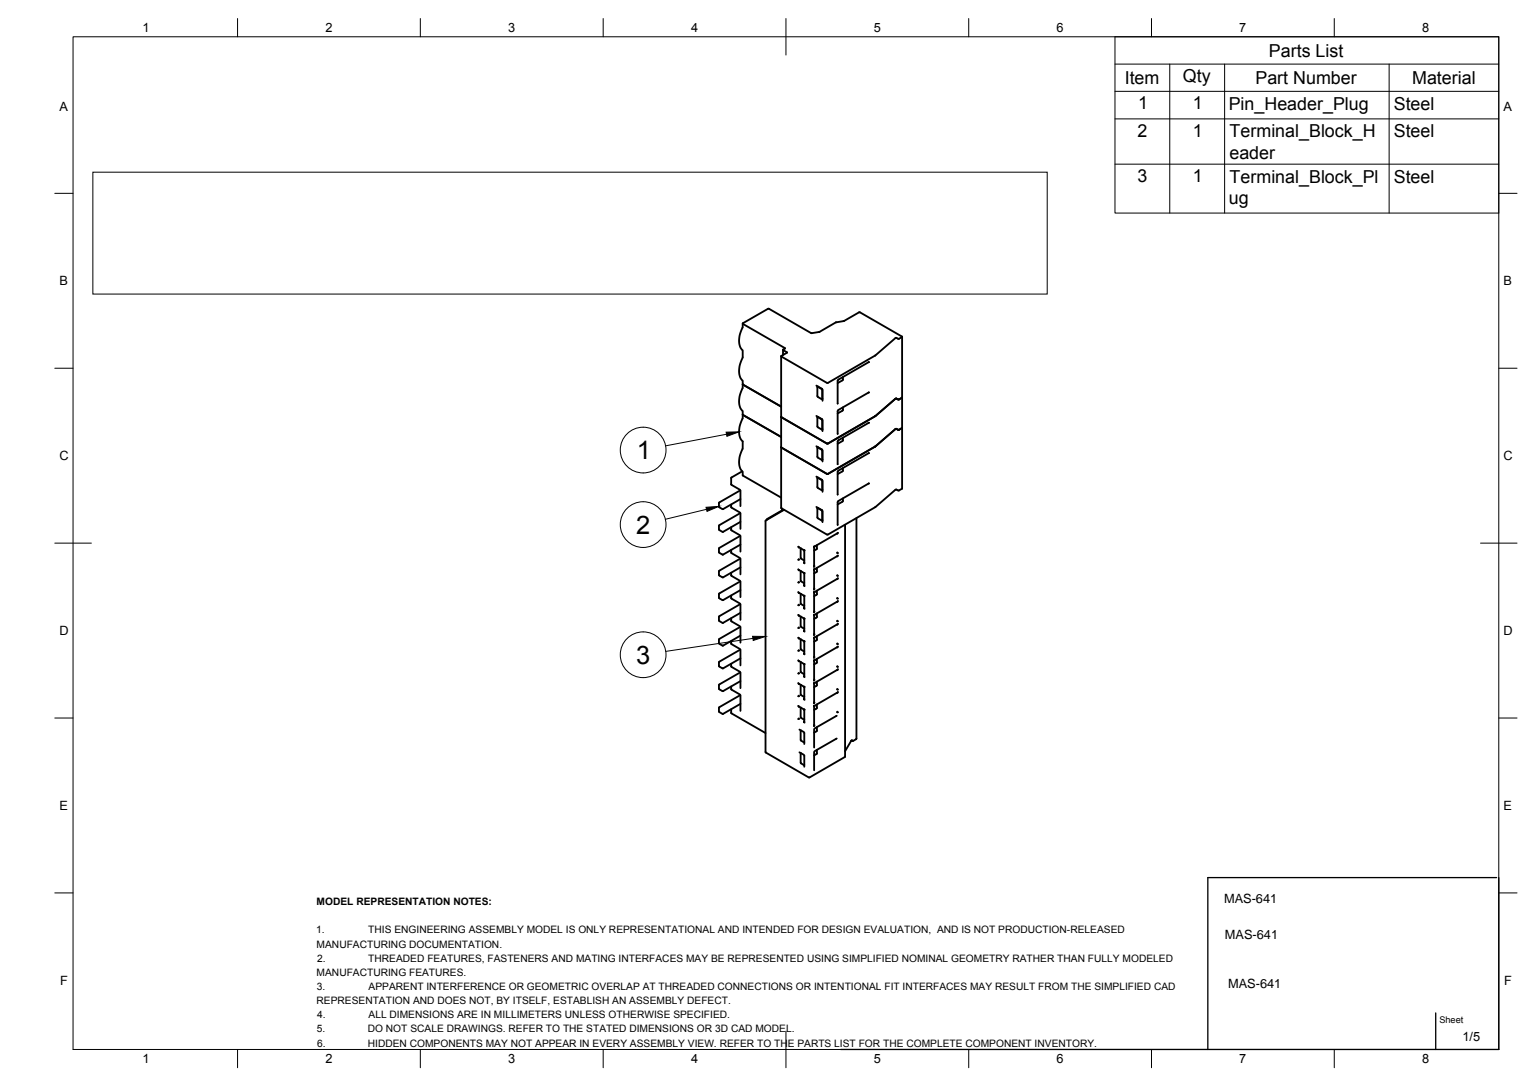
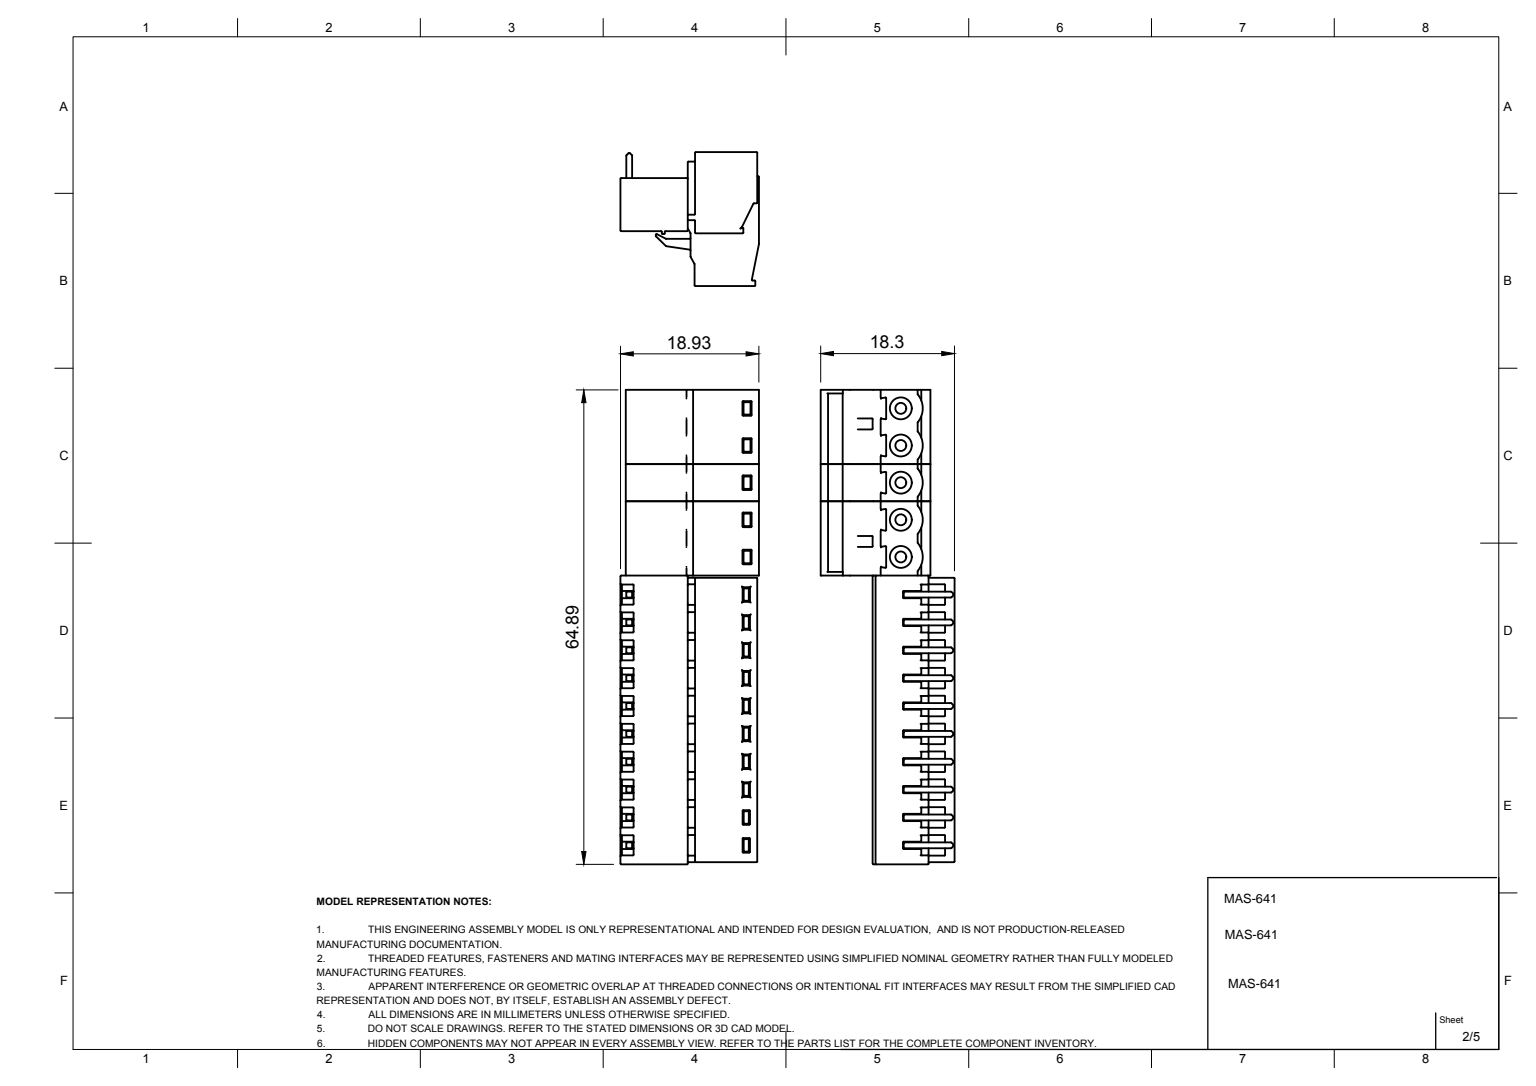
ISO-10303-21;
HEADER;
FILE_DESCRIPTION((''),'2;1');
FILE_NAME('MAS-641','2026-10-09T09:55:32-07:00',(''),(''),'','','');
FILE_SCHEMA (('AUTOMOTIVE_DESIGN { 1 0 10303 214 3 1 1 }'));
ENDSEC;
DATA;
#10 = MECHANICAL_DESIGN_GEOMETRIC_PRESENTATION_REPRESENTATION('',(#79661,
#79662,#79663,#79664,#79665,#79666,#79667,#79668,#79669,#79670,#79671,#79672,
#79673,#79674,#79675,#79676,#79677,#79678,#79679,#79680,#79681,#79682,#79683,
#79684,#79685,#79686,#79687,#79688,#79689,#79690,#79691,#79692,#79693,#79694,
#79695,#79696,#79697,#79698,#79699,#79700,#79701,#79702,#79703,#79704,#79705,
#79706,#79707,#79708,#79709,#79710,#79711,#79712,#79713,#79714,#79715,#79716,
#79717,#79718,#79719,#79720,#79721,#79722,#79723,#79724,#79725,#79726,#79727,
#79728,#79729,#79730,#79731,#79732,#79733,#79734,#79735,#79736,#79737,#79738,
#79739,#79740,#79741,#79742,#79743,#79744,#79745,#79746,#79747,#79748,#79749,
#79750,#79751,#79752,#79753,#79754,#79755,#79756,#79757,#79758,#79759,#79760,
#79761,#79762,#79763,#79764,#79765,#79766,#79767,#79768,#79769,#79770,#79771,
#79772,#79773,#79774,#79775,#79776,#79777,#79778,#79779,#79780,#79781,#79782,
#79783,#79784,#79785,#79786,#79787,#79788,#79789,#79790,#79791,#79792,#79793,
#79794,#79795,#79796,#79797,#79798,#79799,#79800,#79801,#79802,#79803,#79804,
#79805,#79806,#79807,#79808,#79809,#79810,#79811,#79812,#79813,#79814,#79815,
#79816,#79817,#79818,#79819,#79820,#79821,#79822,#79823,#79824,#79825,#79826,
#79827,#79828,#79829,#79830,#79831,#79832,#79833,#79834,#79835,#79836,#79837,
#79838,#79839,#79840,#79841,#79842,#79843,#79844,#79845,#79846,#79847,#79848,
#79849,#79850,#79851,#79852,#79853,#79854,#79855,#79856,#79857,#79858,#79859,
#79860,#79861,#79862,#79863,#79864,#79865,#79866,#79867,#79868,#79869,#79870,
#79871,#79872,#79873,#79874,#79875,#79876,#79877,#79878,#79879,#79880,#79881,
#79882,#79883,#79884,#79885,#79886,#79887,#79888,#79889,#79890,#79891,#79892,
#79893,#79894,#79895,#79896,#79897,#79898,#79899,#79900,#79901,#79902,#79903,
#79904,#79905,#79906,#79907,#79908,#79909,#79910,#79911,#79912,#79913,#79914,
#79915,#79916,#79917,#79918,#79919,#79920,#79921,#79922,#79923,#79924,#79925,
#79926,#79927,#79928,#79929,#79930,#79931,#79932,#79933,#79934,#79935,#79936,
#79937,#79938,#79939,#79940,#79941,#79942,#79943,#79944,#79945,#79946,#79947,
#79948,#79949,#79950,#79951,#79952,#79953,#79954,#79955,#79956,#79957,#79958,
#79959,#79960,#79961,#79962,#79963,#79964,#79965,#79966,#79967,#79968,#79969,
#79970,#79971,#79972,#79973,#79974,#79975,#79976,#79977,#79978,#79979,#79980,
#79981,#79982,#79983,#79984,#79985,#79986,#79987,#79988,#79989,#79990,#79991,
#79992,#79993,#79994,#79995,#79996,#79997,#79998,#79999,#80000,#80001,#80002,
#80003,#80004,#80005,#80006,#80007,#80008,#80009,#80010,#80011,#80012,#80013,
#80014,#80015,#80016,#80017,#80018,#80019,#80020,#80021,#80022,#80023,#80024,
#80025,#80026,#80027,#80028,#80029,#80030,#80031,#80032,#80033,#80034,#80035,
#80036,#80037,#80038,#80039,#80040,#80041,#80042,#80043,#80044,#80045,#80046,
#80047,#80048,#80049,#80050,#80051,#80052,#80053,#80054,#80055,#80056,#80057,
#80058,#80059,#80060,#80061,#80062,#80063,#80064,#80065,#80066,#80067,#80068,
#80069,#80070,#80071,#80072,#80073,#80074,#80075,#80076,#80077,#80078,#80079,
#80080,#80081,#80082,#80083,#80084,#80085,#80086,#80087,#80088,#80089,#80090,
#80091,#80092,#80093,#80094,#80095,#80096,#80097,#80098,#80099,#80100,#80101,
#80102,#80103,#80104,#80105,#80106,#80107,#80108,#80109,#80110,#80111,#80112,
#80113,#80114,#80115,#80116,#80117,#80118,#80119,#80120,#80121,#80122,#80123,
#80124,#80125,#80126,#80127,#80128,#80129,#80130,#80131,#80132,#80133,#80134,
#80135,#80136,#80137,#80138,#80139,#80140,#80141,#80142,#80143,#80144,#80145,
#80146,#80147,#80148,#80149,#80150,#80151,#80152,#80153,#80154,#80155,#80156,
#80157,#80158,#80159,#80160,#80161,#80162,#80163,#80164,#80165,#80166,#80167,
#80168,#80169,#80170,#80171,#80172,#80173,#80174,#80175,#80176,#80177,#80178,
#80179,#80180,#80181,#80182,#80183,#80184,#80185,#80186,#80187,#80188,#80189,
#80190,#80191,#80192,#80193,#80194,#80195,#80196,#80197,#80198,#80199,#80200,
#80201,#80202,#80203,#80204,#80205,#80206,#80207,#80208,#80209,#80210,#80211,
#80212,#80213,#80214,#80215,#80216,#80217,#80218,#80219,#80220,#80221,#80222,
#80223,#80224,#80225,#80226,#80227,#80228,#80229,#80230,#80231,#80232,#80233,
#80234,#80235,#80236,#80237,#80238,#80239,#80240,#80241,#80242,#80243,#80244,
#80245,#80246,#80247,#80248,#80249,#80250,#80251,#80252,#80253,#80254,#80255,
#80256,#80257,#80258,#80259,#80260,#80261,#80262,#80263,#80264,#80265,#80266,
#80267,#80268,#80269,#80270,#80271,#80272,#80273,#80274,#80275,#80276,#80277,
#80278,#80279,#80280,#80281,#80282,#80283,#80284,#80285,#80286,#80287,#80288,
#80289,#80290,#80291,#80292,#80293,#80294,#80295,#80296,#80297,#80298,#80299,
#80300,#80301,#80302,#80303,#80304,#80305,#80306,#80307,#80308,#80309,#80310,
#80311,#80312,#80313,#80314,#80315,#80316,#80317,#80318,#80319,#80320,#80321,
#80322,#80323,#80324,#80325,#80326,#80327,#80328,#80329,#80330,#80331,#80332,
#80333,#80334,#80335,#80336,#80337,#80338,#80339,#80340,#80341,#80342,#80343,
#80344,#80345,#80346,#80347,#80348,#80349,#80350,#80351,#80352,#80353,#80354,
#80355,#80356,#80357,#80358,#80359,#80360,#80361,#80362,#80363,#80364,#80365,
#80366,#80367,#80368,#80369,#80370,#80371,#80372,#80373,#80374,#80375,#80376,
#80377,#80378,#80379,#80380,#80381,#80382,#80383,#80384,#80385,#80386,#80387,
#80388,#80389,#80390,#80391,#80392,#80393,#80394,#80395,#80396,#80397,#80398,
#80399,#80400,#80401,#80402,#80403,#80404,#80405,#80406,#80407,#80408,#80409,
#80410,#80411,#80412,#80413,#80414,#80415,#80416,#80417,#80418,#80419,#80420,
#80421,#80422,#80423,#80424,#80425,#80426,#80427,#80428,#80429,#80430,#80431,
#80432,#80433,#80434,#80435,#80436,#80437,#80438,#80439,#80440,#80441,#80442,
#80443,#80444,#80445,#80446,#80447,#80448,#80449,#80450,#80451,#80452,#80453,
#80454,#80455,#80456,#80457,#80458,#80459,#80460,#80461,#80462,#80463,#80464,
#80465,#80466,#80467,#80468,#80469,#80470,#80471,#80472,#80473,#80474,#80475,
#80476,#80477,#80478,#80479,#80480,#80481,#80482,#80483,#80484,#80485,#80486,
#80487,#80488,#80489,#80490,#80491,#80492,#80493,#80494,#80495,#80496,#80497,
#80498,#80499,#80500,#80501,#80502,#80503,#80504,#80505,#80506,#80507,#80508,
#80509,#80510,#80511,#80512,#80513,#80514,#80515,#80516,#80517,#80518,#80519,
#80520,#80521,#80522,#80523,#80524,#80525,#80526,#80527,#80528,#80529,#80530,
#80531,#80532,#80533,#80534,#80535,#80536,#80537,#80538,#80539,#80540,#80541,
#80542,#80543,#80544,#80545,#80546,#80547,#80548,#80549,#80550,#80551,#80552,
#80553,#80554,#80555,#80556,#80557,#80558,#80559,#80560,#80561,#80562,#80563,
#80564,#80565,#80566,#80567,#80568,#80569,#80570,#80571,#80572,#80573,#80574,
#80575,#80576,#80577,#80578,#80579,#80580,#80581,#80582,#80583,#80584,#80585,
#80586,#80587,#80588,#80589,#80590,#80591,#80592,#80593,#80594,#80595,#80596,
#80597,#80598,#80599,#80600,#80601,#80602,#80603,#80604,#80605,#80606,#80607,
#80608,#80609,#80610,#80611,#80612,#80613,#80614,#80615,#80616,#80617,#80618,
#80619,#80620,#80621,#80622,#80623,#80624,#80625,#80626,#80627,#80628,#80629,
#80630,#80631,#80632,#80633,#80634,#80635,#80636,#80637,#80638,#80639,#80640,
#80641,#80642,#80643,#80644,#80645,#80646,#80647,#80648,#80649,#80650,#80651,
#80652,#80653,#80654,#80655,#80656,#80657,#80658,#80659,#80660,#80661,#80662,
#80663,#80664,#80665,#80666,#80667,#80668,#80669,#80670,#80671,#80672,#80673,
#80674,#80675,#80676,#80677,#80678,#80679,#80680,#80681,#80682,#80683,#80684,
#80685,#80686,#80687,#80688,#80689,#80690,#80691,#80692,#80693,#80694,#80695,
#80696,#80697,#80698,#80699,#80700,#80701,#80702,#80703,#80704,#80705,#80706,
#80707,#80708,#80709,#80710,#80711,#80712,#80713,#80714,#80715,#80716,#80717,
#80718,#80719,#80720,#80721,#80722,#80723,#80724,#80725,#80726,#80727,#80728,
#80729,#80730,#80731,#80732,#80733,#80734,#80735,#80736,#80737,#80738,#80739,
#80740,#80741,#80742,#80743,#80744,#80745,#80746,#80747,#80748,#80749,#80750,
#80751,#80752,#80753,#80754,#80755,#80756,#80757,#80758,#80759,#80760,#80761,
#80762,#80763,#80764,#80765,#80766,#80767,#80768,#80769,#80770,#80771,#80772,
#80773,#80774,#80775,#80776,#80777,#80778,#80779,#80780,#80781,#80782,#80783,
#80784,#80785,#80786,#80787,#80788,#80789,#80790,#80791,#80792,#80793,#80794,
#80795,#80796,#80797,#80798,#80799,#80800,#80801,#80802,#80803,#80804,#80805,
#80806,#80807,#80808,#80809,#80810,#80811,#80812,#80813,#80814,#80815,#80816,
#80817,#80818,#80819,#80820,#80821,#80822,#80823,#80824,#80825,#80826,#80827,
#80828,#80829,#80830,#80831,#80832,#80833,#80834,#80835,#80836,#80837,#80838,
#80839,#80840,#80841,#80842,#80843,#80844,#80845,#80846,#80847,#80848,#80849,
#80850,#80851,#80852,#80853,#80854,#80855,#80856,#80857,#80858,#80859,#80860,
#80861,#80862,#80863,#80864,#80865,#80866,#80867,#80868,#80869,#80870,#80871,
#80872,#80873,#80874,#80875,#80876,#80877,#80878,#80879,#80880,#80881,#80882,
#80883,#80884,#80885,#80886,#80887,#80888,#80889,#80890,#80891,#80892,#80893,
#80894,#80895,#80896,#80897,#80898,#80899,#80900,#80901,#80902,#80903,#80904,
#80905,#80906,#80907,#80908,#80909,#80910,#80911,#80912,#80913,#80914,#80915,
#80916,#80917,#80918,#80919,#80920,#80921,#80922,#80923,#80924,#80925,#80926,
#80927,#80928,#80929,#80930,#80931,#80932,#80933,#80934,#80935,#80936,#80937,
#80938,#80939,#80940,#80941,#80942,#80943,#80944,#80945,#80946,#80947,#80948,
#80949,#80950,#80951,#80952,#80953,#80954,#80955,#80956,#80957,#80958,#80959,
#80960,#80961,#80962,#80963,#80964,#80965,#80966,#80967,#80968,#80969,#80970,
#80971,#80972,#80973,#80974,#80975,#80976,#80977,#80978,#80979,#80980,#80981,
#80982,#80983,#80984,#80985,#80986,#80987,#80988,#80989,#80990,#80991,#80992,
#80993,#80994,#80995,#80996,#80997,#80998,#80999,#81000,#81001,#81002,#81003,
#81004,#81005,#81006,#81007,#81008,#81009,#81010,#81011,#81012,#81013,#81014,
#81015,#81016,#81017,#81018,#81019,#81020,#81021,#81022,#81023,#81024,#81025,
#81026,#81027,#81028,#81029,#81030,#81031,#81032,#81033,#81034,#81035,#81036,
#81037,#81038,#81039,#81040,#81041,#81042,#81043,#81044,#81045,#81046,#81047,
#81048,#81049,#81050,#81051,#81052,#81053,#81054,#81055,#81056,#81057,#81058,
#81059,#81060,#81061,#81062,#81063,#81064,#81065,#81066,#81067,#81068,#81069,
#81070,#81071,#81072,#81073,#81074,#81075,#81076,#81077,#81078,#81079,#81080,
#81081,#81082,#81083,#81084,#81085,#81086,#81087,#81088,#81089,#81090,#81091,
#81092,#81093,#81094,#81095,#81096,#81097,#81098,#81099,#81100,#81101,#81102,
#81103,#81104,#81105,#81106,#81107,#81108,#81109,#81110,#81111,#81112,#81113,
#81114,#81115,#81116,#81117,#81118,#81119,#81120,#81121,#81122,#81123,#81124,
#81125,#81126,#81127,#81128,#81129,#81130,#81131,#81132,#81133,#81134,#81135,
#81136,#81137,#81138,#81139,#81140,#81141,#81142,#81143,#81144,#81145,#81146,
#81147,#81148,#81149,#81150,#81151,#81152,#81153,#81154,#81155,#81156,#81157,
#81158,#81159,#81160,#81161,#81162,#81163,#81164,#81165,#81166,#81167,#81168,
#81169,#81170,#81171,#81172,#81173,#81174,#81175,#81176,#81177,#81178,#81179,
#81180,#81181,#81182,#81183,#81184,#81185,#81186,#81187,#81188,#81189,#81190,
#81191,#81192,#81193,#81194,#81195,#81196,#81197,#81198,#81199,#81200,#81201,
#81202,#81203,#81204,#81205,#81206,#81207,#81208,#81209,#81210,#81211,#81212,
#81213,#81214,#81215,#81216,#81217,#81218,#81219,#81220,#81221,#81222,#81223,
#81224,#81225,#81226,#81227,#81228,#81229,#81230,#81231,#81232,#81233,#81234,
#81235,#81236,#81237,#81238,#81239,#81240,#81241,#81242,#81243,#81244,#81245,
#81246,#81247,#81248,#81249,#81250,#81251,#81252,#81253,#81254,#81255,#81256,
#81257,#81258,#81259,#81260,#81261,#81262,#81263,#81264,#81265,#81266,#81267,
#81268,#81269,#81270,#81271,#81272,#81273,#81274,#81275,#81276,#81277,#81278,
#81279,#81280,#81281,#81282,#81283,#81284,#81285,#81286,#81287,#81288,#81289,
#81290,#81291,#81292,#81293,#81294,#81295,#81296,#81297,#81298,#81299,#81300,
#81301,#81302,#81303,#81304,#81305,#81306,#81307,#81308,#81309,#81310,#81311,
#81312,#81313,#81314,#81315,#81316,#81317,#81318,#81319,#81320,#81321,#81322,
#81323,#81324,#81325,#81326,#81327,#81328,#81329,#81330,#81331,#81332,#81333,
#81334,#81335,#81336,#81337,#81338,#81339,#81340,#81341,#81342,#81343,#81344,
#81345,#81346,#81347,#81348,#81349,#81350,#81351,#81352,#81353,#81354,#81355,
#81356,#81357,#81358,#81359,#81360,#81361,#81362,#81363,#81364,#81365,#81366,
#81367,#81368,#81369,#81370,#81371,#81372,#81373,#81374,#81375,#81376,#81377,
#81378,#81379,#81380,#81381,#81382,#81383,#81384,#81385,#81386,#81387,#81388,
#81389,#81390,#81391,#81392,#81393,#81394,#81395,#81396,#81397,#81398,#81399,
#81400,#81401,#81402,#81403,#81404,#81405,#81406,#81407,#81408,#81409,#81410,
#81411,#81412,#81413,#81414,#81415,#81416,#81417,#81418,#81419,#81420,#81421,
#81422,#81423,#81424,#81425,#81426,#81427,#81428,#81429,#81430,#81431,#81432,
#81433,#81434,#81435,#81436,#81437,#81438,#81439,#81440,#81441,#81442,#81443,
#81444,#81445,#81446,#81447,#81448,#81449,#81450,#81451,#81452,#81453,#81454,
#81455,#81456,#81457,#81458,#81459,#81460,#81461,#81462,#81463,#81464,#81465,
#81466,#81467,#81468,#81469,#81470,#81471,#81472,#81473,#81474,#81475,#81476,
#81477,#81478,#81479,#81480,#81481,#81482,#81483,#81484,#81485,#81486,#81487,
#81488,#81489,#81490,#81491,#81492,#81493,#81494,#81495,#81496,#81497,#81498,
#81499,#81500,#81501,#81502,#81503,#81504,#81505,#81506,#81507,#81508,#81509,
#81510,#81511,#81512,#81513,#81514,#81515,#81516,#81517,#81518,#81519,#81520,
#81521,#81522,#81523,#81524,#81525,#81526,#81527,#81528,#81529,#81530,#81531,
#81532,#81533,#81534,#81535,#81536,#81537,#81538,#81539,#81540,#81541,#81542,
#81543,#81544,#81545,#81546,#81547,#81548,#81549,#81550,#81551,#81552,#81553,
#81554,#81555,#81556,#81557,#81558,#81559,#81560,#81561,#81562,#81563,#81564,
#81565,#81566,#81567,#81568,#81569,#81570,#81571,#81572,#81573,#81574,#81575,
#81576,#81577,#81578,#81579,#81580,#81581,#81582,#81583,#81584,#81585,#81586,
#81587,#81588,#81589,#81590,#81591,#81592,#81593,#81594,#81595,#81596,#81597,
#81598,#81599,#81600,#81601,#81602,#81603,#81604,#81605,#81606,#81607,#81608,
#81609,#81610,#81611,#81612,#81613,#81614,#81615,#81616,#81617,#81618,#81619,
#81620,#81621,#81622,#81623,#81624,#81625,#81626,#81627,#81628,#81629,#81630,
#81631,#81632,#81633,#81634,#81635,#81636,#81637,#81638,#81639,#81640,#81641,
#81642,#81643,#81644,#81645,#81646,#81647,#81648,#81649,#81650,#81651,#81652,
#81653,#81654,#81655,#81656,#81657,#81658,#81659,#81660,#81661,#81662,#81663,
#81664,#81665,#81666,#81667,#81668,#81669,#81670,#81671,#81672,#81673,#81674,
#81675,#81676,#81677,#81678,#81679,#81680,#81681,#81682,#81683,#81684,#81685,
#81686,#81687,#81688,#81689,#81690,#81691,#81692,#81693,#81694,#81695,#81696,
#81697,#81698,#81699,#81700,#81701,#81702,#81703,#81704,#81705,#81706,#81707,
#81708,#81709,#81710,#81711,#81712,#81713,#81714,#81715,#81716,#81717,#81718,
#81719,#81720,#81721,#81722,#81723,#81724,#81725,#81726,#81727,#81728,#81729,
#81730,#81731,#81732,#81733,#81734,#81735,#81736,#81737,#81738,#81739,#81740,
#81741,#81742,#81743,#81744,#81745,#81746,#81747,#81748,#81749,#81750,#81751,
#81752,#81753,#81754,#81755,#81756,#81757,#81758,#81759,#81760,#81761,#81762,
#81763,#81764,#81765,#81766,#81767,#81768,#81769,#81770,#81771,#81772,#81773,
#81774,#81775,#81776,#81777,#81778,#81779,#81780,#81781,#81782,#81783,#81784,
#81785,#81786,#81787,#81788,#81789,#81790,#81791,#81792,#81793,#81794,#81795,
#81796,#81797,#81798,#81799,#81800,#81801,#81802,#81803,#81804,#81805,#81806,
#81807,#81808,#81809,#81810,#81811,#81812,#81813,#81814,#81815,#81816,#81817,
#81818,#81819,#81820,#81821,#81822,#81823,#81824,#81825,#81826,#81827,#81828,
#81829,#81830,#81831,#81832,#81833,#81834,#81835,#81836,#81837,#81838,#81839,
#81840,#81841,#81842,#81843,#81844,#81845,#81846,#81847,#81848,#81849,#81850,
#81851,#81852,#81853,#81854,#81855,#81856,#81857,#81858,#81859,#81860,#81861,
#81862,#81863,#81864,#81865,#81866,#81867,#81868,#81869,#81870,#81871,#81872,
#81873,#81874,#81875,#81876,#81877,#81878,#81879,#81880,#81881,#81882,#81883,
#81884,#81885,#81886,#81887,#81888,#81889,#81890,#81891,#81892,#81893,#81894,
#81895,#81896,#81897,#81898,#81899,#81900,#81901,#81902,#81903,#81904,#81905,
#81906,#81907,#81908,#81909,#81910,#81911,#81912,#81913,#81914,#81915,#81916,
#81917,#81918,#81919,#81920,#81921,#81922,#81923,#81924,#81925,#81926,#81927,
#81928,#81929,#81930,#81931,#81932,#81933,#81934,#81935,#81936,#81937,#81938,
#81939,#81940,#81941,#81942,#81943,#81944,#81945,#81946,#81947,#81948,#81949,
#81950,#81951,#81952,#81953,#81954,#81955,#81956,#81957,#81958,#81959,#81960,
#81961,#81962,#81963,#81964,#81965,#81966,#81967,#81968,#81969,#81970,#81971,
#81972,#81973,#81974,#81975,#81976,#81977,#81978,#81979,#81980,#81981,#81982,
#81983,#81984,#81985,#81986,#81987,#81988,#81989,#81990,#81991,#81992,#81993,
#81994,#81995,#81996,#81997,#81998,#81999,#82000,#82001,#82002,#82003,#82004,
#82005,#82006,#82007,#82008,#82009,#82010,#82011,#82012,#82013,#82014,#82015,
#82016,#82017,#82018,#82019,#82020,#82021,#82022,#82023,#82024,#82025,#82026,
#82027,#82028,#82029,#82030,#82031,#82032,#82033,#82034,#82035,#82036,#82037,
#82038,#82039,#82040,#82041,#82042,#82043,#82044,#82045,#82046,#82047,#82048,
#82049,#82050,#82051,#82052,#82053,#82054,#82055,#82056,#82057,#82058,#82059,
#82060,#82061,#82062,#82063,#82064,#82065,#82066,#82067,#82068,#82069,#82070,
#82071,#82072,#82073,#82074,#82075,#82076,#82077,#82078,#82079,#82080,#82081,
#82082,#82083,#82084,#82085,#82086,#82087,#82088,#82089,#82090,#82091,#82092,
#82093,#82094,#82095,#82096,#82097,#82098,#82099,#82100,#82101,#82102,#82103,
#82104,#82105,#82106,#82107,#82108,#82109,#82110,#82111,#82112,#82113,#82114,
#82115,#82116,#82117,#82118,#82119,#82120,#82121,#82122,#82123,#82124,#82125,
#82126,#82127,#82128,#82129,#82130,#82131,#82132,#82133,#82134,#82135,#82136,
#82137,#82138,#82139,#82140,#82141,#82142,#82143,#82144,#82145,#82146,#82147,
#82148,#82149,#82150,#82151,#82152,#82153,#82154,#82155,#82156,#82157,#82158,
#82159,#82160,#82161,#82162,#82163,#82164,#82165,#82166,#82167,#82168,#82169,
#82170,#82171,#82172,#82173,#82174,#82175,#82176,#82177,#82178,#82179,#82180,
#82181,#82182,#82183,#82184,#82185,#82186,#82187,#82188,#82189,#82190,#82191,
#82192,#82193,#82194,#82195,#82196,#82197,#82198,#82199,#82200,#82201,#82202,
#82203,#82204,#82205,#82206,#82207,#82208,#82209,#82210,#82211,#82212,#82213,
#82214,#82215,#82216,#82217,#82218,#82219,#82220,#82221,#82222,#82223,#82224,
#82225,#82226,#82227,#82228,#82229,#82230,#82231,#82232,#82233,#82234,#82235,
#82236,#82237,#82238,#82239,#82240,#82241,#82242,#82243,#82244,#82245,#82246,
#82247,#82248,#82249,#82250,#82251,#82252,#82253,#82254,#82255,#82256,#82257,
#82258,#82259,#82260,#82261,#82262,#82263,#82264,#82265,#82266,#82267,#82268,
#82269,#82270,#82271,#82272,#82273,#82274,#82275,#82276,#82277,#82278,#82279,
#82280,#82281,#82282,#82283,#82284,#82285,#82286,#82287,#82288,#82289,#82290,
#82291,#82292,#82293,#82294,#82295,#82296,#82297,#82298,#82299,#82300,#82301,
#82302,#82303,#82304,#82305,#82306,#82307,#82308,#82309,#82310,#82311,#82312,
#82313,#82314,#82315,#82316,#82317,#82318,#82319,#82320,#82321,#82322,#82323,
#82324,#82325,#82326,#82327,#82328,#82329,#82330,#82331,#82332,#82333,#82334,
#82335,#82336,#82337,#82338,#82339,#82340,#82341,#82342,#82343,#82344,#82345,
#82346,#82347,#82348,#82349,#82350,#82351,#82352,#82353,#82354,#82355,#82356,
#82357,#82358,#82359,#82360,#82361,#82362,#82363,#82364,#82365,#82366,#82367,
#82368,#82369,#82370,#82371,#82372,#82373,#82374,#82375,#82376,#82377,#82378,
#82379,#82380,#82381,#82382,#82383,#82384,#82385,#82386,#82387,#82388,#82389,
#82390,#82391,#82392,#82393,#82394,#82395,#82396,#82397,#82398,#82399,#82400,
#82401,#82402,#82403,#82404,#82405,#82406,#82407,#82408,#82409,#82410,#82411,
#82412,#82413,#82414,#82415,#82416,#82417,#82418,#82419,#82420,#82421,#82422,
#82423,#82424,#82425,#82426,#82427,#82428,#82429,#82430,#82431,#82432,#82433,
#82434,#82435,#82436,#82437,#82438,#82439,#82440,#82441,#82442,#82443,#82444,
#82445,#82446,#82447,#82448,#82449,#82450,#82451,#82452,#82453,#82454,#82455,
#82456,#82457,#82458,#82459,#82460,#82461,#82462,#82463,#82464,#82465,#82466,
#82467,#82468,#82469,#82470,#82471,#82472,#82473,#82474,#82475,#82476,#82477,
#82478,#82479,#82480,#82481,#82482,#82483,#82484,#82485,#82486,#82487,#82488,
#82489,#82490,#82491,#82492,#82493,#82494,#82495,#82496,#82497,#82498,#82499,
#82500,#82501,#82502,#82503,#82504,#82505,#82506,#82507,#82508,#82509,#82510,
#82511,#82512,#82513,#82514,#82515,#82516,#82517,#82518,#82519,#82520,#82521,
#82522,#82523,#82524,#82525,#82526,#82527,#82528,#82529,#82530,#82531,#82532,
#82533,#82534,#82535,#82536,#82537,#82538,#82539,#82540,#82541,#82542,#82543,
#82544,#82545,#82546,#82547,#82548,#82549,#82550,#82551,#82552,#82553,#82554,
#82555,#82556,#82557,#82558,#82559,#82560,#82561,#82562,#82563,#82564,#82565,
#82566,#82567,#82568,#82569,#82570,#82571,#82572,#82573,#82574,#82575,#82576,
#82577,#82578,#82579,#82580,#82581,#82582,#82583,#82584,#82585,#82586,#82587,
#82588,#82589,#82590,#82591,#82592,#82593,#82594,#82595,#82596,#82597,#82598,
#82599,#82600,#82601,#82602,#82603,#82604,#82605,#82606,#82607,#82608,#82609,
#82610,#82611,#82612,#82613,#82614,#82615,#82616,#82617,#82618,#82619,#82620,
#82621,#82622,#82623,#82624,#82625,#82626,#82627,#82628,#82629,#82630,#82631,
#82632,#82633,#82634,#82635,#82636,#82637,#82638,#82639,#82640,#82641,#82642,
#82643,#82644,#82645,#82646,#82647,#82648,#82649,#82650,#82651,#82652,#82653,
#82654,#82655,#82656,#82657,#82658,#82659,#82660,#82661,#82662,#82663,#82664,
#82665,#82666,#82667,#82668,#82669,#82670,#82671,#82672,#82673,#82674,#82675,
#82676,#82677,#82678,#82679,#82680,#82681,#82682,#82683,#82684,#82685,#82686,
#82687,#82688,#82689,#82690,#82691,#82692,#82693,#82694,#82695,#82696,#82697,
#82698,#82699,#82700,#82701,#82702,#82703,#82704,#82705,#82706,#82707,#82708,
#82709,#82710,#82711,#82712,#82713,#82714,#82715,#82716,#82717,#82718,#82719,
#82720,#82721,#82722,#82723,#82724,#82725,#82726,#82727,#82728,#82729,#82730,
#82731,#82732,#82733,#82734,#82735,#82736,#82737,#82738,#82739,#82740,#82741,
#82742,#82743,#82744,#82745,#82746,#82747,#82748,#82749,#82750,#82751,#82752,
#82753,#82754,#82755,#82756,#82757,#82758,#82759,#82760,#82761,#82762,#82763,
#82764,#82765,#82766,#82767,#82768,#82769,#82770,#82771,#82772,#82773,#82774,
#82775,#82776,#82777,#82778,#82779,#82780,#82781,#82782,#82783,#82784,#82785,
#82786,#82787,#82788,#82789,#82790,#82791,#82792,#82793,#82794,#82795,#82796,
#82797,#82798,#82799,#82800,#82801,#82802,#82803,#82804,#82805,#82806,#82807,
#82808,#82809,#82810,#82811,#82812,#82813,#82814,#82815,#82816,#82817,#82818,
#82819,#82820,#82821,#82822,#82823,#82824,#82825,#82826,#82827,#82828,#82829,
#82830,#82831,#82832,#82833,#82834,#82835,#82836,#82837,#82838,#82839,#82840,
#82841,#82842,#82843,#82844,#82845,#82846,#82847,#82848,#82849,#82850,#82851,
#82852,#82853,#82854,#82855,#82856,#82857,#82858,#82859,#82860,#82861,#82862,
#82863,#82864,#82865,#82866,#82867,#82868,#82869,#82870,#82871,#82872,#82873,
#82874,#82875,#82876,#82877,#82878,#82879,#82880,#82881,#82882,#82883,#82884,
#82885,#82886,#82887,#82888,#82889,#82890,#82891,#82892,#82893,#82894,#82895,
#82896,#82897,#82898,#82899,#82900,#82901,#82902,#82903,#82904,#82905,#82906,
#82907,#82908,#82909,#82910,#82911,#82912,#82913,#82914,#82915,#82916,#82917,
#82918,#82919,#82920,#82921,#82922,#82923,#82924,#82925,#82926,#82927,#82928,
#82929,#82930,#82931,#82932,#82933,#82934,#82935,#82936,#82937,#82938,#82939,
#82940,#82941,#82942,#82943,#82944,#82945,#82946,#82947,#82948,#82949,#82950,
#82951,#82952,#82953,#82954,#82955,#82956,#82957,#82958,#82959,#82960,#82961,
#82962,#82963,#82964,#82965,#82966,#82967,#82968,#82969,#82970,#82971,#82972,
#82973,#82974,#82975,#82976,#82977,#82978,#82979,#82980,#82981,#82982,#82983,
#82984,#82985,#82986,#82987,#82988,#82989,#82990,#82991,#82992,#82993,#82994,
#82995,#82996,#82997,#82998,#82999,#83000,#83001,#83002,#83003,#83004,#83005,
#83006,#83007,#83008,#83009,#83010,#83011,#83012,#83013,#83014,#83015,#83016,
#83017,#83018,#83019,#83020,#83021,#83022,#83023,#83024,#83025,#83026,#83027,
#83028,#83029,#83030,#83031,#83032,#83033,#83034,#83035,#83036,#83037,#83038,
#83039,#83040,#83041,#83042,#83043,#83044,#83045,#83046,#83047,#83048,#83049,
#83050,#83051,#83052,#83053,#83054,#83055,#83056,#83057,#83058,#83059,#83060,
#83061,#83062,#83063,#83064,#83065,#83066,#83067,#83068,#83069,#83070,#83071,
#83072,#83073,#83074,#83075,#83076,#83077,#83078,#83079,#83080,#83081,#83082,
#83083,#83084,#83085,#83086,#83087,#83088,#83089,#83090,#83091,#83092,#83093,
#83094,#83095,#83096,#83097,#83098,#83099,#83100,#83101,#83102,#83103,#83104,
#83105,#83106,#83107,#83108,#83109,#83110,#83111,#83112,#83113,#83114,#83115,
#83116,#83117,#83118,#83119,#83120,#83121,#83122,#83123,#83124,#83125,#83126,
#83127,#83128,#83129,#83130,#83131,#83132,#83133,#83134,#83135,#83136,#83137,
#83138,#83139,#83140,#83141,#83142,#83143,#83144,#83145,#83146,#83147,#83148,
#83149,#83150,#83151,#83152,#83153,#83154,#83155,#83156,#83157,#83158,#83159,
#83160,#83161,#83162,#83163,#83164,#83165,#83166,#83167,#83168,#83169,#83170,
#83171,#83172,#83173,#83174,#83175,#83176,#83177,#83178,#83179,#83180,#83181,
#83182,#83183,#83184,#83185,#83186,#83187,#83188,#83189,#83190,#83191,#83192,
#83193,#83194,#83195,#83196,#83197,#83198,#83199,#83200,#83201,#83202,#83203,
#83204,#83205,#83206,#83207,#83208,#83209,#83210,#83211,#83212,#83213,#83214,
#83215,#83216,#83217,#83218,#83219,#83220,#83221,#83222,#83223,#83224,#83225,
#83226,#83227,#83228,#83229,#83230,#83231,#83232,#83233,#83234,#83235,#83236,
#83237,#83238,#83239,#83240,#83241,#83242,#83243,#83244,#83245,#83246,#83247,
#83248,#83249,#83250,#83251,#83252,#83253,#83254,#83255,#83256,#83257,#83258,
#83259,#83260,#83261,#83262,#83263,#83264,#83265,#83266,#83267,#83268,#83269,
#83270,#83271,#83272,#83273,#83274,#83275,#83276,#83277,#83278,#83279,#83280,
#83281,#83282,#83283,#83284,#83285,#83286,#83287,#83288,#83289,#83290,#83291,
#83292,#83293,#83294,#83295,#83296,#83297,#83298,#83299,#83300,#83301,#83302,
#83303,#83304,#83305,#83306,#83307,#83308,#83309,#83310,#83311,#83312,#83313,
#83314,#83315,#83316,#83317,#83318,#83319,#83320,#83321,#83322,#83323,#83324,
#83325,#83326,#83327,#83328,#83329,#83330,#83331,#83332,#83333,#83334,#83335,
#83336,#83337,#83338,#83339,#83340,#83341,#83342,#83343,#83344,#83345,#83346,
#83347,#83348,#83349,#83350,#83351,#83352,#83353,#83354,#83355,#83356,#83357,
#83358,#83359,#83360,#83361,#83362,#83363,#83364,#83365,#83366,#83367,#83368,
#83369,#83370,#83371,#83372,#83373,#83374,#83375,#83376,#83377,#83378,#83379,
#83380,#83381,#83382,#83383,#83384,#83385,#83386,#83387,#83388,#83389,#83390,
#83391,#83392,#83393,#83394,#83395,#83396,#83397,#83398,#83399,#83400,#83401,
#83402,#83403,#83404,#83405,#83406,#83407,#83408,#83409,#83410,#83411,#83412,
#83413,#83414,#83415,#83416,#83417,#83418,#83419,#83420,#83421,#83422,#83423,
#83424,#83425,#83426,#83427,#83428,#83429,#83430,#83431,#83432,#83433,#83434,
#83435,#83436,#83437,#83438,#83439,#83440,#83441,#83442,#83443,#83444,#83445,
#83446,#83447,#83448,#83449,#83450,#83451,#83452,#83453,#83454,#83455,#83456,
#83457,#83458,#83459,#83460,#83461,#83462,#83463,#83464,#83465,#83466,#83467,
#83468,#83469,#83470,#83471,#83472,#83473,#83474,#83475,#83476,#83477,#83478,
#83479,#83480,#83481,#83482,#83483,#83484,#83485,#83486,#83487,#83488,#83489,
#83490,#83491,#83492,#83493,#83494,#83495,#83496,#83497,#83498,#83499,#83500,
#83501,#83502,#83503,#83504,#83505,#83506,#83507,#83508,#83509,#83510,#83511,
#83512,#83513,#83514,#83515,#83516,#83517,#83518,#83519,#83520,#83521,#83522,
#83523,#83524,#83525,#83526,#83527,#83528,#83529,#83530,#83531,#83532,#83533,
#83534,#83535,#83536,#83537,#83538,#83539,#83540,#83541,#83542,#83543,#83544,
#83545,#83546,#83547,#83548,#83549,#83550,#83551,#83552,#83553,#83554,#83555,
#83556,#83557,#83558,#83559,#83560,#83561,#83562,#83563,#83564,#83565,#83566,
#83567,#83568,#83569,#83570,#83571,#83572,#83573,#83574,#83575,#83576,#83577,
#83578,#83579,#83580,#83581,#83582,#83583,#83584,#83585,#83586,#83587,#83588,
#83589,#83590,#83591,#83592,#83593,#83594,#83595,#83596,#83597,#83598,#83599,
#83600,#83601,#83602,#83603,#83604,#83605,#83606,#83607,#83608,#83609,#83610,
#83611,#83612,#83613,#83614,#83615,#83616,#83617,#83618,#83619,#83620,#83621,
#83622,#83623,#83624,#83625,#83626,#83627,#83628,#83629,#83630,#83631,#83632,
#83633,#83634,#83635,#83636,#83637,#83638,#83639,#83640,#83641,#83642,#83643,
#83644,#83645,#83646,#83647,#83648,#83649,#83650,#83651,#83652,#83653,#83654,
#83655,#83656,#83657,#83658,#83659,#83660,#83661,#83662,#83663,#83664,#83665,
#83666,#83667,#83668,#83669,#83670,#83671,#83672,#83673,#83674,#83675,#83676,
#83677,#83678,#83679,#83680,#83681,#83682,#83683,#83684,#83685,#83686,#83687,
#83688,#83689,#83690,#83691,#83692,#83693,#83694,#83695,#83696,#83697,#83698,
#83699,#83700,#83701,#83702,#83703,#83704,#83705,#83706,#83707,#83708,#83709,
#83710,#83711,#83712,#83713,#83714,#83715,#83716,#83717,#83718,#83719,#83720,
#83721,#83722,#83723,#83724,#83725,#83726,#83727,#83728,#83729,#83730,#83731,
#83732,#83733,#83734,#83735,#83736,#83737,#83738,#83739,#83740,#83741,#83742,
#83743,#83744,#83745,#83746,#83747,#83748,#83749,#83750,#83751,#83752,#83753,
#83754,#83755,#83756,#83757,#83758,#83759,#83760,#83761,#83762,#83763,#83764,
#83765,#83766,#83767,#83768,#83769,#83770,#83771,#83772,#83773,#83774,#83775,
#83776,#83777,#83778,#83779,#83780,#83781,#83782,#83783,#83784,#83785,#83786,
#83787,#83788,#83789,#83790,#83791,#83792,#83793,#83794,#83795,#83796,#83797,
#83798,#83799,#83800,#83801,#83802,#83803,#83804,#83805,#83806,#83807,#83808,
#83809,#83810,#83811,#83812,#83813,#83814,#83815,#83816,#83817,#83818,#83819,
#83820,#83821,#83822,#83823,#83824,#83825,#83826,#83827,#83828,#83829,#83830,
#83831,#83832,#83833,#83834,#83835,#83836,#83837,#83838,#83839,#83840,#83841,
#83842,#83843,#83844,#83845,#83846,#83847,#83848,#83849,#83850,#83851,#83852,
#83853,#83854,#83855,#83856,#83857,#83858,#83859,#83860,#83861,#83862,#83863,
#83864,#83865,#83866,#83867,#83868,#83869,#83870,#83871,#83872,#83873,#83874,
#83875,#83876,#83877,#83878,#83879,#83880,#83881,#83882,#83883,#83884,#83885,
#83886,#83887,#83888,#83889,#83890,#83891,#83892,#83893,#83894,#83895,#83896,
#83897,#83898,#83899,#83900,#83901,#83902,#83903,#83904,#83905,#83906,#83907,
#83908,#83909,#83910,#83911,#83912,#83913,#83914,#83915,#83916,#83917,#83918,
#83919,#83920,#83921,#83922,#83923,#83924,#83925,#83926,#83927,#83928,#83929,
#83930,#83931,#83932,#83933,#83934,#83935,#83936,#83937,#83938,#83939,#83940,
#83941,#83942,#83943,#83944,#83945,#83946,#83947,#83948,#83949,#83950,#83951,
#83952,#83953,#83954,#83955,#83956,#83957,#83958,#83959,#83960,#83961,#83962,
#83963,#83964,#83965,#83966,#83967,#83968,#83969,#83970,#83971,#83972,#83973,
#83974,#83975,#83976,#83977,#83978,#83979,#83980,#83981,#83982,#83983,#83984,
#83985,#83986,#83987,#83988,#83989,#83990,#83991,#83992,#83993,#83994,#83995,
#83996,#83997,#83998,#83999,#84000,#84001,#84002,#84003,#84004,#84005,#84006,
#84007,#84008,#84009,#84010,#84011,#84012,#84013,#84014,#84015,#84016,#84017,
#84018,#84019,#84020,#84021,#84022,#84023,#84024,#84025,#84026,#84027,#84028,
#84029,#84030,#84031,#84032,#84033,#84034,#84035,#84036,#84037,#84038,#84039,
#84040,#84041,#84042,#84043,#84044,#84045,#84046,#84047,#84048,#84049,#84050,
#84051,#84052,#84053,#84054,#84055,#84056,#84057,#84058,#84059,#84060,#84061,
#84062,#84063,#84064,#84065,#84066,#84067,#84068,#84069,#84070,#84071,#84072,
#84073,#84074,#84075,#84076,#84077,#84078,#84079,#84080,#84081,#84082,#84083,
#84084,#84085,#84086,#84087,#84088,#84089,#84090,#84091,#84092,#84093,#84094,
#84095,#84096,#84097,#84098,#84099,#84100,#84101,#84102,#84103,#84104,#84105,
#84106,#84107,#84108,#84109,#84110,#84111,#84112,#84113,#84114,#84115,#84116,
#84117,#84118,#84119,#84120,#84121,#84122,#84123,#84124,#84125,#84126,#84127,
#84128,#84129,#84130,#84131,#84132,#84133,#84134,#84135,#84136,#84137,#84138,
#84139,#84140,#84141,#84142,#84143,#84144,#84145,#84146,#84147,#84148,#84149,
#84150,#84151,#84152,#84153,#84154,#84155,#84156,#84157,#84158,#84159,#84160,
#84161,#84162,#84163,#84164,#84165,#84166,#84167,#84168,#84169,#84170,#84171,
#84172,#84173,#84174,#84175,#84176,#84177,#84178,#84179,#84180,#84181,#84182,
#84183,#84184,#84185,#84186,#84187,#84188,#84189,#84190,#84191,#84192,#84193,
#84194,#84195,#84196,#84197,#84198,#84199,#84200,#84201,#84202,#84203,#84204,
#84205,#84206,#84207,#84208,#84209,#84210,#84211,#84212,#84213,#84214,#84215,
#84216,#84217,#84218,#84219,#84220,#84221,#84222,#84223,#84224,#84225,#84226,
#84227,#84228,#84229,#84230,#84231,#84232,#84233,#84234,#84235,#84236,#84237,
#84238,#84239,#84240,#84241,#84242,#84243,#84244,#84245,#84246,#84247,#84248,
#84249,#84250,#84251,#84252,#84253,#84254,#84255,#84256,#84257,#84258,#84259,
#84260,#84261,#84262,#84263,#84264,#84265,#84266,#84267,#84268,#84269,#84270,
#84271,#84272,#84273,#84274,#84275,#84276,#84277,#84278,#84279,#84280,#84281,
#84282,#84283,#84284,#84285,#84286,#84287,#84288,#84289,#84290,#84291,#84292,
#84293,#84294,#84295,#84296,#84297,#84298,#84299,#84300,#84301,#84302,#84303,
#84304,#84305,#84306,#84307,#84308,#84309,#84310,#84311,#84312,#84313,#84314,
#84315,#84316,#84317,#84318,#84319,#84320,#84321,#84322,#84323,#84324,#84325,
#84326,#84327,#84328,#84329,#84330,#84331,#84332,#84333,#84334,#84335,#84336,
#84337,#84338,#84339,#84340,#84341,#84342,#84343,#84344,#84345,#84346,#84347,
#84348,#84349,#84350,#84351,#84352,#84353,#84354,#84355,#84356,#84357,#84358,
#84359,#84360,#84361,#84362,#84363,#84364,#84365,#84366,#84367,#84368,#84369,
#84370,#84371,#84372,#84373,#84374,#84375,#84376,#84377,#84378,#84379,#84380,
#84381,#84382,#84383,#84384,#84385,#84386,#84387,#84388,#84389,#84390,#84391,
#84392,#84393,#84394,#84395,#84396,#84397,#84398,#84399,#84400,#84401,#84402,
#84403,#84404,#84405,#84406,#84407,#84408,#84409,#84410,#84411,#84412,#84413,
#84414,#84415,#84416,#84417,#84418,#84419,#84420,#84421,#84422,#84423,#84424,
#84425,#84426,#84427,#84428,#84429,#84430,#84431,#84432,#84433,#84434,#84435,
#84436,#84437,#84438,#84439,#84440,#84441,#84442,#84443,#84444,#84445,#84446,
#84447,#84448,#84449,#84450,#84451,#84452,#84453,#84454,#84455,#84456,#84457,
#84458,#84459,#84460,#84461,#84462,#84463,#84464,#84465,#84466,#84467,#84468,
#84469,#84470,#84471,#84472,#84473,#84474,#84475,#84476,#84477,#84478,#84479,
#84480,#84481,#84482,#84483,#84484,#84485,#84486,#84487,#84488,#84489,#84490,
#84491,#84492,#84493,#84494,#84495,#84496,#84497,#84498,#84499,#84500,#84501,
#84502,#84503,#84504,#84505,#84506,#84507,#84508,#84509,#84510,#84511,#84512,
#84513,#84514,#84515,#84516,#84517,#84518,#84519,#84520,#84521,#84522,#84523,
#84524,#84525,#84526,#84527,#84528,#84529,#84530,#84531,#84532,#84533,#84534,
#84535,#84536,#84537,#84538,#84539,#84540,#84541,#84542,#84543,#84544,#84545,
#84546,#84547,#84548,#84549,#84550,#84551,#84552,#84553,#84554,#84555,#84556,
#84557,#84558,#84559,#84560,#84561,#84562,#84563,#84564,#84565,#84566,#84567,
#84568,#84569,#84570,#84571,#84572,#84573,#84574,#84575,#84576,#84577,#84578,
#84579,#84580,#84581,#84582,#84583,#84584,#84585,#84586,#84587,#84588,#84589,
#84590,#84591,#84592,#84593,#84594,#84595,#84596,#84597,#84598,#84599,#84600,
#84601,#84602,#84603,#84604,#84605,#84606,#84607,#84608,#84609,#84610,#84611,
#84612,#84613,#84614,#84615,#84616,#84617,#84618,#84619,#84620,#84621,#84622,
#84623,#84624,#84625,#84626,#84627,#84628,#84629,#84630,#84631,#84632,#84633,
#84634,#84635,#84636,#84637,#84638,#84639,#84640,#84641,#84642,#84643,#84644,
#84645,#84646,#84647,#84648,#84649,#84650,#84651,#84652,#84653,#84654,#84655,
#84656,#84657,#84658,#84659,#84660,#84661,#84662,#84663,#84664,#84665,#84666,
#84667,#84668,#84669,#84670,#84671,#84672,#84673,#84674,#84675,#84676,#84677,
#84678,#84679,#84680,#84681,#84682,#84683,#84684,#84685,#84686,#84687,#84688,
#84689,#84690,#84691,#84692,#84693,#84694,#84695,#84696,#84697,#84698,#84699,
#84700,#84701,#84702,#84703,#84704,#84705,#84706,#84707,#84708,#84709,#84710,
#84711,#84712,#84713,#84714,#84715,#84716,#84717,#84718,#84719,#84720,#84721,
#84722,#84723,#84724,#84725,#84726,#84727,#84728,#84729,#84730,#84731,#84732,
#84733,#84734,#84735,#84736,#84737,#84738,#84739,#84740,#84741,#84742,#84743,
#84744,#84745,#84746,#84747,#84748,#84749,#84750,#84751,#84752,#84753,#84754,
#84755,#84756,#84757,#84758,#84759,#84760,#84761,#84762,#84763,#84764,#84765,
#84766,#84767,#84768,#84769,#84770,#84771,#84772,#84773,#84774,#84775,#84776,
#84777,#84778,#84779,#84780,#84781,#84782,#84783,#84784,#84785,#84786,#84787,
#84788,#84789,#84790,#84791,#84792,#84793,#84794,#84795,#84796,#84797,#84798,
#84799,#84800,#84801,#84802,#84803,#84804,#84805,#84806,#84807,#84808,#84809,
#84810,#84811,#84812,#84813,#84814,#84815,#84816,#84817,#84818,#84819,#84820,
#84821,#84822,#84823,#84824,#84825,#84826,#84827,#84828,#84829,#84830,#84831,
#84832,#84833,#84834,#84835,#84836,#84837,#84838,#84839,#84840,#84841,#84842,
#84843,#84844,#84845,#84846,#84847,#84848,#84849,#84850,#84851,#84852,#84853,
#84854,#84855,#84856,#84857,#84858,#84859,#84860,#84861,#84862,#84863,#84864,
#84865,#84866,#84867,#84868,#84869,#84870,#84871,#84872,#84873,#84874,#84875,
#84876,#84877,#84878,#84879,#84880,#84881,#84882,#84883,#84884,#84885,#84886,
#84887,#84888,#84889,#84890,#84891,#84892,#84893,#84894,#84895,#84896,#84897,
#84898,#84899,#84900,#84901,#84902,#84903,#84904,#84905,#84906,#84907,#84908,
#84909,#84910,#84911,#84912,#84913,#84914,#84915,#84916,#84917,#84918,#84919,
#84920,#84921,#84922,#84923,#84924,#84925,#84926,#84927,#84928,#84929,#84930,
#84931,#84932,#84933,#84934,#84935,#84936,#84937,#84938,#84939,#84940,#84941,
#84942,#84943,#84944,#84945,#84946,#84947,#84948,#84949,#84950,#84951,#84952,
#84953,#84954,#84955,#84956,#84957,#84958,#84959,#84960,#84961,#84962,#84963,
#84964,#84965,#84966,#84967,#84968,#84969,#84970,#84971,#84972,#84973,#84974,
#84975,#84976,#84977,#84978,#84979,#84980,#84981,#84982,#84983,#84984,#84985,
#84986,#84987,#84988,#84989,#84990,#84991,#84992,#84993,#84994,#84995,#84996,
#84997,#84998,#84999,#85000,#85001,#85002,#85003,#85004,#85005,#85006,#85007,
#85008,#85009,#85010,#85011,#85012,#85013,#85014,#85015,#85016,#85017,#85018,
#85019,#85020,#85021,#85022,#85023,#85024,#85025,#85026,#85027,#85028,#85029,
#85030,#85031,#85032,#85033,#85034,#85035,#85036,#85037,#85038,#85039,#85040,
#85041,#85042,#85043,#85044,#85045,#85046,#85047,#85048,#85049,#85050,#85051,
#85052,#85053,#85054,#85055,#85056,#85057,#85058,#85059,#85060,#85061,#85062,
#85063,#85064,#85065,#85066,#85067,#85068,#85069,#85070,#85071,#85072,#85073,
#85074,#85075,#85076,#85077,#85078,#85079,#85080,#85081,#85082,#85083,#85084,
#85085,#85086,#85087,#85088,#85089,#85090,#85091,#85092,#85093,#85094,#85095,
#85096,#85097,#85098,#85099,#85100,#85101,#85102,#85103,#85104,#85105,#85106,
#85107,#85108,#85109,#85110,#85111,#85112,#85113,#85114,#85115,#85116,#85117,
#85118,#85119,#85120,#85121,#85122,#85123,#85124,#85125,#85126,#85127,#85128,
#85129,#85130,#85131,#85132,#85133,#85134,#85135,#85136,#85137,#85138,#85139,
#85140,#85141,#85142,#85143,#85144,#85145,#85146,#85147,#85148,#85149,#85150,
#85151,#85152,#85153,#85154,#85155,#85156,#85157,#85158,#85159,#85160,#85161,
#85162,#85163,#85164,#85165,#85166,#85167,#85168,#85169,#85170,#85171,#85172,
#85173,#85174,#85175,#85176,#85177,#85178,#85179,#85180,#85181,#85182,#85183,
#85184,#85185,#85186,#85187,#85188,#85189,#85190,#85191,#85192,#85193,#85194,
#85195,#85196,#85197,#85198,#85199,#85200,#85201,#85202,#85203,#85204,#85205,
#85206,#85207,#85208,#85209,#85210,#85211,#85212,#85213,#85214,#85215,#85216,
#85217,#85218,#85219,#85220,#85221,#85222,#85223,#85224,#85225,#85226,#85227,
#85228,#85229,#85230,#85231,#85232,#85233,#85234,#85235,#85236,#85237,#85238,
#85239,#85240,#85241,#85242,#85243,#85244,#85245,#85246,#85247,#85248,#85249,
#85250,#85251,#85252,#85253,#85254,#85255,#85256,#85257,#85258,#85259,#85260,
#85261,#85262,#85263,#85264,#85265,#85266,#85267,#85268,#85269,#85270,#85271,
#85272,#85273,#85274,#85275,#85276,#85277,#85278,#85279,#85280,#85281,#85282,
#85283,#85284,#85285,#85286,#85287,#85288,#85289,#85290,#85291,#85292,#85293,
#85294,#85295,#85296,#85297,#85298,#85299,#85300,#85301,#85302,#85303,#85304,
#85305,#85306,#85307,#85308,#85309,#85310,#85311,#85312,#85313,#85314,#85315,
#85316,#85317,#85318,#85319,#85320,#85321,#85322,#85323,#85324,#85325,#85326,
#85327,#85328,#85329,#85330,#85331,#85332,#85333,#85334,#85335,#85336,#85337,
#85338,#85339,#85340,#85341,#85342,#85343,#85344,#85345,#85346,#85347,#85348,
#85349,#85350,#85351,#85352,#85353,#85354,#85355,#85356,#85357,#85358,#85359,
#85360,#85361,#85362,#85363,#85364,#85365,#85366),#170127) ;
#11 = ITEM_DEFINED_TRANSFORMATION($,$,#91123,#103077) ;
#12 = ITEM_DEFINED_TRANSFORMATION($,$,#93348,#103078) ;
#13 = ITEM_DEFINED_TRANSFORMATION($,$,#98151,#103079) ;
#14 = (
REPRESENTATION_RELATIONSHIP($,$,#170144,#170143)
REPRESENTATION_RELATIONSHIP_WITH_TRANSFORMATION(#11)
SHAPE_REPRESENTATION_RELATIONSHIP()
) ;
#15 = (
REPRESENTATION_RELATIONSHIP($,$,#170145,#170143)
REPRESENTATION_RELATIONSHIP_WITH_TRANSFORMATION(#12)
SHAPE_REPRESENTATION_RELATIONSHIP()
) ;
#16 = (
REPRESENTATION_RELATIONSHIP($,$,#170146,#170143)
REPRESENTATION_RELATIONSHIP_WITH_TRANSFORMATION(#13)
SHAPE_REPRESENTATION_RELATIONSHIP()
) ;
#17 = CONTEXT_DEPENDENT_SHAPE_REPRESENTATION(#14,#170140) ;
#18 = CONTEXT_DEPENDENT_SHAPE_REPRESENTATION(#15,#170141) ;
#19 = CONTEXT_DEPENDENT_SHAPE_REPRESENTATION(#16,#170142) ;
#20 = NEXT_ASSEMBLY_USAGE_OCCURRENCE('Pin_Header_Plug:1',
'Pin_Header_Plug:1','Pin_Header_Plug:1',#170148,#170149,
'Pin_Header_Plug:1') ;
#21 = NEXT_ASSEMBLY_USAGE_OCCURRENCE('Terminal_Block_Header:1',
'Terminal_Block_Header:1','Terminal_Block_Header:1',#170148,#170150,
'Terminal_Block_Header:1') ;
#22 = NEXT_ASSEMBLY_USAGE_OCCURRENCE('Terminal_Block_Plug:1',
'Terminal_Block_Plug:1','Terminal_Block_Plug:1',#170148,#170151,
'Terminal_Block_Plug:1') ;
#23 = SHAPE_REPRESENTATION_RELATIONSHIP('SRR','None',#170144,#26) ;
#24 = SHAPE_REPRESENTATION_RELATIONSHIP('SRR','None',#170145,#27) ;
#25 = SHAPE_REPRESENTATION_RELATIONSHIP('SRR','None',#170146,#28) ;
#26 = ADVANCED_BREP_SHAPE_REPRESENTATION('',(#29,#30,#31),#170124) ;
#27 = ADVANCED_BREP_SHAPE_REPRESENTATION('',(#32),#170125) ;
#28 = ADVANCED_BREP_SHAPE_REPRESENTATION('',(#33),#170126) ;
#29 = MANIFOLD_SOLID_BREP('Body1',#91083) ;
#30 = MANIFOLD_SOLID_BREP('Body2',#91084) ;
#31 = MANIFOLD_SOLID_BREP('Body3',#91085) ;
#32 = MANIFOLD_SOLID_BREP('Body1',#91086) ;
#33 = MANIFOLD_SOLID_BREP('Body1',#91087) ;
#34 = (
BOUNDED_SURFACE()
B_SPLINE_SURFACE(3,2,((#133940,#133941,#133942),(#133943,#133944,#133945),
(#133946,#133947,#133948),(#133949,#133950,#133951),(#133952,#133953,#133954),
(#133955,#133956,#133957)),.UNSPECIFIED.,.F.,.F.,.F.)
B_SPLINE_SURFACE_WITH_KNOTS((4,2,4),(3,3),(3.14159265358979,3.92699081698724,
4.71238898038469),(0.,1.),.UNSPECIFIED.)
GEOMETRIC_REPRESENTATION_ITEM()
RATIONAL_B_SPLINE_SURFACE(((1.,0.934721701546417,1.),(1.,0.934869636336921,
1.),(1.,0.913780519322362,1.),(1.,0.83464631504231,1.),(1.,0.776518516961033,
1.),(1.,0.707106781186548,1.)))
REPRESENTATION_ITEM('')
SURFACE()
) ;
#35 = (
BOUNDED_SURFACE()
B_SPLINE_SURFACE(3,2,((#133968,#133969,#133970),(#133971,#133972,#133973),
(#133974,#133975,#133976),(#133977,#133978,#133979)),.UNSPECIFIED.,.F.,
 .F.,.F.)
B_SPLINE_SURFACE_WITH_KNOTS((4,4),(3,3),(1.5707963267949,2.41495031290807),
(0.,1.),.UNSPECIFIED.)
GEOMETRIC_REPRESENTATION_ITEM()
RATIONAL_B_SPLINE_SURFACE(((1.,0.707106781186547,1.),(1.,0.730803471035897,
1.),(1.,0.752906082887246,1.),(1.,0.76729220397862,1.)))
REPRESENTATION_ITEM('')
SURFACE()
) ;
#36 = (
BOUNDED_SURFACE()
B_SPLINE_SURFACE(3,2,((#133996,#133997,#133998),(#133999,#134000,#134001),
(#134002,#134003,#134004),(#134005,#134006,#134007),(#134008,#134009,#134010),
(#134011,#134012,#134013)),.UNSPECIFIED.,.F.,.F.,.F.)
B_SPLINE_SURFACE_WITH_KNOTS((4,2,4),(3,3),(1.56955149927804,2.35619449019234,
3.14283748110665),(-0.00124482751686043,1.),.UNSPECIFIED.)
GEOMETRIC_REPRESENTATION_ITEM()
RATIONAL_B_SPLINE_SURFACE(((1.00073060381457,0.70654415785643,1.),(1.00062673753069,
0.748263304672891,1.),(1.00053422463656,0.785422225437728,1.),(1.00040682904418,
0.836592203069559,1.),(1.00037181710676,0.850655170404881,1.),(1.00037229282027,
0.850464094333141,1.)))
REPRESENTATION_ITEM('')
SURFACE()
) ;
#37 = (
BOUNDED_SURFACE()
B_SPLINE_SURFACE(3,2,((#134016,#134017,#134018),(#134019,#134020,#134021),
(#134022,#134023,#134024),(#134025,#134026,#134027),(#134028,#134029,#134030),
(#134031,#134032,#134033)),.UNSPECIFIED.,.F.,.F.,.F.)
B_SPLINE_SURFACE_WITH_KNOTS((4,2,4),(3,3),(4.71238898038469,5.49778714378214,
6.28318530717959),(0.,1.),.UNSPECIFIED.)
GEOMETRIC_REPRESENTATION_ITEM()
RATIONAL_B_SPLINE_SURFACE(((1.,0.707106781186548,1.),(1.,0.776518516961036,
1.),(1.,0.834646315042305,1.),(1.,0.913780519322366,1.),(1.,0.934869636336917,
1.),(1.,0.934721701546417,1.)))
REPRESENTATION_ITEM('')
SURFACE()
) ;
#38 = (
BOUNDED_SURFACE()
B_SPLINE_SURFACE(3,2,((#134041,#134042,#134043),(#134044,#134045,#134046),
(#134047,#134048,#134049),(#134050,#134051,#134052)),.UNSPECIFIED.,.F.,
 .F.,.F.)
B_SPLINE_SURFACE_WITH_KNOTS((4,4),(3,3),(0.726642340681724,1.5707963267949),
(0.,1.),.UNSPECIFIED.)
GEOMETRIC_REPRESENTATION_ITEM()
RATIONAL_B_SPLINE_SURFACE(((1.,0.76729220397862,1.),(1.,0.752906082887247,
1.),(1.,0.730803471035896,1.),(1.,0.707106781186548,1.)))
REPRESENTATION_ITEM('')
SURFACE()
) ;
#39 = (
BOUNDED_SURFACE()
B_SPLINE_SURFACE(3,2,((#134068,#134069,#134070),(#134071,#134072,#134073),
(#134074,#134075,#134076),(#134077,#134078,#134079),(#134080,#134081,#134082),
(#134083,#134084,#134085)),.UNSPECIFIED.,.F.,.F.,.F.)
B_SPLINE_SURFACE_WITH_KNOTS((4,2,4),(3,3),(-0.00124482751684684,0.785398163397448,
1.57204115431174),(-0.00124482751684684,1.),.UNSPECIFIED.)
GEOMETRIC_REPRESENTATION_ITEM()
RATIONAL_B_SPLINE_SURFACE(((1.00037229282026,0.850464094333143,1.),(1.00037181710676,
0.850655170404876,1.),(1.00040682904417,0.83659220306957,1.),(1.00053422463656,
0.785422225437723,1.),(1.00062673753069,0.748263304672901,1.),(1.00073060381456,
0.706544157856436,1.)))
REPRESENTATION_ITEM('')
SURFACE()
) ;
#40 = (
BOUNDED_SURFACE()
B_SPLINE_SURFACE(3,2,((#134097,#134098,#134099),(#134100,#134101,#134102),
(#134103,#134104,#134105),(#134106,#134107,#134108)),.UNSPECIFIED.,.F.,
 .F.,.F.)
B_SPLINE_SURFACE_WITH_KNOTS((4,4),(3,3),(1.10714871779409,1.5707963267949),
(0.,1.),.UNSPECIFIED.)
GEOMETRIC_REPRESENTATION_ITEM()
RATIONAL_B_SPLINE_SURFACE(((1.,0.743704326447946,1.),(1.,0.73267692820235,
1.),(1.,0.720087778783133,1.),(1.,0.707106781186547,1.)))
REPRESENTATION_ITEM('')
SURFACE()
) ;
#41 = (
BOUNDED_SURFACE()
B_SPLINE_SURFACE(3,2,((#134116,#134117,#134118),(#134119,#134120,#134121),
(#134122,#134123,#134124),(#134125,#134126,#134127)),.UNSPECIFIED.,.F.,
 .F.,.F.)
B_SPLINE_SURFACE_WITH_KNOTS((4,4),(3,3),(1.5707963267949,2.0344439357957),
(0.,1.),.UNSPECIFIED.)
GEOMETRIC_REPRESENTATION_ITEM()
RATIONAL_B_SPLINE_SURFACE(((1.,0.707106781186547,1.),(1.,0.720087778783132,
1.),(1.,0.73267692820235,1.),(1.,0.743704326447946,1.)))
REPRESENTATION_ITEM('')
SURFACE()
) ;
#42 = (
BOUNDED_SURFACE()
B_SPLINE_SURFACE(3,2,((#134402,#134403,#134404),(#134405,#134406,#134407),
(#134408,#134409,#134410),(#134411,#134412,#134413)),.UNSPECIFIED.,.F.,
 .F.,.F.)
B_SPLINE_SURFACE_WITH_KNOTS((4,4),(3,3),(0.000111059871785624,0.00024129664665087),
(0.,1.00030059112233),.UNSPECIFIED.)
GEOMETRIC_REPRESENTATION_ITEM()
RATIONAL_B_SPLINE_SURFACE(((1.,0.839985548969888,1.00009619784685),(1.,
0.797322032917078,1.00012184639519),(1.,0.734686009440384,1.00015950206038),
(1.,0.707018740085181,1.00017613513148)))
REPRESENTATION_ITEM('')
SURFACE()
) ;
#43 = (
BOUNDED_SURFACE()
B_SPLINE_SURFACE(3,2,((#134415,#134416,#134417),(#134418,#134419,#134420),
(#134421,#134422,#134423),(#134424,#134425,#134426)),.UNSPECIFIED.,.F.,
 .F.,.F.)
B_SPLINE_SURFACE_WITH_KNOTS((4,4),(3,3),(3.14159265358979,3.68974201455418),
(0.,1.),.UNSPECIFIED.)
GEOMETRIC_REPRESENTATION_ITEM()
RATIONAL_B_SPLINE_SURFACE(((1.,0.860789971413512,1.),(1.,0.86080954675505,
1.),(1.,0.853709425573778,1.),(1.,0.840033633436872,1.)))
REPRESENTATION_ITEM('')
SURFACE()
) ;
#44 = (
BOUNDED_SURFACE()
B_SPLINE_SURFACE(3,2,((#134432,#134433,#134434),(#134435,#134436,#134437),
(#134438,#134439,#134440),(#134441,#134442,#134443)),.UNSPECIFIED.,.F.,
 .F.,.F.)
B_SPLINE_SURFACE_WITH_KNOTS((4,4),(3,3),(2.59344329260966,3.14159265358979),
(0.,1.),.UNSPECIFIED.)
GEOMETRIC_REPRESENTATION_ITEM()
RATIONAL_B_SPLINE_SURFACE(((1.,0.840033633435697,1.),(1.,0.853709425573365,
1.),(1.,0.860809546755054,1.),(1.,0.860789971413512,1.)))
REPRESENTATION_ITEM('')
SURFACE()
) ;
#45 = (
BOUNDED_SURFACE()
B_SPLINE_SURFACE(3,2,((#134445,#134446,#134447),(#134448,#134449,#134450),
(#134451,#134452,#134453),(#134454,#134455,#134456)),.UNSPECIFIED.,.F.,
 .F.,.F.)
B_SPLINE_SURFACE_WITH_KNOTS((4,4),(3,3),(0.000111059871788868,0.00024129664665087),
(-0.000300086749770041,1.),.UNSPECIFIED.)
GEOMETRIC_REPRESENTATION_ITEM()
RATIONAL_B_SPLINE_SURFACE(((1.00009603638463,0.839985629649273,1.),(1.00012164188345,
0.797322135108583,1.),(1.0001592343459,0.734686143216499,1.),(1.0001758394994,
0.707018887812483,1.)))
REPRESENTATION_ITEM('')
SURFACE()
) ;
#46 = (
BOUNDED_SURFACE()
B_SPLINE_SURFACE(3,2,((#134540,#134541,#134542),(#134543,#134544,#134545),
(#134546,#134547,#134548),(#134549,#134550,#134551),(#134552,#134553,#134554),
(#134555,#134556,#134557),(#134558,#134559,#134560),(#134561,#134562,#134563),
(#134564,#134565,#134566),(#134567,#134568,#134569)),.UNSPECIFIED.,.F.,
 .F.,.F.)
B_SPLINE_SURFACE_WITH_KNOTS((4,2,2,2,4),(3,3),(0.00112100122803332,0.00145633576709043,
0.0015908372445872,0.00165808798333558,0.00178849406635728),(-0.000893324189270442,
1.00101552458207),.UNSPECIFIED.)
GEOMETRIC_REPRESENTATION_ITEM()
RATIONAL_B_SPLINE_SURFACE(((1.00061830890916,0.653576280075622,1.00070297498515),
(1.00045188087569,0.746821933830033,1.00051375768191),(1.00032243686652,
0.819346321742885,1.00036658868746),(1.00017052538066,0.904458700444864,
1.00019387570704),(1.00013074576008,0.926746272131238,1.0001486489963),
(1.00007983643892,0.955269549338581,1.0000907685764),(1.00006394848111,
0.964171192776746,1.00007270505389),(1.00002748579919,0.98460036292333,
1.00003124947579),(1.00001632684003,0.990852461324379,1.00001856250163),
(1.00006581963707,0.963122828765907,1.00007483243037)))
REPRESENTATION_ITEM('')
SURFACE()
) ;
#47 = (
BOUNDED_SURFACE()
B_SPLINE_SURFACE(3,2,((#134611,#134612,#134613),(#134614,#134615,#134616),
(#134617,#134618,#134619),(#134620,#134621,#134622),(#134623,#134624,#134625),
(#134626,#134627,#134628),(#134629,#134630,#134631),(#134632,#134633,#134634),
(#134635,#134636,#134637),(#134638,#134639,#134640)),.UNSPECIFIED.,.F.,
 .F.,.F.)
B_SPLINE_SURFACE_WITH_KNOTS((4,2,2,2,4),(3,3),(0.00112100122803331,0.00145633576709043,
0.00159083724458721,0.00165808798333559,0.00178849406635727),(-0.00113559264167203,
1.),.UNSPECIFIED.)
GEOMETRIC_REPRESENTATION_ITEM()
RATIONAL_B_SPLINE_SURFACE(((1.0007861837978,0.65384427084655,1.),(1.00057456947123,
0.747017790468101,1.),(1.00040998057203,0.819486074062728,1.),(1.00021682413014,
0.904532610471948,1.),(1.00016624408395,0.926802940661382,1.),(1.00010151255112,
0.955304152477056,1.),(1.00008131090948,0.964198909671164,1.),(1.00003494837236,
0.984612275966157,1.),(1.00002075968326,0.990859537791147,1.),(1.00008369009644,
0.963151356666802,0.999999999999999)))
REPRESENTATION_ITEM('')
SURFACE()
) ;
#48 = (
BOUNDED_SURFACE()
B_SPLINE_SURFACE(3,2,((#134677,#134678,#134679),(#134680,#134681,#134682),
(#134683,#134684,#134685),(#134686,#134687,#134688),(#134689,#134690,#134691),
(#134692,#134693,#134694),(#134695,#134696,#134697),(#134698,#134699,#134700),
(#134701,#134702,#134703),(#134704,#134705,#134706),(#134707,#134708,#134709),
(#134710,#134711,#134712),(#134713,#134714,#134715),(#134716,#134717,#134718),
(#134719,#134720,#134721),(#134722,#134723,#134724)),.UNSPECIFIED.,.F.,
 .F.,.F.)
B_SPLINE_SURFACE_WITH_KNOTS((4,2,2,2,2,2,2,4),(3,3),(5.62831031780675E-15,
3.85995771599554E-5,5.7899365737119E-5,6.75492600257008E-5,7.23742071699917E-5,
7.47866807421371E-5,7.59929175282099E-5,7.71991543142826E-5),(0.,1.00107899067816),
 .UNSPECIFIED.)
GEOMETRIC_REPRESENTATION_ITEM()
RATIONAL_B_SPLINE_SURFACE(((1.,0.976255617118809,1.00005123993557),(1.,
0.981339981891257,1.00004026797119),(1.,0.986086237829177,1.00003002563936),
(1.,0.992269463037034,1.00001668235464),(1.,0.994174411180039,1.00001257151206),
(1.,0.996706913506704,1.00000710641926),(1.,0.997492596832092,1.00000541092929),
(1.,0.998537621803389,1.00000315578488),(1.,0.998865045809511,1.00000244920998),
(1.,0.999323526852931,1.00000145981644),(1.,0.999468419970869,1.00000114713979),
(1.,0.99959844684718,1.00000086654422),(1.,0.999614491362717,1.00000083192045),
(1.,0.999732489024762,1.0000005772837),(1.,0.999724369239699,1.00000059480604),
(1.,1.,1.)))
REPRESENTATION_ITEM('')
SURFACE()
) ;
#49 = (
BOUNDED_SURFACE()
B_SPLINE_SURFACE(3,2,((#134726,#134727,#134728),(#134729,#134730,#134731),
(#134732,#134733,#134734),(#134735,#134736,#134737),(#134738,#134739,#134740),
(#134741,#134742,#134743),(#134744,#134745,#134746),(#134747,#134748,#134749),
(#134750,#134751,#134752),(#134753,#134754,#134755)),.UNSPECIFIED.,.F.,
 .F.,.F.)
B_SPLINE_SURFACE_WITH_KNOTS((4,2,2,2,4),(3,3),(-0.000110707928511331,0.000553539642556654,
0.000830309463834981,0.000968694374474144,0.00121778721363011),(0.,1.00563383762696),
 .UNSPECIFIED.)
GEOMETRIC_REPRESENTATION_ITEM()
RATIONAL_B_SPLINE_SURFACE(((1.,0.710139408519195,1.00326605501372),(1.,
0.691948125896918,1.00347102847876),(1.,0.728232377173825,1.00306218931854),
(1.,0.818030374423679,1.00205037464707),(1.,0.849110759469254,1.00170017096161),
(1.,0.897979778369935,1.00114953072666),(1.,0.914666724297516,1.00096150763897),
(1.,0.961090538823392,1.00043841917284),(1.,0.990973799041213,1.00010170430118),
(1.,0.9924634551618,1.00008491933977)))
REPRESENTATION_ITEM('')
SURFACE()
) ;
#50 = (
BOUNDED_SURFACE()
B_SPLINE_SURFACE(3,2,((#134757,#134758,#134759),(#134760,#134761,#134762),
(#134763,#134764,#134765),(#134766,#134767,#134768),(#134769,#134770,#134771),
(#134772,#134773,#134774),(#134775,#134776,#134777),(#134778,#134779,#134780),
(#134781,#134782,#134783),(#134784,#134785,#134786)),.UNSPECIFIED.,.F.,
 .F.,.F.)
B_SPLINE_SURFACE_WITH_KNOTS((4,2,2,2,4),(3,3),(-0.000137915648493858,0.000139027965246065,
0.000278055930499747,0.00055611186100711,0.00125013859505181),(-0.000741678185408241,
1.00283457365794),.UNSPECIFIED.)
GEOMETRIC_REPRESENTATION_ITEM()
RATIONAL_B_SPLINE_SURFACE(((1.00001340810331,0.990935328833035,1.00005135076282),
(1.00000300543757,0.997968146378466,1.00001151031642),(1.00005311279897,
0.964092605306839,1.00020341301682),(1.00012590576281,0.914880254704014,
1.00048219772916),(1.00015093966337,0.897955856705928,1.00057807332481),
(1.00022375355351,0.84872935869733,1.00085693818127),(1.00026920263019,
0.818003093714666,1.00103100044084),(1.00040494517418,0.726233102310977,
1.0015508713745),(1.00045889592378,0.689759203409617,1.00175749360019),
(1.00042429005305,0.71315481959354,1.00162495898138)))
REPRESENTATION_ITEM('')
SURFACE()
) ;
#51 = (
BOUNDED_SURFACE()
B_SPLINE_SURFACE(3,2,((#134788,#134789,#134790),(#134791,#134792,#134793),
(#134794,#134795,#134796),(#134797,#134798,#134799),(#134800,#134801,#134802),
(#134803,#134804,#134805),(#134806,#134807,#134808),(#134809,#134810,#134811),
(#134812,#134813,#134814),(#134815,#134816,#134817),(#134818,#134819,#134820),
(#134821,#134822,#134823),(#134824,#134825,#134826),(#134827,#134828,#134829),
(#134830,#134831,#134832),(#134833,#134834,#134835)),.UNSPECIFIED.,.F.,
 .F.,.F.)
B_SPLINE_SURFACE_WITH_KNOTS((4,2,2,2,2,2,2,4),(3,3),(7.77892019462184E-15,
3.88447601478312E-5,5.82671402178573E-5,6.79783302528704E-5,7.28339252703769E-5,
7.52617227791302E-5,7.64756215335068E-5,7.76895202878834E-5),(-0.00120945525754678,
1.01080070868962),.UNSPECIFIED.)
GEOMETRIC_REPRESENTATION_ITEM()
RATIONAL_B_SPLINE_SURFACE(((1.00005744302265,0.975995723233526,1.00051789333956),
(1.00004519813151,0.981112615457369,1.0004074961621),(1.00003362760161,
0.985947705765597,1.00030317887351),(1.00001854219783,0.992251590743247,
1.00016717227456),(1.00001393966879,0.994174894491123,1.0001256769106),
(1.00000788875349,0.996703449551652,1.00007112322264),(1.00000601414708,
0.997486809637524,1.00005422219392),(1.00000351698944,0.998530321282699,
1.00003170838373),(1.00000273459082,0.998857269833632,1.0000246544542),
(1.00000163903614,0.999315079966001,1.00001477718022),(1.00000129000885,
0.999460931405222,1.00001163042892),(1.0000009745592,0.999592751431242,
1.000008786406),(1.00000093560708,0.99960902873406,1.00000843522246),(1.00000065019919,
0.999728294915416,1.00000586204929),(1.00000066918571,0.99972036083143,
1.00000603322751),(1.,1.,1.)))
REPRESENTATION_ITEM('')
SURFACE()
) ;
#52 = (
BOUNDED_SURFACE()
B_SPLINE_SURFACE(3,2,((#135308,#135309,#135310),(#135311,#135312,#135313),
(#135314,#135315,#135316),(#135317,#135318,#135319),(#135320,#135321,#135322),
(#135323,#135324,#135325)),.UNSPECIFIED.,.F.,.F.,.F.)
B_SPLINE_SURFACE_WITH_KNOTS((4,2,4),(3,3),(3.14159265358979,3.92699081698724,
4.71238898038469),(0.,1.),.UNSPECIFIED.)
GEOMETRIC_REPRESENTATION_ITEM()
RATIONAL_B_SPLINE_SURFACE(((1.,0.934721701546417,1.),(1.,0.934869636336909,
1.),(1.,0.913780519322377,1.),(1.,0.834646315042295,1.),(1.,0.776518516961044,
1.),(1.,0.707106781186548,1.)))
REPRESENTATION_ITEM('')
SURFACE()
) ;
#53 = (
BOUNDED_SURFACE()
B_SPLINE_SURFACE(3,2,((#135336,#135337,#135338),(#135339,#135340,#135341),
(#135342,#135343,#135344),(#135345,#135346,#135347)),.UNSPECIFIED.,.F.,
 .F.,.F.)
B_SPLINE_SURFACE_WITH_KNOTS((4,4),(3,3),(1.5707963267949,2.41495031290807),
(0.,1.),.UNSPECIFIED.)
GEOMETRIC_REPRESENTATION_ITEM()
RATIONAL_B_SPLINE_SURFACE(((1.,0.707106781186547,1.),(1.,0.730803471035898,
1.),(1.,0.752906082887245,1.),(1.,0.76729220397862,1.)))
REPRESENTATION_ITEM('')
SURFACE()
) ;
#54 = (
BOUNDED_SURFACE()
B_SPLINE_SURFACE(3,2,((#135364,#135365,#135366),(#135367,#135368,#135369),
(#135370,#135371,#135372),(#135373,#135374,#135375),(#135376,#135377,#135378),
(#135379,#135380,#135381)),.UNSPECIFIED.,.F.,.F.,.F.)
B_SPLINE_SURFACE_WITH_KNOTS((4,2,4),(3,3),(1.5695514992781,2.35619449019234,
3.14283748110659),(-0.00124482751679711,1.),.UNSPECIFIED.)
GEOMETRIC_REPRESENTATION_ITEM()
RATIONAL_B_SPLINE_SURFACE(((1.00073060381453,0.706544157856458,1.),(1.00062673753066,
0.748263304672962,1.),(1.00053422463654,0.785422225437678,1.),(1.00040682904416,
0.836592203069638,1.),(1.00037181710674,0.850655170404834,1.),(1.00037229282025,
0.850464094333151,1.)))
REPRESENTATION_ITEM('')
SURFACE()
) ;
#55 = (
BOUNDED_SURFACE()
B_SPLINE_SURFACE(3,2,((#135384,#135385,#135386),(#135387,#135388,#135389),
(#135390,#135391,#135392),(#135393,#135394,#135395),(#135396,#135397,#135398),
(#135399,#135400,#135401)),.UNSPECIFIED.,.F.,.F.,.F.)
B_SPLINE_SURFACE_WITH_KNOTS((4,2,4),(3,3),(4.71238898038469,5.49778714378214,
6.28318530717959),(0.,1.),.UNSPECIFIED.)
GEOMETRIC_REPRESENTATION_ITEM()
RATIONAL_B_SPLINE_SURFACE(((1.,0.707106781186548,1.),(1.,0.776518516961043,
1.),(1.,0.834646315042294,1.),(1.,0.913780519322378,1.),(1.,0.934869636336909,
1.),(1.,0.934721701546417,1.)))
REPRESENTATION_ITEM('')
SURFACE()
) ;
#56 = (
BOUNDED_SURFACE()
B_SPLINE_SURFACE(3,2,((#135409,#135410,#135411),(#135412,#135413,#135414),
(#135415,#135416,#135417),(#135418,#135419,#135420)),.UNSPECIFIED.,.F.,
 .F.,.F.)
B_SPLINE_SURFACE_WITH_KNOTS((4,4),(3,3),(0.726642340681723,1.5707963267949),
(0.,1.),.UNSPECIFIED.)
GEOMETRIC_REPRESENTATION_ITEM()
RATIONAL_B_SPLINE_SURFACE(((1.,0.767292203978618,1.),(1.,0.752906082887251,
1.),(1.,0.730803471035892,1.),(1.,0.70710678118655,1.)))
REPRESENTATION_ITEM('')
SURFACE()
) ;
#57 = (
BOUNDED_SURFACE()
B_SPLINE_SURFACE(3,2,((#135436,#135437,#135438),(#135439,#135440,#135441),
(#135442,#135443,#135444),(#135445,#135446,#135447),(#135448,#135449,#135450),
(#135451,#135452,#135453)),.UNSPECIFIED.,.F.,.F.,.F.)
B_SPLINE_SURFACE_WITH_KNOTS((4,2,4),(3,3),(-0.00124482751677724,0.785398163397448,
1.57204115431167),(-0.00124482751677724,1.),.UNSPECIFIED.)
GEOMETRIC_REPRESENTATION_ITEM()
RATIONAL_B_SPLINE_SURFACE(((1.00037229282024,0.850464094333154,1.),(1.00037181710674,
0.850655170404788,1.),(1.00040682904415,0.836592203069706,1.),(1.00053422463653,
0.785422225437613,1.),(1.00062673753065,0.748263304673021,1.),(1.00073060381452,
0.706544157856467,1.)))
REPRESENTATION_ITEM('')
SURFACE()
) ;
#58 = (
BOUNDED_SURFACE()
B_SPLINE_SURFACE(3,2,((#135465,#135466,#135467),(#135468,#135469,#135470),
(#135471,#135472,#135473),(#135474,#135475,#135476)),.UNSPECIFIED.,.F.,
 .F.,.F.)
B_SPLINE_SURFACE_WITH_KNOTS((4,4),(3,3),(1.10714871779409,1.5707963267949),
(0.,1.),.UNSPECIFIED.)
GEOMETRIC_REPRESENTATION_ITEM()
RATIONAL_B_SPLINE_SURFACE(((1.,0.743704326447947,1.),(1.,0.732676928202351,
1.),(1.,0.720087778783133,1.),(1.,0.707106781186548,1.)))
REPRESENTATION_ITEM('')
SURFACE()
) ;
#59 = (
BOUNDED_SURFACE()
B_SPLINE_SURFACE(3,2,((#135484,#135485,#135486),(#135487,#135488,#135489),
(#135490,#135491,#135492),(#135493,#135494,#135495)),.UNSPECIFIED.,.F.,
 .F.,.F.)
B_SPLINE_SURFACE_WITH_KNOTS((4,4),(3,3),(1.5707963267949,2.0344439357957),
(0.,1.),.UNSPECIFIED.)
GEOMETRIC_REPRESENTATION_ITEM()
RATIONAL_B_SPLINE_SURFACE(((1.,0.707106781186548,1.),(1.,0.720087778783135,
1.),(1.,0.732676928202346,1.),(1.,0.74370432644795,1.)))
REPRESENTATION_ITEM('')
SURFACE()
) ;
#60 = (
BOUNDED_SURFACE()
B_SPLINE_SURFACE(3,2,((#135745,#135746,#135747),(#135748,#135749,#135750),
(#135751,#135752,#135753),(#135754,#135755,#135756)),.UNSPECIFIED.,.F.,
 .F.,.F.)
B_SPLINE_SURFACE_WITH_KNOTS((4,4),(3,3),(0.000111059871785624,0.00024129664665087),
(0.,1.00030059112235),.UNSPECIFIED.)
GEOMETRIC_REPRESENTATION_ITEM()
RATIONAL_B_SPLINE_SURFACE(((1.,0.839985548969885,1.00009619784685),(1.,
0.797322032917072,1.0001218463952),(1.,0.734686009440383,1.00015950206039),
(1.,0.707018740085174,1.00017613513149)))
REPRESENTATION_ITEM('')
SURFACE()
) ;
#61 = (
BOUNDED_SURFACE()
B_SPLINE_SURFACE(3,2,((#135758,#135759,#135760),(#135761,#135762,#135763),
(#135764,#135765,#135766),(#135767,#135768,#135769)),.UNSPECIFIED.,.F.,
 .F.,.F.)
B_SPLINE_SURFACE_WITH_KNOTS((4,4),(3,3),(3.14159265358979,3.68974201455419),
(0.,1.),.UNSPECIFIED.)
GEOMETRIC_REPRESENTATION_ITEM()
RATIONAL_B_SPLINE_SURFACE(((1.,0.860789971413512,1.),(1.,0.860809546755051,
1.),(1.,0.853709425573777,1.),(1.,0.840033633436872,1.)))
REPRESENTATION_ITEM('')
SURFACE()
) ;
#62 = (
BOUNDED_SURFACE()
B_SPLINE_SURFACE(3,2,((#135772,#135773,#135774),(#135775,#135776,#135777),
(#135778,#135779,#135780),(#135781,#135782,#135783)),.UNSPECIFIED.,.F.,
 .F.,.F.)
B_SPLINE_SURFACE_WITH_KNOTS((4,4),(3,3),(2.59344329260966,3.14159265358979),
(0.,1.),.UNSPECIFIED.)
GEOMETRIC_REPRESENTATION_ITEM()
RATIONAL_B_SPLINE_SURFACE(((1.,0.840033633435696,1.),(1.,0.853709425573366,
1.),(1.,0.860809546755054,1.),(1.,0.860789971413512,1.)))
REPRESENTATION_ITEM('')
SURFACE()
) ;
#63 = (
BOUNDED_SURFACE()
B_SPLINE_SURFACE(3,2,((#135785,#135786,#135787),(#135788,#135789,#135790),
(#135791,#135792,#135793),(#135794,#135795,#135796)),.UNSPECIFIED.,.F.,
 .F.,.F.)
B_SPLINE_SURFACE_WITH_KNOTS((4,4),(3,3),(0.000111059871788867,0.00024129664665087),
(-0.000300086749674745,1.),.UNSPECIFIED.)
GEOMETRIC_REPRESENTATION_ITEM()
RATIONAL_B_SPLINE_SURFACE(((1.0000960363846,0.839985629649289,1.),(1.00012164188341,
0.797322135108605,1.),(1.00015923434585,0.734686143216524,1.),(1.00017583949934,
0.707018887812511,1.)))
REPRESENTATION_ITEM('')
SURFACE()
) ;
#64 = (
BOUNDED_SURFACE()
B_SPLINE_SURFACE(3,2,((#135878,#135879,#135880),(#135881,#135882,#135883),
(#135884,#135885,#135886),(#135887,#135888,#135889),(#135890,#135891,#135892),
(#135893,#135894,#135895),(#135896,#135897,#135898),(#135899,#135900,#135901),
(#135902,#135903,#135904),(#135905,#135906,#135907)),.UNSPECIFIED.,.F.,
 .F.,.F.)
B_SPLINE_SURFACE_WITH_KNOTS((4,2,2,2,4),(3,3),(0.00112100122803333,0.00145633576709043,
0.0015908372445872,0.00165808798333558,0.00178849406635727),(-0.000893324189226138,
1.00101552458159),.UNSPECIFIED.)
GEOMETRIC_REPRESENTATION_ITEM()
RATIONAL_B_SPLINE_SURFACE(((1.00061830890913,0.653576280075824,1.00070297498481),
(1.00045188087567,0.746821933830164,1.00051375768166),(1.0003224368665,
0.819346321742989,1.00036658868727),(1.00017052538065,0.904458700444912,
1.00019387570695),(1.00013074576007,0.926746272131305,1.00014864899623),
(1.00007983643891,0.955269549338591,1.00009076857636),(1.00006394848111,
0.964171192776766,1.00007270505385),(1.00002748579919,0.984600362923336,
1.00003124947577),(1.00001632684003,0.99085246132439,1.00001856250162),
(1.00006581963707,0.963122828765912,1.00007483243033)))
REPRESENTATION_ITEM('')
SURFACE()
) ;
#65 = (
BOUNDED_SURFACE()
B_SPLINE_SURFACE(3,2,((#135948,#135949,#135950),(#135951,#135952,#135953),
(#135954,#135955,#135956),(#135957,#135958,#135959),(#135960,#135961,#135962),
(#135963,#135964,#135965),(#135966,#135967,#135968),(#135969,#135970,#135971),
(#135972,#135973,#135974),(#135975,#135976,#135977)),.UNSPECIFIED.,.F.,
 .F.,.F.)
B_SPLINE_SURFACE_WITH_KNOTS((4,2,2,2,4),(3,3),(0.00112100122803332,0.00145633576709043,
0.00159083724458721,0.00165808798333559,0.00178849406635728),(-0.00113559264173565,
1.),.UNSPECIFIED.)
GEOMETRIC_REPRESENTATION_ITEM()
RATIONAL_B_SPLINE_SURFACE(((1.00078618379784,0.653844270846546,1.),(1.00057456947127,
0.747017790468067,1.),(1.00040998057205,0.819486074062731,1.),(1.00021682413015,
0.904532610471937,1.),(1.00016624408396,0.926802940661352,1.),(1.00010151255113,
0.955304152477066,1.),(1.00008131090949,0.964198909671163,1.),(1.00003494837236,
0.984612275966154,1.),(1.00002075968326,0.990859537791153,1.),(1.00008369009645,
0.963151356666784,1.)))
REPRESENTATION_ITEM('')
SURFACE()
) ;
#66 = (
BOUNDED_SURFACE()
B_SPLINE_SURFACE(3,2,((#136014,#136015,#136016),(#136017,#136018,#136019),
(#136020,#136021,#136022),(#136023,#136024,#136025),(#136026,#136027,#136028),
(#136029,#136030,#136031),(#136032,#136033,#136034),(#136035,#136036,#136037),
(#136038,#136039,#136040),(#136041,#136042,#136043),(#136044,#136045,#136046),
(#136047,#136048,#136049),(#136050,#136051,#136052),(#136053,#136054,#136055),
(#136056,#136057,#136058),(#136059,#136060,#136061)),.UNSPECIFIED.,.F.,
 .F.,.F.)
B_SPLINE_SURFACE_WITH_KNOTS((4,2,2,2,2,2,2,4),(3,3),(5.62805281979079E-15,
3.85995771599553E-5,5.7899365737119E-5,6.75492600257008E-5,7.23742071699917E-5,
7.47866807421372E-5,7.59929175282099E-5,7.71991543142826E-5),(0.,1.00107899067844),
 .UNSPECIFIED.)
GEOMETRIC_REPRESENTATION_ITEM()
RATIONAL_B_SPLINE_SURFACE(((1.,0.976255617118803,1.00005123993559),(1.,
0.981339981891199,1.0000402679712),(1.,0.986086237829182,1.00003002563937),
(1.,0.992269463037027,1.00001668235464),(1.,0.994174411180035,1.00001257151207),
(1.,0.996706913506705,1.00000710641926),(1.,0.997492596832093,1.00000541092929),
(1.,0.998537621803387,1.00000315578488),(1.,0.998865045809509,1.00000244920998),
(1.,0.999323526852929,1.00000145981644),(1.,0.999468419970868,1.00000114713979),
(1.,0.999598446847179,1.00000086654422),(1.,0.999614491362717,1.00000083192045),
(1.,0.999732489024762,1.0000005772837),(1.,0.999724369239699,1.00000059480604),
(1.,1.,1.)))
REPRESENTATION_ITEM('')
SURFACE()
) ;
#67 = (
BOUNDED_SURFACE()
B_SPLINE_SURFACE(3,2,((#136063,#136064,#136065),(#136066,#136067,#136068),
(#136069,#136070,#136071),(#136072,#136073,#136074),(#136075,#136076,#136077),
(#136078,#136079,#136080),(#136081,#136082,#136083),(#136084,#136085,#136086),
(#136087,#136088,#136089),(#136090,#136091,#136092)),.UNSPECIFIED.,.F.,
 .F.,.F.)
B_SPLINE_SURFACE_WITH_KNOTS((4,2,2,2,4),(3,3),(-0.000110707928511331,0.000553539642556654,
0.000830309463834981,0.000968694374474145,0.00121778721363011),(0.,1.00563383762722),
 .UNSPECIFIED.)
GEOMETRIC_REPRESENTATION_ITEM()
RATIONAL_B_SPLINE_SURFACE(((1.,0.710139408519121,1.00326605501387),(1.,
0.691948125896839,1.00347102847892),(1.,0.728232377173756,1.00306218931868),
(1.,0.818030374423633,1.00205037464717),(1.,0.849110759469252,1.00170017096169),
(1.,0.897979778369892,1.00114953072671),(1.,0.914666724297501,1.00096150763901),
(1.,0.961090538823375,1.00043841917286),(1.,0.990973799041227,1.00010170430118),
(1.,0.992463455161771,1.00008491933978)))
REPRESENTATION_ITEM('')
SURFACE()
) ;
#68 = (
BOUNDED_SURFACE()
B_SPLINE_SURFACE(3,2,((#136094,#136095,#136096),(#136097,#136098,#136099),
(#136100,#136101,#136102),(#136103,#136104,#136105),(#136106,#136107,#136108),
(#136109,#136110,#136111),(#136112,#136113,#136114),(#136115,#136116,#136117),
(#136118,#136119,#136120),(#136121,#136122,#136123)),.UNSPECIFIED.,.F.,
 .F.,.F.)
B_SPLINE_SURFACE_WITH_KNOTS((4,2,2,2,4),(3,3),(-0.000137915648493859,0.000139027965246065,
0.000278055930499747,0.000556111861007111,0.00125013859505181),(-0.000741678185857755,
1.00283457365566),.UNSPECIFIED.)
GEOMETRIC_REPRESENTATION_ITEM()
RATIONAL_B_SPLINE_SURFACE(((1.00001340810332,0.990935328833157,1.00005135076278),
(1.00000300543756,0.997968146378419,1.00001151031642),(1.00005311279899,
0.96409260530692,1.00020341301665),(1.00012590576288,0.914880254704161,
1.00048219772877),(1.00015093966347,0.897955856706116,1.00057807332434),
(1.00022375355364,0.8487293586976,1.00085693818058),(1.00026920263035,0.818003093714992,
1.00103100044001),(1.00040494517442,0.726233102311489,1.00155087137326),
(1.00045889592406,0.689759203410164,1.00175749359878),(1.0004242900533,
0.713154819594072,1.00162495898007)))
REPRESENTATION_ITEM('')
SURFACE()
) ;
#69 = (
BOUNDED_SURFACE()
B_SPLINE_SURFACE(3,2,((#136125,#136126,#136127),(#136128,#136129,#136130),
(#136131,#136132,#136133),(#136134,#136135,#136136),(#136137,#136138,#136139),
(#136140,#136141,#136142),(#136143,#136144,#136145),(#136146,#136147,#136148),
(#136149,#136150,#136151),(#136152,#136153,#136154),(#136155,#136156,#136157),
(#136158,#136159,#136160),(#136161,#136162,#136163),(#136164,#136165,#136166),
(#136167,#136168,#136169),(#136170,#136171,#136172)),.UNSPECIFIED.,.F.,
 .F.,.F.)
B_SPLINE_SURFACE_WITH_KNOTS((4,2,2,2,2,2,2,4),(3,3),(7.77840519858991E-15,
3.8844760147831E-5,5.82671402178573E-5,6.79783302528705E-5,7.28339252703771E-5,
7.52617227791304E-5,7.6475621533507E-5,7.76895202878836E-5),(-0.00120945525754052,
1.01080070868977),.UNSPECIFIED.)
GEOMETRIC_REPRESENTATION_ITEM()
RATIONAL_B_SPLINE_SURFACE(((1.00005744302265,0.975995723233522,1.00051789333957),
(1.00004519813151,0.981112615457372,1.0004074961621),(1.00003362760161,
0.985947705765589,1.00030317887352),(1.00001854219783,0.992251590743248,
1.00016717227456),(1.00001393966879,0.994174894491119,1.0001256769106),
(1.00000788875349,0.996703449551654,1.00007112322264),(1.00000601414708,
0.997486809637525,1.00005422219392),(1.00000351698944,0.9985303212827,1.00003170838373),
(1.00000273459082,0.998857269833632,1.0000246544542),(1.00000163903614,
0.999315079965995,1.00001477718022),(1.00000129000885,0.999460931405222,
1.00001163042892),(1.0000009745592,0.999592751431241,1.000008786406),(1.00000093560708,
0.999609028734061,1.00000843522246),(1.00000065019919,0.999728294915418,
1.00000586204929),(1.00000066918571,0.999720360831427,1.00000603322751),
(1.,1.,1.)))
REPRESENTATION_ITEM('')
SURFACE()
) ;
#70 = (
BOUNDED_SURFACE()
B_SPLINE_SURFACE(3,2,((#136214,#136215,#136216),(#136217,#136218,#136219),
(#136220,#136221,#136222),(#136223,#136224,#136225)),.UNSPECIFIED.,.F.,
 .F.,.F.)
B_SPLINE_SURFACE_WITH_KNOTS((4,4),(3,3),(3.14159265358979,4.71238898038469),
(0.,1.),.UNSPECIFIED.)
GEOMETRIC_REPRESENTATION_ITEM()
RATIONAL_B_SPLINE_SURFACE(((1.,0.75750200074082,1.),(1.,0.758151925542941,
1.),(1.,0.735025202593057,1.),(1.,0.707106781186548,1.)))
REPRESENTATION_ITEM('')
SURFACE()
) ;
#71 = (
BOUNDED_SURFACE()
B_SPLINE_SURFACE(3,2,((#136227,#136228,#136229),(#136230,#136231,#136232),
(#136233,#136234,#136235),(#136236,#136237,#136238)),.UNSPECIFIED.,.F.,
 .F.,.F.)
B_SPLINE_SURFACE_WITH_KNOTS((4,4),(3,3),(4.71238898038469,6.28318530717959),
(0.,1.),.UNSPECIFIED.)
GEOMETRIC_REPRESENTATION_ITEM()
RATIONAL_B_SPLINE_SURFACE(((1.,0.707106781186548,1.),(1.,0.735025202593054,
1.),(1.,0.758151925542943,1.),(1.,0.75750200074082,1.)))
REPRESENTATION_ITEM('')
SURFACE()
) ;
#72 = (
BOUNDED_SURFACE()
B_SPLINE_SURFACE(3,2,((#137643,#137644,#137645),(#137646,#137647,#137648),
(#137649,#137650,#137651),(#137652,#137653,#137654),(#137655,#137656,#137657),
(#137658,#137659,#137660)),.UNSPECIFIED.,.F.,.F.,.F.)
B_SPLINE_SURFACE_WITH_KNOTS((4,2,4),(3,3),(3.14159265358979,3.92699081698724,
4.71238898038469),(0.,1.),.UNSPECIFIED.)
GEOMETRIC_REPRESENTATION_ITEM()
RATIONAL_B_SPLINE_SURFACE(((1.,0.934721701546417,1.),(1.,0.934869636336908,
1.),(1.,0.913780519322379,1.),(1.,0.834646315042289,1.),(1.,0.776518516961048,
1.),(1.,0.707106781186548,1.)))
REPRESENTATION_ITEM('')
SURFACE()
) ;
#73 = (
BOUNDED_SURFACE()
B_SPLINE_SURFACE(3,2,((#137671,#137672,#137673),(#137674,#137675,#137676),
(#137677,#137678,#137679),(#137680,#137681,#137682)),.UNSPECIFIED.,.F.,
 .F.,.F.)
B_SPLINE_SURFACE_WITH_KNOTS((4,4),(3,3),(1.5707963267949,2.41495031290807),
(0.,1.),.UNSPECIFIED.)
GEOMETRIC_REPRESENTATION_ITEM()
RATIONAL_B_SPLINE_SURFACE(((1.,0.707106781186547,1.),(1.,0.730803471035896,
1.),(1.,0.752906082887246,1.),(1.,0.767292203978619,1.)))
REPRESENTATION_ITEM('')
SURFACE()
) ;
#74 = (
BOUNDED_SURFACE()
B_SPLINE_SURFACE(3,2,((#137699,#137700,#137701),(#137702,#137703,#137704),
(#137705,#137706,#137707),(#137708,#137709,#137710),(#137711,#137712,#137713),
(#137714,#137715,#137716)),.UNSPECIFIED.,.F.,.F.,.F.)
B_SPLINE_SURFACE_WITH_KNOTS((4,2,4),(3,3),(1.56955149927807,2.35619449019234,
3.14283748110662),(-0.00124482751682279,1.),.UNSPECIFIED.)
GEOMETRIC_REPRESENTATION_ITEM()
RATIONAL_B_SPLINE_SURFACE(((1.00073060381455,0.706544157856447,1.),(1.00062673753067,
0.748263304672953,1.),(1.00053422463655,0.78542222543767,1.),(1.00040682904416,
0.836592203069634,1.),(1.00037181710675,0.850655170404833,1.),(1.00037229282025,
0.850464094333147,1.)))
REPRESENTATION_ITEM('')
SURFACE()
) ;
#75 = (
BOUNDED_SURFACE()
B_SPLINE_SURFACE(3,2,((#137719,#137720,#137721),(#137722,#137723,#137724),
(#137725,#137726,#137727),(#137728,#137729,#137730),(#137731,#137732,#137733),
(#137734,#137735,#137736)),.UNSPECIFIED.,.F.,.F.,.F.)
B_SPLINE_SURFACE_WITH_KNOTS((4,2,4),(3,3),(4.71238898038469,5.49778714378214,
6.28318530717959),(0.,1.),.UNSPECIFIED.)
GEOMETRIC_REPRESENTATION_ITEM()
RATIONAL_B_SPLINE_SURFACE(((1.,0.707106781186548,1.),(1.,0.776518516961086,
1.),(1.,0.83464631504224,1.),(1.,0.913780519322428,1.),(1.,0.934869636336872,
1.),(1.,0.934721701546417,1.)))
REPRESENTATION_ITEM('')
SURFACE()
) ;
#76 = (
BOUNDED_SURFACE()
B_SPLINE_SURFACE(3,2,((#137744,#137745,#137746),(#137747,#137748,#137749),
(#137750,#137751,#137752),(#137753,#137754,#137755)),.UNSPECIFIED.,.F.,
 .F.,.F.)
B_SPLINE_SURFACE_WITH_KNOTS((4,4),(3,3),(0.726642340681723,1.5707963267949),
(0.,1.),.UNSPECIFIED.)
GEOMETRIC_REPRESENTATION_ITEM()
RATIONAL_B_SPLINE_SURFACE(((1.,0.767292203978619,1.),(1.,0.752906082887264,
1.),(1.,0.730803471035884,1.),(1.,0.707106781186547,1.)))
REPRESENTATION_ITEM('')
SURFACE()
) ;
#77 = (
BOUNDED_SURFACE()
B_SPLINE_SURFACE(3,2,((#137771,#137772,#137773),(#137774,#137775,#137776),
(#137777,#137778,#137779),(#137780,#137781,#137782),(#137783,#137784,#137785),
(#137786,#137787,#137788)),.UNSPECIFIED.,.F.,.F.,.F.)
B_SPLINE_SURFACE_WITH_KNOTS((4,2,4),(3,3),(-0.00124482751685595,0.785398163397448,
1.57204115431175),(-0.00124482751685595,1.),.UNSPECIFIED.)
GEOMETRIC_REPRESENTATION_ITEM()
RATIONAL_B_SPLINE_SURFACE(((1.00037229282026,0.850464094333142,1.),(1.00037181710676,
0.850655170404827,1.),(1.00040682904418,0.836592203069629,1.),(1.00053422463656,
0.785422225437663,1.),(1.00062673753069,0.748263304672945,1.),(1.00073060381456,
0.706544157856431,1.)))
REPRESENTATION_ITEM('')
SURFACE()
) ;
#78 = (
BOUNDED_SURFACE()
B_SPLINE_SURFACE(3,2,((#137800,#137801,#137802),(#137803,#137804,#137805),
(#137806,#137807,#137808),(#137809,#137810,#137811)),.UNSPECIFIED.,.F.,
 .F.,.F.)
B_SPLINE_SURFACE_WITH_KNOTS((4,4),(3,3),(1.10714871779409,1.5707963267949),
(0.,1.),.UNSPECIFIED.)
GEOMETRIC_REPRESENTATION_ITEM()
RATIONAL_B_SPLINE_SURFACE(((1.,0.743704326447947,1.),(1.,0.732676928202348,
1.),(1.,0.720087778783133,1.),(1.,0.707106781186548,1.)))
REPRESENTATION_ITEM('')
SURFACE()
) ;
#79 = (
BOUNDED_SURFACE()
B_SPLINE_SURFACE(3,2,((#137819,#137820,#137821),(#137822,#137823,#137824),
(#137825,#137826,#137827),(#137828,#137829,#137830)),.UNSPECIFIED.,.F.,
 .F.,.F.)
B_SPLINE_SURFACE_WITH_KNOTS((4,4),(3,3),(1.5707963267949,2.0344439357957),
(0.,1.),.UNSPECIFIED.)
GEOMETRIC_REPRESENTATION_ITEM()
RATIONAL_B_SPLINE_SURFACE(((1.,0.707106781186548,1.),(1.,0.720087778783145,
1.),(1.,0.732676928202328,1.),(1.,0.743704326447957,1.)))
REPRESENTATION_ITEM('')
SURFACE()
) ;
#80 = (
BOUNDED_SURFACE()
B_SPLINE_SURFACE(3,2,((#138105,#138106,#138107),(#138108,#138109,#138110),
(#138111,#138112,#138113),(#138114,#138115,#138116)),.UNSPECIFIED.,.F.,
 .F.,.F.)
B_SPLINE_SURFACE_WITH_KNOTS((4,4),(3,3),(0.000111059871785624,0.000241296646650869),
(0.,1.00030059112236),.UNSPECIFIED.)
GEOMETRIC_REPRESENTATION_ITEM()
RATIONAL_B_SPLINE_SURFACE(((1.,0.839985548969886,1.00009619784686),(1.,
0.79732203291707,1.0001218463952),(1.,0.73468600944038,1.0001595020604),
(1.,0.707018740085173,1.00017613513149)))
REPRESENTATION_ITEM('')
SURFACE()
) ;
#81 = (
BOUNDED_SURFACE()
B_SPLINE_SURFACE(3,2,((#138118,#138119,#138120),(#138121,#138122,#138123),
(#138124,#138125,#138126),(#138127,#138128,#138129)),.UNSPECIFIED.,.F.,
 .F.,.F.)
B_SPLINE_SURFACE_WITH_KNOTS((4,4),(3,3),(3.14159265358979,3.68974201455418),
(0.,1.),.UNSPECIFIED.)
GEOMETRIC_REPRESENTATION_ITEM()
RATIONAL_B_SPLINE_SURFACE(((1.,0.860789971413512,1.),(1.,0.860809546755052,
1.),(1.,0.853709425573776,1.),(1.,0.840033633436873,1.)))
REPRESENTATION_ITEM('')
SURFACE()
) ;
#82 = (
BOUNDED_SURFACE()
B_SPLINE_SURFACE(3,2,((#138135,#138136,#138137),(#138138,#138139,#138140),
(#138141,#138142,#138143),(#138144,#138145,#138146)),.UNSPECIFIED.,.F.,
 .F.,.F.)
B_SPLINE_SURFACE_WITH_KNOTS((4,4),(3,3),(2.59344329260967,3.14159265358979),
(0.,1.),.UNSPECIFIED.)
GEOMETRIC_REPRESENTATION_ITEM()
RATIONAL_B_SPLINE_SURFACE(((1.,0.840033633435699,1.),(1.,0.853709425573365,
1.),(1.,0.860809546755054,1.),(1.,0.860789971413512,1.)))
REPRESENTATION_ITEM('')
SURFACE()
) ;
#83 = (
BOUNDED_SURFACE()
B_SPLINE_SURFACE(3,2,((#138148,#138149,#138150),(#138151,#138152,#138153),
(#138154,#138155,#138156),(#138157,#138158,#138159)),.UNSPECIFIED.,.F.,
 .F.,.F.)
B_SPLINE_SURFACE_WITH_KNOTS((4,4),(3,3),(0.000111059871788868,0.000241296646650869),
(-0.000300086750004719,1.),.UNSPECIFIED.)
GEOMETRIC_REPRESENTATION_ITEM()
RATIONAL_B_SPLINE_SURFACE(((1.00009603638471,0.839985629649231,1.),(1.00012164188355,
0.797322135108548,1.),(1.00015923434603,0.734686143216427,1.),(1.00017583949954,
0.707018887812415,1.)))
REPRESENTATION_ITEM('')
SURFACE()
) ;
#84 = (
BOUNDED_SURFACE()
B_SPLINE_SURFACE(3,2,((#138244,#138245,#138246),(#138247,#138248,#138249),
(#138250,#138251,#138252),(#138253,#138254,#138255),(#138256,#138257,#138258),
(#138259,#138260,#138261),(#138262,#138263,#138264),(#138265,#138266,#138267),
(#138268,#138269,#138270),(#138271,#138272,#138273)),.UNSPECIFIED.,.F.,
 .F.,.F.)
B_SPLINE_SURFACE_WITH_KNOTS((4,2,2,2,4),(3,3),(0.00112100122803336,0.00145633576709043,
0.0015908372445872,0.00165808798333558,0.00178849406635727),(-0.000893324189260702,
1.00101552458171),.UNSPECIFIED.)
GEOMETRIC_REPRESENTATION_ITEM()
RATIONAL_B_SPLINE_SURFACE(((1.00061830890916,0.653576280075716,1.0007029749849),
(1.00045188087569,0.746821933830268,1.00051375768173),(1.00032243686651,
0.819346321742879,1.00036658868733),(1.00017052538065,0.904458700444932,
1.00019387570697),(1.00013074576008,0.926746272131252,1.00014864899624),
(1.00007983643892,0.955269549338603,1.00009076857637),(1.00006394848111,
0.964171192776776,1.00007270505386),(1.00002748579919,0.984600362923306,
1.00003124947578),(1.00001632684003,0.990852461324469,1.00001856250162),
(1.00006581963707,0.963122828765763,1.00007483243035)))
REPRESENTATION_ITEM('')
SURFACE()
) ;
#85 = (
BOUNDED_SURFACE()
B_SPLINE_SURFACE(3,2,((#138314,#138315,#138316),(#138317,#138318,#138319),
(#138320,#138321,#138322),(#138323,#138324,#138325),(#138326,#138327,#138328),
(#138329,#138330,#138331),(#138332,#138333,#138334),(#138335,#138336,#138337),
(#138338,#138339,#138340),(#138341,#138342,#138343)),.UNSPECIFIED.,.F.,
 .F.,.F.)
B_SPLINE_SURFACE_WITH_KNOTS((4,2,2,2,4),(3,3),(0.00112100122803338,0.00145633576709043,
0.00159083724458721,0.00165808798333559,0.00178849406635728),(-0.00113559264167306,
1.),.UNSPECIFIED.)
GEOMETRIC_REPRESENTATION_ITEM()
RATIONAL_B_SPLINE_SURFACE(((1.0007861837978,0.653844270846518,1.),(1.00057456947124,
0.747017790468252,1.),(1.00040998057203,0.81948607406265,1.),(1.00021682413014,
0.904532610471983,1.),(1.00016624408395,0.926802940661303,1.),(1.00010151255112,
0.955304152477097,1.),(1.00008131090948,0.964198909671178,1.),(1.00003494837236,
0.984612275966134,1.),(1.00002075968324,0.990859537791216,1.),(1.00008369009644,
0.963151356666673,1.)))
REPRESENTATION_ITEM('')
SURFACE()
) ;
#86 = (
BOUNDED_SURFACE()
B_SPLINE_SURFACE(3,2,((#138380,#138381,#138382),(#138383,#138384,#138385),
(#138386,#138387,#138388),(#138389,#138390,#138391),(#138392,#138393,#138394),
(#138395,#138396,#138397),(#138398,#138399,#138400),(#138401,#138402,#138403),
(#138404,#138405,#138406),(#138407,#138408,#138409),(#138410,#138411,#138412),
(#138413,#138414,#138415),(#138416,#138417,#138418),(#138419,#138420,#138421),
(#138422,#138423,#138424),(#138425,#138426,#138427)),.UNSPECIFIED.,.F.,
 .F.,.F.)
B_SPLINE_SURFACE_WITH_KNOTS((4,2,2,2,2,2,2,4),(3,3),(5.6285407107684E-15,
3.85995771599558E-5,5.78993657371195E-5,6.75492600257013E-5,7.23742071699922E-5,
7.47866807421377E-5,7.59929175282104E-5,7.71991543142831E-5),(0.,1.00107899067822),
 .UNSPECIFIED.)
GEOMETRIC_REPRESENTATION_ITEM()
RATIONAL_B_SPLINE_SURFACE(((1.,0.976255617118807,1.00005123993558),(1.,
0.981339981891218,1.00004026797119),(1.,0.986086237829171,1.00003002563936),
(1.,0.992269463037035,1.00001668235464),(1.,0.994174411180035,1.00001257151206),
(1.,0.996706913506707,1.00000710641926),(1.,0.997492596832092,1.00000541092929),
(1.,0.998537621803386,1.00000315578488),(1.,0.998865045809506,1.00000244920998),
(1.,0.999323526852926,1.00000145981644),(1.,0.999468419970867,1.00000114713979),
(1.,0.99959844684718,1.00000086654422),(1.,0.999614491362716,1.00000083192045),
(1.,0.999732489024761,1.0000005772837),(1.,0.999724369239699,1.00000059480604),
(1.,1.,1.)))
REPRESENTATION_ITEM('')
SURFACE()
) ;
#87 = (
BOUNDED_SURFACE()
B_SPLINE_SURFACE(3,2,((#138429,#138430,#138431),(#138432,#138433,#138434),
(#138435,#138436,#138437),(#138438,#138439,#138440),(#138441,#138442,#138443),
(#138444,#138445,#138446),(#138447,#138448,#138449),(#138450,#138451,#138452),
(#138453,#138454,#138455),(#138456,#138457,#138458)),.UNSPECIFIED.,.F.,
 .F.,.F.)
B_SPLINE_SURFACE_WITH_KNOTS((4,2,2,2,4),(3,3),(-0.00011070792851133,0.000553539642556655,
0.000830309463834981,0.000968694374474145,0.00121778721363011),(0.,1.00563383762715),
 .UNSPECIFIED.)
GEOMETRIC_REPRESENTATION_ITEM()
RATIONAL_B_SPLINE_SURFACE(((1.,0.710139408519237,1.00326605501383),(1.,
0.691948125896667,1.00347102847888),(1.,0.728232377173921,1.00306218931864),
(1.,0.818030374423583,1.00205037464714),(1.,0.8491107594692,1.00170017096167),
(1.,0.897979778369929,1.0011495307267),(1.,0.914666724297522,1.000961507639),
(1.,0.961090538823349,1.00043841917286),(1.,0.990973799041317,1.00010170430118),
(1.,0.992463455161609,1.00008491933978)))
REPRESENTATION_ITEM('')
SURFACE()
) ;
#88 = (
BOUNDED_SURFACE()
B_SPLINE_SURFACE(3,2,((#138460,#138461,#138462),(#138463,#138464,#138465),
(#138466,#138467,#138468),(#138469,#138470,#138471),(#138472,#138473,#138474),
(#138475,#138476,#138477),(#138478,#138479,#138480),(#138481,#138482,#138483),
(#138484,#138485,#138486),(#138487,#138488,#138489)),.UNSPECIFIED.,.F.,
 .F.,.F.)
B_SPLINE_SURFACE_WITH_KNOTS((4,2,2,2,4),(3,3),(-0.000137915648493747,0.000139027965246066,
0.000278055930499748,0.000556111861007113,0.00125013859505175),(-0.000741678186154432,
1.00283457365368),.UNSPECIFIED.)
GEOMETRIC_REPRESENTATION_ITEM()
RATIONAL_B_SPLINE_SURFACE(((1.00001340810332,0.990935328832712,1.00005135076275),
(1.00000300543757,0.997968146378609,1.00001151031641),(1.00005311279901,
0.964092605306906,1.0002034130165),(1.00012590576293,0.914880254704336,
1.00048219772843),(1.00015093966353,0.897955856706345,1.00057807332394),
(1.00022375355373,0.848729358697742,1.00085693817998),(1.00026920263046,
0.818003093715361,1.00103100043929),(1.00040494517458,0.726233102311804,
1.00155087137217),(1.00045889592424,0.689759203410913,1.00175749359754),
(1.00042429005347,0.713154819594415,1.00162495897893)))
REPRESENTATION_ITEM('')
SURFACE()
) ;
#89 = (
BOUNDED_SURFACE()
B_SPLINE_SURFACE(3,2,((#138491,#138492,#138493),(#138494,#138495,#138496),
(#138497,#138498,#138499),(#138500,#138501,#138502),(#138503,#138504,#138505),
(#138506,#138507,#138508),(#138509,#138510,#138511),(#138512,#138513,#138514),
(#138515,#138516,#138517),(#138518,#138519,#138520),(#138521,#138522,#138523),
(#138524,#138525,#138526),(#138527,#138528,#138529),(#138530,#138531,#138532),
(#138533,#138534,#138535),(#138536,#138537,#138538)),.UNSPECIFIED.,.F.,
 .F.,.F.)
B_SPLINE_SURFACE_WITH_KNOTS((4,2,2,2,2,2,2,4),(3,3),(7.7799501866857E-15,
3.88447601478329E-5,5.82671402178594E-5,6.79783302528727E-5,7.28339252703793E-5,
7.52617227791326E-5,7.64756215335093E-5,7.76895202878859E-5),(-0.00120945525743048,
1.010800708689),.UNSPECIFIED.)
GEOMETRIC_REPRESENTATION_ITEM()
RATIONAL_B_SPLINE_SURFACE(((1.00005744302265,0.975995723233542,1.00051789333953),
(1.00004519813151,0.98111261545739,1.00040749616208),(1.00003362760161,
0.985947705765599,1.00030317887349),(1.00001854219782,0.992251590743256,
1.00016717227455),(1.00001393966879,0.994174894491125,1.0001256769106),
(1.00000788875349,0.996703449551656,1.00007112322263),(1.00000601414708,
0.997486809637528,1.00005422219392),(1.00000351698944,0.998530321282699,
1.00003170838373),(1.00000273459082,0.998857269833612,1.0000246544542),
(1.00000163903614,0.999315079966002,1.00001477718022),(1.00000129000885,
0.999460931405225,1.00001163042892),(1.0000009745592,0.99959275143124,1.000008786406),
(1.00000093560708,0.99960902873406,1.00000843522246),(1.00000065019919,
0.999728294915416,1.00000586204929),(1.00000066918571,0.99972036083143,
1.00000603322751),(1.,1.,1.)))
REPRESENTATION_ITEM('')
SURFACE()
) ;
#90 = (
BOUNDED_SURFACE()
B_SPLINE_SURFACE(3,2,((#139011,#139012,#139013),(#139014,#139015,#139016),
(#139017,#139018,#139019),(#139020,#139021,#139022),(#139023,#139024,#139025),
(#139026,#139027,#139028)),.UNSPECIFIED.,.F.,.F.,.F.)
B_SPLINE_SURFACE_WITH_KNOTS((4,2,4),(3,3),(3.14159265358979,3.92699081698724,
4.71238898038469),(0.,1.),.UNSPECIFIED.)
GEOMETRIC_REPRESENTATION_ITEM()
RATIONAL_B_SPLINE_SURFACE(((1.,0.934721701546417,1.),(1.,0.934869636336949,
1.),(1.,0.913780519322321,1.),(1.,0.834646315042351,1.),(1.,0.776518516961002,
1.),(1.,0.707106781186548,1.)))
REPRESENTATION_ITEM('')
SURFACE()
) ;
#91 = (
BOUNDED_SURFACE()
B_SPLINE_SURFACE(3,2,((#139039,#139040,#139041),(#139042,#139043,#139044),
(#139045,#139046,#139047),(#139048,#139049,#139050)),.UNSPECIFIED.,.F.,
 .F.,.F.)
B_SPLINE_SURFACE_WITH_KNOTS((4,4),(3,3),(1.5707963267949,2.41495031290807),
(0.,1.),.UNSPECIFIED.)
GEOMETRIC_REPRESENTATION_ITEM()
RATIONAL_B_SPLINE_SURFACE(((1.,0.707106781186553,1.),(1.,0.730803471035898,
1.),(1.,0.752906082887247,1.),(1.,0.76729220397862,1.)))
REPRESENTATION_ITEM('')
SURFACE()
) ;
#92 = (
BOUNDED_SURFACE()
B_SPLINE_SURFACE(3,2,((#139067,#139068,#139069),(#139070,#139071,#139072),
(#139073,#139074,#139075),(#139076,#139077,#139078),(#139079,#139080,#139081),
(#139082,#139083,#139084)),.UNSPECIFIED.,.F.,.F.,.F.)
B_SPLINE_SURFACE_WITH_KNOTS((4,2,4),(3,3),(1.56955149927814,2.35619449019234,
3.14283748110655),(-0.00124482751675719,1.),.UNSPECIFIED.)
GEOMETRIC_REPRESENTATION_ITEM()
RATIONAL_B_SPLINE_SURFACE(((1.00073060381451,0.706544157856477,1.),(1.00062673753064,
0.748263304672955,1.),(1.00053422463652,0.785422225437717,1.),(1.00040682904414,
0.83659220306961,1.),(1.00037181710673,0.850655170404864,1.),(1.00037229282023,
0.850464094333156,1.)))
REPRESENTATION_ITEM('')
SURFACE()
) ;
#93 = (
BOUNDED_SURFACE()
B_SPLINE_SURFACE(3,2,((#139087,#139088,#139089),(#139090,#139091,#139092),
(#139093,#139094,#139095),(#139096,#139097,#139098),(#139099,#139100,#139101),
(#139102,#139103,#139104)),.UNSPECIFIED.,.F.,.F.,.F.)
B_SPLINE_SURFACE_WITH_KNOTS((4,2,4),(3,3),(4.71238898038469,5.49778714378214,
6.28318530717959),(0.,1.),.UNSPECIFIED.)
GEOMETRIC_REPRESENTATION_ITEM()
RATIONAL_B_SPLINE_SURFACE(((1.,0.707106781186548,1.),(1.,0.776518516960999,
1.),(1.,0.834646315042352,1.),(1.,0.913780519322316,1.),(1.,0.934869636336956,
1.),(1.,0.934721701546417,1.)))
REPRESENTATION_ITEM('')
SURFACE()
) ;
#94 = (
BOUNDED_SURFACE()
B_SPLINE_SURFACE(3,2,((#139112,#139113,#139114),(#139115,#139116,#139117),
(#139118,#139119,#139120),(#139121,#139122,#139123)),.UNSPECIFIED.,.F.,
 .F.,.F.)
B_SPLINE_SURFACE_WITH_KNOTS((4,4),(3,3),(0.726642340681723,1.5707963267949),
(0.,1.),.UNSPECIFIED.)
GEOMETRIC_REPRESENTATION_ITEM()
RATIONAL_B_SPLINE_SURFACE(((1.,0.767292203978619,1.),(1.,0.752906082887246,
1.),(1.,0.730803471035896,1.),(1.,0.707106781186547,1.)))
REPRESENTATION_ITEM('')
SURFACE()
) ;
#95 = (
BOUNDED_SURFACE()
B_SPLINE_SURFACE(3,2,((#139139,#139140,#139141),(#139142,#139143,#139144),
(#139145,#139146,#139147),(#139148,#139149,#139150),(#139151,#139152,#139153),
(#139154,#139155,#139156)),.UNSPECIFIED.,.F.,.F.,.F.)
B_SPLINE_SURFACE_WITH_KNOTS((4,2,4),(3,3),(-0.00124482751681696,0.785398163397448,
1.57204115431171),(-0.00124482751681696,1.),.UNSPECIFIED.)
GEOMETRIC_REPRESENTATION_ITEM()
RATIONAL_B_SPLINE_SURFACE(((1.00037229282025,0.850464094333147,1.),(1.00037181710675,
0.850655170404832,1.),(1.00040682904416,0.836592203069633,1.),(1.00053422463654,
0.785422225437673,1.),(1.00062673753067,0.748263304672954,1.),(1.00073060381454,
0.706544157856449,1.)))
REPRESENTATION_ITEM('')
SURFACE()
) ;
#96 = (
BOUNDED_SURFACE()
B_SPLINE_SURFACE(3,2,((#139168,#139169,#139170),(#139171,#139172,#139173),
(#139174,#139175,#139176),(#139177,#139178,#139179)),.UNSPECIFIED.,.F.,
 .F.,.F.)
B_SPLINE_SURFACE_WITH_KNOTS((4,4),(3,3),(1.10714871779409,1.5707963267949),
(0.,1.),.UNSPECIFIED.)
GEOMETRIC_REPRESENTATION_ITEM()
RATIONAL_B_SPLINE_SURFACE(((1.,0.743704326447947,1.),(1.,0.732676928202349,
1.),(1.,0.720087778783133,1.),(1.,0.707106781186553,1.)))
REPRESENTATION_ITEM('')
SURFACE()
) ;
#97 = (
BOUNDED_SURFACE()
B_SPLINE_SURFACE(3,2,((#139187,#139188,#139189),(#139190,#139191,#139192),
(#139193,#139194,#139195),(#139196,#139197,#139198)),.UNSPECIFIED.,.F.,
 .F.,.F.)
B_SPLINE_SURFACE_WITH_KNOTS((4,4),(3,3),(1.5707963267949,2.0344439357957),
(0.,1.),.UNSPECIFIED.)
GEOMETRIC_REPRESENTATION_ITEM()
RATIONAL_B_SPLINE_SURFACE(((1.,0.707106781186548,1.),(1.,0.720087778783133,
1.),(1.,0.73267692820235,1.),(1.,0.743704326447947,1.)))
REPRESENTATION_ITEM('')
SURFACE()
) ;
#98 = (
BOUNDED_SURFACE()
B_SPLINE_SURFACE(3,2,((#139448,#139449,#139450),(#139451,#139452,#139453),
(#139454,#139455,#139456),(#139457,#139458,#139459)),.UNSPECIFIED.,.F.,
 .F.,.F.)
B_SPLINE_SURFACE_WITH_KNOTS((4,4),(3,3),(0.000111059871785622,0.000241296646650869),
(0.,1.00030059112227),.UNSPECIFIED.)
GEOMETRIC_REPRESENTATION_ITEM()
RATIONAL_B_SPLINE_SURFACE(((1.,0.839985548969898,1.00009619784683),(1.,
0.797322032917094,1.00012184639517),(1.,0.734686009440392,1.00015950206035),
(1.,0.707018740085205,1.00017613513144)))
REPRESENTATION_ITEM('')
SURFACE()
) ;
#99 = (
BOUNDED_SURFACE()
B_SPLINE_SURFACE(3,2,((#139461,#139462,#139463),(#139464,#139465,#139466),
(#139467,#139468,#139469),(#139470,#139471,#139472)),.UNSPECIFIED.,.F.,
 .F.,.F.)
B_SPLINE_SURFACE_WITH_KNOTS((4,4),(3,3),(3.14159265358979,3.68974201455418),
(0.,1.),.UNSPECIFIED.)
GEOMETRIC_REPRESENTATION_ITEM()
RATIONAL_B_SPLINE_SURFACE(((1.,0.860789971413512,1.),(1.,0.860809546755051,
1.),(1.,0.853709425573778,1.),(1.,0.840033633436873,1.)))
REPRESENTATION_ITEM('')
SURFACE()
) ;
#100 = (
BOUNDED_SURFACE()
B_SPLINE_SURFACE(3,2,((#139475,#139476,#139477),(#139478,#139479,#139480),
(#139481,#139482,#139483),(#139484,#139485,#139486)),.UNSPECIFIED.,.F.,
 .F.,.F.)
B_SPLINE_SURFACE_WITH_KNOTS((4,4),(3,3),(2.59344329260967,3.14159265358979),
(0.,1.),.UNSPECIFIED.)
GEOMETRIC_REPRESENTATION_ITEM()
RATIONAL_B_SPLINE_SURFACE(((1.,0.840033633435699,1.),(1.,0.853709425573363,
1.),(1.,0.860809546755055,1.),(1.,0.860789971413512,1.)))
REPRESENTATION_ITEM('')
SURFACE()
) ;
#101 = (
BOUNDED_SURFACE()
B_SPLINE_SURFACE(3,2,((#139488,#139489,#139490),(#139491,#139492,#139493),
(#139494,#139495,#139496),(#139497,#139498,#139499)),.UNSPECIFIED.,.F.,
 .F.,.F.)
B_SPLINE_SURFACE_WITH_KNOTS((4,4),(3,3),(0.000111059871788868,0.000241296646650869),
(-0.000300086750003606,1.),.UNSPECIFIED.)
GEOMETRIC_REPRESENTATION_ITEM()
RATIONAL_B_SPLINE_SURFACE(((1.0000960363847,0.839985629649235,1.),(1.00012164188355,
0.797322135108538,1.),(1.00015923434603,0.734686143216438,1.),(1.00017583949954,
0.707018887812415,1.)))
REPRESENTATION_ITEM('')
SURFACE()
) ;
#102 = (
BOUNDED_SURFACE()
B_SPLINE_SURFACE(3,2,((#139583,#139584,#139585),(#139586,#139587,#139588),
(#139589,#139590,#139591),(#139592,#139593,#139594),(#139595,#139596,#139597),
(#139598,#139599,#139600),(#139601,#139602,#139603),(#139604,#139605,#139606),
(#139607,#139608,#139609),(#139610,#139611,#139612)),.UNSPECIFIED.,.F.,
 .F.,.F.)
B_SPLINE_SURFACE_WITH_KNOTS((4,2,2,2,4),(3,3),(0.00112100122803331,0.00145633576709043,
0.0015908372445872,0.00165808798333558,0.00178849406635728),(-0.000893324189052896,
1.00101552458165),.UNSPECIFIED.)
GEOMETRIC_REPRESENTATION_ITEM()
RATIONAL_B_SPLINE_SURFACE(((1.00061830890902,0.653576280075841,1.00070297498485),
(1.00045188087558,0.746821933830185,1.0005137576817),(1.00032243686644,
0.819346321743005,1.0003665886873),(1.00017052538062,0.904458700444923,
1.00019387570696),(1.00013074576005,0.926746272131313,1.00014864899624),
(1.0000798364389,0.955269549338596,1.00009076857636),(1.0000639484811,0.964171192776782,
1.00007270505386),(1.00002748579918,0.984600362923314,1.00003124947578),
(1.00001632684004,0.990852461324472,1.00001856250162),(1.00006581963706,
0.963122828765752,1.00007483243035)))
REPRESENTATION_ITEM('')
SURFACE()
) ;
#103 = (
BOUNDED_SURFACE()
B_SPLINE_SURFACE(3,2,((#139651,#139652,#139653),(#139654,#139655,#139656),
(#139657,#139658,#139659),(#139660,#139661,#139662),(#139663,#139664,#139665),
(#139666,#139667,#139668),(#139669,#139670,#139671),(#139672,#139673,#139674),
(#139675,#139676,#139677),(#139678,#139679,#139680)),.UNSPECIFIED.,.F.,
 .F.,.F.)
B_SPLINE_SURFACE_WITH_KNOTS((4,2,2,2,4),(3,3),(0.00112100122803326,0.00145633576709043,
0.00159083724458721,0.00165808798333559,0.00178849406635729),(-0.00113559264180098,
1.),.UNSPECIFIED.)
GEOMETRIC_REPRESENTATION_ITEM()
RATIONAL_B_SPLINE_SURFACE(((1.00078618379789,0.653844270846382,1.),(1.0005745694713,
0.747017790468173,1.),(1.00040998057207,0.819486074062609,1.),(1.00021682413016,
0.904532610471971,1.),(1.00016624408397,0.926802940661278,1.),(1.00010151255113,
0.955304152477099,1.),(1.00008131090949,0.964198909671174,1.),(1.00003494837237,
0.984612275966134,1.),(1.00002075968325,0.990859537791216,1.),(1.00008369009645,
0.963151356666666,1.)))
REPRESENTATION_ITEM('')
SURFACE()
) ;
#104 = (
BOUNDED_SURFACE()
B_SPLINE_SURFACE(3,2,((#139717,#139718,#139719),(#139720,#139721,#139722),
(#139723,#139724,#139725),(#139726,#139727,#139728),(#139729,#139730,#139731),
(#139732,#139733,#139734),(#139735,#139736,#139737),(#139738,#139739,#139740),
(#139741,#139742,#139743),(#139744,#139745,#139746),(#139747,#139748,#139749),
(#139750,#139751,#139752),(#139753,#139754,#139755),(#139756,#139757,#139758),
(#139759,#139760,#139761),(#139762,#139763,#139764)),.UNSPECIFIED.,.F.,
 .F.,.F.)
B_SPLINE_SURFACE_WITH_KNOTS((4,2,2,2,2,2,2,4),(3,3),(5.6278630844106E-15,
3.85995771599556E-5,5.78993657371195E-5,6.75492600257015E-5,7.23742071699924E-5,
7.47866807421379E-5,7.59929175282107E-5,7.71991543142834E-5),(0.,1.00107899067813),
 .UNSPECIFIED.)
GEOMETRIC_REPRESENTATION_ITEM()
RATIONAL_B_SPLINE_SURFACE(((1.,0.976255617118809,1.00005123993557),(1.,
0.981339981891254,1.00004026797119),(1.,0.986086237829182,1.00003002563936),
(1.,0.992269463037031,1.00001668235464),(1.,0.994174411180037,1.00001257151206),
(1.,0.996706913506705,1.00000710641926),(1.,0.997492596832093,1.00000541092929),
(1.,0.99853762180339,1.00000315578488),(1.,0.998865045809501,1.00000244920998),
(1.,0.999323526852926,1.00000145981644),(1.,0.999468419970872,1.00000114713979),
(1.,0.999598446847179,1.00000086654422),(1.,0.999614491362717,1.00000083192045),
(1.,0.999732489024762,1.0000005772837),(1.,0.999724369239697,1.00000059480604),
(1.,1.,1.)))
REPRESENTATION_ITEM('')
SURFACE()
) ;
#105 = (
BOUNDED_SURFACE()
B_SPLINE_SURFACE(3,2,((#139766,#139767,#139768),(#139769,#139770,#139771),
(#139772,#139773,#139774),(#139775,#139776,#139777),(#139778,#139779,#139780),
(#139781,#139782,#139783),(#139784,#139785,#139786),(#139787,#139788,#139789),
(#139790,#139791,#139792),(#139793,#139794,#139795)),.UNSPECIFIED.,.F.,
 .F.,.F.)
B_SPLINE_SURFACE_WITH_KNOTS((4,2,2,2,4),(3,3),(-0.000110707928511331,0.000553539642556653,
0.00083030946383498,0.000968694374474144,0.00121778721363011),(0.,1.00563383762645),
 .UNSPECIFIED.)
GEOMETRIC_REPRESENTATION_ITEM()
RATIONAL_B_SPLINE_SURFACE(((1.,0.710139408519343,1.00326605501342),(1.,
0.691948125897072,1.00347102847844),(1.,0.728232377173963,1.00306218931826),
(1.,0.818030374423771,1.00205037464689),(1.,0.849110759469331,1.00170017096146),
(1.,0.897979778369987,1.00114953072656),(1.,0.914666724297546,1.00096150763888),
(1.,0.961090538823436,1.0004384191728),(1.,0.990973799041145,1.00010170430117),
(1.,0.992463455161931,1.00008491933976)))
REPRESENTATION_ITEM('')
SURFACE()
) ;
#106 = (
BOUNDED_SURFACE()
B_SPLINE_SURFACE(3,2,((#139797,#139798,#139799),(#139800,#139801,#139802),
(#139803,#139804,#139805),(#139806,#139807,#139808),(#139809,#139810,#139811),
(#139812,#139813,#139814),(#139815,#139816,#139817),(#139818,#139819,#139820),
(#139821,#139822,#139823),(#139824,#139825,#139826)),.UNSPECIFIED.,.F.,
 .F.,.F.)
B_SPLINE_SURFACE_WITH_KNOTS((4,2,2,2,4),(3,3),(-0.000137915648493774,0.000139027965246066,
0.000278055930499748,0.000556111861007112,0.00125013859505186),(-0.000741678186100512,
1.00283457365347),.UNSPECIFIED.)
GEOMETRIC_REPRESENTATION_ITEM()
RATIONAL_B_SPLINE_SURFACE(((1.00001340810332,0.990935328832901,1.00005135076275),
(1.00000300543757,0.997968146378528,1.0000115103164),(1.00005311279901,
0.964092605306946,1.00020341301648),(1.00012590576293,0.914880254704346,
1.00048219772839),(1.00015093966352,0.897955856706357,1.00057807332389),
(1.00022375355372,0.848729358697813,1.00085693817992),(1.00026920263044,
0.818003093715353,1.00103100043921),(1.00040494517455,0.726233102312007,
1.00155087137205),(1.0004588959242,0.689759203410784,1.00175749359741),
(1.00042429005344,0.713154819594625,1.00162495897881)))
REPRESENTATION_ITEM('')
SURFACE()
) ;
#107 = (
BOUNDED_SURFACE()
B_SPLINE_SURFACE(3,2,((#139828,#139829,#139830),(#139831,#139832,#139833),
(#139834,#139835,#139836),(#139837,#139838,#139839),(#139840,#139841,#139842),
(#139843,#139844,#139845),(#139846,#139847,#139848),(#139849,#139850,#139851),
(#139852,#139853,#139854),(#139855,#139856,#139857),(#139858,#139859,#139860),
(#139861,#139862,#139863),(#139864,#139865,#139866),(#139867,#139868,#139869),
(#139870,#139871,#139872),(#139873,#139874,#139875)),.UNSPECIFIED.,.F.,
 .F.,.F.)
B_SPLINE_SURFACE_WITH_KNOTS((4,2,2,2,2,2,2,4),(3,3),(7.7799501866857E-15,
3.88447601478329E-5,5.82671402178594E-5,6.79783302528727E-5,7.28339252703793E-5,
7.52617227791326E-5,7.64756215335093E-5,7.76895202878859E-5),(-0.00120945525752119,
1.01080070868862),.UNSPECIFIED.)
GEOMETRIC_REPRESENTATION_ITEM()
RATIONAL_B_SPLINE_SURFACE(((1.00005744302265,0.975995723233548,1.00051789333951),
(1.00004519813151,0.981112615457395,1.00040749616206),(1.00003362760161,
0.985947705765603,1.00030317887348),(1.00001854219783,0.992251590743258,
1.00016717227455),(1.00001393966879,0.994174894491126,1.00012567691059),
(1.00000788875349,0.996703449551657,1.00007112322263),(1.00000601414708,
0.997486809637528,1.00005422219392),(1.00000351698944,0.9985303212827,1.00003170838373),
(1.00000273459082,0.998857269833613,1.0000246544542),(1.00000163903614,
0.999315079966002,1.00001477718021),(1.00000129000885,0.999460931405225,
1.00001163042892),(1.0000009745592,0.99959275143124,1.00000878640599),(1.00000093560708,
0.99960902873406,1.00000843522246),(1.00000065019919,0.999728294915417,
1.00000586204929),(1.00000066918571,0.99972036083143,1.00000603322751),
(1.,1.,1.)))
REPRESENTATION_ITEM('')
SURFACE()
) ;
#108 = (
BOUNDED_SURFACE()
B_SPLINE_SURFACE(3,2,((#139917,#139918,#139919),(#139920,#139921,#139922),
(#139923,#139924,#139925),(#139926,#139927,#139928)),.UNSPECIFIED.,.F.,
 .F.,.F.)
B_SPLINE_SURFACE_WITH_KNOTS((4,4),(3,3),(3.14159265358979,4.71238898038469),
(0.,1.),.UNSPECIFIED.)
GEOMETRIC_REPRESENTATION_ITEM()
RATIONAL_B_SPLINE_SURFACE(((1.,0.75750200074082,1.),(1.,0.758151925542946,
1.),(1.,0.735025202593052,1.),(1.,0.707106781186548,1.)))
REPRESENTATION_ITEM('')
SURFACE()
) ;
#109 = (
BOUNDED_SURFACE()
B_SPLINE_SURFACE(3,2,((#139930,#139931,#139932),(#139933,#139934,#139935),
(#139936,#139937,#139938),(#139939,#139940,#139941)),.UNSPECIFIED.,.F.,
 .F.,.F.)
B_SPLINE_SURFACE_WITH_KNOTS((4,4),(3,3),(4.71238898038469,6.28318530717959),
(0.,1.),.UNSPECIFIED.)
GEOMETRIC_REPRESENTATION_ITEM()
RATIONAL_B_SPLINE_SURFACE(((1.,0.707106781186548,1.),(1.,0.735025202593053,
1.),(1.,0.758151925542945,1.),(1.,0.75750200074082,1.)))
REPRESENTATION_ITEM('')
SURFACE()
) ;
#110 = (
BOUNDED_SURFACE()
B_SPLINE_SURFACE(3,2,((#140939,#140940,#140941),(#140942,#140943,#140944),
(#140945,#140946,#140947),(#140948,#140949,#140950),(#140951,#140952,#140953),
(#140954,#140955,#140956)),.UNSPECIFIED.,.F.,.F.,.F.)
B_SPLINE_SURFACE_WITH_KNOTS((4,2,4),(3,3),(3.14159265358979,3.92699081698724,
4.71238898038469),(0.,1.),.UNSPECIFIED.)
GEOMETRIC_REPRESENTATION_ITEM()
RATIONAL_B_SPLINE_SURFACE(((1.,0.934721701546417,1.),(1.,0.934869636336908,
1.),(1.,0.913780519322377,1.),(1.,0.834646315042295,1.),(1.,0.776518516961044,
1.),(1.,0.707106781186548,1.)))
REPRESENTATION_ITEM('')
SURFACE()
) ;
#111 = (
BOUNDED_SURFACE()
B_SPLINE_SURFACE(3,2,((#140967,#140968,#140969),(#140970,#140971,#140972),
(#140973,#140974,#140975),(#140976,#140977,#140978)),.UNSPECIFIED.,.F.,
 .F.,.F.)
B_SPLINE_SURFACE_WITH_KNOTS((4,4),(3,3),(1.5707963267949,2.41495031290807),
(0.,1.),.UNSPECIFIED.)
GEOMETRIC_REPRESENTATION_ITEM()
RATIONAL_B_SPLINE_SURFACE(((1.,0.707106781186547,1.),(1.,0.730803471035897,
1.),(1.,0.752906082887246,1.),(1.,0.76729220397862,1.)))
REPRESENTATION_ITEM('')
SURFACE()
) ;
#112 = (
BOUNDED_SURFACE()
B_SPLINE_SURFACE(3,2,((#140995,#140996,#140997),(#140998,#140999,#141000),
(#141001,#141002,#141003),(#141004,#141005,#141006),(#141007,#141008,#141009),
(#141010,#141011,#141012)),.UNSPECIFIED.,.F.,.F.,.F.)
B_SPLINE_SURFACE_WITH_KNOTS((4,2,4),(3,3),(1.56955149927815,2.35619449019234,
3.14283748110654),(-0.00124482751675201,1.),.UNSPECIFIED.)
GEOMETRIC_REPRESENTATION_ITEM()
RATIONAL_B_SPLINE_SURFACE(((1.0007306038145,0.706544157856479,1.),(1.00062673753064,
0.748263304672957,1.),(1.00053422463652,0.785422225437718,1.),(1.00040682904414,
0.83659220306961,1.),(1.00037181710673,0.850655170404865,1.),(1.00037229282023,
0.850464094333157,1.)))
REPRESENTATION_ITEM('')
SURFACE()
) ;
#113 = (
BOUNDED_SURFACE()
B_SPLINE_SURFACE(3,2,((#141015,#141016,#141017),(#141018,#141019,#141020),
(#141021,#141022,#141023),(#141024,#141025,#141026),(#141027,#141028,#141029),
(#141030,#141031,#141032)),.UNSPECIFIED.,.F.,.F.,.F.)
B_SPLINE_SURFACE_WITH_KNOTS((4,2,4),(3,3),(4.71238898038469,5.49778714378214,
6.28318530717959),(0.,1.),.UNSPECIFIED.)
GEOMETRIC_REPRESENTATION_ITEM()
RATIONAL_B_SPLINE_SURFACE(((1.,0.707106781186548,1.),(1.,0.776518516961005,
1.),(1.,0.834646315042348,1.),(1.,0.913780519322327,1.),(1.,0.934869636336944,
1.),(1.,0.934721701546417,1.)))
REPRESENTATION_ITEM('')
SURFACE()
) ;
#114 = (
BOUNDED_SURFACE()
B_SPLINE_SURFACE(3,2,((#141040,#141041,#141042),(#141043,#141044,#141045),
(#141046,#141047,#141048),(#141049,#141050,#141051)),.UNSPECIFIED.,.F.,
 .F.,.F.)
B_SPLINE_SURFACE_WITH_KNOTS((4,4),(3,3),(0.726642340681723,1.5707963267949),
(0.,1.),.UNSPECIFIED.)
GEOMETRIC_REPRESENTATION_ITEM()
RATIONAL_B_SPLINE_SURFACE(((1.,0.76729220397862,1.),(1.,0.752906082887249,
1.),(1.,0.730803471035892,1.),(1.,0.707106781186547,1.)))
REPRESENTATION_ITEM('')
SURFACE()
) ;
#115 = (
BOUNDED_SURFACE()
B_SPLINE_SURFACE(3,2,((#141067,#141068,#141069),(#141070,#141071,#141072),
(#141073,#141074,#141075),(#141076,#141077,#141078),(#141079,#141080,#141081),
(#141082,#141083,#141084)),.UNSPECIFIED.,.F.,.F.,.F.)
B_SPLINE_SURFACE_WITH_KNOTS((4,2,4),(3,3),(-0.001244827516706,0.785398163397448,
1.5720411543116),(-0.001244827516706,1.),.UNSPECIFIED.)
GEOMETRIC_REPRESENTATION_ITEM()
RATIONAL_B_SPLINE_SURFACE(((1.00037229282022,0.850464094333164,1.),(1.00037181710672,
0.850655170404816,1.),(1.00040682904413,0.836592203069687,1.),(1.0005342246365,
0.785422225437665,1.),(1.00062673753062,0.748263304673023,1.),(1.00073060381448,
0.7065441578565,1.)))
REPRESENTATION_ITEM('')
SURFACE()
) ;
#116 = (
BOUNDED_SURFACE()
B_SPLINE_SURFACE(3,2,((#141096,#141097,#141098),(#141099,#141100,#141101),
(#141102,#141103,#141104),(#141105,#141106,#141107)),.UNSPECIFIED.,.F.,
 .F.,.F.)
B_SPLINE_SURFACE_WITH_KNOTS((4,4),(3,3),(1.10714871779409,1.5707963267949),
(0.,1.),.UNSPECIFIED.)
GEOMETRIC_REPRESENTATION_ITEM()
RATIONAL_B_SPLINE_SURFACE(((1.,0.743704326447947,1.),(1.,0.732676928202348,
1.),(1.,0.720087778783135,1.),(1.,0.707106781186548,1.)))
REPRESENTATION_ITEM('')
SURFACE()
) ;
#117 = (
BOUNDED_SURFACE()
B_SPLINE_SURFACE(3,2,((#141115,#141116,#141117),(#141118,#141119,#141120),
(#141121,#141122,#141123),(#141124,#141125,#141126)),.UNSPECIFIED.,.F.,
 .F.,.F.)
B_SPLINE_SURFACE_WITH_KNOTS((4,4),(3,3),(1.5707963267949,2.0344439357957),
(0.,1.),.UNSPECIFIED.)
GEOMETRIC_REPRESENTATION_ITEM()
RATIONAL_B_SPLINE_SURFACE(((1.,0.707106781186548,1.),(1.,0.720087778783125,
1.),(1.,0.732676928202353,1.),(1.,0.743704326447947,1.)))
REPRESENTATION_ITEM('')
SURFACE()
) ;
#118 = (
BOUNDED_SURFACE()
B_SPLINE_SURFACE(3,2,((#141394,#141395,#141396),(#141397,#141398,#141399),
(#141400,#141401,#141402),(#141403,#141404,#141405)),.UNSPECIFIED.,.F.,
 .F.,.F.)
B_SPLINE_SURFACE_WITH_KNOTS((4,4),(3,3),(0.000111059871785624,0.00024129664665087),
(0.,1.00030059112224),.UNSPECIFIED.)
GEOMETRIC_REPRESENTATION_ITEM()
RATIONAL_B_SPLINE_SURFACE(((1.,0.839985548969901,1.00009619784682),(1.,
0.797322032917093,1.00012184639516),(1.,0.734686009440409,1.00015950206034),
(1.,0.707018740085206,1.00017613513143)))
REPRESENTATION_ITEM('')
SURFACE()
) ;
#119 = (
BOUNDED_SURFACE()
B_SPLINE_SURFACE(3,2,((#141407,#141408,#141409),(#141410,#141411,#141412),
(#141413,#141414,#141415),(#141416,#141417,#141418)),.UNSPECIFIED.,.F.,
 .F.,.F.)
B_SPLINE_SURFACE_WITH_KNOTS((4,4),(3,3),(3.14159265358979,3.68974201455418),
(0.,1.),.UNSPECIFIED.)
GEOMETRIC_REPRESENTATION_ITEM()
RATIONAL_B_SPLINE_SURFACE(((1.,0.860789971413512,1.),(1.,0.860809546755051,
1.),(1.,0.853709425573777,1.),(1.,0.840033633436873,1.)))
REPRESENTATION_ITEM('')
SURFACE()
) ;
#120 = (
BOUNDED_SURFACE()
B_SPLINE_SURFACE(3,2,((#141423,#141424,#141425),(#141426,#141427,#141428),
(#141429,#141430,#141431),(#141432,#141433,#141434)),.UNSPECIFIED.,.F.,
 .F.,.F.)
B_SPLINE_SURFACE_WITH_KNOTS((4,4),(3,3),(2.59344329260965,3.14159265358979),
(0.,1.),.UNSPECIFIED.)
GEOMETRIC_REPRESENTATION_ITEM()
RATIONAL_B_SPLINE_SURFACE(((1.,0.840033633435695,1.),(1.,0.853709425573363,
1.),(1.,0.860809546755055,1.),(1.,0.860789971413512,1.)))
REPRESENTATION_ITEM('')
SURFACE()
) ;
#121 = (
BOUNDED_SURFACE()
B_SPLINE_SURFACE(3,2,((#141436,#141437,#141438),(#141439,#141440,#141441),
(#141442,#141443,#141444),(#141445,#141446,#141447)),.UNSPECIFIED.,.F.,
 .F.,.F.)
B_SPLINE_SURFACE_WITH_KNOTS((4,4),(3,3),(0.000111059871788868,0.00024129664665087),
(-0.000300086749610278,1.),.UNSPECIFIED.)
GEOMETRIC_REPRESENTATION_ITEM()
RATIONAL_B_SPLINE_SURFACE(((1.00009603638458,0.839985629649299,1.),(1.00012164188339,
0.797322135108613,1.),(1.00015923434582,0.734686143216544,1.),(1.00017583949931,
0.70701888781253,1.)))
REPRESENTATION_ITEM('')
SURFACE()
) ;
#122 = (
BOUNDED_SURFACE()
B_SPLINE_SURFACE(3,2,((#141531,#141532,#141533),(#141534,#141535,#141536),
(#141537,#141538,#141539),(#141540,#141541,#141542),(#141543,#141544,#141545),
(#141546,#141547,#141548),(#141549,#141550,#141551),(#141552,#141553,#141554),
(#141555,#141556,#141557),(#141558,#141559,#141560)),.UNSPECIFIED.,.F.,
 .F.,.F.)
B_SPLINE_SURFACE_WITH_KNOTS((4,2,2,2,4),(3,3),(0.00112100122803331,0.00145633576709043,
0.0015908372445872,0.00165808798333558,0.00178849406635726),(-0.000893324189041646,
1.00101552458189),.UNSPECIFIED.)
GEOMETRIC_REPRESENTATION_ITEM()
RATIONAL_B_SPLINE_SURFACE(((1.00061830890901,0.653576280075763,1.00070297498501),
(1.00045188087558,0.74682193383013,1.00051375768181),(1.00032243686644,
0.819346321742964,1.00036658868739),(1.00017052538061,0.904458700444901,
1.000193875707),(1.00013074576005,0.926746272131261,1.00014864899627),(1.0000798364389,
0.955269549338603,1.00009076857638),(1.0000639484811,0.964171192776774,
1.00007270505388),(1.00002748579918,0.98460036292331,1.00003124947578),
(1.00001632684003,0.990852461324468,1.00001856250162),(1.00006581963706,
0.96312282876575,1.00007483243036)))
REPRESENTATION_ITEM('')
SURFACE()
) ;
#123 = (
BOUNDED_SURFACE()
B_SPLINE_SURFACE(3,2,((#141601,#141602,#141603),(#141604,#141605,#141606),
(#141607,#141608,#141609),(#141610,#141611,#141612),(#141613,#141614,#141615),
(#141616,#141617,#141618),(#141619,#141620,#141621),(#141622,#141623,#141624),
(#141625,#141626,#141627),(#141628,#141629,#141630)),.UNSPECIFIED.,.F.,
 .F.,.F.)
B_SPLINE_SURFACE_WITH_KNOTS((4,2,2,2,4),(3,3),(0.00112100122803333,0.00145633576709044,
0.00159083724458721,0.00165808798333559,0.00178849406635728),(-0.00113559264181192,
1.),.UNSPECIFIED.)
GEOMETRIC_REPRESENTATION_ITEM()
RATIONAL_B_SPLINE_SURFACE(((1.0007861837979,0.653844270846462,0.999999999999999),
(1.00057456947131,0.747017790468138,1.),(1.00040998057208,0.819486074062655,
1.),(1.00021682413016,0.904532610471955,1.),(1.00016624408397,0.926802940661334,
1.),(1.00010151255113,0.955304152477068,1.),(1.00008131090949,0.964198909671162,
1.),(1.00003494837237,0.984612275966151,1.),(1.00002075968325,0.990859537791165,
1.),(1.00008369009645,0.963151356666752,1.)))
REPRESENTATION_ITEM('')
SURFACE()
) ;
#124 = (
BOUNDED_SURFACE()
B_SPLINE_SURFACE(3,2,((#141667,#141668,#141669),(#141670,#141671,#141672),
(#141673,#141674,#141675),(#141676,#141677,#141678),(#141679,#141680,#141681),
(#141682,#141683,#141684),(#141685,#141686,#141687),(#141688,#141689,#141690),
(#141691,#141692,#141693),(#141694,#141695,#141696),(#141697,#141698,#141699),
(#141700,#141701,#141702),(#141703,#141704,#141705),(#141706,#141707,#141708),
(#141709,#141710,#141711),(#141712,#141713,#141714)),.UNSPECIFIED.,.F.,
 .F.,.F.)
B_SPLINE_SURFACE_WITH_KNOTS((4,2,2,2,2,2,2,4),(3,3),(5.6278630844106E-15,
3.85995771599548E-5,5.78993657371183E-5,6.75492600257001E-5,7.23742071699909E-5,
7.47866807421364E-5,7.59929175282091E-5,7.71991543142818E-5),(0.,1.00107899067834),
 .UNSPECIFIED.)
GEOMETRIC_REPRESENTATION_ITEM()
RATIONAL_B_SPLINE_SURFACE(((1.,0.976255617118804,1.00005123993558),(1.,
0.981339981891258,1.00004026797119),(1.,0.986086237829169,1.00003002563937),
(1.,0.992269463037034,1.00001668235464),(1.,0.994174411180042,1.00001257151207),
(1.,0.996706913506702,1.00000710641926),(1.,0.997492596832094,1.00000541092929),
(1.,0.998537621803387,1.00000315578488),(1.,0.998865045809503,1.00000244920998),
(1.,0.999323526852936,1.00000145981644),(1.,0.999468419970867,1.00000114713979),
(1.,0.99959844684718,1.00000086654422),(1.,0.999614491362718,1.00000083192045),
(1.,0.999732489024762,1.0000005772837),(1.,0.999724369239699,1.00000059480604),
(1.,1.,1.)))
REPRESENTATION_ITEM('')
SURFACE()
) ;
#125 = (
BOUNDED_SURFACE()
B_SPLINE_SURFACE(3,2,((#141716,#141717,#141718),(#141719,#141720,#141721),
(#141722,#141723,#141724),(#141725,#141726,#141727),(#141728,#141729,#141730),
(#141731,#141732,#141733),(#141734,#141735,#141736),(#141737,#141738,#141739),
(#141740,#141741,#141742),(#141743,#141744,#141745)),.UNSPECIFIED.,.F.,
 .F.,.F.)
B_SPLINE_SURFACE_WITH_KNOTS((4,2,2,2,4),(3,3),(-0.000110707928511331,0.000553539642556653,
0.00083030946383498,0.000968694374474144,0.00121778721363011),(0.,1.00563383762648),
 .UNSPECIFIED.)
GEOMETRIC_REPRESENTATION_ITEM()
RATIONAL_B_SPLINE_SURFACE(((1.,0.710139408519336,1.00326605501343),(1.,
0.691948125897064,1.00347102847846),(1.,0.728232377173955,1.00306218931827),
(1.,0.818030374423766,1.0020503746469),(1.,0.849110759469326,1.00170017096147),
(1.,0.897979778369984,1.00114953072656),(1.,0.914666724297552,1.00096150763889),
(1.,0.961090538823421,1.00043841917281),(1.,0.990973799041186,1.00010170430117),
(1.,0.992463455161859,1.00008491933977)))
REPRESENTATION_ITEM('')
SURFACE()
) ;
#126 = (
BOUNDED_SURFACE()
B_SPLINE_SURFACE(3,2,((#141747,#141748,#141749),(#141750,#141751,#141752),
(#141753,#141754,#141755),(#141756,#141757,#141758),(#141759,#141760,#141761),
(#141762,#141763,#141764),(#141765,#141766,#141767),(#141768,#141769,#141770),
(#141771,#141772,#141773),(#141774,#141775,#141776)),.UNSPECIFIED.,.F.,
 .F.,.F.)
B_SPLINE_SURFACE_WITH_KNOTS((4,2,2,2,4),(3,3),(-0.000137915648493739,0.000139027965246064,
0.000278055930499746,0.00055611186100711,0.00125013859505175),(-0.000741678185789884,
1.00283457365337),.UNSPECIFIED.)
GEOMETRIC_REPRESENTATION_ITEM()
RATIONAL_B_SPLINE_SURFACE(((1.00001340810331,0.990935328832968,1.00005135076275),
(1.00000300543756,0.997968146378497,1.0000115103164),(1.00005311279899,
0.96409260530696,1.00020341301648),(1.00012590576287,0.914880254704378,
1.00048219772838),(1.00015093966345,0.897955856706366,1.00057807332388),
(1.00022375355362,0.848729358697935,1.00085693817989),(1.00026920263033,
0.818003093715416,1.00103100043918),(1.00040494517438,0.726233102312152,
1.001550871372),(1.00045889592401,0.689759203410882,1.00175749359735),(1.00042429005326,
0.713154819594753,1.00162495897875)))
REPRESENTATION_ITEM('')
SURFACE()
) ;
#127 = (
BOUNDED_SURFACE()
B_SPLINE_SURFACE(3,2,((#141778,#141779,#141780),(#141781,#141782,#141783),
(#141784,#141785,#141786),(#141787,#141788,#141789),(#141790,#141791,#141792),
(#141793,#141794,#141795),(#141796,#141797,#141798),(#141799,#141800,#141801),
(#141802,#141803,#141804),(#141805,#141806,#141807),(#141808,#141809,#141810),
(#141811,#141812,#141813),(#141814,#141815,#141816),(#141817,#141818,#141819),
(#141820,#141821,#141822),(#141823,#141824,#141825)),.UNSPECIFIED.,.F.,
 .F.,.F.)
B_SPLINE_SURFACE_WITH_KNOTS((4,2,2,2,2,2,2,4),(3,3),(7.77892019462184E-15,
3.88447601478307E-5,5.82671402178566E-5,6.79783302528695E-5,7.2833925270376E-5,
7.52617227791293E-5,7.64756215335059E-5,7.76895202878825E-5),(-0.0012094552576271,
1.01080070868954),.UNSPECIFIED.)
GEOMETRIC_REPRESENTATION_ITEM()
RATIONAL_B_SPLINE_SURFACE(((1.00005744302266,0.975995723233527,1.00051789333955),
(1.00004519813152,0.981112615457371,1.0004074961621),(1.00003362760161,
0.985947705765597,1.00030317887351),(1.00001854219783,0.992251590743248,
1.00016717227456),(1.00001393966879,0.994174894491124,1.0001256769106),
(1.00000788875349,0.996703449551651,1.00007112322264),(1.00000601414708,
0.997486809637525,1.00005422219392),(1.00000351698944,0.998530321282699,
1.00003170838373),(1.00000273459082,0.998857269833631,1.0000246544542),
(1.00000163903614,0.999315079965992,1.00001477718022),(1.00000129000885,
0.999460931405225,1.00001163042892),(1.0000009745592,0.99959275143124,1.000008786406),
(1.00000093560708,0.99960902873406,1.00000843522246),(1.00000065019919,
0.999728294915417,1.00000586204929),(1.00000066918571,0.99972036083143,
1.00000603322751),(1.,1.,1.)))
REPRESENTATION_ITEM('')
SURFACE()
) ;
#128 = (
BOUNDED_SURFACE()
B_SPLINE_SURFACE(3,2,((#157489,#157490,#157491),(#157492,#157493,#157494),
(#157495,#157496,#157497),(#157498,#157499,#157500),(#157501,#157502,#157503),
(#157504,#157505,#157506)),.UNSPECIFIED.,.F.,.F.,.F.)
B_SPLINE_SURFACE_WITH_KNOTS((4,2,4),(3,3),(0.,0.785398163397448,1.5707963267949),
(0.,1.),.UNSPECIFIED.)
GEOMETRIC_REPRESENTATION_ITEM()
RATIONAL_B_SPLINE_SURFACE(((1.,0.923879532511288,1.),(1.,0.924029717224457,
1.),(1.,0.903812846803813,1.),(1.,0.828237960765067,1.),(1.,0.772793297349054,
1.),(1.,0.707106781186551,1.)))
REPRESENTATION_ITEM('')
SURFACE()
) ;
#129 = (
BOUNDED_SURFACE()
B_SPLINE_SURFACE(3,2,((#157529,#157530,#157531),(#157532,#157533,#157534),
(#157535,#157536,#157537),(#157538,#157539,#157540),(#157541,#157542,#157543),
(#157544,#157545,#157546)),.UNSPECIFIED.,.F.,.F.,.F.)
B_SPLINE_SURFACE_WITH_KNOTS((4,2,4),(3,3),(1.5707963267949,2.35619449019234,
3.14159265358979),(0.,1.),.UNSPECIFIED.)
GEOMETRIC_REPRESENTATION_ITEM()
RATIONAL_B_SPLINE_SURFACE(((1.,0.707106781186551,1.),(1.,0.772793297349013,
1.),(1.,0.828237960765125,1.),(1.,0.903812846803755,1.),(1.,0.924029717224501,
1.),(1.,0.923879532511288,1.)))
REPRESENTATION_ITEM('')
SURFACE()
) ;
#130 = (
BOUNDED_SURFACE()
B_SPLINE_SURFACE(3,2,((#157548,#157549,#157550),(#157551,#157552,#157553),
(#157554,#157555,#157556),(#157557,#157558,#157559),(#157560,#157561,#157562),
(#157563,#157564,#157565)),.UNSPECIFIED.,.F.,.F.,.F.)
B_SPLINE_SURFACE_WITH_KNOTS((4,2,4),(3,3),(4.71185725581867,5.49778714378214,
6.2837170317456),(0.,1.00053172456602),.UNSPECIFIED.)
GEOMETRIC_REPRESENTATION_ITEM()
RATIONAL_B_SPLINE_SURFACE(((1.,0.70690521752879,1.00031169139202),(1.,0.729483947708843,
1.00028768006101),(1.,0.750534083362416,1.00026529431252),(1.,0.779901566764209,
1.00023406348779),(1.,0.788212408697306,1.00022522533015),(1.,0.788092590029068,
1.00022535275121)))
REPRESENTATION_ITEM('')
SURFACE()
) ;
#131 = (
BOUNDED_SURFACE()
B_SPLINE_SURFACE(3,2,((#157577,#157578,#157579),(#157580,#157581,#157582),
(#157583,#157584,#157585),(#157586,#157587,#157588),(#157589,#157590,#157591),
(#157592,#157593,#157594)),.UNSPECIFIED.,.F.,.F.,.F.)
B_SPLINE_SURFACE_WITH_KNOTS((4,2,4),(3,3),(3.14106092902388,3.92699081698724,
4.71292070495061),(0.,1.00053172456592),.UNSPECIFIED.)
GEOMETRIC_REPRESENTATION_ITEM()
RATIONAL_B_SPLINE_SURFACE(((1.,0.788092590029089,1.00022535275116),(1.,
0.788212408697304,1.0002252253301),(1.,0.77990156676426,1.00023406348774),
(1.,0.750534083362408,1.00026529431247),(1.,0.729483947708901,1.00028768006096),
(1.,0.706905217528829,1.00031169139196)))
REPRESENTATION_ITEM('')
SURFACE()
) ;
#132 = (
BOUNDED_SURFACE()
B_SPLINE_SURFACE(3,2,((#157852,#157853,#157854),(#157855,#157856,#157857),
(#157858,#157859,#157860),(#157861,#157862,#157863),(#157864,#157865,#157866),
(#157867,#157868,#157869),(#157870,#157871,#157872),(#157873,#157874,#157875),
(#157876,#157877,#157878),(#157879,#157880,#157881)),.UNSPECIFIED.,.F.,
 .F.,.F.)
B_SPLINE_SURFACE_WITH_KNOTS((4,2,2,2,4),(3,3),(-3.3881317890172E-21,5.50005871024832E-5,
0.000110001174204966,0.000165001761307449,0.000220002348409933),(-9.32574651155486E-5,
1.),.UNSPECIFIED.)
GEOMETRIC_REPRESENTATION_ITEM()
RATIONAL_B_SPLINE_SURFACE(((1.00005463405283,0.707079466707411,1.),(1.00005694771662,
0.694674755787634,1.),(1.00005645688428,0.697306353922579,1.),(1.00005591567353,
0.70020805593976,1.),(1.0000556235962,0.701774028840071,1.),(1.00005562454822,
0.701768924610627,1.),(1.00005591789343,0.700196153956614,1.),(1.00005645795057,
0.697300636998118,1.),(1.00005694973354,0.694663942070733,1.),(1.00005463405283,
0.707079466707407,1.)))
REPRESENTATION_ITEM('')
SURFACE()
) ;
#133 = (
BOUNDED_SURFACE()
B_SPLINE_SURFACE(3,2,((#157886,#157887,#157888),(#157889,#157890,#157891),
(#157892,#157893,#157894),(#157895,#157896,#157897),(#157898,#157899,#157900),
(#157901,#157902,#157903),(#157904,#157905,#157906),(#157907,#157908,#157909),
(#157910,#157911,#157912),(#157913,#157914,#157915)),.UNSPECIFIED.,.F.,
 .F.,.F.)
B_SPLINE_SURFACE_WITH_KNOTS((4,2,2,2,4),(3,3),(-1.89735380184963E-19,5.50005871024829E-5,
0.000110001174204966,0.000165001761307449,0.000220002348409932),(0.,1.00009325746512),
 .UNSPECIFIED.)
GEOMETRIC_REPRESENTATION_ITEM()
RATIONAL_B_SPLINE_SURFACE(((1.,0.707079466707407,1.00005463405283),(1.,
0.69467475578763,1.00005694771662),(1.,0.697306353922582,1.00005645688428),
(1.,0.700208055939751,1.00005591567353),(1.,0.701774028840056,1.0000556235962),
(1.,0.701768924610644,1.00005562454822),(1.,0.700196153956613,1.00005591789343),
(1.,0.697300636998124,1.00005645795057),(1.,0.694663942070735,1.00005694973354),
(1.,0.70707946670741,1.00005463405283)))
REPRESENTATION_ITEM('')
SURFACE()
) ;
#134 = (
BOUNDED_SURFACE()
B_SPLINE_SURFACE(3,2,((#163040,#163041,#163042),(#163043,#163044,#163045),
(#163046,#163047,#163048),(#163049,#163050,#163051),(#163052,#163053,#163054),
(#163055,#163056,#163057)),.UNSPECIFIED.,.F.,.F.,.F.)
B_SPLINE_SURFACE_WITH_KNOTS((4,2,4),(3,3),(0.,0.785398163397448,1.5707963267949),
(0.,1.),.UNSPECIFIED.)
GEOMETRIC_REPRESENTATION_ITEM()
RATIONAL_B_SPLINE_SURFACE(((1.,0.923879532511288,1.),(1.,0.924029717224521,
1.),(1.,0.903812846803727,1.),(1.,0.828237960765152,1.),(1.,0.772793297348994,
1.),(1.,0.707106781186548,1.)))
REPRESENTATION_ITEM('')
SURFACE()
) ;
#135 = (
BOUNDED_SURFACE()
B_SPLINE_SURFACE(3,2,((#163080,#163081,#163082),(#163083,#163084,#163085),
(#163086,#163087,#163088),(#163089,#163090,#163091),(#163092,#163093,#163094),
(#163095,#163096,#163097)),.UNSPECIFIED.,.F.,.F.,.F.)
B_SPLINE_SURFACE_WITH_KNOTS((4,2,4),(3,3),(1.5707963267949,2.35619449019234,
3.14159265358979),(0.,1.),.UNSPECIFIED.)
GEOMETRIC_REPRESENTATION_ITEM()
RATIONAL_B_SPLINE_SURFACE(((1.,0.707106781186551,1.),(1.,0.772793297348998,
1.),(1.,0.828237960765139,1.),(1.,0.90381284680374,1.),(1.,0.924029717224511,
1.),(1.,0.923879532511288,1.)))
REPRESENTATION_ITEM('')
SURFACE()
) ;
#136 = (
BOUNDED_SURFACE()
B_SPLINE_SURFACE(3,2,((#163099,#163100,#163101),(#163102,#163103,#163104),
(#163105,#163106,#163107),(#163108,#163109,#163110),(#163111,#163112,#163113),
(#163114,#163115,#163116)),.UNSPECIFIED.,.F.,.F.,.F.)
B_SPLINE_SURFACE_WITH_KNOTS((4,2,4),(3,3),(4.71185725581866,5.49778714378214,
6.28371703174562),(0.,1.00053172456603),.UNSPECIFIED.)
GEOMETRIC_REPRESENTATION_ITEM()
RATIONAL_B_SPLINE_SURFACE(((1.,0.706905217528784,1.00031169139203),(1.,
0.729483947708883,1.00028768006102),(1.,0.750534083362363,1.00026529431253),
(1.,0.779901566764257,1.00023406348779),(1.,0.788212408697267,1.00022522533015),
(1.,0.788092590029066,1.00022535275121)))
REPRESENTATION_ITEM('')
SURFACE()
) ;
#137 = (
BOUNDED_SURFACE()
B_SPLINE_SURFACE(3,2,((#163128,#163129,#163130),(#163131,#163132,#163133),
(#163134,#163135,#163136),(#163137,#163138,#163139),(#163140,#163141,#163142),
(#163143,#163144,#163145)),.UNSPECIFIED.,.F.,.F.,.F.)
B_SPLINE_SURFACE_WITH_KNOTS((4,2,4),(3,3),(3.14106092902389,3.92699081698724,
4.71292070495059),(0.,1.0005317245659),.UNSPECIFIED.)
GEOMETRIC_REPRESENTATION_ITEM()
RATIONAL_B_SPLINE_SURFACE(((1.,0.788092590029092,1.00022535275116),(1.,
0.788212408697299,1.0002252253301),(1.,0.779901566764274,1.00023406348774),
(1.,0.7505340833624,1.00026529431246),(1.,0.729483947708915,1.00028768006095),
(1.,0.706905217528834,1.00031169139195)))
REPRESENTATION_ITEM('')
SURFACE()
) ;
#138 = (
BOUNDED_SURFACE()
B_SPLINE_SURFACE(3,2,((#163546,#163547,#163548),(#163549,#163550,#163551),
(#163552,#163553,#163554),(#163555,#163556,#163557),(#163558,#163559,#163560),
(#163561,#163562,#163563),(#163564,#163565,#163566),(#163567,#163568,#163569)),
 .UNSPECIFIED.,.F.,.F.,.F.)
B_SPLINE_SURFACE_WITH_KNOTS((4,2,2,4),(3,3),(1.5707963267949,2.35619449019234,
2.74889357189107,3.14159265358979),(0.,1.),.UNSPECIFIED.)
GEOMETRIC_REPRESENTATION_ITEM()
RATIONAL_B_SPLINE_SURFACE(((1.,1.,1.),(1.,1.00267605951749,1.),(1.,0.941599607549753,
1.),(1.,0.828238301901781,1.),(1.,0.787677905717216,1.),(1.,0.726552333979994,
1.),(1.,0.706675310150435,1.),(1.,0.707106781186544,1.)))
REPRESENTATION_ITEM('')
SURFACE()
) ;
#139 = (
BOUNDED_SURFACE()
B_SPLINE_SURFACE(3,2,((#163573,#163574,#163575),(#163576,#163577,#163578),
(#163579,#163580,#163581),(#163582,#163583,#163584),(#163585,#163586,#163587),
(#163588,#163589,#163590),(#163591,#163592,#163593),(#163594,#163595,#163596)),
 .UNSPECIFIED.,.F.,.F.,.F.)
B_SPLINE_SURFACE_WITH_KNOTS((4,2,2,4),(3,3),(4.71238898038469,5.49778714378214,
5.89048622548086,6.28318530717959),(0.,1.),.UNSPECIFIED.)
GEOMETRIC_REPRESENTATION_ITEM()
RATIONAL_B_SPLINE_SURFACE(((1.,1.,1.),(1.,1.00267605951751,1.),(1.,0.941599607549725,
1.),(1.,0.828238301901795,1.),(1.,0.787677905717217,1.),(1.,0.726552333979995,
1.),(1.,0.706675310150434,1.),(1.,0.707106781186544,1.)))
REPRESENTATION_ITEM('')
SURFACE()
) ;
#140 = (
BOUNDED_SURFACE()
B_SPLINE_SURFACE(3,2,((#163601,#163602,#163603),(#163604,#163605,#163606),
(#163607,#163608,#163609),(#163610,#163611,#163612),(#163613,#163614,#163615),
(#163616,#163617,#163618),(#163619,#163620,#163621),(#163622,#163623,#163624)),
 .UNSPECIFIED.,.F.,.F.,.F.)
B_SPLINE_SURFACE_WITH_KNOTS((4,2,2,4),(3,3),(1.5707963267949,2.35619449019234,
2.74889357189107,3.14159265358979),(0.,1.),.UNSPECIFIED.)
GEOMETRIC_REPRESENTATION_ITEM()
RATIONAL_B_SPLINE_SURFACE(((1.,1.,1.),(1.,1.00267605951744,1.),(1.,0.941599607549824,
1.),(1.,0.828238301901746,1.),(1.,0.787677905717207,1.),(1.,0.726552333980003,
1.),(1.,0.706675310150422,1.),(1.,0.707106781186548,1.)))
REPRESENTATION_ITEM('')
SURFACE()
) ;
#141 = (
BOUNDED_SURFACE()
B_SPLINE_SURFACE(3,2,((#163646,#163647,#163648),(#163649,#163650,#163651),
(#163652,#163653,#163654),(#163655,#163656,#163657),(#163658,#163659,#163660),
(#163661,#163662,#163663),(#163664,#163665,#163666),(#163667,#163668,#163669)),
 .UNSPECIFIED.,.F.,.F.,.F.)
B_SPLINE_SURFACE_WITH_KNOTS((4,2,2,4),(3,3),(4.71238898038469,5.49778714378214,
5.89048622548086,6.28318530717959),(0.,1.),.UNSPECIFIED.)
GEOMETRIC_REPRESENTATION_ITEM()
RATIONAL_B_SPLINE_SURFACE(((1.,1.,1.),(1.,1.00267605951747,1.),(1.,0.941599607549785,
1.),(1.,0.828238301901765,1.),(1.,0.787677905717207,1.),(1.,0.726552333980003,
1.),(1.,0.706675310150422,1.),(1.,0.707106781186548,1.)))
REPRESENTATION_ITEM('')
SURFACE()
) ;
#142 = (
BOUNDED_SURFACE()
B_SPLINE_SURFACE(3,2,((#163670,#163671,#163672),(#163673,#163674,#163675),
(#163676,#163677,#163678),(#163679,#163680,#163681),(#163682,#163683,#163684),
(#163685,#163686,#163687),(#163688,#163689,#163690),(#163691,#163692,#163693)),
 .UNSPECIFIED.,.F.,.F.,.F.)
B_SPLINE_SURFACE_WITH_KNOTS((4,2,2,4),(3,3),(3.38657131671666,3.71802573263366,
4.04948014855067,4.71238898038469),(-0.000420825309489484,1.00042070189283),
 .UNSPECIFIED.)
GEOMETRIC_REPRESENTATION_ITEM()
RATIONAL_B_SPLINE_SURFACE(((1.00022935632051,0.727377552434629,1.00022928902823),
(1.00021435583198,0.74520775606903,1.00021429294078),(1.00019031910525,
0.773778807684193,1.00019026326634),(1.00013753195033,0.836523812238417,
1.00013749159897),(1.00010896375305,0.870481157936262,1.0001089317835),
(1.00003378452308,0.959842312830291,1.00003377461082),(0.999998875499962,
1.00133662744396,0.999998875829887),(1.,1.,1.)))
REPRESENTATION_ITEM('')
SURFACE()
) ;
#143 = (
BOUNDED_SURFACE()
B_SPLINE_SURFACE(3,2,((#163695,#163696,#163697),(#163698,#163699,#163700),
(#163701,#163702,#163703),(#163704,#163705,#163706)),.UNSPECIFIED.,.F.,
 .F.,.F.)
B_SPLINE_SURFACE_WITH_KNOTS((4,4),(3,3),(1.32581766366803,1.5707963267949),
(0.,1.),.UNSPECIFIED.)
GEOMETRIC_REPRESENTATION_ITEM()
RATIONAL_B_SPLINE_SURFACE(((1.,0.727606875108995,1.),(1.,0.721005575721677,
1.),(1.,0.714109499479742,1.),(1.,0.707106781186548,1.)))
REPRESENTATION_ITEM('')
SURFACE()
) ;
#144 = (
BOUNDED_SURFACE()
B_SPLINE_SURFACE(3,2,((#163722,#163723,#163724),(#163725,#163726,#163727),
(#163728,#163729,#163730),(#163731,#163732,#163733)),.UNSPECIFIED.,.F.,
 .F.,.F.)
B_SPLINE_SURFACE_WITH_KNOTS((4,4),(3,3),(3.92699081698724,4.71238898038469),
(0.,1.),.UNSPECIFIED.)
GEOMETRIC_REPRESENTATION_ITEM()
RATIONAL_B_SPLINE_SURFACE(((1.,0.866025403784441,1.),(1.,0.82836361504933,
1.),(1.,0.772698924407957,1.),(1.,0.707106781186548,1.)))
REPRESENTATION_ITEM('')
SURFACE()
) ;
#145 = (
BOUNDED_SURFACE()
B_SPLINE_SURFACE(3,2,((#163735,#163736,#163737),(#163738,#163739,#163740),
(#163741,#163742,#163743),(#163744,#163745,#163746)),.UNSPECIFIED.,.F.,
 .F.,.F.)
B_SPLINE_SURFACE_WITH_KNOTS((4,4),(3,3),(1.5707963267949,2.35619449019234),
(0.,1.),.UNSPECIFIED.)
GEOMETRIC_REPRESENTATION_ITEM()
RATIONAL_B_SPLINE_SURFACE(((1.,1.,1.),(1.,1.00150544078213,1.),(1.,0.943158245625731,
1.),(1.,0.866025403784441,1.)))
REPRESENTATION_ITEM('')
SURFACE()
) ;
#146 = (
BOUNDED_SURFACE()
B_SPLINE_SURFACE(3,2,((#163747,#163748,#163749),(#163750,#163751,#163752),
(#163753,#163754,#163755),(#163756,#163757,#163758)),.UNSPECIFIED.,.F.,
 .F.,.F.)
B_SPLINE_SURFACE_WITH_KNOTS((4,4),(3,3),(7.06858347057708,7.85398163397448),
(0.,1.),.UNSPECIFIED.)
GEOMETRIC_REPRESENTATION_ITEM()
RATIONAL_B_SPLINE_SURFACE(((1.,0.866025403784455,1.),(1.,0.943158245625741,
1.),(1.,1.00150544078213,1.),(1.,1.,1.)))
REPRESENTATION_ITEM('')
SURFACE()
) ;
#147 = (
BOUNDED_SURFACE()
B_SPLINE_SURFACE(3,2,((#163760,#163761,#163762),(#163763,#163764,#163765),
(#163766,#163767,#163768),(#163769,#163770,#163771)),.UNSPECIFIED.,.F.,
 .F.,.F.)
B_SPLINE_SURFACE_WITH_KNOTS((4,4),(3,3),(1.5707963267949,2.35619449019239),
(0.,1.),.UNSPECIFIED.)
GEOMETRIC_REPRESENTATION_ITEM()
RATIONAL_B_SPLINE_SURFACE(((1.,0.707106781186545,1.),(1.,0.77269892440796,
1.),(1.,0.82836361504934,1.),(1.,0.866025403784447,1.)))
REPRESENTATION_ITEM('')
SURFACE()
) ;
#148 = (
BOUNDED_SURFACE()
B_SPLINE_SURFACE(3,2,((#163787,#163788,#163789),(#163790,#163791,#163792),
(#163793,#163794,#163795),(#163796,#163797,#163798)),.UNSPECIFIED.,.F.,
 .F.,.F.)
B_SPLINE_SURFACE_WITH_KNOTS((4,4),(3,3),(4.71238898038469,4.95736764351155),
(0.,1.),.UNSPECIFIED.)
GEOMETRIC_REPRESENTATION_ITEM()
RATIONAL_B_SPLINE_SURFACE(((1.,0.707106781186548,1.),(1.,0.714109499479746,
1.),(1.,0.721005575721676,1.),(1.,0.727606875108995,1.)))
REPRESENTATION_ITEM('')
SURFACE()
) ;
#149 = (
BOUNDED_SURFACE()
B_SPLINE_SURFACE(3,2,((#163800,#163801,#163802),(#163803,#163804,#163805),
(#163806,#163807,#163808),(#163809,#163810,#163811),(#163812,#163813,#163814),
(#163815,#163816,#163817),(#163818,#163819,#163820),(#163821,#163822,#163823)),
 .UNSPECIFIED.,.F.,.F.,.F.)
B_SPLINE_SURFACE_WITH_KNOTS((4,2,2,4),(3,3),(3.38657131671666,3.71802573263366,
4.04948014855067,4.71238898038469),(-0.000420825307952133,1.00042070189548),
 .UNSPECIFIED.)
GEOMETRIC_REPRESENTATION_ITEM()
RATIONAL_B_SPLINE_SURFACE(((1.00022935631968,0.727377552434324,1.00022928902968),
(1.0002143558312,0.745207756068745,1.00021429294214),(1.00019031910455,
0.77377880768394,1.00019026326754),(1.00013753194982,0.836523812238234,
1.00013749159984),(1.00010896375265,0.87048115793612,1.00010893178419),
(1.00003378452295,0.959842312830239,1.00003377461103),(0.999998875499966,
1.00133662744397,0.99999887582988),(1.,1.,1.)))
REPRESENTATION_ITEM('')
SURFACE()
) ;
#150 = (
BOUNDED_SURFACE()
B_SPLINE_SURFACE(3,2,((#164038,#164039,#164040),(#164041,#164042,#164043),
(#164044,#164045,#164046),(#164047,#164048,#164049),(#164050,#164051,#164052),
(#164053,#164054,#164055),(#164056,#164057,#164058),(#164059,#164060,#164061)),
 .UNSPECIFIED.,.F.,.F.,.F.)
B_SPLINE_SURFACE_WITH_KNOTS((4,2,2,4),(3,3),(1.5707963267949,2.35619449019234,
2.74889357189107,3.14159265358979),(0.,1.),.UNSPECIFIED.)
GEOMETRIC_REPRESENTATION_ITEM()
RATIONAL_B_SPLINE_SURFACE(((1.,1.,1.),(1.,1.00267605951747,1.),(1.,0.941599607549782,
1.),(1.,0.828238301901767,1.),(1.,0.787677905717159,1.),(1.,0.726552333980051,
1.),(1.,0.706675310150383,1.),(1.,0.707106781186548,1.)))
REPRESENTATION_ITEM('')
SURFACE()
) ;
#151 = (
BOUNDED_SURFACE()
B_SPLINE_SURFACE(3,2,((#164065,#164066,#164067),(#164068,#164069,#164070),
(#164071,#164072,#164073),(#164074,#164075,#164076),(#164077,#164078,#164079),
(#164080,#164081,#164082),(#164083,#164084,#164085),(#164086,#164087,#164088)),
 .UNSPECIFIED.,.F.,.F.,.F.)
B_SPLINE_SURFACE_WITH_KNOTS((4,2,2,4),(3,3),(4.71238898038469,5.49778714378214,
5.89048622548086,6.28318530717959),(0.,1.),.UNSPECIFIED.)
GEOMETRIC_REPRESENTATION_ITEM()
RATIONAL_B_SPLINE_SURFACE(((1.,1.,1.),(1.,1.00267605951742,1.),(1.,0.941599607549842,
1.),(1.,0.828238301901737,1.),(1.,0.787677905717144,1.),(1.,0.726552333980065,
1.),(1.,0.706675310150372,1.),(1.,0.707106781186548,1.)))
REPRESENTATION_ITEM('')
SURFACE()
) ;
#152 = (
BOUNDED_SURFACE()
B_SPLINE_SURFACE(3,2,((#164093,#164094,#164095),(#164096,#164097,#164098),
(#164099,#164100,#164101),(#164102,#164103,#164104),(#164105,#164106,#164107),
(#164108,#164109,#164110),(#164111,#164112,#164113),(#164114,#164115,#164116)),
 .UNSPECIFIED.,.F.,.F.,.F.)
B_SPLINE_SURFACE_WITH_KNOTS((4,2,2,4),(3,3),(1.5707963267949,2.35619449019234,
2.74889357189107,3.14159265358979),(0.,1.),.UNSPECIFIED.)
GEOMETRIC_REPRESENTATION_ITEM()
RATIONAL_B_SPLINE_SURFACE(((1.,1.,1.),(1.,1.0026760595174,1.),(1.,0.941599607549881,
1.),(1.,0.828238301901717,1.),(1.,0.787677905717207,1.),(1.,0.726552333980003,
1.),(1.,0.706675310150419,1.),(1.,0.707106781186548,1.)))
REPRESENTATION_ITEM('')
SURFACE()
) ;
#153 = (
BOUNDED_SURFACE()
B_SPLINE_SURFACE(3,2,((#164138,#164139,#164140),(#164141,#164142,#164143),
(#164144,#164145,#164146),(#164147,#164148,#164149),(#164150,#164151,#164152),
(#164153,#164154,#164155),(#164156,#164157,#164158),(#164159,#164160,#164161)),
 .UNSPECIFIED.,.F.,.F.,.F.)
B_SPLINE_SURFACE_WITH_KNOTS((4,2,2,4),(3,3),(4.71238898038469,5.49778714378214,
5.89048622548086,6.28318530717959),(0.,1.),.UNSPECIFIED.)
GEOMETRIC_REPRESENTATION_ITEM()
RATIONAL_B_SPLINE_SURFACE(((1.,1.,1.),(1.,1.00267605951742,1.),(1.,0.941599607549842,
1.),(1.,0.828238301901737,1.),(1.,0.787677905717207,1.),(1.,0.726552333980003,
1.),(1.,0.706675310150423,1.),(1.,0.707106781186548,1.)))
REPRESENTATION_ITEM('')
SURFACE()
) ;
#154 = (
BOUNDED_SURFACE()
B_SPLINE_SURFACE(3,2,((#164162,#164163,#164164),(#164165,#164166,#164167),
(#164168,#164169,#164170),(#164171,#164172,#164173),(#164174,#164175,#164176),
(#164177,#164178,#164179),(#164180,#164181,#164182),(#164183,#164184,#164185)),
 .UNSPECIFIED.,.F.,.F.,.F.)
B_SPLINE_SURFACE_WITH_KNOTS((4,2,2,4),(3,3),(3.38657131671666,3.71802573263366,
4.04948014855067,4.71238898038469),(-0.000420825308263448,1.00042070189224),
 .UNSPECIFIED.)
GEOMETRIC_REPRESENTATION_ITEM()
RATIONAL_B_SPLINE_SURFACE(((1.00022935631984,0.727377552435123,1.00022928902791),
(1.00021435583136,0.745207756069495,1.00021429294048),(1.0001903191047,
0.773778807684603,1.00019026326607),(1.00013753194992,0.836523812238713,
1.00013749159878),(1.00010896375274,0.8704811579365,1.00010893178334),(1.00003378452297,
0.959842312830357,1.00003377461078),(0.999998875499966,1.00133662744397,
0.999998875829888),(1.,1.,1.)))
REPRESENTATION_ITEM('')
SURFACE()
) ;
#155 = (
BOUNDED_SURFACE()
B_SPLINE_SURFACE(3,2,((#164187,#164188,#164189),(#164190,#164191,#164192),
(#164193,#164194,#164195),(#164196,#164197,#164198)),.UNSPECIFIED.,.F.,
 .F.,.F.)
B_SPLINE_SURFACE_WITH_KNOTS((4,4),(3,3),(1.32581766366803,1.5707963267949),
(0.,1.),.UNSPECIFIED.)
GEOMETRIC_REPRESENTATION_ITEM()
RATIONAL_B_SPLINE_SURFACE(((1.,0.727606875108995,1.),(1.,0.721005575721675,
1.),(1.,0.71410949947975,1.),(1.,0.707106781186548,1.)))
REPRESENTATION_ITEM('')
SURFACE()
) ;
#156 = (
BOUNDED_SURFACE()
B_SPLINE_SURFACE(3,2,((#164214,#164215,#164216),(#164217,#164218,#164219),
(#164220,#164221,#164222),(#164223,#164224,#164225)),.UNSPECIFIED.,.F.,
 .F.,.F.)
B_SPLINE_SURFACE_WITH_KNOTS((4,4),(3,3),(3.92699081698723,4.71238898038469),
(0.,1.),.UNSPECIFIED.)
GEOMETRIC_REPRESENTATION_ITEM()
RATIONAL_B_SPLINE_SURFACE(((1.,0.866025403784441,1.),(1.,0.828363615049339,
1.),(1.,0.772698924407948,1.),(1.,0.707106781186548,1.)))
REPRESENTATION_ITEM('')
SURFACE()
) ;
#157 = (
BOUNDED_SURFACE()
B_SPLINE_SURFACE(3,2,((#164227,#164228,#164229),(#164230,#164231,#164232),
(#164233,#164234,#164235),(#164236,#164237,#164238)),.UNSPECIFIED.,.F.,
 .F.,.F.)
B_SPLINE_SURFACE_WITH_KNOTS((4,4),(3,3),(1.5707963267949,2.35619449019234),
(0.,1.),.UNSPECIFIED.)
GEOMETRIC_REPRESENTATION_ITEM()
RATIONAL_B_SPLINE_SURFACE(((1.,1.,1.),(1.,1.00150544078213,1.),(1.,0.943158245625731,
1.),(1.,0.866025403784441,1.)))
REPRESENTATION_ITEM('')
SURFACE()
) ;
#158 = (
BOUNDED_SURFACE()
B_SPLINE_SURFACE(3,2,((#164239,#164240,#164241),(#164242,#164243,#164244),
(#164245,#164246,#164247),(#164248,#164249,#164250)),.UNSPECIFIED.,.F.,
 .F.,.F.)
B_SPLINE_SURFACE_WITH_KNOTS((4,4),(3,3),(7.06858347057708,7.85398163397448),
(0.,1.),.UNSPECIFIED.)
GEOMETRIC_REPRESENTATION_ITEM()
RATIONAL_B_SPLINE_SURFACE(((1.,0.866025403784455,1.),(1.,0.943158245625741,
1.),(1.,1.00150544078213,1.),(1.,1.,1.)))
REPRESENTATION_ITEM('')
SURFACE()
) ;
#159 = (
BOUNDED_SURFACE()
B_SPLINE_SURFACE(3,2,((#164252,#164253,#164254),(#164255,#164256,#164257),
(#164258,#164259,#164260),(#164261,#164262,#164263)),.UNSPECIFIED.,.F.,
 .F.,.F.)
B_SPLINE_SURFACE_WITH_KNOTS((4,4),(3,3),(1.5707963267949,2.35619449019239),
(0.,1.),.UNSPECIFIED.)
GEOMETRIC_REPRESENTATION_ITEM()
RATIONAL_B_SPLINE_SURFACE(((1.,0.707106781186545,1.),(1.,0.772698924407959,
1.),(1.,0.828363615049342,1.),(1.,0.866025403784447,1.)))
REPRESENTATION_ITEM('')
SURFACE()
) ;
#160 = (
BOUNDED_SURFACE()
B_SPLINE_SURFACE(3,2,((#164279,#164280,#164281),(#164282,#164283,#164284),
(#164285,#164286,#164287),(#164288,#164289,#164290)),.UNSPECIFIED.,.F.,
 .F.,.F.)
B_SPLINE_SURFACE_WITH_KNOTS((4,4),(3,3),(4.71238898038469,4.95736764351155),
(0.,1.),.UNSPECIFIED.)
GEOMETRIC_REPRESENTATION_ITEM()
RATIONAL_B_SPLINE_SURFACE(((1.,0.707106781186548,1.),(1.,0.714109499479743,
1.),(1.,0.721005575721684,1.),(1.,0.727606875108989,1.)))
REPRESENTATION_ITEM('')
SURFACE()
) ;
#161 = (
BOUNDED_SURFACE()
B_SPLINE_SURFACE(3,2,((#164292,#164293,#164294),(#164295,#164296,#164297),
(#164298,#164299,#164300),(#164301,#164302,#164303),(#164304,#164305,#164306),
(#164307,#164308,#164309),(#164310,#164311,#164312),(#164313,#164314,#164315)),
 .UNSPECIFIED.,.F.,.F.,.F.)
B_SPLINE_SURFACE_WITH_KNOTS((4,2,2,4),(3,3),(3.38657131671666,3.71802573263366,
4.04948014855067,4.71238898038469),(-0.000420825308919027,1.00042070189557),
 .UNSPECIFIED.)
GEOMETRIC_REPRESENTATION_ITEM()
RATIONAL_B_SPLINE_SURFACE(((1.00022935632021,0.727377552434032,1.00022928902973),
(1.00021435583169,0.745207756068483,1.00021429294218),(1.00019031910499,
0.773778807683706,1.00019026326758),(1.00013753195014,0.836523812238065,
1.00013749159987),(1.0001089637529,0.870481157935983,1.0001089317842),(1.00003378452302,
0.959842312830197,1.00003377461104),(0.999998875499964,1.00133662744398,
0.999998875829879),(1.,1.,1.)))
REPRESENTATION_ITEM('')
SURFACE()
) ;
#162 = (
BOUNDED_SURFACE()
B_SPLINE_SURFACE(3,2,((#164530,#164531,#164532),(#164533,#164534,#164535),
(#164536,#164537,#164538),(#164539,#164540,#164541),(#164542,#164543,#164544),
(#164545,#164546,#164547),(#164548,#164549,#164550),(#164551,#164552,#164553)),
 .UNSPECIFIED.,.F.,.F.,.F.)
B_SPLINE_SURFACE_WITH_KNOTS((4,2,2,4),(3,3),(1.5707963267949,2.35619449019234,
2.74889357189107,3.14159265358979),(0.,1.),.UNSPECIFIED.)
GEOMETRIC_REPRESENTATION_ITEM()
RATIONAL_B_SPLINE_SURFACE(((1.,1.,1.),(1.,1.00267605951747,1.),(1.,0.941599607549782,
1.),(1.,0.828238301901767,1.),(1.,0.787677905717283,1.),(1.,0.726552333979927,
1.),(1.,0.706675310150483,1.),(1.,0.707106781186548,1.)))
REPRESENTATION_ITEM('')
SURFACE()
) ;
#163 = (
BOUNDED_SURFACE()
B_SPLINE_SURFACE(3,2,((#164557,#164558,#164559),(#164560,#164561,#164562),
(#164563,#164564,#164565),(#164566,#164567,#164568),(#164569,#164570,#164571),
(#164572,#164573,#164574),(#164575,#164576,#164577),(#164578,#164579,#164580)),
 .UNSPECIFIED.,.F.,.F.,.F.)
B_SPLINE_SURFACE_WITH_KNOTS((4,2,2,4),(3,3),(4.71238898038469,5.49778714378214,
5.89048622548086,6.28318530717959),(0.,1.),.UNSPECIFIED.)
GEOMETRIC_REPRESENTATION_ITEM()
RATIONAL_B_SPLINE_SURFACE(((1.,1.,1.),(1.,1.00267605951751,1.),(1.,0.941599607549728,
1.),(1.,0.828238301901794,1.),(1.,0.787677905717269,1.),(1.,0.726552333979941,
1.),(1.,0.706675310150473,1.),(1.,0.707106781186548,1.)))
REPRESENTATION_ITEM('')
SURFACE()
) ;
#164 = (
BOUNDED_SURFACE()
B_SPLINE_SURFACE(3,2,((#164585,#164586,#164587),(#164588,#164589,#164590),
(#164591,#164592,#164593),(#164594,#164595,#164596),(#164597,#164598,#164599),
(#164600,#164601,#164602),(#164603,#164604,#164605),(#164606,#164607,#164608)),
 .UNSPECIFIED.,.F.,.F.,.F.)
B_SPLINE_SURFACE_WITH_KNOTS((4,2,2,4),(3,3),(1.5707963267949,2.35619449019234,
2.74889357189107,3.14159265358979),(0.,1.),.UNSPECIFIED.)
GEOMETRIC_REPRESENTATION_ITEM()
RATIONAL_B_SPLINE_SURFACE(((1.,1.,1.),(1.,1.00267605951739,1.),(1.,0.941599607549883,
1.),(1.,0.828238301901719,1.),(1.,0.787677905717209,1.),(1.,0.726552333979999,
1.),(1.,0.706675310150425,1.),(1.,0.707106781186548,1.)))
REPRESENTATION_ITEM('')
SURFACE()
) ;
#165 = (
BOUNDED_SURFACE()
B_SPLINE_SURFACE(3,2,((#164630,#164631,#164632),(#164633,#164634,#164635),
(#164636,#164637,#164638),(#164639,#164640,#164641),(#164642,#164643,#164644),
(#164645,#164646,#164647),(#164648,#164649,#164650),(#164651,#164652,#164653)),
 .UNSPECIFIED.,.F.,.F.,.F.)
B_SPLINE_SURFACE_WITH_KNOTS((4,2,2,4),(3,3),(4.71238898038469,5.49778714378214,
5.89048622548086,6.28318530717959),(0.,1.),.UNSPECIFIED.)
GEOMETRIC_REPRESENTATION_ITEM()
RATIONAL_B_SPLINE_SURFACE(((1.,1.,1.),(1.,1.00267605951742,1.),(1.,0.941599607549841,
1.),(1.,0.82823830190174,1.),(1.,0.787677905717209,1.),(1.,0.726552333979999,
1.),(1.,0.706675310150426,1.),(1.,0.707106781186548,1.)))
REPRESENTATION_ITEM('')
SURFACE()
) ;
#166 = (
BOUNDED_SURFACE()
B_SPLINE_SURFACE(3,2,((#164654,#164655,#164656),(#164657,#164658,#164659),
(#164660,#164661,#164662),(#164663,#164664,#164665),(#164666,#164667,#164668),
(#164669,#164670,#164671),(#164672,#164673,#164674),(#164675,#164676,#164677)),
 .UNSPECIFIED.,.F.,.F.,.F.)
B_SPLINE_SURFACE_WITH_KNOTS((4,2,2,4),(3,3),(3.38657131671666,3.71802573263366,
4.04948014855067,4.71238898038469),(-0.000420825307961358,1.00042070189188),
 .UNSPECIFIED.)
GEOMETRIC_REPRESENTATION_ITEM()
RATIONAL_B_SPLINE_SURFACE(((1.00022935631968,0.727377552435299,1.00022928902772),
(1.00021435583119,0.74520775606967,1.0002142929403),(1.00019031910456,0.773778807684758,
1.00019026326591),(1.00013753194983,0.836523812238825,1.00013749159866),
(1.00010896375265,0.870481157936586,1.00010893178325),(1.00003378452295,
0.959842312830383,1.00003377461075),(0.999998875499967,1.00133662744397,
0.999998875829889),(1.,1.,1.)))
REPRESENTATION_ITEM('')
SURFACE()
) ;
#167 = (
BOUNDED_SURFACE()
B_SPLINE_SURFACE(3,2,((#164679,#164680,#164681),(#164682,#164683,#164684),
(#164685,#164686,#164687),(#164688,#164689,#164690)),.UNSPECIFIED.,.F.,
 .F.,.F.)
B_SPLINE_SURFACE_WITH_KNOTS((4,4),(3,3),(1.32581766366803,1.5707963267949),
(0.,1.),.UNSPECIFIED.)
GEOMETRIC_REPRESENTATION_ITEM()
RATIONAL_B_SPLINE_SURFACE(((1.,0.727606875108989,1.),(1.,0.721005575721685,
1.),(1.,0.714109499479745,1.),(1.,0.707106781186548,1.)))
REPRESENTATION_ITEM('')
SURFACE()
) ;
#168 = (
BOUNDED_SURFACE()
B_SPLINE_SURFACE(3,2,((#164706,#164707,#164708),(#164709,#164710,#164711),
(#164712,#164713,#164714),(#164715,#164716,#164717)),.UNSPECIFIED.,.F.,
 .F.,.F.)
B_SPLINE_SURFACE_WITH_KNOTS((4,4),(3,3),(3.92699081698723,4.71238898038469),
(0.,1.),.UNSPECIFIED.)
GEOMETRIC_REPRESENTATION_ITEM()
RATIONAL_B_SPLINE_SURFACE(((1.,0.866025403784441,1.),(1.,0.828363615049344,
1.),(1.,0.772698924407949,1.),(1.,0.707106781186548,1.)))
REPRESENTATION_ITEM('')
SURFACE()
) ;
#169 = (
BOUNDED_SURFACE()
B_SPLINE_SURFACE(3,2,((#164719,#164720,#164721),(#164722,#164723,#164724),
(#164725,#164726,#164727),(#164728,#164729,#164730)),.UNSPECIFIED.,.F.,
 .F.,.F.)
B_SPLINE_SURFACE_WITH_KNOTS((4,4),(3,3),(1.5707963267949,2.35619449019234),
(0.,1.),.UNSPECIFIED.)
GEOMETRIC_REPRESENTATION_ITEM()
RATIONAL_B_SPLINE_SURFACE(((1.,1.,1.),(1.,1.00150544078213,1.),(1.,0.943158245625731,
1.),(1.,0.866025403784441,1.)))
REPRESENTATION_ITEM('')
SURFACE()
) ;
#170 = (
BOUNDED_SURFACE()
B_SPLINE_SURFACE(3,2,((#164731,#164732,#164733),(#164734,#164735,#164736),
(#164737,#164738,#164739),(#164740,#164741,#164742)),.UNSPECIFIED.,.F.,
 .F.,.F.)
B_SPLINE_SURFACE_WITH_KNOTS((4,4),(3,3),(7.06858347057709,7.85398163397448),
(0.,1.),.UNSPECIFIED.)
GEOMETRIC_REPRESENTATION_ITEM()
RATIONAL_B_SPLINE_SURFACE(((1.,0.866025403784455,1.),(1.,0.943158245625743,
1.),(1.,1.00150544078213,1.),(1.,1.,1.)))
REPRESENTATION_ITEM('')
SURFACE()
) ;
#171 = (
BOUNDED_SURFACE()
B_SPLINE_SURFACE(3,2,((#164744,#164745,#164746),(#164747,#164748,#164749),
(#164750,#164751,#164752),(#164753,#164754,#164755)),.UNSPECIFIED.,.F.,
 .F.,.F.)
B_SPLINE_SURFACE_WITH_KNOTS((4,4),(3,3),(1.5707963267949,2.35619449019239),
(0.,1.),.UNSPECIFIED.)
GEOMETRIC_REPRESENTATION_ITEM()
RATIONAL_B_SPLINE_SURFACE(((1.,0.707106781186545,1.),(1.,0.772698924407961,
1.),(1.,0.828363615049341,1.),(1.,0.866025403784449,1.)))
REPRESENTATION_ITEM('')
SURFACE()
) ;
#172 = (
BOUNDED_SURFACE()
B_SPLINE_SURFACE(3,2,((#164771,#164772,#164773),(#164774,#164775,#164776),
(#164777,#164778,#164779),(#164780,#164781,#164782)),.UNSPECIFIED.,.F.,
 .F.,.F.)
B_SPLINE_SURFACE_WITH_KNOTS((4,4),(3,3),(4.71238898038469,4.95736764351155),
(0.,1.),.UNSPECIFIED.)
GEOMETRIC_REPRESENTATION_ITEM()
RATIONAL_B_SPLINE_SURFACE(((1.,0.707106781186548,1.),(1.,0.714109499479746,
1.),(1.,0.721005575721676,1.),(1.,0.727606875108995,1.)))
REPRESENTATION_ITEM('')
SURFACE()
) ;
#173 = (
BOUNDED_SURFACE()
B_SPLINE_SURFACE(3,2,((#164784,#164785,#164786),(#164787,#164788,#164789),
(#164790,#164791,#164792),(#164793,#164794,#164795),(#164796,#164797,#164798),
(#164799,#164800,#164801),(#164802,#164803,#164804),(#164805,#164806,#164807)),
 .UNSPECIFIED.,.F.,.F.,.F.)
B_SPLINE_SURFACE_WITH_KNOTS((4,2,2,4),(3,3),(3.38657131671666,3.71802573263366,
4.04948014855067,4.71238898038469),(-0.00042082530997056,1.00042070189335),
 .UNSPECIFIED.)
GEOMETRIC_REPRESENTATION_ITEM()
RATIONAL_B_SPLINE_SURFACE(((1.00022935632077,0.727377552434356,1.00022928902852),
(1.00021435583222,0.745207756068763,1.00021429294105),(1.00019031910547,
0.773778807683983,1.00019026326658),(1.00013753195048,0.836523812238235,
1.00013749159914),(1.00010896375318,0.870481157936081,1.00010893178364),
(1.00003378452311,0.95984231283035,1.00003377461086),(0.999998875499962,
1.00133662744389,0.999998875829885),(1.,1.,1.)))
REPRESENTATION_ITEM('')
SURFACE()
) ;
#174 = (
BOUNDED_SURFACE()
B_SPLINE_SURFACE(3,2,((#165022,#165023,#165024),(#165025,#165026,#165027),
(#165028,#165029,#165030),(#165031,#165032,#165033),(#165034,#165035,#165036),
(#165037,#165038,#165039),(#165040,#165041,#165042),(#165043,#165044,#165045)),
 .UNSPECIFIED.,.F.,.F.,.F.)
B_SPLINE_SURFACE_WITH_KNOTS((4,2,2,4),(3,3),(1.5707963267949,2.35619449019234,
2.74889357189107,3.14159265358979),(0.,1.),.UNSPECIFIED.)
GEOMETRIC_REPRESENTATION_ITEM()
RATIONAL_B_SPLINE_SURFACE(((1.,1.,1.),(1.,1.00267605951743,1.),(1.,0.941599607549841,
1.),(1.,0.82823830190174,1.),(1.,0.787677905717223,1.),(1.,0.726552333979985,
1.),(1.,0.706675310150436,1.),(1.,0.707106781186548,1.)))
REPRESENTATION_ITEM('')
SURFACE()
) ;
#175 = (
BOUNDED_SURFACE()
B_SPLINE_SURFACE(3,2,((#165049,#165050,#165051),(#165052,#165053,#165054),
(#165055,#165056,#165057),(#165058,#165059,#165060),(#165061,#165062,#165063),
(#165064,#165065,#165066),(#165067,#165068,#165069),(#165070,#165071,#165072)),
 .UNSPECIFIED.,.F.,.F.,.F.)
B_SPLINE_SURFACE_WITH_KNOTS((4,2,2,4),(3,3),(4.71238898038469,5.49778714378214,
5.89048622548086,6.28318530717959),(0.,1.),.UNSPECIFIED.)
GEOMETRIC_REPRESENTATION_ITEM()
RATIONAL_B_SPLINE_SURFACE(((1.,1.,1.),(1.,1.00267605951742,1.),(1.,0.941599607549841,
1.),(1.,0.82823830190174,1.),(1.,0.787677905717209,1.),(1.,0.726552333979999,
1.),(1.,0.706675310150426,1.),(1.,0.707106781186548,1.)))
REPRESENTATION_ITEM('')
SURFACE()
) ;
#176 = (
BOUNDED_SURFACE()
B_SPLINE_SURFACE(3,2,((#165077,#165078,#165079),(#165080,#165081,#165082),
(#165083,#165084,#165085),(#165086,#165087,#165088),(#165089,#165090,#165091),
(#165092,#165093,#165094),(#165095,#165096,#165097),(#165098,#165099,#165100)),
 .UNSPECIFIED.,.F.,.F.,.F.)
B_SPLINE_SURFACE_WITH_KNOTS((4,2,2,4),(3,3),(1.5707963267949,2.35619449019234,
2.74889357189107,3.14159265358979),(0.,1.),.UNSPECIFIED.)
GEOMETRIC_REPRESENTATION_ITEM()
RATIONAL_B_SPLINE_SURFACE(((1.,1.,1.),(1.,1.00267605951739,1.),(1.,0.941599607549883,
1.),(1.,0.828238301901719,1.),(1.,0.787677905717209,1.),(1.,0.726552333979999,
1.),(1.,0.706675310150425,1.),(1.,0.707106781186548,1.)))
REPRESENTATION_ITEM('')
SURFACE()
) ;
#177 = (
BOUNDED_SURFACE()
B_SPLINE_SURFACE(3,2,((#165122,#165123,#165124),(#165125,#165126,#165127),
(#165128,#165129,#165130),(#165131,#165132,#165133),(#165134,#165135,#165136),
(#165137,#165138,#165139),(#165140,#165141,#165142),(#165143,#165144,#165145)),
 .UNSPECIFIED.,.F.,.F.,.F.)
B_SPLINE_SURFACE_WITH_KNOTS((4,2,2,4),(3,3),(4.71238898038469,5.49778714378214,
5.89048622548086,6.28318530717959),(0.,1.),.UNSPECIFIED.)
GEOMETRIC_REPRESENTATION_ITEM()
RATIONAL_B_SPLINE_SURFACE(((1.,1.,1.),(1.,1.00267605951742,1.),(1.,0.941599607549841,
1.),(1.,0.82823830190174,1.),(1.,0.787677905717209,1.),(1.,0.726552333979999,
1.),(1.,0.706675310150426,1.),(1.,0.707106781186548,1.)))
REPRESENTATION_ITEM('')
SURFACE()
) ;
#178 = (
BOUNDED_SURFACE()
B_SPLINE_SURFACE(3,2,((#165146,#165147,#165148),(#165149,#165150,#165151),
(#165152,#165153,#165154),(#165155,#165156,#165157),(#165158,#165159,#165160),
(#165161,#165162,#165163),(#165164,#165165,#165166),(#165167,#165168,#165169)),
 .UNSPECIFIED.,.F.,.F.,.F.)
B_SPLINE_SURFACE_WITH_KNOTS((4,2,2,4),(3,3),(3.38657131671666,3.71802573263366,
4.04948014855067,4.71238898038469),(-0.000420825307131761,1.00042070189354),
 .UNSPECIFIED.)
GEOMETRIC_REPRESENTATION_ITEM()
RATIONAL_B_SPLINE_SURFACE(((1.00022935631923,0.727377552435078,1.00022928902862),
(1.00021435583078,0.745207756069438,1.00021429294114),(1.00019031910419,
0.773778807684582,1.00019026326667),(1.00013753194956,0.836523812238669,
1.0001374915992),(1.00010896375244,0.870481157936476,1.00010893178368),
(1.00003378452288,0.959842312830354,1.00003377461088),(0.999998875499969,
1.00133662744396,0.999998875829884),(1.,1.,1.)))
REPRESENTATION_ITEM('')
SURFACE()
) ;
#179 = (
BOUNDED_SURFACE()
B_SPLINE_SURFACE(3,2,((#165171,#165172,#165173),(#165174,#165175,#165176),
(#165177,#165178,#165179),(#165180,#165181,#165182)),.UNSPECIFIED.,.F.,
 .F.,.F.)
B_SPLINE_SURFACE_WITH_KNOTS((4,4),(3,3),(1.32581766366803,1.5707963267949),
(0.,1.),.UNSPECIFIED.)
GEOMETRIC_REPRESENTATION_ITEM()
RATIONAL_B_SPLINE_SURFACE(((1.,0.727606875108995,1.),(1.,0.721005575721675,
1.),(1.,0.71410949947975,1.),(1.,0.707106781186548,1.)))
REPRESENTATION_ITEM('')
SURFACE()
) ;
#180 = (
BOUNDED_SURFACE()
B_SPLINE_SURFACE(3,2,((#165198,#165199,#165200),(#165201,#165202,#165203),
(#165204,#165205,#165206),(#165207,#165208,#165209)),.UNSPECIFIED.,.F.,
 .F.,.F.)
B_SPLINE_SURFACE_WITH_KNOTS((4,4),(3,3),(3.92699081698722,4.71238898038469),
(0.,1.),.UNSPECIFIED.)
GEOMETRIC_REPRESENTATION_ITEM()
RATIONAL_B_SPLINE_SURFACE(((1.,0.866025403784442,1.),(1.,0.828363615049333,
1.),(1.,0.772698924407957,1.),(1.,0.707106781186545,1.)))
REPRESENTATION_ITEM('')
SURFACE()
) ;
#181 = (
BOUNDED_SURFACE()
B_SPLINE_SURFACE(3,2,((#165211,#165212,#165213),(#165214,#165215,#165216),
(#165217,#165218,#165219),(#165220,#165221,#165222)),.UNSPECIFIED.,.F.,
 .F.,.F.)
B_SPLINE_SURFACE_WITH_KNOTS((4,4),(3,3),(1.5707963267949,2.35619449019234),
(0.,1.),.UNSPECIFIED.)
GEOMETRIC_REPRESENTATION_ITEM()
RATIONAL_B_SPLINE_SURFACE(((1.,1.,1.),(1.,1.00150544078214,1.),(1.,0.943158245625729,
1.),(1.,0.866025403784442,1.)))
REPRESENTATION_ITEM('')
SURFACE()
) ;
#182 = (
BOUNDED_SURFACE()
B_SPLINE_SURFACE(3,2,((#165223,#165224,#165225),(#165226,#165227,#165228),
(#165229,#165230,#165231),(#165232,#165233,#165234)),.UNSPECIFIED.,.F.,
 .F.,.F.)
B_SPLINE_SURFACE_WITH_KNOTS((4,4),(3,3),(7.06858347057709,7.85398163397448),
(0.,1.),.UNSPECIFIED.)
GEOMETRIC_REPRESENTATION_ITEM()
RATIONAL_B_SPLINE_SURFACE(((1.,0.866025403784455,1.),(1.,0.943158245625743,
1.),(1.,1.00150544078213,1.),(1.,1.,1.)))
REPRESENTATION_ITEM('')
SURFACE()
) ;
#183 = (
BOUNDED_SURFACE()
B_SPLINE_SURFACE(3,2,((#165236,#165237,#165238),(#165239,#165240,#165241),
(#165242,#165243,#165244),(#165245,#165246,#165247)),.UNSPECIFIED.,.F.,
 .F.,.F.)
B_SPLINE_SURFACE_WITH_KNOTS((4,4),(3,3),(1.5707963267949,2.35619449019239),
(0.,1.),.UNSPECIFIED.)
GEOMETRIC_REPRESENTATION_ITEM()
RATIONAL_B_SPLINE_SURFACE(((1.,0.707106781186545,1.),(1.,0.772698924407961,
1.),(1.,0.828363615049341,1.),(1.,0.866025403784449,1.)))
REPRESENTATION_ITEM('')
SURFACE()
) ;
#184 = (
BOUNDED_SURFACE()
B_SPLINE_SURFACE(3,2,((#165263,#165264,#165265),(#165266,#165267,#165268),
(#165269,#165270,#165271),(#165272,#165273,#165274)),.UNSPECIFIED.,.F.,
 .F.,.F.)
B_SPLINE_SURFACE_WITH_KNOTS((4,4),(3,3),(4.71238898038469,4.95736764351155),
(0.,1.),.UNSPECIFIED.)
GEOMETRIC_REPRESENTATION_ITEM()
RATIONAL_B_SPLINE_SURFACE(((1.,0.707106781186548,1.),(1.,0.714109499479746,
1.),(1.,0.721005575721676,1.),(1.,0.727606875108995,1.)))
REPRESENTATION_ITEM('')
SURFACE()
) ;
#185 = (
BOUNDED_SURFACE()
B_SPLINE_SURFACE(3,2,((#165276,#165277,#165278),(#165279,#165280,#165281),
(#165282,#165283,#165284),(#165285,#165286,#165287),(#165288,#165289,#165290),
(#165291,#165292,#165293),(#165294,#165295,#165296),(#165297,#165298,#165299)),
 .UNSPECIFIED.,.F.,.F.,.F.)
B_SPLINE_SURFACE_WITH_KNOTS((4,2,2,4),(3,3),(3.38657131671666,3.71802573263366,
4.04948014855067,4.71238898038469),(-0.000420825309824966,1.00042070189421),
 .UNSPECIFIED.)
GEOMETRIC_REPRESENTATION_ITEM()
RATIONAL_B_SPLINE_SURFACE(((1.0002293563207,0.72737755243416,1.00022928902899),
(1.00021435583215,0.74520775606858,1.00021429294149),(1.0001903191054,0.77377880768382,
1.00019026326696),(1.00013753195043,0.836523812238119,1.00013749159943),
(1.00010896375314,0.870481157935989,1.00010893178386),(1.0000337845231,
0.959842312830321,1.00003377461093),(0.999998875499962,1.0013366274439,
0.999998875829883),(1.,1.,1.)))
REPRESENTATION_ITEM('')
SURFACE()
) ;
#186 = (
BOUNDED_SURFACE()
B_SPLINE_SURFACE(3,2,((#165514,#165515,#165516),(#165517,#165518,#165519),
(#165520,#165521,#165522),(#165523,#165524,#165525),(#165526,#165527,#165528),
(#165529,#165530,#165531),(#165532,#165533,#165534),(#165535,#165536,#165537)),
 .UNSPECIFIED.,.F.,.F.,.F.)
B_SPLINE_SURFACE_WITH_KNOTS((4,2,2,4),(3,3),(1.5707963267949,2.35619449019234,
2.74889357189107,3.14159265358979),(0.,1.),.UNSPECIFIED.)
GEOMETRIC_REPRESENTATION_ITEM()
RATIONAL_B_SPLINE_SURFACE(((1.,1.,1.),(1.,1.00267605951751,1.),(1.,0.94159960754973,
1.),(1.,0.828238301901795,1.),(1.,0.787677905717223,1.),(1.,0.726552333979985,
1.),(1.,0.706675310150446,1.),(1.,0.707106781186535,1.)))
REPRESENTATION_ITEM('')
SURFACE()
) ;
#187 = (
BOUNDED_SURFACE()
B_SPLINE_SURFACE(3,2,((#165541,#165542,#165543),(#165544,#165545,#165546),
(#165547,#165548,#165549),(#165550,#165551,#165552),(#165553,#165554,#165555),
(#165556,#165557,#165558),(#165559,#165560,#165561),(#165562,#165563,#165564)),
 .UNSPECIFIED.,.F.,.F.,.F.)
B_SPLINE_SURFACE_WITH_KNOTS((4,2,2,4),(3,3),(4.71238898038469,5.49778714378214,
5.89048622548086,6.28318530717959),(0.,1.),.UNSPECIFIED.)
GEOMETRIC_REPRESENTATION_ITEM()
RATIONAL_B_SPLINE_SURFACE(((1.,1.,1.),(1.,1.00267605951751,1.),(1.,0.94159960754973,
1.),(1.,0.828238301901796,1.),(1.,0.787677905717209,1.),(1.,0.726552333979999,
1.),(1.,0.706675310150435,1.),(1.,0.707106781186535,1.)))
REPRESENTATION_ITEM('')
SURFACE()
) ;
#188 = (
BOUNDED_SURFACE()
B_SPLINE_SURFACE(3,2,((#165569,#165570,#165571),(#165572,#165573,#165574),
(#165575,#165576,#165577),(#165578,#165579,#165580),(#165581,#165582,#165583),
(#165584,#165585,#165586),(#165587,#165588,#165589),(#165590,#165591,#165592)),
 .UNSPECIFIED.,.F.,.F.,.F.)
B_SPLINE_SURFACE_WITH_KNOTS((4,2,2,4),(3,3),(1.5707963267949,2.35619449019234,
2.74889357189107,3.14159265358979),(0.,1.),.UNSPECIFIED.)
GEOMETRIC_REPRESENTATION_ITEM()
RATIONAL_B_SPLINE_SURFACE(((1.,1.,1.),(1.,1.00267605951731,1.),(1.,0.941599607549997,
1.),(1.,0.828238301901662,1.),(1.,0.787677905717218,1.),(1.,0.726552333980008,
1.),(1.,0.706675310150421,1.),(1.,0.707106781186548,1.)))
REPRESENTATION_ITEM('')
SURFACE()
) ;
#189 = (
BOUNDED_SURFACE()
B_SPLINE_SURFACE(3,2,((#165614,#165615,#165616),(#165617,#165618,#165619),
(#165620,#165621,#165622),(#165623,#165624,#165625),(#165626,#165627,#165628),
(#165629,#165630,#165631),(#165632,#165633,#165634),(#165635,#165636,#165637)),
 .UNSPECIFIED.,.F.,.F.,.F.)
B_SPLINE_SURFACE_WITH_KNOTS((4,2,2,4),(3,3),(4.71238898038469,5.49778714378214,
5.89048622548086,6.28318530717959),(0.,1.),.UNSPECIFIED.)
GEOMETRIC_REPRESENTATION_ITEM()
RATIONAL_B_SPLINE_SURFACE(((1.,1.,1.),(1.,1.00267605951734,1.),(1.,0.941599607549954,
1.),(1.,0.828238301901683,1.),(1.,0.787677905717218,1.),(1.,0.726552333980008,
1.),(1.,0.706675310150422,1.),(1.,0.707106781186548,1.)))
REPRESENTATION_ITEM('')
SURFACE()
) ;
#190 = (
BOUNDED_SURFACE()
B_SPLINE_SURFACE(3,2,((#165638,#165639,#165640),(#165641,#165642,#165643),
(#165644,#165645,#165646),(#165647,#165648,#165649),(#165650,#165651,#165652),
(#165653,#165654,#165655),(#165656,#165657,#165658),(#165659,#165660,#165661)),
 .UNSPECIFIED.,.F.,.F.,.F.)
B_SPLINE_SURFACE_WITH_KNOTS((4,2,2,4),(3,3),(3.38657131671666,3.71802573263366,
4.04948014855067,4.71238898038469),(-0.000420825307381943,1.00042070189293),
 .UNSPECIFIED.)
GEOMETRIC_REPRESENTATION_ITEM()
RATIONAL_B_SPLINE_SURFACE(((1.00022935631936,0.727377552435165,1.00022928902829),
(1.00021435583091,0.745207756069537,1.00021429294084),(1.0001903191043,
0.773778807684663,1.00019026326638),(1.00013753194964,0.836523812238728,
1.000137491599),(1.00010896375251,0.870481157936522,1.00010893178353),(1.0000337845229,
0.959842312830368,1.00003377461083),(0.999998875499968,1.00133662744396,
0.999998875829886),(1.,1.,1.)))
REPRESENTATION_ITEM('')
SURFACE()
) ;
#191 = (
BOUNDED_SURFACE()
B_SPLINE_SURFACE(3,2,((#165663,#165664,#165665),(#165666,#165667,#165668),
(#165669,#165670,#165671),(#165672,#165673,#165674)),.UNSPECIFIED.,.F.,
 .F.,.F.)
B_SPLINE_SURFACE_WITH_KNOTS((4,4),(3,3),(1.32581766366803,1.5707963267949),
(0.,1.),.UNSPECIFIED.)
GEOMETRIC_REPRESENTATION_ITEM()
RATIONAL_B_SPLINE_SURFACE(((1.,0.727606875108984,1.),(1.,0.7210055757217,
1.),(1.,0.714109499479712,1.),(1.,0.70710678118656,1.)))
REPRESENTATION_ITEM('')
SURFACE()
) ;
#192 = (
BOUNDED_SURFACE()
B_SPLINE_SURFACE(3,2,((#165690,#165691,#165692),(#165693,#165694,#165695),
(#165696,#165697,#165698),(#165699,#165700,#165701)),.UNSPECIFIED.,.F.,
 .F.,.F.)
B_SPLINE_SURFACE_WITH_KNOTS((4,4),(3,3),(3.92699081698722,4.71238898038469),
(0.,1.),.UNSPECIFIED.)
GEOMETRIC_REPRESENTATION_ITEM()
RATIONAL_B_SPLINE_SURFACE(((1.,0.866025403784442,1.),(1.,0.82836361504934,
1.),(1.,0.772698924407942,1.),(1.,0.707106781186558,1.)))
REPRESENTATION_ITEM('')
SURFACE()
) ;
#193 = (
BOUNDED_SURFACE()
B_SPLINE_SURFACE(3,2,((#165703,#165704,#165705),(#165706,#165707,#165708),
(#165709,#165710,#165711),(#165712,#165713,#165714)),.UNSPECIFIED.,.F.,
 .F.,.F.)
B_SPLINE_SURFACE_WITH_KNOTS((4,4),(3,3),(1.5707963267949,2.35619449019234),
(0.,1.),.UNSPECIFIED.)
GEOMETRIC_REPRESENTATION_ITEM()
RATIONAL_B_SPLINE_SURFACE(((1.,1.,1.),(1.,1.00150544078214,1.),(1.,0.943158245625727,
1.),(1.,0.866025403784442,1.)))
REPRESENTATION_ITEM('')
SURFACE()
) ;
#194 = (
BOUNDED_SURFACE()
B_SPLINE_SURFACE(3,2,((#165715,#165716,#165717),(#165718,#165719,#165720),
(#165721,#165722,#165723),(#165724,#165725,#165726)),.UNSPECIFIED.,.F.,
 .F.,.F.)
B_SPLINE_SURFACE_WITH_KNOTS((4,4),(3,3),(7.06858347057709,7.85398163397448),
(0.,1.),.UNSPECIFIED.)
GEOMETRIC_REPRESENTATION_ITEM()
RATIONAL_B_SPLINE_SURFACE(((1.,0.866025403784455,1.),(1.,0.943158245625744,
1.),(1.,1.00150544078213,1.),(1.,1.,1.)))
REPRESENTATION_ITEM('')
SURFACE()
) ;
#195 = (
BOUNDED_SURFACE()
B_SPLINE_SURFACE(3,2,((#165728,#165729,#165730),(#165731,#165732,#165733),
(#165734,#165735,#165736),(#165737,#165738,#165739)),.UNSPECIFIED.,.F.,
 .F.,.F.)
B_SPLINE_SURFACE_WITH_KNOTS((4,4),(3,3),(1.5707963267949,2.35619449019239),
(0.,1.),.UNSPECIFIED.)
GEOMETRIC_REPRESENTATION_ITEM()
RATIONAL_B_SPLINE_SURFACE(((1.,0.707106781186533,1.),(1.,0.772698924407975,
1.),(1.,0.828363615049334,1.),(1.,0.866025403784449,1.)))
REPRESENTATION_ITEM('')
SURFACE()
) ;
#196 = (
BOUNDED_SURFACE()
B_SPLINE_SURFACE(3,2,((#165755,#165756,#165757),(#165758,#165759,#165760),
(#165761,#165762,#165763),(#165764,#165765,#165766)),.UNSPECIFIED.,.F.,
 .F.,.F.)
B_SPLINE_SURFACE_WITH_KNOTS((4,4),(3,3),(4.71238898038469,4.95736764351155),
(0.,1.),.UNSPECIFIED.)
GEOMETRIC_REPRESENTATION_ITEM()
RATIONAL_B_SPLINE_SURFACE(((1.,0.707106781186535,1.),(1.,0.714109499479782,
1.),(1.,0.721005575721652,1.),(1.,0.727606875109006,1.)))
REPRESENTATION_ITEM('')
SURFACE()
) ;
#197 = (
BOUNDED_SURFACE()
B_SPLINE_SURFACE(3,2,((#165768,#165769,#165770),(#165771,#165772,#165773),
(#165774,#165775,#165776),(#165777,#165778,#165779),(#165780,#165781,#165782),
(#165783,#165784,#165785),(#165786,#165787,#165788),(#165789,#165790,#165791)),
 .UNSPECIFIED.,.F.,.F.,.F.)
B_SPLINE_SURFACE_WITH_KNOTS((4,2,2,4),(3,3),(3.38657131671666,3.71802573263366,
4.04948014855067,4.71238898038469),(-0.00042082530954674,1.00042070189244),
 .UNSPECIFIED.)
GEOMETRIC_REPRESENTATION_ITEM()
RATIONAL_B_SPLINE_SURFACE(((1.00022935632055,0.727377552434729,1.00022928902802),
(1.000214355832,0.745207756069095,1.00021429294059),(1.00019031910528,0.773778807684285,
1.00019026326617),(1.00013753195035,0.836523812238453,1.00013749159884),
(1.00010896375307,0.870481157936255,1.0001089317834),(1.00003378452308,
0.959842312830403,1.00003377461079),(0.999998875499963,1.00133662744389,
0.999998875829888),(1.,1.,1.)))
REPRESENTATION_ITEM('')
SURFACE()
) ;
#198 = (
BOUNDED_SURFACE()
B_SPLINE_SURFACE(3,2,((#166006,#166007,#166008),(#166009,#166010,#166011),
(#166012,#166013,#166014),(#166015,#166016,#166017),(#166018,#166019,#166020),
(#166021,#166022,#166023),(#166024,#166025,#166026),(#166027,#166028,#166029)),
 .UNSPECIFIED.,.F.,.F.,.F.)
B_SPLINE_SURFACE_WITH_KNOTS((4,2,2,4),(3,3),(1.5707963267949,2.35619449019234,
2.74889357189107,3.14159265358979),(0.,1.),.UNSPECIFIED.)
GEOMETRIC_REPRESENTATION_ITEM()
RATIONAL_B_SPLINE_SURFACE(((1.,1.,1.),(1.,1.00267605951743,1.),(1.,0.941599607549841,
1.),(1.,0.82823830190174,1.),(1.,0.787677905717349,1.),(1.,0.726552333979859,
1.),(1.,0.706675310150533,1.),(1.,0.707106781186548,1.)))
REPRESENTATION_ITEM('')
SURFACE()
) ;
#199 = (
BOUNDED_SURFACE()
B_SPLINE_SURFACE(3,2,((#166033,#166034,#166035),(#166036,#166037,#166038),
(#166039,#166040,#166041),(#166042,#166043,#166044),(#166045,#166046,#166047),
(#166048,#166049,#166050),(#166051,#166052,#166053),(#166054,#166055,#166056)),
 .UNSPECIFIED.,.F.,.F.,.F.)
B_SPLINE_SURFACE_WITH_KNOTS((4,2,2,4),(3,3),(4.71238898038469,5.49778714378214,
5.89048622548086,6.28318530717959),(0.,1.),.UNSPECIFIED.)
GEOMETRIC_REPRESENTATION_ITEM()
RATIONAL_B_SPLINE_SURFACE(((1.,1.,1.),(1.,1.00267605951742,1.),(1.,0.941599607549841,
1.),(1.,0.82823830190174,1.),(1.,0.787677905717335,1.),(1.,0.726552333979873,
1.),(1.,0.706675310150523,1.),(1.,0.707106781186548,1.)))
REPRESENTATION_ITEM('')
SURFACE()
) ;
#200 = (
BOUNDED_SURFACE()
B_SPLINE_SURFACE(3,2,((#166061,#166062,#166063),(#166064,#166065,#166066),
(#166067,#166068,#166069),(#166070,#166071,#166072),(#166073,#166074,#166075),
(#166076,#166077,#166078),(#166079,#166080,#166081),(#166082,#166083,#166084)),
 .UNSPECIFIED.,.F.,.F.,.F.)
B_SPLINE_SURFACE_WITH_KNOTS((4,2,2,4),(3,3),(1.5707963267949,2.35619449019234,
2.74889357189107,3.14159265358979),(0.,1.),.UNSPECIFIED.)
GEOMETRIC_REPRESENTATION_ITEM()
RATIONAL_B_SPLINE_SURFACE(((1.,1.,1.),(1.,1.00267605951739,1.),(1.,0.941599607549887,
1.),(1.,0.828238301901723,1.),(1.,0.787677905717337,1.),(1.,0.726552333979871,
1.),(1.,0.706675310150514,1.),(1.,0.707106781186548,1.)))
REPRESENTATION_ITEM('')
SURFACE()
) ;
#201 = (
BOUNDED_SURFACE()
B_SPLINE_SURFACE(3,2,((#166106,#166107,#166108),(#166109,#166110,#166111),
(#166112,#166113,#166114),(#166115,#166116,#166117),(#166118,#166119,#166120),
(#166121,#166122,#166123),(#166124,#166125,#166126),(#166127,#166128,#166129)),
 .UNSPECIFIED.,.F.,.F.,.F.)
B_SPLINE_SURFACE_WITH_KNOTS((4,2,2,4),(3,3),(4.71238898038469,5.49778714378214,
5.89048622548086,6.28318530717959),(0.,1.),.UNSPECIFIED.)
GEOMETRIC_REPRESENTATION_ITEM()
RATIONAL_B_SPLINE_SURFACE(((1.,1.,1.),(1.,1.00267605951742,1.),(1.,0.941599607549844,
1.),(1.,0.828238301901744,1.),(1.,0.787677905717337,1.),(1.,0.726552333979871,
1.),(1.,0.706675310150515,1.),(1.,0.707106781186548,1.)))
REPRESENTATION_ITEM('')
SURFACE()
) ;
#202 = (
BOUNDED_SURFACE()
B_SPLINE_SURFACE(3,2,((#166130,#166131,#166132),(#166133,#166134,#166135),
(#166136,#166137,#166138),(#166139,#166140,#166141),(#166142,#166143,#166144),
(#166145,#166146,#166147),(#166148,#166149,#166150),(#166151,#166152,#166153)),
 .UNSPECIFIED.,.F.,.F.,.F.)
B_SPLINE_SURFACE_WITH_KNOTS((4,2,2,4),(3,3),(3.38657131671666,3.71802573263366,
4.04948014855067,4.71238898038469),(-0.000420825307658434,1.00042070189319),
 .UNSPECIFIED.)
GEOMETRIC_REPRESENTATION_ITEM()
RATIONAL_B_SPLINE_SURFACE(((1.00022935631952,0.727377552435029,1.00022928902843),
(1.00021435583105,0.745207756069326,1.00021429294096),(1.00019031910442,
0.773778807684626,1.00019026326651),(1.00013753194973,0.836523812238567,
1.00013749159909),(1.00010896375258,0.870481157936425,1.00010893178359),
(1.00003378452293,0.959842312830407,1.00003377461085),(0.999998875499967,
1.00133662744392,0.999998875829886),(1.,1.,1.)))
REPRESENTATION_ITEM('')
SURFACE()
) ;
#203 = (
BOUNDED_SURFACE()
B_SPLINE_SURFACE(3,2,((#166155,#166156,#166157),(#166158,#166159,#166160),
(#166161,#166162,#166163),(#166164,#166165,#166166)),.UNSPECIFIED.,.F.,
 .F.,.F.)
B_SPLINE_SURFACE_WITH_KNOTS((4,4),(3,3),(1.32581766366803,1.5707963267949),
(0.,1.),.UNSPECIFIED.)
GEOMETRIC_REPRESENTATION_ITEM()
RATIONAL_B_SPLINE_SURFACE(((1.,0.727606875108995,1.),(1.,0.72100557572167,
1.),(1.,0.714109499479753,1.),(1.,0.707106781186548,1.)))
REPRESENTATION_ITEM('')
SURFACE()
) ;
#204 = (
BOUNDED_SURFACE()
B_SPLINE_SURFACE(3,2,((#166182,#166183,#166184),(#166185,#166186,#166187),
(#166188,#166189,#166190),(#166191,#166192,#166193)),.UNSPECIFIED.,.F.,
 .F.,.F.)
B_SPLINE_SURFACE_WITH_KNOTS((4,4),(3,3),(3.92699081698722,4.71238898038469),
(0.,1.),.UNSPECIFIED.)
GEOMETRIC_REPRESENTATION_ITEM()
RATIONAL_B_SPLINE_SURFACE(((1.,0.866025403784439,1.),(1.,0.828363615049346,
1.),(1.,0.772698924407957,1.),(1.,0.707106781186545,1.)))
REPRESENTATION_ITEM('')
SURFACE()
) ;
#205 = (
BOUNDED_SURFACE()
B_SPLINE_SURFACE(3,2,((#166195,#166196,#166197),(#166198,#166199,#166200),
(#166201,#166202,#166203),(#166204,#166205,#166206)),.UNSPECIFIED.,.F.,
 .F.,.F.)
B_SPLINE_SURFACE_WITH_KNOTS((4,4),(3,3),(1.5707963267949,2.35619449019234),
(0.,1.),.UNSPECIFIED.)
GEOMETRIC_REPRESENTATION_ITEM()
RATIONAL_B_SPLINE_SURFACE(((1.,1.,1.),(1.,1.00150544078214,1.),(1.,0.943158245625728,
1.),(1.,0.866025403784442,1.)))
REPRESENTATION_ITEM('')
SURFACE()
) ;
#206 = (
BOUNDED_SURFACE()
B_SPLINE_SURFACE(3,2,((#166207,#166208,#166209),(#166210,#166211,#166212),
(#166213,#166214,#166215),(#166216,#166217,#166218)),.UNSPECIFIED.,.F.,
 .F.,.F.)
B_SPLINE_SURFACE_WITH_KNOTS((4,4),(3,3),(7.06858347057709,7.85398163397448),
(0.,1.),.UNSPECIFIED.)
GEOMETRIC_REPRESENTATION_ITEM()
RATIONAL_B_SPLINE_SURFACE(((1.,0.866025403784455,1.),(1.,0.943158245625744,
1.),(1.,1.00150544078213,1.),(1.,1.,1.)))
REPRESENTATION_ITEM('')
SURFACE()
) ;
#207 = (
BOUNDED_SURFACE()
B_SPLINE_SURFACE(3,2,((#166220,#166221,#166222),(#166223,#166224,#166225),
(#166226,#166227,#166228),(#166229,#166230,#166231)),.UNSPECIFIED.,.F.,
 .F.,.F.)
B_SPLINE_SURFACE_WITH_KNOTS((4,4),(3,3),(1.5707963267949,2.35619449019239),
(0.,1.),.UNSPECIFIED.)
GEOMETRIC_REPRESENTATION_ITEM()
RATIONAL_B_SPLINE_SURFACE(((1.,0.707106781186545,1.),(1.,0.772698924407971,
1.),(1.,0.828363615049334,1.),(1.,0.866025403784449,1.)))
REPRESENTATION_ITEM('')
SURFACE()
) ;
#208 = (
BOUNDED_SURFACE()
B_SPLINE_SURFACE(3,2,((#166247,#166248,#166249),(#166250,#166251,#166252),
(#166253,#166254,#166255),(#166256,#166257,#166258)),.UNSPECIFIED.,.F.,
 .F.,.F.)
B_SPLINE_SURFACE_WITH_KNOTS((4,4),(3,3),(4.71238898038469,4.95736764351155),
(0.,1.),.UNSPECIFIED.)
GEOMETRIC_REPRESENTATION_ITEM()
RATIONAL_B_SPLINE_SURFACE(((1.,0.707106781186548,1.),(1.,0.714109499479749,
1.),(1.,0.721005575721671,1.),(1.,0.727606875108995,1.)))
REPRESENTATION_ITEM('')
SURFACE()
) ;
#209 = (
BOUNDED_SURFACE()
B_SPLINE_SURFACE(3,2,((#166260,#166261,#166262),(#166263,#166264,#166265),
(#166266,#166267,#166268),(#166269,#166270,#166271),(#166272,#166273,#166274),
(#166275,#166276,#166277),(#166278,#166279,#166280),(#166281,#166282,#166283)),
 .UNSPECIFIED.,.F.,.F.,.F.)
B_SPLINE_SURFACE_WITH_KNOTS((4,2,2,4),(3,3),(3.38657131671666,3.71802573263366,
4.04948014855067,4.71238898038469),(-0.00042082530851535,1.00042070189436),
 .UNSPECIFIED.)
GEOMETRIC_REPRESENTATION_ITEM()
RATIONAL_B_SPLINE_SURFACE(((1.00022935631998,0.727377552434477,1.00022928902906),
(1.00021435583148,0.745207756068811,1.00021429294157),(1.00019031910481,
0.773778807684169,1.00019026326703),(1.00013753195001,0.836523812238236,
1.00013749159947),(1.0001089637528,0.870481157936111,1.0001089317839),(1.00003378452299,
0.95984231283043,1.00003377461095),(0.999998875499966,1.00133662744384,
0.999998875829883),(1.,1.,1.)))
REPRESENTATION_ITEM('')
SURFACE()
) ;
#210 = (
BOUNDED_SURFACE()
B_SPLINE_SURFACE(3,2,((#166498,#166499,#166500),(#166501,#166502,#166503),
(#166504,#166505,#166506),(#166507,#166508,#166509),(#166510,#166511,#166512),
(#166513,#166514,#166515),(#166516,#166517,#166518),(#166519,#166520,#166521)),
 .UNSPECIFIED.,.F.,.F.,.F.)
B_SPLINE_SURFACE_WITH_KNOTS((4,2,2,4),(3,3),(1.5707963267949,2.35619449019234,
2.74889357189107,3.14159265358979),(0.,1.),.UNSPECIFIED.)
GEOMETRIC_REPRESENTATION_ITEM()
RATIONAL_B_SPLINE_SURFACE(((1.,1.,1.),(1.,1.00267605951734,1.),(1.,0.941599607549954,
1.),(1.,0.828238301901683,1.),(1.,0.787677905717223,1.),(1.,0.726552333979985,
1.),(1.,0.706675310150426,1.),(1.,0.70710678118656,1.)))
REPRESENTATION_ITEM('')
SURFACE()
) ;
#211 = (
BOUNDED_SURFACE()
B_SPLINE_SURFACE(3,2,((#166525,#166526,#166527),(#166528,#166529,#166530),
(#166531,#166532,#166533),(#166534,#166535,#166536),(#166537,#166538,#166539),
(#166540,#166541,#166542),(#166543,#166544,#166545),(#166546,#166547,#166548)),
 .UNSPECIFIED.,.F.,.F.,.F.)
B_SPLINE_SURFACE_WITH_KNOTS((4,2,2,4),(3,3),(4.71238898038469,5.49778714378214,
5.89048622548086,6.28318530717959),(0.,1.),.UNSPECIFIED.)
GEOMETRIC_REPRESENTATION_ITEM()
RATIONAL_B_SPLINE_SURFACE(((1.,1.,1.),(1.,1.00267605951734,1.),(1.,0.941599607549954,
1.),(1.,0.828238301901683,1.),(1.,0.787677905717209,1.),(1.,0.726552333979999,
1.),(1.,0.706675310150416,1.),(1.,0.70710678118656,1.)))
REPRESENTATION_ITEM('')
SURFACE()
) ;
#212 = (
BOUNDED_SURFACE()
B_SPLINE_SURFACE(3,2,((#166553,#166554,#166555),(#166556,#166557,#166558),
(#166559,#166560,#166561),(#166562,#166563,#166564),(#166565,#166566,#166567),
(#166568,#166569,#166570),(#166571,#166572,#166573),(#166574,#166575,#166576)),
 .UNSPECIFIED.,.F.,.F.,.F.)
B_SPLINE_SURFACE_WITH_KNOTS((4,2,2,4),(3,3),(1.5707963267949,2.35619449019234,
2.74889357189107,3.14159265358979),(0.,1.),.UNSPECIFIED.)
GEOMETRIC_REPRESENTATION_ITEM()
RATIONAL_B_SPLINE_SURFACE(((1.,1.,1.),(1.,1.00267605951746,1.),(1.,0.941599607549799,
1.),(1.,0.828238301901763,1.),(1.,0.787677905717196,1.),(1.,0.72655233398001,
1.),(1.,0.706675310150416,1.),(1.,0.707106781186548,1.)))
REPRESENTATION_ITEM('')
SURFACE()
) ;
#213 = (
BOUNDED_SURFACE()
B_SPLINE_SURFACE(3,2,((#166598,#166599,#166600),(#166601,#166602,#166603),
(#166604,#166605,#166606),(#166607,#166608,#166609),(#166610,#166611,#166612),
(#166613,#166614,#166615),(#166616,#166617,#166618),(#166619,#166620,#166621)),
 .UNSPECIFIED.,.F.,.F.,.F.)
B_SPLINE_SURFACE_WITH_KNOTS((4,2,2,4),(3,3),(4.71238898038469,5.49778714378214,
5.89048622548086,6.28318530717959),(0.,1.),.UNSPECIFIED.)
GEOMETRIC_REPRESENTATION_ITEM()
RATIONAL_B_SPLINE_SURFACE(((1.,1.,1.),(1.,1.00267605951749,1.),(1.,0.941599607549756,
1.),(1.,0.828238301901784,1.),(1.,0.787677905717196,1.),(1.,0.72655233398001,
1.),(1.,0.706675310150417,1.),(1.,0.707106781186548,1.)))
REPRESENTATION_ITEM('')
SURFACE()
) ;
#214 = (
BOUNDED_SURFACE()
B_SPLINE_SURFACE(3,2,((#166622,#166623,#166624),(#166625,#166626,#166627),
(#166628,#166629,#166630),(#166631,#166632,#166633),(#166634,#166635,#166636),
(#166637,#166638,#166639),(#166640,#166641,#166642),(#166643,#166644,#166645)),
 .UNSPECIFIED.,.F.,.F.,.F.)
B_SPLINE_SURFACE_WITH_KNOTS((4,2,2,4),(3,3),(3.38657131671666,3.71802573263366,
4.04948014855067,4.71238898038469),(-0.000420825308972864,1.00042070189455),
 .UNSPECIFIED.)
GEOMETRIC_REPRESENTATION_ITEM()
RATIONAL_B_SPLINE_SURFACE(((1.00022935632023,0.727377552434312,1.00022928902917),
(1.00021435583172,0.745207756068707,1.00021429294166),(1.00019031910501,
0.773778807683938,1.00019026326711),(1.00013753195016,0.836523812238204,
1.00013749159953),(1.00010896375292,0.870481157936108,1.00010893178394),
(1.00003378452303,0.959842312830239,1.00003377461096),(0.999998875499964,
1.00133662744397,0.999998875829882),(1.,1.,1.)))
REPRESENTATION_ITEM('')
SURFACE()
) ;
#215 = (
BOUNDED_SURFACE()
B_SPLINE_SURFACE(3,2,((#166647,#166648,#166649),(#166650,#166651,#166652),
(#166653,#166654,#166655),(#166656,#166657,#166658)),.UNSPECIFIED.,.F.,
 .F.,.F.)
B_SPLINE_SURFACE_WITH_KNOTS((4,4),(3,3),(1.32581766366803,1.5707963267949),
(0.,1.),.UNSPECIFIED.)
GEOMETRIC_REPRESENTATION_ITEM()
RATIONAL_B_SPLINE_SURFACE(((1.,0.727606875109006,1.),(1.,0.72100557572165,
1.),(1.,0.714109499479786,1.),(1.,0.707106781186535,1.)))
REPRESENTATION_ITEM('')
SURFACE()
) ;
#216 = (
BOUNDED_SURFACE()
B_SPLINE_SURFACE(3,2,((#166674,#166675,#166676),(#166677,#166678,#166679),
(#166680,#166681,#166682),(#166683,#166684,#166685)),.UNSPECIFIED.,.F.,
 .F.,.F.)
B_SPLINE_SURFACE_WITH_KNOTS((4,4),(3,3),(3.92699081698722,4.71238898038469),
(0.,1.),.UNSPECIFIED.)
GEOMETRIC_REPRESENTATION_ITEM()
RATIONAL_B_SPLINE_SURFACE(((1.,0.866025403784442,1.),(1.,0.828363615049326,
1.),(1.,0.772698924407971,1.),(1.,0.707106781186533,1.)))
REPRESENTATION_ITEM('')
SURFACE()
) ;
#217 = (
BOUNDED_SURFACE()
B_SPLINE_SURFACE(3,2,((#166687,#166688,#166689),(#166690,#166691,#166692),
(#166693,#166694,#166695),(#166696,#166697,#166698)),.UNSPECIFIED.,.F.,
 .F.,.F.)
B_SPLINE_SURFACE_WITH_KNOTS((4,4),(3,3),(1.5707963267949,2.35619449019234),
(0.,1.),.UNSPECIFIED.)
GEOMETRIC_REPRESENTATION_ITEM()
RATIONAL_B_SPLINE_SURFACE(((1.,1.,1.),(1.,1.00150544078214,1.),(1.,0.943158245625729,
1.),(1.,0.866025403784442,1.)))
REPRESENTATION_ITEM('')
SURFACE()
) ;
#218 = (
BOUNDED_SURFACE()
B_SPLINE_SURFACE(3,2,((#166699,#166700,#166701),(#166702,#166703,#166704),
(#166705,#166706,#166707),(#166708,#166709,#166710)),.UNSPECIFIED.,.F.,
 .F.,.F.)
B_SPLINE_SURFACE_WITH_KNOTS((4,4),(3,3),(7.06858347057706,7.85398163397448),
(0.,1.),.UNSPECIFIED.)
GEOMETRIC_REPRESENTATION_ITEM()
RATIONAL_B_SPLINE_SURFACE(((1.,0.866025403784446,1.),(1.,0.943158245625744,
1.),(1.,1.00150544078213,1.),(1.,1.,1.)))
REPRESENTATION_ITEM('')
SURFACE()
) ;
#219 = (
BOUNDED_SURFACE()
B_SPLINE_SURFACE(3,2,((#166712,#166713,#166714),(#166715,#166716,#166717),
(#166718,#166719,#166720),(#166721,#166722,#166723)),.UNSPECIFIED.,.F.,
 .F.,.F.)
B_SPLINE_SURFACE_WITH_KNOTS((4,4),(3,3),(1.5707963267949,2.35619449019237),
(0.,1.),.UNSPECIFIED.)
GEOMETRIC_REPRESENTATION_ITEM()
RATIONAL_B_SPLINE_SURFACE(((1.,0.707106781186545,1.),(1.,0.772698924407959,
1.),(1.,0.828363615049336,1.),(1.,0.86602540378444,1.)))
REPRESENTATION_ITEM('')
SURFACE()
) ;
#220 = (
BOUNDED_SURFACE()
B_SPLINE_SURFACE(3,2,((#166739,#166740,#166741),(#166742,#166743,#166744),
(#166745,#166746,#166747),(#166748,#166749,#166750)),.UNSPECIFIED.,.F.,
 .F.,.F.)
B_SPLINE_SURFACE_WITH_KNOTS((4,4),(3,3),(4.71238898038469,4.95736764351155),
(0.,1.),.UNSPECIFIED.)
GEOMETRIC_REPRESENTATION_ITEM()
RATIONAL_B_SPLINE_SURFACE(((1.,0.707106781186548,1.),(1.,0.714109499479746,
1.),(1.,0.721005575721677,1.),(1.,0.727606875108994,1.)))
REPRESENTATION_ITEM('')
SURFACE()
) ;
#221 = (
BOUNDED_SURFACE()
B_SPLINE_SURFACE(3,2,((#166752,#166753,#166754),(#166755,#166756,#166757),
(#166758,#166759,#166760),(#166761,#166762,#166763),(#166764,#166765,#166766),
(#166767,#166768,#166769),(#166770,#166771,#166772),(#166773,#166774,#166775)),
 .UNSPECIFIED.,.F.,.F.,.F.)
B_SPLINE_SURFACE_WITH_KNOTS((4,2,2,4),(3,3),(3.38657131671663,3.71802573263365,
4.04948014855066,4.71238898038469),(-0.000420825310317862,1.0004207018963),
 .UNSPECIFIED.)
GEOMETRIC_REPRESENTATION_ITEM()
RATIONAL_B_SPLINE_SURFACE(((1.00022935632096,0.72737755243345,1.00022928903013),
(1.0002143558324,0.745207756067913,1.00021429294255),(1.00019031910563,
0.773778807683235,1.00019026326791),(1.0001375319506,0.83652381223769,1.00013749160011),
(1.00010896375327,0.870481157935671,1.0001089317844),(1.00003378452314,
0.959842312830171,1.0000337746111),(0.99999887549996,1.00133662744394,0.999998875829878),
(1.,1.,1.)))
REPRESENTATION_ITEM('')
SURFACE()
) ;
#222 = (
BOUNDED_SURFACE()
B_SPLINE_SURFACE(3,2,((#166990,#166991,#166992),(#166993,#166994,#166995),
(#166996,#166997,#166998),(#166999,#167000,#167001),(#167002,#167003,#167004),
(#167005,#167006,#167007),(#167008,#167009,#167010),(#167011,#167012,#167013)),
 .UNSPECIFIED.,.F.,.F.,.F.)
B_SPLINE_SURFACE_WITH_KNOTS((4,2,2,4),(3,3),(1.5707963267949,2.35619449019234,
2.74889357189107,3.14159265358979),(0.,1.),.UNSPECIFIED.)
GEOMETRIC_REPRESENTATION_ITEM()
RATIONAL_B_SPLINE_SURFACE(((1.,1.,1.),(1.,1.00267605951749,1.),(1.,0.94159960754976,
1.),(1.,0.828238301901782,1.),(1.,0.787677905717208,1.),(1.,0.726552333979998,
1.),(1.,0.706675310150427,1.),(1.,0.707106781186548,1.)))
REPRESENTATION_ITEM('')
SURFACE()
) ;
#223 = (
BOUNDED_SURFACE()
B_SPLINE_SURFACE(3,2,((#167017,#167018,#167019),(#167020,#167021,#167022),
(#167023,#167024,#167025),(#167026,#167027,#167028),(#167029,#167030,#167031),
(#167032,#167033,#167034),(#167035,#167036,#167037),(#167038,#167039,#167040)),
 .UNSPECIFIED.,.F.,.F.,.F.)
B_SPLINE_SURFACE_WITH_KNOTS((4,2,2,4),(3,3),(4.71238898038469,5.49778714378214,
5.89048622548086,6.28318530717959),(0.,1.),.UNSPECIFIED.)
GEOMETRIC_REPRESENTATION_ITEM()
RATIONAL_B_SPLINE_SURFACE(((1.,1.,1.),(1.,1.00267605951749,1.),(1.,0.941599607549756,
1.),(1.,0.828238301901784,1.),(1.,0.787677905717196,1.),(1.,0.72655233398001,
1.),(1.,0.706675310150417,1.),(1.,0.707106781186548,1.)))
REPRESENTATION_ITEM('')
SURFACE()
) ;
#224 = (
BOUNDED_SURFACE()
B_SPLINE_SURFACE(3,2,((#167045,#167046,#167047),(#167048,#167049,#167050),
(#167051,#167052,#167053),(#167054,#167055,#167056),(#167057,#167058,#167059),
(#167060,#167061,#167062),(#167063,#167064,#167065),(#167066,#167067,#167068)),
 .UNSPECIFIED.,.F.,.F.,.F.)
B_SPLINE_SURFACE_WITH_KNOTS((4,2,2,4),(3,3),(1.5707963267949,2.35619449019234,
2.74889357189107,3.14159265358979),(0.,1.),.UNSPECIFIED.)
GEOMETRIC_REPRESENTATION_ITEM()
RATIONAL_B_SPLINE_SURFACE(((1.,1.,1.),(1.,1.00267605951746,1.),(1.,0.941599607549799,
1.),(1.,0.828238301901763,1.),(1.,0.787677905717196,1.),(1.,0.72655233398001,
1.),(1.,0.706675310150416,1.),(1.,0.707106781186548,1.)))
REPRESENTATION_ITEM('')
SURFACE()
) ;
#225 = (
BOUNDED_SURFACE()
B_SPLINE_SURFACE(3,2,((#167090,#167091,#167092),(#167093,#167094,#167095),
(#167096,#167097,#167098),(#167099,#167100,#167101),(#167102,#167103,#167104),
(#167105,#167106,#167107),(#167108,#167109,#167110),(#167111,#167112,#167113)),
 .UNSPECIFIED.,.F.,.F.,.F.)
B_SPLINE_SURFACE_WITH_KNOTS((4,2,2,4),(3,3),(4.71238898038469,5.49778714378214,
5.89048622548086,6.28318530717959),(0.,1.),.UNSPECIFIED.)
GEOMETRIC_REPRESENTATION_ITEM()
RATIONAL_B_SPLINE_SURFACE(((1.,1.,1.),(1.,1.00267605951749,1.),(1.,0.941599607549756,
1.),(1.,0.828238301901784,1.),(1.,0.787677905717196,1.),(1.,0.72655233398001,
1.),(1.,0.706675310150417,1.),(1.,0.707106781186548,1.)))
REPRESENTATION_ITEM('')
SURFACE()
) ;
#226 = (
BOUNDED_SURFACE()
B_SPLINE_SURFACE(3,2,((#167114,#167115,#167116),(#167117,#167118,#167119),
(#167120,#167121,#167122),(#167123,#167124,#167125),(#167126,#167127,#167128),
(#167129,#167130,#167131),(#167132,#167133,#167134),(#167135,#167136,#167137)),
 .UNSPECIFIED.,.F.,.F.,.F.)
B_SPLINE_SURFACE_WITH_KNOTS((4,2,2,4),(3,3),(3.38657131671664,3.71802573263365,
4.04948014855067,4.71238898038469),(-0.000420825293764194,1.00042070189636),
 .UNSPECIFIED.)
GEOMETRIC_REPRESENTATION_ITEM()
RATIONAL_B_SPLINE_SURFACE(((1.00022935631194,0.727377552437947,1.00022928903016),
(1.00021435582396,0.745207756072161,1.00021429294259),(1.00019031909813,
0.773778807686912,1.00019026326795),(1.00013753194518,0.836523812240446,
1.00013749160012),(1.00010896374898,0.870481157937832,1.00010893178441),
(1.00003378452181,0.959842312830787,1.0000337746111),(0.999998875500004,
1.00133662744395,0.999998875829878),(1.,1.,1.)))
REPRESENTATION_ITEM('')
SURFACE()
) ;
#227 = (
BOUNDED_SURFACE()
B_SPLINE_SURFACE(3,2,((#167139,#167140,#167141),(#167142,#167143,#167144),
(#167145,#167146,#167147),(#167148,#167149,#167150)),.UNSPECIFIED.,.F.,
 .F.,.F.)
B_SPLINE_SURFACE_WITH_KNOTS((4,4),(3,3),(1.32581766366803,1.5707963267949),
(0.,1.),.UNSPECIFIED.)
GEOMETRIC_REPRESENTATION_ITEM()
RATIONAL_B_SPLINE_SURFACE(((1.,0.727606875108994,1.),(1.,0.721005575721676,
1.),(1.,0.714109499479749,1.),(1.,0.707106781186548,1.)))
REPRESENTATION_ITEM('')
SURFACE()
) ;
#228 = (
BOUNDED_SURFACE()
B_SPLINE_SURFACE(3,2,((#167166,#167167,#167168),(#167169,#167170,#167171),
(#167172,#167173,#167174),(#167175,#167176,#167177)),.UNSPECIFIED.,.F.,
 .F.,.F.)
B_SPLINE_SURFACE_WITH_KNOTS((4,4),(3,3),(3.92699081698722,4.71238898038469),
(0.,1.),.UNSPECIFIED.)
GEOMETRIC_REPRESENTATION_ITEM()
RATIONAL_B_SPLINE_SURFACE(((1.,0.866025403784442,1.),(1.,0.828363615049332,
1.),(1.,0.772698924407958,1.),(1.,0.707106781186545,1.)))
REPRESENTATION_ITEM('')
SURFACE()
) ;
#229 = (
BOUNDED_SURFACE()
B_SPLINE_SURFACE(3,2,((#167179,#167180,#167181),(#167182,#167183,#167184),
(#167185,#167186,#167187),(#167188,#167189,#167190)),.UNSPECIFIED.,.F.,
 .F.,.F.)
B_SPLINE_SURFACE_WITH_KNOTS((4,4),(3,3),(1.5707963267949,2.35619449019233),
(0.,1.),.UNSPECIFIED.)
GEOMETRIC_REPRESENTATION_ITEM()
RATIONAL_B_SPLINE_SURFACE(((1.,1.,1.),(1.,1.00150544078213,1.),(1.,0.943158245625741,
1.),(1.,0.866025403784444,1.)))
REPRESENTATION_ITEM('')
SURFACE()
) ;
#230 = (
BOUNDED_SURFACE()
B_SPLINE_SURFACE(3,2,((#167191,#167192,#167193),(#167194,#167195,#167196),
(#167197,#167198,#167199),(#167200,#167201,#167202)),.UNSPECIFIED.,.F.,
 .F.,.F.)
B_SPLINE_SURFACE_WITH_KNOTS((4,4),(3,3),(7.06858347057706,7.85398163397448),
(0.,1.),.UNSPECIFIED.)
GEOMETRIC_REPRESENTATION_ITEM()
RATIONAL_B_SPLINE_SURFACE(((1.,0.866025403784446,1.),(1.,0.943158245625744,
1.),(1.,1.00150544078213,1.),(1.,1.,1.)))
REPRESENTATION_ITEM('')
SURFACE()
) ;
#231 = (
BOUNDED_SURFACE()
B_SPLINE_SURFACE(3,2,((#167204,#167205,#167206),(#167207,#167208,#167209),
(#167210,#167211,#167212),(#167213,#167214,#167215)),.UNSPECIFIED.,.F.,
 .F.,.F.)
B_SPLINE_SURFACE_WITH_KNOTS((4,4),(3,3),(1.5707963267949,2.35619449019237),
(0.,1.),.UNSPECIFIED.)
GEOMETRIC_REPRESENTATION_ITEM()
RATIONAL_B_SPLINE_SURFACE(((1.,0.707106781186545,1.),(1.,0.772698924407959,
1.),(1.,0.828363615049336,1.),(1.,0.86602540378444,1.)))
REPRESENTATION_ITEM('')
SURFACE()
) ;
#232 = (
BOUNDED_SURFACE()
B_SPLINE_SURFACE(3,2,((#167231,#167232,#167233),(#167234,#167235,#167236),
(#167237,#167238,#167239),(#167240,#167241,#167242)),.UNSPECIFIED.,.F.,
 .F.,.F.)
B_SPLINE_SURFACE_WITH_KNOTS((4,4),(3,3),(4.71238898038469,4.95736764351155),
(0.,1.),.UNSPECIFIED.)
GEOMETRIC_REPRESENTATION_ITEM()
RATIONAL_B_SPLINE_SURFACE(((1.,0.707106781186548,1.),(1.,0.714109499479746,
1.),(1.,0.721005575721677,1.),(1.,0.727606875108994,1.)))
REPRESENTATION_ITEM('')
SURFACE()
) ;
#233 = (
BOUNDED_SURFACE()
B_SPLINE_SURFACE(3,2,((#167244,#167245,#167246),(#167247,#167248,#167249),
(#167250,#167251,#167252),(#167253,#167254,#167255),(#167256,#167257,#167258),
(#167259,#167260,#167261),(#167262,#167263,#167264),(#167265,#167266,#167267)),
 .UNSPECIFIED.,.F.,.F.,.F.)
B_SPLINE_SURFACE_WITH_KNOTS((4,2,2,4),(3,3),(3.38657131671663,3.71802573263365,
4.04948014855066,4.71238898038469),(-0.00042082531042703,1.00042070189448),
 .UNSPECIFIED.)
GEOMETRIC_REPRESENTATION_ITEM()
RATIONAL_B_SPLINE_SURFACE(((1.00022935632103,0.727377552433915,1.00022928902914),
(1.00021435583246,0.745207756068348,1.00021429294162),(1.00019031910567,
0.773778807683621,1.00019026326709),(1.00013753195063,0.836523812237968,
1.00013749159951),(1.00010896375329,0.870481157935892,1.00010893178393),
(1.00003378452315,0.959842312830238,1.00003377461096),(0.99999887549996,
1.00133662744394,0.999998875829883),(1.,1.,1.)))
REPRESENTATION_ITEM('')
SURFACE()
) ;
#234 = (
BOUNDED_SURFACE()
B_SPLINE_SURFACE(3,2,((#168899,#168900,#168901),(#168902,#168903,#168904),
(#168905,#168906,#168907),(#168908,#168909,#168910),(#168911,#168912,#168913),
(#168914,#168915,#168916),(#168917,#168918,#168919),(#168920,#168921,#168922),
(#168923,#168924,#168925),(#168926,#168927,#168928)),.UNSPECIFIED.,.F.,
 .F.,.F.)
B_SPLINE_SURFACE_WITH_KNOTS((4,2,2,2,4),(3,3),(-3.3881317890172E-21,5.50005871024831E-5,
0.000110001174204966,0.000165001761307449,0.000220002348409932),(-9.32574651119021E-5,
1.),.UNSPECIFIED.)
GEOMETRIC_REPRESENTATION_ITEM()
RATIONAL_B_SPLINE_SURFACE(((1.00005463405283,0.707079466707422,1.),(1.00005694771662,
0.694674755787659,1.),(1.00005645688428,0.697306353922547,1.),(1.00005591567353,
0.700208055939803,1.),(1.0000556235962,0.701774028840045,1.),(1.00005562454822,
0.70176892461066,1.),(1.00005591789343,0.70019615395662,1.),(1.00005645795057,
0.697300636998116,1.),(1.00005694973354,0.694663942070735,1.),(1.00005463405283,
0.707079466707408,1.)))
REPRESENTATION_ITEM('')
SURFACE()
) ;
#235 = (
BOUNDED_SURFACE()
B_SPLINE_SURFACE(3,2,((#168933,#168934,#168935),(#168936,#168937,#168938),
(#168939,#168940,#168941),(#168942,#168943,#168944),(#168945,#168946,#168947),
(#168948,#168949,#168950),(#168951,#168952,#168953),(#168954,#168955,#168956),
(#168957,#168958,#168959),(#168960,#168961,#168962)),.UNSPECIFIED.,.F.,
 .F.,.F.)
B_SPLINE_SURFACE_WITH_KNOTS((4,2,2,2,4),(3,3),(-3.3881317890172E-21,5.50005871024829E-5,
0.000110001174204966,0.000165001761307449,0.000220002348409932),(0.,1.00009325746509),
 .UNSPECIFIED.)
GEOMETRIC_REPRESENTATION_ITEM()
RATIONAL_B_SPLINE_SURFACE(((1.,0.707079466707414,1.00005463405282),(1.,
0.694674755787651,1.00005694771661),(1.,0.697306353922573,1.00005645688426),
(1.,0.700208055939776,1.00005591567352),(1.,0.701774028840086,1.00005562359619),
(1.,0.701768924610626,1.0000556245482),(1.,0.700196153956618,1.00005591789341),
(1.,0.697300636998131,1.00005645795056),(1.,0.694663942070735,1.00005694973353),
(1.,0.707079466707415,1.00005463405282)))
REPRESENTATION_ITEM('')
SURFACE()
) ;
#236 = (
BOUNDED_SURFACE()
B_SPLINE_SURFACE(3,2,((#168967,#168968,#168969),(#168970,#168971,#168972),
(#168973,#168974,#168975),(#168976,#168977,#168978),(#168979,#168980,#168981),
(#168982,#168983,#168984),(#168985,#168986,#168987),(#168988,#168989,#168990),
(#168991,#168992,#168993),(#168994,#168995,#168996)),.UNSPECIFIED.,.F.,
 .F.,.F.)
B_SPLINE_SURFACE_WITH_KNOTS((4,2,2,2,4),(3,3),(0.,5.5000587102484E-5,0.000110001174204968,
0.000165001761307452,0.000220002348409936),(-9.32574651108896E-5,1.),
 .UNSPECIFIED.)
GEOMETRIC_REPRESENTATION_ITEM()
RATIONAL_B_SPLINE_SURFACE(((1.00005463405283,0.707079466707377,1.),(1.00005694771662,
0.694674755787608,1.),(1.00005645688428,0.697306353922581,1.),(1.00005591567353,
0.700208055939738,1.),(1.0000556235962,0.7017740288401,1.),(1.00005562454822,
0.701768924610595,1.),(1.00005591789342,0.700196153956602,1.),(1.00005645795057,
0.697300636998131,1.),(1.00005694973354,0.694663942070724,1.),(1.00005463405283,
0.70707946670741,1.)))
REPRESENTATION_ITEM('')
SURFACE()
) ;
#237 = (
BOUNDED_SURFACE()
B_SPLINE_SURFACE(3,2,((#169001,#169002,#169003),(#169004,#169005,#169006),
(#169007,#169008,#169009),(#169010,#169011,#169012),(#169013,#169014,#169015),
(#169016,#169017,#169018),(#169019,#169020,#169021),(#169022,#169023,#169024),
(#169025,#169026,#169027),(#169028,#169029,#169030)),.UNSPECIFIED.,.F.,
 .F.,.F.)
B_SPLINE_SURFACE_WITH_KNOTS((4,2,2,2,4),(3,3),(0.,5.5000587102483E-5,0.000110001174204966,
0.000165001761307449,0.000220002348409932),(0.,1.00009325746509),
 .UNSPECIFIED.)
GEOMETRIC_REPRESENTATION_ITEM()
RATIONAL_B_SPLINE_SURFACE(((1.,0.707079466707415,1.00005463405282),(1.,
0.694674755787641,1.00005694771661),(1.,0.697306353922585,1.00005645688426),
(1.,0.700208055939766,1.00005591567351),(1.,0.701774028840102,1.00005562359619),
(1.,0.701768924610621,1.0000556245482),(1.,0.700196153956564,1.00005591789341),
(1.,0.697300636998199,1.00005645795056),(1.,0.694663942070693,1.00005694973353),
(1.,0.707079466707429,1.00005463405282)))
REPRESENTATION_ITEM('')
SURFACE()
) ;
#238 = (
BOUNDED_SURFACE()
B_SPLINE_SURFACE(3,2,((#169035,#169036,#169037),(#169038,#169039,#169040),
(#169041,#169042,#169043),(#169044,#169045,#169046),(#169047,#169048,#169049),
(#169050,#169051,#169052),(#169053,#169054,#169055),(#169056,#169057,#169058),
(#169059,#169060,#169061),(#169062,#169063,#169064)),.UNSPECIFIED.,.F.,
 .F.,.F.)
B_SPLINE_SURFACE_WITH_KNOTS((4,2,2,2,4),(3,3),(6.7762635780344E-21,5.50005871024835E-5,
0.000110001174204967,0.00016500176130745,0.000220002348409934),(-9.32574651090946E-5,
1.),.UNSPECIFIED.)
GEOMETRIC_REPRESENTATION_ITEM()
RATIONAL_B_SPLINE_SURFACE(((1.00005463405283,0.707079466707396,1.),(1.00005694771662,
0.694674755787625,1.),(1.00005645688428,0.697306353922589,1.),(1.00005591567353,
0.700208055939743,1.),(1.0000556235962,0.701774028840088,1.),(1.00005562454822,
0.701768924610605,1.),(1.00005591789342,0.700196153956601,1.),(1.00005645795057,
0.697300636998125,1.),(1.00005694973354,0.694663942070733,1.),(1.00005463405283,
0.707079466707409,1.)))
REPRESENTATION_ITEM('')
SURFACE()
) ;
#239 = (
BOUNDED_SURFACE()
B_SPLINE_SURFACE(3,2,((#169069,#169070,#169071),(#169072,#169073,#169074),
(#169075,#169076,#169077),(#169078,#169079,#169080),(#169081,#169082,#169083),
(#169084,#169085,#169086),(#169087,#169088,#169089),(#169090,#169091,#169092),
(#169093,#169094,#169095),(#169096,#169097,#169098)),.UNSPECIFIED.,.F.,
 .F.,.F.)
B_SPLINE_SURFACE_WITH_KNOTS((4,2,2,2,4),(3,3),(3.3881317890172E-21,5.50005871024834E-5,
0.000110001174204967,0.00016500176130745,0.000220002348409934),(0.,1.00009325746519),
 .UNSPECIFIED.)
GEOMETRIC_REPRESENTATION_ITEM()
RATIONAL_B_SPLINE_SURFACE(((1.,0.707079466707384,1.00005463405288),(1.,
0.694674755787592,1.00005694771667),(1.,0.697306353922578,1.00005645688433),
(1.,0.700208055939709,1.00005591567358),(1.,0.701774028840076,1.00005562359625),
(1.,0.701768924610577,1.00005562454827),(1.,0.700196153956582,1.00005591789348),
(1.,0.697300636998093,1.00005645795062),(1.,0.694663942070696,1.00005694973359),
(1.,0.70707946670737,1.00005463405288)))
REPRESENTATION_ITEM('')
SURFACE()
) ;
#240 = (
BOUNDED_SURFACE()
B_SPLINE_SURFACE(3,2,((#169103,#169104,#169105),(#169106,#169107,#169108),
(#169109,#169110,#169111),(#169112,#169113,#169114),(#169115,#169116,#169117),
(#169118,#169119,#169120),(#169121,#169122,#169123),(#169124,#169125,#169126),
(#169127,#169128,#169129),(#169130,#169131,#169132)),.UNSPECIFIED.,.F.,
 .F.,.F.)
B_SPLINE_SURFACE_WITH_KNOTS((4,2,2,2,4),(3,3),(-3.3881317890172E-21,5.50005871024834E-5,
0.000110001174204967,0.00016500176130745,0.000220002348409933),(-9.32574651049742E-5,
1.),.UNSPECIFIED.)
GEOMETRIC_REPRESENTATION_ITEM()
RATIONAL_B_SPLINE_SURFACE(((1.00005463405282,0.707079466707415,1.),(1.00005694771662,
0.694674755787666,1.),(1.00005645688427,0.697306353922507,1.),(1.00005591567352,
0.700208055939813,1.),(1.0000556235962,0.701774028840077,1.),(1.00005562454821,
0.701768924610621,1.),(1.00005591789342,0.700196153956683,1.),(1.00005645795056,
0.697300636998053,1.),(1.00005694973354,0.694663942070781,1.),(1.00005463405282,
0.707079466707411,1.)))
REPRESENTATION_ITEM('')
SURFACE()
) ;
#241 = (
BOUNDED_SURFACE()
B_SPLINE_SURFACE(3,2,((#169137,#169138,#169139),(#169140,#169141,#169142),
(#169143,#169144,#169145),(#169146,#169147,#169148),(#169149,#169150,#169151),
(#169152,#169153,#169154),(#169155,#169156,#169157),(#169158,#169159,#169160),
(#169161,#169162,#169163),(#169164,#169165,#169166)),.UNSPECIFIED.,.F.,
 .F.,.F.)
B_SPLINE_SURFACE_WITH_KNOTS((4,2,2,2,4),(3,3),(3.3881317890172E-21,5.50005871024834E-5,
0.000110001174204967,0.00016500176130745,0.000220002348409934),(0.,1.00009325746519),
 .UNSPECIFIED.)
GEOMETRIC_REPRESENTATION_ITEM()
RATIONAL_B_SPLINE_SURFACE(((1.,0.707079466707385,1.00005463405287),(1.,
0.694674755787593,1.00005694771667),(1.,0.69730635392258,1.00005645688432),
(1.,0.70020805593971,1.00005591567357),(1.,0.701774028840128,1.00005562359625),
(1.,0.701768924610516,1.00005562454826),(1.,0.700196153956523,1.00005591789347),
(1.,0.697300636998155,1.00005645795062),(1.,0.694663942070652,1.00005694973359),
(1.,0.707079466707371,1.00005463405287)))
REPRESENTATION_ITEM('')
SURFACE()
) ;
#242 = (
BOUNDED_SURFACE()
B_SPLINE_SURFACE(3,2,((#169171,#169172,#169173),(#169174,#169175,#169176),
(#169177,#169178,#169179),(#169180,#169181,#169182),(#169183,#169184,#169185),
(#169186,#169187,#169188),(#169189,#169190,#169191),(#169192,#169193,#169194),
(#169195,#169196,#169197),(#169198,#169199,#169200)),.UNSPECIFIED.,.F.,
 .F.,.F.)
B_SPLINE_SURFACE_WITH_KNOTS((4,2,2,2,4),(3,3),(-3.3881317890172E-21,5.50005871024834E-5,
0.000110001174204967,0.00016500176130745,0.000220002348409933),(-9.3257465103702E-5,
1.),.UNSPECIFIED.)
GEOMETRIC_REPRESENTATION_ITEM()
RATIONAL_B_SPLINE_SURFACE(((1.00005463405282,0.707079466707416,1.),(1.00005694771662,
0.694674755787666,1.),(1.00005645688427,0.697306353922507,1.),(1.00005591567352,
0.700208055939814,1.),(1.0000556235962,0.701774028840078,1.),(1.00005562454821,
0.701768924610622,1.),(1.00005591789342,0.700196153956684,1.),(1.00005645795056,
0.697300636998054,1.),(1.00005694973353,0.694663942070781,1.),(1.00005463405282,
0.707079466707412,1.)))
REPRESENTATION_ITEM('')
SURFACE()
) ;
#243 = (
BOUNDED_SURFACE()
B_SPLINE_SURFACE(3,2,((#169205,#169206,#169207),(#169208,#169209,#169210),
(#169211,#169212,#169213),(#169214,#169215,#169216),(#169217,#169218,#169219),
(#169220,#169221,#169222),(#169223,#169224,#169225),(#169226,#169227,#169228),
(#169229,#169230,#169231),(#169232,#169233,#169234)),.UNSPECIFIED.,.F.,
 .F.,.F.)
B_SPLINE_SURFACE_WITH_KNOTS((4,2,2,2,4),(3,3),(3.3881317890172E-21,5.50005871024832E-5,
0.000110001174204966,0.00016500176130745,0.000220002348409933),(0.,1.00009325746505),
 .UNSPECIFIED.)
GEOMETRIC_REPRESENTATION_ITEM()
RATIONAL_B_SPLINE_SURFACE(((1.,0.707079466707425,1.00005463405279),(1.,
0.694674755787719,1.00005694771658),(1.,0.697306353922511,1.00005645688424),
(1.,0.700208055939858,1.00005591567349),(1.,0.701774028840035,1.00005562359617),
(1.,0.701768924610702,1.00005562454818),(1.,0.700196153956624,1.00005591789339),
(1.,0.697300636998136,1.00005645795053),(1.,0.694663942070728,1.0000569497335),
(1.,0.707079466707431,1.00005463405279)))
REPRESENTATION_ITEM('')
SURFACE()
) ;
#244 = (
BOUNDED_SURFACE()
B_SPLINE_SURFACE(3,2,((#169239,#169240,#169241),(#169242,#169243,#169244),
(#169245,#169246,#169247),(#169248,#169249,#169250),(#169251,#169252,#169253),
(#169254,#169255,#169256),(#169257,#169258,#169259),(#169260,#169261,#169262),
(#169263,#169264,#169265),(#169266,#169267,#169268)),.UNSPECIFIED.,.F.,
 .F.,.F.)
B_SPLINE_SURFACE_WITH_KNOTS((4,2,2,2,4),(3,3),(-3.3881317890172E-21,5.50005871024834E-5,
0.000110001174204967,0.00016500176130745,0.000220002348409933),(-9.32574651063451E-5,
1.),.UNSPECIFIED.)
GEOMETRIC_REPRESENTATION_ITEM()
RATIONAL_B_SPLINE_SURFACE(((1.00005463405282,0.707079466707415,1.),(1.00005694771662,
0.694674755787663,1.),(1.00005645688427,0.697306353922506,1.),(1.00005591567352,
0.700208055939813,1.),(1.0000556235962,0.701774028840077,1.),(1.00005562454821,
0.701768924610621,1.),(1.00005591789342,0.700196153956578,1.),(1.00005645795057,
0.697300636998158,1.),(1.00005694973354,0.6946639420707,1.),(1.00005463405282,
0.707079466707411,1.)))
REPRESENTATION_ITEM('')
SURFACE()
) ;
#245 = (
BOUNDED_SURFACE()
B_SPLINE_SURFACE(3,2,((#169273,#169274,#169275),(#169276,#169277,#169278),
(#169279,#169280,#169281),(#169282,#169283,#169284),(#169285,#169286,#169287),
(#169288,#169289,#169290),(#169291,#169292,#169293),(#169294,#169295,#169296),
(#169297,#169298,#169299),(#169300,#169301,#169302)),.UNSPECIFIED.,.F.,
 .F.,.F.)
B_SPLINE_SURFACE_WITH_KNOTS((4,2,2,2,4),(3,3),(3.3881317890172E-21,5.50005871024832E-5,
0.000110001174204966,0.00016500176130745,0.000220002348409933),(0.,1.00009325746505),
 .UNSPECIFIED.)
GEOMETRIC_REPRESENTATION_ITEM()
RATIONAL_B_SPLINE_SURFACE(((1.,0.707079466707427,1.00005463405279),(1.,
0.694674755787585,1.00005694771658),(1.,0.6973063539227,1.00005645688424),
(1.,0.700208055939672,1.00005591567349),(1.,0.70177402884015,1.00005562359616),
(1.,0.701768924610591,1.00005562454818),(1.,0.700196153956506,1.00005591789339),
(1.,0.697300636998258,1.00005645795053),(1.,0.694663942070653,1.0000569497335),
(1.,0.707079466707433,1.00005463405279)))
REPRESENTATION_ITEM('')
SURFACE()
) ;
#246 = (
BOUNDED_SURFACE()
B_SPLINE_SURFACE(3,2,((#169307,#169308,#169309),(#169310,#169311,#169312),
(#169313,#169314,#169315),(#169316,#169317,#169318),(#169319,#169320,#169321),
(#169322,#169323,#169324),(#169325,#169326,#169327),(#169328,#169329,#169330),
(#169331,#169332,#169333),(#169334,#169335,#169336)),.UNSPECIFIED.,.F.,
 .F.,.F.)
B_SPLINE_SURFACE_WITH_KNOTS((4,2,2,2,4),(3,3),(-3.3881317890172E-21,5.50005871024834E-5,
0.000110001174204967,0.00016500176130745,0.000220002348409933),(-9.32574651063668E-5,
1.),.UNSPECIFIED.)
GEOMETRIC_REPRESENTATION_ITEM()
RATIONAL_B_SPLINE_SURFACE(((1.00005463405283,0.707079466707403,1.),(1.00005694771662,
0.694674755787773,1.),(1.00005645688427,0.697306353922386,1.),(1.00005591567352,
0.700208055939933,1.),(1.0000556235962,0.701774028840204,1.),(1.00005562454821,
0.701768924610519,1.),(1.00005591789342,0.700196153956681,1.),(1.00005645795057,
0.697300636998076,1.),(1.00005694973354,0.694663942070754,1.),(1.00005463405283,
0.707079466707411,1.)))
REPRESENTATION_ITEM('')
SURFACE()
) ;
#247 = (
BOUNDED_SURFACE()
B_SPLINE_SURFACE(3,2,((#169341,#169342,#169343),(#169344,#169345,#169346),
(#169347,#169348,#169349),(#169350,#169351,#169352),(#169353,#169354,#169355),
(#169356,#169357,#169358),(#169359,#169360,#169361),(#169362,#169363,#169364),
(#169365,#169366,#169367),(#169368,#169369,#169370)),.UNSPECIFIED.,.F.,
 .F.,.F.)
B_SPLINE_SURFACE_WITH_KNOTS((4,2,2,2,4),(3,3),(3.3881317890172E-21,5.50005871024832E-5,
0.000110001174204966,0.00016500176130745,0.000220002348409933),(0.,1.00009325746505),
 .UNSPECIFIED.)
GEOMETRIC_REPRESENTATION_ITEM()
RATIONAL_B_SPLINE_SURFACE(((1.,0.707079466707425,1.00005463405279),(1.,
0.694674755787727,1.00005694771658),(1.,0.69730635392251,1.00005645688424),
(1.,0.700208055939857,1.00005591567349),(1.,0.701774028839934,1.00005562359617),
(1.,0.701768924610827,1.00005562454818),(1.,0.700196153956623,1.00005591789339),
(1.,0.697300636998135,1.00005645795053),(1.,0.694663942070729,1.0000569497335),
(1.,0.707079466707418,1.00005463405279)))
REPRESENTATION_ITEM('')
SURFACE()
) ;
#248 = (
BOUNDED_SURFACE()
B_SPLINE_SURFACE(3,2,((#169375,#169376,#169377),(#169378,#169379,#169380),
(#169381,#169382,#169383),(#169384,#169385,#169386),(#169387,#169388,#169389),
(#169390,#169391,#169392),(#169393,#169394,#169395),(#169396,#169397,#169398),
(#169399,#169400,#169401),(#169402,#169403,#169404)),.UNSPECIFIED.,.F.,
 .F.,.F.)
B_SPLINE_SURFACE_WITH_KNOTS((4,2,2,2,4),(3,3),(-3.3881317890172E-21,5.50005871024821E-5,
0.000110001174204964,0.000165001761307446,0.000220002348409928),(-9.325746516207E-5,
1.),.UNSPECIFIED.)
GEOMETRIC_REPRESENTATION_ITEM()
RATIONAL_B_SPLINE_SURFACE(((1.00005463405286,0.707079466707472,1.),(1.00005694771665,
0.6946747557876,1.),(1.00005645688431,0.697306353922669,1.),(1.00005591567356,
0.700208055939717,1.),(1.00005562359623,0.701774028840023,1.),(1.00005562454825,
0.701768924610666,1.),(1.00005591789346,0.700196153956725,1.),(1.0000564579506,
0.697300636997996,1.),(1.00005694973357,0.694663942070795,1.),(1.00005463405286,
0.707079466707395,1.)))
REPRESENTATION_ITEM('')
SURFACE()
) ;
#249 = (
BOUNDED_SURFACE()
B_SPLINE_SURFACE(3,2,((#169409,#169410,#169411),(#169412,#169413,#169414),
(#169415,#169416,#169417),(#169418,#169419,#169420),(#169421,#169422,#169423),
(#169424,#169425,#169426),(#169427,#169428,#169429),(#169430,#169431,#169432),
(#169433,#169434,#169435),(#169436,#169437,#169438)),.UNSPECIFIED.,.F.,
 .F.,.F.)
B_SPLINE_SURFACE_WITH_KNOTS((4,2,2,2,4),(3,3),(3.3881317890172E-21,5.50005871024832E-5,
0.000110001174204966,0.00016500176130745,0.000220002348409933),(0.,1.00009325746505),
 .UNSPECIFIED.)
GEOMETRIC_REPRESENTATION_ITEM()
RATIONAL_B_SPLINE_SURFACE(((1.,0.707079466707427,1.00005463405279),(1.,
0.694674755787857,1.00005694771658),(1.,0.697306353922324,1.00005645688424),
(1.,0.700208055940047,1.00005591567349),(1.,0.701774028839924,1.00005562359616),
(1.,0.701768924610816,1.00005562454818),(1.,0.700196153956747,1.00005591789339),
(1.,0.697300636998016,1.00005645795053),(1.,0.694663942070808,1.0000569497335),
(1.,0.707079466707432,1.00005463405279)))
REPRESENTATION_ITEM('')
SURFACE()
) ;
#250 = (
BOUNDED_SURFACE()
B_SPLINE_SURFACE(3,2,((#169443,#169444,#169445),(#169446,#169447,#169448),
(#169449,#169450,#169451),(#169452,#169453,#169454),(#169455,#169456,#169457),
(#169458,#169459,#169460),(#169461,#169462,#169463),(#169464,#169465,#169466),
(#169467,#169468,#169469),(#169470,#169471,#169472)),.UNSPECIFIED.,.F.,
 .F.,.F.)
B_SPLINE_SURFACE_WITH_KNOTS((4,2,2,2,4),(3,3),(-3.3881317890172E-21,5.50005871024821E-5,
0.000110001174204964,0.000165001761307446,0.000220002348409928),(-9.32574651622988E-5,
1.),.UNSPECIFIED.)
GEOMETRIC_REPRESENTATION_ITEM()
RATIONAL_B_SPLINE_SURFACE(((1.00005463405286,0.707079466707472,1.),(1.00005694771665,
0.6946747557876,1.),(1.00005645688431,0.697306353922669,1.),(1.00005591567356,
0.700208055939717,1.),(1.00005562359623,0.701774028840023,1.),(1.00005562454825,
0.701768924610666,1.),(1.00005591789346,0.700196153956725,1.),(1.0000564579506,
0.697300636997996,1.),(1.00005694973357,0.694663942070795,1.),(1.00005463405286,
0.707079466707394,1.)))
REPRESENTATION_ITEM('')
SURFACE()
) ;
#251 = (
BOUNDED_SURFACE()
B_SPLINE_SURFACE(3,2,((#169477,#169478,#169479),(#169480,#169481,#169482),
(#169483,#169484,#169485),(#169486,#169487,#169488),(#169489,#169490,#169491),
(#169492,#169493,#169494),(#169495,#169496,#169497),(#169498,#169499,#169500),
(#169501,#169502,#169503),(#169504,#169505,#169506)),.UNSPECIFIED.,.F.,
 .F.,.F.)
B_SPLINE_SURFACE_WITH_KNOTS((4,2,2,2,4),(3,3),(0.,5.50005871024826E-5,0.000110001174204965,
0.000165001761307448,0.00022000234840993),(0.,1.00009325746516),
 .UNSPECIFIED.)
GEOMETRIC_REPRESENTATION_ITEM()
RATIONAL_B_SPLINE_SURFACE(((1.,0.707079466707393,1.00005463405286),(1.,
0.6946747557876,1.00005694771665),(1.,0.697306353922587,1.00005645688431),
(1.,0.700208055939715,1.00005591567356),(1.,0.701774028840065,1.00005562359623),
(1.,0.701768924610603,1.00005562454825),(1.,0.700196153956427,1.00005591789346),
(1.,0.697300636998359,1.0000564579506),(1.,0.694663942070582,1.00005694973357),
(1.,0.707079466707472,1.00005463405286)))
REPRESENTATION_ITEM('')
SURFACE()
) ;
#252 = (
BOUNDED_SURFACE()
B_SPLINE_SURFACE(3,2,((#169610,#169611,#169612),(#169613,#169614,#169615),
(#169616,#169617,#169618),(#169619,#169620,#169621),(#169622,#169623,#169624),
(#169625,#169626,#169627),(#169628,#169629,#169630),(#169631,#169632,#169633),
(#169634,#169635,#169636),(#169637,#169638,#169639)),.UNSPECIFIED.,.F.,
 .F.,.F.)
B_SPLINE_SURFACE_WITH_KNOTS((4,2,2,2,4),(3,3),(-8.470329472543E-22,1.20923255006762E-5,
2.41846510013524E-5,4.83693020027048E-5,9.67386040054096E-5),(-0.000804444758851847,
1.00077659724948),.UNSPECIFIED.)
GEOMETRIC_REPRESENTATION_ITEM()
RATIONAL_B_SPLINE_SURFACE(((1.00092876437359,0.422280884438106,1.00089658833676),
(1.00092908313811,0.422082603407448,1.00089689605803),(1.00086201767711,
0.46379931855613,1.00083215400736),(1.00071445154572,0.555589849432173,
1.00068970014494),(1.00063665558035,0.603981258051229,1.00061459933661),
(1.00042751802664,0.734071048305621,1.00041270712717),(1.00031984666358,
0.801045844505129,1.00030876592199),(1.0000701654339,0.956355009333009,
1.00006773462836),(1.00000277537655,0.998273633088197,1.00000267922663),
(1.,1.,1.)))
REPRESENTATION_ITEM('')
SURFACE()
) ;
#253 = (
BOUNDED_SURFACE()
B_SPLINE_SURFACE(3,2,((#169641,#169642,#169643),(#169644,#169645,#169646),
(#169647,#169648,#169649),(#169650,#169651,#169652),(#169653,#169654,#169655),
(#169656,#169657,#169658),(#169659,#169660,#169661),(#169662,#169663,#169664),
(#169665,#169666,#169667),(#169668,#169669,#169670)),.UNSPECIFIED.,.F.,
 .F.,.F.)
B_SPLINE_SURFACE_WITH_KNOTS((4,2,2,2,4),(3,3),(0.,9.64580201362678E-6,1.92916040272536E-5,
3.85832080545071E-5,7.71664161090142E-5),(-0.000370411631943625,1.00037041163331),
 .UNSPECIFIED.)
GEOMETRIC_REPRESENTATION_ITEM()
RATIONAL_B_SPLINE_SURFACE(((1.00032019601253,0.567623377417556,1.00032019601371),
(1.00032045653552,0.567271580252903,1.0003204565367),(1.00030818786187,
0.583838581291787,1.00030818786301),(1.00027173235979,0.63306626136058,
1.0002717323608),(1.00024819709674,0.664847099196012,1.00024819709766),
(1.00017892209811,0.758392579986913,1.00017892209877),(1.000134718753,0.818082558353675,
1.0001347187535),(1.00003314780627,0.955238866321452,1.00003314780639),
(0.999999834267815,1.00022379642419,0.999999834267814),(1.,1.,1.)))
REPRESENTATION_ITEM('')
SURFACE()
) ;
#254 = (
BOUNDED_SURFACE()
B_SPLINE_SURFACE(3,2,((#169672,#169673,#169674),(#169675,#169676,#169677),
(#169678,#169679,#169680),(#169681,#169682,#169683),(#169684,#169685,#169686),
(#169687,#169688,#169689),(#169690,#169691,#169692),(#169693,#169694,#169695),
(#169696,#169697,#169698),(#169699,#169700,#169701)),.UNSPECIFIED.,.F.,
 .F.,.F.)
B_SPLINE_SURFACE_WITH_KNOTS((4,2,2,2,4),(3,3),(0.,9.64580201362836E-6,1.92916040272567E-5,
3.85832080545134E-5,7.71664161090269E-5),(-0.000370411633304617,1.00037041163335),
 .UNSPECIFIED.)
GEOMETRIC_REPRESENTATION_ITEM()
RATIONAL_B_SPLINE_SURFACE(((1.0003201960137,0.56762337741697,1.00032019601374),
(1.00032045653669,0.567271580252287,1.00032045653673),(1.00030818786301,
0.583838581291198,1.00030818786303),(1.00027173236079,0.633066261360079,
1.00027173236081),(1.00024819709765,0.664847099195498,1.00024819709767),
(1.00017892209876,0.758392579986697,1.00017892209878),(1.0001347187535,
0.818082558353415,1.00013471875351),(1.00003314780639,0.955238866321388,
1.00003314780639),(0.999999834267815,1.0002237964242,0.999999834267813),
(1.,1.,1.)))
REPRESENTATION_ITEM('')
SURFACE()
) ;
#255 = (
BOUNDED_SURFACE()
B_SPLINE_SURFACE(3,2,((#169703,#169704,#169705),(#169706,#169707,#169708),
(#169709,#169710,#169711),(#169712,#169713,#169714),(#169715,#169716,#169717),
(#169718,#169719,#169720),(#169721,#169722,#169723),(#169724,#169725,#169726),
(#169727,#169728,#169729),(#169730,#169731,#169732)),.UNSPECIFIED.,.F.,
 .F.,.F.)
B_SPLINE_SURFACE_WITH_KNOTS((4,2,2,2,4),(3,3),(0.,9.64580201362833E-6,1.92916040272567E-5,
3.85832080545133E-5,7.71664161090267E-5),(-0.000370411633799105,1.00037041163132),
 .UNSPECIFIED.)
GEOMETRIC_REPRESENTATION_ITEM()
RATIONAL_B_SPLINE_SURFACE(((1.00032019601413,0.567623377417628,1.00032019601199),
(1.00032045653712,0.567271580252937,1.00032045653497),(1.00030818786341,
0.583838581291844,1.00030818786135),(1.00027173236115,0.63306626136063,
1.00027173235934),(1.00024819709798,0.66484709919601,1.00024819709632),
(1.000178922099,0.758392579987061,1.0001789220978),(1.00013471875369,0.818082558353688,
1.00013471875278),(1.00003314780643,0.955238866321459,1.00003314780621),
(0.999999834267814,1.00022379642419,0.999999834267815),(1.,1.,1.)))
REPRESENTATION_ITEM('')
SURFACE()
) ;
#256 = (
BOUNDED_SURFACE()
B_SPLINE_SURFACE(3,2,((#169734,#169735,#169736),(#169737,#169738,#169739),
(#169740,#169741,#169742),(#169743,#169744,#169745),(#169746,#169747,#169748),
(#169749,#169750,#169751),(#169752,#169753,#169754),(#169755,#169756,#169757),
(#169758,#169759,#169760),(#169761,#169762,#169763)),.UNSPECIFIED.,.F.,
 .F.,.F.)
B_SPLINE_SURFACE_WITH_KNOTS((4,2,2,2,4),(3,3),(-4.25210539521659E-19,9.64580201362817E-6,
1.92916040272568E-5,3.8583208054514E-5,7.71664161090284E-5),(-0.00037041163343029,
1.00037041163324),.UNSPECIFIED.)
GEOMETRIC_REPRESENTATION_ITEM()
RATIONAL_B_SPLINE_SURFACE(((1.00032019601381,0.567623377416959,1.00032019601364),
(1.0003204565368,0.56727158025228,1.00032045653663),(1.00030818786311,0.583838581291188,
1.00030818786295),(1.00027173236089,0.633066261360063,1.00027173236074),
(1.00024819709774,0.664847099195502,1.00024819709761),(1.00017892209882,
0.758392579986709,1.00017892209873),(1.00013471875355,0.818082558353424,
1.00013471875348),(1.0000331478064,0.955238866321397,1.00003314780639),
(0.999999834267814,1.00022379642418,0.999999834267814),(1.,1.,1.)))
REPRESENTATION_ITEM('')
SURFACE()
) ;
#257 = (
BOUNDED_SURFACE()
B_SPLINE_SURFACE(3,2,((#169765,#169766,#169767),(#169768,#169769,#169770),
(#169771,#169772,#169773),(#169774,#169775,#169776),(#169777,#169778,#169779),
(#169780,#169781,#169782),(#169783,#169784,#169785),(#169786,#169787,#169788),
(#169789,#169790,#169791),(#169792,#169793,#169794)),.UNSPECIFIED.,.F.,
 .F.,.F.)
B_SPLINE_SURFACE_WITH_KNOTS((4,2,2,2,4),(3,3),(-4.25210539521659E-19,9.64580201362817E-6,
1.92916040272568E-5,3.8583208054514E-5,7.71664161090284E-5),(-0.000370411633405951,
1.00037041163366),.UNSPECIFIED.)
GEOMETRIC_REPRESENTATION_ITEM()
RATIONAL_B_SPLINE_SURFACE(((1.00032019601379,0.567623377416788,1.00032019601401),
(1.00032045653678,0.567271580252109,1.00032045653699),(1.00030818786309,
0.583838581291024,1.0003081878633),(1.00027173236087,0.633066261359918,
1.00027173236105),(1.00024819709772,0.66484709919537,1.00024819709789),
(1.00017892209881,0.758392579986613,1.00017892209894),(1.00013471875354,
0.818082558353352,1.00013471875363),(1.0000331478064,0.955238866321379,
1.00003314780643),(0.999999834267814,1.00022379642418,0.999999834267814),
(1.,1.,1.)))
REPRESENTATION_ITEM('')
SURFACE()
) ;
#258 = (
BOUNDED_SURFACE()
B_SPLINE_SURFACE(3,2,((#169796,#169797,#169798),(#169799,#169800,#169801),
(#169802,#169803,#169804),(#169805,#169806,#169807),(#169808,#169809,#169810),
(#169811,#169812,#169813),(#169814,#169815,#169816),(#169817,#169818,#169819),
(#169820,#169821,#169822),(#169823,#169824,#169825)),.UNSPECIFIED.,.F.,
 .F.,.F.)
B_SPLINE_SURFACE_WITH_KNOTS((4,2,2,2,4),(3,3),(-8.92772726406033E-19,9.64580201362776E-6,
1.92916040272564E-5,3.85832080545137E-5,7.71664161090283E-5),(-0.000370411626210755,
1.00037041164027),.UNSPECIFIED.)
GEOMETRIC_REPRESENTATION_ITEM()
RATIONAL_B_SPLINE_SURFACE(((1.00032019600757,0.567623377417044,1.00032019601972),
(1.00032045653055,0.567271580252367,1.00032045654271),(1.0003081878571,
0.583838581291261,1.0003081878688),(1.00027173235558,0.633066261360144,
1.0002717323659),(1.0002481970929,0.664847099195559,1.00024819710231),(1.00017892209533,
0.758392579986733,1.00017892210213),(1.00013471875092,0.818082558353452,
1.00013471875604),(1.00003314780575,0.955238866321398,1.00003314780701),
(0.999999834267817,1.00022379642419,0.99999983426781),(1.,1.,1.)))
REPRESENTATION_ITEM('')
SURFACE()
) ;
#259 = (
BOUNDED_SURFACE()
B_SPLINE_SURFACE(3,2,((#169827,#169828,#169829),(#169830,#169831,#169832),
(#169833,#169834,#169835),(#169836,#169837,#169838),(#169839,#169840,#169841),
(#169842,#169843,#169844),(#169845,#169846,#169847),(#169848,#169849,#169850),
(#169851,#169852,#169853),(#169854,#169855,#169856)),.UNSPECIFIED.,.F.,
 .F.,.F.)
B_SPLINE_SURFACE_WITH_KNOTS((4,2,2,2,4),(3,3),(0.,9.64580201362838E-6,1.92916040272568E-5,
3.85832080545135E-5,7.71664161090271E-5),(-0.000370411640884523,1.00037041162619),
 .UNSPECIFIED.)
GEOMETRIC_REPRESENTATION_ITEM()
RATIONAL_B_SPLINE_SURFACE(((1.00032019602025,0.567623377416787,1.00032019600755),
(1.00032045654325,0.567271580252103,1.00032045653053),(1.00030818786931,
0.58383858129102,1.00030818785708),(1.00027173236636,0.633066261359912,
1.00027173235557),(1.00024819710274,0.66484709919538,1.00024819709289),
(1.00017892210243,0.758392579986544,1.00017892209533),(1.00013471875626,
0.81808255835334,1.00013471875092),(1.00003314780707,0.955238866321376,
1.00003314780575),(0.99999983426781,1.00022379642419,0.999999834267817),
(1.,1.,1.)))
REPRESENTATION_ITEM('')
SURFACE()
) ;
#260 = (
BOUNDED_SURFACE()
B_SPLINE_SURFACE(3,2,((#169858,#169859,#169860),(#169861,#169862,#169863),
(#169864,#169865,#169866),(#169867,#169868,#169869),(#169870,#169871,#169872),
(#169873,#169874,#169875),(#169876,#169877,#169878),(#169879,#169880,#169881),
(#169882,#169883,#169884),(#169885,#169886,#169887)),.UNSPECIFIED.,.F.,
 .F.,.F.)
B_SPLINE_SURFACE_WITH_KNOTS((4,2,2,2,4),(3,3),(0.,9.64580201362832E-6,1.92916040272566E-5,
3.85832080545133E-5,7.71664161090265E-5),(-0.000370411633605454,1.00037041163324),
 .UNSPECIFIED.)
GEOMETRIC_REPRESENTATION_ITEM()
RATIONAL_B_SPLINE_SURFACE(((1.00032019601396,0.567623377416892,1.00032019601364),
(1.00032045653695,0.567271580252197,1.00032045653663),(1.00030818786325,
0.583838581291129,1.00030818786294),(1.00027173236101,0.633066261360012,
1.00027173236073),(1.00024819709786,0.664847099195459,1.00024819709761),
(1.00017892209891,0.758392579986615,1.00017892209872),(1.00013471875361,
0.8180825583534,1.00013471875347),(1.00003314780642,0.955238866321366,1.00003314780638),
(0.999999834267813,1.0002237964242,0.999999834267813),(1.,1.,1.)))
REPRESENTATION_ITEM('')
SURFACE()
) ;
#261 = (
BOUNDED_SURFACE()
B_SPLINE_SURFACE(3,2,((#169893,#169894,#169895),(#169896,#169897,#169898),
(#169899,#169900,#169901),(#169902,#169903,#169904),(#169905,#169906,#169907),
(#169908,#169909,#169910),(#169911,#169912,#169913),(#169914,#169915,#169916),
(#169917,#169918,#169919),(#169920,#169921,#169922)),.UNSPECIFIED.,.F.,
 .F.,.F.)
B_SPLINE_SURFACE_WITH_KNOTS((4,2,2,2,4),(3,3),(0.,9.6458020136283E-6,1.92916040272566E-5,
3.85832080545132E-5,7.71664161090264E-5),(-0.000370411633385564,1.00037041163303),
 .UNSPECIFIED.)
GEOMETRIC_REPRESENTATION_ITEM()
RATIONAL_B_SPLINE_SURFACE(((1.00032019601377,0.567623377417072,1.00032019601346),
(1.00032045653676,0.567271580252374,1.00032045653645),(1.00030818786307,
0.58383858129131,1.00030818786277),(1.00027173236085,0.633066261360156,
1.00027173236059),(1.00024819709771,0.664847099195593,1.00024819709747),
(1.0001789220988,0.758392579986717,1.00017892209863),(1.00013471875353,
0.81808255835345,1.0001347187534),(1.0000331478064,0.955238866321428,1.00003314780636),
(0.999999834267813,1.00022379642417,0.999999834267814),(1.,1.,1.)))
REPRESENTATION_ITEM('')
SURFACE()
) ;
#262 = (
BOUNDED_SURFACE()
B_SPLINE_SURFACE(3,2,((#169928,#169929,#169930),(#169931,#169932,#169933),
(#169934,#169935,#169936),(#169937,#169938,#169939),(#169940,#169941,#169942),
(#169943,#169944,#169945),(#169946,#169947,#169948),(#169949,#169950,#169951),
(#169952,#169953,#169954),(#169955,#169956,#169957)),.UNSPECIFIED.,.F.,
 .F.,.F.)
B_SPLINE_SURFACE_WITH_KNOTS((4,2,2,2,4),(3,3),(-4.26904605416167E-19,1.20923255006779E-5,
2.41846510013563E-5,4.8369302002713E-5,9.67386040054264E-5),(-0.000768510511548604,
1.00084741984056),.UNSPECIFIED.)
GEOMETRIC_REPRESENTATION_ITEM()
RATIONAL_B_SPLINE_SURFACE(((1.00088724495747,0.422260730021251,1.00097842287518),
(1.00088754947197,0.422062442073261,1.00097875868317),(1.00082348210054,
0.463780612559125,1.00090810741463),(1.00068251275493,0.555574345656711,
1.00075265132409),(1.00060819457483,0.603967442467466,1.00067069582031),
(1.00040840629136,0.734061771058594,1.0004503762512),(1.00030554826122,
0.801038903753378,1.00033694799359),(1.00006702876336,0.95635348672563,
1.00007391698856),(1.00000265130631,0.9982735728619,1.00000292376837),(1.,
1.,1.)))
REPRESENTATION_ITEM('')
SURFACE()
) ;
#263 = (
BOUNDED_SURFACE()
B_SPLINE_SURFACE(3,2,((#170041,#170042,#170043),(#170044,#170045,#170046),
(#170047,#170048,#170049),(#170050,#170051,#170052),(#170053,#170054,#170055),
(#170056,#170057,#170058),(#170059,#170060,#170061),(#170062,#170063,#170064)),
 .UNSPECIFIED.,.F.,.F.,.F.)
B_SPLINE_SURFACE_WITH_KNOTS((4,2,2,4),(3,3),(3.40064005737571,3.72857728812795,
4.0565145188802,4.71238898038469),(0.,1.00035627873587),.UNSPECIFIED.)
GEOMETRIC_REPRESENTATION_ITEM()
RATIONAL_B_SPLINE_SURFACE(((1.,0.571144599242878,1.00030558412011),(1.,
0.605472570854249,1.00028112346745),(1.,0.655758245054346,1.00024529203457),
(1.,0.758559230914953,1.000172040424),(1.,0.810907017329345,1.00013473961766),
(1.,0.944519775683756,1.00003953284837),(1.,1.00147328708535,0.999998950198279),
(1.,1.,1.)))
REPRESENTATION_ITEM('')
SURFACE()
) ;
#264 = (
BOUNDED_SURFACE()
B_SPLINE_SURFACE(3,2,((#170066,#170067,#170068),(#170069,#170070,#170071),
(#170072,#170073,#170074),(#170075,#170076,#170077)),.UNSPECIFIED.,.F.,
 .F.,.F.)
B_SPLINE_SURFACE_WITH_KNOTS((4,4),(3,3),(0.000567067675011747,0.00061979582196747),
(0.,1.),.UNSPECIFIED.)
GEOMETRIC_REPRESENTATION_ITEM()
RATIONAL_B_SPLINE_SURFACE(((1.,0.571297336894462,1.),(1.,0.558391514685631,
1.),(1.,0.550506809043631,1.),(1.,0.550571663591217,1.)))
REPRESENTATION_ITEM('')
SURFACE()
) ;
#265 = (
BOUNDED_SURFACE()
B_SPLINE_SURFACE(3,2,((#170078,#170079,#170080),(#170081,#170082,#170083),
(#170084,#170085,#170086),(#170087,#170088,#170089),(#170090,#170091,#170092),
(#170093,#170094,#170095),(#170096,#170097,#170098),(#170099,#170100,#170101)),
 .UNSPECIFIED.,.F.,.F.,.F.)
B_SPLINE_SURFACE_WITH_KNOTS((4,2,2,4),(3,3),(6.54223271101527,6.87016994175507,
7.19810717249488,7.85398163397448),(-0.000356360340643563,1.00035627873694),
 .UNSPECIFIED.)
GEOMETRIC_REPRESENTATION_ITEM()
RATIONAL_B_SPLINE_SURFACE(((1.00030565413832,0.570991717771645,1.00030558412101),
(1.00028118788101,0.605331926871258,1.00028112346828),(1.00024534823811,
0.655635527273589,1.0002452920353),(1.00017207984346,0.758473160372548,
1.0001720404245),(1.00013477049042,0.810839608102769,1.00013473961805),
(1.00003954190649,0.944499997695579,1.00003953284848),(0.999998949957739,
1.00147381229284,0.999998950198277),(1.,1.,1.)))
REPRESENTATION_ITEM('')
SURFACE()
) ;
#266 = (
BOUNDED_SURFACE()
B_SPLINE_SURFACE(3,2,((#170103,#170104,#170105),(#170106,#170107,#170108),
(#170109,#170110,#170111),(#170112,#170113,#170114)),.UNSPECIFIED.,.F.,
 .F.,.F.)
B_SPLINE_SURFACE_WITH_KNOTS((4,4),(3,3),(0.000567067675015788,0.000619795821981054),
(0.,1.00004537587559),.UNSPECIFIED.)
GEOMETRIC_REPRESENTATION_ITEM()
RATIONAL_B_SPLINE_SURFACE(((1.,0.571277884142694,1.00003890728278),(1.,
0.558371476316907,1.0000400785619),(1.,0.55048641289642,1.00004079414521),
(1.,0.550551270386939,1.00004078825928)))
REPRESENTATION_ITEM('')
SURFACE()
) ;
#267 = ELLIPSE('',#91249,0.191322338734783,0.178429548359619) ;
#268 = ELLIPSE('',#91250,0.19132233878183,0.178429548383724) ;
#269 = ELLIPSE('',#91251,0.191322338731802,0.178429548357439) ;
#270 = ELLIPSE('',#91252,0.191322338779123,0.17842954838245) ;
#271 = ELLIPSE('',#91300,0.190951225717336,0.171364150514683) ;
#272 = ELLIPSE('',#91301,0.184110979856706,0.15942086075581) ;
#273 = ELLIPSE('',#91303,0.102944309528002,0.0999999999999975) ;
#274 = ELLIPSE('',#91304,0.102944309527982,0.0999999999999795) ;
#275 = ELLIPSE('',#91305,0.102944309527979,0.0999999999999756) ;
#276 = ELLIPSE('',#91306,0.102944309527978,0.0999999999999751) ;
#277 = ELLIPSE('',#91308,0.184110979853722,0.159420860750542) ;
#278 = ELLIPSE('',#91309,0.19095122571746,0.171364150514935) ;
#279 = ELLIPSE('',#91378,0.102447207929153,0.0855466862257129) ;
#280 = ELLIPSE('',#91388,0.102447207928901,0.0855466862253011) ;
#281 = ELLIPSE('',#91393,0.141421356237246,0.099999999999956) ;
#282 = ELLIPSE('',#91411,0.141421356237246,0.0999999999999589) ;
#283 = ELLIPSE('',#91422,0.111310931434027,0.0999999999994426) ;
#284 = ELLIPSE('',#91426,0.111310931436794,0.100000000004093) ;
#285 = ELLIPSE('',#91433,0.126113554280143,0.0912763326628817) ;
#286 = ELLIPSE('',#91447,0.126113554274935,0.0912763326607385) ;
#287 = ELLIPSE('',#91665,0.190951225717095,0.171364150514224) ;
#288 = ELLIPSE('',#91666,0.18411097985465,0.159420860752213) ;
#289 = ELLIPSE('',#91668,0.102944309528002,0.0999999999999973) ;
#290 = ELLIPSE('',#91669,0.102944309528015,0.100000000000011) ;
#291 = ELLIPSE('',#91670,0.102944309528021,0.100000000000013) ;
#292 = ELLIPSE('',#91671,0.102944309527952,0.0999999999999486) ;
#293 = ELLIPSE('',#91673,0.184110979853536,0.159420860750266) ;
#294 = ELLIPSE('',#91674,0.19095122571723,0.17136415051449) ;
#295 = ELLIPSE('',#91743,0.102447207929021,0.085546686225496) ;
#296 = ELLIPSE('',#91753,0.102447207929205,0.0855466862258343) ;
#297 = ELLIPSE('',#91758,0.14142135623734,0.100000000000021) ;
#298 = ELLIPSE('',#91776,0.141421356237089,0.0999999999998527) ;
#299 = ELLIPSE('',#91787,0.11131093143594,0.100000000002612) ;
#300 = ELLIPSE('',#91791,0.111310931435708,0.10000000000223) ;
#301 = ELLIPSE('',#91798,0.126113554274573,0.0912763326605795) ;
#302 = ELLIPSE('',#91811,0.126113554276116,0.0912763326612655) ;
#303 = ELLIPSE('',#92137,0.191322338736984,0.178429548360737) ;
#304 = ELLIPSE('',#92138,0.191322338786359,0.178429548386577) ;
#305 = ELLIPSE('',#92139,0.191322338724264,0.17842954835187) ;
#306 = ELLIPSE('',#92140,0.191322338783867,0.178429548384638) ;
#307 = ELLIPSE('',#92189,0.190951225717061,0.171364150514171) ;
#308 = ELLIPSE('',#92190,0.184110979854607,0.159420860752121) ;
#309 = ELLIPSE('',#92192,0.102944309527925,0.0999999999999341) ;
#310 = ELLIPSE('',#92193,0.102944309528208,0.100000000000198) ;
#311 = ELLIPSE('',#92194,0.102944309528197,0.100000000000187) ;
#312 = ELLIPSE('',#92195,0.10294430952777,0.0999999999997609) ;
#313 = ELLIPSE('',#92197,0.184110979849685,0.159420860743423) ;
#314 = ELLIPSE('',#92198,0.190951225717448,0.171364150514883) ;
#315 = ELLIPSE('',#92267,0.102447207929559,0.0855466862264446) ;
#316 = ELLIPSE('',#92277,0.102447207929716,0.0855466862267171) ;
#317 = ELLIPSE('',#92282,0.141421356237578,0.100000000000185) ;
#318 = ELLIPSE('',#92300,0.141421356237136,0.0999999999998538) ;
#319 = ELLIPSE('',#92311,0.111310931434914,0.100000000000826) ;
#320 = ELLIPSE('',#92315,0.111310931434193,0.099999999999555) ;
#321 = ELLIPSE('',#92322,0.12611355428909,0.0912763326666119) ;
#322 = ELLIPSE('',#92336,0.126113554268033,0.0912763326579103) ;
#323 = ELLIPSE('',#92554,0.190951225717901,0.171364150515768) ;
#324 = ELLIPSE('',#92555,0.184110979854194,0.159420860751403) ;
#325 = ELLIPSE('',#92557,0.102944309528061,0.100000000000057) ;
#326 = ELLIPSE('',#92558,0.102944309528071,0.100000000000074) ;
#327 = ELLIPSE('',#92559,0.102944309527994,0.0999999999999879) ;
#328 = ELLIPSE('',#92560,0.102944309527827,0.0999999999998399) ;
#329 = ELLIPSE('',#92562,0.184110979851928,0.159420860747419) ;
#330 = ELLIPSE('',#92563,0.190951225717375,0.17136415051477) ;
#331 = ELLIPSE('',#92632,0.102447207928804,0.0855466862251576) ;
#332 = ELLIPSE('',#92642,0.102447207929456,0.0855466862262483) ;
#333 = ELLIPSE('',#92647,0.141421356237259,0.0999999999999835) ;
#334 = ELLIPSE('',#92665,0.141421356237111,0.0999999999998622) ;
#335 = ELLIPSE('',#92676,0.111310931436081,0.100000000002901) ;
#336 = ELLIPSE('',#92680,0.111310931433336,0.0999999999981691) ;
#337 = ELLIPSE('',#92686,0.126113554288552,0.0912763326663696) ;
#338 = ELLIPSE('',#92700,0.126113554294105,0.0912763326688326) ;
#339 = ELLIPSE('',#92960,0.191322338738038,0.178429548361451) ;
#340 = ELLIPSE('',#92961,0.191322338777325,0.178429548380458) ;
#341 = ELLIPSE('',#93028,0.190951225717903,0.171364150515775) ;
#342 = ELLIPSE('',#93029,0.184110979854543,0.159420860752014) ;
#343 = ELLIPSE('',#93031,0.10294430952807,0.100000000000064) ;
#344 = ELLIPSE('',#93032,0.102944309528103,0.1000000000001) ;
#345 = ELLIPSE('',#93033,0.102944309528091,0.100000000000089) ;
#346 = ELLIPSE('',#93034,0.102944309527858,0.0999999999998653) ;
#347 = ELLIPSE('',#93036,0.184110979854767,0.159420860752386) ;
#348 = ELLIPSE('',#93037,0.190951225717425,0.171364150514857) ;
#349 = ELLIPSE('',#93106,0.102447207929024,0.0855466862255089) ;
#350 = ELLIPSE('',#93116,0.102447207928841,0.0855466862251956) ;
#351 = ELLIPSE('',#93121,0.141421356237363,0.100000000000039) ;
#352 = ELLIPSE('',#93139,0.141421356237142,0.0999999999998897) ;
#353 = ELLIPSE('',#93150,0.111310931435548,0.10000000000196) ;
#354 = ELLIPSE('',#93154,0.111310931436154,0.100000000003053) ;
#355 = ELLIPSE('',#93161,0.126113554273832,0.0912763326602602) ;
#356 = ELLIPSE('',#93175,0.126113554282611,0.0912763326639418) ;
#357 = ELLIPSE('',#93363,0.141421356226833,0.0999999999854714) ;
#358 = ELLIPSE('',#93380,0.141421356205715,0.0999999999561054) ;
#359 = ELLIPSE('',#93397,0.141421356206211,0.0999999999568741) ;
#360 = ELLIPSE('',#93414,0.14142135619891,0.0999999999469108) ;
#361 = ELLIPSE('',#93431,0.14142135620716,0.0999999999583245) ;
#362 = ELLIPSE('',#93448,0.141421356264666,0.100000000037862) ;
#363 = ELLIPSE('',#93465,0.141421356235352,0.0999999999972513) ;
#364 = ELLIPSE('',#93482,0.141421356240128,0.100000000003844) ;
#365 = ELLIPSE('',#93544,0.141421356242718,0.100000000007393) ;
#366 = ELLIPSE('',#93593,0.141421356244824,0.100000000010334) ;
#367 = ELLIPSE('',#98719,0.113705760628021,0.0999999999999901) ;
#368 = ELLIPSE('',#98720,0.149345237620599,0.0999999999999305) ;
#369 = ELLIPSE('',#98721,0.149345237620645,0.0999999999999468) ;
#370 = ELLIPSE('',#98722,0.113705760627924,0.0999999999999499) ;
#371 = ELLIPSE('',#98829,0.37480415029708,0.108393547954855) ;
#372 = ELLIPSE('',#98830,0.293533022904216,0.0776808743108713) ;
#373 = ELLIPSE('',#98841,0.0594417542785182,0.0546700434940687) ;
#374 = ELLIPSE('',#98843,0.335126724531724,0.0994337530748851) ;
#375 = ELLIPSE('',#98844,0.35994804660384,0.105243435885102) ;
#376 = ELLIPSE('',#98845,0.108850968875591,0.0580464239932984) ;
#377 = ELLIPSE('',#98864,0.0629103936951647,0.0573206382682852) ;
#378 = ELLIPSE('',#98870,0.335126724504839,0.0994337530612308) ;
#379 = ELLIPSE('',#98871,0.359948046537181,0.105243435873707) ;
#380 = ELLIPSE('',#98875,0.0702807513773626,0.0453069706635111) ;
#381 = ELLIPSE('',#98876,0.359930277252907,0.105237474483862) ;
#382 = ELLIPSE('',#98877,0.335173749742838,0.0994597385892411) ;
#383 = ELLIPSE('',#99074,0.111803398874898,0.0999999999999263) ;
#384 = ELLIPSE('',#99089,0.111803398874933,0.0999999999999485) ;
#385 = ELLIPSE('',#99211,0.113705760627989,0.0999999999999707) ;
#386 = ELLIPSE('',#99212,0.149345237619608,0.0999999999995642) ;
#387 = ELLIPSE('',#99213,0.149345237620654,0.0999999999999208) ;
#388 = ELLIPSE('',#99214,0.113705760628105,0.100000000000041) ;
#389 = ELLIPSE('',#99220,0.113705760628277,0.100000000000111) ;
#390 = ELLIPSE('',#99221,0.149345237618997,0.0999999999993761) ;
#391 = ELLIPSE('',#99222,0.149345237620065,0.0999999999997663) ;
#392 = ELLIPSE('',#99223,0.113705760628311,0.100000000000123) ;
#393 = ELLIPSE('',#99229,0.113705760628234,0.100000000000072) ;
#394 = ELLIPSE('',#99230,0.149345237619401,0.0999999999995206) ;
#395 = ELLIPSE('',#99231,0.149345237620857,0.100000000000031) ;
#396 = ELLIPSE('',#99232,0.113705760627957,0.0999999999999554) ;
#397 = ELLIPSE('',#99238,0.113705760628047,0.100000000000004) ;
#398 = ELLIPSE('',#99239,0.149345237619215,0.0999999999994726) ;
#399 = ELLIPSE('',#99240,0.14934523762126,0.10000000000015) ;
#400 = ELLIPSE('',#99241,0.113705760628205,0.100000000000077) ;
#401 = ELLIPSE('',#99247,0.113705760628038,0.0999999999999974) ;
#402 = ELLIPSE('',#99248,0.149345237619726,0.0999999999996396) ;
#403 = ELLIPSE('',#99249,0.149345237619801,0.0999999999996606) ;
#404 = ELLIPSE('',#99250,0.11370576062794,0.0999999999999675) ;
#405 = ELLIPSE('',#99256,0.113705760628114,0.100000000000042) ;
#406 = ELLIPSE('',#99257,0.149345237621322,0.100000000000178) ;
#407 = ELLIPSE('',#99258,0.14934523761991,0.0999999999997026) ;
#408 = ELLIPSE('',#99259,0.113705760627855,0.0999999999999047) ;
#409 = ELLIPSE('',#99265,0.113705760627948,0.099999999999958) ;
#410 = ELLIPSE('',#99266,0.149345237620904,0.100000000000041) ;
#411 = ELLIPSE('',#99267,0.149345237620801,0.100000000000004) ;
#412 = ELLIPSE('',#99268,0.113705760627834,0.0999999999999106) ;
#413 = ELLIPSE('',#99274,0.113705760628053,0.100000000000007) ;
#414 = ELLIPSE('',#99275,0.149345237620591,0.0999999999999292) ;
#415 = ELLIPSE('',#99276,0.149345237621263,0.100000000000161) ;
#416 = ELLIPSE('',#99277,0.113705760627995,0.0999999999999786) ;
#417 = ELLIPSE('',#99283,0.113705760627941,0.0999999999999602) ;
#418 = ELLIPSE('',#99284,0.149345237620714,0.0999999999999713) ;
#419 = ELLIPSE('',#99285,0.149345237620732,0.0999999999999782) ;
#420 = ELLIPSE('',#99286,0.113705760627987,0.0999999999999783) ;
#421 = ELLIPSE('',#99291,0.180453309435584,0.153056323384521) ;
#422 = ELLIPSE('',#99292,0.180453309425237,0.153056323367989) ;
#423 = ELLIPSE('',#99294,0.18045330947415,0.153056323451711) ;
#424 = ELLIPSE('',#99295,0.180453309589905,0.153056323648943) ;
#425 = ELLIPSE('',#99297,0.180453309654479,0.153056323758989) ;
#426 = ELLIPSE('',#99298,0.180453309391707,0.15305632331313) ;
#427 = ELLIPSE('',#99300,0.180453309365101,0.153056323267468) ;
#428 = ELLIPSE('',#99301,0.180453309556384,0.153056323594097) ;
#429 = ELLIPSE('',#99303,0.180453309198145,0.153056322983094) ;
#430 = ELLIPSE('',#99304,0.180453309480796,0.153056323464846) ;
#431 = ELLIPSE('',#99306,0.180453309173328,0.153056322941511) ;
#432 = ELLIPSE('',#99307,0.180453309202449,0.153056322990444) ;
#433 = ELLIPSE('',#99309,0.180453309242158,0.153056323057428) ;
#434 = ELLIPSE('',#99310,0.180453309451238,0.153056323414422) ;
#435 = ELLIPSE('',#99312,0.180453309481229,0.153056323465124) ;
#436 = ELLIPSE('',#99313,0.180453309451544,0.153056323414031) ;
#437 = ELLIPSE('',#99316,0.25539026404391,0.166311404124396) ;
#438 = ELLIPSE('',#99317,0.255390264039982,0.166311404121025) ;
#439 = ELLIPSE('',#99319,0.255390264047263,0.166311404128388) ;
#440 = ELLIPSE('',#99320,0.255390264044952,0.166311404125431) ;
#441 = ELLIPSE('',#99322,0.255390264049319,0.166311404131415) ;
#442 = ELLIPSE('',#99323,0.255390264043609,0.166311404123759) ;
#443 = ELLIPSE('',#99325,0.255390264047487,0.166311404129269) ;
#444 = ELLIPSE('',#99326,0.255390264041227,0.166311404120253) ;
#445 = ELLIPSE('',#99328,0.255390264048306,0.166311404130063) ;
#446 = ELLIPSE('',#99329,0.255390264042795,0.166311404122152) ;
#447 = ELLIPSE('',#99331,0.255390264044007,0.166311404124825) ;
#448 = ELLIPSE('',#99332,0.255390264041525,0.166311404120579) ;
#449 = ELLIPSE('',#99334,0.255390264028709,0.166311404112411) ;
#450 = ELLIPSE('',#99335,0.255390264039117,0.166311404117828) ;
#451 = ELLIPSE('',#99337,0.255390264033842,0.166311404118425) ;
#452 = ELLIPSE('',#99338,0.255390264029649,0.166311404113467) ;
#453 = ELLIPSE('',#100045,0.239471272541672,0.104190452490447) ;
#454 = ELLIPSE('',#100046,0.239594752726074,0.104223676986789) ;
#455 = ELLIPSE('',#100048,0.239594752697272,0.104223676980424) ;
#456 = ELLIPSE('',#100049,0.239471272492843,0.104190452477864) ;
#457 = ELLIPSE('',#100051,0.239594752684102,0.1042236769773) ;
#458 = ELLIPSE('',#100052,0.239471272466969,0.10419045247166) ;
#459 = ELLIPSE('',#100054,0.239594752734068,0.104223676990242) ;
#460 = ELLIPSE('',#100055,0.239471272561877,0.104190452494461) ;
#461 = ELLIPSE('',#100057,0.239471272527132,0.104190452486722) ;
#462 = ELLIPSE('',#100058,0.239594752734183,0.104223676988681) ;
#463 = ELLIPSE('',#100060,0.23959475268759,0.104223676978089) ;
#464 = ELLIPSE('',#100061,0.239471272489249,0.104190452477087) ;
#465 = ELLIPSE('',#100063,0.2395947526905,0.104223676978911) ;
#466 = ELLIPSE('',#100064,0.239471272497335,0.104190452479123) ;
#467 = ELLIPSE('',#100066,0.239594752708729,0.104223676983616) ;
#468 = ELLIPSE('',#100067,0.239471272526268,0.104190452487083) ;
#469 = ELLIPSE('',#100069,0.239471272514144,0.104190452483521) ;
#470 = ELLIPSE('',#100070,0.239594752716605,0.104223676986095) ;
#471 = ELLIPSE('',#100072,0.239594752699331,0.104223676981028) ;
#472 = ELLIPSE('',#100073,0.239471272496544,0.10419045247883) ;
#473 = ELLIPSE('',#100075,0.239594752723358,0.10422367698701) ;
#474 = ELLIPSE('',#100076,0.239471272495837,0.104190452478645) ;
#475 = ELLIPSE('',#100078,0.239594752698616,0.104223676981038) ;
#476 = ELLIPSE('',#100079,0.239471272522506,0.104190452485985) ;
#477 = ELLIPSE('',#100081,0.239471272517247,0.104190452484287) ;
#478 = ELLIPSE('',#100082,0.239594752720674,0.104223676987029) ;
#479 = ELLIPSE('',#100084,0.239594752709324,0.104223676983649) ;
#480 = ELLIPSE('',#100085,0.239471272554278,0.104190452493733) ;
#481 = ELLIPSE('',#100087,0.239594752719202,0.104223676985857) ;
#482 = ELLIPSE('',#100088,0.239471272507799,0.104190452481569) ;
#483 = ELLIPSE('',#100090,0.239594752706474,0.104223676983052) ;
#484 = ELLIPSE('',#100091,0.239471272527043,0.104190452487123) ;
#485 = ELLIPSE('',#100093,0.239471272527633,0.104190452486785) ;
#486 = ELLIPSE('',#100094,0.239594752719546,0.104223676986731) ;
#487 = ELLIPSE('',#100096,0.239594752703205,0.10422367698204) ;
#488 = ELLIPSE('',#100097,0.239471272482974,0.10419045247551) ;
#489 = ELLIPSE('',#100099,0.23959475271894,0.104223676985872) ;
#490 = ELLIPSE('',#100100,0.239471272513673,0.104190452482924) ;
#491 = ELLIPSE('',#100102,0.239594752701382,0.104223676981721) ;
#492 = ELLIPSE('',#100103,0.239471272535599,0.104190452489416) ;
#493 = ELLIPSE('',#100105,0.239471272525269,0.104190452486334) ;
#494 = ELLIPSE('',#100106,0.239594752716578,0.104223676986044) ;
#495 = ELLIPSE('',#100108,0.23959475276603,0.104223676998289) ;
#496 = ELLIPSE('',#100109,0.239471272489896,0.104190452477545) ;
#497 = ELLIPSE('',#100111,0.239594752717894,0.104223676985692) ;
#498 = ELLIPSE('',#100112,0.239471272524125,0.10419045248605) ;
#499 = ELLIPSE('',#100114,0.239594752691381,0.104223676979494) ;
#500 = ELLIPSE('',#100115,0.239471272558152,0.10419045249462) ;
#501 = ELLIPSE('',#100117,0.239471272517302,0.104190452484572) ;
#502 = ELLIPSE('',#100118,0.239594752726099,0.104223676988114) ;
#503 = ELLIPSE('',#100120,0.239594752760816,0.104223676997006) ;
#504 = ELLIPSE('',#100121,0.239471272488601,0.104190452477342) ;
#505 = ELLIPSE('',#100123,0.239594752734497,0.104223676990487) ;
#506 = ELLIPSE('',#100124,0.239471272528897,0.104190452487192) ;
#507 = ELLIPSE('',#100126,0.239594752719834,0.104223676986734) ;
#508 = ELLIPSE('',#100127,0.239471272551583,0.104190452493005) ;
#509 = ELLIPSE('',#100129,0.239471272526413,0.1041904524868) ;
#510 = ELLIPSE('',#100130,0.239594752719693,0.104223676986493) ;
#511 = ELLIPSE('',#100132,0.23959475272552,0.104223676988002) ;
#512 = ELLIPSE('',#100133,0.23947127255968,0.104190452495628) ;
#513 = ELLIPSE('',#100135,0.239594752745901,0.104223676993333) ;
#514 = ELLIPSE('',#100136,0.239471272534012,0.104190452488509) ;
#515 = ELLIPSE('',#100138,0.239594752723728,0.104223676987511) ;
#516 = ELLIPSE('',#100139,0.239471272544375,0.10419045249119) ;
#517 = ELLIPSE('',#100231,0.111803398874902,0.0999999999999214) ;
#518 = ELLIPSE('',#100246,0.111803398875015,0.100000000000024) ;
#519 = ELLIPSE('',#100249,0.19738899237826,0.0801201351308594) ;
#520 = ELLIPSE('',#100250,0.197388988783904,0.0801201312644544) ;
#521 = ELLIPSE('',#100251,0.111803398883664,0.100000000015977) ;
#522 = ELLIPSE('',#100252,0.236436524449966,0.104276779744234) ;
#523 = ELLIPSE('',#100253,0.222726289984573,0.0995178910570516) ;
#524 = ELLIPSE('',#100255,0.222704123466412,0.099498796196121) ;
#525 = ELLIPSE('',#100256,0.236408404049101,0.104269413800199) ;
#526 = ELLIPSE('',#100257,0.236436524432732,0.104276779737213) ;
#527 = ELLIPSE('',#100258,0.222726289984934,0.0995178910577687) ;
#528 = ELLIPSE('',#100260,0.197388992378616,0.0801201351309043) ;
#529 = ELLIPSE('',#100261,0.197388992379545,0.080120135131515) ;
#530 = ELLIPSE('',#100263,0.222704123474636,0.0994987962024968) ;
#531 = ELLIPSE('',#100264,0.236408404032557,0.104269413795424) ;
#532 = ELLIPSE('',#100265,0.111803398978043,0.100000000180811) ;
#533 = ELLIPSE('',#100266,0.197388988784215,0.080120131264687) ;
#534 = ELLIPSE('',#100267,0.197388992379424,0.0801201351317529) ;
#535 = ELLIPSE('',#100269,0.197388992379045,0.0801201351315553) ;
#536 = ELLIPSE('',#100270,0.197388988782772,0.0801201312636463) ;
#537 = ELLIPSE('',#100271,0.111803398854216,0.0999999999644239) ;
#538 = ELLIPSE('',#100272,0.236436524483533,0.104276779754402) ;
#539 = ELLIPSE('',#100273,0.222726289977912,0.0995178910519717) ;
#540 = ELLIPSE('',#100275,0.2227041234645,0.0994987961949076) ;
#541 = ELLIPSE('',#100276,0.236408403975384,0.104269413775528) ;
#542 = ELLIPSE('',#100277,0.236436524415503,0.104276779732904) ;
#543 = ELLIPSE('',#100278,0.222726289980937,0.0995178910544354) ;
#544 = ELLIPSE('',#100280,0.197388992380326,0.0801201351322599) ;
#545 = ELLIPSE('',#100281,0.197388992379516,0.0801201351314597) ;
#546 = ELLIPSE('',#100283,0.222704123471206,0.0994987961995229) ;
#547 = ELLIPSE('',#100284,0.236408404041556,0.104269413798962) ;
#548 = ELLIPSE('',#100285,0.1118033989916,0.100000000205665) ;
#549 = ELLIPSE('',#100286,0.197388988782326,0.0801201312633943) ;
#550 = ELLIPSE('',#100287,0.197388992380803,0.0801201351327621) ;
#551 = ELLIPSE('',#100289,0.197388992379311,0.0801201351317526) ;
#552 = ELLIPSE('',#100290,0.197388988782863,0.0801201312636897) ;
#553 = ELLIPSE('',#100291,0.111803398885653,0.100000000017746) ;
#554 = ELLIPSE('',#100292,0.236436524510541,0.104276779762262) ;
#555 = ELLIPSE('',#100293,0.222726289989238,0.0995178910616732) ;
#556 = ELLIPSE('',#100295,0.222704123468478,0.099498796197896) ;
#557 = ELLIPSE('',#100296,0.236408403942723,0.10426941376595) ;
#558 = ELLIPSE('',#100297,0.236436524607894,0.10427677979644) ;
#559 = ELLIPSE('',#100298,0.222726289996681,0.0995178910669966) ;
#560 = ELLIPSE('',#100300,0.197388992379108,0.0801201351314067) ;
#561 = ELLIPSE('',#100301,0.197388992378061,0.0801201351307853) ;
#562 = ELLIPSE('',#100303,0.222704123464741,0.0994987961955434) ;
#563 = ELLIPSE('',#100304,0.236408404096636,0.104269413815376) ;
#564 = ELLIPSE('',#100305,0.111803399145635,0.100000000475424) ;
#565 = ELLIPSE('',#100306,0.197388988779542,0.0801201312609667) ;
#566 = ELLIPSE('',#100307,0.197388992378485,0.0801201351306929) ;
#567 = ELLIPSE('',#100309,0.197388992378957,0.0801201351310294) ;
#568 = ELLIPSE('',#100310,0.19738898878374,0.0801201312642938) ;
#569 = ELLIPSE('',#100311,0.111803399036703,0.100000000285152) ;
#570 = ELLIPSE('',#100312,0.236436524495273,0.104276779757397) ;
#571 = ELLIPSE('',#100313,0.222726289990922,0.099517891062712) ;
#572 = ELLIPSE('',#100315,0.222704123464531,0.0994987961947874) ;
#573 = ELLIPSE('',#100316,0.236408404057535,0.10426941380379) ;
#574 = ELLIPSE('',#100317,0.236436524486579,0.104276779756148) ;
#575 = ELLIPSE('',#100318,0.222726289984491,0.0995178910572093) ;
#576 = ELLIPSE('',#100320,0.197388992378839,0.0801201351314571) ;
#577 = ELLIPSE('',#100321,0.197388992377843,0.0801201351307153) ;
#578 = ELLIPSE('',#100323,0.222704123467226,0.0994987961965839) ;
#579 = ELLIPSE('',#100324,0.236408404080475,0.104269413810236) ;
#580 = ELLIPSE('',#100325,0.111803399487092,0.100000001075964) ;
#581 = ELLIPSE('',#100326,0.197388988782072,0.080120131262859) ;
#582 = ELLIPSE('',#100327,0.197388992379507,0.0801201351315046) ;
#583 = ELLIPSE('',#100329,0.19738899237792,0.0801201351302709) ;
#584 = ELLIPSE('',#100330,0.197388988782827,0.0801201312637812) ;
#585 = ELLIPSE('',#100331,0.111803399293401,0.100000000733944) ;
#586 = ELLIPSE('',#100332,0.236436524534394,0.104276779769979) ;
#587 = ELLIPSE('',#100333,0.22272629000147,0.0995178910705121) ;
#588 = ELLIPSE('',#100335,0.222704123464496,0.0994987961947227) ;
#589 = ELLIPSE('',#100336,0.236408403913088,0.104269413756808) ;
#590 = ELLIPSE('',#100337,0.236436524427347,0.104276779737167) ;
#591 = ELLIPSE('',#100338,0.222726289994107,0.0995178910649231) ;
#592 = ELLIPSE('',#100340,0.197388992379256,0.0801201351317907) ;
#593 = ELLIPSE('',#100341,0.19738899237989,0.0801201351321866) ;
#594 = ELLIPSE('',#100343,0.222704123455483,0.0994987961875182) ;
#595 = ELLIPSE('',#100344,0.236408404037391,0.104269413796386) ;
#596 = ELLIPSE('',#100345,0.111803399309713,0.100000000765477) ;
#597 = ELLIPSE('',#100346,0.197388988785316,0.0801201312652288) ;
#598 = ELLIPSE('',#100347,0.197388992379548,0.0801201351314808) ;
#599 = ELLIPSE('',#100349,0.19738899237924,0.0801201351312266) ;
#600 = ELLIPSE('',#100350,0.197388988776506,0.0801201312591199) ;
#601 = ELLIPSE('',#100351,0.111803398888132,0.100000000025592) ;
#602 = ELLIPSE('',#100352,0.236436524490662,0.104276779756003) ;
#603 = ELLIPSE('',#100353,0.222726290011381,0.0995178910787348) ;
#604 = ELLIPSE('',#100355,0.222704123464471,0.0994987961944618) ;
#605 = ELLIPSE('',#100356,0.236408403978192,0.104269413778509) ;
#606 = ELLIPSE('',#100357,0.236436524480116,0.104276779754641) ;
#607 = ELLIPSE('',#100358,0.222726289983351,0.0995178910561129) ;
#608 = ELLIPSE('',#100360,0.197388992377652,0.080120135130641) ;
#609 = ELLIPSE('',#100361,0.197388992377957,0.0801201351307889) ;
#610 = ELLIPSE('',#100363,0.222704123465533,0.0994987961961162) ;
#611 = ELLIPSE('',#100364,0.236408404086778,0.104269413812232) ;
#612 = ELLIPSE('',#100365,0.111803400137024,0.100000002213876) ;
#613 = ELLIPSE('',#100366,0.1973889887795,0.0801201312608118) ;
#614 = ELLIPSE('',#100367,0.197388992378253,0.0801201351305352) ;
#615 = ELLIPSE('',#100369,0.197388992377339,0.080120135129837) ;
#616 = ELLIPSE('',#100370,0.197388988783307,0.0801201312640243) ;
#617 = ELLIPSE('',#100371,0.11180339860087,0.0999999995158049) ;
#618 = ELLIPSE('',#100372,0.236436524487559,0.104276779755015) ;
#619 = ELLIPSE('',#100373,0.222726290004162,0.0995178910729244) ;
#620 = ELLIPSE('',#100375,0.222704123462615,0.0994987961928787) ;
#621 = ELLIPSE('',#100376,0.236408404066321,0.104269413806983) ;
#622 = ELLIPSE('',#100377,0.236436524282318,0.104276779688654) ;
#623 = ELLIPSE('',#100378,0.222726289995458,0.0995178910658395) ;
#624 = ELLIPSE('',#100380,0.197388992379746,0.0801201351321519) ;
#625 = ELLIPSE('',#100381,0.197388992378042,0.0801201351301879) ;
#626 = ELLIPSE('',#100383,0.222704123484497,0.099498796209647) ;
#627 = ELLIPSE('',#100384,0.236408404052811,0.104269413801709) ;
#628 = ELLIPSE('',#100385,0.111803399379941,0.100000000890385) ;
#629 = ELLIPSE('',#100386,0.197388988782014,0.0801201312627937) ;
#630 = ELLIPSE('',#100387,0.197388992380941,0.0801201351337526) ;
#631 = ELLIPSE('',#100389,0.19738899238036,0.0801201351332252) ;
#632 = ELLIPSE('',#100390,0.197388988775444,0.0801201312580623) ;
#633 = ELLIPSE('',#100391,0.111803398688121,0.0999999996752641) ;
#634 = ELLIPSE('',#100392,0.236436524475147,0.104276779747239) ;
#635 = ELLIPSE('',#100393,0.222726289922601,0.0995178910101093) ;
#636 = ELLIPSE('',#100395,0.222704123486384,0.0994987962122068) ;
#637 = ELLIPSE('',#100396,0.236408404061106,0.104269413803139) ;
#638 = ELLIPSE('',#100397,0.236436524346302,0.104276779709588) ;
#639 = ELLIPSE('',#100398,0.22272628996843,0.0995178910441956) ;
#640 = ELLIPSE('',#100400,0.197388992380072,0.0801201351314788) ;
#641 = ELLIPSE('',#100401,0.197388992377762,0.0801201351300403) ;
#642 = ELLIPSE('',#100403,0.22270412347746,0.0994987962033312) ;
#643 = ELLIPSE('',#100404,0.236408404072224,0.104269413808533) ;
#644 = ELLIPSE('',#100405,0.11180339854823,0.0999999994295695) ;
#645 = ELLIPSE('',#100406,0.197388988782537,0.0801201312629481) ;
#646 = ELLIPSE('',#100407,0.197388992380398,0.0801201351334049) ;
#647 = FACE_BOUND('',#22787,.T.) ;
#648 = FACE_BOUND('',#22800,.T.) ;
#649 = FACE_BOUND('',#22801,.T.) ;
#650 = FACE_BOUND('',#22807,.T.) ;
#651 = FACE_BOUND('',#22808,.T.) ;
#652 = FACE_BOUND('',#22809,.T.) ;
#653 = FACE_BOUND('',#22810,.T.) ;
#654 = FACE_BOUND('',#22815,.T.) ;
#655 = FACE_BOUND('',#22816,.T.) ;
#656 = FACE_BOUND('',#22818,.T.) ;
#657 = FACE_BOUND('',#22819,.T.) ;
#658 = FACE_BOUND('',#22839,.T.) ;
#659 = FACE_BOUND('',#22858,.T.) ;
#660 = FACE_BOUND('',#23042,.T.) ;
#661 = FACE_BOUND('',#23061,.T.) ;
#662 = FACE_BOUND('',#23250,.T.) ;
#663 = FACE_BOUND('',#23263,.T.) ;
#664 = FACE_BOUND('',#23264,.T.) ;
#665 = FACE_BOUND('',#23270,.T.) ;
#666 = FACE_BOUND('',#23271,.T.) ;
#667 = FACE_BOUND('',#23272,.T.) ;
#668 = FACE_BOUND('',#23273,.T.) ;
#669 = FACE_BOUND('',#23278,.T.) ;
#670 = FACE_BOUND('',#23279,.T.) ;
#671 = FACE_BOUND('',#23281,.T.) ;
#672 = FACE_BOUND('',#23282,.T.) ;
#673 = FACE_BOUND('',#23302,.T.) ;
#674 = FACE_BOUND('',#23321,.T.) ;
#675 = FACE_BOUND('',#23505,.T.) ;
#676 = FACE_BOUND('',#23524,.T.) ;
#677 = FACE_BOUND('',#23706,.T.) ;
#678 = FACE_BOUND('',#23716,.T.) ;
#679 = FACE_BOUND('',#23717,.T.) ;
#680 = FACE_BOUND('',#23722,.T.) ;
#681 = FACE_BOUND('',#23724,.T.) ;
#682 = FACE_BOUND('',#23745,.T.) ;
#683 = FACE_BOUND('',#23764,.T.) ;
#684 = FACE_BOUND('',#24047,.T.) ;
#685 = FACE_BOUND('',#24048,.T.) ;
#686 = FACE_BOUND('',#24049,.T.) ;
#687 = FACE_BOUND('',#24050,.T.) ;
#688 = FACE_BOUND('',#24051,.T.) ;
#689 = FACE_BOUND('',#24052,.T.) ;
#690 = FACE_BOUND('',#24053,.T.) ;
#691 = FACE_BOUND('',#24054,.T.) ;
#692 = FACE_BOUND('',#24055,.T.) ;
#693 = FACE_BOUND('',#24056,.T.) ;
#694 = FACE_BOUND('',#24093,.T.) ;
#695 = FACE_BOUND('',#24095,.T.) ;
#696 = FACE_BOUND('',#24382,.T.) ;
#697 = FACE_BOUND('',#24411,.T.) ;
#698 = FACE_BOUND('',#24440,.T.) ;
#699 = FACE_BOUND('',#24469,.T.) ;
#700 = FACE_BOUND('',#24498,.T.) ;
#701 = FACE_BOUND('',#24527,.T.) ;
#702 = FACE_BOUND('',#24556,.T.) ;
#703 = FACE_BOUND('',#24585,.T.) ;
#704 = FACE_BOUND('',#24614,.T.) ;
#705 = FACE_BOUND('',#24616,.T.) ;
#706 = FACE_BOUND('',#24618,.T.) ;
#707 = FACE_BOUND('',#24620,.T.) ;
#708 = FACE_BOUND('',#24622,.T.) ;
#709 = FACE_BOUND('',#24624,.T.) ;
#710 = FACE_BOUND('',#24626,.T.) ;
#711 = FACE_BOUND('',#24628,.T.) ;
#712 = FACE_BOUND('',#24630,.T.) ;
#713 = FACE_BOUND('',#24632,.T.) ;
#714 = FACE_BOUND('',#26275,.T.) ;
#715 = FACE_BOUND('',#26276,.T.) ;
#716 = FACE_BOUND('',#26277,.T.) ;
#717 = FACE_BOUND('',#26278,.T.) ;
#718 = FACE_BOUND('',#26279,.T.) ;
#719 = FACE_BOUND('',#26280,.T.) ;
#720 = FACE_BOUND('',#26281,.T.) ;
#721 = FACE_BOUND('',#26282,.T.) ;
#722 = FACE_BOUND('',#26283,.T.) ;
#723 = FACE_BOUND('',#26284,.T.) ;
#724 = FACE_BOUND('',#26285,.T.) ;
#725 = FACE_BOUND('',#26286,.T.) ;
#726 = FACE_BOUND('',#26287,.T.) ;
#727 = FACE_BOUND('',#26288,.T.) ;
#728 = FACE_BOUND('',#26289,.T.) ;
#729 = FACE_BOUND('',#26290,.T.) ;
#730 = FACE_BOUND('',#26291,.T.) ;
#731 = FACE_BOUND('',#26292,.T.) ;
#732 = FACE_BOUND('',#26293,.T.) ;
#733 = FACE_BOUND('',#26294,.T.) ;
#734 = FACE_BOUND('',#26296,.T.) ;
#735 = FACE_BOUND('',#26298,.T.) ;
#736 = FACE_BOUND('',#26300,.T.) ;
#737 = FACE_BOUND('',#26302,.T.) ;
#738 = FACE_BOUND('',#26304,.T.) ;
#739 = FACE_BOUND('',#26306,.T.) ;
#740 = FACE_BOUND('',#26308,.T.) ;
#741 = FACE_BOUND('',#26310,.T.) ;
#742 = FACE_BOUND('',#26312,.T.) ;
#743 = FACE_BOUND('',#26337,.T.) ;
#744 = FACE_BOUND('',#26338,.T.) ;
#745 = FACE_BOUND('',#26339,.T.) ;
#746 = FACE_BOUND('',#26340,.T.) ;
#747 = FACE_BOUND('',#26341,.T.) ;
#748 = FACE_BOUND('',#26342,.T.) ;
#749 = FACE_BOUND('',#26343,.T.) ;
#750 = FACE_BOUND('',#26344,.T.) ;
#751 = FACE_BOUND('',#26345,.T.) ;
#752 = FACE_BOUND('',#26346,.T.) ;
#753 = FACE_BOUND('',#26348,.T.) ;
#754 = FACE_BOUND('',#26356,.T.) ;
#755 = FACE_BOUND('',#26357,.T.) ;
#756 = FACE_BOUND('',#26358,.T.) ;
#757 = FACE_BOUND('',#26359,.T.) ;
#758 = FACE_BOUND('',#26360,.T.) ;
#759 = FACE_BOUND('',#26361,.T.) ;
#760 = FACE_BOUND('',#26362,.T.) ;
#761 = FACE_BOUND('',#26363,.T.) ;
#762 = FACE_BOUND('',#26364,.T.) ;
#763 = FACE_BOUND('',#26365,.T.) ;
#764 = FACE_BOUND('',#26380,.T.) ;
#765 = FACE_BOUND('',#26396,.T.) ;
#766 = FACE_BOUND('',#26403,.T.) ;
#767 = FACE_BOUND('',#26715,.T.) ;
#768 = FACE_BOUND('',#26721,.T.) ;
#769 = FACE_BOUND('',#26727,.T.) ;
#770 = FACE_BOUND('',#26733,.T.) ;
#771 = FACE_BOUND('',#26739,.T.) ;
#772 = FACE_BOUND('',#26745,.T.) ;
#773 = FACE_BOUND('',#26751,.T.) ;
#774 = FACE_BOUND('',#26757,.T.) ;
#775 = FACE_BOUND('',#26763,.T.) ;
#776 = FACE_BOUND('',#26817,.T.) ;
#777 = FACE_BOUND('',#26822,.T.) ;
#778 = FACE_BOUND('',#26827,.T.) ;
#779 = FACE_BOUND('',#26832,.T.) ;
#780 = FACE_BOUND('',#26837,.T.) ;
#781 = FACE_BOUND('',#26842,.T.) ;
#782 = FACE_BOUND('',#26847,.T.) ;
#783 = FACE_BOUND('',#26852,.T.) ;
#784 = FACE_BOUND('',#26857,.T.) ;
#785 = FACE_BOUND('',#26904,.T.) ;
#786 = FACE_BOUND('',#26910,.T.) ;
#787 = FACE_BOUND('',#26916,.T.) ;
#788 = FACE_BOUND('',#26922,.T.) ;
#789 = FACE_BOUND('',#26928,.T.) ;
#790 = FACE_BOUND('',#26934,.T.) ;
#791 = FACE_BOUND('',#26940,.T.) ;
#792 = FACE_BOUND('',#26946,.T.) ;
#793 = FACE_BOUND('',#26952,.T.) ;
#794 = PLANE('',#91213) ;
#795 = PLANE('',#91216) ;
#796 = PLANE('',#91217) ;
#797 = PLANE('',#91218) ;
#798 = PLANE('',#91232) ;
#799 = PLANE('',#91235) ;
#800 = PLANE('',#91236) ;
#801 = PLANE('',#91237) ;
#802 = PLANE('',#91238) ;
#803 = PLANE('',#91247) ;
#804 = PLANE('',#91248) ;
#805 = PLANE('',#91253) ;
#806 = PLANE('',#91254) ;
#807 = PLANE('',#91255) ;
#808 = PLANE('',#91264) ;
#809 = PLANE('',#91265) ;
#810 = PLANE('',#91266) ;
#811 = PLANE('',#91267) ;
#812 = PLANE('',#91268) ;
#813 = PLANE('',#91277) ;
#814 = PLANE('',#91278) ;
#815 = PLANE('',#91279) ;
#816 = PLANE('',#91281) ;
#817 = PLANE('',#91282) ;
#818 = PLANE('',#91297) ;
#819 = PLANE('',#91298) ;
#820 = PLANE('',#91299) ;
#821 = PLANE('',#91302) ;
#822 = PLANE('',#91307) ;
#823 = PLANE('',#91310) ;
#824 = PLANE('',#91311) ;
#825 = PLANE('',#91312) ;
#826 = PLANE('',#91313) ;
#827 = PLANE('',#91314) ;
#828 = PLANE('',#91315) ;
#829 = PLANE('',#91316) ;
#830 = PLANE('',#91317) ;
#831 = PLANE('',#91318) ;
#832 = PLANE('',#91325) ;
#833 = PLANE('',#91328) ;
#834 = PLANE('',#91331) ;
#835 = PLANE('',#91334) ;
#836 = PLANE('',#91335) ;
#837 = PLANE('',#91336) ;
#838 = PLANE('',#91337) ;
#839 = PLANE('',#91338) ;
#840 = PLANE('',#91339) ;
#841 = PLANE('',#91340) ;
#842 = PLANE('',#91341) ;
#843 = PLANE('',#91342) ;
#844 = PLANE('',#91343) ;
#845 = PLANE('',#91344) ;
#846 = PLANE('',#91351) ;
#847 = PLANE('',#91354) ;
#848 = PLANE('',#91357) ;
#849 = PLANE('',#91360) ;
#850 = PLANE('',#91361) ;
#851 = PLANE('',#91362) ;
#852 = PLANE('',#91363) ;
#853 = PLANE('',#91364) ;
#854 = PLANE('',#91365) ;
#855 = PLANE('',#91367) ;
#856 = PLANE('',#91629) ;
#857 = PLANE('',#91630) ;
#858 = PLANE('',#91634) ;
#859 = PLANE('',#91638) ;
#860 = PLANE('',#91642) ;
#861 = PLANE('',#91646) ;
#862 = PLANE('',#91647) ;
#863 = PLANE('',#91649) ;
#864 = PLANE('',#91651) ;
#865 = PLANE('',#91653) ;
#866 = PLANE('',#91654) ;
#867 = PLANE('',#91655) ;
#868 = PLANE('',#91656) ;
#869 = PLANE('',#91662) ;
#870 = PLANE('',#91663) ;
#871 = PLANE('',#91664) ;
#872 = PLANE('',#91667) ;
#873 = PLANE('',#91672) ;
#874 = PLANE('',#91675) ;
#875 = PLANE('',#91676) ;
#876 = PLANE('',#91677) ;
#877 = PLANE('',#91678) ;
#878 = PLANE('',#91679) ;
#879 = PLANE('',#91680) ;
#880 = PLANE('',#91681) ;
#881 = PLANE('',#91682) ;
#882 = PLANE('',#91683) ;
#883 = PLANE('',#91690) ;
#884 = PLANE('',#91693) ;
#885 = PLANE('',#91696) ;
#886 = PLANE('',#91699) ;
#887 = PLANE('',#91700) ;
#888 = PLANE('',#91701) ;
#889 = PLANE('',#91702) ;
#890 = PLANE('',#91703) ;
#891 = PLANE('',#91704) ;
#892 = PLANE('',#91705) ;
#893 = PLANE('',#91706) ;
#894 = PLANE('',#91707) ;
#895 = PLANE('',#91708) ;
#896 = PLANE('',#91709) ;
#897 = PLANE('',#91716) ;
#898 = PLANE('',#91719) ;
#899 = PLANE('',#91722) ;
#900 = PLANE('',#91725) ;
#901 = PLANE('',#91726) ;
#902 = PLANE('',#91727) ;
#903 = PLANE('',#91728) ;
#904 = PLANE('',#91729) ;
#905 = PLANE('',#91730) ;
#906 = PLANE('',#91732) ;
#907 = PLANE('',#92102) ;
#908 = PLANE('',#92105) ;
#909 = PLANE('',#92106) ;
#910 = PLANE('',#92107) ;
#911 = PLANE('',#92121) ;
#912 = PLANE('',#92123) ;
#913 = PLANE('',#92124) ;
#914 = PLANE('',#92125) ;
#915 = PLANE('',#92126) ;
#916 = PLANE('',#92135) ;
#917 = PLANE('',#92136) ;
#918 = PLANE('',#92141) ;
#919 = PLANE('',#92142) ;
#920 = PLANE('',#92143) ;
#921 = PLANE('',#92152) ;
#922 = PLANE('',#92153) ;
#923 = PLANE('',#92154) ;
#924 = PLANE('',#92155) ;
#925 = PLANE('',#92156) ;
#926 = PLANE('',#92165) ;
#927 = PLANE('',#92166) ;
#928 = PLANE('',#92167) ;
#929 = PLANE('',#92170) ;
#930 = PLANE('',#92171) ;
#931 = PLANE('',#92186) ;
#932 = PLANE('',#92187) ;
#933 = PLANE('',#92188) ;
#934 = PLANE('',#92191) ;
#935 = PLANE('',#92196) ;
#936 = PLANE('',#92199) ;
#937 = PLANE('',#92200) ;
#938 = PLANE('',#92201) ;
#939 = PLANE('',#92202) ;
#940 = PLANE('',#92203) ;
#941 = PLANE('',#92204) ;
#942 = PLANE('',#92205) ;
#943 = PLANE('',#92206) ;
#944 = PLANE('',#92207) ;
#945 = PLANE('',#92214) ;
#946 = PLANE('',#92217) ;
#947 = PLANE('',#92220) ;
#948 = PLANE('',#92223) ;
#949 = PLANE('',#92224) ;
#950 = PLANE('',#92225) ;
#951 = PLANE('',#92226) ;
#952 = PLANE('',#92227) ;
#953 = PLANE('',#92228) ;
#954 = PLANE('',#92229) ;
#955 = PLANE('',#92230) ;
#956 = PLANE('',#92231) ;
#957 = PLANE('',#92232) ;
#958 = PLANE('',#92233) ;
#959 = PLANE('',#92240) ;
#960 = PLANE('',#92243) ;
#961 = PLANE('',#92246) ;
#962 = PLANE('',#92249) ;
#963 = PLANE('',#92250) ;
#964 = PLANE('',#92251) ;
#965 = PLANE('',#92252) ;
#966 = PLANE('',#92253) ;
#967 = PLANE('',#92254) ;
#968 = PLANE('',#92256) ;
#969 = PLANE('',#92518) ;
#970 = PLANE('',#92519) ;
#971 = PLANE('',#92523) ;
#972 = PLANE('',#92527) ;
#973 = PLANE('',#92531) ;
#974 = PLANE('',#92535) ;
#975 = PLANE('',#92536) ;
#976 = PLANE('',#92538) ;
#977 = PLANE('',#92540) ;
#978 = PLANE('',#92541) ;
#979 = PLANE('',#92542) ;
#980 = PLANE('',#92543) ;
#981 = PLANE('',#92545) ;
#982 = PLANE('',#92551) ;
#983 = PLANE('',#92552) ;
#984 = PLANE('',#92553) ;
#985 = PLANE('',#92556) ;
#986 = PLANE('',#92561) ;
#987 = PLANE('',#92564) ;
#988 = PLANE('',#92565) ;
#989 = PLANE('',#92566) ;
#990 = PLANE('',#92567) ;
#991 = PLANE('',#92568) ;
#992 = PLANE('',#92569) ;
#993 = PLANE('',#92570) ;
#994 = PLANE('',#92571) ;
#995 = PLANE('',#92572) ;
#996 = PLANE('',#92579) ;
#997 = PLANE('',#92582) ;
#998 = PLANE('',#92585) ;
#999 = PLANE('',#92588) ;
#1000 = PLANE('',#92589) ;
#1001 = PLANE('',#92590) ;
#1002 = PLANE('',#92591) ;
#1003 = PLANE('',#92592) ;
#1004 = PLANE('',#92593) ;
#1005 = PLANE('',#92594) ;
#1006 = PLANE('',#92595) ;
#1007 = PLANE('',#92596) ;
#1008 = PLANE('',#92597) ;
#1009 = PLANE('',#92598) ;
#1010 = PLANE('',#92605) ;
#1011 = PLANE('',#92608) ;
#1012 = PLANE('',#92611) ;
#1013 = PLANE('',#92614) ;
#1014 = PLANE('',#92615) ;
#1015 = PLANE('',#92616) ;
#1016 = PLANE('',#92617) ;
#1017 = PLANE('',#92618) ;
#1018 = PLANE('',#92619) ;
#1019 = PLANE('',#92621) ;
#1020 = PLANE('',#92948) ;
#1021 = PLANE('',#92950) ;
#1022 = PLANE('',#92951) ;
#1023 = PLANE('',#92952) ;
#1024 = PLANE('',#92953) ;
#1025 = PLANE('',#92958) ;
#1026 = PLANE('',#92959) ;
#1027 = PLANE('',#92962) ;
#1028 = PLANE('',#92963) ;
#1029 = PLANE('',#92964) ;
#1030 = PLANE('',#92965) ;
#1031 = PLANE('',#92966) ;
#1032 = PLANE('',#92967) ;
#1033 = PLANE('',#92968) ;
#1034 = PLANE('',#92973) ;
#1035 = PLANE('',#92974) ;
#1036 = PLANE('',#92975) ;
#1037 = PLANE('',#92976) ;
#1038 = PLANE('',#92977) ;
#1039 = PLANE('',#92982) ;
#1040 = PLANE('',#92983) ;
#1041 = PLANE('',#92984) ;
#1042 = PLANE('',#92986) ;
#1043 = PLANE('',#92987) ;
#1044 = PLANE('',#93006) ;
#1045 = PLANE('',#93025) ;
#1046 = PLANE('',#93026) ;
#1047 = PLANE('',#93027) ;
#1048 = PLANE('',#93030) ;
#1049 = PLANE('',#93035) ;
#1050 = PLANE('',#93038) ;
#1051 = PLANE('',#93039) ;
#1052 = PLANE('',#93040) ;
#1053 = PLANE('',#93041) ;
#1054 = PLANE('',#93042) ;
#1055 = PLANE('',#93043) ;
#1056 = PLANE('',#93044) ;
#1057 = PLANE('',#93045) ;
#1058 = PLANE('',#93046) ;
#1059 = PLANE('',#93053) ;
#1060 = PLANE('',#93056) ;
#1061 = PLANE('',#93059) ;
#1062 = PLANE('',#93062) ;
#1063 = PLANE('',#93063) ;
#1064 = PLANE('',#93064) ;
#1065 = PLANE('',#93065) ;
#1066 = PLANE('',#93066) ;
#1067 = PLANE('',#93067) ;
#1068 = PLANE('',#93068) ;
#1069 = PLANE('',#93069) ;
#1070 = PLANE('',#93070) ;
#1071 = PLANE('',#93071) ;
#1072 = PLANE('',#93072) ;
#1073 = PLANE('',#93079) ;
#1074 = PLANE('',#93082) ;
#1075 = PLANE('',#93085) ;
#1076 = PLANE('',#93088) ;
#1077 = PLANE('',#93089) ;
#1078 = PLANE('',#93090) ;
#1079 = PLANE('',#93091) ;
#1080 = PLANE('',#93092) ;
#1081 = PLANE('',#93093) ;
#1082 = PLANE('',#93095) ;
#1083 = PLANE('',#93599) ;
#1084 = PLANE('',#93604) ;
#1085 = PLANE('',#93609) ;
#1086 = PLANE('',#93614) ;
#1087 = PLANE('',#93619) ;
#1088 = PLANE('',#93624) ;
#1089 = PLANE('',#93629) ;
#1090 = PLANE('',#93634) ;
#1091 = PLANE('',#93639) ;
#1092 = PLANE('',#93644) ;
#1093 = PLANE('',#93646) ;
#1094 = PLANE('',#93648) ;
#1095 = PLANE('',#93650) ;
#1096 = PLANE('',#93652) ;
#1097 = PLANE('',#93654) ;
#1098 = PLANE('',#93656) ;
#1099 = PLANE('',#93658) ;
#1100 = PLANE('',#93660) ;
#1101 = PLANE('',#93662) ;
#1102 = PLANE('',#93664) ;
#1103 = PLANE('',#93666) ;
#1104 = PLANE('',#93668) ;
#1105 = PLANE('',#93670) ;
#1106 = PLANE('',#93672) ;
#1107 = PLANE('',#93674) ;
#1108 = PLANE('',#93676) ;
#1109 = PLANE('',#93678) ;
#1110 = PLANE('',#93707) ;
#1111 = PLANE('',#93712) ;
#1112 = PLANE('',#93714) ;
#1113 = PLANE('',#93722) ;
#1114 = PLANE('',#93746) ;
#1115 = PLANE('',#93770) ;
#1116 = PLANE('',#93774) ;
#1117 = PLANE('',#93778) ;
#1118 = PLANE('',#93782) ;
#1119 = PLANE('',#93786) ;
#1120 = PLANE('',#93790) ;
#1121 = PLANE('',#93891) ;
#1122 = PLANE('',#93894) ;
#1123 = PLANE('',#93897) ;
#1124 = PLANE('',#93900) ;
#1125 = PLANE('',#93901) ;
#1126 = PLANE('',#93902) ;
#1127 = PLANE('',#93903) ;
#1128 = PLANE('',#93904) ;
#1129 = PLANE('',#93908) ;
#1130 = PLANE('',#93912) ;
#1131 = PLANE('',#93916) ;
#1132 = PLANE('',#93919) ;
#1133 = PLANE('',#93920) ;
#1134 = PLANE('',#93924) ;
#1135 = PLANE('',#93928) ;
#1136 = PLANE('',#93932) ;
#1137 = PLANE('',#93936) ;
#1138 = PLANE('',#93940) ;
#1139 = PLANE('',#93950) ;
#1140 = PLANE('',#93954) ;
#1141 = PLANE('',#93958) ;
#1142 = PLANE('',#93959) ;
#1143 = PLANE('',#93965) ;
#1144 = PLANE('',#94240) ;
#1145 = PLANE('',#94241) ;
#1146 = PLANE('',#94242) ;
#1147 = PLANE('',#94243) ;
#1148 = PLANE('',#94244) ;
#1149 = PLANE('',#94245) ;
#1150 = PLANE('',#94248) ;
#1151 = PLANE('',#94257) ;
#1152 = PLANE('',#94258) ;
#1153 = PLANE('',#94259) ;
#1154 = PLANE('',#94260) ;
#1155 = PLANE('',#94261) ;
#1156 = PLANE('',#94262) ;
#1157 = PLANE('',#94263) ;
#1158 = PLANE('',#94264) ;
#1159 = PLANE('',#94265) ;
#1160 = PLANE('',#94266) ;
#1161 = PLANE('',#94267) ;
#1162 = PLANE('',#94380) ;
#1163 = PLANE('',#94383) ;
#1164 = PLANE('',#94386) ;
#1165 = PLANE('',#94389) ;
#1166 = PLANE('',#94392) ;
#1167 = PLANE('',#94395) ;
#1168 = PLANE('',#94398) ;
#1169 = PLANE('',#94401) ;
#1170 = PLANE('',#94404) ;
#1171 = PLANE('',#94407) ;
#1172 = PLANE('',#94408) ;
#1173 = PLANE('',#94409) ;
#1174 = PLANE('',#94410) ;
#1175 = PLANE('',#94411) ;
#1176 = PLANE('',#94412) ;
#1177 = PLANE('',#94413) ;
#1178 = PLANE('',#94414) ;
#1179 = PLANE('',#94415) ;
#1180 = PLANE('',#94416) ;
#1181 = PLANE('',#94417) ;
#1182 = PLANE('',#94418) ;
#1183 = PLANE('',#94419) ;
#1184 = PLANE('',#94420) ;
#1185 = PLANE('',#94421) ;
#1186 = PLANE('',#94422) ;
#1187 = PLANE('',#94423) ;
#1188 = PLANE('',#94424) ;
#1189 = PLANE('',#94425) ;
#1190 = PLANE('',#94426) ;
#1191 = PLANE('',#94427) ;
#1192 = PLANE('',#94428) ;
#1193 = PLANE('',#94429) ;
#1194 = PLANE('',#94430) ;
#1195 = PLANE('',#94431) ;
#1196 = PLANE('',#94432) ;
#1197 = PLANE('',#94433) ;
#1198 = PLANE('',#94434) ;
#1199 = PLANE('',#94435) ;
#1200 = PLANE('',#94436) ;
#1201 = PLANE('',#94437) ;
#1202 = PLANE('',#94438) ;
#1203 = PLANE('',#94439) ;
#1204 = PLANE('',#94440) ;
#1205 = PLANE('',#94441) ;
#1206 = PLANE('',#94442) ;
#1207 = PLANE('',#94443) ;
#1208 = PLANE('',#94444) ;
#1209 = PLANE('',#94445) ;
#1210 = PLANE('',#94446) ;
#1211 = PLANE('',#94447) ;
#1212 = PLANE('',#94448) ;
#1213 = PLANE('',#94449) ;
#1214 = PLANE('',#94450) ;
#1215 = PLANE('',#94451) ;
#1216 = PLANE('',#94455) ;
#1217 = PLANE('',#94459) ;
#1218 = PLANE('',#94463) ;
#1219 = PLANE('',#94466) ;
#1220 = PLANE('',#94467) ;
#1221 = PLANE('',#94471) ;
#1222 = PLANE('',#94475) ;
#1223 = PLANE('',#94479) ;
#1224 = PLANE('',#94483) ;
#1225 = PLANE('',#94487) ;
#1226 = PLANE('',#94497) ;
#1227 = PLANE('',#94501) ;
#1228 = PLANE('',#94505) ;
#1229 = PLANE('',#94506) ;
#1230 = PLANE('',#94515) ;
#1231 = PLANE('',#94519) ;
#1232 = PLANE('',#94523) ;
#1233 = PLANE('',#94526) ;
#1234 = PLANE('',#94527) ;
#1235 = PLANE('',#94531) ;
#1236 = PLANE('',#94535) ;
#1237 = PLANE('',#94539) ;
#1238 = PLANE('',#94543) ;
#1239 = PLANE('',#94547) ;
#1240 = PLANE('',#94557) ;
#1241 = PLANE('',#94561) ;
#1242 = PLANE('',#94565) ;
#1243 = PLANE('',#94566) ;
#1244 = PLANE('',#94575) ;
#1245 = PLANE('',#94579) ;
#1246 = PLANE('',#94583) ;
#1247 = PLANE('',#94586) ;
#1248 = PLANE('',#94587) ;
#1249 = PLANE('',#94591) ;
#1250 = PLANE('',#94595) ;
#1251 = PLANE('',#94599) ;
#1252 = PLANE('',#94603) ;
#1253 = PLANE('',#94607) ;
#1254 = PLANE('',#94617) ;
#1255 = PLANE('',#94621) ;
#1256 = PLANE('',#94625) ;
#1257 = PLANE('',#94626) ;
#1258 = PLANE('',#94635) ;
#1259 = PLANE('',#94639) ;
#1260 = PLANE('',#94643) ;
#1261 = PLANE('',#94646) ;
#1262 = PLANE('',#94647) ;
#1263 = PLANE('',#94651) ;
#1264 = PLANE('',#94655) ;
#1265 = PLANE('',#94659) ;
#1266 = PLANE('',#94663) ;
#1267 = PLANE('',#94667) ;
#1268 = PLANE('',#94677) ;
#1269 = PLANE('',#94681) ;
#1270 = PLANE('',#94685) ;
#1271 = PLANE('',#94686) ;
#1272 = PLANE('',#94695) ;
#1273 = PLANE('',#94699) ;
#1274 = PLANE('',#94703) ;
#1275 = PLANE('',#94706) ;
#1276 = PLANE('',#94707) ;
#1277 = PLANE('',#94711) ;
#1278 = PLANE('',#94715) ;
#1279 = PLANE('',#94719) ;
#1280 = PLANE('',#94723) ;
#1281 = PLANE('',#94727) ;
#1282 = PLANE('',#94737) ;
#1283 = PLANE('',#94741) ;
#1284 = PLANE('',#94745) ;
#1285 = PLANE('',#94746) ;
#1286 = PLANE('',#94755) ;
#1287 = PLANE('',#94759) ;
#1288 = PLANE('',#94763) ;
#1289 = PLANE('',#94766) ;
#1290 = PLANE('',#94767) ;
#1291 = PLANE('',#94771) ;
#1292 = PLANE('',#94775) ;
#1293 = PLANE('',#94779) ;
#1294 = PLANE('',#94783) ;
#1295 = PLANE('',#94787) ;
#1296 = PLANE('',#94797) ;
#1297 = PLANE('',#94801) ;
#1298 = PLANE('',#94805) ;
#1299 = PLANE('',#94806) ;
#1300 = PLANE('',#94815) ;
#1301 = PLANE('',#94819) ;
#1302 = PLANE('',#94823) ;
#1303 = PLANE('',#94826) ;
#1304 = PLANE('',#94827) ;
#1305 = PLANE('',#94831) ;
#1306 = PLANE('',#94835) ;
#1307 = PLANE('',#94839) ;
#1308 = PLANE('',#94843) ;
#1309 = PLANE('',#94847) ;
#1310 = PLANE('',#94857) ;
#1311 = PLANE('',#94861) ;
#1312 = PLANE('',#94865) ;
#1313 = PLANE('',#94866) ;
#1314 = PLANE('',#94875) ;
#1315 = PLANE('',#94879) ;
#1316 = PLANE('',#94883) ;
#1317 = PLANE('',#94886) ;
#1318 = PLANE('',#94887) ;
#1319 = PLANE('',#94891) ;
#1320 = PLANE('',#94895) ;
#1321 = PLANE('',#94899) ;
#1322 = PLANE('',#94903) ;
#1323 = PLANE('',#94907) ;
#1324 = PLANE('',#94917) ;
#1325 = PLANE('',#94921) ;
#1326 = PLANE('',#94925) ;
#1327 = PLANE('',#94926) ;
#1328 = PLANE('',#94935) ;
#1329 = PLANE('',#94939) ;
#1330 = PLANE('',#94943) ;
#1331 = PLANE('',#94946) ;
#1332 = PLANE('',#94947) ;
#1333 = PLANE('',#94951) ;
#1334 = PLANE('',#94955) ;
#1335 = PLANE('',#94959) ;
#1336 = PLANE('',#94963) ;
#1337 = PLANE('',#94967) ;
#1338 = PLANE('',#94977) ;
#1339 = PLANE('',#94981) ;
#1340 = PLANE('',#94985) ;
#1341 = PLANE('',#94986) ;
#1342 = PLANE('',#94992) ;
#1343 = PLANE('',#94997) ;
#1344 = PLANE('',#95002) ;
#1345 = PLANE('',#95007) ;
#1346 = PLANE('',#95012) ;
#1347 = PLANE('',#95017) ;
#1348 = PLANE('',#95022) ;
#1349 = PLANE('',#95027) ;
#1350 = PLANE('',#95032) ;
#1351 = PLANE('',#96891) ;
#1352 = PLANE('',#96892) ;
#1353 = PLANE('',#96893) ;
#1354 = PLANE('',#96894) ;
#1355 = PLANE('',#96895) ;
#1356 = PLANE('',#96896) ;
#1357 = PLANE('',#96899) ;
#1358 = PLANE('',#96908) ;
#1359 = PLANE('',#96909) ;
#1360 = PLANE('',#96910) ;
#1361 = PLANE('',#96911) ;
#1362 = PLANE('',#96912) ;
#1363 = PLANE('',#96913) ;
#1364 = PLANE('',#96914) ;
#1365 = PLANE('',#96915) ;
#1366 = PLANE('',#96916) ;
#1367 = PLANE('',#96917) ;
#1368 = PLANE('',#96918) ;
#1369 = PLANE('',#96919) ;
#1370 = PLANE('',#96920) ;
#1371 = PLANE('',#96923) ;
#1372 = PLANE('',#96932) ;
#1373 = PLANE('',#96933) ;
#1374 = PLANE('',#96934) ;
#1375 = PLANE('',#96935) ;
#1376 = PLANE('',#96936) ;
#1377 = PLANE('',#96937) ;
#1378 = PLANE('',#96938) ;
#1379 = PLANE('',#96939) ;
#1380 = PLANE('',#96940) ;
#1381 = PLANE('',#96941) ;
#1382 = PLANE('',#96942) ;
#1383 = PLANE('',#96943) ;
#1384 = PLANE('',#96944) ;
#1385 = PLANE('',#96947) ;
#1386 = PLANE('',#96956) ;
#1387 = PLANE('',#96957) ;
#1388 = PLANE('',#96958) ;
#1389 = PLANE('',#96959) ;
#1390 = PLANE('',#96960) ;
#1391 = PLANE('',#96961) ;
#1392 = PLANE('',#96962) ;
#1393 = PLANE('',#96963) ;
#1394 = PLANE('',#96964) ;
#1395 = PLANE('',#96965) ;
#1396 = PLANE('',#96966) ;
#1397 = PLANE('',#96967) ;
#1398 = PLANE('',#96968) ;
#1399 = PLANE('',#96971) ;
#1400 = PLANE('',#96980) ;
#1401 = PLANE('',#96981) ;
#1402 = PLANE('',#96982) ;
#1403 = PLANE('',#96983) ;
#1404 = PLANE('',#96984) ;
#1405 = PLANE('',#96985) ;
#1406 = PLANE('',#96986) ;
#1407 = PLANE('',#96987) ;
#1408 = PLANE('',#96988) ;
#1409 = PLANE('',#96989) ;
#1410 = PLANE('',#96990) ;
#1411 = PLANE('',#96991) ;
#1412 = PLANE('',#96992) ;
#1413 = PLANE('',#96995) ;
#1414 = PLANE('',#97004) ;
#1415 = PLANE('',#97005) ;
#1416 = PLANE('',#97006) ;
#1417 = PLANE('',#97007) ;
#1418 = PLANE('',#97008) ;
#1419 = PLANE('',#97009) ;
#1420 = PLANE('',#97010) ;
#1421 = PLANE('',#97011) ;
#1422 = PLANE('',#97012) ;
#1423 = PLANE('',#97013) ;
#1424 = PLANE('',#97014) ;
#1425 = PLANE('',#97015) ;
#1426 = PLANE('',#97016) ;
#1427 = PLANE('',#97019) ;
#1428 = PLANE('',#97028) ;
#1429 = PLANE('',#97029) ;
#1430 = PLANE('',#97030) ;
#1431 = PLANE('',#97031) ;
#1432 = PLANE('',#97032) ;
#1433 = PLANE('',#97033) ;
#1434 = PLANE('',#97034) ;
#1435 = PLANE('',#97035) ;
#1436 = PLANE('',#97036) ;
#1437 = PLANE('',#97037) ;
#1438 = PLANE('',#97038) ;
#1439 = PLANE('',#97039) ;
#1440 = PLANE('',#97040) ;
#1441 = PLANE('',#97043) ;
#1442 = PLANE('',#97052) ;
#1443 = PLANE('',#97053) ;
#1444 = PLANE('',#97054) ;
#1445 = PLANE('',#97055) ;
#1446 = PLANE('',#97056) ;
#1447 = PLANE('',#97057) ;
#1448 = PLANE('',#97058) ;
#1449 = PLANE('',#97059) ;
#1450 = PLANE('',#97060) ;
#1451 = PLANE('',#97061) ;
#1452 = PLANE('',#97062) ;
#1453 = PLANE('',#97063) ;
#1454 = PLANE('',#97064) ;
#1455 = PLANE('',#97067) ;
#1456 = PLANE('',#97076) ;
#1457 = PLANE('',#97077) ;
#1458 = PLANE('',#97078) ;
#1459 = PLANE('',#97079) ;
#1460 = PLANE('',#97080) ;
#1461 = PLANE('',#97081) ;
#1462 = PLANE('',#97082) ;
#1463 = PLANE('',#97083) ;
#1464 = PLANE('',#97084) ;
#1465 = PLANE('',#97085) ;
#1466 = PLANE('',#97086) ;
#1467 = PLANE('',#97087) ;
#1468 = PLANE('',#97088) ;
#1469 = PLANE('',#97091) ;
#1470 = PLANE('',#97100) ;
#1471 = PLANE('',#97101) ;
#1472 = PLANE('',#97102) ;
#1473 = PLANE('',#97103) ;
#1474 = PLANE('',#97104) ;
#1475 = PLANE('',#97105) ;
#1476 = PLANE('',#97106) ;
#1477 = PLANE('',#97107) ;
#1478 = PLANE('',#97108) ;
#1479 = PLANE('',#97109) ;
#1480 = PLANE('',#97110) ;
#1481 = PLANE('',#97111) ;
#1482 = PLANE('',#97112) ;
#1483 = PLANE('',#97113) ;
#1484 = PLANE('',#97114) ;
#1485 = PLANE('',#97115) ;
#1486 = PLANE('',#97116) ;
#1487 = PLANE('',#97117) ;
#1488 = PLANE('',#97118) ;
#1489 = PLANE('',#97119) ;
#1490 = PLANE('',#97120) ;
#1491 = PLANE('',#97121) ;
#1492 = PLANE('',#97122) ;
#1493 = PLANE('',#97123) ;
#1494 = PLANE('',#97124) ;
#1495 = PLANE('',#97125) ;
#1496 = PLANE('',#97126) ;
#1497 = PLANE('',#97127) ;
#1498 = PLANE('',#97128) ;
#1499 = PLANE('',#97129) ;
#1500 = PLANE('',#97130) ;
#1501 = PLANE('',#97131) ;
#1502 = PLANE('',#97132) ;
#1503 = PLANE('',#97133) ;
#1504 = PLANE('',#97134) ;
#1505 = PLANE('',#97135) ;
#1506 = PLANE('',#97136) ;
#1507 = PLANE('',#97137) ;
#1508 = PLANE('',#97138) ;
#1509 = PLANE('',#97139) ;
#1510 = PLANE('',#97140) ;
#1511 = PLANE('',#97141) ;
#1512 = PLANE('',#97142) ;
#1513 = PLANE('',#98472) ;
#1514 = PLANE('',#98523) ;
#1515 = PLANE('',#98528) ;
#1516 = PLANE('',#98533) ;
#1517 = PLANE('',#98538) ;
#1518 = PLANE('',#98543) ;
#1519 = PLANE('',#98548) ;
#1520 = PLANE('',#98553) ;
#1521 = PLANE('',#98558) ;
#1522 = PLANE('',#98563) ;
#1523 = PLANE('',#98568) ;
#1524 = PLANE('',#98569) ;
#1525 = PLANE('',#98570) ;
#1526 = PLANE('',#98571) ;
#1527 = PLANE('',#98572) ;
#1528 = PLANE('',#98573) ;
#1529 = PLANE('',#98574) ;
#1530 = PLANE('',#98575) ;
#1531 = PLANE('',#98576) ;
#1532 = PLANE('',#98577) ;
#1533 = PLANE('',#98618) ;
#1534 = PLANE('',#98622) ;
#1535 = PLANE('',#98626) ;
#1536 = PLANE('',#98630) ;
#1537 = PLANE('',#98634) ;
#1538 = PLANE('',#98638) ;
#1539 = PLANE('',#98642) ;
#1540 = PLANE('',#98646) ;
#1541 = PLANE('',#98650) ;
#1542 = PLANE('',#98654) ;
#1543 = PLANE('',#98655) ;
#1544 = PLANE('',#98684) ;
#1545 = PLANE('',#98685) ;
#1546 = PLANE('',#98690) ;
#1547 = PLANE('',#98691) ;
#1548 = PLANE('',#98692) ;
#1549 = PLANE('',#98696) ;
#1550 = PLANE('',#98697) ;
#1551 = PLANE('',#98698) ;
#1552 = PLANE('',#98699) ;
#1553 = PLANE('',#98708) ;
#1554 = PLANE('',#98712) ;
#1555 = PLANE('',#98716) ;
#1556 = PLANE('',#98717) ;
#1557 = PLANE('',#98718) ;
#1558 = PLANE('',#98723) ;
#1559 = PLANE('',#98724) ;
#1560 = PLANE('',#98725) ;
#1561 = PLANE('',#98726) ;
#1562 = PLANE('',#98727) ;
#1563 = PLANE('',#98728) ;
#1564 = PLANE('',#98729) ;
#1565 = PLANE('',#98730) ;
#1566 = PLANE('',#98731) ;
#1567 = PLANE('',#98736) ;
#1568 = PLANE('',#98737) ;
#1569 = PLANE('',#98738) ;
#1570 = PLANE('',#98739) ;
#1571 = PLANE('',#98740) ;
#1572 = PLANE('',#98741) ;
#1573 = PLANE('',#98744) ;
#1574 = PLANE('',#98745) ;
#1575 = PLANE('',#98749) ;
#1576 = PLANE('',#98750) ;
#1577 = PLANE('',#98754) ;
#1578 = PLANE('',#98755) ;
#1579 = PLANE('',#98756) ;
#1580 = PLANE('',#98760) ;
#1581 = PLANE('',#98762) ;
#1582 = PLANE('',#98763) ;
#1583 = PLANE('',#98764) ;
#1584 = PLANE('',#98765) ;
#1585 = PLANE('',#98766) ;
#1586 = PLANE('',#98767) ;
#1587 = PLANE('',#98772) ;
#1588 = PLANE('',#98773) ;
#1589 = PLANE('',#98774) ;
#1590 = PLANE('',#98775) ;
#1591 = PLANE('',#98776) ;
#1592 = PLANE('',#98777) ;
#1593 = PLANE('',#98778) ;
#1594 = PLANE('',#98779) ;
#1595 = PLANE('',#98780) ;
#1596 = PLANE('',#98785) ;
#1597 = PLANE('',#98786) ;
#1598 = PLANE('',#98794) ;
#1599 = PLANE('',#98798) ;
#1600 = PLANE('',#98802) ;
#1601 = PLANE('',#98806) ;
#1602 = PLANE('',#98807) ;
#1603 = PLANE('',#99208) ;
#1604 = PLANE('',#99209) ;
#1605 = PLANE('',#99210) ;
#1606 = PLANE('',#99215) ;
#1607 = PLANE('',#99216) ;
#1608 = PLANE('',#99217) ;
#1609 = PLANE('',#99218) ;
#1610 = PLANE('',#99219) ;
#1611 = PLANE('',#99224) ;
#1612 = PLANE('',#99225) ;
#1613 = PLANE('',#99226) ;
#1614 = PLANE('',#99227) ;
#1615 = PLANE('',#99228) ;
#1616 = PLANE('',#99233) ;
#1617 = PLANE('',#99234) ;
#1618 = PLANE('',#99235) ;
#1619 = PLANE('',#99236) ;
#1620 = PLANE('',#99237) ;
#1621 = PLANE('',#99242) ;
#1622 = PLANE('',#99243) ;
#1623 = PLANE('',#99244) ;
#1624 = PLANE('',#99245) ;
#1625 = PLANE('',#99246) ;
#1626 = PLANE('',#99251) ;
#1627 = PLANE('',#99252) ;
#1628 = PLANE('',#99253) ;
#1629 = PLANE('',#99254) ;
#1630 = PLANE('',#99255) ;
#1631 = PLANE('',#99260) ;
#1632 = PLANE('',#99261) ;
#1633 = PLANE('',#99262) ;
#1634 = PLANE('',#99263) ;
#1635 = PLANE('',#99264) ;
#1636 = PLANE('',#99269) ;
#1637 = PLANE('',#99270) ;
#1638 = PLANE('',#99271) ;
#1639 = PLANE('',#99272) ;
#1640 = PLANE('',#99273) ;
#1641 = PLANE('',#99278) ;
#1642 = PLANE('',#99279) ;
#1643 = PLANE('',#99280) ;
#1644 = PLANE('',#99281) ;
#1645 = PLANE('',#99282) ;
#1646 = PLANE('',#99287) ;
#1647 = PLANE('',#99288) ;
#1648 = PLANE('',#99289) ;
#1649 = PLANE('',#99290) ;
#1650 = PLANE('',#99293) ;
#1651 = PLANE('',#99296) ;
#1652 = PLANE('',#99299) ;
#1653 = PLANE('',#99302) ;
#1654 = PLANE('',#99305) ;
#1655 = PLANE('',#99308) ;
#1656 = PLANE('',#99311) ;
#1657 = PLANE('',#99314) ;
#1658 = PLANE('',#99315) ;
#1659 = PLANE('',#99318) ;
#1660 = PLANE('',#99321) ;
#1661 = PLANE('',#99324) ;
#1662 = PLANE('',#99327) ;
#1663 = PLANE('',#99330) ;
#1664 = PLANE('',#99333) ;
#1665 = PLANE('',#99336) ;
#1666 = PLANE('',#99339) ;
#1667 = PLANE('',#99340) ;
#1668 = PLANE('',#99341) ;
#1669 = PLANE('',#99342) ;
#1670 = PLANE('',#99343) ;
#1671 = PLANE('',#99344) ;
#1672 = PLANE('',#99345) ;
#1673 = PLANE('',#99346) ;
#1674 = PLANE('',#99347) ;
#1675 = PLANE('',#99348) ;
#1676 = PLANE('',#99349) ;
#1677 = PLANE('',#99350) ;
#1678 = PLANE('',#99351) ;
#1679 = PLANE('',#99352) ;
#1680 = PLANE('',#99353) ;
#1681 = PLANE('',#99354) ;
#1682 = PLANE('',#99355) ;
#1683 = PLANE('',#99356) ;
#1684 = PLANE('',#99357) ;
#1685 = PLANE('',#99358) ;
#1686 = PLANE('',#99359) ;
#1687 = PLANE('',#99360) ;
#1688 = PLANE('',#99361) ;
#1689 = PLANE('',#99362) ;
#1690 = PLANE('',#99363) ;
#1691 = PLANE('',#99364) ;
#1692 = PLANE('',#99365) ;
#1693 = PLANE('',#99366) ;
#1694 = PLANE('',#99367) ;
#1695 = PLANE('',#99368) ;
#1696 = PLANE('',#99369) ;
#1697 = PLANE('',#99370) ;
#1698 = PLANE('',#99371) ;
#1699 = PLANE('',#99372) ;
#1700 = PLANE('',#99373) ;
#1701 = PLANE('',#99374) ;
#1702 = PLANE('',#99375) ;
#1703 = PLANE('',#99380) ;
#1704 = PLANE('',#99381) ;
#1705 = PLANE('',#99382) ;
#1706 = PLANE('',#99383) ;
#1707 = PLANE('',#99384) ;
#1708 = PLANE('',#99389) ;
#1709 = PLANE('',#99390) ;
#1710 = PLANE('',#99391) ;
#1711 = PLANE('',#99392) ;
#1712 = PLANE('',#99393) ;
#1713 = PLANE('',#99398) ;
#1714 = PLANE('',#99399) ;
#1715 = PLANE('',#99400) ;
#1716 = PLANE('',#99401) ;
#1717 = PLANE('',#99402) ;
#1718 = PLANE('',#99407) ;
#1719 = PLANE('',#99408) ;
#1720 = PLANE('',#99409) ;
#1721 = PLANE('',#99410) ;
#1722 = PLANE('',#99411) ;
#1723 = PLANE('',#99416) ;
#1724 = PLANE('',#99417) ;
#1725 = PLANE('',#99418) ;
#1726 = PLANE('',#99419) ;
#1727 = PLANE('',#99420) ;
#1728 = PLANE('',#99425) ;
#1729 = PLANE('',#99426) ;
#1730 = PLANE('',#99427) ;
#1731 = PLANE('',#99428) ;
#1732 = PLANE('',#99429) ;
#1733 = PLANE('',#99434) ;
#1734 = PLANE('',#99435) ;
#1735 = PLANE('',#99436) ;
#1736 = PLANE('',#99437) ;
#1737 = PLANE('',#99438) ;
#1738 = PLANE('',#99443) ;
#1739 = PLANE('',#99444) ;
#1740 = PLANE('',#99445) ;
#1741 = PLANE('',#99446) ;
#1742 = PLANE('',#99447) ;
#1743 = PLANE('',#99452) ;
#1744 = PLANE('',#99453) ;
#1745 = PLANE('',#99454) ;
#1746 = PLANE('',#99455) ;
#1747 = PLANE('',#99456) ;
#1748 = PLANE('',#99457) ;
#1749 = PLANE('',#99458) ;
#1750 = PLANE('',#99459) ;
#1751 = PLANE('',#99460) ;
#1752 = PLANE('',#99461) ;
#1753 = PLANE('',#99462) ;
#1754 = PLANE('',#99463) ;
#1755 = PLANE('',#99464) ;
#1756 = PLANE('',#99465) ;
#1757 = PLANE('',#99469) ;
#1758 = PLANE('',#99470) ;
#1759 = PLANE('',#99474) ;
#1760 = PLANE('',#99475) ;
#1761 = PLANE('',#99479) ;
#1762 = PLANE('',#99480) ;
#1763 = PLANE('',#99484) ;
#1764 = PLANE('',#99485) ;
#1765 = PLANE('',#99489) ;
#1766 = PLANE('',#99490) ;
#1767 = PLANE('',#99494) ;
#1768 = PLANE('',#99495) ;
#1769 = PLANE('',#99499) ;
#1770 = PLANE('',#99500) ;
#1771 = PLANE('',#99504) ;
#1772 = PLANE('',#99505) ;
#1773 = PLANE('',#99509) ;
#1774 = PLANE('',#99510) ;
#1775 = PLANE('',#99514) ;
#1776 = PLANE('',#99515) ;
#1777 = PLANE('',#99519) ;
#1778 = PLANE('',#99520) ;
#1779 = PLANE('',#99524) ;
#1780 = PLANE('',#99525) ;
#1781 = PLANE('',#99529) ;
#1782 = PLANE('',#99530) ;
#1783 = PLANE('',#99534) ;
#1784 = PLANE('',#99535) ;
#1785 = PLANE('',#99539) ;
#1786 = PLANE('',#99540) ;
#1787 = PLANE('',#99544) ;
#1788 = PLANE('',#99545) ;
#1789 = PLANE('',#99549) ;
#1790 = PLANE('',#99550) ;
#1791 = PLANE('',#99554) ;
#1792 = PLANE('',#99555) ;
#1793 = PLANE('',#99556) ;
#1794 = PLANE('',#99560) ;
#1795 = PLANE('',#99562) ;
#1796 = PLANE('',#99563) ;
#1797 = PLANE('',#99567) ;
#1798 = PLANE('',#99569) ;
#1799 = PLANE('',#99570) ;
#1800 = PLANE('',#99574) ;
#1801 = PLANE('',#99576) ;
#1802 = PLANE('',#99577) ;
#1803 = PLANE('',#99581) ;
#1804 = PLANE('',#99583) ;
#1805 = PLANE('',#99584) ;
#1806 = PLANE('',#99588) ;
#1807 = PLANE('',#99590) ;
#1808 = PLANE('',#99591) ;
#1809 = PLANE('',#99595) ;
#1810 = PLANE('',#99597) ;
#1811 = PLANE('',#99598) ;
#1812 = PLANE('',#99602) ;
#1813 = PLANE('',#99604) ;
#1814 = PLANE('',#99605) ;
#1815 = PLANE('',#99609) ;
#1816 = PLANE('',#99611) ;
#1817 = PLANE('',#99612) ;
#1818 = PLANE('',#99616) ;
#1819 = PLANE('',#99618) ;
#1820 = PLANE('',#99619) ;
#1821 = PLANE('',#99620) ;
#1822 = PLANE('',#99621) ;
#1823 = PLANE('',#99622) ;
#1824 = PLANE('',#99623) ;
#1825 = PLANE('',#99624) ;
#1826 = PLANE('',#99625) ;
#1827 = PLANE('',#99626) ;
#1828 = PLANE('',#99627) ;
#1829 = PLANE('',#99628) ;
#1830 = PLANE('',#99629) ;
#1831 = PLANE('',#99630) ;
#1832 = PLANE('',#99631) ;
#1833 = PLANE('',#99632) ;
#1834 = PLANE('',#99633) ;
#1835 = PLANE('',#99634) ;
#1836 = PLANE('',#99635) ;
#1837 = PLANE('',#99636) ;
#1838 = PLANE('',#99637) ;
#1839 = PLANE('',#99638) ;
#1840 = PLANE('',#99639) ;
#1841 = PLANE('',#99640) ;
#1842 = PLANE('',#99641) ;
#1843 = PLANE('',#99642) ;
#1844 = PLANE('',#99643) ;
#1845 = PLANE('',#99644) ;
#1846 = PLANE('',#99645) ;
#1847 = PLANE('',#99646) ;
#1848 = PLANE('',#99647) ;
#1849 = PLANE('',#99648) ;
#1850 = PLANE('',#99649) ;
#1851 = PLANE('',#99650) ;
#1852 = PLANE('',#99651) ;
#1853 = PLANE('',#99652) ;
#1854 = PLANE('',#99653) ;
#1855 = PLANE('',#99654) ;
#1856 = PLANE('',#99655) ;
#1857 = PLANE('',#99656) ;
#1858 = PLANE('',#99657) ;
#1859 = PLANE('',#99658) ;
#1860 = PLANE('',#99659) ;
#1861 = PLANE('',#99660) ;
#1862 = PLANE('',#99661) ;
#1863 = PLANE('',#99662) ;
#1864 = PLANE('',#99663) ;
#1865 = PLANE('',#99668) ;
#1866 = PLANE('',#99669) ;
#1867 = PLANE('',#99670) ;
#1868 = PLANE('',#99671) ;
#1869 = PLANE('',#99672) ;
#1870 = PLANE('',#99677) ;
#1871 = PLANE('',#99678) ;
#1872 = PLANE('',#99679) ;
#1873 = PLANE('',#99680) ;
#1874 = PLANE('',#99681) ;
#1875 = PLANE('',#99686) ;
#1876 = PLANE('',#99687) ;
#1877 = PLANE('',#99688) ;
#1878 = PLANE('',#99689) ;
#1879 = PLANE('',#99690) ;
#1880 = PLANE('',#99695) ;
#1881 = PLANE('',#99696) ;
#1882 = PLANE('',#99697) ;
#1883 = PLANE('',#99698) ;
#1884 = PLANE('',#99699) ;
#1885 = PLANE('',#99704) ;
#1886 = PLANE('',#99705) ;
#1887 = PLANE('',#99706) ;
#1888 = PLANE('',#99707) ;
#1889 = PLANE('',#99708) ;
#1890 = PLANE('',#99713) ;
#1891 = PLANE('',#99714) ;
#1892 = PLANE('',#99715) ;
#1893 = PLANE('',#99716) ;
#1894 = PLANE('',#99717) ;
#1895 = PLANE('',#99722) ;
#1896 = PLANE('',#99723) ;
#1897 = PLANE('',#99724) ;
#1898 = PLANE('',#99725) ;
#1899 = PLANE('',#99726) ;
#1900 = PLANE('',#99731) ;
#1901 = PLANE('',#99732) ;
#1902 = PLANE('',#99733) ;
#1903 = PLANE('',#99734) ;
#1904 = PLANE('',#99735) ;
#1905 = PLANE('',#99740) ;
#1906 = PLANE('',#99741) ;
#1907 = PLANE('',#99742) ;
#1908 = PLANE('',#99743) ;
#1909 = PLANE('',#99744) ;
#1910 = PLANE('',#99745) ;
#1911 = PLANE('',#99746) ;
#1912 = PLANE('',#99747) ;
#1913 = PLANE('',#99748) ;
#1914 = PLANE('',#99749) ;
#1915 = PLANE('',#99750) ;
#1916 = PLANE('',#99751) ;
#1917 = PLANE('',#99752) ;
#1918 = PLANE('',#99753) ;
#1919 = PLANE('',#99754) ;
#1920 = PLANE('',#99755) ;
#1921 = PLANE('',#99756) ;
#1922 = PLANE('',#99757) ;
#1923 = PLANE('',#99758) ;
#1924 = PLANE('',#99759) ;
#1925 = PLANE('',#99760) ;
#1926 = PLANE('',#99761) ;
#1927 = PLANE('',#99762) ;
#1928 = PLANE('',#99763) ;
#1929 = PLANE('',#99764) ;
#1930 = PLANE('',#99765) ;
#1931 = PLANE('',#99766) ;
#1932 = PLANE('',#99767) ;
#1933 = PLANE('',#99768) ;
#1934 = PLANE('',#99769) ;
#1935 = PLANE('',#99770) ;
#1936 = PLANE('',#99771) ;
#1937 = PLANE('',#99772) ;
#1938 = PLANE('',#99773) ;
#1939 = PLANE('',#99774) ;
#1940 = PLANE('',#99775) ;
#1941 = PLANE('',#99776) ;
#1942 = PLANE('',#99777) ;
#1943 = PLANE('',#99778) ;
#1944 = PLANE('',#99779) ;
#1945 = PLANE('',#99780) ;
#1946 = PLANE('',#99781) ;
#1947 = PLANE('',#99782) ;
#1948 = PLANE('',#99783) ;
#1949 = PLANE('',#99784) ;
#1950 = PLANE('',#99785) ;
#1951 = PLANE('',#99786) ;
#1952 = PLANE('',#99787) ;
#1953 = PLANE('',#99788) ;
#1954 = PLANE('',#99792) ;
#1955 = PLANE('',#99796) ;
#1956 = PLANE('',#99800) ;
#1957 = PLANE('',#99804) ;
#1958 = PLANE('',#99805) ;
#1959 = PLANE('',#99809) ;
#1960 = PLANE('',#99813) ;
#1961 = PLANE('',#99817) ;
#1962 = PLANE('',#99821) ;
#1963 = PLANE('',#99822) ;
#1964 = PLANE('',#99826) ;
#1965 = PLANE('',#99830) ;
#1966 = PLANE('',#99834) ;
#1967 = PLANE('',#99838) ;
#1968 = PLANE('',#99839) ;
#1969 = PLANE('',#99843) ;
#1970 = PLANE('',#99847) ;
#1971 = PLANE('',#99851) ;
#1972 = PLANE('',#99855) ;
#1973 = PLANE('',#99856) ;
#1974 = PLANE('',#99860) ;
#1975 = PLANE('',#99864) ;
#1976 = PLANE('',#99868) ;
#1977 = PLANE('',#99872) ;
#1978 = PLANE('',#99873) ;
#1979 = PLANE('',#99877) ;
#1980 = PLANE('',#99881) ;
#1981 = PLANE('',#99885) ;
#1982 = PLANE('',#99889) ;
#1983 = PLANE('',#99890) ;
#1984 = PLANE('',#99894) ;
#1985 = PLANE('',#99898) ;
#1986 = PLANE('',#99902) ;
#1987 = PLANE('',#99906) ;
#1988 = PLANE('',#99907) ;
#1989 = PLANE('',#99911) ;
#1990 = PLANE('',#99915) ;
#1991 = PLANE('',#99919) ;
#1992 = PLANE('',#99923) ;
#1993 = PLANE('',#99924) ;
#1994 = PLANE('',#99928) ;
#1995 = PLANE('',#99932) ;
#1996 = PLANE('',#99936) ;
#1997 = PLANE('',#99940) ;
#1998 = PLANE('',#99941) ;
#1999 = B_SPLINE_CURVE_WITH_KNOTS('',3,(#132623,#132624,#132625,#132626,#132627,
#132628,#132629,#132630,#132631,#132632),.UNSPECIFIED.,.F.,.F.,(4,2,2,2,
4),(0.0155454932989835,0.0194994353522834,0.0234533774055832,0.0272081302045205,
0.0309628830034577),.UNSPECIFIED.) ;
#2000 = B_SPLINE_CURVE_WITH_KNOTS('',3,(#132636,#132637,#132638,#132639,#132640,
#132641,#132642,#132643,#132644,#132645),.UNSPECIFIED.,.F.,.F.,(4,2,2,2,
4),(-0.0304888223793686,-0.0267236306519753,-0.0229584389245819,-0.0190821381960852,
-0.0152058374675885),.UNSPECIFIED.) ;
#2001 = B_SPLINE_CURVE_WITH_KNOTS('',3,(#132649,#132650,#132651,#132652,#132653,
#132654,#132655,#132656,#132657,#132658),.UNSPECIFIED.,.F.,.F.,(4,2,2,2,
4),(-0.0457718072911488,-0.041895506562652,-0.0380192058341553,-0.034254014106762,
-0.0304888223793686),.UNSPECIFIED.) ;
#2002 = B_SPLINE_CURVE_WITH_KNOTS('',3,(#132662,#132663,#132664,#132665,#132666,
#132667,#132668,#132669,#132670,#132671,#132672,#132673,#132674,#132675,
#132676,#132677,#132678,#132679,#132680,#132681,#132682,#132683,#132684,
#132685,#132686,#132687,#132688,#132689,#132690,#132691,#132692),
 .UNSPECIFIED.,.F.,.F.,(4,3,3,3,3,3,3,3,3,3,4),(0.,1.73748728562045E-5,
3.26506729531324E-5,5.02804002574634E-5,6.52741227887637E-5,8.3439070256478E-5,
9.83241608049985E-5,0.00011756895656783,0.00013250051079383,0.000151525967767889,
0.000159849152172774),.UNSPECIFIED.) ;
#2003 = B_SPLINE_CURVE_WITH_KNOTS('',3,(#132696,#132697,#132698,#132699,#132700,
#132701,#132702,#132703,#132704,#132705),.UNSPECIFIED.,.F.,.F.,(4,2,2,2,
4),(0.0155454932989835,0.0194994353522834,0.0234533774055832,0.0272081302045204,
0.0309628830034577),.UNSPECIFIED.) ;
#2004 = B_SPLINE_CURVE_WITH_KNOTS('',3,(#132709,#132710,#132711,#132712,#132713,
#132714,#132715,#132716,#132717,#132718),.UNSPECIFIED.,.F.,.F.,(4,2,2,2,
4),(-0.0304888223793686,-0.0267236306519752,-0.0229584389245819,-0.0190821381960852,
-0.0152058374675885),.UNSPECIFIED.) ;
#2005 = B_SPLINE_CURVE_WITH_KNOTS('',3,(#132722,#132723,#132724,#132725,#132726,
#132727,#132728,#132729,#132730,#132731),.UNSPECIFIED.,.F.,.F.,(4,2,2,2,
4),(-0.0457718072911488,-0.0418955065626521,-0.0380192058341553,-0.034254014106762,
-0.0304888223793686),.UNSPECIFIED.) ;
#2006 = B_SPLINE_CURVE_WITH_KNOTS('',3,(#132735,#132736,#132737,#132738,#132739,
#132740,#132741,#132742,#132743,#132744,#132745,#132746,#132747,#132748,
#132749,#132750,#132751,#132752,#132753,#132754,#132755,#132756,#132757,
#132758,#132759,#132760,#132761,#132762,#132763,#132764,#132765),
 .UNSPECIFIED.,.F.,.F.,(4,3,3,3,3,3,3,3,3,3,4),(0.,1.73748728562068E-5,
3.26506729531323E-5,5.02804002574648E-5,6.52741227887635E-5,8.34390702564692E-5,
9.83241608049985E-5,0.000117568956567848,0.00013250051079383,0.000151525967767866,
0.000159849152172774),.UNSPECIFIED.) ;
#2007 = B_SPLINE_CURVE_WITH_KNOTS('',3,(#132848,#132849,#132850,#132851,#132852,
#132853,#132854,#132855,#132856,#132857),.UNSPECIFIED.,.F.,.F.,(4,2,2,2,
4),(0.0155454932989836,0.0194994353522834,0.0234533774055832,0.0272081302045205,
0.0309628830034577),.UNSPECIFIED.) ;
#2008 = B_SPLINE_CURVE_WITH_KNOTS('',3,(#132861,#132862,#132863,#132864,#132865,
#132866,#132867,#132868,#132869,#132870),.UNSPECIFIED.,.F.,.F.,(4,2,2,2,
4),(-0.0304888223793686,-0.0267236306519753,-0.0229584389245819,-0.0190821381960852,
-0.0152058374675885),.UNSPECIFIED.) ;
#2009 = B_SPLINE_CURVE_WITH_KNOTS('',3,(#132874,#132875,#132876,#132877,#132878,
#132879,#132880,#132881,#132882,#132883),.UNSPECIFIED.,.F.,.F.,(4,2,2,2,
4),(-0.0457718072911489,-0.0418955065626522,-0.0380192058341554,-0.0342540141067621,
-0.0304888223793687),.UNSPECIFIED.) ;
#2010 = B_SPLINE_CURVE_WITH_KNOTS('',3,(#132887,#132888,#132889,#132890,#132891,
#132892,#132893,#132894,#132895,#132896,#132897,#132898,#132899,#132900,
#132901,#132902,#132903,#132904,#132905,#132906,#132907,#132908,#132909,
#132910,#132911,#132912,#132913,#132914,#132915,#132916,#132917),
 .UNSPECIFIED.,.F.,.F.,(4,3,3,3,3,3,3,3,3,3,4),(0.,1.73748728562045E-5,
3.26506729531323E-5,5.02804002574719E-5,6.52741227887636E-5,8.34390702564519E-5,
9.83241608049985E-5,0.000117568956567851,0.00013250051079383,0.00015152596776785,
0.000159849152172774),.UNSPECIFIED.) ;
#2011 = B_SPLINE_CURVE_WITH_KNOTS('',3,(#132921,#132922,#132923,#132924,#132925,
#132926,#132927,#132928,#132929,#132930),.UNSPECIFIED.,.F.,.F.,(4,2,2,2,
4),(0.0155454932989836,0.0194994353522834,0.0234533774055832,0.0272081302045205,
0.0309628830034577),.UNSPECIFIED.) ;
#2012 = B_SPLINE_CURVE_WITH_KNOTS('',3,(#132934,#132935,#132936,#132937,#132938,
#132939,#132940,#132941,#132942,#132943),.UNSPECIFIED.,.F.,.F.,(4,2,2,2,
4),(-0.0304888223793687,-0.0267236306519753,-0.022958438924582,-0.0190821381960853,
-0.0152058374675885),.UNSPECIFIED.) ;
#2013 = B_SPLINE_CURVE_WITH_KNOTS('',3,(#132947,#132948,#132949,#132950,#132951,
#132952,#132953,#132954,#132955,#132956),.UNSPECIFIED.,.F.,.F.,(4,2,2,2,
4),(-0.0457718072911488,-0.0418955065626521,-0.0380192058341554,-0.034254014106762,
-0.0304888223793687),.UNSPECIFIED.) ;
#2014 = B_SPLINE_CURVE_WITH_KNOTS('',3,(#132960,#132961,#132962,#132963,#132964,
#132965,#132966,#132967,#132968,#132969,#132970,#132971,#132972,#132973,
#132974,#132975,#132976,#132977,#132978,#132979,#132980,#132981,#132982,
#132983,#132984,#132985,#132986,#132987,#132988,#132989,#132990),
 .UNSPECIFIED.,.F.,.F.,(4,3,3,3,3,3,3,3,3,3,4),(0.,1.73748728562037E-5,
3.26506729531323E-5,5.02804002574677E-5,6.52741227887636E-5,8.34390702564633E-5,
9.83241608049985E-5,0.000117568956567858,0.00013250051079383,0.000151525967767868,
0.000159849152172774),.UNSPECIFIED.) ;
#2015 = B_SPLINE_CURVE_WITH_KNOTS('',3,(#133008,#133009,#133010,#133011),
 .UNSPECIFIED.,.F.,.F.,(4,4),(0.,1.5707963267949),.UNSPECIFIED.) ;
#2016 = B_SPLINE_CURVE_WITH_KNOTS('',3,(#133015,#133016,#133017,#133018),
 .UNSPECIFIED.,.F.,.F.,(4,4),(1.5707963267949,3.14159265358979),
 .UNSPECIFIED.) ;
#2017 = B_SPLINE_CURVE_WITH_KNOTS('',3,(#133260,#133261,#133262,#133263,#133264,
#133265),.UNSPECIFIED.,.F.,.F.,(4,2,4),(3.14159265358979,3.92699081698724,
4.71238898038469),.UNSPECIFIED.) ;
#2018 = B_SPLINE_CURVE_WITH_KNOTS('',3,(#133269,#133270,#133271,#133272,#133273,
#133274),.UNSPECIFIED.,.F.,.F.,(4,2,4),(3.14159265358979,3.92699081698724,
4.71238898038469),.UNSPECIFIED.) ;
#2019 = B_SPLINE_CURVE_WITH_KNOTS('',3,(#133278,#133279,#133280,#133281,#133282,
#133283),.UNSPECIFIED.,.F.,.F.,(4,2,4),(4.71238898038469,5.49778714378214,
6.28318530717959),.UNSPECIFIED.) ;
#2020 = B_SPLINE_CURVE_WITH_KNOTS('',3,(#133286,#133287,#133288,#133289,#133290,
#133291),.UNSPECIFIED.,.F.,.F.,(4,2,4),(4.71238898038469,5.49778714378214,
6.28318530717959),.UNSPECIFIED.) ;
#2021 = B_SPLINE_CURVE_WITH_KNOTS('',3,(#133296,#133297,#133298,#133299,#133300,
#133301),.UNSPECIFIED.,.F.,.F.,(4,2,4),(3.14159265358979,3.92699081698724,
4.71238898038469),.UNSPECIFIED.) ;
#2022 = B_SPLINE_CURVE_WITH_KNOTS('',3,(#133305,#133306,#133307,#133308,#133309,
#133310),.UNSPECIFIED.,.F.,.F.,(4,2,4),(3.14159265358979,3.92699081698724,
4.71238898038469),.UNSPECIFIED.) ;
#2023 = B_SPLINE_CURVE_WITH_KNOTS('',3,(#133314,#133315,#133316,#133317,#133318,
#133319),.UNSPECIFIED.,.F.,.F.,(4,2,4),(4.71238898038469,5.49778714378214,
6.28318530717959),.UNSPECIFIED.) ;
#2024 = B_SPLINE_CURVE_WITH_KNOTS('',3,(#133322,#133323,#133324,#133325,#133326,
#133327),.UNSPECIFIED.,.F.,.F.,(4,2,4),(4.71238898038469,5.49778714378214,
6.28318530717959),.UNSPECIFIED.) ;
#2025 = B_SPLINE_CURVE_WITH_KNOTS('',3,(#133381,#133382,#133383,#133384,#133385,
#133386,#133387,#133388,#133389,#133390,#133391,#133392,#133393,#133394,
#133395,#133396,#133397,#133398,#133399,#133400,#133401,#133402,#133403,
#133404,#133405,#133406,#133407,#133408),.UNSPECIFIED.,.F.,.F.,(4,3,3,3,
3,3,3,3,3,4),(2.16840434497101E-19,0.00010866297864345,0.0002173259572869,
0.000239795331094194,0.000268321712743107,0.000359692996641291,0.000370380550777844,
0.000402443213187502,0.000469559030214579,0.000479590662188387),
 .UNSPECIFIED.) ;
#2026 = B_SPLINE_CURVE_WITH_KNOTS('',3,(#133410,#133411,#133412,#133413,#133414,
#133415,#133416,#133417,#133418,#133419),.UNSPECIFIED.,.F.,.F.,(4,2,2,2,
4),(4.46821448257462E-15,0.000139027965256961,0.000278055930509455,0.000556111861014442,
0.00111222372202442),.UNSPECIFIED.) ;
#2027 = B_SPLINE_CURVE_WITH_KNOTS('',3,(#133421,#133422,#133423,#133424,#133425,
#133426,#133427,#133428,#133429,#133430,#133431,#133432,#133433,#133434,
#133435,#133436,#133437,#133438,#133439,#133440,#133441,#133442,#133443,
#133444,#133445),.UNSPECIFIED.,.F.,.F.,(4,3,3,3,3,3,3,3,4),(0.,0.000553539642553921,
0.000830309463830882,0.000968694374469362,0.000985992488299172,0.00104653588670351,
0.00108059154830595,0.00109383541670689,0.00110707928510784),
 .UNSPECIFIED.) ;
#2028 = B_SPLINE_CURVE_WITH_KNOTS('',3,(#133447,#133448,#133449,#133450,#133451,
#133452,#133453,#133454,#133455,#133456,#133457,#133458,#133459,#133460,
#133461,#133462),.UNSPECIFIED.,.F.,.F.,(4,2,2,2,2,2,2,4),(2.46381126959653E-5,
3.49307346223092E-5,0.000103812737360936,0.000147753773859884,0.000241616793832017,
0.000270869435023803,0.000448933238085274,0.000517100757351641),
 .UNSPECIFIED.) ;
#2029 = B_SPLINE_CURVE_WITH_KNOTS('',3,(#133474,#133475,#133476,#133477,#133478,
#133479,#133480,#133481,#133482,#133483,#133484,#133485,#133486,#133487,
#133488,#133489,#133490,#133491,#133492,#133493,#133494,#133495,#133496,
#133497,#133498,#133499,#133500,#133501),.UNSPECIFIED.,.F.,.F.,(4,3,3,3,
3,3,3,3,3,4),(0.,0.000108662978644149,0.000217325957288299,0.000239795331094193,
0.000268321712743106,0.00035969299664129,0.000370380550777843,0.000402443213187502,
0.000469559030214579,0.000479590662188388),.UNSPECIFIED.) ;
#2030 = B_SPLINE_CURVE_WITH_KNOTS('',3,(#133503,#133504,#133505,#133506,#133507,
#133508,#133509,#133510,#133511,#133512),.UNSPECIFIED.,.F.,.F.,(4,2,2,2,
4),(4.4671593419464E-15,0.000139027965256961,0.000278055930509454,0.000556111861014442,
0.00111222372202441),.UNSPECIFIED.) ;
#2031 = B_SPLINE_CURVE_WITH_KNOTS('',3,(#133514,#133515,#133516,#133517,#133518,
#133519,#133520,#133521,#133522,#133523,#133524,#133525,#133526,#133527,
#133528,#133529,#133530,#133531,#133532,#133533,#133534,#133535,#133536,
#133537,#133538),.UNSPECIFIED.,.F.,.F.,(4,3,3,3,3,3,3,3,4),(0.,0.000553539642553921,
0.000830309463830883,0.000968694374469362,0.000985992488299172,0.00104653588670351,
0.00108059154830595,0.00109383541670689,0.00110707928510784),
 .UNSPECIFIED.) ;
#2032 = B_SPLINE_CURVE_WITH_KNOTS('',3,(#133540,#133541,#133542,#133543,#133544,
#133545,#133546,#133547,#133548,#133549,#133550,#133551,#133552,#133553,
#133554,#133555),.UNSPECIFIED.,.F.,.F.,(4,2,2,2,2,2,2,4),(2.46381126959657E-5,
3.49307346223102E-5,0.000103812737360935,0.000147753773859885,0.000241616793832018,
0.000270869435023804,0.000448933238082175,0.00051710075735164),
 .UNSPECIFIED.) ;
#2033 = B_SPLINE_CURVE_WITH_KNOTS('',3,(#133959,#133960,#133961,#133962,#133963,
#133964),.UNSPECIFIED.,.F.,.F.,(4,2,4),(1.5707963267949,2.35619449019234,
3.14159265358979),.UNSPECIFIED.) ;
#2034 = B_SPLINE_CURVE_WITH_KNOTS('',3,(#134035,#134036,#134037,#134038,#134039,
#134040),.UNSPECIFIED.,.F.,.F.,(4,2,4),(0.,0.785398163397445,1.57079632679489),
 .UNSPECIFIED.) ;
#2035 = B_SPLINE_CURVE_WITH_KNOTS('',3,(#134134,#134135,#134136,#134137,#134138,
#134139,#134140,#134141,#134142,#134143,#134144,#134145,#134146,#134147,
#134148,#134149,#134150,#134151,#134152),.UNSPECIFIED.,.F.,.F.,(4,3,3,3,
3,3,4),(5.8575878041605E-5,6.39772274846954E-5,8.50081925564311E-5,0.000101719137060913,
0.000115369906146044,0.000121992710600423,0.000127737589255657),
 .UNSPECIFIED.) ;
#2036 = B_SPLINE_CURVE_WITH_KNOTS('',3,(#134159,#134160,#134161,#134162,#134163,
#134164,#134165,#134166,#134167,#134168,#134169,#134170,#134171,#134172),
 .UNSPECIFIED.,.F.,.F.,(4,2,2,2,2,2,4),(0.000106030898883045,0.000114450588602972,
0.0001358619160635,0.000155180925252374,0.000169070632935497,0.000187290067688934,
0.000202757041675869),.UNSPECIFIED.) ;
#2037 = B_SPLINE_CURVE_WITH_KNOTS('',3,(#134173,#134174,#134175,#134176,#134177,
#134178,#134179,#134180,#134181,#134182,#134183,#134184,#134185,#134186),
 .UNSPECIFIED.,.F.,.F.,(4,2,2,2,2,2,4),(0.,1.81852425157699E-5,3.36231897823057E-5,
5.26817905680866E-5,7.3668643005217E-5,8.81407292049458E-5,9.65446177718808E-5),
 .UNSPECIFIED.) ;
#2038 = B_SPLINE_CURVE_WITH_KNOTS('',3,(#134196,#134197,#134198,#134199,#134200,
#134201,#134202,#134203,#134204,#134205,#134206,#134207,#134208,#134209,
#134210,#134211,#134212,#134213,#134214),.UNSPECIFIED.,.F.,.F.,(4,3,3,3,
3,3,4),(0.,1.26126247467577E-5,2.08447799633808E-5,2.61321988210988E-5,
4.72564717706651E-5,6.39499555081058E-5,6.93621596435636E-5),
 .UNSPECIFIED.) ;
#2039 = B_SPLINE_CURVE_WITH_KNOTS('',3,(#134324,#134325,#134326,#134327,#134328,
#134329,#134330,#134331,#134332,#134333,#134334,#134335),.UNSPECIFIED.,
 .F.,.F.,(4,2,2,2,2,4),(2.16840434497101E-19,0.000230913708713648,0.000346370563070472,
0.000404098990248884,0.00043296320383809,0.000461827417427296),
 .UNSPECIFIED.) ;
#2040 = B_SPLINE_CURVE_WITH_KNOTS('',3,(#134362,#134363,#134364,#134365,#134366,
#134367,#134368,#134369,#134370,#134371,#134372,#134373),.UNSPECIFIED.,
 .F.,.F.,(4,2,2,2,2,4),(0.,2.92942635586613E-5,5.85885271173226E-5,0.000117177054234646,
0.000234354108469295,0.000468708216938589),.UNSPECIFIED.) ;
#2041 = B_SPLINE_CURVE_WITH_KNOTS('',3,(#134463,#134464,#134465,#134466,#134467,
#134468,#134469,#134470,#134471,#134472,#134473,#134474),.UNSPECIFIED.,
 .F.,.F.,(4,2,2,2,2,4),(7.70621319460113E-10,0.000528455713264078,0.000792683184585458,
0.000924796920246148,0.000990853788076493,0.00105691065590684),
 .UNSPECIFIED.) ;
#2042 = B_SPLINE_CURVE_WITH_KNOTS('',3,(#134475,#134476,#134477,#134478,#134479,
#134480,#134481,#134482,#134483,#134484,#134485,#134486,#134487,#134488,
#134489,#134490,#134491,#134492,#134493,#134494,#134495,#134496,#134497,
#134498,#134499,#134500,#134501,#134502),.UNSPECIFIED.,.F.,.F.,(4,2,2,2,
2,2,2,2,2,2,2,2,2,4),(0.,1.88814447164022E-5,2.66390109708352E-5,2.82246506940909E-5,
2.82548001019668E-5,4.36852952398544E-5,4.37205777570019E-5,4.63087975636132E-5,
5.19857273366478E-5,5.63013930903595E-5,5.77982263345347E-5,5.8493669267456E-5,
5.96281966878496E-5,6.07824730943691E-5),.UNSPECIFIED.) ;
#2043 = B_SPLINE_CURVE_WITH_KNOTS('',3,(#134504,#134505,#134506,#134507,#134508,
#134509,#134510,#134511,#134512,#134513,#134514,#134515,#134516,#134517,
#134518,#134519,#134520,#134521,#134522,#134523,#134524,#134525),
 .UNSPECIFIED.,.F.,.F.,(4,2,2,2,2,2,2,2,2,2,4),(-2.98424671548918E-6,-1.83179854035004E-6,
-6.78494605943823E-7,0.,1.61207185756534E-6,5.98431127542647E-6,1.25056665528015E-5,
1.40350946485193E-5,2.93914218611999E-5,4.85423642734616E-5,5.82245408950306E-5),
 .UNSPECIFIED.) ;
#2044 = B_SPLINE_CURVE_WITH_KNOTS('',3,(#134526,#134527,#134528,#134529,#134530,
#134531,#134532,#134533,#134534,#134535,#134536,#134537),.UNSPECIFIED.,
 .F.,.F.,(4,2,2,2,2,4),(0.,6.61189708719518E-5,0.000132237941743904,0.000264475883487807,
0.000528951766975614,0.00105790353395123),.UNSPECIFIED.) ;
#2045 = B_SPLINE_CURVE_WITH_KNOTS('',3,(#134570,#134571,#134572,#134573,#134574,
#134575,#134576,#134577,#134578,#134579,#134580,#134581,#134582,#134583,
#134584,#134585,#134586,#134587,#134588,#134589,#134590,#134591,#134592,
#134593,#134594,#134595,#134596,#134597,#134598,#134599,#134600,#134601,
#134602,#134603,#134604,#134605,#134606,#134607),.UNSPECIFIED.,.F.,.F.,
(4,2,2,2,2,2,2,2,2,2,2,2,2,2,2,2,2,2,4),(4.08242498362039E-13,1.91825894880777E-5,
2.29499826201368E-5,2.74799101222728E-5,3.52358269328764E-5,4.12198651829317E-5,
4.25319315563255E-5,4.54442131893302E-5,4.69409045132628E-5,4.80898427132611E-5,
4.9446473946099E-5,4.96432742482141E-5,5.04298720437356E-5,5.14115331535164E-5,
5.17333590635578E-5,5.22889985287821E-5,5.29242843672018E-5,5.37719008581487E-5,
5.49598202435906E-5),.UNSPECIFIED.) ;
#2046 = B_SPLINE_CURVE_WITH_KNOTS('',3,(#134641,#134642,#134643,#134644,#134645,
#134646,#134647,#134648,#134649,#134650,#134651,#134652,#134653,#134654,
#134655,#134656,#134657,#134658,#134659,#134660,#134661,#134662,#134663,
#134664,#134665,#134666,#134667,#134668,#134669,#134670,#134671,#134672,
#134673,#134674,#134675,#134676),.UNSPECIFIED.,.F.,.F.,(4,2,2,2,2,2,2,2,
2,2,2,2,2,2,2,2,2,4),(-2.90335387328764E-6,-1.36780202085548E-6,-6.41515161605833E-7,
-6.4061093095502E-8,3.81173304657634E-7,1.44450314270962E-6,2.24472183150878E-6,
2.5078329807616E-6,3.96662365739235E-6,5.28616271355818E-6,8.35978425194598E-6,
9.71024741494835E-6,1.08366011880723E-5,1.65505252295058E-5,2.45765562494323E-5,
2.90642498315122E-5,4.41638722239744E-5,5.20477084101052E-5),
 .UNSPECIFIED.) ;
#2047 = B_SPLINE_CURVE_WITH_KNOTS('',3,(#135327,#135328,#135329,#135330,#135331,
#135332),.UNSPECIFIED.,.F.,.F.,(4,2,4),(1.5707963267949,2.35619449019234,
3.14159265358979),.UNSPECIFIED.) ;
#2048 = B_SPLINE_CURVE_WITH_KNOTS('',3,(#135403,#135404,#135405,#135406,#135407,
#135408),.UNSPECIFIED.,.F.,.F.,(4,2,4),(0.,0.785398163397448,1.57079632679489),
 .UNSPECIFIED.) ;
#2049 = B_SPLINE_CURVE_WITH_KNOTS('',3,(#135502,#135503,#135504,#135505,#135506,
#135507,#135508,#135509,#135510,#135511,#135512,#135513,#135514,#135515,
#135516,#135517,#135518,#135519,#135520),.UNSPECIFIED.,.F.,.F.,(4,3,3,3,
3,3,4),(5.85758780416049E-5,6.39772274846956E-5,8.50081925566845E-5,0.000101719137060913,
0.000115369906146169,0.000121992710600423,0.000127737589255657),
 .UNSPECIFIED.) ;
#2050 = B_SPLINE_CURVE_WITH_KNOTS('',3,(#135527,#135528,#135529,#135530,#135531,
#135532,#135533,#135534,#135535,#135536,#135537,#135538,#135539,#135540),
 .UNSPECIFIED.,.F.,.F.,(4,2,2,2,2,2,4),(0.000106030898883045,0.000114450588602972,
0.000135861916063515,0.000155180925252387,0.000169070632935497,0.000187290067688863,
0.000202757041675869),.UNSPECIFIED.) ;
#2051 = B_SPLINE_CURVE_WITH_KNOTS('',3,(#135541,#135542,#135543,#135544,#135545,
#135546,#135547,#135548,#135549,#135550,#135551,#135552,#135553,#135554),
 .UNSPECIFIED.,.F.,.F.,(4,2,2,2,2,2,4),(0.,1.81852425155684E-5,3.36231897823057E-5,
5.26817905680615E-5,7.36686430051892E-5,8.81407292049454E-5,9.65446177718809E-5),
 .UNSPECIFIED.) ;
#2052 = B_SPLINE_CURVE_WITH_KNOTS('',3,(#135563,#135564,#135565,#135566,#135567,
#135568,#135569,#135570,#135571,#135572,#135573,#135574,#135575,#135576,
#135577,#135578,#135579,#135580,#135581),.UNSPECIFIED.,.F.,.F.,(4,3,3,3,
3,3,4),(0.,1.26126247467848E-5,2.08447799633808E-5,2.61321988210988E-5,
4.72564717709744E-5,6.39499555081057E-5,6.93621596435632E-5),
 .UNSPECIFIED.) ;
#2053 = B_SPLINE_CURVE_WITH_KNOTS('',3,(#135691,#135692,#135693,#135694,#135695,
#135696,#135697,#135698,#135699,#135700,#135701,#135702),.UNSPECIFIED.,
 .F.,.F.,(4,2,2,2,2,4),(4.33680868994202E-19,0.000230913708713649,0.000346370563070474,
0.000404098990248885,0.000432963203838091,0.000461827417427296),
 .UNSPECIFIED.) ;
#2054 = B_SPLINE_CURVE_WITH_KNOTS('',3,(#135723,#135724,#135725,#135726,#135727,
#135728,#135729,#135730,#135731,#135732,#135733,#135734),.UNSPECIFIED.,
 .F.,.F.,(4,2,2,2,2,4),(0.,2.92942635586604E-5,5.85885271173207E-5,0.000117177054234645,
0.000234354108469293,0.000468708216938593),.UNSPECIFIED.) ;
#2055 = B_SPLINE_CURVE_WITH_KNOTS('',3,(#135803,#135804,#135805,#135806,#135807,
#135808,#135809,#135810,#135811,#135812,#135813,#135814),.UNSPECIFIED.,
 .F.,.F.,(4,2,2,2,2,4),(7.70621318557099E-10,0.000528455713264077,0.000792683184585457,
0.000924796920246147,0.000990853788076492,0.00105691065590684),
 .UNSPECIFIED.) ;
#2056 = B_SPLINE_CURVE_WITH_KNOTS('',3,(#135815,#135816,#135817,#135818,#135819,
#135820,#135821,#135822,#135823,#135824,#135825,#135826,#135827,#135828,
#135829,#135830,#135831,#135832,#135833,#135834,#135835,#135836,#135837,
#135838,#135839,#135840,#135841,#135842),.UNSPECIFIED.,.F.,.F.,(4,2,2,2,
2,2,2,2,2,2,2,2,2,4),(0.,1.88814447164821E-5,2.66390109708352E-5,2.82246506940927E-5,
2.82548001019694E-5,4.36852952398541E-5,4.37205777570016E-5,4.63087975636134E-5,
5.19857273366473E-5,5.63013930903587E-5,5.77982263345345E-5,5.84936692674544E-5,
5.96281966878474E-5,6.07824730943697E-5),.UNSPECIFIED.) ;
#2057 = B_SPLINE_CURVE_WITH_KNOTS('',3,(#135844,#135845,#135846,#135847,#135848,
#135849,#135850,#135851,#135852,#135853,#135854,#135855,#135856,#135857,
#135858,#135859,#135860,#135861,#135862,#135863,#135864,#135865),
 .UNSPECIFIED.,.F.,.F.,(4,2,2,2,2,2,2,2,2,2,4),(-2.98424671548898E-6,-1.83179854035005E-6,
-6.78494605944079E-7,0.,1.61207185756418E-6,5.9843112754236E-6,1.25056665528019E-5,
1.40350946485009E-5,2.93914218611391E-5,4.85423642729475E-5,5.82245408950306E-5),
 .UNSPECIFIED.) ;
#2058 = B_SPLINE_CURVE_WITH_KNOTS('',3,(#135866,#135867,#135868,#135869,#135870,
#135871,#135872,#135873,#135874,#135875,#135876,#135877),.UNSPECIFIED.,
 .F.,.F.,(4,2,2,2,2,4),(0.,6.61189708719504E-5,0.000132237941743901,0.000264475883487804,
0.000528951766975613,0.00105790353395123),.UNSPECIFIED.) ;
#2059 = B_SPLINE_CURVE_WITH_KNOTS('',3,(#135908,#135909,#135910,#135911,#135912,
#135913,#135914,#135915,#135916,#135917,#135918,#135919,#135920,#135921,
#135922,#135923,#135924,#135925,#135926,#135927,#135928,#135929,#135930,
#135931,#135932,#135933,#135934,#135935,#135936,#135937,#135938,#135939,
#135940,#135941,#135942,#135943,#135944,#135945),.UNSPECIFIED.,.F.,.F.,
(4,2,2,2,2,2,2,2,2,2,2,2,2,2,2,2,2,2,4),(4.08242998125434E-13,1.91825894890263E-5,
2.29499826201337E-5,2.74799101222727E-5,3.52358269328724E-5,4.12198651829315E-5,
4.25319315563219E-5,4.54442131893529E-5,4.694090451326E-5,4.8089842713261E-5,
4.94464739460923E-5,4.9643274248211E-5,5.04298720437361E-5,5.14115331535221E-5,
5.17333590635549E-5,5.22889985287794E-5,5.29242843671993E-5,5.3771900858147E-5,
5.49598202435904E-5),.UNSPECIFIED.) ;
#2060 = B_SPLINE_CURVE_WITH_KNOTS('',3,(#135978,#135979,#135980,#135981,#135982,
#135983,#135984,#135985,#135986,#135987,#135988,#135989,#135990,#135991,
#135992,#135993,#135994,#135995,#135996,#135997,#135998,#135999,#136000,
#136001,#136002,#136003,#136004,#136005,#136006,#136007,#136008,#136009,
#136010,#136011,#136012,#136013),.UNSPECIFIED.,.F.,.F.,(4,2,2,2,2,2,2,2,
2,2,2,2,2,2,2,2,2,4),(-2.90335387328765E-6,-1.36780202088648E-6,-6.41515161635526E-7,
-6.40610931249841E-8,3.81173304645144E-7,1.44450314269772E-6,2.24472183150306E-6,
2.5078329807503E-6,3.96662365739234E-6,5.28616271355017E-6,8.35978425189786E-6,
9.71024741494142E-6,1.08366011880723E-5,1.65505252294989E-5,2.45765562494323E-5,
2.9064249831501E-5,4.41638722239248E-5,5.20477084101053E-5),
 .UNSPECIFIED.) ;
#2061 = B_SPLINE_CURVE_WITH_KNOTS('',3,(#136198,#136199,#136200,#136201),
 .UNSPECIFIED.,.F.,.F.,(4,4),(3.14159265358979,4.71238898038469),
 .UNSPECIFIED.) ;
#2062 = B_SPLINE_CURVE_WITH_KNOTS('',3,(#136206,#136207,#136208,#136209),
 .UNSPECIFIED.,.F.,.F.,(4,4),(4.71238898038469,6.28318530717959),
 .UNSPECIFIED.) ;
#2063 = B_SPLINE_CURVE_WITH_KNOTS('',3,(#136326,#136327,#136328,#136329,#136330,
#136331,#136332,#136333,#136334,#136335),.UNSPECIFIED.,.F.,.F.,(4,2,2,2,
4),(0.0155454932989846,0.0194994353522841,0.0234533774055837,0.0272081302045207,
0.0309628830034577),.UNSPECIFIED.) ;
#2064 = B_SPLINE_CURVE_WITH_KNOTS('',3,(#136339,#136340,#136341,#136342,#136343,
#136344,#136345,#136346,#136347,#136348),.UNSPECIFIED.,.F.,.F.,(4,2,2,2,
4),(-0.0304888223793687,-0.0267236306519748,-0.0229584389245809,-0.0190821381960837,
-0.0152058374675865),.UNSPECIFIED.) ;
#2065 = B_SPLINE_CURVE_WITH_KNOTS('',3,(#136352,#136353,#136354,#136355,#136356,
#136357,#136358,#136359,#136360,#136361),.UNSPECIFIED.,.F.,.F.,(4,2,2,2,
4),(-0.0457718072911502,-0.0418955065626531,-0.038019205834156,-0.0342540141067624,
-0.0304888223793687),.UNSPECIFIED.) ;
#2066 = B_SPLINE_CURVE_WITH_KNOTS('',3,(#136365,#136366,#136367,#136368,#136369,
#136370,#136371,#136372,#136373,#136374,#136375,#136376,#136377,#136378,
#136379,#136380,#136381,#136382,#136383,#136384,#136385,#136386,#136387,
#136388,#136389,#136390,#136391,#136392,#136393,#136394,#136395),
 .UNSPECIFIED.,.F.,.F.,(4,3,3,3,3,3,3,3,3,3,4),(0.,1.73748728561907E-5,
3.26506729531324E-5,5.02804002574635E-5,6.52741227887648E-5,8.34390702564386E-5,
9.83241608050006E-5,0.000117568956567835,0.000132500510793831,0.000151525967767874,
0.000159849152172776),.UNSPECIFIED.) ;
#2067 = B_SPLINE_CURVE_WITH_KNOTS('',3,(#136399,#136400,#136401,#136402,#136403,
#136404,#136405,#136406,#136407,#136408),.UNSPECIFIED.,.F.,.F.,(4,2,2,2,
4),(0.015545493298985,0.0194994353522845,0.023453377405584,0.0272081302045209,
0.0309628830034578),.UNSPECIFIED.) ;
#2068 = B_SPLINE_CURVE_WITH_KNOTS('',3,(#136412,#136413,#136414,#136415,#136416,
#136417,#136418,#136419,#136420,#136421),.UNSPECIFIED.,.F.,.F.,(4,2,2,2,
4),(-0.0304888223793687,-0.0267236306519748,-0.0229584389245809,-0.0190821381960837,
-0.0152058374675865),.UNSPECIFIED.) ;
#2069 = B_SPLINE_CURVE_WITH_KNOTS('',3,(#136425,#136426,#136427,#136428,#136429,
#136430,#136431,#136432,#136433,#136434),.UNSPECIFIED.,.F.,.F.,(4,2,2,2,
4),(-0.0457718072911503,-0.0418955065626532,-0.0380192058341561,-0.0342540141067624,
-0.0304888223793688),.UNSPECIFIED.) ;
#2070 = B_SPLINE_CURVE_WITH_KNOTS('',3,(#136438,#136439,#136440,#136441,#136442,
#136443,#136444,#136445,#136446,#136447,#136448,#136449,#136450,#136451,
#136452,#136453,#136454,#136455,#136456,#136457,#136458,#136459,#136460,
#136461,#136462,#136463,#136464,#136465,#136466,#136467,#136468),
 .UNSPECIFIED.,.F.,.F.,(4,3,3,3,3,3,3,3,3,3,4),(0.,1.73748728562053E-5,
3.26506729531322E-5,5.02804002574541E-5,6.52741227887639E-5,8.34390702564725E-5,
9.8324160804999E-5,0.000117568956567813,0.00013250051079383,0.000151525967767858,
0.000159849152172774),.UNSPECIFIED.) ;
#2071 = B_SPLINE_CURVE_WITH_KNOTS('',3,(#136551,#136552,#136553,#136554,#136555,
#136556,#136557,#136558,#136559,#136560),.UNSPECIFIED.,.F.,.F.,(4,2,2,2,
4),(0.0155454932989845,0.019499435352284,0.0234533774055836,0.0272081302045206,
0.0309628830034576),.UNSPECIFIED.) ;
#2072 = B_SPLINE_CURVE_WITH_KNOTS('',3,(#136564,#136565,#136566,#136567,#136568,
#136569,#136570,#136571,#136572,#136573),.UNSPECIFIED.,.F.,.F.,(4,2,2,2,
4),(-0.0304888223793686,-0.0267236306519753,-0.0229584389245819,-0.0190821381960852,
-0.0152058374675885),.UNSPECIFIED.) ;
#2073 = B_SPLINE_CURVE_WITH_KNOTS('',3,(#136577,#136578,#136579,#136580,#136581,
#136582,#136583,#136584,#136585,#136586),.UNSPECIFIED.,.F.,.F.,(4,2,2,2,
4),(-0.04577180729115,-0.041895506562653,-0.0380192058341561,-0.0342540141067623,
-0.0304888223793686),.UNSPECIFIED.) ;
#2074 = B_SPLINE_CURVE_WITH_KNOTS('',3,(#136590,#136591,#136592,#136593,#136594,
#136595,#136596,#136597,#136598,#136599,#136600,#136601,#136602,#136603,
#136604,#136605,#136606,#136607,#136608,#136609,#136610,#136611,#136612,
#136613,#136614,#136615,#136616,#136617,#136618,#136619,#136620),
 .UNSPECIFIED.,.F.,.F.,(4,3,3,3,3,3,3,3,3,3,4),(0.,1.73748728562061E-5,
3.26506729531324E-5,5.02804002574579E-5,6.52741227887648E-5,8.34390702564438E-5,
9.83241608050006E-5,0.000117568956567808,0.000132500510793831,0.000151525967767823,
0.000159849152172776),.UNSPECIFIED.) ;
#2075 = B_SPLINE_CURVE_WITH_KNOTS('',3,(#136624,#136625,#136626,#136627,#136628,
#136629,#136630,#136631,#136632,#136633),.UNSPECIFIED.,.F.,.F.,(4,2,2,2,
4),(0.0155454932989848,0.0194994353522843,0.0234533774055838,0.0272081302045207,
0.0309628830034576),.UNSPECIFIED.) ;
#2076 = B_SPLINE_CURVE_WITH_KNOTS('',3,(#136637,#136638,#136639,#136640,#136641,
#136642,#136643,#136644,#136645,#136646),.UNSPECIFIED.,.F.,.F.,(4,2,2,2,
4),(-0.0304888223793686,-0.0267236306519748,-0.0229584389245809,-0.0190821381960837,
-0.0152058374675865),.UNSPECIFIED.) ;
#2077 = B_SPLINE_CURVE_WITH_KNOTS('',3,(#136650,#136651,#136652,#136653,#136654,
#136655,#136656,#136657,#136658,#136659),.UNSPECIFIED.,.F.,.F.,(4,2,2,2,
4),(-0.04577180729115,-0.041895506562653,-0.038019205834156,-0.0342540141067624,
-0.0304888223793687),.UNSPECIFIED.) ;
#2078 = B_SPLINE_CURVE_WITH_KNOTS('',3,(#136663,#136664,#136665,#136666,#136667,
#136668,#136669,#136670,#136671,#136672,#136673,#136674,#136675,#136676,
#136677,#136678,#136679,#136680,#136681,#136682,#136683,#136684,#136685,
#136686,#136687,#136688,#136689,#136690,#136691,#136692,#136693),
 .UNSPECIFIED.,.F.,.F.,(4,3,3,3,3,3,3,3,3,3,4),(0.,1.73748728562032E-5,
3.26506729531328E-5,5.02804002574436E-5,6.52741227887643E-5,8.34390702564541E-5,
9.83241608049997E-5,0.000117568956567832,0.00013250051079383,0.000151525967767753,
0.000159849152172774),.UNSPECIFIED.) ;
#2079 = B_SPLINE_CURVE_WITH_KNOTS('',3,(#136711,#136712,#136713,#136714),
 .UNSPECIFIED.,.F.,.F.,(4,4),(0.,1.5707963267949),.UNSPECIFIED.) ;
#2080 = B_SPLINE_CURVE_WITH_KNOTS('',3,(#136718,#136719,#136720,#136721),
 .UNSPECIFIED.,.F.,.F.,(4,4),(1.5707963267949,3.14159265358979),
 .UNSPECIFIED.) ;
#2081 = B_SPLINE_CURVE_WITH_KNOTS('',3,(#136963,#136964,#136965,#136966,#136967,
#136968),.UNSPECIFIED.,.F.,.F.,(4,2,4),(3.14159265358979,3.92699081698724,
4.71238898038469),.UNSPECIFIED.) ;
#2082 = B_SPLINE_CURVE_WITH_KNOTS('',3,(#136972,#136973,#136974,#136975,#136976,
#136977),.UNSPECIFIED.,.F.,.F.,(4,2,4),(3.14159265358979,3.92699081698724,
4.71238898038469),.UNSPECIFIED.) ;
#2083 = B_SPLINE_CURVE_WITH_KNOTS('',3,(#136981,#136982,#136983,#136984,#136985,
#136986),.UNSPECIFIED.,.F.,.F.,(4,2,4),(4.71238898038469,5.49778714378214,
6.28318530717959),.UNSPECIFIED.) ;
#2084 = B_SPLINE_CURVE_WITH_KNOTS('',3,(#136989,#136990,#136991,#136992,#136993,
#136994),.UNSPECIFIED.,.F.,.F.,(4,2,4),(4.71238898038469,5.49778714378214,
6.28318530717959),.UNSPECIFIED.) ;
#2085 = B_SPLINE_CURVE_WITH_KNOTS('',3,(#136999,#137000,#137001,#137002,#137003,
#137004),.UNSPECIFIED.,.F.,.F.,(4,2,4),(3.14159265358979,3.92699081698724,
4.71238898038469),.UNSPECIFIED.) ;
#2086 = B_SPLINE_CURVE_WITH_KNOTS('',3,(#137008,#137009,#137010,#137011,#137012,
#137013),.UNSPECIFIED.,.F.,.F.,(4,2,4),(3.14159265358979,3.92699081698724,
4.71238898038469),.UNSPECIFIED.) ;
#2087 = B_SPLINE_CURVE_WITH_KNOTS('',3,(#137017,#137018,#137019,#137020,#137021,
#137022),.UNSPECIFIED.,.F.,.F.,(4,2,4),(4.71238898038469,5.49778714378214,
6.28318530717959),.UNSPECIFIED.) ;
#2088 = B_SPLINE_CURVE_WITH_KNOTS('',3,(#137025,#137026,#137027,#137028,#137029,
#137030),.UNSPECIFIED.,.F.,.F.,(4,2,4),(4.71238898038469,5.49778714378214,
6.28318530717959),.UNSPECIFIED.) ;
#2089 = B_SPLINE_CURVE_WITH_KNOTS('',3,(#137084,#137085,#137086,#137087,#137088,
#137089,#137090,#137091,#137092,#137093,#137094,#137095,#137096,#137097,
#137098,#137099,#137100,#137101,#137102,#137103,#137104,#137105,#137106,
#137107,#137108,#137109,#137110,#137111),.UNSPECIFIED.,.F.,.F.,(4,3,3,3,
3,3,3,3,3,4),(0.,0.000108662978650454,0.000217325957300909,0.000239795331094189,
0.00026832171274309,0.000359692996641288,0.000370380550777836,0.000402443213187482,
0.000469559030214573,0.000479590662188388),.UNSPECIFIED.) ;
#2090 = B_SPLINE_CURVE_WITH_KNOTS('',3,(#137113,#137114,#137115,#137116,#137117,
#137118,#137119,#137120,#137121,#137122),.UNSPECIFIED.,.F.,.F.,(4,2,2,2,
4),(4.46893664505693E-15,0.00013902796525696,0.000278055930509451,0.000556111861014443,
0.00111222372202442),.UNSPECIFIED.) ;
#2091 = B_SPLINE_CURVE_WITH_KNOTS('',3,(#137124,#137125,#137126,#137127,#137128,
#137129,#137130,#137131,#137132,#137133,#137134,#137135,#137136,#137137,
#137138,#137139,#137140,#137141,#137142,#137143,#137144,#137145,#137146,
#137147,#137148),.UNSPECIFIED.,.F.,.F.,(4,3,3,3,3,3,3,3,4),(0.,0.000553539642553915,
0.000830309463830878,0.000968694374469359,0.000985992488299169,0.0010465358867035,
0.00108059154830594,0.00109383541670689,0.00110707928510784),
 .UNSPECIFIED.) ;
#2092 = B_SPLINE_CURVE_WITH_KNOTS('',3,(#137150,#137151,#137152,#137153,#137154,
#137155,#137156,#137157,#137158,#137159,#137160,#137161,#137162,#137163,
#137164,#137165),.UNSPECIFIED.,.F.,.F.,(4,2,2,2,2,2,2,4),(2.46381126959637E-5,
3.49307346222979E-5,0.000103812737360902,0.00014775377385988,0.000241616793832009,
0.000270869435023796,0.000448933238137038,0.000517100757351638),
 .UNSPECIFIED.) ;
#2093 = B_SPLINE_CURVE_WITH_KNOTS('',3,(#137169,#137170,#137171,#137172,#137173,
#137174,#137175,#137176,#137177,#137178,#137179,#137180,#137181,#137182,
#137183,#137184,#137185,#137186,#137187,#137188,#137189,#137190,#137191,
#137192,#137193,#137194,#137195,#137196),.UNSPECIFIED.,.F.,.F.,(4,3,3,3,
3,3,3,3,3,4),(0.,0.000108662978648,0.000217325957296001,0.000239795331094189,
0.000268321712743099,0.000359692996641288,0.000370380550777836,0.00040244321318748,
0.000469559030214573,0.000479590662188388),.UNSPECIFIED.) ;
#2094 = B_SPLINE_CURVE_WITH_KNOTS('',3,(#137198,#137199,#137200,#137201,#137202,
#137203,#137204,#137205,#137206,#137207),.UNSPECIFIED.,.F.,.F.,(4,2,2,2,
4),(4.46893664505693E-15,0.00013902796525696,0.00027805593050945,0.000556111861014442,
0.00111222372202442),.UNSPECIFIED.) ;
#2095 = B_SPLINE_CURVE_WITH_KNOTS('',3,(#137209,#137210,#137211,#137212,#137213,
#137214,#137215,#137216,#137217,#137218,#137219,#137220,#137221,#137222,
#137223,#137224,#137225,#137226,#137227,#137228,#137229,#137230,#137231,
#137232,#137233),.UNSPECIFIED.,.F.,.F.,(4,3,3,3,3,3,3,3,4),(0.,0.000553539642553922,
0.00083030946383088,0.000968694374469362,0.000985992488299172,0.00104653588670351,
0.00108059154830595,0.00109383541670689,0.00110707928510784),
 .UNSPECIFIED.) ;
#2096 = B_SPLINE_CURVE_WITH_KNOTS('',3,(#137235,#137236,#137237,#137238,#137239,
#137240,#137241,#137242,#137243,#137244,#137245,#137246,#137247,#137248,
#137249,#137250),.UNSPECIFIED.,.F.,.F.,(4,2,2,2,2,2,2,4),(2.46381126959657E-5,
3.49307346222963E-5,0.000103812737360898,0.000147753773859885,0.000241616793832011,
0.000270869435023803,0.000448933238140248,0.00051710075735164),
 .UNSPECIFIED.) ;
#2097 = B_SPLINE_CURVE_WITH_KNOTS('',3,(#137662,#137663,#137664,#137665,#137666,
#137667),.UNSPECIFIED.,.F.,.F.,(4,2,4),(1.5707963267949,2.35619449019234,
3.14159265358979),.UNSPECIFIED.) ;
#2098 = B_SPLINE_CURVE_WITH_KNOTS('',3,(#137738,#137739,#137740,#137741,#137742,
#137743),.UNSPECIFIED.,.F.,.F.,(4,2,4),(0.,0.785398163397447,1.57079632679489),
 .UNSPECIFIED.) ;
#2099 = B_SPLINE_CURVE_WITH_KNOTS('',3,(#137837,#137838,#137839,#137840,#137841,
#137842,#137843,#137844,#137845,#137846,#137847,#137848,#137849,#137850,
#137851,#137852,#137853,#137854,#137855),.UNSPECIFIED.,.F.,.F.,(4,3,3,3,
3,3,4),(5.85758780416038E-5,6.39772274846938E-5,8.50081925559283E-5,0.000101719137060913,
0.000115369906146282,0.000121992710600423,0.000127737589255657),
 .UNSPECIFIED.) ;
#2100 = B_SPLINE_CURVE_WITH_KNOTS('',3,(#137862,#137863,#137864,#137865,#137866,
#137867,#137868,#137869,#137870,#137871,#137872,#137873,#137874,#137875),
 .UNSPECIFIED.,.F.,.F.,(4,2,2,2,2,2,4),(0.000106030898883045,0.000114450588602971,
0.000135861916063415,0.000155180925252132,0.000169070632935497,0.000187290067688046,
0.000202757041675868),.UNSPECIFIED.) ;
#2101 = B_SPLINE_CURVE_WITH_KNOTS('',3,(#137876,#137877,#137878,#137879,#137880,
#137881,#137882,#137883,#137884,#137885,#137886,#137887,#137888,#137889),
 .UNSPECIFIED.,.F.,.F.,(4,2,2,2,2,2,4),(0.,1.81852425150456E-5,3.36231897823044E-5,
5.26817905679537E-5,7.36686430049931E-5,8.81407292049456E-5,9.65446177718811E-5),
 .UNSPECIFIED.) ;
#2102 = B_SPLINE_CURVE_WITH_KNOTS('',3,(#137899,#137900,#137901,#137902,#137903,
#137904,#137905,#137906,#137907,#137908,#137909,#137910,#137911,#137912,
#137913,#137914,#137915,#137916,#137917),.UNSPECIFIED.,.F.,.F.,(4,3,3,3,
3,3,4),(0.,1.26126247466114E-5,2.08447799633796E-5,2.61321988210975E-5,
4.72564717703709E-5,6.3949955508106E-5,6.93621596435493E-5),
 .UNSPECIFIED.) ;
#2103 = B_SPLINE_CURVE_WITH_KNOTS('',3,(#138027,#138028,#138029,#138030,#138031,
#138032,#138033,#138034,#138035,#138036,#138037,#138038),.UNSPECIFIED.,
 .F.,.F.,(4,2,2,2,2,4),(0.,0.000230913708713649,0.000346370563070478,0.000404098990248888,
0.000432963203838092,0.000461827417427297),.UNSPECIFIED.) ;
#2104 = B_SPLINE_CURVE_WITH_KNOTS('',3,(#138065,#138066,#138067,#138068,#138069,
#138070,#138071,#138072,#138073,#138074,#138075,#138076),.UNSPECIFIED.,
 .F.,.F.,(4,2,2,2,2,4),(0.,2.92942635586651E-5,5.85885271173302E-5,0.00011717705423465,
0.000234354108469299,0.000468708216938598),.UNSPECIFIED.) ;
#2105 = B_SPLINE_CURVE_WITH_KNOTS('',3,(#138166,#138167,#138168,#138169,#138170,
#138171,#138172,#138173,#138174,#138175,#138176,#138177),.UNSPECIFIED.,
 .F.,.F.,(4,2,2,2,2,4),(7.70621319424336E-10,0.000528455713264088,0.000792683184585472,
0.00092479692024616,0.000990853788076498,0.00105691065590684),
 .UNSPECIFIED.) ;
#2106 = B_SPLINE_CURVE_WITH_KNOTS('',3,(#138178,#138179,#138180,#138181,#138182,
#138183,#138184,#138185,#138186,#138187,#138188,#138189,#138190,#138191,
#138192,#138193,#138194,#138195,#138196,#138197,#138198,#138199,#138200,
#138201,#138202,#138203,#138204,#138205),.UNSPECIFIED.,.F.,.F.,(4,2,2,2,
2,2,2,2,2,2,2,2,2,4),(0.,1.88814447163025E-5,2.66390109708352E-5,2.82246506940943E-5,
2.82548001019656E-5,4.36852952398557E-5,4.3720577757044E-5,4.63087975636134E-5,
5.19857273366473E-5,5.63013930903634E-5,5.77982263345347E-5,5.84936692674664E-5,
5.96281966878638E-5,6.07824730943714E-5),.UNSPECIFIED.) ;
#2107 = B_SPLINE_CURVE_WITH_KNOTS('',3,(#138207,#138208,#138209,#138210,#138211,
#138212,#138213,#138214,#138215,#138216,#138217,#138218,#138219,#138220,
#138221,#138222,#138223,#138224,#138225,#138226,#138227,#138228),
 .UNSPECIFIED.,.F.,.F.,(4,2,2,2,2,2,2,2,2,2,4),(-2.98424671549139E-6,-1.83179854035283E-6,
-6.78494605945076E-7,0.,1.61207185756484E-6,5.98431127542434E-6,1.25056665527988E-5,
1.40350946484969E-5,2.93914218611264E-5,4.85423642724965E-5,5.82245408950303E-5),
 .UNSPECIFIED.) ;
#2108 = B_SPLINE_CURVE_WITH_KNOTS('',3,(#138229,#138230,#138231,#138232,#138233,
#138234,#138235,#138236,#138237,#138238,#138239,#138240),.UNSPECIFIED.,
 .F.,.F.,(4,2,2,2,2,4),(0.,6.61189708719449E-5,0.00013223794174389,0.00026447588348779,
0.000528951766975601,0.00105790353395122),.UNSPECIFIED.) ;
#2109 = B_SPLINE_CURVE_WITH_KNOTS('',3,(#138274,#138275,#138276,#138277,#138278,
#138279,#138280,#138281,#138282,#138283,#138284,#138285,#138286,#138287,
#138288,#138289,#138290,#138291,#138292,#138293,#138294,#138295,#138296,
#138297,#138298,#138299,#138300,#138301,#138302,#138303,#138304,#138305,
#138306,#138307,#138308,#138309,#138310,#138311),.UNSPECIFIED.,.F.,.F.,
(4,2,2,2,2,2,2,2,2,2,2,2,2,2,2,2,2,2,4),(4.08239077498685E-13,1.91825894886969E-5,
2.29499826201334E-5,2.74799101222721E-5,3.52358269328737E-5,4.1219865182931E-5,
4.25319315563233E-5,4.54442131892892E-5,4.69409045132602E-5,4.80898427132604E-5,
4.94464739460608E-5,4.9643274248212E-5,5.04298720437271E-5,5.14115331534997E-5,
5.17333590635563E-5,5.22889985287807E-5,5.29242843672003E-5,5.37719008581471E-5,
5.49598202435899E-5),.UNSPECIFIED.) ;
#2110 = B_SPLINE_CURVE_WITH_KNOTS('',3,(#138344,#138345,#138346,#138347,#138348,
#138349,#138350,#138351,#138352,#138353,#138354,#138355,#138356,#138357,
#138358,#138359,#138360,#138361,#138362,#138363,#138364,#138365,#138366,
#138367,#138368,#138369,#138370,#138371,#138372,#138373,#138374,#138375,
#138376,#138377,#138378,#138379),.UNSPECIFIED.,.F.,.F.,(4,2,2,2,2,2,2,2,
2,2,2,2,2,2,2,2,2,4),(-2.90335387328777E-6,-1.36780202097199E-6,-6.41515161704647E-7,
-6.40610931867504E-8,3.8117330464249E-7,1.44450314269995E-6,2.24472183151459E-6,
2.50783298075742E-6,3.9666236573922E-6,5.28616271357864E-6,8.35978425016734E-6,
9.71024741498647E-6,1.08366011880722E-5,1.65505252295115E-5,2.45765562494321E-5,
2.90642498314919E-5,4.41638722245607E-5,5.20477084101079E-5),
 .UNSPECIFIED.) ;
#2111 = B_SPLINE_CURVE_WITH_KNOTS('',3,(#139030,#139031,#139032,#139033,#139034,
#139035),.UNSPECIFIED.,.F.,.F.,(4,2,4),(1.5707963267949,2.35619449019234,
3.14159265358979),.UNSPECIFIED.) ;
#2112 = B_SPLINE_CURVE_WITH_KNOTS('',3,(#139106,#139107,#139108,#139109,#139110,
#139111),.UNSPECIFIED.,.F.,.F.,(4,2,4),(0.,0.785398163397446,1.57079632679489),
 .UNSPECIFIED.) ;
#2113 = B_SPLINE_CURVE_WITH_KNOTS('',3,(#139204,#139205,#139206,#139207,#139208,
#139209,#139210,#139211,#139212,#139213,#139214,#139215,#139216,#139217,
#139218,#139219,#139220,#139221,#139222),.UNSPECIFIED.,.F.,.F.,(4,3,3,3,
3,3,4),(5.85758780416038E-5,6.39772274846938E-5,8.5008192556256E-5,0.000101719137060913,
0.000115369906146167,0.000121992710600423,0.000127737589255657),
 .UNSPECIFIED.) ;
#2114 = B_SPLINE_CURVE_WITH_KNOTS('',3,(#139229,#139230,#139231,#139232,#139233,
#139234,#139235,#139236,#139237,#139238,#139239,#139240,#139241,#139242),
 .UNSPECIFIED.,.F.,.F.,(4,2,2,2,2,2,4),(0.000106030898883045,0.000114450588602972,
0.00013586191606343,0.000155180925252192,0.000169070632935497,0.00018729006768833,
0.000202757041675869),.UNSPECIFIED.) ;
#2115 = B_SPLINE_CURVE_WITH_KNOTS('',3,(#139243,#139244,#139245,#139246,#139247,
#139248,#139249,#139250,#139251,#139252,#139253,#139254,#139255,#139256),
 .UNSPECIFIED.,.F.,.F.,(4,2,2,2,2,2,4),(0.,1.81852425150232E-5,3.36231897823044E-5,
5.26817905679335E-5,7.36686430049626E-5,8.81407292049456E-5,9.65446177718811E-5),
 .UNSPECIFIED.) ;
#2116 = B_SPLINE_CURVE_WITH_KNOTS('',3,(#139266,#139267,#139268,#139269,#139270,
#139271,#139272,#139273,#139274,#139275,#139276,#139277,#139278,#139279,
#139280,#139281,#139282,#139283,#139284),.UNSPECIFIED.,.F.,.F.,(4,3,3,3,
3,3,4),(0.,1.26126247466293E-5,2.08447799633812E-5,2.61321988210992E-5,
4.72564717703644E-5,6.39499555081068E-5,6.93621596435509E-5),
 .UNSPECIFIED.) ;
#2117 = B_SPLINE_CURVE_WITH_KNOTS('',3,(#139394,#139395,#139396,#139397,#139398,
#139399,#139400,#139401,#139402,#139403,#139404,#139405),.UNSPECIFIED.,
 .F.,.F.,(4,2,2,2,2,4),(0.,0.000230913708713646,0.000346370563070469,0.00040409899024888,
0.000432963203838088,0.000461827417427296),.UNSPECIFIED.) ;
#2118 = B_SPLINE_CURVE_WITH_KNOTS('',3,(#139426,#139427,#139428,#139429,#139430,
#139431,#139432,#139433,#139434,#139435,#139436,#139437),.UNSPECIFIED.,
 .F.,.F.,(4,2,2,2,2,4),(0.,2.92942635586651E-5,5.85885271173302E-5,0.00011717705423465,
0.000234354108469299,0.000468708216938598),.UNSPECIFIED.) ;
#2119 = B_SPLINE_CURVE_WITH_KNOTS('',3,(#139506,#139507,#139508,#139509,#139510,
#139511,#139512,#139513,#139514,#139515,#139516,#139517),.UNSPECIFIED.,
 .F.,.F.,(4,2,2,2,2,4),(7.70621319424336E-10,0.000528455713264091,0.000792683184585474,
0.00092479692024616,0.000990853788076498,0.00105691065590684),
 .UNSPECIFIED.) ;
#2120 = B_SPLINE_CURVE_WITH_KNOTS('',3,(#139518,#139519,#139520,#139521,#139522,
#139523,#139524,#139525,#139526,#139527,#139528,#139529,#139530,#139531,
#139532,#139533,#139534,#139535,#139536,#139537,#139538,#139539,#139540,
#139541,#139542,#139543,#139544,#139545),.UNSPECIFIED.,.F.,.F.,(4,2,2,2,
2,2,2,2,2,2,2,2,2,4),(0.,1.88814447163332E-5,2.66390109708352E-5,2.82246506940923E-5,
2.82548001019634E-5,4.36852952398549E-5,4.37205777570411E-5,4.63087975636134E-5,
5.1985727336649E-5,5.6301393090365E-5,5.77982263345347E-5,5.84936692674662E-5,
5.96281966878616E-5,6.07824730943714E-5),.UNSPECIFIED.) ;
#2121 = B_SPLINE_CURVE_WITH_KNOTS('',3,(#139547,#139548,#139549,#139550,#139551,
#139552,#139553,#139554,#139555,#139556,#139557,#139558,#139559,#139560,
#139561,#139562,#139563,#139564,#139565,#139566,#139567,#139568),
 .UNSPECIFIED.,.F.,.F.,(4,2,2,2,2,2,2,2,2,2,4),(-2.98424671548978E-6,-1.83179854034966E-6,
-6.78494605943072E-7,0.,1.6120718575636E-6,5.9843112754229E-6,1.25056665528019E-5,
1.40350946485183E-5,2.93914218612042E-5,4.85423642734593E-5,5.82245408950314E-5),
 .UNSPECIFIED.) ;
#2122 = B_SPLINE_CURVE_WITH_KNOTS('',3,(#139569,#139570,#139571,#139572,#139573,
#139574,#139575,#139576,#139577,#139578,#139579,#139580),.UNSPECIFIED.,
 .F.,.F.,(4,2,2,2,2,4),(0.,6.61189708719511E-5,0.000132237941743902,0.000264475883487804,
0.000528951766975613,0.00105790353395123),.UNSPECIFIED.) ;
#2123 = B_SPLINE_CURVE_WITH_KNOTS('',3,(#139613,#139614,#139615,#139616,#139617,
#139618,#139619,#139620,#139621,#139622,#139623,#139624,#139625,#139626,
#139627,#139628,#139629,#139630,#139631,#139632,#139633,#139634,#139635,
#139636,#139637,#139638,#139639,#139640,#139641,#139642,#139643,#139644,
#139645,#139646,#139647,#139648,#139649,#139650),.UNSPECIFIED.,.F.,.F.,
(4,2,2,2,2,2,2,2,2,2,2,2,2,2,2,2,2,2,4),(4.08242776004549E-13,1.91825894880122E-5,
2.29499826201316E-5,2.7479910122273E-5,3.52358269328682E-5,4.1219865182932E-5,
4.25319315563182E-5,4.54442131889642E-5,4.6940904513264E-5,4.80898427132615E-5,
4.94464739459852E-5,4.96432742482264E-5,5.04298720437672E-5,5.14115331535745E-5,
5.17333590635751E-5,5.22889985288004E-5,5.2924284367221E-5,5.37719008581647E-5,
5.4959820243591E-5),.UNSPECIFIED.) ;
#2124 = B_SPLINE_CURVE_WITH_KNOTS('',3,(#139681,#139682,#139683,#139684,#139685,
#139686,#139687,#139688,#139689,#139690,#139691,#139692,#139693,#139694,
#139695,#139696,#139697,#139698,#139699,#139700,#139701,#139702,#139703,
#139704,#139705,#139706,#139707,#139708,#139709,#139710,#139711,#139712,
#139713,#139714,#139715,#139716),.UNSPECIFIED.,.F.,.F.,(4,2,2,2,2,2,2,2,
2,2,2,2,2,2,2,2,2,4),(-2.90335387328777E-6,-1.36780202111177E-6,-6.41515161821873E-7,
-6.40610932957299E-8,3.81173304625258E-7,1.44450314268527E-6,2.24472183149534E-6,
2.50783298074528E-6,3.9666236573922E-6,5.28616271357869E-6,8.35978424998975E-6,
9.71024741500059E-6,1.08366011880722E-5,1.65505252295281E-5,2.45765562494321E-5,
2.90642498314901E-5,4.41638722228978E-5,5.20477084101061E-5),
 .UNSPECIFIED.) ;
#2125 = B_SPLINE_CURVE_WITH_KNOTS('',3,(#139901,#139902,#139903,#139904),
 .UNSPECIFIED.,.F.,.F.,(4,4),(3.14159265358979,4.71238898038469),
 .UNSPECIFIED.) ;
#2126 = B_SPLINE_CURVE_WITH_KNOTS('',3,(#139909,#139910,#139911,#139912),
 .UNSPECIFIED.,.F.,.F.,(4,4),(4.71238898038469,6.28318530717959),
 .UNSPECIFIED.) ;
#2127 = B_SPLINE_CURVE_WITH_KNOTS('',3,(#140038,#140039,#140040,#140041,#140042,
#140043,#140044,#140045,#140046,#140047),.UNSPECIFIED.,.F.,.F.,(4,2,2,2,
4),(0.0155454932989836,0.0194994353522834,0.0234533774055832,0.0272081302045205,
0.0309628830034577),.UNSPECIFIED.) ;
#2128 = B_SPLINE_CURVE_WITH_KNOTS('',3,(#140051,#140052,#140053,#140054,#140055,
#140056,#140057,#140058,#140059,#140060),.UNSPECIFIED.,.F.,.F.,(4,2,2,2,
4),(-0.0304888223793687,-0.0267236306519753,-0.0229584389245819,-0.0190821381960852,
-0.0152058374675885),.UNSPECIFIED.) ;
#2129 = B_SPLINE_CURVE_WITH_KNOTS('',3,(#140064,#140065,#140066,#140067,#140068,
#140069,#140070,#140071,#140072,#140073),.UNSPECIFIED.,.F.,.F.,(4,2,2,2,
4),(-0.0457718072911489,-0.0418955065626522,-0.0380192058341555,-0.0342540141067621,
-0.0304888223793687),.UNSPECIFIED.) ;
#2130 = B_SPLINE_CURVE_WITH_KNOTS('',3,(#140077,#140078,#140079,#140080,#140081,
#140082,#140083,#140084,#140085,#140086,#140087,#140088,#140089,#140090,
#140091,#140092,#140093,#140094,#140095,#140096,#140097,#140098,#140099,
#140100,#140101,#140102,#140103,#140104,#140105,#140106,#140107),
 .UNSPECIFIED.,.F.,.F.,(4,3,3,3,3,3,3,3,3,3,4),(0.,1.73748728562024E-5,
3.26506729531322E-5,5.028040025746E-5,6.5274122788763E-5,8.34390702564348E-5,
9.83241608049979E-5,0.000117568956567809,0.000132500510793829,0.000151525967767831,
0.000159849152172774),.UNSPECIFIED.) ;
#2131 = B_SPLINE_CURVE_WITH_KNOTS('',3,(#140111,#140112,#140113,#140114,#140115,
#140116,#140117,#140118,#140119,#140120),.UNSPECIFIED.,.F.,.F.,(4,2,2,2,
4),(0.0155454932989836,0.0194994353522835,0.0234533774055833,0.0272081302045205,
0.0309628830034578),.UNSPECIFIED.) ;
#2132 = B_SPLINE_CURVE_WITH_KNOTS('',3,(#140124,#140125,#140126,#140127,#140128,
#140129,#140130,#140131,#140132,#140133),.UNSPECIFIED.,.F.,.F.,(4,2,2,2,
4),(-0.0304888223793687,-0.0267236306519753,-0.022958438924582,-0.0190821381960853,
-0.0152058374675886),.UNSPECIFIED.) ;
#2133 = B_SPLINE_CURVE_WITH_KNOTS('',3,(#140137,#140138,#140139,#140140,#140141,
#140142,#140143,#140144,#140145,#140146),.UNSPECIFIED.,.F.,.F.,(4,2,2,2,
4),(-0.0457718072911489,-0.0418955065626522,-0.0380192058341554,-0.0342540141067621,
-0.0304888223793687),.UNSPECIFIED.) ;
#2134 = B_SPLINE_CURVE_WITH_KNOTS('',3,(#140150,#140151,#140152,#140153,#140154,
#140155,#140156,#140157,#140158,#140159,#140160,#140161,#140162,#140163,
#140164,#140165,#140166,#140167,#140168,#140169,#140170,#140171,#140172,
#140173,#140174,#140175,#140176,#140177,#140178,#140179,#140180),
 .UNSPECIFIED.,.F.,.F.,(4,3,3,3,3,3,3,3,3,3,4),(0.,1.73748728562086E-5,
3.2650672953132E-5,5.02804002574591E-5,6.52741227887635E-5,8.34390702564457E-5,
9.83241608049975E-5,0.000117568956567842,0.000132500510793829,0.000151525967767912,
0.000159849152172773),.UNSPECIFIED.) ;
#2135 = B_SPLINE_CURVE_WITH_KNOTS('',3,(#140373,#140374,#140375,#140376,#140377,
#140378),.UNSPECIFIED.,.F.,.F.,(4,2,4),(3.14159265358979,3.92699081698724,
4.71238898038469),.UNSPECIFIED.) ;
#2136 = B_SPLINE_CURVE_WITH_KNOTS('',3,(#140382,#140383,#140384,#140385,#140386,
#140387),.UNSPECIFIED.,.F.,.F.,(4,2,4),(3.14159265358979,3.92699081698724,
4.71238898038469),.UNSPECIFIED.) ;
#2137 = B_SPLINE_CURVE_WITH_KNOTS('',3,(#140391,#140392,#140393,#140394,#140395,
#140396),.UNSPECIFIED.,.F.,.F.,(4,2,4),(4.71238898038469,5.49778714378214,
6.28318530717959),.UNSPECIFIED.) ;
#2138 = B_SPLINE_CURVE_WITH_KNOTS('',3,(#140399,#140400,#140401,#140402,#140403,
#140404),.UNSPECIFIED.,.F.,.F.,(4,2,4),(4.71238898038469,5.49778714378214,
6.28318530717959),.UNSPECIFIED.) ;
#2139 = B_SPLINE_CURVE_WITH_KNOTS('',3,(#140442,#140443,#140444,#140445,#140446,
#140447,#140448,#140449,#140450,#140451,#140452,#140453,#140454,#140455,
#140456,#140457,#140458,#140459,#140460,#140461,#140462,#140463,#140464,
#140465,#140466,#140467,#140468,#140469),.UNSPECIFIED.,.F.,.F.,(4,3,3,3,
3,3,3,3,3,4),(0.,0.000108662978633385,0.00021732595726677,0.000239795331094194,
0.000268321712743107,0.000359692996641291,0.000370380550777844,0.000402443213187504,
0.000469559030214583,0.000479590662188388),.UNSPECIFIED.) ;
#2140 = B_SPLINE_CURVE_WITH_KNOTS('',3,(#140471,#140472,#140473,#140474,#140475,
#140476,#140477,#140478,#140479,#140480),.UNSPECIFIED.,.F.,.F.,(4,2,2,2,
4),(4.46838099282933E-15,0.000139027965256961,0.000278055930509455,0.000556111861014441,
0.00111222372202441),.UNSPECIFIED.) ;
#2141 = B_SPLINE_CURVE_WITH_KNOTS('',3,(#140482,#140483,#140484,#140485,#140486,
#140487,#140488,#140489,#140490,#140491,#140492,#140493,#140494,#140495,
#140496,#140497,#140498,#140499,#140500,#140501,#140502,#140503,#140504,
#140505,#140506),.UNSPECIFIED.,.F.,.F.,(4,3,3,3,3,3,3,3,4),(0.,0.000553539642553922,
0.000830309463830885,0.000968694374469364,0.000985992488299174,0.00104653588670351,
0.00108059154830595,0.0010938354167069,0.00110707928510784),
 .UNSPECIFIED.) ;
#2142 = B_SPLINE_CURVE_WITH_KNOTS('',3,(#140508,#140509,#140510,#140511,#140512,
#140513,#140514,#140515,#140516,#140517,#140518,#140519,#140520,#140521,
#140522,#140523),.UNSPECIFIED.,.F.,.F.,(4,2,2,2,2,2,2,4),(2.46381126959657E-5,
3.49307346223165E-5,0.000103812737360941,0.000147753773859885,0.000241616793832021,
0.000270869435023803,0.00044893323810819,0.00051710075735164),
 .UNSPECIFIED.) ;
#2143 = B_SPLINE_CURVE_WITH_KNOTS('',3,(#140958,#140959,#140960,#140961,#140962,
#140963),.UNSPECIFIED.,.F.,.F.,(4,2,4),(1.5707963267949,2.35619449019235,
3.14159265358979),.UNSPECIFIED.) ;
#2144 = B_SPLINE_CURVE_WITH_KNOTS('',3,(#141034,#141035,#141036,#141037,#141038,
#141039),.UNSPECIFIED.,.F.,.F.,(4,2,4),(0.,0.785398163397447,1.57079632679489),
 .UNSPECIFIED.) ;
#2145 = B_SPLINE_CURVE_WITH_KNOTS('',3,(#141133,#141134,#141135,#141136,#141137,
#141138,#141139,#141140,#141141,#141142,#141143,#141144,#141145,#141146,
#141147,#141148,#141149,#141150,#141151),.UNSPECIFIED.,.F.,.F.,(4,3,3,3,
3,3,4),(5.85758780416056E-5,6.39772274846961E-5,8.50081925558201E-5,0.000101719137060913,
0.000115369906146294,0.000121992710600423,0.000127737589255657),
 .UNSPECIFIED.) ;
#2146 = B_SPLINE_CURVE_WITH_KNOTS('',3,(#141158,#141159,#141160,#141161,#141162,
#141163,#141164,#141165,#141166,#141167,#141168,#141169,#141170,#141171),
 .UNSPECIFIED.,.F.,.F.,(4,2,2,2,2,2,4),(0.000106030898883045,0.000114450588602972,
0.000135861916063444,0.00015518092525221,0.000169070632935497,0.00018729006768838,
0.000202757041675869),.UNSPECIFIED.) ;
#2147 = B_SPLINE_CURVE_WITH_KNOTS('',3,(#141172,#141173,#141174,#141175,#141176,
#141177,#141178,#141179,#141180,#141181,#141182,#141183,#141184,#141185),
 .UNSPECIFIED.,.F.,.F.,(4,2,2,2,2,2,4),(0.,1.81852425165316E-5,3.36231897823057E-5,
5.26817905682147E-5,7.36686430054364E-5,8.81407292049455E-5,9.65446177718808E-5),
 .UNSPECIFIED.) ;
#2148 = B_SPLINE_CURVE_WITH_KNOTS('',3,(#141195,#141196,#141197,#141198,#141199,
#141200,#141201,#141202,#141203,#141204,#141205,#141206,#141207,#141208,
#141209,#141210,#141211,#141212,#141213),.UNSPECIFIED.,.F.,.F.,(4,3,3,3,
3,3,4),(0.,1.2612624746691E-5,2.08447799633812E-5,2.61321988210992E-5,4.72564717707153E-5,
6.39499555081056E-5,6.93621596435645E-5),.UNSPECIFIED.) ;
#2149 = B_SPLINE_CURVE_WITH_KNOTS('',3,(#141323,#141324,#141325,#141326,#141327,
#141328,#141329,#141330,#141331,#141332,#141333,#141334),.UNSPECIFIED.,
 .F.,.F.,(4,2,2,2,2,4),(0.,0.000230913708713651,0.000346370563070476,0.000404098990248888,
0.000432963203838092,0.000461827417427296),.UNSPECIFIED.) ;
#2150 = B_SPLINE_CURVE_WITH_KNOTS('',3,(#141359,#141360,#141361,#141362,#141363,
#141364,#141365,#141366,#141367,#141368,#141369,#141370),.UNSPECIFIED.,
 .F.,.F.,(4,2,2,2,2,4),(0.,2.92942635586625E-5,5.85885271173251E-5,0.000117177054234649,
0.000234354108469297,0.000468708216938592),.UNSPECIFIED.) ;
#2151 = B_SPLINE_CURVE_WITH_KNOTS('',3,(#141454,#141455,#141456,#141457,#141458,
#141459,#141460,#141461,#141462,#141463,#141464,#141465),.UNSPECIFIED.,
 .F.,.F.,(4,2,2,2,2,4),(7.70621319424336E-10,0.000528455713264076,0.000792683184585456,
0.000924796920246147,0.000990853788076492,0.00105691065590684),
 .UNSPECIFIED.) ;
#2152 = B_SPLINE_CURVE_WITH_KNOTS('',3,(#141466,#141467,#141468,#141469,#141470,
#141471,#141472,#141473,#141474,#141475,#141476,#141477,#141478,#141479,
#141480,#141481,#141482,#141483,#141484,#141485,#141486,#141487,#141488,
#141489,#141490,#141491,#141492,#141493),.UNSPECIFIED.,.F.,.F.,(4,2,2,2,
2,2,2,2,2,2,2,2,2,4),(0.,1.88814447164933E-5,2.66390109708352E-5,2.82246506940905E-5,
2.8254800101963E-5,4.36852952398535E-5,4.37205777570259E-5,4.63087975636133E-5,
5.19857273366466E-5,5.63013930903582E-5,5.77982263345344E-5,5.84936692674549E-5,
5.96281966878481E-5,6.07824730943679E-5),.UNSPECIFIED.) ;
#2153 = B_SPLINE_CURVE_WITH_KNOTS('',3,(#141495,#141496,#141497,#141498,#141499,
#141500,#141501,#141502,#141503,#141504,#141505,#141506,#141507,#141508,
#141509,#141510,#141511,#141512,#141513,#141514,#141515,#141516),
 .UNSPECIFIED.,.F.,.F.,(4,2,2,2,2,2,2,2,2,2,4),(-2.98424671548817E-6,-1.8317985403492E-6,
-6.78494605942832E-7,0.,1.61207185756534E-6,5.98431127542578E-6,1.25056665528019E-5,
1.40350946485201E-5,2.93914218612042E-5,4.85423642732289E-5,5.82245408950313E-5),
 .UNSPECIFIED.) ;
#2154 = B_SPLINE_CURVE_WITH_KNOTS('',3,(#141517,#141518,#141519,#141520,#141521,
#141522,#141523,#141524,#141525,#141526,#141527,#141528),.UNSPECIFIED.,
 .F.,.F.,(4,2,2,2,2,4),(0.,6.6118970871953E-5,0.000132237941743906,0.000264475883487812,
0.000528951766975618,0.00105790353395123),.UNSPECIFIED.) ;
#2155 = B_SPLINE_CURVE_WITH_KNOTS('',3,(#141561,#141562,#141563,#141564,#141565,
#141566,#141567,#141568,#141569,#141570,#141571,#141572,#141573,#141574,
#141575,#141576,#141577,#141578,#141579,#141580,#141581,#141582,#141583,
#141584,#141585,#141586,#141587,#141588,#141589,#141590,#141591,#141592,
#141593,#141594,#141595,#141596,#141597,#141598),.UNSPECIFIED.,.F.,.F.,
(4,2,2,2,2,2,2,2,2,2,2,2,2,2,2,2,2,2,4),(4.08242331775179E-13,1.91825894882532E-5,
2.29499826201334E-5,2.7479910122273E-5,3.52358269328724E-5,4.1219865182932E-5,
4.25319315563226E-5,4.54442131889474E-5,4.69409045132582E-5,4.80898427132615E-5,
4.9446473946197E-5,4.96432742482032E-5,5.04298720437313E-5,5.1411533153523E-5,
5.17333590635443E-5,5.2288998528769E-5,5.29242843671897E-5,5.37719008581445E-5,
5.4959820243591E-5),.UNSPECIFIED.) ;
#2156 = B_SPLINE_CURVE_WITH_KNOTS('',3,(#141631,#141632,#141633,#141634,#141635,
#141636,#141637,#141638,#141639,#141640,#141641,#141642,#141643,#141644,
#141645,#141646,#141647,#141648,#141649,#141650,#141651,#141652,#141653,
#141654,#141655,#141656,#141657,#141658,#141659,#141660,#141661,#141662,
#141663,#141664,#141665,#141666),.UNSPECIFIED.,.F.,.F.,(4,2,2,2,2,2,2,2,
2,2,2,2,2,2,2,2,2,4),(-2.90335387328765E-6,-1.36780202118156E-6,-6.41515161884124E-7,
-6.40610933545424E-8,3.81173304600826E-7,1.44450314266245E-6,2.2447218314835E-6,
2.50783298072407E-6,3.96662365739231E-6,5.28616271356407E-6,8.35978425208288E-6,
9.71024741497824E-6,1.08366011880723E-5,1.65505252295101E-5,2.45765562494322E-5,
2.90642498314973E-5,4.41638722243032E-5,5.20477084101071E-5),
 .UNSPECIFIED.) ;
#2157 = B_SPLINE_CURVE_WITH_KNOTS('',3,(#141862,#141863,#141864,#141865,#141866,
#141867,#141868,#141869),.UNSPECIFIED.,.F.,.F.,(4,2,2,4),(-0.0212593174733862,
-0.0176486602253693,-0.0143243289552082,-0.0134403252720105),
 .UNSPECIFIED.) ;
#2158 = B_SPLINE_CURVE_WITH_KNOTS('',3,(#141905,#141906,#141907,#141908,#141909,
#141910,#141911,#141912),.UNSPECIFIED.,.F.,.F.,(4,2,2,4),(-0.021259317482921,
-0.0176486602328459,-0.0143243289609224,-0.0134403252772803),
 .UNSPECIFIED.) ;
#2159 = B_SPLINE_CURVE_WITH_KNOTS('',3,(#141948,#141949,#141950,#141951,#141952,
#141953,#141954,#141955),.UNSPECIFIED.,.F.,.F.,(4,2,2,4),(-0.0212593174877944,
-0.0176486602368674,-0.0143243289641644,-0.0134403252803157),
 .UNSPECIFIED.) ;
#2160 = B_SPLINE_CURVE_WITH_KNOTS('',3,(#141991,#141992,#141993,#141994,#141995,
#141996,#141997,#141998),.UNSPECIFIED.,.F.,.F.,(4,2,2,4),(-0.0212593174829433,
-0.0176486602328601,-0.014324328960934,-0.0134403252772914),
 .UNSPECIFIED.) ;
#2161 = B_SPLINE_CURVE_WITH_KNOTS('',3,(#142034,#142035,#142036,#142037,#142038,
#142039,#142040,#142041),.UNSPECIFIED.,.F.,.F.,(4,2,2,4),(-0.0212593174732112,
-0.0176486602254681,-0.0143243289554829,-0.0134403252723181),
 .UNSPECIFIED.) ;
#2162 = B_SPLINE_CURVE_WITH_KNOTS('',3,(#142077,#142078,#142079,#142080,#142081,
#142082,#142083,#142084),.UNSPECIFIED.,.F.,.F.,(4,2,2,4),(-0.0212593174781932,
-0.0176486602293651,-0.0143243289584549,-0.0134403252750573),
 .UNSPECIFIED.) ;
#2163 = B_SPLINE_CURVE_WITH_KNOTS('',3,(#142120,#142121,#142122,#142123,#142124,
#142125,#142126,#142127),.UNSPECIFIED.,.F.,.F.,(4,2,2,4),(-0.0212593174830444,
-0.0176486602331658,-0.0143243289613579,-0.0134403252777338),
 .UNSPECIFIED.) ;
#2164 = B_SPLINE_CURVE_WITH_KNOTS('',3,(#142163,#142164,#142165,#142166,#142167,
#142168,#142169,#142170),.UNSPECIFIED.,.F.,.F.,(4,2,2,4),(-0.021259317485983,
-0.017648660235379,-0.0143243289629727,-0.0134403252792024),
 .UNSPECIFIED.) ;
#2165 = B_SPLINE_CURVE_WITH_KNOTS('',3,(#142287,#142288,#142289,#142290,#142291,
#142292,#142293,#142294),.UNSPECIFIED.,.F.,.F.,(4,2,2,4),(-0.0212593174838741,
-0.0176486602337396,-0.0143243289617316,-0.0134403252780616),
 .UNSPECIFIED.) ;
#2166 = B_SPLINE_CURVE_WITH_KNOTS('',3,(#142411,#142412,#142413,#142414,#142415,
#142416,#142417,#142418),.UNSPECIFIED.,.F.,.F.,(4,2,2,4),(-0.021259317485706,
-0.0176486602351398,-0.0143243289627718,-0.013440325279013),
 .UNSPECIFIED.) ;
#2167 = B_SPLINE_CURVE_WITH_KNOTS('',3,(#144015,#144016,#144017,#144018,#144019,
#144020,#144021,#144022),.UNSPECIFIED.,.F.,.F.,(4,2,2,4),(-0.052701717162025,
-0.0518504523811948,-0.0480303917439054,-0.04467544736819),
 .UNSPECIFIED.) ;
#2168 = B_SPLINE_CURVE_WITH_KNOTS('',3,(#144026,#144027,#144028,#144029,#144030,
#144031,#144032,#144033,#144034,#144035,#144036,#144037,#144038,#144039,
#144040,#144041,#144042,#144043,#144044,#144045,#144046,#144047,#144048,
#144049,#144050,#144051,#144052,#144053,#144054,#144055,#144056),
 .UNSPECIFIED.,.F.,.F.,(4,3,3,3,3,3,3,3,3,3,4),(0.,1.7911486298437E-5,3.35636550441565E-5,
5.14128838689559E-5,6.71346369544057E-5,8.50076921954425E-5,0.000100614915215922,
0.000118595988596762,0.000134133865285036,0.000151845157316713,0.0001565184788544),
 .UNSPECIFIED.) ;
#2169 = B_SPLINE_CURVE_WITH_KNOTS('',3,(#144058,#144059,#144060,#144061,#144062,
#144063,#144064,#144065,#144066,#144067,#144068,#144069,#144070,#144071,
#144072,#144073,#144074,#144075,#144076,#144077,#144078,#144079),
 .UNSPECIFIED.,.F.,.F.,(4,2,2,2,2,2,2,2,2,2,4),(-0.0842935807175857,-0.0841564124762399,
-0.0836958438579189,-0.0829341784875174,-0.0805923611130053,-0.0773601159115686,
-0.0742136752654363,-0.071123820447877,-0.0675672289498007,-0.0637829215046486,
-0.0629274139192696),.UNSPECIFIED.) ;
#2170 = B_SPLINE_CURVE_WITH_KNOTS('',3,(#147077,#147078,#147079,#147080,#147081,
#147082,#147083,#147084),.UNSPECIFIED.,.F.,.F.,(4,2,2,4),(-0.0527017171620382,
-0.0518504523812081,-0.0480303917439178,-0.0446754473682008),
 .UNSPECIFIED.) ;
#2171 = B_SPLINE_CURVE_WITH_KNOTS('',3,(#147088,#147089,#147090,#147091,#147092,
#147093,#147094,#147095,#147096,#147097,#147098,#147099,#147100,#147101,
#147102,#147103,#147104,#147105,#147106,#147107,#147108,#147109,#147110,
#147111,#147112,#147113,#147114,#147115,#147116,#147117,#147118),
 .UNSPECIFIED.,.F.,.F.,(4,3,3,3,3,3,3,3,3,3,4),(0.,1.79114862984415E-5,
3.35636550441565E-5,5.14128838689557E-5,6.7134636954406E-5,8.50076921954395E-5,
0.000100614915215921,0.000118595988596772,0.000134133865285036,0.000151845157316653,
0.0001565184788544),.UNSPECIFIED.) ;
#2172 = B_SPLINE_CURVE_WITH_KNOTS('',3,(#147120,#147121,#147122,#147123,#147124,
#147125,#147126,#147127,#147128,#147129,#147130,#147131,#147132,#147133,
#147134,#147135,#147136,#147137,#147138,#147139,#147140,#147141),
 .UNSPECIFIED.,.F.,.F.,(4,2,2,2,2,2,2,2,2,2,4),(-0.0842935807153196,-0.0841564124739783,
-0.0836958438556783,-0.0829341784853091,-0.0805923611108952,-0.0773601159095917,
-0.0742136752635866,-0.0711238204461505,-0.0675672289482145,-0.0637829215032092,
-0.062927413917864),.UNSPECIFIED.) ;
#2173 = B_SPLINE_CURVE_WITH_KNOTS('',3,(#147781,#147782,#147783,#147784,#147785,
#147786,#147787,#147788),.UNSPECIFIED.,.F.,.F.,(4,2,2,4),(-0.0527017171621304,
-0.0518504523813015,-0.0480303917440028,-0.0446754473682719),
 .UNSPECIFIED.) ;
#2174 = B_SPLINE_CURVE_WITH_KNOTS('',3,(#147792,#147793,#147794,#147795,#147796,
#147797,#147798,#147799,#147800,#147801,#147802,#147803,#147804,#147805,
#147806,#147807,#147808,#147809,#147810,#147811,#147812,#147813,#147814,
#147815,#147816,#147817,#147818,#147819,#147820,#147821,#147822),
 .UNSPECIFIED.,.F.,.F.,(4,3,3,3,3,3,3,3,3,3,4),(0.,1.79114862984384E-5,
3.35636550441566E-5,5.14128838689606E-5,6.7134636954406E-5,8.50076921954722E-5,
0.000100614915215922,0.000118595988596755,0.000134133865285036,0.00015184515731678,
0.0001565184788544),.UNSPECIFIED.) ;
#2175 = B_SPLINE_CURVE_WITH_KNOTS('',3,(#147824,#147825,#147826,#147827,#147828,
#147829,#147830,#147831,#147832,#147833,#147834,#147835,#147836,#147837,
#147838,#147839,#147840,#147841,#147842,#147843,#147844,#147845),
 .UNSPECIFIED.,.F.,.F.,(4,2,2,2,2,2,2,2,2,2,4),(-0.0842935807419127,-0.0841564125005222,
-0.0836958438819682,-0.082934178511186,-0.0805923611355419,-0.0773601159325885,
-0.0742136752850249,-0.0711238204661043,-0.0675672289665108,-0.0637829215197928,
-0.0629274139340661),.UNSPECIFIED.) ;
#2176 = B_SPLINE_CURVE_WITH_KNOTS('',3,(#148008,#148009,#148010,#148011,#148012,
#148013,#148014,#148015),.UNSPECIFIED.,.F.,.F.,(4,2,2,4),(-0.0527017171621393,
-0.0518504523813096,-0.0480303917440155,-0.0446754473682944),
 .UNSPECIFIED.) ;
#2177 = B_SPLINE_CURVE_WITH_KNOTS('',3,(#148019,#148020,#148021,#148022,#148023,
#148024,#148025,#148026,#148027,#148028,#148029,#148030,#148031,#148032,
#148033,#148034,#148035,#148036,#148037,#148038,#148039,#148040,#148041,
#148042,#148043,#148044,#148045,#148046,#148047,#148048,#148049),
 .UNSPECIFIED.,.F.,.F.,(4,3,3,3,3,3,3,3,3,3,4),(0.,1.7911486298444E-5,3.35636550441567E-5,
5.14128838689174E-5,6.71346369544062E-5,8.50076921954515E-5,0.000100614915215921,
0.000118595988596814,0.000134133865285036,0.000151845157316771,0.0001565184788544),
 .UNSPECIFIED.) ;
#2178 = B_SPLINE_CURVE_WITH_KNOTS('',3,(#148051,#148052,#148053,#148054,#148055,
#148056,#148057,#148058,#148059,#148060,#148061,#148062,#148063,#148064,
#148065,#148066,#148067,#148068,#148069,#148070,#148071,#148072),
 .UNSPECIFIED.,.F.,.F.,(4,2,2,2,2,2,2,2,2,2,4),(-0.0842935808351552,-0.0841564125935704,
-0.0836958439740798,-0.0829341786018125,-0.0805923612217205,-0.077360116012801,
-0.0742136753596006,-0.0711238205353107,-0.0675672290297288,-0.0637829215768355,
-0.0629274139897445),.UNSPECIFIED.) ;
#2179 = B_SPLINE_CURVE_WITH_KNOTS('',3,(#148235,#148236,#148237,#148238,#148239,
#148240,#148241,#148242),.UNSPECIFIED.,.F.,.F.,(4,2,2,4),(-0.0527017171620452,
-0.0518504523812172,-0.0480303917439374,-0.04467544736823),
 .UNSPECIFIED.) ;
#2180 = B_SPLINE_CURVE_WITH_KNOTS('',3,(#148246,#148247,#148248,#148249,#148250,
#148251,#148252,#148253,#148254,#148255,#148256,#148257,#148258,#148259,
#148260,#148261,#148262,#148263,#148264,#148265,#148266,#148267,#148268,
#148269,#148270,#148271,#148272,#148273,#148274,#148275,#148276),
 .UNSPECIFIED.,.F.,.F.,(4,3,3,3,3,3,3,3,3,3,4),(0.,1.79114862984569E-5,
3.35636550441567E-5,5.14128838689565E-5,6.71346369544062E-5,8.50076921954284E-5,
0.000100614915215921,0.000118595988596684,0.000134133865285036,0.000151845157316633,
0.0001565184788544),.UNSPECIFIED.) ;
#2181 = B_SPLINE_CURVE_WITH_KNOTS('',3,(#148278,#148279,#148280,#148281,#148282,
#148283,#148284,#148285,#148286,#148287,#148288,#148289,#148290,#148291,
#148292,#148293,#148294,#148295,#148296,#148297,#148298,#148299),
 .UNSPECIFIED.,.F.,.F.,(4,2,2,2,2,2,2,2,2,2,4),(-0.0842935807861705,-0.0841564125446822,
-0.08369584392567,-0.0829341785541707,-0.0805923611763772,-0.0773601159705437,
-0.0742136753202586,-0.0711238204987475,-0.0675672289962676,-0.0637829215465878,
-0.0629274139602073),.UNSPECIFIED.) ;
#2182 = B_SPLINE_CURVE_WITH_KNOTS('',3,(#148462,#148463,#148464,#148465,#148466,
#148467,#148468,#148469),.UNSPECIFIED.,.F.,.F.,(4,2,2,4),(-0.0527017171621833,
-0.0518504523813524,-0.0480303917440445,-0.044675447368305),
 .UNSPECIFIED.) ;
#2183 = B_SPLINE_CURVE_WITH_KNOTS('',3,(#148473,#148474,#148475,#148476,#148477,
#148478,#148479,#148480,#148481,#148482,#148483,#148484,#148485,#148486,
#148487,#148488,#148489,#148490,#148491,#148492,#148493,#148494,#148495,
#148496,#148497,#148498,#148499,#148500,#148501,#148502,#148503),
 .UNSPECIFIED.,.F.,.F.,(4,3,3,3,3,3,3,3,3,3,4),(0.,1.791148629847E-5,3.35636550441561E-5,
5.14128838689644E-5,6.71346369544058E-5,8.50076921954764E-5,0.000100614915215921,
0.000118595988596817,0.000134133865285032,0.000151845157316703,0.000156518478854398),
 .UNSPECIFIED.) ;
#2184 = B_SPLINE_CURVE_WITH_KNOTS('',3,(#148505,#148506,#148507,#148508,#148509,
#148510,#148511,#148512,#148513,#148514,#148515,#148516,#148517,#148518,
#148519,#148520,#148521,#148522,#148523,#148524,#148525,#148526),
 .UNSPECIFIED.,.F.,.F.,(4,2,2,2,2,2,2,2,2,2,4),(-0.0842935807861705,-0.0841564125446822,
-0.08369584392567,-0.0829341785541707,-0.0805923611763772,-0.0773601159705437,
-0.0742136753202586,-0.0711238204987475,-0.0675672289962676,-0.0637829215465878,
-0.0629274139602073),.UNSPECIFIED.) ;
#2185 = B_SPLINE_CURVE_WITH_KNOTS('',3,(#148689,#148690,#148691,#148692,#148693,
#148694,#148695,#148696),.UNSPECIFIED.,.F.,.F.,(4,2,2,4),(-0.0527017171619057,
-0.0518504523810739,-0.0480303917437878,-0.0446754473680843),
 .UNSPECIFIED.) ;
#2186 = B_SPLINE_CURVE_WITH_KNOTS('',3,(#148700,#148701,#148702,#148703,#148704,
#148705,#148706,#148707,#148708,#148709,#148710,#148711,#148712,#148713,
#148714,#148715,#148716,#148717,#148718,#148719,#148720,#148721,#148722,
#148723,#148724,#148725,#148726,#148727,#148728,#148729,#148730),
 .UNSPECIFIED.,.F.,.F.,(4,3,3,3,3,3,3,3,3,3,4),(0.,1.79114862984022E-5,
3.35636550441561E-5,5.14128838690747E-5,6.71346369544058E-5,8.50076921955029E-5,
0.000100614915215921,0.000118595988596949,0.000134133865285032,0.000151845157316721,
0.000156518478854398),.UNSPECIFIED.) ;
#2187 = B_SPLINE_CURVE_WITH_KNOTS('',3,(#148732,#148733,#148734,#148735,#148736,
#148737,#148738,#148739,#148740,#148741,#148742,#148743,#148744,#148745,
#148746,#148747,#148748,#148749,#148750,#148751,#148752,#148753),
 .UNSPECIFIED.,.F.,.F.,(4,2,2,2,2,2,2,2,2,2,4),(-0.0842935806846017,-0.0841564124433096,
-0.0836958438252493,-0.0829341784552694,-0.0805923610820353,-0.0773601158823278,
-0.0742136752378489,-0.07112382042188,-0.0675672289255957,-0.0637829214823062,
-0.0629274138973503),.UNSPECIFIED.) ;
#2188 = B_SPLINE_CURVE_WITH_KNOTS('',3,(#148916,#148917,#148918,#148919,#148920,
#148921,#148922,#148923),.UNSPECIFIED.,.F.,.F.,(4,2,2,4),(-0.0527017171620534,
-0.0518504523812236,-0.0480303917439217,-0.0446754473681886),
 .UNSPECIFIED.) ;
#2189 = B_SPLINE_CURVE_WITH_KNOTS('',3,(#148927,#148928,#148929,#148930,#148931,
#148932,#148933,#148934,#148935,#148936,#148937,#148938,#148939,#148940,
#148941,#148942,#148943,#148944,#148945,#148946,#148947,#148948,#148949,
#148950,#148951,#148952,#148953,#148954,#148955,#148956,#148957),
 .UNSPECIFIED.,.F.,.F.,(4,3,3,3,3,3,3,3,3,3,4),(0.,1.79114862984111E-5,
3.35636550441561E-5,5.1412883869035E-5,6.71346369544058E-5,8.50076921954072E-5,
0.000100614915215921,0.000118595988596959,0.000134133865285032,0.000151845157317271,
0.000156518478854398),.UNSPECIFIED.) ;
#2190 = B_SPLINE_CURVE_WITH_KNOTS('',3,(#148959,#148960,#148961,#148962,#148963,
#148964,#148965,#148966,#148967,#148968,#148969,#148970,#148971,#148972,
#148973,#148974,#148975,#148976,#148977,#148978,#148979,#148980),
 .UNSPECIFIED.,.F.,.F.,(4,2,2,2,2,2,2,2,2,2,4),(-0.0842935807784001,-0.0841564125369118,
-0.0836958439179285,-0.0829341785465007,-0.080592361168928,-0.0773601159633862,
-0.0742136753133782,-0.071123820492143,-0.0675672289899856,-0.063782921540619,
-0.0629274139542864),.UNSPECIFIED.) ;
#2191 = B_SPLINE_CURVE_WITH_KNOTS('',3,(#149143,#149144,#149145,#149146,#149147,
#149148,#149149,#149150),.UNSPECIFIED.,.F.,.F.,(4,2,2,4),(-0.0527017171619366,
-0.0518504523811075,-0.0480303917438238,-0.0446754473681228),
 .UNSPECIFIED.) ;
#2192 = B_SPLINE_CURVE_WITH_KNOTS('',3,(#149154,#149155,#149156,#149157,#149158,
#149159,#149160,#149161,#149162,#149163,#149164,#149165,#149166,#149167,
#149168,#149169,#149170,#149171,#149172,#149173,#149174,#149175,#149176,
#149177,#149178,#149179,#149180,#149181,#149182,#149183,#149184),
 .UNSPECIFIED.,.F.,.F.,(4,3,3,3,3,3,3,3,3,3,4),(0.,1.7911486298388E-5,3.35636550441561E-5,
5.14128838690249E-5,6.71346369544058E-5,8.50076921954834E-5,0.000100614915215921,
0.000118595988596784,0.000134133865285032,0.000151845157317113,0.000156518478854398),
 .UNSPECIFIED.) ;
#2193 = B_SPLINE_CURVE_WITH_KNOTS('',3,(#149186,#149187,#149188,#149189,#149190,
#149191,#149192,#149193,#149194,#149195,#149196,#149197,#149198,#149199,
#149200,#149201,#149202,#149203,#149204,#149205,#149206,#149207),
 .UNSPECIFIED.,.F.,.F.,(4,2,2,2,2,2,2,2,2,2,4),(-0.0842935807784001,-0.0841564125369118,
-0.0836958439179285,-0.0829341785465007,-0.080592361168928,-0.0773601159633862,
-0.0742136753133782,-0.071123820492143,-0.0675672289899856,-0.063782921540619,
-0.0629274139542864),.UNSPECIFIED.) ;
#2194 = B_SPLINE_CURVE_WITH_KNOTS('',3,(#149370,#149371,#149372,#149373,#149374,
#149375,#149376,#149377),.UNSPECIFIED.,.F.,.F.,(4,2,2,4),(-0.0527017171617456,
-0.0518504523809185,-0.0480303917436524,-0.0446754473679689),
 .UNSPECIFIED.) ;
#2195 = B_SPLINE_CURVE_WITH_KNOTS('',3,(#149381,#149382,#149383,#149384,#149385,
#149386,#149387,#149388,#149389,#149390,#149391,#149392,#149393,#149394,
#149395,#149396,#149397,#149398,#149399,#149400,#149401,#149402,#149403,
#149404,#149405,#149406,#149407,#149408,#149409,#149410,#149411),
 .UNSPECIFIED.,.F.,.F.,(4,3,3,3,3,3,3,3,3,3,4),(0.,1.79114862983986E-5,
3.35636550441583E-5,5.14128838688763E-5,6.71346369544075E-5,8.5007692195462E-5,
0.000100614915215918,0.000118595988596873,0.000134133865285036,0.000151845157315814,
0.000156518478854401),.UNSPECIFIED.) ;
#2196 = B_SPLINE_CURVE_WITH_KNOTS('',3,(#149413,#149414,#149415,#149416,#149417,
#149418,#149419,#149420,#149421,#149422,#149423,#149424,#149425,#149426,
#149427,#149428,#149429,#149430,#149431,#149432,#149433,#149434),
 .UNSPECIFIED.,.F.,.F.,(4,2,2,2,2,2,2,2,2,2,4),(-0.0842935807784001,-0.0841564125369118,
-0.0836958439179285,-0.0829341785465007,-0.080592361168928,-0.0773601159633862,
-0.0742136753133782,-0.071123820492143,-0.0675672289899856,-0.063782921540619,
-0.0629274139542864),.UNSPECIFIED.) ;
#2197 = B_SPLINE_CURVE_WITH_KNOTS('',3,(#152042,#152043,#152044,#152045,#152046,
#152047,#152048,#152049,#152050,#152051,#152052,#152053,#152054,#152055,
#152056,#152057,#152058,#152059,#152060,#152061,#152062,#152063,#152064,
#152065,#152066,#152067,#152068,#152069,#152070,#152071,#152072,#152073,
#152074,#152075,#152076,#152077,#152078,#152079,#152080,#152081,#152082,
#152083,#152084,#152085,#152086,#152087,#152088,#152089,#152090,#152091,
#152092,#152093,#152094,#152095,#152096,#152097,#152098,#152099,#152100,
#152101,#152102,#152103,#152104,#152105,#152106,#152107,#152108,#152109,
#152110,#152111,#152112,#152113,#152114,#152115,#152116,#152117,#152118,
#152119,#152120),.UNSPECIFIED.,.F.,.F.,(4,2,2,2,2,2,2,2,2,1,2,2,2,2,2,2,
2,2,1,2,2,2,2,2,2,2,2,2,2,1,2,2,2,2,2,2,2,2,2,2,4),(-2.04439259789017E-6,
0.,1.16813469870535E-6,2.3362693974107E-6,4.67253879482139E-6,9.34507758964279E-6,
1.56893443514872E-5,2.5897054707271E-5,3.53798289796446E-5,3.67345110185551E-5,
3.74570081059741E-5,3.91084300200745E-5,4.3512221791009E-5,4.45654530819768E-5,
6.26353541277857E-5,6.56193588433549E-5,7.12078702674521E-5,7.16407948146347E-5,
7.25009999533889E-5,7.34840915405366E-5,7.61056691062638E-5,8.65919793691728E-5,
8.89786567925481E-5,9.40446697643188E-5,9.57333407549091E-5,9.79849020756961E-5,
0.000106991147358844,0.000113571562047159,0.000119834164740902,0.000121170237394284,
0.000122506310047666,0.00012517845535443,0.000130522745967958,0.000132049686143252,
0.000136121526610702,0.000138121518246153,0.000141418986123913,0.000147599170335016,
0.000149659231738717,0.000157899477353521,0.000165007876130274),
 .UNSPECIFIED.) ;
#2198 = B_SPLINE_CURVE_WITH_KNOTS('',3,(#152123,#152124,#152125,#152126,#152127,
#152128,#152129,#152130,#152131,#152132,#152133,#152134,#152135,#152136,
#152137,#152138,#152139,#152140,#152141,#152142,#152143,#152144,#152145,
#152146,#152147,#152148,#152149,#152150,#152151,#152152,#152153,#152154,
#152155,#152156,#152157,#152158,#152159,#152160,#152161,#152162,#152163,
#152164,#152165,#152166,#152167,#152168,#152169,#152170,#152171,#152172),
 .UNSPECIFIED.,.F.,.F.,(4,2,2,2,2,2,2,2,2,2,2,2,2,2,2,2,2,2,2,2,2,2,2,2,
4),(-2.08053324537705E-6,4.2351647362715E-22,1.73126834661496E-6,3.96468142042611E-6,
7.52178969731147E-6,1.32303807352218E-5,2.25750184175543E-5,3.87948997653528E-5,
5.72367363101908E-5,6.41156850334219E-5,7.29633420205792E-5,7.57300836966956E-5,
9.46996266571652E-5,9.75514675378546E-5,0.000111620796538317,0.000116439892133749,
0.000117409636556728,0.000134179897042086,0.000142027094744281,0.000142768074549618,
0.000154973322944091,0.000157365523939564,0.000159579629273015,0.000173553148900826,
0.000174961243144783),.UNSPECIFIED.) ;
#2199 = B_SPLINE_CURVE_WITH_KNOTS('',3,(#152186,#152187,#152188,#152189,#152190,
#152191,#152192,#152193,#152194,#152195,#152196,#152197,#152198,#152199,
#152200,#152201,#152202,#152203,#152204,#152205,#152206,#152207,#152208,
#152209,#152210,#152211,#152212,#152213,#152214,#152215,#152216,#152217,
#152218,#152219,#152220,#152221,#152222,#152223,#152224,#152225,#152226,
#152227,#152228,#152229,#152230,#152231,#152232,#152233,#152234,#152235,
#152236,#152237,#152238,#152239,#152240,#152241,#152242,#152243,#152244,
#152245,#152246,#152247,#152248,#152249,#152250,#152251,#152252,#152253,
#152254,#152255,#152256,#152257,#152258,#152259,#152260,#152261,#152262,
#152263,#152264),.UNSPECIFIED.,.F.,.F.,(4,2,2,2,2,2,2,2,2,1,2,2,2,2,2,2,
2,2,1,2,2,2,2,2,2,2,2,2,2,1,2,2,2,2,2,2,2,2,2,2,4),(-2.0443925978901E-6,
-4.2351647362715E-22,1.16813469870574E-6,2.33626939741147E-6,4.67253879482294E-6,
9.34507758964589E-6,1.56893443514892E-5,2.5897054707273E-5,3.53798289796464E-5,
3.67345110185569E-5,3.74570081059758E-5,3.91084300200762E-5,4.35122217910106E-5,
4.45654530819776E-5,6.26353541267333E-5,6.56193588433769E-5,7.12078702674526E-5,
7.16407948146629E-5,7.2500999953418E-5,7.34840915405668E-5,7.61056691062967E-5,
8.65919793692166E-5,8.89786567925514E-5,9.40446697643274E-5,9.57333407549194E-5,
9.79849020757087E-5,0.000106991147358866,0.000113571562047158,0.000119834164740905,
0.000121170237394289,0.000122506310047672,0.000125178455354439,0.000130522745967973,
0.000132049686143269,0.000136121526610723,0.000138121518246146,0.000141418986123914,
0.000147599170335021,0.000149659231738723,0.000157899477353533,0.000165007876130275),
 .UNSPECIFIED.) ;
#2200 = B_SPLINE_CURVE_WITH_KNOTS('',3,(#152267,#152268,#152269,#152270,#152271,
#152272,#152273,#152274,#152275,#152276,#152277,#152278,#152279,#152280,
#152281,#152282,#152283,#152284,#152285,#152286,#152287,#152288,#152289,
#152290,#152291,#152292,#152293,#152294,#152295,#152296,#152297,#152298,
#152299,#152300,#152301,#152302,#152303,#152304,#152305,#152306,#152307,
#152308,#152309,#152310,#152311,#152312,#152313,#152314,#152315,#152316,
#152317,#152318,#152319,#152320,#152321,#152322,#152323,#152324,#152325,
#152326,#152327,#152328,#152329,#152330,#152331,#152332,#152333,#152334,
#152335,#152336,#152337,#152338,#152339,#152340,#152341,#152342,#152343,
#152344,#152345,#152346,#152347),.UNSPECIFIED.,.F.,.F.,(4,2,2,2,2,2,2,2,
2,2,1,2,2,2,2,2,2,2,2,1,2,2,2,2,2,2,2,2,2,2,1,2,2,2,2,2,2,2,2,2,2,4),(-2.04439259788975E-6,
-1.02219629894488E-6,0.,1.16813469870559E-6,2.33626939741118E-6,4.67253879482236E-6,
9.34507758964471E-6,1.56893443514874E-5,2.58970547072708E-5,3.53798289796441E-5,
3.67345110185546E-5,3.74570081059735E-5,3.91084300200739E-5,4.35122217910083E-5,
4.45654530819754E-5,6.26353541276203E-5,6.56193588433579E-5,7.12078702674436E-5,
7.1640794814638E-5,7.25009999533923E-5,7.348409154054E-5,7.61056691062674E-5,
8.65919793691769E-5,8.89786567925471E-5,9.40446697643204E-5,9.57333407549114E-5,
9.79849020756996E-5,0.000106991147358852,0.000113571562047158,0.000119834164740902,
0.000121170237394284,0.000122506310047666,0.00012517845535443,0.000130522745967958,
0.000132049686143252,0.000136121526610702,0.000138121518246153,0.000141418986123913,
0.000147599170335002,0.000149659231738699,0.000157899477353485,0.000165007876130273),
 .UNSPECIFIED.) ;
#2201 = B_SPLINE_CURVE_WITH_KNOTS('',3,(#152361,#152362,#152363,#152364,#152365,
#152366,#152367,#152368,#152369,#152370,#152371,#152372,#152373,#152374,
#152375,#152376,#152377,#152378,#152379,#152380,#152381,#152382,#152383,
#152384,#152385,#152386,#152387,#152388,#152389,#152390,#152391,#152392,
#152393,#152394,#152395,#152396,#152397,#152398,#152399,#152400,#152401,
#152402,#152403,#152404,#152405,#152406,#152407,#152408,#152409,#152410,
#152411,#152412,#152413,#152414,#152415,#152416,#152417,#152418,#152419,
#152420,#152421,#152422,#152423,#152424,#152425,#152426,#152427,#152428,
#152429,#152430,#152431,#152432,#152433,#152434,#152435,#152436,#152437,
#152438,#152439,#152440,#152441,#152442),.UNSPECIFIED.,.F.,.F.,(4,2,1,2,
2,2,2,2,2,2,2,1,2,2,2,2,2,2,2,2,1,2,2,2,2,2,2,2,2,2,2,1,2,2,2,2,2,2,2,2,
2,2,4),(-2.04439246668907E-6,-1.98050532921559E-6,-1.02219629894998E-6,
0.,1.16813469870384E-6,2.33626939740767E-6,4.67253879481535E-6,9.34507758963069E-6,
1.56893443514762E-5,2.58970547072613E-5,3.53798289796358E-5,3.67345110185464E-5,
3.74570081059654E-5,3.9108430020066E-5,4.35122217910009E-5,4.45654530819649E-5,
6.26353541268739E-5,6.56193588433615E-5,7.12078702674378E-5,7.16407948146413E-5,
7.25009999533956E-5,7.34840915405433E-5,7.61056691062706E-5,8.65919793691797E-5,
8.89786567925395E-5,9.40446697643135E-5,9.57333407549048E-5,9.79849020756933E-5,
0.000106991147358847,0.000113571562047149,0.000119834164740893,0.000121170237394276,
0.00012250631004766,0.000125178455354427,0.000130522745967961,0.000132049686143256,
0.000136121526610711,0.00013812151824614,0.000141418986123901,0.000147599170334991,
0.000149659231738688,0.000157899477353475,0.000165007876130261),
 .UNSPECIFIED.) ;
#2202 = B_SPLINE_CURVE_WITH_KNOTS('',3,(#152445,#152446,#152447,#152448,#152449,
#152450,#152451,#152452,#152453,#152454,#152455,#152456,#152457,#152458,
#152459,#152460,#152461,#152462,#152463,#152464,#152465,#152466,#152467,
#152468,#152469,#152470,#152471,#152472,#152473,#152474,#152475,#152476,
#152477,#152478,#152479,#152480,#152481,#152482,#152483,#152484,#152485,
#152486,#152487,#152488,#152489,#152490,#152491,#152492,#152493,#152494,
#152495,#152496,#152497,#152498,#152499,#152500,#152501,#152502,#152503,
#152504,#152505,#152506,#152507,#152508,#152509,#152510,#152511,#152512,
#152513,#152514,#152515,#152516,#152517,#152518,#152519,#152520,#152521,
#152522,#152523),.UNSPECIFIED.,.F.,.F.,(4,2,2,2,2,2,2,2,2,1,2,2,2,2,2,2,
2,2,1,2,2,2,2,2,2,2,2,2,2,1,2,2,2,2,2,2,2,2,2,2,4),(-2.04439259788986E-6,
0.,1.16813469870571E-6,2.33626939741142E-6,4.67253879482284E-6,9.34507758964569E-6,
1.56893443514882E-5,2.58970547072723E-5,3.53798289796464E-5,3.6734511018557E-5,
3.7457008105976E-5,3.91084300200765E-5,4.35122217910112E-5,4.45654530819765E-5,
6.26353541265572E-5,6.56193588433932E-5,7.12078702674494E-5,7.16407948146812E-5,
7.25009999534366E-5,7.34840915405856E-5,7.61056691063164E-5,8.65919793692397E-5,
8.89786567925485E-5,9.40446697643211E-5,9.57333407549119E-5,9.79849020756997E-5,
0.000106991147358851,0.000113571562047157,0.000119834164740902,0.000121170237394286,
0.000122506310047671,0.000125178455354439,0.000130522745967977,0.000132049686143273,
0.00013612152661073,0.00013812151824615,0.000141418986123912,0.000147599170335004,
0.000149659231738701,0.000157899477353491,0.000165007876130273),
 .UNSPECIFIED.) ;
#2203 = B_SPLINE_CURVE_WITH_KNOTS('',3,(#152537,#152538,#152539,#152540,#152541,
#152542,#152543,#152544,#152545,#152546,#152547,#152548,#152549,#152550,
#152551,#152552,#152553,#152554,#152555,#152556,#152557,#152558,#152559,
#152560,#152561,#152562,#152563,#152564,#152565,#152566,#152567,#152568,
#152569,#152570,#152571,#152572,#152573,#152574,#152575,#152576,#152577,
#152578,#152579,#152580,#152581,#152582,#152583,#152584,#152585,#152586,
#152587,#152588,#152589,#152590,#152591,#152592,#152593,#152594,#152595,
#152596,#152597,#152598,#152599,#152600,#152601,#152602,#152603,#152604,
#152605,#152606,#152607,#152608,#152609,#152610,#152611,#152612,#152613,
#152614,#152615,#152616),.UNSPECIFIED.,.F.,.F.,(4,1,2,2,2,2,2,2,2,2,1,2,
2,2,2,2,2,2,2,1,2,2,2,2,2,2,2,2,2,2,1,2,2,2,2,2,2,2,2,2,2,4),(-2.04439259788173E-6,
-1.02219629894086E-6,0.,1.16813469870681E-6,2.33626939741361E-6,4.67253879482722E-6,
9.34507758965445E-6,1.56893443514986E-5,2.58970547072802E-5,3.53798289796539E-5,
3.67345110185645E-5,3.74570081059834E-5,3.91084300200839E-5,4.35122217910184E-5,
4.45654530819858E-5,6.26353541299918E-5,6.56193588433716E-5,7.1207870267458E-5,
7.16407948146529E-5,7.25009999534074E-5,7.34840915405553E-5,7.61056691062832E-5,
8.65919793691949E-5,8.89786567925583E-5,9.40446697643248E-5,9.57333407549136E-5,
9.79849020756987E-5,0.000106991147358839,0.000113571562047167,0.000119834164740911,
0.000121170237394293,0.000122506310047674,0.000125178455354437,0.000130522745967964,
0.000132049686143257,0.000136121526610706,0.000138121518246156,0.00014141898612392,
0.000147599170335024,0.000149659231738725,0.00015789947735353,0.000165007876130282),
 .UNSPECIFIED.) ;
#2204 = B_SPLINE_CURVE_WITH_KNOTS('',3,(#152619,#152620,#152621,#152622,#152623,
#152624,#152625,#152626,#152627,#152628,#152629,#152630,#152631,#152632,
#152633,#152634,#152635,#152636,#152637,#152638,#152639,#152640,#152641,
#152642,#152643,#152644,#152645,#152646,#152647,#152648,#152649,#152650,
#152651,#152652,#152653,#152654,#152655,#152656,#152657,#152658,#152659,
#152660,#152661,#152662,#152663,#152664,#152665,#152666,#152667,#152668,
#152669,#152670,#152671,#152672,#152673,#152674,#152675,#152676,#152677,
#152678,#152679,#152680,#152681,#152682,#152683,#152684,#152685,#152686,
#152687,#152688,#152689,#152690,#152691,#152692,#152693,#152694,#152695,
#152696,#152697,#152698,#152699),.UNSPECIFIED.,.F.,.F.,(4,2,2,2,2,2,2,2,
2,2,1,2,2,2,2,2,2,2,2,1,2,2,2,2,2,2,2,2,2,2,1,2,2,2,2,2,2,2,2,2,2,4),(-2.0443925978812E-6,
-1.0221962989406E-6,4.2351647362715E-22,1.1681346987067E-6,2.33626939741339E-6,
4.67253879482678E-6,9.34507758965356E-6,1.56893443514987E-5,2.58970547072825E-5,
3.53798289796548E-5,3.67345110185651E-5,3.7457008105984E-5,3.91084300200842E-5,
4.35122217910181E-5,4.45654530819845E-5,6.2635354127915E-5,6.56193588433688E-5,
7.12078702674513E-5,7.16407948146474E-5,7.25009999534015E-5,7.3484091540549E-5,
7.61056691062757E-5,8.65919793691826E-5,8.89786567925572E-5,9.40446697643321E-5,
9.57333407549237E-5,9.79849020757126E-5,0.000106991147358868,0.000113571562047162,
0.000119834164740911,0.000121170237394293,0.000122506310047674,0.000125178455354437,
0.000130522745967964,0.000132049686143257,0.000136121526610706,0.000138121518246158,
0.000141418986123922,0.00014759917033502,0.00014965923173872,0.000157899477353517,
0.000165007876130284),.UNSPECIFIED.) ;
#2205 = B_SPLINE_CURVE_WITH_KNOTS('',3,(#152713,#152714,#152715,#152716,#152717,
#152718,#152719,#152720,#152721,#152722,#152723,#152724,#152725,#152726,
#152727,#152728,#152729,#152730,#152731,#152732,#152733,#152734,#152735,
#152736,#152737,#152738,#152739,#152740,#152741,#152742,#152743,#152744,
#152745,#152746,#152747,#152748,#152749,#152750,#152751,#152752,#152753,
#152754,#152755,#152756,#152757,#152758,#152759,#152760,#152761,#152762,
#152763,#152764,#152765,#152766,#152767,#152768,#152769,#152770,#152771,
#152772,#152773,#152774,#152775,#152776,#152777,#152778,#152779,#152780,
#152781,#152782,#152783,#152784,#152785,#152786,#152787,#152788,#152789,
#152790,#152791),.UNSPECIFIED.,.F.,.F.,(4,2,2,2,2,2,2,2,2,1,2,2,2,2,2,2,
2,2,1,2,2,2,2,2,2,2,2,2,2,1,2,2,2,2,2,2,2,2,2,2,4),(-2.04439259789012E-6,
-4.2351647362715E-22,1.16813469870576E-6,2.33626939741152E-6,4.67253879482304E-6,
9.34507758964607E-6,1.56893443514891E-5,2.5897054707274E-5,3.53798289796481E-5,
3.67345110185587E-5,3.74570081059777E-5,3.91084300200782E-5,4.35122217910129E-5,
4.45654530819766E-5,6.26353541292069E-5,6.56193588434199E-5,7.12078702674474E-5,
7.16407948147103E-5,7.25009999534661E-5,7.34840915406156E-5,7.61056691063475E-5,
8.6591979369275E-5,8.89786567925508E-5,9.40446697643281E-5,9.57333407549205E-5,
9.79849020757104E-5,0.00010699114735887,0.000113571562047157,0.000119834164740904,
0.00012117023739429,0.000122506310047677,0.00012517845535445,0.000130522745967996,
0.000132049686143294,0.000136121526610758,0.000138121518246149,0.000141418986123913,
0.000147599170334991,0.000149659231738683,0.000157899477353454,0.000165007876130274),
 .UNSPECIFIED.) ;
#2206 = B_SPLINE_CURVE_WITH_KNOTS('',3,(#152794,#152795,#152796,#152797,#152798,
#152799,#152800,#152801,#152802,#152803,#152804,#152805,#152806,#152807,
#152808,#152809,#152810,#152811,#152812,#152813,#152814,#152815,#152816,
#152817,#152818,#152819,#152820,#152821,#152822,#152823,#152824,#152825,
#152826,#152827,#152828,#152829,#152830,#152831,#152832,#152833,#152834,
#152835,#152836,#152837,#152838,#152839,#152840,#152841,#152842,#152843,
#152844,#152845,#152846,#152847,#152848,#152849,#152850,#152851,#152852,
#152853,#152854,#152855,#152856,#152857,#152858,#152859,#152860,#152861,
#152862,#152863,#152864,#152865,#152866,#152867,#152868,#152869,#152870,
#152871,#152872,#152873,#152874),.UNSPECIFIED.,.F.,.F.,(4,2,2,2,2,2,2,2,
2,2,1,2,2,2,2,2,2,2,2,1,2,2,2,2,2,2,2,2,2,2,1,2,2,2,2,2,2,2,2,2,2,4),(-2.04439259790034E-6,
-1.02219629895017E-6,0.,1.16813469870406E-6,2.33626939740812E-6,4.67253879481623E-6,
9.34507758963246E-6,1.56893443514797E-5,2.58970547072656E-5,3.53798289796408E-5,
3.67345110185516E-5,3.74570081059706E-5,3.91084300200713E-5,4.35122217910066E-5,
4.45654530819667E-5,6.26353541284101E-5,6.5619358843395E-5,7.12078702674452E-5,
7.1640794814688E-5,7.25009999534442E-5,7.34840915405941E-5,7.61056691063271E-5,
8.65919793692592E-5,8.89786567925412E-5,9.40446697643201E-5,9.5733340754913E-5,
9.79849020757036E-5,0.000106991147358866,0.000113571562047154,0.000119834164740894,
0.000121170237394276,0.000122506310047659,0.000125178455354423,0.000130522745967953,
0.000132049686143247,0.000136121526610698,0.000138121518246142,0.000141418986123903,
0.000147599170334999,0.000149659231738698,0.000157899477353493,0.000165007876130263),
 .UNSPECIFIED.) ;
#2207 = B_SPLINE_CURVE_WITH_KNOTS('',3,(#152888,#152889,#152890,#152891,#152892,
#152893,#152894,#152895,#152896,#152897,#152898,#152899,#152900,#152901,
#152902,#152903,#152904,#152905,#152906,#152907,#152908,#152909,#152910,
#152911,#152912,#152913,#152914,#152915,#152916,#152917,#152918,#152919,
#152920,#152921,#152922,#152923,#152924,#152925,#152926,#152927,#152928,
#152929,#152930,#152931,#152932,#152933,#152934,#152935,#152936,#152937,
#152938,#152939,#152940,#152941,#152942,#152943,#152944,#152945,#152946,
#152947,#152948,#152949,#152950,#152951,#152952,#152953,#152954,#152955,
#152956,#152957,#152958,#152959,#152960,#152961,#152962,#152963,#152964,
#152965,#152966),.UNSPECIFIED.,.F.,.F.,(4,2,2,2,2,2,2,2,2,1,2,2,2,2,2,2,
2,2,1,2,2,2,2,2,2,2,2,2,2,1,2,2,2,2,2,2,2,2,2,2,4),(-2.04439259789012E-6,
-4.2351647362715E-22,1.16813469870576E-6,2.33626939741152E-6,4.67253879482304E-6,
9.34507758964607E-6,1.56893443514891E-5,2.5897054707274E-5,3.53798289796481E-5,
3.67345110185587E-5,3.74570081059777E-5,3.91084300200782E-5,4.35122217910129E-5,
4.45654530819766E-5,6.26353541312969E-5,6.56193588434229E-5,7.12078702674478E-5,
7.16407948147216E-5,7.25009999534786E-5,7.34840915406294E-5,7.61056691063649E-5,
8.65919793693069E-5,8.89786567925508E-5,9.4044669764314E-5,9.57333407549018E-5,
9.79849020756854E-5,0.00010699114735882,0.00011357156204716,0.000119834164740904,
0.000121170237394285,0.000122506310047666,0.000125178455354429,0.000130522745967953,
0.000132049686143246,0.000136121526610693,0.000138121518246146,0.000141418986123913,
0.00014759917033499,0.000149659231738683,0.000157899477353452,0.000165007876130274),
 .UNSPECIFIED.) ;
#2208 = B_SPLINE_CURVE_WITH_KNOTS('',3,(#152969,#152970,#152971,#152972,#152973,
#152974,#152975,#152976,#152977,#152978,#152979,#152980,#152981,#152982,
#152983,#152984,#152985,#152986,#152987,#152988,#152989,#152990,#152991,
#152992,#152993,#152994,#152995,#152996,#152997,#152998,#152999,#153000,
#153001,#153002,#153003,#153004,#153005,#153006,#153007,#153008,#153009,
#153010,#153011,#153012,#153013,#153014,#153015,#153016,#153017,#153018,
#153019,#153020,#153021,#153022,#153023,#153024,#153025,#153026,#153027,
#153028,#153029,#153030,#153031,#153032,#153033,#153034,#153035,#153036,
#153037,#153038,#153039,#153040,#153041,#153042,#153043,#153044,#153045,
#153046,#153047,#153048,#153049),.UNSPECIFIED.,.F.,.F.,(4,2,2,2,2,2,2,2,
2,2,1,2,2,2,2,2,2,2,2,1,2,2,2,2,2,2,2,2,2,2,1,2,2,2,2,2,2,2,2,2,2,4),(-2.04439259789012E-6,
-1.02219629894506E-6,-4.2351647362715E-22,1.16813469870576E-6,2.33626939741152E-6,
4.67253879482304E-6,9.34507758964607E-6,1.56893443514891E-5,2.5897054707274E-5,
3.53798289796481E-5,3.67345110185587E-5,3.74570081059777E-5,3.91084300200782E-5,
4.35122217910129E-5,4.45654530819766E-5,6.26353541222793E-5,6.56193588434281E-5,
7.12078702674497E-5,7.16407948147244E-5,7.2500999953481E-5,7.34840915406315E-5,
7.61056691063659E-5,8.65919793693037E-5,8.89786567925508E-5,9.40446697643295E-5,
9.57333407549224E-5,9.79849020757129E-5,0.000106991147358875,0.000113571562047159,
0.000119834164740904,0.000121170237394286,0.000122506310047668,0.000125178455354432,
0.00013052274596796,0.000132049686143254,0.000136121526610704,0.000138121518246146,
0.000141418986123913,0.000147599170335,0.000149659231738696,0.000157899477353478,
0.000165007876130274),.UNSPECIFIED.) ;
#2209 = B_SPLINE_CURVE_WITH_KNOTS('',3,(#153063,#153064,#153065,#153066,#153067,
#153068,#153069,#153070,#153071,#153072,#153073,#153074,#153075,#153076,
#153077,#153078,#153079,#153080,#153081,#153082,#153083,#153084,#153085,
#153086,#153087,#153088,#153089,#153090,#153091,#153092,#153093,#153094,
#153095,#153096,#153097,#153098,#153099,#153100,#153101,#153102,#153103,
#153104,#153105,#153106,#153107,#153108,#153109,#153110,#153111,#153112,
#153113,#153114,#153115,#153116,#153117,#153118,#153119,#153120,#153121,
#153122,#153123,#153124,#153125,#153126,#153127,#153128,#153129,#153130,
#153131,#153132,#153133,#153134,#153135,#153136,#153137,#153138,#153139,
#153140,#153141),.UNSPECIFIED.,.F.,.F.,(4,2,2,2,2,2,2,2,2,1,2,2,2,2,2,2,
2,2,1,2,2,2,2,2,2,2,2,2,2,1,2,2,2,2,2,2,2,2,2,2,4),(-2.04439259789117E-6,
4.2351647362715E-22,1.16813469870585E-6,2.3362693974117E-6,4.67253879482341E-6,
9.34507758964682E-6,1.56893443514892E-5,2.58970547072705E-5,3.53798289796436E-5,
3.67345110185541E-5,3.7457008105973E-5,3.91084300200733E-5,4.35122217910076E-5,
4.45654530819785E-5,6.26353541292637E-5,6.56193588433652E-5,7.12078702674523E-5,
7.16407948146479E-5,7.25009999534026E-5,7.34840915405508E-5,7.61056691062794E-5,
8.65919793691936E-5,8.89786567925488E-5,9.40446697643019E-5,9.57333407548862E-5,
9.79849020756654E-5,0.000106991147358782,0.000113571562047156,0.000119834164740906,
0.000121170237394291,0.000122506310047676,0.000125178455354446,0.000130522745967985,
0.000132049686143282,0.000136121526610741,0.000138121518246147,0.000141418986123914,
0.000147599170334984,0.000149659231738674,0.000157899477353434,0.000165007876130277),
 .UNSPECIFIED.) ;
#2210 = B_SPLINE_CURVE_WITH_KNOTS('',3,(#153144,#153145,#153146,#153147,#153148,
#153149,#153150,#153151,#153152,#153153,#153154,#153155,#153156,#153157,
#153158,#153159,#153160,#153161,#153162,#153163,#153164,#153165,#153166,
#153167,#153168,#153169,#153170,#153171,#153172,#153173,#153174,#153175,
#153176,#153177,#153178,#153179,#153180,#153181,#153182,#153183,#153184,
#153185,#153186,#153187,#153188,#153189,#153190,#153191,#153192,#153193,
#153194,#153195,#153196,#153197,#153198,#153199,#153200,#153201,#153202,
#153203,#153204,#153205,#153206,#153207,#153208,#153209,#153210,#153211,
#153212,#153213,#153214,#153215,#153216,#153217,#153218,#153219,#153220,
#153221,#153222,#153223,#153224),.UNSPECIFIED.,.F.,.F.,(4,2,2,2,2,2,2,2,
2,2,1,2,2,2,2,2,2,2,2,1,2,2,2,2,2,2,2,2,2,2,1,2,2,2,2,2,2,2,2,2,2,4),(-2.04439259789012E-6,
-1.02219629894506E-6,-4.2351647362715E-22,1.16813469870576E-6,2.33626939741152E-6,
4.67253879482304E-6,9.34507758964607E-6,1.56893443514891E-5,2.5897054707274E-5,
3.53798289796481E-5,3.67345110185587E-5,3.74570081059777E-5,3.91084300200782E-5,
4.35122217910129E-5,4.45654530819766E-5,6.26353541228085E-5,6.56193588434328E-5,
7.12078702674523E-5,7.16407948147346E-5,7.2500999953492E-5,7.34840915406433E-5,
7.61056691063801E-5,8.65919793693274E-5,8.89786567925508E-5,9.40446697643413E-5,
9.57333407549381E-5,9.79849020757339E-5,0.000106991147358917,0.000113571562047154,
0.000119834164740904,0.000121170237394293,0.000122506310047682,0.000125178455354461,
0.000130522745968017,0.000132049686143319,0.000136121526610791,0.000138121518246147,
0.000141418986123913,0.000147599170334984,0.000149659231738674,0.000157899477353436,
0.000165007876130274),.UNSPECIFIED.) ;
#2211 = B_SPLINE_CURVE_WITH_KNOTS('',3,(#153238,#153239,#153240,#153241,#153242,
#153243,#153244,#153245,#153246,#153247,#153248,#153249,#153250,#153251,
#153252,#153253,#153254,#153255,#153256,#153257,#153258,#153259,#153260,
#153261,#153262,#153263,#153264,#153265,#153266,#153267,#153268,#153269,
#153270,#153271,#153272,#153273,#153274,#153275,#153276,#153277,#153278,
#153279,#153280,#153281,#153282,#153283,#153284,#153285,#153286,#153287,
#153288,#153289,#153290,#153291,#153292,#153293,#153294,#153295,#153296,
#153297,#153298,#153299,#153300,#153301,#153302,#153303,#153304,#153305,
#153306,#153307,#153308,#153309,#153310,#153311,#153312,#153313,#153314,
#153315,#153316,#153317,#153318),.UNSPECIFIED.,.F.,.F.,(4,2,2,2,2,2,2,2,
2,2,1,2,2,2,2,2,2,2,2,1,2,2,2,2,2,2,2,2,2,2,1,2,2,2,2,2,2,2,2,2,2,4),(-2.04439259788935E-6,
-1.02219629894467E-6,0.,1.16813469870576E-6,2.33626939741152E-6,4.67253879482303E-6,
9.34507758964606E-6,1.56893443514906E-5,2.5897054707276E-5,3.53798289796491E-5,
3.67345110185596E-5,3.74570081059785E-5,3.91084300200788E-5,4.35122217910131E-5,
4.45654530819802E-5,6.26353541287885E-5,6.56193588433466E-5,7.12078702674531E-5,
7.16407948146223E-5,7.25009999533759E-5,7.3484091540523E-5,7.61056691062484E-5,
8.65919793691503E-5,8.89786567925503E-5,9.40446697643058E-5,9.57333407548909E-5,
9.79849020756711E-5,0.000106991147358792,0.000113571562047162,0.000119834164740905,
0.000121170237394295,0.000122506310047685,0.000125178455354465,0.000130522745968025,
0.000132049686143328,0.000136121526610802,0.000138121518246146,0.000141418986123915,
0.000147599170335001,0.000149659231738696,0.000157899477353478,0.000165007876130276),
 .UNSPECIFIED.) ;
#2212 = B_SPLINE_CURVE_WITH_KNOTS('',3,(#153321,#153322,#153323,#153324,#153325,
#153326,#153327,#153328,#153329,#153330,#153331,#153332,#153333,#153334,
#153335,#153336,#153337,#153338,#153339,#153340,#153341,#153342,#153343,
#153344,#153345,#153346,#153347,#153348,#153349,#153350,#153351,#153352,
#153353,#153354,#153355,#153356,#153357,#153358,#153359,#153360,#153361,
#153362,#153363,#153364,#153365,#153366,#153367,#153368,#153369,#153370,
#153371,#153372,#153373,#153374,#153375,#153376,#153377,#153378,#153379,
#153380,#153381,#153382,#153383,#153384,#153385,#153386,#153387,#153388,
#153389,#153390,#153391,#153392,#153393,#153394,#153395,#153396,#153397,
#153398,#153399,#153400),.UNSPECIFIED.,.F.,.F.,(4,1,2,2,2,2,2,2,2,2,1,2,
2,2,2,2,2,2,2,1,2,2,2,2,2,2,2,2,2,2,1,2,2,2,2,2,2,2,2,2,2,4),(-2.04439259788868E-6,
-1.02219629894434E-6,0.,1.16813469870521E-6,2.33626939741041E-6,4.67253879482083E-6,
9.34507758964166E-6,1.56893443514874E-5,2.58970547072727E-5,3.53798289796463E-5,
3.67345110185568E-5,3.74570081059758E-5,3.91084300200762E-5,4.35122217910107E-5,
4.45654530819764E-5,6.26353541299785E-5,6.56193588432828E-5,7.1207870267458E-5,
7.16407948145442E-5,7.25009999532958E-5,7.34840915404405E-5,7.61056691061598E-5,
8.65919793690367E-5,8.89786567925501E-5,9.40446697643433E-5,9.57333407549411E-5,
9.7984902075738E-5,0.000106991147358926,0.000113571562047156,0.0001198341647409,
0.000121170237394275,0.00012250631004765,0.000125178455354399,0.000130522745967899,
0.000132049686143184,0.000136121526610612,0.000138121518246142,0.000141418986123913,
0.000147599170335002,0.000149659231738699,0.000157899477353484,0.000165007876130273),
 .UNSPECIFIED.) ;
#2213 = B_SPLINE_CURVE_WITH_KNOTS('',3,(#153414,#153415,#153416,#153417,#153418,
#153419,#153420,#153421,#153422,#153423,#153424,#153425,#153426,#153427,
#153428,#153429,#153430,#153431,#153432,#153433,#153434,#153435,#153436,
#153437,#153438,#153439,#153440,#153441,#153442,#153443,#153444,#153445,
#153446,#153447,#153448,#153449,#153450,#153451,#153452,#153453,#153454,
#153455,#153456,#153457,#153458,#153459,#153460,#153461,#153462,#153463,
#153464,#153465,#153466,#153467,#153468,#153469,#153470,#153471,#153472,
#153473,#153474,#153475,#153476,#153477,#153478,#153479,#153480,#153481,
#153482,#153483,#153484,#153485,#153486,#153487,#153488,#153489,#153490,
#153491,#153492,#153493),.UNSPECIFIED.,.F.,.F.,(4,1,2,2,2,2,2,2,2,2,1,2,
2,2,2,2,2,2,2,1,2,2,2,2,2,2,2,2,2,2,1,2,2,2,2,2,2,2,2,2,2,4),(-2.04439259788983E-6,
-1.02219629894492E-6,0.,1.16813469870562E-6,2.33626939741123E-6,4.67253879482247E-6,
9.34507758964493E-6,1.56893443514854E-5,2.58970547072686E-5,3.537982897964E-5,
3.67345110185502E-5,3.7457008105969E-5,3.9108430020069E-5,4.35122217910025E-5,
4.45654530819757E-5,6.26353541202787E-5,6.56193588433876E-5,7.12078702674454E-5,
7.16407948146769E-5,7.25009999534325E-5,7.34840915405817E-5,7.61056691063131E-5,
8.65919793692386E-5,8.89786567925425E-5,9.40446697643215E-5,9.57333407549146E-5,
9.79849020757052E-5,0.000106991147358868,0.000113571562047158,0.000119834164740895,
0.000121170237394282,0.000122506310047669,0.000125178455354443,0.000130522745967992,
0.000132049686143291,0.000136121526610757,0.000138121518246138,0.000141418986123904,
0.000147599170334986,0.000149659231738681,0.000157899477353457,0.000165007876130264),
 .UNSPECIFIED.) ;
#2214 = B_SPLINE_CURVE_WITH_KNOTS('',3,(#153496,#153497,#153498,#153499,#153500,
#153501,#153502,#153503,#153504,#153505,#153506,#153507,#153508,#153509,
#153510,#153511,#153512,#153513,#153514,#153515,#153516,#153517,#153518,
#153519,#153520,#153521,#153522,#153523,#153524,#153525,#153526,#153527,
#153528,#153529,#153530,#153531,#153532,#153533,#153534,#153535,#153536,
#153537,#153538,#153539,#153540,#153541,#153542,#153543,#153544,#153545,
#153546,#153547,#153548,#153549,#153550,#153551,#153552,#153553,#153554,
#153555,#153556,#153557,#153558,#153559,#153560,#153561,#153562,#153563,
#153564,#153565,#153566,#153567,#153568,#153569,#153570,#153571,#153572,
#153573,#153574),.UNSPECIFIED.,.F.,.F.,(4,2,2,2,2,2,2,2,2,1,2,2,2,2,2,2,
2,2,1,2,2,2,2,2,2,2,2,2,2,1,2,2,2,2,2,2,2,2,2,2,4),(-2.04439259789041E-6,
0.,1.16813469870559E-6,2.33626939741119E-6,4.67253879482237E-6,9.34507758964474E-6,
1.56893443514909E-5,2.5897054707274E-5,3.53798289796484E-5,3.6734511018559E-5,
3.74570081059781E-5,3.91084300200786E-5,4.35122217910135E-5,4.4565453081976E-5,
6.26353541290543E-5,6.56193588433348E-5,7.12078702674495E-5,7.16407948146086E-5,
7.2500999953362E-5,7.34840915405088E-5,7.61056691062334E-5,8.6591979369132E-5,
8.89786567925493E-5,9.4044669764311E-5,9.57333407548982E-5,9.79849020756812E-5,
0.000106991147358813,0.00011357156204716,0.000119834164740903,0.000121170237394283,
0.000122506310047663,0.000125178455354423,0.000130522745967942,0.000132049686143234,
0.000136121526610677,0.000138121518246148,0.000141418986123912,0.000147599170335,
0.000149659231738696,0.000157899477353481,0.000165007876130272),
 .UNSPECIFIED.) ;
#2215 = B_SPLINE_CURVE_WITH_KNOTS('',3,(#153588,#153589,#153590,#153591,#153592,
#153593,#153594,#153595,#153596,#153597,#153598,#153599,#153600,#153601,
#153602,#153603,#153604,#153605,#153606,#153607,#153608,#153609,#153610,
#153611,#153612,#153613,#153614,#153615,#153616,#153617,#153618,#153619,
#153620,#153621,#153622,#153623,#153624,#153625,#153626,#153627,#153628,
#153629,#153630,#153631,#153632,#153633,#153634,#153635,#153636,#153637),
 .UNSPECIFIED.,.F.,.F.,(4,2,2,2,2,2,2,2,2,2,2,2,2,2,2,2,2,2,2,2,2,2,2,2,
4),(-2.0805332453777E-6,-4.2351647362715E-22,1.73126834661512E-6,3.9646814204225E-6,
7.52178969731448E-6,1.32303807352205E-5,2.25750184175528E-5,3.87948997653525E-5,
5.72571304993316E-5,6.41156850332471E-5,7.29633420187519E-5,7.57300836966873E-5,
9.46996265562493E-5,9.75514675378132E-5,0.000111620796538463,0.000116439892133737,
0.00011740963655672,0.000134179897041995,0.000142027094744273,0.000142768074549612,
0.000154973322948364,0.000157365523939684,0.000159579629273007,0.000173553148905421,
0.000174961243144775),.UNSPECIFIED.) ;
#2216 = B_SPLINE_CURVE_WITH_KNOTS('',3,(#153640,#153641,#153642,#153643,#153644,
#153645,#153646,#153647,#153648,#153649,#153650,#153651,#153652,#153653,
#153654,#153655,#153656,#153657,#153658,#153659,#153660,#153661,#153662,
#153663,#153664,#153665,#153666,#153667,#153668,#153669,#153670,#153671,
#153672,#153673,#153674,#153675,#153676,#153677,#153678,#153679,#153680,
#153681,#153682,#153683,#153684,#153685,#153686,#153687,#153688,#153689,
#153690,#153691,#153692,#153693,#153694,#153695,#153696,#153697,#153698,
#153699,#153700,#153701,#153702,#153703,#153704,#153705,#153706,#153707,
#153708,#153709,#153710,#153711,#153712,#153713,#153714,#153715,#153716,
#153717,#153718),.UNSPECIFIED.,.F.,.F.,(4,2,2,2,2,2,2,2,2,1,2,2,2,2,2,2,
2,2,1,2,2,2,2,2,2,2,2,2,2,1,2,2,2,2,2,2,2,2,2,2,4),(-2.04439259789194E-6,
0.,1.16813469870674E-6,2.33626939741348E-6,4.67253879482696E-6,9.34507758965391E-6,
1.5689344351494E-5,2.58970547072731E-5,3.5379828979644E-5,3.67345110185541E-5,
3.74570081059728E-5,3.91084300200728E-5,4.3512221791006E-5,4.45654530819813E-5,
6.26353541219344E-5,6.56193588435038E-5,7.12078702674442E-5,7.16407948148223E-5,
7.25009999535821E-5,7.34840915407362E-5,7.61056691064803E-5,8.65919793694568E-5,
8.8978656792545E-5,9.4044669764307E-5,9.57333407548944E-5,9.79849020756775E-5,
0.00010699114735881,0.000113571562047152,0.000119834164740901,0.000121170237394268,
0.000122506310047635,0.000125178455354369,0.000130522745967838,0.000132049686143115,
0.000136121526610519,0.000138121518246145,0.000141418986123913,0.000147599170334989,
0.000149659231738682,0.00015789947735345,0.000165007876130276),
 .UNSPECIFIED.) ;
#2217 = B_SPLINE_CURVE_WITH_KNOTS('',3,(#153914,#153915,#153916,#153917,#153918,
#153919,#153920,#153921,#153922,#153923),.UNSPECIFIED.,.F.,.F.,(4,2,2,2,
4),(0.015568479421891,0.0195166960586068,0.0234649126953226,0.0272193439053862,
0.0309737751154498),.UNSPECIFIED.) ;
#2218 = B_SPLINE_CURVE_WITH_KNOTS('',3,(#153927,#153928,#153929,#153930,#153931,
#153932,#153933,#153934,#153935,#153936),.UNSPECIFIED.,.F.,.F.,(4,2,2,2,
4),(-0.0304066187772768,-0.0266397364244227,-0.0228728540715686,-0.0190171760180443,
-0.0151614979645201),.UNSPECIFIED.) ;
#2219 = B_SPLINE_CURVE_WITH_KNOTS('',3,(#153940,#153941,#153942,#153943,#153944,
#153945,#153946,#153947,#153948,#153949),.UNSPECIFIED.,.F.,.F.,(4,2,2,2,
4),(-0.045651798047763,-0.0418195667444863,-0.0379873354412096,-0.0341969771092432,
-0.0304066187772768),.UNSPECIFIED.) ;
#2220 = B_SPLINE_CURVE_WITH_KNOTS('',3,(#153953,#153954,#153955,#153956,#153957,
#153958,#153959,#153960,#153961,#153962,#153963,#153964,#153965,#153966,
#153967,#153968,#153969,#153970,#153971,#153972,#153973,#153974,#153975,
#153976,#153977,#153978,#153979,#153980,#153981,#153982,#153983),
 .UNSPECIFIED.,.F.,.F.,(4,3,3,3,3,3,3,3,3,3,4),(0.,1.7421454496146E-5,3.27267941377286E-5,
5.03532648038955E-5,6.54304063451112E-5,8.35242149508461E-5,9.84987277349577E-5,
0.000117634019508126,0.000132578862231984,0.000151533502617316,0.000159722162354116),
 .UNSPECIFIED.) ;
#2221 = B_SPLINE_CURVE_WITH_KNOTS('',3,(#153987,#153988,#153989,#153990,#153991,
#153992,#153993,#153994,#153995,#153996),.UNSPECIFIED.,.F.,.F.,(4,2,2,2,
4),(0.015568479421891,0.0195166960586069,0.0234649126953227,0.0272193439053863,
0.0309737751154499),.UNSPECIFIED.) ;
#2222 = B_SPLINE_CURVE_WITH_KNOTS('',3,(#154000,#154001,#154002,#154003,#154004,
#154005,#154006,#154007,#154008,#154009),.UNSPECIFIED.,.F.,.F.,(4,2,2,2,
4),(-0.0304066810505573,-0.0266163227185909,-0.0228259643866245,-0.0189937330833478,
-0.0151615017800711),.UNSPECIFIED.) ;
#2223 = B_SPLINE_CURVE_WITH_KNOTS('',3,(#154013,#154014,#154015,#154016,#154017,
#154018,#154019,#154020,#154021,#154022),.UNSPECIFIED.,.F.,.F.,(4,2,2,2,
4),(-0.045651801863314,-0.0417961238097898,-0.0379404457562656,-0.0341735634034114,
-0.0304066810505573),.UNSPECIFIED.) ;
#2224 = B_SPLINE_CURVE_WITH_KNOTS('',3,(#154026,#154027,#154028,#154029,#154030,
#154031,#154032,#154033,#154034,#154035,#154036,#154037,#154038,#154039,
#154040,#154041,#154042,#154043,#154044,#154045,#154046,#154047,#154048,
#154049,#154050,#154051,#154052,#154053,#154054,#154055,#154056),
 .UNSPECIFIED.,.F.,.F.,(4,3,3,3,3,3,3,3,3,3,4),(0.,1.74214544961505E-5,
3.27267941377285E-5,5.03532648039079E-5,6.54304063451121E-5,8.35242149508558E-5,
9.84987277349571E-5,0.000117634019508131,0.000132578862231983,0.0001515335026173,
0.000159722162354115),.UNSPECIFIED.) ;
#2225 = B_SPLINE_CURVE_WITH_KNOTS('',3,(#154064,#154065,#154066,#154067,#154068,
#154069,#154070,#154071,#154072,#154073),.UNSPECIFIED.,.F.,.F.,(4,2,2,2,
4),(0.0155684794218909,0.0195166960586067,0.0234649126953226,0.0272193439053862,
0.0309737751154498),.UNSPECIFIED.) ;
#2226 = B_SPLINE_CURVE_WITH_KNOTS('',3,(#154077,#154078,#154079,#154080,#154081,
#154082,#154083,#154084,#154085,#154086),.UNSPECIFIED.,.F.,.F.,(4,2,2,2,
4),(-0.0304066187772767,-0.0266397364244226,-0.0228728540715685,-0.0190171760180443,
-0.0151614979645201),.UNSPECIFIED.) ;
#2227 = B_SPLINE_CURVE_WITH_KNOTS('',3,(#154090,#154091,#154092,#154093,#154094,
#154095,#154096,#154097,#154098,#154099),.UNSPECIFIED.,.F.,.F.,(4,2,2,2,
4),(-0.0456517980477629,-0.0418195667444862,-0.0379873354412095,-0.0341969771092431,
-0.0304066187772767),.UNSPECIFIED.) ;
#2228 = B_SPLINE_CURVE_WITH_KNOTS('',3,(#154103,#154104,#154105,#154106,#154107,
#154108,#154109,#154110,#154111,#154112,#154113,#154114,#154115,#154116,
#154117,#154118,#154119,#154120,#154121,#154122,#154123,#154124,#154125,
#154126,#154127,#154128,#154129,#154130,#154131,#154132,#154133),
 .UNSPECIFIED.,.F.,.F.,(4,3,3,3,3,3,3,3,3,3,4),(0.,1.74214544961512E-5,
3.27267941377284E-5,5.0353264803915E-5,6.54304063451114E-5,8.35242149508516E-5,
9.84987277349568E-5,0.000117634019508137,0.000132578862231983,0.0001515335026173,
0.000159722162354115),.UNSPECIFIED.) ;
#2229 = B_SPLINE_CURVE_WITH_KNOTS('',3,(#154137,#154138,#154139,#154140,#154141,
#154142,#154143,#154144,#154145,#154146),.UNSPECIFIED.,.F.,.F.,(4,2,2,2,
4),(0.0155684794218909,0.0195166960586068,0.0234649126953226,0.0272193439053862,
0.0309737751154498),.UNSPECIFIED.) ;
#2230 = B_SPLINE_CURVE_WITH_KNOTS('',3,(#154150,#154151,#154152,#154153,#154154,
#154155,#154156,#154157,#154158,#154159),.UNSPECIFIED.,.F.,.F.,(4,2,2,2,
4),(-0.0304066810505572,-0.0266163227185908,-0.0228259643866244,-0.0189937330833477,
-0.015161501780071),.UNSPECIFIED.) ;
#2231 = B_SPLINE_CURVE_WITH_KNOTS('',3,(#154163,#154164,#154165,#154166,#154167,
#154168,#154169,#154170,#154171,#154172),.UNSPECIFIED.,.F.,.F.,(4,2,2,2,
4),(-0.0456518018633139,-0.0417961238097897,-0.0379404457562655,-0.0341735634034114,
-0.0304066810505572),.UNSPECIFIED.) ;
#2232 = B_SPLINE_CURVE_WITH_KNOTS('',3,(#154176,#154177,#154178,#154179,#154180,
#154181,#154182,#154183,#154184,#154185,#154186,#154187,#154188,#154189,
#154190,#154191,#154192,#154193,#154194,#154195,#154196,#154197,#154198,
#154199,#154200,#154201,#154202,#154203,#154204,#154205,#154206),
 .UNSPECIFIED.,.F.,.F.,(4,3,3,3,3,3,3,3,3,3,4),(0.,1.74214544961498E-5,
3.27267941377288E-5,5.03532648039088E-5,6.54304063451117E-5,8.35242149508504E-5,
9.84987277349565E-5,0.000117634019508152,0.000132578862231984,0.000151533502617308,
0.000159722162354116),.UNSPECIFIED.) ;
#2233 = B_SPLINE_CURVE_WITH_KNOTS('',3,(#154214,#154215,#154216,#154217,#154218,
#154219,#154220,#154221,#154222,#154223),.UNSPECIFIED.,.F.,.F.,(4,2,2,2,
4),(0.015568479421891,0.0195166960586068,0.0234649126953226,0.0272193439053862,
0.0309737751154498),.UNSPECIFIED.) ;
#2234 = B_SPLINE_CURVE_WITH_KNOTS('',3,(#154227,#154228,#154229,#154230,#154231,
#154232,#154233,#154234,#154235,#154236),.UNSPECIFIED.,.F.,.F.,(4,2,2,2,
4),(-0.0304066187772769,-0.0266397364244227,-0.0228728540715686,-0.0190171760180443,
-0.0151614979645201),.UNSPECIFIED.) ;
#2235 = B_SPLINE_CURVE_WITH_KNOTS('',3,(#154240,#154241,#154242,#154243,#154244,
#154245,#154246,#154247,#154248,#154249),.UNSPECIFIED.,.F.,.F.,(4,2,2,2,
4),(-0.0456517980477632,-0.0418195667444864,-0.0379873354412097,-0.0341969771092433,
-0.0304066187772769),.UNSPECIFIED.) ;
#2236 = B_SPLINE_CURVE_WITH_KNOTS('',3,(#154253,#154254,#154255,#154256,#154257,
#154258,#154259,#154260,#154261,#154262,#154263,#154264,#154265,#154266,
#154267,#154268,#154269,#154270,#154271,#154272,#154273,#154274,#154275,
#154276,#154277,#154278,#154279,#154280,#154281,#154282,#154283),
 .UNSPECIFIED.,.F.,.F.,(4,3,3,3,3,3,3,3,3,3,4),(0.,1.74214544961577E-5,
3.27267941377284E-5,5.0353264803909E-5,6.54304063451126E-5,8.35242149508578E-5,
9.84987277349568E-5,0.000117634019508136,0.000132578862231983,0.000151533502617318,
0.000159722162354101),.UNSPECIFIED.) ;
#2237 = B_SPLINE_CURVE_WITH_KNOTS('',3,(#154287,#154288,#154289,#154290,#154291,
#154292,#154293,#154294,#154295,#154296),.UNSPECIFIED.,.F.,.F.,(4,2,2,2,
4),(0.015568479421891,0.0195166960586068,0.0234649126953226,0.0272193439053862,
0.0309737751154499),.UNSPECIFIED.) ;
#2238 = B_SPLINE_CURVE_WITH_KNOTS('',3,(#154300,#154301,#154302,#154303,#154304,
#154305,#154306,#154307,#154308,#154309),.UNSPECIFIED.,.F.,.F.,(4,2,2,2,
4),(-0.0304066810505573,-0.0266163227185909,-0.0228259643866245,-0.0189937330833478,
-0.0151615017800711),.UNSPECIFIED.) ;
#2239 = B_SPLINE_CURVE_WITH_KNOTS('',3,(#154313,#154314,#154315,#154316,#154317,
#154318,#154319,#154320,#154321,#154322),.UNSPECIFIED.,.F.,.F.,(4,2,2,2,
4),(-0.045651801863314,-0.0417961238097898,-0.0379404457562655,-0.0341735634034114,
-0.0304066810505573),.UNSPECIFIED.) ;
#2240 = B_SPLINE_CURVE_WITH_KNOTS('',3,(#154326,#154327,#154328,#154329,#154330,
#154331,#154332,#154333,#154334,#154335,#154336,#154337,#154338,#154339,
#154340,#154341,#154342,#154343,#154344,#154345,#154346,#154347,#154348,
#154349,#154350,#154351,#154352,#154353,#154354,#154355,#154356),
 .UNSPECIFIED.,.F.,.F.,(4,3,3,3,3,3,3,3,3,3,4),(0.,1.74214544961458E-5,
3.27267941377285E-5,5.03532648039101E-5,6.54304063451128E-5,8.35242149508591E-5,
9.84987277349573E-5,0.000117634019508134,0.000132578862231983,0.000151533502617299,
0.000159722162354101),.UNSPECIFIED.) ;
#2241 = B_SPLINE_CURVE_WITH_KNOTS('',3,(#154364,#154365,#154366,#154367,#154368,
#154369,#154370,#154371,#154372,#154373),.UNSPECIFIED.,.F.,.F.,(4,2,2,2,
4),(0.015568479421891,0.0195166960586068,0.0234649126953226,0.0272193439053863,
0.0309737751154499),.UNSPECIFIED.) ;
#2242 = B_SPLINE_CURVE_WITH_KNOTS('',3,(#154377,#154378,#154379,#154380,#154381,
#154382,#154383,#154384,#154385,#154386),.UNSPECIFIED.,.F.,.F.,(4,2,2,2,
4),(-0.0304066187772769,-0.0266397364244227,-0.0228728540715686,-0.0190171760180443,
-0.0151614979645201),.UNSPECIFIED.) ;
#2243 = B_SPLINE_CURVE_WITH_KNOTS('',3,(#154390,#154391,#154392,#154393,#154394,
#154395,#154396,#154397,#154398,#154399),.UNSPECIFIED.,.F.,.F.,(4,2,2,2,
4),(-0.0456517980477631,-0.0418195667444864,-0.0379873354412096,-0.0341969771092433,
-0.0304066187772769),.UNSPECIFIED.) ;
#2244 = B_SPLINE_CURVE_WITH_KNOTS('',3,(#154403,#154404,#154405,#154406,#154407,
#154408,#154409,#154410,#154411,#154412,#154413,#154414,#154415,#154416,
#154417,#154418,#154419,#154420,#154421,#154422,#154423,#154424,#154425,
#154426,#154427,#154428,#154429,#154430,#154431,#154432,#154433),
 .UNSPECIFIED.,.F.,.F.,(4,3,3,3,3,3,3,3,3,3,4),(0.,1.74214544961475E-5,
3.27267941377288E-5,5.03532648039243E-5,6.54304063451135E-5,8.35242149508581E-5,
9.84987277349581E-5,0.000117634019508135,0.000132578862231985,0.000151533502617287,
0.000159722162354101),.UNSPECIFIED.) ;
#2245 = B_SPLINE_CURVE_WITH_KNOTS('',3,(#154437,#154438,#154439,#154440,#154441,
#154442,#154443,#154444,#154445,#154446),.UNSPECIFIED.,.F.,.F.,(4,2,2,2,
4),(0.015568479421891,0.0195166960586068,0.0234649126953226,0.0272193439053862,
0.0309737751154498),.UNSPECIFIED.) ;
#2246 = B_SPLINE_CURVE_WITH_KNOTS('',3,(#154450,#154451,#154452,#154453,#154454,
#154455,#154456,#154457,#154458,#154459),.UNSPECIFIED.,.F.,.F.,(4,2,2,2,
4),(-0.0304066810505574,-0.026616322718591,-0.0228259643866246,-0.0189937330833478,
-0.0151615017800711),.UNSPECIFIED.) ;
#2247 = B_SPLINE_CURVE_WITH_KNOTS('',3,(#154463,#154464,#154465,#154466,#154467,
#154468,#154469,#154470,#154471,#154472),.UNSPECIFIED.,.F.,.F.,(4,2,2,2,
4),(-0.0456518018633141,-0.0417961238097898,-0.0379404457562656,-0.0341735634034115,
-0.0304066810505573),.UNSPECIFIED.) ;
#2248 = B_SPLINE_CURVE_WITH_KNOTS('',3,(#154476,#154477,#154478,#154479,#154480,
#154481,#154482,#154483,#154484,#154485,#154486,#154487,#154488,#154489,
#154490,#154491,#154492,#154493,#154494,#154495,#154496,#154497,#154498,
#154499,#154500,#154501,#154502,#154503,#154504,#154505,#154506),
 .UNSPECIFIED.,.F.,.F.,(4,3,3,3,3,3,3,3,3,3,4),(0.,1.74214544961482E-5,
3.27267941377286E-5,5.03532648038853E-5,6.54304063451119E-5,8.3524214950871E-5,
9.84987277349562E-5,0.000117634019508187,0.000132578862231985,0.000151533502617321,
0.000159722162354102),.UNSPECIFIED.) ;
#2249 = B_SPLINE_CURVE_WITH_KNOTS('',3,(#154514,#154515,#154516,#154517,#154518,
#154519,#154520,#154521,#154522,#154523),.UNSPECIFIED.,.F.,.F.,(4,2,2,2,
4),(0.0155684794218922,0.0195166960586076,0.023464912695323,0.0272193439053864,
0.0309737751154497),.UNSPECIFIED.) ;
#2250 = B_SPLINE_CURVE_WITH_KNOTS('',3,(#154527,#154528,#154529,#154530,#154531,
#154532,#154533,#154534,#154535,#154536),.UNSPECIFIED.,.F.,.F.,(4,2,2,2,
4),(-0.0304066187772768,-0.0266397364244227,-0.0228728540715685,-0.0190171760180443,
-0.0151614979645201),.UNSPECIFIED.) ;
#2251 = B_SPLINE_CURVE_WITH_KNOTS('',3,(#154540,#154541,#154542,#154543,#154544,
#154545,#154546,#154547,#154548,#154549),.UNSPECIFIED.,.F.,.F.,(4,2,2,2,
4),(-0.0456517980477629,-0.0418195667444862,-0.0379873354412095,-0.0341969771092431,
-0.0304066187772767),.UNSPECIFIED.) ;
#2252 = B_SPLINE_CURVE_WITH_KNOTS('',3,(#154553,#154554,#154555,#154556,#154557,
#154558,#154559,#154560,#154561,#154562,#154563,#154564,#154565,#154566,
#154567,#154568,#154569,#154570,#154571,#154572,#154573,#154574,#154575,
#154576,#154577,#154578,#154579,#154580,#154581,#154582,#154583),
 .UNSPECIFIED.,.F.,.F.,(4,3,3,3,3,3,3,3,3,3,4),(0.,1.74214544961346E-5,
3.27267941377278E-5,5.03532648038744E-5,6.54304063451099E-5,8.35242149508715E-5,
9.84987277349543E-5,0.000117634019508116,0.000132578862231983,0.000151533502617351,
0.000159722162354115),.UNSPECIFIED.) ;
#2253 = B_SPLINE_CURVE_WITH_KNOTS('',3,(#154587,#154588,#154589,#154590,#154591,
#154592,#154593,#154594,#154595,#154596),.UNSPECIFIED.,.F.,.F.,(4,2,2,2,
4),(0.0155684794218919,0.0195166960586074,0.0234649126953229,0.0272193439053863,
0.0309737751154497),.UNSPECIFIED.) ;
#2254 = B_SPLINE_CURVE_WITH_KNOTS('',3,(#154600,#154601,#154602,#154603,#154604,
#154605,#154606,#154607,#154608,#154609),.UNSPECIFIED.,.F.,.F.,(4,2,2,2,
4),(-0.0304066810505573,-0.0266163227185909,-0.0228259643866245,-0.0189937330833478,
-0.0151615017800711),.UNSPECIFIED.) ;
#2255 = B_SPLINE_CURVE_WITH_KNOTS('',3,(#154613,#154614,#154615,#154616,#154617,
#154618,#154619,#154620,#154621,#154622),.UNSPECIFIED.,.F.,.F.,(4,2,2,2,
4),(-0.0456518018633141,-0.0417961238097899,-0.0379404457562657,-0.0341735634034116,
-0.0304066810505575),.UNSPECIFIED.) ;
#2256 = B_SPLINE_CURVE_WITH_KNOTS('',3,(#154626,#154627,#154628,#154629,#154630,
#154631,#154632,#154633,#154634,#154635,#154636,#154637,#154638,#154639,
#154640,#154641,#154642,#154643,#154644,#154645,#154646,#154647,#154648,
#154649,#154650,#154651,#154652,#154653,#154654,#154655,#154656),
 .UNSPECIFIED.,.F.,.F.,(4,3,3,3,3,3,3,3,3,3,4),(0.,1.74214544961505E-5,
3.27267941377287E-5,5.03532648039035E-5,6.54304063451121E-5,8.35242149508726E-5,
9.84987277349566E-5,0.000117634019508169,0.000132578862231986,0.000151533502617341,
0.000159722162354098),.UNSPECIFIED.) ;
#2257 = B_SPLINE_CURVE_WITH_KNOTS('',3,(#154664,#154665,#154666,#154667,#154668,
#154669,#154670,#154671,#154672,#154673),.UNSPECIFIED.,.F.,.F.,(4,2,2,2,
4),(0.0155684794218919,0.0195166960586075,0.023464912695323,0.0272193439053864,
0.0309737751154497),.UNSPECIFIED.) ;
#2258 = B_SPLINE_CURVE_WITH_KNOTS('',3,(#154677,#154678,#154679,#154680,#154681,
#154682,#154683,#154684,#154685,#154686),.UNSPECIFIED.,.F.,.F.,(4,2,2,2,
4),(-0.0304066187772767,-0.0266397364244226,-0.0228728540715685,-0.0190171760180443,
-0.0151614979645201),.UNSPECIFIED.) ;
#2259 = B_SPLINE_CURVE_WITH_KNOTS('',3,(#154690,#154691,#154692,#154693,#154694,
#154695,#154696,#154697,#154698,#154699),.UNSPECIFIED.,.F.,.F.,(4,2,2,2,
4),(-0.0456517980477628,-0.0418195667444863,-0.0379873354412098,-0.0341969771092433,
-0.0304066187772768),.UNSPECIFIED.) ;
#2260 = B_SPLINE_CURVE_WITH_KNOTS('',3,(#154703,#154704,#154705,#154706,#154707,
#154708,#154709,#154710,#154711,#154712,#154713,#154714,#154715,#154716,
#154717,#154718,#154719,#154720,#154721,#154722,#154723,#154724,#154725,
#154726,#154727,#154728,#154729,#154730,#154731,#154732,#154733),
 .UNSPECIFIED.,.F.,.F.,(4,3,3,3,3,3,3,3,3,3,4),(0.,1.74214544961313E-5,
3.27267941377278E-5,5.03532648038729E-5,6.54304063451099E-5,8.35242149508288E-5,
9.84987277349543E-5,0.000117634019508168,0.000132578862231983,0.000151533502617396,
0.000159722162354101),.UNSPECIFIED.) ;
#2261 = B_SPLINE_CURVE_WITH_KNOTS('',3,(#154737,#154738,#154739,#154740,#154741,
#154742,#154743,#154744,#154745,#154746),.UNSPECIFIED.,.F.,.F.,(4,2,2,2,
4),(0.0155684794218909,0.0195166960586067,0.0234649126953226,0.0272193439053862,
0.0309737751154498),.UNSPECIFIED.) ;
#2262 = B_SPLINE_CURVE_WITH_KNOTS('',3,(#154750,#154751,#154752,#154753,#154754,
#154755,#154756,#154757,#154758,#154759),.UNSPECIFIED.,.F.,.F.,(4,2,2,2,
4),(-0.0304066810505572,-0.0266163227185908,-0.0228259643866244,-0.0189937330833477,
-0.0151615017800711),.UNSPECIFIED.) ;
#2263 = B_SPLINE_CURVE_WITH_KNOTS('',3,(#154763,#154764,#154765,#154766,#154767,
#154768,#154769,#154770,#154771,#154772),.UNSPECIFIED.,.F.,.F.,(4,2,2,2,
4),(-0.0456518018633141,-0.0417961238097899,-0.0379404457562657,-0.0341735634034116,
-0.0304066810505575),.UNSPECIFIED.) ;
#2264 = B_SPLINE_CURVE_WITH_KNOTS('',3,(#154776,#154777,#154778,#154779,#154780,
#154781,#154782,#154783,#154784,#154785,#154786,#154787,#154788,#154789,
#154790,#154791,#154792,#154793,#154794,#154795,#154796,#154797,#154798,
#154799,#154800,#154801,#154802,#154803,#154804,#154805,#154806),
 .UNSPECIFIED.,.F.,.F.,(4,3,3,3,3,3,3,3,3,3,4),(0.,1.74214544961324E-5,
3.27267941377287E-5,5.03532648039218E-5,6.54304063451121E-5,8.35242149508849E-5,
9.84987277349566E-5,0.000117634019508209,0.000132578862231986,0.000151533502617305,
0.000159722162354113),.UNSPECIFIED.) ;
#2265 = B_SPLINE_CURVE_WITH_KNOTS('',3,(#154814,#154815,#154816,#154817,#154818,
#154819,#154820,#154821,#154822,#154823),.UNSPECIFIED.,.F.,.F.,(4,2,2,2,
4),(0.0155684794218922,0.0195166960586077,0.0234649126953232,0.0272193439053865,
0.0309737751154498),.UNSPECIFIED.) ;
#2266 = B_SPLINE_CURVE_WITH_KNOTS('',3,(#154827,#154828,#154829,#154830,#154831,
#154832,#154833,#154834,#154835,#154836),.UNSPECIFIED.,.F.,.F.,(4,2,2,2,
4),(-0.0304066187772767,-0.0266397364244226,-0.0228728540715685,-0.0190171760180443,
-0.0151614979645201),.UNSPECIFIED.) ;
#2267 = B_SPLINE_CURVE_WITH_KNOTS('',3,(#154840,#154841,#154842,#154843,#154844,
#154845,#154846,#154847,#154848,#154849),.UNSPECIFIED.,.F.,.F.,(4,2,2,2,
4),(-0.0456517980477626,-0.0418195667444861,-0.0379873354412096,-0.0341969771092432,
-0.0304066187772767),.UNSPECIFIED.) ;
#2268 = B_SPLINE_CURVE_WITH_KNOTS('',3,(#154853,#154854,#154855,#154856,#154857,
#154858,#154859,#154860,#154861,#154862,#154863,#154864,#154865,#154866,
#154867,#154868,#154869,#154870,#154871,#154872,#154873,#154874,#154875,
#154876,#154877,#154878,#154879,#154880,#154881,#154882,#154883),
 .UNSPECIFIED.,.F.,.F.,(4,3,3,3,3,3,3,3,3,3,4),(0.,1.74214544961345E-5,
3.27267941377278E-5,5.03532648038844E-5,6.54304063451099E-5,8.3524214950855E-5,
9.84987277349543E-5,0.000117634019508163,0.000132578862231983,0.00015153350261733,
0.000159722162354115),.UNSPECIFIED.) ;
#2269 = B_SPLINE_CURVE_WITH_KNOTS('',3,(#154887,#154888,#154889,#154890,#154891,
#154892,#154893,#154894,#154895,#154896),.UNSPECIFIED.,.F.,.F.,(4,2,2,2,
4),(0.0155684794218909,0.0195166960586067,0.0234649126953226,0.0272193439053862,
0.0309737751154498),.UNSPECIFIED.) ;
#2270 = B_SPLINE_CURVE_WITH_KNOTS('',3,(#154900,#154901,#154902,#154903,#154904,
#154905,#154906,#154907,#154908,#154909),.UNSPECIFIED.,.F.,.F.,(4,2,2,2,
4),(-0.0304066810505572,-0.0266163227185908,-0.0228259643866244,-0.0189937330833477,
-0.0151615017800711),.UNSPECIFIED.) ;
#2271 = B_SPLINE_CURVE_WITH_KNOTS('',3,(#154913,#154914,#154915,#154916,#154917,
#154918,#154919,#154920,#154921,#154922),.UNSPECIFIED.,.F.,.F.,(4,2,2,2,
4),(-0.0456518018633141,-0.0417961238097899,-0.0379404457562657,-0.0341735634034116,
-0.0304066810505575),.UNSPECIFIED.) ;
#2272 = B_SPLINE_CURVE_WITH_KNOTS('',3,(#154926,#154927,#154928,#154929,#154930,
#154931,#154932,#154933,#154934,#154935,#154936,#154937,#154938,#154939,
#154940,#154941,#154942,#154943,#154944,#154945,#154946,#154947,#154948,
#154949,#154950,#154951,#154952,#154953,#154954,#154955,#154956),
 .UNSPECIFIED.,.F.,.F.,(4,3,3,3,3,3,3,3,3,3,4),(0.,1.74214544961354E-5,
3.27267941377287E-5,5.03532648039094E-5,6.54304063451121E-5,8.35242149508793E-5,
9.84987277349566E-5,0.000117634019508197,0.000132578862231986,0.000151533502617206,
0.000159722162354098),.UNSPECIFIED.) ;
#2273 = B_SPLINE_CURVE_WITH_KNOTS('',3,(#154964,#154965,#154966,#154967,#154968,
#154969,#154970,#154971,#154972,#154973),.UNSPECIFIED.,.F.,.F.,(4,2,2,2,
4),(0.0155684794218921,0.0195166960586076,0.0234649126953232,0.0272193439053865,
0.0309737751154498),.UNSPECIFIED.) ;
#2274 = B_SPLINE_CURVE_WITH_KNOTS('',3,(#154977,#154978,#154979,#154980,#154981,
#154982,#154983,#154984,#154985,#154986),.UNSPECIFIED.,.F.,.F.,(4,2,2,2,
4),(-0.0304066187772767,-0.0266397364244226,-0.0228728540715685,-0.0190171760180442,
-0.01516149796452),.UNSPECIFIED.) ;
#2275 = B_SPLINE_CURVE_WITH_KNOTS('',3,(#154990,#154991,#154992,#154993,#154994,
#154995,#154996,#154997,#154998,#154999),.UNSPECIFIED.,.F.,.F.,(4,2,2,2,
4),(-0.0456517980477622,-0.0418195667444857,-0.0379873354412092,-0.0341969771092428,
-0.0304066187772765),.UNSPECIFIED.) ;
#2276 = B_SPLINE_CURVE_WITH_KNOTS('',3,(#155003,#155004,#155005,#155006,#155007,
#155008,#155009,#155010,#155011,#155012,#155013,#155014,#155015,#155016,
#155017,#155018,#155019,#155020,#155021,#155022,#155023,#155024,#155025,
#155026,#155027,#155028,#155029,#155030,#155031,#155032,#155033),
 .UNSPECIFIED.,.F.,.F.,(4,3,3,3,3,3,3,3,3,3,4),(0.,1.74214544961244E-5,
3.27267941377278E-5,5.03532648038767E-5,6.54304063451099E-5,8.3524214950855E-5,
9.84987277349543E-5,0.000117634019508207,0.000132578862231983,0.000151533502617196,
0.000159722162354101),.UNSPECIFIED.) ;
#2277 = B_SPLINE_CURVE_WITH_KNOTS('',3,(#155037,#155038,#155039,#155040,#155041,
#155042,#155043,#155044,#155045,#155046),.UNSPECIFIED.,.F.,.F.,(4,2,2,2,
4),(0.015568479421892,0.0195166960586076,0.0234649126953231,0.0272193439053864,
0.0309737751154497),.UNSPECIFIED.) ;
#2278 = B_SPLINE_CURVE_WITH_KNOTS('',3,(#155050,#155051,#155052,#155053,#155054,
#155055,#155056,#155057,#155058,#155059),.UNSPECIFIED.,.F.,.F.,(4,2,2,2,
4),(-0.0304066810505572,-0.0266163227185908,-0.0228259643866244,-0.0189937330833477,
-0.0151615017800711),.UNSPECIFIED.) ;
#2279 = B_SPLINE_CURVE_WITH_KNOTS('',3,(#155063,#155064,#155065,#155066,#155067,
#155068,#155069,#155070,#155071,#155072),.UNSPECIFIED.,.F.,.F.,(4,2,2,2,
4),(-0.0456518018633141,-0.0417961238097899,-0.0379404457562657,-0.0341735634034116,
-0.0304066810505575),.UNSPECIFIED.) ;
#2280 = B_SPLINE_CURVE_WITH_KNOTS('',3,(#155076,#155077,#155078,#155079,#155080,
#155081,#155082,#155083,#155084,#155085,#155086,#155087,#155088,#155089,
#155090,#155091,#155092,#155093,#155094,#155095,#155096,#155097,#155098,
#155099,#155100,#155101,#155102,#155103,#155104,#155105,#155106),
 .UNSPECIFIED.,.F.,.F.,(4,3,3,3,3,3,3,3,3,3,4),(0.,1.74214544961202E-5,
3.27267941377275E-5,5.03532648039345E-5,6.54304063451101E-5,8.35242149508574E-5,
9.84987277349543E-5,0.000117634019508031,0.000132578862231981,0.000151533502617366,
0.000159722162354098),.UNSPECIFIED.) ;
#2281 = B_SPLINE_CURVE_WITH_KNOTS('',3,(#155114,#155115,#155116,#155117,#155118,
#155119,#155120,#155121,#155122,#155123),.UNSPECIFIED.,.F.,.F.,(4,2,2,2,
4),(0.0155684794218921,0.0195166960586076,0.0234649126953232,0.0272193439053865,
0.0309737751154498),.UNSPECIFIED.) ;
#2282 = B_SPLINE_CURVE_WITH_KNOTS('',3,(#155127,#155128,#155129,#155130,#155131,
#155132,#155133,#155134,#155135,#155136),.UNSPECIFIED.,.F.,.F.,(4,2,2,2,
4),(-0.0304066187772767,-0.0266397364244226,-0.0228728540715685,-0.0190171760180442,
-0.01516149796452),.UNSPECIFIED.) ;
#2283 = B_SPLINE_CURVE_WITH_KNOTS('',3,(#155140,#155141,#155142,#155143,#155144,
#155145,#155146,#155147,#155148,#155149),.UNSPECIFIED.,.F.,.F.,(4,2,2,2,
4),(-0.0456517980477626,-0.041819566744486,-0.0379873354412094,-0.034196977109243,
-0.0304066187772766),.UNSPECIFIED.) ;
#2284 = B_SPLINE_CURVE_WITH_KNOTS('',3,(#155153,#155154,#155155,#155156,#155157,
#155158,#155159,#155160,#155161,#155162,#155163,#155164,#155165,#155166,
#155167,#155168,#155169,#155170,#155171,#155172,#155173,#155174,#155175,
#155176,#155177,#155178,#155179,#155180,#155181,#155182,#155183),
 .UNSPECIFIED.,.F.,.F.,(4,3,3,3,3,3,3,3,3,3,4),(0.,1.74214544961506E-5,
3.27267941377281E-5,5.03532648039511E-5,6.54304063451099E-5,8.35242149508654E-5,
9.84987277349558E-5,0.000117634019508106,0.000132578862231983,0.000151533502617118,
0.000159722162354107),.UNSPECIFIED.) ;
#2285 = B_SPLINE_CURVE_WITH_KNOTS('',3,(#155187,#155188,#155189,#155190,#155191,
#155192,#155193,#155194,#155195,#155196),.UNSPECIFIED.,.F.,.F.,(4,2,2,2,
4),(0.0155684794218909,0.0195166960586068,0.0234649126953227,0.0272193439053862,
0.0309737751154498),.UNSPECIFIED.) ;
#2286 = B_SPLINE_CURVE_WITH_KNOTS('',3,(#155200,#155201,#155202,#155203,#155204,
#155205,#155206,#155207,#155208,#155209),.UNSPECIFIED.,.F.,.F.,(4,2,2,2,
4),(-0.0304066810505572,-0.0266163227185907,-0.0228259643866243,-0.0189937330833476,
-0.0151615017800709),.UNSPECIFIED.) ;
#2287 = B_SPLINE_CURVE_WITH_KNOTS('',3,(#155213,#155214,#155215,#155216,#155217,
#155218,#155219,#155220,#155221,#155222),.UNSPECIFIED.,.F.,.F.,(4,2,2,2,
4),(-0.0456518018633141,-0.0417961238097899,-0.0379404457562657,-0.0341735634034116,
-0.0304066810505575),.UNSPECIFIED.) ;
#2288 = B_SPLINE_CURVE_WITH_KNOTS('',3,(#155226,#155227,#155228,#155229,#155230,
#155231,#155232,#155233,#155234,#155235,#155236,#155237,#155238,#155239,
#155240,#155241,#155242,#155243,#155244,#155245,#155246,#155247,#155248,
#155249,#155250,#155251,#155252,#155253,#155254,#155255,#155256),
 .UNSPECIFIED.,.F.,.F.,(4,3,3,3,3,3,3,3,3,3,4),(0.,1.74214544961235E-5,
3.27267941377286E-5,5.03532648039153E-5,6.54304063451125E-5,8.35242149508653E-5,
9.84987277349577E-5,0.000117634019508158,0.000132578862231986,0.000151533502617377,
0.000159722162354107),.UNSPECIFIED.) ;
#2289 = B_SPLINE_CURVE_WITH_KNOTS('',3,(#155354,#155355,#155356,#155357,#155358,
#155359,#155360,#155361,#155362,#155363),.UNSPECIFIED.,.F.,.F.,(4,2,2,2,
4),(0.015568479421891,0.0195166960586068,0.0234649126953226,0.0272193439053862,
0.0309737751154498),.UNSPECIFIED.) ;
#2290 = B_SPLINE_CURVE_WITH_KNOTS('',3,(#155367,#155368,#155369,#155370,#155371,
#155372,#155373,#155374,#155375,#155376),.UNSPECIFIED.,.F.,.F.,(4,2,2,2,
4),(-0.0304066187772769,-0.0266397364244227,-0.0228728540715685,-0.0190171760180443,
-0.0151614979645201),.UNSPECIFIED.) ;
#2291 = B_SPLINE_CURVE_WITH_KNOTS('',3,(#155380,#155381,#155382,#155383,#155384,
#155385,#155386,#155387,#155388,#155389),.UNSPECIFIED.,.F.,.F.,(4,2,2,2,
4),(-0.0456517980477631,-0.0418195667444864,-0.0379873354412096,-0.0341969771092432,
-0.0304066187772769),.UNSPECIFIED.) ;
#2292 = B_SPLINE_CURVE_WITH_KNOTS('',3,(#155393,#155394,#155395,#155396,#155397,
#155398,#155399,#155400,#155401,#155402,#155403,#155404,#155405,#155406,
#155407,#155408,#155409,#155410,#155411,#155412,#155413,#155414,#155415,
#155416,#155417,#155418,#155419,#155420,#155421,#155422,#155423),
 .UNSPECIFIED.,.F.,.F.,(4,3,3,3,3,3,3,3,3,3,4),(0.,1.74214544961506E-5,
3.27267941377286E-5,5.03532648039032E-5,6.54304063451112E-5,8.35242149508585E-5,
9.8498727734957E-5,0.000117634019508128,0.000132578862231984,0.000151533502617294,
0.000159722162354116),.UNSPECIFIED.) ;
#2293 = B_SPLINE_CURVE_WITH_KNOTS('',3,(#155427,#155428,#155429,#155430,#155431,
#155432,#155433,#155434,#155435,#155436),.UNSPECIFIED.,.F.,.F.,(4,2,2,2,
4),(0.015568479421891,0.0195166960586068,0.0234649126953226,0.0272193439053862,
0.0309737751154498),.UNSPECIFIED.) ;
#2294 = B_SPLINE_CURVE_WITH_KNOTS('',3,(#155440,#155441,#155442,#155443,#155444,
#155445,#155446,#155447,#155448,#155449),.UNSPECIFIED.,.F.,.F.,(4,2,2,2,
4),(-0.0304066810505573,-0.0266163227185909,-0.0228259643866245,-0.0189937330833478,
-0.0151615017800711),.UNSPECIFIED.) ;
#2295 = B_SPLINE_CURVE_WITH_KNOTS('',3,(#155453,#155454,#155455,#155456,#155457,
#155458,#155459,#155460,#155461,#155462),.UNSPECIFIED.,.F.,.F.,(4,2,2,2,
4),(-0.045651801863314,-0.0417961238097898,-0.0379404457562656,-0.0341735634034115,
-0.0304066810505573),.UNSPECIFIED.) ;
#2296 = B_SPLINE_CURVE_WITH_KNOTS('',3,(#155466,#155467,#155468,#155469,#155470,
#155471,#155472,#155473,#155474,#155475,#155476,#155477,#155478,#155479,
#155480,#155481,#155482,#155483,#155484,#155485,#155486,#155487,#155488,
#155489,#155490,#155491,#155492,#155493,#155494,#155495,#155496),
 .UNSPECIFIED.,.F.,.F.,(4,3,3,3,3,3,3,3,3,3,4),(0.,1.74214544961524E-5,
3.27267941377286E-5,5.03532648039125E-5,6.54304063451117E-5,8.35242149508611E-5,
9.84987277349575E-5,0.000117634019508132,0.000132578862231984,0.000151533502617307,
0.000159722162354116),.UNSPECIFIED.) ;
#2297 = B_SPLINE_CURVE_WITH_KNOTS('',3,(#156379,#156380,#156381,#156382,#156383,
#156384),.UNSPECIFIED.,.F.,.F.,(4,2,4),(3.14159265358979,3.92699081698724,
4.71238898038469),.UNSPECIFIED.) ;
#2298 = B_SPLINE_CURVE_WITH_KNOTS('',3,(#156388,#156389,#156390,#156391,#156392,
#156393),.UNSPECIFIED.,.F.,.F.,(4,2,4),(4.71238898038469,5.49778714378214,
6.28318530717959),.UNSPECIFIED.) ;
#2299 = B_SPLINE_CURVE_WITH_KNOTS('',3,(#156397,#156398,#156399,#156400,#156401,
#156402),.UNSPECIFIED.,.F.,.F.,(4,2,4),(0.,0.785398163397448,1.5707963267949),
 .UNSPECIFIED.) ;
#2300 = B_SPLINE_CURVE_WITH_KNOTS('',3,(#156406,#156407,#156408,#156409,#156410,
#156411),.UNSPECIFIED.,.F.,.F.,(4,2,4),(1.5707963267949,2.35619449019234,
3.14159265358979),.UNSPECIFIED.) ;
#2301 = B_SPLINE_CURVE_WITH_KNOTS('',3,(#156479,#156480,#156481,#156482,#156483,
#156484),.UNSPECIFIED.,.F.,.F.,(4,2,4),(3.14159265358979,3.92699081698724,
4.71238898038469),.UNSPECIFIED.) ;
#2302 = B_SPLINE_CURVE_WITH_KNOTS('',3,(#156488,#156489,#156490,#156491,#156492,
#156493),.UNSPECIFIED.,.F.,.F.,(4,2,4),(4.71238898038469,5.49778714378214,
6.28318530717959),.UNSPECIFIED.) ;
#2303 = B_SPLINE_CURVE_WITH_KNOTS('',3,(#156497,#156498,#156499,#156500,#156501,
#156502),.UNSPECIFIED.,.F.,.F.,(4,2,4),(0.,0.785398163397448,1.5707963267949),
 .UNSPECIFIED.) ;
#2304 = B_SPLINE_CURVE_WITH_KNOTS('',3,(#156506,#156507,#156508,#156509,#156510,
#156511),.UNSPECIFIED.,.F.,.F.,(4,2,4),(1.5707963267949,2.35619449019234,
3.14159265358979),.UNSPECIFIED.) ;
#2305 = B_SPLINE_CURVE_WITH_KNOTS('',3,(#157479,#157480,#157481,#157482,#157483,
#157484),.UNSPECIFIED.,.F.,.F.,(4,2,4),(4.71238898038469,5.49778714378214,
6.28318530717959),.UNSPECIFIED.) ;
#2306 = B_SPLINE_CURVE_WITH_KNOTS('',3,(#157514,#157515,#157516,#157517,#157518,
#157519),.UNSPECIFIED.,.F.,.F.,(4,2,4),(3.14159265358979,3.92699081698724,
4.71238898038469),.UNSPECIFIED.) ;
#2307 = B_SPLINE_CURVE_WITH_KNOTS('',3,(#157689,#157690,#157691,#157692,#157693,
#157694,#157695,#157696,#157697,#157698,#157699,#157700,#157701,#157702,
#157703,#157704,#157705,#157706,#157707,#157708,#157709,#157710,#157711,
#157712,#157713,#157714,#157715,#157716,#157717,#157718,#157719,#157720,
#157721,#157722),.UNSPECIFIED.,.F.,.F.,(4,2,2,2,2,2,2,2,2,2,2,2,2,2,2,2,
4),(0.,8.71783727051651E-6,1.76441105356865E-5,3.58270994901032E-5,4.83658434534696E-5,
6.68919645678521E-5,7.05613987999434E-5,8.27232142756399E-5,9.8736263280299E-5,
0.000104111574538336,0.000114567411933631,0.000115616565506963,0.000123791392829713,
0.00012426720927833,0.000126967031952651,0.00013254691974501,0.000134871234237328),
 .UNSPECIFIED.) ;
#2308 = B_SPLINE_CURVE_WITH_KNOTS('',3,(#157729,#157730,#157731,#157732,#157733,
#157734,#157735,#157736,#157737,#157738,#157739,#157740,#157741,#157742,
#157743,#157744,#157745,#157746,#157747,#157748,#157749,#157750,#157751,
#157752,#157753,#157754),.UNSPECIFIED.,.F.,.F.,(4,2,2,2,2,2,2,2,2,2,2,2,
4),(0.,5.70004774914365E-6,8.25511347640861E-6,9.93040049428829E-6,2.64556965229606E-5,
3.0587336112473E-5,4.24593515817714E-5,6.43784914888441E-5,7.66562101644909E-5,
9.74321373320278E-5,9.92796257088233E-5,0.000111632960404945,0.000135309975333051),
 .UNSPECIFIED.) ;
#2309 = B_SPLINE_CURVE_WITH_KNOTS('',3,(#157757,#157758,#157759,#157760,#157761,
#157762,#157763,#157764,#157765,#157766,#157767,#157768,#157769,#157770,
#157771,#157772,#157773,#157774,#157775,#157776,#157777,#157778,#157779,
#157780,#157781,#157782,#157783,#157784,#157785,#157786,#157787,#157788,
#157789,#157790,#157791,#157792,#157793,#157794,#157795,#157796,#157797,
#157798,#157799,#157800,#157801,#157802,#157803,#157804,#157805,#157806,
#157807,#157808,#157809,#157810,#157811),.UNSPECIFIED.,.F.,.F.,(4,3,3,3,
3,3,3,3,3,3,3,3,3,3,3,3,3,3,4),(0.,1.96170179200463E-5,2.35258500143173E-5,
3.58003153605657E-5,5.29187212185648E-5,5.64435994881288E-5,5.82792926524093E-5,
7.046492538053E-5,8.72923312905478E-5,9.05038369578109E-5,9.22578228185112E-5,
0.000103663146463144,0.000113866005521512,0.000117768598772948,0.000124579094175181,
0.000129312863866852,0.000130178750830806,0.000132692979584748,0.000134419842078312),
 .UNSPECIFIED.) ;
#2310 = B_SPLINE_CURVE_WITH_KNOTS('',3,(#157820,#157821,#157822,#157823,#157824,
#157825,#157826,#157827,#157828,#157829,#157830,#157831,#157832,#157833,
#157834,#157835,#157836,#157837,#157838,#157839,#157840,#157841,#157842,
#157843,#157844,#157845),.UNSPECIFIED.,.F.,.F.,(4,2,2,2,2,2,2,2,2,2,2,2,
4),(2.16840434497101E-19,5.55321021973507E-6,8.2551134764302E-6,1.91711188535186E-5,
3.04852632940551E-5,5.08165579103458E-5,5.19149958125389E-5,6.39742577536716E-5,
8.61162395509796E-5,9.85980048375157E-5,0.000117622240611177,0.000125683481931498,
0.000134262298488522),.UNSPECIFIED.) ;
#2311 = B_SPLINE_CURVE_WITH_KNOTS('',3,(#161903,#161904,#161905,#161906,#161907,
#161908,#161909,#161910,#161911,#161912,#161913,#161914,#161915,#161916),
 .UNSPECIFIED.,.F.,.F.,(4,2,2,2,2,2,4),(0.784956998631289,0.966941694311738,
1.14311721215536,1.16348181627601,1.34745079132926,1.51752882030803,1.5707963267949),
 .UNSPECIFIED.) ;
#2312 = B_SPLINE_CURVE_WITH_KNOTS('',3,(#161918,#161919,#161920,#161921,#161922,
#161923,#161924,#161925,#161926,#161927,#161928,#161929,#161930,#161931),
 .UNSPECIFIED.,.F.,.F.,(4,2,2,2,2,2,4),(1.5707963267949,1.74016540886056,
1.92604436639238,2.10178657601615,2.12292067848492,2.30714825223632,2.35663565495862),
 .UNSPECIFIED.) ;
#2313 = B_SPLINE_CURVE_WITH_KNOTS('',3,(#161935,#161936,#161937,#161938,#161939,
#161940,#161941,#161942,#161943,#161944,#161945,#161946,#161947,#161948),
 .UNSPECIFIED.,.F.,.F.,(4,2,2,2,2,2,4),(1.5707963267949,1.74016540886327,
1.92604436640156,2.10178657606191,2.12292067849459,2.30714825224118,2.35663565495873),
 .UNSPECIFIED.) ;
#2314 = B_SPLINE_CURVE_WITH_KNOTS('',3,(#161952,#161953,#161954,#161955,#161956,
#161957,#161958,#161959,#161960,#161961,#161962,#161963,#161964,#161965),
 .UNSPECIFIED.,.F.,.F.,(4,2,2,2,2,2,4),(3.92654965222093,4.10853434790149,
4.28470986572121,4.30507446986523,4.48904344491852,4.65912147389766,4.71238898038469),
 .UNSPECIFIED.) ;
#2315 = B_SPLINE_CURVE_WITH_KNOTS('',3,(#161968,#161969,#161970,#161971,#161972,
#161973,#161974,#161975,#161976,#161977,#161978,#161979,#161980,#161981),
 .UNSPECIFIED.,.F.,.F.,(4,2,2,2,2,2,4),(4.71238898038469,4.88175806245295,
5.06763701999115,5.24337922965399,5.26451333208407,5.44874090583052,5.49822830854846),
 .UNSPECIFIED.) ;
#2316 = B_SPLINE_CURVE_WITH_KNOTS('',3,(#161985,#161986,#161987,#161988,#161989,
#161990,#161991,#161992,#161993,#161994,#161995,#161996,#161997,#161998),
 .UNSPECIFIED.,.F.,.F.,(4,2,2,2,2,2,4),(0.784956998631145,0.96694169431173,
1.14311721212928,1.16348181627549,1.34745079132874,1.51752882030789,1.5707963267949),
 .UNSPECIFIED.) ;
#2317 = B_SPLINE_CURVE_WITH_KNOTS('',3,(#162001,#162002,#162003,#162004,#162005,
#162006,#162007,#162008,#162009,#162010,#162011,#162012,#162013,#162014),
 .UNSPECIFIED.,.F.,.F.,(4,2,2,2,2,2,4),(4.71238898038469,4.88175806245252,
5.06763701999072,5.24337922963828,5.26451333208419,5.44874090583056,5.49822830854825),
 .UNSPECIFIED.) ;
#2318 = B_SPLINE_CURVE_WITH_KNOTS('',3,(#162018,#162019,#162020,#162021,#162022,
#162023,#162024,#162025,#162026,#162027,#162028,#162029,#162030,#162031),
 .UNSPECIFIED.,.F.,.F.,(4,2,2,2,2,2,4),(3.92654965222105,4.1085343479052,
4.28470986576985,4.30507446986799,4.48904344491476,4.65912147389089,4.71238898038469),
 .UNSPECIFIED.) ;
#2319 = B_SPLINE_CURVE_WITH_KNOTS('',3,(#162035,#162036,#162037,#162038,#162039,
#162040,#162041,#162042,#162043,#162044,#162045,#162046,#162047,#162048),
 .UNSPECIFIED.,.F.,.F.,(4,2,2,2,2,2,4),(0.784956998631336,0.966941694311724,
1.14311721213576,1.16348181627607,1.34745079132915,1.51752882030789,1.5707963267949),
 .UNSPECIFIED.) ;
#2320 = B_SPLINE_CURVE_WITH_KNOTS('',3,(#162050,#162051,#162052,#162053,#162054,
#162055,#162056,#162057,#162058,#162059,#162060,#162061,#162062,#162063),
 .UNSPECIFIED.,.F.,.F.,(4,2,2,2,2,2,4),(1.5707963267949,1.74016540886059,
1.92604436639241,2.10178657602066,2.122920678485,2.30714825223642,2.35663565495861),
 .UNSPECIFIED.) ;
#2321 = B_SPLINE_CURVE_WITH_KNOTS('',3,(#162067,#162068,#162069,#162070,#162071,
#162072,#162073,#162074,#162075,#162076,#162077,#162078,#162079,#162080),
 .UNSPECIFIED.,.F.,.F.,(4,2,2,2,2,2,4),(1.5707963267949,1.74016540886221,
1.92604436639984,2.10178657605964,2.12292067849308,2.30714825223984,2.3566356549586),
 .UNSPECIFIED.) ;
#2322 = B_SPLINE_CURVE_WITH_KNOTS('',3,(#162084,#162085,#162086,#162087,#162088,
#162089,#162090,#162091,#162092,#162093,#162094,#162095,#162096,#162097),
 .UNSPECIFIED.,.F.,.F.,(4,2,2,2,2,2,4),(3.92654965222098,4.10853434790153,
4.28470986572269,4.30507446986533,4.48904344491862,4.6591214738977,4.71238898038469),
 .UNSPECIFIED.) ;
#2323 = B_SPLINE_CURVE_WITH_KNOTS('',3,(#162100,#162101,#162102,#162103,#162104,
#162105,#162106,#162107,#162108,#162109,#162110,#162111,#162112,#162113),
 .UNSPECIFIED.,.F.,.F.,(4,2,2,2,2,2,4),(4.71238898038469,4.88175806245294,
5.06763701999115,5.24337922965432,5.26451333208408,5.44874090583055,5.49822830854844),
 .UNSPECIFIED.) ;
#2324 = B_SPLINE_CURVE_WITH_KNOTS('',3,(#162117,#162118,#162119,#162120,#162121,
#162122,#162123,#162124,#162125,#162126,#162127,#162128,#162129,#162130),
 .UNSPECIFIED.,.F.,.F.,(4,2,2,2,2,2,4),(0.784956998631396,0.96694169431207,
1.14311721213661,1.16348181627586,1.34745079132829,1.51752882030632,1.5707963267949),
 .UNSPECIFIED.) ;
#2325 = B_SPLINE_CURVE_WITH_KNOTS('',3,(#162133,#162134,#162135,#162136,#162137,
#162138,#162139,#162140,#162141,#162142,#162143,#162144,#162145,#162146),
 .UNSPECIFIED.,.F.,.F.,(4,2,2,2,2,2,4),(4.71238898038469,4.88175806245104,
5.06763701998726,5.243379229698,5.26451333208011,5.44874090582758,5.49822830854818),
 .UNSPECIFIED.) ;
#2326 = B_SPLINE_CURVE_WITH_KNOTS('',3,(#162150,#162151,#162152,#162153,#162154,
#162155,#162156,#162157,#162158,#162159,#162160,#162161,#162162,#162163),
 .UNSPECIFIED.,.F.,.F.,(4,2,2,2,2,2,4),(3.92654965222123,4.1085343479017,
4.28470986568251,4.30507446986548,4.48904344491786,4.65912147389568,4.71238898038469),
 .UNSPECIFIED.) ;
#2327 = B_SPLINE_CURVE_WITH_KNOTS('',3,(#162167,#162168,#162169,#162170,#162171,
#162172,#162173,#162174,#162175,#162176,#162177,#162178,#162179,#162180),
 .UNSPECIFIED.,.F.,.F.,(4,2,2,2,2,2,4),(0.784956998631411,0.966941694312594,
1.14311721209517,1.16348181627623,1.3474507913276,1.51752882030504,1.5707963267949),
 .UNSPECIFIED.) ;
#2328 = B_SPLINE_CURVE_WITH_KNOTS('',3,(#162182,#162183,#162184,#162185,#162186,
#162187,#162188,#162189,#162190,#162191,#162192,#162193,#162194,#162195),
 .UNSPECIFIED.,.F.,.F.,(4,2,2,2,2,2,4),(1.5707963267949,1.74016540886207,
1.92604436639947,2.10178657612721,2.12292067849245,2.30714825223912,2.35663565495845),
 .UNSPECIFIED.) ;
#2329 = B_SPLINE_CURVE_WITH_KNOTS('',3,(#162199,#162200,#162201,#162202,#162203,
#162204,#162205,#162206,#162207,#162208,#162209,#162210,#162211,#162212),
 .UNSPECIFIED.,.F.,.F.,(4,2,2,2,2,2,4),(1.5707963267949,1.74016540886209,
1.92604436639968,2.10178657607307,2.12292067849299,2.30714825223981,2.35663565495851),
 .UNSPECIFIED.) ;
#2330 = B_SPLINE_CURVE_WITH_KNOTS('',3,(#162216,#162217,#162218,#162219,#162220,
#162221,#162222,#162223,#162224,#162225,#162226,#162227,#162228,#162229),
 .UNSPECIFIED.,.F.,.F.,(4,2,2,2,2,2,4),(3.92654965222121,4.10853434790169,
4.28470986572592,4.30507446986558,4.48904344491809,4.65912147389607,4.71238898038469),
 .UNSPECIFIED.) ;
#2331 = B_SPLINE_CURVE_WITH_KNOTS('',3,(#162232,#162233,#162234,#162235,#162236,
#162237,#162238,#162239,#162240,#162241,#162242,#162243,#162244,#162245),
 .UNSPECIFIED.,.F.,.F.,(4,2,2,2,2,2,4),(4.71238898038469,4.88175806245171,
5.06763701998878,5.24337922965182,5.26451333208185,5.44874090582863,5.49822830854819),
 .UNSPECIFIED.) ;
#2332 = B_SPLINE_CURVE_WITH_KNOTS('',3,(#162249,#162250,#162251,#162252,#162253,
#162254,#162255,#162256,#162257,#162258,#162259,#162260,#162261,#162262),
 .UNSPECIFIED.,.F.,.F.,(4,2,2,2,2,2,4),(0.784956998631413,0.966941694312171,
1.14311721212413,1.163481816276,1.34745079132843,1.51752882030641,1.5707963267949),
 .UNSPECIFIED.) ;
#2333 = B_SPLINE_CURVE_WITH_KNOTS('',3,(#162265,#162266,#162267,#162268,#162269,
#162270,#162271,#162272,#162273,#162274,#162275,#162276,#162277,#162278),
 .UNSPECIFIED.,.F.,.F.,(4,2,2,2,2,2,4),(4.71238898038469,4.88175806245124,
5.06763701998751,5.24337922969634,5.2645133320804,5.44874090582779,5.49822830854818),
 .UNSPECIFIED.) ;
#2334 = B_SPLINE_CURVE_WITH_KNOTS('',3,(#162282,#162283,#162284,#162285,#162286,
#162287,#162288,#162289,#162290,#162291,#162292,#162293,#162294,#162295),
 .UNSPECIFIED.,.F.,.F.,(4,2,2,2,2,2,4),(3.92654965222121,4.10853434790165,
4.28470986568095,4.30507446986543,4.48904344491779,4.65912147389564,4.71238898038469),
 .UNSPECIFIED.) ;
#2335 = B_SPLINE_CURVE_WITH_KNOTS('',3,(#162299,#162300,#162301,#162302,#162303,
#162304,#162305,#162306,#162307,#162308,#162309,#162310,#162311,#162312),
 .UNSPECIFIED.,.F.,.F.,(4,2,2,2,2,2,4),(0.784956998631375,0.966941694312727,
1.14311721209632,1.16348181627625,1.34745079132752,1.51752882030494,1.5707963267949),
 .UNSPECIFIED.) ;
#2336 = B_SPLINE_CURVE_WITH_KNOTS('',3,(#162314,#162315,#162316,#162317,#162318,
#162319,#162320,#162321,#162322,#162323,#162324,#162325,#162326,#162327),
 .UNSPECIFIED.,.F.,.F.,(4,2,2,2,2,2,4),(1.5707963267949,1.74016540886203,
1.9260443663994,2.10178657612866,2.1229206784924,2.30714825223906,2.35663565495846),
 .UNSPECIFIED.) ;
#2337 = B_SPLINE_CURVE_WITH_KNOTS('',3,(#162331,#162332,#162333,#162334,#162335,
#162336,#162337,#162338,#162339,#162340,#162341,#162342,#162343,#162344),
 .UNSPECIFIED.,.F.,.F.,(4,2,2,2,2,2,4),(1.5707963267949,1.74016540886207,
1.92604436639964,2.10178657606564,2.122920678493,2.30714825223986,2.35663565495852),
 .UNSPECIFIED.) ;
#2338 = B_SPLINE_CURVE_WITH_KNOTS('',3,(#162348,#162349,#162350,#162351,#162352,
#162353,#162354,#162355,#162356,#162357,#162358,#162359,#162360,#162361),
 .UNSPECIFIED.,.F.,.F.,(4,2,2,2,2,2,4),(3.92654965222121,4.10853434790162,
4.28470986571305,4.30507446986553,4.48904344491808,4.65912147389608,4.71238898038469),
 .UNSPECIFIED.) ;
#2339 = B_SPLINE_CURVE_WITH_KNOTS('',3,(#162364,#162365,#162366,#162367,#162368,
#162369,#162370,#162371,#162372,#162373,#162374,#162375,#162376,#162377),
 .UNSPECIFIED.,.F.,.F.,(4,2,2,2,2,2,4),(4.71238898038469,4.88175806245168,
5.06763701998876,5.24337922964848,5.26451333208179,5.44874090582859,5.49822830854817),
 .UNSPECIFIED.) ;
#2340 = B_SPLINE_CURVE_WITH_KNOTS('',3,(#162381,#162382,#162383,#162384,#162385,
#162386,#162387,#162388,#162389,#162390,#162391,#162392,#162393,#162394),
 .UNSPECIFIED.,.F.,.F.,(4,2,2,2,2,2,4),(0.784956998631362,0.966941694311931,
1.14311721213235,1.16348181627574,1.34745079132811,1.51752882030616,1.5707963267949),
 .UNSPECIFIED.) ;
#2341 = B_SPLINE_CURVE_WITH_KNOTS('',3,(#162397,#162398,#162399,#162400,#162401,
#162402,#162403,#162404,#162405,#162406,#162407,#162408,#162409,#162410),
 .UNSPECIFIED.,.F.,.F.,(4,2,2,2,2,2,4),(4.71238898038469,4.88175806245117,
5.06763701998738,5.24337922970193,5.26451333208026,5.44874090582769,5.49822830854819),
 .UNSPECIFIED.) ;
#2342 = B_SPLINE_CURVE_WITH_KNOTS('',3,(#162414,#162415,#162416,#162417,#162418,
#162419,#162420,#162421,#162422,#162423,#162424,#162425,#162426,#162427),
 .UNSPECIFIED.,.F.,.F.,(4,2,2,2,2,2,4),(3.92654965222123,4.1085343479017,
4.28470986570811,4.30507446986548,4.48904344491786,4.65912147389568,4.71238898038469),
 .UNSPECIFIED.) ;
#2343 = B_SPLINE_CURVE_WITH_KNOTS('',3,(#162431,#162432,#162433,#162434,#162435,
#162436,#162437,#162438,#162439,#162440,#162441,#162442,#162443,#162444),
 .UNSPECIFIED.,.F.,.F.,(4,2,2,2,2,2,4),(0.784956998631398,0.966941694312289,
1.14311721210181,1.16348181627595,1.34745079132735,1.51752882030477,1.5707963267949),
 .UNSPECIFIED.) ;
#2344 = B_SPLINE_CURVE_WITH_KNOTS('',3,(#162446,#162447,#162448,#162449,#162450,
#162451,#162452,#162453,#162454,#162455,#162456,#162457,#162458,#162459),
 .UNSPECIFIED.,.F.,.F.,(4,2,2,2,2,2,4),(1.5707963267949,1.74016540886207,
1.92604436639947,2.10178657613724,2.12292067849245,2.3071482522391,2.35663565495846),
 .UNSPECIFIED.) ;
#2345 = B_SPLINE_CURVE_WITH_KNOTS('',3,(#162463,#162464,#162465,#162466,#162467,
#162468,#162469,#162470,#162471,#162472,#162473,#162474,#162475,#162476),
 .UNSPECIFIED.,.F.,.F.,(4,2,2,2,2,2,4),(1.5707963267949,1.74016540886204,
1.9260443663996,2.10178657605896,2.12292067849293,2.30714825223977,2.35663565495851),
 .UNSPECIFIED.) ;
#2346 = B_SPLINE_CURVE_WITH_KNOTS('',3,(#162480,#162481,#162482,#162483,#162484,
#162485,#162486,#162487,#162488,#162489,#162490,#162491,#162492,#162493),
 .UNSPECIFIED.,.F.,.F.,(4,2,2,2,2,2,4),(3.92654965222119,4.10853434790172,
4.28470986572196,4.3050744698657,4.48904344491821,4.6591214738962,4.71238898038469),
 .UNSPECIFIED.) ;
#2347 = B_SPLINE_CURVE_WITH_KNOTS('',3,(#162496,#162497,#162498,#162499,#162500,
#162501,#162502,#162503,#162504,#162505,#162506,#162507,#162508,#162509),
 .UNSPECIFIED.,.F.,.F.,(4,2,2,2,2,2,4),(4.71238898038469,4.88175806245162,
5.06763701998873,5.2433792296528,5.26451333208183,5.44874090582879,5.49822830854821),
 .UNSPECIFIED.) ;
#2348 = B_SPLINE_CURVE_WITH_KNOTS('',3,(#162513,#162514,#162515,#162516,#162517,
#162518,#162519,#162520,#162521,#162522,#162523,#162524,#162525,#162526),
 .UNSPECIFIED.,.F.,.F.,(4,2,2,2,2,2,4),(0.784956998631419,0.966941694312359,
1.14311721212337,1.16348181627619,1.34745079132836,1.51752882030628,1.5707963267949),
 .UNSPECIFIED.) ;
#2349 = B_SPLINE_CURVE_WITH_KNOTS('',3,(#162529,#162530,#162531,#162532,#162533,
#162534,#162535,#162536,#162537,#162538,#162539,#162540,#162541,#162542),
 .UNSPECIFIED.,.F.,.F.,(4,2,2,2,2,2,4),(4.71238898038469,4.88175806245117,
5.06763701998736,5.24337922970041,5.26451333208017,5.44874090582767,5.49822830854818),
 .UNSPECIFIED.) ;
#2350 = B_SPLINE_CURVE_WITH_KNOTS('',3,(#162546,#162547,#162548,#162549,#162550,
#162551,#162552,#162553,#162554,#162555,#162556,#162557,#162558,#162559),
 .UNSPECIFIED.,.F.,.F.,(4,2,2,2,2,2,4),(3.92654965222123,4.10853434790176,
4.28470986571068,4.30507446986555,4.48904344491787,4.65912147389569,4.71238898038469),
 .UNSPECIFIED.) ;
#2351 = B_SPLINE_CURVE_WITH_KNOTS('',3,(#162563,#162564,#162565,#162566,#162567,
#162568,#162569,#162570,#162571,#162572,#162573,#162574,#162575,#162576),
 .UNSPECIFIED.,.F.,.F.,(4,2,2,2,2,2,4),(0.784956998631419,0.966941694312394,
1.14311721209636,1.16348181627596,1.34745079132737,1.51752882030475,1.5707963267949),
 .UNSPECIFIED.) ;
#2352 = B_SPLINE_CURVE_WITH_KNOTS('',3,(#162578,#162579,#162580,#162581,#162582,
#162583,#162584,#162585,#162586,#162587,#162588,#162589,#162590,#162591),
 .UNSPECIFIED.,.F.,.F.,(4,2,2,2,2,2,4),(1.5707963267949,1.74016540886206,
1.92604436639944,2.1017865761314,2.1229206784924,2.30714825223909,2.35663565495846),
 .UNSPECIFIED.) ;
#2353 = B_SPLINE_CURVE_WITH_KNOTS('',3,(#162595,#162596,#162597,#162598,#162599,
#162600,#162601,#162602,#162603,#162604,#162605,#162606,#162607,#162608),
 .UNSPECIFIED.,.F.,.F.,(4,2,2,2,2,2,4),(1.5707963267949,1.74016540886189,
1.92604436639889,2.10178657606285,2.12292067849207,2.30714825223932,2.35663565495855),
 .UNSPECIFIED.) ;
#2354 = B_SPLINE_CURVE_WITH_KNOTS('',3,(#162612,#162613,#162614,#162615,#162616,
#162617,#162618,#162619,#162620,#162621,#162622,#162623,#162624,#162625),
 .UNSPECIFIED.,.F.,.F.,(4,2,2,2,2,2,4),(3.92654965222116,4.10853434790171,
4.28470986572152,4.30507446986565,4.48904344491819,4.65912147389622,4.71238898038469),
 .UNSPECIFIED.) ;
#2355 = B_SPLINE_CURVE_WITH_KNOTS('',3,(#162628,#162629,#162630,#162631,#162632,
#162633,#162634,#162635,#162636,#162637,#162638,#162639,#162640,#162641),
 .UNSPECIFIED.,.F.,.F.,(4,2,2,2,2,2,4),(4.71238898038469,4.88175806245176,
5.06763701998884,5.24337922965909,5.26451333208186,5.44874090582875,5.49822830854823),
 .UNSPECIFIED.) ;
#2356 = B_SPLINE_CURVE_WITH_KNOTS('',3,(#162645,#162646,#162647,#162648,#162649,
#162650,#162651,#162652,#162653,#162654,#162655,#162656,#162657,#162658),
 .UNSPECIFIED.,.F.,.F.,(4,2,2,2,2,2,4),(0.784956998631252,0.966941694313067,
1.14311721213665,1.16348181627663,1.34745079132838,1.51752882030642,1.5707963267949),
 .UNSPECIFIED.) ;
#2357 = B_SPLINE_CURVE_WITH_KNOTS('',3,(#162661,#162662,#162663,#162664,#162665,
#162666,#162667,#162668,#162669,#162670,#162671,#162672,#162673,#162674),
 .UNSPECIFIED.,.F.,.F.,(4,2,2,2,2,2,4),(4.71238898038469,4.88175806245219,
5.06763701999001,5.24337922963567,5.26451333208336,5.44874090582993,5.4982283085483),
 .UNSPECIFIED.) ;
#2358 = B_SPLINE_CURVE_WITH_KNOTS('',3,(#162678,#162679,#162680,#162681,#162682,
#162683,#162684,#162685,#162686,#162687,#162688,#162689,#162690,#162691),
 .UNSPECIFIED.,.F.,.F.,(4,2,2,2,2,2,4),(3.92654965222115,4.10853434790203,
4.28470986568823,4.3050744698658,4.48904344491754,4.65912147389529,4.71238898038469),
 .UNSPECIFIED.) ;
#2359 = B_SPLINE_CURVE_WITH_KNOTS('',3,(#162695,#162696,#162697,#162698,#162699,
#162700,#162701,#162702,#162703,#162704,#162705,#162706,#162707,#162708),
 .UNSPECIFIED.,.F.,.F.,(4,2,2,2,2,2,4),(0.784956998631286,0.966941694311768,
1.14311721213309,1.16348181627596,1.34745079132886,1.5175288203073,1.5707963267949),
 .UNSPECIFIED.) ;
#2360 = B_SPLINE_CURVE_WITH_KNOTS('',3,(#162710,#162711,#162712,#162713,#162714,
#162715,#162716,#162717,#162718,#162719,#162720,#162721,#162722,#162723),
 .UNSPECIFIED.,.F.,.F.,(4,2,2,2,2,2,4),(1.5707963267949,1.74016540886205,
1.926044366399,2.10178657613527,2.12292067849206,2.30714825223934,2.35663565495854),
 .UNSPECIFIED.) ;
#2361 = B_SPLINE_CURVE_WITH_KNOTS('',3,(#162727,#162728,#162729,#162730,#162731,
#162732,#162733,#162734,#162735,#162736,#162737,#162738,#162739,#162740),
 .UNSPECIFIED.,.F.,.F.,(4,2,2,2,2,2,4),(1.5707963267949,1.74016540886187,
1.9260443663989,2.10178657606494,2.1229206784921,2.30714825223936,2.35663565495855),
 .UNSPECIFIED.) ;
#2362 = B_SPLINE_CURVE_WITH_KNOTS('',3,(#162744,#162745,#162746,#162747,#162748,
#162749,#162750,#162751,#162752,#162753,#162754,#162755,#162756,#162757),
 .UNSPECIFIED.,.F.,.F.,(4,2,2,2,2,2,4),(3.92654965222115,4.10853434790176,
4.28470986571692,4.3050744698657,4.48904344491822,4.65912147389629,4.71238898038469),
 .UNSPECIFIED.) ;
#2363 = B_SPLINE_CURVE_WITH_KNOTS('',3,(#162760,#162761,#162762,#162763,#162764,
#162765,#162766,#162767,#162768,#162769,#162770,#162771,#162772,#162773),
 .UNSPECIFIED.,.F.,.F.,(4,2,2,2,2,2,4),(4.71238898038469,4.88175806245178,
5.06763701998822,5.24337922965634,5.26451333208117,5.44874090582883,5.4982283085483),
 .UNSPECIFIED.) ;
#2364 = B_SPLINE_CURVE_WITH_KNOTS('',3,(#162777,#162778,#162779,#162780,#162781,
#162782,#162783,#162784,#162785,#162786,#162787,#162788,#162789,#162790),
 .UNSPECIFIED.,.F.,.F.,(4,2,2,2,2,2,4),(0.784956998631253,0.966941694312816,
1.1431172121299,1.16348181627639,1.34745079132795,1.51752882030599,1.5707963267949),
 .UNSPECIFIED.) ;
#2365 = B_SPLINE_CURVE_WITH_KNOTS('',3,(#162793,#162794,#162795,#162796,#162797,
#162798,#162799,#162800,#162801,#162802,#162803,#162804,#162805,#162806),
 .UNSPECIFIED.,.F.,.F.,(4,2,2,2,2,2,4),(4.71238898038469,4.88175806245208,
5.06763701998989,5.24337922963223,5.26451333208325,5.4487409058299,5.49822830854831),
 .UNSPECIFIED.) ;
#2366 = B_SPLINE_CURVE_WITH_KNOTS('',3,(#162810,#162811,#162812,#162813,#162814,
#162815,#162816,#162817,#162818,#162819,#162820,#162821,#162822,#162823),
 .UNSPECIFIED.,.F.,.F.,(4,2,2,2,2,2,4),(3.92654965222114,4.10853434790186,
4.2847098656881,4.30507446986561,4.48904344491734,4.65912147389511,4.71238898038469),
 .UNSPECIFIED.) ;
#2367 = B_SPLINE_CURVE_WITH_KNOTS('',3,(#162827,#162828,#162829,#162830,#162831,
#162832,#162833,#162834,#162835,#162836,#162837,#162838,#162839,#162840),
 .UNSPECIFIED.,.F.,.F.,(4,2,2,2,2,2,4),(0.784956998631275,0.966941694311846,
1.14311721212765,1.16348181627603,1.34745079132913,1.51752882030757,1.5707963267949),
 .UNSPECIFIED.) ;
#2368 = B_SPLINE_CURVE_WITH_KNOTS('',3,(#162842,#162843,#162844,#162845,#162846,
#162847,#162848,#162849,#162850,#162851,#162852,#162853,#162854,#162855),
 .UNSPECIFIED.,.F.,.F.,(4,2,2,2,2,2,4),(1.5707963267949,1.74016540886206,
1.92604436639903,2.10178657606026,2.12292067849211,2.30714825223937,2.35663565495855),
 .UNSPECIFIED.) ;
#2369 = B_SPLINE_CURVE_WITH_KNOTS('',3,(#162859,#162860,#162861,#162862,#162863,
#162864,#162865,#162866,#162867,#162868,#162869,#162870,#162871,#162872),
 .UNSPECIFIED.,.F.,.F.,(4,2,2,2,2,2,4),(1.5707963267949,1.74016540886233,
1.92604436640004,2.10178657606526,2.12292067849322,2.30714825223986,2.35663565495855),
 .UNSPECIFIED.) ;
#2370 = B_SPLINE_CURVE_WITH_KNOTS('',3,(#162876,#162877,#162878,#162879,#162880,
#162881,#162882,#162883,#162884,#162885,#162886,#162887,#162888,#162889),
 .UNSPECIFIED.,.F.,.F.,(4,2,2,2,2,2,4),(3.92654965222116,4.10853434790169,
4.28470986572823,4.30507446986562,4.48904344491821,4.65912147389623,4.71238898038469),
 .UNSPECIFIED.) ;
#2371 = B_SPLINE_CURVE_WITH_KNOTS('',3,(#162892,#162893,#162894,#162895,#162896,
#162897,#162898,#162899,#162900,#162901,#162902,#162903,#162904,#162905),
 .UNSPECIFIED.,.F.,.F.,(4,2,2,2,2,2,4),(4.71238898038469,4.88175806245184,
5.06763701998833,5.24337922965272,5.26451333208122,5.44874090582878,5.49822830854832),
 .UNSPECIFIED.) ;
#2372 = B_SPLINE_CURVE_WITH_KNOTS('',3,(#162909,#162910,#162911,#162912,#162913,
#162914,#162915,#162916,#162917,#162918,#162919,#162920,#162921,#162922),
 .UNSPECIFIED.,.F.,.F.,(4,2,2,2,2,2,4),(0.784956998631356,0.966941694311965,
1.14311721213089,1.16348181627574,1.34745079132755,1.51752882030535,1.5707963267949),
 .UNSPECIFIED.) ;
#2373 = B_SPLINE_CURVE_WITH_KNOTS('',3,(#162925,#162926,#162927,#162928,#162929,
#162930,#162931,#162932,#162933,#162934,#162935,#162936,#162937,#162938),
 .UNSPECIFIED.,.F.,.F.,(4,2,2,2,2,2,4),(4.71238898038469,4.88175806245187,
5.06763701998943,5.24337922964722,5.26451333208265,5.44874090582937,5.49822830854828),
 .UNSPECIFIED.) ;
#2374 = B_SPLINE_CURVE_WITH_KNOTS('',3,(#162942,#162943,#162944,#162945,#162946,
#162947,#162948,#162949,#162950,#162951,#162952,#162953,#162954,#162955),
 .UNSPECIFIED.,.F.,.F.,(4,2,2,2,2,2,4),(3.92654965222114,4.10853434790249,
4.28470986571866,4.30507446986622,4.48904344491771,4.65912147389542,4.71238898038469),
 .UNSPECIFIED.) ;
#2375 = B_SPLINE_CURVE_WITH_KNOTS('',3,(#163030,#163031,#163032,#163033,#163034,
#163035),.UNSPECIFIED.,.F.,.F.,(4,2,4),(4.71238898038469,5.49778714378214,
6.28318530717959),.UNSPECIFIED.) ;
#2376 = B_SPLINE_CURVE_WITH_KNOTS('',3,(#163065,#163066,#163067,#163068,#163069,
#163070),.UNSPECIFIED.,.F.,.F.,(4,2,4),(3.14159265358979,3.92699081698724,
4.71238898038469),.UNSPECIFIED.) ;
#2377 = B_SPLINE_CURVE_WITH_KNOTS('',3,(#167426,#167427,#167428,#167429,#167430,
#167431,#167432,#167433,#167434,#167435,#167436,#167437,#167438,#167439,
#167440,#167441,#167442,#167443,#167444,#167445,#167446,#167447,#167448,
#167449,#167450,#167451),.UNSPECIFIED.,.F.,.F.,(4,2,2,2,2,2,2,2,2,2,2,2,
4),(6.1331736667335E-19,5.70004774914534E-6,8.25511347640713E-6,9.93040049428836E-6,
2.64556965228396E-5,3.0587336112471E-5,4.24593515817707E-5,6.43784914888407E-5,
7.6656210164489E-5,9.74321373319979E-5,9.92796257088188E-5,0.000111632960404942,
0.000135309975333047),.UNSPECIFIED.) ;
#2378 = B_SPLINE_CURVE_WITH_KNOTS('',3,(#167458,#167459,#167460,#167461,#167462,
#167463,#167464,#167465,#167466,#167467,#167468,#167469,#167470,#167471,
#167472,#167473,#167474,#167475,#167476,#167477,#167478,#167479,#167480,
#167481,#167482,#167483,#167484,#167485,#167486,#167487,#167488,#167489,
#167490,#167491),.UNSPECIFIED.,.F.,.F.,(4,2,2,2,2,2,2,2,2,2,2,2,2,2,2,2,
4),(0.,8.71783727051893E-6,1.76441105360345E-5,3.58270994901034E-5,4.83658434534685E-5,
6.68919645679043E-5,7.05613987999435E-5,8.27232142756391E-5,9.87362632805838E-5,
0.000104111574538336,0.000114567411933464,0.000115616565506961,0.000123791392829615,
0.000124267209278334,0.000126967031952647,0.000132546919744955,0.000134871234237328),
 .UNSPECIFIED.) ;
#2379 = B_SPLINE_CURVE_WITH_KNOTS('',3,(#167493,#167494,#167495,#167496,#167497,
#167498,#167499,#167500,#167501,#167502,#167503,#167504,#167505,#167506,
#167507,#167508,#167509,#167510,#167511,#167512,#167513,#167514,#167515,
#167516,#167517,#167518),.UNSPECIFIED.,.F.,.F.,(4,2,2,2,2,2,2,2,2,2,2,2,
4),(4.33680868994202E-19,5.700047749144E-6,8.25511347640865E-6,9.93040049428814E-6,
2.64556965230734E-5,3.05873361124735E-5,4.24593515817708E-5,6.43784914888414E-5,
7.66562101644896E-5,9.74321373319674E-5,9.92796257088195E-5,0.000111632960404942,
0.000135309975333047),.UNSPECIFIED.) ;
#2380 = B_SPLINE_CURVE_WITH_KNOTS('',3,(#167522,#167523,#167524,#167525,#167526,
#167527,#167528,#167529,#167530,#167531,#167532,#167533,#167534,#167535,
#167536,#167537,#167538,#167539,#167540,#167541,#167542,#167543,#167544,
#167545,#167546,#167547),.UNSPECIFIED.,.F.,.F.,(4,2,2,2,2,2,2,2,2,2,2,2,
4),(9.69739903612216E-19,5.70004774917064E-6,8.25511347641042E-6,9.93040049429001E-6,
2.64556965230525E-5,3.05873361124729E-5,4.24593515817735E-5,6.43784914888468E-5,
7.6656210164492E-5,9.74321373319885E-5,9.92796257088266E-5,0.000111632960404945,
0.000135309975333051),.UNSPECIFIED.) ;
#2381 = B_SPLINE_CURVE_WITH_KNOTS('',3,(#167554,#167555,#167556,#167557,#167558,
#167559,#167560,#167561,#167562,#167563,#167564,#167565,#167566,#167567,
#167568,#167569,#167570,#167571,#167572,#167573,#167574,#167575,#167576,
#167577,#167578,#167579,#167580,#167581,#167582,#167583,#167584,#167585,
#167586,#167587),.UNSPECIFIED.,.F.,.F.,(4,2,2,2,2,2,2,2,2,2,2,2,2,2,2,2,
4),(0.,8.71783727085515E-6,1.7644110536621E-5,3.58270994901043E-5,4.83658434534726E-5,
6.68919645677967E-5,7.05613987999456E-5,8.27232142756448E-5,9.87362632804046E-5,
0.000104111574538337,0.00011456741193359,0.000115616565506969,0.000123791392829788,
0.000124267209278257,0.00012696703195266,0.000132546919745185,0.000134871234237334),
 .UNSPECIFIED.) ;
#2382 = B_SPLINE_CURVE_WITH_KNOTS('',3,(#167591,#167592,#167593,#167594,#167595,
#167596,#167597,#167598,#167599,#167600,#167601,#167602,#167603,#167604,
#167605,#167606,#167607,#167608,#167609,#167610,#167611,#167612,#167613,
#167614,#167615,#167616),.UNSPECIFIED.,.F.,.F.,(4,2,2,2,2,2,2,2,2,2,2,2,
4),(9.69739903612216E-19,5.70004774915885E-6,8.25511347641042E-6,9.93040049429001E-6,
2.64556965230698E-5,3.05873361124735E-5,4.24593515817735E-5,6.43784914888452E-5,
7.6656210164492E-5,9.74321373321103E-5,9.92796257088256E-5,0.000111632960404945,
0.000135309975333051),.UNSPECIFIED.) ;
#2383 = B_SPLINE_CURVE_WITH_KNOTS('',3,(#167623,#167624,#167625,#167626,#167627,
#167628,#167629,#167630,#167631,#167632,#167633,#167634,#167635,#167636,
#167637,#167638,#167639,#167640,#167641,#167642,#167643,#167644,#167645,
#167646,#167647,#167648,#167649,#167650,#167651,#167652,#167653,#167654,
#167655,#167656),.UNSPECIFIED.,.F.,.F.,(4,2,2,2,2,2,2,2,2,2,2,2,2,2,2,2,
4),(0.,8.717837270643E-6,1.76441105351036E-5,3.58270994901016E-5,4.83658434534694E-5,
6.68919645660009E-5,7.05613987999433E-5,8.27232142756404E-5,9.8736263280134E-5,
0.000104111574538333,0.000114567411932816,0.000115616565506965,0.000123791392829682,
0.000124267209278245,0.000126967031952653,0.000132546919745188,0.00013487123423733),
 .UNSPECIFIED.) ;
#2384 = B_SPLINE_CURVE_WITH_KNOTS('',3,(#167660,#167661,#167662,#167663,#167664,
#167665,#167666,#167667,#167668,#167669,#167670,#167671,#167672,#167673,
#167674,#167675,#167676,#167677,#167678,#167679,#167680,#167681,#167682,
#167683,#167684,#167685),.UNSPECIFIED.,.F.,.F.,(4,2,2,2,2,2,2,2,2,2,2,2,
4),(0.,5.70004774913574E-6,8.2551134764029E-6,9.93040049428637E-6,2.64556965229031E-5,
3.05873361124737E-5,4.24593515817696E-5,6.43784914888402E-5,7.66562101644865E-5,
9.74321373305911E-5,9.92796257088035E-5,0.000111632960404936,0.00013530997533304),
 .UNSPECIFIED.) ;
#2385 = B_SPLINE_CURVE_WITH_KNOTS('',3,(#167692,#167693,#167694,#167695,#167696,
#167697,#167698,#167699,#167700,#167701,#167702,#167703,#167704,#167705,
#167706,#167707,#167708,#167709,#167710,#167711,#167712,#167713,#167714,
#167715,#167716,#167717,#167718,#167719,#167720,#167721,#167722,#167723,
#167724,#167725),.UNSPECIFIED.,.F.,.F.,(4,2,2,2,2,2,2,2,2,2,2,2,2,2,2,2,
4),(0.,1.27221745291788E-5,3.17734837391886E-5,3.5827099490101E-5,4.83658434534691E-5,
6.6891964566145E-5,7.0561398799944E-5,8.272321427564E-5,9.87362632794886E-5,
0.00010411157453835,0.000114567411933352,0.000115616565506964,0.000123791392830442,
0.00012426720927844,0.000126967031952657,0.000132546919744853,0.000134871234237328),
 .UNSPECIFIED.) ;
#2386 = B_SPLINE_CURVE_WITH_KNOTS('',3,(#167729,#167730,#167731,#167732,#167733,
#167734,#167735,#167736,#167737,#167738,#167739,#167740,#167741,#167742,
#167743,#167744,#167745,#167746,#167747,#167748,#167749,#167750,#167751,
#167752,#167753,#167754),.UNSPECIFIED.,.F.,.F.,(4,2,2,2,2,2,2,2,2,2,2,2,
4),(0.,5.70004774912575E-6,8.2551134764029E-6,9.93040049428637E-6,2.64556965228879E-5,
3.05873361124728E-5,4.24593515817696E-5,6.43784914888337E-5,7.66562101644865E-5,
9.74321373308457E-5,9.92796257088009E-5,0.000111632960404936,0.00013530997533304),
 .UNSPECIFIED.) ;
#2387 = B_SPLINE_CURVE_WITH_KNOTS('',3,(#167761,#167762,#167763,#167764,#167765,
#167766,#167767,#167768,#167769,#167770,#167771,#167772,#167773,#167774,
#167775,#167776,#167777,#167778,#167779,#167780,#167781,#167782,#167783,
#167784,#167785,#167786,#167787,#167788,#167789,#167790,#167791,#167792,
#167793,#167794),.UNSPECIFIED.,.F.,.F.,(4,2,2,2,2,2,2,2,2,2,2,2,2,2,2,2,
4),(0.,8.71783727022481E-6,1.7644110536595E-5,3.58270994901018E-5,4.83658434534691E-5,
6.68919645661972E-5,7.05613987999443E-5,8.272321427564E-5,9.87362632793253E-5,
0.00010411157453835,0.000114567411933539,0.000115616565506964,0.000123791392830457,
0.000124267209278436,0.000126967031952657,0.000132546919744863,0.000134871234237328),
 .UNSPECIFIED.) ;
#2388 = B_SPLINE_CURVE_WITH_KNOTS('',3,(#167798,#167799,#167800,#167801,#167802,
#167803,#167804,#167805,#167806,#167807,#167808,#167809,#167810,#167811,
#167812,#167813,#167814,#167815,#167816,#167817,#167818,#167819,#167820,
#167821,#167822,#167823),.UNSPECIFIED.,.F.,.F.,(4,2,2,2,2,2,2,2,2,2,2,2,
4),(0.,5.70004774913546E-6,8.2551134764029E-6,9.93040049428637E-6,2.64556965229398E-5,
3.05873361124753E-5,4.24593515817696E-5,6.43784914888368E-5,7.66562101644865E-5,
9.74321373310438E-5,9.92796257088069E-5,0.000111632960404936,0.00013530997533304),
 .UNSPECIFIED.) ;
#2389 = B_SPLINE_CURVE_WITH_KNOTS('',3,(#167830,#167831,#167832,#167833,#167834,
#167835,#167836,#167837,#167838,#167839,#167840,#167841,#167842,#167843,
#167844,#167845,#167846,#167847,#167848,#167849,#167850,#167851,#167852,
#167853,#167854,#167855,#167856,#167857,#167858,#167859,#167860,#167861,
#167862,#167863),.UNSPECIFIED.,.F.,.F.,(4,2,2,2,2,2,2,2,2,2,2,2,2,2,2,2,
4),(0.,8.7178372714199E-6,1.76441105365042E-5,3.58270994900995E-5,4.83658434534691E-5,
6.68919645658283E-5,7.0561398799945E-5,8.272321427564E-5,9.87362632792552E-5,
0.000104111574538349,0.000114567411933256,0.000115616565506964,0.000123791392830476,
0.000124267209278436,0.000126967031952657,0.000132546919744827,0.000134871234237328),
 .UNSPECIFIED.) ;
#2390 = B_SPLINE_CURVE_WITH_KNOTS('',3,(#167867,#167868,#167869,#167870,#167871,
#167872,#167873,#167874,#167875,#167876,#167877,#167878,#167879,#167880,
#167881,#167882,#167883,#167884,#167885,#167886,#167887,#167888,#167889,
#167890,#167891,#167892),.UNSPECIFIED.,.F.,.F.,(4,2,2,2,2,2,2,2,2,2,2,2,
4),(0.,5.7000477491356E-6,8.2551134764029E-6,9.93040049428637E-6,2.64556965228419E-5,
3.05873361124732E-5,4.24593515817696E-5,6.43784914888367E-5,7.66562101644865E-5,
9.74321373305317E-5,9.92796257088022E-5,0.000111632960404936,0.00013530997533304),
 .UNSPECIFIED.) ;
#2391 = B_SPLINE_CURVE_WITH_KNOTS('',3,(#167899,#167900,#167901,#167902,#167903,
#167904,#167905,#167906,#167907,#167908,#167909,#167910,#167911,#167912,
#167913,#167914,#167915,#167916,#167917,#167918,#167919,#167920,#167921,
#167922,#167923,#167924,#167925,#167926,#167927,#167928,#167929,#167930,
#167931,#167932),.UNSPECIFIED.,.F.,.F.,(4,2,2,2,2,2,2,2,2,2,2,2,2,2,2,2,
4),(0.,1.27221745291788E-5,3.17734837391183E-5,3.58270994901062E-5,4.83658434534691E-5,
6.68919645661017E-5,7.05613987999452E-5,8.272321427564E-5,9.87362632793197E-5,
0.000104111574538349,0.00011456741193351,0.000115616565506964,0.000123791392830282,
0.000124267209278427,0.000126967031952657,0.000132546919744846,0.000134871234237328),
 .UNSPECIFIED.) ;
#2392 = B_SPLINE_CURVE_WITH_KNOTS('',3,(#167936,#167937,#167938,#167939,#167940,
#167941,#167942,#167943,#167944,#167945,#167946,#167947,#167948,#167949,
#167950,#167951,#167952,#167953,#167954,#167955,#167956,#167957,#167958,
#167959,#167960,#167961),.UNSPECIFIED.,.F.,.F.,(4,2,2,2,2,2,2,2,2,2,2,2,
4),(5.65450672847475E-18,5.70004774919696E-6,8.25511347639078E-6,9.93040049428371E-6,
2.64556965223417E-5,3.05873361124641E-5,4.24593515817652E-5,6.43784914888292E-5,
7.66562101644793E-5,9.74321373329595E-5,9.92796257088198E-5,0.000111632960404932,
0.000135309975333043),.UNSPECIFIED.) ;
#2393 = B_SPLINE_CURVE_WITH_KNOTS('',3,(#167968,#167969,#167970,#167971,#167972,
#167973,#167974,#167975,#167976,#167977,#167978,#167979,#167980,#167981,
#167982,#167983,#167984,#167985,#167986,#167987,#167988,#167989,#167990,
#167991,#167992,#167993,#167994,#167995,#167996,#167997,#167998,#167999,
#168000,#168001),.UNSPECIFIED.,.F.,.F.,(4,2,2,2,2,2,2,2,2,2,2,2,2,2,2,2,
4),(0.,1.27221745291825E-5,3.17734837389246E-5,3.58270994900963E-5,4.8365843453465E-5,
6.68919645660607E-5,7.05613987999433E-5,8.27232142756395E-5,9.87362632792754E-5,
0.000104111574538343,0.000114567411932696,0.000115616565506954,0.000123791392829404,
0.000124267209278547,0.000126967031952634,0.000132546919744699,0.000134871234237319),
 .UNSPECIFIED.) ;
#2394 = B_SPLINE_CURVE_WITH_KNOTS('',3,(#168008,#168009,#168010,#168011,#168012,
#168013,#168014,#168015,#168016,#168017,#168018,#168019,#168020,#168021,
#168022,#168023,#168024,#168025,#168026,#168027,#168028,#168029,#168030,
#168031,#168032,#168033,#168034,#168035,#168036,#168037,#168038,#168039,
#168040,#168041),.UNSPECIFIED.,.F.,.F.,(4,2,2,2,2,2,2,2,2,2,2,2,2,2,2,2,
4),(0.,1.27221745291825E-5,3.17734837389621E-5,3.58270994901002E-5,4.8365843453465E-5,
6.68919645658703E-5,7.05613987999433E-5,8.27232142756395E-5,9.87362632795784E-5,
0.000104111574538341,0.000114567411933155,0.000115616565506954,0.000123791392830688,
0.00012426720927855,0.000126967031952634,0.000132546919744675,0.000134871234237319),
 .UNSPECIFIED.) ;
#2395 = B_SPLINE_CURVE_WITH_KNOTS('',3,(#168044,#168045,#168046,#168047,#168048,
#168049,#168050,#168051,#168052,#168053,#168054,#168055,#168056,#168057,
#168058,#168059,#168060,#168061,#168062,#168063,#168064,#168065,#168066,
#168067,#168068,#168069,#168070,#168071,#168072,#168073,#168074,#168075,
#168076,#168077,#168078,#168079,#168080,#168081,#168082,#168083,#168084,
#168085,#168086,#168087,#168088,#168089,#168090,#168091,#168092,#168093,
#168094,#168095,#168096,#168097,#168098),.UNSPECIFIED.,.F.,.F.,(4,3,3,3,
3,3,3,3,3,3,3,3,3,3,3,3,3,3,4),(0.,1.96170179200497E-5,2.35258500143173E-5,
3.58003153605656E-5,5.29187212186161E-5,5.64435994880342E-5,5.827929265241E-5,
7.04649253805291E-5,8.72923312913114E-5,9.05038369578067E-5,9.22578228185119E-5,
0.000103663146463146,0.00011386600552152,0.000117768598772948,0.000124579094175181,
0.000129312863866763,0.000130178750830829,0.000132692979584749,0.000134419842078313),
 .UNSPECIFIED.) ;
#2396 = B_SPLINE_CURVE_WITH_KNOTS('',3,(#168107,#168108,#168109,#168110,#168111,
#168112,#168113,#168114,#168115,#168116,#168117,#168118,#168119,#168120,
#168121,#168122,#168123,#168124,#168125,#168126,#168127,#168128,#168129,
#168130,#168131,#168132),.UNSPECIFIED.,.F.,.F.,(4,2,2,2,2,2,2,2,2,2,2,2,
4),(0.,5.55321021973765E-6,8.25511347643081E-6,1.91711188535185E-5,3.04852632940538E-5,
5.08165579102967E-5,5.19149958125378E-5,6.39742577536705E-5,8.61162395509785E-5,
9.85980048375137E-5,0.000117622240611127,0.000125683481931241,0.00013426229848852),
 .UNSPECIFIED.) ;
#2397 = B_SPLINE_CURVE_WITH_KNOTS('',3,(#168139,#168140,#168141,#168142,#168143,
#168144,#168145,#168146,#168147,#168148,#168149,#168150,#168151,#168152,
#168153,#168154,#168155,#168156,#168157,#168158,#168159,#168160,#168161,
#168162,#168163,#168164,#168165,#168166,#168167,#168168,#168169,#168170,
#168171,#168172,#168173,#168174,#168175,#168176,#168177,#168178,#168179,
#168180,#168181,#168182,#168183,#168184,#168185,#168186,#168187,#168188,
#168189,#168190,#168191,#168192,#168193),.UNSPECIFIED.,.F.,.F.,(4,3,3,3,
3,3,3,3,3,3,3,3,3,3,3,3,3,3,4),(0.,1.96170179200542E-5,2.35258500143173E-5,
3.58003153605654E-5,5.29187212186038E-5,5.64435994880909E-5,5.8279292652409E-5,
7.04649253805292E-5,8.72923312915481E-5,9.05038369577458E-5,9.22578228185104E-5,
0.000103663146463144,0.000113866005521528,0.000117768598772953,0.00012457909417518,
0.000129312863866768,0.00013017875083082,0.000132692979584748,0.000134419842078312),
 .UNSPECIFIED.) ;
#2398 = B_SPLINE_CURVE_WITH_KNOTS('',3,(#168202,#168203,#168204,#168205,#168206,
#168207,#168208,#168209,#168210,#168211,#168212,#168213,#168214,#168215,
#168216,#168217,#168218,#168219,#168220,#168221,#168222,#168223,#168224,
#168225,#168226,#168227),.UNSPECIFIED.,.F.,.F.,(4,2,2,2,2,2,2,2,2,2,2,2,
4),(0.,5.55321021971803E-6,8.2551134764307E-6,1.91711188535182E-5,3.04852632940564E-5,
5.08165579104009E-5,5.1914995812538E-5,6.39742577536707E-5,8.61162395509773E-5,
9.85980048375135E-5,0.000117622240611135,0.000125683481931497,0.00013426229848852),
 .UNSPECIFIED.) ;
#2399 = B_SPLINE_CURVE_WITH_KNOTS('',3,(#168234,#168235,#168236,#168237,#168238,
#168239,#168240,#168241,#168242,#168243,#168244,#168245,#168246,#168247,
#168248,#168249,#168250,#168251,#168252,#168253,#168254,#168255,#168256,
#168257,#168258,#168259,#168260,#168261,#168262,#168263,#168264,#168265,
#168266,#168267,#168268,#168269,#168270,#168271,#168272,#168273,#168274,
#168275,#168276,#168277,#168278,#168279,#168280,#168281,#168282,#168283,
#168284,#168285,#168286,#168287,#168288),.UNSPECIFIED.,.F.,.F.,(4,3,3,3,
3,3,3,3,3,3,3,3,3,3,3,3,3,3,4),(0.,1.96170179192311E-5,2.35258500143173E-5,
3.58003153605661E-5,5.29187212162782E-5,5.6443599488185E-5,5.82792926524099E-5,
7.046492538053E-5,8.72923312900606E-5,9.05038369578505E-5,9.22578228185119E-5,
0.000103663146463143,0.000113866005521194,0.000117768598772959,0.000124579094175181,
0.000129312863866605,0.000130178750830851,0.000132692979584745,0.000134419842078313),
 .UNSPECIFIED.) ;
#2400 = B_SPLINE_CURVE_WITH_KNOTS('',3,(#168297,#168298,#168299,#168300,#168301,
#168302,#168303,#168304,#168305,#168306,#168307,#168308,#168309,#168310,
#168311,#168312,#168313,#168314,#168315,#168316,#168317,#168318,#168319,
#168320,#168321,#168322),.UNSPECIFIED.,.F.,.F.,(4,2,2,2,2,2,2,2,2,2,2,2,
4),(0.,5.55321021971055E-6,8.25511347643257E-6,1.91711188535176E-5,3.04852632940549E-5,
5.08165579107018E-5,5.19149958125369E-5,6.39742577536715E-5,8.61162395509772E-5,
9.85980048375149E-5,0.000117622240611143,0.00012568348193157,0.00013426229848852),
 .UNSPECIFIED.) ;
#2401 = B_SPLINE_CURVE_WITH_KNOTS('',3,(#168329,#168330,#168331,#168332,#168333,
#168334,#168335,#168336,#168337,#168338,#168339,#168340,#168341,#168342,
#168343,#168344,#168345,#168346,#168347,#168348,#168349,#168350,#168351,
#168352,#168353,#168354,#168355,#168356,#168357,#168358,#168359,#168360,
#168361,#168362,#168363,#168364,#168365,#168366,#168367,#168368,#168369,
#168370,#168371,#168372,#168373,#168374,#168375,#168376,#168377,#168378,
#168379,#168380,#168381,#168382,#168383),.UNSPECIFIED.,.F.,.F.,(4,3,3,3,
3,3,3,3,3,3,3,3,3,3,3,3,3,3,4),(0.,1.96170179203663E-5,2.35258500143174E-5,
3.58003153605658E-5,5.2918721219628E-5,5.64435994880167E-5,5.82792926524091E-5,
7.04649253805322E-5,8.72923312915083E-5,9.05038369581538E-5,9.2257822818511E-5,
0.000103663146463142,0.00011386600552163,0.000117768598772992,0.000124579094175182,
0.000129312863867062,0.0001301787508309,0.000132692979584746,0.000134419842078314),
 .UNSPECIFIED.) ;
#2402 = B_SPLINE_CURVE_WITH_KNOTS('',3,(#168392,#168393,#168394,#168395,#168396,
#168397,#168398,#168399,#168400,#168401,#168402,#168403,#168404,#168405,
#168406,#168407,#168408,#168409,#168410,#168411,#168412,#168413,#168414,
#168415,#168416,#168417),.UNSPECIFIED.,.F.,.F.,(4,2,2,2,2,2,2,2,2,2,2,2,
4),(0.,5.55321021972969E-6,8.25511347643257E-6,1.91711188535176E-5,3.04852632940556E-5,
5.08165579107454E-5,5.19149958125369E-5,6.39742577536697E-5,8.61162395509772E-5,
9.85980048375132E-5,0.000117622240611155,0.00012568348193195,0.00013426229848852),
 .UNSPECIFIED.) ;
#2403 = B_SPLINE_CURVE_WITH_KNOTS('',3,(#168424,#168425,#168426,#168427,#168428,
#168429,#168430,#168431,#168432,#168433,#168434,#168435,#168436,#168437,
#168438,#168439,#168440,#168441,#168442,#168443,#168444,#168445,#168446,
#168447,#168448,#168449,#168450,#168451,#168452,#168453,#168454,#168455,
#168456,#168457,#168458,#168459,#168460,#168461,#168462,#168463,#168464,
#168465,#168466,#168467,#168468,#168469,#168470,#168471,#168472,#168473,
#168474,#168475,#168476,#168477,#168478),.UNSPECIFIED.,.F.,.F.,(4,3,3,3,
3,3,3,3,3,3,3,3,3,3,3,3,3,3,4),(0.,1.96170179208962E-5,2.35258500143174E-5,
3.58003153605662E-5,5.29187212198585E-5,5.64435994880185E-5,5.82792926524091E-5,
7.04649253805333E-5,8.72923312910633E-5,9.05038369581232E-5,9.2257822818511E-5,
0.000103663146463146,0.000113866005521589,0.000117768598772995,0.000124579094175182,
0.000129312863867127,0.000130178750830904,0.000132692979584746,0.000134419842078314),
 .UNSPECIFIED.) ;
#2404 = B_SPLINE_CURVE_WITH_KNOTS('',3,(#168487,#168488,#168489,#168490,#168491,
#168492,#168493,#168494,#168495,#168496,#168497,#168498,#168499,#168500,
#168501,#168502,#168503,#168504,#168505,#168506,#168507,#168508,#168509,
#168510,#168511,#168512),.UNSPECIFIED.,.F.,.F.,(4,2,2,2,2,2,2,2,2,2,2,2,
4),(0.,5.55321021973998E-6,8.25511347643153E-6,1.91711188535163E-5,3.0485263294052E-5,
5.0816557910318E-5,5.19149958125372E-5,6.39742577536688E-5,8.61162395509784E-5,
9.85980048375113E-5,0.000117622240611307,0.000125683481932561,0.000134262298488521),
 .UNSPECIFIED.) ;
#2405 = B_SPLINE_CURVE_WITH_KNOTS('',3,(#168519,#168520,#168521,#168522,#168523,
#168524,#168525,#168526,#168527,#168528,#168529,#168530,#168531,#168532,
#168533,#168534,#168535,#168536,#168537,#168538,#168539,#168540,#168541,
#168542,#168543,#168544,#168545,#168546,#168547,#168548,#168549,#168550,
#168551,#168552,#168553,#168554,#168555,#168556,#168557,#168558,#168559,
#168560,#168561,#168562,#168563,#168564,#168565,#168566,#168567,#168568,
#168569,#168570,#168571,#168572,#168573),.UNSPECIFIED.,.F.,.F.,(4,3,3,3,
3,3,3,3,3,3,3,3,3,3,3,3,3,3,4),(0.,1.96170179192042E-5,2.35258500143174E-5,
3.58003153605655E-5,5.2918721218618E-5,5.64435994880514E-5,5.82792926524091E-5,
7.04649253805306E-5,8.72923312917556E-5,9.05038369587251E-5,9.2257822818511E-5,
0.000103663146463134,0.000113866005521224,0.000117768598772955,0.000124579094175182,
0.0001293128638668,0.000130178750830747,0.000132692979584746,0.000134419842078314),
 .UNSPECIFIED.) ;
#2406 = B_SPLINE_CURVE_WITH_KNOTS('',3,(#168582,#168583,#168584,#168585,#168586,
#168587,#168588,#168589,#168590,#168591,#168592,#168593,#168594,#168595,
#168596,#168597,#168598,#168599,#168600,#168601,#168602,#168603,#168604,
#168605,#168606,#168607),.UNSPECIFIED.,.F.,.F.,(4,2,2,2,2,2,2,2,2,2,2,2,
4),(0.,5.55321021976979E-6,8.25511347643153E-6,1.91711188535163E-5,3.0485263294054E-5,
5.08165579104287E-5,5.19149958125372E-5,6.39742577536726E-5,8.61162395509784E-5,
9.85980048375128E-5,0.000117622240611284,0.000125683481932007,0.000134262298488521),
 .UNSPECIFIED.) ;
#2407 = B_SPLINE_CURVE_WITH_KNOTS('',3,(#168614,#168615,#168616,#168617,#168618,
#168619,#168620,#168621,#168622,#168623,#168624,#168625,#168626,#168627,
#168628,#168629,#168630,#168631,#168632,#168633,#168634,#168635,#168636,
#168637,#168638,#168639,#168640,#168641,#168642,#168643,#168644,#168645,
#168646,#168647,#168648,#168649,#168650,#168651,#168652,#168653,#168654,
#168655,#168656,#168657,#168658,#168659,#168660,#168661,#168662,#168663,
#168664,#168665,#168666,#168667,#168668),.UNSPECIFIED.,.F.,.F.,(4,3,3,3,
3,3,3,3,3,3,3,3,3,3,3,3,3,3,4),(0.,1.96170179208898E-5,2.35258500143174E-5,
3.58003153605655E-5,5.29187212199216E-5,5.64435994880236E-5,5.82792926524091E-5,
7.04649253805303E-5,8.7292331290714E-5,9.05038369585905E-5,9.2257822818511E-5,
0.000103663146463137,0.00011386600552116,0.000117768598772957,0.000124579094175182,
0.000129312863866651,0.000130178750830784,0.000132692979584746,0.000134419842078314),
 .UNSPECIFIED.) ;
#2408 = B_SPLINE_CURVE_WITH_KNOTS('',3,(#168677,#168678,#168679,#168680,#168681,
#168682,#168683,#168684,#168685,#168686,#168687,#168688,#168689,#168690,
#168691,#168692,#168693,#168694,#168695,#168696,#168697,#168698,#168699,
#168700,#168701,#168702),.UNSPECIFIED.,.F.,.F.,(4,2,2,2,2,2,2,2,2,2,2,2,
4),(0.,5.55321021976964E-6,8.25511347643153E-6,1.91711188535163E-5,3.04852632940513E-5,
5.08165579102757E-5,5.19149958125372E-5,6.39742577536695E-5,8.61162395509784E-5,
9.85980048375118E-5,0.000117622240611266,0.000125683481932165,0.000134262298488521),
 .UNSPECIFIED.) ;
#2409 = B_SPLINE_CURVE_WITH_KNOTS('',3,(#168709,#168710,#168711,#168712,#168713,
#168714,#168715,#168716,#168717,#168718,#168719,#168720,#168721,#168722,
#168723,#168724,#168725,#168726,#168727,#168728,#168729,#168730,#168731,
#168732,#168733,#168734,#168735,#168736,#168737,#168738,#168739,#168740,
#168741,#168742,#168743,#168744,#168745,#168746,#168747,#168748,#168749,
#168750,#168751,#168752,#168753,#168754,#168755,#168756,#168757,#168758,
#168759,#168760,#168761,#168762,#168763),.UNSPECIFIED.,.F.,.F.,(4,3,3,3,
3,3,3,3,3,3,3,3,3,3,3,3,3,3,4),(0.,1.96170179198987E-5,2.35258500143176E-5,
3.58003153605645E-5,5.29187212179511E-5,5.64435994874837E-5,5.82792926524096E-5,
7.04649253805232E-5,8.72923312922054E-5,9.05038369575662E-5,9.22578228185116E-5,
0.000103663146463143,0.000113866005521635,0.000117768598772949,0.000124579094175177,
0.000129312863866761,0.000130178750830864,0.000132692979584753,0.000134419842078312),
 .UNSPECIFIED.) ;
#2410 = B_SPLINE_CURVE_WITH_KNOTS('',3,(#168772,#168773,#168774,#168775,#168776,
#168777,#168778,#168779,#168780,#168781,#168782,#168783,#168784,#168785,
#168786,#168787,#168788,#168789,#168790,#168791,#168792,#168793,#168794,
#168795,#168796,#168797),.UNSPECIFIED.,.F.,.F.,(4,2,2,2,2,2,2,2,2,2,2,2,
4),(0.,5.55321021972859E-6,8.25511347643153E-6,1.91711188535163E-5,3.0485263294052E-5,
5.08165579103031E-5,5.19149958125372E-5,6.39742577536713E-5,8.61162395509784E-5,
9.85980048375125E-5,0.000117622240611228,0.000125683481931749,0.000134262298488521),
 .UNSPECIFIED.) ;
#2411 = B_SPLINE_CURVE_WITH_KNOTS('',3,(#168804,#168805,#168806,#168807,#168808,
#168809,#168810,#168811,#168812,#168813,#168814,#168815,#168816,#168817,
#168818,#168819,#168820,#168821,#168822,#168823,#168824,#168825,#168826,
#168827,#168828,#168829,#168830,#168831,#168832,#168833,#168834,#168835,
#168836,#168837,#168838,#168839,#168840,#168841,#168842,#168843,#168844,
#168845,#168846,#168847,#168848,#168849,#168850,#168851,#168852,#168853,
#168854,#168855,#168856,#168857,#168858),.UNSPECIFIED.,.F.,.F.,(4,3,3,3,
3,3,3,3,3,3,3,3,3,3,3,3,3,3,4),(0.,1.96170179200225E-5,2.35258500143176E-5,
3.58003153605643E-5,5.29187212193709E-5,5.64435994873347E-5,5.82792926524096E-5,
7.04649253805203E-5,8.72923312916406E-5,9.05038369574672E-5,9.22578228185116E-5,
0.000103663146463146,0.000113866005521278,0.000117768598772934,0.000124579094175177,
0.00012931286386678,0.00013017875083066,0.000132692979584753,0.000134419842078312),
 .UNSPECIFIED.) ;
#2412 = B_SPLINE_CURVE_WITH_KNOTS('',3,(#168867,#168868,#168869,#168870,#168871,
#168872,#168873,#168874,#168875,#168876,#168877,#168878,#168879,#168880,
#168881,#168882,#168883,#168884,#168885,#168886,#168887,#168888,#168889,
#168890,#168891,#168892),.UNSPECIFIED.,.F.,.F.,(4,2,2,2,2,2,2,2,2,2,2,2,
4),(0.,5.55321021961745E-6,8.25511347643483E-6,1.91711188535197E-5,3.04852632940677E-5,
5.08165579107201E-5,5.19149958125403E-5,6.39742577536799E-5,8.61162395509805E-5,
9.85980048375172E-5,0.000117622240610844,0.000125683481932884,0.000134262298488518),
 .UNSPECIFIED.) ;
#2413 = B_SPLINE_CURVE_WITH_KNOTS('',3,(#169558,#169559,#169560,#169561,#169562,
#169563,#169564,#169565,#169566,#169567,#169568,#169569,#169570,#169571,
#169572,#169573,#169574,#169575,#169576,#169577,#169578,#169579,#169580,
#169581,#169582,#169583,#169584,#169585,#169586,#169587,#169588,#169589,
#169590,#169591,#169592,#169593,#169594,#169595,#169596,#169597,#169598,
#169599,#169600,#169601,#169602,#169603,#169604,#169605,#169606,#169607),
 .UNSPECIFIED.,.F.,.F.,(4,2,2,2,2,2,2,2,2,2,2,2,2,2,2,2,2,2,2,2,2,2,2,2,
4),(-2.08039868634433E-6,0.,1.80285080514979E-6,4.0751335740202E-6,7.68982405736938E-6,
1.34802948057236E-5,2.29326054193163E-5,3.92630132602966E-5,5.80367880477344E-5,
6.50818237188975E-5,7.31401178077086E-5,7.59246603911382E-5,9.50727127604295E-5,
9.80359284023885E-5,0.000112225222383658,0.000116796661227539,0.000117770724301747,
0.000134602167593749,0.000142446541904567,0.000143188584796264,0.000155450849073387,
0.000157760323312202,0.000160014008022128,0.000173898693194695,0.000175397121695959),
 .UNSPECIFIED.) ;
#2414 = B_SPLINE_CURVE_WITH_KNOTS('',3,(#169958,#169959,#169960,#169961,#169962,
#169963,#169964,#169965,#169966,#169967,#169968,#169969,#169970,#169971,
#169972,#169973,#169974,#169975,#169976,#169977,#169978,#169979,#169980,
#169981,#169982,#169983,#169984,#169985,#169986,#169987,#169988,#169989,
#169990,#169991,#169992,#169993,#169994,#169995,#169996,#169997,#169998,
#169999,#170000,#170001,#170002,#170003,#170004,#170005,#170006,#170007),
 .UNSPECIFIED.,.F.,.F.,(4,2,2,2,2,2,2,2,2,2,2,2,2,2,2,2,2,2,2,2,2,2,2,2,
4),(-2.08039868634673E-6,0.,1.80285080513718E-6,4.07513357401502E-6,7.68982405736462E-6,
1.34802948057175E-5,2.29326054193016E-5,3.92630132602916E-5,5.80367882596256E-5,
6.50818237191735E-5,7.31401178093195E-5,7.59246603911372E-5,9.50727128359684E-5,
9.80359284024087E-5,0.000112225222382539,0.000116796661227535,0.00011777072430175,
0.000134602167593809,0.000142446541904572,0.000143188584796265,0.000155450849073815,
0.000157760323312273,0.000160014008022131,0.000173898693194877,0.000175397121695963),
 .UNSPECIFIED.) ;
#2415 = CONICAL_SURFACE('',#91158,1.5,0.78539816339745) ;
#2416 = CONICAL_SURFACE('',#91204,1.5,0.78539816339745) ;
#2417 = CONICAL_SURFACE('',#92047,1.5,0.78539816339745) ;
#2418 = CONICAL_SURFACE('',#92093,1.5,0.78539816339745) ;
#2419 = CONICAL_SURFACE('',#92939,1.5,0.78539816339745) ;
#2420 = CONICAL_SURFACE('',#98416,1.,0.78539816339745) ;
#2421 = CONICAL_SURFACE('',#98418,1.,0.78539816339745) ;
#2422 = CONICAL_SURFACE('',#98420,1.,0.78539816339745) ;
#2423 = CONICAL_SURFACE('',#98422,1.,0.78539816339745) ;
#2424 = CONICAL_SURFACE('',#98424,1.,0.78539816339745) ;
#2425 = CONICAL_SURFACE('',#98426,1.,0.78539816339745) ;
#2426 = CONICAL_SURFACE('',#98428,1.,0.78539816339745) ;
#2427 = CONICAL_SURFACE('',#98430,0.999999999999999,0.78539816339745) ;
#2428 = CONICAL_SURFACE('',#98432,1.,0.78539816339745) ;
#2429 = CONICAL_SURFACE('',#98469,1.,0.78539816339745) ;
#2430 = LINE('',#132601,#7984) ;
#2431 = LINE('',#132604,#7985) ;
#2432 = LINE('',#132615,#7986) ;
#2433 = LINE('',#132617,#7987) ;
#2434 = LINE('',#132634,#7988) ;
#2435 = LINE('',#132660,#7989) ;
#2436 = LINE('',#132707,#7990) ;
#2437 = LINE('',#132733,#7991) ;
#2438 = LINE('',#132767,#7992) ;
#2439 = LINE('',#132782,#7993) ;
#2440 = LINE('',#132785,#7994) ;
#2441 = LINE('',#132826,#7995) ;
#2442 = LINE('',#132829,#7996) ;
#2443 = LINE('',#132840,#7997) ;
#2444 = LINE('',#132842,#7998) ;
#2445 = LINE('',#132859,#7999) ;
#2446 = LINE('',#132885,#8000) ;
#2447 = LINE('',#132932,#8001) ;
#2448 = LINE('',#132958,#8002) ;
#2449 = LINE('',#132992,#8003) ;
#2450 = LINE('',#132996,#8004) ;
#2451 = LINE('',#132998,#8005) ;
#2452 = LINE('',#133000,#8006) ;
#2453 = LINE('',#133001,#8007) ;
#2454 = LINE('',#133006,#8008) ;
#2455 = LINE('',#133013,#8009) ;
#2456 = LINE('',#133020,#8010) ;
#2457 = LINE('',#133023,#8011) ;
#2458 = LINE('',#133027,#8012) ;
#2459 = LINE('',#133029,#8013) ;
#2460 = LINE('',#133031,#8014) ;
#2461 = LINE('',#133032,#8015) ;
#2462 = LINE('',#133036,#8016) ;
#2463 = LINE('',#133038,#8017) ;
#2464 = LINE('',#133040,#8018) ;
#2465 = LINE('',#133041,#8019) ;
#2466 = LINE('',#133045,#8020) ;
#2467 = LINE('',#133047,#8021) ;
#2468 = LINE('',#133049,#8022) ;
#2469 = LINE('',#133050,#8023) ;
#2470 = LINE('',#133054,#8024) ;
#2471 = LINE('',#133067,#8025) ;
#2472 = LINE('',#133071,#8026) ;
#2473 = LINE('',#133078,#8027) ;
#2474 = LINE('',#133081,#8028) ;
#2475 = LINE('',#133085,#8029) ;
#2476 = LINE('',#133087,#8030) ;
#2477 = LINE('',#133089,#8031) ;
#2478 = LINE('',#133090,#8032) ;
#2479 = LINE('',#133092,#8033) ;
#2480 = LINE('',#133094,#8034) ;
#2481 = LINE('',#133096,#8035) ;
#2482 = LINE('',#133097,#8036) ;
#2483 = LINE('',#133099,#8037) ;
#2484 = LINE('',#133101,#8038) ;
#2485 = LINE('',#133103,#8039) ;
#2486 = LINE('',#133105,#8040) ;
#2487 = LINE('',#133107,#8041) ;
#2488 = LINE('',#133115,#8042) ;
#2489 = LINE('',#133123,#8043) ;
#2490 = LINE('',#133125,#8044) ;
#2491 = LINE('',#133126,#8045) ;
#2492 = LINE('',#133128,#8046) ;
#2493 = LINE('',#133131,#8047) ;
#2494 = LINE('',#133132,#8048) ;
#2495 = LINE('',#133133,#8049) ;
#2496 = LINE('',#133135,#8050) ;
#2497 = LINE('',#133138,#8051) ;
#2498 = LINE('',#133141,#8052) ;
#2499 = LINE('',#133143,#8053) ;
#2500 = LINE('',#133145,#8054) ;
#2501 = LINE('',#133146,#8055) ;
#2502 = LINE('',#133150,#8056) ;
#2503 = LINE('',#133152,#8057) ;
#2504 = LINE('',#133156,#8058) ;
#2505 = LINE('',#133160,#8059) ;
#2506 = LINE('',#133164,#8060) ;
#2507 = LINE('',#133168,#8061) ;
#2508 = LINE('',#133170,#8062) ;
#2509 = LINE('',#133171,#8063) ;
#2510 = LINE('',#133175,#8064) ;
#2511 = LINE('',#133176,#8065) ;
#2512 = LINE('',#133177,#8066) ;
#2513 = LINE('',#133180,#8067) ;
#2514 = LINE('',#133182,#8068) ;
#2515 = LINE('',#133183,#8069) ;
#2516 = LINE('',#133184,#8070) ;
#2517 = LINE('',#133188,#8071) ;
#2518 = LINE('',#133190,#8072) ;
#2519 = LINE('',#133192,#8073) ;
#2520 = LINE('',#133193,#8074) ;
#2521 = LINE('',#133198,#8075) ;
#2522 = LINE('',#133202,#8076) ;
#2523 = LINE('',#133206,#8077) ;
#2524 = LINE('',#133209,#8078) ;
#2525 = LINE('',#133214,#8079) ;
#2526 = LINE('',#133218,#8080) ;
#2527 = LINE('',#133222,#8081) ;
#2528 = LINE('',#133225,#8082) ;
#2529 = LINE('',#133229,#8083) ;
#2530 = LINE('',#133231,#8084) ;
#2531 = LINE('',#133233,#8085) ;
#2532 = LINE('',#133234,#8086) ;
#2533 = LINE('',#133238,#8087) ;
#2534 = LINE('',#133239,#8088) ;
#2535 = LINE('',#133240,#8089) ;
#2536 = LINE('',#133243,#8090) ;
#2537 = LINE('',#133245,#8091) ;
#2538 = LINE('',#133246,#8092) ;
#2539 = LINE('',#133250,#8093) ;
#2540 = LINE('',#133252,#8094) ;
#2541 = LINE('',#133254,#8095) ;
#2542 = LINE('',#133255,#8096) ;
#2543 = LINE('',#133258,#8097) ;
#2544 = LINE('',#133267,#8098) ;
#2545 = LINE('',#133276,#8099) ;
#2546 = LINE('',#133285,#8100) ;
#2547 = LINE('',#133294,#8101) ;
#2548 = LINE('',#133303,#8102) ;
#2549 = LINE('',#133312,#8103) ;
#2550 = LINE('',#133321,#8104) ;
#2551 = LINE('',#133331,#8105) ;
#2552 = LINE('',#133333,#8106) ;
#2553 = LINE('',#133335,#8107) ;
#2554 = LINE('',#133336,#8108) ;
#2555 = LINE('',#133341,#8109) ;
#2556 = LINE('',#133345,#8110) ;
#2557 = LINE('',#133349,#8111) ;
#2558 = LINE('',#133352,#8112) ;
#2559 = LINE('',#133357,#8113) ;
#2560 = LINE('',#133361,#8114) ;
#2561 = LINE('',#133365,#8115) ;
#2562 = LINE('',#133368,#8116) ;
#2563 = LINE('',#133372,#8117) ;
#2564 = LINE('',#133374,#8118) ;
#2565 = LINE('',#133376,#8119) ;
#2566 = LINE('',#133377,#8120) ;
#2567 = LINE('',#133464,#8121) ;
#2568 = LINE('',#133466,#8122) ;
#2569 = LINE('',#133468,#8123) ;
#2570 = LINE('',#133470,#8124) ;
#2571 = LINE('',#133472,#8125) ;
#2572 = LINE('',#133556,#8126) ;
#2573 = LINE('',#133560,#8127) ;
#2574 = LINE('',#133562,#8128) ;
#2575 = LINE('',#133565,#8129) ;
#2576 = LINE('',#133569,#8130) ;
#2577 = LINE('',#133571,#8131) ;
#2578 = LINE('',#133573,#8132) ;
#2579 = LINE('',#133574,#8133) ;
#2580 = LINE('',#133593,#8134) ;
#2581 = LINE('',#133595,#8135) ;
#2582 = LINE('',#133597,#8136) ;
#2583 = LINE('',#133598,#8137) ;
#2584 = LINE('',#133602,#8138) ;
#2585 = LINE('',#133604,#8139) ;
#2586 = LINE('',#133606,#8140) ;
#2587 = LINE('',#133607,#8141) ;
#2588 = LINE('',#133613,#8142) ;
#2589 = LINE('',#133615,#8143) ;
#2590 = LINE('',#133617,#8144) ;
#2591 = LINE('',#133621,#8145) ;
#2592 = LINE('',#133623,#8146) ;
#2593 = LINE('',#133624,#8147) ;
#2594 = LINE('',#133628,#8148) ;
#2595 = LINE('',#133632,#8149) ;
#2596 = LINE('',#133637,#8150) ;
#2597 = LINE('',#133643,#8151) ;
#2598 = LINE('',#133645,#8152) ;
#2599 = LINE('',#133649,#8153) ;
#2600 = LINE('',#133651,#8154) ;
#2601 = LINE('',#133652,#8155) ;
#2602 = LINE('',#133655,#8156) ;
#2603 = LINE('',#133657,#8157) ;
#2604 = LINE('',#133658,#8158) ;
#2605 = LINE('',#133661,#8159) ;
#2606 = LINE('',#133663,#8160) ;
#2607 = LINE('',#133664,#8161) ;
#2608 = LINE('',#133668,#8162) ;
#2609 = LINE('',#133670,#8163) ;
#2610 = LINE('',#133672,#8164) ;
#2611 = LINE('',#133674,#8165) ;
#2612 = LINE('',#133676,#8166) ;
#2613 = LINE('',#133677,#8167) ;
#2614 = LINE('',#133681,#8168) ;
#2615 = LINE('',#133683,#8169) ;
#2616 = LINE('',#133685,#8170) ;
#2617 = LINE('',#133687,#8171) ;
#2618 = LINE('',#133689,#8172) ;
#2619 = LINE('',#133690,#8173) ;
#2620 = LINE('',#133694,#8174) ;
#2621 = LINE('',#133696,#8175) ;
#2622 = LINE('',#133698,#8176) ;
#2623 = LINE('',#133699,#8177) ;
#2624 = LINE('',#133703,#8178) ;
#2625 = LINE('',#133705,#8179) ;
#2626 = LINE('',#133707,#8180) ;
#2627 = LINE('',#133708,#8181) ;
#2628 = LINE('',#133712,#8182) ;
#2629 = LINE('',#133714,#8183) ;
#2630 = LINE('',#133716,#8184) ;
#2631 = LINE('',#133717,#8185) ;
#2632 = LINE('',#133721,#8186) ;
#2633 = LINE('',#133723,#8187) ;
#2634 = LINE('',#133725,#8188) ;
#2635 = LINE('',#133726,#8189) ;
#2636 = LINE('',#133730,#8190) ;
#2637 = LINE('',#133732,#8191) ;
#2638 = LINE('',#133734,#8192) ;
#2639 = LINE('',#133735,#8193) ;
#2640 = LINE('',#133738,#8194) ;
#2641 = LINE('',#133742,#8195) ;
#2642 = LINE('',#133746,#8196) ;
#2643 = LINE('',#133750,#8197) ;
#2644 = LINE('',#133756,#8198) ;
#2645 = LINE('',#133757,#8199) ;
#2646 = LINE('',#133760,#8200) ;
#2647 = LINE('',#133761,#8201) ;
#2648 = LINE('',#133765,#8202) ;
#2649 = LINE('',#133768,#8203) ;
#2650 = LINE('',#133769,#8204) ;
#2651 = LINE('',#133773,#8205) ;
#2652 = LINE('',#133776,#8206) ;
#2653 = LINE('',#133777,#8207) ;
#2654 = LINE('',#133781,#8208) ;
#2655 = LINE('',#133783,#8209) ;
#2656 = LINE('',#133786,#8210) ;
#2657 = LINE('',#133788,#8211) ;
#2658 = LINE('',#133789,#8212) ;
#2659 = LINE('',#133791,#8213) ;
#2660 = LINE('',#133792,#8214) ;
#2661 = LINE('',#133794,#8215) ;
#2662 = LINE('',#133795,#8216) ;
#2663 = LINE('',#133799,#8217) ;
#2664 = LINE('',#133801,#8218) ;
#2665 = LINE('',#133803,#8219) ;
#2666 = LINE('',#133804,#8220) ;
#2667 = LINE('',#133808,#8221) ;
#2668 = LINE('',#133810,#8222) ;
#2669 = LINE('',#133812,#8223) ;
#2670 = LINE('',#133813,#8224) ;
#2671 = LINE('',#133817,#8225) ;
#2672 = LINE('',#133819,#8226) ;
#2673 = LINE('',#133821,#8227) ;
#2674 = LINE('',#133822,#8228) ;
#2675 = LINE('',#133826,#8229) ;
#2676 = LINE('',#133828,#8230) ;
#2677 = LINE('',#133830,#8231) ;
#2678 = LINE('',#133831,#8232) ;
#2679 = LINE('',#133835,#8233) ;
#2680 = LINE('',#133837,#8234) ;
#2681 = LINE('',#133839,#8235) ;
#2682 = LINE('',#133840,#8236) ;
#2683 = LINE('',#133843,#8237) ;
#2684 = LINE('',#133847,#8238) ;
#2685 = LINE('',#133851,#8239) ;
#2686 = LINE('',#133855,#8240) ;
#2687 = LINE('',#133859,#8241) ;
#2688 = LINE('',#133862,#8242) ;
#2689 = LINE('',#133865,#8243) ;
#2690 = LINE('',#133866,#8244) ;
#2691 = LINE('',#133870,#8245) ;
#2692 = LINE('',#133873,#8246) ;
#2693 = LINE('',#133874,#8247) ;
#2694 = LINE('',#133878,#8248) ;
#2695 = LINE('',#133881,#8249) ;
#2696 = LINE('',#133882,#8250) ;
#2697 = LINE('',#133886,#8251) ;
#2698 = LINE('',#133888,#8252) ;
#2699 = LINE('',#133892,#8253) ;
#2700 = LINE('',#133894,#8254) ;
#2701 = LINE('',#133896,#8255) ;
#2702 = LINE('',#133897,#8256) ;
#2703 = LINE('',#133899,#8257) ;
#2704 = LINE('',#133901,#8258) ;
#2705 = LINE('',#133903,#8259) ;
#2706 = LINE('',#133904,#8260) ;
#2707 = LINE('',#133907,#8261) ;
#2708 = LINE('',#133909,#8262) ;
#2709 = LINE('',#133910,#8263) ;
#2710 = LINE('',#133913,#8264) ;
#2711 = LINE('',#133914,#8265) ;
#2712 = LINE('',#133915,#8266) ;
#2713 = LINE('',#133918,#8267) ;
#2714 = LINE('',#133922,#8268) ;
#2715 = LINE('',#133924,#8269) ;
#2716 = LINE('',#133925,#8270) ;
#2717 = LINE('',#133936,#8271) ;
#2718 = LINE('',#133939,#8272) ;
#2719 = LINE('',#134840,#8273) ;
#2720 = LINE('',#134842,#8274) ;
#2721 = LINE('',#134844,#8275) ;
#2722 = LINE('',#134845,#8276) ;
#2723 = LINE('',#134850,#8277) ;
#2724 = LINE('',#134854,#8278) ;
#2725 = LINE('',#134856,#8279) ;
#2726 = LINE('',#134857,#8280) ;
#2727 = LINE('',#134862,#8281) ;
#2728 = LINE('',#134866,#8282) ;
#2729 = LINE('',#134868,#8283) ;
#2730 = LINE('',#134869,#8284) ;
#2731 = LINE('',#134874,#8285) ;
#2732 = LINE('',#134878,#8286) ;
#2733 = LINE('',#134880,#8287) ;
#2734 = LINE('',#134881,#8288) ;
#2735 = LINE('',#134886,#8289) ;
#2736 = LINE('',#134890,#8290) ;
#2737 = LINE('',#134892,#8291) ;
#2738 = LINE('',#134893,#8292) ;
#2739 = LINE('',#134899,#8293) ;
#2740 = LINE('',#134901,#8294) ;
#2741 = LINE('',#134903,#8295) ;
#2742 = LINE('',#134905,#8296) ;
#2743 = LINE('',#134907,#8297) ;
#2744 = LINE('',#134908,#8298) ;
#2745 = LINE('',#134912,#8299) ;
#2746 = LINE('',#134914,#8300) ;
#2747 = LINE('',#134916,#8301) ;
#2748 = LINE('',#134918,#8302) ;
#2749 = LINE('',#134922,#8303) ;
#2750 = LINE('',#134923,#8304) ;
#2751 = LINE('',#134929,#8305) ;
#2752 = LINE('',#134931,#8306) ;
#2753 = LINE('',#134932,#8307) ;
#2754 = LINE('',#134936,#8308) ;
#2755 = LINE('',#134938,#8309) ;
#2756 = LINE('',#134939,#8310) ;
#2757 = LINE('',#134940,#8311) ;
#2758 = LINE('',#134942,#8312) ;
#2759 = LINE('',#134946,#8313) ;
#2760 = LINE('',#134948,#8314) ;
#2761 = LINE('',#134950,#8315) ;
#2762 = LINE('',#134951,#8316) ;
#2763 = LINE('',#134961,#8317) ;
#2764 = LINE('',#134963,#8318) ;
#2765 = LINE('',#134965,#8319) ;
#2766 = LINE('',#134966,#8320) ;
#2767 = LINE('',#134970,#8321) ;
#2768 = LINE('',#134972,#8322) ;
#2769 = LINE('',#134974,#8323) ;
#2770 = LINE('',#134975,#8324) ;
#2771 = LINE('',#134981,#8325) ;
#2772 = LINE('',#134983,#8326) ;
#2773 = LINE('',#134985,#8327) ;
#2774 = LINE('',#134989,#8328) ;
#2775 = LINE('',#134991,#8329) ;
#2776 = LINE('',#134992,#8330) ;
#2777 = LINE('',#134996,#8331) ;
#2778 = LINE('',#135000,#8332) ;
#2779 = LINE('',#135005,#8333) ;
#2780 = LINE('',#135011,#8334) ;
#2781 = LINE('',#135013,#8335) ;
#2782 = LINE('',#135017,#8336) ;
#2783 = LINE('',#135019,#8337) ;
#2784 = LINE('',#135020,#8338) ;
#2785 = LINE('',#135023,#8339) ;
#2786 = LINE('',#135025,#8340) ;
#2787 = LINE('',#135026,#8341) ;
#2788 = LINE('',#135029,#8342) ;
#2789 = LINE('',#135031,#8343) ;
#2790 = LINE('',#135032,#8344) ;
#2791 = LINE('',#135036,#8345) ;
#2792 = LINE('',#135038,#8346) ;
#2793 = LINE('',#135040,#8347) ;
#2794 = LINE('',#135042,#8348) ;
#2795 = LINE('',#135044,#8349) ;
#2796 = LINE('',#135045,#8350) ;
#2797 = LINE('',#135049,#8351) ;
#2798 = LINE('',#135051,#8352) ;
#2799 = LINE('',#135053,#8353) ;
#2800 = LINE('',#135055,#8354) ;
#2801 = LINE('',#135057,#8355) ;
#2802 = LINE('',#135058,#8356) ;
#2803 = LINE('',#135062,#8357) ;
#2804 = LINE('',#135064,#8358) ;
#2805 = LINE('',#135066,#8359) ;
#2806 = LINE('',#135067,#8360) ;
#2807 = LINE('',#135071,#8361) ;
#2808 = LINE('',#135073,#8362) ;
#2809 = LINE('',#135075,#8363) ;
#2810 = LINE('',#135076,#8364) ;
#2811 = LINE('',#135080,#8365) ;
#2812 = LINE('',#135082,#8366) ;
#2813 = LINE('',#135084,#8367) ;
#2814 = LINE('',#135085,#8368) ;
#2815 = LINE('',#135089,#8369) ;
#2816 = LINE('',#135091,#8370) ;
#2817 = LINE('',#135093,#8371) ;
#2818 = LINE('',#135094,#8372) ;
#2819 = LINE('',#135098,#8373) ;
#2820 = LINE('',#135100,#8374) ;
#2821 = LINE('',#135102,#8375) ;
#2822 = LINE('',#135103,#8376) ;
#2823 = LINE('',#135106,#8377) ;
#2824 = LINE('',#135110,#8378) ;
#2825 = LINE('',#135114,#8379) ;
#2826 = LINE('',#135118,#8380) ;
#2827 = LINE('',#135124,#8381) ;
#2828 = LINE('',#135125,#8382) ;
#2829 = LINE('',#135128,#8383) ;
#2830 = LINE('',#135129,#8384) ;
#2831 = LINE('',#135133,#8385) ;
#2832 = LINE('',#135136,#8386) ;
#2833 = LINE('',#135137,#8387) ;
#2834 = LINE('',#135141,#8388) ;
#2835 = LINE('',#135144,#8389) ;
#2836 = LINE('',#135145,#8390) ;
#2837 = LINE('',#135149,#8391) ;
#2838 = LINE('',#135151,#8392) ;
#2839 = LINE('',#135154,#8393) ;
#2840 = LINE('',#135156,#8394) ;
#2841 = LINE('',#135157,#8395) ;
#2842 = LINE('',#135159,#8396) ;
#2843 = LINE('',#135160,#8397) ;
#2844 = LINE('',#135162,#8398) ;
#2845 = LINE('',#135163,#8399) ;
#2846 = LINE('',#135167,#8400) ;
#2847 = LINE('',#135169,#8401) ;
#2848 = LINE('',#135171,#8402) ;
#2849 = LINE('',#135172,#8403) ;
#2850 = LINE('',#135176,#8404) ;
#2851 = LINE('',#135178,#8405) ;
#2852 = LINE('',#135180,#8406) ;
#2853 = LINE('',#135181,#8407) ;
#2854 = LINE('',#135185,#8408) ;
#2855 = LINE('',#135187,#8409) ;
#2856 = LINE('',#135189,#8410) ;
#2857 = LINE('',#135190,#8411) ;
#2858 = LINE('',#135194,#8412) ;
#2859 = LINE('',#135196,#8413) ;
#2860 = LINE('',#135198,#8414) ;
#2861 = LINE('',#135199,#8415) ;
#2862 = LINE('',#135203,#8416) ;
#2863 = LINE('',#135205,#8417) ;
#2864 = LINE('',#135207,#8418) ;
#2865 = LINE('',#135208,#8419) ;
#2866 = LINE('',#135211,#8420) ;
#2867 = LINE('',#135215,#8421) ;
#2868 = LINE('',#135219,#8422) ;
#2869 = LINE('',#135223,#8423) ;
#2870 = LINE('',#135227,#8424) ;
#2871 = LINE('',#135230,#8425) ;
#2872 = LINE('',#135233,#8426) ;
#2873 = LINE('',#135234,#8427) ;
#2874 = LINE('',#135238,#8428) ;
#2875 = LINE('',#135241,#8429) ;
#2876 = LINE('',#135242,#8430) ;
#2877 = LINE('',#135246,#8431) ;
#2878 = LINE('',#135249,#8432) ;
#2879 = LINE('',#135250,#8433) ;
#2880 = LINE('',#135254,#8434) ;
#2881 = LINE('',#135256,#8435) ;
#2882 = LINE('',#135260,#8436) ;
#2883 = LINE('',#135262,#8437) ;
#2884 = LINE('',#135264,#8438) ;
#2885 = LINE('',#135265,#8439) ;
#2886 = LINE('',#135267,#8440) ;
#2887 = LINE('',#135269,#8441) ;
#2888 = LINE('',#135271,#8442) ;
#2889 = LINE('',#135272,#8443) ;
#2890 = LINE('',#135275,#8444) ;
#2891 = LINE('',#135277,#8445) ;
#2892 = LINE('',#135278,#8446) ;
#2893 = LINE('',#135281,#8447) ;
#2894 = LINE('',#135282,#8448) ;
#2895 = LINE('',#135283,#8449) ;
#2896 = LINE('',#135286,#8450) ;
#2897 = LINE('',#135290,#8451) ;
#2898 = LINE('',#135292,#8452) ;
#2899 = LINE('',#135293,#8453) ;
#2900 = LINE('',#135304,#8454) ;
#2901 = LINE('',#135307,#8455) ;
#2902 = LINE('',#136304,#8456) ;
#2903 = LINE('',#136307,#8457) ;
#2904 = LINE('',#136318,#8458) ;
#2905 = LINE('',#136320,#8459) ;
#2906 = LINE('',#136337,#8460) ;
#2907 = LINE('',#136363,#8461) ;
#2908 = LINE('',#136410,#8462) ;
#2909 = LINE('',#136436,#8463) ;
#2910 = LINE('',#136470,#8464) ;
#2911 = LINE('',#136485,#8465) ;
#2912 = LINE('',#136488,#8466) ;
#2913 = LINE('',#136529,#8467) ;
#2914 = LINE('',#136532,#8468) ;
#2915 = LINE('',#136543,#8469) ;
#2916 = LINE('',#136545,#8470) ;
#2917 = LINE('',#136562,#8471) ;
#2918 = LINE('',#136588,#8472) ;
#2919 = LINE('',#136635,#8473) ;
#2920 = LINE('',#136661,#8474) ;
#2921 = LINE('',#136695,#8475) ;
#2922 = LINE('',#136699,#8476) ;
#2923 = LINE('',#136701,#8477) ;
#2924 = LINE('',#136703,#8478) ;
#2925 = LINE('',#136704,#8479) ;
#2926 = LINE('',#136709,#8480) ;
#2927 = LINE('',#136716,#8481) ;
#2928 = LINE('',#136723,#8482) ;
#2929 = LINE('',#136726,#8483) ;
#2930 = LINE('',#136730,#8484) ;
#2931 = LINE('',#136732,#8485) ;
#2932 = LINE('',#136734,#8486) ;
#2933 = LINE('',#136735,#8487) ;
#2934 = LINE('',#136739,#8488) ;
#2935 = LINE('',#136741,#8489) ;
#2936 = LINE('',#136743,#8490) ;
#2937 = LINE('',#136744,#8491) ;
#2938 = LINE('',#136748,#8492) ;
#2939 = LINE('',#136750,#8493) ;
#2940 = LINE('',#136752,#8494) ;
#2941 = LINE('',#136753,#8495) ;
#2942 = LINE('',#136758,#8496) ;
#2943 = LINE('',#136771,#8497) ;
#2944 = LINE('',#136775,#8498) ;
#2945 = LINE('',#136781,#8499) ;
#2946 = LINE('',#136783,#8500) ;
#2947 = LINE('',#136784,#8501) ;
#2948 = LINE('',#136788,#8502) ;
#2949 = LINE('',#136790,#8503) ;
#2950 = LINE('',#136792,#8504) ;
#2951 = LINE('',#136793,#8505) ;
#2952 = LINE('',#136797,#8506) ;
#2953 = LINE('',#136799,#8507) ;
#2954 = LINE('',#136800,#8508) ;
#2955 = LINE('',#136801,#8509) ;
#2956 = LINE('',#136803,#8510) ;
#2957 = LINE('',#136805,#8511) ;
#2958 = LINE('',#136806,#8512) ;
#2959 = LINE('',#136808,#8513) ;
#2960 = LINE('',#136811,#8514) ;
#2961 = LINE('',#136812,#8515) ;
#2962 = LINE('',#136814,#8516) ;
#2963 = LINE('',#136816,#8517) ;
#2964 = LINE('',#136818,#8518) ;
#2965 = LINE('',#136826,#8519) ;
#2966 = LINE('',#136834,#8520) ;
#2967 = LINE('',#136836,#8521) ;
#2968 = LINE('',#136837,#8522) ;
#2969 = LINE('',#136839,#8523) ;
#2970 = LINE('',#136842,#8524) ;
#2971 = LINE('',#136845,#8525) ;
#2972 = LINE('',#136847,#8526) ;
#2973 = LINE('',#136848,#8527) ;
#2974 = LINE('',#136849,#8528) ;
#2975 = LINE('',#136853,#8529) ;
#2976 = LINE('',#136855,#8530) ;
#2977 = LINE('',#136857,#8531) ;
#2978 = LINE('',#136861,#8532) ;
#2979 = LINE('',#136865,#8533) ;
#2980 = LINE('',#136869,#8534) ;
#2981 = LINE('',#136873,#8535) ;
#2982 = LINE('',#136874,#8536) ;
#2983 = LINE('',#136877,#8537) ;
#2984 = LINE('',#136879,#8538) ;
#2985 = LINE('',#136880,#8539) ;
#2986 = LINE('',#136883,#8540) ;
#2987 = LINE('',#136885,#8541) ;
#2988 = LINE('',#136886,#8542) ;
#2989 = LINE('',#136887,#8543) ;
#2990 = LINE('',#136891,#8544) ;
#2991 = LINE('',#136893,#8545) ;
#2992 = LINE('',#136895,#8546) ;
#2993 = LINE('',#136896,#8547) ;
#2994 = LINE('',#136901,#8548) ;
#2995 = LINE('',#136905,#8549) ;
#2996 = LINE('',#136909,#8550) ;
#2997 = LINE('',#136912,#8551) ;
#2998 = LINE('',#136917,#8552) ;
#2999 = LINE('',#136921,#8553) ;
#3000 = LINE('',#136925,#8554) ;
#3001 = LINE('',#136928,#8555) ;
#3002 = LINE('',#136932,#8556) ;
#3003 = LINE('',#136934,#8557) ;
#3004 = LINE('',#136936,#8558) ;
#3005 = LINE('',#136937,#8559) ;
#3006 = LINE('',#136940,#8560) ;
#3007 = LINE('',#136942,#8561) ;
#3008 = LINE('',#136943,#8562) ;
#3009 = LINE('',#136946,#8563) ;
#3010 = LINE('',#136948,#8564) ;
#3011 = LINE('',#136949,#8565) ;
#3012 = LINE('',#136953,#8566) ;
#3013 = LINE('',#136955,#8567) ;
#3014 = LINE('',#136957,#8568) ;
#3015 = LINE('',#136958,#8569) ;
#3016 = LINE('',#136961,#8570) ;
#3017 = LINE('',#136970,#8571) ;
#3018 = LINE('',#136979,#8572) ;
#3019 = LINE('',#136988,#8573) ;
#3020 = LINE('',#136997,#8574) ;
#3021 = LINE('',#137006,#8575) ;
#3022 = LINE('',#137015,#8576) ;
#3023 = LINE('',#137024,#8577) ;
#3024 = LINE('',#137034,#8578) ;
#3025 = LINE('',#137036,#8579) ;
#3026 = LINE('',#137038,#8580) ;
#3027 = LINE('',#137039,#8581) ;
#3028 = LINE('',#137044,#8582) ;
#3029 = LINE('',#137048,#8583) ;
#3030 = LINE('',#137052,#8584) ;
#3031 = LINE('',#137055,#8585) ;
#3032 = LINE('',#137060,#8586) ;
#3033 = LINE('',#137064,#8587) ;
#3034 = LINE('',#137068,#8588) ;
#3035 = LINE('',#137071,#8589) ;
#3036 = LINE('',#137075,#8590) ;
#3037 = LINE('',#137077,#8591) ;
#3038 = LINE('',#137079,#8592) ;
#3039 = LINE('',#137080,#8593) ;
#3040 = LINE('',#137167,#8594) ;
#3041 = LINE('',#137252,#8595) ;
#3042 = LINE('',#137254,#8596) ;
#3043 = LINE('',#137256,#8597) ;
#3044 = LINE('',#137258,#8598) ;
#3045 = LINE('',#137259,#8599) ;
#3046 = LINE('',#137263,#8600) ;
#3047 = LINE('',#137267,#8601) ;
#3048 = LINE('',#137272,#8602) ;
#3049 = LINE('',#137274,#8603) ;
#3050 = LINE('',#137276,#8604) ;
#3051 = LINE('',#137277,#8605) ;
#3052 = LINE('',#137296,#8606) ;
#3053 = LINE('',#137298,#8607) ;
#3054 = LINE('',#137300,#8608) ;
#3055 = LINE('',#137301,#8609) ;
#3056 = LINE('',#137305,#8610) ;
#3057 = LINE('',#137307,#8611) ;
#3058 = LINE('',#137309,#8612) ;
#3059 = LINE('',#137310,#8613) ;
#3060 = LINE('',#137316,#8614) ;
#3061 = LINE('',#137318,#8615) ;
#3062 = LINE('',#137320,#8616) ;
#3063 = LINE('',#137324,#8617) ;
#3064 = LINE('',#137326,#8618) ;
#3065 = LINE('',#137327,#8619) ;
#3066 = LINE('',#137331,#8620) ;
#3067 = LINE('',#137335,#8621) ;
#3068 = LINE('',#137340,#8622) ;
#3069 = LINE('',#137346,#8623) ;
#3070 = LINE('',#137348,#8624) ;
#3071 = LINE('',#137352,#8625) ;
#3072 = LINE('',#137354,#8626) ;
#3073 = LINE('',#137355,#8627) ;
#3074 = LINE('',#137358,#8628) ;
#3075 = LINE('',#137360,#8629) ;
#3076 = LINE('',#137361,#8630) ;
#3077 = LINE('',#137364,#8631) ;
#3078 = LINE('',#137366,#8632) ;
#3079 = LINE('',#137367,#8633) ;
#3080 = LINE('',#137371,#8634) ;
#3081 = LINE('',#137373,#8635) ;
#3082 = LINE('',#137375,#8636) ;
#3083 = LINE('',#137377,#8637) ;
#3084 = LINE('',#137379,#8638) ;
#3085 = LINE('',#137380,#8639) ;
#3086 = LINE('',#137384,#8640) ;
#3087 = LINE('',#137386,#8641) ;
#3088 = LINE('',#137388,#8642) ;
#3089 = LINE('',#137390,#8643) ;
#3090 = LINE('',#137392,#8644) ;
#3091 = LINE('',#137393,#8645) ;
#3092 = LINE('',#137397,#8646) ;
#3093 = LINE('',#137399,#8647) ;
#3094 = LINE('',#137401,#8648) ;
#3095 = LINE('',#137402,#8649) ;
#3096 = LINE('',#137406,#8650) ;
#3097 = LINE('',#137408,#8651) ;
#3098 = LINE('',#137410,#8652) ;
#3099 = LINE('',#137411,#8653) ;
#3100 = LINE('',#137415,#8654) ;
#3101 = LINE('',#137417,#8655) ;
#3102 = LINE('',#137419,#8656) ;
#3103 = LINE('',#137420,#8657) ;
#3104 = LINE('',#137424,#8658) ;
#3105 = LINE('',#137426,#8659) ;
#3106 = LINE('',#137428,#8660) ;
#3107 = LINE('',#137429,#8661) ;
#3108 = LINE('',#137433,#8662) ;
#3109 = LINE('',#137435,#8663) ;
#3110 = LINE('',#137437,#8664) ;
#3111 = LINE('',#137438,#8665) ;
#3112 = LINE('',#137441,#8666) ;
#3113 = LINE('',#137445,#8667) ;
#3114 = LINE('',#137449,#8668) ;
#3115 = LINE('',#137453,#8669) ;
#3116 = LINE('',#137459,#8670) ;
#3117 = LINE('',#137460,#8671) ;
#3118 = LINE('',#137463,#8672) ;
#3119 = LINE('',#137464,#8673) ;
#3120 = LINE('',#137468,#8674) ;
#3121 = LINE('',#137471,#8675) ;
#3122 = LINE('',#137472,#8676) ;
#3123 = LINE('',#137476,#8677) ;
#3124 = LINE('',#137479,#8678) ;
#3125 = LINE('',#137480,#8679) ;
#3126 = LINE('',#137484,#8680) ;
#3127 = LINE('',#137486,#8681) ;
#3128 = LINE('',#137489,#8682) ;
#3129 = LINE('',#137491,#8683) ;
#3130 = LINE('',#137492,#8684) ;
#3131 = LINE('',#137494,#8685) ;
#3132 = LINE('',#137495,#8686) ;
#3133 = LINE('',#137497,#8687) ;
#3134 = LINE('',#137498,#8688) ;
#3135 = LINE('',#137502,#8689) ;
#3136 = LINE('',#137504,#8690) ;
#3137 = LINE('',#137506,#8691) ;
#3138 = LINE('',#137507,#8692) ;
#3139 = LINE('',#137511,#8693) ;
#3140 = LINE('',#137513,#8694) ;
#3141 = LINE('',#137515,#8695) ;
#3142 = LINE('',#137516,#8696) ;
#3143 = LINE('',#137520,#8697) ;
#3144 = LINE('',#137522,#8698) ;
#3145 = LINE('',#137524,#8699) ;
#3146 = LINE('',#137525,#8700) ;
#3147 = LINE('',#137529,#8701) ;
#3148 = LINE('',#137531,#8702) ;
#3149 = LINE('',#137533,#8703) ;
#3150 = LINE('',#137534,#8704) ;
#3151 = LINE('',#137538,#8705) ;
#3152 = LINE('',#137540,#8706) ;
#3153 = LINE('',#137542,#8707) ;
#3154 = LINE('',#137543,#8708) ;
#3155 = LINE('',#137546,#8709) ;
#3156 = LINE('',#137550,#8710) ;
#3157 = LINE('',#137554,#8711) ;
#3158 = LINE('',#137558,#8712) ;
#3159 = LINE('',#137562,#8713) ;
#3160 = LINE('',#137565,#8714) ;
#3161 = LINE('',#137568,#8715) ;
#3162 = LINE('',#137569,#8716) ;
#3163 = LINE('',#137573,#8717) ;
#3164 = LINE('',#137576,#8718) ;
#3165 = LINE('',#137577,#8719) ;
#3166 = LINE('',#137581,#8720) ;
#3167 = LINE('',#137584,#8721) ;
#3168 = LINE('',#137585,#8722) ;
#3169 = LINE('',#137589,#8723) ;
#3170 = LINE('',#137591,#8724) ;
#3171 = LINE('',#137595,#8725) ;
#3172 = LINE('',#137597,#8726) ;
#3173 = LINE('',#137599,#8727) ;
#3174 = LINE('',#137600,#8728) ;
#3175 = LINE('',#137602,#8729) ;
#3176 = LINE('',#137604,#8730) ;
#3177 = LINE('',#137606,#8731) ;
#3178 = LINE('',#137607,#8732) ;
#3179 = LINE('',#137610,#8733) ;
#3180 = LINE('',#137612,#8734) ;
#3181 = LINE('',#137613,#8735) ;
#3182 = LINE('',#137616,#8736) ;
#3183 = LINE('',#137617,#8737) ;
#3184 = LINE('',#137618,#8738) ;
#3185 = LINE('',#137621,#8739) ;
#3186 = LINE('',#137625,#8740) ;
#3187 = LINE('',#137627,#8741) ;
#3188 = LINE('',#137628,#8742) ;
#3189 = LINE('',#137639,#8743) ;
#3190 = LINE('',#137642,#8744) ;
#3191 = LINE('',#138543,#8745) ;
#3192 = LINE('',#138545,#8746) ;
#3193 = LINE('',#138547,#8747) ;
#3194 = LINE('',#138548,#8748) ;
#3195 = LINE('',#138553,#8749) ;
#3196 = LINE('',#138557,#8750) ;
#3197 = LINE('',#138559,#8751) ;
#3198 = LINE('',#138560,#8752) ;
#3199 = LINE('',#138565,#8753) ;
#3200 = LINE('',#138569,#8754) ;
#3201 = LINE('',#138571,#8755) ;
#3202 = LINE('',#138572,#8756) ;
#3203 = LINE('',#138577,#8757) ;
#3204 = LINE('',#138581,#8758) ;
#3205 = LINE('',#138583,#8759) ;
#3206 = LINE('',#138584,#8760) ;
#3207 = LINE('',#138589,#8761) ;
#3208 = LINE('',#138593,#8762) ;
#3209 = LINE('',#138595,#8763) ;
#3210 = LINE('',#138596,#8764) ;
#3211 = LINE('',#138602,#8765) ;
#3212 = LINE('',#138604,#8766) ;
#3213 = LINE('',#138606,#8767) ;
#3214 = LINE('',#138608,#8768) ;
#3215 = LINE('',#138610,#8769) ;
#3216 = LINE('',#138611,#8770) ;
#3217 = LINE('',#138615,#8771) ;
#3218 = LINE('',#138617,#8772) ;
#3219 = LINE('',#138619,#8773) ;
#3220 = LINE('',#138621,#8774) ;
#3221 = LINE('',#138625,#8775) ;
#3222 = LINE('',#138626,#8776) ;
#3223 = LINE('',#138630,#8777) ;
#3224 = LINE('',#138632,#8778) ;
#3225 = LINE('',#138634,#8779) ;
#3226 = LINE('',#138635,#8780) ;
#3227 = LINE('',#138637,#8781) ;
#3228 = LINE('',#138640,#8782) ;
#3229 = LINE('',#138642,#8783) ;
#3230 = LINE('',#138644,#8784) ;
#3231 = LINE('',#138645,#8785) ;
#3232 = LINE('',#138649,#8786) ;
#3233 = LINE('',#138651,#8787) ;
#3234 = LINE('',#138654,#8788) ;
#3235 = LINE('',#138664,#8789) ;
#3236 = LINE('',#138666,#8790) ;
#3237 = LINE('',#138668,#8791) ;
#3238 = LINE('',#138669,#8792) ;
#3239 = LINE('',#138673,#8793) ;
#3240 = LINE('',#138675,#8794) ;
#3241 = LINE('',#138677,#8795) ;
#3242 = LINE('',#138678,#8796) ;
#3243 = LINE('',#138684,#8797) ;
#3244 = LINE('',#138686,#8798) ;
#3245 = LINE('',#138688,#8799) ;
#3246 = LINE('',#138692,#8800) ;
#3247 = LINE('',#138694,#8801) ;
#3248 = LINE('',#138695,#8802) ;
#3249 = LINE('',#138699,#8803) ;
#3250 = LINE('',#138703,#8804) ;
#3251 = LINE('',#138708,#8805) ;
#3252 = LINE('',#138714,#8806) ;
#3253 = LINE('',#138716,#8807) ;
#3254 = LINE('',#138720,#8808) ;
#3255 = LINE('',#138722,#8809) ;
#3256 = LINE('',#138723,#8810) ;
#3257 = LINE('',#138726,#8811) ;
#3258 = LINE('',#138728,#8812) ;
#3259 = LINE('',#138729,#8813) ;
#3260 = LINE('',#138732,#8814) ;
#3261 = LINE('',#138734,#8815) ;
#3262 = LINE('',#138735,#8816) ;
#3263 = LINE('',#138739,#8817) ;
#3264 = LINE('',#138741,#8818) ;
#3265 = LINE('',#138743,#8819) ;
#3266 = LINE('',#138745,#8820) ;
#3267 = LINE('',#138747,#8821) ;
#3268 = LINE('',#138748,#8822) ;
#3269 = LINE('',#138752,#8823) ;
#3270 = LINE('',#138754,#8824) ;
#3271 = LINE('',#138756,#8825) ;
#3272 = LINE('',#138758,#8826) ;
#3273 = LINE('',#138760,#8827) ;
#3274 = LINE('',#138761,#8828) ;
#3275 = LINE('',#138765,#8829) ;
#3276 = LINE('',#138767,#8830) ;
#3277 = LINE('',#138769,#8831) ;
#3278 = LINE('',#138770,#8832) ;
#3279 = LINE('',#138774,#8833) ;
#3280 = LINE('',#138776,#8834) ;
#3281 = LINE('',#138778,#8835) ;
#3282 = LINE('',#138779,#8836) ;
#3283 = LINE('',#138783,#8837) ;
#3284 = LINE('',#138785,#8838) ;
#3285 = LINE('',#138787,#8839) ;
#3286 = LINE('',#138788,#8840) ;
#3287 = LINE('',#138792,#8841) ;
#3288 = LINE('',#138794,#8842) ;
#3289 = LINE('',#138796,#8843) ;
#3290 = LINE('',#138797,#8844) ;
#3291 = LINE('',#138801,#8845) ;
#3292 = LINE('',#138803,#8846) ;
#3293 = LINE('',#138805,#8847) ;
#3294 = LINE('',#138806,#8848) ;
#3295 = LINE('',#138809,#8849) ;
#3296 = LINE('',#138813,#8850) ;
#3297 = LINE('',#138817,#8851) ;
#3298 = LINE('',#138821,#8852) ;
#3299 = LINE('',#138827,#8853) ;
#3300 = LINE('',#138828,#8854) ;
#3301 = LINE('',#138831,#8855) ;
#3302 = LINE('',#138832,#8856) ;
#3303 = LINE('',#138836,#8857) ;
#3304 = LINE('',#138839,#8858) ;
#3305 = LINE('',#138840,#8859) ;
#3306 = LINE('',#138844,#8860) ;
#3307 = LINE('',#138847,#8861) ;
#3308 = LINE('',#138848,#8862) ;
#3309 = LINE('',#138852,#8863) ;
#3310 = LINE('',#138854,#8864) ;
#3311 = LINE('',#138857,#8865) ;
#3312 = LINE('',#138859,#8866) ;
#3313 = LINE('',#138860,#8867) ;
#3314 = LINE('',#138862,#8868) ;
#3315 = LINE('',#138863,#8869) ;
#3316 = LINE('',#138865,#8870) ;
#3317 = LINE('',#138866,#8871) ;
#3318 = LINE('',#138870,#8872) ;
#3319 = LINE('',#138872,#8873) ;
#3320 = LINE('',#138874,#8874) ;
#3321 = LINE('',#138875,#8875) ;
#3322 = LINE('',#138879,#8876) ;
#3323 = LINE('',#138881,#8877) ;
#3324 = LINE('',#138883,#8878) ;
#3325 = LINE('',#138884,#8879) ;
#3326 = LINE('',#138888,#8880) ;
#3327 = LINE('',#138890,#8881) ;
#3328 = LINE('',#138892,#8882) ;
#3329 = LINE('',#138893,#8883) ;
#3330 = LINE('',#138897,#8884) ;
#3331 = LINE('',#138899,#8885) ;
#3332 = LINE('',#138901,#8886) ;
#3333 = LINE('',#138902,#8887) ;
#3334 = LINE('',#138906,#8888) ;
#3335 = LINE('',#138908,#8889) ;
#3336 = LINE('',#138910,#8890) ;
#3337 = LINE('',#138911,#8891) ;
#3338 = LINE('',#138914,#8892) ;
#3339 = LINE('',#138918,#8893) ;
#3340 = LINE('',#138922,#8894) ;
#3341 = LINE('',#138926,#8895) ;
#3342 = LINE('',#138930,#8896) ;
#3343 = LINE('',#138933,#8897) ;
#3344 = LINE('',#138936,#8898) ;
#3345 = LINE('',#138937,#8899) ;
#3346 = LINE('',#138941,#8900) ;
#3347 = LINE('',#138944,#8901) ;
#3348 = LINE('',#138945,#8902) ;
#3349 = LINE('',#138949,#8903) ;
#3350 = LINE('',#138952,#8904) ;
#3351 = LINE('',#138953,#8905) ;
#3352 = LINE('',#138957,#8906) ;
#3353 = LINE('',#138959,#8907) ;
#3354 = LINE('',#138963,#8908) ;
#3355 = LINE('',#138965,#8909) ;
#3356 = LINE('',#138967,#8910) ;
#3357 = LINE('',#138968,#8911) ;
#3358 = LINE('',#138970,#8912) ;
#3359 = LINE('',#138972,#8913) ;
#3360 = LINE('',#138974,#8914) ;
#3361 = LINE('',#138975,#8915) ;
#3362 = LINE('',#138978,#8916) ;
#3363 = LINE('',#138980,#8917) ;
#3364 = LINE('',#138981,#8918) ;
#3365 = LINE('',#138984,#8919) ;
#3366 = LINE('',#138985,#8920) ;
#3367 = LINE('',#138986,#8921) ;
#3368 = LINE('',#138989,#8922) ;
#3369 = LINE('',#138993,#8923) ;
#3370 = LINE('',#138995,#8924) ;
#3371 = LINE('',#138996,#8925) ;
#3372 = LINE('',#139007,#8926) ;
#3373 = LINE('',#139010,#8927) ;
#3374 = LINE('',#139972,#8928) ;
#3375 = LINE('',#139975,#8929) ;
#3376 = LINE('',#140016,#8930) ;
#3377 = LINE('',#140019,#8931) ;
#3378 = LINE('',#140030,#8932) ;
#3379 = LINE('',#140032,#8933) ;
#3380 = LINE('',#140049,#8934) ;
#3381 = LINE('',#140075,#8935) ;
#3382 = LINE('',#140122,#8936) ;
#3383 = LINE('',#140148,#8937) ;
#3384 = LINE('',#140182,#8938) ;
#3385 = LINE('',#140188,#8939) ;
#3386 = LINE('',#140190,#8940) ;
#3387 = LINE('',#140191,#8941) ;
#3388 = LINE('',#140195,#8942) ;
#3389 = LINE('',#140197,#8943) ;
#3390 = LINE('',#140199,#8944) ;
#3391 = LINE('',#140200,#8945) ;
#3392 = LINE('',#140204,#8946) ;
#3393 = LINE('',#140206,#8947) ;
#3394 = LINE('',#140207,#8948) ;
#3395 = LINE('',#140208,#8949) ;
#3396 = LINE('',#140210,#8950) ;
#3397 = LINE('',#140212,#8951) ;
#3398 = LINE('',#140214,#8952) ;
#3399 = LINE('',#140216,#8953) ;
#3400 = LINE('',#140218,#8954) ;
#3401 = LINE('',#140226,#8955) ;
#3402 = LINE('',#140228,#8956) ;
#3403 = LINE('',#140229,#8957) ;
#3404 = LINE('',#140231,#8958) ;
#3405 = LINE('',#140234,#8959) ;
#3406 = LINE('',#140237,#8960) ;
#3407 = LINE('',#140239,#8961) ;
#3408 = LINE('',#140241,#8962) ;
#3409 = LINE('',#140242,#8963) ;
#3410 = LINE('',#140246,#8964) ;
#3411 = LINE('',#140248,#8965) ;
#3412 = LINE('',#140252,#8966) ;
#3413 = LINE('',#140256,#8967) ;
#3414 = LINE('',#140258,#8968) ;
#3415 = LINE('',#140259,#8969) ;
#3416 = LINE('',#140263,#8970) ;
#3417 = LINE('',#140265,#8971) ;
#3418 = LINE('',#140267,#8972) ;
#3419 = LINE('',#140268,#8973) ;
#3420 = LINE('',#140272,#8974) ;
#3421 = LINE('',#140274,#8975) ;
#3422 = LINE('',#140276,#8976) ;
#3423 = LINE('',#140277,#8977) ;
#3424 = LINE('',#140281,#8978) ;
#3425 = LINE('',#140283,#8979) ;
#3426 = LINE('',#140285,#8980) ;
#3427 = LINE('',#140286,#8981) ;
#3428 = LINE('',#140290,#8982) ;
#3429 = LINE('',#140292,#8983) ;
#3430 = LINE('',#140294,#8984) ;
#3431 = LINE('',#140295,#8985) ;
#3432 = LINE('',#140299,#8986) ;
#3433 = LINE('',#140301,#8987) ;
#3434 = LINE('',#140303,#8988) ;
#3435 = LINE('',#140304,#8989) ;
#3436 = LINE('',#140308,#8990) ;
#3437 = LINE('',#140310,#8991) ;
#3438 = LINE('',#140312,#8992) ;
#3439 = LINE('',#140313,#8993) ;
#3440 = LINE('',#140317,#8994) ;
#3441 = LINE('',#140319,#8995) ;
#3442 = LINE('',#140321,#8996) ;
#3443 = LINE('',#140322,#8997) ;
#3444 = LINE('',#140327,#8998) ;
#3445 = LINE('',#140331,#8999) ;
#3446 = LINE('',#140335,#9000) ;
#3447 = LINE('',#140338,#9001) ;
#3448 = LINE('',#140342,#9002) ;
#3449 = LINE('',#140344,#9003) ;
#3450 = LINE('',#140346,#9004) ;
#3451 = LINE('',#140347,#9005) ;
#3452 = LINE('',#140350,#9006) ;
#3453 = LINE('',#140352,#9007) ;
#3454 = LINE('',#140353,#9008) ;
#3455 = LINE('',#140356,#9009) ;
#3456 = LINE('',#140358,#9010) ;
#3457 = LINE('',#140359,#9011) ;
#3458 = LINE('',#140363,#9012) ;
#3459 = LINE('',#140365,#9013) ;
#3460 = LINE('',#140367,#9014) ;
#3461 = LINE('',#140368,#9015) ;
#3462 = LINE('',#140371,#9016) ;
#3463 = LINE('',#140380,#9017) ;
#3464 = LINE('',#140389,#9018) ;
#3465 = LINE('',#140398,#9019) ;
#3466 = LINE('',#140408,#9020) ;
#3467 = LINE('',#140410,#9021) ;
#3468 = LINE('',#140412,#9022) ;
#3469 = LINE('',#140413,#9023) ;
#3470 = LINE('',#140418,#9024) ;
#3471 = LINE('',#140422,#9025) ;
#3472 = LINE('',#140426,#9026) ;
#3473 = LINE('',#140429,#9027) ;
#3474 = LINE('',#140433,#9028) ;
#3475 = LINE('',#140435,#9029) ;
#3476 = LINE('',#140437,#9030) ;
#3477 = LINE('',#140438,#9031) ;
#3478 = LINE('',#140525,#9032) ;
#3479 = LINE('',#140527,#9033) ;
#3480 = LINE('',#140529,#9034) ;
#3481 = LINE('',#140531,#9035) ;
#3482 = LINE('',#140532,#9036) ;
#3483 = LINE('',#140536,#9037) ;
#3484 = LINE('',#140538,#9038) ;
#3485 = LINE('',#140541,#9039) ;
#3486 = LINE('',#140545,#9040) ;
#3487 = LINE('',#140547,#9041) ;
#3488 = LINE('',#140549,#9042) ;
#3489 = LINE('',#140550,#9043) ;
#3490 = LINE('',#140592,#9044) ;
#3491 = LINE('',#140594,#9045) ;
#3492 = LINE('',#140596,#9046) ;
#3493 = LINE('',#140597,#9047) ;
#3494 = LINE('',#140601,#9048) ;
#3495 = LINE('',#140603,#9049) ;
#3496 = LINE('',#140605,#9050) ;
#3497 = LINE('',#140606,#9051) ;
#3498 = LINE('',#140612,#9052) ;
#3499 = LINE('',#140614,#9053) ;
#3500 = LINE('',#140616,#9054) ;
#3501 = LINE('',#140620,#9055) ;
#3502 = LINE('',#140622,#9056) ;
#3503 = LINE('',#140623,#9057) ;
#3504 = LINE('',#140627,#9058) ;
#3505 = LINE('',#140631,#9059) ;
#3506 = LINE('',#140636,#9060) ;
#3507 = LINE('',#140642,#9061) ;
#3508 = LINE('',#140644,#9062) ;
#3509 = LINE('',#140648,#9063) ;
#3510 = LINE('',#140650,#9064) ;
#3511 = LINE('',#140651,#9065) ;
#3512 = LINE('',#140654,#9066) ;
#3513 = LINE('',#140656,#9067) ;
#3514 = LINE('',#140657,#9068) ;
#3515 = LINE('',#140660,#9069) ;
#3516 = LINE('',#140662,#9070) ;
#3517 = LINE('',#140663,#9071) ;
#3518 = LINE('',#140667,#9072) ;
#3519 = LINE('',#140669,#9073) ;
#3520 = LINE('',#140671,#9074) ;
#3521 = LINE('',#140673,#9075) ;
#3522 = LINE('',#140675,#9076) ;
#3523 = LINE('',#140676,#9077) ;
#3524 = LINE('',#140680,#9078) ;
#3525 = LINE('',#140682,#9079) ;
#3526 = LINE('',#140684,#9080) ;
#3527 = LINE('',#140686,#9081) ;
#3528 = LINE('',#140688,#9082) ;
#3529 = LINE('',#140689,#9083) ;
#3530 = LINE('',#140693,#9084) ;
#3531 = LINE('',#140695,#9085) ;
#3532 = LINE('',#140697,#9086) ;
#3533 = LINE('',#140698,#9087) ;
#3534 = LINE('',#140702,#9088) ;
#3535 = LINE('',#140704,#9089) ;
#3536 = LINE('',#140706,#9090) ;
#3537 = LINE('',#140707,#9091) ;
#3538 = LINE('',#140711,#9092) ;
#3539 = LINE('',#140713,#9093) ;
#3540 = LINE('',#140715,#9094) ;
#3541 = LINE('',#140716,#9095) ;
#3542 = LINE('',#140720,#9096) ;
#3543 = LINE('',#140722,#9097) ;
#3544 = LINE('',#140724,#9098) ;
#3545 = LINE('',#140725,#9099) ;
#3546 = LINE('',#140729,#9100) ;
#3547 = LINE('',#140731,#9101) ;
#3548 = LINE('',#140733,#9102) ;
#3549 = LINE('',#140734,#9103) ;
#3550 = LINE('',#140737,#9104) ;
#3551 = LINE('',#140741,#9105) ;
#3552 = LINE('',#140745,#9106) ;
#3553 = LINE('',#140749,#9107) ;
#3554 = LINE('',#140755,#9108) ;
#3555 = LINE('',#140756,#9109) ;
#3556 = LINE('',#140759,#9110) ;
#3557 = LINE('',#140760,#9111) ;
#3558 = LINE('',#140764,#9112) ;
#3559 = LINE('',#140767,#9113) ;
#3560 = LINE('',#140768,#9114) ;
#3561 = LINE('',#140772,#9115) ;
#3562 = LINE('',#140775,#9116) ;
#3563 = LINE('',#140776,#9117) ;
#3564 = LINE('',#140780,#9118) ;
#3565 = LINE('',#140782,#9119) ;
#3566 = LINE('',#140785,#9120) ;
#3567 = LINE('',#140787,#9121) ;
#3568 = LINE('',#140788,#9122) ;
#3569 = LINE('',#140790,#9123) ;
#3570 = LINE('',#140791,#9124) ;
#3571 = LINE('',#140793,#9125) ;
#3572 = LINE('',#140794,#9126) ;
#3573 = LINE('',#140798,#9127) ;
#3574 = LINE('',#140800,#9128) ;
#3575 = LINE('',#140802,#9129) ;
#3576 = LINE('',#140803,#9130) ;
#3577 = LINE('',#140807,#9131) ;
#3578 = LINE('',#140809,#9132) ;
#3579 = LINE('',#140811,#9133) ;
#3580 = LINE('',#140812,#9134) ;
#3581 = LINE('',#140816,#9135) ;
#3582 = LINE('',#140818,#9136) ;
#3583 = LINE('',#140820,#9137) ;
#3584 = LINE('',#140821,#9138) ;
#3585 = LINE('',#140825,#9139) ;
#3586 = LINE('',#140827,#9140) ;
#3587 = LINE('',#140829,#9141) ;
#3588 = LINE('',#140830,#9142) ;
#3589 = LINE('',#140834,#9143) ;
#3590 = LINE('',#140836,#9144) ;
#3591 = LINE('',#140838,#9145) ;
#3592 = LINE('',#140839,#9146) ;
#3593 = LINE('',#140842,#9147) ;
#3594 = LINE('',#140846,#9148) ;
#3595 = LINE('',#140850,#9149) ;
#3596 = LINE('',#140854,#9150) ;
#3597 = LINE('',#140858,#9151) ;
#3598 = LINE('',#140861,#9152) ;
#3599 = LINE('',#140864,#9153) ;
#3600 = LINE('',#140865,#9154) ;
#3601 = LINE('',#140869,#9155) ;
#3602 = LINE('',#140872,#9156) ;
#3603 = LINE('',#140873,#9157) ;
#3604 = LINE('',#140877,#9158) ;
#3605 = LINE('',#140880,#9159) ;
#3606 = LINE('',#140881,#9160) ;
#3607 = LINE('',#140885,#9161) ;
#3608 = LINE('',#140887,#9162) ;
#3609 = LINE('',#140891,#9163) ;
#3610 = LINE('',#140893,#9164) ;
#3611 = LINE('',#140895,#9165) ;
#3612 = LINE('',#140896,#9166) ;
#3613 = LINE('',#140898,#9167) ;
#3614 = LINE('',#140900,#9168) ;
#3615 = LINE('',#140902,#9169) ;
#3616 = LINE('',#140903,#9170) ;
#3617 = LINE('',#140906,#9171) ;
#3618 = LINE('',#140908,#9172) ;
#3619 = LINE('',#140909,#9173) ;
#3620 = LINE('',#140912,#9174) ;
#3621 = LINE('',#140913,#9175) ;
#3622 = LINE('',#140914,#9176) ;
#3623 = LINE('',#140917,#9177) ;
#3624 = LINE('',#140921,#9178) ;
#3625 = LINE('',#140923,#9179) ;
#3626 = LINE('',#140924,#9180) ;
#3627 = LINE('',#140935,#9181) ;
#3628 = LINE('',#140938,#9182) ;
#3629 = LINE('',#141855,#9183) ;
#3630 = LINE('',#141859,#9184) ;
#3631 = LINE('',#141861,#9185) ;
#3632 = LINE('',#141898,#9186) ;
#3633 = LINE('',#141902,#9187) ;
#3634 = LINE('',#141904,#9188) ;
#3635 = LINE('',#141941,#9189) ;
#3636 = LINE('',#141945,#9190) ;
#3637 = LINE('',#141947,#9191) ;
#3638 = LINE('',#141984,#9192) ;
#3639 = LINE('',#141988,#9193) ;
#3640 = LINE('',#141990,#9194) ;
#3641 = LINE('',#142027,#9195) ;
#3642 = LINE('',#142031,#9196) ;
#3643 = LINE('',#142033,#9197) ;
#3644 = LINE('',#142070,#9198) ;
#3645 = LINE('',#142074,#9199) ;
#3646 = LINE('',#142076,#9200) ;
#3647 = LINE('',#142113,#9201) ;
#3648 = LINE('',#142117,#9202) ;
#3649 = LINE('',#142119,#9203) ;
#3650 = LINE('',#142156,#9204) ;
#3651 = LINE('',#142160,#9205) ;
#3652 = LINE('',#142162,#9206) ;
#3653 = LINE('',#142280,#9207) ;
#3654 = LINE('',#142284,#9208) ;
#3655 = LINE('',#142286,#9209) ;
#3656 = LINE('',#142296,#9210) ;
#3657 = LINE('',#142298,#9211) ;
#3658 = LINE('',#142300,#9212) ;
#3659 = LINE('',#142302,#9213) ;
#3660 = LINE('',#142304,#9214) ;
#3661 = LINE('',#142306,#9215) ;
#3662 = LINE('',#142308,#9216) ;
#3663 = LINE('',#142310,#9217) ;
#3664 = LINE('',#142312,#9218) ;
#3665 = LINE('',#142317,#9219) ;
#3666 = LINE('',#142318,#9220) ;
#3667 = LINE('',#142323,#9221) ;
#3668 = LINE('',#142324,#9222) ;
#3669 = LINE('',#142329,#9223) ;
#3670 = LINE('',#142330,#9224) ;
#3671 = LINE('',#142335,#9225) ;
#3672 = LINE('',#142336,#9226) ;
#3673 = LINE('',#142341,#9227) ;
#3674 = LINE('',#142342,#9228) ;
#3675 = LINE('',#142347,#9229) ;
#3676 = LINE('',#142348,#9230) ;
#3677 = LINE('',#142353,#9231) ;
#3678 = LINE('',#142354,#9232) ;
#3679 = LINE('',#142359,#9233) ;
#3680 = LINE('',#142360,#9234) ;
#3681 = LINE('',#142365,#9235) ;
#3682 = LINE('',#142366,#9236) ;
#3683 = LINE('',#142404,#9237) ;
#3684 = LINE('',#142408,#9238) ;
#3685 = LINE('',#142410,#9239) ;
#3686 = LINE('',#142420,#9240) ;
#3687 = LINE('',#142425,#9241) ;
#3688 = LINE('',#142426,#9242) ;
#3689 = LINE('',#142430,#9243) ;
#3690 = LINE('',#142434,#9244) ;
#3691 = LINE('',#142439,#9245) ;
#3692 = LINE('',#142441,#9246) ;
#3693 = LINE('',#142443,#9247) ;
#3694 = LINE('',#142445,#9248) ;
#3695 = LINE('',#142447,#9249) ;
#3696 = LINE('',#142452,#9250) ;
#3697 = LINE('',#142456,#9251) ;
#3698 = LINE('',#142461,#9252) ;
#3699 = LINE('',#142463,#9253) ;
#3700 = LINE('',#142465,#9254) ;
#3701 = LINE('',#142467,#9255) ;
#3702 = LINE('',#142469,#9256) ;
#3703 = LINE('',#142474,#9257) ;
#3704 = LINE('',#142478,#9258) ;
#3705 = LINE('',#142483,#9259) ;
#3706 = LINE('',#142485,#9260) ;
#3707 = LINE('',#142487,#9261) ;
#3708 = LINE('',#142489,#9262) ;
#3709 = LINE('',#142491,#9263) ;
#3710 = LINE('',#142496,#9264) ;
#3711 = LINE('',#142500,#9265) ;
#3712 = LINE('',#142505,#9266) ;
#3713 = LINE('',#142507,#9267) ;
#3714 = LINE('',#142509,#9268) ;
#3715 = LINE('',#142511,#9269) ;
#3716 = LINE('',#142513,#9270) ;
#3717 = LINE('',#142518,#9271) ;
#3718 = LINE('',#142522,#9272) ;
#3719 = LINE('',#142527,#9273) ;
#3720 = LINE('',#142529,#9274) ;
#3721 = LINE('',#142531,#9275) ;
#3722 = LINE('',#142533,#9276) ;
#3723 = LINE('',#142535,#9277) ;
#3724 = LINE('',#142540,#9278) ;
#3725 = LINE('',#142544,#9279) ;
#3726 = LINE('',#142549,#9280) ;
#3727 = LINE('',#142551,#9281) ;
#3728 = LINE('',#142553,#9282) ;
#3729 = LINE('',#142555,#9283) ;
#3730 = LINE('',#142557,#9284) ;
#3731 = LINE('',#142562,#9285) ;
#3732 = LINE('',#142566,#9286) ;
#3733 = LINE('',#142571,#9287) ;
#3734 = LINE('',#142573,#9288) ;
#3735 = LINE('',#142575,#9289) ;
#3736 = LINE('',#142577,#9290) ;
#3737 = LINE('',#142579,#9291) ;
#3738 = LINE('',#142584,#9292) ;
#3739 = LINE('',#142588,#9293) ;
#3740 = LINE('',#142593,#9294) ;
#3741 = LINE('',#142595,#9295) ;
#3742 = LINE('',#142597,#9296) ;
#3743 = LINE('',#142599,#9297) ;
#3744 = LINE('',#142601,#9298) ;
#3745 = LINE('',#142606,#9299) ;
#3746 = LINE('',#142610,#9300) ;
#3747 = LINE('',#142615,#9301) ;
#3748 = LINE('',#142617,#9302) ;
#3749 = LINE('',#142619,#9303) ;
#3750 = LINE('',#142621,#9304) ;
#3751 = LINE('',#142623,#9305) ;
#3752 = LINE('',#142630,#9306) ;
#3753 = LINE('',#142632,#9307) ;
#3754 = LINE('',#142634,#9308) ;
#3755 = LINE('',#142635,#9309) ;
#3756 = LINE('',#142641,#9310) ;
#3757 = LINE('',#142643,#9311) ;
#3758 = LINE('',#142645,#9312) ;
#3759 = LINE('',#142646,#9313) ;
#3760 = LINE('',#142652,#9314) ;
#3761 = LINE('',#142654,#9315) ;
#3762 = LINE('',#142656,#9316) ;
#3763 = LINE('',#142657,#9317) ;
#3764 = LINE('',#142663,#9318) ;
#3765 = LINE('',#142665,#9319) ;
#3766 = LINE('',#142667,#9320) ;
#3767 = LINE('',#142668,#9321) ;
#3768 = LINE('',#142674,#9322) ;
#3769 = LINE('',#142676,#9323) ;
#3770 = LINE('',#142678,#9324) ;
#3771 = LINE('',#142679,#9325) ;
#3772 = LINE('',#142685,#9326) ;
#3773 = LINE('',#142687,#9327) ;
#3774 = LINE('',#142689,#9328) ;
#3775 = LINE('',#142690,#9329) ;
#3776 = LINE('',#142696,#9330) ;
#3777 = LINE('',#142698,#9331) ;
#3778 = LINE('',#142700,#9332) ;
#3779 = LINE('',#142701,#9333) ;
#3780 = LINE('',#142707,#9334) ;
#3781 = LINE('',#142709,#9335) ;
#3782 = LINE('',#142711,#9336) ;
#3783 = LINE('',#142712,#9337) ;
#3784 = LINE('',#142718,#9338) ;
#3785 = LINE('',#142720,#9339) ;
#3786 = LINE('',#142722,#9340) ;
#3787 = LINE('',#142723,#9341) ;
#3788 = LINE('',#142729,#9342) ;
#3789 = LINE('',#142731,#9343) ;
#3790 = LINE('',#142733,#9344) ;
#3791 = LINE('',#142734,#9345) ;
#3792 = LINE('',#142740,#9346) ;
#3793 = LINE('',#142742,#9347) ;
#3794 = LINE('',#142744,#9348) ;
#3795 = LINE('',#142745,#9349) ;
#3796 = LINE('',#142751,#9350) ;
#3797 = LINE('',#142753,#9351) ;
#3798 = LINE('',#142755,#9352) ;
#3799 = LINE('',#142756,#9353) ;
#3800 = LINE('',#142762,#9354) ;
#3801 = LINE('',#142764,#9355) ;
#3802 = LINE('',#142766,#9356) ;
#3803 = LINE('',#142767,#9357) ;
#3804 = LINE('',#142773,#9358) ;
#3805 = LINE('',#142775,#9359) ;
#3806 = LINE('',#142777,#9360) ;
#3807 = LINE('',#142778,#9361) ;
#3808 = LINE('',#142784,#9362) ;
#3809 = LINE('',#142786,#9363) ;
#3810 = LINE('',#142788,#9364) ;
#3811 = LINE('',#142789,#9365) ;
#3812 = LINE('',#142795,#9366) ;
#3813 = LINE('',#142797,#9367) ;
#3814 = LINE('',#142799,#9368) ;
#3815 = LINE('',#142800,#9369) ;
#3816 = LINE('',#142806,#9370) ;
#3817 = LINE('',#142808,#9371) ;
#3818 = LINE('',#142810,#9372) ;
#3819 = LINE('',#142811,#9373) ;
#3820 = LINE('',#142817,#9374) ;
#3821 = LINE('',#142819,#9375) ;
#3822 = LINE('',#142821,#9376) ;
#3823 = LINE('',#142822,#9377) ;
#3824 = LINE('',#142826,#9378) ;
#3825 = LINE('',#142830,#9379) ;
#3826 = LINE('',#142835,#9380) ;
#3827 = LINE('',#142839,#9381) ;
#3828 = LINE('',#142844,#9382) ;
#3829 = LINE('',#142848,#9383) ;
#3830 = LINE('',#142853,#9384) ;
#3831 = LINE('',#142857,#9385) ;
#3832 = LINE('',#142862,#9386) ;
#3833 = LINE('',#142866,#9387) ;
#3834 = LINE('',#142871,#9388) ;
#3835 = LINE('',#142875,#9389) ;
#3836 = LINE('',#142880,#9390) ;
#3837 = LINE('',#142884,#9391) ;
#3838 = LINE('',#142889,#9392) ;
#3839 = LINE('',#142893,#9393) ;
#3840 = LINE('',#142898,#9394) ;
#3841 = LINE('',#142902,#9395) ;
#3842 = LINE('',#142907,#9396) ;
#3843 = LINE('',#142911,#9397) ;
#3844 = LINE('',#142916,#9398) ;
#3845 = LINE('',#142918,#9399) ;
#3846 = LINE('',#142920,#9400) ;
#3847 = LINE('',#142922,#9401) ;
#3848 = LINE('',#142924,#9402) ;
#3849 = LINE('',#142931,#9403) ;
#3850 = LINE('',#142933,#9404) ;
#3851 = LINE('',#142935,#9405) ;
#3852 = LINE('',#142936,#9406) ;
#3853 = LINE('',#142942,#9407) ;
#3854 = LINE('',#142944,#9408) ;
#3855 = LINE('',#142946,#9409) ;
#3856 = LINE('',#142947,#9410) ;
#3857 = LINE('',#142951,#9411) ;
#3858 = LINE('',#142955,#9412) ;
#3859 = LINE('',#142960,#9413) ;
#3860 = LINE('',#142964,#9414) ;
#3861 = LINE('',#142971,#9415) ;
#3862 = LINE('',#142973,#9416) ;
#3863 = LINE('',#142974,#9417) ;
#3864 = LINE('',#142975,#9418) ;
#3865 = LINE('',#142977,#9419) ;
#3866 = LINE('',#142981,#9420) ;
#3867 = LINE('',#142984,#9421) ;
#3868 = LINE('',#142986,#9422) ;
#3869 = LINE('',#142990,#9423) ;
#3870 = LINE('',#142993,#9424) ;
#3871 = LINE('',#142995,#9425) ;
#3872 = LINE('',#142999,#9426) ;
#3873 = LINE('',#143002,#9427) ;
#3874 = LINE('',#143004,#9428) ;
#3875 = LINE('',#143008,#9429) ;
#3876 = LINE('',#143011,#9430) ;
#3877 = LINE('',#143013,#9431) ;
#3878 = LINE('',#143017,#9432) ;
#3879 = LINE('',#143020,#9433) ;
#3880 = LINE('',#143022,#9434) ;
#3881 = LINE('',#143026,#9435) ;
#3882 = LINE('',#143029,#9436) ;
#3883 = LINE('',#143031,#9437) ;
#3884 = LINE('',#143035,#9438) ;
#3885 = LINE('',#143038,#9439) ;
#3886 = LINE('',#143040,#9440) ;
#3887 = LINE('',#143044,#9441) ;
#3888 = LINE('',#143047,#9442) ;
#3889 = LINE('',#143049,#9443) ;
#3890 = LINE('',#143053,#9444) ;
#3891 = LINE('',#143056,#9445) ;
#3892 = LINE('',#143058,#9446) ;
#3893 = LINE('',#143061,#9447) ;
#3894 = LINE('',#143066,#9448) ;
#3895 = LINE('',#143072,#9449) ;
#3896 = LINE('',#143074,#9450) ;
#3897 = LINE('',#143078,#9451) ;
#3898 = LINE('',#143081,#9452) ;
#3899 = LINE('',#143083,#9453) ;
#3900 = LINE('',#143087,#9454) ;
#3901 = LINE('',#143090,#9455) ;
#3902 = LINE('',#143092,#9456) ;
#3903 = LINE('',#143096,#9457) ;
#3904 = LINE('',#143099,#9458) ;
#3905 = LINE('',#143101,#9459) ;
#3906 = LINE('',#143105,#9460) ;
#3907 = LINE('',#143108,#9461) ;
#3908 = LINE('',#143110,#9462) ;
#3909 = LINE('',#143114,#9463) ;
#3910 = LINE('',#143117,#9464) ;
#3911 = LINE('',#143119,#9465) ;
#3912 = LINE('',#143123,#9466) ;
#3913 = LINE('',#143126,#9467) ;
#3914 = LINE('',#143128,#9468) ;
#3915 = LINE('',#143132,#9469) ;
#3916 = LINE('',#143135,#9470) ;
#3917 = LINE('',#143137,#9471) ;
#3918 = LINE('',#143141,#9472) ;
#3919 = LINE('',#143144,#9473) ;
#3920 = LINE('',#143146,#9474) ;
#3921 = LINE('',#143150,#9475) ;
#3922 = LINE('',#143153,#9476) ;
#3923 = LINE('',#143155,#9477) ;
#3924 = LINE('',#143157,#9478) ;
#3925 = LINE('',#143158,#9479) ;
#3926 = LINE('',#143160,#9480) ;
#3927 = LINE('',#143163,#9481) ;
#3928 = LINE('',#143167,#9482) ;
#3929 = LINE('',#143173,#9483) ;
#3930 = LINE('',#143174,#9484) ;
#3931 = LINE('',#143175,#9485) ;
#3932 = LINE('',#143179,#9486) ;
#3933 = LINE('',#143185,#9487) ;
#3934 = LINE('',#143186,#9488) ;
#3935 = LINE('',#143187,#9489) ;
#3936 = LINE('',#143191,#9490) ;
#3937 = LINE('',#143197,#9491) ;
#3938 = LINE('',#143198,#9492) ;
#3939 = LINE('',#143199,#9493) ;
#3940 = LINE('',#143203,#9494) ;
#3941 = LINE('',#143209,#9495) ;
#3942 = LINE('',#143210,#9496) ;
#3943 = LINE('',#143211,#9497) ;
#3944 = LINE('',#143215,#9498) ;
#3945 = LINE('',#143221,#9499) ;
#3946 = LINE('',#143222,#9500) ;
#3947 = LINE('',#143223,#9501) ;
#3948 = LINE('',#143227,#9502) ;
#3949 = LINE('',#143231,#9503) ;
#3950 = LINE('',#143232,#9504) ;
#3951 = LINE('',#143237,#9505) ;
#3952 = LINE('',#143239,#9506) ;
#3953 = LINE('',#143241,#9507) ;
#3954 = LINE('',#143245,#9508) ;
#3955 = LINE('',#143248,#9509) ;
#3956 = LINE('',#143250,#9510) ;
#3957 = LINE('',#143254,#9511) ;
#3958 = LINE('',#143256,#9512) ;
#3959 = LINE('',#143258,#9513) ;
#3960 = LINE('',#143262,#9514) ;
#3961 = LINE('',#143266,#9515) ;
#3962 = LINE('',#143274,#9516) ;
#3963 = LINE('',#143277,#9517) ;
#3964 = LINE('',#143282,#9518) ;
#3965 = LINE('',#143284,#9519) ;
#3966 = LINE('',#143286,#9520) ;
#3967 = LINE('',#143290,#9521) ;
#3968 = LINE('',#143293,#9522) ;
#3969 = LINE('',#143295,#9523) ;
#3970 = LINE('',#143299,#9524) ;
#3971 = LINE('',#143301,#9525) ;
#3972 = LINE('',#143303,#9526) ;
#3973 = LINE('',#143307,#9527) ;
#3974 = LINE('',#143311,#9528) ;
#3975 = LINE('',#143319,#9529) ;
#3976 = LINE('',#143322,#9530) ;
#3977 = LINE('',#143327,#9531) ;
#3978 = LINE('',#143329,#9532) ;
#3979 = LINE('',#143331,#9533) ;
#3980 = LINE('',#143335,#9534) ;
#3981 = LINE('',#143338,#9535) ;
#3982 = LINE('',#143340,#9536) ;
#3983 = LINE('',#143344,#9537) ;
#3984 = LINE('',#143346,#9538) ;
#3985 = LINE('',#143348,#9539) ;
#3986 = LINE('',#143352,#9540) ;
#3987 = LINE('',#143356,#9541) ;
#3988 = LINE('',#143364,#9542) ;
#3989 = LINE('',#143367,#9543) ;
#3990 = LINE('',#143372,#9544) ;
#3991 = LINE('',#143374,#9545) ;
#3992 = LINE('',#143376,#9546) ;
#3993 = LINE('',#143380,#9547) ;
#3994 = LINE('',#143383,#9548) ;
#3995 = LINE('',#143385,#9549) ;
#3996 = LINE('',#143389,#9550) ;
#3997 = LINE('',#143391,#9551) ;
#3998 = LINE('',#143393,#9552) ;
#3999 = LINE('',#143397,#9553) ;
#4000 = LINE('',#143401,#9554) ;
#4001 = LINE('',#143409,#9555) ;
#4002 = LINE('',#143412,#9556) ;
#4003 = LINE('',#143417,#9557) ;
#4004 = LINE('',#143419,#9558) ;
#4005 = LINE('',#143421,#9559) ;
#4006 = LINE('',#143425,#9560) ;
#4007 = LINE('',#143428,#9561) ;
#4008 = LINE('',#143430,#9562) ;
#4009 = LINE('',#143434,#9563) ;
#4010 = LINE('',#143436,#9564) ;
#4011 = LINE('',#143438,#9565) ;
#4012 = LINE('',#143442,#9566) ;
#4013 = LINE('',#143446,#9567) ;
#4014 = LINE('',#143454,#9568) ;
#4015 = LINE('',#143457,#9569) ;
#4016 = LINE('',#143462,#9570) ;
#4017 = LINE('',#143464,#9571) ;
#4018 = LINE('',#143466,#9572) ;
#4019 = LINE('',#143470,#9573) ;
#4020 = LINE('',#143473,#9574) ;
#4021 = LINE('',#143475,#9575) ;
#4022 = LINE('',#143479,#9576) ;
#4023 = LINE('',#143481,#9577) ;
#4024 = LINE('',#143483,#9578) ;
#4025 = LINE('',#143487,#9579) ;
#4026 = LINE('',#143491,#9580) ;
#4027 = LINE('',#143499,#9581) ;
#4028 = LINE('',#143502,#9582) ;
#4029 = LINE('',#143507,#9583) ;
#4030 = LINE('',#143509,#9584) ;
#4031 = LINE('',#143511,#9585) ;
#4032 = LINE('',#143515,#9586) ;
#4033 = LINE('',#143518,#9587) ;
#4034 = LINE('',#143520,#9588) ;
#4035 = LINE('',#143524,#9589) ;
#4036 = LINE('',#143526,#9590) ;
#4037 = LINE('',#143528,#9591) ;
#4038 = LINE('',#143532,#9592) ;
#4039 = LINE('',#143536,#9593) ;
#4040 = LINE('',#143544,#9594) ;
#4041 = LINE('',#143547,#9595) ;
#4042 = LINE('',#143552,#9596) ;
#4043 = LINE('',#143554,#9597) ;
#4044 = LINE('',#143556,#9598) ;
#4045 = LINE('',#143560,#9599) ;
#4046 = LINE('',#143563,#9600) ;
#4047 = LINE('',#143565,#9601) ;
#4048 = LINE('',#143569,#9602) ;
#4049 = LINE('',#143571,#9603) ;
#4050 = LINE('',#143573,#9604) ;
#4051 = LINE('',#143577,#9605) ;
#4052 = LINE('',#143581,#9606) ;
#4053 = LINE('',#143589,#9607) ;
#4054 = LINE('',#143592,#9608) ;
#4055 = LINE('',#143597,#9609) ;
#4056 = LINE('',#143599,#9610) ;
#4057 = LINE('',#143601,#9611) ;
#4058 = LINE('',#143605,#9612) ;
#4059 = LINE('',#143608,#9613) ;
#4060 = LINE('',#143610,#9614) ;
#4061 = LINE('',#143614,#9615) ;
#4062 = LINE('',#143616,#9616) ;
#4063 = LINE('',#143618,#9617) ;
#4064 = LINE('',#143622,#9618) ;
#4065 = LINE('',#143626,#9619) ;
#4066 = LINE('',#143634,#9620) ;
#4067 = LINE('',#143637,#9621) ;
#4068 = LINE('',#143642,#9622) ;
#4069 = LINE('',#143644,#9623) ;
#4070 = LINE('',#143646,#9624) ;
#4071 = LINE('',#143650,#9625) ;
#4072 = LINE('',#143653,#9626) ;
#4073 = LINE('',#143655,#9627) ;
#4074 = LINE('',#143659,#9628) ;
#4075 = LINE('',#143661,#9629) ;
#4076 = LINE('',#143663,#9630) ;
#4077 = LINE('',#143667,#9631) ;
#4078 = LINE('',#143671,#9632) ;
#4079 = LINE('',#143679,#9633) ;
#4080 = LINE('',#143682,#9634) ;
#4081 = LINE('',#143686,#9635) ;
#4082 = LINE('',#143688,#9636) ;
#4083 = LINE('',#143690,#9637) ;
#4084 = LINE('',#143692,#9638) ;
#4085 = LINE('',#143696,#9639) ;
#4086 = LINE('',#143698,#9640) ;
#4087 = LINE('',#143700,#9641) ;
#4088 = LINE('',#143703,#9642) ;
#4089 = LINE('',#143707,#9643) ;
#4090 = LINE('',#143709,#9644) ;
#4091 = LINE('',#143711,#9645) ;
#4092 = LINE('',#143713,#9646) ;
#4093 = LINE('',#143717,#9647) ;
#4094 = LINE('',#143719,#9648) ;
#4095 = LINE('',#143721,#9649) ;
#4096 = LINE('',#143724,#9650) ;
#4097 = LINE('',#143728,#9651) ;
#4098 = LINE('',#143730,#9652) ;
#4099 = LINE('',#143732,#9653) ;
#4100 = LINE('',#143734,#9654) ;
#4101 = LINE('',#143736,#9655) ;
#4102 = LINE('',#143738,#9656) ;
#4103 = LINE('',#143742,#9657) ;
#4104 = LINE('',#143745,#9658) ;
#4105 = LINE('',#143749,#9659) ;
#4106 = LINE('',#143751,#9660) ;
#4107 = LINE('',#143753,#9661) ;
#4108 = LINE('',#143754,#9662) ;
#4109 = LINE('',#143757,#9663) ;
#4110 = LINE('',#143759,#9664) ;
#4111 = LINE('',#143760,#9665) ;
#4112 = LINE('',#143764,#9666) ;
#4113 = LINE('',#143766,#9667) ;
#4114 = LINE('',#143768,#9668) ;
#4115 = LINE('',#143769,#9669) ;
#4116 = LINE('',#143773,#9670) ;
#4117 = LINE('',#143775,#9671) ;
#4118 = LINE('',#143777,#9672) ;
#4119 = LINE('',#143778,#9673) ;
#4120 = LINE('',#143782,#9674) ;
#4121 = LINE('',#143784,#9675) ;
#4122 = LINE('',#143786,#9676) ;
#4123 = LINE('',#143787,#9677) ;
#4124 = LINE('',#143791,#9678) ;
#4125 = LINE('',#143795,#9679) ;
#4126 = LINE('',#143799,#9680) ;
#4127 = LINE('',#143801,#9681) ;
#4128 = LINE('',#143802,#9682) ;
#4129 = LINE('',#143807,#9683) ;
#4130 = LINE('',#143811,#9684) ;
#4131 = LINE('',#143813,#9685) ;
#4132 = LINE('',#143814,#9686) ;
#4133 = LINE('',#143819,#9687) ;
#4134 = LINE('',#143822,#9688) ;
#4135 = LINE('',#143824,#9689) ;
#4136 = LINE('',#143825,#9690) ;
#4137 = LINE('',#143828,#9691) ;
#4138 = LINE('',#143831,#9692) ;
#4139 = LINE('',#143832,#9693) ;
#4140 = LINE('',#143835,#9694) ;
#4141 = LINE('',#143837,#9695) ;
#4142 = LINE('',#143838,#9696) ;
#4143 = LINE('',#143843,#9697) ;
#4144 = LINE('',#143847,#9698) ;
#4145 = LINE('',#143849,#9699) ;
#4146 = LINE('',#143850,#9700) ;
#4147 = LINE('',#143855,#9701) ;
#4148 = LINE('',#143859,#9702) ;
#4149 = LINE('',#143861,#9703) ;
#4150 = LINE('',#143862,#9704) ;
#4151 = LINE('',#143867,#9705) ;
#4152 = LINE('',#143871,#9706) ;
#4153 = LINE('',#143873,#9707) ;
#4154 = LINE('',#143874,#9708) ;
#4155 = LINE('',#143879,#9709) ;
#4156 = LINE('',#143883,#9710) ;
#4157 = LINE('',#143885,#9711) ;
#4158 = LINE('',#143886,#9712) ;
#4159 = LINE('',#143891,#9713) ;
#4160 = LINE('',#143895,#9714) ;
#4161 = LINE('',#143897,#9715) ;
#4162 = LINE('',#143898,#9716) ;
#4163 = LINE('',#143903,#9717) ;
#4164 = LINE('',#143909,#9718) ;
#4165 = LINE('',#143915,#9719) ;
#4166 = LINE('',#143919,#9720) ;
#4167 = LINE('',#143921,#9721) ;
#4168 = LINE('',#143922,#9722) ;
#4169 = LINE('',#143927,#9723) ;
#4170 = LINE('',#143931,#9724) ;
#4171 = LINE('',#143933,#9725) ;
#4172 = LINE('',#143934,#9726) ;
#4173 = LINE('',#143939,#9727) ;
#4174 = LINE('',#143942,#9728) ;
#4175 = LINE('',#143943,#9729) ;
#4176 = LINE('',#143949,#9730) ;
#4177 = LINE('',#143953,#9731) ;
#4178 = LINE('',#143955,#9732) ;
#4179 = LINE('',#143957,#9733) ;
#4180 = LINE('',#143961,#9734) ;
#4181 = LINE('',#143963,#9735) ;
#4182 = LINE('',#143965,#9736) ;
#4183 = LINE('',#143969,#9737) ;
#4184 = LINE('',#143973,#9738) ;
#4185 = LINE('',#143975,#9739) ;
#4186 = LINE('',#143976,#9740) ;
#4187 = LINE('',#143978,#9741) ;
#4188 = LINE('',#143979,#9742) ;
#4189 = LINE('',#143983,#9743) ;
#4190 = LINE('',#143987,#9744) ;
#4191 = LINE('',#143991,#9745) ;
#4192 = LINE('',#143995,#9746) ;
#4193 = LINE('',#144023,#9747) ;
#4194 = LINE('',#144080,#9748) ;
#4195 = LINE('',#144105,#9749) ;
#4196 = LINE('',#144137,#9750) ;
#4197 = LINE('',#144163,#9751) ;
#4198 = LINE('',#144344,#9752) ;
#4199 = LINE('',#144346,#9753) ;
#4200 = LINE('',#144348,#9754) ;
#4201 = LINE('',#144349,#9755) ;
#4202 = LINE('',#144353,#9756) ;
#4203 = LINE('',#144355,#9757) ;
#4204 = LINE('',#144357,#9758) ;
#4205 = LINE('',#144358,#9759) ;
#4206 = LINE('',#144362,#9760) ;
#4207 = LINE('',#144364,#9761) ;
#4208 = LINE('',#144366,#9762) ;
#4209 = LINE('',#144367,#9763) ;
#4210 = LINE('',#144371,#9764) ;
#4211 = LINE('',#144373,#9765) ;
#4212 = LINE('',#144375,#9766) ;
#4213 = LINE('',#144376,#9767) ;
#4214 = LINE('',#144380,#9768) ;
#4215 = LINE('',#144382,#9769) ;
#4216 = LINE('',#144384,#9770) ;
#4217 = LINE('',#144385,#9771) ;
#4218 = LINE('',#144389,#9772) ;
#4219 = LINE('',#144394,#9773) ;
#4220 = LINE('',#144395,#9774) ;
#4221 = LINE('',#144399,#9775) ;
#4222 = LINE('',#144404,#9776) ;
#4223 = LINE('',#144405,#9777) ;
#4224 = LINE('',#144415,#9778) ;
#4225 = LINE('',#144417,#9779) ;
#4226 = LINE('',#144419,#9780) ;
#4227 = LINE('',#144420,#9781) ;
#4228 = LINE('',#144424,#9782) ;
#4229 = LINE('',#144425,#9783) ;
#4230 = LINE('',#144426,#9784) ;
#4231 = LINE('',#144429,#9785) ;
#4232 = LINE('',#144431,#9786) ;
#4233 = LINE('',#144432,#9787) ;
#4234 = LINE('',#144436,#9788) ;
#4235 = LINE('',#144438,#9789) ;
#4236 = LINE('',#144440,#9790) ;
#4237 = LINE('',#144441,#9791) ;
#4238 = LINE('',#144445,#9792) ;
#4239 = LINE('',#144447,#9793) ;
#4240 = LINE('',#144449,#9794) ;
#4241 = LINE('',#144450,#9795) ;
#4242 = LINE('',#144454,#9796) ;
#4243 = LINE('',#144455,#9797) ;
#4244 = LINE('',#144456,#9798) ;
#4245 = LINE('',#144459,#9799) ;
#4246 = LINE('',#144461,#9800) ;
#4247 = LINE('',#144462,#9801) ;
#4248 = LINE('',#144466,#9802) ;
#4249 = LINE('',#144468,#9803) ;
#4250 = LINE('',#144470,#9804) ;
#4251 = LINE('',#144471,#9805) ;
#4252 = LINE('',#144475,#9806) ;
#4253 = LINE('',#144477,#9807) ;
#4254 = LINE('',#144479,#9808) ;
#4255 = LINE('',#144480,#9809) ;
#4256 = LINE('',#144484,#9810) ;
#4257 = LINE('',#144486,#9811) ;
#4258 = LINE('',#144488,#9812) ;
#4259 = LINE('',#144489,#9813) ;
#4260 = LINE('',#144493,#9814) ;
#4261 = LINE('',#144495,#9815) ;
#4262 = LINE('',#144497,#9816) ;
#4263 = LINE('',#144498,#9817) ;
#4264 = LINE('',#144614,#9818) ;
#4265 = LINE('',#144616,#9819) ;
#4266 = LINE('',#144618,#9820) ;
#4267 = LINE('',#144620,#9821) ;
#4268 = LINE('',#144622,#9822) ;
#4269 = LINE('',#144624,#9823) ;
#4270 = LINE('',#144628,#9824) ;
#4271 = LINE('',#144631,#9825) ;
#4272 = LINE('',#144635,#9826) ;
#4273 = LINE('',#144637,#9827) ;
#4274 = LINE('',#144639,#9828) ;
#4275 = LINE('',#144641,#9829) ;
#4276 = LINE('',#144643,#9830) ;
#4277 = LINE('',#144645,#9831) ;
#4278 = LINE('',#144649,#9832) ;
#4279 = LINE('',#144652,#9833) ;
#4280 = LINE('',#144656,#9834) ;
#4281 = LINE('',#144658,#9835) ;
#4282 = LINE('',#144660,#9836) ;
#4283 = LINE('',#144662,#9837) ;
#4284 = LINE('',#144664,#9838) ;
#4285 = LINE('',#144666,#9839) ;
#4286 = LINE('',#144670,#9840) ;
#4287 = LINE('',#144673,#9841) ;
#4288 = LINE('',#144677,#9842) ;
#4289 = LINE('',#144679,#9843) ;
#4290 = LINE('',#144681,#9844) ;
#4291 = LINE('',#144683,#9845) ;
#4292 = LINE('',#144685,#9846) ;
#4293 = LINE('',#144687,#9847) ;
#4294 = LINE('',#144691,#9848) ;
#4295 = LINE('',#144694,#9849) ;
#4296 = LINE('',#144698,#9850) ;
#4297 = LINE('',#144700,#9851) ;
#4298 = LINE('',#144702,#9852) ;
#4299 = LINE('',#144704,#9853) ;
#4300 = LINE('',#144706,#9854) ;
#4301 = LINE('',#144708,#9855) ;
#4302 = LINE('',#144712,#9856) ;
#4303 = LINE('',#144715,#9857) ;
#4304 = LINE('',#144719,#9858) ;
#4305 = LINE('',#144721,#9859) ;
#4306 = LINE('',#144723,#9860) ;
#4307 = LINE('',#144725,#9861) ;
#4308 = LINE('',#144727,#9862) ;
#4309 = LINE('',#144729,#9863) ;
#4310 = LINE('',#144733,#9864) ;
#4311 = LINE('',#144736,#9865) ;
#4312 = LINE('',#144740,#9866) ;
#4313 = LINE('',#144742,#9867) ;
#4314 = LINE('',#144744,#9868) ;
#4315 = LINE('',#144746,#9869) ;
#4316 = LINE('',#144748,#9870) ;
#4317 = LINE('',#144750,#9871) ;
#4318 = LINE('',#144754,#9872) ;
#4319 = LINE('',#144757,#9873) ;
#4320 = LINE('',#144761,#9874) ;
#4321 = LINE('',#144763,#9875) ;
#4322 = LINE('',#144765,#9876) ;
#4323 = LINE('',#144767,#9877) ;
#4324 = LINE('',#144769,#9878) ;
#4325 = LINE('',#144771,#9879) ;
#4326 = LINE('',#144775,#9880) ;
#4327 = LINE('',#144778,#9881) ;
#4328 = LINE('',#144782,#9882) ;
#4329 = LINE('',#144784,#9883) ;
#4330 = LINE('',#144786,#9884) ;
#4331 = LINE('',#144788,#9885) ;
#4332 = LINE('',#144790,#9886) ;
#4333 = LINE('',#144792,#9887) ;
#4334 = LINE('',#144796,#9888) ;
#4335 = LINE('',#144799,#9889) ;
#4336 = LINE('',#144803,#9890) ;
#4337 = LINE('',#144805,#9891) ;
#4338 = LINE('',#144807,#9892) ;
#4339 = LINE('',#144808,#9893) ;
#4340 = LINE('',#144811,#9894) ;
#4341 = LINE('',#144813,#9895) ;
#4342 = LINE('',#144814,#9896) ;
#4343 = LINE('',#144818,#9897) ;
#4344 = LINE('',#144820,#9898) ;
#4345 = LINE('',#144822,#9899) ;
#4346 = LINE('',#144823,#9900) ;
#4347 = LINE('',#144827,#9901) ;
#4348 = LINE('',#144829,#9902) ;
#4349 = LINE('',#144831,#9903) ;
#4350 = LINE('',#144832,#9904) ;
#4351 = LINE('',#144836,#9905) ;
#4352 = LINE('',#144838,#9906) ;
#4353 = LINE('',#144840,#9907) ;
#4354 = LINE('',#144841,#9908) ;
#4355 = LINE('',#144845,#9909) ;
#4356 = LINE('',#144847,#9910) ;
#4357 = LINE('',#144849,#9911) ;
#4358 = LINE('',#144850,#9912) ;
#4359 = LINE('',#144853,#9913) ;
#4360 = LINE('',#144855,#9914) ;
#4361 = LINE('',#144856,#9915) ;
#4362 = LINE('',#144860,#9916) ;
#4363 = LINE('',#144862,#9917) ;
#4364 = LINE('',#144864,#9918) ;
#4365 = LINE('',#144865,#9919) ;
#4366 = LINE('',#144869,#9920) ;
#4367 = LINE('',#144871,#9921) ;
#4368 = LINE('',#144873,#9922) ;
#4369 = LINE('',#144874,#9923) ;
#4370 = LINE('',#144878,#9924) ;
#4371 = LINE('',#144880,#9925) ;
#4372 = LINE('',#144882,#9926) ;
#4373 = LINE('',#144883,#9927) ;
#4374 = LINE('',#144887,#9928) ;
#4375 = LINE('',#144889,#9929) ;
#4376 = LINE('',#144891,#9930) ;
#4377 = LINE('',#144892,#9931) ;
#4378 = LINE('',#144895,#9932) ;
#4379 = LINE('',#144897,#9933) ;
#4380 = LINE('',#144898,#9934) ;
#4381 = LINE('',#144902,#9935) ;
#4382 = LINE('',#144904,#9936) ;
#4383 = LINE('',#144906,#9937) ;
#4384 = LINE('',#144907,#9938) ;
#4385 = LINE('',#144911,#9939) ;
#4386 = LINE('',#144913,#9940) ;
#4387 = LINE('',#144915,#9941) ;
#4388 = LINE('',#144916,#9942) ;
#4389 = LINE('',#144920,#9943) ;
#4390 = LINE('',#144922,#9944) ;
#4391 = LINE('',#144924,#9945) ;
#4392 = LINE('',#144925,#9946) ;
#4393 = LINE('',#144929,#9947) ;
#4394 = LINE('',#144931,#9948) ;
#4395 = LINE('',#144933,#9949) ;
#4396 = LINE('',#144934,#9950) ;
#4397 = LINE('',#144937,#9951) ;
#4398 = LINE('',#144939,#9952) ;
#4399 = LINE('',#144940,#9953) ;
#4400 = LINE('',#144944,#9954) ;
#4401 = LINE('',#144946,#9955) ;
#4402 = LINE('',#144948,#9956) ;
#4403 = LINE('',#144949,#9957) ;
#4404 = LINE('',#144953,#9958) ;
#4405 = LINE('',#144955,#9959) ;
#4406 = LINE('',#144957,#9960) ;
#4407 = LINE('',#144958,#9961) ;
#4408 = LINE('',#144962,#9962) ;
#4409 = LINE('',#144964,#9963) ;
#4410 = LINE('',#144966,#9964) ;
#4411 = LINE('',#144967,#9965) ;
#4412 = LINE('',#144971,#9966) ;
#4413 = LINE('',#144973,#9967) ;
#4414 = LINE('',#144975,#9968) ;
#4415 = LINE('',#144976,#9969) ;
#4416 = LINE('',#144979,#9970) ;
#4417 = LINE('',#144981,#9971) ;
#4418 = LINE('',#144982,#9972) ;
#4419 = LINE('',#144986,#9973) ;
#4420 = LINE('',#144988,#9974) ;
#4421 = LINE('',#144990,#9975) ;
#4422 = LINE('',#144991,#9976) ;
#4423 = LINE('',#144995,#9977) ;
#4424 = LINE('',#144997,#9978) ;
#4425 = LINE('',#144999,#9979) ;
#4426 = LINE('',#145000,#9980) ;
#4427 = LINE('',#145004,#9981) ;
#4428 = LINE('',#145006,#9982) ;
#4429 = LINE('',#145008,#9983) ;
#4430 = LINE('',#145009,#9984) ;
#4431 = LINE('',#145013,#9985) ;
#4432 = LINE('',#145015,#9986) ;
#4433 = LINE('',#145017,#9987) ;
#4434 = LINE('',#145018,#9988) ;
#4435 = LINE('',#145021,#9989) ;
#4436 = LINE('',#145023,#9990) ;
#4437 = LINE('',#145024,#9991) ;
#4438 = LINE('',#145028,#9992) ;
#4439 = LINE('',#145030,#9993) ;
#4440 = LINE('',#145032,#9994) ;
#4441 = LINE('',#145033,#9995) ;
#4442 = LINE('',#145037,#9996) ;
#4443 = LINE('',#145039,#9997) ;
#4444 = LINE('',#145041,#9998) ;
#4445 = LINE('',#145042,#9999) ;
#4446 = LINE('',#145046,#10000) ;
#4447 = LINE('',#145048,#10001) ;
#4448 = LINE('',#145050,#10002) ;
#4449 = LINE('',#145051,#10003) ;
#4450 = LINE('',#145055,#10004) ;
#4451 = LINE('',#145057,#10005) ;
#4452 = LINE('',#145059,#10006) ;
#4453 = LINE('',#145060,#10007) ;
#4454 = LINE('',#145063,#10008) ;
#4455 = LINE('',#145065,#10009) ;
#4456 = LINE('',#145066,#10010) ;
#4457 = LINE('',#145070,#10011) ;
#4458 = LINE('',#145072,#10012) ;
#4459 = LINE('',#145074,#10013) ;
#4460 = LINE('',#145075,#10014) ;
#4461 = LINE('',#145079,#10015) ;
#4462 = LINE('',#145081,#10016) ;
#4463 = LINE('',#145083,#10017) ;
#4464 = LINE('',#145084,#10018) ;
#4465 = LINE('',#145088,#10019) ;
#4466 = LINE('',#145090,#10020) ;
#4467 = LINE('',#145092,#10021) ;
#4468 = LINE('',#145093,#10022) ;
#4469 = LINE('',#145097,#10023) ;
#4470 = LINE('',#145099,#10024) ;
#4471 = LINE('',#145101,#10025) ;
#4472 = LINE('',#145102,#10026) ;
#4473 = LINE('',#145105,#10027) ;
#4474 = LINE('',#145107,#10028) ;
#4475 = LINE('',#145108,#10029) ;
#4476 = LINE('',#145112,#10030) ;
#4477 = LINE('',#145114,#10031) ;
#4478 = LINE('',#145116,#10032) ;
#4479 = LINE('',#145117,#10033) ;
#4480 = LINE('',#145121,#10034) ;
#4481 = LINE('',#145123,#10035) ;
#4482 = LINE('',#145125,#10036) ;
#4483 = LINE('',#145126,#10037) ;
#4484 = LINE('',#145130,#10038) ;
#4485 = LINE('',#145132,#10039) ;
#4486 = LINE('',#145134,#10040) ;
#4487 = LINE('',#145135,#10041) ;
#4488 = LINE('',#145139,#10042) ;
#4489 = LINE('',#145141,#10043) ;
#4490 = LINE('',#145143,#10044) ;
#4491 = LINE('',#145144,#10045) ;
#4492 = LINE('',#145147,#10046) ;
#4493 = LINE('',#145149,#10047) ;
#4494 = LINE('',#145150,#10048) ;
#4495 = LINE('',#145154,#10049) ;
#4496 = LINE('',#145156,#10050) ;
#4497 = LINE('',#145158,#10051) ;
#4498 = LINE('',#145159,#10052) ;
#4499 = LINE('',#145163,#10053) ;
#4500 = LINE('',#145165,#10054) ;
#4501 = LINE('',#145167,#10055) ;
#4502 = LINE('',#145168,#10056) ;
#4503 = LINE('',#145172,#10057) ;
#4504 = LINE('',#145174,#10058) ;
#4505 = LINE('',#145176,#10059) ;
#4506 = LINE('',#145177,#10060) ;
#4507 = LINE('',#145181,#10061) ;
#4508 = LINE('',#145185,#10062) ;
#4509 = LINE('',#145189,#10063) ;
#4510 = LINE('',#145191,#10064) ;
#4511 = LINE('',#145192,#10065) ;
#4512 = LINE('',#145197,#10066) ;
#4513 = LINE('',#145201,#10067) ;
#4514 = LINE('',#145203,#10068) ;
#4515 = LINE('',#145204,#10069) ;
#4516 = LINE('',#145209,#10070) ;
#4517 = LINE('',#145212,#10071) ;
#4518 = LINE('',#145214,#10072) ;
#4519 = LINE('',#145215,#10073) ;
#4520 = LINE('',#145218,#10074) ;
#4521 = LINE('',#145221,#10075) ;
#4522 = LINE('',#145222,#10076) ;
#4523 = LINE('',#145225,#10077) ;
#4524 = LINE('',#145227,#10078) ;
#4525 = LINE('',#145228,#10079) ;
#4526 = LINE('',#145233,#10080) ;
#4527 = LINE('',#145237,#10081) ;
#4528 = LINE('',#145239,#10082) ;
#4529 = LINE('',#145240,#10083) ;
#4530 = LINE('',#145245,#10084) ;
#4531 = LINE('',#145249,#10085) ;
#4532 = LINE('',#145251,#10086) ;
#4533 = LINE('',#145252,#10087) ;
#4534 = LINE('',#145257,#10088) ;
#4535 = LINE('',#145261,#10089) ;
#4536 = LINE('',#145263,#10090) ;
#4537 = LINE('',#145264,#10091) ;
#4538 = LINE('',#145269,#10092) ;
#4539 = LINE('',#145273,#10093) ;
#4540 = LINE('',#145275,#10094) ;
#4541 = LINE('',#145276,#10095) ;
#4542 = LINE('',#145281,#10096) ;
#4543 = LINE('',#145285,#10097) ;
#4544 = LINE('',#145287,#10098) ;
#4545 = LINE('',#145288,#10099) ;
#4546 = LINE('',#145293,#10100) ;
#4547 = LINE('',#145299,#10101) ;
#4548 = LINE('',#145305,#10102) ;
#4549 = LINE('',#145309,#10103) ;
#4550 = LINE('',#145311,#10104) ;
#4551 = LINE('',#145312,#10105) ;
#4552 = LINE('',#145317,#10106) ;
#4553 = LINE('',#145321,#10107) ;
#4554 = LINE('',#145323,#10108) ;
#4555 = LINE('',#145324,#10109) ;
#4556 = LINE('',#145329,#10110) ;
#4557 = LINE('',#145332,#10111) ;
#4558 = LINE('',#145333,#10112) ;
#4559 = LINE('',#145339,#10113) ;
#4560 = LINE('',#145343,#10114) ;
#4561 = LINE('',#145345,#10115) ;
#4562 = LINE('',#145347,#10116) ;
#4563 = LINE('',#145351,#10117) ;
#4564 = LINE('',#145353,#10118) ;
#4565 = LINE('',#145355,#10119) ;
#4566 = LINE('',#145359,#10120) ;
#4567 = LINE('',#145363,#10121) ;
#4568 = LINE('',#145365,#10122) ;
#4569 = LINE('',#145366,#10123) ;
#4570 = LINE('',#145368,#10124) ;
#4571 = LINE('',#145369,#10125) ;
#4572 = LINE('',#145373,#10126) ;
#4573 = LINE('',#145377,#10127) ;
#4574 = LINE('',#145381,#10128) ;
#4575 = LINE('',#145383,#10129) ;
#4576 = LINE('',#145384,#10130) ;
#4577 = LINE('',#145389,#10131) ;
#4578 = LINE('',#145393,#10132) ;
#4579 = LINE('',#145395,#10133) ;
#4580 = LINE('',#145396,#10134) ;
#4581 = LINE('',#145401,#10135) ;
#4582 = LINE('',#145404,#10136) ;
#4583 = LINE('',#145406,#10137) ;
#4584 = LINE('',#145407,#10138) ;
#4585 = LINE('',#145410,#10139) ;
#4586 = LINE('',#145413,#10140) ;
#4587 = LINE('',#145414,#10141) ;
#4588 = LINE('',#145417,#10142) ;
#4589 = LINE('',#145419,#10143) ;
#4590 = LINE('',#145420,#10144) ;
#4591 = LINE('',#145425,#10145) ;
#4592 = LINE('',#145429,#10146) ;
#4593 = LINE('',#145431,#10147) ;
#4594 = LINE('',#145432,#10148) ;
#4595 = LINE('',#145437,#10149) ;
#4596 = LINE('',#145441,#10150) ;
#4597 = LINE('',#145443,#10151) ;
#4598 = LINE('',#145444,#10152) ;
#4599 = LINE('',#145449,#10153) ;
#4600 = LINE('',#145453,#10154) ;
#4601 = LINE('',#145455,#10155) ;
#4602 = LINE('',#145456,#10156) ;
#4603 = LINE('',#145461,#10157) ;
#4604 = LINE('',#145465,#10158) ;
#4605 = LINE('',#145467,#10159) ;
#4606 = LINE('',#145468,#10160) ;
#4607 = LINE('',#145473,#10161) ;
#4608 = LINE('',#145477,#10162) ;
#4609 = LINE('',#145479,#10163) ;
#4610 = LINE('',#145480,#10164) ;
#4611 = LINE('',#145485,#10165) ;
#4612 = LINE('',#145491,#10166) ;
#4613 = LINE('',#145497,#10167) ;
#4614 = LINE('',#145501,#10168) ;
#4615 = LINE('',#145503,#10169) ;
#4616 = LINE('',#145504,#10170) ;
#4617 = LINE('',#145509,#10171) ;
#4618 = LINE('',#145513,#10172) ;
#4619 = LINE('',#145515,#10173) ;
#4620 = LINE('',#145516,#10174) ;
#4621 = LINE('',#145521,#10175) ;
#4622 = LINE('',#145524,#10176) ;
#4623 = LINE('',#145525,#10177) ;
#4624 = LINE('',#145531,#10178) ;
#4625 = LINE('',#145535,#10179) ;
#4626 = LINE('',#145537,#10180) ;
#4627 = LINE('',#145539,#10181) ;
#4628 = LINE('',#145543,#10182) ;
#4629 = LINE('',#145545,#10183) ;
#4630 = LINE('',#145547,#10184) ;
#4631 = LINE('',#145551,#10185) ;
#4632 = LINE('',#145555,#10186) ;
#4633 = LINE('',#145557,#10187) ;
#4634 = LINE('',#145558,#10188) ;
#4635 = LINE('',#145560,#10189) ;
#4636 = LINE('',#145561,#10190) ;
#4637 = LINE('',#145565,#10191) ;
#4638 = LINE('',#145569,#10192) ;
#4639 = LINE('',#145573,#10193) ;
#4640 = LINE('',#145575,#10194) ;
#4641 = LINE('',#145576,#10195) ;
#4642 = LINE('',#145581,#10196) ;
#4643 = LINE('',#145585,#10197) ;
#4644 = LINE('',#145587,#10198) ;
#4645 = LINE('',#145588,#10199) ;
#4646 = LINE('',#145593,#10200) ;
#4647 = LINE('',#145596,#10201) ;
#4648 = LINE('',#145598,#10202) ;
#4649 = LINE('',#145599,#10203) ;
#4650 = LINE('',#145602,#10204) ;
#4651 = LINE('',#145605,#10205) ;
#4652 = LINE('',#145606,#10206) ;
#4653 = LINE('',#145609,#10207) ;
#4654 = LINE('',#145611,#10208) ;
#4655 = LINE('',#145612,#10209) ;
#4656 = LINE('',#145617,#10210) ;
#4657 = LINE('',#145621,#10211) ;
#4658 = LINE('',#145623,#10212) ;
#4659 = LINE('',#145624,#10213) ;
#4660 = LINE('',#145629,#10214) ;
#4661 = LINE('',#145633,#10215) ;
#4662 = LINE('',#145635,#10216) ;
#4663 = LINE('',#145636,#10217) ;
#4664 = LINE('',#145641,#10218) ;
#4665 = LINE('',#145645,#10219) ;
#4666 = LINE('',#145647,#10220) ;
#4667 = LINE('',#145648,#10221) ;
#4668 = LINE('',#145653,#10222) ;
#4669 = LINE('',#145657,#10223) ;
#4670 = LINE('',#145659,#10224) ;
#4671 = LINE('',#145660,#10225) ;
#4672 = LINE('',#145665,#10226) ;
#4673 = LINE('',#145669,#10227) ;
#4674 = LINE('',#145671,#10228) ;
#4675 = LINE('',#145672,#10229) ;
#4676 = LINE('',#145677,#10230) ;
#4677 = LINE('',#145683,#10231) ;
#4678 = LINE('',#145689,#10232) ;
#4679 = LINE('',#145693,#10233) ;
#4680 = LINE('',#145695,#10234) ;
#4681 = LINE('',#145696,#10235) ;
#4682 = LINE('',#145701,#10236) ;
#4683 = LINE('',#145705,#10237) ;
#4684 = LINE('',#145707,#10238) ;
#4685 = LINE('',#145708,#10239) ;
#4686 = LINE('',#145713,#10240) ;
#4687 = LINE('',#145716,#10241) ;
#4688 = LINE('',#145717,#10242) ;
#4689 = LINE('',#145723,#10243) ;
#4690 = LINE('',#145727,#10244) ;
#4691 = LINE('',#145729,#10245) ;
#4692 = LINE('',#145731,#10246) ;
#4693 = LINE('',#145735,#10247) ;
#4694 = LINE('',#145737,#10248) ;
#4695 = LINE('',#145739,#10249) ;
#4696 = LINE('',#145743,#10250) ;
#4697 = LINE('',#145747,#10251) ;
#4698 = LINE('',#145749,#10252) ;
#4699 = LINE('',#145750,#10253) ;
#4700 = LINE('',#145752,#10254) ;
#4701 = LINE('',#145753,#10255) ;
#4702 = LINE('',#145757,#10256) ;
#4703 = LINE('',#145761,#10257) ;
#4704 = LINE('',#145765,#10258) ;
#4705 = LINE('',#145767,#10259) ;
#4706 = LINE('',#145768,#10260) ;
#4707 = LINE('',#145773,#10261) ;
#4708 = LINE('',#145777,#10262) ;
#4709 = LINE('',#145779,#10263) ;
#4710 = LINE('',#145780,#10264) ;
#4711 = LINE('',#145785,#10265) ;
#4712 = LINE('',#145788,#10266) ;
#4713 = LINE('',#145790,#10267) ;
#4714 = LINE('',#145791,#10268) ;
#4715 = LINE('',#145794,#10269) ;
#4716 = LINE('',#145797,#10270) ;
#4717 = LINE('',#145798,#10271) ;
#4718 = LINE('',#145801,#10272) ;
#4719 = LINE('',#145803,#10273) ;
#4720 = LINE('',#145804,#10274) ;
#4721 = LINE('',#145809,#10275) ;
#4722 = LINE('',#145813,#10276) ;
#4723 = LINE('',#145815,#10277) ;
#4724 = LINE('',#145816,#10278) ;
#4725 = LINE('',#145821,#10279) ;
#4726 = LINE('',#145825,#10280) ;
#4727 = LINE('',#145827,#10281) ;
#4728 = LINE('',#145828,#10282) ;
#4729 = LINE('',#145833,#10283) ;
#4730 = LINE('',#145837,#10284) ;
#4731 = LINE('',#145839,#10285) ;
#4732 = LINE('',#145840,#10286) ;
#4733 = LINE('',#145845,#10287) ;
#4734 = LINE('',#145849,#10288) ;
#4735 = LINE('',#145851,#10289) ;
#4736 = LINE('',#145852,#10290) ;
#4737 = LINE('',#145857,#10291) ;
#4738 = LINE('',#145861,#10292) ;
#4739 = LINE('',#145863,#10293) ;
#4740 = LINE('',#145864,#10294) ;
#4741 = LINE('',#145869,#10295) ;
#4742 = LINE('',#145875,#10296) ;
#4743 = LINE('',#145881,#10297) ;
#4744 = LINE('',#145885,#10298) ;
#4745 = LINE('',#145887,#10299) ;
#4746 = LINE('',#145888,#10300) ;
#4747 = LINE('',#145893,#10301) ;
#4748 = LINE('',#145897,#10302) ;
#4749 = LINE('',#145899,#10303) ;
#4750 = LINE('',#145900,#10304) ;
#4751 = LINE('',#145905,#10305) ;
#4752 = LINE('',#145908,#10306) ;
#4753 = LINE('',#145909,#10307) ;
#4754 = LINE('',#145915,#10308) ;
#4755 = LINE('',#145919,#10309) ;
#4756 = LINE('',#145921,#10310) ;
#4757 = LINE('',#145923,#10311) ;
#4758 = LINE('',#145927,#10312) ;
#4759 = LINE('',#145929,#10313) ;
#4760 = LINE('',#145931,#10314) ;
#4761 = LINE('',#145935,#10315) ;
#4762 = LINE('',#145939,#10316) ;
#4763 = LINE('',#145941,#10317) ;
#4764 = LINE('',#145942,#10318) ;
#4765 = LINE('',#145944,#10319) ;
#4766 = LINE('',#145945,#10320) ;
#4767 = LINE('',#145949,#10321) ;
#4768 = LINE('',#145953,#10322) ;
#4769 = LINE('',#145957,#10323) ;
#4770 = LINE('',#145959,#10324) ;
#4771 = LINE('',#145960,#10325) ;
#4772 = LINE('',#145965,#10326) ;
#4773 = LINE('',#145969,#10327) ;
#4774 = LINE('',#145971,#10328) ;
#4775 = LINE('',#145972,#10329) ;
#4776 = LINE('',#145977,#10330) ;
#4777 = LINE('',#145980,#10331) ;
#4778 = LINE('',#145982,#10332) ;
#4779 = LINE('',#145983,#10333) ;
#4780 = LINE('',#145986,#10334) ;
#4781 = LINE('',#145989,#10335) ;
#4782 = LINE('',#145990,#10336) ;
#4783 = LINE('',#145993,#10337) ;
#4784 = LINE('',#145995,#10338) ;
#4785 = LINE('',#145996,#10339) ;
#4786 = LINE('',#146001,#10340) ;
#4787 = LINE('',#146005,#10341) ;
#4788 = LINE('',#146007,#10342) ;
#4789 = LINE('',#146008,#10343) ;
#4790 = LINE('',#146013,#10344) ;
#4791 = LINE('',#146017,#10345) ;
#4792 = LINE('',#146019,#10346) ;
#4793 = LINE('',#146020,#10347) ;
#4794 = LINE('',#146025,#10348) ;
#4795 = LINE('',#146029,#10349) ;
#4796 = LINE('',#146031,#10350) ;
#4797 = LINE('',#146032,#10351) ;
#4798 = LINE('',#146037,#10352) ;
#4799 = LINE('',#146041,#10353) ;
#4800 = LINE('',#146043,#10354) ;
#4801 = LINE('',#146044,#10355) ;
#4802 = LINE('',#146049,#10356) ;
#4803 = LINE('',#146053,#10357) ;
#4804 = LINE('',#146055,#10358) ;
#4805 = LINE('',#146056,#10359) ;
#4806 = LINE('',#146061,#10360) ;
#4807 = LINE('',#146067,#10361) ;
#4808 = LINE('',#146073,#10362) ;
#4809 = LINE('',#146077,#10363) ;
#4810 = LINE('',#146079,#10364) ;
#4811 = LINE('',#146080,#10365) ;
#4812 = LINE('',#146085,#10366) ;
#4813 = LINE('',#146089,#10367) ;
#4814 = LINE('',#146091,#10368) ;
#4815 = LINE('',#146092,#10369) ;
#4816 = LINE('',#146097,#10370) ;
#4817 = LINE('',#146100,#10371) ;
#4818 = LINE('',#146101,#10372) ;
#4819 = LINE('',#146107,#10373) ;
#4820 = LINE('',#146111,#10374) ;
#4821 = LINE('',#146113,#10375) ;
#4822 = LINE('',#146115,#10376) ;
#4823 = LINE('',#146119,#10377) ;
#4824 = LINE('',#146121,#10378) ;
#4825 = LINE('',#146123,#10379) ;
#4826 = LINE('',#146127,#10380) ;
#4827 = LINE('',#146131,#10381) ;
#4828 = LINE('',#146133,#10382) ;
#4829 = LINE('',#146134,#10383) ;
#4830 = LINE('',#146136,#10384) ;
#4831 = LINE('',#146137,#10385) ;
#4832 = LINE('',#146141,#10386) ;
#4833 = LINE('',#146145,#10387) ;
#4834 = LINE('',#146149,#10388) ;
#4835 = LINE('',#146151,#10389) ;
#4836 = LINE('',#146152,#10390) ;
#4837 = LINE('',#146157,#10391) ;
#4838 = LINE('',#146161,#10392) ;
#4839 = LINE('',#146163,#10393) ;
#4840 = LINE('',#146164,#10394) ;
#4841 = LINE('',#146169,#10395) ;
#4842 = LINE('',#146172,#10396) ;
#4843 = LINE('',#146174,#10397) ;
#4844 = LINE('',#146175,#10398) ;
#4845 = LINE('',#146178,#10399) ;
#4846 = LINE('',#146181,#10400) ;
#4847 = LINE('',#146182,#10401) ;
#4848 = LINE('',#146185,#10402) ;
#4849 = LINE('',#146187,#10403) ;
#4850 = LINE('',#146188,#10404) ;
#4851 = LINE('',#146193,#10405) ;
#4852 = LINE('',#146197,#10406) ;
#4853 = LINE('',#146199,#10407) ;
#4854 = LINE('',#146200,#10408) ;
#4855 = LINE('',#146205,#10409) ;
#4856 = LINE('',#146209,#10410) ;
#4857 = LINE('',#146211,#10411) ;
#4858 = LINE('',#146212,#10412) ;
#4859 = LINE('',#146217,#10413) ;
#4860 = LINE('',#146221,#10414) ;
#4861 = LINE('',#146223,#10415) ;
#4862 = LINE('',#146224,#10416) ;
#4863 = LINE('',#146229,#10417) ;
#4864 = LINE('',#146233,#10418) ;
#4865 = LINE('',#146235,#10419) ;
#4866 = LINE('',#146236,#10420) ;
#4867 = LINE('',#146241,#10421) ;
#4868 = LINE('',#146245,#10422) ;
#4869 = LINE('',#146247,#10423) ;
#4870 = LINE('',#146248,#10424) ;
#4871 = LINE('',#146253,#10425) ;
#4872 = LINE('',#146259,#10426) ;
#4873 = LINE('',#146265,#10427) ;
#4874 = LINE('',#146269,#10428) ;
#4875 = LINE('',#146271,#10429) ;
#4876 = LINE('',#146272,#10430) ;
#4877 = LINE('',#146277,#10431) ;
#4878 = LINE('',#146281,#10432) ;
#4879 = LINE('',#146283,#10433) ;
#4880 = LINE('',#146284,#10434) ;
#4881 = LINE('',#146289,#10435) ;
#4882 = LINE('',#146292,#10436) ;
#4883 = LINE('',#146293,#10437) ;
#4884 = LINE('',#146299,#10438) ;
#4885 = LINE('',#146303,#10439) ;
#4886 = LINE('',#146305,#10440) ;
#4887 = LINE('',#146307,#10441) ;
#4888 = LINE('',#146311,#10442) ;
#4889 = LINE('',#146313,#10443) ;
#4890 = LINE('',#146315,#10444) ;
#4891 = LINE('',#146319,#10445) ;
#4892 = LINE('',#146323,#10446) ;
#4893 = LINE('',#146325,#10447) ;
#4894 = LINE('',#146326,#10448) ;
#4895 = LINE('',#146328,#10449) ;
#4896 = LINE('',#146329,#10450) ;
#4897 = LINE('',#146333,#10451) ;
#4898 = LINE('',#146337,#10452) ;
#4899 = LINE('',#146341,#10453) ;
#4900 = LINE('',#146343,#10454) ;
#4901 = LINE('',#146344,#10455) ;
#4902 = LINE('',#146349,#10456) ;
#4903 = LINE('',#146353,#10457) ;
#4904 = LINE('',#146355,#10458) ;
#4905 = LINE('',#146356,#10459) ;
#4906 = LINE('',#146361,#10460) ;
#4907 = LINE('',#146364,#10461) ;
#4908 = LINE('',#146366,#10462) ;
#4909 = LINE('',#146367,#10463) ;
#4910 = LINE('',#146370,#10464) ;
#4911 = LINE('',#146373,#10465) ;
#4912 = LINE('',#146374,#10466) ;
#4913 = LINE('',#146377,#10467) ;
#4914 = LINE('',#146379,#10468) ;
#4915 = LINE('',#146380,#10469) ;
#4916 = LINE('',#146385,#10470) ;
#4917 = LINE('',#146389,#10471) ;
#4918 = LINE('',#146391,#10472) ;
#4919 = LINE('',#146392,#10473) ;
#4920 = LINE('',#146397,#10474) ;
#4921 = LINE('',#146401,#10475) ;
#4922 = LINE('',#146403,#10476) ;
#4923 = LINE('',#146404,#10477) ;
#4924 = LINE('',#146409,#10478) ;
#4925 = LINE('',#146413,#10479) ;
#4926 = LINE('',#146415,#10480) ;
#4927 = LINE('',#146416,#10481) ;
#4928 = LINE('',#146421,#10482) ;
#4929 = LINE('',#146425,#10483) ;
#4930 = LINE('',#146427,#10484) ;
#4931 = LINE('',#146428,#10485) ;
#4932 = LINE('',#146433,#10486) ;
#4933 = LINE('',#146437,#10487) ;
#4934 = LINE('',#146439,#10488) ;
#4935 = LINE('',#146440,#10489) ;
#4936 = LINE('',#146445,#10490) ;
#4937 = LINE('',#146451,#10491) ;
#4938 = LINE('',#146457,#10492) ;
#4939 = LINE('',#146461,#10493) ;
#4940 = LINE('',#146463,#10494) ;
#4941 = LINE('',#146464,#10495) ;
#4942 = LINE('',#146469,#10496) ;
#4943 = LINE('',#146473,#10497) ;
#4944 = LINE('',#146475,#10498) ;
#4945 = LINE('',#146476,#10499) ;
#4946 = LINE('',#146481,#10500) ;
#4947 = LINE('',#146484,#10501) ;
#4948 = LINE('',#146485,#10502) ;
#4949 = LINE('',#146491,#10503) ;
#4950 = LINE('',#146495,#10504) ;
#4951 = LINE('',#146497,#10505) ;
#4952 = LINE('',#146499,#10506) ;
#4953 = LINE('',#146503,#10507) ;
#4954 = LINE('',#146505,#10508) ;
#4955 = LINE('',#146507,#10509) ;
#4956 = LINE('',#146511,#10510) ;
#4957 = LINE('',#146515,#10511) ;
#4958 = LINE('',#146517,#10512) ;
#4959 = LINE('',#146518,#10513) ;
#4960 = LINE('',#146520,#10514) ;
#4961 = LINE('',#146521,#10515) ;
#4962 = LINE('',#146525,#10516) ;
#4963 = LINE('',#146529,#10517) ;
#4964 = LINE('',#146533,#10518) ;
#4965 = LINE('',#146535,#10519) ;
#4966 = LINE('',#146536,#10520) ;
#4967 = LINE('',#146541,#10521) ;
#4968 = LINE('',#146545,#10522) ;
#4969 = LINE('',#146547,#10523) ;
#4970 = LINE('',#146548,#10524) ;
#4971 = LINE('',#146553,#10525) ;
#4972 = LINE('',#146556,#10526) ;
#4973 = LINE('',#146558,#10527) ;
#4974 = LINE('',#146559,#10528) ;
#4975 = LINE('',#146562,#10529) ;
#4976 = LINE('',#146565,#10530) ;
#4977 = LINE('',#146566,#10531) ;
#4978 = LINE('',#146569,#10532) ;
#4979 = LINE('',#146571,#10533) ;
#4980 = LINE('',#146572,#10534) ;
#4981 = LINE('',#146577,#10535) ;
#4982 = LINE('',#146581,#10536) ;
#4983 = LINE('',#146583,#10537) ;
#4984 = LINE('',#146584,#10538) ;
#4985 = LINE('',#146589,#10539) ;
#4986 = LINE('',#146593,#10540) ;
#4987 = LINE('',#146595,#10541) ;
#4988 = LINE('',#146596,#10542) ;
#4989 = LINE('',#146601,#10543) ;
#4990 = LINE('',#146605,#10544) ;
#4991 = LINE('',#146607,#10545) ;
#4992 = LINE('',#146608,#10546) ;
#4993 = LINE('',#146613,#10547) ;
#4994 = LINE('',#146617,#10548) ;
#4995 = LINE('',#146619,#10549) ;
#4996 = LINE('',#146620,#10550) ;
#4997 = LINE('',#146625,#10551) ;
#4998 = LINE('',#146629,#10552) ;
#4999 = LINE('',#146631,#10553) ;
#5000 = LINE('',#146632,#10554) ;
#5001 = LINE('',#146637,#10555) ;
#5002 = LINE('',#146643,#10556) ;
#5003 = LINE('',#146649,#10557) ;
#5004 = LINE('',#146653,#10558) ;
#5005 = LINE('',#146655,#10559) ;
#5006 = LINE('',#146656,#10560) ;
#5007 = LINE('',#146661,#10561) ;
#5008 = LINE('',#146665,#10562) ;
#5009 = LINE('',#146667,#10563) ;
#5010 = LINE('',#146668,#10564) ;
#5011 = LINE('',#146673,#10565) ;
#5012 = LINE('',#146676,#10566) ;
#5013 = LINE('',#146677,#10567) ;
#5014 = LINE('',#146683,#10568) ;
#5015 = LINE('',#146687,#10569) ;
#5016 = LINE('',#146689,#10570) ;
#5017 = LINE('',#146691,#10571) ;
#5018 = LINE('',#146695,#10572) ;
#5019 = LINE('',#146697,#10573) ;
#5020 = LINE('',#146699,#10574) ;
#5021 = LINE('',#146703,#10575) ;
#5022 = LINE('',#146707,#10576) ;
#5023 = LINE('',#146709,#10577) ;
#5024 = LINE('',#146710,#10578) ;
#5025 = LINE('',#146712,#10579) ;
#5026 = LINE('',#146713,#10580) ;
#5027 = LINE('',#146717,#10581) ;
#5028 = LINE('',#146721,#10582) ;
#5029 = LINE('',#146725,#10583) ;
#5030 = LINE('',#146727,#10584) ;
#5031 = LINE('',#146728,#10585) ;
#5032 = LINE('',#146733,#10586) ;
#5033 = LINE('',#146737,#10587) ;
#5034 = LINE('',#146739,#10588) ;
#5035 = LINE('',#146740,#10589) ;
#5036 = LINE('',#146745,#10590) ;
#5037 = LINE('',#146748,#10591) ;
#5038 = LINE('',#146750,#10592) ;
#5039 = LINE('',#146751,#10593) ;
#5040 = LINE('',#146754,#10594) ;
#5041 = LINE('',#146757,#10595) ;
#5042 = LINE('',#146758,#10596) ;
#5043 = LINE('',#146761,#10597) ;
#5044 = LINE('',#146763,#10598) ;
#5045 = LINE('',#146764,#10599) ;
#5046 = LINE('',#146769,#10600) ;
#5047 = LINE('',#146773,#10601) ;
#5048 = LINE('',#146775,#10602) ;
#5049 = LINE('',#146776,#10603) ;
#5050 = LINE('',#146781,#10604) ;
#5051 = LINE('',#146785,#10605) ;
#5052 = LINE('',#146787,#10606) ;
#5053 = LINE('',#146788,#10607) ;
#5054 = LINE('',#146793,#10608) ;
#5055 = LINE('',#146797,#10609) ;
#5056 = LINE('',#146799,#10610) ;
#5057 = LINE('',#146800,#10611) ;
#5058 = LINE('',#146805,#10612) ;
#5059 = LINE('',#146809,#10613) ;
#5060 = LINE('',#146811,#10614) ;
#5061 = LINE('',#146812,#10615) ;
#5062 = LINE('',#146817,#10616) ;
#5063 = LINE('',#146821,#10617) ;
#5064 = LINE('',#146823,#10618) ;
#5065 = LINE('',#146824,#10619) ;
#5066 = LINE('',#146829,#10620) ;
#5067 = LINE('',#146835,#10621) ;
#5068 = LINE('',#146841,#10622) ;
#5069 = LINE('',#146845,#10623) ;
#5070 = LINE('',#146847,#10624) ;
#5071 = LINE('',#146848,#10625) ;
#5072 = LINE('',#146853,#10626) ;
#5073 = LINE('',#146857,#10627) ;
#5074 = LINE('',#146859,#10628) ;
#5075 = LINE('',#146860,#10629) ;
#5076 = LINE('',#146865,#10630) ;
#5077 = LINE('',#146868,#10631) ;
#5078 = LINE('',#146869,#10632) ;
#5079 = LINE('',#146875,#10633) ;
#5080 = LINE('',#146879,#10634) ;
#5081 = LINE('',#146881,#10635) ;
#5082 = LINE('',#146883,#10636) ;
#5083 = LINE('',#146887,#10637) ;
#5084 = LINE('',#146889,#10638) ;
#5085 = LINE('',#146891,#10639) ;
#5086 = LINE('',#146895,#10640) ;
#5087 = LINE('',#146899,#10641) ;
#5088 = LINE('',#146901,#10642) ;
#5089 = LINE('',#146902,#10643) ;
#5090 = LINE('',#146904,#10644) ;
#5091 = LINE('',#146905,#10645) ;
#5092 = LINE('',#146909,#10646) ;
#5093 = LINE('',#146913,#10647) ;
#5094 = LINE('',#146917,#10648) ;
#5095 = LINE('',#146921,#10649) ;
#5096 = LINE('',#146926,#10650) ;
#5097 = LINE('',#146930,#10651) ;
#5098 = LINE('',#146934,#10652) ;
#5099 = LINE('',#146938,#10653) ;
#5100 = LINE('',#146943,#10654) ;
#5101 = LINE('',#146947,#10655) ;
#5102 = LINE('',#146951,#10656) ;
#5103 = LINE('',#146955,#10657) ;
#5104 = LINE('',#146960,#10658) ;
#5105 = LINE('',#146964,#10659) ;
#5106 = LINE('',#146968,#10660) ;
#5107 = LINE('',#146972,#10661) ;
#5108 = LINE('',#146977,#10662) ;
#5109 = LINE('',#146981,#10663) ;
#5110 = LINE('',#146985,#10664) ;
#5111 = LINE('',#146989,#10665) ;
#5112 = LINE('',#146994,#10666) ;
#5113 = LINE('',#146998,#10667) ;
#5114 = LINE('',#147002,#10668) ;
#5115 = LINE('',#147006,#10669) ;
#5116 = LINE('',#147011,#10670) ;
#5117 = LINE('',#147015,#10671) ;
#5118 = LINE('',#147019,#10672) ;
#5119 = LINE('',#147023,#10673) ;
#5120 = LINE('',#147028,#10674) ;
#5121 = LINE('',#147032,#10675) ;
#5122 = LINE('',#147036,#10676) ;
#5123 = LINE('',#147040,#10677) ;
#5124 = LINE('',#147045,#10678) ;
#5125 = LINE('',#147049,#10679) ;
#5126 = LINE('',#147053,#10680) ;
#5127 = LINE('',#147057,#10681) ;
#5128 = LINE('',#147085,#10682) ;
#5129 = LINE('',#147142,#10683) ;
#5130 = LINE('',#147167,#10684) ;
#5131 = LINE('',#147199,#10685) ;
#5132 = LINE('',#147225,#10686) ;
#5133 = LINE('',#147789,#10687) ;
#5134 = LINE('',#147846,#10688) ;
#5135 = LINE('',#147871,#10689) ;
#5136 = LINE('',#147903,#10690) ;
#5137 = LINE('',#147929,#10691) ;
#5138 = LINE('',#148016,#10692) ;
#5139 = LINE('',#148073,#10693) ;
#5140 = LINE('',#148098,#10694) ;
#5141 = LINE('',#148130,#10695) ;
#5142 = LINE('',#148156,#10696) ;
#5143 = LINE('',#148243,#10697) ;
#5144 = LINE('',#148300,#10698) ;
#5145 = LINE('',#148325,#10699) ;
#5146 = LINE('',#148357,#10700) ;
#5147 = LINE('',#148383,#10701) ;
#5148 = LINE('',#148470,#10702) ;
#5149 = LINE('',#148527,#10703) ;
#5150 = LINE('',#148552,#10704) ;
#5151 = LINE('',#148584,#10705) ;
#5152 = LINE('',#148610,#10706) ;
#5153 = LINE('',#148697,#10707) ;
#5154 = LINE('',#148754,#10708) ;
#5155 = LINE('',#148779,#10709) ;
#5156 = LINE('',#148811,#10710) ;
#5157 = LINE('',#148837,#10711) ;
#5158 = LINE('',#148924,#10712) ;
#5159 = LINE('',#148981,#10713) ;
#5160 = LINE('',#149006,#10714) ;
#5161 = LINE('',#149038,#10715) ;
#5162 = LINE('',#149064,#10716) ;
#5163 = LINE('',#149151,#10717) ;
#5164 = LINE('',#149208,#10718) ;
#5165 = LINE('',#149233,#10719) ;
#5166 = LINE('',#149265,#10720) ;
#5167 = LINE('',#149291,#10721) ;
#5168 = LINE('',#149378,#10722) ;
#5169 = LINE('',#149435,#10723) ;
#5170 = LINE('',#149460,#10724) ;
#5171 = LINE('',#149492,#10725) ;
#5172 = LINE('',#149518,#10726) ;
#5173 = LINE('',#149582,#10727) ;
#5174 = LINE('',#149584,#10728) ;
#5175 = LINE('',#149586,#10729) ;
#5176 = LINE('',#149587,#10730) ;
#5177 = LINE('',#149591,#10731) ;
#5178 = LINE('',#149593,#10732) ;
#5179 = LINE('',#149595,#10733) ;
#5180 = LINE('',#149596,#10734) ;
#5181 = LINE('',#149600,#10735) ;
#5182 = LINE('',#149602,#10736) ;
#5183 = LINE('',#149604,#10737) ;
#5184 = LINE('',#149605,#10738) ;
#5185 = LINE('',#149609,#10739) ;
#5186 = LINE('',#149611,#10740) ;
#5187 = LINE('',#149613,#10741) ;
#5188 = LINE('',#149614,#10742) ;
#5189 = LINE('',#149618,#10743) ;
#5190 = LINE('',#149620,#10744) ;
#5191 = LINE('',#149622,#10745) ;
#5192 = LINE('',#149623,#10746) ;
#5193 = LINE('',#149627,#10747) ;
#5194 = LINE('',#149632,#10748) ;
#5195 = LINE('',#149633,#10749) ;
#5196 = LINE('',#149637,#10750) ;
#5197 = LINE('',#149642,#10751) ;
#5198 = LINE('',#149643,#10752) ;
#5199 = LINE('',#149653,#10753) ;
#5200 = LINE('',#149655,#10754) ;
#5201 = LINE('',#149657,#10755) ;
#5202 = LINE('',#149658,#10756) ;
#5203 = LINE('',#149662,#10757) ;
#5204 = LINE('',#149663,#10758) ;
#5205 = LINE('',#149664,#10759) ;
#5206 = LINE('',#149667,#10760) ;
#5207 = LINE('',#149669,#10761) ;
#5208 = LINE('',#149670,#10762) ;
#5209 = LINE('',#149674,#10763) ;
#5210 = LINE('',#149676,#10764) ;
#5211 = LINE('',#149678,#10765) ;
#5212 = LINE('',#149679,#10766) ;
#5213 = LINE('',#149683,#10767) ;
#5214 = LINE('',#149685,#10768) ;
#5215 = LINE('',#149687,#10769) ;
#5216 = LINE('',#149688,#10770) ;
#5217 = LINE('',#149692,#10771) ;
#5218 = LINE('',#149693,#10772) ;
#5219 = LINE('',#149694,#10773) ;
#5220 = LINE('',#149697,#10774) ;
#5221 = LINE('',#149699,#10775) ;
#5222 = LINE('',#149700,#10776) ;
#5223 = LINE('',#149704,#10777) ;
#5224 = LINE('',#149706,#10778) ;
#5225 = LINE('',#149708,#10779) ;
#5226 = LINE('',#149709,#10780) ;
#5227 = LINE('',#149713,#10781) ;
#5228 = LINE('',#149715,#10782) ;
#5229 = LINE('',#149717,#10783) ;
#5230 = LINE('',#149718,#10784) ;
#5231 = LINE('',#149722,#10785) ;
#5232 = LINE('',#149724,#10786) ;
#5233 = LINE('',#149726,#10787) ;
#5234 = LINE('',#149727,#10788) ;
#5235 = LINE('',#149731,#10789) ;
#5236 = LINE('',#149733,#10790) ;
#5237 = LINE('',#149735,#10791) ;
#5238 = LINE('',#149736,#10792) ;
#5239 = LINE('',#149740,#10793) ;
#5240 = LINE('',#149742,#10794) ;
#5241 = LINE('',#149744,#10795) ;
#5242 = LINE('',#149745,#10796) ;
#5243 = LINE('',#149749,#10797) ;
#5244 = LINE('',#149754,#10798) ;
#5245 = LINE('',#149755,#10799) ;
#5246 = LINE('',#149759,#10800) ;
#5247 = LINE('',#149764,#10801) ;
#5248 = LINE('',#149765,#10802) ;
#5249 = LINE('',#149775,#10803) ;
#5250 = LINE('',#149777,#10804) ;
#5251 = LINE('',#149779,#10805) ;
#5252 = LINE('',#149780,#10806) ;
#5253 = LINE('',#149784,#10807) ;
#5254 = LINE('',#149785,#10808) ;
#5255 = LINE('',#149786,#10809) ;
#5256 = LINE('',#149789,#10810) ;
#5257 = LINE('',#149791,#10811) ;
#5258 = LINE('',#149792,#10812) ;
#5259 = LINE('',#149796,#10813) ;
#5260 = LINE('',#149798,#10814) ;
#5261 = LINE('',#149800,#10815) ;
#5262 = LINE('',#149801,#10816) ;
#5263 = LINE('',#149805,#10817) ;
#5264 = LINE('',#149807,#10818) ;
#5265 = LINE('',#149809,#10819) ;
#5266 = LINE('',#149810,#10820) ;
#5267 = LINE('',#149814,#10821) ;
#5268 = LINE('',#149815,#10822) ;
#5269 = LINE('',#149816,#10823) ;
#5270 = LINE('',#149819,#10824) ;
#5271 = LINE('',#149821,#10825) ;
#5272 = LINE('',#149822,#10826) ;
#5273 = LINE('',#149826,#10827) ;
#5274 = LINE('',#149828,#10828) ;
#5275 = LINE('',#149830,#10829) ;
#5276 = LINE('',#149831,#10830) ;
#5277 = LINE('',#149835,#10831) ;
#5278 = LINE('',#149837,#10832) ;
#5279 = LINE('',#149839,#10833) ;
#5280 = LINE('',#149840,#10834) ;
#5281 = LINE('',#149844,#10835) ;
#5282 = LINE('',#149846,#10836) ;
#5283 = LINE('',#149848,#10837) ;
#5284 = LINE('',#149849,#10838) ;
#5285 = LINE('',#149853,#10839) ;
#5286 = LINE('',#149855,#10840) ;
#5287 = LINE('',#149857,#10841) ;
#5288 = LINE('',#149858,#10842) ;
#5289 = LINE('',#149862,#10843) ;
#5290 = LINE('',#149864,#10844) ;
#5291 = LINE('',#149866,#10845) ;
#5292 = LINE('',#149867,#10846) ;
#5293 = LINE('',#149871,#10847) ;
#5294 = LINE('',#149876,#10848) ;
#5295 = LINE('',#149877,#10849) ;
#5296 = LINE('',#149881,#10850) ;
#5297 = LINE('',#149886,#10851) ;
#5298 = LINE('',#149887,#10852) ;
#5299 = LINE('',#149897,#10853) ;
#5300 = LINE('',#149899,#10854) ;
#5301 = LINE('',#149901,#10855) ;
#5302 = LINE('',#149902,#10856) ;
#5303 = LINE('',#149906,#10857) ;
#5304 = LINE('',#149907,#10858) ;
#5305 = LINE('',#149908,#10859) ;
#5306 = LINE('',#149911,#10860) ;
#5307 = LINE('',#149913,#10861) ;
#5308 = LINE('',#149914,#10862) ;
#5309 = LINE('',#149918,#10863) ;
#5310 = LINE('',#149920,#10864) ;
#5311 = LINE('',#149922,#10865) ;
#5312 = LINE('',#149923,#10866) ;
#5313 = LINE('',#149927,#10867) ;
#5314 = LINE('',#149929,#10868) ;
#5315 = LINE('',#149931,#10869) ;
#5316 = LINE('',#149932,#10870) ;
#5317 = LINE('',#149936,#10871) ;
#5318 = LINE('',#149937,#10872) ;
#5319 = LINE('',#149938,#10873) ;
#5320 = LINE('',#149941,#10874) ;
#5321 = LINE('',#149943,#10875) ;
#5322 = LINE('',#149944,#10876) ;
#5323 = LINE('',#149948,#10877) ;
#5324 = LINE('',#149950,#10878) ;
#5325 = LINE('',#149952,#10879) ;
#5326 = LINE('',#149953,#10880) ;
#5327 = LINE('',#149957,#10881) ;
#5328 = LINE('',#149959,#10882) ;
#5329 = LINE('',#149961,#10883) ;
#5330 = LINE('',#149962,#10884) ;
#5331 = LINE('',#149966,#10885) ;
#5332 = LINE('',#149968,#10886) ;
#5333 = LINE('',#149970,#10887) ;
#5334 = LINE('',#149971,#10888) ;
#5335 = LINE('',#149975,#10889) ;
#5336 = LINE('',#149977,#10890) ;
#5337 = LINE('',#149979,#10891) ;
#5338 = LINE('',#149980,#10892) ;
#5339 = LINE('',#149984,#10893) ;
#5340 = LINE('',#149986,#10894) ;
#5341 = LINE('',#149988,#10895) ;
#5342 = LINE('',#149989,#10896) ;
#5343 = LINE('',#149993,#10897) ;
#5344 = LINE('',#149998,#10898) ;
#5345 = LINE('',#149999,#10899) ;
#5346 = LINE('',#150003,#10900) ;
#5347 = LINE('',#150008,#10901) ;
#5348 = LINE('',#150009,#10902) ;
#5349 = LINE('',#150019,#10903) ;
#5350 = LINE('',#150021,#10904) ;
#5351 = LINE('',#150023,#10905) ;
#5352 = LINE('',#150024,#10906) ;
#5353 = LINE('',#150028,#10907) ;
#5354 = LINE('',#150029,#10908) ;
#5355 = LINE('',#150030,#10909) ;
#5356 = LINE('',#150033,#10910) ;
#5357 = LINE('',#150035,#10911) ;
#5358 = LINE('',#150036,#10912) ;
#5359 = LINE('',#150040,#10913) ;
#5360 = LINE('',#150042,#10914) ;
#5361 = LINE('',#150044,#10915) ;
#5362 = LINE('',#150045,#10916) ;
#5363 = LINE('',#150049,#10917) ;
#5364 = LINE('',#150051,#10918) ;
#5365 = LINE('',#150053,#10919) ;
#5366 = LINE('',#150054,#10920) ;
#5367 = LINE('',#150058,#10921) ;
#5368 = LINE('',#150059,#10922) ;
#5369 = LINE('',#150060,#10923) ;
#5370 = LINE('',#150063,#10924) ;
#5371 = LINE('',#150065,#10925) ;
#5372 = LINE('',#150066,#10926) ;
#5373 = LINE('',#150070,#10927) ;
#5374 = LINE('',#150072,#10928) ;
#5375 = LINE('',#150074,#10929) ;
#5376 = LINE('',#150075,#10930) ;
#5377 = LINE('',#150079,#10931) ;
#5378 = LINE('',#150081,#10932) ;
#5379 = LINE('',#150083,#10933) ;
#5380 = LINE('',#150084,#10934) ;
#5381 = LINE('',#150088,#10935) ;
#5382 = LINE('',#150090,#10936) ;
#5383 = LINE('',#150092,#10937) ;
#5384 = LINE('',#150093,#10938) ;
#5385 = LINE('',#150097,#10939) ;
#5386 = LINE('',#150099,#10940) ;
#5387 = LINE('',#150101,#10941) ;
#5388 = LINE('',#150102,#10942) ;
#5389 = LINE('',#150106,#10943) ;
#5390 = LINE('',#150108,#10944) ;
#5391 = LINE('',#150110,#10945) ;
#5392 = LINE('',#150111,#10946) ;
#5393 = LINE('',#150115,#10947) ;
#5394 = LINE('',#150120,#10948) ;
#5395 = LINE('',#150121,#10949) ;
#5396 = LINE('',#150125,#10950) ;
#5397 = LINE('',#150130,#10951) ;
#5398 = LINE('',#150131,#10952) ;
#5399 = LINE('',#150141,#10953) ;
#5400 = LINE('',#150143,#10954) ;
#5401 = LINE('',#150145,#10955) ;
#5402 = LINE('',#150146,#10956) ;
#5403 = LINE('',#150150,#10957) ;
#5404 = LINE('',#150151,#10958) ;
#5405 = LINE('',#150152,#10959) ;
#5406 = LINE('',#150155,#10960) ;
#5407 = LINE('',#150157,#10961) ;
#5408 = LINE('',#150158,#10962) ;
#5409 = LINE('',#150162,#10963) ;
#5410 = LINE('',#150164,#10964) ;
#5411 = LINE('',#150166,#10965) ;
#5412 = LINE('',#150167,#10966) ;
#5413 = LINE('',#150171,#10967) ;
#5414 = LINE('',#150173,#10968) ;
#5415 = LINE('',#150175,#10969) ;
#5416 = LINE('',#150176,#10970) ;
#5417 = LINE('',#150180,#10971) ;
#5418 = LINE('',#150181,#10972) ;
#5419 = LINE('',#150182,#10973) ;
#5420 = LINE('',#150185,#10974) ;
#5421 = LINE('',#150187,#10975) ;
#5422 = LINE('',#150188,#10976) ;
#5423 = LINE('',#150192,#10977) ;
#5424 = LINE('',#150194,#10978) ;
#5425 = LINE('',#150196,#10979) ;
#5426 = LINE('',#150197,#10980) ;
#5427 = LINE('',#150201,#10981) ;
#5428 = LINE('',#150203,#10982) ;
#5429 = LINE('',#150205,#10983) ;
#5430 = LINE('',#150206,#10984) ;
#5431 = LINE('',#150210,#10985) ;
#5432 = LINE('',#150212,#10986) ;
#5433 = LINE('',#150214,#10987) ;
#5434 = LINE('',#150215,#10988) ;
#5435 = LINE('',#150219,#10989) ;
#5436 = LINE('',#150221,#10990) ;
#5437 = LINE('',#150223,#10991) ;
#5438 = LINE('',#150224,#10992) ;
#5439 = LINE('',#150228,#10993) ;
#5440 = LINE('',#150230,#10994) ;
#5441 = LINE('',#150232,#10995) ;
#5442 = LINE('',#150233,#10996) ;
#5443 = LINE('',#150237,#10997) ;
#5444 = LINE('',#150242,#10998) ;
#5445 = LINE('',#150243,#10999) ;
#5446 = LINE('',#150247,#11000) ;
#5447 = LINE('',#150252,#11001) ;
#5448 = LINE('',#150253,#11002) ;
#5449 = LINE('',#150263,#11003) ;
#5450 = LINE('',#150265,#11004) ;
#5451 = LINE('',#150267,#11005) ;
#5452 = LINE('',#150268,#11006) ;
#5453 = LINE('',#150272,#11007) ;
#5454 = LINE('',#150273,#11008) ;
#5455 = LINE('',#150274,#11009) ;
#5456 = LINE('',#150277,#11010) ;
#5457 = LINE('',#150279,#11011) ;
#5458 = LINE('',#150280,#11012) ;
#5459 = LINE('',#150284,#11013) ;
#5460 = LINE('',#150286,#11014) ;
#5461 = LINE('',#150288,#11015) ;
#5462 = LINE('',#150289,#11016) ;
#5463 = LINE('',#150293,#11017) ;
#5464 = LINE('',#150295,#11018) ;
#5465 = LINE('',#150297,#11019) ;
#5466 = LINE('',#150298,#11020) ;
#5467 = LINE('',#150302,#11021) ;
#5468 = LINE('',#150303,#11022) ;
#5469 = LINE('',#150304,#11023) ;
#5470 = LINE('',#150307,#11024) ;
#5471 = LINE('',#150309,#11025) ;
#5472 = LINE('',#150310,#11026) ;
#5473 = LINE('',#150314,#11027) ;
#5474 = LINE('',#150316,#11028) ;
#5475 = LINE('',#150318,#11029) ;
#5476 = LINE('',#150319,#11030) ;
#5477 = LINE('',#150323,#11031) ;
#5478 = LINE('',#150325,#11032) ;
#5479 = LINE('',#150327,#11033) ;
#5480 = LINE('',#150328,#11034) ;
#5481 = LINE('',#150332,#11035) ;
#5482 = LINE('',#150334,#11036) ;
#5483 = LINE('',#150336,#11037) ;
#5484 = LINE('',#150337,#11038) ;
#5485 = LINE('',#150341,#11039) ;
#5486 = LINE('',#150343,#11040) ;
#5487 = LINE('',#150345,#11041) ;
#5488 = LINE('',#150346,#11042) ;
#5489 = LINE('',#150350,#11043) ;
#5490 = LINE('',#150352,#11044) ;
#5491 = LINE('',#150354,#11045) ;
#5492 = LINE('',#150355,#11046) ;
#5493 = LINE('',#150359,#11047) ;
#5494 = LINE('',#150364,#11048) ;
#5495 = LINE('',#150365,#11049) ;
#5496 = LINE('',#150369,#11050) ;
#5497 = LINE('',#150374,#11051) ;
#5498 = LINE('',#150375,#11052) ;
#5499 = LINE('',#150385,#11053) ;
#5500 = LINE('',#150387,#11054) ;
#5501 = LINE('',#150389,#11055) ;
#5502 = LINE('',#150390,#11056) ;
#5503 = LINE('',#150394,#11057) ;
#5504 = LINE('',#150395,#11058) ;
#5505 = LINE('',#150396,#11059) ;
#5506 = LINE('',#150399,#11060) ;
#5507 = LINE('',#150401,#11061) ;
#5508 = LINE('',#150402,#11062) ;
#5509 = LINE('',#150406,#11063) ;
#5510 = LINE('',#150408,#11064) ;
#5511 = LINE('',#150410,#11065) ;
#5512 = LINE('',#150411,#11066) ;
#5513 = LINE('',#150415,#11067) ;
#5514 = LINE('',#150417,#11068) ;
#5515 = LINE('',#150419,#11069) ;
#5516 = LINE('',#150420,#11070) ;
#5517 = LINE('',#150424,#11071) ;
#5518 = LINE('',#150425,#11072) ;
#5519 = LINE('',#150426,#11073) ;
#5520 = LINE('',#150429,#11074) ;
#5521 = LINE('',#150431,#11075) ;
#5522 = LINE('',#150432,#11076) ;
#5523 = LINE('',#150436,#11077) ;
#5524 = LINE('',#150438,#11078) ;
#5525 = LINE('',#150440,#11079) ;
#5526 = LINE('',#150441,#11080) ;
#5527 = LINE('',#150445,#11081) ;
#5528 = LINE('',#150447,#11082) ;
#5529 = LINE('',#150449,#11083) ;
#5530 = LINE('',#150450,#11084) ;
#5531 = LINE('',#150454,#11085) ;
#5532 = LINE('',#150456,#11086) ;
#5533 = LINE('',#150458,#11087) ;
#5534 = LINE('',#150459,#11088) ;
#5535 = LINE('',#150463,#11089) ;
#5536 = LINE('',#150465,#11090) ;
#5537 = LINE('',#150467,#11091) ;
#5538 = LINE('',#150468,#11092) ;
#5539 = LINE('',#150472,#11093) ;
#5540 = LINE('',#150474,#11094) ;
#5541 = LINE('',#150476,#11095) ;
#5542 = LINE('',#150477,#11096) ;
#5543 = LINE('',#150481,#11097) ;
#5544 = LINE('',#150486,#11098) ;
#5545 = LINE('',#150487,#11099) ;
#5546 = LINE('',#150491,#11100) ;
#5547 = LINE('',#150496,#11101) ;
#5548 = LINE('',#150497,#11102) ;
#5549 = LINE('',#150507,#11103) ;
#5550 = LINE('',#150509,#11104) ;
#5551 = LINE('',#150511,#11105) ;
#5552 = LINE('',#150512,#11106) ;
#5553 = LINE('',#150516,#11107) ;
#5554 = LINE('',#150517,#11108) ;
#5555 = LINE('',#150518,#11109) ;
#5556 = LINE('',#150521,#11110) ;
#5557 = LINE('',#150523,#11111) ;
#5558 = LINE('',#150524,#11112) ;
#5559 = LINE('',#150528,#11113) ;
#5560 = LINE('',#150530,#11114) ;
#5561 = LINE('',#150532,#11115) ;
#5562 = LINE('',#150533,#11116) ;
#5563 = LINE('',#150537,#11117) ;
#5564 = LINE('',#150539,#11118) ;
#5565 = LINE('',#150541,#11119) ;
#5566 = LINE('',#150542,#11120) ;
#5567 = LINE('',#150546,#11121) ;
#5568 = LINE('',#150547,#11122) ;
#5569 = LINE('',#150548,#11123) ;
#5570 = LINE('',#150551,#11124) ;
#5571 = LINE('',#150553,#11125) ;
#5572 = LINE('',#150554,#11126) ;
#5573 = LINE('',#150558,#11127) ;
#5574 = LINE('',#150560,#11128) ;
#5575 = LINE('',#150562,#11129) ;
#5576 = LINE('',#150563,#11130) ;
#5577 = LINE('',#150567,#11131) ;
#5578 = LINE('',#150569,#11132) ;
#5579 = LINE('',#150571,#11133) ;
#5580 = LINE('',#150572,#11134) ;
#5581 = LINE('',#150576,#11135) ;
#5582 = LINE('',#150578,#11136) ;
#5583 = LINE('',#150580,#11137) ;
#5584 = LINE('',#150581,#11138) ;
#5585 = LINE('',#150585,#11139) ;
#5586 = LINE('',#150587,#11140) ;
#5587 = LINE('',#150589,#11141) ;
#5588 = LINE('',#150590,#11142) ;
#5589 = LINE('',#150594,#11143) ;
#5590 = LINE('',#150596,#11144) ;
#5591 = LINE('',#150598,#11145) ;
#5592 = LINE('',#150599,#11146) ;
#5593 = LINE('',#150603,#11147) ;
#5594 = LINE('',#150608,#11148) ;
#5595 = LINE('',#150609,#11149) ;
#5596 = LINE('',#150613,#11150) ;
#5597 = LINE('',#150618,#11151) ;
#5598 = LINE('',#150619,#11152) ;
#5599 = LINE('',#150629,#11153) ;
#5600 = LINE('',#150631,#11154) ;
#5601 = LINE('',#150633,#11155) ;
#5602 = LINE('',#150634,#11156) ;
#5603 = LINE('',#150638,#11157) ;
#5604 = LINE('',#150639,#11158) ;
#5605 = LINE('',#150640,#11159) ;
#5606 = LINE('',#150643,#11160) ;
#5607 = LINE('',#150645,#11161) ;
#5608 = LINE('',#150646,#11162) ;
#5609 = LINE('',#150650,#11163) ;
#5610 = LINE('',#150652,#11164) ;
#5611 = LINE('',#150654,#11165) ;
#5612 = LINE('',#150655,#11166) ;
#5613 = LINE('',#150659,#11167) ;
#5614 = LINE('',#150661,#11168) ;
#5615 = LINE('',#150663,#11169) ;
#5616 = LINE('',#150664,#11170) ;
#5617 = LINE('',#150668,#11171) ;
#5618 = LINE('',#150669,#11172) ;
#5619 = LINE('',#150670,#11173) ;
#5620 = LINE('',#150673,#11174) ;
#5621 = LINE('',#150675,#11175) ;
#5622 = LINE('',#150676,#11176) ;
#5623 = LINE('',#150680,#11177) ;
#5624 = LINE('',#150682,#11178) ;
#5625 = LINE('',#150684,#11179) ;
#5626 = LINE('',#150685,#11180) ;
#5627 = LINE('',#150689,#11181) ;
#5628 = LINE('',#150691,#11182) ;
#5629 = LINE('',#150693,#11183) ;
#5630 = LINE('',#150694,#11184) ;
#5631 = LINE('',#150698,#11185) ;
#5632 = LINE('',#150700,#11186) ;
#5633 = LINE('',#150702,#11187) ;
#5634 = LINE('',#150703,#11188) ;
#5635 = LINE('',#150707,#11189) ;
#5636 = LINE('',#150709,#11190) ;
#5637 = LINE('',#150711,#11191) ;
#5638 = LINE('',#150712,#11192) ;
#5639 = LINE('',#150716,#11193) ;
#5640 = LINE('',#150718,#11194) ;
#5641 = LINE('',#150720,#11195) ;
#5642 = LINE('',#150721,#11196) ;
#5643 = LINE('',#150725,#11197) ;
#5644 = LINE('',#150727,#11198) ;
#5645 = LINE('',#150729,#11199) ;
#5646 = LINE('',#150730,#11200) ;
#5647 = LINE('',#150734,#11201) ;
#5648 = LINE('',#150736,#11202) ;
#5649 = LINE('',#150738,#11203) ;
#5650 = LINE('',#150739,#11204) ;
#5651 = LINE('',#150743,#11205) ;
#5652 = LINE('',#150745,#11206) ;
#5653 = LINE('',#150747,#11207) ;
#5654 = LINE('',#150748,#11208) ;
#5655 = LINE('',#150752,#11209) ;
#5656 = LINE('',#150754,#11210) ;
#5657 = LINE('',#150756,#11211) ;
#5658 = LINE('',#150757,#11212) ;
#5659 = LINE('',#150761,#11213) ;
#5660 = LINE('',#150763,#11214) ;
#5661 = LINE('',#150765,#11215) ;
#5662 = LINE('',#150766,#11216) ;
#5663 = LINE('',#150770,#11217) ;
#5664 = LINE('',#150772,#11218) ;
#5665 = LINE('',#150774,#11219) ;
#5666 = LINE('',#150775,#11220) ;
#5667 = LINE('',#150779,#11221) ;
#5668 = LINE('',#150781,#11222) ;
#5669 = LINE('',#150783,#11223) ;
#5670 = LINE('',#150784,#11224) ;
#5671 = LINE('',#150788,#11225) ;
#5672 = LINE('',#150790,#11226) ;
#5673 = LINE('',#150792,#11227) ;
#5674 = LINE('',#150793,#11228) ;
#5675 = LINE('',#150797,#11229) ;
#5676 = LINE('',#150799,#11230) ;
#5677 = LINE('',#150801,#11231) ;
#5678 = LINE('',#150802,#11232) ;
#5679 = LINE('',#150806,#11233) ;
#5680 = LINE('',#150808,#11234) ;
#5681 = LINE('',#150810,#11235) ;
#5682 = LINE('',#150811,#11236) ;
#5683 = LINE('',#150815,#11237) ;
#5684 = LINE('',#150817,#11238) ;
#5685 = LINE('',#150819,#11239) ;
#5686 = LINE('',#150820,#11240) ;
#5687 = LINE('',#150824,#11241) ;
#5688 = LINE('',#150826,#11242) ;
#5689 = LINE('',#150828,#11243) ;
#5690 = LINE('',#150829,#11244) ;
#5691 = LINE('',#150833,#11245) ;
#5692 = LINE('',#150835,#11246) ;
#5693 = LINE('',#150837,#11247) ;
#5694 = LINE('',#150838,#11248) ;
#5695 = LINE('',#150842,#11249) ;
#5696 = LINE('',#150844,#11250) ;
#5697 = LINE('',#150846,#11251) ;
#5698 = LINE('',#150847,#11252) ;
#5699 = LINE('',#150851,#11253) ;
#5700 = LINE('',#150853,#11254) ;
#5701 = LINE('',#150855,#11255) ;
#5702 = LINE('',#150856,#11256) ;
#5703 = LINE('',#150860,#11257) ;
#5704 = LINE('',#150862,#11258) ;
#5705 = LINE('',#150864,#11259) ;
#5706 = LINE('',#150865,#11260) ;
#5707 = LINE('',#150869,#11261) ;
#5708 = LINE('',#150871,#11262) ;
#5709 = LINE('',#150873,#11263) ;
#5710 = LINE('',#150874,#11264) ;
#5711 = LINE('',#150878,#11265) ;
#5712 = LINE('',#150880,#11266) ;
#5713 = LINE('',#150882,#11267) ;
#5714 = LINE('',#150883,#11268) ;
#5715 = LINE('',#150887,#11269) ;
#5716 = LINE('',#150889,#11270) ;
#5717 = LINE('',#150891,#11271) ;
#5718 = LINE('',#150892,#11272) ;
#5719 = LINE('',#150896,#11273) ;
#5720 = LINE('',#150898,#11274) ;
#5721 = LINE('',#150900,#11275) ;
#5722 = LINE('',#150901,#11276) ;
#5723 = LINE('',#150905,#11277) ;
#5724 = LINE('',#150907,#11278) ;
#5725 = LINE('',#150909,#11279) ;
#5726 = LINE('',#150910,#11280) ;
#5727 = LINE('',#150914,#11281) ;
#5728 = LINE('',#150916,#11282) ;
#5729 = LINE('',#150918,#11283) ;
#5730 = LINE('',#150919,#11284) ;
#5731 = LINE('',#150923,#11285) ;
#5732 = LINE('',#150925,#11286) ;
#5733 = LINE('',#150927,#11287) ;
#5734 = LINE('',#150928,#11288) ;
#5735 = LINE('',#150932,#11289) ;
#5736 = LINE('',#150934,#11290) ;
#5737 = LINE('',#150936,#11291) ;
#5738 = LINE('',#150937,#11292) ;
#5739 = LINE('',#150941,#11293) ;
#5740 = LINE('',#150943,#11294) ;
#5741 = LINE('',#150945,#11295) ;
#5742 = LINE('',#150946,#11296) ;
#5743 = LINE('',#150950,#11297) ;
#5744 = LINE('',#150952,#11298) ;
#5745 = LINE('',#150954,#11299) ;
#5746 = LINE('',#150955,#11300) ;
#5747 = LINE('',#150959,#11301) ;
#5748 = LINE('',#150961,#11302) ;
#5749 = LINE('',#150963,#11303) ;
#5750 = LINE('',#150964,#11304) ;
#5751 = LINE('',#150968,#11305) ;
#5752 = LINE('',#150970,#11306) ;
#5753 = LINE('',#150972,#11307) ;
#5754 = LINE('',#150973,#11308) ;
#5755 = LINE('',#150977,#11309) ;
#5756 = LINE('',#150979,#11310) ;
#5757 = LINE('',#150981,#11311) ;
#5758 = LINE('',#150982,#11312) ;
#5759 = LINE('',#150986,#11313) ;
#5760 = LINE('',#150988,#11314) ;
#5761 = LINE('',#150990,#11315) ;
#5762 = LINE('',#150991,#11316) ;
#5763 = LINE('',#150995,#11317) ;
#5764 = LINE('',#150997,#11318) ;
#5765 = LINE('',#150999,#11319) ;
#5766 = LINE('',#151000,#11320) ;
#5767 = LINE('',#152015,#11321) ;
#5768 = LINE('',#152018,#11322) ;
#5769 = LINE('',#153721,#11323) ;
#5770 = LINE('',#153722,#11324) ;
#5771 = LINE('',#153725,#11325) ;
#5772 = LINE('',#153726,#11326) ;
#5773 = LINE('',#153729,#11327) ;
#5774 = LINE('',#153730,#11328) ;
#5775 = LINE('',#153733,#11329) ;
#5776 = LINE('',#153734,#11330) ;
#5777 = LINE('',#153737,#11331) ;
#5778 = LINE('',#153738,#11332) ;
#5779 = LINE('',#153741,#11333) ;
#5780 = LINE('',#153742,#11334) ;
#5781 = LINE('',#153745,#11335) ;
#5782 = LINE('',#153746,#11336) ;
#5783 = LINE('',#153925,#11337) ;
#5784 = LINE('',#153951,#11338) ;
#5785 = LINE('',#153998,#11339) ;
#5786 = LINE('',#154024,#11340) ;
#5787 = LINE('',#154058,#11341) ;
#5788 = LINE('',#154075,#11342) ;
#5789 = LINE('',#154101,#11343) ;
#5790 = LINE('',#154148,#11344) ;
#5791 = LINE('',#154174,#11345) ;
#5792 = LINE('',#154208,#11346) ;
#5793 = LINE('',#154225,#11347) ;
#5794 = LINE('',#154251,#11348) ;
#5795 = LINE('',#154298,#11349) ;
#5796 = LINE('',#154324,#11350) ;
#5797 = LINE('',#154358,#11351) ;
#5798 = LINE('',#154375,#11352) ;
#5799 = LINE('',#154401,#11353) ;
#5800 = LINE('',#154448,#11354) ;
#5801 = LINE('',#154474,#11355) ;
#5802 = LINE('',#154508,#11356) ;
#5803 = LINE('',#154525,#11357) ;
#5804 = LINE('',#154551,#11358) ;
#5805 = LINE('',#154598,#11359) ;
#5806 = LINE('',#154624,#11360) ;
#5807 = LINE('',#154658,#11361) ;
#5808 = LINE('',#154675,#11362) ;
#5809 = LINE('',#154701,#11363) ;
#5810 = LINE('',#154748,#11364) ;
#5811 = LINE('',#154774,#11365) ;
#5812 = LINE('',#154808,#11366) ;
#5813 = LINE('',#154825,#11367) ;
#5814 = LINE('',#154851,#11368) ;
#5815 = LINE('',#154898,#11369) ;
#5816 = LINE('',#154924,#11370) ;
#5817 = LINE('',#154958,#11371) ;
#5818 = LINE('',#154975,#11372) ;
#5819 = LINE('',#155001,#11373) ;
#5820 = LINE('',#155048,#11374) ;
#5821 = LINE('',#155074,#11375) ;
#5822 = LINE('',#155108,#11376) ;
#5823 = LINE('',#155125,#11377) ;
#5824 = LINE('',#155151,#11378) ;
#5825 = LINE('',#155198,#11379) ;
#5826 = LINE('',#155224,#11380) ;
#5827 = LINE('',#155258,#11381) ;
#5828 = LINE('',#155262,#11382) ;
#5829 = LINE('',#155266,#11383) ;
#5830 = LINE('',#155270,#11384) ;
#5831 = LINE('',#155274,#11385) ;
#5832 = LINE('',#155278,#11386) ;
#5833 = LINE('',#155282,#11387) ;
#5834 = LINE('',#155286,#11388) ;
#5835 = LINE('',#155290,#11389) ;
#5836 = LINE('',#155294,#11390) ;
#5837 = LINE('',#155296,#11391) ;
#5838 = LINE('',#155298,#11392) ;
#5839 = LINE('',#155300,#11393) ;
#5840 = LINE('',#155302,#11394) ;
#5841 = LINE('',#155304,#11395) ;
#5842 = LINE('',#155306,#11396) ;
#5843 = LINE('',#155308,#11397) ;
#5844 = LINE('',#155310,#11398) ;
#5845 = LINE('',#155312,#11399) ;
#5846 = LINE('',#155333,#11400) ;
#5847 = LINE('',#155334,#11401) ;
#5848 = LINE('',#155338,#11402) ;
#5849 = LINE('',#155339,#11403) ;
#5850 = LINE('',#155343,#11404) ;
#5851 = LINE('',#155344,#11405) ;
#5852 = LINE('',#155347,#11406) ;
#5853 = LINE('',#155348,#11407) ;
#5854 = LINE('',#155365,#11408) ;
#5855 = LINE('',#155391,#11409) ;
#5856 = LINE('',#155438,#11410) ;
#5857 = LINE('',#155464,#11411) ;
#5858 = LINE('',#155498,#11412) ;
#5859 = LINE('',#155502,#11413) ;
#5860 = LINE('',#155504,#11414) ;
#5861 = LINE('',#155508,#11415) ;
#5862 = LINE('',#155510,#11416) ;
#5863 = LINE('',#155512,#11417) ;
#5864 = LINE('',#155513,#11418) ;
#5865 = LINE('',#155525,#11419) ;
#5866 = LINE('',#155527,#11420) ;
#5867 = LINE('',#155528,#11421) ;
#5868 = LINE('',#155533,#11422) ;
#5869 = LINE('',#155537,#11423) ;
#5870 = LINE('',#155541,#11424) ;
#5871 = LINE('',#155544,#11425) ;
#5872 = LINE('',#155549,#11426) ;
#5873 = LINE('',#155553,#11427) ;
#5874 = LINE('',#155557,#11428) ;
#5875 = LINE('',#155560,#11429) ;
#5876 = LINE('',#155565,#11430) ;
#5877 = LINE('',#155569,#11431) ;
#5878 = LINE('',#155573,#11432) ;
#5879 = LINE('',#155576,#11433) ;
#5880 = LINE('',#155581,#11434) ;
#5881 = LINE('',#155585,#11435) ;
#5882 = LINE('',#155589,#11436) ;
#5883 = LINE('',#155592,#11437) ;
#5884 = LINE('',#155597,#11438) ;
#5885 = LINE('',#155601,#11439) ;
#5886 = LINE('',#155605,#11440) ;
#5887 = LINE('',#155608,#11441) ;
#5888 = LINE('',#155613,#11442) ;
#5889 = LINE('',#155617,#11443) ;
#5890 = LINE('',#155621,#11444) ;
#5891 = LINE('',#155624,#11445) ;
#5892 = LINE('',#155629,#11446) ;
#5893 = LINE('',#155633,#11447) ;
#5894 = LINE('',#155637,#11448) ;
#5895 = LINE('',#155640,#11449) ;
#5896 = LINE('',#155645,#11450) ;
#5897 = LINE('',#155649,#11451) ;
#5898 = LINE('',#155653,#11452) ;
#5899 = LINE('',#155656,#11453) ;
#5900 = LINE('',#155661,#11454) ;
#5901 = LINE('',#155665,#11455) ;
#5902 = LINE('',#155669,#11456) ;
#5903 = LINE('',#155672,#11457) ;
#5904 = LINE('',#155677,#11458) ;
#5905 = LINE('',#155681,#11459) ;
#5906 = LINE('',#155685,#11460) ;
#5907 = LINE('',#155688,#11461) ;
#5908 = LINE('',#155692,#11462) ;
#5909 = LINE('',#155694,#11463) ;
#5910 = LINE('',#155696,#11464) ;
#5911 = LINE('',#155697,#11465) ;
#5912 = LINE('',#155700,#11466) ;
#5913 = LINE('',#155704,#11467) ;
#5914 = LINE('',#155708,#11468) ;
#5915 = LINE('',#155712,#11469) ;
#5916 = LINE('',#155717,#11470) ;
#5917 = LINE('',#155719,#11471) ;
#5918 = LINE('',#155721,#11472) ;
#5919 = LINE('',#155722,#11473) ;
#5920 = LINE('',#155725,#11474) ;
#5921 = LINE('',#155729,#11475) ;
#5922 = LINE('',#155733,#11476) ;
#5923 = LINE('',#155737,#11477) ;
#5924 = LINE('',#155742,#11478) ;
#5925 = LINE('',#155744,#11479) ;
#5926 = LINE('',#155746,#11480) ;
#5927 = LINE('',#155747,#11481) ;
#5928 = LINE('',#155750,#11482) ;
#5929 = LINE('',#155754,#11483) ;
#5930 = LINE('',#155758,#11484) ;
#5931 = LINE('',#155762,#11485) ;
#5932 = LINE('',#155767,#11486) ;
#5933 = LINE('',#155769,#11487) ;
#5934 = LINE('',#155771,#11488) ;
#5935 = LINE('',#155772,#11489) ;
#5936 = LINE('',#155775,#11490) ;
#5937 = LINE('',#155779,#11491) ;
#5938 = LINE('',#155783,#11492) ;
#5939 = LINE('',#155787,#11493) ;
#5940 = LINE('',#155792,#11494) ;
#5941 = LINE('',#155794,#11495) ;
#5942 = LINE('',#155796,#11496) ;
#5943 = LINE('',#155797,#11497) ;
#5944 = LINE('',#155800,#11498) ;
#5945 = LINE('',#155804,#11499) ;
#5946 = LINE('',#155808,#11500) ;
#5947 = LINE('',#155812,#11501) ;
#5948 = LINE('',#155817,#11502) ;
#5949 = LINE('',#155819,#11503) ;
#5950 = LINE('',#155821,#11504) ;
#5951 = LINE('',#155822,#11505) ;
#5952 = LINE('',#155825,#11506) ;
#5953 = LINE('',#155829,#11507) ;
#5954 = LINE('',#155833,#11508) ;
#5955 = LINE('',#155837,#11509) ;
#5956 = LINE('',#155842,#11510) ;
#5957 = LINE('',#155844,#11511) ;
#5958 = LINE('',#155846,#11512) ;
#5959 = LINE('',#155847,#11513) ;
#5960 = LINE('',#155850,#11514) ;
#5961 = LINE('',#155854,#11515) ;
#5962 = LINE('',#155858,#11516) ;
#5963 = LINE('',#155862,#11517) ;
#5964 = LINE('',#155867,#11518) ;
#5965 = LINE('',#155869,#11519) ;
#5966 = LINE('',#155871,#11520) ;
#5967 = LINE('',#155872,#11521) ;
#5968 = LINE('',#155875,#11522) ;
#5969 = LINE('',#155879,#11523) ;
#5970 = LINE('',#155883,#11524) ;
#5971 = LINE('',#155887,#11525) ;
#5972 = LINE('',#155892,#11526) ;
#5973 = LINE('',#155894,#11527) ;
#5974 = LINE('',#155896,#11528) ;
#5975 = LINE('',#155897,#11529) ;
#5976 = LINE('',#155900,#11530) ;
#5977 = LINE('',#155904,#11531) ;
#5978 = LINE('',#155908,#11532) ;
#5979 = LINE('',#155912,#11533) ;
#5980 = LINE('',#155915,#11534) ;
#5981 = LINE('',#155917,#11535) ;
#5982 = LINE('',#155919,#11536) ;
#5983 = LINE('',#155921,#11537) ;
#5984 = LINE('',#155923,#11538) ;
#5985 = LINE('',#155925,#11539) ;
#5986 = LINE('',#155927,#11540) ;
#5987 = LINE('',#155929,#11541) ;
#5988 = LINE('',#155931,#11542) ;
#5989 = LINE('',#155935,#11543) ;
#5990 = LINE('',#155937,#11544) ;
#5991 = LINE('',#155939,#11545) ;
#5992 = LINE('',#155941,#11546) ;
#5993 = LINE('',#155943,#11547) ;
#5994 = LINE('',#155949,#11548) ;
#5995 = LINE('',#155955,#11549) ;
#5996 = LINE('',#155961,#11550) ;
#5997 = LINE('',#155967,#11551) ;
#5998 = LINE('',#155973,#11552) ;
#5999 = LINE('',#155979,#11553) ;
#6000 = LINE('',#155985,#11554) ;
#6001 = LINE('',#155991,#11555) ;
#6002 = LINE('',#155997,#11556) ;
#6003 = LINE('',#156003,#11557) ;
#6004 = LINE('',#156009,#11558) ;
#6005 = LINE('',#156015,#11559) ;
#6006 = LINE('',#156021,#11560) ;
#6007 = LINE('',#156027,#11561) ;
#6008 = LINE('',#156033,#11562) ;
#6009 = LINE('',#156039,#11563) ;
#6010 = LINE('',#156045,#11564) ;
#6011 = LINE('',#156051,#11565) ;
#6012 = LINE('',#156057,#11566) ;
#6013 = LINE('',#156066,#11567) ;
#6014 = LINE('',#156068,#11568) ;
#6015 = LINE('',#156070,#11569) ;
#6016 = LINE('',#156072,#11570) ;
#6017 = LINE('',#156074,#11571) ;
#6018 = LINE('',#156083,#11572) ;
#6019 = LINE('',#156085,#11573) ;
#6020 = LINE('',#156087,#11574) ;
#6021 = LINE('',#156089,#11575) ;
#6022 = LINE('',#156091,#11576) ;
#6023 = LINE('',#156100,#11577) ;
#6024 = LINE('',#156102,#11578) ;
#6025 = LINE('',#156104,#11579) ;
#6026 = LINE('',#156106,#11580) ;
#6027 = LINE('',#156108,#11581) ;
#6028 = LINE('',#156117,#11582) ;
#6029 = LINE('',#156119,#11583) ;
#6030 = LINE('',#156121,#11584) ;
#6031 = LINE('',#156123,#11585) ;
#6032 = LINE('',#156125,#11586) ;
#6033 = LINE('',#156134,#11587) ;
#6034 = LINE('',#156136,#11588) ;
#6035 = LINE('',#156138,#11589) ;
#6036 = LINE('',#156140,#11590) ;
#6037 = LINE('',#156142,#11591) ;
#6038 = LINE('',#156151,#11592) ;
#6039 = LINE('',#156153,#11593) ;
#6040 = LINE('',#156155,#11594) ;
#6041 = LINE('',#156157,#11595) ;
#6042 = LINE('',#156159,#11596) ;
#6043 = LINE('',#156168,#11597) ;
#6044 = LINE('',#156170,#11598) ;
#6045 = LINE('',#156172,#11599) ;
#6046 = LINE('',#156174,#11600) ;
#6047 = LINE('',#156176,#11601) ;
#6048 = LINE('',#156185,#11602) ;
#6049 = LINE('',#156187,#11603) ;
#6050 = LINE('',#156189,#11604) ;
#6051 = LINE('',#156191,#11605) ;
#6052 = LINE('',#156193,#11606) ;
#6053 = LINE('',#156202,#11607) ;
#6054 = LINE('',#156204,#11608) ;
#6055 = LINE('',#156206,#11609) ;
#6056 = LINE('',#156208,#11610) ;
#6057 = LINE('',#156210,#11611) ;
#6058 = LINE('',#156217,#11612) ;
#6059 = LINE('',#156219,#11613) ;
#6060 = LINE('',#156221,#11614) ;
#6061 = LINE('',#156222,#11615) ;
#6062 = LINE('',#156226,#11616) ;
#6063 = LINE('',#156228,#11617) ;
#6064 = LINE('',#156230,#11618) ;
#6065 = LINE('',#156232,#11619) ;
#6066 = LINE('',#156236,#11620) ;
#6067 = LINE('',#156240,#11621) ;
#6068 = LINE('',#156242,#11622) ;
#6069 = LINE('',#156244,#11623) ;
#6070 = LINE('',#156248,#11624) ;
#6071 = LINE('',#156252,#11625) ;
#6072 = LINE('',#156254,#11626) ;
#6073 = LINE('',#156256,#11627) ;
#6074 = LINE('',#156260,#11628) ;
#6075 = LINE('',#156264,#11629) ;
#6076 = LINE('',#156266,#11630) ;
#6077 = LINE('',#156268,#11631) ;
#6078 = LINE('',#156272,#11632) ;
#6079 = LINE('',#156276,#11633) ;
#6080 = LINE('',#156278,#11634) ;
#6081 = LINE('',#156280,#11635) ;
#6082 = LINE('',#156284,#11636) ;
#6083 = LINE('',#156288,#11637) ;
#6084 = LINE('',#156290,#11638) ;
#6085 = LINE('',#156292,#11639) ;
#6086 = LINE('',#156296,#11640) ;
#6087 = LINE('',#156300,#11641) ;
#6088 = LINE('',#156302,#11642) ;
#6089 = LINE('',#156304,#11643) ;
#6090 = LINE('',#156308,#11644) ;
#6091 = LINE('',#156312,#11645) ;
#6092 = LINE('',#156314,#11646) ;
#6093 = LINE('',#156316,#11647) ;
#6094 = LINE('',#156320,#11648) ;
#6095 = LINE('',#156324,#11649) ;
#6096 = LINE('',#156326,#11650) ;
#6097 = LINE('',#156328,#11651) ;
#6098 = LINE('',#156332,#11652) ;
#6099 = LINE('',#156336,#11653) ;
#6100 = LINE('',#156338,#11654) ;
#6101 = LINE('',#156340,#11655) ;
#6102 = LINE('',#156344,#11656) ;
#6103 = LINE('',#156348,#11657) ;
#6104 = LINE('',#156350,#11658) ;
#6105 = LINE('',#156351,#11659) ;
#6106 = LINE('',#156355,#11660) ;
#6107 = LINE('',#156361,#11661) ;
#6108 = LINE('',#156371,#11662) ;
#6109 = LINE('',#156373,#11663) ;
#6110 = LINE('',#156375,#11664) ;
#6111 = LINE('',#156376,#11665) ;
#6112 = LINE('',#156386,#11666) ;
#6113 = LINE('',#156395,#11667) ;
#6114 = LINE('',#156404,#11668) ;
#6115 = LINE('',#156412,#11669) ;
#6116 = LINE('',#156415,#11670) ;
#6117 = LINE('',#156417,#11671) ;
#6118 = LINE('',#156419,#11672) ;
#6119 = LINE('',#156420,#11673) ;
#6120 = LINE('',#156423,#11674) ;
#6121 = LINE('',#156425,#11675) ;
#6122 = LINE('',#156427,#11676) ;
#6123 = LINE('',#156428,#11677) ;
#6124 = LINE('',#156431,#11678) ;
#6125 = LINE('',#156433,#11679) ;
#6126 = LINE('',#156435,#11680) ;
#6127 = LINE('',#156436,#11681) ;
#6128 = LINE('',#156439,#11682) ;
#6129 = LINE('',#156441,#11683) ;
#6130 = LINE('',#156443,#11684) ;
#6131 = LINE('',#156444,#11685) ;
#6132 = LINE('',#156447,#11686) ;
#6133 = LINE('',#156449,#11687) ;
#6134 = LINE('',#156451,#11688) ;
#6135 = LINE('',#156452,#11689) ;
#6136 = LINE('',#156455,#11690) ;
#6137 = LINE('',#156457,#11691) ;
#6138 = LINE('',#156459,#11692) ;
#6139 = LINE('',#156460,#11693) ;
#6140 = LINE('',#156463,#11694) ;
#6141 = LINE('',#156465,#11695) ;
#6142 = LINE('',#156467,#11696) ;
#6143 = LINE('',#156468,#11697) ;
#6144 = LINE('',#156471,#11698) ;
#6145 = LINE('',#156473,#11699) ;
#6146 = LINE('',#156475,#11700) ;
#6147 = LINE('',#156476,#11701) ;
#6148 = LINE('',#156486,#11702) ;
#6149 = LINE('',#156495,#11703) ;
#6150 = LINE('',#156504,#11704) ;
#6151 = LINE('',#156512,#11705) ;
#6152 = LINE('',#156516,#11706) ;
#6153 = LINE('',#156518,#11707) ;
#6154 = LINE('',#156520,#11708) ;
#6155 = LINE('',#156521,#11709) ;
#6156 = LINE('',#156524,#11710) ;
#6157 = LINE('',#156528,#11711) ;
#6158 = LINE('',#156532,#11712) ;
#6159 = LINE('',#156536,#11713) ;
#6160 = LINE('',#156541,#11714) ;
#6161 = LINE('',#156543,#11715) ;
#6162 = LINE('',#156545,#11716) ;
#6163 = LINE('',#156546,#11717) ;
#6164 = LINE('',#156548,#11718) ;
#6165 = LINE('',#156552,#11719) ;
#6166 = LINE('',#156554,#11720) ;
#6167 = LINE('',#156556,#11721) ;
#6168 = LINE('',#156558,#11722) ;
#6169 = LINE('',#156565,#11723) ;
#6170 = LINE('',#156569,#11724) ;
#6171 = LINE('',#156571,#11725) ;
#6172 = LINE('',#156573,#11726) ;
#6173 = LINE('',#156574,#11727) ;
#6174 = LINE('',#156577,#11728) ;
#6175 = LINE('',#156579,#11729) ;
#6176 = LINE('',#156580,#11730) ;
#6177 = LINE('',#156584,#11731) ;
#6178 = LINE('',#156586,#11732) ;
#6179 = LINE('',#156588,#11733) ;
#6180 = LINE('',#156589,#11734) ;
#6181 = LINE('',#156593,#11735) ;
#6182 = LINE('',#156595,#11736) ;
#6183 = LINE('',#156597,#11737) ;
#6184 = LINE('',#156598,#11738) ;
#6185 = LINE('',#156601,#11739) ;
#6186 = LINE('',#156603,#11740) ;
#6187 = LINE('',#156605,#11741) ;
#6188 = LINE('',#156606,#11742) ;
#6189 = LINE('',#156609,#11743) ;
#6190 = LINE('',#156611,#11744) ;
#6191 = LINE('',#156613,#11745) ;
#6192 = LINE('',#156614,#11746) ;
#6193 = LINE('',#156617,#11747) ;
#6194 = LINE('',#156619,#11748) ;
#6195 = LINE('',#156621,#11749) ;
#6196 = LINE('',#156622,#11750) ;
#6197 = LINE('',#156625,#11751) ;
#6198 = LINE('',#156627,#11752) ;
#6199 = LINE('',#156629,#11753) ;
#6200 = LINE('',#156630,#11754) ;
#6201 = LINE('',#156633,#11755) ;
#6202 = LINE('',#156635,#11756) ;
#6203 = LINE('',#156637,#11757) ;
#6204 = LINE('',#156638,#11758) ;
#6205 = LINE('',#156641,#11759) ;
#6206 = LINE('',#156643,#11760) ;
#6207 = LINE('',#156645,#11761) ;
#6208 = LINE('',#156646,#11762) ;
#6209 = LINE('',#156649,#11763) ;
#6210 = LINE('',#156651,#11764) ;
#6211 = LINE('',#156653,#11765) ;
#6212 = LINE('',#156654,#11766) ;
#6213 = LINE('',#156657,#11767) ;
#6214 = LINE('',#156659,#11768) ;
#6215 = LINE('',#156661,#11769) ;
#6216 = LINE('',#156662,#11770) ;
#6217 = LINE('',#156667,#11771) ;
#6218 = LINE('',#156671,#11772) ;
#6219 = LINE('',#156675,#11773) ;
#6220 = LINE('',#156678,#11774) ;
#6221 = LINE('',#156683,#11775) ;
#6222 = LINE('',#156687,#11776) ;
#6223 = LINE('',#156691,#11777) ;
#6224 = LINE('',#156694,#11778) ;
#6225 = LINE('',#156698,#11779) ;
#6226 = LINE('',#156700,#11780) ;
#6227 = LINE('',#156702,#11781) ;
#6228 = LINE('',#156706,#11782) ;
#6229 = LINE('',#156708,#11783) ;
#6230 = LINE('',#156710,#11784) ;
#6231 = LINE('',#156714,#11785) ;
#6232 = LINE('',#156716,#11786) ;
#6233 = LINE('',#156718,#11787) ;
#6234 = LINE('',#156720,#11788) ;
#6235 = LINE('',#156724,#11789) ;
#6236 = LINE('',#156725,#11790) ;
#6237 = LINE('',#156729,#11791) ;
#6238 = LINE('',#156731,#11792) ;
#6239 = LINE('',#156733,#11793) ;
#6240 = LINE('',#156735,#11794) ;
#6241 = LINE('',#156737,#11795) ;
#6242 = LINE('',#156741,#11796) ;
#6243 = LINE('',#156743,#11797) ;
#6244 = LINE('',#156745,#11798) ;
#6245 = LINE('',#156747,#11799) ;
#6246 = LINE('',#156751,#11800) ;
#6247 = LINE('',#156753,#11801) ;
#6248 = LINE('',#156755,#11802) ;
#6249 = LINE('',#156760,#11803) ;
#6250 = LINE('',#156762,#11804) ;
#6251 = LINE('',#156764,#11805) ;
#6252 = LINE('',#156765,#11806) ;
#6253 = LINE('',#156769,#11807) ;
#6254 = LINE('',#156771,#11808) ;
#6255 = LINE('',#156773,#11809) ;
#6256 = LINE('',#156774,#11810) ;
#6257 = LINE('',#156778,#11811) ;
#6258 = LINE('',#156782,#11812) ;
#6259 = LINE('',#156786,#11813) ;
#6260 = LINE('',#156791,#11814) ;
#6261 = LINE('',#156793,#11815) ;
#6262 = LINE('',#156794,#11816) ;
#6263 = LINE('',#156798,#11817) ;
#6264 = LINE('',#156800,#11818) ;
#6265 = LINE('',#156802,#11819) ;
#6266 = LINE('',#156803,#11820) ;
#6267 = LINE('',#156807,#11821) ;
#6268 = LINE('',#156808,#11822) ;
#6269 = LINE('',#156810,#11823) ;
#6270 = LINE('',#156812,#11824) ;
#6271 = LINE('',#156813,#11825) ;
#6272 = LINE('',#156817,#11826) ;
#6273 = LINE('',#156818,#11827) ;
#6274 = LINE('',#156820,#11828) ;
#6275 = LINE('',#156822,#11829) ;
#6276 = LINE('',#156823,#11830) ;
#6277 = LINE('',#156827,#11831) ;
#6278 = LINE('',#156829,#11832) ;
#6279 = LINE('',#156831,#11833) ;
#6280 = LINE('',#156832,#11834) ;
#6281 = LINE('',#156836,#11835) ;
#6282 = LINE('',#156838,#11836) ;
#6283 = LINE('',#156840,#11837) ;
#6284 = LINE('',#156841,#11838) ;
#6285 = LINE('',#156845,#11839) ;
#6286 = LINE('',#156847,#11840) ;
#6287 = LINE('',#156849,#11841) ;
#6288 = LINE('',#156850,#11842) ;
#6289 = LINE('',#156854,#11843) ;
#6290 = LINE('',#156856,#11844) ;
#6291 = LINE('',#156858,#11845) ;
#6292 = LINE('',#156859,#11846) ;
#6293 = LINE('',#156863,#11847) ;
#6294 = LINE('',#156865,#11848) ;
#6295 = LINE('',#156867,#11849) ;
#6296 = LINE('',#156868,#11850) ;
#6297 = LINE('',#156871,#11851) ;
#6298 = LINE('',#156875,#11852) ;
#6299 = LINE('',#156879,#11853) ;
#6300 = LINE('',#156883,#11854) ;
#6301 = LINE('',#156887,#11855) ;
#6302 = LINE('',#156889,#11856) ;
#6303 = LINE('',#156890,#11857) ;
#6304 = LINE('',#156893,#11858) ;
#6305 = LINE('',#156895,#11859) ;
#6306 = LINE('',#156896,#11860) ;
#6307 = LINE('',#156900,#11861) ;
#6308 = LINE('',#156901,#11862) ;
#6309 = LINE('',#156902,#11863) ;
#6310 = LINE('',#156905,#11864) ;
#6311 = LINE('',#156907,#11865) ;
#6312 = LINE('',#156908,#11866) ;
#6313 = LINE('',#156912,#11867) ;
#6314 = LINE('',#156914,#11868) ;
#6315 = LINE('',#156916,#11869) ;
#6316 = LINE('',#156917,#11870) ;
#6317 = LINE('',#156920,#11871) ;
#6318 = LINE('',#156922,#11872) ;
#6319 = LINE('',#156925,#11873) ;
#6320 = LINE('',#156927,#11874) ;
#6321 = LINE('',#156931,#11875) ;
#6322 = LINE('',#156932,#11876) ;
#6323 = LINE('',#156936,#11877) ;
#6324 = LINE('',#156938,#11878) ;
#6325 = LINE('',#156940,#11879) ;
#6326 = LINE('',#156941,#11880) ;
#6327 = LINE('',#156949,#11881) ;
#6328 = LINE('',#156951,#11882) ;
#6329 = LINE('',#156953,#11883) ;
#6330 = LINE('',#156955,#11884) ;
#6331 = LINE('',#156959,#11885) ;
#6332 = LINE('',#156961,#11886) ;
#6333 = LINE('',#156962,#11887) ;
#6334 = LINE('',#156966,#11888) ;
#6335 = LINE('',#156968,#11889) ;
#6336 = LINE('',#156970,#11890) ;
#6337 = LINE('',#156971,#11891) ;
#6338 = LINE('',#156975,#11892) ;
#6339 = LINE('',#156981,#11893) ;
#6340 = LINE('',#156983,#11894) ;
#6341 = LINE('',#156985,#11895) ;
#6342 = LINE('',#156989,#11896) ;
#6343 = LINE('',#156991,#11897) ;
#6344 = LINE('',#156992,#11898) ;
#6345 = LINE('',#156995,#11899) ;
#6346 = LINE('',#156997,#11900) ;
#6347 = LINE('',#156998,#11901) ;
#6348 = LINE('',#157002,#11902) ;
#6349 = LINE('',#157004,#11903) ;
#6350 = LINE('',#157006,#11904) ;
#6351 = LINE('',#157007,#11905) ;
#6352 = LINE('',#157011,#11906) ;
#6353 = LINE('',#157013,#11907) ;
#6354 = LINE('',#157015,#11908) ;
#6355 = LINE('',#157016,#11909) ;
#6356 = LINE('',#157020,#11910) ;
#6357 = LINE('',#157024,#11911) ;
#6358 = LINE('',#157029,#11912) ;
#6359 = LINE('',#157033,#11913) ;
#6360 = LINE('',#157035,#11914) ;
#6361 = LINE('',#157037,#11915) ;
#6362 = LINE('',#157038,#11916) ;
#6363 = LINE('',#157043,#11917) ;
#6364 = LINE('',#157045,#11918) ;
#6365 = LINE('',#157047,#11919) ;
#6366 = LINE('',#157048,#11920) ;
#6367 = LINE('',#157052,#11921) ;
#6368 = LINE('',#157054,#11922) ;
#6369 = LINE('',#157056,#11923) ;
#6370 = LINE('',#157057,#11924) ;
#6371 = LINE('',#157061,#11925) ;
#6372 = LINE('',#157063,#11926) ;
#6373 = LINE('',#157065,#11927) ;
#6374 = LINE('',#157066,#11928) ;
#6375 = LINE('',#157070,#11929) ;
#6376 = LINE('',#157072,#11930) ;
#6377 = LINE('',#157074,#11931) ;
#6378 = LINE('',#157075,#11932) ;
#6379 = LINE('',#157079,#11933) ;
#6380 = LINE('',#157081,#11934) ;
#6381 = LINE('',#157083,#11935) ;
#6382 = LINE('',#157084,#11936) ;
#6383 = LINE('',#157087,#11937) ;
#6384 = LINE('',#157091,#11938) ;
#6385 = LINE('',#157095,#11939) ;
#6386 = LINE('',#157099,#11940) ;
#6387 = LINE('',#157104,#11941) ;
#6388 = LINE('',#157105,#11942) ;
#6389 = LINE('',#157106,#11943) ;
#6390 = LINE('',#157110,#11944) ;
#6391 = LINE('',#157111,#11945) ;
#6392 = LINE('',#157112,#11946) ;
#6393 = LINE('',#157115,#11947) ;
#6394 = LINE('',#157117,#11948) ;
#6395 = LINE('',#157118,#11949) ;
#6396 = LINE('',#157122,#11950) ;
#6397 = LINE('',#157123,#11951) ;
#6398 = LINE('',#157124,#11952) ;
#6399 = LINE('',#157128,#11953) ;
#6400 = LINE('',#157130,#11954) ;
#6401 = LINE('',#157132,#11955) ;
#6402 = LINE('',#157133,#11956) ;
#6403 = LINE('',#157135,#11957) ;
#6404 = LINE('',#157137,#11958) ;
#6405 = LINE('',#157138,#11959) ;
#6406 = LINE('',#157140,#11960) ;
#6407 = LINE('',#157141,#11961) ;
#6408 = LINE('',#157143,#11962) ;
#6409 = LINE('',#157144,#11963) ;
#6410 = LINE('',#157151,#11964) ;
#6411 = LINE('',#157153,#11965) ;
#6412 = LINE('',#157154,#11966) ;
#6413 = LINE('',#157158,#11967) ;
#6414 = LINE('',#157159,#11968) ;
#6415 = LINE('',#157160,#11969) ;
#6416 = LINE('',#157168,#11970) ;
#6417 = LINE('',#157172,#11971) ;
#6418 = LINE('',#157176,#11972) ;
#6419 = LINE('',#157178,#11973) ;
#6420 = LINE('',#157179,#11974) ;
#6421 = LINE('',#157184,#11975) ;
#6422 = LINE('',#157188,#11976) ;
#6423 = LINE('',#157190,#11977) ;
#6424 = LINE('',#157191,#11978) ;
#6425 = LINE('',#157196,#11979) ;
#6426 = LINE('',#157200,#11980) ;
#6427 = LINE('',#157202,#11981) ;
#6428 = LINE('',#157203,#11982) ;
#6429 = LINE('',#157208,#11983) ;
#6430 = LINE('',#157211,#11984) ;
#6431 = LINE('',#157212,#11985) ;
#6432 = LINE('',#157216,#11986) ;
#6433 = LINE('',#157218,#11987) ;
#6434 = LINE('',#157220,#11988) ;
#6435 = LINE('',#157221,#11989) ;
#6436 = LINE('',#157921,#11990) ;
#6437 = LINE('',#157923,#11991) ;
#6438 = LINE('',#157925,#11992) ;
#6439 = LINE('',#157926,#11993) ;
#6440 = LINE('',#157930,#11994) ;
#6441 = LINE('',#157932,#11995) ;
#6442 = LINE('',#157934,#11996) ;
#6443 = LINE('',#157935,#11997) ;
#6444 = LINE('',#157939,#11998) ;
#6445 = LINE('',#157943,#11999) ;
#6446 = LINE('',#157947,#12000) ;
#6447 = LINE('',#157952,#12001) ;
#6448 = LINE('',#157954,#12002) ;
#6449 = LINE('',#157955,#12003) ;
#6450 = LINE('',#157959,#12004) ;
#6451 = LINE('',#157961,#12005) ;
#6452 = LINE('',#157963,#12006) ;
#6453 = LINE('',#157964,#12007) ;
#6454 = LINE('',#157968,#12008) ;
#6455 = LINE('',#157970,#12009) ;
#6456 = LINE('',#157972,#12010) ;
#6457 = LINE('',#157973,#12011) ;
#6458 = LINE('',#157977,#12012) ;
#6459 = LINE('',#157979,#12013) ;
#6460 = LINE('',#157981,#12014) ;
#6461 = LINE('',#157982,#12015) ;
#6462 = LINE('',#157986,#12016) ;
#6463 = LINE('',#157990,#12017) ;
#6464 = LINE('',#157994,#12018) ;
#6465 = LINE('',#157999,#12019) ;
#6466 = LINE('',#158001,#12020) ;
#6467 = LINE('',#158002,#12021) ;
#6468 = LINE('',#158006,#12022) ;
#6469 = LINE('',#158008,#12023) ;
#6470 = LINE('',#158010,#12024) ;
#6471 = LINE('',#158011,#12025) ;
#6472 = LINE('',#158015,#12026) ;
#6473 = LINE('',#158017,#12027) ;
#6474 = LINE('',#158019,#12028) ;
#6475 = LINE('',#158020,#12029) ;
#6476 = LINE('',#158024,#12030) ;
#6477 = LINE('',#158026,#12031) ;
#6478 = LINE('',#158028,#12032) ;
#6479 = LINE('',#158029,#12033) ;
#6480 = LINE('',#158033,#12034) ;
#6481 = LINE('',#158037,#12035) ;
#6482 = LINE('',#158041,#12036) ;
#6483 = LINE('',#158046,#12037) ;
#6484 = LINE('',#158048,#12038) ;
#6485 = LINE('',#158049,#12039) ;
#6486 = LINE('',#158053,#12040) ;
#6487 = LINE('',#158055,#12041) ;
#6488 = LINE('',#158057,#12042) ;
#6489 = LINE('',#158058,#12043) ;
#6490 = LINE('',#158062,#12044) ;
#6491 = LINE('',#158064,#12045) ;
#6492 = LINE('',#158066,#12046) ;
#6493 = LINE('',#158067,#12047) ;
#6494 = LINE('',#158071,#12048) ;
#6495 = LINE('',#158073,#12049) ;
#6496 = LINE('',#158075,#12050) ;
#6497 = LINE('',#158076,#12051) ;
#6498 = LINE('',#158080,#12052) ;
#6499 = LINE('',#158084,#12053) ;
#6500 = LINE('',#158088,#12054) ;
#6501 = LINE('',#158093,#12055) ;
#6502 = LINE('',#158095,#12056) ;
#6503 = LINE('',#158096,#12057) ;
#6504 = LINE('',#158100,#12058) ;
#6505 = LINE('',#158102,#12059) ;
#6506 = LINE('',#158104,#12060) ;
#6507 = LINE('',#158105,#12061) ;
#6508 = LINE('',#158109,#12062) ;
#6509 = LINE('',#158111,#12063) ;
#6510 = LINE('',#158113,#12064) ;
#6511 = LINE('',#158114,#12065) ;
#6512 = LINE('',#158118,#12066) ;
#6513 = LINE('',#158120,#12067) ;
#6514 = LINE('',#158122,#12068) ;
#6515 = LINE('',#158123,#12069) ;
#6516 = LINE('',#158127,#12070) ;
#6517 = LINE('',#158131,#12071) ;
#6518 = LINE('',#158135,#12072) ;
#6519 = LINE('',#158140,#12073) ;
#6520 = LINE('',#158142,#12074) ;
#6521 = LINE('',#158143,#12075) ;
#6522 = LINE('',#158147,#12076) ;
#6523 = LINE('',#158149,#12077) ;
#6524 = LINE('',#158151,#12078) ;
#6525 = LINE('',#158152,#12079) ;
#6526 = LINE('',#158156,#12080) ;
#6527 = LINE('',#158158,#12081) ;
#6528 = LINE('',#158160,#12082) ;
#6529 = LINE('',#158161,#12083) ;
#6530 = LINE('',#158165,#12084) ;
#6531 = LINE('',#158167,#12085) ;
#6532 = LINE('',#158169,#12086) ;
#6533 = LINE('',#158170,#12087) ;
#6534 = LINE('',#158174,#12088) ;
#6535 = LINE('',#158178,#12089) ;
#6536 = LINE('',#158182,#12090) ;
#6537 = LINE('',#158187,#12091) ;
#6538 = LINE('',#158189,#12092) ;
#6539 = LINE('',#158190,#12093) ;
#6540 = LINE('',#158194,#12094) ;
#6541 = LINE('',#158196,#12095) ;
#6542 = LINE('',#158198,#12096) ;
#6543 = LINE('',#158199,#12097) ;
#6544 = LINE('',#158203,#12098) ;
#6545 = LINE('',#158205,#12099) ;
#6546 = LINE('',#158207,#12100) ;
#6547 = LINE('',#158208,#12101) ;
#6548 = LINE('',#158212,#12102) ;
#6549 = LINE('',#158214,#12103) ;
#6550 = LINE('',#158216,#12104) ;
#6551 = LINE('',#158217,#12105) ;
#6552 = LINE('',#158221,#12106) ;
#6553 = LINE('',#158225,#12107) ;
#6554 = LINE('',#158229,#12108) ;
#6555 = LINE('',#158234,#12109) ;
#6556 = LINE('',#158236,#12110) ;
#6557 = LINE('',#158237,#12111) ;
#6558 = LINE('',#158241,#12112) ;
#6559 = LINE('',#158243,#12113) ;
#6560 = LINE('',#158245,#12114) ;
#6561 = LINE('',#158246,#12115) ;
#6562 = LINE('',#158250,#12116) ;
#6563 = LINE('',#158252,#12117) ;
#6564 = LINE('',#158254,#12118) ;
#6565 = LINE('',#158255,#12119) ;
#6566 = LINE('',#158259,#12120) ;
#6567 = LINE('',#158261,#12121) ;
#6568 = LINE('',#158263,#12122) ;
#6569 = LINE('',#158264,#12123) ;
#6570 = LINE('',#158268,#12124) ;
#6571 = LINE('',#158272,#12125) ;
#6572 = LINE('',#158276,#12126) ;
#6573 = LINE('',#158281,#12127) ;
#6574 = LINE('',#158283,#12128) ;
#6575 = LINE('',#158284,#12129) ;
#6576 = LINE('',#158288,#12130) ;
#6577 = LINE('',#158290,#12131) ;
#6578 = LINE('',#158292,#12132) ;
#6579 = LINE('',#158293,#12133) ;
#6580 = LINE('',#158297,#12134) ;
#6581 = LINE('',#158299,#12135) ;
#6582 = LINE('',#158301,#12136) ;
#6583 = LINE('',#158302,#12137) ;
#6584 = LINE('',#158306,#12138) ;
#6585 = LINE('',#158308,#12139) ;
#6586 = LINE('',#158310,#12140) ;
#6587 = LINE('',#158311,#12141) ;
#6588 = LINE('',#158315,#12142) ;
#6589 = LINE('',#158319,#12143) ;
#6590 = LINE('',#158323,#12144) ;
#6591 = LINE('',#158328,#12145) ;
#6592 = LINE('',#158330,#12146) ;
#6593 = LINE('',#158331,#12147) ;
#6594 = LINE('',#158335,#12148) ;
#6595 = LINE('',#158337,#12149) ;
#6596 = LINE('',#158339,#12150) ;
#6597 = LINE('',#158340,#12151) ;
#6598 = LINE('',#158344,#12152) ;
#6599 = LINE('',#158345,#12153) ;
#6600 = LINE('',#158347,#12154) ;
#6601 = LINE('',#158349,#12155) ;
#6602 = LINE('',#158350,#12156) ;
#6603 = LINE('',#158354,#12157) ;
#6604 = LINE('',#158358,#12158) ;
#6605 = LINE('',#158359,#12159) ;
#6606 = LINE('',#158361,#12160) ;
#6607 = LINE('',#158363,#12161) ;
#6608 = LINE('',#158368,#12162) ;
#6609 = LINE('',#158372,#12163) ;
#6610 = LINE('',#158373,#12164) ;
#6611 = LINE('',#158375,#12165) ;
#6612 = LINE('',#158377,#12166) ;
#6613 = LINE('',#158382,#12167) ;
#6614 = LINE('',#158386,#12168) ;
#6615 = LINE('',#158387,#12169) ;
#6616 = LINE('',#158389,#12170) ;
#6617 = LINE('',#158391,#12171) ;
#6618 = LINE('',#158396,#12172) ;
#6619 = LINE('',#158400,#12173) ;
#6620 = LINE('',#158401,#12174) ;
#6621 = LINE('',#158403,#12175) ;
#6622 = LINE('',#158405,#12176) ;
#6623 = LINE('',#158410,#12177) ;
#6624 = LINE('',#158414,#12178) ;
#6625 = LINE('',#158415,#12179) ;
#6626 = LINE('',#158417,#12180) ;
#6627 = LINE('',#158419,#12181) ;
#6628 = LINE('',#158424,#12182) ;
#6629 = LINE('',#158428,#12183) ;
#6630 = LINE('',#158429,#12184) ;
#6631 = LINE('',#158431,#12185) ;
#6632 = LINE('',#158433,#12186) ;
#6633 = LINE('',#158438,#12187) ;
#6634 = LINE('',#158442,#12188) ;
#6635 = LINE('',#158443,#12189) ;
#6636 = LINE('',#158445,#12190) ;
#6637 = LINE('',#158447,#12191) ;
#6638 = LINE('',#158452,#12192) ;
#6639 = LINE('',#158456,#12193) ;
#6640 = LINE('',#158457,#12194) ;
#6641 = LINE('',#158459,#12195) ;
#6642 = LINE('',#158461,#12196) ;
#6643 = LINE('',#158466,#12197) ;
#6644 = LINE('',#158467,#12198) ;
#6645 = LINE('',#158469,#12199) ;
#6646 = LINE('',#158471,#12200) ;
#6647 = LINE('',#158472,#12201) ;
#6648 = LINE('',#158476,#12202) ;
#6649 = LINE('',#158480,#12203) ;
#6650 = LINE('',#158481,#12204) ;
#6651 = LINE('',#158483,#12205) ;
#6652 = LINE('',#158485,#12206) ;
#6653 = LINE('',#158490,#12207) ;
#6654 = LINE('',#158494,#12208) ;
#6655 = LINE('',#158495,#12209) ;
#6656 = LINE('',#158497,#12210) ;
#6657 = LINE('',#158499,#12211) ;
#6658 = LINE('',#158504,#12212) ;
#6659 = LINE('',#158508,#12213) ;
#6660 = LINE('',#158509,#12214) ;
#6661 = LINE('',#158511,#12215) ;
#6662 = LINE('',#158513,#12216) ;
#6663 = LINE('',#158518,#12217) ;
#6664 = LINE('',#158522,#12218) ;
#6665 = LINE('',#158523,#12219) ;
#6666 = LINE('',#158525,#12220) ;
#6667 = LINE('',#158527,#12221) ;
#6668 = LINE('',#158532,#12222) ;
#6669 = LINE('',#158536,#12223) ;
#6670 = LINE('',#158537,#12224) ;
#6671 = LINE('',#158539,#12225) ;
#6672 = LINE('',#158541,#12226) ;
#6673 = LINE('',#158546,#12227) ;
#6674 = LINE('',#158550,#12228) ;
#6675 = LINE('',#158551,#12229) ;
#6676 = LINE('',#158553,#12230) ;
#6677 = LINE('',#158555,#12231) ;
#6678 = LINE('',#158560,#12232) ;
#6679 = LINE('',#158564,#12233) ;
#6680 = LINE('',#158565,#12234) ;
#6681 = LINE('',#158567,#12235) ;
#6682 = LINE('',#158569,#12236) ;
#6683 = LINE('',#158574,#12237) ;
#6684 = LINE('',#158578,#12238) ;
#6685 = LINE('',#158579,#12239) ;
#6686 = LINE('',#158581,#12240) ;
#6687 = LINE('',#158583,#12241) ;
#6688 = LINE('',#158588,#12242) ;
#6689 = LINE('',#158590,#12243) ;
#6690 = LINE('',#158592,#12244) ;
#6691 = LINE('',#158593,#12245) ;
#6692 = LINE('',#158597,#12246) ;
#6693 = LINE('',#158599,#12247) ;
#6694 = LINE('',#158601,#12248) ;
#6695 = LINE('',#158602,#12249) ;
#6696 = LINE('',#158606,#12250) ;
#6697 = LINE('',#158608,#12251) ;
#6698 = LINE('',#158610,#12252) ;
#6699 = LINE('',#158611,#12253) ;
#6700 = LINE('',#158615,#12254) ;
#6701 = LINE('',#158617,#12255) ;
#6702 = LINE('',#158619,#12256) ;
#6703 = LINE('',#158620,#12257) ;
#6704 = LINE('',#158624,#12258) ;
#6705 = LINE('',#158626,#12259) ;
#6706 = LINE('',#158628,#12260) ;
#6707 = LINE('',#158629,#12261) ;
#6708 = LINE('',#158633,#12262) ;
#6709 = LINE('',#158635,#12263) ;
#6710 = LINE('',#158637,#12264) ;
#6711 = LINE('',#158638,#12265) ;
#6712 = LINE('',#158642,#12266) ;
#6713 = LINE('',#158644,#12267) ;
#6714 = LINE('',#158646,#12268) ;
#6715 = LINE('',#158647,#12269) ;
#6716 = LINE('',#158651,#12270) ;
#6717 = LINE('',#158653,#12271) ;
#6718 = LINE('',#158655,#12272) ;
#6719 = LINE('',#158656,#12273) ;
#6720 = LINE('',#158660,#12274) ;
#6721 = LINE('',#158662,#12275) ;
#6722 = LINE('',#158664,#12276) ;
#6723 = LINE('',#158665,#12277) ;
#6724 = LINE('',#158669,#12278) ;
#6725 = LINE('',#158671,#12279) ;
#6726 = LINE('',#158673,#12280) ;
#6727 = LINE('',#158674,#12281) ;
#6728 = LINE('',#158678,#12282) ;
#6729 = LINE('',#158680,#12283) ;
#6730 = LINE('',#158682,#12284) ;
#6731 = LINE('',#158683,#12285) ;
#6732 = LINE('',#158687,#12286) ;
#6733 = LINE('',#158689,#12287) ;
#6734 = LINE('',#158691,#12288) ;
#6735 = LINE('',#158692,#12289) ;
#6736 = LINE('',#158696,#12290) ;
#6737 = LINE('',#158698,#12291) ;
#6738 = LINE('',#158700,#12292) ;
#6739 = LINE('',#158701,#12293) ;
#6740 = LINE('',#158705,#12294) ;
#6741 = LINE('',#158707,#12295) ;
#6742 = LINE('',#158709,#12296) ;
#6743 = LINE('',#158710,#12297) ;
#6744 = LINE('',#158714,#12298) ;
#6745 = LINE('',#158716,#12299) ;
#6746 = LINE('',#158718,#12300) ;
#6747 = LINE('',#158719,#12301) ;
#6748 = LINE('',#158723,#12302) ;
#6749 = LINE('',#158725,#12303) ;
#6750 = LINE('',#158727,#12304) ;
#6751 = LINE('',#158728,#12305) ;
#6752 = LINE('',#158732,#12306) ;
#6753 = LINE('',#158734,#12307) ;
#6754 = LINE('',#158736,#12308) ;
#6755 = LINE('',#158737,#12309) ;
#6756 = LINE('',#158741,#12310) ;
#6757 = LINE('',#158743,#12311) ;
#6758 = LINE('',#158745,#12312) ;
#6759 = LINE('',#158746,#12313) ;
#6760 = LINE('',#158750,#12314) ;
#6761 = LINE('',#158752,#12315) ;
#6762 = LINE('',#158754,#12316) ;
#6763 = LINE('',#158755,#12317) ;
#6764 = LINE('',#158759,#12318) ;
#6765 = LINE('',#158761,#12319) ;
#6766 = LINE('',#158763,#12320) ;
#6767 = LINE('',#158764,#12321) ;
#6768 = LINE('',#158768,#12322) ;
#6769 = LINE('',#158770,#12323) ;
#6770 = LINE('',#158772,#12324) ;
#6771 = LINE('',#158773,#12325) ;
#6772 = LINE('',#158777,#12326) ;
#6773 = LINE('',#158779,#12327) ;
#6774 = LINE('',#158781,#12328) ;
#6775 = LINE('',#158782,#12329) ;
#6776 = LINE('',#158786,#12330) ;
#6777 = LINE('',#158788,#12331) ;
#6778 = LINE('',#158790,#12332) ;
#6779 = LINE('',#158791,#12333) ;
#6780 = LINE('',#158795,#12334) ;
#6781 = LINE('',#158797,#12335) ;
#6782 = LINE('',#158799,#12336) ;
#6783 = LINE('',#158800,#12337) ;
#6784 = LINE('',#158804,#12338) ;
#6785 = LINE('',#158806,#12339) ;
#6786 = LINE('',#158808,#12340) ;
#6787 = LINE('',#158809,#12341) ;
#6788 = LINE('',#158813,#12342) ;
#6789 = LINE('',#158815,#12343) ;
#6790 = LINE('',#158817,#12344) ;
#6791 = LINE('',#158818,#12345) ;
#6792 = LINE('',#158822,#12346) ;
#6793 = LINE('',#158824,#12347) ;
#6794 = LINE('',#158826,#12348) ;
#6795 = LINE('',#158827,#12349) ;
#6796 = LINE('',#158831,#12350) ;
#6797 = LINE('',#158833,#12351) ;
#6798 = LINE('',#158835,#12352) ;
#6799 = LINE('',#158836,#12353) ;
#6800 = LINE('',#158840,#12354) ;
#6801 = LINE('',#158842,#12355) ;
#6802 = LINE('',#158844,#12356) ;
#6803 = LINE('',#158845,#12357) ;
#6804 = LINE('',#158849,#12358) ;
#6805 = LINE('',#158851,#12359) ;
#6806 = LINE('',#158853,#12360) ;
#6807 = LINE('',#158854,#12361) ;
#6808 = LINE('',#158858,#12362) ;
#6809 = LINE('',#158860,#12363) ;
#6810 = LINE('',#158862,#12364) ;
#6811 = LINE('',#158863,#12365) ;
#6812 = LINE('',#158867,#12366) ;
#6813 = LINE('',#158869,#12367) ;
#6814 = LINE('',#158871,#12368) ;
#6815 = LINE('',#158872,#12369) ;
#6816 = LINE('',#158876,#12370) ;
#6817 = LINE('',#158878,#12371) ;
#6818 = LINE('',#158880,#12372) ;
#6819 = LINE('',#158881,#12373) ;
#6820 = LINE('',#158885,#12374) ;
#6821 = LINE('',#158887,#12375) ;
#6822 = LINE('',#158889,#12376) ;
#6823 = LINE('',#158890,#12377) ;
#6824 = LINE('',#158894,#12378) ;
#6825 = LINE('',#158896,#12379) ;
#6826 = LINE('',#158898,#12380) ;
#6827 = LINE('',#158899,#12381) ;
#6828 = LINE('',#158903,#12382) ;
#6829 = LINE('',#158905,#12383) ;
#6830 = LINE('',#158907,#12384) ;
#6831 = LINE('',#158908,#12385) ;
#6832 = LINE('',#158912,#12386) ;
#6833 = LINE('',#158914,#12387) ;
#6834 = LINE('',#158916,#12388) ;
#6835 = LINE('',#158917,#12389) ;
#6836 = LINE('',#158920,#12390) ;
#6837 = LINE('',#158924,#12391) ;
#6838 = LINE('',#158928,#12392) ;
#6839 = LINE('',#158932,#12393) ;
#6840 = LINE('',#158936,#12394) ;
#6841 = LINE('',#158938,#12395) ;
#6842 = LINE('',#158939,#12396) ;
#6843 = LINE('',#158942,#12397) ;
#6844 = LINE('',#158944,#12398) ;
#6845 = LINE('',#158945,#12399) ;
#6846 = LINE('',#158949,#12400) ;
#6847 = LINE('',#158950,#12401) ;
#6848 = LINE('',#158951,#12402) ;
#6849 = LINE('',#158954,#12403) ;
#6850 = LINE('',#158956,#12404) ;
#6851 = LINE('',#158957,#12405) ;
#6852 = LINE('',#158961,#12406) ;
#6853 = LINE('',#158963,#12407) ;
#6854 = LINE('',#158965,#12408) ;
#6855 = LINE('',#158966,#12409) ;
#6856 = LINE('',#158969,#12410) ;
#6857 = LINE('',#158973,#12411) ;
#6858 = LINE('',#158977,#12412) ;
#6859 = LINE('',#158981,#12413) ;
#6860 = LINE('',#158985,#12414) ;
#6861 = LINE('',#158987,#12415) ;
#6862 = LINE('',#158988,#12416) ;
#6863 = LINE('',#158991,#12417) ;
#6864 = LINE('',#158993,#12418) ;
#6865 = LINE('',#158994,#12419) ;
#6866 = LINE('',#158998,#12420) ;
#6867 = LINE('',#158999,#12421) ;
#6868 = LINE('',#159000,#12422) ;
#6869 = LINE('',#159003,#12423) ;
#6870 = LINE('',#159005,#12424) ;
#6871 = LINE('',#159006,#12425) ;
#6872 = LINE('',#159010,#12426) ;
#6873 = LINE('',#159012,#12427) ;
#6874 = LINE('',#159014,#12428) ;
#6875 = LINE('',#159015,#12429) ;
#6876 = LINE('',#159018,#12430) ;
#6877 = LINE('',#159022,#12431) ;
#6878 = LINE('',#159026,#12432) ;
#6879 = LINE('',#159030,#12433) ;
#6880 = LINE('',#159034,#12434) ;
#6881 = LINE('',#159036,#12435) ;
#6882 = LINE('',#159037,#12436) ;
#6883 = LINE('',#159040,#12437) ;
#6884 = LINE('',#159042,#12438) ;
#6885 = LINE('',#159043,#12439) ;
#6886 = LINE('',#159047,#12440) ;
#6887 = LINE('',#159048,#12441) ;
#6888 = LINE('',#159049,#12442) ;
#6889 = LINE('',#159052,#12443) ;
#6890 = LINE('',#159054,#12444) ;
#6891 = LINE('',#159055,#12445) ;
#6892 = LINE('',#159059,#12446) ;
#6893 = LINE('',#159061,#12447) ;
#6894 = LINE('',#159063,#12448) ;
#6895 = LINE('',#159064,#12449) ;
#6896 = LINE('',#159067,#12450) ;
#6897 = LINE('',#159071,#12451) ;
#6898 = LINE('',#159075,#12452) ;
#6899 = LINE('',#159079,#12453) ;
#6900 = LINE('',#159083,#12454) ;
#6901 = LINE('',#159085,#12455) ;
#6902 = LINE('',#159086,#12456) ;
#6903 = LINE('',#159089,#12457) ;
#6904 = LINE('',#159091,#12458) ;
#6905 = LINE('',#159092,#12459) ;
#6906 = LINE('',#159096,#12460) ;
#6907 = LINE('',#159097,#12461) ;
#6908 = LINE('',#159098,#12462) ;
#6909 = LINE('',#159101,#12463) ;
#6910 = LINE('',#159103,#12464) ;
#6911 = LINE('',#159104,#12465) ;
#6912 = LINE('',#159108,#12466) ;
#6913 = LINE('',#159110,#12467) ;
#6914 = LINE('',#159112,#12468) ;
#6915 = LINE('',#159113,#12469) ;
#6916 = LINE('',#159116,#12470) ;
#6917 = LINE('',#159120,#12471) ;
#6918 = LINE('',#159124,#12472) ;
#6919 = LINE('',#159128,#12473) ;
#6920 = LINE('',#159132,#12474) ;
#6921 = LINE('',#159134,#12475) ;
#6922 = LINE('',#159135,#12476) ;
#6923 = LINE('',#159138,#12477) ;
#6924 = LINE('',#159140,#12478) ;
#6925 = LINE('',#159141,#12479) ;
#6926 = LINE('',#159145,#12480) ;
#6927 = LINE('',#159146,#12481) ;
#6928 = LINE('',#159147,#12482) ;
#6929 = LINE('',#159150,#12483) ;
#6930 = LINE('',#159152,#12484) ;
#6931 = LINE('',#159153,#12485) ;
#6932 = LINE('',#159157,#12486) ;
#6933 = LINE('',#159159,#12487) ;
#6934 = LINE('',#159161,#12488) ;
#6935 = LINE('',#159162,#12489) ;
#6936 = LINE('',#159165,#12490) ;
#6937 = LINE('',#159169,#12491) ;
#6938 = LINE('',#159173,#12492) ;
#6939 = LINE('',#159177,#12493) ;
#6940 = LINE('',#159181,#12494) ;
#6941 = LINE('',#159183,#12495) ;
#6942 = LINE('',#159184,#12496) ;
#6943 = LINE('',#159187,#12497) ;
#6944 = LINE('',#159189,#12498) ;
#6945 = LINE('',#159190,#12499) ;
#6946 = LINE('',#159194,#12500) ;
#6947 = LINE('',#159195,#12501) ;
#6948 = LINE('',#159196,#12502) ;
#6949 = LINE('',#159199,#12503) ;
#6950 = LINE('',#159201,#12504) ;
#6951 = LINE('',#159202,#12505) ;
#6952 = LINE('',#159206,#12506) ;
#6953 = LINE('',#159208,#12507) ;
#6954 = LINE('',#159210,#12508) ;
#6955 = LINE('',#159211,#12509) ;
#6956 = LINE('',#159214,#12510) ;
#6957 = LINE('',#159218,#12511) ;
#6958 = LINE('',#159222,#12512) ;
#6959 = LINE('',#159226,#12513) ;
#6960 = LINE('',#159230,#12514) ;
#6961 = LINE('',#159232,#12515) ;
#6962 = LINE('',#159233,#12516) ;
#6963 = LINE('',#159236,#12517) ;
#6964 = LINE('',#159238,#12518) ;
#6965 = LINE('',#159239,#12519) ;
#6966 = LINE('',#159243,#12520) ;
#6967 = LINE('',#159244,#12521) ;
#6968 = LINE('',#159245,#12522) ;
#6969 = LINE('',#159248,#12523) ;
#6970 = LINE('',#159250,#12524) ;
#6971 = LINE('',#159251,#12525) ;
#6972 = LINE('',#159255,#12526) ;
#6973 = LINE('',#159257,#12527) ;
#6974 = LINE('',#159259,#12528) ;
#6975 = LINE('',#159260,#12529) ;
#6976 = LINE('',#159263,#12530) ;
#6977 = LINE('',#159267,#12531) ;
#6978 = LINE('',#159271,#12532) ;
#6979 = LINE('',#159275,#12533) ;
#6980 = LINE('',#159279,#12534) ;
#6981 = LINE('',#159281,#12535) ;
#6982 = LINE('',#159282,#12536) ;
#6983 = LINE('',#159285,#12537) ;
#6984 = LINE('',#159287,#12538) ;
#6985 = LINE('',#159288,#12539) ;
#6986 = LINE('',#159292,#12540) ;
#6987 = LINE('',#159293,#12541) ;
#6988 = LINE('',#159294,#12542) ;
#6989 = LINE('',#159297,#12543) ;
#6990 = LINE('',#159299,#12544) ;
#6991 = LINE('',#159300,#12545) ;
#6992 = LINE('',#159304,#12546) ;
#6993 = LINE('',#159306,#12547) ;
#6994 = LINE('',#159308,#12548) ;
#6995 = LINE('',#159309,#12549) ;
#6996 = LINE('',#159312,#12550) ;
#6997 = LINE('',#159316,#12551) ;
#6998 = LINE('',#159320,#12552) ;
#6999 = LINE('',#159324,#12553) ;
#7000 = LINE('',#159328,#12554) ;
#7001 = LINE('',#159330,#12555) ;
#7002 = LINE('',#159331,#12556) ;
#7003 = LINE('',#159334,#12557) ;
#7004 = LINE('',#159336,#12558) ;
#7005 = LINE('',#159337,#12559) ;
#7006 = LINE('',#159341,#12560) ;
#7007 = LINE('',#159342,#12561) ;
#7008 = LINE('',#159343,#12562) ;
#7009 = LINE('',#159346,#12563) ;
#7010 = LINE('',#159348,#12564) ;
#7011 = LINE('',#159349,#12565) ;
#7012 = LINE('',#159353,#12566) ;
#7013 = LINE('',#159355,#12567) ;
#7014 = LINE('',#159357,#12568) ;
#7015 = LINE('',#159358,#12569) ;
#7016 = LINE('',#159362,#12570) ;
#7017 = LINE('',#159364,#12571) ;
#7018 = LINE('',#159366,#12572) ;
#7019 = LINE('',#159367,#12573) ;
#7020 = LINE('',#159371,#12574) ;
#7021 = LINE('',#159373,#12575) ;
#7022 = LINE('',#159375,#12576) ;
#7023 = LINE('',#159376,#12577) ;
#7024 = LINE('',#159380,#12578) ;
#7025 = LINE('',#159382,#12579) ;
#7026 = LINE('',#159384,#12580) ;
#7027 = LINE('',#159385,#12581) ;
#7028 = LINE('',#159389,#12582) ;
#7029 = LINE('',#159391,#12583) ;
#7030 = LINE('',#159393,#12584) ;
#7031 = LINE('',#159394,#12585) ;
#7032 = LINE('',#159398,#12586) ;
#7033 = LINE('',#159400,#12587) ;
#7034 = LINE('',#159402,#12588) ;
#7035 = LINE('',#159403,#12589) ;
#7036 = LINE('',#159407,#12590) ;
#7037 = LINE('',#159409,#12591) ;
#7038 = LINE('',#159411,#12592) ;
#7039 = LINE('',#159412,#12593) ;
#7040 = LINE('',#159416,#12594) ;
#7041 = LINE('',#159418,#12595) ;
#7042 = LINE('',#159420,#12596) ;
#7043 = LINE('',#159421,#12597) ;
#7044 = LINE('',#159425,#12598) ;
#7045 = LINE('',#159427,#12599) ;
#7046 = LINE('',#159429,#12600) ;
#7047 = LINE('',#159430,#12601) ;
#7048 = LINE('',#159438,#12602) ;
#7049 = LINE('',#159440,#12603) ;
#7050 = LINE('',#159442,#12604) ;
#7051 = LINE('',#159444,#12605) ;
#7052 = LINE('',#159448,#12606) ;
#7053 = LINE('',#159450,#12607) ;
#7054 = LINE('',#159451,#12608) ;
#7055 = LINE('',#159455,#12609) ;
#7056 = LINE('',#159457,#12610) ;
#7057 = LINE('',#159459,#12611) ;
#7058 = LINE('',#159460,#12612) ;
#7059 = LINE('',#159464,#12613) ;
#7060 = LINE('',#159470,#12614) ;
#7061 = LINE('',#159472,#12615) ;
#7062 = LINE('',#159474,#12616) ;
#7063 = LINE('',#159478,#12617) ;
#7064 = LINE('',#159480,#12618) ;
#7065 = LINE('',#159481,#12619) ;
#7066 = LINE('',#159485,#12620) ;
#7067 = LINE('',#159487,#12621) ;
#7068 = LINE('',#159489,#12622) ;
#7069 = LINE('',#159490,#12623) ;
#7070 = LINE('',#159498,#12624) ;
#7071 = LINE('',#159500,#12625) ;
#7072 = LINE('',#159502,#12626) ;
#7073 = LINE('',#159504,#12627) ;
#7074 = LINE('',#159508,#12628) ;
#7075 = LINE('',#159510,#12629) ;
#7076 = LINE('',#159511,#12630) ;
#7077 = LINE('',#159515,#12631) ;
#7078 = LINE('',#159517,#12632) ;
#7079 = LINE('',#159519,#12633) ;
#7080 = LINE('',#159520,#12634) ;
#7081 = LINE('',#159524,#12635) ;
#7082 = LINE('',#159530,#12636) ;
#7083 = LINE('',#159532,#12637) ;
#7084 = LINE('',#159534,#12638) ;
#7085 = LINE('',#159538,#12639) ;
#7086 = LINE('',#159540,#12640) ;
#7087 = LINE('',#159541,#12641) ;
#7088 = LINE('',#159545,#12642) ;
#7089 = LINE('',#159547,#12643) ;
#7090 = LINE('',#159549,#12644) ;
#7091 = LINE('',#159550,#12645) ;
#7092 = LINE('',#159558,#12646) ;
#7093 = LINE('',#159560,#12647) ;
#7094 = LINE('',#159562,#12648) ;
#7095 = LINE('',#159564,#12649) ;
#7096 = LINE('',#159568,#12650) ;
#7097 = LINE('',#159570,#12651) ;
#7098 = LINE('',#159571,#12652) ;
#7099 = LINE('',#159575,#12653) ;
#7100 = LINE('',#159577,#12654) ;
#7101 = LINE('',#159579,#12655) ;
#7102 = LINE('',#159580,#12656) ;
#7103 = LINE('',#159584,#12657) ;
#7104 = LINE('',#159590,#12658) ;
#7105 = LINE('',#159592,#12659) ;
#7106 = LINE('',#159594,#12660) ;
#7107 = LINE('',#159598,#12661) ;
#7108 = LINE('',#159600,#12662) ;
#7109 = LINE('',#159601,#12663) ;
#7110 = LINE('',#159605,#12664) ;
#7111 = LINE('',#159607,#12665) ;
#7112 = LINE('',#159609,#12666) ;
#7113 = LINE('',#159610,#12667) ;
#7114 = LINE('',#159618,#12668) ;
#7115 = LINE('',#159620,#12669) ;
#7116 = LINE('',#159622,#12670) ;
#7117 = LINE('',#159624,#12671) ;
#7118 = LINE('',#159628,#12672) ;
#7119 = LINE('',#159630,#12673) ;
#7120 = LINE('',#159631,#12674) ;
#7121 = LINE('',#159635,#12675) ;
#7122 = LINE('',#159637,#12676) ;
#7123 = LINE('',#159639,#12677) ;
#7124 = LINE('',#159640,#12678) ;
#7125 = LINE('',#159644,#12679) ;
#7126 = LINE('',#159650,#12680) ;
#7127 = LINE('',#159652,#12681) ;
#7128 = LINE('',#159654,#12682) ;
#7129 = LINE('',#159658,#12683) ;
#7130 = LINE('',#159660,#12684) ;
#7131 = LINE('',#159661,#12685) ;
#7132 = LINE('',#159665,#12686) ;
#7133 = LINE('',#159667,#12687) ;
#7134 = LINE('',#159669,#12688) ;
#7135 = LINE('',#159670,#12689) ;
#7136 = LINE('',#159678,#12690) ;
#7137 = LINE('',#159680,#12691) ;
#7138 = LINE('',#159682,#12692) ;
#7139 = LINE('',#159684,#12693) ;
#7140 = LINE('',#159688,#12694) ;
#7141 = LINE('',#159690,#12695) ;
#7142 = LINE('',#159691,#12696) ;
#7143 = LINE('',#159695,#12697) ;
#7144 = LINE('',#159697,#12698) ;
#7145 = LINE('',#159699,#12699) ;
#7146 = LINE('',#159700,#12700) ;
#7147 = LINE('',#159704,#12701) ;
#7148 = LINE('',#159710,#12702) ;
#7149 = LINE('',#159712,#12703) ;
#7150 = LINE('',#159714,#12704) ;
#7151 = LINE('',#159718,#12705) ;
#7152 = LINE('',#159720,#12706) ;
#7153 = LINE('',#159721,#12707) ;
#7154 = LINE('',#159725,#12708) ;
#7155 = LINE('',#159727,#12709) ;
#7156 = LINE('',#159729,#12710) ;
#7157 = LINE('',#159730,#12711) ;
#7158 = LINE('',#159738,#12712) ;
#7159 = LINE('',#159740,#12713) ;
#7160 = LINE('',#159742,#12714) ;
#7161 = LINE('',#159744,#12715) ;
#7162 = LINE('',#159748,#12716) ;
#7163 = LINE('',#159750,#12717) ;
#7164 = LINE('',#159751,#12718) ;
#7165 = LINE('',#159755,#12719) ;
#7166 = LINE('',#159757,#12720) ;
#7167 = LINE('',#159759,#12721) ;
#7168 = LINE('',#159760,#12722) ;
#7169 = LINE('',#159764,#12723) ;
#7170 = LINE('',#159770,#12724) ;
#7171 = LINE('',#159772,#12725) ;
#7172 = LINE('',#159774,#12726) ;
#7173 = LINE('',#159778,#12727) ;
#7174 = LINE('',#159780,#12728) ;
#7175 = LINE('',#159781,#12729) ;
#7176 = LINE('',#159785,#12730) ;
#7177 = LINE('',#159787,#12731) ;
#7178 = LINE('',#159789,#12732) ;
#7179 = LINE('',#159790,#12733) ;
#7180 = LINE('',#159798,#12734) ;
#7181 = LINE('',#159800,#12735) ;
#7182 = LINE('',#159802,#12736) ;
#7183 = LINE('',#159804,#12737) ;
#7184 = LINE('',#159808,#12738) ;
#7185 = LINE('',#159810,#12739) ;
#7186 = LINE('',#159811,#12740) ;
#7187 = LINE('',#159815,#12741) ;
#7188 = LINE('',#159817,#12742) ;
#7189 = LINE('',#159819,#12743) ;
#7190 = LINE('',#159820,#12744) ;
#7191 = LINE('',#159824,#12745) ;
#7192 = LINE('',#159830,#12746) ;
#7193 = LINE('',#159832,#12747) ;
#7194 = LINE('',#159834,#12748) ;
#7195 = LINE('',#159838,#12749) ;
#7196 = LINE('',#159840,#12750) ;
#7197 = LINE('',#159841,#12751) ;
#7198 = LINE('',#159845,#12752) ;
#7199 = LINE('',#159847,#12753) ;
#7200 = LINE('',#159849,#12754) ;
#7201 = LINE('',#159850,#12755) ;
#7202 = LINE('',#159858,#12756) ;
#7203 = LINE('',#159860,#12757) ;
#7204 = LINE('',#159862,#12758) ;
#7205 = LINE('',#159864,#12759) ;
#7206 = LINE('',#159868,#12760) ;
#7207 = LINE('',#159870,#12761) ;
#7208 = LINE('',#159871,#12762) ;
#7209 = LINE('',#159875,#12763) ;
#7210 = LINE('',#159877,#12764) ;
#7211 = LINE('',#159879,#12765) ;
#7212 = LINE('',#159880,#12766) ;
#7213 = LINE('',#159884,#12767) ;
#7214 = LINE('',#159890,#12768) ;
#7215 = LINE('',#159892,#12769) ;
#7216 = LINE('',#159894,#12770) ;
#7217 = LINE('',#159898,#12771) ;
#7218 = LINE('',#159900,#12772) ;
#7219 = LINE('',#159901,#12773) ;
#7220 = LINE('',#159905,#12774) ;
#7221 = LINE('',#159907,#12775) ;
#7222 = LINE('',#159909,#12776) ;
#7223 = LINE('',#159910,#12777) ;
#7224 = LINE('',#159918,#12778) ;
#7225 = LINE('',#159920,#12779) ;
#7226 = LINE('',#159922,#12780) ;
#7227 = LINE('',#159924,#12781) ;
#7228 = LINE('',#159928,#12782) ;
#7229 = LINE('',#159930,#12783) ;
#7230 = LINE('',#159931,#12784) ;
#7231 = LINE('',#159935,#12785) ;
#7232 = LINE('',#159937,#12786) ;
#7233 = LINE('',#159939,#12787) ;
#7234 = LINE('',#159940,#12788) ;
#7235 = LINE('',#159944,#12789) ;
#7236 = LINE('',#159950,#12790) ;
#7237 = LINE('',#159952,#12791) ;
#7238 = LINE('',#159954,#12792) ;
#7239 = LINE('',#159958,#12793) ;
#7240 = LINE('',#159960,#12794) ;
#7241 = LINE('',#159961,#12795) ;
#7242 = LINE('',#159965,#12796) ;
#7243 = LINE('',#159967,#12797) ;
#7244 = LINE('',#159969,#12798) ;
#7245 = LINE('',#159970,#12799) ;
#7246 = LINE('',#159974,#12800) ;
#7247 = LINE('',#159976,#12801) ;
#7248 = LINE('',#159978,#12802) ;
#7249 = LINE('',#159979,#12803) ;
#7250 = LINE('',#159983,#12804) ;
#7251 = LINE('',#159985,#12805) ;
#7252 = LINE('',#159987,#12806) ;
#7253 = LINE('',#159988,#12807) ;
#7254 = LINE('',#159992,#12808) ;
#7255 = LINE('',#159996,#12809) ;
#7256 = LINE('',#160001,#12810) ;
#7257 = LINE('',#160005,#12811) ;
#7258 = LINE('',#160007,#12812) ;
#7259 = LINE('',#160009,#12813) ;
#7260 = LINE('',#160010,#12814) ;
#7261 = LINE('',#160014,#12815) ;
#7262 = LINE('',#160016,#12816) ;
#7263 = LINE('',#160018,#12817) ;
#7264 = LINE('',#160019,#12818) ;
#7265 = LINE('',#160023,#12819) ;
#7266 = LINE('',#160025,#12820) ;
#7267 = LINE('',#160027,#12821) ;
#7268 = LINE('',#160028,#12822) ;
#7269 = LINE('',#160032,#12823) ;
#7270 = LINE('',#160036,#12824) ;
#7271 = LINE('',#160041,#12825) ;
#7272 = LINE('',#160045,#12826) ;
#7273 = LINE('',#160047,#12827) ;
#7274 = LINE('',#160049,#12828) ;
#7275 = LINE('',#160050,#12829) ;
#7276 = LINE('',#160054,#12830) ;
#7277 = LINE('',#160056,#12831) ;
#7278 = LINE('',#160058,#12832) ;
#7279 = LINE('',#160059,#12833) ;
#7280 = LINE('',#160063,#12834) ;
#7281 = LINE('',#160065,#12835) ;
#7282 = LINE('',#160067,#12836) ;
#7283 = LINE('',#160068,#12837) ;
#7284 = LINE('',#160072,#12838) ;
#7285 = LINE('',#160076,#12839) ;
#7286 = LINE('',#160081,#12840) ;
#7287 = LINE('',#160085,#12841) ;
#7288 = LINE('',#160087,#12842) ;
#7289 = LINE('',#160089,#12843) ;
#7290 = LINE('',#160090,#12844) ;
#7291 = LINE('',#160094,#12845) ;
#7292 = LINE('',#160096,#12846) ;
#7293 = LINE('',#160098,#12847) ;
#7294 = LINE('',#160099,#12848) ;
#7295 = LINE('',#160103,#12849) ;
#7296 = LINE('',#160105,#12850) ;
#7297 = LINE('',#160107,#12851) ;
#7298 = LINE('',#160108,#12852) ;
#7299 = LINE('',#160112,#12853) ;
#7300 = LINE('',#160116,#12854) ;
#7301 = LINE('',#160121,#12855) ;
#7302 = LINE('',#160125,#12856) ;
#7303 = LINE('',#160127,#12857) ;
#7304 = LINE('',#160129,#12858) ;
#7305 = LINE('',#160130,#12859) ;
#7306 = LINE('',#160134,#12860) ;
#7307 = LINE('',#160136,#12861) ;
#7308 = LINE('',#160138,#12862) ;
#7309 = LINE('',#160139,#12863) ;
#7310 = LINE('',#160143,#12864) ;
#7311 = LINE('',#160145,#12865) ;
#7312 = LINE('',#160147,#12866) ;
#7313 = LINE('',#160148,#12867) ;
#7314 = LINE('',#160152,#12868) ;
#7315 = LINE('',#160156,#12869) ;
#7316 = LINE('',#160161,#12870) ;
#7317 = LINE('',#160165,#12871) ;
#7318 = LINE('',#160167,#12872) ;
#7319 = LINE('',#160169,#12873) ;
#7320 = LINE('',#160170,#12874) ;
#7321 = LINE('',#160174,#12875) ;
#7322 = LINE('',#160176,#12876) ;
#7323 = LINE('',#160178,#12877) ;
#7324 = LINE('',#160179,#12878) ;
#7325 = LINE('',#160183,#12879) ;
#7326 = LINE('',#160185,#12880) ;
#7327 = LINE('',#160187,#12881) ;
#7328 = LINE('',#160188,#12882) ;
#7329 = LINE('',#160192,#12883) ;
#7330 = LINE('',#160196,#12884) ;
#7331 = LINE('',#160201,#12885) ;
#7332 = LINE('',#160205,#12886) ;
#7333 = LINE('',#160207,#12887) ;
#7334 = LINE('',#160209,#12888) ;
#7335 = LINE('',#160210,#12889) ;
#7336 = LINE('',#160214,#12890) ;
#7337 = LINE('',#160216,#12891) ;
#7338 = LINE('',#160218,#12892) ;
#7339 = LINE('',#160219,#12893) ;
#7340 = LINE('',#160223,#12894) ;
#7341 = LINE('',#160225,#12895) ;
#7342 = LINE('',#160227,#12896) ;
#7343 = LINE('',#160228,#12897) ;
#7344 = LINE('',#160232,#12898) ;
#7345 = LINE('',#160236,#12899) ;
#7346 = LINE('',#160241,#12900) ;
#7347 = LINE('',#160245,#12901) ;
#7348 = LINE('',#160247,#12902) ;
#7349 = LINE('',#160249,#12903) ;
#7350 = LINE('',#160250,#12904) ;
#7351 = LINE('',#160254,#12905) ;
#7352 = LINE('',#160256,#12906) ;
#7353 = LINE('',#160258,#12907) ;
#7354 = LINE('',#160259,#12908) ;
#7355 = LINE('',#160263,#12909) ;
#7356 = LINE('',#160265,#12910) ;
#7357 = LINE('',#160267,#12911) ;
#7358 = LINE('',#160268,#12912) ;
#7359 = LINE('',#160272,#12913) ;
#7360 = LINE('',#160276,#12914) ;
#7361 = LINE('',#160281,#12915) ;
#7362 = LINE('',#160285,#12916) ;
#7363 = LINE('',#160287,#12917) ;
#7364 = LINE('',#160289,#12918) ;
#7365 = LINE('',#160290,#12919) ;
#7366 = LINE('',#160294,#12920) ;
#7367 = LINE('',#160296,#12921) ;
#7368 = LINE('',#160298,#12922) ;
#7369 = LINE('',#160299,#12923) ;
#7370 = LINE('',#160303,#12924) ;
#7371 = LINE('',#160305,#12925) ;
#7372 = LINE('',#160307,#12926) ;
#7373 = LINE('',#160308,#12927) ;
#7374 = LINE('',#160312,#12928) ;
#7375 = LINE('',#160316,#12929) ;
#7376 = LINE('',#160321,#12930) ;
#7377 = LINE('',#160325,#12931) ;
#7378 = LINE('',#160327,#12932) ;
#7379 = LINE('',#160329,#12933) ;
#7380 = LINE('',#160330,#12934) ;
#7381 = LINE('',#160343,#12935) ;
#7382 = LINE('',#160345,#12936) ;
#7383 = LINE('',#160347,#12937) ;
#7384 = LINE('',#160348,#12938) ;
#7385 = LINE('',#160352,#12939) ;
#7386 = LINE('',#160354,#12940) ;
#7387 = LINE('',#160356,#12941) ;
#7388 = LINE('',#160357,#12942) ;
#7389 = LINE('',#160361,#12943) ;
#7390 = LINE('',#160363,#12944) ;
#7391 = LINE('',#160365,#12945) ;
#7392 = LINE('',#160366,#12946) ;
#7393 = LINE('',#160370,#12947) ;
#7394 = LINE('',#160372,#12948) ;
#7395 = LINE('',#160374,#12949) ;
#7396 = LINE('',#160375,#12950) ;
#7397 = LINE('',#160379,#12951) ;
#7398 = LINE('',#160381,#12952) ;
#7399 = LINE('',#160383,#12953) ;
#7400 = LINE('',#160384,#12954) ;
#7401 = LINE('',#160388,#12955) ;
#7402 = LINE('',#160390,#12956) ;
#7403 = LINE('',#160392,#12957) ;
#7404 = LINE('',#160393,#12958) ;
#7405 = LINE('',#160397,#12959) ;
#7406 = LINE('',#160399,#12960) ;
#7407 = LINE('',#160401,#12961) ;
#7408 = LINE('',#160402,#12962) ;
#7409 = LINE('',#160406,#12963) ;
#7410 = LINE('',#160408,#12964) ;
#7411 = LINE('',#160410,#12965) ;
#7412 = LINE('',#160411,#12966) ;
#7413 = LINE('',#160415,#12967) ;
#7414 = LINE('',#160417,#12968) ;
#7415 = LINE('',#160419,#12969) ;
#7416 = LINE('',#160420,#12970) ;
#7417 = LINE('',#160424,#12971) ;
#7418 = LINE('',#160426,#12972) ;
#7419 = LINE('',#160428,#12973) ;
#7420 = LINE('',#160429,#12974) ;
#7421 = LINE('',#160433,#12975) ;
#7422 = LINE('',#160435,#12976) ;
#7423 = LINE('',#160437,#12977) ;
#7424 = LINE('',#160438,#12978) ;
#7425 = LINE('',#160442,#12979) ;
#7426 = LINE('',#160444,#12980) ;
#7427 = LINE('',#160446,#12981) ;
#7428 = LINE('',#160447,#12982) ;
#7429 = LINE('',#160451,#12983) ;
#7430 = LINE('',#160453,#12984) ;
#7431 = LINE('',#160455,#12985) ;
#7432 = LINE('',#160456,#12986) ;
#7433 = LINE('',#160460,#12987) ;
#7434 = LINE('',#160462,#12988) ;
#7435 = LINE('',#160464,#12989) ;
#7436 = LINE('',#160465,#12990) ;
#7437 = LINE('',#160469,#12991) ;
#7438 = LINE('',#160471,#12992) ;
#7439 = LINE('',#160473,#12993) ;
#7440 = LINE('',#160474,#12994) ;
#7441 = LINE('',#160478,#12995) ;
#7442 = LINE('',#160480,#12996) ;
#7443 = LINE('',#160482,#12997) ;
#7444 = LINE('',#160483,#12998) ;
#7445 = LINE('',#160487,#12999) ;
#7446 = LINE('',#160489,#13000) ;
#7447 = LINE('',#160491,#13001) ;
#7448 = LINE('',#160492,#13002) ;
#7449 = LINE('',#160496,#13003) ;
#7450 = LINE('',#160498,#13004) ;
#7451 = LINE('',#160500,#13005) ;
#7452 = LINE('',#160501,#13006) ;
#7453 = LINE('',#160505,#13007) ;
#7454 = LINE('',#160507,#13008) ;
#7455 = LINE('',#160509,#13009) ;
#7456 = LINE('',#160510,#13010) ;
#7457 = LINE('',#160514,#13011) ;
#7458 = LINE('',#160516,#13012) ;
#7459 = LINE('',#160518,#13013) ;
#7460 = LINE('',#160519,#13014) ;
#7461 = LINE('',#160523,#13015) ;
#7462 = LINE('',#160525,#13016) ;
#7463 = LINE('',#160527,#13017) ;
#7464 = LINE('',#160528,#13018) ;
#7465 = LINE('',#160532,#13019) ;
#7466 = LINE('',#160534,#13020) ;
#7467 = LINE('',#160536,#13021) ;
#7468 = LINE('',#160537,#13022) ;
#7469 = LINE('',#160541,#13023) ;
#7470 = LINE('',#160543,#13024) ;
#7471 = LINE('',#160545,#13025) ;
#7472 = LINE('',#160546,#13026) ;
#7473 = LINE('',#160550,#13027) ;
#7474 = LINE('',#160552,#13028) ;
#7475 = LINE('',#160554,#13029) ;
#7476 = LINE('',#160555,#13030) ;
#7477 = LINE('',#160559,#13031) ;
#7478 = LINE('',#160561,#13032) ;
#7479 = LINE('',#160563,#13033) ;
#7480 = LINE('',#160564,#13034) ;
#7481 = LINE('',#160568,#13035) ;
#7482 = LINE('',#160570,#13036) ;
#7483 = LINE('',#160572,#13037) ;
#7484 = LINE('',#160573,#13038) ;
#7485 = LINE('',#160577,#13039) ;
#7486 = LINE('',#160579,#13040) ;
#7487 = LINE('',#160581,#13041) ;
#7488 = LINE('',#160582,#13042) ;
#7489 = LINE('',#160586,#13043) ;
#7490 = LINE('',#160588,#13044) ;
#7491 = LINE('',#160590,#13045) ;
#7492 = LINE('',#160591,#13046) ;
#7493 = LINE('',#160595,#13047) ;
#7494 = LINE('',#160597,#13048) ;
#7495 = LINE('',#160599,#13049) ;
#7496 = LINE('',#160600,#13050) ;
#7497 = LINE('',#160604,#13051) ;
#7498 = LINE('',#160606,#13052) ;
#7499 = LINE('',#160608,#13053) ;
#7500 = LINE('',#160609,#13054) ;
#7501 = LINE('',#160613,#13055) ;
#7502 = LINE('',#160615,#13056) ;
#7503 = LINE('',#160617,#13057) ;
#7504 = LINE('',#160618,#13058) ;
#7505 = LINE('',#160622,#13059) ;
#7506 = LINE('',#160624,#13060) ;
#7507 = LINE('',#160626,#13061) ;
#7508 = LINE('',#160627,#13062) ;
#7509 = LINE('',#160631,#13063) ;
#7510 = LINE('',#160633,#13064) ;
#7511 = LINE('',#160635,#13065) ;
#7512 = LINE('',#160636,#13066) ;
#7513 = LINE('',#160640,#13067) ;
#7514 = LINE('',#160642,#13068) ;
#7515 = LINE('',#160644,#13069) ;
#7516 = LINE('',#160645,#13070) ;
#7517 = LINE('',#160649,#13071) ;
#7518 = LINE('',#160651,#13072) ;
#7519 = LINE('',#160653,#13073) ;
#7520 = LINE('',#160654,#13074) ;
#7521 = LINE('',#160658,#13075) ;
#7522 = LINE('',#160660,#13076) ;
#7523 = LINE('',#160662,#13077) ;
#7524 = LINE('',#160663,#13078) ;
#7525 = LINE('',#160667,#13079) ;
#7526 = LINE('',#160669,#13080) ;
#7527 = LINE('',#160671,#13081) ;
#7528 = LINE('',#160672,#13082) ;
#7529 = LINE('',#160675,#13083) ;
#7530 = LINE('',#160679,#13084) ;
#7531 = LINE('',#160683,#13085) ;
#7532 = LINE('',#160687,#13086) ;
#7533 = LINE('',#160692,#13087) ;
#7534 = LINE('',#160693,#13088) ;
#7535 = LINE('',#160694,#13089) ;
#7536 = LINE('',#160698,#13090) ;
#7537 = LINE('',#160699,#13091) ;
#7538 = LINE('',#160700,#13092) ;
#7539 = LINE('',#160703,#13093) ;
#7540 = LINE('',#160705,#13094) ;
#7541 = LINE('',#160706,#13095) ;
#7542 = LINE('',#160710,#13096) ;
#7543 = LINE('',#160711,#13097) ;
#7544 = LINE('',#160712,#13098) ;
#7545 = LINE('',#160716,#13099) ;
#7546 = LINE('',#160718,#13100) ;
#7547 = LINE('',#160720,#13101) ;
#7548 = LINE('',#160721,#13102) ;
#7549 = LINE('',#160724,#13103) ;
#7550 = LINE('',#160728,#13104) ;
#7551 = LINE('',#160732,#13105) ;
#7552 = LINE('',#160736,#13106) ;
#7553 = LINE('',#160741,#13107) ;
#7554 = LINE('',#160742,#13108) ;
#7555 = LINE('',#160743,#13109) ;
#7556 = LINE('',#160747,#13110) ;
#7557 = LINE('',#160748,#13111) ;
#7558 = LINE('',#160749,#13112) ;
#7559 = LINE('',#160752,#13113) ;
#7560 = LINE('',#160754,#13114) ;
#7561 = LINE('',#160755,#13115) ;
#7562 = LINE('',#160759,#13116) ;
#7563 = LINE('',#160760,#13117) ;
#7564 = LINE('',#160761,#13118) ;
#7565 = LINE('',#160765,#13119) ;
#7566 = LINE('',#160767,#13120) ;
#7567 = LINE('',#160769,#13121) ;
#7568 = LINE('',#160770,#13122) ;
#7569 = LINE('',#160773,#13123) ;
#7570 = LINE('',#160777,#13124) ;
#7571 = LINE('',#160781,#13125) ;
#7572 = LINE('',#160785,#13126) ;
#7573 = LINE('',#160790,#13127) ;
#7574 = LINE('',#160791,#13128) ;
#7575 = LINE('',#160792,#13129) ;
#7576 = LINE('',#160796,#13130) ;
#7577 = LINE('',#160797,#13131) ;
#7578 = LINE('',#160798,#13132) ;
#7579 = LINE('',#160801,#13133) ;
#7580 = LINE('',#160803,#13134) ;
#7581 = LINE('',#160804,#13135) ;
#7582 = LINE('',#160808,#13136) ;
#7583 = LINE('',#160809,#13137) ;
#7584 = LINE('',#160810,#13138) ;
#7585 = LINE('',#160814,#13139) ;
#7586 = LINE('',#160816,#13140) ;
#7587 = LINE('',#160818,#13141) ;
#7588 = LINE('',#160819,#13142) ;
#7589 = LINE('',#160822,#13143) ;
#7590 = LINE('',#160826,#13144) ;
#7591 = LINE('',#160830,#13145) ;
#7592 = LINE('',#160834,#13146) ;
#7593 = LINE('',#160839,#13147) ;
#7594 = LINE('',#160840,#13148) ;
#7595 = LINE('',#160841,#13149) ;
#7596 = LINE('',#160845,#13150) ;
#7597 = LINE('',#160846,#13151) ;
#7598 = LINE('',#160847,#13152) ;
#7599 = LINE('',#160850,#13153) ;
#7600 = LINE('',#160852,#13154) ;
#7601 = LINE('',#160853,#13155) ;
#7602 = LINE('',#160857,#13156) ;
#7603 = LINE('',#160858,#13157) ;
#7604 = LINE('',#160859,#13158) ;
#7605 = LINE('',#160863,#13159) ;
#7606 = LINE('',#160865,#13160) ;
#7607 = LINE('',#160867,#13161) ;
#7608 = LINE('',#160868,#13162) ;
#7609 = LINE('',#160871,#13163) ;
#7610 = LINE('',#160875,#13164) ;
#7611 = LINE('',#160879,#13165) ;
#7612 = LINE('',#160883,#13166) ;
#7613 = LINE('',#160888,#13167) ;
#7614 = LINE('',#160889,#13168) ;
#7615 = LINE('',#160890,#13169) ;
#7616 = LINE('',#160894,#13170) ;
#7617 = LINE('',#160895,#13171) ;
#7618 = LINE('',#160896,#13172) ;
#7619 = LINE('',#160899,#13173) ;
#7620 = LINE('',#160901,#13174) ;
#7621 = LINE('',#160902,#13175) ;
#7622 = LINE('',#160906,#13176) ;
#7623 = LINE('',#160907,#13177) ;
#7624 = LINE('',#160908,#13178) ;
#7625 = LINE('',#160912,#13179) ;
#7626 = LINE('',#160914,#13180) ;
#7627 = LINE('',#160916,#13181) ;
#7628 = LINE('',#160917,#13182) ;
#7629 = LINE('',#160920,#13183) ;
#7630 = LINE('',#160924,#13184) ;
#7631 = LINE('',#160928,#13185) ;
#7632 = LINE('',#160932,#13186) ;
#7633 = LINE('',#160937,#13187) ;
#7634 = LINE('',#160938,#13188) ;
#7635 = LINE('',#160939,#13189) ;
#7636 = LINE('',#160943,#13190) ;
#7637 = LINE('',#160944,#13191) ;
#7638 = LINE('',#160945,#13192) ;
#7639 = LINE('',#160948,#13193) ;
#7640 = LINE('',#160950,#13194) ;
#7641 = LINE('',#160951,#13195) ;
#7642 = LINE('',#160955,#13196) ;
#7643 = LINE('',#160956,#13197) ;
#7644 = LINE('',#160957,#13198) ;
#7645 = LINE('',#160961,#13199) ;
#7646 = LINE('',#160963,#13200) ;
#7647 = LINE('',#160965,#13201) ;
#7648 = LINE('',#160966,#13202) ;
#7649 = LINE('',#160969,#13203) ;
#7650 = LINE('',#160973,#13204) ;
#7651 = LINE('',#160977,#13205) ;
#7652 = LINE('',#160981,#13206) ;
#7653 = LINE('',#160986,#13207) ;
#7654 = LINE('',#160987,#13208) ;
#7655 = LINE('',#160988,#13209) ;
#7656 = LINE('',#160992,#13210) ;
#7657 = LINE('',#160993,#13211) ;
#7658 = LINE('',#160994,#13212) ;
#7659 = LINE('',#160997,#13213) ;
#7660 = LINE('',#160999,#13214) ;
#7661 = LINE('',#161000,#13215) ;
#7662 = LINE('',#161004,#13216) ;
#7663 = LINE('',#161005,#13217) ;
#7664 = LINE('',#161006,#13218) ;
#7665 = LINE('',#161010,#13219) ;
#7666 = LINE('',#161012,#13220) ;
#7667 = LINE('',#161014,#13221) ;
#7668 = LINE('',#161015,#13222) ;
#7669 = LINE('',#161018,#13223) ;
#7670 = LINE('',#161022,#13224) ;
#7671 = LINE('',#161026,#13225) ;
#7672 = LINE('',#161030,#13226) ;
#7673 = LINE('',#161035,#13227) ;
#7674 = LINE('',#161036,#13228) ;
#7675 = LINE('',#161037,#13229) ;
#7676 = LINE('',#161041,#13230) ;
#7677 = LINE('',#161042,#13231) ;
#7678 = LINE('',#161043,#13232) ;
#7679 = LINE('',#161046,#13233) ;
#7680 = LINE('',#161048,#13234) ;
#7681 = LINE('',#161049,#13235) ;
#7682 = LINE('',#161053,#13236) ;
#7683 = LINE('',#161054,#13237) ;
#7684 = LINE('',#161055,#13238) ;
#7685 = LINE('',#161059,#13239) ;
#7686 = LINE('',#161061,#13240) ;
#7687 = LINE('',#161063,#13241) ;
#7688 = LINE('',#161064,#13242) ;
#7689 = LINE('',#161067,#13243) ;
#7690 = LINE('',#161071,#13244) ;
#7691 = LINE('',#161075,#13245) ;
#7692 = LINE('',#161079,#13246) ;
#7693 = LINE('',#161084,#13247) ;
#7694 = LINE('',#161085,#13248) ;
#7695 = LINE('',#161086,#13249) ;
#7696 = LINE('',#161090,#13250) ;
#7697 = LINE('',#161091,#13251) ;
#7698 = LINE('',#161092,#13252) ;
#7699 = LINE('',#161095,#13253) ;
#7700 = LINE('',#161097,#13254) ;
#7701 = LINE('',#161098,#13255) ;
#7702 = LINE('',#161102,#13256) ;
#7703 = LINE('',#161103,#13257) ;
#7704 = LINE('',#161104,#13258) ;
#7705 = LINE('',#161108,#13259) ;
#7706 = LINE('',#161110,#13260) ;
#7707 = LINE('',#161112,#13261) ;
#7708 = LINE('',#161113,#13262) ;
#7709 = LINE('',#161117,#13263) ;
#7710 = LINE('',#161119,#13264) ;
#7711 = LINE('',#161121,#13265) ;
#7712 = LINE('',#161122,#13266) ;
#7713 = LINE('',#161126,#13267) ;
#7714 = LINE('',#161128,#13268) ;
#7715 = LINE('',#161130,#13269) ;
#7716 = LINE('',#161131,#13270) ;
#7717 = LINE('',#161135,#13271) ;
#7718 = LINE('',#161137,#13272) ;
#7719 = LINE('',#161139,#13273) ;
#7720 = LINE('',#161140,#13274) ;
#7721 = LINE('',#161144,#13275) ;
#7722 = LINE('',#161146,#13276) ;
#7723 = LINE('',#161148,#13277) ;
#7724 = LINE('',#161149,#13278) ;
#7725 = LINE('',#161153,#13279) ;
#7726 = LINE('',#161155,#13280) ;
#7727 = LINE('',#161157,#13281) ;
#7728 = LINE('',#161158,#13282) ;
#7729 = LINE('',#161162,#13283) ;
#7730 = LINE('',#161164,#13284) ;
#7731 = LINE('',#161166,#13285) ;
#7732 = LINE('',#161167,#13286) ;
#7733 = LINE('',#161171,#13287) ;
#7734 = LINE('',#161173,#13288) ;
#7735 = LINE('',#161175,#13289) ;
#7736 = LINE('',#161176,#13290) ;
#7737 = LINE('',#161180,#13291) ;
#7738 = LINE('',#161182,#13292) ;
#7739 = LINE('',#161184,#13293) ;
#7740 = LINE('',#161185,#13294) ;
#7741 = LINE('',#161187,#13295) ;
#7742 = LINE('',#161189,#13296) ;
#7743 = LINE('',#161191,#13297) ;
#7744 = LINE('',#161193,#13298) ;
#7745 = LINE('',#161195,#13299) ;
#7746 = LINE('',#161197,#13300) ;
#7747 = LINE('',#161199,#13301) ;
#7748 = LINE('',#161201,#13302) ;
#7749 = LINE('',#161203,#13303) ;
#7750 = LINE('',#161205,#13304) ;
#7751 = LINE('',#161206,#13305) ;
#7752 = LINE('',#161208,#13306) ;
#7753 = LINE('',#161209,#13307) ;
#7754 = LINE('',#161211,#13308) ;
#7755 = LINE('',#161212,#13309) ;
#7756 = LINE('',#161214,#13310) ;
#7757 = LINE('',#161215,#13311) ;
#7758 = LINE('',#161217,#13312) ;
#7759 = LINE('',#161218,#13313) ;
#7760 = LINE('',#161220,#13314) ;
#7761 = LINE('',#161221,#13315) ;
#7762 = LINE('',#161223,#13316) ;
#7763 = LINE('',#161224,#13317) ;
#7764 = LINE('',#161226,#13318) ;
#7765 = LINE('',#161227,#13319) ;
#7766 = LINE('',#161229,#13320) ;
#7767 = LINE('',#161230,#13321) ;
#7768 = LINE('',#161232,#13322) ;
#7769 = LINE('',#161233,#13323) ;
#7770 = LINE('',#161235,#13324) ;
#7771 = LINE('',#161236,#13325) ;
#7772 = LINE('',#161238,#13326) ;
#7773 = LINE('',#161239,#13327) ;
#7774 = LINE('',#161241,#13328) ;
#7775 = LINE('',#161242,#13329) ;
#7776 = LINE('',#161244,#13330) ;
#7777 = LINE('',#161245,#13331) ;
#7778 = LINE('',#161247,#13332) ;
#7779 = LINE('',#161248,#13333) ;
#7780 = LINE('',#161250,#13334) ;
#7781 = LINE('',#161251,#13335) ;
#7782 = LINE('',#161253,#13336) ;
#7783 = LINE('',#161254,#13337) ;
#7784 = LINE('',#161256,#13338) ;
#7785 = LINE('',#161257,#13339) ;
#7786 = LINE('',#161259,#13340) ;
#7787 = LINE('',#161260,#13341) ;
#7788 = LINE('',#161262,#13342) ;
#7789 = LINE('',#161263,#13343) ;
#7790 = LINE('',#161265,#13344) ;
#7791 = LINE('',#161266,#13345) ;
#7792 = LINE('',#161268,#13346) ;
#7793 = LINE('',#161269,#13347) ;
#7794 = LINE('',#161271,#13348) ;
#7795 = LINE('',#161272,#13349) ;
#7796 = LINE('',#161274,#13350) ;
#7797 = LINE('',#161275,#13351) ;
#7798 = LINE('',#161277,#13352) ;
#7799 = LINE('',#161278,#13353) ;
#7800 = LINE('',#161280,#13354) ;
#7801 = LINE('',#161281,#13355) ;
#7802 = LINE('',#161283,#13356) ;
#7803 = LINE('',#161284,#13357) ;
#7804 = LINE('',#161288,#13358) ;
#7805 = LINE('',#161292,#13359) ;
#7806 = LINE('',#161296,#13360) ;
#7807 = LINE('',#161298,#13361) ;
#7808 = LINE('',#161299,#13362) ;
#7809 = LINE('',#161304,#13363) ;
#7810 = LINE('',#161308,#13364) ;
#7811 = LINE('',#161310,#13365) ;
#7812 = LINE('',#161311,#13366) ;
#7813 = LINE('',#161316,#13367) ;
#7814 = LINE('',#161320,#13368) ;
#7815 = LINE('',#161322,#13369) ;
#7816 = LINE('',#161323,#13370) ;
#7817 = LINE('',#161328,#13371) ;
#7818 = LINE('',#161331,#13372) ;
#7819 = LINE('',#161332,#13373) ;
#7820 = LINE('',#161336,#13374) ;
#7821 = LINE('',#161338,#13375) ;
#7822 = LINE('',#161340,#13376) ;
#7823 = LINE('',#161341,#13377) ;
#7824 = LINE('',#161345,#13378) ;
#7825 = LINE('',#161349,#13379) ;
#7826 = LINE('',#161353,#13380) ;
#7827 = LINE('',#161355,#13381) ;
#7828 = LINE('',#161356,#13382) ;
#7829 = LINE('',#161361,#13383) ;
#7830 = LINE('',#161365,#13384) ;
#7831 = LINE('',#161367,#13385) ;
#7832 = LINE('',#161368,#13386) ;
#7833 = LINE('',#161373,#13387) ;
#7834 = LINE('',#161377,#13388) ;
#7835 = LINE('',#161379,#13389) ;
#7836 = LINE('',#161380,#13390) ;
#7837 = LINE('',#161385,#13391) ;
#7838 = LINE('',#161388,#13392) ;
#7839 = LINE('',#161389,#13393) ;
#7840 = LINE('',#161393,#13394) ;
#7841 = LINE('',#161395,#13395) ;
#7842 = LINE('',#161397,#13396) ;
#7843 = LINE('',#161398,#13397) ;
#7844 = LINE('',#161402,#13398) ;
#7845 = LINE('',#161406,#13399) ;
#7846 = LINE('',#161410,#13400) ;
#7847 = LINE('',#161412,#13401) ;
#7848 = LINE('',#161413,#13402) ;
#7849 = LINE('',#161418,#13403) ;
#7850 = LINE('',#161422,#13404) ;
#7851 = LINE('',#161424,#13405) ;
#7852 = LINE('',#161425,#13406) ;
#7853 = LINE('',#161430,#13407) ;
#7854 = LINE('',#161434,#13408) ;
#7855 = LINE('',#161436,#13409) ;
#7856 = LINE('',#161437,#13410) ;
#7857 = LINE('',#161442,#13411) ;
#7858 = LINE('',#161445,#13412) ;
#7859 = LINE('',#161446,#13413) ;
#7860 = LINE('',#161450,#13414) ;
#7861 = LINE('',#161452,#13415) ;
#7862 = LINE('',#161454,#13416) ;
#7863 = LINE('',#161455,#13417) ;
#7864 = LINE('',#161459,#13418) ;
#7865 = LINE('',#161463,#13419) ;
#7866 = LINE('',#161467,#13420) ;
#7867 = LINE('',#161469,#13421) ;
#7868 = LINE('',#161470,#13422) ;
#7869 = LINE('',#161475,#13423) ;
#7870 = LINE('',#161479,#13424) ;
#7871 = LINE('',#161481,#13425) ;
#7872 = LINE('',#161482,#13426) ;
#7873 = LINE('',#161487,#13427) ;
#7874 = LINE('',#161491,#13428) ;
#7875 = LINE('',#161493,#13429) ;
#7876 = LINE('',#161494,#13430) ;
#7877 = LINE('',#161499,#13431) ;
#7878 = LINE('',#161502,#13432) ;
#7879 = LINE('',#161503,#13433) ;
#7880 = LINE('',#161507,#13434) ;
#7881 = LINE('',#161509,#13435) ;
#7882 = LINE('',#161511,#13436) ;
#7883 = LINE('',#161512,#13437) ;
#7884 = LINE('',#161516,#13438) ;
#7885 = LINE('',#161520,#13439) ;
#7886 = LINE('',#161524,#13440) ;
#7887 = LINE('',#161526,#13441) ;
#7888 = LINE('',#161527,#13442) ;
#7889 = LINE('',#161532,#13443) ;
#7890 = LINE('',#161536,#13444) ;
#7891 = LINE('',#161538,#13445) ;
#7892 = LINE('',#161539,#13446) ;
#7893 = LINE('',#161544,#13447) ;
#7894 = LINE('',#161548,#13448) ;
#7895 = LINE('',#161550,#13449) ;
#7896 = LINE('',#161551,#13450) ;
#7897 = LINE('',#161556,#13451) ;
#7898 = LINE('',#161559,#13452) ;
#7899 = LINE('',#161560,#13453) ;
#7900 = LINE('',#161564,#13454) ;
#7901 = LINE('',#161566,#13455) ;
#7902 = LINE('',#161568,#13456) ;
#7903 = LINE('',#161569,#13457) ;
#7904 = LINE('',#161573,#13458) ;
#7905 = LINE('',#161577,#13459) ;
#7906 = LINE('',#161581,#13460) ;
#7907 = LINE('',#161583,#13461) ;
#7908 = LINE('',#161584,#13462) ;
#7909 = LINE('',#161589,#13463) ;
#7910 = LINE('',#161593,#13464) ;
#7911 = LINE('',#161595,#13465) ;
#7912 = LINE('',#161596,#13466) ;
#7913 = LINE('',#161601,#13467) ;
#7914 = LINE('',#161605,#13468) ;
#7915 = LINE('',#161607,#13469) ;
#7916 = LINE('',#161608,#13470) ;
#7917 = LINE('',#161613,#13471) ;
#7918 = LINE('',#161616,#13472) ;
#7919 = LINE('',#161617,#13473) ;
#7920 = LINE('',#161621,#13474) ;
#7921 = LINE('',#161623,#13475) ;
#7922 = LINE('',#161625,#13476) ;
#7923 = LINE('',#161626,#13477) ;
#7924 = LINE('',#161630,#13478) ;
#7925 = LINE('',#161634,#13479) ;
#7926 = LINE('',#161638,#13480) ;
#7927 = LINE('',#161640,#13481) ;
#7928 = LINE('',#161641,#13482) ;
#7929 = LINE('',#161646,#13483) ;
#7930 = LINE('',#161650,#13484) ;
#7931 = LINE('',#161652,#13485) ;
#7932 = LINE('',#161653,#13486) ;
#7933 = LINE('',#161658,#13487) ;
#7934 = LINE('',#161662,#13488) ;
#7935 = LINE('',#161664,#13489) ;
#7936 = LINE('',#161665,#13490) ;
#7937 = LINE('',#161670,#13491) ;
#7938 = LINE('',#161673,#13492) ;
#7939 = LINE('',#161674,#13493) ;
#7940 = LINE('',#161678,#13494) ;
#7941 = LINE('',#161680,#13495) ;
#7942 = LINE('',#161682,#13496) ;
#7943 = LINE('',#161683,#13497) ;
#7944 = LINE('',#161687,#13498) ;
#7945 = LINE('',#161691,#13499) ;
#7946 = LINE('',#161695,#13500) ;
#7947 = LINE('',#161697,#13501) ;
#7948 = LINE('',#161698,#13502) ;
#7949 = LINE('',#161703,#13503) ;
#7950 = LINE('',#161707,#13504) ;
#7951 = LINE('',#161709,#13505) ;
#7952 = LINE('',#161710,#13506) ;
#7953 = LINE('',#161715,#13507) ;
#7954 = LINE('',#161719,#13508) ;
#7955 = LINE('',#161721,#13509) ;
#7956 = LINE('',#161722,#13510) ;
#7957 = LINE('',#161727,#13511) ;
#7958 = LINE('',#161730,#13512) ;
#7959 = LINE('',#161731,#13513) ;
#7960 = LINE('',#161735,#13514) ;
#7961 = LINE('',#161737,#13515) ;
#7962 = LINE('',#161739,#13516) ;
#7963 = LINE('',#161740,#13517) ;
#7964 = LINE('',#161744,#13518) ;
#7965 = LINE('',#161748,#13519) ;
#7966 = LINE('',#161752,#13520) ;
#7967 = LINE('',#161754,#13521) ;
#7968 = LINE('',#161755,#13522) ;
#7969 = LINE('',#161760,#13523) ;
#7970 = LINE('',#161764,#13524) ;
#7971 = LINE('',#161766,#13525) ;
#7972 = LINE('',#161767,#13526) ;
#7973 = LINE('',#161772,#13527) ;
#7974 = LINE('',#161776,#13528) ;
#7975 = LINE('',#161778,#13529) ;
#7976 = LINE('',#161779,#13530) ;
#7977 = LINE('',#161784,#13531) ;
#7978 = LINE('',#161787,#13532) ;
#7979 = LINE('',#161788,#13533) ;
#7980 = LINE('',#161792,#13534) ;
#7981 = LINE('',#161794,#13535) ;
#7982 = LINE('',#161796,#13536) ;
#7983 = LINE('',#161797,#13537) ;
#7984 = VECTOR('',#103142,1000.) ;
#7985 = VECTOR('',#103145,1000.) ;
#7986 = VECTOR('',#103158,1.5) ;
#7987 = VECTOR('',#103161,1.5) ;
#7988 = VECTOR('',#103166,1000.) ;
#7989 = VECTOR('',#103169,1000.) ;
#7990 = VECTOR('',#103172,1000.) ;
#7991 = VECTOR('',#103175,1000.) ;
#7992 = VECTOR('',#103178,1.9) ;
#7993 = VECTOR('',#103193,1000.) ;
#7994 = VECTOR('',#103196,1000.) ;
#7995 = VECTOR('',#103245,1000.) ;
#7996 = VECTOR('',#103248,1000.) ;
#7997 = VECTOR('',#103261,1.5) ;
#7998 = VECTOR('',#103264,1.5) ;
#7999 = VECTOR('',#103269,1000.) ;
#8000 = VECTOR('',#103272,1000.) ;
#8001 = VECTOR('',#103275,1000.) ;
#8002 = VECTOR('',#103278,1000.) ;
#8003 = VECTOR('',#103281,1.9) ;
#8004 = VECTOR('',#103284,1000.) ;
#8005 = VECTOR('',#103285,1000.) ;
#8006 = VECTOR('',#103286,1000.) ;
#8007 = VECTOR('',#103287,1000.) ;
#8008 = VECTOR('',#103290,1000.) ;
#8009 = VECTOR('',#103291,1000.) ;
#8010 = VECTOR('',#103292,1000.) ;
#8011 = VECTOR('',#103295,1000.) ;
#8012 = VECTOR('',#103298,1000.) ;
#8013 = VECTOR('',#103299,1000.) ;
#8014 = VECTOR('',#103300,1000.) ;
#8015 = VECTOR('',#103301,1000.) ;
#8016 = VECTOR('',#103304,1000.) ;
#8017 = VECTOR('',#103305,1000.) ;
#8018 = VECTOR('',#103306,1000.) ;
#8019 = VECTOR('',#103307,1000.) ;
#8020 = VECTOR('',#103310,1000.) ;
#8021 = VECTOR('',#103311,1000.) ;
#8022 = VECTOR('',#103312,1000.) ;
#8023 = VECTOR('',#103313,1000.) ;
#8024 = VECTOR('',#103316,1000.) ;
#8025 = VECTOR('',#103337,1000.) ;
#8026 = VECTOR('',#103340,1000.) ;
#8027 = VECTOR('',#103347,1000.) ;
#8028 = VECTOR('',#103350,1000.) ;
#8029 = VECTOR('',#103353,1000.) ;
#8030 = VECTOR('',#103354,1000.) ;
#8031 = VECTOR('',#103355,1000.) ;
#8032 = VECTOR('',#103356,1000.) ;
#8033 = VECTOR('',#103359,1000.) ;
#8034 = VECTOR('',#103360,1000.) ;
#8035 = VECTOR('',#103361,1000.) ;
#8036 = VECTOR('',#103362,1000.) ;
#8037 = VECTOR('',#103365,1000.) ;
#8038 = VECTOR('',#103368,1000.) ;
#8039 = VECTOR('',#103369,1000.) ;
#8040 = VECTOR('',#103370,1000.) ;
#8041 = VECTOR('',#103371,1000.) ;
#8042 = VECTOR('',#103378,1000.) ;
#8043 = VECTOR('',#103385,1000.) ;
#8044 = VECTOR('',#103386,1000.) ;
#8045 = VECTOR('',#103387,1000.) ;
#8046 = VECTOR('',#103388,1000.) ;
#8047 = VECTOR('',#103391,1000.) ;
#8048 = VECTOR('',#103392,1000.) ;
#8049 = VECTOR('',#103393,1000.) ;
#8050 = VECTOR('',#103394,1000.) ;
#8051 = VECTOR('',#103397,1000.) ;
#8052 = VECTOR('',#103400,1000.) ;
#8053 = VECTOR('',#103401,1000.) ;
#8054 = VECTOR('',#103402,1000.) ;
#8055 = VECTOR('',#103403,1000.) ;
#8056 = VECTOR('',#103406,1000.) ;
#8057 = VECTOR('',#103407,1000.) ;
#8058 = VECTOR('',#103410,1000.) ;
#8059 = VECTOR('',#103413,1000.) ;
#8060 = VECTOR('',#103416,1000.) ;
#8061 = VECTOR('',#103419,1000.) ;
#8062 = VECTOR('',#103420,1000.) ;
#8063 = VECTOR('',#103421,1000.) ;
#8064 = VECTOR('',#103424,1000.) ;
#8065 = VECTOR('',#103425,1000.) ;
#8066 = VECTOR('',#103426,1000.) ;
#8067 = VECTOR('',#103429,1000.) ;
#8068 = VECTOR('',#103430,1000.) ;
#8069 = VECTOR('',#103431,1000.) ;
#8070 = VECTOR('',#103432,1000.) ;
#8071 = VECTOR('',#103435,1000.) ;
#8072 = VECTOR('',#103436,1000.) ;
#8073 = VECTOR('',#103437,1000.) ;
#8074 = VECTOR('',#103438,1000.) ;
#8075 = VECTOR('',#103441,1000.) ;
#8076 = VECTOR('',#103444,1000.) ;
#8077 = VECTOR('',#103447,1000.) ;
#8078 = VECTOR('',#103450,1000.) ;
#8079 = VECTOR('',#103453,1000.) ;
#8080 = VECTOR('',#103456,1000.) ;
#8081 = VECTOR('',#103459,1000.) ;
#8082 = VECTOR('',#103462,1000.) ;
#8083 = VECTOR('',#103465,1000.) ;
#8084 = VECTOR('',#103466,1000.) ;
#8085 = VECTOR('',#103467,1000.) ;
#8086 = VECTOR('',#103468,1000.) ;
#8087 = VECTOR('',#103471,1000.) ;
#8088 = VECTOR('',#103472,1000.) ;
#8089 = VECTOR('',#103473,1000.) ;
#8090 = VECTOR('',#103476,1000.) ;
#8091 = VECTOR('',#103477,1000.) ;
#8092 = VECTOR('',#103478,1000.) ;
#8093 = VECTOR('',#103481,1000.) ;
#8094 = VECTOR('',#103482,1000.) ;
#8095 = VECTOR('',#103483,1000.) ;
#8096 = VECTOR('',#103484,1000.) ;
#8097 = VECTOR('',#103485,1000.) ;
#8098 = VECTOR('',#103486,1000.) ;
#8099 = VECTOR('',#103487,1000.) ;
#8100 = VECTOR('',#103488,1000.) ;
#8101 = VECTOR('',#103489,1000.) ;
#8102 = VECTOR('',#103490,1000.) ;
#8103 = VECTOR('',#103491,1000.) ;
#8104 = VECTOR('',#103492,1000.) ;
#8105 = VECTOR('',#103495,1000.) ;
#8106 = VECTOR('',#103496,1000.) ;
#8107 = VECTOR('',#103497,1000.) ;
#8108 = VECTOR('',#103498,1000.) ;
#8109 = VECTOR('',#103501,1000.) ;
#8110 = VECTOR('',#103504,1000.) ;
#8111 = VECTOR('',#103507,1000.) ;
#8112 = VECTOR('',#103510,1000.) ;
#8113 = VECTOR('',#103513,1000.) ;
#8114 = VECTOR('',#103516,1000.) ;
#8115 = VECTOR('',#103519,1000.) ;
#8116 = VECTOR('',#103522,1000.) ;
#8117 = VECTOR('',#103525,1000.) ;
#8118 = VECTOR('',#103526,1000.) ;
#8119 = VECTOR('',#103527,1000.) ;
#8120 = VECTOR('',#103528,1000.) ;
#8121 = VECTOR('',#103531,1000.) ;
#8122 = VECTOR('',#103532,1000.) ;
#8123 = VECTOR('',#103533,1000.) ;
#8124 = VECTOR('',#103534,1000.) ;
#8125 = VECTOR('',#103535,1000.) ;
#8126 = VECTOR('',#103536,1000.) ;
#8127 = VECTOR('',#103539,1000.) ;
#8128 = VECTOR('',#103540,1000.) ;
#8129 = VECTOR('',#103543,1000.) ;
#8130 = VECTOR('',#103546,1000.) ;
#8131 = VECTOR('',#103547,1000.) ;
#8132 = VECTOR('',#103548,1000.) ;
#8133 = VECTOR('',#103549,1000.) ;
#8134 = VECTOR('',#103582,1000.) ;
#8135 = VECTOR('',#103583,1000.) ;
#8136 = VECTOR('',#103584,1000.) ;
#8137 = VECTOR('',#103585,1000.) ;
#8138 = VECTOR('',#103588,1000.) ;
#8139 = VECTOR('',#103589,1000.) ;
#8140 = VECTOR('',#103590,1000.) ;
#8141 = VECTOR('',#103591,1000.) ;
#8142 = VECTOR('',#103596,1000.) ;
#8143 = VECTOR('',#103597,1000.) ;
#8144 = VECTOR('',#103598,1000.) ;
#8145 = VECTOR('',#103601,1000.) ;
#8146 = VECTOR('',#103602,1000.) ;
#8147 = VECTOR('',#103603,1000.) ;
#8148 = VECTOR('',#103606,1000.) ;
#8149 = VECTOR('',#103609,1000.) ;
#8150 = VECTOR('',#103614,1000.) ;
#8151 = VECTOR('',#103621,1000.) ;
#8152 = VECTOR('',#103622,1000.) ;
#8153 = VECTOR('',#103625,1000.) ;
#8154 = VECTOR('',#103626,1000.) ;
#8155 = VECTOR('',#103627,1000.) ;
#8156 = VECTOR('',#103630,1000.) ;
#8157 = VECTOR('',#103631,1000.) ;
#8158 = VECTOR('',#103632,1000.) ;
#8159 = VECTOR('',#103635,1000.) ;
#8160 = VECTOR('',#103636,1000.) ;
#8161 = VECTOR('',#103637,1000.) ;
#8162 = VECTOR('',#103640,1000.) ;
#8163 = VECTOR('',#103641,1000.) ;
#8164 = VECTOR('',#103642,1000.) ;
#8165 = VECTOR('',#103643,1000.) ;
#8166 = VECTOR('',#103644,1000.) ;
#8167 = VECTOR('',#103645,1000.) ;
#8168 = VECTOR('',#103648,1000.) ;
#8169 = VECTOR('',#103649,1000.) ;
#8170 = VECTOR('',#103650,1000.) ;
#8171 = VECTOR('',#103651,1000.) ;
#8172 = VECTOR('',#103652,1000.) ;
#8173 = VECTOR('',#103653,1000.) ;
#8174 = VECTOR('',#103656,1000.) ;
#8175 = VECTOR('',#103657,1000.) ;
#8176 = VECTOR('',#103658,1000.) ;
#8177 = VECTOR('',#103659,1000.) ;
#8178 = VECTOR('',#103662,1000.) ;
#8179 = VECTOR('',#103663,1000.) ;
#8180 = VECTOR('',#103664,1000.) ;
#8181 = VECTOR('',#103665,1000.) ;
#8182 = VECTOR('',#103668,1000.) ;
#8183 = VECTOR('',#103669,1000.) ;
#8184 = VECTOR('',#103670,1000.) ;
#8185 = VECTOR('',#103671,1000.) ;
#8186 = VECTOR('',#103674,1000.) ;
#8187 = VECTOR('',#103675,1000.) ;
#8188 = VECTOR('',#103676,1000.) ;
#8189 = VECTOR('',#103677,1000.) ;
#8190 = VECTOR('',#103680,1000.) ;
#8191 = VECTOR('',#103681,1000.) ;
#8192 = VECTOR('',#103682,1000.) ;
#8193 = VECTOR('',#103683,1000.) ;
#8194 = VECTOR('',#103684,1000.) ;
#8195 = VECTOR('',#103687,1000.) ;
#8196 = VECTOR('',#103690,1000.) ;
#8197 = VECTOR('',#103693,1000.) ;
#8198 = VECTOR('',#103700,1000.) ;
#8199 = VECTOR('',#103701,1000.) ;
#8200 = VECTOR('',#103704,1000.) ;
#8201 = VECTOR('',#103705,1000.) ;
#8202 = VECTOR('',#103710,1000.) ;
#8203 = VECTOR('',#103713,1000.) ;
#8204 = VECTOR('',#103714,1000.) ;
#8205 = VECTOR('',#103719,1000.) ;
#8206 = VECTOR('',#103722,1000.) ;
#8207 = VECTOR('',#103723,1000.) ;
#8208 = VECTOR('',#103728,1000.) ;
#8209 = VECTOR('',#103731,1000.) ;
#8210 = VECTOR('',#103736,1000.) ;
#8211 = VECTOR('',#103739,1000.) ;
#8212 = VECTOR('',#103740,1000.) ;
#8213 = VECTOR('',#103743,1000.) ;
#8214 = VECTOR('',#103744,1000.) ;
#8215 = VECTOR('',#103747,1000.) ;
#8216 = VECTOR('',#103748,1000.) ;
#8217 = VECTOR('',#103751,1000.) ;
#8218 = VECTOR('',#103752,1000.) ;
#8219 = VECTOR('',#103753,1000.) ;
#8220 = VECTOR('',#103754,1000.) ;
#8221 = VECTOR('',#103757,1000.) ;
#8222 = VECTOR('',#103758,1000.) ;
#8223 = VECTOR('',#103759,1000.) ;
#8224 = VECTOR('',#103760,1000.) ;
#8225 = VECTOR('',#103763,1000.) ;
#8226 = VECTOR('',#103764,1000.) ;
#8227 = VECTOR('',#103765,1000.) ;
#8228 = VECTOR('',#103766,1000.) ;
#8229 = VECTOR('',#103769,1000.) ;
#8230 = VECTOR('',#103770,1000.) ;
#8231 = VECTOR('',#103771,1000.) ;
#8232 = VECTOR('',#103772,1000.) ;
#8233 = VECTOR('',#103775,1000.) ;
#8234 = VECTOR('',#103776,1000.) ;
#8235 = VECTOR('',#103777,1000.) ;
#8236 = VECTOR('',#103778,1000.) ;
#8237 = VECTOR('',#103779,1000.) ;
#8238 = VECTOR('',#103782,1000.) ;
#8239 = VECTOR('',#103785,1000.) ;
#8240 = VECTOR('',#103788,1000.) ;
#8241 = VECTOR('',#103793,1000.) ;
#8242 = VECTOR('',#103796,1000.) ;
#8243 = VECTOR('',#103799,1000.) ;
#8244 = VECTOR('',#103800,1000.) ;
#8245 = VECTOR('',#103805,1000.) ;
#8246 = VECTOR('',#103808,1000.) ;
#8247 = VECTOR('',#103809,1000.) ;
#8248 = VECTOR('',#103814,1000.) ;
#8249 = VECTOR('',#103817,1000.) ;
#8250 = VECTOR('',#103818,1000.) ;
#8251 = VECTOR('',#103823,1000.) ;
#8252 = VECTOR('',#103826,1000.) ;
#8253 = VECTOR('',#103829,1000.) ;
#8254 = VECTOR('',#103830,1000.) ;
#8255 = VECTOR('',#103831,1000.) ;
#8256 = VECTOR('',#103832,1000.) ;
#8257 = VECTOR('',#103835,1000.) ;
#8258 = VECTOR('',#103836,1000.) ;
#8259 = VECTOR('',#103837,1000.) ;
#8260 = VECTOR('',#103838,1000.) ;
#8261 = VECTOR('',#103841,1000.) ;
#8262 = VECTOR('',#103842,1000.) ;
#8263 = VECTOR('',#103843,1000.) ;
#8264 = VECTOR('',#103846,1000.) ;
#8265 = VECTOR('',#103847,1000.) ;
#8266 = VECTOR('',#103848,1000.) ;
#8267 = VECTOR('',#103851,1000.) ;
#8268 = VECTOR('',#103854,1000.) ;
#8269 = VECTOR('',#103855,1000.) ;
#8270 = VECTOR('',#103856,1000.) ;
#8271 = VECTOR('',#103867,1000.) ;
#8272 = VECTOR('',#103870,1000.) ;
#8273 = VECTOR('',#104387,1000.) ;
#8274 = VECTOR('',#104388,1000.) ;
#8275 = VECTOR('',#104389,1000.) ;
#8276 = VECTOR('',#104390,1000.) ;
#8277 = VECTOR('',#104395,1000.) ;
#8278 = VECTOR('',#104400,1000.) ;
#8279 = VECTOR('',#104401,1000.) ;
#8280 = VECTOR('',#104402,1000.) ;
#8281 = VECTOR('',#104407,1000.) ;
#8282 = VECTOR('',#104412,1000.) ;
#8283 = VECTOR('',#104413,1000.) ;
#8284 = VECTOR('',#104414,1000.) ;
#8285 = VECTOR('',#104419,1000.) ;
#8286 = VECTOR('',#104424,1000.) ;
#8287 = VECTOR('',#104425,1000.) ;
#8288 = VECTOR('',#104426,1000.) ;
#8289 = VECTOR('',#104431,1000.) ;
#8290 = VECTOR('',#104436,1000.) ;
#8291 = VECTOR('',#104437,1000.) ;
#8292 = VECTOR('',#104438,1000.) ;
#8293 = VECTOR('',#104443,1000.) ;
#8294 = VECTOR('',#104444,1000.) ;
#8295 = VECTOR('',#104445,1000.) ;
#8296 = VECTOR('',#104446,1000.) ;
#8297 = VECTOR('',#104447,1000.) ;
#8298 = VECTOR('',#104448,1000.) ;
#8299 = VECTOR('',#104451,1000.) ;
#8300 = VECTOR('',#104452,1000.) ;
#8301 = VECTOR('',#104453,1000.) ;
#8302 = VECTOR('',#104454,1000.) ;
#8303 = VECTOR('',#104457,1000.) ;
#8304 = VECTOR('',#104458,1000.) ;
#8305 = VECTOR('',#104463,1000.) ;
#8306 = VECTOR('',#104464,1000.) ;
#8307 = VECTOR('',#104465,1000.) ;
#8308 = VECTOR('',#104468,1000.) ;
#8309 = VECTOR('',#104469,1000.) ;
#8310 = VECTOR('',#104470,1000.) ;
#8311 = VECTOR('',#104471,1000.) ;
#8312 = VECTOR('',#104474,1000.) ;
#8313 = VECTOR('',#104477,1000.) ;
#8314 = VECTOR('',#104478,1000.) ;
#8315 = VECTOR('',#104479,1000.) ;
#8316 = VECTOR('',#104480,1000.) ;
#8317 = VECTOR('',#104495,1000.) ;
#8318 = VECTOR('',#104496,1000.) ;
#8319 = VECTOR('',#104497,1000.) ;
#8320 = VECTOR('',#104498,1000.) ;
#8321 = VECTOR('',#104501,1000.) ;
#8322 = VECTOR('',#104502,1000.) ;
#8323 = VECTOR('',#104503,1000.) ;
#8324 = VECTOR('',#104504,1000.) ;
#8325 = VECTOR('',#104509,1000.) ;
#8326 = VECTOR('',#104510,1000.) ;
#8327 = VECTOR('',#104511,1000.) ;
#8328 = VECTOR('',#104514,1000.) ;
#8329 = VECTOR('',#104515,1000.) ;
#8330 = VECTOR('',#104516,1000.) ;
#8331 = VECTOR('',#104519,1000.) ;
#8332 = VECTOR('',#104522,1000.) ;
#8333 = VECTOR('',#104527,1000.) ;
#8334 = VECTOR('',#104534,1000.) ;
#8335 = VECTOR('',#104535,1000.) ;
#8336 = VECTOR('',#104538,1000.) ;
#8337 = VECTOR('',#104539,1000.) ;
#8338 = VECTOR('',#104540,1000.) ;
#8339 = VECTOR('',#104543,1000.) ;
#8340 = VECTOR('',#104544,1000.) ;
#8341 = VECTOR('',#104545,1000.) ;
#8342 = VECTOR('',#104548,1000.) ;
#8343 = VECTOR('',#104549,1000.) ;
#8344 = VECTOR('',#104550,1000.) ;
#8345 = VECTOR('',#104553,1000.) ;
#8346 = VECTOR('',#104554,1000.) ;
#8347 = VECTOR('',#104555,1000.) ;
#8348 = VECTOR('',#104556,1000.) ;
#8349 = VECTOR('',#104557,1000.) ;
#8350 = VECTOR('',#104558,1000.) ;
#8351 = VECTOR('',#104561,1000.) ;
#8352 = VECTOR('',#104562,1000.) ;
#8353 = VECTOR('',#104563,1000.) ;
#8354 = VECTOR('',#104564,1000.) ;
#8355 = VECTOR('',#104565,1000.) ;
#8356 = VECTOR('',#104566,1000.) ;
#8357 = VECTOR('',#104569,1000.) ;
#8358 = VECTOR('',#104570,1000.) ;
#8359 = VECTOR('',#104571,1000.) ;
#8360 = VECTOR('',#104572,1000.) ;
#8361 = VECTOR('',#104575,1000.) ;
#8362 = VECTOR('',#104576,1000.) ;
#8363 = VECTOR('',#104577,1000.) ;
#8364 = VECTOR('',#104578,1000.) ;
#8365 = VECTOR('',#104581,1000.) ;
#8366 = VECTOR('',#104582,1000.) ;
#8367 = VECTOR('',#104583,1000.) ;
#8368 = VECTOR('',#104584,1000.) ;
#8369 = VECTOR('',#104587,1000.) ;
#8370 = VECTOR('',#104588,1000.) ;
#8371 = VECTOR('',#104589,1000.) ;
#8372 = VECTOR('',#104590,1000.) ;
#8373 = VECTOR('',#104593,1000.) ;
#8374 = VECTOR('',#104594,1000.) ;
#8375 = VECTOR('',#104595,1000.) ;
#8376 = VECTOR('',#104596,1000.) ;
#8377 = VECTOR('',#104597,1000.) ;
#8378 = VECTOR('',#104600,1000.) ;
#8379 = VECTOR('',#104603,1000.) ;
#8380 = VECTOR('',#104606,1000.) ;
#8381 = VECTOR('',#104613,1000.) ;
#8382 = VECTOR('',#104614,1000.) ;
#8383 = VECTOR('',#104617,1000.) ;
#8384 = VECTOR('',#104618,1000.) ;
#8385 = VECTOR('',#104623,1000.) ;
#8386 = VECTOR('',#104626,1000.) ;
#8387 = VECTOR('',#104627,1000.) ;
#8388 = VECTOR('',#104632,1000.) ;
#8389 = VECTOR('',#104635,1000.) ;
#8390 = VECTOR('',#104636,1000.) ;
#8391 = VECTOR('',#104641,1000.) ;
#8392 = VECTOR('',#104644,1000.) ;
#8393 = VECTOR('',#104649,1000.) ;
#8394 = VECTOR('',#104652,1000.) ;
#8395 = VECTOR('',#104653,1000.) ;
#8396 = VECTOR('',#104656,1000.) ;
#8397 = VECTOR('',#104657,1000.) ;
#8398 = VECTOR('',#104660,1000.) ;
#8399 = VECTOR('',#104661,1000.) ;
#8400 = VECTOR('',#104664,1000.) ;
#8401 = VECTOR('',#104665,1000.) ;
#8402 = VECTOR('',#104666,1000.) ;
#8403 = VECTOR('',#104667,1000.) ;
#8404 = VECTOR('',#104670,1000.) ;
#8405 = VECTOR('',#104671,1000.) ;
#8406 = VECTOR('',#104672,1000.) ;
#8407 = VECTOR('',#104673,1000.) ;
#8408 = VECTOR('',#104676,1000.) ;
#8409 = VECTOR('',#104677,1000.) ;
#8410 = VECTOR('',#104678,1000.) ;
#8411 = VECTOR('',#104679,1000.) ;
#8412 = VECTOR('',#104682,1000.) ;
#8413 = VECTOR('',#104683,1000.) ;
#8414 = VECTOR('',#104684,1000.) ;
#8415 = VECTOR('',#104685,1000.) ;
#8416 = VECTOR('',#104688,1000.) ;
#8417 = VECTOR('',#104689,1000.) ;
#8418 = VECTOR('',#104690,1000.) ;
#8419 = VECTOR('',#104691,1000.) ;
#8420 = VECTOR('',#104692,1000.) ;
#8421 = VECTOR('',#104695,1000.) ;
#8422 = VECTOR('',#104698,1000.) ;
#8423 = VECTOR('',#104701,1000.) ;
#8424 = VECTOR('',#104706,1000.) ;
#8425 = VECTOR('',#104709,1000.) ;
#8426 = VECTOR('',#104712,1000.) ;
#8427 = VECTOR('',#104713,1000.) ;
#8428 = VECTOR('',#104718,1000.) ;
#8429 = VECTOR('',#104721,1000.) ;
#8430 = VECTOR('',#104722,1000.) ;
#8431 = VECTOR('',#104727,1000.) ;
#8432 = VECTOR('',#104730,1000.) ;
#8433 = VECTOR('',#104731,1000.) ;
#8434 = VECTOR('',#104736,1000.) ;
#8435 = VECTOR('',#104739,1000.) ;
#8436 = VECTOR('',#104742,1000.) ;
#8437 = VECTOR('',#104743,1000.) ;
#8438 = VECTOR('',#104744,1000.) ;
#8439 = VECTOR('',#104745,1000.) ;
#8440 = VECTOR('',#104748,1000.) ;
#8441 = VECTOR('',#104749,1000.) ;
#8442 = VECTOR('',#104750,1000.) ;
#8443 = VECTOR('',#104751,1000.) ;
#8444 = VECTOR('',#104754,1000.) ;
#8445 = VECTOR('',#104755,1000.) ;
#8446 = VECTOR('',#104756,1000.) ;
#8447 = VECTOR('',#104759,1000.) ;
#8448 = VECTOR('',#104760,1000.) ;
#8449 = VECTOR('',#104761,1000.) ;
#8450 = VECTOR('',#104764,1000.) ;
#8451 = VECTOR('',#104767,1000.) ;
#8452 = VECTOR('',#104768,1000.) ;
#8453 = VECTOR('',#104769,1000.) ;
#8454 = VECTOR('',#104780,1000.) ;
#8455 = VECTOR('',#104783,1000.) ;
#8456 = VECTOR('',#105392,1000.) ;
#8457 = VECTOR('',#105395,1000.) ;
#8458 = VECTOR('',#105408,1.5) ;
#8459 = VECTOR('',#105411,1.5) ;
#8460 = VECTOR('',#105416,1000.) ;
#8461 = VECTOR('',#105419,1000.) ;
#8462 = VECTOR('',#105422,1000.) ;
#8463 = VECTOR('',#105425,1000.) ;
#8464 = VECTOR('',#105428,1.9) ;
#8465 = VECTOR('',#105443,1000.) ;
#8466 = VECTOR('',#105446,1000.) ;
#8467 = VECTOR('',#105495,1000.) ;
#8468 = VECTOR('',#105498,1000.) ;
#8469 = VECTOR('',#105511,1.5) ;
#8470 = VECTOR('',#105514,1.5) ;
#8471 = VECTOR('',#105519,1000.) ;
#8472 = VECTOR('',#105522,1000.) ;
#8473 = VECTOR('',#105525,1000.) ;
#8474 = VECTOR('',#105528,1000.) ;
#8475 = VECTOR('',#105531,1.9) ;
#8476 = VECTOR('',#105534,1000.) ;
#8477 = VECTOR('',#105535,1000.) ;
#8478 = VECTOR('',#105536,1000.) ;
#8479 = VECTOR('',#105537,1000.) ;
#8480 = VECTOR('',#105540,1000.) ;
#8481 = VECTOR('',#105541,1000.) ;
#8482 = VECTOR('',#105542,1000.) ;
#8483 = VECTOR('',#105545,1000.) ;
#8484 = VECTOR('',#105548,1000.) ;
#8485 = VECTOR('',#105549,1000.) ;
#8486 = VECTOR('',#105550,1000.) ;
#8487 = VECTOR('',#105551,1000.) ;
#8488 = VECTOR('',#105554,1000.) ;
#8489 = VECTOR('',#105555,1000.) ;
#8490 = VECTOR('',#105556,1000.) ;
#8491 = VECTOR('',#105557,1000.) ;
#8492 = VECTOR('',#105560,1000.) ;
#8493 = VECTOR('',#105561,1000.) ;
#8494 = VECTOR('',#105562,1000.) ;
#8495 = VECTOR('',#105563,1000.) ;
#8496 = VECTOR('',#105568,1000.) ;
#8497 = VECTOR('',#105587,1000.) ;
#8498 = VECTOR('',#105592,1000.) ;
#8499 = VECTOR('',#105597,1000.) ;
#8500 = VECTOR('',#105598,1000.) ;
#8501 = VECTOR('',#105599,1000.) ;
#8502 = VECTOR('',#105602,1000.) ;
#8503 = VECTOR('',#105603,1000.) ;
#8504 = VECTOR('',#105604,1000.) ;
#8505 = VECTOR('',#105605,1000.) ;
#8506 = VECTOR('',#105608,1000.) ;
#8507 = VECTOR('',#105609,1000.) ;
#8508 = VECTOR('',#105610,1000.) ;
#8509 = VECTOR('',#105611,1000.) ;
#8510 = VECTOR('',#105614,1000.) ;
#8511 = VECTOR('',#105617,1000.) ;
#8512 = VECTOR('',#105618,1000.) ;
#8513 = VECTOR('',#105619,1000.) ;
#8514 = VECTOR('',#105622,1000.) ;
#8515 = VECTOR('',#105623,1000.) ;
#8516 = VECTOR('',#105624,1000.) ;
#8517 = VECTOR('',#105625,1000.) ;
#8518 = VECTOR('',#105626,1000.) ;
#8519 = VECTOR('',#105633,1000.) ;
#8520 = VECTOR('',#105640,1000.) ;
#8521 = VECTOR('',#105641,1000.) ;
#8522 = VECTOR('',#105642,1000.) ;
#8523 = VECTOR('',#105643,1000.) ;
#8524 = VECTOR('',#105646,1000.) ;
#8525 = VECTOR('',#105649,1000.) ;
#8526 = VECTOR('',#105650,1000.) ;
#8527 = VECTOR('',#105651,1000.) ;
#8528 = VECTOR('',#105652,1000.) ;
#8529 = VECTOR('',#105655,1000.) ;
#8530 = VECTOR('',#105656,1000.) ;
#8531 = VECTOR('',#105657,1000.) ;
#8532 = VECTOR('',#105660,1000.) ;
#8533 = VECTOR('',#105663,1000.) ;
#8534 = VECTOR('',#105666,1000.) ;
#8535 = VECTOR('',#105669,1000.) ;
#8536 = VECTOR('',#105670,1000.) ;
#8537 = VECTOR('',#105673,1000.) ;
#8538 = VECTOR('',#105674,1000.) ;
#8539 = VECTOR('',#105675,1000.) ;
#8540 = VECTOR('',#105678,1000.) ;
#8541 = VECTOR('',#105679,1000.) ;
#8542 = VECTOR('',#105680,1000.) ;
#8543 = VECTOR('',#105681,1000.) ;
#8544 = VECTOR('',#105684,1000.) ;
#8545 = VECTOR('',#105685,1000.) ;
#8546 = VECTOR('',#105686,1000.) ;
#8547 = VECTOR('',#105687,1000.) ;
#8548 = VECTOR('',#105690,1000.) ;
#8549 = VECTOR('',#105693,1000.) ;
#8550 = VECTOR('',#105696,1000.) ;
#8551 = VECTOR('',#105699,1000.) ;
#8552 = VECTOR('',#105702,1000.) ;
#8553 = VECTOR('',#105705,1000.) ;
#8554 = VECTOR('',#105708,1000.) ;
#8555 = VECTOR('',#105711,1000.) ;
#8556 = VECTOR('',#105714,1000.) ;
#8557 = VECTOR('',#105715,1000.) ;
#8558 = VECTOR('',#105716,1000.) ;
#8559 = VECTOR('',#105717,1000.) ;
#8560 = VECTOR('',#105720,1000.) ;
#8561 = VECTOR('',#105721,1000.) ;
#8562 = VECTOR('',#105722,1000.) ;
#8563 = VECTOR('',#105725,1000.) ;
#8564 = VECTOR('',#105726,1000.) ;
#8565 = VECTOR('',#105727,1000.) ;
#8566 = VECTOR('',#105730,1000.) ;
#8567 = VECTOR('',#105731,1000.) ;
#8568 = VECTOR('',#105732,1000.) ;
#8569 = VECTOR('',#105733,1000.) ;
#8570 = VECTOR('',#105734,1000.) ;
#8571 = VECTOR('',#105735,1000.) ;
#8572 = VECTOR('',#105736,1000.) ;
#8573 = VECTOR('',#105737,1000.) ;
#8574 = VECTOR('',#105738,1000.) ;
#8575 = VECTOR('',#105739,1000.) ;
#8576 = VECTOR('',#105740,1000.) ;
#8577 = VECTOR('',#105741,1000.) ;
#8578 = VECTOR('',#105744,1000.) ;
#8579 = VECTOR('',#105745,1000.) ;
#8580 = VECTOR('',#105746,1000.) ;
#8581 = VECTOR('',#105747,1000.) ;
#8582 = VECTOR('',#105750,1000.) ;
#8583 = VECTOR('',#105753,1000.) ;
#8584 = VECTOR('',#105756,1000.) ;
#8585 = VECTOR('',#105759,1000.) ;
#8586 = VECTOR('',#105762,1000.) ;
#8587 = VECTOR('',#105765,1000.) ;
#8588 = VECTOR('',#105768,1000.) ;
#8589 = VECTOR('',#105771,1000.) ;
#8590 = VECTOR('',#105774,1000.) ;
#8591 = VECTOR('',#105775,1000.) ;
#8592 = VECTOR('',#105776,1000.) ;
#8593 = VECTOR('',#105777,1000.) ;
#8594 = VECTOR('',#105780,1000.) ;
#8595 = VECTOR('',#105781,1000.) ;
#8596 = VECTOR('',#105782,1000.) ;
#8597 = VECTOR('',#105783,1000.) ;
#8598 = VECTOR('',#105784,1000.) ;
#8599 = VECTOR('',#105785,1000.) ;
#8600 = VECTOR('',#105788,1000.) ;
#8601 = VECTOR('',#105791,1000.) ;
#8602 = VECTOR('',#105796,1000.) ;
#8603 = VECTOR('',#105797,1000.) ;
#8604 = VECTOR('',#105798,1000.) ;
#8605 = VECTOR('',#105799,1000.) ;
#8606 = VECTOR('',#105832,1000.) ;
#8607 = VECTOR('',#105833,1000.) ;
#8608 = VECTOR('',#105834,1000.) ;
#8609 = VECTOR('',#105835,1000.) ;
#8610 = VECTOR('',#105838,1000.) ;
#8611 = VECTOR('',#105839,1000.) ;
#8612 = VECTOR('',#105840,1000.) ;
#8613 = VECTOR('',#105841,1000.) ;
#8614 = VECTOR('',#105846,1000.) ;
#8615 = VECTOR('',#105847,1000.) ;
#8616 = VECTOR('',#105848,1000.) ;
#8617 = VECTOR('',#105851,1000.) ;
#8618 = VECTOR('',#105852,1000.) ;
#8619 = VECTOR('',#105853,1000.) ;
#8620 = VECTOR('',#105856,1000.) ;
#8621 = VECTOR('',#105859,1000.) ;
#8622 = VECTOR('',#105864,1000.) ;
#8623 = VECTOR('',#105871,1000.) ;
#8624 = VECTOR('',#105872,1000.) ;
#8625 = VECTOR('',#105875,1000.) ;
#8626 = VECTOR('',#105876,1000.) ;
#8627 = VECTOR('',#105877,1000.) ;
#8628 = VECTOR('',#105880,1000.) ;
#8629 = VECTOR('',#105881,1000.) ;
#8630 = VECTOR('',#105882,1000.) ;
#8631 = VECTOR('',#105885,1000.) ;
#8632 = VECTOR('',#105886,1000.) ;
#8633 = VECTOR('',#105887,1000.) ;
#8634 = VECTOR('',#105890,1000.) ;
#8635 = VECTOR('',#105891,1000.) ;
#8636 = VECTOR('',#105892,1000.) ;
#8637 = VECTOR('',#105893,1000.) ;
#8638 = VECTOR('',#105894,1000.) ;
#8639 = VECTOR('',#105895,1000.) ;
#8640 = VECTOR('',#105898,1000.) ;
#8641 = VECTOR('',#105899,1000.) ;
#8642 = VECTOR('',#105900,1000.) ;
#8643 = VECTOR('',#105901,1000.) ;
#8644 = VECTOR('',#105902,1000.) ;
#8645 = VECTOR('',#105903,1000.) ;
#8646 = VECTOR('',#105906,1000.) ;
#8647 = VECTOR('',#105907,1000.) ;
#8648 = VECTOR('',#105908,1000.) ;
#8649 = VECTOR('',#105909,1000.) ;
#8650 = VECTOR('',#105912,1000.) ;
#8651 = VECTOR('',#105913,1000.) ;
#8652 = VECTOR('',#105914,1000.) ;
#8653 = VECTOR('',#105915,1000.) ;
#8654 = VECTOR('',#105918,1000.) ;
#8655 = VECTOR('',#105919,1000.) ;
#8656 = VECTOR('',#105920,1000.) ;
#8657 = VECTOR('',#105921,1000.) ;
#8658 = VECTOR('',#105924,1000.) ;
#8659 = VECTOR('',#105925,1000.) ;
#8660 = VECTOR('',#105926,1000.) ;
#8661 = VECTOR('',#105927,1000.) ;
#8662 = VECTOR('',#105930,1000.) ;
#8663 = VECTOR('',#105931,1000.) ;
#8664 = VECTOR('',#105932,1000.) ;
#8665 = VECTOR('',#105933,1000.) ;
#8666 = VECTOR('',#105934,1000.) ;
#8667 = VECTOR('',#105937,1000.) ;
#8668 = VECTOR('',#105940,1000.) ;
#8669 = VECTOR('',#105943,1000.) ;
#8670 = VECTOR('',#105950,1000.) ;
#8671 = VECTOR('',#105951,1000.) ;
#8672 = VECTOR('',#105954,1000.) ;
#8673 = VECTOR('',#105955,1000.) ;
#8674 = VECTOR('',#105960,1000.) ;
#8675 = VECTOR('',#105963,1000.) ;
#8676 = VECTOR('',#105964,1000.) ;
#8677 = VECTOR('',#105969,1000.) ;
#8678 = VECTOR('',#105972,1000.) ;
#8679 = VECTOR('',#105973,1000.) ;
#8680 = VECTOR('',#105978,1000.) ;
#8681 = VECTOR('',#105981,1000.) ;
#8682 = VECTOR('',#105986,1000.) ;
#8683 = VECTOR('',#105989,1000.) ;
#8684 = VECTOR('',#105990,1000.) ;
#8685 = VECTOR('',#105993,1000.) ;
#8686 = VECTOR('',#105994,1000.) ;
#8687 = VECTOR('',#105997,1000.) ;
#8688 = VECTOR('',#105998,1000.) ;
#8689 = VECTOR('',#106001,1000.) ;
#8690 = VECTOR('',#106002,1000.) ;
#8691 = VECTOR('',#106003,1000.) ;
#8692 = VECTOR('',#106004,1000.) ;
#8693 = VECTOR('',#106007,1000.) ;
#8694 = VECTOR('',#106008,1000.) ;
#8695 = VECTOR('',#106009,1000.) ;
#8696 = VECTOR('',#106010,1000.) ;
#8697 = VECTOR('',#106013,1000.) ;
#8698 = VECTOR('',#106014,1000.) ;
#8699 = VECTOR('',#106015,1000.) ;
#8700 = VECTOR('',#106016,1000.) ;
#8701 = VECTOR('',#106019,1000.) ;
#8702 = VECTOR('',#106020,1000.) ;
#8703 = VECTOR('',#106021,1000.) ;
#8704 = VECTOR('',#106022,1000.) ;
#8705 = VECTOR('',#106025,1000.) ;
#8706 = VECTOR('',#106026,1000.) ;
#8707 = VECTOR('',#106027,1000.) ;
#8708 = VECTOR('',#106028,1000.) ;
#8709 = VECTOR('',#106029,1000.) ;
#8710 = VECTOR('',#106032,1000.) ;
#8711 = VECTOR('',#106035,1000.) ;
#8712 = VECTOR('',#106038,1000.) ;
#8713 = VECTOR('',#106043,1000.) ;
#8714 = VECTOR('',#106046,1000.) ;
#8715 = VECTOR('',#106049,1000.) ;
#8716 = VECTOR('',#106050,1000.) ;
#8717 = VECTOR('',#106055,1000.) ;
#8718 = VECTOR('',#106058,1000.) ;
#8719 = VECTOR('',#106059,1000.) ;
#8720 = VECTOR('',#106064,1000.) ;
#8721 = VECTOR('',#106067,1000.) ;
#8722 = VECTOR('',#106068,1000.) ;
#8723 = VECTOR('',#106073,1000.) ;
#8724 = VECTOR('',#106076,1000.) ;
#8725 = VECTOR('',#106079,1000.) ;
#8726 = VECTOR('',#106080,1000.) ;
#8727 = VECTOR('',#106081,1000.) ;
#8728 = VECTOR('',#106082,1000.) ;
#8729 = VECTOR('',#106085,1000.) ;
#8730 = VECTOR('',#106086,1000.) ;
#8731 = VECTOR('',#106087,1000.) ;
#8732 = VECTOR('',#106088,1000.) ;
#8733 = VECTOR('',#106091,1000.) ;
#8734 = VECTOR('',#106092,1000.) ;
#8735 = VECTOR('',#106093,1000.) ;
#8736 = VECTOR('',#106096,1000.) ;
#8737 = VECTOR('',#106097,1000.) ;
#8738 = VECTOR('',#106098,1000.) ;
#8739 = VECTOR('',#106101,1000.) ;
#8740 = VECTOR('',#106104,1000.) ;
#8741 = VECTOR('',#106105,1000.) ;
#8742 = VECTOR('',#106106,1000.) ;
#8743 = VECTOR('',#106117,1000.) ;
#8744 = VECTOR('',#106120,1000.) ;
#8745 = VECTOR('',#106637,1000.) ;
#8746 = VECTOR('',#106638,1000.) ;
#8747 = VECTOR('',#106639,1000.) ;
#8748 = VECTOR('',#106640,1000.) ;
#8749 = VECTOR('',#106645,1000.) ;
#8750 = VECTOR('',#106650,1000.) ;
#8751 = VECTOR('',#106651,1000.) ;
#8752 = VECTOR('',#106652,1000.) ;
#8753 = VECTOR('',#106657,1000.) ;
#8754 = VECTOR('',#106662,1000.) ;
#8755 = VECTOR('',#106663,1000.) ;
#8756 = VECTOR('',#106664,1000.) ;
#8757 = VECTOR('',#106669,1000.) ;
#8758 = VECTOR('',#106674,1000.) ;
#8759 = VECTOR('',#106675,1000.) ;
#8760 = VECTOR('',#106676,1000.) ;
#8761 = VECTOR('',#106681,1000.) ;
#8762 = VECTOR('',#106686,1000.) ;
#8763 = VECTOR('',#106687,1000.) ;
#8764 = VECTOR('',#106688,1000.) ;
#8765 = VECTOR('',#106693,1000.) ;
#8766 = VECTOR('',#106694,1000.) ;
#8767 = VECTOR('',#106695,1000.) ;
#8768 = VECTOR('',#106696,1000.) ;
#8769 = VECTOR('',#106697,1000.) ;
#8770 = VECTOR('',#106698,1000.) ;
#8771 = VECTOR('',#106701,1000.) ;
#8772 = VECTOR('',#106702,1000.) ;
#8773 = VECTOR('',#106703,1000.) ;
#8774 = VECTOR('',#106704,1000.) ;
#8775 = VECTOR('',#106707,1000.) ;
#8776 = VECTOR('',#106708,1000.) ;
#8777 = VECTOR('',#106711,1000.) ;
#8778 = VECTOR('',#106712,1000.) ;
#8779 = VECTOR('',#106713,1000.) ;
#8780 = VECTOR('',#106714,1000.) ;
#8781 = VECTOR('',#106717,1000.) ;
#8782 = VECTOR('',#106720,1000.) ;
#8783 = VECTOR('',#106721,1000.) ;
#8784 = VECTOR('',#106722,1000.) ;
#8785 = VECTOR('',#106723,1000.) ;
#8786 = VECTOR('',#106726,1000.) ;
#8787 = VECTOR('',#106727,1000.) ;
#8788 = VECTOR('',#106730,1000.) ;
#8789 = VECTOR('',#106745,1000.) ;
#8790 = VECTOR('',#106746,1000.) ;
#8791 = VECTOR('',#106747,1000.) ;
#8792 = VECTOR('',#106748,1000.) ;
#8793 = VECTOR('',#106751,1000.) ;
#8794 = VECTOR('',#106752,1000.) ;
#8795 = VECTOR('',#106753,1000.) ;
#8796 = VECTOR('',#106754,1000.) ;
#8797 = VECTOR('',#106759,1000.) ;
#8798 = VECTOR('',#106760,1000.) ;
#8799 = VECTOR('',#106761,1000.) ;
#8800 = VECTOR('',#106764,1000.) ;
#8801 = VECTOR('',#106765,1000.) ;
#8802 = VECTOR('',#106766,1000.) ;
#8803 = VECTOR('',#106769,1000.) ;
#8804 = VECTOR('',#106772,1000.) ;
#8805 = VECTOR('',#106777,1000.) ;
#8806 = VECTOR('',#106784,1000.) ;
#8807 = VECTOR('',#106785,1000.) ;
#8808 = VECTOR('',#106788,1000.) ;
#8809 = VECTOR('',#106789,1000.) ;
#8810 = VECTOR('',#106790,1000.) ;
#8811 = VECTOR('',#106793,1000.) ;
#8812 = VECTOR('',#106794,1000.) ;
#8813 = VECTOR('',#106795,1000.) ;
#8814 = VECTOR('',#106798,1000.) ;
#8815 = VECTOR('',#106799,1000.) ;
#8816 = VECTOR('',#106800,1000.) ;
#8817 = VECTOR('',#106803,1000.) ;
#8818 = VECTOR('',#106804,1000.) ;
#8819 = VECTOR('',#106805,1000.) ;
#8820 = VECTOR('',#106806,1000.) ;
#8821 = VECTOR('',#106807,1000.) ;
#8822 = VECTOR('',#106808,1000.) ;
#8823 = VECTOR('',#106811,1000.) ;
#8824 = VECTOR('',#106812,1000.) ;
#8825 = VECTOR('',#106813,1000.) ;
#8826 = VECTOR('',#106814,1000.) ;
#8827 = VECTOR('',#106815,1000.) ;
#8828 = VECTOR('',#106816,1000.) ;
#8829 = VECTOR('',#106819,1000.) ;
#8830 = VECTOR('',#106820,1000.) ;
#8831 = VECTOR('',#106821,1000.) ;
#8832 = VECTOR('',#106822,1000.) ;
#8833 = VECTOR('',#106825,1000.) ;
#8834 = VECTOR('',#106826,1000.) ;
#8835 = VECTOR('',#106827,1000.) ;
#8836 = VECTOR('',#106828,1000.) ;
#8837 = VECTOR('',#106831,1000.) ;
#8838 = VECTOR('',#106832,1000.) ;
#8839 = VECTOR('',#106833,1000.) ;
#8840 = VECTOR('',#106834,1000.) ;
#8841 = VECTOR('',#106837,1000.) ;
#8842 = VECTOR('',#106838,1000.) ;
#8843 = VECTOR('',#106839,1000.) ;
#8844 = VECTOR('',#106840,1000.) ;
#8845 = VECTOR('',#106843,1000.) ;
#8846 = VECTOR('',#106844,1000.) ;
#8847 = VECTOR('',#106845,1000.) ;
#8848 = VECTOR('',#106846,1000.) ;
#8849 = VECTOR('',#106847,1000.) ;
#8850 = VECTOR('',#106850,1000.) ;
#8851 = VECTOR('',#106853,1000.) ;
#8852 = VECTOR('',#106856,1000.) ;
#8853 = VECTOR('',#106863,1000.) ;
#8854 = VECTOR('',#106864,1000.) ;
#8855 = VECTOR('',#106867,1000.) ;
#8856 = VECTOR('',#106868,1000.) ;
#8857 = VECTOR('',#106873,1000.) ;
#8858 = VECTOR('',#106876,1000.) ;
#8859 = VECTOR('',#106877,1000.) ;
#8860 = VECTOR('',#106882,1000.) ;
#8861 = VECTOR('',#106885,1000.) ;
#8862 = VECTOR('',#106886,1000.) ;
#8863 = VECTOR('',#106891,1000.) ;
#8864 = VECTOR('',#106894,1000.) ;
#8865 = VECTOR('',#106899,1000.) ;
#8866 = VECTOR('',#106902,1000.) ;
#8867 = VECTOR('',#106903,1000.) ;
#8868 = VECTOR('',#106906,1000.) ;
#8869 = VECTOR('',#106907,1000.) ;
#8870 = VECTOR('',#106910,1000.) ;
#8871 = VECTOR('',#106911,1000.) ;
#8872 = VECTOR('',#106914,1000.) ;
#8873 = VECTOR('',#106915,1000.) ;
#8874 = VECTOR('',#106916,1000.) ;
#8875 = VECTOR('',#106917,1000.) ;
#8876 = VECTOR('',#106920,1000.) ;
#8877 = VECTOR('',#106921,1000.) ;
#8878 = VECTOR('',#106922,1000.) ;
#8879 = VECTOR('',#106923,1000.) ;
#8880 = VECTOR('',#106926,1000.) ;
#8881 = VECTOR('',#106927,1000.) ;
#8882 = VECTOR('',#106928,1000.) ;
#8883 = VECTOR('',#106929,1000.) ;
#8884 = VECTOR('',#106932,1000.) ;
#8885 = VECTOR('',#106933,1000.) ;
#8886 = VECTOR('',#106934,1000.) ;
#8887 = VECTOR('',#106935,1000.) ;
#8888 = VECTOR('',#106938,1000.) ;
#8889 = VECTOR('',#106939,1000.) ;
#8890 = VECTOR('',#106940,1000.) ;
#8891 = VECTOR('',#106941,1000.) ;
#8892 = VECTOR('',#106942,1000.) ;
#8893 = VECTOR('',#106945,1000.) ;
#8894 = VECTOR('',#106948,1000.) ;
#8895 = VECTOR('',#106951,1000.) ;
#8896 = VECTOR('',#106956,1000.) ;
#8897 = VECTOR('',#106959,1000.) ;
#8898 = VECTOR('',#106962,1000.) ;
#8899 = VECTOR('',#106963,1000.) ;
#8900 = VECTOR('',#106968,1000.) ;
#8901 = VECTOR('',#106971,1000.) ;
#8902 = VECTOR('',#106972,1000.) ;
#8903 = VECTOR('',#106977,1000.) ;
#8904 = VECTOR('',#106980,1000.) ;
#8905 = VECTOR('',#106981,1000.) ;
#8906 = VECTOR('',#106986,1000.) ;
#8907 = VECTOR('',#106989,1000.) ;
#8908 = VECTOR('',#106992,1000.) ;
#8909 = VECTOR('',#106993,1000.) ;
#8910 = VECTOR('',#106994,1000.) ;
#8911 = VECTOR('',#106995,1000.) ;
#8912 = VECTOR('',#106998,1000.) ;
#8913 = VECTOR('',#106999,1000.) ;
#8914 = VECTOR('',#107000,1000.) ;
#8915 = VECTOR('',#107001,1000.) ;
#8916 = VECTOR('',#107004,1000.) ;
#8917 = VECTOR('',#107005,1000.) ;
#8918 = VECTOR('',#107006,1000.) ;
#8919 = VECTOR('',#107009,1000.) ;
#8920 = VECTOR('',#107010,1000.) ;
#8921 = VECTOR('',#107011,1000.) ;
#8922 = VECTOR('',#107014,1000.) ;
#8923 = VECTOR('',#107017,1000.) ;
#8924 = VECTOR('',#107018,1000.) ;
#8925 = VECTOR('',#107019,1000.) ;
#8926 = VECTOR('',#107030,1000.) ;
#8927 = VECTOR('',#107033,1000.) ;
#8928 = VECTOR('',#107598,1000.) ;
#8929 = VECTOR('',#107601,1000.) ;
#8930 = VECTOR('',#107650,1000.) ;
#8931 = VECTOR('',#107653,1000.) ;
#8932 = VECTOR('',#107666,1.5) ;
#8933 = VECTOR('',#107669,1.5) ;
#8934 = VECTOR('',#107674,1000.) ;
#8935 = VECTOR('',#107677,1000.) ;
#8936 = VECTOR('',#107680,1000.) ;
#8937 = VECTOR('',#107683,1000.) ;
#8938 = VECTOR('',#107686,1.9) ;
#8939 = VECTOR('',#107691,1000.) ;
#8940 = VECTOR('',#107692,1000.) ;
#8941 = VECTOR('',#107693,1000.) ;
#8942 = VECTOR('',#107696,1000.) ;
#8943 = VECTOR('',#107697,1000.) ;
#8944 = VECTOR('',#107698,1000.) ;
#8945 = VECTOR('',#107699,1000.) ;
#8946 = VECTOR('',#107702,1000.) ;
#8947 = VECTOR('',#107703,1000.) ;
#8948 = VECTOR('',#107704,1000.) ;
#8949 = VECTOR('',#107705,1000.) ;
#8950 = VECTOR('',#107708,1000.) ;
#8951 = VECTOR('',#107711,1000.) ;
#8952 = VECTOR('',#107712,1000.) ;
#8953 = VECTOR('',#107713,1000.) ;
#8954 = VECTOR('',#107714,1000.) ;
#8955 = VECTOR('',#107721,1000.) ;
#8956 = VECTOR('',#107722,1000.) ;
#8957 = VECTOR('',#107723,1000.) ;
#8958 = VECTOR('',#107724,1000.) ;
#8959 = VECTOR('',#107727,1000.) ;
#8960 = VECTOR('',#107730,1000.) ;
#8961 = VECTOR('',#107731,1000.) ;
#8962 = VECTOR('',#107732,1000.) ;
#8963 = VECTOR('',#107733,1000.) ;
#8964 = VECTOR('',#107736,1000.) ;
#8965 = VECTOR('',#107737,1000.) ;
#8966 = VECTOR('',#107740,1000.) ;
#8967 = VECTOR('',#107743,1000.) ;
#8968 = VECTOR('',#107744,1000.) ;
#8969 = VECTOR('',#107745,1000.) ;
#8970 = VECTOR('',#107748,1000.) ;
#8971 = VECTOR('',#107749,1000.) ;
#8972 = VECTOR('',#107750,1000.) ;
#8973 = VECTOR('',#107751,1000.) ;
#8974 = VECTOR('',#107754,1000.) ;
#8975 = VECTOR('',#107755,1000.) ;
#8976 = VECTOR('',#107756,1000.) ;
#8977 = VECTOR('',#107757,1000.) ;
#8978 = VECTOR('',#107760,1000.) ;
#8979 = VECTOR('',#107761,1000.) ;
#8980 = VECTOR('',#107762,1000.) ;
#8981 = VECTOR('',#107763,1000.) ;
#8982 = VECTOR('',#107766,1000.) ;
#8983 = VECTOR('',#107767,1000.) ;
#8984 = VECTOR('',#107768,1000.) ;
#8985 = VECTOR('',#107769,1000.) ;
#8986 = VECTOR('',#107772,1000.) ;
#8987 = VECTOR('',#107773,1000.) ;
#8988 = VECTOR('',#107774,1000.) ;
#8989 = VECTOR('',#107775,1000.) ;
#8990 = VECTOR('',#107778,1000.) ;
#8991 = VECTOR('',#107779,1000.) ;
#8992 = VECTOR('',#107780,1000.) ;
#8993 = VECTOR('',#107781,1000.) ;
#8994 = VECTOR('',#107784,1000.) ;
#8995 = VECTOR('',#107785,1000.) ;
#8996 = VECTOR('',#107786,1000.) ;
#8997 = VECTOR('',#107787,1000.) ;
#8998 = VECTOR('',#107790,1000.) ;
#8999 = VECTOR('',#107793,1000.) ;
#9000 = VECTOR('',#107796,1000.) ;
#9001 = VECTOR('',#107799,1000.) ;
#9002 = VECTOR('',#107802,1000.) ;
#9003 = VECTOR('',#107803,1000.) ;
#9004 = VECTOR('',#107804,1000.) ;
#9005 = VECTOR('',#107805,1000.) ;
#9006 = VECTOR('',#107808,1000.) ;
#9007 = VECTOR('',#107809,1000.) ;
#9008 = VECTOR('',#107810,1000.) ;
#9009 = VECTOR('',#107813,1000.) ;
#9010 = VECTOR('',#107814,1000.) ;
#9011 = VECTOR('',#107815,1000.) ;
#9012 = VECTOR('',#107818,1000.) ;
#9013 = VECTOR('',#107819,1000.) ;
#9014 = VECTOR('',#107820,1000.) ;
#9015 = VECTOR('',#107821,1000.) ;
#9016 = VECTOR('',#107822,1000.) ;
#9017 = VECTOR('',#107823,1000.) ;
#9018 = VECTOR('',#107824,1000.) ;
#9019 = VECTOR('',#107825,1000.) ;
#9020 = VECTOR('',#107828,1000.) ;
#9021 = VECTOR('',#107829,1000.) ;
#9022 = VECTOR('',#107830,1000.) ;
#9023 = VECTOR('',#107831,1000.) ;
#9024 = VECTOR('',#107834,1000.) ;
#9025 = VECTOR('',#107837,1000.) ;
#9026 = VECTOR('',#107840,1000.) ;
#9027 = VECTOR('',#107843,1000.) ;
#9028 = VECTOR('',#107846,1000.) ;
#9029 = VECTOR('',#107847,1000.) ;
#9030 = VECTOR('',#107848,1000.) ;
#9031 = VECTOR('',#107849,1000.) ;
#9032 = VECTOR('',#107852,1000.) ;
#9033 = VECTOR('',#107853,1000.) ;
#9034 = VECTOR('',#107854,1000.) ;
#9035 = VECTOR('',#107855,1000.) ;
#9036 = VECTOR('',#107856,1000.) ;
#9037 = VECTOR('',#107859,1000.) ;
#9038 = VECTOR('',#107860,1000.) ;
#9039 = VECTOR('',#107863,1000.) ;
#9040 = VECTOR('',#107866,1000.) ;
#9041 = VECTOR('',#107867,1000.) ;
#9042 = VECTOR('',#107868,1000.) ;
#9043 = VECTOR('',#107869,1000.) ;
#9044 = VECTOR('',#107948,1000.) ;
#9045 = VECTOR('',#107949,1000.) ;
#9046 = VECTOR('',#107950,1000.) ;
#9047 = VECTOR('',#107951,1000.) ;
#9048 = VECTOR('',#107954,1000.) ;
#9049 = VECTOR('',#107955,1000.) ;
#9050 = VECTOR('',#107956,1000.) ;
#9051 = VECTOR('',#107957,1000.) ;
#9052 = VECTOR('',#107962,1000.) ;
#9053 = VECTOR('',#107963,1000.) ;
#9054 = VECTOR('',#107964,1000.) ;
#9055 = VECTOR('',#107967,1000.) ;
#9056 = VECTOR('',#107968,1000.) ;
#9057 = VECTOR('',#107969,1000.) ;
#9058 = VECTOR('',#107972,1000.) ;
#9059 = VECTOR('',#107975,1000.) ;
#9060 = VECTOR('',#107980,1000.) ;
#9061 = VECTOR('',#107987,1000.) ;
#9062 = VECTOR('',#107988,1000.) ;
#9063 = VECTOR('',#107991,1000.) ;
#9064 = VECTOR('',#107992,1000.) ;
#9065 = VECTOR('',#107993,1000.) ;
#9066 = VECTOR('',#107996,1000.) ;
#9067 = VECTOR('',#107997,1000.) ;
#9068 = VECTOR('',#107998,1000.) ;
#9069 = VECTOR('',#108001,1000.) ;
#9070 = VECTOR('',#108002,1000.) ;
#9071 = VECTOR('',#108003,1000.) ;
#9072 = VECTOR('',#108006,1000.) ;
#9073 = VECTOR('',#108007,1000.) ;
#9074 = VECTOR('',#108008,1000.) ;
#9075 = VECTOR('',#108009,1000.) ;
#9076 = VECTOR('',#108010,1000.) ;
#9077 = VECTOR('',#108011,1000.) ;
#9078 = VECTOR('',#108014,1000.) ;
#9079 = VECTOR('',#108015,1000.) ;
#9080 = VECTOR('',#108016,1000.) ;
#9081 = VECTOR('',#108017,1000.) ;
#9082 = VECTOR('',#108018,1000.) ;
#9083 = VECTOR('',#108019,1000.) ;
#9084 = VECTOR('',#108022,1000.) ;
#9085 = VECTOR('',#108023,1000.) ;
#9086 = VECTOR('',#108024,1000.) ;
#9087 = VECTOR('',#108025,1000.) ;
#9088 = VECTOR('',#108028,1000.) ;
#9089 = VECTOR('',#108029,1000.) ;
#9090 = VECTOR('',#108030,1000.) ;
#9091 = VECTOR('',#108031,1000.) ;
#9092 = VECTOR('',#108034,1000.) ;
#9093 = VECTOR('',#108035,1000.) ;
#9094 = VECTOR('',#108036,1000.) ;
#9095 = VECTOR('',#108037,1000.) ;
#9096 = VECTOR('',#108040,1000.) ;
#9097 = VECTOR('',#108041,1000.) ;
#9098 = VECTOR('',#108042,1000.) ;
#9099 = VECTOR('',#108043,1000.) ;
#9100 = VECTOR('',#108046,1000.) ;
#9101 = VECTOR('',#108047,1000.) ;
#9102 = VECTOR('',#108048,1000.) ;
#9103 = VECTOR('',#108049,1000.) ;
#9104 = VECTOR('',#108050,1000.) ;
#9105 = VECTOR('',#108053,1000.) ;
#9106 = VECTOR('',#108056,1000.) ;
#9107 = VECTOR('',#108059,1000.) ;
#9108 = VECTOR('',#108066,1000.) ;
#9109 = VECTOR('',#108067,1000.) ;
#9110 = VECTOR('',#108070,1000.) ;
#9111 = VECTOR('',#108071,1000.) ;
#9112 = VECTOR('',#108076,1000.) ;
#9113 = VECTOR('',#108079,1000.) ;
#9114 = VECTOR('',#108080,1000.) ;
#9115 = VECTOR('',#108085,1000.) ;
#9116 = VECTOR('',#108088,1000.) ;
#9117 = VECTOR('',#108089,1000.) ;
#9118 = VECTOR('',#108094,1000.) ;
#9119 = VECTOR('',#108097,1000.) ;
#9120 = VECTOR('',#108102,1000.) ;
#9121 = VECTOR('',#108105,1000.) ;
#9122 = VECTOR('',#108106,1000.) ;
#9123 = VECTOR('',#108109,1000.) ;
#9124 = VECTOR('',#108110,1000.) ;
#9125 = VECTOR('',#108113,1000.) ;
#9126 = VECTOR('',#108114,1000.) ;
#9127 = VECTOR('',#108117,1000.) ;
#9128 = VECTOR('',#108118,1000.) ;
#9129 = VECTOR('',#108119,1000.) ;
#9130 = VECTOR('',#108120,1000.) ;
#9131 = VECTOR('',#108123,1000.) ;
#9132 = VECTOR('',#108124,1000.) ;
#9133 = VECTOR('',#108125,1000.) ;
#9134 = VECTOR('',#108126,1000.) ;
#9135 = VECTOR('',#108129,1000.) ;
#9136 = VECTOR('',#108130,1000.) ;
#9137 = VECTOR('',#108131,1000.) ;
#9138 = VECTOR('',#108132,1000.) ;
#9139 = VECTOR('',#108135,1000.) ;
#9140 = VECTOR('',#108136,1000.) ;
#9141 = VECTOR('',#108137,1000.) ;
#9142 = VECTOR('',#108138,1000.) ;
#9143 = VECTOR('',#108141,1000.) ;
#9144 = VECTOR('',#108142,1000.) ;
#9145 = VECTOR('',#108143,1000.) ;
#9146 = VECTOR('',#108144,1000.) ;
#9147 = VECTOR('',#108145,1000.) ;
#9148 = VECTOR('',#108148,1000.) ;
#9149 = VECTOR('',#108151,1000.) ;
#9150 = VECTOR('',#108154,1000.) ;
#9151 = VECTOR('',#108159,1000.) ;
#9152 = VECTOR('',#108162,1000.) ;
#9153 = VECTOR('',#108165,1000.) ;
#9154 = VECTOR('',#108166,1000.) ;
#9155 = VECTOR('',#108171,1000.) ;
#9156 = VECTOR('',#108174,1000.) ;
#9157 = VECTOR('',#108175,1000.) ;
#9158 = VECTOR('',#108180,1000.) ;
#9159 = VECTOR('',#108183,1000.) ;
#9160 = VECTOR('',#108184,1000.) ;
#9161 = VECTOR('',#108189,1000.) ;
#9162 = VECTOR('',#108192,1000.) ;
#9163 = VECTOR('',#108195,1000.) ;
#9164 = VECTOR('',#108196,1000.) ;
#9165 = VECTOR('',#108197,1000.) ;
#9166 = VECTOR('',#108198,1000.) ;
#9167 = VECTOR('',#108201,1000.) ;
#9168 = VECTOR('',#108202,1000.) ;
#9169 = VECTOR('',#108203,1000.) ;
#9170 = VECTOR('',#108204,1000.) ;
#9171 = VECTOR('',#108207,1000.) ;
#9172 = VECTOR('',#108208,1000.) ;
#9173 = VECTOR('',#108209,1000.) ;
#9174 = VECTOR('',#108212,1000.) ;
#9175 = VECTOR('',#108213,1000.) ;
#9176 = VECTOR('',#108214,1000.) ;
#9177 = VECTOR('',#108217,1000.) ;
#9178 = VECTOR('',#108220,1000.) ;
#9179 = VECTOR('',#108221,1000.) ;
#9180 = VECTOR('',#108222,1000.) ;
#9181 = VECTOR('',#108233,1000.) ;
#9182 = VECTOR('',#108236,1000.) ;
#9183 = VECTOR('',#108765,1000.) ;
#9184 = VECTOR('',#108768,1000.) ;
#9185 = VECTOR('',#108769,1000.) ;
#9186 = VECTOR('',#108802,1000.) ;
#9187 = VECTOR('',#108805,1000.) ;
#9188 = VECTOR('',#108806,1000.) ;
#9189 = VECTOR('',#108839,1000.) ;
#9190 = VECTOR('',#108842,1000.) ;
#9191 = VECTOR('',#108843,1000.) ;
#9192 = VECTOR('',#108876,1000.) ;
#9193 = VECTOR('',#108879,1000.) ;
#9194 = VECTOR('',#108880,1000.) ;
#9195 = VECTOR('',#108913,1000.) ;
#9196 = VECTOR('',#108916,1000.) ;
#9197 = VECTOR('',#108917,1000.) ;
#9198 = VECTOR('',#108950,1000.) ;
#9199 = VECTOR('',#108953,1000.) ;
#9200 = VECTOR('',#108954,1000.) ;
#9201 = VECTOR('',#108987,1000.) ;
#9202 = VECTOR('',#108990,1000.) ;
#9203 = VECTOR('',#108991,1000.) ;
#9204 = VECTOR('',#109024,1000.) ;
#9205 = VECTOR('',#109027,1000.) ;
#9206 = VECTOR('',#109028,1000.) ;
#9207 = VECTOR('',#109151,1000.) ;
#9208 = VECTOR('',#109154,1000.) ;
#9209 = VECTOR('',#109155,1000.) ;
#9210 = VECTOR('',#109158,1.) ;
#9211 = VECTOR('',#109161,1.) ;
#9212 = VECTOR('',#109164,1.) ;
#9213 = VECTOR('',#109167,1.) ;
#9214 = VECTOR('',#109170,1.) ;
#9215 = VECTOR('',#109173,0.999999999999999) ;
#9216 = VECTOR('',#109176,0.999999999999999) ;
#9217 = VECTOR('',#109179,1.) ;
#9218 = VECTOR('',#109182,1.) ;
#9219 = VECTOR('',#109187,1000.) ;
#9220 = VECTOR('',#109188,1000.) ;
#9221 = VECTOR('',#109193,1000.) ;
#9222 = VECTOR('',#109194,1000.) ;
#9223 = VECTOR('',#109199,1000.) ;
#9224 = VECTOR('',#109200,1000.) ;
#9225 = VECTOR('',#109205,1000.) ;
#9226 = VECTOR('',#109206,1000.) ;
#9227 = VECTOR('',#109211,1000.) ;
#9228 = VECTOR('',#109212,1000.) ;
#9229 = VECTOR('',#109217,1000.) ;
#9230 = VECTOR('',#109218,1000.) ;
#9231 = VECTOR('',#109223,1000.) ;
#9232 = VECTOR('',#109224,1000.) ;
#9233 = VECTOR('',#109229,1000.) ;
#9234 = VECTOR('',#109230,1000.) ;
#9235 = VECTOR('',#109235,1000.) ;
#9236 = VECTOR('',#109236,1000.) ;
#9237 = VECTOR('',#109279,1000.) ;
#9238 = VECTOR('',#109282,1000.) ;
#9239 = VECTOR('',#109283,1000.) ;
#9240 = VECTOR('',#109286,1.) ;
#9241 = VECTOR('',#109291,1000.) ;
#9242 = VECTOR('',#109292,1000.) ;
#9243 = VECTOR('',#109295,1000.) ;
#9244 = VECTOR('',#109298,1000.) ;
#9245 = VECTOR('',#109303,1000.) ;
#9246 = VECTOR('',#109304,1000.) ;
#9247 = VECTOR('',#109305,1000.) ;
#9248 = VECTOR('',#109306,1000.) ;
#9249 = VECTOR('',#109307,1000.) ;
#9250 = VECTOR('',#109312,1000.) ;
#9251 = VECTOR('',#109315,1000.) ;
#9252 = VECTOR('',#109320,1000.) ;
#9253 = VECTOR('',#109321,1000.) ;
#9254 = VECTOR('',#109322,1000.) ;
#9255 = VECTOR('',#109323,1000.) ;
#9256 = VECTOR('',#109324,1000.) ;
#9257 = VECTOR('',#109329,1000.) ;
#9258 = VECTOR('',#109332,1000.) ;
#9259 = VECTOR('',#109337,1000.) ;
#9260 = VECTOR('',#109338,1000.) ;
#9261 = VECTOR('',#109339,1000.) ;
#9262 = VECTOR('',#109340,1000.) ;
#9263 = VECTOR('',#109341,1000.) ;
#9264 = VECTOR('',#109346,1000.) ;
#9265 = VECTOR('',#109349,1000.) ;
#9266 = VECTOR('',#109354,1000.) ;
#9267 = VECTOR('',#109355,1000.) ;
#9268 = VECTOR('',#109356,1000.) ;
#9269 = VECTOR('',#109357,1000.) ;
#9270 = VECTOR('',#109358,1000.) ;
#9271 = VECTOR('',#109363,1000.) ;
#9272 = VECTOR('',#109366,1000.) ;
#9273 = VECTOR('',#109371,1000.) ;
#9274 = VECTOR('',#109372,1000.) ;
#9275 = VECTOR('',#109373,1000.) ;
#9276 = VECTOR('',#109374,1000.) ;
#9277 = VECTOR('',#109375,1000.) ;
#9278 = VECTOR('',#109380,1000.) ;
#9279 = VECTOR('',#109383,1000.) ;
#9280 = VECTOR('',#109388,1000.) ;
#9281 = VECTOR('',#109389,1000.) ;
#9282 = VECTOR('',#109390,1000.) ;
#9283 = VECTOR('',#109391,1000.) ;
#9284 = VECTOR('',#109392,1000.) ;
#9285 = VECTOR('',#109397,1000.) ;
#9286 = VECTOR('',#109400,1000.) ;
#9287 = VECTOR('',#109405,1000.) ;
#9288 = VECTOR('',#109406,1000.) ;
#9289 = VECTOR('',#109407,1000.) ;
#9290 = VECTOR('',#109408,1000.) ;
#9291 = VECTOR('',#109409,1000.) ;
#9292 = VECTOR('',#109414,1000.) ;
#9293 = VECTOR('',#109417,1000.) ;
#9294 = VECTOR('',#109422,1000.) ;
#9295 = VECTOR('',#109423,1000.) ;
#9296 = VECTOR('',#109424,1000.) ;
#9297 = VECTOR('',#109425,1000.) ;
#9298 = VECTOR('',#109426,1000.) ;
#9299 = VECTOR('',#109431,1000.) ;
#9300 = VECTOR('',#109434,1000.) ;
#9301 = VECTOR('',#109439,1000.) ;
#9302 = VECTOR('',#109440,1000.) ;
#9303 = VECTOR('',#109441,1000.) ;
#9304 = VECTOR('',#109442,1000.) ;
#9305 = VECTOR('',#109443,1000.) ;
#9306 = VECTOR('',#109450,1000.) ;
#9307 = VECTOR('',#109451,1000.) ;
#9308 = VECTOR('',#109452,1000.) ;
#9309 = VECTOR('',#109453,1000.) ;
#9310 = VECTOR('',#109458,1000.) ;
#9311 = VECTOR('',#109459,1000.) ;
#9312 = VECTOR('',#109460,1000.) ;
#9313 = VECTOR('',#109461,1000.) ;
#9314 = VECTOR('',#109466,1000.) ;
#9315 = VECTOR('',#109467,1000.) ;
#9316 = VECTOR('',#109468,1000.) ;
#9317 = VECTOR('',#109469,1000.) ;
#9318 = VECTOR('',#109474,1000.) ;
#9319 = VECTOR('',#109475,1000.) ;
#9320 = VECTOR('',#109476,1000.) ;
#9321 = VECTOR('',#109477,1000.) ;
#9322 = VECTOR('',#109482,1000.) ;
#9323 = VECTOR('',#109483,1000.) ;
#9324 = VECTOR('',#109484,1000.) ;
#9325 = VECTOR('',#109485,1000.) ;
#9326 = VECTOR('',#109490,1000.) ;
#9327 = VECTOR('',#109491,1000.) ;
#9328 = VECTOR('',#109492,1000.) ;
#9329 = VECTOR('',#109493,1000.) ;
#9330 = VECTOR('',#109498,1000.) ;
#9331 = VECTOR('',#109499,1000.) ;
#9332 = VECTOR('',#109500,1000.) ;
#9333 = VECTOR('',#109501,1000.) ;
#9334 = VECTOR('',#109506,1000.) ;
#9335 = VECTOR('',#109507,1000.) ;
#9336 = VECTOR('',#109508,1000.) ;
#9337 = VECTOR('',#109509,1000.) ;
#9338 = VECTOR('',#109514,1000.) ;
#9339 = VECTOR('',#109515,1000.) ;
#9340 = VECTOR('',#109516,1000.) ;
#9341 = VECTOR('',#109517,1000.) ;
#9342 = VECTOR('',#109522,1000.) ;
#9343 = VECTOR('',#109523,1000.) ;
#9344 = VECTOR('',#109524,1000.) ;
#9345 = VECTOR('',#109525,1000.) ;
#9346 = VECTOR('',#109530,1000.) ;
#9347 = VECTOR('',#109531,1000.) ;
#9348 = VECTOR('',#109532,1000.) ;
#9349 = VECTOR('',#109533,1000.) ;
#9350 = VECTOR('',#109538,1000.) ;
#9351 = VECTOR('',#109539,1000.) ;
#9352 = VECTOR('',#109540,1000.) ;
#9353 = VECTOR('',#109541,1000.) ;
#9354 = VECTOR('',#109546,1000.) ;
#9355 = VECTOR('',#109547,1000.) ;
#9356 = VECTOR('',#109548,1000.) ;
#9357 = VECTOR('',#109549,1000.) ;
#9358 = VECTOR('',#109554,1000.) ;
#9359 = VECTOR('',#109555,1000.) ;
#9360 = VECTOR('',#109556,1000.) ;
#9361 = VECTOR('',#109557,1000.) ;
#9362 = VECTOR('',#109562,1000.) ;
#9363 = VECTOR('',#109563,1000.) ;
#9364 = VECTOR('',#109564,1000.) ;
#9365 = VECTOR('',#109565,1000.) ;
#9366 = VECTOR('',#109570,1000.) ;
#9367 = VECTOR('',#109571,1000.) ;
#9368 = VECTOR('',#109572,1000.) ;
#9369 = VECTOR('',#109573,1000.) ;
#9370 = VECTOR('',#109578,1000.) ;
#9371 = VECTOR('',#109579,1000.) ;
#9372 = VECTOR('',#109580,1000.) ;
#9373 = VECTOR('',#109581,1000.) ;
#9374 = VECTOR('',#109586,1000.) ;
#9375 = VECTOR('',#109587,1000.) ;
#9376 = VECTOR('',#109588,1000.) ;
#9377 = VECTOR('',#109589,1000.) ;
#9378 = VECTOR('',#109592,1000.) ;
#9379 = VECTOR('',#109595,1000.) ;
#9380 = VECTOR('',#109600,1000.) ;
#9381 = VECTOR('',#109603,1000.) ;
#9382 = VECTOR('',#109608,1000.) ;
#9383 = VECTOR('',#109611,1000.) ;
#9384 = VECTOR('',#109616,1000.) ;
#9385 = VECTOR('',#109619,1000.) ;
#9386 = VECTOR('',#109624,1000.) ;
#9387 = VECTOR('',#109627,1000.) ;
#9388 = VECTOR('',#109632,1000.) ;
#9389 = VECTOR('',#109635,1000.) ;
#9390 = VECTOR('',#109640,1000.) ;
#9391 = VECTOR('',#109643,1000.) ;
#9392 = VECTOR('',#109648,1000.) ;
#9393 = VECTOR('',#109651,1000.) ;
#9394 = VECTOR('',#109656,1000.) ;
#9395 = VECTOR('',#109659,1000.) ;
#9396 = VECTOR('',#109664,1000.) ;
#9397 = VECTOR('',#109667,1000.) ;
#9398 = VECTOR('',#109672,1000.) ;
#9399 = VECTOR('',#109673,1000.) ;
#9400 = VECTOR('',#109674,1000.) ;
#9401 = VECTOR('',#109675,1000.) ;
#9402 = VECTOR('',#109676,1000.) ;
#9403 = VECTOR('',#109683,1000.) ;
#9404 = VECTOR('',#109684,1000.) ;
#9405 = VECTOR('',#109685,1000.) ;
#9406 = VECTOR('',#109686,1000.) ;
#9407 = VECTOR('',#109691,1000.) ;
#9408 = VECTOR('',#109692,1000.) ;
#9409 = VECTOR('',#109693,1000.) ;
#9410 = VECTOR('',#109694,1000.) ;
#9411 = VECTOR('',#109697,1000.) ;
#9412 = VECTOR('',#109700,1000.) ;
#9413 = VECTOR('',#109705,1000.) ;
#9414 = VECTOR('',#109708,1000.) ;
#9415 = VECTOR('',#109715,1000.) ;
#9416 = VECTOR('',#109716,1000.) ;
#9417 = VECTOR('',#109717,1000.) ;
#9418 = VECTOR('',#109718,1000.) ;
#9419 = VECTOR('',#109719,1000.) ;
#9420 = VECTOR('',#109722,1000.) ;
#9421 = VECTOR('',#109725,1000.) ;
#9422 = VECTOR('',#109726,1000.) ;
#9423 = VECTOR('',#109729,1000.) ;
#9424 = VECTOR('',#109732,1000.) ;
#9425 = VECTOR('',#109733,1000.) ;
#9426 = VECTOR('',#109736,1000.) ;
#9427 = VECTOR('',#109739,1000.) ;
#9428 = VECTOR('',#109740,1000.) ;
#9429 = VECTOR('',#109743,1000.) ;
#9430 = VECTOR('',#109746,1000.) ;
#9431 = VECTOR('',#109747,1000.) ;
#9432 = VECTOR('',#109750,1000.) ;
#9433 = VECTOR('',#109753,1000.) ;
#9434 = VECTOR('',#109754,1000.) ;
#9435 = VECTOR('',#109757,1000.) ;
#9436 = VECTOR('',#109760,1000.) ;
#9437 = VECTOR('',#109761,1000.) ;
#9438 = VECTOR('',#109764,1000.) ;
#9439 = VECTOR('',#109767,1000.) ;
#9440 = VECTOR('',#109768,1000.) ;
#9441 = VECTOR('',#109771,1000.) ;
#9442 = VECTOR('',#109774,1000.) ;
#9443 = VECTOR('',#109775,1000.) ;
#9444 = VECTOR('',#109778,1000.) ;
#9445 = VECTOR('',#109781,1000.) ;
#9446 = VECTOR('',#109782,1000.) ;
#9447 = VECTOR('',#109785,1000.) ;
#9448 = VECTOR('',#109790,1000.) ;
#9449 = VECTOR('',#109797,1000.) ;
#9450 = VECTOR('',#109798,1000.) ;
#9451 = VECTOR('',#109801,1000.) ;
#9452 = VECTOR('',#109804,1000.) ;
#9453 = VECTOR('',#109805,1000.) ;
#9454 = VECTOR('',#109808,1000.) ;
#9455 = VECTOR('',#109811,1000.) ;
#9456 = VECTOR('',#109812,1000.) ;
#9457 = VECTOR('',#109815,1000.) ;
#9458 = VECTOR('',#109818,1000.) ;
#9459 = VECTOR('',#109819,1000.) ;
#9460 = VECTOR('',#109822,1000.) ;
#9461 = VECTOR('',#109825,1000.) ;
#9462 = VECTOR('',#109826,1000.) ;
#9463 = VECTOR('',#109829,1000.) ;
#9464 = VECTOR('',#109832,1000.) ;
#9465 = VECTOR('',#109833,1000.) ;
#9466 = VECTOR('',#109836,1000.) ;
#9467 = VECTOR('',#109839,1000.) ;
#9468 = VECTOR('',#109840,1000.) ;
#9469 = VECTOR('',#109843,1000.) ;
#9470 = VECTOR('',#109846,1000.) ;
#9471 = VECTOR('',#109847,1000.) ;
#9472 = VECTOR('',#109850,1000.) ;
#9473 = VECTOR('',#109853,1000.) ;
#9474 = VECTOR('',#109854,1000.) ;
#9475 = VECTOR('',#109857,1000.) ;
#9476 = VECTOR('',#109860,1000.) ;
#9477 = VECTOR('',#109861,1000.) ;
#9478 = VECTOR('',#109862,1000.) ;
#9479 = VECTOR('',#109863,1000.) ;
#9480 = VECTOR('',#109864,1000.) ;
#9481 = VECTOR('',#109867,1000.) ;
#9482 = VECTOR('',#109870,1000.) ;
#9483 = VECTOR('',#109877,1000.) ;
#9484 = VECTOR('',#109878,1000.) ;
#9485 = VECTOR('',#109879,1000.) ;
#9486 = VECTOR('',#109882,1000.) ;
#9487 = VECTOR('',#109889,1000.) ;
#9488 = VECTOR('',#109890,1000.) ;
#9489 = VECTOR('',#109891,1000.) ;
#9490 = VECTOR('',#109894,1000.) ;
#9491 = VECTOR('',#109901,1000.) ;
#9492 = VECTOR('',#109902,1000.) ;
#9493 = VECTOR('',#109903,1000.) ;
#9494 = VECTOR('',#109906,1000.) ;
#9495 = VECTOR('',#109913,1000.) ;
#9496 = VECTOR('',#109914,1000.) ;
#9497 = VECTOR('',#109915,1000.) ;
#9498 = VECTOR('',#109918,1000.) ;
#9499 = VECTOR('',#109925,1000.) ;
#9500 = VECTOR('',#109926,1000.) ;
#9501 = VECTOR('',#109927,1000.) ;
#9502 = VECTOR('',#109930,1000.) ;
#9503 = VECTOR('',#109937,1000.) ;
#9504 = VECTOR('',#109938,1000.) ;
#9505 = VECTOR('',#109941,1000.) ;
#9506 = VECTOR('',#109942,1000.) ;
#9507 = VECTOR('',#109943,1000.) ;
#9508 = VECTOR('',#109946,1000.) ;
#9509 = VECTOR('',#109949,1000.) ;
#9510 = VECTOR('',#109950,1000.) ;
#9511 = VECTOR('',#109953,1000.) ;
#9512 = VECTOR('',#109954,1000.) ;
#9513 = VECTOR('',#109955,1000.) ;
#9514 = VECTOR('',#109958,1000.) ;
#9515 = VECTOR('',#109961,1000.) ;
#9516 = VECTOR('',#109968,1000.) ;
#9517 = VECTOR('',#109971,1000.) ;
#9518 = VECTOR('',#109974,1000.) ;
#9519 = VECTOR('',#109975,1000.) ;
#9520 = VECTOR('',#109976,1000.) ;
#9521 = VECTOR('',#109979,1000.) ;
#9522 = VECTOR('',#109982,1000.) ;
#9523 = VECTOR('',#109983,1000.) ;
#9524 = VECTOR('',#109986,1000.) ;
#9525 = VECTOR('',#109987,1000.) ;
#9526 = VECTOR('',#109988,1000.) ;
#9527 = VECTOR('',#109991,1000.) ;
#9528 = VECTOR('',#109994,1000.) ;
#9529 = VECTOR('',#110001,1000.) ;
#9530 = VECTOR('',#110004,1000.) ;
#9531 = VECTOR('',#110007,1000.) ;
#9532 = VECTOR('',#110008,1000.) ;
#9533 = VECTOR('',#110009,1000.) ;
#9534 = VECTOR('',#110012,1000.) ;
#9535 = VECTOR('',#110015,1000.) ;
#9536 = VECTOR('',#110016,1000.) ;
#9537 = VECTOR('',#110019,1000.) ;
#9538 = VECTOR('',#110020,1000.) ;
#9539 = VECTOR('',#110021,1000.) ;
#9540 = VECTOR('',#110024,1000.) ;
#9541 = VECTOR('',#110027,1000.) ;
#9542 = VECTOR('',#110034,1000.) ;
#9543 = VECTOR('',#110037,1000.) ;
#9544 = VECTOR('',#110040,1000.) ;
#9545 = VECTOR('',#110041,1000.) ;
#9546 = VECTOR('',#110042,1000.) ;
#9547 = VECTOR('',#110045,1000.) ;
#9548 = VECTOR('',#110048,1000.) ;
#9549 = VECTOR('',#110049,1000.) ;
#9550 = VECTOR('',#110052,1000.) ;
#9551 = VECTOR('',#110053,1000.) ;
#9552 = VECTOR('',#110054,1000.) ;
#9553 = VECTOR('',#110057,1000.) ;
#9554 = VECTOR('',#110060,1000.) ;
#9555 = VECTOR('',#110067,1000.) ;
#9556 = VECTOR('',#110070,1000.) ;
#9557 = VECTOR('',#110073,1000.) ;
#9558 = VECTOR('',#110074,1000.) ;
#9559 = VECTOR('',#110075,1000.) ;
#9560 = VECTOR('',#110078,1000.) ;
#9561 = VECTOR('',#110081,1000.) ;
#9562 = VECTOR('',#110082,1000.) ;
#9563 = VECTOR('',#110085,1000.) ;
#9564 = VECTOR('',#110086,1000.) ;
#9565 = VECTOR('',#110087,1000.) ;
#9566 = VECTOR('',#110090,1000.) ;
#9567 = VECTOR('',#110093,1000.) ;
#9568 = VECTOR('',#110100,1000.) ;
#9569 = VECTOR('',#110103,1000.) ;
#9570 = VECTOR('',#110106,1000.) ;
#9571 = VECTOR('',#110107,1000.) ;
#9572 = VECTOR('',#110108,1000.) ;
#9573 = VECTOR('',#110111,1000.) ;
#9574 = VECTOR('',#110114,1000.) ;
#9575 = VECTOR('',#110115,1000.) ;
#9576 = VECTOR('',#110118,1000.) ;
#9577 = VECTOR('',#110119,1000.) ;
#9578 = VECTOR('',#110120,1000.) ;
#9579 = VECTOR('',#110123,1000.) ;
#9580 = VECTOR('',#110126,1000.) ;
#9581 = VECTOR('',#110133,1000.) ;
#9582 = VECTOR('',#110136,1000.) ;
#9583 = VECTOR('',#110139,1000.) ;
#9584 = VECTOR('',#110140,1000.) ;
#9585 = VECTOR('',#110141,1000.) ;
#9586 = VECTOR('',#110144,1000.) ;
#9587 = VECTOR('',#110147,1000.) ;
#9588 = VECTOR('',#110148,1000.) ;
#9589 = VECTOR('',#110151,1000.) ;
#9590 = VECTOR('',#110152,1000.) ;
#9591 = VECTOR('',#110153,1000.) ;
#9592 = VECTOR('',#110156,1000.) ;
#9593 = VECTOR('',#110159,1000.) ;
#9594 = VECTOR('',#110166,1000.) ;
#9595 = VECTOR('',#110169,1000.) ;
#9596 = VECTOR('',#110172,1000.) ;
#9597 = VECTOR('',#110173,1000.) ;
#9598 = VECTOR('',#110174,1000.) ;
#9599 = VECTOR('',#110177,1000.) ;
#9600 = VECTOR('',#110180,1000.) ;
#9601 = VECTOR('',#110181,1000.) ;
#9602 = VECTOR('',#110184,1000.) ;
#9603 = VECTOR('',#110185,1000.) ;
#9604 = VECTOR('',#110186,1000.) ;
#9605 = VECTOR('',#110189,1000.) ;
#9606 = VECTOR('',#110192,1000.) ;
#9607 = VECTOR('',#110199,1000.) ;
#9608 = VECTOR('',#110202,1000.) ;
#9609 = VECTOR('',#110205,1000.) ;
#9610 = VECTOR('',#110206,1000.) ;
#9611 = VECTOR('',#110207,1000.) ;
#9612 = VECTOR('',#110210,1000.) ;
#9613 = VECTOR('',#110213,1000.) ;
#9614 = VECTOR('',#110214,1000.) ;
#9615 = VECTOR('',#110217,1000.) ;
#9616 = VECTOR('',#110218,1000.) ;
#9617 = VECTOR('',#110219,1000.) ;
#9618 = VECTOR('',#110222,1000.) ;
#9619 = VECTOR('',#110225,1000.) ;
#9620 = VECTOR('',#110232,1000.) ;
#9621 = VECTOR('',#110235,1000.) ;
#9622 = VECTOR('',#110238,1000.) ;
#9623 = VECTOR('',#110239,1000.) ;
#9624 = VECTOR('',#110240,1000.) ;
#9625 = VECTOR('',#110243,1000.) ;
#9626 = VECTOR('',#110246,1000.) ;
#9627 = VECTOR('',#110247,1000.) ;
#9628 = VECTOR('',#110250,1000.) ;
#9629 = VECTOR('',#110251,1000.) ;
#9630 = VECTOR('',#110252,1000.) ;
#9631 = VECTOR('',#110255,1000.) ;
#9632 = VECTOR('',#110258,1000.) ;
#9633 = VECTOR('',#110265,1000.) ;
#9634 = VECTOR('',#110268,1000.) ;
#9635 = VECTOR('',#110271,1000.) ;
#9636 = VECTOR('',#110272,1000.) ;
#9637 = VECTOR('',#110273,1000.) ;
#9638 = VECTOR('',#110274,1000.) ;
#9639 = VECTOR('',#110277,1000.) ;
#9640 = VECTOR('',#110278,1000.) ;
#9641 = VECTOR('',#110279,1000.) ;
#9642 = VECTOR('',#110282,1000.) ;
#9643 = VECTOR('',#110285,1000.) ;
#9644 = VECTOR('',#110286,1000.) ;
#9645 = VECTOR('',#110287,1000.) ;
#9646 = VECTOR('',#110288,1000.) ;
#9647 = VECTOR('',#110291,1000.) ;
#9648 = VECTOR('',#110292,1000.) ;
#9649 = VECTOR('',#110293,1000.) ;
#9650 = VECTOR('',#110296,1000.) ;
#9651 = VECTOR('',#110299,1000.) ;
#9652 = VECTOR('',#110300,1000.) ;
#9653 = VECTOR('',#110301,1000.) ;
#9654 = VECTOR('',#110302,1000.) ;
#9655 = VECTOR('',#110303,1000.) ;
#9656 = VECTOR('',#110304,1000.) ;
#9657 = VECTOR('',#110307,1000.) ;
#9658 = VECTOR('',#110310,1000.) ;
#9659 = VECTOR('',#110313,1000.) ;
#9660 = VECTOR('',#110314,1000.) ;
#9661 = VECTOR('',#110315,1000.) ;
#9662 = VECTOR('',#110316,1000.) ;
#9663 = VECTOR('',#110319,1000.) ;
#9664 = VECTOR('',#110320,1000.) ;
#9665 = VECTOR('',#110321,1000.) ;
#9666 = VECTOR('',#110324,1000.) ;
#9667 = VECTOR('',#110325,1000.) ;
#9668 = VECTOR('',#110326,1000.) ;
#9669 = VECTOR('',#110327,1000.) ;
#9670 = VECTOR('',#110330,1000.) ;
#9671 = VECTOR('',#110331,1000.) ;
#9672 = VECTOR('',#110332,1000.) ;
#9673 = VECTOR('',#110333,1000.) ;
#9674 = VECTOR('',#110336,1000.) ;
#9675 = VECTOR('',#110337,1000.) ;
#9676 = VECTOR('',#110338,1000.) ;
#9677 = VECTOR('',#110339,1000.) ;
#9678 = VECTOR('',#110342,1000.) ;
#9679 = VECTOR('',#110345,1000.) ;
#9680 = VECTOR('',#110350,1000.) ;
#9681 = VECTOR('',#110351,1000.) ;
#9682 = VECTOR('',#110352,1000.) ;
#9683 = VECTOR('',#110357,1000.) ;
#9684 = VECTOR('',#110362,1000.) ;
#9685 = VECTOR('',#110363,1000.) ;
#9686 = VECTOR('',#110364,1000.) ;
#9687 = VECTOR('',#110369,1000.) ;
#9688 = VECTOR('',#110374,1000.) ;
#9689 = VECTOR('',#110375,1000.) ;
#9690 = VECTOR('',#110376,1000.) ;
#9691 = VECTOR('',#110379,1000.) ;
#9692 = VECTOR('',#110384,1000.) ;
#9693 = VECTOR('',#110385,1000.) ;
#9694 = VECTOR('',#110388,1000.) ;
#9695 = VECTOR('',#110389,1000.) ;
#9696 = VECTOR('',#110390,1000.) ;
#9697 = VECTOR('',#110395,1000.) ;
#9698 = VECTOR('',#110400,1000.) ;
#9699 = VECTOR('',#110401,1000.) ;
#9700 = VECTOR('',#110402,1000.) ;
#9701 = VECTOR('',#110407,1000.) ;
#9702 = VECTOR('',#110412,1000.) ;
#9703 = VECTOR('',#110413,1000.) ;
#9704 = VECTOR('',#110414,1000.) ;
#9705 = VECTOR('',#110419,1000.) ;
#9706 = VECTOR('',#110424,1000.) ;
#9707 = VECTOR('',#110425,1000.) ;
#9708 = VECTOR('',#110426,1000.) ;
#9709 = VECTOR('',#110431,1000.) ;
#9710 = VECTOR('',#110436,1000.) ;
#9711 = VECTOR('',#110437,1000.) ;
#9712 = VECTOR('',#110438,1000.) ;
#9713 = VECTOR('',#110443,1000.) ;
#9714 = VECTOR('',#110448,1000.) ;
#9715 = VECTOR('',#110449,1000.) ;
#9716 = VECTOR('',#110450,1000.) ;
#9717 = VECTOR('',#110455,1000.) ;
#9718 = VECTOR('',#110462,1000.) ;
#9719 = VECTOR('',#110469,1000.) ;
#9720 = VECTOR('',#110474,1000.) ;
#9721 = VECTOR('',#110475,1000.) ;
#9722 = VECTOR('',#110476,1000.) ;
#9723 = VECTOR('',#110481,1000.) ;
#9724 = VECTOR('',#110486,1000.) ;
#9725 = VECTOR('',#110487,1000.) ;
#9726 = VECTOR('',#110488,1000.) ;
#9727 = VECTOR('',#110493,1000.) ;
#9728 = VECTOR('',#110498,1000.) ;
#9729 = VECTOR('',#110499,1000.) ;
#9730 = VECTOR('',#110504,1000.) ;
#9731 = VECTOR('',#110507,1000.) ;
#9732 = VECTOR('',#110508,1000.) ;
#9733 = VECTOR('',#110509,1000.) ;
#9734 = VECTOR('',#110512,1000.) ;
#9735 = VECTOR('',#110513,1000.) ;
#9736 = VECTOR('',#110514,1000.) ;
#9737 = VECTOR('',#110517,1000.) ;
#9738 = VECTOR('',#110520,1000.) ;
#9739 = VECTOR('',#110521,1000.) ;
#9740 = VECTOR('',#110522,1000.) ;
#9741 = VECTOR('',#110523,1000.) ;
#9742 = VECTOR('',#110524,1000.) ;
#9743 = VECTOR('',#110527,1000.) ;
#9744 = VECTOR('',#110530,1000.) ;
#9745 = VECTOR('',#110533,1000.) ;
#9746 = VECTOR('',#110536,1000.) ;
#9747 = VECTOR('',#110571,1000.) ;
#9748 = VECTOR('',#110574,1000.) ;
#9749 = VECTOR('',#110621,1000.) ;
#9750 = VECTOR('',#110680,1000.) ;
#9751 = VECTOR('',#110729,1000.) ;
#9752 = VECTOR('',#111086,1000.) ;
#9753 = VECTOR('',#111087,1000.) ;
#9754 = VECTOR('',#111088,1000.) ;
#9755 = VECTOR('',#111089,1000.) ;
#9756 = VECTOR('',#111092,1000.) ;
#9757 = VECTOR('',#111093,1000.) ;
#9758 = VECTOR('',#111094,1000.) ;
#9759 = VECTOR('',#111095,1000.) ;
#9760 = VECTOR('',#111098,1000.) ;
#9761 = VECTOR('',#111099,1000.) ;
#9762 = VECTOR('',#111100,1000.) ;
#9763 = VECTOR('',#111101,1000.) ;
#9764 = VECTOR('',#111104,1000.) ;
#9765 = VECTOR('',#111105,1000.) ;
#9766 = VECTOR('',#111106,1000.) ;
#9767 = VECTOR('',#111107,1000.) ;
#9768 = VECTOR('',#111110,1000.) ;
#9769 = VECTOR('',#111111,1000.) ;
#9770 = VECTOR('',#111112,1000.) ;
#9771 = VECTOR('',#111113,1000.) ;
#9772 = VECTOR('',#111116,1000.) ;
#9773 = VECTOR('',#111121,1000.) ;
#9774 = VECTOR('',#111122,1000.) ;
#9775 = VECTOR('',#111125,1000.) ;
#9776 = VECTOR('',#111130,1000.) ;
#9777 = VECTOR('',#111131,1000.) ;
#9778 = VECTOR('',#111146,1000.) ;
#9779 = VECTOR('',#111147,1000.) ;
#9780 = VECTOR('',#111148,1000.) ;
#9781 = VECTOR('',#111149,1000.) ;
#9782 = VECTOR('',#111152,1000.) ;
#9783 = VECTOR('',#111153,1000.) ;
#9784 = VECTOR('',#111154,1000.) ;
#9785 = VECTOR('',#111157,1000.) ;
#9786 = VECTOR('',#111158,1000.) ;
#9787 = VECTOR('',#111159,1000.) ;
#9788 = VECTOR('',#111162,1000.) ;
#9789 = VECTOR('',#111163,1000.) ;
#9790 = VECTOR('',#111164,1000.) ;
#9791 = VECTOR('',#111165,1000.) ;
#9792 = VECTOR('',#111168,1000.) ;
#9793 = VECTOR('',#111169,1000.) ;
#9794 = VECTOR('',#111170,1000.) ;
#9795 = VECTOR('',#111171,1000.) ;
#9796 = VECTOR('',#111174,1000.) ;
#9797 = VECTOR('',#111175,1000.) ;
#9798 = VECTOR('',#111176,1000.) ;
#9799 = VECTOR('',#111179,1000.) ;
#9800 = VECTOR('',#111180,1000.) ;
#9801 = VECTOR('',#111181,1000.) ;
#9802 = VECTOR('',#111184,1000.) ;
#9803 = VECTOR('',#111185,1000.) ;
#9804 = VECTOR('',#111186,1000.) ;
#9805 = VECTOR('',#111187,1000.) ;
#9806 = VECTOR('',#111190,1000.) ;
#9807 = VECTOR('',#111191,1000.) ;
#9808 = VECTOR('',#111192,1000.) ;
#9809 = VECTOR('',#111193,1000.) ;
#9810 = VECTOR('',#111196,1000.) ;
#9811 = VECTOR('',#111197,1000.) ;
#9812 = VECTOR('',#111198,1000.) ;
#9813 = VECTOR('',#111199,1000.) ;
#9814 = VECTOR('',#111202,1000.) ;
#9815 = VECTOR('',#111203,1000.) ;
#9816 = VECTOR('',#111204,1000.) ;
#9817 = VECTOR('',#111205,1000.) ;
#9818 = VECTOR('',#111432,1000.) ;
#9819 = VECTOR('',#111433,1000.) ;
#9820 = VECTOR('',#111434,1000.) ;
#9821 = VECTOR('',#111435,1000.) ;
#9822 = VECTOR('',#111436,1000.) ;
#9823 = VECTOR('',#111437,1000.) ;
#9824 = VECTOR('',#111440,1000.) ;
#9825 = VECTOR('',#111443,1000.) ;
#9826 = VECTOR('',#111446,1000.) ;
#9827 = VECTOR('',#111447,1000.) ;
#9828 = VECTOR('',#111448,1000.) ;
#9829 = VECTOR('',#111449,1000.) ;
#9830 = VECTOR('',#111450,1000.) ;
#9831 = VECTOR('',#111451,1000.) ;
#9832 = VECTOR('',#111454,1000.) ;
#9833 = VECTOR('',#111457,1000.) ;
#9834 = VECTOR('',#111460,1000.) ;
#9835 = VECTOR('',#111461,1000.) ;
#9836 = VECTOR('',#111462,1000.) ;
#9837 = VECTOR('',#111463,1000.) ;
#9838 = VECTOR('',#111464,1000.) ;
#9839 = VECTOR('',#111465,1000.) ;
#9840 = VECTOR('',#111468,1000.) ;
#9841 = VECTOR('',#111471,1000.) ;
#9842 = VECTOR('',#111474,1000.) ;
#9843 = VECTOR('',#111475,1000.) ;
#9844 = VECTOR('',#111476,1000.) ;
#9845 = VECTOR('',#111477,1000.) ;
#9846 = VECTOR('',#111478,1000.) ;
#9847 = VECTOR('',#111479,1000.) ;
#9848 = VECTOR('',#111482,1000.) ;
#9849 = VECTOR('',#111485,1000.) ;
#9850 = VECTOR('',#111488,1000.) ;
#9851 = VECTOR('',#111489,1000.) ;
#9852 = VECTOR('',#111490,1000.) ;
#9853 = VECTOR('',#111491,1000.) ;
#9854 = VECTOR('',#111492,1000.) ;
#9855 = VECTOR('',#111493,1000.) ;
#9856 = VECTOR('',#111496,1000.) ;
#9857 = VECTOR('',#111499,1000.) ;
#9858 = VECTOR('',#111502,1000.) ;
#9859 = VECTOR('',#111503,1000.) ;
#9860 = VECTOR('',#111504,1000.) ;
#9861 = VECTOR('',#111505,1000.) ;
#9862 = VECTOR('',#111506,1000.) ;
#9863 = VECTOR('',#111507,1000.) ;
#9864 = VECTOR('',#111510,1000.) ;
#9865 = VECTOR('',#111513,1000.) ;
#9866 = VECTOR('',#111516,1000.) ;
#9867 = VECTOR('',#111517,1000.) ;
#9868 = VECTOR('',#111518,1000.) ;
#9869 = VECTOR('',#111519,1000.) ;
#9870 = VECTOR('',#111520,1000.) ;
#9871 = VECTOR('',#111521,1000.) ;
#9872 = VECTOR('',#111524,1000.) ;
#9873 = VECTOR('',#111527,1000.) ;
#9874 = VECTOR('',#111530,1000.) ;
#9875 = VECTOR('',#111531,1000.) ;
#9876 = VECTOR('',#111532,1000.) ;
#9877 = VECTOR('',#111533,1000.) ;
#9878 = VECTOR('',#111534,1000.) ;
#9879 = VECTOR('',#111535,1000.) ;
#9880 = VECTOR('',#111538,1000.) ;
#9881 = VECTOR('',#111541,1000.) ;
#9882 = VECTOR('',#111544,1000.) ;
#9883 = VECTOR('',#111545,1000.) ;
#9884 = VECTOR('',#111546,1000.) ;
#9885 = VECTOR('',#111547,1000.) ;
#9886 = VECTOR('',#111548,1000.) ;
#9887 = VECTOR('',#111549,1000.) ;
#9888 = VECTOR('',#111552,1000.) ;
#9889 = VECTOR('',#111555,1000.) ;
#9890 = VECTOR('',#111558,1000.) ;
#9891 = VECTOR('',#111559,1000.) ;
#9892 = VECTOR('',#111560,1000.) ;
#9893 = VECTOR('',#111561,1000.) ;
#9894 = VECTOR('',#111564,1000.) ;
#9895 = VECTOR('',#111565,1000.) ;
#9896 = VECTOR('',#111566,1000.) ;
#9897 = VECTOR('',#111569,1000.) ;
#9898 = VECTOR('',#111570,1000.) ;
#9899 = VECTOR('',#111571,1000.) ;
#9900 = VECTOR('',#111572,1000.) ;
#9901 = VECTOR('',#111575,1000.) ;
#9902 = VECTOR('',#111576,1000.) ;
#9903 = VECTOR('',#111577,1000.) ;
#9904 = VECTOR('',#111578,1000.) ;
#9905 = VECTOR('',#111581,1000.) ;
#9906 = VECTOR('',#111582,1000.) ;
#9907 = VECTOR('',#111583,1000.) ;
#9908 = VECTOR('',#111584,1000.) ;
#9909 = VECTOR('',#111587,1000.) ;
#9910 = VECTOR('',#111588,1000.) ;
#9911 = VECTOR('',#111589,1000.) ;
#9912 = VECTOR('',#111590,1000.) ;
#9913 = VECTOR('',#111593,1000.) ;
#9914 = VECTOR('',#111594,1000.) ;
#9915 = VECTOR('',#111595,1000.) ;
#9916 = VECTOR('',#111598,1000.) ;
#9917 = VECTOR('',#111599,1000.) ;
#9918 = VECTOR('',#111600,1000.) ;
#9919 = VECTOR('',#111601,1000.) ;
#9920 = VECTOR('',#111604,1000.) ;
#9921 = VECTOR('',#111605,1000.) ;
#9922 = VECTOR('',#111606,1000.) ;
#9923 = VECTOR('',#111607,1000.) ;
#9924 = VECTOR('',#111610,1000.) ;
#9925 = VECTOR('',#111611,1000.) ;
#9926 = VECTOR('',#111612,1000.) ;
#9927 = VECTOR('',#111613,1000.) ;
#9928 = VECTOR('',#111616,1000.) ;
#9929 = VECTOR('',#111617,1000.) ;
#9930 = VECTOR('',#111618,1000.) ;
#9931 = VECTOR('',#111619,1000.) ;
#9932 = VECTOR('',#111622,1000.) ;
#9933 = VECTOR('',#111623,1000.) ;
#9934 = VECTOR('',#111624,1000.) ;
#9935 = VECTOR('',#111627,1000.) ;
#9936 = VECTOR('',#111628,1000.) ;
#9937 = VECTOR('',#111629,1000.) ;
#9938 = VECTOR('',#111630,1000.) ;
#9939 = VECTOR('',#111633,1000.) ;
#9940 = VECTOR('',#111634,1000.) ;
#9941 = VECTOR('',#111635,1000.) ;
#9942 = VECTOR('',#111636,1000.) ;
#9943 = VECTOR('',#111639,1000.) ;
#9944 = VECTOR('',#111640,1000.) ;
#9945 = VECTOR('',#111641,1000.) ;
#9946 = VECTOR('',#111642,1000.) ;
#9947 = VECTOR('',#111645,1000.) ;
#9948 = VECTOR('',#111646,1000.) ;
#9949 = VECTOR('',#111647,1000.) ;
#9950 = VECTOR('',#111648,1000.) ;
#9951 = VECTOR('',#111651,1000.) ;
#9952 = VECTOR('',#111652,1000.) ;
#9953 = VECTOR('',#111653,1000.) ;
#9954 = VECTOR('',#111656,1000.) ;
#9955 = VECTOR('',#111657,1000.) ;
#9956 = VECTOR('',#111658,1000.) ;
#9957 = VECTOR('',#111659,1000.) ;
#9958 = VECTOR('',#111662,1000.) ;
#9959 = VECTOR('',#111663,1000.) ;
#9960 = VECTOR('',#111664,1000.) ;
#9961 = VECTOR('',#111665,1000.) ;
#9962 = VECTOR('',#111668,1000.) ;
#9963 = VECTOR('',#111669,1000.) ;
#9964 = VECTOR('',#111670,1000.) ;
#9965 = VECTOR('',#111671,1000.) ;
#9966 = VECTOR('',#111674,1000.) ;
#9967 = VECTOR('',#111675,1000.) ;
#9968 = VECTOR('',#111676,1000.) ;
#9969 = VECTOR('',#111677,1000.) ;
#9970 = VECTOR('',#111680,1000.) ;
#9971 = VECTOR('',#111681,1000.) ;
#9972 = VECTOR('',#111682,1000.) ;
#9973 = VECTOR('',#111685,1000.) ;
#9974 = VECTOR('',#111686,1000.) ;
#9975 = VECTOR('',#111687,1000.) ;
#9976 = VECTOR('',#111688,1000.) ;
#9977 = VECTOR('',#111691,1000.) ;
#9978 = VECTOR('',#111692,1000.) ;
#9979 = VECTOR('',#111693,1000.) ;
#9980 = VECTOR('',#111694,1000.) ;
#9981 = VECTOR('',#111697,1000.) ;
#9982 = VECTOR('',#111698,1000.) ;
#9983 = VECTOR('',#111699,1000.) ;
#9984 = VECTOR('',#111700,1000.) ;
#9985 = VECTOR('',#111703,1000.) ;
#9986 = VECTOR('',#111704,1000.) ;
#9987 = VECTOR('',#111705,1000.) ;
#9988 = VECTOR('',#111706,1000.) ;
#9989 = VECTOR('',#111709,1000.) ;
#9990 = VECTOR('',#111710,1000.) ;
#9991 = VECTOR('',#111711,1000.) ;
#9992 = VECTOR('',#111714,1000.) ;
#9993 = VECTOR('',#111715,1000.) ;
#9994 = VECTOR('',#111716,1000.) ;
#9995 = VECTOR('',#111717,1000.) ;
#9996 = VECTOR('',#111720,1000.) ;
#9997 = VECTOR('',#111721,1000.) ;
#9998 = VECTOR('',#111722,1000.) ;
#9999 = VECTOR('',#111723,1000.) ;
#10000 = VECTOR('',#111726,1000.) ;
#10001 = VECTOR('',#111727,1000.) ;
#10002 = VECTOR('',#111728,1000.) ;
#10003 = VECTOR('',#111729,1000.) ;
#10004 = VECTOR('',#111732,1000.) ;
#10005 = VECTOR('',#111733,1000.) ;
#10006 = VECTOR('',#111734,1000.) ;
#10007 = VECTOR('',#111735,1000.) ;
#10008 = VECTOR('',#111738,1000.) ;
#10009 = VECTOR('',#111739,1000.) ;
#10010 = VECTOR('',#111740,1000.) ;
#10011 = VECTOR('',#111743,1000.) ;
#10012 = VECTOR('',#111744,1000.) ;
#10013 = VECTOR('',#111745,1000.) ;
#10014 = VECTOR('',#111746,1000.) ;
#10015 = VECTOR('',#111749,1000.) ;
#10016 = VECTOR('',#111750,1000.) ;
#10017 = VECTOR('',#111751,1000.) ;
#10018 = VECTOR('',#111752,1000.) ;
#10019 = VECTOR('',#111755,1000.) ;
#10020 = VECTOR('',#111756,1000.) ;
#10021 = VECTOR('',#111757,1000.) ;
#10022 = VECTOR('',#111758,1000.) ;
#10023 = VECTOR('',#111761,1000.) ;
#10024 = VECTOR('',#111762,1000.) ;
#10025 = VECTOR('',#111763,1000.) ;
#10026 = VECTOR('',#111764,1000.) ;
#10027 = VECTOR('',#111767,1000.) ;
#10028 = VECTOR('',#111768,1000.) ;
#10029 = VECTOR('',#111769,1000.) ;
#10030 = VECTOR('',#111772,1000.) ;
#10031 = VECTOR('',#111773,1000.) ;
#10032 = VECTOR('',#111774,1000.) ;
#10033 = VECTOR('',#111775,1000.) ;
#10034 = VECTOR('',#111778,1000.) ;
#10035 = VECTOR('',#111779,1000.) ;
#10036 = VECTOR('',#111780,1000.) ;
#10037 = VECTOR('',#111781,1000.) ;
#10038 = VECTOR('',#111784,1000.) ;
#10039 = VECTOR('',#111785,1000.) ;
#10040 = VECTOR('',#111786,1000.) ;
#10041 = VECTOR('',#111787,1000.) ;
#10042 = VECTOR('',#111790,1000.) ;
#10043 = VECTOR('',#111791,1000.) ;
#10044 = VECTOR('',#111792,1000.) ;
#10045 = VECTOR('',#111793,1000.) ;
#10046 = VECTOR('',#111796,1000.) ;
#10047 = VECTOR('',#111797,1000.) ;
#10048 = VECTOR('',#111798,1000.) ;
#10049 = VECTOR('',#111801,1000.) ;
#10050 = VECTOR('',#111802,1000.) ;
#10051 = VECTOR('',#111803,1000.) ;
#10052 = VECTOR('',#111804,1000.) ;
#10053 = VECTOR('',#111807,1000.) ;
#10054 = VECTOR('',#111808,1000.) ;
#10055 = VECTOR('',#111809,1000.) ;
#10056 = VECTOR('',#111810,1000.) ;
#10057 = VECTOR('',#111813,1000.) ;
#10058 = VECTOR('',#111814,1000.) ;
#10059 = VECTOR('',#111815,1000.) ;
#10060 = VECTOR('',#111816,1000.) ;
#10061 = VECTOR('',#111819,1000.) ;
#10062 = VECTOR('',#111822,1000.) ;
#10063 = VECTOR('',#111827,1000.) ;
#10064 = VECTOR('',#111828,1000.) ;
#10065 = VECTOR('',#111829,1000.) ;
#10066 = VECTOR('',#111834,1000.) ;
#10067 = VECTOR('',#111839,1000.) ;
#10068 = VECTOR('',#111840,1000.) ;
#10069 = VECTOR('',#111841,1000.) ;
#10070 = VECTOR('',#111846,1000.) ;
#10071 = VECTOR('',#111851,1000.) ;
#10072 = VECTOR('',#111852,1000.) ;
#10073 = VECTOR('',#111853,1000.) ;
#10074 = VECTOR('',#111856,1000.) ;
#10075 = VECTOR('',#111861,1000.) ;
#10076 = VECTOR('',#111862,1000.) ;
#10077 = VECTOR('',#111865,1000.) ;
#10078 = VECTOR('',#111866,1000.) ;
#10079 = VECTOR('',#111867,1000.) ;
#10080 = VECTOR('',#111872,1000.) ;
#10081 = VECTOR('',#111877,1000.) ;
#10082 = VECTOR('',#111878,1000.) ;
#10083 = VECTOR('',#111879,1000.) ;
#10084 = VECTOR('',#111884,1000.) ;
#10085 = VECTOR('',#111889,1000.) ;
#10086 = VECTOR('',#111890,1000.) ;
#10087 = VECTOR('',#111891,1000.) ;
#10088 = VECTOR('',#111896,1000.) ;
#10089 = VECTOR('',#111901,1000.) ;
#10090 = VECTOR('',#111902,1000.) ;
#10091 = VECTOR('',#111903,1000.) ;
#10092 = VECTOR('',#111908,1000.) ;
#10093 = VECTOR('',#111913,1000.) ;
#10094 = VECTOR('',#111914,1000.) ;
#10095 = VECTOR('',#111915,1000.) ;
#10096 = VECTOR('',#111920,1000.) ;
#10097 = VECTOR('',#111925,1000.) ;
#10098 = VECTOR('',#111926,1000.) ;
#10099 = VECTOR('',#111927,1000.) ;
#10100 = VECTOR('',#111932,1000.) ;
#10101 = VECTOR('',#111939,1000.) ;
#10102 = VECTOR('',#111946,1000.) ;
#10103 = VECTOR('',#111951,1000.) ;
#10104 = VECTOR('',#111952,1000.) ;
#10105 = VECTOR('',#111953,1000.) ;
#10106 = VECTOR('',#111958,1000.) ;
#10107 = VECTOR('',#111963,1000.) ;
#10108 = VECTOR('',#111964,1000.) ;
#10109 = VECTOR('',#111965,1000.) ;
#10110 = VECTOR('',#111970,1000.) ;
#10111 = VECTOR('',#111975,1000.) ;
#10112 = VECTOR('',#111976,1000.) ;
#10113 = VECTOR('',#111981,1000.) ;
#10114 = VECTOR('',#111984,1000.) ;
#10115 = VECTOR('',#111985,1000.) ;
#10116 = VECTOR('',#111986,1000.) ;
#10117 = VECTOR('',#111989,1000.) ;
#10118 = VECTOR('',#111990,1000.) ;
#10119 = VECTOR('',#111991,1000.) ;
#10120 = VECTOR('',#111994,1000.) ;
#10121 = VECTOR('',#111997,1000.) ;
#10122 = VECTOR('',#111998,1000.) ;
#10123 = VECTOR('',#111999,1000.) ;
#10124 = VECTOR('',#112000,1000.) ;
#10125 = VECTOR('',#112001,1000.) ;
#10126 = VECTOR('',#112004,1000.) ;
#10127 = VECTOR('',#112007,1000.) ;
#10128 = VECTOR('',#112012,1000.) ;
#10129 = VECTOR('',#112013,1000.) ;
#10130 = VECTOR('',#112014,1000.) ;
#10131 = VECTOR('',#112019,1000.) ;
#10132 = VECTOR('',#112024,1000.) ;
#10133 = VECTOR('',#112025,1000.) ;
#10134 = VECTOR('',#112026,1000.) ;
#10135 = VECTOR('',#112031,1000.) ;
#10136 = VECTOR('',#112036,1000.) ;
#10137 = VECTOR('',#112037,1000.) ;
#10138 = VECTOR('',#112038,1000.) ;
#10139 = VECTOR('',#112041,1000.) ;
#10140 = VECTOR('',#112046,1000.) ;
#10141 = VECTOR('',#112047,1000.) ;
#10142 = VECTOR('',#112050,1000.) ;
#10143 = VECTOR('',#112051,1000.) ;
#10144 = VECTOR('',#112052,1000.) ;
#10145 = VECTOR('',#112057,1000.) ;
#10146 = VECTOR('',#112062,1000.) ;
#10147 = VECTOR('',#112063,1000.) ;
#10148 = VECTOR('',#112064,1000.) ;
#10149 = VECTOR('',#112069,1000.) ;
#10150 = VECTOR('',#112074,1000.) ;
#10151 = VECTOR('',#112075,1000.) ;
#10152 = VECTOR('',#112076,1000.) ;
#10153 = VECTOR('',#112081,1000.) ;
#10154 = VECTOR('',#112086,1000.) ;
#10155 = VECTOR('',#112087,1000.) ;
#10156 = VECTOR('',#112088,1000.) ;
#10157 = VECTOR('',#112093,1000.) ;
#10158 = VECTOR('',#112098,1000.) ;
#10159 = VECTOR('',#112099,1000.) ;
#10160 = VECTOR('',#112100,1000.) ;
#10161 = VECTOR('',#112105,1000.) ;
#10162 = VECTOR('',#112110,1000.) ;
#10163 = VECTOR('',#112111,1000.) ;
#10164 = VECTOR('',#112112,1000.) ;
#10165 = VECTOR('',#112117,1000.) ;
#10166 = VECTOR('',#112124,1000.) ;
#10167 = VECTOR('',#112131,1000.) ;
#10168 = VECTOR('',#112136,1000.) ;
#10169 = VECTOR('',#112137,1000.) ;
#10170 = VECTOR('',#112138,1000.) ;
#10171 = VECTOR('',#112143,1000.) ;
#10172 = VECTOR('',#112148,1000.) ;
#10173 = VECTOR('',#112149,1000.) ;
#10174 = VECTOR('',#112150,1000.) ;
#10175 = VECTOR('',#112155,1000.) ;
#10176 = VECTOR('',#112160,1000.) ;
#10177 = VECTOR('',#112161,1000.) ;
#10178 = VECTOR('',#112166,1000.) ;
#10179 = VECTOR('',#112169,1000.) ;
#10180 = VECTOR('',#112170,1000.) ;
#10181 = VECTOR('',#112171,1000.) ;
#10182 = VECTOR('',#112174,1000.) ;
#10183 = VECTOR('',#112175,1000.) ;
#10184 = VECTOR('',#112176,1000.) ;
#10185 = VECTOR('',#112179,1000.) ;
#10186 = VECTOR('',#112182,1000.) ;
#10187 = VECTOR('',#112183,1000.) ;
#10188 = VECTOR('',#112184,1000.) ;
#10189 = VECTOR('',#112185,1000.) ;
#10190 = VECTOR('',#112186,1000.) ;
#10191 = VECTOR('',#112189,1000.) ;
#10192 = VECTOR('',#112192,1000.) ;
#10193 = VECTOR('',#112197,1000.) ;
#10194 = VECTOR('',#112198,1000.) ;
#10195 = VECTOR('',#112199,1000.) ;
#10196 = VECTOR('',#112204,1000.) ;
#10197 = VECTOR('',#112209,1000.) ;
#10198 = VECTOR('',#112210,1000.) ;
#10199 = VECTOR('',#112211,1000.) ;
#10200 = VECTOR('',#112216,1000.) ;
#10201 = VECTOR('',#112221,1000.) ;
#10202 = VECTOR('',#112222,1000.) ;
#10203 = VECTOR('',#112223,1000.) ;
#10204 = VECTOR('',#112226,1000.) ;
#10205 = VECTOR('',#112231,1000.) ;
#10206 = VECTOR('',#112232,1000.) ;
#10207 = VECTOR('',#112235,1000.) ;
#10208 = VECTOR('',#112236,1000.) ;
#10209 = VECTOR('',#112237,1000.) ;
#10210 = VECTOR('',#112242,1000.) ;
#10211 = VECTOR('',#112247,1000.) ;
#10212 = VECTOR('',#112248,1000.) ;
#10213 = VECTOR('',#112249,1000.) ;
#10214 = VECTOR('',#112254,1000.) ;
#10215 = VECTOR('',#112259,1000.) ;
#10216 = VECTOR('',#112260,1000.) ;
#10217 = VECTOR('',#112261,1000.) ;
#10218 = VECTOR('',#112266,1000.) ;
#10219 = VECTOR('',#112271,1000.) ;
#10220 = VECTOR('',#112272,1000.) ;
#10221 = VECTOR('',#112273,1000.) ;
#10222 = VECTOR('',#112278,1000.) ;
#10223 = VECTOR('',#112283,1000.) ;
#10224 = VECTOR('',#112284,1000.) ;
#10225 = VECTOR('',#112285,1000.) ;
#10226 = VECTOR('',#112290,1000.) ;
#10227 = VECTOR('',#112295,1000.) ;
#10228 = VECTOR('',#112296,1000.) ;
#10229 = VECTOR('',#112297,1000.) ;
#10230 = VECTOR('',#112302,1000.) ;
#10231 = VECTOR('',#112309,1000.) ;
#10232 = VECTOR('',#112316,1000.) ;
#10233 = VECTOR('',#112321,1000.) ;
#10234 = VECTOR('',#112322,1000.) ;
#10235 = VECTOR('',#112323,1000.) ;
#10236 = VECTOR('',#112328,1000.) ;
#10237 = VECTOR('',#112333,1000.) ;
#10238 = VECTOR('',#112334,1000.) ;
#10239 = VECTOR('',#112335,1000.) ;
#10240 = VECTOR('',#112340,1000.) ;
#10241 = VECTOR('',#112345,1000.) ;
#10242 = VECTOR('',#112346,1000.) ;
#10243 = VECTOR('',#112351,1000.) ;
#10244 = VECTOR('',#112354,1000.) ;
#10245 = VECTOR('',#112355,1000.) ;
#10246 = VECTOR('',#112356,1000.) ;
#10247 = VECTOR('',#112359,1000.) ;
#10248 = VECTOR('',#112360,1000.) ;
#10249 = VECTOR('',#112361,1000.) ;
#10250 = VECTOR('',#112364,1000.) ;
#10251 = VECTOR('',#112367,1000.) ;
#10252 = VECTOR('',#112368,1000.) ;
#10253 = VECTOR('',#112369,1000.) ;
#10254 = VECTOR('',#112370,1000.) ;
#10255 = VECTOR('',#112371,1000.) ;
#10256 = VECTOR('',#112374,1000.) ;
#10257 = VECTOR('',#112377,1000.) ;
#10258 = VECTOR('',#112382,1000.) ;
#10259 = VECTOR('',#112383,1000.) ;
#10260 = VECTOR('',#112384,1000.) ;
#10261 = VECTOR('',#112389,1000.) ;
#10262 = VECTOR('',#112394,1000.) ;
#10263 = VECTOR('',#112395,1000.) ;
#10264 = VECTOR('',#112396,1000.) ;
#10265 = VECTOR('',#112401,1000.) ;
#10266 = VECTOR('',#112406,1000.) ;
#10267 = VECTOR('',#112407,1000.) ;
#10268 = VECTOR('',#112408,1000.) ;
#10269 = VECTOR('',#112411,1000.) ;
#10270 = VECTOR('',#112416,1000.) ;
#10271 = VECTOR('',#112417,1000.) ;
#10272 = VECTOR('',#112420,1000.) ;
#10273 = VECTOR('',#112421,1000.) ;
#10274 = VECTOR('',#112422,1000.) ;
#10275 = VECTOR('',#112427,1000.) ;
#10276 = VECTOR('',#112432,1000.) ;
#10277 = VECTOR('',#112433,1000.) ;
#10278 = VECTOR('',#112434,1000.) ;
#10279 = VECTOR('',#112439,1000.) ;
#10280 = VECTOR('',#112444,1000.) ;
#10281 = VECTOR('',#112445,1000.) ;
#10282 = VECTOR('',#112446,1000.) ;
#10283 = VECTOR('',#112451,1000.) ;
#10284 = VECTOR('',#112456,1000.) ;
#10285 = VECTOR('',#112457,1000.) ;
#10286 = VECTOR('',#112458,1000.) ;
#10287 = VECTOR('',#112463,1000.) ;
#10288 = VECTOR('',#112468,1000.) ;
#10289 = VECTOR('',#112469,1000.) ;
#10290 = VECTOR('',#112470,1000.) ;
#10291 = VECTOR('',#112475,1000.) ;
#10292 = VECTOR('',#112480,1000.) ;
#10293 = VECTOR('',#112481,1000.) ;
#10294 = VECTOR('',#112482,1000.) ;
#10295 = VECTOR('',#112487,1000.) ;
#10296 = VECTOR('',#112494,1000.) ;
#10297 = VECTOR('',#112501,1000.) ;
#10298 = VECTOR('',#112506,1000.) ;
#10299 = VECTOR('',#112507,1000.) ;
#10300 = VECTOR('',#112508,1000.) ;
#10301 = VECTOR('',#112513,1000.) ;
#10302 = VECTOR('',#112518,1000.) ;
#10303 = VECTOR('',#112519,1000.) ;
#10304 = VECTOR('',#112520,1000.) ;
#10305 = VECTOR('',#112525,1000.) ;
#10306 = VECTOR('',#112530,1000.) ;
#10307 = VECTOR('',#112531,1000.) ;
#10308 = VECTOR('',#112536,1000.) ;
#10309 = VECTOR('',#112539,1000.) ;
#10310 = VECTOR('',#112540,1000.) ;
#10311 = VECTOR('',#112541,1000.) ;
#10312 = VECTOR('',#112544,1000.) ;
#10313 = VECTOR('',#112545,1000.) ;
#10314 = VECTOR('',#112546,1000.) ;
#10315 = VECTOR('',#112549,1000.) ;
#10316 = VECTOR('',#112552,1000.) ;
#10317 = VECTOR('',#112553,1000.) ;
#10318 = VECTOR('',#112554,1000.) ;
#10319 = VECTOR('',#112555,1000.) ;
#10320 = VECTOR('',#112556,1000.) ;
#10321 = VECTOR('',#112559,1000.) ;
#10322 = VECTOR('',#112562,1000.) ;
#10323 = VECTOR('',#112567,1000.) ;
#10324 = VECTOR('',#112568,1000.) ;
#10325 = VECTOR('',#112569,1000.) ;
#10326 = VECTOR('',#112574,1000.) ;
#10327 = VECTOR('',#112579,1000.) ;
#10328 = VECTOR('',#112580,1000.) ;
#10329 = VECTOR('',#112581,1000.) ;
#10330 = VECTOR('',#112586,1000.) ;
#10331 = VECTOR('',#112591,1000.) ;
#10332 = VECTOR('',#112592,1000.) ;
#10333 = VECTOR('',#112593,1000.) ;
#10334 = VECTOR('',#112596,1000.) ;
#10335 = VECTOR('',#112601,1000.) ;
#10336 = VECTOR('',#112602,1000.) ;
#10337 = VECTOR('',#112605,1000.) ;
#10338 = VECTOR('',#112606,1000.) ;
#10339 = VECTOR('',#112607,1000.) ;
#10340 = VECTOR('',#112612,1000.) ;
#10341 = VECTOR('',#112617,1000.) ;
#10342 = VECTOR('',#112618,1000.) ;
#10343 = VECTOR('',#112619,1000.) ;
#10344 = VECTOR('',#112624,1000.) ;
#10345 = VECTOR('',#112629,1000.) ;
#10346 = VECTOR('',#112630,1000.) ;
#10347 = VECTOR('',#112631,1000.) ;
#10348 = VECTOR('',#112636,1000.) ;
#10349 = VECTOR('',#112641,1000.) ;
#10350 = VECTOR('',#112642,1000.) ;
#10351 = VECTOR('',#112643,1000.) ;
#10352 = VECTOR('',#112648,1000.) ;
#10353 = VECTOR('',#112653,1000.) ;
#10354 = VECTOR('',#112654,1000.) ;
#10355 = VECTOR('',#112655,1000.) ;
#10356 = VECTOR('',#112660,1000.) ;
#10357 = VECTOR('',#112665,1000.) ;
#10358 = VECTOR('',#112666,1000.) ;
#10359 = VECTOR('',#112667,1000.) ;
#10360 = VECTOR('',#112672,1000.) ;
#10361 = VECTOR('',#112679,1000.) ;
#10362 = VECTOR('',#112686,1000.) ;
#10363 = VECTOR('',#112691,1000.) ;
#10364 = VECTOR('',#112692,1000.) ;
#10365 = VECTOR('',#112693,1000.) ;
#10366 = VECTOR('',#112698,1000.) ;
#10367 = VECTOR('',#112703,1000.) ;
#10368 = VECTOR('',#112704,1000.) ;
#10369 = VECTOR('',#112705,1000.) ;
#10370 = VECTOR('',#112710,1000.) ;
#10371 = VECTOR('',#112715,1000.) ;
#10372 = VECTOR('',#112716,1000.) ;
#10373 = VECTOR('',#112721,1000.) ;
#10374 = VECTOR('',#112724,1000.) ;
#10375 = VECTOR('',#112725,1000.) ;
#10376 = VECTOR('',#112726,1000.) ;
#10377 = VECTOR('',#112729,1000.) ;
#10378 = VECTOR('',#112730,1000.) ;
#10379 = VECTOR('',#112731,1000.) ;
#10380 = VECTOR('',#112734,1000.) ;
#10381 = VECTOR('',#112737,1000.) ;
#10382 = VECTOR('',#112738,1000.) ;
#10383 = VECTOR('',#112739,1000.) ;
#10384 = VECTOR('',#112740,1000.) ;
#10385 = VECTOR('',#112741,1000.) ;
#10386 = VECTOR('',#112744,1000.) ;
#10387 = VECTOR('',#112747,1000.) ;
#10388 = VECTOR('',#112752,1000.) ;
#10389 = VECTOR('',#112753,1000.) ;
#10390 = VECTOR('',#112754,1000.) ;
#10391 = VECTOR('',#112759,1000.) ;
#10392 = VECTOR('',#112764,1000.) ;
#10393 = VECTOR('',#112765,1000.) ;
#10394 = VECTOR('',#112766,1000.) ;
#10395 = VECTOR('',#112771,1000.) ;
#10396 = VECTOR('',#112776,1000.) ;
#10397 = VECTOR('',#112777,1000.) ;
#10398 = VECTOR('',#112778,1000.) ;
#10399 = VECTOR('',#112781,1000.) ;
#10400 = VECTOR('',#112786,1000.) ;
#10401 = VECTOR('',#112787,1000.) ;
#10402 = VECTOR('',#112790,1000.) ;
#10403 = VECTOR('',#112791,1000.) ;
#10404 = VECTOR('',#112792,1000.) ;
#10405 = VECTOR('',#112797,1000.) ;
#10406 = VECTOR('',#112802,1000.) ;
#10407 = VECTOR('',#112803,1000.) ;
#10408 = VECTOR('',#112804,1000.) ;
#10409 = VECTOR('',#112809,1000.) ;
#10410 = VECTOR('',#112814,1000.) ;
#10411 = VECTOR('',#112815,1000.) ;
#10412 = VECTOR('',#112816,1000.) ;
#10413 = VECTOR('',#112821,1000.) ;
#10414 = VECTOR('',#112826,1000.) ;
#10415 = VECTOR('',#112827,1000.) ;
#10416 = VECTOR('',#112828,1000.) ;
#10417 = VECTOR('',#112833,1000.) ;
#10418 = VECTOR('',#112838,1000.) ;
#10419 = VECTOR('',#112839,1000.) ;
#10420 = VECTOR('',#112840,1000.) ;
#10421 = VECTOR('',#112845,1000.) ;
#10422 = VECTOR('',#112850,1000.) ;
#10423 = VECTOR('',#112851,1000.) ;
#10424 = VECTOR('',#112852,1000.) ;
#10425 = VECTOR('',#112857,1000.) ;
#10426 = VECTOR('',#112864,1000.) ;
#10427 = VECTOR('',#112871,1000.) ;
#10428 = VECTOR('',#112876,1000.) ;
#10429 = VECTOR('',#112877,1000.) ;
#10430 = VECTOR('',#112878,1000.) ;
#10431 = VECTOR('',#112883,1000.) ;
#10432 = VECTOR('',#112888,1000.) ;
#10433 = VECTOR('',#112889,1000.) ;
#10434 = VECTOR('',#112890,1000.) ;
#10435 = VECTOR('',#112895,1000.) ;
#10436 = VECTOR('',#112900,1000.) ;
#10437 = VECTOR('',#112901,1000.) ;
#10438 = VECTOR('',#112906,1000.) ;
#10439 = VECTOR('',#112909,1000.) ;
#10440 = VECTOR('',#112910,1000.) ;
#10441 = VECTOR('',#112911,1000.) ;
#10442 = VECTOR('',#112914,1000.) ;
#10443 = VECTOR('',#112915,1000.) ;
#10444 = VECTOR('',#112916,1000.) ;
#10445 = VECTOR('',#112919,1000.) ;
#10446 = VECTOR('',#112922,1000.) ;
#10447 = VECTOR('',#112923,1000.) ;
#10448 = VECTOR('',#112924,1000.) ;
#10449 = VECTOR('',#112925,1000.) ;
#10450 = VECTOR('',#112926,1000.) ;
#10451 = VECTOR('',#112929,1000.) ;
#10452 = VECTOR('',#112932,1000.) ;
#10453 = VECTOR('',#112937,1000.) ;
#10454 = VECTOR('',#112938,1000.) ;
#10455 = VECTOR('',#112939,1000.) ;
#10456 = VECTOR('',#112944,1000.) ;
#10457 = VECTOR('',#112949,1000.) ;
#10458 = VECTOR('',#112950,1000.) ;
#10459 = VECTOR('',#112951,1000.) ;
#10460 = VECTOR('',#112956,1000.) ;
#10461 = VECTOR('',#112961,1000.) ;
#10462 = VECTOR('',#112962,1000.) ;
#10463 = VECTOR('',#112963,1000.) ;
#10464 = VECTOR('',#112966,1000.) ;
#10465 = VECTOR('',#112971,1000.) ;
#10466 = VECTOR('',#112972,1000.) ;
#10467 = VECTOR('',#112975,1000.) ;
#10468 = VECTOR('',#112976,1000.) ;
#10469 = VECTOR('',#112977,1000.) ;
#10470 = VECTOR('',#112982,1000.) ;
#10471 = VECTOR('',#112987,1000.) ;
#10472 = VECTOR('',#112988,1000.) ;
#10473 = VECTOR('',#112989,1000.) ;
#10474 = VECTOR('',#112994,1000.) ;
#10475 = VECTOR('',#112999,1000.) ;
#10476 = VECTOR('',#113000,1000.) ;
#10477 = VECTOR('',#113001,1000.) ;
#10478 = VECTOR('',#113006,1000.) ;
#10479 = VECTOR('',#113011,1000.) ;
#10480 = VECTOR('',#113012,1000.) ;
#10481 = VECTOR('',#113013,1000.) ;
#10482 = VECTOR('',#113018,1000.) ;
#10483 = VECTOR('',#113023,1000.) ;
#10484 = VECTOR('',#113024,1000.) ;
#10485 = VECTOR('',#113025,1000.) ;
#10486 = VECTOR('',#113030,1000.) ;
#10487 = VECTOR('',#113035,1000.) ;
#10488 = VECTOR('',#113036,1000.) ;
#10489 = VECTOR('',#113037,1000.) ;
#10490 = VECTOR('',#113042,1000.) ;
#10491 = VECTOR('',#113049,1000.) ;
#10492 = VECTOR('',#113056,1000.) ;
#10493 = VECTOR('',#113061,1000.) ;
#10494 = VECTOR('',#113062,1000.) ;
#10495 = VECTOR('',#113063,1000.) ;
#10496 = VECTOR('',#113068,1000.) ;
#10497 = VECTOR('',#113073,1000.) ;
#10498 = VECTOR('',#113074,1000.) ;
#10499 = VECTOR('',#113075,1000.) ;
#10500 = VECTOR('',#113080,1000.) ;
#10501 = VECTOR('',#113085,1000.) ;
#10502 = VECTOR('',#113086,1000.) ;
#10503 = VECTOR('',#113091,1000.) ;
#10504 = VECTOR('',#113094,1000.) ;
#10505 = VECTOR('',#113095,1000.) ;
#10506 = VECTOR('',#113096,1000.) ;
#10507 = VECTOR('',#113099,1000.) ;
#10508 = VECTOR('',#113100,1000.) ;
#10509 = VECTOR('',#113101,1000.) ;
#10510 = VECTOR('',#113104,1000.) ;
#10511 = VECTOR('',#113107,1000.) ;
#10512 = VECTOR('',#113108,1000.) ;
#10513 = VECTOR('',#113109,1000.) ;
#10514 = VECTOR('',#113110,1000.) ;
#10515 = VECTOR('',#113111,1000.) ;
#10516 = VECTOR('',#113114,1000.) ;
#10517 = VECTOR('',#113117,1000.) ;
#10518 = VECTOR('',#113122,1000.) ;
#10519 = VECTOR('',#113123,1000.) ;
#10520 = VECTOR('',#113124,1000.) ;
#10521 = VECTOR('',#113129,1000.) ;
#10522 = VECTOR('',#113134,1000.) ;
#10523 = VECTOR('',#113135,1000.) ;
#10524 = VECTOR('',#113136,1000.) ;
#10525 = VECTOR('',#113141,1000.) ;
#10526 = VECTOR('',#113146,1000.) ;
#10527 = VECTOR('',#113147,1000.) ;
#10528 = VECTOR('',#113148,1000.) ;
#10529 = VECTOR('',#113151,1000.) ;
#10530 = VECTOR('',#113156,1000.) ;
#10531 = VECTOR('',#113157,1000.) ;
#10532 = VECTOR('',#113160,1000.) ;
#10533 = VECTOR('',#113161,1000.) ;
#10534 = VECTOR('',#113162,1000.) ;
#10535 = VECTOR('',#113167,1000.) ;
#10536 = VECTOR('',#113172,1000.) ;
#10537 = VECTOR('',#113173,1000.) ;
#10538 = VECTOR('',#113174,1000.) ;
#10539 = VECTOR('',#113179,1000.) ;
#10540 = VECTOR('',#113184,1000.) ;
#10541 = VECTOR('',#113185,1000.) ;
#10542 = VECTOR('',#113186,1000.) ;
#10543 = VECTOR('',#113191,1000.) ;
#10544 = VECTOR('',#113196,1000.) ;
#10545 = VECTOR('',#113197,1000.) ;
#10546 = VECTOR('',#113198,1000.) ;
#10547 = VECTOR('',#113203,1000.) ;
#10548 = VECTOR('',#113208,1000.) ;
#10549 = VECTOR('',#113209,1000.) ;
#10550 = VECTOR('',#113210,1000.) ;
#10551 = VECTOR('',#113215,1000.) ;
#10552 = VECTOR('',#113220,1000.) ;
#10553 = VECTOR('',#113221,1000.) ;
#10554 = VECTOR('',#113222,1000.) ;
#10555 = VECTOR('',#113227,1000.) ;
#10556 = VECTOR('',#113234,1000.) ;
#10557 = VECTOR('',#113241,1000.) ;
#10558 = VECTOR('',#113246,1000.) ;
#10559 = VECTOR('',#113247,1000.) ;
#10560 = VECTOR('',#113248,1000.) ;
#10561 = VECTOR('',#113253,1000.) ;
#10562 = VECTOR('',#113258,1000.) ;
#10563 = VECTOR('',#113259,1000.) ;
#10564 = VECTOR('',#113260,1000.) ;
#10565 = VECTOR('',#113265,1000.) ;
#10566 = VECTOR('',#113270,1000.) ;
#10567 = VECTOR('',#113271,1000.) ;
#10568 = VECTOR('',#113276,1000.) ;
#10569 = VECTOR('',#113279,1000.) ;
#10570 = VECTOR('',#113280,1000.) ;
#10571 = VECTOR('',#113281,1000.) ;
#10572 = VECTOR('',#113284,1000.) ;
#10573 = VECTOR('',#113285,1000.) ;
#10574 = VECTOR('',#113286,1000.) ;
#10575 = VECTOR('',#113289,1000.) ;
#10576 = VECTOR('',#113292,1000.) ;
#10577 = VECTOR('',#113293,1000.) ;
#10578 = VECTOR('',#113294,1000.) ;
#10579 = VECTOR('',#113295,1000.) ;
#10580 = VECTOR('',#113296,1000.) ;
#10581 = VECTOR('',#113299,1000.) ;
#10582 = VECTOR('',#113302,1000.) ;
#10583 = VECTOR('',#113307,1000.) ;
#10584 = VECTOR('',#113308,1000.) ;
#10585 = VECTOR('',#113309,1000.) ;
#10586 = VECTOR('',#113314,1000.) ;
#10587 = VECTOR('',#113319,1000.) ;
#10588 = VECTOR('',#113320,1000.) ;
#10589 = VECTOR('',#113321,1000.) ;
#10590 = VECTOR('',#113326,1000.) ;
#10591 = VECTOR('',#113331,1000.) ;
#10592 = VECTOR('',#113332,1000.) ;
#10593 = VECTOR('',#113333,1000.) ;
#10594 = VECTOR('',#113336,1000.) ;
#10595 = VECTOR('',#113341,1000.) ;
#10596 = VECTOR('',#113342,1000.) ;
#10597 = VECTOR('',#113345,1000.) ;
#10598 = VECTOR('',#113346,1000.) ;
#10599 = VECTOR('',#113347,1000.) ;
#10600 = VECTOR('',#113352,1000.) ;
#10601 = VECTOR('',#113357,1000.) ;
#10602 = VECTOR('',#113358,1000.) ;
#10603 = VECTOR('',#113359,1000.) ;
#10604 = VECTOR('',#113364,1000.) ;
#10605 = VECTOR('',#113369,1000.) ;
#10606 = VECTOR('',#113370,1000.) ;
#10607 = VECTOR('',#113371,1000.) ;
#10608 = VECTOR('',#113376,1000.) ;
#10609 = VECTOR('',#113381,1000.) ;
#10610 = VECTOR('',#113382,1000.) ;
#10611 = VECTOR('',#113383,1000.) ;
#10612 = VECTOR('',#113388,1000.) ;
#10613 = VECTOR('',#113393,1000.) ;
#10614 = VECTOR('',#113394,1000.) ;
#10615 = VECTOR('',#113395,1000.) ;
#10616 = VECTOR('',#113400,1000.) ;
#10617 = VECTOR('',#113405,1000.) ;
#10618 = VECTOR('',#113406,1000.) ;
#10619 = VECTOR('',#113407,1000.) ;
#10620 = VECTOR('',#113412,1000.) ;
#10621 = VECTOR('',#113419,1000.) ;
#10622 = VECTOR('',#113426,1000.) ;
#10623 = VECTOR('',#113431,1000.) ;
#10624 = VECTOR('',#113432,1000.) ;
#10625 = VECTOR('',#113433,1000.) ;
#10626 = VECTOR('',#113438,1000.) ;
#10627 = VECTOR('',#113443,1000.) ;
#10628 = VECTOR('',#113444,1000.) ;
#10629 = VECTOR('',#113445,1000.) ;
#10630 = VECTOR('',#113450,1000.) ;
#10631 = VECTOR('',#113455,1000.) ;
#10632 = VECTOR('',#113456,1000.) ;
#10633 = VECTOR('',#113461,1000.) ;
#10634 = VECTOR('',#113464,1000.) ;
#10635 = VECTOR('',#113465,1000.) ;
#10636 = VECTOR('',#113466,1000.) ;
#10637 = VECTOR('',#113469,1000.) ;
#10638 = VECTOR('',#113470,1000.) ;
#10639 = VECTOR('',#113471,1000.) ;
#10640 = VECTOR('',#113474,1000.) ;
#10641 = VECTOR('',#113477,1000.) ;
#10642 = VECTOR('',#113478,1000.) ;
#10643 = VECTOR('',#113479,1000.) ;
#10644 = VECTOR('',#113480,1000.) ;
#10645 = VECTOR('',#113481,1000.) ;
#10646 = VECTOR('',#113484,1000.) ;
#10647 = VECTOR('',#113487,1000.) ;
#10648 = VECTOR('',#113490,1000.) ;
#10649 = VECTOR('',#113493,1000.) ;
#10650 = VECTOR('',#113498,1000.) ;
#10651 = VECTOR('',#113501,1000.) ;
#10652 = VECTOR('',#113504,1000.) ;
#10653 = VECTOR('',#113507,1000.) ;
#10654 = VECTOR('',#113512,1000.) ;
#10655 = VECTOR('',#113515,1000.) ;
#10656 = VECTOR('',#113518,1000.) ;
#10657 = VECTOR('',#113521,1000.) ;
#10658 = VECTOR('',#113526,1000.) ;
#10659 = VECTOR('',#113529,1000.) ;
#10660 = VECTOR('',#113532,1000.) ;
#10661 = VECTOR('',#113535,1000.) ;
#10662 = VECTOR('',#113540,1000.) ;
#10663 = VECTOR('',#113543,1000.) ;
#10664 = VECTOR('',#113546,1000.) ;
#10665 = VECTOR('',#113549,1000.) ;
#10666 = VECTOR('',#113554,1000.) ;
#10667 = VECTOR('',#113557,1000.) ;
#10668 = VECTOR('',#113560,1000.) ;
#10669 = VECTOR('',#113563,1000.) ;
#10670 = VECTOR('',#113568,1000.) ;
#10671 = VECTOR('',#113571,1000.) ;
#10672 = VECTOR('',#113574,1000.) ;
#10673 = VECTOR('',#113577,1000.) ;
#10674 = VECTOR('',#113582,1000.) ;
#10675 = VECTOR('',#113585,1000.) ;
#10676 = VECTOR('',#113588,1000.) ;
#10677 = VECTOR('',#113591,1000.) ;
#10678 = VECTOR('',#113596,1000.) ;
#10679 = VECTOR('',#113599,1000.) ;
#10680 = VECTOR('',#113602,1000.) ;
#10681 = VECTOR('',#113605,1000.) ;
#10682 = VECTOR('',#113640,1000.) ;
#10683 = VECTOR('',#113643,1000.) ;
#10684 = VECTOR('',#113690,1000.) ;
#10685 = VECTOR('',#113749,1000.) ;
#10686 = VECTOR('',#113798,1000.) ;
#10687 = VECTOR('',#114905,1000.) ;
#10688 = VECTOR('',#114908,1000.) ;
#10689 = VECTOR('',#114955,1000.) ;
#10690 = VECTOR('',#115014,1000.) ;
#10691 = VECTOR('',#115063,1000.) ;
#10692 = VECTOR('',#115216,1000.) ;
#10693 = VECTOR('',#115219,1000.) ;
#10694 = VECTOR('',#115266,1000.) ;
#10695 = VECTOR('',#115325,1000.) ;
#10696 = VECTOR('',#115374,1000.) ;
#10697 = VECTOR('',#115527,1000.) ;
#10698 = VECTOR('',#115530,1000.) ;
#10699 = VECTOR('',#115577,1000.) ;
#10700 = VECTOR('',#115636,1000.) ;
#10701 = VECTOR('',#115685,1000.) ;
#10702 = VECTOR('',#115838,1000.) ;
#10703 = VECTOR('',#115841,1000.) ;
#10704 = VECTOR('',#115888,1000.) ;
#10705 = VECTOR('',#115947,1000.) ;
#10706 = VECTOR('',#115996,1000.) ;
#10707 = VECTOR('',#116149,1000.) ;
#10708 = VECTOR('',#116152,1000.) ;
#10709 = VECTOR('',#116199,1000.) ;
#10710 = VECTOR('',#116258,1000.) ;
#10711 = VECTOR('',#116307,1000.) ;
#10712 = VECTOR('',#116460,1000.) ;
#10713 = VECTOR('',#116463,1000.) ;
#10714 = VECTOR('',#116510,1000.) ;
#10715 = VECTOR('',#116569,1000.) ;
#10716 = VECTOR('',#116618,1000.) ;
#10717 = VECTOR('',#116771,1000.) ;
#10718 = VECTOR('',#116774,1000.) ;
#10719 = VECTOR('',#116821,1000.) ;
#10720 = VECTOR('',#116880,1000.) ;
#10721 = VECTOR('',#116929,1000.) ;
#10722 = VECTOR('',#117082,1000.) ;
#10723 = VECTOR('',#117085,1000.) ;
#10724 = VECTOR('',#117132,1000.) ;
#10725 = VECTOR('',#117191,1000.) ;
#10726 = VECTOR('',#117240,1000.) ;
#10727 = VECTOR('',#117363,1000.) ;
#10728 = VECTOR('',#117364,1000.) ;
#10729 = VECTOR('',#117365,1000.) ;
#10730 = VECTOR('',#117366,1000.) ;
#10731 = VECTOR('',#117369,1000.) ;
#10732 = VECTOR('',#117370,1000.) ;
#10733 = VECTOR('',#117371,1000.) ;
#10734 = VECTOR('',#117372,1000.) ;
#10735 = VECTOR('',#117375,1000.) ;
#10736 = VECTOR('',#117376,1000.) ;
#10737 = VECTOR('',#117377,1000.) ;
#10738 = VECTOR('',#117378,1000.) ;
#10739 = VECTOR('',#117381,1000.) ;
#10740 = VECTOR('',#117382,1000.) ;
#10741 = VECTOR('',#117383,1000.) ;
#10742 = VECTOR('',#117384,1000.) ;
#10743 = VECTOR('',#117387,1000.) ;
#10744 = VECTOR('',#117388,1000.) ;
#10745 = VECTOR('',#117389,1000.) ;
#10746 = VECTOR('',#117390,1000.) ;
#10747 = VECTOR('',#117393,1000.) ;
#10748 = VECTOR('',#117398,1000.) ;
#10749 = VECTOR('',#117399,1000.) ;
#10750 = VECTOR('',#117402,1000.) ;
#10751 = VECTOR('',#117407,1000.) ;
#10752 = VECTOR('',#117408,1000.) ;
#10753 = VECTOR('',#117423,1000.) ;
#10754 = VECTOR('',#117424,1000.) ;
#10755 = VECTOR('',#117425,1000.) ;
#10756 = VECTOR('',#117426,1000.) ;
#10757 = VECTOR('',#117429,1000.) ;
#10758 = VECTOR('',#117430,1000.) ;
#10759 = VECTOR('',#117431,1000.) ;
#10760 = VECTOR('',#117434,1000.) ;
#10761 = VECTOR('',#117435,1000.) ;
#10762 = VECTOR('',#117436,1000.) ;
#10763 = VECTOR('',#117439,1000.) ;
#10764 = VECTOR('',#117440,1000.) ;
#10765 = VECTOR('',#117441,1000.) ;
#10766 = VECTOR('',#117442,1000.) ;
#10767 = VECTOR('',#117445,1000.) ;
#10768 = VECTOR('',#117446,1000.) ;
#10769 = VECTOR('',#117447,1000.) ;
#10770 = VECTOR('',#117448,1000.) ;
#10771 = VECTOR('',#117451,1000.) ;
#10772 = VECTOR('',#117452,1000.) ;
#10773 = VECTOR('',#117453,1000.) ;
#10774 = VECTOR('',#117456,1000.) ;
#10775 = VECTOR('',#117457,1000.) ;
#10776 = VECTOR('',#117458,1000.) ;
#10777 = VECTOR('',#117461,1000.) ;
#10778 = VECTOR('',#117462,1000.) ;
#10779 = VECTOR('',#117463,1000.) ;
#10780 = VECTOR('',#117464,1000.) ;
#10781 = VECTOR('',#117467,1000.) ;
#10782 = VECTOR('',#117468,1000.) ;
#10783 = VECTOR('',#117469,1000.) ;
#10784 = VECTOR('',#117470,1000.) ;
#10785 = VECTOR('',#117473,1000.) ;
#10786 = VECTOR('',#117474,1000.) ;
#10787 = VECTOR('',#117475,1000.) ;
#10788 = VECTOR('',#117476,1000.) ;
#10789 = VECTOR('',#117479,1000.) ;
#10790 = VECTOR('',#117480,1000.) ;
#10791 = VECTOR('',#117481,1000.) ;
#10792 = VECTOR('',#117482,1000.) ;
#10793 = VECTOR('',#117485,1000.) ;
#10794 = VECTOR('',#117486,1000.) ;
#10795 = VECTOR('',#117487,1000.) ;
#10796 = VECTOR('',#117488,1000.) ;
#10797 = VECTOR('',#117491,1000.) ;
#10798 = VECTOR('',#117496,1000.) ;
#10799 = VECTOR('',#117497,1000.) ;
#10800 = VECTOR('',#117500,1000.) ;
#10801 = VECTOR('',#117505,1000.) ;
#10802 = VECTOR('',#117506,1000.) ;
#10803 = VECTOR('',#117521,1000.) ;
#10804 = VECTOR('',#117522,1000.) ;
#10805 = VECTOR('',#117523,1000.) ;
#10806 = VECTOR('',#117524,1000.) ;
#10807 = VECTOR('',#117527,1000.) ;
#10808 = VECTOR('',#117528,1000.) ;
#10809 = VECTOR('',#117529,1000.) ;
#10810 = VECTOR('',#117532,1000.) ;
#10811 = VECTOR('',#117533,1000.) ;
#10812 = VECTOR('',#117534,1000.) ;
#10813 = VECTOR('',#117537,1000.) ;
#10814 = VECTOR('',#117538,1000.) ;
#10815 = VECTOR('',#117539,1000.) ;
#10816 = VECTOR('',#117540,1000.) ;
#10817 = VECTOR('',#117543,1000.) ;
#10818 = VECTOR('',#117544,1000.) ;
#10819 = VECTOR('',#117545,1000.) ;
#10820 = VECTOR('',#117546,1000.) ;
#10821 = VECTOR('',#117549,1000.) ;
#10822 = VECTOR('',#117550,1000.) ;
#10823 = VECTOR('',#117551,1000.) ;
#10824 = VECTOR('',#117554,1000.) ;
#10825 = VECTOR('',#117555,1000.) ;
#10826 = VECTOR('',#117556,1000.) ;
#10827 = VECTOR('',#117559,1000.) ;
#10828 = VECTOR('',#117560,1000.) ;
#10829 = VECTOR('',#117561,1000.) ;
#10830 = VECTOR('',#117562,1000.) ;
#10831 = VECTOR('',#117565,1000.) ;
#10832 = VECTOR('',#117566,1000.) ;
#10833 = VECTOR('',#117567,1000.) ;
#10834 = VECTOR('',#117568,1000.) ;
#10835 = VECTOR('',#117571,1000.) ;
#10836 = VECTOR('',#117572,1000.) ;
#10837 = VECTOR('',#117573,1000.) ;
#10838 = VECTOR('',#117574,1000.) ;
#10839 = VECTOR('',#117577,1000.) ;
#10840 = VECTOR('',#117578,1000.) ;
#10841 = VECTOR('',#117579,1000.) ;
#10842 = VECTOR('',#117580,1000.) ;
#10843 = VECTOR('',#117583,1000.) ;
#10844 = VECTOR('',#117584,1000.) ;
#10845 = VECTOR('',#117585,1000.) ;
#10846 = VECTOR('',#117586,1000.) ;
#10847 = VECTOR('',#117589,1000.) ;
#10848 = VECTOR('',#117594,1000.) ;
#10849 = VECTOR('',#117595,1000.) ;
#10850 = VECTOR('',#117598,1000.) ;
#10851 = VECTOR('',#117603,1000.) ;
#10852 = VECTOR('',#117604,1000.) ;
#10853 = VECTOR('',#117619,1000.) ;
#10854 = VECTOR('',#117620,1000.) ;
#10855 = VECTOR('',#117621,1000.) ;
#10856 = VECTOR('',#117622,1000.) ;
#10857 = VECTOR('',#117625,1000.) ;
#10858 = VECTOR('',#117626,1000.) ;
#10859 = VECTOR('',#117627,1000.) ;
#10860 = VECTOR('',#117630,1000.) ;
#10861 = VECTOR('',#117631,1000.) ;
#10862 = VECTOR('',#117632,1000.) ;
#10863 = VECTOR('',#117635,1000.) ;
#10864 = VECTOR('',#117636,1000.) ;
#10865 = VECTOR('',#117637,1000.) ;
#10866 = VECTOR('',#117638,1000.) ;
#10867 = VECTOR('',#117641,1000.) ;
#10868 = VECTOR('',#117642,1000.) ;
#10869 = VECTOR('',#117643,1000.) ;
#10870 = VECTOR('',#117644,1000.) ;
#10871 = VECTOR('',#117647,1000.) ;
#10872 = VECTOR('',#117648,1000.) ;
#10873 = VECTOR('',#117649,1000.) ;
#10874 = VECTOR('',#117652,1000.) ;
#10875 = VECTOR('',#117653,1000.) ;
#10876 = VECTOR('',#117654,1000.) ;
#10877 = VECTOR('',#117657,1000.) ;
#10878 = VECTOR('',#117658,1000.) ;
#10879 = VECTOR('',#117659,1000.) ;
#10880 = VECTOR('',#117660,1000.) ;
#10881 = VECTOR('',#117663,1000.) ;
#10882 = VECTOR('',#117664,1000.) ;
#10883 = VECTOR('',#117665,1000.) ;
#10884 = VECTOR('',#117666,1000.) ;
#10885 = VECTOR('',#117669,1000.) ;
#10886 = VECTOR('',#117670,1000.) ;
#10887 = VECTOR('',#117671,1000.) ;
#10888 = VECTOR('',#117672,1000.) ;
#10889 = VECTOR('',#117675,1000.) ;
#10890 = VECTOR('',#117676,1000.) ;
#10891 = VECTOR('',#117677,1000.) ;
#10892 = VECTOR('',#117678,1000.) ;
#10893 = VECTOR('',#117681,1000.) ;
#10894 = VECTOR('',#117682,1000.) ;
#10895 = VECTOR('',#117683,1000.) ;
#10896 = VECTOR('',#117684,1000.) ;
#10897 = VECTOR('',#117687,1000.) ;
#10898 = VECTOR('',#117692,1000.) ;
#10899 = VECTOR('',#117693,1000.) ;
#10900 = VECTOR('',#117696,1000.) ;
#10901 = VECTOR('',#117701,1000.) ;
#10902 = VECTOR('',#117702,1000.) ;
#10903 = VECTOR('',#117717,1000.) ;
#10904 = VECTOR('',#117718,1000.) ;
#10905 = VECTOR('',#117719,1000.) ;
#10906 = VECTOR('',#117720,1000.) ;
#10907 = VECTOR('',#117723,1000.) ;
#10908 = VECTOR('',#117724,1000.) ;
#10909 = VECTOR('',#117725,1000.) ;
#10910 = VECTOR('',#117728,1000.) ;
#10911 = VECTOR('',#117729,1000.) ;
#10912 = VECTOR('',#117730,1000.) ;
#10913 = VECTOR('',#117733,1000.) ;
#10914 = VECTOR('',#117734,1000.) ;
#10915 = VECTOR('',#117735,1000.) ;
#10916 = VECTOR('',#117736,1000.) ;
#10917 = VECTOR('',#117739,1000.) ;
#10918 = VECTOR('',#117740,1000.) ;
#10919 = VECTOR('',#117741,1000.) ;
#10920 = VECTOR('',#117742,1000.) ;
#10921 = VECTOR('',#117745,1000.) ;
#10922 = VECTOR('',#117746,1000.) ;
#10923 = VECTOR('',#117747,1000.) ;
#10924 = VECTOR('',#117750,1000.) ;
#10925 = VECTOR('',#117751,1000.) ;
#10926 = VECTOR('',#117752,1000.) ;
#10927 = VECTOR('',#117755,1000.) ;
#10928 = VECTOR('',#117756,1000.) ;
#10929 = VECTOR('',#117757,1000.) ;
#10930 = VECTOR('',#117758,1000.) ;
#10931 = VECTOR('',#117761,1000.) ;
#10932 = VECTOR('',#117762,1000.) ;
#10933 = VECTOR('',#117763,1000.) ;
#10934 = VECTOR('',#117764,1000.) ;
#10935 = VECTOR('',#117767,1000.) ;
#10936 = VECTOR('',#117768,1000.) ;
#10937 = VECTOR('',#117769,1000.) ;
#10938 = VECTOR('',#117770,1000.) ;
#10939 = VECTOR('',#117773,1000.) ;
#10940 = VECTOR('',#117774,1000.) ;
#10941 = VECTOR('',#117775,1000.) ;
#10942 = VECTOR('',#117776,1000.) ;
#10943 = VECTOR('',#117779,1000.) ;
#10944 = VECTOR('',#117780,1000.) ;
#10945 = VECTOR('',#117781,1000.) ;
#10946 = VECTOR('',#117782,1000.) ;
#10947 = VECTOR('',#117785,1000.) ;
#10948 = VECTOR('',#117790,1000.) ;
#10949 = VECTOR('',#117791,1000.) ;
#10950 = VECTOR('',#117794,1000.) ;
#10951 = VECTOR('',#117799,1000.) ;
#10952 = VECTOR('',#117800,1000.) ;
#10953 = VECTOR('',#117815,1000.) ;
#10954 = VECTOR('',#117816,1000.) ;
#10955 = VECTOR('',#117817,1000.) ;
#10956 = VECTOR('',#117818,1000.) ;
#10957 = VECTOR('',#117821,1000.) ;
#10958 = VECTOR('',#117822,1000.) ;
#10959 = VECTOR('',#117823,1000.) ;
#10960 = VECTOR('',#117826,1000.) ;
#10961 = VECTOR('',#117827,1000.) ;
#10962 = VECTOR('',#117828,1000.) ;
#10963 = VECTOR('',#117831,1000.) ;
#10964 = VECTOR('',#117832,1000.) ;
#10965 = VECTOR('',#117833,1000.) ;
#10966 = VECTOR('',#117834,1000.) ;
#10967 = VECTOR('',#117837,1000.) ;
#10968 = VECTOR('',#117838,1000.) ;
#10969 = VECTOR('',#117839,1000.) ;
#10970 = VECTOR('',#117840,1000.) ;
#10971 = VECTOR('',#117843,1000.) ;
#10972 = VECTOR('',#117844,1000.) ;
#10973 = VECTOR('',#117845,1000.) ;
#10974 = VECTOR('',#117848,1000.) ;
#10975 = VECTOR('',#117849,1000.) ;
#10976 = VECTOR('',#117850,1000.) ;
#10977 = VECTOR('',#117853,1000.) ;
#10978 = VECTOR('',#117854,1000.) ;
#10979 = VECTOR('',#117855,1000.) ;
#10980 = VECTOR('',#117856,1000.) ;
#10981 = VECTOR('',#117859,1000.) ;
#10982 = VECTOR('',#117860,1000.) ;
#10983 = VECTOR('',#117861,1000.) ;
#10984 = VECTOR('',#117862,1000.) ;
#10985 = VECTOR('',#117865,1000.) ;
#10986 = VECTOR('',#117866,1000.) ;
#10987 = VECTOR('',#117867,1000.) ;
#10988 = VECTOR('',#117868,1000.) ;
#10989 = VECTOR('',#117871,1000.) ;
#10990 = VECTOR('',#117872,1000.) ;
#10991 = VECTOR('',#117873,1000.) ;
#10992 = VECTOR('',#117874,1000.) ;
#10993 = VECTOR('',#117877,1000.) ;
#10994 = VECTOR('',#117878,1000.) ;
#10995 = VECTOR('',#117879,1000.) ;
#10996 = VECTOR('',#117880,1000.) ;
#10997 = VECTOR('',#117883,1000.) ;
#10998 = VECTOR('',#117888,1000.) ;
#10999 = VECTOR('',#117889,1000.) ;
#11000 = VECTOR('',#117892,1000.) ;
#11001 = VECTOR('',#117897,1000.) ;
#11002 = VECTOR('',#117898,1000.) ;
#11003 = VECTOR('',#117913,1000.) ;
#11004 = VECTOR('',#117914,1000.) ;
#11005 = VECTOR('',#117915,1000.) ;
#11006 = VECTOR('',#117916,1000.) ;
#11007 = VECTOR('',#117919,1000.) ;
#11008 = VECTOR('',#117920,1000.) ;
#11009 = VECTOR('',#117921,1000.) ;
#11010 = VECTOR('',#117924,1000.) ;
#11011 = VECTOR('',#117925,1000.) ;
#11012 = VECTOR('',#117926,1000.) ;
#11013 = VECTOR('',#117929,1000.) ;
#11014 = VECTOR('',#117930,1000.) ;
#11015 = VECTOR('',#117931,1000.) ;
#11016 = VECTOR('',#117932,1000.) ;
#11017 = VECTOR('',#117935,1000.) ;
#11018 = VECTOR('',#117936,1000.) ;
#11019 = VECTOR('',#117937,1000.) ;
#11020 = VECTOR('',#117938,1000.) ;
#11021 = VECTOR('',#117941,1000.) ;
#11022 = VECTOR('',#117942,1000.) ;
#11023 = VECTOR('',#117943,1000.) ;
#11024 = VECTOR('',#117946,1000.) ;
#11025 = VECTOR('',#117947,1000.) ;
#11026 = VECTOR('',#117948,1000.) ;
#11027 = VECTOR('',#117951,1000.) ;
#11028 = VECTOR('',#117952,1000.) ;
#11029 = VECTOR('',#117953,1000.) ;
#11030 = VECTOR('',#117954,1000.) ;
#11031 = VECTOR('',#117957,1000.) ;
#11032 = VECTOR('',#117958,1000.) ;
#11033 = VECTOR('',#117959,1000.) ;
#11034 = VECTOR('',#117960,1000.) ;
#11035 = VECTOR('',#117963,1000.) ;
#11036 = VECTOR('',#117964,1000.) ;
#11037 = VECTOR('',#117965,1000.) ;
#11038 = VECTOR('',#117966,1000.) ;
#11039 = VECTOR('',#117969,1000.) ;
#11040 = VECTOR('',#117970,1000.) ;
#11041 = VECTOR('',#117971,1000.) ;
#11042 = VECTOR('',#117972,1000.) ;
#11043 = VECTOR('',#117975,1000.) ;
#11044 = VECTOR('',#117976,1000.) ;
#11045 = VECTOR('',#117977,1000.) ;
#11046 = VECTOR('',#117978,1000.) ;
#11047 = VECTOR('',#117981,1000.) ;
#11048 = VECTOR('',#117986,1000.) ;
#11049 = VECTOR('',#117987,1000.) ;
#11050 = VECTOR('',#117990,1000.) ;
#11051 = VECTOR('',#117995,1000.) ;
#11052 = VECTOR('',#117996,1000.) ;
#11053 = VECTOR('',#118011,1000.) ;
#11054 = VECTOR('',#118012,1000.) ;
#11055 = VECTOR('',#118013,1000.) ;
#11056 = VECTOR('',#118014,1000.) ;
#11057 = VECTOR('',#118017,1000.) ;
#11058 = VECTOR('',#118018,1000.) ;
#11059 = VECTOR('',#118019,1000.) ;
#11060 = VECTOR('',#118022,1000.) ;
#11061 = VECTOR('',#118023,1000.) ;
#11062 = VECTOR('',#118024,1000.) ;
#11063 = VECTOR('',#118027,1000.) ;
#11064 = VECTOR('',#118028,1000.) ;
#11065 = VECTOR('',#118029,1000.) ;
#11066 = VECTOR('',#118030,1000.) ;
#11067 = VECTOR('',#118033,1000.) ;
#11068 = VECTOR('',#118034,1000.) ;
#11069 = VECTOR('',#118035,1000.) ;
#11070 = VECTOR('',#118036,1000.) ;
#11071 = VECTOR('',#118039,1000.) ;
#11072 = VECTOR('',#118040,1000.) ;
#11073 = VECTOR('',#118041,1000.) ;
#11074 = VECTOR('',#118044,1000.) ;
#11075 = VECTOR('',#118045,1000.) ;
#11076 = VECTOR('',#118046,1000.) ;
#11077 = VECTOR('',#118049,1000.) ;
#11078 = VECTOR('',#118050,1000.) ;
#11079 = VECTOR('',#118051,1000.) ;
#11080 = VECTOR('',#118052,1000.) ;
#11081 = VECTOR('',#118055,1000.) ;
#11082 = VECTOR('',#118056,1000.) ;
#11083 = VECTOR('',#118057,1000.) ;
#11084 = VECTOR('',#118058,1000.) ;
#11085 = VECTOR('',#118061,1000.) ;
#11086 = VECTOR('',#118062,1000.) ;
#11087 = VECTOR('',#118063,1000.) ;
#11088 = VECTOR('',#118064,1000.) ;
#11089 = VECTOR('',#118067,1000.) ;
#11090 = VECTOR('',#118068,1000.) ;
#11091 = VECTOR('',#118069,1000.) ;
#11092 = VECTOR('',#118070,1000.) ;
#11093 = VECTOR('',#118073,1000.) ;
#11094 = VECTOR('',#118074,1000.) ;
#11095 = VECTOR('',#118075,1000.) ;
#11096 = VECTOR('',#118076,1000.) ;
#11097 = VECTOR('',#118079,1000.) ;
#11098 = VECTOR('',#118084,1000.) ;
#11099 = VECTOR('',#118085,1000.) ;
#11100 = VECTOR('',#118088,1000.) ;
#11101 = VECTOR('',#118093,1000.) ;
#11102 = VECTOR('',#118094,1000.) ;
#11103 = VECTOR('',#118109,1000.) ;
#11104 = VECTOR('',#118110,1000.) ;
#11105 = VECTOR('',#118111,1000.) ;
#11106 = VECTOR('',#118112,1000.) ;
#11107 = VECTOR('',#118115,1000.) ;
#11108 = VECTOR('',#118116,1000.) ;
#11109 = VECTOR('',#118117,1000.) ;
#11110 = VECTOR('',#118120,1000.) ;
#11111 = VECTOR('',#118121,1000.) ;
#11112 = VECTOR('',#118122,1000.) ;
#11113 = VECTOR('',#118125,1000.) ;
#11114 = VECTOR('',#118126,1000.) ;
#11115 = VECTOR('',#118127,1000.) ;
#11116 = VECTOR('',#118128,1000.) ;
#11117 = VECTOR('',#118131,1000.) ;
#11118 = VECTOR('',#118132,1000.) ;
#11119 = VECTOR('',#118133,1000.) ;
#11120 = VECTOR('',#118134,1000.) ;
#11121 = VECTOR('',#118137,1000.) ;
#11122 = VECTOR('',#118138,1000.) ;
#11123 = VECTOR('',#118139,1000.) ;
#11124 = VECTOR('',#118142,1000.) ;
#11125 = VECTOR('',#118143,1000.) ;
#11126 = VECTOR('',#118144,1000.) ;
#11127 = VECTOR('',#118147,1000.) ;
#11128 = VECTOR('',#118148,1000.) ;
#11129 = VECTOR('',#118149,1000.) ;
#11130 = VECTOR('',#118150,1000.) ;
#11131 = VECTOR('',#118153,1000.) ;
#11132 = VECTOR('',#118154,1000.) ;
#11133 = VECTOR('',#118155,1000.) ;
#11134 = VECTOR('',#118156,1000.) ;
#11135 = VECTOR('',#118159,1000.) ;
#11136 = VECTOR('',#118160,1000.) ;
#11137 = VECTOR('',#118161,1000.) ;
#11138 = VECTOR('',#118162,1000.) ;
#11139 = VECTOR('',#118165,1000.) ;
#11140 = VECTOR('',#118166,1000.) ;
#11141 = VECTOR('',#118167,1000.) ;
#11142 = VECTOR('',#118168,1000.) ;
#11143 = VECTOR('',#118171,1000.) ;
#11144 = VECTOR('',#118172,1000.) ;
#11145 = VECTOR('',#118173,1000.) ;
#11146 = VECTOR('',#118174,1000.) ;
#11147 = VECTOR('',#118177,1000.) ;
#11148 = VECTOR('',#118182,1000.) ;
#11149 = VECTOR('',#118183,1000.) ;
#11150 = VECTOR('',#118186,1000.) ;
#11151 = VECTOR('',#118191,1000.) ;
#11152 = VECTOR('',#118192,1000.) ;
#11153 = VECTOR('',#118207,1000.) ;
#11154 = VECTOR('',#118208,1000.) ;
#11155 = VECTOR('',#118209,1000.) ;
#11156 = VECTOR('',#118210,1000.) ;
#11157 = VECTOR('',#118213,1000.) ;
#11158 = VECTOR('',#118214,1000.) ;
#11159 = VECTOR('',#118215,1000.) ;
#11160 = VECTOR('',#118218,1000.) ;
#11161 = VECTOR('',#118219,1000.) ;
#11162 = VECTOR('',#118220,1000.) ;
#11163 = VECTOR('',#118223,1000.) ;
#11164 = VECTOR('',#118224,1000.) ;
#11165 = VECTOR('',#118225,1000.) ;
#11166 = VECTOR('',#118226,1000.) ;
#11167 = VECTOR('',#118229,1000.) ;
#11168 = VECTOR('',#118230,1000.) ;
#11169 = VECTOR('',#118231,1000.) ;
#11170 = VECTOR('',#118232,1000.) ;
#11171 = VECTOR('',#118235,1000.) ;
#11172 = VECTOR('',#118236,1000.) ;
#11173 = VECTOR('',#118237,1000.) ;
#11174 = VECTOR('',#118240,1000.) ;
#11175 = VECTOR('',#118241,1000.) ;
#11176 = VECTOR('',#118242,1000.) ;
#11177 = VECTOR('',#118245,1000.) ;
#11178 = VECTOR('',#118246,1000.) ;
#11179 = VECTOR('',#118247,1000.) ;
#11180 = VECTOR('',#118248,1000.) ;
#11181 = VECTOR('',#118251,1000.) ;
#11182 = VECTOR('',#118252,1000.) ;
#11183 = VECTOR('',#118253,1000.) ;
#11184 = VECTOR('',#118254,1000.) ;
#11185 = VECTOR('',#118257,1000.) ;
#11186 = VECTOR('',#118258,1000.) ;
#11187 = VECTOR('',#118259,1000.) ;
#11188 = VECTOR('',#118260,1000.) ;
#11189 = VECTOR('',#118263,1000.) ;
#11190 = VECTOR('',#118264,1000.) ;
#11191 = VECTOR('',#118265,1000.) ;
#11192 = VECTOR('',#118266,1000.) ;
#11193 = VECTOR('',#118269,1000.) ;
#11194 = VECTOR('',#118270,1000.) ;
#11195 = VECTOR('',#118271,1000.) ;
#11196 = VECTOR('',#118272,1000.) ;
#11197 = VECTOR('',#118275,1000.) ;
#11198 = VECTOR('',#118276,1000.) ;
#11199 = VECTOR('',#118277,1000.) ;
#11200 = VECTOR('',#118278,1000.) ;
#11201 = VECTOR('',#118281,1000.) ;
#11202 = VECTOR('',#118282,1000.) ;
#11203 = VECTOR('',#118283,1000.) ;
#11204 = VECTOR('',#118284,1000.) ;
#11205 = VECTOR('',#118287,1000.) ;
#11206 = VECTOR('',#118288,1000.) ;
#11207 = VECTOR('',#118289,1000.) ;
#11208 = VECTOR('',#118290,1000.) ;
#11209 = VECTOR('',#118293,1000.) ;
#11210 = VECTOR('',#118294,1000.) ;
#11211 = VECTOR('',#118295,1000.) ;
#11212 = VECTOR('',#118296,1000.) ;
#11213 = VECTOR('',#118299,1000.) ;
#11214 = VECTOR('',#118300,1000.) ;
#11215 = VECTOR('',#118301,1000.) ;
#11216 = VECTOR('',#118302,1000.) ;
#11217 = VECTOR('',#118305,1000.) ;
#11218 = VECTOR('',#118306,1000.) ;
#11219 = VECTOR('',#118307,1000.) ;
#11220 = VECTOR('',#118308,1000.) ;
#11221 = VECTOR('',#118311,1000.) ;
#11222 = VECTOR('',#118312,1000.) ;
#11223 = VECTOR('',#118313,1000.) ;
#11224 = VECTOR('',#118314,1000.) ;
#11225 = VECTOR('',#118317,1000.) ;
#11226 = VECTOR('',#118318,1000.) ;
#11227 = VECTOR('',#118319,1000.) ;
#11228 = VECTOR('',#118320,1000.) ;
#11229 = VECTOR('',#118323,1000.) ;
#11230 = VECTOR('',#118324,1000.) ;
#11231 = VECTOR('',#118325,1000.) ;
#11232 = VECTOR('',#118326,1000.) ;
#11233 = VECTOR('',#118329,1000.) ;
#11234 = VECTOR('',#118330,1000.) ;
#11235 = VECTOR('',#118331,1000.) ;
#11236 = VECTOR('',#118332,1000.) ;
#11237 = VECTOR('',#118335,1000.) ;
#11238 = VECTOR('',#118336,1000.) ;
#11239 = VECTOR('',#118337,1000.) ;
#11240 = VECTOR('',#118338,1000.) ;
#11241 = VECTOR('',#118341,1000.) ;
#11242 = VECTOR('',#118342,1000.) ;
#11243 = VECTOR('',#118343,1000.) ;
#11244 = VECTOR('',#118344,1000.) ;
#11245 = VECTOR('',#118347,1000.) ;
#11246 = VECTOR('',#118348,1000.) ;
#11247 = VECTOR('',#118349,1000.) ;
#11248 = VECTOR('',#118350,1000.) ;
#11249 = VECTOR('',#118353,1000.) ;
#11250 = VECTOR('',#118354,1000.) ;
#11251 = VECTOR('',#118355,1000.) ;
#11252 = VECTOR('',#118356,1000.) ;
#11253 = VECTOR('',#118359,1000.) ;
#11254 = VECTOR('',#118360,1000.) ;
#11255 = VECTOR('',#118361,1000.) ;
#11256 = VECTOR('',#118362,1000.) ;
#11257 = VECTOR('',#118365,1000.) ;
#11258 = VECTOR('',#118366,1000.) ;
#11259 = VECTOR('',#118367,1000.) ;
#11260 = VECTOR('',#118368,1000.) ;
#11261 = VECTOR('',#118371,1000.) ;
#11262 = VECTOR('',#118372,1000.) ;
#11263 = VECTOR('',#118373,1000.) ;
#11264 = VECTOR('',#118374,1000.) ;
#11265 = VECTOR('',#118377,1000.) ;
#11266 = VECTOR('',#118378,1000.) ;
#11267 = VECTOR('',#118379,1000.) ;
#11268 = VECTOR('',#118380,1000.) ;
#11269 = VECTOR('',#118383,1000.) ;
#11270 = VECTOR('',#118384,1000.) ;
#11271 = VECTOR('',#118385,1000.) ;
#11272 = VECTOR('',#118386,1000.) ;
#11273 = VECTOR('',#118389,1000.) ;
#11274 = VECTOR('',#118390,1000.) ;
#11275 = VECTOR('',#118391,1000.) ;
#11276 = VECTOR('',#118392,1000.) ;
#11277 = VECTOR('',#118395,1000.) ;
#11278 = VECTOR('',#118396,1000.) ;
#11279 = VECTOR('',#118397,1000.) ;
#11280 = VECTOR('',#118398,1000.) ;
#11281 = VECTOR('',#118401,1000.) ;
#11282 = VECTOR('',#118402,1000.) ;
#11283 = VECTOR('',#118403,1000.) ;
#11284 = VECTOR('',#118404,1000.) ;
#11285 = VECTOR('',#118407,1000.) ;
#11286 = VECTOR('',#118408,1000.) ;
#11287 = VECTOR('',#118409,1000.) ;
#11288 = VECTOR('',#118410,1000.) ;
#11289 = VECTOR('',#118413,1000.) ;
#11290 = VECTOR('',#118414,1000.) ;
#11291 = VECTOR('',#118415,1000.) ;
#11292 = VECTOR('',#118416,1000.) ;
#11293 = VECTOR('',#118419,1000.) ;
#11294 = VECTOR('',#118420,1000.) ;
#11295 = VECTOR('',#118421,1000.) ;
#11296 = VECTOR('',#118422,1000.) ;
#11297 = VECTOR('',#118425,1000.) ;
#11298 = VECTOR('',#118426,1000.) ;
#11299 = VECTOR('',#118427,1000.) ;
#11300 = VECTOR('',#118428,1000.) ;
#11301 = VECTOR('',#118431,1000.) ;
#11302 = VECTOR('',#118432,1000.) ;
#11303 = VECTOR('',#118433,1000.) ;
#11304 = VECTOR('',#118434,1000.) ;
#11305 = VECTOR('',#118437,1000.) ;
#11306 = VECTOR('',#118438,1000.) ;
#11307 = VECTOR('',#118439,1000.) ;
#11308 = VECTOR('',#118440,1000.) ;
#11309 = VECTOR('',#118443,1000.) ;
#11310 = VECTOR('',#118444,1000.) ;
#11311 = VECTOR('',#118445,1000.) ;
#11312 = VECTOR('',#118446,1000.) ;
#11313 = VECTOR('',#118449,1000.) ;
#11314 = VECTOR('',#118450,1000.) ;
#11315 = VECTOR('',#118451,1000.) ;
#11316 = VECTOR('',#118452,1000.) ;
#11317 = VECTOR('',#118455,1000.) ;
#11318 = VECTOR('',#118456,1000.) ;
#11319 = VECTOR('',#118457,1000.) ;
#11320 = VECTOR('',#118458,1000.) ;
#11321 = VECTOR('',#120481,1000.) ;
#11322 = VECTOR('',#120484,1000.) ;
#11323 = VECTOR('',#120659,1000.) ;
#11324 = VECTOR('',#120660,1000.) ;
#11325 = VECTOR('',#120665,1000.) ;
#11326 = VECTOR('',#120666,1000.) ;
#11327 = VECTOR('',#120671,1000.) ;
#11328 = VECTOR('',#120672,1000.) ;
#11329 = VECTOR('',#120677,1000.) ;
#11330 = VECTOR('',#120678,1000.) ;
#11331 = VECTOR('',#120683,1000.) ;
#11332 = VECTOR('',#120684,1000.) ;
#11333 = VECTOR('',#120689,1000.) ;
#11334 = VECTOR('',#120690,1000.) ;
#11335 = VECTOR('',#120695,1000.) ;
#11336 = VECTOR('',#120696,1000.) ;
#11337 = VECTOR('',#120917,1000.) ;
#11338 = VECTOR('',#120920,1000.) ;
#11339 = VECTOR('',#120923,1000.) ;
#11340 = VECTOR('',#120926,1000.) ;
#11341 = VECTOR('',#120929,1.5) ;
#11342 = VECTOR('',#120934,1000.) ;
#11343 = VECTOR('',#120937,1000.) ;
#11344 = VECTOR('',#120940,1000.) ;
#11345 = VECTOR('',#120943,1000.) ;
#11346 = VECTOR('',#120946,1.5) ;
#11347 = VECTOR('',#120951,1000.) ;
#11348 = VECTOR('',#120954,1000.) ;
#11349 = VECTOR('',#120957,1000.) ;
#11350 = VECTOR('',#120960,1000.) ;
#11351 = VECTOR('',#120963,1.5) ;
#11352 = VECTOR('',#120968,1000.) ;
#11353 = VECTOR('',#120971,1000.) ;
#11354 = VECTOR('',#120974,1000.) ;
#11355 = VECTOR('',#120977,1000.) ;
#11356 = VECTOR('',#120980,1.5) ;
#11357 = VECTOR('',#120985,1000.) ;
#11358 = VECTOR('',#120988,1000.) ;
#11359 = VECTOR('',#120991,1000.) ;
#11360 = VECTOR('',#120994,1000.) ;
#11361 = VECTOR('',#120997,1.5) ;
#11362 = VECTOR('',#121002,1000.) ;
#11363 = VECTOR('',#121005,1000.) ;
#11364 = VECTOR('',#121008,1000.) ;
#11365 = VECTOR('',#121011,1000.) ;
#11366 = VECTOR('',#121014,1.5) ;
#11367 = VECTOR('',#121019,1000.) ;
#11368 = VECTOR('',#121022,1000.) ;
#11369 = VECTOR('',#121025,1000.) ;
#11370 = VECTOR('',#121028,1000.) ;
#11371 = VECTOR('',#121031,1.5) ;
#11372 = VECTOR('',#121036,1000.) ;
#11373 = VECTOR('',#121039,1000.) ;
#11374 = VECTOR('',#121042,1000.) ;
#11375 = VECTOR('',#121045,1000.) ;
#11376 = VECTOR('',#121048,1.5) ;
#11377 = VECTOR('',#121053,1000.) ;
#11378 = VECTOR('',#121056,1000.) ;
#11379 = VECTOR('',#121059,1000.) ;
#11380 = VECTOR('',#121062,1000.) ;
#11381 = VECTOR('',#121065,1.5) ;
#11382 = VECTOR('',#121070,1.) ;
#11383 = VECTOR('',#121075,1.) ;
#11384 = VECTOR('',#121080,1.) ;
#11385 = VECTOR('',#121085,1.) ;
#11386 = VECTOR('',#121090,1.) ;
#11387 = VECTOR('',#121095,1.) ;
#11388 = VECTOR('',#121100,1.) ;
#11389 = VECTOR('',#121105,0.999999999999999) ;
#11390 = VECTOR('',#121110,1.) ;
#11391 = VECTOR('',#121113,1.) ;
#11392 = VECTOR('',#121116,0.999999999999999) ;
#11393 = VECTOR('',#121119,1.) ;
#11394 = VECTOR('',#121122,1.) ;
#11395 = VECTOR('',#121125,1.) ;
#11396 = VECTOR('',#121128,1.) ;
#11397 = VECTOR('',#121131,1.) ;
#11398 = VECTOR('',#121134,1.) ;
#11399 = VECTOR('',#121137,1.) ;
#11400 = VECTOR('',#121166,1000.) ;
#11401 = VECTOR('',#121167,1000.) ;
#11402 = VECTOR('',#121172,1000.) ;
#11403 = VECTOR('',#121173,1000.) ;
#11404 = VECTOR('',#121178,1000.) ;
#11405 = VECTOR('',#121179,1000.) ;
#11406 = VECTOR('',#121184,1000.) ;
#11407 = VECTOR('',#121185,1000.) ;
#11408 = VECTOR('',#121190,1000.) ;
#11409 = VECTOR('',#121193,1000.) ;
#11410 = VECTOR('',#121196,1000.) ;
#11411 = VECTOR('',#121199,1000.) ;
#11412 = VECTOR('',#121202,1.5) ;
#11413 = VECTOR('',#121207,1.) ;
#11414 = VECTOR('',#121210,1.) ;
#11415 = VECTOR('',#121213,1000.) ;
#11416 = VECTOR('',#121214,1000.) ;
#11417 = VECTOR('',#121215,1000.) ;
#11418 = VECTOR('',#121216,1000.) ;
#11419 = VECTOR('',#121237,1000.) ;
#11420 = VECTOR('',#121238,1000.) ;
#11421 = VECTOR('',#121239,1000.) ;
#11422 = VECTOR('',#121242,1000.) ;
#11423 = VECTOR('',#121245,1000.) ;
#11424 = VECTOR('',#121248,1000.) ;
#11425 = VECTOR('',#121251,1000.) ;
#11426 = VECTOR('',#121254,1000.) ;
#11427 = VECTOR('',#121257,1000.) ;
#11428 = VECTOR('',#121260,1000.) ;
#11429 = VECTOR('',#121263,1000.) ;
#11430 = VECTOR('',#121266,1000.) ;
#11431 = VECTOR('',#121269,1000.) ;
#11432 = VECTOR('',#121272,1000.) ;
#11433 = VECTOR('',#121275,1000.) ;
#11434 = VECTOR('',#121278,1000.) ;
#11435 = VECTOR('',#121281,1000.) ;
#11436 = VECTOR('',#121284,1000.) ;
#11437 = VECTOR('',#121287,1000.) ;
#11438 = VECTOR('',#121290,1000.) ;
#11439 = VECTOR('',#121293,1000.) ;
#11440 = VECTOR('',#121296,1000.) ;
#11441 = VECTOR('',#121299,1000.) ;
#11442 = VECTOR('',#121302,1000.) ;
#11443 = VECTOR('',#121305,1000.) ;
#11444 = VECTOR('',#121308,1000.) ;
#11445 = VECTOR('',#121311,1000.) ;
#11446 = VECTOR('',#121314,1000.) ;
#11447 = VECTOR('',#121317,1000.) ;
#11448 = VECTOR('',#121320,1000.) ;
#11449 = VECTOR('',#121323,1000.) ;
#11450 = VECTOR('',#121326,1000.) ;
#11451 = VECTOR('',#121329,1000.) ;
#11452 = VECTOR('',#121332,1000.) ;
#11453 = VECTOR('',#121335,1000.) ;
#11454 = VECTOR('',#121338,1000.) ;
#11455 = VECTOR('',#121341,1000.) ;
#11456 = VECTOR('',#121344,1000.) ;
#11457 = VECTOR('',#121347,1000.) ;
#11458 = VECTOR('',#121350,1000.) ;
#11459 = VECTOR('',#121353,1000.) ;
#11460 = VECTOR('',#121356,1000.) ;
#11461 = VECTOR('',#121359,1000.) ;
#11462 = VECTOR('',#121362,1000.) ;
#11463 = VECTOR('',#121363,1000.) ;
#11464 = VECTOR('',#121364,1000.) ;
#11465 = VECTOR('',#121365,1000.) ;
#11466 = VECTOR('',#121366,1000.) ;
#11467 = VECTOR('',#121369,1000.) ;
#11468 = VECTOR('',#121372,1000.) ;
#11469 = VECTOR('',#121375,1000.) ;
#11470 = VECTOR('',#121380,1000.) ;
#11471 = VECTOR('',#121381,1000.) ;
#11472 = VECTOR('',#121382,1000.) ;
#11473 = VECTOR('',#121383,1000.) ;
#11474 = VECTOR('',#121384,1000.) ;
#11475 = VECTOR('',#121387,1000.) ;
#11476 = VECTOR('',#121390,1000.) ;
#11477 = VECTOR('',#121393,1000.) ;
#11478 = VECTOR('',#121398,1000.) ;
#11479 = VECTOR('',#121399,1000.) ;
#11480 = VECTOR('',#121400,1000.) ;
#11481 = VECTOR('',#121401,1000.) ;
#11482 = VECTOR('',#121402,1000.) ;
#11483 = VECTOR('',#121405,1000.) ;
#11484 = VECTOR('',#121408,1000.) ;
#11485 = VECTOR('',#121411,1000.) ;
#11486 = VECTOR('',#121416,1000.) ;
#11487 = VECTOR('',#121417,1000.) ;
#11488 = VECTOR('',#121418,1000.) ;
#11489 = VECTOR('',#121419,1000.) ;
#11490 = VECTOR('',#121420,1000.) ;
#11491 = VECTOR('',#121423,1000.) ;
#11492 = VECTOR('',#121426,1000.) ;
#11493 = VECTOR('',#121429,1000.) ;
#11494 = VECTOR('',#121434,1000.) ;
#11495 = VECTOR('',#121435,1000.) ;
#11496 = VECTOR('',#121436,1000.) ;
#11497 = VECTOR('',#121437,1000.) ;
#11498 = VECTOR('',#121438,1000.) ;
#11499 = VECTOR('',#121441,1000.) ;
#11500 = VECTOR('',#121444,1000.) ;
#11501 = VECTOR('',#121447,1000.) ;
#11502 = VECTOR('',#121452,1000.) ;
#11503 = VECTOR('',#121453,1000.) ;
#11504 = VECTOR('',#121454,1000.) ;
#11505 = VECTOR('',#121455,1000.) ;
#11506 = VECTOR('',#121456,1000.) ;
#11507 = VECTOR('',#121459,1000.) ;
#11508 = VECTOR('',#121462,1000.) ;
#11509 = VECTOR('',#121465,1000.) ;
#11510 = VECTOR('',#121470,1000.) ;
#11511 = VECTOR('',#121471,1000.) ;
#11512 = VECTOR('',#121472,1000.) ;
#11513 = VECTOR('',#121473,1000.) ;
#11514 = VECTOR('',#121474,1000.) ;
#11515 = VECTOR('',#121477,1000.) ;
#11516 = VECTOR('',#121480,1000.) ;
#11517 = VECTOR('',#121483,1000.) ;
#11518 = VECTOR('',#121488,1000.) ;
#11519 = VECTOR('',#121489,1000.) ;
#11520 = VECTOR('',#121490,1000.) ;
#11521 = VECTOR('',#121491,1000.) ;
#11522 = VECTOR('',#121492,1000.) ;
#11523 = VECTOR('',#121495,1000.) ;
#11524 = VECTOR('',#121498,1000.) ;
#11525 = VECTOR('',#121501,1000.) ;
#11526 = VECTOR('',#121506,1000.) ;
#11527 = VECTOR('',#121507,1000.) ;
#11528 = VECTOR('',#121508,1000.) ;
#11529 = VECTOR('',#121509,1000.) ;
#11530 = VECTOR('',#121510,1000.) ;
#11531 = VECTOR('',#121513,1000.) ;
#11532 = VECTOR('',#121516,1000.) ;
#11533 = VECTOR('',#121519,1000.) ;
#11534 = VECTOR('',#121524,1000.) ;
#11535 = VECTOR('',#121527,1000.) ;
#11536 = VECTOR('',#121530,1000.) ;
#11537 = VECTOR('',#121533,1000.) ;
#11538 = VECTOR('',#121536,1000.) ;
#11539 = VECTOR('',#121539,1000.) ;
#11540 = VECTOR('',#121542,1000.) ;
#11541 = VECTOR('',#121545,1000.) ;
#11542 = VECTOR('',#121548,1000.) ;
#11543 = VECTOR('',#121551,1000.) ;
#11544 = VECTOR('',#121552,1000.) ;
#11545 = VECTOR('',#121553,1000.) ;
#11546 = VECTOR('',#121554,1000.) ;
#11547 = VECTOR('',#121555,1000.) ;
#11548 = VECTOR('',#121560,1000.) ;
#11549 = VECTOR('',#121565,1000.) ;
#11550 = VECTOR('',#121570,1000.) ;
#11551 = VECTOR('',#121575,1000.) ;
#11552 = VECTOR('',#121580,1000.) ;
#11553 = VECTOR('',#121585,1000.) ;
#11554 = VECTOR('',#121590,1000.) ;
#11555 = VECTOR('',#121595,1000.) ;
#11556 = VECTOR('',#121600,1000.) ;
#11557 = VECTOR('',#121605,1000.) ;
#11558 = VECTOR('',#121610,1000.) ;
#11559 = VECTOR('',#121615,1000.) ;
#11560 = VECTOR('',#121620,1000.) ;
#11561 = VECTOR('',#121625,1000.) ;
#11562 = VECTOR('',#121630,1000.) ;
#11563 = VECTOR('',#121635,1000.) ;
#11564 = VECTOR('',#121640,1000.) ;
#11565 = VECTOR('',#121645,1000.) ;
#11566 = VECTOR('',#121650,1000.) ;
#11567 = VECTOR('',#121659,1000.) ;
#11568 = VECTOR('',#121660,1000.) ;
#11569 = VECTOR('',#121661,1000.) ;
#11570 = VECTOR('',#121662,1000.) ;
#11571 = VECTOR('',#121663,1000.) ;
#11572 = VECTOR('',#121672,1000.) ;
#11573 = VECTOR('',#121673,1000.) ;
#11574 = VECTOR('',#121674,1000.) ;
#11575 = VECTOR('',#121675,1000.) ;
#11576 = VECTOR('',#121676,1000.) ;
#11577 = VECTOR('',#121685,1000.) ;
#11578 = VECTOR('',#121686,1000.) ;
#11579 = VECTOR('',#121687,1000.) ;
#11580 = VECTOR('',#121688,1000.) ;
#11581 = VECTOR('',#121689,1000.) ;
#11582 = VECTOR('',#121698,1000.) ;
#11583 = VECTOR('',#121699,1000.) ;
#11584 = VECTOR('',#121700,1000.) ;
#11585 = VECTOR('',#121701,1000.) ;
#11586 = VECTOR('',#121702,1000.) ;
#11587 = VECTOR('',#121711,1000.) ;
#11588 = VECTOR('',#121712,1000.) ;
#11589 = VECTOR('',#121713,1000.) ;
#11590 = VECTOR('',#121714,1000.) ;
#11591 = VECTOR('',#121715,1000.) ;
#11592 = VECTOR('',#121724,1000.) ;
#11593 = VECTOR('',#121725,1000.) ;
#11594 = VECTOR('',#121726,1000.) ;
#11595 = VECTOR('',#121727,1000.) ;
#11596 = VECTOR('',#121728,1000.) ;
#11597 = VECTOR('',#121737,1000.) ;
#11598 = VECTOR('',#121738,1000.) ;
#11599 = VECTOR('',#121739,1000.) ;
#11600 = VECTOR('',#121740,1000.) ;
#11601 = VECTOR('',#121741,1000.) ;
#11602 = VECTOR('',#121750,1000.) ;
#11603 = VECTOR('',#121751,1000.) ;
#11604 = VECTOR('',#121752,1000.) ;
#11605 = VECTOR('',#121753,1000.) ;
#11606 = VECTOR('',#121754,1000.) ;
#11607 = VECTOR('',#121763,1000.) ;
#11608 = VECTOR('',#121764,1000.) ;
#11609 = VECTOR('',#121765,1000.) ;
#11610 = VECTOR('',#121766,1000.) ;
#11611 = VECTOR('',#121767,1000.) ;
#11612 = VECTOR('',#121774,1000.) ;
#11613 = VECTOR('',#121775,1000.) ;
#11614 = VECTOR('',#121776,1000.) ;
#11615 = VECTOR('',#121777,1000.) ;
#11616 = VECTOR('',#121780,1000.) ;
#11617 = VECTOR('',#121781,1000.) ;
#11618 = VECTOR('',#121782,1000.) ;
#11619 = VECTOR('',#121783,1000.) ;
#11620 = VECTOR('',#121786,1000.) ;
#11621 = VECTOR('',#121789,1000.) ;
#11622 = VECTOR('',#121790,1000.) ;
#11623 = VECTOR('',#121791,1000.) ;
#11624 = VECTOR('',#121794,1000.) ;
#11625 = VECTOR('',#121797,1000.) ;
#11626 = VECTOR('',#121798,1000.) ;
#11627 = VECTOR('',#121799,1000.) ;
#11628 = VECTOR('',#121802,1000.) ;
#11629 = VECTOR('',#121805,1000.) ;
#11630 = VECTOR('',#121806,1000.) ;
#11631 = VECTOR('',#121807,1000.) ;
#11632 = VECTOR('',#121810,1000.) ;
#11633 = VECTOR('',#121813,1000.) ;
#11634 = VECTOR('',#121814,1000.) ;
#11635 = VECTOR('',#121815,1000.) ;
#11636 = VECTOR('',#121818,1000.) ;
#11637 = VECTOR('',#121821,1000.) ;
#11638 = VECTOR('',#121822,1000.) ;
#11639 = VECTOR('',#121823,1000.) ;
#11640 = VECTOR('',#121826,1000.) ;
#11641 = VECTOR('',#121829,1000.) ;
#11642 = VECTOR('',#121830,1000.) ;
#11643 = VECTOR('',#121831,1000.) ;
#11644 = VECTOR('',#121834,1000.) ;
#11645 = VECTOR('',#121837,1000.) ;
#11646 = VECTOR('',#121838,1000.) ;
#11647 = VECTOR('',#121839,1000.) ;
#11648 = VECTOR('',#121842,1000.) ;
#11649 = VECTOR('',#121845,1000.) ;
#11650 = VECTOR('',#121846,1000.) ;
#11651 = VECTOR('',#121847,1000.) ;
#11652 = VECTOR('',#121850,1000.) ;
#11653 = VECTOR('',#121853,1000.) ;
#11654 = VECTOR('',#121854,1000.) ;
#11655 = VECTOR('',#121855,1000.) ;
#11656 = VECTOR('',#121858,1000.) ;
#11657 = VECTOR('',#121861,1000.) ;
#11658 = VECTOR('',#121862,1000.) ;
#11659 = VECTOR('',#121863,1000.) ;
#11660 = VECTOR('',#121866,1000.) ;
#11661 = VECTOR('',#121873,1000.) ;
#11662 = VECTOR('',#121884,1000.) ;
#11663 = VECTOR('',#121885,1000.) ;
#11664 = VECTOR('',#121886,1000.) ;
#11665 = VECTOR('',#121887,1000.) ;
#11666 = VECTOR('',#121888,1000.) ;
#11667 = VECTOR('',#121889,1000.) ;
#11668 = VECTOR('',#121890,1000.) ;
#11669 = VECTOR('',#121891,1000.) ;
#11670 = VECTOR('',#121892,1000.) ;
#11671 = VECTOR('',#121893,1000.) ;
#11672 = VECTOR('',#121894,1000.) ;
#11673 = VECTOR('',#121895,1000.) ;
#11674 = VECTOR('',#121896,1000.) ;
#11675 = VECTOR('',#121897,1000.) ;
#11676 = VECTOR('',#121898,1000.) ;
#11677 = VECTOR('',#121899,1000.) ;
#11678 = VECTOR('',#121900,1000.) ;
#11679 = VECTOR('',#121901,1000.) ;
#11680 = VECTOR('',#121902,1000.) ;
#11681 = VECTOR('',#121903,1000.) ;
#11682 = VECTOR('',#121904,1000.) ;
#11683 = VECTOR('',#121905,1000.) ;
#11684 = VECTOR('',#121906,1000.) ;
#11685 = VECTOR('',#121907,1000.) ;
#11686 = VECTOR('',#121908,1000.) ;
#11687 = VECTOR('',#121909,1000.) ;
#11688 = VECTOR('',#121910,1000.) ;
#11689 = VECTOR('',#121911,1000.) ;
#11690 = VECTOR('',#121912,1000.) ;
#11691 = VECTOR('',#121913,1000.) ;
#11692 = VECTOR('',#121914,1000.) ;
#11693 = VECTOR('',#121915,1000.) ;
#11694 = VECTOR('',#121916,1000.) ;
#11695 = VECTOR('',#121917,1000.) ;
#11696 = VECTOR('',#121918,1000.) ;
#11697 = VECTOR('',#121919,1000.) ;
#11698 = VECTOR('',#121920,1000.) ;
#11699 = VECTOR('',#121921,1000.) ;
#11700 = VECTOR('',#121922,1000.) ;
#11701 = VECTOR('',#121923,1000.) ;
#11702 = VECTOR('',#121924,1000.) ;
#11703 = VECTOR('',#121925,1000.) ;
#11704 = VECTOR('',#121926,1000.) ;
#11705 = VECTOR('',#121927,1000.) ;
#11706 = VECTOR('',#121930,1000.) ;
#11707 = VECTOR('',#121931,1000.) ;
#11708 = VECTOR('',#121932,1000.) ;
#11709 = VECTOR('',#121933,1000.) ;
#11710 = VECTOR('',#121934,1000.) ;
#11711 = VECTOR('',#121937,1000.) ;
#11712 = VECTOR('',#121940,1000.) ;
#11713 = VECTOR('',#121943,1000.) ;
#11714 = VECTOR('',#121948,1000.) ;
#11715 = VECTOR('',#121949,1000.) ;
#11716 = VECTOR('',#121950,1000.) ;
#11717 = VECTOR('',#121951,1000.) ;
#11718 = VECTOR('',#121954,1000.) ;
#11719 = VECTOR('',#121957,1000.) ;
#11720 = VECTOR('',#121958,1000.) ;
#11721 = VECTOR('',#121959,1000.) ;
#11722 = VECTOR('',#121960,1000.) ;
#11723 = VECTOR('',#121967,1000.) ;
#11724 = VECTOR('',#121970,1000.) ;
#11725 = VECTOR('',#121971,1000.) ;
#11726 = VECTOR('',#121972,1000.) ;
#11727 = VECTOR('',#121973,1000.) ;
#11728 = VECTOR('',#121976,1000.) ;
#11729 = VECTOR('',#121977,1000.) ;
#11730 = VECTOR('',#121978,1000.) ;
#11731 = VECTOR('',#121981,1000.) ;
#11732 = VECTOR('',#121982,1000.) ;
#11733 = VECTOR('',#121983,1000.) ;
#11734 = VECTOR('',#121984,1000.) ;
#11735 = VECTOR('',#121987,1000.) ;
#11736 = VECTOR('',#121988,1000.) ;
#11737 = VECTOR('',#121989,1000.) ;
#11738 = VECTOR('',#121990,1000.) ;
#11739 = VECTOR('',#121991,1000.) ;
#11740 = VECTOR('',#121992,1000.) ;
#11741 = VECTOR('',#121993,1000.) ;
#11742 = VECTOR('',#121994,1000.) ;
#11743 = VECTOR('',#121995,1000.) ;
#11744 = VECTOR('',#121996,1000.) ;
#11745 = VECTOR('',#121997,1000.) ;
#11746 = VECTOR('',#121998,1000.) ;
#11747 = VECTOR('',#121999,1000.) ;
#11748 = VECTOR('',#122000,1000.) ;
#11749 = VECTOR('',#122001,1000.) ;
#11750 = VECTOR('',#122002,1000.) ;
#11751 = VECTOR('',#122003,1000.) ;
#11752 = VECTOR('',#122004,1000.) ;
#11753 = VECTOR('',#122005,1000.) ;
#11754 = VECTOR('',#122006,1000.) ;
#11755 = VECTOR('',#122007,1000.) ;
#11756 = VECTOR('',#122008,1000.) ;
#11757 = VECTOR('',#122009,1000.) ;
#11758 = VECTOR('',#122010,1000.) ;
#11759 = VECTOR('',#122011,1000.) ;
#11760 = VECTOR('',#122012,1000.) ;
#11761 = VECTOR('',#122013,1000.) ;
#11762 = VECTOR('',#122014,1000.) ;
#11763 = VECTOR('',#122015,1000.) ;
#11764 = VECTOR('',#122016,1000.) ;
#11765 = VECTOR('',#122017,1000.) ;
#11766 = VECTOR('',#122018,1000.) ;
#11767 = VECTOR('',#122019,1000.) ;
#11768 = VECTOR('',#122020,1000.) ;
#11769 = VECTOR('',#122021,1000.) ;
#11770 = VECTOR('',#122022,1000.) ;
#11771 = VECTOR('',#122025,1000.) ;
#11772 = VECTOR('',#122028,1000.) ;
#11773 = VECTOR('',#122031,1000.) ;
#11774 = VECTOR('',#122034,1000.) ;
#11775 = VECTOR('',#122037,1000.) ;
#11776 = VECTOR('',#122040,1000.) ;
#11777 = VECTOR('',#122043,1000.) ;
#11778 = VECTOR('',#122046,1000.) ;
#11779 = VECTOR('',#122049,1000.) ;
#11780 = VECTOR('',#122050,1000.) ;
#11781 = VECTOR('',#122051,1000.) ;
#11782 = VECTOR('',#122054,1000.) ;
#11783 = VECTOR('',#122055,1000.) ;
#11784 = VECTOR('',#122056,1000.) ;
#11785 = VECTOR('',#122059,1000.) ;
#11786 = VECTOR('',#122060,1000.) ;
#11787 = VECTOR('',#122061,1000.) ;
#11788 = VECTOR('',#122062,1000.) ;
#11789 = VECTOR('',#122065,1000.) ;
#11790 = VECTOR('',#122066,1000.) ;
#11791 = VECTOR('',#122069,1000.) ;
#11792 = VECTOR('',#122070,1000.) ;
#11793 = VECTOR('',#122071,1000.) ;
#11794 = VECTOR('',#122072,1000.) ;
#11795 = VECTOR('',#122073,1000.) ;
#11796 = VECTOR('',#122076,1000.) ;
#11797 = VECTOR('',#122077,1000.) ;
#11798 = VECTOR('',#122078,1000.) ;
#11799 = VECTOR('',#122079,1000.) ;
#11800 = VECTOR('',#122082,1000.) ;
#11801 = VECTOR('',#122083,1000.) ;
#11802 = VECTOR('',#122084,1000.) ;
#11803 = VECTOR('',#122089,1000.) ;
#11804 = VECTOR('',#122090,1000.) ;
#11805 = VECTOR('',#122091,1000.) ;
#11806 = VECTOR('',#122092,1000.) ;
#11807 = VECTOR('',#122095,1000.) ;
#11808 = VECTOR('',#122096,1000.) ;
#11809 = VECTOR('',#122097,1000.) ;
#11810 = VECTOR('',#122098,1000.) ;
#11811 = VECTOR('',#122101,1000.) ;
#11812 = VECTOR('',#122104,1000.) ;
#11813 = VECTOR('',#122107,1000.) ;
#11814 = VECTOR('',#122114,1000.) ;
#11815 = VECTOR('',#122115,1000.) ;
#11816 = VECTOR('',#122116,1000.) ;
#11817 = VECTOR('',#122119,1000.) ;
#11818 = VECTOR('',#122120,1000.) ;
#11819 = VECTOR('',#122121,1000.) ;
#11820 = VECTOR('',#122122,1000.) ;
#11821 = VECTOR('',#122125,1000.) ;
#11822 = VECTOR('',#122126,1000.) ;
#11823 = VECTOR('',#122127,1000.) ;
#11824 = VECTOR('',#122128,1000.) ;
#11825 = VECTOR('',#122129,1000.) ;
#11826 = VECTOR('',#122132,1000.) ;
#11827 = VECTOR('',#122133,1000.) ;
#11828 = VECTOR('',#122134,1000.) ;
#11829 = VECTOR('',#122135,1000.) ;
#11830 = VECTOR('',#122136,1000.) ;
#11831 = VECTOR('',#122139,1000.) ;
#11832 = VECTOR('',#122140,1000.) ;
#11833 = VECTOR('',#122141,1000.) ;
#11834 = VECTOR('',#122142,1000.) ;
#11835 = VECTOR('',#122145,1000.) ;
#11836 = VECTOR('',#122146,1000.) ;
#11837 = VECTOR('',#122147,1000.) ;
#11838 = VECTOR('',#122148,1000.) ;
#11839 = VECTOR('',#122151,1000.) ;
#11840 = VECTOR('',#122152,1000.) ;
#11841 = VECTOR('',#122153,1000.) ;
#11842 = VECTOR('',#122154,1000.) ;
#11843 = VECTOR('',#122157,1000.) ;
#11844 = VECTOR('',#122158,1000.) ;
#11845 = VECTOR('',#122159,1000.) ;
#11846 = VECTOR('',#122160,1000.) ;
#11847 = VECTOR('',#122163,1000.) ;
#11848 = VECTOR('',#122164,1000.) ;
#11849 = VECTOR('',#122165,1000.) ;
#11850 = VECTOR('',#122166,1000.) ;
#11851 = VECTOR('',#122167,1000.) ;
#11852 = VECTOR('',#122170,1000.) ;
#11853 = VECTOR('',#122173,1000.) ;
#11854 = VECTOR('',#122176,1000.) ;
#11855 = VECTOR('',#122181,1000.) ;
#11856 = VECTOR('',#122182,1000.) ;
#11857 = VECTOR('',#122183,1000.) ;
#11858 = VECTOR('',#122186,1000.) ;
#11859 = VECTOR('',#122187,1000.) ;
#11860 = VECTOR('',#122188,1000.) ;
#11861 = VECTOR('',#122191,1000.) ;
#11862 = VECTOR('',#122192,1000.) ;
#11863 = VECTOR('',#122193,1000.) ;
#11864 = VECTOR('',#122196,1000.) ;
#11865 = VECTOR('',#122197,1000.) ;
#11866 = VECTOR('',#122198,1000.) ;
#11867 = VECTOR('',#122201,1000.) ;
#11868 = VECTOR('',#122202,1000.) ;
#11869 = VECTOR('',#122203,1000.) ;
#11870 = VECTOR('',#122204,1000.) ;
#11871 = VECTOR('',#122207,1000.) ;
#11872 = VECTOR('',#122208,1000.) ;
#11873 = VECTOR('',#122211,1000.) ;
#11874 = VECTOR('',#122212,1000.) ;
#11875 = VECTOR('',#122215,1000.) ;
#11876 = VECTOR('',#122216,1000.) ;
#11877 = VECTOR('',#122219,1000.) ;
#11878 = VECTOR('',#122220,1000.) ;
#11879 = VECTOR('',#122221,1000.) ;
#11880 = VECTOR('',#122222,1000.) ;
#11881 = VECTOR('',#122229,1000.) ;
#11882 = VECTOR('',#122230,1000.) ;
#11883 = VECTOR('',#122231,1000.) ;
#11884 = VECTOR('',#122232,1000.) ;
#11885 = VECTOR('',#122235,1000.) ;
#11886 = VECTOR('',#122236,1000.) ;
#11887 = VECTOR('',#122237,1000.) ;
#11888 = VECTOR('',#122240,1000.) ;
#11889 = VECTOR('',#122241,1000.) ;
#11890 = VECTOR('',#122242,1000.) ;
#11891 = VECTOR('',#122243,1000.) ;
#11892 = VECTOR('',#122246,1000.) ;
#11893 = VECTOR('',#122251,1000.) ;
#11894 = VECTOR('',#122252,1000.) ;
#11895 = VECTOR('',#122253,1000.) ;
#11896 = VECTOR('',#122256,1000.) ;
#11897 = VECTOR('',#122257,1000.) ;
#11898 = VECTOR('',#122258,1000.) ;
#11899 = VECTOR('',#122261,1000.) ;
#11900 = VECTOR('',#122262,1000.) ;
#11901 = VECTOR('',#122263,1000.) ;
#11902 = VECTOR('',#122266,1000.) ;
#11903 = VECTOR('',#122267,1000.) ;
#11904 = VECTOR('',#122268,1000.) ;
#11905 = VECTOR('',#122269,1000.) ;
#11906 = VECTOR('',#122272,1000.) ;
#11907 = VECTOR('',#122273,1000.) ;
#11908 = VECTOR('',#122274,1000.) ;
#11909 = VECTOR('',#122275,1000.) ;
#11910 = VECTOR('',#122278,1000.) ;
#11911 = VECTOR('',#122281,1000.) ;
#11912 = VECTOR('',#122286,1000.) ;
#11913 = VECTOR('',#122289,1000.) ;
#11914 = VECTOR('',#122290,1000.) ;
#11915 = VECTOR('',#122291,1000.) ;
#11916 = VECTOR('',#122292,1000.) ;
#11917 = VECTOR('',#122297,1000.) ;
#11918 = VECTOR('',#122298,1000.) ;
#11919 = VECTOR('',#122299,1000.) ;
#11920 = VECTOR('',#122300,1000.) ;
#11921 = VECTOR('',#122303,1000.) ;
#11922 = VECTOR('',#122304,1000.) ;
#11923 = VECTOR('',#122305,1000.) ;
#11924 = VECTOR('',#122306,1000.) ;
#11925 = VECTOR('',#122309,1000.) ;
#11926 = VECTOR('',#122310,1000.) ;
#11927 = VECTOR('',#122311,1000.) ;
#11928 = VECTOR('',#122312,1000.) ;
#11929 = VECTOR('',#122315,1000.) ;
#11930 = VECTOR('',#122316,1000.) ;
#11931 = VECTOR('',#122317,1000.) ;
#11932 = VECTOR('',#122318,1000.) ;
#11933 = VECTOR('',#122321,1000.) ;
#11934 = VECTOR('',#122322,1000.) ;
#11935 = VECTOR('',#122323,1000.) ;
#11936 = VECTOR('',#122324,1000.) ;
#11937 = VECTOR('',#122325,1000.) ;
#11938 = VECTOR('',#122328,1000.) ;
#11939 = VECTOR('',#122331,1000.) ;
#11940 = VECTOR('',#122334,1000.) ;
#11941 = VECTOR('',#122339,1000.) ;
#11942 = VECTOR('',#122340,1000.) ;
#11943 = VECTOR('',#122341,1000.) ;
#11944 = VECTOR('',#122344,1000.) ;
#11945 = VECTOR('',#122345,1000.) ;
#11946 = VECTOR('',#122346,1000.) ;
#11947 = VECTOR('',#122349,1000.) ;
#11948 = VECTOR('',#122350,1000.) ;
#11949 = VECTOR('',#122351,1000.) ;
#11950 = VECTOR('',#122354,1000.) ;
#11951 = VECTOR('',#122355,1000.) ;
#11952 = VECTOR('',#122356,1000.) ;
#11953 = VECTOR('',#122359,1000.) ;
#11954 = VECTOR('',#122360,1000.) ;
#11955 = VECTOR('',#122361,1000.) ;
#11956 = VECTOR('',#122362,1000.) ;
#11957 = VECTOR('',#122365,1000.) ;
#11958 = VECTOR('',#122368,1000.) ;
#11959 = VECTOR('',#122369,1000.) ;
#11960 = VECTOR('',#122372,1000.) ;
#11961 = VECTOR('',#122373,1000.) ;
#11962 = VECTOR('',#122376,1000.) ;
#11963 = VECTOR('',#122377,1000.) ;
#11964 = VECTOR('',#122388,1000.) ;
#11965 = VECTOR('',#122389,1000.) ;
#11966 = VECTOR('',#122390,1000.) ;
#11967 = VECTOR('',#122393,1000.) ;
#11968 = VECTOR('',#122394,1000.) ;
#11969 = VECTOR('',#122395,1000.) ;
#11970 = VECTOR('',#122406,1000.) ;
#11971 = VECTOR('',#122409,1000.) ;
#11972 = VECTOR('',#122414,1000.) ;
#11973 = VECTOR('',#122415,1000.) ;
#11974 = VECTOR('',#122416,1000.) ;
#11975 = VECTOR('',#122421,1000.) ;
#11976 = VECTOR('',#122426,1000.) ;
#11977 = VECTOR('',#122427,1000.) ;
#11978 = VECTOR('',#122428,1000.) ;
#11979 = VECTOR('',#122433,1000.) ;
#11980 = VECTOR('',#122438,1000.) ;
#11981 = VECTOR('',#122439,1000.) ;
#11982 = VECTOR('',#122440,1000.) ;
#11983 = VECTOR('',#122445,1000.) ;
#11984 = VECTOR('',#122450,1000.) ;
#11985 = VECTOR('',#122451,1000.) ;
#11986 = VECTOR('',#122454,1000.) ;
#11987 = VECTOR('',#122455,1000.) ;
#11988 = VECTOR('',#122456,1000.) ;
#11989 = VECTOR('',#122457,1000.) ;
#11990 = VECTOR('',#123260,1000.) ;
#11991 = VECTOR('',#123261,1000.) ;
#11992 = VECTOR('',#123262,1000.) ;
#11993 = VECTOR('',#123263,1000.) ;
#11994 = VECTOR('',#123266,1000.) ;
#11995 = VECTOR('',#123267,1000.) ;
#11996 = VECTOR('',#123268,1000.) ;
#11997 = VECTOR('',#123269,1000.) ;
#11998 = VECTOR('',#123272,1000.) ;
#11999 = VECTOR('',#123275,1000.) ;
#12000 = VECTOR('',#123278,1000.) ;
#12001 = VECTOR('',#123285,1000.) ;
#12002 = VECTOR('',#123286,1000.) ;
#12003 = VECTOR('',#123287,1000.) ;
#12004 = VECTOR('',#123290,1000.) ;
#12005 = VECTOR('',#123291,1000.) ;
#12006 = VECTOR('',#123292,1000.) ;
#12007 = VECTOR('',#123293,1000.) ;
#12008 = VECTOR('',#123296,1000.) ;
#12009 = VECTOR('',#123297,1000.) ;
#12010 = VECTOR('',#123298,1000.) ;
#12011 = VECTOR('',#123299,1000.) ;
#12012 = VECTOR('',#123302,1000.) ;
#12013 = VECTOR('',#123303,1000.) ;
#12014 = VECTOR('',#123304,1000.) ;
#12015 = VECTOR('',#123305,1000.) ;
#12016 = VECTOR('',#123308,1000.) ;
#12017 = VECTOR('',#123311,1000.) ;
#12018 = VECTOR('',#123314,1000.) ;
#12019 = VECTOR('',#123321,1000.) ;
#12020 = VECTOR('',#123322,1000.) ;
#12021 = VECTOR('',#123323,1000.) ;
#12022 = VECTOR('',#123326,1000.) ;
#12023 = VECTOR('',#123327,1000.) ;
#12024 = VECTOR('',#123328,1000.) ;
#12025 = VECTOR('',#123329,1000.) ;
#12026 = VECTOR('',#123332,1000.) ;
#12027 = VECTOR('',#123333,1000.) ;
#12028 = VECTOR('',#123334,1000.) ;
#12029 = VECTOR('',#123335,1000.) ;
#12030 = VECTOR('',#123338,1000.) ;
#12031 = VECTOR('',#123339,1000.) ;
#12032 = VECTOR('',#123340,1000.) ;
#12033 = VECTOR('',#123341,1000.) ;
#12034 = VECTOR('',#123344,1000.) ;
#12035 = VECTOR('',#123347,1000.) ;
#12036 = VECTOR('',#123350,1000.) ;
#12037 = VECTOR('',#123357,1000.) ;
#12038 = VECTOR('',#123358,1000.) ;
#12039 = VECTOR('',#123359,1000.) ;
#12040 = VECTOR('',#123362,1000.) ;
#12041 = VECTOR('',#123363,1000.) ;
#12042 = VECTOR('',#123364,1000.) ;
#12043 = VECTOR('',#123365,1000.) ;
#12044 = VECTOR('',#123368,1000.) ;
#12045 = VECTOR('',#123369,1000.) ;
#12046 = VECTOR('',#123370,1000.) ;
#12047 = VECTOR('',#123371,1000.) ;
#12048 = VECTOR('',#123374,1000.) ;
#12049 = VECTOR('',#123375,1000.) ;
#12050 = VECTOR('',#123376,1000.) ;
#12051 = VECTOR('',#123377,1000.) ;
#12052 = VECTOR('',#123380,1000.) ;
#12053 = VECTOR('',#123383,1000.) ;
#12054 = VECTOR('',#123386,1000.) ;
#12055 = VECTOR('',#123393,1000.) ;
#12056 = VECTOR('',#123394,1000.) ;
#12057 = VECTOR('',#123395,1000.) ;
#12058 = VECTOR('',#123398,1000.) ;
#12059 = VECTOR('',#123399,1000.) ;
#12060 = VECTOR('',#123400,1000.) ;
#12061 = VECTOR('',#123401,1000.) ;
#12062 = VECTOR('',#123404,1000.) ;
#12063 = VECTOR('',#123405,1000.) ;
#12064 = VECTOR('',#123406,1000.) ;
#12065 = VECTOR('',#123407,1000.) ;
#12066 = VECTOR('',#123410,1000.) ;
#12067 = VECTOR('',#123411,1000.) ;
#12068 = VECTOR('',#123412,1000.) ;
#12069 = VECTOR('',#123413,1000.) ;
#12070 = VECTOR('',#123416,1000.) ;
#12071 = VECTOR('',#123419,1000.) ;
#12072 = VECTOR('',#123422,1000.) ;
#12073 = VECTOR('',#123429,1000.) ;
#12074 = VECTOR('',#123430,1000.) ;
#12075 = VECTOR('',#123431,1000.) ;
#12076 = VECTOR('',#123434,1000.) ;
#12077 = VECTOR('',#123435,1000.) ;
#12078 = VECTOR('',#123436,1000.) ;
#12079 = VECTOR('',#123437,1000.) ;
#12080 = VECTOR('',#123440,1000.) ;
#12081 = VECTOR('',#123441,1000.) ;
#12082 = VECTOR('',#123442,1000.) ;
#12083 = VECTOR('',#123443,1000.) ;
#12084 = VECTOR('',#123446,1000.) ;
#12085 = VECTOR('',#123447,1000.) ;
#12086 = VECTOR('',#123448,1000.) ;
#12087 = VECTOR('',#123449,1000.) ;
#12088 = VECTOR('',#123452,1000.) ;
#12089 = VECTOR('',#123455,1000.) ;
#12090 = VECTOR('',#123458,1000.) ;
#12091 = VECTOR('',#123465,1000.) ;
#12092 = VECTOR('',#123466,1000.) ;
#12093 = VECTOR('',#123467,1000.) ;
#12094 = VECTOR('',#123470,1000.) ;
#12095 = VECTOR('',#123471,1000.) ;
#12096 = VECTOR('',#123472,1000.) ;
#12097 = VECTOR('',#123473,1000.) ;
#12098 = VECTOR('',#123476,1000.) ;
#12099 = VECTOR('',#123477,1000.) ;
#12100 = VECTOR('',#123478,1000.) ;
#12101 = VECTOR('',#123479,1000.) ;
#12102 = VECTOR('',#123482,1000.) ;
#12103 = VECTOR('',#123483,1000.) ;
#12104 = VECTOR('',#123484,1000.) ;
#12105 = VECTOR('',#123485,1000.) ;
#12106 = VECTOR('',#123488,1000.) ;
#12107 = VECTOR('',#123491,1000.) ;
#12108 = VECTOR('',#123494,1000.) ;
#12109 = VECTOR('',#123501,1000.) ;
#12110 = VECTOR('',#123502,1000.) ;
#12111 = VECTOR('',#123503,1000.) ;
#12112 = VECTOR('',#123506,1000.) ;
#12113 = VECTOR('',#123507,1000.) ;
#12114 = VECTOR('',#123508,1000.) ;
#12115 = VECTOR('',#123509,1000.) ;
#12116 = VECTOR('',#123512,1000.) ;
#12117 = VECTOR('',#123513,1000.) ;
#12118 = VECTOR('',#123514,1000.) ;
#12119 = VECTOR('',#123515,1000.) ;
#12120 = VECTOR('',#123518,1000.) ;
#12121 = VECTOR('',#123519,1000.) ;
#12122 = VECTOR('',#123520,1000.) ;
#12123 = VECTOR('',#123521,1000.) ;
#12124 = VECTOR('',#123524,1000.) ;
#12125 = VECTOR('',#123527,1000.) ;
#12126 = VECTOR('',#123530,1000.) ;
#12127 = VECTOR('',#123537,1000.) ;
#12128 = VECTOR('',#123538,1000.) ;
#12129 = VECTOR('',#123539,1000.) ;
#12130 = VECTOR('',#123542,1000.) ;
#12131 = VECTOR('',#123543,1000.) ;
#12132 = VECTOR('',#123544,1000.) ;
#12133 = VECTOR('',#123545,1000.) ;
#12134 = VECTOR('',#123548,1000.) ;
#12135 = VECTOR('',#123549,1000.) ;
#12136 = VECTOR('',#123550,1000.) ;
#12137 = VECTOR('',#123551,1000.) ;
#12138 = VECTOR('',#123554,1000.) ;
#12139 = VECTOR('',#123555,1000.) ;
#12140 = VECTOR('',#123556,1000.) ;
#12141 = VECTOR('',#123557,1000.) ;
#12142 = VECTOR('',#123560,1000.) ;
#12143 = VECTOR('',#123563,1000.) ;
#12144 = VECTOR('',#123566,1000.) ;
#12145 = VECTOR('',#123573,1000.) ;
#12146 = VECTOR('',#123574,1000.) ;
#12147 = VECTOR('',#123575,1000.) ;
#12148 = VECTOR('',#123578,1000.) ;
#12149 = VECTOR('',#123579,1000.) ;
#12150 = VECTOR('',#123580,1000.) ;
#12151 = VECTOR('',#123581,1000.) ;
#12152 = VECTOR('',#123584,1000.) ;
#12153 = VECTOR('',#123585,1000.) ;
#12154 = VECTOR('',#123586,1000.) ;
#12155 = VECTOR('',#123587,1000.) ;
#12156 = VECTOR('',#123588,1000.) ;
#12157 = VECTOR('',#123591,1000.) ;
#12158 = VECTOR('',#123594,1000.) ;
#12159 = VECTOR('',#123595,1000.) ;
#12160 = VECTOR('',#123596,1000.) ;
#12161 = VECTOR('',#123597,1000.) ;
#12162 = VECTOR('',#123602,1000.) ;
#12163 = VECTOR('',#123605,1000.) ;
#12164 = VECTOR('',#123606,1000.) ;
#12165 = VECTOR('',#123607,1000.) ;
#12166 = VECTOR('',#123608,1000.) ;
#12167 = VECTOR('',#123613,1000.) ;
#12168 = VECTOR('',#123616,1000.) ;
#12169 = VECTOR('',#123617,1000.) ;
#12170 = VECTOR('',#123618,1000.) ;
#12171 = VECTOR('',#123619,1000.) ;
#12172 = VECTOR('',#123624,1000.) ;
#12173 = VECTOR('',#123627,1000.) ;
#12174 = VECTOR('',#123628,1000.) ;
#12175 = VECTOR('',#123629,1000.) ;
#12176 = VECTOR('',#123630,1000.) ;
#12177 = VECTOR('',#123635,1000.) ;
#12178 = VECTOR('',#123638,1000.) ;
#12179 = VECTOR('',#123639,1000.) ;
#12180 = VECTOR('',#123640,1000.) ;
#12181 = VECTOR('',#123641,1000.) ;
#12182 = VECTOR('',#123646,1000.) ;
#12183 = VECTOR('',#123649,1000.) ;
#12184 = VECTOR('',#123650,1000.) ;
#12185 = VECTOR('',#123651,1000.) ;
#12186 = VECTOR('',#123652,1000.) ;
#12187 = VECTOR('',#123657,1000.) ;
#12188 = VECTOR('',#123660,1000.) ;
#12189 = VECTOR('',#123661,1000.) ;
#12190 = VECTOR('',#123662,1000.) ;
#12191 = VECTOR('',#123663,1000.) ;
#12192 = VECTOR('',#123668,1000.) ;
#12193 = VECTOR('',#123671,1000.) ;
#12194 = VECTOR('',#123672,1000.) ;
#12195 = VECTOR('',#123673,1000.) ;
#12196 = VECTOR('',#123674,1000.) ;
#12197 = VECTOR('',#123679,1000.) ;
#12198 = VECTOR('',#123680,1000.) ;
#12199 = VECTOR('',#123681,1000.) ;
#12200 = VECTOR('',#123682,1000.) ;
#12201 = VECTOR('',#123683,1000.) ;
#12202 = VECTOR('',#123686,1000.) ;
#12203 = VECTOR('',#123689,1000.) ;
#12204 = VECTOR('',#123690,1000.) ;
#12205 = VECTOR('',#123691,1000.) ;
#12206 = VECTOR('',#123692,1000.) ;
#12207 = VECTOR('',#123697,1000.) ;
#12208 = VECTOR('',#123700,1000.) ;
#12209 = VECTOR('',#123701,1000.) ;
#12210 = VECTOR('',#123702,1000.) ;
#12211 = VECTOR('',#123703,1000.) ;
#12212 = VECTOR('',#123708,1000.) ;
#12213 = VECTOR('',#123711,1000.) ;
#12214 = VECTOR('',#123712,1000.) ;
#12215 = VECTOR('',#123713,1000.) ;
#12216 = VECTOR('',#123714,1000.) ;
#12217 = VECTOR('',#123719,1000.) ;
#12218 = VECTOR('',#123722,1000.) ;
#12219 = VECTOR('',#123723,1000.) ;
#12220 = VECTOR('',#123724,1000.) ;
#12221 = VECTOR('',#123725,1000.) ;
#12222 = VECTOR('',#123730,1000.) ;
#12223 = VECTOR('',#123733,1000.) ;
#12224 = VECTOR('',#123734,1000.) ;
#12225 = VECTOR('',#123735,1000.) ;
#12226 = VECTOR('',#123736,1000.) ;
#12227 = VECTOR('',#123741,1000.) ;
#12228 = VECTOR('',#123744,1000.) ;
#12229 = VECTOR('',#123745,1000.) ;
#12230 = VECTOR('',#123746,1000.) ;
#12231 = VECTOR('',#123747,1000.) ;
#12232 = VECTOR('',#123752,1000.) ;
#12233 = VECTOR('',#123755,1000.) ;
#12234 = VECTOR('',#123756,1000.) ;
#12235 = VECTOR('',#123757,1000.) ;
#12236 = VECTOR('',#123758,1000.) ;
#12237 = VECTOR('',#123763,1000.) ;
#12238 = VECTOR('',#123766,1000.) ;
#12239 = VECTOR('',#123767,1000.) ;
#12240 = VECTOR('',#123768,1000.) ;
#12241 = VECTOR('',#123769,1000.) ;
#12242 = VECTOR('',#123774,1000.) ;
#12243 = VECTOR('',#123775,1000.) ;
#12244 = VECTOR('',#123776,1000.) ;
#12245 = VECTOR('',#123777,1000.) ;
#12246 = VECTOR('',#123780,1000.) ;
#12247 = VECTOR('',#123781,1000.) ;
#12248 = VECTOR('',#123782,1000.) ;
#12249 = VECTOR('',#123783,1000.) ;
#12250 = VECTOR('',#123786,1000.) ;
#12251 = VECTOR('',#123787,1000.) ;
#12252 = VECTOR('',#123788,1000.) ;
#12253 = VECTOR('',#123789,1000.) ;
#12254 = VECTOR('',#123792,1000.) ;
#12255 = VECTOR('',#123793,1000.) ;
#12256 = VECTOR('',#123794,1000.) ;
#12257 = VECTOR('',#123795,1000.) ;
#12258 = VECTOR('',#123798,1000.) ;
#12259 = VECTOR('',#123799,1000.) ;
#12260 = VECTOR('',#123800,1000.) ;
#12261 = VECTOR('',#123801,1000.) ;
#12262 = VECTOR('',#123804,1000.) ;
#12263 = VECTOR('',#123805,1000.) ;
#12264 = VECTOR('',#123806,1000.) ;
#12265 = VECTOR('',#123807,1000.) ;
#12266 = VECTOR('',#123810,1000.) ;
#12267 = VECTOR('',#123811,1000.) ;
#12268 = VECTOR('',#123812,1000.) ;
#12269 = VECTOR('',#123813,1000.) ;
#12270 = VECTOR('',#123816,1000.) ;
#12271 = VECTOR('',#123817,1000.) ;
#12272 = VECTOR('',#123818,1000.) ;
#12273 = VECTOR('',#123819,1000.) ;
#12274 = VECTOR('',#123822,1000.) ;
#12275 = VECTOR('',#123823,1000.) ;
#12276 = VECTOR('',#123824,1000.) ;
#12277 = VECTOR('',#123825,1000.) ;
#12278 = VECTOR('',#123828,1000.) ;
#12279 = VECTOR('',#123829,1000.) ;
#12280 = VECTOR('',#123830,1000.) ;
#12281 = VECTOR('',#123831,1000.) ;
#12282 = VECTOR('',#123834,1000.) ;
#12283 = VECTOR('',#123835,1000.) ;
#12284 = VECTOR('',#123836,1000.) ;
#12285 = VECTOR('',#123837,1000.) ;
#12286 = VECTOR('',#123840,1000.) ;
#12287 = VECTOR('',#123841,1000.) ;
#12288 = VECTOR('',#123842,1000.) ;
#12289 = VECTOR('',#123843,1000.) ;
#12290 = VECTOR('',#123846,1000.) ;
#12291 = VECTOR('',#123847,1000.) ;
#12292 = VECTOR('',#123848,1000.) ;
#12293 = VECTOR('',#123849,1000.) ;
#12294 = VECTOR('',#123852,1000.) ;
#12295 = VECTOR('',#123853,1000.) ;
#12296 = VECTOR('',#123854,1000.) ;
#12297 = VECTOR('',#123855,1000.) ;
#12298 = VECTOR('',#123858,1000.) ;
#12299 = VECTOR('',#123859,1000.) ;
#12300 = VECTOR('',#123860,1000.) ;
#12301 = VECTOR('',#123861,1000.) ;
#12302 = VECTOR('',#123864,1000.) ;
#12303 = VECTOR('',#123865,1000.) ;
#12304 = VECTOR('',#123866,1000.) ;
#12305 = VECTOR('',#123867,1000.) ;
#12306 = VECTOR('',#123870,1000.) ;
#12307 = VECTOR('',#123871,1000.) ;
#12308 = VECTOR('',#123872,1000.) ;
#12309 = VECTOR('',#123873,1000.) ;
#12310 = VECTOR('',#123876,1000.) ;
#12311 = VECTOR('',#123877,1000.) ;
#12312 = VECTOR('',#123878,1000.) ;
#12313 = VECTOR('',#123879,1000.) ;
#12314 = VECTOR('',#123882,1000.) ;
#12315 = VECTOR('',#123883,1000.) ;
#12316 = VECTOR('',#123884,1000.) ;
#12317 = VECTOR('',#123885,1000.) ;
#12318 = VECTOR('',#123888,1000.) ;
#12319 = VECTOR('',#123889,1000.) ;
#12320 = VECTOR('',#123890,1000.) ;
#12321 = VECTOR('',#123891,1000.) ;
#12322 = VECTOR('',#123894,1000.) ;
#12323 = VECTOR('',#123895,1000.) ;
#12324 = VECTOR('',#123896,1000.) ;
#12325 = VECTOR('',#123897,1000.) ;
#12326 = VECTOR('',#123900,1000.) ;
#12327 = VECTOR('',#123901,1000.) ;
#12328 = VECTOR('',#123902,1000.) ;
#12329 = VECTOR('',#123903,1000.) ;
#12330 = VECTOR('',#123906,1000.) ;
#12331 = VECTOR('',#123907,1000.) ;
#12332 = VECTOR('',#123908,1000.) ;
#12333 = VECTOR('',#123909,1000.) ;
#12334 = VECTOR('',#123912,1000.) ;
#12335 = VECTOR('',#123913,1000.) ;
#12336 = VECTOR('',#123914,1000.) ;
#12337 = VECTOR('',#123915,1000.) ;
#12338 = VECTOR('',#123918,1000.) ;
#12339 = VECTOR('',#123919,1000.) ;
#12340 = VECTOR('',#123920,1000.) ;
#12341 = VECTOR('',#123921,1000.) ;
#12342 = VECTOR('',#123924,1000.) ;
#12343 = VECTOR('',#123925,1000.) ;
#12344 = VECTOR('',#123926,1000.) ;
#12345 = VECTOR('',#123927,1000.) ;
#12346 = VECTOR('',#123930,1000.) ;
#12347 = VECTOR('',#123931,1000.) ;
#12348 = VECTOR('',#123932,1000.) ;
#12349 = VECTOR('',#123933,1000.) ;
#12350 = VECTOR('',#123936,1000.) ;
#12351 = VECTOR('',#123937,1000.) ;
#12352 = VECTOR('',#123938,1000.) ;
#12353 = VECTOR('',#123939,1000.) ;
#12354 = VECTOR('',#123942,1000.) ;
#12355 = VECTOR('',#123943,1000.) ;
#12356 = VECTOR('',#123944,1000.) ;
#12357 = VECTOR('',#123945,1000.) ;
#12358 = VECTOR('',#123948,1000.) ;
#12359 = VECTOR('',#123949,1000.) ;
#12360 = VECTOR('',#123950,1000.) ;
#12361 = VECTOR('',#123951,1000.) ;
#12362 = VECTOR('',#123954,1000.) ;
#12363 = VECTOR('',#123955,1000.) ;
#12364 = VECTOR('',#123956,1000.) ;
#12365 = VECTOR('',#123957,1000.) ;
#12366 = VECTOR('',#123960,1000.) ;
#12367 = VECTOR('',#123961,1000.) ;
#12368 = VECTOR('',#123962,1000.) ;
#12369 = VECTOR('',#123963,1000.) ;
#12370 = VECTOR('',#123966,1000.) ;
#12371 = VECTOR('',#123967,1000.) ;
#12372 = VECTOR('',#123968,1000.) ;
#12373 = VECTOR('',#123969,1000.) ;
#12374 = VECTOR('',#123972,1000.) ;
#12375 = VECTOR('',#123973,1000.) ;
#12376 = VECTOR('',#123974,1000.) ;
#12377 = VECTOR('',#123975,1000.) ;
#12378 = VECTOR('',#123978,1000.) ;
#12379 = VECTOR('',#123979,1000.) ;
#12380 = VECTOR('',#123980,1000.) ;
#12381 = VECTOR('',#123981,1000.) ;
#12382 = VECTOR('',#123984,1000.) ;
#12383 = VECTOR('',#123985,1000.) ;
#12384 = VECTOR('',#123986,1000.) ;
#12385 = VECTOR('',#123987,1000.) ;
#12386 = VECTOR('',#123990,1000.) ;
#12387 = VECTOR('',#123991,1000.) ;
#12388 = VECTOR('',#123992,1000.) ;
#12389 = VECTOR('',#123993,1000.) ;
#12390 = VECTOR('',#123994,1000.) ;
#12391 = VECTOR('',#123997,1000.) ;
#12392 = VECTOR('',#124000,1000.) ;
#12393 = VECTOR('',#124003,1000.) ;
#12394 = VECTOR('',#124008,1000.) ;
#12395 = VECTOR('',#124009,1000.) ;
#12396 = VECTOR('',#124010,1000.) ;
#12397 = VECTOR('',#124013,1000.) ;
#12398 = VECTOR('',#124014,1000.) ;
#12399 = VECTOR('',#124015,1000.) ;
#12400 = VECTOR('',#124018,1000.) ;
#12401 = VECTOR('',#124019,1000.) ;
#12402 = VECTOR('',#124020,1000.) ;
#12403 = VECTOR('',#124023,1000.) ;
#12404 = VECTOR('',#124024,1000.) ;
#12405 = VECTOR('',#124025,1000.) ;
#12406 = VECTOR('',#124028,1000.) ;
#12407 = VECTOR('',#124029,1000.) ;
#12408 = VECTOR('',#124030,1000.) ;
#12409 = VECTOR('',#124031,1000.) ;
#12410 = VECTOR('',#124032,1000.) ;
#12411 = VECTOR('',#124035,1000.) ;
#12412 = VECTOR('',#124038,1000.) ;
#12413 = VECTOR('',#124041,1000.) ;
#12414 = VECTOR('',#124046,1000.) ;
#12415 = VECTOR('',#124047,1000.) ;
#12416 = VECTOR('',#124048,1000.) ;
#12417 = VECTOR('',#124051,1000.) ;
#12418 = VECTOR('',#124052,1000.) ;
#12419 = VECTOR('',#124053,1000.) ;
#12420 = VECTOR('',#124056,1000.) ;
#12421 = VECTOR('',#124057,1000.) ;
#12422 = VECTOR('',#124058,1000.) ;
#12423 = VECTOR('',#124061,1000.) ;
#12424 = VECTOR('',#124062,1000.) ;
#12425 = VECTOR('',#124063,1000.) ;
#12426 = VECTOR('',#124066,1000.) ;
#12427 = VECTOR('',#124067,1000.) ;
#12428 = VECTOR('',#124068,1000.) ;
#12429 = VECTOR('',#124069,1000.) ;
#12430 = VECTOR('',#124070,1000.) ;
#12431 = VECTOR('',#124073,1000.) ;
#12432 = VECTOR('',#124076,1000.) ;
#12433 = VECTOR('',#124079,1000.) ;
#12434 = VECTOR('',#124084,1000.) ;
#12435 = VECTOR('',#124085,1000.) ;
#12436 = VECTOR('',#124086,1000.) ;
#12437 = VECTOR('',#124089,1000.) ;
#12438 = VECTOR('',#124090,1000.) ;
#12439 = VECTOR('',#124091,1000.) ;
#12440 = VECTOR('',#124094,1000.) ;
#12441 = VECTOR('',#124095,1000.) ;
#12442 = VECTOR('',#124096,1000.) ;
#12443 = VECTOR('',#124099,1000.) ;
#12444 = VECTOR('',#124100,1000.) ;
#12445 = VECTOR('',#124101,1000.) ;
#12446 = VECTOR('',#124104,1000.) ;
#12447 = VECTOR('',#124105,1000.) ;
#12448 = VECTOR('',#124106,1000.) ;
#12449 = VECTOR('',#124107,1000.) ;
#12450 = VECTOR('',#124108,1000.) ;
#12451 = VECTOR('',#124111,1000.) ;
#12452 = VECTOR('',#124114,1000.) ;
#12453 = VECTOR('',#124117,1000.) ;
#12454 = VECTOR('',#124122,1000.) ;
#12455 = VECTOR('',#124123,1000.) ;
#12456 = VECTOR('',#124124,1000.) ;
#12457 = VECTOR('',#124127,1000.) ;
#12458 = VECTOR('',#124128,1000.) ;
#12459 = VECTOR('',#124129,1000.) ;
#12460 = VECTOR('',#124132,1000.) ;
#12461 = VECTOR('',#124133,1000.) ;
#12462 = VECTOR('',#124134,1000.) ;
#12463 = VECTOR('',#124137,1000.) ;
#12464 = VECTOR('',#124138,1000.) ;
#12465 = VECTOR('',#124139,1000.) ;
#12466 = VECTOR('',#124142,1000.) ;
#12467 = VECTOR('',#124143,1000.) ;
#12468 = VECTOR('',#124144,1000.) ;
#12469 = VECTOR('',#124145,1000.) ;
#12470 = VECTOR('',#124146,1000.) ;
#12471 = VECTOR('',#124149,1000.) ;
#12472 = VECTOR('',#124152,1000.) ;
#12473 = VECTOR('',#124155,1000.) ;
#12474 = VECTOR('',#124160,1000.) ;
#12475 = VECTOR('',#124161,1000.) ;
#12476 = VECTOR('',#124162,1000.) ;
#12477 = VECTOR('',#124165,1000.) ;
#12478 = VECTOR('',#124166,1000.) ;
#12479 = VECTOR('',#124167,1000.) ;
#12480 = VECTOR('',#124170,1000.) ;
#12481 = VECTOR('',#124171,1000.) ;
#12482 = VECTOR('',#124172,1000.) ;
#12483 = VECTOR('',#124175,1000.) ;
#12484 = VECTOR('',#124176,1000.) ;
#12485 = VECTOR('',#124177,1000.) ;
#12486 = VECTOR('',#124180,1000.) ;
#12487 = VECTOR('',#124181,1000.) ;
#12488 = VECTOR('',#124182,1000.) ;
#12489 = VECTOR('',#124183,1000.) ;
#12490 = VECTOR('',#124184,1000.) ;
#12491 = VECTOR('',#124187,1000.) ;
#12492 = VECTOR('',#124190,1000.) ;
#12493 = VECTOR('',#124193,1000.) ;
#12494 = VECTOR('',#124198,1000.) ;
#12495 = VECTOR('',#124199,1000.) ;
#12496 = VECTOR('',#124200,1000.) ;
#12497 = VECTOR('',#124203,1000.) ;
#12498 = VECTOR('',#124204,1000.) ;
#12499 = VECTOR('',#124205,1000.) ;
#12500 = VECTOR('',#124208,1000.) ;
#12501 = VECTOR('',#124209,1000.) ;
#12502 = VECTOR('',#124210,1000.) ;
#12503 = VECTOR('',#124213,1000.) ;
#12504 = VECTOR('',#124214,1000.) ;
#12505 = VECTOR('',#124215,1000.) ;
#12506 = VECTOR('',#124218,1000.) ;
#12507 = VECTOR('',#124219,1000.) ;
#12508 = VECTOR('',#124220,1000.) ;
#12509 = VECTOR('',#124221,1000.) ;
#12510 = VECTOR('',#124222,1000.) ;
#12511 = VECTOR('',#124225,1000.) ;
#12512 = VECTOR('',#124228,1000.) ;
#12513 = VECTOR('',#124231,1000.) ;
#12514 = VECTOR('',#124236,1000.) ;
#12515 = VECTOR('',#124237,1000.) ;
#12516 = VECTOR('',#124238,1000.) ;
#12517 = VECTOR('',#124241,1000.) ;
#12518 = VECTOR('',#124242,1000.) ;
#12519 = VECTOR('',#124243,1000.) ;
#12520 = VECTOR('',#124246,1000.) ;
#12521 = VECTOR('',#124247,1000.) ;
#12522 = VECTOR('',#124248,1000.) ;
#12523 = VECTOR('',#124251,1000.) ;
#12524 = VECTOR('',#124252,1000.) ;
#12525 = VECTOR('',#124253,1000.) ;
#12526 = VECTOR('',#124256,1000.) ;
#12527 = VECTOR('',#124257,1000.) ;
#12528 = VECTOR('',#124258,1000.) ;
#12529 = VECTOR('',#124259,1000.) ;
#12530 = VECTOR('',#124260,1000.) ;
#12531 = VECTOR('',#124263,1000.) ;
#12532 = VECTOR('',#124266,1000.) ;
#12533 = VECTOR('',#124269,1000.) ;
#12534 = VECTOR('',#124274,1000.) ;
#12535 = VECTOR('',#124275,1000.) ;
#12536 = VECTOR('',#124276,1000.) ;
#12537 = VECTOR('',#124279,1000.) ;
#12538 = VECTOR('',#124280,1000.) ;
#12539 = VECTOR('',#124281,1000.) ;
#12540 = VECTOR('',#124284,1000.) ;
#12541 = VECTOR('',#124285,1000.) ;
#12542 = VECTOR('',#124286,1000.) ;
#12543 = VECTOR('',#124289,1000.) ;
#12544 = VECTOR('',#124290,1000.) ;
#12545 = VECTOR('',#124291,1000.) ;
#12546 = VECTOR('',#124294,1000.) ;
#12547 = VECTOR('',#124295,1000.) ;
#12548 = VECTOR('',#124296,1000.) ;
#12549 = VECTOR('',#124297,1000.) ;
#12550 = VECTOR('',#124298,1000.) ;
#12551 = VECTOR('',#124301,1000.) ;
#12552 = VECTOR('',#124304,1000.) ;
#12553 = VECTOR('',#124307,1000.) ;
#12554 = VECTOR('',#124312,1000.) ;
#12555 = VECTOR('',#124313,1000.) ;
#12556 = VECTOR('',#124314,1000.) ;
#12557 = VECTOR('',#124317,1000.) ;
#12558 = VECTOR('',#124318,1000.) ;
#12559 = VECTOR('',#124319,1000.) ;
#12560 = VECTOR('',#124322,1000.) ;
#12561 = VECTOR('',#124323,1000.) ;
#12562 = VECTOR('',#124324,1000.) ;
#12563 = VECTOR('',#124327,1000.) ;
#12564 = VECTOR('',#124328,1000.) ;
#12565 = VECTOR('',#124329,1000.) ;
#12566 = VECTOR('',#124332,1000.) ;
#12567 = VECTOR('',#124333,1000.) ;
#12568 = VECTOR('',#124334,1000.) ;
#12569 = VECTOR('',#124335,1000.) ;
#12570 = VECTOR('',#124338,1000.) ;
#12571 = VECTOR('',#124339,1000.) ;
#12572 = VECTOR('',#124340,1000.) ;
#12573 = VECTOR('',#124341,1000.) ;
#12574 = VECTOR('',#124344,1000.) ;
#12575 = VECTOR('',#124345,1000.) ;
#12576 = VECTOR('',#124346,1000.) ;
#12577 = VECTOR('',#124347,1000.) ;
#12578 = VECTOR('',#124350,1000.) ;
#12579 = VECTOR('',#124351,1000.) ;
#12580 = VECTOR('',#124352,1000.) ;
#12581 = VECTOR('',#124353,1000.) ;
#12582 = VECTOR('',#124356,1000.) ;
#12583 = VECTOR('',#124357,1000.) ;
#12584 = VECTOR('',#124358,1000.) ;
#12585 = VECTOR('',#124359,1000.) ;
#12586 = VECTOR('',#124362,1000.) ;
#12587 = VECTOR('',#124363,1000.) ;
#12588 = VECTOR('',#124364,1000.) ;
#12589 = VECTOR('',#124365,1000.) ;
#12590 = VECTOR('',#124368,1000.) ;
#12591 = VECTOR('',#124369,1000.) ;
#12592 = VECTOR('',#124370,1000.) ;
#12593 = VECTOR('',#124371,1000.) ;
#12594 = VECTOR('',#124374,1000.) ;
#12595 = VECTOR('',#124375,1000.) ;
#12596 = VECTOR('',#124376,1000.) ;
#12597 = VECTOR('',#124377,1000.) ;
#12598 = VECTOR('',#124380,1000.) ;
#12599 = VECTOR('',#124381,1000.) ;
#12600 = VECTOR('',#124382,1000.) ;
#12601 = VECTOR('',#124383,1000.) ;
#12602 = VECTOR('',#124390,1000.) ;
#12603 = VECTOR('',#124391,1000.) ;
#12604 = VECTOR('',#124392,1000.) ;
#12605 = VECTOR('',#124393,1000.) ;
#12606 = VECTOR('',#124396,1000.) ;
#12607 = VECTOR('',#124397,1000.) ;
#12608 = VECTOR('',#124398,1000.) ;
#12609 = VECTOR('',#124401,1000.) ;
#12610 = VECTOR('',#124402,1000.) ;
#12611 = VECTOR('',#124403,1000.) ;
#12612 = VECTOR('',#124404,1000.) ;
#12613 = VECTOR('',#124407,1000.) ;
#12614 = VECTOR('',#124412,1000.) ;
#12615 = VECTOR('',#124413,1000.) ;
#12616 = VECTOR('',#124414,1000.) ;
#12617 = VECTOR('',#124417,1000.) ;
#12618 = VECTOR('',#124418,1000.) ;
#12619 = VECTOR('',#124419,1000.) ;
#12620 = VECTOR('',#124422,1000.) ;
#12621 = VECTOR('',#124423,1000.) ;
#12622 = VECTOR('',#124424,1000.) ;
#12623 = VECTOR('',#124425,1000.) ;
#12624 = VECTOR('',#124432,1000.) ;
#12625 = VECTOR('',#124433,1000.) ;
#12626 = VECTOR('',#124434,1000.) ;
#12627 = VECTOR('',#124435,1000.) ;
#12628 = VECTOR('',#124438,1000.) ;
#12629 = VECTOR('',#124439,1000.) ;
#12630 = VECTOR('',#124440,1000.) ;
#12631 = VECTOR('',#124443,1000.) ;
#12632 = VECTOR('',#124444,1000.) ;
#12633 = VECTOR('',#124445,1000.) ;
#12634 = VECTOR('',#124446,1000.) ;
#12635 = VECTOR('',#124449,1000.) ;
#12636 = VECTOR('',#124454,1000.) ;
#12637 = VECTOR('',#124455,1000.) ;
#12638 = VECTOR('',#124456,1000.) ;
#12639 = VECTOR('',#124459,1000.) ;
#12640 = VECTOR('',#124460,1000.) ;
#12641 = VECTOR('',#124461,1000.) ;
#12642 = VECTOR('',#124464,1000.) ;
#12643 = VECTOR('',#124465,1000.) ;
#12644 = VECTOR('',#124466,1000.) ;
#12645 = VECTOR('',#124467,1000.) ;
#12646 = VECTOR('',#124474,1000.) ;
#12647 = VECTOR('',#124475,1000.) ;
#12648 = VECTOR('',#124476,1000.) ;
#12649 = VECTOR('',#124477,1000.) ;
#12650 = VECTOR('',#124480,1000.) ;
#12651 = VECTOR('',#124481,1000.) ;
#12652 = VECTOR('',#124482,1000.) ;
#12653 = VECTOR('',#124485,1000.) ;
#12654 = VECTOR('',#124486,1000.) ;
#12655 = VECTOR('',#124487,1000.) ;
#12656 = VECTOR('',#124488,1000.) ;
#12657 = VECTOR('',#124491,1000.) ;
#12658 = VECTOR('',#124496,1000.) ;
#12659 = VECTOR('',#124497,1000.) ;
#12660 = VECTOR('',#124498,1000.) ;
#12661 = VECTOR('',#124501,1000.) ;
#12662 = VECTOR('',#124502,1000.) ;
#12663 = VECTOR('',#124503,1000.) ;
#12664 = VECTOR('',#124506,1000.) ;
#12665 = VECTOR('',#124507,1000.) ;
#12666 = VECTOR('',#124508,1000.) ;
#12667 = VECTOR('',#124509,1000.) ;
#12668 = VECTOR('',#124516,1000.) ;
#12669 = VECTOR('',#124517,1000.) ;
#12670 = VECTOR('',#124518,1000.) ;
#12671 = VECTOR('',#124519,1000.) ;
#12672 = VECTOR('',#124522,1000.) ;
#12673 = VECTOR('',#124523,1000.) ;
#12674 = VECTOR('',#124524,1000.) ;
#12675 = VECTOR('',#124527,1000.) ;
#12676 = VECTOR('',#124528,1000.) ;
#12677 = VECTOR('',#124529,1000.) ;
#12678 = VECTOR('',#124530,1000.) ;
#12679 = VECTOR('',#124533,1000.) ;
#12680 = VECTOR('',#124538,1000.) ;
#12681 = VECTOR('',#124539,1000.) ;
#12682 = VECTOR('',#124540,1000.) ;
#12683 = VECTOR('',#124543,1000.) ;
#12684 = VECTOR('',#124544,1000.) ;
#12685 = VECTOR('',#124545,1000.) ;
#12686 = VECTOR('',#124548,1000.) ;
#12687 = VECTOR('',#124549,1000.) ;
#12688 = VECTOR('',#124550,1000.) ;
#12689 = VECTOR('',#124551,1000.) ;
#12690 = VECTOR('',#124558,1000.) ;
#12691 = VECTOR('',#124559,1000.) ;
#12692 = VECTOR('',#124560,1000.) ;
#12693 = VECTOR('',#124561,1000.) ;
#12694 = VECTOR('',#124564,1000.) ;
#12695 = VECTOR('',#124565,1000.) ;
#12696 = VECTOR('',#124566,1000.) ;
#12697 = VECTOR('',#124569,1000.) ;
#12698 = VECTOR('',#124570,1000.) ;
#12699 = VECTOR('',#124571,1000.) ;
#12700 = VECTOR('',#124572,1000.) ;
#12701 = VECTOR('',#124575,1000.) ;
#12702 = VECTOR('',#124580,1000.) ;
#12703 = VECTOR('',#124581,1000.) ;
#12704 = VECTOR('',#124582,1000.) ;
#12705 = VECTOR('',#124585,1000.) ;
#12706 = VECTOR('',#124586,1000.) ;
#12707 = VECTOR('',#124587,1000.) ;
#12708 = VECTOR('',#124590,1000.) ;
#12709 = VECTOR('',#124591,1000.) ;
#12710 = VECTOR('',#124592,1000.) ;
#12711 = VECTOR('',#124593,1000.) ;
#12712 = VECTOR('',#124600,1000.) ;
#12713 = VECTOR('',#124601,1000.) ;
#12714 = VECTOR('',#124602,1000.) ;
#12715 = VECTOR('',#124603,1000.) ;
#12716 = VECTOR('',#124606,1000.) ;
#12717 = VECTOR('',#124607,1000.) ;
#12718 = VECTOR('',#124608,1000.) ;
#12719 = VECTOR('',#124611,1000.) ;
#12720 = VECTOR('',#124612,1000.) ;
#12721 = VECTOR('',#124613,1000.) ;
#12722 = VECTOR('',#124614,1000.) ;
#12723 = VECTOR('',#124617,1000.) ;
#12724 = VECTOR('',#124622,1000.) ;
#12725 = VECTOR('',#124623,1000.) ;
#12726 = VECTOR('',#124624,1000.) ;
#12727 = VECTOR('',#124627,1000.) ;
#12728 = VECTOR('',#124628,1000.) ;
#12729 = VECTOR('',#124629,1000.) ;
#12730 = VECTOR('',#124632,1000.) ;
#12731 = VECTOR('',#124633,1000.) ;
#12732 = VECTOR('',#124634,1000.) ;
#12733 = VECTOR('',#124635,1000.) ;
#12734 = VECTOR('',#124642,1000.) ;
#12735 = VECTOR('',#124643,1000.) ;
#12736 = VECTOR('',#124644,1000.) ;
#12737 = VECTOR('',#124645,1000.) ;
#12738 = VECTOR('',#124648,1000.) ;
#12739 = VECTOR('',#124649,1000.) ;
#12740 = VECTOR('',#124650,1000.) ;
#12741 = VECTOR('',#124653,1000.) ;
#12742 = VECTOR('',#124654,1000.) ;
#12743 = VECTOR('',#124655,1000.) ;
#12744 = VECTOR('',#124656,1000.) ;
#12745 = VECTOR('',#124659,1000.) ;
#12746 = VECTOR('',#124664,1000.) ;
#12747 = VECTOR('',#124665,1000.) ;
#12748 = VECTOR('',#124666,1000.) ;
#12749 = VECTOR('',#124669,1000.) ;
#12750 = VECTOR('',#124670,1000.) ;
#12751 = VECTOR('',#124671,1000.) ;
#12752 = VECTOR('',#124674,1000.) ;
#12753 = VECTOR('',#124675,1000.) ;
#12754 = VECTOR('',#124676,1000.) ;
#12755 = VECTOR('',#124677,1000.) ;
#12756 = VECTOR('',#124684,1000.) ;
#12757 = VECTOR('',#124685,1000.) ;
#12758 = VECTOR('',#124686,1000.) ;
#12759 = VECTOR('',#124687,1000.) ;
#12760 = VECTOR('',#124690,1000.) ;
#12761 = VECTOR('',#124691,1000.) ;
#12762 = VECTOR('',#124692,1000.) ;
#12763 = VECTOR('',#124695,1000.) ;
#12764 = VECTOR('',#124696,1000.) ;
#12765 = VECTOR('',#124697,1000.) ;
#12766 = VECTOR('',#124698,1000.) ;
#12767 = VECTOR('',#124701,1000.) ;
#12768 = VECTOR('',#124706,1000.) ;
#12769 = VECTOR('',#124707,1000.) ;
#12770 = VECTOR('',#124708,1000.) ;
#12771 = VECTOR('',#124711,1000.) ;
#12772 = VECTOR('',#124712,1000.) ;
#12773 = VECTOR('',#124713,1000.) ;
#12774 = VECTOR('',#124716,1000.) ;
#12775 = VECTOR('',#124717,1000.) ;
#12776 = VECTOR('',#124718,1000.) ;
#12777 = VECTOR('',#124719,1000.) ;
#12778 = VECTOR('',#124726,1000.) ;
#12779 = VECTOR('',#124727,1000.) ;
#12780 = VECTOR('',#124728,1000.) ;
#12781 = VECTOR('',#124729,1000.) ;
#12782 = VECTOR('',#124732,1000.) ;
#12783 = VECTOR('',#124733,1000.) ;
#12784 = VECTOR('',#124734,1000.) ;
#12785 = VECTOR('',#124737,1000.) ;
#12786 = VECTOR('',#124738,1000.) ;
#12787 = VECTOR('',#124739,1000.) ;
#12788 = VECTOR('',#124740,1000.) ;
#12789 = VECTOR('',#124743,1000.) ;
#12790 = VECTOR('',#124748,1000.) ;
#12791 = VECTOR('',#124749,1000.) ;
#12792 = VECTOR('',#124750,1000.) ;
#12793 = VECTOR('',#124753,1000.) ;
#12794 = VECTOR('',#124754,1000.) ;
#12795 = VECTOR('',#124755,1000.) ;
#12796 = VECTOR('',#124758,1000.) ;
#12797 = VECTOR('',#124759,1000.) ;
#12798 = VECTOR('',#124760,1000.) ;
#12799 = VECTOR('',#124761,1000.) ;
#12800 = VECTOR('',#124764,1000.) ;
#12801 = VECTOR('',#124765,1000.) ;
#12802 = VECTOR('',#124766,1000.) ;
#12803 = VECTOR('',#124767,1000.) ;
#12804 = VECTOR('',#124770,1000.) ;
#12805 = VECTOR('',#124771,1000.) ;
#12806 = VECTOR('',#124772,1000.) ;
#12807 = VECTOR('',#124773,1000.) ;
#12808 = VECTOR('',#124776,1000.) ;
#12809 = VECTOR('',#124779,1000.) ;
#12810 = VECTOR('',#124784,1000.) ;
#12811 = VECTOR('',#124787,1000.) ;
#12812 = VECTOR('',#124788,1000.) ;
#12813 = VECTOR('',#124789,1000.) ;
#12814 = VECTOR('',#124790,1000.) ;
#12815 = VECTOR('',#124793,1000.) ;
#12816 = VECTOR('',#124794,1000.) ;
#12817 = VECTOR('',#124795,1000.) ;
#12818 = VECTOR('',#124796,1000.) ;
#12819 = VECTOR('',#124799,1000.) ;
#12820 = VECTOR('',#124800,1000.) ;
#12821 = VECTOR('',#124801,1000.) ;
#12822 = VECTOR('',#124802,1000.) ;
#12823 = VECTOR('',#124805,1000.) ;
#12824 = VECTOR('',#124808,1000.) ;
#12825 = VECTOR('',#124813,1000.) ;
#12826 = VECTOR('',#124816,1000.) ;
#12827 = VECTOR('',#124817,1000.) ;
#12828 = VECTOR('',#124818,1000.) ;
#12829 = VECTOR('',#124819,1000.) ;
#12830 = VECTOR('',#124822,1000.) ;
#12831 = VECTOR('',#124823,1000.) ;
#12832 = VECTOR('',#124824,1000.) ;
#12833 = VECTOR('',#124825,1000.) ;
#12834 = VECTOR('',#124828,1000.) ;
#12835 = VECTOR('',#124829,1000.) ;
#12836 = VECTOR('',#124830,1000.) ;
#12837 = VECTOR('',#124831,1000.) ;
#12838 = VECTOR('',#124834,1000.) ;
#12839 = VECTOR('',#124837,1000.) ;
#12840 = VECTOR('',#124842,1000.) ;
#12841 = VECTOR('',#124845,1000.) ;
#12842 = VECTOR('',#124846,1000.) ;
#12843 = VECTOR('',#124847,1000.) ;
#12844 = VECTOR('',#124848,1000.) ;
#12845 = VECTOR('',#124851,1000.) ;
#12846 = VECTOR('',#124852,1000.) ;
#12847 = VECTOR('',#124853,1000.) ;
#12848 = VECTOR('',#124854,1000.) ;
#12849 = VECTOR('',#124857,1000.) ;
#12850 = VECTOR('',#124858,1000.) ;
#12851 = VECTOR('',#124859,1000.) ;
#12852 = VECTOR('',#124860,1000.) ;
#12853 = VECTOR('',#124863,1000.) ;
#12854 = VECTOR('',#124866,1000.) ;
#12855 = VECTOR('',#124871,1000.) ;
#12856 = VECTOR('',#124874,1000.) ;
#12857 = VECTOR('',#124875,1000.) ;
#12858 = VECTOR('',#124876,1000.) ;
#12859 = VECTOR('',#124877,1000.) ;
#12860 = VECTOR('',#124880,1000.) ;
#12861 = VECTOR('',#124881,1000.) ;
#12862 = VECTOR('',#124882,1000.) ;
#12863 = VECTOR('',#124883,1000.) ;
#12864 = VECTOR('',#124886,1000.) ;
#12865 = VECTOR('',#124887,1000.) ;
#12866 = VECTOR('',#124888,1000.) ;
#12867 = VECTOR('',#124889,1000.) ;
#12868 = VECTOR('',#124892,1000.) ;
#12869 = VECTOR('',#124895,1000.) ;
#12870 = VECTOR('',#124900,1000.) ;
#12871 = VECTOR('',#124903,1000.) ;
#12872 = VECTOR('',#124904,1000.) ;
#12873 = VECTOR('',#124905,1000.) ;
#12874 = VECTOR('',#124906,1000.) ;
#12875 = VECTOR('',#124909,1000.) ;
#12876 = VECTOR('',#124910,1000.) ;
#12877 = VECTOR('',#124911,1000.) ;
#12878 = VECTOR('',#124912,1000.) ;
#12879 = VECTOR('',#124915,1000.) ;
#12880 = VECTOR('',#124916,1000.) ;
#12881 = VECTOR('',#124917,1000.) ;
#12882 = VECTOR('',#124918,1000.) ;
#12883 = VECTOR('',#124921,1000.) ;
#12884 = VECTOR('',#124924,1000.) ;
#12885 = VECTOR('',#124929,1000.) ;
#12886 = VECTOR('',#124932,1000.) ;
#12887 = VECTOR('',#124933,1000.) ;
#12888 = VECTOR('',#124934,1000.) ;
#12889 = VECTOR('',#124935,1000.) ;
#12890 = VECTOR('',#124938,1000.) ;
#12891 = VECTOR('',#124939,1000.) ;
#12892 = VECTOR('',#124940,1000.) ;
#12893 = VECTOR('',#124941,1000.) ;
#12894 = VECTOR('',#124944,1000.) ;
#12895 = VECTOR('',#124945,1000.) ;
#12896 = VECTOR('',#124946,1000.) ;
#12897 = VECTOR('',#124947,1000.) ;
#12898 = VECTOR('',#124950,1000.) ;
#12899 = VECTOR('',#124953,1000.) ;
#12900 = VECTOR('',#124958,1000.) ;
#12901 = VECTOR('',#124961,1000.) ;
#12902 = VECTOR('',#124962,1000.) ;
#12903 = VECTOR('',#124963,1000.) ;
#12904 = VECTOR('',#124964,1000.) ;
#12905 = VECTOR('',#124967,1000.) ;
#12906 = VECTOR('',#124968,1000.) ;
#12907 = VECTOR('',#124969,1000.) ;
#12908 = VECTOR('',#124970,1000.) ;
#12909 = VECTOR('',#124973,1000.) ;
#12910 = VECTOR('',#124974,1000.) ;
#12911 = VECTOR('',#124975,1000.) ;
#12912 = VECTOR('',#124976,1000.) ;
#12913 = VECTOR('',#124979,1000.) ;
#12914 = VECTOR('',#124982,1000.) ;
#12915 = VECTOR('',#124987,1000.) ;
#12916 = VECTOR('',#124990,1000.) ;
#12917 = VECTOR('',#124991,1000.) ;
#12918 = VECTOR('',#124992,1000.) ;
#12919 = VECTOR('',#124993,1000.) ;
#12920 = VECTOR('',#124996,1000.) ;
#12921 = VECTOR('',#124997,1000.) ;
#12922 = VECTOR('',#124998,1000.) ;
#12923 = VECTOR('',#124999,1000.) ;
#12924 = VECTOR('',#125002,1000.) ;
#12925 = VECTOR('',#125003,1000.) ;
#12926 = VECTOR('',#125004,1000.) ;
#12927 = VECTOR('',#125005,1000.) ;
#12928 = VECTOR('',#125008,1000.) ;
#12929 = VECTOR('',#125011,1000.) ;
#12930 = VECTOR('',#125016,1000.) ;
#12931 = VECTOR('',#125019,1000.) ;
#12932 = VECTOR('',#125020,1000.) ;
#12933 = VECTOR('',#125021,1000.) ;
#12934 = VECTOR('',#125022,1000.) ;
#12935 = VECTOR('',#125043,1000.) ;
#12936 = VECTOR('',#125044,1000.) ;
#12937 = VECTOR('',#125045,1000.) ;
#12938 = VECTOR('',#125046,1000.) ;
#12939 = VECTOR('',#125049,1000.) ;
#12940 = VECTOR('',#125050,1000.) ;
#12941 = VECTOR('',#125051,1000.) ;
#12942 = VECTOR('',#125052,1000.) ;
#12943 = VECTOR('',#125055,1000.) ;
#12944 = VECTOR('',#125056,1000.) ;
#12945 = VECTOR('',#125057,1000.) ;
#12946 = VECTOR('',#125058,1000.) ;
#12947 = VECTOR('',#125061,1000.) ;
#12948 = VECTOR('',#125062,1000.) ;
#12949 = VECTOR('',#125063,1000.) ;
#12950 = VECTOR('',#125064,1000.) ;
#12951 = VECTOR('',#125067,1000.) ;
#12952 = VECTOR('',#125068,1000.) ;
#12953 = VECTOR('',#125069,1000.) ;
#12954 = VECTOR('',#125070,1000.) ;
#12955 = VECTOR('',#125073,1000.) ;
#12956 = VECTOR('',#125074,1000.) ;
#12957 = VECTOR('',#125075,1000.) ;
#12958 = VECTOR('',#125076,1000.) ;
#12959 = VECTOR('',#125079,1000.) ;
#12960 = VECTOR('',#125080,1000.) ;
#12961 = VECTOR('',#125081,1000.) ;
#12962 = VECTOR('',#125082,1000.) ;
#12963 = VECTOR('',#125085,1000.) ;
#12964 = VECTOR('',#125086,1000.) ;
#12965 = VECTOR('',#125087,1000.) ;
#12966 = VECTOR('',#125088,1000.) ;
#12967 = VECTOR('',#125091,1000.) ;
#12968 = VECTOR('',#125092,1000.) ;
#12969 = VECTOR('',#125093,1000.) ;
#12970 = VECTOR('',#125094,1000.) ;
#12971 = VECTOR('',#125097,1000.) ;
#12972 = VECTOR('',#125098,1000.) ;
#12973 = VECTOR('',#125099,1000.) ;
#12974 = VECTOR('',#125100,1000.) ;
#12975 = VECTOR('',#125103,1000.) ;
#12976 = VECTOR('',#125104,1000.) ;
#12977 = VECTOR('',#125105,1000.) ;
#12978 = VECTOR('',#125106,1000.) ;
#12979 = VECTOR('',#125109,1000.) ;
#12980 = VECTOR('',#125110,1000.) ;
#12981 = VECTOR('',#125111,1000.) ;
#12982 = VECTOR('',#125112,1000.) ;
#12983 = VECTOR('',#125115,1000.) ;
#12984 = VECTOR('',#125116,1000.) ;
#12985 = VECTOR('',#125117,1000.) ;
#12986 = VECTOR('',#125118,1000.) ;
#12987 = VECTOR('',#125121,1000.) ;
#12988 = VECTOR('',#125122,1000.) ;
#12989 = VECTOR('',#125123,1000.) ;
#12990 = VECTOR('',#125124,1000.) ;
#12991 = VECTOR('',#125127,1000.) ;
#12992 = VECTOR('',#125128,1000.) ;
#12993 = VECTOR('',#125129,1000.) ;
#12994 = VECTOR('',#125130,1000.) ;
#12995 = VECTOR('',#125133,1000.) ;
#12996 = VECTOR('',#125134,1000.) ;
#12997 = VECTOR('',#125135,1000.) ;
#12998 = VECTOR('',#125136,1000.) ;
#12999 = VECTOR('',#125139,1000.) ;
#13000 = VECTOR('',#125140,1000.) ;
#13001 = VECTOR('',#125141,1000.) ;
#13002 = VECTOR('',#125142,1000.) ;
#13003 = VECTOR('',#125145,1000.) ;
#13004 = VECTOR('',#125146,1000.) ;
#13005 = VECTOR('',#125147,1000.) ;
#13006 = VECTOR('',#125148,1000.) ;
#13007 = VECTOR('',#125151,1000.) ;
#13008 = VECTOR('',#125152,1000.) ;
#13009 = VECTOR('',#125153,1000.) ;
#13010 = VECTOR('',#125154,1000.) ;
#13011 = VECTOR('',#125157,1000.) ;
#13012 = VECTOR('',#125158,1000.) ;
#13013 = VECTOR('',#125159,1000.) ;
#13014 = VECTOR('',#125160,1000.) ;
#13015 = VECTOR('',#125163,1000.) ;
#13016 = VECTOR('',#125164,1000.) ;
#13017 = VECTOR('',#125165,1000.) ;
#13018 = VECTOR('',#125166,1000.) ;
#13019 = VECTOR('',#125169,1000.) ;
#13020 = VECTOR('',#125170,1000.) ;
#13021 = VECTOR('',#125171,1000.) ;
#13022 = VECTOR('',#125172,1000.) ;
#13023 = VECTOR('',#125175,1000.) ;
#13024 = VECTOR('',#125176,1000.) ;
#13025 = VECTOR('',#125177,1000.) ;
#13026 = VECTOR('',#125178,1000.) ;
#13027 = VECTOR('',#125181,1000.) ;
#13028 = VECTOR('',#125182,1000.) ;
#13029 = VECTOR('',#125183,1000.) ;
#13030 = VECTOR('',#125184,1000.) ;
#13031 = VECTOR('',#125187,1000.) ;
#13032 = VECTOR('',#125188,1000.) ;
#13033 = VECTOR('',#125189,1000.) ;
#13034 = VECTOR('',#125190,1000.) ;
#13035 = VECTOR('',#125193,1000.) ;
#13036 = VECTOR('',#125194,1000.) ;
#13037 = VECTOR('',#125195,1000.) ;
#13038 = VECTOR('',#125196,1000.) ;
#13039 = VECTOR('',#125199,1000.) ;
#13040 = VECTOR('',#125200,1000.) ;
#13041 = VECTOR('',#125201,1000.) ;
#13042 = VECTOR('',#125202,1000.) ;
#13043 = VECTOR('',#125205,1000.) ;
#13044 = VECTOR('',#125206,1000.) ;
#13045 = VECTOR('',#125207,1000.) ;
#13046 = VECTOR('',#125208,1000.) ;
#13047 = VECTOR('',#125211,1000.) ;
#13048 = VECTOR('',#125212,1000.) ;
#13049 = VECTOR('',#125213,1000.) ;
#13050 = VECTOR('',#125214,1000.) ;
#13051 = VECTOR('',#125217,1000.) ;
#13052 = VECTOR('',#125218,1000.) ;
#13053 = VECTOR('',#125219,1000.) ;
#13054 = VECTOR('',#125220,1000.) ;
#13055 = VECTOR('',#125223,1000.) ;
#13056 = VECTOR('',#125224,1000.) ;
#13057 = VECTOR('',#125225,1000.) ;
#13058 = VECTOR('',#125226,1000.) ;
#13059 = VECTOR('',#125229,1000.) ;
#13060 = VECTOR('',#125230,1000.) ;
#13061 = VECTOR('',#125231,1000.) ;
#13062 = VECTOR('',#125232,1000.) ;
#13063 = VECTOR('',#125235,1000.) ;
#13064 = VECTOR('',#125236,1000.) ;
#13065 = VECTOR('',#125237,1000.) ;
#13066 = VECTOR('',#125238,1000.) ;
#13067 = VECTOR('',#125241,1000.) ;
#13068 = VECTOR('',#125242,1000.) ;
#13069 = VECTOR('',#125243,1000.) ;
#13070 = VECTOR('',#125244,1000.) ;
#13071 = VECTOR('',#125247,1000.) ;
#13072 = VECTOR('',#125248,1000.) ;
#13073 = VECTOR('',#125249,1000.) ;
#13074 = VECTOR('',#125250,1000.) ;
#13075 = VECTOR('',#125253,1000.) ;
#13076 = VECTOR('',#125254,1000.) ;
#13077 = VECTOR('',#125255,1000.) ;
#13078 = VECTOR('',#125256,1000.) ;
#13079 = VECTOR('',#125259,1000.) ;
#13080 = VECTOR('',#125260,1000.) ;
#13081 = VECTOR('',#125261,1000.) ;
#13082 = VECTOR('',#125262,1000.) ;
#13083 = VECTOR('',#125263,1000.) ;
#13084 = VECTOR('',#125266,1000.) ;
#13085 = VECTOR('',#125269,1000.) ;
#13086 = VECTOR('',#125272,1000.) ;
#13087 = VECTOR('',#125277,1000.) ;
#13088 = VECTOR('',#125278,1000.) ;
#13089 = VECTOR('',#125279,1000.) ;
#13090 = VECTOR('',#125282,1000.) ;
#13091 = VECTOR('',#125283,1000.) ;
#13092 = VECTOR('',#125284,1000.) ;
#13093 = VECTOR('',#125287,1000.) ;
#13094 = VECTOR('',#125288,1000.) ;
#13095 = VECTOR('',#125289,1000.) ;
#13096 = VECTOR('',#125292,1000.) ;
#13097 = VECTOR('',#125293,1000.) ;
#13098 = VECTOR('',#125294,1000.) ;
#13099 = VECTOR('',#125297,1000.) ;
#13100 = VECTOR('',#125298,1000.) ;
#13101 = VECTOR('',#125299,1000.) ;
#13102 = VECTOR('',#125300,1000.) ;
#13103 = VECTOR('',#125301,1000.) ;
#13104 = VECTOR('',#125304,1000.) ;
#13105 = VECTOR('',#125307,1000.) ;
#13106 = VECTOR('',#125310,1000.) ;
#13107 = VECTOR('',#125315,1000.) ;
#13108 = VECTOR('',#125316,1000.) ;
#13109 = VECTOR('',#125317,1000.) ;
#13110 = VECTOR('',#125320,1000.) ;
#13111 = VECTOR('',#125321,1000.) ;
#13112 = VECTOR('',#125322,1000.) ;
#13113 = VECTOR('',#125325,1000.) ;
#13114 = VECTOR('',#125326,1000.) ;
#13115 = VECTOR('',#125327,1000.) ;
#13116 = VECTOR('',#125330,1000.) ;
#13117 = VECTOR('',#125331,1000.) ;
#13118 = VECTOR('',#125332,1000.) ;
#13119 = VECTOR('',#125335,1000.) ;
#13120 = VECTOR('',#125336,1000.) ;
#13121 = VECTOR('',#125337,1000.) ;
#13122 = VECTOR('',#125338,1000.) ;
#13123 = VECTOR('',#125339,1000.) ;
#13124 = VECTOR('',#125342,1000.) ;
#13125 = VECTOR('',#125345,1000.) ;
#13126 = VECTOR('',#125348,1000.) ;
#13127 = VECTOR('',#125353,1000.) ;
#13128 = VECTOR('',#125354,1000.) ;
#13129 = VECTOR('',#125355,1000.) ;
#13130 = VECTOR('',#125358,1000.) ;
#13131 = VECTOR('',#125359,1000.) ;
#13132 = VECTOR('',#125360,1000.) ;
#13133 = VECTOR('',#125363,1000.) ;
#13134 = VECTOR('',#125364,1000.) ;
#13135 = VECTOR('',#125365,1000.) ;
#13136 = VECTOR('',#125368,1000.) ;
#13137 = VECTOR('',#125369,1000.) ;
#13138 = VECTOR('',#125370,1000.) ;
#13139 = VECTOR('',#125373,1000.) ;
#13140 = VECTOR('',#125374,1000.) ;
#13141 = VECTOR('',#125375,1000.) ;
#13142 = VECTOR('',#125376,1000.) ;
#13143 = VECTOR('',#125377,1000.) ;
#13144 = VECTOR('',#125380,1000.) ;
#13145 = VECTOR('',#125383,1000.) ;
#13146 = VECTOR('',#125386,1000.) ;
#13147 = VECTOR('',#125391,1000.) ;
#13148 = VECTOR('',#125392,1000.) ;
#13149 = VECTOR('',#125393,1000.) ;
#13150 = VECTOR('',#125396,1000.) ;
#13151 = VECTOR('',#125397,1000.) ;
#13152 = VECTOR('',#125398,1000.) ;
#13153 = VECTOR('',#125401,1000.) ;
#13154 = VECTOR('',#125402,1000.) ;
#13155 = VECTOR('',#125403,1000.) ;
#13156 = VECTOR('',#125406,1000.) ;
#13157 = VECTOR('',#125407,1000.) ;
#13158 = VECTOR('',#125408,1000.) ;
#13159 = VECTOR('',#125411,1000.) ;
#13160 = VECTOR('',#125412,1000.) ;
#13161 = VECTOR('',#125413,1000.) ;
#13162 = VECTOR('',#125414,1000.) ;
#13163 = VECTOR('',#125415,1000.) ;
#13164 = VECTOR('',#125418,1000.) ;
#13165 = VECTOR('',#125421,1000.) ;
#13166 = VECTOR('',#125424,1000.) ;
#13167 = VECTOR('',#125429,1000.) ;
#13168 = VECTOR('',#125430,1000.) ;
#13169 = VECTOR('',#125431,1000.) ;
#13170 = VECTOR('',#125434,1000.) ;
#13171 = VECTOR('',#125435,1000.) ;
#13172 = VECTOR('',#125436,1000.) ;
#13173 = VECTOR('',#125439,1000.) ;
#13174 = VECTOR('',#125440,1000.) ;
#13175 = VECTOR('',#125441,1000.) ;
#13176 = VECTOR('',#125444,1000.) ;
#13177 = VECTOR('',#125445,1000.) ;
#13178 = VECTOR('',#125446,1000.) ;
#13179 = VECTOR('',#125449,1000.) ;
#13180 = VECTOR('',#125450,1000.) ;
#13181 = VECTOR('',#125451,1000.) ;
#13182 = VECTOR('',#125452,1000.) ;
#13183 = VECTOR('',#125453,1000.) ;
#13184 = VECTOR('',#125456,1000.) ;
#13185 = VECTOR('',#125459,1000.) ;
#13186 = VECTOR('',#125462,1000.) ;
#13187 = VECTOR('',#125467,1000.) ;
#13188 = VECTOR('',#125468,1000.) ;
#13189 = VECTOR('',#125469,1000.) ;
#13190 = VECTOR('',#125472,1000.) ;
#13191 = VECTOR('',#125473,1000.) ;
#13192 = VECTOR('',#125474,1000.) ;
#13193 = VECTOR('',#125477,1000.) ;
#13194 = VECTOR('',#125478,1000.) ;
#13195 = VECTOR('',#125479,1000.) ;
#13196 = VECTOR('',#125482,1000.) ;
#13197 = VECTOR('',#125483,1000.) ;
#13198 = VECTOR('',#125484,1000.) ;
#13199 = VECTOR('',#125487,1000.) ;
#13200 = VECTOR('',#125488,1000.) ;
#13201 = VECTOR('',#125489,1000.) ;
#13202 = VECTOR('',#125490,1000.) ;
#13203 = VECTOR('',#125491,1000.) ;
#13204 = VECTOR('',#125494,1000.) ;
#13205 = VECTOR('',#125497,1000.) ;
#13206 = VECTOR('',#125500,1000.) ;
#13207 = VECTOR('',#125505,1000.) ;
#13208 = VECTOR('',#125506,1000.) ;
#13209 = VECTOR('',#125507,1000.) ;
#13210 = VECTOR('',#125510,1000.) ;
#13211 = VECTOR('',#125511,1000.) ;
#13212 = VECTOR('',#125512,1000.) ;
#13213 = VECTOR('',#125515,1000.) ;
#13214 = VECTOR('',#125516,1000.) ;
#13215 = VECTOR('',#125517,1000.) ;
#13216 = VECTOR('',#125520,1000.) ;
#13217 = VECTOR('',#125521,1000.) ;
#13218 = VECTOR('',#125522,1000.) ;
#13219 = VECTOR('',#125525,1000.) ;
#13220 = VECTOR('',#125526,1000.) ;
#13221 = VECTOR('',#125527,1000.) ;
#13222 = VECTOR('',#125528,1000.) ;
#13223 = VECTOR('',#125529,1000.) ;
#13224 = VECTOR('',#125532,1000.) ;
#13225 = VECTOR('',#125535,1000.) ;
#13226 = VECTOR('',#125538,1000.) ;
#13227 = VECTOR('',#125543,1000.) ;
#13228 = VECTOR('',#125544,1000.) ;
#13229 = VECTOR('',#125545,1000.) ;
#13230 = VECTOR('',#125548,1000.) ;
#13231 = VECTOR('',#125549,1000.) ;
#13232 = VECTOR('',#125550,1000.) ;
#13233 = VECTOR('',#125553,1000.) ;
#13234 = VECTOR('',#125554,1000.) ;
#13235 = VECTOR('',#125555,1000.) ;
#13236 = VECTOR('',#125558,1000.) ;
#13237 = VECTOR('',#125559,1000.) ;
#13238 = VECTOR('',#125560,1000.) ;
#13239 = VECTOR('',#125563,1000.) ;
#13240 = VECTOR('',#125564,1000.) ;
#13241 = VECTOR('',#125565,1000.) ;
#13242 = VECTOR('',#125566,1000.) ;
#13243 = VECTOR('',#125567,1000.) ;
#13244 = VECTOR('',#125570,1000.) ;
#13245 = VECTOR('',#125573,1000.) ;
#13246 = VECTOR('',#125576,1000.) ;
#13247 = VECTOR('',#125581,1000.) ;
#13248 = VECTOR('',#125582,1000.) ;
#13249 = VECTOR('',#125583,1000.) ;
#13250 = VECTOR('',#125586,1000.) ;
#13251 = VECTOR('',#125587,1000.) ;
#13252 = VECTOR('',#125588,1000.) ;
#13253 = VECTOR('',#125591,1000.) ;
#13254 = VECTOR('',#125592,1000.) ;
#13255 = VECTOR('',#125593,1000.) ;
#13256 = VECTOR('',#125596,1000.) ;
#13257 = VECTOR('',#125597,1000.) ;
#13258 = VECTOR('',#125598,1000.) ;
#13259 = VECTOR('',#125601,1000.) ;
#13260 = VECTOR('',#125602,1000.) ;
#13261 = VECTOR('',#125603,1000.) ;
#13262 = VECTOR('',#125604,1000.) ;
#13263 = VECTOR('',#125607,1000.) ;
#13264 = VECTOR('',#125608,1000.) ;
#13265 = VECTOR('',#125609,1000.) ;
#13266 = VECTOR('',#125610,1000.) ;
#13267 = VECTOR('',#125613,1000.) ;
#13268 = VECTOR('',#125614,1000.) ;
#13269 = VECTOR('',#125615,1000.) ;
#13270 = VECTOR('',#125616,1000.) ;
#13271 = VECTOR('',#125619,1000.) ;
#13272 = VECTOR('',#125620,1000.) ;
#13273 = VECTOR('',#125621,1000.) ;
#13274 = VECTOR('',#125622,1000.) ;
#13275 = VECTOR('',#125625,1000.) ;
#13276 = VECTOR('',#125626,1000.) ;
#13277 = VECTOR('',#125627,1000.) ;
#13278 = VECTOR('',#125628,1000.) ;
#13279 = VECTOR('',#125631,1000.) ;
#13280 = VECTOR('',#125632,1000.) ;
#13281 = VECTOR('',#125633,1000.) ;
#13282 = VECTOR('',#125634,1000.) ;
#13283 = VECTOR('',#125637,1000.) ;
#13284 = VECTOR('',#125638,1000.) ;
#13285 = VECTOR('',#125639,1000.) ;
#13286 = VECTOR('',#125640,1000.) ;
#13287 = VECTOR('',#125643,1000.) ;
#13288 = VECTOR('',#125644,1000.) ;
#13289 = VECTOR('',#125645,1000.) ;
#13290 = VECTOR('',#125646,1000.) ;
#13291 = VECTOR('',#125649,1000.) ;
#13292 = VECTOR('',#125650,1000.) ;
#13293 = VECTOR('',#125651,1000.) ;
#13294 = VECTOR('',#125652,1000.) ;
#13295 = VECTOR('',#125655,1000.) ;
#13296 = VECTOR('',#125658,1000.) ;
#13297 = VECTOR('',#125661,1000.) ;
#13298 = VECTOR('',#125664,1000.) ;
#13299 = VECTOR('',#125667,1000.) ;
#13300 = VECTOR('',#125670,1000.) ;
#13301 = VECTOR('',#125673,1000.) ;
#13302 = VECTOR('',#125676,1000.) ;
#13303 = VECTOR('',#125679,1000.) ;
#13304 = VECTOR('',#125682,1000.) ;
#13305 = VECTOR('',#125683,1000.) ;
#13306 = VECTOR('',#125686,1000.) ;
#13307 = VECTOR('',#125687,1000.) ;
#13308 = VECTOR('',#125690,1000.) ;
#13309 = VECTOR('',#125691,1000.) ;
#13310 = VECTOR('',#125694,1000.) ;
#13311 = VECTOR('',#125695,1000.) ;
#13312 = VECTOR('',#125698,1000.) ;
#13313 = VECTOR('',#125699,1000.) ;
#13314 = VECTOR('',#125702,1000.) ;
#13315 = VECTOR('',#125703,1000.) ;
#13316 = VECTOR('',#125706,1000.) ;
#13317 = VECTOR('',#125707,1000.) ;
#13318 = VECTOR('',#125710,1000.) ;
#13319 = VECTOR('',#125711,1000.) ;
#13320 = VECTOR('',#125714,1000.) ;
#13321 = VECTOR('',#125715,1000.) ;
#13322 = VECTOR('',#125718,1000.) ;
#13323 = VECTOR('',#125719,1000.) ;
#13324 = VECTOR('',#125722,1000.) ;
#13325 = VECTOR('',#125723,1000.) ;
#13326 = VECTOR('',#125726,1000.) ;
#13327 = VECTOR('',#125727,1000.) ;
#13328 = VECTOR('',#125730,1000.) ;
#13329 = VECTOR('',#125731,1000.) ;
#13330 = VECTOR('',#125734,1000.) ;
#13331 = VECTOR('',#125735,1000.) ;
#13332 = VECTOR('',#125738,1000.) ;
#13333 = VECTOR('',#125739,1000.) ;
#13334 = VECTOR('',#125742,1000.) ;
#13335 = VECTOR('',#125743,1000.) ;
#13336 = VECTOR('',#125746,1000.) ;
#13337 = VECTOR('',#125747,1000.) ;
#13338 = VECTOR('',#125750,1000.) ;
#13339 = VECTOR('',#125751,1000.) ;
#13340 = VECTOR('',#125754,1000.) ;
#13341 = VECTOR('',#125755,1000.) ;
#13342 = VECTOR('',#125758,1000.) ;
#13343 = VECTOR('',#125759,1000.) ;
#13344 = VECTOR('',#125762,1000.) ;
#13345 = VECTOR('',#125763,1000.) ;
#13346 = VECTOR('',#125766,1000.) ;
#13347 = VECTOR('',#125767,1000.) ;
#13348 = VECTOR('',#125770,1000.) ;
#13349 = VECTOR('',#125771,1000.) ;
#13350 = VECTOR('',#125774,1000.) ;
#13351 = VECTOR('',#125775,1000.) ;
#13352 = VECTOR('',#125778,1000.) ;
#13353 = VECTOR('',#125779,1000.) ;
#13354 = VECTOR('',#125782,1000.) ;
#13355 = VECTOR('',#125783,1000.) ;
#13356 = VECTOR('',#125786,1000.) ;
#13357 = VECTOR('',#125787,1000.) ;
#13358 = VECTOR('',#125790,1000.) ;
#13359 = VECTOR('',#125793,1000.) ;
#13360 = VECTOR('',#125798,1000.) ;
#13361 = VECTOR('',#125799,1000.) ;
#13362 = VECTOR('',#125800,1000.) ;
#13363 = VECTOR('',#125805,1000.) ;
#13364 = VECTOR('',#125810,1000.) ;
#13365 = VECTOR('',#125811,1000.) ;
#13366 = VECTOR('',#125812,1000.) ;
#13367 = VECTOR('',#125817,1000.) ;
#13368 = VECTOR('',#125822,1000.) ;
#13369 = VECTOR('',#125823,1000.) ;
#13370 = VECTOR('',#125824,1000.) ;
#13371 = VECTOR('',#125829,1000.) ;
#13372 = VECTOR('',#125834,1000.) ;
#13373 = VECTOR('',#125835,1000.) ;
#13374 = VECTOR('',#125838,1000.) ;
#13375 = VECTOR('',#125839,1000.) ;
#13376 = VECTOR('',#125840,1000.) ;
#13377 = VECTOR('',#125841,1000.) ;
#13378 = VECTOR('',#125844,1000.) ;
#13379 = VECTOR('',#125847,1000.) ;
#13380 = VECTOR('',#125852,1000.) ;
#13381 = VECTOR('',#125853,1000.) ;
#13382 = VECTOR('',#125854,1000.) ;
#13383 = VECTOR('',#125859,1000.) ;
#13384 = VECTOR('',#125864,1000.) ;
#13385 = VECTOR('',#125865,1000.) ;
#13386 = VECTOR('',#125866,1000.) ;
#13387 = VECTOR('',#125871,1000.) ;
#13388 = VECTOR('',#125876,1000.) ;
#13389 = VECTOR('',#125877,1000.) ;
#13390 = VECTOR('',#125878,1000.) ;
#13391 = VECTOR('',#125883,1000.) ;
#13392 = VECTOR('',#125888,1000.) ;
#13393 = VECTOR('',#125889,1000.) ;
#13394 = VECTOR('',#125892,1000.) ;
#13395 = VECTOR('',#125893,1000.) ;
#13396 = VECTOR('',#125894,1000.) ;
#13397 = VECTOR('',#125895,1000.) ;
#13398 = VECTOR('',#125898,1000.) ;
#13399 = VECTOR('',#125901,1000.) ;
#13400 = VECTOR('',#125906,1000.) ;
#13401 = VECTOR('',#125907,1000.) ;
#13402 = VECTOR('',#125908,1000.) ;
#13403 = VECTOR('',#125913,1000.) ;
#13404 = VECTOR('',#125918,1000.) ;
#13405 = VECTOR('',#125919,1000.) ;
#13406 = VECTOR('',#125920,1000.) ;
#13407 = VECTOR('',#125925,1000.) ;
#13408 = VECTOR('',#125930,1000.) ;
#13409 = VECTOR('',#125931,1000.) ;
#13410 = VECTOR('',#125932,1000.) ;
#13411 = VECTOR('',#125937,1000.) ;
#13412 = VECTOR('',#125942,1000.) ;
#13413 = VECTOR('',#125943,1000.) ;
#13414 = VECTOR('',#125946,1000.) ;
#13415 = VECTOR('',#125947,1000.) ;
#13416 = VECTOR('',#125948,1000.) ;
#13417 = VECTOR('',#125949,1000.) ;
#13418 = VECTOR('',#125952,1000.) ;
#13419 = VECTOR('',#125955,1000.) ;
#13420 = VECTOR('',#125960,1000.) ;
#13421 = VECTOR('',#125961,1000.) ;
#13422 = VECTOR('',#125962,1000.) ;
#13423 = VECTOR('',#125967,1000.) ;
#13424 = VECTOR('',#125972,1000.) ;
#13425 = VECTOR('',#125973,1000.) ;
#13426 = VECTOR('',#125974,1000.) ;
#13427 = VECTOR('',#125979,1000.) ;
#13428 = VECTOR('',#125984,1000.) ;
#13429 = VECTOR('',#125985,1000.) ;
#13430 = VECTOR('',#125986,1000.) ;
#13431 = VECTOR('',#125991,1000.) ;
#13432 = VECTOR('',#125996,1000.) ;
#13433 = VECTOR('',#125997,1000.) ;
#13434 = VECTOR('',#126000,1000.) ;
#13435 = VECTOR('',#126001,1000.) ;
#13436 = VECTOR('',#126002,1000.) ;
#13437 = VECTOR('',#126003,1000.) ;
#13438 = VECTOR('',#126006,1000.) ;
#13439 = VECTOR('',#126009,1000.) ;
#13440 = VECTOR('',#126014,1000.) ;
#13441 = VECTOR('',#126015,1000.) ;
#13442 = VECTOR('',#126016,1000.) ;
#13443 = VECTOR('',#126021,1000.) ;
#13444 = VECTOR('',#126026,1000.) ;
#13445 = VECTOR('',#126027,1000.) ;
#13446 = VECTOR('',#126028,1000.) ;
#13447 = VECTOR('',#126033,1000.) ;
#13448 = VECTOR('',#126038,1000.) ;
#13449 = VECTOR('',#126039,1000.) ;
#13450 = VECTOR('',#126040,1000.) ;
#13451 = VECTOR('',#126045,1000.) ;
#13452 = VECTOR('',#126050,1000.) ;
#13453 = VECTOR('',#126051,1000.) ;
#13454 = VECTOR('',#126054,1000.) ;
#13455 = VECTOR('',#126055,1000.) ;
#13456 = VECTOR('',#126056,1000.) ;
#13457 = VECTOR('',#126057,1000.) ;
#13458 = VECTOR('',#126060,1000.) ;
#13459 = VECTOR('',#126063,1000.) ;
#13460 = VECTOR('',#126068,1000.) ;
#13461 = VECTOR('',#126069,1000.) ;
#13462 = VECTOR('',#126070,1000.) ;
#13463 = VECTOR('',#126075,1000.) ;
#13464 = VECTOR('',#126080,1000.) ;
#13465 = VECTOR('',#126081,1000.) ;
#13466 = VECTOR('',#126082,1000.) ;
#13467 = VECTOR('',#126087,1000.) ;
#13468 = VECTOR('',#126092,1000.) ;
#13469 = VECTOR('',#126093,1000.) ;
#13470 = VECTOR('',#126094,1000.) ;
#13471 = VECTOR('',#126099,1000.) ;
#13472 = VECTOR('',#126104,1000.) ;
#13473 = VECTOR('',#126105,1000.) ;
#13474 = VECTOR('',#126108,1000.) ;
#13475 = VECTOR('',#126109,1000.) ;
#13476 = VECTOR('',#126110,1000.) ;
#13477 = VECTOR('',#126111,1000.) ;
#13478 = VECTOR('',#126114,1000.) ;
#13479 = VECTOR('',#126117,1000.) ;
#13480 = VECTOR('',#126122,1000.) ;
#13481 = VECTOR('',#126123,1000.) ;
#13482 = VECTOR('',#126124,1000.) ;
#13483 = VECTOR('',#126129,1000.) ;
#13484 = VECTOR('',#126134,1000.) ;
#13485 = VECTOR('',#126135,1000.) ;
#13486 = VECTOR('',#126136,1000.) ;
#13487 = VECTOR('',#126141,1000.) ;
#13488 = VECTOR('',#126146,1000.) ;
#13489 = VECTOR('',#126147,1000.) ;
#13490 = VECTOR('',#126148,1000.) ;
#13491 = VECTOR('',#126153,1000.) ;
#13492 = VECTOR('',#126158,1000.) ;
#13493 = VECTOR('',#126159,1000.) ;
#13494 = VECTOR('',#126162,1000.) ;
#13495 = VECTOR('',#126163,1000.) ;
#13496 = VECTOR('',#126164,1000.) ;
#13497 = VECTOR('',#126165,1000.) ;
#13498 = VECTOR('',#126168,1000.) ;
#13499 = VECTOR('',#126171,1000.) ;
#13500 = VECTOR('',#126176,1000.) ;
#13501 = VECTOR('',#126177,1000.) ;
#13502 = VECTOR('',#126178,1000.) ;
#13503 = VECTOR('',#126183,1000.) ;
#13504 = VECTOR('',#126188,1000.) ;
#13505 = VECTOR('',#126189,1000.) ;
#13506 = VECTOR('',#126190,1000.) ;
#13507 = VECTOR('',#126195,1000.) ;
#13508 = VECTOR('',#126200,1000.) ;
#13509 = VECTOR('',#126201,1000.) ;
#13510 = VECTOR('',#126202,1000.) ;
#13511 = VECTOR('',#126207,1000.) ;
#13512 = VECTOR('',#126212,1000.) ;
#13513 = VECTOR('',#126213,1000.) ;
#13514 = VECTOR('',#126216,1000.) ;
#13515 = VECTOR('',#126217,1000.) ;
#13516 = VECTOR('',#126218,1000.) ;
#13517 = VECTOR('',#126219,1000.) ;
#13518 = VECTOR('',#126222,1000.) ;
#13519 = VECTOR('',#126225,1000.) ;
#13520 = VECTOR('',#126230,1000.) ;
#13521 = VECTOR('',#126231,1000.) ;
#13522 = VECTOR('',#126232,1000.) ;
#13523 = VECTOR('',#126237,1000.) ;
#13524 = VECTOR('',#126242,1000.) ;
#13525 = VECTOR('',#126243,1000.) ;
#13526 = VECTOR('',#126244,1000.) ;
#13527 = VECTOR('',#126249,1000.) ;
#13528 = VECTOR('',#126254,1000.) ;
#13529 = VECTOR('',#126255,1000.) ;
#13530 = VECTOR('',#126256,1000.) ;
#13531 = VECTOR('',#126261,1000.) ;
#13532 = VECTOR('',#126266,1000.) ;
#13533 = VECTOR('',#126267,1000.) ;
#13534 = VECTOR('',#126270,1000.) ;
#13535 = VECTOR('',#126271,1000.) ;
#13536 = VECTOR('',#126272,1000.) ;
#13537 = VECTOR('',#126273,1000.) ;
#13538 = CYLINDRICAL_SURFACE('',#91152,0.0999999999999998) ;
#13539 = CYLINDRICAL_SURFACE('',#91160,1.5) ;
#13540 = CYLINDRICAL_SURFACE('',#91161,1.9) ;
#13541 = CYLINDRICAL_SURFACE('',#91172,0.1) ;
#13542 = CYLINDRICAL_SURFACE('',#91198,0.1) ;
#13543 = CYLINDRICAL_SURFACE('',#91206,1.5) ;
#13544 = CYLINDRICAL_SURFACE('',#91207,1.9) ;
#13545 = CYLINDRICAL_SURFACE('',#91219,0.0999999999999998) ;
#13546 = CYLINDRICAL_SURFACE('',#91222,0.0999999999999998) ;
#13547 = CYLINDRICAL_SURFACE('',#91225,0.0999999999999998) ;
#13548 = CYLINDRICAL_SURFACE('',#91228,0.0999999999999998) ;
#13549 = CYLINDRICAL_SURFACE('',#91323,0.1) ;
#13550 = CYLINDRICAL_SURFACE('',#91326,0.1) ;
#13551 = CYLINDRICAL_SURFACE('',#91329,0.1) ;
#13552 = CYLINDRICAL_SURFACE('',#91332,0.1) ;
#13553 = CYLINDRICAL_SURFACE('',#91349,0.1) ;
#13554 = CYLINDRICAL_SURFACE('',#91352,0.1) ;
#13555 = CYLINDRICAL_SURFACE('',#91355,0.1) ;
#13556 = CYLINDRICAL_SURFACE('',#91358,0.1) ;
#13557 = CYLINDRICAL_SURFACE('',#91368,3.) ;
#13558 = CYLINDRICAL_SURFACE('',#91375,0.1) ;
#13559 = CYLINDRICAL_SURFACE('',#91379,0.0999999999999997) ;
#13560 = CYLINDRICAL_SURFACE('',#91381,0.0999999999999997) ;
#13561 = CYLINDRICAL_SURFACE('',#91383,0.0999999999999998) ;
#13562 = CYLINDRICAL_SURFACE('',#91385,0.1) ;
#13563 = CYLINDRICAL_SURFACE('',#91387,0.0999999999999998) ;
#13564 = CYLINDRICAL_SURFACE('',#91389,0.0999999999999999) ;
#13565 = CYLINDRICAL_SURFACE('',#91397,0.1) ;
#13566 = CYLINDRICAL_SURFACE('',#91399,0.0999999999999999) ;
#13567 = CYLINDRICAL_SURFACE('',#91401,0.1) ;
#13568 = CYLINDRICAL_SURFACE('',#91403,0.0999999999999998) ;
#13569 = CYLINDRICAL_SURFACE('',#91405,0.0999999999999997) ;
#13570 = CYLINDRICAL_SURFACE('',#91407,0.1) ;
#13571 = CYLINDRICAL_SURFACE('',#91414,0.1) ;
#13572 = CYLINDRICAL_SURFACE('',#91416,0.0999999999999999) ;
#13573 = CYLINDRICAL_SURFACE('',#91418,0.0999999999999999) ;
#13574 = CYLINDRICAL_SURFACE('',#91420,0.1) ;
#13575 = CYLINDRICAL_SURFACE('',#91425,0.0999999999999998) ;
#13576 = CYLINDRICAL_SURFACE('',#91427,0.1) ;
#13577 = CYLINDRICAL_SURFACE('',#91430,0.1) ;
#13578 = CYLINDRICAL_SURFACE('',#91431,0.0999999999999994) ;
#13579 = CYLINDRICAL_SURFACE('',#91432,0.0999999999999998) ;
#13580 = CYLINDRICAL_SURFACE('',#91434,0.1) ;
#13581 = CYLINDRICAL_SURFACE('',#91437,0.1) ;
#13582 = CYLINDRICAL_SURFACE('',#91439,0.1) ;
#13583 = CYLINDRICAL_SURFACE('',#91440,0.1) ;
#13584 = CYLINDRICAL_SURFACE('',#91445,0.0999999999999994) ;
#13585 = CYLINDRICAL_SURFACE('',#91446,0.0999999999999998) ;
#13586 = CYLINDRICAL_SURFACE('',#91449,0.0999999999999994) ;
#13587 = CYLINDRICAL_SURFACE('',#91450,0.1) ;
#13588 = CYLINDRICAL_SURFACE('',#91454,0.1) ;
#13589 = CYLINDRICAL_SURFACE('',#91456,0.0999999999999998) ;
#13590 = CYLINDRICAL_SURFACE('',#91462,0.0999999999999998) ;
#13591 = CYLINDRICAL_SURFACE('',#91464,0.1) ;
#13592 = CYLINDRICAL_SURFACE('',#91467,0.0999999999999998) ;
#13593 = CYLINDRICAL_SURFACE('',#91476,0.1) ;
#13594 = CYLINDRICAL_SURFACE('',#91478,0.1) ;
#13595 = CYLINDRICAL_SURFACE('',#91480,0.0999999999999998) ;
#13596 = CYLINDRICAL_SURFACE('',#91483,0.1) ;
#13597 = CYLINDRICAL_SURFACE('',#91485,0.1) ;
#13598 = CYLINDRICAL_SURFACE('',#91487,0.1) ;
#13599 = CYLINDRICAL_SURFACE('',#91498,0.1) ;
#13600 = CYLINDRICAL_SURFACE('',#91500,0.1) ;
#13601 = CYLINDRICAL_SURFACE('',#91502,0.1) ;
#13602 = CYLINDRICAL_SURFACE('',#91504,0.1) ;
#13603 = CYLINDRICAL_SURFACE('',#91510,0.1) ;
#13604 = CYLINDRICAL_SURFACE('',#91511,0.0999999999999998) ;
#13605 = CYLINDRICAL_SURFACE('',#91520,0.1) ;
#13606 = CYLINDRICAL_SURFACE('',#91522,0.1) ;
#13607 = CYLINDRICAL_SURFACE('',#91524,0.0999999999999998) ;
#13608 = CYLINDRICAL_SURFACE('',#91527,0.1) ;
#13609 = CYLINDRICAL_SURFACE('',#91529,0.1) ;
#13610 = CYLINDRICAL_SURFACE('',#91531,0.0999999999999998) ;
#13611 = CYLINDRICAL_SURFACE('',#91542,0.1) ;
#13612 = CYLINDRICAL_SURFACE('',#91544,0.1) ;
#13613 = CYLINDRICAL_SURFACE('',#91546,0.1) ;
#13614 = CYLINDRICAL_SURFACE('',#91548,0.1) ;
#13615 = CYLINDRICAL_SURFACE('',#91554,0.0999999999999998) ;
#13616 = CYLINDRICAL_SURFACE('',#91557,0.1) ;
#13617 = CYLINDRICAL_SURFACE('',#91561,0.1) ;
#13618 = CYLINDRICAL_SURFACE('',#91563,0.0999999999999994) ;
#13619 = CYLINDRICAL_SURFACE('',#91569,0.0999999999999994) ;
#13620 = CYLINDRICAL_SURFACE('',#91574,0.0999999999999998) ;
#13621 = CYLINDRICAL_SURFACE('',#91576,0.1) ;
#13622 = CYLINDRICAL_SURFACE('',#91582,0.0999999999999998) ;
#13623 = CYLINDRICAL_SURFACE('',#91584,0.0999999999999998) ;
#13624 = CYLINDRICAL_SURFACE('',#91586,0.1) ;
#13625 = CYLINDRICAL_SURFACE('',#91588,0.1) ;
#13626 = CYLINDRICAL_SURFACE('',#91590,0.1) ;
#13627 = CYLINDRICAL_SURFACE('',#91592,0.1) ;
#13628 = CYLINDRICAL_SURFACE('',#91594,0.1) ;
#13629 = CYLINDRICAL_SURFACE('',#91595,0.1) ;
#13630 = CYLINDRICAL_SURFACE('',#91596,0.1) ;
#13631 = CYLINDRICAL_SURFACE('',#91597,0.0999999999999999) ;
#13632 = CYLINDRICAL_SURFACE('',#91598,0.0999999999999998) ;
#13633 = CYLINDRICAL_SURFACE('',#91600,0.0999999999999998) ;
#13634 = CYLINDRICAL_SURFACE('',#91602,0.1) ;
#13635 = CYLINDRICAL_SURFACE('',#91606,0.1) ;
#13636 = CYLINDRICAL_SURFACE('',#91612,0.1) ;
#13637 = CYLINDRICAL_SURFACE('',#91613,0.1) ;
#13638 = CYLINDRICAL_SURFACE('',#91617,0.1) ;
#13639 = CYLINDRICAL_SURFACE('',#91621,0.1) ;
#13640 = CYLINDRICAL_SURFACE('',#91623,0.1) ;
#13641 = CYLINDRICAL_SURFACE('',#91631,0.100000000000001) ;
#13642 = CYLINDRICAL_SURFACE('',#91635,0.0999999999999994) ;
#13643 = CYLINDRICAL_SURFACE('',#91639,0.100000000000001) ;
#13644 = CYLINDRICAL_SURFACE('',#91643,0.0999999999999994) ;
#13645 = CYLINDRICAL_SURFACE('',#91688,0.1) ;
#13646 = CYLINDRICAL_SURFACE('',#91691,0.1) ;
#13647 = CYLINDRICAL_SURFACE('',#91694,0.1) ;
#13648 = CYLINDRICAL_SURFACE('',#91697,0.1) ;
#13649 = CYLINDRICAL_SURFACE('',#91714,0.1) ;
#13650 = CYLINDRICAL_SURFACE('',#91717,0.1) ;
#13651 = CYLINDRICAL_SURFACE('',#91720,0.1) ;
#13652 = CYLINDRICAL_SURFACE('',#91723,0.1) ;
#13653 = CYLINDRICAL_SURFACE('',#91733,3.) ;
#13654 = CYLINDRICAL_SURFACE('',#91740,0.1) ;
#13655 = CYLINDRICAL_SURFACE('',#91744,0.0999999999999997) ;
#13656 = CYLINDRICAL_SURFACE('',#91746,0.0999999999999997) ;
#13657 = CYLINDRICAL_SURFACE('',#91748,0.0999999999999998) ;
#13658 = CYLINDRICAL_SURFACE('',#91750,0.1) ;
#13659 = CYLINDRICAL_SURFACE('',#91752,0.0999999999999998) ;
#13660 = CYLINDRICAL_SURFACE('',#91754,0.0999999999999999) ;
#13661 = CYLINDRICAL_SURFACE('',#91762,0.0999999999999998) ;
#13662 = CYLINDRICAL_SURFACE('',#91764,0.0999999999999999) ;
#13663 = CYLINDRICAL_SURFACE('',#91766,0.1) ;
#13664 = CYLINDRICAL_SURFACE('',#91768,0.1) ;
#13665 = CYLINDRICAL_SURFACE('',#91770,0.0999999999999997) ;
#13666 = CYLINDRICAL_SURFACE('',#91772,0.1) ;
#13667 = CYLINDRICAL_SURFACE('',#91779,0.0999999999999999) ;
#13668 = CYLINDRICAL_SURFACE('',#91781,0.0999999999999999) ;
#13669 = CYLINDRICAL_SURFACE('',#91783,0.0999999999999999) ;
#13670 = CYLINDRICAL_SURFACE('',#91785,0.1) ;
#13671 = CYLINDRICAL_SURFACE('',#91790,0.0999999999999998) ;
#13672 = CYLINDRICAL_SURFACE('',#91792,0.1) ;
#13673 = CYLINDRICAL_SURFACE('',#91795,0.0999999999999999) ;
#13674 = CYLINDRICAL_SURFACE('',#91796,0.0999999999999994) ;
#13675 = CYLINDRICAL_SURFACE('',#91797,0.0999999999999998) ;
#13676 = CYLINDRICAL_SURFACE('',#91799,0.1) ;
#13677 = CYLINDRICAL_SURFACE('',#91802,0.1) ;
#13678 = CYLINDRICAL_SURFACE('',#91804,0.1) ;
#13679 = CYLINDRICAL_SURFACE('',#91805,0.1) ;
#13680 = CYLINDRICAL_SURFACE('',#91810,0.0999999999999998) ;
#13681 = CYLINDRICAL_SURFACE('',#91813,0.0999999999999994) ;
#13682 = CYLINDRICAL_SURFACE('',#91814,0.0999999999999999) ;
#13683 = CYLINDRICAL_SURFACE('',#91818,0.1) ;
#13684 = CYLINDRICAL_SURFACE('',#91820,0.0999999999999998) ;
#13685 = CYLINDRICAL_SURFACE('',#91826,0.0999999999999998) ;
#13686 = CYLINDRICAL_SURFACE('',#91828,0.1) ;
#13687 = CYLINDRICAL_SURFACE('',#91831,0.0999999999999998) ;
#13688 = CYLINDRICAL_SURFACE('',#91840,0.0999999999999998) ;
#13689 = CYLINDRICAL_SURFACE('',#91842,0.1) ;
#13690 = CYLINDRICAL_SURFACE('',#91844,0.0999999999999998) ;
#13691 = CYLINDRICAL_SURFACE('',#91847,0.1) ;
#13692 = CYLINDRICAL_SURFACE('',#91849,0.1) ;
#13693 = CYLINDRICAL_SURFACE('',#91851,0.1) ;
#13694 = CYLINDRICAL_SURFACE('',#91862,0.1) ;
#13695 = CYLINDRICAL_SURFACE('',#91864,0.1) ;
#13696 = CYLINDRICAL_SURFACE('',#91866,0.1) ;
#13697 = CYLINDRICAL_SURFACE('',#91868,0.1) ;
#13698 = CYLINDRICAL_SURFACE('',#91874,0.1) ;
#13699 = CYLINDRICAL_SURFACE('',#91875,0.0999999999999998) ;
#13700 = CYLINDRICAL_SURFACE('',#91884,0.1) ;
#13701 = CYLINDRICAL_SURFACE('',#91886,0.1) ;
#13702 = CYLINDRICAL_SURFACE('',#91888,0.0999999999999998) ;
#13703 = CYLINDRICAL_SURFACE('',#91891,0.1) ;
#13704 = CYLINDRICAL_SURFACE('',#91893,0.1) ;
#13705 = CYLINDRICAL_SURFACE('',#91895,0.0999999999999998) ;
#13706 = CYLINDRICAL_SURFACE('',#91906,0.1) ;
#13707 = CYLINDRICAL_SURFACE('',#91908,0.1) ;
#13708 = CYLINDRICAL_SURFACE('',#91910,0.1) ;
#13709 = CYLINDRICAL_SURFACE('',#91912,0.1) ;
#13710 = CYLINDRICAL_SURFACE('',#91918,0.0999999999999998) ;
#13711 = CYLINDRICAL_SURFACE('',#91923,0.0999999999999998) ;
#13712 = CYLINDRICAL_SURFACE('',#91929,0.0999999999999994) ;
#13713 = CYLINDRICAL_SURFACE('',#91933,0.1) ;
#13714 = CYLINDRICAL_SURFACE('',#91935,0.1) ;
#13715 = CYLINDRICAL_SURFACE('',#91940,0.0999999999999998) ;
#13716 = CYLINDRICAL_SURFACE('',#91941,0.0999999999999998) ;
#13717 = CYLINDRICAL_SURFACE('',#91942,0.1) ;
#13718 = CYLINDRICAL_SURFACE('',#91943,0.1) ;
#13719 = CYLINDRICAL_SURFACE('',#91946,0.0999999999999999) ;
#13720 = CYLINDRICAL_SURFACE('',#91951,0.1) ;
#13721 = CYLINDRICAL_SURFACE('',#91954,0.1) ;
#13722 = CYLINDRICAL_SURFACE('',#91958,0.1) ;
#13723 = CYLINDRICAL_SURFACE('',#91969,0.0999999999999998) ;
#13724 = CYLINDRICAL_SURFACE('',#91971,0.1) ;
#13725 = CYLINDRICAL_SURFACE('',#91973,0.1) ;
#13726 = CYLINDRICAL_SURFACE('',#91975,0.1) ;
#13727 = CYLINDRICAL_SURFACE('',#91985,0.1) ;
#13728 = CYLINDRICAL_SURFACE('',#91987,0.1) ;
#13729 = CYLINDRICAL_SURFACE('',#91988,0.1) ;
#13730 = CYLINDRICAL_SURFACE('',#91991,0.1) ;
#13731 = CYLINDRICAL_SURFACE('',#91992,0.1) ;
#13732 = CYLINDRICAL_SURFACE('',#92000,0.1) ;
#13733 = CYLINDRICAL_SURFACE('',#92002,0.0999999999999998) ;
#13734 = CYLINDRICAL_SURFACE('',#92004,0.1) ;
#13735 = CYLINDRICAL_SURFACE('',#92006,0.1) ;
#13736 = CYLINDRICAL_SURFACE('',#92012,0.1) ;
#13737 = CYLINDRICAL_SURFACE('',#92041,0.0999999999999994) ;
#13738 = CYLINDRICAL_SURFACE('',#92049,1.5) ;
#13739 = CYLINDRICAL_SURFACE('',#92050,1.9) ;
#13740 = CYLINDRICAL_SURFACE('',#92061,0.1) ;
#13741 = CYLINDRICAL_SURFACE('',#92087,0.0999999999999994) ;
#13742 = CYLINDRICAL_SURFACE('',#92095,1.5) ;
#13743 = CYLINDRICAL_SURFACE('',#92096,1.9) ;
#13744 = CYLINDRICAL_SURFACE('',#92108,0.0999999999999998) ;
#13745 = CYLINDRICAL_SURFACE('',#92111,0.0999999999999998) ;
#13746 = CYLINDRICAL_SURFACE('',#92114,0.0999999999999998) ;
#13747 = CYLINDRICAL_SURFACE('',#92117,0.0999999999999998) ;
#13748 = CYLINDRICAL_SURFACE('',#92212,0.0999999999999994) ;
#13749 = CYLINDRICAL_SURFACE('',#92215,0.0999999999999994) ;
#13750 = CYLINDRICAL_SURFACE('',#92218,0.0999999999999994) ;
#13751 = CYLINDRICAL_SURFACE('',#92221,0.0999999999999994) ;
#13752 = CYLINDRICAL_SURFACE('',#92238,0.0999999999999994) ;
#13753 = CYLINDRICAL_SURFACE('',#92241,0.0999999999999994) ;
#13754 = CYLINDRICAL_SURFACE('',#92244,0.0999999999999994) ;
#13755 = CYLINDRICAL_SURFACE('',#92247,0.0999999999999994) ;
#13756 = CYLINDRICAL_SURFACE('',#92257,3.) ;
#13757 = CYLINDRICAL_SURFACE('',#92264,0.100000000000002) ;
#13758 = CYLINDRICAL_SURFACE('',#92268,0.0999999999999997) ;
#13759 = CYLINDRICAL_SURFACE('',#92270,0.0999999999999997) ;
#13760 = CYLINDRICAL_SURFACE('',#92272,0.0999999999999994) ;
#13761 = CYLINDRICAL_SURFACE('',#92274,0.1) ;
#13762 = CYLINDRICAL_SURFACE('',#92276,0.0999999999999998) ;
#13763 = CYLINDRICAL_SURFACE('',#92278,0.100000000000002) ;
#13764 = CYLINDRICAL_SURFACE('',#92286,0.0999999999999994) ;
#13765 = CYLINDRICAL_SURFACE('',#92288,0.0999999999999999) ;
#13766 = CYLINDRICAL_SURFACE('',#92290,0.1) ;
#13767 = CYLINDRICAL_SURFACE('',#92292,0.0999999999999994) ;
#13768 = CYLINDRICAL_SURFACE('',#92294,0.0999999999999997) ;
#13769 = CYLINDRICAL_SURFACE('',#92296,0.1) ;
#13770 = CYLINDRICAL_SURFACE('',#92303,0.100000000000002) ;
#13771 = CYLINDRICAL_SURFACE('',#92305,0.0999999999999999) ;
#13772 = CYLINDRICAL_SURFACE('',#92307,0.0999999999999999) ;
#13773 = CYLINDRICAL_SURFACE('',#92309,0.0999999999999994) ;
#13774 = CYLINDRICAL_SURFACE('',#92314,0.0999999999999998) ;
#13775 = CYLINDRICAL_SURFACE('',#92316,0.1) ;
#13776 = CYLINDRICAL_SURFACE('',#92319,0.100000000000002) ;
#13777 = CYLINDRICAL_SURFACE('',#92320,0.0999999999999994) ;
#13778 = CYLINDRICAL_SURFACE('',#92321,0.0999999999999998) ;
#13779 = CYLINDRICAL_SURFACE('',#92323,0.0999999999999994) ;
#13780 = CYLINDRICAL_SURFACE('',#92326,0.0999999999999994) ;
#13781 = CYLINDRICAL_SURFACE('',#92328,0.1) ;
#13782 = CYLINDRICAL_SURFACE('',#92329,0.1) ;
#13783 = CYLINDRICAL_SURFACE('',#92334,0.0999999999999994) ;
#13784 = CYLINDRICAL_SURFACE('',#92335,0.0999999999999998) ;
#13785 = CYLINDRICAL_SURFACE('',#92338,0.0999999999999994) ;
#13786 = CYLINDRICAL_SURFACE('',#92339,0.0999999999999994) ;
#13787 = CYLINDRICAL_SURFACE('',#92343,0.0999999999999994) ;
#13788 = CYLINDRICAL_SURFACE('',#92345,0.0999999999999998) ;
#13789 = CYLINDRICAL_SURFACE('',#92351,0.0999999999999998) ;
#13790 = CYLINDRICAL_SURFACE('',#92353,0.0999999999999994) ;
#13791 = CYLINDRICAL_SURFACE('',#92356,0.0999999999999998) ;
#13792 = CYLINDRICAL_SURFACE('',#92365,0.0999999999999994) ;
#13793 = CYLINDRICAL_SURFACE('',#92367,0.0999999999999994) ;
#13794 = CYLINDRICAL_SURFACE('',#92369,0.0999999999999998) ;
#13795 = CYLINDRICAL_SURFACE('',#92372,0.0999999999999994) ;
#13796 = CYLINDRICAL_SURFACE('',#92374,0.0999999999999994) ;
#13797 = CYLINDRICAL_SURFACE('',#92376,0.1) ;
#13798 = CYLINDRICAL_SURFACE('',#92387,0.0999999999999994) ;
#13799 = CYLINDRICAL_SURFACE('',#92389,0.0999999999999994) ;
#13800 = CYLINDRICAL_SURFACE('',#92391,0.0999999999999994) ;
#13801 = CYLINDRICAL_SURFACE('',#92393,0.0999999999999994) ;
#13802 = CYLINDRICAL_SURFACE('',#92399,0.1) ;
#13803 = CYLINDRICAL_SURFACE('',#92400,0.0999999999999998) ;
#13804 = CYLINDRICAL_SURFACE('',#92409,0.0999999999999994) ;
#13805 = CYLINDRICAL_SURFACE('',#92411,0.0999999999999994) ;
#13806 = CYLINDRICAL_SURFACE('',#92413,0.0999999999999998) ;
#13807 = CYLINDRICAL_SURFACE('',#92416,0.0999999999999994) ;
#13808 = CYLINDRICAL_SURFACE('',#92418,0.0999999999999994) ;
#13809 = CYLINDRICAL_SURFACE('',#92420,0.0999999999999998) ;
#13810 = CYLINDRICAL_SURFACE('',#92431,0.0999999999999994) ;
#13811 = CYLINDRICAL_SURFACE('',#92433,0.0999999999999994) ;
#13812 = CYLINDRICAL_SURFACE('',#92435,0.0999999999999994) ;
#13813 = CYLINDRICAL_SURFACE('',#92437,0.0999999999999994) ;
#13814 = CYLINDRICAL_SURFACE('',#92443,0.0999999999999998) ;
#13815 = CYLINDRICAL_SURFACE('',#92446,0.1) ;
#13816 = CYLINDRICAL_SURFACE('',#92451,0.0999999999999994) ;
#13817 = CYLINDRICAL_SURFACE('',#92453,0.0999999999999994) ;
#13818 = CYLINDRICAL_SURFACE('',#92460,0.0999999999999994) ;
#13819 = CYLINDRICAL_SURFACE('',#92464,0.0999999999999994) ;
#13820 = CYLINDRICAL_SURFACE('',#92466,0.1) ;
#13821 = CYLINDRICAL_SURFACE('',#92471,0.0999999999999998) ;
#13822 = CYLINDRICAL_SURFACE('',#92473,0.0999999999999998) ;
#13823 = CYLINDRICAL_SURFACE('',#92475,0.1) ;
#13824 = CYLINDRICAL_SURFACE('',#92477,0.1) ;
#13825 = CYLINDRICAL_SURFACE('',#92479,0.1) ;
#13826 = CYLINDRICAL_SURFACE('',#92481,0.1) ;
#13827 = CYLINDRICAL_SURFACE('',#92483,0.0999999999999995) ;
#13828 = CYLINDRICAL_SURFACE('',#92484,0.0999999999999995) ;
#13829 = CYLINDRICAL_SURFACE('',#92485,0.0999999999999995) ;
#13830 = CYLINDRICAL_SURFACE('',#92486,0.0999999999999995) ;
#13831 = CYLINDRICAL_SURFACE('',#92487,0.0999999999999998) ;
#13832 = CYLINDRICAL_SURFACE('',#92489,0.0999999999999998) ;
#13833 = CYLINDRICAL_SURFACE('',#92491,0.1) ;
#13834 = CYLINDRICAL_SURFACE('',#92495,0.0999999999999994) ;
#13835 = CYLINDRICAL_SURFACE('',#92501,0.1) ;
#13836 = CYLINDRICAL_SURFACE('',#92503,0.1) ;
#13837 = CYLINDRICAL_SURFACE('',#92506,0.0999999999999994) ;
#13838 = CYLINDRICAL_SURFACE('',#92510,0.1) ;
#13839 = CYLINDRICAL_SURFACE('',#92513,0.1) ;
#13840 = CYLINDRICAL_SURFACE('',#92520,0.100000000000001) ;
#13841 = CYLINDRICAL_SURFACE('',#92524,0.0999999999999994) ;
#13842 = CYLINDRICAL_SURFACE('',#92528,0.100000000000001) ;
#13843 = CYLINDRICAL_SURFACE('',#92532,0.0999999999999994) ;
#13844 = CYLINDRICAL_SURFACE('',#92577,0.0999999999999994) ;
#13845 = CYLINDRICAL_SURFACE('',#92580,0.0999999999999994) ;
#13846 = CYLINDRICAL_SURFACE('',#92583,0.0999999999999994) ;
#13847 = CYLINDRICAL_SURFACE('',#92586,0.0999999999999994) ;
#13848 = CYLINDRICAL_SURFACE('',#92603,0.0999999999999994) ;
#13849 = CYLINDRICAL_SURFACE('',#92606,0.0999999999999994) ;
#13850 = CYLINDRICAL_SURFACE('',#92609,0.0999999999999994) ;
#13851 = CYLINDRICAL_SURFACE('',#92612,0.0999999999999994) ;
#13852 = CYLINDRICAL_SURFACE('',#92622,3.) ;
#13853 = CYLINDRICAL_SURFACE('',#92629,0.1) ;
#13854 = CYLINDRICAL_SURFACE('',#92633,0.0999999999999997) ;
#13855 = CYLINDRICAL_SURFACE('',#92635,0.0999999999999997) ;
#13856 = CYLINDRICAL_SURFACE('',#92637,0.0999999999999994) ;
#13857 = CYLINDRICAL_SURFACE('',#92639,0.1) ;
#13858 = CYLINDRICAL_SURFACE('',#92641,0.0999999999999998) ;
#13859 = CYLINDRICAL_SURFACE('',#92643,0.100000000000002) ;
#13860 = CYLINDRICAL_SURFACE('',#92651,0.0999999999999994) ;
#13861 = CYLINDRICAL_SURFACE('',#92653,0.0999999999999999) ;
#13862 = CYLINDRICAL_SURFACE('',#92655,0.1) ;
#13863 = CYLINDRICAL_SURFACE('',#92657,0.0999999999999994) ;
#13864 = CYLINDRICAL_SURFACE('',#92659,0.0999999999999997) ;
#13865 = CYLINDRICAL_SURFACE('',#92661,0.1) ;
#13866 = CYLINDRICAL_SURFACE('',#92668,0.0999999999999999) ;
#13867 = CYLINDRICAL_SURFACE('',#92670,0.0999999999999999) ;
#13868 = CYLINDRICAL_SURFACE('',#92672,0.0999999999999999) ;
#13869 = CYLINDRICAL_SURFACE('',#92674,0.0999999999999994) ;
#13870 = CYLINDRICAL_SURFACE('',#92679,0.0999999999999998) ;
#13871 = CYLINDRICAL_SURFACE('',#92681,0.1) ;
#13872 = CYLINDRICAL_SURFACE('',#92684,0.100000000000002) ;
#13873 = CYLINDRICAL_SURFACE('',#92685,0.0999999999999998) ;
#13874 = CYLINDRICAL_SURFACE('',#92687,0.0999999999999994) ;
#13875 = CYLINDRICAL_SURFACE('',#92690,0.0999999999999994) ;
#13876 = CYLINDRICAL_SURFACE('',#92692,0.1) ;
#13877 = CYLINDRICAL_SURFACE('',#92693,0.1) ;
#13878 = CYLINDRICAL_SURFACE('',#92698,0.0999999999999994) ;
#13879 = CYLINDRICAL_SURFACE('',#92699,0.0999999999999998) ;
#13880 = CYLINDRICAL_SURFACE('',#92702,0.0999999999999994) ;
#13881 = CYLINDRICAL_SURFACE('',#92703,0.0999999999999994) ;
#13882 = CYLINDRICAL_SURFACE('',#92707,0.0999999999999994) ;
#13883 = CYLINDRICAL_SURFACE('',#92709,0.0999999999999998) ;
#13884 = CYLINDRICAL_SURFACE('',#92715,0.0999999999999998) ;
#13885 = CYLINDRICAL_SURFACE('',#92717,0.0999999999999994) ;
#13886 = CYLINDRICAL_SURFACE('',#92720,0.0999999999999998) ;
#13887 = CYLINDRICAL_SURFACE('',#92729,0.0999999999999994) ;
#13888 = CYLINDRICAL_SURFACE('',#92731,0.0999999999999994) ;
#13889 = CYLINDRICAL_SURFACE('',#92733,0.0999999999999998) ;
#13890 = CYLINDRICAL_SURFACE('',#92736,0.0999999999999994) ;
#13891 = CYLINDRICAL_SURFACE('',#92738,0.0999999999999994) ;
#13892 = CYLINDRICAL_SURFACE('',#92740,0.1) ;
#13893 = CYLINDRICAL_SURFACE('',#92751,0.0999999999999994) ;
#13894 = CYLINDRICAL_SURFACE('',#92753,0.0999999999999994) ;
#13895 = CYLINDRICAL_SURFACE('',#92755,0.0999999999999994) ;
#13896 = CYLINDRICAL_SURFACE('',#92757,0.0999999999999994) ;
#13897 = CYLINDRICAL_SURFACE('',#92763,0.1) ;
#13898 = CYLINDRICAL_SURFACE('',#92764,0.0999999999999998) ;
#13899 = CYLINDRICAL_SURFACE('',#92773,0.0999999999999994) ;
#13900 = CYLINDRICAL_SURFACE('',#92775,0.0999999999999994) ;
#13901 = CYLINDRICAL_SURFACE('',#92777,0.0999999999999998) ;
#13902 = CYLINDRICAL_SURFACE('',#92780,0.0999999999999994) ;
#13903 = CYLINDRICAL_SURFACE('',#92782,0.0999999999999994) ;
#13904 = CYLINDRICAL_SURFACE('',#92784,0.0999999999999998) ;
#13905 = CYLINDRICAL_SURFACE('',#92795,0.0999999999999994) ;
#13906 = CYLINDRICAL_SURFACE('',#92797,0.0999999999999994) ;
#13907 = CYLINDRICAL_SURFACE('',#92799,0.0999999999999994) ;
#13908 = CYLINDRICAL_SURFACE('',#92801,0.0999999999999994) ;
#13909 = CYLINDRICAL_SURFACE('',#92807,0.0999999999999998) ;
#13910 = CYLINDRICAL_SURFACE('',#92810,0.1) ;
#13911 = CYLINDRICAL_SURFACE('',#92814,0.0999999999999994) ;
#13912 = CYLINDRICAL_SURFACE('',#92816,0.0999999999999994) ;
#13913 = CYLINDRICAL_SURFACE('',#92824,0.0999999999999994) ;
#13914 = CYLINDRICAL_SURFACE('',#92829,0.1) ;
#13915 = CYLINDRICAL_SURFACE('',#92830,0.1) ;
#13916 = CYLINDRICAL_SURFACE('',#92831,0.1) ;
#13917 = CYLINDRICAL_SURFACE('',#92832,0.1) ;
#13918 = CYLINDRICAL_SURFACE('',#92835,0.0999999999999994) ;
#13919 = CYLINDRICAL_SURFACE('',#92841,0.1) ;
#13920 = CYLINDRICAL_SURFACE('',#92843,0.0999999999999994) ;
#13921 = CYLINDRICAL_SURFACE('',#92847,0.1) ;
#13922 = CYLINDRICAL_SURFACE('',#92858,0.0999999999999994) ;
#13923 = CYLINDRICAL_SURFACE('',#92860,0.1) ;
#13924 = CYLINDRICAL_SURFACE('',#92862,0.1) ;
#13925 = CYLINDRICAL_SURFACE('',#92864,0.0999999999999994) ;
#13926 = CYLINDRICAL_SURFACE('',#92874,0.1) ;
#13927 = CYLINDRICAL_SURFACE('',#92876,0.1) ;
#13928 = CYLINDRICAL_SURFACE('',#92877,0.1) ;
#13929 = CYLINDRICAL_SURFACE('',#92880,0.1) ;
#13930 = CYLINDRICAL_SURFACE('',#92881,0.1) ;
#13931 = CYLINDRICAL_SURFACE('',#92889,0.1) ;
#13932 = CYLINDRICAL_SURFACE('',#92891,0.0999999999999994) ;
#13933 = CYLINDRICAL_SURFACE('',#92893,0.0999999999999994) ;
#13934 = CYLINDRICAL_SURFACE('',#92895,0.1) ;
#13935 = CYLINDRICAL_SURFACE('',#92901,0.1) ;
#13936 = CYLINDRICAL_SURFACE('',#92907,0.1) ;
#13937 = CYLINDRICAL_SURFACE('',#92933,0.0999999999999994) ;
#13938 = CYLINDRICAL_SURFACE('',#92941,1.5) ;
#13939 = CYLINDRICAL_SURFACE('',#92942,1.9) ;
#13940 = CYLINDRICAL_SURFACE('',#93051,0.0999999999999994) ;
#13941 = CYLINDRICAL_SURFACE('',#93054,0.0999999999999994) ;
#13942 = CYLINDRICAL_SURFACE('',#93057,0.0999999999999994) ;
#13943 = CYLINDRICAL_SURFACE('',#93060,0.0999999999999994) ;
#13944 = CYLINDRICAL_SURFACE('',#93077,0.0999999999999994) ;
#13945 = CYLINDRICAL_SURFACE('',#93080,0.0999999999999994) ;
#13946 = CYLINDRICAL_SURFACE('',#93083,0.0999999999999994) ;
#13947 = CYLINDRICAL_SURFACE('',#93086,0.0999999999999994) ;
#13948 = CYLINDRICAL_SURFACE('',#93096,3.) ;
#13949 = CYLINDRICAL_SURFACE('',#93103,0.1) ;
#13950 = CYLINDRICAL_SURFACE('',#93107,0.0999999999999997) ;
#13951 = CYLINDRICAL_SURFACE('',#93109,0.0999999999999997) ;
#13952 = CYLINDRICAL_SURFACE('',#93111,0.0999999999999994) ;
#13953 = CYLINDRICAL_SURFACE('',#93113,0.1) ;
#13954 = CYLINDRICAL_SURFACE('',#93115,0.0999999999999998) ;
#13955 = CYLINDRICAL_SURFACE('',#93117,0.0999999999999999) ;
#13956 = CYLINDRICAL_SURFACE('',#93125,0.0999999999999994) ;
#13957 = CYLINDRICAL_SURFACE('',#93127,0.0999999999999999) ;
#13958 = CYLINDRICAL_SURFACE('',#93129,0.1) ;
#13959 = CYLINDRICAL_SURFACE('',#93131,0.0999999999999994) ;
#13960 = CYLINDRICAL_SURFACE('',#93133,0.0999999999999997) ;
#13961 = CYLINDRICAL_SURFACE('',#93135,0.1) ;
#13962 = CYLINDRICAL_SURFACE('',#93142,0.0999999999999999) ;
#13963 = CYLINDRICAL_SURFACE('',#93144,0.0999999999999999) ;
#13964 = CYLINDRICAL_SURFACE('',#93146,0.0999999999999999) ;
#13965 = CYLINDRICAL_SURFACE('',#93148,0.0999999999999994) ;
#13966 = CYLINDRICAL_SURFACE('',#93153,0.0999999999999998) ;
#13967 = CYLINDRICAL_SURFACE('',#93155,0.1) ;
#13968 = CYLINDRICAL_SURFACE('',#93158,0.0999999999999999) ;
#13969 = CYLINDRICAL_SURFACE('',#93159,0.0999999999999994) ;
#13970 = CYLINDRICAL_SURFACE('',#93160,0.0999999999999998) ;
#13971 = CYLINDRICAL_SURFACE('',#93162,0.0999999999999994) ;
#13972 = CYLINDRICAL_SURFACE('',#93165,0.0999999999999994) ;
#13973 = CYLINDRICAL_SURFACE('',#93167,0.1) ;
#13974 = CYLINDRICAL_SURFACE('',#93168,0.1) ;
#13975 = CYLINDRICAL_SURFACE('',#93173,0.0999999999999994) ;
#13976 = CYLINDRICAL_SURFACE('',#93174,0.0999999999999998) ;
#13977 = CYLINDRICAL_SURFACE('',#93177,0.0999999999999994) ;
#13978 = CYLINDRICAL_SURFACE('',#93178,0.0999999999999994) ;
#13979 = CYLINDRICAL_SURFACE('',#93182,0.0999999999999994) ;
#13980 = CYLINDRICAL_SURFACE('',#93184,0.0999999999999998) ;
#13981 = CYLINDRICAL_SURFACE('',#93190,0.0999999999999998) ;
#13982 = CYLINDRICAL_SURFACE('',#93192,0.0999999999999994) ;
#13983 = CYLINDRICAL_SURFACE('',#93195,0.0999999999999998) ;
#13984 = CYLINDRICAL_SURFACE('',#93204,0.0999999999999994) ;
#13985 = CYLINDRICAL_SURFACE('',#93206,0.0999999999999994) ;
#13986 = CYLINDRICAL_SURFACE('',#93208,0.0999999999999998) ;
#13987 = CYLINDRICAL_SURFACE('',#93211,0.0999999999999994) ;
#13988 = CYLINDRICAL_SURFACE('',#93213,0.0999999999999994) ;
#13989 = CYLINDRICAL_SURFACE('',#93215,0.1) ;
#13990 = CYLINDRICAL_SURFACE('',#93226,0.0999999999999994) ;
#13991 = CYLINDRICAL_SURFACE('',#93228,0.0999999999999994) ;
#13992 = CYLINDRICAL_SURFACE('',#93230,0.0999999999999994) ;
#13993 = CYLINDRICAL_SURFACE('',#93232,0.0999999999999994) ;
#13994 = CYLINDRICAL_SURFACE('',#93238,0.1) ;
#13995 = CYLINDRICAL_SURFACE('',#93239,0.0999999999999998) ;
#13996 = CYLINDRICAL_SURFACE('',#93248,0.0999999999999994) ;
#13997 = CYLINDRICAL_SURFACE('',#93250,0.0999999999999994) ;
#13998 = CYLINDRICAL_SURFACE('',#93252,0.0999999999999998) ;
#13999 = CYLINDRICAL_SURFACE('',#93255,0.0999999999999994) ;
#14000 = CYLINDRICAL_SURFACE('',#93257,0.0999999999999994) ;
#14001 = CYLINDRICAL_SURFACE('',#93259,0.0999999999999998) ;
#14002 = CYLINDRICAL_SURFACE('',#93270,0.0999999999999994) ;
#14003 = CYLINDRICAL_SURFACE('',#93272,0.0999999999999994) ;
#14004 = CYLINDRICAL_SURFACE('',#93274,0.0999999999999994) ;
#14005 = CYLINDRICAL_SURFACE('',#93276,0.0999999999999994) ;
#14006 = CYLINDRICAL_SURFACE('',#93282,0.0999999999999998) ;
#14007 = CYLINDRICAL_SURFACE('',#93285,0.1) ;
#14008 = CYLINDRICAL_SURFACE('',#93289,0.0999999999999994) ;
#14009 = CYLINDRICAL_SURFACE('',#93291,0.0999999999999994) ;
#14010 = CYLINDRICAL_SURFACE('',#93297,0.0999999999999994) ;
#14011 = CYLINDRICAL_SURFACE('',#93301,0.0999999999999994) ;
#14012 = CYLINDRICAL_SURFACE('',#93303,0.1) ;
#14013 = CYLINDRICAL_SURFACE('',#93308,0.0999999999999998) ;
#14014 = CYLINDRICAL_SURFACE('',#93309,0.0999999999999998) ;
#14015 = CYLINDRICAL_SURFACE('',#93310,0.1) ;
#14016 = CYLINDRICAL_SURFACE('',#93311,0.1) ;
#14017 = CYLINDRICAL_SURFACE('',#93312,0.1) ;
#14018 = CYLINDRICAL_SURFACE('',#93313,0.1) ;
#14019 = CYLINDRICAL_SURFACE('',#93314,0.1) ;
#14020 = CYLINDRICAL_SURFACE('',#93315,0.1) ;
#14021 = CYLINDRICAL_SURFACE('',#93316,0.1) ;
#14022 = CYLINDRICAL_SURFACE('',#93317,0.1) ;
#14023 = CYLINDRICAL_SURFACE('',#93318,0.0999999999999998) ;
#14024 = CYLINDRICAL_SURFACE('',#93319,0.0999999999999998) ;
#14025 = CYLINDRICAL_SURFACE('',#93320,0.0999999999999998) ;
#14026 = CYLINDRICAL_SURFACE('',#93321,0.0999999999999998) ;
#14027 = CYLINDRICAL_SURFACE('',#93322,0.0999999999999998) ;
#14028 = CYLINDRICAL_SURFACE('',#93323,0.0999999999999998) ;
#14029 = CYLINDRICAL_SURFACE('',#93324,0.1) ;
#14030 = CYLINDRICAL_SURFACE('',#93327,0.0999999999999994) ;
#14031 = CYLINDRICAL_SURFACE('',#93333,0.1) ;
#14032 = CYLINDRICAL_SURFACE('',#93334,0.1) ;
#14033 = CYLINDRICAL_SURFACE('',#93337,0.0999999999999994) ;
#14034 = CYLINDRICAL_SURFACE('',#93341,0.1) ;
#14035 = CYLINDRICAL_SURFACE('',#93343,0.1) ;
#14036 = CYLINDRICAL_SURFACE('',#93362,0.1) ;
#14037 = CYLINDRICAL_SURFACE('',#93379,0.1) ;
#14038 = CYLINDRICAL_SURFACE('',#93396,0.1) ;
#14039 = CYLINDRICAL_SURFACE('',#93413,0.1) ;
#14040 = CYLINDRICAL_SURFACE('',#93430,0.1) ;
#14041 = CYLINDRICAL_SURFACE('',#93447,0.1) ;
#14042 = CYLINDRICAL_SURFACE('',#93464,0.1) ;
#14043 = CYLINDRICAL_SURFACE('',#93481,0.1) ;
#14044 = CYLINDRICAL_SURFACE('',#93543,0.1) ;
#14045 = CYLINDRICAL_SURFACE('',#93547,1.) ;
#14046 = CYLINDRICAL_SURFACE('',#93548,1.) ;
#14047 = CYLINDRICAL_SURFACE('',#93549,1.) ;
#14048 = CYLINDRICAL_SURFACE('',#93550,1.) ;
#14049 = CYLINDRICAL_SURFACE('',#93551,1.) ;
#14050 = CYLINDRICAL_SURFACE('',#93552,0.999999999999999) ;
#14051 = CYLINDRICAL_SURFACE('',#93553,0.999999999999999) ;
#14052 = CYLINDRICAL_SURFACE('',#93554,1.) ;
#14053 = CYLINDRICAL_SURFACE('',#93555,1.) ;
#14054 = CYLINDRICAL_SURFACE('',#93556,0.1) ;
#14055 = CYLINDRICAL_SURFACE('',#93558,0.100000000000001) ;
#14056 = CYLINDRICAL_SURFACE('',#93560,0.100000000000001) ;
#14057 = CYLINDRICAL_SURFACE('',#93562,0.0999999999999994) ;
#14058 = CYLINDRICAL_SURFACE('',#93564,0.0999999999999994) ;
#14059 = CYLINDRICAL_SURFACE('',#93566,0.0999999999999994) ;
#14060 = CYLINDRICAL_SURFACE('',#93568,0.0999999999999994) ;
#14061 = CYLINDRICAL_SURFACE('',#93570,0.100000000000003) ;
#14062 = CYLINDRICAL_SURFACE('',#93572,0.100000000000003) ;
#14063 = CYLINDRICAL_SURFACE('',#93592,0.1) ;
#14064 = CYLINDRICAL_SURFACE('',#93596,1.) ;
#14065 = CYLINDRICAL_SURFACE('',#93597,0.1) ;
#14066 = CYLINDRICAL_SURFACE('',#93680,0.1) ;
#14067 = CYLINDRICAL_SURFACE('',#93683,0.1) ;
#14068 = CYLINDRICAL_SURFACE('',#93686,0.1) ;
#14069 = CYLINDRICAL_SURFACE('',#93689,0.1) ;
#14070 = CYLINDRICAL_SURFACE('',#93692,0.1) ;
#14071 = CYLINDRICAL_SURFACE('',#93695,0.1) ;
#14072 = CYLINDRICAL_SURFACE('',#93698,0.1) ;
#14073 = CYLINDRICAL_SURFACE('',#93701,0.1) ;
#14074 = CYLINDRICAL_SURFACE('',#93704,0.1) ;
#14075 = CYLINDRICAL_SURFACE('',#93716,0.1) ;
#14076 = CYLINDRICAL_SURFACE('',#93719,0.0999999999999994) ;
#14077 = CYLINDRICAL_SURFACE('',#93743,0.1) ;
#14078 = CYLINDRICAL_SURFACE('',#93767,0.1) ;
#14079 = CYLINDRICAL_SURFACE('',#93771,0.1) ;
#14080 = CYLINDRICAL_SURFACE('',#93775,0.1) ;
#14081 = CYLINDRICAL_SURFACE('',#93779,0.100000000000001) ;
#14082 = CYLINDRICAL_SURFACE('',#93783,0.1) ;
#14083 = CYLINDRICAL_SURFACE('',#93787,0.0999999999999994) ;
#14084 = CYLINDRICAL_SURFACE('',#93905,0.1) ;
#14085 = CYLINDRICAL_SURFACE('',#93909,0.1) ;
#14086 = CYLINDRICAL_SURFACE('',#93913,0.0999999999999994) ;
#14087 = CYLINDRICAL_SURFACE('',#93917,0.1) ;
#14088 = CYLINDRICAL_SURFACE('',#93921,0.1) ;
#14089 = CYLINDRICAL_SURFACE('',#93925,0.1) ;
#14090 = CYLINDRICAL_SURFACE('',#93929,0.1) ;
#14091 = CYLINDRICAL_SURFACE('',#93933,0.1) ;
#14092 = CYLINDRICAL_SURFACE('',#93937,0.1) ;
#14093 = CYLINDRICAL_SURFACE('',#93941,0.1) ;
#14094 = CYLINDRICAL_SURFACE('',#93944,1.65625) ;
#14095 = CYLINDRICAL_SURFACE('',#93947,0.1) ;
#14096 = CYLINDRICAL_SURFACE('',#93951,0.1) ;
#14097 = CYLINDRICAL_SURFACE('',#93955,0.1) ;
#14098 = CYLINDRICAL_SURFACE('',#93970,0.1) ;
#14099 = CYLINDRICAL_SURFACE('',#93973,0.1) ;
#14100 = CYLINDRICAL_SURFACE('',#93984,0.1) ;
#14101 = CYLINDRICAL_SURFACE('',#93986,0.1) ;
#14102 = CYLINDRICAL_SURFACE('',#93988,0.1) ;
#14103 = CYLINDRICAL_SURFACE('',#93990,0.1) ;
#14104 = CYLINDRICAL_SURFACE('',#93992,0.1) ;
#14105 = CYLINDRICAL_SURFACE('',#93994,0.1) ;
#14106 = CYLINDRICAL_SURFACE('',#94005,0.1) ;
#14107 = CYLINDRICAL_SURFACE('',#94007,0.0999999999999998) ;
#14108 = CYLINDRICAL_SURFACE('',#94009,0.1) ;
#14109 = CYLINDRICAL_SURFACE('',#94011,0.1) ;
#14110 = CYLINDRICAL_SURFACE('',#94013,0.1) ;
#14111 = CYLINDRICAL_SURFACE('',#94023,0.1) ;
#14112 = CYLINDRICAL_SURFACE('',#94030,0.1) ;
#14113 = CYLINDRICAL_SURFACE('',#94032,0.1) ;
#14114 = CYLINDRICAL_SURFACE('',#94034,0.1) ;
#14115 = CYLINDRICAL_SURFACE('',#94038,0.1) ;
#14116 = CYLINDRICAL_SURFACE('',#94040,0.1) ;
#14117 = CYLINDRICAL_SURFACE('',#94042,0.0999999999999998) ;
#14118 = CYLINDRICAL_SURFACE('',#94049,0.1) ;
#14119 = CYLINDRICAL_SURFACE('',#94056,0.1) ;
#14120 = CYLINDRICAL_SURFACE('',#94058,0.1) ;
#14121 = CYLINDRICAL_SURFACE('',#94062,0.1) ;
#14122 = CYLINDRICAL_SURFACE('',#94065,0.1) ;
#14123 = CYLINDRICAL_SURFACE('',#94067,0.1) ;
#14124 = CYLINDRICAL_SURFACE('',#94073,0.100000000000003) ;
#14125 = CYLINDRICAL_SURFACE('',#94075,0.100000000000003) ;
#14126 = CYLINDRICAL_SURFACE('',#94081,0.1) ;
#14127 = CYLINDRICAL_SURFACE('',#94083,0.1) ;
#14128 = CYLINDRICAL_SURFACE('',#94089,0.1) ;
#14129 = CYLINDRICAL_SURFACE('',#94091,0.1) ;
#14130 = CYLINDRICAL_SURFACE('',#94097,0.100000000000003) ;
#14131 = CYLINDRICAL_SURFACE('',#94099,0.100000000000003) ;
#14132 = CYLINDRICAL_SURFACE('',#94105,0.0999999999999998) ;
#14133 = CYLINDRICAL_SURFACE('',#94107,0.0999999999999998) ;
#14134 = CYLINDRICAL_SURFACE('',#94113,0.1) ;
#14135 = CYLINDRICAL_SURFACE('',#94115,0.1) ;
#14136 = CYLINDRICAL_SURFACE('',#94121,0.1) ;
#14137 = CYLINDRICAL_SURFACE('',#94123,0.1) ;
#14138 = CYLINDRICAL_SURFACE('',#94129,0.0999999999999998) ;
#14139 = CYLINDRICAL_SURFACE('',#94131,0.0999999999999998) ;
#14140 = CYLINDRICAL_SURFACE('',#94134,0.1) ;
#14141 = CYLINDRICAL_SURFACE('',#94141,0.1) ;
#14142 = CYLINDRICAL_SURFACE('',#94143,0.1) ;
#14143 = CYLINDRICAL_SURFACE('',#94149,0.1) ;
#14144 = CYLINDRICAL_SURFACE('',#94151,0.1) ;
#14145 = CYLINDRICAL_SURFACE('',#94157,0.0999999999999999) ;
#14146 = CYLINDRICAL_SURFACE('',#94165,0.1) ;
#14147 = CYLINDRICAL_SURFACE('',#94166,0.1) ;
#14148 = CYLINDRICAL_SURFACE('',#94170,0.1) ;
#14149 = CYLINDRICAL_SURFACE('',#94172,0.1) ;
#14150 = CYLINDRICAL_SURFACE('',#94178,0.0999999999999998) ;
#14151 = CYLINDRICAL_SURFACE('',#94180,0.1) ;
#14152 = CYLINDRICAL_SURFACE('',#94186,0.1) ;
#14153 = CYLINDRICAL_SURFACE('',#94187,0.1) ;
#14154 = CYLINDRICAL_SURFACE('',#94194,0.0999999999999994) ;
#14155 = CYLINDRICAL_SURFACE('',#94196,0.1) ;
#14156 = CYLINDRICAL_SURFACE('',#94202,0.1) ;
#14157 = CYLINDRICAL_SURFACE('',#94203,0.1) ;
#14158 = CYLINDRICAL_SURFACE('',#94207,0.1) ;
#14159 = CYLINDRICAL_SURFACE('',#94209,0.0999999999999994) ;
#14160 = CYLINDRICAL_SURFACE('',#94215,0.1) ;
#14161 = CYLINDRICAL_SURFACE('',#94223,0.0999999999999998) ;
#14162 = CYLINDRICAL_SURFACE('',#94225,0.0999999999999994) ;
#14163 = CYLINDRICAL_SURFACE('',#94231,0.1) ;
#14164 = CYLINDRICAL_SURFACE('',#94233,0.1) ;
#14165 = CYLINDRICAL_SURFACE('',#94239,0.1) ;
#14166 = CYLINDRICAL_SURFACE('',#94251,1.) ;
#14167 = CYLINDRICAL_SURFACE('',#94254,0.2) ;
#14168 = CYLINDRICAL_SURFACE('',#94268,0.1) ;
#14169 = CYLINDRICAL_SURFACE('',#94271,0.1) ;
#14170 = CYLINDRICAL_SURFACE('',#94277,0.1) ;
#14171 = CYLINDRICAL_SURFACE('',#94280,0.1) ;
#14172 = CYLINDRICAL_SURFACE('',#94282,0.1) ;
#14173 = CYLINDRICAL_SURFACE('',#94289,0.1) ;
#14174 = CYLINDRICAL_SURFACE('',#94291,0.1) ;
#14175 = CYLINDRICAL_SURFACE('',#94293,0.1) ;
#14176 = CYLINDRICAL_SURFACE('',#94297,0.1) ;
#14177 = CYLINDRICAL_SURFACE('',#94300,0.1) ;
#14178 = CYLINDRICAL_SURFACE('',#94302,0.1) ;
#14179 = CYLINDRICAL_SURFACE('',#94305,0.1) ;
#14180 = CYLINDRICAL_SURFACE('',#94311,0.1) ;
#14181 = CYLINDRICAL_SURFACE('',#94314,0.1) ;
#14182 = CYLINDRICAL_SURFACE('',#94316,0.1) ;
#14183 = CYLINDRICAL_SURFACE('',#94323,0.1) ;
#14184 = CYLINDRICAL_SURFACE('',#94325,0.1) ;
#14185 = CYLINDRICAL_SURFACE('',#94327,0.1) ;
#14186 = CYLINDRICAL_SURFACE('',#94331,0.1) ;
#14187 = CYLINDRICAL_SURFACE('',#94334,0.1) ;
#14188 = CYLINDRICAL_SURFACE('',#94338,0.1) ;
#14189 = CYLINDRICAL_SURFACE('',#94342,0.1) ;
#14190 = CYLINDRICAL_SURFACE('',#94346,0.1) ;
#14191 = CYLINDRICAL_SURFACE('',#94351,0.1) ;
#14192 = CYLINDRICAL_SURFACE('',#94355,0.1) ;
#14193 = CYLINDRICAL_SURFACE('',#94359,0.1) ;
#14194 = CYLINDRICAL_SURFACE('',#94362,0.1) ;
#14195 = CYLINDRICAL_SURFACE('',#94366,0.1) ;
#14196 = CYLINDRICAL_SURFACE('',#94370,0.1) ;
#14197 = CYLINDRICAL_SURFACE('',#94371,0.1) ;
#14198 = CYLINDRICAL_SURFACE('',#94375,0.1) ;
#14199 = CYLINDRICAL_SURFACE('',#94377,0.1) ;
#14200 = CYLINDRICAL_SURFACE('',#94452,0.100000000000003) ;
#14201 = CYLINDRICAL_SURFACE('',#94456,0.100000000000003) ;
#14202 = CYLINDRICAL_SURFACE('',#94460,0.0999999999999959) ;
#14203 = CYLINDRICAL_SURFACE('',#94464,0.100000000000003) ;
#14204 = CYLINDRICAL_SURFACE('',#94468,0.100000000000003) ;
#14205 = CYLINDRICAL_SURFACE('',#94472,0.100000000000003) ;
#14206 = CYLINDRICAL_SURFACE('',#94476,0.100000000000003) ;
#14207 = CYLINDRICAL_SURFACE('',#94480,0.100000000000003) ;
#14208 = CYLINDRICAL_SURFACE('',#94484,0.100000000000003) ;
#14209 = CYLINDRICAL_SURFACE('',#94488,0.100000000000003) ;
#14210 = CYLINDRICAL_SURFACE('',#94491,1.65625) ;
#14211 = CYLINDRICAL_SURFACE('',#94494,0.100000000000003) ;
#14212 = CYLINDRICAL_SURFACE('',#94498,0.100000000000003) ;
#14213 = CYLINDRICAL_SURFACE('',#94502,0.100000000000003) ;
#14214 = CYLINDRICAL_SURFACE('',#94512,0.0999999999999994) ;
#14215 = CYLINDRICAL_SURFACE('',#94516,0.0999999999999994) ;
#14216 = CYLINDRICAL_SURFACE('',#94520,0.0999999999999994) ;
#14217 = CYLINDRICAL_SURFACE('',#94524,0.0999999999999994) ;
#14218 = CYLINDRICAL_SURFACE('',#94528,0.100000000000003) ;
#14219 = CYLINDRICAL_SURFACE('',#94532,0.0999999999999994) ;
#14220 = CYLINDRICAL_SURFACE('',#94536,0.0999999999999994) ;
#14221 = CYLINDRICAL_SURFACE('',#94540,0.100000000000003) ;
#14222 = CYLINDRICAL_SURFACE('',#94544,0.100000000000003) ;
#14223 = CYLINDRICAL_SURFACE('',#94548,0.100000000000003) ;
#14224 = CYLINDRICAL_SURFACE('',#94551,1.65625) ;
#14225 = CYLINDRICAL_SURFACE('',#94554,0.0999999999999994) ;
#14226 = CYLINDRICAL_SURFACE('',#94558,0.0999999999999994) ;
#14227 = CYLINDRICAL_SURFACE('',#94562,0.0999999999999994) ;
#14228 = CYLINDRICAL_SURFACE('',#94572,0.0999999999999994) ;
#14229 = CYLINDRICAL_SURFACE('',#94576,0.0999999999999994) ;
#14230 = CYLINDRICAL_SURFACE('',#94580,0.0999999999999994) ;
#14231 = CYLINDRICAL_SURFACE('',#94584,0.0999999999999994) ;
#14232 = CYLINDRICAL_SURFACE('',#94588,0.0999999999999994) ;
#14233 = CYLINDRICAL_SURFACE('',#94592,0.0999999999999994) ;
#14234 = CYLINDRICAL_SURFACE('',#94596,0.0999999999999994) ;
#14235 = CYLINDRICAL_SURFACE('',#94600,0.0999999999999994) ;
#14236 = CYLINDRICAL_SURFACE('',#94604,0.0999999999999994) ;
#14237 = CYLINDRICAL_SURFACE('',#94608,0.0999999999999994) ;
#14238 = CYLINDRICAL_SURFACE('',#94611,1.65625) ;
#14239 = CYLINDRICAL_SURFACE('',#94614,0.0999999999999994) ;
#14240 = CYLINDRICAL_SURFACE('',#94618,0.0999999999999994) ;
#14241 = CYLINDRICAL_SURFACE('',#94622,0.0999999999999994) ;
#14242 = CYLINDRICAL_SURFACE('',#94632,0.0999999999999994) ;
#14243 = CYLINDRICAL_SURFACE('',#94636,0.0999999999999994) ;
#14244 = CYLINDRICAL_SURFACE('',#94640,0.0999999999999994) ;
#14245 = CYLINDRICAL_SURFACE('',#94644,0.0999999999999994) ;
#14246 = CYLINDRICAL_SURFACE('',#94648,0.0999999999999994) ;
#14247 = CYLINDRICAL_SURFACE('',#94652,0.0999999999999994) ;
#14248 = CYLINDRICAL_SURFACE('',#94656,0.0999999999999994) ;
#14249 = CYLINDRICAL_SURFACE('',#94660,0.0999999999999994) ;
#14250 = CYLINDRICAL_SURFACE('',#94664,0.0999999999999994) ;
#14251 = CYLINDRICAL_SURFACE('',#94668,0.0999999999999994) ;
#14252 = CYLINDRICAL_SURFACE('',#94671,1.65625) ;
#14253 = CYLINDRICAL_SURFACE('',#94674,0.0999999999999994) ;
#14254 = CYLINDRICAL_SURFACE('',#94678,0.0999999999999994) ;
#14255 = CYLINDRICAL_SURFACE('',#94682,0.0999999999999994) ;
#14256 = CYLINDRICAL_SURFACE('',#94692,0.0999999999999994) ;
#14257 = CYLINDRICAL_SURFACE('',#94696,0.0999999999999994) ;
#14258 = CYLINDRICAL_SURFACE('',#94700,0.0999999999999994) ;
#14259 = CYLINDRICAL_SURFACE('',#94704,0.0999999999999994) ;
#14260 = CYLINDRICAL_SURFACE('',#94708,0.0999999999999994) ;
#14261 = CYLINDRICAL_SURFACE('',#94712,0.0999999999999994) ;
#14262 = CYLINDRICAL_SURFACE('',#94716,0.0999999999999994) ;
#14263 = CYLINDRICAL_SURFACE('',#94720,0.0999999999999994) ;
#14264 = CYLINDRICAL_SURFACE('',#94724,0.0999999999999994) ;
#14265 = CYLINDRICAL_SURFACE('',#94728,0.0999999999999994) ;
#14266 = CYLINDRICAL_SURFACE('',#94731,1.65625) ;
#14267 = CYLINDRICAL_SURFACE('',#94734,0.0999999999999994) ;
#14268 = CYLINDRICAL_SURFACE('',#94738,0.0999999999999994) ;
#14269 = CYLINDRICAL_SURFACE('',#94742,0.0999999999999994) ;
#14270 = CYLINDRICAL_SURFACE('',#94752,0.0999999999999994) ;
#14271 = CYLINDRICAL_SURFACE('',#94756,0.0999999999999994) ;
#14272 = CYLINDRICAL_SURFACE('',#94760,0.0999999999999994) ;
#14273 = CYLINDRICAL_SURFACE('',#94764,0.100000000000001) ;
#14274 = CYLINDRICAL_SURFACE('',#94768,0.0999999999999994) ;
#14275 = CYLINDRICAL_SURFACE('',#94772,0.0999999999999994) ;
#14276 = CYLINDRICAL_SURFACE('',#94776,0.0999999999999994) ;
#14277 = CYLINDRICAL_SURFACE('',#94780,0.0999999999999994) ;
#14278 = CYLINDRICAL_SURFACE('',#94784,0.0999999999999994) ;
#14279 = CYLINDRICAL_SURFACE('',#94788,0.0999999999999994) ;
#14280 = CYLINDRICAL_SURFACE('',#94791,1.65625) ;
#14281 = CYLINDRICAL_SURFACE('',#94794,0.0999999999999994) ;
#14282 = CYLINDRICAL_SURFACE('',#94798,0.0999999999999994) ;
#14283 = CYLINDRICAL_SURFACE('',#94802,0.0999999999999994) ;
#14284 = CYLINDRICAL_SURFACE('',#94812,0.0999999999999994) ;
#14285 = CYLINDRICAL_SURFACE('',#94816,0.0999999999999994) ;
#14286 = CYLINDRICAL_SURFACE('',#94820,0.0999999999999994) ;
#14287 = CYLINDRICAL_SURFACE('',#94824,0.100000000000001) ;
#14288 = CYLINDRICAL_SURFACE('',#94828,0.100000000000001) ;
#14289 = CYLINDRICAL_SURFACE('',#94832,0.0999999999999994) ;
#14290 = CYLINDRICAL_SURFACE('',#94836,0.0999999999999994) ;
#14291 = CYLINDRICAL_SURFACE('',#94840,0.0999999999999994) ;
#14292 = CYLINDRICAL_SURFACE('',#94844,0.0999999999999994) ;
#14293 = CYLINDRICAL_SURFACE('',#94848,0.0999999999999994) ;
#14294 = CYLINDRICAL_SURFACE('',#94851,1.65625) ;
#14295 = CYLINDRICAL_SURFACE('',#94854,0.0999999999999994) ;
#14296 = CYLINDRICAL_SURFACE('',#94858,0.0999999999999994) ;
#14297 = CYLINDRICAL_SURFACE('',#94862,0.0999999999999994) ;
#14298 = CYLINDRICAL_SURFACE('',#94872,0.1) ;
#14299 = CYLINDRICAL_SURFACE('',#94876,0.1) ;
#14300 = CYLINDRICAL_SURFACE('',#94880,0.0999999999999994) ;
#14301 = CYLINDRICAL_SURFACE('',#94884,0.1) ;
#14302 = CYLINDRICAL_SURFACE('',#94888,0.100000000000001) ;
#14303 = CYLINDRICAL_SURFACE('',#94892,0.0999999999999994) ;
#14304 = CYLINDRICAL_SURFACE('',#94896,0.0999999999999994) ;
#14305 = CYLINDRICAL_SURFACE('',#94900,0.0999999999999994) ;
#14306 = CYLINDRICAL_SURFACE('',#94904,0.0999999999999994) ;
#14307 = CYLINDRICAL_SURFACE('',#94908,0.0999999999999994) ;
#14308 = CYLINDRICAL_SURFACE('',#94911,1.65625) ;
#14309 = CYLINDRICAL_SURFACE('',#94914,0.1) ;
#14310 = CYLINDRICAL_SURFACE('',#94918,0.1) ;
#14311 = CYLINDRICAL_SURFACE('',#94922,0.1) ;
#14312 = CYLINDRICAL_SURFACE('',#94932,0.0999999999999998) ;
#14313 = CYLINDRICAL_SURFACE('',#94936,0.0999999999999998) ;
#14314 = CYLINDRICAL_SURFACE('',#94940,0.0999999999999994) ;
#14315 = CYLINDRICAL_SURFACE('',#94944,0.100000000000001) ;
#14316 = CYLINDRICAL_SURFACE('',#94948,0.1) ;
#14317 = CYLINDRICAL_SURFACE('',#94952,0.1) ;
#14318 = CYLINDRICAL_SURFACE('',#94956,0.1) ;
#14319 = CYLINDRICAL_SURFACE('',#94960,0.1) ;
#14320 = CYLINDRICAL_SURFACE('',#94964,0.1) ;
#14321 = CYLINDRICAL_SURFACE('',#94968,0.1) ;
#14322 = CYLINDRICAL_SURFACE('',#94971,1.65625) ;
#14323 = CYLINDRICAL_SURFACE('',#94974,0.0999999999999998) ;
#14324 = CYLINDRICAL_SURFACE('',#94978,0.0999999999999998) ;
#14325 = CYLINDRICAL_SURFACE('',#94982,0.1) ;
#14326 = CYLINDRICAL_SURFACE('',#95037,0.1) ;
#14327 = CYLINDRICAL_SURFACE('',#95040,0.1) ;
#14328 = CYLINDRICAL_SURFACE('',#95051,0.1) ;
#14329 = CYLINDRICAL_SURFACE('',#95053,0.1) ;
#14330 = CYLINDRICAL_SURFACE('',#95055,0.1) ;
#14331 = CYLINDRICAL_SURFACE('',#95057,0.1) ;
#14332 = CYLINDRICAL_SURFACE('',#95059,0.1) ;
#14333 = CYLINDRICAL_SURFACE('',#95061,0.1) ;
#14334 = CYLINDRICAL_SURFACE('',#95072,0.1) ;
#14335 = CYLINDRICAL_SURFACE('',#95074,0.0999999999999998) ;
#14336 = CYLINDRICAL_SURFACE('',#95076,0.1) ;
#14337 = CYLINDRICAL_SURFACE('',#95078,0.1) ;
#14338 = CYLINDRICAL_SURFACE('',#95080,0.1) ;
#14339 = CYLINDRICAL_SURFACE('',#95090,0.1) ;
#14340 = CYLINDRICAL_SURFACE('',#95097,0.1) ;
#14341 = CYLINDRICAL_SURFACE('',#95099,0.1) ;
#14342 = CYLINDRICAL_SURFACE('',#95101,0.0999999999999998) ;
#14343 = CYLINDRICAL_SURFACE('',#95105,0.1) ;
#14344 = CYLINDRICAL_SURFACE('',#95107,0.1) ;
#14345 = CYLINDRICAL_SURFACE('',#95109,0.0999999999999998) ;
#14346 = CYLINDRICAL_SURFACE('',#95116,0.1) ;
#14347 = CYLINDRICAL_SURFACE('',#95123,0.1) ;
#14348 = CYLINDRICAL_SURFACE('',#95125,0.1) ;
#14349 = CYLINDRICAL_SURFACE('',#95129,0.1) ;
#14350 = CYLINDRICAL_SURFACE('',#95132,0.1) ;
#14351 = CYLINDRICAL_SURFACE('',#95134,0.1) ;
#14352 = CYLINDRICAL_SURFACE('',#95137,0.1) ;
#14353 = CYLINDRICAL_SURFACE('',#95144,0.1) ;
#14354 = CYLINDRICAL_SURFACE('',#95146,0.1) ;
#14355 = CYLINDRICAL_SURFACE('',#95152,0.1) ;
#14356 = CYLINDRICAL_SURFACE('',#95154,0.1) ;
#14357 = CYLINDRICAL_SURFACE('',#95160,0.1) ;
#14358 = CYLINDRICAL_SURFACE('',#95168,0.1) ;
#14359 = CYLINDRICAL_SURFACE('',#95169,0.1) ;
#14360 = CYLINDRICAL_SURFACE('',#95173,0.1) ;
#14361 = CYLINDRICAL_SURFACE('',#95175,0.0999999999999998) ;
#14362 = CYLINDRICAL_SURFACE('',#95181,0.0999999999999998) ;
#14363 = CYLINDRICAL_SURFACE('',#95183,0.1) ;
#14364 = CYLINDRICAL_SURFACE('',#95189,0.0999999999999998) ;
#14365 = CYLINDRICAL_SURFACE('',#95190,0.100000000000003) ;
#14366 = CYLINDRICAL_SURFACE('',#95197,0.0999999999999994) ;
#14367 = CYLINDRICAL_SURFACE('',#95199,0.1) ;
#14368 = CYLINDRICAL_SURFACE('',#95205,0.0999999999999989) ;
#14369 = CYLINDRICAL_SURFACE('',#95206,0.100000000000003) ;
#14370 = CYLINDRICAL_SURFACE('',#95210,0.1) ;
#14371 = CYLINDRICAL_SURFACE('',#95212,0.0999999999999994) ;
#14372 = CYLINDRICAL_SURFACE('',#95218,0.0999999999999989) ;
#14373 = CYLINDRICAL_SURFACE('',#95226,0.0999999999999998) ;
#14374 = CYLINDRICAL_SURFACE('',#95228,0.0999999999999994) ;
#14375 = CYLINDRICAL_SURFACE('',#95234,0.100000000000003) ;
#14376 = CYLINDRICAL_SURFACE('',#95236,0.100000000000003) ;
#14377 = CYLINDRICAL_SURFACE('',#95242,0.1) ;
#14378 = CYLINDRICAL_SURFACE('',#95243,0.0999999999999994) ;
#14379 = CYLINDRICAL_SURFACE('',#95250,0.0999999999999994) ;
#14380 = CYLINDRICAL_SURFACE('',#95252,0.1) ;
#14381 = CYLINDRICAL_SURFACE('',#95258,0.0999999999999989) ;
#14382 = CYLINDRICAL_SURFACE('',#95259,0.100000000000003) ;
#14383 = CYLINDRICAL_SURFACE('',#95263,0.1) ;
#14384 = CYLINDRICAL_SURFACE('',#95265,0.0999999999999994) ;
#14385 = CYLINDRICAL_SURFACE('',#95271,0.0999999999999989) ;
#14386 = CYLINDRICAL_SURFACE('',#95279,0.0999999999999998) ;
#14387 = CYLINDRICAL_SURFACE('',#95281,0.0999999999999994) ;
#14388 = CYLINDRICAL_SURFACE('',#95287,0.0999999999999994) ;
#14389 = CYLINDRICAL_SURFACE('',#95289,0.0999999999999994) ;
#14390 = CYLINDRICAL_SURFACE('',#95295,0.1) ;
#14391 = CYLINDRICAL_SURFACE('',#95296,0.0999999999999994) ;
#14392 = CYLINDRICAL_SURFACE('',#95303,0.0999999999999994) ;
#14393 = CYLINDRICAL_SURFACE('',#95305,0.1) ;
#14394 = CYLINDRICAL_SURFACE('',#95311,0.0999999999999989) ;
#14395 = CYLINDRICAL_SURFACE('',#95312,0.0999999999999994) ;
#14396 = CYLINDRICAL_SURFACE('',#95316,0.1) ;
#14397 = CYLINDRICAL_SURFACE('',#95318,0.0999999999999994) ;
#14398 = CYLINDRICAL_SURFACE('',#95324,0.0999999999999989) ;
#14399 = CYLINDRICAL_SURFACE('',#95332,0.0999999999999998) ;
#14400 = CYLINDRICAL_SURFACE('',#95334,0.0999999999999994) ;
#14401 = CYLINDRICAL_SURFACE('',#95340,0.0999999999999994) ;
#14402 = CYLINDRICAL_SURFACE('',#95342,0.0999999999999994) ;
#14403 = CYLINDRICAL_SURFACE('',#95348,0.1) ;
#14404 = CYLINDRICAL_SURFACE('',#95349,0.0999999999999994) ;
#14405 = CYLINDRICAL_SURFACE('',#95356,0.0999999999999994) ;
#14406 = CYLINDRICAL_SURFACE('',#95358,0.1) ;
#14407 = CYLINDRICAL_SURFACE('',#95364,0.0999999999999989) ;
#14408 = CYLINDRICAL_SURFACE('',#95365,0.0999999999999994) ;
#14409 = CYLINDRICAL_SURFACE('',#95369,0.1) ;
#14410 = CYLINDRICAL_SURFACE('',#95371,0.0999999999999994) ;
#14411 = CYLINDRICAL_SURFACE('',#95377,0.0999999999999989) ;
#14412 = CYLINDRICAL_SURFACE('',#95385,0.0999999999999998) ;
#14413 = CYLINDRICAL_SURFACE('',#95387,0.0999999999999994) ;
#14414 = CYLINDRICAL_SURFACE('',#95393,0.0999999999999994) ;
#14415 = CYLINDRICAL_SURFACE('',#95395,0.0999999999999994) ;
#14416 = CYLINDRICAL_SURFACE('',#95401,0.1) ;
#14417 = CYLINDRICAL_SURFACE('',#95402,0.0999999999999994) ;
#14418 = CYLINDRICAL_SURFACE('',#95409,0.0999999999999994) ;
#14419 = CYLINDRICAL_SURFACE('',#95411,0.1) ;
#14420 = CYLINDRICAL_SURFACE('',#95417,0.0999999999999989) ;
#14421 = CYLINDRICAL_SURFACE('',#95418,0.0999999999999994) ;
#14422 = CYLINDRICAL_SURFACE('',#95422,0.1) ;
#14423 = CYLINDRICAL_SURFACE('',#95424,0.0999999999999994) ;
#14424 = CYLINDRICAL_SURFACE('',#95430,0.0999999999999989) ;
#14425 = CYLINDRICAL_SURFACE('',#95438,0.0999999999999998) ;
#14426 = CYLINDRICAL_SURFACE('',#95440,0.0999999999999994) ;
#14427 = CYLINDRICAL_SURFACE('',#95446,0.0999999999999994) ;
#14428 = CYLINDRICAL_SURFACE('',#95448,0.0999999999999994) ;
#14429 = CYLINDRICAL_SURFACE('',#95454,0.1) ;
#14430 = CYLINDRICAL_SURFACE('',#95455,0.0999999999999994) ;
#14431 = CYLINDRICAL_SURFACE('',#95462,0.0999999999999994) ;
#14432 = CYLINDRICAL_SURFACE('',#95464,0.1) ;
#14433 = CYLINDRICAL_SURFACE('',#95470,0.0999999999999989) ;
#14434 = CYLINDRICAL_SURFACE('',#95471,0.0999999999999994) ;
#14435 = CYLINDRICAL_SURFACE('',#95475,0.1) ;
#14436 = CYLINDRICAL_SURFACE('',#95477,0.0999999999999994) ;
#14437 = CYLINDRICAL_SURFACE('',#95483,0.1) ;
#14438 = CYLINDRICAL_SURFACE('',#95491,0.0999999999999998) ;
#14439 = CYLINDRICAL_SURFACE('',#95493,0.0999999999999994) ;
#14440 = CYLINDRICAL_SURFACE('',#95499,0.0999999999999994) ;
#14441 = CYLINDRICAL_SURFACE('',#95501,0.0999999999999994) ;
#14442 = CYLINDRICAL_SURFACE('',#95507,0.1) ;
#14443 = CYLINDRICAL_SURFACE('',#95508,0.0999999999999994) ;
#14444 = CYLINDRICAL_SURFACE('',#95515,0.0999999999999994) ;
#14445 = CYLINDRICAL_SURFACE('',#95517,0.1) ;
#14446 = CYLINDRICAL_SURFACE('',#95523,0.1) ;
#14447 = CYLINDRICAL_SURFACE('',#95524,0.0999999999999994) ;
#14448 = CYLINDRICAL_SURFACE('',#95528,0.1) ;
#14449 = CYLINDRICAL_SURFACE('',#95530,0.0999999999999994) ;
#14450 = CYLINDRICAL_SURFACE('',#95536,0.1) ;
#14451 = CYLINDRICAL_SURFACE('',#95544,0.0999999999999998) ;
#14452 = CYLINDRICAL_SURFACE('',#95546,0.0999999999999994) ;
#14453 = CYLINDRICAL_SURFACE('',#95552,0.0999999999999994) ;
#14454 = CYLINDRICAL_SURFACE('',#95554,0.0999999999999994) ;
#14455 = CYLINDRICAL_SURFACE('',#95560,0.1) ;
#14456 = CYLINDRICAL_SURFACE('',#95561,0.0999999999999994) ;
#14457 = CYLINDRICAL_SURFACE('',#95568,0.0999999999999994) ;
#14458 = CYLINDRICAL_SURFACE('',#95570,0.1) ;
#14459 = CYLINDRICAL_SURFACE('',#95576,0.1) ;
#14460 = CYLINDRICAL_SURFACE('',#95577,0.0999999999999994) ;
#14461 = CYLINDRICAL_SURFACE('',#95581,0.1) ;
#14462 = CYLINDRICAL_SURFACE('',#95583,0.0999999999999994) ;
#14463 = CYLINDRICAL_SURFACE('',#95589,0.1) ;
#14464 = CYLINDRICAL_SURFACE('',#95597,0.0999999999999998) ;
#14465 = CYLINDRICAL_SURFACE('',#95599,0.0999999999999994) ;
#14466 = CYLINDRICAL_SURFACE('',#95605,0.1) ;
#14467 = CYLINDRICAL_SURFACE('',#95607,0.1) ;
#14468 = CYLINDRICAL_SURFACE('',#95613,0.1) ;
#14469 = CYLINDRICAL_SURFACE('',#95614,0.1) ;
#14470 = CYLINDRICAL_SURFACE('',#95621,0.0999999999999994) ;
#14471 = CYLINDRICAL_SURFACE('',#95623,0.1) ;
#14472 = CYLINDRICAL_SURFACE('',#95629,0.1) ;
#14473 = CYLINDRICAL_SURFACE('',#95630,0.1) ;
#14474 = CYLINDRICAL_SURFACE('',#95634,0.1) ;
#14475 = CYLINDRICAL_SURFACE('',#95636,0.0999999999999994) ;
#14476 = CYLINDRICAL_SURFACE('',#95642,0.1) ;
#14477 = CYLINDRICAL_SURFACE('',#95650,0.0999999999999998) ;
#14478 = CYLINDRICAL_SURFACE('',#95652,0.0999999999999994) ;
#14479 = CYLINDRICAL_SURFACE('',#95658,0.0999999999999998) ;
#14480 = CYLINDRICAL_SURFACE('',#95660,0.0999999999999998) ;
#14481 = CYLINDRICAL_SURFACE('',#95666,0.1) ;
#14482 = CYLINDRICAL_SURFACE('',#95667,0.1) ;
#14483 = CYLINDRICAL_SURFACE('',#95670,0.1) ;
#14484 = CYLINDRICAL_SURFACE('',#95681,0.1) ;
#14485 = CYLINDRICAL_SURFACE('',#95683,0.1) ;
#14486 = CYLINDRICAL_SURFACE('',#95685,0.1) ;
#14487 = CYLINDRICAL_SURFACE('',#95687,0.1) ;
#14488 = CYLINDRICAL_SURFACE('',#95689,0.1) ;
#14489 = CYLINDRICAL_SURFACE('',#95691,0.1) ;
#14490 = CYLINDRICAL_SURFACE('',#95702,0.1) ;
#14491 = CYLINDRICAL_SURFACE('',#95704,0.0999999999999998) ;
#14492 = CYLINDRICAL_SURFACE('',#95706,0.1) ;
#14493 = CYLINDRICAL_SURFACE('',#95708,0.1) ;
#14494 = CYLINDRICAL_SURFACE('',#95710,0.1) ;
#14495 = CYLINDRICAL_SURFACE('',#95720,0.1) ;
#14496 = CYLINDRICAL_SURFACE('',#95727,0.1) ;
#14497 = CYLINDRICAL_SURFACE('',#95729,0.1) ;
#14498 = CYLINDRICAL_SURFACE('',#95731,0.1) ;
#14499 = CYLINDRICAL_SURFACE('',#95735,0.1) ;
#14500 = CYLINDRICAL_SURFACE('',#95737,0.1) ;
#14501 = CYLINDRICAL_SURFACE('',#95739,0.0999999999999998) ;
#14502 = CYLINDRICAL_SURFACE('',#95746,0.1) ;
#14503 = CYLINDRICAL_SURFACE('',#95753,0.1) ;
#14504 = CYLINDRICAL_SURFACE('',#95755,0.1) ;
#14505 = CYLINDRICAL_SURFACE('',#95759,0.1) ;
#14506 = CYLINDRICAL_SURFACE('',#95762,0.1) ;
#14507 = CYLINDRICAL_SURFACE('',#95764,0.0999999999999994) ;
#14508 = CYLINDRICAL_SURFACE('',#95767,0.1) ;
#14509 = CYLINDRICAL_SURFACE('',#95774,0.0999999999999994) ;
#14510 = CYLINDRICAL_SURFACE('',#95776,0.0999999999999994) ;
#14511 = CYLINDRICAL_SURFACE('',#95782,0.1) ;
#14512 = CYLINDRICAL_SURFACE('',#95784,0.1) ;
#14513 = CYLINDRICAL_SURFACE('',#95790,0.1) ;
#14514 = CYLINDRICAL_SURFACE('',#95798,0.1) ;
#14515 = CYLINDRICAL_SURFACE('',#95799,0.1) ;
#14516 = CYLINDRICAL_SURFACE('',#95803,0.1) ;
#14517 = CYLINDRICAL_SURFACE('',#95805,0.1) ;
#14518 = CYLINDRICAL_SURFACE('',#95811,0.0999999999999998) ;
#14519 = CYLINDRICAL_SURFACE('',#95813,0.1) ;
#14520 = CYLINDRICAL_SURFACE('',#95819,0.1) ;
#14521 = CYLINDRICAL_SURFACE('',#95820,0.1) ;
#14522 = CYLINDRICAL_SURFACE('',#95823,0.1) ;
#14523 = CYLINDRICAL_SURFACE('',#95834,0.1) ;
#14524 = CYLINDRICAL_SURFACE('',#95836,0.1) ;
#14525 = CYLINDRICAL_SURFACE('',#95838,0.1) ;
#14526 = CYLINDRICAL_SURFACE('',#95840,0.1) ;
#14527 = CYLINDRICAL_SURFACE('',#95842,0.1) ;
#14528 = CYLINDRICAL_SURFACE('',#95844,0.1) ;
#14529 = CYLINDRICAL_SURFACE('',#95855,0.1) ;
#14530 = CYLINDRICAL_SURFACE('',#95857,0.0999999999999998) ;
#14531 = CYLINDRICAL_SURFACE('',#95859,0.1) ;
#14532 = CYLINDRICAL_SURFACE('',#95861,0.1) ;
#14533 = CYLINDRICAL_SURFACE('',#95863,0.1) ;
#14534 = CYLINDRICAL_SURFACE('',#95873,0.1) ;
#14535 = CYLINDRICAL_SURFACE('',#95880,0.1) ;
#14536 = CYLINDRICAL_SURFACE('',#95882,0.1) ;
#14537 = CYLINDRICAL_SURFACE('',#95884,0.0999999999999994) ;
#14538 = CYLINDRICAL_SURFACE('',#95888,0.1) ;
#14539 = CYLINDRICAL_SURFACE('',#95890,0.1) ;
#14540 = CYLINDRICAL_SURFACE('',#95892,0.0999999999999998) ;
#14541 = CYLINDRICAL_SURFACE('',#95899,0.1) ;
#14542 = CYLINDRICAL_SURFACE('',#95906,0.1) ;
#14543 = CYLINDRICAL_SURFACE('',#95908,0.1) ;
#14544 = CYLINDRICAL_SURFACE('',#95912,0.1) ;
#14545 = CYLINDRICAL_SURFACE('',#95915,0.1) ;
#14546 = CYLINDRICAL_SURFACE('',#95917,0.0999999999999994) ;
#14547 = CYLINDRICAL_SURFACE('',#95920,0.1) ;
#14548 = CYLINDRICAL_SURFACE('',#95927,0.0999999999999994) ;
#14549 = CYLINDRICAL_SURFACE('',#95929,0.0999999999999994) ;
#14550 = CYLINDRICAL_SURFACE('',#95935,0.1) ;
#14551 = CYLINDRICAL_SURFACE('',#95937,0.1) ;
#14552 = CYLINDRICAL_SURFACE('',#95943,0.1) ;
#14553 = CYLINDRICAL_SURFACE('',#95951,0.1) ;
#14554 = CYLINDRICAL_SURFACE('',#95952,0.1) ;
#14555 = CYLINDRICAL_SURFACE('',#95956,0.1) ;
#14556 = CYLINDRICAL_SURFACE('',#95958,0.0999999999999994) ;
#14557 = CYLINDRICAL_SURFACE('',#95964,0.0999999999999998) ;
#14558 = CYLINDRICAL_SURFACE('',#95966,0.1) ;
#14559 = CYLINDRICAL_SURFACE('',#95972,0.0999999999999994) ;
#14560 = CYLINDRICAL_SURFACE('',#95973,0.1) ;
#14561 = CYLINDRICAL_SURFACE('',#95976,0.1) ;
#14562 = CYLINDRICAL_SURFACE('',#95987,0.1) ;
#14563 = CYLINDRICAL_SURFACE('',#95989,0.1) ;
#14564 = CYLINDRICAL_SURFACE('',#95991,0.1) ;
#14565 = CYLINDRICAL_SURFACE('',#95993,0.1) ;
#14566 = CYLINDRICAL_SURFACE('',#95995,0.1) ;
#14567 = CYLINDRICAL_SURFACE('',#95997,0.1) ;
#14568 = CYLINDRICAL_SURFACE('',#96008,0.1) ;
#14569 = CYLINDRICAL_SURFACE('',#96010,0.0999999999999998) ;
#14570 = CYLINDRICAL_SURFACE('',#96012,0.1) ;
#14571 = CYLINDRICAL_SURFACE('',#96014,0.1) ;
#14572 = CYLINDRICAL_SURFACE('',#96016,0.1) ;
#14573 = CYLINDRICAL_SURFACE('',#96026,0.1) ;
#14574 = CYLINDRICAL_SURFACE('',#96033,0.1) ;
#14575 = CYLINDRICAL_SURFACE('',#96035,0.1) ;
#14576 = CYLINDRICAL_SURFACE('',#96037,0.0999999999999994) ;
#14577 = CYLINDRICAL_SURFACE('',#96041,0.1) ;
#14578 = CYLINDRICAL_SURFACE('',#96043,0.1) ;
#14579 = CYLINDRICAL_SURFACE('',#96045,0.0999999999999998) ;
#14580 = CYLINDRICAL_SURFACE('',#96052,0.1) ;
#14581 = CYLINDRICAL_SURFACE('',#96059,0.1) ;
#14582 = CYLINDRICAL_SURFACE('',#96061,0.1) ;
#14583 = CYLINDRICAL_SURFACE('',#96065,0.1) ;
#14584 = CYLINDRICAL_SURFACE('',#96068,0.1) ;
#14585 = CYLINDRICAL_SURFACE('',#96070,0.0999999999999994) ;
#14586 = CYLINDRICAL_SURFACE('',#96073,0.1) ;
#14587 = CYLINDRICAL_SURFACE('',#96080,0.0999999999999994) ;
#14588 = CYLINDRICAL_SURFACE('',#96082,0.0999999999999994) ;
#14589 = CYLINDRICAL_SURFACE('',#96088,0.1) ;
#14590 = CYLINDRICAL_SURFACE('',#96090,0.1) ;
#14591 = CYLINDRICAL_SURFACE('',#96096,0.1) ;
#14592 = CYLINDRICAL_SURFACE('',#96104,0.1) ;
#14593 = CYLINDRICAL_SURFACE('',#96105,0.1) ;
#14594 = CYLINDRICAL_SURFACE('',#96109,0.1) ;
#14595 = CYLINDRICAL_SURFACE('',#96111,0.0999999999999994) ;
#14596 = CYLINDRICAL_SURFACE('',#96117,0.0999999999999998) ;
#14597 = CYLINDRICAL_SURFACE('',#96119,0.1) ;
#14598 = CYLINDRICAL_SURFACE('',#96125,0.0999999999999994) ;
#14599 = CYLINDRICAL_SURFACE('',#96126,0.1) ;
#14600 = CYLINDRICAL_SURFACE('',#96129,0.1) ;
#14601 = CYLINDRICAL_SURFACE('',#96140,0.1) ;
#14602 = CYLINDRICAL_SURFACE('',#96142,0.1) ;
#14603 = CYLINDRICAL_SURFACE('',#96144,0.1) ;
#14604 = CYLINDRICAL_SURFACE('',#96146,0.1) ;
#14605 = CYLINDRICAL_SURFACE('',#96148,0.1) ;
#14606 = CYLINDRICAL_SURFACE('',#96150,0.1) ;
#14607 = CYLINDRICAL_SURFACE('',#96161,0.1) ;
#14608 = CYLINDRICAL_SURFACE('',#96163,0.0999999999999998) ;
#14609 = CYLINDRICAL_SURFACE('',#96165,0.1) ;
#14610 = CYLINDRICAL_SURFACE('',#96167,0.1) ;
#14611 = CYLINDRICAL_SURFACE('',#96169,0.1) ;
#14612 = CYLINDRICAL_SURFACE('',#96179,0.1) ;
#14613 = CYLINDRICAL_SURFACE('',#96186,0.1) ;
#14614 = CYLINDRICAL_SURFACE('',#96188,0.1) ;
#14615 = CYLINDRICAL_SURFACE('',#96190,0.0999999999999994) ;
#14616 = CYLINDRICAL_SURFACE('',#96194,0.1) ;
#14617 = CYLINDRICAL_SURFACE('',#96196,0.1) ;
#14618 = CYLINDRICAL_SURFACE('',#96198,0.0999999999999998) ;
#14619 = CYLINDRICAL_SURFACE('',#96205,0.1) ;
#14620 = CYLINDRICAL_SURFACE('',#96212,0.1) ;
#14621 = CYLINDRICAL_SURFACE('',#96214,0.1) ;
#14622 = CYLINDRICAL_SURFACE('',#96218,0.1) ;
#14623 = CYLINDRICAL_SURFACE('',#96221,0.1) ;
#14624 = CYLINDRICAL_SURFACE('',#96223,0.0999999999999994) ;
#14625 = CYLINDRICAL_SURFACE('',#96226,0.1) ;
#14626 = CYLINDRICAL_SURFACE('',#96233,0.0999999999999994) ;
#14627 = CYLINDRICAL_SURFACE('',#96235,0.0999999999999994) ;
#14628 = CYLINDRICAL_SURFACE('',#96241,0.1) ;
#14629 = CYLINDRICAL_SURFACE('',#96243,0.1) ;
#14630 = CYLINDRICAL_SURFACE('',#96249,0.0999999999999988) ;
#14631 = CYLINDRICAL_SURFACE('',#96257,0.1) ;
#14632 = CYLINDRICAL_SURFACE('',#96258,0.1) ;
#14633 = CYLINDRICAL_SURFACE('',#96262,0.0999999999999989) ;
#14634 = CYLINDRICAL_SURFACE('',#96264,0.0999999999999994) ;
#14635 = CYLINDRICAL_SURFACE('',#96270,0.0999999999999998) ;
#14636 = CYLINDRICAL_SURFACE('',#96272,0.1) ;
#14637 = CYLINDRICAL_SURFACE('',#96278,0.0999999999999994) ;
#14638 = CYLINDRICAL_SURFACE('',#96279,0.1) ;
#14639 = CYLINDRICAL_SURFACE('',#96282,0.1) ;
#14640 = CYLINDRICAL_SURFACE('',#96293,0.1) ;
#14641 = CYLINDRICAL_SURFACE('',#96295,0.1) ;
#14642 = CYLINDRICAL_SURFACE('',#96297,0.1) ;
#14643 = CYLINDRICAL_SURFACE('',#96299,0.1) ;
#14644 = CYLINDRICAL_SURFACE('',#96301,0.1) ;
#14645 = CYLINDRICAL_SURFACE('',#96303,0.1) ;
#14646 = CYLINDRICAL_SURFACE('',#96314,0.1) ;
#14647 = CYLINDRICAL_SURFACE('',#96316,0.0999999999999998) ;
#14648 = CYLINDRICAL_SURFACE('',#96318,0.1) ;
#14649 = CYLINDRICAL_SURFACE('',#96320,0.1) ;
#14650 = CYLINDRICAL_SURFACE('',#96322,0.1) ;
#14651 = CYLINDRICAL_SURFACE('',#96332,0.1) ;
#14652 = CYLINDRICAL_SURFACE('',#96339,0.1) ;
#14653 = CYLINDRICAL_SURFACE('',#96341,0.1) ;
#14654 = CYLINDRICAL_SURFACE('',#96343,0.0999999999999994) ;
#14655 = CYLINDRICAL_SURFACE('',#96347,0.1) ;
#14656 = CYLINDRICAL_SURFACE('',#96349,0.1) ;
#14657 = CYLINDRICAL_SURFACE('',#96351,0.0999999999999998) ;
#14658 = CYLINDRICAL_SURFACE('',#96358,0.1) ;
#14659 = CYLINDRICAL_SURFACE('',#96365,0.1) ;
#14660 = CYLINDRICAL_SURFACE('',#96367,0.1) ;
#14661 = CYLINDRICAL_SURFACE('',#96371,0.1) ;
#14662 = CYLINDRICAL_SURFACE('',#96374,0.1) ;
#14663 = CYLINDRICAL_SURFACE('',#96376,0.0999999999999994) ;
#14664 = CYLINDRICAL_SURFACE('',#96379,0.1) ;
#14665 = CYLINDRICAL_SURFACE('',#96386,0.0999999999999994) ;
#14666 = CYLINDRICAL_SURFACE('',#96388,0.0999999999999994) ;
#14667 = CYLINDRICAL_SURFACE('',#96394,0.1) ;
#14668 = CYLINDRICAL_SURFACE('',#96396,0.1) ;
#14669 = CYLINDRICAL_SURFACE('',#96402,0.0999999999999988) ;
#14670 = CYLINDRICAL_SURFACE('',#96410,0.1) ;
#14671 = CYLINDRICAL_SURFACE('',#96411,0.1) ;
#14672 = CYLINDRICAL_SURFACE('',#96415,0.0999999999999989) ;
#14673 = CYLINDRICAL_SURFACE('',#96417,0.0999999999999994) ;
#14674 = CYLINDRICAL_SURFACE('',#96423,0.0999999999999998) ;
#14675 = CYLINDRICAL_SURFACE('',#96425,0.1) ;
#14676 = CYLINDRICAL_SURFACE('',#96431,0.0999999999999994) ;
#14677 = CYLINDRICAL_SURFACE('',#96432,0.1) ;
#14678 = CYLINDRICAL_SURFACE('',#96435,0.1) ;
#14679 = CYLINDRICAL_SURFACE('',#96446,0.1) ;
#14680 = CYLINDRICAL_SURFACE('',#96448,0.1) ;
#14681 = CYLINDRICAL_SURFACE('',#96450,0.1) ;
#14682 = CYLINDRICAL_SURFACE('',#96452,0.1) ;
#14683 = CYLINDRICAL_SURFACE('',#96454,0.1) ;
#14684 = CYLINDRICAL_SURFACE('',#96456,0.1) ;
#14685 = CYLINDRICAL_SURFACE('',#96467,0.1) ;
#14686 = CYLINDRICAL_SURFACE('',#96469,0.0999999999999998) ;
#14687 = CYLINDRICAL_SURFACE('',#96471,0.1) ;
#14688 = CYLINDRICAL_SURFACE('',#96473,0.1) ;
#14689 = CYLINDRICAL_SURFACE('',#96475,0.1) ;
#14690 = CYLINDRICAL_SURFACE('',#96485,0.1) ;
#14691 = CYLINDRICAL_SURFACE('',#96492,0.1) ;
#14692 = CYLINDRICAL_SURFACE('',#96494,0.1) ;
#14693 = CYLINDRICAL_SURFACE('',#96496,0.0999999999999994) ;
#14694 = CYLINDRICAL_SURFACE('',#96500,0.1) ;
#14695 = CYLINDRICAL_SURFACE('',#96502,0.1) ;
#14696 = CYLINDRICAL_SURFACE('',#96504,0.0999999999999998) ;
#14697 = CYLINDRICAL_SURFACE('',#96511,0.1) ;
#14698 = CYLINDRICAL_SURFACE('',#96518,0.1) ;
#14699 = CYLINDRICAL_SURFACE('',#96520,0.1) ;
#14700 = CYLINDRICAL_SURFACE('',#96524,0.1) ;
#14701 = CYLINDRICAL_SURFACE('',#96527,0.1) ;
#14702 = CYLINDRICAL_SURFACE('',#96529,0.0999999999999994) ;
#14703 = CYLINDRICAL_SURFACE('',#96532,0.1) ;
#14704 = CYLINDRICAL_SURFACE('',#96539,0.0999999999999994) ;
#14705 = CYLINDRICAL_SURFACE('',#96541,0.0999999999999994) ;
#14706 = CYLINDRICAL_SURFACE('',#96547,0.1) ;
#14707 = CYLINDRICAL_SURFACE('',#96549,0.1) ;
#14708 = CYLINDRICAL_SURFACE('',#96555,0.0999999999999988) ;
#14709 = CYLINDRICAL_SURFACE('',#96563,0.1) ;
#14710 = CYLINDRICAL_SURFACE('',#96564,0.1) ;
#14711 = CYLINDRICAL_SURFACE('',#96568,0.0999999999999989) ;
#14712 = CYLINDRICAL_SURFACE('',#96570,0.0999999999999994) ;
#14713 = CYLINDRICAL_SURFACE('',#96576,0.0999999999999998) ;
#14714 = CYLINDRICAL_SURFACE('',#96578,0.1) ;
#14715 = CYLINDRICAL_SURFACE('',#96584,0.0999999999999994) ;
#14716 = CYLINDRICAL_SURFACE('',#96585,0.1) ;
#14717 = CYLINDRICAL_SURFACE('',#96588,0.1) ;
#14718 = CYLINDRICAL_SURFACE('',#96599,0.1) ;
#14719 = CYLINDRICAL_SURFACE('',#96601,0.1) ;
#14720 = CYLINDRICAL_SURFACE('',#96603,0.1) ;
#14721 = CYLINDRICAL_SURFACE('',#96605,0.1) ;
#14722 = CYLINDRICAL_SURFACE('',#96607,0.1) ;
#14723 = CYLINDRICAL_SURFACE('',#96609,0.1) ;
#14724 = CYLINDRICAL_SURFACE('',#96620,0.1) ;
#14725 = CYLINDRICAL_SURFACE('',#96622,0.0999999999999998) ;
#14726 = CYLINDRICAL_SURFACE('',#96624,0.1) ;
#14727 = CYLINDRICAL_SURFACE('',#96626,0.1) ;
#14728 = CYLINDRICAL_SURFACE('',#96628,0.1) ;
#14729 = CYLINDRICAL_SURFACE('',#96638,0.1) ;
#14730 = CYLINDRICAL_SURFACE('',#96645,0.1) ;
#14731 = CYLINDRICAL_SURFACE('',#96647,0.1) ;
#14732 = CYLINDRICAL_SURFACE('',#96649,0.0999999999999994) ;
#14733 = CYLINDRICAL_SURFACE('',#96653,0.1) ;
#14734 = CYLINDRICAL_SURFACE('',#96655,0.1) ;
#14735 = CYLINDRICAL_SURFACE('',#96657,0.0999999999999998) ;
#14736 = CYLINDRICAL_SURFACE('',#96664,0.1) ;
#14737 = CYLINDRICAL_SURFACE('',#96671,0.1) ;
#14738 = CYLINDRICAL_SURFACE('',#96673,0.1) ;
#14739 = CYLINDRICAL_SURFACE('',#96677,0.1) ;
#14740 = CYLINDRICAL_SURFACE('',#96680,0.1) ;
#14741 = CYLINDRICAL_SURFACE('',#96682,0.100000000000003) ;
#14742 = CYLINDRICAL_SURFACE('',#96685,0.1) ;
#14743 = CYLINDRICAL_SURFACE('',#96692,0.0999999999999994) ;
#14744 = CYLINDRICAL_SURFACE('',#96694,0.100000000000003) ;
#14745 = CYLINDRICAL_SURFACE('',#96700,0.1) ;
#14746 = CYLINDRICAL_SURFACE('',#96702,0.1) ;
#14747 = CYLINDRICAL_SURFACE('',#96708,0.0999999999999988) ;
#14748 = CYLINDRICAL_SURFACE('',#96716,0.1) ;
#14749 = CYLINDRICAL_SURFACE('',#96717,0.1) ;
#14750 = CYLINDRICAL_SURFACE('',#96721,0.0999999999999989) ;
#14751 = CYLINDRICAL_SURFACE('',#96723,0.0999999999999994) ;
#14752 = CYLINDRICAL_SURFACE('',#96729,0.0999999999999998) ;
#14753 = CYLINDRICAL_SURFACE('',#96731,0.1) ;
#14754 = CYLINDRICAL_SURFACE('',#96737,0.0999999999999994) ;
#14755 = CYLINDRICAL_SURFACE('',#96738,0.1) ;
#14756 = CYLINDRICAL_SURFACE('',#96741,0.1) ;
#14757 = CYLINDRICAL_SURFACE('',#96752,0.1) ;
#14758 = CYLINDRICAL_SURFACE('',#96754,0.1) ;
#14759 = CYLINDRICAL_SURFACE('',#96756,0.1) ;
#14760 = CYLINDRICAL_SURFACE('',#96758,0.1) ;
#14761 = CYLINDRICAL_SURFACE('',#96760,0.1) ;
#14762 = CYLINDRICAL_SURFACE('',#96762,0.1) ;
#14763 = CYLINDRICAL_SURFACE('',#96773,0.1) ;
#14764 = CYLINDRICAL_SURFACE('',#96775,0.0999999999999998) ;
#14765 = CYLINDRICAL_SURFACE('',#96777,0.1) ;
#14766 = CYLINDRICAL_SURFACE('',#96779,0.1) ;
#14767 = CYLINDRICAL_SURFACE('',#96781,0.1) ;
#14768 = CYLINDRICAL_SURFACE('',#96791,0.1) ;
#14769 = CYLINDRICAL_SURFACE('',#96798,0.1) ;
#14770 = CYLINDRICAL_SURFACE('',#96800,0.1) ;
#14771 = CYLINDRICAL_SURFACE('',#96802,0.100000000000003) ;
#14772 = CYLINDRICAL_SURFACE('',#96806,0.1) ;
#14773 = CYLINDRICAL_SURFACE('',#96808,0.1) ;
#14774 = CYLINDRICAL_SURFACE('',#96810,0.0999999999999998) ;
#14775 = CYLINDRICAL_SURFACE('',#96817,0.1) ;
#14776 = CYLINDRICAL_SURFACE('',#96824,0.1) ;
#14777 = CYLINDRICAL_SURFACE('',#96826,0.1) ;
#14778 = CYLINDRICAL_SURFACE('',#96830,0.1) ;
#14779 = CYLINDRICAL_SURFACE('',#96833,0.1) ;
#14780 = CYLINDRICAL_SURFACE('',#96835,0.100000000000003) ;
#14781 = CYLINDRICAL_SURFACE('',#96838,0.1) ;
#14782 = CYLINDRICAL_SURFACE('',#96845,0.100000000000003) ;
#14783 = CYLINDRICAL_SURFACE('',#96847,0.100000000000003) ;
#14784 = CYLINDRICAL_SURFACE('',#96853,0.1) ;
#14785 = CYLINDRICAL_SURFACE('',#96855,0.1) ;
#14786 = CYLINDRICAL_SURFACE('',#96861,0.0999999999999988) ;
#14787 = CYLINDRICAL_SURFACE('',#96869,0.1) ;
#14788 = CYLINDRICAL_SURFACE('',#96870,0.1) ;
#14789 = CYLINDRICAL_SURFACE('',#96874,0.0999999999999989) ;
#14790 = CYLINDRICAL_SURFACE('',#96876,0.100000000000003) ;
#14791 = CYLINDRICAL_SURFACE('',#96882,0.0999999999999998) ;
#14792 = CYLINDRICAL_SURFACE('',#96884,0.1) ;
#14793 = CYLINDRICAL_SURFACE('',#96890,0.100000000000003) ;
#14794 = CYLINDRICAL_SURFACE('',#96902,1.) ;
#14795 = CYLINDRICAL_SURFACE('',#96905,0.2) ;
#14796 = CYLINDRICAL_SURFACE('',#96926,1.) ;
#14797 = CYLINDRICAL_SURFACE('',#96929,0.2) ;
#14798 = CYLINDRICAL_SURFACE('',#96950,1.) ;
#14799 = CYLINDRICAL_SURFACE('',#96953,0.2) ;
#14800 = CYLINDRICAL_SURFACE('',#96974,1.) ;
#14801 = CYLINDRICAL_SURFACE('',#96977,0.2) ;
#14802 = CYLINDRICAL_SURFACE('',#96998,1.) ;
#14803 = CYLINDRICAL_SURFACE('',#97001,0.2) ;
#14804 = CYLINDRICAL_SURFACE('',#97022,1.) ;
#14805 = CYLINDRICAL_SURFACE('',#97025,0.2) ;
#14806 = CYLINDRICAL_SURFACE('',#97046,1.) ;
#14807 = CYLINDRICAL_SURFACE('',#97049,0.2) ;
#14808 = CYLINDRICAL_SURFACE('',#97070,1.) ;
#14809 = CYLINDRICAL_SURFACE('',#97073,0.2) ;
#14810 = CYLINDRICAL_SURFACE('',#97094,1.) ;
#14811 = CYLINDRICAL_SURFACE('',#97097,0.2) ;
#14812 = CYLINDRICAL_SURFACE('',#97143,0.0999999999999999) ;
#14813 = CYLINDRICAL_SURFACE('',#97146,0.1) ;
#14814 = CYLINDRICAL_SURFACE('',#97152,0.0999999999999999) ;
#14815 = CYLINDRICAL_SURFACE('',#97155,0.1) ;
#14816 = CYLINDRICAL_SURFACE('',#97157,0.0999999999999998) ;
#14817 = CYLINDRICAL_SURFACE('',#97164,0.0999999999999998) ;
#14818 = CYLINDRICAL_SURFACE('',#97166,0.1) ;
#14819 = CYLINDRICAL_SURFACE('',#97168,0.1) ;
#14820 = CYLINDRICAL_SURFACE('',#97172,0.1) ;
#14821 = CYLINDRICAL_SURFACE('',#97175,0.0999999999999999) ;
#14822 = CYLINDRICAL_SURFACE('',#97177,0.1) ;
#14823 = CYLINDRICAL_SURFACE('',#97180,0.1) ;
#14824 = CYLINDRICAL_SURFACE('',#97186,0.1) ;
#14825 = CYLINDRICAL_SURFACE('',#97189,0.1) ;
#14826 = CYLINDRICAL_SURFACE('',#97191,0.0999999999999998) ;
#14827 = CYLINDRICAL_SURFACE('',#97198,0.0999999999999998) ;
#14828 = CYLINDRICAL_SURFACE('',#97200,0.1) ;
#14829 = CYLINDRICAL_SURFACE('',#97202,0.1) ;
#14830 = CYLINDRICAL_SURFACE('',#97206,0.1) ;
#14831 = CYLINDRICAL_SURFACE('',#97209,0.1) ;
#14832 = CYLINDRICAL_SURFACE('',#97211,0.1) ;
#14833 = CYLINDRICAL_SURFACE('',#97214,0.1) ;
#14834 = CYLINDRICAL_SURFACE('',#97220,0.1) ;
#14835 = CYLINDRICAL_SURFACE('',#97223,0.1) ;
#14836 = CYLINDRICAL_SURFACE('',#97225,0.1) ;
#14837 = CYLINDRICAL_SURFACE('',#97232,0.1) ;
#14838 = CYLINDRICAL_SURFACE('',#97234,0.1) ;
#14839 = CYLINDRICAL_SURFACE('',#97236,0.1) ;
#14840 = CYLINDRICAL_SURFACE('',#97240,0.1) ;
#14841 = CYLINDRICAL_SURFACE('',#97243,0.1) ;
#14842 = CYLINDRICAL_SURFACE('',#97245,0.1) ;
#14843 = CYLINDRICAL_SURFACE('',#97248,0.1) ;
#14844 = CYLINDRICAL_SURFACE('',#97254,0.1) ;
#14845 = CYLINDRICAL_SURFACE('',#97257,0.1) ;
#14846 = CYLINDRICAL_SURFACE('',#97259,0.1) ;
#14847 = CYLINDRICAL_SURFACE('',#97266,0.1) ;
#14848 = CYLINDRICAL_SURFACE('',#97268,0.1) ;
#14849 = CYLINDRICAL_SURFACE('',#97270,0.1) ;
#14850 = CYLINDRICAL_SURFACE('',#97274,0.1) ;
#14851 = CYLINDRICAL_SURFACE('',#97277,0.1) ;
#14852 = CYLINDRICAL_SURFACE('',#97279,0.1) ;
#14853 = CYLINDRICAL_SURFACE('',#97282,0.1) ;
#14854 = CYLINDRICAL_SURFACE('',#97288,0.1) ;
#14855 = CYLINDRICAL_SURFACE('',#97291,0.1) ;
#14856 = CYLINDRICAL_SURFACE('',#97293,0.0999999999999994) ;
#14857 = CYLINDRICAL_SURFACE('',#97300,0.0999999999999994) ;
#14858 = CYLINDRICAL_SURFACE('',#97302,0.1) ;
#14859 = CYLINDRICAL_SURFACE('',#97304,0.1) ;
#14860 = CYLINDRICAL_SURFACE('',#97308,0.1) ;
#14861 = CYLINDRICAL_SURFACE('',#97311,0.1) ;
#14862 = CYLINDRICAL_SURFACE('',#97313,0.1) ;
#14863 = CYLINDRICAL_SURFACE('',#97316,0.1) ;
#14864 = CYLINDRICAL_SURFACE('',#97322,0.1) ;
#14865 = CYLINDRICAL_SURFACE('',#97325,0.1) ;
#14866 = CYLINDRICAL_SURFACE('',#97327,0.0999999999999994) ;
#14867 = CYLINDRICAL_SURFACE('',#97334,0.0999999999999994) ;
#14868 = CYLINDRICAL_SURFACE('',#97336,0.1) ;
#14869 = CYLINDRICAL_SURFACE('',#97338,0.1) ;
#14870 = CYLINDRICAL_SURFACE('',#97342,0.1) ;
#14871 = CYLINDRICAL_SURFACE('',#97345,0.1) ;
#14872 = CYLINDRICAL_SURFACE('',#97347,0.1) ;
#14873 = CYLINDRICAL_SURFACE('',#97350,0.1) ;
#14874 = CYLINDRICAL_SURFACE('',#97356,0.1) ;
#14875 = CYLINDRICAL_SURFACE('',#97359,0.1) ;
#14876 = CYLINDRICAL_SURFACE('',#97361,0.0999999999999994) ;
#14877 = CYLINDRICAL_SURFACE('',#97368,0.0999999999999994) ;
#14878 = CYLINDRICAL_SURFACE('',#97370,0.1) ;
#14879 = CYLINDRICAL_SURFACE('',#97372,0.1) ;
#14880 = CYLINDRICAL_SURFACE('',#97376,0.1) ;
#14881 = CYLINDRICAL_SURFACE('',#97379,0.1) ;
#14882 = CYLINDRICAL_SURFACE('',#97381,0.1) ;
#14883 = CYLINDRICAL_SURFACE('',#97384,0.1) ;
#14884 = CYLINDRICAL_SURFACE('',#97390,0.1) ;
#14885 = CYLINDRICAL_SURFACE('',#97393,0.1) ;
#14886 = CYLINDRICAL_SURFACE('',#97395,0.0999999999999994) ;
#14887 = CYLINDRICAL_SURFACE('',#97402,0.0999999999999994) ;
#14888 = CYLINDRICAL_SURFACE('',#97404,0.1) ;
#14889 = CYLINDRICAL_SURFACE('',#97406,0.1) ;
#14890 = CYLINDRICAL_SURFACE('',#97410,0.1) ;
#14891 = CYLINDRICAL_SURFACE('',#97413,0.1) ;
#14892 = CYLINDRICAL_SURFACE('',#97415,0.099999999999999) ;
#14893 = CYLINDRICAL_SURFACE('',#97418,0.1) ;
#14894 = CYLINDRICAL_SURFACE('',#97424,0.099999999999999) ;
#14895 = CYLINDRICAL_SURFACE('',#97427,0.1) ;
#14896 = CYLINDRICAL_SURFACE('',#97429,0.0999999999999994) ;
#14897 = CYLINDRICAL_SURFACE('',#97436,0.0999999999999994) ;
#14898 = CYLINDRICAL_SURFACE('',#97438,0.1) ;
#14899 = CYLINDRICAL_SURFACE('',#97440,0.099999999999999) ;
#14900 = CYLINDRICAL_SURFACE('',#97444,0.1) ;
#14901 = CYLINDRICAL_SURFACE('',#97447,0.099999999999999) ;
#14902 = CYLINDRICAL_SURFACE('',#97449,0.0999999999999989) ;
#14903 = CYLINDRICAL_SURFACE('',#97452,0.1) ;
#14904 = CYLINDRICAL_SURFACE('',#97458,0.0999999999999989) ;
#14905 = CYLINDRICAL_SURFACE('',#97461,0.1) ;
#14906 = CYLINDRICAL_SURFACE('',#97463,0.0999999999999994) ;
#14907 = CYLINDRICAL_SURFACE('',#97470,0.0999999999999994) ;
#14908 = CYLINDRICAL_SURFACE('',#97472,0.1) ;
#14909 = CYLINDRICAL_SURFACE('',#97474,0.0999999999999989) ;
#14910 = CYLINDRICAL_SURFACE('',#97478,0.1) ;
#14911 = CYLINDRICAL_SURFACE('',#97481,0.0999999999999989) ;
#14912 = CYLINDRICAL_SURFACE('',#97483,0.099999999999999) ;
#14913 = CYLINDRICAL_SURFACE('',#97486,0.1) ;
#14914 = CYLINDRICAL_SURFACE('',#97492,0.099999999999999) ;
#14915 = CYLINDRICAL_SURFACE('',#97495,0.1) ;
#14916 = CYLINDRICAL_SURFACE('',#97497,0.0999999999999994) ;
#14917 = CYLINDRICAL_SURFACE('',#97504,0.0999999999999994) ;
#14918 = CYLINDRICAL_SURFACE('',#97506,0.1) ;
#14919 = CYLINDRICAL_SURFACE('',#97508,0.099999999999999) ;
#14920 = CYLINDRICAL_SURFACE('',#97512,0.1) ;
#14921 = CYLINDRICAL_SURFACE('',#97515,0.099999999999999) ;
#14922 = CYLINDRICAL_SURFACE('',#97517,0.0999999999999989) ;
#14923 = CYLINDRICAL_SURFACE('',#97520,0.1) ;
#14924 = CYLINDRICAL_SURFACE('',#97526,0.0999999999999989) ;
#14925 = CYLINDRICAL_SURFACE('',#97529,0.1) ;
#14926 = CYLINDRICAL_SURFACE('',#97531,0.0999999999999994) ;
#14927 = CYLINDRICAL_SURFACE('',#97538,0.0999999999999994) ;
#14928 = CYLINDRICAL_SURFACE('',#97540,0.1) ;
#14929 = CYLINDRICAL_SURFACE('',#97542,0.0999999999999989) ;
#14930 = CYLINDRICAL_SURFACE('',#97546,0.1) ;
#14931 = CYLINDRICAL_SURFACE('',#97549,0.0999999999999989) ;
#14932 = CYLINDRICAL_SURFACE('',#97551,0.099999999999999) ;
#14933 = CYLINDRICAL_SURFACE('',#97554,0.1) ;
#14934 = CYLINDRICAL_SURFACE('',#97560,0.099999999999999) ;
#14935 = CYLINDRICAL_SURFACE('',#97563,0.1) ;
#14936 = CYLINDRICAL_SURFACE('',#97565,0.0999999999999994) ;
#14937 = CYLINDRICAL_SURFACE('',#97572,0.0999999999999994) ;
#14938 = CYLINDRICAL_SURFACE('',#97574,0.1) ;
#14939 = CYLINDRICAL_SURFACE('',#97576,0.099999999999999) ;
#14940 = CYLINDRICAL_SURFACE('',#97580,0.1) ;
#14941 = CYLINDRICAL_SURFACE('',#97583,0.099999999999999) ;
#14942 = CYLINDRICAL_SURFACE('',#97585,0.0999999999999989) ;
#14943 = CYLINDRICAL_SURFACE('',#97588,0.1) ;
#14944 = CYLINDRICAL_SURFACE('',#97594,0.0999999999999989) ;
#14945 = CYLINDRICAL_SURFACE('',#97597,0.1) ;
#14946 = CYLINDRICAL_SURFACE('',#97599,0.0999999999999994) ;
#14947 = CYLINDRICAL_SURFACE('',#97606,0.0999999999999994) ;
#14948 = CYLINDRICAL_SURFACE('',#97608,0.1) ;
#14949 = CYLINDRICAL_SURFACE('',#97610,0.0999999999999989) ;
#14950 = CYLINDRICAL_SURFACE('',#97614,0.1) ;
#14951 = CYLINDRICAL_SURFACE('',#97617,0.0999999999999989) ;
#14952 = CYLINDRICAL_SURFACE('',#97619,0.099999999999999) ;
#14953 = CYLINDRICAL_SURFACE('',#97622,0.1) ;
#14954 = CYLINDRICAL_SURFACE('',#97628,0.099999999999999) ;
#14955 = CYLINDRICAL_SURFACE('',#97631,0.1) ;
#14956 = CYLINDRICAL_SURFACE('',#97633,0.0999999999999994) ;
#14957 = CYLINDRICAL_SURFACE('',#97640,0.0999999999999994) ;
#14958 = CYLINDRICAL_SURFACE('',#97642,0.1) ;
#14959 = CYLINDRICAL_SURFACE('',#97644,0.099999999999999) ;
#14960 = CYLINDRICAL_SURFACE('',#97648,0.1) ;
#14961 = CYLINDRICAL_SURFACE('',#97651,0.099999999999999) ;
#14962 = CYLINDRICAL_SURFACE('',#97653,0.0999999999999989) ;
#14963 = CYLINDRICAL_SURFACE('',#97656,0.1) ;
#14964 = CYLINDRICAL_SURFACE('',#97662,0.0999999999999989) ;
#14965 = CYLINDRICAL_SURFACE('',#97665,0.1) ;
#14966 = CYLINDRICAL_SURFACE('',#97667,0.0999999999999994) ;
#14967 = CYLINDRICAL_SURFACE('',#97674,0.0999999999999994) ;
#14968 = CYLINDRICAL_SURFACE('',#97676,0.1) ;
#14969 = CYLINDRICAL_SURFACE('',#97678,0.0999999999999989) ;
#14970 = CYLINDRICAL_SURFACE('',#97682,0.1) ;
#14971 = CYLINDRICAL_SURFACE('',#97685,0.0999999999999989) ;
#14972 = CYLINDRICAL_SURFACE('',#97687,0.099999999999999) ;
#14973 = CYLINDRICAL_SURFACE('',#97690,0.1) ;
#14974 = CYLINDRICAL_SURFACE('',#97696,0.099999999999999) ;
#14975 = CYLINDRICAL_SURFACE('',#97699,0.1) ;
#14976 = CYLINDRICAL_SURFACE('',#97701,0.100000000000003) ;
#14977 = CYLINDRICAL_SURFACE('',#97708,0.100000000000003) ;
#14978 = CYLINDRICAL_SURFACE('',#97710,0.1) ;
#14979 = CYLINDRICAL_SURFACE('',#97712,0.099999999999999) ;
#14980 = CYLINDRICAL_SURFACE('',#97716,0.1) ;
#14981 = CYLINDRICAL_SURFACE('',#97719,0.099999999999999) ;
#14982 = CYLINDRICAL_SURFACE('',#97721,0.0999999999999989) ;
#14983 = CYLINDRICAL_SURFACE('',#97724,0.1) ;
#14984 = CYLINDRICAL_SURFACE('',#97730,0.0999999999999989) ;
#14985 = CYLINDRICAL_SURFACE('',#97733,0.1) ;
#14986 = CYLINDRICAL_SURFACE('',#97735,0.100000000000003) ;
#14987 = CYLINDRICAL_SURFACE('',#97742,0.100000000000003) ;
#14988 = CYLINDRICAL_SURFACE('',#97744,0.1) ;
#14989 = CYLINDRICAL_SURFACE('',#97746,0.0999999999999989) ;
#14990 = CYLINDRICAL_SURFACE('',#97750,0.1) ;
#14991 = CYLINDRICAL_SURFACE('',#97753,0.0999999999999989) ;
#14992 = CYLINDRICAL_SURFACE('',#97757,0.1) ;
#14993 = CYLINDRICAL_SURFACE('',#97761,0.1) ;
#14994 = CYLINDRICAL_SURFACE('',#97765,0.1) ;
#14995 = CYLINDRICAL_SURFACE('',#97770,0.1) ;
#14996 = CYLINDRICAL_SURFACE('',#97774,0.1) ;
#14997 = CYLINDRICAL_SURFACE('',#97778,0.1) ;
#14998 = CYLINDRICAL_SURFACE('',#97781,0.1) ;
#14999 = CYLINDRICAL_SURFACE('',#97785,0.1) ;
#15000 = CYLINDRICAL_SURFACE('',#97789,0.1) ;
#15001 = CYLINDRICAL_SURFACE('',#97790,0.1) ;
#15002 = CYLINDRICAL_SURFACE('',#97794,0.1) ;
#15003 = CYLINDRICAL_SURFACE('',#97796,0.1) ;
#15004 = CYLINDRICAL_SURFACE('',#97801,0.1) ;
#15005 = CYLINDRICAL_SURFACE('',#97805,0.1) ;
#15006 = CYLINDRICAL_SURFACE('',#97809,0.1) ;
#15007 = CYLINDRICAL_SURFACE('',#97814,0.1) ;
#15008 = CYLINDRICAL_SURFACE('',#97818,0.1) ;
#15009 = CYLINDRICAL_SURFACE('',#97822,0.1) ;
#15010 = CYLINDRICAL_SURFACE('',#97825,0.1) ;
#15011 = CYLINDRICAL_SURFACE('',#97829,0.1) ;
#15012 = CYLINDRICAL_SURFACE('',#97833,0.1) ;
#15013 = CYLINDRICAL_SURFACE('',#97834,0.1) ;
#15014 = CYLINDRICAL_SURFACE('',#97838,0.1) ;
#15015 = CYLINDRICAL_SURFACE('',#97840,0.1) ;
#15016 = CYLINDRICAL_SURFACE('',#97845,0.1) ;
#15017 = CYLINDRICAL_SURFACE('',#97849,0.1) ;
#15018 = CYLINDRICAL_SURFACE('',#97853,0.1) ;
#15019 = CYLINDRICAL_SURFACE('',#97858,0.1) ;
#15020 = CYLINDRICAL_SURFACE('',#97862,0.1) ;
#15021 = CYLINDRICAL_SURFACE('',#97866,0.1) ;
#15022 = CYLINDRICAL_SURFACE('',#97869,0.1) ;
#15023 = CYLINDRICAL_SURFACE('',#97873,0.1) ;
#15024 = CYLINDRICAL_SURFACE('',#97877,0.1) ;
#15025 = CYLINDRICAL_SURFACE('',#97878,0.1) ;
#15026 = CYLINDRICAL_SURFACE('',#97882,0.1) ;
#15027 = CYLINDRICAL_SURFACE('',#97884,0.1) ;
#15028 = CYLINDRICAL_SURFACE('',#97889,0.1) ;
#15029 = CYLINDRICAL_SURFACE('',#97893,0.1) ;
#15030 = CYLINDRICAL_SURFACE('',#97897,0.1) ;
#15031 = CYLINDRICAL_SURFACE('',#97902,0.1) ;
#15032 = CYLINDRICAL_SURFACE('',#97906,0.1) ;
#15033 = CYLINDRICAL_SURFACE('',#97910,0.1) ;
#15034 = CYLINDRICAL_SURFACE('',#97913,0.1) ;
#15035 = CYLINDRICAL_SURFACE('',#97917,0.1) ;
#15036 = CYLINDRICAL_SURFACE('',#97921,0.1) ;
#15037 = CYLINDRICAL_SURFACE('',#97922,0.1) ;
#15038 = CYLINDRICAL_SURFACE('',#97926,0.1) ;
#15039 = CYLINDRICAL_SURFACE('',#97928,0.1) ;
#15040 = CYLINDRICAL_SURFACE('',#97933,0.1) ;
#15041 = CYLINDRICAL_SURFACE('',#97937,0.1) ;
#15042 = CYLINDRICAL_SURFACE('',#97941,0.1) ;
#15043 = CYLINDRICAL_SURFACE('',#97946,0.1) ;
#15044 = CYLINDRICAL_SURFACE('',#97950,0.1) ;
#15045 = CYLINDRICAL_SURFACE('',#97954,0.1) ;
#15046 = CYLINDRICAL_SURFACE('',#97957,0.1) ;
#15047 = CYLINDRICAL_SURFACE('',#97961,0.1) ;
#15048 = CYLINDRICAL_SURFACE('',#97965,0.1) ;
#15049 = CYLINDRICAL_SURFACE('',#97966,0.1) ;
#15050 = CYLINDRICAL_SURFACE('',#97970,0.1) ;
#15051 = CYLINDRICAL_SURFACE('',#97972,0.1) ;
#15052 = CYLINDRICAL_SURFACE('',#97977,0.1) ;
#15053 = CYLINDRICAL_SURFACE('',#97981,0.1) ;
#15054 = CYLINDRICAL_SURFACE('',#97985,0.1) ;
#15055 = CYLINDRICAL_SURFACE('',#97990,0.1) ;
#15056 = CYLINDRICAL_SURFACE('',#97994,0.1) ;
#15057 = CYLINDRICAL_SURFACE('',#97998,0.1) ;
#15058 = CYLINDRICAL_SURFACE('',#98001,0.1) ;
#15059 = CYLINDRICAL_SURFACE('',#98005,0.1) ;
#15060 = CYLINDRICAL_SURFACE('',#98009,0.1) ;
#15061 = CYLINDRICAL_SURFACE('',#98010,0.1) ;
#15062 = CYLINDRICAL_SURFACE('',#98014,0.1) ;
#15063 = CYLINDRICAL_SURFACE('',#98016,0.1) ;
#15064 = CYLINDRICAL_SURFACE('',#98021,0.1) ;
#15065 = CYLINDRICAL_SURFACE('',#98025,0.1) ;
#15066 = CYLINDRICAL_SURFACE('',#98029,0.1) ;
#15067 = CYLINDRICAL_SURFACE('',#98034,0.1) ;
#15068 = CYLINDRICAL_SURFACE('',#98038,0.1) ;
#15069 = CYLINDRICAL_SURFACE('',#98042,0.1) ;
#15070 = CYLINDRICAL_SURFACE('',#98045,0.1) ;
#15071 = CYLINDRICAL_SURFACE('',#98049,0.1) ;
#15072 = CYLINDRICAL_SURFACE('',#98053,0.1) ;
#15073 = CYLINDRICAL_SURFACE('',#98054,0.1) ;
#15074 = CYLINDRICAL_SURFACE('',#98058,0.1) ;
#15075 = CYLINDRICAL_SURFACE('',#98060,0.1) ;
#15076 = CYLINDRICAL_SURFACE('',#98065,0.1) ;
#15077 = CYLINDRICAL_SURFACE('',#98069,0.1) ;
#15078 = CYLINDRICAL_SURFACE('',#98073,0.1) ;
#15079 = CYLINDRICAL_SURFACE('',#98078,0.1) ;
#15080 = CYLINDRICAL_SURFACE('',#98082,0.1) ;
#15081 = CYLINDRICAL_SURFACE('',#98086,0.1) ;
#15082 = CYLINDRICAL_SURFACE('',#98089,0.1) ;
#15083 = CYLINDRICAL_SURFACE('',#98093,0.1) ;
#15084 = CYLINDRICAL_SURFACE('',#98097,0.1) ;
#15085 = CYLINDRICAL_SURFACE('',#98098,0.1) ;
#15086 = CYLINDRICAL_SURFACE('',#98102,0.1) ;
#15087 = CYLINDRICAL_SURFACE('',#98104,0.1) ;
#15088 = CYLINDRICAL_SURFACE('',#98109,0.1) ;
#15089 = CYLINDRICAL_SURFACE('',#98113,0.1) ;
#15090 = CYLINDRICAL_SURFACE('',#98117,0.1) ;
#15091 = CYLINDRICAL_SURFACE('',#98122,0.1) ;
#15092 = CYLINDRICAL_SURFACE('',#98126,0.1) ;
#15093 = CYLINDRICAL_SURFACE('',#98130,0.1) ;
#15094 = CYLINDRICAL_SURFACE('',#98133,0.1) ;
#15095 = CYLINDRICAL_SURFACE('',#98137,0.1) ;
#15096 = CYLINDRICAL_SURFACE('',#98141,0.1) ;
#15097 = CYLINDRICAL_SURFACE('',#98142,0.1) ;
#15098 = CYLINDRICAL_SURFACE('',#98146,0.1) ;
#15099 = CYLINDRICAL_SURFACE('',#98148,0.1) ;
#15100 = CYLINDRICAL_SURFACE('',#98152,0.0999999999999998) ;
#15101 = CYLINDRICAL_SURFACE('',#98240,0.0645125000000003) ;
#15102 = CYLINDRICAL_SURFACE('',#98242,0.0645125000000003) ;
#15103 = CYLINDRICAL_SURFACE('',#98244,0.0645125000000003) ;
#15104 = CYLINDRICAL_SURFACE('',#98246,0.0645125000000003) ;
#15105 = CYLINDRICAL_SURFACE('',#98248,0.0645125000000003) ;
#15106 = CYLINDRICAL_SURFACE('',#98250,0.0645125000000003) ;
#15107 = CYLINDRICAL_SURFACE('',#98252,0.0645125000000003) ;
#15108 = CYLINDRICAL_SURFACE('',#98362,1.5) ;
#15109 = CYLINDRICAL_SURFACE('',#98368,1.5) ;
#15110 = CYLINDRICAL_SURFACE('',#98374,1.5) ;
#15111 = CYLINDRICAL_SURFACE('',#98380,1.5) ;
#15112 = CYLINDRICAL_SURFACE('',#98386,1.5) ;
#15113 = CYLINDRICAL_SURFACE('',#98392,1.5) ;
#15114 = CYLINDRICAL_SURFACE('',#98398,1.5) ;
#15115 = CYLINDRICAL_SURFACE('',#98404,1.5) ;
#15116 = CYLINDRICAL_SURFACE('',#98410,1.5) ;
#15117 = CYLINDRICAL_SURFACE('',#98434,1.) ;
#15118 = CYLINDRICAL_SURFACE('',#98435,0.999999999999999) ;
#15119 = CYLINDRICAL_SURFACE('',#98436,1.) ;
#15120 = CYLINDRICAL_SURFACE('',#98437,1.) ;
#15121 = CYLINDRICAL_SURFACE('',#98438,1.) ;
#15122 = CYLINDRICAL_SURFACE('',#98439,1.) ;
#15123 = CYLINDRICAL_SURFACE('',#98440,1.) ;
#15124 = CYLINDRICAL_SURFACE('',#98441,1.) ;
#15125 = CYLINDRICAL_SURFACE('',#98442,1.) ;
#15126 = CYLINDRICAL_SURFACE('',#98455,0.0645125000000055) ;
#15127 = CYLINDRICAL_SURFACE('',#98457,0.0645125000000061) ;
#15128 = CYLINDRICAL_SURFACE('',#98459,0.0645124999999998) ;
#15129 = CYLINDRICAL_SURFACE('',#98461,0.0645125000000003) ;
#15130 = CYLINDRICAL_SURFACE('',#98463,1.5) ;
#15131 = CYLINDRICAL_SURFACE('',#98471,1.) ;
#15132 = CYLINDRICAL_SURFACE('',#98676,0.0999999999999998) ;
#15133 = CYLINDRICAL_SURFACE('',#98679,0.0999999999999998) ;
#15134 = CYLINDRICAL_SURFACE('',#98757,1.65625) ;
#15135 = CYLINDRICAL_SURFACE('',#98781,2.25) ;
#15136 = CYLINDRICAL_SURFACE('',#98783,2.25) ;
#15137 = CYLINDRICAL_SURFACE('',#98787,2.25) ;
#15138 = CYLINDRICAL_SURFACE('',#98789,2.25) ;
#15139 = CYLINDRICAL_SURFACE('',#98791,0.0999999999999997) ;
#15140 = CYLINDRICAL_SURFACE('',#98795,0.1) ;
#15141 = CYLINDRICAL_SURFACE('',#98799,0.1) ;
#15142 = CYLINDRICAL_SURFACE('',#98803,0.0999999999999997) ;
#15143 = CYLINDRICAL_SURFACE('',#98808,0.0999999999999998) ;
#15144 = CYLINDRICAL_SURFACE('',#98814,0.0999999999999998) ;
#15145 = CYLINDRICAL_SURFACE('',#98817,0.1) ;
#15146 = CYLINDRICAL_SURFACE('',#98819,0.1) ;
#15147 = CYLINDRICAL_SURFACE('',#98821,0.100000000000003) ;
#15148 = CYLINDRICAL_SURFACE('',#98824,0.0999999999999998) ;
#15149 = CYLINDRICAL_SURFACE('',#98827,0.0999999999999998) ;
#15150 = CYLINDRICAL_SURFACE('',#98836,0.0999999999999998) ;
#15151 = CYLINDRICAL_SURFACE('',#98842,0.1) ;
#15152 = CYLINDRICAL_SURFACE('',#98847,0.0999999999999998) ;
#15153 = CYLINDRICAL_SURFACE('',#98849,0.1) ;
#15154 = CYLINDRICAL_SURFACE('',#98851,0.1) ;
#15155 = CYLINDRICAL_SURFACE('',#98853,0.100000000000003) ;
#15156 = CYLINDRICAL_SURFACE('',#98856,0.0999999999999998) ;
#15157 = CYLINDRICAL_SURFACE('',#98865,0.1) ;
#15158 = CYLINDRICAL_SURFACE('',#98867,0.100000000000003) ;
#15159 = CYLINDRICAL_SURFACE('',#98869,0.100000000000003) ;
#15160 = CYLINDRICAL_SURFACE('',#98874,0.1) ;
#15161 = CYLINDRICAL_SURFACE('',#98884,0.1) ;
#15162 = CYLINDRICAL_SURFACE('',#98886,0.0999999999999994) ;
#15163 = CYLINDRICAL_SURFACE('',#98888,0.1) ;
#15164 = CYLINDRICAL_SURFACE('',#98891,0.0999999999999994) ;
#15165 = CYLINDRICAL_SURFACE('',#98902,0.1) ;
#15166 = CYLINDRICAL_SURFACE('',#98905,0.0999999999999994) ;
#15167 = CYLINDRICAL_SURFACE('',#98907,0.1) ;
#15168 = CYLINDRICAL_SURFACE('',#98911,0.0999999999999998) ;
#15169 = CYLINDRICAL_SURFACE('',#98913,0.1) ;
#15170 = CYLINDRICAL_SURFACE('',#98921,0.1) ;
#15171 = CYLINDRICAL_SURFACE('',#98923,0.0999999999999998) ;
#15172 = CYLINDRICAL_SURFACE('',#98925,0.1) ;
#15173 = CYLINDRICAL_SURFACE('',#98927,0.1) ;
#15174 = CYLINDRICAL_SURFACE('',#98930,0.1) ;
#15175 = CYLINDRICAL_SURFACE('',#98940,0.1) ;
#15176 = CYLINDRICAL_SURFACE('',#98942,0.0999999999999998) ;
#15177 = CYLINDRICAL_SURFACE('',#98944,0.1) ;
#15178 = CYLINDRICAL_SURFACE('',#98946,0.1) ;
#15179 = CYLINDRICAL_SURFACE('',#98952,0.1) ;
#15180 = CYLINDRICAL_SURFACE('',#98955,0.1) ;
#15181 = CYLINDRICAL_SURFACE('',#98958,0.1) ;
#15182 = CYLINDRICAL_SURFACE('',#98960,0.0999999999999998) ;
#15183 = CYLINDRICAL_SURFACE('',#98966,0.1) ;
#15184 = CYLINDRICAL_SURFACE('',#98970,0.1) ;
#15185 = CYLINDRICAL_SURFACE('',#98972,0.1) ;
#15186 = CYLINDRICAL_SURFACE('',#98978,0.1) ;
#15187 = CYLINDRICAL_SURFACE('',#98980,0.0999999999999994) ;
#15188 = CYLINDRICAL_SURFACE('',#98983,0.1) ;
#15189 = CYLINDRICAL_SURFACE('',#98992,0.1) ;
#15190 = CYLINDRICAL_SURFACE('',#98994,0.1) ;
#15191 = CYLINDRICAL_SURFACE('',#98996,0.1) ;
#15192 = CYLINDRICAL_SURFACE('',#98999,0.1) ;
#15193 = CYLINDRICAL_SURFACE('',#99001,0.0999999999999998) ;
#15194 = CYLINDRICAL_SURFACE('',#99003,0.1) ;
#15195 = CYLINDRICAL_SURFACE('',#99014,0.1) ;
#15196 = CYLINDRICAL_SURFACE('',#99016,0.1) ;
#15197 = CYLINDRICAL_SURFACE('',#99018,0.0999999999999998) ;
#15198 = CYLINDRICAL_SURFACE('',#99020,0.1) ;
#15199 = CYLINDRICAL_SURFACE('',#99026,0.1) ;
#15200 = CYLINDRICAL_SURFACE('',#99027,0.1) ;
#15201 = CYLINDRICAL_SURFACE('',#99029,0.1) ;
#15202 = CYLINDRICAL_SURFACE('',#99032,0.1) ;
#15203 = CYLINDRICAL_SURFACE('',#99038,0.1) ;
#15204 = CYLINDRICAL_SURFACE('',#99040,0.1) ;
#15205 = CYLINDRICAL_SURFACE('',#99042,0.1) ;
#15206 = CYLINDRICAL_SURFACE('',#99044,0.1) ;
#15207 = CYLINDRICAL_SURFACE('',#99050,0.1) ;
#15208 = CYLINDRICAL_SURFACE('',#99051,0.1) ;
#15209 = CYLINDRICAL_SURFACE('',#99056,0.1) ;
#15210 = CYLINDRICAL_SURFACE('',#99057,0.1) ;
#15211 = CYLINDRICAL_SURFACE('',#99059,0.1) ;
#15212 = CYLINDRICAL_SURFACE('',#99065,0.1) ;
#15213 = CYLINDRICAL_SURFACE('',#99067,0.1) ;
#15214 = CYLINDRICAL_SURFACE('',#99069,0.1) ;
#15215 = CYLINDRICAL_SURFACE('',#99071,0.1) ;
#15216 = CYLINDRICAL_SURFACE('',#99073,0.1) ;
#15217 = CYLINDRICAL_SURFACE('',#99079,0.1) ;
#15218 = CYLINDRICAL_SURFACE('',#99081,0.1) ;
#15219 = CYLINDRICAL_SURFACE('',#99083,0.1) ;
#15220 = CYLINDRICAL_SURFACE('',#99085,0.1) ;
#15221 = CYLINDRICAL_SURFACE('',#99090,0.1) ;
#15222 = CYLINDRICAL_SURFACE('',#99091,0.1) ;
#15223 = CYLINDRICAL_SURFACE('',#99100,0.0999999999999998) ;
#15224 = CYLINDRICAL_SURFACE('',#99102,0.0999999999999998) ;
#15225 = CYLINDRICAL_SURFACE('',#99104,0.1) ;
#15226 = CYLINDRICAL_SURFACE('',#99107,0.0999999999999998) ;
#15227 = CYLINDRICAL_SURFACE('',#99109,0.1) ;
#15228 = CYLINDRICAL_SURFACE('',#99111,0.1) ;
#15229 = CYLINDRICAL_SURFACE('',#99122,0.0999999999999998) ;
#15230 = CYLINDRICAL_SURFACE('',#99124,0.0999999999999998) ;
#15231 = CYLINDRICAL_SURFACE('',#99126,0.0999999999999998) ;
#15232 = CYLINDRICAL_SURFACE('',#99128,0.0999999999999998) ;
#15233 = CYLINDRICAL_SURFACE('',#99134,0.1) ;
#15234 = CYLINDRICAL_SURFACE('',#99135,0.1) ;
#15235 = CYLINDRICAL_SURFACE('',#99137,0.0999999999999998) ;
#15236 = CYLINDRICAL_SURFACE('',#99140,0.1) ;
#15237 = CYLINDRICAL_SURFACE('',#99146,0.1) ;
#15238 = CYLINDRICAL_SURFACE('',#99148,0.1) ;
#15239 = CYLINDRICAL_SURFACE('',#99150,0.1) ;
#15240 = CYLINDRICAL_SURFACE('',#99152,0.1) ;
#15241 = CYLINDRICAL_SURFACE('',#99158,0.0999999999999998) ;
#15242 = CYLINDRICAL_SURFACE('',#99159,0.0999999999999994) ;
#15243 = CYLINDRICAL_SURFACE('',#99166,0.1) ;
#15244 = CYLINDRICAL_SURFACE('',#99168,0.1) ;
#15245 = CYLINDRICAL_SURFACE('',#99174,0.0999999999999994) ;
#15246 = CYLINDRICAL_SURFACE('',#99175,0.1) ;
#15247 = CYLINDRICAL_SURFACE('',#99176,0.1) ;
#15248 = CYLINDRICAL_SURFACE('',#99177,0.1) ;
#15249 = CYLINDRICAL_SURFACE('',#99178,0.1) ;
#15250 = CYLINDRICAL_SURFACE('',#99179,0.0999999999999998) ;
#15251 = CYLINDRICAL_SURFACE('',#99183,0.0999999999999998) ;
#15252 = CYLINDRICAL_SURFACE('',#99190,0.1) ;
#15253 = CYLINDRICAL_SURFACE('',#99196,0.1) ;
#15254 = CYLINDRICAL_SURFACE('',#99557,1.65625) ;
#15255 = CYLINDRICAL_SURFACE('',#99564,1.65625) ;
#15256 = CYLINDRICAL_SURFACE('',#99571,1.65625) ;
#15257 = CYLINDRICAL_SURFACE('',#99578,1.65625) ;
#15258 = CYLINDRICAL_SURFACE('',#99585,1.65625) ;
#15259 = CYLINDRICAL_SURFACE('',#99592,1.65625) ;
#15260 = CYLINDRICAL_SURFACE('',#99599,1.65625) ;
#15261 = CYLINDRICAL_SURFACE('',#99606,1.65625) ;
#15262 = CYLINDRICAL_SURFACE('',#99613,1.65625) ;
#15263 = CYLINDRICAL_SURFACE('',#99789,0.0999999999999994) ;
#15264 = CYLINDRICAL_SURFACE('',#99793,0.1) ;
#15265 = CYLINDRICAL_SURFACE('',#99797,0.1) ;
#15266 = CYLINDRICAL_SURFACE('',#99801,0.0999999999999998) ;
#15267 = CYLINDRICAL_SURFACE('',#99806,0.0999999999999994) ;
#15268 = CYLINDRICAL_SURFACE('',#99810,0.0999999999999994) ;
#15269 = CYLINDRICAL_SURFACE('',#99814,0.1) ;
#15270 = CYLINDRICAL_SURFACE('',#99818,0.0999999999999994) ;
#15271 = CYLINDRICAL_SURFACE('',#99823,0.0999999999999994) ;
#15272 = CYLINDRICAL_SURFACE('',#99827,0.0999999999999994) ;
#15273 = CYLINDRICAL_SURFACE('',#99831,0.0999999999999994) ;
#15274 = CYLINDRICAL_SURFACE('',#99835,0.0999999999999994) ;
#15275 = CYLINDRICAL_SURFACE('',#99840,0.0999999999999994) ;
#15276 = CYLINDRICAL_SURFACE('',#99844,0.0999999999999994) ;
#15277 = CYLINDRICAL_SURFACE('',#99848,0.0999999999999994) ;
#15278 = CYLINDRICAL_SURFACE('',#99852,0.0999999999999994) ;
#15279 = CYLINDRICAL_SURFACE('',#99857,0.0999999999999994) ;
#15280 = CYLINDRICAL_SURFACE('',#99861,0.0999999999999994) ;
#15281 = CYLINDRICAL_SURFACE('',#99865,0.0999999999999994) ;
#15282 = CYLINDRICAL_SURFACE('',#99869,0.0999999999999994) ;
#15283 = CYLINDRICAL_SURFACE('',#99874,0.0999999999999994) ;
#15284 = CYLINDRICAL_SURFACE('',#99878,0.0999999999999994) ;
#15285 = CYLINDRICAL_SURFACE('',#99882,0.0999999999999994) ;
#15286 = CYLINDRICAL_SURFACE('',#99886,0.0999999999999994) ;
#15287 = CYLINDRICAL_SURFACE('',#99891,0.0999999999999994) ;
#15288 = CYLINDRICAL_SURFACE('',#99895,0.0999999999999994) ;
#15289 = CYLINDRICAL_SURFACE('',#99899,0.0999999999999994) ;
#15290 = CYLINDRICAL_SURFACE('',#99903,0.0999999999999994) ;
#15291 = CYLINDRICAL_SURFACE('',#99908,0.0999999999999994) ;
#15292 = CYLINDRICAL_SURFACE('',#99912,0.0999999999999994) ;
#15293 = CYLINDRICAL_SURFACE('',#99916,0.0999999999999994) ;
#15294 = CYLINDRICAL_SURFACE('',#99920,0.0999999999999994) ;
#15295 = CYLINDRICAL_SURFACE('',#99925,0.100000000000003) ;
#15296 = CYLINDRICAL_SURFACE('',#99929,0.100000000000003) ;
#15297 = CYLINDRICAL_SURFACE('',#99933,0.100000000000003) ;
#15298 = CYLINDRICAL_SURFACE('',#99937,0.100000000000003) ;
#15299 = CYLINDRICAL_SURFACE('',#99948,0.1) ;
#15300 = CYLINDRICAL_SURFACE('',#99950,0.0999999999999994) ;
#15301 = CYLINDRICAL_SURFACE('',#99952,0.1) ;
#15302 = CYLINDRICAL_SURFACE('',#99955,0.0999999999999994) ;
#15303 = CYLINDRICAL_SURFACE('',#99966,0.0999999999999998) ;
#15304 = CYLINDRICAL_SURFACE('',#99969,0.0999999999999994) ;
#15305 = CYLINDRICAL_SURFACE('',#99971,0.0999999999999998) ;
#15306 = CYLINDRICAL_SURFACE('',#99975,0.0999999999999998) ;
#15307 = CYLINDRICAL_SURFACE('',#99977,0.1) ;
#15308 = CYLINDRICAL_SURFACE('',#99985,0.0999999999999998) ;
#15309 = CYLINDRICAL_SURFACE('',#99987,0.0999999999999998) ;
#15310 = CYLINDRICAL_SURFACE('',#99989,0.1) ;
#15311 = CYLINDRICAL_SURFACE('',#99991,0.1) ;
#15312 = CYLINDRICAL_SURFACE('',#99994,0.1) ;
#15313 = CYLINDRICAL_SURFACE('',#100004,0.0999999999999998) ;
#15314 = CYLINDRICAL_SURFACE('',#100006,0.0999999999999998) ;
#15315 = CYLINDRICAL_SURFACE('',#100008,0.1) ;
#15316 = CYLINDRICAL_SURFACE('',#100010,0.1) ;
#15317 = CYLINDRICAL_SURFACE('',#100016,0.1) ;
#15318 = CYLINDRICAL_SURFACE('',#100019,0.1) ;
#15319 = CYLINDRICAL_SURFACE('',#100021,0.0999999999999998) ;
#15320 = CYLINDRICAL_SURFACE('',#100027,0.0999999999999998) ;
#15321 = CYLINDRICAL_SURFACE('',#100031,0.1) ;
#15322 = CYLINDRICAL_SURFACE('',#100033,0.1) ;
#15323 = CYLINDRICAL_SURFACE('',#100039,0.0999999999999998) ;
#15324 = CYLINDRICAL_SURFACE('',#100041,0.0999999999999994) ;
#15325 = CYLINDRICAL_SURFACE('',#100044,0.100000000000003) ;
#15326 = CYLINDRICAL_SURFACE('',#100047,0.0999999999999998) ;
#15327 = CYLINDRICAL_SURFACE('',#100050,0.1) ;
#15328 = CYLINDRICAL_SURFACE('',#100053,0.100000000000003) ;
#15329 = CYLINDRICAL_SURFACE('',#100056,0.100000000000003) ;
#15330 = CYLINDRICAL_SURFACE('',#100059,0.0999999999999998) ;
#15331 = CYLINDRICAL_SURFACE('',#100062,0.1) ;
#15332 = CYLINDRICAL_SURFACE('',#100065,0.0999999999999994) ;
#15333 = CYLINDRICAL_SURFACE('',#100068,0.0999999999999994) ;
#15334 = CYLINDRICAL_SURFACE('',#100071,0.0999999999999998) ;
#15335 = CYLINDRICAL_SURFACE('',#100074,0.1) ;
#15336 = CYLINDRICAL_SURFACE('',#100077,0.0999999999999994) ;
#15337 = CYLINDRICAL_SURFACE('',#100080,0.0999999999999994) ;
#15338 = CYLINDRICAL_SURFACE('',#100083,0.0999999999999998) ;
#15339 = CYLINDRICAL_SURFACE('',#100086,0.1) ;
#15340 = CYLINDRICAL_SURFACE('',#100089,0.0999999999999994) ;
#15341 = CYLINDRICAL_SURFACE('',#100092,0.0999999999999994) ;
#15342 = CYLINDRICAL_SURFACE('',#100095,0.0999999999999998) ;
#15343 = CYLINDRICAL_SURFACE('',#100098,0.1) ;
#15344 = CYLINDRICAL_SURFACE('',#100101,0.0999999999999994) ;
#15345 = CYLINDRICAL_SURFACE('',#100104,0.0999999999999994) ;
#15346 = CYLINDRICAL_SURFACE('',#100107,0.0999999999999998) ;
#15347 = CYLINDRICAL_SURFACE('',#100110,0.1) ;
#15348 = CYLINDRICAL_SURFACE('',#100113,0.0999999999999994) ;
#15349 = CYLINDRICAL_SURFACE('',#100116,0.0999999999999994) ;
#15350 = CYLINDRICAL_SURFACE('',#100119,0.0999999999999998) ;
#15351 = CYLINDRICAL_SURFACE('',#100122,0.1) ;
#15352 = CYLINDRICAL_SURFACE('',#100125,0.0999999999999994) ;
#15353 = CYLINDRICAL_SURFACE('',#100128,0.0999999999999994) ;
#15354 = CYLINDRICAL_SURFACE('',#100131,0.0999999999999998) ;
#15355 = CYLINDRICAL_SURFACE('',#100134,0.1) ;
#15356 = CYLINDRICAL_SURFACE('',#100137,0.1) ;
#15357 = CYLINDRICAL_SURFACE('',#100140,0.0999999999999998) ;
#15358 = CYLINDRICAL_SURFACE('',#100149,0.1) ;
#15359 = CYLINDRICAL_SURFACE('',#100151,0.0999999999999998) ;
#15360 = CYLINDRICAL_SURFACE('',#100153,0.0999999999999998) ;
#15361 = CYLINDRICAL_SURFACE('',#100156,0.0999999999999998) ;
#15362 = CYLINDRICAL_SURFACE('',#100158,0.0999999999999998) ;
#15363 = CYLINDRICAL_SURFACE('',#100160,0.1) ;
#15364 = CYLINDRICAL_SURFACE('',#100171,0.1) ;
#15365 = CYLINDRICAL_SURFACE('',#100173,0.1) ;
#15366 = CYLINDRICAL_SURFACE('',#100175,0.0999999999999998) ;
#15367 = CYLINDRICAL_SURFACE('',#100177,0.1) ;
#15368 = CYLINDRICAL_SURFACE('',#100183,0.1) ;
#15369 = CYLINDRICAL_SURFACE('',#100184,0.0999999999999998) ;
#15370 = CYLINDRICAL_SURFACE('',#100186,0.1) ;
#15371 = CYLINDRICAL_SURFACE('',#100189,0.1) ;
#15372 = CYLINDRICAL_SURFACE('',#100195,0.0999999999999998) ;
#15373 = CYLINDRICAL_SURFACE('',#100197,0.0999999999999998) ;
#15374 = CYLINDRICAL_SURFACE('',#100199,0.1) ;
#15375 = CYLINDRICAL_SURFACE('',#100201,0.1) ;
#15376 = CYLINDRICAL_SURFACE('',#100207,0.1) ;
#15377 = CYLINDRICAL_SURFACE('',#100208,0.1) ;
#15378 = CYLINDRICAL_SURFACE('',#100213,0.0999999999999998) ;
#15379 = CYLINDRICAL_SURFACE('',#100214,0.1) ;
#15380 = CYLINDRICAL_SURFACE('',#100216,0.1) ;
#15381 = CYLINDRICAL_SURFACE('',#100222,0.1) ;
#15382 = CYLINDRICAL_SURFACE('',#100224,0.1) ;
#15383 = CYLINDRICAL_SURFACE('',#100226,0.1) ;
#15384 = CYLINDRICAL_SURFACE('',#100228,0.1) ;
#15385 = CYLINDRICAL_SURFACE('',#100230,0.1) ;
#15386 = CYLINDRICAL_SURFACE('',#100236,0.0999999999999998) ;
#15387 = CYLINDRICAL_SURFACE('',#100238,0.0999999999999998) ;
#15388 = CYLINDRICAL_SURFACE('',#100240,0.1) ;
#15389 = CYLINDRICAL_SURFACE('',#100242,0.1) ;
#15390 = CYLINDRICAL_SURFACE('',#100247,0.1) ;
#15391 = CYLINDRICAL_SURFACE('',#100248,0.1) ;
#15392 = CYLINDRICAL_SURFACE('',#100254,0.1) ;
#15393 = CYLINDRICAL_SURFACE('',#100259,0.1) ;
#15394 = CYLINDRICAL_SURFACE('',#100262,0.1) ;
#15395 = CYLINDRICAL_SURFACE('',#100268,0.1) ;
#15396 = CYLINDRICAL_SURFACE('',#100274,0.1) ;
#15397 = CYLINDRICAL_SURFACE('',#100279,0.1) ;
#15398 = CYLINDRICAL_SURFACE('',#100282,0.1) ;
#15399 = CYLINDRICAL_SURFACE('',#100288,0.1) ;
#15400 = CYLINDRICAL_SURFACE('',#100294,0.1) ;
#15401 = CYLINDRICAL_SURFACE('',#100299,0.1) ;
#15402 = CYLINDRICAL_SURFACE('',#100302,0.1) ;
#15403 = CYLINDRICAL_SURFACE('',#100308,0.1) ;
#15404 = CYLINDRICAL_SURFACE('',#100314,0.1) ;
#15405 = CYLINDRICAL_SURFACE('',#100319,0.1) ;
#15406 = CYLINDRICAL_SURFACE('',#100322,0.1) ;
#15407 = CYLINDRICAL_SURFACE('',#100328,0.1) ;
#15408 = CYLINDRICAL_SURFACE('',#100334,0.1) ;
#15409 = CYLINDRICAL_SURFACE('',#100339,0.1) ;
#15410 = CYLINDRICAL_SURFACE('',#100342,0.1) ;
#15411 = CYLINDRICAL_SURFACE('',#100348,0.1) ;
#15412 = CYLINDRICAL_SURFACE('',#100354,0.1) ;
#15413 = CYLINDRICAL_SURFACE('',#100359,0.1) ;
#15414 = CYLINDRICAL_SURFACE('',#100362,0.1) ;
#15415 = CYLINDRICAL_SURFACE('',#100368,0.1) ;
#15416 = CYLINDRICAL_SURFACE('',#100374,0.1) ;
#15417 = CYLINDRICAL_SURFACE('',#100379,0.1) ;
#15418 = CYLINDRICAL_SURFACE('',#100382,0.1) ;
#15419 = CYLINDRICAL_SURFACE('',#100388,0.1) ;
#15420 = CYLINDRICAL_SURFACE('',#100394,0.1) ;
#15421 = CYLINDRICAL_SURFACE('',#100399,0.1) ;
#15422 = CYLINDRICAL_SURFACE('',#100402,0.1) ;
#15423 = CYLINDRICAL_SURFACE('',#100408,0.1) ;
#15424 = CYLINDRICAL_SURFACE('',#100417,0.0999999999999998) ;
#15425 = CYLINDRICAL_SURFACE('',#100419,0.0999999999999998) ;
#15426 = CYLINDRICAL_SURFACE('',#100421,0.1) ;
#15427 = CYLINDRICAL_SURFACE('',#100424,0.0999999999999998) ;
#15428 = CYLINDRICAL_SURFACE('',#100426,0.1) ;
#15429 = CYLINDRICAL_SURFACE('',#100428,0.0999999999999998) ;
#15430 = CYLINDRICAL_SURFACE('',#100439,0.0999999999999998) ;
#15431 = CYLINDRICAL_SURFACE('',#100441,0.0999999999999998) ;
#15432 = CYLINDRICAL_SURFACE('',#100443,0.0999999999999998) ;
#15433 = CYLINDRICAL_SURFACE('',#100445,0.0999999999999998) ;
#15434 = CYLINDRICAL_SURFACE('',#100451,0.0999999999999998) ;
#15435 = CYLINDRICAL_SURFACE('',#100452,0.1) ;
#15436 = CYLINDRICAL_SURFACE('',#100454,0.0999999999999998) ;
#15437 = CYLINDRICAL_SURFACE('',#100457,0.0999999999999998) ;
#15438 = CYLINDRICAL_SURFACE('',#100463,0.1) ;
#15439 = CYLINDRICAL_SURFACE('',#100465,0.1) ;
#15440 = CYLINDRICAL_SURFACE('',#100467,0.0999999999999998) ;
#15441 = CYLINDRICAL_SURFACE('',#100469,0.0999999999999998) ;
#15442 = CYLINDRICAL_SURFACE('',#100475,0.0999999999999998) ;
#15443 = CYLINDRICAL_SURFACE('',#100476,0.0999999999999994) ;
#15444 = CYLINDRICAL_SURFACE('',#100483,0.0999999999999998) ;
#15445 = CYLINDRICAL_SURFACE('',#100485,0.1) ;
#15446 = CYLINDRICAL_SURFACE('',#100491,0.0999999999999994) ;
#15447 = CYLINDRICAL_SURFACE('',#100492,0.1) ;
#15448 = CYLINDRICAL_SURFACE('',#100493,0.1) ;
#15449 = CYLINDRICAL_SURFACE('',#100494,0.1) ;
#15450 = CYLINDRICAL_SURFACE('',#100495,0.1) ;
#15451 = CYLINDRICAL_SURFACE('',#100500,0.0999999999999994) ;
#15452 = CYLINDRICAL_SURFACE('',#100502,0.1) ;
#15453 = CYLINDRICAL_SURFACE('',#100506,0.1) ;
#15454 = CYLINDRICAL_SURFACE('',#100517,0.0999999999999994) ;
#15455 = CYLINDRICAL_SURFACE('',#100520,0.1) ;
#15456 = CYLINDRICAL_SURFACE('',#100522,0.0999999999999998) ;
#15457 = CYLINDRICAL_SURFACE('',#100526,0.0999999999999994) ;
#15458 = CYLINDRICAL_SURFACE('',#100528,0.0999999999999994) ;
#15459 = CYLINDRICAL_SURFACE('',#100530,0.0999999999999994) ;
#15460 = CYLINDRICAL_SURFACE('',#100539,0.1) ;
#15461 = CYLINDRICAL_SURFACE('',#100542,0.1) ;
#15462 = CYLINDRICAL_SURFACE('',#100544,0.0999999999999998) ;
#15463 = CYLINDRICAL_SURFACE('',#100546,0.0999999999999994) ;
#15464 = CYLINDRICAL_SURFACE('',#100555,0.1) ;
#15465 = CYLINDRICAL_SURFACE('',#100557,0.1) ;
#15466 = CYLINDRICAL_SURFACE('',#100559,0.0999999999999998) ;
#15467 = CYLINDRICAL_SURFACE('',#100561,0.0999999999999994) ;
#15468 = CYLINDRICAL_SURFACE('',#100567,0.0999999999999998) ;
#15469 = CYLINDRICAL_SURFACE('',#100569,0.1) ;
#15470 = CYLINDRICAL_SURFACE('',#100571,0.1) ;
#15471 = CYLINDRICAL_SURFACE('',#100574,0.1) ;
#15472 = CYLINDRICAL_SURFACE('',#100581,0.0999999999999994) ;
#15473 = CYLINDRICAL_SURFACE('',#100583,0.1) ;
#15474 = CYLINDRICAL_SURFACE('',#100590,0.1) ;
#15475 = CYLINDRICAL_SURFACE('',#100592,0.1) ;
#15476 = CYLINDRICAL_SURFACE('',#100594,0.0999999999999998) ;
#15477 = CYLINDRICAL_SURFACE('',#100596,0.0999999999999994) ;
#15478 = CYLINDRICAL_SURFACE('',#100602,0.1) ;
#15479 = CYLINDRICAL_SURFACE('',#100604,0.0999999999999994) ;
#15480 = CYLINDRICAL_SURFACE('',#100608,0.0999999999999994) ;
#15481 = CYLINDRICAL_SURFACE('',#100612,0.1) ;
#15482 = CYLINDRICAL_SURFACE('',#100614,0.1) ;
#15483 = CYLINDRICAL_SURFACE('',#100618,0.1) ;
#15484 = CYLINDRICAL_SURFACE('',#100620,0.1) ;
#15485 = CYLINDRICAL_SURFACE('',#100624,0.1) ;
#15486 = CYLINDRICAL_SURFACE('',#100629,0.0999999999999998) ;
#15487 = CYLINDRICAL_SURFACE('',#100631,0.1) ;
#15488 = CYLINDRICAL_SURFACE('',#100635,0.0999999999999994) ;
#15489 = CYLINDRICAL_SURFACE('',#100637,0.0999999999999994) ;
#15490 = CYLINDRICAL_SURFACE('',#100641,0.1) ;
#15491 = CYLINDRICAL_SURFACE('',#100647,0.1) ;
#15492 = CYLINDRICAL_SURFACE('',#100649,0.0999999999999994) ;
#15493 = CYLINDRICAL_SURFACE('',#100655,0.1) ;
#15494 = CYLINDRICAL_SURFACE('',#100657,0.0999999999999994) ;
#15495 = CYLINDRICAL_SURFACE('',#100660,0.1) ;
#15496 = CYLINDRICAL_SURFACE('',#100662,0.1) ;
#15497 = CYLINDRICAL_SURFACE('',#100665,0.0999999999999994) ;
#15498 = CYLINDRICAL_SURFACE('',#100671,0.1) ;
#15499 = CYLINDRICAL_SURFACE('',#100673,0.1) ;
#15500 = CYLINDRICAL_SURFACE('',#100675,0.0999999999999994) ;
#15501 = CYLINDRICAL_SURFACE('',#100677,0.0999999999999994) ;
#15502 = CYLINDRICAL_SURFACE('',#100683,0.1) ;
#15503 = CYLINDRICAL_SURFACE('',#100684,0.0999999999999994) ;
#15504 = CYLINDRICAL_SURFACE('',#100693,0.0999999999999998) ;
#15505 = CYLINDRICAL_SURFACE('',#100695,0.0999999999999998) ;
#15506 = CYLINDRICAL_SURFACE('',#100697,0.0999999999999994) ;
#15507 = CYLINDRICAL_SURFACE('',#100700,0.0999999999999998) ;
#15508 = CYLINDRICAL_SURFACE('',#100702,0.1) ;
#15509 = CYLINDRICAL_SURFACE('',#100704,0.1) ;
#15510 = CYLINDRICAL_SURFACE('',#100715,0.0999999999999998) ;
#15511 = CYLINDRICAL_SURFACE('',#100717,0.0999999999999998) ;
#15512 = CYLINDRICAL_SURFACE('',#100719,0.0999999999999998) ;
#15513 = CYLINDRICAL_SURFACE('',#100721,0.0999999999999998) ;
#15514 = CYLINDRICAL_SURFACE('',#100727,0.1) ;
#15515 = CYLINDRICAL_SURFACE('',#100728,0.0999999999999994) ;
#15516 = CYLINDRICAL_SURFACE('',#100730,0.0999999999999998) ;
#15517 = CYLINDRICAL_SURFACE('',#100733,0.1) ;
#15518 = CYLINDRICAL_SURFACE('',#100739,0.0999999999999994) ;
#15519 = CYLINDRICAL_SURFACE('',#100741,0.0999999999999994) ;
#15520 = CYLINDRICAL_SURFACE('',#100743,0.1) ;
#15521 = CYLINDRICAL_SURFACE('',#100745,0.1) ;
#15522 = CYLINDRICAL_SURFACE('',#100751,0.0999999999999998) ;
#15523 = CYLINDRICAL_SURFACE('',#100752,0.0999999999999994) ;
#15524 = CYLINDRICAL_SURFACE('',#100759,0.1) ;
#15525 = CYLINDRICAL_SURFACE('',#100761,0.0999999999999994) ;
#15526 = CYLINDRICAL_SURFACE('',#100767,0.0999999999999994) ;
#15527 = CYLINDRICAL_SURFACE('',#100768,0.0999999999999998) ;
#15528 = CYLINDRICAL_SURFACE('',#100769,0.0999999999999998) ;
#15529 = CYLINDRICAL_SURFACE('',#100770,0.0999999999999998) ;
#15530 = CYLINDRICAL_SURFACE('',#100771,0.0999999999999998) ;
#15531 = CYLINDRICAL_SURFACE('',#100776,0.0999999999999994) ;
#15532 = CYLINDRICAL_SURFACE('',#100778,0.0999999999999994) ;
#15533 = CYLINDRICAL_SURFACE('',#100782,0.0999999999999994) ;
#15534 = CYLINDRICAL_SURFACE('',#100793,0.0999999999999994) ;
#15535 = CYLINDRICAL_SURFACE('',#100796,0.0999999999999994) ;
#15536 = CYLINDRICAL_SURFACE('',#100798,0.0999999999999998) ;
#15537 = CYLINDRICAL_SURFACE('',#100802,0.0999999999999994) ;
#15538 = CYLINDRICAL_SURFACE('',#100804,0.0999999999999994) ;
#15539 = CYLINDRICAL_SURFACE('',#100806,0.0999999999999994) ;
#15540 = CYLINDRICAL_SURFACE('',#100815,0.1) ;
#15541 = CYLINDRICAL_SURFACE('',#100818,0.0999999999999994) ;
#15542 = CYLINDRICAL_SURFACE('',#100820,0.0999999999999998) ;
#15543 = CYLINDRICAL_SURFACE('',#100822,0.0999999999999994) ;
#15544 = CYLINDRICAL_SURFACE('',#100831,0.0999999999999994) ;
#15545 = CYLINDRICAL_SURFACE('',#100833,0.1) ;
#15546 = CYLINDRICAL_SURFACE('',#100835,0.0999999999999998) ;
#15547 = CYLINDRICAL_SURFACE('',#100837,0.0999999999999994) ;
#15548 = CYLINDRICAL_SURFACE('',#100843,0.0999999999999998) ;
#15549 = CYLINDRICAL_SURFACE('',#100845,0.1) ;
#15550 = CYLINDRICAL_SURFACE('',#100847,0.1) ;
#15551 = CYLINDRICAL_SURFACE('',#100850,0.1) ;
#15552 = CYLINDRICAL_SURFACE('',#100857,0.0999999999999994) ;
#15553 = CYLINDRICAL_SURFACE('',#100859,0.0999999999999994) ;
#15554 = CYLINDRICAL_SURFACE('',#100866,0.0999999999999994) ;
#15555 = CYLINDRICAL_SURFACE('',#100868,0.0999999999999994) ;
#15556 = CYLINDRICAL_SURFACE('',#100870,0.0999999999999998) ;
#15557 = CYLINDRICAL_SURFACE('',#100872,0.0999999999999994) ;
#15558 = CYLINDRICAL_SURFACE('',#100878,0.1) ;
#15559 = CYLINDRICAL_SURFACE('',#100880,0.0999999999999994) ;
#15560 = CYLINDRICAL_SURFACE('',#100884,0.0999999999999994) ;
#15561 = CYLINDRICAL_SURFACE('',#100888,0.1) ;
#15562 = CYLINDRICAL_SURFACE('',#100890,0.0999999999999994) ;
#15563 = CYLINDRICAL_SURFACE('',#100894,0.0999999999999994) ;
#15564 = CYLINDRICAL_SURFACE('',#100896,0.1) ;
#15565 = CYLINDRICAL_SURFACE('',#100900,0.1) ;
#15566 = CYLINDRICAL_SURFACE('',#100905,0.0999999999999998) ;
#15567 = CYLINDRICAL_SURFACE('',#100907,0.1) ;
#15568 = CYLINDRICAL_SURFACE('',#100911,0.0999999999999994) ;
#15569 = CYLINDRICAL_SURFACE('',#100913,0.0999999999999994) ;
#15570 = CYLINDRICAL_SURFACE('',#100917,0.1) ;
#15571 = CYLINDRICAL_SURFACE('',#100923,0.1) ;
#15572 = CYLINDRICAL_SURFACE('',#100925,0.0999999999999994) ;
#15573 = CYLINDRICAL_SURFACE('',#100931,0.0999999999999994) ;
#15574 = CYLINDRICAL_SURFACE('',#100933,0.0999999999999994) ;
#15575 = CYLINDRICAL_SURFACE('',#100936,0.0999999999999994) ;
#15576 = CYLINDRICAL_SURFACE('',#100938,0.1) ;
#15577 = CYLINDRICAL_SURFACE('',#100941,0.0999999999999994) ;
#15578 = CYLINDRICAL_SURFACE('',#100947,0.0999999999999994) ;
#15579 = CYLINDRICAL_SURFACE('',#100949,0.0999999999999994) ;
#15580 = CYLINDRICAL_SURFACE('',#100951,0.0999999999999994) ;
#15581 = CYLINDRICAL_SURFACE('',#100953,0.0999999999999994) ;
#15582 = CYLINDRICAL_SURFACE('',#100959,0.1) ;
#15583 = CYLINDRICAL_SURFACE('',#100960,0.0999999999999994) ;
#15584 = CYLINDRICAL_SURFACE('',#100969,0.0999999999999998) ;
#15585 = CYLINDRICAL_SURFACE('',#100971,0.0999999999999998) ;
#15586 = CYLINDRICAL_SURFACE('',#100973,0.0999999999999994) ;
#15587 = CYLINDRICAL_SURFACE('',#100976,0.0999999999999998) ;
#15588 = CYLINDRICAL_SURFACE('',#100978,0.1) ;
#15589 = CYLINDRICAL_SURFACE('',#100980,0.0999999999999994) ;
#15590 = CYLINDRICAL_SURFACE('',#100991,0.0999999999999998) ;
#15591 = CYLINDRICAL_SURFACE('',#100993,0.0999999999999998) ;
#15592 = CYLINDRICAL_SURFACE('',#100995,0.0999999999999998) ;
#15593 = CYLINDRICAL_SURFACE('',#100997,0.0999999999999998) ;
#15594 = CYLINDRICAL_SURFACE('',#101003,0.0999999999999994) ;
#15595 = CYLINDRICAL_SURFACE('',#101004,0.0999999999999994) ;
#15596 = CYLINDRICAL_SURFACE('',#101006,0.0999999999999998) ;
#15597 = CYLINDRICAL_SURFACE('',#101009,0.0999999999999994) ;
#15598 = CYLINDRICAL_SURFACE('',#101015,0.0999999999999994) ;
#15599 = CYLINDRICAL_SURFACE('',#101017,0.0999999999999994) ;
#15600 = CYLINDRICAL_SURFACE('',#101019,0.0999999999999994) ;
#15601 = CYLINDRICAL_SURFACE('',#101021,0.0999999999999994) ;
#15602 = CYLINDRICAL_SURFACE('',#101027,0.0999999999999998) ;
#15603 = CYLINDRICAL_SURFACE('',#101028,0.0999999999999994) ;
#15604 = CYLINDRICAL_SURFACE('',#101035,0.0999999999999994) ;
#15605 = CYLINDRICAL_SURFACE('',#101037,0.0999999999999994) ;
#15606 = CYLINDRICAL_SURFACE('',#101043,0.0999999999999994) ;
#15607 = CYLINDRICAL_SURFACE('',#101044,0.1) ;
#15608 = CYLINDRICAL_SURFACE('',#101045,0.1) ;
#15609 = CYLINDRICAL_SURFACE('',#101046,0.1) ;
#15610 = CYLINDRICAL_SURFACE('',#101047,0.1) ;
#15611 = CYLINDRICAL_SURFACE('',#101052,0.0999999999999994) ;
#15612 = CYLINDRICAL_SURFACE('',#101054,0.0999999999999994) ;
#15613 = CYLINDRICAL_SURFACE('',#101058,0.0999999999999994) ;
#15614 = CYLINDRICAL_SURFACE('',#101069,0.0999999999999994) ;
#15615 = CYLINDRICAL_SURFACE('',#101072,0.0999999999999994) ;
#15616 = CYLINDRICAL_SURFACE('',#101074,0.0999999999999998) ;
#15617 = CYLINDRICAL_SURFACE('',#101078,0.0999999999999994) ;
#15618 = CYLINDRICAL_SURFACE('',#101080,0.0999999999999994) ;
#15619 = CYLINDRICAL_SURFACE('',#101082,0.0999999999999994) ;
#15620 = CYLINDRICAL_SURFACE('',#101091,0.1) ;
#15621 = CYLINDRICAL_SURFACE('',#101094,0.0999999999999994) ;
#15622 = CYLINDRICAL_SURFACE('',#101096,0.0999999999999998) ;
#15623 = CYLINDRICAL_SURFACE('',#101098,0.0999999999999994) ;
#15624 = CYLINDRICAL_SURFACE('',#101107,0.0999999999999994) ;
#15625 = CYLINDRICAL_SURFACE('',#101109,0.1) ;
#15626 = CYLINDRICAL_SURFACE('',#101111,0.0999999999999998) ;
#15627 = CYLINDRICAL_SURFACE('',#101113,0.0999999999999994) ;
#15628 = CYLINDRICAL_SURFACE('',#101119,0.0999999999999998) ;
#15629 = CYLINDRICAL_SURFACE('',#101121,0.1) ;
#15630 = CYLINDRICAL_SURFACE('',#101123,0.1) ;
#15631 = CYLINDRICAL_SURFACE('',#101126,0.1) ;
#15632 = CYLINDRICAL_SURFACE('',#101133,0.0999999999999994) ;
#15633 = CYLINDRICAL_SURFACE('',#101135,0.0999999999999994) ;
#15634 = CYLINDRICAL_SURFACE('',#101142,0.0999999999999994) ;
#15635 = CYLINDRICAL_SURFACE('',#101144,0.0999999999999994) ;
#15636 = CYLINDRICAL_SURFACE('',#101146,0.0999999999999998) ;
#15637 = CYLINDRICAL_SURFACE('',#101148,0.0999999999999994) ;
#15638 = CYLINDRICAL_SURFACE('',#101154,0.1) ;
#15639 = CYLINDRICAL_SURFACE('',#101156,0.0999999999999994) ;
#15640 = CYLINDRICAL_SURFACE('',#101160,0.0999999999999994) ;
#15641 = CYLINDRICAL_SURFACE('',#101164,0.1) ;
#15642 = CYLINDRICAL_SURFACE('',#101166,0.0999999999999994) ;
#15643 = CYLINDRICAL_SURFACE('',#101170,0.0999999999999994) ;
#15644 = CYLINDRICAL_SURFACE('',#101172,0.1) ;
#15645 = CYLINDRICAL_SURFACE('',#101176,0.1) ;
#15646 = CYLINDRICAL_SURFACE('',#101181,0.0999999999999998) ;
#15647 = CYLINDRICAL_SURFACE('',#101183,0.1) ;
#15648 = CYLINDRICAL_SURFACE('',#101187,0.0999999999999994) ;
#15649 = CYLINDRICAL_SURFACE('',#101189,0.0999999999999994) ;
#15650 = CYLINDRICAL_SURFACE('',#101193,0.1) ;
#15651 = CYLINDRICAL_SURFACE('',#101199,0.1) ;
#15652 = CYLINDRICAL_SURFACE('',#101201,0.0999999999999994) ;
#15653 = CYLINDRICAL_SURFACE('',#101207,0.0999999999999994) ;
#15654 = CYLINDRICAL_SURFACE('',#101209,0.0999999999999994) ;
#15655 = CYLINDRICAL_SURFACE('',#101212,0.0999999999999994) ;
#15656 = CYLINDRICAL_SURFACE('',#101214,0.1) ;
#15657 = CYLINDRICAL_SURFACE('',#101217,0.0999999999999994) ;
#15658 = CYLINDRICAL_SURFACE('',#101223,0.0999999999999994) ;
#15659 = CYLINDRICAL_SURFACE('',#101225,0.0999999999999994) ;
#15660 = CYLINDRICAL_SURFACE('',#101227,0.0999999999999994) ;
#15661 = CYLINDRICAL_SURFACE('',#101229,0.0999999999999994) ;
#15662 = CYLINDRICAL_SURFACE('',#101235,0.1) ;
#15663 = CYLINDRICAL_SURFACE('',#101236,0.0999999999999994) ;
#15664 = CYLINDRICAL_SURFACE('',#101245,0.0999999999999998) ;
#15665 = CYLINDRICAL_SURFACE('',#101247,0.0999999999999998) ;
#15666 = CYLINDRICAL_SURFACE('',#101249,0.0999999999999994) ;
#15667 = CYLINDRICAL_SURFACE('',#101252,0.0999999999999998) ;
#15668 = CYLINDRICAL_SURFACE('',#101254,0.1) ;
#15669 = CYLINDRICAL_SURFACE('',#101256,0.0999999999999994) ;
#15670 = CYLINDRICAL_SURFACE('',#101267,0.0999999999999998) ;
#15671 = CYLINDRICAL_SURFACE('',#101269,0.0999999999999998) ;
#15672 = CYLINDRICAL_SURFACE('',#101271,0.0999999999999998) ;
#15673 = CYLINDRICAL_SURFACE('',#101273,0.0999999999999998) ;
#15674 = CYLINDRICAL_SURFACE('',#101279,0.0999999999999994) ;
#15675 = CYLINDRICAL_SURFACE('',#101280,0.0999999999999994) ;
#15676 = CYLINDRICAL_SURFACE('',#101282,0.0999999999999998) ;
#15677 = CYLINDRICAL_SURFACE('',#101285,0.0999999999999994) ;
#15678 = CYLINDRICAL_SURFACE('',#101291,0.0999999999999994) ;
#15679 = CYLINDRICAL_SURFACE('',#101293,0.0999999999999994) ;
#15680 = CYLINDRICAL_SURFACE('',#101295,0.0999999999999994) ;
#15681 = CYLINDRICAL_SURFACE('',#101297,0.0999999999999994) ;
#15682 = CYLINDRICAL_SURFACE('',#101303,0.0999999999999998) ;
#15683 = CYLINDRICAL_SURFACE('',#101304,0.0999999999999994) ;
#15684 = CYLINDRICAL_SURFACE('',#101311,0.0999999999999994) ;
#15685 = CYLINDRICAL_SURFACE('',#101313,0.0999999999999994) ;
#15686 = CYLINDRICAL_SURFACE('',#101319,0.0999999999999994) ;
#15687 = CYLINDRICAL_SURFACE('',#101320,0.1) ;
#15688 = CYLINDRICAL_SURFACE('',#101321,0.1) ;
#15689 = CYLINDRICAL_SURFACE('',#101322,0.1) ;
#15690 = CYLINDRICAL_SURFACE('',#101323,0.1) ;
#15691 = CYLINDRICAL_SURFACE('',#101328,0.0999999999999994) ;
#15692 = CYLINDRICAL_SURFACE('',#101330,0.0999999999999994) ;
#15693 = CYLINDRICAL_SURFACE('',#101334,0.0999999999999994) ;
#15694 = CYLINDRICAL_SURFACE('',#101345,0.0999999999999994) ;
#15695 = CYLINDRICAL_SURFACE('',#101348,0.0999999999999994) ;
#15696 = CYLINDRICAL_SURFACE('',#101350,0.0999999999999998) ;
#15697 = CYLINDRICAL_SURFACE('',#101354,0.0999999999999994) ;
#15698 = CYLINDRICAL_SURFACE('',#101356,0.0999999999999994) ;
#15699 = CYLINDRICAL_SURFACE('',#101358,0.0999999999999994) ;
#15700 = CYLINDRICAL_SURFACE('',#101367,0.1) ;
#15701 = CYLINDRICAL_SURFACE('',#101370,0.0999999999999994) ;
#15702 = CYLINDRICAL_SURFACE('',#101372,0.0999999999999998) ;
#15703 = CYLINDRICAL_SURFACE('',#101374,0.0999999999999994) ;
#15704 = CYLINDRICAL_SURFACE('',#101383,0.0999999999999994) ;
#15705 = CYLINDRICAL_SURFACE('',#101385,0.1) ;
#15706 = CYLINDRICAL_SURFACE('',#101387,0.0999999999999998) ;
#15707 = CYLINDRICAL_SURFACE('',#101389,0.0999999999999994) ;
#15708 = CYLINDRICAL_SURFACE('',#101395,0.0999999999999998) ;
#15709 = CYLINDRICAL_SURFACE('',#101397,0.1) ;
#15710 = CYLINDRICAL_SURFACE('',#101399,0.1) ;
#15711 = CYLINDRICAL_SURFACE('',#101402,0.1) ;
#15712 = CYLINDRICAL_SURFACE('',#101409,0.0999999999999994) ;
#15713 = CYLINDRICAL_SURFACE('',#101411,0.0999999999999994) ;
#15714 = CYLINDRICAL_SURFACE('',#101418,0.0999999999999994) ;
#15715 = CYLINDRICAL_SURFACE('',#101420,0.0999999999999994) ;
#15716 = CYLINDRICAL_SURFACE('',#101422,0.0999999999999998) ;
#15717 = CYLINDRICAL_SURFACE('',#101424,0.0999999999999994) ;
#15718 = CYLINDRICAL_SURFACE('',#101430,0.1) ;
#15719 = CYLINDRICAL_SURFACE('',#101432,0.0999999999999994) ;
#15720 = CYLINDRICAL_SURFACE('',#101436,0.0999999999999994) ;
#15721 = CYLINDRICAL_SURFACE('',#101440,0.1) ;
#15722 = CYLINDRICAL_SURFACE('',#101442,0.0999999999999994) ;
#15723 = CYLINDRICAL_SURFACE('',#101446,0.0999999999999994) ;
#15724 = CYLINDRICAL_SURFACE('',#101448,0.1) ;
#15725 = CYLINDRICAL_SURFACE('',#101452,0.1) ;
#15726 = CYLINDRICAL_SURFACE('',#101457,0.0999999999999998) ;
#15727 = CYLINDRICAL_SURFACE('',#101459,0.1) ;
#15728 = CYLINDRICAL_SURFACE('',#101463,0.0999999999999994) ;
#15729 = CYLINDRICAL_SURFACE('',#101465,0.0999999999999994) ;
#15730 = CYLINDRICAL_SURFACE('',#101469,0.1) ;
#15731 = CYLINDRICAL_SURFACE('',#101475,0.1) ;
#15732 = CYLINDRICAL_SURFACE('',#101477,0.0999999999999994) ;
#15733 = CYLINDRICAL_SURFACE('',#101483,0.0999999999999994) ;
#15734 = CYLINDRICAL_SURFACE('',#101485,0.0999999999999994) ;
#15735 = CYLINDRICAL_SURFACE('',#101488,0.0999999999999994) ;
#15736 = CYLINDRICAL_SURFACE('',#101490,0.1) ;
#15737 = CYLINDRICAL_SURFACE('',#101493,0.0999999999999994) ;
#15738 = CYLINDRICAL_SURFACE('',#101499,0.0999999999999994) ;
#15739 = CYLINDRICAL_SURFACE('',#101501,0.0999999999999994) ;
#15740 = CYLINDRICAL_SURFACE('',#101503,0.0999999999999994) ;
#15741 = CYLINDRICAL_SURFACE('',#101505,0.0999999999999994) ;
#15742 = CYLINDRICAL_SURFACE('',#101511,0.1) ;
#15743 = CYLINDRICAL_SURFACE('',#101512,0.0999999999999994) ;
#15744 = CYLINDRICAL_SURFACE('',#101521,0.0999999999999998) ;
#15745 = CYLINDRICAL_SURFACE('',#101523,0.0999999999999998) ;
#15746 = CYLINDRICAL_SURFACE('',#101525,0.0999999999999994) ;
#15747 = CYLINDRICAL_SURFACE('',#101528,0.0999999999999998) ;
#15748 = CYLINDRICAL_SURFACE('',#101530,0.1) ;
#15749 = CYLINDRICAL_SURFACE('',#101532,0.0999999999999994) ;
#15750 = CYLINDRICAL_SURFACE('',#101543,0.0999999999999998) ;
#15751 = CYLINDRICAL_SURFACE('',#101545,0.0999999999999998) ;
#15752 = CYLINDRICAL_SURFACE('',#101547,0.0999999999999998) ;
#15753 = CYLINDRICAL_SURFACE('',#101549,0.0999999999999998) ;
#15754 = CYLINDRICAL_SURFACE('',#101555,0.0999999999999994) ;
#15755 = CYLINDRICAL_SURFACE('',#101556,0.0999999999999994) ;
#15756 = CYLINDRICAL_SURFACE('',#101558,0.0999999999999998) ;
#15757 = CYLINDRICAL_SURFACE('',#101561,0.0999999999999994) ;
#15758 = CYLINDRICAL_SURFACE('',#101567,0.0999999999999994) ;
#15759 = CYLINDRICAL_SURFACE('',#101569,0.0999999999999994) ;
#15760 = CYLINDRICAL_SURFACE('',#101571,0.0999999999999994) ;
#15761 = CYLINDRICAL_SURFACE('',#101573,0.0999999999999994) ;
#15762 = CYLINDRICAL_SURFACE('',#101579,0.0999999999999998) ;
#15763 = CYLINDRICAL_SURFACE('',#101580,0.0999999999999994) ;
#15764 = CYLINDRICAL_SURFACE('',#101587,0.0999999999999994) ;
#15765 = CYLINDRICAL_SURFACE('',#101589,0.0999999999999994) ;
#15766 = CYLINDRICAL_SURFACE('',#101595,0.0999999999999994) ;
#15767 = CYLINDRICAL_SURFACE('',#101596,0.0999999999999995) ;
#15768 = CYLINDRICAL_SURFACE('',#101597,0.0999999999999995) ;
#15769 = CYLINDRICAL_SURFACE('',#101598,0.0999999999999995) ;
#15770 = CYLINDRICAL_SURFACE('',#101599,0.0999999999999995) ;
#15771 = CYLINDRICAL_SURFACE('',#101604,0.0999999999999994) ;
#15772 = CYLINDRICAL_SURFACE('',#101606,0.0999999999999994) ;
#15773 = CYLINDRICAL_SURFACE('',#101610,0.0999999999999994) ;
#15774 = CYLINDRICAL_SURFACE('',#101621,0.0999999999999994) ;
#15775 = CYLINDRICAL_SURFACE('',#101624,0.0999999999999994) ;
#15776 = CYLINDRICAL_SURFACE('',#101626,0.0999999999999998) ;
#15777 = CYLINDRICAL_SURFACE('',#101630,0.0999999999999994) ;
#15778 = CYLINDRICAL_SURFACE('',#101632,0.0999999999999994) ;
#15779 = CYLINDRICAL_SURFACE('',#101634,0.0999999999999994) ;
#15780 = CYLINDRICAL_SURFACE('',#101643,0.1) ;
#15781 = CYLINDRICAL_SURFACE('',#101646,0.0999999999999994) ;
#15782 = CYLINDRICAL_SURFACE('',#101648,0.0999999999999998) ;
#15783 = CYLINDRICAL_SURFACE('',#101650,0.0999999999999994) ;
#15784 = CYLINDRICAL_SURFACE('',#101659,0.0999999999999994) ;
#15785 = CYLINDRICAL_SURFACE('',#101661,0.1) ;
#15786 = CYLINDRICAL_SURFACE('',#101663,0.0999999999999998) ;
#15787 = CYLINDRICAL_SURFACE('',#101665,0.0999999999999994) ;
#15788 = CYLINDRICAL_SURFACE('',#101671,0.0999999999999998) ;
#15789 = CYLINDRICAL_SURFACE('',#101673,0.1) ;
#15790 = CYLINDRICAL_SURFACE('',#101675,0.1) ;
#15791 = CYLINDRICAL_SURFACE('',#101678,0.1) ;
#15792 = CYLINDRICAL_SURFACE('',#101685,0.0999999999999994) ;
#15793 = CYLINDRICAL_SURFACE('',#101687,0.0999999999999994) ;
#15794 = CYLINDRICAL_SURFACE('',#101694,0.0999999999999994) ;
#15795 = CYLINDRICAL_SURFACE('',#101696,0.0999999999999994) ;
#15796 = CYLINDRICAL_SURFACE('',#101698,0.0999999999999998) ;
#15797 = CYLINDRICAL_SURFACE('',#101700,0.0999999999999994) ;
#15798 = CYLINDRICAL_SURFACE('',#101706,0.1) ;
#15799 = CYLINDRICAL_SURFACE('',#101708,0.0999999999999994) ;
#15800 = CYLINDRICAL_SURFACE('',#101712,0.0999999999999994) ;
#15801 = CYLINDRICAL_SURFACE('',#101716,0.1) ;
#15802 = CYLINDRICAL_SURFACE('',#101718,0.0999999999999994) ;
#15803 = CYLINDRICAL_SURFACE('',#101722,0.0999999999999994) ;
#15804 = CYLINDRICAL_SURFACE('',#101724,0.1) ;
#15805 = CYLINDRICAL_SURFACE('',#101728,0.1) ;
#15806 = CYLINDRICAL_SURFACE('',#101733,0.0999999999999998) ;
#15807 = CYLINDRICAL_SURFACE('',#101735,0.1) ;
#15808 = CYLINDRICAL_SURFACE('',#101739,0.0999999999999994) ;
#15809 = CYLINDRICAL_SURFACE('',#101741,0.0999999999999994) ;
#15810 = CYLINDRICAL_SURFACE('',#101745,0.1) ;
#15811 = CYLINDRICAL_SURFACE('',#101751,0.1) ;
#15812 = CYLINDRICAL_SURFACE('',#101753,0.0999999999999994) ;
#15813 = CYLINDRICAL_SURFACE('',#101759,0.0999999999999994) ;
#15814 = CYLINDRICAL_SURFACE('',#101761,0.0999999999999994) ;
#15815 = CYLINDRICAL_SURFACE('',#101764,0.0999999999999994) ;
#15816 = CYLINDRICAL_SURFACE('',#101766,0.1) ;
#15817 = CYLINDRICAL_SURFACE('',#101769,0.0999999999999994) ;
#15818 = CYLINDRICAL_SURFACE('',#101775,0.0999999999999994) ;
#15819 = CYLINDRICAL_SURFACE('',#101777,0.0999999999999994) ;
#15820 = CYLINDRICAL_SURFACE('',#101779,0.0999999999999994) ;
#15821 = CYLINDRICAL_SURFACE('',#101781,0.0999999999999994) ;
#15822 = CYLINDRICAL_SURFACE('',#101787,0.1) ;
#15823 = CYLINDRICAL_SURFACE('',#101788,0.0999999999999994) ;
#15824 = CYLINDRICAL_SURFACE('',#101797,0.0999999999999998) ;
#15825 = CYLINDRICAL_SURFACE('',#101799,0.0999999999999998) ;
#15826 = CYLINDRICAL_SURFACE('',#101801,0.0999999999999994) ;
#15827 = CYLINDRICAL_SURFACE('',#101804,0.0999999999999998) ;
#15828 = CYLINDRICAL_SURFACE('',#101806,0.1) ;
#15829 = CYLINDRICAL_SURFACE('',#101808,0.0999999999999994) ;
#15830 = CYLINDRICAL_SURFACE('',#101819,0.0999999999999998) ;
#15831 = CYLINDRICAL_SURFACE('',#101821,0.0999999999999998) ;
#15832 = CYLINDRICAL_SURFACE('',#101823,0.0999999999999998) ;
#15833 = CYLINDRICAL_SURFACE('',#101825,0.0999999999999998) ;
#15834 = CYLINDRICAL_SURFACE('',#101831,0.0999999999999994) ;
#15835 = CYLINDRICAL_SURFACE('',#101832,0.0999999999999994) ;
#15836 = CYLINDRICAL_SURFACE('',#101834,0.0999999999999998) ;
#15837 = CYLINDRICAL_SURFACE('',#101837,0.0999999999999994) ;
#15838 = CYLINDRICAL_SURFACE('',#101843,0.0999999999999994) ;
#15839 = CYLINDRICAL_SURFACE('',#101845,0.0999999999999994) ;
#15840 = CYLINDRICAL_SURFACE('',#101847,0.0999999999999994) ;
#15841 = CYLINDRICAL_SURFACE('',#101849,0.0999999999999994) ;
#15842 = CYLINDRICAL_SURFACE('',#101855,0.0999999999999998) ;
#15843 = CYLINDRICAL_SURFACE('',#101856,0.0999999999999994) ;
#15844 = CYLINDRICAL_SURFACE('',#101863,0.0999999999999994) ;
#15845 = CYLINDRICAL_SURFACE('',#101865,0.0999999999999994) ;
#15846 = CYLINDRICAL_SURFACE('',#101871,0.0999999999999994) ;
#15847 = CYLINDRICAL_SURFACE('',#101872,0.0999999999999995) ;
#15848 = CYLINDRICAL_SURFACE('',#101873,0.0999999999999995) ;
#15849 = CYLINDRICAL_SURFACE('',#101874,0.0999999999999995) ;
#15850 = CYLINDRICAL_SURFACE('',#101875,0.0999999999999995) ;
#15851 = CYLINDRICAL_SURFACE('',#101880,0.0999999999999994) ;
#15852 = CYLINDRICAL_SURFACE('',#101882,0.0999999999999994) ;
#15853 = CYLINDRICAL_SURFACE('',#101886,0.0999999999999994) ;
#15854 = CYLINDRICAL_SURFACE('',#101897,0.0999999999999994) ;
#15855 = CYLINDRICAL_SURFACE('',#101900,0.0999999999999994) ;
#15856 = CYLINDRICAL_SURFACE('',#101902,0.0999999999999998) ;
#15857 = CYLINDRICAL_SURFACE('',#101906,0.0999999999999994) ;
#15858 = CYLINDRICAL_SURFACE('',#101908,0.0999999999999994) ;
#15859 = CYLINDRICAL_SURFACE('',#101910,0.0999999999999994) ;
#15860 = CYLINDRICAL_SURFACE('',#101919,0.1) ;
#15861 = CYLINDRICAL_SURFACE('',#101922,0.0999999999999994) ;
#15862 = CYLINDRICAL_SURFACE('',#101924,0.0999999999999998) ;
#15863 = CYLINDRICAL_SURFACE('',#101926,0.0999999999999994) ;
#15864 = CYLINDRICAL_SURFACE('',#101935,0.0999999999999994) ;
#15865 = CYLINDRICAL_SURFACE('',#101937,0.1) ;
#15866 = CYLINDRICAL_SURFACE('',#101939,0.0999999999999998) ;
#15867 = CYLINDRICAL_SURFACE('',#101941,0.0999999999999994) ;
#15868 = CYLINDRICAL_SURFACE('',#101947,0.0999999999999998) ;
#15869 = CYLINDRICAL_SURFACE('',#101949,0.1) ;
#15870 = CYLINDRICAL_SURFACE('',#101951,0.1) ;
#15871 = CYLINDRICAL_SURFACE('',#101954,0.1) ;
#15872 = CYLINDRICAL_SURFACE('',#101961,0.0999999999999994) ;
#15873 = CYLINDRICAL_SURFACE('',#101963,0.0999999999999994) ;
#15874 = CYLINDRICAL_SURFACE('',#101970,0.0999999999999994) ;
#15875 = CYLINDRICAL_SURFACE('',#101972,0.0999999999999994) ;
#15876 = CYLINDRICAL_SURFACE('',#101974,0.0999999999999998) ;
#15877 = CYLINDRICAL_SURFACE('',#101976,0.0999999999999994) ;
#15878 = CYLINDRICAL_SURFACE('',#101982,0.1) ;
#15879 = CYLINDRICAL_SURFACE('',#101984,0.0999999999999994) ;
#15880 = CYLINDRICAL_SURFACE('',#101988,0.0999999999999994) ;
#15881 = CYLINDRICAL_SURFACE('',#101992,0.1) ;
#15882 = CYLINDRICAL_SURFACE('',#101994,0.0999999999999994) ;
#15883 = CYLINDRICAL_SURFACE('',#101998,0.0999999999999994) ;
#15884 = CYLINDRICAL_SURFACE('',#102000,0.1) ;
#15885 = CYLINDRICAL_SURFACE('',#102004,0.1) ;
#15886 = CYLINDRICAL_SURFACE('',#102009,0.0999999999999998) ;
#15887 = CYLINDRICAL_SURFACE('',#102011,0.1) ;
#15888 = CYLINDRICAL_SURFACE('',#102015,0.0999999999999994) ;
#15889 = CYLINDRICAL_SURFACE('',#102017,0.0999999999999994) ;
#15890 = CYLINDRICAL_SURFACE('',#102021,0.1) ;
#15891 = CYLINDRICAL_SURFACE('',#102027,0.1) ;
#15892 = CYLINDRICAL_SURFACE('',#102029,0.0999999999999994) ;
#15893 = CYLINDRICAL_SURFACE('',#102035,0.0999999999999994) ;
#15894 = CYLINDRICAL_SURFACE('',#102037,0.0999999999999994) ;
#15895 = CYLINDRICAL_SURFACE('',#102040,0.0999999999999994) ;
#15896 = CYLINDRICAL_SURFACE('',#102042,0.1) ;
#15897 = CYLINDRICAL_SURFACE('',#102045,0.0999999999999994) ;
#15898 = CYLINDRICAL_SURFACE('',#102051,0.0999999999999994) ;
#15899 = CYLINDRICAL_SURFACE('',#102053,0.0999999999999994) ;
#15900 = CYLINDRICAL_SURFACE('',#102055,0.0999999999999994) ;
#15901 = CYLINDRICAL_SURFACE('',#102057,0.0999999999999994) ;
#15902 = CYLINDRICAL_SURFACE('',#102063,0.1) ;
#15903 = CYLINDRICAL_SURFACE('',#102064,0.0999999999999994) ;
#15904 = CYLINDRICAL_SURFACE('',#102073,0.0999999999999998) ;
#15905 = CYLINDRICAL_SURFACE('',#102075,0.0999999999999998) ;
#15906 = CYLINDRICAL_SURFACE('',#102077,0.0999999999999994) ;
#15907 = CYLINDRICAL_SURFACE('',#102080,0.0999999999999998) ;
#15908 = CYLINDRICAL_SURFACE('',#102082,0.1) ;
#15909 = CYLINDRICAL_SURFACE('',#102084,0.0999999999999994) ;
#15910 = CYLINDRICAL_SURFACE('',#102095,0.0999999999999998) ;
#15911 = CYLINDRICAL_SURFACE('',#102097,0.0999999999999998) ;
#15912 = CYLINDRICAL_SURFACE('',#102099,0.0999999999999998) ;
#15913 = CYLINDRICAL_SURFACE('',#102101,0.0999999999999998) ;
#15914 = CYLINDRICAL_SURFACE('',#102107,0.0999999999999994) ;
#15915 = CYLINDRICAL_SURFACE('',#102108,0.0999999999999994) ;
#15916 = CYLINDRICAL_SURFACE('',#102110,0.0999999999999998) ;
#15917 = CYLINDRICAL_SURFACE('',#102113,0.0999999999999994) ;
#15918 = CYLINDRICAL_SURFACE('',#102119,0.0999999999999994) ;
#15919 = CYLINDRICAL_SURFACE('',#102121,0.0999999999999994) ;
#15920 = CYLINDRICAL_SURFACE('',#102123,0.0999999999999994) ;
#15921 = CYLINDRICAL_SURFACE('',#102125,0.0999999999999994) ;
#15922 = CYLINDRICAL_SURFACE('',#102131,0.0999999999999998) ;
#15923 = CYLINDRICAL_SURFACE('',#102132,0.0999999999999994) ;
#15924 = CYLINDRICAL_SURFACE('',#102139,0.0999999999999994) ;
#15925 = CYLINDRICAL_SURFACE('',#102141,0.0999999999999994) ;
#15926 = CYLINDRICAL_SURFACE('',#102147,0.0999999999999994) ;
#15927 = CYLINDRICAL_SURFACE('',#102148,0.0999999999999995) ;
#15928 = CYLINDRICAL_SURFACE('',#102149,0.0999999999999995) ;
#15929 = CYLINDRICAL_SURFACE('',#102150,0.0999999999999995) ;
#15930 = CYLINDRICAL_SURFACE('',#102151,0.0999999999999995) ;
#15931 = CYLINDRICAL_SURFACE('',#102156,0.0999999999999994) ;
#15932 = CYLINDRICAL_SURFACE('',#102158,0.0999999999999994) ;
#15933 = CYLINDRICAL_SURFACE('',#102162,0.0999999999999994) ;
#15934 = CYLINDRICAL_SURFACE('',#102173,0.0999999999999994) ;
#15935 = CYLINDRICAL_SURFACE('',#102176,0.0999999999999994) ;
#15936 = CYLINDRICAL_SURFACE('',#102178,0.0999999999999998) ;
#15937 = CYLINDRICAL_SURFACE('',#102182,0.100000000000003) ;
#15938 = CYLINDRICAL_SURFACE('',#102184,0.0999999999999994) ;
#15939 = CYLINDRICAL_SURFACE('',#102186,0.100000000000003) ;
#15940 = CYLINDRICAL_SURFACE('',#102195,0.1) ;
#15941 = CYLINDRICAL_SURFACE('',#102198,0.0999999999999994) ;
#15942 = CYLINDRICAL_SURFACE('',#102200,0.0999999999999998) ;
#15943 = CYLINDRICAL_SURFACE('',#102202,0.100000000000003) ;
#15944 = CYLINDRICAL_SURFACE('',#102211,0.0999999999999994) ;
#15945 = CYLINDRICAL_SURFACE('',#102213,0.1) ;
#15946 = CYLINDRICAL_SURFACE('',#102215,0.0999999999999998) ;
#15947 = CYLINDRICAL_SURFACE('',#102217,0.100000000000003) ;
#15948 = CYLINDRICAL_SURFACE('',#102223,0.0999999999999998) ;
#15949 = CYLINDRICAL_SURFACE('',#102225,0.1) ;
#15950 = CYLINDRICAL_SURFACE('',#102227,0.1) ;
#15951 = CYLINDRICAL_SURFACE('',#102230,0.1) ;
#15952 = CYLINDRICAL_SURFACE('',#102237,0.100000000000003) ;
#15953 = CYLINDRICAL_SURFACE('',#102239,0.0999999999999994) ;
#15954 = CYLINDRICAL_SURFACE('',#102246,0.0999999999999994) ;
#15955 = CYLINDRICAL_SURFACE('',#102248,0.0999999999999994) ;
#15956 = CYLINDRICAL_SURFACE('',#102250,0.0999999999999998) ;
#15957 = CYLINDRICAL_SURFACE('',#102252,0.100000000000003) ;
#15958 = CYLINDRICAL_SURFACE('',#102258,0.1) ;
#15959 = CYLINDRICAL_SURFACE('',#102260,0.100000000000003) ;
#15960 = CYLINDRICAL_SURFACE('',#102264,0.100000000000003) ;
#15961 = CYLINDRICAL_SURFACE('',#102268,0.1) ;
#15962 = CYLINDRICAL_SURFACE('',#102270,0.0999999999999994) ;
#15963 = CYLINDRICAL_SURFACE('',#102274,0.0999999999999994) ;
#15964 = CYLINDRICAL_SURFACE('',#102276,0.1) ;
#15965 = CYLINDRICAL_SURFACE('',#102280,0.1) ;
#15966 = CYLINDRICAL_SURFACE('',#102285,0.0999999999999998) ;
#15967 = CYLINDRICAL_SURFACE('',#102287,0.1) ;
#15968 = CYLINDRICAL_SURFACE('',#102291,0.100000000000003) ;
#15969 = CYLINDRICAL_SURFACE('',#102293,0.0999999999999994) ;
#15970 = CYLINDRICAL_SURFACE('',#102297,0.1) ;
#15971 = CYLINDRICAL_SURFACE('',#102303,0.1) ;
#15972 = CYLINDRICAL_SURFACE('',#102305,0.0999999999999994) ;
#15973 = CYLINDRICAL_SURFACE('',#102311,0.0999999999999994) ;
#15974 = CYLINDRICAL_SURFACE('',#102313,0.0999999999999994) ;
#15975 = CYLINDRICAL_SURFACE('',#102316,0.0999999999999994) ;
#15976 = CYLINDRICAL_SURFACE('',#102318,0.1) ;
#15977 = CYLINDRICAL_SURFACE('',#102321,0.0999999999999994) ;
#15978 = CYLINDRICAL_SURFACE('',#102327,0.0999999999999994) ;
#15979 = CYLINDRICAL_SURFACE('',#102329,0.0999999999999994) ;
#15980 = CYLINDRICAL_SURFACE('',#102331,0.0999999999999994) ;
#15981 = CYLINDRICAL_SURFACE('',#102333,0.0999999999999994) ;
#15982 = CYLINDRICAL_SURFACE('',#102339,0.1) ;
#15983 = CYLINDRICAL_SURFACE('',#102340,0.100000000000003) ;
#15984 = CYLINDRICAL_SURFACE('',#102349,0.0999999999999998) ;
#15985 = CYLINDRICAL_SURFACE('',#102351,0.0999999999999998) ;
#15986 = CYLINDRICAL_SURFACE('',#102353,0.100000000000003) ;
#15987 = CYLINDRICAL_SURFACE('',#102356,0.0999999999999998) ;
#15988 = CYLINDRICAL_SURFACE('',#102358,0.1) ;
#15989 = CYLINDRICAL_SURFACE('',#102360,0.0999999999999994) ;
#15990 = CYLINDRICAL_SURFACE('',#102371,0.0999999999999998) ;
#15991 = CYLINDRICAL_SURFACE('',#102373,0.0999999999999998) ;
#15992 = CYLINDRICAL_SURFACE('',#102375,0.0999999999999998) ;
#15993 = CYLINDRICAL_SURFACE('',#102377,0.0999999999999998) ;
#15994 = CYLINDRICAL_SURFACE('',#102383,0.0999999999999994) ;
#15995 = CYLINDRICAL_SURFACE('',#102384,0.0999999999999994) ;
#15996 = CYLINDRICAL_SURFACE('',#102386,0.0999999999999998) ;
#15997 = CYLINDRICAL_SURFACE('',#102389,0.0999999999999994) ;
#15998 = CYLINDRICAL_SURFACE('',#102395,0.0999999999999994) ;
#15999 = CYLINDRICAL_SURFACE('',#102397,0.0999999999999994) ;
#16000 = CYLINDRICAL_SURFACE('',#102399,0.0999999999999994) ;
#16001 = CYLINDRICAL_SURFACE('',#102401,0.0999999999999994) ;
#16002 = CYLINDRICAL_SURFACE('',#102407,0.0999999999999998) ;
#16003 = CYLINDRICAL_SURFACE('',#102408,0.0999999999999994) ;
#16004 = CYLINDRICAL_SURFACE('',#102415,0.0999999999999994) ;
#16005 = CYLINDRICAL_SURFACE('',#102417,0.0999999999999994) ;
#16006 = CYLINDRICAL_SURFACE('',#102423,0.0999999999999994) ;
#16007 = CYLINDRICAL_SURFACE('',#102424,0.0999999999999995) ;
#16008 = CYLINDRICAL_SURFACE('',#102425,0.0999999999999995) ;
#16009 = CYLINDRICAL_SURFACE('',#102426,0.0999999999999995) ;
#16010 = CYLINDRICAL_SURFACE('',#102427,0.0999999999999995) ;
#16011 = CYLINDRICAL_SURFACE('',#102432,0.0999999999999994) ;
#16012 = CYLINDRICAL_SURFACE('',#102434,0.100000000000003) ;
#16013 = CYLINDRICAL_SURFACE('',#102438,0.100000000000003) ;
#16014 = CYLINDRICAL_SURFACE('',#102449,0.0999999999999994) ;
#16015 = CYLINDRICAL_SURFACE('',#102452,0.100000000000003) ;
#16016 = CYLINDRICAL_SURFACE('',#102454,0.0999999999999998) ;
#16017 = CYLINDRICAL_SURFACE('',#102458,0.100000000000003) ;
#16018 = CYLINDRICAL_SURFACE('',#102460,0.0999999999999994) ;
#16019 = CYLINDRICAL_SURFACE('',#102462,0.100000000000003) ;
#16020 = CYLINDRICAL_SURFACE('',#102471,0.1) ;
#16021 = CYLINDRICAL_SURFACE('',#102474,0.100000000000003) ;
#16022 = CYLINDRICAL_SURFACE('',#102476,0.0999999999999998) ;
#16023 = CYLINDRICAL_SURFACE('',#102478,0.100000000000003) ;
#16024 = CYLINDRICAL_SURFACE('',#102487,0.100000000000003) ;
#16025 = CYLINDRICAL_SURFACE('',#102489,0.1) ;
#16026 = CYLINDRICAL_SURFACE('',#102491,0.0999999999999998) ;
#16027 = CYLINDRICAL_SURFACE('',#102493,0.100000000000003) ;
#16028 = CYLINDRICAL_SURFACE('',#102499,0.0999999999999998) ;
#16029 = CYLINDRICAL_SURFACE('',#102501,0.1) ;
#16030 = CYLINDRICAL_SURFACE('',#102503,0.1) ;
#16031 = CYLINDRICAL_SURFACE('',#102506,0.1) ;
#16032 = CYLINDRICAL_SURFACE('',#102513,0.100000000000003) ;
#16033 = CYLINDRICAL_SURFACE('',#102515,0.100000000000003) ;
#16034 = CYLINDRICAL_SURFACE('',#102522,0.100000000000003) ;
#16035 = CYLINDRICAL_SURFACE('',#102524,0.100000000000003) ;
#16036 = CYLINDRICAL_SURFACE('',#102526,0.0999999999999998) ;
#16037 = CYLINDRICAL_SURFACE('',#102528,0.100000000000003) ;
#16038 = CYLINDRICAL_SURFACE('',#102534,0.1) ;
#16039 = CYLINDRICAL_SURFACE('',#102536,0.100000000000003) ;
#16040 = CYLINDRICAL_SURFACE('',#102540,0.100000000000003) ;
#16041 = CYLINDRICAL_SURFACE('',#102544,0.1) ;
#16042 = CYLINDRICAL_SURFACE('',#102546,0.0999999999999994) ;
#16043 = CYLINDRICAL_SURFACE('',#102550,0.100000000000003) ;
#16044 = CYLINDRICAL_SURFACE('',#102552,0.1) ;
#16045 = CYLINDRICAL_SURFACE('',#102556,0.1) ;
#16046 = CYLINDRICAL_SURFACE('',#102561,0.0999999999999998) ;
#16047 = CYLINDRICAL_SURFACE('',#102563,0.1) ;
#16048 = CYLINDRICAL_SURFACE('',#102567,0.100000000000003) ;
#16049 = CYLINDRICAL_SURFACE('',#102569,0.0999999999999994) ;
#16050 = CYLINDRICAL_SURFACE('',#102573,0.1) ;
#16051 = CYLINDRICAL_SURFACE('',#102579,0.1) ;
#16052 = CYLINDRICAL_SURFACE('',#102581,0.100000000000003) ;
#16053 = CYLINDRICAL_SURFACE('',#102587,0.100000000000003) ;
#16054 = CYLINDRICAL_SURFACE('',#102589,0.0999999999999994) ;
#16055 = CYLINDRICAL_SURFACE('',#102592,0.100000000000003) ;
#16056 = CYLINDRICAL_SURFACE('',#102594,0.1) ;
#16057 = CYLINDRICAL_SURFACE('',#102597,0.100000000000003) ;
#16058 = CYLINDRICAL_SURFACE('',#102603,0.100000000000003) ;
#16059 = CYLINDRICAL_SURFACE('',#102605,0.100000000000003) ;
#16060 = CYLINDRICAL_SURFACE('',#102607,0.100000000000003) ;
#16061 = CYLINDRICAL_SURFACE('',#102609,0.100000000000003) ;
#16062 = CYLINDRICAL_SURFACE('',#102615,0.1) ;
#16063 = CYLINDRICAL_SURFACE('',#102616,0.100000000000003) ;
#16064 = CYLINDRICAL_SURFACE('',#102625,0.0999999999999998) ;
#16065 = CYLINDRICAL_SURFACE('',#102627,0.0999999999999998) ;
#16066 = CYLINDRICAL_SURFACE('',#102629,0.100000000000003) ;
#16067 = CYLINDRICAL_SURFACE('',#102632,0.0999999999999998) ;
#16068 = CYLINDRICAL_SURFACE('',#102634,0.1) ;
#16069 = CYLINDRICAL_SURFACE('',#102636,0.100000000000003) ;
#16070 = CYLINDRICAL_SURFACE('',#102647,0.0999999999999998) ;
#16071 = CYLINDRICAL_SURFACE('',#102649,0.0999999999999998) ;
#16072 = CYLINDRICAL_SURFACE('',#102651,0.0999999999999998) ;
#16073 = CYLINDRICAL_SURFACE('',#102653,0.0999999999999998) ;
#16074 = CYLINDRICAL_SURFACE('',#102659,0.100000000000003) ;
#16075 = CYLINDRICAL_SURFACE('',#102660,0.100000000000003) ;
#16076 = CYLINDRICAL_SURFACE('',#102662,0.0999999999999998) ;
#16077 = CYLINDRICAL_SURFACE('',#102665,0.100000000000003) ;
#16078 = CYLINDRICAL_SURFACE('',#102671,0.100000000000003) ;
#16079 = CYLINDRICAL_SURFACE('',#102673,0.100000000000003) ;
#16080 = CYLINDRICAL_SURFACE('',#102675,0.100000000000003) ;
#16081 = CYLINDRICAL_SURFACE('',#102677,0.100000000000003) ;
#16082 = CYLINDRICAL_SURFACE('',#102683,0.0999999999999998) ;
#16083 = CYLINDRICAL_SURFACE('',#102684,0.0999999999999994) ;
#16084 = CYLINDRICAL_SURFACE('',#102691,0.100000000000003) ;
#16085 = CYLINDRICAL_SURFACE('',#102693,0.100000000000003) ;
#16086 = CYLINDRICAL_SURFACE('',#102699,0.0999999999999994) ;
#16087 = CYLINDRICAL_SURFACE('',#102700,0.0999999999999995) ;
#16088 = CYLINDRICAL_SURFACE('',#102701,0.0999999999999995) ;
#16089 = CYLINDRICAL_SURFACE('',#102702,0.0999999999999995) ;
#16090 = CYLINDRICAL_SURFACE('',#102703,0.0999999999999995) ;
#16091 = CYLINDRICAL_SURFACE('',#102704,0.0999999999999998) ;
#16092 = CYLINDRICAL_SURFACE('',#102707,0.0999999999999998) ;
#16093 = CYLINDRICAL_SURFACE('',#102710,0.0999999999999998) ;
#16094 = CYLINDRICAL_SURFACE('',#102713,0.0999999999999998) ;
#16095 = CYLINDRICAL_SURFACE('',#102716,0.0999999999999998) ;
#16096 = CYLINDRICAL_SURFACE('',#102719,0.0999999999999998) ;
#16097 = CYLINDRICAL_SURFACE('',#102722,0.0999999999999998) ;
#16098 = CYLINDRICAL_SURFACE('',#102725,0.0999999999999998) ;
#16099 = CYLINDRICAL_SURFACE('',#102728,0.0999999999999998) ;
#16100 = CYLINDRICAL_SURFACE('',#102733,0.0999999999999998) ;
#16101 = CYLINDRICAL_SURFACE('',#102741,0.0999999999999998) ;
#16102 = CYLINDRICAL_SURFACE('',#102748,0.0999999999999998) ;
#16103 = CYLINDRICAL_SURFACE('',#102755,0.0999999999999998) ;
#16104 = CYLINDRICAL_SURFACE('',#102762,0.0999999999999998) ;
#16105 = CYLINDRICAL_SURFACE('',#102769,0.0999999999999998) ;
#16106 = CYLINDRICAL_SURFACE('',#102776,0.0999999999999998) ;
#16107 = CYLINDRICAL_SURFACE('',#102783,0.0999999999999998) ;
#16108 = CYLINDRICAL_SURFACE('',#102788,0.0999999999999998) ;
#16109 = CYLINDRICAL_SURFACE('',#102795,0.1) ;
#16110 = CYLINDRICAL_SURFACE('',#102801,0.0999999999999998) ;
#16111 = CYLINDRICAL_SURFACE('',#102807,0.0999999999999994) ;
#16112 = CYLINDRICAL_SURFACE('',#102813,0.1) ;
#16113 = CYLINDRICAL_SURFACE('',#102819,0.0999999999999994) ;
#16114 = CYLINDRICAL_SURFACE('',#102825,0.0999999999999994) ;
#16115 = CYLINDRICAL_SURFACE('',#102831,0.0999999999999994) ;
#16116 = CYLINDRICAL_SURFACE('',#102837,0.0999999999999994) ;
#16117 = CYLINDRICAL_SURFACE('',#102843,0.0999999999999994) ;
#16118 = CYLINDRICAL_SURFACE('',#102849,0.0999999999999994) ;
#16119 = CYLINDRICAL_SURFACE('',#102855,0.0999999999999994) ;
#16120 = CYLINDRICAL_SURFACE('',#102861,0.0999999999999994) ;
#16121 = CYLINDRICAL_SURFACE('',#102867,0.0999999999999994) ;
#16122 = CYLINDRICAL_SURFACE('',#102873,0.0999999999999994) ;
#16123 = CYLINDRICAL_SURFACE('',#102879,0.100000000000003) ;
#16124 = CYLINDRICAL_SURFACE('',#102885,0.0999999999999994) ;
#16125 = CYLINDRICAL_SURFACE('',#102891,0.100000000000003) ;
#16126 = CYLINDRICAL_SURFACE('',#102897,0.100000000000003) ;
#16127 = CYLINDRICAL_SURFACE('',#102973,2.25) ;
#16128 = CYLINDRICAL_SURFACE('',#102975,2.25) ;
#16129 = CYLINDRICAL_SURFACE('',#102977,2.25) ;
#16130 = CYLINDRICAL_SURFACE('',#102979,2.25) ;
#16131 = CYLINDRICAL_SURFACE('',#102981,2.25) ;
#16132 = CYLINDRICAL_SURFACE('',#102983,2.25) ;
#16133 = CYLINDRICAL_SURFACE('',#102987,0.0999999999999998) ;
#16134 = CYLINDRICAL_SURFACE('',#102991,0.0999999999999998) ;
#16135 = CYLINDRICAL_SURFACE('',#102995,0.100000000000003) ;
#16136 = CYLINDRICAL_SURFACE('',#102999,0.0999999999999998) ;
#16137 = CYLINDRICAL_SURFACE('',#103006,0.1) ;
#16138 = CYLINDRICAL_SURFACE('',#103008,0.0999999999999998) ;
#16139 = CYLINDRICAL_SURFACE('',#103010,0.0999999999999998) ;
#16140 = CYLINDRICAL_SURFACE('',#103017,0.0999999999999998) ;
#16141 = CYLINDRICAL_SURFACE('',#103019,0.0999999999999998) ;
#16142 = CYLINDRICAL_SURFACE('',#103021,0.0999999999999998) ;
#16143 = CYLINDRICAL_SURFACE('',#103024,0.1) ;
#16144 = CYLINDRICAL_SURFACE('',#103035,0.0999999999999998) ;
#16145 = CYLINDRICAL_SURFACE('',#103040,0.0999999999999998) ;
#16146 = CYLINDRICAL_SURFACE('',#103045,0.1) ;
#16147 = CYLINDRICAL_SURFACE('',#103047,0.0999999999999998) ;
#16148 = CYLINDRICAL_SURFACE('',#103054,0.1) ;
#16149 = CYLINDRICAL_SURFACE('',#103056,0.0999999999999998) ;
#16150 = CYLINDRICAL_SURFACE('',#103058,0.0999999999999998) ;
#16151 = CYLINDRICAL_SURFACE('',#103060,0.0999999999999998) ;
#16152 = CYLINDRICAL_SURFACE('',#103066,0.0999999999999998) ;
#16153 = CYLINDRICAL_SURFACE('',#103068,0.0999999999999998) ;
#16154 = CYLINDRICAL_SURFACE('',#103072,0.1) ;
#16155 = SPHERICAL_SURFACE('',#91148,0.1) ;
#16156 = SPHERICAL_SURFACE('',#91154,0.1) ;
#16157 = SPHERICAL_SURFACE('',#91194,0.1) ;
#16158 = SPHERICAL_SURFACE('',#91200,0.1) ;
#16159 = SPHERICAL_SURFACE('',#91391,0.1) ;
#16160 = SPHERICAL_SURFACE('',#91409,0.1) ;
#16161 = SPHERICAL_SURFACE('',#91412,0.1) ;
#16162 = SPHERICAL_SURFACE('',#91423,0.1) ;
#16163 = SPHERICAL_SURFACE('',#91451,0.1) ;
#16164 = SPHERICAL_SURFACE('',#91458,0.1) ;
#16165 = SPHERICAL_SURFACE('',#91460,0.1) ;
#16166 = SPHERICAL_SURFACE('',#91466,0.1) ;
#16167 = SPHERICAL_SURFACE('',#91492,0.1) ;
#16168 = SPHERICAL_SURFACE('',#91494,0.1) ;
#16169 = SPHERICAL_SURFACE('',#91506,0.1) ;
#16170 = SPHERICAL_SURFACE('',#91508,0.1) ;
#16171 = SPHERICAL_SURFACE('',#91536,0.1) ;
#16172 = SPHERICAL_SURFACE('',#91538,0.1) ;
#16173 = SPHERICAL_SURFACE('',#91550,0.1) ;
#16174 = SPHERICAL_SURFACE('',#91552,0.1) ;
#16175 = SPHERICAL_SURFACE('',#91559,0.1) ;
#16176 = SPHERICAL_SURFACE('',#91579,0.1) ;
#16177 = SPHERICAL_SURFACE('',#91604,0.1) ;
#16178 = SPHERICAL_SURFACE('',#91619,0.1) ;
#16179 = SPHERICAL_SURFACE('',#91756,0.1) ;
#16180 = SPHERICAL_SURFACE('',#91774,0.1) ;
#16181 = SPHERICAL_SURFACE('',#91777,0.1) ;
#16182 = SPHERICAL_SURFACE('',#91788,0.1) ;
#16183 = SPHERICAL_SURFACE('',#91815,0.1) ;
#16184 = SPHERICAL_SURFACE('',#91822,0.1) ;
#16185 = SPHERICAL_SURFACE('',#91824,0.1) ;
#16186 = SPHERICAL_SURFACE('',#91830,0.1) ;
#16187 = SPHERICAL_SURFACE('',#91856,0.1) ;
#16188 = SPHERICAL_SURFACE('',#91858,0.1) ;
#16189 = SPHERICAL_SURFACE('',#91870,0.1) ;
#16190 = SPHERICAL_SURFACE('',#91872,0.1) ;
#16191 = SPHERICAL_SURFACE('',#91900,0.1) ;
#16192 = SPHERICAL_SURFACE('',#91902,0.1) ;
#16193 = SPHERICAL_SURFACE('',#91914,0.1) ;
#16194 = SPHERICAL_SURFACE('',#91916,0.1) ;
#16195 = SPHERICAL_SURFACE('',#91921,0.1) ;
#16196 = SPHERICAL_SURFACE('',#91937,0.1) ;
#16197 = SPHERICAL_SURFACE('',#91944,0.1) ;
#16198 = SPHERICAL_SURFACE('',#91956,0.1) ;
#16199 = SPHERICAL_SURFACE('',#91963,0.1) ;
#16200 = SPHERICAL_SURFACE('',#91966,0.1) ;
#16201 = SPHERICAL_SURFACE('',#91977,0.1) ;
#16202 = SPHERICAL_SURFACE('',#91979,0.1) ;
#16203 = SPHERICAL_SURFACE('',#91981,0.1) ;
#16204 = SPHERICAL_SURFACE('',#91983,0.1) ;
#16205 = SPHERICAL_SURFACE('',#92037,0.1) ;
#16206 = SPHERICAL_SURFACE('',#92043,0.1) ;
#16207 = SPHERICAL_SURFACE('',#92083,0.1) ;
#16208 = SPHERICAL_SURFACE('',#92089,0.1) ;
#16209 = SPHERICAL_SURFACE('',#92280,0.1) ;
#16210 = SPHERICAL_SURFACE('',#92298,0.1) ;
#16211 = SPHERICAL_SURFACE('',#92301,0.1) ;
#16212 = SPHERICAL_SURFACE('',#92312,0.1) ;
#16213 = SPHERICAL_SURFACE('',#92340,0.1) ;
#16214 = SPHERICAL_SURFACE('',#92347,0.1) ;
#16215 = SPHERICAL_SURFACE('',#92349,0.1) ;
#16216 = SPHERICAL_SURFACE('',#92355,0.1) ;
#16217 = SPHERICAL_SURFACE('',#92381,0.1) ;
#16218 = SPHERICAL_SURFACE('',#92383,0.1) ;
#16219 = SPHERICAL_SURFACE('',#92395,0.1) ;
#16220 = SPHERICAL_SURFACE('',#92397,0.1) ;
#16221 = SPHERICAL_SURFACE('',#92425,0.1) ;
#16222 = SPHERICAL_SURFACE('',#92427,0.1) ;
#16223 = SPHERICAL_SURFACE('',#92439,0.1) ;
#16224 = SPHERICAL_SURFACE('',#92441,0.1) ;
#16225 = SPHERICAL_SURFACE('',#92449,0.1) ;
#16226 = SPHERICAL_SURFACE('',#92468,0.1) ;
#16227 = SPHERICAL_SURFACE('',#92493,0.1) ;
#16228 = SPHERICAL_SURFACE('',#92508,0.1) ;
#16229 = SPHERICAL_SURFACE('',#92645,0.1) ;
#16230 = SPHERICAL_SURFACE('',#92663,0.1) ;
#16231 = SPHERICAL_SURFACE('',#92666,0.1) ;
#16232 = SPHERICAL_SURFACE('',#92677,0.1) ;
#16233 = SPHERICAL_SURFACE('',#92704,0.1) ;
#16234 = SPHERICAL_SURFACE('',#92711,0.1) ;
#16235 = SPHERICAL_SURFACE('',#92713,0.1) ;
#16236 = SPHERICAL_SURFACE('',#92719,0.1) ;
#16237 = SPHERICAL_SURFACE('',#92745,0.1) ;
#16238 = SPHERICAL_SURFACE('',#92747,0.1) ;
#16239 = SPHERICAL_SURFACE('',#92759,0.1) ;
#16240 = SPHERICAL_SURFACE('',#92761,0.1) ;
#16241 = SPHERICAL_SURFACE('',#92789,0.1) ;
#16242 = SPHERICAL_SURFACE('',#92791,0.1) ;
#16243 = SPHERICAL_SURFACE('',#92803,0.1) ;
#16244 = SPHERICAL_SURFACE('',#92805,0.1) ;
#16245 = SPHERICAL_SURFACE('',#92812,0.1) ;
#16246 = SPHERICAL_SURFACE('',#92826,0.1) ;
#16247 = SPHERICAL_SURFACE('',#92833,0.1) ;
#16248 = SPHERICAL_SURFACE('',#92845,0.1) ;
#16249 = SPHERICAL_SURFACE('',#92852,0.1) ;
#16250 = SPHERICAL_SURFACE('',#92855,0.1) ;
#16251 = SPHERICAL_SURFACE('',#92866,0.1) ;
#16252 = SPHERICAL_SURFACE('',#92868,0.1) ;
#16253 = SPHERICAL_SURFACE('',#92870,0.1) ;
#16254 = SPHERICAL_SURFACE('',#92872,0.1) ;
#16255 = SPHERICAL_SURFACE('',#92929,0.1) ;
#16256 = SPHERICAL_SURFACE('',#92935,0.1) ;
#16257 = SPHERICAL_SURFACE('',#93119,0.1) ;
#16258 = SPHERICAL_SURFACE('',#93137,0.1) ;
#16259 = SPHERICAL_SURFACE('',#93140,0.1) ;
#16260 = SPHERICAL_SURFACE('',#93151,0.1) ;
#16261 = SPHERICAL_SURFACE('',#93179,0.1) ;
#16262 = SPHERICAL_SURFACE('',#93186,0.1) ;
#16263 = SPHERICAL_SURFACE('',#93188,0.1) ;
#16264 = SPHERICAL_SURFACE('',#93194,0.1) ;
#16265 = SPHERICAL_SURFACE('',#93220,0.1) ;
#16266 = SPHERICAL_SURFACE('',#93222,0.1) ;
#16267 = SPHERICAL_SURFACE('',#93234,0.1) ;
#16268 = SPHERICAL_SURFACE('',#93236,0.1) ;
#16269 = SPHERICAL_SURFACE('',#93264,0.1) ;
#16270 = SPHERICAL_SURFACE('',#93266,0.1) ;
#16271 = SPHERICAL_SURFACE('',#93278,0.1) ;
#16272 = SPHERICAL_SURFACE('',#93280,0.1) ;
#16273 = SPHERICAL_SURFACE('',#93287,0.1) ;
#16274 = SPHERICAL_SURFACE('',#93305,0.1) ;
#16275 = SPHERICAL_SURFACE('',#93325,0.1) ;
#16276 = SPHERICAL_SURFACE('',#93339,0.1) ;
#16277 = SPHERICAL_SURFACE('',#93358,0.1) ;
#16278 = SPHERICAL_SURFACE('',#93375,0.1) ;
#16279 = SPHERICAL_SURFACE('',#93392,0.1) ;
#16280 = SPHERICAL_SURFACE('',#93409,0.1) ;
#16281 = SPHERICAL_SURFACE('',#93426,0.1) ;
#16282 = SPHERICAL_SURFACE('',#93443,0.1) ;
#16283 = SPHERICAL_SURFACE('',#93460,0.1) ;
#16284 = SPHERICAL_SURFACE('',#93477,0.1) ;
#16285 = SPHERICAL_SURFACE('',#93539,0.1) ;
#16286 = SPHERICAL_SURFACE('',#93588,0.1) ;
#16287 = SPHERICAL_SURFACE('',#93976,0.1) ;
#16288 = SPHERICAL_SURFACE('',#93979,0.1) ;
#16289 = SPHERICAL_SURFACE('',#93997,0.1) ;
#16290 = SPHERICAL_SURFACE('',#94018,0.1) ;
#16291 = SPHERICAL_SURFACE('',#94020,0.1) ;
#16292 = SPHERICAL_SURFACE('',#94025,0.1) ;
#16293 = SPHERICAL_SURFACE('',#94028,0.1) ;
#16294 = SPHERICAL_SURFACE('',#94045,0.1) ;
#16295 = SPHERICAL_SURFACE('',#94051,0.1) ;
#16296 = SPHERICAL_SURFACE('',#94069,0.1) ;
#16297 = SPHERICAL_SURFACE('',#94070,0.1) ;
#16298 = SPHERICAL_SURFACE('',#94079,0.1) ;
#16299 = SPHERICAL_SURFACE('',#94085,0.1) ;
#16300 = SPHERICAL_SURFACE('',#94093,0.1) ;
#16301 = SPHERICAL_SURFACE('',#94095,0.1) ;
#16302 = SPHERICAL_SURFACE('',#94101,0.1) ;
#16303 = SPHERICAL_SURFACE('',#94102,0.1) ;
#16304 = SPHERICAL_SURFACE('',#94111,0.1) ;
#16305 = SPHERICAL_SURFACE('',#94117,0.1) ;
#16306 = SPHERICAL_SURFACE('',#94125,0.1) ;
#16307 = SPHERICAL_SURFACE('',#94127,0.1) ;
#16308 = SPHERICAL_SURFACE('',#94133,0.1) ;
#16309 = SPHERICAL_SURFACE('',#94139,0.1) ;
#16310 = SPHERICAL_SURFACE('',#94147,0.1) ;
#16311 = SPHERICAL_SURFACE('',#94153,0.1) ;
#16312 = SPHERICAL_SURFACE('',#94155,0.1) ;
#16313 = SPHERICAL_SURFACE('',#94161,0.1) ;
#16314 = SPHERICAL_SURFACE('',#94163,0.1) ;
#16315 = SPHERICAL_SURFACE('',#94168,0.1) ;
#16316 = SPHERICAL_SURFACE('',#94174,0.1) ;
#16317 = SPHERICAL_SURFACE('',#94176,0.1) ;
#16318 = SPHERICAL_SURFACE('',#94190,0.1) ;
#16319 = SPHERICAL_SURFACE('',#94192,0.1) ;
#16320 = SPHERICAL_SURFACE('',#94227,0.1) ;
#16321 = SPHERICAL_SURFACE('',#94235,0.1) ;
#16322 = SPHERICAL_SURFACE('',#94274,0.1) ;
#16323 = SPHERICAL_SURFACE('',#94284,0.1) ;
#16324 = SPHERICAL_SURFACE('',#94286,0.1) ;
#16325 = SPHERICAL_SURFACE('',#94295,0.1) ;
#16326 = SPHERICAL_SURFACE('',#94308,0.1) ;
#16327 = SPHERICAL_SURFACE('',#94318,0.1) ;
#16328 = SPHERICAL_SURFACE('',#94320,0.1) ;
#16329 = SPHERICAL_SURFACE('',#94329,0.1) ;
#16330 = SPHERICAL_SURFACE('',#94340,0.1) ;
#16331 = SPHERICAL_SURFACE('',#94344,0.1) ;
#16332 = SPHERICAL_SURFACE('',#94353,0.1) ;
#16333 = SPHERICAL_SURFACE('',#94357,0.1) ;
#16334 = SPHERICAL_SURFACE('',#94364,0.1) ;
#16335 = SPHERICAL_SURFACE('',#94368,0.1) ;
#16336 = SPHERICAL_SURFACE('',#94373,0.1) ;
#16337 = SPHERICAL_SURFACE('',#94379,0.1) ;
#16338 = SPHERICAL_SURFACE('',#95043,0.1) ;
#16339 = SPHERICAL_SURFACE('',#95046,0.1) ;
#16340 = SPHERICAL_SURFACE('',#95064,0.1) ;
#16341 = SPHERICAL_SURFACE('',#95085,0.1) ;
#16342 = SPHERICAL_SURFACE('',#95087,0.1) ;
#16343 = SPHERICAL_SURFACE('',#95092,0.1) ;
#16344 = SPHERICAL_SURFACE('',#95095,0.1) ;
#16345 = SPHERICAL_SURFACE('',#95112,0.1) ;
#16346 = SPHERICAL_SURFACE('',#95118,0.1) ;
#16347 = SPHERICAL_SURFACE('',#95136,0.1) ;
#16348 = SPHERICAL_SURFACE('',#95142,0.1) ;
#16349 = SPHERICAL_SURFACE('',#95150,0.1) ;
#16350 = SPHERICAL_SURFACE('',#95156,0.1) ;
#16351 = SPHERICAL_SURFACE('',#95158,0.1) ;
#16352 = SPHERICAL_SURFACE('',#95164,0.1) ;
#16353 = SPHERICAL_SURFACE('',#95166,0.1) ;
#16354 = SPHERICAL_SURFACE('',#95171,0.1) ;
#16355 = SPHERICAL_SURFACE('',#95177,0.1) ;
#16356 = SPHERICAL_SURFACE('',#95179,0.1) ;
#16357 = SPHERICAL_SURFACE('',#95193,0.1) ;
#16358 = SPHERICAL_SURFACE('',#95195,0.1) ;
#16359 = SPHERICAL_SURFACE('',#95230,0.1) ;
#16360 = SPHERICAL_SURFACE('',#95238,0.1) ;
#16361 = SPHERICAL_SURFACE('',#95246,0.1) ;
#16362 = SPHERICAL_SURFACE('',#95248,0.1) ;
#16363 = SPHERICAL_SURFACE('',#95283,0.1) ;
#16364 = SPHERICAL_SURFACE('',#95291,0.1) ;
#16365 = SPHERICAL_SURFACE('',#95299,0.1) ;
#16366 = SPHERICAL_SURFACE('',#95301,0.1) ;
#16367 = SPHERICAL_SURFACE('',#95336,0.1) ;
#16368 = SPHERICAL_SURFACE('',#95344,0.1) ;
#16369 = SPHERICAL_SURFACE('',#95352,0.1) ;
#16370 = SPHERICAL_SURFACE('',#95354,0.1) ;
#16371 = SPHERICAL_SURFACE('',#95389,0.1) ;
#16372 = SPHERICAL_SURFACE('',#95397,0.1) ;
#16373 = SPHERICAL_SURFACE('',#95405,0.1) ;
#16374 = SPHERICAL_SURFACE('',#95407,0.1) ;
#16375 = SPHERICAL_SURFACE('',#95442,0.1) ;
#16376 = SPHERICAL_SURFACE('',#95450,0.1) ;
#16377 = SPHERICAL_SURFACE('',#95458,0.1) ;
#16378 = SPHERICAL_SURFACE('',#95460,0.1) ;
#16379 = SPHERICAL_SURFACE('',#95495,0.1) ;
#16380 = SPHERICAL_SURFACE('',#95503,0.1) ;
#16381 = SPHERICAL_SURFACE('',#95511,0.1) ;
#16382 = SPHERICAL_SURFACE('',#95513,0.1) ;
#16383 = SPHERICAL_SURFACE('',#95548,0.1) ;
#16384 = SPHERICAL_SURFACE('',#95556,0.1) ;
#16385 = SPHERICAL_SURFACE('',#95564,0.1) ;
#16386 = SPHERICAL_SURFACE('',#95566,0.1) ;
#16387 = SPHERICAL_SURFACE('',#95601,0.1) ;
#16388 = SPHERICAL_SURFACE('',#95609,0.1) ;
#16389 = SPHERICAL_SURFACE('',#95617,0.1) ;
#16390 = SPHERICAL_SURFACE('',#95619,0.1) ;
#16391 = SPHERICAL_SURFACE('',#95654,0.1) ;
#16392 = SPHERICAL_SURFACE('',#95662,0.1) ;
#16393 = SPHERICAL_SURFACE('',#95673,0.1) ;
#16394 = SPHERICAL_SURFACE('',#95676,0.1) ;
#16395 = SPHERICAL_SURFACE('',#95694,0.1) ;
#16396 = SPHERICAL_SURFACE('',#95715,0.1) ;
#16397 = SPHERICAL_SURFACE('',#95717,0.1) ;
#16398 = SPHERICAL_SURFACE('',#95722,0.1) ;
#16399 = SPHERICAL_SURFACE('',#95725,0.1) ;
#16400 = SPHERICAL_SURFACE('',#95742,0.1) ;
#16401 = SPHERICAL_SURFACE('',#95748,0.1) ;
#16402 = SPHERICAL_SURFACE('',#95766,0.1) ;
#16403 = SPHERICAL_SURFACE('',#95772,0.1) ;
#16404 = SPHERICAL_SURFACE('',#95780,0.1) ;
#16405 = SPHERICAL_SURFACE('',#95786,0.1) ;
#16406 = SPHERICAL_SURFACE('',#95788,0.1) ;
#16407 = SPHERICAL_SURFACE('',#95794,0.1) ;
#16408 = SPHERICAL_SURFACE('',#95796,0.1) ;
#16409 = SPHERICAL_SURFACE('',#95801,0.1) ;
#16410 = SPHERICAL_SURFACE('',#95807,0.1) ;
#16411 = SPHERICAL_SURFACE('',#95809,0.1) ;
#16412 = SPHERICAL_SURFACE('',#95826,0.1) ;
#16413 = SPHERICAL_SURFACE('',#95829,0.1) ;
#16414 = SPHERICAL_SURFACE('',#95847,0.1) ;
#16415 = SPHERICAL_SURFACE('',#95868,0.1) ;
#16416 = SPHERICAL_SURFACE('',#95870,0.1) ;
#16417 = SPHERICAL_SURFACE('',#95875,0.1) ;
#16418 = SPHERICAL_SURFACE('',#95878,0.1) ;
#16419 = SPHERICAL_SURFACE('',#95895,0.1) ;
#16420 = SPHERICAL_SURFACE('',#95901,0.1) ;
#16421 = SPHERICAL_SURFACE('',#95919,0.1) ;
#16422 = SPHERICAL_SURFACE('',#95925,0.1) ;
#16423 = SPHERICAL_SURFACE('',#95933,0.1) ;
#16424 = SPHERICAL_SURFACE('',#95939,0.1) ;
#16425 = SPHERICAL_SURFACE('',#95941,0.1) ;
#16426 = SPHERICAL_SURFACE('',#95947,0.1) ;
#16427 = SPHERICAL_SURFACE('',#95949,0.1) ;
#16428 = SPHERICAL_SURFACE('',#95954,0.1) ;
#16429 = SPHERICAL_SURFACE('',#95960,0.1) ;
#16430 = SPHERICAL_SURFACE('',#95962,0.1) ;
#16431 = SPHERICAL_SURFACE('',#95979,0.1) ;
#16432 = SPHERICAL_SURFACE('',#95982,0.1) ;
#16433 = SPHERICAL_SURFACE('',#96000,0.1) ;
#16434 = SPHERICAL_SURFACE('',#96021,0.1) ;
#16435 = SPHERICAL_SURFACE('',#96023,0.1) ;
#16436 = SPHERICAL_SURFACE('',#96028,0.1) ;
#16437 = SPHERICAL_SURFACE('',#96031,0.1) ;
#16438 = SPHERICAL_SURFACE('',#96048,0.1) ;
#16439 = SPHERICAL_SURFACE('',#96054,0.1) ;
#16440 = SPHERICAL_SURFACE('',#96072,0.1) ;
#16441 = SPHERICAL_SURFACE('',#96078,0.1) ;
#16442 = SPHERICAL_SURFACE('',#96086,0.1) ;
#16443 = SPHERICAL_SURFACE('',#96092,0.1) ;
#16444 = SPHERICAL_SURFACE('',#96094,0.1) ;
#16445 = SPHERICAL_SURFACE('',#96100,0.1) ;
#16446 = SPHERICAL_SURFACE('',#96102,0.1) ;
#16447 = SPHERICAL_SURFACE('',#96107,0.1) ;
#16448 = SPHERICAL_SURFACE('',#96113,0.1) ;
#16449 = SPHERICAL_SURFACE('',#96115,0.1) ;
#16450 = SPHERICAL_SURFACE('',#96132,0.1) ;
#16451 = SPHERICAL_SURFACE('',#96135,0.1) ;
#16452 = SPHERICAL_SURFACE('',#96153,0.1) ;
#16453 = SPHERICAL_SURFACE('',#96174,0.1) ;
#16454 = SPHERICAL_SURFACE('',#96176,0.1) ;
#16455 = SPHERICAL_SURFACE('',#96181,0.1) ;
#16456 = SPHERICAL_SURFACE('',#96184,0.1) ;
#16457 = SPHERICAL_SURFACE('',#96201,0.1) ;
#16458 = SPHERICAL_SURFACE('',#96207,0.1) ;
#16459 = SPHERICAL_SURFACE('',#96225,0.1) ;
#16460 = SPHERICAL_SURFACE('',#96231,0.1) ;
#16461 = SPHERICAL_SURFACE('',#96239,0.1) ;
#16462 = SPHERICAL_SURFACE('',#96245,0.1) ;
#16463 = SPHERICAL_SURFACE('',#96247,0.1) ;
#16464 = SPHERICAL_SURFACE('',#96253,0.1) ;
#16465 = SPHERICAL_SURFACE('',#96255,0.1) ;
#16466 = SPHERICAL_SURFACE('',#96260,0.1) ;
#16467 = SPHERICAL_SURFACE('',#96266,0.1) ;
#16468 = SPHERICAL_SURFACE('',#96268,0.1) ;
#16469 = SPHERICAL_SURFACE('',#96285,0.1) ;
#16470 = SPHERICAL_SURFACE('',#96288,0.1) ;
#16471 = SPHERICAL_SURFACE('',#96306,0.1) ;
#16472 = SPHERICAL_SURFACE('',#96327,0.1) ;
#16473 = SPHERICAL_SURFACE('',#96329,0.1) ;
#16474 = SPHERICAL_SURFACE('',#96334,0.1) ;
#16475 = SPHERICAL_SURFACE('',#96337,0.1) ;
#16476 = SPHERICAL_SURFACE('',#96354,0.1) ;
#16477 = SPHERICAL_SURFACE('',#96360,0.1) ;
#16478 = SPHERICAL_SURFACE('',#96378,0.1) ;
#16479 = SPHERICAL_SURFACE('',#96384,0.1) ;
#16480 = SPHERICAL_SURFACE('',#96392,0.1) ;
#16481 = SPHERICAL_SURFACE('',#96398,0.1) ;
#16482 = SPHERICAL_SURFACE('',#96400,0.1) ;
#16483 = SPHERICAL_SURFACE('',#96406,0.1) ;
#16484 = SPHERICAL_SURFACE('',#96408,0.1) ;
#16485 = SPHERICAL_SURFACE('',#96413,0.1) ;
#16486 = SPHERICAL_SURFACE('',#96419,0.1) ;
#16487 = SPHERICAL_SURFACE('',#96421,0.1) ;
#16488 = SPHERICAL_SURFACE('',#96438,0.1) ;
#16489 = SPHERICAL_SURFACE('',#96441,0.1) ;
#16490 = SPHERICAL_SURFACE('',#96459,0.1) ;
#16491 = SPHERICAL_SURFACE('',#96480,0.1) ;
#16492 = SPHERICAL_SURFACE('',#96482,0.1) ;
#16493 = SPHERICAL_SURFACE('',#96487,0.1) ;
#16494 = SPHERICAL_SURFACE('',#96490,0.1) ;
#16495 = SPHERICAL_SURFACE('',#96507,0.1) ;
#16496 = SPHERICAL_SURFACE('',#96513,0.1) ;
#16497 = SPHERICAL_SURFACE('',#96531,0.1) ;
#16498 = SPHERICAL_SURFACE('',#96537,0.1) ;
#16499 = SPHERICAL_SURFACE('',#96545,0.1) ;
#16500 = SPHERICAL_SURFACE('',#96551,0.1) ;
#16501 = SPHERICAL_SURFACE('',#96553,0.1) ;
#16502 = SPHERICAL_SURFACE('',#96559,0.1) ;
#16503 = SPHERICAL_SURFACE('',#96561,0.1) ;
#16504 = SPHERICAL_SURFACE('',#96566,0.1) ;
#16505 = SPHERICAL_SURFACE('',#96572,0.1) ;
#16506 = SPHERICAL_SURFACE('',#96574,0.1) ;
#16507 = SPHERICAL_SURFACE('',#96591,0.1) ;
#16508 = SPHERICAL_SURFACE('',#96594,0.1) ;
#16509 = SPHERICAL_SURFACE('',#96612,0.1) ;
#16510 = SPHERICAL_SURFACE('',#96633,0.1) ;
#16511 = SPHERICAL_SURFACE('',#96635,0.1) ;
#16512 = SPHERICAL_SURFACE('',#96640,0.1) ;
#16513 = SPHERICAL_SURFACE('',#96643,0.1) ;
#16514 = SPHERICAL_SURFACE('',#96660,0.1) ;
#16515 = SPHERICAL_SURFACE('',#96666,0.1) ;
#16516 = SPHERICAL_SURFACE('',#96684,0.1) ;
#16517 = SPHERICAL_SURFACE('',#96690,0.1) ;
#16518 = SPHERICAL_SURFACE('',#96698,0.1) ;
#16519 = SPHERICAL_SURFACE('',#96704,0.1) ;
#16520 = SPHERICAL_SURFACE('',#96706,0.1) ;
#16521 = SPHERICAL_SURFACE('',#96712,0.1) ;
#16522 = SPHERICAL_SURFACE('',#96714,0.1) ;
#16523 = SPHERICAL_SURFACE('',#96719,0.1) ;
#16524 = SPHERICAL_SURFACE('',#96725,0.1) ;
#16525 = SPHERICAL_SURFACE('',#96727,0.1) ;
#16526 = SPHERICAL_SURFACE('',#96744,0.1) ;
#16527 = SPHERICAL_SURFACE('',#96747,0.1) ;
#16528 = SPHERICAL_SURFACE('',#96765,0.1) ;
#16529 = SPHERICAL_SURFACE('',#96786,0.1) ;
#16530 = SPHERICAL_SURFACE('',#96788,0.1) ;
#16531 = SPHERICAL_SURFACE('',#96793,0.1) ;
#16532 = SPHERICAL_SURFACE('',#96796,0.1) ;
#16533 = SPHERICAL_SURFACE('',#96813,0.1) ;
#16534 = SPHERICAL_SURFACE('',#96819,0.1) ;
#16535 = SPHERICAL_SURFACE('',#96837,0.1) ;
#16536 = SPHERICAL_SURFACE('',#96843,0.1) ;
#16537 = SPHERICAL_SURFACE('',#96851,0.1) ;
#16538 = SPHERICAL_SURFACE('',#96857,0.1) ;
#16539 = SPHERICAL_SURFACE('',#96859,0.1) ;
#16540 = SPHERICAL_SURFACE('',#96865,0.1) ;
#16541 = SPHERICAL_SURFACE('',#96867,0.1) ;
#16542 = SPHERICAL_SURFACE('',#96872,0.1) ;
#16543 = SPHERICAL_SURFACE('',#96878,0.1) ;
#16544 = SPHERICAL_SURFACE('',#96880,0.1) ;
#16545 = SPHERICAL_SURFACE('',#97149,0.1) ;
#16546 = SPHERICAL_SURFACE('',#97159,0.1) ;
#16547 = SPHERICAL_SURFACE('',#97161,0.1) ;
#16548 = SPHERICAL_SURFACE('',#97170,0.1) ;
#16549 = SPHERICAL_SURFACE('',#97183,0.1) ;
#16550 = SPHERICAL_SURFACE('',#97193,0.1) ;
#16551 = SPHERICAL_SURFACE('',#97195,0.1) ;
#16552 = SPHERICAL_SURFACE('',#97204,0.1) ;
#16553 = SPHERICAL_SURFACE('',#97217,0.1) ;
#16554 = SPHERICAL_SURFACE('',#97227,0.1) ;
#16555 = SPHERICAL_SURFACE('',#97229,0.1) ;
#16556 = SPHERICAL_SURFACE('',#97238,0.1) ;
#16557 = SPHERICAL_SURFACE('',#97251,0.1) ;
#16558 = SPHERICAL_SURFACE('',#97261,0.1) ;
#16559 = SPHERICAL_SURFACE('',#97263,0.1) ;
#16560 = SPHERICAL_SURFACE('',#97272,0.1) ;
#16561 = SPHERICAL_SURFACE('',#97285,0.1) ;
#16562 = SPHERICAL_SURFACE('',#97295,0.1) ;
#16563 = SPHERICAL_SURFACE('',#97297,0.1) ;
#16564 = SPHERICAL_SURFACE('',#97306,0.1) ;
#16565 = SPHERICAL_SURFACE('',#97319,0.1) ;
#16566 = SPHERICAL_SURFACE('',#97329,0.1) ;
#16567 = SPHERICAL_SURFACE('',#97331,0.1) ;
#16568 = SPHERICAL_SURFACE('',#97340,0.1) ;
#16569 = SPHERICAL_SURFACE('',#97353,0.1) ;
#16570 = SPHERICAL_SURFACE('',#97363,0.1) ;
#16571 = SPHERICAL_SURFACE('',#97365,0.1) ;
#16572 = SPHERICAL_SURFACE('',#97374,0.1) ;
#16573 = SPHERICAL_SURFACE('',#97387,0.1) ;
#16574 = SPHERICAL_SURFACE('',#97397,0.1) ;
#16575 = SPHERICAL_SURFACE('',#97399,0.1) ;
#16576 = SPHERICAL_SURFACE('',#97408,0.1) ;
#16577 = SPHERICAL_SURFACE('',#97421,0.1) ;
#16578 = SPHERICAL_SURFACE('',#97431,0.1) ;
#16579 = SPHERICAL_SURFACE('',#97433,0.1) ;
#16580 = SPHERICAL_SURFACE('',#97442,0.1) ;
#16581 = SPHERICAL_SURFACE('',#97455,0.1) ;
#16582 = SPHERICAL_SURFACE('',#97465,0.1) ;
#16583 = SPHERICAL_SURFACE('',#97467,0.1) ;
#16584 = SPHERICAL_SURFACE('',#97476,0.1) ;
#16585 = SPHERICAL_SURFACE('',#97489,0.1) ;
#16586 = SPHERICAL_SURFACE('',#97499,0.1) ;
#16587 = SPHERICAL_SURFACE('',#97501,0.1) ;
#16588 = SPHERICAL_SURFACE('',#97510,0.1) ;
#16589 = SPHERICAL_SURFACE('',#97523,0.1) ;
#16590 = SPHERICAL_SURFACE('',#97533,0.1) ;
#16591 = SPHERICAL_SURFACE('',#97535,0.1) ;
#16592 = SPHERICAL_SURFACE('',#97544,0.1) ;
#16593 = SPHERICAL_SURFACE('',#97557,0.1) ;
#16594 = SPHERICAL_SURFACE('',#97567,0.1) ;
#16595 = SPHERICAL_SURFACE('',#97569,0.1) ;
#16596 = SPHERICAL_SURFACE('',#97578,0.1) ;
#16597 = SPHERICAL_SURFACE('',#97591,0.1) ;
#16598 = SPHERICAL_SURFACE('',#97601,0.1) ;
#16599 = SPHERICAL_SURFACE('',#97603,0.1) ;
#16600 = SPHERICAL_SURFACE('',#97612,0.1) ;
#16601 = SPHERICAL_SURFACE('',#97625,0.1) ;
#16602 = SPHERICAL_SURFACE('',#97635,0.1) ;
#16603 = SPHERICAL_SURFACE('',#97637,0.1) ;
#16604 = SPHERICAL_SURFACE('',#97646,0.1) ;
#16605 = SPHERICAL_SURFACE('',#97659,0.1) ;
#16606 = SPHERICAL_SURFACE('',#97669,0.1) ;
#16607 = SPHERICAL_SURFACE('',#97671,0.1) ;
#16608 = SPHERICAL_SURFACE('',#97680,0.1) ;
#16609 = SPHERICAL_SURFACE('',#97693,0.1) ;
#16610 = SPHERICAL_SURFACE('',#97703,0.1) ;
#16611 = SPHERICAL_SURFACE('',#97705,0.1) ;
#16612 = SPHERICAL_SURFACE('',#97714,0.1) ;
#16613 = SPHERICAL_SURFACE('',#97727,0.1) ;
#16614 = SPHERICAL_SURFACE('',#97737,0.1) ;
#16615 = SPHERICAL_SURFACE('',#97739,0.1) ;
#16616 = SPHERICAL_SURFACE('',#97748,0.1) ;
#16617 = SPHERICAL_SURFACE('',#97759,0.1) ;
#16618 = SPHERICAL_SURFACE('',#97763,0.1) ;
#16619 = SPHERICAL_SURFACE('',#97772,0.1) ;
#16620 = SPHERICAL_SURFACE('',#97776,0.1) ;
#16621 = SPHERICAL_SURFACE('',#97783,0.1) ;
#16622 = SPHERICAL_SURFACE('',#97787,0.1) ;
#16623 = SPHERICAL_SURFACE('',#97792,0.1) ;
#16624 = SPHERICAL_SURFACE('',#97798,0.1) ;
#16625 = SPHERICAL_SURFACE('',#97803,0.1) ;
#16626 = SPHERICAL_SURFACE('',#97807,0.1) ;
#16627 = SPHERICAL_SURFACE('',#97816,0.1) ;
#16628 = SPHERICAL_SURFACE('',#97820,0.1) ;
#16629 = SPHERICAL_SURFACE('',#97827,0.1) ;
#16630 = SPHERICAL_SURFACE('',#97831,0.1) ;
#16631 = SPHERICAL_SURFACE('',#97836,0.1) ;
#16632 = SPHERICAL_SURFACE('',#97842,0.1) ;
#16633 = SPHERICAL_SURFACE('',#97847,0.1) ;
#16634 = SPHERICAL_SURFACE('',#97851,0.1) ;
#16635 = SPHERICAL_SURFACE('',#97860,0.1) ;
#16636 = SPHERICAL_SURFACE('',#97864,0.1) ;
#16637 = SPHERICAL_SURFACE('',#97871,0.1) ;
#16638 = SPHERICAL_SURFACE('',#97875,0.1) ;
#16639 = SPHERICAL_SURFACE('',#97880,0.1) ;
#16640 = SPHERICAL_SURFACE('',#97886,0.1) ;
#16641 = SPHERICAL_SURFACE('',#97891,0.1) ;
#16642 = SPHERICAL_SURFACE('',#97895,0.1) ;
#16643 = SPHERICAL_SURFACE('',#97904,0.1) ;
#16644 = SPHERICAL_SURFACE('',#97908,0.1) ;
#16645 = SPHERICAL_SURFACE('',#97915,0.1) ;
#16646 = SPHERICAL_SURFACE('',#97919,0.1) ;
#16647 = SPHERICAL_SURFACE('',#97924,0.1) ;
#16648 = SPHERICAL_SURFACE('',#97930,0.1) ;
#16649 = SPHERICAL_SURFACE('',#97935,0.1) ;
#16650 = SPHERICAL_SURFACE('',#97939,0.1) ;
#16651 = SPHERICAL_SURFACE('',#97948,0.1) ;
#16652 = SPHERICAL_SURFACE('',#97952,0.1) ;
#16653 = SPHERICAL_SURFACE('',#97959,0.1) ;
#16654 = SPHERICAL_SURFACE('',#97963,0.1) ;
#16655 = SPHERICAL_SURFACE('',#97968,0.1) ;
#16656 = SPHERICAL_SURFACE('',#97974,0.1) ;
#16657 = SPHERICAL_SURFACE('',#97979,0.1) ;
#16658 = SPHERICAL_SURFACE('',#97983,0.1) ;
#16659 = SPHERICAL_SURFACE('',#97992,0.1) ;
#16660 = SPHERICAL_SURFACE('',#97996,0.1) ;
#16661 = SPHERICAL_SURFACE('',#98003,0.1) ;
#16662 = SPHERICAL_SURFACE('',#98007,0.1) ;
#16663 = SPHERICAL_SURFACE('',#98012,0.1) ;
#16664 = SPHERICAL_SURFACE('',#98018,0.1) ;
#16665 = SPHERICAL_SURFACE('',#98023,0.1) ;
#16666 = SPHERICAL_SURFACE('',#98027,0.1) ;
#16667 = SPHERICAL_SURFACE('',#98036,0.1) ;
#16668 = SPHERICAL_SURFACE('',#98040,0.1) ;
#16669 = SPHERICAL_SURFACE('',#98047,0.1) ;
#16670 = SPHERICAL_SURFACE('',#98051,0.1) ;
#16671 = SPHERICAL_SURFACE('',#98056,0.1) ;
#16672 = SPHERICAL_SURFACE('',#98062,0.1) ;
#16673 = SPHERICAL_SURFACE('',#98067,0.1) ;
#16674 = SPHERICAL_SURFACE('',#98071,0.1) ;
#16675 = SPHERICAL_SURFACE('',#98080,0.1) ;
#16676 = SPHERICAL_SURFACE('',#98084,0.1) ;
#16677 = SPHERICAL_SURFACE('',#98091,0.1) ;
#16678 = SPHERICAL_SURFACE('',#98095,0.1) ;
#16679 = SPHERICAL_SURFACE('',#98100,0.1) ;
#16680 = SPHERICAL_SURFACE('',#98106,0.1) ;
#16681 = SPHERICAL_SURFACE('',#98111,0.1) ;
#16682 = SPHERICAL_SURFACE('',#98115,0.1) ;
#16683 = SPHERICAL_SURFACE('',#98124,0.1) ;
#16684 = SPHERICAL_SURFACE('',#98128,0.1) ;
#16685 = SPHERICAL_SURFACE('',#98135,0.1) ;
#16686 = SPHERICAL_SURFACE('',#98139,0.1) ;
#16687 = SPHERICAL_SURFACE('',#98144,0.1) ;
#16688 = SPHERICAL_SURFACE('',#98150,0.1) ;
#16689 = SPHERICAL_SURFACE('',#98811,0.1) ;
#16690 = SPHERICAL_SURFACE('',#98831,0.1) ;
#16691 = SPHERICAL_SURFACE('',#98834,0.1) ;
#16692 = SPHERICAL_SURFACE('',#98839,0.1) ;
#16693 = SPHERICAL_SURFACE('',#98860,0.1) ;
#16694 = SPHERICAL_SURFACE('',#98862,0.1) ;
#16695 = SPHERICAL_SURFACE('',#98878,0.1) ;
#16696 = SPHERICAL_SURFACE('',#98894,0.1) ;
#16697 = SPHERICAL_SURFACE('',#98900,0.1) ;
#16698 = SPHERICAL_SURFACE('',#98915,0.1) ;
#16699 = SPHERICAL_SURFACE('',#98935,0.1) ;
#16700 = SPHERICAL_SURFACE('',#98938,0.1) ;
#16701 = SPHERICAL_SURFACE('',#98948,0.1) ;
#16702 = SPHERICAL_SURFACE('',#98962,0.1) ;
#16703 = SPHERICAL_SURFACE('',#99008,0.1) ;
#16704 = SPHERICAL_SURFACE('',#99010,0.1) ;
#16705 = SPHERICAL_SURFACE('',#99022,0.1) ;
#16706 = SPHERICAL_SURFACE('',#99024,0.1) ;
#16707 = SPHERICAL_SURFACE('',#99034,0.1) ;
#16708 = SPHERICAL_SURFACE('',#99036,0.1) ;
#16709 = SPHERICAL_SURFACE('',#99046,0.1) ;
#16710 = SPHERICAL_SURFACE('',#99048,0.1) ;
#16711 = SPHERICAL_SURFACE('',#99053,0.1) ;
#16712 = SPHERICAL_SURFACE('',#99063,0.1) ;
#16713 = SPHERICAL_SURFACE('',#99075,0.1) ;
#16714 = SPHERICAL_SURFACE('',#99087,0.1) ;
#16715 = SPHERICAL_SURFACE('',#99116,0.1) ;
#16716 = SPHERICAL_SURFACE('',#99118,0.1) ;
#16717 = SPHERICAL_SURFACE('',#99130,0.1) ;
#16718 = SPHERICAL_SURFACE('',#99132,0.1) ;
#16719 = SPHERICAL_SURFACE('',#99142,0.1) ;
#16720 = SPHERICAL_SURFACE('',#99144,0.1) ;
#16721 = SPHERICAL_SURFACE('',#99154,0.1) ;
#16722 = SPHERICAL_SURFACE('',#99156,0.1) ;
#16723 = SPHERICAL_SURFACE('',#99162,0.1) ;
#16724 = SPHERICAL_SURFACE('',#99164,0.1) ;
#16725 = SPHERICAL_SURFACE('',#99170,0.1) ;
#16726 = SPHERICAL_SURFACE('',#99172,0.1) ;
#16727 = SPHERICAL_SURFACE('',#99193,0.1) ;
#16728 = SPHERICAL_SURFACE('',#99199,0.1) ;
#16729 = SPHERICAL_SURFACE('',#99942,0.1) ;
#16730 = SPHERICAL_SURFACE('',#99958,0.1) ;
#16731 = SPHERICAL_SURFACE('',#99964,0.1) ;
#16732 = SPHERICAL_SURFACE('',#99979,0.1) ;
#16733 = SPHERICAL_SURFACE('',#99999,0.1) ;
#16734 = SPHERICAL_SURFACE('',#100002,0.1) ;
#16735 = SPHERICAL_SURFACE('',#100012,0.1) ;
#16736 = SPHERICAL_SURFACE('',#100023,0.1) ;
#16737 = SPHERICAL_SURFACE('',#100165,0.1) ;
#16738 = SPHERICAL_SURFACE('',#100167,0.1) ;
#16739 = SPHERICAL_SURFACE('',#100179,0.1) ;
#16740 = SPHERICAL_SURFACE('',#100181,0.1) ;
#16741 = SPHERICAL_SURFACE('',#100191,0.1) ;
#16742 = SPHERICAL_SURFACE('',#100193,0.1) ;
#16743 = SPHERICAL_SURFACE('',#100203,0.1) ;
#16744 = SPHERICAL_SURFACE('',#100205,0.1) ;
#16745 = SPHERICAL_SURFACE('',#100210,0.1) ;
#16746 = SPHERICAL_SURFACE('',#100220,0.1) ;
#16747 = SPHERICAL_SURFACE('',#100232,0.1) ;
#16748 = SPHERICAL_SURFACE('',#100244,0.1) ;
#16749 = SPHERICAL_SURFACE('',#100433,0.1) ;
#16750 = SPHERICAL_SURFACE('',#100435,0.1) ;
#16751 = SPHERICAL_SURFACE('',#100447,0.1) ;
#16752 = SPHERICAL_SURFACE('',#100449,0.1) ;
#16753 = SPHERICAL_SURFACE('',#100459,0.1) ;
#16754 = SPHERICAL_SURFACE('',#100461,0.1) ;
#16755 = SPHERICAL_SURFACE('',#100471,0.1) ;
#16756 = SPHERICAL_SURFACE('',#100473,0.1) ;
#16757 = SPHERICAL_SURFACE('',#100479,0.1) ;
#16758 = SPHERICAL_SURFACE('',#100481,0.1) ;
#16759 = SPHERICAL_SURFACE('',#100487,0.1) ;
#16760 = SPHERICAL_SURFACE('',#100489,0.1) ;
#16761 = SPHERICAL_SURFACE('',#100496,0.1) ;
#16762 = SPHERICAL_SURFACE('',#100509,0.1) ;
#16763 = SPHERICAL_SURFACE('',#100514,0.1) ;
#16764 = SPHERICAL_SURFACE('',#100537,0.1) ;
#16765 = SPHERICAL_SURFACE('',#100548,0.1) ;
#16766 = SPHERICAL_SURFACE('',#100550,0.1) ;
#16767 = SPHERICAL_SURFACE('',#100565,0.1) ;
#16768 = SPHERICAL_SURFACE('',#100579,0.1) ;
#16769 = SPHERICAL_SURFACE('',#100586,0.1) ;
#16770 = SPHERICAL_SURFACE('',#100598,0.1) ;
#16771 = SPHERICAL_SURFACE('',#100600,0.1) ;
#16772 = SPHERICAL_SURFACE('',#100606,0.1) ;
#16773 = SPHERICAL_SURFACE('',#100616,0.1) ;
#16774 = SPHERICAL_SURFACE('',#100622,0.1) ;
#16775 = SPHERICAL_SURFACE('',#100633,0.1) ;
#16776 = SPHERICAL_SURFACE('',#100639,0.1) ;
#16777 = SPHERICAL_SURFACE('',#100667,0.1) ;
#16778 = SPHERICAL_SURFACE('',#100669,0.1) ;
#16779 = SPHERICAL_SURFACE('',#100679,0.1) ;
#16780 = SPHERICAL_SURFACE('',#100681,0.1) ;
#16781 = SPHERICAL_SURFACE('',#100709,0.1) ;
#16782 = SPHERICAL_SURFACE('',#100711,0.1) ;
#16783 = SPHERICAL_SURFACE('',#100723,0.1) ;
#16784 = SPHERICAL_SURFACE('',#100725,0.1) ;
#16785 = SPHERICAL_SURFACE('',#100735,0.1) ;
#16786 = SPHERICAL_SURFACE('',#100737,0.1) ;
#16787 = SPHERICAL_SURFACE('',#100747,0.1) ;
#16788 = SPHERICAL_SURFACE('',#100749,0.1) ;
#16789 = SPHERICAL_SURFACE('',#100755,0.1) ;
#16790 = SPHERICAL_SURFACE('',#100757,0.1) ;
#16791 = SPHERICAL_SURFACE('',#100763,0.1) ;
#16792 = SPHERICAL_SURFACE('',#100765,0.1) ;
#16793 = SPHERICAL_SURFACE('',#100772,0.1) ;
#16794 = SPHERICAL_SURFACE('',#100785,0.1) ;
#16795 = SPHERICAL_SURFACE('',#100790,0.1) ;
#16796 = SPHERICAL_SURFACE('',#100813,0.1) ;
#16797 = SPHERICAL_SURFACE('',#100824,0.1) ;
#16798 = SPHERICAL_SURFACE('',#100826,0.1) ;
#16799 = SPHERICAL_SURFACE('',#100841,0.1) ;
#16800 = SPHERICAL_SURFACE('',#100855,0.1) ;
#16801 = SPHERICAL_SURFACE('',#100862,0.1) ;
#16802 = SPHERICAL_SURFACE('',#100874,0.1) ;
#16803 = SPHERICAL_SURFACE('',#100876,0.1) ;
#16804 = SPHERICAL_SURFACE('',#100882,0.1) ;
#16805 = SPHERICAL_SURFACE('',#100892,0.1) ;
#16806 = SPHERICAL_SURFACE('',#100898,0.1) ;
#16807 = SPHERICAL_SURFACE('',#100909,0.1) ;
#16808 = SPHERICAL_SURFACE('',#100915,0.1) ;
#16809 = SPHERICAL_SURFACE('',#100943,0.1) ;
#16810 = SPHERICAL_SURFACE('',#100945,0.1) ;
#16811 = SPHERICAL_SURFACE('',#100955,0.1) ;
#16812 = SPHERICAL_SURFACE('',#100957,0.1) ;
#16813 = SPHERICAL_SURFACE('',#100985,0.1) ;
#16814 = SPHERICAL_SURFACE('',#100987,0.1) ;
#16815 = SPHERICAL_SURFACE('',#100999,0.1) ;
#16816 = SPHERICAL_SURFACE('',#101001,0.1) ;
#16817 = SPHERICAL_SURFACE('',#101011,0.1) ;
#16818 = SPHERICAL_SURFACE('',#101013,0.1) ;
#16819 = SPHERICAL_SURFACE('',#101023,0.1) ;
#16820 = SPHERICAL_SURFACE('',#101025,0.1) ;
#16821 = SPHERICAL_SURFACE('',#101031,0.1) ;
#16822 = SPHERICAL_SURFACE('',#101033,0.1) ;
#16823 = SPHERICAL_SURFACE('',#101039,0.1) ;
#16824 = SPHERICAL_SURFACE('',#101041,0.1) ;
#16825 = SPHERICAL_SURFACE('',#101048,0.1) ;
#16826 = SPHERICAL_SURFACE('',#101061,0.1) ;
#16827 = SPHERICAL_SURFACE('',#101066,0.1) ;
#16828 = SPHERICAL_SURFACE('',#101089,0.1) ;
#16829 = SPHERICAL_SURFACE('',#101100,0.1) ;
#16830 = SPHERICAL_SURFACE('',#101102,0.1) ;
#16831 = SPHERICAL_SURFACE('',#101117,0.1) ;
#16832 = SPHERICAL_SURFACE('',#101131,0.1) ;
#16833 = SPHERICAL_SURFACE('',#101138,0.1) ;
#16834 = SPHERICAL_SURFACE('',#101150,0.1) ;
#16835 = SPHERICAL_SURFACE('',#101152,0.1) ;
#16836 = SPHERICAL_SURFACE('',#101158,0.1) ;
#16837 = SPHERICAL_SURFACE('',#101168,0.1) ;
#16838 = SPHERICAL_SURFACE('',#101174,0.1) ;
#16839 = SPHERICAL_SURFACE('',#101185,0.1) ;
#16840 = SPHERICAL_SURFACE('',#101191,0.1) ;
#16841 = SPHERICAL_SURFACE('',#101219,0.1) ;
#16842 = SPHERICAL_SURFACE('',#101221,0.1) ;
#16843 = SPHERICAL_SURFACE('',#101231,0.1) ;
#16844 = SPHERICAL_SURFACE('',#101233,0.1) ;
#16845 = SPHERICAL_SURFACE('',#101261,0.1) ;
#16846 = SPHERICAL_SURFACE('',#101263,0.1) ;
#16847 = SPHERICAL_SURFACE('',#101275,0.1) ;
#16848 = SPHERICAL_SURFACE('',#101277,0.1) ;
#16849 = SPHERICAL_SURFACE('',#101287,0.1) ;
#16850 = SPHERICAL_SURFACE('',#101289,0.1) ;
#16851 = SPHERICAL_SURFACE('',#101299,0.1) ;
#16852 = SPHERICAL_SURFACE('',#101301,0.1) ;
#16853 = SPHERICAL_SURFACE('',#101307,0.1) ;
#16854 = SPHERICAL_SURFACE('',#101309,0.1) ;
#16855 = SPHERICAL_SURFACE('',#101315,0.1) ;
#16856 = SPHERICAL_SURFACE('',#101317,0.1) ;
#16857 = SPHERICAL_SURFACE('',#101324,0.1) ;
#16858 = SPHERICAL_SURFACE('',#101337,0.1) ;
#16859 = SPHERICAL_SURFACE('',#101342,0.1) ;
#16860 = SPHERICAL_SURFACE('',#101365,0.1) ;
#16861 = SPHERICAL_SURFACE('',#101376,0.1) ;
#16862 = SPHERICAL_SURFACE('',#101378,0.1) ;
#16863 = SPHERICAL_SURFACE('',#101393,0.1) ;
#16864 = SPHERICAL_SURFACE('',#101407,0.1) ;
#16865 = SPHERICAL_SURFACE('',#101414,0.1) ;
#16866 = SPHERICAL_SURFACE('',#101426,0.1) ;
#16867 = SPHERICAL_SURFACE('',#101428,0.1) ;
#16868 = SPHERICAL_SURFACE('',#101434,0.1) ;
#16869 = SPHERICAL_SURFACE('',#101444,0.1) ;
#16870 = SPHERICAL_SURFACE('',#101450,0.1) ;
#16871 = SPHERICAL_SURFACE('',#101461,0.1) ;
#16872 = SPHERICAL_SURFACE('',#101467,0.1) ;
#16873 = SPHERICAL_SURFACE('',#101495,0.1) ;
#16874 = SPHERICAL_SURFACE('',#101497,0.1) ;
#16875 = SPHERICAL_SURFACE('',#101507,0.1) ;
#16876 = SPHERICAL_SURFACE('',#101509,0.1) ;
#16877 = SPHERICAL_SURFACE('',#101537,0.1) ;
#16878 = SPHERICAL_SURFACE('',#101539,0.1) ;
#16879 = SPHERICAL_SURFACE('',#101551,0.1) ;
#16880 = SPHERICAL_SURFACE('',#101553,0.1) ;
#16881 = SPHERICAL_SURFACE('',#101563,0.1) ;
#16882 = SPHERICAL_SURFACE('',#101565,0.1) ;
#16883 = SPHERICAL_SURFACE('',#101575,0.1) ;
#16884 = SPHERICAL_SURFACE('',#101577,0.1) ;
#16885 = SPHERICAL_SURFACE('',#101583,0.1) ;
#16886 = SPHERICAL_SURFACE('',#101585,0.1) ;
#16887 = SPHERICAL_SURFACE('',#101591,0.1) ;
#16888 = SPHERICAL_SURFACE('',#101593,0.1) ;
#16889 = SPHERICAL_SURFACE('',#101600,0.1) ;
#16890 = SPHERICAL_SURFACE('',#101613,0.1) ;
#16891 = SPHERICAL_SURFACE('',#101618,0.1) ;
#16892 = SPHERICAL_SURFACE('',#101641,0.1) ;
#16893 = SPHERICAL_SURFACE('',#101652,0.1) ;
#16894 = SPHERICAL_SURFACE('',#101654,0.1) ;
#16895 = SPHERICAL_SURFACE('',#101669,0.1) ;
#16896 = SPHERICAL_SURFACE('',#101683,0.1) ;
#16897 = SPHERICAL_SURFACE('',#101690,0.1) ;
#16898 = SPHERICAL_SURFACE('',#101702,0.1) ;
#16899 = SPHERICAL_SURFACE('',#101704,0.1) ;
#16900 = SPHERICAL_SURFACE('',#101710,0.1) ;
#16901 = SPHERICAL_SURFACE('',#101720,0.1) ;
#16902 = SPHERICAL_SURFACE('',#101726,0.1) ;
#16903 = SPHERICAL_SURFACE('',#101737,0.1) ;
#16904 = SPHERICAL_SURFACE('',#101743,0.1) ;
#16905 = SPHERICAL_SURFACE('',#101771,0.1) ;
#16906 = SPHERICAL_SURFACE('',#101773,0.1) ;
#16907 = SPHERICAL_SURFACE('',#101783,0.1) ;
#16908 = SPHERICAL_SURFACE('',#101785,0.1) ;
#16909 = SPHERICAL_SURFACE('',#101813,0.1) ;
#16910 = SPHERICAL_SURFACE('',#101815,0.1) ;
#16911 = SPHERICAL_SURFACE('',#101827,0.1) ;
#16912 = SPHERICAL_SURFACE('',#101829,0.1) ;
#16913 = SPHERICAL_SURFACE('',#101839,0.1) ;
#16914 = SPHERICAL_SURFACE('',#101841,0.1) ;
#16915 = SPHERICAL_SURFACE('',#101851,0.1) ;
#16916 = SPHERICAL_SURFACE('',#101853,0.1) ;
#16917 = SPHERICAL_SURFACE('',#101859,0.1) ;
#16918 = SPHERICAL_SURFACE('',#101861,0.1) ;
#16919 = SPHERICAL_SURFACE('',#101867,0.1) ;
#16920 = SPHERICAL_SURFACE('',#101869,0.1) ;
#16921 = SPHERICAL_SURFACE('',#101876,0.1) ;
#16922 = SPHERICAL_SURFACE('',#101889,0.1) ;
#16923 = SPHERICAL_SURFACE('',#101894,0.1) ;
#16924 = SPHERICAL_SURFACE('',#101917,0.1) ;
#16925 = SPHERICAL_SURFACE('',#101928,0.1) ;
#16926 = SPHERICAL_SURFACE('',#101930,0.1) ;
#16927 = SPHERICAL_SURFACE('',#101945,0.1) ;
#16928 = SPHERICAL_SURFACE('',#101959,0.1) ;
#16929 = SPHERICAL_SURFACE('',#101966,0.1) ;
#16930 = SPHERICAL_SURFACE('',#101978,0.1) ;
#16931 = SPHERICAL_SURFACE('',#101980,0.1) ;
#16932 = SPHERICAL_SURFACE('',#101986,0.1) ;
#16933 = SPHERICAL_SURFACE('',#101996,0.1) ;
#16934 = SPHERICAL_SURFACE('',#102002,0.1) ;
#16935 = SPHERICAL_SURFACE('',#102013,0.1) ;
#16936 = SPHERICAL_SURFACE('',#102019,0.1) ;
#16937 = SPHERICAL_SURFACE('',#102047,0.1) ;
#16938 = SPHERICAL_SURFACE('',#102049,0.1) ;
#16939 = SPHERICAL_SURFACE('',#102059,0.1) ;
#16940 = SPHERICAL_SURFACE('',#102061,0.1) ;
#16941 = SPHERICAL_SURFACE('',#102089,0.1) ;
#16942 = SPHERICAL_SURFACE('',#102091,0.1) ;
#16943 = SPHERICAL_SURFACE('',#102103,0.1) ;
#16944 = SPHERICAL_SURFACE('',#102105,0.1) ;
#16945 = SPHERICAL_SURFACE('',#102115,0.1) ;
#16946 = SPHERICAL_SURFACE('',#102117,0.1) ;
#16947 = SPHERICAL_SURFACE('',#102127,0.1) ;
#16948 = SPHERICAL_SURFACE('',#102129,0.1) ;
#16949 = SPHERICAL_SURFACE('',#102135,0.1) ;
#16950 = SPHERICAL_SURFACE('',#102137,0.1) ;
#16951 = SPHERICAL_SURFACE('',#102143,0.1) ;
#16952 = SPHERICAL_SURFACE('',#102145,0.1) ;
#16953 = SPHERICAL_SURFACE('',#102152,0.1) ;
#16954 = SPHERICAL_SURFACE('',#102165,0.1) ;
#16955 = SPHERICAL_SURFACE('',#102170,0.1) ;
#16956 = SPHERICAL_SURFACE('',#102193,0.1) ;
#16957 = SPHERICAL_SURFACE('',#102204,0.1) ;
#16958 = SPHERICAL_SURFACE('',#102206,0.1) ;
#16959 = SPHERICAL_SURFACE('',#102221,0.1) ;
#16960 = SPHERICAL_SURFACE('',#102235,0.1) ;
#16961 = SPHERICAL_SURFACE('',#102242,0.1) ;
#16962 = SPHERICAL_SURFACE('',#102254,0.1) ;
#16963 = SPHERICAL_SURFACE('',#102256,0.1) ;
#16964 = SPHERICAL_SURFACE('',#102262,0.1) ;
#16965 = SPHERICAL_SURFACE('',#102272,0.1) ;
#16966 = SPHERICAL_SURFACE('',#102278,0.1) ;
#16967 = SPHERICAL_SURFACE('',#102289,0.1) ;
#16968 = SPHERICAL_SURFACE('',#102295,0.1) ;
#16969 = SPHERICAL_SURFACE('',#102323,0.1) ;
#16970 = SPHERICAL_SURFACE('',#102325,0.1) ;
#16971 = SPHERICAL_SURFACE('',#102335,0.1) ;
#16972 = SPHERICAL_SURFACE('',#102337,0.1) ;
#16973 = SPHERICAL_SURFACE('',#102365,0.1) ;
#16974 = SPHERICAL_SURFACE('',#102367,0.1) ;
#16975 = SPHERICAL_SURFACE('',#102379,0.1) ;
#16976 = SPHERICAL_SURFACE('',#102381,0.1) ;
#16977 = SPHERICAL_SURFACE('',#102391,0.1) ;
#16978 = SPHERICAL_SURFACE('',#102393,0.1) ;
#16979 = SPHERICAL_SURFACE('',#102403,0.1) ;
#16980 = SPHERICAL_SURFACE('',#102405,0.1) ;
#16981 = SPHERICAL_SURFACE('',#102411,0.1) ;
#16982 = SPHERICAL_SURFACE('',#102413,0.1) ;
#16983 = SPHERICAL_SURFACE('',#102419,0.1) ;
#16984 = SPHERICAL_SURFACE('',#102421,0.1) ;
#16985 = SPHERICAL_SURFACE('',#102428,0.1) ;
#16986 = SPHERICAL_SURFACE('',#102441,0.1) ;
#16987 = SPHERICAL_SURFACE('',#102446,0.1) ;
#16988 = SPHERICAL_SURFACE('',#102469,0.1) ;
#16989 = SPHERICAL_SURFACE('',#102480,0.1) ;
#16990 = SPHERICAL_SURFACE('',#102482,0.1) ;
#16991 = SPHERICAL_SURFACE('',#102497,0.1) ;
#16992 = SPHERICAL_SURFACE('',#102511,0.1) ;
#16993 = SPHERICAL_SURFACE('',#102518,0.1) ;
#16994 = SPHERICAL_SURFACE('',#102530,0.1) ;
#16995 = SPHERICAL_SURFACE('',#102532,0.1) ;
#16996 = SPHERICAL_SURFACE('',#102538,0.1) ;
#16997 = SPHERICAL_SURFACE('',#102548,0.1) ;
#16998 = SPHERICAL_SURFACE('',#102554,0.1) ;
#16999 = SPHERICAL_SURFACE('',#102565,0.1) ;
#17000 = SPHERICAL_SURFACE('',#102571,0.1) ;
#17001 = SPHERICAL_SURFACE('',#102599,0.1) ;
#17002 = SPHERICAL_SURFACE('',#102601,0.1) ;
#17003 = SPHERICAL_SURFACE('',#102611,0.1) ;
#17004 = SPHERICAL_SURFACE('',#102613,0.1) ;
#17005 = SPHERICAL_SURFACE('',#102641,0.1) ;
#17006 = SPHERICAL_SURFACE('',#102643,0.1) ;
#17007 = SPHERICAL_SURFACE('',#102655,0.1) ;
#17008 = SPHERICAL_SURFACE('',#102657,0.1) ;
#17009 = SPHERICAL_SURFACE('',#102667,0.1) ;
#17010 = SPHERICAL_SURFACE('',#102669,0.1) ;
#17011 = SPHERICAL_SURFACE('',#102679,0.1) ;
#17012 = SPHERICAL_SURFACE('',#102681,0.1) ;
#17013 = SPHERICAL_SURFACE('',#102687,0.1) ;
#17014 = SPHERICAL_SURFACE('',#102689,0.1) ;
#17015 = SPHERICAL_SURFACE('',#102695,0.1) ;
#17016 = SPHERICAL_SURFACE('',#102697,0.1) ;
#17017 = SPHERICAL_SURFACE('',#102798,0.1) ;
#17018 = SPHERICAL_SURFACE('',#102804,0.1) ;
#17019 = SPHERICAL_SURFACE('',#102810,0.1) ;
#17020 = SPHERICAL_SURFACE('',#102816,0.1) ;
#17021 = SPHERICAL_SURFACE('',#102822,0.1) ;
#17022 = SPHERICAL_SURFACE('',#102828,0.1) ;
#17023 = SPHERICAL_SURFACE('',#102834,0.1) ;
#17024 = SPHERICAL_SURFACE('',#102840,0.1) ;
#17025 = SPHERICAL_SURFACE('',#102846,0.1) ;
#17026 = SPHERICAL_SURFACE('',#102852,0.1) ;
#17027 = SPHERICAL_SURFACE('',#102858,0.1) ;
#17028 = SPHERICAL_SURFACE('',#102864,0.1) ;
#17029 = SPHERICAL_SURFACE('',#102870,0.1) ;
#17030 = SPHERICAL_SURFACE('',#102876,0.1) ;
#17031 = SPHERICAL_SURFACE('',#102882,0.1) ;
#17032 = SPHERICAL_SURFACE('',#102888,0.1) ;
#17033 = SPHERICAL_SURFACE('',#102894,0.1) ;
#17034 = SPHERICAL_SURFACE('',#102900,0.1) ;
#17035 = SPHERICAL_SURFACE('',#102985,0.1) ;
#17036 = SPHERICAL_SURFACE('',#102993,0.1) ;
#17037 = SPHERICAL_SURFACE('',#102997,0.1) ;
#17038 = SPHERICAL_SURFACE('',#103001,0.1) ;
#17039 = SPHERICAL_SURFACE('',#103012,0.1) ;
#17040 = SPHERICAL_SURFACE('',#103022,0.1) ;
#17041 = SPHERICAL_SURFACE('',#103032,0.1) ;
#17042 = SPHERICAL_SURFACE('',#103042,0.1) ;
#17043 = SPHERICAL_SURFACE('',#103052,0.1) ;
#17044 = SPHERICAL_SURFACE('',#103062,0.1) ;
#17045 = SPHERICAL_SURFACE('',#103070,0.1) ;
#17046 = SPHERICAL_SURFACE('',#103074,0.1) ;
#17047 = FACE_OUTER_BOUND('',#22763,.T.) ;
#17048 = FACE_OUTER_BOUND('',#22764,.T.) ;
#17049 = FACE_OUTER_BOUND('',#22765,.T.) ;
#17050 = FACE_OUTER_BOUND('',#22766,.T.) ;
#17051 = FACE_OUTER_BOUND('',#22767,.T.) ;
#17052 = FACE_OUTER_BOUND('',#22768,.T.) ;
#17053 = FACE_OUTER_BOUND('',#22769,.T.) ;
#17054 = FACE_OUTER_BOUND('',#22770,.T.) ;
#17055 = FACE_OUTER_BOUND('',#22771,.T.) ;
#17056 = FACE_OUTER_BOUND('',#22772,.T.) ;
#17057 = FACE_OUTER_BOUND('',#22773,.T.) ;
#17058 = FACE_OUTER_BOUND('',#22774,.T.) ;
#17059 = FACE_OUTER_BOUND('',#22775,.T.) ;
#17060 = FACE_OUTER_BOUND('',#22776,.T.) ;
#17061 = FACE_OUTER_BOUND('',#22777,.T.) ;
#17062 = FACE_OUTER_BOUND('',#22778,.T.) ;
#17063 = FACE_OUTER_BOUND('',#22779,.T.) ;
#17064 = FACE_OUTER_BOUND('',#22780,.T.) ;
#17065 = FACE_OUTER_BOUND('',#22781,.T.) ;
#17066 = FACE_OUTER_BOUND('',#22782,.T.) ;
#17067 = FACE_OUTER_BOUND('',#22783,.T.) ;
#17068 = FACE_OUTER_BOUND('',#22784,.T.) ;
#17069 = FACE_OUTER_BOUND('',#22785,.T.) ;
#17070 = FACE_OUTER_BOUND('',#22786,.T.) ;
#17071 = FACE_OUTER_BOUND('',#22788,.T.) ;
#17072 = FACE_OUTER_BOUND('',#22789,.T.) ;
#17073 = FACE_OUTER_BOUND('',#22790,.T.) ;
#17074 = FACE_OUTER_BOUND('',#22791,.T.) ;
#17075 = FACE_OUTER_BOUND('',#22792,.T.) ;
#17076 = FACE_OUTER_BOUND('',#22793,.T.) ;
#17077 = FACE_OUTER_BOUND('',#22794,.T.) ;
#17078 = FACE_OUTER_BOUND('',#22795,.T.) ;
#17079 = FACE_OUTER_BOUND('',#22796,.T.) ;
#17080 = FACE_OUTER_BOUND('',#22797,.T.) ;
#17081 = FACE_OUTER_BOUND('',#22798,.T.) ;
#17082 = FACE_OUTER_BOUND('',#22799,.T.) ;
#17083 = FACE_OUTER_BOUND('',#22802,.T.) ;
#17084 = FACE_OUTER_BOUND('',#22803,.T.) ;
#17085 = FACE_OUTER_BOUND('',#22804,.T.) ;
#17086 = FACE_OUTER_BOUND('',#22805,.T.) ;
#17087 = FACE_OUTER_BOUND('',#22806,.T.) ;
#17088 = FACE_OUTER_BOUND('',#22811,.T.) ;
#17089 = FACE_OUTER_BOUND('',#22812,.T.) ;
#17090 = FACE_OUTER_BOUND('',#22813,.T.) ;
#17091 = FACE_OUTER_BOUND('',#22814,.T.) ;
#17092 = FACE_OUTER_BOUND('',#22817,.T.) ;
#17093 = FACE_OUTER_BOUND('',#22820,.T.) ;
#17094 = FACE_OUTER_BOUND('',#22821,.T.) ;
#17095 = FACE_OUTER_BOUND('',#22822,.T.) ;
#17096 = FACE_OUTER_BOUND('',#22823,.T.) ;
#17097 = FACE_OUTER_BOUND('',#22824,.T.) ;
#17098 = FACE_OUTER_BOUND('',#22825,.T.) ;
#17099 = FACE_OUTER_BOUND('',#22826,.T.) ;
#17100 = FACE_OUTER_BOUND('',#22827,.T.) ;
#17101 = FACE_OUTER_BOUND('',#22828,.T.) ;
#17102 = FACE_OUTER_BOUND('',#22829,.T.) ;
#17103 = FACE_OUTER_BOUND('',#22830,.T.) ;
#17104 = FACE_OUTER_BOUND('',#22831,.T.) ;
#17105 = FACE_OUTER_BOUND('',#22832,.T.) ;
#17106 = FACE_OUTER_BOUND('',#22833,.T.) ;
#17107 = FACE_OUTER_BOUND('',#22834,.T.) ;
#17108 = FACE_OUTER_BOUND('',#22835,.T.) ;
#17109 = FACE_OUTER_BOUND('',#22836,.T.) ;
#17110 = FACE_OUTER_BOUND('',#22837,.T.) ;
#17111 = FACE_OUTER_BOUND('',#22838,.T.) ;
#17112 = FACE_OUTER_BOUND('',#22840,.T.) ;
#17113 = FACE_OUTER_BOUND('',#22841,.T.) ;
#17114 = FACE_OUTER_BOUND('',#22842,.T.) ;
#17115 = FACE_OUTER_BOUND('',#22843,.T.) ;
#17116 = FACE_OUTER_BOUND('',#22844,.T.) ;
#17117 = FACE_OUTER_BOUND('',#22845,.T.) ;
#17118 = FACE_OUTER_BOUND('',#22846,.T.) ;
#17119 = FACE_OUTER_BOUND('',#22847,.T.) ;
#17120 = FACE_OUTER_BOUND('',#22848,.T.) ;
#17121 = FACE_OUTER_BOUND('',#22849,.T.) ;
#17122 = FACE_OUTER_BOUND('',#22850,.T.) ;
#17123 = FACE_OUTER_BOUND('',#22851,.T.) ;
#17124 = FACE_OUTER_BOUND('',#22852,.T.) ;
#17125 = FACE_OUTER_BOUND('',#22853,.T.) ;
#17126 = FACE_OUTER_BOUND('',#22854,.T.) ;
#17127 = FACE_OUTER_BOUND('',#22855,.T.) ;
#17128 = FACE_OUTER_BOUND('',#22856,.T.) ;
#17129 = FACE_OUTER_BOUND('',#22857,.T.) ;
#17130 = FACE_OUTER_BOUND('',#22859,.T.) ;
#17131 = FACE_OUTER_BOUND('',#22860,.T.) ;
#17132 = FACE_OUTER_BOUND('',#22861,.T.) ;
#17133 = FACE_OUTER_BOUND('',#22862,.T.) ;
#17134 = FACE_OUTER_BOUND('',#22863,.T.) ;
#17135 = FACE_OUTER_BOUND('',#22864,.T.) ;
#17136 = FACE_OUTER_BOUND('',#22865,.T.) ;
#17137 = FACE_OUTER_BOUND('',#22866,.T.) ;
#17138 = FACE_OUTER_BOUND('',#22867,.T.) ;
#17139 = FACE_OUTER_BOUND('',#22868,.T.) ;
#17140 = FACE_OUTER_BOUND('',#22869,.T.) ;
#17141 = FACE_OUTER_BOUND('',#22870,.T.) ;
#17142 = FACE_OUTER_BOUND('',#22871,.T.) ;
#17143 = FACE_OUTER_BOUND('',#22872,.T.) ;
#17144 = FACE_OUTER_BOUND('',#22873,.T.) ;
#17145 = FACE_OUTER_BOUND('',#22874,.T.) ;
#17146 = FACE_OUTER_BOUND('',#22875,.T.) ;
#17147 = FACE_OUTER_BOUND('',#22876,.T.) ;
#17148 = FACE_OUTER_BOUND('',#22877,.T.) ;
#17149 = FACE_OUTER_BOUND('',#22878,.T.) ;
#17150 = FACE_OUTER_BOUND('',#22879,.T.) ;
#17151 = FACE_OUTER_BOUND('',#22880,.T.) ;
#17152 = FACE_OUTER_BOUND('',#22881,.T.) ;
#17153 = FACE_OUTER_BOUND('',#22882,.T.) ;
#17154 = FACE_OUTER_BOUND('',#22883,.T.) ;
#17155 = FACE_OUTER_BOUND('',#22884,.T.) ;
#17156 = FACE_OUTER_BOUND('',#22885,.T.) ;
#17157 = FACE_OUTER_BOUND('',#22886,.T.) ;
#17158 = FACE_OUTER_BOUND('',#22887,.T.) ;
#17159 = FACE_OUTER_BOUND('',#22888,.T.) ;
#17160 = FACE_OUTER_BOUND('',#22889,.T.) ;
#17161 = FACE_OUTER_BOUND('',#22890,.T.) ;
#17162 = FACE_OUTER_BOUND('',#22891,.T.) ;
#17163 = FACE_OUTER_BOUND('',#22892,.T.) ;
#17164 = FACE_OUTER_BOUND('',#22893,.T.) ;
#17165 = FACE_OUTER_BOUND('',#22894,.T.) ;
#17166 = FACE_OUTER_BOUND('',#22895,.T.) ;
#17167 = FACE_OUTER_BOUND('',#22896,.T.) ;
#17168 = FACE_OUTER_BOUND('',#22897,.T.) ;
#17169 = FACE_OUTER_BOUND('',#22898,.T.) ;
#17170 = FACE_OUTER_BOUND('',#22899,.T.) ;
#17171 = FACE_OUTER_BOUND('',#22900,.T.) ;
#17172 = FACE_OUTER_BOUND('',#22901,.T.) ;
#17173 = FACE_OUTER_BOUND('',#22902,.T.) ;
#17174 = FACE_OUTER_BOUND('',#22903,.T.) ;
#17175 = FACE_OUTER_BOUND('',#22904,.T.) ;
#17176 = FACE_OUTER_BOUND('',#22905,.T.) ;
#17177 = FACE_OUTER_BOUND('',#22906,.T.) ;
#17178 = FACE_OUTER_BOUND('',#22907,.T.) ;
#17179 = FACE_OUTER_BOUND('',#22908,.T.) ;
#17180 = FACE_OUTER_BOUND('',#22909,.T.) ;
#17181 = FACE_OUTER_BOUND('',#22910,.T.) ;
#17182 = FACE_OUTER_BOUND('',#22911,.T.) ;
#17183 = FACE_OUTER_BOUND('',#22912,.T.) ;
#17184 = FACE_OUTER_BOUND('',#22913,.T.) ;
#17185 = FACE_OUTER_BOUND('',#22914,.T.) ;
#17186 = FACE_OUTER_BOUND('',#22915,.T.) ;
#17187 = FACE_OUTER_BOUND('',#22916,.T.) ;
#17188 = FACE_OUTER_BOUND('',#22917,.T.) ;
#17189 = FACE_OUTER_BOUND('',#22918,.T.) ;
#17190 = FACE_OUTER_BOUND('',#22919,.T.) ;
#17191 = FACE_OUTER_BOUND('',#22920,.T.) ;
#17192 = FACE_OUTER_BOUND('',#22921,.T.) ;
#17193 = FACE_OUTER_BOUND('',#22922,.T.) ;
#17194 = FACE_OUTER_BOUND('',#22923,.T.) ;
#17195 = FACE_OUTER_BOUND('',#22924,.T.) ;
#17196 = FACE_OUTER_BOUND('',#22925,.T.) ;
#17197 = FACE_OUTER_BOUND('',#22926,.T.) ;
#17198 = FACE_OUTER_BOUND('',#22927,.T.) ;
#17199 = FACE_OUTER_BOUND('',#22928,.T.) ;
#17200 = FACE_OUTER_BOUND('',#22929,.T.) ;
#17201 = FACE_OUTER_BOUND('',#22930,.T.) ;
#17202 = FACE_OUTER_BOUND('',#22931,.T.) ;
#17203 = FACE_OUTER_BOUND('',#22932,.T.) ;
#17204 = FACE_OUTER_BOUND('',#22933,.T.) ;
#17205 = FACE_OUTER_BOUND('',#22934,.T.) ;
#17206 = FACE_OUTER_BOUND('',#22935,.T.) ;
#17207 = FACE_OUTER_BOUND('',#22936,.T.) ;
#17208 = FACE_OUTER_BOUND('',#22937,.T.) ;
#17209 = FACE_OUTER_BOUND('',#22938,.T.) ;
#17210 = FACE_OUTER_BOUND('',#22939,.T.) ;
#17211 = FACE_OUTER_BOUND('',#22940,.T.) ;
#17212 = FACE_OUTER_BOUND('',#22941,.T.) ;
#17213 = FACE_OUTER_BOUND('',#22942,.T.) ;
#17214 = FACE_OUTER_BOUND('',#22943,.T.) ;
#17215 = FACE_OUTER_BOUND('',#22944,.T.) ;
#17216 = FACE_OUTER_BOUND('',#22945,.T.) ;
#17217 = FACE_OUTER_BOUND('',#22946,.T.) ;
#17218 = FACE_OUTER_BOUND('',#22947,.T.) ;
#17219 = FACE_OUTER_BOUND('',#22948,.T.) ;
#17220 = FACE_OUTER_BOUND('',#22949,.T.) ;
#17221 = FACE_OUTER_BOUND('',#22950,.T.) ;
#17222 = FACE_OUTER_BOUND('',#22951,.T.) ;
#17223 = FACE_OUTER_BOUND('',#22952,.T.) ;
#17224 = FACE_OUTER_BOUND('',#22953,.T.) ;
#17225 = FACE_OUTER_BOUND('',#22954,.T.) ;
#17226 = FACE_OUTER_BOUND('',#22955,.T.) ;
#17227 = FACE_OUTER_BOUND('',#22956,.T.) ;
#17228 = FACE_OUTER_BOUND('',#22957,.T.) ;
#17229 = FACE_OUTER_BOUND('',#22958,.T.) ;
#17230 = FACE_OUTER_BOUND('',#22959,.T.) ;
#17231 = FACE_OUTER_BOUND('',#22960,.T.) ;
#17232 = FACE_OUTER_BOUND('',#22961,.T.) ;
#17233 = FACE_OUTER_BOUND('',#22962,.T.) ;
#17234 = FACE_OUTER_BOUND('',#22963,.T.) ;
#17235 = FACE_OUTER_BOUND('',#22964,.T.) ;
#17236 = FACE_OUTER_BOUND('',#22965,.T.) ;
#17237 = FACE_OUTER_BOUND('',#22966,.T.) ;
#17238 = FACE_OUTER_BOUND('',#22967,.T.) ;
#17239 = FACE_OUTER_BOUND('',#22968,.T.) ;
#17240 = FACE_OUTER_BOUND('',#22969,.T.) ;
#17241 = FACE_OUTER_BOUND('',#22970,.T.) ;
#17242 = FACE_OUTER_BOUND('',#22971,.T.) ;
#17243 = FACE_OUTER_BOUND('',#22972,.T.) ;
#17244 = FACE_OUTER_BOUND('',#22973,.T.) ;
#17245 = FACE_OUTER_BOUND('',#22974,.T.) ;
#17246 = FACE_OUTER_BOUND('',#22975,.T.) ;
#17247 = FACE_OUTER_BOUND('',#22976,.T.) ;
#17248 = FACE_OUTER_BOUND('',#22977,.T.) ;
#17249 = FACE_OUTER_BOUND('',#22978,.T.) ;
#17250 = FACE_OUTER_BOUND('',#22979,.T.) ;
#17251 = FACE_OUTER_BOUND('',#22980,.T.) ;
#17252 = FACE_OUTER_BOUND('',#22981,.T.) ;
#17253 = FACE_OUTER_BOUND('',#22982,.T.) ;
#17254 = FACE_OUTER_BOUND('',#22983,.T.) ;
#17255 = FACE_OUTER_BOUND('',#22984,.T.) ;
#17256 = FACE_OUTER_BOUND('',#22985,.T.) ;
#17257 = FACE_OUTER_BOUND('',#22986,.T.) ;
#17258 = FACE_OUTER_BOUND('',#22987,.T.) ;
#17259 = FACE_OUTER_BOUND('',#22988,.T.) ;
#17260 = FACE_OUTER_BOUND('',#22989,.T.) ;
#17261 = FACE_OUTER_BOUND('',#22990,.T.) ;
#17262 = FACE_OUTER_BOUND('',#22991,.T.) ;
#17263 = FACE_OUTER_BOUND('',#22992,.T.) ;
#17264 = FACE_OUTER_BOUND('',#22993,.T.) ;
#17265 = FACE_OUTER_BOUND('',#22994,.T.) ;
#17266 = FACE_OUTER_BOUND('',#22995,.T.) ;
#17267 = FACE_OUTER_BOUND('',#22996,.T.) ;
#17268 = FACE_OUTER_BOUND('',#22997,.T.) ;
#17269 = FACE_OUTER_BOUND('',#22998,.T.) ;
#17270 = FACE_OUTER_BOUND('',#22999,.T.) ;
#17271 = FACE_OUTER_BOUND('',#23000,.T.) ;
#17272 = FACE_OUTER_BOUND('',#23001,.T.) ;
#17273 = FACE_OUTER_BOUND('',#23002,.T.) ;
#17274 = FACE_OUTER_BOUND('',#23003,.T.) ;
#17275 = FACE_OUTER_BOUND('',#23004,.T.) ;
#17276 = FACE_OUTER_BOUND('',#23005,.T.) ;
#17277 = FACE_OUTER_BOUND('',#23006,.T.) ;
#17278 = FACE_OUTER_BOUND('',#23007,.T.) ;
#17279 = FACE_OUTER_BOUND('',#23008,.T.) ;
#17280 = FACE_OUTER_BOUND('',#23009,.T.) ;
#17281 = FACE_OUTER_BOUND('',#23010,.T.) ;
#17282 = FACE_OUTER_BOUND('',#23011,.T.) ;
#17283 = FACE_OUTER_BOUND('',#23012,.T.) ;
#17284 = FACE_OUTER_BOUND('',#23013,.T.) ;
#17285 = FACE_OUTER_BOUND('',#23014,.T.) ;
#17286 = FACE_OUTER_BOUND('',#23015,.T.) ;
#17287 = FACE_OUTER_BOUND('',#23016,.T.) ;
#17288 = FACE_OUTER_BOUND('',#23017,.T.) ;
#17289 = FACE_OUTER_BOUND('',#23018,.T.) ;
#17290 = FACE_OUTER_BOUND('',#23019,.T.) ;
#17291 = FACE_OUTER_BOUND('',#23020,.T.) ;
#17292 = FACE_OUTER_BOUND('',#23021,.T.) ;
#17293 = FACE_OUTER_BOUND('',#23022,.T.) ;
#17294 = FACE_OUTER_BOUND('',#23023,.T.) ;
#17295 = FACE_OUTER_BOUND('',#23024,.T.) ;
#17296 = FACE_OUTER_BOUND('',#23025,.T.) ;
#17297 = FACE_OUTER_BOUND('',#23026,.T.) ;
#17298 = FACE_OUTER_BOUND('',#23027,.T.) ;
#17299 = FACE_OUTER_BOUND('',#23028,.T.) ;
#17300 = FACE_OUTER_BOUND('',#23029,.T.) ;
#17301 = FACE_OUTER_BOUND('',#23030,.T.) ;
#17302 = FACE_OUTER_BOUND('',#23031,.T.) ;
#17303 = FACE_OUTER_BOUND('',#23032,.T.) ;
#17304 = FACE_OUTER_BOUND('',#23033,.T.) ;
#17305 = FACE_OUTER_BOUND('',#23034,.T.) ;
#17306 = FACE_OUTER_BOUND('',#23035,.T.) ;
#17307 = FACE_OUTER_BOUND('',#23036,.T.) ;
#17308 = FACE_OUTER_BOUND('',#23037,.T.) ;
#17309 = FACE_OUTER_BOUND('',#23038,.T.) ;
#17310 = FACE_OUTER_BOUND('',#23039,.T.) ;
#17311 = FACE_OUTER_BOUND('',#23040,.T.) ;
#17312 = FACE_OUTER_BOUND('',#23041,.T.) ;
#17313 = FACE_OUTER_BOUND('',#23043,.T.) ;
#17314 = FACE_OUTER_BOUND('',#23044,.T.) ;
#17315 = FACE_OUTER_BOUND('',#23045,.T.) ;
#17316 = FACE_OUTER_BOUND('',#23046,.T.) ;
#17317 = FACE_OUTER_BOUND('',#23047,.T.) ;
#17318 = FACE_OUTER_BOUND('',#23048,.T.) ;
#17319 = FACE_OUTER_BOUND('',#23049,.T.) ;
#17320 = FACE_OUTER_BOUND('',#23050,.T.) ;
#17321 = FACE_OUTER_BOUND('',#23051,.T.) ;
#17322 = FACE_OUTER_BOUND('',#23052,.T.) ;
#17323 = FACE_OUTER_BOUND('',#23053,.T.) ;
#17324 = FACE_OUTER_BOUND('',#23054,.T.) ;
#17325 = FACE_OUTER_BOUND('',#23055,.T.) ;
#17326 = FACE_OUTER_BOUND('',#23056,.T.) ;
#17327 = FACE_OUTER_BOUND('',#23057,.T.) ;
#17328 = FACE_OUTER_BOUND('',#23058,.T.) ;
#17329 = FACE_OUTER_BOUND('',#23059,.T.) ;
#17330 = FACE_OUTER_BOUND('',#23060,.T.) ;
#17331 = FACE_OUTER_BOUND('',#23062,.T.) ;
#17332 = FACE_OUTER_BOUND('',#23063,.T.) ;
#17333 = FACE_OUTER_BOUND('',#23064,.T.) ;
#17334 = FACE_OUTER_BOUND('',#23065,.T.) ;
#17335 = FACE_OUTER_BOUND('',#23066,.T.) ;
#17336 = FACE_OUTER_BOUND('',#23067,.T.) ;
#17337 = FACE_OUTER_BOUND('',#23068,.T.) ;
#17338 = FACE_OUTER_BOUND('',#23069,.T.) ;
#17339 = FACE_OUTER_BOUND('',#23070,.T.) ;
#17340 = FACE_OUTER_BOUND('',#23071,.T.) ;
#17341 = FACE_OUTER_BOUND('',#23072,.T.) ;
#17342 = FACE_OUTER_BOUND('',#23073,.T.) ;
#17343 = FACE_OUTER_BOUND('',#23074,.T.) ;
#17344 = FACE_OUTER_BOUND('',#23075,.T.) ;
#17345 = FACE_OUTER_BOUND('',#23076,.T.) ;
#17346 = FACE_OUTER_BOUND('',#23077,.T.) ;
#17347 = FACE_OUTER_BOUND('',#23078,.T.) ;
#17348 = FACE_OUTER_BOUND('',#23079,.T.) ;
#17349 = FACE_OUTER_BOUND('',#23080,.T.) ;
#17350 = FACE_OUTER_BOUND('',#23081,.T.) ;
#17351 = FACE_OUTER_BOUND('',#23082,.T.) ;
#17352 = FACE_OUTER_BOUND('',#23083,.T.) ;
#17353 = FACE_OUTER_BOUND('',#23084,.T.) ;
#17354 = FACE_OUTER_BOUND('',#23085,.T.) ;
#17355 = FACE_OUTER_BOUND('',#23086,.T.) ;
#17356 = FACE_OUTER_BOUND('',#23087,.T.) ;
#17357 = FACE_OUTER_BOUND('',#23088,.T.) ;
#17358 = FACE_OUTER_BOUND('',#23089,.T.) ;
#17359 = FACE_OUTER_BOUND('',#23090,.T.) ;
#17360 = FACE_OUTER_BOUND('',#23091,.T.) ;
#17361 = FACE_OUTER_BOUND('',#23092,.T.) ;
#17362 = FACE_OUTER_BOUND('',#23093,.T.) ;
#17363 = FACE_OUTER_BOUND('',#23094,.T.) ;
#17364 = FACE_OUTER_BOUND('',#23095,.T.) ;
#17365 = FACE_OUTER_BOUND('',#23096,.T.) ;
#17366 = FACE_OUTER_BOUND('',#23097,.T.) ;
#17367 = FACE_OUTER_BOUND('',#23098,.T.) ;
#17368 = FACE_OUTER_BOUND('',#23099,.T.) ;
#17369 = FACE_OUTER_BOUND('',#23100,.T.) ;
#17370 = FACE_OUTER_BOUND('',#23101,.T.) ;
#17371 = FACE_OUTER_BOUND('',#23102,.T.) ;
#17372 = FACE_OUTER_BOUND('',#23103,.T.) ;
#17373 = FACE_OUTER_BOUND('',#23104,.T.) ;
#17374 = FACE_OUTER_BOUND('',#23105,.T.) ;
#17375 = FACE_OUTER_BOUND('',#23106,.T.) ;
#17376 = FACE_OUTER_BOUND('',#23107,.T.) ;
#17377 = FACE_OUTER_BOUND('',#23108,.T.) ;
#17378 = FACE_OUTER_BOUND('',#23109,.T.) ;
#17379 = FACE_OUTER_BOUND('',#23110,.T.) ;
#17380 = FACE_OUTER_BOUND('',#23111,.T.) ;
#17381 = FACE_OUTER_BOUND('',#23112,.T.) ;
#17382 = FACE_OUTER_BOUND('',#23113,.T.) ;
#17383 = FACE_OUTER_BOUND('',#23114,.T.) ;
#17384 = FACE_OUTER_BOUND('',#23115,.T.) ;
#17385 = FACE_OUTER_BOUND('',#23116,.T.) ;
#17386 = FACE_OUTER_BOUND('',#23117,.T.) ;
#17387 = FACE_OUTER_BOUND('',#23118,.T.) ;
#17388 = FACE_OUTER_BOUND('',#23119,.T.) ;
#17389 = FACE_OUTER_BOUND('',#23120,.T.) ;
#17390 = FACE_OUTER_BOUND('',#23121,.T.) ;
#17391 = FACE_OUTER_BOUND('',#23122,.T.) ;
#17392 = FACE_OUTER_BOUND('',#23123,.T.) ;
#17393 = FACE_OUTER_BOUND('',#23124,.T.) ;
#17394 = FACE_OUTER_BOUND('',#23125,.T.) ;
#17395 = FACE_OUTER_BOUND('',#23126,.T.) ;
#17396 = FACE_OUTER_BOUND('',#23127,.T.) ;
#17397 = FACE_OUTER_BOUND('',#23128,.T.) ;
#17398 = FACE_OUTER_BOUND('',#23129,.T.) ;
#17399 = FACE_OUTER_BOUND('',#23130,.T.) ;
#17400 = FACE_OUTER_BOUND('',#23131,.T.) ;
#17401 = FACE_OUTER_BOUND('',#23132,.T.) ;
#17402 = FACE_OUTER_BOUND('',#23133,.T.) ;
#17403 = FACE_OUTER_BOUND('',#23134,.T.) ;
#17404 = FACE_OUTER_BOUND('',#23135,.T.) ;
#17405 = FACE_OUTER_BOUND('',#23136,.T.) ;
#17406 = FACE_OUTER_BOUND('',#23137,.T.) ;
#17407 = FACE_OUTER_BOUND('',#23138,.T.) ;
#17408 = FACE_OUTER_BOUND('',#23139,.T.) ;
#17409 = FACE_OUTER_BOUND('',#23140,.T.) ;
#17410 = FACE_OUTER_BOUND('',#23141,.T.) ;
#17411 = FACE_OUTER_BOUND('',#23142,.T.) ;
#17412 = FACE_OUTER_BOUND('',#23143,.T.) ;
#17413 = FACE_OUTER_BOUND('',#23144,.T.) ;
#17414 = FACE_OUTER_BOUND('',#23145,.T.) ;
#17415 = FACE_OUTER_BOUND('',#23146,.T.) ;
#17416 = FACE_OUTER_BOUND('',#23147,.T.) ;
#17417 = FACE_OUTER_BOUND('',#23148,.T.) ;
#17418 = FACE_OUTER_BOUND('',#23149,.T.) ;
#17419 = FACE_OUTER_BOUND('',#23150,.T.) ;
#17420 = FACE_OUTER_BOUND('',#23151,.T.) ;
#17421 = FACE_OUTER_BOUND('',#23152,.T.) ;
#17422 = FACE_OUTER_BOUND('',#23153,.T.) ;
#17423 = FACE_OUTER_BOUND('',#23154,.T.) ;
#17424 = FACE_OUTER_BOUND('',#23155,.T.) ;
#17425 = FACE_OUTER_BOUND('',#23156,.T.) ;
#17426 = FACE_OUTER_BOUND('',#23157,.T.) ;
#17427 = FACE_OUTER_BOUND('',#23158,.T.) ;
#17428 = FACE_OUTER_BOUND('',#23159,.T.) ;
#17429 = FACE_OUTER_BOUND('',#23160,.T.) ;
#17430 = FACE_OUTER_BOUND('',#23161,.T.) ;
#17431 = FACE_OUTER_BOUND('',#23162,.T.) ;
#17432 = FACE_OUTER_BOUND('',#23163,.T.) ;
#17433 = FACE_OUTER_BOUND('',#23164,.T.) ;
#17434 = FACE_OUTER_BOUND('',#23165,.T.) ;
#17435 = FACE_OUTER_BOUND('',#23166,.T.) ;
#17436 = FACE_OUTER_BOUND('',#23167,.T.) ;
#17437 = FACE_OUTER_BOUND('',#23168,.T.) ;
#17438 = FACE_OUTER_BOUND('',#23169,.T.) ;
#17439 = FACE_OUTER_BOUND('',#23170,.T.) ;
#17440 = FACE_OUTER_BOUND('',#23171,.T.) ;
#17441 = FACE_OUTER_BOUND('',#23172,.T.) ;
#17442 = FACE_OUTER_BOUND('',#23173,.T.) ;
#17443 = FACE_OUTER_BOUND('',#23174,.T.) ;
#17444 = FACE_OUTER_BOUND('',#23175,.T.) ;
#17445 = FACE_OUTER_BOUND('',#23176,.T.) ;
#17446 = FACE_OUTER_BOUND('',#23177,.T.) ;
#17447 = FACE_OUTER_BOUND('',#23178,.T.) ;
#17448 = FACE_OUTER_BOUND('',#23179,.T.) ;
#17449 = FACE_OUTER_BOUND('',#23180,.T.) ;
#17450 = FACE_OUTER_BOUND('',#23181,.T.) ;
#17451 = FACE_OUTER_BOUND('',#23182,.T.) ;
#17452 = FACE_OUTER_BOUND('',#23183,.T.) ;
#17453 = FACE_OUTER_BOUND('',#23184,.T.) ;
#17454 = FACE_OUTER_BOUND('',#23185,.T.) ;
#17455 = FACE_OUTER_BOUND('',#23186,.T.) ;
#17456 = FACE_OUTER_BOUND('',#23187,.T.) ;
#17457 = FACE_OUTER_BOUND('',#23188,.T.) ;
#17458 = FACE_OUTER_BOUND('',#23189,.T.) ;
#17459 = FACE_OUTER_BOUND('',#23190,.T.) ;
#17460 = FACE_OUTER_BOUND('',#23191,.T.) ;
#17461 = FACE_OUTER_BOUND('',#23192,.T.) ;
#17462 = FACE_OUTER_BOUND('',#23193,.T.) ;
#17463 = FACE_OUTER_BOUND('',#23194,.T.) ;
#17464 = FACE_OUTER_BOUND('',#23195,.T.) ;
#17465 = FACE_OUTER_BOUND('',#23196,.T.) ;
#17466 = FACE_OUTER_BOUND('',#23197,.T.) ;
#17467 = FACE_OUTER_BOUND('',#23198,.T.) ;
#17468 = FACE_OUTER_BOUND('',#23199,.T.) ;
#17469 = FACE_OUTER_BOUND('',#23200,.T.) ;
#17470 = FACE_OUTER_BOUND('',#23201,.T.) ;
#17471 = FACE_OUTER_BOUND('',#23202,.T.) ;
#17472 = FACE_OUTER_BOUND('',#23203,.T.) ;
#17473 = FACE_OUTER_BOUND('',#23204,.T.) ;
#17474 = FACE_OUTER_BOUND('',#23205,.T.) ;
#17475 = FACE_OUTER_BOUND('',#23206,.T.) ;
#17476 = FACE_OUTER_BOUND('',#23207,.T.) ;
#17477 = FACE_OUTER_BOUND('',#23208,.T.) ;
#17478 = FACE_OUTER_BOUND('',#23209,.T.) ;
#17479 = FACE_OUTER_BOUND('',#23210,.T.) ;
#17480 = FACE_OUTER_BOUND('',#23211,.T.) ;
#17481 = FACE_OUTER_BOUND('',#23212,.T.) ;
#17482 = FACE_OUTER_BOUND('',#23213,.T.) ;
#17483 = FACE_OUTER_BOUND('',#23214,.T.) ;
#17484 = FACE_OUTER_BOUND('',#23215,.T.) ;
#17485 = FACE_OUTER_BOUND('',#23216,.T.) ;
#17486 = FACE_OUTER_BOUND('',#23217,.T.) ;
#17487 = FACE_OUTER_BOUND('',#23218,.T.) ;
#17488 = FACE_OUTER_BOUND('',#23219,.T.) ;
#17489 = FACE_OUTER_BOUND('',#23220,.T.) ;
#17490 = FACE_OUTER_BOUND('',#23221,.T.) ;
#17491 = FACE_OUTER_BOUND('',#23222,.T.) ;
#17492 = FACE_OUTER_BOUND('',#23223,.T.) ;
#17493 = FACE_OUTER_BOUND('',#23224,.T.) ;
#17494 = FACE_OUTER_BOUND('',#23225,.T.) ;
#17495 = FACE_OUTER_BOUND('',#23226,.T.) ;
#17496 = FACE_OUTER_BOUND('',#23227,.T.) ;
#17497 = FACE_OUTER_BOUND('',#23228,.T.) ;
#17498 = FACE_OUTER_BOUND('',#23229,.T.) ;
#17499 = FACE_OUTER_BOUND('',#23230,.T.) ;
#17500 = FACE_OUTER_BOUND('',#23231,.T.) ;
#17501 = FACE_OUTER_BOUND('',#23232,.T.) ;
#17502 = FACE_OUTER_BOUND('',#23233,.T.) ;
#17503 = FACE_OUTER_BOUND('',#23234,.T.) ;
#17504 = FACE_OUTER_BOUND('',#23235,.T.) ;
#17505 = FACE_OUTER_BOUND('',#23236,.T.) ;
#17506 = FACE_OUTER_BOUND('',#23237,.T.) ;
#17507 = FACE_OUTER_BOUND('',#23238,.T.) ;
#17508 = FACE_OUTER_BOUND('',#23239,.T.) ;
#17509 = FACE_OUTER_BOUND('',#23240,.T.) ;
#17510 = FACE_OUTER_BOUND('',#23241,.T.) ;
#17511 = FACE_OUTER_BOUND('',#23242,.T.) ;
#17512 = FACE_OUTER_BOUND('',#23243,.T.) ;
#17513 = FACE_OUTER_BOUND('',#23244,.T.) ;
#17514 = FACE_OUTER_BOUND('',#23245,.T.) ;
#17515 = FACE_OUTER_BOUND('',#23246,.T.) ;
#17516 = FACE_OUTER_BOUND('',#23247,.T.) ;
#17517 = FACE_OUTER_BOUND('',#23248,.T.) ;
#17518 = FACE_OUTER_BOUND('',#23249,.T.) ;
#17519 = FACE_OUTER_BOUND('',#23251,.T.) ;
#17520 = FACE_OUTER_BOUND('',#23252,.T.) ;
#17521 = FACE_OUTER_BOUND('',#23253,.T.) ;
#17522 = FACE_OUTER_BOUND('',#23254,.T.) ;
#17523 = FACE_OUTER_BOUND('',#23255,.T.) ;
#17524 = FACE_OUTER_BOUND('',#23256,.T.) ;
#17525 = FACE_OUTER_BOUND('',#23257,.T.) ;
#17526 = FACE_OUTER_BOUND('',#23258,.T.) ;
#17527 = FACE_OUTER_BOUND('',#23259,.T.) ;
#17528 = FACE_OUTER_BOUND('',#23260,.T.) ;
#17529 = FACE_OUTER_BOUND('',#23261,.T.) ;
#17530 = FACE_OUTER_BOUND('',#23262,.T.) ;
#17531 = FACE_OUTER_BOUND('',#23265,.T.) ;
#17532 = FACE_OUTER_BOUND('',#23266,.T.) ;
#17533 = FACE_OUTER_BOUND('',#23267,.T.) ;
#17534 = FACE_OUTER_BOUND('',#23268,.T.) ;
#17535 = FACE_OUTER_BOUND('',#23269,.T.) ;
#17536 = FACE_OUTER_BOUND('',#23274,.T.) ;
#17537 = FACE_OUTER_BOUND('',#23275,.T.) ;
#17538 = FACE_OUTER_BOUND('',#23276,.T.) ;
#17539 = FACE_OUTER_BOUND('',#23277,.T.) ;
#17540 = FACE_OUTER_BOUND('',#23280,.T.) ;
#17541 = FACE_OUTER_BOUND('',#23283,.T.) ;
#17542 = FACE_OUTER_BOUND('',#23284,.T.) ;
#17543 = FACE_OUTER_BOUND('',#23285,.T.) ;
#17544 = FACE_OUTER_BOUND('',#23286,.T.) ;
#17545 = FACE_OUTER_BOUND('',#23287,.T.) ;
#17546 = FACE_OUTER_BOUND('',#23288,.T.) ;
#17547 = FACE_OUTER_BOUND('',#23289,.T.) ;
#17548 = FACE_OUTER_BOUND('',#23290,.T.) ;
#17549 = FACE_OUTER_BOUND('',#23291,.T.) ;
#17550 = FACE_OUTER_BOUND('',#23292,.T.) ;
#17551 = FACE_OUTER_BOUND('',#23293,.T.) ;
#17552 = FACE_OUTER_BOUND('',#23294,.T.) ;
#17553 = FACE_OUTER_BOUND('',#23295,.T.) ;
#17554 = FACE_OUTER_BOUND('',#23296,.T.) ;
#17555 = FACE_OUTER_BOUND('',#23297,.T.) ;
#17556 = FACE_OUTER_BOUND('',#23298,.T.) ;
#17557 = FACE_OUTER_BOUND('',#23299,.T.) ;
#17558 = FACE_OUTER_BOUND('',#23300,.T.) ;
#17559 = FACE_OUTER_BOUND('',#23301,.T.) ;
#17560 = FACE_OUTER_BOUND('',#23303,.T.) ;
#17561 = FACE_OUTER_BOUND('',#23304,.T.) ;
#17562 = FACE_OUTER_BOUND('',#23305,.T.) ;
#17563 = FACE_OUTER_BOUND('',#23306,.T.) ;
#17564 = FACE_OUTER_BOUND('',#23307,.T.) ;
#17565 = FACE_OUTER_BOUND('',#23308,.T.) ;
#17566 = FACE_OUTER_BOUND('',#23309,.T.) ;
#17567 = FACE_OUTER_BOUND('',#23310,.T.) ;
#17568 = FACE_OUTER_BOUND('',#23311,.T.) ;
#17569 = FACE_OUTER_BOUND('',#23312,.T.) ;
#17570 = FACE_OUTER_BOUND('',#23313,.T.) ;
#17571 = FACE_OUTER_BOUND('',#23314,.T.) ;
#17572 = FACE_OUTER_BOUND('',#23315,.T.) ;
#17573 = FACE_OUTER_BOUND('',#23316,.T.) ;
#17574 = FACE_OUTER_BOUND('',#23317,.T.) ;
#17575 = FACE_OUTER_BOUND('',#23318,.T.) ;
#17576 = FACE_OUTER_BOUND('',#23319,.T.) ;
#17577 = FACE_OUTER_BOUND('',#23320,.T.) ;
#17578 = FACE_OUTER_BOUND('',#23322,.T.) ;
#17579 = FACE_OUTER_BOUND('',#23323,.T.) ;
#17580 = FACE_OUTER_BOUND('',#23324,.T.) ;
#17581 = FACE_OUTER_BOUND('',#23325,.T.) ;
#17582 = FACE_OUTER_BOUND('',#23326,.T.) ;
#17583 = FACE_OUTER_BOUND('',#23327,.T.) ;
#17584 = FACE_OUTER_BOUND('',#23328,.T.) ;
#17585 = FACE_OUTER_BOUND('',#23329,.T.) ;
#17586 = FACE_OUTER_BOUND('',#23330,.T.) ;
#17587 = FACE_OUTER_BOUND('',#23331,.T.) ;
#17588 = FACE_OUTER_BOUND('',#23332,.T.) ;
#17589 = FACE_OUTER_BOUND('',#23333,.T.) ;
#17590 = FACE_OUTER_BOUND('',#23334,.T.) ;
#17591 = FACE_OUTER_BOUND('',#23335,.T.) ;
#17592 = FACE_OUTER_BOUND('',#23336,.T.) ;
#17593 = FACE_OUTER_BOUND('',#23337,.T.) ;
#17594 = FACE_OUTER_BOUND('',#23338,.T.) ;
#17595 = FACE_OUTER_BOUND('',#23339,.T.) ;
#17596 = FACE_OUTER_BOUND('',#23340,.T.) ;
#17597 = FACE_OUTER_BOUND('',#23341,.T.) ;
#17598 = FACE_OUTER_BOUND('',#23342,.T.) ;
#17599 = FACE_OUTER_BOUND('',#23343,.T.) ;
#17600 = FACE_OUTER_BOUND('',#23344,.T.) ;
#17601 = FACE_OUTER_BOUND('',#23345,.T.) ;
#17602 = FACE_OUTER_BOUND('',#23346,.T.) ;
#17603 = FACE_OUTER_BOUND('',#23347,.T.) ;
#17604 = FACE_OUTER_BOUND('',#23348,.T.) ;
#17605 = FACE_OUTER_BOUND('',#23349,.T.) ;
#17606 = FACE_OUTER_BOUND('',#23350,.T.) ;
#17607 = FACE_OUTER_BOUND('',#23351,.T.) ;
#17608 = FACE_OUTER_BOUND('',#23352,.T.) ;
#17609 = FACE_OUTER_BOUND('',#23353,.T.) ;
#17610 = FACE_OUTER_BOUND('',#23354,.T.) ;
#17611 = FACE_OUTER_BOUND('',#23355,.T.) ;
#17612 = FACE_OUTER_BOUND('',#23356,.T.) ;
#17613 = FACE_OUTER_BOUND('',#23357,.T.) ;
#17614 = FACE_OUTER_BOUND('',#23358,.T.) ;
#17615 = FACE_OUTER_BOUND('',#23359,.T.) ;
#17616 = FACE_OUTER_BOUND('',#23360,.T.) ;
#17617 = FACE_OUTER_BOUND('',#23361,.T.) ;
#17618 = FACE_OUTER_BOUND('',#23362,.T.) ;
#17619 = FACE_OUTER_BOUND('',#23363,.T.) ;
#17620 = FACE_OUTER_BOUND('',#23364,.T.) ;
#17621 = FACE_OUTER_BOUND('',#23365,.T.) ;
#17622 = FACE_OUTER_BOUND('',#23366,.T.) ;
#17623 = FACE_OUTER_BOUND('',#23367,.T.) ;
#17624 = FACE_OUTER_BOUND('',#23368,.T.) ;
#17625 = FACE_OUTER_BOUND('',#23369,.T.) ;
#17626 = FACE_OUTER_BOUND('',#23370,.T.) ;
#17627 = FACE_OUTER_BOUND('',#23371,.T.) ;
#17628 = FACE_OUTER_BOUND('',#23372,.T.) ;
#17629 = FACE_OUTER_BOUND('',#23373,.T.) ;
#17630 = FACE_OUTER_BOUND('',#23374,.T.) ;
#17631 = FACE_OUTER_BOUND('',#23375,.T.) ;
#17632 = FACE_OUTER_BOUND('',#23376,.T.) ;
#17633 = FACE_OUTER_BOUND('',#23377,.T.) ;
#17634 = FACE_OUTER_BOUND('',#23378,.T.) ;
#17635 = FACE_OUTER_BOUND('',#23379,.T.) ;
#17636 = FACE_OUTER_BOUND('',#23380,.T.) ;
#17637 = FACE_OUTER_BOUND('',#23381,.T.) ;
#17638 = FACE_OUTER_BOUND('',#23382,.T.) ;
#17639 = FACE_OUTER_BOUND('',#23383,.T.) ;
#17640 = FACE_OUTER_BOUND('',#23384,.T.) ;
#17641 = FACE_OUTER_BOUND('',#23385,.T.) ;
#17642 = FACE_OUTER_BOUND('',#23386,.T.) ;
#17643 = FACE_OUTER_BOUND('',#23387,.T.) ;
#17644 = FACE_OUTER_BOUND('',#23388,.T.) ;
#17645 = FACE_OUTER_BOUND('',#23389,.T.) ;
#17646 = FACE_OUTER_BOUND('',#23390,.T.) ;
#17647 = FACE_OUTER_BOUND('',#23391,.T.) ;
#17648 = FACE_OUTER_BOUND('',#23392,.T.) ;
#17649 = FACE_OUTER_BOUND('',#23393,.T.) ;
#17650 = FACE_OUTER_BOUND('',#23394,.T.) ;
#17651 = FACE_OUTER_BOUND('',#23395,.T.) ;
#17652 = FACE_OUTER_BOUND('',#23396,.T.) ;
#17653 = FACE_OUTER_BOUND('',#23397,.T.) ;
#17654 = FACE_OUTER_BOUND('',#23398,.T.) ;
#17655 = FACE_OUTER_BOUND('',#23399,.T.) ;
#17656 = FACE_OUTER_BOUND('',#23400,.T.) ;
#17657 = FACE_OUTER_BOUND('',#23401,.T.) ;
#17658 = FACE_OUTER_BOUND('',#23402,.T.) ;
#17659 = FACE_OUTER_BOUND('',#23403,.T.) ;
#17660 = FACE_OUTER_BOUND('',#23404,.T.) ;
#17661 = FACE_OUTER_BOUND('',#23405,.T.) ;
#17662 = FACE_OUTER_BOUND('',#23406,.T.) ;
#17663 = FACE_OUTER_BOUND('',#23407,.T.) ;
#17664 = FACE_OUTER_BOUND('',#23408,.T.) ;
#17665 = FACE_OUTER_BOUND('',#23409,.T.) ;
#17666 = FACE_OUTER_BOUND('',#23410,.T.) ;
#17667 = FACE_OUTER_BOUND('',#23411,.T.) ;
#17668 = FACE_OUTER_BOUND('',#23412,.T.) ;
#17669 = FACE_OUTER_BOUND('',#23413,.T.) ;
#17670 = FACE_OUTER_BOUND('',#23414,.T.) ;
#17671 = FACE_OUTER_BOUND('',#23415,.T.) ;
#17672 = FACE_OUTER_BOUND('',#23416,.T.) ;
#17673 = FACE_OUTER_BOUND('',#23417,.T.) ;
#17674 = FACE_OUTER_BOUND('',#23418,.T.) ;
#17675 = FACE_OUTER_BOUND('',#23419,.T.) ;
#17676 = FACE_OUTER_BOUND('',#23420,.T.) ;
#17677 = FACE_OUTER_BOUND('',#23421,.T.) ;
#17678 = FACE_OUTER_BOUND('',#23422,.T.) ;
#17679 = FACE_OUTER_BOUND('',#23423,.T.) ;
#17680 = FACE_OUTER_BOUND('',#23424,.T.) ;
#17681 = FACE_OUTER_BOUND('',#23425,.T.) ;
#17682 = FACE_OUTER_BOUND('',#23426,.T.) ;
#17683 = FACE_OUTER_BOUND('',#23427,.T.) ;
#17684 = FACE_OUTER_BOUND('',#23428,.T.) ;
#17685 = FACE_OUTER_BOUND('',#23429,.T.) ;
#17686 = FACE_OUTER_BOUND('',#23430,.T.) ;
#17687 = FACE_OUTER_BOUND('',#23431,.T.) ;
#17688 = FACE_OUTER_BOUND('',#23432,.T.) ;
#17689 = FACE_OUTER_BOUND('',#23433,.T.) ;
#17690 = FACE_OUTER_BOUND('',#23434,.T.) ;
#17691 = FACE_OUTER_BOUND('',#23435,.T.) ;
#17692 = FACE_OUTER_BOUND('',#23436,.T.) ;
#17693 = FACE_OUTER_BOUND('',#23437,.T.) ;
#17694 = FACE_OUTER_BOUND('',#23438,.T.) ;
#17695 = FACE_OUTER_BOUND('',#23439,.T.) ;
#17696 = FACE_OUTER_BOUND('',#23440,.T.) ;
#17697 = FACE_OUTER_BOUND('',#23441,.T.) ;
#17698 = FACE_OUTER_BOUND('',#23442,.T.) ;
#17699 = FACE_OUTER_BOUND('',#23443,.T.) ;
#17700 = FACE_OUTER_BOUND('',#23444,.T.) ;
#17701 = FACE_OUTER_BOUND('',#23445,.T.) ;
#17702 = FACE_OUTER_BOUND('',#23446,.T.) ;
#17703 = FACE_OUTER_BOUND('',#23447,.T.) ;
#17704 = FACE_OUTER_BOUND('',#23448,.T.) ;
#17705 = FACE_OUTER_BOUND('',#23449,.T.) ;
#17706 = FACE_OUTER_BOUND('',#23450,.T.) ;
#17707 = FACE_OUTER_BOUND('',#23451,.T.) ;
#17708 = FACE_OUTER_BOUND('',#23452,.T.) ;
#17709 = FACE_OUTER_BOUND('',#23453,.T.) ;
#17710 = FACE_OUTER_BOUND('',#23454,.T.) ;
#17711 = FACE_OUTER_BOUND('',#23455,.T.) ;
#17712 = FACE_OUTER_BOUND('',#23456,.T.) ;
#17713 = FACE_OUTER_BOUND('',#23457,.T.) ;
#17714 = FACE_OUTER_BOUND('',#23458,.T.) ;
#17715 = FACE_OUTER_BOUND('',#23459,.T.) ;
#17716 = FACE_OUTER_BOUND('',#23460,.T.) ;
#17717 = FACE_OUTER_BOUND('',#23461,.T.) ;
#17718 = FACE_OUTER_BOUND('',#23462,.T.) ;
#17719 = FACE_OUTER_BOUND('',#23463,.T.) ;
#17720 = FACE_OUTER_BOUND('',#23464,.T.) ;
#17721 = FACE_OUTER_BOUND('',#23465,.T.) ;
#17722 = FACE_OUTER_BOUND('',#23466,.T.) ;
#17723 = FACE_OUTER_BOUND('',#23467,.T.) ;
#17724 = FACE_OUTER_BOUND('',#23468,.T.) ;
#17725 = FACE_OUTER_BOUND('',#23469,.T.) ;
#17726 = FACE_OUTER_BOUND('',#23470,.T.) ;
#17727 = FACE_OUTER_BOUND('',#23471,.T.) ;
#17728 = FACE_OUTER_BOUND('',#23472,.T.) ;
#17729 = FACE_OUTER_BOUND('',#23473,.T.) ;
#17730 = FACE_OUTER_BOUND('',#23474,.T.) ;
#17731 = FACE_OUTER_BOUND('',#23475,.T.) ;
#17732 = FACE_OUTER_BOUND('',#23476,.T.) ;
#17733 = FACE_OUTER_BOUND('',#23477,.T.) ;
#17734 = FACE_OUTER_BOUND('',#23478,.T.) ;
#17735 = FACE_OUTER_BOUND('',#23479,.T.) ;
#17736 = FACE_OUTER_BOUND('',#23480,.T.) ;
#17737 = FACE_OUTER_BOUND('',#23481,.T.) ;
#17738 = FACE_OUTER_BOUND('',#23482,.T.) ;
#17739 = FACE_OUTER_BOUND('',#23483,.T.) ;
#17740 = FACE_OUTER_BOUND('',#23484,.T.) ;
#17741 = FACE_OUTER_BOUND('',#23485,.T.) ;
#17742 = FACE_OUTER_BOUND('',#23486,.T.) ;
#17743 = FACE_OUTER_BOUND('',#23487,.T.) ;
#17744 = FACE_OUTER_BOUND('',#23488,.T.) ;
#17745 = FACE_OUTER_BOUND('',#23489,.T.) ;
#17746 = FACE_OUTER_BOUND('',#23490,.T.) ;
#17747 = FACE_OUTER_BOUND('',#23491,.T.) ;
#17748 = FACE_OUTER_BOUND('',#23492,.T.) ;
#17749 = FACE_OUTER_BOUND('',#23493,.T.) ;
#17750 = FACE_OUTER_BOUND('',#23494,.T.) ;
#17751 = FACE_OUTER_BOUND('',#23495,.T.) ;
#17752 = FACE_OUTER_BOUND('',#23496,.T.) ;
#17753 = FACE_OUTER_BOUND('',#23497,.T.) ;
#17754 = FACE_OUTER_BOUND('',#23498,.T.) ;
#17755 = FACE_OUTER_BOUND('',#23499,.T.) ;
#17756 = FACE_OUTER_BOUND('',#23500,.T.) ;
#17757 = FACE_OUTER_BOUND('',#23501,.T.) ;
#17758 = FACE_OUTER_BOUND('',#23502,.T.) ;
#17759 = FACE_OUTER_BOUND('',#23503,.T.) ;
#17760 = FACE_OUTER_BOUND('',#23504,.T.) ;
#17761 = FACE_OUTER_BOUND('',#23506,.T.) ;
#17762 = FACE_OUTER_BOUND('',#23507,.T.) ;
#17763 = FACE_OUTER_BOUND('',#23508,.T.) ;
#17764 = FACE_OUTER_BOUND('',#23509,.T.) ;
#17765 = FACE_OUTER_BOUND('',#23510,.T.) ;
#17766 = FACE_OUTER_BOUND('',#23511,.T.) ;
#17767 = FACE_OUTER_BOUND('',#23512,.T.) ;
#17768 = FACE_OUTER_BOUND('',#23513,.T.) ;
#17769 = FACE_OUTER_BOUND('',#23514,.T.) ;
#17770 = FACE_OUTER_BOUND('',#23515,.T.) ;
#17771 = FACE_OUTER_BOUND('',#23516,.T.) ;
#17772 = FACE_OUTER_BOUND('',#23517,.T.) ;
#17773 = FACE_OUTER_BOUND('',#23518,.T.) ;
#17774 = FACE_OUTER_BOUND('',#23519,.T.) ;
#17775 = FACE_OUTER_BOUND('',#23520,.T.) ;
#17776 = FACE_OUTER_BOUND('',#23521,.T.) ;
#17777 = FACE_OUTER_BOUND('',#23522,.T.) ;
#17778 = FACE_OUTER_BOUND('',#23523,.T.) ;
#17779 = FACE_OUTER_BOUND('',#23525,.T.) ;
#17780 = FACE_OUTER_BOUND('',#23526,.T.) ;
#17781 = FACE_OUTER_BOUND('',#23527,.T.) ;
#17782 = FACE_OUTER_BOUND('',#23528,.T.) ;
#17783 = FACE_OUTER_BOUND('',#23529,.T.) ;
#17784 = FACE_OUTER_BOUND('',#23530,.T.) ;
#17785 = FACE_OUTER_BOUND('',#23531,.T.) ;
#17786 = FACE_OUTER_BOUND('',#23532,.T.) ;
#17787 = FACE_OUTER_BOUND('',#23533,.T.) ;
#17788 = FACE_OUTER_BOUND('',#23534,.T.) ;
#17789 = FACE_OUTER_BOUND('',#23535,.T.) ;
#17790 = FACE_OUTER_BOUND('',#23536,.T.) ;
#17791 = FACE_OUTER_BOUND('',#23537,.T.) ;
#17792 = FACE_OUTER_BOUND('',#23538,.T.) ;
#17793 = FACE_OUTER_BOUND('',#23539,.T.) ;
#17794 = FACE_OUTER_BOUND('',#23540,.T.) ;
#17795 = FACE_OUTER_BOUND('',#23541,.T.) ;
#17796 = FACE_OUTER_BOUND('',#23542,.T.) ;
#17797 = FACE_OUTER_BOUND('',#23543,.T.) ;
#17798 = FACE_OUTER_BOUND('',#23544,.T.) ;
#17799 = FACE_OUTER_BOUND('',#23545,.T.) ;
#17800 = FACE_OUTER_BOUND('',#23546,.T.) ;
#17801 = FACE_OUTER_BOUND('',#23547,.T.) ;
#17802 = FACE_OUTER_BOUND('',#23548,.T.) ;
#17803 = FACE_OUTER_BOUND('',#23549,.T.) ;
#17804 = FACE_OUTER_BOUND('',#23550,.T.) ;
#17805 = FACE_OUTER_BOUND('',#23551,.T.) ;
#17806 = FACE_OUTER_BOUND('',#23552,.T.) ;
#17807 = FACE_OUTER_BOUND('',#23553,.T.) ;
#17808 = FACE_OUTER_BOUND('',#23554,.T.) ;
#17809 = FACE_OUTER_BOUND('',#23555,.T.) ;
#17810 = FACE_OUTER_BOUND('',#23556,.T.) ;
#17811 = FACE_OUTER_BOUND('',#23557,.T.) ;
#17812 = FACE_OUTER_BOUND('',#23558,.T.) ;
#17813 = FACE_OUTER_BOUND('',#23559,.T.) ;
#17814 = FACE_OUTER_BOUND('',#23560,.T.) ;
#17815 = FACE_OUTER_BOUND('',#23561,.T.) ;
#17816 = FACE_OUTER_BOUND('',#23562,.T.) ;
#17817 = FACE_OUTER_BOUND('',#23563,.T.) ;
#17818 = FACE_OUTER_BOUND('',#23564,.T.) ;
#17819 = FACE_OUTER_BOUND('',#23565,.T.) ;
#17820 = FACE_OUTER_BOUND('',#23566,.T.) ;
#17821 = FACE_OUTER_BOUND('',#23567,.T.) ;
#17822 = FACE_OUTER_BOUND('',#23568,.T.) ;
#17823 = FACE_OUTER_BOUND('',#23569,.T.) ;
#17824 = FACE_OUTER_BOUND('',#23570,.T.) ;
#17825 = FACE_OUTER_BOUND('',#23571,.T.) ;
#17826 = FACE_OUTER_BOUND('',#23572,.T.) ;
#17827 = FACE_OUTER_BOUND('',#23573,.T.) ;
#17828 = FACE_OUTER_BOUND('',#23574,.T.) ;
#17829 = FACE_OUTER_BOUND('',#23575,.T.) ;
#17830 = FACE_OUTER_BOUND('',#23576,.T.) ;
#17831 = FACE_OUTER_BOUND('',#23577,.T.) ;
#17832 = FACE_OUTER_BOUND('',#23578,.T.) ;
#17833 = FACE_OUTER_BOUND('',#23579,.T.) ;
#17834 = FACE_OUTER_BOUND('',#23580,.T.) ;
#17835 = FACE_OUTER_BOUND('',#23581,.T.) ;
#17836 = FACE_OUTER_BOUND('',#23582,.T.) ;
#17837 = FACE_OUTER_BOUND('',#23583,.T.) ;
#17838 = FACE_OUTER_BOUND('',#23584,.T.) ;
#17839 = FACE_OUTER_BOUND('',#23585,.T.) ;
#17840 = FACE_OUTER_BOUND('',#23586,.T.) ;
#17841 = FACE_OUTER_BOUND('',#23587,.T.) ;
#17842 = FACE_OUTER_BOUND('',#23588,.T.) ;
#17843 = FACE_OUTER_BOUND('',#23589,.T.) ;
#17844 = FACE_OUTER_BOUND('',#23590,.T.) ;
#17845 = FACE_OUTER_BOUND('',#23591,.T.) ;
#17846 = FACE_OUTER_BOUND('',#23592,.T.) ;
#17847 = FACE_OUTER_BOUND('',#23593,.T.) ;
#17848 = FACE_OUTER_BOUND('',#23594,.T.) ;
#17849 = FACE_OUTER_BOUND('',#23595,.T.) ;
#17850 = FACE_OUTER_BOUND('',#23596,.T.) ;
#17851 = FACE_OUTER_BOUND('',#23597,.T.) ;
#17852 = FACE_OUTER_BOUND('',#23598,.T.) ;
#17853 = FACE_OUTER_BOUND('',#23599,.T.) ;
#17854 = FACE_OUTER_BOUND('',#23600,.T.) ;
#17855 = FACE_OUTER_BOUND('',#23601,.T.) ;
#17856 = FACE_OUTER_BOUND('',#23602,.T.) ;
#17857 = FACE_OUTER_BOUND('',#23603,.T.) ;
#17858 = FACE_OUTER_BOUND('',#23604,.T.) ;
#17859 = FACE_OUTER_BOUND('',#23605,.T.) ;
#17860 = FACE_OUTER_BOUND('',#23606,.T.) ;
#17861 = FACE_OUTER_BOUND('',#23607,.T.) ;
#17862 = FACE_OUTER_BOUND('',#23608,.T.) ;
#17863 = FACE_OUTER_BOUND('',#23609,.T.) ;
#17864 = FACE_OUTER_BOUND('',#23610,.T.) ;
#17865 = FACE_OUTER_BOUND('',#23611,.T.) ;
#17866 = FACE_OUTER_BOUND('',#23612,.T.) ;
#17867 = FACE_OUTER_BOUND('',#23613,.T.) ;
#17868 = FACE_OUTER_BOUND('',#23614,.T.) ;
#17869 = FACE_OUTER_BOUND('',#23615,.T.) ;
#17870 = FACE_OUTER_BOUND('',#23616,.T.) ;
#17871 = FACE_OUTER_BOUND('',#23617,.T.) ;
#17872 = FACE_OUTER_BOUND('',#23618,.T.) ;
#17873 = FACE_OUTER_BOUND('',#23619,.T.) ;
#17874 = FACE_OUTER_BOUND('',#23620,.T.) ;
#17875 = FACE_OUTER_BOUND('',#23621,.T.) ;
#17876 = FACE_OUTER_BOUND('',#23622,.T.) ;
#17877 = FACE_OUTER_BOUND('',#23623,.T.) ;
#17878 = FACE_OUTER_BOUND('',#23624,.T.) ;
#17879 = FACE_OUTER_BOUND('',#23625,.T.) ;
#17880 = FACE_OUTER_BOUND('',#23626,.T.) ;
#17881 = FACE_OUTER_BOUND('',#23627,.T.) ;
#17882 = FACE_OUTER_BOUND('',#23628,.T.) ;
#17883 = FACE_OUTER_BOUND('',#23629,.T.) ;
#17884 = FACE_OUTER_BOUND('',#23630,.T.) ;
#17885 = FACE_OUTER_BOUND('',#23631,.T.) ;
#17886 = FACE_OUTER_BOUND('',#23632,.T.) ;
#17887 = FACE_OUTER_BOUND('',#23633,.T.) ;
#17888 = FACE_OUTER_BOUND('',#23634,.T.) ;
#17889 = FACE_OUTER_BOUND('',#23635,.T.) ;
#17890 = FACE_OUTER_BOUND('',#23636,.T.) ;
#17891 = FACE_OUTER_BOUND('',#23637,.T.) ;
#17892 = FACE_OUTER_BOUND('',#23638,.T.) ;
#17893 = FACE_OUTER_BOUND('',#23639,.T.) ;
#17894 = FACE_OUTER_BOUND('',#23640,.T.) ;
#17895 = FACE_OUTER_BOUND('',#23641,.T.) ;
#17896 = FACE_OUTER_BOUND('',#23642,.T.) ;
#17897 = FACE_OUTER_BOUND('',#23643,.T.) ;
#17898 = FACE_OUTER_BOUND('',#23644,.T.) ;
#17899 = FACE_OUTER_BOUND('',#23645,.T.) ;
#17900 = FACE_OUTER_BOUND('',#23646,.T.) ;
#17901 = FACE_OUTER_BOUND('',#23647,.T.) ;
#17902 = FACE_OUTER_BOUND('',#23648,.T.) ;
#17903 = FACE_OUTER_BOUND('',#23649,.T.) ;
#17904 = FACE_OUTER_BOUND('',#23650,.T.) ;
#17905 = FACE_OUTER_BOUND('',#23651,.T.) ;
#17906 = FACE_OUTER_BOUND('',#23652,.T.) ;
#17907 = FACE_OUTER_BOUND('',#23653,.T.) ;
#17908 = FACE_OUTER_BOUND('',#23654,.T.) ;
#17909 = FACE_OUTER_BOUND('',#23655,.T.) ;
#17910 = FACE_OUTER_BOUND('',#23656,.T.) ;
#17911 = FACE_OUTER_BOUND('',#23657,.T.) ;
#17912 = FACE_OUTER_BOUND('',#23658,.T.) ;
#17913 = FACE_OUTER_BOUND('',#23659,.T.) ;
#17914 = FACE_OUTER_BOUND('',#23660,.T.) ;
#17915 = FACE_OUTER_BOUND('',#23661,.T.) ;
#17916 = FACE_OUTER_BOUND('',#23662,.T.) ;
#17917 = FACE_OUTER_BOUND('',#23663,.T.) ;
#17918 = FACE_OUTER_BOUND('',#23664,.T.) ;
#17919 = FACE_OUTER_BOUND('',#23665,.T.) ;
#17920 = FACE_OUTER_BOUND('',#23666,.T.) ;
#17921 = FACE_OUTER_BOUND('',#23667,.T.) ;
#17922 = FACE_OUTER_BOUND('',#23668,.T.) ;
#17923 = FACE_OUTER_BOUND('',#23669,.T.) ;
#17924 = FACE_OUTER_BOUND('',#23670,.T.) ;
#17925 = FACE_OUTER_BOUND('',#23671,.T.) ;
#17926 = FACE_OUTER_BOUND('',#23672,.T.) ;
#17927 = FACE_OUTER_BOUND('',#23673,.T.) ;
#17928 = FACE_OUTER_BOUND('',#23674,.T.) ;
#17929 = FACE_OUTER_BOUND('',#23675,.T.) ;
#17930 = FACE_OUTER_BOUND('',#23676,.T.) ;
#17931 = FACE_OUTER_BOUND('',#23677,.T.) ;
#17932 = FACE_OUTER_BOUND('',#23678,.T.) ;
#17933 = FACE_OUTER_BOUND('',#23679,.T.) ;
#17934 = FACE_OUTER_BOUND('',#23680,.T.) ;
#17935 = FACE_OUTER_BOUND('',#23681,.T.) ;
#17936 = FACE_OUTER_BOUND('',#23682,.T.) ;
#17937 = FACE_OUTER_BOUND('',#23683,.T.) ;
#17938 = FACE_OUTER_BOUND('',#23684,.T.) ;
#17939 = FACE_OUTER_BOUND('',#23685,.T.) ;
#17940 = FACE_OUTER_BOUND('',#23686,.T.) ;
#17941 = FACE_OUTER_BOUND('',#23687,.T.) ;
#17942 = FACE_OUTER_BOUND('',#23688,.T.) ;
#17943 = FACE_OUTER_BOUND('',#23689,.T.) ;
#17944 = FACE_OUTER_BOUND('',#23690,.T.) ;
#17945 = FACE_OUTER_BOUND('',#23691,.T.) ;
#17946 = FACE_OUTER_BOUND('',#23692,.T.) ;
#17947 = FACE_OUTER_BOUND('',#23693,.T.) ;
#17948 = FACE_OUTER_BOUND('',#23694,.T.) ;
#17949 = FACE_OUTER_BOUND('',#23695,.T.) ;
#17950 = FACE_OUTER_BOUND('',#23696,.T.) ;
#17951 = FACE_OUTER_BOUND('',#23697,.T.) ;
#17952 = FACE_OUTER_BOUND('',#23698,.T.) ;
#17953 = FACE_OUTER_BOUND('',#23699,.T.) ;
#17954 = FACE_OUTER_BOUND('',#23700,.T.) ;
#17955 = FACE_OUTER_BOUND('',#23701,.T.) ;
#17956 = FACE_OUTER_BOUND('',#23702,.T.) ;
#17957 = FACE_OUTER_BOUND('',#23703,.T.) ;
#17958 = FACE_OUTER_BOUND('',#23704,.T.) ;
#17959 = FACE_OUTER_BOUND('',#23705,.T.) ;
#17960 = FACE_OUTER_BOUND('',#23707,.T.) ;
#17961 = FACE_OUTER_BOUND('',#23708,.T.) ;
#17962 = FACE_OUTER_BOUND('',#23709,.T.) ;
#17963 = FACE_OUTER_BOUND('',#23710,.T.) ;
#17964 = FACE_OUTER_BOUND('',#23711,.T.) ;
#17965 = FACE_OUTER_BOUND('',#23712,.T.) ;
#17966 = FACE_OUTER_BOUND('',#23713,.T.) ;
#17967 = FACE_OUTER_BOUND('',#23714,.T.) ;
#17968 = FACE_OUTER_BOUND('',#23715,.T.) ;
#17969 = FACE_OUTER_BOUND('',#23718,.T.) ;
#17970 = FACE_OUTER_BOUND('',#23719,.T.) ;
#17971 = FACE_OUTER_BOUND('',#23720,.T.) ;
#17972 = FACE_OUTER_BOUND('',#23721,.T.) ;
#17973 = FACE_OUTER_BOUND('',#23723,.T.) ;
#17974 = FACE_OUTER_BOUND('',#23725,.T.) ;
#17975 = FACE_OUTER_BOUND('',#23726,.T.) ;
#17976 = FACE_OUTER_BOUND('',#23727,.T.) ;
#17977 = FACE_OUTER_BOUND('',#23728,.T.) ;
#17978 = FACE_OUTER_BOUND('',#23729,.T.) ;
#17979 = FACE_OUTER_BOUND('',#23730,.T.) ;
#17980 = FACE_OUTER_BOUND('',#23731,.T.) ;
#17981 = FACE_OUTER_BOUND('',#23732,.T.) ;
#17982 = FACE_OUTER_BOUND('',#23733,.T.) ;
#17983 = FACE_OUTER_BOUND('',#23734,.T.) ;
#17984 = FACE_OUTER_BOUND('',#23735,.T.) ;
#17985 = FACE_OUTER_BOUND('',#23736,.T.) ;
#17986 = FACE_OUTER_BOUND('',#23737,.T.) ;
#17987 = FACE_OUTER_BOUND('',#23738,.T.) ;
#17988 = FACE_OUTER_BOUND('',#23739,.T.) ;
#17989 = FACE_OUTER_BOUND('',#23740,.T.) ;
#17990 = FACE_OUTER_BOUND('',#23741,.T.) ;
#17991 = FACE_OUTER_BOUND('',#23742,.T.) ;
#17992 = FACE_OUTER_BOUND('',#23743,.T.) ;
#17993 = FACE_OUTER_BOUND('',#23744,.T.) ;
#17994 = FACE_OUTER_BOUND('',#23746,.T.) ;
#17995 = FACE_OUTER_BOUND('',#23747,.T.) ;
#17996 = FACE_OUTER_BOUND('',#23748,.T.) ;
#17997 = FACE_OUTER_BOUND('',#23749,.T.) ;
#17998 = FACE_OUTER_BOUND('',#23750,.T.) ;
#17999 = FACE_OUTER_BOUND('',#23751,.T.) ;
#18000 = FACE_OUTER_BOUND('',#23752,.T.) ;
#18001 = FACE_OUTER_BOUND('',#23753,.T.) ;
#18002 = FACE_OUTER_BOUND('',#23754,.T.) ;
#18003 = FACE_OUTER_BOUND('',#23755,.T.) ;
#18004 = FACE_OUTER_BOUND('',#23756,.T.) ;
#18005 = FACE_OUTER_BOUND('',#23757,.T.) ;
#18006 = FACE_OUTER_BOUND('',#23758,.T.) ;
#18007 = FACE_OUTER_BOUND('',#23759,.T.) ;
#18008 = FACE_OUTER_BOUND('',#23760,.T.) ;
#18009 = FACE_OUTER_BOUND('',#23761,.T.) ;
#18010 = FACE_OUTER_BOUND('',#23762,.T.) ;
#18011 = FACE_OUTER_BOUND('',#23763,.T.) ;
#18012 = FACE_OUTER_BOUND('',#23765,.T.) ;
#18013 = FACE_OUTER_BOUND('',#23766,.T.) ;
#18014 = FACE_OUTER_BOUND('',#23767,.T.) ;
#18015 = FACE_OUTER_BOUND('',#23768,.T.) ;
#18016 = FACE_OUTER_BOUND('',#23769,.T.) ;
#18017 = FACE_OUTER_BOUND('',#23770,.T.) ;
#18018 = FACE_OUTER_BOUND('',#23771,.T.) ;
#18019 = FACE_OUTER_BOUND('',#23772,.T.) ;
#18020 = FACE_OUTER_BOUND('',#23773,.T.) ;
#18021 = FACE_OUTER_BOUND('',#23774,.T.) ;
#18022 = FACE_OUTER_BOUND('',#23775,.T.) ;
#18023 = FACE_OUTER_BOUND('',#23776,.T.) ;
#18024 = FACE_OUTER_BOUND('',#23777,.T.) ;
#18025 = FACE_OUTER_BOUND('',#23778,.T.) ;
#18026 = FACE_OUTER_BOUND('',#23779,.T.) ;
#18027 = FACE_OUTER_BOUND('',#23780,.T.) ;
#18028 = FACE_OUTER_BOUND('',#23781,.T.) ;
#18029 = FACE_OUTER_BOUND('',#23782,.T.) ;
#18030 = FACE_OUTER_BOUND('',#23783,.T.) ;
#18031 = FACE_OUTER_BOUND('',#23784,.T.) ;
#18032 = FACE_OUTER_BOUND('',#23785,.T.) ;
#18033 = FACE_OUTER_BOUND('',#23786,.T.) ;
#18034 = FACE_OUTER_BOUND('',#23787,.T.) ;
#18035 = FACE_OUTER_BOUND('',#23788,.T.) ;
#18036 = FACE_OUTER_BOUND('',#23789,.T.) ;
#18037 = FACE_OUTER_BOUND('',#23790,.T.) ;
#18038 = FACE_OUTER_BOUND('',#23791,.T.) ;
#18039 = FACE_OUTER_BOUND('',#23792,.T.) ;
#18040 = FACE_OUTER_BOUND('',#23793,.T.) ;
#18041 = FACE_OUTER_BOUND('',#23794,.T.) ;
#18042 = FACE_OUTER_BOUND('',#23795,.T.) ;
#18043 = FACE_OUTER_BOUND('',#23796,.T.) ;
#18044 = FACE_OUTER_BOUND('',#23797,.T.) ;
#18045 = FACE_OUTER_BOUND('',#23798,.T.) ;
#18046 = FACE_OUTER_BOUND('',#23799,.T.) ;
#18047 = FACE_OUTER_BOUND('',#23800,.T.) ;
#18048 = FACE_OUTER_BOUND('',#23801,.T.) ;
#18049 = FACE_OUTER_BOUND('',#23802,.T.) ;
#18050 = FACE_OUTER_BOUND('',#23803,.T.) ;
#18051 = FACE_OUTER_BOUND('',#23804,.T.) ;
#18052 = FACE_OUTER_BOUND('',#23805,.T.) ;
#18053 = FACE_OUTER_BOUND('',#23806,.T.) ;
#18054 = FACE_OUTER_BOUND('',#23807,.T.) ;
#18055 = FACE_OUTER_BOUND('',#23808,.T.) ;
#18056 = FACE_OUTER_BOUND('',#23809,.T.) ;
#18057 = FACE_OUTER_BOUND('',#23810,.T.) ;
#18058 = FACE_OUTER_BOUND('',#23811,.T.) ;
#18059 = FACE_OUTER_BOUND('',#23812,.T.) ;
#18060 = FACE_OUTER_BOUND('',#23813,.T.) ;
#18061 = FACE_OUTER_BOUND('',#23814,.T.) ;
#18062 = FACE_OUTER_BOUND('',#23815,.T.) ;
#18063 = FACE_OUTER_BOUND('',#23816,.T.) ;
#18064 = FACE_OUTER_BOUND('',#23817,.T.) ;
#18065 = FACE_OUTER_BOUND('',#23818,.T.) ;
#18066 = FACE_OUTER_BOUND('',#23819,.T.) ;
#18067 = FACE_OUTER_BOUND('',#23820,.T.) ;
#18068 = FACE_OUTER_BOUND('',#23821,.T.) ;
#18069 = FACE_OUTER_BOUND('',#23822,.T.) ;
#18070 = FACE_OUTER_BOUND('',#23823,.T.) ;
#18071 = FACE_OUTER_BOUND('',#23824,.T.) ;
#18072 = FACE_OUTER_BOUND('',#23825,.T.) ;
#18073 = FACE_OUTER_BOUND('',#23826,.T.) ;
#18074 = FACE_OUTER_BOUND('',#23827,.T.) ;
#18075 = FACE_OUTER_BOUND('',#23828,.T.) ;
#18076 = FACE_OUTER_BOUND('',#23829,.T.) ;
#18077 = FACE_OUTER_BOUND('',#23830,.T.) ;
#18078 = FACE_OUTER_BOUND('',#23831,.T.) ;
#18079 = FACE_OUTER_BOUND('',#23832,.T.) ;
#18080 = FACE_OUTER_BOUND('',#23833,.T.) ;
#18081 = FACE_OUTER_BOUND('',#23834,.T.) ;
#18082 = FACE_OUTER_BOUND('',#23835,.T.) ;
#18083 = FACE_OUTER_BOUND('',#23836,.T.) ;
#18084 = FACE_OUTER_BOUND('',#23837,.T.) ;
#18085 = FACE_OUTER_BOUND('',#23838,.T.) ;
#18086 = FACE_OUTER_BOUND('',#23839,.T.) ;
#18087 = FACE_OUTER_BOUND('',#23840,.T.) ;
#18088 = FACE_OUTER_BOUND('',#23841,.T.) ;
#18089 = FACE_OUTER_BOUND('',#23842,.T.) ;
#18090 = FACE_OUTER_BOUND('',#23843,.T.) ;
#18091 = FACE_OUTER_BOUND('',#23844,.T.) ;
#18092 = FACE_OUTER_BOUND('',#23845,.T.) ;
#18093 = FACE_OUTER_BOUND('',#23846,.T.) ;
#18094 = FACE_OUTER_BOUND('',#23847,.T.) ;
#18095 = FACE_OUTER_BOUND('',#23848,.T.) ;
#18096 = FACE_OUTER_BOUND('',#23849,.T.) ;
#18097 = FACE_OUTER_BOUND('',#23850,.T.) ;
#18098 = FACE_OUTER_BOUND('',#23851,.T.) ;
#18099 = FACE_OUTER_BOUND('',#23852,.T.) ;
#18100 = FACE_OUTER_BOUND('',#23853,.T.) ;
#18101 = FACE_OUTER_BOUND('',#23854,.T.) ;
#18102 = FACE_OUTER_BOUND('',#23855,.T.) ;
#18103 = FACE_OUTER_BOUND('',#23856,.T.) ;
#18104 = FACE_OUTER_BOUND('',#23857,.T.) ;
#18105 = FACE_OUTER_BOUND('',#23858,.T.) ;
#18106 = FACE_OUTER_BOUND('',#23859,.T.) ;
#18107 = FACE_OUTER_BOUND('',#23860,.T.) ;
#18108 = FACE_OUTER_BOUND('',#23861,.T.) ;
#18109 = FACE_OUTER_BOUND('',#23862,.T.) ;
#18110 = FACE_OUTER_BOUND('',#23863,.T.) ;
#18111 = FACE_OUTER_BOUND('',#23864,.T.) ;
#18112 = FACE_OUTER_BOUND('',#23865,.T.) ;
#18113 = FACE_OUTER_BOUND('',#23866,.T.) ;
#18114 = FACE_OUTER_BOUND('',#23867,.T.) ;
#18115 = FACE_OUTER_BOUND('',#23868,.T.) ;
#18116 = FACE_OUTER_BOUND('',#23869,.T.) ;
#18117 = FACE_OUTER_BOUND('',#23870,.T.) ;
#18118 = FACE_OUTER_BOUND('',#23871,.T.) ;
#18119 = FACE_OUTER_BOUND('',#23872,.T.) ;
#18120 = FACE_OUTER_BOUND('',#23873,.T.) ;
#18121 = FACE_OUTER_BOUND('',#23874,.T.) ;
#18122 = FACE_OUTER_BOUND('',#23875,.T.) ;
#18123 = FACE_OUTER_BOUND('',#23876,.T.) ;
#18124 = FACE_OUTER_BOUND('',#23877,.T.) ;
#18125 = FACE_OUTER_BOUND('',#23878,.T.) ;
#18126 = FACE_OUTER_BOUND('',#23879,.T.) ;
#18127 = FACE_OUTER_BOUND('',#23880,.T.) ;
#18128 = FACE_OUTER_BOUND('',#23881,.T.) ;
#18129 = FACE_OUTER_BOUND('',#23882,.T.) ;
#18130 = FACE_OUTER_BOUND('',#23883,.T.) ;
#18131 = FACE_OUTER_BOUND('',#23884,.T.) ;
#18132 = FACE_OUTER_BOUND('',#23885,.T.) ;
#18133 = FACE_OUTER_BOUND('',#23886,.T.) ;
#18134 = FACE_OUTER_BOUND('',#23887,.T.) ;
#18135 = FACE_OUTER_BOUND('',#23888,.T.) ;
#18136 = FACE_OUTER_BOUND('',#23889,.T.) ;
#18137 = FACE_OUTER_BOUND('',#23890,.T.) ;
#18138 = FACE_OUTER_BOUND('',#23891,.T.) ;
#18139 = FACE_OUTER_BOUND('',#23892,.T.) ;
#18140 = FACE_OUTER_BOUND('',#23893,.T.) ;
#18141 = FACE_OUTER_BOUND('',#23894,.T.) ;
#18142 = FACE_OUTER_BOUND('',#23895,.T.) ;
#18143 = FACE_OUTER_BOUND('',#23896,.T.) ;
#18144 = FACE_OUTER_BOUND('',#23897,.T.) ;
#18145 = FACE_OUTER_BOUND('',#23898,.T.) ;
#18146 = FACE_OUTER_BOUND('',#23899,.T.) ;
#18147 = FACE_OUTER_BOUND('',#23900,.T.) ;
#18148 = FACE_OUTER_BOUND('',#23901,.T.) ;
#18149 = FACE_OUTER_BOUND('',#23902,.T.) ;
#18150 = FACE_OUTER_BOUND('',#23903,.T.) ;
#18151 = FACE_OUTER_BOUND('',#23904,.T.) ;
#18152 = FACE_OUTER_BOUND('',#23905,.T.) ;
#18153 = FACE_OUTER_BOUND('',#23906,.T.) ;
#18154 = FACE_OUTER_BOUND('',#23907,.T.) ;
#18155 = FACE_OUTER_BOUND('',#23908,.T.) ;
#18156 = FACE_OUTER_BOUND('',#23909,.T.) ;
#18157 = FACE_OUTER_BOUND('',#23910,.T.) ;
#18158 = FACE_OUTER_BOUND('',#23911,.T.) ;
#18159 = FACE_OUTER_BOUND('',#23912,.T.) ;
#18160 = FACE_OUTER_BOUND('',#23913,.T.) ;
#18161 = FACE_OUTER_BOUND('',#23914,.T.) ;
#18162 = FACE_OUTER_BOUND('',#23915,.T.) ;
#18163 = FACE_OUTER_BOUND('',#23916,.T.) ;
#18164 = FACE_OUTER_BOUND('',#23917,.T.) ;
#18165 = FACE_OUTER_BOUND('',#23918,.T.) ;
#18166 = FACE_OUTER_BOUND('',#23919,.T.) ;
#18167 = FACE_OUTER_BOUND('',#23920,.T.) ;
#18168 = FACE_OUTER_BOUND('',#23921,.T.) ;
#18169 = FACE_OUTER_BOUND('',#23922,.T.) ;
#18170 = FACE_OUTER_BOUND('',#23923,.T.) ;
#18171 = FACE_OUTER_BOUND('',#23924,.T.) ;
#18172 = FACE_OUTER_BOUND('',#23925,.T.) ;
#18173 = FACE_OUTER_BOUND('',#23926,.T.) ;
#18174 = FACE_OUTER_BOUND('',#23927,.T.) ;
#18175 = FACE_OUTER_BOUND('',#23928,.T.) ;
#18176 = FACE_OUTER_BOUND('',#23929,.T.) ;
#18177 = FACE_OUTER_BOUND('',#23930,.T.) ;
#18178 = FACE_OUTER_BOUND('',#23931,.T.) ;
#18179 = FACE_OUTER_BOUND('',#23932,.T.) ;
#18180 = FACE_OUTER_BOUND('',#23933,.T.) ;
#18181 = FACE_OUTER_BOUND('',#23934,.T.) ;
#18182 = FACE_OUTER_BOUND('',#23935,.T.) ;
#18183 = FACE_OUTER_BOUND('',#23936,.T.) ;
#18184 = FACE_OUTER_BOUND('',#23937,.T.) ;
#18185 = FACE_OUTER_BOUND('',#23938,.T.) ;
#18186 = FACE_OUTER_BOUND('',#23939,.T.) ;
#18187 = FACE_OUTER_BOUND('',#23940,.T.) ;
#18188 = FACE_OUTER_BOUND('',#23941,.T.) ;
#18189 = FACE_OUTER_BOUND('',#23942,.T.) ;
#18190 = FACE_OUTER_BOUND('',#23943,.T.) ;
#18191 = FACE_OUTER_BOUND('',#23944,.T.) ;
#18192 = FACE_OUTER_BOUND('',#23945,.T.) ;
#18193 = FACE_OUTER_BOUND('',#23946,.T.) ;
#18194 = FACE_OUTER_BOUND('',#23947,.T.) ;
#18195 = FACE_OUTER_BOUND('',#23948,.T.) ;
#18196 = FACE_OUTER_BOUND('',#23949,.T.) ;
#18197 = FACE_OUTER_BOUND('',#23950,.T.) ;
#18198 = FACE_OUTER_BOUND('',#23951,.T.) ;
#18199 = FACE_OUTER_BOUND('',#23952,.T.) ;
#18200 = FACE_OUTER_BOUND('',#23953,.T.) ;
#18201 = FACE_OUTER_BOUND('',#23954,.T.) ;
#18202 = FACE_OUTER_BOUND('',#23955,.T.) ;
#18203 = FACE_OUTER_BOUND('',#23956,.T.) ;
#18204 = FACE_OUTER_BOUND('',#23957,.T.) ;
#18205 = FACE_OUTER_BOUND('',#23958,.T.) ;
#18206 = FACE_OUTER_BOUND('',#23959,.T.) ;
#18207 = FACE_OUTER_BOUND('',#23960,.T.) ;
#18208 = FACE_OUTER_BOUND('',#23961,.T.) ;
#18209 = FACE_OUTER_BOUND('',#23962,.T.) ;
#18210 = FACE_OUTER_BOUND('',#23963,.T.) ;
#18211 = FACE_OUTER_BOUND('',#23964,.T.) ;
#18212 = FACE_OUTER_BOUND('',#23965,.T.) ;
#18213 = FACE_OUTER_BOUND('',#23966,.T.) ;
#18214 = FACE_OUTER_BOUND('',#23967,.T.) ;
#18215 = FACE_OUTER_BOUND('',#23968,.T.) ;
#18216 = FACE_OUTER_BOUND('',#23969,.T.) ;
#18217 = FACE_OUTER_BOUND('',#23970,.T.) ;
#18218 = FACE_OUTER_BOUND('',#23971,.T.) ;
#18219 = FACE_OUTER_BOUND('',#23972,.T.) ;
#18220 = FACE_OUTER_BOUND('',#23973,.T.) ;
#18221 = FACE_OUTER_BOUND('',#23974,.T.) ;
#18222 = FACE_OUTER_BOUND('',#23975,.T.) ;
#18223 = FACE_OUTER_BOUND('',#23976,.T.) ;
#18224 = FACE_OUTER_BOUND('',#23977,.T.) ;
#18225 = FACE_OUTER_BOUND('',#23978,.T.) ;
#18226 = FACE_OUTER_BOUND('',#23979,.T.) ;
#18227 = FACE_OUTER_BOUND('',#23980,.T.) ;
#18228 = FACE_OUTER_BOUND('',#23981,.T.) ;
#18229 = FACE_OUTER_BOUND('',#23982,.T.) ;
#18230 = FACE_OUTER_BOUND('',#23983,.T.) ;
#18231 = FACE_OUTER_BOUND('',#23984,.T.) ;
#18232 = FACE_OUTER_BOUND('',#23985,.T.) ;
#18233 = FACE_OUTER_BOUND('',#23986,.T.) ;
#18234 = FACE_OUTER_BOUND('',#23987,.T.) ;
#18235 = FACE_OUTER_BOUND('',#23988,.T.) ;
#18236 = FACE_OUTER_BOUND('',#23989,.T.) ;
#18237 = FACE_OUTER_BOUND('',#23990,.T.) ;
#18238 = FACE_OUTER_BOUND('',#23991,.T.) ;
#18239 = FACE_OUTER_BOUND('',#23992,.T.) ;
#18240 = FACE_OUTER_BOUND('',#23993,.T.) ;
#18241 = FACE_OUTER_BOUND('',#23994,.T.) ;
#18242 = FACE_OUTER_BOUND('',#23995,.T.) ;
#18243 = FACE_OUTER_BOUND('',#23996,.T.) ;
#18244 = FACE_OUTER_BOUND('',#23997,.T.) ;
#18245 = FACE_OUTER_BOUND('',#23998,.T.) ;
#18246 = FACE_OUTER_BOUND('',#23999,.T.) ;
#18247 = FACE_OUTER_BOUND('',#24000,.T.) ;
#18248 = FACE_OUTER_BOUND('',#24001,.T.) ;
#18249 = FACE_OUTER_BOUND('',#24002,.T.) ;
#18250 = FACE_OUTER_BOUND('',#24003,.T.) ;
#18251 = FACE_OUTER_BOUND('',#24004,.T.) ;
#18252 = FACE_OUTER_BOUND('',#24005,.T.) ;
#18253 = FACE_OUTER_BOUND('',#24006,.T.) ;
#18254 = FACE_OUTER_BOUND('',#24007,.T.) ;
#18255 = FACE_OUTER_BOUND('',#24008,.T.) ;
#18256 = FACE_OUTER_BOUND('',#24009,.T.) ;
#18257 = FACE_OUTER_BOUND('',#24010,.T.) ;
#18258 = FACE_OUTER_BOUND('',#24011,.T.) ;
#18259 = FACE_OUTER_BOUND('',#24012,.T.) ;
#18260 = FACE_OUTER_BOUND('',#24013,.T.) ;
#18261 = FACE_OUTER_BOUND('',#24014,.T.) ;
#18262 = FACE_OUTER_BOUND('',#24015,.T.) ;
#18263 = FACE_OUTER_BOUND('',#24016,.T.) ;
#18264 = FACE_OUTER_BOUND('',#24017,.T.) ;
#18265 = FACE_OUTER_BOUND('',#24018,.T.) ;
#18266 = FACE_OUTER_BOUND('',#24019,.T.) ;
#18267 = FACE_OUTER_BOUND('',#24020,.T.) ;
#18268 = FACE_OUTER_BOUND('',#24021,.T.) ;
#18269 = FACE_OUTER_BOUND('',#24022,.T.) ;
#18270 = FACE_OUTER_BOUND('',#24023,.T.) ;
#18271 = FACE_OUTER_BOUND('',#24024,.T.) ;
#18272 = FACE_OUTER_BOUND('',#24025,.T.) ;
#18273 = FACE_OUTER_BOUND('',#24026,.T.) ;
#18274 = FACE_OUTER_BOUND('',#24027,.T.) ;
#18275 = FACE_OUTER_BOUND('',#24028,.T.) ;
#18276 = FACE_OUTER_BOUND('',#24029,.T.) ;
#18277 = FACE_OUTER_BOUND('',#24030,.T.) ;
#18278 = FACE_OUTER_BOUND('',#24031,.T.) ;
#18279 = FACE_OUTER_BOUND('',#24032,.T.) ;
#18280 = FACE_OUTER_BOUND('',#24033,.T.) ;
#18281 = FACE_OUTER_BOUND('',#24034,.T.) ;
#18282 = FACE_OUTER_BOUND('',#24035,.T.) ;
#18283 = FACE_OUTER_BOUND('',#24036,.T.) ;
#18284 = FACE_OUTER_BOUND('',#24037,.T.) ;
#18285 = FACE_OUTER_BOUND('',#24038,.T.) ;
#18286 = FACE_OUTER_BOUND('',#24039,.T.) ;
#18287 = FACE_OUTER_BOUND('',#24040,.T.) ;
#18288 = FACE_OUTER_BOUND('',#24041,.T.) ;
#18289 = FACE_OUTER_BOUND('',#24042,.T.) ;
#18290 = FACE_OUTER_BOUND('',#24043,.T.) ;
#18291 = FACE_OUTER_BOUND('',#24044,.T.) ;
#18292 = FACE_OUTER_BOUND('',#24045,.T.) ;
#18293 = FACE_OUTER_BOUND('',#24046,.T.) ;
#18294 = FACE_OUTER_BOUND('',#24057,.T.) ;
#18295 = FACE_OUTER_BOUND('',#24058,.T.) ;
#18296 = FACE_OUTER_BOUND('',#24059,.T.) ;
#18297 = FACE_OUTER_BOUND('',#24060,.T.) ;
#18298 = FACE_OUTER_BOUND('',#24061,.T.) ;
#18299 = FACE_OUTER_BOUND('',#24062,.T.) ;
#18300 = FACE_OUTER_BOUND('',#24063,.T.) ;
#18301 = FACE_OUTER_BOUND('',#24064,.T.) ;
#18302 = FACE_OUTER_BOUND('',#24065,.T.) ;
#18303 = FACE_OUTER_BOUND('',#24066,.T.) ;
#18304 = FACE_OUTER_BOUND('',#24067,.T.) ;
#18305 = FACE_OUTER_BOUND('',#24068,.T.) ;
#18306 = FACE_OUTER_BOUND('',#24069,.T.) ;
#18307 = FACE_OUTER_BOUND('',#24070,.T.) ;
#18308 = FACE_OUTER_BOUND('',#24071,.T.) ;
#18309 = FACE_OUTER_BOUND('',#24072,.T.) ;
#18310 = FACE_OUTER_BOUND('',#24073,.T.) ;
#18311 = FACE_OUTER_BOUND('',#24074,.T.) ;
#18312 = FACE_OUTER_BOUND('',#24075,.T.) ;
#18313 = FACE_OUTER_BOUND('',#24076,.T.) ;
#18314 = FACE_OUTER_BOUND('',#24077,.T.) ;
#18315 = FACE_OUTER_BOUND('',#24078,.T.) ;
#18316 = FACE_OUTER_BOUND('',#24079,.T.) ;
#18317 = FACE_OUTER_BOUND('',#24080,.T.) ;
#18318 = FACE_OUTER_BOUND('',#24081,.T.) ;
#18319 = FACE_OUTER_BOUND('',#24082,.T.) ;
#18320 = FACE_OUTER_BOUND('',#24083,.T.) ;
#18321 = FACE_OUTER_BOUND('',#24084,.T.) ;
#18322 = FACE_OUTER_BOUND('',#24085,.T.) ;
#18323 = FACE_OUTER_BOUND('',#24086,.T.) ;
#18324 = FACE_OUTER_BOUND('',#24087,.T.) ;
#18325 = FACE_OUTER_BOUND('',#24088,.T.) ;
#18326 = FACE_OUTER_BOUND('',#24089,.T.) ;
#18327 = FACE_OUTER_BOUND('',#24090,.T.) ;
#18328 = FACE_OUTER_BOUND('',#24091,.T.) ;
#18329 = FACE_OUTER_BOUND('',#24092,.T.) ;
#18330 = FACE_OUTER_BOUND('',#24094,.T.) ;
#18331 = FACE_OUTER_BOUND('',#24096,.T.) ;
#18332 = FACE_OUTER_BOUND('',#24097,.T.) ;
#18333 = FACE_OUTER_BOUND('',#24098,.T.) ;
#18334 = FACE_OUTER_BOUND('',#24099,.T.) ;
#18335 = FACE_OUTER_BOUND('',#24100,.T.) ;
#18336 = FACE_OUTER_BOUND('',#24101,.T.) ;
#18337 = FACE_OUTER_BOUND('',#24102,.T.) ;
#18338 = FACE_OUTER_BOUND('',#24103,.T.) ;
#18339 = FACE_OUTER_BOUND('',#24104,.T.) ;
#18340 = FACE_OUTER_BOUND('',#24105,.T.) ;
#18341 = FACE_OUTER_BOUND('',#24106,.T.) ;
#18342 = FACE_OUTER_BOUND('',#24107,.T.) ;
#18343 = FACE_OUTER_BOUND('',#24108,.T.) ;
#18344 = FACE_OUTER_BOUND('',#24109,.T.) ;
#18345 = FACE_OUTER_BOUND('',#24110,.T.) ;
#18346 = FACE_OUTER_BOUND('',#24111,.T.) ;
#18347 = FACE_OUTER_BOUND('',#24112,.T.) ;
#18348 = FACE_OUTER_BOUND('',#24113,.T.) ;
#18349 = FACE_OUTER_BOUND('',#24114,.T.) ;
#18350 = FACE_OUTER_BOUND('',#24115,.T.) ;
#18351 = FACE_OUTER_BOUND('',#24116,.T.) ;
#18352 = FACE_OUTER_BOUND('',#24117,.T.) ;
#18353 = FACE_OUTER_BOUND('',#24118,.T.) ;
#18354 = FACE_OUTER_BOUND('',#24119,.T.) ;
#18355 = FACE_OUTER_BOUND('',#24120,.T.) ;
#18356 = FACE_OUTER_BOUND('',#24121,.T.) ;
#18357 = FACE_OUTER_BOUND('',#24122,.T.) ;
#18358 = FACE_OUTER_BOUND('',#24123,.T.) ;
#18359 = FACE_OUTER_BOUND('',#24124,.T.) ;
#18360 = FACE_OUTER_BOUND('',#24125,.T.) ;
#18361 = FACE_OUTER_BOUND('',#24126,.T.) ;
#18362 = FACE_OUTER_BOUND('',#24127,.T.) ;
#18363 = FACE_OUTER_BOUND('',#24128,.T.) ;
#18364 = FACE_OUTER_BOUND('',#24129,.T.) ;
#18365 = FACE_OUTER_BOUND('',#24130,.T.) ;
#18366 = FACE_OUTER_BOUND('',#24131,.T.) ;
#18367 = FACE_OUTER_BOUND('',#24132,.T.) ;
#18368 = FACE_OUTER_BOUND('',#24133,.T.) ;
#18369 = FACE_OUTER_BOUND('',#24134,.T.) ;
#18370 = FACE_OUTER_BOUND('',#24135,.T.) ;
#18371 = FACE_OUTER_BOUND('',#24136,.T.) ;
#18372 = FACE_OUTER_BOUND('',#24137,.T.) ;
#18373 = FACE_OUTER_BOUND('',#24138,.T.) ;
#18374 = FACE_OUTER_BOUND('',#24139,.T.) ;
#18375 = FACE_OUTER_BOUND('',#24140,.T.) ;
#18376 = FACE_OUTER_BOUND('',#24141,.T.) ;
#18377 = FACE_OUTER_BOUND('',#24142,.T.) ;
#18378 = FACE_OUTER_BOUND('',#24143,.T.) ;
#18379 = FACE_OUTER_BOUND('',#24144,.T.) ;
#18380 = FACE_OUTER_BOUND('',#24145,.T.) ;
#18381 = FACE_OUTER_BOUND('',#24146,.T.) ;
#18382 = FACE_OUTER_BOUND('',#24147,.T.) ;
#18383 = FACE_OUTER_BOUND('',#24148,.T.) ;
#18384 = FACE_OUTER_BOUND('',#24149,.T.) ;
#18385 = FACE_OUTER_BOUND('',#24150,.T.) ;
#18386 = FACE_OUTER_BOUND('',#24151,.T.) ;
#18387 = FACE_OUTER_BOUND('',#24152,.T.) ;
#18388 = FACE_OUTER_BOUND('',#24153,.T.) ;
#18389 = FACE_OUTER_BOUND('',#24154,.T.) ;
#18390 = FACE_OUTER_BOUND('',#24155,.T.) ;
#18391 = FACE_OUTER_BOUND('',#24156,.T.) ;
#18392 = FACE_OUTER_BOUND('',#24157,.T.) ;
#18393 = FACE_OUTER_BOUND('',#24158,.T.) ;
#18394 = FACE_OUTER_BOUND('',#24159,.T.) ;
#18395 = FACE_OUTER_BOUND('',#24160,.T.) ;
#18396 = FACE_OUTER_BOUND('',#24161,.T.) ;
#18397 = FACE_OUTER_BOUND('',#24162,.T.) ;
#18398 = FACE_OUTER_BOUND('',#24163,.T.) ;
#18399 = FACE_OUTER_BOUND('',#24164,.T.) ;
#18400 = FACE_OUTER_BOUND('',#24165,.T.) ;
#18401 = FACE_OUTER_BOUND('',#24166,.T.) ;
#18402 = FACE_OUTER_BOUND('',#24167,.T.) ;
#18403 = FACE_OUTER_BOUND('',#24168,.T.) ;
#18404 = FACE_OUTER_BOUND('',#24169,.T.) ;
#18405 = FACE_OUTER_BOUND('',#24170,.T.) ;
#18406 = FACE_OUTER_BOUND('',#24171,.T.) ;
#18407 = FACE_OUTER_BOUND('',#24172,.T.) ;
#18408 = FACE_OUTER_BOUND('',#24173,.T.) ;
#18409 = FACE_OUTER_BOUND('',#24174,.T.) ;
#18410 = FACE_OUTER_BOUND('',#24175,.T.) ;
#18411 = FACE_OUTER_BOUND('',#24176,.T.) ;
#18412 = FACE_OUTER_BOUND('',#24177,.T.) ;
#18413 = FACE_OUTER_BOUND('',#24178,.T.) ;
#18414 = FACE_OUTER_BOUND('',#24179,.T.) ;
#18415 = FACE_OUTER_BOUND('',#24180,.T.) ;
#18416 = FACE_OUTER_BOUND('',#24181,.T.) ;
#18417 = FACE_OUTER_BOUND('',#24182,.T.) ;
#18418 = FACE_OUTER_BOUND('',#24183,.T.) ;
#18419 = FACE_OUTER_BOUND('',#24184,.T.) ;
#18420 = FACE_OUTER_BOUND('',#24185,.T.) ;
#18421 = FACE_OUTER_BOUND('',#24186,.T.) ;
#18422 = FACE_OUTER_BOUND('',#24187,.T.) ;
#18423 = FACE_OUTER_BOUND('',#24188,.T.) ;
#18424 = FACE_OUTER_BOUND('',#24189,.T.) ;
#18425 = FACE_OUTER_BOUND('',#24190,.T.) ;
#18426 = FACE_OUTER_BOUND('',#24191,.T.) ;
#18427 = FACE_OUTER_BOUND('',#24192,.T.) ;
#18428 = FACE_OUTER_BOUND('',#24193,.T.) ;
#18429 = FACE_OUTER_BOUND('',#24194,.T.) ;
#18430 = FACE_OUTER_BOUND('',#24195,.T.) ;
#18431 = FACE_OUTER_BOUND('',#24196,.T.) ;
#18432 = FACE_OUTER_BOUND('',#24197,.T.) ;
#18433 = FACE_OUTER_BOUND('',#24198,.T.) ;
#18434 = FACE_OUTER_BOUND('',#24199,.T.) ;
#18435 = FACE_OUTER_BOUND('',#24200,.T.) ;
#18436 = FACE_OUTER_BOUND('',#24201,.T.) ;
#18437 = FACE_OUTER_BOUND('',#24202,.T.) ;
#18438 = FACE_OUTER_BOUND('',#24203,.T.) ;
#18439 = FACE_OUTER_BOUND('',#24204,.T.) ;
#18440 = FACE_OUTER_BOUND('',#24205,.T.) ;
#18441 = FACE_OUTER_BOUND('',#24206,.T.) ;
#18442 = FACE_OUTER_BOUND('',#24207,.T.) ;
#18443 = FACE_OUTER_BOUND('',#24208,.T.) ;
#18444 = FACE_OUTER_BOUND('',#24209,.T.) ;
#18445 = FACE_OUTER_BOUND('',#24210,.T.) ;
#18446 = FACE_OUTER_BOUND('',#24211,.T.) ;
#18447 = FACE_OUTER_BOUND('',#24212,.T.) ;
#18448 = FACE_OUTER_BOUND('',#24213,.T.) ;
#18449 = FACE_OUTER_BOUND('',#24214,.T.) ;
#18450 = FACE_OUTER_BOUND('',#24215,.T.) ;
#18451 = FACE_OUTER_BOUND('',#24216,.T.) ;
#18452 = FACE_OUTER_BOUND('',#24217,.T.) ;
#18453 = FACE_OUTER_BOUND('',#24218,.T.) ;
#18454 = FACE_OUTER_BOUND('',#24219,.T.) ;
#18455 = FACE_OUTER_BOUND('',#24220,.T.) ;
#18456 = FACE_OUTER_BOUND('',#24221,.T.) ;
#18457 = FACE_OUTER_BOUND('',#24222,.T.) ;
#18458 = FACE_OUTER_BOUND('',#24223,.T.) ;
#18459 = FACE_OUTER_BOUND('',#24224,.T.) ;
#18460 = FACE_OUTER_BOUND('',#24225,.T.) ;
#18461 = FACE_OUTER_BOUND('',#24226,.T.) ;
#18462 = FACE_OUTER_BOUND('',#24227,.T.) ;
#18463 = FACE_OUTER_BOUND('',#24228,.T.) ;
#18464 = FACE_OUTER_BOUND('',#24229,.T.) ;
#18465 = FACE_OUTER_BOUND('',#24230,.T.) ;
#18466 = FACE_OUTER_BOUND('',#24231,.T.) ;
#18467 = FACE_OUTER_BOUND('',#24232,.T.) ;
#18468 = FACE_OUTER_BOUND('',#24233,.T.) ;
#18469 = FACE_OUTER_BOUND('',#24234,.T.) ;
#18470 = FACE_OUTER_BOUND('',#24235,.T.) ;
#18471 = FACE_OUTER_BOUND('',#24236,.T.) ;
#18472 = FACE_OUTER_BOUND('',#24237,.T.) ;
#18473 = FACE_OUTER_BOUND('',#24238,.T.) ;
#18474 = FACE_OUTER_BOUND('',#24239,.T.) ;
#18475 = FACE_OUTER_BOUND('',#24240,.T.) ;
#18476 = FACE_OUTER_BOUND('',#24241,.T.) ;
#18477 = FACE_OUTER_BOUND('',#24242,.T.) ;
#18478 = FACE_OUTER_BOUND('',#24243,.T.) ;
#18479 = FACE_OUTER_BOUND('',#24244,.T.) ;
#18480 = FACE_OUTER_BOUND('',#24245,.T.) ;
#18481 = FACE_OUTER_BOUND('',#24246,.T.) ;
#18482 = FACE_OUTER_BOUND('',#24247,.T.) ;
#18483 = FACE_OUTER_BOUND('',#24248,.T.) ;
#18484 = FACE_OUTER_BOUND('',#24249,.T.) ;
#18485 = FACE_OUTER_BOUND('',#24250,.T.) ;
#18486 = FACE_OUTER_BOUND('',#24251,.T.) ;
#18487 = FACE_OUTER_BOUND('',#24252,.T.) ;
#18488 = FACE_OUTER_BOUND('',#24253,.T.) ;
#18489 = FACE_OUTER_BOUND('',#24254,.T.) ;
#18490 = FACE_OUTER_BOUND('',#24255,.T.) ;
#18491 = FACE_OUTER_BOUND('',#24256,.T.) ;
#18492 = FACE_OUTER_BOUND('',#24257,.T.) ;
#18493 = FACE_OUTER_BOUND('',#24258,.T.) ;
#18494 = FACE_OUTER_BOUND('',#24259,.T.) ;
#18495 = FACE_OUTER_BOUND('',#24260,.T.) ;
#18496 = FACE_OUTER_BOUND('',#24261,.T.) ;
#18497 = FACE_OUTER_BOUND('',#24262,.T.) ;
#18498 = FACE_OUTER_BOUND('',#24263,.T.) ;
#18499 = FACE_OUTER_BOUND('',#24264,.T.) ;
#18500 = FACE_OUTER_BOUND('',#24265,.T.) ;
#18501 = FACE_OUTER_BOUND('',#24266,.T.) ;
#18502 = FACE_OUTER_BOUND('',#24267,.T.) ;
#18503 = FACE_OUTER_BOUND('',#24268,.T.) ;
#18504 = FACE_OUTER_BOUND('',#24269,.T.) ;
#18505 = FACE_OUTER_BOUND('',#24270,.T.) ;
#18506 = FACE_OUTER_BOUND('',#24271,.T.) ;
#18507 = FACE_OUTER_BOUND('',#24272,.T.) ;
#18508 = FACE_OUTER_BOUND('',#24273,.T.) ;
#18509 = FACE_OUTER_BOUND('',#24274,.T.) ;
#18510 = FACE_OUTER_BOUND('',#24275,.T.) ;
#18511 = FACE_OUTER_BOUND('',#24276,.T.) ;
#18512 = FACE_OUTER_BOUND('',#24277,.T.) ;
#18513 = FACE_OUTER_BOUND('',#24278,.T.) ;
#18514 = FACE_OUTER_BOUND('',#24279,.T.) ;
#18515 = FACE_OUTER_BOUND('',#24280,.T.) ;
#18516 = FACE_OUTER_BOUND('',#24281,.T.) ;
#18517 = FACE_OUTER_BOUND('',#24282,.T.) ;
#18518 = FACE_OUTER_BOUND('',#24283,.T.) ;
#18519 = FACE_OUTER_BOUND('',#24284,.T.) ;
#18520 = FACE_OUTER_BOUND('',#24285,.T.) ;
#18521 = FACE_OUTER_BOUND('',#24286,.T.) ;
#18522 = FACE_OUTER_BOUND('',#24287,.T.) ;
#18523 = FACE_OUTER_BOUND('',#24288,.T.) ;
#18524 = FACE_OUTER_BOUND('',#24289,.T.) ;
#18525 = FACE_OUTER_BOUND('',#24290,.T.) ;
#18526 = FACE_OUTER_BOUND('',#24291,.T.) ;
#18527 = FACE_OUTER_BOUND('',#24292,.T.) ;
#18528 = FACE_OUTER_BOUND('',#24293,.T.) ;
#18529 = FACE_OUTER_BOUND('',#24294,.T.) ;
#18530 = FACE_OUTER_BOUND('',#24295,.T.) ;
#18531 = FACE_OUTER_BOUND('',#24296,.T.) ;
#18532 = FACE_OUTER_BOUND('',#24297,.T.) ;
#18533 = FACE_OUTER_BOUND('',#24298,.T.) ;
#18534 = FACE_OUTER_BOUND('',#24299,.T.) ;
#18535 = FACE_OUTER_BOUND('',#24300,.T.) ;
#18536 = FACE_OUTER_BOUND('',#24301,.T.) ;
#18537 = FACE_OUTER_BOUND('',#24302,.T.) ;
#18538 = FACE_OUTER_BOUND('',#24303,.T.) ;
#18539 = FACE_OUTER_BOUND('',#24304,.T.) ;
#18540 = FACE_OUTER_BOUND('',#24305,.T.) ;
#18541 = FACE_OUTER_BOUND('',#24306,.T.) ;
#18542 = FACE_OUTER_BOUND('',#24307,.T.) ;
#18543 = FACE_OUTER_BOUND('',#24308,.T.) ;
#18544 = FACE_OUTER_BOUND('',#24309,.T.) ;
#18545 = FACE_OUTER_BOUND('',#24310,.T.) ;
#18546 = FACE_OUTER_BOUND('',#24311,.T.) ;
#18547 = FACE_OUTER_BOUND('',#24312,.T.) ;
#18548 = FACE_OUTER_BOUND('',#24313,.T.) ;
#18549 = FACE_OUTER_BOUND('',#24314,.T.) ;
#18550 = FACE_OUTER_BOUND('',#24315,.T.) ;
#18551 = FACE_OUTER_BOUND('',#24316,.T.) ;
#18552 = FACE_OUTER_BOUND('',#24317,.T.) ;
#18553 = FACE_OUTER_BOUND('',#24318,.T.) ;
#18554 = FACE_OUTER_BOUND('',#24319,.T.) ;
#18555 = FACE_OUTER_BOUND('',#24320,.T.) ;
#18556 = FACE_OUTER_BOUND('',#24321,.T.) ;
#18557 = FACE_OUTER_BOUND('',#24322,.T.) ;
#18558 = FACE_OUTER_BOUND('',#24323,.T.) ;
#18559 = FACE_OUTER_BOUND('',#24324,.T.) ;
#18560 = FACE_OUTER_BOUND('',#24325,.T.) ;
#18561 = FACE_OUTER_BOUND('',#24326,.T.) ;
#18562 = FACE_OUTER_BOUND('',#24327,.T.) ;
#18563 = FACE_OUTER_BOUND('',#24328,.T.) ;
#18564 = FACE_OUTER_BOUND('',#24329,.T.) ;
#18565 = FACE_OUTER_BOUND('',#24330,.T.) ;
#18566 = FACE_OUTER_BOUND('',#24331,.T.) ;
#18567 = FACE_OUTER_BOUND('',#24332,.T.) ;
#18568 = FACE_OUTER_BOUND('',#24333,.T.) ;
#18569 = FACE_OUTER_BOUND('',#24334,.T.) ;
#18570 = FACE_OUTER_BOUND('',#24335,.T.) ;
#18571 = FACE_OUTER_BOUND('',#24336,.T.) ;
#18572 = FACE_OUTER_BOUND('',#24337,.T.) ;
#18573 = FACE_OUTER_BOUND('',#24338,.T.) ;
#18574 = FACE_OUTER_BOUND('',#24339,.T.) ;
#18575 = FACE_OUTER_BOUND('',#24340,.T.) ;
#18576 = FACE_OUTER_BOUND('',#24341,.T.) ;
#18577 = FACE_OUTER_BOUND('',#24342,.T.) ;
#18578 = FACE_OUTER_BOUND('',#24343,.T.) ;
#18579 = FACE_OUTER_BOUND('',#24344,.T.) ;
#18580 = FACE_OUTER_BOUND('',#24345,.T.) ;
#18581 = FACE_OUTER_BOUND('',#24346,.T.) ;
#18582 = FACE_OUTER_BOUND('',#24347,.T.) ;
#18583 = FACE_OUTER_BOUND('',#24348,.T.) ;
#18584 = FACE_OUTER_BOUND('',#24349,.T.) ;
#18585 = FACE_OUTER_BOUND('',#24350,.T.) ;
#18586 = FACE_OUTER_BOUND('',#24351,.T.) ;
#18587 = FACE_OUTER_BOUND('',#24352,.T.) ;
#18588 = FACE_OUTER_BOUND('',#24353,.T.) ;
#18589 = FACE_OUTER_BOUND('',#24354,.T.) ;
#18590 = FACE_OUTER_BOUND('',#24355,.T.) ;
#18591 = FACE_OUTER_BOUND('',#24356,.T.) ;
#18592 = FACE_OUTER_BOUND('',#24357,.T.) ;
#18593 = FACE_OUTER_BOUND('',#24358,.T.) ;
#18594 = FACE_OUTER_BOUND('',#24359,.T.) ;
#18595 = FACE_OUTER_BOUND('',#24360,.T.) ;
#18596 = FACE_OUTER_BOUND('',#24361,.T.) ;
#18597 = FACE_OUTER_BOUND('',#24362,.T.) ;
#18598 = FACE_OUTER_BOUND('',#24363,.T.) ;
#18599 = FACE_OUTER_BOUND('',#24364,.T.) ;
#18600 = FACE_OUTER_BOUND('',#24365,.T.) ;
#18601 = FACE_OUTER_BOUND('',#24366,.T.) ;
#18602 = FACE_OUTER_BOUND('',#24367,.T.) ;
#18603 = FACE_OUTER_BOUND('',#24368,.T.) ;
#18604 = FACE_OUTER_BOUND('',#24369,.T.) ;
#18605 = FACE_OUTER_BOUND('',#24370,.T.) ;
#18606 = FACE_OUTER_BOUND('',#24371,.T.) ;
#18607 = FACE_OUTER_BOUND('',#24372,.T.) ;
#18608 = FACE_OUTER_BOUND('',#24373,.T.) ;
#18609 = FACE_OUTER_BOUND('',#24374,.T.) ;
#18610 = FACE_OUTER_BOUND('',#24375,.T.) ;
#18611 = FACE_OUTER_BOUND('',#24376,.T.) ;
#18612 = FACE_OUTER_BOUND('',#24377,.T.) ;
#18613 = FACE_OUTER_BOUND('',#24378,.T.) ;
#18614 = FACE_OUTER_BOUND('',#24379,.T.) ;
#18615 = FACE_OUTER_BOUND('',#24380,.T.) ;
#18616 = FACE_OUTER_BOUND('',#24381,.T.) ;
#18617 = FACE_OUTER_BOUND('',#24383,.T.) ;
#18618 = FACE_OUTER_BOUND('',#24384,.T.) ;
#18619 = FACE_OUTER_BOUND('',#24385,.T.) ;
#18620 = FACE_OUTER_BOUND('',#24386,.T.) ;
#18621 = FACE_OUTER_BOUND('',#24387,.T.) ;
#18622 = FACE_OUTER_BOUND('',#24388,.T.) ;
#18623 = FACE_OUTER_BOUND('',#24389,.T.) ;
#18624 = FACE_OUTER_BOUND('',#24390,.T.) ;
#18625 = FACE_OUTER_BOUND('',#24391,.T.) ;
#18626 = FACE_OUTER_BOUND('',#24392,.T.) ;
#18627 = FACE_OUTER_BOUND('',#24393,.T.) ;
#18628 = FACE_OUTER_BOUND('',#24394,.T.) ;
#18629 = FACE_OUTER_BOUND('',#24395,.T.) ;
#18630 = FACE_OUTER_BOUND('',#24396,.T.) ;
#18631 = FACE_OUTER_BOUND('',#24397,.T.) ;
#18632 = FACE_OUTER_BOUND('',#24398,.T.) ;
#18633 = FACE_OUTER_BOUND('',#24399,.T.) ;
#18634 = FACE_OUTER_BOUND('',#24400,.T.) ;
#18635 = FACE_OUTER_BOUND('',#24401,.T.) ;
#18636 = FACE_OUTER_BOUND('',#24402,.T.) ;
#18637 = FACE_OUTER_BOUND('',#24403,.T.) ;
#18638 = FACE_OUTER_BOUND('',#24404,.T.) ;
#18639 = FACE_OUTER_BOUND('',#24405,.T.) ;
#18640 = FACE_OUTER_BOUND('',#24406,.T.) ;
#18641 = FACE_OUTER_BOUND('',#24407,.T.) ;
#18642 = FACE_OUTER_BOUND('',#24408,.T.) ;
#18643 = FACE_OUTER_BOUND('',#24409,.T.) ;
#18644 = FACE_OUTER_BOUND('',#24410,.T.) ;
#18645 = FACE_OUTER_BOUND('',#24412,.T.) ;
#18646 = FACE_OUTER_BOUND('',#24413,.T.) ;
#18647 = FACE_OUTER_BOUND('',#24414,.T.) ;
#18648 = FACE_OUTER_BOUND('',#24415,.T.) ;
#18649 = FACE_OUTER_BOUND('',#24416,.T.) ;
#18650 = FACE_OUTER_BOUND('',#24417,.T.) ;
#18651 = FACE_OUTER_BOUND('',#24418,.T.) ;
#18652 = FACE_OUTER_BOUND('',#24419,.T.) ;
#18653 = FACE_OUTER_BOUND('',#24420,.T.) ;
#18654 = FACE_OUTER_BOUND('',#24421,.T.) ;
#18655 = FACE_OUTER_BOUND('',#24422,.T.) ;
#18656 = FACE_OUTER_BOUND('',#24423,.T.) ;
#18657 = FACE_OUTER_BOUND('',#24424,.T.) ;
#18658 = FACE_OUTER_BOUND('',#24425,.T.) ;
#18659 = FACE_OUTER_BOUND('',#24426,.T.) ;
#18660 = FACE_OUTER_BOUND('',#24427,.T.) ;
#18661 = FACE_OUTER_BOUND('',#24428,.T.) ;
#18662 = FACE_OUTER_BOUND('',#24429,.T.) ;
#18663 = FACE_OUTER_BOUND('',#24430,.T.) ;
#18664 = FACE_OUTER_BOUND('',#24431,.T.) ;
#18665 = FACE_OUTER_BOUND('',#24432,.T.) ;
#18666 = FACE_OUTER_BOUND('',#24433,.T.) ;
#18667 = FACE_OUTER_BOUND('',#24434,.T.) ;
#18668 = FACE_OUTER_BOUND('',#24435,.T.) ;
#18669 = FACE_OUTER_BOUND('',#24436,.T.) ;
#18670 = FACE_OUTER_BOUND('',#24437,.T.) ;
#18671 = FACE_OUTER_BOUND('',#24438,.T.) ;
#18672 = FACE_OUTER_BOUND('',#24439,.T.) ;
#18673 = FACE_OUTER_BOUND('',#24441,.T.) ;
#18674 = FACE_OUTER_BOUND('',#24442,.T.) ;
#18675 = FACE_OUTER_BOUND('',#24443,.T.) ;
#18676 = FACE_OUTER_BOUND('',#24444,.T.) ;
#18677 = FACE_OUTER_BOUND('',#24445,.T.) ;
#18678 = FACE_OUTER_BOUND('',#24446,.T.) ;
#18679 = FACE_OUTER_BOUND('',#24447,.T.) ;
#18680 = FACE_OUTER_BOUND('',#24448,.T.) ;
#18681 = FACE_OUTER_BOUND('',#24449,.T.) ;
#18682 = FACE_OUTER_BOUND('',#24450,.T.) ;
#18683 = FACE_OUTER_BOUND('',#24451,.T.) ;
#18684 = FACE_OUTER_BOUND('',#24452,.T.) ;
#18685 = FACE_OUTER_BOUND('',#24453,.T.) ;
#18686 = FACE_OUTER_BOUND('',#24454,.T.) ;
#18687 = FACE_OUTER_BOUND('',#24455,.T.) ;
#18688 = FACE_OUTER_BOUND('',#24456,.T.) ;
#18689 = FACE_OUTER_BOUND('',#24457,.T.) ;
#18690 = FACE_OUTER_BOUND('',#24458,.T.) ;
#18691 = FACE_OUTER_BOUND('',#24459,.T.) ;
#18692 = FACE_OUTER_BOUND('',#24460,.T.) ;
#18693 = FACE_OUTER_BOUND('',#24461,.T.) ;
#18694 = FACE_OUTER_BOUND('',#24462,.T.) ;
#18695 = FACE_OUTER_BOUND('',#24463,.T.) ;
#18696 = FACE_OUTER_BOUND('',#24464,.T.) ;
#18697 = FACE_OUTER_BOUND('',#24465,.T.) ;
#18698 = FACE_OUTER_BOUND('',#24466,.T.) ;
#18699 = FACE_OUTER_BOUND('',#24467,.T.) ;
#18700 = FACE_OUTER_BOUND('',#24468,.T.) ;
#18701 = FACE_OUTER_BOUND('',#24470,.T.) ;
#18702 = FACE_OUTER_BOUND('',#24471,.T.) ;
#18703 = FACE_OUTER_BOUND('',#24472,.T.) ;
#18704 = FACE_OUTER_BOUND('',#24473,.T.) ;
#18705 = FACE_OUTER_BOUND('',#24474,.T.) ;
#18706 = FACE_OUTER_BOUND('',#24475,.T.) ;
#18707 = FACE_OUTER_BOUND('',#24476,.T.) ;
#18708 = FACE_OUTER_BOUND('',#24477,.T.) ;
#18709 = FACE_OUTER_BOUND('',#24478,.T.) ;
#18710 = FACE_OUTER_BOUND('',#24479,.T.) ;
#18711 = FACE_OUTER_BOUND('',#24480,.T.) ;
#18712 = FACE_OUTER_BOUND('',#24481,.T.) ;
#18713 = FACE_OUTER_BOUND('',#24482,.T.) ;
#18714 = FACE_OUTER_BOUND('',#24483,.T.) ;
#18715 = FACE_OUTER_BOUND('',#24484,.T.) ;
#18716 = FACE_OUTER_BOUND('',#24485,.T.) ;
#18717 = FACE_OUTER_BOUND('',#24486,.T.) ;
#18718 = FACE_OUTER_BOUND('',#24487,.T.) ;
#18719 = FACE_OUTER_BOUND('',#24488,.T.) ;
#18720 = FACE_OUTER_BOUND('',#24489,.T.) ;
#18721 = FACE_OUTER_BOUND('',#24490,.T.) ;
#18722 = FACE_OUTER_BOUND('',#24491,.T.) ;
#18723 = FACE_OUTER_BOUND('',#24492,.T.) ;
#18724 = FACE_OUTER_BOUND('',#24493,.T.) ;
#18725 = FACE_OUTER_BOUND('',#24494,.T.) ;
#18726 = FACE_OUTER_BOUND('',#24495,.T.) ;
#18727 = FACE_OUTER_BOUND('',#24496,.T.) ;
#18728 = FACE_OUTER_BOUND('',#24497,.T.) ;
#18729 = FACE_OUTER_BOUND('',#24499,.T.) ;
#18730 = FACE_OUTER_BOUND('',#24500,.T.) ;
#18731 = FACE_OUTER_BOUND('',#24501,.T.) ;
#18732 = FACE_OUTER_BOUND('',#24502,.T.) ;
#18733 = FACE_OUTER_BOUND('',#24503,.T.) ;
#18734 = FACE_OUTER_BOUND('',#24504,.T.) ;
#18735 = FACE_OUTER_BOUND('',#24505,.T.) ;
#18736 = FACE_OUTER_BOUND('',#24506,.T.) ;
#18737 = FACE_OUTER_BOUND('',#24507,.T.) ;
#18738 = FACE_OUTER_BOUND('',#24508,.T.) ;
#18739 = FACE_OUTER_BOUND('',#24509,.T.) ;
#18740 = FACE_OUTER_BOUND('',#24510,.T.) ;
#18741 = FACE_OUTER_BOUND('',#24511,.T.) ;
#18742 = FACE_OUTER_BOUND('',#24512,.T.) ;
#18743 = FACE_OUTER_BOUND('',#24513,.T.) ;
#18744 = FACE_OUTER_BOUND('',#24514,.T.) ;
#18745 = FACE_OUTER_BOUND('',#24515,.T.) ;
#18746 = FACE_OUTER_BOUND('',#24516,.T.) ;
#18747 = FACE_OUTER_BOUND('',#24517,.T.) ;
#18748 = FACE_OUTER_BOUND('',#24518,.T.) ;
#18749 = FACE_OUTER_BOUND('',#24519,.T.) ;
#18750 = FACE_OUTER_BOUND('',#24520,.T.) ;
#18751 = FACE_OUTER_BOUND('',#24521,.T.) ;
#18752 = FACE_OUTER_BOUND('',#24522,.T.) ;
#18753 = FACE_OUTER_BOUND('',#24523,.T.) ;
#18754 = FACE_OUTER_BOUND('',#24524,.T.) ;
#18755 = FACE_OUTER_BOUND('',#24525,.T.) ;
#18756 = FACE_OUTER_BOUND('',#24526,.T.) ;
#18757 = FACE_OUTER_BOUND('',#24528,.T.) ;
#18758 = FACE_OUTER_BOUND('',#24529,.T.) ;
#18759 = FACE_OUTER_BOUND('',#24530,.T.) ;
#18760 = FACE_OUTER_BOUND('',#24531,.T.) ;
#18761 = FACE_OUTER_BOUND('',#24532,.T.) ;
#18762 = FACE_OUTER_BOUND('',#24533,.T.) ;
#18763 = FACE_OUTER_BOUND('',#24534,.T.) ;
#18764 = FACE_OUTER_BOUND('',#24535,.T.) ;
#18765 = FACE_OUTER_BOUND('',#24536,.T.) ;
#18766 = FACE_OUTER_BOUND('',#24537,.T.) ;
#18767 = FACE_OUTER_BOUND('',#24538,.T.) ;
#18768 = FACE_OUTER_BOUND('',#24539,.T.) ;
#18769 = FACE_OUTER_BOUND('',#24540,.T.) ;
#18770 = FACE_OUTER_BOUND('',#24541,.T.) ;
#18771 = FACE_OUTER_BOUND('',#24542,.T.) ;
#18772 = FACE_OUTER_BOUND('',#24543,.T.) ;
#18773 = FACE_OUTER_BOUND('',#24544,.T.) ;
#18774 = FACE_OUTER_BOUND('',#24545,.T.) ;
#18775 = FACE_OUTER_BOUND('',#24546,.T.) ;
#18776 = FACE_OUTER_BOUND('',#24547,.T.) ;
#18777 = FACE_OUTER_BOUND('',#24548,.T.) ;
#18778 = FACE_OUTER_BOUND('',#24549,.T.) ;
#18779 = FACE_OUTER_BOUND('',#24550,.T.) ;
#18780 = FACE_OUTER_BOUND('',#24551,.T.) ;
#18781 = FACE_OUTER_BOUND('',#24552,.T.) ;
#18782 = FACE_OUTER_BOUND('',#24553,.T.) ;
#18783 = FACE_OUTER_BOUND('',#24554,.T.) ;
#18784 = FACE_OUTER_BOUND('',#24555,.T.) ;
#18785 = FACE_OUTER_BOUND('',#24557,.T.) ;
#18786 = FACE_OUTER_BOUND('',#24558,.T.) ;
#18787 = FACE_OUTER_BOUND('',#24559,.T.) ;
#18788 = FACE_OUTER_BOUND('',#24560,.T.) ;
#18789 = FACE_OUTER_BOUND('',#24561,.T.) ;
#18790 = FACE_OUTER_BOUND('',#24562,.T.) ;
#18791 = FACE_OUTER_BOUND('',#24563,.T.) ;
#18792 = FACE_OUTER_BOUND('',#24564,.T.) ;
#18793 = FACE_OUTER_BOUND('',#24565,.T.) ;
#18794 = FACE_OUTER_BOUND('',#24566,.T.) ;
#18795 = FACE_OUTER_BOUND('',#24567,.T.) ;
#18796 = FACE_OUTER_BOUND('',#24568,.T.) ;
#18797 = FACE_OUTER_BOUND('',#24569,.T.) ;
#18798 = FACE_OUTER_BOUND('',#24570,.T.) ;
#18799 = FACE_OUTER_BOUND('',#24571,.T.) ;
#18800 = FACE_OUTER_BOUND('',#24572,.T.) ;
#18801 = FACE_OUTER_BOUND('',#24573,.T.) ;
#18802 = FACE_OUTER_BOUND('',#24574,.T.) ;
#18803 = FACE_OUTER_BOUND('',#24575,.T.) ;
#18804 = FACE_OUTER_BOUND('',#24576,.T.) ;
#18805 = FACE_OUTER_BOUND('',#24577,.T.) ;
#18806 = FACE_OUTER_BOUND('',#24578,.T.) ;
#18807 = FACE_OUTER_BOUND('',#24579,.T.) ;
#18808 = FACE_OUTER_BOUND('',#24580,.T.) ;
#18809 = FACE_OUTER_BOUND('',#24581,.T.) ;
#18810 = FACE_OUTER_BOUND('',#24582,.T.) ;
#18811 = FACE_OUTER_BOUND('',#24583,.T.) ;
#18812 = FACE_OUTER_BOUND('',#24584,.T.) ;
#18813 = FACE_OUTER_BOUND('',#24586,.T.) ;
#18814 = FACE_OUTER_BOUND('',#24587,.T.) ;
#18815 = FACE_OUTER_BOUND('',#24588,.T.) ;
#18816 = FACE_OUTER_BOUND('',#24589,.T.) ;
#18817 = FACE_OUTER_BOUND('',#24590,.T.) ;
#18818 = FACE_OUTER_BOUND('',#24591,.T.) ;
#18819 = FACE_OUTER_BOUND('',#24592,.T.) ;
#18820 = FACE_OUTER_BOUND('',#24593,.T.) ;
#18821 = FACE_OUTER_BOUND('',#24594,.T.) ;
#18822 = FACE_OUTER_BOUND('',#24595,.T.) ;
#18823 = FACE_OUTER_BOUND('',#24596,.T.) ;
#18824 = FACE_OUTER_BOUND('',#24597,.T.) ;
#18825 = FACE_OUTER_BOUND('',#24598,.T.) ;
#18826 = FACE_OUTER_BOUND('',#24599,.T.) ;
#18827 = FACE_OUTER_BOUND('',#24600,.T.) ;
#18828 = FACE_OUTER_BOUND('',#24601,.T.) ;
#18829 = FACE_OUTER_BOUND('',#24602,.T.) ;
#18830 = FACE_OUTER_BOUND('',#24603,.T.) ;
#18831 = FACE_OUTER_BOUND('',#24604,.T.) ;
#18832 = FACE_OUTER_BOUND('',#24605,.T.) ;
#18833 = FACE_OUTER_BOUND('',#24606,.T.) ;
#18834 = FACE_OUTER_BOUND('',#24607,.T.) ;
#18835 = FACE_OUTER_BOUND('',#24608,.T.) ;
#18836 = FACE_OUTER_BOUND('',#24609,.T.) ;
#18837 = FACE_OUTER_BOUND('',#24610,.T.) ;
#18838 = FACE_OUTER_BOUND('',#24611,.T.) ;
#18839 = FACE_OUTER_BOUND('',#24612,.T.) ;
#18840 = FACE_OUTER_BOUND('',#24613,.T.) ;
#18841 = FACE_OUTER_BOUND('',#24615,.T.) ;
#18842 = FACE_OUTER_BOUND('',#24617,.T.) ;
#18843 = FACE_OUTER_BOUND('',#24619,.T.) ;
#18844 = FACE_OUTER_BOUND('',#24621,.T.) ;
#18845 = FACE_OUTER_BOUND('',#24623,.T.) ;
#18846 = FACE_OUTER_BOUND('',#24625,.T.) ;
#18847 = FACE_OUTER_BOUND('',#24627,.T.) ;
#18848 = FACE_OUTER_BOUND('',#24629,.T.) ;
#18849 = FACE_OUTER_BOUND('',#24631,.T.) ;
#18850 = FACE_OUTER_BOUND('',#24633,.T.) ;
#18851 = FACE_OUTER_BOUND('',#24634,.T.) ;
#18852 = FACE_OUTER_BOUND('',#24635,.T.) ;
#18853 = FACE_OUTER_BOUND('',#24636,.T.) ;
#18854 = FACE_OUTER_BOUND('',#24637,.T.) ;
#18855 = FACE_OUTER_BOUND('',#24638,.T.) ;
#18856 = FACE_OUTER_BOUND('',#24639,.T.) ;
#18857 = FACE_OUTER_BOUND('',#24640,.T.) ;
#18858 = FACE_OUTER_BOUND('',#24641,.T.) ;
#18859 = FACE_OUTER_BOUND('',#24642,.T.) ;
#18860 = FACE_OUTER_BOUND('',#24643,.T.) ;
#18861 = FACE_OUTER_BOUND('',#24644,.T.) ;
#18862 = FACE_OUTER_BOUND('',#24645,.T.) ;
#18863 = FACE_OUTER_BOUND('',#24646,.T.) ;
#18864 = FACE_OUTER_BOUND('',#24647,.T.) ;
#18865 = FACE_OUTER_BOUND('',#24648,.T.) ;
#18866 = FACE_OUTER_BOUND('',#24649,.T.) ;
#18867 = FACE_OUTER_BOUND('',#24650,.T.) ;
#18868 = FACE_OUTER_BOUND('',#24651,.T.) ;
#18869 = FACE_OUTER_BOUND('',#24652,.T.) ;
#18870 = FACE_OUTER_BOUND('',#24653,.T.) ;
#18871 = FACE_OUTER_BOUND('',#24654,.T.) ;
#18872 = FACE_OUTER_BOUND('',#24655,.T.) ;
#18873 = FACE_OUTER_BOUND('',#24656,.T.) ;
#18874 = FACE_OUTER_BOUND('',#24657,.T.) ;
#18875 = FACE_OUTER_BOUND('',#24658,.T.) ;
#18876 = FACE_OUTER_BOUND('',#24659,.T.) ;
#18877 = FACE_OUTER_BOUND('',#24660,.T.) ;
#18878 = FACE_OUTER_BOUND('',#24661,.T.) ;
#18879 = FACE_OUTER_BOUND('',#24662,.T.) ;
#18880 = FACE_OUTER_BOUND('',#24663,.T.) ;
#18881 = FACE_OUTER_BOUND('',#24664,.T.) ;
#18882 = FACE_OUTER_BOUND('',#24665,.T.) ;
#18883 = FACE_OUTER_BOUND('',#24666,.T.) ;
#18884 = FACE_OUTER_BOUND('',#24667,.T.) ;
#18885 = FACE_OUTER_BOUND('',#24668,.T.) ;
#18886 = FACE_OUTER_BOUND('',#24669,.T.) ;
#18887 = FACE_OUTER_BOUND('',#24670,.T.) ;
#18888 = FACE_OUTER_BOUND('',#24671,.T.) ;
#18889 = FACE_OUTER_BOUND('',#24672,.T.) ;
#18890 = FACE_OUTER_BOUND('',#24673,.T.) ;
#18891 = FACE_OUTER_BOUND('',#24674,.T.) ;
#18892 = FACE_OUTER_BOUND('',#24675,.T.) ;
#18893 = FACE_OUTER_BOUND('',#24676,.T.) ;
#18894 = FACE_OUTER_BOUND('',#24677,.T.) ;
#18895 = FACE_OUTER_BOUND('',#24678,.T.) ;
#18896 = FACE_OUTER_BOUND('',#24679,.T.) ;
#18897 = FACE_OUTER_BOUND('',#24680,.T.) ;
#18898 = FACE_OUTER_BOUND('',#24681,.T.) ;
#18899 = FACE_OUTER_BOUND('',#24682,.T.) ;
#18900 = FACE_OUTER_BOUND('',#24683,.T.) ;
#18901 = FACE_OUTER_BOUND('',#24684,.T.) ;
#18902 = FACE_OUTER_BOUND('',#24685,.T.) ;
#18903 = FACE_OUTER_BOUND('',#24686,.T.) ;
#18904 = FACE_OUTER_BOUND('',#24687,.T.) ;
#18905 = FACE_OUTER_BOUND('',#24688,.T.) ;
#18906 = FACE_OUTER_BOUND('',#24689,.T.) ;
#18907 = FACE_OUTER_BOUND('',#24690,.T.) ;
#18908 = FACE_OUTER_BOUND('',#24691,.T.) ;
#18909 = FACE_OUTER_BOUND('',#24692,.T.) ;
#18910 = FACE_OUTER_BOUND('',#24693,.T.) ;
#18911 = FACE_OUTER_BOUND('',#24694,.T.) ;
#18912 = FACE_OUTER_BOUND('',#24695,.T.) ;
#18913 = FACE_OUTER_BOUND('',#24696,.T.) ;
#18914 = FACE_OUTER_BOUND('',#24697,.T.) ;
#18915 = FACE_OUTER_BOUND('',#24698,.T.) ;
#18916 = FACE_OUTER_BOUND('',#24699,.T.) ;
#18917 = FACE_OUTER_BOUND('',#24700,.T.) ;
#18918 = FACE_OUTER_BOUND('',#24701,.T.) ;
#18919 = FACE_OUTER_BOUND('',#24702,.T.) ;
#18920 = FACE_OUTER_BOUND('',#24703,.T.) ;
#18921 = FACE_OUTER_BOUND('',#24704,.T.) ;
#18922 = FACE_OUTER_BOUND('',#24705,.T.) ;
#18923 = FACE_OUTER_BOUND('',#24706,.T.) ;
#18924 = FACE_OUTER_BOUND('',#24707,.T.) ;
#18925 = FACE_OUTER_BOUND('',#24708,.T.) ;
#18926 = FACE_OUTER_BOUND('',#24709,.T.) ;
#18927 = FACE_OUTER_BOUND('',#24710,.T.) ;
#18928 = FACE_OUTER_BOUND('',#24711,.T.) ;
#18929 = FACE_OUTER_BOUND('',#24712,.T.) ;
#18930 = FACE_OUTER_BOUND('',#24713,.T.) ;
#18931 = FACE_OUTER_BOUND('',#24714,.T.) ;
#18932 = FACE_OUTER_BOUND('',#24715,.T.) ;
#18933 = FACE_OUTER_BOUND('',#24716,.T.) ;
#18934 = FACE_OUTER_BOUND('',#24717,.T.) ;
#18935 = FACE_OUTER_BOUND('',#24718,.T.) ;
#18936 = FACE_OUTER_BOUND('',#24719,.T.) ;
#18937 = FACE_OUTER_BOUND('',#24720,.T.) ;
#18938 = FACE_OUTER_BOUND('',#24721,.T.) ;
#18939 = FACE_OUTER_BOUND('',#24722,.T.) ;
#18940 = FACE_OUTER_BOUND('',#24723,.T.) ;
#18941 = FACE_OUTER_BOUND('',#24724,.T.) ;
#18942 = FACE_OUTER_BOUND('',#24725,.T.) ;
#18943 = FACE_OUTER_BOUND('',#24726,.T.) ;
#18944 = FACE_OUTER_BOUND('',#24727,.T.) ;
#18945 = FACE_OUTER_BOUND('',#24728,.T.) ;
#18946 = FACE_OUTER_BOUND('',#24729,.T.) ;
#18947 = FACE_OUTER_BOUND('',#24730,.T.) ;
#18948 = FACE_OUTER_BOUND('',#24731,.T.) ;
#18949 = FACE_OUTER_BOUND('',#24732,.T.) ;
#18950 = FACE_OUTER_BOUND('',#24733,.T.) ;
#18951 = FACE_OUTER_BOUND('',#24734,.T.) ;
#18952 = FACE_OUTER_BOUND('',#24735,.T.) ;
#18953 = FACE_OUTER_BOUND('',#24736,.T.) ;
#18954 = FACE_OUTER_BOUND('',#24737,.T.) ;
#18955 = FACE_OUTER_BOUND('',#24738,.T.) ;
#18956 = FACE_OUTER_BOUND('',#24739,.T.) ;
#18957 = FACE_OUTER_BOUND('',#24740,.T.) ;
#18958 = FACE_OUTER_BOUND('',#24741,.T.) ;
#18959 = FACE_OUTER_BOUND('',#24742,.T.) ;
#18960 = FACE_OUTER_BOUND('',#24743,.T.) ;
#18961 = FACE_OUTER_BOUND('',#24744,.T.) ;
#18962 = FACE_OUTER_BOUND('',#24745,.T.) ;
#18963 = FACE_OUTER_BOUND('',#24746,.T.) ;
#18964 = FACE_OUTER_BOUND('',#24747,.T.) ;
#18965 = FACE_OUTER_BOUND('',#24748,.T.) ;
#18966 = FACE_OUTER_BOUND('',#24749,.T.) ;
#18967 = FACE_OUTER_BOUND('',#24750,.T.) ;
#18968 = FACE_OUTER_BOUND('',#24751,.T.) ;
#18969 = FACE_OUTER_BOUND('',#24752,.T.) ;
#18970 = FACE_OUTER_BOUND('',#24753,.T.) ;
#18971 = FACE_OUTER_BOUND('',#24754,.T.) ;
#18972 = FACE_OUTER_BOUND('',#24755,.T.) ;
#18973 = FACE_OUTER_BOUND('',#24756,.T.) ;
#18974 = FACE_OUTER_BOUND('',#24757,.T.) ;
#18975 = FACE_OUTER_BOUND('',#24758,.T.) ;
#18976 = FACE_OUTER_BOUND('',#24759,.T.) ;
#18977 = FACE_OUTER_BOUND('',#24760,.T.) ;
#18978 = FACE_OUTER_BOUND('',#24761,.T.) ;
#18979 = FACE_OUTER_BOUND('',#24762,.T.) ;
#18980 = FACE_OUTER_BOUND('',#24763,.T.) ;
#18981 = FACE_OUTER_BOUND('',#24764,.T.) ;
#18982 = FACE_OUTER_BOUND('',#24765,.T.) ;
#18983 = FACE_OUTER_BOUND('',#24766,.T.) ;
#18984 = FACE_OUTER_BOUND('',#24767,.T.) ;
#18985 = FACE_OUTER_BOUND('',#24768,.T.) ;
#18986 = FACE_OUTER_BOUND('',#24769,.T.) ;
#18987 = FACE_OUTER_BOUND('',#24770,.T.) ;
#18988 = FACE_OUTER_BOUND('',#24771,.T.) ;
#18989 = FACE_OUTER_BOUND('',#24772,.T.) ;
#18990 = FACE_OUTER_BOUND('',#24773,.T.) ;
#18991 = FACE_OUTER_BOUND('',#24774,.T.) ;
#18992 = FACE_OUTER_BOUND('',#24775,.T.) ;
#18993 = FACE_OUTER_BOUND('',#24776,.T.) ;
#18994 = FACE_OUTER_BOUND('',#24777,.T.) ;
#18995 = FACE_OUTER_BOUND('',#24778,.T.) ;
#18996 = FACE_OUTER_BOUND('',#24779,.T.) ;
#18997 = FACE_OUTER_BOUND('',#24780,.T.) ;
#18998 = FACE_OUTER_BOUND('',#24781,.T.) ;
#18999 = FACE_OUTER_BOUND('',#24782,.T.) ;
#19000 = FACE_OUTER_BOUND('',#24783,.T.) ;
#19001 = FACE_OUTER_BOUND('',#24784,.T.) ;
#19002 = FACE_OUTER_BOUND('',#24785,.T.) ;
#19003 = FACE_OUTER_BOUND('',#24786,.T.) ;
#19004 = FACE_OUTER_BOUND('',#24787,.T.) ;
#19005 = FACE_OUTER_BOUND('',#24788,.T.) ;
#19006 = FACE_OUTER_BOUND('',#24789,.T.) ;
#19007 = FACE_OUTER_BOUND('',#24790,.T.) ;
#19008 = FACE_OUTER_BOUND('',#24791,.T.) ;
#19009 = FACE_OUTER_BOUND('',#24792,.T.) ;
#19010 = FACE_OUTER_BOUND('',#24793,.T.) ;
#19011 = FACE_OUTER_BOUND('',#24794,.T.) ;
#19012 = FACE_OUTER_BOUND('',#24795,.T.) ;
#19013 = FACE_OUTER_BOUND('',#24796,.T.) ;
#19014 = FACE_OUTER_BOUND('',#24797,.T.) ;
#19015 = FACE_OUTER_BOUND('',#24798,.T.) ;
#19016 = FACE_OUTER_BOUND('',#24799,.T.) ;
#19017 = FACE_OUTER_BOUND('',#24800,.T.) ;
#19018 = FACE_OUTER_BOUND('',#24801,.T.) ;
#19019 = FACE_OUTER_BOUND('',#24802,.T.) ;
#19020 = FACE_OUTER_BOUND('',#24803,.T.) ;
#19021 = FACE_OUTER_BOUND('',#24804,.T.) ;
#19022 = FACE_OUTER_BOUND('',#24805,.T.) ;
#19023 = FACE_OUTER_BOUND('',#24806,.T.) ;
#19024 = FACE_OUTER_BOUND('',#24807,.T.) ;
#19025 = FACE_OUTER_BOUND('',#24808,.T.) ;
#19026 = FACE_OUTER_BOUND('',#24809,.T.) ;
#19027 = FACE_OUTER_BOUND('',#24810,.T.) ;
#19028 = FACE_OUTER_BOUND('',#24811,.T.) ;
#19029 = FACE_OUTER_BOUND('',#24812,.T.) ;
#19030 = FACE_OUTER_BOUND('',#24813,.T.) ;
#19031 = FACE_OUTER_BOUND('',#24814,.T.) ;
#19032 = FACE_OUTER_BOUND('',#24815,.T.) ;
#19033 = FACE_OUTER_BOUND('',#24816,.T.) ;
#19034 = FACE_OUTER_BOUND('',#24817,.T.) ;
#19035 = FACE_OUTER_BOUND('',#24818,.T.) ;
#19036 = FACE_OUTER_BOUND('',#24819,.T.) ;
#19037 = FACE_OUTER_BOUND('',#24820,.T.) ;
#19038 = FACE_OUTER_BOUND('',#24821,.T.) ;
#19039 = FACE_OUTER_BOUND('',#24822,.T.) ;
#19040 = FACE_OUTER_BOUND('',#24823,.T.) ;
#19041 = FACE_OUTER_BOUND('',#24824,.T.) ;
#19042 = FACE_OUTER_BOUND('',#24825,.T.) ;
#19043 = FACE_OUTER_BOUND('',#24826,.T.) ;
#19044 = FACE_OUTER_BOUND('',#24827,.T.) ;
#19045 = FACE_OUTER_BOUND('',#24828,.T.) ;
#19046 = FACE_OUTER_BOUND('',#24829,.T.) ;
#19047 = FACE_OUTER_BOUND('',#24830,.T.) ;
#19048 = FACE_OUTER_BOUND('',#24831,.T.) ;
#19049 = FACE_OUTER_BOUND('',#24832,.T.) ;
#19050 = FACE_OUTER_BOUND('',#24833,.T.) ;
#19051 = FACE_OUTER_BOUND('',#24834,.T.) ;
#19052 = FACE_OUTER_BOUND('',#24835,.T.) ;
#19053 = FACE_OUTER_BOUND('',#24836,.T.) ;
#19054 = FACE_OUTER_BOUND('',#24837,.T.) ;
#19055 = FACE_OUTER_BOUND('',#24838,.T.) ;
#19056 = FACE_OUTER_BOUND('',#24839,.T.) ;
#19057 = FACE_OUTER_BOUND('',#24840,.T.) ;
#19058 = FACE_OUTER_BOUND('',#24841,.T.) ;
#19059 = FACE_OUTER_BOUND('',#24842,.T.) ;
#19060 = FACE_OUTER_BOUND('',#24843,.T.) ;
#19061 = FACE_OUTER_BOUND('',#24844,.T.) ;
#19062 = FACE_OUTER_BOUND('',#24845,.T.) ;
#19063 = FACE_OUTER_BOUND('',#24846,.T.) ;
#19064 = FACE_OUTER_BOUND('',#24847,.T.) ;
#19065 = FACE_OUTER_BOUND('',#24848,.T.) ;
#19066 = FACE_OUTER_BOUND('',#24849,.T.) ;
#19067 = FACE_OUTER_BOUND('',#24850,.T.) ;
#19068 = FACE_OUTER_BOUND('',#24851,.T.) ;
#19069 = FACE_OUTER_BOUND('',#24852,.T.) ;
#19070 = FACE_OUTER_BOUND('',#24853,.T.) ;
#19071 = FACE_OUTER_BOUND('',#24854,.T.) ;
#19072 = FACE_OUTER_BOUND('',#24855,.T.) ;
#19073 = FACE_OUTER_BOUND('',#24856,.T.) ;
#19074 = FACE_OUTER_BOUND('',#24857,.T.) ;
#19075 = FACE_OUTER_BOUND('',#24858,.T.) ;
#19076 = FACE_OUTER_BOUND('',#24859,.T.) ;
#19077 = FACE_OUTER_BOUND('',#24860,.T.) ;
#19078 = FACE_OUTER_BOUND('',#24861,.T.) ;
#19079 = FACE_OUTER_BOUND('',#24862,.T.) ;
#19080 = FACE_OUTER_BOUND('',#24863,.T.) ;
#19081 = FACE_OUTER_BOUND('',#24864,.T.) ;
#19082 = FACE_OUTER_BOUND('',#24865,.T.) ;
#19083 = FACE_OUTER_BOUND('',#24866,.T.) ;
#19084 = FACE_OUTER_BOUND('',#24867,.T.) ;
#19085 = FACE_OUTER_BOUND('',#24868,.T.) ;
#19086 = FACE_OUTER_BOUND('',#24869,.T.) ;
#19087 = FACE_OUTER_BOUND('',#24870,.T.) ;
#19088 = FACE_OUTER_BOUND('',#24871,.T.) ;
#19089 = FACE_OUTER_BOUND('',#24872,.T.) ;
#19090 = FACE_OUTER_BOUND('',#24873,.T.) ;
#19091 = FACE_OUTER_BOUND('',#24874,.T.) ;
#19092 = FACE_OUTER_BOUND('',#24875,.T.) ;
#19093 = FACE_OUTER_BOUND('',#24876,.T.) ;
#19094 = FACE_OUTER_BOUND('',#24877,.T.) ;
#19095 = FACE_OUTER_BOUND('',#24878,.T.) ;
#19096 = FACE_OUTER_BOUND('',#24879,.T.) ;
#19097 = FACE_OUTER_BOUND('',#24880,.T.) ;
#19098 = FACE_OUTER_BOUND('',#24881,.T.) ;
#19099 = FACE_OUTER_BOUND('',#24882,.T.) ;
#19100 = FACE_OUTER_BOUND('',#24883,.T.) ;
#19101 = FACE_OUTER_BOUND('',#24884,.T.) ;
#19102 = FACE_OUTER_BOUND('',#24885,.T.) ;
#19103 = FACE_OUTER_BOUND('',#24886,.T.) ;
#19104 = FACE_OUTER_BOUND('',#24887,.T.) ;
#19105 = FACE_OUTER_BOUND('',#24888,.T.) ;
#19106 = FACE_OUTER_BOUND('',#24889,.T.) ;
#19107 = FACE_OUTER_BOUND('',#24890,.T.) ;
#19108 = FACE_OUTER_BOUND('',#24891,.T.) ;
#19109 = FACE_OUTER_BOUND('',#24892,.T.) ;
#19110 = FACE_OUTER_BOUND('',#24893,.T.) ;
#19111 = FACE_OUTER_BOUND('',#24894,.T.) ;
#19112 = FACE_OUTER_BOUND('',#24895,.T.) ;
#19113 = FACE_OUTER_BOUND('',#24896,.T.) ;
#19114 = FACE_OUTER_BOUND('',#24897,.T.) ;
#19115 = FACE_OUTER_BOUND('',#24898,.T.) ;
#19116 = FACE_OUTER_BOUND('',#24899,.T.) ;
#19117 = FACE_OUTER_BOUND('',#24900,.T.) ;
#19118 = FACE_OUTER_BOUND('',#24901,.T.) ;
#19119 = FACE_OUTER_BOUND('',#24902,.T.) ;
#19120 = FACE_OUTER_BOUND('',#24903,.T.) ;
#19121 = FACE_OUTER_BOUND('',#24904,.T.) ;
#19122 = FACE_OUTER_BOUND('',#24905,.T.) ;
#19123 = FACE_OUTER_BOUND('',#24906,.T.) ;
#19124 = FACE_OUTER_BOUND('',#24907,.T.) ;
#19125 = FACE_OUTER_BOUND('',#24908,.T.) ;
#19126 = FACE_OUTER_BOUND('',#24909,.T.) ;
#19127 = FACE_OUTER_BOUND('',#24910,.T.) ;
#19128 = FACE_OUTER_BOUND('',#24911,.T.) ;
#19129 = FACE_OUTER_BOUND('',#24912,.T.) ;
#19130 = FACE_OUTER_BOUND('',#24913,.T.) ;
#19131 = FACE_OUTER_BOUND('',#24914,.T.) ;
#19132 = FACE_OUTER_BOUND('',#24915,.T.) ;
#19133 = FACE_OUTER_BOUND('',#24916,.T.) ;
#19134 = FACE_OUTER_BOUND('',#24917,.T.) ;
#19135 = FACE_OUTER_BOUND('',#24918,.T.) ;
#19136 = FACE_OUTER_BOUND('',#24919,.T.) ;
#19137 = FACE_OUTER_BOUND('',#24920,.T.) ;
#19138 = FACE_OUTER_BOUND('',#24921,.T.) ;
#19139 = FACE_OUTER_BOUND('',#24922,.T.) ;
#19140 = FACE_OUTER_BOUND('',#24923,.T.) ;
#19141 = FACE_OUTER_BOUND('',#24924,.T.) ;
#19142 = FACE_OUTER_BOUND('',#24925,.T.) ;
#19143 = FACE_OUTER_BOUND('',#24926,.T.) ;
#19144 = FACE_OUTER_BOUND('',#24927,.T.) ;
#19145 = FACE_OUTER_BOUND('',#24928,.T.) ;
#19146 = FACE_OUTER_BOUND('',#24929,.T.) ;
#19147 = FACE_OUTER_BOUND('',#24930,.T.) ;
#19148 = FACE_OUTER_BOUND('',#24931,.T.) ;
#19149 = FACE_OUTER_BOUND('',#24932,.T.) ;
#19150 = FACE_OUTER_BOUND('',#24933,.T.) ;
#19151 = FACE_OUTER_BOUND('',#24934,.T.) ;
#19152 = FACE_OUTER_BOUND('',#24935,.T.) ;
#19153 = FACE_OUTER_BOUND('',#24936,.T.) ;
#19154 = FACE_OUTER_BOUND('',#24937,.T.) ;
#19155 = FACE_OUTER_BOUND('',#24938,.T.) ;
#19156 = FACE_OUTER_BOUND('',#24939,.T.) ;
#19157 = FACE_OUTER_BOUND('',#24940,.T.) ;
#19158 = FACE_OUTER_BOUND('',#24941,.T.) ;
#19159 = FACE_OUTER_BOUND('',#24942,.T.) ;
#19160 = FACE_OUTER_BOUND('',#24943,.T.) ;
#19161 = FACE_OUTER_BOUND('',#24944,.T.) ;
#19162 = FACE_OUTER_BOUND('',#24945,.T.) ;
#19163 = FACE_OUTER_BOUND('',#24946,.T.) ;
#19164 = FACE_OUTER_BOUND('',#24947,.T.) ;
#19165 = FACE_OUTER_BOUND('',#24948,.T.) ;
#19166 = FACE_OUTER_BOUND('',#24949,.T.) ;
#19167 = FACE_OUTER_BOUND('',#24950,.T.) ;
#19168 = FACE_OUTER_BOUND('',#24951,.T.) ;
#19169 = FACE_OUTER_BOUND('',#24952,.T.) ;
#19170 = FACE_OUTER_BOUND('',#24953,.T.) ;
#19171 = FACE_OUTER_BOUND('',#24954,.T.) ;
#19172 = FACE_OUTER_BOUND('',#24955,.T.) ;
#19173 = FACE_OUTER_BOUND('',#24956,.T.) ;
#19174 = FACE_OUTER_BOUND('',#24957,.T.) ;
#19175 = FACE_OUTER_BOUND('',#24958,.T.) ;
#19176 = FACE_OUTER_BOUND('',#24959,.T.) ;
#19177 = FACE_OUTER_BOUND('',#24960,.T.) ;
#19178 = FACE_OUTER_BOUND('',#24961,.T.) ;
#19179 = FACE_OUTER_BOUND('',#24962,.T.) ;
#19180 = FACE_OUTER_BOUND('',#24963,.T.) ;
#19181 = FACE_OUTER_BOUND('',#24964,.T.) ;
#19182 = FACE_OUTER_BOUND('',#24965,.T.) ;
#19183 = FACE_OUTER_BOUND('',#24966,.T.) ;
#19184 = FACE_OUTER_BOUND('',#24967,.T.) ;
#19185 = FACE_OUTER_BOUND('',#24968,.T.) ;
#19186 = FACE_OUTER_BOUND('',#24969,.T.) ;
#19187 = FACE_OUTER_BOUND('',#24970,.T.) ;
#19188 = FACE_OUTER_BOUND('',#24971,.T.) ;
#19189 = FACE_OUTER_BOUND('',#24972,.T.) ;
#19190 = FACE_OUTER_BOUND('',#24973,.T.) ;
#19191 = FACE_OUTER_BOUND('',#24974,.T.) ;
#19192 = FACE_OUTER_BOUND('',#24975,.T.) ;
#19193 = FACE_OUTER_BOUND('',#24976,.T.) ;
#19194 = FACE_OUTER_BOUND('',#24977,.T.) ;
#19195 = FACE_OUTER_BOUND('',#24978,.T.) ;
#19196 = FACE_OUTER_BOUND('',#24979,.T.) ;
#19197 = FACE_OUTER_BOUND('',#24980,.T.) ;
#19198 = FACE_OUTER_BOUND('',#24981,.T.) ;
#19199 = FACE_OUTER_BOUND('',#24982,.T.) ;
#19200 = FACE_OUTER_BOUND('',#24983,.T.) ;
#19201 = FACE_OUTER_BOUND('',#24984,.T.) ;
#19202 = FACE_OUTER_BOUND('',#24985,.T.) ;
#19203 = FACE_OUTER_BOUND('',#24986,.T.) ;
#19204 = FACE_OUTER_BOUND('',#24987,.T.) ;
#19205 = FACE_OUTER_BOUND('',#24988,.T.) ;
#19206 = FACE_OUTER_BOUND('',#24989,.T.) ;
#19207 = FACE_OUTER_BOUND('',#24990,.T.) ;
#19208 = FACE_OUTER_BOUND('',#24991,.T.) ;
#19209 = FACE_OUTER_BOUND('',#24992,.T.) ;
#19210 = FACE_OUTER_BOUND('',#24993,.T.) ;
#19211 = FACE_OUTER_BOUND('',#24994,.T.) ;
#19212 = FACE_OUTER_BOUND('',#24995,.T.) ;
#19213 = FACE_OUTER_BOUND('',#24996,.T.) ;
#19214 = FACE_OUTER_BOUND('',#24997,.T.) ;
#19215 = FACE_OUTER_BOUND('',#24998,.T.) ;
#19216 = FACE_OUTER_BOUND('',#24999,.T.) ;
#19217 = FACE_OUTER_BOUND('',#25000,.T.) ;
#19218 = FACE_OUTER_BOUND('',#25001,.T.) ;
#19219 = FACE_OUTER_BOUND('',#25002,.T.) ;
#19220 = FACE_OUTER_BOUND('',#25003,.T.) ;
#19221 = FACE_OUTER_BOUND('',#25004,.T.) ;
#19222 = FACE_OUTER_BOUND('',#25005,.T.) ;
#19223 = FACE_OUTER_BOUND('',#25006,.T.) ;
#19224 = FACE_OUTER_BOUND('',#25007,.T.) ;
#19225 = FACE_OUTER_BOUND('',#25008,.T.) ;
#19226 = FACE_OUTER_BOUND('',#25009,.T.) ;
#19227 = FACE_OUTER_BOUND('',#25010,.T.) ;
#19228 = FACE_OUTER_BOUND('',#25011,.T.) ;
#19229 = FACE_OUTER_BOUND('',#25012,.T.) ;
#19230 = FACE_OUTER_BOUND('',#25013,.T.) ;
#19231 = FACE_OUTER_BOUND('',#25014,.T.) ;
#19232 = FACE_OUTER_BOUND('',#25015,.T.) ;
#19233 = FACE_OUTER_BOUND('',#25016,.T.) ;
#19234 = FACE_OUTER_BOUND('',#25017,.T.) ;
#19235 = FACE_OUTER_BOUND('',#25018,.T.) ;
#19236 = FACE_OUTER_BOUND('',#25019,.T.) ;
#19237 = FACE_OUTER_BOUND('',#25020,.T.) ;
#19238 = FACE_OUTER_BOUND('',#25021,.T.) ;
#19239 = FACE_OUTER_BOUND('',#25022,.T.) ;
#19240 = FACE_OUTER_BOUND('',#25023,.T.) ;
#19241 = FACE_OUTER_BOUND('',#25024,.T.) ;
#19242 = FACE_OUTER_BOUND('',#25025,.T.) ;
#19243 = FACE_OUTER_BOUND('',#25026,.T.) ;
#19244 = FACE_OUTER_BOUND('',#25027,.T.) ;
#19245 = FACE_OUTER_BOUND('',#25028,.T.) ;
#19246 = FACE_OUTER_BOUND('',#25029,.T.) ;
#19247 = FACE_OUTER_BOUND('',#25030,.T.) ;
#19248 = FACE_OUTER_BOUND('',#25031,.T.) ;
#19249 = FACE_OUTER_BOUND('',#25032,.T.) ;
#19250 = FACE_OUTER_BOUND('',#25033,.T.) ;
#19251 = FACE_OUTER_BOUND('',#25034,.T.) ;
#19252 = FACE_OUTER_BOUND('',#25035,.T.) ;
#19253 = FACE_OUTER_BOUND('',#25036,.T.) ;
#19254 = FACE_OUTER_BOUND('',#25037,.T.) ;
#19255 = FACE_OUTER_BOUND('',#25038,.T.) ;
#19256 = FACE_OUTER_BOUND('',#25039,.T.) ;
#19257 = FACE_OUTER_BOUND('',#25040,.T.) ;
#19258 = FACE_OUTER_BOUND('',#25041,.T.) ;
#19259 = FACE_OUTER_BOUND('',#25042,.T.) ;
#19260 = FACE_OUTER_BOUND('',#25043,.T.) ;
#19261 = FACE_OUTER_BOUND('',#25044,.T.) ;
#19262 = FACE_OUTER_BOUND('',#25045,.T.) ;
#19263 = FACE_OUTER_BOUND('',#25046,.T.) ;
#19264 = FACE_OUTER_BOUND('',#25047,.T.) ;
#19265 = FACE_OUTER_BOUND('',#25048,.T.) ;
#19266 = FACE_OUTER_BOUND('',#25049,.T.) ;
#19267 = FACE_OUTER_BOUND('',#25050,.T.) ;
#19268 = FACE_OUTER_BOUND('',#25051,.T.) ;
#19269 = FACE_OUTER_BOUND('',#25052,.T.) ;
#19270 = FACE_OUTER_BOUND('',#25053,.T.) ;
#19271 = FACE_OUTER_BOUND('',#25054,.T.) ;
#19272 = FACE_OUTER_BOUND('',#25055,.T.) ;
#19273 = FACE_OUTER_BOUND('',#25056,.T.) ;
#19274 = FACE_OUTER_BOUND('',#25057,.T.) ;
#19275 = FACE_OUTER_BOUND('',#25058,.T.) ;
#19276 = FACE_OUTER_BOUND('',#25059,.T.) ;
#19277 = FACE_OUTER_BOUND('',#25060,.T.) ;
#19278 = FACE_OUTER_BOUND('',#25061,.T.) ;
#19279 = FACE_OUTER_BOUND('',#25062,.T.) ;
#19280 = FACE_OUTER_BOUND('',#25063,.T.) ;
#19281 = FACE_OUTER_BOUND('',#25064,.T.) ;
#19282 = FACE_OUTER_BOUND('',#25065,.T.) ;
#19283 = FACE_OUTER_BOUND('',#25066,.T.) ;
#19284 = FACE_OUTER_BOUND('',#25067,.T.) ;
#19285 = FACE_OUTER_BOUND('',#25068,.T.) ;
#19286 = FACE_OUTER_BOUND('',#25069,.T.) ;
#19287 = FACE_OUTER_BOUND('',#25070,.T.) ;
#19288 = FACE_OUTER_BOUND('',#25071,.T.) ;
#19289 = FACE_OUTER_BOUND('',#25072,.T.) ;
#19290 = FACE_OUTER_BOUND('',#25073,.T.) ;
#19291 = FACE_OUTER_BOUND('',#25074,.T.) ;
#19292 = FACE_OUTER_BOUND('',#25075,.T.) ;
#19293 = FACE_OUTER_BOUND('',#25076,.T.) ;
#19294 = FACE_OUTER_BOUND('',#25077,.T.) ;
#19295 = FACE_OUTER_BOUND('',#25078,.T.) ;
#19296 = FACE_OUTER_BOUND('',#25079,.T.) ;
#19297 = FACE_OUTER_BOUND('',#25080,.T.) ;
#19298 = FACE_OUTER_BOUND('',#25081,.T.) ;
#19299 = FACE_OUTER_BOUND('',#25082,.T.) ;
#19300 = FACE_OUTER_BOUND('',#25083,.T.) ;
#19301 = FACE_OUTER_BOUND('',#25084,.T.) ;
#19302 = FACE_OUTER_BOUND('',#25085,.T.) ;
#19303 = FACE_OUTER_BOUND('',#25086,.T.) ;
#19304 = FACE_OUTER_BOUND('',#25087,.T.) ;
#19305 = FACE_OUTER_BOUND('',#25088,.T.) ;
#19306 = FACE_OUTER_BOUND('',#25089,.T.) ;
#19307 = FACE_OUTER_BOUND('',#25090,.T.) ;
#19308 = FACE_OUTER_BOUND('',#25091,.T.) ;
#19309 = FACE_OUTER_BOUND('',#25092,.T.) ;
#19310 = FACE_OUTER_BOUND('',#25093,.T.) ;
#19311 = FACE_OUTER_BOUND('',#25094,.T.) ;
#19312 = FACE_OUTER_BOUND('',#25095,.T.) ;
#19313 = FACE_OUTER_BOUND('',#25096,.T.) ;
#19314 = FACE_OUTER_BOUND('',#25097,.T.) ;
#19315 = FACE_OUTER_BOUND('',#25098,.T.) ;
#19316 = FACE_OUTER_BOUND('',#25099,.T.) ;
#19317 = FACE_OUTER_BOUND('',#25100,.T.) ;
#19318 = FACE_OUTER_BOUND('',#25101,.T.) ;
#19319 = FACE_OUTER_BOUND('',#25102,.T.) ;
#19320 = FACE_OUTER_BOUND('',#25103,.T.) ;
#19321 = FACE_OUTER_BOUND('',#25104,.T.) ;
#19322 = FACE_OUTER_BOUND('',#25105,.T.) ;
#19323 = FACE_OUTER_BOUND('',#25106,.T.) ;
#19324 = FACE_OUTER_BOUND('',#25107,.T.) ;
#19325 = FACE_OUTER_BOUND('',#25108,.T.) ;
#19326 = FACE_OUTER_BOUND('',#25109,.T.) ;
#19327 = FACE_OUTER_BOUND('',#25110,.T.) ;
#19328 = FACE_OUTER_BOUND('',#25111,.T.) ;
#19329 = FACE_OUTER_BOUND('',#25112,.T.) ;
#19330 = FACE_OUTER_BOUND('',#25113,.T.) ;
#19331 = FACE_OUTER_BOUND('',#25114,.T.) ;
#19332 = FACE_OUTER_BOUND('',#25115,.T.) ;
#19333 = FACE_OUTER_BOUND('',#25116,.T.) ;
#19334 = FACE_OUTER_BOUND('',#25117,.T.) ;
#19335 = FACE_OUTER_BOUND('',#25118,.T.) ;
#19336 = FACE_OUTER_BOUND('',#25119,.T.) ;
#19337 = FACE_OUTER_BOUND('',#25120,.T.) ;
#19338 = FACE_OUTER_BOUND('',#25121,.T.) ;
#19339 = FACE_OUTER_BOUND('',#25122,.T.) ;
#19340 = FACE_OUTER_BOUND('',#25123,.T.) ;
#19341 = FACE_OUTER_BOUND('',#25124,.T.) ;
#19342 = FACE_OUTER_BOUND('',#25125,.T.) ;
#19343 = FACE_OUTER_BOUND('',#25126,.T.) ;
#19344 = FACE_OUTER_BOUND('',#25127,.T.) ;
#19345 = FACE_OUTER_BOUND('',#25128,.T.) ;
#19346 = FACE_OUTER_BOUND('',#25129,.T.) ;
#19347 = FACE_OUTER_BOUND('',#25130,.T.) ;
#19348 = FACE_OUTER_BOUND('',#25131,.T.) ;
#19349 = FACE_OUTER_BOUND('',#25132,.T.) ;
#19350 = FACE_OUTER_BOUND('',#25133,.T.) ;
#19351 = FACE_OUTER_BOUND('',#25134,.T.) ;
#19352 = FACE_OUTER_BOUND('',#25135,.T.) ;
#19353 = FACE_OUTER_BOUND('',#25136,.T.) ;
#19354 = FACE_OUTER_BOUND('',#25137,.T.) ;
#19355 = FACE_OUTER_BOUND('',#25138,.T.) ;
#19356 = FACE_OUTER_BOUND('',#25139,.T.) ;
#19357 = FACE_OUTER_BOUND('',#25140,.T.) ;
#19358 = FACE_OUTER_BOUND('',#25141,.T.) ;
#19359 = FACE_OUTER_BOUND('',#25142,.T.) ;
#19360 = FACE_OUTER_BOUND('',#25143,.T.) ;
#19361 = FACE_OUTER_BOUND('',#25144,.T.) ;
#19362 = FACE_OUTER_BOUND('',#25145,.T.) ;
#19363 = FACE_OUTER_BOUND('',#25146,.T.) ;
#19364 = FACE_OUTER_BOUND('',#25147,.T.) ;
#19365 = FACE_OUTER_BOUND('',#25148,.T.) ;
#19366 = FACE_OUTER_BOUND('',#25149,.T.) ;
#19367 = FACE_OUTER_BOUND('',#25150,.T.) ;
#19368 = FACE_OUTER_BOUND('',#25151,.T.) ;
#19369 = FACE_OUTER_BOUND('',#25152,.T.) ;
#19370 = FACE_OUTER_BOUND('',#25153,.T.) ;
#19371 = FACE_OUTER_BOUND('',#25154,.T.) ;
#19372 = FACE_OUTER_BOUND('',#25155,.T.) ;
#19373 = FACE_OUTER_BOUND('',#25156,.T.) ;
#19374 = FACE_OUTER_BOUND('',#25157,.T.) ;
#19375 = FACE_OUTER_BOUND('',#25158,.T.) ;
#19376 = FACE_OUTER_BOUND('',#25159,.T.) ;
#19377 = FACE_OUTER_BOUND('',#25160,.T.) ;
#19378 = FACE_OUTER_BOUND('',#25161,.T.) ;
#19379 = FACE_OUTER_BOUND('',#25162,.T.) ;
#19380 = FACE_OUTER_BOUND('',#25163,.T.) ;
#19381 = FACE_OUTER_BOUND('',#25164,.T.) ;
#19382 = FACE_OUTER_BOUND('',#25165,.T.) ;
#19383 = FACE_OUTER_BOUND('',#25166,.T.) ;
#19384 = FACE_OUTER_BOUND('',#25167,.T.) ;
#19385 = FACE_OUTER_BOUND('',#25168,.T.) ;
#19386 = FACE_OUTER_BOUND('',#25169,.T.) ;
#19387 = FACE_OUTER_BOUND('',#25170,.T.) ;
#19388 = FACE_OUTER_BOUND('',#25171,.T.) ;
#19389 = FACE_OUTER_BOUND('',#25172,.T.) ;
#19390 = FACE_OUTER_BOUND('',#25173,.T.) ;
#19391 = FACE_OUTER_BOUND('',#25174,.T.) ;
#19392 = FACE_OUTER_BOUND('',#25175,.T.) ;
#19393 = FACE_OUTER_BOUND('',#25176,.T.) ;
#19394 = FACE_OUTER_BOUND('',#25177,.T.) ;
#19395 = FACE_OUTER_BOUND('',#25178,.T.) ;
#19396 = FACE_OUTER_BOUND('',#25179,.T.) ;
#19397 = FACE_OUTER_BOUND('',#25180,.T.) ;
#19398 = FACE_OUTER_BOUND('',#25181,.T.) ;
#19399 = FACE_OUTER_BOUND('',#25182,.T.) ;
#19400 = FACE_OUTER_BOUND('',#25183,.T.) ;
#19401 = FACE_OUTER_BOUND('',#25184,.T.) ;
#19402 = FACE_OUTER_BOUND('',#25185,.T.) ;
#19403 = FACE_OUTER_BOUND('',#25186,.T.) ;
#19404 = FACE_OUTER_BOUND('',#25187,.T.) ;
#19405 = FACE_OUTER_BOUND('',#25188,.T.) ;
#19406 = FACE_OUTER_BOUND('',#25189,.T.) ;
#19407 = FACE_OUTER_BOUND('',#25190,.T.) ;
#19408 = FACE_OUTER_BOUND('',#25191,.T.) ;
#19409 = FACE_OUTER_BOUND('',#25192,.T.) ;
#19410 = FACE_OUTER_BOUND('',#25193,.T.) ;
#19411 = FACE_OUTER_BOUND('',#25194,.T.) ;
#19412 = FACE_OUTER_BOUND('',#25195,.T.) ;
#19413 = FACE_OUTER_BOUND('',#25196,.T.) ;
#19414 = FACE_OUTER_BOUND('',#25197,.T.) ;
#19415 = FACE_OUTER_BOUND('',#25198,.T.) ;
#19416 = FACE_OUTER_BOUND('',#25199,.T.) ;
#19417 = FACE_OUTER_BOUND('',#25200,.T.) ;
#19418 = FACE_OUTER_BOUND('',#25201,.T.) ;
#19419 = FACE_OUTER_BOUND('',#25202,.T.) ;
#19420 = FACE_OUTER_BOUND('',#25203,.T.) ;
#19421 = FACE_OUTER_BOUND('',#25204,.T.) ;
#19422 = FACE_OUTER_BOUND('',#25205,.T.) ;
#19423 = FACE_OUTER_BOUND('',#25206,.T.) ;
#19424 = FACE_OUTER_BOUND('',#25207,.T.) ;
#19425 = FACE_OUTER_BOUND('',#25208,.T.) ;
#19426 = FACE_OUTER_BOUND('',#25209,.T.) ;
#19427 = FACE_OUTER_BOUND('',#25210,.T.) ;
#19428 = FACE_OUTER_BOUND('',#25211,.T.) ;
#19429 = FACE_OUTER_BOUND('',#25212,.T.) ;
#19430 = FACE_OUTER_BOUND('',#25213,.T.) ;
#19431 = FACE_OUTER_BOUND('',#25214,.T.) ;
#19432 = FACE_OUTER_BOUND('',#25215,.T.) ;
#19433 = FACE_OUTER_BOUND('',#25216,.T.) ;
#19434 = FACE_OUTER_BOUND('',#25217,.T.) ;
#19435 = FACE_OUTER_BOUND('',#25218,.T.) ;
#19436 = FACE_OUTER_BOUND('',#25219,.T.) ;
#19437 = FACE_OUTER_BOUND('',#25220,.T.) ;
#19438 = FACE_OUTER_BOUND('',#25221,.T.) ;
#19439 = FACE_OUTER_BOUND('',#25222,.T.) ;
#19440 = FACE_OUTER_BOUND('',#25223,.T.) ;
#19441 = FACE_OUTER_BOUND('',#25224,.T.) ;
#19442 = FACE_OUTER_BOUND('',#25225,.T.) ;
#19443 = FACE_OUTER_BOUND('',#25226,.T.) ;
#19444 = FACE_OUTER_BOUND('',#25227,.T.) ;
#19445 = FACE_OUTER_BOUND('',#25228,.T.) ;
#19446 = FACE_OUTER_BOUND('',#25229,.T.) ;
#19447 = FACE_OUTER_BOUND('',#25230,.T.) ;
#19448 = FACE_OUTER_BOUND('',#25231,.T.) ;
#19449 = FACE_OUTER_BOUND('',#25232,.T.) ;
#19450 = FACE_OUTER_BOUND('',#25233,.T.) ;
#19451 = FACE_OUTER_BOUND('',#25234,.T.) ;
#19452 = FACE_OUTER_BOUND('',#25235,.T.) ;
#19453 = FACE_OUTER_BOUND('',#25236,.T.) ;
#19454 = FACE_OUTER_BOUND('',#25237,.T.) ;
#19455 = FACE_OUTER_BOUND('',#25238,.T.) ;
#19456 = FACE_OUTER_BOUND('',#25239,.T.) ;
#19457 = FACE_OUTER_BOUND('',#25240,.T.) ;
#19458 = FACE_OUTER_BOUND('',#25241,.T.) ;
#19459 = FACE_OUTER_BOUND('',#25242,.T.) ;
#19460 = FACE_OUTER_BOUND('',#25243,.T.) ;
#19461 = FACE_OUTER_BOUND('',#25244,.T.) ;
#19462 = FACE_OUTER_BOUND('',#25245,.T.) ;
#19463 = FACE_OUTER_BOUND('',#25246,.T.) ;
#19464 = FACE_OUTER_BOUND('',#25247,.T.) ;
#19465 = FACE_OUTER_BOUND('',#25248,.T.) ;
#19466 = FACE_OUTER_BOUND('',#25249,.T.) ;
#19467 = FACE_OUTER_BOUND('',#25250,.T.) ;
#19468 = FACE_OUTER_BOUND('',#25251,.T.) ;
#19469 = FACE_OUTER_BOUND('',#25252,.T.) ;
#19470 = FACE_OUTER_BOUND('',#25253,.T.) ;
#19471 = FACE_OUTER_BOUND('',#25254,.T.) ;
#19472 = FACE_OUTER_BOUND('',#25255,.T.) ;
#19473 = FACE_OUTER_BOUND('',#25256,.T.) ;
#19474 = FACE_OUTER_BOUND('',#25257,.T.) ;
#19475 = FACE_OUTER_BOUND('',#25258,.T.) ;
#19476 = FACE_OUTER_BOUND('',#25259,.T.) ;
#19477 = FACE_OUTER_BOUND('',#25260,.T.) ;
#19478 = FACE_OUTER_BOUND('',#25261,.T.) ;
#19479 = FACE_OUTER_BOUND('',#25262,.T.) ;
#19480 = FACE_OUTER_BOUND('',#25263,.T.) ;
#19481 = FACE_OUTER_BOUND('',#25264,.T.) ;
#19482 = FACE_OUTER_BOUND('',#25265,.T.) ;
#19483 = FACE_OUTER_BOUND('',#25266,.T.) ;
#19484 = FACE_OUTER_BOUND('',#25267,.T.) ;
#19485 = FACE_OUTER_BOUND('',#25268,.T.) ;
#19486 = FACE_OUTER_BOUND('',#25269,.T.) ;
#19487 = FACE_OUTER_BOUND('',#25270,.T.) ;
#19488 = FACE_OUTER_BOUND('',#25271,.T.) ;
#19489 = FACE_OUTER_BOUND('',#25272,.T.) ;
#19490 = FACE_OUTER_BOUND('',#25273,.T.) ;
#19491 = FACE_OUTER_BOUND('',#25274,.T.) ;
#19492 = FACE_OUTER_BOUND('',#25275,.T.) ;
#19493 = FACE_OUTER_BOUND('',#25276,.T.) ;
#19494 = FACE_OUTER_BOUND('',#25277,.T.) ;
#19495 = FACE_OUTER_BOUND('',#25278,.T.) ;
#19496 = FACE_OUTER_BOUND('',#25279,.T.) ;
#19497 = FACE_OUTER_BOUND('',#25280,.T.) ;
#19498 = FACE_OUTER_BOUND('',#25281,.T.) ;
#19499 = FACE_OUTER_BOUND('',#25282,.T.) ;
#19500 = FACE_OUTER_BOUND('',#25283,.T.) ;
#19501 = FACE_OUTER_BOUND('',#25284,.T.) ;
#19502 = FACE_OUTER_BOUND('',#25285,.T.) ;
#19503 = FACE_OUTER_BOUND('',#25286,.T.) ;
#19504 = FACE_OUTER_BOUND('',#25287,.T.) ;
#19505 = FACE_OUTER_BOUND('',#25288,.T.) ;
#19506 = FACE_OUTER_BOUND('',#25289,.T.) ;
#19507 = FACE_OUTER_BOUND('',#25290,.T.) ;
#19508 = FACE_OUTER_BOUND('',#25291,.T.) ;
#19509 = FACE_OUTER_BOUND('',#25292,.T.) ;
#19510 = FACE_OUTER_BOUND('',#25293,.T.) ;
#19511 = FACE_OUTER_BOUND('',#25294,.T.) ;
#19512 = FACE_OUTER_BOUND('',#25295,.T.) ;
#19513 = FACE_OUTER_BOUND('',#25296,.T.) ;
#19514 = FACE_OUTER_BOUND('',#25297,.T.) ;
#19515 = FACE_OUTER_BOUND('',#25298,.T.) ;
#19516 = FACE_OUTER_BOUND('',#25299,.T.) ;
#19517 = FACE_OUTER_BOUND('',#25300,.T.) ;
#19518 = FACE_OUTER_BOUND('',#25301,.T.) ;
#19519 = FACE_OUTER_BOUND('',#25302,.T.) ;
#19520 = FACE_OUTER_BOUND('',#25303,.T.) ;
#19521 = FACE_OUTER_BOUND('',#25304,.T.) ;
#19522 = FACE_OUTER_BOUND('',#25305,.T.) ;
#19523 = FACE_OUTER_BOUND('',#25306,.T.) ;
#19524 = FACE_OUTER_BOUND('',#25307,.T.) ;
#19525 = FACE_OUTER_BOUND('',#25308,.T.) ;
#19526 = FACE_OUTER_BOUND('',#25309,.T.) ;
#19527 = FACE_OUTER_BOUND('',#25310,.T.) ;
#19528 = FACE_OUTER_BOUND('',#25311,.T.) ;
#19529 = FACE_OUTER_BOUND('',#25312,.T.) ;
#19530 = FACE_OUTER_BOUND('',#25313,.T.) ;
#19531 = FACE_OUTER_BOUND('',#25314,.T.) ;
#19532 = FACE_OUTER_BOUND('',#25315,.T.) ;
#19533 = FACE_OUTER_BOUND('',#25316,.T.) ;
#19534 = FACE_OUTER_BOUND('',#25317,.T.) ;
#19535 = FACE_OUTER_BOUND('',#25318,.T.) ;
#19536 = FACE_OUTER_BOUND('',#25319,.T.) ;
#19537 = FACE_OUTER_BOUND('',#25320,.T.) ;
#19538 = FACE_OUTER_BOUND('',#25321,.T.) ;
#19539 = FACE_OUTER_BOUND('',#25322,.T.) ;
#19540 = FACE_OUTER_BOUND('',#25323,.T.) ;
#19541 = FACE_OUTER_BOUND('',#25324,.T.) ;
#19542 = FACE_OUTER_BOUND('',#25325,.T.) ;
#19543 = FACE_OUTER_BOUND('',#25326,.T.) ;
#19544 = FACE_OUTER_BOUND('',#25327,.T.) ;
#19545 = FACE_OUTER_BOUND('',#25328,.T.) ;
#19546 = FACE_OUTER_BOUND('',#25329,.T.) ;
#19547 = FACE_OUTER_BOUND('',#25330,.T.) ;
#19548 = FACE_OUTER_BOUND('',#25331,.T.) ;
#19549 = FACE_OUTER_BOUND('',#25332,.T.) ;
#19550 = FACE_OUTER_BOUND('',#25333,.T.) ;
#19551 = FACE_OUTER_BOUND('',#25334,.T.) ;
#19552 = FACE_OUTER_BOUND('',#25335,.T.) ;
#19553 = FACE_OUTER_BOUND('',#25336,.T.) ;
#19554 = FACE_OUTER_BOUND('',#25337,.T.) ;
#19555 = FACE_OUTER_BOUND('',#25338,.T.) ;
#19556 = FACE_OUTER_BOUND('',#25339,.T.) ;
#19557 = FACE_OUTER_BOUND('',#25340,.T.) ;
#19558 = FACE_OUTER_BOUND('',#25341,.T.) ;
#19559 = FACE_OUTER_BOUND('',#25342,.T.) ;
#19560 = FACE_OUTER_BOUND('',#25343,.T.) ;
#19561 = FACE_OUTER_BOUND('',#25344,.T.) ;
#19562 = FACE_OUTER_BOUND('',#25345,.T.) ;
#19563 = FACE_OUTER_BOUND('',#25346,.T.) ;
#19564 = FACE_OUTER_BOUND('',#25347,.T.) ;
#19565 = FACE_OUTER_BOUND('',#25348,.T.) ;
#19566 = FACE_OUTER_BOUND('',#25349,.T.) ;
#19567 = FACE_OUTER_BOUND('',#25350,.T.) ;
#19568 = FACE_OUTER_BOUND('',#25351,.T.) ;
#19569 = FACE_OUTER_BOUND('',#25352,.T.) ;
#19570 = FACE_OUTER_BOUND('',#25353,.T.) ;
#19571 = FACE_OUTER_BOUND('',#25354,.T.) ;
#19572 = FACE_OUTER_BOUND('',#25355,.T.) ;
#19573 = FACE_OUTER_BOUND('',#25356,.T.) ;
#19574 = FACE_OUTER_BOUND('',#25357,.T.) ;
#19575 = FACE_OUTER_BOUND('',#25358,.T.) ;
#19576 = FACE_OUTER_BOUND('',#25359,.T.) ;
#19577 = FACE_OUTER_BOUND('',#25360,.T.) ;
#19578 = FACE_OUTER_BOUND('',#25361,.T.) ;
#19579 = FACE_OUTER_BOUND('',#25362,.T.) ;
#19580 = FACE_OUTER_BOUND('',#25363,.T.) ;
#19581 = FACE_OUTER_BOUND('',#25364,.T.) ;
#19582 = FACE_OUTER_BOUND('',#25365,.T.) ;
#19583 = FACE_OUTER_BOUND('',#25366,.T.) ;
#19584 = FACE_OUTER_BOUND('',#25367,.T.) ;
#19585 = FACE_OUTER_BOUND('',#25368,.T.) ;
#19586 = FACE_OUTER_BOUND('',#25369,.T.) ;
#19587 = FACE_OUTER_BOUND('',#25370,.T.) ;
#19588 = FACE_OUTER_BOUND('',#25371,.T.) ;
#19589 = FACE_OUTER_BOUND('',#25372,.T.) ;
#19590 = FACE_OUTER_BOUND('',#25373,.T.) ;
#19591 = FACE_OUTER_BOUND('',#25374,.T.) ;
#19592 = FACE_OUTER_BOUND('',#25375,.T.) ;
#19593 = FACE_OUTER_BOUND('',#25376,.T.) ;
#19594 = FACE_OUTER_BOUND('',#25377,.T.) ;
#19595 = FACE_OUTER_BOUND('',#25378,.T.) ;
#19596 = FACE_OUTER_BOUND('',#25379,.T.) ;
#19597 = FACE_OUTER_BOUND('',#25380,.T.) ;
#19598 = FACE_OUTER_BOUND('',#25381,.T.) ;
#19599 = FACE_OUTER_BOUND('',#25382,.T.) ;
#19600 = FACE_OUTER_BOUND('',#25383,.T.) ;
#19601 = FACE_OUTER_BOUND('',#25384,.T.) ;
#19602 = FACE_OUTER_BOUND('',#25385,.T.) ;
#19603 = FACE_OUTER_BOUND('',#25386,.T.) ;
#19604 = FACE_OUTER_BOUND('',#25387,.T.) ;
#19605 = FACE_OUTER_BOUND('',#25388,.T.) ;
#19606 = FACE_OUTER_BOUND('',#25389,.T.) ;
#19607 = FACE_OUTER_BOUND('',#25390,.T.) ;
#19608 = FACE_OUTER_BOUND('',#25391,.T.) ;
#19609 = FACE_OUTER_BOUND('',#25392,.T.) ;
#19610 = FACE_OUTER_BOUND('',#25393,.T.) ;
#19611 = FACE_OUTER_BOUND('',#25394,.T.) ;
#19612 = FACE_OUTER_BOUND('',#25395,.T.) ;
#19613 = FACE_OUTER_BOUND('',#25396,.T.) ;
#19614 = FACE_OUTER_BOUND('',#25397,.T.) ;
#19615 = FACE_OUTER_BOUND('',#25398,.T.) ;
#19616 = FACE_OUTER_BOUND('',#25399,.T.) ;
#19617 = FACE_OUTER_BOUND('',#25400,.T.) ;
#19618 = FACE_OUTER_BOUND('',#25401,.T.) ;
#19619 = FACE_OUTER_BOUND('',#25402,.T.) ;
#19620 = FACE_OUTER_BOUND('',#25403,.T.) ;
#19621 = FACE_OUTER_BOUND('',#25404,.T.) ;
#19622 = FACE_OUTER_BOUND('',#25405,.T.) ;
#19623 = FACE_OUTER_BOUND('',#25406,.T.) ;
#19624 = FACE_OUTER_BOUND('',#25407,.T.) ;
#19625 = FACE_OUTER_BOUND('',#25408,.T.) ;
#19626 = FACE_OUTER_BOUND('',#25409,.T.) ;
#19627 = FACE_OUTER_BOUND('',#25410,.T.) ;
#19628 = FACE_OUTER_BOUND('',#25411,.T.) ;
#19629 = FACE_OUTER_BOUND('',#25412,.T.) ;
#19630 = FACE_OUTER_BOUND('',#25413,.T.) ;
#19631 = FACE_OUTER_BOUND('',#25414,.T.) ;
#19632 = FACE_OUTER_BOUND('',#25415,.T.) ;
#19633 = FACE_OUTER_BOUND('',#25416,.T.) ;
#19634 = FACE_OUTER_BOUND('',#25417,.T.) ;
#19635 = FACE_OUTER_BOUND('',#25418,.T.) ;
#19636 = FACE_OUTER_BOUND('',#25419,.T.) ;
#19637 = FACE_OUTER_BOUND('',#25420,.T.) ;
#19638 = FACE_OUTER_BOUND('',#25421,.T.) ;
#19639 = FACE_OUTER_BOUND('',#25422,.T.) ;
#19640 = FACE_OUTER_BOUND('',#25423,.T.) ;
#19641 = FACE_OUTER_BOUND('',#25424,.T.) ;
#19642 = FACE_OUTER_BOUND('',#25425,.T.) ;
#19643 = FACE_OUTER_BOUND('',#25426,.T.) ;
#19644 = FACE_OUTER_BOUND('',#25427,.T.) ;
#19645 = FACE_OUTER_BOUND('',#25428,.T.) ;
#19646 = FACE_OUTER_BOUND('',#25429,.T.) ;
#19647 = FACE_OUTER_BOUND('',#25430,.T.) ;
#19648 = FACE_OUTER_BOUND('',#25431,.T.) ;
#19649 = FACE_OUTER_BOUND('',#25432,.T.) ;
#19650 = FACE_OUTER_BOUND('',#25433,.T.) ;
#19651 = FACE_OUTER_BOUND('',#25434,.T.) ;
#19652 = FACE_OUTER_BOUND('',#25435,.T.) ;
#19653 = FACE_OUTER_BOUND('',#25436,.T.) ;
#19654 = FACE_OUTER_BOUND('',#25437,.T.) ;
#19655 = FACE_OUTER_BOUND('',#25438,.T.) ;
#19656 = FACE_OUTER_BOUND('',#25439,.T.) ;
#19657 = FACE_OUTER_BOUND('',#25440,.T.) ;
#19658 = FACE_OUTER_BOUND('',#25441,.T.) ;
#19659 = FACE_OUTER_BOUND('',#25442,.T.) ;
#19660 = FACE_OUTER_BOUND('',#25443,.T.) ;
#19661 = FACE_OUTER_BOUND('',#25444,.T.) ;
#19662 = FACE_OUTER_BOUND('',#25445,.T.) ;
#19663 = FACE_OUTER_BOUND('',#25446,.T.) ;
#19664 = FACE_OUTER_BOUND('',#25447,.T.) ;
#19665 = FACE_OUTER_BOUND('',#25448,.T.) ;
#19666 = FACE_OUTER_BOUND('',#25449,.T.) ;
#19667 = FACE_OUTER_BOUND('',#25450,.T.) ;
#19668 = FACE_OUTER_BOUND('',#25451,.T.) ;
#19669 = FACE_OUTER_BOUND('',#25452,.T.) ;
#19670 = FACE_OUTER_BOUND('',#25453,.T.) ;
#19671 = FACE_OUTER_BOUND('',#25454,.T.) ;
#19672 = FACE_OUTER_BOUND('',#25455,.T.) ;
#19673 = FACE_OUTER_BOUND('',#25456,.T.) ;
#19674 = FACE_OUTER_BOUND('',#25457,.T.) ;
#19675 = FACE_OUTER_BOUND('',#25458,.T.) ;
#19676 = FACE_OUTER_BOUND('',#25459,.T.) ;
#19677 = FACE_OUTER_BOUND('',#25460,.T.) ;
#19678 = FACE_OUTER_BOUND('',#25461,.T.) ;
#19679 = FACE_OUTER_BOUND('',#25462,.T.) ;
#19680 = FACE_OUTER_BOUND('',#25463,.T.) ;
#19681 = FACE_OUTER_BOUND('',#25464,.T.) ;
#19682 = FACE_OUTER_BOUND('',#25465,.T.) ;
#19683 = FACE_OUTER_BOUND('',#25466,.T.) ;
#19684 = FACE_OUTER_BOUND('',#25467,.T.) ;
#19685 = FACE_OUTER_BOUND('',#25468,.T.) ;
#19686 = FACE_OUTER_BOUND('',#25469,.T.) ;
#19687 = FACE_OUTER_BOUND('',#25470,.T.) ;
#19688 = FACE_OUTER_BOUND('',#25471,.T.) ;
#19689 = FACE_OUTER_BOUND('',#25472,.T.) ;
#19690 = FACE_OUTER_BOUND('',#25473,.T.) ;
#19691 = FACE_OUTER_BOUND('',#25474,.T.) ;
#19692 = FACE_OUTER_BOUND('',#25475,.T.) ;
#19693 = FACE_OUTER_BOUND('',#25476,.T.) ;
#19694 = FACE_OUTER_BOUND('',#25477,.T.) ;
#19695 = FACE_OUTER_BOUND('',#25478,.T.) ;
#19696 = FACE_OUTER_BOUND('',#25479,.T.) ;
#19697 = FACE_OUTER_BOUND('',#25480,.T.) ;
#19698 = FACE_OUTER_BOUND('',#25481,.T.) ;
#19699 = FACE_OUTER_BOUND('',#25482,.T.) ;
#19700 = FACE_OUTER_BOUND('',#25483,.T.) ;
#19701 = FACE_OUTER_BOUND('',#25484,.T.) ;
#19702 = FACE_OUTER_BOUND('',#25485,.T.) ;
#19703 = FACE_OUTER_BOUND('',#25486,.T.) ;
#19704 = FACE_OUTER_BOUND('',#25487,.T.) ;
#19705 = FACE_OUTER_BOUND('',#25488,.T.) ;
#19706 = FACE_OUTER_BOUND('',#25489,.T.) ;
#19707 = FACE_OUTER_BOUND('',#25490,.T.) ;
#19708 = FACE_OUTER_BOUND('',#25491,.T.) ;
#19709 = FACE_OUTER_BOUND('',#25492,.T.) ;
#19710 = FACE_OUTER_BOUND('',#25493,.T.) ;
#19711 = FACE_OUTER_BOUND('',#25494,.T.) ;
#19712 = FACE_OUTER_BOUND('',#25495,.T.) ;
#19713 = FACE_OUTER_BOUND('',#25496,.T.) ;
#19714 = FACE_OUTER_BOUND('',#25497,.T.) ;
#19715 = FACE_OUTER_BOUND('',#25498,.T.) ;
#19716 = FACE_OUTER_BOUND('',#25499,.T.) ;
#19717 = FACE_OUTER_BOUND('',#25500,.T.) ;
#19718 = FACE_OUTER_BOUND('',#25501,.T.) ;
#19719 = FACE_OUTER_BOUND('',#25502,.T.) ;
#19720 = FACE_OUTER_BOUND('',#25503,.T.) ;
#19721 = FACE_OUTER_BOUND('',#25504,.T.) ;
#19722 = FACE_OUTER_BOUND('',#25505,.T.) ;
#19723 = FACE_OUTER_BOUND('',#25506,.T.) ;
#19724 = FACE_OUTER_BOUND('',#25507,.T.) ;
#19725 = FACE_OUTER_BOUND('',#25508,.T.) ;
#19726 = FACE_OUTER_BOUND('',#25509,.T.) ;
#19727 = FACE_OUTER_BOUND('',#25510,.T.) ;
#19728 = FACE_OUTER_BOUND('',#25511,.T.) ;
#19729 = FACE_OUTER_BOUND('',#25512,.T.) ;
#19730 = FACE_OUTER_BOUND('',#25513,.T.) ;
#19731 = FACE_OUTER_BOUND('',#25514,.T.) ;
#19732 = FACE_OUTER_BOUND('',#25515,.T.) ;
#19733 = FACE_OUTER_BOUND('',#25516,.T.) ;
#19734 = FACE_OUTER_BOUND('',#25517,.T.) ;
#19735 = FACE_OUTER_BOUND('',#25518,.T.) ;
#19736 = FACE_OUTER_BOUND('',#25519,.T.) ;
#19737 = FACE_OUTER_BOUND('',#25520,.T.) ;
#19738 = FACE_OUTER_BOUND('',#25521,.T.) ;
#19739 = FACE_OUTER_BOUND('',#25522,.T.) ;
#19740 = FACE_OUTER_BOUND('',#25523,.T.) ;
#19741 = FACE_OUTER_BOUND('',#25524,.T.) ;
#19742 = FACE_OUTER_BOUND('',#25525,.T.) ;
#19743 = FACE_OUTER_BOUND('',#25526,.T.) ;
#19744 = FACE_OUTER_BOUND('',#25527,.T.) ;
#19745 = FACE_OUTER_BOUND('',#25528,.T.) ;
#19746 = FACE_OUTER_BOUND('',#25529,.T.) ;
#19747 = FACE_OUTER_BOUND('',#25530,.T.) ;
#19748 = FACE_OUTER_BOUND('',#25531,.T.) ;
#19749 = FACE_OUTER_BOUND('',#25532,.T.) ;
#19750 = FACE_OUTER_BOUND('',#25533,.T.) ;
#19751 = FACE_OUTER_BOUND('',#25534,.T.) ;
#19752 = FACE_OUTER_BOUND('',#25535,.T.) ;
#19753 = FACE_OUTER_BOUND('',#25536,.T.) ;
#19754 = FACE_OUTER_BOUND('',#25537,.T.) ;
#19755 = FACE_OUTER_BOUND('',#25538,.T.) ;
#19756 = FACE_OUTER_BOUND('',#25539,.T.) ;
#19757 = FACE_OUTER_BOUND('',#25540,.T.) ;
#19758 = FACE_OUTER_BOUND('',#25541,.T.) ;
#19759 = FACE_OUTER_BOUND('',#25542,.T.) ;
#19760 = FACE_OUTER_BOUND('',#25543,.T.) ;
#19761 = FACE_OUTER_BOUND('',#25544,.T.) ;
#19762 = FACE_OUTER_BOUND('',#25545,.T.) ;
#19763 = FACE_OUTER_BOUND('',#25546,.T.) ;
#19764 = FACE_OUTER_BOUND('',#25547,.T.) ;
#19765 = FACE_OUTER_BOUND('',#25548,.T.) ;
#19766 = FACE_OUTER_BOUND('',#25549,.T.) ;
#19767 = FACE_OUTER_BOUND('',#25550,.T.) ;
#19768 = FACE_OUTER_BOUND('',#25551,.T.) ;
#19769 = FACE_OUTER_BOUND('',#25552,.T.) ;
#19770 = FACE_OUTER_BOUND('',#25553,.T.) ;
#19771 = FACE_OUTER_BOUND('',#25554,.T.) ;
#19772 = FACE_OUTER_BOUND('',#25555,.T.) ;
#19773 = FACE_OUTER_BOUND('',#25556,.T.) ;
#19774 = FACE_OUTER_BOUND('',#25557,.T.) ;
#19775 = FACE_OUTER_BOUND('',#25558,.T.) ;
#19776 = FACE_OUTER_BOUND('',#25559,.T.) ;
#19777 = FACE_OUTER_BOUND('',#25560,.T.) ;
#19778 = FACE_OUTER_BOUND('',#25561,.T.) ;
#19779 = FACE_OUTER_BOUND('',#25562,.T.) ;
#19780 = FACE_OUTER_BOUND('',#25563,.T.) ;
#19781 = FACE_OUTER_BOUND('',#25564,.T.) ;
#19782 = FACE_OUTER_BOUND('',#25565,.T.) ;
#19783 = FACE_OUTER_BOUND('',#25566,.T.) ;
#19784 = FACE_OUTER_BOUND('',#25567,.T.) ;
#19785 = FACE_OUTER_BOUND('',#25568,.T.) ;
#19786 = FACE_OUTER_BOUND('',#25569,.T.) ;
#19787 = FACE_OUTER_BOUND('',#25570,.T.) ;
#19788 = FACE_OUTER_BOUND('',#25571,.T.) ;
#19789 = FACE_OUTER_BOUND('',#25572,.T.) ;
#19790 = FACE_OUTER_BOUND('',#25573,.T.) ;
#19791 = FACE_OUTER_BOUND('',#25574,.T.) ;
#19792 = FACE_OUTER_BOUND('',#25575,.T.) ;
#19793 = FACE_OUTER_BOUND('',#25576,.T.) ;
#19794 = FACE_OUTER_BOUND('',#25577,.T.) ;
#19795 = FACE_OUTER_BOUND('',#25578,.T.) ;
#19796 = FACE_OUTER_BOUND('',#25579,.T.) ;
#19797 = FACE_OUTER_BOUND('',#25580,.T.) ;
#19798 = FACE_OUTER_BOUND('',#25581,.T.) ;
#19799 = FACE_OUTER_BOUND('',#25582,.T.) ;
#19800 = FACE_OUTER_BOUND('',#25583,.T.) ;
#19801 = FACE_OUTER_BOUND('',#25584,.T.) ;
#19802 = FACE_OUTER_BOUND('',#25585,.T.) ;
#19803 = FACE_OUTER_BOUND('',#25586,.T.) ;
#19804 = FACE_OUTER_BOUND('',#25587,.T.) ;
#19805 = FACE_OUTER_BOUND('',#25588,.T.) ;
#19806 = FACE_OUTER_BOUND('',#25589,.T.) ;
#19807 = FACE_OUTER_BOUND('',#25590,.T.) ;
#19808 = FACE_OUTER_BOUND('',#25591,.T.) ;
#19809 = FACE_OUTER_BOUND('',#25592,.T.) ;
#19810 = FACE_OUTER_BOUND('',#25593,.T.) ;
#19811 = FACE_OUTER_BOUND('',#25594,.T.) ;
#19812 = FACE_OUTER_BOUND('',#25595,.T.) ;
#19813 = FACE_OUTER_BOUND('',#25596,.T.) ;
#19814 = FACE_OUTER_BOUND('',#25597,.T.) ;
#19815 = FACE_OUTER_BOUND('',#25598,.T.) ;
#19816 = FACE_OUTER_BOUND('',#25599,.T.) ;
#19817 = FACE_OUTER_BOUND('',#25600,.T.) ;
#19818 = FACE_OUTER_BOUND('',#25601,.T.) ;
#19819 = FACE_OUTER_BOUND('',#25602,.T.) ;
#19820 = FACE_OUTER_BOUND('',#25603,.T.) ;
#19821 = FACE_OUTER_BOUND('',#25604,.T.) ;
#19822 = FACE_OUTER_BOUND('',#25605,.T.) ;
#19823 = FACE_OUTER_BOUND('',#25606,.T.) ;
#19824 = FACE_OUTER_BOUND('',#25607,.T.) ;
#19825 = FACE_OUTER_BOUND('',#25608,.T.) ;
#19826 = FACE_OUTER_BOUND('',#25609,.T.) ;
#19827 = FACE_OUTER_BOUND('',#25610,.T.) ;
#19828 = FACE_OUTER_BOUND('',#25611,.T.) ;
#19829 = FACE_OUTER_BOUND('',#25612,.T.) ;
#19830 = FACE_OUTER_BOUND('',#25613,.T.) ;
#19831 = FACE_OUTER_BOUND('',#25614,.T.) ;
#19832 = FACE_OUTER_BOUND('',#25615,.T.) ;
#19833 = FACE_OUTER_BOUND('',#25616,.T.) ;
#19834 = FACE_OUTER_BOUND('',#25617,.T.) ;
#19835 = FACE_OUTER_BOUND('',#25618,.T.) ;
#19836 = FACE_OUTER_BOUND('',#25619,.T.) ;
#19837 = FACE_OUTER_BOUND('',#25620,.T.) ;
#19838 = FACE_OUTER_BOUND('',#25621,.T.) ;
#19839 = FACE_OUTER_BOUND('',#25622,.T.) ;
#19840 = FACE_OUTER_BOUND('',#25623,.T.) ;
#19841 = FACE_OUTER_BOUND('',#25624,.T.) ;
#19842 = FACE_OUTER_BOUND('',#25625,.T.) ;
#19843 = FACE_OUTER_BOUND('',#25626,.T.) ;
#19844 = FACE_OUTER_BOUND('',#25627,.T.) ;
#19845 = FACE_OUTER_BOUND('',#25628,.T.) ;
#19846 = FACE_OUTER_BOUND('',#25629,.T.) ;
#19847 = FACE_OUTER_BOUND('',#25630,.T.) ;
#19848 = FACE_OUTER_BOUND('',#25631,.T.) ;
#19849 = FACE_OUTER_BOUND('',#25632,.T.) ;
#19850 = FACE_OUTER_BOUND('',#25633,.T.) ;
#19851 = FACE_OUTER_BOUND('',#25634,.T.) ;
#19852 = FACE_OUTER_BOUND('',#25635,.T.) ;
#19853 = FACE_OUTER_BOUND('',#25636,.T.) ;
#19854 = FACE_OUTER_BOUND('',#25637,.T.) ;
#19855 = FACE_OUTER_BOUND('',#25638,.T.) ;
#19856 = FACE_OUTER_BOUND('',#25639,.T.) ;
#19857 = FACE_OUTER_BOUND('',#25640,.T.) ;
#19858 = FACE_OUTER_BOUND('',#25641,.T.) ;
#19859 = FACE_OUTER_BOUND('',#25642,.T.) ;
#19860 = FACE_OUTER_BOUND('',#25643,.T.) ;
#19861 = FACE_OUTER_BOUND('',#25644,.T.) ;
#19862 = FACE_OUTER_BOUND('',#25645,.T.) ;
#19863 = FACE_OUTER_BOUND('',#25646,.T.) ;
#19864 = FACE_OUTER_BOUND('',#25647,.T.) ;
#19865 = FACE_OUTER_BOUND('',#25648,.T.) ;
#19866 = FACE_OUTER_BOUND('',#25649,.T.) ;
#19867 = FACE_OUTER_BOUND('',#25650,.T.) ;
#19868 = FACE_OUTER_BOUND('',#25651,.T.) ;
#19869 = FACE_OUTER_BOUND('',#25652,.T.) ;
#19870 = FACE_OUTER_BOUND('',#25653,.T.) ;
#19871 = FACE_OUTER_BOUND('',#25654,.T.) ;
#19872 = FACE_OUTER_BOUND('',#25655,.T.) ;
#19873 = FACE_OUTER_BOUND('',#25656,.T.) ;
#19874 = FACE_OUTER_BOUND('',#25657,.T.) ;
#19875 = FACE_OUTER_BOUND('',#25658,.T.) ;
#19876 = FACE_OUTER_BOUND('',#25659,.T.) ;
#19877 = FACE_OUTER_BOUND('',#25660,.T.) ;
#19878 = FACE_OUTER_BOUND('',#25661,.T.) ;
#19879 = FACE_OUTER_BOUND('',#25662,.T.) ;
#19880 = FACE_OUTER_BOUND('',#25663,.T.) ;
#19881 = FACE_OUTER_BOUND('',#25664,.T.) ;
#19882 = FACE_OUTER_BOUND('',#25665,.T.) ;
#19883 = FACE_OUTER_BOUND('',#25666,.T.) ;
#19884 = FACE_OUTER_BOUND('',#25667,.T.) ;
#19885 = FACE_OUTER_BOUND('',#25668,.T.) ;
#19886 = FACE_OUTER_BOUND('',#25669,.T.) ;
#19887 = FACE_OUTER_BOUND('',#25670,.T.) ;
#19888 = FACE_OUTER_BOUND('',#25671,.T.) ;
#19889 = FACE_OUTER_BOUND('',#25672,.T.) ;
#19890 = FACE_OUTER_BOUND('',#25673,.T.) ;
#19891 = FACE_OUTER_BOUND('',#25674,.T.) ;
#19892 = FACE_OUTER_BOUND('',#25675,.T.) ;
#19893 = FACE_OUTER_BOUND('',#25676,.T.) ;
#19894 = FACE_OUTER_BOUND('',#25677,.T.) ;
#19895 = FACE_OUTER_BOUND('',#25678,.T.) ;
#19896 = FACE_OUTER_BOUND('',#25679,.T.) ;
#19897 = FACE_OUTER_BOUND('',#25680,.T.) ;
#19898 = FACE_OUTER_BOUND('',#25681,.T.) ;
#19899 = FACE_OUTER_BOUND('',#25682,.T.) ;
#19900 = FACE_OUTER_BOUND('',#25683,.T.) ;
#19901 = FACE_OUTER_BOUND('',#25684,.T.) ;
#19902 = FACE_OUTER_BOUND('',#25685,.T.) ;
#19903 = FACE_OUTER_BOUND('',#25686,.T.) ;
#19904 = FACE_OUTER_BOUND('',#25687,.T.) ;
#19905 = FACE_OUTER_BOUND('',#25688,.T.) ;
#19906 = FACE_OUTER_BOUND('',#25689,.T.) ;
#19907 = FACE_OUTER_BOUND('',#25690,.T.) ;
#19908 = FACE_OUTER_BOUND('',#25691,.T.) ;
#19909 = FACE_OUTER_BOUND('',#25692,.T.) ;
#19910 = FACE_OUTER_BOUND('',#25693,.T.) ;
#19911 = FACE_OUTER_BOUND('',#25694,.T.) ;
#19912 = FACE_OUTER_BOUND('',#25695,.T.) ;
#19913 = FACE_OUTER_BOUND('',#25696,.T.) ;
#19914 = FACE_OUTER_BOUND('',#25697,.T.) ;
#19915 = FACE_OUTER_BOUND('',#25698,.T.) ;
#19916 = FACE_OUTER_BOUND('',#25699,.T.) ;
#19917 = FACE_OUTER_BOUND('',#25700,.T.) ;
#19918 = FACE_OUTER_BOUND('',#25701,.T.) ;
#19919 = FACE_OUTER_BOUND('',#25702,.T.) ;
#19920 = FACE_OUTER_BOUND('',#25703,.T.) ;
#19921 = FACE_OUTER_BOUND('',#25704,.T.) ;
#19922 = FACE_OUTER_BOUND('',#25705,.T.) ;
#19923 = FACE_OUTER_BOUND('',#25706,.T.) ;
#19924 = FACE_OUTER_BOUND('',#25707,.T.) ;
#19925 = FACE_OUTER_BOUND('',#25708,.T.) ;
#19926 = FACE_OUTER_BOUND('',#25709,.T.) ;
#19927 = FACE_OUTER_BOUND('',#25710,.T.) ;
#19928 = FACE_OUTER_BOUND('',#25711,.T.) ;
#19929 = FACE_OUTER_BOUND('',#25712,.T.) ;
#19930 = FACE_OUTER_BOUND('',#25713,.T.) ;
#19931 = FACE_OUTER_BOUND('',#25714,.T.) ;
#19932 = FACE_OUTER_BOUND('',#25715,.T.) ;
#19933 = FACE_OUTER_BOUND('',#25716,.T.) ;
#19934 = FACE_OUTER_BOUND('',#25717,.T.) ;
#19935 = FACE_OUTER_BOUND('',#25718,.T.) ;
#19936 = FACE_OUTER_BOUND('',#25719,.T.) ;
#19937 = FACE_OUTER_BOUND('',#25720,.T.) ;
#19938 = FACE_OUTER_BOUND('',#25721,.T.) ;
#19939 = FACE_OUTER_BOUND('',#25722,.T.) ;
#19940 = FACE_OUTER_BOUND('',#25723,.T.) ;
#19941 = FACE_OUTER_BOUND('',#25724,.T.) ;
#19942 = FACE_OUTER_BOUND('',#25725,.T.) ;
#19943 = FACE_OUTER_BOUND('',#25726,.T.) ;
#19944 = FACE_OUTER_BOUND('',#25727,.T.) ;
#19945 = FACE_OUTER_BOUND('',#25728,.T.) ;
#19946 = FACE_OUTER_BOUND('',#25729,.T.) ;
#19947 = FACE_OUTER_BOUND('',#25730,.T.) ;
#19948 = FACE_OUTER_BOUND('',#25731,.T.) ;
#19949 = FACE_OUTER_BOUND('',#25732,.T.) ;
#19950 = FACE_OUTER_BOUND('',#25733,.T.) ;
#19951 = FACE_OUTER_BOUND('',#25734,.T.) ;
#19952 = FACE_OUTER_BOUND('',#25735,.T.) ;
#19953 = FACE_OUTER_BOUND('',#25736,.T.) ;
#19954 = FACE_OUTER_BOUND('',#25737,.T.) ;
#19955 = FACE_OUTER_BOUND('',#25738,.T.) ;
#19956 = FACE_OUTER_BOUND('',#25739,.T.) ;
#19957 = FACE_OUTER_BOUND('',#25740,.T.) ;
#19958 = FACE_OUTER_BOUND('',#25741,.T.) ;
#19959 = FACE_OUTER_BOUND('',#25742,.T.) ;
#19960 = FACE_OUTER_BOUND('',#25743,.T.) ;
#19961 = FACE_OUTER_BOUND('',#25744,.T.) ;
#19962 = FACE_OUTER_BOUND('',#25745,.T.) ;
#19963 = FACE_OUTER_BOUND('',#25746,.T.) ;
#19964 = FACE_OUTER_BOUND('',#25747,.T.) ;
#19965 = FACE_OUTER_BOUND('',#25748,.T.) ;
#19966 = FACE_OUTER_BOUND('',#25749,.T.) ;
#19967 = FACE_OUTER_BOUND('',#25750,.T.) ;
#19968 = FACE_OUTER_BOUND('',#25751,.T.) ;
#19969 = FACE_OUTER_BOUND('',#25752,.T.) ;
#19970 = FACE_OUTER_BOUND('',#25753,.T.) ;
#19971 = FACE_OUTER_BOUND('',#25754,.T.) ;
#19972 = FACE_OUTER_BOUND('',#25755,.T.) ;
#19973 = FACE_OUTER_BOUND('',#25756,.T.) ;
#19974 = FACE_OUTER_BOUND('',#25757,.T.) ;
#19975 = FACE_OUTER_BOUND('',#25758,.T.) ;
#19976 = FACE_OUTER_BOUND('',#25759,.T.) ;
#19977 = FACE_OUTER_BOUND('',#25760,.T.) ;
#19978 = FACE_OUTER_BOUND('',#25761,.T.) ;
#19979 = FACE_OUTER_BOUND('',#25762,.T.) ;
#19980 = FACE_OUTER_BOUND('',#25763,.T.) ;
#19981 = FACE_OUTER_BOUND('',#25764,.T.) ;
#19982 = FACE_OUTER_BOUND('',#25765,.T.) ;
#19983 = FACE_OUTER_BOUND('',#25766,.T.) ;
#19984 = FACE_OUTER_BOUND('',#25767,.T.) ;
#19985 = FACE_OUTER_BOUND('',#25768,.T.) ;
#19986 = FACE_OUTER_BOUND('',#25769,.T.) ;
#19987 = FACE_OUTER_BOUND('',#25770,.T.) ;
#19988 = FACE_OUTER_BOUND('',#25771,.T.) ;
#19989 = FACE_OUTER_BOUND('',#25772,.T.) ;
#19990 = FACE_OUTER_BOUND('',#25773,.T.) ;
#19991 = FACE_OUTER_BOUND('',#25774,.T.) ;
#19992 = FACE_OUTER_BOUND('',#25775,.T.) ;
#19993 = FACE_OUTER_BOUND('',#25776,.T.) ;
#19994 = FACE_OUTER_BOUND('',#25777,.T.) ;
#19995 = FACE_OUTER_BOUND('',#25778,.T.) ;
#19996 = FACE_OUTER_BOUND('',#25779,.T.) ;
#19997 = FACE_OUTER_BOUND('',#25780,.T.) ;
#19998 = FACE_OUTER_BOUND('',#25781,.T.) ;
#19999 = FACE_OUTER_BOUND('',#25782,.T.) ;
#20000 = FACE_OUTER_BOUND('',#25783,.T.) ;
#20001 = FACE_OUTER_BOUND('',#25784,.T.) ;
#20002 = FACE_OUTER_BOUND('',#25785,.T.) ;
#20003 = FACE_OUTER_BOUND('',#25786,.T.) ;
#20004 = FACE_OUTER_BOUND('',#25787,.T.) ;
#20005 = FACE_OUTER_BOUND('',#25788,.T.) ;
#20006 = FACE_OUTER_BOUND('',#25789,.T.) ;
#20007 = FACE_OUTER_BOUND('',#25790,.T.) ;
#20008 = FACE_OUTER_BOUND('',#25791,.T.) ;
#20009 = FACE_OUTER_BOUND('',#25792,.T.) ;
#20010 = FACE_OUTER_BOUND('',#25793,.T.) ;
#20011 = FACE_OUTER_BOUND('',#25794,.T.) ;
#20012 = FACE_OUTER_BOUND('',#25795,.T.) ;
#20013 = FACE_OUTER_BOUND('',#25796,.T.) ;
#20014 = FACE_OUTER_BOUND('',#25797,.T.) ;
#20015 = FACE_OUTER_BOUND('',#25798,.T.) ;
#20016 = FACE_OUTER_BOUND('',#25799,.T.) ;
#20017 = FACE_OUTER_BOUND('',#25800,.T.) ;
#20018 = FACE_OUTER_BOUND('',#25801,.T.) ;
#20019 = FACE_OUTER_BOUND('',#25802,.T.) ;
#20020 = FACE_OUTER_BOUND('',#25803,.T.) ;
#20021 = FACE_OUTER_BOUND('',#25804,.T.) ;
#20022 = FACE_OUTER_BOUND('',#25805,.T.) ;
#20023 = FACE_OUTER_BOUND('',#25806,.T.) ;
#20024 = FACE_OUTER_BOUND('',#25807,.T.) ;
#20025 = FACE_OUTER_BOUND('',#25808,.T.) ;
#20026 = FACE_OUTER_BOUND('',#25809,.T.) ;
#20027 = FACE_OUTER_BOUND('',#25810,.T.) ;
#20028 = FACE_OUTER_BOUND('',#25811,.T.) ;
#20029 = FACE_OUTER_BOUND('',#25812,.T.) ;
#20030 = FACE_OUTER_BOUND('',#25813,.T.) ;
#20031 = FACE_OUTER_BOUND('',#25814,.T.) ;
#20032 = FACE_OUTER_BOUND('',#25815,.T.) ;
#20033 = FACE_OUTER_BOUND('',#25816,.T.) ;
#20034 = FACE_OUTER_BOUND('',#25817,.T.) ;
#20035 = FACE_OUTER_BOUND('',#25818,.T.) ;
#20036 = FACE_OUTER_BOUND('',#25819,.T.) ;
#20037 = FACE_OUTER_BOUND('',#25820,.T.) ;
#20038 = FACE_OUTER_BOUND('',#25821,.T.) ;
#20039 = FACE_OUTER_BOUND('',#25822,.T.) ;
#20040 = FACE_OUTER_BOUND('',#25823,.T.) ;
#20041 = FACE_OUTER_BOUND('',#25824,.T.) ;
#20042 = FACE_OUTER_BOUND('',#25825,.T.) ;
#20043 = FACE_OUTER_BOUND('',#25826,.T.) ;
#20044 = FACE_OUTER_BOUND('',#25827,.T.) ;
#20045 = FACE_OUTER_BOUND('',#25828,.T.) ;
#20046 = FACE_OUTER_BOUND('',#25829,.T.) ;
#20047 = FACE_OUTER_BOUND('',#25830,.T.) ;
#20048 = FACE_OUTER_BOUND('',#25831,.T.) ;
#20049 = FACE_OUTER_BOUND('',#25832,.T.) ;
#20050 = FACE_OUTER_BOUND('',#25833,.T.) ;
#20051 = FACE_OUTER_BOUND('',#25834,.T.) ;
#20052 = FACE_OUTER_BOUND('',#25835,.T.) ;
#20053 = FACE_OUTER_BOUND('',#25836,.T.) ;
#20054 = FACE_OUTER_BOUND('',#25837,.T.) ;
#20055 = FACE_OUTER_BOUND('',#25838,.T.) ;
#20056 = FACE_OUTER_BOUND('',#25839,.T.) ;
#20057 = FACE_OUTER_BOUND('',#25840,.T.) ;
#20058 = FACE_OUTER_BOUND('',#25841,.T.) ;
#20059 = FACE_OUTER_BOUND('',#25842,.T.) ;
#20060 = FACE_OUTER_BOUND('',#25843,.T.) ;
#20061 = FACE_OUTER_BOUND('',#25844,.T.) ;
#20062 = FACE_OUTER_BOUND('',#25845,.T.) ;
#20063 = FACE_OUTER_BOUND('',#25846,.T.) ;
#20064 = FACE_OUTER_BOUND('',#25847,.T.) ;
#20065 = FACE_OUTER_BOUND('',#25848,.T.) ;
#20066 = FACE_OUTER_BOUND('',#25849,.T.) ;
#20067 = FACE_OUTER_BOUND('',#25850,.T.) ;
#20068 = FACE_OUTER_BOUND('',#25851,.T.) ;
#20069 = FACE_OUTER_BOUND('',#25852,.T.) ;
#20070 = FACE_OUTER_BOUND('',#25853,.T.) ;
#20071 = FACE_OUTER_BOUND('',#25854,.T.) ;
#20072 = FACE_OUTER_BOUND('',#25855,.T.) ;
#20073 = FACE_OUTER_BOUND('',#25856,.T.) ;
#20074 = FACE_OUTER_BOUND('',#25857,.T.) ;
#20075 = FACE_OUTER_BOUND('',#25858,.T.) ;
#20076 = FACE_OUTER_BOUND('',#25859,.T.) ;
#20077 = FACE_OUTER_BOUND('',#25860,.T.) ;
#20078 = FACE_OUTER_BOUND('',#25861,.T.) ;
#20079 = FACE_OUTER_BOUND('',#25862,.T.) ;
#20080 = FACE_OUTER_BOUND('',#25863,.T.) ;
#20081 = FACE_OUTER_BOUND('',#25864,.T.) ;
#20082 = FACE_OUTER_BOUND('',#25865,.T.) ;
#20083 = FACE_OUTER_BOUND('',#25866,.T.) ;
#20084 = FACE_OUTER_BOUND('',#25867,.T.) ;
#20085 = FACE_OUTER_BOUND('',#25868,.T.) ;
#20086 = FACE_OUTER_BOUND('',#25869,.T.) ;
#20087 = FACE_OUTER_BOUND('',#25870,.T.) ;
#20088 = FACE_OUTER_BOUND('',#25871,.T.) ;
#20089 = FACE_OUTER_BOUND('',#25872,.T.) ;
#20090 = FACE_OUTER_BOUND('',#25873,.T.) ;
#20091 = FACE_OUTER_BOUND('',#25874,.T.) ;
#20092 = FACE_OUTER_BOUND('',#25875,.T.) ;
#20093 = FACE_OUTER_BOUND('',#25876,.T.) ;
#20094 = FACE_OUTER_BOUND('',#25877,.T.) ;
#20095 = FACE_OUTER_BOUND('',#25878,.T.) ;
#20096 = FACE_OUTER_BOUND('',#25879,.T.) ;
#20097 = FACE_OUTER_BOUND('',#25880,.T.) ;
#20098 = FACE_OUTER_BOUND('',#25881,.T.) ;
#20099 = FACE_OUTER_BOUND('',#25882,.T.) ;
#20100 = FACE_OUTER_BOUND('',#25883,.T.) ;
#20101 = FACE_OUTER_BOUND('',#25884,.T.) ;
#20102 = FACE_OUTER_BOUND('',#25885,.T.) ;
#20103 = FACE_OUTER_BOUND('',#25886,.T.) ;
#20104 = FACE_OUTER_BOUND('',#25887,.T.) ;
#20105 = FACE_OUTER_BOUND('',#25888,.T.) ;
#20106 = FACE_OUTER_BOUND('',#25889,.T.) ;
#20107 = FACE_OUTER_BOUND('',#25890,.T.) ;
#20108 = FACE_OUTER_BOUND('',#25891,.T.) ;
#20109 = FACE_OUTER_BOUND('',#25892,.T.) ;
#20110 = FACE_OUTER_BOUND('',#25893,.T.) ;
#20111 = FACE_OUTER_BOUND('',#25894,.T.) ;
#20112 = FACE_OUTER_BOUND('',#25895,.T.) ;
#20113 = FACE_OUTER_BOUND('',#25896,.T.) ;
#20114 = FACE_OUTER_BOUND('',#25897,.T.) ;
#20115 = FACE_OUTER_BOUND('',#25898,.T.) ;
#20116 = FACE_OUTER_BOUND('',#25899,.T.) ;
#20117 = FACE_OUTER_BOUND('',#25900,.T.) ;
#20118 = FACE_OUTER_BOUND('',#25901,.T.) ;
#20119 = FACE_OUTER_BOUND('',#25902,.T.) ;
#20120 = FACE_OUTER_BOUND('',#25903,.T.) ;
#20121 = FACE_OUTER_BOUND('',#25904,.T.) ;
#20122 = FACE_OUTER_BOUND('',#25905,.T.) ;
#20123 = FACE_OUTER_BOUND('',#25906,.T.) ;
#20124 = FACE_OUTER_BOUND('',#25907,.T.) ;
#20125 = FACE_OUTER_BOUND('',#25908,.T.) ;
#20126 = FACE_OUTER_BOUND('',#25909,.T.) ;
#20127 = FACE_OUTER_BOUND('',#25910,.T.) ;
#20128 = FACE_OUTER_BOUND('',#25911,.T.) ;
#20129 = FACE_OUTER_BOUND('',#25912,.T.) ;
#20130 = FACE_OUTER_BOUND('',#25913,.T.) ;
#20131 = FACE_OUTER_BOUND('',#25914,.T.) ;
#20132 = FACE_OUTER_BOUND('',#25915,.T.) ;
#20133 = FACE_OUTER_BOUND('',#25916,.T.) ;
#20134 = FACE_OUTER_BOUND('',#25917,.T.) ;
#20135 = FACE_OUTER_BOUND('',#25918,.T.) ;
#20136 = FACE_OUTER_BOUND('',#25919,.T.) ;
#20137 = FACE_OUTER_BOUND('',#25920,.T.) ;
#20138 = FACE_OUTER_BOUND('',#25921,.T.) ;
#20139 = FACE_OUTER_BOUND('',#25922,.T.) ;
#20140 = FACE_OUTER_BOUND('',#25923,.T.) ;
#20141 = FACE_OUTER_BOUND('',#25924,.T.) ;
#20142 = FACE_OUTER_BOUND('',#25925,.T.) ;
#20143 = FACE_OUTER_BOUND('',#25926,.T.) ;
#20144 = FACE_OUTER_BOUND('',#25927,.T.) ;
#20145 = FACE_OUTER_BOUND('',#25928,.T.) ;
#20146 = FACE_OUTER_BOUND('',#25929,.T.) ;
#20147 = FACE_OUTER_BOUND('',#25930,.T.) ;
#20148 = FACE_OUTER_BOUND('',#25931,.T.) ;
#20149 = FACE_OUTER_BOUND('',#25932,.T.) ;
#20150 = FACE_OUTER_BOUND('',#25933,.T.) ;
#20151 = FACE_OUTER_BOUND('',#25934,.T.) ;
#20152 = FACE_OUTER_BOUND('',#25935,.T.) ;
#20153 = FACE_OUTER_BOUND('',#25936,.T.) ;
#20154 = FACE_OUTER_BOUND('',#25937,.T.) ;
#20155 = FACE_OUTER_BOUND('',#25938,.T.) ;
#20156 = FACE_OUTER_BOUND('',#25939,.T.) ;
#20157 = FACE_OUTER_BOUND('',#25940,.T.) ;
#20158 = FACE_OUTER_BOUND('',#25941,.T.) ;
#20159 = FACE_OUTER_BOUND('',#25942,.T.) ;
#20160 = FACE_OUTER_BOUND('',#25943,.T.) ;
#20161 = FACE_OUTER_BOUND('',#25944,.T.) ;
#20162 = FACE_OUTER_BOUND('',#25945,.T.) ;
#20163 = FACE_OUTER_BOUND('',#25946,.T.) ;
#20164 = FACE_OUTER_BOUND('',#25947,.T.) ;
#20165 = FACE_OUTER_BOUND('',#25948,.T.) ;
#20166 = FACE_OUTER_BOUND('',#25949,.T.) ;
#20167 = FACE_OUTER_BOUND('',#25950,.T.) ;
#20168 = FACE_OUTER_BOUND('',#25951,.T.) ;
#20169 = FACE_OUTER_BOUND('',#25952,.T.) ;
#20170 = FACE_OUTER_BOUND('',#25953,.T.) ;
#20171 = FACE_OUTER_BOUND('',#25954,.T.) ;
#20172 = FACE_OUTER_BOUND('',#25955,.T.) ;
#20173 = FACE_OUTER_BOUND('',#25956,.T.) ;
#20174 = FACE_OUTER_BOUND('',#25957,.T.) ;
#20175 = FACE_OUTER_BOUND('',#25958,.T.) ;
#20176 = FACE_OUTER_BOUND('',#25959,.T.) ;
#20177 = FACE_OUTER_BOUND('',#25960,.T.) ;
#20178 = FACE_OUTER_BOUND('',#25961,.T.) ;
#20179 = FACE_OUTER_BOUND('',#25962,.T.) ;
#20180 = FACE_OUTER_BOUND('',#25963,.T.) ;
#20181 = FACE_OUTER_BOUND('',#25964,.T.) ;
#20182 = FACE_OUTER_BOUND('',#25965,.T.) ;
#20183 = FACE_OUTER_BOUND('',#25966,.T.) ;
#20184 = FACE_OUTER_BOUND('',#25967,.T.) ;
#20185 = FACE_OUTER_BOUND('',#25968,.T.) ;
#20186 = FACE_OUTER_BOUND('',#25969,.T.) ;
#20187 = FACE_OUTER_BOUND('',#25970,.T.) ;
#20188 = FACE_OUTER_BOUND('',#25971,.T.) ;
#20189 = FACE_OUTER_BOUND('',#25972,.T.) ;
#20190 = FACE_OUTER_BOUND('',#25973,.T.) ;
#20191 = FACE_OUTER_BOUND('',#25974,.T.) ;
#20192 = FACE_OUTER_BOUND('',#25975,.T.) ;
#20193 = FACE_OUTER_BOUND('',#25976,.T.) ;
#20194 = FACE_OUTER_BOUND('',#25977,.T.) ;
#20195 = FACE_OUTER_BOUND('',#25978,.T.) ;
#20196 = FACE_OUTER_BOUND('',#25979,.T.) ;
#20197 = FACE_OUTER_BOUND('',#25980,.T.) ;
#20198 = FACE_OUTER_BOUND('',#25981,.T.) ;
#20199 = FACE_OUTER_BOUND('',#25982,.T.) ;
#20200 = FACE_OUTER_BOUND('',#25983,.T.) ;
#20201 = FACE_OUTER_BOUND('',#25984,.T.) ;
#20202 = FACE_OUTER_BOUND('',#25985,.T.) ;
#20203 = FACE_OUTER_BOUND('',#25986,.T.) ;
#20204 = FACE_OUTER_BOUND('',#25987,.T.) ;
#20205 = FACE_OUTER_BOUND('',#25988,.T.) ;
#20206 = FACE_OUTER_BOUND('',#25989,.T.) ;
#20207 = FACE_OUTER_BOUND('',#25990,.T.) ;
#20208 = FACE_OUTER_BOUND('',#25991,.T.) ;
#20209 = FACE_OUTER_BOUND('',#25992,.T.) ;
#20210 = FACE_OUTER_BOUND('',#25993,.T.) ;
#20211 = FACE_OUTER_BOUND('',#25994,.T.) ;
#20212 = FACE_OUTER_BOUND('',#25995,.T.) ;
#20213 = FACE_OUTER_BOUND('',#25996,.T.) ;
#20214 = FACE_OUTER_BOUND('',#25997,.T.) ;
#20215 = FACE_OUTER_BOUND('',#25998,.T.) ;
#20216 = FACE_OUTER_BOUND('',#25999,.T.) ;
#20217 = FACE_OUTER_BOUND('',#26000,.T.) ;
#20218 = FACE_OUTER_BOUND('',#26001,.T.) ;
#20219 = FACE_OUTER_BOUND('',#26002,.T.) ;
#20220 = FACE_OUTER_BOUND('',#26003,.T.) ;
#20221 = FACE_OUTER_BOUND('',#26004,.T.) ;
#20222 = FACE_OUTER_BOUND('',#26005,.T.) ;
#20223 = FACE_OUTER_BOUND('',#26006,.T.) ;
#20224 = FACE_OUTER_BOUND('',#26007,.T.) ;
#20225 = FACE_OUTER_BOUND('',#26008,.T.) ;
#20226 = FACE_OUTER_BOUND('',#26009,.T.) ;
#20227 = FACE_OUTER_BOUND('',#26010,.T.) ;
#20228 = FACE_OUTER_BOUND('',#26011,.T.) ;
#20229 = FACE_OUTER_BOUND('',#26012,.T.) ;
#20230 = FACE_OUTER_BOUND('',#26013,.T.) ;
#20231 = FACE_OUTER_BOUND('',#26014,.T.) ;
#20232 = FACE_OUTER_BOUND('',#26015,.T.) ;
#20233 = FACE_OUTER_BOUND('',#26016,.T.) ;
#20234 = FACE_OUTER_BOUND('',#26017,.T.) ;
#20235 = FACE_OUTER_BOUND('',#26018,.T.) ;
#20236 = FACE_OUTER_BOUND('',#26019,.T.) ;
#20237 = FACE_OUTER_BOUND('',#26020,.T.) ;
#20238 = FACE_OUTER_BOUND('',#26021,.T.) ;
#20239 = FACE_OUTER_BOUND('',#26022,.T.) ;
#20240 = FACE_OUTER_BOUND('',#26023,.T.) ;
#20241 = FACE_OUTER_BOUND('',#26024,.T.) ;
#20242 = FACE_OUTER_BOUND('',#26025,.T.) ;
#20243 = FACE_OUTER_BOUND('',#26026,.T.) ;
#20244 = FACE_OUTER_BOUND('',#26027,.T.) ;
#20245 = FACE_OUTER_BOUND('',#26028,.T.) ;
#20246 = FACE_OUTER_BOUND('',#26029,.T.) ;
#20247 = FACE_OUTER_BOUND('',#26030,.T.) ;
#20248 = FACE_OUTER_BOUND('',#26031,.T.) ;
#20249 = FACE_OUTER_BOUND('',#26032,.T.) ;
#20250 = FACE_OUTER_BOUND('',#26033,.T.) ;
#20251 = FACE_OUTER_BOUND('',#26034,.T.) ;
#20252 = FACE_OUTER_BOUND('',#26035,.T.) ;
#20253 = FACE_OUTER_BOUND('',#26036,.T.) ;
#20254 = FACE_OUTER_BOUND('',#26037,.T.) ;
#20255 = FACE_OUTER_BOUND('',#26038,.T.) ;
#20256 = FACE_OUTER_BOUND('',#26039,.T.) ;
#20257 = FACE_OUTER_BOUND('',#26040,.T.) ;
#20258 = FACE_OUTER_BOUND('',#26041,.T.) ;
#20259 = FACE_OUTER_BOUND('',#26042,.T.) ;
#20260 = FACE_OUTER_BOUND('',#26043,.T.) ;
#20261 = FACE_OUTER_BOUND('',#26044,.T.) ;
#20262 = FACE_OUTER_BOUND('',#26045,.T.) ;
#20263 = FACE_OUTER_BOUND('',#26046,.T.) ;
#20264 = FACE_OUTER_BOUND('',#26047,.T.) ;
#20265 = FACE_OUTER_BOUND('',#26048,.T.) ;
#20266 = FACE_OUTER_BOUND('',#26049,.T.) ;
#20267 = FACE_OUTER_BOUND('',#26050,.T.) ;
#20268 = FACE_OUTER_BOUND('',#26051,.T.) ;
#20269 = FACE_OUTER_BOUND('',#26052,.T.) ;
#20270 = FACE_OUTER_BOUND('',#26053,.T.) ;
#20271 = FACE_OUTER_BOUND('',#26054,.T.) ;
#20272 = FACE_OUTER_BOUND('',#26055,.T.) ;
#20273 = FACE_OUTER_BOUND('',#26056,.T.) ;
#20274 = FACE_OUTER_BOUND('',#26057,.T.) ;
#20275 = FACE_OUTER_BOUND('',#26058,.T.) ;
#20276 = FACE_OUTER_BOUND('',#26059,.T.) ;
#20277 = FACE_OUTER_BOUND('',#26060,.T.) ;
#20278 = FACE_OUTER_BOUND('',#26061,.T.) ;
#20279 = FACE_OUTER_BOUND('',#26062,.T.) ;
#20280 = FACE_OUTER_BOUND('',#26063,.T.) ;
#20281 = FACE_OUTER_BOUND('',#26064,.T.) ;
#20282 = FACE_OUTER_BOUND('',#26065,.T.) ;
#20283 = FACE_OUTER_BOUND('',#26066,.T.) ;
#20284 = FACE_OUTER_BOUND('',#26067,.T.) ;
#20285 = FACE_OUTER_BOUND('',#26068,.T.) ;
#20286 = FACE_OUTER_BOUND('',#26069,.T.) ;
#20287 = FACE_OUTER_BOUND('',#26070,.T.) ;
#20288 = FACE_OUTER_BOUND('',#26071,.T.) ;
#20289 = FACE_OUTER_BOUND('',#26072,.T.) ;
#20290 = FACE_OUTER_BOUND('',#26073,.T.) ;
#20291 = FACE_OUTER_BOUND('',#26074,.T.) ;
#20292 = FACE_OUTER_BOUND('',#26075,.T.) ;
#20293 = FACE_OUTER_BOUND('',#26076,.T.) ;
#20294 = FACE_OUTER_BOUND('',#26077,.T.) ;
#20295 = FACE_OUTER_BOUND('',#26078,.T.) ;
#20296 = FACE_OUTER_BOUND('',#26079,.T.) ;
#20297 = FACE_OUTER_BOUND('',#26080,.T.) ;
#20298 = FACE_OUTER_BOUND('',#26081,.T.) ;
#20299 = FACE_OUTER_BOUND('',#26082,.T.) ;
#20300 = FACE_OUTER_BOUND('',#26083,.T.) ;
#20301 = FACE_OUTER_BOUND('',#26084,.T.) ;
#20302 = FACE_OUTER_BOUND('',#26085,.T.) ;
#20303 = FACE_OUTER_BOUND('',#26086,.T.) ;
#20304 = FACE_OUTER_BOUND('',#26087,.T.) ;
#20305 = FACE_OUTER_BOUND('',#26088,.T.) ;
#20306 = FACE_OUTER_BOUND('',#26089,.T.) ;
#20307 = FACE_OUTER_BOUND('',#26090,.T.) ;
#20308 = FACE_OUTER_BOUND('',#26091,.T.) ;
#20309 = FACE_OUTER_BOUND('',#26092,.T.) ;
#20310 = FACE_OUTER_BOUND('',#26093,.T.) ;
#20311 = FACE_OUTER_BOUND('',#26094,.T.) ;
#20312 = FACE_OUTER_BOUND('',#26095,.T.) ;
#20313 = FACE_OUTER_BOUND('',#26096,.T.) ;
#20314 = FACE_OUTER_BOUND('',#26097,.T.) ;
#20315 = FACE_OUTER_BOUND('',#26098,.T.) ;
#20316 = FACE_OUTER_BOUND('',#26099,.T.) ;
#20317 = FACE_OUTER_BOUND('',#26100,.T.) ;
#20318 = FACE_OUTER_BOUND('',#26101,.T.) ;
#20319 = FACE_OUTER_BOUND('',#26102,.T.) ;
#20320 = FACE_OUTER_BOUND('',#26103,.T.) ;
#20321 = FACE_OUTER_BOUND('',#26104,.T.) ;
#20322 = FACE_OUTER_BOUND('',#26105,.T.) ;
#20323 = FACE_OUTER_BOUND('',#26106,.T.) ;
#20324 = FACE_OUTER_BOUND('',#26107,.T.) ;
#20325 = FACE_OUTER_BOUND('',#26108,.T.) ;
#20326 = FACE_OUTER_BOUND('',#26109,.T.) ;
#20327 = FACE_OUTER_BOUND('',#26110,.T.) ;
#20328 = FACE_OUTER_BOUND('',#26111,.T.) ;
#20329 = FACE_OUTER_BOUND('',#26112,.T.) ;
#20330 = FACE_OUTER_BOUND('',#26113,.T.) ;
#20331 = FACE_OUTER_BOUND('',#26114,.T.) ;
#20332 = FACE_OUTER_BOUND('',#26115,.T.) ;
#20333 = FACE_OUTER_BOUND('',#26116,.T.) ;
#20334 = FACE_OUTER_BOUND('',#26117,.T.) ;
#20335 = FACE_OUTER_BOUND('',#26118,.T.) ;
#20336 = FACE_OUTER_BOUND('',#26119,.T.) ;
#20337 = FACE_OUTER_BOUND('',#26120,.T.) ;
#20338 = FACE_OUTER_BOUND('',#26121,.T.) ;
#20339 = FACE_OUTER_BOUND('',#26122,.T.) ;
#20340 = FACE_OUTER_BOUND('',#26123,.T.) ;
#20341 = FACE_OUTER_BOUND('',#26124,.T.) ;
#20342 = FACE_OUTER_BOUND('',#26125,.T.) ;
#20343 = FACE_OUTER_BOUND('',#26126,.T.) ;
#20344 = FACE_OUTER_BOUND('',#26127,.T.) ;
#20345 = FACE_OUTER_BOUND('',#26128,.T.) ;
#20346 = FACE_OUTER_BOUND('',#26129,.T.) ;
#20347 = FACE_OUTER_BOUND('',#26130,.T.) ;
#20348 = FACE_OUTER_BOUND('',#26131,.T.) ;
#20349 = FACE_OUTER_BOUND('',#26132,.T.) ;
#20350 = FACE_OUTER_BOUND('',#26133,.T.) ;
#20351 = FACE_OUTER_BOUND('',#26134,.T.) ;
#20352 = FACE_OUTER_BOUND('',#26135,.T.) ;
#20353 = FACE_OUTER_BOUND('',#26136,.T.) ;
#20354 = FACE_OUTER_BOUND('',#26137,.T.) ;
#20355 = FACE_OUTER_BOUND('',#26138,.T.) ;
#20356 = FACE_OUTER_BOUND('',#26139,.T.) ;
#20357 = FACE_OUTER_BOUND('',#26140,.T.) ;
#20358 = FACE_OUTER_BOUND('',#26141,.T.) ;
#20359 = FACE_OUTER_BOUND('',#26142,.T.) ;
#20360 = FACE_OUTER_BOUND('',#26143,.T.) ;
#20361 = FACE_OUTER_BOUND('',#26144,.T.) ;
#20362 = FACE_OUTER_BOUND('',#26145,.T.) ;
#20363 = FACE_OUTER_BOUND('',#26146,.T.) ;
#20364 = FACE_OUTER_BOUND('',#26147,.T.) ;
#20365 = FACE_OUTER_BOUND('',#26148,.T.) ;
#20366 = FACE_OUTER_BOUND('',#26149,.T.) ;
#20367 = FACE_OUTER_BOUND('',#26150,.T.) ;
#20368 = FACE_OUTER_BOUND('',#26151,.T.) ;
#20369 = FACE_OUTER_BOUND('',#26152,.T.) ;
#20370 = FACE_OUTER_BOUND('',#26153,.T.) ;
#20371 = FACE_OUTER_BOUND('',#26154,.T.) ;
#20372 = FACE_OUTER_BOUND('',#26155,.T.) ;
#20373 = FACE_OUTER_BOUND('',#26156,.T.) ;
#20374 = FACE_OUTER_BOUND('',#26157,.T.) ;
#20375 = FACE_OUTER_BOUND('',#26158,.T.) ;
#20376 = FACE_OUTER_BOUND('',#26159,.T.) ;
#20377 = FACE_OUTER_BOUND('',#26160,.T.) ;
#20378 = FACE_OUTER_BOUND('',#26161,.T.) ;
#20379 = FACE_OUTER_BOUND('',#26162,.T.) ;
#20380 = FACE_OUTER_BOUND('',#26163,.T.) ;
#20381 = FACE_OUTER_BOUND('',#26164,.T.) ;
#20382 = FACE_OUTER_BOUND('',#26165,.T.) ;
#20383 = FACE_OUTER_BOUND('',#26166,.T.) ;
#20384 = FACE_OUTER_BOUND('',#26167,.T.) ;
#20385 = FACE_OUTER_BOUND('',#26168,.T.) ;
#20386 = FACE_OUTER_BOUND('',#26169,.T.) ;
#20387 = FACE_OUTER_BOUND('',#26170,.T.) ;
#20388 = FACE_OUTER_BOUND('',#26171,.T.) ;
#20389 = FACE_OUTER_BOUND('',#26172,.T.) ;
#20390 = FACE_OUTER_BOUND('',#26173,.T.) ;
#20391 = FACE_OUTER_BOUND('',#26174,.T.) ;
#20392 = FACE_OUTER_BOUND('',#26175,.T.) ;
#20393 = FACE_OUTER_BOUND('',#26176,.T.) ;
#20394 = FACE_OUTER_BOUND('',#26177,.T.) ;
#20395 = FACE_OUTER_BOUND('',#26178,.T.) ;
#20396 = FACE_OUTER_BOUND('',#26179,.T.) ;
#20397 = FACE_OUTER_BOUND('',#26180,.T.) ;
#20398 = FACE_OUTER_BOUND('',#26181,.T.) ;
#20399 = FACE_OUTER_BOUND('',#26182,.T.) ;
#20400 = FACE_OUTER_BOUND('',#26183,.T.) ;
#20401 = FACE_OUTER_BOUND('',#26184,.T.) ;
#20402 = FACE_OUTER_BOUND('',#26185,.T.) ;
#20403 = FACE_OUTER_BOUND('',#26186,.T.) ;
#20404 = FACE_OUTER_BOUND('',#26187,.T.) ;
#20405 = FACE_OUTER_BOUND('',#26188,.T.) ;
#20406 = FACE_OUTER_BOUND('',#26189,.T.) ;
#20407 = FACE_OUTER_BOUND('',#26190,.T.) ;
#20408 = FACE_OUTER_BOUND('',#26191,.T.) ;
#20409 = FACE_OUTER_BOUND('',#26192,.T.) ;
#20410 = FACE_OUTER_BOUND('',#26193,.T.) ;
#20411 = FACE_OUTER_BOUND('',#26194,.T.) ;
#20412 = FACE_OUTER_BOUND('',#26195,.T.) ;
#20413 = FACE_OUTER_BOUND('',#26196,.T.) ;
#20414 = FACE_OUTER_BOUND('',#26197,.T.) ;
#20415 = FACE_OUTER_BOUND('',#26198,.T.) ;
#20416 = FACE_OUTER_BOUND('',#26199,.T.) ;
#20417 = FACE_OUTER_BOUND('',#26200,.T.) ;
#20418 = FACE_OUTER_BOUND('',#26201,.T.) ;
#20419 = FACE_OUTER_BOUND('',#26202,.T.) ;
#20420 = FACE_OUTER_BOUND('',#26203,.T.) ;
#20421 = FACE_OUTER_BOUND('',#26204,.T.) ;
#20422 = FACE_OUTER_BOUND('',#26205,.T.) ;
#20423 = FACE_OUTER_BOUND('',#26206,.T.) ;
#20424 = FACE_OUTER_BOUND('',#26207,.T.) ;
#20425 = FACE_OUTER_BOUND('',#26208,.T.) ;
#20426 = FACE_OUTER_BOUND('',#26209,.T.) ;
#20427 = FACE_OUTER_BOUND('',#26210,.T.) ;
#20428 = FACE_OUTER_BOUND('',#26211,.T.) ;
#20429 = FACE_OUTER_BOUND('',#26212,.T.) ;
#20430 = FACE_OUTER_BOUND('',#26213,.T.) ;
#20431 = FACE_OUTER_BOUND('',#26214,.T.) ;
#20432 = FACE_OUTER_BOUND('',#26215,.T.) ;
#20433 = FACE_OUTER_BOUND('',#26216,.T.) ;
#20434 = FACE_OUTER_BOUND('',#26217,.T.) ;
#20435 = FACE_OUTER_BOUND('',#26218,.T.) ;
#20436 = FACE_OUTER_BOUND('',#26219,.T.) ;
#20437 = FACE_OUTER_BOUND('',#26220,.T.) ;
#20438 = FACE_OUTER_BOUND('',#26221,.T.) ;
#20439 = FACE_OUTER_BOUND('',#26222,.T.) ;
#20440 = FACE_OUTER_BOUND('',#26223,.T.) ;
#20441 = FACE_OUTER_BOUND('',#26224,.T.) ;
#20442 = FACE_OUTER_BOUND('',#26225,.T.) ;
#20443 = FACE_OUTER_BOUND('',#26226,.T.) ;
#20444 = FACE_OUTER_BOUND('',#26227,.T.) ;
#20445 = FACE_OUTER_BOUND('',#26228,.T.) ;
#20446 = FACE_OUTER_BOUND('',#26229,.T.) ;
#20447 = FACE_OUTER_BOUND('',#26230,.T.) ;
#20448 = FACE_OUTER_BOUND('',#26231,.T.) ;
#20449 = FACE_OUTER_BOUND('',#26232,.T.) ;
#20450 = FACE_OUTER_BOUND('',#26233,.T.) ;
#20451 = FACE_OUTER_BOUND('',#26234,.T.) ;
#20452 = FACE_OUTER_BOUND('',#26235,.T.) ;
#20453 = FACE_OUTER_BOUND('',#26236,.T.) ;
#20454 = FACE_OUTER_BOUND('',#26237,.T.) ;
#20455 = FACE_OUTER_BOUND('',#26238,.T.) ;
#20456 = FACE_OUTER_BOUND('',#26239,.T.) ;
#20457 = FACE_OUTER_BOUND('',#26240,.T.) ;
#20458 = FACE_OUTER_BOUND('',#26241,.T.) ;
#20459 = FACE_OUTER_BOUND('',#26242,.T.) ;
#20460 = FACE_OUTER_BOUND('',#26243,.T.) ;
#20461 = FACE_OUTER_BOUND('',#26244,.T.) ;
#20462 = FACE_OUTER_BOUND('',#26245,.T.) ;
#20463 = FACE_OUTER_BOUND('',#26246,.T.) ;
#20464 = FACE_OUTER_BOUND('',#26247,.T.) ;
#20465 = FACE_OUTER_BOUND('',#26248,.T.) ;
#20466 = FACE_OUTER_BOUND('',#26249,.T.) ;
#20467 = FACE_OUTER_BOUND('',#26250,.T.) ;
#20468 = FACE_OUTER_BOUND('',#26251,.T.) ;
#20469 = FACE_OUTER_BOUND('',#26252,.T.) ;
#20470 = FACE_OUTER_BOUND('',#26253,.T.) ;
#20471 = FACE_OUTER_BOUND('',#26254,.T.) ;
#20472 = FACE_OUTER_BOUND('',#26255,.T.) ;
#20473 = FACE_OUTER_BOUND('',#26256,.T.) ;
#20474 = FACE_OUTER_BOUND('',#26257,.T.) ;
#20475 = FACE_OUTER_BOUND('',#26258,.T.) ;
#20476 = FACE_OUTER_BOUND('',#26259,.T.) ;
#20477 = FACE_OUTER_BOUND('',#26260,.T.) ;
#20478 = FACE_OUTER_BOUND('',#26261,.T.) ;
#20479 = FACE_OUTER_BOUND('',#26262,.T.) ;
#20480 = FACE_OUTER_BOUND('',#26263,.T.) ;
#20481 = FACE_OUTER_BOUND('',#26264,.T.) ;
#20482 = FACE_OUTER_BOUND('',#26265,.T.) ;
#20483 = FACE_OUTER_BOUND('',#26266,.T.) ;
#20484 = FACE_OUTER_BOUND('',#26267,.T.) ;
#20485 = FACE_OUTER_BOUND('',#26268,.T.) ;
#20486 = FACE_OUTER_BOUND('',#26269,.T.) ;
#20487 = FACE_OUTER_BOUND('',#26270,.T.) ;
#20488 = FACE_OUTER_BOUND('',#26271,.T.) ;
#20489 = FACE_OUTER_BOUND('',#26272,.T.) ;
#20490 = FACE_OUTER_BOUND('',#26273,.T.) ;
#20491 = FACE_OUTER_BOUND('',#26274,.T.) ;
#20492 = FACE_OUTER_BOUND('',#26295,.T.) ;
#20493 = FACE_OUTER_BOUND('',#26297,.T.) ;
#20494 = FACE_OUTER_BOUND('',#26299,.T.) ;
#20495 = FACE_OUTER_BOUND('',#26301,.T.) ;
#20496 = FACE_OUTER_BOUND('',#26303,.T.) ;
#20497 = FACE_OUTER_BOUND('',#26305,.T.) ;
#20498 = FACE_OUTER_BOUND('',#26307,.T.) ;
#20499 = FACE_OUTER_BOUND('',#26309,.T.) ;
#20500 = FACE_OUTER_BOUND('',#26311,.T.) ;
#20501 = FACE_OUTER_BOUND('',#26313,.T.) ;
#20502 = FACE_OUTER_BOUND('',#26314,.T.) ;
#20503 = FACE_OUTER_BOUND('',#26315,.T.) ;
#20504 = FACE_OUTER_BOUND('',#26316,.T.) ;
#20505 = FACE_OUTER_BOUND('',#26317,.T.) ;
#20506 = FACE_OUTER_BOUND('',#26318,.T.) ;
#20507 = FACE_OUTER_BOUND('',#26319,.T.) ;
#20508 = FACE_OUTER_BOUND('',#26320,.T.) ;
#20509 = FACE_OUTER_BOUND('',#26321,.T.) ;
#20510 = FACE_OUTER_BOUND('',#26322,.T.) ;
#20511 = FACE_OUTER_BOUND('',#26323,.T.) ;
#20512 = FACE_OUTER_BOUND('',#26324,.T.) ;
#20513 = FACE_OUTER_BOUND('',#26325,.T.) ;
#20514 = FACE_OUTER_BOUND('',#26326,.T.) ;
#20515 = FACE_OUTER_BOUND('',#26327,.T.) ;
#20516 = FACE_OUTER_BOUND('',#26328,.T.) ;
#20517 = FACE_OUTER_BOUND('',#26329,.T.) ;
#20518 = FACE_OUTER_BOUND('',#26330,.T.) ;
#20519 = FACE_OUTER_BOUND('',#26331,.T.) ;
#20520 = FACE_OUTER_BOUND('',#26332,.T.) ;
#20521 = FACE_OUTER_BOUND('',#26333,.T.) ;
#20522 = FACE_OUTER_BOUND('',#26334,.T.) ;
#20523 = FACE_OUTER_BOUND('',#26335,.T.) ;
#20524 = FACE_OUTER_BOUND('',#26336,.T.) ;
#20525 = FACE_OUTER_BOUND('',#26347,.T.) ;
#20526 = FACE_OUTER_BOUND('',#26349,.T.) ;
#20527 = FACE_OUTER_BOUND('',#26350,.T.) ;
#20528 = FACE_OUTER_BOUND('',#26351,.T.) ;
#20529 = FACE_OUTER_BOUND('',#26352,.T.) ;
#20530 = FACE_OUTER_BOUND('',#26353,.T.) ;
#20531 = FACE_OUTER_BOUND('',#26354,.T.) ;
#20532 = FACE_OUTER_BOUND('',#26355,.T.) ;
#20533 = FACE_OUTER_BOUND('',#26366,.T.) ;
#20534 = FACE_OUTER_BOUND('',#26367,.T.) ;
#20535 = FACE_OUTER_BOUND('',#26368,.T.) ;
#20536 = FACE_OUTER_BOUND('',#26369,.T.) ;
#20537 = FACE_OUTER_BOUND('',#26370,.T.) ;
#20538 = FACE_OUTER_BOUND('',#26371,.T.) ;
#20539 = FACE_OUTER_BOUND('',#26372,.T.) ;
#20540 = FACE_OUTER_BOUND('',#26373,.T.) ;
#20541 = FACE_OUTER_BOUND('',#26374,.T.) ;
#20542 = FACE_OUTER_BOUND('',#26375,.T.) ;
#20543 = FACE_OUTER_BOUND('',#26376,.T.) ;
#20544 = FACE_OUTER_BOUND('',#26377,.T.) ;
#20545 = FACE_OUTER_BOUND('',#26378,.T.) ;
#20546 = FACE_OUTER_BOUND('',#26379,.T.) ;
#20547 = FACE_OUTER_BOUND('',#26381,.T.) ;
#20548 = FACE_OUTER_BOUND('',#26382,.T.) ;
#20549 = FACE_OUTER_BOUND('',#26383,.T.) ;
#20550 = FACE_OUTER_BOUND('',#26384,.T.) ;
#20551 = FACE_OUTER_BOUND('',#26385,.T.) ;
#20552 = FACE_OUTER_BOUND('',#26386,.T.) ;
#20553 = FACE_OUTER_BOUND('',#26387,.T.) ;
#20554 = FACE_OUTER_BOUND('',#26388,.T.) ;
#20555 = FACE_OUTER_BOUND('',#26389,.T.) ;
#20556 = FACE_OUTER_BOUND('',#26390,.T.) ;
#20557 = FACE_OUTER_BOUND('',#26391,.T.) ;
#20558 = FACE_OUTER_BOUND('',#26392,.T.) ;
#20559 = FACE_OUTER_BOUND('',#26393,.T.) ;
#20560 = FACE_OUTER_BOUND('',#26394,.T.) ;
#20561 = FACE_OUTER_BOUND('',#26395,.T.) ;
#20562 = FACE_OUTER_BOUND('',#26397,.T.) ;
#20563 = FACE_OUTER_BOUND('',#26398,.T.) ;
#20564 = FACE_OUTER_BOUND('',#26399,.T.) ;
#20565 = FACE_OUTER_BOUND('',#26400,.T.) ;
#20566 = FACE_OUTER_BOUND('',#26401,.T.) ;
#20567 = FACE_OUTER_BOUND('',#26402,.T.) ;
#20568 = FACE_OUTER_BOUND('',#26404,.T.) ;
#20569 = FACE_OUTER_BOUND('',#26405,.T.) ;
#20570 = FACE_OUTER_BOUND('',#26406,.T.) ;
#20571 = FACE_OUTER_BOUND('',#26407,.T.) ;
#20572 = FACE_OUTER_BOUND('',#26408,.T.) ;
#20573 = FACE_OUTER_BOUND('',#26409,.T.) ;
#20574 = FACE_OUTER_BOUND('',#26410,.T.) ;
#20575 = FACE_OUTER_BOUND('',#26411,.T.) ;
#20576 = FACE_OUTER_BOUND('',#26412,.T.) ;
#20577 = FACE_OUTER_BOUND('',#26413,.T.) ;
#20578 = FACE_OUTER_BOUND('',#26414,.T.) ;
#20579 = FACE_OUTER_BOUND('',#26415,.T.) ;
#20580 = FACE_OUTER_BOUND('',#26416,.T.) ;
#20581 = FACE_OUTER_BOUND('',#26417,.T.) ;
#20582 = FACE_OUTER_BOUND('',#26418,.T.) ;
#20583 = FACE_OUTER_BOUND('',#26419,.T.) ;
#20584 = FACE_OUTER_BOUND('',#26420,.T.) ;
#20585 = FACE_OUTER_BOUND('',#26421,.T.) ;
#20586 = FACE_OUTER_BOUND('',#26422,.T.) ;
#20587 = FACE_OUTER_BOUND('',#26423,.T.) ;
#20588 = FACE_OUTER_BOUND('',#26424,.T.) ;
#20589 = FACE_OUTER_BOUND('',#26425,.T.) ;
#20590 = FACE_OUTER_BOUND('',#26426,.T.) ;
#20591 = FACE_OUTER_BOUND('',#26427,.T.) ;
#20592 = FACE_OUTER_BOUND('',#26428,.T.) ;
#20593 = FACE_OUTER_BOUND('',#26429,.T.) ;
#20594 = FACE_OUTER_BOUND('',#26430,.T.) ;
#20595 = FACE_OUTER_BOUND('',#26431,.T.) ;
#20596 = FACE_OUTER_BOUND('',#26432,.T.) ;
#20597 = FACE_OUTER_BOUND('',#26433,.T.) ;
#20598 = FACE_OUTER_BOUND('',#26434,.T.) ;
#20599 = FACE_OUTER_BOUND('',#26435,.T.) ;
#20600 = FACE_OUTER_BOUND('',#26436,.T.) ;
#20601 = FACE_OUTER_BOUND('',#26437,.T.) ;
#20602 = FACE_OUTER_BOUND('',#26438,.T.) ;
#20603 = FACE_OUTER_BOUND('',#26439,.T.) ;
#20604 = FACE_OUTER_BOUND('',#26440,.T.) ;
#20605 = FACE_OUTER_BOUND('',#26441,.T.) ;
#20606 = FACE_OUTER_BOUND('',#26442,.T.) ;
#20607 = FACE_OUTER_BOUND('',#26443,.T.) ;
#20608 = FACE_OUTER_BOUND('',#26444,.T.) ;
#20609 = FACE_OUTER_BOUND('',#26445,.T.) ;
#20610 = FACE_OUTER_BOUND('',#26446,.T.) ;
#20611 = FACE_OUTER_BOUND('',#26447,.T.) ;
#20612 = FACE_OUTER_BOUND('',#26448,.T.) ;
#20613 = FACE_OUTER_BOUND('',#26449,.T.) ;
#20614 = FACE_OUTER_BOUND('',#26450,.T.) ;
#20615 = FACE_OUTER_BOUND('',#26451,.T.) ;
#20616 = FACE_OUTER_BOUND('',#26452,.T.) ;
#20617 = FACE_OUTER_BOUND('',#26453,.T.) ;
#20618 = FACE_OUTER_BOUND('',#26454,.T.) ;
#20619 = FACE_OUTER_BOUND('',#26455,.T.) ;
#20620 = FACE_OUTER_BOUND('',#26456,.T.) ;
#20621 = FACE_OUTER_BOUND('',#26457,.T.) ;
#20622 = FACE_OUTER_BOUND('',#26458,.T.) ;
#20623 = FACE_OUTER_BOUND('',#26459,.T.) ;
#20624 = FACE_OUTER_BOUND('',#26460,.T.) ;
#20625 = FACE_OUTER_BOUND('',#26461,.T.) ;
#20626 = FACE_OUTER_BOUND('',#26462,.T.) ;
#20627 = FACE_OUTER_BOUND('',#26463,.T.) ;
#20628 = FACE_OUTER_BOUND('',#26464,.T.) ;
#20629 = FACE_OUTER_BOUND('',#26465,.T.) ;
#20630 = FACE_OUTER_BOUND('',#26466,.T.) ;
#20631 = FACE_OUTER_BOUND('',#26467,.T.) ;
#20632 = FACE_OUTER_BOUND('',#26468,.T.) ;
#20633 = FACE_OUTER_BOUND('',#26469,.T.) ;
#20634 = FACE_OUTER_BOUND('',#26470,.T.) ;
#20635 = FACE_OUTER_BOUND('',#26471,.T.) ;
#20636 = FACE_OUTER_BOUND('',#26472,.T.) ;
#20637 = FACE_OUTER_BOUND('',#26473,.T.) ;
#20638 = FACE_OUTER_BOUND('',#26474,.T.) ;
#20639 = FACE_OUTER_BOUND('',#26475,.T.) ;
#20640 = FACE_OUTER_BOUND('',#26476,.T.) ;
#20641 = FACE_OUTER_BOUND('',#26477,.T.) ;
#20642 = FACE_OUTER_BOUND('',#26478,.T.) ;
#20643 = FACE_OUTER_BOUND('',#26479,.T.) ;
#20644 = FACE_OUTER_BOUND('',#26480,.T.) ;
#20645 = FACE_OUTER_BOUND('',#26481,.T.) ;
#20646 = FACE_OUTER_BOUND('',#26482,.T.) ;
#20647 = FACE_OUTER_BOUND('',#26483,.T.) ;
#20648 = FACE_OUTER_BOUND('',#26484,.T.) ;
#20649 = FACE_OUTER_BOUND('',#26485,.T.) ;
#20650 = FACE_OUTER_BOUND('',#26486,.T.) ;
#20651 = FACE_OUTER_BOUND('',#26487,.T.) ;
#20652 = FACE_OUTER_BOUND('',#26488,.T.) ;
#20653 = FACE_OUTER_BOUND('',#26489,.T.) ;
#20654 = FACE_OUTER_BOUND('',#26490,.T.) ;
#20655 = FACE_OUTER_BOUND('',#26491,.T.) ;
#20656 = FACE_OUTER_BOUND('',#26492,.T.) ;
#20657 = FACE_OUTER_BOUND('',#26493,.T.) ;
#20658 = FACE_OUTER_BOUND('',#26494,.T.) ;
#20659 = FACE_OUTER_BOUND('',#26495,.T.) ;
#20660 = FACE_OUTER_BOUND('',#26496,.T.) ;
#20661 = FACE_OUTER_BOUND('',#26497,.T.) ;
#20662 = FACE_OUTER_BOUND('',#26498,.T.) ;
#20663 = FACE_OUTER_BOUND('',#26499,.T.) ;
#20664 = FACE_OUTER_BOUND('',#26500,.T.) ;
#20665 = FACE_OUTER_BOUND('',#26501,.T.) ;
#20666 = FACE_OUTER_BOUND('',#26502,.T.) ;
#20667 = FACE_OUTER_BOUND('',#26503,.T.) ;
#20668 = FACE_OUTER_BOUND('',#26504,.T.) ;
#20669 = FACE_OUTER_BOUND('',#26505,.T.) ;
#20670 = FACE_OUTER_BOUND('',#26506,.T.) ;
#20671 = FACE_OUTER_BOUND('',#26507,.T.) ;
#20672 = FACE_OUTER_BOUND('',#26508,.T.) ;
#20673 = FACE_OUTER_BOUND('',#26509,.T.) ;
#20674 = FACE_OUTER_BOUND('',#26510,.T.) ;
#20675 = FACE_OUTER_BOUND('',#26511,.T.) ;
#20676 = FACE_OUTER_BOUND('',#26512,.T.) ;
#20677 = FACE_OUTER_BOUND('',#26513,.T.) ;
#20678 = FACE_OUTER_BOUND('',#26514,.T.) ;
#20679 = FACE_OUTER_BOUND('',#26515,.T.) ;
#20680 = FACE_OUTER_BOUND('',#26516,.T.) ;
#20681 = FACE_OUTER_BOUND('',#26517,.T.) ;
#20682 = FACE_OUTER_BOUND('',#26518,.T.) ;
#20683 = FACE_OUTER_BOUND('',#26519,.T.) ;
#20684 = FACE_OUTER_BOUND('',#26520,.T.) ;
#20685 = FACE_OUTER_BOUND('',#26521,.T.) ;
#20686 = FACE_OUTER_BOUND('',#26522,.T.) ;
#20687 = FACE_OUTER_BOUND('',#26523,.T.) ;
#20688 = FACE_OUTER_BOUND('',#26524,.T.) ;
#20689 = FACE_OUTER_BOUND('',#26525,.T.) ;
#20690 = FACE_OUTER_BOUND('',#26526,.T.) ;
#20691 = FACE_OUTER_BOUND('',#26527,.T.) ;
#20692 = FACE_OUTER_BOUND('',#26528,.T.) ;
#20693 = FACE_OUTER_BOUND('',#26529,.T.) ;
#20694 = FACE_OUTER_BOUND('',#26530,.T.) ;
#20695 = FACE_OUTER_BOUND('',#26531,.T.) ;
#20696 = FACE_OUTER_BOUND('',#26532,.T.) ;
#20697 = FACE_OUTER_BOUND('',#26533,.T.) ;
#20698 = FACE_OUTER_BOUND('',#26534,.T.) ;
#20699 = FACE_OUTER_BOUND('',#26535,.T.) ;
#20700 = FACE_OUTER_BOUND('',#26536,.T.) ;
#20701 = FACE_OUTER_BOUND('',#26537,.T.) ;
#20702 = FACE_OUTER_BOUND('',#26538,.T.) ;
#20703 = FACE_OUTER_BOUND('',#26539,.T.) ;
#20704 = FACE_OUTER_BOUND('',#26540,.T.) ;
#20705 = FACE_OUTER_BOUND('',#26541,.T.) ;
#20706 = FACE_OUTER_BOUND('',#26542,.T.) ;
#20707 = FACE_OUTER_BOUND('',#26543,.T.) ;
#20708 = FACE_OUTER_BOUND('',#26544,.T.) ;
#20709 = FACE_OUTER_BOUND('',#26545,.T.) ;
#20710 = FACE_OUTER_BOUND('',#26546,.T.) ;
#20711 = FACE_OUTER_BOUND('',#26547,.T.) ;
#20712 = FACE_OUTER_BOUND('',#26548,.T.) ;
#20713 = FACE_OUTER_BOUND('',#26549,.T.) ;
#20714 = FACE_OUTER_BOUND('',#26550,.T.) ;
#20715 = FACE_OUTER_BOUND('',#26551,.T.) ;
#20716 = FACE_OUTER_BOUND('',#26552,.T.) ;
#20717 = FACE_OUTER_BOUND('',#26553,.T.) ;
#20718 = FACE_OUTER_BOUND('',#26554,.T.) ;
#20719 = FACE_OUTER_BOUND('',#26555,.T.) ;
#20720 = FACE_OUTER_BOUND('',#26556,.T.) ;
#20721 = FACE_OUTER_BOUND('',#26557,.T.) ;
#20722 = FACE_OUTER_BOUND('',#26558,.T.) ;
#20723 = FACE_OUTER_BOUND('',#26559,.T.) ;
#20724 = FACE_OUTER_BOUND('',#26560,.T.) ;
#20725 = FACE_OUTER_BOUND('',#26561,.T.) ;
#20726 = FACE_OUTER_BOUND('',#26562,.T.) ;
#20727 = FACE_OUTER_BOUND('',#26563,.T.) ;
#20728 = FACE_OUTER_BOUND('',#26564,.T.) ;
#20729 = FACE_OUTER_BOUND('',#26565,.T.) ;
#20730 = FACE_OUTER_BOUND('',#26566,.T.) ;
#20731 = FACE_OUTER_BOUND('',#26567,.T.) ;
#20732 = FACE_OUTER_BOUND('',#26568,.T.) ;
#20733 = FACE_OUTER_BOUND('',#26569,.T.) ;
#20734 = FACE_OUTER_BOUND('',#26570,.T.) ;
#20735 = FACE_OUTER_BOUND('',#26571,.T.) ;
#20736 = FACE_OUTER_BOUND('',#26572,.T.) ;
#20737 = FACE_OUTER_BOUND('',#26573,.T.) ;
#20738 = FACE_OUTER_BOUND('',#26574,.T.) ;
#20739 = FACE_OUTER_BOUND('',#26575,.T.) ;
#20740 = FACE_OUTER_BOUND('',#26576,.T.) ;
#20741 = FACE_OUTER_BOUND('',#26577,.T.) ;
#20742 = FACE_OUTER_BOUND('',#26578,.T.) ;
#20743 = FACE_OUTER_BOUND('',#26579,.T.) ;
#20744 = FACE_OUTER_BOUND('',#26580,.T.) ;
#20745 = FACE_OUTER_BOUND('',#26581,.T.) ;
#20746 = FACE_OUTER_BOUND('',#26582,.T.) ;
#20747 = FACE_OUTER_BOUND('',#26583,.T.) ;
#20748 = FACE_OUTER_BOUND('',#26584,.T.) ;
#20749 = FACE_OUTER_BOUND('',#26585,.T.) ;
#20750 = FACE_OUTER_BOUND('',#26586,.T.) ;
#20751 = FACE_OUTER_BOUND('',#26587,.T.) ;
#20752 = FACE_OUTER_BOUND('',#26588,.T.) ;
#20753 = FACE_OUTER_BOUND('',#26589,.T.) ;
#20754 = FACE_OUTER_BOUND('',#26590,.T.) ;
#20755 = FACE_OUTER_BOUND('',#26591,.T.) ;
#20756 = FACE_OUTER_BOUND('',#26592,.T.) ;
#20757 = FACE_OUTER_BOUND('',#26593,.T.) ;
#20758 = FACE_OUTER_BOUND('',#26594,.T.) ;
#20759 = FACE_OUTER_BOUND('',#26595,.T.) ;
#20760 = FACE_OUTER_BOUND('',#26596,.T.) ;
#20761 = FACE_OUTER_BOUND('',#26597,.T.) ;
#20762 = FACE_OUTER_BOUND('',#26598,.T.) ;
#20763 = FACE_OUTER_BOUND('',#26599,.T.) ;
#20764 = FACE_OUTER_BOUND('',#26600,.T.) ;
#20765 = FACE_OUTER_BOUND('',#26601,.T.) ;
#20766 = FACE_OUTER_BOUND('',#26602,.T.) ;
#20767 = FACE_OUTER_BOUND('',#26603,.T.) ;
#20768 = FACE_OUTER_BOUND('',#26604,.T.) ;
#20769 = FACE_OUTER_BOUND('',#26605,.T.) ;
#20770 = FACE_OUTER_BOUND('',#26606,.T.) ;
#20771 = FACE_OUTER_BOUND('',#26607,.T.) ;
#20772 = FACE_OUTER_BOUND('',#26608,.T.) ;
#20773 = FACE_OUTER_BOUND('',#26609,.T.) ;
#20774 = FACE_OUTER_BOUND('',#26610,.T.) ;
#20775 = FACE_OUTER_BOUND('',#26611,.T.) ;
#20776 = FACE_OUTER_BOUND('',#26612,.T.) ;
#20777 = FACE_OUTER_BOUND('',#26613,.T.) ;
#20778 = FACE_OUTER_BOUND('',#26614,.T.) ;
#20779 = FACE_OUTER_BOUND('',#26615,.T.) ;
#20780 = FACE_OUTER_BOUND('',#26616,.T.) ;
#20781 = FACE_OUTER_BOUND('',#26617,.T.) ;
#20782 = FACE_OUTER_BOUND('',#26618,.T.) ;
#20783 = FACE_OUTER_BOUND('',#26619,.T.) ;
#20784 = FACE_OUTER_BOUND('',#26620,.T.) ;
#20785 = FACE_OUTER_BOUND('',#26621,.T.) ;
#20786 = FACE_OUTER_BOUND('',#26622,.T.) ;
#20787 = FACE_OUTER_BOUND('',#26623,.T.) ;
#20788 = FACE_OUTER_BOUND('',#26624,.T.) ;
#20789 = FACE_OUTER_BOUND('',#26625,.T.) ;
#20790 = FACE_OUTER_BOUND('',#26626,.T.) ;
#20791 = FACE_OUTER_BOUND('',#26627,.T.) ;
#20792 = FACE_OUTER_BOUND('',#26628,.T.) ;
#20793 = FACE_OUTER_BOUND('',#26629,.T.) ;
#20794 = FACE_OUTER_BOUND('',#26630,.T.) ;
#20795 = FACE_OUTER_BOUND('',#26631,.T.) ;
#20796 = FACE_OUTER_BOUND('',#26632,.T.) ;
#20797 = FACE_OUTER_BOUND('',#26633,.T.) ;
#20798 = FACE_OUTER_BOUND('',#26634,.T.) ;
#20799 = FACE_OUTER_BOUND('',#26635,.T.) ;
#20800 = FACE_OUTER_BOUND('',#26636,.T.) ;
#20801 = FACE_OUTER_BOUND('',#26637,.T.) ;
#20802 = FACE_OUTER_BOUND('',#26638,.T.) ;
#20803 = FACE_OUTER_BOUND('',#26639,.T.) ;
#20804 = FACE_OUTER_BOUND('',#26640,.T.) ;
#20805 = FACE_OUTER_BOUND('',#26641,.T.) ;
#20806 = FACE_OUTER_BOUND('',#26642,.T.) ;
#20807 = FACE_OUTER_BOUND('',#26643,.T.) ;
#20808 = FACE_OUTER_BOUND('',#26644,.T.) ;
#20809 = FACE_OUTER_BOUND('',#26645,.T.) ;
#20810 = FACE_OUTER_BOUND('',#26646,.T.) ;
#20811 = FACE_OUTER_BOUND('',#26647,.T.) ;
#20812 = FACE_OUTER_BOUND('',#26648,.T.) ;
#20813 = FACE_OUTER_BOUND('',#26649,.T.) ;
#20814 = FACE_OUTER_BOUND('',#26650,.T.) ;
#20815 = FACE_OUTER_BOUND('',#26651,.T.) ;
#20816 = FACE_OUTER_BOUND('',#26652,.T.) ;
#20817 = FACE_OUTER_BOUND('',#26653,.T.) ;
#20818 = FACE_OUTER_BOUND('',#26654,.T.) ;
#20819 = FACE_OUTER_BOUND('',#26655,.T.) ;
#20820 = FACE_OUTER_BOUND('',#26656,.T.) ;
#20821 = FACE_OUTER_BOUND('',#26657,.T.) ;
#20822 = FACE_OUTER_BOUND('',#26658,.T.) ;
#20823 = FACE_OUTER_BOUND('',#26659,.T.) ;
#20824 = FACE_OUTER_BOUND('',#26660,.T.) ;
#20825 = FACE_OUTER_BOUND('',#26661,.T.) ;
#20826 = FACE_OUTER_BOUND('',#26662,.T.) ;
#20827 = FACE_OUTER_BOUND('',#26663,.T.) ;
#20828 = FACE_OUTER_BOUND('',#26664,.T.) ;
#20829 = FACE_OUTER_BOUND('',#26665,.T.) ;
#20830 = FACE_OUTER_BOUND('',#26666,.T.) ;
#20831 = FACE_OUTER_BOUND('',#26667,.T.) ;
#20832 = FACE_OUTER_BOUND('',#26668,.T.) ;
#20833 = FACE_OUTER_BOUND('',#26669,.T.) ;
#20834 = FACE_OUTER_BOUND('',#26670,.T.) ;
#20835 = FACE_OUTER_BOUND('',#26671,.T.) ;
#20836 = FACE_OUTER_BOUND('',#26672,.T.) ;
#20837 = FACE_OUTER_BOUND('',#26673,.T.) ;
#20838 = FACE_OUTER_BOUND('',#26674,.T.) ;
#20839 = FACE_OUTER_BOUND('',#26675,.T.) ;
#20840 = FACE_OUTER_BOUND('',#26676,.T.) ;
#20841 = FACE_OUTER_BOUND('',#26677,.T.) ;
#20842 = FACE_OUTER_BOUND('',#26678,.T.) ;
#20843 = FACE_OUTER_BOUND('',#26679,.T.) ;
#20844 = FACE_OUTER_BOUND('',#26680,.T.) ;
#20845 = FACE_OUTER_BOUND('',#26681,.T.) ;
#20846 = FACE_OUTER_BOUND('',#26682,.T.) ;
#20847 = FACE_OUTER_BOUND('',#26683,.T.) ;
#20848 = FACE_OUTER_BOUND('',#26684,.T.) ;
#20849 = FACE_OUTER_BOUND('',#26685,.T.) ;
#20850 = FACE_OUTER_BOUND('',#26686,.T.) ;
#20851 = FACE_OUTER_BOUND('',#26687,.T.) ;
#20852 = FACE_OUTER_BOUND('',#26688,.T.) ;
#20853 = FACE_OUTER_BOUND('',#26689,.T.) ;
#20854 = FACE_OUTER_BOUND('',#26690,.T.) ;
#20855 = FACE_OUTER_BOUND('',#26691,.T.) ;
#20856 = FACE_OUTER_BOUND('',#26692,.T.) ;
#20857 = FACE_OUTER_BOUND('',#26693,.T.) ;
#20858 = FACE_OUTER_BOUND('',#26694,.T.) ;
#20859 = FACE_OUTER_BOUND('',#26695,.T.) ;
#20860 = FACE_OUTER_BOUND('',#26696,.T.) ;
#20861 = FACE_OUTER_BOUND('',#26697,.T.) ;
#20862 = FACE_OUTER_BOUND('',#26698,.T.) ;
#20863 = FACE_OUTER_BOUND('',#26699,.T.) ;
#20864 = FACE_OUTER_BOUND('',#26700,.T.) ;
#20865 = FACE_OUTER_BOUND('',#26701,.T.) ;
#20866 = FACE_OUTER_BOUND('',#26702,.T.) ;
#20867 = FACE_OUTER_BOUND('',#26703,.T.) ;
#20868 = FACE_OUTER_BOUND('',#26704,.T.) ;
#20869 = FACE_OUTER_BOUND('',#26705,.T.) ;
#20870 = FACE_OUTER_BOUND('',#26706,.T.) ;
#20871 = FACE_OUTER_BOUND('',#26707,.T.) ;
#20872 = FACE_OUTER_BOUND('',#26708,.T.) ;
#20873 = FACE_OUTER_BOUND('',#26709,.T.) ;
#20874 = FACE_OUTER_BOUND('',#26710,.T.) ;
#20875 = FACE_OUTER_BOUND('',#26711,.T.) ;
#20876 = FACE_OUTER_BOUND('',#26712,.T.) ;
#20877 = FACE_OUTER_BOUND('',#26713,.T.) ;
#20878 = FACE_OUTER_BOUND('',#26714,.T.) ;
#20879 = FACE_OUTER_BOUND('',#26716,.T.) ;
#20880 = FACE_OUTER_BOUND('',#26717,.T.) ;
#20881 = FACE_OUTER_BOUND('',#26718,.T.) ;
#20882 = FACE_OUTER_BOUND('',#26719,.T.) ;
#20883 = FACE_OUTER_BOUND('',#26720,.T.) ;
#20884 = FACE_OUTER_BOUND('',#26722,.T.) ;
#20885 = FACE_OUTER_BOUND('',#26723,.T.) ;
#20886 = FACE_OUTER_BOUND('',#26724,.T.) ;
#20887 = FACE_OUTER_BOUND('',#26725,.T.) ;
#20888 = FACE_OUTER_BOUND('',#26726,.T.) ;
#20889 = FACE_OUTER_BOUND('',#26728,.T.) ;
#20890 = FACE_OUTER_BOUND('',#26729,.T.) ;
#20891 = FACE_OUTER_BOUND('',#26730,.T.) ;
#20892 = FACE_OUTER_BOUND('',#26731,.T.) ;
#20893 = FACE_OUTER_BOUND('',#26732,.T.) ;
#20894 = FACE_OUTER_BOUND('',#26734,.T.) ;
#20895 = FACE_OUTER_BOUND('',#26735,.T.) ;
#20896 = FACE_OUTER_BOUND('',#26736,.T.) ;
#20897 = FACE_OUTER_BOUND('',#26737,.T.) ;
#20898 = FACE_OUTER_BOUND('',#26738,.T.) ;
#20899 = FACE_OUTER_BOUND('',#26740,.T.) ;
#20900 = FACE_OUTER_BOUND('',#26741,.T.) ;
#20901 = FACE_OUTER_BOUND('',#26742,.T.) ;
#20902 = FACE_OUTER_BOUND('',#26743,.T.) ;
#20903 = FACE_OUTER_BOUND('',#26744,.T.) ;
#20904 = FACE_OUTER_BOUND('',#26746,.T.) ;
#20905 = FACE_OUTER_BOUND('',#26747,.T.) ;
#20906 = FACE_OUTER_BOUND('',#26748,.T.) ;
#20907 = FACE_OUTER_BOUND('',#26749,.T.) ;
#20908 = FACE_OUTER_BOUND('',#26750,.T.) ;
#20909 = FACE_OUTER_BOUND('',#26752,.T.) ;
#20910 = FACE_OUTER_BOUND('',#26753,.T.) ;
#20911 = FACE_OUTER_BOUND('',#26754,.T.) ;
#20912 = FACE_OUTER_BOUND('',#26755,.T.) ;
#20913 = FACE_OUTER_BOUND('',#26756,.T.) ;
#20914 = FACE_OUTER_BOUND('',#26758,.T.) ;
#20915 = FACE_OUTER_BOUND('',#26759,.T.) ;
#20916 = FACE_OUTER_BOUND('',#26760,.T.) ;
#20917 = FACE_OUTER_BOUND('',#26761,.T.) ;
#20918 = FACE_OUTER_BOUND('',#26762,.T.) ;
#20919 = FACE_OUTER_BOUND('',#26764,.T.) ;
#20920 = FACE_OUTER_BOUND('',#26765,.T.) ;
#20921 = FACE_OUTER_BOUND('',#26766,.T.) ;
#20922 = FACE_OUTER_BOUND('',#26767,.T.) ;
#20923 = FACE_OUTER_BOUND('',#26768,.T.) ;
#20924 = FACE_OUTER_BOUND('',#26769,.T.) ;
#20925 = FACE_OUTER_BOUND('',#26770,.T.) ;
#20926 = FACE_OUTER_BOUND('',#26771,.T.) ;
#20927 = FACE_OUTER_BOUND('',#26772,.T.) ;
#20928 = FACE_OUTER_BOUND('',#26773,.T.) ;
#20929 = FACE_OUTER_BOUND('',#26774,.T.) ;
#20930 = FACE_OUTER_BOUND('',#26775,.T.) ;
#20931 = FACE_OUTER_BOUND('',#26776,.T.) ;
#20932 = FACE_OUTER_BOUND('',#26777,.T.) ;
#20933 = FACE_OUTER_BOUND('',#26778,.T.) ;
#20934 = FACE_OUTER_BOUND('',#26779,.T.) ;
#20935 = FACE_OUTER_BOUND('',#26780,.T.) ;
#20936 = FACE_OUTER_BOUND('',#26781,.T.) ;
#20937 = FACE_OUTER_BOUND('',#26782,.T.) ;
#20938 = FACE_OUTER_BOUND('',#26783,.T.) ;
#20939 = FACE_OUTER_BOUND('',#26784,.T.) ;
#20940 = FACE_OUTER_BOUND('',#26785,.T.) ;
#20941 = FACE_OUTER_BOUND('',#26786,.T.) ;
#20942 = FACE_OUTER_BOUND('',#26787,.T.) ;
#20943 = FACE_OUTER_BOUND('',#26788,.T.) ;
#20944 = FACE_OUTER_BOUND('',#26789,.T.) ;
#20945 = FACE_OUTER_BOUND('',#26790,.T.) ;
#20946 = FACE_OUTER_BOUND('',#26791,.T.) ;
#20947 = FACE_OUTER_BOUND('',#26792,.T.) ;
#20948 = FACE_OUTER_BOUND('',#26793,.T.) ;
#20949 = FACE_OUTER_BOUND('',#26794,.T.) ;
#20950 = FACE_OUTER_BOUND('',#26795,.T.) ;
#20951 = FACE_OUTER_BOUND('',#26796,.T.) ;
#20952 = FACE_OUTER_BOUND('',#26797,.T.) ;
#20953 = FACE_OUTER_BOUND('',#26798,.T.) ;
#20954 = FACE_OUTER_BOUND('',#26799,.T.) ;
#20955 = FACE_OUTER_BOUND('',#26800,.T.) ;
#20956 = FACE_OUTER_BOUND('',#26801,.T.) ;
#20957 = FACE_OUTER_BOUND('',#26802,.T.) ;
#20958 = FACE_OUTER_BOUND('',#26803,.T.) ;
#20959 = FACE_OUTER_BOUND('',#26804,.T.) ;
#20960 = FACE_OUTER_BOUND('',#26805,.T.) ;
#20961 = FACE_OUTER_BOUND('',#26806,.T.) ;
#20962 = FACE_OUTER_BOUND('',#26807,.T.) ;
#20963 = FACE_OUTER_BOUND('',#26808,.T.) ;
#20964 = FACE_OUTER_BOUND('',#26809,.T.) ;
#20965 = FACE_OUTER_BOUND('',#26810,.T.) ;
#20966 = FACE_OUTER_BOUND('',#26811,.T.) ;
#20967 = FACE_OUTER_BOUND('',#26812,.T.) ;
#20968 = FACE_OUTER_BOUND('',#26813,.T.) ;
#20969 = FACE_OUTER_BOUND('',#26814,.T.) ;
#20970 = FACE_OUTER_BOUND('',#26815,.T.) ;
#20971 = FACE_OUTER_BOUND('',#26816,.T.) ;
#20972 = FACE_OUTER_BOUND('',#26818,.T.) ;
#20973 = FACE_OUTER_BOUND('',#26819,.T.) ;
#20974 = FACE_OUTER_BOUND('',#26820,.T.) ;
#20975 = FACE_OUTER_BOUND('',#26821,.T.) ;
#20976 = FACE_OUTER_BOUND('',#26823,.T.) ;
#20977 = FACE_OUTER_BOUND('',#26824,.T.) ;
#20978 = FACE_OUTER_BOUND('',#26825,.T.) ;
#20979 = FACE_OUTER_BOUND('',#26826,.T.) ;
#20980 = FACE_OUTER_BOUND('',#26828,.T.) ;
#20981 = FACE_OUTER_BOUND('',#26829,.T.) ;
#20982 = FACE_OUTER_BOUND('',#26830,.T.) ;
#20983 = FACE_OUTER_BOUND('',#26831,.T.) ;
#20984 = FACE_OUTER_BOUND('',#26833,.T.) ;
#20985 = FACE_OUTER_BOUND('',#26834,.T.) ;
#20986 = FACE_OUTER_BOUND('',#26835,.T.) ;
#20987 = FACE_OUTER_BOUND('',#26836,.T.) ;
#20988 = FACE_OUTER_BOUND('',#26838,.T.) ;
#20989 = FACE_OUTER_BOUND('',#26839,.T.) ;
#20990 = FACE_OUTER_BOUND('',#26840,.T.) ;
#20991 = FACE_OUTER_BOUND('',#26841,.T.) ;
#20992 = FACE_OUTER_BOUND('',#26843,.T.) ;
#20993 = FACE_OUTER_BOUND('',#26844,.T.) ;
#20994 = FACE_OUTER_BOUND('',#26845,.T.) ;
#20995 = FACE_OUTER_BOUND('',#26846,.T.) ;
#20996 = FACE_OUTER_BOUND('',#26848,.T.) ;
#20997 = FACE_OUTER_BOUND('',#26849,.T.) ;
#20998 = FACE_OUTER_BOUND('',#26850,.T.) ;
#20999 = FACE_OUTER_BOUND('',#26851,.T.) ;
#21000 = FACE_OUTER_BOUND('',#26853,.T.) ;
#21001 = FACE_OUTER_BOUND('',#26854,.T.) ;
#21002 = FACE_OUTER_BOUND('',#26855,.T.) ;
#21003 = FACE_OUTER_BOUND('',#26856,.T.) ;
#21004 = FACE_OUTER_BOUND('',#26858,.T.) ;
#21005 = FACE_OUTER_BOUND('',#26859,.T.) ;
#21006 = FACE_OUTER_BOUND('',#26860,.T.) ;
#21007 = FACE_OUTER_BOUND('',#26861,.T.) ;
#21008 = FACE_OUTER_BOUND('',#26862,.T.) ;
#21009 = FACE_OUTER_BOUND('',#26863,.T.) ;
#21010 = FACE_OUTER_BOUND('',#26864,.T.) ;
#21011 = FACE_OUTER_BOUND('',#26865,.T.) ;
#21012 = FACE_OUTER_BOUND('',#26866,.T.) ;
#21013 = FACE_OUTER_BOUND('',#26867,.T.) ;
#21014 = FACE_OUTER_BOUND('',#26868,.T.) ;
#21015 = FACE_OUTER_BOUND('',#26869,.T.) ;
#21016 = FACE_OUTER_BOUND('',#26870,.T.) ;
#21017 = FACE_OUTER_BOUND('',#26871,.T.) ;
#21018 = FACE_OUTER_BOUND('',#26872,.T.) ;
#21019 = FACE_OUTER_BOUND('',#26873,.T.) ;
#21020 = FACE_OUTER_BOUND('',#26874,.T.) ;
#21021 = FACE_OUTER_BOUND('',#26875,.T.) ;
#21022 = FACE_OUTER_BOUND('',#26876,.T.) ;
#21023 = FACE_OUTER_BOUND('',#26877,.T.) ;
#21024 = FACE_OUTER_BOUND('',#26878,.T.) ;
#21025 = FACE_OUTER_BOUND('',#26879,.T.) ;
#21026 = FACE_OUTER_BOUND('',#26880,.T.) ;
#21027 = FACE_OUTER_BOUND('',#26881,.T.) ;
#21028 = FACE_OUTER_BOUND('',#26882,.T.) ;
#21029 = FACE_OUTER_BOUND('',#26883,.T.) ;
#21030 = FACE_OUTER_BOUND('',#26884,.T.) ;
#21031 = FACE_OUTER_BOUND('',#26885,.T.) ;
#21032 = FACE_OUTER_BOUND('',#26886,.T.) ;
#21033 = FACE_OUTER_BOUND('',#26887,.T.) ;
#21034 = FACE_OUTER_BOUND('',#26888,.T.) ;
#21035 = FACE_OUTER_BOUND('',#26889,.T.) ;
#21036 = FACE_OUTER_BOUND('',#26890,.T.) ;
#21037 = FACE_OUTER_BOUND('',#26891,.T.) ;
#21038 = FACE_OUTER_BOUND('',#26892,.T.) ;
#21039 = FACE_OUTER_BOUND('',#26893,.T.) ;
#21040 = FACE_OUTER_BOUND('',#26894,.T.) ;
#21041 = FACE_OUTER_BOUND('',#26895,.T.) ;
#21042 = FACE_OUTER_BOUND('',#26896,.T.) ;
#21043 = FACE_OUTER_BOUND('',#26897,.T.) ;
#21044 = FACE_OUTER_BOUND('',#26898,.T.) ;
#21045 = FACE_OUTER_BOUND('',#26899,.T.) ;
#21046 = FACE_OUTER_BOUND('',#26900,.T.) ;
#21047 = FACE_OUTER_BOUND('',#26901,.T.) ;
#21048 = FACE_OUTER_BOUND('',#26902,.T.) ;
#21049 = FACE_OUTER_BOUND('',#26903,.T.) ;
#21050 = FACE_OUTER_BOUND('',#26905,.T.) ;
#21051 = FACE_OUTER_BOUND('',#26906,.T.) ;
#21052 = FACE_OUTER_BOUND('',#26907,.T.) ;
#21053 = FACE_OUTER_BOUND('',#26908,.T.) ;
#21054 = FACE_OUTER_BOUND('',#26909,.T.) ;
#21055 = FACE_OUTER_BOUND('',#26911,.T.) ;
#21056 = FACE_OUTER_BOUND('',#26912,.T.) ;
#21057 = FACE_OUTER_BOUND('',#26913,.T.) ;
#21058 = FACE_OUTER_BOUND('',#26914,.T.) ;
#21059 = FACE_OUTER_BOUND('',#26915,.T.) ;
#21060 = FACE_OUTER_BOUND('',#26917,.T.) ;
#21061 = FACE_OUTER_BOUND('',#26918,.T.) ;
#21062 = FACE_OUTER_BOUND('',#26919,.T.) ;
#21063 = FACE_OUTER_BOUND('',#26920,.T.) ;
#21064 = FACE_OUTER_BOUND('',#26921,.T.) ;
#21065 = FACE_OUTER_BOUND('',#26923,.T.) ;
#21066 = FACE_OUTER_BOUND('',#26924,.T.) ;
#21067 = FACE_OUTER_BOUND('',#26925,.T.) ;
#21068 = FACE_OUTER_BOUND('',#26926,.T.) ;
#21069 = FACE_OUTER_BOUND('',#26927,.T.) ;
#21070 = FACE_OUTER_BOUND('',#26929,.T.) ;
#21071 = FACE_OUTER_BOUND('',#26930,.T.) ;
#21072 = FACE_OUTER_BOUND('',#26931,.T.) ;
#21073 = FACE_OUTER_BOUND('',#26932,.T.) ;
#21074 = FACE_OUTER_BOUND('',#26933,.T.) ;
#21075 = FACE_OUTER_BOUND('',#26935,.T.) ;
#21076 = FACE_OUTER_BOUND('',#26936,.T.) ;
#21077 = FACE_OUTER_BOUND('',#26937,.T.) ;
#21078 = FACE_OUTER_BOUND('',#26938,.T.) ;
#21079 = FACE_OUTER_BOUND('',#26939,.T.) ;
#21080 = FACE_OUTER_BOUND('',#26941,.T.) ;
#21081 = FACE_OUTER_BOUND('',#26942,.T.) ;
#21082 = FACE_OUTER_BOUND('',#26943,.T.) ;
#21083 = FACE_OUTER_BOUND('',#26944,.T.) ;
#21084 = FACE_OUTER_BOUND('',#26945,.T.) ;
#21085 = FACE_OUTER_BOUND('',#26947,.T.) ;
#21086 = FACE_OUTER_BOUND('',#26948,.T.) ;
#21087 = FACE_OUTER_BOUND('',#26949,.T.) ;
#21088 = FACE_OUTER_BOUND('',#26950,.T.) ;
#21089 = FACE_OUTER_BOUND('',#26951,.T.) ;
#21090 = FACE_OUTER_BOUND('',#26953,.T.) ;
#21091 = FACE_OUTER_BOUND('',#26954,.T.) ;
#21092 = FACE_OUTER_BOUND('',#26955,.T.) ;
#21093 = FACE_OUTER_BOUND('',#26956,.T.) ;
#21094 = FACE_OUTER_BOUND('',#26957,.T.) ;
#21095 = FACE_OUTER_BOUND('',#26958,.T.) ;
#21096 = FACE_OUTER_BOUND('',#26959,.T.) ;
#21097 = FACE_OUTER_BOUND('',#26960,.T.) ;
#21098 = FACE_OUTER_BOUND('',#26961,.T.) ;
#21099 = FACE_OUTER_BOUND('',#26962,.T.) ;
#21100 = FACE_OUTER_BOUND('',#26963,.T.) ;
#21101 = FACE_OUTER_BOUND('',#26964,.T.) ;
#21102 = FACE_OUTER_BOUND('',#26965,.T.) ;
#21103 = FACE_OUTER_BOUND('',#26966,.T.) ;
#21104 = FACE_OUTER_BOUND('',#26967,.T.) ;
#21105 = FACE_OUTER_BOUND('',#26968,.T.) ;
#21106 = FACE_OUTER_BOUND('',#26969,.T.) ;
#21107 = FACE_OUTER_BOUND('',#26970,.T.) ;
#21108 = FACE_OUTER_BOUND('',#26971,.T.) ;
#21109 = FACE_OUTER_BOUND('',#26972,.T.) ;
#21110 = FACE_OUTER_BOUND('',#26973,.T.) ;
#21111 = FACE_OUTER_BOUND('',#26974,.T.) ;
#21112 = FACE_OUTER_BOUND('',#26975,.T.) ;
#21113 = FACE_OUTER_BOUND('',#26976,.T.) ;
#21114 = FACE_OUTER_BOUND('',#26977,.T.) ;
#21115 = FACE_OUTER_BOUND('',#26978,.T.) ;
#21116 = FACE_OUTER_BOUND('',#26979,.T.) ;
#21117 = FACE_OUTER_BOUND('',#26980,.T.) ;
#21118 = FACE_OUTER_BOUND('',#26981,.T.) ;
#21119 = FACE_OUTER_BOUND('',#26982,.T.) ;
#21120 = FACE_OUTER_BOUND('',#26983,.T.) ;
#21121 = FACE_OUTER_BOUND('',#26984,.T.) ;
#21122 = FACE_OUTER_BOUND('',#26985,.T.) ;
#21123 = FACE_OUTER_BOUND('',#26986,.T.) ;
#21124 = FACE_OUTER_BOUND('',#26987,.T.) ;
#21125 = FACE_OUTER_BOUND('',#26988,.T.) ;
#21126 = FACE_OUTER_BOUND('',#26989,.T.) ;
#21127 = FACE_OUTER_BOUND('',#26990,.T.) ;
#21128 = FACE_OUTER_BOUND('',#26991,.T.) ;
#21129 = FACE_OUTER_BOUND('',#26992,.T.) ;
#21130 = FACE_OUTER_BOUND('',#26993,.T.) ;
#21131 = FACE_OUTER_BOUND('',#26994,.T.) ;
#21132 = FACE_OUTER_BOUND('',#26995,.T.) ;
#21133 = FACE_OUTER_BOUND('',#26996,.T.) ;
#21134 = FACE_OUTER_BOUND('',#26997,.T.) ;
#21135 = FACE_OUTER_BOUND('',#26998,.T.) ;
#21136 = FACE_OUTER_BOUND('',#26999,.T.) ;
#21137 = FACE_OUTER_BOUND('',#27000,.T.) ;
#21138 = FACE_OUTER_BOUND('',#27001,.T.) ;
#21139 = FACE_OUTER_BOUND('',#27002,.T.) ;
#21140 = FACE_OUTER_BOUND('',#27003,.T.) ;
#21141 = FACE_OUTER_BOUND('',#27004,.T.) ;
#21142 = FACE_OUTER_BOUND('',#27005,.T.) ;
#21143 = FACE_OUTER_BOUND('',#27006,.T.) ;
#21144 = FACE_OUTER_BOUND('',#27007,.T.) ;
#21145 = FACE_OUTER_BOUND('',#27008,.T.) ;
#21146 = FACE_OUTER_BOUND('',#27009,.T.) ;
#21147 = FACE_OUTER_BOUND('',#27010,.T.) ;
#21148 = FACE_OUTER_BOUND('',#27011,.T.) ;
#21149 = FACE_OUTER_BOUND('',#27012,.T.) ;
#21150 = FACE_OUTER_BOUND('',#27013,.T.) ;
#21151 = FACE_OUTER_BOUND('',#27014,.T.) ;
#21152 = FACE_OUTER_BOUND('',#27015,.T.) ;
#21153 = FACE_OUTER_BOUND('',#27016,.T.) ;
#21154 = FACE_OUTER_BOUND('',#27017,.T.) ;
#21155 = FACE_OUTER_BOUND('',#27018,.T.) ;
#21156 = FACE_OUTER_BOUND('',#27019,.T.) ;
#21157 = FACE_OUTER_BOUND('',#27020,.T.) ;
#21158 = FACE_OUTER_BOUND('',#27021,.T.) ;
#21159 = FACE_OUTER_BOUND('',#27022,.T.) ;
#21160 = FACE_OUTER_BOUND('',#27023,.T.) ;
#21161 = FACE_OUTER_BOUND('',#27024,.T.) ;
#21162 = FACE_OUTER_BOUND('',#27025,.T.) ;
#21163 = FACE_OUTER_BOUND('',#27026,.T.) ;
#21164 = FACE_OUTER_BOUND('',#27027,.T.) ;
#21165 = FACE_OUTER_BOUND('',#27028,.T.) ;
#21166 = FACE_OUTER_BOUND('',#27029,.T.) ;
#21167 = FACE_OUTER_BOUND('',#27030,.T.) ;
#21168 = FACE_OUTER_BOUND('',#27031,.T.) ;
#21169 = FACE_OUTER_BOUND('',#27032,.T.) ;
#21170 = FACE_OUTER_BOUND('',#27033,.T.) ;
#21171 = FACE_OUTER_BOUND('',#27034,.T.) ;
#21172 = FACE_OUTER_BOUND('',#27035,.T.) ;
#21173 = FACE_OUTER_BOUND('',#27036,.T.) ;
#21174 = FACE_OUTER_BOUND('',#27037,.T.) ;
#21175 = FACE_OUTER_BOUND('',#27038,.T.) ;
#21176 = FACE_OUTER_BOUND('',#27039,.T.) ;
#21177 = FACE_OUTER_BOUND('',#27040,.T.) ;
#21178 = FACE_OUTER_BOUND('',#27041,.T.) ;
#21179 = FACE_OUTER_BOUND('',#27042,.T.) ;
#21180 = FACE_OUTER_BOUND('',#27043,.T.) ;
#21181 = FACE_OUTER_BOUND('',#27044,.T.) ;
#21182 = FACE_OUTER_BOUND('',#27045,.T.) ;
#21183 = FACE_OUTER_BOUND('',#27046,.T.) ;
#21184 = FACE_OUTER_BOUND('',#27047,.T.) ;
#21185 = FACE_OUTER_BOUND('',#27048,.T.) ;
#21186 = FACE_OUTER_BOUND('',#27049,.T.) ;
#21187 = FACE_OUTER_BOUND('',#27050,.T.) ;
#21188 = FACE_OUTER_BOUND('',#27051,.T.) ;
#21189 = FACE_OUTER_BOUND('',#27052,.T.) ;
#21190 = FACE_OUTER_BOUND('',#27053,.T.) ;
#21191 = FACE_OUTER_BOUND('',#27054,.T.) ;
#21192 = FACE_OUTER_BOUND('',#27055,.T.) ;
#21193 = FACE_OUTER_BOUND('',#27056,.T.) ;
#21194 = FACE_OUTER_BOUND('',#27057,.T.) ;
#21195 = FACE_OUTER_BOUND('',#27058,.T.) ;
#21196 = FACE_OUTER_BOUND('',#27059,.T.) ;
#21197 = FACE_OUTER_BOUND('',#27060,.T.) ;
#21198 = FACE_OUTER_BOUND('',#27061,.T.) ;
#21199 = FACE_OUTER_BOUND('',#27062,.T.) ;
#21200 = FACE_OUTER_BOUND('',#27063,.T.) ;
#21201 = FACE_OUTER_BOUND('',#27064,.T.) ;
#21202 = FACE_OUTER_BOUND('',#27065,.T.) ;
#21203 = FACE_OUTER_BOUND('',#27066,.T.) ;
#21204 = FACE_OUTER_BOUND('',#27067,.T.) ;
#21205 = FACE_OUTER_BOUND('',#27068,.T.) ;
#21206 = FACE_OUTER_BOUND('',#27069,.T.) ;
#21207 = FACE_OUTER_BOUND('',#27070,.T.) ;
#21208 = FACE_OUTER_BOUND('',#27071,.T.) ;
#21209 = FACE_OUTER_BOUND('',#27072,.T.) ;
#21210 = FACE_OUTER_BOUND('',#27073,.T.) ;
#21211 = FACE_OUTER_BOUND('',#27074,.T.) ;
#21212 = FACE_OUTER_BOUND('',#27075,.T.) ;
#21213 = FACE_OUTER_BOUND('',#27076,.T.) ;
#21214 = FACE_OUTER_BOUND('',#27077,.T.) ;
#21215 = FACE_OUTER_BOUND('',#27078,.T.) ;
#21216 = FACE_OUTER_BOUND('',#27079,.T.) ;
#21217 = FACE_OUTER_BOUND('',#27080,.T.) ;
#21218 = FACE_OUTER_BOUND('',#27081,.T.) ;
#21219 = FACE_OUTER_BOUND('',#27082,.T.) ;
#21220 = FACE_OUTER_BOUND('',#27083,.T.) ;
#21221 = FACE_OUTER_BOUND('',#27084,.T.) ;
#21222 = FACE_OUTER_BOUND('',#27085,.T.) ;
#21223 = FACE_OUTER_BOUND('',#27086,.T.) ;
#21224 = FACE_OUTER_BOUND('',#27087,.T.) ;
#21225 = FACE_OUTER_BOUND('',#27088,.T.) ;
#21226 = FACE_OUTER_BOUND('',#27089,.T.) ;
#21227 = FACE_OUTER_BOUND('',#27090,.T.) ;
#21228 = FACE_OUTER_BOUND('',#27091,.T.) ;
#21229 = FACE_OUTER_BOUND('',#27092,.T.) ;
#21230 = FACE_OUTER_BOUND('',#27093,.T.) ;
#21231 = FACE_OUTER_BOUND('',#27094,.T.) ;
#21232 = FACE_OUTER_BOUND('',#27095,.T.) ;
#21233 = FACE_OUTER_BOUND('',#27096,.T.) ;
#21234 = FACE_OUTER_BOUND('',#27097,.T.) ;
#21235 = FACE_OUTER_BOUND('',#27098,.T.) ;
#21236 = FACE_OUTER_BOUND('',#27099,.T.) ;
#21237 = FACE_OUTER_BOUND('',#27100,.T.) ;
#21238 = FACE_OUTER_BOUND('',#27101,.T.) ;
#21239 = FACE_OUTER_BOUND('',#27102,.T.) ;
#21240 = FACE_OUTER_BOUND('',#27103,.T.) ;
#21241 = FACE_OUTER_BOUND('',#27104,.T.) ;
#21242 = FACE_OUTER_BOUND('',#27105,.T.) ;
#21243 = FACE_OUTER_BOUND('',#27106,.T.) ;
#21244 = FACE_OUTER_BOUND('',#27107,.T.) ;
#21245 = FACE_OUTER_BOUND('',#27108,.T.) ;
#21246 = FACE_OUTER_BOUND('',#27109,.T.) ;
#21247 = FACE_OUTER_BOUND('',#27110,.T.) ;
#21248 = FACE_OUTER_BOUND('',#27111,.T.) ;
#21249 = FACE_OUTER_BOUND('',#27112,.T.) ;
#21250 = FACE_OUTER_BOUND('',#27113,.T.) ;
#21251 = FACE_OUTER_BOUND('',#27114,.T.) ;
#21252 = FACE_OUTER_BOUND('',#27115,.T.) ;
#21253 = FACE_OUTER_BOUND('',#27116,.T.) ;
#21254 = FACE_OUTER_BOUND('',#27117,.T.) ;
#21255 = FACE_OUTER_BOUND('',#27118,.T.) ;
#21256 = FACE_OUTER_BOUND('',#27119,.T.) ;
#21257 = FACE_OUTER_BOUND('',#27120,.T.) ;
#21258 = FACE_OUTER_BOUND('',#27121,.T.) ;
#21259 = FACE_OUTER_BOUND('',#27122,.T.) ;
#21260 = FACE_OUTER_BOUND('',#27123,.T.) ;
#21261 = FACE_OUTER_BOUND('',#27124,.T.) ;
#21262 = FACE_OUTER_BOUND('',#27125,.T.) ;
#21263 = FACE_OUTER_BOUND('',#27126,.T.) ;
#21264 = FACE_OUTER_BOUND('',#27127,.T.) ;
#21265 = FACE_OUTER_BOUND('',#27128,.T.) ;
#21266 = FACE_OUTER_BOUND('',#27129,.T.) ;
#21267 = FACE_OUTER_BOUND('',#27130,.T.) ;
#21268 = FACE_OUTER_BOUND('',#27131,.T.) ;
#21269 = FACE_OUTER_BOUND('',#27132,.T.) ;
#21270 = FACE_OUTER_BOUND('',#27133,.T.) ;
#21271 = FACE_OUTER_BOUND('',#27134,.T.) ;
#21272 = FACE_OUTER_BOUND('',#27135,.T.) ;
#21273 = FACE_OUTER_BOUND('',#27136,.T.) ;
#21274 = FACE_OUTER_BOUND('',#27137,.T.) ;
#21275 = FACE_OUTER_BOUND('',#27138,.T.) ;
#21276 = FACE_OUTER_BOUND('',#27139,.T.) ;
#21277 = FACE_OUTER_BOUND('',#27140,.T.) ;
#21278 = FACE_OUTER_BOUND('',#27141,.T.) ;
#21279 = FACE_OUTER_BOUND('',#27142,.T.) ;
#21280 = FACE_OUTER_BOUND('',#27143,.T.) ;
#21281 = FACE_OUTER_BOUND('',#27144,.T.) ;
#21282 = FACE_OUTER_BOUND('',#27145,.T.) ;
#21283 = FACE_OUTER_BOUND('',#27146,.T.) ;
#21284 = FACE_OUTER_BOUND('',#27147,.T.) ;
#21285 = FACE_OUTER_BOUND('',#27148,.T.) ;
#21286 = FACE_OUTER_BOUND('',#27149,.T.) ;
#21287 = FACE_OUTER_BOUND('',#27150,.T.) ;
#21288 = FACE_OUTER_BOUND('',#27151,.T.) ;
#21289 = FACE_OUTER_BOUND('',#27152,.T.) ;
#21290 = FACE_OUTER_BOUND('',#27153,.T.) ;
#21291 = FACE_OUTER_BOUND('',#27154,.T.) ;
#21292 = FACE_OUTER_BOUND('',#27155,.T.) ;
#21293 = FACE_OUTER_BOUND('',#27156,.T.) ;
#21294 = FACE_OUTER_BOUND('',#27157,.T.) ;
#21295 = FACE_OUTER_BOUND('',#27158,.T.) ;
#21296 = FACE_OUTER_BOUND('',#27159,.T.) ;
#21297 = FACE_OUTER_BOUND('',#27160,.T.) ;
#21298 = FACE_OUTER_BOUND('',#27161,.T.) ;
#21299 = FACE_OUTER_BOUND('',#27162,.T.) ;
#21300 = FACE_OUTER_BOUND('',#27163,.T.) ;
#21301 = FACE_OUTER_BOUND('',#27164,.T.) ;
#21302 = FACE_OUTER_BOUND('',#27165,.T.) ;
#21303 = FACE_OUTER_BOUND('',#27166,.T.) ;
#21304 = FACE_OUTER_BOUND('',#27167,.T.) ;
#21305 = FACE_OUTER_BOUND('',#27168,.T.) ;
#21306 = FACE_OUTER_BOUND('',#27169,.T.) ;
#21307 = FACE_OUTER_BOUND('',#27170,.T.) ;
#21308 = FACE_OUTER_BOUND('',#27171,.T.) ;
#21309 = FACE_OUTER_BOUND('',#27172,.T.) ;
#21310 = FACE_OUTER_BOUND('',#27173,.T.) ;
#21311 = FACE_OUTER_BOUND('',#27174,.T.) ;
#21312 = FACE_OUTER_BOUND('',#27175,.T.) ;
#21313 = FACE_OUTER_BOUND('',#27176,.T.) ;
#21314 = FACE_OUTER_BOUND('',#27177,.T.) ;
#21315 = FACE_OUTER_BOUND('',#27178,.T.) ;
#21316 = FACE_OUTER_BOUND('',#27179,.T.) ;
#21317 = FACE_OUTER_BOUND('',#27180,.T.) ;
#21318 = FACE_OUTER_BOUND('',#27181,.T.) ;
#21319 = FACE_OUTER_BOUND('',#27182,.T.) ;
#21320 = FACE_OUTER_BOUND('',#27183,.T.) ;
#21321 = FACE_OUTER_BOUND('',#27184,.T.) ;
#21322 = FACE_OUTER_BOUND('',#27185,.T.) ;
#21323 = FACE_OUTER_BOUND('',#27186,.T.) ;
#21324 = FACE_OUTER_BOUND('',#27187,.T.) ;
#21325 = FACE_OUTER_BOUND('',#27188,.T.) ;
#21326 = FACE_OUTER_BOUND('',#27189,.T.) ;
#21327 = FACE_OUTER_BOUND('',#27190,.T.) ;
#21328 = FACE_OUTER_BOUND('',#27191,.T.) ;
#21329 = FACE_OUTER_BOUND('',#27192,.T.) ;
#21330 = FACE_OUTER_BOUND('',#27193,.T.) ;
#21331 = FACE_OUTER_BOUND('',#27194,.T.) ;
#21332 = FACE_OUTER_BOUND('',#27195,.T.) ;
#21333 = FACE_OUTER_BOUND('',#27196,.T.) ;
#21334 = FACE_OUTER_BOUND('',#27197,.T.) ;
#21335 = FACE_OUTER_BOUND('',#27198,.T.) ;
#21336 = FACE_OUTER_BOUND('',#27199,.T.) ;
#21337 = FACE_OUTER_BOUND('',#27200,.T.) ;
#21338 = FACE_OUTER_BOUND('',#27201,.T.) ;
#21339 = FACE_OUTER_BOUND('',#27202,.T.) ;
#21340 = FACE_OUTER_BOUND('',#27203,.T.) ;
#21341 = FACE_OUTER_BOUND('',#27204,.T.) ;
#21342 = FACE_OUTER_BOUND('',#27205,.T.) ;
#21343 = FACE_OUTER_BOUND('',#27206,.T.) ;
#21344 = FACE_OUTER_BOUND('',#27207,.T.) ;
#21345 = FACE_OUTER_BOUND('',#27208,.T.) ;
#21346 = FACE_OUTER_BOUND('',#27209,.T.) ;
#21347 = FACE_OUTER_BOUND('',#27210,.T.) ;
#21348 = FACE_OUTER_BOUND('',#27211,.T.) ;
#21349 = FACE_OUTER_BOUND('',#27212,.T.) ;
#21350 = FACE_OUTER_BOUND('',#27213,.T.) ;
#21351 = FACE_OUTER_BOUND('',#27214,.T.) ;
#21352 = FACE_OUTER_BOUND('',#27215,.T.) ;
#21353 = FACE_OUTER_BOUND('',#27216,.T.) ;
#21354 = FACE_OUTER_BOUND('',#27217,.T.) ;
#21355 = FACE_OUTER_BOUND('',#27218,.T.) ;
#21356 = FACE_OUTER_BOUND('',#27219,.T.) ;
#21357 = FACE_OUTER_BOUND('',#27220,.T.) ;
#21358 = FACE_OUTER_BOUND('',#27221,.T.) ;
#21359 = FACE_OUTER_BOUND('',#27222,.T.) ;
#21360 = FACE_OUTER_BOUND('',#27223,.T.) ;
#21361 = FACE_OUTER_BOUND('',#27224,.T.) ;
#21362 = FACE_OUTER_BOUND('',#27225,.T.) ;
#21363 = FACE_OUTER_BOUND('',#27226,.T.) ;
#21364 = FACE_OUTER_BOUND('',#27227,.T.) ;
#21365 = FACE_OUTER_BOUND('',#27228,.T.) ;
#21366 = FACE_OUTER_BOUND('',#27229,.T.) ;
#21367 = FACE_OUTER_BOUND('',#27230,.T.) ;
#21368 = FACE_OUTER_BOUND('',#27231,.T.) ;
#21369 = FACE_OUTER_BOUND('',#27232,.T.) ;
#21370 = FACE_OUTER_BOUND('',#27233,.T.) ;
#21371 = FACE_OUTER_BOUND('',#27234,.T.) ;
#21372 = FACE_OUTER_BOUND('',#27235,.T.) ;
#21373 = FACE_OUTER_BOUND('',#27236,.T.) ;
#21374 = FACE_OUTER_BOUND('',#27237,.T.) ;
#21375 = FACE_OUTER_BOUND('',#27238,.T.) ;
#21376 = FACE_OUTER_BOUND('',#27239,.T.) ;
#21377 = FACE_OUTER_BOUND('',#27240,.T.) ;
#21378 = FACE_OUTER_BOUND('',#27241,.T.) ;
#21379 = FACE_OUTER_BOUND('',#27242,.T.) ;
#21380 = FACE_OUTER_BOUND('',#27243,.T.) ;
#21381 = FACE_OUTER_BOUND('',#27244,.T.) ;
#21382 = FACE_OUTER_BOUND('',#27245,.T.) ;
#21383 = FACE_OUTER_BOUND('',#27246,.T.) ;
#21384 = FACE_OUTER_BOUND('',#27247,.T.) ;
#21385 = FACE_OUTER_BOUND('',#27248,.T.) ;
#21386 = FACE_OUTER_BOUND('',#27249,.T.) ;
#21387 = FACE_OUTER_BOUND('',#27250,.T.) ;
#21388 = FACE_OUTER_BOUND('',#27251,.T.) ;
#21389 = FACE_OUTER_BOUND('',#27252,.T.) ;
#21390 = FACE_OUTER_BOUND('',#27253,.T.) ;
#21391 = FACE_OUTER_BOUND('',#27254,.T.) ;
#21392 = FACE_OUTER_BOUND('',#27255,.T.) ;
#21393 = FACE_OUTER_BOUND('',#27256,.T.) ;
#21394 = FACE_OUTER_BOUND('',#27257,.T.) ;
#21395 = FACE_OUTER_BOUND('',#27258,.T.) ;
#21396 = FACE_OUTER_BOUND('',#27259,.T.) ;
#21397 = FACE_OUTER_BOUND('',#27260,.T.) ;
#21398 = FACE_OUTER_BOUND('',#27261,.T.) ;
#21399 = FACE_OUTER_BOUND('',#27262,.T.) ;
#21400 = FACE_OUTER_BOUND('',#27263,.T.) ;
#21401 = FACE_OUTER_BOUND('',#27264,.T.) ;
#21402 = FACE_OUTER_BOUND('',#27265,.T.) ;
#21403 = FACE_OUTER_BOUND('',#27266,.T.) ;
#21404 = FACE_OUTER_BOUND('',#27267,.T.) ;
#21405 = FACE_OUTER_BOUND('',#27268,.T.) ;
#21406 = FACE_OUTER_BOUND('',#27269,.T.) ;
#21407 = FACE_OUTER_BOUND('',#27270,.T.) ;
#21408 = FACE_OUTER_BOUND('',#27271,.T.) ;
#21409 = FACE_OUTER_BOUND('',#27272,.T.) ;
#21410 = FACE_OUTER_BOUND('',#27273,.T.) ;
#21411 = FACE_OUTER_BOUND('',#27274,.T.) ;
#21412 = FACE_OUTER_BOUND('',#27275,.T.) ;
#21413 = FACE_OUTER_BOUND('',#27276,.T.) ;
#21414 = FACE_OUTER_BOUND('',#27277,.T.) ;
#21415 = FACE_OUTER_BOUND('',#27278,.T.) ;
#21416 = FACE_OUTER_BOUND('',#27279,.T.) ;
#21417 = FACE_OUTER_BOUND('',#27280,.T.) ;
#21418 = FACE_OUTER_BOUND('',#27281,.T.) ;
#21419 = FACE_OUTER_BOUND('',#27282,.T.) ;
#21420 = FACE_OUTER_BOUND('',#27283,.T.) ;
#21421 = FACE_OUTER_BOUND('',#27284,.T.) ;
#21422 = FACE_OUTER_BOUND('',#27285,.T.) ;
#21423 = FACE_OUTER_BOUND('',#27286,.T.) ;
#21424 = FACE_OUTER_BOUND('',#27287,.T.) ;
#21425 = FACE_OUTER_BOUND('',#27288,.T.) ;
#21426 = FACE_OUTER_BOUND('',#27289,.T.) ;
#21427 = FACE_OUTER_BOUND('',#27290,.T.) ;
#21428 = FACE_OUTER_BOUND('',#27291,.T.) ;
#21429 = FACE_OUTER_BOUND('',#27292,.T.) ;
#21430 = FACE_OUTER_BOUND('',#27293,.T.) ;
#21431 = FACE_OUTER_BOUND('',#27294,.T.) ;
#21432 = FACE_OUTER_BOUND('',#27295,.T.) ;
#21433 = FACE_OUTER_BOUND('',#27296,.T.) ;
#21434 = FACE_OUTER_BOUND('',#27297,.T.) ;
#21435 = FACE_OUTER_BOUND('',#27298,.T.) ;
#21436 = FACE_OUTER_BOUND('',#27299,.T.) ;
#21437 = FACE_OUTER_BOUND('',#27300,.T.) ;
#21438 = FACE_OUTER_BOUND('',#27301,.T.) ;
#21439 = FACE_OUTER_BOUND('',#27302,.T.) ;
#21440 = FACE_OUTER_BOUND('',#27303,.T.) ;
#21441 = FACE_OUTER_BOUND('',#27304,.T.) ;
#21442 = FACE_OUTER_BOUND('',#27305,.T.) ;
#21443 = FACE_OUTER_BOUND('',#27306,.T.) ;
#21444 = FACE_OUTER_BOUND('',#27307,.T.) ;
#21445 = FACE_OUTER_BOUND('',#27308,.T.) ;
#21446 = FACE_OUTER_BOUND('',#27309,.T.) ;
#21447 = FACE_OUTER_BOUND('',#27310,.T.) ;
#21448 = FACE_OUTER_BOUND('',#27311,.T.) ;
#21449 = FACE_OUTER_BOUND('',#27312,.T.) ;
#21450 = FACE_OUTER_BOUND('',#27313,.T.) ;
#21451 = FACE_OUTER_BOUND('',#27314,.T.) ;
#21452 = FACE_OUTER_BOUND('',#27315,.T.) ;
#21453 = FACE_OUTER_BOUND('',#27316,.T.) ;
#21454 = FACE_OUTER_BOUND('',#27317,.T.) ;
#21455 = FACE_OUTER_BOUND('',#27318,.T.) ;
#21456 = FACE_OUTER_BOUND('',#27319,.T.) ;
#21457 = FACE_OUTER_BOUND('',#27320,.T.) ;
#21458 = FACE_OUTER_BOUND('',#27321,.T.) ;
#21459 = FACE_OUTER_BOUND('',#27322,.T.) ;
#21460 = FACE_OUTER_BOUND('',#27323,.T.) ;
#21461 = FACE_OUTER_BOUND('',#27324,.T.) ;
#21462 = FACE_OUTER_BOUND('',#27325,.T.) ;
#21463 = FACE_OUTER_BOUND('',#27326,.T.) ;
#21464 = FACE_OUTER_BOUND('',#27327,.T.) ;
#21465 = FACE_OUTER_BOUND('',#27328,.T.) ;
#21466 = FACE_OUTER_BOUND('',#27329,.T.) ;
#21467 = FACE_OUTER_BOUND('',#27330,.T.) ;
#21468 = FACE_OUTER_BOUND('',#27331,.T.) ;
#21469 = FACE_OUTER_BOUND('',#27332,.T.) ;
#21470 = FACE_OUTER_BOUND('',#27333,.T.) ;
#21471 = FACE_OUTER_BOUND('',#27334,.T.) ;
#21472 = FACE_OUTER_BOUND('',#27335,.T.) ;
#21473 = FACE_OUTER_BOUND('',#27336,.T.) ;
#21474 = FACE_OUTER_BOUND('',#27337,.T.) ;
#21475 = FACE_OUTER_BOUND('',#27338,.T.) ;
#21476 = FACE_OUTER_BOUND('',#27339,.T.) ;
#21477 = FACE_OUTER_BOUND('',#27340,.T.) ;
#21478 = FACE_OUTER_BOUND('',#27341,.T.) ;
#21479 = FACE_OUTER_BOUND('',#27342,.T.) ;
#21480 = FACE_OUTER_BOUND('',#27343,.T.) ;
#21481 = FACE_OUTER_BOUND('',#27344,.T.) ;
#21482 = FACE_OUTER_BOUND('',#27345,.T.) ;
#21483 = FACE_OUTER_BOUND('',#27346,.T.) ;
#21484 = FACE_OUTER_BOUND('',#27347,.T.) ;
#21485 = FACE_OUTER_BOUND('',#27348,.T.) ;
#21486 = FACE_OUTER_BOUND('',#27349,.T.) ;
#21487 = FACE_OUTER_BOUND('',#27350,.T.) ;
#21488 = FACE_OUTER_BOUND('',#27351,.T.) ;
#21489 = FACE_OUTER_BOUND('',#27352,.T.) ;
#21490 = FACE_OUTER_BOUND('',#27353,.T.) ;
#21491 = FACE_OUTER_BOUND('',#27354,.T.) ;
#21492 = FACE_OUTER_BOUND('',#27355,.T.) ;
#21493 = FACE_OUTER_BOUND('',#27356,.T.) ;
#21494 = FACE_OUTER_BOUND('',#27357,.T.) ;
#21495 = FACE_OUTER_BOUND('',#27358,.T.) ;
#21496 = FACE_OUTER_BOUND('',#27359,.T.) ;
#21497 = FACE_OUTER_BOUND('',#27360,.T.) ;
#21498 = FACE_OUTER_BOUND('',#27361,.T.) ;
#21499 = FACE_OUTER_BOUND('',#27362,.T.) ;
#21500 = FACE_OUTER_BOUND('',#27363,.T.) ;
#21501 = FACE_OUTER_BOUND('',#27364,.T.) ;
#21502 = FACE_OUTER_BOUND('',#27365,.T.) ;
#21503 = FACE_OUTER_BOUND('',#27366,.T.) ;
#21504 = FACE_OUTER_BOUND('',#27367,.T.) ;
#21505 = FACE_OUTER_BOUND('',#27368,.T.) ;
#21506 = FACE_OUTER_BOUND('',#27369,.T.) ;
#21507 = FACE_OUTER_BOUND('',#27370,.T.) ;
#21508 = FACE_OUTER_BOUND('',#27371,.T.) ;
#21509 = FACE_OUTER_BOUND('',#27372,.T.) ;
#21510 = FACE_OUTER_BOUND('',#27373,.T.) ;
#21511 = FACE_OUTER_BOUND('',#27374,.T.) ;
#21512 = FACE_OUTER_BOUND('',#27375,.T.) ;
#21513 = FACE_OUTER_BOUND('',#27376,.T.) ;
#21514 = FACE_OUTER_BOUND('',#27377,.T.) ;
#21515 = FACE_OUTER_BOUND('',#27378,.T.) ;
#21516 = FACE_OUTER_BOUND('',#27379,.T.) ;
#21517 = FACE_OUTER_BOUND('',#27380,.T.) ;
#21518 = FACE_OUTER_BOUND('',#27381,.T.) ;
#21519 = FACE_OUTER_BOUND('',#27382,.T.) ;
#21520 = FACE_OUTER_BOUND('',#27383,.T.) ;
#21521 = FACE_OUTER_BOUND('',#27384,.T.) ;
#21522 = FACE_OUTER_BOUND('',#27385,.T.) ;
#21523 = FACE_OUTER_BOUND('',#27386,.T.) ;
#21524 = FACE_OUTER_BOUND('',#27387,.T.) ;
#21525 = FACE_OUTER_BOUND('',#27388,.T.) ;
#21526 = FACE_OUTER_BOUND('',#27389,.T.) ;
#21527 = FACE_OUTER_BOUND('',#27390,.T.) ;
#21528 = FACE_OUTER_BOUND('',#27391,.T.) ;
#21529 = FACE_OUTER_BOUND('',#27392,.T.) ;
#21530 = FACE_OUTER_BOUND('',#27393,.T.) ;
#21531 = FACE_OUTER_BOUND('',#27394,.T.) ;
#21532 = FACE_OUTER_BOUND('',#27395,.T.) ;
#21533 = FACE_OUTER_BOUND('',#27396,.T.) ;
#21534 = FACE_OUTER_BOUND('',#27397,.T.) ;
#21535 = FACE_OUTER_BOUND('',#27398,.T.) ;
#21536 = FACE_OUTER_BOUND('',#27399,.T.) ;
#21537 = FACE_OUTER_BOUND('',#27400,.T.) ;
#21538 = FACE_OUTER_BOUND('',#27401,.T.) ;
#21539 = FACE_OUTER_BOUND('',#27402,.T.) ;
#21540 = FACE_OUTER_BOUND('',#27403,.T.) ;
#21541 = FACE_OUTER_BOUND('',#27404,.T.) ;
#21542 = FACE_OUTER_BOUND('',#27405,.T.) ;
#21543 = FACE_OUTER_BOUND('',#27406,.T.) ;
#21544 = FACE_OUTER_BOUND('',#27407,.T.) ;
#21545 = FACE_OUTER_BOUND('',#27408,.T.) ;
#21546 = FACE_OUTER_BOUND('',#27409,.T.) ;
#21547 = FACE_OUTER_BOUND('',#27410,.T.) ;
#21548 = FACE_OUTER_BOUND('',#27411,.T.) ;
#21549 = FACE_OUTER_BOUND('',#27412,.T.) ;
#21550 = FACE_OUTER_BOUND('',#27413,.T.) ;
#21551 = FACE_OUTER_BOUND('',#27414,.T.) ;
#21552 = FACE_OUTER_BOUND('',#27415,.T.) ;
#21553 = FACE_OUTER_BOUND('',#27416,.T.) ;
#21554 = FACE_OUTER_BOUND('',#27417,.T.) ;
#21555 = FACE_OUTER_BOUND('',#27418,.T.) ;
#21556 = FACE_OUTER_BOUND('',#27419,.T.) ;
#21557 = FACE_OUTER_BOUND('',#27420,.T.) ;
#21558 = FACE_OUTER_BOUND('',#27421,.T.) ;
#21559 = FACE_OUTER_BOUND('',#27422,.T.) ;
#21560 = FACE_OUTER_BOUND('',#27423,.T.) ;
#21561 = FACE_OUTER_BOUND('',#27424,.T.) ;
#21562 = FACE_OUTER_BOUND('',#27425,.T.) ;
#21563 = FACE_OUTER_BOUND('',#27426,.T.) ;
#21564 = FACE_OUTER_BOUND('',#27427,.T.) ;
#21565 = FACE_OUTER_BOUND('',#27428,.T.) ;
#21566 = FACE_OUTER_BOUND('',#27429,.T.) ;
#21567 = FACE_OUTER_BOUND('',#27430,.T.) ;
#21568 = FACE_OUTER_BOUND('',#27431,.T.) ;
#21569 = FACE_OUTER_BOUND('',#27432,.T.) ;
#21570 = FACE_OUTER_BOUND('',#27433,.T.) ;
#21571 = FACE_OUTER_BOUND('',#27434,.T.) ;
#21572 = FACE_OUTER_BOUND('',#27435,.T.) ;
#21573 = FACE_OUTER_BOUND('',#27436,.T.) ;
#21574 = FACE_OUTER_BOUND('',#27437,.T.) ;
#21575 = FACE_OUTER_BOUND('',#27438,.T.) ;
#21576 = FACE_OUTER_BOUND('',#27439,.T.) ;
#21577 = FACE_OUTER_BOUND('',#27440,.T.) ;
#21578 = FACE_OUTER_BOUND('',#27441,.T.) ;
#21579 = FACE_OUTER_BOUND('',#27442,.T.) ;
#21580 = FACE_OUTER_BOUND('',#27443,.T.) ;
#21581 = FACE_OUTER_BOUND('',#27444,.T.) ;
#21582 = FACE_OUTER_BOUND('',#27445,.T.) ;
#21583 = FACE_OUTER_BOUND('',#27446,.T.) ;
#21584 = FACE_OUTER_BOUND('',#27447,.T.) ;
#21585 = FACE_OUTER_BOUND('',#27448,.T.) ;
#21586 = FACE_OUTER_BOUND('',#27449,.T.) ;
#21587 = FACE_OUTER_BOUND('',#27450,.T.) ;
#21588 = FACE_OUTER_BOUND('',#27451,.T.) ;
#21589 = FACE_OUTER_BOUND('',#27452,.T.) ;
#21590 = FACE_OUTER_BOUND('',#27453,.T.) ;
#21591 = FACE_OUTER_BOUND('',#27454,.T.) ;
#21592 = FACE_OUTER_BOUND('',#27455,.T.) ;
#21593 = FACE_OUTER_BOUND('',#27456,.T.) ;
#21594 = FACE_OUTER_BOUND('',#27457,.T.) ;
#21595 = FACE_OUTER_BOUND('',#27458,.T.) ;
#21596 = FACE_OUTER_BOUND('',#27459,.T.) ;
#21597 = FACE_OUTER_BOUND('',#27460,.T.) ;
#21598 = FACE_OUTER_BOUND('',#27461,.T.) ;
#21599 = FACE_OUTER_BOUND('',#27462,.T.) ;
#21600 = FACE_OUTER_BOUND('',#27463,.T.) ;
#21601 = FACE_OUTER_BOUND('',#27464,.T.) ;
#21602 = FACE_OUTER_BOUND('',#27465,.T.) ;
#21603 = FACE_OUTER_BOUND('',#27466,.T.) ;
#21604 = FACE_OUTER_BOUND('',#27467,.T.) ;
#21605 = FACE_OUTER_BOUND('',#27468,.T.) ;
#21606 = FACE_OUTER_BOUND('',#27469,.T.) ;
#21607 = FACE_OUTER_BOUND('',#27470,.T.) ;
#21608 = FACE_OUTER_BOUND('',#27471,.T.) ;
#21609 = FACE_OUTER_BOUND('',#27472,.T.) ;
#21610 = FACE_OUTER_BOUND('',#27473,.T.) ;
#21611 = FACE_OUTER_BOUND('',#27474,.T.) ;
#21612 = FACE_OUTER_BOUND('',#27475,.T.) ;
#21613 = FACE_OUTER_BOUND('',#27476,.T.) ;
#21614 = FACE_OUTER_BOUND('',#27477,.T.) ;
#21615 = FACE_OUTER_BOUND('',#27478,.T.) ;
#21616 = FACE_OUTER_BOUND('',#27479,.T.) ;
#21617 = FACE_OUTER_BOUND('',#27480,.T.) ;
#21618 = FACE_OUTER_BOUND('',#27481,.T.) ;
#21619 = FACE_OUTER_BOUND('',#27482,.T.) ;
#21620 = FACE_OUTER_BOUND('',#27483,.T.) ;
#21621 = FACE_OUTER_BOUND('',#27484,.T.) ;
#21622 = FACE_OUTER_BOUND('',#27485,.T.) ;
#21623 = FACE_OUTER_BOUND('',#27486,.T.) ;
#21624 = FACE_OUTER_BOUND('',#27487,.T.) ;
#21625 = FACE_OUTER_BOUND('',#27488,.T.) ;
#21626 = FACE_OUTER_BOUND('',#27489,.T.) ;
#21627 = FACE_OUTER_BOUND('',#27490,.T.) ;
#21628 = FACE_OUTER_BOUND('',#27491,.T.) ;
#21629 = FACE_OUTER_BOUND('',#27492,.T.) ;
#21630 = FACE_OUTER_BOUND('',#27493,.T.) ;
#21631 = FACE_OUTER_BOUND('',#27494,.T.) ;
#21632 = FACE_OUTER_BOUND('',#27495,.T.) ;
#21633 = FACE_OUTER_BOUND('',#27496,.T.) ;
#21634 = FACE_OUTER_BOUND('',#27497,.T.) ;
#21635 = FACE_OUTER_BOUND('',#27498,.T.) ;
#21636 = FACE_OUTER_BOUND('',#27499,.T.) ;
#21637 = FACE_OUTER_BOUND('',#27500,.T.) ;
#21638 = FACE_OUTER_BOUND('',#27501,.T.) ;
#21639 = FACE_OUTER_BOUND('',#27502,.T.) ;
#21640 = FACE_OUTER_BOUND('',#27503,.T.) ;
#21641 = FACE_OUTER_BOUND('',#27504,.T.) ;
#21642 = FACE_OUTER_BOUND('',#27505,.T.) ;
#21643 = FACE_OUTER_BOUND('',#27506,.T.) ;
#21644 = FACE_OUTER_BOUND('',#27507,.T.) ;
#21645 = FACE_OUTER_BOUND('',#27508,.T.) ;
#21646 = FACE_OUTER_BOUND('',#27509,.T.) ;
#21647 = FACE_OUTER_BOUND('',#27510,.T.) ;
#21648 = FACE_OUTER_BOUND('',#27511,.T.) ;
#21649 = FACE_OUTER_BOUND('',#27512,.T.) ;
#21650 = FACE_OUTER_BOUND('',#27513,.T.) ;
#21651 = FACE_OUTER_BOUND('',#27514,.T.) ;
#21652 = FACE_OUTER_BOUND('',#27515,.T.) ;
#21653 = FACE_OUTER_BOUND('',#27516,.T.) ;
#21654 = FACE_OUTER_BOUND('',#27517,.T.) ;
#21655 = FACE_OUTER_BOUND('',#27518,.T.) ;
#21656 = FACE_OUTER_BOUND('',#27519,.T.) ;
#21657 = FACE_OUTER_BOUND('',#27520,.T.) ;
#21658 = FACE_OUTER_BOUND('',#27521,.T.) ;
#21659 = FACE_OUTER_BOUND('',#27522,.T.) ;
#21660 = FACE_OUTER_BOUND('',#27523,.T.) ;
#21661 = FACE_OUTER_BOUND('',#27524,.T.) ;
#21662 = FACE_OUTER_BOUND('',#27525,.T.) ;
#21663 = FACE_OUTER_BOUND('',#27526,.T.) ;
#21664 = FACE_OUTER_BOUND('',#27527,.T.) ;
#21665 = FACE_OUTER_BOUND('',#27528,.T.) ;
#21666 = FACE_OUTER_BOUND('',#27529,.T.) ;
#21667 = FACE_OUTER_BOUND('',#27530,.T.) ;
#21668 = FACE_OUTER_BOUND('',#27531,.T.) ;
#21669 = FACE_OUTER_BOUND('',#27532,.T.) ;
#21670 = FACE_OUTER_BOUND('',#27533,.T.) ;
#21671 = FACE_OUTER_BOUND('',#27534,.T.) ;
#21672 = FACE_OUTER_BOUND('',#27535,.T.) ;
#21673 = FACE_OUTER_BOUND('',#27536,.T.) ;
#21674 = FACE_OUTER_BOUND('',#27537,.T.) ;
#21675 = FACE_OUTER_BOUND('',#27538,.T.) ;
#21676 = FACE_OUTER_BOUND('',#27539,.T.) ;
#21677 = FACE_OUTER_BOUND('',#27540,.T.) ;
#21678 = FACE_OUTER_BOUND('',#27541,.T.) ;
#21679 = FACE_OUTER_BOUND('',#27542,.T.) ;
#21680 = FACE_OUTER_BOUND('',#27543,.T.) ;
#21681 = FACE_OUTER_BOUND('',#27544,.T.) ;
#21682 = FACE_OUTER_BOUND('',#27545,.T.) ;
#21683 = FACE_OUTER_BOUND('',#27546,.T.) ;
#21684 = FACE_OUTER_BOUND('',#27547,.T.) ;
#21685 = FACE_OUTER_BOUND('',#27548,.T.) ;
#21686 = FACE_OUTER_BOUND('',#27549,.T.) ;
#21687 = FACE_OUTER_BOUND('',#27550,.T.) ;
#21688 = FACE_OUTER_BOUND('',#27551,.T.) ;
#21689 = FACE_OUTER_BOUND('',#27552,.T.) ;
#21690 = FACE_OUTER_BOUND('',#27553,.T.) ;
#21691 = FACE_OUTER_BOUND('',#27554,.T.) ;
#21692 = FACE_OUTER_BOUND('',#27555,.T.) ;
#21693 = FACE_OUTER_BOUND('',#27556,.T.) ;
#21694 = FACE_OUTER_BOUND('',#27557,.T.) ;
#21695 = FACE_OUTER_BOUND('',#27558,.T.) ;
#21696 = FACE_OUTER_BOUND('',#27559,.T.) ;
#21697 = FACE_OUTER_BOUND('',#27560,.T.) ;
#21698 = FACE_OUTER_BOUND('',#27561,.T.) ;
#21699 = FACE_OUTER_BOUND('',#27562,.T.) ;
#21700 = FACE_OUTER_BOUND('',#27563,.T.) ;
#21701 = FACE_OUTER_BOUND('',#27564,.T.) ;
#21702 = FACE_OUTER_BOUND('',#27565,.T.) ;
#21703 = FACE_OUTER_BOUND('',#27566,.T.) ;
#21704 = FACE_OUTER_BOUND('',#27567,.T.) ;
#21705 = FACE_OUTER_BOUND('',#27568,.T.) ;
#21706 = FACE_OUTER_BOUND('',#27569,.T.) ;
#21707 = FACE_OUTER_BOUND('',#27570,.T.) ;
#21708 = FACE_OUTER_BOUND('',#27571,.T.) ;
#21709 = FACE_OUTER_BOUND('',#27572,.T.) ;
#21710 = FACE_OUTER_BOUND('',#27573,.T.) ;
#21711 = FACE_OUTER_BOUND('',#27574,.T.) ;
#21712 = FACE_OUTER_BOUND('',#27575,.T.) ;
#21713 = FACE_OUTER_BOUND('',#27576,.T.) ;
#21714 = FACE_OUTER_BOUND('',#27577,.T.) ;
#21715 = FACE_OUTER_BOUND('',#27578,.T.) ;
#21716 = FACE_OUTER_BOUND('',#27579,.T.) ;
#21717 = FACE_OUTER_BOUND('',#27580,.T.) ;
#21718 = FACE_OUTER_BOUND('',#27581,.T.) ;
#21719 = FACE_OUTER_BOUND('',#27582,.T.) ;
#21720 = FACE_OUTER_BOUND('',#27583,.T.) ;
#21721 = FACE_OUTER_BOUND('',#27584,.T.) ;
#21722 = FACE_OUTER_BOUND('',#27585,.T.) ;
#21723 = FACE_OUTER_BOUND('',#27586,.T.) ;
#21724 = FACE_OUTER_BOUND('',#27587,.T.) ;
#21725 = FACE_OUTER_BOUND('',#27588,.T.) ;
#21726 = FACE_OUTER_BOUND('',#27589,.T.) ;
#21727 = FACE_OUTER_BOUND('',#27590,.T.) ;
#21728 = FACE_OUTER_BOUND('',#27591,.T.) ;
#21729 = FACE_OUTER_BOUND('',#27592,.T.) ;
#21730 = FACE_OUTER_BOUND('',#27593,.T.) ;
#21731 = FACE_OUTER_BOUND('',#27594,.T.) ;
#21732 = FACE_OUTER_BOUND('',#27595,.T.) ;
#21733 = FACE_OUTER_BOUND('',#27596,.T.) ;
#21734 = FACE_OUTER_BOUND('',#27597,.T.) ;
#21735 = FACE_OUTER_BOUND('',#27598,.T.) ;
#21736 = FACE_OUTER_BOUND('',#27599,.T.) ;
#21737 = FACE_OUTER_BOUND('',#27600,.T.) ;
#21738 = FACE_OUTER_BOUND('',#27601,.T.) ;
#21739 = FACE_OUTER_BOUND('',#27602,.T.) ;
#21740 = FACE_OUTER_BOUND('',#27603,.T.) ;
#21741 = FACE_OUTER_BOUND('',#27604,.T.) ;
#21742 = FACE_OUTER_BOUND('',#27605,.T.) ;
#21743 = FACE_OUTER_BOUND('',#27606,.T.) ;
#21744 = FACE_OUTER_BOUND('',#27607,.T.) ;
#21745 = FACE_OUTER_BOUND('',#27608,.T.) ;
#21746 = FACE_OUTER_BOUND('',#27609,.T.) ;
#21747 = FACE_OUTER_BOUND('',#27610,.T.) ;
#21748 = FACE_OUTER_BOUND('',#27611,.T.) ;
#21749 = FACE_OUTER_BOUND('',#27612,.T.) ;
#21750 = FACE_OUTER_BOUND('',#27613,.T.) ;
#21751 = FACE_OUTER_BOUND('',#27614,.T.) ;
#21752 = FACE_OUTER_BOUND('',#27615,.T.) ;
#21753 = FACE_OUTER_BOUND('',#27616,.T.) ;
#21754 = FACE_OUTER_BOUND('',#27617,.T.) ;
#21755 = FACE_OUTER_BOUND('',#27618,.T.) ;
#21756 = FACE_OUTER_BOUND('',#27619,.T.) ;
#21757 = FACE_OUTER_BOUND('',#27620,.T.) ;
#21758 = FACE_OUTER_BOUND('',#27621,.T.) ;
#21759 = FACE_OUTER_BOUND('',#27622,.T.) ;
#21760 = FACE_OUTER_BOUND('',#27623,.T.) ;
#21761 = FACE_OUTER_BOUND('',#27624,.T.) ;
#21762 = FACE_OUTER_BOUND('',#27625,.T.) ;
#21763 = FACE_OUTER_BOUND('',#27626,.T.) ;
#21764 = FACE_OUTER_BOUND('',#27627,.T.) ;
#21765 = FACE_OUTER_BOUND('',#27628,.T.) ;
#21766 = FACE_OUTER_BOUND('',#27629,.T.) ;
#21767 = FACE_OUTER_BOUND('',#27630,.T.) ;
#21768 = FACE_OUTER_BOUND('',#27631,.T.) ;
#21769 = FACE_OUTER_BOUND('',#27632,.T.) ;
#21770 = FACE_OUTER_BOUND('',#27633,.T.) ;
#21771 = FACE_OUTER_BOUND('',#27634,.T.) ;
#21772 = FACE_OUTER_BOUND('',#27635,.T.) ;
#21773 = FACE_OUTER_BOUND('',#27636,.T.) ;
#21774 = FACE_OUTER_BOUND('',#27637,.T.) ;
#21775 = FACE_OUTER_BOUND('',#27638,.T.) ;
#21776 = FACE_OUTER_BOUND('',#27639,.T.) ;
#21777 = FACE_OUTER_BOUND('',#27640,.T.) ;
#21778 = FACE_OUTER_BOUND('',#27641,.T.) ;
#21779 = FACE_OUTER_BOUND('',#27642,.T.) ;
#21780 = FACE_OUTER_BOUND('',#27643,.T.) ;
#21781 = FACE_OUTER_BOUND('',#27644,.T.) ;
#21782 = FACE_OUTER_BOUND('',#27645,.T.) ;
#21783 = FACE_OUTER_BOUND('',#27646,.T.) ;
#21784 = FACE_OUTER_BOUND('',#27647,.T.) ;
#21785 = FACE_OUTER_BOUND('',#27648,.T.) ;
#21786 = FACE_OUTER_BOUND('',#27649,.T.) ;
#21787 = FACE_OUTER_BOUND('',#27650,.T.) ;
#21788 = FACE_OUTER_BOUND('',#27651,.T.) ;
#21789 = FACE_OUTER_BOUND('',#27652,.T.) ;
#21790 = FACE_OUTER_BOUND('',#27653,.T.) ;
#21791 = FACE_OUTER_BOUND('',#27654,.T.) ;
#21792 = FACE_OUTER_BOUND('',#27655,.T.) ;
#21793 = FACE_OUTER_BOUND('',#27656,.T.) ;
#21794 = FACE_OUTER_BOUND('',#27657,.T.) ;
#21795 = FACE_OUTER_BOUND('',#27658,.T.) ;
#21796 = FACE_OUTER_BOUND('',#27659,.T.) ;
#21797 = FACE_OUTER_BOUND('',#27660,.T.) ;
#21798 = FACE_OUTER_BOUND('',#27661,.T.) ;
#21799 = FACE_OUTER_BOUND('',#27662,.T.) ;
#21800 = FACE_OUTER_BOUND('',#27663,.T.) ;
#21801 = FACE_OUTER_BOUND('',#27664,.T.) ;
#21802 = FACE_OUTER_BOUND('',#27665,.T.) ;
#21803 = FACE_OUTER_BOUND('',#27666,.T.) ;
#21804 = FACE_OUTER_BOUND('',#27667,.T.) ;
#21805 = FACE_OUTER_BOUND('',#27668,.T.) ;
#21806 = FACE_OUTER_BOUND('',#27669,.T.) ;
#21807 = FACE_OUTER_BOUND('',#27670,.T.) ;
#21808 = FACE_OUTER_BOUND('',#27671,.T.) ;
#21809 = FACE_OUTER_BOUND('',#27672,.T.) ;
#21810 = FACE_OUTER_BOUND('',#27673,.T.) ;
#21811 = FACE_OUTER_BOUND('',#27674,.T.) ;
#21812 = FACE_OUTER_BOUND('',#27675,.T.) ;
#21813 = FACE_OUTER_BOUND('',#27676,.T.) ;
#21814 = FACE_OUTER_BOUND('',#27677,.T.) ;
#21815 = FACE_OUTER_BOUND('',#27678,.T.) ;
#21816 = FACE_OUTER_BOUND('',#27679,.T.) ;
#21817 = FACE_OUTER_BOUND('',#27680,.T.) ;
#21818 = FACE_OUTER_BOUND('',#27681,.T.) ;
#21819 = FACE_OUTER_BOUND('',#27682,.T.) ;
#21820 = FACE_OUTER_BOUND('',#27683,.T.) ;
#21821 = FACE_OUTER_BOUND('',#27684,.T.) ;
#21822 = FACE_OUTER_BOUND('',#27685,.T.) ;
#21823 = FACE_OUTER_BOUND('',#27686,.T.) ;
#21824 = FACE_OUTER_BOUND('',#27687,.T.) ;
#21825 = FACE_OUTER_BOUND('',#27688,.T.) ;
#21826 = FACE_OUTER_BOUND('',#27689,.T.) ;
#21827 = FACE_OUTER_BOUND('',#27690,.T.) ;
#21828 = FACE_OUTER_BOUND('',#27691,.T.) ;
#21829 = FACE_OUTER_BOUND('',#27692,.T.) ;
#21830 = FACE_OUTER_BOUND('',#27693,.T.) ;
#21831 = FACE_OUTER_BOUND('',#27694,.T.) ;
#21832 = FACE_OUTER_BOUND('',#27695,.T.) ;
#21833 = FACE_OUTER_BOUND('',#27696,.T.) ;
#21834 = FACE_OUTER_BOUND('',#27697,.T.) ;
#21835 = FACE_OUTER_BOUND('',#27698,.T.) ;
#21836 = FACE_OUTER_BOUND('',#27699,.T.) ;
#21837 = FACE_OUTER_BOUND('',#27700,.T.) ;
#21838 = FACE_OUTER_BOUND('',#27701,.T.) ;
#21839 = FACE_OUTER_BOUND('',#27702,.T.) ;
#21840 = FACE_OUTER_BOUND('',#27703,.T.) ;
#21841 = FACE_OUTER_BOUND('',#27704,.T.) ;
#21842 = FACE_OUTER_BOUND('',#27705,.T.) ;
#21843 = FACE_OUTER_BOUND('',#27706,.T.) ;
#21844 = FACE_OUTER_BOUND('',#27707,.T.) ;
#21845 = FACE_OUTER_BOUND('',#27708,.T.) ;
#21846 = FACE_OUTER_BOUND('',#27709,.T.) ;
#21847 = FACE_OUTER_BOUND('',#27710,.T.) ;
#21848 = FACE_OUTER_BOUND('',#27711,.T.) ;
#21849 = FACE_OUTER_BOUND('',#27712,.T.) ;
#21850 = FACE_OUTER_BOUND('',#27713,.T.) ;
#21851 = FACE_OUTER_BOUND('',#27714,.T.) ;
#21852 = FACE_OUTER_BOUND('',#27715,.T.) ;
#21853 = FACE_OUTER_BOUND('',#27716,.T.) ;
#21854 = FACE_OUTER_BOUND('',#27717,.T.) ;
#21855 = FACE_OUTER_BOUND('',#27718,.T.) ;
#21856 = FACE_OUTER_BOUND('',#27719,.T.) ;
#21857 = FACE_OUTER_BOUND('',#27720,.T.) ;
#21858 = FACE_OUTER_BOUND('',#27721,.T.) ;
#21859 = FACE_OUTER_BOUND('',#27722,.T.) ;
#21860 = FACE_OUTER_BOUND('',#27723,.T.) ;
#21861 = FACE_OUTER_BOUND('',#27724,.T.) ;
#21862 = FACE_OUTER_BOUND('',#27725,.T.) ;
#21863 = FACE_OUTER_BOUND('',#27726,.T.) ;
#21864 = FACE_OUTER_BOUND('',#27727,.T.) ;
#21865 = FACE_OUTER_BOUND('',#27728,.T.) ;
#21866 = FACE_OUTER_BOUND('',#27729,.T.) ;
#21867 = FACE_OUTER_BOUND('',#27730,.T.) ;
#21868 = FACE_OUTER_BOUND('',#27731,.T.) ;
#21869 = FACE_OUTER_BOUND('',#27732,.T.) ;
#21870 = FACE_OUTER_BOUND('',#27733,.T.) ;
#21871 = FACE_OUTER_BOUND('',#27734,.T.) ;
#21872 = FACE_OUTER_BOUND('',#27735,.T.) ;
#21873 = FACE_OUTER_BOUND('',#27736,.T.) ;
#21874 = FACE_OUTER_BOUND('',#27737,.T.) ;
#21875 = FACE_OUTER_BOUND('',#27738,.T.) ;
#21876 = FACE_OUTER_BOUND('',#27739,.T.) ;
#21877 = FACE_OUTER_BOUND('',#27740,.T.) ;
#21878 = FACE_OUTER_BOUND('',#27741,.T.) ;
#21879 = FACE_OUTER_BOUND('',#27742,.T.) ;
#21880 = FACE_OUTER_BOUND('',#27743,.T.) ;
#21881 = FACE_OUTER_BOUND('',#27744,.T.) ;
#21882 = FACE_OUTER_BOUND('',#27745,.T.) ;
#21883 = FACE_OUTER_BOUND('',#27746,.T.) ;
#21884 = FACE_OUTER_BOUND('',#27747,.T.) ;
#21885 = FACE_OUTER_BOUND('',#27748,.T.) ;
#21886 = FACE_OUTER_BOUND('',#27749,.T.) ;
#21887 = FACE_OUTER_BOUND('',#27750,.T.) ;
#21888 = FACE_OUTER_BOUND('',#27751,.T.) ;
#21889 = FACE_OUTER_BOUND('',#27752,.T.) ;
#21890 = FACE_OUTER_BOUND('',#27753,.T.) ;
#21891 = FACE_OUTER_BOUND('',#27754,.T.) ;
#21892 = FACE_OUTER_BOUND('',#27755,.T.) ;
#21893 = FACE_OUTER_BOUND('',#27756,.T.) ;
#21894 = FACE_OUTER_BOUND('',#27757,.T.) ;
#21895 = FACE_OUTER_BOUND('',#27758,.T.) ;
#21896 = FACE_OUTER_BOUND('',#27759,.T.) ;
#21897 = FACE_OUTER_BOUND('',#27760,.T.) ;
#21898 = FACE_OUTER_BOUND('',#27761,.T.) ;
#21899 = FACE_OUTER_BOUND('',#27762,.T.) ;
#21900 = FACE_OUTER_BOUND('',#27763,.T.) ;
#21901 = FACE_OUTER_BOUND('',#27764,.T.) ;
#21902 = FACE_OUTER_BOUND('',#27765,.T.) ;
#21903 = FACE_OUTER_BOUND('',#27766,.T.) ;
#21904 = FACE_OUTER_BOUND('',#27767,.T.) ;
#21905 = FACE_OUTER_BOUND('',#27768,.T.) ;
#21906 = FACE_OUTER_BOUND('',#27769,.T.) ;
#21907 = FACE_OUTER_BOUND('',#27770,.T.) ;
#21908 = FACE_OUTER_BOUND('',#27771,.T.) ;
#21909 = FACE_OUTER_BOUND('',#27772,.T.) ;
#21910 = FACE_OUTER_BOUND('',#27773,.T.) ;
#21911 = FACE_OUTER_BOUND('',#27774,.T.) ;
#21912 = FACE_OUTER_BOUND('',#27775,.T.) ;
#21913 = FACE_OUTER_BOUND('',#27776,.T.) ;
#21914 = FACE_OUTER_BOUND('',#27777,.T.) ;
#21915 = FACE_OUTER_BOUND('',#27778,.T.) ;
#21916 = FACE_OUTER_BOUND('',#27779,.T.) ;
#21917 = FACE_OUTER_BOUND('',#27780,.T.) ;
#21918 = FACE_OUTER_BOUND('',#27781,.T.) ;
#21919 = FACE_OUTER_BOUND('',#27782,.T.) ;
#21920 = FACE_OUTER_BOUND('',#27783,.T.) ;
#21921 = FACE_OUTER_BOUND('',#27784,.T.) ;
#21922 = FACE_OUTER_BOUND('',#27785,.T.) ;
#21923 = FACE_OUTER_BOUND('',#27786,.T.) ;
#21924 = FACE_OUTER_BOUND('',#27787,.T.) ;
#21925 = FACE_OUTER_BOUND('',#27788,.T.) ;
#21926 = FACE_OUTER_BOUND('',#27789,.T.) ;
#21927 = FACE_OUTER_BOUND('',#27790,.T.) ;
#21928 = FACE_OUTER_BOUND('',#27791,.T.) ;
#21929 = FACE_OUTER_BOUND('',#27792,.T.) ;
#21930 = FACE_OUTER_BOUND('',#27793,.T.) ;
#21931 = FACE_OUTER_BOUND('',#27794,.T.) ;
#21932 = FACE_OUTER_BOUND('',#27795,.T.) ;
#21933 = FACE_OUTER_BOUND('',#27796,.T.) ;
#21934 = FACE_OUTER_BOUND('',#27797,.T.) ;
#21935 = FACE_OUTER_BOUND('',#27798,.T.) ;
#21936 = FACE_OUTER_BOUND('',#27799,.T.) ;
#21937 = FACE_OUTER_BOUND('',#27800,.T.) ;
#21938 = FACE_OUTER_BOUND('',#27801,.T.) ;
#21939 = FACE_OUTER_BOUND('',#27802,.T.) ;
#21940 = FACE_OUTER_BOUND('',#27803,.T.) ;
#21941 = FACE_OUTER_BOUND('',#27804,.T.) ;
#21942 = FACE_OUTER_BOUND('',#27805,.T.) ;
#21943 = FACE_OUTER_BOUND('',#27806,.T.) ;
#21944 = FACE_OUTER_BOUND('',#27807,.T.) ;
#21945 = FACE_OUTER_BOUND('',#27808,.T.) ;
#21946 = FACE_OUTER_BOUND('',#27809,.T.) ;
#21947 = FACE_OUTER_BOUND('',#27810,.T.) ;
#21948 = FACE_OUTER_BOUND('',#27811,.T.) ;
#21949 = FACE_OUTER_BOUND('',#27812,.T.) ;
#21950 = FACE_OUTER_BOUND('',#27813,.T.) ;
#21951 = FACE_OUTER_BOUND('',#27814,.T.) ;
#21952 = FACE_OUTER_BOUND('',#27815,.T.) ;
#21953 = FACE_OUTER_BOUND('',#27816,.T.) ;
#21954 = FACE_OUTER_BOUND('',#27817,.T.) ;
#21955 = FACE_OUTER_BOUND('',#27818,.T.) ;
#21956 = FACE_OUTER_BOUND('',#27819,.T.) ;
#21957 = FACE_OUTER_BOUND('',#27820,.T.) ;
#21958 = FACE_OUTER_BOUND('',#27821,.T.) ;
#21959 = FACE_OUTER_BOUND('',#27822,.T.) ;
#21960 = FACE_OUTER_BOUND('',#27823,.T.) ;
#21961 = FACE_OUTER_BOUND('',#27824,.T.) ;
#21962 = FACE_OUTER_BOUND('',#27825,.T.) ;
#21963 = FACE_OUTER_BOUND('',#27826,.T.) ;
#21964 = FACE_OUTER_BOUND('',#27827,.T.) ;
#21965 = FACE_OUTER_BOUND('',#27828,.T.) ;
#21966 = FACE_OUTER_BOUND('',#27829,.T.) ;
#21967 = FACE_OUTER_BOUND('',#27830,.T.) ;
#21968 = FACE_OUTER_BOUND('',#27831,.T.) ;
#21969 = FACE_OUTER_BOUND('',#27832,.T.) ;
#21970 = FACE_OUTER_BOUND('',#27833,.T.) ;
#21971 = FACE_OUTER_BOUND('',#27834,.T.) ;
#21972 = FACE_OUTER_BOUND('',#27835,.T.) ;
#21973 = FACE_OUTER_BOUND('',#27836,.T.) ;
#21974 = FACE_OUTER_BOUND('',#27837,.T.) ;
#21975 = FACE_OUTER_BOUND('',#27838,.T.) ;
#21976 = FACE_OUTER_BOUND('',#27839,.T.) ;
#21977 = FACE_OUTER_BOUND('',#27840,.T.) ;
#21978 = FACE_OUTER_BOUND('',#27841,.T.) ;
#21979 = FACE_OUTER_BOUND('',#27842,.T.) ;
#21980 = FACE_OUTER_BOUND('',#27843,.T.) ;
#21981 = FACE_OUTER_BOUND('',#27844,.T.) ;
#21982 = FACE_OUTER_BOUND('',#27845,.T.) ;
#21983 = FACE_OUTER_BOUND('',#27846,.T.) ;
#21984 = FACE_OUTER_BOUND('',#27847,.T.) ;
#21985 = FACE_OUTER_BOUND('',#27848,.T.) ;
#21986 = FACE_OUTER_BOUND('',#27849,.T.) ;
#21987 = FACE_OUTER_BOUND('',#27850,.T.) ;
#21988 = FACE_OUTER_BOUND('',#27851,.T.) ;
#21989 = FACE_OUTER_BOUND('',#27852,.T.) ;
#21990 = FACE_OUTER_BOUND('',#27853,.T.) ;
#21991 = FACE_OUTER_BOUND('',#27854,.T.) ;
#21992 = FACE_OUTER_BOUND('',#27855,.T.) ;
#21993 = FACE_OUTER_BOUND('',#27856,.T.) ;
#21994 = FACE_OUTER_BOUND('',#27857,.T.) ;
#21995 = FACE_OUTER_BOUND('',#27858,.T.) ;
#21996 = FACE_OUTER_BOUND('',#27859,.T.) ;
#21997 = FACE_OUTER_BOUND('',#27860,.T.) ;
#21998 = FACE_OUTER_BOUND('',#27861,.T.) ;
#21999 = FACE_OUTER_BOUND('',#27862,.T.) ;
#22000 = FACE_OUTER_BOUND('',#27863,.T.) ;
#22001 = FACE_OUTER_BOUND('',#27864,.T.) ;
#22002 = FACE_OUTER_BOUND('',#27865,.T.) ;
#22003 = FACE_OUTER_BOUND('',#27866,.T.) ;
#22004 = FACE_OUTER_BOUND('',#27867,.T.) ;
#22005 = FACE_OUTER_BOUND('',#27868,.T.) ;
#22006 = FACE_OUTER_BOUND('',#27869,.T.) ;
#22007 = FACE_OUTER_BOUND('',#27870,.T.) ;
#22008 = FACE_OUTER_BOUND('',#27871,.T.) ;
#22009 = FACE_OUTER_BOUND('',#27872,.T.) ;
#22010 = FACE_OUTER_BOUND('',#27873,.T.) ;
#22011 = FACE_OUTER_BOUND('',#27874,.T.) ;
#22012 = FACE_OUTER_BOUND('',#27875,.T.) ;
#22013 = FACE_OUTER_BOUND('',#27876,.T.) ;
#22014 = FACE_OUTER_BOUND('',#27877,.T.) ;
#22015 = FACE_OUTER_BOUND('',#27878,.T.) ;
#22016 = FACE_OUTER_BOUND('',#27879,.T.) ;
#22017 = FACE_OUTER_BOUND('',#27880,.T.) ;
#22018 = FACE_OUTER_BOUND('',#27881,.T.) ;
#22019 = FACE_OUTER_BOUND('',#27882,.T.) ;
#22020 = FACE_OUTER_BOUND('',#27883,.T.) ;
#22021 = FACE_OUTER_BOUND('',#27884,.T.) ;
#22022 = FACE_OUTER_BOUND('',#27885,.T.) ;
#22023 = FACE_OUTER_BOUND('',#27886,.T.) ;
#22024 = FACE_OUTER_BOUND('',#27887,.T.) ;
#22025 = FACE_OUTER_BOUND('',#27888,.T.) ;
#22026 = FACE_OUTER_BOUND('',#27889,.T.) ;
#22027 = FACE_OUTER_BOUND('',#27890,.T.) ;
#22028 = FACE_OUTER_BOUND('',#27891,.T.) ;
#22029 = FACE_OUTER_BOUND('',#27892,.T.) ;
#22030 = FACE_OUTER_BOUND('',#27893,.T.) ;
#22031 = FACE_OUTER_BOUND('',#27894,.T.) ;
#22032 = FACE_OUTER_BOUND('',#27895,.T.) ;
#22033 = FACE_OUTER_BOUND('',#27896,.T.) ;
#22034 = FACE_OUTER_BOUND('',#27897,.T.) ;
#22035 = FACE_OUTER_BOUND('',#27898,.T.) ;
#22036 = FACE_OUTER_BOUND('',#27899,.T.) ;
#22037 = FACE_OUTER_BOUND('',#27900,.T.) ;
#22038 = FACE_OUTER_BOUND('',#27901,.T.) ;
#22039 = FACE_OUTER_BOUND('',#27902,.T.) ;
#22040 = FACE_OUTER_BOUND('',#27903,.T.) ;
#22041 = FACE_OUTER_BOUND('',#27904,.T.) ;
#22042 = FACE_OUTER_BOUND('',#27905,.T.) ;
#22043 = FACE_OUTER_BOUND('',#27906,.T.) ;
#22044 = FACE_OUTER_BOUND('',#27907,.T.) ;
#22045 = FACE_OUTER_BOUND('',#27908,.T.) ;
#22046 = FACE_OUTER_BOUND('',#27909,.T.) ;
#22047 = FACE_OUTER_BOUND('',#27910,.T.) ;
#22048 = FACE_OUTER_BOUND('',#27911,.T.) ;
#22049 = FACE_OUTER_BOUND('',#27912,.T.) ;
#22050 = FACE_OUTER_BOUND('',#27913,.T.) ;
#22051 = FACE_OUTER_BOUND('',#27914,.T.) ;
#22052 = FACE_OUTER_BOUND('',#27915,.T.) ;
#22053 = FACE_OUTER_BOUND('',#27916,.T.) ;
#22054 = FACE_OUTER_BOUND('',#27917,.T.) ;
#22055 = FACE_OUTER_BOUND('',#27918,.T.) ;
#22056 = FACE_OUTER_BOUND('',#27919,.T.) ;
#22057 = FACE_OUTER_BOUND('',#27920,.T.) ;
#22058 = FACE_OUTER_BOUND('',#27921,.T.) ;
#22059 = FACE_OUTER_BOUND('',#27922,.T.) ;
#22060 = FACE_OUTER_BOUND('',#27923,.T.) ;
#22061 = FACE_OUTER_BOUND('',#27924,.T.) ;
#22062 = FACE_OUTER_BOUND('',#27925,.T.) ;
#22063 = FACE_OUTER_BOUND('',#27926,.T.) ;
#22064 = FACE_OUTER_BOUND('',#27927,.T.) ;
#22065 = FACE_OUTER_BOUND('',#27928,.T.) ;
#22066 = FACE_OUTER_BOUND('',#27929,.T.) ;
#22067 = FACE_OUTER_BOUND('',#27930,.T.) ;
#22068 = FACE_OUTER_BOUND('',#27931,.T.) ;
#22069 = FACE_OUTER_BOUND('',#27932,.T.) ;
#22070 = FACE_OUTER_BOUND('',#27933,.T.) ;
#22071 = FACE_OUTER_BOUND('',#27934,.T.) ;
#22072 = FACE_OUTER_BOUND('',#27935,.T.) ;
#22073 = FACE_OUTER_BOUND('',#27936,.T.) ;
#22074 = FACE_OUTER_BOUND('',#27937,.T.) ;
#22075 = FACE_OUTER_BOUND('',#27938,.T.) ;
#22076 = FACE_OUTER_BOUND('',#27939,.T.) ;
#22077 = FACE_OUTER_BOUND('',#27940,.T.) ;
#22078 = FACE_OUTER_BOUND('',#27941,.T.) ;
#22079 = FACE_OUTER_BOUND('',#27942,.T.) ;
#22080 = FACE_OUTER_BOUND('',#27943,.T.) ;
#22081 = FACE_OUTER_BOUND('',#27944,.T.) ;
#22082 = FACE_OUTER_BOUND('',#27945,.T.) ;
#22083 = FACE_OUTER_BOUND('',#27946,.T.) ;
#22084 = FACE_OUTER_BOUND('',#27947,.T.) ;
#22085 = FACE_OUTER_BOUND('',#27948,.T.) ;
#22086 = FACE_OUTER_BOUND('',#27949,.T.) ;
#22087 = FACE_OUTER_BOUND('',#27950,.T.) ;
#22088 = FACE_OUTER_BOUND('',#27951,.T.) ;
#22089 = FACE_OUTER_BOUND('',#27952,.T.) ;
#22090 = FACE_OUTER_BOUND('',#27953,.T.) ;
#22091 = FACE_OUTER_BOUND('',#27954,.T.) ;
#22092 = FACE_OUTER_BOUND('',#27955,.T.) ;
#22093 = FACE_OUTER_BOUND('',#27956,.T.) ;
#22094 = FACE_OUTER_BOUND('',#27957,.T.) ;
#22095 = FACE_OUTER_BOUND('',#27958,.T.) ;
#22096 = FACE_OUTER_BOUND('',#27959,.T.) ;
#22097 = FACE_OUTER_BOUND('',#27960,.T.) ;
#22098 = FACE_OUTER_BOUND('',#27961,.T.) ;
#22099 = FACE_OUTER_BOUND('',#27962,.T.) ;
#22100 = FACE_OUTER_BOUND('',#27963,.T.) ;
#22101 = FACE_OUTER_BOUND('',#27964,.T.) ;
#22102 = FACE_OUTER_BOUND('',#27965,.T.) ;
#22103 = FACE_OUTER_BOUND('',#27966,.T.) ;
#22104 = FACE_OUTER_BOUND('',#27967,.T.) ;
#22105 = FACE_OUTER_BOUND('',#27968,.T.) ;
#22106 = FACE_OUTER_BOUND('',#27969,.T.) ;
#22107 = FACE_OUTER_BOUND('',#27970,.T.) ;
#22108 = FACE_OUTER_BOUND('',#27971,.T.) ;
#22109 = FACE_OUTER_BOUND('',#27972,.T.) ;
#22110 = FACE_OUTER_BOUND('',#27973,.T.) ;
#22111 = FACE_OUTER_BOUND('',#27974,.T.) ;
#22112 = FACE_OUTER_BOUND('',#27975,.T.) ;
#22113 = FACE_OUTER_BOUND('',#27976,.T.) ;
#22114 = FACE_OUTER_BOUND('',#27977,.T.) ;
#22115 = FACE_OUTER_BOUND('',#27978,.T.) ;
#22116 = FACE_OUTER_BOUND('',#27979,.T.) ;
#22117 = FACE_OUTER_BOUND('',#27980,.T.) ;
#22118 = FACE_OUTER_BOUND('',#27981,.T.) ;
#22119 = FACE_OUTER_BOUND('',#27982,.T.) ;
#22120 = FACE_OUTER_BOUND('',#27983,.T.) ;
#22121 = FACE_OUTER_BOUND('',#27984,.T.) ;
#22122 = FACE_OUTER_BOUND('',#27985,.T.) ;
#22123 = FACE_OUTER_BOUND('',#27986,.T.) ;
#22124 = FACE_OUTER_BOUND('',#27987,.T.) ;
#22125 = FACE_OUTER_BOUND('',#27988,.T.) ;
#22126 = FACE_OUTER_BOUND('',#27989,.T.) ;
#22127 = FACE_OUTER_BOUND('',#27990,.T.) ;
#22128 = FACE_OUTER_BOUND('',#27991,.T.) ;
#22129 = FACE_OUTER_BOUND('',#27992,.T.) ;
#22130 = FACE_OUTER_BOUND('',#27993,.T.) ;
#22131 = FACE_OUTER_BOUND('',#27994,.T.) ;
#22132 = FACE_OUTER_BOUND('',#27995,.T.) ;
#22133 = FACE_OUTER_BOUND('',#27996,.T.) ;
#22134 = FACE_OUTER_BOUND('',#27997,.T.) ;
#22135 = FACE_OUTER_BOUND('',#27998,.T.) ;
#22136 = FACE_OUTER_BOUND('',#27999,.T.) ;
#22137 = FACE_OUTER_BOUND('',#28000,.T.) ;
#22138 = FACE_OUTER_BOUND('',#28001,.T.) ;
#22139 = FACE_OUTER_BOUND('',#28002,.T.) ;
#22140 = FACE_OUTER_BOUND('',#28003,.T.) ;
#22141 = FACE_OUTER_BOUND('',#28004,.T.) ;
#22142 = FACE_OUTER_BOUND('',#28005,.T.) ;
#22143 = FACE_OUTER_BOUND('',#28006,.T.) ;
#22144 = FACE_OUTER_BOUND('',#28007,.T.) ;
#22145 = FACE_OUTER_BOUND('',#28008,.T.) ;
#22146 = FACE_OUTER_BOUND('',#28009,.T.) ;
#22147 = FACE_OUTER_BOUND('',#28010,.T.) ;
#22148 = FACE_OUTER_BOUND('',#28011,.T.) ;
#22149 = FACE_OUTER_BOUND('',#28012,.T.) ;
#22150 = FACE_OUTER_BOUND('',#28013,.T.) ;
#22151 = FACE_OUTER_BOUND('',#28014,.T.) ;
#22152 = FACE_OUTER_BOUND('',#28015,.T.) ;
#22153 = FACE_OUTER_BOUND('',#28016,.T.) ;
#22154 = FACE_OUTER_BOUND('',#28017,.T.) ;
#22155 = FACE_OUTER_BOUND('',#28018,.T.) ;
#22156 = FACE_OUTER_BOUND('',#28019,.T.) ;
#22157 = FACE_OUTER_BOUND('',#28020,.T.) ;
#22158 = FACE_OUTER_BOUND('',#28021,.T.) ;
#22159 = FACE_OUTER_BOUND('',#28022,.T.) ;
#22160 = FACE_OUTER_BOUND('',#28023,.T.) ;
#22161 = FACE_OUTER_BOUND('',#28024,.T.) ;
#22162 = FACE_OUTER_BOUND('',#28025,.T.) ;
#22163 = FACE_OUTER_BOUND('',#28026,.T.) ;
#22164 = FACE_OUTER_BOUND('',#28027,.T.) ;
#22165 = FACE_OUTER_BOUND('',#28028,.T.) ;
#22166 = FACE_OUTER_BOUND('',#28029,.T.) ;
#22167 = FACE_OUTER_BOUND('',#28030,.T.) ;
#22168 = FACE_OUTER_BOUND('',#28031,.T.) ;
#22169 = FACE_OUTER_BOUND('',#28032,.T.) ;
#22170 = FACE_OUTER_BOUND('',#28033,.T.) ;
#22171 = FACE_OUTER_BOUND('',#28034,.T.) ;
#22172 = FACE_OUTER_BOUND('',#28035,.T.) ;
#22173 = FACE_OUTER_BOUND('',#28036,.T.) ;
#22174 = FACE_OUTER_BOUND('',#28037,.T.) ;
#22175 = FACE_OUTER_BOUND('',#28038,.T.) ;
#22176 = FACE_OUTER_BOUND('',#28039,.T.) ;
#22177 = FACE_OUTER_BOUND('',#28040,.T.) ;
#22178 = FACE_OUTER_BOUND('',#28041,.T.) ;
#22179 = FACE_OUTER_BOUND('',#28042,.T.) ;
#22180 = FACE_OUTER_BOUND('',#28043,.T.) ;
#22181 = FACE_OUTER_BOUND('',#28044,.T.) ;
#22182 = FACE_OUTER_BOUND('',#28045,.T.) ;
#22183 = FACE_OUTER_BOUND('',#28046,.T.) ;
#22184 = FACE_OUTER_BOUND('',#28047,.T.) ;
#22185 = FACE_OUTER_BOUND('',#28048,.T.) ;
#22186 = FACE_OUTER_BOUND('',#28049,.T.) ;
#22187 = FACE_OUTER_BOUND('',#28050,.T.) ;
#22188 = FACE_OUTER_BOUND('',#28051,.T.) ;
#22189 = FACE_OUTER_BOUND('',#28052,.T.) ;
#22190 = FACE_OUTER_BOUND('',#28053,.T.) ;
#22191 = FACE_OUTER_BOUND('',#28054,.T.) ;
#22192 = FACE_OUTER_BOUND('',#28055,.T.) ;
#22193 = FACE_OUTER_BOUND('',#28056,.T.) ;
#22194 = FACE_OUTER_BOUND('',#28057,.T.) ;
#22195 = FACE_OUTER_BOUND('',#28058,.T.) ;
#22196 = FACE_OUTER_BOUND('',#28059,.T.) ;
#22197 = FACE_OUTER_BOUND('',#28060,.T.) ;
#22198 = FACE_OUTER_BOUND('',#28061,.T.) ;
#22199 = FACE_OUTER_BOUND('',#28062,.T.) ;
#22200 = FACE_OUTER_BOUND('',#28063,.T.) ;
#22201 = FACE_OUTER_BOUND('',#28064,.T.) ;
#22202 = FACE_OUTER_BOUND('',#28065,.T.) ;
#22203 = FACE_OUTER_BOUND('',#28066,.T.) ;
#22204 = FACE_OUTER_BOUND('',#28067,.T.) ;
#22205 = FACE_OUTER_BOUND('',#28068,.T.) ;
#22206 = FACE_OUTER_BOUND('',#28069,.T.) ;
#22207 = FACE_OUTER_BOUND('',#28070,.T.) ;
#22208 = FACE_OUTER_BOUND('',#28071,.T.) ;
#22209 = FACE_OUTER_BOUND('',#28072,.T.) ;
#22210 = FACE_OUTER_BOUND('',#28073,.T.) ;
#22211 = FACE_OUTER_BOUND('',#28074,.T.) ;
#22212 = FACE_OUTER_BOUND('',#28075,.T.) ;
#22213 = FACE_OUTER_BOUND('',#28076,.T.) ;
#22214 = FACE_OUTER_BOUND('',#28077,.T.) ;
#22215 = FACE_OUTER_BOUND('',#28078,.T.) ;
#22216 = FACE_OUTER_BOUND('',#28079,.T.) ;
#22217 = FACE_OUTER_BOUND('',#28080,.T.) ;
#22218 = FACE_OUTER_BOUND('',#28081,.T.) ;
#22219 = FACE_OUTER_BOUND('',#28082,.T.) ;
#22220 = FACE_OUTER_BOUND('',#28083,.T.) ;
#22221 = FACE_OUTER_BOUND('',#28084,.T.) ;
#22222 = FACE_OUTER_BOUND('',#28085,.T.) ;
#22223 = FACE_OUTER_BOUND('',#28086,.T.) ;
#22224 = FACE_OUTER_BOUND('',#28087,.T.) ;
#22225 = FACE_OUTER_BOUND('',#28088,.T.) ;
#22226 = FACE_OUTER_BOUND('',#28089,.T.) ;
#22227 = FACE_OUTER_BOUND('',#28090,.T.) ;
#22228 = FACE_OUTER_BOUND('',#28091,.T.) ;
#22229 = FACE_OUTER_BOUND('',#28092,.T.) ;
#22230 = FACE_OUTER_BOUND('',#28093,.T.) ;
#22231 = FACE_OUTER_BOUND('',#28094,.T.) ;
#22232 = FACE_OUTER_BOUND('',#28095,.T.) ;
#22233 = FACE_OUTER_BOUND('',#28096,.T.) ;
#22234 = FACE_OUTER_BOUND('',#28097,.T.) ;
#22235 = FACE_OUTER_BOUND('',#28098,.T.) ;
#22236 = FACE_OUTER_BOUND('',#28099,.T.) ;
#22237 = FACE_OUTER_BOUND('',#28100,.T.) ;
#22238 = FACE_OUTER_BOUND('',#28101,.T.) ;
#22239 = FACE_OUTER_BOUND('',#28102,.T.) ;
#22240 = FACE_OUTER_BOUND('',#28103,.T.) ;
#22241 = FACE_OUTER_BOUND('',#28104,.T.) ;
#22242 = FACE_OUTER_BOUND('',#28105,.T.) ;
#22243 = FACE_OUTER_BOUND('',#28106,.T.) ;
#22244 = FACE_OUTER_BOUND('',#28107,.T.) ;
#22245 = FACE_OUTER_BOUND('',#28108,.T.) ;
#22246 = FACE_OUTER_BOUND('',#28109,.T.) ;
#22247 = FACE_OUTER_BOUND('',#28110,.T.) ;
#22248 = FACE_OUTER_BOUND('',#28111,.T.) ;
#22249 = FACE_OUTER_BOUND('',#28112,.T.) ;
#22250 = FACE_OUTER_BOUND('',#28113,.T.) ;
#22251 = FACE_OUTER_BOUND('',#28114,.T.) ;
#22252 = FACE_OUTER_BOUND('',#28115,.T.) ;
#22253 = FACE_OUTER_BOUND('',#28116,.T.) ;
#22254 = FACE_OUTER_BOUND('',#28117,.T.) ;
#22255 = FACE_OUTER_BOUND('',#28118,.T.) ;
#22256 = FACE_OUTER_BOUND('',#28119,.T.) ;
#22257 = FACE_OUTER_BOUND('',#28120,.T.) ;
#22258 = FACE_OUTER_BOUND('',#28121,.T.) ;
#22259 = FACE_OUTER_BOUND('',#28122,.T.) ;
#22260 = FACE_OUTER_BOUND('',#28123,.T.) ;
#22261 = FACE_OUTER_BOUND('',#28124,.T.) ;
#22262 = FACE_OUTER_BOUND('',#28125,.T.) ;
#22263 = FACE_OUTER_BOUND('',#28126,.T.) ;
#22264 = FACE_OUTER_BOUND('',#28127,.T.) ;
#22265 = FACE_OUTER_BOUND('',#28128,.T.) ;
#22266 = FACE_OUTER_BOUND('',#28129,.T.) ;
#22267 = FACE_OUTER_BOUND('',#28130,.T.) ;
#22268 = FACE_OUTER_BOUND('',#28131,.T.) ;
#22269 = FACE_OUTER_BOUND('',#28132,.T.) ;
#22270 = FACE_OUTER_BOUND('',#28133,.T.) ;
#22271 = FACE_OUTER_BOUND('',#28134,.T.) ;
#22272 = FACE_OUTER_BOUND('',#28135,.T.) ;
#22273 = FACE_OUTER_BOUND('',#28136,.T.) ;
#22274 = FACE_OUTER_BOUND('',#28137,.T.) ;
#22275 = FACE_OUTER_BOUND('',#28138,.T.) ;
#22276 = FACE_OUTER_BOUND('',#28139,.T.) ;
#22277 = FACE_OUTER_BOUND('',#28140,.T.) ;
#22278 = FACE_OUTER_BOUND('',#28141,.T.) ;
#22279 = FACE_OUTER_BOUND('',#28142,.T.) ;
#22280 = FACE_OUTER_BOUND('',#28143,.T.) ;
#22281 = FACE_OUTER_BOUND('',#28144,.T.) ;
#22282 = FACE_OUTER_BOUND('',#28145,.T.) ;
#22283 = FACE_OUTER_BOUND('',#28146,.T.) ;
#22284 = FACE_OUTER_BOUND('',#28147,.T.) ;
#22285 = FACE_OUTER_BOUND('',#28148,.T.) ;
#22286 = FACE_OUTER_BOUND('',#28149,.T.) ;
#22287 = FACE_OUTER_BOUND('',#28150,.T.) ;
#22288 = FACE_OUTER_BOUND('',#28151,.T.) ;
#22289 = FACE_OUTER_BOUND('',#28152,.T.) ;
#22290 = FACE_OUTER_BOUND('',#28153,.T.) ;
#22291 = FACE_OUTER_BOUND('',#28154,.T.) ;
#22292 = FACE_OUTER_BOUND('',#28155,.T.) ;
#22293 = FACE_OUTER_BOUND('',#28156,.T.) ;
#22294 = FACE_OUTER_BOUND('',#28157,.T.) ;
#22295 = FACE_OUTER_BOUND('',#28158,.T.) ;
#22296 = FACE_OUTER_BOUND('',#28159,.T.) ;
#22297 = FACE_OUTER_BOUND('',#28160,.T.) ;
#22298 = FACE_OUTER_BOUND('',#28161,.T.) ;
#22299 = FACE_OUTER_BOUND('',#28162,.T.) ;
#22300 = FACE_OUTER_BOUND('',#28163,.T.) ;
#22301 = FACE_OUTER_BOUND('',#28164,.T.) ;
#22302 = FACE_OUTER_BOUND('',#28165,.T.) ;
#22303 = FACE_OUTER_BOUND('',#28166,.T.) ;
#22304 = FACE_OUTER_BOUND('',#28167,.T.) ;
#22305 = FACE_OUTER_BOUND('',#28168,.T.) ;
#22306 = FACE_OUTER_BOUND('',#28169,.T.) ;
#22307 = FACE_OUTER_BOUND('',#28170,.T.) ;
#22308 = FACE_OUTER_BOUND('',#28171,.T.) ;
#22309 = FACE_OUTER_BOUND('',#28172,.T.) ;
#22310 = FACE_OUTER_BOUND('',#28173,.T.) ;
#22311 = FACE_OUTER_BOUND('',#28174,.T.) ;
#22312 = FACE_OUTER_BOUND('',#28175,.T.) ;
#22313 = FACE_OUTER_BOUND('',#28176,.T.) ;
#22314 = FACE_OUTER_BOUND('',#28177,.T.) ;
#22315 = FACE_OUTER_BOUND('',#28178,.T.) ;
#22316 = FACE_OUTER_BOUND('',#28179,.T.) ;
#22317 = FACE_OUTER_BOUND('',#28180,.T.) ;
#22318 = FACE_OUTER_BOUND('',#28181,.T.) ;
#22319 = FACE_OUTER_BOUND('',#28182,.T.) ;
#22320 = FACE_OUTER_BOUND('',#28183,.T.) ;
#22321 = FACE_OUTER_BOUND('',#28184,.T.) ;
#22322 = FACE_OUTER_BOUND('',#28185,.T.) ;
#22323 = FACE_OUTER_BOUND('',#28186,.T.) ;
#22324 = FACE_OUTER_BOUND('',#28187,.T.) ;
#22325 = FACE_OUTER_BOUND('',#28188,.T.) ;
#22326 = FACE_OUTER_BOUND('',#28189,.T.) ;
#22327 = FACE_OUTER_BOUND('',#28190,.T.) ;
#22328 = FACE_OUTER_BOUND('',#28191,.T.) ;
#22329 = FACE_OUTER_BOUND('',#28192,.T.) ;
#22330 = FACE_OUTER_BOUND('',#28193,.T.) ;
#22331 = FACE_OUTER_BOUND('',#28194,.T.) ;
#22332 = FACE_OUTER_BOUND('',#28195,.T.) ;
#22333 = FACE_OUTER_BOUND('',#28196,.T.) ;
#22334 = FACE_OUTER_BOUND('',#28197,.T.) ;
#22335 = FACE_OUTER_BOUND('',#28198,.T.) ;
#22336 = FACE_OUTER_BOUND('',#28199,.T.) ;
#22337 = FACE_OUTER_BOUND('',#28200,.T.) ;
#22338 = FACE_OUTER_BOUND('',#28201,.T.) ;
#22339 = FACE_OUTER_BOUND('',#28202,.T.) ;
#22340 = FACE_OUTER_BOUND('',#28203,.T.) ;
#22341 = FACE_OUTER_BOUND('',#28204,.T.) ;
#22342 = FACE_OUTER_BOUND('',#28205,.T.) ;
#22343 = FACE_OUTER_BOUND('',#28206,.T.) ;
#22344 = FACE_OUTER_BOUND('',#28207,.T.) ;
#22345 = FACE_OUTER_BOUND('',#28208,.T.) ;
#22346 = FACE_OUTER_BOUND('',#28209,.T.) ;
#22347 = FACE_OUTER_BOUND('',#28210,.T.) ;
#22348 = FACE_OUTER_BOUND('',#28211,.T.) ;
#22349 = FACE_OUTER_BOUND('',#28212,.T.) ;
#22350 = FACE_OUTER_BOUND('',#28213,.T.) ;
#22351 = FACE_OUTER_BOUND('',#28214,.T.) ;
#22352 = FACE_OUTER_BOUND('',#28215,.T.) ;
#22353 = FACE_OUTER_BOUND('',#28216,.T.) ;
#22354 = FACE_OUTER_BOUND('',#28217,.T.) ;
#22355 = FACE_OUTER_BOUND('',#28218,.T.) ;
#22356 = FACE_OUTER_BOUND('',#28219,.T.) ;
#22357 = FACE_OUTER_BOUND('',#28220,.T.) ;
#22358 = FACE_OUTER_BOUND('',#28221,.T.) ;
#22359 = FACE_OUTER_BOUND('',#28222,.T.) ;
#22360 = FACE_OUTER_BOUND('',#28223,.T.) ;
#22361 = FACE_OUTER_BOUND('',#28224,.T.) ;
#22362 = FACE_OUTER_BOUND('',#28225,.T.) ;
#22363 = FACE_OUTER_BOUND('',#28226,.T.) ;
#22364 = FACE_OUTER_BOUND('',#28227,.T.) ;
#22365 = FACE_OUTER_BOUND('',#28228,.T.) ;
#22366 = FACE_OUTER_BOUND('',#28229,.T.) ;
#22367 = FACE_OUTER_BOUND('',#28230,.T.) ;
#22368 = FACE_OUTER_BOUND('',#28231,.T.) ;
#22369 = FACE_OUTER_BOUND('',#28232,.T.) ;
#22370 = FACE_OUTER_BOUND('',#28233,.T.) ;
#22371 = FACE_OUTER_BOUND('',#28234,.T.) ;
#22372 = FACE_OUTER_BOUND('',#28235,.T.) ;
#22373 = FACE_OUTER_BOUND('',#28236,.T.) ;
#22374 = FACE_OUTER_BOUND('',#28237,.T.) ;
#22375 = FACE_OUTER_BOUND('',#28238,.T.) ;
#22376 = FACE_OUTER_BOUND('',#28239,.T.) ;
#22377 = FACE_OUTER_BOUND('',#28240,.T.) ;
#22378 = FACE_OUTER_BOUND('',#28241,.T.) ;
#22379 = FACE_OUTER_BOUND('',#28242,.T.) ;
#22380 = FACE_OUTER_BOUND('',#28243,.T.) ;
#22381 = FACE_OUTER_BOUND('',#28244,.T.) ;
#22382 = FACE_OUTER_BOUND('',#28245,.T.) ;
#22383 = FACE_OUTER_BOUND('',#28246,.T.) ;
#22384 = FACE_OUTER_BOUND('',#28247,.T.) ;
#22385 = FACE_OUTER_BOUND('',#28248,.T.) ;
#22386 = FACE_OUTER_BOUND('',#28249,.T.) ;
#22387 = FACE_OUTER_BOUND('',#28250,.T.) ;
#22388 = FACE_OUTER_BOUND('',#28251,.T.) ;
#22389 = FACE_OUTER_BOUND('',#28252,.T.) ;
#22390 = FACE_OUTER_BOUND('',#28253,.T.) ;
#22391 = FACE_OUTER_BOUND('',#28254,.T.) ;
#22392 = FACE_OUTER_BOUND('',#28255,.T.) ;
#22393 = FACE_OUTER_BOUND('',#28256,.T.) ;
#22394 = FACE_OUTER_BOUND('',#28257,.T.) ;
#22395 = FACE_OUTER_BOUND('',#28258,.T.) ;
#22396 = FACE_OUTER_BOUND('',#28259,.T.) ;
#22397 = FACE_OUTER_BOUND('',#28260,.T.) ;
#22398 = FACE_OUTER_BOUND('',#28261,.T.) ;
#22399 = FACE_OUTER_BOUND('',#28262,.T.) ;
#22400 = FACE_OUTER_BOUND('',#28263,.T.) ;
#22401 = FACE_OUTER_BOUND('',#28264,.T.) ;
#22402 = FACE_OUTER_BOUND('',#28265,.T.) ;
#22403 = FACE_OUTER_BOUND('',#28266,.T.) ;
#22404 = FACE_OUTER_BOUND('',#28267,.T.) ;
#22405 = FACE_OUTER_BOUND('',#28268,.T.) ;
#22406 = FACE_OUTER_BOUND('',#28269,.T.) ;
#22407 = FACE_OUTER_BOUND('',#28270,.T.) ;
#22408 = FACE_OUTER_BOUND('',#28271,.T.) ;
#22409 = FACE_OUTER_BOUND('',#28272,.T.) ;
#22410 = FACE_OUTER_BOUND('',#28273,.T.) ;
#22411 = FACE_OUTER_BOUND('',#28274,.T.) ;
#22412 = FACE_OUTER_BOUND('',#28275,.T.) ;
#22413 = FACE_OUTER_BOUND('',#28276,.T.) ;
#22414 = FACE_OUTER_BOUND('',#28277,.T.) ;
#22415 = FACE_OUTER_BOUND('',#28278,.T.) ;
#22416 = FACE_OUTER_BOUND('',#28279,.T.) ;
#22417 = FACE_OUTER_BOUND('',#28280,.T.) ;
#22418 = FACE_OUTER_BOUND('',#28281,.T.) ;
#22419 = FACE_OUTER_BOUND('',#28282,.T.) ;
#22420 = FACE_OUTER_BOUND('',#28283,.T.) ;
#22421 = FACE_OUTER_BOUND('',#28284,.T.) ;
#22422 = FACE_OUTER_BOUND('',#28285,.T.) ;
#22423 = FACE_OUTER_BOUND('',#28286,.T.) ;
#22424 = FACE_OUTER_BOUND('',#28287,.T.) ;
#22425 = FACE_OUTER_BOUND('',#28288,.T.) ;
#22426 = FACE_OUTER_BOUND('',#28289,.T.) ;
#22427 = FACE_OUTER_BOUND('',#28290,.T.) ;
#22428 = FACE_OUTER_BOUND('',#28291,.T.) ;
#22429 = FACE_OUTER_BOUND('',#28292,.T.) ;
#22430 = FACE_OUTER_BOUND('',#28293,.T.) ;
#22431 = FACE_OUTER_BOUND('',#28294,.T.) ;
#22432 = FACE_OUTER_BOUND('',#28295,.T.) ;
#22433 = FACE_OUTER_BOUND('',#28296,.T.) ;
#22434 = FACE_OUTER_BOUND('',#28297,.T.) ;
#22435 = FACE_OUTER_BOUND('',#28298,.T.) ;
#22436 = FACE_OUTER_BOUND('',#28299,.T.) ;
#22437 = FACE_OUTER_BOUND('',#28300,.T.) ;
#22438 = FACE_OUTER_BOUND('',#28301,.T.) ;
#22439 = FACE_OUTER_BOUND('',#28302,.T.) ;
#22440 = FACE_OUTER_BOUND('',#28303,.T.) ;
#22441 = FACE_OUTER_BOUND('',#28304,.T.) ;
#22442 = FACE_OUTER_BOUND('',#28305,.T.) ;
#22443 = FACE_OUTER_BOUND('',#28306,.T.) ;
#22444 = FACE_OUTER_BOUND('',#28307,.T.) ;
#22445 = FACE_OUTER_BOUND('',#28308,.T.) ;
#22446 = FACE_OUTER_BOUND('',#28309,.T.) ;
#22447 = FACE_OUTER_BOUND('',#28310,.T.) ;
#22448 = FACE_OUTER_BOUND('',#28311,.T.) ;
#22449 = FACE_OUTER_BOUND('',#28312,.T.) ;
#22450 = FACE_OUTER_BOUND('',#28313,.T.) ;
#22451 = FACE_OUTER_BOUND('',#28314,.T.) ;
#22452 = FACE_OUTER_BOUND('',#28315,.T.) ;
#22453 = FACE_OUTER_BOUND('',#28316,.T.) ;
#22454 = FACE_OUTER_BOUND('',#28317,.T.) ;
#22455 = FACE_OUTER_BOUND('',#28318,.T.) ;
#22456 = FACE_OUTER_BOUND('',#28319,.T.) ;
#22457 = FACE_OUTER_BOUND('',#28320,.T.) ;
#22458 = FACE_OUTER_BOUND('',#28321,.T.) ;
#22459 = FACE_OUTER_BOUND('',#28322,.T.) ;
#22460 = FACE_OUTER_BOUND('',#28323,.T.) ;
#22461 = FACE_OUTER_BOUND('',#28324,.T.) ;
#22462 = FACE_OUTER_BOUND('',#28325,.T.) ;
#22463 = FACE_OUTER_BOUND('',#28326,.T.) ;
#22464 = FACE_OUTER_BOUND('',#28327,.T.) ;
#22465 = FACE_OUTER_BOUND('',#28328,.T.) ;
#22466 = FACE_OUTER_BOUND('',#28329,.T.) ;
#22467 = FACE_OUTER_BOUND('',#28330,.T.) ;
#22468 = FACE_OUTER_BOUND('',#28331,.T.) ;
#22469 = FACE_OUTER_BOUND('',#28332,.T.) ;
#22470 = FACE_OUTER_BOUND('',#28333,.T.) ;
#22471 = FACE_OUTER_BOUND('',#28334,.T.) ;
#22472 = FACE_OUTER_BOUND('',#28335,.T.) ;
#22473 = FACE_OUTER_BOUND('',#28336,.T.) ;
#22474 = FACE_OUTER_BOUND('',#28337,.T.) ;
#22475 = FACE_OUTER_BOUND('',#28338,.T.) ;
#22476 = FACE_OUTER_BOUND('',#28339,.T.) ;
#22477 = FACE_OUTER_BOUND('',#28340,.T.) ;
#22478 = FACE_OUTER_BOUND('',#28341,.T.) ;
#22479 = FACE_OUTER_BOUND('',#28342,.T.) ;
#22480 = FACE_OUTER_BOUND('',#28343,.T.) ;
#22481 = FACE_OUTER_BOUND('',#28344,.T.) ;
#22482 = FACE_OUTER_BOUND('',#28345,.T.) ;
#22483 = FACE_OUTER_BOUND('',#28346,.T.) ;
#22484 = FACE_OUTER_BOUND('',#28347,.T.) ;
#22485 = FACE_OUTER_BOUND('',#28348,.T.) ;
#22486 = FACE_OUTER_BOUND('',#28349,.T.) ;
#22487 = FACE_OUTER_BOUND('',#28350,.T.) ;
#22488 = FACE_OUTER_BOUND('',#28351,.T.) ;
#22489 = FACE_OUTER_BOUND('',#28352,.T.) ;
#22490 = FACE_OUTER_BOUND('',#28353,.T.) ;
#22491 = FACE_OUTER_BOUND('',#28354,.T.) ;
#22492 = FACE_OUTER_BOUND('',#28355,.T.) ;
#22493 = FACE_OUTER_BOUND('',#28356,.T.) ;
#22494 = FACE_OUTER_BOUND('',#28357,.T.) ;
#22495 = FACE_OUTER_BOUND('',#28358,.T.) ;
#22496 = FACE_OUTER_BOUND('',#28359,.T.) ;
#22497 = FACE_OUTER_BOUND('',#28360,.T.) ;
#22498 = FACE_OUTER_BOUND('',#28361,.T.) ;
#22499 = FACE_OUTER_BOUND('',#28362,.T.) ;
#22500 = FACE_OUTER_BOUND('',#28363,.T.) ;
#22501 = FACE_OUTER_BOUND('',#28364,.T.) ;
#22502 = FACE_OUTER_BOUND('',#28365,.T.) ;
#22503 = FACE_OUTER_BOUND('',#28366,.T.) ;
#22504 = FACE_OUTER_BOUND('',#28367,.T.) ;
#22505 = FACE_OUTER_BOUND('',#28368,.T.) ;
#22506 = FACE_OUTER_BOUND('',#28369,.T.) ;
#22507 = FACE_OUTER_BOUND('',#28370,.T.) ;
#22508 = FACE_OUTER_BOUND('',#28371,.T.) ;
#22509 = FACE_OUTER_BOUND('',#28372,.T.) ;
#22510 = FACE_OUTER_BOUND('',#28373,.T.) ;
#22511 = FACE_OUTER_BOUND('',#28374,.T.) ;
#22512 = FACE_OUTER_BOUND('',#28375,.T.) ;
#22513 = FACE_OUTER_BOUND('',#28376,.T.) ;
#22514 = FACE_OUTER_BOUND('',#28377,.T.) ;
#22515 = FACE_OUTER_BOUND('',#28378,.T.) ;
#22516 = FACE_OUTER_BOUND('',#28379,.T.) ;
#22517 = FACE_OUTER_BOUND('',#28380,.T.) ;
#22518 = FACE_OUTER_BOUND('',#28381,.T.) ;
#22519 = FACE_OUTER_BOUND('',#28382,.T.) ;
#22520 = FACE_OUTER_BOUND('',#28383,.T.) ;
#22521 = FACE_OUTER_BOUND('',#28384,.T.) ;
#22522 = FACE_OUTER_BOUND('',#28385,.T.) ;
#22523 = FACE_OUTER_BOUND('',#28386,.T.) ;
#22524 = FACE_OUTER_BOUND('',#28387,.T.) ;
#22525 = FACE_OUTER_BOUND('',#28388,.T.) ;
#22526 = FACE_OUTER_BOUND('',#28389,.T.) ;
#22527 = FACE_OUTER_BOUND('',#28390,.T.) ;
#22528 = FACE_OUTER_BOUND('',#28391,.T.) ;
#22529 = FACE_OUTER_BOUND('',#28392,.T.) ;
#22530 = FACE_OUTER_BOUND('',#28393,.T.) ;
#22531 = FACE_OUTER_BOUND('',#28394,.T.) ;
#22532 = FACE_OUTER_BOUND('',#28395,.T.) ;
#22533 = FACE_OUTER_BOUND('',#28396,.T.) ;
#22534 = FACE_OUTER_BOUND('',#28397,.T.) ;
#22535 = FACE_OUTER_BOUND('',#28398,.T.) ;
#22536 = FACE_OUTER_BOUND('',#28399,.T.) ;
#22537 = FACE_OUTER_BOUND('',#28400,.T.) ;
#22538 = FACE_OUTER_BOUND('',#28401,.T.) ;
#22539 = FACE_OUTER_BOUND('',#28402,.T.) ;
#22540 = FACE_OUTER_BOUND('',#28403,.T.) ;
#22541 = FACE_OUTER_BOUND('',#28404,.T.) ;
#22542 = FACE_OUTER_BOUND('',#28405,.T.) ;
#22543 = FACE_OUTER_BOUND('',#28406,.T.) ;
#22544 = FACE_OUTER_BOUND('',#28407,.T.) ;
#22545 = FACE_OUTER_BOUND('',#28408,.T.) ;
#22546 = FACE_OUTER_BOUND('',#28409,.T.) ;
#22547 = FACE_OUTER_BOUND('',#28410,.T.) ;
#22548 = FACE_OUTER_BOUND('',#28411,.T.) ;
#22549 = FACE_OUTER_BOUND('',#28412,.T.) ;
#22550 = FACE_OUTER_BOUND('',#28413,.T.) ;
#22551 = FACE_OUTER_BOUND('',#28414,.T.) ;
#22552 = FACE_OUTER_BOUND('',#28415,.T.) ;
#22553 = FACE_OUTER_BOUND('',#28416,.T.) ;
#22554 = FACE_OUTER_BOUND('',#28417,.T.) ;
#22555 = FACE_OUTER_BOUND('',#28418,.T.) ;
#22556 = FACE_OUTER_BOUND('',#28419,.T.) ;
#22557 = FACE_OUTER_BOUND('',#28420,.T.) ;
#22558 = FACE_OUTER_BOUND('',#28421,.T.) ;
#22559 = FACE_OUTER_BOUND('',#28422,.T.) ;
#22560 = FACE_OUTER_BOUND('',#28423,.T.) ;
#22561 = FACE_OUTER_BOUND('',#28424,.T.) ;
#22562 = FACE_OUTER_BOUND('',#28425,.T.) ;
#22563 = FACE_OUTER_BOUND('',#28426,.T.) ;
#22564 = FACE_OUTER_BOUND('',#28427,.T.) ;
#22565 = FACE_OUTER_BOUND('',#28428,.T.) ;
#22566 = FACE_OUTER_BOUND('',#28429,.T.) ;
#22567 = FACE_OUTER_BOUND('',#28430,.T.) ;
#22568 = FACE_OUTER_BOUND('',#28431,.T.) ;
#22569 = FACE_OUTER_BOUND('',#28432,.T.) ;
#22570 = FACE_OUTER_BOUND('',#28433,.T.) ;
#22571 = FACE_OUTER_BOUND('',#28434,.T.) ;
#22572 = FACE_OUTER_BOUND('',#28435,.T.) ;
#22573 = FACE_OUTER_BOUND('',#28436,.T.) ;
#22574 = FACE_OUTER_BOUND('',#28437,.T.) ;
#22575 = FACE_OUTER_BOUND('',#28438,.T.) ;
#22576 = FACE_OUTER_BOUND('',#28439,.T.) ;
#22577 = FACE_OUTER_BOUND('',#28440,.T.) ;
#22578 = FACE_OUTER_BOUND('',#28441,.T.) ;
#22579 = FACE_OUTER_BOUND('',#28442,.T.) ;
#22580 = FACE_OUTER_BOUND('',#28443,.T.) ;
#22581 = FACE_OUTER_BOUND('',#28444,.T.) ;
#22582 = FACE_OUTER_BOUND('',#28445,.T.) ;
#22583 = FACE_OUTER_BOUND('',#28446,.T.) ;
#22584 = FACE_OUTER_BOUND('',#28447,.T.) ;
#22585 = FACE_OUTER_BOUND('',#28448,.T.) ;
#22586 = FACE_OUTER_BOUND('',#28449,.T.) ;
#22587 = FACE_OUTER_BOUND('',#28450,.T.) ;
#22588 = FACE_OUTER_BOUND('',#28451,.T.) ;
#22589 = FACE_OUTER_BOUND('',#28452,.T.) ;
#22590 = FACE_OUTER_BOUND('',#28453,.T.) ;
#22591 = FACE_OUTER_BOUND('',#28454,.T.) ;
#22592 = FACE_OUTER_BOUND('',#28455,.T.) ;
#22593 = FACE_OUTER_BOUND('',#28456,.T.) ;
#22594 = FACE_OUTER_BOUND('',#28457,.T.) ;
#22595 = FACE_OUTER_BOUND('',#28458,.T.) ;
#22596 = FACE_OUTER_BOUND('',#28459,.T.) ;
#22597 = FACE_OUTER_BOUND('',#28460,.T.) ;
#22598 = FACE_OUTER_BOUND('',#28461,.T.) ;
#22599 = FACE_OUTER_BOUND('',#28462,.T.) ;
#22600 = FACE_OUTER_BOUND('',#28463,.T.) ;
#22601 = FACE_OUTER_BOUND('',#28464,.T.) ;
#22602 = FACE_OUTER_BOUND('',#28465,.T.) ;
#22603 = FACE_OUTER_BOUND('',#28466,.T.) ;
#22604 = FACE_OUTER_BOUND('',#28467,.T.) ;
#22605 = FACE_OUTER_BOUND('',#28468,.T.) ;
#22606 = FACE_OUTER_BOUND('',#28469,.T.) ;
#22607 = FACE_OUTER_BOUND('',#28470,.T.) ;
#22608 = FACE_OUTER_BOUND('',#28471,.T.) ;
#22609 = FACE_OUTER_BOUND('',#28472,.T.) ;
#22610 = FACE_OUTER_BOUND('',#28473,.T.) ;
#22611 = FACE_OUTER_BOUND('',#28474,.T.) ;
#22612 = FACE_OUTER_BOUND('',#28475,.T.) ;
#22613 = FACE_OUTER_BOUND('',#28476,.T.) ;
#22614 = FACE_OUTER_BOUND('',#28477,.T.) ;
#22615 = FACE_OUTER_BOUND('',#28478,.T.) ;
#22616 = FACE_OUTER_BOUND('',#28479,.T.) ;
#22617 = FACE_OUTER_BOUND('',#28480,.T.) ;
#22618 = FACE_OUTER_BOUND('',#28481,.T.) ;
#22619 = FACE_OUTER_BOUND('',#28482,.T.) ;
#22620 = FACE_OUTER_BOUND('',#28483,.T.) ;
#22621 = FACE_OUTER_BOUND('',#28484,.T.) ;
#22622 = FACE_OUTER_BOUND('',#28485,.T.) ;
#22623 = FACE_OUTER_BOUND('',#28486,.T.) ;
#22624 = FACE_OUTER_BOUND('',#28487,.T.) ;
#22625 = FACE_OUTER_BOUND('',#28488,.T.) ;
#22626 = FACE_OUTER_BOUND('',#28489,.T.) ;
#22627 = FACE_OUTER_BOUND('',#28490,.T.) ;
#22628 = FACE_OUTER_BOUND('',#28491,.T.) ;
#22629 = FACE_OUTER_BOUND('',#28492,.T.) ;
#22630 = FACE_OUTER_BOUND('',#28493,.T.) ;
#22631 = FACE_OUTER_BOUND('',#28494,.T.) ;
#22632 = FACE_OUTER_BOUND('',#28495,.T.) ;
#22633 = FACE_OUTER_BOUND('',#28496,.T.) ;
#22634 = FACE_OUTER_BOUND('',#28497,.T.) ;
#22635 = FACE_OUTER_BOUND('',#28498,.T.) ;
#22636 = FACE_OUTER_BOUND('',#28499,.T.) ;
#22637 = FACE_OUTER_BOUND('',#28500,.T.) ;
#22638 = FACE_OUTER_BOUND('',#28501,.T.) ;
#22639 = FACE_OUTER_BOUND('',#28502,.T.) ;
#22640 = FACE_OUTER_BOUND('',#28503,.T.) ;
#22641 = FACE_OUTER_BOUND('',#28504,.T.) ;
#22642 = FACE_OUTER_BOUND('',#28505,.T.) ;
#22643 = FACE_OUTER_BOUND('',#28506,.T.) ;
#22644 = FACE_OUTER_BOUND('',#28507,.T.) ;
#22645 = FACE_OUTER_BOUND('',#28508,.T.) ;
#22646 = FACE_OUTER_BOUND('',#28509,.T.) ;
#22647 = FACE_OUTER_BOUND('',#28510,.T.) ;
#22648 = FACE_OUTER_BOUND('',#28511,.T.) ;
#22649 = FACE_OUTER_BOUND('',#28512,.T.) ;
#22650 = FACE_OUTER_BOUND('',#28513,.T.) ;
#22651 = FACE_OUTER_BOUND('',#28514,.T.) ;
#22652 = FACE_OUTER_BOUND('',#28515,.T.) ;
#22653 = FACE_OUTER_BOUND('',#28516,.T.) ;
#22654 = FACE_OUTER_BOUND('',#28517,.T.) ;
#22655 = FACE_OUTER_BOUND('',#28518,.T.) ;
#22656 = FACE_OUTER_BOUND('',#28519,.T.) ;
#22657 = FACE_OUTER_BOUND('',#28520,.T.) ;
#22658 = FACE_OUTER_BOUND('',#28521,.T.) ;
#22659 = FACE_OUTER_BOUND('',#28522,.T.) ;
#22660 = FACE_OUTER_BOUND('',#28523,.T.) ;
#22661 = FACE_OUTER_BOUND('',#28524,.T.) ;
#22662 = FACE_OUTER_BOUND('',#28525,.T.) ;
#22663 = FACE_OUTER_BOUND('',#28526,.T.) ;
#22664 = FACE_OUTER_BOUND('',#28527,.T.) ;
#22665 = FACE_OUTER_BOUND('',#28528,.T.) ;
#22666 = FACE_OUTER_BOUND('',#28529,.T.) ;
#22667 = FACE_OUTER_BOUND('',#28530,.T.) ;
#22668 = FACE_OUTER_BOUND('',#28531,.T.) ;
#22669 = FACE_OUTER_BOUND('',#28532,.T.) ;
#22670 = FACE_OUTER_BOUND('',#28533,.T.) ;
#22671 = FACE_OUTER_BOUND('',#28534,.T.) ;
#22672 = FACE_OUTER_BOUND('',#28535,.T.) ;
#22673 = FACE_OUTER_BOUND('',#28536,.T.) ;
#22674 = FACE_OUTER_BOUND('',#28537,.T.) ;
#22675 = FACE_OUTER_BOUND('',#28538,.T.) ;
#22676 = FACE_OUTER_BOUND('',#28539,.T.) ;
#22677 = FACE_OUTER_BOUND('',#28540,.T.) ;
#22678 = FACE_OUTER_BOUND('',#28541,.T.) ;
#22679 = FACE_OUTER_BOUND('',#28542,.T.) ;
#22680 = FACE_OUTER_BOUND('',#28543,.T.) ;
#22681 = FACE_OUTER_BOUND('',#28544,.T.) ;
#22682 = FACE_OUTER_BOUND('',#28545,.T.) ;
#22683 = FACE_OUTER_BOUND('',#28546,.T.) ;
#22684 = FACE_OUTER_BOUND('',#28547,.T.) ;
#22685 = FACE_OUTER_BOUND('',#28548,.T.) ;
#22686 = FACE_OUTER_BOUND('',#28549,.T.) ;
#22687 = FACE_OUTER_BOUND('',#28550,.T.) ;
#22688 = FACE_OUTER_BOUND('',#28551,.T.) ;
#22689 = FACE_OUTER_BOUND('',#28552,.T.) ;
#22690 = FACE_OUTER_BOUND('',#28553,.T.) ;
#22691 = FACE_OUTER_BOUND('',#28554,.T.) ;
#22692 = FACE_OUTER_BOUND('',#28555,.T.) ;
#22693 = FACE_OUTER_BOUND('',#28556,.T.) ;
#22694 = FACE_OUTER_BOUND('',#28557,.T.) ;
#22695 = FACE_OUTER_BOUND('',#28558,.T.) ;
#22696 = FACE_OUTER_BOUND('',#28559,.T.) ;
#22697 = FACE_OUTER_BOUND('',#28560,.T.) ;
#22698 = FACE_OUTER_BOUND('',#28561,.T.) ;
#22699 = FACE_OUTER_BOUND('',#28562,.T.) ;
#22700 = FACE_OUTER_BOUND('',#28563,.T.) ;
#22701 = FACE_OUTER_BOUND('',#28564,.T.) ;
#22702 = FACE_OUTER_BOUND('',#28565,.T.) ;
#22703 = FACE_OUTER_BOUND('',#28566,.T.) ;
#22704 = FACE_OUTER_BOUND('',#28567,.T.) ;
#22705 = FACE_OUTER_BOUND('',#28568,.T.) ;
#22706 = FACE_OUTER_BOUND('',#28569,.T.) ;
#22707 = FACE_OUTER_BOUND('',#28570,.T.) ;
#22708 = FACE_OUTER_BOUND('',#28571,.T.) ;
#22709 = FACE_OUTER_BOUND('',#28572,.T.) ;
#22710 = FACE_OUTER_BOUND('',#28573,.T.) ;
#22711 = FACE_OUTER_BOUND('',#28574,.T.) ;
#22712 = FACE_OUTER_BOUND('',#28575,.T.) ;
#22713 = FACE_OUTER_BOUND('',#28576,.T.) ;
#22714 = FACE_OUTER_BOUND('',#28577,.T.) ;
#22715 = FACE_OUTER_BOUND('',#28578,.T.) ;
#22716 = FACE_OUTER_BOUND('',#28579,.T.) ;
#22717 = FACE_OUTER_BOUND('',#28580,.T.) ;
#22718 = FACE_OUTER_BOUND('',#28581,.T.) ;
#22719 = FACE_OUTER_BOUND('',#28582,.T.) ;
#22720 = FACE_OUTER_BOUND('',#28583,.T.) ;
#22721 = FACE_OUTER_BOUND('',#28584,.T.) ;
#22722 = FACE_OUTER_BOUND('',#28585,.T.) ;
#22723 = FACE_OUTER_BOUND('',#28586,.T.) ;
#22724 = FACE_OUTER_BOUND('',#28587,.T.) ;
#22725 = FACE_OUTER_BOUND('',#28588,.T.) ;
#22726 = FACE_OUTER_BOUND('',#28589,.T.) ;
#22727 = FACE_OUTER_BOUND('',#28590,.T.) ;
#22728 = FACE_OUTER_BOUND('',#28591,.T.) ;
#22729 = FACE_OUTER_BOUND('',#28592,.T.) ;
#22730 = FACE_OUTER_BOUND('',#28593,.T.) ;
#22731 = FACE_OUTER_BOUND('',#28594,.T.) ;
#22732 = FACE_OUTER_BOUND('',#28595,.T.) ;
#22733 = FACE_OUTER_BOUND('',#28596,.T.) ;
#22734 = FACE_OUTER_BOUND('',#28597,.T.) ;
#22735 = FACE_OUTER_BOUND('',#28598,.T.) ;
#22736 = FACE_OUTER_BOUND('',#28599,.T.) ;
#22737 = FACE_OUTER_BOUND('',#28600,.T.) ;
#22738 = FACE_OUTER_BOUND('',#28601,.T.) ;
#22739 = FACE_OUTER_BOUND('',#28602,.T.) ;
#22740 = FACE_OUTER_BOUND('',#28603,.T.) ;
#22741 = FACE_OUTER_BOUND('',#28604,.T.) ;
#22742 = FACE_OUTER_BOUND('',#28605,.T.) ;
#22743 = FACE_OUTER_BOUND('',#28606,.T.) ;
#22744 = FACE_OUTER_BOUND('',#28607,.T.) ;
#22745 = FACE_OUTER_BOUND('',#28608,.T.) ;
#22746 = FACE_OUTER_BOUND('',#28609,.T.) ;
#22747 = FACE_OUTER_BOUND('',#28610,.T.) ;
#22748 = FACE_OUTER_BOUND('',#28611,.T.) ;
#22749 = FACE_OUTER_BOUND('',#28612,.T.) ;
#22750 = FACE_OUTER_BOUND('',#28613,.T.) ;
#22751 = FACE_OUTER_BOUND('',#28614,.T.) ;
#22752 = FACE_OUTER_BOUND('',#28615,.T.) ;
#22753 = FACE_OUTER_BOUND('',#28616,.T.) ;
#22754 = FACE_OUTER_BOUND('',#28617,.T.) ;
#22755 = FACE_OUTER_BOUND('',#28618,.T.) ;
#22756 = FACE_OUTER_BOUND('',#28619,.T.) ;
#22757 = FACE_OUTER_BOUND('',#28620,.T.) ;
#22758 = FACE_OUTER_BOUND('',#28621,.T.) ;
#22759 = FACE_OUTER_BOUND('',#28622,.T.) ;
#22760 = FACE_OUTER_BOUND('',#28623,.T.) ;
#22761 = FACE_OUTER_BOUND('',#28624,.T.) ;
#22762 = FACE_OUTER_BOUND('',#28625,.T.) ;
#22763 = EDGE_LOOP('',(#54031,#54032,#54033,#54034)) ;
#22764 = EDGE_LOOP('',(#54035,#54036,#54037,#54038,#54039)) ;
#22765 = EDGE_LOOP('',(#54040,#54041,#54042,#54043)) ;
#22766 = EDGE_LOOP('',(#54044,#54045,#54046,#54047,#54048)) ;
#22767 = EDGE_LOOP('',(#54049,#54050,#54051,#54052)) ;
#22768 = EDGE_LOOP('',(#54053,#54054,#54055)) ;
#22769 = EDGE_LOOP('',(#54056,#54057,#54058,#54059)) ;
#22770 = EDGE_LOOP('',(#54060,#54061,#54062)) ;
#22771 = EDGE_LOOP('',(#54063,#54064,#54065,#54066)) ;
#22772 = EDGE_LOOP('',(#54067,#54068,#54069,#54070,#54071)) ;
#22773 = EDGE_LOOP('',(#54072,#54073,#54074,#54075,#54076,#54077,#54078,#54079,
#54080,#54081,#54082,#54083,#54084,#54085,#54086,#54087,#54088,#54089,#54090,
#54091,#54092)) ;
#22774 = EDGE_LOOP('',(#54093,#54094,#54095,#54096)) ;
#22775 = EDGE_LOOP('',(#54097,#54098,#54099,#54100)) ;
#22776 = EDGE_LOOP('',(#54101,#54102,#54103,#54104,#54105)) ;
#22777 = EDGE_LOOP('',(#54106,#54107,#54108,#54109)) ;
#22778 = EDGE_LOOP('',(#54110,#54111,#54112,#54113,#54114)) ;
#22779 = EDGE_LOOP('',(#54115,#54116,#54117,#54118)) ;
#22780 = EDGE_LOOP('',(#54119,#54120,#54121)) ;
#22781 = EDGE_LOOP('',(#54122,#54123,#54124,#54125)) ;
#22782 = EDGE_LOOP('',(#54126,#54127,#54128)) ;
#22783 = EDGE_LOOP('',(#54129,#54130,#54131,#54132)) ;
#22784 = EDGE_LOOP('',(#54133,#54134,#54135,#54136,#54137)) ;
#22785 = EDGE_LOOP('',(#54138,#54139,#54140,#54141,#54142,#54143,#54144,#54145,
#54146,#54147,#54148,#54149,#54150,#54151,#54152,#54153,#54154,#54155,#54156,
#54157,#54158)) ;
#22786 = EDGE_LOOP('',(#54159,#54160,#54161,#54162)) ;
#22787 = EDGE_LOOP('',(#54163,#54164,#54165,#54166,#54167,#54168,#54169,#54170)) ;
#22788 = EDGE_LOOP('',(#54171,#54172,#54173,#54174)) ;
#22789 = EDGE_LOOP('',(#54175,#54176,#54177,#54178)) ;
#22790 = EDGE_LOOP('',(#54179,#54180,#54181,#54182)) ;
#22791 = EDGE_LOOP('',(#54183,#54184,#54185,#54186)) ;
#22792 = EDGE_LOOP('',(#54187,#54188,#54189,#54190)) ;
#22793 = EDGE_LOOP('',(#54191,#54192,#54193,#54194)) ;
#22794 = EDGE_LOOP('',(#54195,#54196,#54197,#54198,#54199,#54200)) ;
#22795 = EDGE_LOOP('',(#54201,#54202,#54203,#54204)) ;
#22796 = EDGE_LOOP('',(#54205,#54206,#54207,#54208)) ;
#22797 = EDGE_LOOP('',(#54209,#54210,#54211,#54212)) ;
#22798 = EDGE_LOOP('',(#54213,#54214,#54215)) ;
#22799 = EDGE_LOOP('',(#54216,#54217,#54218,#54219,#54220,#54221,#54222,#54223,
#54224,#54225,#54226,#54227,#54228,#54229,#54230,#54231,#54232,#54233,#54234,
#54235,#54236,#54237,#54238,#54239)) ;
#22800 = EDGE_LOOP('',(#54240)) ;
#22801 = EDGE_LOOP('',(#54241)) ;
#22802 = EDGE_LOOP('',(#54242,#54243,#54244,#54245)) ;
#22803 = EDGE_LOOP('',(#54246,#54247,#54248,#54249,#54250,#54251,#54252,#54253,
#54254,#54255,#54256,#54257)) ;
#22804 = EDGE_LOOP('',(#54258,#54259,#54260,#54261)) ;
#22805 = EDGE_LOOP('',(#54262,#54263,#54264,#54265,#54266,#54267)) ;
#22806 = EDGE_LOOP('',(#54268,#54269,#54270,#54271)) ;
#22807 = EDGE_LOOP('',(#54272,#54273,#54274,#54275,#54276,#54277,#54278,#54279)) ;
#22808 = EDGE_LOOP('',(#54280)) ;
#22809 = EDGE_LOOP('',(#54281,#54282,#54283,#54284,#54285,#54286,#54287,#54288)) ;
#22810 = EDGE_LOOP('',(#54289)) ;
#22811 = EDGE_LOOP('',(#54290,#54291,#54292,#54293)) ;
#22812 = EDGE_LOOP('',(#54294,#54295,#54296,#54297)) ;
#22813 = EDGE_LOOP('',(#54298,#54299,#54300,#54301)) ;
#22814 = EDGE_LOOP('',(#54302,#54303,#54304,#54305)) ;
#22815 = EDGE_LOOP('',(#54306,#54307,#54308,#54309,#54310,#54311,#54312,#54313)) ;
#22816 = EDGE_LOOP('',(#54314,#54315,#54316,#54317,#54318,#54319,#54320,#54321)) ;
#22817 = EDGE_LOOP('',(#54322,#54323,#54324,#54325)) ;
#22818 = EDGE_LOOP('',(#54326,#54327,#54328,#54329,#54330,#54331,#54332,#54333)) ;
#22819 = EDGE_LOOP('',(#54334,#54335,#54336,#54337,#54338,#54339,#54340,#54341)) ;
#22820 = EDGE_LOOP('',(#54342,#54343,#54344,#54345)) ;
#22821 = EDGE_LOOP('',(#54346,#54347,#54348,#54349,#54350,#54351,#54352,#54353,
#54354,#54355,#54356,#54357,#54358,#54359)) ;
#22822 = EDGE_LOOP('',(#54360,#54361,#54362,#54363)) ;
#22823 = EDGE_LOOP('',(#54364,#54365,#54366,#54367)) ;
#22824 = EDGE_LOOP('',(#54368,#54369,#54370,#54371,#54372,#54373,#54374,#54375,
#54376,#54377,#54378,#54379,#54380,#54381,#54382,#54383,#54384,#54385,#54386,
#54387,#54388,#54389,#54390,#54391,#54392,#54393,#54394,#54395,#54396,#54397,
#54398,#54399)) ;
#22825 = EDGE_LOOP('',(#54400,#54401,#54402,#54403)) ;
#22826 = EDGE_LOOP('',(#54404,#54405,#54406,#54407)) ;
#22827 = EDGE_LOOP('',(#54408,#54409,#54410,#54411,#54412,#54413,#54414,#54415)) ;
#22828 = EDGE_LOOP('',(#54416,#54417,#54418,#54419,#54420,#54421,#54422,#54423)) ;
#22829 = EDGE_LOOP('',(#54424,#54425,#54426,#54427,#54428,#54429,#54430,#54431)) ;
#22830 = EDGE_LOOP('',(#54432,#54433,#54434,#54435)) ;
#22831 = EDGE_LOOP('',(#54436,#54437,#54438,#54439)) ;
#22832 = EDGE_LOOP('',(#54440,#54441,#54442,#54443,#54444,#54445)) ;
#22833 = EDGE_LOOP('',(#54446,#54447,#54448,#54449,#54450,#54451)) ;
#22834 = EDGE_LOOP('',(#54452,#54453,#54454,#54455)) ;
#22835 = EDGE_LOOP('',(#54456,#54457,#54458,#54459)) ;
#22836 = EDGE_LOOP('',(#54460,#54461,#54462,#54463)) ;
#22837 = EDGE_LOOP('',(#54464,#54465,#54466,#54467)) ;
#22838 = EDGE_LOOP('',(#54468,#54469,#54470,#54471)) ;
#22839 = EDGE_LOOP('',(#54472,#54473,#54474,#54475,#54476,#54477,#54478,#54479)) ;
#22840 = EDGE_LOOP('',(#54480,#54481,#54482,#54483)) ;
#22841 = EDGE_LOOP('',(#54484,#54485,#54486,#54487)) ;
#22842 = EDGE_LOOP('',(#54488,#54489,#54490,#54491)) ;
#22843 = EDGE_LOOP('',(#54492,#54493,#54494,#54495)) ;
#22844 = EDGE_LOOP('',(#54496,#54497,#54498,#54499)) ;
#22845 = EDGE_LOOP('',(#54500,#54501,#54502,#54503)) ;
#22846 = EDGE_LOOP('',(#54504,#54505,#54506,#54507)) ;
#22847 = EDGE_LOOP('',(#54508,#54509,#54510,#54511)) ;
#22848 = EDGE_LOOP('',(#54512,#54513,#54514,#54515,#54516,#54517,#54518,#54519)) ;
#22849 = EDGE_LOOP('',(#54520,#54521)) ;
#22850 = EDGE_LOOP('',(#54522,#54523,#54524,#54525)) ;
#22851 = EDGE_LOOP('',(#54526,#54527,#54528,#54529)) ;
#22852 = EDGE_LOOP('',(#54530,#54531,#54532,#54533)) ;
#22853 = EDGE_LOOP('',(#54534,#54535,#54536,#54537)) ;
#22854 = EDGE_LOOP('',(#54538,#54539,#54540,#54541)) ;
#22855 = EDGE_LOOP('',(#54542,#54543,#54544,#54545)) ;
#22856 = EDGE_LOOP('',(#54546,#54547,#54548,#54549)) ;
#22857 = EDGE_LOOP('',(#54550,#54551,#54552,#54553)) ;
#22858 = EDGE_LOOP('',(#54554,#54555,#54556,#54557,#54558,#54559,#54560,#54561)) ;
#22859 = EDGE_LOOP('',(#54562,#54563,#54564,#54565)) ;
#22860 = EDGE_LOOP('',(#54566,#54567,#54568,#54569)) ;
#22861 = EDGE_LOOP('',(#54570,#54571,#54572,#54573)) ;
#22862 = EDGE_LOOP('',(#54574,#54575,#54576,#54577)) ;
#22863 = EDGE_LOOP('',(#54578,#54579,#54580,#54581)) ;
#22864 = EDGE_LOOP('',(#54582,#54583,#54584,#54585)) ;
#22865 = EDGE_LOOP('',(#54586,#54587,#54588,#54589)) ;
#22866 = EDGE_LOOP('',(#54590,#54591,#54592,#54593)) ;
#22867 = EDGE_LOOP('',(#54594,#54595,#54596,#54597)) ;
#22868 = EDGE_LOOP('',(#54598,#54599,#54600,#54601)) ;
#22869 = EDGE_LOOP('',(#54602,#54603,#54604,#54605)) ;
#22870 = EDGE_LOOP('',(#54606,#54607,#54608,#54609)) ;
#22871 = EDGE_LOOP('',(#54610,#54611,#54612,#54613,#54614,#54615)) ;
#22872 = EDGE_LOOP('',(#54616)) ;
#22873 = EDGE_LOOP('',(#54617,#54618,#54619,#54620,#54621,#54622)) ;
#22874 = EDGE_LOOP('',(#54623,#54624,#54625,#54626)) ;
#22875 = EDGE_LOOP('',(#54627,#54628,#54629,#54630)) ;
#22876 = EDGE_LOOP('',(#54631,#54632,#54633,#54634)) ;
#22877 = EDGE_LOOP('',(#54635,#54636,#54637,#54638)) ;
#22878 = EDGE_LOOP('',(#54639,#54640,#54641,#54642)) ;
#22879 = EDGE_LOOP('',(#54643,#54644,#54645,#54646)) ;
#22880 = EDGE_LOOP('',(#54647,#54648,#54649,#54650)) ;
#22881 = EDGE_LOOP('',(#54651,#54652,#54653,#54654)) ;
#22882 = EDGE_LOOP('',(#54655,#54656,#54657,#54658)) ;
#22883 = EDGE_LOOP('',(#54659,#54660,#54661)) ;
#22884 = EDGE_LOOP('',(#54662,#54663,#54664,#54665)) ;
#22885 = EDGE_LOOP('',(#54666,#54667,#54668,#54669)) ;
#22886 = EDGE_LOOP('',(#54670,#54671,#54672,#54673)) ;
#22887 = EDGE_LOOP('',(#54674,#54675,#54676,#54677)) ;
#22888 = EDGE_LOOP('',(#54678,#54679,#54680,#54681)) ;
#22889 = EDGE_LOOP('',(#54682,#54683,#54684,#54685)) ;
#22890 = EDGE_LOOP('',(#54686,#54687,#54688,#54689)) ;
#22891 = EDGE_LOOP('',(#54690,#54691,#54692,#54693)) ;
#22892 = EDGE_LOOP('',(#54694,#54695,#54696,#54697)) ;
#22893 = EDGE_LOOP('',(#54698,#54699,#54700)) ;
#22894 = EDGE_LOOP('',(#54701,#54702,#54703,#54704)) ;
#22895 = EDGE_LOOP('',(#54705,#54706,#54707)) ;
#22896 = EDGE_LOOP('',(#54708,#54709,#54710,#54711)) ;
#22897 = EDGE_LOOP('',(#54712,#54713,#54714,#54715)) ;
#22898 = EDGE_LOOP('',(#54716,#54717,#54718,#54719)) ;
#22899 = EDGE_LOOP('',(#54720,#54721,#54722,#54723)) ;
#22900 = EDGE_LOOP('',(#54724,#54725,#54726,#54727)) ;
#22901 = EDGE_LOOP('',(#54728,#54729,#54730)) ;
#22902 = EDGE_LOOP('',(#54731,#54732,#54733,#54734)) ;
#22903 = EDGE_LOOP('',(#54735,#54736,#54737,#54738)) ;
#22904 = EDGE_LOOP('',(#54739,#54740,#54741,#54742)) ;
#22905 = EDGE_LOOP('',(#54743,#54744,#54745,#54746)) ;
#22906 = EDGE_LOOP('',(#54747,#54748,#54749,#54750)) ;
#22907 = EDGE_LOOP('',(#54751,#54752,#54753,#54754,#54755,#54756)) ;
#22908 = EDGE_LOOP('',(#54757,#54758,#54759,#54760)) ;
#22909 = EDGE_LOOP('',(#54761,#54762,#54763,#54764)) ;
#22910 = EDGE_LOOP('',(#54765,#54766,#54767,#54768)) ;
#22911 = EDGE_LOOP('',(#54769,#54770,#54771,#54772)) ;
#22912 = EDGE_LOOP('',(#54773,#54774,#54775,#54776)) ;
#22913 = EDGE_LOOP('',(#54777,#54778,#54779,#54780)) ;
#22914 = EDGE_LOOP('',(#54781,#54782,#54783,#54784,#54785,#54786)) ;
#22915 = EDGE_LOOP('',(#54787,#54788,#54789,#54790)) ;
#22916 = EDGE_LOOP('',(#54791,#54792,#54793,#54794)) ;
#22917 = EDGE_LOOP('',(#54795,#54796,#54797)) ;
#22918 = EDGE_LOOP('',(#54798,#54799,#54800,#54801)) ;
#22919 = EDGE_LOOP('',(#54802,#54803,#54804,#54805)) ;
#22920 = EDGE_LOOP('',(#54806,#54807,#54808)) ;
#22921 = EDGE_LOOP('',(#54809,#54810,#54811)) ;
#22922 = EDGE_LOOP('',(#54812,#54813,#54814,#54815)) ;
#22923 = EDGE_LOOP('',(#54816,#54817,#54818,#54819)) ;
#22924 = EDGE_LOOP('',(#54820,#54821,#54822)) ;
#22925 = EDGE_LOOP('',(#54823,#54824,#54825,#54826)) ;
#22926 = EDGE_LOOP('',(#54827,#54828,#54829,#54830)) ;
#22927 = EDGE_LOOP('',(#54831,#54832,#54833,#54834)) ;
#22928 = EDGE_LOOP('',(#54835,#54836,#54837,#54838)) ;
#22929 = EDGE_LOOP('',(#54839,#54840,#54841,#54842)) ;
#22930 = EDGE_LOOP('',(#54843,#54844,#54845,#54846)) ;
#22931 = EDGE_LOOP('',(#54847,#54848,#54849,#54850)) ;
#22932 = EDGE_LOOP('',(#54851,#54852,#54853,#54854)) ;
#22933 = EDGE_LOOP('',(#54855,#54856,#54857,#54858)) ;
#22934 = EDGE_LOOP('',(#54859,#54860,#54861,#54862)) ;
#22935 = EDGE_LOOP('',(#54863,#54864,#54865)) ;
#22936 = EDGE_LOOP('',(#54866,#54867,#54868)) ;
#22937 = EDGE_LOOP('',(#54869,#54870,#54871,#54872)) ;
#22938 = EDGE_LOOP('',(#54873,#54874,#54875,#54876)) ;
#22939 = EDGE_LOOP('',(#54877,#54878,#54879,#54880)) ;
#22940 = EDGE_LOOP('',(#54881,#54882,#54883,#54884)) ;
#22941 = EDGE_LOOP('',(#54885,#54886,#54887,#54888)) ;
#22942 = EDGE_LOOP('',(#54889,#54890,#54891)) ;
#22943 = EDGE_LOOP('',(#54892,#54893,#54894)) ;
#22944 = EDGE_LOOP('',(#54895,#54896,#54897,#54898)) ;
#22945 = EDGE_LOOP('',(#54899,#54900,#54901,#54902)) ;
#22946 = EDGE_LOOP('',(#54903,#54904,#54905,#54906)) ;
#22947 = EDGE_LOOP('',(#54907,#54908,#54909,#54910)) ;
#22948 = EDGE_LOOP('',(#54911,#54912,#54913,#54914)) ;
#22949 = EDGE_LOOP('',(#54915,#54916,#54917,#54918)) ;
#22950 = EDGE_LOOP('',(#54919,#54920,#54921,#54922)) ;
#22951 = EDGE_LOOP('',(#54923,#54924,#54925,#54926)) ;
#22952 = EDGE_LOOP('',(#54927,#54928,#54929,#54930)) ;
#22953 = EDGE_LOOP('',(#54931,#54932,#54933,#54934)) ;
#22954 = EDGE_LOOP('',(#54935,#54936,#54937,#54938)) ;
#22955 = EDGE_LOOP('',(#54939,#54940,#54941)) ;
#22956 = EDGE_LOOP('',(#54942,#54943,#54944)) ;
#22957 = EDGE_LOOP('',(#54945,#54946,#54947,#54948)) ;
#22958 = EDGE_LOOP('',(#54949,#54950,#54951,#54952)) ;
#22959 = EDGE_LOOP('',(#54953,#54954,#54955,#54956)) ;
#22960 = EDGE_LOOP('',(#54957,#54958,#54959,#54960)) ;
#22961 = EDGE_LOOP('',(#54961,#54962,#54963,#54964)) ;
#22962 = EDGE_LOOP('',(#54965,#54966,#54967)) ;
#22963 = EDGE_LOOP('',(#54968,#54969,#54970)) ;
#22964 = EDGE_LOOP('',(#54971,#54972,#54973,#54974)) ;
#22965 = EDGE_LOOP('',(#54975,#54976,#54977,#54978)) ;
#22966 = EDGE_LOOP('',(#54979,#54980,#54981,#54982)) ;
#22967 = EDGE_LOOP('',(#54983,#54984,#54985)) ;
#22968 = EDGE_LOOP('',(#54986,#54987,#54988,#54989)) ;
#22969 = EDGE_LOOP('',(#54990,#54991,#54992,#54993)) ;
#22970 = EDGE_LOOP('',(#54994,#54995,#54996,#54997)) ;
#22971 = EDGE_LOOP('',(#54998,#54999,#55000,#55001)) ;
#22972 = EDGE_LOOP('',(#55002,#55003,#55004,#55005)) ;
#22973 = EDGE_LOOP('',(#55006,#55007,#55008,#55009)) ;
#22974 = EDGE_LOOP('',(#55010,#55011,#55012,#55013)) ;
#22975 = EDGE_LOOP('',(#55014,#55015,#55016,#55017)) ;
#22976 = EDGE_LOOP('',(#55018,#55019,#55020)) ;
#22977 = EDGE_LOOP('',(#55021,#55022,#55023,#55024)) ;
#22978 = EDGE_LOOP('',(#55025,#55026,#55027,#55028)) ;
#22979 = EDGE_LOOP('',(#55029,#55030,#55031,#55032)) ;
#22980 = EDGE_LOOP('',(#55033,#55034,#55035,#55036)) ;
#22981 = EDGE_LOOP('',(#55037,#55038,#55039,#55040)) ;
#22982 = EDGE_LOOP('',(#55041,#55042,#55043,#55044)) ;
#22983 = EDGE_LOOP('',(#55045,#55046,#55047,#55048)) ;
#22984 = EDGE_LOOP('',(#55049,#55050,#55051,#55052)) ;
#22985 = EDGE_LOOP('',(#55053,#55054,#55055,#55056)) ;
#22986 = EDGE_LOOP('',(#55057,#55058,#55059,#55060)) ;
#22987 = EDGE_LOOP('',(#55061,#55062,#55063,#55064)) ;
#22988 = EDGE_LOOP('',(#55065,#55066,#55067,#55068)) ;
#22989 = EDGE_LOOP('',(#55069,#55070,#55071,#55072)) ;
#22990 = EDGE_LOOP('',(#55073,#55074,#55075,#55076)) ;
#22991 = EDGE_LOOP('',(#55077,#55078,#55079)) ;
#22992 = EDGE_LOOP('',(#55080,#55081,#55082,#55083)) ;
#22993 = EDGE_LOOP('',(#55084,#55085,#55086,#55087)) ;
#22994 = EDGE_LOOP('',(#55088,#55089,#55090,#55091)) ;
#22995 = EDGE_LOOP('',(#55092,#55093,#55094,#55095)) ;
#22996 = EDGE_LOOP('',(#55096,#55097,#55098,#55099)) ;
#22997 = EDGE_LOOP('',(#55100,#55101,#55102,#55103)) ;
#22998 = EDGE_LOOP('',(#55104,#55105,#55106,#55107)) ;
#22999 = EDGE_LOOP('',(#55108,#55109,#55110,#55111)) ;
#23000 = EDGE_LOOP('',(#55112,#55113,#55114,#55115)) ;
#23001 = EDGE_LOOP('',(#55116,#55117,#55118)) ;
#23002 = EDGE_LOOP('',(#55119,#55120,#55121,#55122,#55123)) ;
#23003 = EDGE_LOOP('',(#55124,#55125,#55126,#55127)) ;
#23004 = EDGE_LOOP('',(#55128,#55129,#55130,#55131)) ;
#23005 = EDGE_LOOP('',(#55132,#55133,#55134,#55135)) ;
#23006 = EDGE_LOOP('',(#55136,#55137,#55138,#55139)) ;
#23007 = EDGE_LOOP('',(#55140,#55141,#55142)) ;
#23008 = EDGE_LOOP('',(#55143,#55144,#55145,#55146)) ;
#23009 = EDGE_LOOP('',(#55147,#55148,#55149,#55150)) ;
#23010 = EDGE_LOOP('',(#55151,#55152,#55153)) ;
#23011 = EDGE_LOOP('',(#55154,#55155,#55156,#55157,#55158,#55159,#55160,#55161)) ;
#23012 = EDGE_LOOP('',(#55162,#55163,#55164,#55165)) ;
#23013 = EDGE_LOOP('',(#55166,#55167,#55168,#55169)) ;
#23014 = EDGE_LOOP('',(#55170,#55171,#55172,#55173)) ;
#23015 = EDGE_LOOP('',(#55174,#55175,#55176,#55177)) ;
#23016 = EDGE_LOOP('',(#55178,#55179,#55180,#55181)) ;
#23017 = EDGE_LOOP('',(#55182,#55183,#55184,#55185)) ;
#23018 = EDGE_LOOP('',(#55186,#55187,#55188,#55189)) ;
#23019 = EDGE_LOOP('',(#55190,#55191,#55192,#55193)) ;
#23020 = EDGE_LOOP('',(#55194,#55195,#55196,#55197)) ;
#23021 = EDGE_LOOP('',(#55198,#55199,#55200,#55201,#55202,#55203,#55204)) ;
#23022 = EDGE_LOOP('',(#55205,#55206,#55207,#55208,#55209,#55210,#55211)) ;
#23023 = EDGE_LOOP('',(#55212,#55213,#55214,#55215)) ;
#23024 = EDGE_LOOP('',(#55216,#55217,#55218,#55219)) ;
#23025 = EDGE_LOOP('',(#55220,#55221,#55222)) ;
#23026 = EDGE_LOOP('',(#55223,#55224,#55225,#55226)) ;
#23027 = EDGE_LOOP('',(#55227,#55228,#55229,#55230,#55231,#55232,#55233,#55234,
#55235,#55236,#55237,#55238,#55239,#55240,#55241,#55242,#55243,#55244,#55245,
#55246,#55247,#55248,#55249,#55250,#55251,#55252,#55253,#55254,#55255,#55256,
#55257,#55258,#55259,#55260,#55261,#55262,#55263,#55264)) ;
#23028 = EDGE_LOOP('',(#55265,#55266,#55267,#55268)) ;
#23029 = EDGE_LOOP('',(#55269,#55270,#55271,#55272)) ;
#23030 = EDGE_LOOP('',(#55273,#55274,#55275,#55276,#55277,#55278,#55279,#55280)) ;
#23031 = EDGE_LOOP('',(#55281,#55282,#55283,#55284,#55285,#55286,#55287,#55288)) ;
#23032 = EDGE_LOOP('',(#55289,#55290,#55291,#55292,#55293,#55294,#55295,#55296)) ;
#23033 = EDGE_LOOP('',(#55297,#55298,#55299,#55300)) ;
#23034 = EDGE_LOOP('',(#55301,#55302,#55303,#55304)) ;
#23035 = EDGE_LOOP('',(#55305,#55306,#55307,#55308,#55309,#55310)) ;
#23036 = EDGE_LOOP('',(#55311,#55312,#55313,#55314,#55315,#55316)) ;
#23037 = EDGE_LOOP('',(#55317,#55318,#55319,#55320)) ;
#23038 = EDGE_LOOP('',(#55321,#55322,#55323,#55324)) ;
#23039 = EDGE_LOOP('',(#55325,#55326,#55327,#55328)) ;
#23040 = EDGE_LOOP('',(#55329,#55330,#55331,#55332)) ;
#23041 = EDGE_LOOP('',(#55333,#55334,#55335,#55336)) ;
#23042 = EDGE_LOOP('',(#55337,#55338,#55339,#55340,#55341,#55342,#55343,#55344)) ;
#23043 = EDGE_LOOP('',(#55345,#55346,#55347,#55348)) ;
#23044 = EDGE_LOOP('',(#55349,#55350,#55351,#55352)) ;
#23045 = EDGE_LOOP('',(#55353,#55354,#55355,#55356)) ;
#23046 = EDGE_LOOP('',(#55357,#55358,#55359,#55360)) ;
#23047 = EDGE_LOOP('',(#55361,#55362,#55363,#55364)) ;
#23048 = EDGE_LOOP('',(#55365,#55366,#55367,#55368)) ;
#23049 = EDGE_LOOP('',(#55369,#55370,#55371,#55372)) ;
#23050 = EDGE_LOOP('',(#55373,#55374,#55375,#55376)) ;
#23051 = EDGE_LOOP('',(#55377,#55378,#55379,#55380,#55381,#55382,#55383,#55384)) ;
#23052 = EDGE_LOOP('',(#55385,#55386)) ;
#23053 = EDGE_LOOP('',(#55387,#55388,#55389,#55390)) ;
#23054 = EDGE_LOOP('',(#55391,#55392,#55393,#55394)) ;
#23055 = EDGE_LOOP('',(#55395,#55396,#55397,#55398)) ;
#23056 = EDGE_LOOP('',(#55399,#55400,#55401,#55402)) ;
#23057 = EDGE_LOOP('',(#55403,#55404,#55405,#55406)) ;
#23058 = EDGE_LOOP('',(#55407,#55408,#55409,#55410)) ;
#23059 = EDGE_LOOP('',(#55411,#55412,#55413,#55414)) ;
#23060 = EDGE_LOOP('',(#55415,#55416,#55417,#55418)) ;
#23061 = EDGE_LOOP('',(#55419,#55420,#55421,#55422,#55423,#55424,#55425,#55426)) ;
#23062 = EDGE_LOOP('',(#55427,#55428,#55429,#55430)) ;
#23063 = EDGE_LOOP('',(#55431,#55432,#55433,#55434)) ;
#23064 = EDGE_LOOP('',(#55435,#55436,#55437,#55438)) ;
#23065 = EDGE_LOOP('',(#55439,#55440,#55441,#55442)) ;
#23066 = EDGE_LOOP('',(#55443,#55444,#55445,#55446)) ;
#23067 = EDGE_LOOP('',(#55447,#55448,#55449,#55450)) ;
#23068 = EDGE_LOOP('',(#55451,#55452,#55453,#55454)) ;
#23069 = EDGE_LOOP('',(#55455,#55456,#55457,#55458)) ;
#23070 = EDGE_LOOP('',(#55459,#55460,#55461,#55462)) ;
#23071 = EDGE_LOOP('',(#55463,#55464,#55465,#55466)) ;
#23072 = EDGE_LOOP('',(#55467,#55468,#55469,#55470)) ;
#23073 = EDGE_LOOP('',(#55471,#55472,#55473,#55474)) ;
#23074 = EDGE_LOOP('',(#55475,#55476,#55477,#55478,#55479,#55480)) ;
#23075 = EDGE_LOOP('',(#55481)) ;
#23076 = EDGE_LOOP('',(#55482,#55483,#55484,#55485,#55486,#55487)) ;
#23077 = EDGE_LOOP('',(#55488,#55489,#55490,#55491)) ;
#23078 = EDGE_LOOP('',(#55492,#55493,#55494,#55495)) ;
#23079 = EDGE_LOOP('',(#55496,#55497,#55498,#55499)) ;
#23080 = EDGE_LOOP('',(#55500,#55501,#55502,#55503)) ;
#23081 = EDGE_LOOP('',(#55504,#55505,#55506,#55507)) ;
#23082 = EDGE_LOOP('',(#55508,#55509,#55510,#55511)) ;
#23083 = EDGE_LOOP('',(#55512,#55513,#55514,#55515)) ;
#23084 = EDGE_LOOP('',(#55516,#55517,#55518,#55519)) ;
#23085 = EDGE_LOOP('',(#55520,#55521,#55522,#55523)) ;
#23086 = EDGE_LOOP('',(#55524,#55525,#55526)) ;
#23087 = EDGE_LOOP('',(#55527,#55528,#55529,#55530)) ;
#23088 = EDGE_LOOP('',(#55531,#55532,#55533,#55534)) ;
#23089 = EDGE_LOOP('',(#55535,#55536,#55537,#55538)) ;
#23090 = EDGE_LOOP('',(#55539,#55540,#55541,#55542)) ;
#23091 = EDGE_LOOP('',(#55543,#55544,#55545,#55546)) ;
#23092 = EDGE_LOOP('',(#55547,#55548,#55549,#55550)) ;
#23093 = EDGE_LOOP('',(#55551,#55552,#55553,#55554)) ;
#23094 = EDGE_LOOP('',(#55555,#55556,#55557,#55558)) ;
#23095 = EDGE_LOOP('',(#55559,#55560,#55561,#55562)) ;
#23096 = EDGE_LOOP('',(#55563,#55564,#55565)) ;
#23097 = EDGE_LOOP('',(#55566,#55567,#55568,#55569)) ;
#23098 = EDGE_LOOP('',(#55570,#55571,#55572)) ;
#23099 = EDGE_LOOP('',(#55573,#55574,#55575,#55576)) ;
#23100 = EDGE_LOOP('',(#55577,#55578,#55579,#55580)) ;
#23101 = EDGE_LOOP('',(#55581,#55582,#55583,#55584)) ;
#23102 = EDGE_LOOP('',(#55585,#55586,#55587,#55588)) ;
#23103 = EDGE_LOOP('',(#55589,#55590,#55591,#55592)) ;
#23104 = EDGE_LOOP('',(#55593,#55594,#55595)) ;
#23105 = EDGE_LOOP('',(#55596,#55597,#55598,#55599)) ;
#23106 = EDGE_LOOP('',(#55600,#55601,#55602,#55603)) ;
#23107 = EDGE_LOOP('',(#55604,#55605,#55606,#55607)) ;
#23108 = EDGE_LOOP('',(#55608,#55609,#55610,#55611)) ;
#23109 = EDGE_LOOP('',(#55612,#55613,#55614,#55615)) ;
#23110 = EDGE_LOOP('',(#55616,#55617,#55618,#55619,#55620,#55621)) ;
#23111 = EDGE_LOOP('',(#55622,#55623,#55624,#55625)) ;
#23112 = EDGE_LOOP('',(#55626,#55627,#55628,#55629)) ;
#23113 = EDGE_LOOP('',(#55630,#55631,#55632,#55633)) ;
#23114 = EDGE_LOOP('',(#55634,#55635,#55636,#55637)) ;
#23115 = EDGE_LOOP('',(#55638,#55639,#55640,#55641)) ;
#23116 = EDGE_LOOP('',(#55642,#55643,#55644,#55645,#55646,#55647)) ;
#23117 = EDGE_LOOP('',(#55648,#55649,#55650,#55651)) ;
#23118 = EDGE_LOOP('',(#55652,#55653,#55654,#55655)) ;
#23119 = EDGE_LOOP('',(#55656,#55657,#55658)) ;
#23120 = EDGE_LOOP('',(#55659,#55660,#55661,#55662)) ;
#23121 = EDGE_LOOP('',(#55663,#55664,#55665,#55666)) ;
#23122 = EDGE_LOOP('',(#55667,#55668,#55669)) ;
#23123 = EDGE_LOOP('',(#55670,#55671,#55672)) ;
#23124 = EDGE_LOOP('',(#55673,#55674,#55675,#55676)) ;
#23125 = EDGE_LOOP('',(#55677,#55678,#55679,#55680)) ;
#23126 = EDGE_LOOP('',(#55681,#55682,#55683)) ;
#23127 = EDGE_LOOP('',(#55684,#55685,#55686,#55687)) ;
#23128 = EDGE_LOOP('',(#55688,#55689,#55690,#55691)) ;
#23129 = EDGE_LOOP('',(#55692,#55693,#55694,#55695)) ;
#23130 = EDGE_LOOP('',(#55696,#55697,#55698,#55699)) ;
#23131 = EDGE_LOOP('',(#55700,#55701,#55702,#55703)) ;
#23132 = EDGE_LOOP('',(#55704,#55705,#55706,#55707)) ;
#23133 = EDGE_LOOP('',(#55708,#55709,#55710,#55711)) ;
#23134 = EDGE_LOOP('',(#55712,#55713,#55714,#55715)) ;
#23135 = EDGE_LOOP('',(#55716,#55717,#55718,#55719)) ;
#23136 = EDGE_LOOP('',(#55720,#55721,#55722,#55723)) ;
#23137 = EDGE_LOOP('',(#55724,#55725,#55726)) ;
#23138 = EDGE_LOOP('',(#55727,#55728,#55729)) ;
#23139 = EDGE_LOOP('',(#55730,#55731,#55732,#55733)) ;
#23140 = EDGE_LOOP('',(#55734,#55735,#55736,#55737)) ;
#23141 = EDGE_LOOP('',(#55738,#55739,#55740,#55741)) ;
#23142 = EDGE_LOOP('',(#55742,#55743,#55744,#55745)) ;
#23143 = EDGE_LOOP('',(#55746,#55747,#55748,#55749)) ;
#23144 = EDGE_LOOP('',(#55750,#55751,#55752)) ;
#23145 = EDGE_LOOP('',(#55753,#55754,#55755)) ;
#23146 = EDGE_LOOP('',(#55756,#55757,#55758,#55759)) ;
#23147 = EDGE_LOOP('',(#55760,#55761,#55762,#55763)) ;
#23148 = EDGE_LOOP('',(#55764,#55765,#55766,#55767)) ;
#23149 = EDGE_LOOP('',(#55768,#55769,#55770,#55771)) ;
#23150 = EDGE_LOOP('',(#55772,#55773,#55774,#55775)) ;
#23151 = EDGE_LOOP('',(#55776,#55777,#55778,#55779)) ;
#23152 = EDGE_LOOP('',(#55780,#55781,#55782,#55783)) ;
#23153 = EDGE_LOOP('',(#55784,#55785,#55786,#55787)) ;
#23154 = EDGE_LOOP('',(#55788,#55789,#55790,#55791)) ;
#23155 = EDGE_LOOP('',(#55792,#55793,#55794,#55795)) ;
#23156 = EDGE_LOOP('',(#55796,#55797,#55798,#55799)) ;
#23157 = EDGE_LOOP('',(#55800,#55801,#55802)) ;
#23158 = EDGE_LOOP('',(#55803,#55804,#55805)) ;
#23159 = EDGE_LOOP('',(#55806,#55807,#55808,#55809)) ;
#23160 = EDGE_LOOP('',(#55810,#55811,#55812,#55813)) ;
#23161 = EDGE_LOOP('',(#55814,#55815,#55816,#55817)) ;
#23162 = EDGE_LOOP('',(#55818,#55819,#55820,#55821)) ;
#23163 = EDGE_LOOP('',(#55822,#55823,#55824,#55825)) ;
#23164 = EDGE_LOOP('',(#55826,#55827,#55828)) ;
#23165 = EDGE_LOOP('',(#55829,#55830,#55831)) ;
#23166 = EDGE_LOOP('',(#55832,#55833,#55834,#55835)) ;
#23167 = EDGE_LOOP('',(#55836,#55837,#55838,#55839)) ;
#23168 = EDGE_LOOP('',(#55840,#55841,#55842)) ;
#23169 = EDGE_LOOP('',(#55843,#55844,#55845,#55846)) ;
#23170 = EDGE_LOOP('',(#55847,#55848,#55849,#55850)) ;
#23171 = EDGE_LOOP('',(#55851,#55852,#55853,#55854)) ;
#23172 = EDGE_LOOP('',(#55855,#55856,#55857,#55858)) ;
#23173 = EDGE_LOOP('',(#55859,#55860,#55861,#55862)) ;
#23174 = EDGE_LOOP('',(#55863,#55864,#55865,#55866)) ;
#23175 = EDGE_LOOP('',(#55867,#55868,#55869,#55870)) ;
#23176 = EDGE_LOOP('',(#55871,#55872,#55873)) ;
#23177 = EDGE_LOOP('',(#55874,#55875,#55876,#55877)) ;
#23178 = EDGE_LOOP('',(#55878,#55879,#55880,#55881)) ;
#23179 = EDGE_LOOP('',(#55882,#55883,#55884,#55885)) ;
#23180 = EDGE_LOOP('',(#55886,#55887,#55888,#55889)) ;
#23181 = EDGE_LOOP('',(#55890,#55891,#55892,#55893)) ;
#23182 = EDGE_LOOP('',(#55894,#55895,#55896)) ;
#23183 = EDGE_LOOP('',(#55897,#55898,#55899,#55900)) ;
#23184 = EDGE_LOOP('',(#55901,#55902,#55903,#55904)) ;
#23185 = EDGE_LOOP('',(#55905,#55906,#55907,#55908)) ;
#23186 = EDGE_LOOP('',(#55909,#55910,#55911,#55912)) ;
#23187 = EDGE_LOOP('',(#55913,#55914,#55915,#55916)) ;
#23188 = EDGE_LOOP('',(#55917,#55918,#55919,#55920)) ;
#23189 = EDGE_LOOP('',(#55921,#55922,#55923,#55924)) ;
#23190 = EDGE_LOOP('',(#55925,#55926,#55927,#55928)) ;
#23191 = EDGE_LOOP('',(#55929,#55930,#55931)) ;
#23192 = EDGE_LOOP('',(#55932,#55933,#55934,#55935,#55936)) ;
#23193 = EDGE_LOOP('',(#55937,#55938,#55939,#55940)) ;
#23194 = EDGE_LOOP('',(#55941,#55942,#55943,#55944)) ;
#23195 = EDGE_LOOP('',(#55945,#55946,#55947,#55948)) ;
#23196 = EDGE_LOOP('',(#55949,#55950,#55951)) ;
#23197 = EDGE_LOOP('',(#55952,#55953,#55954,#55955)) ;
#23198 = EDGE_LOOP('',(#55956,#55957,#55958,#55959)) ;
#23199 = EDGE_LOOP('',(#55960,#55961,#55962)) ;
#23200 = EDGE_LOOP('',(#55963,#55964,#55965)) ;
#23201 = EDGE_LOOP('',(#55966,#55967,#55968)) ;
#23202 = EDGE_LOOP('',(#55969,#55970,#55971,#55972)) ;
#23203 = EDGE_LOOP('',(#55973,#55974,#55975,#55976)) ;
#23204 = EDGE_LOOP('',(#55977,#55978,#55979,#55980)) ;
#23205 = EDGE_LOOP('',(#55981,#55982,#55983,#55984)) ;
#23206 = EDGE_LOOP('',(#55985,#55986,#55987)) ;
#23207 = EDGE_LOOP('',(#55988,#55989,#55990)) ;
#23208 = EDGE_LOOP('',(#55991,#55992,#55993)) ;
#23209 = EDGE_LOOP('',(#55994,#55995,#55996)) ;
#23210 = EDGE_LOOP('',(#55997,#55998,#55999,#56000)) ;
#23211 = EDGE_LOOP('',(#56001,#56002,#56003,#56004)) ;
#23212 = EDGE_LOOP('',(#56005,#56006,#56007,#56008)) ;
#23213 = EDGE_LOOP('',(#56009,#56010,#56011,#56012)) ;
#23214 = EDGE_LOOP('',(#56013,#56014,#56015,#56016)) ;
#23215 = EDGE_LOOP('',(#56017,#56018,#56019,#56020)) ;
#23216 = EDGE_LOOP('',(#56021,#56022,#56023,#56024)) ;
#23217 = EDGE_LOOP('',(#56025,#56026,#56027,#56028)) ;
#23218 = EDGE_LOOP('',(#56029,#56030,#56031,#56032)) ;
#23219 = EDGE_LOOP('',(#56033,#56034,#56035,#56036)) ;
#23220 = EDGE_LOOP('',(#56037,#56038,#56039,#56040)) ;
#23221 = EDGE_LOOP('',(#56041,#56042,#56043,#56044)) ;
#23222 = EDGE_LOOP('',(#56045,#56046,#56047,#56048)) ;
#23223 = EDGE_LOOP('',(#56049,#56050,#56051,#56052)) ;
#23224 = EDGE_LOOP('',(#56053,#56054,#56055,#56056)) ;
#23225 = EDGE_LOOP('',(#56057,#56058,#56059,#56060)) ;
#23226 = EDGE_LOOP('',(#56061,#56062,#56063,#56064)) ;
#23227 = EDGE_LOOP('',(#56065,#56066,#56067,#56068,#56069)) ;
#23228 = EDGE_LOOP('',(#56070,#56071,#56072,#56073)) ;
#23229 = EDGE_LOOP('',(#56074,#56075,#56076,#56077,#56078)) ;
#23230 = EDGE_LOOP('',(#56079,#56080,#56081,#56082)) ;
#23231 = EDGE_LOOP('',(#56083,#56084,#56085)) ;
#23232 = EDGE_LOOP('',(#56086,#56087,#56088,#56089)) ;
#23233 = EDGE_LOOP('',(#56090,#56091,#56092)) ;
#23234 = EDGE_LOOP('',(#56093,#56094,#56095,#56096)) ;
#23235 = EDGE_LOOP('',(#56097,#56098,#56099,#56100,#56101)) ;
#23236 = EDGE_LOOP('',(#56102,#56103,#56104,#56105,#56106,#56107,#56108,#56109,
#56110,#56111,#56112,#56113,#56114,#56115,#56116,#56117,#56118,#56119,#56120,
#56121,#56122)) ;
#23237 = EDGE_LOOP('',(#56123,#56124,#56125,#56126)) ;
#23238 = EDGE_LOOP('',(#56127,#56128,#56129,#56130)) ;
#23239 = EDGE_LOOP('',(#56131,#56132,#56133,#56134,#56135)) ;
#23240 = EDGE_LOOP('',(#56136,#56137,#56138,#56139)) ;
#23241 = EDGE_LOOP('',(#56140,#56141,#56142,#56143,#56144)) ;
#23242 = EDGE_LOOP('',(#56145,#56146,#56147,#56148)) ;
#23243 = EDGE_LOOP('',(#56149,#56150,#56151)) ;
#23244 = EDGE_LOOP('',(#56152,#56153,#56154,#56155)) ;
#23245 = EDGE_LOOP('',(#56156,#56157,#56158)) ;
#23246 = EDGE_LOOP('',(#56159,#56160,#56161,#56162)) ;
#23247 = EDGE_LOOP('',(#56163,#56164,#56165,#56166,#56167)) ;
#23248 = EDGE_LOOP('',(#56168,#56169,#56170,#56171,#56172,#56173,#56174,#56175,
#56176,#56177,#56178,#56179,#56180,#56181,#56182,#56183,#56184,#56185,#56186,
#56187,#56188)) ;
#23249 = EDGE_LOOP('',(#56189,#56190,#56191,#56192)) ;
#23250 = EDGE_LOOP('',(#56193,#56194,#56195,#56196,#56197,#56198,#56199,#56200)) ;
#23251 = EDGE_LOOP('',(#56201,#56202,#56203,#56204)) ;
#23252 = EDGE_LOOP('',(#56205,#56206,#56207,#56208)) ;
#23253 = EDGE_LOOP('',(#56209,#56210,#56211,#56212)) ;
#23254 = EDGE_LOOP('',(#56213,#56214,#56215,#56216)) ;
#23255 = EDGE_LOOP('',(#56217,#56218,#56219,#56220)) ;
#23256 = EDGE_LOOP('',(#56221,#56222,#56223,#56224)) ;
#23257 = EDGE_LOOP('',(#56225,#56226,#56227,#56228,#56229,#56230)) ;
#23258 = EDGE_LOOP('',(#56231,#56232,#56233,#56234)) ;
#23259 = EDGE_LOOP('',(#56235,#56236,#56237,#56238)) ;
#23260 = EDGE_LOOP('',(#56239,#56240,#56241,#56242)) ;
#23261 = EDGE_LOOP('',(#56243,#56244,#56245)) ;
#23262 = EDGE_LOOP('',(#56246,#56247,#56248,#56249,#56250,#56251,#56252,#56253,
#56254,#56255,#56256,#56257,#56258,#56259,#56260,#56261,#56262,#56263,#56264,
#56265,#56266,#56267,#56268,#56269)) ;
#23263 = EDGE_LOOP('',(#56270)) ;
#23264 = EDGE_LOOP('',(#56271)) ;
#23265 = EDGE_LOOP('',(#56272,#56273,#56274,#56275)) ;
#23266 = EDGE_LOOP('',(#56276,#56277,#56278,#56279,#56280,#56281,#56282,#56283,
#56284,#56285,#56286,#56287)) ;
#23267 = EDGE_LOOP('',(#56288,#56289,#56290,#56291)) ;
#23268 = EDGE_LOOP('',(#56292,#56293,#56294,#56295,#56296,#56297)) ;
#23269 = EDGE_LOOP('',(#56298,#56299,#56300,#56301)) ;
#23270 = EDGE_LOOP('',(#56302,#56303,#56304,#56305,#56306,#56307,#56308,#56309)) ;
#23271 = EDGE_LOOP('',(#56310)) ;
#23272 = EDGE_LOOP('',(#56311,#56312,#56313,#56314,#56315,#56316,#56317,#56318)) ;
#23273 = EDGE_LOOP('',(#56319)) ;
#23274 = EDGE_LOOP('',(#56320,#56321,#56322,#56323)) ;
#23275 = EDGE_LOOP('',(#56324,#56325,#56326,#56327)) ;
#23276 = EDGE_LOOP('',(#56328,#56329,#56330,#56331)) ;
#23277 = EDGE_LOOP('',(#56332,#56333,#56334,#56335)) ;
#23278 = EDGE_LOOP('',(#56336,#56337,#56338,#56339,#56340,#56341,#56342,#56343)) ;
#23279 = EDGE_LOOP('',(#56344,#56345,#56346,#56347,#56348,#56349,#56350,#56351)) ;
#23280 = EDGE_LOOP('',(#56352,#56353,#56354,#56355)) ;
#23281 = EDGE_LOOP('',(#56356,#56357,#56358,#56359,#56360,#56361,#56362,#56363)) ;
#23282 = EDGE_LOOP('',(#56364,#56365,#56366,#56367,#56368,#56369,#56370,#56371)) ;
#23283 = EDGE_LOOP('',(#56372,#56373,#56374,#56375)) ;
#23284 = EDGE_LOOP('',(#56376,#56377,#56378,#56379,#56380,#56381,#56382,#56383,
#56384,#56385,#56386,#56387,#56388,#56389)) ;
#23285 = EDGE_LOOP('',(#56390,#56391,#56392,#56393)) ;
#23286 = EDGE_LOOP('',(#56394,#56395,#56396,#56397)) ;
#23287 = EDGE_LOOP('',(#56398,#56399,#56400,#56401,#56402,#56403,#56404,#56405,
#56406,#56407,#56408,#56409,#56410,#56411,#56412,#56413,#56414,#56415,#56416,
#56417,#56418,#56419,#56420,#56421,#56422,#56423,#56424,#56425,#56426,#56427,
#56428,#56429)) ;
#23288 = EDGE_LOOP('',(#56430,#56431,#56432,#56433)) ;
#23289 = EDGE_LOOP('',(#56434,#56435,#56436,#56437)) ;
#23290 = EDGE_LOOP('',(#56438,#56439,#56440,#56441,#56442,#56443,#56444,#56445)) ;
#23291 = EDGE_LOOP('',(#56446,#56447,#56448,#56449,#56450,#56451,#56452,#56453)) ;
#23292 = EDGE_LOOP('',(#56454,#56455,#56456,#56457,#56458,#56459,#56460,#56461)) ;
#23293 = EDGE_LOOP('',(#56462,#56463,#56464,#56465)) ;
#23294 = EDGE_LOOP('',(#56466,#56467,#56468,#56469)) ;
#23295 = EDGE_LOOP('',(#56470,#56471,#56472,#56473,#56474,#56475)) ;
#23296 = EDGE_LOOP('',(#56476,#56477,#56478,#56479,#56480,#56481)) ;
#23297 = EDGE_LOOP('',(#56482,#56483,#56484,#56485)) ;
#23298 = EDGE_LOOP('',(#56486,#56487,#56488,#56489)) ;
#23299 = EDGE_LOOP('',(#56490,#56491,#56492,#56493)) ;
#23300 = EDGE_LOOP('',(#56494,#56495,#56496,#56497)) ;
#23301 = EDGE_LOOP('',(#56498,#56499,#56500,#56501)) ;
#23302 = EDGE_LOOP('',(#56502,#56503,#56504,#56505,#56506,#56507,#56508,#56509)) ;
#23303 = EDGE_LOOP('',(#56510,#56511,#56512,#56513)) ;
#23304 = EDGE_LOOP('',(#56514,#56515,#56516,#56517)) ;
#23305 = EDGE_LOOP('',(#56518,#56519,#56520,#56521)) ;
#23306 = EDGE_LOOP('',(#56522,#56523,#56524,#56525)) ;
#23307 = EDGE_LOOP('',(#56526,#56527,#56528,#56529)) ;
#23308 = EDGE_LOOP('',(#56530,#56531,#56532,#56533)) ;
#23309 = EDGE_LOOP('',(#56534,#56535,#56536,#56537)) ;
#23310 = EDGE_LOOP('',(#56538,#56539,#56540,#56541)) ;
#23311 = EDGE_LOOP('',(#56542,#56543,#56544,#56545,#56546,#56547,#56548,#56549)) ;
#23312 = EDGE_LOOP('',(#56550,#56551)) ;
#23313 = EDGE_LOOP('',(#56552,#56553,#56554,#56555)) ;
#23314 = EDGE_LOOP('',(#56556,#56557,#56558,#56559)) ;
#23315 = EDGE_LOOP('',(#56560,#56561,#56562,#56563)) ;
#23316 = EDGE_LOOP('',(#56564,#56565,#56566,#56567)) ;
#23317 = EDGE_LOOP('',(#56568,#56569,#56570,#56571)) ;
#23318 = EDGE_LOOP('',(#56572,#56573,#56574,#56575)) ;
#23319 = EDGE_LOOP('',(#56576,#56577,#56578,#56579)) ;
#23320 = EDGE_LOOP('',(#56580,#56581,#56582,#56583)) ;
#23321 = EDGE_LOOP('',(#56584,#56585,#56586,#56587,#56588,#56589,#56590,#56591)) ;
#23322 = EDGE_LOOP('',(#56592,#56593,#56594,#56595)) ;
#23323 = EDGE_LOOP('',(#56596,#56597,#56598,#56599)) ;
#23324 = EDGE_LOOP('',(#56600,#56601,#56602,#56603)) ;
#23325 = EDGE_LOOP('',(#56604,#56605,#56606,#56607)) ;
#23326 = EDGE_LOOP('',(#56608,#56609,#56610,#56611)) ;
#23327 = EDGE_LOOP('',(#56612,#56613,#56614,#56615)) ;
#23328 = EDGE_LOOP('',(#56616,#56617,#56618,#56619)) ;
#23329 = EDGE_LOOP('',(#56620,#56621,#56622,#56623)) ;
#23330 = EDGE_LOOP('',(#56624,#56625,#56626,#56627)) ;
#23331 = EDGE_LOOP('',(#56628,#56629,#56630,#56631)) ;
#23332 = EDGE_LOOP('',(#56632,#56633,#56634,#56635)) ;
#23333 = EDGE_LOOP('',(#56636,#56637,#56638,#56639)) ;
#23334 = EDGE_LOOP('',(#56640,#56641,#56642,#56643,#56644,#56645)) ;
#23335 = EDGE_LOOP('',(#56646)) ;
#23336 = EDGE_LOOP('',(#56647,#56648,#56649,#56650,#56651,#56652)) ;
#23337 = EDGE_LOOP('',(#56653,#56654,#56655,#56656)) ;
#23338 = EDGE_LOOP('',(#56657,#56658,#56659,#56660)) ;
#23339 = EDGE_LOOP('',(#56661,#56662,#56663,#56664)) ;
#23340 = EDGE_LOOP('',(#56665,#56666,#56667,#56668)) ;
#23341 = EDGE_LOOP('',(#56669,#56670,#56671,#56672)) ;
#23342 = EDGE_LOOP('',(#56673,#56674,#56675,#56676)) ;
#23343 = EDGE_LOOP('',(#56677,#56678,#56679,#56680)) ;
#23344 = EDGE_LOOP('',(#56681,#56682,#56683,#56684)) ;
#23345 = EDGE_LOOP('',(#56685,#56686,#56687,#56688)) ;
#23346 = EDGE_LOOP('',(#56689,#56690,#56691)) ;
#23347 = EDGE_LOOP('',(#56692,#56693,#56694,#56695)) ;
#23348 = EDGE_LOOP('',(#56696,#56697,#56698,#56699)) ;
#23349 = EDGE_LOOP('',(#56700,#56701,#56702,#56703)) ;
#23350 = EDGE_LOOP('',(#56704,#56705,#56706,#56707)) ;
#23351 = EDGE_LOOP('',(#56708,#56709,#56710,#56711)) ;
#23352 = EDGE_LOOP('',(#56712,#56713,#56714,#56715)) ;
#23353 = EDGE_LOOP('',(#56716,#56717,#56718,#56719)) ;
#23354 = EDGE_LOOP('',(#56720,#56721,#56722,#56723)) ;
#23355 = EDGE_LOOP('',(#56724,#56725,#56726,#56727)) ;
#23356 = EDGE_LOOP('',(#56728,#56729,#56730)) ;
#23357 = EDGE_LOOP('',(#56731,#56732,#56733,#56734)) ;
#23358 = EDGE_LOOP('',(#56735,#56736,#56737)) ;
#23359 = EDGE_LOOP('',(#56738,#56739,#56740,#56741)) ;
#23360 = EDGE_LOOP('',(#56742,#56743,#56744,#56745)) ;
#23361 = EDGE_LOOP('',(#56746,#56747,#56748,#56749)) ;
#23362 = EDGE_LOOP('',(#56750,#56751,#56752,#56753)) ;
#23363 = EDGE_LOOP('',(#56754,#56755,#56756,#56757)) ;
#23364 = EDGE_LOOP('',(#56758,#56759,#56760)) ;
#23365 = EDGE_LOOP('',(#56761,#56762,#56763,#56764)) ;
#23366 = EDGE_LOOP('',(#56765,#56766,#56767,#56768)) ;
#23367 = EDGE_LOOP('',(#56769,#56770,#56771,#56772)) ;
#23368 = EDGE_LOOP('',(#56773,#56774,#56775,#56776)) ;
#23369 = EDGE_LOOP('',(#56777,#56778,#56779,#56780)) ;
#23370 = EDGE_LOOP('',(#56781,#56782,#56783,#56784,#56785,#56786)) ;
#23371 = EDGE_LOOP('',(#56787,#56788,#56789,#56790)) ;
#23372 = EDGE_LOOP('',(#56791,#56792,#56793,#56794)) ;
#23373 = EDGE_LOOP('',(#56795,#56796,#56797,#56798)) ;
#23374 = EDGE_LOOP('',(#56799,#56800,#56801,#56802)) ;
#23375 = EDGE_LOOP('',(#56803,#56804,#56805,#56806)) ;
#23376 = EDGE_LOOP('',(#56807,#56808,#56809,#56810)) ;
#23377 = EDGE_LOOP('',(#56811,#56812,#56813,#56814,#56815,#56816)) ;
#23378 = EDGE_LOOP('',(#56817,#56818,#56819,#56820)) ;
#23379 = EDGE_LOOP('',(#56821,#56822,#56823,#56824)) ;
#23380 = EDGE_LOOP('',(#56825,#56826,#56827)) ;
#23381 = EDGE_LOOP('',(#56828,#56829,#56830,#56831)) ;
#23382 = EDGE_LOOP('',(#56832,#56833,#56834,#56835)) ;
#23383 = EDGE_LOOP('',(#56836,#56837,#56838)) ;
#23384 = EDGE_LOOP('',(#56839,#56840,#56841)) ;
#23385 = EDGE_LOOP('',(#56842,#56843,#56844,#56845)) ;
#23386 = EDGE_LOOP('',(#56846,#56847,#56848,#56849)) ;
#23387 = EDGE_LOOP('',(#56850,#56851,#56852)) ;
#23388 = EDGE_LOOP('',(#56853,#56854,#56855,#56856)) ;
#23389 = EDGE_LOOP('',(#56857,#56858,#56859,#56860)) ;
#23390 = EDGE_LOOP('',(#56861,#56862,#56863,#56864)) ;
#23391 = EDGE_LOOP('',(#56865,#56866,#56867,#56868)) ;
#23392 = EDGE_LOOP('',(#56869,#56870,#56871,#56872)) ;
#23393 = EDGE_LOOP('',(#56873,#56874,#56875,#56876)) ;
#23394 = EDGE_LOOP('',(#56877,#56878,#56879,#56880)) ;
#23395 = EDGE_LOOP('',(#56881,#56882,#56883,#56884)) ;
#23396 = EDGE_LOOP('',(#56885,#56886,#56887,#56888)) ;
#23397 = EDGE_LOOP('',(#56889,#56890,#56891,#56892)) ;
#23398 = EDGE_LOOP('',(#56893,#56894,#56895)) ;
#23399 = EDGE_LOOP('',(#56896,#56897,#56898)) ;
#23400 = EDGE_LOOP('',(#56899,#56900,#56901,#56902)) ;
#23401 = EDGE_LOOP('',(#56903,#56904,#56905,#56906)) ;
#23402 = EDGE_LOOP('',(#56907,#56908,#56909,#56910)) ;
#23403 = EDGE_LOOP('',(#56911,#56912,#56913,#56914)) ;
#23404 = EDGE_LOOP('',(#56915,#56916,#56917,#56918)) ;
#23405 = EDGE_LOOP('',(#56919,#56920,#56921)) ;
#23406 = EDGE_LOOP('',(#56922,#56923,#56924)) ;
#23407 = EDGE_LOOP('',(#56925,#56926,#56927,#56928)) ;
#23408 = EDGE_LOOP('',(#56929,#56930,#56931,#56932)) ;
#23409 = EDGE_LOOP('',(#56933,#56934,#56935,#56936)) ;
#23410 = EDGE_LOOP('',(#56937,#56938,#56939,#56940)) ;
#23411 = EDGE_LOOP('',(#56941,#56942,#56943,#56944)) ;
#23412 = EDGE_LOOP('',(#56945,#56946,#56947,#56948)) ;
#23413 = EDGE_LOOP('',(#56949,#56950,#56951,#56952)) ;
#23414 = EDGE_LOOP('',(#56953,#56954,#56955,#56956)) ;
#23415 = EDGE_LOOP('',(#56957,#56958,#56959,#56960)) ;
#23416 = EDGE_LOOP('',(#56961,#56962,#56963,#56964)) ;
#23417 = EDGE_LOOP('',(#56965,#56966,#56967,#56968)) ;
#23418 = EDGE_LOOP('',(#56969,#56970,#56971)) ;
#23419 = EDGE_LOOP('',(#56972,#56973,#56974)) ;
#23420 = EDGE_LOOP('',(#56975,#56976,#56977,#56978)) ;
#23421 = EDGE_LOOP('',(#56979,#56980,#56981,#56982)) ;
#23422 = EDGE_LOOP('',(#56983,#56984,#56985,#56986)) ;
#23423 = EDGE_LOOP('',(#56987,#56988,#56989,#56990)) ;
#23424 = EDGE_LOOP('',(#56991,#56992,#56993,#56994)) ;
#23425 = EDGE_LOOP('',(#56995,#56996,#56997)) ;
#23426 = EDGE_LOOP('',(#56998,#56999,#57000)) ;
#23427 = EDGE_LOOP('',(#57001,#57002,#57003,#57004)) ;
#23428 = EDGE_LOOP('',(#57005,#57006,#57007,#57008)) ;
#23429 = EDGE_LOOP('',(#57009,#57010,#57011,#57012)) ;
#23430 = EDGE_LOOP('',(#57013,#57014,#57015)) ;
#23431 = EDGE_LOOP('',(#57016,#57017,#57018,#57019)) ;
#23432 = EDGE_LOOP('',(#57020,#57021,#57022,#57023)) ;
#23433 = EDGE_LOOP('',(#57024,#57025,#57026,#57027)) ;
#23434 = EDGE_LOOP('',(#57028,#57029,#57030,#57031)) ;
#23435 = EDGE_LOOP('',(#57032,#57033,#57034,#57035)) ;
#23436 = EDGE_LOOP('',(#57036,#57037,#57038,#57039)) ;
#23437 = EDGE_LOOP('',(#57040,#57041,#57042,#57043)) ;
#23438 = EDGE_LOOP('',(#57044,#57045,#57046,#57047)) ;
#23439 = EDGE_LOOP('',(#57048,#57049,#57050)) ;
#23440 = EDGE_LOOP('',(#57051,#57052,#57053,#57054)) ;
#23441 = EDGE_LOOP('',(#57055,#57056,#57057,#57058)) ;
#23442 = EDGE_LOOP('',(#57059,#57060,#57061,#57062)) ;
#23443 = EDGE_LOOP('',(#57063,#57064,#57065,#57066)) ;
#23444 = EDGE_LOOP('',(#57067,#57068,#57069,#57070)) ;
#23445 = EDGE_LOOP('',(#57071,#57072,#57073,#57074)) ;
#23446 = EDGE_LOOP('',(#57075,#57076,#57077,#57078)) ;
#23447 = EDGE_LOOP('',(#57079,#57080,#57081,#57082)) ;
#23448 = EDGE_LOOP('',(#57083,#57084,#57085,#57086)) ;
#23449 = EDGE_LOOP('',(#57087,#57088,#57089,#57090)) ;
#23450 = EDGE_LOOP('',(#57091,#57092,#57093,#57094)) ;
#23451 = EDGE_LOOP('',(#57095,#57096,#57097,#57098)) ;
#23452 = EDGE_LOOP('',(#57099,#57100,#57101,#57102)) ;
#23453 = EDGE_LOOP('',(#57103,#57104,#57105,#57106)) ;
#23454 = EDGE_LOOP('',(#57107,#57108,#57109)) ;
#23455 = EDGE_LOOP('',(#57110,#57111,#57112,#57113)) ;
#23456 = EDGE_LOOP('',(#57114,#57115,#57116,#57117)) ;
#23457 = EDGE_LOOP('',(#57118,#57119,#57120,#57121)) ;
#23458 = EDGE_LOOP('',(#57122,#57123,#57124,#57125)) ;
#23459 = EDGE_LOOP('',(#57126,#57127,#57128,#57129)) ;
#23460 = EDGE_LOOP('',(#57130,#57131,#57132,#57133)) ;
#23461 = EDGE_LOOP('',(#57134,#57135,#57136,#57137)) ;
#23462 = EDGE_LOOP('',(#57138,#57139,#57140,#57141)) ;
#23463 = EDGE_LOOP('',(#57142,#57143,#57144,#57145)) ;
#23464 = EDGE_LOOP('',(#57146,#57147,#57148)) ;
#23465 = EDGE_LOOP('',(#57149,#57150,#57151,#57152,#57153)) ;
#23466 = EDGE_LOOP('',(#57154,#57155,#57156,#57157)) ;
#23467 = EDGE_LOOP('',(#57158,#57159,#57160,#57161)) ;
#23468 = EDGE_LOOP('',(#57162,#57163,#57164,#57165)) ;
#23469 = EDGE_LOOP('',(#57166,#57167,#57168,#57169)) ;
#23470 = EDGE_LOOP('',(#57170,#57171,#57172)) ;
#23471 = EDGE_LOOP('',(#57173,#57174,#57175,#57176)) ;
#23472 = EDGE_LOOP('',(#57177,#57178,#57179,#57180)) ;
#23473 = EDGE_LOOP('',(#57181,#57182,#57183)) ;
#23474 = EDGE_LOOP('',(#57184,#57185,#57186,#57187,#57188,#57189,#57190,#57191)) ;
#23475 = EDGE_LOOP('',(#57192,#57193,#57194,#57195)) ;
#23476 = EDGE_LOOP('',(#57196,#57197,#57198,#57199)) ;
#23477 = EDGE_LOOP('',(#57200,#57201,#57202,#57203)) ;
#23478 = EDGE_LOOP('',(#57204,#57205,#57206,#57207)) ;
#23479 = EDGE_LOOP('',(#57208,#57209,#57210,#57211)) ;
#23480 = EDGE_LOOP('',(#57212,#57213,#57214,#57215)) ;
#23481 = EDGE_LOOP('',(#57216,#57217,#57218,#57219)) ;
#23482 = EDGE_LOOP('',(#57220,#57221,#57222,#57223)) ;
#23483 = EDGE_LOOP('',(#57224,#57225,#57226,#57227)) ;
#23484 = EDGE_LOOP('',(#57228,#57229,#57230,#57231,#57232,#57233,#57234)) ;
#23485 = EDGE_LOOP('',(#57235,#57236,#57237,#57238,#57239,#57240,#57241)) ;
#23486 = EDGE_LOOP('',(#57242,#57243,#57244,#57245)) ;
#23487 = EDGE_LOOP('',(#57246,#57247,#57248)) ;
#23488 = EDGE_LOOP('',(#57249,#57250,#57251,#57252)) ;
#23489 = EDGE_LOOP('',(#57253,#57254,#57255,#57256)) ;
#23490 = EDGE_LOOP('',(#57257,#57258,#57259,#57260,#57261,#57262,#57263,#57264,
#57265,#57266,#57267,#57268,#57269,#57270,#57271,#57272,#57273,#57274,#57275,
#57276,#57277,#57278,#57279,#57280,#57281,#57282,#57283,#57284,#57285,#57286,
#57287,#57288,#57289,#57290,#57291,#57292,#57293,#57294)) ;
#23491 = EDGE_LOOP('',(#57295,#57296,#57297,#57298)) ;
#23492 = EDGE_LOOP('',(#57299,#57300,#57301,#57302)) ;
#23493 = EDGE_LOOP('',(#57303,#57304,#57305,#57306,#57307,#57308,#57309,#57310)) ;
#23494 = EDGE_LOOP('',(#57311,#57312,#57313,#57314,#57315,#57316,#57317,#57318)) ;
#23495 = EDGE_LOOP('',(#57319,#57320,#57321,#57322,#57323,#57324,#57325,#57326)) ;
#23496 = EDGE_LOOP('',(#57327,#57328,#57329,#57330)) ;
#23497 = EDGE_LOOP('',(#57331,#57332,#57333,#57334)) ;
#23498 = EDGE_LOOP('',(#57335,#57336,#57337,#57338,#57339,#57340)) ;
#23499 = EDGE_LOOP('',(#57341,#57342,#57343,#57344,#57345,#57346)) ;
#23500 = EDGE_LOOP('',(#57347,#57348,#57349,#57350)) ;
#23501 = EDGE_LOOP('',(#57351,#57352,#57353,#57354)) ;
#23502 = EDGE_LOOP('',(#57355,#57356,#57357,#57358)) ;
#23503 = EDGE_LOOP('',(#57359,#57360,#57361,#57362)) ;
#23504 = EDGE_LOOP('',(#57363,#57364,#57365,#57366)) ;
#23505 = EDGE_LOOP('',(#57367,#57368,#57369,#57370,#57371,#57372,#57373,#57374)) ;
#23506 = EDGE_LOOP('',(#57375,#57376,#57377,#57378)) ;
#23507 = EDGE_LOOP('',(#57379,#57380,#57381,#57382)) ;
#23508 = EDGE_LOOP('',(#57383,#57384,#57385,#57386)) ;
#23509 = EDGE_LOOP('',(#57387,#57388,#57389,#57390)) ;
#23510 = EDGE_LOOP('',(#57391,#57392,#57393,#57394)) ;
#23511 = EDGE_LOOP('',(#57395,#57396,#57397,#57398)) ;
#23512 = EDGE_LOOP('',(#57399,#57400,#57401,#57402)) ;
#23513 = EDGE_LOOP('',(#57403,#57404,#57405,#57406)) ;
#23514 = EDGE_LOOP('',(#57407,#57408,#57409,#57410,#57411,#57412,#57413,#57414)) ;
#23515 = EDGE_LOOP('',(#57415,#57416)) ;
#23516 = EDGE_LOOP('',(#57417,#57418,#57419,#57420)) ;
#23517 = EDGE_LOOP('',(#57421,#57422,#57423,#57424)) ;
#23518 = EDGE_LOOP('',(#57425,#57426,#57427,#57428)) ;
#23519 = EDGE_LOOP('',(#57429,#57430,#57431,#57432)) ;
#23520 = EDGE_LOOP('',(#57433,#57434,#57435,#57436)) ;
#23521 = EDGE_LOOP('',(#57437,#57438,#57439,#57440)) ;
#23522 = EDGE_LOOP('',(#57441,#57442,#57443,#57444)) ;
#23523 = EDGE_LOOP('',(#57445,#57446,#57447,#57448)) ;
#23524 = EDGE_LOOP('',(#57449,#57450,#57451,#57452,#57453,#57454,#57455,#57456)) ;
#23525 = EDGE_LOOP('',(#57457,#57458,#57459,#57460)) ;
#23526 = EDGE_LOOP('',(#57461,#57462,#57463,#57464)) ;
#23527 = EDGE_LOOP('',(#57465,#57466,#57467,#57468)) ;
#23528 = EDGE_LOOP('',(#57469,#57470,#57471,#57472)) ;
#23529 = EDGE_LOOP('',(#57473,#57474,#57475,#57476)) ;
#23530 = EDGE_LOOP('',(#57477,#57478,#57479,#57480)) ;
#23531 = EDGE_LOOP('',(#57481,#57482,#57483,#57484)) ;
#23532 = EDGE_LOOP('',(#57485,#57486,#57487,#57488)) ;
#23533 = EDGE_LOOP('',(#57489,#57490,#57491,#57492)) ;
#23534 = EDGE_LOOP('',(#57493,#57494,#57495,#57496)) ;
#23535 = EDGE_LOOP('',(#57497,#57498,#57499,#57500)) ;
#23536 = EDGE_LOOP('',(#57501,#57502,#57503,#57504)) ;
#23537 = EDGE_LOOP('',(#57505,#57506,#57507,#57508,#57509,#57510)) ;
#23538 = EDGE_LOOP('',(#57511)) ;
#23539 = EDGE_LOOP('',(#57512,#57513,#57514,#57515,#57516,#57517)) ;
#23540 = EDGE_LOOP('',(#57518,#57519,#57520,#57521)) ;
#23541 = EDGE_LOOP('',(#57522,#57523,#57524,#57525)) ;
#23542 = EDGE_LOOP('',(#57526,#57527,#57528,#57529)) ;
#23543 = EDGE_LOOP('',(#57530,#57531,#57532,#57533)) ;
#23544 = EDGE_LOOP('',(#57534,#57535,#57536,#57537)) ;
#23545 = EDGE_LOOP('',(#57538,#57539,#57540,#57541)) ;
#23546 = EDGE_LOOP('',(#57542,#57543,#57544,#57545)) ;
#23547 = EDGE_LOOP('',(#57546,#57547,#57548,#57549)) ;
#23548 = EDGE_LOOP('',(#57550,#57551,#57552,#57553)) ;
#23549 = EDGE_LOOP('',(#57554,#57555,#57556)) ;
#23550 = EDGE_LOOP('',(#57557,#57558,#57559,#57560)) ;
#23551 = EDGE_LOOP('',(#57561,#57562,#57563,#57564)) ;
#23552 = EDGE_LOOP('',(#57565,#57566,#57567,#57568)) ;
#23553 = EDGE_LOOP('',(#57569,#57570,#57571,#57572)) ;
#23554 = EDGE_LOOP('',(#57573,#57574,#57575,#57576)) ;
#23555 = EDGE_LOOP('',(#57577,#57578,#57579,#57580)) ;
#23556 = EDGE_LOOP('',(#57581,#57582,#57583,#57584)) ;
#23557 = EDGE_LOOP('',(#57585,#57586,#57587,#57588)) ;
#23558 = EDGE_LOOP('',(#57589,#57590,#57591,#57592)) ;
#23559 = EDGE_LOOP('',(#57593,#57594,#57595)) ;
#23560 = EDGE_LOOP('',(#57596,#57597,#57598,#57599)) ;
#23561 = EDGE_LOOP('',(#57600,#57601,#57602)) ;
#23562 = EDGE_LOOP('',(#57603,#57604,#57605,#57606)) ;
#23563 = EDGE_LOOP('',(#57607,#57608,#57609,#57610)) ;
#23564 = EDGE_LOOP('',(#57611,#57612,#57613,#57614)) ;
#23565 = EDGE_LOOP('',(#57615,#57616,#57617,#57618)) ;
#23566 = EDGE_LOOP('',(#57619,#57620,#57621,#57622)) ;
#23567 = EDGE_LOOP('',(#57623,#57624,#57625)) ;
#23568 = EDGE_LOOP('',(#57626,#57627,#57628,#57629)) ;
#23569 = EDGE_LOOP('',(#57630,#57631,#57632,#57633)) ;
#23570 = EDGE_LOOP('',(#57634,#57635,#57636,#57637)) ;
#23571 = EDGE_LOOP('',(#57638,#57639,#57640,#57641)) ;
#23572 = EDGE_LOOP('',(#57642,#57643,#57644,#57645,#57646,#57647)) ;
#23573 = EDGE_LOOP('',(#57648,#57649,#57650,#57651)) ;
#23574 = EDGE_LOOP('',(#57652,#57653,#57654,#57655)) ;
#23575 = EDGE_LOOP('',(#57656,#57657,#57658,#57659)) ;
#23576 = EDGE_LOOP('',(#57660,#57661,#57662,#57663)) ;
#23577 = EDGE_LOOP('',(#57664,#57665,#57666,#57667)) ;
#23578 = EDGE_LOOP('',(#57668,#57669,#57670,#57671)) ;
#23579 = EDGE_LOOP('',(#57672,#57673,#57674,#57675,#57676,#57677)) ;
#23580 = EDGE_LOOP('',(#57678,#57679,#57680,#57681)) ;
#23581 = EDGE_LOOP('',(#57682,#57683,#57684,#57685)) ;
#23582 = EDGE_LOOP('',(#57686,#57687,#57688)) ;
#23583 = EDGE_LOOP('',(#57689,#57690,#57691,#57692)) ;
#23584 = EDGE_LOOP('',(#57693,#57694,#57695,#57696)) ;
#23585 = EDGE_LOOP('',(#57697,#57698,#57699)) ;
#23586 = EDGE_LOOP('',(#57700,#57701,#57702)) ;
#23587 = EDGE_LOOP('',(#57703,#57704,#57705,#57706)) ;
#23588 = EDGE_LOOP('',(#57707,#57708,#57709,#57710)) ;
#23589 = EDGE_LOOP('',(#57711,#57712,#57713)) ;
#23590 = EDGE_LOOP('',(#57714,#57715,#57716,#57717)) ;
#23591 = EDGE_LOOP('',(#57718,#57719,#57720,#57721)) ;
#23592 = EDGE_LOOP('',(#57722,#57723,#57724,#57725)) ;
#23593 = EDGE_LOOP('',(#57726,#57727,#57728,#57729)) ;
#23594 = EDGE_LOOP('',(#57730,#57731,#57732,#57733)) ;
#23595 = EDGE_LOOP('',(#57734,#57735,#57736,#57737)) ;
#23596 = EDGE_LOOP('',(#57738,#57739,#57740,#57741)) ;
#23597 = EDGE_LOOP('',(#57742,#57743,#57744,#57745)) ;
#23598 = EDGE_LOOP('',(#57746,#57747,#57748,#57749)) ;
#23599 = EDGE_LOOP('',(#57750,#57751,#57752,#57753)) ;
#23600 = EDGE_LOOP('',(#57754,#57755,#57756)) ;
#23601 = EDGE_LOOP('',(#57757,#57758,#57759)) ;
#23602 = EDGE_LOOP('',(#57760,#57761,#57762,#57763)) ;
#23603 = EDGE_LOOP('',(#57764,#57765,#57766,#57767)) ;
#23604 = EDGE_LOOP('',(#57768,#57769,#57770,#57771)) ;
#23605 = EDGE_LOOP('',(#57772,#57773,#57774,#57775)) ;
#23606 = EDGE_LOOP('',(#57776,#57777,#57778,#57779)) ;
#23607 = EDGE_LOOP('',(#57780,#57781,#57782)) ;
#23608 = EDGE_LOOP('',(#57783,#57784,#57785)) ;
#23609 = EDGE_LOOP('',(#57786,#57787,#57788,#57789)) ;
#23610 = EDGE_LOOP('',(#57790,#57791,#57792,#57793)) ;
#23611 = EDGE_LOOP('',(#57794,#57795,#57796,#57797)) ;
#23612 = EDGE_LOOP('',(#57798,#57799,#57800,#57801)) ;
#23613 = EDGE_LOOP('',(#57802,#57803,#57804,#57805)) ;
#23614 = EDGE_LOOP('',(#57806,#57807,#57808,#57809)) ;
#23615 = EDGE_LOOP('',(#57810,#57811,#57812,#57813)) ;
#23616 = EDGE_LOOP('',(#57814,#57815,#57816,#57817)) ;
#23617 = EDGE_LOOP('',(#57818,#57819,#57820,#57821)) ;
#23618 = EDGE_LOOP('',(#57822,#57823,#57824,#57825)) ;
#23619 = EDGE_LOOP('',(#57826,#57827,#57828,#57829)) ;
#23620 = EDGE_LOOP('',(#57830,#57831,#57832)) ;
#23621 = EDGE_LOOP('',(#57833,#57834,#57835)) ;
#23622 = EDGE_LOOP('',(#57836,#57837,#57838,#57839)) ;
#23623 = EDGE_LOOP('',(#57840,#57841,#57842,#57843)) ;
#23624 = EDGE_LOOP('',(#57844,#57845,#57846,#57847)) ;
#23625 = EDGE_LOOP('',(#57848,#57849,#57850,#57851)) ;
#23626 = EDGE_LOOP('',(#57852,#57853,#57854,#57855)) ;
#23627 = EDGE_LOOP('',(#57856,#57857,#57858)) ;
#23628 = EDGE_LOOP('',(#57859,#57860,#57861)) ;
#23629 = EDGE_LOOP('',(#57862,#57863,#57864,#57865)) ;
#23630 = EDGE_LOOP('',(#57866,#57867,#57868,#57869)) ;
#23631 = EDGE_LOOP('',(#57870,#57871,#57872,#57873)) ;
#23632 = EDGE_LOOP('',(#57874,#57875,#57876)) ;
#23633 = EDGE_LOOP('',(#57877,#57878,#57879,#57880)) ;
#23634 = EDGE_LOOP('',(#57881,#57882,#57883,#57884)) ;
#23635 = EDGE_LOOP('',(#57885,#57886,#57887,#57888)) ;
#23636 = EDGE_LOOP('',(#57889,#57890,#57891,#57892)) ;
#23637 = EDGE_LOOP('',(#57893,#57894,#57895,#57896)) ;
#23638 = EDGE_LOOP('',(#57897,#57898,#57899,#57900)) ;
#23639 = EDGE_LOOP('',(#57901,#57902,#57903)) ;
#23640 = EDGE_LOOP('',(#57904,#57905,#57906,#57907)) ;
#23641 = EDGE_LOOP('',(#57908,#57909,#57910,#57911)) ;
#23642 = EDGE_LOOP('',(#57912,#57913,#57914,#57915)) ;
#23643 = EDGE_LOOP('',(#57916,#57917,#57918,#57919)) ;
#23644 = EDGE_LOOP('',(#57920,#57921,#57922,#57923)) ;
#23645 = EDGE_LOOP('',(#57924,#57925,#57926)) ;
#23646 = EDGE_LOOP('',(#57927,#57928,#57929,#57930)) ;
#23647 = EDGE_LOOP('',(#57931,#57932,#57933,#57934)) ;
#23648 = EDGE_LOOP('',(#57935,#57936,#57937,#57938)) ;
#23649 = EDGE_LOOP('',(#57939,#57940,#57941,#57942)) ;
#23650 = EDGE_LOOP('',(#57943,#57944,#57945,#57946)) ;
#23651 = EDGE_LOOP('',(#57947,#57948,#57949,#57950)) ;
#23652 = EDGE_LOOP('',(#57951,#57952,#57953,#57954)) ;
#23653 = EDGE_LOOP('',(#57955,#57956,#57957,#57958)) ;
#23654 = EDGE_LOOP('',(#57959,#57960,#57961)) ;
#23655 = EDGE_LOOP('',(#57962,#57963,#57964,#57965,#57966)) ;
#23656 = EDGE_LOOP('',(#57967,#57968,#57969,#57970)) ;
#23657 = EDGE_LOOP('',(#57971,#57972,#57973,#57974)) ;
#23658 = EDGE_LOOP('',(#57975,#57976,#57977,#57978)) ;
#23659 = EDGE_LOOP('',(#57979,#57980,#57981)) ;
#23660 = EDGE_LOOP('',(#57982,#57983,#57984,#57985)) ;
#23661 = EDGE_LOOP('',(#57986,#57987,#57988,#57989)) ;
#23662 = EDGE_LOOP('',(#57990,#57991,#57992)) ;
#23663 = EDGE_LOOP('',(#57993,#57994,#57995)) ;
#23664 = EDGE_LOOP('',(#57996,#57997,#57998)) ;
#23665 = EDGE_LOOP('',(#57999,#58000,#58001,#58002)) ;
#23666 = EDGE_LOOP('',(#58003,#58004,#58005,#58006)) ;
#23667 = EDGE_LOOP('',(#58007,#58008,#58009,#58010)) ;
#23668 = EDGE_LOOP('',(#58011,#58012,#58013,#58014)) ;
#23669 = EDGE_LOOP('',(#58015,#58016,#58017)) ;
#23670 = EDGE_LOOP('',(#58018,#58019,#58020)) ;
#23671 = EDGE_LOOP('',(#58021,#58022,#58023)) ;
#23672 = EDGE_LOOP('',(#58024,#58025,#58026)) ;
#23673 = EDGE_LOOP('',(#58027,#58028,#58029,#58030)) ;
#23674 = EDGE_LOOP('',(#58031,#58032,#58033,#58034)) ;
#23675 = EDGE_LOOP('',(#58035,#58036,#58037,#58038)) ;
#23676 = EDGE_LOOP('',(#58039,#58040,#58041,#58042)) ;
#23677 = EDGE_LOOP('',(#58043,#58044,#58045,#58046)) ;
#23678 = EDGE_LOOP('',(#58047,#58048,#58049,#58050)) ;
#23679 = EDGE_LOOP('',(#58051,#58052,#58053,#58054)) ;
#23680 = EDGE_LOOP('',(#58055,#58056,#58057,#58058)) ;
#23681 = EDGE_LOOP('',(#58059,#58060,#58061,#58062)) ;
#23682 = EDGE_LOOP('',(#58063,#58064,#58065,#58066)) ;
#23683 = EDGE_LOOP('',(#58067,#58068,#58069,#58070)) ;
#23684 = EDGE_LOOP('',(#58071,#58072,#58073,#58074)) ;
#23685 = EDGE_LOOP('',(#58075,#58076,#58077,#58078)) ;
#23686 = EDGE_LOOP('',(#58079,#58080,#58081,#58082)) ;
#23687 = EDGE_LOOP('',(#58083,#58084,#58085,#58086)) ;
#23688 = EDGE_LOOP('',(#58087,#58088,#58089,#58090)) ;
#23689 = EDGE_LOOP('',(#58091,#58092,#58093,#58094)) ;
#23690 = EDGE_LOOP('',(#58095,#58096,#58097,#58098)) ;
#23691 = EDGE_LOOP('',(#58099,#58100,#58101,#58102,#58103)) ;
#23692 = EDGE_LOOP('',(#58104,#58105,#58106,#58107)) ;
#23693 = EDGE_LOOP('',(#58108,#58109,#58110,#58111,#58112)) ;
#23694 = EDGE_LOOP('',(#58113,#58114,#58115,#58116)) ;
#23695 = EDGE_LOOP('',(#58117,#58118,#58119)) ;
#23696 = EDGE_LOOP('',(#58120,#58121,#58122,#58123)) ;
#23697 = EDGE_LOOP('',(#58124,#58125,#58126)) ;
#23698 = EDGE_LOOP('',(#58127,#58128,#58129,#58130)) ;
#23699 = EDGE_LOOP('',(#58131,#58132,#58133,#58134,#58135)) ;
#23700 = EDGE_LOOP('',(#58136,#58137,#58138,#58139,#58140,#58141,#58142,#58143,
#58144,#58145,#58146,#58147,#58148,#58149,#58150,#58151,#58152,#58153,#58154,
#58155,#58156)) ;
#23701 = EDGE_LOOP('',(#58157,#58158,#58159,#58160)) ;
#23702 = EDGE_LOOP('',(#58161,#58162,#58163,#58164)) ;
#23703 = EDGE_LOOP('',(#58165,#58166,#58167,#58168)) ;
#23704 = EDGE_LOOP('',(#58169,#58170,#58171)) ;
#23705 = EDGE_LOOP('',(#58172,#58173,#58174,#58175,#58176,#58177,#58178,#58179,
#58180,#58181,#58182,#58183,#58184,#58185)) ;
#23706 = EDGE_LOOP('',(#58186)) ;
#23707 = EDGE_LOOP('',(#58187,#58188,#58189,#58190)) ;
#23708 = EDGE_LOOP('',(#58191,#58192,#58193,#58194,#58195,#58196,#58197,#58198)) ;
#23709 = EDGE_LOOP('',(#58199,#58200,#58201,#58202)) ;
#23710 = EDGE_LOOP('',(#58203,#58204,#58205,#58206)) ;
#23711 = EDGE_LOOP('',(#58207,#58208,#58209,#58210)) ;
#23712 = EDGE_LOOP('',(#58211,#58212,#58213,#58214)) ;
#23713 = EDGE_LOOP('',(#58215,#58216,#58217,#58218)) ;
#23714 = EDGE_LOOP('',(#58219,#58220,#58221,#58222)) ;
#23715 = EDGE_LOOP('',(#58223,#58224,#58225,#58226)) ;
#23716 = EDGE_LOOP('',(#58227,#58228,#58229,#58230,#58231,#58232,#58233,#58234)) ;
#23717 = EDGE_LOOP('',(#58235)) ;
#23718 = EDGE_LOOP('',(#58236,#58237,#58238,#58239)) ;
#23719 = EDGE_LOOP('',(#58240,#58241,#58242,#58243)) ;
#23720 = EDGE_LOOP('',(#58244,#58245,#58246,#58247)) ;
#23721 = EDGE_LOOP('',(#58248,#58249,#58250,#58251)) ;
#23722 = EDGE_LOOP('',(#58252,#58253,#58254,#58255,#58256,#58257,#58258,#58259)) ;
#23723 = EDGE_LOOP('',(#58260,#58261,#58262,#58263)) ;
#23724 = EDGE_LOOP('',(#58264,#58265,#58266,#58267,#58268,#58269,#58270,#58271)) ;
#23725 = EDGE_LOOP('',(#58272,#58273,#58274,#58275)) ;
#23726 = EDGE_LOOP('',(#58276,#58277,#58278,#58279,#58280,#58281,#58282,#58283,
#58284)) ;
#23727 = EDGE_LOOP('',(#58285,#58286,#58287,#58288)) ;
#23728 = EDGE_LOOP('',(#58289,#58290,#58291,#58292)) ;
#23729 = EDGE_LOOP('',(#58293,#58294,#58295,#58296,#58297,#58298,#58299,#58300,
#58301,#58302,#58303,#58304,#58305,#58306,#58307,#58308,#58309,#58310,#58311,
#58312,#58313,#58314,#58315,#58316,#58317,#58318,#58319,#58320,#58321,#58322,
#58323,#58324,#58325,#58326,#58327,#58328,#58329,#58330)) ;
#23730 = EDGE_LOOP('',(#58331,#58332,#58333,#58334,#58335,#58336,#58337,#58338,
#58339,#58340,#58341,#58342,#58343,#58344,#58345,#58346,#58347,#58348,#58349,
#58350,#58351,#58352,#58353,#58354,#58355,#58356,#58357,#58358,#58359,#58360,
#58361,#58362,#58363,#58364,#58365,#58366,#58367,#58368)) ;
#23731 = EDGE_LOOP('',(#58369,#58370,#58371,#58372)) ;
#23732 = EDGE_LOOP('',(#58373,#58374,#58375,#58376)) ;
#23733 = EDGE_LOOP('',(#58377,#58378,#58379,#58380,#58381,#58382,#58383,#58384)) ;
#23734 = EDGE_LOOP('',(#58385,#58386,#58387,#58388,#58389,#58390,#58391,#58392)) ;
#23735 = EDGE_LOOP('',(#58393,#58394,#58395,#58396,#58397,#58398,#58399,#58400)) ;
#23736 = EDGE_LOOP('',(#58401,#58402,#58403,#58404)) ;
#23737 = EDGE_LOOP('',(#58405,#58406,#58407,#58408)) ;
#23738 = EDGE_LOOP('',(#58409,#58410,#58411,#58412,#58413,#58414)) ;
#23739 = EDGE_LOOP('',(#58415,#58416,#58417,#58418,#58419,#58420)) ;
#23740 = EDGE_LOOP('',(#58421,#58422,#58423,#58424)) ;
#23741 = EDGE_LOOP('',(#58425,#58426,#58427,#58428)) ;
#23742 = EDGE_LOOP('',(#58429,#58430,#58431,#58432)) ;
#23743 = EDGE_LOOP('',(#58433,#58434,#58435,#58436)) ;
#23744 = EDGE_LOOP('',(#58437,#58438,#58439,#58440)) ;
#23745 = EDGE_LOOP('',(#58441,#58442,#58443,#58444,#58445,#58446,#58447,#58448)) ;
#23746 = EDGE_LOOP('',(#58449,#58450,#58451,#58452)) ;
#23747 = EDGE_LOOP('',(#58453,#58454,#58455,#58456)) ;
#23748 = EDGE_LOOP('',(#58457,#58458,#58459,#58460)) ;
#23749 = EDGE_LOOP('',(#58461,#58462,#58463,#58464)) ;
#23750 = EDGE_LOOP('',(#58465,#58466,#58467,#58468)) ;
#23751 = EDGE_LOOP('',(#58469,#58470,#58471,#58472)) ;
#23752 = EDGE_LOOP('',(#58473,#58474,#58475,#58476)) ;
#23753 = EDGE_LOOP('',(#58477,#58478,#58479,#58480)) ;
#23754 = EDGE_LOOP('',(#58481,#58482,#58483,#58484,#58485,#58486,#58487,#58488)) ;
#23755 = EDGE_LOOP('',(#58489,#58490)) ;
#23756 = EDGE_LOOP('',(#58491,#58492,#58493,#58494)) ;
#23757 = EDGE_LOOP('',(#58495,#58496,#58497,#58498)) ;
#23758 = EDGE_LOOP('',(#58499,#58500,#58501,#58502)) ;
#23759 = EDGE_LOOP('',(#58503,#58504,#58505,#58506)) ;
#23760 = EDGE_LOOP('',(#58507,#58508,#58509,#58510)) ;
#23761 = EDGE_LOOP('',(#58511,#58512,#58513,#58514)) ;
#23762 = EDGE_LOOP('',(#58515,#58516,#58517,#58518)) ;
#23763 = EDGE_LOOP('',(#58519,#58520,#58521,#58522)) ;
#23764 = EDGE_LOOP('',(#58523,#58524,#58525,#58526,#58527,#58528,#58529,#58530)) ;
#23765 = EDGE_LOOP('',(#58531,#58532,#58533,#58534)) ;
#23766 = EDGE_LOOP('',(#58535,#58536,#58537,#58538)) ;
#23767 = EDGE_LOOP('',(#58539,#58540,#58541,#58542)) ;
#23768 = EDGE_LOOP('',(#58543,#58544,#58545,#58546)) ;
#23769 = EDGE_LOOP('',(#58547,#58548,#58549,#58550)) ;
#23770 = EDGE_LOOP('',(#58551,#58552,#58553,#58554)) ;
#23771 = EDGE_LOOP('',(#58555,#58556,#58557,#58558)) ;
#23772 = EDGE_LOOP('',(#58559,#58560,#58561,#58562)) ;
#23773 = EDGE_LOOP('',(#58563,#58564,#58565,#58566)) ;
#23774 = EDGE_LOOP('',(#58567,#58568,#58569,#58570)) ;
#23775 = EDGE_LOOP('',(#58571,#58572,#58573,#58574)) ;
#23776 = EDGE_LOOP('',(#58575,#58576,#58577,#58578)) ;
#23777 = EDGE_LOOP('',(#58579,#58580,#58581,#58582,#58583,#58584)) ;
#23778 = EDGE_LOOP('',(#58585)) ;
#23779 = EDGE_LOOP('',(#58586,#58587,#58588,#58589,#58590,#58591)) ;
#23780 = EDGE_LOOP('',(#58592,#58593,#58594,#58595)) ;
#23781 = EDGE_LOOP('',(#58596,#58597,#58598,#58599)) ;
#23782 = EDGE_LOOP('',(#58600,#58601,#58602,#58603)) ;
#23783 = EDGE_LOOP('',(#58604,#58605,#58606,#58607)) ;
#23784 = EDGE_LOOP('',(#58608,#58609,#58610,#58611)) ;
#23785 = EDGE_LOOP('',(#58612,#58613,#58614,#58615)) ;
#23786 = EDGE_LOOP('',(#58616,#58617,#58618,#58619)) ;
#23787 = EDGE_LOOP('',(#58620,#58621,#58622,#58623)) ;
#23788 = EDGE_LOOP('',(#58624,#58625,#58626,#58627)) ;
#23789 = EDGE_LOOP('',(#58628,#58629,#58630)) ;
#23790 = EDGE_LOOP('',(#58631,#58632,#58633,#58634)) ;
#23791 = EDGE_LOOP('',(#58635,#58636,#58637,#58638)) ;
#23792 = EDGE_LOOP('',(#58639,#58640,#58641,#58642)) ;
#23793 = EDGE_LOOP('',(#58643,#58644,#58645,#58646)) ;
#23794 = EDGE_LOOP('',(#58647,#58648,#58649,#58650)) ;
#23795 = EDGE_LOOP('',(#58651,#58652,#58653,#58654)) ;
#23796 = EDGE_LOOP('',(#58655,#58656,#58657,#58658)) ;
#23797 = EDGE_LOOP('',(#58659,#58660,#58661,#58662)) ;
#23798 = EDGE_LOOP('',(#58663,#58664,#58665,#58666)) ;
#23799 = EDGE_LOOP('',(#58667,#58668,#58669)) ;
#23800 = EDGE_LOOP('',(#58670,#58671,#58672,#58673)) ;
#23801 = EDGE_LOOP('',(#58674,#58675,#58676)) ;
#23802 = EDGE_LOOP('',(#58677,#58678,#58679,#58680)) ;
#23803 = EDGE_LOOP('',(#58681,#58682,#58683,#58684)) ;
#23804 = EDGE_LOOP('',(#58685,#58686,#58687,#58688)) ;
#23805 = EDGE_LOOP('',(#58689,#58690,#58691,#58692)) ;
#23806 = EDGE_LOOP('',(#58693,#58694,#58695,#58696)) ;
#23807 = EDGE_LOOP('',(#58697,#58698,#58699)) ;
#23808 = EDGE_LOOP('',(#58700,#58701,#58702,#58703)) ;
#23809 = EDGE_LOOP('',(#58704,#58705,#58706,#58707)) ;
#23810 = EDGE_LOOP('',(#58708,#58709,#58710,#58711)) ;
#23811 = EDGE_LOOP('',(#58712,#58713,#58714,#58715)) ;
#23812 = EDGE_LOOP('',(#58716,#58717,#58718,#58719)) ;
#23813 = EDGE_LOOP('',(#58720,#58721,#58722,#58723,#58724,#58725)) ;
#23814 = EDGE_LOOP('',(#58726,#58727,#58728,#58729)) ;
#23815 = EDGE_LOOP('',(#58730,#58731,#58732,#58733)) ;
#23816 = EDGE_LOOP('',(#58734,#58735,#58736,#58737)) ;
#23817 = EDGE_LOOP('',(#58738,#58739,#58740,#58741)) ;
#23818 = EDGE_LOOP('',(#58742,#58743,#58744,#58745)) ;
#23819 = EDGE_LOOP('',(#58746,#58747,#58748,#58749)) ;
#23820 = EDGE_LOOP('',(#58750,#58751,#58752,#58753,#58754,#58755)) ;
#23821 = EDGE_LOOP('',(#58756,#58757,#58758,#58759)) ;
#23822 = EDGE_LOOP('',(#58760,#58761,#58762,#58763)) ;
#23823 = EDGE_LOOP('',(#58764,#58765,#58766)) ;
#23824 = EDGE_LOOP('',(#58767,#58768,#58769,#58770)) ;
#23825 = EDGE_LOOP('',(#58771,#58772,#58773,#58774)) ;
#23826 = EDGE_LOOP('',(#58775,#58776,#58777)) ;
#23827 = EDGE_LOOP('',(#58778,#58779,#58780)) ;
#23828 = EDGE_LOOP('',(#58781,#58782,#58783,#58784)) ;
#23829 = EDGE_LOOP('',(#58785,#58786,#58787,#58788)) ;
#23830 = EDGE_LOOP('',(#58789,#58790,#58791)) ;
#23831 = EDGE_LOOP('',(#58792,#58793,#58794,#58795)) ;
#23832 = EDGE_LOOP('',(#58796,#58797,#58798,#58799)) ;
#23833 = EDGE_LOOP('',(#58800,#58801,#58802,#58803)) ;
#23834 = EDGE_LOOP('',(#58804,#58805,#58806,#58807)) ;
#23835 = EDGE_LOOP('',(#58808,#58809,#58810,#58811)) ;
#23836 = EDGE_LOOP('',(#58812,#58813,#58814,#58815)) ;
#23837 = EDGE_LOOP('',(#58816,#58817,#58818,#58819)) ;
#23838 = EDGE_LOOP('',(#58820,#58821,#58822,#58823)) ;
#23839 = EDGE_LOOP('',(#58824,#58825,#58826,#58827)) ;
#23840 = EDGE_LOOP('',(#58828,#58829,#58830,#58831)) ;
#23841 = EDGE_LOOP('',(#58832,#58833,#58834)) ;
#23842 = EDGE_LOOP('',(#58835,#58836,#58837)) ;
#23843 = EDGE_LOOP('',(#58838,#58839,#58840,#58841)) ;
#23844 = EDGE_LOOP('',(#58842,#58843,#58844,#58845)) ;
#23845 = EDGE_LOOP('',(#58846,#58847,#58848,#58849)) ;
#23846 = EDGE_LOOP('',(#58850,#58851,#58852,#58853)) ;
#23847 = EDGE_LOOP('',(#58854,#58855,#58856,#58857)) ;
#23848 = EDGE_LOOP('',(#58858,#58859,#58860)) ;
#23849 = EDGE_LOOP('',(#58861,#58862,#58863)) ;
#23850 = EDGE_LOOP('',(#58864,#58865,#58866,#58867)) ;
#23851 = EDGE_LOOP('',(#58868,#58869,#58870,#58871)) ;
#23852 = EDGE_LOOP('',(#58872,#58873,#58874,#58875)) ;
#23853 = EDGE_LOOP('',(#58876,#58877,#58878,#58879)) ;
#23854 = EDGE_LOOP('',(#58880,#58881,#58882,#58883)) ;
#23855 = EDGE_LOOP('',(#58884,#58885,#58886,#58887)) ;
#23856 = EDGE_LOOP('',(#58888,#58889,#58890,#58891)) ;
#23857 = EDGE_LOOP('',(#58892,#58893,#58894,#58895)) ;
#23858 = EDGE_LOOP('',(#58896,#58897,#58898,#58899)) ;
#23859 = EDGE_LOOP('',(#58900,#58901,#58902,#58903)) ;
#23860 = EDGE_LOOP('',(#58904,#58905,#58906,#58907)) ;
#23861 = EDGE_LOOP('',(#58908,#58909,#58910)) ;
#23862 = EDGE_LOOP('',(#58911,#58912,#58913)) ;
#23863 = EDGE_LOOP('',(#58914,#58915,#58916,#58917)) ;
#23864 = EDGE_LOOP('',(#58918,#58919,#58920,#58921)) ;
#23865 = EDGE_LOOP('',(#58922,#58923,#58924,#58925)) ;
#23866 = EDGE_LOOP('',(#58926,#58927,#58928,#58929)) ;
#23867 = EDGE_LOOP('',(#58930,#58931,#58932,#58933)) ;
#23868 = EDGE_LOOP('',(#58934,#58935,#58936)) ;
#23869 = EDGE_LOOP('',(#58937,#58938,#58939)) ;
#23870 = EDGE_LOOP('',(#58940,#58941,#58942,#58943)) ;
#23871 = EDGE_LOOP('',(#58944,#58945,#58946,#58947)) ;
#23872 = EDGE_LOOP('',(#58948,#58949,#58950,#58951)) ;
#23873 = EDGE_LOOP('',(#58952,#58953,#58954)) ;
#23874 = EDGE_LOOP('',(#58955,#58956,#58957,#58958)) ;
#23875 = EDGE_LOOP('',(#58959,#58960,#58961,#58962)) ;
#23876 = EDGE_LOOP('',(#58963,#58964,#58965,#58966)) ;
#23877 = EDGE_LOOP('',(#58967,#58968,#58969,#58970)) ;
#23878 = EDGE_LOOP('',(#58971,#58972,#58973,#58974)) ;
#23879 = EDGE_LOOP('',(#58975,#58976,#58977,#58978)) ;
#23880 = EDGE_LOOP('',(#58979,#58980,#58981,#58982)) ;
#23881 = EDGE_LOOP('',(#58983,#58984,#58985,#58986)) ;
#23882 = EDGE_LOOP('',(#58987,#58988,#58989)) ;
#23883 = EDGE_LOOP('',(#58990,#58991,#58992,#58993)) ;
#23884 = EDGE_LOOP('',(#58994,#58995,#58996,#58997)) ;
#23885 = EDGE_LOOP('',(#58998,#58999,#59000,#59001)) ;
#23886 = EDGE_LOOP('',(#59002,#59003,#59004,#59005)) ;
#23887 = EDGE_LOOP('',(#59006,#59007,#59008,#59009)) ;
#23888 = EDGE_LOOP('',(#59010,#59011,#59012,#59013)) ;
#23889 = EDGE_LOOP('',(#59014,#59015,#59016,#59017)) ;
#23890 = EDGE_LOOP('',(#59018,#59019,#59020,#59021)) ;
#23891 = EDGE_LOOP('',(#59022,#59023,#59024,#59025)) ;
#23892 = EDGE_LOOP('',(#59026,#59027,#59028,#59029)) ;
#23893 = EDGE_LOOP('',(#59030,#59031,#59032,#59033)) ;
#23894 = EDGE_LOOP('',(#59034,#59035,#59036,#59037)) ;
#23895 = EDGE_LOOP('',(#59038,#59039,#59040,#59041)) ;
#23896 = EDGE_LOOP('',(#59042,#59043,#59044,#59045)) ;
#23897 = EDGE_LOOP('',(#59046,#59047,#59048,#59049)) ;
#23898 = EDGE_LOOP('',(#59050,#59051,#59052,#59053)) ;
#23899 = EDGE_LOOP('',(#59054,#59055,#59056,#59057)) ;
#23900 = EDGE_LOOP('',(#59058,#59059,#59060,#59061)) ;
#23901 = EDGE_LOOP('',(#59062,#59063,#59064)) ;
#23902 = EDGE_LOOP('',(#59065,#59066,#59067,#59068)) ;
#23903 = EDGE_LOOP('',(#59069,#59070,#59071,#59072)) ;
#23904 = EDGE_LOOP('',(#59073,#59074,#59075,#59076)) ;
#23905 = EDGE_LOOP('',(#59077,#59078,#59079,#59080)) ;
#23906 = EDGE_LOOP('',(#59081,#59082,#59083,#59084)) ;
#23907 = EDGE_LOOP('',(#59085,#59086,#59087,#59088)) ;
#23908 = EDGE_LOOP('',(#59089,#59090,#59091,#59092)) ;
#23909 = EDGE_LOOP('',(#59093,#59094,#59095,#59096)) ;
#23910 = EDGE_LOOP('',(#59097,#59098,#59099,#59100)) ;
#23911 = EDGE_LOOP('',(#59101,#59102,#59103)) ;
#23912 = EDGE_LOOP('',(#59104,#59105,#59106,#59107,#59108)) ;
#23913 = EDGE_LOOP('',(#59109,#59110,#59111,#59112)) ;
#23914 = EDGE_LOOP('',(#59113,#59114,#59115,#59116)) ;
#23915 = EDGE_LOOP('',(#59117,#59118,#59119,#59120)) ;
#23916 = EDGE_LOOP('',(#59121,#59122,#59123,#59124)) ;
#23917 = EDGE_LOOP('',(#59125,#59126,#59127)) ;
#23918 = EDGE_LOOP('',(#59128,#59129,#59130,#59131)) ;
#23919 = EDGE_LOOP('',(#59132,#59133,#59134,#59135)) ;
#23920 = EDGE_LOOP('',(#59136,#59137,#59138)) ;
#23921 = EDGE_LOOP('',(#59139,#59140,#59141,#59142,#59143)) ;
#23922 = EDGE_LOOP('',(#59144,#59145,#59146,#59147)) ;
#23923 = EDGE_LOOP('',(#59148,#59149,#59150)) ;
#23924 = EDGE_LOOP('',(#59151,#59152,#59153,#59154,#59155,#59156,#59157)) ;
#23925 = EDGE_LOOP('',(#59158,#59159,#59160,#59161,#59162)) ;
#23926 = EDGE_LOOP('',(#59163,#59164,#59165,#59166)) ;
#23927 = EDGE_LOOP('',(#59167,#59168,#59169)) ;
#23928 = EDGE_LOOP('',(#59170,#59171,#59172,#59173,#59174,#59175,#59176)) ;
#23929 = EDGE_LOOP('',(#59177,#59178,#59179,#59180,#59181)) ;
#23930 = EDGE_LOOP('',(#59182,#59183,#59184,#59185)) ;
#23931 = EDGE_LOOP('',(#59186,#59187,#59188)) ;
#23932 = EDGE_LOOP('',(#59189,#59190,#59191,#59192,#59193,#59194,#59195)) ;
#23933 = EDGE_LOOP('',(#59196,#59197,#59198,#59199,#59200)) ;
#23934 = EDGE_LOOP('',(#59201,#59202,#59203,#59204)) ;
#23935 = EDGE_LOOP('',(#59205,#59206,#59207)) ;
#23936 = EDGE_LOOP('',(#59208,#59209,#59210,#59211,#59212,#59213,#59214)) ;
#23937 = EDGE_LOOP('',(#59215,#59216,#59217,#59218,#59219)) ;
#23938 = EDGE_LOOP('',(#59220,#59221,#59222,#59223)) ;
#23939 = EDGE_LOOP('',(#59224,#59225,#59226)) ;
#23940 = EDGE_LOOP('',(#59227,#59228,#59229,#59230,#59231,#59232,#59233)) ;
#23941 = EDGE_LOOP('',(#59234,#59235,#59236,#59237,#59238)) ;
#23942 = EDGE_LOOP('',(#59239,#59240,#59241,#59242)) ;
#23943 = EDGE_LOOP('',(#59243,#59244,#59245)) ;
#23944 = EDGE_LOOP('',(#59246,#59247,#59248,#59249,#59250,#59251,#59252)) ;
#23945 = EDGE_LOOP('',(#59253,#59254,#59255,#59256,#59257)) ;
#23946 = EDGE_LOOP('',(#59258,#59259,#59260,#59261)) ;
#23947 = EDGE_LOOP('',(#59262,#59263,#59264)) ;
#23948 = EDGE_LOOP('',(#59265,#59266,#59267,#59268,#59269,#59270,#59271)) ;
#23949 = EDGE_LOOP('',(#59272,#59273,#59274,#59275,#59276)) ;
#23950 = EDGE_LOOP('',(#59277,#59278,#59279,#59280)) ;
#23951 = EDGE_LOOP('',(#59281,#59282,#59283)) ;
#23952 = EDGE_LOOP('',(#59284,#59285,#59286,#59287,#59288,#59289,#59290)) ;
#23953 = EDGE_LOOP('',(#59291,#59292,#59293,#59294,#59295)) ;
#23954 = EDGE_LOOP('',(#59296,#59297,#59298,#59299)) ;
#23955 = EDGE_LOOP('',(#59300,#59301,#59302,#59303)) ;
#23956 = EDGE_LOOP('',(#59304,#59305,#59306,#59307)) ;
#23957 = EDGE_LOOP('',(#59308,#59309,#59310,#59311)) ;
#23958 = EDGE_LOOP('',(#59312,#59313,#59314,#59315)) ;
#23959 = EDGE_LOOP('',(#59316,#59317,#59318,#59319)) ;
#23960 = EDGE_LOOP('',(#59320,#59321,#59322,#59323)) ;
#23961 = EDGE_LOOP('',(#59324,#59325,#59326,#59327)) ;
#23962 = EDGE_LOOP('',(#59328,#59329,#59330,#59331)) ;
#23963 = EDGE_LOOP('',(#59332,#59333,#59334,#59335)) ;
#23964 = EDGE_LOOP('',(#59336,#59337,#59338)) ;
#23965 = EDGE_LOOP('',(#59339,#59340,#59341,#59342,#59343,#59344,#59345)) ;
#23966 = EDGE_LOOP('',(#59346,#59347,#59348,#59349,#59350)) ;
#23967 = EDGE_LOOP('',(#59351,#59352,#59353,#59354,#59355)) ;
#23968 = EDGE_LOOP('',(#59356,#59357,#59358,#59359,#59360)) ;
#23969 = EDGE_LOOP('',(#59361,#59362,#59363,#59364,#59365)) ;
#23970 = EDGE_LOOP('',(#59366,#59367,#59368,#59369,#59370)) ;
#23971 = EDGE_LOOP('',(#59371,#59372,#59373,#59374,#59375)) ;
#23972 = EDGE_LOOP('',(#59376,#59377,#59378,#59379,#59380)) ;
#23973 = EDGE_LOOP('',(#59381,#59382,#59383,#59384,#59385)) ;
#23974 = EDGE_LOOP('',(#59386,#59387,#59388,#59389,#59390)) ;
#23975 = EDGE_LOOP('',(#59391,#59392,#59393,#59394)) ;
#23976 = EDGE_LOOP('',(#59395,#59396,#59397,#59398)) ;
#23977 = EDGE_LOOP('',(#59399,#59400,#59401,#59402)) ;
#23978 = EDGE_LOOP('',(#59403,#59404,#59405,#59406)) ;
#23979 = EDGE_LOOP('',(#59407,#59408,#59409,#59410)) ;
#23980 = EDGE_LOOP('',(#59411,#59412,#59413,#59414)) ;
#23981 = EDGE_LOOP('',(#59415,#59416,#59417,#59418)) ;
#23982 = EDGE_LOOP('',(#59419,#59420,#59421,#59422)) ;
#23983 = EDGE_LOOP('',(#59423,#59424,#59425,#59426)) ;
#23984 = EDGE_LOOP('',(#59427,#59428,#59429,#59430,#59431)) ;
#23985 = EDGE_LOOP('',(#59432,#59433,#59434,#59435)) ;
#23986 = EDGE_LOOP('',(#59436,#59437,#59438,#59439)) ;
#23987 = EDGE_LOOP('',(#59440,#59441,#59442)) ;
#23988 = EDGE_LOOP('',(#59443,#59444,#59445,#59446,#59447,#59448,#59449)) ;
#23989 = EDGE_LOOP('',(#59450,#59451,#59452,#59453,#59454)) ;
#23990 = EDGE_LOOP('',(#59455,#59456,#59457,#59458)) ;
#23991 = EDGE_LOOP('',(#59459,#59460,#59461,#59462,#59463,#59464,#59465,#59466,
#59467,#59468,#59469,#59470)) ;
#23992 = EDGE_LOOP('',(#59471,#59472,#59473,#59474,#59475,#59476,#59477,#59478,
#59479,#59480,#59481,#59482)) ;
#23993 = EDGE_LOOP('',(#59483,#59484,#59485,#59486,#59487,#59488,#59489,#59490,
#59491,#59492,#59493,#59494)) ;
#23994 = EDGE_LOOP('',(#59495,#59496,#59497,#59498,#59499,#59500,#59501,#59502,
#59503,#59504,#59505,#59506)) ;
#23995 = EDGE_LOOP('',(#59507,#59508,#59509,#59510,#59511,#59512,#59513,#59514,
#59515,#59516,#59517,#59518)) ;
#23996 = EDGE_LOOP('',(#59519,#59520,#59521,#59522,#59523,#59524,#59525,#59526,
#59527,#59528,#59529,#59530)) ;
#23997 = EDGE_LOOP('',(#59531,#59532,#59533,#59534,#59535,#59536,#59537,#59538,
#59539,#59540,#59541,#59542)) ;
#23998 = EDGE_LOOP('',(#59543,#59544,#59545,#59546,#59547,#59548,#59549,#59550,
#59551,#59552,#59553,#59554)) ;
#23999 = EDGE_LOOP('',(#59555,#59556,#59557,#59558,#59559,#59560,#59561,#59562,
#59563,#59564,#59565,#59566)) ;
#24000 = EDGE_LOOP('',(#59567,#59568,#59569,#59570,#59571)) ;
#24001 = EDGE_LOOP('',(#59572,#59573,#59574,#59575,#59576)) ;
#24002 = EDGE_LOOP('',(#59577,#59578,#59579,#59580,#59581)) ;
#24003 = EDGE_LOOP('',(#59582,#59583,#59584,#59585,#59586)) ;
#24004 = EDGE_LOOP('',(#59587,#59588,#59589,#59590,#59591)) ;
#24005 = EDGE_LOOP('',(#59592,#59593,#59594,#59595,#59596)) ;
#24006 = EDGE_LOOP('',(#59597,#59598,#59599,#59600,#59601)) ;
#24007 = EDGE_LOOP('',(#59602,#59603,#59604,#59605,#59606)) ;
#24008 = EDGE_LOOP('',(#59607,#59608,#59609,#59610,#59611)) ;
#24009 = EDGE_LOOP('',(#59612,#59613,#59614,#59615,#59616)) ;
#24010 = EDGE_LOOP('',(#59617,#59618,#59619,#59620,#59621)) ;
#24011 = EDGE_LOOP('',(#59622,#59623,#59624,#59625,#59626)) ;
#24012 = EDGE_LOOP('',(#59627,#59628,#59629,#59630,#59631)) ;
#24013 = EDGE_LOOP('',(#59632,#59633,#59634,#59635,#59636)) ;
#24014 = EDGE_LOOP('',(#59637,#59638,#59639,#59640,#59641)) ;
#24015 = EDGE_LOOP('',(#59642,#59643,#59644,#59645,#59646)) ;
#24016 = EDGE_LOOP('',(#59647,#59648,#59649,#59650,#59651)) ;
#24017 = EDGE_LOOP('',(#59652,#59653,#59654,#59655,#59656)) ;
#24018 = EDGE_LOOP('',(#59657,#59658,#59659,#59660)) ;
#24019 = EDGE_LOOP('',(#59661,#59662,#59663,#59664)) ;
#24020 = EDGE_LOOP('',(#59665,#59666,#59667,#59668)) ;
#24021 = EDGE_LOOP('',(#59669,#59670,#59671,#59672)) ;
#24022 = EDGE_LOOP('',(#59673,#59674,#59675,#59676)) ;
#24023 = EDGE_LOOP('',(#59677,#59678,#59679,#59680)) ;
#24024 = EDGE_LOOP('',(#59681,#59682,#59683,#59684)) ;
#24025 = EDGE_LOOP('',(#59685,#59686,#59687,#59688)) ;
#24026 = EDGE_LOOP('',(#59689,#59690,#59691,#59692)) ;
#24027 = EDGE_LOOP('',(#59693,#59694,#59695,#59696,#59697,#59698,#59699,#59700,
#59701,#59702,#59703,#59704)) ;
#24028 = EDGE_LOOP('',(#59705,#59706,#59707,#59708,#59709)) ;
#24029 = EDGE_LOOP('',(#59710,#59711,#59712,#59713,#59714)) ;
#24030 = EDGE_LOOP('',(#59715,#59716,#59717,#59718)) ;
#24031 = EDGE_LOOP('',(#59719,#59720,#59721,#59722)) ;
#24032 = EDGE_LOOP('',(#59723,#59724,#59725,#59726,#59727,#59728,#59729,#59730,
#59731,#59732,#59733,#59734,#59735,#59736,#59737,#59738,#59739,#59740,#59741,
#59742,#59743,#59744,#59745,#59746,#59747,#59748,#59749,#59750,#59751,#59752,
#59753,#59754,#59755,#59756,#59757,#59758,#59759,#59760,#59761,#59762,#59763,
#59764,#59765,#59766,#59767,#59768,#59769,#59770,#59771,#59772,#59773,#59774,
#59775,#59776,#59777,#59778,#59779,#59780,#59781,#59782,#59783,#59784,#59785,
#59786)) ;
#24033 = EDGE_LOOP('',(#59787,#59788,#59789,#59790)) ;
#24034 = EDGE_LOOP('',(#59791,#59792,#59793,#59794,#59795,#59796,#59797,#59798,
#59799,#59800,#59801,#59802,#59803,#59804,#59805,#59806,#59807,#59808,#59809,
#59810,#59811,#59812,#59813,#59814,#59815,#59816,#59817,#59818,#59819,#59820,
#59821,#59822,#59823,#59824,#59825,#59826,#59827,#59828,#59829,#59830,#59831,
#59832,#59833,#59834,#59835,#59836,#59837,#59838,#59839,#59840,#59841,#59842,
#59843,#59844,#59845,#59846,#59847,#59848,#59849,#59850,#59851,#59852,#59853,
#59854)) ;
#24035 = EDGE_LOOP('',(#59855,#59856,#59857,#59858)) ;
#24036 = EDGE_LOOP('',(#59859,#59860,#59861,#59862)) ;
#24037 = EDGE_LOOP('',(#59863,#59864,#59865,#59866)) ;
#24038 = EDGE_LOOP('',(#59867,#59868,#59869,#59870)) ;
#24039 = EDGE_LOOP('',(#59871,#59872,#59873,#59874)) ;
#24040 = EDGE_LOOP('',(#59875,#59876,#59877,#59878)) ;
#24041 = EDGE_LOOP('',(#59879,#59880,#59881,#59882)) ;
#24042 = EDGE_LOOP('',(#59883,#59884,#59885,#59886)) ;
#24043 = EDGE_LOOP('',(#59887,#59888,#59889,#59890)) ;
#24044 = EDGE_LOOP('',(#59891,#59892,#59893,#59894)) ;
#24045 = EDGE_LOOP('',(#59895,#59896,#59897,#59898)) ;
#24046 = EDGE_LOOP('',(#59899,#59900,#59901,#59902)) ;
#24047 = EDGE_LOOP('',(#59903,#59904,#59905,#59906,#59907,#59908,#59909,#59910,
#59911,#59912,#59913,#59914,#59915,#59916,#59917,#59918,#59919,#59920,#59921,
#59922,#59923,#59924,#59925,#59926)) ;
#24048 = EDGE_LOOP('',(#59927,#59928,#59929,#59930,#59931,#59932,#59933,#59934,
#59935,#59936,#59937,#59938,#59939,#59940,#59941,#59942,#59943,#59944,#59945,
#59946,#59947,#59948,#59949,#59950)) ;
#24049 = EDGE_LOOP('',(#59951,#59952,#59953,#59954,#59955,#59956,#59957,#59958,
#59959,#59960,#59961,#59962,#59963,#59964,#59965,#59966,#59967,#59968,#59969,
#59970,#59971,#59972,#59973,#59974)) ;
#24050 = EDGE_LOOP('',(#59975,#59976,#59977,#59978,#59979,#59980,#59981,#59982,
#59983,#59984,#59985,#59986,#59987,#59988,#59989,#59990,#59991,#59992,#59993,
#59994,#59995,#59996,#59997,#59998)) ;
#24051 = EDGE_LOOP('',(#59999,#60000,#60001,#60002,#60003,#60004,#60005,#60006,
#60007,#60008,#60009,#60010,#60011,#60012,#60013,#60014,#60015,#60016,#60017,
#60018,#60019,#60020,#60021,#60022)) ;
#24052 = EDGE_LOOP('',(#60023,#60024,#60025,#60026,#60027,#60028,#60029,#60030,
#60031,#60032,#60033,#60034,#60035,#60036,#60037,#60038,#60039,#60040,#60041,
#60042,#60043,#60044,#60045,#60046)) ;
#24053 = EDGE_LOOP('',(#60047,#60048,#60049,#60050,#60051,#60052,#60053,#60054,
#60055,#60056,#60057,#60058,#60059,#60060,#60061,#60062,#60063,#60064,#60065,
#60066,#60067,#60068,#60069,#60070)) ;
#24054 = EDGE_LOOP('',(#60071,#60072,#60073,#60074,#60075,#60076,#60077,#60078,
#60079,#60080,#60081,#60082,#60083,#60084,#60085,#60086,#60087,#60088,#60089,
#60090,#60091,#60092,#60093,#60094)) ;
#24055 = EDGE_LOOP('',(#60095,#60096,#60097,#60098,#60099,#60100,#60101,#60102,
#60103,#60104,#60105,#60106,#60107,#60108,#60109,#60110,#60111,#60112,#60113,
#60114,#60115,#60116,#60117,#60118)) ;
#24056 = EDGE_LOOP('',(#60119,#60120,#60121,#60122,#60123,#60124,#60125,#60126,
#60127,#60128,#60129,#60130,#60131,#60132,#60133,#60134,#60135,#60136,#60137,
#60138,#60139,#60140,#60141,#60142)) ;
#24057 = EDGE_LOOP('',(#60143,#60144,#60145,#60146,#60147,#60148,#60149,#60150,
#60151,#60152)) ;
#24058 = EDGE_LOOP('',(#60153,#60154,#60155,#60156,#60157,#60158,#60159,#60160,
#60161,#60162)) ;
#24059 = EDGE_LOOP('',(#60163,#60164,#60165,#60166,#60167,#60168,#60169,#60170,
#60171,#60172)) ;
#24060 = EDGE_LOOP('',(#60173,#60174,#60175,#60176)) ;
#24061 = EDGE_LOOP('',(#60177,#60178,#60179,#60180)) ;
#24062 = EDGE_LOOP('',(#60181,#60182,#60183,#60184)) ;
#24063 = EDGE_LOOP('',(#60185,#60186,#60187,#60188)) ;
#24064 = EDGE_LOOP('',(#60189,#60190,#60191,#60192)) ;
#24065 = EDGE_LOOP('',(#60193,#60194,#60195,#60196)) ;
#24066 = EDGE_LOOP('',(#60197,#60198,#60199,#60200)) ;
#24067 = EDGE_LOOP('',(#60201,#60202,#60203,#60204)) ;
#24068 = EDGE_LOOP('',(#60205,#60206,#60207,#60208)) ;
#24069 = EDGE_LOOP('',(#60209,#60210,#60211,#60212)) ;
#24070 = EDGE_LOOP('',(#60213,#60214,#60215,#60216)) ;
#24071 = EDGE_LOOP('',(#60217,#60218,#60219,#60220)) ;
#24072 = EDGE_LOOP('',(#60221,#60222,#60223,#60224)) ;
#24073 = EDGE_LOOP('',(#60225,#60226,#60227,#60228)) ;
#24074 = EDGE_LOOP('',(#60229,#60230,#60231,#60232)) ;
#24075 = EDGE_LOOP('',(#60233,#60234,#60235,#60236)) ;
#24076 = EDGE_LOOP('',(#60237,#60238,#60239,#60240)) ;
#24077 = EDGE_LOOP('',(#60241,#60242,#60243,#60244)) ;
#24078 = EDGE_LOOP('',(#60245,#60246,#60247,#60248)) ;
#24079 = EDGE_LOOP('',(#60249,#60250,#60251,#60252)) ;
#24080 = EDGE_LOOP('',(#60253,#60254,#60255,#60256)) ;
#24081 = EDGE_LOOP('',(#60257,#60258,#60259,#60260)) ;
#24082 = EDGE_LOOP('',(#60261,#60262,#60263,#60264)) ;
#24083 = EDGE_LOOP('',(#60265,#60266,#60267,#60268)) ;
#24084 = EDGE_LOOP('',(#60269,#60270,#60271,#60272)) ;
#24085 = EDGE_LOOP('',(#60273,#60274,#60275,#60276)) ;
#24086 = EDGE_LOOP('',(#60277,#60278,#60279,#60280)) ;
#24087 = EDGE_LOOP('',(#60281,#60282,#60283,#60284)) ;
#24088 = EDGE_LOOP('',(#60285,#60286,#60287,#60288)) ;
#24089 = EDGE_LOOP('',(#60289,#60290,#60291,#60292)) ;
#24090 = EDGE_LOOP('',(#60293,#60294,#60295,#60296)) ;
#24091 = EDGE_LOOP('',(#60297,#60298,#60299,#60300)) ;
#24092 = EDGE_LOOP('',(#60301,#60302,#60303,#60304,#60305,#60306,#60307,#60308,
#60309,#60310,#60311,#60312,#60313,#60314,#60315,#60316,#60317,#60318)) ;
#24093 = EDGE_LOOP('',(#60319)) ;
#24094 = EDGE_LOOP('',(#60320)) ;
#24095 = EDGE_LOOP('',(#60321,#60322,#60323,#60324,#60325,#60326,#60327,#60328)) ;
#24096 = EDGE_LOOP('',(#60329,#60330,#60331,#60332)) ;
#24097 = EDGE_LOOP('',(#60333,#60334,#60335,#60336)) ;
#24098 = EDGE_LOOP('',(#60337,#60338,#60339)) ;
#24099 = EDGE_LOOP('',(#60340,#60341,#60342)) ;
#24100 = EDGE_LOOP('',(#60343,#60344,#60345,#60346)) ;
#24101 = EDGE_LOOP('',(#60347,#60348,#60349,#60350,#60351,#60352)) ;
#24102 = EDGE_LOOP('',(#60353,#60354,#60355,#60356,#60357,#60358,#60359)) ;
#24103 = EDGE_LOOP('',(#60360,#60361,#60362,#60363)) ;
#24104 = EDGE_LOOP('',(#60364,#60365,#60366,#60367)) ;
#24105 = EDGE_LOOP('',(#60368,#60369,#60370,#60371)) ;
#24106 = EDGE_LOOP('',(#60372,#60373,#60374,#60375)) ;
#24107 = EDGE_LOOP('',(#60376,#60377,#60378)) ;
#24108 = EDGE_LOOP('',(#60379,#60380,#60381,#60382)) ;
#24109 = EDGE_LOOP('',(#60383,#60384,#60385,#60386)) ;
#24110 = EDGE_LOOP('',(#60387,#60388,#60389,#60390)) ;
#24111 = EDGE_LOOP('',(#60391,#60392,#60393,#60394)) ;
#24112 = EDGE_LOOP('',(#60395,#60396,#60397,#60398)) ;
#24113 = EDGE_LOOP('',(#60399,#60400,#60401,#60402)) ;
#24114 = EDGE_LOOP('',(#60403,#60404,#60405,#60406)) ;
#24115 = EDGE_LOOP('',(#60407,#60408,#60409,#60410)) ;
#24116 = EDGE_LOOP('',(#60411,#60412,#60413,#60414)) ;
#24117 = EDGE_LOOP('',(#60415,#60416,#60417)) ;
#24118 = EDGE_LOOP('',(#60418,#60419,#60420)) ;
#24119 = EDGE_LOOP('',(#60421,#60422,#60423,#60424,#60425)) ;
#24120 = EDGE_LOOP('',(#60426,#60427,#60428)) ;
#24121 = EDGE_LOOP('',(#60429,#60430,#60431)) ;
#24122 = EDGE_LOOP('',(#60432,#60433,#60434,#60435)) ;
#24123 = EDGE_LOOP('',(#60436,#60437,#60438,#60439)) ;
#24124 = EDGE_LOOP('',(#60440,#60441,#60442,#60443)) ;
#24125 = EDGE_LOOP('',(#60444,#60445,#60446,#60447)) ;
#24126 = EDGE_LOOP('',(#60448,#60449,#60450,#60451)) ;
#24127 = EDGE_LOOP('',(#60452,#60453,#60454,#60455)) ;
#24128 = EDGE_LOOP('',(#60456,#60457,#60458,#60459)) ;
#24129 = EDGE_LOOP('',(#60460,#60461,#60462)) ;
#24130 = EDGE_LOOP('',(#60463,#60464,#60465,#60466)) ;
#24131 = EDGE_LOOP('',(#60467,#60468,#60469,#60470)) ;
#24132 = EDGE_LOOP('',(#60471,#60472,#60473)) ;
#24133 = EDGE_LOOP('',(#60474,#60475,#60476,#60477)) ;
#24134 = EDGE_LOOP('',(#60478,#60479,#60480,#60481)) ;
#24135 = EDGE_LOOP('',(#60482,#60483,#60484,#60485)) ;
#24136 = EDGE_LOOP('',(#60486,#60487,#60488,#60489)) ;
#24137 = EDGE_LOOP('',(#60490,#60491,#60492,#60493)) ;
#24138 = EDGE_LOOP('',(#60494,#60495,#60496,#60497)) ;
#24139 = EDGE_LOOP('',(#60498,#60499,#60500,#60501,#60502)) ;
#24140 = EDGE_LOOP('',(#60503,#60504,#60505,#60506)) ;
#24141 = EDGE_LOOP('',(#60507,#60508,#60509)) ;
#24142 = EDGE_LOOP('',(#60510,#60511,#60512)) ;
#24143 = EDGE_LOOP('',(#60513,#60514,#60515,#60516)) ;
#24144 = EDGE_LOOP('',(#60517,#60518,#60519,#60520)) ;
#24145 = EDGE_LOOP('',(#60521,#60522,#60523,#60524)) ;
#24146 = EDGE_LOOP('',(#60525,#60526,#60527)) ;
#24147 = EDGE_LOOP('',(#60528,#60529,#60530,#60531)) ;
#24148 = EDGE_LOOP('',(#60532,#60533,#60534,#60535)) ;
#24149 = EDGE_LOOP('',(#60536,#60537,#60538)) ;
#24150 = EDGE_LOOP('',(#60539,#60540,#60541,#60542)) ;
#24151 = EDGE_LOOP('',(#60543,#60544,#60545,#60546)) ;
#24152 = EDGE_LOOP('',(#60547,#60548,#60549,#60550)) ;
#24153 = EDGE_LOOP('',(#60551,#60552,#60553)) ;
#24154 = EDGE_LOOP('',(#60554,#60555,#60556)) ;
#24155 = EDGE_LOOP('',(#60557,#60558,#60559,#60560)) ;
#24156 = EDGE_LOOP('',(#60561,#60562,#60563,#60564)) ;
#24157 = EDGE_LOOP('',(#60565,#60566,#60567)) ;
#24158 = EDGE_LOOP('',(#60568,#60569,#60570)) ;
#24159 = EDGE_LOOP('',(#60571,#60572,#60573,#60574)) ;
#24160 = EDGE_LOOP('',(#60575,#60576,#60577,#60578)) ;
#24161 = EDGE_LOOP('',(#60579,#60580,#60581,#60582)) ;
#24162 = EDGE_LOOP('',(#60583,#60584,#60585)) ;
#24163 = EDGE_LOOP('',(#60586,#60587,#60588,#60589)) ;
#24164 = EDGE_LOOP('',(#60590,#60591,#60592,#60593)) ;
#24165 = EDGE_LOOP('',(#60594,#60595,#60596)) ;
#24166 = EDGE_LOOP('',(#60597,#60598,#60599,#60600)) ;
#24167 = EDGE_LOOP('',(#60601,#60602,#60603,#60604)) ;
#24168 = EDGE_LOOP('',(#60605,#60606,#60607,#60608)) ;
#24169 = EDGE_LOOP('',(#60609,#60610,#60611)) ;
#24170 = EDGE_LOOP('',(#60612,#60613,#60614)) ;
#24171 = EDGE_LOOP('',(#60615,#60616,#60617,#60618)) ;
#24172 = EDGE_LOOP('',(#60619,#60620,#60621,#60622)) ;
#24173 = EDGE_LOOP('',(#60623,#60624,#60625)) ;
#24174 = EDGE_LOOP('',(#60626,#60627,#60628,#60629)) ;
#24175 = EDGE_LOOP('',(#60630,#60631,#60632,#60633)) ;
#24176 = EDGE_LOOP('',(#60634,#60635,#60636)) ;
#24177 = EDGE_LOOP('',(#60637,#60638,#60639,#60640)) ;
#24178 = EDGE_LOOP('',(#60641,#60642,#60643,#60644)) ;
#24179 = EDGE_LOOP('',(#60645,#60646,#60647,#60648)) ;
#24180 = EDGE_LOOP('',(#60649,#60650,#60651)) ;
#24181 = EDGE_LOOP('',(#60652,#60653,#60654,#60655)) ;
#24182 = EDGE_LOOP('',(#60656,#60657,#60658,#60659)) ;
#24183 = EDGE_LOOP('',(#60660,#60661,#60662)) ;
#24184 = EDGE_LOOP('',(#60663,#60664,#60665)) ;
#24185 = EDGE_LOOP('',(#60666,#60667,#60668,#60669)) ;
#24186 = EDGE_LOOP('',(#60670,#60671,#60672,#60673)) ;
#24187 = EDGE_LOOP('',(#60674,#60675,#60676)) ;
#24188 = EDGE_LOOP('',(#60677,#60678,#60679)) ;
#24189 = EDGE_LOOP('',(#60680,#60681,#60682,#60683)) ;
#24190 = EDGE_LOOP('',(#60684,#60685,#60686,#60687)) ;
#24191 = EDGE_LOOP('',(#60688,#60689,#60690)) ;
#24192 = EDGE_LOOP('',(#60691,#60692,#60693,#60694)) ;
#24193 = EDGE_LOOP('',(#60695,#60696,#60697,#60698)) ;
#24194 = EDGE_LOOP('',(#60699,#60700,#60701)) ;
#24195 = EDGE_LOOP('',(#60702,#60703,#60704)) ;
#24196 = EDGE_LOOP('',(#60705,#60706,#60707,#60708)) ;
#24197 = EDGE_LOOP('',(#60709,#60710,#60711,#60712)) ;
#24198 = EDGE_LOOP('',(#60713,#60714,#60715,#60716)) ;
#24199 = EDGE_LOOP('',(#60717,#60718,#60719,#60720)) ;
#24200 = EDGE_LOOP('',(#60721,#60722,#60723,#60724)) ;
#24201 = EDGE_LOOP('',(#60725,#60726,#60727,#60728)) ;
#24202 = EDGE_LOOP('',(#60729,#60730,#60731)) ;
#24203 = EDGE_LOOP('',(#60732,#60733,#60734)) ;
#24204 = EDGE_LOOP('',(#60735,#60736,#60737,#60738)) ;
#24205 = EDGE_LOOP('',(#60739,#60740,#60741,#60742)) ;
#24206 = EDGE_LOOP('',(#60743,#60744,#60745,#60746)) ;
#24207 = EDGE_LOOP('',(#60747,#60748,#60749,#60750)) ;
#24208 = EDGE_LOOP('',(#60751,#60752,#60753,#60754)) ;
#24209 = EDGE_LOOP('',(#60755,#60756,#60757,#60758)) ;
#24210 = EDGE_LOOP('',(#60759,#60760,#60761,#60762)) ;
#24211 = EDGE_LOOP('',(#60763,#60764,#60765,#60766)) ;
#24212 = EDGE_LOOP('',(#60767,#60768,#60769,#60770)) ;
#24213 = EDGE_LOOP('',(#60771,#60772,#60773,#60774)) ;
#24214 = EDGE_LOOP('',(#60775,#60776,#60777,#60778)) ;
#24215 = EDGE_LOOP('',(#60779,#60780,#60781,#60782)) ;
#24216 = EDGE_LOOP('',(#60783,#60784,#60785,#60786)) ;
#24217 = EDGE_LOOP('',(#60787,#60788,#60789,#60790)) ;
#24218 = EDGE_LOOP('',(#60791,#60792,#60793,#60794)) ;
#24219 = EDGE_LOOP('',(#60795,#60796,#60797,#60798)) ;
#24220 = EDGE_LOOP('',(#60799,#60800,#60801,#60802)) ;
#24221 = EDGE_LOOP('',(#60803,#60804,#60805)) ;
#24222 = EDGE_LOOP('',(#60806,#60807,#60808,#60809)) ;
#24223 = EDGE_LOOP('',(#60810,#60811,#60812,#60813)) ;
#24224 = EDGE_LOOP('',(#60814,#60815,#60816,#60817)) ;
#24225 = EDGE_LOOP('',(#60818,#60819,#60820)) ;
#24226 = EDGE_LOOP('',(#60821,#60822,#60823,#60824)) ;
#24227 = EDGE_LOOP('',(#60825,#60826,#60827,#60828)) ;
#24228 = EDGE_LOOP('',(#60829,#60830,#60831,#60832)) ;
#24229 = EDGE_LOOP('',(#60833,#60834,#60835,#60836)) ;
#24230 = EDGE_LOOP('',(#60837,#60838,#60839,#60840)) ;
#24231 = EDGE_LOOP('',(#60841,#60842,#60843,#60844)) ;
#24232 = EDGE_LOOP('',(#60845,#60846,#60847,#60848)) ;
#24233 = EDGE_LOOP('',(#60849,#60850,#60851,#60852,#60853,#60854)) ;
#24234 = EDGE_LOOP('',(#60855,#60856,#60857,#60858,#60859,#60860)) ;
#24235 = EDGE_LOOP('',(#60861,#60862,#60863,#60864,#60865)) ;
#24236 = EDGE_LOOP('',(#60866,#60867,#60868,#60869)) ;
#24237 = EDGE_LOOP('',(#60870,#60871,#60872,#60873)) ;
#24238 = EDGE_LOOP('',(#60874,#60875,#60876,#60877)) ;
#24239 = EDGE_LOOP('',(#60878,#60879,#60880,#60881)) ;
#24240 = EDGE_LOOP('',(#60882,#60883,#60884,#60885)) ;
#24241 = EDGE_LOOP('',(#60886,#60887,#60888,#60889)) ;
#24242 = EDGE_LOOP('',(#60890,#60891,#60892,#60893)) ;
#24243 = EDGE_LOOP('',(#60894,#60895,#60896,#60897)) ;
#24244 = EDGE_LOOP('',(#60898,#60899,#60900,#60901)) ;
#24245 = EDGE_LOOP('',(#60902,#60903,#60904,#60905)) ;
#24246 = EDGE_LOOP('',(#60906,#60907,#60908,#60909)) ;
#24247 = EDGE_LOOP('',(#60910,#60911,#60912,#60913)) ;
#24248 = EDGE_LOOP('',(#60914,#60915,#60916,#60917)) ;
#24249 = EDGE_LOOP('',(#60918,#60919,#60920,#60921)) ;
#24250 = EDGE_LOOP('',(#60922,#60923,#60924)) ;
#24251 = EDGE_LOOP('',(#60925,#60926,#60927,#60928)) ;
#24252 = EDGE_LOOP('',(#60929,#60930,#60931,#60932)) ;
#24253 = EDGE_LOOP('',(#60933,#60934,#60935,#60936)) ;
#24254 = EDGE_LOOP('',(#60937,#60938,#60939)) ;
#24255 = EDGE_LOOP('',(#60940,#60941,#60942)) ;
#24256 = EDGE_LOOP('',(#60943,#60944,#60945,#60946)) ;
#24257 = EDGE_LOOP('',(#60947,#60948,#60949,#60950)) ;
#24258 = EDGE_LOOP('',(#60951,#60952,#60953,#60954)) ;
#24259 = EDGE_LOOP('',(#60955,#60956,#60957)) ;
#24260 = EDGE_LOOP('',(#60958,#60959,#60960,#60961)) ;
#24261 = EDGE_LOOP('',(#60962,#60963,#60964,#60965)) ;
#24262 = EDGE_LOOP('',(#60966,#60967,#60968,#60969)) ;
#24263 = EDGE_LOOP('',(#60970,#60971,#60972,#60973)) ;
#24264 = EDGE_LOOP('',(#60974,#60975,#60976)) ;
#24265 = EDGE_LOOP('',(#60977,#60978,#60979,#60980)) ;
#24266 = EDGE_LOOP('',(#60981,#60982,#60983,#60984)) ;
#24267 = EDGE_LOOP('',(#60985,#60986,#60987,#60988)) ;
#24268 = EDGE_LOOP('',(#60989,#60990,#60991)) ;
#24269 = EDGE_LOOP('',(#60992,#60993,#60994)) ;
#24270 = EDGE_LOOP('',(#60995,#60996,#60997,#60998)) ;
#24271 = EDGE_LOOP('',(#60999,#61000,#61001,#61002)) ;
#24272 = EDGE_LOOP('',(#61003,#61004,#61005,#61006)) ;
#24273 = EDGE_LOOP('',(#61007,#61008,#61009)) ;
#24274 = EDGE_LOOP('',(#61010,#61011,#61012,#61013)) ;
#24275 = EDGE_LOOP('',(#61014,#61015,#61016,#61017)) ;
#24276 = EDGE_LOOP('',(#61018,#61019,#61020,#61021)) ;
#24277 = EDGE_LOOP('',(#61022,#61023,#61024,#61025)) ;
#24278 = EDGE_LOOP('',(#61026,#61027,#61028,#61029)) ;
#24279 = EDGE_LOOP('',(#61030,#61031,#61032,#61033)) ;
#24280 = EDGE_LOOP('',(#61034,#61035,#61036,#61037)) ;
#24281 = EDGE_LOOP('',(#61038,#61039,#61040,#61041)) ;
#24282 = EDGE_LOOP('',(#61042,#61043,#61044,#61045,#61046)) ;
#24283 = EDGE_LOOP('',(#61047,#61048,#61049,#61050)) ;
#24284 = EDGE_LOOP('',(#61051,#61052,#61053,#61054)) ;
#24285 = EDGE_LOOP('',(#61055,#61056,#61057,#61058)) ;
#24286 = EDGE_LOOP('',(#61059,#61060,#61061,#61062)) ;
#24287 = EDGE_LOOP('',(#61063,#61064,#61065,#61066)) ;
#24288 = EDGE_LOOP('',(#61067,#61068,#61069,#61070)) ;
#24289 = EDGE_LOOP('',(#61071,#61072,#61073,#61074)) ;
#24290 = EDGE_LOOP('',(#61075,#61076,#61077,#61078)) ;
#24291 = EDGE_LOOP('',(#61079,#61080,#61081,#61082)) ;
#24292 = EDGE_LOOP('',(#61083,#61084,#61085,#61086)) ;
#24293 = EDGE_LOOP('',(#61087,#61088,#61089,#61090)) ;
#24294 = EDGE_LOOP('',(#61091,#61092,#61093,#61094)) ;
#24295 = EDGE_LOOP('',(#61095,#61096,#61097,#61098)) ;
#24296 = EDGE_LOOP('',(#61099,#61100,#61101,#61102)) ;
#24297 = EDGE_LOOP('',(#61103,#61104,#61105,#61106)) ;
#24298 = EDGE_LOOP('',(#61107,#61108,#61109,#61110)) ;
#24299 = EDGE_LOOP('',(#61111,#61112,#61113,#61114)) ;
#24300 = EDGE_LOOP('',(#61115,#61116,#61117,#61118,#61119,#61120,#61121,#61122,
#61123,#61124)) ;
#24301 = EDGE_LOOP('',(#61125,#61126,#61127,#61128,#61129,#61130,#61131,#61132,
#61133,#61134)) ;
#24302 = EDGE_LOOP('',(#61135,#61136,#61137,#61138,#61139,#61140,#61141,#61142,
#61143,#61144)) ;
#24303 = EDGE_LOOP('',(#61145,#61146,#61147,#61148,#61149,#61150,#61151,#61152,
#61153,#61154)) ;
#24304 = EDGE_LOOP('',(#61155,#61156,#61157,#61158,#61159,#61160,#61161,#61162,
#61163,#61164)) ;
#24305 = EDGE_LOOP('',(#61165,#61166,#61167,#61168,#61169,#61170,#61171,#61172,
#61173,#61174)) ;
#24306 = EDGE_LOOP('',(#61175,#61176,#61177,#61178,#61179,#61180,#61181,#61182,
#61183,#61184)) ;
#24307 = EDGE_LOOP('',(#61185,#61186,#61187,#61188,#61189,#61190,#61191,#61192,
#61193,#61194)) ;
#24308 = EDGE_LOOP('',(#61195,#61196,#61197,#61198,#61199,#61200,#61201,#61202,
#61203,#61204)) ;
#24309 = EDGE_LOOP('',(#61205,#61206,#61207,#61208)) ;
#24310 = EDGE_LOOP('',(#61209,#61210,#61211,#61212)) ;
#24311 = EDGE_LOOP('',(#61213,#61214,#61215,#61216)) ;
#24312 = EDGE_LOOP('',(#61217,#61218,#61219,#61220)) ;
#24313 = EDGE_LOOP('',(#61221,#61222,#61223,#61224)) ;
#24314 = EDGE_LOOP('',(#61225,#61226,#61227,#61228)) ;
#24315 = EDGE_LOOP('',(#61229,#61230,#61231,#61232)) ;
#24316 = EDGE_LOOP('',(#61233,#61234,#61235,#61236)) ;
#24317 = EDGE_LOOP('',(#61237,#61238,#61239,#61240)) ;
#24318 = EDGE_LOOP('',(#61241,#61242,#61243,#61244)) ;
#24319 = EDGE_LOOP('',(#61245,#61246,#61247,#61248)) ;
#24320 = EDGE_LOOP('',(#61249,#61250,#61251,#61252)) ;
#24321 = EDGE_LOOP('',(#61253,#61254,#61255,#61256)) ;
#24322 = EDGE_LOOP('',(#61257,#61258,#61259,#61260)) ;
#24323 = EDGE_LOOP('',(#61261,#61262,#61263,#61264)) ;
#24324 = EDGE_LOOP('',(#61265,#61266,#61267,#61268)) ;
#24325 = EDGE_LOOP('',(#61269,#61270,#61271,#61272)) ;
#24326 = EDGE_LOOP('',(#61273,#61274,#61275,#61276)) ;
#24327 = EDGE_LOOP('',(#61277,#61278,#61279,#61280)) ;
#24328 = EDGE_LOOP('',(#61281,#61282,#61283,#61284)) ;
#24329 = EDGE_LOOP('',(#61285,#61286,#61287,#61288)) ;
#24330 = EDGE_LOOP('',(#61289,#61290,#61291,#61292)) ;
#24331 = EDGE_LOOP('',(#61293,#61294,#61295,#61296)) ;
#24332 = EDGE_LOOP('',(#61297,#61298,#61299,#61300)) ;
#24333 = EDGE_LOOP('',(#61301,#61302,#61303,#61304)) ;
#24334 = EDGE_LOOP('',(#61305,#61306,#61307,#61308)) ;
#24335 = EDGE_LOOP('',(#61309,#61310,#61311,#61312)) ;
#24336 = EDGE_LOOP('',(#61313,#61314,#61315,#61316)) ;
#24337 = EDGE_LOOP('',(#61317,#61318,#61319,#61320)) ;
#24338 = EDGE_LOOP('',(#61321,#61322,#61323,#61324)) ;
#24339 = EDGE_LOOP('',(#61325,#61326,#61327,#61328)) ;
#24340 = EDGE_LOOP('',(#61329,#61330,#61331,#61332)) ;
#24341 = EDGE_LOOP('',(#61333,#61334,#61335,#61336)) ;
#24342 = EDGE_LOOP('',(#61337,#61338,#61339,#61340)) ;
#24343 = EDGE_LOOP('',(#61341,#61342,#61343,#61344)) ;
#24344 = EDGE_LOOP('',(#61345,#61346,#61347,#61348)) ;
#24345 = EDGE_LOOP('',(#61349,#61350,#61351,#61352)) ;
#24346 = EDGE_LOOP('',(#61353,#61354,#61355,#61356)) ;
#24347 = EDGE_LOOP('',(#61357,#61358,#61359,#61360)) ;
#24348 = EDGE_LOOP('',(#61361,#61362,#61363,#61364)) ;
#24349 = EDGE_LOOP('',(#61365,#61366,#61367,#61368)) ;
#24350 = EDGE_LOOP('',(#61369,#61370,#61371,#61372)) ;
#24351 = EDGE_LOOP('',(#61373,#61374,#61375,#61376)) ;
#24352 = EDGE_LOOP('',(#61377,#61378,#61379,#61380)) ;
#24353 = EDGE_LOOP('',(#61381,#61382,#61383,#61384)) ;
#24354 = EDGE_LOOP('',(#61385,#61386,#61387,#61388)) ;
#24355 = EDGE_LOOP('',(#61389,#61390,#61391,#61392)) ;
#24356 = EDGE_LOOP('',(#61393,#61394,#61395,#61396)) ;
#24357 = EDGE_LOOP('',(#61397,#61398,#61399,#61400)) ;
#24358 = EDGE_LOOP('',(#61401,#61402,#61403,#61404)) ;
#24359 = EDGE_LOOP('',(#61405,#61406,#61407,#61408)) ;
#24360 = EDGE_LOOP('',(#61409,#61410,#61411,#61412)) ;
#24361 = EDGE_LOOP('',(#61413,#61414,#61415,#61416)) ;
#24362 = EDGE_LOOP('',(#61417,#61418,#61419,#61420)) ;
#24363 = EDGE_LOOP('',(#61421,#61422,#61423,#61424)) ;
#24364 = EDGE_LOOP('',(#61425,#61426,#61427,#61428)) ;
#24365 = EDGE_LOOP('',(#61429,#61430,#61431,#61432)) ;
#24366 = EDGE_LOOP('',(#61433,#61434,#61435,#61436)) ;
#24367 = EDGE_LOOP('',(#61437,#61438,#61439,#61440)) ;
#24368 = EDGE_LOOP('',(#61441,#61442,#61443,#61444)) ;
#24369 = EDGE_LOOP('',(#61445,#61446,#61447,#61448)) ;
#24370 = EDGE_LOOP('',(#61449,#61450,#61451,#61452)) ;
#24371 = EDGE_LOOP('',(#61453,#61454,#61455,#61456)) ;
#24372 = EDGE_LOOP('',(#61457,#61458,#61459,#61460)) ;
#24373 = EDGE_LOOP('',(#61461,#61462,#61463,#61464)) ;
#24374 = EDGE_LOOP('',(#61465,#61466,#61467,#61468)) ;
#24375 = EDGE_LOOP('',(#61469,#61470,#61471,#61472)) ;
#24376 = EDGE_LOOP('',(#61473,#61474,#61475,#61476)) ;
#24377 = EDGE_LOOP('',(#61477,#61478,#61479,#61480)) ;
#24378 = EDGE_LOOP('',(#61481,#61482,#61483,#61484)) ;
#24379 = EDGE_LOOP('',(#61485,#61486,#61487,#61488)) ;
#24380 = EDGE_LOOP('',(#61489,#61490,#61491,#61492)) ;
#24381 = EDGE_LOOP('',(#61493,#61494,#61495,#61496,#61497,#61498,#61499,#61500,
#61501,#61502,#61503,#61504,#61505,#61506,#61507,#61508,#61509,#61510)) ;
#24382 = EDGE_LOOP('',(#61511)) ;
#24383 = EDGE_LOOP('',(#61512,#61513,#61514,#61515)) ;
#24384 = EDGE_LOOP('',(#61516,#61517,#61518,#61519)) ;
#24385 = EDGE_LOOP('',(#61520,#61521,#61522,#61523)) ;
#24386 = EDGE_LOOP('',(#61524,#61525,#61526,#61527)) ;
#24387 = EDGE_LOOP('',(#61528,#61529,#61530,#61531)) ;
#24388 = EDGE_LOOP('',(#61532,#61533,#61534,#61535)) ;
#24389 = EDGE_LOOP('',(#61536,#61537,#61538,#61539)) ;
#24390 = EDGE_LOOP('',(#61540,#61541,#61542,#61543)) ;
#24391 = EDGE_LOOP('',(#61544,#61545,#61546,#61547)) ;
#24392 = EDGE_LOOP('',(#61548,#61549,#61550,#61551)) ;
#24393 = EDGE_LOOP('',(#61552,#61553,#61554,#61555)) ;
#24394 = EDGE_LOOP('',(#61556,#61557,#61558,#61559)) ;
#24395 = EDGE_LOOP('',(#61560,#61561,#61562,#61563)) ;
#24396 = EDGE_LOOP('',(#61564,#61565,#61566,#61567)) ;
#24397 = EDGE_LOOP('',(#61568,#61569,#61570,#61571)) ;
#24398 = EDGE_LOOP('',(#61572,#61573,#61574,#61575)) ;
#24399 = EDGE_LOOP('',(#61576,#61577,#61578,#61579)) ;
#24400 = EDGE_LOOP('',(#61580,#61581,#61582,#61583)) ;
#24401 = EDGE_LOOP('',(#61584,#61585,#61586,#61587)) ;
#24402 = EDGE_LOOP('',(#61588,#61589,#61590,#61591)) ;
#24403 = EDGE_LOOP('',(#61592,#61593,#61594,#61595)) ;
#24404 = EDGE_LOOP('',(#61596,#61597,#61598,#61599)) ;
#24405 = EDGE_LOOP('',(#61600,#61601,#61602,#61603)) ;
#24406 = EDGE_LOOP('',(#61604,#61605,#61606,#61607)) ;
#24407 = EDGE_LOOP('',(#61608,#61609,#61610,#61611)) ;
#24408 = EDGE_LOOP('',(#61612,#61613,#61614,#61615)) ;
#24409 = EDGE_LOOP('',(#61616,#61617,#61618,#61619)) ;
#24410 = EDGE_LOOP('',(#61620,#61621,#61622,#61623,#61624,#61625,#61626,#61627,
#61628,#61629,#61630,#61631,#61632,#61633,#61634,#61635,#61636,#61637)) ;
#24411 = EDGE_LOOP('',(#61638)) ;
#24412 = EDGE_LOOP('',(#61639,#61640,#61641,#61642)) ;
#24413 = EDGE_LOOP('',(#61643,#61644,#61645,#61646)) ;
#24414 = EDGE_LOOP('',(#61647,#61648,#61649,#61650)) ;
#24415 = EDGE_LOOP('',(#61651,#61652,#61653,#61654)) ;
#24416 = EDGE_LOOP('',(#61655,#61656,#61657,#61658)) ;
#24417 = EDGE_LOOP('',(#61659,#61660,#61661,#61662)) ;
#24418 = EDGE_LOOP('',(#61663,#61664,#61665,#61666)) ;
#24419 = EDGE_LOOP('',(#61667,#61668,#61669,#61670)) ;
#24420 = EDGE_LOOP('',(#61671,#61672,#61673,#61674)) ;
#24421 = EDGE_LOOP('',(#61675,#61676,#61677,#61678)) ;
#24422 = EDGE_LOOP('',(#61679,#61680,#61681,#61682)) ;
#24423 = EDGE_LOOP('',(#61683,#61684,#61685,#61686)) ;
#24424 = EDGE_LOOP('',(#61687,#61688,#61689,#61690)) ;
#24425 = EDGE_LOOP('',(#61691,#61692,#61693,#61694)) ;
#24426 = EDGE_LOOP('',(#61695,#61696,#61697,#61698)) ;
#24427 = EDGE_LOOP('',(#61699,#61700,#61701,#61702)) ;
#24428 = EDGE_LOOP('',(#61703,#61704,#61705,#61706)) ;
#24429 = EDGE_LOOP('',(#61707,#61708,#61709,#61710)) ;
#24430 = EDGE_LOOP('',(#61711,#61712,#61713,#61714)) ;
#24431 = EDGE_LOOP('',(#61715,#61716,#61717,#61718)) ;
#24432 = EDGE_LOOP('',(#61719,#61720,#61721,#61722)) ;
#24433 = EDGE_LOOP('',(#61723,#61724,#61725,#61726)) ;
#24434 = EDGE_LOOP('',(#61727,#61728,#61729,#61730)) ;
#24435 = EDGE_LOOP('',(#61731,#61732,#61733,#61734)) ;
#24436 = EDGE_LOOP('',(#61735,#61736,#61737,#61738)) ;
#24437 = EDGE_LOOP('',(#61739,#61740,#61741,#61742)) ;
#24438 = EDGE_LOOP('',(#61743,#61744,#61745,#61746)) ;
#24439 = EDGE_LOOP('',(#61747,#61748,#61749,#61750,#61751,#61752,#61753,#61754,
#61755,#61756,#61757,#61758,#61759,#61760,#61761,#61762,#61763,#61764)) ;
#24440 = EDGE_LOOP('',(#61765)) ;
#24441 = EDGE_LOOP('',(#61766,#61767,#61768,#61769)) ;
#24442 = EDGE_LOOP('',(#61770,#61771,#61772,#61773)) ;
#24443 = EDGE_LOOP('',(#61774,#61775,#61776,#61777)) ;
#24444 = EDGE_LOOP('',(#61778,#61779,#61780,#61781)) ;
#24445 = EDGE_LOOP('',(#61782,#61783,#61784,#61785)) ;
#24446 = EDGE_LOOP('',(#61786,#61787,#61788,#61789)) ;
#24447 = EDGE_LOOP('',(#61790,#61791,#61792,#61793)) ;
#24448 = EDGE_LOOP('',(#61794,#61795,#61796,#61797)) ;
#24449 = EDGE_LOOP('',(#61798,#61799,#61800,#61801)) ;
#24450 = EDGE_LOOP('',(#61802,#61803,#61804,#61805)) ;
#24451 = EDGE_LOOP('',(#61806,#61807,#61808,#61809)) ;
#24452 = EDGE_LOOP('',(#61810,#61811,#61812,#61813)) ;
#24453 = EDGE_LOOP('',(#61814,#61815,#61816,#61817)) ;
#24454 = EDGE_LOOP('',(#61818,#61819,#61820,#61821)) ;
#24455 = EDGE_LOOP('',(#61822,#61823,#61824,#61825)) ;
#24456 = EDGE_LOOP('',(#61826,#61827,#61828,#61829)) ;
#24457 = EDGE_LOOP('',(#61830,#61831,#61832,#61833)) ;
#24458 = EDGE_LOOP('',(#61834,#61835,#61836,#61837)) ;
#24459 = EDGE_LOOP('',(#61838,#61839,#61840,#61841)) ;
#24460 = EDGE_LOOP('',(#61842,#61843,#61844,#61845)) ;
#24461 = EDGE_LOOP('',(#61846,#61847,#61848,#61849)) ;
#24462 = EDGE_LOOP('',(#61850,#61851,#61852,#61853)) ;
#24463 = EDGE_LOOP('',(#61854,#61855,#61856,#61857)) ;
#24464 = EDGE_LOOP('',(#61858,#61859,#61860,#61861)) ;
#24465 = EDGE_LOOP('',(#61862,#61863,#61864,#61865)) ;
#24466 = EDGE_LOOP('',(#61866,#61867,#61868,#61869)) ;
#24467 = EDGE_LOOP('',(#61870,#61871,#61872,#61873)) ;
#24468 = EDGE_LOOP('',(#61874,#61875,#61876,#61877,#61878,#61879,#61880,#61881,
#61882,#61883,#61884,#61885,#61886,#61887,#61888,#61889,#61890,#61891)) ;
#24469 = EDGE_LOOP('',(#61892)) ;
#24470 = EDGE_LOOP('',(#61893,#61894,#61895,#61896)) ;
#24471 = EDGE_LOOP('',(#61897,#61898,#61899,#61900)) ;
#24472 = EDGE_LOOP('',(#61901,#61902,#61903,#61904)) ;
#24473 = EDGE_LOOP('',(#61905,#61906,#61907,#61908)) ;
#24474 = EDGE_LOOP('',(#61909,#61910,#61911,#61912)) ;
#24475 = EDGE_LOOP('',(#61913,#61914,#61915,#61916)) ;
#24476 = EDGE_LOOP('',(#61917,#61918,#61919,#61920)) ;
#24477 = EDGE_LOOP('',(#61921,#61922,#61923,#61924)) ;
#24478 = EDGE_LOOP('',(#61925,#61926,#61927,#61928)) ;
#24479 = EDGE_LOOP('',(#61929,#61930,#61931,#61932)) ;
#24480 = EDGE_LOOP('',(#61933,#61934,#61935,#61936)) ;
#24481 = EDGE_LOOP('',(#61937,#61938,#61939,#61940)) ;
#24482 = EDGE_LOOP('',(#61941,#61942,#61943,#61944)) ;
#24483 = EDGE_LOOP('',(#61945,#61946,#61947,#61948)) ;
#24484 = EDGE_LOOP('',(#61949,#61950,#61951,#61952)) ;
#24485 = EDGE_LOOP('',(#61953,#61954,#61955,#61956)) ;
#24486 = EDGE_LOOP('',(#61957,#61958,#61959,#61960)) ;
#24487 = EDGE_LOOP('',(#61961,#61962,#61963,#61964)) ;
#24488 = EDGE_LOOP('',(#61965,#61966,#61967,#61968)) ;
#24489 = EDGE_LOOP('',(#61969,#61970,#61971,#61972)) ;
#24490 = EDGE_LOOP('',(#61973,#61974,#61975,#61976)) ;
#24491 = EDGE_LOOP('',(#61977,#61978,#61979,#61980)) ;
#24492 = EDGE_LOOP('',(#61981,#61982,#61983,#61984)) ;
#24493 = EDGE_LOOP('',(#61985,#61986,#61987,#61988)) ;
#24494 = EDGE_LOOP('',(#61989,#61990,#61991,#61992)) ;
#24495 = EDGE_LOOP('',(#61993,#61994,#61995,#61996)) ;
#24496 = EDGE_LOOP('',(#61997,#61998,#61999,#62000)) ;
#24497 = EDGE_LOOP('',(#62001,#62002,#62003,#62004,#62005,#62006,#62007,#62008,
#62009,#62010,#62011,#62012,#62013,#62014,#62015,#62016,#62017,#62018)) ;
#24498 = EDGE_LOOP('',(#62019)) ;
#24499 = EDGE_LOOP('',(#62020,#62021,#62022,#62023)) ;
#24500 = EDGE_LOOP('',(#62024,#62025,#62026,#62027)) ;
#24501 = EDGE_LOOP('',(#62028,#62029,#62030,#62031)) ;
#24502 = EDGE_LOOP('',(#62032,#62033,#62034,#62035)) ;
#24503 = EDGE_LOOP('',(#62036,#62037,#62038,#62039)) ;
#24504 = EDGE_LOOP('',(#62040,#62041,#62042,#62043)) ;
#24505 = EDGE_LOOP('',(#62044,#62045,#62046,#62047)) ;
#24506 = EDGE_LOOP('',(#62048,#62049,#62050,#62051)) ;
#24507 = EDGE_LOOP('',(#62052,#62053,#62054,#62055)) ;
#24508 = EDGE_LOOP('',(#62056,#62057,#62058,#62059)) ;
#24509 = EDGE_LOOP('',(#62060,#62061,#62062,#62063)) ;
#24510 = EDGE_LOOP('',(#62064,#62065,#62066,#62067)) ;
#24511 = EDGE_LOOP('',(#62068,#62069,#62070,#62071)) ;
#24512 = EDGE_LOOP('',(#62072,#62073,#62074,#62075)) ;
#24513 = EDGE_LOOP('',(#62076,#62077,#62078,#62079)) ;
#24514 = EDGE_LOOP('',(#62080,#62081,#62082,#62083)) ;
#24515 = EDGE_LOOP('',(#62084,#62085,#62086,#62087)) ;
#24516 = EDGE_LOOP('',(#62088,#62089,#62090,#62091)) ;
#24517 = EDGE_LOOP('',(#62092,#62093,#62094,#62095)) ;
#24518 = EDGE_LOOP('',(#62096,#62097,#62098,#62099)) ;
#24519 = EDGE_LOOP('',(#62100,#62101,#62102,#62103)) ;
#24520 = EDGE_LOOP('',(#62104,#62105,#62106,#62107)) ;
#24521 = EDGE_LOOP('',(#62108,#62109,#62110,#62111)) ;
#24522 = EDGE_LOOP('',(#62112,#62113,#62114,#62115)) ;
#24523 = EDGE_LOOP('',(#62116,#62117,#62118,#62119)) ;
#24524 = EDGE_LOOP('',(#62120,#62121,#62122,#62123)) ;
#24525 = EDGE_LOOP('',(#62124,#62125,#62126,#62127)) ;
#24526 = EDGE_LOOP('',(#62128,#62129,#62130,#62131,#62132,#62133,#62134,#62135,
#62136,#62137,#62138,#62139,#62140,#62141,#62142,#62143,#62144,#62145)) ;
#24527 = EDGE_LOOP('',(#62146)) ;
#24528 = EDGE_LOOP('',(#62147,#62148,#62149,#62150)) ;
#24529 = EDGE_LOOP('',(#62151,#62152,#62153,#62154)) ;
#24530 = EDGE_LOOP('',(#62155,#62156,#62157,#62158)) ;
#24531 = EDGE_LOOP('',(#62159,#62160,#62161,#62162)) ;
#24532 = EDGE_LOOP('',(#62163,#62164,#62165,#62166)) ;
#24533 = EDGE_LOOP('',(#62167,#62168,#62169,#62170)) ;
#24534 = EDGE_LOOP('',(#62171,#62172,#62173,#62174)) ;
#24535 = EDGE_LOOP('',(#62175,#62176,#62177,#62178)) ;
#24536 = EDGE_LOOP('',(#62179,#62180,#62181,#62182)) ;
#24537 = EDGE_LOOP('',(#62183,#62184,#62185,#62186)) ;
#24538 = EDGE_LOOP('',(#62187,#62188,#62189,#62190)) ;
#24539 = EDGE_LOOP('',(#62191,#62192,#62193,#62194)) ;
#24540 = EDGE_LOOP('',(#62195,#62196,#62197,#62198)) ;
#24541 = EDGE_LOOP('',(#62199,#62200,#62201,#62202)) ;
#24542 = EDGE_LOOP('',(#62203,#62204,#62205,#62206)) ;
#24543 = EDGE_LOOP('',(#62207,#62208,#62209,#62210)) ;
#24544 = EDGE_LOOP('',(#62211,#62212,#62213,#62214)) ;
#24545 = EDGE_LOOP('',(#62215,#62216,#62217,#62218)) ;
#24546 = EDGE_LOOP('',(#62219,#62220,#62221,#62222)) ;
#24547 = EDGE_LOOP('',(#62223,#62224,#62225,#62226)) ;
#24548 = EDGE_LOOP('',(#62227,#62228,#62229,#62230)) ;
#24549 = EDGE_LOOP('',(#62231,#62232,#62233,#62234)) ;
#24550 = EDGE_LOOP('',(#62235,#62236,#62237,#62238)) ;
#24551 = EDGE_LOOP('',(#62239,#62240,#62241,#62242)) ;
#24552 = EDGE_LOOP('',(#62243,#62244,#62245,#62246)) ;
#24553 = EDGE_LOOP('',(#62247,#62248,#62249,#62250)) ;
#24554 = EDGE_LOOP('',(#62251,#62252,#62253,#62254)) ;
#24555 = EDGE_LOOP('',(#62255,#62256,#62257,#62258,#62259,#62260,#62261,#62262,
#62263,#62264,#62265,#62266,#62267,#62268,#62269,#62270,#62271,#62272)) ;
#24556 = EDGE_LOOP('',(#62273)) ;
#24557 = EDGE_LOOP('',(#62274,#62275,#62276,#62277)) ;
#24558 = EDGE_LOOP('',(#62278,#62279,#62280,#62281)) ;
#24559 = EDGE_LOOP('',(#62282,#62283,#62284,#62285)) ;
#24560 = EDGE_LOOP('',(#62286,#62287,#62288,#62289)) ;
#24561 = EDGE_LOOP('',(#62290,#62291,#62292,#62293)) ;
#24562 = EDGE_LOOP('',(#62294,#62295,#62296,#62297)) ;
#24563 = EDGE_LOOP('',(#62298,#62299,#62300,#62301)) ;
#24564 = EDGE_LOOP('',(#62302,#62303,#62304,#62305)) ;
#24565 = EDGE_LOOP('',(#62306,#62307,#62308,#62309)) ;
#24566 = EDGE_LOOP('',(#62310,#62311,#62312,#62313)) ;
#24567 = EDGE_LOOP('',(#62314,#62315,#62316,#62317)) ;
#24568 = EDGE_LOOP('',(#62318,#62319,#62320,#62321)) ;
#24569 = EDGE_LOOP('',(#62322,#62323,#62324,#62325)) ;
#24570 = EDGE_LOOP('',(#62326,#62327,#62328,#62329)) ;
#24571 = EDGE_LOOP('',(#62330,#62331,#62332,#62333)) ;
#24572 = EDGE_LOOP('',(#62334,#62335,#62336,#62337)) ;
#24573 = EDGE_LOOP('',(#62338,#62339,#62340,#62341)) ;
#24574 = EDGE_LOOP('',(#62342,#62343,#62344,#62345)) ;
#24575 = EDGE_LOOP('',(#62346,#62347,#62348,#62349)) ;
#24576 = EDGE_LOOP('',(#62350,#62351,#62352,#62353)) ;
#24577 = EDGE_LOOP('',(#62354,#62355,#62356,#62357)) ;
#24578 = EDGE_LOOP('',(#62358,#62359,#62360,#62361)) ;
#24579 = EDGE_LOOP('',(#62362,#62363,#62364,#62365)) ;
#24580 = EDGE_LOOP('',(#62366,#62367,#62368,#62369)) ;
#24581 = EDGE_LOOP('',(#62370,#62371,#62372,#62373)) ;
#24582 = EDGE_LOOP('',(#62374,#62375,#62376,#62377)) ;
#24583 = EDGE_LOOP('',(#62378,#62379,#62380,#62381)) ;
#24584 = EDGE_LOOP('',(#62382,#62383,#62384,#62385,#62386,#62387,#62388,#62389,
#62390,#62391,#62392,#62393,#62394,#62395,#62396,#62397,#62398,#62399)) ;
#24585 = EDGE_LOOP('',(#62400)) ;
#24586 = EDGE_LOOP('',(#62401,#62402,#62403,#62404)) ;
#24587 = EDGE_LOOP('',(#62405,#62406,#62407,#62408)) ;
#24588 = EDGE_LOOP('',(#62409,#62410,#62411,#62412)) ;
#24589 = EDGE_LOOP('',(#62413,#62414,#62415,#62416)) ;
#24590 = EDGE_LOOP('',(#62417,#62418,#62419,#62420)) ;
#24591 = EDGE_LOOP('',(#62421,#62422,#62423,#62424)) ;
#24592 = EDGE_LOOP('',(#62425,#62426,#62427,#62428)) ;
#24593 = EDGE_LOOP('',(#62429,#62430,#62431,#62432)) ;
#24594 = EDGE_LOOP('',(#62433,#62434,#62435,#62436)) ;
#24595 = EDGE_LOOP('',(#62437,#62438,#62439,#62440)) ;
#24596 = EDGE_LOOP('',(#62441,#62442,#62443,#62444)) ;
#24597 = EDGE_LOOP('',(#62445,#62446,#62447,#62448)) ;
#24598 = EDGE_LOOP('',(#62449,#62450,#62451,#62452)) ;
#24599 = EDGE_LOOP('',(#62453,#62454,#62455,#62456)) ;
#24600 = EDGE_LOOP('',(#62457,#62458,#62459,#62460)) ;
#24601 = EDGE_LOOP('',(#62461,#62462,#62463,#62464)) ;
#24602 = EDGE_LOOP('',(#62465,#62466,#62467,#62468)) ;
#24603 = EDGE_LOOP('',(#62469,#62470,#62471,#62472)) ;
#24604 = EDGE_LOOP('',(#62473,#62474,#62475,#62476)) ;
#24605 = EDGE_LOOP('',(#62477,#62478,#62479,#62480)) ;
#24606 = EDGE_LOOP('',(#62481,#62482,#62483,#62484)) ;
#24607 = EDGE_LOOP('',(#62485,#62486,#62487,#62488)) ;
#24608 = EDGE_LOOP('',(#62489,#62490,#62491,#62492)) ;
#24609 = EDGE_LOOP('',(#62493,#62494,#62495,#62496)) ;
#24610 = EDGE_LOOP('',(#62497,#62498,#62499,#62500)) ;
#24611 = EDGE_LOOP('',(#62501,#62502,#62503,#62504)) ;
#24612 = EDGE_LOOP('',(#62505,#62506,#62507,#62508)) ;
#24613 = EDGE_LOOP('',(#62509,#62510,#62511,#62512,#62513,#62514,#62515,#62516,
#62517,#62518,#62519,#62520,#62521,#62522,#62523,#62524,#62525,#62526)) ;
#24614 = EDGE_LOOP('',(#62527)) ;
#24615 = EDGE_LOOP('',(#62528)) ;
#24616 = EDGE_LOOP('',(#62529,#62530,#62531,#62532,#62533,#62534,#62535,#62536)) ;
#24617 = EDGE_LOOP('',(#62537)) ;
#24618 = EDGE_LOOP('',(#62538,#62539,#62540,#62541,#62542,#62543,#62544,#62545)) ;
#24619 = EDGE_LOOP('',(#62546)) ;
#24620 = EDGE_LOOP('',(#62547,#62548,#62549,#62550,#62551,#62552,#62553,#62554)) ;
#24621 = EDGE_LOOP('',(#62555)) ;
#24622 = EDGE_LOOP('',(#62556,#62557,#62558,#62559,#62560,#62561,#62562,#62563)) ;
#24623 = EDGE_LOOP('',(#62564)) ;
#24624 = EDGE_LOOP('',(#62565,#62566,#62567,#62568,#62569,#62570,#62571,#62572)) ;
#24625 = EDGE_LOOP('',(#62573)) ;
#24626 = EDGE_LOOP('',(#62574,#62575,#62576,#62577,#62578,#62579,#62580,#62581)) ;
#24627 = EDGE_LOOP('',(#62582)) ;
#24628 = EDGE_LOOP('',(#62583,#62584,#62585,#62586,#62587,#62588,#62589,#62590)) ;
#24629 = EDGE_LOOP('',(#62591)) ;
#24630 = EDGE_LOOP('',(#62592,#62593,#62594,#62595,#62596,#62597,#62598,#62599)) ;
#24631 = EDGE_LOOP('',(#62600)) ;
#24632 = EDGE_LOOP('',(#62601,#62602,#62603,#62604,#62605,#62606,#62607,#62608)) ;
#24633 = EDGE_LOOP('',(#62609,#62610,#62611,#62612)) ;
#24634 = EDGE_LOOP('',(#62613,#62614,#62615,#62616)) ;
#24635 = EDGE_LOOP('',(#62617,#62618,#62619)) ;
#24636 = EDGE_LOOP('',(#62620,#62621,#62622)) ;
#24637 = EDGE_LOOP('',(#62623,#62624,#62625,#62626)) ;
#24638 = EDGE_LOOP('',(#62627,#62628,#62629,#62630,#62631,#62632)) ;
#24639 = EDGE_LOOP('',(#62633,#62634,#62635,#62636,#62637,#62638,#62639)) ;
#24640 = EDGE_LOOP('',(#62640,#62641,#62642,#62643)) ;
#24641 = EDGE_LOOP('',(#62644,#62645,#62646,#62647)) ;
#24642 = EDGE_LOOP('',(#62648,#62649,#62650,#62651)) ;
#24643 = EDGE_LOOP('',(#62652,#62653,#62654,#62655)) ;
#24644 = EDGE_LOOP('',(#62656,#62657,#62658)) ;
#24645 = EDGE_LOOP('',(#62659,#62660,#62661,#62662)) ;
#24646 = EDGE_LOOP('',(#62663,#62664,#62665,#62666)) ;
#24647 = EDGE_LOOP('',(#62667,#62668,#62669,#62670)) ;
#24648 = EDGE_LOOP('',(#62671,#62672,#62673,#62674)) ;
#24649 = EDGE_LOOP('',(#62675,#62676,#62677,#62678)) ;
#24650 = EDGE_LOOP('',(#62679,#62680,#62681,#62682)) ;
#24651 = EDGE_LOOP('',(#62683,#62684,#62685,#62686)) ;
#24652 = EDGE_LOOP('',(#62687,#62688,#62689,#62690)) ;
#24653 = EDGE_LOOP('',(#62691,#62692,#62693,#62694)) ;
#24654 = EDGE_LOOP('',(#62695,#62696,#62697)) ;
#24655 = EDGE_LOOP('',(#62698,#62699,#62700)) ;
#24656 = EDGE_LOOP('',(#62701,#62702,#62703,#62704,#62705)) ;
#24657 = EDGE_LOOP('',(#62706,#62707,#62708)) ;
#24658 = EDGE_LOOP('',(#62709,#62710,#62711)) ;
#24659 = EDGE_LOOP('',(#62712,#62713,#62714,#62715)) ;
#24660 = EDGE_LOOP('',(#62716,#62717,#62718,#62719)) ;
#24661 = EDGE_LOOP('',(#62720,#62721,#62722,#62723)) ;
#24662 = EDGE_LOOP('',(#62724,#62725,#62726,#62727)) ;
#24663 = EDGE_LOOP('',(#62728,#62729,#62730,#62731)) ;
#24664 = EDGE_LOOP('',(#62732,#62733,#62734,#62735)) ;
#24665 = EDGE_LOOP('',(#62736,#62737,#62738,#62739)) ;
#24666 = EDGE_LOOP('',(#62740,#62741,#62742)) ;
#24667 = EDGE_LOOP('',(#62743,#62744,#62745,#62746)) ;
#24668 = EDGE_LOOP('',(#62747,#62748,#62749,#62750)) ;
#24669 = EDGE_LOOP('',(#62751,#62752,#62753)) ;
#24670 = EDGE_LOOP('',(#62754,#62755,#62756,#62757)) ;
#24671 = EDGE_LOOP('',(#62758,#62759,#62760,#62761)) ;
#24672 = EDGE_LOOP('',(#62762,#62763,#62764,#62765)) ;
#24673 = EDGE_LOOP('',(#62766,#62767,#62768,#62769)) ;
#24674 = EDGE_LOOP('',(#62770,#62771,#62772,#62773)) ;
#24675 = EDGE_LOOP('',(#62774,#62775,#62776,#62777)) ;
#24676 = EDGE_LOOP('',(#62778,#62779,#62780,#62781,#62782)) ;
#24677 = EDGE_LOOP('',(#62783,#62784,#62785,#62786)) ;
#24678 = EDGE_LOOP('',(#62787,#62788,#62789)) ;
#24679 = EDGE_LOOP('',(#62790,#62791,#62792,#62793)) ;
#24680 = EDGE_LOOP('',(#62794,#62795,#62796,#62797)) ;
#24681 = EDGE_LOOP('',(#62798,#62799,#62800)) ;
#24682 = EDGE_LOOP('',(#62801,#62802,#62803,#62804)) ;
#24683 = EDGE_LOOP('',(#62805,#62806,#62807,#62808)) ;
#24684 = EDGE_LOOP('',(#62809,#62810,#62811,#62812)) ;
#24685 = EDGE_LOOP('',(#62813,#62814,#62815)) ;
#24686 = EDGE_LOOP('',(#62816,#62817,#62818,#62819)) ;
#24687 = EDGE_LOOP('',(#62820,#62821,#62822,#62823)) ;
#24688 = EDGE_LOOP('',(#62824,#62825,#62826)) ;
#24689 = EDGE_LOOP('',(#62827,#62828,#62829)) ;
#24690 = EDGE_LOOP('',(#62830,#62831,#62832,#62833)) ;
#24691 = EDGE_LOOP('',(#62834,#62835,#62836,#62837)) ;
#24692 = EDGE_LOOP('',(#62838,#62839,#62840)) ;
#24693 = EDGE_LOOP('',(#62841,#62842,#62843)) ;
#24694 = EDGE_LOOP('',(#62844,#62845,#62846,#62847)) ;
#24695 = EDGE_LOOP('',(#62848,#62849,#62850,#62851)) ;
#24696 = EDGE_LOOP('',(#62852,#62853,#62854)) ;
#24697 = EDGE_LOOP('',(#62855,#62856,#62857,#62858)) ;
#24698 = EDGE_LOOP('',(#62859,#62860,#62861,#62862)) ;
#24699 = EDGE_LOOP('',(#62863,#62864,#62865)) ;
#24700 = EDGE_LOOP('',(#62866,#62867,#62868)) ;
#24701 = EDGE_LOOP('',(#62869,#62870,#62871,#62872)) ;
#24702 = EDGE_LOOP('',(#62873,#62874,#62875,#62876)) ;
#24703 = EDGE_LOOP('',(#62877,#62878,#62879,#62880)) ;
#24704 = EDGE_LOOP('',(#62881,#62882,#62883,#62884)) ;
#24705 = EDGE_LOOP('',(#62885,#62886,#62887,#62888)) ;
#24706 = EDGE_LOOP('',(#62889,#62890,#62891,#62892)) ;
#24707 = EDGE_LOOP('',(#62893,#62894,#62895)) ;
#24708 = EDGE_LOOP('',(#62896,#62897,#62898)) ;
#24709 = EDGE_LOOP('',(#62899,#62900,#62901,#62902)) ;
#24710 = EDGE_LOOP('',(#62903,#62904,#62905,#62906)) ;
#24711 = EDGE_LOOP('',(#62907,#62908,#62909,#62910)) ;
#24712 = EDGE_LOOP('',(#62911,#62912,#62913,#62914)) ;
#24713 = EDGE_LOOP('',(#62915,#62916,#62917,#62918)) ;
#24714 = EDGE_LOOP('',(#62919,#62920,#62921,#62922)) ;
#24715 = EDGE_LOOP('',(#62923,#62924,#62925,#62926)) ;
#24716 = EDGE_LOOP('',(#62927,#62928,#62929,#62930)) ;
#24717 = EDGE_LOOP('',(#62931,#62932,#62933,#62934)) ;
#24718 = EDGE_LOOP('',(#62935,#62936,#62937,#62938)) ;
#24719 = EDGE_LOOP('',(#62939,#62940,#62941,#62942)) ;
#24720 = EDGE_LOOP('',(#62943,#62944,#62945,#62946)) ;
#24721 = EDGE_LOOP('',(#62947,#62948,#62949,#62950)) ;
#24722 = EDGE_LOOP('',(#62951,#62952,#62953,#62954)) ;
#24723 = EDGE_LOOP('',(#62955,#62956,#62957,#62958)) ;
#24724 = EDGE_LOOP('',(#62959,#62960,#62961,#62962)) ;
#24725 = EDGE_LOOP('',(#62963,#62964,#62965,#62966)) ;
#24726 = EDGE_LOOP('',(#62967,#62968,#62969)) ;
#24727 = EDGE_LOOP('',(#62970,#62971,#62972,#62973)) ;
#24728 = EDGE_LOOP('',(#62974,#62975,#62976,#62977)) ;
#24729 = EDGE_LOOP('',(#62978,#62979,#62980,#62981)) ;
#24730 = EDGE_LOOP('',(#62982,#62983,#62984)) ;
#24731 = EDGE_LOOP('',(#62985,#62986,#62987,#62988)) ;
#24732 = EDGE_LOOP('',(#62989,#62990,#62991,#62992)) ;
#24733 = EDGE_LOOP('',(#62993,#62994,#62995,#62996)) ;
#24734 = EDGE_LOOP('',(#62997,#62998,#62999)) ;
#24735 = EDGE_LOOP('',(#63000,#63001,#63002)) ;
#24736 = EDGE_LOOP('',(#63003,#63004,#63005,#63006)) ;
#24737 = EDGE_LOOP('',(#63007,#63008,#63009,#63010)) ;
#24738 = EDGE_LOOP('',(#63011,#63012,#63013,#63014)) ;
#24739 = EDGE_LOOP('',(#63015,#63016,#63017,#63018)) ;
#24740 = EDGE_LOOP('',(#63019,#63020,#63021,#63022)) ;
#24741 = EDGE_LOOP('',(#63023,#63024,#63025,#63026)) ;
#24742 = EDGE_LOOP('',(#63027,#63028,#63029,#63030)) ;
#24743 = EDGE_LOOP('',(#63031,#63032,#63033,#63034)) ;
#24744 = EDGE_LOOP('',(#63035,#63036,#63037,#63038)) ;
#24745 = EDGE_LOOP('',(#63039,#63040,#63041,#63042)) ;
#24746 = EDGE_LOOP('',(#63043,#63044,#63045,#63046)) ;
#24747 = EDGE_LOOP('',(#63047,#63048,#63049,#63050)) ;
#24748 = EDGE_LOOP('',(#63051,#63052,#63053,#63054)) ;
#24749 = EDGE_LOOP('',(#63055,#63056,#63057,#63058)) ;
#24750 = EDGE_LOOP('',(#63059,#63060,#63061,#63062)) ;
#24751 = EDGE_LOOP('',(#63063,#63064,#63065,#63066)) ;
#24752 = EDGE_LOOP('',(#63067,#63068,#63069,#63070)) ;
#24753 = EDGE_LOOP('',(#63071,#63072,#63073)) ;
#24754 = EDGE_LOOP('',(#63074,#63075,#63076,#63077)) ;
#24755 = EDGE_LOOP('',(#63078,#63079,#63080,#63081)) ;
#24756 = EDGE_LOOP('',(#63082,#63083,#63084,#63085)) ;
#24757 = EDGE_LOOP('',(#63086,#63087,#63088)) ;
#24758 = EDGE_LOOP('',(#63089,#63090,#63091,#63092)) ;
#24759 = EDGE_LOOP('',(#63093,#63094,#63095,#63096)) ;
#24760 = EDGE_LOOP('',(#63097,#63098,#63099,#63100)) ;
#24761 = EDGE_LOOP('',(#63101,#63102,#63103)) ;
#24762 = EDGE_LOOP('',(#63104,#63105,#63106)) ;
#24763 = EDGE_LOOP('',(#63107,#63108,#63109,#63110)) ;
#24764 = EDGE_LOOP('',(#63111,#63112,#63113,#63114)) ;
#24765 = EDGE_LOOP('',(#63115,#63116,#63117,#63118)) ;
#24766 = EDGE_LOOP('',(#63119,#63120,#63121,#63122)) ;
#24767 = EDGE_LOOP('',(#63123,#63124,#63125,#63126)) ;
#24768 = EDGE_LOOP('',(#63127,#63128,#63129,#63130)) ;
#24769 = EDGE_LOOP('',(#63131,#63132,#63133,#63134)) ;
#24770 = EDGE_LOOP('',(#63135,#63136,#63137,#63138)) ;
#24771 = EDGE_LOOP('',(#63139,#63140,#63141,#63142)) ;
#24772 = EDGE_LOOP('',(#63143,#63144,#63145,#63146)) ;
#24773 = EDGE_LOOP('',(#63147,#63148,#63149,#63150)) ;
#24774 = EDGE_LOOP('',(#63151,#63152,#63153,#63154)) ;
#24775 = EDGE_LOOP('',(#63155,#63156,#63157,#63158)) ;
#24776 = EDGE_LOOP('',(#63159,#63160,#63161,#63162)) ;
#24777 = EDGE_LOOP('',(#63163,#63164,#63165,#63166)) ;
#24778 = EDGE_LOOP('',(#63167,#63168,#63169,#63170)) ;
#24779 = EDGE_LOOP('',(#63171,#63172,#63173,#63174)) ;
#24780 = EDGE_LOOP('',(#63175,#63176,#63177)) ;
#24781 = EDGE_LOOP('',(#63178,#63179,#63180,#63181)) ;
#24782 = EDGE_LOOP('',(#63182,#63183,#63184,#63185)) ;
#24783 = EDGE_LOOP('',(#63186,#63187,#63188,#63189)) ;
#24784 = EDGE_LOOP('',(#63190,#63191,#63192)) ;
#24785 = EDGE_LOOP('',(#63193,#63194,#63195,#63196)) ;
#24786 = EDGE_LOOP('',(#63197,#63198,#63199,#63200)) ;
#24787 = EDGE_LOOP('',(#63201,#63202,#63203,#63204)) ;
#24788 = EDGE_LOOP('',(#63205,#63206,#63207)) ;
#24789 = EDGE_LOOP('',(#63208,#63209,#63210)) ;
#24790 = EDGE_LOOP('',(#63211,#63212,#63213,#63214)) ;
#24791 = EDGE_LOOP('',(#63215,#63216,#63217,#63218)) ;
#24792 = EDGE_LOOP('',(#63219,#63220,#63221,#63222)) ;
#24793 = EDGE_LOOP('',(#63223,#63224,#63225,#63226)) ;
#24794 = EDGE_LOOP('',(#63227,#63228,#63229,#63230)) ;
#24795 = EDGE_LOOP('',(#63231,#63232,#63233,#63234)) ;
#24796 = EDGE_LOOP('',(#63235,#63236,#63237,#63238)) ;
#24797 = EDGE_LOOP('',(#63239,#63240,#63241,#63242)) ;
#24798 = EDGE_LOOP('',(#63243,#63244,#63245,#63246)) ;
#24799 = EDGE_LOOP('',(#63247,#63248,#63249,#63250)) ;
#24800 = EDGE_LOOP('',(#63251,#63252,#63253,#63254)) ;
#24801 = EDGE_LOOP('',(#63255,#63256,#63257,#63258)) ;
#24802 = EDGE_LOOP('',(#63259,#63260,#63261,#63262)) ;
#24803 = EDGE_LOOP('',(#63263,#63264,#63265,#63266)) ;
#24804 = EDGE_LOOP('',(#63267,#63268,#63269,#63270)) ;
#24805 = EDGE_LOOP('',(#63271,#63272,#63273,#63274)) ;
#24806 = EDGE_LOOP('',(#63275,#63276,#63277,#63278)) ;
#24807 = EDGE_LOOP('',(#63279,#63280,#63281)) ;
#24808 = EDGE_LOOP('',(#63282,#63283,#63284,#63285)) ;
#24809 = EDGE_LOOP('',(#63286,#63287,#63288,#63289)) ;
#24810 = EDGE_LOOP('',(#63290,#63291,#63292,#63293)) ;
#24811 = EDGE_LOOP('',(#63294,#63295,#63296)) ;
#24812 = EDGE_LOOP('',(#63297,#63298,#63299,#63300)) ;
#24813 = EDGE_LOOP('',(#63301,#63302,#63303,#63304)) ;
#24814 = EDGE_LOOP('',(#63305,#63306,#63307,#63308)) ;
#24815 = EDGE_LOOP('',(#63309,#63310,#63311)) ;
#24816 = EDGE_LOOP('',(#63312,#63313,#63314)) ;
#24817 = EDGE_LOOP('',(#63315,#63316,#63317,#63318)) ;
#24818 = EDGE_LOOP('',(#63319,#63320,#63321,#63322)) ;
#24819 = EDGE_LOOP('',(#63323,#63324,#63325,#63326)) ;
#24820 = EDGE_LOOP('',(#63327,#63328,#63329,#63330)) ;
#24821 = EDGE_LOOP('',(#63331,#63332,#63333,#63334)) ;
#24822 = EDGE_LOOP('',(#63335,#63336,#63337,#63338)) ;
#24823 = EDGE_LOOP('',(#63339,#63340,#63341,#63342)) ;
#24824 = EDGE_LOOP('',(#63343,#63344,#63345,#63346)) ;
#24825 = EDGE_LOOP('',(#63347,#63348,#63349,#63350)) ;
#24826 = EDGE_LOOP('',(#63351,#63352,#63353,#63354)) ;
#24827 = EDGE_LOOP('',(#63355,#63356,#63357,#63358)) ;
#24828 = EDGE_LOOP('',(#63359,#63360,#63361,#63362)) ;
#24829 = EDGE_LOOP('',(#63363,#63364,#63365,#63366)) ;
#24830 = EDGE_LOOP('',(#63367,#63368,#63369,#63370)) ;
#24831 = EDGE_LOOP('',(#63371,#63372,#63373,#63374)) ;
#24832 = EDGE_LOOP('',(#63375,#63376,#63377,#63378)) ;
#24833 = EDGE_LOOP('',(#63379,#63380,#63381,#63382)) ;
#24834 = EDGE_LOOP('',(#63383,#63384,#63385)) ;
#24835 = EDGE_LOOP('',(#63386,#63387,#63388,#63389)) ;
#24836 = EDGE_LOOP('',(#63390,#63391,#63392,#63393)) ;
#24837 = EDGE_LOOP('',(#63394,#63395,#63396,#63397)) ;
#24838 = EDGE_LOOP('',(#63398,#63399,#63400)) ;
#24839 = EDGE_LOOP('',(#63401,#63402,#63403,#63404)) ;
#24840 = EDGE_LOOP('',(#63405,#63406,#63407,#63408)) ;
#24841 = EDGE_LOOP('',(#63409,#63410,#63411,#63412)) ;
#24842 = EDGE_LOOP('',(#63413,#63414,#63415)) ;
#24843 = EDGE_LOOP('',(#63416,#63417,#63418)) ;
#24844 = EDGE_LOOP('',(#63419,#63420,#63421,#63422)) ;
#24845 = EDGE_LOOP('',(#63423,#63424,#63425,#63426)) ;
#24846 = EDGE_LOOP('',(#63427,#63428,#63429,#63430)) ;
#24847 = EDGE_LOOP('',(#63431,#63432,#63433,#63434)) ;
#24848 = EDGE_LOOP('',(#63435,#63436,#63437,#63438)) ;
#24849 = EDGE_LOOP('',(#63439,#63440,#63441,#63442)) ;
#24850 = EDGE_LOOP('',(#63443,#63444,#63445,#63446)) ;
#24851 = EDGE_LOOP('',(#63447,#63448,#63449,#63450)) ;
#24852 = EDGE_LOOP('',(#63451,#63452,#63453,#63454)) ;
#24853 = EDGE_LOOP('',(#63455,#63456,#63457,#63458)) ;
#24854 = EDGE_LOOP('',(#63459,#63460,#63461,#63462)) ;
#24855 = EDGE_LOOP('',(#63463,#63464,#63465,#63466)) ;
#24856 = EDGE_LOOP('',(#63467,#63468,#63469,#63470)) ;
#24857 = EDGE_LOOP('',(#63471,#63472,#63473,#63474)) ;
#24858 = EDGE_LOOP('',(#63475,#63476,#63477,#63478)) ;
#24859 = EDGE_LOOP('',(#63479,#63480,#63481,#63482)) ;
#24860 = EDGE_LOOP('',(#63483,#63484,#63485,#63486)) ;
#24861 = EDGE_LOOP('',(#63487,#63488,#63489)) ;
#24862 = EDGE_LOOP('',(#63490,#63491,#63492,#63493)) ;
#24863 = EDGE_LOOP('',(#63494,#63495,#63496,#63497)) ;
#24864 = EDGE_LOOP('',(#63498,#63499,#63500,#63501)) ;
#24865 = EDGE_LOOP('',(#63502,#63503,#63504)) ;
#24866 = EDGE_LOOP('',(#63505,#63506,#63507,#63508)) ;
#24867 = EDGE_LOOP('',(#63509,#63510,#63511,#63512)) ;
#24868 = EDGE_LOOP('',(#63513,#63514,#63515,#63516)) ;
#24869 = EDGE_LOOP('',(#63517,#63518,#63519)) ;
#24870 = EDGE_LOOP('',(#63520,#63521,#63522)) ;
#24871 = EDGE_LOOP('',(#63523,#63524,#63525,#63526)) ;
#24872 = EDGE_LOOP('',(#63527,#63528,#63529,#63530)) ;
#24873 = EDGE_LOOP('',(#63531,#63532,#63533,#63534)) ;
#24874 = EDGE_LOOP('',(#63535,#63536,#63537,#63538)) ;
#24875 = EDGE_LOOP('',(#63539,#63540,#63541,#63542)) ;
#24876 = EDGE_LOOP('',(#63543,#63544,#63545,#63546)) ;
#24877 = EDGE_LOOP('',(#63547,#63548,#63549,#63550)) ;
#24878 = EDGE_LOOP('',(#63551,#63552,#63553,#63554)) ;
#24879 = EDGE_LOOP('',(#63555,#63556,#63557,#63558)) ;
#24880 = EDGE_LOOP('',(#63559,#63560,#63561,#63562)) ;
#24881 = EDGE_LOOP('',(#63563,#63564,#63565,#63566)) ;
#24882 = EDGE_LOOP('',(#63567,#63568,#63569,#63570)) ;
#24883 = EDGE_LOOP('',(#63571,#63572,#63573,#63574)) ;
#24884 = EDGE_LOOP('',(#63575,#63576,#63577,#63578)) ;
#24885 = EDGE_LOOP('',(#63579,#63580,#63581,#63582)) ;
#24886 = EDGE_LOOP('',(#63583,#63584,#63585,#63586)) ;
#24887 = EDGE_LOOP('',(#63587,#63588,#63589,#63590)) ;
#24888 = EDGE_LOOP('',(#63591,#63592,#63593)) ;
#24889 = EDGE_LOOP('',(#63594,#63595,#63596,#63597)) ;
#24890 = EDGE_LOOP('',(#63598,#63599,#63600,#63601)) ;
#24891 = EDGE_LOOP('',(#63602,#63603,#63604,#63605)) ;
#24892 = EDGE_LOOP('',(#63606,#63607,#63608)) ;
#24893 = EDGE_LOOP('',(#63609,#63610,#63611,#63612)) ;
#24894 = EDGE_LOOP('',(#63613,#63614,#63615,#63616)) ;
#24895 = EDGE_LOOP('',(#63617,#63618,#63619,#63620)) ;
#24896 = EDGE_LOOP('',(#63621,#63622,#63623)) ;
#24897 = EDGE_LOOP('',(#63624,#63625,#63626)) ;
#24898 = EDGE_LOOP('',(#63627,#63628,#63629,#63630)) ;
#24899 = EDGE_LOOP('',(#63631,#63632,#63633,#63634)) ;
#24900 = EDGE_LOOP('',(#63635,#63636,#63637,#63638)) ;
#24901 = EDGE_LOOP('',(#63639,#63640,#63641,#63642)) ;
#24902 = EDGE_LOOP('',(#63643,#63644,#63645,#63646)) ;
#24903 = EDGE_LOOP('',(#63647,#63648,#63649,#63650)) ;
#24904 = EDGE_LOOP('',(#63651,#63652,#63653,#63654)) ;
#24905 = EDGE_LOOP('',(#63655,#63656,#63657,#63658)) ;
#24906 = EDGE_LOOP('',(#63659,#63660,#63661,#63662)) ;
#24907 = EDGE_LOOP('',(#63663,#63664,#63665,#63666)) ;
#24908 = EDGE_LOOP('',(#63667,#63668,#63669,#63670)) ;
#24909 = EDGE_LOOP('',(#63671,#63672,#63673,#63674)) ;
#24910 = EDGE_LOOP('',(#63675,#63676,#63677,#63678)) ;
#24911 = EDGE_LOOP('',(#63679,#63680,#63681,#63682)) ;
#24912 = EDGE_LOOP('',(#63683,#63684,#63685,#63686)) ;
#24913 = EDGE_LOOP('',(#63687,#63688,#63689,#63690)) ;
#24914 = EDGE_LOOP('',(#63691,#63692,#63693,#63694)) ;
#24915 = EDGE_LOOP('',(#63695,#63696,#63697)) ;
#24916 = EDGE_LOOP('',(#63698,#63699,#63700,#63701)) ;
#24917 = EDGE_LOOP('',(#63702,#63703,#63704,#63705)) ;
#24918 = EDGE_LOOP('',(#63706,#63707,#63708,#63709)) ;
#24919 = EDGE_LOOP('',(#63710,#63711,#63712)) ;
#24920 = EDGE_LOOP('',(#63713,#63714,#63715,#63716)) ;
#24921 = EDGE_LOOP('',(#63717,#63718,#63719,#63720)) ;
#24922 = EDGE_LOOP('',(#63721,#63722,#63723,#63724)) ;
#24923 = EDGE_LOOP('',(#63725,#63726,#63727)) ;
#24924 = EDGE_LOOP('',(#63728,#63729,#63730)) ;
#24925 = EDGE_LOOP('',(#63731,#63732,#63733,#63734)) ;
#24926 = EDGE_LOOP('',(#63735,#63736,#63737,#63738)) ;
#24927 = EDGE_LOOP('',(#63739,#63740,#63741,#63742)) ;
#24928 = EDGE_LOOP('',(#63743,#63744,#63745,#63746)) ;
#24929 = EDGE_LOOP('',(#63747,#63748,#63749,#63750)) ;
#24930 = EDGE_LOOP('',(#63751,#63752,#63753,#63754)) ;
#24931 = EDGE_LOOP('',(#63755,#63756,#63757,#63758)) ;
#24932 = EDGE_LOOP('',(#63759,#63760,#63761,#63762)) ;
#24933 = EDGE_LOOP('',(#63763,#63764,#63765,#63766)) ;
#24934 = EDGE_LOOP('',(#63767,#63768,#63769,#63770)) ;
#24935 = EDGE_LOOP('',(#63771,#63772,#63773,#63774)) ;
#24936 = EDGE_LOOP('',(#63775,#63776,#63777,#63778)) ;
#24937 = EDGE_LOOP('',(#63779,#63780,#63781,#63782)) ;
#24938 = EDGE_LOOP('',(#63783,#63784,#63785,#63786)) ;
#24939 = EDGE_LOOP('',(#63787,#63788,#63789,#63790)) ;
#24940 = EDGE_LOOP('',(#63791,#63792,#63793,#63794)) ;
#24941 = EDGE_LOOP('',(#63795,#63796,#63797,#63798)) ;
#24942 = EDGE_LOOP('',(#63799,#63800,#63801)) ;
#24943 = EDGE_LOOP('',(#63802,#63803,#63804,#63805)) ;
#24944 = EDGE_LOOP('',(#63806,#63807,#63808,#63809)) ;
#24945 = EDGE_LOOP('',(#63810,#63811,#63812,#63813)) ;
#24946 = EDGE_LOOP('',(#63814,#63815,#63816)) ;
#24947 = EDGE_LOOP('',(#63817,#63818,#63819,#63820)) ;
#24948 = EDGE_LOOP('',(#63821,#63822,#63823,#63824)) ;
#24949 = EDGE_LOOP('',(#63825,#63826,#63827,#63828)) ;
#24950 = EDGE_LOOP('',(#63829,#63830,#63831,#63832)) ;
#24951 = EDGE_LOOP('',(#63833,#63834,#63835)) ;
#24952 = EDGE_LOOP('',(#63836,#63837,#63838)) ;
#24953 = EDGE_LOOP('',(#63839,#63840,#63841,#63842)) ;
#24954 = EDGE_LOOP('',(#63843,#63844,#63845,#63846,#63847,#63848)) ;
#24955 = EDGE_LOOP('',(#63849,#63850,#63851,#63852,#63853,#63854,#63855)) ;
#24956 = EDGE_LOOP('',(#63856,#63857,#63858,#63859)) ;
#24957 = EDGE_LOOP('',(#63860,#63861,#63862,#63863)) ;
#24958 = EDGE_LOOP('',(#63864,#63865,#63866,#63867)) ;
#24959 = EDGE_LOOP('',(#63868,#63869,#63870,#63871)) ;
#24960 = EDGE_LOOP('',(#63872,#63873,#63874)) ;
#24961 = EDGE_LOOP('',(#63875,#63876,#63877,#63878)) ;
#24962 = EDGE_LOOP('',(#63879,#63880,#63881,#63882)) ;
#24963 = EDGE_LOOP('',(#63883,#63884,#63885,#63886)) ;
#24964 = EDGE_LOOP('',(#63887,#63888,#63889,#63890)) ;
#24965 = EDGE_LOOP('',(#63891,#63892,#63893,#63894)) ;
#24966 = EDGE_LOOP('',(#63895,#63896,#63897,#63898)) ;
#24967 = EDGE_LOOP('',(#63899,#63900,#63901,#63902)) ;
#24968 = EDGE_LOOP('',(#63903,#63904,#63905,#63906)) ;
#24969 = EDGE_LOOP('',(#63907,#63908,#63909,#63910)) ;
#24970 = EDGE_LOOP('',(#63911,#63912,#63913)) ;
#24971 = EDGE_LOOP('',(#63914,#63915,#63916)) ;
#24972 = EDGE_LOOP('',(#63917,#63918,#63919,#63920,#63921)) ;
#24973 = EDGE_LOOP('',(#63922,#63923,#63924)) ;
#24974 = EDGE_LOOP('',(#63925,#63926,#63927)) ;
#24975 = EDGE_LOOP('',(#63928,#63929,#63930,#63931)) ;
#24976 = EDGE_LOOP('',(#63932,#63933,#63934,#63935)) ;
#24977 = EDGE_LOOP('',(#63936,#63937,#63938,#63939)) ;
#24978 = EDGE_LOOP('',(#63940,#63941,#63942,#63943)) ;
#24979 = EDGE_LOOP('',(#63944,#63945,#63946,#63947)) ;
#24980 = EDGE_LOOP('',(#63948,#63949,#63950,#63951)) ;
#24981 = EDGE_LOOP('',(#63952,#63953,#63954,#63955)) ;
#24982 = EDGE_LOOP('',(#63956,#63957,#63958)) ;
#24983 = EDGE_LOOP('',(#63959,#63960,#63961,#63962)) ;
#24984 = EDGE_LOOP('',(#63963,#63964,#63965,#63966)) ;
#24985 = EDGE_LOOP('',(#63967,#63968,#63969)) ;
#24986 = EDGE_LOOP('',(#63970,#63971,#63972,#63973)) ;
#24987 = EDGE_LOOP('',(#63974,#63975,#63976,#63977)) ;
#24988 = EDGE_LOOP('',(#63978,#63979,#63980,#63981)) ;
#24989 = EDGE_LOOP('',(#63982,#63983,#63984,#63985)) ;
#24990 = EDGE_LOOP('',(#63986,#63987,#63988,#63989)) ;
#24991 = EDGE_LOOP('',(#63990,#63991,#63992,#63993)) ;
#24992 = EDGE_LOOP('',(#63994,#63995,#63996,#63997,#63998)) ;
#24993 = EDGE_LOOP('',(#63999,#64000,#64001,#64002)) ;
#24994 = EDGE_LOOP('',(#64003,#64004,#64005)) ;
#24995 = EDGE_LOOP('',(#64006,#64007,#64008,#64009)) ;
#24996 = EDGE_LOOP('',(#64010,#64011,#64012,#64013)) ;
#24997 = EDGE_LOOP('',(#64014,#64015,#64016)) ;
#24998 = EDGE_LOOP('',(#64017,#64018,#64019,#64020)) ;
#24999 = EDGE_LOOP('',(#64021,#64022,#64023,#64024)) ;
#25000 = EDGE_LOOP('',(#64025,#64026,#64027,#64028)) ;
#25001 = EDGE_LOOP('',(#64029,#64030,#64031)) ;
#25002 = EDGE_LOOP('',(#64032,#64033,#64034,#64035)) ;
#25003 = EDGE_LOOP('',(#64036,#64037,#64038,#64039)) ;
#25004 = EDGE_LOOP('',(#64040,#64041,#64042)) ;
#25005 = EDGE_LOOP('',(#64043,#64044,#64045)) ;
#25006 = EDGE_LOOP('',(#64046,#64047,#64048,#64049)) ;
#25007 = EDGE_LOOP('',(#64050,#64051,#64052,#64053)) ;
#25008 = EDGE_LOOP('',(#64054,#64055,#64056)) ;
#25009 = EDGE_LOOP('',(#64057,#64058,#64059)) ;
#25010 = EDGE_LOOP('',(#64060,#64061,#64062,#64063)) ;
#25011 = EDGE_LOOP('',(#64064,#64065,#64066,#64067)) ;
#25012 = EDGE_LOOP('',(#64068,#64069,#64070)) ;
#25013 = EDGE_LOOP('',(#64071,#64072,#64073,#64074)) ;
#25014 = EDGE_LOOP('',(#64075,#64076,#64077,#64078)) ;
#25015 = EDGE_LOOP('',(#64079,#64080,#64081)) ;
#25016 = EDGE_LOOP('',(#64082,#64083,#64084)) ;
#25017 = EDGE_LOOP('',(#64085,#64086,#64087,#64088)) ;
#25018 = EDGE_LOOP('',(#64089,#64090,#64091,#64092)) ;
#25019 = EDGE_LOOP('',(#64093,#64094,#64095,#64096)) ;
#25020 = EDGE_LOOP('',(#64097,#64098,#64099,#64100)) ;
#25021 = EDGE_LOOP('',(#64101,#64102,#64103,#64104)) ;
#25022 = EDGE_LOOP('',(#64105,#64106,#64107,#64108)) ;
#25023 = EDGE_LOOP('',(#64109,#64110,#64111,#64112)) ;
#25024 = EDGE_LOOP('',(#64113,#64114,#64115)) ;
#25025 = EDGE_LOOP('',(#64116,#64117,#64118)) ;
#25026 = EDGE_LOOP('',(#64119,#64120,#64121,#64122)) ;
#25027 = EDGE_LOOP('',(#64123,#64124,#64125,#64126,#64127,#64128)) ;
#25028 = EDGE_LOOP('',(#64129,#64130,#64131,#64132,#64133,#64134,#64135)) ;
#25029 = EDGE_LOOP('',(#64136,#64137,#64138,#64139)) ;
#25030 = EDGE_LOOP('',(#64140,#64141,#64142,#64143)) ;
#25031 = EDGE_LOOP('',(#64144,#64145,#64146,#64147)) ;
#25032 = EDGE_LOOP('',(#64148,#64149,#64150,#64151)) ;
#25033 = EDGE_LOOP('',(#64152,#64153,#64154)) ;
#25034 = EDGE_LOOP('',(#64155,#64156,#64157,#64158)) ;
#25035 = EDGE_LOOP('',(#64159,#64160,#64161,#64162)) ;
#25036 = EDGE_LOOP('',(#64163,#64164,#64165,#64166)) ;
#25037 = EDGE_LOOP('',(#64167,#64168,#64169,#64170)) ;
#25038 = EDGE_LOOP('',(#64171,#64172,#64173,#64174)) ;
#25039 = EDGE_LOOP('',(#64175,#64176,#64177,#64178)) ;
#25040 = EDGE_LOOP('',(#64179,#64180,#64181,#64182)) ;
#25041 = EDGE_LOOP('',(#64183,#64184,#64185,#64186)) ;
#25042 = EDGE_LOOP('',(#64187,#64188,#64189,#64190)) ;
#25043 = EDGE_LOOP('',(#64191,#64192,#64193)) ;
#25044 = EDGE_LOOP('',(#64194,#64195,#64196)) ;
#25045 = EDGE_LOOP('',(#64197,#64198,#64199,#64200,#64201)) ;
#25046 = EDGE_LOOP('',(#64202,#64203,#64204)) ;
#25047 = EDGE_LOOP('',(#64205,#64206,#64207)) ;
#25048 = EDGE_LOOP('',(#64208,#64209,#64210,#64211)) ;
#25049 = EDGE_LOOP('',(#64212,#64213,#64214,#64215)) ;
#25050 = EDGE_LOOP('',(#64216,#64217,#64218,#64219)) ;
#25051 = EDGE_LOOP('',(#64220,#64221,#64222,#64223)) ;
#25052 = EDGE_LOOP('',(#64224,#64225,#64226,#64227)) ;
#25053 = EDGE_LOOP('',(#64228,#64229,#64230,#64231)) ;
#25054 = EDGE_LOOP('',(#64232,#64233,#64234,#64235)) ;
#25055 = EDGE_LOOP('',(#64236,#64237,#64238)) ;
#25056 = EDGE_LOOP('',(#64239,#64240,#64241,#64242)) ;
#25057 = EDGE_LOOP('',(#64243,#64244,#64245,#64246)) ;
#25058 = EDGE_LOOP('',(#64247,#64248,#64249)) ;
#25059 = EDGE_LOOP('',(#64250,#64251,#64252,#64253)) ;
#25060 = EDGE_LOOP('',(#64254,#64255,#64256,#64257)) ;
#25061 = EDGE_LOOP('',(#64258,#64259,#64260,#64261)) ;
#25062 = EDGE_LOOP('',(#64262,#64263,#64264,#64265)) ;
#25063 = EDGE_LOOP('',(#64266,#64267,#64268,#64269)) ;
#25064 = EDGE_LOOP('',(#64270,#64271,#64272,#64273)) ;
#25065 = EDGE_LOOP('',(#64274,#64275,#64276,#64277,#64278)) ;
#25066 = EDGE_LOOP('',(#64279,#64280,#64281,#64282)) ;
#25067 = EDGE_LOOP('',(#64283,#64284,#64285)) ;
#25068 = EDGE_LOOP('',(#64286,#64287,#64288,#64289)) ;
#25069 = EDGE_LOOP('',(#64290,#64291,#64292,#64293)) ;
#25070 = EDGE_LOOP('',(#64294,#64295,#64296)) ;
#25071 = EDGE_LOOP('',(#64297,#64298,#64299,#64300)) ;
#25072 = EDGE_LOOP('',(#64301,#64302,#64303,#64304)) ;
#25073 = EDGE_LOOP('',(#64305,#64306,#64307,#64308)) ;
#25074 = EDGE_LOOP('',(#64309,#64310,#64311)) ;
#25075 = EDGE_LOOP('',(#64312,#64313,#64314,#64315)) ;
#25076 = EDGE_LOOP('',(#64316,#64317,#64318,#64319)) ;
#25077 = EDGE_LOOP('',(#64320,#64321,#64322)) ;
#25078 = EDGE_LOOP('',(#64323,#64324,#64325)) ;
#25079 = EDGE_LOOP('',(#64326,#64327,#64328,#64329)) ;
#25080 = EDGE_LOOP('',(#64330,#64331,#64332,#64333)) ;
#25081 = EDGE_LOOP('',(#64334,#64335,#64336)) ;
#25082 = EDGE_LOOP('',(#64337,#64338,#64339)) ;
#25083 = EDGE_LOOP('',(#64340,#64341,#64342,#64343)) ;
#25084 = EDGE_LOOP('',(#64344,#64345,#64346,#64347)) ;
#25085 = EDGE_LOOP('',(#64348,#64349,#64350)) ;
#25086 = EDGE_LOOP('',(#64351,#64352,#64353,#64354)) ;
#25087 = EDGE_LOOP('',(#64355,#64356,#64357,#64358)) ;
#25088 = EDGE_LOOP('',(#64359,#64360,#64361)) ;
#25089 = EDGE_LOOP('',(#64362,#64363,#64364)) ;
#25090 = EDGE_LOOP('',(#64365,#64366,#64367,#64368)) ;
#25091 = EDGE_LOOP('',(#64369,#64370,#64371,#64372)) ;
#25092 = EDGE_LOOP('',(#64373,#64374,#64375,#64376)) ;
#25093 = EDGE_LOOP('',(#64377,#64378,#64379,#64380)) ;
#25094 = EDGE_LOOP('',(#64381,#64382,#64383,#64384)) ;
#25095 = EDGE_LOOP('',(#64385,#64386,#64387,#64388)) ;
#25096 = EDGE_LOOP('',(#64389,#64390,#64391,#64392)) ;
#25097 = EDGE_LOOP('',(#64393,#64394,#64395)) ;
#25098 = EDGE_LOOP('',(#64396,#64397,#64398)) ;
#25099 = EDGE_LOOP('',(#64399,#64400,#64401,#64402)) ;
#25100 = EDGE_LOOP('',(#64403,#64404,#64405,#64406,#64407,#64408)) ;
#25101 = EDGE_LOOP('',(#64409,#64410,#64411,#64412,#64413,#64414,#64415)) ;
#25102 = EDGE_LOOP('',(#64416,#64417,#64418,#64419)) ;
#25103 = EDGE_LOOP('',(#64420,#64421,#64422,#64423)) ;
#25104 = EDGE_LOOP('',(#64424,#64425,#64426,#64427)) ;
#25105 = EDGE_LOOP('',(#64428,#64429,#64430,#64431)) ;
#25106 = EDGE_LOOP('',(#64432,#64433,#64434)) ;
#25107 = EDGE_LOOP('',(#64435,#64436,#64437,#64438)) ;
#25108 = EDGE_LOOP('',(#64439,#64440,#64441,#64442)) ;
#25109 = EDGE_LOOP('',(#64443,#64444,#64445,#64446)) ;
#25110 = EDGE_LOOP('',(#64447,#64448,#64449,#64450)) ;
#25111 = EDGE_LOOP('',(#64451,#64452,#64453,#64454)) ;
#25112 = EDGE_LOOP('',(#64455,#64456,#64457,#64458)) ;
#25113 = EDGE_LOOP('',(#64459,#64460,#64461,#64462)) ;
#25114 = EDGE_LOOP('',(#64463,#64464,#64465,#64466)) ;
#25115 = EDGE_LOOP('',(#64467,#64468,#64469,#64470)) ;
#25116 = EDGE_LOOP('',(#64471,#64472,#64473)) ;
#25117 = EDGE_LOOP('',(#64474,#64475,#64476)) ;
#25118 = EDGE_LOOP('',(#64477,#64478,#64479,#64480,#64481)) ;
#25119 = EDGE_LOOP('',(#64482,#64483,#64484)) ;
#25120 = EDGE_LOOP('',(#64485,#64486,#64487)) ;
#25121 = EDGE_LOOP('',(#64488,#64489,#64490,#64491)) ;
#25122 = EDGE_LOOP('',(#64492,#64493,#64494,#64495)) ;
#25123 = EDGE_LOOP('',(#64496,#64497,#64498,#64499)) ;
#25124 = EDGE_LOOP('',(#64500,#64501,#64502,#64503)) ;
#25125 = EDGE_LOOP('',(#64504,#64505,#64506,#64507)) ;
#25126 = EDGE_LOOP('',(#64508,#64509,#64510,#64511)) ;
#25127 = EDGE_LOOP('',(#64512,#64513,#64514,#64515)) ;
#25128 = EDGE_LOOP('',(#64516,#64517,#64518)) ;
#25129 = EDGE_LOOP('',(#64519,#64520,#64521,#64522)) ;
#25130 = EDGE_LOOP('',(#64523,#64524,#64525,#64526)) ;
#25131 = EDGE_LOOP('',(#64527,#64528,#64529)) ;
#25132 = EDGE_LOOP('',(#64530,#64531,#64532,#64533)) ;
#25133 = EDGE_LOOP('',(#64534,#64535,#64536,#64537)) ;
#25134 = EDGE_LOOP('',(#64538,#64539,#64540,#64541)) ;
#25135 = EDGE_LOOP('',(#64542,#64543,#64544,#64545)) ;
#25136 = EDGE_LOOP('',(#64546,#64547,#64548,#64549)) ;
#25137 = EDGE_LOOP('',(#64550,#64551,#64552,#64553)) ;
#25138 = EDGE_LOOP('',(#64554,#64555,#64556,#64557,#64558)) ;
#25139 = EDGE_LOOP('',(#64559,#64560,#64561,#64562)) ;
#25140 = EDGE_LOOP('',(#64563,#64564,#64565)) ;
#25141 = EDGE_LOOP('',(#64566,#64567,#64568,#64569)) ;
#25142 = EDGE_LOOP('',(#64570,#64571,#64572,#64573)) ;
#25143 = EDGE_LOOP('',(#64574,#64575,#64576)) ;
#25144 = EDGE_LOOP('',(#64577,#64578,#64579,#64580)) ;
#25145 = EDGE_LOOP('',(#64581,#64582,#64583,#64584)) ;
#25146 = EDGE_LOOP('',(#64585,#64586,#64587,#64588)) ;
#25147 = EDGE_LOOP('',(#64589,#64590,#64591)) ;
#25148 = EDGE_LOOP('',(#64592,#64593,#64594,#64595)) ;
#25149 = EDGE_LOOP('',(#64596,#64597,#64598,#64599)) ;
#25150 = EDGE_LOOP('',(#64600,#64601,#64602)) ;
#25151 = EDGE_LOOP('',(#64603,#64604,#64605)) ;
#25152 = EDGE_LOOP('',(#64606,#64607,#64608,#64609)) ;
#25153 = EDGE_LOOP('',(#64610,#64611,#64612,#64613)) ;
#25154 = EDGE_LOOP('',(#64614,#64615,#64616)) ;
#25155 = EDGE_LOOP('',(#64617,#64618,#64619)) ;
#25156 = EDGE_LOOP('',(#64620,#64621,#64622,#64623)) ;
#25157 = EDGE_LOOP('',(#64624,#64625,#64626,#64627)) ;
#25158 = EDGE_LOOP('',(#64628,#64629,#64630)) ;
#25159 = EDGE_LOOP('',(#64631,#64632,#64633,#64634)) ;
#25160 = EDGE_LOOP('',(#64635,#64636,#64637,#64638)) ;
#25161 = EDGE_LOOP('',(#64639,#64640,#64641)) ;
#25162 = EDGE_LOOP('',(#64642,#64643,#64644)) ;
#25163 = EDGE_LOOP('',(#64645,#64646,#64647,#64648)) ;
#25164 = EDGE_LOOP('',(#64649,#64650,#64651,#64652)) ;
#25165 = EDGE_LOOP('',(#64653,#64654,#64655,#64656)) ;
#25166 = EDGE_LOOP('',(#64657,#64658,#64659,#64660)) ;
#25167 = EDGE_LOOP('',(#64661,#64662,#64663,#64664)) ;
#25168 = EDGE_LOOP('',(#64665,#64666,#64667,#64668)) ;
#25169 = EDGE_LOOP('',(#64669,#64670,#64671,#64672)) ;
#25170 = EDGE_LOOP('',(#64673,#64674,#64675)) ;
#25171 = EDGE_LOOP('',(#64676,#64677,#64678)) ;
#25172 = EDGE_LOOP('',(#64679,#64680,#64681,#64682)) ;
#25173 = EDGE_LOOP('',(#64683,#64684,#64685,#64686,#64687,#64688)) ;
#25174 = EDGE_LOOP('',(#64689,#64690,#64691,#64692,#64693,#64694,#64695)) ;
#25175 = EDGE_LOOP('',(#64696,#64697,#64698,#64699)) ;
#25176 = EDGE_LOOP('',(#64700,#64701,#64702,#64703)) ;
#25177 = EDGE_LOOP('',(#64704,#64705,#64706,#64707)) ;
#25178 = EDGE_LOOP('',(#64708,#64709,#64710,#64711)) ;
#25179 = EDGE_LOOP('',(#64712,#64713,#64714)) ;
#25180 = EDGE_LOOP('',(#64715,#64716,#64717,#64718)) ;
#25181 = EDGE_LOOP('',(#64719,#64720,#64721,#64722)) ;
#25182 = EDGE_LOOP('',(#64723,#64724,#64725,#64726)) ;
#25183 = EDGE_LOOP('',(#64727,#64728,#64729,#64730)) ;
#25184 = EDGE_LOOP('',(#64731,#64732,#64733,#64734)) ;
#25185 = EDGE_LOOP('',(#64735,#64736,#64737,#64738)) ;
#25186 = EDGE_LOOP('',(#64739,#64740,#64741,#64742)) ;
#25187 = EDGE_LOOP('',(#64743,#64744,#64745,#64746)) ;
#25188 = EDGE_LOOP('',(#64747,#64748,#64749,#64750)) ;
#25189 = EDGE_LOOP('',(#64751,#64752,#64753)) ;
#25190 = EDGE_LOOP('',(#64754,#64755,#64756)) ;
#25191 = EDGE_LOOP('',(#64757,#64758,#64759,#64760,#64761)) ;
#25192 = EDGE_LOOP('',(#64762,#64763,#64764)) ;
#25193 = EDGE_LOOP('',(#64765,#64766,#64767)) ;
#25194 = EDGE_LOOP('',(#64768,#64769,#64770,#64771)) ;
#25195 = EDGE_LOOP('',(#64772,#64773,#64774,#64775)) ;
#25196 = EDGE_LOOP('',(#64776,#64777,#64778,#64779)) ;
#25197 = EDGE_LOOP('',(#64780,#64781,#64782,#64783)) ;
#25198 = EDGE_LOOP('',(#64784,#64785,#64786,#64787)) ;
#25199 = EDGE_LOOP('',(#64788,#64789,#64790,#64791)) ;
#25200 = EDGE_LOOP('',(#64792,#64793,#64794,#64795)) ;
#25201 = EDGE_LOOP('',(#64796,#64797,#64798)) ;
#25202 = EDGE_LOOP('',(#64799,#64800,#64801,#64802)) ;
#25203 = EDGE_LOOP('',(#64803,#64804,#64805,#64806)) ;
#25204 = EDGE_LOOP('',(#64807,#64808,#64809)) ;
#25205 = EDGE_LOOP('',(#64810,#64811,#64812,#64813)) ;
#25206 = EDGE_LOOP('',(#64814,#64815,#64816,#64817)) ;
#25207 = EDGE_LOOP('',(#64818,#64819,#64820,#64821)) ;
#25208 = EDGE_LOOP('',(#64822,#64823,#64824,#64825)) ;
#25209 = EDGE_LOOP('',(#64826,#64827,#64828,#64829)) ;
#25210 = EDGE_LOOP('',(#64830,#64831,#64832,#64833)) ;
#25211 = EDGE_LOOP('',(#64834,#64835,#64836,#64837,#64838)) ;
#25212 = EDGE_LOOP('',(#64839,#64840,#64841,#64842)) ;
#25213 = EDGE_LOOP('',(#64843,#64844,#64845)) ;
#25214 = EDGE_LOOP('',(#64846,#64847,#64848,#64849)) ;
#25215 = EDGE_LOOP('',(#64850,#64851,#64852,#64853)) ;
#25216 = EDGE_LOOP('',(#64854,#64855,#64856)) ;
#25217 = EDGE_LOOP('',(#64857,#64858,#64859,#64860)) ;
#25218 = EDGE_LOOP('',(#64861,#64862,#64863,#64864)) ;
#25219 = EDGE_LOOP('',(#64865,#64866,#64867,#64868)) ;
#25220 = EDGE_LOOP('',(#64869,#64870,#64871)) ;
#25221 = EDGE_LOOP('',(#64872,#64873,#64874,#64875)) ;
#25222 = EDGE_LOOP('',(#64876,#64877,#64878,#64879)) ;
#25223 = EDGE_LOOP('',(#64880,#64881,#64882)) ;
#25224 = EDGE_LOOP('',(#64883,#64884,#64885)) ;
#25225 = EDGE_LOOP('',(#64886,#64887,#64888,#64889)) ;
#25226 = EDGE_LOOP('',(#64890,#64891,#64892,#64893)) ;
#25227 = EDGE_LOOP('',(#64894,#64895,#64896)) ;
#25228 = EDGE_LOOP('',(#64897,#64898,#64899)) ;
#25229 = EDGE_LOOP('',(#64900,#64901,#64902,#64903)) ;
#25230 = EDGE_LOOP('',(#64904,#64905,#64906,#64907)) ;
#25231 = EDGE_LOOP('',(#64908,#64909,#64910)) ;
#25232 = EDGE_LOOP('',(#64911,#64912,#64913,#64914)) ;
#25233 = EDGE_LOOP('',(#64915,#64916,#64917,#64918)) ;
#25234 = EDGE_LOOP('',(#64919,#64920,#64921)) ;
#25235 = EDGE_LOOP('',(#64922,#64923,#64924)) ;
#25236 = EDGE_LOOP('',(#64925,#64926,#64927,#64928)) ;
#25237 = EDGE_LOOP('',(#64929,#64930,#64931,#64932)) ;
#25238 = EDGE_LOOP('',(#64933,#64934,#64935,#64936)) ;
#25239 = EDGE_LOOP('',(#64937,#64938,#64939,#64940)) ;
#25240 = EDGE_LOOP('',(#64941,#64942,#64943,#64944)) ;
#25241 = EDGE_LOOP('',(#64945,#64946,#64947,#64948)) ;
#25242 = EDGE_LOOP('',(#64949,#64950,#64951,#64952)) ;
#25243 = EDGE_LOOP('',(#64953,#64954,#64955)) ;
#25244 = EDGE_LOOP('',(#64956,#64957,#64958)) ;
#25245 = EDGE_LOOP('',(#64959,#64960,#64961,#64962)) ;
#25246 = EDGE_LOOP('',(#64963,#64964,#64965,#64966,#64967,#64968)) ;
#25247 = EDGE_LOOP('',(#64969,#64970,#64971,#64972,#64973,#64974,#64975)) ;
#25248 = EDGE_LOOP('',(#64976,#64977,#64978,#64979)) ;
#25249 = EDGE_LOOP('',(#64980,#64981,#64982,#64983)) ;
#25250 = EDGE_LOOP('',(#64984,#64985,#64986,#64987)) ;
#25251 = EDGE_LOOP('',(#64988,#64989,#64990,#64991)) ;
#25252 = EDGE_LOOP('',(#64992,#64993,#64994)) ;
#25253 = EDGE_LOOP('',(#64995,#64996,#64997,#64998)) ;
#25254 = EDGE_LOOP('',(#64999,#65000,#65001,#65002)) ;
#25255 = EDGE_LOOP('',(#65003,#65004,#65005,#65006)) ;
#25256 = EDGE_LOOP('',(#65007,#65008,#65009,#65010)) ;
#25257 = EDGE_LOOP('',(#65011,#65012,#65013,#65014)) ;
#25258 = EDGE_LOOP('',(#65015,#65016,#65017,#65018)) ;
#25259 = EDGE_LOOP('',(#65019,#65020,#65021,#65022)) ;
#25260 = EDGE_LOOP('',(#65023,#65024,#65025,#65026)) ;
#25261 = EDGE_LOOP('',(#65027,#65028,#65029,#65030)) ;
#25262 = EDGE_LOOP('',(#65031,#65032,#65033)) ;
#25263 = EDGE_LOOP('',(#65034,#65035,#65036)) ;
#25264 = EDGE_LOOP('',(#65037,#65038,#65039,#65040,#65041)) ;
#25265 = EDGE_LOOP('',(#65042,#65043,#65044)) ;
#25266 = EDGE_LOOP('',(#65045,#65046,#65047)) ;
#25267 = EDGE_LOOP('',(#65048,#65049,#65050,#65051)) ;
#25268 = EDGE_LOOP('',(#65052,#65053,#65054,#65055)) ;
#25269 = EDGE_LOOP('',(#65056,#65057,#65058,#65059)) ;
#25270 = EDGE_LOOP('',(#65060,#65061,#65062,#65063)) ;
#25271 = EDGE_LOOP('',(#65064,#65065,#65066,#65067)) ;
#25272 = EDGE_LOOP('',(#65068,#65069,#65070,#65071)) ;
#25273 = EDGE_LOOP('',(#65072,#65073,#65074,#65075)) ;
#25274 = EDGE_LOOP('',(#65076,#65077,#65078)) ;
#25275 = EDGE_LOOP('',(#65079,#65080,#65081,#65082)) ;
#25276 = EDGE_LOOP('',(#65083,#65084,#65085,#65086)) ;
#25277 = EDGE_LOOP('',(#65087,#65088,#65089)) ;
#25278 = EDGE_LOOP('',(#65090,#65091,#65092,#65093)) ;
#25279 = EDGE_LOOP('',(#65094,#65095,#65096,#65097)) ;
#25280 = EDGE_LOOP('',(#65098,#65099,#65100,#65101)) ;
#25281 = EDGE_LOOP('',(#65102,#65103,#65104,#65105)) ;
#25282 = EDGE_LOOP('',(#65106,#65107,#65108,#65109)) ;
#25283 = EDGE_LOOP('',(#65110,#65111,#65112,#65113)) ;
#25284 = EDGE_LOOP('',(#65114,#65115,#65116,#65117,#65118)) ;
#25285 = EDGE_LOOP('',(#65119,#65120,#65121,#65122)) ;
#25286 = EDGE_LOOP('',(#65123,#65124,#65125)) ;
#25287 = EDGE_LOOP('',(#65126,#65127,#65128,#65129)) ;
#25288 = EDGE_LOOP('',(#65130,#65131,#65132,#65133)) ;
#25289 = EDGE_LOOP('',(#65134,#65135,#65136)) ;
#25290 = EDGE_LOOP('',(#65137,#65138,#65139,#65140)) ;
#25291 = EDGE_LOOP('',(#65141,#65142,#65143,#65144)) ;
#25292 = EDGE_LOOP('',(#65145,#65146,#65147,#65148)) ;
#25293 = EDGE_LOOP('',(#65149,#65150,#65151)) ;
#25294 = EDGE_LOOP('',(#65152,#65153,#65154,#65155)) ;
#25295 = EDGE_LOOP('',(#65156,#65157,#65158,#65159)) ;
#25296 = EDGE_LOOP('',(#65160,#65161,#65162)) ;
#25297 = EDGE_LOOP('',(#65163,#65164,#65165)) ;
#25298 = EDGE_LOOP('',(#65166,#65167,#65168,#65169)) ;
#25299 = EDGE_LOOP('',(#65170,#65171,#65172,#65173)) ;
#25300 = EDGE_LOOP('',(#65174,#65175,#65176)) ;
#25301 = EDGE_LOOP('',(#65177,#65178,#65179)) ;
#25302 = EDGE_LOOP('',(#65180,#65181,#65182,#65183)) ;
#25303 = EDGE_LOOP('',(#65184,#65185,#65186,#65187)) ;
#25304 = EDGE_LOOP('',(#65188,#65189,#65190)) ;
#25305 = EDGE_LOOP('',(#65191,#65192,#65193,#65194)) ;
#25306 = EDGE_LOOP('',(#65195,#65196,#65197,#65198)) ;
#25307 = EDGE_LOOP('',(#65199,#65200,#65201)) ;
#25308 = EDGE_LOOP('',(#65202,#65203,#65204)) ;
#25309 = EDGE_LOOP('',(#65205,#65206,#65207,#65208)) ;
#25310 = EDGE_LOOP('',(#65209,#65210,#65211,#65212)) ;
#25311 = EDGE_LOOP('',(#65213,#65214,#65215,#65216)) ;
#25312 = EDGE_LOOP('',(#65217,#65218,#65219,#65220)) ;
#25313 = EDGE_LOOP('',(#65221,#65222,#65223,#65224)) ;
#25314 = EDGE_LOOP('',(#65225,#65226,#65227,#65228)) ;
#25315 = EDGE_LOOP('',(#65229,#65230,#65231,#65232)) ;
#25316 = EDGE_LOOP('',(#65233,#65234,#65235)) ;
#25317 = EDGE_LOOP('',(#65236,#65237,#65238)) ;
#25318 = EDGE_LOOP('',(#65239,#65240,#65241,#65242)) ;
#25319 = EDGE_LOOP('',(#65243,#65244,#65245,#65246,#65247,#65248)) ;
#25320 = EDGE_LOOP('',(#65249,#65250,#65251,#65252,#65253,#65254,#65255)) ;
#25321 = EDGE_LOOP('',(#65256,#65257,#65258,#65259)) ;
#25322 = EDGE_LOOP('',(#65260,#65261,#65262,#65263)) ;
#25323 = EDGE_LOOP('',(#65264,#65265,#65266,#65267)) ;
#25324 = EDGE_LOOP('',(#65268,#65269,#65270,#65271)) ;
#25325 = EDGE_LOOP('',(#65272,#65273,#65274)) ;
#25326 = EDGE_LOOP('',(#65275,#65276,#65277,#65278)) ;
#25327 = EDGE_LOOP('',(#65279,#65280,#65281,#65282)) ;
#25328 = EDGE_LOOP('',(#65283,#65284,#65285,#65286)) ;
#25329 = EDGE_LOOP('',(#65287,#65288,#65289,#65290)) ;
#25330 = EDGE_LOOP('',(#65291,#65292,#65293,#65294)) ;
#25331 = EDGE_LOOP('',(#65295,#65296,#65297,#65298)) ;
#25332 = EDGE_LOOP('',(#65299,#65300,#65301,#65302)) ;
#25333 = EDGE_LOOP('',(#65303,#65304,#65305,#65306)) ;
#25334 = EDGE_LOOP('',(#65307,#65308,#65309,#65310)) ;
#25335 = EDGE_LOOP('',(#65311,#65312,#65313)) ;
#25336 = EDGE_LOOP('',(#65314,#65315,#65316)) ;
#25337 = EDGE_LOOP('',(#65317,#65318,#65319,#65320,#65321)) ;
#25338 = EDGE_LOOP('',(#65322,#65323,#65324)) ;
#25339 = EDGE_LOOP('',(#65325,#65326,#65327)) ;
#25340 = EDGE_LOOP('',(#65328,#65329,#65330,#65331)) ;
#25341 = EDGE_LOOP('',(#65332,#65333,#65334,#65335)) ;
#25342 = EDGE_LOOP('',(#65336,#65337,#65338,#65339)) ;
#25343 = EDGE_LOOP('',(#65340,#65341,#65342,#65343)) ;
#25344 = EDGE_LOOP('',(#65344,#65345,#65346,#65347)) ;
#25345 = EDGE_LOOP('',(#65348,#65349,#65350,#65351)) ;
#25346 = EDGE_LOOP('',(#65352,#65353,#65354,#65355)) ;
#25347 = EDGE_LOOP('',(#65356,#65357,#65358)) ;
#25348 = EDGE_LOOP('',(#65359,#65360,#65361,#65362)) ;
#25349 = EDGE_LOOP('',(#65363,#65364,#65365,#65366)) ;
#25350 = EDGE_LOOP('',(#65367,#65368,#65369)) ;
#25351 = EDGE_LOOP('',(#65370,#65371,#65372,#65373)) ;
#25352 = EDGE_LOOP('',(#65374,#65375,#65376,#65377)) ;
#25353 = EDGE_LOOP('',(#65378,#65379,#65380,#65381)) ;
#25354 = EDGE_LOOP('',(#65382,#65383,#65384,#65385)) ;
#25355 = EDGE_LOOP('',(#65386,#65387,#65388,#65389)) ;
#25356 = EDGE_LOOP('',(#65390,#65391,#65392,#65393)) ;
#25357 = EDGE_LOOP('',(#65394,#65395,#65396,#65397,#65398)) ;
#25358 = EDGE_LOOP('',(#65399,#65400,#65401,#65402)) ;
#25359 = EDGE_LOOP('',(#65403,#65404,#65405)) ;
#25360 = EDGE_LOOP('',(#65406,#65407,#65408,#65409)) ;
#25361 = EDGE_LOOP('',(#65410,#65411,#65412,#65413)) ;
#25362 = EDGE_LOOP('',(#65414,#65415,#65416)) ;
#25363 = EDGE_LOOP('',(#65417,#65418,#65419,#65420)) ;
#25364 = EDGE_LOOP('',(#65421,#65422,#65423,#65424)) ;
#25365 = EDGE_LOOP('',(#65425,#65426,#65427,#65428)) ;
#25366 = EDGE_LOOP('',(#65429,#65430,#65431)) ;
#25367 = EDGE_LOOP('',(#65432,#65433,#65434,#65435)) ;
#25368 = EDGE_LOOP('',(#65436,#65437,#65438,#65439)) ;
#25369 = EDGE_LOOP('',(#65440,#65441,#65442)) ;
#25370 = EDGE_LOOP('',(#65443,#65444,#65445)) ;
#25371 = EDGE_LOOP('',(#65446,#65447,#65448,#65449)) ;
#25372 = EDGE_LOOP('',(#65450,#65451,#65452,#65453)) ;
#25373 = EDGE_LOOP('',(#65454,#65455,#65456)) ;
#25374 = EDGE_LOOP('',(#65457,#65458,#65459)) ;
#25375 = EDGE_LOOP('',(#65460,#65461,#65462,#65463)) ;
#25376 = EDGE_LOOP('',(#65464,#65465,#65466,#65467)) ;
#25377 = EDGE_LOOP('',(#65468,#65469,#65470)) ;
#25378 = EDGE_LOOP('',(#65471,#65472,#65473,#65474)) ;
#25379 = EDGE_LOOP('',(#65475,#65476,#65477,#65478)) ;
#25380 = EDGE_LOOP('',(#65479,#65480,#65481)) ;
#25381 = EDGE_LOOP('',(#65482,#65483,#65484)) ;
#25382 = EDGE_LOOP('',(#65485,#65486,#65487,#65488)) ;
#25383 = EDGE_LOOP('',(#65489,#65490,#65491,#65492)) ;
#25384 = EDGE_LOOP('',(#65493,#65494,#65495,#65496)) ;
#25385 = EDGE_LOOP('',(#65497,#65498,#65499,#65500)) ;
#25386 = EDGE_LOOP('',(#65501,#65502,#65503,#65504)) ;
#25387 = EDGE_LOOP('',(#65505,#65506,#65507,#65508)) ;
#25388 = EDGE_LOOP('',(#65509,#65510,#65511,#65512)) ;
#25389 = EDGE_LOOP('',(#65513,#65514,#65515)) ;
#25390 = EDGE_LOOP('',(#65516,#65517,#65518)) ;
#25391 = EDGE_LOOP('',(#65519,#65520,#65521,#65522)) ;
#25392 = EDGE_LOOP('',(#65523,#65524,#65525,#65526,#65527,#65528)) ;
#25393 = EDGE_LOOP('',(#65529,#65530,#65531,#65532,#65533,#65534,#65535)) ;
#25394 = EDGE_LOOP('',(#65536,#65537,#65538,#65539)) ;
#25395 = EDGE_LOOP('',(#65540,#65541,#65542,#65543)) ;
#25396 = EDGE_LOOP('',(#65544,#65545,#65546,#65547)) ;
#25397 = EDGE_LOOP('',(#65548,#65549,#65550,#65551)) ;
#25398 = EDGE_LOOP('',(#65552,#65553,#65554)) ;
#25399 = EDGE_LOOP('',(#65555,#65556,#65557,#65558)) ;
#25400 = EDGE_LOOP('',(#65559,#65560,#65561,#65562)) ;
#25401 = EDGE_LOOP('',(#65563,#65564,#65565,#65566)) ;
#25402 = EDGE_LOOP('',(#65567,#65568,#65569,#65570)) ;
#25403 = EDGE_LOOP('',(#65571,#65572,#65573,#65574)) ;
#25404 = EDGE_LOOP('',(#65575,#65576,#65577,#65578)) ;
#25405 = EDGE_LOOP('',(#65579,#65580,#65581,#65582)) ;
#25406 = EDGE_LOOP('',(#65583,#65584,#65585,#65586)) ;
#25407 = EDGE_LOOP('',(#65587,#65588,#65589,#65590)) ;
#25408 = EDGE_LOOP('',(#65591,#65592,#65593)) ;
#25409 = EDGE_LOOP('',(#65594,#65595,#65596)) ;
#25410 = EDGE_LOOP('',(#65597,#65598,#65599,#65600,#65601)) ;
#25411 = EDGE_LOOP('',(#65602,#65603,#65604)) ;
#25412 = EDGE_LOOP('',(#65605,#65606,#65607)) ;
#25413 = EDGE_LOOP('',(#65608,#65609,#65610,#65611)) ;
#25414 = EDGE_LOOP('',(#65612,#65613,#65614,#65615)) ;
#25415 = EDGE_LOOP('',(#65616,#65617,#65618,#65619)) ;
#25416 = EDGE_LOOP('',(#65620,#65621,#65622,#65623)) ;
#25417 = EDGE_LOOP('',(#65624,#65625,#65626,#65627)) ;
#25418 = EDGE_LOOP('',(#65628,#65629,#65630,#65631)) ;
#25419 = EDGE_LOOP('',(#65632,#65633,#65634,#65635)) ;
#25420 = EDGE_LOOP('',(#65636,#65637,#65638)) ;
#25421 = EDGE_LOOP('',(#65639,#65640,#65641,#65642)) ;
#25422 = EDGE_LOOP('',(#65643,#65644,#65645,#65646)) ;
#25423 = EDGE_LOOP('',(#65647,#65648,#65649)) ;
#25424 = EDGE_LOOP('',(#65650,#65651,#65652,#65653)) ;
#25425 = EDGE_LOOP('',(#65654,#65655,#65656,#65657)) ;
#25426 = EDGE_LOOP('',(#65658,#65659,#65660,#65661)) ;
#25427 = EDGE_LOOP('',(#65662,#65663,#65664,#65665)) ;
#25428 = EDGE_LOOP('',(#65666,#65667,#65668,#65669)) ;
#25429 = EDGE_LOOP('',(#65670,#65671,#65672,#65673)) ;
#25430 = EDGE_LOOP('',(#65674,#65675,#65676,#65677,#65678)) ;
#25431 = EDGE_LOOP('',(#65679,#65680,#65681,#65682)) ;
#25432 = EDGE_LOOP('',(#65683,#65684,#65685)) ;
#25433 = EDGE_LOOP('',(#65686,#65687,#65688,#65689)) ;
#25434 = EDGE_LOOP('',(#65690,#65691,#65692,#65693)) ;
#25435 = EDGE_LOOP('',(#65694,#65695,#65696)) ;
#25436 = EDGE_LOOP('',(#65697,#65698,#65699,#65700)) ;
#25437 = EDGE_LOOP('',(#65701,#65702,#65703,#65704)) ;
#25438 = EDGE_LOOP('',(#65705,#65706,#65707,#65708)) ;
#25439 = EDGE_LOOP('',(#65709,#65710,#65711)) ;
#25440 = EDGE_LOOP('',(#65712,#65713,#65714,#65715)) ;
#25441 = EDGE_LOOP('',(#65716,#65717,#65718,#65719)) ;
#25442 = EDGE_LOOP('',(#65720,#65721,#65722)) ;
#25443 = EDGE_LOOP('',(#65723,#65724,#65725)) ;
#25444 = EDGE_LOOP('',(#65726,#65727,#65728,#65729)) ;
#25445 = EDGE_LOOP('',(#65730,#65731,#65732,#65733)) ;
#25446 = EDGE_LOOP('',(#65734,#65735,#65736)) ;
#25447 = EDGE_LOOP('',(#65737,#65738,#65739)) ;
#25448 = EDGE_LOOP('',(#65740,#65741,#65742,#65743)) ;
#25449 = EDGE_LOOP('',(#65744,#65745,#65746,#65747)) ;
#25450 = EDGE_LOOP('',(#65748,#65749,#65750)) ;
#25451 = EDGE_LOOP('',(#65751,#65752,#65753,#65754)) ;
#25452 = EDGE_LOOP('',(#65755,#65756,#65757,#65758)) ;
#25453 = EDGE_LOOP('',(#65759,#65760,#65761)) ;
#25454 = EDGE_LOOP('',(#65762,#65763,#65764)) ;
#25455 = EDGE_LOOP('',(#65765,#65766,#65767,#65768)) ;
#25456 = EDGE_LOOP('',(#65769,#65770,#65771,#65772)) ;
#25457 = EDGE_LOOP('',(#65773,#65774,#65775,#65776)) ;
#25458 = EDGE_LOOP('',(#65777,#65778,#65779,#65780)) ;
#25459 = EDGE_LOOP('',(#65781,#65782,#65783,#65784)) ;
#25460 = EDGE_LOOP('',(#65785,#65786,#65787,#65788)) ;
#25461 = EDGE_LOOP('',(#65789,#65790,#65791,#65792)) ;
#25462 = EDGE_LOOP('',(#65793,#65794,#65795)) ;
#25463 = EDGE_LOOP('',(#65796,#65797,#65798)) ;
#25464 = EDGE_LOOP('',(#65799,#65800,#65801,#65802)) ;
#25465 = EDGE_LOOP('',(#65803,#65804,#65805,#65806,#65807,#65808)) ;
#25466 = EDGE_LOOP('',(#65809,#65810,#65811,#65812,#65813,#65814,#65815)) ;
#25467 = EDGE_LOOP('',(#65816,#65817,#65818,#65819)) ;
#25468 = EDGE_LOOP('',(#65820,#65821,#65822,#65823)) ;
#25469 = EDGE_LOOP('',(#65824,#65825,#65826,#65827)) ;
#25470 = EDGE_LOOP('',(#65828,#65829,#65830,#65831)) ;
#25471 = EDGE_LOOP('',(#65832,#65833,#65834)) ;
#25472 = EDGE_LOOP('',(#65835,#65836,#65837,#65838)) ;
#25473 = EDGE_LOOP('',(#65839,#65840,#65841,#65842)) ;
#25474 = EDGE_LOOP('',(#65843,#65844,#65845,#65846)) ;
#25475 = EDGE_LOOP('',(#65847,#65848,#65849,#65850)) ;
#25476 = EDGE_LOOP('',(#65851,#65852,#65853,#65854)) ;
#25477 = EDGE_LOOP('',(#65855,#65856,#65857,#65858)) ;
#25478 = EDGE_LOOP('',(#65859,#65860,#65861,#65862)) ;
#25479 = EDGE_LOOP('',(#65863,#65864,#65865,#65866)) ;
#25480 = EDGE_LOOP('',(#65867,#65868,#65869,#65870)) ;
#25481 = EDGE_LOOP('',(#65871,#65872,#65873)) ;
#25482 = EDGE_LOOP('',(#65874,#65875,#65876)) ;
#25483 = EDGE_LOOP('',(#65877,#65878,#65879,#65880,#65881)) ;
#25484 = EDGE_LOOP('',(#65882,#65883,#65884)) ;
#25485 = EDGE_LOOP('',(#65885,#65886,#65887)) ;
#25486 = EDGE_LOOP('',(#65888,#65889,#65890,#65891)) ;
#25487 = EDGE_LOOP('',(#65892,#65893,#65894,#65895)) ;
#25488 = EDGE_LOOP('',(#65896,#65897,#65898,#65899)) ;
#25489 = EDGE_LOOP('',(#65900,#65901,#65902,#65903)) ;
#25490 = EDGE_LOOP('',(#65904,#65905,#65906,#65907)) ;
#25491 = EDGE_LOOP('',(#65908,#65909,#65910,#65911)) ;
#25492 = EDGE_LOOP('',(#65912,#65913,#65914,#65915)) ;
#25493 = EDGE_LOOP('',(#65916,#65917,#65918)) ;
#25494 = EDGE_LOOP('',(#65919,#65920,#65921,#65922)) ;
#25495 = EDGE_LOOP('',(#65923,#65924,#65925,#65926)) ;
#25496 = EDGE_LOOP('',(#65927,#65928,#65929)) ;
#25497 = EDGE_LOOP('',(#65930,#65931,#65932,#65933)) ;
#25498 = EDGE_LOOP('',(#65934,#65935,#65936,#65937)) ;
#25499 = EDGE_LOOP('',(#65938,#65939,#65940,#65941)) ;
#25500 = EDGE_LOOP('',(#65942,#65943,#65944,#65945)) ;
#25501 = EDGE_LOOP('',(#65946,#65947,#65948,#65949)) ;
#25502 = EDGE_LOOP('',(#65950,#65951,#65952,#65953)) ;
#25503 = EDGE_LOOP('',(#65954,#65955,#65956,#65957,#65958)) ;
#25504 = EDGE_LOOP('',(#65959,#65960,#65961,#65962)) ;
#25505 = EDGE_LOOP('',(#65963,#65964,#65965)) ;
#25506 = EDGE_LOOP('',(#65966,#65967,#65968,#65969)) ;
#25507 = EDGE_LOOP('',(#65970,#65971,#65972,#65973)) ;
#25508 = EDGE_LOOP('',(#65974,#65975,#65976)) ;
#25509 = EDGE_LOOP('',(#65977,#65978,#65979,#65980)) ;
#25510 = EDGE_LOOP('',(#65981,#65982,#65983,#65984)) ;
#25511 = EDGE_LOOP('',(#65985,#65986,#65987,#65988)) ;
#25512 = EDGE_LOOP('',(#65989,#65990,#65991)) ;
#25513 = EDGE_LOOP('',(#65992,#65993,#65994,#65995)) ;
#25514 = EDGE_LOOP('',(#65996,#65997,#65998,#65999)) ;
#25515 = EDGE_LOOP('',(#66000,#66001,#66002)) ;
#25516 = EDGE_LOOP('',(#66003,#66004,#66005)) ;
#25517 = EDGE_LOOP('',(#66006,#66007,#66008,#66009)) ;
#25518 = EDGE_LOOP('',(#66010,#66011,#66012,#66013)) ;
#25519 = EDGE_LOOP('',(#66014,#66015,#66016)) ;
#25520 = EDGE_LOOP('',(#66017,#66018,#66019)) ;
#25521 = EDGE_LOOP('',(#66020,#66021,#66022,#66023)) ;
#25522 = EDGE_LOOP('',(#66024,#66025,#66026,#66027)) ;
#25523 = EDGE_LOOP('',(#66028,#66029,#66030)) ;
#25524 = EDGE_LOOP('',(#66031,#66032,#66033,#66034)) ;
#25525 = EDGE_LOOP('',(#66035,#66036,#66037,#66038)) ;
#25526 = EDGE_LOOP('',(#66039,#66040,#66041)) ;
#25527 = EDGE_LOOP('',(#66042,#66043,#66044)) ;
#25528 = EDGE_LOOP('',(#66045,#66046,#66047,#66048)) ;
#25529 = EDGE_LOOP('',(#66049,#66050,#66051,#66052)) ;
#25530 = EDGE_LOOP('',(#66053,#66054,#66055,#66056)) ;
#25531 = EDGE_LOOP('',(#66057,#66058,#66059,#66060)) ;
#25532 = EDGE_LOOP('',(#66061,#66062,#66063,#66064)) ;
#25533 = EDGE_LOOP('',(#66065,#66066,#66067,#66068)) ;
#25534 = EDGE_LOOP('',(#66069,#66070,#66071,#66072)) ;
#25535 = EDGE_LOOP('',(#66073,#66074,#66075,#66076)) ;
#25536 = EDGE_LOOP('',(#66077,#66078,#66079,#66080)) ;
#25537 = EDGE_LOOP('',(#66081,#66082,#66083,#66084)) ;
#25538 = EDGE_LOOP('',(#66085,#66086,#66087,#66088,#66089,#66090)) ;
#25539 = EDGE_LOOP('',(#66091,#66092,#66093,#66094,#66095,#66096)) ;
#25540 = EDGE_LOOP('',(#66097,#66098,#66099,#66100,#66101)) ;
#25541 = EDGE_LOOP('',(#66102,#66103,#66104,#66105)) ;
#25542 = EDGE_LOOP('',(#66106,#66107,#66108,#66109)) ;
#25543 = EDGE_LOOP('',(#66110,#66111,#66112,#66113)) ;
#25544 = EDGE_LOOP('',(#66114,#66115,#66116,#66117)) ;
#25545 = EDGE_LOOP('',(#66118,#66119,#66120,#66121)) ;
#25546 = EDGE_LOOP('',(#66122,#66123,#66124,#66125)) ;
#25547 = EDGE_LOOP('',(#66126,#66127,#66128,#66129)) ;
#25548 = EDGE_LOOP('',(#66130,#66131,#66132,#66133)) ;
#25549 = EDGE_LOOP('',(#66134,#66135,#66136,#66137)) ;
#25550 = EDGE_LOOP('',(#66138,#66139,#66140,#66141)) ;
#25551 = EDGE_LOOP('',(#66142,#66143,#66144,#66145)) ;
#25552 = EDGE_LOOP('',(#66146,#66147,#66148,#66149)) ;
#25553 = EDGE_LOOP('',(#66150,#66151,#66152,#66153)) ;
#25554 = EDGE_LOOP('',(#66154,#66155,#66156,#66157,#66158,#66159)) ;
#25555 = EDGE_LOOP('',(#66160,#66161,#66162,#66163,#66164,#66165)) ;
#25556 = EDGE_LOOP('',(#66166,#66167,#66168,#66169,#66170)) ;
#25557 = EDGE_LOOP('',(#66171,#66172,#66173,#66174)) ;
#25558 = EDGE_LOOP('',(#66175,#66176,#66177,#66178)) ;
#25559 = EDGE_LOOP('',(#66179,#66180,#66181,#66182)) ;
#25560 = EDGE_LOOP('',(#66183,#66184,#66185,#66186)) ;
#25561 = EDGE_LOOP('',(#66187,#66188,#66189,#66190)) ;
#25562 = EDGE_LOOP('',(#66191,#66192,#66193,#66194)) ;
#25563 = EDGE_LOOP('',(#66195,#66196,#66197,#66198)) ;
#25564 = EDGE_LOOP('',(#66199,#66200,#66201,#66202)) ;
#25565 = EDGE_LOOP('',(#66203,#66204,#66205,#66206)) ;
#25566 = EDGE_LOOP('',(#66207,#66208,#66209,#66210)) ;
#25567 = EDGE_LOOP('',(#66211,#66212,#66213,#66214)) ;
#25568 = EDGE_LOOP('',(#66215,#66216,#66217,#66218)) ;
#25569 = EDGE_LOOP('',(#66219,#66220,#66221,#66222)) ;
#25570 = EDGE_LOOP('',(#66223,#66224,#66225,#66226,#66227,#66228)) ;
#25571 = EDGE_LOOP('',(#66229,#66230,#66231,#66232,#66233,#66234)) ;
#25572 = EDGE_LOOP('',(#66235,#66236,#66237,#66238,#66239)) ;
#25573 = EDGE_LOOP('',(#66240,#66241,#66242,#66243)) ;
#25574 = EDGE_LOOP('',(#66244,#66245,#66246,#66247)) ;
#25575 = EDGE_LOOP('',(#66248,#66249,#66250,#66251)) ;
#25576 = EDGE_LOOP('',(#66252,#66253,#66254,#66255)) ;
#25577 = EDGE_LOOP('',(#66256,#66257,#66258,#66259)) ;
#25578 = EDGE_LOOP('',(#66260,#66261,#66262,#66263)) ;
#25579 = EDGE_LOOP('',(#66264,#66265,#66266,#66267)) ;
#25580 = EDGE_LOOP('',(#66268,#66269,#66270,#66271)) ;
#25581 = EDGE_LOOP('',(#66272,#66273,#66274,#66275)) ;
#25582 = EDGE_LOOP('',(#66276,#66277,#66278,#66279)) ;
#25583 = EDGE_LOOP('',(#66280,#66281,#66282,#66283)) ;
#25584 = EDGE_LOOP('',(#66284,#66285,#66286,#66287)) ;
#25585 = EDGE_LOOP('',(#66288,#66289,#66290,#66291)) ;
#25586 = EDGE_LOOP('',(#66292,#66293,#66294,#66295,#66296,#66297)) ;
#25587 = EDGE_LOOP('',(#66298,#66299,#66300,#66301,#66302,#66303)) ;
#25588 = EDGE_LOOP('',(#66304,#66305,#66306,#66307,#66308)) ;
#25589 = EDGE_LOOP('',(#66309,#66310,#66311,#66312)) ;
#25590 = EDGE_LOOP('',(#66313,#66314,#66315,#66316)) ;
#25591 = EDGE_LOOP('',(#66317,#66318,#66319,#66320)) ;
#25592 = EDGE_LOOP('',(#66321,#66322,#66323,#66324)) ;
#25593 = EDGE_LOOP('',(#66325,#66326,#66327,#66328)) ;
#25594 = EDGE_LOOP('',(#66329,#66330,#66331,#66332)) ;
#25595 = EDGE_LOOP('',(#66333,#66334,#66335,#66336)) ;
#25596 = EDGE_LOOP('',(#66337,#66338,#66339,#66340)) ;
#25597 = EDGE_LOOP('',(#66341,#66342,#66343,#66344)) ;
#25598 = EDGE_LOOP('',(#66345,#66346,#66347,#66348)) ;
#25599 = EDGE_LOOP('',(#66349,#66350,#66351,#66352)) ;
#25600 = EDGE_LOOP('',(#66353,#66354,#66355,#66356)) ;
#25601 = EDGE_LOOP('',(#66357,#66358,#66359,#66360)) ;
#25602 = EDGE_LOOP('',(#66361,#66362,#66363,#66364,#66365,#66366)) ;
#25603 = EDGE_LOOP('',(#66367,#66368,#66369,#66370,#66371,#66372)) ;
#25604 = EDGE_LOOP('',(#66373,#66374,#66375,#66376,#66377)) ;
#25605 = EDGE_LOOP('',(#66378,#66379,#66380,#66381)) ;
#25606 = EDGE_LOOP('',(#66382,#66383,#66384,#66385)) ;
#25607 = EDGE_LOOP('',(#66386,#66387,#66388,#66389)) ;
#25608 = EDGE_LOOP('',(#66390,#66391,#66392,#66393)) ;
#25609 = EDGE_LOOP('',(#66394,#66395,#66396,#66397)) ;
#25610 = EDGE_LOOP('',(#66398,#66399,#66400,#66401)) ;
#25611 = EDGE_LOOP('',(#66402,#66403,#66404,#66405)) ;
#25612 = EDGE_LOOP('',(#66406,#66407,#66408,#66409)) ;
#25613 = EDGE_LOOP('',(#66410,#66411,#66412,#66413)) ;
#25614 = EDGE_LOOP('',(#66414,#66415,#66416,#66417)) ;
#25615 = EDGE_LOOP('',(#66418,#66419,#66420,#66421)) ;
#25616 = EDGE_LOOP('',(#66422,#66423,#66424,#66425)) ;
#25617 = EDGE_LOOP('',(#66426,#66427,#66428,#66429)) ;
#25618 = EDGE_LOOP('',(#66430,#66431,#66432,#66433,#66434,#66435)) ;
#25619 = EDGE_LOOP('',(#66436,#66437,#66438,#66439,#66440,#66441)) ;
#25620 = EDGE_LOOP('',(#66442,#66443,#66444,#66445,#66446)) ;
#25621 = EDGE_LOOP('',(#66447,#66448,#66449,#66450)) ;
#25622 = EDGE_LOOP('',(#66451,#66452,#66453,#66454)) ;
#25623 = EDGE_LOOP('',(#66455,#66456,#66457,#66458)) ;
#25624 = EDGE_LOOP('',(#66459,#66460,#66461,#66462)) ;
#25625 = EDGE_LOOP('',(#66463,#66464,#66465,#66466)) ;
#25626 = EDGE_LOOP('',(#66467,#66468,#66469,#66470)) ;
#25627 = EDGE_LOOP('',(#66471,#66472,#66473,#66474)) ;
#25628 = EDGE_LOOP('',(#66475,#66476,#66477,#66478)) ;
#25629 = EDGE_LOOP('',(#66479,#66480,#66481,#66482)) ;
#25630 = EDGE_LOOP('',(#66483,#66484,#66485,#66486)) ;
#25631 = EDGE_LOOP('',(#66487,#66488,#66489,#66490)) ;
#25632 = EDGE_LOOP('',(#66491,#66492,#66493,#66494)) ;
#25633 = EDGE_LOOP('',(#66495,#66496,#66497,#66498)) ;
#25634 = EDGE_LOOP('',(#66499,#66500,#66501,#66502,#66503,#66504)) ;
#25635 = EDGE_LOOP('',(#66505,#66506,#66507,#66508,#66509,#66510)) ;
#25636 = EDGE_LOOP('',(#66511,#66512,#66513,#66514,#66515)) ;
#25637 = EDGE_LOOP('',(#66516,#66517,#66518,#66519)) ;
#25638 = EDGE_LOOP('',(#66520,#66521,#66522,#66523)) ;
#25639 = EDGE_LOOP('',(#66524,#66525,#66526,#66527)) ;
#25640 = EDGE_LOOP('',(#66528,#66529,#66530,#66531)) ;
#25641 = EDGE_LOOP('',(#66532,#66533,#66534,#66535)) ;
#25642 = EDGE_LOOP('',(#66536,#66537,#66538,#66539)) ;
#25643 = EDGE_LOOP('',(#66540,#66541,#66542,#66543)) ;
#25644 = EDGE_LOOP('',(#66544,#66545,#66546,#66547)) ;
#25645 = EDGE_LOOP('',(#66548,#66549,#66550,#66551)) ;
#25646 = EDGE_LOOP('',(#66552,#66553,#66554,#66555)) ;
#25647 = EDGE_LOOP('',(#66556,#66557,#66558,#66559)) ;
#25648 = EDGE_LOOP('',(#66560,#66561,#66562,#66563)) ;
#25649 = EDGE_LOOP('',(#66564,#66565,#66566,#66567)) ;
#25650 = EDGE_LOOP('',(#66568,#66569,#66570,#66571,#66572,#66573)) ;
#25651 = EDGE_LOOP('',(#66574,#66575,#66576,#66577,#66578,#66579)) ;
#25652 = EDGE_LOOP('',(#66580,#66581,#66582,#66583,#66584)) ;
#25653 = EDGE_LOOP('',(#66585,#66586,#66587,#66588)) ;
#25654 = EDGE_LOOP('',(#66589,#66590,#66591,#66592)) ;
#25655 = EDGE_LOOP('',(#66593,#66594,#66595,#66596)) ;
#25656 = EDGE_LOOP('',(#66597,#66598,#66599,#66600)) ;
#25657 = EDGE_LOOP('',(#66601,#66602,#66603,#66604)) ;
#25658 = EDGE_LOOP('',(#66605,#66606,#66607,#66608)) ;
#25659 = EDGE_LOOP('',(#66609,#66610,#66611,#66612)) ;
#25660 = EDGE_LOOP('',(#66613,#66614,#66615,#66616)) ;
#25661 = EDGE_LOOP('',(#66617,#66618,#66619,#66620)) ;
#25662 = EDGE_LOOP('',(#66621,#66622,#66623,#66624)) ;
#25663 = EDGE_LOOP('',(#66625,#66626,#66627,#66628)) ;
#25664 = EDGE_LOOP('',(#66629,#66630,#66631,#66632)) ;
#25665 = EDGE_LOOP('',(#66633,#66634,#66635,#66636)) ;
#25666 = EDGE_LOOP('',(#66637,#66638,#66639,#66640,#66641,#66642)) ;
#25667 = EDGE_LOOP('',(#66643,#66644,#66645,#66646,#66647,#66648)) ;
#25668 = EDGE_LOOP('',(#66649,#66650,#66651,#66652,#66653)) ;
#25669 = EDGE_LOOP('',(#66654,#66655,#66656,#66657)) ;
#25670 = EDGE_LOOP('',(#66658,#66659,#66660,#66661)) ;
#25671 = EDGE_LOOP('',(#66662,#66663,#66664,#66665)) ;
#25672 = EDGE_LOOP('',(#66666,#66667,#66668,#66669)) ;
#25673 = EDGE_LOOP('',(#66670,#66671,#66672,#66673)) ;
#25674 = EDGE_LOOP('',(#66674,#66675,#66676,#66677)) ;
#25675 = EDGE_LOOP('',(#66678,#66679,#66680,#66681)) ;
#25676 = EDGE_LOOP('',(#66682,#66683,#66684,#66685)) ;
#25677 = EDGE_LOOP('',(#66686,#66687,#66688,#66689)) ;
#25678 = EDGE_LOOP('',(#66690,#66691,#66692,#66693)) ;
#25679 = EDGE_LOOP('',(#66694,#66695,#66696,#66697)) ;
#25680 = EDGE_LOOP('',(#66698,#66699,#66700,#66701)) ;
#25681 = EDGE_LOOP('',(#66702,#66703,#66704,#66705)) ;
#25682 = EDGE_LOOP('',(#66706,#66707,#66708,#66709)) ;
#25683 = EDGE_LOOP('',(#66710,#66711,#66712,#66713)) ;
#25684 = EDGE_LOOP('',(#66714,#66715,#66716,#66717)) ;
#25685 = EDGE_LOOP('',(#66718,#66719,#66720,#66721)) ;
#25686 = EDGE_LOOP('',(#66722,#66723,#66724,#66725)) ;
#25687 = EDGE_LOOP('',(#66726,#66727,#66728,#66729)) ;
#25688 = EDGE_LOOP('',(#66730,#66731,#66732,#66733)) ;
#25689 = EDGE_LOOP('',(#66734,#66735,#66736,#66737)) ;
#25690 = EDGE_LOOP('',(#66738,#66739,#66740,#66741)) ;
#25691 = EDGE_LOOP('',(#66742,#66743,#66744,#66745)) ;
#25692 = EDGE_LOOP('',(#66746,#66747,#66748,#66749)) ;
#25693 = EDGE_LOOP('',(#66750,#66751,#66752,#66753)) ;
#25694 = EDGE_LOOP('',(#66754,#66755,#66756,#66757)) ;
#25695 = EDGE_LOOP('',(#66758,#66759,#66760,#66761)) ;
#25696 = EDGE_LOOP('',(#66762,#66763,#66764,#66765)) ;
#25697 = EDGE_LOOP('',(#66766,#66767,#66768,#66769)) ;
#25698 = EDGE_LOOP('',(#66770,#66771,#66772,#66773)) ;
#25699 = EDGE_LOOP('',(#66774,#66775,#66776,#66777)) ;
#25700 = EDGE_LOOP('',(#66778,#66779,#66780,#66781)) ;
#25701 = EDGE_LOOP('',(#66782,#66783,#66784,#66785)) ;
#25702 = EDGE_LOOP('',(#66786,#66787,#66788,#66789)) ;
#25703 = EDGE_LOOP('',(#66790,#66791,#66792,#66793)) ;
#25704 = EDGE_LOOP('',(#66794,#66795,#66796,#66797)) ;
#25705 = EDGE_LOOP('',(#66798,#66799,#66800,#66801)) ;
#25706 = EDGE_LOOP('',(#66802,#66803,#66804,#66805)) ;
#25707 = EDGE_LOOP('',(#66806,#66807,#66808,#66809)) ;
#25708 = EDGE_LOOP('',(#66810,#66811,#66812,#66813)) ;
#25709 = EDGE_LOOP('',(#66814,#66815,#66816,#66817)) ;
#25710 = EDGE_LOOP('',(#66818,#66819,#66820,#66821)) ;
#25711 = EDGE_LOOP('',(#66822,#66823,#66824,#66825)) ;
#25712 = EDGE_LOOP('',(#66826,#66827,#66828,#66829)) ;
#25713 = EDGE_LOOP('',(#66830,#66831,#66832,#66833)) ;
#25714 = EDGE_LOOP('',(#66834,#66835,#66836,#66837)) ;
#25715 = EDGE_LOOP('',(#66838,#66839,#66840)) ;
#25716 = EDGE_LOOP('',(#66841,#66842,#66843,#66844)) ;
#25717 = EDGE_LOOP('',(#66845,#66846,#66847,#66848)) ;
#25718 = EDGE_LOOP('',(#66849,#66850,#66851,#66852)) ;
#25719 = EDGE_LOOP('',(#66853,#66854,#66855)) ;
#25720 = EDGE_LOOP('',(#66856,#66857,#66858)) ;
#25721 = EDGE_LOOP('',(#66859,#66860,#66861,#66862)) ;
#25722 = EDGE_LOOP('',(#66863,#66864,#66865,#66866)) ;
#25723 = EDGE_LOOP('',(#66867,#66868,#66869,#66870)) ;
#25724 = EDGE_LOOP('',(#66871,#66872,#66873)) ;
#25725 = EDGE_LOOP('',(#66874,#66875,#66876,#66877)) ;
#25726 = EDGE_LOOP('',(#66878,#66879,#66880,#66881)) ;
#25727 = EDGE_LOOP('',(#66882,#66883,#66884,#66885)) ;
#25728 = EDGE_LOOP('',(#66886,#66887,#66888,#66889)) ;
#25729 = EDGE_LOOP('',(#66890,#66891,#66892)) ;
#25730 = EDGE_LOOP('',(#66893,#66894,#66895,#66896)) ;
#25731 = EDGE_LOOP('',(#66897,#66898,#66899,#66900)) ;
#25732 = EDGE_LOOP('',(#66901,#66902,#66903,#66904)) ;
#25733 = EDGE_LOOP('',(#66905,#66906,#66907)) ;
#25734 = EDGE_LOOP('',(#66908,#66909,#66910)) ;
#25735 = EDGE_LOOP('',(#66911,#66912,#66913,#66914)) ;
#25736 = EDGE_LOOP('',(#66915,#66916,#66917,#66918)) ;
#25737 = EDGE_LOOP('',(#66919,#66920,#66921,#66922)) ;
#25738 = EDGE_LOOP('',(#66923,#66924,#66925)) ;
#25739 = EDGE_LOOP('',(#66926,#66927,#66928,#66929)) ;
#25740 = EDGE_LOOP('',(#66930,#66931,#66932,#66933)) ;
#25741 = EDGE_LOOP('',(#66934,#66935,#66936,#66937)) ;
#25742 = EDGE_LOOP('',(#66938,#66939,#66940,#66941)) ;
#25743 = EDGE_LOOP('',(#66942,#66943,#66944)) ;
#25744 = EDGE_LOOP('',(#66945,#66946,#66947,#66948)) ;
#25745 = EDGE_LOOP('',(#66949,#66950,#66951,#66952)) ;
#25746 = EDGE_LOOP('',(#66953,#66954,#66955,#66956)) ;
#25747 = EDGE_LOOP('',(#66957,#66958,#66959)) ;
#25748 = EDGE_LOOP('',(#66960,#66961,#66962)) ;
#25749 = EDGE_LOOP('',(#66963,#66964,#66965,#66966)) ;
#25750 = EDGE_LOOP('',(#66967,#66968,#66969,#66970)) ;
#25751 = EDGE_LOOP('',(#66971,#66972,#66973,#66974)) ;
#25752 = EDGE_LOOP('',(#66975,#66976,#66977)) ;
#25753 = EDGE_LOOP('',(#66978,#66979,#66980,#66981)) ;
#25754 = EDGE_LOOP('',(#66982,#66983,#66984,#66985)) ;
#25755 = EDGE_LOOP('',(#66986,#66987,#66988,#66989)) ;
#25756 = EDGE_LOOP('',(#66990,#66991,#66992,#66993)) ;
#25757 = EDGE_LOOP('',(#66994,#66995,#66996)) ;
#25758 = EDGE_LOOP('',(#66997,#66998,#66999,#67000)) ;
#25759 = EDGE_LOOP('',(#67001,#67002,#67003,#67004)) ;
#25760 = EDGE_LOOP('',(#67005,#67006,#67007,#67008)) ;
#25761 = EDGE_LOOP('',(#67009,#67010,#67011)) ;
#25762 = EDGE_LOOP('',(#67012,#67013,#67014)) ;
#25763 = EDGE_LOOP('',(#67015,#67016,#67017,#67018)) ;
#25764 = EDGE_LOOP('',(#67019,#67020,#67021,#67022)) ;
#25765 = EDGE_LOOP('',(#67023,#67024,#67025,#67026)) ;
#25766 = EDGE_LOOP('',(#67027,#67028,#67029)) ;
#25767 = EDGE_LOOP('',(#67030,#67031,#67032,#67033)) ;
#25768 = EDGE_LOOP('',(#67034,#67035,#67036,#67037)) ;
#25769 = EDGE_LOOP('',(#67038,#67039,#67040,#67041)) ;
#25770 = EDGE_LOOP('',(#67042,#67043,#67044,#67045)) ;
#25771 = EDGE_LOOP('',(#67046,#67047,#67048)) ;
#25772 = EDGE_LOOP('',(#67049,#67050,#67051,#67052)) ;
#25773 = EDGE_LOOP('',(#67053,#67054,#67055,#67056)) ;
#25774 = EDGE_LOOP('',(#67057,#67058,#67059,#67060)) ;
#25775 = EDGE_LOOP('',(#67061,#67062,#67063)) ;
#25776 = EDGE_LOOP('',(#67064,#67065,#67066)) ;
#25777 = EDGE_LOOP('',(#67067,#67068,#67069,#67070)) ;
#25778 = EDGE_LOOP('',(#67071,#67072,#67073,#67074)) ;
#25779 = EDGE_LOOP('',(#67075,#67076,#67077,#67078)) ;
#25780 = EDGE_LOOP('',(#67079,#67080,#67081)) ;
#25781 = EDGE_LOOP('',(#67082,#67083,#67084,#67085)) ;
#25782 = EDGE_LOOP('',(#67086,#67087,#67088,#67089)) ;
#25783 = EDGE_LOOP('',(#67090,#67091,#67092,#67093)) ;
#25784 = EDGE_LOOP('',(#67094,#67095,#67096,#67097)) ;
#25785 = EDGE_LOOP('',(#67098,#67099,#67100)) ;
#25786 = EDGE_LOOP('',(#67101,#67102,#67103,#67104)) ;
#25787 = EDGE_LOOP('',(#67105,#67106,#67107,#67108)) ;
#25788 = EDGE_LOOP('',(#67109,#67110,#67111,#67112)) ;
#25789 = EDGE_LOOP('',(#67113,#67114,#67115)) ;
#25790 = EDGE_LOOP('',(#67116,#67117,#67118)) ;
#25791 = EDGE_LOOP('',(#67119,#67120,#67121,#67122)) ;
#25792 = EDGE_LOOP('',(#67123,#67124,#67125,#67126)) ;
#25793 = EDGE_LOOP('',(#67127,#67128,#67129,#67130)) ;
#25794 = EDGE_LOOP('',(#67131,#67132,#67133)) ;
#25795 = EDGE_LOOP('',(#67134,#67135,#67136,#67137)) ;
#25796 = EDGE_LOOP('',(#67138,#67139,#67140,#67141)) ;
#25797 = EDGE_LOOP('',(#67142,#67143,#67144,#67145)) ;
#25798 = EDGE_LOOP('',(#67146,#67147,#67148,#67149)) ;
#25799 = EDGE_LOOP('',(#67150,#67151,#67152)) ;
#25800 = EDGE_LOOP('',(#67153,#67154,#67155,#67156)) ;
#25801 = EDGE_LOOP('',(#67157,#67158,#67159,#67160)) ;
#25802 = EDGE_LOOP('',(#67161,#67162,#67163,#67164)) ;
#25803 = EDGE_LOOP('',(#67165,#67166,#67167)) ;
#25804 = EDGE_LOOP('',(#67168,#67169,#67170)) ;
#25805 = EDGE_LOOP('',(#67171,#67172,#67173,#67174)) ;
#25806 = EDGE_LOOP('',(#67175,#67176,#67177,#67178)) ;
#25807 = EDGE_LOOP('',(#67179,#67180,#67181,#67182)) ;
#25808 = EDGE_LOOP('',(#67183,#67184,#67185)) ;
#25809 = EDGE_LOOP('',(#67186,#67187,#67188,#67189)) ;
#25810 = EDGE_LOOP('',(#67190,#67191,#67192,#67193)) ;
#25811 = EDGE_LOOP('',(#67194,#67195,#67196,#67197)) ;
#25812 = EDGE_LOOP('',(#67198,#67199,#67200,#67201)) ;
#25813 = EDGE_LOOP('',(#67202,#67203,#67204)) ;
#25814 = EDGE_LOOP('',(#67205,#67206,#67207,#67208)) ;
#25815 = EDGE_LOOP('',(#67209,#67210,#67211,#67212)) ;
#25816 = EDGE_LOOP('',(#67213,#67214,#67215,#67216)) ;
#25817 = EDGE_LOOP('',(#67217,#67218,#67219)) ;
#25818 = EDGE_LOOP('',(#67220,#67221,#67222)) ;
#25819 = EDGE_LOOP('',(#67223,#67224,#67225,#67226)) ;
#25820 = EDGE_LOOP('',(#67227,#67228,#67229,#67230)) ;
#25821 = EDGE_LOOP('',(#67231,#67232,#67233,#67234)) ;
#25822 = EDGE_LOOP('',(#67235,#67236,#67237)) ;
#25823 = EDGE_LOOP('',(#67238,#67239,#67240,#67241)) ;
#25824 = EDGE_LOOP('',(#67242,#67243,#67244,#67245)) ;
#25825 = EDGE_LOOP('',(#67246,#67247,#67248,#67249)) ;
#25826 = EDGE_LOOP('',(#67250,#67251,#67252,#67253)) ;
#25827 = EDGE_LOOP('',(#67254,#67255,#67256)) ;
#25828 = EDGE_LOOP('',(#67257,#67258,#67259,#67260)) ;
#25829 = EDGE_LOOP('',(#67261,#67262,#67263,#67264)) ;
#25830 = EDGE_LOOP('',(#67265,#67266,#67267,#67268)) ;
#25831 = EDGE_LOOP('',(#67269,#67270,#67271)) ;
#25832 = EDGE_LOOP('',(#67272,#67273,#67274)) ;
#25833 = EDGE_LOOP('',(#67275,#67276,#67277,#67278)) ;
#25834 = EDGE_LOOP('',(#67279,#67280,#67281,#67282)) ;
#25835 = EDGE_LOOP('',(#67283,#67284,#67285,#67286)) ;
#25836 = EDGE_LOOP('',(#67287,#67288,#67289)) ;
#25837 = EDGE_LOOP('',(#67290,#67291,#67292,#67293)) ;
#25838 = EDGE_LOOP('',(#67294,#67295,#67296,#67297)) ;
#25839 = EDGE_LOOP('',(#67298,#67299,#67300,#67301)) ;
#25840 = EDGE_LOOP('',(#67302,#67303,#67304,#67305)) ;
#25841 = EDGE_LOOP('',(#67306,#67307,#67308)) ;
#25842 = EDGE_LOOP('',(#67309,#67310,#67311,#67312)) ;
#25843 = EDGE_LOOP('',(#67313,#67314,#67315,#67316)) ;
#25844 = EDGE_LOOP('',(#67317,#67318,#67319,#67320)) ;
#25845 = EDGE_LOOP('',(#67321,#67322,#67323)) ;
#25846 = EDGE_LOOP('',(#67324,#67325,#67326)) ;
#25847 = EDGE_LOOP('',(#67327,#67328,#67329,#67330)) ;
#25848 = EDGE_LOOP('',(#67331,#67332,#67333,#67334)) ;
#25849 = EDGE_LOOP('',(#67335,#67336,#67337,#67338)) ;
#25850 = EDGE_LOOP('',(#67339,#67340,#67341)) ;
#25851 = EDGE_LOOP('',(#67342,#67343,#67344,#67345)) ;
#25852 = EDGE_LOOP('',(#67346,#67347,#67348,#67349)) ;
#25853 = EDGE_LOOP('',(#67350,#67351,#67352,#67353)) ;
#25854 = EDGE_LOOP('',(#67354,#67355,#67356,#67357)) ;
#25855 = EDGE_LOOP('',(#67358,#67359,#67360)) ;
#25856 = EDGE_LOOP('',(#67361,#67362,#67363,#67364)) ;
#25857 = EDGE_LOOP('',(#67365,#67366,#67367,#67368)) ;
#25858 = EDGE_LOOP('',(#67369,#67370,#67371,#67372)) ;
#25859 = EDGE_LOOP('',(#67373,#67374,#67375)) ;
#25860 = EDGE_LOOP('',(#67376,#67377,#67378)) ;
#25861 = EDGE_LOOP('',(#67379,#67380,#67381,#67382)) ;
#25862 = EDGE_LOOP('',(#67383,#67384,#67385,#67386)) ;
#25863 = EDGE_LOOP('',(#67387,#67388,#67389,#67390)) ;
#25864 = EDGE_LOOP('',(#67391,#67392,#67393)) ;
#25865 = EDGE_LOOP('',(#67394,#67395,#67396,#67397)) ;
#25866 = EDGE_LOOP('',(#67398,#67399,#67400,#67401)) ;
#25867 = EDGE_LOOP('',(#67402,#67403,#67404,#67405)) ;
#25868 = EDGE_LOOP('',(#67406,#67407,#67408,#67409)) ;
#25869 = EDGE_LOOP('',(#67410,#67411,#67412)) ;
#25870 = EDGE_LOOP('',(#67413,#67414,#67415,#67416)) ;
#25871 = EDGE_LOOP('',(#67417,#67418,#67419,#67420)) ;
#25872 = EDGE_LOOP('',(#67421,#67422,#67423,#67424)) ;
#25873 = EDGE_LOOP('',(#67425,#67426,#67427)) ;
#25874 = EDGE_LOOP('',(#67428,#67429,#67430)) ;
#25875 = EDGE_LOOP('',(#67431,#67432,#67433,#67434)) ;
#25876 = EDGE_LOOP('',(#67435,#67436,#67437,#67438)) ;
#25877 = EDGE_LOOP('',(#67439,#67440,#67441,#67442)) ;
#25878 = EDGE_LOOP('',(#67443,#67444,#67445)) ;
#25879 = EDGE_LOOP('',(#67446,#67447,#67448,#67449)) ;
#25880 = EDGE_LOOP('',(#67450,#67451,#67452,#67453)) ;
#25881 = EDGE_LOOP('',(#67454,#67455,#67456,#67457)) ;
#25882 = EDGE_LOOP('',(#67458,#67459,#67460,#67461)) ;
#25883 = EDGE_LOOP('',(#67462,#67463,#67464)) ;
#25884 = EDGE_LOOP('',(#67465,#67466,#67467,#67468)) ;
#25885 = EDGE_LOOP('',(#67469,#67470,#67471,#67472)) ;
#25886 = EDGE_LOOP('',(#67473,#67474,#67475,#67476)) ;
#25887 = EDGE_LOOP('',(#67477,#67478,#67479)) ;
#25888 = EDGE_LOOP('',(#67480,#67481,#67482)) ;
#25889 = EDGE_LOOP('',(#67483,#67484,#67485,#67486)) ;
#25890 = EDGE_LOOP('',(#67487,#67488,#67489,#67490)) ;
#25891 = EDGE_LOOP('',(#67491,#67492,#67493,#67494)) ;
#25892 = EDGE_LOOP('',(#67495,#67496,#67497)) ;
#25893 = EDGE_LOOP('',(#67498,#67499,#67500,#67501)) ;
#25894 = EDGE_LOOP('',(#67502,#67503,#67504,#67505)) ;
#25895 = EDGE_LOOP('',(#67506,#67507,#67508,#67509)) ;
#25896 = EDGE_LOOP('',(#67510,#67511,#67512,#67513)) ;
#25897 = EDGE_LOOP('',(#67514,#67515,#67516)) ;
#25898 = EDGE_LOOP('',(#67517,#67518,#67519,#67520)) ;
#25899 = EDGE_LOOP('',(#67521,#67522,#67523,#67524)) ;
#25900 = EDGE_LOOP('',(#67525,#67526,#67527,#67528)) ;
#25901 = EDGE_LOOP('',(#67529,#67530,#67531)) ;
#25902 = EDGE_LOOP('',(#67532,#67533,#67534)) ;
#25903 = EDGE_LOOP('',(#67535,#67536,#67537,#67538)) ;
#25904 = EDGE_LOOP('',(#67539,#67540,#67541,#67542)) ;
#25905 = EDGE_LOOP('',(#67543,#67544,#67545,#67546)) ;
#25906 = EDGE_LOOP('',(#67547,#67548,#67549)) ;
#25907 = EDGE_LOOP('',(#67550,#67551,#67552,#67553)) ;
#25908 = EDGE_LOOP('',(#67554,#67555,#67556,#67557)) ;
#25909 = EDGE_LOOP('',(#67558,#67559,#67560,#67561)) ;
#25910 = EDGE_LOOP('',(#67562,#67563,#67564,#67565)) ;
#25911 = EDGE_LOOP('',(#67566,#67567,#67568)) ;
#25912 = EDGE_LOOP('',(#67569,#67570,#67571,#67572)) ;
#25913 = EDGE_LOOP('',(#67573,#67574,#67575,#67576)) ;
#25914 = EDGE_LOOP('',(#67577,#67578,#67579,#67580)) ;
#25915 = EDGE_LOOP('',(#67581,#67582,#67583)) ;
#25916 = EDGE_LOOP('',(#67584,#67585,#67586)) ;
#25917 = EDGE_LOOP('',(#67587,#67588,#67589,#67590)) ;
#25918 = EDGE_LOOP('',(#67591,#67592,#67593,#67594)) ;
#25919 = EDGE_LOOP('',(#67595,#67596,#67597,#67598)) ;
#25920 = EDGE_LOOP('',(#67599,#67600,#67601)) ;
#25921 = EDGE_LOOP('',(#67602,#67603,#67604,#67605)) ;
#25922 = EDGE_LOOP('',(#67606,#67607,#67608,#67609)) ;
#25923 = EDGE_LOOP('',(#67610,#67611,#67612,#67613)) ;
#25924 = EDGE_LOOP('',(#67614,#67615,#67616,#67617)) ;
#25925 = EDGE_LOOP('',(#67618,#67619,#67620)) ;
#25926 = EDGE_LOOP('',(#67621,#67622,#67623,#67624)) ;
#25927 = EDGE_LOOP('',(#67625,#67626,#67627,#67628)) ;
#25928 = EDGE_LOOP('',(#67629,#67630,#67631,#67632)) ;
#25929 = EDGE_LOOP('',(#67633,#67634,#67635)) ;
#25930 = EDGE_LOOP('',(#67636,#67637,#67638)) ;
#25931 = EDGE_LOOP('',(#67639,#67640,#67641,#67642)) ;
#25932 = EDGE_LOOP('',(#67643,#67644,#67645,#67646)) ;
#25933 = EDGE_LOOP('',(#67647,#67648,#67649,#67650)) ;
#25934 = EDGE_LOOP('',(#67651,#67652,#67653)) ;
#25935 = EDGE_LOOP('',(#67654,#67655,#67656,#67657)) ;
#25936 = EDGE_LOOP('',(#67658,#67659,#67660,#67661)) ;
#25937 = EDGE_LOOP('',(#67662,#67663,#67664,#67665)) ;
#25938 = EDGE_LOOP('',(#67666,#67667,#67668,#67669)) ;
#25939 = EDGE_LOOP('',(#67670,#67671,#67672)) ;
#25940 = EDGE_LOOP('',(#67673,#67674,#67675,#67676)) ;
#25941 = EDGE_LOOP('',(#67677,#67678,#67679,#67680)) ;
#25942 = EDGE_LOOP('',(#67681,#67682,#67683,#67684)) ;
#25943 = EDGE_LOOP('',(#67685,#67686,#67687)) ;
#25944 = EDGE_LOOP('',(#67688,#67689,#67690)) ;
#25945 = EDGE_LOOP('',(#67691,#67692,#67693,#67694)) ;
#25946 = EDGE_LOOP('',(#67695,#67696,#67697,#67698)) ;
#25947 = EDGE_LOOP('',(#67699,#67700,#67701,#67702)) ;
#25948 = EDGE_LOOP('',(#67703,#67704,#67705)) ;
#25949 = EDGE_LOOP('',(#67706,#67707,#67708,#67709)) ;
#25950 = EDGE_LOOP('',(#67710,#67711,#67712,#67713)) ;
#25951 = EDGE_LOOP('',(#67714,#67715,#67716,#67717)) ;
#25952 = EDGE_LOOP('',(#67718,#67719,#67720,#67721)) ;
#25953 = EDGE_LOOP('',(#67722,#67723,#67724)) ;
#25954 = EDGE_LOOP('',(#67725,#67726,#67727,#67728)) ;
#25955 = EDGE_LOOP('',(#67729,#67730,#67731,#67732)) ;
#25956 = EDGE_LOOP('',(#67733,#67734,#67735,#67736)) ;
#25957 = EDGE_LOOP('',(#67737,#67738,#67739)) ;
#25958 = EDGE_LOOP('',(#67740,#67741,#67742)) ;
#25959 = EDGE_LOOP('',(#67743,#67744,#67745,#67746)) ;
#25960 = EDGE_LOOP('',(#67747,#67748,#67749,#67750)) ;
#25961 = EDGE_LOOP('',(#67751,#67752,#67753,#67754)) ;
#25962 = EDGE_LOOP('',(#67755,#67756,#67757)) ;
#25963 = EDGE_LOOP('',(#67758,#67759,#67760,#67761)) ;
#25964 = EDGE_LOOP('',(#67762,#67763,#67764,#67765)) ;
#25965 = EDGE_LOOP('',(#67766,#67767,#67768,#67769)) ;
#25966 = EDGE_LOOP('',(#67770,#67771,#67772,#67773)) ;
#25967 = EDGE_LOOP('',(#67774,#67775,#67776,#67777)) ;
#25968 = EDGE_LOOP('',(#67778,#67779,#67780,#67781)) ;
#25969 = EDGE_LOOP('',(#67782,#67783,#67784,#67785)) ;
#25970 = EDGE_LOOP('',(#67786,#67787,#67788,#67789)) ;
#25971 = EDGE_LOOP('',(#67790,#67791,#67792,#67793,#67794)) ;
#25972 = EDGE_LOOP('',(#67795,#67796,#67797,#67798)) ;
#25973 = EDGE_LOOP('',(#67799,#67800,#67801,#67802)) ;
#25974 = EDGE_LOOP('',(#67803,#67804,#67805,#67806)) ;
#25975 = EDGE_LOOP('',(#67807,#67808,#67809,#67810)) ;
#25976 = EDGE_LOOP('',(#67811,#67812,#67813,#67814)) ;
#25977 = EDGE_LOOP('',(#67815,#67816,#67817,#67818)) ;
#25978 = EDGE_LOOP('',(#67819,#67820,#67821,#67822)) ;
#25979 = EDGE_LOOP('',(#67823,#67824,#67825,#67826)) ;
#25980 = EDGE_LOOP('',(#67827,#67828,#67829,#67830)) ;
#25981 = EDGE_LOOP('',(#67831,#67832,#67833,#67834)) ;
#25982 = EDGE_LOOP('',(#67835,#67836,#67837,#67838)) ;
#25983 = EDGE_LOOP('',(#67839,#67840,#67841,#67842)) ;
#25984 = EDGE_LOOP('',(#67843,#67844,#67845,#67846)) ;
#25985 = EDGE_LOOP('',(#67847,#67848,#67849,#67850)) ;
#25986 = EDGE_LOOP('',(#67851,#67852,#67853,#67854)) ;
#25987 = EDGE_LOOP('',(#67855,#67856,#67857,#67858)) ;
#25988 = EDGE_LOOP('',(#67859,#67860,#67861,#67862)) ;
#25989 = EDGE_LOOP('',(#67863,#67864,#67865,#67866)) ;
#25990 = EDGE_LOOP('',(#67867,#67868,#67869,#67870)) ;
#25991 = EDGE_LOOP('',(#67871,#67872,#67873,#67874)) ;
#25992 = EDGE_LOOP('',(#67875,#67876,#67877,#67878)) ;
#25993 = EDGE_LOOP('',(#67879,#67880,#67881,#67882)) ;
#25994 = EDGE_LOOP('',(#67883,#67884,#67885,#67886)) ;
#25995 = EDGE_LOOP('',(#67887,#67888,#67889,#67890,#67891)) ;
#25996 = EDGE_LOOP('',(#67892,#67893,#67894,#67895)) ;
#25997 = EDGE_LOOP('',(#67896,#67897,#67898,#67899)) ;
#25998 = EDGE_LOOP('',(#67900,#67901,#67902,#67903)) ;
#25999 = EDGE_LOOP('',(#67904,#67905,#67906,#67907)) ;
#26000 = EDGE_LOOP('',(#67908,#67909,#67910,#67911)) ;
#26001 = EDGE_LOOP('',(#67912,#67913,#67914,#67915)) ;
#26002 = EDGE_LOOP('',(#67916,#67917,#67918,#67919)) ;
#26003 = EDGE_LOOP('',(#67920,#67921,#67922,#67923)) ;
#26004 = EDGE_LOOP('',(#67924,#67925,#67926,#67927)) ;
#26005 = EDGE_LOOP('',(#67928,#67929,#67930,#67931)) ;
#26006 = EDGE_LOOP('',(#67932,#67933,#67934,#67935)) ;
#26007 = EDGE_LOOP('',(#67936,#67937,#67938,#67939)) ;
#26008 = EDGE_LOOP('',(#67940,#67941,#67942,#67943)) ;
#26009 = EDGE_LOOP('',(#67944,#67945,#67946,#67947)) ;
#26010 = EDGE_LOOP('',(#67948,#67949,#67950,#67951)) ;
#26011 = EDGE_LOOP('',(#67952,#67953,#67954,#67955)) ;
#26012 = EDGE_LOOP('',(#67956,#67957,#67958,#67959)) ;
#26013 = EDGE_LOOP('',(#67960,#67961,#67962,#67963)) ;
#26014 = EDGE_LOOP('',(#67964,#67965,#67966,#67967)) ;
#26015 = EDGE_LOOP('',(#67968,#67969,#67970,#67971)) ;
#26016 = EDGE_LOOP('',(#67972,#67973,#67974,#67975)) ;
#26017 = EDGE_LOOP('',(#67976,#67977,#67978,#67979)) ;
#26018 = EDGE_LOOP('',(#67980,#67981,#67982,#67983)) ;
#26019 = EDGE_LOOP('',(#67984,#67985,#67986,#67987,#67988)) ;
#26020 = EDGE_LOOP('',(#67989,#67990,#67991,#67992)) ;
#26021 = EDGE_LOOP('',(#67993,#67994,#67995,#67996)) ;
#26022 = EDGE_LOOP('',(#67997,#67998,#67999,#68000)) ;
#26023 = EDGE_LOOP('',(#68001,#68002,#68003,#68004)) ;
#26024 = EDGE_LOOP('',(#68005,#68006,#68007,#68008)) ;
#26025 = EDGE_LOOP('',(#68009,#68010,#68011,#68012)) ;
#26026 = EDGE_LOOP('',(#68013,#68014,#68015,#68016)) ;
#26027 = EDGE_LOOP('',(#68017,#68018,#68019,#68020)) ;
#26028 = EDGE_LOOP('',(#68021,#68022,#68023,#68024)) ;
#26029 = EDGE_LOOP('',(#68025,#68026,#68027,#68028)) ;
#26030 = EDGE_LOOP('',(#68029,#68030,#68031,#68032)) ;
#26031 = EDGE_LOOP('',(#68033,#68034,#68035,#68036)) ;
#26032 = EDGE_LOOP('',(#68037,#68038,#68039,#68040)) ;
#26033 = EDGE_LOOP('',(#68041,#68042,#68043,#68044)) ;
#26034 = EDGE_LOOP('',(#68045,#68046,#68047,#68048)) ;
#26035 = EDGE_LOOP('',(#68049,#68050,#68051,#68052)) ;
#26036 = EDGE_LOOP('',(#68053,#68054,#68055,#68056)) ;
#26037 = EDGE_LOOP('',(#68057,#68058,#68059,#68060)) ;
#26038 = EDGE_LOOP('',(#68061,#68062,#68063,#68064)) ;
#26039 = EDGE_LOOP('',(#68065,#68066,#68067,#68068)) ;
#26040 = EDGE_LOOP('',(#68069,#68070,#68071,#68072)) ;
#26041 = EDGE_LOOP('',(#68073,#68074,#68075,#68076)) ;
#26042 = EDGE_LOOP('',(#68077,#68078,#68079,#68080)) ;
#26043 = EDGE_LOOP('',(#68081,#68082,#68083,#68084,#68085)) ;
#26044 = EDGE_LOOP('',(#68086,#68087,#68088,#68089)) ;
#26045 = EDGE_LOOP('',(#68090,#68091,#68092,#68093)) ;
#26046 = EDGE_LOOP('',(#68094,#68095,#68096,#68097)) ;
#26047 = EDGE_LOOP('',(#68098,#68099,#68100,#68101)) ;
#26048 = EDGE_LOOP('',(#68102,#68103,#68104,#68105)) ;
#26049 = EDGE_LOOP('',(#68106,#68107,#68108,#68109)) ;
#26050 = EDGE_LOOP('',(#68110,#68111,#68112,#68113)) ;
#26051 = EDGE_LOOP('',(#68114,#68115,#68116,#68117)) ;
#26052 = EDGE_LOOP('',(#68118,#68119,#68120,#68121)) ;
#26053 = EDGE_LOOP('',(#68122,#68123,#68124,#68125)) ;
#26054 = EDGE_LOOP('',(#68126,#68127,#68128,#68129)) ;
#26055 = EDGE_LOOP('',(#68130,#68131,#68132,#68133)) ;
#26056 = EDGE_LOOP('',(#68134,#68135,#68136,#68137)) ;
#26057 = EDGE_LOOP('',(#68138,#68139,#68140,#68141)) ;
#26058 = EDGE_LOOP('',(#68142,#68143,#68144,#68145)) ;
#26059 = EDGE_LOOP('',(#68146,#68147,#68148,#68149)) ;
#26060 = EDGE_LOOP('',(#68150,#68151,#68152,#68153)) ;
#26061 = EDGE_LOOP('',(#68154,#68155,#68156,#68157)) ;
#26062 = EDGE_LOOP('',(#68158,#68159,#68160,#68161)) ;
#26063 = EDGE_LOOP('',(#68162,#68163,#68164,#68165)) ;
#26064 = EDGE_LOOP('',(#68166,#68167,#68168,#68169)) ;
#26065 = EDGE_LOOP('',(#68170,#68171,#68172,#68173)) ;
#26066 = EDGE_LOOP('',(#68174,#68175,#68176,#68177)) ;
#26067 = EDGE_LOOP('',(#68178,#68179,#68180,#68181,#68182)) ;
#26068 = EDGE_LOOP('',(#68183,#68184,#68185,#68186)) ;
#26069 = EDGE_LOOP('',(#68187,#68188,#68189,#68190)) ;
#26070 = EDGE_LOOP('',(#68191,#68192,#68193,#68194)) ;
#26071 = EDGE_LOOP('',(#68195,#68196,#68197,#68198)) ;
#26072 = EDGE_LOOP('',(#68199,#68200,#68201,#68202)) ;
#26073 = EDGE_LOOP('',(#68203,#68204,#68205,#68206)) ;
#26074 = EDGE_LOOP('',(#68207,#68208,#68209,#68210)) ;
#26075 = EDGE_LOOP('',(#68211,#68212,#68213,#68214)) ;
#26076 = EDGE_LOOP('',(#68215,#68216,#68217,#68218)) ;
#26077 = EDGE_LOOP('',(#68219,#68220,#68221,#68222)) ;
#26078 = EDGE_LOOP('',(#68223,#68224,#68225,#68226)) ;
#26079 = EDGE_LOOP('',(#68227,#68228,#68229,#68230)) ;
#26080 = EDGE_LOOP('',(#68231,#68232,#68233,#68234)) ;
#26081 = EDGE_LOOP('',(#68235,#68236,#68237,#68238)) ;
#26082 = EDGE_LOOP('',(#68239,#68240,#68241,#68242)) ;
#26083 = EDGE_LOOP('',(#68243,#68244,#68245,#68246)) ;
#26084 = EDGE_LOOP('',(#68247,#68248,#68249,#68250)) ;
#26085 = EDGE_LOOP('',(#68251,#68252,#68253,#68254)) ;
#26086 = EDGE_LOOP('',(#68255,#68256,#68257,#68258)) ;
#26087 = EDGE_LOOP('',(#68259,#68260,#68261,#68262)) ;
#26088 = EDGE_LOOP('',(#68263,#68264,#68265,#68266)) ;
#26089 = EDGE_LOOP('',(#68267,#68268,#68269,#68270)) ;
#26090 = EDGE_LOOP('',(#68271,#68272,#68273,#68274)) ;
#26091 = EDGE_LOOP('',(#68275,#68276,#68277,#68278,#68279)) ;
#26092 = EDGE_LOOP('',(#68280,#68281,#68282,#68283)) ;
#26093 = EDGE_LOOP('',(#68284,#68285,#68286,#68287)) ;
#26094 = EDGE_LOOP('',(#68288,#68289,#68290,#68291)) ;
#26095 = EDGE_LOOP('',(#68292,#68293,#68294,#68295)) ;
#26096 = EDGE_LOOP('',(#68296,#68297,#68298,#68299)) ;
#26097 = EDGE_LOOP('',(#68300,#68301,#68302,#68303)) ;
#26098 = EDGE_LOOP('',(#68304,#68305,#68306,#68307)) ;
#26099 = EDGE_LOOP('',(#68308,#68309,#68310,#68311)) ;
#26100 = EDGE_LOOP('',(#68312,#68313,#68314,#68315)) ;
#26101 = EDGE_LOOP('',(#68316,#68317,#68318,#68319)) ;
#26102 = EDGE_LOOP('',(#68320,#68321,#68322,#68323)) ;
#26103 = EDGE_LOOP('',(#68324,#68325,#68326,#68327)) ;
#26104 = EDGE_LOOP('',(#68328,#68329,#68330,#68331)) ;
#26105 = EDGE_LOOP('',(#68332,#68333,#68334,#68335)) ;
#26106 = EDGE_LOOP('',(#68336,#68337,#68338,#68339)) ;
#26107 = EDGE_LOOP('',(#68340,#68341,#68342,#68343)) ;
#26108 = EDGE_LOOP('',(#68344,#68345,#68346,#68347)) ;
#26109 = EDGE_LOOP('',(#68348,#68349,#68350,#68351)) ;
#26110 = EDGE_LOOP('',(#68352,#68353,#68354,#68355)) ;
#26111 = EDGE_LOOP('',(#68356,#68357,#68358,#68359)) ;
#26112 = EDGE_LOOP('',(#68360,#68361,#68362,#68363)) ;
#26113 = EDGE_LOOP('',(#68364,#68365,#68366,#68367)) ;
#26114 = EDGE_LOOP('',(#68368,#68369,#68370,#68371)) ;
#26115 = EDGE_LOOP('',(#68372,#68373,#68374,#68375,#68376)) ;
#26116 = EDGE_LOOP('',(#68377,#68378,#68379,#68380)) ;
#26117 = EDGE_LOOP('',(#68381,#68382,#68383,#68384)) ;
#26118 = EDGE_LOOP('',(#68385,#68386,#68387,#68388)) ;
#26119 = EDGE_LOOP('',(#68389,#68390,#68391,#68392)) ;
#26120 = EDGE_LOOP('',(#68393,#68394,#68395,#68396)) ;
#26121 = EDGE_LOOP('',(#68397,#68398,#68399,#68400)) ;
#26122 = EDGE_LOOP('',(#68401,#68402,#68403,#68404)) ;
#26123 = EDGE_LOOP('',(#68405,#68406,#68407,#68408)) ;
#26124 = EDGE_LOOP('',(#68409,#68410,#68411,#68412)) ;
#26125 = EDGE_LOOP('',(#68413,#68414,#68415,#68416)) ;
#26126 = EDGE_LOOP('',(#68417,#68418,#68419,#68420)) ;
#26127 = EDGE_LOOP('',(#68421,#68422,#68423,#68424)) ;
#26128 = EDGE_LOOP('',(#68425,#68426,#68427,#68428)) ;
#26129 = EDGE_LOOP('',(#68429,#68430,#68431,#68432)) ;
#26130 = EDGE_LOOP('',(#68433,#68434,#68435,#68436)) ;
#26131 = EDGE_LOOP('',(#68437,#68438,#68439,#68440)) ;
#26132 = EDGE_LOOP('',(#68441,#68442,#68443,#68444)) ;
#26133 = EDGE_LOOP('',(#68445,#68446,#68447,#68448)) ;
#26134 = EDGE_LOOP('',(#68449,#68450,#68451,#68452)) ;
#26135 = EDGE_LOOP('',(#68453,#68454,#68455,#68456)) ;
#26136 = EDGE_LOOP('',(#68457,#68458,#68459,#68460)) ;
#26137 = EDGE_LOOP('',(#68461,#68462,#68463,#68464)) ;
#26138 = EDGE_LOOP('',(#68465,#68466,#68467,#68468)) ;
#26139 = EDGE_LOOP('',(#68469,#68470,#68471,#68472,#68473)) ;
#26140 = EDGE_LOOP('',(#68474,#68475,#68476,#68477)) ;
#26141 = EDGE_LOOP('',(#68478,#68479,#68480,#68481)) ;
#26142 = EDGE_LOOP('',(#68482,#68483,#68484,#68485)) ;
#26143 = EDGE_LOOP('',(#68486,#68487,#68488,#68489)) ;
#26144 = EDGE_LOOP('',(#68490,#68491,#68492,#68493)) ;
#26145 = EDGE_LOOP('',(#68494,#68495,#68496,#68497)) ;
#26146 = EDGE_LOOP('',(#68498,#68499,#68500,#68501)) ;
#26147 = EDGE_LOOP('',(#68502,#68503,#68504,#68505)) ;
#26148 = EDGE_LOOP('',(#68506,#68507,#68508,#68509)) ;
#26149 = EDGE_LOOP('',(#68510,#68511,#68512,#68513)) ;
#26150 = EDGE_LOOP('',(#68514,#68515,#68516,#68517)) ;
#26151 = EDGE_LOOP('',(#68518,#68519,#68520,#68521)) ;
#26152 = EDGE_LOOP('',(#68522,#68523,#68524,#68525)) ;
#26153 = EDGE_LOOP('',(#68526,#68527,#68528,#68529)) ;
#26154 = EDGE_LOOP('',(#68530,#68531,#68532,#68533)) ;
#26155 = EDGE_LOOP('',(#68534,#68535,#68536,#68537)) ;
#26156 = EDGE_LOOP('',(#68538,#68539,#68540,#68541)) ;
#26157 = EDGE_LOOP('',(#68542,#68543,#68544,#68545)) ;
#26158 = EDGE_LOOP('',(#68546,#68547,#68548,#68549)) ;
#26159 = EDGE_LOOP('',(#68550,#68551,#68552,#68553)) ;
#26160 = EDGE_LOOP('',(#68554,#68555,#68556,#68557)) ;
#26161 = EDGE_LOOP('',(#68558,#68559,#68560,#68561)) ;
#26162 = EDGE_LOOP('',(#68562,#68563,#68564,#68565)) ;
#26163 = EDGE_LOOP('',(#68566,#68567,#68568,#68569,#68570)) ;
#26164 = EDGE_LOOP('',(#68571,#68572,#68573,#68574)) ;
#26165 = EDGE_LOOP('',(#68575,#68576,#68577,#68578)) ;
#26166 = EDGE_LOOP('',(#68579,#68580,#68581,#68582)) ;
#26167 = EDGE_LOOP('',(#68583,#68584,#68585,#68586)) ;
#26168 = EDGE_LOOP('',(#68587,#68588,#68589,#68590)) ;
#26169 = EDGE_LOOP('',(#68591,#68592,#68593,#68594)) ;
#26170 = EDGE_LOOP('',(#68595,#68596,#68597,#68598)) ;
#26171 = EDGE_LOOP('',(#68599,#68600,#68601,#68602)) ;
#26172 = EDGE_LOOP('',(#68603,#68604,#68605,#68606)) ;
#26173 = EDGE_LOOP('',(#68607,#68608,#68609,#68610)) ;
#26174 = EDGE_LOOP('',(#68611,#68612,#68613,#68614)) ;
#26175 = EDGE_LOOP('',(#68615,#68616,#68617,#68618)) ;
#26176 = EDGE_LOOP('',(#68619,#68620,#68621,#68622)) ;
#26177 = EDGE_LOOP('',(#68623,#68624,#68625,#68626)) ;
#26178 = EDGE_LOOP('',(#68627,#68628,#68629,#68630)) ;
#26179 = EDGE_LOOP('',(#68631,#68632,#68633,#68634)) ;
#26180 = EDGE_LOOP('',(#68635,#68636,#68637,#68638)) ;
#26181 = EDGE_LOOP('',(#68639,#68640,#68641,#68642)) ;
#26182 = EDGE_LOOP('',(#68643,#68644,#68645,#68646)) ;
#26183 = EDGE_LOOP('',(#68647,#68648,#68649,#68650)) ;
#26184 = EDGE_LOOP('',(#68651,#68652,#68653,#68654)) ;
#26185 = EDGE_LOOP('',(#68655,#68656,#68657,#68658)) ;
#26186 = EDGE_LOOP('',(#68659,#68660,#68661,#68662)) ;
#26187 = EDGE_LOOP('',(#68663,#68664,#68665,#68666)) ;
#26188 = EDGE_LOOP('',(#68667,#68668,#68669,#68670)) ;
#26189 = EDGE_LOOP('',(#68671,#68672,#68673,#68674)) ;
#26190 = EDGE_LOOP('',(#68675,#68676,#68677,#68678)) ;
#26191 = EDGE_LOOP('',(#68679,#68680,#68681,#68682)) ;
#26192 = EDGE_LOOP('',(#68683,#68684,#68685,#68686)) ;
#26193 = EDGE_LOOP('',(#68687,#68688,#68689,#68690)) ;
#26194 = EDGE_LOOP('',(#68691,#68692,#68693,#68694)) ;
#26195 = EDGE_LOOP('',(#68695,#68696,#68697,#68698)) ;
#26196 = EDGE_LOOP('',(#68699,#68700,#68701,#68702)) ;
#26197 = EDGE_LOOP('',(#68703,#68704,#68705,#68706)) ;
#26198 = EDGE_LOOP('',(#68707,#68708,#68709,#68710)) ;
#26199 = EDGE_LOOP('',(#68711,#68712,#68713,#68714)) ;
#26200 = EDGE_LOOP('',(#68715,#68716,#68717,#68718)) ;
#26201 = EDGE_LOOP('',(#68719,#68720,#68721,#68722)) ;
#26202 = EDGE_LOOP('',(#68723,#68724,#68725,#68726)) ;
#26203 = EDGE_LOOP('',(#68727,#68728,#68729,#68730)) ;
#26204 = EDGE_LOOP('',(#68731,#68732,#68733,#68734)) ;
#26205 = EDGE_LOOP('',(#68735,#68736,#68737,#68738)) ;
#26206 = EDGE_LOOP('',(#68739,#68740,#68741,#68742)) ;
#26207 = EDGE_LOOP('',(#68743,#68744,#68745,#68746)) ;
#26208 = EDGE_LOOP('',(#68747,#68748,#68749,#68750)) ;
#26209 = EDGE_LOOP('',(#68751,#68752,#68753,#68754)) ;
#26210 = EDGE_LOOP('',(#68755,#68756,#68757,#68758)) ;
#26211 = EDGE_LOOP('',(#68759,#68760,#68761,#68762)) ;
#26212 = EDGE_LOOP('',(#68763,#68764,#68765,#68766)) ;
#26213 = EDGE_LOOP('',(#68767,#68768,#68769,#68770)) ;
#26214 = EDGE_LOOP('',(#68771,#68772,#68773,#68774)) ;
#26215 = EDGE_LOOP('',(#68775,#68776,#68777,#68778)) ;
#26216 = EDGE_LOOP('',(#68779,#68780,#68781,#68782)) ;
#26217 = EDGE_LOOP('',(#68783,#68784,#68785,#68786)) ;
#26218 = EDGE_LOOP('',(#68787,#68788,#68789,#68790)) ;
#26219 = EDGE_LOOP('',(#68791,#68792,#68793,#68794)) ;
#26220 = EDGE_LOOP('',(#68795,#68796,#68797,#68798)) ;
#26221 = EDGE_LOOP('',(#68799,#68800,#68801,#68802)) ;
#26222 = EDGE_LOOP('',(#68803,#68804,#68805,#68806)) ;
#26223 = EDGE_LOOP('',(#68807,#68808,#68809,#68810)) ;
#26224 = EDGE_LOOP('',(#68811,#68812,#68813,#68814)) ;
#26225 = EDGE_LOOP('',(#68815,#68816,#68817,#68818)) ;
#26226 = EDGE_LOOP('',(#68819,#68820,#68821,#68822)) ;
#26227 = EDGE_LOOP('',(#68823,#68824,#68825,#68826)) ;
#26228 = EDGE_LOOP('',(#68827,#68828,#68829,#68830)) ;
#26229 = EDGE_LOOP('',(#68831,#68832,#68833,#68834)) ;
#26230 = EDGE_LOOP('',(#68835,#68836,#68837,#68838)) ;
#26231 = EDGE_LOOP('',(#68839,#68840,#68841,#68842)) ;
#26232 = EDGE_LOOP('',(#68843,#68844,#68845,#68846)) ;
#26233 = EDGE_LOOP('',(#68847,#68848,#68849,#68850)) ;
#26234 = EDGE_LOOP('',(#68851,#68852,#68853,#68854)) ;
#26235 = EDGE_LOOP('',(#68855,#68856,#68857,#68858)) ;
#26236 = EDGE_LOOP('',(#68859,#68860,#68861,#68862)) ;
#26237 = EDGE_LOOP('',(#68863,#68864,#68865,#68866,#68867,#68868,#68869,#68870,
#68871,#68872,#68873,#68874,#68875,#68876,#68877,#68878,#68879,#68880,#68881,
#68882)) ;
#26238 = EDGE_LOOP('',(#68883,#68884,#68885,#68886,#68887,#68888,#68889,#68890,
#68891,#68892,#68893,#68894,#68895,#68896,#68897,#68898,#68899,#68900,#68901,
#68902)) ;
#26239 = EDGE_LOOP('',(#68903,#68904,#68905,#68906,#68907,#68908,#68909,#68910,
#68911,#68912,#68913,#68914,#68915,#68916,#68917,#68918,#68919,#68920,#68921,
#68922)) ;
#26240 = EDGE_LOOP('',(#68923,#68924,#68925,#68926,#68927,#68928,#68929,#68930,
#68931,#68932,#68933,#68934,#68935,#68936,#68937,#68938,#68939,#68940,#68941,
#68942)) ;
#26241 = EDGE_LOOP('',(#68943,#68944,#68945,#68946,#68947,#68948,#68949,#68950,
#68951,#68952,#68953,#68954,#68955,#68956,#68957,#68958,#68959,#68960,#68961,
#68962)) ;
#26242 = EDGE_LOOP('',(#68963,#68964,#68965,#68966,#68967,#68968,#68969,#68970,
#68971,#68972,#68973,#68974,#68975,#68976,#68977,#68978,#68979,#68980,#68981,
#68982)) ;
#26243 = EDGE_LOOP('',(#68983,#68984,#68985,#68986,#68987,#68988,#68989,#68990,
#68991,#68992,#68993,#68994,#68995,#68996,#68997,#68998,#68999,#69000,#69001,
#69002)) ;
#26244 = EDGE_LOOP('',(#69003,#69004,#69005,#69006,#69007,#69008,#69009,#69010,
#69011,#69012,#69013,#69014,#69015,#69016,#69017,#69018,#69019,#69020,#69021,
#69022)) ;
#26245 = EDGE_LOOP('',(#69023,#69024,#69025,#69026,#69027,#69028,#69029,#69030,
#69031,#69032,#69033,#69034,#69035,#69036,#69037,#69038,#69039,#69040,#69041,
#69042)) ;
#26246 = EDGE_LOOP('',(#69043,#69044,#69045,#69046)) ;
#26247 = EDGE_LOOP('',(#69047,#69048,#69049,#69050)) ;
#26248 = EDGE_LOOP('',(#69051,#69052,#69053,#69054)) ;
#26249 = EDGE_LOOP('',(#69055,#69056,#69057,#69058)) ;
#26250 = EDGE_LOOP('',(#69059,#69060,#69061,#69062)) ;
#26251 = EDGE_LOOP('',(#69063,#69064,#69065,#69066)) ;
#26252 = EDGE_LOOP('',(#69067,#69068,#69069,#69070)) ;
#26253 = EDGE_LOOP('',(#69071,#69072,#69073,#69074)) ;
#26254 = EDGE_LOOP('',(#69075,#69076,#69077,#69078)) ;
#26255 = EDGE_LOOP('',(#69079,#69080,#69081,#69082)) ;
#26256 = EDGE_LOOP('',(#69083,#69084,#69085,#69086)) ;
#26257 = EDGE_LOOP('',(#69087,#69088,#69089,#69090)) ;
#26258 = EDGE_LOOP('',(#69091,#69092,#69093,#69094)) ;
#26259 = EDGE_LOOP('',(#69095,#69096,#69097,#69098)) ;
#26260 = EDGE_LOOP('',(#69099,#69100,#69101,#69102)) ;
#26261 = EDGE_LOOP('',(#69103,#69104,#69105,#69106)) ;
#26262 = EDGE_LOOP('',(#69107,#69108,#69109,#69110)) ;
#26263 = EDGE_LOOP('',(#69111,#69112,#69113,#69114)) ;
#26264 = EDGE_LOOP('',(#69115,#69116,#69117,#69118)) ;
#26265 = EDGE_LOOP('',(#69119,#69120,#69121,#69122)) ;
#26266 = EDGE_LOOP('',(#69123,#69124,#69125,#69126)) ;
#26267 = EDGE_LOOP('',(#69127,#69128,#69129,#69130)) ;
#26268 = EDGE_LOOP('',(#69131,#69132,#69133,#69134)) ;
#26269 = EDGE_LOOP('',(#69135,#69136,#69137,#69138)) ;
#26270 = EDGE_LOOP('',(#69139,#69140,#69141,#69142)) ;
#26271 = EDGE_LOOP('',(#69143,#69144,#69145,#69146,#69147,#69148,#69149,#69150,
#69151,#69152,#69153,#69154,#69155,#69156,#69157,#69158,#69159,#69160,#69161,
#69162)) ;
#26272 = EDGE_LOOP('',(#69163,#69164,#69165,#69166)) ;
#26273 = EDGE_LOOP('',(#69167,#69168,#69169,#69170)) ;
#26274 = EDGE_LOOP('',(#69171,#69172,#69173,#69174,#69175,#69176,#69177,#69178,
#69179,#69180,#69181,#69182,#69183,#69184,#69185,#69186,#69187,#69188,#69189,
#69190,#69191,#69192,#69193,#69194,#69195,#69196,#69197,#69198)) ;
#26275 = EDGE_LOOP('',(#69199,#69200,#69201,#69202,#69203,#69204,#69205,#69206)) ;
#26276 = EDGE_LOOP('',(#69207)) ;
#26277 = EDGE_LOOP('',(#69208,#69209,#69210,#69211,#69212,#69213,#69214,#69215)) ;
#26278 = EDGE_LOOP('',(#69216)) ;
#26279 = EDGE_LOOP('',(#69217,#69218,#69219,#69220,#69221,#69222,#69223,#69224)) ;
#26280 = EDGE_LOOP('',(#69225)) ;
#26281 = EDGE_LOOP('',(#69226,#69227,#69228,#69229,#69230,#69231,#69232,#69233)) ;
#26282 = EDGE_LOOP('',(#69234)) ;
#26283 = EDGE_LOOP('',(#69235,#69236,#69237,#69238,#69239,#69240,#69241,#69242)) ;
#26284 = EDGE_LOOP('',(#69243)) ;
#26285 = EDGE_LOOP('',(#69244)) ;
#26286 = EDGE_LOOP('',(#69245,#69246,#69247,#69248,#69249,#69250,#69251,#69252)) ;
#26287 = EDGE_LOOP('',(#69253)) ;
#26288 = EDGE_LOOP('',(#69254,#69255,#69256,#69257,#69258,#69259,#69260,#69261)) ;
#26289 = EDGE_LOOP('',(#69262)) ;
#26290 = EDGE_LOOP('',(#69263,#69264,#69265,#69266,#69267,#69268,#69269,#69270)) ;
#26291 = EDGE_LOOP('',(#69271)) ;
#26292 = EDGE_LOOP('',(#69272,#69273,#69274,#69275,#69276,#69277,#69278,#69279)) ;
#26293 = EDGE_LOOP('',(#69280)) ;
#26294 = EDGE_LOOP('',(#69281,#69282,#69283,#69284,#69285,#69286,#69287,#69288)) ;
#26295 = EDGE_LOOP('',(#69289,#69290,#69291,#69292)) ;
#26296 = EDGE_LOOP('',(#69293,#69294,#69295,#69296,#69297,#69298,#69299,#69300)) ;
#26297 = EDGE_LOOP('',(#69301,#69302,#69303,#69304)) ;
#26298 = EDGE_LOOP('',(#69305,#69306,#69307,#69308,#69309,#69310,#69311,#69312)) ;
#26299 = EDGE_LOOP('',(#69313,#69314,#69315,#69316)) ;
#26300 = EDGE_LOOP('',(#69317,#69318,#69319,#69320,#69321,#69322,#69323,#69324)) ;
#26301 = EDGE_LOOP('',(#69325,#69326,#69327,#69328)) ;
#26302 = EDGE_LOOP('',(#69329,#69330,#69331,#69332,#69333,#69334,#69335,#69336)) ;
#26303 = EDGE_LOOP('',(#69337,#69338,#69339,#69340)) ;
#26304 = EDGE_LOOP('',(#69341,#69342,#69343,#69344,#69345,#69346,#69347,#69348)) ;
#26305 = EDGE_LOOP('',(#69349,#69350,#69351,#69352)) ;
#26306 = EDGE_LOOP('',(#69353,#69354,#69355,#69356,#69357,#69358,#69359,#69360)) ;
#26307 = EDGE_LOOP('',(#69361,#69362,#69363,#69364)) ;
#26308 = EDGE_LOOP('',(#69365,#69366,#69367,#69368,#69369,#69370,#69371,#69372)) ;
#26309 = EDGE_LOOP('',(#69373,#69374,#69375,#69376)) ;
#26310 = EDGE_LOOP('',(#69377,#69378,#69379,#69380,#69381,#69382,#69383,#69384)) ;
#26311 = EDGE_LOOP('',(#69385,#69386,#69387,#69388)) ;
#26312 = EDGE_LOOP('',(#69389,#69390,#69391,#69392,#69393,#69394,#69395,#69396)) ;
#26313 = EDGE_LOOP('',(#69397,#69398)) ;
#26314 = EDGE_LOOP('',(#69399,#69400)) ;
#26315 = EDGE_LOOP('',(#69401,#69402)) ;
#26316 = EDGE_LOOP('',(#69403,#69404)) ;
#26317 = EDGE_LOOP('',(#69405,#69406)) ;
#26318 = EDGE_LOOP('',(#69407,#69408)) ;
#26319 = EDGE_LOOP('',(#69409,#69410)) ;
#26320 = EDGE_LOOP('',(#69411,#69412)) ;
#26321 = EDGE_LOOP('',(#69413,#69414)) ;
#26322 = EDGE_LOOP('',(#69415,#69416,#69417,#69418,#69419,#69420,#69421,#69422,
#69423,#69424,#69425,#69426,#69427,#69428,#69429,#69430,#69431,#69432,#69433,
#69434,#69435,#69436,#69437,#69438,#69439,#69440,#69441,#69442,#69443,#69444,
#69445,#69446,#69447,#69448,#69449,#69450,#69451,#69452,#69453,#69454,#69455,
#69456,#69457,#69458,#69459,#69460,#69461,#69462,#69463,#69464,#69465,#69466,
#69467,#69468,#69469,#69470,#69471,#69472,#69473,#69474,#69475,#69476,#69477,
#69478)) ;
#26323 = EDGE_LOOP('',(#69479,#69480,#69481,#69482,#69483,#69484,#69485,#69486)) ;
#26324 = EDGE_LOOP('',(#69487,#69488,#69489,#69490,#69491,#69492,#69493,#69494)) ;
#26325 = EDGE_LOOP('',(#69495,#69496,#69497,#69498,#69499,#69500,#69501,#69502)) ;
#26326 = EDGE_LOOP('',(#69503,#69504,#69505,#69506,#69507,#69508,#69509,#69510)) ;
#26327 = EDGE_LOOP('',(#69511,#69512,#69513,#69514,#69515,#69516,#69517,#69518)) ;
#26328 = EDGE_LOOP('',(#69519,#69520,#69521,#69522,#69523,#69524,#69525,#69526)) ;
#26329 = EDGE_LOOP('',(#69527,#69528,#69529,#69530,#69531,#69532,#69533,#69534)) ;
#26330 = EDGE_LOOP('',(#69535,#69536,#69537,#69538,#69539,#69540,#69541,#69542)) ;
#26331 = EDGE_LOOP('',(#69543,#69544,#69545,#69546,#69547,#69548,#69549,#69550)) ;
#26332 = EDGE_LOOP('',(#69551,#69552,#69553,#69554)) ;
#26333 = EDGE_LOOP('',(#69555,#69556,#69557,#69558,#69559,#69560,#69561,#69562,
#69563,#69564,#69565,#69566,#69567,#69568,#69569,#69570,#69571,#69572,#69573,
#69574,#69575,#69576,#69577,#69578,#69579,#69580,#69581,#69582,#69583,#69584,
#69585,#69586,#69587,#69588,#69589,#69590,#69591,#69592,#69593,#69594,#69595,
#69596,#69597,#69598,#69599,#69600,#69601,#69602,#69603,#69604,#69605,#69606,
#69607,#69608,#69609,#69610,#69611,#69612,#69613,#69614,#69615,#69616,#69617,
#69618)) ;
#26334 = EDGE_LOOP('',(#69619,#69620,#69621,#69622)) ;
#26335 = EDGE_LOOP('',(#69623,#69624,#69625,#69626,#69627,#69628)) ;
#26336 = EDGE_LOOP('',(#69629,#69630,#69631,#69632)) ;
#26337 = EDGE_LOOP('',(#69633,#69634,#69635,#69636,#69637,#69638,#69639,#69640)) ;
#26338 = EDGE_LOOP('',(#69641,#69642,#69643,#69644)) ;
#26339 = EDGE_LOOP('',(#69645,#69646,#69647,#69648)) ;
#26340 = EDGE_LOOP('',(#69649,#69650,#69651,#69652)) ;
#26341 = EDGE_LOOP('',(#69653,#69654,#69655,#69656)) ;
#26342 = EDGE_LOOP('',(#69657,#69658,#69659,#69660)) ;
#26343 = EDGE_LOOP('',(#69661,#69662,#69663,#69664)) ;
#26344 = EDGE_LOOP('',(#69665,#69666,#69667,#69668)) ;
#26345 = EDGE_LOOP('',(#69669,#69670,#69671,#69672)) ;
#26346 = EDGE_LOOP('',(#69673,#69674,#69675,#69676,#69677,#69678,#69679,#69680)) ;
#26347 = EDGE_LOOP('',(#69681,#69682,#69683,#69684)) ;
#26348 = EDGE_LOOP('',(#69685,#69686,#69687,#69688,#69689,#69690,#69691,#69692)) ;
#26349 = EDGE_LOOP('',(#69693,#69694,#69695,#69696)) ;
#26350 = EDGE_LOOP('',(#69697,#69698)) ;
#26351 = EDGE_LOOP('',(#69699,#69700,#69701,#69702,#69703,#69704,#69705,#69706)) ;
#26352 = EDGE_LOOP('',(#69707,#69708,#69709,#69710)) ;
#26353 = EDGE_LOOP('',(#69711,#69712,#69713,#69714)) ;
#26354 = EDGE_LOOP('',(#69715,#69716,#69717,#69718)) ;
#26355 = EDGE_LOOP('',(#69719,#69720,#69721,#69722)) ;
#26356 = EDGE_LOOP('',(#69723,#69724,#69725,#69726)) ;
#26357 = EDGE_LOOP('',(#69727,#69728,#69729,#69730)) ;
#26358 = EDGE_LOOP('',(#69731,#69732,#69733,#69734)) ;
#26359 = EDGE_LOOP('',(#69735,#69736,#69737,#69738)) ;
#26360 = EDGE_LOOP('',(#69739,#69740,#69741,#69742)) ;
#26361 = EDGE_LOOP('',(#69743,#69744,#69745,#69746)) ;
#26362 = EDGE_LOOP('',(#69747,#69748,#69749,#69750)) ;
#26363 = EDGE_LOOP('',(#69751,#69752,#69753,#69754)) ;
#26364 = EDGE_LOOP('',(#69755,#69756,#69757,#69758,#69759,#69760,#69761,#69762)) ;
#26365 = EDGE_LOOP('',(#69763,#69764,#69765,#69766,#69767,#69768,#69769,#69770)) ;
#26366 = EDGE_LOOP('',(#69771,#69772,#69773,#69774,#69775,#69776,#69777,#69778,
#69779,#69780,#69781,#69782,#69783,#69784,#69785)) ;
#26367 = EDGE_LOOP('',(#69786,#69787,#69788,#69789,#69790,#69791,#69792,#69793,
#69794,#69795,#69796,#69797,#69798,#69799,#69800)) ;
#26368 = EDGE_LOOP('',(#69801,#69802,#69803,#69804)) ;
#26369 = EDGE_LOOP('',(#69805,#69806,#69807,#69808)) ;
#26370 = EDGE_LOOP('',(#69809,#69810,#69811,#69812,#69813,#69814,#69815,#69816)) ;
#26371 = EDGE_LOOP('',(#69817,#69818,#69819,#69820)) ;
#26372 = EDGE_LOOP('',(#69821,#69822,#69823,#69824)) ;
#26373 = EDGE_LOOP('',(#69825,#69826,#69827,#69828,#69829,#69830)) ;
#26374 = EDGE_LOOP('',(#69831,#69832,#69833,#69834,#69835,#69836)) ;
#26375 = EDGE_LOOP('',(#69837,#69838,#69839,#69840)) ;
#26376 = EDGE_LOOP('',(#69841,#69842,#69843,#69844)) ;
#26377 = EDGE_LOOP('',(#69845,#69846,#69847,#69848)) ;
#26378 = EDGE_LOOP('',(#69849,#69850,#69851,#69852)) ;
#26379 = EDGE_LOOP('',(#69853,#69854,#69855,#69856)) ;
#26380 = EDGE_LOOP('',(#69857,#69858,#69859,#69860,#69861,#69862,#69863,#69864)) ;
#26381 = EDGE_LOOP('',(#69865,#69866,#69867,#69868)) ;
#26382 = EDGE_LOOP('',(#69869,#69870,#69871,#69872)) ;
#26383 = EDGE_LOOP('',(#69873,#69874,#69875,#69876)) ;
#26384 = EDGE_LOOP('',(#69877,#69878,#69879,#69880)) ;
#26385 = EDGE_LOOP('',(#69881,#69882,#69883,#69884)) ;
#26386 = EDGE_LOOP('',(#69885,#69886,#69887,#69888,#69889,#69890,#69891,#69892,
#69893,#69894,#69895,#69896,#69897,#69898,#69899,#69900,#69901,#69902,#69903)) ;
#26387 = EDGE_LOOP('',(#69904,#69905,#69906,#69907)) ;
#26388 = EDGE_LOOP('',(#69908,#69909,#69910,#69911,#69912,#69913,#69914,#69915,
#69916,#69917)) ;
#26389 = EDGE_LOOP('',(#69918,#69919,#69920,#69921)) ;
#26390 = EDGE_LOOP('',(#69922,#69923,#69924,#69925,#69926,#69927,#69928,#69929,
#69930,#69931)) ;
#26391 = EDGE_LOOP('',(#69932,#69933,#69934,#69935)) ;
#26392 = EDGE_LOOP('',(#69936,#69937,#69938,#69939)) ;
#26393 = EDGE_LOOP('',(#69940,#69941,#69942,#69943)) ;
#26394 = EDGE_LOOP('',(#69944,#69945,#69946,#69947)) ;
#26395 = EDGE_LOOP('',(#69948,#69949,#69950,#69951,#69952,#69953)) ;
#26396 = EDGE_LOOP('',(#69954)) ;
#26397 = EDGE_LOOP('',(#69955)) ;
#26398 = EDGE_LOOP('',(#69956,#69957,#69958,#69959)) ;
#26399 = EDGE_LOOP('',(#69960,#69961,#69962,#69963)) ;
#26400 = EDGE_LOOP('',(#69964,#69965,#69966,#69967)) ;
#26401 = EDGE_LOOP('',(#69968,#69969,#69970,#69971)) ;
#26402 = EDGE_LOOP('',(#69972,#69973,#69974,#69975)) ;
#26403 = EDGE_LOOP('',(#69976,#69977,#69978,#69979,#69980,#69981,#69982,#69983)) ;
#26404 = EDGE_LOOP('',(#69984,#69985,#69986,#69987)) ;
#26405 = EDGE_LOOP('',(#69988,#69989,#69990,#69991)) ;
#26406 = EDGE_LOOP('',(#69992,#69993,#69994,#69995)) ;
#26407 = EDGE_LOOP('',(#69996,#69997,#69998,#69999)) ;
#26408 = EDGE_LOOP('',(#70000,#70001,#70002,#70003)) ;
#26409 = EDGE_LOOP('',(#70004,#70005,#70006)) ;
#26410 = EDGE_LOOP('',(#70007,#70008,#70009,#70010)) ;
#26411 = EDGE_LOOP('',(#70011,#70012,#70013,#70014)) ;
#26412 = EDGE_LOOP('',(#70015,#70016,#70017,#70018)) ;
#26413 = EDGE_LOOP('',(#70019,#70020,#70021,#70022)) ;
#26414 = EDGE_LOOP('',(#70023,#70024,#70025,#70026)) ;
#26415 = EDGE_LOOP('',(#70027,#70028,#70029,#70030)) ;
#26416 = EDGE_LOOP('',(#70031,#70032,#70033,#70034)) ;
#26417 = EDGE_LOOP('',(#70035,#70036,#70037,#70038)) ;
#26418 = EDGE_LOOP('',(#70039,#70040,#70041,#70042)) ;
#26419 = EDGE_LOOP('',(#70043,#70044,#70045,#70046)) ;
#26420 = EDGE_LOOP('',(#70047,#70048,#70049,#70050)) ;
#26421 = EDGE_LOOP('',(#70051,#70052,#70053,#70054)) ;
#26422 = EDGE_LOOP('',(#70055,#70056,#70057,#70058)) ;
#26423 = EDGE_LOOP('',(#70059,#70060,#70061,#70062)) ;
#26424 = EDGE_LOOP('',(#70063,#70064,#70065,#70066)) ;
#26425 = EDGE_LOOP('',(#70067,#70068,#70069,#70070)) ;
#26426 = EDGE_LOOP('',(#70071,#70072,#70073,#70074)) ;
#26427 = EDGE_LOOP('',(#70075,#70076,#70077,#70078)) ;
#26428 = EDGE_LOOP('',(#70079,#70080,#70081,#70082)) ;
#26429 = EDGE_LOOP('',(#70083,#70084,#70085)) ;
#26430 = EDGE_LOOP('',(#70086,#70087,#70088,#70089)) ;
#26431 = EDGE_LOOP('',(#70090,#70091,#70092,#70093)) ;
#26432 = EDGE_LOOP('',(#70094,#70095,#70096,#70097)) ;
#26433 = EDGE_LOOP('',(#70098,#70099,#70100,#70101)) ;
#26434 = EDGE_LOOP('',(#70102,#70103,#70104,#70105)) ;
#26435 = EDGE_LOOP('',(#70106,#70107,#70108,#70109)) ;
#26436 = EDGE_LOOP('',(#70110,#70111,#70112)) ;
#26437 = EDGE_LOOP('',(#70113,#70114,#70115)) ;
#26438 = EDGE_LOOP('',(#70116,#70117,#70118,#70119)) ;
#26439 = EDGE_LOOP('',(#70120,#70121,#70122,#70123)) ;
#26440 = EDGE_LOOP('',(#70124,#70125,#70126,#70127,#70128,#70129)) ;
#26441 = EDGE_LOOP('',(#70130,#70131,#70132,#70133)) ;
#26442 = EDGE_LOOP('',(#70134,#70135,#70136,#70137)) ;
#26443 = EDGE_LOOP('',(#70138,#70139,#70140,#70141)) ;
#26444 = EDGE_LOOP('',(#70142,#70143,#70144,#70145)) ;
#26445 = EDGE_LOOP('',(#70146,#70147,#70148,#70149)) ;
#26446 = EDGE_LOOP('',(#70150,#70151,#70152,#70153)) ;
#26447 = EDGE_LOOP('',(#70154,#70155,#70156)) ;
#26448 = EDGE_LOOP('',(#70157,#70158,#70159,#70160)) ;
#26449 = EDGE_LOOP('',(#70161,#70162,#70163,#70164)) ;
#26450 = EDGE_LOOP('',(#70165,#70166,#70167,#70168)) ;
#26451 = EDGE_LOOP('',(#70169,#70170,#70171,#70172)) ;
#26452 = EDGE_LOOP('',(#70173,#70174,#70175,#70176)) ;
#26453 = EDGE_LOOP('',(#70177,#70178,#70179,#70180,#70181,#70182)) ;
#26454 = EDGE_LOOP('',(#70183,#70184,#70185)) ;
#26455 = EDGE_LOOP('',(#70186,#70187,#70188,#70189)) ;
#26456 = EDGE_LOOP('',(#70190,#70191,#70192,#70193)) ;
#26457 = EDGE_LOOP('',(#70194,#70195,#70196,#70197)) ;
#26458 = EDGE_LOOP('',(#70198,#70199,#70200,#70201)) ;
#26459 = EDGE_LOOP('',(#70202,#70203,#70204,#70205)) ;
#26460 = EDGE_LOOP('',(#70206,#70207,#70208)) ;
#26461 = EDGE_LOOP('',(#70209,#70210,#70211,#70212)) ;
#26462 = EDGE_LOOP('',(#70213,#70214,#70215)) ;
#26463 = EDGE_LOOP('',(#70216,#70217,#70218,#70219)) ;
#26464 = EDGE_LOOP('',(#70220,#70221,#70222,#70223)) ;
#26465 = EDGE_LOOP('',(#70224,#70225,#70226,#70227)) ;
#26466 = EDGE_LOOP('',(#70228,#70229,#70230,#70231)) ;
#26467 = EDGE_LOOP('',(#70232,#70233,#70234,#70235)) ;
#26468 = EDGE_LOOP('',(#70236,#70237,#70238,#70239)) ;
#26469 = EDGE_LOOP('',(#70240,#70241,#70242)) ;
#26470 = EDGE_LOOP('',(#70243,#70244,#70245,#70246)) ;
#26471 = EDGE_LOOP('',(#70247,#70248,#70249,#70250)) ;
#26472 = EDGE_LOOP('',(#70251,#70252,#70253,#70254)) ;
#26473 = EDGE_LOOP('',(#70255,#70256,#70257,#70258)) ;
#26474 = EDGE_LOOP('',(#70259,#70260,#70261,#70262)) ;
#26475 = EDGE_LOOP('',(#70263,#70264,#70265,#70266)) ;
#26476 = EDGE_LOOP('',(#70267,#70268,#70269,#70270)) ;
#26477 = EDGE_LOOP('',(#70271,#70272,#70273,#70274)) ;
#26478 = EDGE_LOOP('',(#70275,#70276,#70277)) ;
#26479 = EDGE_LOOP('',(#70278,#70279,#70280)) ;
#26480 = EDGE_LOOP('',(#70281,#70282,#70283,#70284)) ;
#26481 = EDGE_LOOP('',(#70285,#70286,#70287,#70288)) ;
#26482 = EDGE_LOOP('',(#70289,#70290,#70291,#70292)) ;
#26483 = EDGE_LOOP('',(#70293,#70294,#70295,#70296)) ;
#26484 = EDGE_LOOP('',(#70297,#70298,#70299)) ;
#26485 = EDGE_LOOP('',(#70300,#70301,#70302,#70303)) ;
#26486 = EDGE_LOOP('',(#70304,#70305,#70306,#70307)) ;
#26487 = EDGE_LOOP('',(#70308,#70309,#70310,#70311)) ;
#26488 = EDGE_LOOP('',(#70312,#70313,#70314,#70315)) ;
#26489 = EDGE_LOOP('',(#70316,#70317,#70318,#70319)) ;
#26490 = EDGE_LOOP('',(#70320,#70321,#70322)) ;
#26491 = EDGE_LOOP('',(#70323,#70324,#70325,#70326)) ;
#26492 = EDGE_LOOP('',(#70327,#70328,#70329,#70330)) ;
#26493 = EDGE_LOOP('',(#70331,#70332,#70333,#70334)) ;
#26494 = EDGE_LOOP('',(#70335,#70336,#70337,#70338)) ;
#26495 = EDGE_LOOP('',(#70339,#70340,#70341,#70342)) ;
#26496 = EDGE_LOOP('',(#70343,#70344,#70345,#70346)) ;
#26497 = EDGE_LOOP('',(#70347,#70348,#70349,#70350)) ;
#26498 = EDGE_LOOP('',(#70351,#70352,#70353,#70354)) ;
#26499 = EDGE_LOOP('',(#70355,#70356,#70357,#70358)) ;
#26500 = EDGE_LOOP('',(#70359,#70360,#70361,#70362)) ;
#26501 = EDGE_LOOP('',(#70363,#70364,#70365,#70366)) ;
#26502 = EDGE_LOOP('',(#70367,#70368,#70369,#70370)) ;
#26503 = EDGE_LOOP('',(#70371,#70372,#70373,#70374)) ;
#26504 = EDGE_LOOP('',(#70375,#70376,#70377,#70378)) ;
#26505 = EDGE_LOOP('',(#70379,#70380,#70381,#70382)) ;
#26506 = EDGE_LOOP('',(#70383,#70384,#70385,#70386)) ;
#26507 = EDGE_LOOP('',(#70387,#70388,#70389,#70390)) ;
#26508 = EDGE_LOOP('',(#70391,#70392,#70393,#70394)) ;
#26509 = EDGE_LOOP('',(#70395,#70396,#70397,#70398)) ;
#26510 = EDGE_LOOP('',(#70399,#70400,#70401,#70402)) ;
#26511 = EDGE_LOOP('',(#70403,#70404,#70405)) ;
#26512 = EDGE_LOOP('',(#70406,#70407,#70408)) ;
#26513 = EDGE_LOOP('',(#70409,#70410,#70411,#70412)) ;
#26514 = EDGE_LOOP('',(#70413,#70414,#70415,#70416)) ;
#26515 = EDGE_LOOP('',(#70417,#70418,#70419,#70420)) ;
#26516 = EDGE_LOOP('',(#70421,#70422,#70423,#70424)) ;
#26517 = EDGE_LOOP('',(#70425,#70426,#70427,#70428)) ;
#26518 = EDGE_LOOP('',(#70429,#70430,#70431)) ;
#26519 = EDGE_LOOP('',(#70432,#70433,#70434)) ;
#26520 = EDGE_LOOP('',(#70435,#70436,#70437,#70438)) ;
#26521 = EDGE_LOOP('',(#70439,#70440,#70441,#70442)) ;
#26522 = EDGE_LOOP('',(#70443,#70444,#70445,#70446)) ;
#26523 = EDGE_LOOP('',(#70447,#70448,#70449,#70450)) ;
#26524 = EDGE_LOOP('',(#70451,#70452,#70453)) ;
#26525 = EDGE_LOOP('',(#70454,#70455,#70456)) ;
#26526 = EDGE_LOOP('',(#70457,#70458,#70459,#70460)) ;
#26527 = EDGE_LOOP('',(#70461,#70462,#70463,#70464)) ;
#26528 = EDGE_LOOP('',(#70465,#70466,#70467,#70468)) ;
#26529 = EDGE_LOOP('',(#70469,#70470,#70471,#70472)) ;
#26530 = EDGE_LOOP('',(#70473,#70474,#70475)) ;
#26531 = EDGE_LOOP('',(#70476,#70477,#70478)) ;
#26532 = EDGE_LOOP('',(#70479,#70480,#70481,#70482)) ;
#26533 = EDGE_LOOP('',(#70483,#70484,#70485,#70486)) ;
#26534 = EDGE_LOOP('',(#70487,#70488,#70489)) ;
#26535 = EDGE_LOOP('',(#70490,#70491,#70492,#70493)) ;
#26536 = EDGE_LOOP('',(#70494,#70495,#70496,#70497)) ;
#26537 = EDGE_LOOP('',(#70498,#70499,#70500,#70501)) ;
#26538 = EDGE_LOOP('',(#70502,#70503,#70504,#70505)) ;
#26539 = EDGE_LOOP('',(#70506,#70507,#70508)) ;
#26540 = EDGE_LOOP('',(#70509,#70510,#70511,#70512)) ;
#26541 = EDGE_LOOP('',(#70513,#70514,#70515,#70516)) ;
#26542 = EDGE_LOOP('',(#70517,#70518,#70519,#70520)) ;
#26543 = EDGE_LOOP('',(#70521,#70522,#70523,#70524)) ;
#26544 = EDGE_LOOP('',(#70525,#70526,#70527,#70528)) ;
#26545 = EDGE_LOOP('',(#70529,#70530,#70531)) ;
#26546 = EDGE_LOOP('',(#70532,#70533,#70534,#70535)) ;
#26547 = EDGE_LOOP('',(#70536,#70537,#70538,#70539)) ;
#26548 = EDGE_LOOP('',(#70540,#70541,#70542,#70543)) ;
#26549 = EDGE_LOOP('',(#70544,#70545,#70546,#70547)) ;
#26550 = EDGE_LOOP('',(#70548,#70549,#70550,#70551)) ;
#26551 = EDGE_LOOP('',(#70552,#70553,#70554,#70555)) ;
#26552 = EDGE_LOOP('',(#70556,#70557,#70558)) ;
#26553 = EDGE_LOOP('',(#70559,#70560,#70561,#70562)) ;
#26554 = EDGE_LOOP('',(#70563,#70564,#70565,#70566)) ;
#26555 = EDGE_LOOP('',(#70567,#70568,#70569,#70570)) ;
#26556 = EDGE_LOOP('',(#70571,#70572,#70573,#70574)) ;
#26557 = EDGE_LOOP('',(#70575,#70576,#70577,#70578)) ;
#26558 = EDGE_LOOP('',(#70579,#70580,#70581,#70582)) ;
#26559 = EDGE_LOOP('',(#70583,#70584,#70585,#70586)) ;
#26560 = EDGE_LOOP('',(#70587,#70588,#70589,#70590)) ;
#26561 = EDGE_LOOP('',(#70591,#70592,#70593,#70594)) ;
#26562 = EDGE_LOOP('',(#70595,#70596,#70597,#70598)) ;
#26563 = EDGE_LOOP('',(#70599,#70600,#70601,#70602)) ;
#26564 = EDGE_LOOP('',(#70603,#70604,#70605,#70606)) ;
#26565 = EDGE_LOOP('',(#70607,#70608,#70609)) ;
#26566 = EDGE_LOOP('',(#70610,#70611,#70612)) ;
#26567 = EDGE_LOOP('',(#70613,#70614,#70615,#70616)) ;
#26568 = EDGE_LOOP('',(#70617,#70618,#70619,#70620)) ;
#26569 = EDGE_LOOP('',(#70621,#70622,#70623,#70624)) ;
#26570 = EDGE_LOOP('',(#70625,#70626,#70627,#70628)) ;
#26571 = EDGE_LOOP('',(#70629,#70630,#70631,#70632)) ;
#26572 = EDGE_LOOP('',(#70633,#70634,#70635)) ;
#26573 = EDGE_LOOP('',(#70636,#70637,#70638)) ;
#26574 = EDGE_LOOP('',(#70639,#70640,#70641,#70642)) ;
#26575 = EDGE_LOOP('',(#70643,#70644,#70645,#70646)) ;
#26576 = EDGE_LOOP('',(#70647,#70648,#70649,#70650)) ;
#26577 = EDGE_LOOP('',(#70651,#70652,#70653,#70654)) ;
#26578 = EDGE_LOOP('',(#70655,#70656,#70657)) ;
#26579 = EDGE_LOOP('',(#70658,#70659,#70660)) ;
#26580 = EDGE_LOOP('',(#70661,#70662,#70663,#70664)) ;
#26581 = EDGE_LOOP('',(#70665,#70666,#70667,#70668)) ;
#26582 = EDGE_LOOP('',(#70669,#70670,#70671,#70672)) ;
#26583 = EDGE_LOOP('',(#70673,#70674,#70675,#70676)) ;
#26584 = EDGE_LOOP('',(#70677,#70678,#70679)) ;
#26585 = EDGE_LOOP('',(#70680,#70681,#70682)) ;
#26586 = EDGE_LOOP('',(#70683,#70684,#70685,#70686)) ;
#26587 = EDGE_LOOP('',(#70687,#70688,#70689,#70690)) ;
#26588 = EDGE_LOOP('',(#70691,#70692,#70693)) ;
#26589 = EDGE_LOOP('',(#70694,#70695,#70696)) ;
#26590 = EDGE_LOOP('',(#70697,#70698,#70699,#70700)) ;
#26591 = EDGE_LOOP('',(#70701,#70702,#70703,#70704)) ;
#26592 = EDGE_LOOP('',(#70705,#70706,#70707)) ;
#26593 = EDGE_LOOP('',(#70708,#70709,#70710)) ;
#26594 = EDGE_LOOP('',(#70711,#70712,#70713,#70714)) ;
#26595 = EDGE_LOOP('',(#70715,#70716,#70717,#70718)) ;
#26596 = EDGE_LOOP('',(#70719,#70720,#70721,#70722)) ;
#26597 = EDGE_LOOP('',(#70723,#70724,#70725,#70726)) ;
#26598 = EDGE_LOOP('',(#70727,#70728,#70729,#70730)) ;
#26599 = EDGE_LOOP('',(#70731,#70732,#70733,#70734)) ;
#26600 = EDGE_LOOP('',(#70735,#70736,#70737)) ;
#26601 = EDGE_LOOP('',(#70738,#70739,#70740,#70741,#70742)) ;
#26602 = EDGE_LOOP('',(#70743,#70744,#70745)) ;
#26603 = EDGE_LOOP('',(#70746,#70747,#70748)) ;
#26604 = EDGE_LOOP('',(#70749,#70750,#70751,#70752,#70753)) ;
#26605 = EDGE_LOOP('',(#70754,#70755,#70756)) ;
#26606 = EDGE_LOOP('',(#70757,#70758,#70759)) ;
#26607 = EDGE_LOOP('',(#70760,#70761,#70762,#70763,#70764)) ;
#26608 = EDGE_LOOP('',(#70765,#70766,#70767)) ;
#26609 = EDGE_LOOP('',(#70768,#70769,#70770,#70771)) ;
#26610 = EDGE_LOOP('',(#70772,#70773,#70774,#70775)) ;
#26611 = EDGE_LOOP('',(#70776,#70777,#70778,#70779)) ;
#26612 = EDGE_LOOP('',(#70780,#70781,#70782,#70783)) ;
#26613 = EDGE_LOOP('',(#70784,#70785,#70786,#70787)) ;
#26614 = EDGE_LOOP('',(#70788,#70789,#70790,#70791)) ;
#26615 = EDGE_LOOP('',(#70792,#70793,#70794,#70795)) ;
#26616 = EDGE_LOOP('',(#70796,#70797,#70798,#70799)) ;
#26617 = EDGE_LOOP('',(#70800,#70801,#70802,#70803,#70804,#70805,#70806,#70807)) ;
#26618 = EDGE_LOOP('',(#70808,#70809,#70810,#70811)) ;
#26619 = EDGE_LOOP('',(#70812,#70813,#70814,#70815)) ;
#26620 = EDGE_LOOP('',(#70816,#70817,#70818,#70819)) ;
#26621 = EDGE_LOOP('',(#70820,#70821,#70822,#70823)) ;
#26622 = EDGE_LOOP('',(#70824,#70825,#70826,#70827,#70828,#70829,#70830,#70831)) ;
#26623 = EDGE_LOOP('',(#70832,#70833,#70834,#70835)) ;
#26624 = EDGE_LOOP('',(#70836,#70837,#70838,#70839)) ;
#26625 = EDGE_LOOP('',(#70840,#70841,#70842,#70843)) ;
#26626 = EDGE_LOOP('',(#70844,#70845,#70846,#70847)) ;
#26627 = EDGE_LOOP('',(#70848,#70849,#70850,#70851,#70852,#70853,#70854,#70855)) ;
#26628 = EDGE_LOOP('',(#70856,#70857,#70858,#70859)) ;
#26629 = EDGE_LOOP('',(#70860,#70861,#70862,#70863)) ;
#26630 = EDGE_LOOP('',(#70864,#70865,#70866,#70867)) ;
#26631 = EDGE_LOOP('',(#70868,#70869,#70870,#70871)) ;
#26632 = EDGE_LOOP('',(#70872,#70873,#70874,#70875,#70876,#70877,#70878,#70879)) ;
#26633 = EDGE_LOOP('',(#70880,#70881,#70882,#70883)) ;
#26634 = EDGE_LOOP('',(#70884,#70885,#70886,#70887)) ;
#26635 = EDGE_LOOP('',(#70888,#70889,#70890,#70891)) ;
#26636 = EDGE_LOOP('',(#70892,#70893,#70894,#70895)) ;
#26637 = EDGE_LOOP('',(#70896,#70897,#70898,#70899,#70900,#70901,#70902,#70903)) ;
#26638 = EDGE_LOOP('',(#70904,#70905,#70906,#70907)) ;
#26639 = EDGE_LOOP('',(#70908,#70909,#70910,#70911)) ;
#26640 = EDGE_LOOP('',(#70912,#70913,#70914,#70915)) ;
#26641 = EDGE_LOOP('',(#70916,#70917,#70918,#70919)) ;
#26642 = EDGE_LOOP('',(#70920,#70921,#70922,#70923,#70924,#70925,#70926,#70927)) ;
#26643 = EDGE_LOOP('',(#70928,#70929,#70930,#70931)) ;
#26644 = EDGE_LOOP('',(#70932,#70933,#70934,#70935)) ;
#26645 = EDGE_LOOP('',(#70936,#70937,#70938,#70939)) ;
#26646 = EDGE_LOOP('',(#70940,#70941,#70942,#70943)) ;
#26647 = EDGE_LOOP('',(#70944,#70945,#70946,#70947,#70948,#70949,#70950,#70951)) ;
#26648 = EDGE_LOOP('',(#70952,#70953,#70954,#70955)) ;
#26649 = EDGE_LOOP('',(#70956,#70957,#70958,#70959)) ;
#26650 = EDGE_LOOP('',(#70960,#70961,#70962,#70963)) ;
#26651 = EDGE_LOOP('',(#70964,#70965,#70966,#70967)) ;
#26652 = EDGE_LOOP('',(#70968,#70969,#70970,#70971,#70972,#70973,#70974,#70975)) ;
#26653 = EDGE_LOOP('',(#70976,#70977,#70978,#70979)) ;
#26654 = EDGE_LOOP('',(#70980,#70981,#70982,#70983)) ;
#26655 = EDGE_LOOP('',(#70984,#70985,#70986,#70987)) ;
#26656 = EDGE_LOOP('',(#70988,#70989,#70990,#70991)) ;
#26657 = EDGE_LOOP('',(#70992,#70993,#70994,#70995,#70996,#70997,#70998,#70999)) ;
#26658 = EDGE_LOOP('',(#71000,#71001,#71002,#71003)) ;
#26659 = EDGE_LOOP('',(#71004,#71005,#71006,#71007)) ;
#26660 = EDGE_LOOP('',(#71008,#71009,#71010,#71011,#71012,#71013)) ;
#26661 = EDGE_LOOP('',(#71014,#71015,#71016,#71017,#71018,#71019,#71020,#71021)) ;
#26662 = EDGE_LOOP('',(#71022,#71023,#71024,#71025,#71026,#71027,#71028,#71029)) ;
#26663 = EDGE_LOOP('',(#71030,#71031,#71032,#71033,#71034,#71035,#71036,#71037)) ;
#26664 = EDGE_LOOP('',(#71038,#71039,#71040,#71041,#71042,#71043,#71044,#71045)) ;
#26665 = EDGE_LOOP('',(#71046,#71047,#71048,#71049,#71050,#71051,#71052,#71053)) ;
#26666 = EDGE_LOOP('',(#71054,#71055,#71056,#71057,#71058,#71059,#71060,#71061)) ;
#26667 = EDGE_LOOP('',(#71062,#71063,#71064,#71065,#71066,#71067,#71068,#71069)) ;
#26668 = EDGE_LOOP('',(#71070,#71071,#71072,#71073,#71074,#71075,#71076,#71077)) ;
#26669 = EDGE_LOOP('',(#71078,#71079,#71080,#71081,#71082,#71083)) ;
#26670 = EDGE_LOOP('',(#71084,#71085,#71086,#71087,#71088,#71089,#71090,#71091)) ;
#26671 = EDGE_LOOP('',(#71092,#71093,#71094,#71095,#71096,#71097,#71098,#71099)) ;
#26672 = EDGE_LOOP('',(#71100,#71101,#71102,#71103,#71104,#71105,#71106,#71107)) ;
#26673 = EDGE_LOOP('',(#71108,#71109,#71110,#71111,#71112,#71113,#71114,#71115)) ;
#26674 = EDGE_LOOP('',(#71116,#71117,#71118,#71119,#71120,#71121,#71122,#71123)) ;
#26675 = EDGE_LOOP('',(#71124,#71125,#71126,#71127,#71128,#71129,#71130,#71131)) ;
#26676 = EDGE_LOOP('',(#71132,#71133,#71134,#71135,#71136,#71137,#71138,#71139)) ;
#26677 = EDGE_LOOP('',(#71140,#71141,#71142,#71143,#71144,#71145,#71146,#71147)) ;
#26678 = EDGE_LOOP('',(#71148,#71149,#71150,#71151)) ;
#26679 = EDGE_LOOP('',(#71152,#71153,#71154,#71155)) ;
#26680 = EDGE_LOOP('',(#71156,#71157,#71158,#71159)) ;
#26681 = EDGE_LOOP('',(#71160,#71161,#71162,#71163)) ;
#26682 = EDGE_LOOP('',(#71164,#71165,#71166,#71167)) ;
#26683 = EDGE_LOOP('',(#71168,#71169,#71170,#71171)) ;
#26684 = EDGE_LOOP('',(#71172,#71173,#71174,#71175)) ;
#26685 = EDGE_LOOP('',(#71176,#71177,#71178,#71179)) ;
#26686 = EDGE_LOOP('',(#71180,#71181,#71182,#71183)) ;
#26687 = EDGE_LOOP('',(#71184,#71185,#71186,#71187)) ;
#26688 = EDGE_LOOP('',(#71188,#71189,#71190,#71191)) ;
#26689 = EDGE_LOOP('',(#71192,#71193,#71194,#71195)) ;
#26690 = EDGE_LOOP('',(#71196,#71197,#71198,#71199)) ;
#26691 = EDGE_LOOP('',(#71200,#71201,#71202,#71203)) ;
#26692 = EDGE_LOOP('',(#71204,#71205,#71206,#71207)) ;
#26693 = EDGE_LOOP('',(#71208,#71209,#71210,#71211)) ;
#26694 = EDGE_LOOP('',(#71212,#71213,#71214,#71215)) ;
#26695 = EDGE_LOOP('',(#71216,#71217,#71218,#71219)) ;
#26696 = EDGE_LOOP('',(#71220,#71221,#71222,#71223)) ;
#26697 = EDGE_LOOP('',(#71224,#71225,#71226,#71227)) ;
#26698 = EDGE_LOOP('',(#71228,#71229,#71230,#71231)) ;
#26699 = EDGE_LOOP('',(#71232,#71233,#71234,#71235)) ;
#26700 = EDGE_LOOP('',(#71236,#71237,#71238,#71239)) ;
#26701 = EDGE_LOOP('',(#71240,#71241,#71242,#71243)) ;
#26702 = EDGE_LOOP('',(#71244,#71245,#71246,#71247)) ;
#26703 = EDGE_LOOP('',(#71248,#71249,#71250,#71251)) ;
#26704 = EDGE_LOOP('',(#71252,#71253,#71254,#71255)) ;
#26705 = EDGE_LOOP('',(#71256,#71257,#71258,#71259)) ;
#26706 = EDGE_LOOP('',(#71260,#71261,#71262,#71263)) ;
#26707 = EDGE_LOOP('',(#71264,#71265,#71266,#71267)) ;
#26708 = EDGE_LOOP('',(#71268,#71269,#71270,#71271)) ;
#26709 = EDGE_LOOP('',(#71272,#71273,#71274,#71275)) ;
#26710 = EDGE_LOOP('',(#71276,#71277,#71278,#71279)) ;
#26711 = EDGE_LOOP('',(#71280,#71281,#71282,#71283)) ;
#26712 = EDGE_LOOP('',(#71284,#71285,#71286,#71287)) ;
#26713 = EDGE_LOOP('',(#71288,#71289,#71290,#71291)) ;
#26714 = EDGE_LOOP('',(#71292,#71293,#71294,#71295)) ;
#26715 = EDGE_LOOP('',(#71296,#71297,#71298,#71299,#71300,#71301,#71302,#71303)) ;
#26716 = EDGE_LOOP('',(#71304,#71305,#71306,#71307)) ;
#26717 = EDGE_LOOP('',(#71308,#71309,#71310,#71311)) ;
#26718 = EDGE_LOOP('',(#71312,#71313,#71314,#71315)) ;
#26719 = EDGE_LOOP('',(#71316,#71317,#71318,#71319)) ;
#26720 = EDGE_LOOP('',(#71320,#71321,#71322,#71323)) ;
#26721 = EDGE_LOOP('',(#71324,#71325,#71326,#71327,#71328,#71329,#71330,#71331)) ;
#26722 = EDGE_LOOP('',(#71332,#71333,#71334,#71335)) ;
#26723 = EDGE_LOOP('',(#71336,#71337,#71338,#71339)) ;
#26724 = EDGE_LOOP('',(#71340,#71341,#71342,#71343)) ;
#26725 = EDGE_LOOP('',(#71344,#71345,#71346,#71347)) ;
#26726 = EDGE_LOOP('',(#71348,#71349,#71350,#71351)) ;
#26727 = EDGE_LOOP('',(#71352,#71353,#71354,#71355,#71356,#71357,#71358,#71359)) ;
#26728 = EDGE_LOOP('',(#71360,#71361,#71362,#71363)) ;
#26729 = EDGE_LOOP('',(#71364,#71365,#71366,#71367)) ;
#26730 = EDGE_LOOP('',(#71368,#71369,#71370,#71371)) ;
#26731 = EDGE_LOOP('',(#71372,#71373,#71374,#71375)) ;
#26732 = EDGE_LOOP('',(#71376,#71377,#71378,#71379)) ;
#26733 = EDGE_LOOP('',(#71380,#71381,#71382,#71383,#71384,#71385,#71386,#71387)) ;
#26734 = EDGE_LOOP('',(#71388,#71389,#71390,#71391)) ;
#26735 = EDGE_LOOP('',(#71392,#71393,#71394,#71395)) ;
#26736 = EDGE_LOOP('',(#71396,#71397,#71398,#71399)) ;
#26737 = EDGE_LOOP('',(#71400,#71401,#71402,#71403)) ;
#26738 = EDGE_LOOP('',(#71404,#71405,#71406,#71407)) ;
#26739 = EDGE_LOOP('',(#71408,#71409,#71410,#71411,#71412,#71413,#71414,#71415)) ;
#26740 = EDGE_LOOP('',(#71416,#71417,#71418,#71419)) ;
#26741 = EDGE_LOOP('',(#71420,#71421,#71422,#71423)) ;
#26742 = EDGE_LOOP('',(#71424,#71425,#71426,#71427)) ;
#26743 = EDGE_LOOP('',(#71428,#71429,#71430,#71431)) ;
#26744 = EDGE_LOOP('',(#71432,#71433,#71434,#71435)) ;
#26745 = EDGE_LOOP('',(#71436,#71437,#71438,#71439,#71440,#71441,#71442,#71443)) ;
#26746 = EDGE_LOOP('',(#71444,#71445,#71446,#71447)) ;
#26747 = EDGE_LOOP('',(#71448,#71449,#71450,#71451)) ;
#26748 = EDGE_LOOP('',(#71452,#71453,#71454,#71455)) ;
#26749 = EDGE_LOOP('',(#71456,#71457,#71458,#71459)) ;
#26750 = EDGE_LOOP('',(#71460,#71461,#71462,#71463)) ;
#26751 = EDGE_LOOP('',(#71464,#71465,#71466,#71467,#71468,#71469,#71470,#71471)) ;
#26752 = EDGE_LOOP('',(#71472,#71473,#71474,#71475)) ;
#26753 = EDGE_LOOP('',(#71476,#71477,#71478,#71479)) ;
#26754 = EDGE_LOOP('',(#71480,#71481,#71482,#71483)) ;
#26755 = EDGE_LOOP('',(#71484,#71485,#71486,#71487)) ;
#26756 = EDGE_LOOP('',(#71488,#71489,#71490,#71491)) ;
#26757 = EDGE_LOOP('',(#71492,#71493,#71494,#71495,#71496,#71497,#71498,#71499)) ;
#26758 = EDGE_LOOP('',(#71500,#71501,#71502,#71503)) ;
#26759 = EDGE_LOOP('',(#71504,#71505,#71506,#71507)) ;
#26760 = EDGE_LOOP('',(#71508,#71509,#71510,#71511)) ;
#26761 = EDGE_LOOP('',(#71512,#71513,#71514,#71515)) ;
#26762 = EDGE_LOOP('',(#71516,#71517,#71518,#71519)) ;
#26763 = EDGE_LOOP('',(#71520,#71521,#71522,#71523,#71524,#71525,#71526,#71527)) ;
#26764 = EDGE_LOOP('',(#71528,#71529,#71530,#71531)) ;
#26765 = EDGE_LOOP('',(#71532,#71533,#71534,#71535)) ;
#26766 = EDGE_LOOP('',(#71536,#71537,#71538,#71539)) ;
#26767 = EDGE_LOOP('',(#71540,#71541,#71542,#71543)) ;
#26768 = EDGE_LOOP('',(#71544,#71545,#71546,#71547)) ;
#26769 = EDGE_LOOP('',(#71548,#71549,#71550,#71551)) ;
#26770 = EDGE_LOOP('',(#71552,#71553,#71554,#71555)) ;
#26771 = EDGE_LOOP('',(#71556,#71557,#71558,#71559)) ;
#26772 = EDGE_LOOP('',(#71560,#71561,#71562,#71563)) ;
#26773 = EDGE_LOOP('',(#71564,#71565,#71566,#71567)) ;
#26774 = EDGE_LOOP('',(#71568,#71569,#71570,#71571)) ;
#26775 = EDGE_LOOP('',(#71572,#71573,#71574,#71575)) ;
#26776 = EDGE_LOOP('',(#71576,#71577,#71578,#71579)) ;
#26777 = EDGE_LOOP('',(#71580,#71581,#71582,#71583,#71584,#71585,#71586,#71587,
#71588,#71589)) ;
#26778 = EDGE_LOOP('',(#71590,#71591,#71592,#71593)) ;
#26779 = EDGE_LOOP('',(#71594,#71595,#71596,#71597,#71598,#71599,#71600,#71601,
#71602,#71603)) ;
#26780 = EDGE_LOOP('',(#71604,#71605,#71606,#71607)) ;
#26781 = EDGE_LOOP('',(#71608,#71609,#71610,#71611,#71612,#71613,#71614,#71615,
#71616,#71617)) ;
#26782 = EDGE_LOOP('',(#71618,#71619,#71620,#71621)) ;
#26783 = EDGE_LOOP('',(#71622,#71623,#71624,#71625,#71626,#71627,#71628,#71629,
#71630,#71631)) ;
#26784 = EDGE_LOOP('',(#71632,#71633,#71634,#71635)) ;
#26785 = EDGE_LOOP('',(#71636,#71637,#71638,#71639,#71640,#71641,#71642,#71643,
#71644,#71645)) ;
#26786 = EDGE_LOOP('',(#71646,#71647,#71648,#71649)) ;
#26787 = EDGE_LOOP('',(#71650,#71651,#71652,#71653,#71654,#71655,#71656,#71657,
#71658,#71659)) ;
#26788 = EDGE_LOOP('',(#71660,#71661,#71662,#71663)) ;
#26789 = EDGE_LOOP('',(#71664,#71665,#71666,#71667,#71668,#71669,#71670,#71671,
#71672,#71673)) ;
#26790 = EDGE_LOOP('',(#71674,#71675,#71676,#71677)) ;
#26791 = EDGE_LOOP('',(#71678,#71679,#71680,#71681,#71682,#71683,#71684,#71685,
#71686,#71687)) ;
#26792 = EDGE_LOOP('',(#71688,#71689,#71690,#71691)) ;
#26793 = EDGE_LOOP('',(#71692,#71693,#71694,#71695,#71696,#71697,#71698,#71699,
#71700,#71701)) ;
#26794 = EDGE_LOOP('',(#71702,#71703,#71704,#71705)) ;
#26795 = EDGE_LOOP('',(#71706,#71707,#71708,#71709,#71710,#71711,#71712,#71713,
#71714,#71715)) ;
#26796 = EDGE_LOOP('',(#71716,#71717,#71718,#71719)) ;
#26797 = EDGE_LOOP('',(#71720,#71721,#71722,#71723,#71724,#71725,#71726,#71727,
#71728,#71729)) ;
#26798 = EDGE_LOOP('',(#71730,#71731,#71732,#71733)) ;
#26799 = EDGE_LOOP('',(#71734,#71735,#71736,#71737,#71738,#71739,#71740,#71741,
#71742,#71743)) ;
#26800 = EDGE_LOOP('',(#71744,#71745,#71746,#71747)) ;
#26801 = EDGE_LOOP('',(#71748,#71749,#71750,#71751,#71752,#71753,#71754,#71755,
#71756,#71757)) ;
#26802 = EDGE_LOOP('',(#71758,#71759,#71760,#71761)) ;
#26803 = EDGE_LOOP('',(#71762,#71763,#71764,#71765,#71766,#71767,#71768,#71769,
#71770,#71771)) ;
#26804 = EDGE_LOOP('',(#71772,#71773,#71774,#71775)) ;
#26805 = EDGE_LOOP('',(#71776,#71777,#71778,#71779,#71780,#71781,#71782,#71783,
#71784,#71785)) ;
#26806 = EDGE_LOOP('',(#71786,#71787,#71788,#71789)) ;
#26807 = EDGE_LOOP('',(#71790,#71791,#71792,#71793,#71794,#71795,#71796,#71797,
#71798,#71799)) ;
#26808 = EDGE_LOOP('',(#71800,#71801,#71802,#71803)) ;
#26809 = EDGE_LOOP('',(#71804,#71805,#71806,#71807,#71808,#71809,#71810,#71811,
#71812,#71813)) ;
#26810 = EDGE_LOOP('',(#71814,#71815,#71816,#71817)) ;
#26811 = EDGE_LOOP('',(#71818,#71819,#71820,#71821,#71822,#71823,#71824,#71825,
#71826,#71827)) ;
#26812 = EDGE_LOOP('',(#71828,#71829,#71830,#71831)) ;
#26813 = EDGE_LOOP('',(#71832,#71833,#71834,#71835)) ;
#26814 = EDGE_LOOP('',(#71836,#71837,#71838,#71839)) ;
#26815 = EDGE_LOOP('',(#71840,#71841,#71842,#71843)) ;
#26816 = EDGE_LOOP('',(#71844,#71845,#71846,#71847,#71848,#71849)) ;
#26817 = EDGE_LOOP('',(#71850)) ;
#26818 = EDGE_LOOP('',(#71851,#71852,#71853,#71854)) ;
#26819 = EDGE_LOOP('',(#71855,#71856,#71857,#71858)) ;
#26820 = EDGE_LOOP('',(#71859,#71860,#71861,#71862)) ;
#26821 = EDGE_LOOP('',(#71863,#71864,#71865,#71866,#71867,#71868)) ;
#26822 = EDGE_LOOP('',(#71869)) ;
#26823 = EDGE_LOOP('',(#71870,#71871,#71872,#71873)) ;
#26824 = EDGE_LOOP('',(#71874,#71875,#71876,#71877)) ;
#26825 = EDGE_LOOP('',(#71878,#71879,#71880,#71881)) ;
#26826 = EDGE_LOOP('',(#71882,#71883,#71884,#71885,#71886,#71887)) ;
#26827 = EDGE_LOOP('',(#71888)) ;
#26828 = EDGE_LOOP('',(#71889,#71890,#71891,#71892)) ;
#26829 = EDGE_LOOP('',(#71893,#71894,#71895,#71896)) ;
#26830 = EDGE_LOOP('',(#71897,#71898,#71899,#71900)) ;
#26831 = EDGE_LOOP('',(#71901,#71902,#71903,#71904,#71905,#71906)) ;
#26832 = EDGE_LOOP('',(#71907)) ;
#26833 = EDGE_LOOP('',(#71908,#71909,#71910,#71911)) ;
#26834 = EDGE_LOOP('',(#71912,#71913,#71914,#71915)) ;
#26835 = EDGE_LOOP('',(#71916,#71917,#71918,#71919)) ;
#26836 = EDGE_LOOP('',(#71920,#71921,#71922,#71923,#71924,#71925)) ;
#26837 = EDGE_LOOP('',(#71926)) ;
#26838 = EDGE_LOOP('',(#71927,#71928,#71929,#71930)) ;
#26839 = EDGE_LOOP('',(#71931,#71932,#71933,#71934)) ;
#26840 = EDGE_LOOP('',(#71935,#71936,#71937,#71938)) ;
#26841 = EDGE_LOOP('',(#71939,#71940,#71941,#71942,#71943,#71944)) ;
#26842 = EDGE_LOOP('',(#71945)) ;
#26843 = EDGE_LOOP('',(#71946,#71947,#71948,#71949)) ;
#26844 = EDGE_LOOP('',(#71950,#71951,#71952,#71953)) ;
#26845 = EDGE_LOOP('',(#71954,#71955,#71956,#71957)) ;
#26846 = EDGE_LOOP('',(#71958,#71959,#71960,#71961,#71962,#71963)) ;
#26847 = EDGE_LOOP('',(#71964)) ;
#26848 = EDGE_LOOP('',(#71965,#71966,#71967,#71968)) ;
#26849 = EDGE_LOOP('',(#71969,#71970,#71971,#71972)) ;
#26850 = EDGE_LOOP('',(#71973,#71974,#71975,#71976)) ;
#26851 = EDGE_LOOP('',(#71977,#71978,#71979,#71980,#71981,#71982)) ;
#26852 = EDGE_LOOP('',(#71983)) ;
#26853 = EDGE_LOOP('',(#71984,#71985,#71986,#71987)) ;
#26854 = EDGE_LOOP('',(#71988,#71989,#71990,#71991)) ;
#26855 = EDGE_LOOP('',(#71992,#71993,#71994,#71995)) ;
#26856 = EDGE_LOOP('',(#71996,#71997,#71998,#71999,#72000,#72001)) ;
#26857 = EDGE_LOOP('',(#72002)) ;
#26858 = EDGE_LOOP('',(#72003)) ;
#26859 = EDGE_LOOP('',(#72004)) ;
#26860 = EDGE_LOOP('',(#72005)) ;
#26861 = EDGE_LOOP('',(#72006)) ;
#26862 = EDGE_LOOP('',(#72007)) ;
#26863 = EDGE_LOOP('',(#72008)) ;
#26864 = EDGE_LOOP('',(#72009)) ;
#26865 = EDGE_LOOP('',(#72010)) ;
#26866 = EDGE_LOOP('',(#72011)) ;
#26867 = EDGE_LOOP('',(#72012,#72013,#72014,#72015)) ;
#26868 = EDGE_LOOP('',(#72016,#72017,#72018,#72019)) ;
#26869 = EDGE_LOOP('',(#72020,#72021,#72022,#72023)) ;
#26870 = EDGE_LOOP('',(#72024,#72025,#72026,#72027)) ;
#26871 = EDGE_LOOP('',(#72028,#72029,#72030,#72031)) ;
#26872 = EDGE_LOOP('',(#72032,#72033,#72034,#72035)) ;
#26873 = EDGE_LOOP('',(#72036,#72037,#72038,#72039)) ;
#26874 = EDGE_LOOP('',(#72040,#72041,#72042,#72043)) ;
#26875 = EDGE_LOOP('',(#72044,#72045,#72046,#72047)) ;
#26876 = EDGE_LOOP('',(#72048,#72049,#72050,#72051)) ;
#26877 = EDGE_LOOP('',(#72052,#72053,#72054,#72055)) ;
#26878 = EDGE_LOOP('',(#72056,#72057,#72058,#72059)) ;
#26879 = EDGE_LOOP('',(#72060,#72061,#72062,#72063)) ;
#26880 = EDGE_LOOP('',(#72064,#72065,#72066,#72067)) ;
#26881 = EDGE_LOOP('',(#72068,#72069,#72070,#72071)) ;
#26882 = EDGE_LOOP('',(#72072,#72073,#72074,#72075)) ;
#26883 = EDGE_LOOP('',(#72076,#72077,#72078,#72079)) ;
#26884 = EDGE_LOOP('',(#72080,#72081,#72082,#72083)) ;
#26885 = EDGE_LOOP('',(#72084,#72085,#72086,#72087)) ;
#26886 = EDGE_LOOP('',(#72088,#72089,#72090,#72091)) ;
#26887 = EDGE_LOOP('',(#72092,#72093,#72094,#72095)) ;
#26888 = EDGE_LOOP('',(#72096,#72097,#72098,#72099)) ;
#26889 = EDGE_LOOP('',(#72100,#72101,#72102,#72103)) ;
#26890 = EDGE_LOOP('',(#72104,#72105,#72106,#72107)) ;
#26891 = EDGE_LOOP('',(#72108,#72109,#72110,#72111)) ;
#26892 = EDGE_LOOP('',(#72112,#72113,#72114,#72115)) ;
#26893 = EDGE_LOOP('',(#72116,#72117,#72118,#72119)) ;
#26894 = EDGE_LOOP('',(#72120,#72121,#72122,#72123)) ;
#26895 = EDGE_LOOP('',(#72124,#72125,#72126,#72127)) ;
#26896 = EDGE_LOOP('',(#72128,#72129,#72130,#72131)) ;
#26897 = EDGE_LOOP('',(#72132,#72133,#72134,#72135)) ;
#26898 = EDGE_LOOP('',(#72136,#72137,#72138,#72139)) ;
#26899 = EDGE_LOOP('',(#72140,#72141,#72142,#72143)) ;
#26900 = EDGE_LOOP('',(#72144,#72145,#72146,#72147)) ;
#26901 = EDGE_LOOP('',(#72148,#72149,#72150,#72151)) ;
#26902 = EDGE_LOOP('',(#72152,#72153,#72154,#72155)) ;
#26903 = EDGE_LOOP('',(#72156,#72157,#72158,#72159)) ;
#26904 = EDGE_LOOP('',(#72160,#72161,#72162,#72163,#72164,#72165,#72166,#72167)) ;
#26905 = EDGE_LOOP('',(#72168,#72169,#72170,#72171)) ;
#26906 = EDGE_LOOP('',(#72172,#72173,#72174,#72175)) ;
#26907 = EDGE_LOOP('',(#72176,#72177,#72178,#72179)) ;
#26908 = EDGE_LOOP('',(#72180,#72181,#72182,#72183)) ;
#26909 = EDGE_LOOP('',(#72184,#72185,#72186,#72187)) ;
#26910 = EDGE_LOOP('',(#72188,#72189,#72190,#72191,#72192,#72193,#72194,#72195)) ;
#26911 = EDGE_LOOP('',(#72196,#72197,#72198,#72199)) ;
#26912 = EDGE_LOOP('',(#72200,#72201,#72202,#72203)) ;
#26913 = EDGE_LOOP('',(#72204,#72205,#72206,#72207)) ;
#26914 = EDGE_LOOP('',(#72208,#72209,#72210,#72211)) ;
#26915 = EDGE_LOOP('',(#72212,#72213,#72214,#72215)) ;
#26916 = EDGE_LOOP('',(#72216,#72217,#72218,#72219,#72220,#72221,#72222,#72223)) ;
#26917 = EDGE_LOOP('',(#72224,#72225,#72226,#72227)) ;
#26918 = EDGE_LOOP('',(#72228,#72229,#72230,#72231)) ;
#26919 = EDGE_LOOP('',(#72232,#72233,#72234,#72235)) ;
#26920 = EDGE_LOOP('',(#72236,#72237,#72238,#72239)) ;
#26921 = EDGE_LOOP('',(#72240,#72241,#72242,#72243)) ;
#26922 = EDGE_LOOP('',(#72244,#72245,#72246,#72247,#72248,#72249,#72250,#72251)) ;
#26923 = EDGE_LOOP('',(#72252,#72253,#72254,#72255)) ;
#26924 = EDGE_LOOP('',(#72256,#72257,#72258,#72259)) ;
#26925 = EDGE_LOOP('',(#72260,#72261,#72262,#72263)) ;
#26926 = EDGE_LOOP('',(#72264,#72265,#72266,#72267)) ;
#26927 = EDGE_LOOP('',(#72268,#72269,#72270,#72271)) ;
#26928 = EDGE_LOOP('',(#72272,#72273,#72274,#72275,#72276,#72277,#72278,#72279)) ;
#26929 = EDGE_LOOP('',(#72280,#72281,#72282,#72283)) ;
#26930 = EDGE_LOOP('',(#72284,#72285,#72286,#72287)) ;
#26931 = EDGE_LOOP('',(#72288,#72289,#72290,#72291)) ;
#26932 = EDGE_LOOP('',(#72292,#72293,#72294,#72295)) ;
#26933 = EDGE_LOOP('',(#72296,#72297,#72298,#72299)) ;
#26934 = EDGE_LOOP('',(#72300,#72301,#72302,#72303,#72304,#72305,#72306,#72307)) ;
#26935 = EDGE_LOOP('',(#72308,#72309,#72310,#72311)) ;
#26936 = EDGE_LOOP('',(#72312,#72313,#72314,#72315)) ;
#26937 = EDGE_LOOP('',(#72316,#72317,#72318,#72319)) ;
#26938 = EDGE_LOOP('',(#72320,#72321,#72322,#72323)) ;
#26939 = EDGE_LOOP('',(#72324,#72325,#72326,#72327)) ;
#26940 = EDGE_LOOP('',(#72328,#72329,#72330,#72331,#72332,#72333,#72334,#72335)) ;
#26941 = EDGE_LOOP('',(#72336,#72337,#72338,#72339)) ;
#26942 = EDGE_LOOP('',(#72340,#72341,#72342,#72343)) ;
#26943 = EDGE_LOOP('',(#72344,#72345,#72346,#72347)) ;
#26944 = EDGE_LOOP('',(#72348,#72349,#72350,#72351)) ;
#26945 = EDGE_LOOP('',(#72352,#72353,#72354,#72355)) ;
#26946 = EDGE_LOOP('',(#72356,#72357,#72358,#72359,#72360,#72361,#72362,#72363)) ;
#26947 = EDGE_LOOP('',(#72364,#72365,#72366,#72367)) ;
#26948 = EDGE_LOOP('',(#72368,#72369,#72370,#72371)) ;
#26949 = EDGE_LOOP('',(#72372,#72373,#72374,#72375)) ;
#26950 = EDGE_LOOP('',(#72376,#72377,#72378,#72379)) ;
#26951 = EDGE_LOOP('',(#72380,#72381,#72382,#72383)) ;
#26952 = EDGE_LOOP('',(#72384,#72385,#72386,#72387,#72388,#72389,#72390,#72391)) ;
#26953 = EDGE_LOOP('',(#72392,#72393,#72394,#72395)) ;
#26954 = EDGE_LOOP('',(#72396,#72397,#72398,#72399)) ;
#26955 = EDGE_LOOP('',(#72400,#72401,#72402,#72403)) ;
#26956 = EDGE_LOOP('',(#72404,#72405,#72406,#72407)) ;
#26957 = EDGE_LOOP('',(#72408,#72409,#72410,#72411)) ;
#26958 = EDGE_LOOP('',(#72412,#72413,#72414,#72415)) ;
#26959 = EDGE_LOOP('',(#72416,#72417,#72418,#72419)) ;
#26960 = EDGE_LOOP('',(#72420,#72421,#72422,#72423)) ;
#26961 = EDGE_LOOP('',(#72424,#72425,#72426,#72427)) ;
#26962 = EDGE_LOOP('',(#72428,#72429,#72430,#72431)) ;
#26963 = EDGE_LOOP('',(#72432,#72433,#72434,#72435)) ;
#26964 = EDGE_LOOP('',(#72436,#72437,#72438,#72439)) ;
#26965 = EDGE_LOOP('',(#72440,#72441,#72442,#72443)) ;
#26966 = EDGE_LOOP('',(#72444,#72445,#72446)) ;
#26967 = EDGE_LOOP('',(#72447,#72448,#72449)) ;
#26968 = EDGE_LOOP('',(#72450,#72451,#72452)) ;
#26969 = EDGE_LOOP('',(#72453,#72454,#72455)) ;
#26970 = EDGE_LOOP('',(#72456,#72457,#72458)) ;
#26971 = EDGE_LOOP('',(#72459,#72460,#72461)) ;
#26972 = EDGE_LOOP('',(#72462,#72463,#72464)) ;
#26973 = EDGE_LOOP('',(#72465,#72466,#72467)) ;
#26974 = EDGE_LOOP('',(#72468,#72469,#72470)) ;
#26975 = EDGE_LOOP('',(#72471,#72472,#72473,#72474)) ;
#26976 = EDGE_LOOP('',(#72475,#72476,#72477,#72478)) ;
#26977 = EDGE_LOOP('',(#72479,#72480,#72481,#72482)) ;
#26978 = EDGE_LOOP('',(#72483,#72484,#72485,#72486)) ;
#26979 = EDGE_LOOP('',(#72487,#72488,#72489,#72490)) ;
#26980 = EDGE_LOOP('',(#72491,#72492,#72493,#72494)) ;
#26981 = EDGE_LOOP('',(#72495,#72496,#72497,#72498)) ;
#26982 = EDGE_LOOP('',(#72499,#72500,#72501,#72502)) ;
#26983 = EDGE_LOOP('',(#72503,#72504,#72505,#72506)) ;
#26984 = EDGE_LOOP('',(#72507,#72508,#72509,#72510)) ;
#26985 = EDGE_LOOP('',(#72511,#72512,#72513,#72514)) ;
#26986 = EDGE_LOOP('',(#72515,#72516,#72517,#72518)) ;
#26987 = EDGE_LOOP('',(#72519,#72520,#72521,#72522)) ;
#26988 = EDGE_LOOP('',(#72523,#72524,#72525,#72526)) ;
#26989 = EDGE_LOOP('',(#72527,#72528,#72529,#72530)) ;
#26990 = EDGE_LOOP('',(#72531,#72532,#72533,#72534)) ;
#26991 = EDGE_LOOP('',(#72535,#72536,#72537,#72538)) ;
#26992 = EDGE_LOOP('',(#72539,#72540,#72541,#72542)) ;
#26993 = EDGE_LOOP('',(#72543,#72544,#72545,#72546)) ;
#26994 = EDGE_LOOP('',(#72547,#72548,#72549,#72550)) ;
#26995 = EDGE_LOOP('',(#72551,#72552,#72553,#72554)) ;
#26996 = EDGE_LOOP('',(#72555,#72556,#72557,#72558)) ;
#26997 = EDGE_LOOP('',(#72559,#72560,#72561,#72562)) ;
#26998 = EDGE_LOOP('',(#72563,#72564,#72565,#72566)) ;
#26999 = EDGE_LOOP('',(#72567,#72568,#72569,#72570)) ;
#27000 = EDGE_LOOP('',(#72571,#72572,#72573,#72574)) ;
#27001 = EDGE_LOOP('',(#72575,#72576,#72577,#72578)) ;
#27002 = EDGE_LOOP('',(#72579,#72580,#72581,#72582)) ;
#27003 = EDGE_LOOP('',(#72583,#72584,#72585,#72586)) ;
#27004 = EDGE_LOOP('',(#72587,#72588,#72589,#72590)) ;
#27005 = EDGE_LOOP('',(#72591,#72592,#72593,#72594)) ;
#27006 = EDGE_LOOP('',(#72595,#72596,#72597,#72598)) ;
#27007 = EDGE_LOOP('',(#72599,#72600,#72601,#72602)) ;
#27008 = EDGE_LOOP('',(#72603,#72604,#72605,#72606)) ;
#27009 = EDGE_LOOP('',(#72607,#72608,#72609,#72610)) ;
#27010 = EDGE_LOOP('',(#72611,#72612,#72613,#72614)) ;
#27011 = EDGE_LOOP('',(#72615,#72616,#72617,#72618)) ;
#27012 = EDGE_LOOP('',(#72619,#72620,#72621,#72622)) ;
#27013 = EDGE_LOOP('',(#72623,#72624,#72625,#72626)) ;
#27014 = EDGE_LOOP('',(#72627,#72628,#72629,#72630)) ;
#27015 = EDGE_LOOP('',(#72631,#72632,#72633,#72634)) ;
#27016 = EDGE_LOOP('',(#72635,#72636,#72637,#72638)) ;
#27017 = EDGE_LOOP('',(#72639,#72640,#72641,#72642)) ;
#27018 = EDGE_LOOP('',(#72643,#72644,#72645,#72646)) ;
#27019 = EDGE_LOOP('',(#72647,#72648,#72649,#72650)) ;
#27020 = EDGE_LOOP('',(#72651,#72652,#72653,#72654)) ;
#27021 = EDGE_LOOP('',(#72655,#72656,#72657,#72658)) ;
#27022 = EDGE_LOOP('',(#72659,#72660,#72661,#72662)) ;
#27023 = EDGE_LOOP('',(#72663,#72664,#72665,#72666)) ;
#27024 = EDGE_LOOP('',(#72667,#72668,#72669,#72670)) ;
#27025 = EDGE_LOOP('',(#72671,#72672,#72673,#72674)) ;
#27026 = EDGE_LOOP('',(#72675,#72676,#72677,#72678)) ;
#27027 = EDGE_LOOP('',(#72679,#72680,#72681,#72682)) ;
#27028 = EDGE_LOOP('',(#72683,#72684,#72685,#72686)) ;
#27029 = EDGE_LOOP('',(#72687,#72688,#72689,#72690)) ;
#27030 = EDGE_LOOP('',(#72691,#72692,#72693,#72694)) ;
#27031 = EDGE_LOOP('',(#72695,#72696,#72697,#72698)) ;
#27032 = EDGE_LOOP('',(#72699,#72700,#72701,#72702)) ;
#27033 = EDGE_LOOP('',(#72703,#72704,#72705,#72706)) ;
#27034 = EDGE_LOOP('',(#72707,#72708,#72709,#72710)) ;
#27035 = EDGE_LOOP('',(#72711,#72712,#72713,#72714)) ;
#27036 = EDGE_LOOP('',(#72715,#72716,#72717,#72718)) ;
#27037 = EDGE_LOOP('',(#72719,#72720,#72721,#72722)) ;
#27038 = EDGE_LOOP('',(#72723,#72724,#72725,#72726)) ;
#27039 = EDGE_LOOP('',(#72727,#72728,#72729,#72730)) ;
#27040 = EDGE_LOOP('',(#72731,#72732,#72733,#72734)) ;
#27041 = EDGE_LOOP('',(#72735,#72736,#72737,#72738)) ;
#27042 = EDGE_LOOP('',(#72739,#72740,#72741,#72742)) ;
#27043 = EDGE_LOOP('',(#72743,#72744,#72745,#72746)) ;
#27044 = EDGE_LOOP('',(#72747,#72748,#72749,#72750)) ;
#27045 = EDGE_LOOP('',(#72751,#72752,#72753,#72754)) ;
#27046 = EDGE_LOOP('',(#72755,#72756,#72757,#72758)) ;
#27047 = EDGE_LOOP('',(#72759,#72760,#72761,#72762)) ;
#27048 = EDGE_LOOP('',(#72763,#72764,#72765,#72766)) ;
#27049 = EDGE_LOOP('',(#72767,#72768,#72769,#72770)) ;
#27050 = EDGE_LOOP('',(#72771,#72772,#72773,#72774)) ;
#27051 = EDGE_LOOP('',(#72775,#72776,#72777,#72778)) ;
#27052 = EDGE_LOOP('',(#72779,#72780,#72781,#72782)) ;
#27053 = EDGE_LOOP('',(#72783,#72784,#72785,#72786)) ;
#27054 = EDGE_LOOP('',(#72787,#72788,#72789,#72790)) ;
#27055 = EDGE_LOOP('',(#72791,#72792,#72793,#72794)) ;
#27056 = EDGE_LOOP('',(#72795,#72796,#72797,#72798)) ;
#27057 = EDGE_LOOP('',(#72799,#72800,#72801,#72802)) ;
#27058 = EDGE_LOOP('',(#72803,#72804,#72805,#72806)) ;
#27059 = EDGE_LOOP('',(#72807,#72808,#72809,#72810)) ;
#27060 = EDGE_LOOP('',(#72811,#72812,#72813,#72814)) ;
#27061 = EDGE_LOOP('',(#72815,#72816,#72817,#72818)) ;
#27062 = EDGE_LOOP('',(#72819,#72820,#72821,#72822)) ;
#27063 = EDGE_LOOP('',(#72823,#72824,#72825,#72826)) ;
#27064 = EDGE_LOOP('',(#72827,#72828,#72829,#72830)) ;
#27065 = EDGE_LOOP('',(#72831,#72832,#72833,#72834)) ;
#27066 = EDGE_LOOP('',(#72835,#72836,#72837,#72838)) ;
#27067 = EDGE_LOOP('',(#72839,#72840,#72841,#72842)) ;
#27068 = EDGE_LOOP('',(#72843,#72844,#72845,#72846)) ;
#27069 = EDGE_LOOP('',(#72847,#72848,#72849,#72850)) ;
#27070 = EDGE_LOOP('',(#72851,#72852,#72853,#72854)) ;
#27071 = EDGE_LOOP('',(#72855,#72856,#72857,#72858)) ;
#27072 = EDGE_LOOP('',(#72859,#72860,#72861,#72862)) ;
#27073 = EDGE_LOOP('',(#72863,#72864,#72865,#72866)) ;
#27074 = EDGE_LOOP('',(#72867,#72868,#72869,#72870)) ;
#27075 = EDGE_LOOP('',(#72871,#72872,#72873,#72874)) ;
#27076 = EDGE_LOOP('',(#72875,#72876,#72877,#72878)) ;
#27077 = EDGE_LOOP('',(#72879,#72880,#72881,#72882)) ;
#27078 = EDGE_LOOP('',(#72883,#72884,#72885,#72886)) ;
#27079 = EDGE_LOOP('',(#72887,#72888,#72889,#72890)) ;
#27080 = EDGE_LOOP('',(#72891,#72892,#72893,#72894)) ;
#27081 = EDGE_LOOP('',(#72895,#72896,#72897,#72898)) ;
#27082 = EDGE_LOOP('',(#72899,#72900,#72901,#72902)) ;
#27083 = EDGE_LOOP('',(#72903,#72904,#72905)) ;
#27084 = EDGE_LOOP('',(#72906,#72907,#72908,#72909)) ;
#27085 = EDGE_LOOP('',(#72910,#72911,#72912,#72913)) ;
#27086 = EDGE_LOOP('',(#72914,#72915,#72916,#72917)) ;
#27087 = EDGE_LOOP('',(#72918,#72919,#72920,#72921)) ;
#27088 = EDGE_LOOP('',(#72922,#72923,#72924,#72925)) ;
#27089 = EDGE_LOOP('',(#72926,#72927,#72928)) ;
#27090 = EDGE_LOOP('',(#72929,#72930,#72931,#72932)) ;
#27091 = EDGE_LOOP('',(#72933,#72934,#72935)) ;
#27092 = EDGE_LOOP('',(#72936,#72937,#72938,#72939)) ;
#27093 = EDGE_LOOP('',(#72940,#72941,#72942,#72943)) ;
#27094 = EDGE_LOOP('',(#72944,#72945,#72946,#72947)) ;
#27095 = EDGE_LOOP('',(#72948,#72949,#72950,#72951)) ;
#27096 = EDGE_LOOP('',(#72952,#72953,#72954,#72955)) ;
#27097 = EDGE_LOOP('',(#72956,#72957,#72958,#72959)) ;
#27098 = EDGE_LOOP('',(#72960,#72961,#72962)) ;
#27099 = EDGE_LOOP('',(#72963,#72964,#72965,#72966)) ;
#27100 = EDGE_LOOP('',(#72967,#72968,#72969,#72970)) ;
#27101 = EDGE_LOOP('',(#72971,#72972,#72973,#72974)) ;
#27102 = EDGE_LOOP('',(#72975,#72976,#72977,#72978)) ;
#27103 = EDGE_LOOP('',(#72979,#72980,#72981,#72982)) ;
#27104 = EDGE_LOOP('',(#72983,#72984,#72985,#72986)) ;
#27105 = EDGE_LOOP('',(#72987,#72988,#72989,#72990)) ;
#27106 = EDGE_LOOP('',(#72991,#72992,#72993,#72994)) ;
#27107 = EDGE_LOOP('',(#72995,#72996,#72997)) ;
#27108 = EDGE_LOOP('',(#72998,#72999,#73000)) ;
#27109 = EDGE_LOOP('',(#73001,#73002,#73003,#73004)) ;
#27110 = EDGE_LOOP('',(#73005,#73006,#73007,#73008)) ;
#27111 = EDGE_LOOP('',(#73009,#73010,#73011,#73012)) ;
#27112 = EDGE_LOOP('',(#73013,#73014,#73015,#73016)) ;
#27113 = EDGE_LOOP('',(#73017,#73018,#73019)) ;
#27114 = EDGE_LOOP('',(#73020,#73021,#73022,#73023)) ;
#27115 = EDGE_LOOP('',(#73024,#73025,#73026,#73027)) ;
#27116 = EDGE_LOOP('',(#73028,#73029,#73030,#73031)) ;
#27117 = EDGE_LOOP('',(#73032,#73033,#73034,#73035)) ;
#27118 = EDGE_LOOP('',(#73036,#73037,#73038)) ;
#27119 = EDGE_LOOP('',(#73039,#73040,#73041,#73042)) ;
#27120 = EDGE_LOOP('',(#73043,#73044,#73045,#73046)) ;
#27121 = EDGE_LOOP('',(#73047,#73048,#73049,#73050)) ;
#27122 = EDGE_LOOP('',(#73051,#73052,#73053,#73054)) ;
#27123 = EDGE_LOOP('',(#73055,#73056,#73057,#73058)) ;
#27124 = EDGE_LOOP('',(#73059,#73060,#73061,#73062)) ;
#27125 = EDGE_LOOP('',(#73063,#73064,#73065,#73066)) ;
#27126 = EDGE_LOOP('',(#73067,#73068,#73069,#73070)) ;
#27127 = EDGE_LOOP('',(#73071,#73072,#73073,#73074)) ;
#27128 = EDGE_LOOP('',(#73075,#73076,#73077,#73078)) ;
#27129 = EDGE_LOOP('',(#73079,#73080,#73081,#73082,#73083,#73084)) ;
#27130 = EDGE_LOOP('',(#73085,#73086,#73087,#73088,#73089,#73090)) ;
#27131 = EDGE_LOOP('',(#73091,#73092,#73093,#73094,#73095,#73096)) ;
#27132 = EDGE_LOOP('',(#73097,#73098,#73099,#73100,#73101,#73102)) ;
#27133 = EDGE_LOOP('',(#73103,#73104,#73105,#73106,#73107,#73108)) ;
#27134 = EDGE_LOOP('',(#73109,#73110,#73111,#73112,#73113,#73114)) ;
#27135 = EDGE_LOOP('',(#73115,#73116,#73117,#73118,#73119,#73120)) ;
#27136 = EDGE_LOOP('',(#73121,#73122,#73123,#73124,#73125,#73126)) ;
#27137 = EDGE_LOOP('',(#73127,#73128,#73129,#73130,#73131,#73132)) ;
#27138 = EDGE_LOOP('',(#73133,#73134,#73135,#73136,#73137,#73138)) ;
#27139 = EDGE_LOOP('',(#73139,#73140,#73141,#73142,#73143,#73144)) ;
#27140 = EDGE_LOOP('',(#73145,#73146,#73147,#73148,#73149,#73150)) ;
#27141 = EDGE_LOOP('',(#73151,#73152,#73153,#73154,#73155,#73156)) ;
#27142 = EDGE_LOOP('',(#73157,#73158,#73159,#73160,#73161,#73162)) ;
#27143 = EDGE_LOOP('',(#73163,#73164,#73165,#73166,#73167,#73168)) ;
#27144 = EDGE_LOOP('',(#73169,#73170,#73171,#73172,#73173,#73174)) ;
#27145 = EDGE_LOOP('',(#73175,#73176,#73177,#73178,#73179,#73180)) ;
#27146 = EDGE_LOOP('',(#73181,#73182,#73183,#73184,#73185,#73186)) ;
#27147 = EDGE_LOOP('',(#73187,#73188,#73189,#73190,#73191,#73192)) ;
#27148 = EDGE_LOOP('',(#73193,#73194,#73195,#73196,#73197,#73198)) ;
#27149 = EDGE_LOOP('',(#73199,#73200,#73201,#73202,#73203,#73204)) ;
#27150 = EDGE_LOOP('',(#73205,#73206,#73207,#73208,#73209,#73210)) ;
#27151 = EDGE_LOOP('',(#73211,#73212,#73213,#73214,#73215,#73216)) ;
#27152 = EDGE_LOOP('',(#73217,#73218,#73219,#73220,#73221,#73222)) ;
#27153 = EDGE_LOOP('',(#73223,#73224,#73225,#73226,#73227,#73228)) ;
#27154 = EDGE_LOOP('',(#73229,#73230,#73231,#73232,#73233,#73234)) ;
#27155 = EDGE_LOOP('',(#73235,#73236,#73237,#73238,#73239,#73240)) ;
#27156 = EDGE_LOOP('',(#73241,#73242,#73243,#73244,#73245,#73246)) ;
#27157 = EDGE_LOOP('',(#73247,#73248,#73249,#73250,#73251,#73252)) ;
#27158 = EDGE_LOOP('',(#73253,#73254,#73255,#73256,#73257,#73258)) ;
#27159 = EDGE_LOOP('',(#73259,#73260,#73261,#73262,#73263,#73264)) ;
#27160 = EDGE_LOOP('',(#73265,#73266,#73267,#73268,#73269,#73270)) ;
#27161 = EDGE_LOOP('',(#73271,#73272,#73273,#73274)) ;
#27162 = EDGE_LOOP('',(#73275,#73276,#73277,#73278)) ;
#27163 = EDGE_LOOP('',(#73279,#73280,#73281,#73282)) ;
#27164 = EDGE_LOOP('',(#73283,#73284,#73285,#73286)) ;
#27165 = EDGE_LOOP('',(#73287,#73288,#73289,#73290)) ;
#27166 = EDGE_LOOP('',(#73291,#73292,#73293,#73294)) ;
#27167 = EDGE_LOOP('',(#73295,#73296,#73297,#73298)) ;
#27168 = EDGE_LOOP('',(#73299,#73300,#73301,#73302)) ;
#27169 = EDGE_LOOP('',(#73303,#73304,#73305,#73306)) ;
#27170 = EDGE_LOOP('',(#73307,#73308,#73309,#73310)) ;
#27171 = EDGE_LOOP('',(#73311,#73312,#73313)) ;
#27172 = EDGE_LOOP('',(#73314,#73315,#73316)) ;
#27173 = EDGE_LOOP('',(#73317,#73318,#73319,#73320)) ;
#27174 = EDGE_LOOP('',(#73321,#73322,#73323,#73324)) ;
#27175 = EDGE_LOOP('',(#73325,#73326,#73327,#73328)) ;
#27176 = EDGE_LOOP('',(#73329,#73330,#73331,#73332)) ;
#27177 = EDGE_LOOP('',(#73333,#73334,#73335,#73336)) ;
#27178 = EDGE_LOOP('',(#73337,#73338,#73339)) ;
#27179 = EDGE_LOOP('',(#73340,#73341,#73342)) ;
#27180 = EDGE_LOOP('',(#73343,#73344,#73345,#73346)) ;
#27181 = EDGE_LOOP('',(#73347,#73348,#73349,#73350)) ;
#27182 = EDGE_LOOP('',(#73351,#73352,#73353,#73354)) ;
#27183 = EDGE_LOOP('',(#73355,#73356,#73357,#73358)) ;
#27184 = EDGE_LOOP('',(#73359,#73360,#73361)) ;
#27185 = EDGE_LOOP('',(#73362,#73363,#73364)) ;
#27186 = EDGE_LOOP('',(#73365,#73366,#73367,#73368)) ;
#27187 = EDGE_LOOP('',(#73369,#73370,#73371,#73372)) ;
#27188 = EDGE_LOOP('',(#73373,#73374,#73375,#73376)) ;
#27189 = EDGE_LOOP('',(#73377,#73378,#73379,#73380)) ;
#27190 = EDGE_LOOP('',(#73381,#73382,#73383)) ;
#27191 = EDGE_LOOP('',(#73384,#73385,#73386)) ;
#27192 = EDGE_LOOP('',(#73387,#73388,#73389,#73390)) ;
#27193 = EDGE_LOOP('',(#73391,#73392,#73393,#73394)) ;
#27194 = EDGE_LOOP('',(#73395,#73396,#73397)) ;
#27195 = EDGE_LOOP('',(#73398,#73399,#73400,#73401)) ;
#27196 = EDGE_LOOP('',(#73402,#73403,#73404,#73405)) ;
#27197 = EDGE_LOOP('',(#73406,#73407,#73408,#73409)) ;
#27198 = EDGE_LOOP('',(#73410,#73411,#73412,#73413)) ;
#27199 = EDGE_LOOP('',(#73414,#73415,#73416)) ;
#27200 = EDGE_LOOP('',(#73417,#73418,#73419,#73420)) ;
#27201 = EDGE_LOOP('',(#73421,#73422,#73423,#73424)) ;
#27202 = EDGE_LOOP('',(#73425,#73426,#73427,#73428)) ;
#27203 = EDGE_LOOP('',(#73429,#73430,#73431,#73432)) ;
#27204 = EDGE_LOOP('',(#73433,#73434,#73435,#73436)) ;
#27205 = EDGE_LOOP('',(#73437,#73438,#73439)) ;
#27206 = EDGE_LOOP('',(#73440,#73441,#73442,#73443)) ;
#27207 = EDGE_LOOP('',(#73444,#73445,#73446,#73447)) ;
#27208 = EDGE_LOOP('',(#73448,#73449,#73450,#73451)) ;
#27209 = EDGE_LOOP('',(#73452,#73453,#73454,#73455)) ;
#27210 = EDGE_LOOP('',(#73456,#73457,#73458,#73459)) ;
#27211 = EDGE_LOOP('',(#73460,#73461,#73462,#73463)) ;
#27212 = EDGE_LOOP('',(#73464,#73465,#73466)) ;
#27213 = EDGE_LOOP('',(#73467,#73468,#73469,#73470)) ;
#27214 = EDGE_LOOP('',(#73471,#73472,#73473,#73474)) ;
#27215 = EDGE_LOOP('',(#73475,#73476,#73477,#73478,#73479,#73480,#73481)) ;
#27216 = EDGE_LOOP('',(#73482,#73483,#73484,#73485,#73486,#73487)) ;
#27217 = EDGE_LOOP('',(#73488,#73489,#73490,#73491)) ;
#27218 = EDGE_LOOP('',(#73492,#73493,#73494,#73495,#73496,#73497,#73498)) ;
#27219 = EDGE_LOOP('',(#73499,#73500,#73501,#73502,#73503,#73504,#73505)) ;
#27220 = EDGE_LOOP('',(#73506,#73507,#73508,#73509,#73510,#73511)) ;
#27221 = EDGE_LOOP('',(#73512,#73513,#73514,#73515)) ;
#27222 = EDGE_LOOP('',(#73516,#73517,#73518,#73519,#73520,#73521,#73522)) ;
#27223 = EDGE_LOOP('',(#73523,#73524,#73525,#73526,#73527,#73528,#73529)) ;
#27224 = EDGE_LOOP('',(#73530,#73531,#73532,#73533,#73534,#73535)) ;
#27225 = EDGE_LOOP('',(#73536,#73537,#73538,#73539)) ;
#27226 = EDGE_LOOP('',(#73540,#73541,#73542,#73543,#73544,#73545,#73546)) ;
#27227 = EDGE_LOOP('',(#73547,#73548,#73549,#73550,#73551,#73552,#73553)) ;
#27228 = EDGE_LOOP('',(#73554,#73555,#73556,#73557,#73558,#73559)) ;
#27229 = EDGE_LOOP('',(#73560,#73561,#73562,#73563)) ;
#27230 = EDGE_LOOP('',(#73564,#73565,#73566,#73567,#73568,#73569,#73570)) ;
#27231 = EDGE_LOOP('',(#73571,#73572,#73573,#73574,#73575,#73576,#73577)) ;
#27232 = EDGE_LOOP('',(#73578,#73579,#73580,#73581,#73582,#73583)) ;
#27233 = EDGE_LOOP('',(#73584,#73585,#73586,#73587)) ;
#27234 = EDGE_LOOP('',(#73588,#73589,#73590,#73591,#73592,#73593,#73594)) ;
#27235 = EDGE_LOOP('',(#73595,#73596,#73597,#73598,#73599,#73600,#73601)) ;
#27236 = EDGE_LOOP('',(#73602,#73603,#73604,#73605,#73606,#73607)) ;
#27237 = EDGE_LOOP('',(#73608,#73609,#73610,#73611)) ;
#27238 = EDGE_LOOP('',(#73612,#73613,#73614,#73615,#73616,#73617,#73618)) ;
#27239 = EDGE_LOOP('',(#73619,#73620,#73621,#73622,#73623,#73624,#73625)) ;
#27240 = EDGE_LOOP('',(#73626,#73627,#73628,#73629,#73630,#73631)) ;
#27241 = EDGE_LOOP('',(#73632,#73633,#73634,#73635)) ;
#27242 = EDGE_LOOP('',(#73636,#73637,#73638,#73639,#73640,#73641,#73642)) ;
#27243 = EDGE_LOOP('',(#73643,#73644,#73645,#73646,#73647,#73648,#73649)) ;
#27244 = EDGE_LOOP('',(#73650,#73651,#73652,#73653,#73654,#73655)) ;
#27245 = EDGE_LOOP('',(#73656,#73657,#73658,#73659)) ;
#27246 = EDGE_LOOP('',(#73660,#73661,#73662,#73663,#73664,#73665,#73666)) ;
#27247 = EDGE_LOOP('',(#73667,#73668,#73669,#73670)) ;
#27248 = EDGE_LOOP('',(#73671,#73672,#73673,#73674)) ;
#27249 = EDGE_LOOP('',(#73675,#73676,#73677,#73678)) ;
#27250 = EDGE_LOOP('',(#73679,#73680,#73681,#73682)) ;
#27251 = EDGE_LOOP('',(#73683,#73684,#73685,#73686)) ;
#27252 = EDGE_LOOP('',(#73687,#73688,#73689,#73690)) ;
#27253 = EDGE_LOOP('',(#73691,#73692,#73693,#73694)) ;
#27254 = EDGE_LOOP('',(#73695,#73696,#73697,#73698)) ;
#27255 = EDGE_LOOP('',(#73699,#73700,#73701,#73702)) ;
#27256 = EDGE_LOOP('',(#73703,#73704,#73705,#73706)) ;
#27257 = EDGE_LOOP('',(#73707,#73708,#73709)) ;
#27258 = EDGE_LOOP('',(#73710,#73711,#73712)) ;
#27259 = EDGE_LOOP('',(#73713,#73714,#73715,#73716)) ;
#27260 = EDGE_LOOP('',(#73717,#73718,#73719,#73720)) ;
#27261 = EDGE_LOOP('',(#73721,#73722,#73723,#73724)) ;
#27262 = EDGE_LOOP('',(#73725,#73726,#73727,#73728)) ;
#27263 = EDGE_LOOP('',(#73729,#73730,#73731,#73732)) ;
#27264 = EDGE_LOOP('',(#73733,#73734,#73735)) ;
#27265 = EDGE_LOOP('',(#73736,#73737,#73738)) ;
#27266 = EDGE_LOOP('',(#73739,#73740,#73741,#73742)) ;
#27267 = EDGE_LOOP('',(#73743,#73744,#73745,#73746)) ;
#27268 = EDGE_LOOP('',(#73747,#73748,#73749,#73750)) ;
#27269 = EDGE_LOOP('',(#73751,#73752,#73753,#73754)) ;
#27270 = EDGE_LOOP('',(#73755,#73756,#73757)) ;
#27271 = EDGE_LOOP('',(#73758,#73759,#73760)) ;
#27272 = EDGE_LOOP('',(#73761,#73762,#73763,#73764)) ;
#27273 = EDGE_LOOP('',(#73765,#73766,#73767,#73768)) ;
#27274 = EDGE_LOOP('',(#73769,#73770,#73771,#73772)) ;
#27275 = EDGE_LOOP('',(#73773,#73774,#73775,#73776)) ;
#27276 = EDGE_LOOP('',(#73777,#73778,#73779)) ;
#27277 = EDGE_LOOP('',(#73780,#73781,#73782)) ;
#27278 = EDGE_LOOP('',(#73783,#73784,#73785,#73786)) ;
#27279 = EDGE_LOOP('',(#73787,#73788,#73789,#73790)) ;
#27280 = EDGE_LOOP('',(#73791,#73792,#73793)) ;
#27281 = EDGE_LOOP('',(#73794,#73795,#73796)) ;
#27282 = EDGE_LOOP('',(#73797,#73798,#73799,#73800)) ;
#27283 = EDGE_LOOP('',(#73801,#73802,#73803,#73804)) ;
#27284 = EDGE_LOOP('',(#73805,#73806,#73807)) ;
#27285 = EDGE_LOOP('',(#73808,#73809,#73810)) ;
#27286 = EDGE_LOOP('',(#73811,#73812,#73813,#73814)) ;
#27287 = EDGE_LOOP('',(#73815,#73816,#73817,#73818)) ;
#27288 = EDGE_LOOP('',(#73819,#73820,#73821,#73822)) ;
#27289 = EDGE_LOOP('',(#73823,#73824,#73825,#73826)) ;
#27290 = EDGE_LOOP('',(#73827,#73828,#73829,#73830)) ;
#27291 = EDGE_LOOP('',(#73831,#73832,#73833)) ;
#27292 = EDGE_LOOP('',(#73834,#73835,#73836,#73837)) ;
#27293 = EDGE_LOOP('',(#73838,#73839,#73840,#73841)) ;
#27294 = EDGE_LOOP('',(#73842,#73843,#73844,#73845)) ;
#27295 = EDGE_LOOP('',(#73846,#73847,#73848,#73849)) ;
#27296 = EDGE_LOOP('',(#73850,#73851,#73852)) ;
#27297 = EDGE_LOOP('',(#73853,#73854,#73855,#73856)) ;
#27298 = EDGE_LOOP('',(#73857,#73858,#73859)) ;
#27299 = EDGE_LOOP('',(#73860,#73861,#73862,#73863)) ;
#27300 = EDGE_LOOP('',(#73864,#73865,#73866,#73867)) ;
#27301 = EDGE_LOOP('',(#73868,#73869,#73870,#73871)) ;
#27302 = EDGE_LOOP('',(#73872,#73873,#73874,#73875)) ;
#27303 = EDGE_LOOP('',(#73876,#73877,#73878,#73879)) ;
#27304 = EDGE_LOOP('',(#73880,#73881,#73882,#73883)) ;
#27305 = EDGE_LOOP('',(#73884,#73885,#73886,#73887)) ;
#27306 = EDGE_LOOP('',(#73888,#73889,#73890,#73891)) ;
#27307 = EDGE_LOOP('',(#73892,#73893,#73894,#73895)) ;
#27308 = EDGE_LOOP('',(#73896,#73897,#73898)) ;
#27309 = EDGE_LOOP('',(#73899,#73900,#73901,#73902)) ;
#27310 = EDGE_LOOP('',(#73903,#73904,#73905,#73906)) ;
#27311 = EDGE_LOOP('',(#73907,#73908,#73909,#73910)) ;
#27312 = EDGE_LOOP('',(#73911,#73912,#73913,#73914)) ;
#27313 = EDGE_LOOP('',(#73915,#73916,#73917)) ;
#27314 = EDGE_LOOP('',(#73918,#73919,#73920)) ;
#27315 = EDGE_LOOP('',(#73921,#73922,#73923,#73924)) ;
#27316 = EDGE_LOOP('',(#73925,#73926,#73927,#73928)) ;
#27317 = EDGE_LOOP('',(#73929,#73930,#73931,#73932)) ;
#27318 = EDGE_LOOP('',(#73933,#73934,#73935,#73936)) ;
#27319 = EDGE_LOOP('',(#73937,#73938,#73939,#73940)) ;
#27320 = EDGE_LOOP('',(#73941,#73942,#73943,#73944)) ;
#27321 = EDGE_LOOP('',(#73945,#73946,#73947)) ;
#27322 = EDGE_LOOP('',(#73948,#73949,#73950,#73951)) ;
#27323 = EDGE_LOOP('',(#73952,#73953,#73954,#73955)) ;
#27324 = EDGE_LOOP('',(#73956,#73957,#73958,#73959)) ;
#27325 = EDGE_LOOP('',(#73960,#73961,#73962,#73963)) ;
#27326 = EDGE_LOOP('',(#73964,#73965,#73966,#73967)) ;
#27327 = EDGE_LOOP('',(#73968,#73969,#73970)) ;
#27328 = EDGE_LOOP('',(#73971,#73972,#73973,#73974)) ;
#27329 = EDGE_LOOP('',(#73975,#73976,#73977,#73978,#73979)) ;
#27330 = EDGE_LOOP('',(#73980,#73981,#73982,#73983)) ;
#27331 = EDGE_LOOP('',(#73984,#73985,#73986,#73987,#73988)) ;
#27332 = EDGE_LOOP('',(#73989,#73990,#73991)) ;
#27333 = EDGE_LOOP('',(#73992,#73993,#73994,#73995,#73996)) ;
#27334 = EDGE_LOOP('',(#73997,#73998,#73999,#74000)) ;
#27335 = EDGE_LOOP('',(#74001,#74002,#74003,#74004)) ;
#27336 = EDGE_LOOP('',(#74005,#74006,#74007,#74008)) ;
#27337 = EDGE_LOOP('',(#74009,#74010,#74011,#74012)) ;
#27338 = EDGE_LOOP('',(#74013,#74014,#74015)) ;
#27339 = EDGE_LOOP('',(#74016,#74017,#74018)) ;
#27340 = EDGE_LOOP('',(#74019,#74020,#74021,#74022)) ;
#27341 = EDGE_LOOP('',(#74023,#74024,#74025,#74026)) ;
#27342 = EDGE_LOOP('',(#74027,#74028,#74029)) ;
#27343 = EDGE_LOOP('',(#74030,#74031,#74032,#74033)) ;
#27344 = EDGE_LOOP('',(#74034,#74035,#74036,#74037,#74038)) ;
#27345 = EDGE_LOOP('',(#74039,#74040,#74041,#74042,#74043)) ;
#27346 = EDGE_LOOP('',(#74044,#74045,#74046,#74047)) ;
#27347 = EDGE_LOOP('',(#74048,#74049,#74050,#74051)) ;
#27348 = EDGE_LOOP('',(#74052,#74053,#74054,#74055)) ;
#27349 = EDGE_LOOP('',(#74056,#74057,#74058)) ;
#27350 = EDGE_LOOP('',(#74059,#74060,#74061,#74062)) ;
#27351 = EDGE_LOOP('',(#74063,#74064,#74065,#74066)) ;
#27352 = EDGE_LOOP('',(#74067,#74068,#74069)) ;
#27353 = EDGE_LOOP('',(#74070,#74071,#74072,#74073)) ;
#27354 = EDGE_LOOP('',(#74074,#74075,#74076,#74077)) ;
#27355 = EDGE_LOOP('',(#74078,#74079,#74080)) ;
#27356 = EDGE_LOOP('',(#74081,#74082,#74083)) ;
#27357 = EDGE_LOOP('',(#74084,#74085,#74086,#74087)) ;
#27358 = EDGE_LOOP('',(#74088,#74089,#74090,#74091)) ;
#27359 = EDGE_LOOP('',(#74092,#74093,#74094,#74095)) ;
#27360 = EDGE_LOOP('',(#74096,#74097,#74098)) ;
#27361 = EDGE_LOOP('',(#74099,#74100,#74101,#74102)) ;
#27362 = EDGE_LOOP('',(#74103,#74104,#74105,#74106)) ;
#27363 = EDGE_LOOP('',(#74107,#74108,#74109)) ;
#27364 = EDGE_LOOP('',(#74110,#74111,#74112,#74113)) ;
#27365 = EDGE_LOOP('',(#74114,#74115,#74116,#74117)) ;
#27366 = EDGE_LOOP('',(#74118,#74119,#74120,#74121,#74122)) ;
#27367 = EDGE_LOOP('',(#74123,#74124,#74125,#74126)) ;
#27368 = EDGE_LOOP('',(#74127,#74128,#74129,#74130)) ;
#27369 = EDGE_LOOP('',(#74131,#74132,#74133,#74134)) ;
#27370 = EDGE_LOOP('',(#74135,#74136,#74137,#74138)) ;
#27371 = EDGE_LOOP('',(#74139,#74140,#74141,#74142)) ;
#27372 = EDGE_LOOP('',(#74143,#74144,#74145,#74146)) ;
#27373 = EDGE_LOOP('',(#74147,#74148,#74149,#74150)) ;
#27374 = EDGE_LOOP('',(#74151,#74152,#74153,#74154)) ;
#27375 = EDGE_LOOP('',(#74155,#74156,#74157,#74158)) ;
#27376 = EDGE_LOOP('',(#74159,#74160,#74161,#74162)) ;
#27377 = EDGE_LOOP('',(#74163,#74164,#74165,#74166)) ;
#27378 = EDGE_LOOP('',(#74167,#74168,#74169)) ;
#27379 = EDGE_LOOP('',(#74170,#74171,#74172)) ;
#27380 = EDGE_LOOP('',(#74173,#74174,#74175,#74176)) ;
#27381 = EDGE_LOOP('',(#74177,#74178,#74179,#74180)) ;
#27382 = EDGE_LOOP('',(#74181,#74182,#74183,#74184)) ;
#27383 = EDGE_LOOP('',(#74185,#74186,#74187,#74188)) ;
#27384 = EDGE_LOOP('',(#74189,#74190,#74191)) ;
#27385 = EDGE_LOOP('',(#74192,#74193,#74194)) ;
#27386 = EDGE_LOOP('',(#74195,#74196,#74197,#74198)) ;
#27387 = EDGE_LOOP('',(#74199,#74200,#74201,#74202)) ;
#27388 = EDGE_LOOP('',(#74203,#74204,#74205,#74206)) ;
#27389 = EDGE_LOOP('',(#74207,#74208,#74209,#74210)) ;
#27390 = EDGE_LOOP('',(#74211,#74212,#74213,#74214)) ;
#27391 = EDGE_LOOP('',(#74215,#74216,#74217,#74218)) ;
#27392 = EDGE_LOOP('',(#74219,#74220,#74221,#74222)) ;
#27393 = EDGE_LOOP('',(#74223,#74224,#74225,#74226)) ;
#27394 = EDGE_LOOP('',(#74227,#74228,#74229,#74230)) ;
#27395 = EDGE_LOOP('',(#74231,#74232,#74233,#74234)) ;
#27396 = EDGE_LOOP('',(#74235,#74236,#74237,#74238)) ;
#27397 = EDGE_LOOP('',(#74239,#74240,#74241)) ;
#27398 = EDGE_LOOP('',(#74242,#74243,#74244)) ;
#27399 = EDGE_LOOP('',(#74245,#74246,#74247,#74248)) ;
#27400 = EDGE_LOOP('',(#74249,#74250,#74251,#74252)) ;
#27401 = EDGE_LOOP('',(#74253,#74254,#74255,#74256)) ;
#27402 = EDGE_LOOP('',(#74257,#74258,#74259,#74260)) ;
#27403 = EDGE_LOOP('',(#74261,#74262,#74263,#74264)) ;
#27404 = EDGE_LOOP('',(#74265,#74266,#74267)) ;
#27405 = EDGE_LOOP('',(#74268,#74269,#74270)) ;
#27406 = EDGE_LOOP('',(#74271,#74272,#74273,#74274)) ;
#27407 = EDGE_LOOP('',(#74275,#74276,#74277,#74278)) ;
#27408 = EDGE_LOOP('',(#74279,#74280,#74281,#74282)) ;
#27409 = EDGE_LOOP('',(#74283,#74284,#74285,#74286)) ;
#27410 = EDGE_LOOP('',(#74287,#74288,#74289)) ;
#27411 = EDGE_LOOP('',(#74290,#74291,#74292)) ;
#27412 = EDGE_LOOP('',(#74293,#74294,#74295,#74296)) ;
#27413 = EDGE_LOOP('',(#74297,#74298,#74299,#74300)) ;
#27414 = EDGE_LOOP('',(#74301,#74302,#74303,#74304)) ;
#27415 = EDGE_LOOP('',(#74305,#74306,#74307,#74308)) ;
#27416 = EDGE_LOOP('',(#74309,#74310,#74311)) ;
#27417 = EDGE_LOOP('',(#74312,#74313,#74314)) ;
#27418 = EDGE_LOOP('',(#74315,#74316,#74317,#74318)) ;
#27419 = EDGE_LOOP('',(#74319,#74320,#74321,#74322)) ;
#27420 = EDGE_LOOP('',(#74323,#74324,#74325)) ;
#27421 = EDGE_LOOP('',(#74326,#74327,#74328)) ;
#27422 = EDGE_LOOP('',(#74329,#74330,#74331,#74332)) ;
#27423 = EDGE_LOOP('',(#74333,#74334,#74335,#74336)) ;
#27424 = EDGE_LOOP('',(#74337,#74338,#74339)) ;
#27425 = EDGE_LOOP('',(#74340,#74341,#74342)) ;
#27426 = EDGE_LOOP('',(#74343,#74344,#74345,#74346)) ;
#27427 = EDGE_LOOP('',(#74347,#74348,#74349,#74350)) ;
#27428 = EDGE_LOOP('',(#74351,#74352,#74353,#74354)) ;
#27429 = EDGE_LOOP('',(#74355,#74356,#74357,#74358)) ;
#27430 = EDGE_LOOP('',(#74359,#74360,#74361,#74362)) ;
#27431 = EDGE_LOOP('',(#74363,#74364,#74365)) ;
#27432 = EDGE_LOOP('',(#74366,#74367,#74368,#74369)) ;
#27433 = EDGE_LOOP('',(#74370,#74371,#74372,#74373)) ;
#27434 = EDGE_LOOP('',(#74374,#74375,#74376,#74377)) ;
#27435 = EDGE_LOOP('',(#74378,#74379,#74380,#74381)) ;
#27436 = EDGE_LOOP('',(#74382,#74383,#74384)) ;
#27437 = EDGE_LOOP('',(#74385,#74386,#74387,#74388)) ;
#27438 = EDGE_LOOP('',(#74389,#74390,#74391)) ;
#27439 = EDGE_LOOP('',(#74392,#74393,#74394,#74395)) ;
#27440 = EDGE_LOOP('',(#74396,#74397,#74398,#74399)) ;
#27441 = EDGE_LOOP('',(#74400,#74401,#74402,#74403)) ;
#27442 = EDGE_LOOP('',(#74404,#74405,#74406,#74407)) ;
#27443 = EDGE_LOOP('',(#74408,#74409,#74410,#74411)) ;
#27444 = EDGE_LOOP('',(#74412,#74413,#74414,#74415)) ;
#27445 = EDGE_LOOP('',(#74416,#74417,#74418,#74419)) ;
#27446 = EDGE_LOOP('',(#74420,#74421,#74422,#74423)) ;
#27447 = EDGE_LOOP('',(#74424,#74425,#74426,#74427)) ;
#27448 = EDGE_LOOP('',(#74428,#74429,#74430)) ;
#27449 = EDGE_LOOP('',(#74431,#74432,#74433,#74434)) ;
#27450 = EDGE_LOOP('',(#74435,#74436,#74437,#74438)) ;
#27451 = EDGE_LOOP('',(#74439,#74440,#74441,#74442)) ;
#27452 = EDGE_LOOP('',(#74443,#74444,#74445,#74446)) ;
#27453 = EDGE_LOOP('',(#74447,#74448,#74449)) ;
#27454 = EDGE_LOOP('',(#74450,#74451,#74452)) ;
#27455 = EDGE_LOOP('',(#74453,#74454,#74455,#74456)) ;
#27456 = EDGE_LOOP('',(#74457,#74458,#74459,#74460)) ;
#27457 = EDGE_LOOP('',(#74461,#74462,#74463,#74464)) ;
#27458 = EDGE_LOOP('',(#74465,#74466,#74467,#74468)) ;
#27459 = EDGE_LOOP('',(#74469,#74470,#74471,#74472)) ;
#27460 = EDGE_LOOP('',(#74473,#74474,#74475,#74476)) ;
#27461 = EDGE_LOOP('',(#74477,#74478,#74479)) ;
#27462 = EDGE_LOOP('',(#74480,#74481,#74482,#74483)) ;
#27463 = EDGE_LOOP('',(#74484,#74485,#74486,#74487)) ;
#27464 = EDGE_LOOP('',(#74488,#74489,#74490,#74491)) ;
#27465 = EDGE_LOOP('',(#74492,#74493,#74494,#74495)) ;
#27466 = EDGE_LOOP('',(#74496,#74497,#74498,#74499)) ;
#27467 = EDGE_LOOP('',(#74500,#74501,#74502)) ;
#27468 = EDGE_LOOP('',(#74503,#74504,#74505,#74506)) ;
#27469 = EDGE_LOOP('',(#74507,#74508,#74509,#74510,#74511)) ;
#27470 = EDGE_LOOP('',(#74512,#74513,#74514,#74515)) ;
#27471 = EDGE_LOOP('',(#74516,#74517,#74518,#74519,#74520)) ;
#27472 = EDGE_LOOP('',(#74521,#74522,#74523)) ;
#27473 = EDGE_LOOP('',(#74524,#74525,#74526,#74527,#74528)) ;
#27474 = EDGE_LOOP('',(#74529,#74530,#74531,#74532)) ;
#27475 = EDGE_LOOP('',(#74533,#74534,#74535,#74536)) ;
#27476 = EDGE_LOOP('',(#74537,#74538,#74539,#74540)) ;
#27477 = EDGE_LOOP('',(#74541,#74542,#74543,#74544)) ;
#27478 = EDGE_LOOP('',(#74545,#74546,#74547)) ;
#27479 = EDGE_LOOP('',(#74548,#74549,#74550)) ;
#27480 = EDGE_LOOP('',(#74551,#74552,#74553,#74554)) ;
#27481 = EDGE_LOOP('',(#74555,#74556,#74557,#74558)) ;
#27482 = EDGE_LOOP('',(#74559,#74560,#74561)) ;
#27483 = EDGE_LOOP('',(#74562,#74563,#74564,#74565)) ;
#27484 = EDGE_LOOP('',(#74566,#74567,#74568,#74569,#74570)) ;
#27485 = EDGE_LOOP('',(#74571,#74572,#74573,#74574,#74575)) ;
#27486 = EDGE_LOOP('',(#74576,#74577,#74578,#74579)) ;
#27487 = EDGE_LOOP('',(#74580,#74581,#74582,#74583)) ;
#27488 = EDGE_LOOP('',(#74584,#74585,#74586,#74587)) ;
#27489 = EDGE_LOOP('',(#74588,#74589,#74590)) ;
#27490 = EDGE_LOOP('',(#74591,#74592,#74593,#74594)) ;
#27491 = EDGE_LOOP('',(#74595,#74596,#74597,#74598)) ;
#27492 = EDGE_LOOP('',(#74599,#74600,#74601)) ;
#27493 = EDGE_LOOP('',(#74602,#74603,#74604,#74605)) ;
#27494 = EDGE_LOOP('',(#74606,#74607,#74608,#74609)) ;
#27495 = EDGE_LOOP('',(#74610,#74611,#74612)) ;
#27496 = EDGE_LOOP('',(#74613,#74614,#74615)) ;
#27497 = EDGE_LOOP('',(#74616,#74617,#74618,#74619)) ;
#27498 = EDGE_LOOP('',(#74620,#74621,#74622,#74623)) ;
#27499 = EDGE_LOOP('',(#74624,#74625,#74626,#74627)) ;
#27500 = EDGE_LOOP('',(#74628,#74629,#74630)) ;
#27501 = EDGE_LOOP('',(#74631,#74632,#74633,#74634)) ;
#27502 = EDGE_LOOP('',(#74635,#74636,#74637,#74638)) ;
#27503 = EDGE_LOOP('',(#74639,#74640,#74641)) ;
#27504 = EDGE_LOOP('',(#74642,#74643,#74644,#74645)) ;
#27505 = EDGE_LOOP('',(#74646,#74647,#74648,#74649)) ;
#27506 = EDGE_LOOP('',(#74650,#74651,#74652,#74653,#74654)) ;
#27507 = EDGE_LOOP('',(#74655,#74656,#74657,#74658)) ;
#27508 = EDGE_LOOP('',(#74659,#74660,#74661,#74662)) ;
#27509 = EDGE_LOOP('',(#74663,#74664,#74665,#74666)) ;
#27510 = EDGE_LOOP('',(#74667,#74668,#74669,#74670)) ;
#27511 = EDGE_LOOP('',(#74671,#74672,#74673,#74674)) ;
#27512 = EDGE_LOOP('',(#74675,#74676,#74677,#74678)) ;
#27513 = EDGE_LOOP('',(#74679,#74680,#74681,#74682)) ;
#27514 = EDGE_LOOP('',(#74683,#74684,#74685,#74686)) ;
#27515 = EDGE_LOOP('',(#74687,#74688,#74689,#74690)) ;
#27516 = EDGE_LOOP('',(#74691,#74692,#74693,#74694)) ;
#27517 = EDGE_LOOP('',(#74695,#74696,#74697,#74698)) ;
#27518 = EDGE_LOOP('',(#74699,#74700,#74701)) ;
#27519 = EDGE_LOOP('',(#74702,#74703,#74704)) ;
#27520 = EDGE_LOOP('',(#74705,#74706,#74707,#74708)) ;
#27521 = EDGE_LOOP('',(#74709,#74710,#74711,#74712)) ;
#27522 = EDGE_LOOP('',(#74713,#74714,#74715,#74716)) ;
#27523 = EDGE_LOOP('',(#74717,#74718,#74719,#74720)) ;
#27524 = EDGE_LOOP('',(#74721,#74722,#74723)) ;
#27525 = EDGE_LOOP('',(#74724,#74725,#74726)) ;
#27526 = EDGE_LOOP('',(#74727,#74728,#74729,#74730)) ;
#27527 = EDGE_LOOP('',(#74731,#74732,#74733,#74734)) ;
#27528 = EDGE_LOOP('',(#74735,#74736,#74737,#74738)) ;
#27529 = EDGE_LOOP('',(#74739,#74740,#74741,#74742)) ;
#27530 = EDGE_LOOP('',(#74743,#74744,#74745,#74746)) ;
#27531 = EDGE_LOOP('',(#74747,#74748,#74749,#74750)) ;
#27532 = EDGE_LOOP('',(#74751,#74752,#74753,#74754)) ;
#27533 = EDGE_LOOP('',(#74755,#74756,#74757,#74758)) ;
#27534 = EDGE_LOOP('',(#74759,#74760,#74761,#74762)) ;
#27535 = EDGE_LOOP('',(#74763,#74764,#74765,#74766)) ;
#27536 = EDGE_LOOP('',(#74767,#74768,#74769,#74770)) ;
#27537 = EDGE_LOOP('',(#74771,#74772,#74773)) ;
#27538 = EDGE_LOOP('',(#74774,#74775,#74776)) ;
#27539 = EDGE_LOOP('',(#74777,#74778,#74779,#74780)) ;
#27540 = EDGE_LOOP('',(#74781,#74782,#74783,#74784)) ;
#27541 = EDGE_LOOP('',(#74785,#74786,#74787,#74788)) ;
#27542 = EDGE_LOOP('',(#74789,#74790,#74791,#74792)) ;
#27543 = EDGE_LOOP('',(#74793,#74794,#74795,#74796)) ;
#27544 = EDGE_LOOP('',(#74797,#74798,#74799)) ;
#27545 = EDGE_LOOP('',(#74800,#74801,#74802)) ;
#27546 = EDGE_LOOP('',(#74803,#74804,#74805,#74806)) ;
#27547 = EDGE_LOOP('',(#74807,#74808,#74809,#74810)) ;
#27548 = EDGE_LOOP('',(#74811,#74812,#74813,#74814)) ;
#27549 = EDGE_LOOP('',(#74815,#74816,#74817,#74818)) ;
#27550 = EDGE_LOOP('',(#74819,#74820,#74821)) ;
#27551 = EDGE_LOOP('',(#74822,#74823,#74824)) ;
#27552 = EDGE_LOOP('',(#74825,#74826,#74827,#74828)) ;
#27553 = EDGE_LOOP('',(#74829,#74830,#74831,#74832)) ;
#27554 = EDGE_LOOP('',(#74833,#74834,#74835,#74836)) ;
#27555 = EDGE_LOOP('',(#74837,#74838,#74839,#74840)) ;
#27556 = EDGE_LOOP('',(#74841,#74842,#74843)) ;
#27557 = EDGE_LOOP('',(#74844,#74845,#74846)) ;
#27558 = EDGE_LOOP('',(#74847,#74848,#74849,#74850)) ;
#27559 = EDGE_LOOP('',(#74851,#74852,#74853,#74854)) ;
#27560 = EDGE_LOOP('',(#74855,#74856,#74857)) ;
#27561 = EDGE_LOOP('',(#74858,#74859,#74860)) ;
#27562 = EDGE_LOOP('',(#74861,#74862,#74863,#74864)) ;
#27563 = EDGE_LOOP('',(#74865,#74866,#74867,#74868)) ;
#27564 = EDGE_LOOP('',(#74869,#74870,#74871)) ;
#27565 = EDGE_LOOP('',(#74872,#74873,#74874)) ;
#27566 = EDGE_LOOP('',(#74875,#74876,#74877,#74878)) ;
#27567 = EDGE_LOOP('',(#74879,#74880,#74881,#74882)) ;
#27568 = EDGE_LOOP('',(#74883,#74884,#74885,#74886)) ;
#27569 = EDGE_LOOP('',(#74887,#74888,#74889,#74890)) ;
#27570 = EDGE_LOOP('',(#74891,#74892,#74893,#74894)) ;
#27571 = EDGE_LOOP('',(#74895,#74896,#74897)) ;
#27572 = EDGE_LOOP('',(#74898,#74899,#74900,#74901)) ;
#27573 = EDGE_LOOP('',(#74902,#74903,#74904,#74905)) ;
#27574 = EDGE_LOOP('',(#74906,#74907,#74908,#74909)) ;
#27575 = EDGE_LOOP('',(#74910,#74911,#74912,#74913)) ;
#27576 = EDGE_LOOP('',(#74914,#74915,#74916)) ;
#27577 = EDGE_LOOP('',(#74917,#74918,#74919,#74920)) ;
#27578 = EDGE_LOOP('',(#74921,#74922,#74923)) ;
#27579 = EDGE_LOOP('',(#74924,#74925,#74926,#74927)) ;
#27580 = EDGE_LOOP('',(#74928,#74929,#74930,#74931)) ;
#27581 = EDGE_LOOP('',(#74932,#74933,#74934,#74935)) ;
#27582 = EDGE_LOOP('',(#74936,#74937,#74938,#74939)) ;
#27583 = EDGE_LOOP('',(#74940,#74941,#74942,#74943)) ;
#27584 = EDGE_LOOP('',(#74944,#74945,#74946,#74947)) ;
#27585 = EDGE_LOOP('',(#74948,#74949,#74950,#74951)) ;
#27586 = EDGE_LOOP('',(#74952,#74953,#74954,#74955)) ;
#27587 = EDGE_LOOP('',(#74956,#74957,#74958,#74959)) ;
#27588 = EDGE_LOOP('',(#74960,#74961,#74962)) ;
#27589 = EDGE_LOOP('',(#74963,#74964,#74965,#74966)) ;
#27590 = EDGE_LOOP('',(#74967,#74968,#74969,#74970)) ;
#27591 = EDGE_LOOP('',(#74971,#74972,#74973,#74974)) ;
#27592 = EDGE_LOOP('',(#74975,#74976,#74977,#74978)) ;
#27593 = EDGE_LOOP('',(#74979,#74980,#74981)) ;
#27594 = EDGE_LOOP('',(#74982,#74983,#74984)) ;
#27595 = EDGE_LOOP('',(#74985,#74986,#74987,#74988)) ;
#27596 = EDGE_LOOP('',(#74989,#74990,#74991,#74992)) ;
#27597 = EDGE_LOOP('',(#74993,#74994,#74995,#74996)) ;
#27598 = EDGE_LOOP('',(#74997,#74998,#74999,#75000)) ;
#27599 = EDGE_LOOP('',(#75001,#75002,#75003,#75004)) ;
#27600 = EDGE_LOOP('',(#75005,#75006,#75007,#75008)) ;
#27601 = EDGE_LOOP('',(#75009,#75010,#75011)) ;
#27602 = EDGE_LOOP('',(#75012,#75013,#75014,#75015)) ;
#27603 = EDGE_LOOP('',(#75016,#75017,#75018,#75019)) ;
#27604 = EDGE_LOOP('',(#75020,#75021,#75022,#75023)) ;
#27605 = EDGE_LOOP('',(#75024,#75025,#75026,#75027)) ;
#27606 = EDGE_LOOP('',(#75028,#75029,#75030,#75031)) ;
#27607 = EDGE_LOOP('',(#75032,#75033,#75034)) ;
#27608 = EDGE_LOOP('',(#75035,#75036,#75037,#75038)) ;
#27609 = EDGE_LOOP('',(#75039,#75040,#75041,#75042,#75043)) ;
#27610 = EDGE_LOOP('',(#75044,#75045,#75046,#75047)) ;
#27611 = EDGE_LOOP('',(#75048,#75049,#75050,#75051,#75052)) ;
#27612 = EDGE_LOOP('',(#75053,#75054,#75055)) ;
#27613 = EDGE_LOOP('',(#75056,#75057,#75058,#75059,#75060)) ;
#27614 = EDGE_LOOP('',(#75061,#75062,#75063,#75064)) ;
#27615 = EDGE_LOOP('',(#75065,#75066,#75067,#75068)) ;
#27616 = EDGE_LOOP('',(#75069,#75070,#75071,#75072)) ;
#27617 = EDGE_LOOP('',(#75073,#75074,#75075,#75076)) ;
#27618 = EDGE_LOOP('',(#75077,#75078,#75079)) ;
#27619 = EDGE_LOOP('',(#75080,#75081,#75082)) ;
#27620 = EDGE_LOOP('',(#75083,#75084,#75085,#75086)) ;
#27621 = EDGE_LOOP('',(#75087,#75088,#75089,#75090)) ;
#27622 = EDGE_LOOP('',(#75091,#75092,#75093)) ;
#27623 = EDGE_LOOP('',(#75094,#75095,#75096,#75097)) ;
#27624 = EDGE_LOOP('',(#75098,#75099,#75100,#75101,#75102)) ;
#27625 = EDGE_LOOP('',(#75103,#75104,#75105,#75106,#75107)) ;
#27626 = EDGE_LOOP('',(#75108,#75109,#75110,#75111)) ;
#27627 = EDGE_LOOP('',(#75112,#75113,#75114,#75115)) ;
#27628 = EDGE_LOOP('',(#75116,#75117,#75118,#75119)) ;
#27629 = EDGE_LOOP('',(#75120,#75121,#75122)) ;
#27630 = EDGE_LOOP('',(#75123,#75124,#75125,#75126)) ;
#27631 = EDGE_LOOP('',(#75127,#75128,#75129,#75130)) ;
#27632 = EDGE_LOOP('',(#75131,#75132,#75133)) ;
#27633 = EDGE_LOOP('',(#75134,#75135,#75136,#75137)) ;
#27634 = EDGE_LOOP('',(#75138,#75139,#75140,#75141)) ;
#27635 = EDGE_LOOP('',(#75142,#75143,#75144)) ;
#27636 = EDGE_LOOP('',(#75145,#75146,#75147)) ;
#27637 = EDGE_LOOP('',(#75148,#75149,#75150,#75151)) ;
#27638 = EDGE_LOOP('',(#75152,#75153,#75154,#75155)) ;
#27639 = EDGE_LOOP('',(#75156,#75157,#75158,#75159)) ;
#27640 = EDGE_LOOP('',(#75160,#75161,#75162)) ;
#27641 = EDGE_LOOP('',(#75163,#75164,#75165,#75166)) ;
#27642 = EDGE_LOOP('',(#75167,#75168,#75169,#75170)) ;
#27643 = EDGE_LOOP('',(#75171,#75172,#75173)) ;
#27644 = EDGE_LOOP('',(#75174,#75175,#75176,#75177)) ;
#27645 = EDGE_LOOP('',(#75178,#75179,#75180,#75181)) ;
#27646 = EDGE_LOOP('',(#75182,#75183,#75184,#75185,#75186)) ;
#27647 = EDGE_LOOP('',(#75187,#75188,#75189,#75190)) ;
#27648 = EDGE_LOOP('',(#75191,#75192,#75193,#75194)) ;
#27649 = EDGE_LOOP('',(#75195,#75196,#75197,#75198)) ;
#27650 = EDGE_LOOP('',(#75199,#75200,#75201,#75202)) ;
#27651 = EDGE_LOOP('',(#75203,#75204,#75205,#75206)) ;
#27652 = EDGE_LOOP('',(#75207,#75208,#75209,#75210)) ;
#27653 = EDGE_LOOP('',(#75211,#75212,#75213,#75214)) ;
#27654 = EDGE_LOOP('',(#75215,#75216,#75217,#75218)) ;
#27655 = EDGE_LOOP('',(#75219,#75220,#75221,#75222)) ;
#27656 = EDGE_LOOP('',(#75223,#75224,#75225,#75226)) ;
#27657 = EDGE_LOOP('',(#75227,#75228,#75229,#75230)) ;
#27658 = EDGE_LOOP('',(#75231,#75232,#75233)) ;
#27659 = EDGE_LOOP('',(#75234,#75235,#75236)) ;
#27660 = EDGE_LOOP('',(#75237,#75238,#75239,#75240)) ;
#27661 = EDGE_LOOP('',(#75241,#75242,#75243,#75244)) ;
#27662 = EDGE_LOOP('',(#75245,#75246,#75247,#75248)) ;
#27663 = EDGE_LOOP('',(#75249,#75250,#75251,#75252)) ;
#27664 = EDGE_LOOP('',(#75253,#75254,#75255)) ;
#27665 = EDGE_LOOP('',(#75256,#75257,#75258)) ;
#27666 = EDGE_LOOP('',(#75259,#75260,#75261,#75262)) ;
#27667 = EDGE_LOOP('',(#75263,#75264,#75265,#75266)) ;
#27668 = EDGE_LOOP('',(#75267,#75268,#75269,#75270)) ;
#27669 = EDGE_LOOP('',(#75271,#75272,#75273,#75274)) ;
#27670 = EDGE_LOOP('',(#75275,#75276,#75277,#75278)) ;
#27671 = EDGE_LOOP('',(#75279,#75280,#75281,#75282)) ;
#27672 = EDGE_LOOP('',(#75283,#75284,#75285,#75286)) ;
#27673 = EDGE_LOOP('',(#75287,#75288,#75289,#75290)) ;
#27674 = EDGE_LOOP('',(#75291,#75292,#75293,#75294)) ;
#27675 = EDGE_LOOP('',(#75295,#75296,#75297,#75298)) ;
#27676 = EDGE_LOOP('',(#75299,#75300,#75301,#75302)) ;
#27677 = EDGE_LOOP('',(#75303,#75304,#75305)) ;
#27678 = EDGE_LOOP('',(#75306,#75307,#75308)) ;
#27679 = EDGE_LOOP('',(#75309,#75310,#75311,#75312)) ;
#27680 = EDGE_LOOP('',(#75313,#75314,#75315,#75316)) ;
#27681 = EDGE_LOOP('',(#75317,#75318,#75319,#75320)) ;
#27682 = EDGE_LOOP('',(#75321,#75322,#75323,#75324)) ;
#27683 = EDGE_LOOP('',(#75325,#75326,#75327,#75328)) ;
#27684 = EDGE_LOOP('',(#75329,#75330,#75331)) ;
#27685 = EDGE_LOOP('',(#75332,#75333,#75334)) ;
#27686 = EDGE_LOOP('',(#75335,#75336,#75337,#75338)) ;
#27687 = EDGE_LOOP('',(#75339,#75340,#75341,#75342)) ;
#27688 = EDGE_LOOP('',(#75343,#75344,#75345,#75346)) ;
#27689 = EDGE_LOOP('',(#75347,#75348,#75349,#75350)) ;
#27690 = EDGE_LOOP('',(#75351,#75352,#75353)) ;
#27691 = EDGE_LOOP('',(#75354,#75355,#75356)) ;
#27692 = EDGE_LOOP('',(#75357,#75358,#75359,#75360)) ;
#27693 = EDGE_LOOP('',(#75361,#75362,#75363,#75364)) ;
#27694 = EDGE_LOOP('',(#75365,#75366,#75367,#75368)) ;
#27695 = EDGE_LOOP('',(#75369,#75370,#75371,#75372)) ;
#27696 = EDGE_LOOP('',(#75373,#75374,#75375)) ;
#27697 = EDGE_LOOP('',(#75376,#75377,#75378)) ;
#27698 = EDGE_LOOP('',(#75379,#75380,#75381,#75382)) ;
#27699 = EDGE_LOOP('',(#75383,#75384,#75385,#75386)) ;
#27700 = EDGE_LOOP('',(#75387,#75388,#75389)) ;
#27701 = EDGE_LOOP('',(#75390,#75391,#75392)) ;
#27702 = EDGE_LOOP('',(#75393,#75394,#75395,#75396)) ;
#27703 = EDGE_LOOP('',(#75397,#75398,#75399,#75400)) ;
#27704 = EDGE_LOOP('',(#75401,#75402,#75403)) ;
#27705 = EDGE_LOOP('',(#75404,#75405,#75406)) ;
#27706 = EDGE_LOOP('',(#75407,#75408,#75409,#75410)) ;
#27707 = EDGE_LOOP('',(#75411,#75412,#75413,#75414)) ;
#27708 = EDGE_LOOP('',(#75415,#75416,#75417,#75418)) ;
#27709 = EDGE_LOOP('',(#75419,#75420,#75421,#75422)) ;
#27710 = EDGE_LOOP('',(#75423,#75424,#75425,#75426)) ;
#27711 = EDGE_LOOP('',(#75427,#75428,#75429)) ;
#27712 = EDGE_LOOP('',(#75430,#75431,#75432,#75433)) ;
#27713 = EDGE_LOOP('',(#75434,#75435,#75436,#75437)) ;
#27714 = EDGE_LOOP('',(#75438,#75439,#75440,#75441)) ;
#27715 = EDGE_LOOP('',(#75442,#75443,#75444,#75445)) ;
#27716 = EDGE_LOOP('',(#75446,#75447,#75448)) ;
#27717 = EDGE_LOOP('',(#75449,#75450,#75451,#75452)) ;
#27718 = EDGE_LOOP('',(#75453,#75454,#75455)) ;
#27719 = EDGE_LOOP('',(#75456,#75457,#75458,#75459)) ;
#27720 = EDGE_LOOP('',(#75460,#75461,#75462,#75463)) ;
#27721 = EDGE_LOOP('',(#75464,#75465,#75466,#75467)) ;
#27722 = EDGE_LOOP('',(#75468,#75469,#75470,#75471)) ;
#27723 = EDGE_LOOP('',(#75472,#75473,#75474,#75475)) ;
#27724 = EDGE_LOOP('',(#75476,#75477,#75478,#75479)) ;
#27725 = EDGE_LOOP('',(#75480,#75481,#75482,#75483)) ;
#27726 = EDGE_LOOP('',(#75484,#75485,#75486,#75487)) ;
#27727 = EDGE_LOOP('',(#75488,#75489,#75490,#75491)) ;
#27728 = EDGE_LOOP('',(#75492,#75493,#75494)) ;
#27729 = EDGE_LOOP('',(#75495,#75496,#75497,#75498)) ;
#27730 = EDGE_LOOP('',(#75499,#75500,#75501,#75502)) ;
#27731 = EDGE_LOOP('',(#75503,#75504,#75505,#75506)) ;
#27732 = EDGE_LOOP('',(#75507,#75508,#75509,#75510)) ;
#27733 = EDGE_LOOP('',(#75511,#75512,#75513)) ;
#27734 = EDGE_LOOP('',(#75514,#75515,#75516)) ;
#27735 = EDGE_LOOP('',(#75517,#75518,#75519,#75520)) ;
#27736 = EDGE_LOOP('',(#75521,#75522,#75523,#75524)) ;
#27737 = EDGE_LOOP('',(#75525,#75526,#75527,#75528)) ;
#27738 = EDGE_LOOP('',(#75529,#75530,#75531,#75532)) ;
#27739 = EDGE_LOOP('',(#75533,#75534,#75535,#75536)) ;
#27740 = EDGE_LOOP('',(#75537,#75538,#75539,#75540)) ;
#27741 = EDGE_LOOP('',(#75541,#75542,#75543)) ;
#27742 = EDGE_LOOP('',(#75544,#75545,#75546,#75547)) ;
#27743 = EDGE_LOOP('',(#75548,#75549,#75550,#75551)) ;
#27744 = EDGE_LOOP('',(#75552,#75553,#75554,#75555)) ;
#27745 = EDGE_LOOP('',(#75556,#75557,#75558,#75559)) ;
#27746 = EDGE_LOOP('',(#75560,#75561,#75562,#75563)) ;
#27747 = EDGE_LOOP('',(#75564,#75565,#75566)) ;
#27748 = EDGE_LOOP('',(#75567,#75568,#75569,#75570)) ;
#27749 = EDGE_LOOP('',(#75571,#75572,#75573,#75574,#75575)) ;
#27750 = EDGE_LOOP('',(#75576,#75577,#75578,#75579)) ;
#27751 = EDGE_LOOP('',(#75580,#75581,#75582,#75583,#75584)) ;
#27752 = EDGE_LOOP('',(#75585,#75586,#75587)) ;
#27753 = EDGE_LOOP('',(#75588,#75589,#75590,#75591,#75592)) ;
#27754 = EDGE_LOOP('',(#75593,#75594,#75595,#75596)) ;
#27755 = EDGE_LOOP('',(#75597,#75598,#75599,#75600)) ;
#27756 = EDGE_LOOP('',(#75601,#75602,#75603,#75604)) ;
#27757 = EDGE_LOOP('',(#75605,#75606,#75607,#75608)) ;
#27758 = EDGE_LOOP('',(#75609,#75610,#75611)) ;
#27759 = EDGE_LOOP('',(#75612,#75613,#75614)) ;
#27760 = EDGE_LOOP('',(#75615,#75616,#75617,#75618)) ;
#27761 = EDGE_LOOP('',(#75619,#75620,#75621,#75622)) ;
#27762 = EDGE_LOOP('',(#75623,#75624,#75625)) ;
#27763 = EDGE_LOOP('',(#75626,#75627,#75628,#75629)) ;
#27764 = EDGE_LOOP('',(#75630,#75631,#75632,#75633,#75634)) ;
#27765 = EDGE_LOOP('',(#75635,#75636,#75637,#75638,#75639)) ;
#27766 = EDGE_LOOP('',(#75640,#75641,#75642,#75643)) ;
#27767 = EDGE_LOOP('',(#75644,#75645,#75646,#75647)) ;
#27768 = EDGE_LOOP('',(#75648,#75649,#75650,#75651)) ;
#27769 = EDGE_LOOP('',(#75652,#75653,#75654)) ;
#27770 = EDGE_LOOP('',(#75655,#75656,#75657,#75658)) ;
#27771 = EDGE_LOOP('',(#75659,#75660,#75661,#75662)) ;
#27772 = EDGE_LOOP('',(#75663,#75664,#75665)) ;
#27773 = EDGE_LOOP('',(#75666,#75667,#75668,#75669)) ;
#27774 = EDGE_LOOP('',(#75670,#75671,#75672,#75673)) ;
#27775 = EDGE_LOOP('',(#75674,#75675,#75676)) ;
#27776 = EDGE_LOOP('',(#75677,#75678,#75679)) ;
#27777 = EDGE_LOOP('',(#75680,#75681,#75682,#75683)) ;
#27778 = EDGE_LOOP('',(#75684,#75685,#75686,#75687)) ;
#27779 = EDGE_LOOP('',(#75688,#75689,#75690,#75691)) ;
#27780 = EDGE_LOOP('',(#75692,#75693,#75694)) ;
#27781 = EDGE_LOOP('',(#75695,#75696,#75697,#75698)) ;
#27782 = EDGE_LOOP('',(#75699,#75700,#75701,#75702)) ;
#27783 = EDGE_LOOP('',(#75703,#75704,#75705)) ;
#27784 = EDGE_LOOP('',(#75706,#75707,#75708,#75709)) ;
#27785 = EDGE_LOOP('',(#75710,#75711,#75712,#75713)) ;
#27786 = EDGE_LOOP('',(#75714,#75715,#75716,#75717,#75718)) ;
#27787 = EDGE_LOOP('',(#75719,#75720,#75721,#75722)) ;
#27788 = EDGE_LOOP('',(#75723,#75724,#75725,#75726)) ;
#27789 = EDGE_LOOP('',(#75727,#75728,#75729,#75730)) ;
#27790 = EDGE_LOOP('',(#75731,#75732,#75733,#75734)) ;
#27791 = EDGE_LOOP('',(#75735,#75736,#75737,#75738)) ;
#27792 = EDGE_LOOP('',(#75739,#75740,#75741,#75742)) ;
#27793 = EDGE_LOOP('',(#75743,#75744,#75745,#75746)) ;
#27794 = EDGE_LOOP('',(#75747,#75748,#75749,#75750)) ;
#27795 = EDGE_LOOP('',(#75751,#75752,#75753,#75754)) ;
#27796 = EDGE_LOOP('',(#75755,#75756,#75757,#75758)) ;
#27797 = EDGE_LOOP('',(#75759,#75760,#75761,#75762)) ;
#27798 = EDGE_LOOP('',(#75763,#75764,#75765)) ;
#27799 = EDGE_LOOP('',(#75766,#75767,#75768)) ;
#27800 = EDGE_LOOP('',(#75769,#75770,#75771,#75772)) ;
#27801 = EDGE_LOOP('',(#75773,#75774,#75775,#75776)) ;
#27802 = EDGE_LOOP('',(#75777,#75778,#75779,#75780)) ;
#27803 = EDGE_LOOP('',(#75781,#75782,#75783,#75784)) ;
#27804 = EDGE_LOOP('',(#75785,#75786,#75787)) ;
#27805 = EDGE_LOOP('',(#75788,#75789,#75790)) ;
#27806 = EDGE_LOOP('',(#75791,#75792,#75793,#75794)) ;
#27807 = EDGE_LOOP('',(#75795,#75796,#75797,#75798)) ;
#27808 = EDGE_LOOP('',(#75799,#75800,#75801,#75802)) ;
#27809 = EDGE_LOOP('',(#75803,#75804,#75805,#75806)) ;
#27810 = EDGE_LOOP('',(#75807,#75808,#75809,#75810)) ;
#27811 = EDGE_LOOP('',(#75811,#75812,#75813,#75814)) ;
#27812 = EDGE_LOOP('',(#75815,#75816,#75817,#75818)) ;
#27813 = EDGE_LOOP('',(#75819,#75820,#75821,#75822)) ;
#27814 = EDGE_LOOP('',(#75823,#75824,#75825,#75826)) ;
#27815 = EDGE_LOOP('',(#75827,#75828,#75829,#75830)) ;
#27816 = EDGE_LOOP('',(#75831,#75832,#75833,#75834)) ;
#27817 = EDGE_LOOP('',(#75835,#75836,#75837)) ;
#27818 = EDGE_LOOP('',(#75838,#75839,#75840)) ;
#27819 = EDGE_LOOP('',(#75841,#75842,#75843,#75844)) ;
#27820 = EDGE_LOOP('',(#75845,#75846,#75847,#75848)) ;
#27821 = EDGE_LOOP('',(#75849,#75850,#75851,#75852)) ;
#27822 = EDGE_LOOP('',(#75853,#75854,#75855,#75856)) ;
#27823 = EDGE_LOOP('',(#75857,#75858,#75859,#75860)) ;
#27824 = EDGE_LOOP('',(#75861,#75862,#75863)) ;
#27825 = EDGE_LOOP('',(#75864,#75865,#75866)) ;
#27826 = EDGE_LOOP('',(#75867,#75868,#75869,#75870)) ;
#27827 = EDGE_LOOP('',(#75871,#75872,#75873,#75874)) ;
#27828 = EDGE_LOOP('',(#75875,#75876,#75877,#75878)) ;
#27829 = EDGE_LOOP('',(#75879,#75880,#75881,#75882)) ;
#27830 = EDGE_LOOP('',(#75883,#75884,#75885)) ;
#27831 = EDGE_LOOP('',(#75886,#75887,#75888)) ;
#27832 = EDGE_LOOP('',(#75889,#75890,#75891,#75892)) ;
#27833 = EDGE_LOOP('',(#75893,#75894,#75895,#75896)) ;
#27834 = EDGE_LOOP('',(#75897,#75898,#75899,#75900)) ;
#27835 = EDGE_LOOP('',(#75901,#75902,#75903,#75904)) ;
#27836 = EDGE_LOOP('',(#75905,#75906,#75907)) ;
#27837 = EDGE_LOOP('',(#75908,#75909,#75910)) ;
#27838 = EDGE_LOOP('',(#75911,#75912,#75913,#75914)) ;
#27839 = EDGE_LOOP('',(#75915,#75916,#75917,#75918)) ;
#27840 = EDGE_LOOP('',(#75919,#75920,#75921)) ;
#27841 = EDGE_LOOP('',(#75922,#75923,#75924)) ;
#27842 = EDGE_LOOP('',(#75925,#75926,#75927,#75928)) ;
#27843 = EDGE_LOOP('',(#75929,#75930,#75931,#75932)) ;
#27844 = EDGE_LOOP('',(#75933,#75934,#75935)) ;
#27845 = EDGE_LOOP('',(#75936,#75937,#75938)) ;
#27846 = EDGE_LOOP('',(#75939,#75940,#75941,#75942)) ;
#27847 = EDGE_LOOP('',(#75943,#75944,#75945,#75946)) ;
#27848 = EDGE_LOOP('',(#75947,#75948,#75949,#75950)) ;
#27849 = EDGE_LOOP('',(#75951,#75952,#75953,#75954)) ;
#27850 = EDGE_LOOP('',(#75955,#75956,#75957,#75958)) ;
#27851 = EDGE_LOOP('',(#75959,#75960,#75961)) ;
#27852 = EDGE_LOOP('',(#75962,#75963,#75964,#75965)) ;
#27853 = EDGE_LOOP('',(#75966,#75967,#75968,#75969)) ;
#27854 = EDGE_LOOP('',(#75970,#75971,#75972,#75973)) ;
#27855 = EDGE_LOOP('',(#75974,#75975,#75976,#75977)) ;
#27856 = EDGE_LOOP('',(#75978,#75979,#75980)) ;
#27857 = EDGE_LOOP('',(#75981,#75982,#75983,#75984)) ;
#27858 = EDGE_LOOP('',(#75985,#75986,#75987)) ;
#27859 = EDGE_LOOP('',(#75988,#75989,#75990,#75991)) ;
#27860 = EDGE_LOOP('',(#75992,#75993,#75994,#75995)) ;
#27861 = EDGE_LOOP('',(#75996,#75997,#75998,#75999)) ;
#27862 = EDGE_LOOP('',(#76000,#76001,#76002,#76003)) ;
#27863 = EDGE_LOOP('',(#76004,#76005,#76006,#76007)) ;
#27864 = EDGE_LOOP('',(#76008,#76009,#76010,#76011)) ;
#27865 = EDGE_LOOP('',(#76012,#76013,#76014,#76015)) ;
#27866 = EDGE_LOOP('',(#76016,#76017,#76018,#76019)) ;
#27867 = EDGE_LOOP('',(#76020,#76021,#76022,#76023)) ;
#27868 = EDGE_LOOP('',(#76024,#76025,#76026)) ;
#27869 = EDGE_LOOP('',(#76027,#76028,#76029,#76030)) ;
#27870 = EDGE_LOOP('',(#76031,#76032,#76033,#76034)) ;
#27871 = EDGE_LOOP('',(#76035,#76036,#76037,#76038)) ;
#27872 = EDGE_LOOP('',(#76039,#76040,#76041,#76042)) ;
#27873 = EDGE_LOOP('',(#76043,#76044,#76045)) ;
#27874 = EDGE_LOOP('',(#76046,#76047,#76048)) ;
#27875 = EDGE_LOOP('',(#76049,#76050,#76051,#76052)) ;
#27876 = EDGE_LOOP('',(#76053,#76054,#76055,#76056)) ;
#27877 = EDGE_LOOP('',(#76057,#76058,#76059,#76060)) ;
#27878 = EDGE_LOOP('',(#76061,#76062,#76063,#76064)) ;
#27879 = EDGE_LOOP('',(#76065,#76066,#76067,#76068)) ;
#27880 = EDGE_LOOP('',(#76069,#76070,#76071,#76072)) ;
#27881 = EDGE_LOOP('',(#76073,#76074,#76075)) ;
#27882 = EDGE_LOOP('',(#76076,#76077,#76078,#76079)) ;
#27883 = EDGE_LOOP('',(#76080,#76081,#76082,#76083)) ;
#27884 = EDGE_LOOP('',(#76084,#76085,#76086,#76087)) ;
#27885 = EDGE_LOOP('',(#76088,#76089,#76090,#76091)) ;
#27886 = EDGE_LOOP('',(#76092,#76093,#76094,#76095)) ;
#27887 = EDGE_LOOP('',(#76096,#76097,#76098)) ;
#27888 = EDGE_LOOP('',(#76099,#76100,#76101,#76102)) ;
#27889 = EDGE_LOOP('',(#76103,#76104,#76105,#76106,#76107)) ;
#27890 = EDGE_LOOP('',(#76108,#76109,#76110,#76111)) ;
#27891 = EDGE_LOOP('',(#76112,#76113,#76114,#76115,#76116)) ;
#27892 = EDGE_LOOP('',(#76117,#76118,#76119)) ;
#27893 = EDGE_LOOP('',(#76120,#76121,#76122,#76123,#76124)) ;
#27894 = EDGE_LOOP('',(#76125,#76126,#76127,#76128)) ;
#27895 = EDGE_LOOP('',(#76129,#76130,#76131,#76132)) ;
#27896 = EDGE_LOOP('',(#76133,#76134,#76135,#76136)) ;
#27897 = EDGE_LOOP('',(#76137,#76138,#76139,#76140)) ;
#27898 = EDGE_LOOP('',(#76141,#76142,#76143)) ;
#27899 = EDGE_LOOP('',(#76144,#76145,#76146)) ;
#27900 = EDGE_LOOP('',(#76147,#76148,#76149,#76150)) ;
#27901 = EDGE_LOOP('',(#76151,#76152,#76153,#76154)) ;
#27902 = EDGE_LOOP('',(#76155,#76156,#76157)) ;
#27903 = EDGE_LOOP('',(#76158,#76159,#76160,#76161)) ;
#27904 = EDGE_LOOP('',(#76162,#76163,#76164,#76165,#76166)) ;
#27905 = EDGE_LOOP('',(#76167,#76168,#76169,#76170,#76171)) ;
#27906 = EDGE_LOOP('',(#76172,#76173,#76174,#76175)) ;
#27907 = EDGE_LOOP('',(#76176,#76177,#76178,#76179)) ;
#27908 = EDGE_LOOP('',(#76180,#76181,#76182,#76183)) ;
#27909 = EDGE_LOOP('',(#76184,#76185,#76186)) ;
#27910 = EDGE_LOOP('',(#76187,#76188,#76189,#76190)) ;
#27911 = EDGE_LOOP('',(#76191,#76192,#76193,#76194)) ;
#27912 = EDGE_LOOP('',(#76195,#76196,#76197)) ;
#27913 = EDGE_LOOP('',(#76198,#76199,#76200,#76201)) ;
#27914 = EDGE_LOOP('',(#76202,#76203,#76204,#76205)) ;
#27915 = EDGE_LOOP('',(#76206,#76207,#76208)) ;
#27916 = EDGE_LOOP('',(#76209,#76210,#76211)) ;
#27917 = EDGE_LOOP('',(#76212,#76213,#76214,#76215)) ;
#27918 = EDGE_LOOP('',(#76216,#76217,#76218,#76219)) ;
#27919 = EDGE_LOOP('',(#76220,#76221,#76222,#76223)) ;
#27920 = EDGE_LOOP('',(#76224,#76225,#76226)) ;
#27921 = EDGE_LOOP('',(#76227,#76228,#76229,#76230)) ;
#27922 = EDGE_LOOP('',(#76231,#76232,#76233,#76234)) ;
#27923 = EDGE_LOOP('',(#76235,#76236,#76237)) ;
#27924 = EDGE_LOOP('',(#76238,#76239,#76240,#76241)) ;
#27925 = EDGE_LOOP('',(#76242,#76243,#76244,#76245)) ;
#27926 = EDGE_LOOP('',(#76246,#76247,#76248,#76249,#76250)) ;
#27927 = EDGE_LOOP('',(#76251,#76252,#76253,#76254)) ;
#27928 = EDGE_LOOP('',(#76255,#76256,#76257,#76258)) ;
#27929 = EDGE_LOOP('',(#76259,#76260,#76261,#76262)) ;
#27930 = EDGE_LOOP('',(#76263,#76264,#76265,#76266)) ;
#27931 = EDGE_LOOP('',(#76267,#76268,#76269,#76270)) ;
#27932 = EDGE_LOOP('',(#76271,#76272,#76273,#76274)) ;
#27933 = EDGE_LOOP('',(#76275,#76276,#76277,#76278)) ;
#27934 = EDGE_LOOP('',(#76279,#76280,#76281,#76282)) ;
#27935 = EDGE_LOOP('',(#76283,#76284,#76285,#76286)) ;
#27936 = EDGE_LOOP('',(#76287,#76288,#76289,#76290)) ;
#27937 = EDGE_LOOP('',(#76291,#76292,#76293,#76294)) ;
#27938 = EDGE_LOOP('',(#76295,#76296,#76297)) ;
#27939 = EDGE_LOOP('',(#76298,#76299,#76300)) ;
#27940 = EDGE_LOOP('',(#76301,#76302,#76303,#76304)) ;
#27941 = EDGE_LOOP('',(#76305,#76306,#76307,#76308)) ;
#27942 = EDGE_LOOP('',(#76309,#76310,#76311,#76312)) ;
#27943 = EDGE_LOOP('',(#76313,#76314,#76315,#76316)) ;
#27944 = EDGE_LOOP('',(#76317,#76318,#76319)) ;
#27945 = EDGE_LOOP('',(#76320,#76321,#76322)) ;
#27946 = EDGE_LOOP('',(#76323,#76324,#76325,#76326)) ;
#27947 = EDGE_LOOP('',(#76327,#76328,#76329,#76330)) ;
#27948 = EDGE_LOOP('',(#76331,#76332,#76333,#76334)) ;
#27949 = EDGE_LOOP('',(#76335,#76336,#76337,#76338)) ;
#27950 = EDGE_LOOP('',(#76339,#76340,#76341,#76342)) ;
#27951 = EDGE_LOOP('',(#76343,#76344,#76345,#76346)) ;
#27952 = EDGE_LOOP('',(#76347,#76348,#76349,#76350)) ;
#27953 = EDGE_LOOP('',(#76351,#76352,#76353,#76354)) ;
#27954 = EDGE_LOOP('',(#76355,#76356,#76357,#76358)) ;
#27955 = EDGE_LOOP('',(#76359,#76360,#76361,#76362)) ;
#27956 = EDGE_LOOP('',(#76363,#76364,#76365,#76366)) ;
#27957 = EDGE_LOOP('',(#76367,#76368,#76369)) ;
#27958 = EDGE_LOOP('',(#76370,#76371,#76372)) ;
#27959 = EDGE_LOOP('',(#76373,#76374,#76375,#76376)) ;
#27960 = EDGE_LOOP('',(#76377,#76378,#76379,#76380)) ;
#27961 = EDGE_LOOP('',(#76381,#76382,#76383,#76384)) ;
#27962 = EDGE_LOOP('',(#76385,#76386,#76387,#76388)) ;
#27963 = EDGE_LOOP('',(#76389,#76390,#76391,#76392)) ;
#27964 = EDGE_LOOP('',(#76393,#76394,#76395)) ;
#27965 = EDGE_LOOP('',(#76396,#76397,#76398)) ;
#27966 = EDGE_LOOP('',(#76399,#76400,#76401,#76402)) ;
#27967 = EDGE_LOOP('',(#76403,#76404,#76405,#76406)) ;
#27968 = EDGE_LOOP('',(#76407,#76408,#76409,#76410)) ;
#27969 = EDGE_LOOP('',(#76411,#76412,#76413,#76414)) ;
#27970 = EDGE_LOOP('',(#76415,#76416,#76417)) ;
#27971 = EDGE_LOOP('',(#76418,#76419,#76420)) ;
#27972 = EDGE_LOOP('',(#76421,#76422,#76423,#76424)) ;
#27973 = EDGE_LOOP('',(#76425,#76426,#76427,#76428)) ;
#27974 = EDGE_LOOP('',(#76429,#76430,#76431,#76432)) ;
#27975 = EDGE_LOOP('',(#76433,#76434,#76435,#76436)) ;
#27976 = EDGE_LOOP('',(#76437,#76438,#76439)) ;
#27977 = EDGE_LOOP('',(#76440,#76441,#76442)) ;
#27978 = EDGE_LOOP('',(#76443,#76444,#76445,#76446)) ;
#27979 = EDGE_LOOP('',(#76447,#76448,#76449,#76450)) ;
#27980 = EDGE_LOOP('',(#76451,#76452,#76453)) ;
#27981 = EDGE_LOOP('',(#76454,#76455,#76456)) ;
#27982 = EDGE_LOOP('',(#76457,#76458,#76459,#76460)) ;
#27983 = EDGE_LOOP('',(#76461,#76462,#76463,#76464)) ;
#27984 = EDGE_LOOP('',(#76465,#76466,#76467)) ;
#27985 = EDGE_LOOP('',(#76468,#76469,#76470)) ;
#27986 = EDGE_LOOP('',(#76471,#76472,#76473,#76474)) ;
#27987 = EDGE_LOOP('',(#76475,#76476,#76477,#76478)) ;
#27988 = EDGE_LOOP('',(#76479,#76480,#76481,#76482)) ;
#27989 = EDGE_LOOP('',(#76483,#76484,#76485,#76486)) ;
#27990 = EDGE_LOOP('',(#76487,#76488,#76489,#76490)) ;
#27991 = EDGE_LOOP('',(#76491,#76492,#76493)) ;
#27992 = EDGE_LOOP('',(#76494,#76495,#76496,#76497)) ;
#27993 = EDGE_LOOP('',(#76498,#76499,#76500,#76501)) ;
#27994 = EDGE_LOOP('',(#76502,#76503,#76504,#76505)) ;
#27995 = EDGE_LOOP('',(#76506,#76507,#76508,#76509)) ;
#27996 = EDGE_LOOP('',(#76510,#76511,#76512)) ;
#27997 = EDGE_LOOP('',(#76513,#76514,#76515,#76516)) ;
#27998 = EDGE_LOOP('',(#76517,#76518,#76519)) ;
#27999 = EDGE_LOOP('',(#76520,#76521,#76522,#76523)) ;
#28000 = EDGE_LOOP('',(#76524,#76525,#76526,#76527)) ;
#28001 = EDGE_LOOP('',(#76528,#76529,#76530,#76531)) ;
#28002 = EDGE_LOOP('',(#76532,#76533,#76534,#76535)) ;
#28003 = EDGE_LOOP('',(#76536,#76537,#76538,#76539)) ;
#28004 = EDGE_LOOP('',(#76540,#76541,#76542,#76543)) ;
#28005 = EDGE_LOOP('',(#76544,#76545,#76546,#76547)) ;
#28006 = EDGE_LOOP('',(#76548,#76549,#76550,#76551)) ;
#28007 = EDGE_LOOP('',(#76552,#76553,#76554,#76555)) ;
#28008 = EDGE_LOOP('',(#76556,#76557,#76558)) ;
#28009 = EDGE_LOOP('',(#76559,#76560,#76561,#76562)) ;
#28010 = EDGE_LOOP('',(#76563,#76564,#76565,#76566)) ;
#28011 = EDGE_LOOP('',(#76567,#76568,#76569,#76570)) ;
#28012 = EDGE_LOOP('',(#76571,#76572,#76573,#76574)) ;
#28013 = EDGE_LOOP('',(#76575,#76576,#76577)) ;
#28014 = EDGE_LOOP('',(#76578,#76579,#76580)) ;
#28015 = EDGE_LOOP('',(#76581,#76582,#76583,#76584)) ;
#28016 = EDGE_LOOP('',(#76585,#76586,#76587,#76588)) ;
#28017 = EDGE_LOOP('',(#76589,#76590,#76591,#76592)) ;
#28018 = EDGE_LOOP('',(#76593,#76594,#76595,#76596)) ;
#28019 = EDGE_LOOP('',(#76597,#76598,#76599,#76600)) ;
#28020 = EDGE_LOOP('',(#76601,#76602,#76603,#76604)) ;
#28021 = EDGE_LOOP('',(#76605,#76606,#76607)) ;
#28022 = EDGE_LOOP('',(#76608,#76609,#76610,#76611)) ;
#28023 = EDGE_LOOP('',(#76612,#76613,#76614,#76615)) ;
#28024 = EDGE_LOOP('',(#76616,#76617,#76618,#76619)) ;
#28025 = EDGE_LOOP('',(#76620,#76621,#76622,#76623)) ;
#28026 = EDGE_LOOP('',(#76624,#76625,#76626,#76627)) ;
#28027 = EDGE_LOOP('',(#76628,#76629,#76630)) ;
#28028 = EDGE_LOOP('',(#76631,#76632,#76633,#76634)) ;
#28029 = EDGE_LOOP('',(#76635,#76636,#76637,#76638,#76639)) ;
#28030 = EDGE_LOOP('',(#76640,#76641,#76642,#76643)) ;
#28031 = EDGE_LOOP('',(#76644,#76645,#76646,#76647,#76648)) ;
#28032 = EDGE_LOOP('',(#76649,#76650,#76651)) ;
#28033 = EDGE_LOOP('',(#76652,#76653,#76654,#76655,#76656)) ;
#28034 = EDGE_LOOP('',(#76657,#76658,#76659,#76660)) ;
#28035 = EDGE_LOOP('',(#76661,#76662,#76663,#76664)) ;
#28036 = EDGE_LOOP('',(#76665,#76666,#76667,#76668)) ;
#28037 = EDGE_LOOP('',(#76669,#76670,#76671,#76672)) ;
#28038 = EDGE_LOOP('',(#76673,#76674,#76675)) ;
#28039 = EDGE_LOOP('',(#76676,#76677,#76678)) ;
#28040 = EDGE_LOOP('',(#76679,#76680,#76681,#76682)) ;
#28041 = EDGE_LOOP('',(#76683,#76684,#76685,#76686)) ;
#28042 = EDGE_LOOP('',(#76687,#76688,#76689)) ;
#28043 = EDGE_LOOP('',(#76690,#76691,#76692,#76693)) ;
#28044 = EDGE_LOOP('',(#76694,#76695,#76696,#76697,#76698)) ;
#28045 = EDGE_LOOP('',(#76699,#76700,#76701,#76702,#76703)) ;
#28046 = EDGE_LOOP('',(#76704,#76705,#76706,#76707)) ;
#28047 = EDGE_LOOP('',(#76708,#76709,#76710,#76711)) ;
#28048 = EDGE_LOOP('',(#76712,#76713,#76714,#76715)) ;
#28049 = EDGE_LOOP('',(#76716,#76717,#76718)) ;
#28050 = EDGE_LOOP('',(#76719,#76720,#76721,#76722)) ;
#28051 = EDGE_LOOP('',(#76723,#76724,#76725,#76726)) ;
#28052 = EDGE_LOOP('',(#76727,#76728,#76729)) ;
#28053 = EDGE_LOOP('',(#76730,#76731,#76732,#76733)) ;
#28054 = EDGE_LOOP('',(#76734,#76735,#76736,#76737)) ;
#28055 = EDGE_LOOP('',(#76738,#76739,#76740)) ;
#28056 = EDGE_LOOP('',(#76741,#76742,#76743)) ;
#28057 = EDGE_LOOP('',(#76744,#76745,#76746,#76747)) ;
#28058 = EDGE_LOOP('',(#76748,#76749,#76750,#76751)) ;
#28059 = EDGE_LOOP('',(#76752,#76753,#76754,#76755)) ;
#28060 = EDGE_LOOP('',(#76756,#76757,#76758)) ;
#28061 = EDGE_LOOP('',(#76759,#76760,#76761,#76762)) ;
#28062 = EDGE_LOOP('',(#76763,#76764,#76765,#76766)) ;
#28063 = EDGE_LOOP('',(#76767,#76768,#76769)) ;
#28064 = EDGE_LOOP('',(#76770,#76771,#76772,#76773)) ;
#28065 = EDGE_LOOP('',(#76774,#76775,#76776,#76777)) ;
#28066 = EDGE_LOOP('',(#76778,#76779,#76780,#76781,#76782)) ;
#28067 = EDGE_LOOP('',(#76783,#76784,#76785,#76786)) ;
#28068 = EDGE_LOOP('',(#76787,#76788,#76789,#76790)) ;
#28069 = EDGE_LOOP('',(#76791,#76792,#76793,#76794)) ;
#28070 = EDGE_LOOP('',(#76795,#76796,#76797,#76798)) ;
#28071 = EDGE_LOOP('',(#76799,#76800,#76801,#76802)) ;
#28072 = EDGE_LOOP('',(#76803,#76804,#76805,#76806)) ;
#28073 = EDGE_LOOP('',(#76807,#76808,#76809,#76810)) ;
#28074 = EDGE_LOOP('',(#76811,#76812,#76813,#76814)) ;
#28075 = EDGE_LOOP('',(#76815,#76816,#76817,#76818)) ;
#28076 = EDGE_LOOP('',(#76819,#76820,#76821,#76822)) ;
#28077 = EDGE_LOOP('',(#76823,#76824,#76825,#76826)) ;
#28078 = EDGE_LOOP('',(#76827,#76828,#76829)) ;
#28079 = EDGE_LOOP('',(#76830,#76831,#76832)) ;
#28080 = EDGE_LOOP('',(#76833,#76834,#76835,#76836)) ;
#28081 = EDGE_LOOP('',(#76837,#76838,#76839,#76840)) ;
#28082 = EDGE_LOOP('',(#76841,#76842,#76843,#76844)) ;
#28083 = EDGE_LOOP('',(#76845,#76846,#76847,#76848)) ;
#28084 = EDGE_LOOP('',(#76849,#76850,#76851)) ;
#28085 = EDGE_LOOP('',(#76852,#76853,#76854)) ;
#28086 = EDGE_LOOP('',(#76855,#76856,#76857,#76858)) ;
#28087 = EDGE_LOOP('',(#76859,#76860,#76861,#76862)) ;
#28088 = EDGE_LOOP('',(#76863,#76864,#76865,#76866)) ;
#28089 = EDGE_LOOP('',(#76867,#76868,#76869,#76870)) ;
#28090 = EDGE_LOOP('',(#76871,#76872,#76873,#76874)) ;
#28091 = EDGE_LOOP('',(#76875,#76876,#76877,#76878)) ;
#28092 = EDGE_LOOP('',(#76879,#76880,#76881,#76882)) ;
#28093 = EDGE_LOOP('',(#76883,#76884,#76885,#76886)) ;
#28094 = EDGE_LOOP('',(#76887,#76888,#76889,#76890)) ;
#28095 = EDGE_LOOP('',(#76891,#76892,#76893,#76894)) ;
#28096 = EDGE_LOOP('',(#76895,#76896,#76897,#76898)) ;
#28097 = EDGE_LOOP('',(#76899,#76900,#76901)) ;
#28098 = EDGE_LOOP('',(#76902,#76903,#76904)) ;
#28099 = EDGE_LOOP('',(#76905,#76906,#76907,#76908)) ;
#28100 = EDGE_LOOP('',(#76909,#76910,#76911,#76912)) ;
#28101 = EDGE_LOOP('',(#76913,#76914,#76915,#76916)) ;
#28102 = EDGE_LOOP('',(#76917,#76918,#76919,#76920)) ;
#28103 = EDGE_LOOP('',(#76921,#76922,#76923,#76924)) ;
#28104 = EDGE_LOOP('',(#76925,#76926,#76927)) ;
#28105 = EDGE_LOOP('',(#76928,#76929,#76930)) ;
#28106 = EDGE_LOOP('',(#76931,#76932,#76933,#76934)) ;
#28107 = EDGE_LOOP('',(#76935,#76936,#76937,#76938)) ;
#28108 = EDGE_LOOP('',(#76939,#76940,#76941,#76942)) ;
#28109 = EDGE_LOOP('',(#76943,#76944,#76945,#76946)) ;
#28110 = EDGE_LOOP('',(#76947,#76948,#76949)) ;
#28111 = EDGE_LOOP('',(#76950,#76951,#76952)) ;
#28112 = EDGE_LOOP('',(#76953,#76954,#76955,#76956)) ;
#28113 = EDGE_LOOP('',(#76957,#76958,#76959,#76960)) ;
#28114 = EDGE_LOOP('',(#76961,#76962,#76963,#76964)) ;
#28115 = EDGE_LOOP('',(#76965,#76966,#76967,#76968)) ;
#28116 = EDGE_LOOP('',(#76969,#76970,#76971)) ;
#28117 = EDGE_LOOP('',(#76972,#76973,#76974)) ;
#28118 = EDGE_LOOP('',(#76975,#76976,#76977,#76978)) ;
#28119 = EDGE_LOOP('',(#76979,#76980,#76981,#76982)) ;
#28120 = EDGE_LOOP('',(#76983,#76984,#76985)) ;
#28121 = EDGE_LOOP('',(#76986,#76987,#76988)) ;
#28122 = EDGE_LOOP('',(#76989,#76990,#76991,#76992)) ;
#28123 = EDGE_LOOP('',(#76993,#76994,#76995,#76996)) ;
#28124 = EDGE_LOOP('',(#76997,#76998,#76999)) ;
#28125 = EDGE_LOOP('',(#77000,#77001,#77002)) ;
#28126 = EDGE_LOOP('',(#77003,#77004,#77005,#77006)) ;
#28127 = EDGE_LOOP('',(#77007,#77008,#77009,#77010)) ;
#28128 = EDGE_LOOP('',(#77011,#77012,#77013,#77014)) ;
#28129 = EDGE_LOOP('',(#77015,#77016,#77017,#77018)) ;
#28130 = EDGE_LOOP('',(#77019,#77020,#77021,#77022)) ;
#28131 = EDGE_LOOP('',(#77023,#77024,#77025)) ;
#28132 = EDGE_LOOP('',(#77026,#77027,#77028,#77029)) ;
#28133 = EDGE_LOOP('',(#77030,#77031,#77032,#77033)) ;
#28134 = EDGE_LOOP('',(#77034,#77035,#77036,#77037)) ;
#28135 = EDGE_LOOP('',(#77038,#77039,#77040,#77041)) ;
#28136 = EDGE_LOOP('',(#77042,#77043,#77044)) ;
#28137 = EDGE_LOOP('',(#77045,#77046,#77047,#77048)) ;
#28138 = EDGE_LOOP('',(#77049,#77050,#77051)) ;
#28139 = EDGE_LOOP('',(#77052,#77053,#77054,#77055)) ;
#28140 = EDGE_LOOP('',(#77056,#77057,#77058,#77059)) ;
#28141 = EDGE_LOOP('',(#77060,#77061,#77062,#77063)) ;
#28142 = EDGE_LOOP('',(#77064,#77065,#77066,#77067)) ;
#28143 = EDGE_LOOP('',(#77068,#77069,#77070,#77071)) ;
#28144 = EDGE_LOOP('',(#77072,#77073,#77074,#77075)) ;
#28145 = EDGE_LOOP('',(#77076,#77077,#77078,#77079)) ;
#28146 = EDGE_LOOP('',(#77080,#77081,#77082,#77083)) ;
#28147 = EDGE_LOOP('',(#77084,#77085,#77086,#77087)) ;
#28148 = EDGE_LOOP('',(#77088,#77089,#77090)) ;
#28149 = EDGE_LOOP('',(#77091,#77092,#77093,#77094)) ;
#28150 = EDGE_LOOP('',(#77095,#77096,#77097,#77098)) ;
#28151 = EDGE_LOOP('',(#77099,#77100,#77101,#77102)) ;
#28152 = EDGE_LOOP('',(#77103,#77104,#77105,#77106)) ;
#28153 = EDGE_LOOP('',(#77107,#77108,#77109)) ;
#28154 = EDGE_LOOP('',(#77110,#77111,#77112)) ;
#28155 = EDGE_LOOP('',(#77113,#77114,#77115,#77116)) ;
#28156 = EDGE_LOOP('',(#77117,#77118,#77119,#77120)) ;
#28157 = EDGE_LOOP('',(#77121,#77122,#77123,#77124)) ;
#28158 = EDGE_LOOP('',(#77125,#77126,#77127,#77128)) ;
#28159 = EDGE_LOOP('',(#77129,#77130,#77131,#77132)) ;
#28160 = EDGE_LOOP('',(#77133,#77134,#77135,#77136)) ;
#28161 = EDGE_LOOP('',(#77137,#77138,#77139)) ;
#28162 = EDGE_LOOP('',(#77140,#77141,#77142,#77143)) ;
#28163 = EDGE_LOOP('',(#77144,#77145,#77146,#77147)) ;
#28164 = EDGE_LOOP('',(#77148,#77149,#77150,#77151)) ;
#28165 = EDGE_LOOP('',(#77152,#77153,#77154,#77155)) ;
#28166 = EDGE_LOOP('',(#77156,#77157,#77158,#77159)) ;
#28167 = EDGE_LOOP('',(#77160,#77161,#77162)) ;
#28168 = EDGE_LOOP('',(#77163,#77164,#77165,#77166)) ;
#28169 = EDGE_LOOP('',(#77167,#77168,#77169,#77170,#77171)) ;
#28170 = EDGE_LOOP('',(#77172,#77173,#77174,#77175)) ;
#28171 = EDGE_LOOP('',(#77176,#77177,#77178,#77179,#77180)) ;
#28172 = EDGE_LOOP('',(#77181,#77182,#77183)) ;
#28173 = EDGE_LOOP('',(#77184,#77185,#77186,#77187,#77188)) ;
#28174 = EDGE_LOOP('',(#77189,#77190,#77191,#77192)) ;
#28175 = EDGE_LOOP('',(#77193,#77194,#77195,#77196)) ;
#28176 = EDGE_LOOP('',(#77197,#77198,#77199,#77200)) ;
#28177 = EDGE_LOOP('',(#77201,#77202,#77203,#77204)) ;
#28178 = EDGE_LOOP('',(#77205,#77206,#77207)) ;
#28179 = EDGE_LOOP('',(#77208,#77209,#77210)) ;
#28180 = EDGE_LOOP('',(#77211,#77212,#77213,#77214)) ;
#28181 = EDGE_LOOP('',(#77215,#77216,#77217,#77218)) ;
#28182 = EDGE_LOOP('',(#77219,#77220,#77221)) ;
#28183 = EDGE_LOOP('',(#77222,#77223,#77224,#77225)) ;
#28184 = EDGE_LOOP('',(#77226,#77227,#77228,#77229,#77230)) ;
#28185 = EDGE_LOOP('',(#77231,#77232,#77233,#77234,#77235)) ;
#28186 = EDGE_LOOP('',(#77236,#77237,#77238,#77239)) ;
#28187 = EDGE_LOOP('',(#77240,#77241,#77242,#77243)) ;
#28188 = EDGE_LOOP('',(#77244,#77245,#77246,#77247)) ;
#28189 = EDGE_LOOP('',(#77248,#77249,#77250)) ;
#28190 = EDGE_LOOP('',(#77251,#77252,#77253,#77254)) ;
#28191 = EDGE_LOOP('',(#77255,#77256,#77257,#77258)) ;
#28192 = EDGE_LOOP('',(#77259,#77260,#77261)) ;
#28193 = EDGE_LOOP('',(#77262,#77263,#77264,#77265)) ;
#28194 = EDGE_LOOP('',(#77266,#77267,#77268,#77269)) ;
#28195 = EDGE_LOOP('',(#77270,#77271,#77272)) ;
#28196 = EDGE_LOOP('',(#77273,#77274,#77275)) ;
#28197 = EDGE_LOOP('',(#77276,#77277,#77278,#77279)) ;
#28198 = EDGE_LOOP('',(#77280,#77281,#77282,#77283)) ;
#28199 = EDGE_LOOP('',(#77284,#77285,#77286,#77287)) ;
#28200 = EDGE_LOOP('',(#77288,#77289,#77290)) ;
#28201 = EDGE_LOOP('',(#77291,#77292,#77293,#77294)) ;
#28202 = EDGE_LOOP('',(#77295,#77296,#77297,#77298)) ;
#28203 = EDGE_LOOP('',(#77299,#77300,#77301)) ;
#28204 = EDGE_LOOP('',(#77302,#77303,#77304,#77305)) ;
#28205 = EDGE_LOOP('',(#77306,#77307,#77308,#77309)) ;
#28206 = EDGE_LOOP('',(#77310,#77311,#77312,#77313,#77314)) ;
#28207 = EDGE_LOOP('',(#77315,#77316,#77317,#77318)) ;
#28208 = EDGE_LOOP('',(#77319,#77320,#77321,#77322)) ;
#28209 = EDGE_LOOP('',(#77323,#77324,#77325,#77326)) ;
#28210 = EDGE_LOOP('',(#77327,#77328,#77329,#77330)) ;
#28211 = EDGE_LOOP('',(#77331,#77332,#77333,#77334)) ;
#28212 = EDGE_LOOP('',(#77335,#77336,#77337,#77338)) ;
#28213 = EDGE_LOOP('',(#77339,#77340,#77341,#77342)) ;
#28214 = EDGE_LOOP('',(#77343,#77344,#77345,#77346)) ;
#28215 = EDGE_LOOP('',(#77347,#77348,#77349,#77350)) ;
#28216 = EDGE_LOOP('',(#77351,#77352,#77353,#77354)) ;
#28217 = EDGE_LOOP('',(#77355,#77356,#77357,#77358)) ;
#28218 = EDGE_LOOP('',(#77359,#77360,#77361)) ;
#28219 = EDGE_LOOP('',(#77362,#77363,#77364)) ;
#28220 = EDGE_LOOP('',(#77365,#77366,#77367,#77368)) ;
#28221 = EDGE_LOOP('',(#77369,#77370,#77371,#77372)) ;
#28222 = EDGE_LOOP('',(#77373,#77374,#77375,#77376)) ;
#28223 = EDGE_LOOP('',(#77377,#77378,#77379,#77380)) ;
#28224 = EDGE_LOOP('',(#77381,#77382,#77383)) ;
#28225 = EDGE_LOOP('',(#77384,#77385,#77386)) ;
#28226 = EDGE_LOOP('',(#77387,#77388,#77389,#77390)) ;
#28227 = EDGE_LOOP('',(#77391,#77392,#77393,#77394)) ;
#28228 = EDGE_LOOP('',(#77395,#77396,#77397,#77398)) ;
#28229 = EDGE_LOOP('',(#77399,#77400,#77401,#77402)) ;
#28230 = EDGE_LOOP('',(#77403,#77404,#77405,#77406)) ;
#28231 = EDGE_LOOP('',(#77407,#77408,#77409,#77410)) ;
#28232 = EDGE_LOOP('',(#77411,#77412,#77413,#77414)) ;
#28233 = EDGE_LOOP('',(#77415,#77416,#77417,#77418)) ;
#28234 = EDGE_LOOP('',(#77419,#77420,#77421,#77422)) ;
#28235 = EDGE_LOOP('',(#77423,#77424,#77425,#77426)) ;
#28236 = EDGE_LOOP('',(#77427,#77428,#77429,#77430)) ;
#28237 = EDGE_LOOP('',(#77431,#77432,#77433)) ;
#28238 = EDGE_LOOP('',(#77434,#77435,#77436)) ;
#28239 = EDGE_LOOP('',(#77437,#77438,#77439,#77440)) ;
#28240 = EDGE_LOOP('',(#77441,#77442,#77443,#77444)) ;
#28241 = EDGE_LOOP('',(#77445,#77446,#77447,#77448)) ;
#28242 = EDGE_LOOP('',(#77449,#77450,#77451,#77452)) ;
#28243 = EDGE_LOOP('',(#77453,#77454,#77455,#77456)) ;
#28244 = EDGE_LOOP('',(#77457,#77458,#77459)) ;
#28245 = EDGE_LOOP('',(#77460,#77461,#77462)) ;
#28246 = EDGE_LOOP('',(#77463,#77464,#77465,#77466)) ;
#28247 = EDGE_LOOP('',(#77467,#77468,#77469,#77470)) ;
#28248 = EDGE_LOOP('',(#77471,#77472,#77473,#77474)) ;
#28249 = EDGE_LOOP('',(#77475,#77476,#77477,#77478)) ;
#28250 = EDGE_LOOP('',(#77479,#77480,#77481)) ;
#28251 = EDGE_LOOP('',(#77482,#77483,#77484)) ;
#28252 = EDGE_LOOP('',(#77485,#77486,#77487,#77488)) ;
#28253 = EDGE_LOOP('',(#77489,#77490,#77491,#77492)) ;
#28254 = EDGE_LOOP('',(#77493,#77494,#77495,#77496)) ;
#28255 = EDGE_LOOP('',(#77497,#77498,#77499,#77500)) ;
#28256 = EDGE_LOOP('',(#77501,#77502,#77503)) ;
#28257 = EDGE_LOOP('',(#77504,#77505,#77506)) ;
#28258 = EDGE_LOOP('',(#77507,#77508,#77509,#77510)) ;
#28259 = EDGE_LOOP('',(#77511,#77512,#77513,#77514)) ;
#28260 = EDGE_LOOP('',(#77515,#77516,#77517)) ;
#28261 = EDGE_LOOP('',(#77518,#77519,#77520)) ;
#28262 = EDGE_LOOP('',(#77521,#77522,#77523,#77524)) ;
#28263 = EDGE_LOOP('',(#77525,#77526,#77527,#77528)) ;
#28264 = EDGE_LOOP('',(#77529,#77530,#77531)) ;
#28265 = EDGE_LOOP('',(#77532,#77533,#77534)) ;
#28266 = EDGE_LOOP('',(#77535,#77536,#77537,#77538)) ;
#28267 = EDGE_LOOP('',(#77539,#77540,#77541,#77542)) ;
#28268 = EDGE_LOOP('',(#77543,#77544,#77545,#77546)) ;
#28269 = EDGE_LOOP('',(#77547,#77548,#77549,#77550)) ;
#28270 = EDGE_LOOP('',(#77551,#77552,#77553,#77554)) ;
#28271 = EDGE_LOOP('',(#77555,#77556,#77557)) ;
#28272 = EDGE_LOOP('',(#77558,#77559,#77560,#77561)) ;
#28273 = EDGE_LOOP('',(#77562,#77563,#77564,#77565)) ;
#28274 = EDGE_LOOP('',(#77566,#77567,#77568,#77569)) ;
#28275 = EDGE_LOOP('',(#77570,#77571,#77572,#77573)) ;
#28276 = EDGE_LOOP('',(#77574,#77575,#77576)) ;
#28277 = EDGE_LOOP('',(#77577,#77578,#77579,#77580)) ;
#28278 = EDGE_LOOP('',(#77581,#77582,#77583)) ;
#28279 = EDGE_LOOP('',(#77584,#77585,#77586,#77587)) ;
#28280 = EDGE_LOOP('',(#77588,#77589,#77590,#77591)) ;
#28281 = EDGE_LOOP('',(#77592,#77593,#77594,#77595)) ;
#28282 = EDGE_LOOP('',(#77596,#77597,#77598,#77599)) ;
#28283 = EDGE_LOOP('',(#77600,#77601,#77602,#77603)) ;
#28284 = EDGE_LOOP('',(#77604,#77605,#77606,#77607)) ;
#28285 = EDGE_LOOP('',(#77608,#77609,#77610,#77611)) ;
#28286 = EDGE_LOOP('',(#77612,#77613,#77614,#77615)) ;
#28287 = EDGE_LOOP('',(#77616,#77617,#77618,#77619)) ;
#28288 = EDGE_LOOP('',(#77620,#77621,#77622)) ;
#28289 = EDGE_LOOP('',(#77623,#77624,#77625,#77626)) ;
#28290 = EDGE_LOOP('',(#77627,#77628,#77629,#77630)) ;
#28291 = EDGE_LOOP('',(#77631,#77632,#77633,#77634)) ;
#28292 = EDGE_LOOP('',(#77635,#77636,#77637,#77638)) ;
#28293 = EDGE_LOOP('',(#77639,#77640,#77641)) ;
#28294 = EDGE_LOOP('',(#77642,#77643,#77644)) ;
#28295 = EDGE_LOOP('',(#77645,#77646,#77647,#77648)) ;
#28296 = EDGE_LOOP('',(#77649,#77650,#77651,#77652)) ;
#28297 = EDGE_LOOP('',(#77653,#77654,#77655,#77656)) ;
#28298 = EDGE_LOOP('',(#77657,#77658,#77659,#77660)) ;
#28299 = EDGE_LOOP('',(#77661,#77662,#77663,#77664)) ;
#28300 = EDGE_LOOP('',(#77665,#77666,#77667,#77668)) ;
#28301 = EDGE_LOOP('',(#77669,#77670,#77671)) ;
#28302 = EDGE_LOOP('',(#77672,#77673,#77674,#77675)) ;
#28303 = EDGE_LOOP('',(#77676,#77677,#77678,#77679)) ;
#28304 = EDGE_LOOP('',(#77680,#77681,#77682,#77683)) ;
#28305 = EDGE_LOOP('',(#77684,#77685,#77686,#77687)) ;
#28306 = EDGE_LOOP('',(#77688,#77689,#77690,#77691)) ;
#28307 = EDGE_LOOP('',(#77692,#77693,#77694)) ;
#28308 = EDGE_LOOP('',(#77695,#77696,#77697,#77698)) ;
#28309 = EDGE_LOOP('',(#77699,#77700,#77701,#77702,#77703)) ;
#28310 = EDGE_LOOP('',(#77704,#77705,#77706,#77707)) ;
#28311 = EDGE_LOOP('',(#77708,#77709,#77710,#77711,#77712)) ;
#28312 = EDGE_LOOP('',(#77713,#77714,#77715)) ;
#28313 = EDGE_LOOP('',(#77716,#77717,#77718,#77719,#77720)) ;
#28314 = EDGE_LOOP('',(#77721,#77722,#77723,#77724)) ;
#28315 = EDGE_LOOP('',(#77725,#77726,#77727,#77728)) ;
#28316 = EDGE_LOOP('',(#77729,#77730,#77731,#77732)) ;
#28317 = EDGE_LOOP('',(#77733,#77734,#77735,#77736)) ;
#28318 = EDGE_LOOP('',(#77737,#77738,#77739)) ;
#28319 = EDGE_LOOP('',(#77740,#77741,#77742)) ;
#28320 = EDGE_LOOP('',(#77743,#77744,#77745,#77746)) ;
#28321 = EDGE_LOOP('',(#77747,#77748,#77749,#77750)) ;
#28322 = EDGE_LOOP('',(#77751,#77752,#77753)) ;
#28323 = EDGE_LOOP('',(#77754,#77755,#77756,#77757)) ;
#28324 = EDGE_LOOP('',(#77758,#77759,#77760,#77761,#77762)) ;
#28325 = EDGE_LOOP('',(#77763,#77764,#77765,#77766,#77767)) ;
#28326 = EDGE_LOOP('',(#77768,#77769,#77770,#77771)) ;
#28327 = EDGE_LOOP('',(#77772,#77773,#77774,#77775)) ;
#28328 = EDGE_LOOP('',(#77776,#77777,#77778,#77779)) ;
#28329 = EDGE_LOOP('',(#77780,#77781,#77782)) ;
#28330 = EDGE_LOOP('',(#77783,#77784,#77785,#77786)) ;
#28331 = EDGE_LOOP('',(#77787,#77788,#77789,#77790)) ;
#28332 = EDGE_LOOP('',(#77791,#77792,#77793)) ;
#28333 = EDGE_LOOP('',(#77794,#77795,#77796,#77797)) ;
#28334 = EDGE_LOOP('',(#77798,#77799,#77800,#77801)) ;
#28335 = EDGE_LOOP('',(#77802,#77803,#77804)) ;
#28336 = EDGE_LOOP('',(#77805,#77806,#77807)) ;
#28337 = EDGE_LOOP('',(#77808,#77809,#77810,#77811)) ;
#28338 = EDGE_LOOP('',(#77812,#77813,#77814,#77815)) ;
#28339 = EDGE_LOOP('',(#77816,#77817,#77818,#77819)) ;
#28340 = EDGE_LOOP('',(#77820,#77821,#77822)) ;
#28341 = EDGE_LOOP('',(#77823,#77824,#77825,#77826)) ;
#28342 = EDGE_LOOP('',(#77827,#77828,#77829,#77830)) ;
#28343 = EDGE_LOOP('',(#77831,#77832,#77833)) ;
#28344 = EDGE_LOOP('',(#77834,#77835,#77836,#77837)) ;
#28345 = EDGE_LOOP('',(#77838,#77839,#77840,#77841)) ;
#28346 = EDGE_LOOP('',(#77842,#77843,#77844,#77845,#77846)) ;
#28347 = EDGE_LOOP('',(#77847,#77848,#77849,#77850)) ;
#28348 = EDGE_LOOP('',(#77851,#77852,#77853,#77854)) ;
#28349 = EDGE_LOOP('',(#77855,#77856,#77857,#77858)) ;
#28350 = EDGE_LOOP('',(#77859,#77860,#77861,#77862)) ;
#28351 = EDGE_LOOP('',(#77863,#77864,#77865,#77866)) ;
#28352 = EDGE_LOOP('',(#77867,#77868,#77869,#77870)) ;
#28353 = EDGE_LOOP('',(#77871,#77872,#77873,#77874)) ;
#28354 = EDGE_LOOP('',(#77875,#77876,#77877,#77878)) ;
#28355 = EDGE_LOOP('',(#77879,#77880,#77881,#77882)) ;
#28356 = EDGE_LOOP('',(#77883,#77884,#77885,#77886)) ;
#28357 = EDGE_LOOP('',(#77887,#77888,#77889,#77890)) ;
#28358 = EDGE_LOOP('',(#77891,#77892,#77893)) ;
#28359 = EDGE_LOOP('',(#77894,#77895,#77896)) ;
#28360 = EDGE_LOOP('',(#77897,#77898,#77899,#77900)) ;
#28361 = EDGE_LOOP('',(#77901,#77902,#77903,#77904)) ;
#28362 = EDGE_LOOP('',(#77905,#77906,#77907,#77908)) ;
#28363 = EDGE_LOOP('',(#77909,#77910,#77911,#77912)) ;
#28364 = EDGE_LOOP('',(#77913,#77914,#77915)) ;
#28365 = EDGE_LOOP('',(#77916,#77917,#77918)) ;
#28366 = EDGE_LOOP('',(#77919,#77920,#77921,#77922)) ;
#28367 = EDGE_LOOP('',(#77923,#77924,#77925,#77926)) ;
#28368 = EDGE_LOOP('',(#77927,#77928,#77929,#77930)) ;
#28369 = EDGE_LOOP('',(#77931,#77932,#77933,#77934)) ;
#28370 = EDGE_LOOP('',(#77935,#77936,#77937,#77938)) ;
#28371 = EDGE_LOOP('',(#77939,#77940,#77941,#77942)) ;
#28372 = EDGE_LOOP('',(#77943,#77944,#77945,#77946)) ;
#28373 = EDGE_LOOP('',(#77947,#77948,#77949,#77950)) ;
#28374 = EDGE_LOOP('',(#77951,#77952,#77953,#77954)) ;
#28375 = EDGE_LOOP('',(#77955,#77956,#77957,#77958)) ;
#28376 = EDGE_LOOP('',(#77959,#77960,#77961,#77962)) ;
#28377 = EDGE_LOOP('',(#77963,#77964,#77965)) ;
#28378 = EDGE_LOOP('',(#77966,#77967,#77968)) ;
#28379 = EDGE_LOOP('',(#77969,#77970,#77971,#77972)) ;
#28380 = EDGE_LOOP('',(#77973,#77974,#77975,#77976)) ;
#28381 = EDGE_LOOP('',(#77977,#77978,#77979,#77980)) ;
#28382 = EDGE_LOOP('',(#77981,#77982,#77983,#77984)) ;
#28383 = EDGE_LOOP('',(#77985,#77986,#77987,#77988)) ;
#28384 = EDGE_LOOP('',(#77989,#77990,#77991)) ;
#28385 = EDGE_LOOP('',(#77992,#77993,#77994)) ;
#28386 = EDGE_LOOP('',(#77995,#77996,#77997,#77998)) ;
#28387 = EDGE_LOOP('',(#77999,#78000,#78001,#78002)) ;
#28388 = EDGE_LOOP('',(#78003,#78004,#78005,#78006)) ;
#28389 = EDGE_LOOP('',(#78007,#78008,#78009,#78010)) ;
#28390 = EDGE_LOOP('',(#78011,#78012,#78013)) ;
#28391 = EDGE_LOOP('',(#78014,#78015,#78016)) ;
#28392 = EDGE_LOOP('',(#78017,#78018,#78019,#78020)) ;
#28393 = EDGE_LOOP('',(#78021,#78022,#78023,#78024)) ;
#28394 = EDGE_LOOP('',(#78025,#78026,#78027,#78028)) ;
#28395 = EDGE_LOOP('',(#78029,#78030,#78031,#78032)) ;
#28396 = EDGE_LOOP('',(#78033,#78034,#78035)) ;
#28397 = EDGE_LOOP('',(#78036,#78037,#78038)) ;
#28398 = EDGE_LOOP('',(#78039,#78040,#78041,#78042)) ;
#28399 = EDGE_LOOP('',(#78043,#78044,#78045,#78046)) ;
#28400 = EDGE_LOOP('',(#78047,#78048,#78049)) ;
#28401 = EDGE_LOOP('',(#78050,#78051,#78052)) ;
#28402 = EDGE_LOOP('',(#78053,#78054,#78055,#78056)) ;
#28403 = EDGE_LOOP('',(#78057,#78058,#78059,#78060)) ;
#28404 = EDGE_LOOP('',(#78061,#78062,#78063)) ;
#28405 = EDGE_LOOP('',(#78064,#78065,#78066)) ;
#28406 = EDGE_LOOP('',(#78067,#78068,#78069,#78070)) ;
#28407 = EDGE_LOOP('',(#78071,#78072,#78073,#78074)) ;
#28408 = EDGE_LOOP('',(#78075,#78076,#78077,#78078)) ;
#28409 = EDGE_LOOP('',(#78079,#78080,#78081,#78082)) ;
#28410 = EDGE_LOOP('',(#78083,#78084,#78085,#78086)) ;
#28411 = EDGE_LOOP('',(#78087,#78088,#78089,#78090)) ;
#28412 = EDGE_LOOP('',(#78091,#78092,#78093,#78094)) ;
#28413 = EDGE_LOOP('',(#78095,#78096,#78097,#78098)) ;
#28414 = EDGE_LOOP('',(#78099,#78100,#78101,#78102)) ;
#28415 = EDGE_LOOP('',(#78103,#78104,#78105,#78106)) ;
#28416 = EDGE_LOOP('',(#78107,#78108,#78109,#78110)) ;
#28417 = EDGE_LOOP('',(#78111,#78112,#78113,#78114)) ;
#28418 = EDGE_LOOP('',(#78115,#78116,#78117,#78118)) ;
#28419 = EDGE_LOOP('',(#78119,#78120,#78121,#78122)) ;
#28420 = EDGE_LOOP('',(#78123,#78124,#78125)) ;
#28421 = EDGE_LOOP('',(#78126,#78127,#78128,#78129,#78130,#78131)) ;
#28422 = EDGE_LOOP('',(#78132,#78133,#78134)) ;
#28423 = EDGE_LOOP('',(#78135,#78136,#78137)) ;
#28424 = EDGE_LOOP('',(#78138,#78139,#78140)) ;
#28425 = EDGE_LOOP('',(#78141,#78142,#78143,#78144,#78145,#78146)) ;
#28426 = EDGE_LOOP('',(#78147,#78148,#78149)) ;
#28427 = EDGE_LOOP('',(#78150,#78151,#78152)) ;
#28428 = EDGE_LOOP('',(#78153,#78154,#78155,#78156,#78157,#78158)) ;
#28429 = EDGE_LOOP('',(#78159,#78160,#78161)) ;
#28430 = EDGE_LOOP('',(#78162,#78163,#78164)) ;
#28431 = EDGE_LOOP('',(#78165,#78166,#78167,#78168,#78169,#78170)) ;
#28432 = EDGE_LOOP('',(#78171,#78172,#78173)) ;
#28433 = EDGE_LOOP('',(#78174,#78175,#78176)) ;
#28434 = EDGE_LOOP('',(#78177,#78178,#78179,#78180,#78181,#78182)) ;
#28435 = EDGE_LOOP('',(#78183,#78184,#78185)) ;
#28436 = EDGE_LOOP('',(#78186,#78187,#78188)) ;
#28437 = EDGE_LOOP('',(#78189,#78190,#78191,#78192,#78193,#78194)) ;
#28438 = EDGE_LOOP('',(#78195,#78196,#78197)) ;
#28439 = EDGE_LOOP('',(#78198,#78199,#78200)) ;
#28440 = EDGE_LOOP('',(#78201,#78202,#78203,#78204,#78205,#78206)) ;
#28441 = EDGE_LOOP('',(#78207,#78208,#78209)) ;
#28442 = EDGE_LOOP('',(#78210,#78211,#78212)) ;
#28443 = EDGE_LOOP('',(#78213,#78214,#78215,#78216,#78217,#78218)) ;
#28444 = EDGE_LOOP('',(#78219,#78220,#78221)) ;
#28445 = EDGE_LOOP('',(#78222,#78223,#78224,#78225,#78226)) ;
#28446 = EDGE_LOOP('',(#78227,#78228,#78229)) ;
#28447 = EDGE_LOOP('',(#78230,#78231,#78232)) ;
#28448 = EDGE_LOOP('',(#78233,#78234,#78235,#78236,#78237)) ;
#28449 = EDGE_LOOP('',(#78238,#78239,#78240)) ;
#28450 = EDGE_LOOP('',(#78241,#78242,#78243)) ;
#28451 = EDGE_LOOP('',(#78244,#78245,#78246,#78247,#78248)) ;
#28452 = EDGE_LOOP('',(#78249,#78250,#78251)) ;
#28453 = EDGE_LOOP('',(#78252,#78253,#78254)) ;
#28454 = EDGE_LOOP('',(#78255,#78256,#78257,#78258,#78259)) ;
#28455 = EDGE_LOOP('',(#78260,#78261,#78262)) ;
#28456 = EDGE_LOOP('',(#78263,#78264,#78265)) ;
#28457 = EDGE_LOOP('',(#78266,#78267,#78268,#78269,#78270)) ;
#28458 = EDGE_LOOP('',(#78271,#78272,#78273)) ;
#28459 = EDGE_LOOP('',(#78274,#78275,#78276)) ;
#28460 = EDGE_LOOP('',(#78277,#78278,#78279,#78280,#78281)) ;
#28461 = EDGE_LOOP('',(#78282,#78283,#78284)) ;
#28462 = EDGE_LOOP('',(#78285,#78286,#78287)) ;
#28463 = EDGE_LOOP('',(#78288,#78289,#78290,#78291,#78292)) ;
#28464 = EDGE_LOOP('',(#78293,#78294,#78295)) ;
#28465 = EDGE_LOOP('',(#78296,#78297,#78298)) ;
#28466 = EDGE_LOOP('',(#78299,#78300,#78301,#78302,#78303)) ;
#28467 = EDGE_LOOP('',(#78304,#78305,#78306)) ;
#28468 = EDGE_LOOP('',(#78307,#78308,#78309)) ;
#28469 = EDGE_LOOP('',(#78310,#78311,#78312,#78313,#78314)) ;
#28470 = EDGE_LOOP('',(#78315,#78316,#78317)) ;
#28471 = EDGE_LOOP('',(#78318,#78319,#78320)) ;
#28472 = EDGE_LOOP('',(#78321,#78322,#78323,#78324,#78325)) ;
#28473 = EDGE_LOOP('',(#78326,#78327,#78328)) ;
#28474 = EDGE_LOOP('',(#78329,#78330,#78331)) ;
#28475 = EDGE_LOOP('',(#78332,#78333,#78334,#78335,#78336)) ;
#28476 = EDGE_LOOP('',(#78337,#78338,#78339)) ;
#28477 = EDGE_LOOP('',(#78340,#78341,#78342)) ;
#28478 = EDGE_LOOP('',(#78343,#78344,#78345,#78346,#78347)) ;
#28479 = EDGE_LOOP('',(#78348,#78349,#78350)) ;
#28480 = EDGE_LOOP('',(#78351,#78352,#78353)) ;
#28481 = EDGE_LOOP('',(#78354,#78355,#78356,#78357,#78358)) ;
#28482 = EDGE_LOOP('',(#78359,#78360,#78361)) ;
#28483 = EDGE_LOOP('',(#78362,#78363,#78364)) ;
#28484 = EDGE_LOOP('',(#78365,#78366,#78367,#78368,#78369)) ;
#28485 = EDGE_LOOP('',(#78370,#78371,#78372)) ;
#28486 = EDGE_LOOP('',(#78373,#78374,#78375)) ;
#28487 = EDGE_LOOP('',(#78376,#78377,#78378,#78379,#78380)) ;
#28488 = EDGE_LOOP('',(#78381,#78382,#78383)) ;
#28489 = EDGE_LOOP('',(#78384,#78385,#78386)) ;
#28490 = EDGE_LOOP('',(#78387,#78388,#78389,#78390,#78391)) ;
#28491 = EDGE_LOOP('',(#78392,#78393,#78394)) ;
#28492 = EDGE_LOOP('',(#78395,#78396,#78397)) ;
#28493 = EDGE_LOOP('',(#78398,#78399,#78400,#78401,#78402)) ;
#28494 = EDGE_LOOP('',(#78403,#78404,#78405)) ;
#28495 = EDGE_LOOP('',(#78406,#78407,#78408)) ;
#28496 = EDGE_LOOP('',(#78409,#78410,#78411,#78412,#78413)) ;
#28497 = EDGE_LOOP('',(#78414,#78415,#78416)) ;
#28498 = EDGE_LOOP('',(#78417,#78418,#78419)) ;
#28499 = EDGE_LOOP('',(#78420,#78421,#78422,#78423,#78424)) ;
#28500 = EDGE_LOOP('',(#78425,#78426,#78427)) ;
#28501 = EDGE_LOOP('',(#78428,#78429,#78430,#78431)) ;
#28502 = EDGE_LOOP('',(#78432,#78433,#78434,#78435)) ;
#28503 = EDGE_LOOP('',(#78436,#78437,#78438,#78439)) ;
#28504 = EDGE_LOOP('',(#78440,#78441,#78442,#78443)) ;
#28505 = EDGE_LOOP('',(#78444,#78445,#78446,#78447)) ;
#28506 = EDGE_LOOP('',(#78448,#78449,#78450,#78451)) ;
#28507 = EDGE_LOOP('',(#78452,#78453,#78454,#78455)) ;
#28508 = EDGE_LOOP('',(#78456,#78457,#78458,#78459)) ;
#28509 = EDGE_LOOP('',(#78460,#78461,#78462,#78463)) ;
#28510 = EDGE_LOOP('',(#78464,#78465,#78466,#78467)) ;
#28511 = EDGE_LOOP('',(#78468,#78469,#78470,#78471)) ;
#28512 = EDGE_LOOP('',(#78472,#78473,#78474,#78475)) ;
#28513 = EDGE_LOOP('',(#78476,#78477,#78478,#78479)) ;
#28514 = EDGE_LOOP('',(#78480,#78481,#78482,#78483)) ;
#28515 = EDGE_LOOP('',(#78484,#78485,#78486,#78487)) ;
#28516 = EDGE_LOOP('',(#78488,#78489,#78490,#78491)) ;
#28517 = EDGE_LOOP('',(#78492,#78493,#78494,#78495)) ;
#28518 = EDGE_LOOP('',(#78496,#78497,#78498,#78499)) ;
#28519 = EDGE_LOOP('',(#78500,#78501,#78502,#78503)) ;
#28520 = EDGE_LOOP('',(#78504,#78505,#78506,#78507)) ;
#28521 = EDGE_LOOP('',(#78508,#78509,#78510,#78511)) ;
#28522 = EDGE_LOOP('',(#78512,#78513,#78514,#78515)) ;
#28523 = EDGE_LOOP('',(#78516,#78517,#78518,#78519)) ;
#28524 = EDGE_LOOP('',(#78520,#78521,#78522,#78523)) ;
#28525 = EDGE_LOOP('',(#78524,#78525,#78526,#78527)) ;
#28526 = EDGE_LOOP('',(#78528,#78529,#78530,#78531)) ;
#28527 = EDGE_LOOP('',(#78532,#78533,#78534,#78535)) ;
#28528 = EDGE_LOOP('',(#78536,#78537,#78538,#78539)) ;
#28529 = EDGE_LOOP('',(#78540,#78541,#78542,#78543)) ;
#28530 = EDGE_LOOP('',(#78544,#78545,#78546,#78547)) ;
#28531 = EDGE_LOOP('',(#78548,#78549,#78550,#78551)) ;
#28532 = EDGE_LOOP('',(#78552,#78553,#78554,#78555)) ;
#28533 = EDGE_LOOP('',(#78556,#78557,#78558,#78559)) ;
#28534 = EDGE_LOOP('',(#78560,#78561,#78562,#78563)) ;
#28535 = EDGE_LOOP('',(#78564,#78565,#78566,#78567)) ;
#28536 = EDGE_LOOP('',(#78568,#78569,#78570,#78571)) ;
#28537 = EDGE_LOOP('',(#78572,#78573,#78574,#78575)) ;
#28538 = EDGE_LOOP('',(#78576,#78577,#78578,#78579)) ;
#28539 = EDGE_LOOP('',(#78580,#78581,#78582,#78583)) ;
#28540 = EDGE_LOOP('',(#78584,#78585,#78586,#78587)) ;
#28541 = EDGE_LOOP('',(#78588,#78589,#78590,#78591)) ;
#28542 = EDGE_LOOP('',(#78592,#78593,#78594,#78595)) ;
#28543 = EDGE_LOOP('',(#78596,#78597,#78598,#78599)) ;
#28544 = EDGE_LOOP('',(#78600,#78601,#78602,#78603)) ;
#28545 = EDGE_LOOP('',(#78604,#78605,#78606,#78607)) ;
#28546 = EDGE_LOOP('',(#78608,#78609,#78610,#78611)) ;
#28547 = EDGE_LOOP('',(#78612,#78613,#78614,#78615)) ;
#28548 = EDGE_LOOP('',(#78616,#78617,#78618,#78619)) ;
#28549 = EDGE_LOOP('',(#78620,#78621,#78622,#78623)) ;
#28550 = EDGE_LOOP('',(#78624,#78625,#78626,#78627)) ;
#28551 = EDGE_LOOP('',(#78628,#78629,#78630,#78631)) ;
#28552 = EDGE_LOOP('',(#78632,#78633,#78634,#78635)) ;
#28553 = EDGE_LOOP('',(#78636,#78637,#78638,#78639)) ;
#28554 = EDGE_LOOP('',(#78640,#78641,#78642,#78643)) ;
#28555 = EDGE_LOOP('',(#78644,#78645,#78646,#78647)) ;
#28556 = EDGE_LOOP('',(#78648,#78649,#78650,#78651)) ;
#28557 = EDGE_LOOP('',(#78652,#78653,#78654,#78655)) ;
#28558 = EDGE_LOOP('',(#78656,#78657,#78658,#78659)) ;
#28559 = EDGE_LOOP('',(#78660,#78661,#78662,#78663)) ;
#28560 = EDGE_LOOP('',(#78664,#78665,#78666,#78667)) ;
#28561 = EDGE_LOOP('',(#78668,#78669,#78670)) ;
#28562 = EDGE_LOOP('',(#78671,#78672,#78673,#78674)) ;
#28563 = EDGE_LOOP('',(#78675,#78676,#78677,#78678)) ;
#28564 = EDGE_LOOP('',(#78679,#78680,#78681,#78682)) ;
#28565 = EDGE_LOOP('',(#78683,#78684,#78685)) ;
#28566 = EDGE_LOOP('',(#78686,#78687,#78688,#78689)) ;
#28567 = EDGE_LOOP('',(#78690,#78691,#78692)) ;
#28568 = EDGE_LOOP('',(#78693,#78694,#78695,#78696)) ;
#28569 = EDGE_LOOP('',(#78697,#78698,#78699)) ;
#28570 = EDGE_LOOP('',(#78700,#78701,#78702,#78703)) ;
#28571 = EDGE_LOOP('',(#78704,#78705,#78706,#78707)) ;
#28572 = EDGE_LOOP('',(#78708,#78709,#78710,#78711)) ;
#28573 = EDGE_LOOP('',(#78712,#78713,#78714,#78715)) ;
#28574 = EDGE_LOOP('',(#78716,#78717,#78718)) ;
#28575 = EDGE_LOOP('',(#78719,#78720,#78721,#78722)) ;
#28576 = EDGE_LOOP('',(#78723,#78724,#78725,#78726)) ;
#28577 = EDGE_LOOP('',(#78727,#78728,#78729,#78730)) ;
#28578 = EDGE_LOOP('',(#78731,#78732,#78733,#78734)) ;
#28579 = EDGE_LOOP('',(#78735,#78736,#78737)) ;
#28580 = EDGE_LOOP('',(#78738,#78739,#78740)) ;
#28581 = EDGE_LOOP('',(#78741,#78742,#78743,#78744)) ;
#28582 = EDGE_LOOP('',(#78745,#78746,#78747)) ;
#28583 = EDGE_LOOP('',(#78748,#78749,#78750,#78751)) ;
#28584 = EDGE_LOOP('',(#78752,#78753,#78754)) ;
#28585 = EDGE_LOOP('',(#78755,#78756,#78757,#78758)) ;
#28586 = EDGE_LOOP('',(#78759,#78760,#78761)) ;
#28587 = EDGE_LOOP('',(#78762,#78763,#78764,#78765)) ;
#28588 = EDGE_LOOP('',(#78766,#78767,#78768)) ;
#28589 = EDGE_LOOP('',(#78769,#78770,#78771,#78772)) ;
#28590 = EDGE_LOOP('',(#78773,#78774,#78775)) ;
#28591 = EDGE_LOOP('',(#78776,#78777,#78778,#78779)) ;
#28592 = EDGE_LOOP('',(#78780,#78781,#78782)) ;
#28593 = EDGE_LOOP('',(#78783,#78784,#78785,#78786)) ;
#28594 = EDGE_LOOP('',(#78787,#78788,#78789)) ;
#28595 = EDGE_LOOP('',(#78790,#78791,#78792,#78793)) ;
#28596 = EDGE_LOOP('',(#78794,#78795,#78796)) ;
#28597 = EDGE_LOOP('',(#78797,#78798,#78799)) ;
#28598 = EDGE_LOOP('',(#78800,#78801,#78802,#78803)) ;
#28599 = EDGE_LOOP('',(#78804,#78805,#78806,#78807)) ;
#28600 = EDGE_LOOP('',(#78808,#78809,#78810)) ;
#28601 = EDGE_LOOP('',(#78811,#78812,#78813,#78814)) ;
#28602 = EDGE_LOOP('',(#78815,#78816,#78817,#78818)) ;
#28603 = EDGE_LOOP('',(#78819,#78820,#78821,#78822)) ;
#28604 = EDGE_LOOP('',(#78823,#78824,#78825)) ;
#28605 = EDGE_LOOP('',(#78826,#78827,#78828)) ;
#28606 = EDGE_LOOP('',(#78829,#78830,#78831,#78832)) ;
#28607 = EDGE_LOOP('',(#78833,#78834,#78835,#78836)) ;
#28608 = EDGE_LOOP('',(#78837,#78838,#78839,#78840)) ;
#28609 = EDGE_LOOP('',(#78841,#78842,#78843,#78844)) ;
#28610 = EDGE_LOOP('',(#78845,#78846,#78847)) ;
#28611 = EDGE_LOOP('',(#78848,#78849,#78850,#78851)) ;
#28612 = EDGE_LOOP('',(#78852,#78853,#78854,#78855)) ;
#28613 = EDGE_LOOP('',(#78856,#78857,#78858,#78859)) ;
#28614 = EDGE_LOOP('',(#78860,#78861,#78862,#78863)) ;
#28615 = EDGE_LOOP('',(#78864,#78865,#78866)) ;
#28616 = EDGE_LOOP('',(#78867,#78868,#78869,#78870)) ;
#28617 = EDGE_LOOP('',(#78871,#78872,#78873,#78874)) ;
#28618 = EDGE_LOOP('',(#78875,#78876,#78877,#78878)) ;
#28619 = EDGE_LOOP('',(#78879,#78880,#78881)) ;
#28620 = EDGE_LOOP('',(#78882,#78883,#78884,#78885)) ;
#28621 = EDGE_LOOP('',(#78886,#78887,#78888)) ;
#28622 = EDGE_LOOP('',(#78889,#78890,#78891,#78892,#78893)) ;
#28623 = EDGE_LOOP('',(#78894,#78895,#78896,#78897)) ;
#28624 = EDGE_LOOP('',(#78898,#78899,#78900,#78901,#78902)) ;
#28625 = EDGE_LOOP('',(#78903,#78904,#78905,#78906)) ;
#28626 = CIRCLE('',#91125,0.2) ;
#28627 = CIRCLE('',#91126,0.1) ;
#28628 = CIRCLE('',#91127,0.1) ;
#28629 = CIRCLE('',#91128,0.1) ;
#28630 = CIRCLE('',#91130,2.) ;
#28631 = CIRCLE('',#91131,0.1) ;
#28632 = CIRCLE('',#91132,1.9) ;
#28633 = CIRCLE('',#91133,1.9) ;
#28634 = CIRCLE('',#91135,1.47071067811865) ;
#28635 = CIRCLE('',#91136,0.1) ;
#28636 = CIRCLE('',#91137,1.5) ;
#28637 = CIRCLE('',#91139,1.6) ;
#28638 = CIRCLE('',#91140,0.1) ;
#28639 = CIRCLE('',#91141,1.5) ;
#28640 = CIRCLE('',#91142,1.5) ;
#28641 = CIRCLE('',#91144,0.0999999999999998) ;
#28642 = CIRCLE('',#91145,0.0999999999999998) ;
#28643 = CIRCLE('',#91146,0.2) ;
#28644 = CIRCLE('',#91147,0.0999999999999994) ;
#28645 = CIRCLE('',#91149,0.0999999999999998) ;
#28646 = CIRCLE('',#91150,0.0999999999999994) ;
#28647 = CIRCLE('',#91151,0.0999999999999998) ;
#28648 = CIRCLE('',#91153,0.0999999999999998) ;
#28649 = CIRCLE('',#91155,0.1) ;
#28650 = CIRCLE('',#91156,0.0999999999999994) ;
#28651 = CIRCLE('',#91157,0.1) ;
#28652 = CIRCLE('',#91159,0.749999999999996) ;
#28653 = CIRCLE('',#91162,1.9) ;
#28654 = CIRCLE('',#91163,1.9) ;
#28655 = CIRCLE('',#91164,1.9) ;
#28656 = CIRCLE('',#91165,1.9) ;
#28657 = CIRCLE('',#91166,1.9) ;
#28658 = CIRCLE('',#91168,0.2) ;
#28659 = CIRCLE('',#91169,0.1) ;
#28660 = CIRCLE('',#91170,0.1) ;
#28661 = CIRCLE('',#91171,0.1) ;
#28662 = CIRCLE('',#91173,0.1) ;
#28663 = CIRCLE('',#91174,0.1) ;
#28664 = CIRCLE('',#91176,2.) ;
#28665 = CIRCLE('',#91177,0.1) ;
#28666 = CIRCLE('',#91178,1.9) ;
#28667 = CIRCLE('',#91179,1.9) ;
#28668 = CIRCLE('',#91181,1.47071067811866) ;
#28669 = CIRCLE('',#91182,0.1) ;
#28670 = CIRCLE('',#91183,1.5) ;
#28671 = CIRCLE('',#91185,1.6) ;
#28672 = CIRCLE('',#91186,0.1) ;
#28673 = CIRCLE('',#91187,1.5) ;
#28674 = CIRCLE('',#91188,1.5) ;
#28675 = CIRCLE('',#91190,0.1) ;
#28676 = CIRCLE('',#91191,0.1) ;
#28677 = CIRCLE('',#91192,0.2) ;
#28678 = CIRCLE('',#91193,0.0999999999999994) ;
#28679 = CIRCLE('',#91195,0.1) ;
#28680 = CIRCLE('',#91196,0.0999999999999994) ;
#28681 = CIRCLE('',#91197,0.1) ;
#28682 = CIRCLE('',#91199,0.1) ;
#28683 = CIRCLE('',#91201,0.1) ;
#28684 = CIRCLE('',#91202,0.0999999999999994) ;
#28685 = CIRCLE('',#91203,0.1) ;
#28686 = CIRCLE('',#91205,0.749999999999997) ;
#28687 = CIRCLE('',#91208,1.9) ;
#28688 = CIRCLE('',#91209,1.9) ;
#28689 = CIRCLE('',#91210,1.9) ;
#28690 = CIRCLE('',#91211,1.9) ;
#28691 = CIRCLE('',#91212,1.9) ;
#28692 = CIRCLE('',#91214,0.2) ;
#28693 = CIRCLE('',#91215,0.2) ;
#28694 = CIRCLE('',#91220,0.0999999999999994) ;
#28695 = CIRCLE('',#91221,0.0999999999999998) ;
#28696 = CIRCLE('',#91223,0.0999999999999994) ;
#28697 = CIRCLE('',#91224,0.0999999999999998) ;
#28698 = CIRCLE('',#91226,0.0999999999999994) ;
#28699 = CIRCLE('',#91227,0.0999999999999998) ;
#28700 = CIRCLE('',#91229,0.1) ;
#28701 = CIRCLE('',#91230,0.0999999999999998) ;
#28702 = CIRCLE('',#91231,0.0999999999999998) ;
#28703 = CIRCLE('',#91233,3.1) ;
#28704 = CIRCLE('',#91234,3.1) ;
#28705 = CIRCLE('',#91239,0.2) ;
#28706 = CIRCLE('',#91240,2.9) ;
#28707 = CIRCLE('',#91241,0.2) ;
#28708 = CIRCLE('',#91242,0.2) ;
#28709 = CIRCLE('',#91243,2.9) ;
#28710 = CIRCLE('',#91244,0.2) ;
#28711 = CIRCLE('',#91245,0.2) ;
#28712 = CIRCLE('',#91246,0.2) ;
#28713 = CIRCLE('',#91256,0.2) ;
#28714 = CIRCLE('',#91257,0.2) ;
#28715 = CIRCLE('',#91258,0.2) ;
#28716 = CIRCLE('',#91259,0.2) ;
#28717 = CIRCLE('',#91260,0.2) ;
#28718 = CIRCLE('',#91261,0.2) ;
#28719 = CIRCLE('',#91262,0.2) ;
#28720 = CIRCLE('',#91263,0.2) ;
#28721 = CIRCLE('',#91269,0.2) ;
#28722 = CIRCLE('',#91270,0.2) ;
#28723 = CIRCLE('',#91271,0.2) ;
#28724 = CIRCLE('',#91272,0.2) ;
#28725 = CIRCLE('',#91273,0.2) ;
#28726 = CIRCLE('',#91274,0.2) ;
#28727 = CIRCLE('',#91275,0.2) ;
#28728 = CIRCLE('',#91276,0.2) ;
#28729 = CIRCLE('',#91280,3.1) ;
#28730 = CIRCLE('',#91283,0.0999999999999998) ;
#28731 = CIRCLE('',#91284,0.1) ;
#28732 = CIRCLE('',#91285,0.1) ;
#28733 = CIRCLE('',#91286,0.1) ;
#28734 = CIRCLE('',#91287,0.1) ;
#28735 = CIRCLE('',#91288,0.0999999999999998) ;
#28736 = CIRCLE('',#91289,0.0999999999999998) ;
#28737 = CIRCLE('',#91290,0.1) ;
#28738 = CIRCLE('',#91291,0.1) ;
#28739 = CIRCLE('',#91292,0.0999999999999994) ;
#28740 = CIRCLE('',#91293,0.0999999999999994) ;
#28741 = CIRCLE('',#91294,0.1) ;
#28742 = CIRCLE('',#91295,0.1) ;
#28743 = CIRCLE('',#91296,0.0999999999999998) ;
#28744 = CIRCLE('',#91319,0.1) ;
#28745 = CIRCLE('',#91320,0.1) ;
#28746 = CIRCLE('',#91321,0.1) ;
#28747 = CIRCLE('',#91322,0.1) ;
#28748 = CIRCLE('',#91324,0.1) ;
#28749 = CIRCLE('',#91327,0.1) ;
#28750 = CIRCLE('',#91330,0.1) ;
#28751 = CIRCLE('',#91333,0.1) ;
#28752 = CIRCLE('',#91345,0.1) ;
#28753 = CIRCLE('',#91346,0.1) ;
#28754 = CIRCLE('',#91347,0.1) ;
#28755 = CIRCLE('',#91348,0.1) ;
#28756 = CIRCLE('',#91350,0.1) ;
#28757 = CIRCLE('',#91353,0.1) ;
#28758 = CIRCLE('',#91356,0.1) ;
#28759 = CIRCLE('',#91359,0.1) ;
#28760 = CIRCLE('',#91366,0.2) ;
#28761 = CIRCLE('',#91369,3.) ;
#28762 = CIRCLE('',#91370,3.) ;
#28763 = CIRCLE('',#91371,3.) ;
#28764 = CIRCLE('',#91372,3.) ;
#28765 = CIRCLE('',#91373,0.1) ;
#28766 = CIRCLE('',#91374,0.0999999999999998) ;
#28767 = CIRCLE('',#91376,0.1) ;
#28768 = CIRCLE('',#91377,0.0999999999999999) ;
#28769 = CIRCLE('',#91380,0.1) ;
#28770 = CIRCLE('',#91382,0.0999999999999997) ;
#28771 = CIRCLE('',#91384,0.0999999999999998) ;
#28772 = CIRCLE('',#91386,0.1) ;
#28773 = CIRCLE('',#91390,0.1) ;
#28774 = CIRCLE('',#91392,0.1) ;
#28775 = CIRCLE('',#91394,0.1) ;
#28776 = CIRCLE('',#91395,0.0999999999999998) ;
#28777 = CIRCLE('',#91396,0.1) ;
#28778 = CIRCLE('',#91398,0.1) ;
#28779 = CIRCLE('',#91400,0.1) ;
#28780 = CIRCLE('',#91402,0.1) ;
#28781 = CIRCLE('',#91404,0.0999999999999998) ;
#28782 = CIRCLE('',#91406,0.1) ;
#28783 = CIRCLE('',#91408,0.0999999999999998) ;
#28784 = CIRCLE('',#91410,0.0999999999999999) ;
#28785 = CIRCLE('',#91413,0.1) ;
#28786 = CIRCLE('',#91415,0.1) ;
#28787 = CIRCLE('',#91417,0.0999999999999999) ;
#28788 = CIRCLE('',#91419,0.1) ;
#28789 = CIRCLE('',#91421,0.1) ;
#28790 = CIRCLE('',#91424,0.1) ;
#28791 = CIRCLE('',#91428,0.0999999999999999) ;
#28792 = CIRCLE('',#91429,0.1) ;
#28793 = CIRCLE('',#91435,0.1) ;
#28794 = CIRCLE('',#91436,0.1) ;
#28795 = CIRCLE('',#91438,0.1) ;
#28796 = CIRCLE('',#91441,0.1) ;
#28797 = CIRCLE('',#91442,0.1) ;
#28798 = CIRCLE('',#91444,0.0999999999999994) ;
#28799 = CIRCLE('',#91448,0.1) ;
#28800 = CIRCLE('',#91452,0.0999999999999998) ;
#28801 = CIRCLE('',#91453,0.1) ;
#28802 = CIRCLE('',#91455,0.1) ;
#28803 = CIRCLE('',#91457,0.0999999999999998) ;
#28804 = CIRCLE('',#91459,0.0999999999999998) ;
#28805 = CIRCLE('',#91461,0.1) ;
#28806 = CIRCLE('',#91463,0.0999999999999998) ;
#28807 = CIRCLE('',#91465,0.0999999999999994) ;
#28808 = CIRCLE('',#91468,0.0999999999999998) ;
#28809 = CIRCLE('',#91469,0.0999999999999998) ;
#28810 = CIRCLE('',#91471,0.1) ;
#28811 = CIRCLE('',#91472,0.1) ;
#28812 = CIRCLE('',#91474,0.1) ;
#28813 = CIRCLE('',#91475,0.1) ;
#28814 = CIRCLE('',#91477,0.1) ;
#28815 = CIRCLE('',#91479,0.1) ;
#28816 = CIRCLE('',#91481,0.0999999999999998) ;
#28817 = CIRCLE('',#91482,0.0999999999999998) ;
#28818 = CIRCLE('',#91484,0.1) ;
#28819 = CIRCLE('',#91486,0.1) ;
#28820 = CIRCLE('',#91488,0.1) ;
#28821 = CIRCLE('',#91489,0.1) ;
#28822 = CIRCLE('',#91491,0.1) ;
#28823 = CIRCLE('',#91493,0.1) ;
#28824 = CIRCLE('',#91495,0.1) ;
#28825 = CIRCLE('',#91497,0.1) ;
#28826 = CIRCLE('',#91499,0.1) ;
#28827 = CIRCLE('',#91501,0.1) ;
#28828 = CIRCLE('',#91503,0.1) ;
#28829 = CIRCLE('',#91505,0.1) ;
#28830 = CIRCLE('',#91507,0.1) ;
#28831 = CIRCLE('',#91509,0.1) ;
#28832 = CIRCLE('',#91512,0.1) ;
#28833 = CIRCLE('',#91513,0.0999999999999998) ;
#28834 = CIRCLE('',#91515,0.1) ;
#28835 = CIRCLE('',#91516,0.1) ;
#28836 = CIRCLE('',#91518,0.1) ;
#28837 = CIRCLE('',#91519,0.1) ;
#28838 = CIRCLE('',#91521,0.1) ;
#28839 = CIRCLE('',#91523,0.1) ;
#28840 = CIRCLE('',#91525,0.0999999999999998) ;
#28841 = CIRCLE('',#91526,0.0999999999999998) ;
#28842 = CIRCLE('',#91528,0.1) ;
#28843 = CIRCLE('',#91530,0.1) ;
#28844 = CIRCLE('',#91532,0.0999999999999998) ;
#28845 = CIRCLE('',#91533,0.0999999999999998) ;
#28846 = CIRCLE('',#91535,0.1) ;
#28847 = CIRCLE('',#91537,0.1) ;
#28848 = CIRCLE('',#91539,0.1) ;
#28849 = CIRCLE('',#91541,0.1) ;
#28850 = CIRCLE('',#91543,0.1) ;
#28851 = CIRCLE('',#91545,0.1) ;
#28852 = CIRCLE('',#91547,0.1) ;
#28853 = CIRCLE('',#91549,0.1) ;
#28854 = CIRCLE('',#91551,0.0999999999999998) ;
#28855 = CIRCLE('',#91553,0.0999999999999998) ;
#28856 = CIRCLE('',#91556,0.1) ;
#28857 = CIRCLE('',#91558,0.1) ;
#28858 = CIRCLE('',#91560,0.1) ;
#28859 = CIRCLE('',#91562,0.0999999999999998) ;
#28860 = CIRCLE('',#91564,0.0999999999999994) ;
#28861 = CIRCLE('',#91566,0.0999999999999999) ;
#28862 = CIRCLE('',#91568,0.0999999999999999) ;
#28863 = CIRCLE('',#91570,0.0999999999999994) ;
#28864 = CIRCLE('',#91571,0.0999999999999994) ;
#28865 = CIRCLE('',#91573,0.1) ;
#28866 = CIRCLE('',#91575,0.0999999999999998) ;
#28867 = CIRCLE('',#91577,0.1) ;
#28868 = CIRCLE('',#91578,0.0999999999999998) ;
#28869 = CIRCLE('',#91580,0.1) ;
#28870 = CIRCLE('',#91583,0.0999999999999998) ;
#28871 = CIRCLE('',#91585,0.0999999999999998) ;
#28872 = CIRCLE('',#91587,0.1) ;
#28873 = CIRCLE('',#91589,0.1) ;
#28874 = CIRCLE('',#91591,0.1) ;
#28875 = CIRCLE('',#91593,0.1) ;
#28876 = CIRCLE('',#91599,0.0999999999999998) ;
#28877 = CIRCLE('',#91601,0.0999999999999998) ;
#28878 = CIRCLE('',#91603,0.1) ;
#28879 = CIRCLE('',#91605,0.1) ;
#28880 = CIRCLE('',#91607,0.1) ;
#28881 = CIRCLE('',#91609,0.1) ;
#28882 = CIRCLE('',#91610,0.1) ;
#28883 = CIRCLE('',#91611,0.1) ;
#28884 = CIRCLE('',#91614,0.1) ;
#28885 = CIRCLE('',#91615,0.1) ;
#28886 = CIRCLE('',#91616,0.1) ;
#28887 = CIRCLE('',#91618,0.1) ;
#28888 = CIRCLE('',#91622,0.1) ;
#28889 = CIRCLE('',#91624,0.1) ;
#28890 = CIRCLE('',#91625,0.1) ;
#28891 = CIRCLE('',#91626,0.1) ;
#28892 = CIRCLE('',#91627,0.0999999999999998) ;
#28893 = CIRCLE('',#91628,0.1) ;
#28894 = CIRCLE('',#91632,0.100000000000001) ;
#28895 = CIRCLE('',#91633,0.100000000000001) ;
#28896 = CIRCLE('',#91636,0.0999999999999994) ;
#28897 = CIRCLE('',#91637,0.0999999999999994) ;
#28898 = CIRCLE('',#91640,0.100000000000001) ;
#28899 = CIRCLE('',#91641,0.100000000000001) ;
#28900 = CIRCLE('',#91644,0.0999999999999994) ;
#28901 = CIRCLE('',#91645,0.0999999999999994) ;
#28902 = CIRCLE('',#91648,0.199999999999999) ;
#28903 = CIRCLE('',#91650,0.199999999999999) ;
#28904 = CIRCLE('',#91652,3.1) ;
#28905 = CIRCLE('',#91657,0.1) ;
#28906 = CIRCLE('',#91658,0.1) ;
#28907 = CIRCLE('',#91659,0.0999999999999994) ;
#28908 = CIRCLE('',#91660,0.0999999999999994) ;
#28909 = CIRCLE('',#91661,0.1) ;
#28910 = CIRCLE('',#91684,0.1) ;
#28911 = CIRCLE('',#91685,0.1) ;
#28912 = CIRCLE('',#91686,0.1) ;
#28913 = CIRCLE('',#91687,0.1) ;
#28914 = CIRCLE('',#91689,0.1) ;
#28915 = CIRCLE('',#91692,0.1) ;
#28916 = CIRCLE('',#91695,0.1) ;
#28917 = CIRCLE('',#91698,0.1) ;
#28918 = CIRCLE('',#91710,0.1) ;
#28919 = CIRCLE('',#91711,0.1) ;
#28920 = CIRCLE('',#91712,0.1) ;
#28921 = CIRCLE('',#91713,0.1) ;
#28922 = CIRCLE('',#91715,0.1) ;
#28923 = CIRCLE('',#91718,0.1) ;
#28924 = CIRCLE('',#91721,0.1) ;
#28925 = CIRCLE('',#91724,0.1) ;
#28926 = CIRCLE('',#91731,0.2) ;
#28927 = CIRCLE('',#91734,3.) ;
#28928 = CIRCLE('',#91735,3.) ;
#28929 = CIRCLE('',#91736,3.) ;
#28930 = CIRCLE('',#91737,3.) ;
#28931 = CIRCLE('',#91738,0.1) ;
#28932 = CIRCLE('',#91739,0.0999999999999998) ;
#28933 = CIRCLE('',#91741,0.0999999999999999) ;
#28934 = CIRCLE('',#91742,0.0999999999999999) ;
#28935 = CIRCLE('',#91745,0.1) ;
#28936 = CIRCLE('',#91747,0.0999999999999997) ;
#28937 = CIRCLE('',#91749,0.0999999999999998) ;
#28938 = CIRCLE('',#91751,0.1) ;
#28939 = CIRCLE('',#91755,0.0999999999999999) ;
#28940 = CIRCLE('',#91757,0.1) ;
#28941 = CIRCLE('',#91759,0.1) ;
#28942 = CIRCLE('',#91760,0.1) ;
#28943 = CIRCLE('',#91761,0.1) ;
#28944 = CIRCLE('',#91763,0.1) ;
#28945 = CIRCLE('',#91765,0.1) ;
#28946 = CIRCLE('',#91767,0.1) ;
#28947 = CIRCLE('',#91769,0.1) ;
#28948 = CIRCLE('',#91771,0.1) ;
#28949 = CIRCLE('',#91773,0.0999999999999998) ;
#28950 = CIRCLE('',#91775,0.1) ;
#28951 = CIRCLE('',#91778,0.1) ;
#28952 = CIRCLE('',#91780,0.0999999999999999) ;
#28953 = CIRCLE('',#91782,0.0999999999999999) ;
#28954 = CIRCLE('',#91784,0.1) ;
#28955 = CIRCLE('',#91786,0.1) ;
#28956 = CIRCLE('',#91789,0.1) ;
#28957 = CIRCLE('',#91793,0.0999999999999999) ;
#28958 = CIRCLE('',#91794,0.0999999999999999) ;
#28959 = CIRCLE('',#91800,0.1) ;
#28960 = CIRCLE('',#91801,0.1) ;
#28961 = CIRCLE('',#91803,0.1) ;
#28962 = CIRCLE('',#91806,0.1) ;
#28963 = CIRCLE('',#91807,0.1) ;
#28964 = CIRCLE('',#91809,0.0999999999999994) ;
#28965 = CIRCLE('',#91812,0.0999999999999998) ;
#28966 = CIRCLE('',#91816,0.0999999999999998) ;
#28967 = CIRCLE('',#91817,0.1) ;
#28968 = CIRCLE('',#91819,0.1) ;
#28969 = CIRCLE('',#91821,0.0999999999999998) ;
#28970 = CIRCLE('',#91823,0.0999999999999998) ;
#28971 = CIRCLE('',#91825,0.1) ;
#28972 = CIRCLE('',#91827,0.0999999999999998) ;
#28973 = CIRCLE('',#91829,0.0999999999999994) ;
#28974 = CIRCLE('',#91832,0.0999999999999998) ;
#28975 = CIRCLE('',#91833,0.0999999999999998) ;
#28976 = CIRCLE('',#91835,0.1) ;
#28977 = CIRCLE('',#91836,0.1) ;
#28978 = CIRCLE('',#91838,0.1) ;
#28979 = CIRCLE('',#91839,0.1) ;
#28980 = CIRCLE('',#91841,0.0999999999999998) ;
#28981 = CIRCLE('',#91843,0.1) ;
#28982 = CIRCLE('',#91845,0.0999999999999998) ;
#28983 = CIRCLE('',#91846,0.0999999999999998) ;
#28984 = CIRCLE('',#91848,0.1) ;
#28985 = CIRCLE('',#91850,0.1) ;
#28986 = CIRCLE('',#91852,0.1) ;
#28987 = CIRCLE('',#91853,0.1) ;
#28988 = CIRCLE('',#91855,0.1) ;
#28989 = CIRCLE('',#91857,0.1) ;
#28990 = CIRCLE('',#91859,0.1) ;
#28991 = CIRCLE('',#91861,0.1) ;
#28992 = CIRCLE('',#91863,0.1) ;
#28993 = CIRCLE('',#91865,0.1) ;
#28994 = CIRCLE('',#91867,0.1) ;
#28995 = CIRCLE('',#91869,0.1) ;
#28996 = CIRCLE('',#91871,0.1) ;
#28997 = CIRCLE('',#91873,0.1) ;
#28998 = CIRCLE('',#91876,0.1) ;
#28999 = CIRCLE('',#91877,0.0999999999999998) ;
#29000 = CIRCLE('',#91879,0.0999999999999998) ;
#29001 = CIRCLE('',#91880,0.1) ;
#29002 = CIRCLE('',#91882,0.1) ;
#29003 = CIRCLE('',#91883,0.1) ;
#29004 = CIRCLE('',#91885,0.1) ;
#29005 = CIRCLE('',#91887,0.1) ;
#29006 = CIRCLE('',#91889,0.0999999999999998) ;
#29007 = CIRCLE('',#91890,0.0999999999999998) ;
#29008 = CIRCLE('',#91892,0.1) ;
#29009 = CIRCLE('',#91894,0.1) ;
#29010 = CIRCLE('',#91896,0.0999999999999998) ;
#29011 = CIRCLE('',#91897,0.0999999999999998) ;
#29012 = CIRCLE('',#91899,0.1) ;
#29013 = CIRCLE('',#91901,0.1) ;
#29014 = CIRCLE('',#91903,0.1) ;
#29015 = CIRCLE('',#91905,0.1) ;
#29016 = CIRCLE('',#91907,0.1) ;
#29017 = CIRCLE('',#91909,0.1) ;
#29018 = CIRCLE('',#91911,0.1) ;
#29019 = CIRCLE('',#91913,0.1) ;
#29020 = CIRCLE('',#91915,0.0999999999999998) ;
#29021 = CIRCLE('',#91917,0.0999999999999998) ;
#29022 = CIRCLE('',#91920,0.1) ;
#29023 = CIRCLE('',#91922,0.0999999999999998) ;
#29024 = CIRCLE('',#91924,0.0999999999999998) ;
#29025 = CIRCLE('',#91926,0.1) ;
#29026 = CIRCLE('',#91928,0.1) ;
#29027 = CIRCLE('',#91930,0.0999999999999994) ;
#29028 = CIRCLE('',#91932,0.1) ;
#29029 = CIRCLE('',#91934,0.1) ;
#29030 = CIRCLE('',#91936,0.0999999999999998) ;
#29031 = CIRCLE('',#91938,0.1) ;
#29032 = CIRCLE('',#91945,0.0999999999999998) ;
#29033 = CIRCLE('',#91947,0.0999999999999998) ;
#29034 = CIRCLE('',#91949,0.1) ;
#29035 = CIRCLE('',#91950,0.1) ;
#29036 = CIRCLE('',#91952,0.1) ;
#29037 = CIRCLE('',#91953,0.1) ;
#29038 = CIRCLE('',#91955,0.1) ;
#29039 = CIRCLE('',#91959,0.1) ;
#29040 = CIRCLE('',#91960,0.1) ;
#29041 = CIRCLE('',#91961,0.0999999999999998) ;
#29042 = CIRCLE('',#91962,0.1) ;
#29043 = CIRCLE('',#91964,0.0999999999999995) ;
#29044 = CIRCLE('',#91965,0.0999999999999998) ;
#29045 = CIRCLE('',#91967,0.1) ;
#29046 = CIRCLE('',#91968,0.0999999999999995) ;
#29047 = CIRCLE('',#91970,0.0999999999999998) ;
#29048 = CIRCLE('',#91972,0.1) ;
#29049 = CIRCLE('',#91974,0.1) ;
#29050 = CIRCLE('',#91976,0.1) ;
#29051 = CIRCLE('',#91978,0.1) ;
#29052 = CIRCLE('',#91980,0.0999999999999999) ;
#29053 = CIRCLE('',#91982,0.0999999999999999) ;
#29054 = CIRCLE('',#91984,0.1) ;
#29055 = CIRCLE('',#91986,0.1) ;
#29056 = CIRCLE('',#91989,0.1) ;
#29057 = CIRCLE('',#91990,0.1) ;
#29058 = CIRCLE('',#91993,0.0999999999999999) ;
#29059 = CIRCLE('',#91995,0.0999999999999998) ;
#29060 = CIRCLE('',#91996,0.0999999999999998) ;
#29061 = CIRCLE('',#91997,0.1) ;
#29062 = CIRCLE('',#91999,0.1) ;
#29063 = CIRCLE('',#92001,0.0999999999999998) ;
#29064 = CIRCLE('',#92003,0.0999999999999998) ;
#29065 = CIRCLE('',#92005,0.1) ;
#29066 = CIRCLE('',#92007,0.1) ;
#29067 = CIRCLE('',#92009,0.1) ;
#29068 = CIRCLE('',#92011,0.1) ;
#29069 = CIRCLE('',#92014,0.199999999999999) ;
#29070 = CIRCLE('',#92015,0.0999999999999994) ;
#29071 = CIRCLE('',#92016,0.0999999999999994) ;
#29072 = CIRCLE('',#92017,0.100000000000001) ;
#29073 = CIRCLE('',#92019,2.) ;
#29074 = CIRCLE('',#92020,0.1) ;
#29075 = CIRCLE('',#92021,1.9) ;
#29076 = CIRCLE('',#92022,1.9) ;
#29077 = CIRCLE('',#92024,1.47071067811865) ;
#29078 = CIRCLE('',#92025,0.1) ;
#29079 = CIRCLE('',#92026,1.5) ;
#29080 = CIRCLE('',#92028,1.6) ;
#29081 = CIRCLE('',#92029,0.1) ;
#29082 = CIRCLE('',#92030,1.5) ;
#29083 = CIRCLE('',#92031,1.5) ;
#29084 = CIRCLE('',#92033,0.0999999999999994) ;
#29085 = CIRCLE('',#92034,0.0999999999999994) ;
#29086 = CIRCLE('',#92035,0.200000000000001) ;
#29087 = CIRCLE('',#92036,0.0999999999999994) ;
#29088 = CIRCLE('',#92038,0.0999999999999994) ;
#29089 = CIRCLE('',#92039,0.0999999999999994) ;
#29090 = CIRCLE('',#92040,0.0999999999999994) ;
#29091 = CIRCLE('',#92042,0.0999999999999994) ;
#29092 = CIRCLE('',#92044,0.0999999999999994) ;
#29093 = CIRCLE('',#92045,0.0999999999999994) ;
#29094 = CIRCLE('',#92046,0.0999999999999994) ;
#29095 = CIRCLE('',#92048,0.749999999999997) ;
#29096 = CIRCLE('',#92051,1.9) ;
#29097 = CIRCLE('',#92052,1.9) ;
#29098 = CIRCLE('',#92053,1.9) ;
#29099 = CIRCLE('',#92054,1.9) ;
#29100 = CIRCLE('',#92055,1.9) ;
#29101 = CIRCLE('',#92057,0.199999999999999) ;
#29102 = CIRCLE('',#92058,0.0999999999999994) ;
#29103 = CIRCLE('',#92059,0.0999999999999994) ;
#29104 = CIRCLE('',#92060,0.100000000000001) ;
#29105 = CIRCLE('',#92062,0.1) ;
#29106 = CIRCLE('',#92063,0.1) ;
#29107 = CIRCLE('',#92065,2.) ;
#29108 = CIRCLE('',#92066,0.1) ;
#29109 = CIRCLE('',#92067,1.9) ;
#29110 = CIRCLE('',#92068,1.9) ;
#29111 = CIRCLE('',#92070,1.47071067811865) ;
#29112 = CIRCLE('',#92071,0.1) ;
#29113 = CIRCLE('',#92072,1.5) ;
#29114 = CIRCLE('',#92074,1.6) ;
#29115 = CIRCLE('',#92075,0.1) ;
#29116 = CIRCLE('',#92076,1.5) ;
#29117 = CIRCLE('',#92077,1.5) ;
#29118 = CIRCLE('',#92079,0.0999999999999994) ;
#29119 = CIRCLE('',#92080,0.0999999999999994) ;
#29120 = CIRCLE('',#92081,0.199999999999999) ;
#29121 = CIRCLE('',#92082,0.0999999999999994) ;
#29122 = CIRCLE('',#92084,0.0999999999999994) ;
#29123 = CIRCLE('',#92085,0.0999999999999994) ;
#29124 = CIRCLE('',#92086,0.0999999999999994) ;
#29125 = CIRCLE('',#92088,0.0999999999999994) ;
#29126 = CIRCLE('',#92090,0.0999999999999994) ;
#29127 = CIRCLE('',#92091,0.0999999999999994) ;
#29128 = CIRCLE('',#92092,0.0999999999999994) ;
#29129 = CIRCLE('',#92094,0.749999999999997) ;
#29130 = CIRCLE('',#92097,1.9) ;
#29131 = CIRCLE('',#92098,1.9) ;
#29132 = CIRCLE('',#92099,1.9) ;
#29133 = CIRCLE('',#92100,1.9) ;
#29134 = CIRCLE('',#92101,1.9) ;
#29135 = CIRCLE('',#92103,0.199999999999999) ;
#29136 = CIRCLE('',#92104,0.199999999999999) ;
#29137 = CIRCLE('',#92109,0.0999999999999998) ;
#29138 = CIRCLE('',#92110,0.0999999999999998) ;
#29139 = CIRCLE('',#92112,0.0999999999999998) ;
#29140 = CIRCLE('',#92113,0.0999999999999998) ;
#29141 = CIRCLE('',#92115,0.0999999999999998) ;
#29142 = CIRCLE('',#92116,0.0999999999999998) ;
#29143 = CIRCLE('',#92118,0.0999999999999998) ;
#29144 = CIRCLE('',#92119,0.0999999999999998) ;
#29145 = CIRCLE('',#92120,0.0999999999999998) ;
#29146 = CIRCLE('',#92122,3.1) ;
#29147 = CIRCLE('',#92127,0.199999999999999) ;
#29148 = CIRCLE('',#92128,0.200000000000001) ;
#29149 = CIRCLE('',#92129,2.9) ;
#29150 = CIRCLE('',#92130,0.199999999999999) ;
#29151 = CIRCLE('',#92131,0.199999999999999) ;
#29152 = CIRCLE('',#92132,2.9) ;
#29153 = CIRCLE('',#92133,0.199999999999999) ;
#29154 = CIRCLE('',#92134,0.199999999999999) ;
#29155 = CIRCLE('',#92144,0.199999999999999) ;
#29156 = CIRCLE('',#92145,0.200000000000001) ;
#29157 = CIRCLE('',#92146,0.200000000000001) ;
#29158 = CIRCLE('',#92147,0.199999999999999) ;
#29159 = CIRCLE('',#92148,0.199999999999999) ;
#29160 = CIRCLE('',#92149,0.199999999999999) ;
#29161 = CIRCLE('',#92150,0.199999999999999) ;
#29162 = CIRCLE('',#92151,0.199999999999999) ;
#29163 = CIRCLE('',#92157,0.199999999999999) ;
#29164 = CIRCLE('',#92158,0.200000000000001) ;
#29165 = CIRCLE('',#92159,0.200000000000001) ;
#29166 = CIRCLE('',#92160,0.199999999999999) ;
#29167 = CIRCLE('',#92161,0.199999999999999) ;
#29168 = CIRCLE('',#92162,0.199999999999999) ;
#29169 = CIRCLE('',#92163,0.199999999999999) ;
#29170 = CIRCLE('',#92164,0.199999999999999) ;
#29171 = CIRCLE('',#92168,3.1) ;
#29172 = CIRCLE('',#92169,3.1) ;
#29173 = CIRCLE('',#92172,0.0999999999999998) ;
#29174 = CIRCLE('',#92173,0.0999999999999998) ;
#29175 = CIRCLE('',#92174,0.1) ;
#29176 = CIRCLE('',#92175,0.1) ;
#29177 = CIRCLE('',#92176,0.0999999999999994) ;
#29178 = CIRCLE('',#92177,0.0999999999999994) ;
#29179 = CIRCLE('',#92178,0.1) ;
#29180 = CIRCLE('',#92179,0.1) ;
#29181 = CIRCLE('',#92180,0.0999999999999998) ;
#29182 = CIRCLE('',#92181,0.0999999999999998) ;
#29183 = CIRCLE('',#92182,0.1) ;
#29184 = CIRCLE('',#92183,0.1) ;
#29185 = CIRCLE('',#92184,0.1) ;
#29186 = CIRCLE('',#92185,0.1) ;
#29187 = CIRCLE('',#92208,0.0999999999999994) ;
#29188 = CIRCLE('',#92209,0.0999999999999994) ;
#29189 = CIRCLE('',#92210,0.0999999999999994) ;
#29190 = CIRCLE('',#92211,0.0999999999999994) ;
#29191 = CIRCLE('',#92213,0.0999999999999994) ;
#29192 = CIRCLE('',#92216,0.0999999999999994) ;
#29193 = CIRCLE('',#92219,0.0999999999999994) ;
#29194 = CIRCLE('',#92222,0.0999999999999994) ;
#29195 = CIRCLE('',#92234,0.0999999999999994) ;
#29196 = CIRCLE('',#92235,0.0999999999999994) ;
#29197 = CIRCLE('',#92236,0.0999999999999994) ;
#29198 = CIRCLE('',#92237,0.0999999999999994) ;
#29199 = CIRCLE('',#92239,0.0999999999999994) ;
#29200 = CIRCLE('',#92242,0.0999999999999994) ;
#29201 = CIRCLE('',#92245,0.0999999999999994) ;
#29202 = CIRCLE('',#92248,0.0999999999999994) ;
#29203 = CIRCLE('',#92255,0.199999999999999) ;
#29204 = CIRCLE('',#92258,3.) ;
#29205 = CIRCLE('',#92259,3.) ;
#29206 = CIRCLE('',#92260,3.) ;
#29207 = CIRCLE('',#92261,3.) ;
#29208 = CIRCLE('',#92262,0.1) ;
#29209 = CIRCLE('',#92263,0.0999999999999994) ;
#29210 = CIRCLE('',#92265,0.100000000000002) ;
#29211 = CIRCLE('',#92266,0.1) ;
#29212 = CIRCLE('',#92269,0.1) ;
#29213 = CIRCLE('',#92271,0.0999999999999997) ;
#29214 = CIRCLE('',#92273,0.0999999999999994) ;
#29215 = CIRCLE('',#92275,0.1) ;
#29216 = CIRCLE('',#92279,0.100000000000002) ;
#29217 = CIRCLE('',#92281,0.1) ;
#29218 = CIRCLE('',#92283,0.1) ;
#29219 = CIRCLE('',#92284,0.0999999999999994) ;
#29220 = CIRCLE('',#92285,0.0999999999999999) ;
#29221 = CIRCLE('',#92287,0.1) ;
#29222 = CIRCLE('',#92289,0.1) ;
#29223 = CIRCLE('',#92291,0.1) ;
#29224 = CIRCLE('',#92293,0.0999999999999994) ;
#29225 = CIRCLE('',#92295,0.1) ;
#29226 = CIRCLE('',#92297,0.0999999999999998) ;
#29227 = CIRCLE('',#92299,0.0999999999999998) ;
#29228 = CIRCLE('',#92302,0.1) ;
#29229 = CIRCLE('',#92304,0.100000000000002) ;
#29230 = CIRCLE('',#92306,0.0999999999999999) ;
#29231 = CIRCLE('',#92308,0.1) ;
#29232 = CIRCLE('',#92310,0.1) ;
#29233 = CIRCLE('',#92313,0.1) ;
#29234 = CIRCLE('',#92317,0.0999999999999999) ;
#29235 = CIRCLE('',#92318,0.100000000000002) ;
#29236 = CIRCLE('',#92324,0.0999999999999994) ;
#29237 = CIRCLE('',#92325,0.0999999999999994) ;
#29238 = CIRCLE('',#92327,0.0999999999999994) ;
#29239 = CIRCLE('',#92330,0.1) ;
#29240 = CIRCLE('',#92331,0.1) ;
#29241 = CIRCLE('',#92333,0.0999999999999994) ;
#29242 = CIRCLE('',#92337,0.0999999999999994) ;
#29243 = CIRCLE('',#92341,0.0999999999999998) ;
#29244 = CIRCLE('',#92342,0.0999999999999994) ;
#29245 = CIRCLE('',#92344,0.0999999999999994) ;
#29246 = CIRCLE('',#92346,0.0999999999999998) ;
#29247 = CIRCLE('',#92348,0.0999999999999998) ;
#29248 = CIRCLE('',#92350,0.0999999999999994) ;
#29249 = CIRCLE('',#92352,0.0999999999999998) ;
#29250 = CIRCLE('',#92354,0.0999999999999994) ;
#29251 = CIRCLE('',#92357,0.0999999999999998) ;
#29252 = CIRCLE('',#92358,0.0999999999999998) ;
#29253 = CIRCLE('',#92360,0.0999999999999994) ;
#29254 = CIRCLE('',#92361,0.0999999999999994) ;
#29255 = CIRCLE('',#92363,0.0999999999999994) ;
#29256 = CIRCLE('',#92364,0.0999999999999994) ;
#29257 = CIRCLE('',#92366,0.0999999999999994) ;
#29258 = CIRCLE('',#92368,0.0999999999999994) ;
#29259 = CIRCLE('',#92370,0.0999999999999998) ;
#29260 = CIRCLE('',#92371,0.0999999999999998) ;
#29261 = CIRCLE('',#92373,0.0999999999999994) ;
#29262 = CIRCLE('',#92375,0.0999999999999994) ;
#29263 = CIRCLE('',#92377,0.1) ;
#29264 = CIRCLE('',#92378,0.1) ;
#29265 = CIRCLE('',#92380,0.0999999999999994) ;
#29266 = CIRCLE('',#92382,0.0999999999999994) ;
#29267 = CIRCLE('',#92384,0.0999999999999994) ;
#29268 = CIRCLE('',#92386,0.0999999999999994) ;
#29269 = CIRCLE('',#92388,0.0999999999999994) ;
#29270 = CIRCLE('',#92390,0.0999999999999994) ;
#29271 = CIRCLE('',#92392,0.0999999999999994) ;
#29272 = CIRCLE('',#92394,0.0999999999999994) ;
#29273 = CIRCLE('',#92396,0.1) ;
#29274 = CIRCLE('',#92398,0.1) ;
#29275 = CIRCLE('',#92401,0.1) ;
#29276 = CIRCLE('',#92402,0.0999999999999998) ;
#29277 = CIRCLE('',#92404,0.0999999999999994) ;
#29278 = CIRCLE('',#92405,0.0999999999999994) ;
#29279 = CIRCLE('',#92407,0.0999999999999994) ;
#29280 = CIRCLE('',#92408,0.0999999999999994) ;
#29281 = CIRCLE('',#92410,0.0999999999999994) ;
#29282 = CIRCLE('',#92412,0.0999999999999994) ;
#29283 = CIRCLE('',#92414,0.0999999999999998) ;
#29284 = CIRCLE('',#92415,0.0999999999999998) ;
#29285 = CIRCLE('',#92417,0.0999999999999994) ;
#29286 = CIRCLE('',#92419,0.0999999999999994) ;
#29287 = CIRCLE('',#92421,0.0999999999999998) ;
#29288 = CIRCLE('',#92422,0.0999999999999998) ;
#29289 = CIRCLE('',#92424,0.0999999999999994) ;
#29290 = CIRCLE('',#92426,0.0999999999999994) ;
#29291 = CIRCLE('',#92428,0.0999999999999994) ;
#29292 = CIRCLE('',#92430,0.0999999999999994) ;
#29293 = CIRCLE('',#92432,0.0999999999999994) ;
#29294 = CIRCLE('',#92434,0.0999999999999994) ;
#29295 = CIRCLE('',#92436,0.0999999999999994) ;
#29296 = CIRCLE('',#92438,0.0999999999999994) ;
#29297 = CIRCLE('',#92440,0.0999999999999998) ;
#29298 = CIRCLE('',#92442,0.0999999999999998) ;
#29299 = CIRCLE('',#92445,0.100000000000001) ;
#29300 = CIRCLE('',#92447,0.0999999999999998) ;
#29301 = CIRCLE('',#92448,0.1) ;
#29302 = CIRCLE('',#92450,0.0999999999999994) ;
#29303 = CIRCLE('',#92452,0.0999999999999994) ;
#29304 = CIRCLE('',#92454,0.0999999999999994) ;
#29305 = CIRCLE('',#92455,0.0999999999999994) ;
#29306 = CIRCLE('',#92457,0.099999999999999) ;
#29307 = CIRCLE('',#92459,0.099999999999999) ;
#29308 = CIRCLE('',#92461,0.0999999999999994) ;
#29309 = CIRCLE('',#92463,0.0999999999999994) ;
#29310 = CIRCLE('',#92465,0.0999999999999994) ;
#29311 = CIRCLE('',#92467,0.0999999999999998) ;
#29312 = CIRCLE('',#92469,0.099999999999999) ;
#29313 = CIRCLE('',#92472,0.0999999999999998) ;
#29314 = CIRCLE('',#92474,0.0999999999999998) ;
#29315 = CIRCLE('',#92476,0.1) ;
#29316 = CIRCLE('',#92478,0.1) ;
#29317 = CIRCLE('',#92480,0.1) ;
#29318 = CIRCLE('',#92482,0.1) ;
#29319 = CIRCLE('',#92488,0.0999999999999998) ;
#29320 = CIRCLE('',#92490,0.0999999999999998) ;
#29321 = CIRCLE('',#92492,0.1) ;
#29322 = CIRCLE('',#92494,0.0999999999999994) ;
#29323 = CIRCLE('',#92496,0.0999999999999994) ;
#29324 = CIRCLE('',#92498,0.100000000000001) ;
#29325 = CIRCLE('',#92499,0.1) ;
#29326 = CIRCLE('',#92500,0.1) ;
#29327 = CIRCLE('',#92502,0.1) ;
#29328 = CIRCLE('',#92504,0.1) ;
#29329 = CIRCLE('',#92505,0.0999999999999998) ;
#29330 = CIRCLE('',#92507,0.0999999999999994) ;
#29331 = CIRCLE('',#92511,0.1) ;
#29332 = CIRCLE('',#92512,0.1) ;
#29333 = CIRCLE('',#92514,0.1) ;
#29334 = CIRCLE('',#92515,0.100000000000001) ;
#29335 = CIRCLE('',#92516,0.0999999999999998) ;
#29336 = CIRCLE('',#92517,0.100000000000001) ;
#29337 = CIRCLE('',#92521,0.100000000000001) ;
#29338 = CIRCLE('',#92522,0.100000000000001) ;
#29339 = CIRCLE('',#92525,0.0999999999999994) ;
#29340 = CIRCLE('',#92526,0.0999999999999994) ;
#29341 = CIRCLE('',#92529,0.100000000000001) ;
#29342 = CIRCLE('',#92530,0.100000000000001) ;
#29343 = CIRCLE('',#92533,0.0999999999999994) ;
#29344 = CIRCLE('',#92534,0.0999999999999994) ;
#29345 = CIRCLE('',#92537,0.199999999999999) ;
#29346 = CIRCLE('',#92539,0.199999999999999) ;
#29347 = CIRCLE('',#92544,3.1) ;
#29348 = CIRCLE('',#92546,0.1) ;
#29349 = CIRCLE('',#92547,0.1) ;
#29350 = CIRCLE('',#92548,0.0999999999999994) ;
#29351 = CIRCLE('',#92549,0.0999999999999994) ;
#29352 = CIRCLE('',#92550,0.1) ;
#29353 = CIRCLE('',#92573,0.0999999999999994) ;
#29354 = CIRCLE('',#92574,0.0999999999999994) ;
#29355 = CIRCLE('',#92575,0.0999999999999994) ;
#29356 = CIRCLE('',#92576,0.0999999999999994) ;
#29357 = CIRCLE('',#92578,0.0999999999999994) ;
#29358 = CIRCLE('',#92581,0.0999999999999994) ;
#29359 = CIRCLE('',#92584,0.0999999999999994) ;
#29360 = CIRCLE('',#92587,0.0999999999999994) ;
#29361 = CIRCLE('',#92599,0.0999999999999994) ;
#29362 = CIRCLE('',#92600,0.0999999999999994) ;
#29363 = CIRCLE('',#92601,0.0999999999999994) ;
#29364 = CIRCLE('',#92602,0.0999999999999994) ;
#29365 = CIRCLE('',#92604,0.0999999999999994) ;
#29366 = CIRCLE('',#92607,0.0999999999999994) ;
#29367 = CIRCLE('',#92610,0.0999999999999994) ;
#29368 = CIRCLE('',#92613,0.0999999999999994) ;
#29369 = CIRCLE('',#92620,0.200000000000001) ;
#29370 = CIRCLE('',#92623,3.) ;
#29371 = CIRCLE('',#92624,3.) ;
#29372 = CIRCLE('',#92625,3.) ;
#29373 = CIRCLE('',#92626,3.) ;
#29374 = CIRCLE('',#92627,0.1) ;
#29375 = CIRCLE('',#92628,0.0999999999999994) ;
#29376 = CIRCLE('',#92630,0.0999999999999999) ;
#29377 = CIRCLE('',#92631,0.0999999999999999) ;
#29378 = CIRCLE('',#92634,0.1) ;
#29379 = CIRCLE('',#92636,0.0999999999999997) ;
#29380 = CIRCLE('',#92638,0.0999999999999994) ;
#29381 = CIRCLE('',#92640,0.1) ;
#29382 = CIRCLE('',#92644,0.100000000000002) ;
#29383 = CIRCLE('',#92646,0.1) ;
#29384 = CIRCLE('',#92648,0.1) ;
#29385 = CIRCLE('',#92649,0.0999999999999994) ;
#29386 = CIRCLE('',#92650,0.0999999999999999) ;
#29387 = CIRCLE('',#92652,0.1) ;
#29388 = CIRCLE('',#92654,0.1) ;
#29389 = CIRCLE('',#92656,0.1) ;
#29390 = CIRCLE('',#92658,0.0999999999999994) ;
#29391 = CIRCLE('',#92660,0.1) ;
#29392 = CIRCLE('',#92662,0.0999999999999998) ;
#29393 = CIRCLE('',#92664,0.1) ;
#29394 = CIRCLE('',#92667,0.1) ;
#29395 = CIRCLE('',#92669,0.0999999999999999) ;
#29396 = CIRCLE('',#92671,0.0999999999999999) ;
#29397 = CIRCLE('',#92673,0.1) ;
#29398 = CIRCLE('',#92675,0.1) ;
#29399 = CIRCLE('',#92678,0.1) ;
#29400 = CIRCLE('',#92682,0.0999999999999999) ;
#29401 = CIRCLE('',#92683,0.100000000000002) ;
#29402 = CIRCLE('',#92688,0.0999999999999994) ;
#29403 = CIRCLE('',#92689,0.0999999999999994) ;
#29404 = CIRCLE('',#92691,0.0999999999999994) ;
#29405 = CIRCLE('',#92694,0.1) ;
#29406 = CIRCLE('',#92695,0.1) ;
#29407 = CIRCLE('',#92697,0.0999999999999994) ;
#29408 = CIRCLE('',#92701,0.0999999999999994) ;
#29409 = CIRCLE('',#92705,0.0999999999999998) ;
#29410 = CIRCLE('',#92706,0.0999999999999994) ;
#29411 = CIRCLE('',#92708,0.0999999999999994) ;
#29412 = CIRCLE('',#92710,0.0999999999999998) ;
#29413 = CIRCLE('',#92712,0.0999999999999998) ;
#29414 = CIRCLE('',#92714,0.0999999999999994) ;
#29415 = CIRCLE('',#92716,0.0999999999999998) ;
#29416 = CIRCLE('',#92718,0.0999999999999994) ;
#29417 = CIRCLE('',#92721,0.0999999999999998) ;
#29418 = CIRCLE('',#92722,0.0999999999999998) ;
#29419 = CIRCLE('',#92724,0.0999999999999994) ;
#29420 = CIRCLE('',#92725,0.0999999999999994) ;
#29421 = CIRCLE('',#92727,0.0999999999999994) ;
#29422 = CIRCLE('',#92728,0.0999999999999994) ;
#29423 = CIRCLE('',#92730,0.0999999999999994) ;
#29424 = CIRCLE('',#92732,0.0999999999999994) ;
#29425 = CIRCLE('',#92734,0.0999999999999998) ;
#29426 = CIRCLE('',#92735,0.0999999999999998) ;
#29427 = CIRCLE('',#92737,0.0999999999999994) ;
#29428 = CIRCLE('',#92739,0.0999999999999994) ;
#29429 = CIRCLE('',#92741,0.1) ;
#29430 = CIRCLE('',#92742,0.1) ;
#29431 = CIRCLE('',#92744,0.0999999999999994) ;
#29432 = CIRCLE('',#92746,0.0999999999999994) ;
#29433 = CIRCLE('',#92748,0.0999999999999994) ;
#29434 = CIRCLE('',#92750,0.0999999999999994) ;
#29435 = CIRCLE('',#92752,0.0999999999999994) ;
#29436 = CIRCLE('',#92754,0.0999999999999994) ;
#29437 = CIRCLE('',#92756,0.0999999999999994) ;
#29438 = CIRCLE('',#92758,0.0999999999999994) ;
#29439 = CIRCLE('',#92760,0.1) ;
#29440 = CIRCLE('',#92762,0.1) ;
#29441 = CIRCLE('',#92765,0.1) ;
#29442 = CIRCLE('',#92766,0.0999999999999998) ;
#29443 = CIRCLE('',#92768,0.0999999999999994) ;
#29444 = CIRCLE('',#92769,0.0999999999999994) ;
#29445 = CIRCLE('',#92771,0.0999999999999994) ;
#29446 = CIRCLE('',#92772,0.0999999999999994) ;
#29447 = CIRCLE('',#92774,0.0999999999999994) ;
#29448 = CIRCLE('',#92776,0.0999999999999994) ;
#29449 = CIRCLE('',#92778,0.0999999999999998) ;
#29450 = CIRCLE('',#92779,0.0999999999999998) ;
#29451 = CIRCLE('',#92781,0.0999999999999994) ;
#29452 = CIRCLE('',#92783,0.0999999999999994) ;
#29453 = CIRCLE('',#92785,0.0999999999999998) ;
#29454 = CIRCLE('',#92786,0.0999999999999998) ;
#29455 = CIRCLE('',#92788,0.0999999999999994) ;
#29456 = CIRCLE('',#92790,0.0999999999999994) ;
#29457 = CIRCLE('',#92792,0.0999999999999994) ;
#29458 = CIRCLE('',#92794,0.0999999999999994) ;
#29459 = CIRCLE('',#92796,0.0999999999999994) ;
#29460 = CIRCLE('',#92798,0.0999999999999994) ;
#29461 = CIRCLE('',#92800,0.0999999999999994) ;
#29462 = CIRCLE('',#92802,0.0999999999999994) ;
#29463 = CIRCLE('',#92804,0.0999999999999998) ;
#29464 = CIRCLE('',#92806,0.0999999999999998) ;
#29465 = CIRCLE('',#92809,0.0999999999999997) ;
#29466 = CIRCLE('',#92811,0.1) ;
#29467 = CIRCLE('',#92813,0.0999999999999994) ;
#29468 = CIRCLE('',#92815,0.0999999999999994) ;
#29469 = CIRCLE('',#92817,0.0999999999999994) ;
#29470 = CIRCLE('',#92819,0.1) ;
#29471 = CIRCLE('',#92821,0.099999999999999) ;
#29472 = CIRCLE('',#92823,0.0999999999999994) ;
#29473 = CIRCLE('',#92825,0.0999999999999994) ;
#29474 = CIRCLE('',#92827,0.099999999999999) ;
#29475 = CIRCLE('',#92834,0.0999999999999994) ;
#29476 = CIRCLE('',#92836,0.0999999999999994) ;
#29477 = CIRCLE('',#92838,0.0999999999999993) ;
#29478 = CIRCLE('',#92839,0.1) ;
#29479 = CIRCLE('',#92840,0.1) ;
#29480 = CIRCLE('',#92842,0.0999999999999998) ;
#29481 = CIRCLE('',#92844,0.0999999999999994) ;
#29482 = CIRCLE('',#92848,0.1) ;
#29483 = CIRCLE('',#92849,0.0999999999999995) ;
#29484 = CIRCLE('',#92850,0.0999999999999998) ;
#29485 = CIRCLE('',#92851,0.100000000000001) ;
#29486 = CIRCLE('',#92853,0.0999999999999995) ;
#29487 = CIRCLE('',#92854,0.0999999999999994) ;
#29488 = CIRCLE('',#92856,0.0999999999999994) ;
#29489 = CIRCLE('',#92857,0.0999999999999995) ;
#29490 = CIRCLE('',#92859,0.0999999999999994) ;
#29491 = CIRCLE('',#92861,0.1) ;
#29492 = CIRCLE('',#92863,0.1) ;
#29493 = CIRCLE('',#92865,0.0999999999999994) ;
#29494 = CIRCLE('',#92867,0.1) ;
#29495 = CIRCLE('',#92869,0.0999999999999999) ;
#29496 = CIRCLE('',#92871,0.0999999999999999) ;
#29497 = CIRCLE('',#92873,0.1) ;
#29498 = CIRCLE('',#92875,0.1) ;
#29499 = CIRCLE('',#92878,0.1) ;
#29500 = CIRCLE('',#92879,0.1) ;
#29501 = CIRCLE('',#92882,0.1) ;
#29502 = CIRCLE('',#92884,0.0999999999999994) ;
#29503 = CIRCLE('',#92885,0.0999999999999994) ;
#29504 = CIRCLE('',#92886,0.0999999999999994) ;
#29505 = CIRCLE('',#92888,0.0999999999999994) ;
#29506 = CIRCLE('',#92890,0.0999999999999994) ;
#29507 = CIRCLE('',#92892,0.0999999999999994) ;
#29508 = CIRCLE('',#92894,0.0999999999999994) ;
#29509 = CIRCLE('',#92896,0.0999999999999994) ;
#29510 = CIRCLE('',#92898,0.1) ;
#29511 = CIRCLE('',#92900,0.1) ;
#29512 = CIRCLE('',#92903,0.200000000000001) ;
#29513 = CIRCLE('',#92904,0.0999999999999994) ;
#29514 = CIRCLE('',#92905,0.0999999999999994) ;
#29515 = CIRCLE('',#92906,0.0999999999999993) ;
#29516 = CIRCLE('',#92908,0.1) ;
#29517 = CIRCLE('',#92909,0.1) ;
#29518 = CIRCLE('',#92911,2.) ;
#29519 = CIRCLE('',#92912,0.1) ;
#29520 = CIRCLE('',#92913,1.9) ;
#29521 = CIRCLE('',#92914,1.9) ;
#29522 = CIRCLE('',#92916,1.47071067811865) ;
#29523 = CIRCLE('',#92917,0.1) ;
#29524 = CIRCLE('',#92918,1.5) ;
#29525 = CIRCLE('',#92920,1.6) ;
#29526 = CIRCLE('',#92921,0.1) ;
#29527 = CIRCLE('',#92922,1.5) ;
#29528 = CIRCLE('',#92923,1.5) ;
#29529 = CIRCLE('',#92925,0.0999999999999994) ;
#29530 = CIRCLE('',#92926,0.0999999999999994) ;
#29531 = CIRCLE('',#92927,0.200000000000001) ;
#29532 = CIRCLE('',#92928,0.0999999999999994) ;
#29533 = CIRCLE('',#92930,0.0999999999999994) ;
#29534 = CIRCLE('',#92931,0.0999999999999994) ;
#29535 = CIRCLE('',#92932,0.0999999999999994) ;
#29536 = CIRCLE('',#92934,0.0999999999999994) ;
#29537 = CIRCLE('',#92936,0.0999999999999994) ;
#29538 = CIRCLE('',#92937,0.0999999999999994) ;
#29539 = CIRCLE('',#92938,0.0999999999999994) ;
#29540 = CIRCLE('',#92940,0.749999999999997) ;
#29541 = CIRCLE('',#92943,1.9) ;
#29542 = CIRCLE('',#92944,1.9) ;
#29543 = CIRCLE('',#92945,1.9) ;
#29544 = CIRCLE('',#92946,1.9) ;
#29545 = CIRCLE('',#92947,1.9) ;
#29546 = CIRCLE('',#92949,3.1) ;
#29547 = CIRCLE('',#92954,0.200000000000001) ;
#29548 = CIRCLE('',#92955,2.9) ;
#29549 = CIRCLE('',#92956,0.200000000000001) ;
#29550 = CIRCLE('',#92957,0.200000000000001) ;
#29551 = CIRCLE('',#92969,0.200000000000001) ;
#29552 = CIRCLE('',#92970,0.200000000000001) ;
#29553 = CIRCLE('',#92971,0.200000000000001) ;
#29554 = CIRCLE('',#92972,0.200000000000001) ;
#29555 = CIRCLE('',#92978,0.200000000000001) ;
#29556 = CIRCLE('',#92979,0.200000000000001) ;
#29557 = CIRCLE('',#92980,0.200000000000001) ;
#29558 = CIRCLE('',#92981,0.200000000000001) ;
#29559 = CIRCLE('',#92985,3.1) ;
#29560 = CIRCLE('',#92988,0.1) ;
#29561 = CIRCLE('',#92989,0.1) ;
#29562 = CIRCLE('',#92990,0.0999999999999994) ;
#29563 = CIRCLE('',#92991,0.0999999999999994) ;
#29564 = CIRCLE('',#92992,0.1) ;
#29565 = CIRCLE('',#92993,0.1) ;
#29566 = CIRCLE('',#92994,0.0999999999999998) ;
#29567 = CIRCLE('',#92995,0.0999999999999998) ;
#29568 = CIRCLE('',#92996,0.0999999999999998) ;
#29569 = CIRCLE('',#92997,0.0999999999999998) ;
#29570 = CIRCLE('',#92998,0.0999999999999998) ;
#29571 = CIRCLE('',#92999,0.0999999999999998) ;
#29572 = CIRCLE('',#93000,0.1) ;
#29573 = CIRCLE('',#93001,0.1) ;
#29574 = CIRCLE('',#93002,0.1) ;
#29575 = CIRCLE('',#93003,0.1) ;
#29576 = CIRCLE('',#93004,0.0999999999999998) ;
#29577 = CIRCLE('',#93005,0.0999999999999998) ;
#29578 = CIRCLE('',#93007,0.1) ;
#29579 = CIRCLE('',#93008,0.0999999999999998) ;
#29580 = CIRCLE('',#93009,0.0999999999999998) ;
#29581 = CIRCLE('',#93010,0.1) ;
#29582 = CIRCLE('',#93011,0.1) ;
#29583 = CIRCLE('',#93012,0.1) ;
#29584 = CIRCLE('',#93013,0.1) ;
#29585 = CIRCLE('',#93014,0.0999999999999998) ;
#29586 = CIRCLE('',#93015,0.0999999999999998) ;
#29587 = CIRCLE('',#93016,0.0999999999999998) ;
#29588 = CIRCLE('',#93017,0.0999999999999998) ;
#29589 = CIRCLE('',#93018,0.0999999999999998) ;
#29590 = CIRCLE('',#93019,0.0999999999999998) ;
#29591 = CIRCLE('',#93020,0.1) ;
#29592 = CIRCLE('',#93021,0.1) ;
#29593 = CIRCLE('',#93022,0.0999999999999994) ;
#29594 = CIRCLE('',#93023,0.0999999999999994) ;
#29595 = CIRCLE('',#93024,0.1) ;
#29596 = CIRCLE('',#93047,0.0999999999999994) ;
#29597 = CIRCLE('',#93048,0.0999999999999994) ;
#29598 = CIRCLE('',#93049,0.0999999999999994) ;
#29599 = CIRCLE('',#93050,0.0999999999999994) ;
#29600 = CIRCLE('',#93052,0.0999999999999994) ;
#29601 = CIRCLE('',#93055,0.0999999999999994) ;
#29602 = CIRCLE('',#93058,0.0999999999999994) ;
#29603 = CIRCLE('',#93061,0.0999999999999994) ;
#29604 = CIRCLE('',#93073,0.0999999999999994) ;
#29605 = CIRCLE('',#93074,0.0999999999999994) ;
#29606 = CIRCLE('',#93075,0.0999999999999994) ;
#29607 = CIRCLE('',#93076,0.0999999999999994) ;
#29608 = CIRCLE('',#93078,0.0999999999999994) ;
#29609 = CIRCLE('',#93081,0.0999999999999994) ;
#29610 = CIRCLE('',#93084,0.0999999999999994) ;
#29611 = CIRCLE('',#93087,0.0999999999999994) ;
#29612 = CIRCLE('',#93094,0.200000000000001) ;
#29613 = CIRCLE('',#93097,3.) ;
#29614 = CIRCLE('',#93098,3.) ;
#29615 = CIRCLE('',#93099,3.) ;
#29616 = CIRCLE('',#93100,3.) ;
#29617 = CIRCLE('',#93101,0.1) ;
#29618 = CIRCLE('',#93102,0.0999999999999994) ;
#29619 = CIRCLE('',#93104,0.0999999999999999) ;
#29620 = CIRCLE('',#93105,0.1) ;
#29621 = CIRCLE('',#93108,0.1) ;
#29622 = CIRCLE('',#93110,0.0999999999999997) ;
#29623 = CIRCLE('',#93112,0.0999999999999994) ;
#29624 = CIRCLE('',#93114,0.1) ;
#29625 = CIRCLE('',#93118,0.0999999999999999) ;
#29626 = CIRCLE('',#93120,0.1) ;
#29627 = CIRCLE('',#93122,0.1) ;
#29628 = CIRCLE('',#93123,0.0999999999999994) ;
#29629 = CIRCLE('',#93124,0.1) ;
#29630 = CIRCLE('',#93126,0.1) ;
#29631 = CIRCLE('',#93128,0.1) ;
#29632 = CIRCLE('',#93130,0.1) ;
#29633 = CIRCLE('',#93132,0.0999999999999994) ;
#29634 = CIRCLE('',#93134,0.1) ;
#29635 = CIRCLE('',#93136,0.0999999999999998) ;
#29636 = CIRCLE('',#93138,0.1) ;
#29637 = CIRCLE('',#93141,0.1) ;
#29638 = CIRCLE('',#93143,0.0999999999999999) ;
#29639 = CIRCLE('',#93145,0.0999999999999999) ;
#29640 = CIRCLE('',#93147,0.1) ;
#29641 = CIRCLE('',#93149,0.1) ;
#29642 = CIRCLE('',#93152,0.1) ;
#29643 = CIRCLE('',#93156,0.0999999999999999) ;
#29644 = CIRCLE('',#93157,0.0999999999999999) ;
#29645 = CIRCLE('',#93163,0.0999999999999994) ;
#29646 = CIRCLE('',#93164,0.0999999999999994) ;
#29647 = CIRCLE('',#93166,0.0999999999999994) ;
#29648 = CIRCLE('',#93169,0.1) ;
#29649 = CIRCLE('',#93170,0.1) ;
#29650 = CIRCLE('',#93172,0.0999999999999994) ;
#29651 = CIRCLE('',#93176,0.0999999999999994) ;
#29652 = CIRCLE('',#93180,0.0999999999999998) ;
#29653 = CIRCLE('',#93181,0.0999999999999994) ;
#29654 = CIRCLE('',#93183,0.0999999999999994) ;
#29655 = CIRCLE('',#93185,0.0999999999999998) ;
#29656 = CIRCLE('',#93187,0.0999999999999998) ;
#29657 = CIRCLE('',#93189,0.0999999999999994) ;
#29658 = CIRCLE('',#93191,0.0999999999999998) ;
#29659 = CIRCLE('',#93193,0.0999999999999994) ;
#29660 = CIRCLE('',#93196,0.0999999999999998) ;
#29661 = CIRCLE('',#93197,0.0999999999999998) ;
#29662 = CIRCLE('',#93199,0.0999999999999994) ;
#29663 = CIRCLE('',#93200,0.0999999999999994) ;
#29664 = CIRCLE('',#93202,0.0999999999999994) ;
#29665 = CIRCLE('',#93203,0.0999999999999994) ;
#29666 = CIRCLE('',#93205,0.0999999999999994) ;
#29667 = CIRCLE('',#93207,0.0999999999999994) ;
#29668 = CIRCLE('',#93209,0.0999999999999998) ;
#29669 = CIRCLE('',#93210,0.0999999999999998) ;
#29670 = CIRCLE('',#93212,0.0999999999999994) ;
#29671 = CIRCLE('',#93214,0.0999999999999994) ;
#29672 = CIRCLE('',#93216,0.1) ;
#29673 = CIRCLE('',#93217,0.1) ;
#29674 = CIRCLE('',#93219,0.0999999999999994) ;
#29675 = CIRCLE('',#93221,0.0999999999999994) ;
#29676 = CIRCLE('',#93223,0.0999999999999994) ;
#29677 = CIRCLE('',#93225,0.0999999999999994) ;
#29678 = CIRCLE('',#93227,0.0999999999999994) ;
#29679 = CIRCLE('',#93229,0.0999999999999994) ;
#29680 = CIRCLE('',#93231,0.0999999999999994) ;
#29681 = CIRCLE('',#93233,0.0999999999999994) ;
#29682 = CIRCLE('',#93235,0.1) ;
#29683 = CIRCLE('',#93237,0.1) ;
#29684 = CIRCLE('',#93240,0.1) ;
#29685 = CIRCLE('',#93241,0.0999999999999998) ;
#29686 = CIRCLE('',#93243,0.0999999999999994) ;
#29687 = CIRCLE('',#93244,0.0999999999999994) ;
#29688 = CIRCLE('',#93246,0.0999999999999994) ;
#29689 = CIRCLE('',#93247,0.0999999999999994) ;
#29690 = CIRCLE('',#93249,0.0999999999999994) ;
#29691 = CIRCLE('',#93251,0.0999999999999994) ;
#29692 = CIRCLE('',#93253,0.0999999999999998) ;
#29693 = CIRCLE('',#93254,0.0999999999999998) ;
#29694 = CIRCLE('',#93256,0.0999999999999994) ;
#29695 = CIRCLE('',#93258,0.0999999999999994) ;
#29696 = CIRCLE('',#93260,0.0999999999999998) ;
#29697 = CIRCLE('',#93261,0.0999999999999998) ;
#29698 = CIRCLE('',#93263,0.0999999999999994) ;
#29699 = CIRCLE('',#93265,0.0999999999999994) ;
#29700 = CIRCLE('',#93267,0.0999999999999994) ;
#29701 = CIRCLE('',#93269,0.0999999999999994) ;
#29702 = CIRCLE('',#93271,0.0999999999999994) ;
#29703 = CIRCLE('',#93273,0.0999999999999994) ;
#29704 = CIRCLE('',#93275,0.0999999999999994) ;
#29705 = CIRCLE('',#93277,0.0999999999999994) ;
#29706 = CIRCLE('',#93279,0.0999999999999998) ;
#29707 = CIRCLE('',#93281,0.0999999999999998) ;
#29708 = CIRCLE('',#93284,0.0999999999999997) ;
#29709 = CIRCLE('',#93286,0.1) ;
#29710 = CIRCLE('',#93288,0.0999999999999994) ;
#29711 = CIRCLE('',#93290,0.0999999999999994) ;
#29712 = CIRCLE('',#93292,0.0999999999999994) ;
#29713 = CIRCLE('',#93294,0.1) ;
#29714 = CIRCLE('',#93296,0.1) ;
#29715 = CIRCLE('',#93298,0.0999999999999994) ;
#29716 = CIRCLE('',#93300,0.0999999999999994) ;
#29717 = CIRCLE('',#93302,0.0999999999999994) ;
#29718 = CIRCLE('',#93304,0.0999999999999998) ;
#29719 = CIRCLE('',#93306,0.1) ;
#29720 = CIRCLE('',#93326,0.0999999999999994) ;
#29721 = CIRCLE('',#93328,0.0999999999999994) ;
#29722 = CIRCLE('',#93330,0.0999999999999993) ;
#29723 = CIRCLE('',#93331,0.1) ;
#29724 = CIRCLE('',#93332,0.1) ;
#29725 = CIRCLE('',#93335,0.1) ;
#29726 = CIRCLE('',#93336,0.0999999999999998) ;
#29727 = CIRCLE('',#93338,0.0999999999999994) ;
#29728 = CIRCLE('',#93342,0.1) ;
#29729 = CIRCLE('',#93344,0.1) ;
#29730 = CIRCLE('',#93345,0.0999999999999995) ;
#29731 = CIRCLE('',#93346,0.0999999999999998) ;
#29732 = CIRCLE('',#93347,0.0999999999999993) ;
#29733 = CIRCLE('',#93350,0.899999999999998) ;
#29734 = CIRCLE('',#93351,0.1) ;
#29735 = CIRCLE('',#93352,1.) ;
#29736 = CIRCLE('',#93353,1.) ;
#29737 = CIRCLE('',#93355,1.1) ;
#29738 = CIRCLE('',#93356,0.1) ;
#29739 = CIRCLE('',#93357,1.) ;
#29740 = CIRCLE('',#93359,0.100000000000003) ;
#29741 = CIRCLE('',#93360,0.0999999999999999) ;
#29742 = CIRCLE('',#93361,0.1) ;
#29743 = CIRCLE('',#93364,0.1) ;
#29744 = CIRCLE('',#93365,0.100000000000003) ;
#29745 = CIRCLE('',#93367,0.899999999999998) ;
#29746 = CIRCLE('',#93368,0.1) ;
#29747 = CIRCLE('',#93369,1.) ;
#29748 = CIRCLE('',#93370,1.) ;
#29749 = CIRCLE('',#93372,1.1) ;
#29750 = CIRCLE('',#93373,0.1) ;
#29751 = CIRCLE('',#93374,1.) ;
#29752 = CIRCLE('',#93376,0.0999999999999994) ;
#29753 = CIRCLE('',#93377,0.1) ;
#29754 = CIRCLE('',#93378,0.1) ;
#29755 = CIRCLE('',#93381,0.1) ;
#29756 = CIRCLE('',#93382,0.0999999999999994) ;
#29757 = CIRCLE('',#93384,0.899999999999998) ;
#29758 = CIRCLE('',#93385,0.1) ;
#29759 = CIRCLE('',#93386,1.) ;
#29760 = CIRCLE('',#93387,1.) ;
#29761 = CIRCLE('',#93389,1.1) ;
#29762 = CIRCLE('',#93390,0.1) ;
#29763 = CIRCLE('',#93391,1.) ;
#29764 = CIRCLE('',#93393,0.0999999999999994) ;
#29765 = CIRCLE('',#93394,0.1) ;
#29766 = CIRCLE('',#93395,0.1) ;
#29767 = CIRCLE('',#93398,0.1) ;
#29768 = CIRCLE('',#93399,0.0999999999999994) ;
#29769 = CIRCLE('',#93401,0.899999999999998) ;
#29770 = CIRCLE('',#93402,0.1) ;
#29771 = CIRCLE('',#93403,1.) ;
#29772 = CIRCLE('',#93404,1.) ;
#29773 = CIRCLE('',#93406,1.1) ;
#29774 = CIRCLE('',#93407,0.1) ;
#29775 = CIRCLE('',#93408,1.) ;
#29776 = CIRCLE('',#93410,0.0999999999999994) ;
#29777 = CIRCLE('',#93411,0.1) ;
#29778 = CIRCLE('',#93412,0.1) ;
#29779 = CIRCLE('',#93415,0.1) ;
#29780 = CIRCLE('',#93416,0.0999999999999994) ;
#29781 = CIRCLE('',#93418,0.900000000000001) ;
#29782 = CIRCLE('',#93419,0.1) ;
#29783 = CIRCLE('',#93420,1.) ;
#29784 = CIRCLE('',#93421,1.) ;
#29785 = CIRCLE('',#93423,1.1) ;
#29786 = CIRCLE('',#93424,0.1) ;
#29787 = CIRCLE('',#93425,1.) ;
#29788 = CIRCLE('',#93427,0.0999999999999994) ;
#29789 = CIRCLE('',#93428,0.1) ;
#29790 = CIRCLE('',#93429,0.1) ;
#29791 = CIRCLE('',#93432,0.1) ;
#29792 = CIRCLE('',#93433,0.0999999999999994) ;
#29793 = CIRCLE('',#93435,0.900000000000001) ;
#29794 = CIRCLE('',#93436,0.1) ;
#29795 = CIRCLE('',#93437,1.) ;
#29796 = CIRCLE('',#93438,1.) ;
#29797 = CIRCLE('',#93440,1.1) ;
#29798 = CIRCLE('',#93441,0.1) ;
#29799 = CIRCLE('',#93442,0.999999999999999) ;
#29800 = CIRCLE('',#93444,0.100000000000001) ;
#29801 = CIRCLE('',#93445,0.1) ;
#29802 = CIRCLE('',#93446,0.1) ;
#29803 = CIRCLE('',#93449,0.1) ;
#29804 = CIRCLE('',#93450,0.0999999999999994) ;
#29805 = CIRCLE('',#93452,0.9) ;
#29806 = CIRCLE('',#93453,0.1) ;
#29807 = CIRCLE('',#93454,0.999999999999999) ;
#29808 = CIRCLE('',#93455,0.999999999999999) ;
#29809 = CIRCLE('',#93457,1.1) ;
#29810 = CIRCLE('',#93458,0.1) ;
#29811 = CIRCLE('',#93459,0.999999999999999) ;
#29812 = CIRCLE('',#93461,0.100000000000001) ;
#29813 = CIRCLE('',#93462,0.1) ;
#29814 = CIRCLE('',#93463,0.1) ;
#29815 = CIRCLE('',#93466,0.1) ;
#29816 = CIRCLE('',#93467,0.0999999999999994) ;
#29817 = CIRCLE('',#93469,0.9) ;
#29818 = CIRCLE('',#93470,0.1) ;
#29819 = CIRCLE('',#93471,0.999999999999999) ;
#29820 = CIRCLE('',#93472,0.999999999999999) ;
#29821 = CIRCLE('',#93474,1.1) ;
#29822 = CIRCLE('',#93475,0.1) ;
#29823 = CIRCLE('',#93476,1.) ;
#29824 = CIRCLE('',#93478,0.1) ;
#29825 = CIRCLE('',#93479,0.1) ;
#29826 = CIRCLE('',#93480,0.1) ;
#29827 = CIRCLE('',#93483,0.1) ;
#29828 = CIRCLE('',#93484,0.0999999999999994) ;
#29829 = CIRCLE('',#93486,0.9) ;
#29830 = CIRCLE('',#93487,0.1) ;
#29831 = CIRCLE('',#93488,1.) ;
#29832 = CIRCLE('',#93489,1.) ;
#29833 = CIRCLE('',#93491,0.200000000000001) ;
#29834 = CIRCLE('',#93492,0.0999999999999994) ;
#29835 = CIRCLE('',#93493,0.1) ;
#29836 = CIRCLE('',#93494,0.1) ;
#29837 = CIRCLE('',#93496,0.200000000000001) ;
#29838 = CIRCLE('',#93497,0.0999999999999994) ;
#29839 = CIRCLE('',#93498,0.100000000000001) ;
#29840 = CIRCLE('',#93499,0.1) ;
#29841 = CIRCLE('',#93501,0.200000000000001) ;
#29842 = CIRCLE('',#93502,0.0999999999999994) ;
#29843 = CIRCLE('',#93503,0.100000000000001) ;
#29844 = CIRCLE('',#93504,0.1) ;
#29845 = CIRCLE('',#93506,0.199999999999999) ;
#29846 = CIRCLE('',#93507,0.0999999999999994) ;
#29847 = CIRCLE('',#93508,0.0999999999999994) ;
#29848 = CIRCLE('',#93509,0.0999999999999995) ;
#29849 = CIRCLE('',#93511,0.199999999999999) ;
#29850 = CIRCLE('',#93512,0.0999999999999994) ;
#29851 = CIRCLE('',#93513,0.0999999999999994) ;
#29852 = CIRCLE('',#93514,0.0999999999999995) ;
#29853 = CIRCLE('',#93516,0.199999999999999) ;
#29854 = CIRCLE('',#93517,0.0999999999999994) ;
#29855 = CIRCLE('',#93518,0.0999999999999994) ;
#29856 = CIRCLE('',#93519,0.0999999999999995) ;
#29857 = CIRCLE('',#93521,0.199999999999999) ;
#29858 = CIRCLE('',#93522,0.0999999999999994) ;
#29859 = CIRCLE('',#93523,0.0999999999999994) ;
#29860 = CIRCLE('',#93524,0.0999999999999995) ;
#29861 = CIRCLE('',#93526,0.199999999999999) ;
#29862 = CIRCLE('',#93527,0.0999999999999994) ;
#29863 = CIRCLE('',#93528,0.100000000000003) ;
#29864 = CIRCLE('',#93529,0.0999999999999995) ;
#29865 = CIRCLE('',#93531,0.199999999999999) ;
#29866 = CIRCLE('',#93532,0.0999999999999994) ;
#29867 = CIRCLE('',#93533,0.100000000000003) ;
#29868 = CIRCLE('',#93534,0.0999999999999995) ;
#29869 = CIRCLE('',#93536,1.1) ;
#29870 = CIRCLE('',#93537,0.1) ;
#29871 = CIRCLE('',#93538,1.) ;
#29872 = CIRCLE('',#93540,0.100000000000001) ;
#29873 = CIRCLE('',#93541,0.0999999999999998) ;
#29874 = CIRCLE('',#93542,0.1) ;
#29875 = CIRCLE('',#93545,0.1) ;
#29876 = CIRCLE('',#93546,0.1) ;
#29877 = CIRCLE('',#93557,0.1) ;
#29878 = CIRCLE('',#93559,0.100000000000001) ;
#29879 = CIRCLE('',#93561,0.100000000000001) ;
#29880 = CIRCLE('',#93563,0.0999999999999994) ;
#29881 = CIRCLE('',#93565,0.0999999999999994) ;
#29882 = CIRCLE('',#93567,0.0999999999999994) ;
#29883 = CIRCLE('',#93569,0.0999999999999994) ;
#29884 = CIRCLE('',#93571,0.100000000000003) ;
#29885 = CIRCLE('',#93573,0.100000000000003) ;
#29886 = CIRCLE('',#93575,0.9) ;
#29887 = CIRCLE('',#93576,0.1) ;
#29888 = CIRCLE('',#93577,1.) ;
#29889 = CIRCLE('',#93578,1.) ;
#29890 = CIRCLE('',#93580,0.200000000000001) ;
#29891 = CIRCLE('',#93581,0.0999999999999994) ;
#29892 = CIRCLE('',#93582,0.1) ;
#29893 = CIRCLE('',#93583,0.1) ;
#29894 = CIRCLE('',#93585,1.1) ;
#29895 = CIRCLE('',#93586,0.1) ;
#29896 = CIRCLE('',#93587,1.) ;
#29897 = CIRCLE('',#93589,0.1) ;
#29898 = CIRCLE('',#93590,0.1) ;
#29899 = CIRCLE('',#93591,0.1) ;
#29900 = CIRCLE('',#93594,0.1) ;
#29901 = CIRCLE('',#93595,0.1) ;
#29902 = CIRCLE('',#93598,0.1) ;
#29903 = CIRCLE('',#93600,0.1) ;
#29904 = CIRCLE('',#93601,0.1) ;
#29905 = CIRCLE('',#93602,0.2) ;
#29906 = CIRCLE('',#93603,0.2) ;
#29907 = CIRCLE('',#93605,0.1) ;
#29908 = CIRCLE('',#93606,0.1) ;
#29909 = CIRCLE('',#93607,0.2) ;
#29910 = CIRCLE('',#93608,0.2) ;
#29911 = CIRCLE('',#93610,0.1) ;
#29912 = CIRCLE('',#93611,0.1) ;
#29913 = CIRCLE('',#93612,0.2) ;
#29914 = CIRCLE('',#93613,0.2) ;
#29915 = CIRCLE('',#93615,0.1) ;
#29916 = CIRCLE('',#93616,0.1) ;
#29917 = CIRCLE('',#93617,0.2) ;
#29918 = CIRCLE('',#93618,0.2) ;
#29919 = CIRCLE('',#93620,0.1) ;
#29920 = CIRCLE('',#93621,0.1) ;
#29921 = CIRCLE('',#93622,0.2) ;
#29922 = CIRCLE('',#93623,0.2) ;
#29923 = CIRCLE('',#93625,0.1) ;
#29924 = CIRCLE('',#93626,0.1) ;
#29925 = CIRCLE('',#93627,0.2) ;
#29926 = CIRCLE('',#93628,0.2) ;
#29927 = CIRCLE('',#93630,0.1) ;
#29928 = CIRCLE('',#93631,0.1) ;
#29929 = CIRCLE('',#93632,0.2) ;
#29930 = CIRCLE('',#93633,0.2) ;
#29931 = CIRCLE('',#93635,0.1) ;
#29932 = CIRCLE('',#93636,0.1) ;
#29933 = CIRCLE('',#93637,0.2) ;
#29934 = CIRCLE('',#93638,0.2) ;
#29935 = CIRCLE('',#93640,0.1) ;
#29936 = CIRCLE('',#93641,0.1) ;
#29937 = CIRCLE('',#93642,0.2) ;
#29938 = CIRCLE('',#93643,0.2) ;
#29939 = CIRCLE('',#93645,0.2) ;
#29940 = CIRCLE('',#93647,0.2) ;
#29941 = CIRCLE('',#93649,0.2) ;
#29942 = CIRCLE('',#93651,0.2) ;
#29943 = CIRCLE('',#93653,0.2) ;
#29944 = CIRCLE('',#93655,0.2) ;
#29945 = CIRCLE('',#93657,0.2) ;
#29946 = CIRCLE('',#93659,0.2) ;
#29947 = CIRCLE('',#93661,0.2) ;
#29948 = CIRCLE('',#93663,0.2) ;
#29949 = CIRCLE('',#93665,0.2) ;
#29950 = CIRCLE('',#93667,0.2) ;
#29951 = CIRCLE('',#93669,0.2) ;
#29952 = CIRCLE('',#93671,0.2) ;
#29953 = CIRCLE('',#93673,0.2) ;
#29954 = CIRCLE('',#93675,0.2) ;
#29955 = CIRCLE('',#93677,0.2) ;
#29956 = CIRCLE('',#93679,0.2) ;
#29957 = CIRCLE('',#93681,0.1) ;
#29958 = CIRCLE('',#93682,0.1) ;
#29959 = CIRCLE('',#93684,0.1) ;
#29960 = CIRCLE('',#93685,0.1) ;
#29961 = CIRCLE('',#93687,0.1) ;
#29962 = CIRCLE('',#93688,0.1) ;
#29963 = CIRCLE('',#93690,0.1) ;
#29964 = CIRCLE('',#93691,0.1) ;
#29965 = CIRCLE('',#93693,0.1) ;
#29966 = CIRCLE('',#93694,0.1) ;
#29967 = CIRCLE('',#93696,0.1) ;
#29968 = CIRCLE('',#93697,0.1) ;
#29969 = CIRCLE('',#93699,0.1) ;
#29970 = CIRCLE('',#93700,0.1) ;
#29971 = CIRCLE('',#93702,0.1) ;
#29972 = CIRCLE('',#93703,0.1) ;
#29973 = CIRCLE('',#93705,0.1) ;
#29974 = CIRCLE('',#93706,0.1) ;
#29975 = CIRCLE('',#93708,0.1) ;
#29976 = CIRCLE('',#93709,0.1) ;
#29977 = CIRCLE('',#93710,0.2) ;
#29978 = CIRCLE('',#93711,0.2) ;
#29979 = CIRCLE('',#93713,0.2) ;
#29980 = CIRCLE('',#93715,0.2) ;
#29981 = CIRCLE('',#93717,0.1) ;
#29982 = CIRCLE('',#93718,0.1) ;
#29983 = CIRCLE('',#93720,0.0999999999999994) ;
#29984 = CIRCLE('',#93721,0.0999999999999994) ;
#29985 = CIRCLE('',#93723,0.199999999999999) ;
#29986 = CIRCLE('',#93724,0.2) ;
#29987 = CIRCLE('',#93725,0.2) ;
#29988 = CIRCLE('',#93726,0.2) ;
#29989 = CIRCLE('',#93727,0.2) ;
#29990 = CIRCLE('',#93728,0.2) ;
#29991 = CIRCLE('',#93729,0.200000000000001) ;
#29992 = CIRCLE('',#93730,0.200000000000001) ;
#29993 = CIRCLE('',#93731,0.200000000000001) ;
#29994 = CIRCLE('',#93732,0.200000000000001) ;
#29995 = CIRCLE('',#93733,0.199999999999999) ;
#29996 = CIRCLE('',#93734,0.199999999999999) ;
#29997 = CIRCLE('',#93735,0.199999999999999) ;
#29998 = CIRCLE('',#93736,0.199999999999999) ;
#29999 = CIRCLE('',#93737,0.199999999999999) ;
#30000 = CIRCLE('',#93738,0.199999999999999) ;
#30001 = CIRCLE('',#93739,0.199999999999999) ;
#30002 = CIRCLE('',#93740,0.199999999999999) ;
#30003 = CIRCLE('',#93741,0.199999999999999) ;
#30004 = CIRCLE('',#93742,0.199999999999999) ;
#30005 = CIRCLE('',#93744,0.1) ;
#30006 = CIRCLE('',#93745,0.1) ;
#30007 = CIRCLE('',#93747,0.2) ;
#30008 = CIRCLE('',#93748,0.2) ;
#30009 = CIRCLE('',#93749,0.2) ;
#30010 = CIRCLE('',#93750,0.2) ;
#30011 = CIRCLE('',#93751,0.2) ;
#30012 = CIRCLE('',#93752,0.2) ;
#30013 = CIRCLE('',#93753,0.2) ;
#30014 = CIRCLE('',#93754,0.2) ;
#30015 = CIRCLE('',#93755,0.2) ;
#30016 = CIRCLE('',#93756,0.2) ;
#30017 = CIRCLE('',#93757,0.2) ;
#30018 = CIRCLE('',#93758,0.2) ;
#30019 = CIRCLE('',#93759,0.2) ;
#30020 = CIRCLE('',#93760,0.2) ;
#30021 = CIRCLE('',#93761,0.2) ;
#30022 = CIRCLE('',#93762,0.2) ;
#30023 = CIRCLE('',#93763,0.2) ;
#30024 = CIRCLE('',#93764,0.2) ;
#30025 = CIRCLE('',#93765,0.2) ;
#30026 = CIRCLE('',#93766,0.2) ;
#30027 = CIRCLE('',#93768,0.1) ;
#30028 = CIRCLE('',#93769,0.1) ;
#30029 = CIRCLE('',#93772,0.1) ;
#30030 = CIRCLE('',#93773,0.1) ;
#30031 = CIRCLE('',#93776,0.1) ;
#30032 = CIRCLE('',#93777,0.1) ;
#30033 = CIRCLE('',#93780,0.100000000000001) ;
#30034 = CIRCLE('',#93781,0.100000000000001) ;
#30035 = CIRCLE('',#93784,0.1) ;
#30036 = CIRCLE('',#93785,0.1) ;
#30037 = CIRCLE('',#93788,0.0999999999999994) ;
#30038 = CIRCLE('',#93789,0.0999999999999994) ;
#30039 = CIRCLE('',#93791,0.199999999999999) ;
#30040 = CIRCLE('',#93792,0.199999999999999) ;
#30041 = CIRCLE('',#93793,0.199999999999999) ;
#30042 = CIRCLE('',#93794,0.199999999999999) ;
#30043 = CIRCLE('',#93795,0.199999999999999) ;
#30044 = CIRCLE('',#93796,0.199999999999999) ;
#30045 = CIRCLE('',#93797,0.199999999999999) ;
#30046 = CIRCLE('',#93798,1.55625) ;
#30047 = CIRCLE('',#93799,0.199999999999999) ;
#30048 = CIRCLE('',#93800,0.199999999999999) ;
#30049 = CIRCLE('',#93801,0.199999999999999) ;
#30050 = CIRCLE('',#93802,0.199999999999999) ;
#30051 = CIRCLE('',#93803,0.199999999999999) ;
#30052 = CIRCLE('',#93804,0.199999999999999) ;
#30053 = CIRCLE('',#93805,0.199999999999999) ;
#30054 = CIRCLE('',#93806,0.199999999999999) ;
#30055 = CIRCLE('',#93807,0.199999999999999) ;
#30056 = CIRCLE('',#93808,1.55625) ;
#30057 = CIRCLE('',#93809,0.199999999999999) ;
#30058 = CIRCLE('',#93810,0.199999999999999) ;
#30059 = CIRCLE('',#93811,0.199999999999999) ;
#30060 = CIRCLE('',#93812,0.199999999999999) ;
#30061 = CIRCLE('',#93813,0.199999999999999) ;
#30062 = CIRCLE('',#93814,0.199999999999999) ;
#30063 = CIRCLE('',#93815,0.199999999999999) ;
#30064 = CIRCLE('',#93816,0.199999999999999) ;
#30065 = CIRCLE('',#93817,0.199999999999999) ;
#30066 = CIRCLE('',#93818,1.55625) ;
#30067 = CIRCLE('',#93819,0.199999999999999) ;
#30068 = CIRCLE('',#93820,0.199999999999999) ;
#30069 = CIRCLE('',#93821,0.199999999999999) ;
#30070 = CIRCLE('',#93822,0.199999999999999) ;
#30071 = CIRCLE('',#93823,0.199999999999999) ;
#30072 = CIRCLE('',#93824,0.199999999999999) ;
#30073 = CIRCLE('',#93825,0.199999999999999) ;
#30074 = CIRCLE('',#93826,0.199999999999999) ;
#30075 = CIRCLE('',#93827,0.199999999999999) ;
#30076 = CIRCLE('',#93828,1.55625) ;
#30077 = CIRCLE('',#93829,0.199999999999999) ;
#30078 = CIRCLE('',#93830,0.199999999999999) ;
#30079 = CIRCLE('',#93831,0.199999999999999) ;
#30080 = CIRCLE('',#93832,0.199999999999999) ;
#30081 = CIRCLE('',#93833,0.199999999999999) ;
#30082 = CIRCLE('',#93834,0.199999999999999) ;
#30083 = CIRCLE('',#93835,0.199999999999999) ;
#30084 = CIRCLE('',#93836,0.199999999999999) ;
#30085 = CIRCLE('',#93837,0.199999999999999) ;
#30086 = CIRCLE('',#93838,1.55625) ;
#30087 = CIRCLE('',#93839,0.199999999999999) ;
#30088 = CIRCLE('',#93840,0.199999999999999) ;
#30089 = CIRCLE('',#93841,0.200000000000001) ;
#30090 = CIRCLE('',#93842,0.199999999999999) ;
#30091 = CIRCLE('',#93843,0.200000000000001) ;
#30092 = CIRCLE('',#93844,0.199999999999999) ;
#30093 = CIRCLE('',#93845,0.199999999999999) ;
#30094 = CIRCLE('',#93846,0.199999999999999) ;
#30095 = CIRCLE('',#93847,0.199999999999999) ;
#30096 = CIRCLE('',#93848,1.55625) ;
#30097 = CIRCLE('',#93849,0.200000000000001) ;
#30098 = CIRCLE('',#93850,0.200000000000001) ;
#30099 = CIRCLE('',#93851,0.200000000000001) ;
#30100 = CIRCLE('',#93852,0.199999999999999) ;
#30101 = CIRCLE('',#93853,0.200000000000001) ;
#30102 = CIRCLE('',#93854,0.200000000000001) ;
#30103 = CIRCLE('',#93855,0.200000000000001) ;
#30104 = CIRCLE('',#93856,0.200000000000001) ;
#30105 = CIRCLE('',#93857,0.200000000000001) ;
#30106 = CIRCLE('',#93858,1.55625) ;
#30107 = CIRCLE('',#93859,0.200000000000001) ;
#30108 = CIRCLE('',#93860,0.200000000000001) ;
#30109 = CIRCLE('',#93861,0.2) ;
#30110 = CIRCLE('',#93862,0.2) ;
#30111 = CIRCLE('',#93863,0.200000000000001) ;
#30112 = CIRCLE('',#93864,0.200000000000001) ;
#30113 = CIRCLE('',#93865,0.200000000000001) ;
#30114 = CIRCLE('',#93866,0.200000000000001) ;
#30115 = CIRCLE('',#93867,0.200000000000001) ;
#30116 = CIRCLE('',#93868,1.55625) ;
#30117 = CIRCLE('',#93869,0.2) ;
#30118 = CIRCLE('',#93870,0.2) ;
#30119 = CIRCLE('',#93871,0.2) ;
#30120 = CIRCLE('',#93872,0.199999999999999) ;
#30121 = CIRCLE('',#93873,0.200000000000001) ;
#30122 = CIRCLE('',#93874,0.200000000000001) ;
#30123 = CIRCLE('',#93875,0.2) ;
#30124 = CIRCLE('',#93876,0.2) ;
#30125 = CIRCLE('',#93877,0.2) ;
#30126 = CIRCLE('',#93878,1.55625) ;
#30127 = CIRCLE('',#93879,0.2) ;
#30128 = CIRCLE('',#93880,0.2) ;
#30129 = CIRCLE('',#93881,0.2) ;
#30130 = CIRCLE('',#93882,0.199999999999999) ;
#30131 = CIRCLE('',#93883,0.200000000000001) ;
#30132 = CIRCLE('',#93884,0.2) ;
#30133 = CIRCLE('',#93885,0.2) ;
#30134 = CIRCLE('',#93886,0.2) ;
#30135 = CIRCLE('',#93887,0.2) ;
#30136 = CIRCLE('',#93888,1.55625) ;
#30137 = CIRCLE('',#93889,0.2) ;
#30138 = CIRCLE('',#93890,0.2) ;
#30139 = CIRCLE('',#93892,0.200000000000001) ;
#30140 = CIRCLE('',#93893,0.200000000000001) ;
#30141 = CIRCLE('',#93895,0.200000000000001) ;
#30142 = CIRCLE('',#93896,0.200000000000001) ;
#30143 = CIRCLE('',#93898,0.2) ;
#30144 = CIRCLE('',#93899,0.2) ;
#30145 = CIRCLE('',#93906,0.1) ;
#30146 = CIRCLE('',#93907,0.1) ;
#30147 = CIRCLE('',#93910,0.1) ;
#30148 = CIRCLE('',#93911,0.1) ;
#30149 = CIRCLE('',#93914,0.0999999999999994) ;
#30150 = CIRCLE('',#93915,0.0999999999999994) ;
#30151 = CIRCLE('',#93918,0.1) ;
#30152 = CIRCLE('',#93922,0.1) ;
#30153 = CIRCLE('',#93923,0.1) ;
#30154 = CIRCLE('',#93926,0.1) ;
#30155 = CIRCLE('',#93927,0.1) ;
#30156 = CIRCLE('',#93930,0.1) ;
#30157 = CIRCLE('',#93931,0.1) ;
#30158 = CIRCLE('',#93934,0.1) ;
#30159 = CIRCLE('',#93935,0.1) ;
#30160 = CIRCLE('',#93938,0.1) ;
#30161 = CIRCLE('',#93939,0.1) ;
#30162 = CIRCLE('',#93942,0.1) ;
#30163 = CIRCLE('',#93943,0.1) ;
#30164 = CIRCLE('',#93945,1.65625) ;
#30165 = CIRCLE('',#93946,1.65625) ;
#30166 = CIRCLE('',#93948,0.1) ;
#30167 = CIRCLE('',#93949,0.1) ;
#30168 = CIRCLE('',#93952,0.1) ;
#30169 = CIRCLE('',#93953,0.1) ;
#30170 = CIRCLE('',#93956,0.1) ;
#30171 = CIRCLE('',#93957,0.1) ;
#30172 = CIRCLE('',#93960,0.2) ;
#30173 = CIRCLE('',#93961,0.2) ;
#30174 = CIRCLE('',#93962,1.75625) ;
#30175 = CIRCLE('',#93963,0.2) ;
#30176 = CIRCLE('',#93964,0.2) ;
#30177 = CIRCLE('',#93966,0.1) ;
#30178 = CIRCLE('',#93967,0.1) ;
#30179 = CIRCLE('',#93968,0.1) ;
#30180 = CIRCLE('',#93969,0.1) ;
#30181 = CIRCLE('',#93971,0.1) ;
#30182 = CIRCLE('',#93972,0.1) ;
#30183 = CIRCLE('',#93974,0.1) ;
#30184 = CIRCLE('',#93975,0.1) ;
#30185 = CIRCLE('',#93977,0.1) ;
#30186 = CIRCLE('',#93978,0.1) ;
#30187 = CIRCLE('',#93980,0.1) ;
#30188 = CIRCLE('',#93981,0.0999999999999998) ;
#30189 = CIRCLE('',#93983,0.1) ;
#30190 = CIRCLE('',#93985,0.1) ;
#30191 = CIRCLE('',#93987,0.1) ;
#30192 = CIRCLE('',#93989,0.1) ;
#30193 = CIRCLE('',#93991,0.0999999999999998) ;
#30194 = CIRCLE('',#93993,0.1) ;
#30195 = CIRCLE('',#93995,0.1) ;
#30196 = CIRCLE('',#93996,0.1) ;
#30197 = CIRCLE('',#93999,0.1) ;
#30198 = CIRCLE('',#94001,0.1) ;
#30199 = CIRCLE('',#94002,0.1) ;
#30200 = CIRCLE('',#94004,0.1) ;
#30201 = CIRCLE('',#94006,0.1) ;
#30202 = CIRCLE('',#94008,0.1) ;
#30203 = CIRCLE('',#94010,0.1) ;
#30204 = CIRCLE('',#94012,0.1) ;
#30205 = CIRCLE('',#94014,0.1) ;
#30206 = CIRCLE('',#94015,0.1) ;
#30207 = CIRCLE('',#94017,0.1) ;
#30208 = CIRCLE('',#94019,0.1) ;
#30209 = CIRCLE('',#94021,0.0999999999999998) ;
#30210 = CIRCLE('',#94022,0.1) ;
#30211 = CIRCLE('',#94024,0.1) ;
#30212 = CIRCLE('',#94026,0.1) ;
#30213 = CIRCLE('',#94027,0.1) ;
#30214 = CIRCLE('',#94029,0.1) ;
#30215 = CIRCLE('',#94031,0.1) ;
#30216 = CIRCLE('',#94033,0.1) ;
#30217 = CIRCLE('',#94035,0.1) ;
#30218 = CIRCLE('',#94037,0.1) ;
#30219 = CIRCLE('',#94039,0.1) ;
#30220 = CIRCLE('',#94041,0.1) ;
#30221 = CIRCLE('',#94043,0.1) ;
#30222 = CIRCLE('',#94044,0.1) ;
#30223 = CIRCLE('',#94046,0.1) ;
#30224 = CIRCLE('',#94048,0.1) ;
#30225 = CIRCLE('',#94050,0.1) ;
#30226 = CIRCLE('',#94052,0.1) ;
#30227 = CIRCLE('',#94053,0.1) ;
#30228 = CIRCLE('',#94055,0.1) ;
#30229 = CIRCLE('',#94057,0.1) ;
#30230 = CIRCLE('',#94059,0.1) ;
#30231 = CIRCLE('',#94061,0.1) ;
#30232 = CIRCLE('',#94064,0.1) ;
#30233 = CIRCLE('',#94066,0.1) ;
#30234 = CIRCLE('',#94068,0.1) ;
#30235 = CIRCLE('',#94071,0.100000000000003) ;
#30236 = CIRCLE('',#94072,0.100000000000003) ;
#30237 = CIRCLE('',#94074,0.100000000000003) ;
#30238 = CIRCLE('',#94076,0.100000000000003) ;
#30239 = CIRCLE('',#94078,0.1) ;
#30240 = CIRCLE('',#94080,0.100000000000003) ;
#30241 = CIRCLE('',#94082,0.100000000000003) ;
#30242 = CIRCLE('',#94084,0.1) ;
#30243 = CIRCLE('',#94086,0.1) ;
#30244 = CIRCLE('',#94088,0.1) ;
#30245 = CIRCLE('',#94090,0.100000000000003) ;
#30246 = CIRCLE('',#94092,0.100000000000003) ;
#30247 = CIRCLE('',#94094,0.0999999999999998) ;
#30248 = CIRCLE('',#94096,0.100000000000003) ;
#30249 = CIRCLE('',#94098,0.100000000000003) ;
#30250 = CIRCLE('',#94100,0.0999999999999994) ;
#30251 = CIRCLE('',#94103,0.0999999999999998) ;
#30252 = CIRCLE('',#94104,0.0999999999999998) ;
#30253 = CIRCLE('',#94106,0.0999999999999998) ;
#30254 = CIRCLE('',#94108,0.0999999999999998) ;
#30255 = CIRCLE('',#94110,0.0999999999999998) ;
#30256 = CIRCLE('',#94112,0.0999999999999998) ;
#30257 = CIRCLE('',#94114,0.1) ;
#30258 = CIRCLE('',#94116,0.1) ;
#30259 = CIRCLE('',#94118,0.1) ;
#30260 = CIRCLE('',#94120,0.1) ;
#30261 = CIRCLE('',#94122,0.1) ;
#30262 = CIRCLE('',#94124,0.0999999999999998) ;
#30263 = CIRCLE('',#94126,0.0999999999999998) ;
#30264 = CIRCLE('',#94128,0.0999999999999998) ;
#30265 = CIRCLE('',#94130,0.0999999999999998) ;
#30266 = CIRCLE('',#94132,0.0999999999999998) ;
#30267 = CIRCLE('',#94135,0.1) ;
#30268 = CIRCLE('',#94136,0.1) ;
#30269 = CIRCLE('',#94138,0.1) ;
#30270 = CIRCLE('',#94140,0.1) ;
#30271 = CIRCLE('',#94142,0.1) ;
#30272 = CIRCLE('',#94144,0.1) ;
#30273 = CIRCLE('',#94146,0.1) ;
#30274 = CIRCLE('',#94148,0.0999999999999998) ;
#30275 = CIRCLE('',#94150,0.0999999999999998) ;
#30276 = CIRCLE('',#94152,0.1) ;
#30277 = CIRCLE('',#94154,0.1) ;
#30278 = CIRCLE('',#94156,0.1) ;
#30279 = CIRCLE('',#94158,0.1) ;
#30280 = CIRCLE('',#94160,0.1) ;
#30281 = CIRCLE('',#94162,0.1) ;
#30282 = CIRCLE('',#94164,0.1) ;
#30283 = CIRCLE('',#94167,0.1) ;
#30284 = CIRCLE('',#94169,0.1) ;
#30285 = CIRCLE('',#94171,0.1) ;
#30286 = CIRCLE('',#94173,0.1) ;
#30287 = CIRCLE('',#94175,0.0999999999999998) ;
#30288 = CIRCLE('',#94177,0.1) ;
#30289 = CIRCLE('',#94179,0.1) ;
#30290 = CIRCLE('',#94181,0.1) ;
#30291 = CIRCLE('',#94183,0.1) ;
#30292 = CIRCLE('',#94185,0.1) ;
#30293 = CIRCLE('',#94188,0.1) ;
#30294 = CIRCLE('',#94189,0.1) ;
#30295 = CIRCLE('',#94191,0.0999999999999998) ;
#30296 = CIRCLE('',#94193,0.1) ;
#30297 = CIRCLE('',#94195,0.1) ;
#30298 = CIRCLE('',#94197,0.0999999999999998) ;
#30299 = CIRCLE('',#94199,0.1) ;
#30300 = CIRCLE('',#94201,0.1) ;
#30301 = CIRCLE('',#94204,0.1) ;
#30302 = CIRCLE('',#94206,0.0999999999999994) ;
#30303 = CIRCLE('',#94208,0.0999999999999994) ;
#30304 = CIRCLE('',#94210,0.0999999999999994) ;
#30305 = CIRCLE('',#94212,0.1) ;
#30306 = CIRCLE('',#94214,0.1) ;
#30307 = CIRCLE('',#94216,0.1) ;
#30308 = CIRCLE('',#94218,0.1) ;
#30309 = CIRCLE('',#94220,0.0999999999999998) ;
#30310 = CIRCLE('',#94222,0.0999999999999994) ;
#30311 = CIRCLE('',#94224,0.0999999999999998) ;
#30312 = CIRCLE('',#94226,0.0999999999999998) ;
#30313 = CIRCLE('',#94228,0.1) ;
#30314 = CIRCLE('',#94230,0.1) ;
#30315 = CIRCLE('',#94232,0.1) ;
#30316 = CIRCLE('',#94234,0.1) ;
#30317 = CIRCLE('',#94236,0.0999999999999994) ;
#30318 = CIRCLE('',#94238,0.1) ;
#30319 = CIRCLE('',#94246,0.3) ;
#30320 = CIRCLE('',#94247,0.9) ;
#30321 = CIRCLE('',#94249,0.9) ;
#30322 = CIRCLE('',#94250,0.3) ;
#30323 = CIRCLE('',#94252,1.) ;
#30324 = CIRCLE('',#94253,1.) ;
#30325 = CIRCLE('',#94255,0.2) ;
#30326 = CIRCLE('',#94256,0.2) ;
#30327 = CIRCLE('',#94269,0.1) ;
#30328 = CIRCLE('',#94270,0.1) ;
#30329 = CIRCLE('',#94272,0.1) ;
#30330 = CIRCLE('',#94273,0.1) ;
#30331 = CIRCLE('',#94275,0.1) ;
#30332 = CIRCLE('',#94276,0.1) ;
#30333 = CIRCLE('',#94278,0.1) ;
#30334 = CIRCLE('',#94279,0.1) ;
#30335 = CIRCLE('',#94281,0.1) ;
#30336 = CIRCLE('',#94283,0.1) ;
#30337 = CIRCLE('',#94285,0.1) ;
#30338 = CIRCLE('',#94287,0.1) ;
#30339 = CIRCLE('',#94288,0.1) ;
#30340 = CIRCLE('',#94290,0.1) ;
#30341 = CIRCLE('',#94292,0.1) ;
#30342 = CIRCLE('',#94294,0.1) ;
#30343 = CIRCLE('',#94296,0.1) ;
#30344 = CIRCLE('',#94298,0.1) ;
#30345 = CIRCLE('',#94299,0.1) ;
#30346 = CIRCLE('',#94301,0.1) ;
#30347 = CIRCLE('',#94303,0.1) ;
#30348 = CIRCLE('',#94304,0.1) ;
#30349 = CIRCLE('',#94306,0.1) ;
#30350 = CIRCLE('',#94307,0.1) ;
#30351 = CIRCLE('',#94309,0.1) ;
#30352 = CIRCLE('',#94310,0.1) ;
#30353 = CIRCLE('',#94312,0.1) ;
#30354 = CIRCLE('',#94313,0.1) ;
#30355 = CIRCLE('',#94315,0.1) ;
#30356 = CIRCLE('',#94317,0.1) ;
#30357 = CIRCLE('',#94319,0.1) ;
#30358 = CIRCLE('',#94321,0.1) ;
#30359 = CIRCLE('',#94322,0.1) ;
#30360 = CIRCLE('',#94324,0.1) ;
#30361 = CIRCLE('',#94326,0.1) ;
#30362 = CIRCLE('',#94328,0.1) ;
#30363 = CIRCLE('',#94330,0.1) ;
#30364 = CIRCLE('',#94332,0.1) ;
#30365 = CIRCLE('',#94333,0.1) ;
#30366 = CIRCLE('',#94335,0.1) ;
#30367 = CIRCLE('',#94337,0.1) ;
#30368 = CIRCLE('',#94339,0.1) ;
#30369 = CIRCLE('',#94341,0.1) ;
#30370 = CIRCLE('',#94343,0.1) ;
#30371 = CIRCLE('',#94345,0.1) ;
#30372 = CIRCLE('',#94347,0.1) ;
#30373 = CIRCLE('',#94350,0.1) ;
#30374 = CIRCLE('',#94352,0.1) ;
#30375 = CIRCLE('',#94354,0.1) ;
#30376 = CIRCLE('',#94356,0.1) ;
#30377 = CIRCLE('',#94358,0.1) ;
#30378 = CIRCLE('',#94360,0.1) ;
#30379 = CIRCLE('',#94363,0.1) ;
#30380 = CIRCLE('',#94365,0.1) ;
#30381 = CIRCLE('',#94367,0.1) ;
#30382 = CIRCLE('',#94369,0.1) ;
#30383 = CIRCLE('',#94372,0.1) ;
#30384 = CIRCLE('',#94374,0.1) ;
#30385 = CIRCLE('',#94376,0.1) ;
#30386 = CIRCLE('',#94378,0.1) ;
#30387 = CIRCLE('',#94381,0.2) ;
#30388 = CIRCLE('',#94382,0.2) ;
#30389 = CIRCLE('',#94384,0.2) ;
#30390 = CIRCLE('',#94385,0.2) ;
#30391 = CIRCLE('',#94387,0.2) ;
#30392 = CIRCLE('',#94388,0.2) ;
#30393 = CIRCLE('',#94390,0.2) ;
#30394 = CIRCLE('',#94391,0.2) ;
#30395 = CIRCLE('',#94393,0.2) ;
#30396 = CIRCLE('',#94394,0.2) ;
#30397 = CIRCLE('',#94396,0.2) ;
#30398 = CIRCLE('',#94397,0.2) ;
#30399 = CIRCLE('',#94399,0.2) ;
#30400 = CIRCLE('',#94400,0.2) ;
#30401 = CIRCLE('',#94402,0.2) ;
#30402 = CIRCLE('',#94403,0.2) ;
#30403 = CIRCLE('',#94405,0.2) ;
#30404 = CIRCLE('',#94406,0.2) ;
#30405 = CIRCLE('',#94453,0.100000000000003) ;
#30406 = CIRCLE('',#94454,0.100000000000003) ;
#30407 = CIRCLE('',#94457,0.100000000000003) ;
#30408 = CIRCLE('',#94458,0.100000000000003) ;
#30409 = CIRCLE('',#94461,0.0999999999999959) ;
#30410 = CIRCLE('',#94462,0.0999999999999959) ;
#30411 = CIRCLE('',#94465,0.100000000000003) ;
#30412 = CIRCLE('',#94469,0.100000000000003) ;
#30413 = CIRCLE('',#94470,0.100000000000003) ;
#30414 = CIRCLE('',#94473,0.100000000000003) ;
#30415 = CIRCLE('',#94474,0.100000000000003) ;
#30416 = CIRCLE('',#94477,0.100000000000003) ;
#30417 = CIRCLE('',#94478,0.100000000000003) ;
#30418 = CIRCLE('',#94481,0.100000000000003) ;
#30419 = CIRCLE('',#94482,0.100000000000003) ;
#30420 = CIRCLE('',#94485,0.100000000000003) ;
#30421 = CIRCLE('',#94486,0.100000000000003) ;
#30422 = CIRCLE('',#94489,0.100000000000003) ;
#30423 = CIRCLE('',#94490,0.100000000000003) ;
#30424 = CIRCLE('',#94492,1.65625) ;
#30425 = CIRCLE('',#94493,1.65625) ;
#30426 = CIRCLE('',#94495,0.100000000000003) ;
#30427 = CIRCLE('',#94496,0.100000000000003) ;
#30428 = CIRCLE('',#94499,0.100000000000003) ;
#30429 = CIRCLE('',#94500,0.100000000000003) ;
#30430 = CIRCLE('',#94503,0.100000000000003) ;
#30431 = CIRCLE('',#94504,0.100000000000003) ;
#30432 = CIRCLE('',#94507,0.199999999999999) ;
#30433 = CIRCLE('',#94508,0.199999999999999) ;
#30434 = CIRCLE('',#94509,1.75625) ;
#30435 = CIRCLE('',#94510,0.199999999999999) ;
#30436 = CIRCLE('',#94511,0.199999999999999) ;
#30437 = CIRCLE('',#94513,0.0999999999999994) ;
#30438 = CIRCLE('',#94514,0.0999999999999994) ;
#30439 = CIRCLE('',#94517,0.0999999999999994) ;
#30440 = CIRCLE('',#94518,0.0999999999999994) ;
#30441 = CIRCLE('',#94521,0.0999999999999994) ;
#30442 = CIRCLE('',#94522,0.0999999999999994) ;
#30443 = CIRCLE('',#94525,0.0999999999999994) ;
#30444 = CIRCLE('',#94529,0.100000000000003) ;
#30445 = CIRCLE('',#94530,0.100000000000003) ;
#30446 = CIRCLE('',#94533,0.0999999999999994) ;
#30447 = CIRCLE('',#94534,0.0999999999999994) ;
#30448 = CIRCLE('',#94537,0.0999999999999994) ;
#30449 = CIRCLE('',#94538,0.0999999999999994) ;
#30450 = CIRCLE('',#94541,0.100000000000003) ;
#30451 = CIRCLE('',#94542,0.100000000000003) ;
#30452 = CIRCLE('',#94545,0.100000000000003) ;
#30453 = CIRCLE('',#94546,0.100000000000003) ;
#30454 = CIRCLE('',#94549,0.100000000000003) ;
#30455 = CIRCLE('',#94550,0.100000000000003) ;
#30456 = CIRCLE('',#94552,1.65625) ;
#30457 = CIRCLE('',#94553,1.65625) ;
#30458 = CIRCLE('',#94555,0.0999999999999994) ;
#30459 = CIRCLE('',#94556,0.0999999999999994) ;
#30460 = CIRCLE('',#94559,0.0999999999999994) ;
#30461 = CIRCLE('',#94560,0.0999999999999994) ;
#30462 = CIRCLE('',#94563,0.0999999999999994) ;
#30463 = CIRCLE('',#94564,0.0999999999999994) ;
#30464 = CIRCLE('',#94567,0.199999999999999) ;
#30465 = CIRCLE('',#94568,0.199999999999999) ;
#30466 = CIRCLE('',#94569,1.75625) ;
#30467 = CIRCLE('',#94570,0.199999999999999) ;
#30468 = CIRCLE('',#94571,0.199999999999999) ;
#30469 = CIRCLE('',#94573,0.0999999999999994) ;
#30470 = CIRCLE('',#94574,0.0999999999999994) ;
#30471 = CIRCLE('',#94577,0.0999999999999994) ;
#30472 = CIRCLE('',#94578,0.0999999999999994) ;
#30473 = CIRCLE('',#94581,0.0999999999999994) ;
#30474 = CIRCLE('',#94582,0.0999999999999994) ;
#30475 = CIRCLE('',#94585,0.0999999999999994) ;
#30476 = CIRCLE('',#94589,0.0999999999999994) ;
#30477 = CIRCLE('',#94590,0.0999999999999994) ;
#30478 = CIRCLE('',#94593,0.0999999999999994) ;
#30479 = CIRCLE('',#94594,0.0999999999999994) ;
#30480 = CIRCLE('',#94597,0.0999999999999994) ;
#30481 = CIRCLE('',#94598,0.0999999999999994) ;
#30482 = CIRCLE('',#94601,0.0999999999999994) ;
#30483 = CIRCLE('',#94602,0.0999999999999994) ;
#30484 = CIRCLE('',#94605,0.0999999999999994) ;
#30485 = CIRCLE('',#94606,0.0999999999999994) ;
#30486 = CIRCLE('',#94609,0.0999999999999994) ;
#30487 = CIRCLE('',#94610,0.0999999999999994) ;
#30488 = CIRCLE('',#94612,1.65625) ;
#30489 = CIRCLE('',#94613,1.65625) ;
#30490 = CIRCLE('',#94615,0.0999999999999994) ;
#30491 = CIRCLE('',#94616,0.0999999999999994) ;
#30492 = CIRCLE('',#94619,0.0999999999999994) ;
#30493 = CIRCLE('',#94620,0.0999999999999994) ;
#30494 = CIRCLE('',#94623,0.0999999999999994) ;
#30495 = CIRCLE('',#94624,0.0999999999999994) ;
#30496 = CIRCLE('',#94627,0.199999999999999) ;
#30497 = CIRCLE('',#94628,0.199999999999999) ;
#30498 = CIRCLE('',#94629,1.75625) ;
#30499 = CIRCLE('',#94630,0.199999999999999) ;
#30500 = CIRCLE('',#94631,0.199999999999999) ;
#30501 = CIRCLE('',#94633,0.0999999999999994) ;
#30502 = CIRCLE('',#94634,0.0999999999999994) ;
#30503 = CIRCLE('',#94637,0.0999999999999994) ;
#30504 = CIRCLE('',#94638,0.0999999999999994) ;
#30505 = CIRCLE('',#94641,0.0999999999999994) ;
#30506 = CIRCLE('',#94642,0.0999999999999994) ;
#30507 = CIRCLE('',#94645,0.0999999999999994) ;
#30508 = CIRCLE('',#94649,0.0999999999999994) ;
#30509 = CIRCLE('',#94650,0.0999999999999994) ;
#30510 = CIRCLE('',#94653,0.0999999999999994) ;
#30511 = CIRCLE('',#94654,0.0999999999999994) ;
#30512 = CIRCLE('',#94657,0.0999999999999994) ;
#30513 = CIRCLE('',#94658,0.0999999999999994) ;
#30514 = CIRCLE('',#94661,0.0999999999999994) ;
#30515 = CIRCLE('',#94662,0.0999999999999994) ;
#30516 = CIRCLE('',#94665,0.0999999999999994) ;
#30517 = CIRCLE('',#94666,0.0999999999999994) ;
#30518 = CIRCLE('',#94669,0.0999999999999994) ;
#30519 = CIRCLE('',#94670,0.0999999999999994) ;
#30520 = CIRCLE('',#94672,1.65625) ;
#30521 = CIRCLE('',#94673,1.65625) ;
#30522 = CIRCLE('',#94675,0.0999999999999994) ;
#30523 = CIRCLE('',#94676,0.0999999999999994) ;
#30524 = CIRCLE('',#94679,0.0999999999999994) ;
#30525 = CIRCLE('',#94680,0.0999999999999994) ;
#30526 = CIRCLE('',#94683,0.0999999999999994) ;
#30527 = CIRCLE('',#94684,0.0999999999999994) ;
#30528 = CIRCLE('',#94687,0.199999999999999) ;
#30529 = CIRCLE('',#94688,0.199999999999999) ;
#30530 = CIRCLE('',#94689,1.75625) ;
#30531 = CIRCLE('',#94690,0.199999999999999) ;
#30532 = CIRCLE('',#94691,0.199999999999999) ;
#30533 = CIRCLE('',#94693,0.0999999999999994) ;
#30534 = CIRCLE('',#94694,0.0999999999999994) ;
#30535 = CIRCLE('',#94697,0.0999999999999994) ;
#30536 = CIRCLE('',#94698,0.0999999999999994) ;
#30537 = CIRCLE('',#94701,0.0999999999999994) ;
#30538 = CIRCLE('',#94702,0.0999999999999994) ;
#30539 = CIRCLE('',#94705,0.0999999999999994) ;
#30540 = CIRCLE('',#94709,0.0999999999999994) ;
#30541 = CIRCLE('',#94710,0.0999999999999994) ;
#30542 = CIRCLE('',#94713,0.0999999999999994) ;
#30543 = CIRCLE('',#94714,0.0999999999999994) ;
#30544 = CIRCLE('',#94717,0.0999999999999994) ;
#30545 = CIRCLE('',#94718,0.0999999999999994) ;
#30546 = CIRCLE('',#94721,0.0999999999999994) ;
#30547 = CIRCLE('',#94722,0.0999999999999994) ;
#30548 = CIRCLE('',#94725,0.0999999999999994) ;
#30549 = CIRCLE('',#94726,0.0999999999999994) ;
#30550 = CIRCLE('',#94729,0.0999999999999994) ;
#30551 = CIRCLE('',#94730,0.0999999999999994) ;
#30552 = CIRCLE('',#94732,1.65625) ;
#30553 = CIRCLE('',#94733,1.65625) ;
#30554 = CIRCLE('',#94735,0.0999999999999994) ;
#30555 = CIRCLE('',#94736,0.0999999999999994) ;
#30556 = CIRCLE('',#94739,0.0999999999999994) ;
#30557 = CIRCLE('',#94740,0.0999999999999994) ;
#30558 = CIRCLE('',#94743,0.0999999999999994) ;
#30559 = CIRCLE('',#94744,0.0999999999999994) ;
#30560 = CIRCLE('',#94747,0.199999999999999) ;
#30561 = CIRCLE('',#94748,0.199999999999999) ;
#30562 = CIRCLE('',#94749,1.75625) ;
#30563 = CIRCLE('',#94750,0.199999999999999) ;
#30564 = CIRCLE('',#94751,0.199999999999999) ;
#30565 = CIRCLE('',#94753,0.0999999999999994) ;
#30566 = CIRCLE('',#94754,0.0999999999999994) ;
#30567 = CIRCLE('',#94757,0.0999999999999994) ;
#30568 = CIRCLE('',#94758,0.0999999999999994) ;
#30569 = CIRCLE('',#94761,0.0999999999999994) ;
#30570 = CIRCLE('',#94762,0.0999999999999994) ;
#30571 = CIRCLE('',#94765,0.100000000000001) ;
#30572 = CIRCLE('',#94769,0.0999999999999994) ;
#30573 = CIRCLE('',#94770,0.0999999999999994) ;
#30574 = CIRCLE('',#94773,0.0999999999999994) ;
#30575 = CIRCLE('',#94774,0.0999999999999994) ;
#30576 = CIRCLE('',#94777,0.0999999999999994) ;
#30577 = CIRCLE('',#94778,0.0999999999999994) ;
#30578 = CIRCLE('',#94781,0.0999999999999994) ;
#30579 = CIRCLE('',#94782,0.0999999999999994) ;
#30580 = CIRCLE('',#94785,0.0999999999999994) ;
#30581 = CIRCLE('',#94786,0.0999999999999994) ;
#30582 = CIRCLE('',#94789,0.0999999999999994) ;
#30583 = CIRCLE('',#94790,0.0999999999999994) ;
#30584 = CIRCLE('',#94792,1.65625) ;
#30585 = CIRCLE('',#94793,1.65625) ;
#30586 = CIRCLE('',#94795,0.0999999999999994) ;
#30587 = CIRCLE('',#94796,0.0999999999999994) ;
#30588 = CIRCLE('',#94799,0.0999999999999994) ;
#30589 = CIRCLE('',#94800,0.0999999999999994) ;
#30590 = CIRCLE('',#94803,0.0999999999999994) ;
#30591 = CIRCLE('',#94804,0.0999999999999994) ;
#30592 = CIRCLE('',#94807,0.200000000000001) ;
#30593 = CIRCLE('',#94808,0.200000000000001) ;
#30594 = CIRCLE('',#94809,1.75625) ;
#30595 = CIRCLE('',#94810,0.199999999999999) ;
#30596 = CIRCLE('',#94811,0.199999999999999) ;
#30597 = CIRCLE('',#94813,0.0999999999999994) ;
#30598 = CIRCLE('',#94814,0.0999999999999994) ;
#30599 = CIRCLE('',#94817,0.0999999999999994) ;
#30600 = CIRCLE('',#94818,0.0999999999999994) ;
#30601 = CIRCLE('',#94821,0.0999999999999994) ;
#30602 = CIRCLE('',#94822,0.0999999999999994) ;
#30603 = CIRCLE('',#94825,0.100000000000001) ;
#30604 = CIRCLE('',#94829,0.100000000000001) ;
#30605 = CIRCLE('',#94830,0.100000000000001) ;
#30606 = CIRCLE('',#94833,0.0999999999999994) ;
#30607 = CIRCLE('',#94834,0.0999999999999994) ;
#30608 = CIRCLE('',#94837,0.0999999999999994) ;
#30609 = CIRCLE('',#94838,0.0999999999999994) ;
#30610 = CIRCLE('',#94841,0.0999999999999994) ;
#30611 = CIRCLE('',#94842,0.0999999999999994) ;
#30612 = CIRCLE('',#94845,0.0999999999999994) ;
#30613 = CIRCLE('',#94846,0.0999999999999994) ;
#30614 = CIRCLE('',#94849,0.0999999999999994) ;
#30615 = CIRCLE('',#94850,0.0999999999999994) ;
#30616 = CIRCLE('',#94852,1.65625) ;
#30617 = CIRCLE('',#94853,1.65625) ;
#30618 = CIRCLE('',#94855,0.0999999999999994) ;
#30619 = CIRCLE('',#94856,0.0999999999999994) ;
#30620 = CIRCLE('',#94859,0.0999999999999994) ;
#30621 = CIRCLE('',#94860,0.0999999999999994) ;
#30622 = CIRCLE('',#94863,0.0999999999999994) ;
#30623 = CIRCLE('',#94864,0.0999999999999994) ;
#30624 = CIRCLE('',#94867,0.200000000000001) ;
#30625 = CIRCLE('',#94868,0.200000000000001) ;
#30626 = CIRCLE('',#94869,1.75625) ;
#30627 = CIRCLE('',#94870,0.200000000000001) ;
#30628 = CIRCLE('',#94871,0.200000000000001) ;
#30629 = CIRCLE('',#94873,0.1) ;
#30630 = CIRCLE('',#94874,0.1) ;
#30631 = CIRCLE('',#94877,0.1) ;
#30632 = CIRCLE('',#94878,0.1) ;
#30633 = CIRCLE('',#94881,0.0999999999999994) ;
#30634 = CIRCLE('',#94882,0.0999999999999994) ;
#30635 = CIRCLE('',#94885,0.1) ;
#30636 = CIRCLE('',#94889,0.100000000000001) ;
#30637 = CIRCLE('',#94890,0.100000000000001) ;
#30638 = CIRCLE('',#94893,0.0999999999999994) ;
#30639 = CIRCLE('',#94894,0.0999999999999994) ;
#30640 = CIRCLE('',#94897,0.0999999999999994) ;
#30641 = CIRCLE('',#94898,0.0999999999999994) ;
#30642 = CIRCLE('',#94901,0.0999999999999994) ;
#30643 = CIRCLE('',#94902,0.0999999999999994) ;
#30644 = CIRCLE('',#94905,0.0999999999999994) ;
#30645 = CIRCLE('',#94906,0.0999999999999994) ;
#30646 = CIRCLE('',#94909,0.0999999999999994) ;
#30647 = CIRCLE('',#94910,0.0999999999999994) ;
#30648 = CIRCLE('',#94912,1.65625) ;
#30649 = CIRCLE('',#94913,1.65625) ;
#30650 = CIRCLE('',#94915,0.1) ;
#30651 = CIRCLE('',#94916,0.1) ;
#30652 = CIRCLE('',#94919,0.1) ;
#30653 = CIRCLE('',#94920,0.1) ;
#30654 = CIRCLE('',#94923,0.1) ;
#30655 = CIRCLE('',#94924,0.1) ;
#30656 = CIRCLE('',#94927,0.2) ;
#30657 = CIRCLE('',#94928,0.2) ;
#30658 = CIRCLE('',#94929,1.75625) ;
#30659 = CIRCLE('',#94930,0.200000000000001) ;
#30660 = CIRCLE('',#94931,0.200000000000001) ;
#30661 = CIRCLE('',#94933,0.0999999999999998) ;
#30662 = CIRCLE('',#94934,0.0999999999999998) ;
#30663 = CIRCLE('',#94937,0.0999999999999998) ;
#30664 = CIRCLE('',#94938,0.0999999999999998) ;
#30665 = CIRCLE('',#94941,0.0999999999999994) ;
#30666 = CIRCLE('',#94942,0.0999999999999994) ;
#30667 = CIRCLE('',#94945,0.100000000000001) ;
#30668 = CIRCLE('',#94949,0.1) ;
#30669 = CIRCLE('',#94950,0.1) ;
#30670 = CIRCLE('',#94953,0.1) ;
#30671 = CIRCLE('',#94954,0.1) ;
#30672 = CIRCLE('',#94957,0.1) ;
#30673 = CIRCLE('',#94958,0.1) ;
#30674 = CIRCLE('',#94961,0.1) ;
#30675 = CIRCLE('',#94962,0.1) ;
#30676 = CIRCLE('',#94965,0.1) ;
#30677 = CIRCLE('',#94966,0.1) ;
#30678 = CIRCLE('',#94969,0.1) ;
#30679 = CIRCLE('',#94970,0.1) ;
#30680 = CIRCLE('',#94972,1.65625) ;
#30681 = CIRCLE('',#94973,1.65625) ;
#30682 = CIRCLE('',#94975,0.0999999999999998) ;
#30683 = CIRCLE('',#94976,0.0999999999999998) ;
#30684 = CIRCLE('',#94979,0.0999999999999998) ;
#30685 = CIRCLE('',#94980,0.0999999999999998) ;
#30686 = CIRCLE('',#94983,0.1) ;
#30687 = CIRCLE('',#94984,0.1) ;
#30688 = CIRCLE('',#94987,0.2) ;
#30689 = CIRCLE('',#94988,0.2) ;
#30690 = CIRCLE('',#94989,1.75625) ;
#30691 = CIRCLE('',#94990,0.2) ;
#30692 = CIRCLE('',#94991,0.2) ;
#30693 = CIRCLE('',#94993,0.0999999999999998) ;
#30694 = CIRCLE('',#94994,0.1) ;
#30695 = CIRCLE('',#94995,0.1) ;
#30696 = CIRCLE('',#94996,0.0999999999999998) ;
#30697 = CIRCLE('',#94998,0.1) ;
#30698 = CIRCLE('',#94999,0.0999999999999994) ;
#30699 = CIRCLE('',#95000,0.0999999999999994) ;
#30700 = CIRCLE('',#95001,0.1) ;
#30701 = CIRCLE('',#95003,0.0999999999999994) ;
#30702 = CIRCLE('',#95004,0.0999999999999994) ;
#30703 = CIRCLE('',#95005,0.0999999999999994) ;
#30704 = CIRCLE('',#95006,0.0999999999999994) ;
#30705 = CIRCLE('',#95008,0.0999999999999994) ;
#30706 = CIRCLE('',#95009,0.0999999999999994) ;
#30707 = CIRCLE('',#95010,0.0999999999999994) ;
#30708 = CIRCLE('',#95011,0.0999999999999994) ;
#30709 = CIRCLE('',#95013,0.0999999999999994) ;
#30710 = CIRCLE('',#95014,0.0999999999999994) ;
#30711 = CIRCLE('',#95015,0.0999999999999994) ;
#30712 = CIRCLE('',#95016,0.0999999999999994) ;
#30713 = CIRCLE('',#95018,0.0999999999999994) ;
#30714 = CIRCLE('',#95019,0.0999999999999994) ;
#30715 = CIRCLE('',#95020,0.0999999999999994) ;
#30716 = CIRCLE('',#95021,0.0999999999999994) ;
#30717 = CIRCLE('',#95023,0.0999999999999994) ;
#30718 = CIRCLE('',#95024,0.0999999999999994) ;
#30719 = CIRCLE('',#95025,0.0999999999999994) ;
#30720 = CIRCLE('',#95026,0.0999999999999994) ;
#30721 = CIRCLE('',#95028,0.0999999999999994) ;
#30722 = CIRCLE('',#95029,0.0999999999999994) ;
#30723 = CIRCLE('',#95030,0.0999999999999994) ;
#30724 = CIRCLE('',#95031,0.0999999999999994) ;
#30725 = CIRCLE('',#95033,0.100000000000003) ;
#30726 = CIRCLE('',#95034,0.100000000000003) ;
#30727 = CIRCLE('',#95035,0.100000000000003) ;
#30728 = CIRCLE('',#95036,0.100000000000003) ;
#30729 = CIRCLE('',#95038,0.0999999999999998) ;
#30730 = CIRCLE('',#95039,0.0999999999999998) ;
#30731 = CIRCLE('',#95041,0.0999999999999998) ;
#30732 = CIRCLE('',#95042,0.1) ;
#30733 = CIRCLE('',#95044,0.0999999999999998) ;
#30734 = CIRCLE('',#95045,0.1) ;
#30735 = CIRCLE('',#95047,0.1) ;
#30736 = CIRCLE('',#95048,0.0999999999999998) ;
#30737 = CIRCLE('',#95050,0.1) ;
#30738 = CIRCLE('',#95052,0.1) ;
#30739 = CIRCLE('',#95054,0.0999999999999998) ;
#30740 = CIRCLE('',#95056,0.1) ;
#30741 = CIRCLE('',#95058,0.0999999999999998) ;
#30742 = CIRCLE('',#95060,0.1) ;
#30743 = CIRCLE('',#95062,0.1) ;
#30744 = CIRCLE('',#95063,0.1) ;
#30745 = CIRCLE('',#95066,0.1) ;
#30746 = CIRCLE('',#95068,0.0999999999999998) ;
#30747 = CIRCLE('',#95069,0.0999999999999998) ;
#30748 = CIRCLE('',#95071,0.1) ;
#30749 = CIRCLE('',#95073,0.1) ;
#30750 = CIRCLE('',#95075,0.0999999999999998) ;
#30751 = CIRCLE('',#95077,0.0999999999999998) ;
#30752 = CIRCLE('',#95079,0.1) ;
#30753 = CIRCLE('',#95081,0.1) ;
#30754 = CIRCLE('',#95082,0.1) ;
#30755 = CIRCLE('',#95084,0.1) ;
#30756 = CIRCLE('',#95086,0.0999999999999998) ;
#30757 = CIRCLE('',#95088,0.0999999999999998) ;
#30758 = CIRCLE('',#95089,0.1) ;
#30759 = CIRCLE('',#95091,0.0999999999999998) ;
#30760 = CIRCLE('',#95093,0.1) ;
#30761 = CIRCLE('',#95094,0.1) ;
#30762 = CIRCLE('',#95096,0.1) ;
#30763 = CIRCLE('',#95098,0.1) ;
#30764 = CIRCLE('',#95100,0.0999999999999998) ;
#30765 = CIRCLE('',#95102,0.0999999999999998) ;
#30766 = CIRCLE('',#95104,0.1) ;
#30767 = CIRCLE('',#95106,0.1) ;
#30768 = CIRCLE('',#95108,0.1) ;
#30769 = CIRCLE('',#95110,0.1) ;
#30770 = CIRCLE('',#95111,0.1) ;
#30771 = CIRCLE('',#95113,0.1) ;
#30772 = CIRCLE('',#95115,0.1) ;
#30773 = CIRCLE('',#95117,0.1) ;
#30774 = CIRCLE('',#95119,0.1) ;
#30775 = CIRCLE('',#95120,0.1) ;
#30776 = CIRCLE('',#95122,0.1) ;
#30777 = CIRCLE('',#95124,0.1) ;
#30778 = CIRCLE('',#95126,0.1) ;
#30779 = CIRCLE('',#95128,0.1) ;
#30780 = CIRCLE('',#95131,0.1) ;
#30781 = CIRCLE('',#95133,0.1) ;
#30782 = CIRCLE('',#95135,0.1) ;
#30783 = CIRCLE('',#95138,0.1) ;
#30784 = CIRCLE('',#95139,0.1) ;
#30785 = CIRCLE('',#95141,0.1) ;
#30786 = CIRCLE('',#95143,0.1) ;
#30787 = CIRCLE('',#95145,0.1) ;
#30788 = CIRCLE('',#95147,0.1) ;
#30789 = CIRCLE('',#95149,0.1) ;
#30790 = CIRCLE('',#95151,0.1) ;
#30791 = CIRCLE('',#95153,0.1) ;
#30792 = CIRCLE('',#95155,0.1) ;
#30793 = CIRCLE('',#95157,0.1) ;
#30794 = CIRCLE('',#95159,0.1) ;
#30795 = CIRCLE('',#95161,0.0999999999999998) ;
#30796 = CIRCLE('',#95163,0.1) ;
#30797 = CIRCLE('',#95165,0.1) ;
#30798 = CIRCLE('',#95167,0.1) ;
#30799 = CIRCLE('',#95170,0.1) ;
#30800 = CIRCLE('',#95172,0.0999999999999998) ;
#30801 = CIRCLE('',#95174,0.0999999999999998) ;
#30802 = CIRCLE('',#95176,0.0999999999999998) ;
#30803 = CIRCLE('',#95178,0.1) ;
#30804 = CIRCLE('',#95180,0.1) ;
#30805 = CIRCLE('',#95182,0.1) ;
#30806 = CIRCLE('',#95184,0.1) ;
#30807 = CIRCLE('',#95186,0.0999999999999998) ;
#30808 = CIRCLE('',#95188,0.0999999999999998) ;
#30809 = CIRCLE('',#95191,0.100000000000003) ;
#30810 = CIRCLE('',#95192,0.100000000000003) ;
#30811 = CIRCLE('',#95194,0.1) ;
#30812 = CIRCLE('',#95196,0.1) ;
#30813 = CIRCLE('',#95198,0.1) ;
#30814 = CIRCLE('',#95200,0.0999999999999998) ;
#30815 = CIRCLE('',#95202,0.0999999999999998) ;
#30816 = CIRCLE('',#95204,0.100000000000003) ;
#30817 = CIRCLE('',#95207,0.100000000000003) ;
#30818 = CIRCLE('',#95209,0.0999999999999994) ;
#30819 = CIRCLE('',#95211,0.0999999999999994) ;
#30820 = CIRCLE('',#95213,0.0999999999999994) ;
#30821 = CIRCLE('',#95215,0.0999999999999998) ;
#30822 = CIRCLE('',#95217,0.1) ;
#30823 = CIRCLE('',#95219,0.0999999999999995) ;
#30824 = CIRCLE('',#95221,0.1) ;
#30825 = CIRCLE('',#95223,0.1) ;
#30826 = CIRCLE('',#95225,0.0999999999999994) ;
#30827 = CIRCLE('',#95227,0.1) ;
#30828 = CIRCLE('',#95229,0.0999999999999998) ;
#30829 = CIRCLE('',#95231,0.100000000000003) ;
#30830 = CIRCLE('',#95233,0.100000000000003) ;
#30831 = CIRCLE('',#95235,0.100000000000003) ;
#30832 = CIRCLE('',#95237,0.100000000000003) ;
#30833 = CIRCLE('',#95239,0.0999999999999994) ;
#30834 = CIRCLE('',#95241,0.1) ;
#30835 = CIRCLE('',#95244,0.0999999999999994) ;
#30836 = CIRCLE('',#95245,0.0999999999999994) ;
#30837 = CIRCLE('',#95247,0.1) ;
#30838 = CIRCLE('',#95249,0.1) ;
#30839 = CIRCLE('',#95251,0.1) ;
#30840 = CIRCLE('',#95253,0.1) ;
#30841 = CIRCLE('',#95255,0.0999999999999998) ;
#30842 = CIRCLE('',#95257,0.100000000000003) ;
#30843 = CIRCLE('',#95260,0.100000000000003) ;
#30844 = CIRCLE('',#95262,0.0999999999999994) ;
#30845 = CIRCLE('',#95264,0.0999999999999994) ;
#30846 = CIRCLE('',#95266,0.0999999999999994) ;
#30847 = CIRCLE('',#95268,0.1) ;
#30848 = CIRCLE('',#95270,0.1) ;
#30849 = CIRCLE('',#95272,0.0999999999999995) ;
#30850 = CIRCLE('',#95274,0.1) ;
#30851 = CIRCLE('',#95276,0.1) ;
#30852 = CIRCLE('',#95278,0.0999999999999994) ;
#30853 = CIRCLE('',#95280,0.1) ;
#30854 = CIRCLE('',#95282,0.0999999999999994) ;
#30855 = CIRCLE('',#95284,0.0999999999999994) ;
#30856 = CIRCLE('',#95286,0.0999999999999994) ;
#30857 = CIRCLE('',#95288,0.0999999999999994) ;
#30858 = CIRCLE('',#95290,0.0999999999999994) ;
#30859 = CIRCLE('',#95292,0.0999999999999994) ;
#30860 = CIRCLE('',#95294,0.1) ;
#30861 = CIRCLE('',#95297,0.0999999999999994) ;
#30862 = CIRCLE('',#95298,0.0999999999999994) ;
#30863 = CIRCLE('',#95300,0.1) ;
#30864 = CIRCLE('',#95302,0.1) ;
#30865 = CIRCLE('',#95304,0.1) ;
#30866 = CIRCLE('',#95306,0.1) ;
#30867 = CIRCLE('',#95308,0.1) ;
#30868 = CIRCLE('',#95310,0.0999999999999994) ;
#30869 = CIRCLE('',#95313,0.0999999999999994) ;
#30870 = CIRCLE('',#95315,0.0999999999999994) ;
#30871 = CIRCLE('',#95317,0.0999999999999994) ;
#30872 = CIRCLE('',#95319,0.0999999999999994) ;
#30873 = CIRCLE('',#95321,0.1) ;
#30874 = CIRCLE('',#95323,0.1) ;
#30875 = CIRCLE('',#95325,0.0999999999999995) ;
#30876 = CIRCLE('',#95327,0.1) ;
#30877 = CIRCLE('',#95329,0.1) ;
#30878 = CIRCLE('',#95331,0.0999999999999994) ;
#30879 = CIRCLE('',#95333,0.1) ;
#30880 = CIRCLE('',#95335,0.0999999999999994) ;
#30881 = CIRCLE('',#95337,0.0999999999999994) ;
#30882 = CIRCLE('',#95339,0.0999999999999994) ;
#30883 = CIRCLE('',#95341,0.0999999999999994) ;
#30884 = CIRCLE('',#95343,0.0999999999999994) ;
#30885 = CIRCLE('',#95345,0.0999999999999994) ;
#30886 = CIRCLE('',#95347,0.1) ;
#30887 = CIRCLE('',#95350,0.0999999999999994) ;
#30888 = CIRCLE('',#95351,0.0999999999999994) ;
#30889 = CIRCLE('',#95353,0.1) ;
#30890 = CIRCLE('',#95355,0.1) ;
#30891 = CIRCLE('',#95357,0.1) ;
#30892 = CIRCLE('',#95359,0.1) ;
#30893 = CIRCLE('',#95361,0.1) ;
#30894 = CIRCLE('',#95363,0.0999999999999994) ;
#30895 = CIRCLE('',#95366,0.0999999999999994) ;
#30896 = CIRCLE('',#95368,0.0999999999999994) ;
#30897 = CIRCLE('',#95370,0.0999999999999994) ;
#30898 = CIRCLE('',#95372,0.0999999999999994) ;
#30899 = CIRCLE('',#95374,0.1) ;
#30900 = CIRCLE('',#95376,0.1) ;
#30901 = CIRCLE('',#95378,0.0999999999999995) ;
#30902 = CIRCLE('',#95380,0.1) ;
#30903 = CIRCLE('',#95382,0.1) ;
#30904 = CIRCLE('',#95384,0.0999999999999994) ;
#30905 = CIRCLE('',#95386,0.1) ;
#30906 = CIRCLE('',#95388,0.0999999999999994) ;
#30907 = CIRCLE('',#95390,0.0999999999999994) ;
#30908 = CIRCLE('',#95392,0.0999999999999994) ;
#30909 = CIRCLE('',#95394,0.0999999999999994) ;
#30910 = CIRCLE('',#95396,0.0999999999999994) ;
#30911 = CIRCLE('',#95398,0.0999999999999994) ;
#30912 = CIRCLE('',#95400,0.1) ;
#30913 = CIRCLE('',#95403,0.0999999999999994) ;
#30914 = CIRCLE('',#95404,0.0999999999999994) ;
#30915 = CIRCLE('',#95406,0.1) ;
#30916 = CIRCLE('',#95408,0.1) ;
#30917 = CIRCLE('',#95410,0.1) ;
#30918 = CIRCLE('',#95412,0.1) ;
#30919 = CIRCLE('',#95414,0.1) ;
#30920 = CIRCLE('',#95416,0.0999999999999994) ;
#30921 = CIRCLE('',#95419,0.0999999999999994) ;
#30922 = CIRCLE('',#95421,0.0999999999999994) ;
#30923 = CIRCLE('',#95423,0.0999999999999994) ;
#30924 = CIRCLE('',#95425,0.0999999999999994) ;
#30925 = CIRCLE('',#95427,0.1) ;
#30926 = CIRCLE('',#95429,0.1) ;
#30927 = CIRCLE('',#95431,0.0999999999999995) ;
#30928 = CIRCLE('',#95433,0.1) ;
#30929 = CIRCLE('',#95435,0.1) ;
#30930 = CIRCLE('',#95437,0.0999999999999994) ;
#30931 = CIRCLE('',#95439,0.1) ;
#30932 = CIRCLE('',#95441,0.0999999999999994) ;
#30933 = CIRCLE('',#95443,0.0999999999999994) ;
#30934 = CIRCLE('',#95445,0.0999999999999994) ;
#30935 = CIRCLE('',#95447,0.0999999999999994) ;
#30936 = CIRCLE('',#95449,0.0999999999999994) ;
#30937 = CIRCLE('',#95451,0.0999999999999994) ;
#30938 = CIRCLE('',#95453,0.1) ;
#30939 = CIRCLE('',#95456,0.0999999999999994) ;
#30940 = CIRCLE('',#95457,0.0999999999999994) ;
#30941 = CIRCLE('',#95459,0.1) ;
#30942 = CIRCLE('',#95461,0.1) ;
#30943 = CIRCLE('',#95463,0.1) ;
#30944 = CIRCLE('',#95465,0.1) ;
#30945 = CIRCLE('',#95467,0.1) ;
#30946 = CIRCLE('',#95469,0.0999999999999994) ;
#30947 = CIRCLE('',#95472,0.0999999999999994) ;
#30948 = CIRCLE('',#95474,0.0999999999999994) ;
#30949 = CIRCLE('',#95476,0.0999999999999994) ;
#30950 = CIRCLE('',#95478,0.0999999999999994) ;
#30951 = CIRCLE('',#95480,0.1) ;
#30952 = CIRCLE('',#95482,0.1) ;
#30953 = CIRCLE('',#95484,0.1) ;
#30954 = CIRCLE('',#95486,0.1) ;
#30955 = CIRCLE('',#95488,0.1) ;
#30956 = CIRCLE('',#95490,0.0999999999999994) ;
#30957 = CIRCLE('',#95492,0.1) ;
#30958 = CIRCLE('',#95494,0.0999999999999994) ;
#30959 = CIRCLE('',#95496,0.0999999999999994) ;
#30960 = CIRCLE('',#95498,0.0999999999999994) ;
#30961 = CIRCLE('',#95500,0.0999999999999994) ;
#30962 = CIRCLE('',#95502,0.0999999999999994) ;
#30963 = CIRCLE('',#95504,0.0999999999999994) ;
#30964 = CIRCLE('',#95506,0.1) ;
#30965 = CIRCLE('',#95509,0.0999999999999994) ;
#30966 = CIRCLE('',#95510,0.0999999999999994) ;
#30967 = CIRCLE('',#95512,0.1) ;
#30968 = CIRCLE('',#95514,0.1) ;
#30969 = CIRCLE('',#95516,0.1) ;
#30970 = CIRCLE('',#95518,0.1) ;
#30971 = CIRCLE('',#95520,0.1) ;
#30972 = CIRCLE('',#95522,0.0999999999999994) ;
#30973 = CIRCLE('',#95525,0.0999999999999994) ;
#30974 = CIRCLE('',#95527,0.0999999999999994) ;
#30975 = CIRCLE('',#95529,0.0999999999999994) ;
#30976 = CIRCLE('',#95531,0.0999999999999994) ;
#30977 = CIRCLE('',#95533,0.1) ;
#30978 = CIRCLE('',#95535,0.1) ;
#30979 = CIRCLE('',#95537,0.1) ;
#30980 = CIRCLE('',#95539,0.1) ;
#30981 = CIRCLE('',#95541,0.1) ;
#30982 = CIRCLE('',#95543,0.0999999999999994) ;
#30983 = CIRCLE('',#95545,0.1) ;
#30984 = CIRCLE('',#95547,0.0999999999999994) ;
#30985 = CIRCLE('',#95549,0.0999999999999994) ;
#30986 = CIRCLE('',#95551,0.0999999999999994) ;
#30987 = CIRCLE('',#95553,0.0999999999999994) ;
#30988 = CIRCLE('',#95555,0.0999999999999994) ;
#30989 = CIRCLE('',#95557,0.0999999999999994) ;
#30990 = CIRCLE('',#95559,0.1) ;
#30991 = CIRCLE('',#95562,0.0999999999999994) ;
#30992 = CIRCLE('',#95563,0.0999999999999994) ;
#30993 = CIRCLE('',#95565,0.1) ;
#30994 = CIRCLE('',#95567,0.1) ;
#30995 = CIRCLE('',#95569,0.1) ;
#30996 = CIRCLE('',#95571,0.1) ;
#30997 = CIRCLE('',#95573,0.1) ;
#30998 = CIRCLE('',#95575,0.0999999999999994) ;
#30999 = CIRCLE('',#95578,0.0999999999999994) ;
#31000 = CIRCLE('',#95580,0.0999999999999994) ;
#31001 = CIRCLE('',#95582,0.0999999999999994) ;
#31002 = CIRCLE('',#95584,0.0999999999999994) ;
#31003 = CIRCLE('',#95586,0.1) ;
#31004 = CIRCLE('',#95588,0.1) ;
#31005 = CIRCLE('',#95590,0.1) ;
#31006 = CIRCLE('',#95592,0.1) ;
#31007 = CIRCLE('',#95594,0.0999999999999998) ;
#31008 = CIRCLE('',#95596,0.0999999999999994) ;
#31009 = CIRCLE('',#95598,0.1) ;
#31010 = CIRCLE('',#95600,0.0999999999999994) ;
#31011 = CIRCLE('',#95602,0.1) ;
#31012 = CIRCLE('',#95604,0.1) ;
#31013 = CIRCLE('',#95606,0.1) ;
#31014 = CIRCLE('',#95608,0.1) ;
#31015 = CIRCLE('',#95610,0.0999999999999994) ;
#31016 = CIRCLE('',#95612,0.1) ;
#31017 = CIRCLE('',#95615,0.1) ;
#31018 = CIRCLE('',#95616,0.1) ;
#31019 = CIRCLE('',#95618,0.1) ;
#31020 = CIRCLE('',#95620,0.1) ;
#31021 = CIRCLE('',#95622,0.1) ;
#31022 = CIRCLE('',#95624,0.0999999999999998) ;
#31023 = CIRCLE('',#95626,0.1) ;
#31024 = CIRCLE('',#95628,0.1) ;
#31025 = CIRCLE('',#95631,0.1) ;
#31026 = CIRCLE('',#95633,0.0999999999999994) ;
#31027 = CIRCLE('',#95635,0.0999999999999994) ;
#31028 = CIRCLE('',#95637,0.0999999999999994) ;
#31029 = CIRCLE('',#95639,0.0999999999999998) ;
#31030 = CIRCLE('',#95641,0.1) ;
#31031 = CIRCLE('',#95643,0.0999999999999998) ;
#31032 = CIRCLE('',#95645,0.1) ;
#31033 = CIRCLE('',#95647,0.1) ;
#31034 = CIRCLE('',#95649,0.0999999999999994) ;
#31035 = CIRCLE('',#95651,0.0999999999999998) ;
#31036 = CIRCLE('',#95653,0.0999999999999998) ;
#31037 = CIRCLE('',#95655,0.0999999999999998) ;
#31038 = CIRCLE('',#95657,0.0999999999999998) ;
#31039 = CIRCLE('',#95659,0.0999999999999998) ;
#31040 = CIRCLE('',#95661,0.0999999999999998) ;
#31041 = CIRCLE('',#95663,0.0999999999999994) ;
#31042 = CIRCLE('',#95665,0.1) ;
#31043 = CIRCLE('',#95668,0.1) ;
#31044 = CIRCLE('',#95669,0.1) ;
#31045 = CIRCLE('',#95671,0.1) ;
#31046 = CIRCLE('',#95672,0.1) ;
#31047 = CIRCLE('',#95674,0.1) ;
#31048 = CIRCLE('',#95675,0.1) ;
#31049 = CIRCLE('',#95677,0.1) ;
#31050 = CIRCLE('',#95678,0.0999999999999998) ;
#31051 = CIRCLE('',#95680,0.1) ;
#31052 = CIRCLE('',#95682,0.1) ;
#31053 = CIRCLE('',#95684,0.1) ;
#31054 = CIRCLE('',#95686,0.1) ;
#31055 = CIRCLE('',#95688,0.0999999999999998) ;
#31056 = CIRCLE('',#95690,0.1) ;
#31057 = CIRCLE('',#95692,0.0999999999999994) ;
#31058 = CIRCLE('',#95693,0.1) ;
#31059 = CIRCLE('',#95696,0.1) ;
#31060 = CIRCLE('',#95698,0.1) ;
#31061 = CIRCLE('',#95699,0.1) ;
#31062 = CIRCLE('',#95701,0.0999999999999994) ;
#31063 = CIRCLE('',#95703,0.1) ;
#31064 = CIRCLE('',#95705,0.1) ;
#31065 = CIRCLE('',#95707,0.1) ;
#31066 = CIRCLE('',#95709,0.0999999999999994) ;
#31067 = CIRCLE('',#95711,0.1) ;
#31068 = CIRCLE('',#95712,0.0999999999999994) ;
#31069 = CIRCLE('',#95714,0.1) ;
#31070 = CIRCLE('',#95716,0.1) ;
#31071 = CIRCLE('',#95718,0.0999999999999998) ;
#31072 = CIRCLE('',#95719,0.1) ;
#31073 = CIRCLE('',#95721,0.1) ;
#31074 = CIRCLE('',#95723,0.1) ;
#31075 = CIRCLE('',#95724,0.1) ;
#31076 = CIRCLE('',#95726,0.1) ;
#31077 = CIRCLE('',#95728,0.1) ;
#31078 = CIRCLE('',#95730,0.1) ;
#31079 = CIRCLE('',#95732,0.1) ;
#31080 = CIRCLE('',#95734,0.1) ;
#31081 = CIRCLE('',#95736,0.1) ;
#31082 = CIRCLE('',#95738,0.1) ;
#31083 = CIRCLE('',#95740,0.0999999999999994) ;
#31084 = CIRCLE('',#95741,0.0999999999999994) ;
#31085 = CIRCLE('',#95743,0.1) ;
#31086 = CIRCLE('',#95745,0.1) ;
#31087 = CIRCLE('',#95747,0.1) ;
#31088 = CIRCLE('',#95749,0.1) ;
#31089 = CIRCLE('',#95750,0.0999999999999994) ;
#31090 = CIRCLE('',#95752,0.0999999999999994) ;
#31091 = CIRCLE('',#95754,0.0999999999999994) ;
#31092 = CIRCLE('',#95756,0.1) ;
#31093 = CIRCLE('',#95758,0.0999999999999994) ;
#31094 = CIRCLE('',#95761,0.0999999999999994) ;
#31095 = CIRCLE('',#95763,0.1) ;
#31096 = CIRCLE('',#95765,0.0999999999999994) ;
#31097 = CIRCLE('',#95768,0.1) ;
#31098 = CIRCLE('',#95769,0.1) ;
#31099 = CIRCLE('',#95771,0.0999999999999994) ;
#31100 = CIRCLE('',#95773,0.0999999999999994) ;
#31101 = CIRCLE('',#95775,0.0999999999999994) ;
#31102 = CIRCLE('',#95777,0.0999999999999994) ;
#31103 = CIRCLE('',#95779,0.1) ;
#31104 = CIRCLE('',#95781,0.0999999999999998) ;
#31105 = CIRCLE('',#95783,0.1) ;
#31106 = CIRCLE('',#95785,0.1) ;
#31107 = CIRCLE('',#95787,0.1) ;
#31108 = CIRCLE('',#95789,0.1) ;
#31109 = CIRCLE('',#95791,0.1) ;
#31110 = CIRCLE('',#95793,0.1) ;
#31111 = CIRCLE('',#95795,0.1) ;
#31112 = CIRCLE('',#95797,0.1) ;
#31113 = CIRCLE('',#95800,0.1) ;
#31114 = CIRCLE('',#95802,0.1) ;
#31115 = CIRCLE('',#95804,0.1) ;
#31116 = CIRCLE('',#95806,0.1) ;
#31117 = CIRCLE('',#95808,0.0999999999999998) ;
#31118 = CIRCLE('',#95810,0.1) ;
#31119 = CIRCLE('',#95812,0.1) ;
#31120 = CIRCLE('',#95814,0.1) ;
#31121 = CIRCLE('',#95816,0.1) ;
#31122 = CIRCLE('',#95818,0.1) ;
#31123 = CIRCLE('',#95821,0.0999999999999994) ;
#31124 = CIRCLE('',#95822,0.0999999999999994) ;
#31125 = CIRCLE('',#95824,0.0999999999999994) ;
#31126 = CIRCLE('',#95825,0.1) ;
#31127 = CIRCLE('',#95827,0.0999999999999994) ;
#31128 = CIRCLE('',#95828,0.1) ;
#31129 = CIRCLE('',#95830,0.1) ;
#31130 = CIRCLE('',#95831,0.0999999999999998) ;
#31131 = CIRCLE('',#95833,0.1) ;
#31132 = CIRCLE('',#95835,0.1) ;
#31133 = CIRCLE('',#95837,0.0999999999999994) ;
#31134 = CIRCLE('',#95839,0.1) ;
#31135 = CIRCLE('',#95841,0.0999999999999998) ;
#31136 = CIRCLE('',#95843,0.1) ;
#31137 = CIRCLE('',#95845,0.0999999999999994) ;
#31138 = CIRCLE('',#95846,0.1) ;
#31139 = CIRCLE('',#95849,0.1) ;
#31140 = CIRCLE('',#95851,0.0999999999999994) ;
#31141 = CIRCLE('',#95852,0.0999999999999994) ;
#31142 = CIRCLE('',#95854,0.0999999999999994) ;
#31143 = CIRCLE('',#95856,0.1) ;
#31144 = CIRCLE('',#95858,0.0999999999999994) ;
#31145 = CIRCLE('',#95860,0.0999999999999994) ;
#31146 = CIRCLE('',#95862,0.0999999999999994) ;
#31147 = CIRCLE('',#95864,0.1) ;
#31148 = CIRCLE('',#95865,0.0999999999999994) ;
#31149 = CIRCLE('',#95867,0.1) ;
#31150 = CIRCLE('',#95869,0.0999999999999994) ;
#31151 = CIRCLE('',#95871,0.0999999999999998) ;
#31152 = CIRCLE('',#95872,0.1) ;
#31153 = CIRCLE('',#95874,0.0999999999999994) ;
#31154 = CIRCLE('',#95876,0.1) ;
#31155 = CIRCLE('',#95877,0.1) ;
#31156 = CIRCLE('',#95879,0.1) ;
#31157 = CIRCLE('',#95881,0.1) ;
#31158 = CIRCLE('',#95883,0.0999999999999994) ;
#31159 = CIRCLE('',#95885,0.0999999999999994) ;
#31160 = CIRCLE('',#95887,0.1) ;
#31161 = CIRCLE('',#95889,0.1) ;
#31162 = CIRCLE('',#95891,0.1) ;
#31163 = CIRCLE('',#95893,0.0999999999999994) ;
#31164 = CIRCLE('',#95894,0.0999999999999994) ;
#31165 = CIRCLE('',#95896,0.1) ;
#31166 = CIRCLE('',#95898,0.1) ;
#31167 = CIRCLE('',#95900,0.1) ;
#31168 = CIRCLE('',#95902,0.1) ;
#31169 = CIRCLE('',#95903,0.0999999999999994) ;
#31170 = CIRCLE('',#95905,0.0999999999999994) ;
#31171 = CIRCLE('',#95907,0.0999999999999994) ;
#31172 = CIRCLE('',#95909,0.1) ;
#31173 = CIRCLE('',#95911,0.0999999999999994) ;
#31174 = CIRCLE('',#95914,0.0999999999999994) ;
#31175 = CIRCLE('',#95916,0.1) ;
#31176 = CIRCLE('',#95918,0.0999999999999994) ;
#31177 = CIRCLE('',#95921,0.1) ;
#31178 = CIRCLE('',#95922,0.1) ;
#31179 = CIRCLE('',#95924,0.0999999999999994) ;
#31180 = CIRCLE('',#95926,0.0999999999999994) ;
#31181 = CIRCLE('',#95928,0.0999999999999994) ;
#31182 = CIRCLE('',#95930,0.0999999999999994) ;
#31183 = CIRCLE('',#95932,0.1) ;
#31184 = CIRCLE('',#95934,0.0999999999999998) ;
#31185 = CIRCLE('',#95936,0.1) ;
#31186 = CIRCLE('',#95938,0.1) ;
#31187 = CIRCLE('',#95940,0.1) ;
#31188 = CIRCLE('',#95942,0.1) ;
#31189 = CIRCLE('',#95944,0.1) ;
#31190 = CIRCLE('',#95946,0.1) ;
#31191 = CIRCLE('',#95948,0.1) ;
#31192 = CIRCLE('',#95950,0.1) ;
#31193 = CIRCLE('',#95953,0.1) ;
#31194 = CIRCLE('',#95955,0.0999999999999994) ;
#31195 = CIRCLE('',#95957,0.1) ;
#31196 = CIRCLE('',#95959,0.0999999999999994) ;
#31197 = CIRCLE('',#95961,0.1) ;
#31198 = CIRCLE('',#95963,0.1) ;
#31199 = CIRCLE('',#95965,0.1) ;
#31200 = CIRCLE('',#95967,0.1) ;
#31201 = CIRCLE('',#95969,0.0999999999999994) ;
#31202 = CIRCLE('',#95971,0.0999999999999994) ;
#31203 = CIRCLE('',#95974,0.0999999999999994) ;
#31204 = CIRCLE('',#95975,0.0999999999999994) ;
#31205 = CIRCLE('',#95977,0.0999999999999994) ;
#31206 = CIRCLE('',#95978,0.1) ;
#31207 = CIRCLE('',#95980,0.0999999999999994) ;
#31208 = CIRCLE('',#95981,0.1) ;
#31209 = CIRCLE('',#95983,0.1) ;
#31210 = CIRCLE('',#95984,0.0999999999999998) ;
#31211 = CIRCLE('',#95986,0.1) ;
#31212 = CIRCLE('',#95988,0.1) ;
#31213 = CIRCLE('',#95990,0.0999999999999994) ;
#31214 = CIRCLE('',#95992,0.1) ;
#31215 = CIRCLE('',#95994,0.0999999999999998) ;
#31216 = CIRCLE('',#95996,0.1) ;
#31217 = CIRCLE('',#95998,0.0999999999999994) ;
#31218 = CIRCLE('',#95999,0.1) ;
#31219 = CIRCLE('',#96002,0.1) ;
#31220 = CIRCLE('',#96004,0.0999999999999994) ;
#31221 = CIRCLE('',#96005,0.0999999999999994) ;
#31222 = CIRCLE('',#96007,0.0999999999999994) ;
#31223 = CIRCLE('',#96009,0.1) ;
#31224 = CIRCLE('',#96011,0.0999999999999994) ;
#31225 = CIRCLE('',#96013,0.0999999999999994) ;
#31226 = CIRCLE('',#96015,0.0999999999999994) ;
#31227 = CIRCLE('',#96017,0.1) ;
#31228 = CIRCLE('',#96018,0.0999999999999994) ;
#31229 = CIRCLE('',#96020,0.1) ;
#31230 = CIRCLE('',#96022,0.0999999999999994) ;
#31231 = CIRCLE('',#96024,0.0999999999999998) ;
#31232 = CIRCLE('',#96025,0.1) ;
#31233 = CIRCLE('',#96027,0.0999999999999994) ;
#31234 = CIRCLE('',#96029,0.1) ;
#31235 = CIRCLE('',#96030,0.1) ;
#31236 = CIRCLE('',#96032,0.1) ;
#31237 = CIRCLE('',#96034,0.1) ;
#31238 = CIRCLE('',#96036,0.0999999999999994) ;
#31239 = CIRCLE('',#96038,0.0999999999999994) ;
#31240 = CIRCLE('',#96040,0.1) ;
#31241 = CIRCLE('',#96042,0.1) ;
#31242 = CIRCLE('',#96044,0.1) ;
#31243 = CIRCLE('',#96046,0.0999999999999994) ;
#31244 = CIRCLE('',#96047,0.0999999999999994) ;
#31245 = CIRCLE('',#96049,0.1) ;
#31246 = CIRCLE('',#96051,0.1) ;
#31247 = CIRCLE('',#96053,0.1) ;
#31248 = CIRCLE('',#96055,0.1) ;
#31249 = CIRCLE('',#96056,0.0999999999999994) ;
#31250 = CIRCLE('',#96058,0.0999999999999994) ;
#31251 = CIRCLE('',#96060,0.0999999999999994) ;
#31252 = CIRCLE('',#96062,0.1) ;
#31253 = CIRCLE('',#96064,0.0999999999999994) ;
#31254 = CIRCLE('',#96067,0.0999999999999994) ;
#31255 = CIRCLE('',#96069,0.1) ;
#31256 = CIRCLE('',#96071,0.0999999999999994) ;
#31257 = CIRCLE('',#96074,0.1) ;
#31258 = CIRCLE('',#96075,0.1) ;
#31259 = CIRCLE('',#96077,0.0999999999999994) ;
#31260 = CIRCLE('',#96079,0.0999999999999994) ;
#31261 = CIRCLE('',#96081,0.0999999999999994) ;
#31262 = CIRCLE('',#96083,0.0999999999999994) ;
#31263 = CIRCLE('',#96085,0.1) ;
#31264 = CIRCLE('',#96087,0.1) ;
#31265 = CIRCLE('',#96089,0.1) ;
#31266 = CIRCLE('',#96091,0.1) ;
#31267 = CIRCLE('',#96093,0.1) ;
#31268 = CIRCLE('',#96095,0.1) ;
#31269 = CIRCLE('',#96097,0.100000000000001) ;
#31270 = CIRCLE('',#96099,0.1) ;
#31271 = CIRCLE('',#96101,0.1) ;
#31272 = CIRCLE('',#96103,0.1) ;
#31273 = CIRCLE('',#96106,0.1) ;
#31274 = CIRCLE('',#96108,0.0999999999999994) ;
#31275 = CIRCLE('',#96110,0.1) ;
#31276 = CIRCLE('',#96112,0.0999999999999994) ;
#31277 = CIRCLE('',#96114,0.1) ;
#31278 = CIRCLE('',#96116,0.1) ;
#31279 = CIRCLE('',#96118,0.1) ;
#31280 = CIRCLE('',#96120,0.1) ;
#31281 = CIRCLE('',#96122,0.0999999999999994) ;
#31282 = CIRCLE('',#96124,0.0999999999999994) ;
#31283 = CIRCLE('',#96127,0.0999999999999994) ;
#31284 = CIRCLE('',#96128,0.0999999999999994) ;
#31285 = CIRCLE('',#96130,0.0999999999999994) ;
#31286 = CIRCLE('',#96131,0.1) ;
#31287 = CIRCLE('',#96133,0.0999999999999994) ;
#31288 = CIRCLE('',#96134,0.1) ;
#31289 = CIRCLE('',#96136,0.1) ;
#31290 = CIRCLE('',#96137,0.0999999999999998) ;
#31291 = CIRCLE('',#96139,0.1) ;
#31292 = CIRCLE('',#96141,0.1) ;
#31293 = CIRCLE('',#96143,0.0999999999999994) ;
#31294 = CIRCLE('',#96145,0.1) ;
#31295 = CIRCLE('',#96147,0.0999999999999998) ;
#31296 = CIRCLE('',#96149,0.1) ;
#31297 = CIRCLE('',#96151,0.0999999999999994) ;
#31298 = CIRCLE('',#96152,0.1) ;
#31299 = CIRCLE('',#96155,0.1) ;
#31300 = CIRCLE('',#96157,0.0999999999999994) ;
#31301 = CIRCLE('',#96158,0.0999999999999994) ;
#31302 = CIRCLE('',#96160,0.0999999999999994) ;
#31303 = CIRCLE('',#96162,0.1) ;
#31304 = CIRCLE('',#96164,0.0999999999999994) ;
#31305 = CIRCLE('',#96166,0.0999999999999994) ;
#31306 = CIRCLE('',#96168,0.0999999999999994) ;
#31307 = CIRCLE('',#96170,0.1) ;
#31308 = CIRCLE('',#96171,0.0999999999999994) ;
#31309 = CIRCLE('',#96173,0.1) ;
#31310 = CIRCLE('',#96175,0.0999999999999994) ;
#31311 = CIRCLE('',#96177,0.0999999999999998) ;
#31312 = CIRCLE('',#96178,0.1) ;
#31313 = CIRCLE('',#96180,0.0999999999999994) ;
#31314 = CIRCLE('',#96182,0.1) ;
#31315 = CIRCLE('',#96183,0.1) ;
#31316 = CIRCLE('',#96185,0.1) ;
#31317 = CIRCLE('',#96187,0.1) ;
#31318 = CIRCLE('',#96189,0.0999999999999994) ;
#31319 = CIRCLE('',#96191,0.0999999999999994) ;
#31320 = CIRCLE('',#96193,0.1) ;
#31321 = CIRCLE('',#96195,0.1) ;
#31322 = CIRCLE('',#96197,0.1) ;
#31323 = CIRCLE('',#96199,0.0999999999999994) ;
#31324 = CIRCLE('',#96200,0.0999999999999994) ;
#31325 = CIRCLE('',#96202,0.1) ;
#31326 = CIRCLE('',#96204,0.1) ;
#31327 = CIRCLE('',#96206,0.1) ;
#31328 = CIRCLE('',#96208,0.1) ;
#31329 = CIRCLE('',#96209,0.0999999999999994) ;
#31330 = CIRCLE('',#96211,0.0999999999999994) ;
#31331 = CIRCLE('',#96213,0.0999999999999994) ;
#31332 = CIRCLE('',#96215,0.1) ;
#31333 = CIRCLE('',#96217,0.0999999999999994) ;
#31334 = CIRCLE('',#96220,0.0999999999999994) ;
#31335 = CIRCLE('',#96222,0.1) ;
#31336 = CIRCLE('',#96224,0.0999999999999994) ;
#31337 = CIRCLE('',#96227,0.1) ;
#31338 = CIRCLE('',#96228,0.1) ;
#31339 = CIRCLE('',#96230,0.0999999999999994) ;
#31340 = CIRCLE('',#96232,0.0999999999999994) ;
#31341 = CIRCLE('',#96234,0.0999999999999994) ;
#31342 = CIRCLE('',#96236,0.0999999999999994) ;
#31343 = CIRCLE('',#96238,0.1) ;
#31344 = CIRCLE('',#96240,0.1) ;
#31345 = CIRCLE('',#96242,0.1) ;
#31346 = CIRCLE('',#96244,0.1) ;
#31347 = CIRCLE('',#96246,0.1) ;
#31348 = CIRCLE('',#96248,0.1) ;
#31349 = CIRCLE('',#96250,0.0999999999999989) ;
#31350 = CIRCLE('',#96252,0.1) ;
#31351 = CIRCLE('',#96254,0.1) ;
#31352 = CIRCLE('',#96256,0.1) ;
#31353 = CIRCLE('',#96259,0.1) ;
#31354 = CIRCLE('',#96261,0.0999999999999994) ;
#31355 = CIRCLE('',#96263,0.0999999999999995) ;
#31356 = CIRCLE('',#96265,0.0999999999999994) ;
#31357 = CIRCLE('',#96267,0.1) ;
#31358 = CIRCLE('',#96269,0.1) ;
#31359 = CIRCLE('',#96271,0.1) ;
#31360 = CIRCLE('',#96273,0.1) ;
#31361 = CIRCLE('',#96275,0.0999999999999994) ;
#31362 = CIRCLE('',#96277,0.0999999999999994) ;
#31363 = CIRCLE('',#96280,0.0999999999999994) ;
#31364 = CIRCLE('',#96281,0.0999999999999994) ;
#31365 = CIRCLE('',#96283,0.0999999999999994) ;
#31366 = CIRCLE('',#96284,0.1) ;
#31367 = CIRCLE('',#96286,0.0999999999999994) ;
#31368 = CIRCLE('',#96287,0.1) ;
#31369 = CIRCLE('',#96289,0.1) ;
#31370 = CIRCLE('',#96290,0.0999999999999998) ;
#31371 = CIRCLE('',#96292,0.1) ;
#31372 = CIRCLE('',#96294,0.1) ;
#31373 = CIRCLE('',#96296,0.0999999999999994) ;
#31374 = CIRCLE('',#96298,0.1) ;
#31375 = CIRCLE('',#96300,0.0999999999999998) ;
#31376 = CIRCLE('',#96302,0.1) ;
#31377 = CIRCLE('',#96304,0.0999999999999994) ;
#31378 = CIRCLE('',#96305,0.1) ;
#31379 = CIRCLE('',#96308,0.1) ;
#31380 = CIRCLE('',#96310,0.0999999999999994) ;
#31381 = CIRCLE('',#96311,0.0999999999999994) ;
#31382 = CIRCLE('',#96313,0.0999999999999994) ;
#31383 = CIRCLE('',#96315,0.1) ;
#31384 = CIRCLE('',#96317,0.0999999999999994) ;
#31385 = CIRCLE('',#96319,0.0999999999999994) ;
#31386 = CIRCLE('',#96321,0.0999999999999994) ;
#31387 = CIRCLE('',#96323,0.1) ;
#31388 = CIRCLE('',#96324,0.0999999999999994) ;
#31389 = CIRCLE('',#96326,0.1) ;
#31390 = CIRCLE('',#96328,0.0999999999999994) ;
#31391 = CIRCLE('',#96330,0.0999999999999998) ;
#31392 = CIRCLE('',#96331,0.1) ;
#31393 = CIRCLE('',#96333,0.0999999999999994) ;
#31394 = CIRCLE('',#96335,0.1) ;
#31395 = CIRCLE('',#96336,0.1) ;
#31396 = CIRCLE('',#96338,0.1) ;
#31397 = CIRCLE('',#96340,0.1) ;
#31398 = CIRCLE('',#96342,0.0999999999999994) ;
#31399 = CIRCLE('',#96344,0.0999999999999994) ;
#31400 = CIRCLE('',#96346,0.1) ;
#31401 = CIRCLE('',#96348,0.1) ;
#31402 = CIRCLE('',#96350,0.1) ;
#31403 = CIRCLE('',#96352,0.0999999999999994) ;
#31404 = CIRCLE('',#96353,0.0999999999999994) ;
#31405 = CIRCLE('',#96355,0.1) ;
#31406 = CIRCLE('',#96357,0.1) ;
#31407 = CIRCLE('',#96359,0.1) ;
#31408 = CIRCLE('',#96361,0.1) ;
#31409 = CIRCLE('',#96362,0.0999999999999994) ;
#31410 = CIRCLE('',#96364,0.0999999999999994) ;
#31411 = CIRCLE('',#96366,0.0999999999999994) ;
#31412 = CIRCLE('',#96368,0.1) ;
#31413 = CIRCLE('',#96370,0.0999999999999994) ;
#31414 = CIRCLE('',#96373,0.0999999999999994) ;
#31415 = CIRCLE('',#96375,0.1) ;
#31416 = CIRCLE('',#96377,0.0999999999999994) ;
#31417 = CIRCLE('',#96380,0.1) ;
#31418 = CIRCLE('',#96381,0.1) ;
#31419 = CIRCLE('',#96383,0.0999999999999994) ;
#31420 = CIRCLE('',#96385,0.0999999999999994) ;
#31421 = CIRCLE('',#96387,0.0999999999999994) ;
#31422 = CIRCLE('',#96389,0.0999999999999994) ;
#31423 = CIRCLE('',#96391,0.1) ;
#31424 = CIRCLE('',#96393,0.1) ;
#31425 = CIRCLE('',#96395,0.1) ;
#31426 = CIRCLE('',#96397,0.1) ;
#31427 = CIRCLE('',#96399,0.1) ;
#31428 = CIRCLE('',#96401,0.1) ;
#31429 = CIRCLE('',#96403,0.0999999999999989) ;
#31430 = CIRCLE('',#96405,0.1) ;
#31431 = CIRCLE('',#96407,0.1) ;
#31432 = CIRCLE('',#96409,0.1) ;
#31433 = CIRCLE('',#96412,0.1) ;
#31434 = CIRCLE('',#96414,0.0999999999999994) ;
#31435 = CIRCLE('',#96416,0.0999999999999995) ;
#31436 = CIRCLE('',#96418,0.0999999999999994) ;
#31437 = CIRCLE('',#96420,0.1) ;
#31438 = CIRCLE('',#96422,0.1) ;
#31439 = CIRCLE('',#96424,0.1) ;
#31440 = CIRCLE('',#96426,0.1) ;
#31441 = CIRCLE('',#96428,0.0999999999999994) ;
#31442 = CIRCLE('',#96430,0.0999999999999994) ;
#31443 = CIRCLE('',#96433,0.0999999999999994) ;
#31444 = CIRCLE('',#96434,0.0999999999999994) ;
#31445 = CIRCLE('',#96436,0.0999999999999994) ;
#31446 = CIRCLE('',#96437,0.1) ;
#31447 = CIRCLE('',#96439,0.0999999999999994) ;
#31448 = CIRCLE('',#96440,0.1) ;
#31449 = CIRCLE('',#96442,0.1) ;
#31450 = CIRCLE('',#96443,0.0999999999999998) ;
#31451 = CIRCLE('',#96445,0.1) ;
#31452 = CIRCLE('',#96447,0.1) ;
#31453 = CIRCLE('',#96449,0.0999999999999994) ;
#31454 = CIRCLE('',#96451,0.1) ;
#31455 = CIRCLE('',#96453,0.0999999999999998) ;
#31456 = CIRCLE('',#96455,0.1) ;
#31457 = CIRCLE('',#96457,0.0999999999999994) ;
#31458 = CIRCLE('',#96458,0.1) ;
#31459 = CIRCLE('',#96461,0.1) ;
#31460 = CIRCLE('',#96463,0.0999999999999994) ;
#31461 = CIRCLE('',#96464,0.0999999999999994) ;
#31462 = CIRCLE('',#96466,0.0999999999999994) ;
#31463 = CIRCLE('',#96468,0.1) ;
#31464 = CIRCLE('',#96470,0.0999999999999994) ;
#31465 = CIRCLE('',#96472,0.0999999999999994) ;
#31466 = CIRCLE('',#96474,0.0999999999999994) ;
#31467 = CIRCLE('',#96476,0.1) ;
#31468 = CIRCLE('',#96477,0.0999999999999994) ;
#31469 = CIRCLE('',#96479,0.1) ;
#31470 = CIRCLE('',#96481,0.0999999999999994) ;
#31471 = CIRCLE('',#96483,0.0999999999999998) ;
#31472 = CIRCLE('',#96484,0.1) ;
#31473 = CIRCLE('',#96486,0.0999999999999994) ;
#31474 = CIRCLE('',#96488,0.1) ;
#31475 = CIRCLE('',#96489,0.1) ;
#31476 = CIRCLE('',#96491,0.1) ;
#31477 = CIRCLE('',#96493,0.1) ;
#31478 = CIRCLE('',#96495,0.0999999999999994) ;
#31479 = CIRCLE('',#96497,0.0999999999999994) ;
#31480 = CIRCLE('',#96499,0.1) ;
#31481 = CIRCLE('',#96501,0.1) ;
#31482 = CIRCLE('',#96503,0.1) ;
#31483 = CIRCLE('',#96505,0.0999999999999994) ;
#31484 = CIRCLE('',#96506,0.0999999999999994) ;
#31485 = CIRCLE('',#96508,0.1) ;
#31486 = CIRCLE('',#96510,0.1) ;
#31487 = CIRCLE('',#96512,0.1) ;
#31488 = CIRCLE('',#96514,0.1) ;
#31489 = CIRCLE('',#96515,0.0999999999999994) ;
#31490 = CIRCLE('',#96517,0.0999999999999994) ;
#31491 = CIRCLE('',#96519,0.0999999999999994) ;
#31492 = CIRCLE('',#96521,0.1) ;
#31493 = CIRCLE('',#96523,0.0999999999999994) ;
#31494 = CIRCLE('',#96526,0.0999999999999994) ;
#31495 = CIRCLE('',#96528,0.1) ;
#31496 = CIRCLE('',#96530,0.0999999999999994) ;
#31497 = CIRCLE('',#96533,0.1) ;
#31498 = CIRCLE('',#96534,0.1) ;
#31499 = CIRCLE('',#96536,0.0999999999999994) ;
#31500 = CIRCLE('',#96538,0.0999999999999994) ;
#31501 = CIRCLE('',#96540,0.0999999999999994) ;
#31502 = CIRCLE('',#96542,0.0999999999999994) ;
#31503 = CIRCLE('',#96544,0.1) ;
#31504 = CIRCLE('',#96546,0.1) ;
#31505 = CIRCLE('',#96548,0.1) ;
#31506 = CIRCLE('',#96550,0.1) ;
#31507 = CIRCLE('',#96552,0.1) ;
#31508 = CIRCLE('',#96554,0.1) ;
#31509 = CIRCLE('',#96556,0.0999999999999989) ;
#31510 = CIRCLE('',#96558,0.1) ;
#31511 = CIRCLE('',#96560,0.1) ;
#31512 = CIRCLE('',#96562,0.1) ;
#31513 = CIRCLE('',#96565,0.1) ;
#31514 = CIRCLE('',#96567,0.0999999999999994) ;
#31515 = CIRCLE('',#96569,0.0999999999999995) ;
#31516 = CIRCLE('',#96571,0.0999999999999994) ;
#31517 = CIRCLE('',#96573,0.1) ;
#31518 = CIRCLE('',#96575,0.1) ;
#31519 = CIRCLE('',#96577,0.1) ;
#31520 = CIRCLE('',#96579,0.1) ;
#31521 = CIRCLE('',#96581,0.0999999999999994) ;
#31522 = CIRCLE('',#96583,0.0999999999999994) ;
#31523 = CIRCLE('',#96586,0.0999999999999994) ;
#31524 = CIRCLE('',#96587,0.0999999999999994) ;
#31525 = CIRCLE('',#96589,0.0999999999999994) ;
#31526 = CIRCLE('',#96590,0.1) ;
#31527 = CIRCLE('',#96592,0.0999999999999994) ;
#31528 = CIRCLE('',#96593,0.1) ;
#31529 = CIRCLE('',#96595,0.1) ;
#31530 = CIRCLE('',#96596,0.0999999999999998) ;
#31531 = CIRCLE('',#96598,0.1) ;
#31532 = CIRCLE('',#96600,0.1) ;
#31533 = CIRCLE('',#96602,0.0999999999999994) ;
#31534 = CIRCLE('',#96604,0.1) ;
#31535 = CIRCLE('',#96606,0.0999999999999998) ;
#31536 = CIRCLE('',#96608,0.1) ;
#31537 = CIRCLE('',#96610,0.0999999999999994) ;
#31538 = CIRCLE('',#96611,0.1) ;
#31539 = CIRCLE('',#96614,0.1) ;
#31540 = CIRCLE('',#96616,0.0999999999999994) ;
#31541 = CIRCLE('',#96617,0.0999999999999994) ;
#31542 = CIRCLE('',#96619,0.0999999999999994) ;
#31543 = CIRCLE('',#96621,0.1) ;
#31544 = CIRCLE('',#96623,0.0999999999999994) ;
#31545 = CIRCLE('',#96625,0.0999999999999994) ;
#31546 = CIRCLE('',#96627,0.0999999999999994) ;
#31547 = CIRCLE('',#96629,0.1) ;
#31548 = CIRCLE('',#96630,0.0999999999999994) ;
#31549 = CIRCLE('',#96632,0.1) ;
#31550 = CIRCLE('',#96634,0.0999999999999994) ;
#31551 = CIRCLE('',#96636,0.0999999999999998) ;
#31552 = CIRCLE('',#96637,0.1) ;
#31553 = CIRCLE('',#96639,0.0999999999999994) ;
#31554 = CIRCLE('',#96641,0.1) ;
#31555 = CIRCLE('',#96642,0.1) ;
#31556 = CIRCLE('',#96644,0.1) ;
#31557 = CIRCLE('',#96646,0.1) ;
#31558 = CIRCLE('',#96648,0.0999999999999994) ;
#31559 = CIRCLE('',#96650,0.0999999999999994) ;
#31560 = CIRCLE('',#96652,0.1) ;
#31561 = CIRCLE('',#96654,0.1) ;
#31562 = CIRCLE('',#96656,0.1) ;
#31563 = CIRCLE('',#96658,0.100000000000003) ;
#31564 = CIRCLE('',#96659,0.100000000000003) ;
#31565 = CIRCLE('',#96661,0.1) ;
#31566 = CIRCLE('',#96663,0.1) ;
#31567 = CIRCLE('',#96665,0.1) ;
#31568 = CIRCLE('',#96667,0.1) ;
#31569 = CIRCLE('',#96668,0.100000000000003) ;
#31570 = CIRCLE('',#96670,0.100000000000003) ;
#31571 = CIRCLE('',#96672,0.100000000000003) ;
#31572 = CIRCLE('',#96674,0.1) ;
#31573 = CIRCLE('',#96676,0.100000000000003) ;
#31574 = CIRCLE('',#96679,0.100000000000003) ;
#31575 = CIRCLE('',#96681,0.1) ;
#31576 = CIRCLE('',#96683,0.100000000000003) ;
#31577 = CIRCLE('',#96686,0.1) ;
#31578 = CIRCLE('',#96687,0.1) ;
#31579 = CIRCLE('',#96689,0.0999999999999994) ;
#31580 = CIRCLE('',#96691,0.100000000000003) ;
#31581 = CIRCLE('',#96693,0.0999999999999994) ;
#31582 = CIRCLE('',#96695,0.100000000000003) ;
#31583 = CIRCLE('',#96697,0.1) ;
#31584 = CIRCLE('',#96699,0.1) ;
#31585 = CIRCLE('',#96701,0.1) ;
#31586 = CIRCLE('',#96703,0.1) ;
#31587 = CIRCLE('',#96705,0.0999999999999999) ;
#31588 = CIRCLE('',#96707,0.1) ;
#31589 = CIRCLE('',#96709,0.0999999999999992) ;
#31590 = CIRCLE('',#96711,0.1) ;
#31591 = CIRCLE('',#96713,0.1) ;
#31592 = CIRCLE('',#96715,0.1) ;
#31593 = CIRCLE('',#96718,0.1) ;
#31594 = CIRCLE('',#96720,0.0999999999999994) ;
#31595 = CIRCLE('',#96722,0.0999999999999995) ;
#31596 = CIRCLE('',#96724,0.0999999999999994) ;
#31597 = CIRCLE('',#96726,0.1) ;
#31598 = CIRCLE('',#96728,0.1) ;
#31599 = CIRCLE('',#96730,0.1) ;
#31600 = CIRCLE('',#96732,0.1) ;
#31601 = CIRCLE('',#96734,0.0999999999999994) ;
#31602 = CIRCLE('',#96736,0.0999999999999994) ;
#31603 = CIRCLE('',#96739,0.100000000000003) ;
#31604 = CIRCLE('',#96740,0.100000000000003) ;
#31605 = CIRCLE('',#96742,0.100000000000003) ;
#31606 = CIRCLE('',#96743,0.1) ;
#31607 = CIRCLE('',#96745,0.100000000000003) ;
#31608 = CIRCLE('',#96746,0.1) ;
#31609 = CIRCLE('',#96748,0.1) ;
#31610 = CIRCLE('',#96749,0.0999999999999998) ;
#31611 = CIRCLE('',#96751,0.1) ;
#31612 = CIRCLE('',#96753,0.1) ;
#31613 = CIRCLE('',#96755,0.100000000000003) ;
#31614 = CIRCLE('',#96757,0.1) ;
#31615 = CIRCLE('',#96759,0.0999999999999998) ;
#31616 = CIRCLE('',#96761,0.1) ;
#31617 = CIRCLE('',#96763,0.100000000000003) ;
#31618 = CIRCLE('',#96764,0.1) ;
#31619 = CIRCLE('',#96767,0.1) ;
#31620 = CIRCLE('',#96769,0.100000000000003) ;
#31621 = CIRCLE('',#96770,0.100000000000003) ;
#31622 = CIRCLE('',#96772,0.100000000000003) ;
#31623 = CIRCLE('',#96774,0.1) ;
#31624 = CIRCLE('',#96776,0.100000000000003) ;
#31625 = CIRCLE('',#96778,0.100000000000003) ;
#31626 = CIRCLE('',#96780,0.100000000000003) ;
#31627 = CIRCLE('',#96782,0.1) ;
#31628 = CIRCLE('',#96783,0.100000000000003) ;
#31629 = CIRCLE('',#96785,0.1) ;
#31630 = CIRCLE('',#96787,0.100000000000003) ;
#31631 = CIRCLE('',#96789,0.0999999999999998) ;
#31632 = CIRCLE('',#96790,0.1) ;
#31633 = CIRCLE('',#96792,0.100000000000003) ;
#31634 = CIRCLE('',#96794,0.1) ;
#31635 = CIRCLE('',#96795,0.1) ;
#31636 = CIRCLE('',#96797,0.1) ;
#31637 = CIRCLE('',#96799,0.1) ;
#31638 = CIRCLE('',#96801,0.100000000000003) ;
#31639 = CIRCLE('',#96803,0.100000000000003) ;
#31640 = CIRCLE('',#96805,0.1) ;
#31641 = CIRCLE('',#96807,0.1) ;
#31642 = CIRCLE('',#96809,0.1) ;
#31643 = CIRCLE('',#96811,0.100000000000003) ;
#31644 = CIRCLE('',#96812,0.100000000000003) ;
#31645 = CIRCLE('',#96814,0.1) ;
#31646 = CIRCLE('',#96816,0.1) ;
#31647 = CIRCLE('',#96818,0.1) ;
#31648 = CIRCLE('',#96820,0.1) ;
#31649 = CIRCLE('',#96821,0.100000000000003) ;
#31650 = CIRCLE('',#96823,0.100000000000003) ;
#31651 = CIRCLE('',#96825,0.100000000000003) ;
#31652 = CIRCLE('',#96827,0.1) ;
#31653 = CIRCLE('',#96829,0.100000000000003) ;
#31654 = CIRCLE('',#96832,0.100000000000003) ;
#31655 = CIRCLE('',#96834,0.1) ;
#31656 = CIRCLE('',#96836,0.100000000000003) ;
#31657 = CIRCLE('',#96839,0.1) ;
#31658 = CIRCLE('',#96840,0.1) ;
#31659 = CIRCLE('',#96842,0.100000000000003) ;
#31660 = CIRCLE('',#96844,0.100000000000003) ;
#31661 = CIRCLE('',#96846,0.100000000000003) ;
#31662 = CIRCLE('',#96848,0.100000000000003) ;
#31663 = CIRCLE('',#96850,0.1) ;
#31664 = CIRCLE('',#96852,0.1) ;
#31665 = CIRCLE('',#96854,0.1) ;
#31666 = CIRCLE('',#96856,0.1) ;
#31667 = CIRCLE('',#96858,0.0999999999999999) ;
#31668 = CIRCLE('',#96860,0.1) ;
#31669 = CIRCLE('',#96862,0.0999999999999992) ;
#31670 = CIRCLE('',#96864,0.1) ;
#31671 = CIRCLE('',#96866,0.1) ;
#31672 = CIRCLE('',#96868,0.1) ;
#31673 = CIRCLE('',#96871,0.1) ;
#31674 = CIRCLE('',#96873,0.100000000000003) ;
#31675 = CIRCLE('',#96875,0.0999999999999998) ;
#31676 = CIRCLE('',#96877,0.100000000000003) ;
#31677 = CIRCLE('',#96879,0.1) ;
#31678 = CIRCLE('',#96881,0.1) ;
#31679 = CIRCLE('',#96883,0.1) ;
#31680 = CIRCLE('',#96885,0.1) ;
#31681 = CIRCLE('',#96887,0.100000000000003) ;
#31682 = CIRCLE('',#96889,0.100000000000003) ;
#31683 = CIRCLE('',#96897,0.3) ;
#31684 = CIRCLE('',#96898,0.9) ;
#31685 = CIRCLE('',#96900,0.9) ;
#31686 = CIRCLE('',#96901,0.3) ;
#31687 = CIRCLE('',#96903,1.) ;
#31688 = CIRCLE('',#96904,1.) ;
#31689 = CIRCLE('',#96906,0.2) ;
#31690 = CIRCLE('',#96907,0.2) ;
#31691 = CIRCLE('',#96921,0.3) ;
#31692 = CIRCLE('',#96922,0.9) ;
#31693 = CIRCLE('',#96924,0.9) ;
#31694 = CIRCLE('',#96925,0.3) ;
#31695 = CIRCLE('',#96927,1.) ;
#31696 = CIRCLE('',#96928,1.) ;
#31697 = CIRCLE('',#96930,0.2) ;
#31698 = CIRCLE('',#96931,0.2) ;
#31699 = CIRCLE('',#96945,0.3) ;
#31700 = CIRCLE('',#96946,0.9) ;
#31701 = CIRCLE('',#96948,0.9) ;
#31702 = CIRCLE('',#96949,0.3) ;
#31703 = CIRCLE('',#96951,1.) ;
#31704 = CIRCLE('',#96952,1.) ;
#31705 = CIRCLE('',#96954,0.2) ;
#31706 = CIRCLE('',#96955,0.2) ;
#31707 = CIRCLE('',#96969,0.3) ;
#31708 = CIRCLE('',#96970,0.9) ;
#31709 = CIRCLE('',#96972,0.9) ;
#31710 = CIRCLE('',#96973,0.3) ;
#31711 = CIRCLE('',#96975,1.) ;
#31712 = CIRCLE('',#96976,1.) ;
#31713 = CIRCLE('',#96978,0.2) ;
#31714 = CIRCLE('',#96979,0.2) ;
#31715 = CIRCLE('',#96993,0.3) ;
#31716 = CIRCLE('',#96994,0.9) ;
#31717 = CIRCLE('',#96996,0.9) ;
#31718 = CIRCLE('',#96997,0.3) ;
#31719 = CIRCLE('',#96999,1.) ;
#31720 = CIRCLE('',#97000,1.) ;
#31721 = CIRCLE('',#97002,0.2) ;
#31722 = CIRCLE('',#97003,0.2) ;
#31723 = CIRCLE('',#97017,0.3) ;
#31724 = CIRCLE('',#97018,0.9) ;
#31725 = CIRCLE('',#97020,0.9) ;
#31726 = CIRCLE('',#97021,0.3) ;
#31727 = CIRCLE('',#97023,1.) ;
#31728 = CIRCLE('',#97024,1.) ;
#31729 = CIRCLE('',#97026,0.2) ;
#31730 = CIRCLE('',#97027,0.2) ;
#31731 = CIRCLE('',#97041,0.3) ;
#31732 = CIRCLE('',#97042,0.9) ;
#31733 = CIRCLE('',#97044,0.9) ;
#31734 = CIRCLE('',#97045,0.3) ;
#31735 = CIRCLE('',#97047,1.) ;
#31736 = CIRCLE('',#97048,1.) ;
#31737 = CIRCLE('',#97050,0.2) ;
#31738 = CIRCLE('',#97051,0.2) ;
#31739 = CIRCLE('',#97065,0.3) ;
#31740 = CIRCLE('',#97066,0.9) ;
#31741 = CIRCLE('',#97068,0.9) ;
#31742 = CIRCLE('',#97069,0.3) ;
#31743 = CIRCLE('',#97071,1.) ;
#31744 = CIRCLE('',#97072,1.) ;
#31745 = CIRCLE('',#97074,0.2) ;
#31746 = CIRCLE('',#97075,0.2) ;
#31747 = CIRCLE('',#97089,0.3) ;
#31748 = CIRCLE('',#97090,0.9) ;
#31749 = CIRCLE('',#97092,0.9) ;
#31750 = CIRCLE('',#97093,0.3) ;
#31751 = CIRCLE('',#97095,1.) ;
#31752 = CIRCLE('',#97096,1.) ;
#31753 = CIRCLE('',#97098,0.2) ;
#31754 = CIRCLE('',#97099,0.2) ;
#31755 = CIRCLE('',#97144,0.1) ;
#31756 = CIRCLE('',#97145,0.0999999999999998) ;
#31757 = CIRCLE('',#97147,0.1) ;
#31758 = CIRCLE('',#97148,0.1) ;
#31759 = CIRCLE('',#97150,0.0999999999999998) ;
#31760 = CIRCLE('',#97151,0.1) ;
#31761 = CIRCLE('',#97153,0.0999999999999999) ;
#31762 = CIRCLE('',#97154,0.1) ;
#31763 = CIRCLE('',#97156,0.1) ;
#31764 = CIRCLE('',#97158,0.0999999999999998) ;
#31765 = CIRCLE('',#97160,0.0999999999999998) ;
#31766 = CIRCLE('',#97162,0.0999999999999999) ;
#31767 = CIRCLE('',#97163,0.1) ;
#31768 = CIRCLE('',#97165,0.0999999999999998) ;
#31769 = CIRCLE('',#97167,0.1) ;
#31770 = CIRCLE('',#97169,0.1) ;
#31771 = CIRCLE('',#97171,0.0999999999999999) ;
#31772 = CIRCLE('',#97173,0.1) ;
#31773 = CIRCLE('',#97174,0.1) ;
#31774 = CIRCLE('',#97176,0.1) ;
#31775 = CIRCLE('',#97178,0.1) ;
#31776 = CIRCLE('',#97179,0.0999999999999998) ;
#31777 = CIRCLE('',#97181,0.1) ;
#31778 = CIRCLE('',#97182,0.1) ;
#31779 = CIRCLE('',#97184,0.0999999999999998) ;
#31780 = CIRCLE('',#97185,0.1) ;
#31781 = CIRCLE('',#97187,0.1) ;
#31782 = CIRCLE('',#97188,0.1) ;
#31783 = CIRCLE('',#97190,0.1) ;
#31784 = CIRCLE('',#97192,0.1) ;
#31785 = CIRCLE('',#97194,0.0999999999999998) ;
#31786 = CIRCLE('',#97196,0.1) ;
#31787 = CIRCLE('',#97197,0.1) ;
#31788 = CIRCLE('',#97199,0.0999999999999998) ;
#31789 = CIRCLE('',#97201,0.1) ;
#31790 = CIRCLE('',#97203,0.1) ;
#31791 = CIRCLE('',#97205,0.1) ;
#31792 = CIRCLE('',#97207,0.1) ;
#31793 = CIRCLE('',#97208,0.1) ;
#31794 = CIRCLE('',#97210,0.1) ;
#31795 = CIRCLE('',#97212,0.0999999999999997) ;
#31796 = CIRCLE('',#97213,0.0999999999999999) ;
#31797 = CIRCLE('',#97215,0.1) ;
#31798 = CIRCLE('',#97216,0.1) ;
#31799 = CIRCLE('',#97218,0.1) ;
#31800 = CIRCLE('',#97219,0.1) ;
#31801 = CIRCLE('',#97221,0.1) ;
#31802 = CIRCLE('',#97222,0.1) ;
#31803 = CIRCLE('',#97224,0.1) ;
#31804 = CIRCLE('',#97226,0.1) ;
#31805 = CIRCLE('',#97228,0.1) ;
#31806 = CIRCLE('',#97230,0.1) ;
#31807 = CIRCLE('',#97231,0.1) ;
#31808 = CIRCLE('',#97233,0.1) ;
#31809 = CIRCLE('',#97235,0.1) ;
#31810 = CIRCLE('',#97237,0.1) ;
#31811 = CIRCLE('',#97239,0.1) ;
#31812 = CIRCLE('',#97241,0.1) ;
#31813 = CIRCLE('',#97242,0.1) ;
#31814 = CIRCLE('',#97244,0.1) ;
#31815 = CIRCLE('',#97246,0.0999999999999999) ;
#31816 = CIRCLE('',#97247,0.1) ;
#31817 = CIRCLE('',#97249,0.1) ;
#31818 = CIRCLE('',#97250,0.1) ;
#31819 = CIRCLE('',#97252,0.1) ;
#31820 = CIRCLE('',#97253,0.1) ;
#31821 = CIRCLE('',#97255,0.1) ;
#31822 = CIRCLE('',#97256,0.1) ;
#31823 = CIRCLE('',#97258,0.1) ;
#31824 = CIRCLE('',#97260,0.1) ;
#31825 = CIRCLE('',#97262,0.1) ;
#31826 = CIRCLE('',#97264,0.0999999999999999) ;
#31827 = CIRCLE('',#97265,0.1) ;
#31828 = CIRCLE('',#97267,0.1) ;
#31829 = CIRCLE('',#97269,0.1) ;
#31830 = CIRCLE('',#97271,0.1) ;
#31831 = CIRCLE('',#97273,0.1) ;
#31832 = CIRCLE('',#97275,0.1) ;
#31833 = CIRCLE('',#97276,0.1) ;
#31834 = CIRCLE('',#97278,0.0999999999999997) ;
#31835 = CIRCLE('',#97280,0.0999999999999999) ;
#31836 = CIRCLE('',#97281,0.1) ;
#31837 = CIRCLE('',#97283,0.1) ;
#31838 = CIRCLE('',#97284,0.1) ;
#31839 = CIRCLE('',#97286,0.0999999999999994) ;
#31840 = CIRCLE('',#97287,0.1) ;
#31841 = CIRCLE('',#97289,0.1) ;
#31842 = CIRCLE('',#97290,0.1) ;
#31843 = CIRCLE('',#97292,0.1) ;
#31844 = CIRCLE('',#97294,0.0999999999999994) ;
#31845 = CIRCLE('',#97296,0.0999999999999994) ;
#31846 = CIRCLE('',#97298,0.1) ;
#31847 = CIRCLE('',#97299,0.1) ;
#31848 = CIRCLE('',#97301,0.0999999999999994) ;
#31849 = CIRCLE('',#97303,0.1) ;
#31850 = CIRCLE('',#97305,0.1) ;
#31851 = CIRCLE('',#97307,0.0999999999999998) ;
#31852 = CIRCLE('',#97309,0.1) ;
#31853 = CIRCLE('',#97310,0.1) ;
#31854 = CIRCLE('',#97312,0.1) ;
#31855 = CIRCLE('',#97314,0.1) ;
#31856 = CIRCLE('',#97315,0.1) ;
#31857 = CIRCLE('',#97317,0.1) ;
#31858 = CIRCLE('',#97318,0.1) ;
#31859 = CIRCLE('',#97320,0.0999999999999994) ;
#31860 = CIRCLE('',#97321,0.1) ;
#31861 = CIRCLE('',#97323,0.1) ;
#31862 = CIRCLE('',#97324,0.1) ;
#31863 = CIRCLE('',#97326,0.1) ;
#31864 = CIRCLE('',#97328,0.1) ;
#31865 = CIRCLE('',#97330,0.0999999999999994) ;
#31866 = CIRCLE('',#97332,0.1) ;
#31867 = CIRCLE('',#97333,0.1) ;
#31868 = CIRCLE('',#97335,0.0999999999999994) ;
#31869 = CIRCLE('',#97337,0.1) ;
#31870 = CIRCLE('',#97339,0.1) ;
#31871 = CIRCLE('',#97341,0.1) ;
#31872 = CIRCLE('',#97343,0.1) ;
#31873 = CIRCLE('',#97344,0.1) ;
#31874 = CIRCLE('',#97346,0.100000000000001) ;
#31875 = CIRCLE('',#97348,0.0999999999999999) ;
#31876 = CIRCLE('',#97349,0.0999999999999999) ;
#31877 = CIRCLE('',#97351,0.1) ;
#31878 = CIRCLE('',#97352,0.1) ;
#31879 = CIRCLE('',#97354,0.0999999999999994) ;
#31880 = CIRCLE('',#97355,0.1) ;
#31881 = CIRCLE('',#97357,0.1) ;
#31882 = CIRCLE('',#97358,0.1) ;
#31883 = CIRCLE('',#97360,0.1) ;
#31884 = CIRCLE('',#97362,0.0999999999999994) ;
#31885 = CIRCLE('',#97364,0.0999999999999994) ;
#31886 = CIRCLE('',#97366,0.1) ;
#31887 = CIRCLE('',#97367,0.1) ;
#31888 = CIRCLE('',#97369,0.0999999999999994) ;
#31889 = CIRCLE('',#97371,0.1) ;
#31890 = CIRCLE('',#97373,0.1) ;
#31891 = CIRCLE('',#97375,0.0999999999999999) ;
#31892 = CIRCLE('',#97377,0.1) ;
#31893 = CIRCLE('',#97378,0.1) ;
#31894 = CIRCLE('',#97380,0.0999999999999998) ;
#31895 = CIRCLE('',#97382,0.0999999999999999) ;
#31896 = CIRCLE('',#97383,0.0999999999999998) ;
#31897 = CIRCLE('',#97385,0.1) ;
#31898 = CIRCLE('',#97386,0.1) ;
#31899 = CIRCLE('',#97388,0.0999999999999994) ;
#31900 = CIRCLE('',#97389,0.1) ;
#31901 = CIRCLE('',#97391,0.1) ;
#31902 = CIRCLE('',#97392,0.1) ;
#31903 = CIRCLE('',#97394,0.1) ;
#31904 = CIRCLE('',#97396,0.1) ;
#31905 = CIRCLE('',#97398,0.0999999999999994) ;
#31906 = CIRCLE('',#97400,0.1) ;
#31907 = CIRCLE('',#97401,0.1) ;
#31908 = CIRCLE('',#97403,0.0999999999999994) ;
#31909 = CIRCLE('',#97405,0.1) ;
#31910 = CIRCLE('',#97407,0.1) ;
#31911 = CIRCLE('',#97409,0.0999999999999995) ;
#31912 = CIRCLE('',#97411,0.1) ;
#31913 = CIRCLE('',#97412,0.1) ;
#31914 = CIRCLE('',#97414,0.1) ;
#31915 = CIRCLE('',#97416,0.1) ;
#31916 = CIRCLE('',#97417,0.0999999999999999) ;
#31917 = CIRCLE('',#97419,0.1) ;
#31918 = CIRCLE('',#97420,0.1) ;
#31919 = CIRCLE('',#97422,0.0999999999999994) ;
#31920 = CIRCLE('',#97423,0.1) ;
#31921 = CIRCLE('',#97425,0.099999999999999) ;
#31922 = CIRCLE('',#97426,0.1) ;
#31923 = CIRCLE('',#97428,0.1) ;
#31924 = CIRCLE('',#97430,0.0999999999999994) ;
#31925 = CIRCLE('',#97432,0.0999999999999994) ;
#31926 = CIRCLE('',#97434,0.0999999999999999) ;
#31927 = CIRCLE('',#97435,0.1) ;
#31928 = CIRCLE('',#97437,0.0999999999999994) ;
#31929 = CIRCLE('',#97439,0.1) ;
#31930 = CIRCLE('',#97441,0.099999999999999) ;
#31931 = CIRCLE('',#97443,0.1) ;
#31932 = CIRCLE('',#97445,0.1) ;
#31933 = CIRCLE('',#97446,0.1) ;
#31934 = CIRCLE('',#97448,0.0999999999999995) ;
#31935 = CIRCLE('',#97450,0.0999999999999991) ;
#31936 = CIRCLE('',#97451,0.0999999999999995) ;
#31937 = CIRCLE('',#97453,0.1) ;
#31938 = CIRCLE('',#97454,0.1) ;
#31939 = CIRCLE('',#97456,0.0999999999999994) ;
#31940 = CIRCLE('',#97457,0.1) ;
#31941 = CIRCLE('',#97459,0.0999999999999989) ;
#31942 = CIRCLE('',#97460,0.099999999999999) ;
#31943 = CIRCLE('',#97462,0.1) ;
#31944 = CIRCLE('',#97464,0.0999999999999994) ;
#31945 = CIRCLE('',#97466,0.0999999999999994) ;
#31946 = CIRCLE('',#97468,0.1) ;
#31947 = CIRCLE('',#97469,0.1) ;
#31948 = CIRCLE('',#97471,0.0999999999999994) ;
#31949 = CIRCLE('',#97473,0.1) ;
#31950 = CIRCLE('',#97475,0.0999999999999989) ;
#31951 = CIRCLE('',#97477,0.0999999999999999) ;
#31952 = CIRCLE('',#97479,0.1) ;
#31953 = CIRCLE('',#97480,0.1) ;
#31954 = CIRCLE('',#97482,0.0999999999999989) ;
#31955 = CIRCLE('',#97484,0.1) ;
#31956 = CIRCLE('',#97485,0.0999999999999999) ;
#31957 = CIRCLE('',#97487,0.1) ;
#31958 = CIRCLE('',#97488,0.1) ;
#31959 = CIRCLE('',#97490,0.0999999999999994) ;
#31960 = CIRCLE('',#97491,0.1) ;
#31961 = CIRCLE('',#97493,0.099999999999999) ;
#31962 = CIRCLE('',#97494,0.1) ;
#31963 = CIRCLE('',#97496,0.1) ;
#31964 = CIRCLE('',#97498,0.0999999999999994) ;
#31965 = CIRCLE('',#97500,0.0999999999999994) ;
#31966 = CIRCLE('',#97502,0.0999999999999999) ;
#31967 = CIRCLE('',#97503,0.1) ;
#31968 = CIRCLE('',#97505,0.0999999999999994) ;
#31969 = CIRCLE('',#97507,0.1) ;
#31970 = CIRCLE('',#97509,0.099999999999999) ;
#31971 = CIRCLE('',#97511,0.1) ;
#31972 = CIRCLE('',#97513,0.1) ;
#31973 = CIRCLE('',#97514,0.1) ;
#31974 = CIRCLE('',#97516,0.0999999999999995) ;
#31975 = CIRCLE('',#97518,0.0999999999999991) ;
#31976 = CIRCLE('',#97519,0.0999999999999995) ;
#31977 = CIRCLE('',#97521,0.1) ;
#31978 = CIRCLE('',#97522,0.1) ;
#31979 = CIRCLE('',#97524,0.0999999999999994) ;
#31980 = CIRCLE('',#97525,0.1) ;
#31981 = CIRCLE('',#97527,0.0999999999999989) ;
#31982 = CIRCLE('',#97528,0.099999999999999) ;
#31983 = CIRCLE('',#97530,0.1) ;
#31984 = CIRCLE('',#97532,0.0999999999999994) ;
#31985 = CIRCLE('',#97534,0.0999999999999994) ;
#31986 = CIRCLE('',#97536,0.1) ;
#31987 = CIRCLE('',#97537,0.1) ;
#31988 = CIRCLE('',#97539,0.0999999999999994) ;
#31989 = CIRCLE('',#97541,0.1) ;
#31990 = CIRCLE('',#97543,0.0999999999999989) ;
#31991 = CIRCLE('',#97545,0.0999999999999999) ;
#31992 = CIRCLE('',#97547,0.1) ;
#31993 = CIRCLE('',#97548,0.1) ;
#31994 = CIRCLE('',#97550,0.0999999999999989) ;
#31995 = CIRCLE('',#97552,0.1) ;
#31996 = CIRCLE('',#97553,0.0999999999999999) ;
#31997 = CIRCLE('',#97555,0.1) ;
#31998 = CIRCLE('',#97556,0.1) ;
#31999 = CIRCLE('',#97558,0.0999999999999994) ;
#32000 = CIRCLE('',#97559,0.1) ;
#32001 = CIRCLE('',#97561,0.099999999999999) ;
#32002 = CIRCLE('',#97562,0.1) ;
#32003 = CIRCLE('',#97564,0.1) ;
#32004 = CIRCLE('',#97566,0.0999999999999994) ;
#32005 = CIRCLE('',#97568,0.0999999999999994) ;
#32006 = CIRCLE('',#97570,0.0999999999999999) ;
#32007 = CIRCLE('',#97571,0.1) ;
#32008 = CIRCLE('',#97573,0.0999999999999994) ;
#32009 = CIRCLE('',#97575,0.1) ;
#32010 = CIRCLE('',#97577,0.099999999999999) ;
#32011 = CIRCLE('',#97579,0.1) ;
#32012 = CIRCLE('',#97581,0.1) ;
#32013 = CIRCLE('',#97582,0.1) ;
#32014 = CIRCLE('',#97584,0.0999999999999995) ;
#32015 = CIRCLE('',#97586,0.0999999999999991) ;
#32016 = CIRCLE('',#97587,0.0999999999999995) ;
#32017 = CIRCLE('',#97589,0.1) ;
#32018 = CIRCLE('',#97590,0.1) ;
#32019 = CIRCLE('',#97592,0.0999999999999994) ;
#32020 = CIRCLE('',#97593,0.1) ;
#32021 = CIRCLE('',#97595,0.0999999999999989) ;
#32022 = CIRCLE('',#97596,0.099999999999999) ;
#32023 = CIRCLE('',#97598,0.1) ;
#32024 = CIRCLE('',#97600,0.0999999999999994) ;
#32025 = CIRCLE('',#97602,0.0999999999999994) ;
#32026 = CIRCLE('',#97604,0.1) ;
#32027 = CIRCLE('',#97605,0.1) ;
#32028 = CIRCLE('',#97607,0.0999999999999994) ;
#32029 = CIRCLE('',#97609,0.1) ;
#32030 = CIRCLE('',#97611,0.0999999999999989) ;
#32031 = CIRCLE('',#97613,0.0999999999999999) ;
#32032 = CIRCLE('',#97615,0.1) ;
#32033 = CIRCLE('',#97616,0.1) ;
#32034 = CIRCLE('',#97618,0.0999999999999989) ;
#32035 = CIRCLE('',#97620,0.1) ;
#32036 = CIRCLE('',#97621,0.0999999999999999) ;
#32037 = CIRCLE('',#97623,0.1) ;
#32038 = CIRCLE('',#97624,0.1) ;
#32039 = CIRCLE('',#97626,0.0999999999999994) ;
#32040 = CIRCLE('',#97627,0.1) ;
#32041 = CIRCLE('',#97629,0.099999999999999) ;
#32042 = CIRCLE('',#97630,0.1) ;
#32043 = CIRCLE('',#97632,0.1) ;
#32044 = CIRCLE('',#97634,0.0999999999999994) ;
#32045 = CIRCLE('',#97636,0.0999999999999994) ;
#32046 = CIRCLE('',#97638,0.0999999999999999) ;
#32047 = CIRCLE('',#97639,0.1) ;
#32048 = CIRCLE('',#97641,0.0999999999999994) ;
#32049 = CIRCLE('',#97643,0.1) ;
#32050 = CIRCLE('',#97645,0.099999999999999) ;
#32051 = CIRCLE('',#97647,0.1) ;
#32052 = CIRCLE('',#97649,0.1) ;
#32053 = CIRCLE('',#97650,0.1) ;
#32054 = CIRCLE('',#97652,0.0999999999999995) ;
#32055 = CIRCLE('',#97654,0.0999999999999991) ;
#32056 = CIRCLE('',#97655,0.0999999999999995) ;
#32057 = CIRCLE('',#97657,0.1) ;
#32058 = CIRCLE('',#97658,0.1) ;
#32059 = CIRCLE('',#97660,0.0999999999999994) ;
#32060 = CIRCLE('',#97661,0.1) ;
#32061 = CIRCLE('',#97663,0.0999999999999989) ;
#32062 = CIRCLE('',#97664,0.099999999999999) ;
#32063 = CIRCLE('',#97666,0.1) ;
#32064 = CIRCLE('',#97668,0.0999999999999994) ;
#32065 = CIRCLE('',#97670,0.0999999999999994) ;
#32066 = CIRCLE('',#97672,0.1) ;
#32067 = CIRCLE('',#97673,0.1) ;
#32068 = CIRCLE('',#97675,0.0999999999999994) ;
#32069 = CIRCLE('',#97677,0.1) ;
#32070 = CIRCLE('',#97679,0.0999999999999989) ;
#32071 = CIRCLE('',#97681,0.0999999999999999) ;
#32072 = CIRCLE('',#97683,0.1) ;
#32073 = CIRCLE('',#97684,0.1) ;
#32074 = CIRCLE('',#97686,0.0999999999999989) ;
#32075 = CIRCLE('',#97688,0.0999999999999997) ;
#32076 = CIRCLE('',#97689,0.0999999999999995) ;
#32077 = CIRCLE('',#97691,0.1) ;
#32078 = CIRCLE('',#97692,0.1) ;
#32079 = CIRCLE('',#97694,0.100000000000003) ;
#32080 = CIRCLE('',#97695,0.1) ;
#32081 = CIRCLE('',#97697,0.099999999999999) ;
#32082 = CIRCLE('',#97698,0.100000000000001) ;
#32083 = CIRCLE('',#97700,0.1) ;
#32084 = CIRCLE('',#97702,0.100000000000003) ;
#32085 = CIRCLE('',#97704,0.100000000000003) ;
#32086 = CIRCLE('',#97706,0.0999999999999995) ;
#32087 = CIRCLE('',#97707,0.1) ;
#32088 = CIRCLE('',#97709,0.100000000000003) ;
#32089 = CIRCLE('',#97711,0.1) ;
#32090 = CIRCLE('',#97713,0.099999999999999) ;
#32091 = CIRCLE('',#97715,0.1) ;
#32092 = CIRCLE('',#97717,0.1) ;
#32093 = CIRCLE('',#97718,0.1) ;
#32094 = CIRCLE('',#97720,0.0999999999999999) ;
#32095 = CIRCLE('',#97722,0.1) ;
#32096 = CIRCLE('',#97723,0.0999999999999983) ;
#32097 = CIRCLE('',#97725,0.1) ;
#32098 = CIRCLE('',#97726,0.1) ;
#32099 = CIRCLE('',#97728,0.100000000000003) ;
#32100 = CIRCLE('',#97729,0.1) ;
#32101 = CIRCLE('',#97731,0.0999999999999989) ;
#32102 = CIRCLE('',#97732,0.0999999999999998) ;
#32103 = CIRCLE('',#97734,0.1) ;
#32104 = CIRCLE('',#97736,0.1) ;
#32105 = CIRCLE('',#97738,0.100000000000003) ;
#32106 = CIRCLE('',#97740,0.0999999999999998) ;
#32107 = CIRCLE('',#97741,0.1) ;
#32108 = CIRCLE('',#97743,0.100000000000003) ;
#32109 = CIRCLE('',#97745,0.1) ;
#32110 = CIRCLE('',#97747,0.0999999999999989) ;
#32111 = CIRCLE('',#97749,0.1) ;
#32112 = CIRCLE('',#97751,0.1) ;
#32113 = CIRCLE('',#97752,0.1) ;
#32114 = CIRCLE('',#97754,0.100000000000001) ;
#32115 = CIRCLE('',#97756,0.1) ;
#32116 = CIRCLE('',#97758,0.1) ;
#32117 = CIRCLE('',#97760,0.1) ;
#32118 = CIRCLE('',#97762,0.1) ;
#32119 = CIRCLE('',#97764,0.1) ;
#32120 = CIRCLE('',#97766,0.1) ;
#32121 = CIRCLE('',#97769,0.0999999999999998) ;
#32122 = CIRCLE('',#97771,0.0999999999999998) ;
#32123 = CIRCLE('',#97773,0.1) ;
#32124 = CIRCLE('',#97775,0.0999999999999998) ;
#32125 = CIRCLE('',#97777,0.0999999999999998) ;
#32126 = CIRCLE('',#97779,0.0999999999999998) ;
#32127 = CIRCLE('',#97782,0.1) ;
#32128 = CIRCLE('',#97784,0.1) ;
#32129 = CIRCLE('',#97786,0.1) ;
#32130 = CIRCLE('',#97788,0.1) ;
#32131 = CIRCLE('',#97791,0.0999999999999998) ;
#32132 = CIRCLE('',#97793,0.1) ;
#32133 = CIRCLE('',#97795,0.0999999999999998) ;
#32134 = CIRCLE('',#97797,0.0999999999999998) ;
#32135 = CIRCLE('',#97800,0.0999999999999994) ;
#32136 = CIRCLE('',#97802,0.0999999999999994) ;
#32137 = CIRCLE('',#97804,0.1) ;
#32138 = CIRCLE('',#97806,0.0999999999999994) ;
#32139 = CIRCLE('',#97808,0.0999999999999994) ;
#32140 = CIRCLE('',#97810,0.0999999999999994) ;
#32141 = CIRCLE('',#97813,0.1) ;
#32142 = CIRCLE('',#97815,0.1) ;
#32143 = CIRCLE('',#97817,0.1) ;
#32144 = CIRCLE('',#97819,0.1) ;
#32145 = CIRCLE('',#97821,0.1) ;
#32146 = CIRCLE('',#97823,0.1) ;
#32147 = CIRCLE('',#97826,0.0999999999999994) ;
#32148 = CIRCLE('',#97828,0.1) ;
#32149 = CIRCLE('',#97830,0.0999999999999994) ;
#32150 = CIRCLE('',#97832,0.0999999999999994) ;
#32151 = CIRCLE('',#97835,0.1) ;
#32152 = CIRCLE('',#97837,0.1) ;
#32153 = CIRCLE('',#97839,0.1) ;
#32154 = CIRCLE('',#97841,0.1) ;
#32155 = CIRCLE('',#97844,0.0999999999999994) ;
#32156 = CIRCLE('',#97846,0.0999999999999994) ;
#32157 = CIRCLE('',#97848,0.1) ;
#32158 = CIRCLE('',#97850,0.0999999999999994) ;
#32159 = CIRCLE('',#97852,0.0999999999999994) ;
#32160 = CIRCLE('',#97854,0.0999999999999994) ;
#32161 = CIRCLE('',#97857,0.0999999999999994) ;
#32162 = CIRCLE('',#97859,0.0999999999999994) ;
#32163 = CIRCLE('',#97861,0.1) ;
#32164 = CIRCLE('',#97863,0.0999999999999994) ;
#32165 = CIRCLE('',#97865,0.0999999999999994) ;
#32166 = CIRCLE('',#97867,0.0999999999999994) ;
#32167 = CIRCLE('',#97870,0.0999999999999994) ;
#32168 = CIRCLE('',#97872,0.1) ;
#32169 = CIRCLE('',#97874,0.0999999999999994) ;
#32170 = CIRCLE('',#97876,0.0999999999999994) ;
#32171 = CIRCLE('',#97879,0.0999999999999994) ;
#32172 = CIRCLE('',#97881,0.1) ;
#32173 = CIRCLE('',#97883,0.0999999999999994) ;
#32174 = CIRCLE('',#97885,0.0999999999999994) ;
#32175 = CIRCLE('',#97888,0.0999999999999994) ;
#32176 = CIRCLE('',#97890,0.0999999999999994) ;
#32177 = CIRCLE('',#97892,0.0999999999999994) ;
#32178 = CIRCLE('',#97894,0.0999999999999994) ;
#32179 = CIRCLE('',#97896,0.0999999999999994) ;
#32180 = CIRCLE('',#97898,0.0999999999999994) ;
#32181 = CIRCLE('',#97901,0.0999999999999994) ;
#32182 = CIRCLE('',#97903,0.0999999999999994) ;
#32183 = CIRCLE('',#97905,0.1) ;
#32184 = CIRCLE('',#97907,0.0999999999999994) ;
#32185 = CIRCLE('',#97909,0.0999999999999994) ;
#32186 = CIRCLE('',#97911,0.0999999999999994) ;
#32187 = CIRCLE('',#97914,0.100000000000001) ;
#32188 = CIRCLE('',#97916,0.1) ;
#32189 = CIRCLE('',#97918,0.100000000000001) ;
#32190 = CIRCLE('',#97920,0.0999999999999994) ;
#32191 = CIRCLE('',#97923,0.0999999999999994) ;
#32192 = CIRCLE('',#97925,0.1) ;
#32193 = CIRCLE('',#97927,0.0999999999999994) ;
#32194 = CIRCLE('',#97929,0.0999999999999994) ;
#32195 = CIRCLE('',#97932,0.0999999999999994) ;
#32196 = CIRCLE('',#97934,0.0999999999999994) ;
#32197 = CIRCLE('',#97936,0.1) ;
#32198 = CIRCLE('',#97938,0.0999999999999994) ;
#32199 = CIRCLE('',#97940,0.0999999999999994) ;
#32200 = CIRCLE('',#97942,0.0999999999999994) ;
#32201 = CIRCLE('',#97945,0.0999999999999994) ;
#32202 = CIRCLE('',#97947,0.0999999999999994) ;
#32203 = CIRCLE('',#97949,0.1) ;
#32204 = CIRCLE('',#97951,0.0999999999999994) ;
#32205 = CIRCLE('',#97953,0.0999999999999994) ;
#32206 = CIRCLE('',#97955,0.0999999999999994) ;
#32207 = CIRCLE('',#97958,0.0999999999999994) ;
#32208 = CIRCLE('',#97960,0.1) ;
#32209 = CIRCLE('',#97962,0.0999999999999994) ;
#32210 = CIRCLE('',#97964,0.0999999999999994) ;
#32211 = CIRCLE('',#97967,0.0999999999999994) ;
#32212 = CIRCLE('',#97969,0.1) ;
#32213 = CIRCLE('',#97971,0.0999999999999994) ;
#32214 = CIRCLE('',#97973,0.0999999999999994) ;
#32215 = CIRCLE('',#97976,0.0999999999999994) ;
#32216 = CIRCLE('',#97978,0.0999999999999994) ;
#32217 = CIRCLE('',#97980,0.1) ;
#32218 = CIRCLE('',#97982,0.0999999999999994) ;
#32219 = CIRCLE('',#97984,0.0999999999999994) ;
#32220 = CIRCLE('',#97986,0.0999999999999994) ;
#32221 = CIRCLE('',#97989,0.0999999999999994) ;
#32222 = CIRCLE('',#97991,0.0999999999999994) ;
#32223 = CIRCLE('',#97993,0.1) ;
#32224 = CIRCLE('',#97995,0.0999999999999994) ;
#32225 = CIRCLE('',#97997,0.0999999999999994) ;
#32226 = CIRCLE('',#97999,0.0999999999999994) ;
#32227 = CIRCLE('',#98002,0.0999999999999994) ;
#32228 = CIRCLE('',#98004,0.1) ;
#32229 = CIRCLE('',#98006,0.0999999999999994) ;
#32230 = CIRCLE('',#98008,0.0999999999999994) ;
#32231 = CIRCLE('',#98011,0.0999999999999994) ;
#32232 = CIRCLE('',#98013,0.1) ;
#32233 = CIRCLE('',#98015,0.0999999999999994) ;
#32234 = CIRCLE('',#98017,0.0999999999999994) ;
#32235 = CIRCLE('',#98020,0.0999999999999994) ;
#32236 = CIRCLE('',#98022,0.0999999999999994) ;
#32237 = CIRCLE('',#98024,0.1) ;
#32238 = CIRCLE('',#98026,0.0999999999999994) ;
#32239 = CIRCLE('',#98028,0.0999999999999994) ;
#32240 = CIRCLE('',#98030,0.0999999999999994) ;
#32241 = CIRCLE('',#98033,0.0999999999999994) ;
#32242 = CIRCLE('',#98035,0.0999999999999994) ;
#32243 = CIRCLE('',#98037,0.1) ;
#32244 = CIRCLE('',#98039,0.0999999999999994) ;
#32245 = CIRCLE('',#98041,0.0999999999999994) ;
#32246 = CIRCLE('',#98043,0.0999999999999994) ;
#32247 = CIRCLE('',#98046,0.0999999999999994) ;
#32248 = CIRCLE('',#98048,0.1) ;
#32249 = CIRCLE('',#98050,0.0999999999999994) ;
#32250 = CIRCLE('',#98052,0.0999999999999994) ;
#32251 = CIRCLE('',#98055,0.0999999999999994) ;
#32252 = CIRCLE('',#98057,0.1) ;
#32253 = CIRCLE('',#98059,0.0999999999999994) ;
#32254 = CIRCLE('',#98061,0.0999999999999994) ;
#32255 = CIRCLE('',#98064,0.0999999999999994) ;
#32256 = CIRCLE('',#98066,0.0999999999999994) ;
#32257 = CIRCLE('',#98068,0.1) ;
#32258 = CIRCLE('',#98070,0.0999999999999994) ;
#32259 = CIRCLE('',#98072,0.0999999999999994) ;
#32260 = CIRCLE('',#98074,0.0999999999999994) ;
#32261 = CIRCLE('',#98077,0.0999999999999994) ;
#32262 = CIRCLE('',#98079,0.0999999999999994) ;
#32263 = CIRCLE('',#98081,0.1) ;
#32264 = CIRCLE('',#98083,0.0999999999999994) ;
#32265 = CIRCLE('',#98085,0.0999999999999994) ;
#32266 = CIRCLE('',#98087,0.0999999999999994) ;
#32267 = CIRCLE('',#98090,0.0999999999999994) ;
#32268 = CIRCLE('',#98092,0.1) ;
#32269 = CIRCLE('',#98094,0.0999999999999994) ;
#32270 = CIRCLE('',#98096,0.0999999999999994) ;
#32271 = CIRCLE('',#98099,0.0999999999999994) ;
#32272 = CIRCLE('',#98101,0.1) ;
#32273 = CIRCLE('',#98103,0.0999999999999994) ;
#32274 = CIRCLE('',#98105,0.0999999999999994) ;
#32275 = CIRCLE('',#98108,0.100000000000003) ;
#32276 = CIRCLE('',#98110,0.100000000000003) ;
#32277 = CIRCLE('',#98112,0.1) ;
#32278 = CIRCLE('',#98114,0.100000000000003) ;
#32279 = CIRCLE('',#98116,0.100000000000003) ;
#32280 = CIRCLE('',#98118,0.100000000000003) ;
#32281 = CIRCLE('',#98121,0.100000000000003) ;
#32282 = CIRCLE('',#98123,0.100000000000003) ;
#32283 = CIRCLE('',#98125,0.1) ;
#32284 = CIRCLE('',#98127,0.100000000000003) ;
#32285 = CIRCLE('',#98129,0.100000000000003) ;
#32286 = CIRCLE('',#98131,0.100000000000003) ;
#32287 = CIRCLE('',#98134,0.100000000000003) ;
#32288 = CIRCLE('',#98136,0.1) ;
#32289 = CIRCLE('',#98138,0.100000000000003) ;
#32290 = CIRCLE('',#98140,0.100000000000003) ;
#32291 = CIRCLE('',#98143,0.100000000000003) ;
#32292 = CIRCLE('',#98145,0.1) ;
#32293 = CIRCLE('',#98147,0.100000000000003) ;
#32294 = CIRCLE('',#98149,0.100000000000003) ;
#32295 = CIRCLE('',#98153,0.0999999999999998) ;
#32296 = CIRCLE('',#98154,0.0999999999999998) ;
#32297 = CIRCLE('',#98156,0.1645125) ;
#32298 = CIRCLE('',#98157,0.1) ;
#32299 = CIRCLE('',#98158,0.0645124999999998) ;
#32300 = CIRCLE('',#98159,0.1) ;
#32301 = CIRCLE('',#98161,0.1645125) ;
#32302 = CIRCLE('',#98162,0.0999999999999999) ;
#32303 = CIRCLE('',#98163,0.0645125000000003) ;
#32304 = CIRCLE('',#98164,0.1) ;
#32305 = CIRCLE('',#98166,2.35) ;
#32306 = CIRCLE('',#98167,2.25) ;
#32307 = CIRCLE('',#98169,0.1645125) ;
#32308 = CIRCLE('',#98170,0.1) ;
#32309 = CIRCLE('',#98171,0.0645125000000003) ;
#32310 = CIRCLE('',#98172,0.1) ;
#32311 = CIRCLE('',#98174,2.35) ;
#32312 = CIRCLE('',#98175,2.25) ;
#32313 = CIRCLE('',#98177,0.1645125) ;
#32314 = CIRCLE('',#98178,0.1) ;
#32315 = CIRCLE('',#98179,0.0645125000000003) ;
#32316 = CIRCLE('',#98180,0.1) ;
#32317 = CIRCLE('',#98182,2.35) ;
#32318 = CIRCLE('',#98183,2.25) ;
#32319 = CIRCLE('',#98185,0.1645125) ;
#32320 = CIRCLE('',#98186,0.1) ;
#32321 = CIRCLE('',#98187,0.0645125000000003) ;
#32322 = CIRCLE('',#98188,0.1) ;
#32323 = CIRCLE('',#98190,2.35) ;
#32324 = CIRCLE('',#98191,2.25) ;
#32325 = CIRCLE('',#98193,0.1645125) ;
#32326 = CIRCLE('',#98194,0.0999999999999993) ;
#32327 = CIRCLE('',#98195,0.0645125000000003) ;
#32328 = CIRCLE('',#98196,0.0999999999999993) ;
#32329 = CIRCLE('',#98198,2.35) ;
#32330 = CIRCLE('',#98199,2.25) ;
#32331 = CIRCLE('',#98201,0.1645125) ;
#32332 = CIRCLE('',#98202,0.0999999999999993) ;
#32333 = CIRCLE('',#98203,0.0645125000000003) ;
#32334 = CIRCLE('',#98204,0.0999999999999993) ;
#32335 = CIRCLE('',#98206,2.35) ;
#32336 = CIRCLE('',#98207,2.25) ;
#32337 = CIRCLE('',#98209,0.1645125) ;
#32338 = CIRCLE('',#98210,0.0999999999999993) ;
#32339 = CIRCLE('',#98211,0.0645125000000003) ;
#32340 = CIRCLE('',#98212,0.0999999999999993) ;
#32341 = CIRCLE('',#98214,2.35) ;
#32342 = CIRCLE('',#98215,2.25) ;
#32343 = CIRCLE('',#98217,0.1645125) ;
#32344 = CIRCLE('',#98218,0.0999999999999993) ;
#32345 = CIRCLE('',#98219,0.0645125000000003) ;
#32346 = CIRCLE('',#98220,0.0999999999999993) ;
#32347 = CIRCLE('',#98222,2.35) ;
#32348 = CIRCLE('',#98223,2.25) ;
#32349 = CIRCLE('',#98225,0.164512500000005) ;
#32350 = CIRCLE('',#98226,0.0999999999999999) ;
#32351 = CIRCLE('',#98227,0.0645125000000055) ;
#32352 = CIRCLE('',#98228,0.100000000000001) ;
#32353 = CIRCLE('',#98230,2.35) ;
#32354 = CIRCLE('',#98231,2.25) ;
#32355 = CIRCLE('',#98233,0.164512500000006) ;
#32356 = CIRCLE('',#98234,0.0999999999999992) ;
#32357 = CIRCLE('',#98235,0.0645125000000061) ;
#32358 = CIRCLE('',#98236,0.100000000000003) ;
#32359 = CIRCLE('',#98238,2.35) ;
#32360 = CIRCLE('',#98239,2.25) ;
#32361 = CIRCLE('',#98241,0.0645124999999989) ;
#32362 = CIRCLE('',#98243,0.0645124999999989) ;
#32363 = CIRCLE('',#98245,0.0645124999999989) ;
#32364 = CIRCLE('',#98247,0.0645124999999989) ;
#32365 = CIRCLE('',#98249,0.0645125000000003) ;
#32366 = CIRCLE('',#98251,0.0645125000000003) ;
#32367 = CIRCLE('',#98253,0.0645124999999998) ;
#32368 = CIRCLE('',#98255,0.970710678118651) ;
#32369 = CIRCLE('',#98256,0.1) ;
#32370 = CIRCLE('',#98257,1.) ;
#32371 = CIRCLE('',#98259,1.5) ;
#32372 = CIRCLE('',#98260,0.1) ;
#32373 = CIRCLE('',#98261,1.6) ;
#32374 = CIRCLE('',#98263,1.) ;
#32375 = CIRCLE('',#98264,0.1) ;
#32376 = CIRCLE('',#98265,1.1) ;
#32377 = CIRCLE('',#98267,0.970710678118658) ;
#32378 = CIRCLE('',#98268,0.1) ;
#32379 = CIRCLE('',#98269,1.) ;
#32380 = CIRCLE('',#98271,1.5) ;
#32381 = CIRCLE('',#98272,0.1) ;
#32382 = CIRCLE('',#98273,1.6) ;
#32383 = CIRCLE('',#98275,1.) ;
#32384 = CIRCLE('',#98276,0.1) ;
#32385 = CIRCLE('',#98277,1.1) ;
#32386 = CIRCLE('',#98279,0.970710678118658) ;
#32387 = CIRCLE('',#98280,0.1) ;
#32388 = CIRCLE('',#98281,1.) ;
#32389 = CIRCLE('',#98283,1.5) ;
#32390 = CIRCLE('',#98284,0.1) ;
#32391 = CIRCLE('',#98285,1.6) ;
#32392 = CIRCLE('',#98287,1.) ;
#32393 = CIRCLE('',#98288,0.1) ;
#32394 = CIRCLE('',#98289,1.1) ;
#32395 = CIRCLE('',#98291,0.970710678118658) ;
#32396 = CIRCLE('',#98292,0.1) ;
#32397 = CIRCLE('',#98293,1.) ;
#32398 = CIRCLE('',#98295,1.5) ;
#32399 = CIRCLE('',#98296,0.1) ;
#32400 = CIRCLE('',#98297,1.6) ;
#32401 = CIRCLE('',#98299,1.) ;
#32402 = CIRCLE('',#98300,0.1) ;
#32403 = CIRCLE('',#98301,1.1) ;
#32404 = CIRCLE('',#98303,0.970710678118658) ;
#32405 = CIRCLE('',#98304,0.1) ;
#32406 = CIRCLE('',#98305,1.) ;
#32407 = CIRCLE('',#98307,1.5) ;
#32408 = CIRCLE('',#98308,0.1) ;
#32409 = CIRCLE('',#98309,1.6) ;
#32410 = CIRCLE('',#98311,1.) ;
#32411 = CIRCLE('',#98312,0.1) ;
#32412 = CIRCLE('',#98313,1.1) ;
#32413 = CIRCLE('',#98315,0.970710678118658) ;
#32414 = CIRCLE('',#98316,0.1) ;
#32415 = CIRCLE('',#98317,1.) ;
#32416 = CIRCLE('',#98319,1.5) ;
#32417 = CIRCLE('',#98320,0.1) ;
#32418 = CIRCLE('',#98321,1.6) ;
#32419 = CIRCLE('',#98323,1.) ;
#32420 = CIRCLE('',#98324,0.1) ;
#32421 = CIRCLE('',#98325,1.1) ;
#32422 = CIRCLE('',#98327,0.970710678118658) ;
#32423 = CIRCLE('',#98328,0.1) ;
#32424 = CIRCLE('',#98329,1.) ;
#32425 = CIRCLE('',#98331,1.5) ;
#32426 = CIRCLE('',#98332,0.1) ;
#32427 = CIRCLE('',#98333,1.6) ;
#32428 = CIRCLE('',#98335,1.) ;
#32429 = CIRCLE('',#98336,0.1) ;
#32430 = CIRCLE('',#98337,1.1) ;
#32431 = CIRCLE('',#98339,0.970710678118656) ;
#32432 = CIRCLE('',#98340,0.1) ;
#32433 = CIRCLE('',#98341,0.999999999999999) ;
#32434 = CIRCLE('',#98343,1.5) ;
#32435 = CIRCLE('',#98344,0.1) ;
#32436 = CIRCLE('',#98345,1.6) ;
#32437 = CIRCLE('',#98347,0.999999999999999) ;
#32438 = CIRCLE('',#98348,0.1) ;
#32439 = CIRCLE('',#98349,1.1) ;
#32440 = CIRCLE('',#98351,0.970710678118656) ;
#32441 = CIRCLE('',#98352,0.1) ;
#32442 = CIRCLE('',#98353,1.) ;
#32443 = CIRCLE('',#98355,1.5) ;
#32444 = CIRCLE('',#98356,0.1) ;
#32445 = CIRCLE('',#98357,1.6) ;
#32446 = CIRCLE('',#98359,1.) ;
#32447 = CIRCLE('',#98360,0.1) ;
#32448 = CIRCLE('',#98361,1.1) ;
#32449 = CIRCLE('',#98363,1.5) ;
#32450 = CIRCLE('',#98364,1.5) ;
#32451 = CIRCLE('',#98365,1.5) ;
#32452 = CIRCLE('',#98366,1.5) ;
#32453 = CIRCLE('',#98367,1.5) ;
#32454 = CIRCLE('',#98369,1.5) ;
#32455 = CIRCLE('',#98370,1.5) ;
#32456 = CIRCLE('',#98371,1.5) ;
#32457 = CIRCLE('',#98372,1.5) ;
#32458 = CIRCLE('',#98373,1.5) ;
#32459 = CIRCLE('',#98375,1.5) ;
#32460 = CIRCLE('',#98376,1.5) ;
#32461 = CIRCLE('',#98377,1.5) ;
#32462 = CIRCLE('',#98378,1.5) ;
#32463 = CIRCLE('',#98379,1.5) ;
#32464 = CIRCLE('',#98381,1.5) ;
#32465 = CIRCLE('',#98382,1.5) ;
#32466 = CIRCLE('',#98383,1.5) ;
#32467 = CIRCLE('',#98384,1.5) ;
#32468 = CIRCLE('',#98385,1.5) ;
#32469 = CIRCLE('',#98387,1.5) ;
#32470 = CIRCLE('',#98388,1.5) ;
#32471 = CIRCLE('',#98389,1.5) ;
#32472 = CIRCLE('',#98390,1.5) ;
#32473 = CIRCLE('',#98391,1.5) ;
#32474 = CIRCLE('',#98393,1.5) ;
#32475 = CIRCLE('',#98394,1.5) ;
#32476 = CIRCLE('',#98395,1.5) ;
#32477 = CIRCLE('',#98396,1.5) ;
#32478 = CIRCLE('',#98397,1.5) ;
#32479 = CIRCLE('',#98399,1.5) ;
#32480 = CIRCLE('',#98400,1.5) ;
#32481 = CIRCLE('',#98401,1.5) ;
#32482 = CIRCLE('',#98402,1.5) ;
#32483 = CIRCLE('',#98403,1.5) ;
#32484 = CIRCLE('',#98405,1.5) ;
#32485 = CIRCLE('',#98406,1.5) ;
#32486 = CIRCLE('',#98407,1.5) ;
#32487 = CIRCLE('',#98408,1.5) ;
#32488 = CIRCLE('',#98409,1.5) ;
#32489 = CIRCLE('',#98411,1.5) ;
#32490 = CIRCLE('',#98412,1.5) ;
#32491 = CIRCLE('',#98413,1.5) ;
#32492 = CIRCLE('',#98414,1.5) ;
#32493 = CIRCLE('',#98415,1.5) ;
#32494 = CIRCLE('',#98417,0.5) ;
#32495 = CIRCLE('',#98419,0.499999999999997) ;
#32496 = CIRCLE('',#98421,0.499999999999997) ;
#32497 = CIRCLE('',#98423,0.499999999999997) ;
#32498 = CIRCLE('',#98425,0.499999999999997) ;
#32499 = CIRCLE('',#98427,0.499999999999997) ;
#32500 = CIRCLE('',#98429,0.499999999999997) ;
#32501 = CIRCLE('',#98431,0.499999999999997) ;
#32502 = CIRCLE('',#98433,0.499999999999998) ;
#32503 = CIRCLE('',#98444,0.970710678118656) ;
#32504 = CIRCLE('',#98445,0.1) ;
#32505 = CIRCLE('',#98446,1.) ;
#32506 = CIRCLE('',#98448,1.5) ;
#32507 = CIRCLE('',#98449,0.1) ;
#32508 = CIRCLE('',#98450,1.6) ;
#32509 = CIRCLE('',#98452,1.) ;
#32510 = CIRCLE('',#98453,0.1) ;
#32511 = CIRCLE('',#98454,1.1) ;
#32512 = CIRCLE('',#98456,0.0645125000000024) ;
#32513 = CIRCLE('',#98458,0.0645125000000094) ;
#32514 = CIRCLE('',#98460,0.0645125) ;
#32515 = CIRCLE('',#98462,0.0645125) ;
#32516 = CIRCLE('',#98464,1.5) ;
#32517 = CIRCLE('',#98465,1.5) ;
#32518 = CIRCLE('',#98466,1.5) ;
#32519 = CIRCLE('',#98467,1.5) ;
#32520 = CIRCLE('',#98468,1.5) ;
#32521 = CIRCLE('',#98470,0.499999999999998) ;
#32522 = CIRCLE('',#98473,2.15) ;
#32523 = CIRCLE('',#98474,2.15) ;
#32524 = CIRCLE('',#98475,2.15) ;
#32525 = CIRCLE('',#98476,2.15) ;
#32526 = CIRCLE('',#98477,2.15) ;
#32527 = CIRCLE('',#98478,2.15) ;
#32528 = CIRCLE('',#98479,2.15) ;
#32529 = CIRCLE('',#98480,2.15) ;
#32530 = CIRCLE('',#98481,2.15) ;
#32531 = CIRCLE('',#98482,2.15) ;
#32532 = CIRCLE('',#98483,0.2) ;
#32533 = CIRCLE('',#98484,0.2) ;
#32534 = CIRCLE('',#98485,0.2) ;
#32535 = CIRCLE('',#98486,0.2) ;
#32536 = CIRCLE('',#98487,0.2) ;
#32537 = CIRCLE('',#98488,0.2) ;
#32538 = CIRCLE('',#98489,0.2) ;
#32539 = CIRCLE('',#98490,0.2) ;
#32540 = CIRCLE('',#98491,0.2) ;
#32541 = CIRCLE('',#98492,0.2) ;
#32542 = CIRCLE('',#98493,0.2) ;
#32543 = CIRCLE('',#98494,0.2) ;
#32544 = CIRCLE('',#98495,0.2) ;
#32545 = CIRCLE('',#98496,0.2) ;
#32546 = CIRCLE('',#98497,0.2) ;
#32547 = CIRCLE('',#98498,0.2) ;
#32548 = CIRCLE('',#98499,0.2) ;
#32549 = CIRCLE('',#98500,0.2) ;
#32550 = CIRCLE('',#98501,0.2) ;
#32551 = CIRCLE('',#98502,0.2) ;
#32552 = CIRCLE('',#98503,0.2) ;
#32553 = CIRCLE('',#98504,0.2) ;
#32554 = CIRCLE('',#98505,0.2) ;
#32555 = CIRCLE('',#98506,0.2) ;
#32556 = CIRCLE('',#98507,0.2) ;
#32557 = CIRCLE('',#98508,0.2) ;
#32558 = CIRCLE('',#98509,0.2) ;
#32559 = CIRCLE('',#98510,0.2) ;
#32560 = CIRCLE('',#98511,0.2) ;
#32561 = CIRCLE('',#98512,0.2) ;
#32562 = CIRCLE('',#98513,0.2) ;
#32563 = CIRCLE('',#98514,0.2) ;
#32564 = CIRCLE('',#98515,0.2) ;
#32565 = CIRCLE('',#98516,0.2) ;
#32566 = CIRCLE('',#98517,0.2) ;
#32567 = CIRCLE('',#98518,0.2) ;
#32568 = CIRCLE('',#98519,0.2) ;
#32569 = CIRCLE('',#98520,0.2) ;
#32570 = CIRCLE('',#98521,0.2) ;
#32571 = CIRCLE('',#98522,0.2) ;
#32572 = CIRCLE('',#98524,0.199999999999999) ;
#32573 = CIRCLE('',#98525,0.199999999999999) ;
#32574 = CIRCLE('',#98526,0.199999999999999) ;
#32575 = CIRCLE('',#98527,0.199999999999999) ;
#32576 = CIRCLE('',#98529,0.199999999999999) ;
#32577 = CIRCLE('',#98530,0.199999999999999) ;
#32578 = CIRCLE('',#98531,0.199999999999999) ;
#32579 = CIRCLE('',#98532,0.199999999999999) ;
#32580 = CIRCLE('',#98534,0.199999999999999) ;
#32581 = CIRCLE('',#98535,0.199999999999999) ;
#32582 = CIRCLE('',#98536,0.199999999999999) ;
#32583 = CIRCLE('',#98537,0.199999999999999) ;
#32584 = CIRCLE('',#98539,0.199999999999999) ;
#32585 = CIRCLE('',#98540,0.199999999999999) ;
#32586 = CIRCLE('',#98541,0.199999999999999) ;
#32587 = CIRCLE('',#98542,0.199999999999999) ;
#32588 = CIRCLE('',#98544,0.199999999999999) ;
#32589 = CIRCLE('',#98545,0.199999999999999) ;
#32590 = CIRCLE('',#98546,0.199999999999999) ;
#32591 = CIRCLE('',#98547,0.199999999999999) ;
#32592 = CIRCLE('',#98549,0.200000000000001) ;
#32593 = CIRCLE('',#98550,0.200000000000001) ;
#32594 = CIRCLE('',#98551,0.199999999999999) ;
#32595 = CIRCLE('',#98552,0.199999999999999) ;
#32596 = CIRCLE('',#98554,0.200000000000001) ;
#32597 = CIRCLE('',#98555,0.200000000000001) ;
#32598 = CIRCLE('',#98556,0.200000000000001) ;
#32599 = CIRCLE('',#98557,0.200000000000001) ;
#32600 = CIRCLE('',#98559,0.2) ;
#32601 = CIRCLE('',#98560,0.200000000000001) ;
#32602 = CIRCLE('',#98561,0.200000000000001) ;
#32603 = CIRCLE('',#98562,0.200000000000001) ;
#32604 = CIRCLE('',#98564,0.2) ;
#32605 = CIRCLE('',#98565,0.2) ;
#32606 = CIRCLE('',#98566,0.200000000000001) ;
#32607 = CIRCLE('',#98567,0.2) ;
#32608 = CIRCLE('',#98578,0.2) ;
#32609 = CIRCLE('',#98579,0.2) ;
#32610 = CIRCLE('',#98580,0.2) ;
#32611 = CIRCLE('',#98581,0.2) ;
#32612 = CIRCLE('',#98582,0.2) ;
#32613 = CIRCLE('',#98583,0.2) ;
#32614 = CIRCLE('',#98584,0.2) ;
#32615 = CIRCLE('',#98585,0.2) ;
#32616 = CIRCLE('',#98586,0.2) ;
#32617 = CIRCLE('',#98587,0.2) ;
#32618 = CIRCLE('',#98588,0.200000000000001) ;
#32619 = CIRCLE('',#98589,0.200000000000001) ;
#32620 = CIRCLE('',#98590,0.200000000000001) ;
#32621 = CIRCLE('',#98591,0.200000000000001) ;
#32622 = CIRCLE('',#98592,0.200000000000001) ;
#32623 = CIRCLE('',#98593,0.200000000000001) ;
#32624 = CIRCLE('',#98594,0.200000000000001) ;
#32625 = CIRCLE('',#98595,0.200000000000001) ;
#32626 = CIRCLE('',#98596,0.199999999999999) ;
#32627 = CIRCLE('',#98597,0.199999999999999) ;
#32628 = CIRCLE('',#98598,0.199999999999999) ;
#32629 = CIRCLE('',#98599,0.199999999999999) ;
#32630 = CIRCLE('',#98600,0.199999999999999) ;
#32631 = CIRCLE('',#98601,0.199999999999999) ;
#32632 = CIRCLE('',#98602,0.199999999999999) ;
#32633 = CIRCLE('',#98603,0.199999999999999) ;
#32634 = CIRCLE('',#98604,0.199999999999999) ;
#32635 = CIRCLE('',#98605,0.199999999999999) ;
#32636 = CIRCLE('',#98606,0.199999999999999) ;
#32637 = CIRCLE('',#98607,0.199999999999999) ;
#32638 = CIRCLE('',#98608,0.199999999999999) ;
#32639 = CIRCLE('',#98609,0.199999999999999) ;
#32640 = CIRCLE('',#98610,0.199999999999999) ;
#32641 = CIRCLE('',#98611,0.199999999999999) ;
#32642 = CIRCLE('',#98612,0.199999999999999) ;
#32643 = CIRCLE('',#98613,0.199999999999999) ;
#32644 = CIRCLE('',#98614,0.199999999999999) ;
#32645 = CIRCLE('',#98615,0.199999999999999) ;
#32646 = CIRCLE('',#98616,0.199999999999999) ;
#32647 = CIRCLE('',#98617,0.199999999999999) ;
#32648 = CIRCLE('',#98619,0.199999999999999) ;
#32649 = CIRCLE('',#98620,0.199999999999999) ;
#32650 = CIRCLE('',#98621,1.55625) ;
#32651 = CIRCLE('',#98623,0.199999999999999) ;
#32652 = CIRCLE('',#98624,0.199999999999999) ;
#32653 = CIRCLE('',#98625,1.55625) ;
#32654 = CIRCLE('',#98627,0.199999999999999) ;
#32655 = CIRCLE('',#98628,0.199999999999999) ;
#32656 = CIRCLE('',#98629,1.55625) ;
#32657 = CIRCLE('',#98631,0.199999999999999) ;
#32658 = CIRCLE('',#98632,0.199999999999999) ;
#32659 = CIRCLE('',#98633,1.55625) ;
#32660 = CIRCLE('',#98635,0.199999999999999) ;
#32661 = CIRCLE('',#98636,0.199999999999999) ;
#32662 = CIRCLE('',#98637,1.55625) ;
#32663 = CIRCLE('',#98639,0.200000000000001) ;
#32664 = CIRCLE('',#98640,0.199999999999999) ;
#32665 = CIRCLE('',#98641,1.55625) ;
#32666 = CIRCLE('',#98643,0.200000000000001) ;
#32667 = CIRCLE('',#98644,0.200000000000001) ;
#32668 = CIRCLE('',#98645,1.55625) ;
#32669 = CIRCLE('',#98647,0.2) ;
#32670 = CIRCLE('',#98648,0.200000000000001) ;
#32671 = CIRCLE('',#98649,1.55625) ;
#32672 = CIRCLE('',#98651,0.2) ;
#32673 = CIRCLE('',#98652,0.2) ;
#32674 = CIRCLE('',#98653,1.55625) ;
#32675 = CIRCLE('',#98656,0.2) ;
#32676 = CIRCLE('',#98657,0.2) ;
#32677 = CIRCLE('',#98658,0.2) ;
#32678 = CIRCLE('',#98659,0.2) ;
#32679 = CIRCLE('',#98660,0.2) ;
#32680 = CIRCLE('',#98661,0.2) ;
#32681 = CIRCLE('',#98662,0.2) ;
#32682 = CIRCLE('',#98663,0.2) ;
#32683 = CIRCLE('',#98664,0.2) ;
#32684 = CIRCLE('',#98665,0.2) ;
#32685 = CIRCLE('',#98666,0.2) ;
#32686 = CIRCLE('',#98667,0.2) ;
#32687 = CIRCLE('',#98668,0.2) ;
#32688 = CIRCLE('',#98669,0.2) ;
#32689 = CIRCLE('',#98670,0.2) ;
#32690 = CIRCLE('',#98671,0.2) ;
#32691 = CIRCLE('',#98672,0.2) ;
#32692 = CIRCLE('',#98673,0.2) ;
#32693 = CIRCLE('',#98674,0.2) ;
#32694 = CIRCLE('',#98675,0.2) ;
#32695 = CIRCLE('',#98677,0.0999999999999998) ;
#32696 = CIRCLE('',#98678,0.0999999999999998) ;
#32697 = CIRCLE('',#98680,0.0999999999999998) ;
#32698 = CIRCLE('',#98681,0.0999999999999998) ;
#32699 = CIRCLE('',#98682,0.0999999999999998) ;
#32700 = CIRCLE('',#98683,0.0999999999999998) ;
#32701 = CIRCLE('',#98686,0.2) ;
#32702 = CIRCLE('',#98687,0.2) ;
#32703 = CIRCLE('',#98688,0.2) ;
#32704 = CIRCLE('',#98689,0.2) ;
#32705 = CIRCLE('',#98693,0.2) ;
#32706 = CIRCLE('',#98694,1.55625) ;
#32707 = CIRCLE('',#98695,0.2) ;
#32708 = CIRCLE('',#98700,0.2) ;
#32709 = CIRCLE('',#98701,0.2) ;
#32710 = CIRCLE('',#98702,0.2) ;
#32711 = CIRCLE('',#98703,0.2) ;
#32712 = CIRCLE('',#98704,0.2) ;
#32713 = CIRCLE('',#98705,0.2) ;
#32714 = CIRCLE('',#98706,0.2) ;
#32715 = CIRCLE('',#98707,0.2) ;
#32716 = CIRCLE('',#98709,0.2) ;
#32717 = CIRCLE('',#98710,0.2) ;
#32718 = CIRCLE('',#98711,0.2) ;
#32719 = CIRCLE('',#98713,0.2) ;
#32720 = CIRCLE('',#98714,0.2) ;
#32721 = CIRCLE('',#98715,0.2) ;
#32722 = CIRCLE('',#98732,0.1) ;
#32723 = CIRCLE('',#98733,0.1) ;
#32724 = CIRCLE('',#98734,0.1) ;
#32725 = CIRCLE('',#98735,0.1) ;
#32726 = CIRCLE('',#98742,0.2) ;
#32727 = CIRCLE('',#98743,0.2) ;
#32728 = CIRCLE('',#98746,0.2) ;
#32729 = CIRCLE('',#98747,0.2) ;
#32730 = CIRCLE('',#98748,0.2) ;
#32731 = CIRCLE('',#98751,0.2) ;
#32732 = CIRCLE('',#98752,0.2) ;
#32733 = CIRCLE('',#98753,0.2) ;
#32734 = CIRCLE('',#98758,1.65625) ;
#32735 = CIRCLE('',#98759,1.65625) ;
#32736 = CIRCLE('',#98761,1.75625) ;
#32737 = CIRCLE('',#98768,0.1) ;
#32738 = CIRCLE('',#98769,0.1) ;
#32739 = CIRCLE('',#98770,0.1) ;
#32740 = CIRCLE('',#98771,0.1) ;
#32741 = CIRCLE('',#98782,2.25) ;
#32742 = CIRCLE('',#98784,2.25) ;
#32743 = CIRCLE('',#98788,2.25) ;
#32744 = CIRCLE('',#98790,2.25) ;
#32745 = CIRCLE('',#98792,0.0999999999999997) ;
#32746 = CIRCLE('',#98793,0.0999999999999997) ;
#32747 = CIRCLE('',#98796,0.1) ;
#32748 = CIRCLE('',#98797,0.1) ;
#32749 = CIRCLE('',#98800,0.1) ;
#32750 = CIRCLE('',#98801,0.1) ;
#32751 = CIRCLE('',#98804,0.0999999999999997) ;
#32752 = CIRCLE('',#98805,0.0999999999999997) ;
#32753 = CIRCLE('',#98809,0.0999999999999998) ;
#32754 = CIRCLE('',#98810,0.0999999999999998) ;
#32755 = CIRCLE('',#98812,0.1) ;
#32756 = CIRCLE('',#98813,0.0999999999999998) ;
#32757 = CIRCLE('',#98815,0.0999999999999998) ;
#32758 = CIRCLE('',#98816,0.0999999999999998) ;
#32759 = CIRCLE('',#98818,0.0999999999999998) ;
#32760 = CIRCLE('',#98820,0.1) ;
#32761 = CIRCLE('',#98822,0.100000000000003) ;
#32762 = CIRCLE('',#98823,0.100000000000003) ;
#32763 = CIRCLE('',#98825,0.0999999999999998) ;
#32764 = CIRCLE('',#98826,0.0999999999999998) ;
#32765 = CIRCLE('',#98828,0.0999999999999998) ;
#32766 = CIRCLE('',#98832,0.1) ;
#32767 = CIRCLE('',#98833,0.0999999999999998) ;
#32768 = CIRCLE('',#98835,0.100000000000003) ;
#32769 = CIRCLE('',#98837,0.0999999999999998) ;
#32770 = CIRCLE('',#98838,0.0999999999999998) ;
#32771 = CIRCLE('',#98840,0.0999999999999998) ;
#32772 = CIRCLE('',#98846,0.1) ;
#32773 = CIRCLE('',#98848,0.0999999999999998) ;
#32774 = CIRCLE('',#98850,0.1) ;
#32775 = CIRCLE('',#98852,0.100000000000003) ;
#32776 = CIRCLE('',#98854,0.100000000000003) ;
#32777 = CIRCLE('',#98855,0.100000000000003) ;
#32778 = CIRCLE('',#98857,0.0999999999999998) ;
#32779 = CIRCLE('',#98859,0.1) ;
#32780 = CIRCLE('',#98861,0.100000000000003) ;
#32781 = CIRCLE('',#98863,0.100000000000003) ;
#32782 = CIRCLE('',#98866,0.1) ;
#32783 = CIRCLE('',#98868,0.100000000000003) ;
#32784 = CIRCLE('',#98873,0.1) ;
#32785 = CIRCLE('',#98879,0.0999999999999994) ;
#32786 = CIRCLE('',#98880,0.1) ;
#32787 = CIRCLE('',#98881,0.1) ;
#32788 = CIRCLE('',#98883,0.1) ;
#32789 = CIRCLE('',#98885,0.1) ;
#32790 = CIRCLE('',#98887,0.0999999999999994) ;
#32791 = CIRCLE('',#98889,0.1) ;
#32792 = CIRCLE('',#98890,0.1) ;
#32793 = CIRCLE('',#98892,0.0999999999999994) ;
#32794 = CIRCLE('',#98893,0.0999999999999994) ;
#32795 = CIRCLE('',#98895,0.1) ;
#32796 = CIRCLE('',#98896,0.0999999999999998) ;
#32797 = CIRCLE('',#98898,0.0999999999999998) ;
#32798 = CIRCLE('',#98899,0.1) ;
#32799 = CIRCLE('',#98901,0.1) ;
#32800 = CIRCLE('',#98903,0.1) ;
#32801 = CIRCLE('',#98904,0.1) ;
#32802 = CIRCLE('',#98906,0.0999999999999994) ;
#32803 = CIRCLE('',#98908,0.1) ;
#32804 = CIRCLE('',#98910,0.1) ;
#32805 = CIRCLE('',#98912,0.0999999999999998) ;
#32806 = CIRCLE('',#98914,0.1) ;
#32807 = CIRCLE('',#98916,0.1) ;
#32808 = CIRCLE('',#98918,0.0999999999999998) ;
#32809 = CIRCLE('',#98920,0.1) ;
#32810 = CIRCLE('',#98922,0.1) ;
#32811 = CIRCLE('',#98924,0.0999999999999998) ;
#32812 = CIRCLE('',#98926,0.1) ;
#32813 = CIRCLE('',#98928,0.1) ;
#32814 = CIRCLE('',#98929,0.1) ;
#32815 = CIRCLE('',#98931,0.0999999999999998) ;
#32816 = CIRCLE('',#98932,0.0999999999999998) ;
#32817 = CIRCLE('',#98934,0.1) ;
#32818 = CIRCLE('',#98936,0.1) ;
#32819 = CIRCLE('',#98937,0.0999999999999998) ;
#32820 = CIRCLE('',#98939,0.1) ;
#32821 = CIRCLE('',#98941,0.1) ;
#32822 = CIRCLE('',#98943,0.0999999999999998) ;
#32823 = CIRCLE('',#98945,0.1) ;
#32824 = CIRCLE('',#98947,0.1) ;
#32825 = CIRCLE('',#98949,0.1) ;
#32826 = CIRCLE('',#98951,0.0999999999999998) ;
#32827 = CIRCLE('',#98953,0.0999999999999998) ;
#32828 = CIRCLE('',#98954,0.0999999999999998) ;
#32829 = CIRCLE('',#98956,0.1) ;
#32830 = CIRCLE('',#98957,0.1) ;
#32831 = CIRCLE('',#98959,0.1) ;
#32832 = CIRCLE('',#98961,0.0999999999999998) ;
#32833 = CIRCLE('',#98963,0.1) ;
#32834 = CIRCLE('',#98965,0.1) ;
#32835 = CIRCLE('',#98968,0.1) ;
#32836 = CIRCLE('',#98969,0.0999999999999998) ;
#32837 = CIRCLE('',#98971,0.0999999999999998) ;
#32838 = CIRCLE('',#98973,0.1) ;
#32839 = CIRCLE('',#98975,0.1) ;
#32840 = CIRCLE('',#98977,0.0999999999999994) ;
#32841 = CIRCLE('',#98979,0.0999999999999998) ;
#32842 = CIRCLE('',#98981,0.0999999999999994) ;
#32843 = CIRCLE('',#98984,0.1) ;
#32844 = CIRCLE('',#98985,0.1) ;
#32845 = CIRCLE('',#98987,0.1) ;
#32846 = CIRCLE('',#98988,0.1) ;
#32847 = CIRCLE('',#98990,0.1) ;
#32848 = CIRCLE('',#98991,0.0999999999999998) ;
#32849 = CIRCLE('',#98993,0.1) ;
#32850 = CIRCLE('',#98995,0.1) ;
#32851 = CIRCLE('',#98997,0.1) ;
#32852 = CIRCLE('',#98998,0.1) ;
#32853 = CIRCLE('',#99000,0.1) ;
#32854 = CIRCLE('',#99002,0.0999999999999998) ;
#32855 = CIRCLE('',#99004,0.1) ;
#32856 = CIRCLE('',#99005,0.1) ;
#32857 = CIRCLE('',#99007,0.1) ;
#32858 = CIRCLE('',#99009,0.1) ;
#32859 = CIRCLE('',#99011,0.1) ;
#32860 = CIRCLE('',#99013,0.1) ;
#32861 = CIRCLE('',#99015,0.1) ;
#32862 = CIRCLE('',#99017,0.1) ;
#32863 = CIRCLE('',#99019,0.0999999999999998) ;
#32864 = CIRCLE('',#99021,0.1) ;
#32865 = CIRCLE('',#99023,0.1) ;
#32866 = CIRCLE('',#99025,0.1) ;
#32867 = CIRCLE('',#99028,0.1) ;
#32868 = CIRCLE('',#99030,0.1) ;
#32869 = CIRCLE('',#99031,0.1) ;
#32870 = CIRCLE('',#99033,0.1) ;
#32871 = CIRCLE('',#99035,0.1) ;
#32872 = CIRCLE('',#99037,0.1) ;
#32873 = CIRCLE('',#99039,0.1) ;
#32874 = CIRCLE('',#99041,0.1) ;
#32875 = CIRCLE('',#99043,0.1) ;
#32876 = CIRCLE('',#99045,0.1) ;
#32877 = CIRCLE('',#99047,0.1) ;
#32878 = CIRCLE('',#99049,0.1) ;
#32879 = CIRCLE('',#99052,0.0999999999999999) ;
#32880 = CIRCLE('',#99054,0.1) ;
#32881 = CIRCLE('',#99055,0.1) ;
#32882 = CIRCLE('',#99058,0.1) ;
#32883 = CIRCLE('',#99060,0.1) ;
#32884 = CIRCLE('',#99061,0.1) ;
#32885 = CIRCLE('',#99062,0.1) ;
#32886 = CIRCLE('',#99064,0.1) ;
#32887 = CIRCLE('',#99066,0.1) ;
#32888 = CIRCLE('',#99068,0.1) ;
#32889 = CIRCLE('',#99070,0.1) ;
#32890 = CIRCLE('',#99072,0.1) ;
#32891 = CIRCLE('',#99076,0.1) ;
#32892 = CIRCLE('',#99077,0.1) ;
#32893 = CIRCLE('',#99078,0.1) ;
#32894 = CIRCLE('',#99080,0.1) ;
#32895 = CIRCLE('',#99082,0.1) ;
#32896 = CIRCLE('',#99084,0.1) ;
#32897 = CIRCLE('',#99086,0.1) ;
#32898 = CIRCLE('',#99088,0.1) ;
#32899 = CIRCLE('',#99092,0.1) ;
#32900 = CIRCLE('',#99093,0.1) ;
#32901 = CIRCLE('',#99095,0.0999999999999998) ;
#32902 = CIRCLE('',#99096,0.0999999999999998) ;
#32903 = CIRCLE('',#99098,0.0999999999999998) ;
#32904 = CIRCLE('',#99099,0.1) ;
#32905 = CIRCLE('',#99101,0.0999999999999998) ;
#32906 = CIRCLE('',#99103,0.1) ;
#32907 = CIRCLE('',#99105,0.1) ;
#32908 = CIRCLE('',#99106,0.1) ;
#32909 = CIRCLE('',#99108,0.1) ;
#32910 = CIRCLE('',#99110,0.1) ;
#32911 = CIRCLE('',#99112,0.1) ;
#32912 = CIRCLE('',#99113,0.1) ;
#32913 = CIRCLE('',#99115,0.0999999999999998) ;
#32914 = CIRCLE('',#99117,0.0999999999999998) ;
#32915 = CIRCLE('',#99119,0.0999999999999998) ;
#32916 = CIRCLE('',#99121,0.0999999999999998) ;
#32917 = CIRCLE('',#99123,0.1) ;
#32918 = CIRCLE('',#99125,0.0999999999999998) ;
#32919 = CIRCLE('',#99127,0.0999999999999998) ;
#32920 = CIRCLE('',#99129,0.1) ;
#32921 = CIRCLE('',#99131,0.1) ;
#32922 = CIRCLE('',#99133,0.1) ;
#32923 = CIRCLE('',#99136,0.1) ;
#32924 = CIRCLE('',#99138,0.0999999999999998) ;
#32925 = CIRCLE('',#99139,0.0999999999999998) ;
#32926 = CIRCLE('',#99141,0.1) ;
#32927 = CIRCLE('',#99143,0.1) ;
#32928 = CIRCLE('',#99145,0.1) ;
#32929 = CIRCLE('',#99147,0.1) ;
#32930 = CIRCLE('',#99149,0.1) ;
#32931 = CIRCLE('',#99151,0.1) ;
#32932 = CIRCLE('',#99153,0.1) ;
#32933 = CIRCLE('',#99155,0.0999999999999998) ;
#32934 = CIRCLE('',#99157,0.0999999999999998) ;
#32935 = CIRCLE('',#99160,0.1) ;
#32936 = CIRCLE('',#99161,0.0999999999999994) ;
#32937 = CIRCLE('',#99163,0.1) ;
#32938 = CIRCLE('',#99165,0.1) ;
#32939 = CIRCLE('',#99167,0.1) ;
#32940 = CIRCLE('',#99169,0.1) ;
#32941 = CIRCLE('',#99171,0.0999999999999994) ;
#32942 = CIRCLE('',#99173,0.0999999999999994) ;
#32943 = CIRCLE('',#99180,0.0999999999999998) ;
#32944 = CIRCLE('',#99181,0.0999999999999998) ;
#32945 = CIRCLE('',#99184,0.0999999999999998) ;
#32946 = CIRCLE('',#99185,0.0999999999999998) ;
#32947 = CIRCLE('',#99186,0.0999999999999998) ;
#32948 = CIRCLE('',#99189,0.1) ;
#32949 = CIRCLE('',#99191,0.1) ;
#32950 = CIRCLE('',#99192,0.1) ;
#32951 = CIRCLE('',#99195,0.1) ;
#32952 = CIRCLE('',#99197,0.1) ;
#32953 = CIRCLE('',#99198,0.1) ;
#32954 = CIRCLE('',#99201,0.0999999999999998) ;
#32955 = CIRCLE('',#99202,0.1) ;
#32956 = CIRCLE('',#99205,0.1) ;
#32957 = CIRCLE('',#99206,0.0999999999999999) ;
#32958 = CIRCLE('',#99376,0.1) ;
#32959 = CIRCLE('',#99377,0.0999999999999998) ;
#32960 = CIRCLE('',#99378,0.0999999999999998) ;
#32961 = CIRCLE('',#99379,0.1) ;
#32962 = CIRCLE('',#99385,0.0999999999999994) ;
#32963 = CIRCLE('',#99386,0.1) ;
#32964 = CIRCLE('',#99387,0.1) ;
#32965 = CIRCLE('',#99388,0.0999999999999994) ;
#32966 = CIRCLE('',#99394,0.0999999999999994) ;
#32967 = CIRCLE('',#99395,0.0999999999999994) ;
#32968 = CIRCLE('',#99396,0.0999999999999994) ;
#32969 = CIRCLE('',#99397,0.0999999999999994) ;
#32970 = CIRCLE('',#99403,0.0999999999999994) ;
#32971 = CIRCLE('',#99404,0.0999999999999994) ;
#32972 = CIRCLE('',#99405,0.0999999999999994) ;
#32973 = CIRCLE('',#99406,0.0999999999999994) ;
#32974 = CIRCLE('',#99412,0.0999999999999994) ;
#32975 = CIRCLE('',#99413,0.0999999999999994) ;
#32976 = CIRCLE('',#99414,0.0999999999999994) ;
#32977 = CIRCLE('',#99415,0.0999999999999994) ;
#32978 = CIRCLE('',#99421,0.0999999999999994) ;
#32979 = CIRCLE('',#99422,0.0999999999999994) ;
#32980 = CIRCLE('',#99423,0.0999999999999994) ;
#32981 = CIRCLE('',#99424,0.0999999999999994) ;
#32982 = CIRCLE('',#99430,0.0999999999999994) ;
#32983 = CIRCLE('',#99431,0.0999999999999994) ;
#32984 = CIRCLE('',#99432,0.0999999999999994) ;
#32985 = CIRCLE('',#99433,0.0999999999999994) ;
#32986 = CIRCLE('',#99439,0.0999999999999994) ;
#32987 = CIRCLE('',#99440,0.0999999999999994) ;
#32988 = CIRCLE('',#99441,0.0999999999999994) ;
#32989 = CIRCLE('',#99442,0.0999999999999994) ;
#32990 = CIRCLE('',#99448,0.100000000000003) ;
#32991 = CIRCLE('',#99449,0.100000000000003) ;
#32992 = CIRCLE('',#99450,0.100000000000003) ;
#32993 = CIRCLE('',#99451,0.100000000000003) ;
#32994 = CIRCLE('',#99466,0.2) ;
#32995 = CIRCLE('',#99467,0.2) ;
#32996 = CIRCLE('',#99468,0.2) ;
#32997 = CIRCLE('',#99471,0.2) ;
#32998 = CIRCLE('',#99472,0.2) ;
#32999 = CIRCLE('',#99473,0.2) ;
#33000 = CIRCLE('',#99476,0.2) ;
#33001 = CIRCLE('',#99477,0.2) ;
#33002 = CIRCLE('',#99478,0.2) ;
#33003 = CIRCLE('',#99481,0.2) ;
#33004 = CIRCLE('',#99482,0.2) ;
#33005 = CIRCLE('',#99483,0.2) ;
#33006 = CIRCLE('',#99486,0.2) ;
#33007 = CIRCLE('',#99487,0.2) ;
#33008 = CIRCLE('',#99488,0.2) ;
#33009 = CIRCLE('',#99491,0.2) ;
#33010 = CIRCLE('',#99492,0.2) ;
#33011 = CIRCLE('',#99493,0.2) ;
#33012 = CIRCLE('',#99496,0.2) ;
#33013 = CIRCLE('',#99497,0.2) ;
#33014 = CIRCLE('',#99498,0.2) ;
#33015 = CIRCLE('',#99501,0.2) ;
#33016 = CIRCLE('',#99502,0.2) ;
#33017 = CIRCLE('',#99503,0.2) ;
#33018 = CIRCLE('',#99506,0.2) ;
#33019 = CIRCLE('',#99507,0.2) ;
#33020 = CIRCLE('',#99508,0.2) ;
#33021 = CIRCLE('',#99511,0.2) ;
#33022 = CIRCLE('',#99512,0.2) ;
#33023 = CIRCLE('',#99513,0.2) ;
#33024 = CIRCLE('',#99516,0.2) ;
#33025 = CIRCLE('',#99517,0.2) ;
#33026 = CIRCLE('',#99518,0.2) ;
#33027 = CIRCLE('',#99521,0.2) ;
#33028 = CIRCLE('',#99522,0.2) ;
#33029 = CIRCLE('',#99523,0.2) ;
#33030 = CIRCLE('',#99526,0.2) ;
#33031 = CIRCLE('',#99527,0.2) ;
#33032 = CIRCLE('',#99528,0.2) ;
#33033 = CIRCLE('',#99531,0.2) ;
#33034 = CIRCLE('',#99532,0.2) ;
#33035 = CIRCLE('',#99533,0.2) ;
#33036 = CIRCLE('',#99536,0.2) ;
#33037 = CIRCLE('',#99537,0.2) ;
#33038 = CIRCLE('',#99538,0.2) ;
#33039 = CIRCLE('',#99541,0.2) ;
#33040 = CIRCLE('',#99542,0.2) ;
#33041 = CIRCLE('',#99543,0.2) ;
#33042 = CIRCLE('',#99546,0.2) ;
#33043 = CIRCLE('',#99547,0.2) ;
#33044 = CIRCLE('',#99548,0.2) ;
#33045 = CIRCLE('',#99551,0.2) ;
#33046 = CIRCLE('',#99552,0.2) ;
#33047 = CIRCLE('',#99553,0.2) ;
#33048 = CIRCLE('',#99558,1.65625) ;
#33049 = CIRCLE('',#99559,1.65625) ;
#33050 = CIRCLE('',#99561,1.75625) ;
#33051 = CIRCLE('',#99565,1.65625) ;
#33052 = CIRCLE('',#99566,1.65625) ;
#33053 = CIRCLE('',#99568,1.75625) ;
#33054 = CIRCLE('',#99572,1.65625) ;
#33055 = CIRCLE('',#99573,1.65625) ;
#33056 = CIRCLE('',#99575,1.75625) ;
#33057 = CIRCLE('',#99579,1.65625) ;
#33058 = CIRCLE('',#99580,1.65625) ;
#33059 = CIRCLE('',#99582,1.75625) ;
#33060 = CIRCLE('',#99586,1.65625) ;
#33061 = CIRCLE('',#99587,1.65625) ;
#33062 = CIRCLE('',#99589,1.75625) ;
#33063 = CIRCLE('',#99593,1.65625) ;
#33064 = CIRCLE('',#99594,1.65625) ;
#33065 = CIRCLE('',#99596,1.75625) ;
#33066 = CIRCLE('',#99600,1.65625) ;
#33067 = CIRCLE('',#99601,1.65625) ;
#33068 = CIRCLE('',#99603,1.75625) ;
#33069 = CIRCLE('',#99607,1.65625) ;
#33070 = CIRCLE('',#99608,1.65625) ;
#33071 = CIRCLE('',#99610,1.75625) ;
#33072 = CIRCLE('',#99614,1.65625) ;
#33073 = CIRCLE('',#99615,1.65625) ;
#33074 = CIRCLE('',#99617,1.75625) ;
#33075 = CIRCLE('',#99664,0.0999999999999998) ;
#33076 = CIRCLE('',#99665,0.1) ;
#33077 = CIRCLE('',#99666,0.1) ;
#33078 = CIRCLE('',#99667,0.0999999999999998) ;
#33079 = CIRCLE('',#99673,0.1) ;
#33080 = CIRCLE('',#99674,0.0999999999999994) ;
#33081 = CIRCLE('',#99675,0.0999999999999994) ;
#33082 = CIRCLE('',#99676,0.1) ;
#33083 = CIRCLE('',#99682,0.0999999999999994) ;
#33084 = CIRCLE('',#99683,0.0999999999999994) ;
#33085 = CIRCLE('',#99684,0.0999999999999994) ;
#33086 = CIRCLE('',#99685,0.0999999999999994) ;
#33087 = CIRCLE('',#99691,0.0999999999999994) ;
#33088 = CIRCLE('',#99692,0.0999999999999994) ;
#33089 = CIRCLE('',#99693,0.0999999999999994) ;
#33090 = CIRCLE('',#99694,0.0999999999999994) ;
#33091 = CIRCLE('',#99700,0.0999999999999994) ;
#33092 = CIRCLE('',#99701,0.0999999999999994) ;
#33093 = CIRCLE('',#99702,0.0999999999999994) ;
#33094 = CIRCLE('',#99703,0.0999999999999994) ;
#33095 = CIRCLE('',#99709,0.0999999999999994) ;
#33096 = CIRCLE('',#99710,0.0999999999999994) ;
#33097 = CIRCLE('',#99711,0.0999999999999994) ;
#33098 = CIRCLE('',#99712,0.0999999999999994) ;
#33099 = CIRCLE('',#99718,0.0999999999999994) ;
#33100 = CIRCLE('',#99719,0.0999999999999994) ;
#33101 = CIRCLE('',#99720,0.0999999999999994) ;
#33102 = CIRCLE('',#99721,0.0999999999999994) ;
#33103 = CIRCLE('',#99727,0.0999999999999994) ;
#33104 = CIRCLE('',#99728,0.0999999999999994) ;
#33105 = CIRCLE('',#99729,0.0999999999999994) ;
#33106 = CIRCLE('',#99730,0.0999999999999994) ;
#33107 = CIRCLE('',#99736,0.100000000000003) ;
#33108 = CIRCLE('',#99737,0.100000000000003) ;
#33109 = CIRCLE('',#99738,0.100000000000003) ;
#33110 = CIRCLE('',#99739,0.100000000000003) ;
#33111 = CIRCLE('',#99790,0.0999999999999994) ;
#33112 = CIRCLE('',#99791,0.0999999999999994) ;
#33113 = CIRCLE('',#99794,0.1) ;
#33114 = CIRCLE('',#99795,0.1) ;
#33115 = CIRCLE('',#99798,0.1) ;
#33116 = CIRCLE('',#99799,0.1) ;
#33117 = CIRCLE('',#99802,0.0999999999999998) ;
#33118 = CIRCLE('',#99803,0.0999999999999998) ;
#33119 = CIRCLE('',#99807,0.0999999999999994) ;
#33120 = CIRCLE('',#99808,0.0999999999999994) ;
#33121 = CIRCLE('',#99811,0.0999999999999994) ;
#33122 = CIRCLE('',#99812,0.0999999999999994) ;
#33123 = CIRCLE('',#99815,0.1) ;
#33124 = CIRCLE('',#99816,0.1) ;
#33125 = CIRCLE('',#99819,0.0999999999999994) ;
#33126 = CIRCLE('',#99820,0.0999999999999994) ;
#33127 = CIRCLE('',#99824,0.0999999999999994) ;
#33128 = CIRCLE('',#99825,0.0999999999999994) ;
#33129 = CIRCLE('',#99828,0.0999999999999994) ;
#33130 = CIRCLE('',#99829,0.0999999999999994) ;
#33131 = CIRCLE('',#99832,0.0999999999999994) ;
#33132 = CIRCLE('',#99833,0.0999999999999994) ;
#33133 = CIRCLE('',#99836,0.0999999999999994) ;
#33134 = CIRCLE('',#99837,0.0999999999999994) ;
#33135 = CIRCLE('',#99841,0.0999999999999994) ;
#33136 = CIRCLE('',#99842,0.0999999999999994) ;
#33137 = CIRCLE('',#99845,0.0999999999999994) ;
#33138 = CIRCLE('',#99846,0.0999999999999994) ;
#33139 = CIRCLE('',#99849,0.0999999999999994) ;
#33140 = CIRCLE('',#99850,0.0999999999999994) ;
#33141 = CIRCLE('',#99853,0.0999999999999994) ;
#33142 = CIRCLE('',#99854,0.0999999999999994) ;
#33143 = CIRCLE('',#99858,0.0999999999999994) ;
#33144 = CIRCLE('',#99859,0.0999999999999994) ;
#33145 = CIRCLE('',#99862,0.0999999999999994) ;
#33146 = CIRCLE('',#99863,0.0999999999999994) ;
#33147 = CIRCLE('',#99866,0.0999999999999994) ;
#33148 = CIRCLE('',#99867,0.0999999999999994) ;
#33149 = CIRCLE('',#99870,0.0999999999999994) ;
#33150 = CIRCLE('',#99871,0.0999999999999994) ;
#33151 = CIRCLE('',#99875,0.0999999999999994) ;
#33152 = CIRCLE('',#99876,0.0999999999999994) ;
#33153 = CIRCLE('',#99879,0.0999999999999994) ;
#33154 = CIRCLE('',#99880,0.0999999999999994) ;
#33155 = CIRCLE('',#99883,0.0999999999999994) ;
#33156 = CIRCLE('',#99884,0.0999999999999994) ;
#33157 = CIRCLE('',#99887,0.0999999999999994) ;
#33158 = CIRCLE('',#99888,0.0999999999999994) ;
#33159 = CIRCLE('',#99892,0.0999999999999994) ;
#33160 = CIRCLE('',#99893,0.0999999999999994) ;
#33161 = CIRCLE('',#99896,0.0999999999999994) ;
#33162 = CIRCLE('',#99897,0.0999999999999994) ;
#33163 = CIRCLE('',#99900,0.0999999999999994) ;
#33164 = CIRCLE('',#99901,0.0999999999999994) ;
#33165 = CIRCLE('',#99904,0.0999999999999994) ;
#33166 = CIRCLE('',#99905,0.0999999999999994) ;
#33167 = CIRCLE('',#99909,0.0999999999999994) ;
#33168 = CIRCLE('',#99910,0.0999999999999994) ;
#33169 = CIRCLE('',#99913,0.0999999999999994) ;
#33170 = CIRCLE('',#99914,0.0999999999999994) ;
#33171 = CIRCLE('',#99917,0.0999999999999994) ;
#33172 = CIRCLE('',#99918,0.0999999999999994) ;
#33173 = CIRCLE('',#99921,0.0999999999999994) ;
#33174 = CIRCLE('',#99922,0.0999999999999994) ;
#33175 = CIRCLE('',#99926,0.100000000000003) ;
#33176 = CIRCLE('',#99927,0.100000000000003) ;
#33177 = CIRCLE('',#99930,0.100000000000003) ;
#33178 = CIRCLE('',#99931,0.100000000000003) ;
#33179 = CIRCLE('',#99934,0.100000000000003) ;
#33180 = CIRCLE('',#99935,0.100000000000003) ;
#33181 = CIRCLE('',#99938,0.100000000000003) ;
#33182 = CIRCLE('',#99939,0.100000000000003) ;
#33183 = CIRCLE('',#99943,0.0999999999999994) ;
#33184 = CIRCLE('',#99944,0.0999999999999999) ;
#33185 = CIRCLE('',#99945,0.1) ;
#33186 = CIRCLE('',#99947,0.1) ;
#33187 = CIRCLE('',#99949,0.1) ;
#33188 = CIRCLE('',#99951,0.0999999999999998) ;
#33189 = CIRCLE('',#99953,0.1) ;
#33190 = CIRCLE('',#99954,0.1) ;
#33191 = CIRCLE('',#99956,0.0999999999999994) ;
#33192 = CIRCLE('',#99957,0.0999999999999994) ;
#33193 = CIRCLE('',#99959,0.0999999999999998) ;
#33194 = CIRCLE('',#99960,0.0999999999999998) ;
#33195 = CIRCLE('',#99962,0.0999999999999998) ;
#33196 = CIRCLE('',#99963,0.1) ;
#33197 = CIRCLE('',#99965,0.1) ;
#33198 = CIRCLE('',#99967,0.0999999999999998) ;
#33199 = CIRCLE('',#99968,0.0999999999999998) ;
#33200 = CIRCLE('',#99970,0.0999999999999994) ;
#33201 = CIRCLE('',#99972,0.0999999999999998) ;
#33202 = CIRCLE('',#99974,0.1) ;
#33203 = CIRCLE('',#99976,0.0999999999999998) ;
#33204 = CIRCLE('',#99978,0.1) ;
#33205 = CIRCLE('',#99980,0.0999999999999998) ;
#33206 = CIRCLE('',#99982,0.0999999999999998) ;
#33207 = CIRCLE('',#99984,0.1) ;
#33208 = CIRCLE('',#99986,0.0999999999999998) ;
#33209 = CIRCLE('',#99988,0.0999999999999998) ;
#33210 = CIRCLE('',#99990,0.1) ;
#33211 = CIRCLE('',#99992,0.1) ;
#33212 = CIRCLE('',#99993,0.1) ;
#33213 = CIRCLE('',#99995,0.1) ;
#33214 = CIRCLE('',#99996,0.0999999999999998) ;
#33215 = CIRCLE('',#99998,0.0999999999999998) ;
#33216 = CIRCLE('',#100000,0.1) ;
#33217 = CIRCLE('',#100001,0.1) ;
#33218 = CIRCLE('',#100003,0.1) ;
#33219 = CIRCLE('',#100005,0.0999999999999998) ;
#33220 = CIRCLE('',#100007,0.0999999999999998) ;
#33221 = CIRCLE('',#100009,0.1) ;
#33222 = CIRCLE('',#100011,0.1) ;
#33223 = CIRCLE('',#100013,0.0999999999999998) ;
#33224 = CIRCLE('',#100015,0.0999999999999998) ;
#33225 = CIRCLE('',#100017,0.0999999999999998) ;
#33226 = CIRCLE('',#100018,0.0999999999999998) ;
#33227 = CIRCLE('',#100020,0.1) ;
#33228 = CIRCLE('',#100022,0.0999999999999998) ;
#33229 = CIRCLE('',#100024,0.0999999999999998) ;
#33230 = CIRCLE('',#100026,0.0999999999999998) ;
#33231 = CIRCLE('',#100029,0.1) ;
#33232 = CIRCLE('',#100030,0.0999999999999998) ;
#33233 = CIRCLE('',#100032,0.0999999999999998) ;
#33234 = CIRCLE('',#100034,0.1) ;
#33235 = CIRCLE('',#100036,0.0999999999999998) ;
#33236 = CIRCLE('',#100038,0.0999999999999994) ;
#33237 = CIRCLE('',#100040,0.0999999999999998) ;
#33238 = CIRCLE('',#100042,0.0999999999999994) ;
#33239 = CIRCLE('',#100141,0.0999999999999998) ;
#33240 = CIRCLE('',#100142,0.0999999999999998) ;
#33241 = CIRCLE('',#100144,0.1) ;
#33242 = CIRCLE('',#100145,0.0999999999999998) ;
#33243 = CIRCLE('',#100147,0.0999999999999998) ;
#33244 = CIRCLE('',#100148,0.0999999999999998) ;
#33245 = CIRCLE('',#100150,0.1) ;
#33246 = CIRCLE('',#100152,0.0999999999999998) ;
#33247 = CIRCLE('',#100154,0.0999999999999998) ;
#33248 = CIRCLE('',#100155,0.0999999999999998) ;
#33249 = CIRCLE('',#100157,0.0999999999999998) ;
#33250 = CIRCLE('',#100159,0.0999999999999998) ;
#33251 = CIRCLE('',#100161,0.1) ;
#33252 = CIRCLE('',#100162,0.1) ;
#33253 = CIRCLE('',#100164,0.1) ;
#33254 = CIRCLE('',#100166,0.1) ;
#33255 = CIRCLE('',#100168,0.1) ;
#33256 = CIRCLE('',#100170,0.1) ;
#33257 = CIRCLE('',#100172,0.1) ;
#33258 = CIRCLE('',#100174,0.1) ;
#33259 = CIRCLE('',#100176,0.0999999999999998) ;
#33260 = CIRCLE('',#100178,0.1) ;
#33261 = CIRCLE('',#100180,0.1) ;
#33262 = CIRCLE('',#100182,0.1) ;
#33263 = CIRCLE('',#100185,0.0999999999999998) ;
#33264 = CIRCLE('',#100187,0.1) ;
#33265 = CIRCLE('',#100188,0.1) ;
#33266 = CIRCLE('',#100190,0.1) ;
#33267 = CIRCLE('',#100192,0.0999999999999998) ;
#33268 = CIRCLE('',#100194,0.1) ;
#33269 = CIRCLE('',#100196,0.0999999999999998) ;
#33270 = CIRCLE('',#100198,0.0999999999999998) ;
#33271 = CIRCLE('',#100200,0.1) ;
#33272 = CIRCLE('',#100202,0.1) ;
#33273 = CIRCLE('',#100204,0.1) ;
#33274 = CIRCLE('',#100206,0.1) ;
#33275 = CIRCLE('',#100209,0.1) ;
#33276 = CIRCLE('',#100211,0.1) ;
#33277 = CIRCLE('',#100212,0.1) ;
#33278 = CIRCLE('',#100215,0.1) ;
#33279 = CIRCLE('',#100217,0.1) ;
#33280 = CIRCLE('',#100218,0.1) ;
#33281 = CIRCLE('',#100219,0.1) ;
#33282 = CIRCLE('',#100221,0.0999999999999996) ;
#33283 = CIRCLE('',#100223,0.1) ;
#33284 = CIRCLE('',#100225,0.1) ;
#33285 = CIRCLE('',#100227,0.1) ;
#33286 = CIRCLE('',#100229,0.1) ;
#33287 = CIRCLE('',#100233,0.1) ;
#33288 = CIRCLE('',#100234,0.0999999999999998) ;
#33289 = CIRCLE('',#100235,0.1) ;
#33290 = CIRCLE('',#100237,0.0999999999999998) ;
#33291 = CIRCLE('',#100239,0.1) ;
#33292 = CIRCLE('',#100241,0.0999999999999998) ;
#33293 = CIRCLE('',#100243,0.1) ;
#33294 = CIRCLE('',#100245,0.0999999999999996) ;
#33295 = CIRCLE('',#100409,0.1) ;
#33296 = CIRCLE('',#100410,0.1) ;
#33297 = CIRCLE('',#100412,0.0999999999999998) ;
#33298 = CIRCLE('',#100413,0.0999999999999998) ;
#33299 = CIRCLE('',#100415,0.0999999999999998) ;
#33300 = CIRCLE('',#100416,0.1) ;
#33301 = CIRCLE('',#100418,0.0999999999999998) ;
#33302 = CIRCLE('',#100420,0.1) ;
#33303 = CIRCLE('',#100422,0.1) ;
#33304 = CIRCLE('',#100423,0.1) ;
#33305 = CIRCLE('',#100425,0.1) ;
#33306 = CIRCLE('',#100427,0.1) ;
#33307 = CIRCLE('',#100429,0.0999999999999998) ;
#33308 = CIRCLE('',#100430,0.0999999999999998) ;
#33309 = CIRCLE('',#100432,0.0999999999999998) ;
#33310 = CIRCLE('',#100434,0.0999999999999998) ;
#33311 = CIRCLE('',#100436,0.0999999999999998) ;
#33312 = CIRCLE('',#100438,0.0999999999999998) ;
#33313 = CIRCLE('',#100440,0.0999999999999998) ;
#33314 = CIRCLE('',#100442,0.0999999999999998) ;
#33315 = CIRCLE('',#100444,0.1) ;
#33316 = CIRCLE('',#100446,0.0999999999999998) ;
#33317 = CIRCLE('',#100448,0.0999999999999998) ;
#33318 = CIRCLE('',#100450,0.0999999999999998) ;
#33319 = CIRCLE('',#100453,0.1) ;
#33320 = CIRCLE('',#100455,0.0999999999999998) ;
#33321 = CIRCLE('',#100456,0.0999999999999998) ;
#33322 = CIRCLE('',#100458,0.0999999999999998) ;
#33323 = CIRCLE('',#100460,0.1) ;
#33324 = CIRCLE('',#100462,0.0999999999999998) ;
#33325 = CIRCLE('',#100464,0.1) ;
#33326 = CIRCLE('',#100466,0.1) ;
#33327 = CIRCLE('',#100468,0.0999999999999998) ;
#33328 = CIRCLE('',#100470,0.0999999999999998) ;
#33329 = CIRCLE('',#100472,0.0999999999999998) ;
#33330 = CIRCLE('',#100474,0.0999999999999998) ;
#33331 = CIRCLE('',#100477,0.1) ;
#33332 = CIRCLE('',#100478,0.0999999999999994) ;
#33333 = CIRCLE('',#100480,0.0999999999999998) ;
#33334 = CIRCLE('',#100482,0.1) ;
#33335 = CIRCLE('',#100484,0.0999999999999998) ;
#33336 = CIRCLE('',#100486,0.1) ;
#33337 = CIRCLE('',#100488,0.0999999999999994) ;
#33338 = CIRCLE('',#100490,0.0999999999999994) ;
#33339 = CIRCLE('',#100497,0.1) ;
#33340 = CIRCLE('',#100498,0.0999999999999998) ;
#33341 = CIRCLE('',#100499,0.1) ;
#33342 = CIRCLE('',#100501,0.0999999999999994) ;
#33343 = CIRCLE('',#100503,0.1) ;
#33344 = CIRCLE('',#100505,0.1) ;
#33345 = CIRCLE('',#100507,0.1) ;
#33346 = CIRCLE('',#100508,0.1) ;
#33347 = CIRCLE('',#100510,0.1) ;
#33348 = CIRCLE('',#100512,0.1) ;
#33349 = CIRCLE('',#100513,0.0999999999999998) ;
#33350 = CIRCLE('',#100515,0.0999999999999994) ;
#33351 = CIRCLE('',#100516,0.0999999999999994) ;
#33352 = CIRCLE('',#100518,0.0999999999999994) ;
#33353 = CIRCLE('',#100519,0.0999999999999994) ;
#33354 = CIRCLE('',#100521,0.1) ;
#33355 = CIRCLE('',#100523,0.0999999999999998) ;
#33356 = CIRCLE('',#100525,0.1) ;
#33357 = CIRCLE('',#100527,0.0999999999999994) ;
#33358 = CIRCLE('',#100529,0.0999999999999994) ;
#33359 = CIRCLE('',#100531,0.0999999999999994) ;
#33360 = CIRCLE('',#100532,0.0999999999999994) ;
#33361 = CIRCLE('',#100534,0.1) ;
#33362 = CIRCLE('',#100536,0.0999999999999998) ;
#33363 = CIRCLE('',#100538,0.0999999999999994) ;
#33364 = CIRCLE('',#100540,0.1) ;
#33365 = CIRCLE('',#100541,0.1) ;
#33366 = CIRCLE('',#100543,0.1) ;
#33367 = CIRCLE('',#100545,0.0999999999999998) ;
#33368 = CIRCLE('',#100547,0.0999999999999994) ;
#33369 = CIRCLE('',#100549,0.0999999999999998) ;
#33370 = CIRCLE('',#100551,0.0999999999999998) ;
#33371 = CIRCLE('',#100552,0.1) ;
#33372 = CIRCLE('',#100554,0.0999999999999994) ;
#33373 = CIRCLE('',#100556,0.1) ;
#33374 = CIRCLE('',#100558,0.1) ;
#33375 = CIRCLE('',#100560,0.0999999999999998) ;
#33376 = CIRCLE('',#100562,0.0999999999999994) ;
#33377 = CIRCLE('',#100564,0.0999999999999998) ;
#33378 = CIRCLE('',#100566,0.0999999999999994) ;
#33379 = CIRCLE('',#100568,0.0999999999999998) ;
#33380 = CIRCLE('',#100570,0.1) ;
#33381 = CIRCLE('',#100572,0.0999999999999994) ;
#33382 = CIRCLE('',#100573,0.0999999999999994) ;
#33383 = CIRCLE('',#100575,0.1) ;
#33384 = CIRCLE('',#100576,0.0999999999999998) ;
#33385 = CIRCLE('',#100578,0.0999999999999994) ;
#33386 = CIRCLE('',#100580,0.0999999999999994) ;
#33387 = CIRCLE('',#100582,0.1) ;
#33388 = CIRCLE('',#100584,0.1) ;
#33389 = CIRCLE('',#100585,0.1) ;
#33390 = CIRCLE('',#100587,0.1) ;
#33391 = CIRCLE('',#100588,0.1) ;
#33392 = CIRCLE('',#100589,0.0999999999999994) ;
#33393 = CIRCLE('',#100591,0.1) ;
#33394 = CIRCLE('',#100593,0.1) ;
#33395 = CIRCLE('',#100595,0.1) ;
#33396 = CIRCLE('',#100597,0.0999999999999994) ;
#33397 = CIRCLE('',#100599,0.1) ;
#33398 = CIRCLE('',#100601,0.0999999999999994) ;
#33399 = CIRCLE('',#100603,0.1) ;
#33400 = CIRCLE('',#100605,0.0999999999999994) ;
#33401 = CIRCLE('',#100607,0.0999999999999994) ;
#33402 = CIRCLE('',#100609,0.0999999999999994) ;
#33403 = CIRCLE('',#100610,0.0999999999999996) ;
#33404 = CIRCLE('',#100611,0.0999999999999996) ;
#33405 = CIRCLE('',#100613,0.1) ;
#33406 = CIRCLE('',#100615,0.1) ;
#33407 = CIRCLE('',#100617,0.1) ;
#33408 = CIRCLE('',#100619,0.1) ;
#33409 = CIRCLE('',#100621,0.1) ;
#33410 = CIRCLE('',#100623,0.1) ;
#33411 = CIRCLE('',#100625,0.1) ;
#33412 = CIRCLE('',#100626,0.0999999999999995) ;
#33413 = CIRCLE('',#100627,0.0999999999999998) ;
#33414 = CIRCLE('',#100628,0.1) ;
#33415 = CIRCLE('',#100630,0.1) ;
#33416 = CIRCLE('',#100632,0.1) ;
#33417 = CIRCLE('',#100634,0.0999999999999994) ;
#33418 = CIRCLE('',#100636,0.0999999999999994) ;
#33419 = CIRCLE('',#100638,0.1) ;
#33420 = CIRCLE('',#100640,0.1) ;
#33421 = CIRCLE('',#100642,0.0999999999999996) ;
#33422 = CIRCLE('',#100643,0.0999999999999996) ;
#33423 = CIRCLE('',#100645,0.0999999999999994) ;
#33424 = CIRCLE('',#100646,0.1) ;
#33425 = CIRCLE('',#100648,0.0999999999999998) ;
#33426 = CIRCLE('',#100650,0.0999999999999994) ;
#33427 = CIRCLE('',#100652,0.1) ;
#33428 = CIRCLE('',#100654,0.0999999999999994) ;
#33429 = CIRCLE('',#100656,0.0999999999999998) ;
#33430 = CIRCLE('',#100658,0.0999999999999994) ;
#33431 = CIRCLE('',#100661,0.1) ;
#33432 = CIRCLE('',#100663,0.1) ;
#33433 = CIRCLE('',#100664,0.1) ;
#33434 = CIRCLE('',#100666,0.0999999999999994) ;
#33435 = CIRCLE('',#100668,0.1) ;
#33436 = CIRCLE('',#100670,0.0999999999999994) ;
#33437 = CIRCLE('',#100672,0.1) ;
#33438 = CIRCLE('',#100674,0.1) ;
#33439 = CIRCLE('',#100676,0.0999999999999994) ;
#33440 = CIRCLE('',#100678,0.0999999999999994) ;
#33441 = CIRCLE('',#100680,0.1) ;
#33442 = CIRCLE('',#100682,0.1) ;
#33443 = CIRCLE('',#100685,0.0999999999999994) ;
#33444 = CIRCLE('',#100686,0.0999999999999994) ;
#33445 = CIRCLE('',#100688,0.0999999999999998) ;
#33446 = CIRCLE('',#100689,0.0999999999999998) ;
#33447 = CIRCLE('',#100691,0.0999999999999998) ;
#33448 = CIRCLE('',#100692,0.1) ;
#33449 = CIRCLE('',#100694,0.0999999999999998) ;
#33450 = CIRCLE('',#100696,0.0999999999999994) ;
#33451 = CIRCLE('',#100698,0.0999999999999994) ;
#33452 = CIRCLE('',#100699,0.0999999999999994) ;
#33453 = CIRCLE('',#100701,0.0999999999999994) ;
#33454 = CIRCLE('',#100703,0.1) ;
#33455 = CIRCLE('',#100705,0.1) ;
#33456 = CIRCLE('',#100706,0.1) ;
#33457 = CIRCLE('',#100708,0.0999999999999998) ;
#33458 = CIRCLE('',#100710,0.0999999999999998) ;
#33459 = CIRCLE('',#100712,0.0999999999999998) ;
#33460 = CIRCLE('',#100714,0.0999999999999998) ;
#33461 = CIRCLE('',#100716,0.1) ;
#33462 = CIRCLE('',#100718,0.0999999999999998) ;
#33463 = CIRCLE('',#100720,0.0999999999999998) ;
#33464 = CIRCLE('',#100722,0.1) ;
#33465 = CIRCLE('',#100724,0.1) ;
#33466 = CIRCLE('',#100726,0.1) ;
#33467 = CIRCLE('',#100729,0.0999999999999994) ;
#33468 = CIRCLE('',#100731,0.0999999999999998) ;
#33469 = CIRCLE('',#100732,0.0999999999999998) ;
#33470 = CIRCLE('',#100734,0.1) ;
#33471 = CIRCLE('',#100736,0.0999999999999994) ;
#33472 = CIRCLE('',#100738,0.1) ;
#33473 = CIRCLE('',#100740,0.0999999999999994) ;
#33474 = CIRCLE('',#100742,0.0999999999999994) ;
#33475 = CIRCLE('',#100744,0.1) ;
#33476 = CIRCLE('',#100746,0.1) ;
#33477 = CIRCLE('',#100748,0.0999999999999998) ;
#33478 = CIRCLE('',#100750,0.0999999999999998) ;
#33479 = CIRCLE('',#100753,0.1) ;
#33480 = CIRCLE('',#100754,0.0999999999999994) ;
#33481 = CIRCLE('',#100756,0.1) ;
#33482 = CIRCLE('',#100758,0.0999999999999994) ;
#33483 = CIRCLE('',#100760,0.1) ;
#33484 = CIRCLE('',#100762,0.0999999999999994) ;
#33485 = CIRCLE('',#100764,0.0999999999999994) ;
#33486 = CIRCLE('',#100766,0.0999999999999994) ;
#33487 = CIRCLE('',#100773,0.1) ;
#33488 = CIRCLE('',#100774,0.0999999999999998) ;
#33489 = CIRCLE('',#100775,0.0999999999999994) ;
#33490 = CIRCLE('',#100777,0.0999999999999994) ;
#33491 = CIRCLE('',#100779,0.0999999999999994) ;
#33492 = CIRCLE('',#100781,0.1) ;
#33493 = CIRCLE('',#100783,0.0999999999999994) ;
#33494 = CIRCLE('',#100784,0.0999999999999994) ;
#33495 = CIRCLE('',#100786,0.0999999999999994) ;
#33496 = CIRCLE('',#100788,0.1) ;
#33497 = CIRCLE('',#100789,0.0999999999999998) ;
#33498 = CIRCLE('',#100791,0.0999999999999994) ;
#33499 = CIRCLE('',#100792,0.0999999999999994) ;
#33500 = CIRCLE('',#100794,0.0999999999999994) ;
#33501 = CIRCLE('',#100795,0.0999999999999994) ;
#33502 = CIRCLE('',#100797,0.0999999999999994) ;
#33503 = CIRCLE('',#100799,0.0999999999999998) ;
#33504 = CIRCLE('',#100801,0.1) ;
#33505 = CIRCLE('',#100803,0.0999999999999994) ;
#33506 = CIRCLE('',#100805,0.0999999999999994) ;
#33507 = CIRCLE('',#100807,0.0999999999999994) ;
#33508 = CIRCLE('',#100808,0.0999999999999994) ;
#33509 = CIRCLE('',#100810,0.0999999999999994) ;
#33510 = CIRCLE('',#100812,0.0999999999999998) ;
#33511 = CIRCLE('',#100814,0.0999999999999994) ;
#33512 = CIRCLE('',#100816,0.0999999999999994) ;
#33513 = CIRCLE('',#100817,0.0999999999999994) ;
#33514 = CIRCLE('',#100819,0.0999999999999994) ;
#33515 = CIRCLE('',#100821,0.0999999999999998) ;
#33516 = CIRCLE('',#100823,0.0999999999999994) ;
#33517 = CIRCLE('',#100825,0.0999999999999998) ;
#33518 = CIRCLE('',#100827,0.0999999999999998) ;
#33519 = CIRCLE('',#100828,0.0999999999999994) ;
#33520 = CIRCLE('',#100830,0.0999999999999994) ;
#33521 = CIRCLE('',#100832,0.0999999999999994) ;
#33522 = CIRCLE('',#100834,0.1) ;
#33523 = CIRCLE('',#100836,0.0999999999999998) ;
#33524 = CIRCLE('',#100838,0.0999999999999994) ;
#33525 = CIRCLE('',#100840,0.0999999999999998) ;
#33526 = CIRCLE('',#100842,0.0999999999999994) ;
#33527 = CIRCLE('',#100844,0.0999999999999998) ;
#33528 = CIRCLE('',#100846,0.1) ;
#33529 = CIRCLE('',#100848,0.0999999999999994) ;
#33530 = CIRCLE('',#100849,0.0999999999999994) ;
#33531 = CIRCLE('',#100851,0.1) ;
#33532 = CIRCLE('',#100852,0.0999999999999998) ;
#33533 = CIRCLE('',#100854,0.0999999999999994) ;
#33534 = CIRCLE('',#100856,0.0999999999999994) ;
#33535 = CIRCLE('',#100858,0.0999999999999994) ;
#33536 = CIRCLE('',#100860,0.0999999999999994) ;
#33537 = CIRCLE('',#100861,0.0999999999999994) ;
#33538 = CIRCLE('',#100863,0.1) ;
#33539 = CIRCLE('',#100864,0.0999999999999994) ;
#33540 = CIRCLE('',#100865,0.0999999999999994) ;
#33541 = CIRCLE('',#100867,0.0999999999999994) ;
#33542 = CIRCLE('',#100869,0.0999999999999994) ;
#33543 = CIRCLE('',#100871,0.1) ;
#33544 = CIRCLE('',#100873,0.0999999999999994) ;
#33545 = CIRCLE('',#100875,0.1) ;
#33546 = CIRCLE('',#100877,0.0999999999999994) ;
#33547 = CIRCLE('',#100879,0.1) ;
#33548 = CIRCLE('',#100881,0.0999999999999994) ;
#33549 = CIRCLE('',#100883,0.0999999999999994) ;
#33550 = CIRCLE('',#100885,0.0999999999999994) ;
#33551 = CIRCLE('',#100886,0.0999999999999996) ;
#33552 = CIRCLE('',#100887,0.0999999999999996) ;
#33553 = CIRCLE('',#100889,0.0999999999999996) ;
#33554 = CIRCLE('',#100891,0.0999999999999994) ;
#33555 = CIRCLE('',#100893,0.1) ;
#33556 = CIRCLE('',#100895,0.1) ;
#33557 = CIRCLE('',#100897,0.1) ;
#33558 = CIRCLE('',#100899,0.1) ;
#33559 = CIRCLE('',#100901,0.1) ;
#33560 = CIRCLE('',#100902,0.100000000000001) ;
#33561 = CIRCLE('',#100903,0.1) ;
#33562 = CIRCLE('',#100904,0.1) ;
#33563 = CIRCLE('',#100906,0.1) ;
#33564 = CIRCLE('',#100908,0.1) ;
#33565 = CIRCLE('',#100910,0.1) ;
#33566 = CIRCLE('',#100912,0.0999999999999994) ;
#33567 = CIRCLE('',#100914,0.1) ;
#33568 = CIRCLE('',#100916,0.1) ;
#33569 = CIRCLE('',#100918,0.0999999999999996) ;
#33570 = CIRCLE('',#100919,0.0999999999999996) ;
#33571 = CIRCLE('',#100921,0.0999999999999994) ;
#33572 = CIRCLE('',#100922,0.1) ;
#33573 = CIRCLE('',#100924,0.1) ;
#33574 = CIRCLE('',#100926,0.0999999999999994) ;
#33575 = CIRCLE('',#100928,0.0999999999999994) ;
#33576 = CIRCLE('',#100930,0.0999999999999994) ;
#33577 = CIRCLE('',#100932,0.0999999999999998) ;
#33578 = CIRCLE('',#100934,0.0999999999999994) ;
#33579 = CIRCLE('',#100937,0.0999999999999994) ;
#33580 = CIRCLE('',#100939,0.1) ;
#33581 = CIRCLE('',#100940,0.1) ;
#33582 = CIRCLE('',#100942,0.0999999999999994) ;
#33583 = CIRCLE('',#100944,0.0999999999999994) ;
#33584 = CIRCLE('',#100946,0.0999999999999994) ;
#33585 = CIRCLE('',#100948,0.0999999999999994) ;
#33586 = CIRCLE('',#100950,0.0999999999999994) ;
#33587 = CIRCLE('',#100952,0.0999999999999994) ;
#33588 = CIRCLE('',#100954,0.0999999999999994) ;
#33589 = CIRCLE('',#100956,0.1) ;
#33590 = CIRCLE('',#100958,0.1) ;
#33591 = CIRCLE('',#100961,0.0999999999999994) ;
#33592 = CIRCLE('',#100962,0.0999999999999994) ;
#33593 = CIRCLE('',#100964,0.0999999999999998) ;
#33594 = CIRCLE('',#100965,0.0999999999999998) ;
#33595 = CIRCLE('',#100967,0.0999999999999998) ;
#33596 = CIRCLE('',#100968,0.1) ;
#33597 = CIRCLE('',#100970,0.0999999999999998) ;
#33598 = CIRCLE('',#100972,0.0999999999999994) ;
#33599 = CIRCLE('',#100974,0.0999999999999994) ;
#33600 = CIRCLE('',#100975,0.0999999999999994) ;
#33601 = CIRCLE('',#100977,0.0999999999999994) ;
#33602 = CIRCLE('',#100979,0.1) ;
#33603 = CIRCLE('',#100981,0.0999999999999994) ;
#33604 = CIRCLE('',#100982,0.0999999999999994) ;
#33605 = CIRCLE('',#100984,0.0999999999999998) ;
#33606 = CIRCLE('',#100986,0.0999999999999998) ;
#33607 = CIRCLE('',#100988,0.0999999999999998) ;
#33608 = CIRCLE('',#100990,0.0999999999999998) ;
#33609 = CIRCLE('',#100992,0.0999999999999994) ;
#33610 = CIRCLE('',#100994,0.0999999999999998) ;
#33611 = CIRCLE('',#100996,0.0999999999999998) ;
#33612 = CIRCLE('',#100998,0.0999999999999994) ;
#33613 = CIRCLE('',#101000,0.0999999999999994) ;
#33614 = CIRCLE('',#101002,0.0999999999999994) ;
#33615 = CIRCLE('',#101005,0.0999999999999994) ;
#33616 = CIRCLE('',#101007,0.0999999999999998) ;
#33617 = CIRCLE('',#101008,0.0999999999999998) ;
#33618 = CIRCLE('',#101010,0.0999999999999994) ;
#33619 = CIRCLE('',#101012,0.0999999999999994) ;
#33620 = CIRCLE('',#101014,0.0999999999999994) ;
#33621 = CIRCLE('',#101016,0.0999999999999994) ;
#33622 = CIRCLE('',#101018,0.0999999999999994) ;
#33623 = CIRCLE('',#101020,0.0999999999999994) ;
#33624 = CIRCLE('',#101022,0.0999999999999994) ;
#33625 = CIRCLE('',#101024,0.0999999999999998) ;
#33626 = CIRCLE('',#101026,0.0999999999999998) ;
#33627 = CIRCLE('',#101029,0.1) ;
#33628 = CIRCLE('',#101030,0.0999999999999994) ;
#33629 = CIRCLE('',#101032,0.0999999999999994) ;
#33630 = CIRCLE('',#101034,0.0999999999999994) ;
#33631 = CIRCLE('',#101036,0.0999999999999994) ;
#33632 = CIRCLE('',#101038,0.0999999999999994) ;
#33633 = CIRCLE('',#101040,0.0999999999999994) ;
#33634 = CIRCLE('',#101042,0.0999999999999994) ;
#33635 = CIRCLE('',#101049,0.1) ;
#33636 = CIRCLE('',#101050,0.0999999999999998) ;
#33637 = CIRCLE('',#101051,0.0999999999999994) ;
#33638 = CIRCLE('',#101053,0.0999999999999994) ;
#33639 = CIRCLE('',#101055,0.0999999999999994) ;
#33640 = CIRCLE('',#101057,0.1) ;
#33641 = CIRCLE('',#101059,0.0999999999999994) ;
#33642 = CIRCLE('',#101060,0.0999999999999994) ;
#33643 = CIRCLE('',#101062,0.0999999999999994) ;
#33644 = CIRCLE('',#101064,0.1) ;
#33645 = CIRCLE('',#101065,0.0999999999999998) ;
#33646 = CIRCLE('',#101067,0.0999999999999994) ;
#33647 = CIRCLE('',#101068,0.0999999999999994) ;
#33648 = CIRCLE('',#101070,0.0999999999999994) ;
#33649 = CIRCLE('',#101071,0.0999999999999994) ;
#33650 = CIRCLE('',#101073,0.0999999999999994) ;
#33651 = CIRCLE('',#101075,0.0999999999999998) ;
#33652 = CIRCLE('',#101077,0.1) ;
#33653 = CIRCLE('',#101079,0.0999999999999994) ;
#33654 = CIRCLE('',#101081,0.0999999999999994) ;
#33655 = CIRCLE('',#101083,0.0999999999999994) ;
#33656 = CIRCLE('',#101084,0.0999999999999994) ;
#33657 = CIRCLE('',#101086,0.0999999999999994) ;
#33658 = CIRCLE('',#101088,0.0999999999999998) ;
#33659 = CIRCLE('',#101090,0.0999999999999994) ;
#33660 = CIRCLE('',#101092,0.0999999999999994) ;
#33661 = CIRCLE('',#101093,0.0999999999999994) ;
#33662 = CIRCLE('',#101095,0.0999999999999994) ;
#33663 = CIRCLE('',#101097,0.0999999999999998) ;
#33664 = CIRCLE('',#101099,0.0999999999999994) ;
#33665 = CIRCLE('',#101101,0.0999999999999994) ;
#33666 = CIRCLE('',#101103,0.0999999999999998) ;
#33667 = CIRCLE('',#101104,0.0999999999999994) ;
#33668 = CIRCLE('',#101106,0.0999999999999994) ;
#33669 = CIRCLE('',#101108,0.0999999999999994) ;
#33670 = CIRCLE('',#101110,0.1) ;
#33671 = CIRCLE('',#101112,0.0999999999999998) ;
#33672 = CIRCLE('',#101114,0.0999999999999994) ;
#33673 = CIRCLE('',#101116,0.0999999999999998) ;
#33674 = CIRCLE('',#101118,0.0999999999999994) ;
#33675 = CIRCLE('',#101120,0.0999999999999998) ;
#33676 = CIRCLE('',#101122,0.1) ;
#33677 = CIRCLE('',#101124,0.0999999999999994) ;
#33678 = CIRCLE('',#101125,0.0999999999999994) ;
#33679 = CIRCLE('',#101127,0.1) ;
#33680 = CIRCLE('',#101128,0.0999999999999998) ;
#33681 = CIRCLE('',#101130,0.0999999999999994) ;
#33682 = CIRCLE('',#101132,0.0999999999999994) ;
#33683 = CIRCLE('',#101134,0.0999999999999994) ;
#33684 = CIRCLE('',#101136,0.0999999999999994) ;
#33685 = CIRCLE('',#101137,0.0999999999999994) ;
#33686 = CIRCLE('',#101139,0.1) ;
#33687 = CIRCLE('',#101140,0.0999999999999994) ;
#33688 = CIRCLE('',#101141,0.0999999999999994) ;
#33689 = CIRCLE('',#101143,0.0999999999999994) ;
#33690 = CIRCLE('',#101145,0.0999999999999994) ;
#33691 = CIRCLE('',#101147,0.0999999999999998) ;
#33692 = CIRCLE('',#101149,0.0999999999999994) ;
#33693 = CIRCLE('',#101151,0.1) ;
#33694 = CIRCLE('',#101153,0.0999999999999994) ;
#33695 = CIRCLE('',#101155,0.1) ;
#33696 = CIRCLE('',#101157,0.0999999999999994) ;
#33697 = CIRCLE('',#101159,0.0999999999999994) ;
#33698 = CIRCLE('',#101161,0.0999999999999994) ;
#33699 = CIRCLE('',#101162,0.0999999999999996) ;
#33700 = CIRCLE('',#101163,0.0999999999999996) ;
#33701 = CIRCLE('',#101165,0.0999999999999996) ;
#33702 = CIRCLE('',#101167,0.0999999999999994) ;
#33703 = CIRCLE('',#101169,0.1) ;
#33704 = CIRCLE('',#101171,0.1) ;
#33705 = CIRCLE('',#101173,0.1) ;
#33706 = CIRCLE('',#101175,0.1) ;
#33707 = CIRCLE('',#101177,0.1) ;
#33708 = CIRCLE('',#101178,0.100000000000001) ;
#33709 = CIRCLE('',#101179,0.1) ;
#33710 = CIRCLE('',#101180,0.1) ;
#33711 = CIRCLE('',#101182,0.1) ;
#33712 = CIRCLE('',#101184,0.1) ;
#33713 = CIRCLE('',#101186,0.0999999999999994) ;
#33714 = CIRCLE('',#101188,0.0999999999999994) ;
#33715 = CIRCLE('',#101190,0.100000000000001) ;
#33716 = CIRCLE('',#101192,0.0999999999999996) ;
#33717 = CIRCLE('',#101194,0.0999999999999996) ;
#33718 = CIRCLE('',#101195,0.0999999999999996) ;
#33719 = CIRCLE('',#101197,0.0999999999999994) ;
#33720 = CIRCLE('',#101198,0.1) ;
#33721 = CIRCLE('',#101200,0.1) ;
#33722 = CIRCLE('',#101202,0.0999999999999994) ;
#33723 = CIRCLE('',#101204,0.0999999999999994) ;
#33724 = CIRCLE('',#101206,0.0999999999999994) ;
#33725 = CIRCLE('',#101208,0.0999999999999998) ;
#33726 = CIRCLE('',#101210,0.0999999999999994) ;
#33727 = CIRCLE('',#101213,0.0999999999999994) ;
#33728 = CIRCLE('',#101215,0.1) ;
#33729 = CIRCLE('',#101216,0.1) ;
#33730 = CIRCLE('',#101218,0.0999999999999994) ;
#33731 = CIRCLE('',#101220,0.0999999999999994) ;
#33732 = CIRCLE('',#101222,0.0999999999999994) ;
#33733 = CIRCLE('',#101224,0.0999999999999994) ;
#33734 = CIRCLE('',#101226,0.0999999999999994) ;
#33735 = CIRCLE('',#101228,0.0999999999999994) ;
#33736 = CIRCLE('',#101230,0.0999999999999994) ;
#33737 = CIRCLE('',#101232,0.1) ;
#33738 = CIRCLE('',#101234,0.1) ;
#33739 = CIRCLE('',#101237,0.0999999999999994) ;
#33740 = CIRCLE('',#101238,0.0999999999999994) ;
#33741 = CIRCLE('',#101240,0.0999999999999998) ;
#33742 = CIRCLE('',#101241,0.0999999999999998) ;
#33743 = CIRCLE('',#101243,0.0999999999999998) ;
#33744 = CIRCLE('',#101244,0.1) ;
#33745 = CIRCLE('',#101246,0.0999999999999998) ;
#33746 = CIRCLE('',#101248,0.0999999999999994) ;
#33747 = CIRCLE('',#101250,0.0999999999999994) ;
#33748 = CIRCLE('',#101251,0.0999999999999994) ;
#33749 = CIRCLE('',#101253,0.0999999999999994) ;
#33750 = CIRCLE('',#101255,0.1) ;
#33751 = CIRCLE('',#101257,0.0999999999999994) ;
#33752 = CIRCLE('',#101258,0.0999999999999994) ;
#33753 = CIRCLE('',#101260,0.0999999999999998) ;
#33754 = CIRCLE('',#101262,0.0999999999999998) ;
#33755 = CIRCLE('',#101264,0.0999999999999998) ;
#33756 = CIRCLE('',#101266,0.0999999999999998) ;
#33757 = CIRCLE('',#101268,0.0999999999999994) ;
#33758 = CIRCLE('',#101270,0.0999999999999998) ;
#33759 = CIRCLE('',#101272,0.0999999999999998) ;
#33760 = CIRCLE('',#101274,0.0999999999999994) ;
#33761 = CIRCLE('',#101276,0.0999999999999994) ;
#33762 = CIRCLE('',#101278,0.0999999999999994) ;
#33763 = CIRCLE('',#101281,0.0999999999999994) ;
#33764 = CIRCLE('',#101283,0.0999999999999998) ;
#33765 = CIRCLE('',#101284,0.0999999999999998) ;
#33766 = CIRCLE('',#101286,0.0999999999999994) ;
#33767 = CIRCLE('',#101288,0.0999999999999994) ;
#33768 = CIRCLE('',#101290,0.0999999999999994) ;
#33769 = CIRCLE('',#101292,0.0999999999999994) ;
#33770 = CIRCLE('',#101294,0.0999999999999994) ;
#33771 = CIRCLE('',#101296,0.0999999999999994) ;
#33772 = CIRCLE('',#101298,0.0999999999999994) ;
#33773 = CIRCLE('',#101300,0.0999999999999998) ;
#33774 = CIRCLE('',#101302,0.0999999999999998) ;
#33775 = CIRCLE('',#101305,0.1) ;
#33776 = CIRCLE('',#101306,0.0999999999999994) ;
#33777 = CIRCLE('',#101308,0.0999999999999994) ;
#33778 = CIRCLE('',#101310,0.0999999999999994) ;
#33779 = CIRCLE('',#101312,0.0999999999999994) ;
#33780 = CIRCLE('',#101314,0.0999999999999994) ;
#33781 = CIRCLE('',#101316,0.0999999999999994) ;
#33782 = CIRCLE('',#101318,0.0999999999999994) ;
#33783 = CIRCLE('',#101325,0.1) ;
#33784 = CIRCLE('',#101326,0.0999999999999998) ;
#33785 = CIRCLE('',#101327,0.0999999999999994) ;
#33786 = CIRCLE('',#101329,0.0999999999999994) ;
#33787 = CIRCLE('',#101331,0.0999999999999994) ;
#33788 = CIRCLE('',#101333,0.1) ;
#33789 = CIRCLE('',#101335,0.0999999999999994) ;
#33790 = CIRCLE('',#101336,0.0999999999999994) ;
#33791 = CIRCLE('',#101338,0.0999999999999994) ;
#33792 = CIRCLE('',#101340,0.1) ;
#33793 = CIRCLE('',#101341,0.0999999999999998) ;
#33794 = CIRCLE('',#101343,0.0999999999999994) ;
#33795 = CIRCLE('',#101344,0.0999999999999994) ;
#33796 = CIRCLE('',#101346,0.0999999999999994) ;
#33797 = CIRCLE('',#101347,0.0999999999999994) ;
#33798 = CIRCLE('',#101349,0.0999999999999994) ;
#33799 = CIRCLE('',#101351,0.0999999999999998) ;
#33800 = CIRCLE('',#101353,0.1) ;
#33801 = CIRCLE('',#101355,0.0999999999999994) ;
#33802 = CIRCLE('',#101357,0.0999999999999994) ;
#33803 = CIRCLE('',#101359,0.0999999999999994) ;
#33804 = CIRCLE('',#101360,0.0999999999999994) ;
#33805 = CIRCLE('',#101362,0.0999999999999994) ;
#33806 = CIRCLE('',#101364,0.0999999999999998) ;
#33807 = CIRCLE('',#101366,0.0999999999999994) ;
#33808 = CIRCLE('',#101368,0.0999999999999994) ;
#33809 = CIRCLE('',#101369,0.0999999999999994) ;
#33810 = CIRCLE('',#101371,0.0999999999999994) ;
#33811 = CIRCLE('',#101373,0.0999999999999998) ;
#33812 = CIRCLE('',#101375,0.0999999999999994) ;
#33813 = CIRCLE('',#101377,0.0999999999999998) ;
#33814 = CIRCLE('',#101379,0.0999999999999998) ;
#33815 = CIRCLE('',#101380,0.0999999999999994) ;
#33816 = CIRCLE('',#101382,0.0999999999999994) ;
#33817 = CIRCLE('',#101384,0.0999999999999994) ;
#33818 = CIRCLE('',#101386,0.1) ;
#33819 = CIRCLE('',#101388,0.0999999999999998) ;
#33820 = CIRCLE('',#101390,0.0999999999999994) ;
#33821 = CIRCLE('',#101392,0.0999999999999998) ;
#33822 = CIRCLE('',#101394,0.0999999999999994) ;
#33823 = CIRCLE('',#101396,0.0999999999999998) ;
#33824 = CIRCLE('',#101398,0.1) ;
#33825 = CIRCLE('',#101400,0.0999999999999994) ;
#33826 = CIRCLE('',#101401,0.0999999999999994) ;
#33827 = CIRCLE('',#101403,0.1) ;
#33828 = CIRCLE('',#101404,0.0999999999999998) ;
#33829 = CIRCLE('',#101406,0.0999999999999994) ;
#33830 = CIRCLE('',#101408,0.0999999999999994) ;
#33831 = CIRCLE('',#101410,0.0999999999999994) ;
#33832 = CIRCLE('',#101412,0.0999999999999994) ;
#33833 = CIRCLE('',#101413,0.0999999999999994) ;
#33834 = CIRCLE('',#101415,0.1) ;
#33835 = CIRCLE('',#101416,0.0999999999999994) ;
#33836 = CIRCLE('',#101417,0.0999999999999994) ;
#33837 = CIRCLE('',#101419,0.0999999999999994) ;
#33838 = CIRCLE('',#101421,0.0999999999999994) ;
#33839 = CIRCLE('',#101423,0.0999999999999998) ;
#33840 = CIRCLE('',#101425,0.0999999999999994) ;
#33841 = CIRCLE('',#101427,0.1) ;
#33842 = CIRCLE('',#101429,0.0999999999999994) ;
#33843 = CIRCLE('',#101431,0.1) ;
#33844 = CIRCLE('',#101433,0.0999999999999994) ;
#33845 = CIRCLE('',#101435,0.0999999999999994) ;
#33846 = CIRCLE('',#101437,0.0999999999999994) ;
#33847 = CIRCLE('',#101438,0.0999999999999996) ;
#33848 = CIRCLE('',#101439,0.0999999999999996) ;
#33849 = CIRCLE('',#101441,0.1) ;
#33850 = CIRCLE('',#101443,0.0999999999999994) ;
#33851 = CIRCLE('',#101445,0.0999999999999994) ;
#33852 = CIRCLE('',#101447,0.1) ;
#33853 = CIRCLE('',#101449,0.1) ;
#33854 = CIRCLE('',#101451,0.1) ;
#33855 = CIRCLE('',#101453,0.1) ;
#33856 = CIRCLE('',#101454,0.1) ;
#33857 = CIRCLE('',#101455,0.0999999999999998) ;
#33858 = CIRCLE('',#101456,0.1) ;
#33859 = CIRCLE('',#101458,0.1) ;
#33860 = CIRCLE('',#101460,0.1) ;
#33861 = CIRCLE('',#101462,0.0999999999999994) ;
#33862 = CIRCLE('',#101464,0.0999999999999994) ;
#33863 = CIRCLE('',#101466,0.100000000000001) ;
#33864 = CIRCLE('',#101468,0.0999999999999996) ;
#33865 = CIRCLE('',#101470,0.0999999999999996) ;
#33866 = CIRCLE('',#101471,0.0999999999999996) ;
#33867 = CIRCLE('',#101473,0.0999999999999994) ;
#33868 = CIRCLE('',#101474,0.1) ;
#33869 = CIRCLE('',#101476,0.1) ;
#33870 = CIRCLE('',#101478,0.0999999999999994) ;
#33871 = CIRCLE('',#101480,0.0999999999999994) ;
#33872 = CIRCLE('',#101482,0.0999999999999994) ;
#33873 = CIRCLE('',#101484,0.0999999999999998) ;
#33874 = CIRCLE('',#101486,0.0999999999999994) ;
#33875 = CIRCLE('',#101489,0.0999999999999994) ;
#33876 = CIRCLE('',#101491,0.1) ;
#33877 = CIRCLE('',#101492,0.1) ;
#33878 = CIRCLE('',#101494,0.0999999999999994) ;
#33879 = CIRCLE('',#101496,0.0999999999999994) ;
#33880 = CIRCLE('',#101498,0.0999999999999994) ;
#33881 = CIRCLE('',#101500,0.0999999999999994) ;
#33882 = CIRCLE('',#101502,0.0999999999999994) ;
#33883 = CIRCLE('',#101504,0.0999999999999994) ;
#33884 = CIRCLE('',#101506,0.0999999999999994) ;
#33885 = CIRCLE('',#101508,0.1) ;
#33886 = CIRCLE('',#101510,0.1) ;
#33887 = CIRCLE('',#101513,0.0999999999999994) ;
#33888 = CIRCLE('',#101514,0.0999999999999994) ;
#33889 = CIRCLE('',#101516,0.0999999999999998) ;
#33890 = CIRCLE('',#101517,0.0999999999999998) ;
#33891 = CIRCLE('',#101519,0.0999999999999998) ;
#33892 = CIRCLE('',#101520,0.1) ;
#33893 = CIRCLE('',#101522,0.0999999999999998) ;
#33894 = CIRCLE('',#101524,0.0999999999999994) ;
#33895 = CIRCLE('',#101526,0.0999999999999994) ;
#33896 = CIRCLE('',#101527,0.0999999999999994) ;
#33897 = CIRCLE('',#101529,0.0999999999999994) ;
#33898 = CIRCLE('',#101531,0.1) ;
#33899 = CIRCLE('',#101533,0.0999999999999994) ;
#33900 = CIRCLE('',#101534,0.0999999999999994) ;
#33901 = CIRCLE('',#101536,0.0999999999999998) ;
#33902 = CIRCLE('',#101538,0.0999999999999998) ;
#33903 = CIRCLE('',#101540,0.0999999999999998) ;
#33904 = CIRCLE('',#101542,0.0999999999999998) ;
#33905 = CIRCLE('',#101544,0.0999999999999994) ;
#33906 = CIRCLE('',#101546,0.0999999999999998) ;
#33907 = CIRCLE('',#101548,0.0999999999999998) ;
#33908 = CIRCLE('',#101550,0.0999999999999994) ;
#33909 = CIRCLE('',#101552,0.0999999999999994) ;
#33910 = CIRCLE('',#101554,0.0999999999999994) ;
#33911 = CIRCLE('',#101557,0.0999999999999994) ;
#33912 = CIRCLE('',#101559,0.0999999999999998) ;
#33913 = CIRCLE('',#101560,0.0999999999999998) ;
#33914 = CIRCLE('',#101562,0.0999999999999994) ;
#33915 = CIRCLE('',#101564,0.0999999999999994) ;
#33916 = CIRCLE('',#101566,0.0999999999999994) ;
#33917 = CIRCLE('',#101568,0.0999999999999994) ;
#33918 = CIRCLE('',#101570,0.0999999999999994) ;
#33919 = CIRCLE('',#101572,0.0999999999999994) ;
#33920 = CIRCLE('',#101574,0.0999999999999994) ;
#33921 = CIRCLE('',#101576,0.0999999999999998) ;
#33922 = CIRCLE('',#101578,0.0999999999999998) ;
#33923 = CIRCLE('',#101581,0.1) ;
#33924 = CIRCLE('',#101582,0.0999999999999994) ;
#33925 = CIRCLE('',#101584,0.0999999999999994) ;
#33926 = CIRCLE('',#101586,0.0999999999999994) ;
#33927 = CIRCLE('',#101588,0.0999999999999994) ;
#33928 = CIRCLE('',#101590,0.0999999999999994) ;
#33929 = CIRCLE('',#101592,0.0999999999999994) ;
#33930 = CIRCLE('',#101594,0.0999999999999994) ;
#33931 = CIRCLE('',#101601,0.1) ;
#33932 = CIRCLE('',#101602,0.0999999999999998) ;
#33933 = CIRCLE('',#101603,0.0999999999999994) ;
#33934 = CIRCLE('',#101605,0.0999999999999994) ;
#33935 = CIRCLE('',#101607,0.0999999999999994) ;
#33936 = CIRCLE('',#101609,0.1) ;
#33937 = CIRCLE('',#101611,0.0999999999999994) ;
#33938 = CIRCLE('',#101612,0.0999999999999994) ;
#33939 = CIRCLE('',#101614,0.0999999999999994) ;
#33940 = CIRCLE('',#101616,0.1) ;
#33941 = CIRCLE('',#101617,0.0999999999999998) ;
#33942 = CIRCLE('',#101619,0.0999999999999994) ;
#33943 = CIRCLE('',#101620,0.0999999999999994) ;
#33944 = CIRCLE('',#101622,0.0999999999999994) ;
#33945 = CIRCLE('',#101623,0.0999999999999994) ;
#33946 = CIRCLE('',#101625,0.0999999999999994) ;
#33947 = CIRCLE('',#101627,0.0999999999999998) ;
#33948 = CIRCLE('',#101629,0.1) ;
#33949 = CIRCLE('',#101631,0.0999999999999994) ;
#33950 = CIRCLE('',#101633,0.0999999999999994) ;
#33951 = CIRCLE('',#101635,0.0999999999999994) ;
#33952 = CIRCLE('',#101636,0.0999999999999994) ;
#33953 = CIRCLE('',#101638,0.0999999999999994) ;
#33954 = CIRCLE('',#101640,0.0999999999999998) ;
#33955 = CIRCLE('',#101642,0.0999999999999994) ;
#33956 = CIRCLE('',#101644,0.0999999999999994) ;
#33957 = CIRCLE('',#101645,0.0999999999999994) ;
#33958 = CIRCLE('',#101647,0.0999999999999994) ;
#33959 = CIRCLE('',#101649,0.0999999999999998) ;
#33960 = CIRCLE('',#101651,0.0999999999999994) ;
#33961 = CIRCLE('',#101653,0.0999999999999998) ;
#33962 = CIRCLE('',#101655,0.0999999999999998) ;
#33963 = CIRCLE('',#101656,0.0999999999999994) ;
#33964 = CIRCLE('',#101658,0.0999999999999994) ;
#33965 = CIRCLE('',#101660,0.0999999999999994) ;
#33966 = CIRCLE('',#101662,0.1) ;
#33967 = CIRCLE('',#101664,0.0999999999999998) ;
#33968 = CIRCLE('',#101666,0.0999999999999994) ;
#33969 = CIRCLE('',#101668,0.0999999999999998) ;
#33970 = CIRCLE('',#101670,0.0999999999999994) ;
#33971 = CIRCLE('',#101672,0.0999999999999998) ;
#33972 = CIRCLE('',#101674,0.1) ;
#33973 = CIRCLE('',#101676,0.0999999999999994) ;
#33974 = CIRCLE('',#101677,0.0999999999999994) ;
#33975 = CIRCLE('',#101679,0.1) ;
#33976 = CIRCLE('',#101680,0.0999999999999998) ;
#33977 = CIRCLE('',#101682,0.0999999999999994) ;
#33978 = CIRCLE('',#101684,0.0999999999999994) ;
#33979 = CIRCLE('',#101686,0.0999999999999994) ;
#33980 = CIRCLE('',#101688,0.0999999999999994) ;
#33981 = CIRCLE('',#101689,0.0999999999999994) ;
#33982 = CIRCLE('',#101691,0.1) ;
#33983 = CIRCLE('',#101692,0.0999999999999994) ;
#33984 = CIRCLE('',#101693,0.0999999999999994) ;
#33985 = CIRCLE('',#101695,0.0999999999999994) ;
#33986 = CIRCLE('',#101697,0.0999999999999994) ;
#33987 = CIRCLE('',#101699,0.0999999999999998) ;
#33988 = CIRCLE('',#101701,0.0999999999999994) ;
#33989 = CIRCLE('',#101703,0.1) ;
#33990 = CIRCLE('',#101705,0.0999999999999994) ;
#33991 = CIRCLE('',#101707,0.1) ;
#33992 = CIRCLE('',#101709,0.0999999999999994) ;
#33993 = CIRCLE('',#101711,0.0999999999999994) ;
#33994 = CIRCLE('',#101713,0.0999999999999994) ;
#33995 = CIRCLE('',#101714,0.0999999999999996) ;
#33996 = CIRCLE('',#101715,0.0999999999999996) ;
#33997 = CIRCLE('',#101717,0.1) ;
#33998 = CIRCLE('',#101719,0.0999999999999994) ;
#33999 = CIRCLE('',#101721,0.0999999999999994) ;
#34000 = CIRCLE('',#101723,0.1) ;
#34001 = CIRCLE('',#101725,0.1) ;
#34002 = CIRCLE('',#101727,0.1) ;
#34003 = CIRCLE('',#101729,0.1) ;
#34004 = CIRCLE('',#101730,0.1) ;
#34005 = CIRCLE('',#101731,0.0999999999999998) ;
#34006 = CIRCLE('',#101732,0.1) ;
#34007 = CIRCLE('',#101734,0.1) ;
#34008 = CIRCLE('',#101736,0.1) ;
#34009 = CIRCLE('',#101738,0.0999999999999994) ;
#34010 = CIRCLE('',#101740,0.0999999999999994) ;
#34011 = CIRCLE('',#101742,0.100000000000001) ;
#34012 = CIRCLE('',#101744,0.0999999999999996) ;
#34013 = CIRCLE('',#101746,0.0999999999999996) ;
#34014 = CIRCLE('',#101747,0.0999999999999996) ;
#34015 = CIRCLE('',#101749,0.0999999999999994) ;
#34016 = CIRCLE('',#101750,0.1) ;
#34017 = CIRCLE('',#101752,0.0999999999999998) ;
#34018 = CIRCLE('',#101754,0.0999999999999994) ;
#34019 = CIRCLE('',#101756,0.0999999999999994) ;
#34020 = CIRCLE('',#101758,0.0999999999999994) ;
#34021 = CIRCLE('',#101760,0.0999999999999998) ;
#34022 = CIRCLE('',#101762,0.0999999999999994) ;
#34023 = CIRCLE('',#101765,0.0999999999999994) ;
#34024 = CIRCLE('',#101767,0.1) ;
#34025 = CIRCLE('',#101768,0.1) ;
#34026 = CIRCLE('',#101770,0.0999999999999994) ;
#34027 = CIRCLE('',#101772,0.0999999999999994) ;
#34028 = CIRCLE('',#101774,0.0999999999999994) ;
#34029 = CIRCLE('',#101776,0.0999999999999994) ;
#34030 = CIRCLE('',#101778,0.0999999999999994) ;
#34031 = CIRCLE('',#101780,0.0999999999999994) ;
#34032 = CIRCLE('',#101782,0.0999999999999994) ;
#34033 = CIRCLE('',#101784,0.1) ;
#34034 = CIRCLE('',#101786,0.1) ;
#34035 = CIRCLE('',#101789,0.0999999999999994) ;
#34036 = CIRCLE('',#101790,0.0999999999999994) ;
#34037 = CIRCLE('',#101792,0.0999999999999998) ;
#34038 = CIRCLE('',#101793,0.0999999999999998) ;
#34039 = CIRCLE('',#101795,0.0999999999999998) ;
#34040 = CIRCLE('',#101796,0.1) ;
#34041 = CIRCLE('',#101798,0.0999999999999998) ;
#34042 = CIRCLE('',#101800,0.0999999999999994) ;
#34043 = CIRCLE('',#101802,0.0999999999999994) ;
#34044 = CIRCLE('',#101803,0.0999999999999994) ;
#34045 = CIRCLE('',#101805,0.0999999999999994) ;
#34046 = CIRCLE('',#101807,0.1) ;
#34047 = CIRCLE('',#101809,0.0999999999999994) ;
#34048 = CIRCLE('',#101810,0.0999999999999994) ;
#34049 = CIRCLE('',#101812,0.0999999999999998) ;
#34050 = CIRCLE('',#101814,0.0999999999999998) ;
#34051 = CIRCLE('',#101816,0.0999999999999998) ;
#34052 = CIRCLE('',#101818,0.0999999999999998) ;
#34053 = CIRCLE('',#101820,0.0999999999999994) ;
#34054 = CIRCLE('',#101822,0.0999999999999998) ;
#34055 = CIRCLE('',#101824,0.0999999999999998) ;
#34056 = CIRCLE('',#101826,0.0999999999999994) ;
#34057 = CIRCLE('',#101828,0.0999999999999994) ;
#34058 = CIRCLE('',#101830,0.0999999999999994) ;
#34059 = CIRCLE('',#101833,0.0999999999999994) ;
#34060 = CIRCLE('',#101835,0.0999999999999998) ;
#34061 = CIRCLE('',#101836,0.0999999999999998) ;
#34062 = CIRCLE('',#101838,0.0999999999999994) ;
#34063 = CIRCLE('',#101840,0.0999999999999994) ;
#34064 = CIRCLE('',#101842,0.0999999999999994) ;
#34065 = CIRCLE('',#101844,0.0999999999999994) ;
#34066 = CIRCLE('',#101846,0.0999999999999994) ;
#34067 = CIRCLE('',#101848,0.0999999999999994) ;
#34068 = CIRCLE('',#101850,0.0999999999999994) ;
#34069 = CIRCLE('',#101852,0.0999999999999998) ;
#34070 = CIRCLE('',#101854,0.0999999999999998) ;
#34071 = CIRCLE('',#101857,0.1) ;
#34072 = CIRCLE('',#101858,0.0999999999999994) ;
#34073 = CIRCLE('',#101860,0.0999999999999994) ;
#34074 = CIRCLE('',#101862,0.0999999999999994) ;
#34075 = CIRCLE('',#101864,0.0999999999999994) ;
#34076 = CIRCLE('',#101866,0.0999999999999994) ;
#34077 = CIRCLE('',#101868,0.0999999999999994) ;
#34078 = CIRCLE('',#101870,0.0999999999999994) ;
#34079 = CIRCLE('',#101877,0.1) ;
#34080 = CIRCLE('',#101878,0.0999999999999998) ;
#34081 = CIRCLE('',#101879,0.0999999999999994) ;
#34082 = CIRCLE('',#101881,0.0999999999999994) ;
#34083 = CIRCLE('',#101883,0.0999999999999994) ;
#34084 = CIRCLE('',#101885,0.1) ;
#34085 = CIRCLE('',#101887,0.0999999999999994) ;
#34086 = CIRCLE('',#101888,0.0999999999999994) ;
#34087 = CIRCLE('',#101890,0.0999999999999994) ;
#34088 = CIRCLE('',#101892,0.1) ;
#34089 = CIRCLE('',#101893,0.0999999999999998) ;
#34090 = CIRCLE('',#101895,0.0999999999999994) ;
#34091 = CIRCLE('',#101896,0.0999999999999994) ;
#34092 = CIRCLE('',#101898,0.0999999999999994) ;
#34093 = CIRCLE('',#101899,0.0999999999999994) ;
#34094 = CIRCLE('',#101901,0.0999999999999994) ;
#34095 = CIRCLE('',#101903,0.0999999999999998) ;
#34096 = CIRCLE('',#101905,0.1) ;
#34097 = CIRCLE('',#101907,0.0999999999999994) ;
#34098 = CIRCLE('',#101909,0.0999999999999994) ;
#34099 = CIRCLE('',#101911,0.0999999999999994) ;
#34100 = CIRCLE('',#101912,0.0999999999999994) ;
#34101 = CIRCLE('',#101914,0.0999999999999994) ;
#34102 = CIRCLE('',#101916,0.0999999999999998) ;
#34103 = CIRCLE('',#101918,0.0999999999999994) ;
#34104 = CIRCLE('',#101920,0.0999999999999994) ;
#34105 = CIRCLE('',#101921,0.0999999999999994) ;
#34106 = CIRCLE('',#101923,0.0999999999999994) ;
#34107 = CIRCLE('',#101925,0.0999999999999998) ;
#34108 = CIRCLE('',#101927,0.0999999999999994) ;
#34109 = CIRCLE('',#101929,0.0999999999999998) ;
#34110 = CIRCLE('',#101931,0.0999999999999998) ;
#34111 = CIRCLE('',#101932,0.0999999999999994) ;
#34112 = CIRCLE('',#101934,0.0999999999999994) ;
#34113 = CIRCLE('',#101936,0.0999999999999994) ;
#34114 = CIRCLE('',#101938,0.1) ;
#34115 = CIRCLE('',#101940,0.0999999999999998) ;
#34116 = CIRCLE('',#101942,0.0999999999999994) ;
#34117 = CIRCLE('',#101944,0.0999999999999998) ;
#34118 = CIRCLE('',#101946,0.0999999999999994) ;
#34119 = CIRCLE('',#101948,0.0999999999999998) ;
#34120 = CIRCLE('',#101950,0.1) ;
#34121 = CIRCLE('',#101952,0.0999999999999994) ;
#34122 = CIRCLE('',#101953,0.0999999999999994) ;
#34123 = CIRCLE('',#101955,0.1) ;
#34124 = CIRCLE('',#101956,0.0999999999999998) ;
#34125 = CIRCLE('',#101958,0.0999999999999994) ;
#34126 = CIRCLE('',#101960,0.0999999999999994) ;
#34127 = CIRCLE('',#101962,0.0999999999999994) ;
#34128 = CIRCLE('',#101964,0.0999999999999994) ;
#34129 = CIRCLE('',#101965,0.0999999999999994) ;
#34130 = CIRCLE('',#101967,0.1) ;
#34131 = CIRCLE('',#101968,0.0999999999999994) ;
#34132 = CIRCLE('',#101969,0.0999999999999994) ;
#34133 = CIRCLE('',#101971,0.0999999999999994) ;
#34134 = CIRCLE('',#101973,0.0999999999999994) ;
#34135 = CIRCLE('',#101975,0.0999999999999998) ;
#34136 = CIRCLE('',#101977,0.0999999999999994) ;
#34137 = CIRCLE('',#101979,0.1) ;
#34138 = CIRCLE('',#101981,0.0999999999999994) ;
#34139 = CIRCLE('',#101983,0.1) ;
#34140 = CIRCLE('',#101985,0.0999999999999994) ;
#34141 = CIRCLE('',#101987,0.0999999999999994) ;
#34142 = CIRCLE('',#101989,0.0999999999999994) ;
#34143 = CIRCLE('',#101990,0.0999999999999996) ;
#34144 = CIRCLE('',#101991,0.0999999999999996) ;
#34145 = CIRCLE('',#101993,0.1) ;
#34146 = CIRCLE('',#101995,0.0999999999999994) ;
#34147 = CIRCLE('',#101997,0.0999999999999994) ;
#34148 = CIRCLE('',#101999,0.1) ;
#34149 = CIRCLE('',#102001,0.1) ;
#34150 = CIRCLE('',#102003,0.1) ;
#34151 = CIRCLE('',#102005,0.1) ;
#34152 = CIRCLE('',#102006,0.1) ;
#34153 = CIRCLE('',#102007,0.0999999999999998) ;
#34154 = CIRCLE('',#102008,0.1) ;
#34155 = CIRCLE('',#102010,0.1) ;
#34156 = CIRCLE('',#102012,0.1) ;
#34157 = CIRCLE('',#102014,0.0999999999999994) ;
#34158 = CIRCLE('',#102016,0.0999999999999994) ;
#34159 = CIRCLE('',#102018,0.100000000000001) ;
#34160 = CIRCLE('',#102020,0.0999999999999996) ;
#34161 = CIRCLE('',#102022,0.0999999999999996) ;
#34162 = CIRCLE('',#102023,0.0999999999999996) ;
#34163 = CIRCLE('',#102025,0.0999999999999994) ;
#34164 = CIRCLE('',#102026,0.1) ;
#34165 = CIRCLE('',#102028,0.0999999999999998) ;
#34166 = CIRCLE('',#102030,0.0999999999999994) ;
#34167 = CIRCLE('',#102032,0.0999999999999994) ;
#34168 = CIRCLE('',#102034,0.0999999999999994) ;
#34169 = CIRCLE('',#102036,0.0999999999999998) ;
#34170 = CIRCLE('',#102038,0.0999999999999994) ;
#34171 = CIRCLE('',#102041,0.0999999999999994) ;
#34172 = CIRCLE('',#102043,0.1) ;
#34173 = CIRCLE('',#102044,0.1) ;
#34174 = CIRCLE('',#102046,0.0999999999999994) ;
#34175 = CIRCLE('',#102048,0.0999999999999994) ;
#34176 = CIRCLE('',#102050,0.0999999999999994) ;
#34177 = CIRCLE('',#102052,0.0999999999999994) ;
#34178 = CIRCLE('',#102054,0.0999999999999994) ;
#34179 = CIRCLE('',#102056,0.0999999999999994) ;
#34180 = CIRCLE('',#102058,0.0999999999999994) ;
#34181 = CIRCLE('',#102060,0.1) ;
#34182 = CIRCLE('',#102062,0.1) ;
#34183 = CIRCLE('',#102065,0.0999999999999994) ;
#34184 = CIRCLE('',#102066,0.0999999999999994) ;
#34185 = CIRCLE('',#102068,0.0999999999999998) ;
#34186 = CIRCLE('',#102069,0.0999999999999998) ;
#34187 = CIRCLE('',#102071,0.0999999999999998) ;
#34188 = CIRCLE('',#102072,0.1) ;
#34189 = CIRCLE('',#102074,0.0999999999999998) ;
#34190 = CIRCLE('',#102076,0.0999999999999994) ;
#34191 = CIRCLE('',#102078,0.0999999999999994) ;
#34192 = CIRCLE('',#102079,0.0999999999999994) ;
#34193 = CIRCLE('',#102081,0.0999999999999994) ;
#34194 = CIRCLE('',#102083,0.1) ;
#34195 = CIRCLE('',#102085,0.0999999999999994) ;
#34196 = CIRCLE('',#102086,0.0999999999999994) ;
#34197 = CIRCLE('',#102088,0.0999999999999998) ;
#34198 = CIRCLE('',#102090,0.0999999999999998) ;
#34199 = CIRCLE('',#102092,0.0999999999999998) ;
#34200 = CIRCLE('',#102094,0.0999999999999998) ;
#34201 = CIRCLE('',#102096,0.0999999999999994) ;
#34202 = CIRCLE('',#102098,0.0999999999999998) ;
#34203 = CIRCLE('',#102100,0.0999999999999998) ;
#34204 = CIRCLE('',#102102,0.0999999999999994) ;
#34205 = CIRCLE('',#102104,0.0999999999999994) ;
#34206 = CIRCLE('',#102106,0.0999999999999994) ;
#34207 = CIRCLE('',#102109,0.0999999999999994) ;
#34208 = CIRCLE('',#102111,0.0999999999999998) ;
#34209 = CIRCLE('',#102112,0.0999999999999998) ;
#34210 = CIRCLE('',#102114,0.0999999999999994) ;
#34211 = CIRCLE('',#102116,0.0999999999999994) ;
#34212 = CIRCLE('',#102118,0.0999999999999994) ;
#34213 = CIRCLE('',#102120,0.0999999999999994) ;
#34214 = CIRCLE('',#102122,0.0999999999999994) ;
#34215 = CIRCLE('',#102124,0.0999999999999994) ;
#34216 = CIRCLE('',#102126,0.0999999999999994) ;
#34217 = CIRCLE('',#102128,0.0999999999999998) ;
#34218 = CIRCLE('',#102130,0.0999999999999998) ;
#34219 = CIRCLE('',#102133,0.1) ;
#34220 = CIRCLE('',#102134,0.0999999999999994) ;
#34221 = CIRCLE('',#102136,0.0999999999999994) ;
#34222 = CIRCLE('',#102138,0.0999999999999994) ;
#34223 = CIRCLE('',#102140,0.0999999999999994) ;
#34224 = CIRCLE('',#102142,0.0999999999999994) ;
#34225 = CIRCLE('',#102144,0.0999999999999994) ;
#34226 = CIRCLE('',#102146,0.0999999999999994) ;
#34227 = CIRCLE('',#102153,0.1) ;
#34228 = CIRCLE('',#102154,0.0999999999999998) ;
#34229 = CIRCLE('',#102155,0.0999999999999994) ;
#34230 = CIRCLE('',#102157,0.0999999999999994) ;
#34231 = CIRCLE('',#102159,0.0999999999999994) ;
#34232 = CIRCLE('',#102161,0.1) ;
#34233 = CIRCLE('',#102163,0.0999999999999994) ;
#34234 = CIRCLE('',#102164,0.0999999999999994) ;
#34235 = CIRCLE('',#102166,0.0999999999999994) ;
#34236 = CIRCLE('',#102168,0.1) ;
#34237 = CIRCLE('',#102169,0.0999999999999998) ;
#34238 = CIRCLE('',#102171,0.0999999999999994) ;
#34239 = CIRCLE('',#102172,0.100000000000003) ;
#34240 = CIRCLE('',#102174,0.0999999999999994) ;
#34241 = CIRCLE('',#102175,0.0999999999999994) ;
#34242 = CIRCLE('',#102177,0.0999999999999994) ;
#34243 = CIRCLE('',#102179,0.0999999999999998) ;
#34244 = CIRCLE('',#102181,0.1) ;
#34245 = CIRCLE('',#102183,0.100000000000003) ;
#34246 = CIRCLE('',#102185,0.0999999999999994) ;
#34247 = CIRCLE('',#102187,0.100000000000003) ;
#34248 = CIRCLE('',#102188,0.100000000000003) ;
#34249 = CIRCLE('',#102190,0.0999999999999994) ;
#34250 = CIRCLE('',#102192,0.0999999999999998) ;
#34251 = CIRCLE('',#102194,0.100000000000003) ;
#34252 = CIRCLE('',#102196,0.0999999999999994) ;
#34253 = CIRCLE('',#102197,0.0999999999999994) ;
#34254 = CIRCLE('',#102199,0.0999999999999994) ;
#34255 = CIRCLE('',#102201,0.0999999999999998) ;
#34256 = CIRCLE('',#102203,0.100000000000003) ;
#34257 = CIRCLE('',#102205,0.0999999999999994) ;
#34258 = CIRCLE('',#102207,0.0999999999999998) ;
#34259 = CIRCLE('',#102208,0.0999999999999994) ;
#34260 = CIRCLE('',#102210,0.100000000000003) ;
#34261 = CIRCLE('',#102212,0.0999999999999994) ;
#34262 = CIRCLE('',#102214,0.1) ;
#34263 = CIRCLE('',#102216,0.0999999999999998) ;
#34264 = CIRCLE('',#102218,0.100000000000003) ;
#34265 = CIRCLE('',#102220,0.0999999999999998) ;
#34266 = CIRCLE('',#102222,0.100000000000003) ;
#34267 = CIRCLE('',#102224,0.0999999999999998) ;
#34268 = CIRCLE('',#102226,0.1) ;
#34269 = CIRCLE('',#102228,0.100000000000003) ;
#34270 = CIRCLE('',#102229,0.100000000000003) ;
#34271 = CIRCLE('',#102231,0.1) ;
#34272 = CIRCLE('',#102232,0.0999999999999998) ;
#34273 = CIRCLE('',#102234,0.100000000000003) ;
#34274 = CIRCLE('',#102236,0.100000000000003) ;
#34275 = CIRCLE('',#102238,0.0999999999999994) ;
#34276 = CIRCLE('',#102240,0.0999999999999994) ;
#34277 = CIRCLE('',#102241,0.0999999999999994) ;
#34278 = CIRCLE('',#102243,0.1) ;
#34279 = CIRCLE('',#102244,0.0999999999999994) ;
#34280 = CIRCLE('',#102245,0.100000000000003) ;
#34281 = CIRCLE('',#102247,0.0999999999999994) ;
#34282 = CIRCLE('',#102249,0.0999999999999994) ;
#34283 = CIRCLE('',#102251,0.0999999999999998) ;
#34284 = CIRCLE('',#102253,0.100000000000003) ;
#34285 = CIRCLE('',#102255,0.1) ;
#34286 = CIRCLE('',#102257,0.100000000000003) ;
#34287 = CIRCLE('',#102259,0.1) ;
#34288 = CIRCLE('',#102261,0.100000000000003) ;
#34289 = CIRCLE('',#102263,0.100000000000003) ;
#34290 = CIRCLE('',#102265,0.100000000000003) ;
#34291 = CIRCLE('',#102266,0.0999999999999996) ;
#34292 = CIRCLE('',#102267,0.0999999999999996) ;
#34293 = CIRCLE('',#102269,0.1) ;
#34294 = CIRCLE('',#102271,0.0999999999999994) ;
#34295 = CIRCLE('',#102273,0.0999999999999994) ;
#34296 = CIRCLE('',#102275,0.1) ;
#34297 = CIRCLE('',#102277,0.1) ;
#34298 = CIRCLE('',#102279,0.1) ;
#34299 = CIRCLE('',#102281,0.1) ;
#34300 = CIRCLE('',#102282,0.1) ;
#34301 = CIRCLE('',#102283,0.100000000000002) ;
#34302 = CIRCLE('',#102284,0.1) ;
#34303 = CIRCLE('',#102286,0.1) ;
#34304 = CIRCLE('',#102288,0.1) ;
#34305 = CIRCLE('',#102290,0.1) ;
#34306 = CIRCLE('',#102292,0.100000000000003) ;
#34307 = CIRCLE('',#102294,0.0999999999999983) ;
#34308 = CIRCLE('',#102296,0.0999999999999996) ;
#34309 = CIRCLE('',#102298,0.1) ;
#34310 = CIRCLE('',#102299,0.0999999999999969) ;
#34311 = CIRCLE('',#102301,0.0999999999999994) ;
#34312 = CIRCLE('',#102302,0.1) ;
#34313 = CIRCLE('',#102304,0.0999999999999998) ;
#34314 = CIRCLE('',#102306,0.0999999999999994) ;
#34315 = CIRCLE('',#102308,0.0999999999999994) ;
#34316 = CIRCLE('',#102310,0.0999999999999994) ;
#34317 = CIRCLE('',#102312,0.0999999999999998) ;
#34318 = CIRCLE('',#102314,0.0999999999999994) ;
#34319 = CIRCLE('',#102317,0.0999999999999994) ;
#34320 = CIRCLE('',#102319,0.1) ;
#34321 = CIRCLE('',#102320,0.1) ;
#34322 = CIRCLE('',#102322,0.0999999999999994) ;
#34323 = CIRCLE('',#102324,0.0999999999999994) ;
#34324 = CIRCLE('',#102326,0.0999999999999994) ;
#34325 = CIRCLE('',#102328,0.0999999999999994) ;
#34326 = CIRCLE('',#102330,0.0999999999999994) ;
#34327 = CIRCLE('',#102332,0.0999999999999994) ;
#34328 = CIRCLE('',#102334,0.0999999999999994) ;
#34329 = CIRCLE('',#102336,0.1) ;
#34330 = CIRCLE('',#102338,0.1) ;
#34331 = CIRCLE('',#102341,0.100000000000003) ;
#34332 = CIRCLE('',#102342,0.100000000000003) ;
#34333 = CIRCLE('',#102344,0.0999999999999998) ;
#34334 = CIRCLE('',#102345,0.0999999999999998) ;
#34335 = CIRCLE('',#102347,0.0999999999999998) ;
#34336 = CIRCLE('',#102348,0.1) ;
#34337 = CIRCLE('',#102350,0.0999999999999998) ;
#34338 = CIRCLE('',#102352,0.100000000000003) ;
#34339 = CIRCLE('',#102354,0.100000000000003) ;
#34340 = CIRCLE('',#102355,0.100000000000003) ;
#34341 = CIRCLE('',#102357,0.100000000000003) ;
#34342 = CIRCLE('',#102359,0.1) ;
#34343 = CIRCLE('',#102361,0.0999999999999994) ;
#34344 = CIRCLE('',#102362,0.0999999999999994) ;
#34345 = CIRCLE('',#102364,0.0999999999999998) ;
#34346 = CIRCLE('',#102366,0.0999999999999998) ;
#34347 = CIRCLE('',#102368,0.0999999999999998) ;
#34348 = CIRCLE('',#102370,0.0999999999999998) ;
#34349 = CIRCLE('',#102372,0.0999999999999994) ;
#34350 = CIRCLE('',#102374,0.0999999999999998) ;
#34351 = CIRCLE('',#102376,0.0999999999999998) ;
#34352 = CIRCLE('',#102378,0.0999999999999994) ;
#34353 = CIRCLE('',#102380,0.0999999999999994) ;
#34354 = CIRCLE('',#102382,0.0999999999999994) ;
#34355 = CIRCLE('',#102385,0.0999999999999994) ;
#34356 = CIRCLE('',#102387,0.0999999999999998) ;
#34357 = CIRCLE('',#102388,0.0999999999999998) ;
#34358 = CIRCLE('',#102390,0.0999999999999994) ;
#34359 = CIRCLE('',#102392,0.0999999999999994) ;
#34360 = CIRCLE('',#102394,0.0999999999999994) ;
#34361 = CIRCLE('',#102396,0.0999999999999994) ;
#34362 = CIRCLE('',#102398,0.0999999999999994) ;
#34363 = CIRCLE('',#102400,0.0999999999999994) ;
#34364 = CIRCLE('',#102402,0.0999999999999994) ;
#34365 = CIRCLE('',#102404,0.0999999999999998) ;
#34366 = CIRCLE('',#102406,0.0999999999999998) ;
#34367 = CIRCLE('',#102409,0.1) ;
#34368 = CIRCLE('',#102410,0.0999999999999994) ;
#34369 = CIRCLE('',#102412,0.0999999999999994) ;
#34370 = CIRCLE('',#102414,0.0999999999999994) ;
#34371 = CIRCLE('',#102416,0.0999999999999994) ;
#34372 = CIRCLE('',#102418,0.0999999999999994) ;
#34373 = CIRCLE('',#102420,0.0999999999999994) ;
#34374 = CIRCLE('',#102422,0.0999999999999994) ;
#34375 = CIRCLE('',#102429,0.1) ;
#34376 = CIRCLE('',#102430,0.0999999999999998) ;
#34377 = CIRCLE('',#102431,0.100000000000003) ;
#34378 = CIRCLE('',#102433,0.0999999999999994) ;
#34379 = CIRCLE('',#102435,0.100000000000003) ;
#34380 = CIRCLE('',#102437,0.1) ;
#34381 = CIRCLE('',#102439,0.100000000000003) ;
#34382 = CIRCLE('',#102440,0.100000000000003) ;
#34383 = CIRCLE('',#102442,0.100000000000003) ;
#34384 = CIRCLE('',#102444,0.1) ;
#34385 = CIRCLE('',#102445,0.0999999999999998) ;
#34386 = CIRCLE('',#102447,0.0999999999999994) ;
#34387 = CIRCLE('',#102448,0.100000000000003) ;
#34388 = CIRCLE('',#102450,0.0999999999999994) ;
#34389 = CIRCLE('',#102451,0.0999999999999994) ;
#34390 = CIRCLE('',#102453,0.100000000000003) ;
#34391 = CIRCLE('',#102455,0.0999999999999998) ;
#34392 = CIRCLE('',#102457,0.1) ;
#34393 = CIRCLE('',#102459,0.100000000000003) ;
#34394 = CIRCLE('',#102461,0.0999999999999994) ;
#34395 = CIRCLE('',#102463,0.100000000000003) ;
#34396 = CIRCLE('',#102464,0.100000000000003) ;
#34397 = CIRCLE('',#102466,0.100000000000003) ;
#34398 = CIRCLE('',#102468,0.0999999999999998) ;
#34399 = CIRCLE('',#102470,0.100000000000003) ;
#34400 = CIRCLE('',#102472,0.100000000000003) ;
#34401 = CIRCLE('',#102473,0.100000000000003) ;
#34402 = CIRCLE('',#102475,0.100000000000003) ;
#34403 = CIRCLE('',#102477,0.0999999999999998) ;
#34404 = CIRCLE('',#102479,0.100000000000003) ;
#34405 = CIRCLE('',#102481,0.0999999999999998) ;
#34406 = CIRCLE('',#102483,0.0999999999999998) ;
#34407 = CIRCLE('',#102484,0.100000000000003) ;
#34408 = CIRCLE('',#102486,0.100000000000003) ;
#34409 = CIRCLE('',#102488,0.100000000000003) ;
#34410 = CIRCLE('',#102490,0.1) ;
#34411 = CIRCLE('',#102492,0.0999999999999998) ;
#34412 = CIRCLE('',#102494,0.100000000000003) ;
#34413 = CIRCLE('',#102496,0.0999999999999998) ;
#34414 = CIRCLE('',#102498,0.100000000000003) ;
#34415 = CIRCLE('',#102500,0.0999999999999998) ;
#34416 = CIRCLE('',#102502,0.1) ;
#34417 = CIRCLE('',#102504,0.100000000000003) ;
#34418 = CIRCLE('',#102505,0.100000000000003) ;
#34419 = CIRCLE('',#102507,0.0999999999999998) ;
#34420 = CIRCLE('',#102508,0.0999999999999998) ;
#34421 = CIRCLE('',#102510,0.100000000000003) ;
#34422 = CIRCLE('',#102512,0.100000000000003) ;
#34423 = CIRCLE('',#102514,0.100000000000003) ;
#34424 = CIRCLE('',#102516,0.100000000000003) ;
#34425 = CIRCLE('',#102517,0.100000000000003) ;
#34426 = CIRCLE('',#102519,0.1) ;
#34427 = CIRCLE('',#102520,0.100000000000003) ;
#34428 = CIRCLE('',#102521,0.100000000000003) ;
#34429 = CIRCLE('',#102523,0.100000000000003) ;
#34430 = CIRCLE('',#102525,0.100000000000003) ;
#34431 = CIRCLE('',#102527,0.0999999999999998) ;
#34432 = CIRCLE('',#102529,0.100000000000003) ;
#34433 = CIRCLE('',#102531,0.1) ;
#34434 = CIRCLE('',#102533,0.100000000000003) ;
#34435 = CIRCLE('',#102535,0.1) ;
#34436 = CIRCLE('',#102537,0.100000000000003) ;
#34437 = CIRCLE('',#102539,0.100000000000003) ;
#34438 = CIRCLE('',#102541,0.100000000000003) ;
#34439 = CIRCLE('',#102542,0.100000000000003) ;
#34440 = CIRCLE('',#102543,0.0999999999999996) ;
#34441 = CIRCLE('',#102545,0.1) ;
#34442 = CIRCLE('',#102547,0.0999999999999994) ;
#34443 = CIRCLE('',#102549,0.1) ;
#34444 = CIRCLE('',#102551,0.100000000000003) ;
#34445 = CIRCLE('',#102553,0.1) ;
#34446 = CIRCLE('',#102555,0.1) ;
#34447 = CIRCLE('',#102557,0.1) ;
#34448 = CIRCLE('',#102558,0.0999999999999995) ;
#34449 = CIRCLE('',#102559,0.100000000000002) ;
#34450 = CIRCLE('',#102560,0.1) ;
#34451 = CIRCLE('',#102562,0.1) ;
#34452 = CIRCLE('',#102564,0.1) ;
#34453 = CIRCLE('',#102566,0.1) ;
#34454 = CIRCLE('',#102568,0.100000000000003) ;
#34455 = CIRCLE('',#102570,0.0999999999999983) ;
#34456 = CIRCLE('',#102572,0.0999999999999996) ;
#34457 = CIRCLE('',#102574,0.1) ;
#34458 = CIRCLE('',#102575,0.0999999999999969) ;
#34459 = CIRCLE('',#102577,0.100000000000003) ;
#34460 = CIRCLE('',#102578,0.1) ;
#34461 = CIRCLE('',#102580,0.1) ;
#34462 = CIRCLE('',#102582,0.100000000000003) ;
#34463 = CIRCLE('',#102584,0.100000000000003) ;
#34464 = CIRCLE('',#102586,0.0999999999999994) ;
#34465 = CIRCLE('',#102588,0.0999999999999998) ;
#34466 = CIRCLE('',#102590,0.0999999999999994) ;
#34467 = CIRCLE('',#102593,0.100000000000003) ;
#34468 = CIRCLE('',#102595,0.1) ;
#34469 = CIRCLE('',#102596,0.1) ;
#34470 = CIRCLE('',#102598,0.100000000000003) ;
#34471 = CIRCLE('',#102600,0.100000000000003) ;
#34472 = CIRCLE('',#102602,0.100000000000003) ;
#34473 = CIRCLE('',#102604,0.100000000000003) ;
#34474 = CIRCLE('',#102606,0.100000000000003) ;
#34475 = CIRCLE('',#102608,0.100000000000003) ;
#34476 = CIRCLE('',#102610,0.100000000000003) ;
#34477 = CIRCLE('',#102612,0.1) ;
#34478 = CIRCLE('',#102614,0.1) ;
#34479 = CIRCLE('',#102617,0.100000000000003) ;
#34480 = CIRCLE('',#102618,0.100000000000003) ;
#34481 = CIRCLE('',#102620,0.0999999999999998) ;
#34482 = CIRCLE('',#102621,0.0999999999999998) ;
#34483 = CIRCLE('',#102623,0.0999999999999998) ;
#34484 = CIRCLE('',#102624,0.1) ;
#34485 = CIRCLE('',#102626,0.0999999999999998) ;
#34486 = CIRCLE('',#102628,0.100000000000003) ;
#34487 = CIRCLE('',#102630,0.100000000000003) ;
#34488 = CIRCLE('',#102631,0.100000000000003) ;
#34489 = CIRCLE('',#102633,0.100000000000003) ;
#34490 = CIRCLE('',#102635,0.1) ;
#34491 = CIRCLE('',#102637,0.100000000000003) ;
#34492 = CIRCLE('',#102638,0.100000000000003) ;
#34493 = CIRCLE('',#102640,0.0999999999999998) ;
#34494 = CIRCLE('',#102642,0.0999999999999998) ;
#34495 = CIRCLE('',#102644,0.0999999999999998) ;
#34496 = CIRCLE('',#102646,0.0999999999999998) ;
#34497 = CIRCLE('',#102648,0.100000000000003) ;
#34498 = CIRCLE('',#102650,0.0999999999999998) ;
#34499 = CIRCLE('',#102652,0.0999999999999998) ;
#34500 = CIRCLE('',#102654,0.100000000000003) ;
#34501 = CIRCLE('',#102656,0.100000000000003) ;
#34502 = CIRCLE('',#102658,0.100000000000003) ;
#34503 = CIRCLE('',#102661,0.100000000000003) ;
#34504 = CIRCLE('',#102663,0.0999999999999998) ;
#34505 = CIRCLE('',#102664,0.0999999999999998) ;
#34506 = CIRCLE('',#102666,0.100000000000003) ;
#34507 = CIRCLE('',#102668,0.100000000000003) ;
#34508 = CIRCLE('',#102670,0.100000000000003) ;
#34509 = CIRCLE('',#102672,0.100000000000003) ;
#34510 = CIRCLE('',#102674,0.100000000000003) ;
#34511 = CIRCLE('',#102676,0.100000000000003) ;
#34512 = CIRCLE('',#102678,0.100000000000003) ;
#34513 = CIRCLE('',#102680,0.0999999999999998) ;
#34514 = CIRCLE('',#102682,0.0999999999999998) ;
#34515 = CIRCLE('',#102685,0.1) ;
#34516 = CIRCLE('',#102686,0.0999999999999994) ;
#34517 = CIRCLE('',#102688,0.100000000000003) ;
#34518 = CIRCLE('',#102690,0.100000000000003) ;
#34519 = CIRCLE('',#102692,0.100000000000003) ;
#34520 = CIRCLE('',#102694,0.100000000000003) ;
#34521 = CIRCLE('',#102696,0.0999999999999994) ;
#34522 = CIRCLE('',#102698,0.0999999999999994) ;
#34523 = CIRCLE('',#102705,0.0999999999999998) ;
#34524 = CIRCLE('',#102706,0.0999999999999998) ;
#34525 = CIRCLE('',#102708,0.0999999999999998) ;
#34526 = CIRCLE('',#102709,0.0999999999999998) ;
#34527 = CIRCLE('',#102711,0.0999999999999998) ;
#34528 = CIRCLE('',#102712,0.0999999999999998) ;
#34529 = CIRCLE('',#102714,0.0999999999999998) ;
#34530 = CIRCLE('',#102715,0.0999999999999998) ;
#34531 = CIRCLE('',#102717,0.0999999999999998) ;
#34532 = CIRCLE('',#102718,0.0999999999999998) ;
#34533 = CIRCLE('',#102720,0.0999999999999998) ;
#34534 = CIRCLE('',#102721,0.0999999999999998) ;
#34535 = CIRCLE('',#102723,0.0999999999999998) ;
#34536 = CIRCLE('',#102724,0.0999999999999998) ;
#34537 = CIRCLE('',#102726,0.0999999999999998) ;
#34538 = CIRCLE('',#102727,0.0999999999999998) ;
#34539 = CIRCLE('',#102729,0.0999999999999998) ;
#34540 = CIRCLE('',#102730,0.0999999999999998) ;
#34541 = CIRCLE('',#102732,0.0999999999999998) ;
#34542 = CIRCLE('',#102734,0.0999999999999998) ;
#34543 = CIRCLE('',#102735,0.0999999999999998) ;
#34544 = CIRCLE('',#102736,0.0999999999999998) ;
#34545 = CIRCLE('',#102740,0.0999999999999998) ;
#34546 = CIRCLE('',#102742,0.0999999999999998) ;
#34547 = CIRCLE('',#102743,0.0999999999999998) ;
#34548 = CIRCLE('',#102744,0.0999999999999998) ;
#34549 = CIRCLE('',#102747,0.0999999999999998) ;
#34550 = CIRCLE('',#102749,0.0999999999999998) ;
#34551 = CIRCLE('',#102750,0.0999999999999998) ;
#34552 = CIRCLE('',#102751,0.0999999999999998) ;
#34553 = CIRCLE('',#102754,0.0999999999999998) ;
#34554 = CIRCLE('',#102756,0.0999999999999998) ;
#34555 = CIRCLE('',#102757,0.0999999999999998) ;
#34556 = CIRCLE('',#102758,0.0999999999999998) ;
#34557 = CIRCLE('',#102761,0.0999999999999998) ;
#34558 = CIRCLE('',#102763,0.0999999999999998) ;
#34559 = CIRCLE('',#102764,0.0999999999999998) ;
#34560 = CIRCLE('',#102765,0.0999999999999998) ;
#34561 = CIRCLE('',#102768,0.0999999999999998) ;
#34562 = CIRCLE('',#102770,0.0999999999999998) ;
#34563 = CIRCLE('',#102771,0.0999999999999998) ;
#34564 = CIRCLE('',#102772,0.0999999999999998) ;
#34565 = CIRCLE('',#102775,0.0999999999999998) ;
#34566 = CIRCLE('',#102777,0.0999999999999998) ;
#34567 = CIRCLE('',#102778,0.0999999999999998) ;
#34568 = CIRCLE('',#102779,0.0999999999999998) ;
#34569 = CIRCLE('',#102782,0.0999999999999998) ;
#34570 = CIRCLE('',#102784,0.0999999999999998) ;
#34571 = CIRCLE('',#102785,0.0999999999999998) ;
#34572 = CIRCLE('',#102786,0.0999999999999998) ;
#34573 = CIRCLE('',#102789,0.0999999999999998) ;
#34574 = CIRCLE('',#102790,0.0999999999999998) ;
#34575 = CIRCLE('',#102791,0.0999999999999998) ;
#34576 = CIRCLE('',#102794,0.1) ;
#34577 = CIRCLE('',#102796,0.1) ;
#34578 = CIRCLE('',#102797,0.1) ;
#34579 = CIRCLE('',#102800,0.0999999999999998) ;
#34580 = CIRCLE('',#102802,0.0999999999999998) ;
#34581 = CIRCLE('',#102803,0.0999999999999998) ;
#34582 = CIRCLE('',#102806,0.0999999999999994) ;
#34583 = CIRCLE('',#102808,0.0999999999999994) ;
#34584 = CIRCLE('',#102809,0.0999999999999994) ;
#34585 = CIRCLE('',#102812,0.1) ;
#34586 = CIRCLE('',#102814,0.1) ;
#34587 = CIRCLE('',#102815,0.1) ;
#34588 = CIRCLE('',#102818,0.0999999999999994) ;
#34589 = CIRCLE('',#102820,0.0999999999999994) ;
#34590 = CIRCLE('',#102821,0.0999999999999994) ;
#34591 = CIRCLE('',#102824,0.0999999999999994) ;
#34592 = CIRCLE('',#102826,0.0999999999999994) ;
#34593 = CIRCLE('',#102827,0.0999999999999994) ;
#34594 = CIRCLE('',#102830,0.0999999999999994) ;
#34595 = CIRCLE('',#102832,0.0999999999999994) ;
#34596 = CIRCLE('',#102833,0.0999999999999994) ;
#34597 = CIRCLE('',#102836,0.0999999999999994) ;
#34598 = CIRCLE('',#102838,0.0999999999999994) ;
#34599 = CIRCLE('',#102839,0.0999999999999994) ;
#34600 = CIRCLE('',#102842,0.0999999999999994) ;
#34601 = CIRCLE('',#102844,0.0999999999999994) ;
#34602 = CIRCLE('',#102845,0.0999999999999994) ;
#34603 = CIRCLE('',#102848,0.0999999999999994) ;
#34604 = CIRCLE('',#102850,0.0999999999999994) ;
#34605 = CIRCLE('',#102851,0.0999999999999994) ;
#34606 = CIRCLE('',#102854,0.0999999999999994) ;
#34607 = CIRCLE('',#102856,0.0999999999999994) ;
#34608 = CIRCLE('',#102857,0.0999999999999994) ;
#34609 = CIRCLE('',#102860,0.0999999999999994) ;
#34610 = CIRCLE('',#102862,0.0999999999999994) ;
#34611 = CIRCLE('',#102863,0.0999999999999994) ;
#34612 = CIRCLE('',#102866,0.0999999999999994) ;
#34613 = CIRCLE('',#102868,0.0999999999999994) ;
#34614 = CIRCLE('',#102869,0.0999999999999994) ;
#34615 = CIRCLE('',#102872,0.0999999999999994) ;
#34616 = CIRCLE('',#102874,0.0999999999999994) ;
#34617 = CIRCLE('',#102875,0.0999999999999994) ;
#34618 = CIRCLE('',#102878,0.100000000000003) ;
#34619 = CIRCLE('',#102880,0.100000000000003) ;
#34620 = CIRCLE('',#102881,0.100000000000003) ;
#34621 = CIRCLE('',#102884,0.0999999999999994) ;
#34622 = CIRCLE('',#102886,0.0999999999999994) ;
#34623 = CIRCLE('',#102887,0.0999999999999994) ;
#34624 = CIRCLE('',#102890,0.100000000000003) ;
#34625 = CIRCLE('',#102892,0.100000000000003) ;
#34626 = CIRCLE('',#102893,0.100000000000003) ;
#34627 = CIRCLE('',#102896,0.100000000000003) ;
#34628 = CIRCLE('',#102898,0.100000000000003) ;
#34629 = CIRCLE('',#102899,0.100000000000003) ;
#34630 = CIRCLE('',#102902,0.1) ;
#34631 = CIRCLE('',#102903,0.1) ;
#34632 = CIRCLE('',#102906,0.0999999999999999) ;
#34633 = CIRCLE('',#102907,0.1) ;
#34634 = CIRCLE('',#102910,0.0999999999999999) ;
#34635 = CIRCLE('',#102911,0.1) ;
#34636 = CIRCLE('',#102914,0.1) ;
#34637 = CIRCLE('',#102915,0.1) ;
#34638 = CIRCLE('',#102918,0.1) ;
#34639 = CIRCLE('',#102919,0.1) ;
#34640 = CIRCLE('',#102922,0.1) ;
#34641 = CIRCLE('',#102923,0.1) ;
#34642 = CIRCLE('',#102926,0.1) ;
#34643 = CIRCLE('',#102927,0.1) ;
#34644 = CIRCLE('',#102930,0.1) ;
#34645 = CIRCLE('',#102931,0.1) ;
#34646 = CIRCLE('',#102934,0.1) ;
#34647 = CIRCLE('',#102935,0.1) ;
#34648 = CIRCLE('',#102938,0.1) ;
#34649 = CIRCLE('',#102939,0.1) ;
#34650 = CIRCLE('',#102942,0.1) ;
#34651 = CIRCLE('',#102943,0.1) ;
#34652 = CIRCLE('',#102946,0.1) ;
#34653 = CIRCLE('',#102947,0.1) ;
#34654 = CIRCLE('',#102950,0.1) ;
#34655 = CIRCLE('',#102951,0.1) ;
#34656 = CIRCLE('',#102954,0.1) ;
#34657 = CIRCLE('',#102955,0.1) ;
#34658 = CIRCLE('',#102958,0.0999999999999998) ;
#34659 = CIRCLE('',#102959,0.1) ;
#34660 = CIRCLE('',#102962,0.1) ;
#34661 = CIRCLE('',#102963,0.1) ;
#34662 = CIRCLE('',#102966,0.0999999999999998) ;
#34663 = CIRCLE('',#102967,0.1) ;
#34664 = CIRCLE('',#102970,0.1) ;
#34665 = CIRCLE('',#102971,0.1) ;
#34666 = CIRCLE('',#102974,2.25) ;
#34667 = CIRCLE('',#102976,2.25) ;
#34668 = CIRCLE('',#102978,2.25) ;
#34669 = CIRCLE('',#102980,2.25) ;
#34670 = CIRCLE('',#102982,2.25) ;
#34671 = CIRCLE('',#102984,2.25) ;
#34672 = CIRCLE('',#102986,0.0999999999999998) ;
#34673 = CIRCLE('',#102988,0.100000000000003) ;
#34674 = CIRCLE('',#102990,0.100000000000003) ;
#34675 = CIRCLE('',#102992,0.100000000000003) ;
#34676 = CIRCLE('',#102994,0.100000000000003) ;
#34677 = CIRCLE('',#102996,0.100000000000003) ;
#34678 = CIRCLE('',#102998,0.100000000000003) ;
#34679 = CIRCLE('',#103000,0.100000000000003) ;
#34680 = CIRCLE('',#103002,0.100000000000003) ;
#34681 = CIRCLE('',#103004,0.100000000000003) ;
#34682 = CIRCLE('',#103005,0.0999999999999998) ;
#34683 = CIRCLE('',#103007,0.100000000000003) ;
#34684 = CIRCLE('',#103009,0.100000000000003) ;
#34685 = CIRCLE('',#103011,0.0999999999999998) ;
#34686 = CIRCLE('',#103013,0.0999999999999998) ;
#34687 = CIRCLE('',#103015,0.0999999999999998) ;
#34688 = CIRCLE('',#103016,0.100000000000003) ;
#34689 = CIRCLE('',#103018,0.0999999999999998) ;
#34690 = CIRCLE('',#103020,0.100000000000003) ;
#34691 = CIRCLE('',#103023,0.100000000000003) ;
#34692 = CIRCLE('',#103033,0.0999999999999998) ;
#34693 = CIRCLE('',#103036,0.0999999999999998) ;
#34694 = CIRCLE('',#103038,0.0999999999999998) ;
#34695 = CIRCLE('',#103041,0.0999999999999998) ;
#34696 = CIRCLE('',#103043,0.0999999999999998) ;
#34697 = CIRCLE('',#103046,0.1) ;
#34698 = CIRCLE('',#103048,0.0999999999999998) ;
#34699 = CIRCLE('',#103050,0.0999999999999998) ;
#34700 = CIRCLE('',#103051,0.0999999999999998) ;
#34701 = CIRCLE('',#103053,0.0999999999999998) ;
#34702 = CIRCLE('',#103055,0.1) ;
#34703 = CIRCLE('',#103057,0.1) ;
#34704 = CIRCLE('',#103059,0.0999999999999998) ;
#34705 = CIRCLE('',#103061,0.0999999999999998) ;
#34706 = CIRCLE('',#103063,0.0999999999999998) ;
#34707 = CIRCLE('',#103065,0.0999999999999998) ;
#34708 = CIRCLE('',#103067,0.0999999999999998) ;
#34709 = CIRCLE('',#103069,0.0999999999999998) ;
#34710 = CIRCLE('',#103071,0.0999999999999998) ;
#34711 = CIRCLE('',#103073,0.0999999999999998) ;
#34712 = CIRCLE('',#103075,0.1) ;
#34713 = CIRCLE('',#103076,0.100000000000001) ;
#34714 = VERTEX_POINT('',#132553) ;
#34715 = VERTEX_POINT('',#132554) ;
#34716 = VERTEX_POINT('',#132556) ;
#34717 = VERTEX_POINT('',#132558) ;
#34718 = VERTEX_POINT('',#132562) ;
#34719 = VERTEX_POINT('',#132564) ;
#34720 = VERTEX_POINT('',#132566) ;
#34721 = VERTEX_POINT('',#132570) ;
#34722 = VERTEX_POINT('',#132572) ;
#34723 = VERTEX_POINT('',#132576) ;
#34724 = VERTEX_POINT('',#132578) ;
#34725 = VERTEX_POINT('',#132580) ;
#34726 = VERTEX_POINT('',#132584) ;
#34727 = VERTEX_POINT('',#132585) ;
#34728 = VERTEX_POINT('',#132587) ;
#34729 = VERTEX_POINT('',#132589) ;
#34730 = VERTEX_POINT('',#132593) ;
#34731 = VERTEX_POINT('',#132594) ;
#34732 = VERTEX_POINT('',#132596) ;
#34733 = VERTEX_POINT('',#132600) ;
#34734 = VERTEX_POINT('',#132602) ;
#34735 = VERTEX_POINT('',#132606) ;
#34736 = VERTEX_POINT('',#132607) ;
#34737 = VERTEX_POINT('',#132609) ;
#34738 = VERTEX_POINT('',#132613) ;
#34739 = VERTEX_POINT('',#132619) ;
#34740 = VERTEX_POINT('',#132620) ;
#34741 = VERTEX_POINT('',#132622) ;
#34742 = VERTEX_POINT('',#132633) ;
#34743 = VERTEX_POINT('',#132635) ;
#34744 = VERTEX_POINT('',#132646) ;
#34745 = VERTEX_POINT('',#132648) ;
#34746 = VERTEX_POINT('',#132659) ;
#34747 = VERTEX_POINT('',#132661) ;
#34748 = VERTEX_POINT('',#132693) ;
#34749 = VERTEX_POINT('',#132695) ;
#34750 = VERTEX_POINT('',#132706) ;
#34751 = VERTEX_POINT('',#132708) ;
#34752 = VERTEX_POINT('',#132719) ;
#34753 = VERTEX_POINT('',#132721) ;
#34754 = VERTEX_POINT('',#132732) ;
#34755 = VERTEX_POINT('',#132734) ;
#34756 = VERTEX_POINT('',#132769) ;
#34757 = VERTEX_POINT('',#132770) ;
#34758 = VERTEX_POINT('',#132772) ;
#34759 = VERTEX_POINT('',#132774) ;
#34760 = VERTEX_POINT('',#132778) ;
#34761 = VERTEX_POINT('',#132779) ;
#34762 = VERTEX_POINT('',#132781) ;
#34763 = VERTEX_POINT('',#132783) ;
#34764 = VERTEX_POINT('',#132787) ;
#34765 = VERTEX_POINT('',#132789) ;
#34766 = VERTEX_POINT('',#132791) ;
#34767 = VERTEX_POINT('',#132795) ;
#34768 = VERTEX_POINT('',#132797) ;
#34769 = VERTEX_POINT('',#132801) ;
#34770 = VERTEX_POINT('',#132803) ;
#34771 = VERTEX_POINT('',#132805) ;
#34772 = VERTEX_POINT('',#132809) ;
#34773 = VERTEX_POINT('',#132810) ;
#34774 = VERTEX_POINT('',#132812) ;
#34775 = VERTEX_POINT('',#132814) ;
#34776 = VERTEX_POINT('',#132818) ;
#34777 = VERTEX_POINT('',#132819) ;
#34778 = VERTEX_POINT('',#132821) ;
#34779 = VERTEX_POINT('',#132825) ;
#34780 = VERTEX_POINT('',#132827) ;
#34781 = VERTEX_POINT('',#132831) ;
#34782 = VERTEX_POINT('',#132832) ;
#34783 = VERTEX_POINT('',#132834) ;
#34784 = VERTEX_POINT('',#132838) ;
#34785 = VERTEX_POINT('',#132844) ;
#34786 = VERTEX_POINT('',#132845) ;
#34787 = VERTEX_POINT('',#132847) ;
#34788 = VERTEX_POINT('',#132858) ;
#34789 = VERTEX_POINT('',#132860) ;
#34790 = VERTEX_POINT('',#132871) ;
#34791 = VERTEX_POINT('',#132873) ;
#34792 = VERTEX_POINT('',#132884) ;
#34793 = VERTEX_POINT('',#132886) ;
#34794 = VERTEX_POINT('',#132918) ;
#34795 = VERTEX_POINT('',#132920) ;
#34796 = VERTEX_POINT('',#132931) ;
#34797 = VERTEX_POINT('',#132933) ;
#34798 = VERTEX_POINT('',#132944) ;
#34799 = VERTEX_POINT('',#132946) ;
#34800 = VERTEX_POINT('',#132957) ;
#34801 = VERTEX_POINT('',#132959) ;
#34802 = VERTEX_POINT('',#132994) ;
#34803 = VERTEX_POINT('',#132995) ;
#34804 = VERTEX_POINT('',#132997) ;
#34805 = VERTEX_POINT('',#132999) ;
#34806 = VERTEX_POINT('',#133002) ;
#34807 = VERTEX_POINT('',#133003) ;
#34808 = VERTEX_POINT('',#133005) ;
#34809 = VERTEX_POINT('',#133007) ;
#34810 = VERTEX_POINT('',#133012) ;
#34811 = VERTEX_POINT('',#133014) ;
#34812 = VERTEX_POINT('',#133019) ;
#34813 = VERTEX_POINT('',#133021) ;
#34814 = VERTEX_POINT('',#133025) ;
#34815 = VERTEX_POINT('',#133026) ;
#34816 = VERTEX_POINT('',#133028) ;
#34817 = VERTEX_POINT('',#133030) ;
#34818 = VERTEX_POINT('',#133034) ;
#34819 = VERTEX_POINT('',#133035) ;
#34820 = VERTEX_POINT('',#133037) ;
#34821 = VERTEX_POINT('',#133039) ;
#34822 = VERTEX_POINT('',#133043) ;
#34823 = VERTEX_POINT('',#133044) ;
#34824 = VERTEX_POINT('',#133046) ;
#34825 = VERTEX_POINT('',#133048) ;
#34826 = VERTEX_POINT('',#133052) ;
#34827 = VERTEX_POINT('',#133053) ;
#34828 = VERTEX_POINT('',#133064) ;
#34829 = VERTEX_POINT('',#133066) ;
#34830 = VERTEX_POINT('',#133068) ;
#34831 = VERTEX_POINT('',#133070) ;
#34832 = VERTEX_POINT('',#133074) ;
#34833 = VERTEX_POINT('',#133075) ;
#34834 = VERTEX_POINT('',#133077) ;
#34835 = VERTEX_POINT('',#133079) ;
#34836 = VERTEX_POINT('',#133083) ;
#34837 = VERTEX_POINT('',#133084) ;
#34838 = VERTEX_POINT('',#133086) ;
#34839 = VERTEX_POINT('',#133088) ;
#34840 = VERTEX_POINT('',#133093) ;
#34841 = VERTEX_POINT('',#133095) ;
#34842 = VERTEX_POINT('',#133102) ;
#34843 = VERTEX_POINT('',#133104) ;
#34844 = VERTEX_POINT('',#133106) ;
#34845 = VERTEX_POINT('',#133108) ;
#34846 = VERTEX_POINT('',#133110) ;
#34847 = VERTEX_POINT('',#133112) ;
#34848 = VERTEX_POINT('',#133114) ;
#34849 = VERTEX_POINT('',#133116) ;
#34850 = VERTEX_POINT('',#133118) ;
#34851 = VERTEX_POINT('',#133120) ;
#34852 = VERTEX_POINT('',#133122) ;
#34853 = VERTEX_POINT('',#133124) ;
#34854 = VERTEX_POINT('',#133127) ;
#34855 = VERTEX_POINT('',#133129) ;
#34856 = VERTEX_POINT('',#133134) ;
#34857 = VERTEX_POINT('',#133136) ;
#34858 = VERTEX_POINT('',#133140) ;
#34859 = VERTEX_POINT('',#133142) ;
#34860 = VERTEX_POINT('',#133144) ;
#34861 = VERTEX_POINT('',#133148) ;
#34862 = VERTEX_POINT('',#133149) ;
#34863 = VERTEX_POINT('',#133151) ;
#34864 = VERTEX_POINT('',#133153) ;
#34865 = VERTEX_POINT('',#133155) ;
#34866 = VERTEX_POINT('',#133157) ;
#34867 = VERTEX_POINT('',#133159) ;
#34868 = VERTEX_POINT('',#133161) ;
#34869 = VERTEX_POINT('',#133163) ;
#34870 = VERTEX_POINT('',#133165) ;
#34871 = VERTEX_POINT('',#133167) ;
#34872 = VERTEX_POINT('',#133169) ;
#34873 = VERTEX_POINT('',#133173) ;
#34874 = VERTEX_POINT('',#133174) ;
#34875 = VERTEX_POINT('',#133179) ;
#34876 = VERTEX_POINT('',#133181) ;
#34877 = VERTEX_POINT('',#133186) ;
#34878 = VERTEX_POINT('',#133187) ;
#34879 = VERTEX_POINT('',#133189) ;
#34880 = VERTEX_POINT('',#133191) ;
#34881 = VERTEX_POINT('',#133194) ;
#34882 = VERTEX_POINT('',#133195) ;
#34883 = VERTEX_POINT('',#133197) ;
#34884 = VERTEX_POINT('',#133199) ;
#34885 = VERTEX_POINT('',#133201) ;
#34886 = VERTEX_POINT('',#133203) ;
#34887 = VERTEX_POINT('',#133205) ;
#34888 = VERTEX_POINT('',#133207) ;
#34889 = VERTEX_POINT('',#133210) ;
#34890 = VERTEX_POINT('',#133211) ;
#34891 = VERTEX_POINT('',#133213) ;
#34892 = VERTEX_POINT('',#133215) ;
#34893 = VERTEX_POINT('',#133217) ;
#34894 = VERTEX_POINT('',#133219) ;
#34895 = VERTEX_POINT('',#133221) ;
#34896 = VERTEX_POINT('',#133223) ;
#34897 = VERTEX_POINT('',#133227) ;
#34898 = VERTEX_POINT('',#133228) ;
#34899 = VERTEX_POINT('',#133230) ;
#34900 = VERTEX_POINT('',#133232) ;
#34901 = VERTEX_POINT('',#133236) ;
#34902 = VERTEX_POINT('',#133237) ;
#34903 = VERTEX_POINT('',#133242) ;
#34904 = VERTEX_POINT('',#133244) ;
#34905 = VERTEX_POINT('',#133248) ;
#34906 = VERTEX_POINT('',#133249) ;
#34907 = VERTEX_POINT('',#133251) ;
#34908 = VERTEX_POINT('',#133253) ;
#34909 = VERTEX_POINT('',#133256) ;
#34910 = VERTEX_POINT('',#133257) ;
#34911 = VERTEX_POINT('',#133259) ;
#34912 = VERTEX_POINT('',#133266) ;
#34913 = VERTEX_POINT('',#133268) ;
#34914 = VERTEX_POINT('',#133275) ;
#34915 = VERTEX_POINT('',#133277) ;
#34916 = VERTEX_POINT('',#133284) ;
#34917 = VERTEX_POINT('',#133292) ;
#34918 = VERTEX_POINT('',#133293) ;
#34919 = VERTEX_POINT('',#133295) ;
#34920 = VERTEX_POINT('',#133302) ;
#34921 = VERTEX_POINT('',#133304) ;
#34922 = VERTEX_POINT('',#133311) ;
#34923 = VERTEX_POINT('',#133313) ;
#34924 = VERTEX_POINT('',#133320) ;
#34925 = VERTEX_POINT('',#133329) ;
#34926 = VERTEX_POINT('',#133330) ;
#34927 = VERTEX_POINT('',#133332) ;
#34928 = VERTEX_POINT('',#133334) ;
#34929 = VERTEX_POINT('',#133337) ;
#34930 = VERTEX_POINT('',#133338) ;
#34931 = VERTEX_POINT('',#133340) ;
#34932 = VERTEX_POINT('',#133342) ;
#34933 = VERTEX_POINT('',#133344) ;
#34934 = VERTEX_POINT('',#133346) ;
#34935 = VERTEX_POINT('',#133348) ;
#34936 = VERTEX_POINT('',#133350) ;
#34937 = VERTEX_POINT('',#133353) ;
#34938 = VERTEX_POINT('',#133354) ;
#34939 = VERTEX_POINT('',#133356) ;
#34940 = VERTEX_POINT('',#133358) ;
#34941 = VERTEX_POINT('',#133360) ;
#34942 = VERTEX_POINT('',#133362) ;
#34943 = VERTEX_POINT('',#133364) ;
#34944 = VERTEX_POINT('',#133366) ;
#34945 = VERTEX_POINT('',#133370) ;
#34946 = VERTEX_POINT('',#133371) ;
#34947 = VERTEX_POINT('',#133373) ;
#34948 = VERTEX_POINT('',#133375) ;
#34949 = VERTEX_POINT('',#133379) ;
#34950 = VERTEX_POINT('',#133380) ;
#34951 = VERTEX_POINT('',#133409) ;
#34952 = VERTEX_POINT('',#133420) ;
#34953 = VERTEX_POINT('',#133446) ;
#34954 = VERTEX_POINT('',#133463) ;
#34955 = VERTEX_POINT('',#133465) ;
#34956 = VERTEX_POINT('',#133467) ;
#34957 = VERTEX_POINT('',#133469) ;
#34958 = VERTEX_POINT('',#133471) ;
#34959 = VERTEX_POINT('',#133473) ;
#34960 = VERTEX_POINT('',#133502) ;
#34961 = VERTEX_POINT('',#133513) ;
#34962 = VERTEX_POINT('',#133539) ;
#34963 = VERTEX_POINT('',#133558) ;
#34964 = VERTEX_POINT('',#133559) ;
#34965 = VERTEX_POINT('',#133561) ;
#34966 = VERTEX_POINT('',#133563) ;
#34967 = VERTEX_POINT('',#133567) ;
#34968 = VERTEX_POINT('',#133568) ;
#34969 = VERTEX_POINT('',#133570) ;
#34970 = VERTEX_POINT('',#133572) ;
#34971 = VERTEX_POINT('',#133591) ;
#34972 = VERTEX_POINT('',#133592) ;
#34973 = VERTEX_POINT('',#133594) ;
#34974 = VERTEX_POINT('',#133596) ;
#34975 = VERTEX_POINT('',#133600) ;
#34976 = VERTEX_POINT('',#133601) ;
#34977 = VERTEX_POINT('',#133603) ;
#34978 = VERTEX_POINT('',#133605) ;
#34979 = VERTEX_POINT('',#133609) ;
#34980 = VERTEX_POINT('',#133610) ;
#34981 = VERTEX_POINT('',#133612) ;
#34982 = VERTEX_POINT('',#133614) ;
#34983 = VERTEX_POINT('',#133616) ;
#34984 = VERTEX_POINT('',#133618) ;
#34985 = VERTEX_POINT('',#133620) ;
#34986 = VERTEX_POINT('',#133622) ;
#34987 = VERTEX_POINT('',#133626) ;
#34988 = VERTEX_POINT('',#133627) ;
#34989 = VERTEX_POINT('',#133629) ;
#34990 = VERTEX_POINT('',#133631) ;
#34991 = VERTEX_POINT('',#133634) ;
#34992 = VERTEX_POINT('',#133636) ;
#34993 = VERTEX_POINT('',#133640) ;
#34994 = VERTEX_POINT('',#133641) ;
#34995 = VERTEX_POINT('',#133644) ;
#34996 = VERTEX_POINT('',#133646) ;
#34997 = VERTEX_POINT('',#133648) ;
#34998 = VERTEX_POINT('',#133650) ;
#34999 = VERTEX_POINT('',#133654) ;
#35000 = VERTEX_POINT('',#133656) ;
#35001 = VERTEX_POINT('',#133660) ;
#35002 = VERTEX_POINT('',#133662) ;
#35003 = VERTEX_POINT('',#133666) ;
#35004 = VERTEX_POINT('',#133667) ;
#35005 = VERTEX_POINT('',#133669) ;
#35006 = VERTEX_POINT('',#133671) ;
#35007 = VERTEX_POINT('',#133673) ;
#35008 = VERTEX_POINT('',#133675) ;
#35009 = VERTEX_POINT('',#133679) ;
#35010 = VERTEX_POINT('',#133680) ;
#35011 = VERTEX_POINT('',#133682) ;
#35012 = VERTEX_POINT('',#133684) ;
#35013 = VERTEX_POINT('',#133686) ;
#35014 = VERTEX_POINT('',#133688) ;
#35015 = VERTEX_POINT('',#133692) ;
#35016 = VERTEX_POINT('',#133693) ;
#35017 = VERTEX_POINT('',#133695) ;
#35018 = VERTEX_POINT('',#133697) ;
#35019 = VERTEX_POINT('',#133701) ;
#35020 = VERTEX_POINT('',#133702) ;
#35021 = VERTEX_POINT('',#133704) ;
#35022 = VERTEX_POINT('',#133706) ;
#35023 = VERTEX_POINT('',#133710) ;
#35024 = VERTEX_POINT('',#133711) ;
#35025 = VERTEX_POINT('',#133713) ;
#35026 = VERTEX_POINT('',#133715) ;
#35027 = VERTEX_POINT('',#133719) ;
#35028 = VERTEX_POINT('',#133720) ;
#35029 = VERTEX_POINT('',#133722) ;
#35030 = VERTEX_POINT('',#133724) ;
#35031 = VERTEX_POINT('',#133728) ;
#35032 = VERTEX_POINT('',#133729) ;
#35033 = VERTEX_POINT('',#133731) ;
#35034 = VERTEX_POINT('',#133733) ;
#35035 = VERTEX_POINT('',#133736) ;
#35036 = VERTEX_POINT('',#133737) ;
#35037 = VERTEX_POINT('',#133739) ;
#35038 = VERTEX_POINT('',#133741) ;
#35039 = VERTEX_POINT('',#133743) ;
#35040 = VERTEX_POINT('',#133745) ;
#35041 = VERTEX_POINT('',#133747) ;
#35042 = VERTEX_POINT('',#133749) ;
#35043 = VERTEX_POINT('',#133753) ;
#35044 = VERTEX_POINT('',#133754) ;
#35045 = VERTEX_POINT('',#133759) ;
#35046 = VERTEX_POINT('',#133763) ;
#35047 = VERTEX_POINT('',#133767) ;
#35048 = VERTEX_POINT('',#133771) ;
#35049 = VERTEX_POINT('',#133775) ;
#35050 = VERTEX_POINT('',#133779) ;
#35051 = VERTEX_POINT('',#133797) ;
#35052 = VERTEX_POINT('',#133798) ;
#35053 = VERTEX_POINT('',#133800) ;
#35054 = VERTEX_POINT('',#133802) ;
#35055 = VERTEX_POINT('',#133806) ;
#35056 = VERTEX_POINT('',#133807) ;
#35057 = VERTEX_POINT('',#133809) ;
#35058 = VERTEX_POINT('',#133811) ;
#35059 = VERTEX_POINT('',#133815) ;
#35060 = VERTEX_POINT('',#133816) ;
#35061 = VERTEX_POINT('',#133818) ;
#35062 = VERTEX_POINT('',#133820) ;
#35063 = VERTEX_POINT('',#133824) ;
#35064 = VERTEX_POINT('',#133825) ;
#35065 = VERTEX_POINT('',#133827) ;
#35066 = VERTEX_POINT('',#133829) ;
#35067 = VERTEX_POINT('',#133833) ;
#35068 = VERTEX_POINT('',#133834) ;
#35069 = VERTEX_POINT('',#133836) ;
#35070 = VERTEX_POINT('',#133838) ;
#35071 = VERTEX_POINT('',#133841) ;
#35072 = VERTEX_POINT('',#133842) ;
#35073 = VERTEX_POINT('',#133844) ;
#35074 = VERTEX_POINT('',#133846) ;
#35075 = VERTEX_POINT('',#133848) ;
#35076 = VERTEX_POINT('',#133850) ;
#35077 = VERTEX_POINT('',#133852) ;
#35078 = VERTEX_POINT('',#133854) ;
#35079 = VERTEX_POINT('',#133858) ;
#35080 = VERTEX_POINT('',#133860) ;
#35081 = VERTEX_POINT('',#133864) ;
#35082 = VERTEX_POINT('',#133868) ;
#35083 = VERTEX_POINT('',#133872) ;
#35084 = VERTEX_POINT('',#133876) ;
#35085 = VERTEX_POINT('',#133880) ;
#35086 = VERTEX_POINT('',#133884) ;
#35087 = VERTEX_POINT('',#133890) ;
#35088 = VERTEX_POINT('',#133891) ;
#35089 = VERTEX_POINT('',#133893) ;
#35090 = VERTEX_POINT('',#133895) ;
#35091 = VERTEX_POINT('',#133900) ;
#35092 = VERTEX_POINT('',#133902) ;
#35093 = VERTEX_POINT('',#133906) ;
#35094 = VERTEX_POINT('',#133908) ;
#35095 = VERTEX_POINT('',#133912) ;
#35096 = VERTEX_POINT('',#133917) ;
#35097 = VERTEX_POINT('',#133919) ;
#35098 = VERTEX_POINT('',#133921) ;
#35099 = VERTEX_POINT('',#133923) ;
#35100 = VERTEX_POINT('',#133928) ;
#35101 = VERTEX_POINT('',#133929) ;
#35102 = VERTEX_POINT('',#133931) ;
#35103 = VERTEX_POINT('',#133933) ;
#35104 = VERTEX_POINT('',#133935) ;
#35105 = VERTEX_POINT('',#133937) ;
#35106 = VERTEX_POINT('',#134132) ;
#35107 = VERTEX_POINT('',#134194) ;
#35108 = VERTEX_POINT('',#134195) ;
#35109 = VERTEX_POINT('',#134461) ;
#35110 = VERTEX_POINT('',#134462) ;
#35111 = VERTEX_POINT('',#134503) ;
#35112 = VERTEX_POINT('',#134838) ;
#35113 = VERTEX_POINT('',#134839) ;
#35114 = VERTEX_POINT('',#134841) ;
#35115 = VERTEX_POINT('',#134843) ;
#35116 = VERTEX_POINT('',#134847) ;
#35117 = VERTEX_POINT('',#134849) ;
#35118 = VERTEX_POINT('',#134853) ;
#35119 = VERTEX_POINT('',#134855) ;
#35120 = VERTEX_POINT('',#134859) ;
#35121 = VERTEX_POINT('',#134861) ;
#35122 = VERTEX_POINT('',#134865) ;
#35123 = VERTEX_POINT('',#134867) ;
#35124 = VERTEX_POINT('',#134871) ;
#35125 = VERTEX_POINT('',#134873) ;
#35126 = VERTEX_POINT('',#134877) ;
#35127 = VERTEX_POINT('',#134879) ;
#35128 = VERTEX_POINT('',#134883) ;
#35129 = VERTEX_POINT('',#134885) ;
#35130 = VERTEX_POINT('',#134889) ;
#35131 = VERTEX_POINT('',#134891) ;
#35132 = VERTEX_POINT('',#134895) ;
#35133 = VERTEX_POINT('',#134896) ;
#35134 = VERTEX_POINT('',#134898) ;
#35135 = VERTEX_POINT('',#134900) ;
#35136 = VERTEX_POINT('',#134902) ;
#35137 = VERTEX_POINT('',#134904) ;
#35138 = VERTEX_POINT('',#134906) ;
#35139 = VERTEX_POINT('',#134910) ;
#35140 = VERTEX_POINT('',#134911) ;
#35141 = VERTEX_POINT('',#134913) ;
#35142 = VERTEX_POINT('',#134915) ;
#35143 = VERTEX_POINT('',#134917) ;
#35144 = VERTEX_POINT('',#134919) ;
#35145 = VERTEX_POINT('',#134921) ;
#35146 = VERTEX_POINT('',#134925) ;
#35147 = VERTEX_POINT('',#134926) ;
#35148 = VERTEX_POINT('',#134928) ;
#35149 = VERTEX_POINT('',#134930) ;
#35150 = VERTEX_POINT('',#134934) ;
#35151 = VERTEX_POINT('',#134935) ;
#35152 = VERTEX_POINT('',#134937) ;
#35153 = VERTEX_POINT('',#134944) ;
#35154 = VERTEX_POINT('',#134945) ;
#35155 = VERTEX_POINT('',#134947) ;
#35156 = VERTEX_POINT('',#134949) ;
#35157 = VERTEX_POINT('',#134959) ;
#35158 = VERTEX_POINT('',#134960) ;
#35159 = VERTEX_POINT('',#134962) ;
#35160 = VERTEX_POINT('',#134964) ;
#35161 = VERTEX_POINT('',#134968) ;
#35162 = VERTEX_POINT('',#134969) ;
#35163 = VERTEX_POINT('',#134971) ;
#35164 = VERTEX_POINT('',#134973) ;
#35165 = VERTEX_POINT('',#134977) ;
#35166 = VERTEX_POINT('',#134978) ;
#35167 = VERTEX_POINT('',#134980) ;
#35168 = VERTEX_POINT('',#134982) ;
#35169 = VERTEX_POINT('',#134984) ;
#35170 = VERTEX_POINT('',#134986) ;
#35171 = VERTEX_POINT('',#134988) ;
#35172 = VERTEX_POINT('',#134990) ;
#35173 = VERTEX_POINT('',#134994) ;
#35174 = VERTEX_POINT('',#134995) ;
#35175 = VERTEX_POINT('',#134997) ;
#35176 = VERTEX_POINT('',#134999) ;
#35177 = VERTEX_POINT('',#135002) ;
#35178 = VERTEX_POINT('',#135004) ;
#35179 = VERTEX_POINT('',#135008) ;
#35180 = VERTEX_POINT('',#135009) ;
#35181 = VERTEX_POINT('',#135012) ;
#35182 = VERTEX_POINT('',#135014) ;
#35183 = VERTEX_POINT('',#135016) ;
#35184 = VERTEX_POINT('',#135018) ;
#35185 = VERTEX_POINT('',#135022) ;
#35186 = VERTEX_POINT('',#135024) ;
#35187 = VERTEX_POINT('',#135028) ;
#35188 = VERTEX_POINT('',#135030) ;
#35189 = VERTEX_POINT('',#135034) ;
#35190 = VERTEX_POINT('',#135035) ;
#35191 = VERTEX_POINT('',#135037) ;
#35192 = VERTEX_POINT('',#135039) ;
#35193 = VERTEX_POINT('',#135041) ;
#35194 = VERTEX_POINT('',#135043) ;
#35195 = VERTEX_POINT('',#135047) ;
#35196 = VERTEX_POINT('',#135048) ;
#35197 = VERTEX_POINT('',#135050) ;
#35198 = VERTEX_POINT('',#135052) ;
#35199 = VERTEX_POINT('',#135054) ;
#35200 = VERTEX_POINT('',#135056) ;
#35201 = VERTEX_POINT('',#135060) ;
#35202 = VERTEX_POINT('',#135061) ;
#35203 = VERTEX_POINT('',#135063) ;
#35204 = VERTEX_POINT('',#135065) ;
#35205 = VERTEX_POINT('',#135069) ;
#35206 = VERTEX_POINT('',#135070) ;
#35207 = VERTEX_POINT('',#135072) ;
#35208 = VERTEX_POINT('',#135074) ;
#35209 = VERTEX_POINT('',#135078) ;
#35210 = VERTEX_POINT('',#135079) ;
#35211 = VERTEX_POINT('',#135081) ;
#35212 = VERTEX_POINT('',#135083) ;
#35213 = VERTEX_POINT('',#135087) ;
#35214 = VERTEX_POINT('',#135088) ;
#35215 = VERTEX_POINT('',#135090) ;
#35216 = VERTEX_POINT('',#135092) ;
#35217 = VERTEX_POINT('',#135096) ;
#35218 = VERTEX_POINT('',#135097) ;
#35219 = VERTEX_POINT('',#135099) ;
#35220 = VERTEX_POINT('',#135101) ;
#35221 = VERTEX_POINT('',#135104) ;
#35222 = VERTEX_POINT('',#135105) ;
#35223 = VERTEX_POINT('',#135107) ;
#35224 = VERTEX_POINT('',#135109) ;
#35225 = VERTEX_POINT('',#135111) ;
#35226 = VERTEX_POINT('',#135113) ;
#35227 = VERTEX_POINT('',#135115) ;
#35228 = VERTEX_POINT('',#135117) ;
#35229 = VERTEX_POINT('',#135121) ;
#35230 = VERTEX_POINT('',#135122) ;
#35231 = VERTEX_POINT('',#135127) ;
#35232 = VERTEX_POINT('',#135131) ;
#35233 = VERTEX_POINT('',#135135) ;
#35234 = VERTEX_POINT('',#135139) ;
#35235 = VERTEX_POINT('',#135143) ;
#35236 = VERTEX_POINT('',#135147) ;
#35237 = VERTEX_POINT('',#135165) ;
#35238 = VERTEX_POINT('',#135166) ;
#35239 = VERTEX_POINT('',#135168) ;
#35240 = VERTEX_POINT('',#135170) ;
#35241 = VERTEX_POINT('',#135174) ;
#35242 = VERTEX_POINT('',#135175) ;
#35243 = VERTEX_POINT('',#135177) ;
#35244 = VERTEX_POINT('',#135179) ;
#35245 = VERTEX_POINT('',#135183) ;
#35246 = VERTEX_POINT('',#135184) ;
#35247 = VERTEX_POINT('',#135186) ;
#35248 = VERTEX_POINT('',#135188) ;
#35249 = VERTEX_POINT('',#135192) ;
#35250 = VERTEX_POINT('',#135193) ;
#35251 = VERTEX_POINT('',#135195) ;
#35252 = VERTEX_POINT('',#135197) ;
#35253 = VERTEX_POINT('',#135201) ;
#35254 = VERTEX_POINT('',#135202) ;
#35255 = VERTEX_POINT('',#135204) ;
#35256 = VERTEX_POINT('',#135206) ;
#35257 = VERTEX_POINT('',#135209) ;
#35258 = VERTEX_POINT('',#135210) ;
#35259 = VERTEX_POINT('',#135212) ;
#35260 = VERTEX_POINT('',#135214) ;
#35261 = VERTEX_POINT('',#135216) ;
#35262 = VERTEX_POINT('',#135218) ;
#35263 = VERTEX_POINT('',#135220) ;
#35264 = VERTEX_POINT('',#135222) ;
#35265 = VERTEX_POINT('',#135226) ;
#35266 = VERTEX_POINT('',#135228) ;
#35267 = VERTEX_POINT('',#135232) ;
#35268 = VERTEX_POINT('',#135236) ;
#35269 = VERTEX_POINT('',#135240) ;
#35270 = VERTEX_POINT('',#135244) ;
#35271 = VERTEX_POINT('',#135248) ;
#35272 = VERTEX_POINT('',#135252) ;
#35273 = VERTEX_POINT('',#135258) ;
#35274 = VERTEX_POINT('',#135259) ;
#35275 = VERTEX_POINT('',#135261) ;
#35276 = VERTEX_POINT('',#135263) ;
#35277 = VERTEX_POINT('',#135268) ;
#35278 = VERTEX_POINT('',#135270) ;
#35279 = VERTEX_POINT('',#135274) ;
#35280 = VERTEX_POINT('',#135276) ;
#35281 = VERTEX_POINT('',#135280) ;
#35282 = VERTEX_POINT('',#135285) ;
#35283 = VERTEX_POINT('',#135287) ;
#35284 = VERTEX_POINT('',#135289) ;
#35285 = VERTEX_POINT('',#135291) ;
#35286 = VERTEX_POINT('',#135296) ;
#35287 = VERTEX_POINT('',#135297) ;
#35288 = VERTEX_POINT('',#135299) ;
#35289 = VERTEX_POINT('',#135301) ;
#35290 = VERTEX_POINT('',#135303) ;
#35291 = VERTEX_POINT('',#135305) ;
#35292 = VERTEX_POINT('',#135500) ;
#35293 = VERTEX_POINT('',#135561) ;
#35294 = VERTEX_POINT('',#135562) ;
#35295 = VERTEX_POINT('',#135801) ;
#35296 = VERTEX_POINT('',#135802) ;
#35297 = VERTEX_POINT('',#135843) ;
#35298 = VERTEX_POINT('',#136256) ;
#35299 = VERTEX_POINT('',#136257) ;
#35300 = VERTEX_POINT('',#136259) ;
#35301 = VERTEX_POINT('',#136261) ;
#35302 = VERTEX_POINT('',#136265) ;
#35303 = VERTEX_POINT('',#136267) ;
#35304 = VERTEX_POINT('',#136269) ;
#35305 = VERTEX_POINT('',#136273) ;
#35306 = VERTEX_POINT('',#136275) ;
#35307 = VERTEX_POINT('',#136279) ;
#35308 = VERTEX_POINT('',#136281) ;
#35309 = VERTEX_POINT('',#136283) ;
#35310 = VERTEX_POINT('',#136287) ;
#35311 = VERTEX_POINT('',#136288) ;
#35312 = VERTEX_POINT('',#136290) ;
#35313 = VERTEX_POINT('',#136292) ;
#35314 = VERTEX_POINT('',#136296) ;
#35315 = VERTEX_POINT('',#136297) ;
#35316 = VERTEX_POINT('',#136299) ;
#35317 = VERTEX_POINT('',#136303) ;
#35318 = VERTEX_POINT('',#136305) ;
#35319 = VERTEX_POINT('',#136309) ;
#35320 = VERTEX_POINT('',#136310) ;
#35321 = VERTEX_POINT('',#136312) ;
#35322 = VERTEX_POINT('',#136316) ;
#35323 = VERTEX_POINT('',#136322) ;
#35324 = VERTEX_POINT('',#136323) ;
#35325 = VERTEX_POINT('',#136325) ;
#35326 = VERTEX_POINT('',#136336) ;
#35327 = VERTEX_POINT('',#136338) ;
#35328 = VERTEX_POINT('',#136349) ;
#35329 = VERTEX_POINT('',#136351) ;
#35330 = VERTEX_POINT('',#136362) ;
#35331 = VERTEX_POINT('',#136364) ;
#35332 = VERTEX_POINT('',#136396) ;
#35333 = VERTEX_POINT('',#136398) ;
#35334 = VERTEX_POINT('',#136409) ;
#35335 = VERTEX_POINT('',#136411) ;
#35336 = VERTEX_POINT('',#136422) ;
#35337 = VERTEX_POINT('',#136424) ;
#35338 = VERTEX_POINT('',#136435) ;
#35339 = VERTEX_POINT('',#136437) ;
#35340 = VERTEX_POINT('',#136472) ;
#35341 = VERTEX_POINT('',#136473) ;
#35342 = VERTEX_POINT('',#136475) ;
#35343 = VERTEX_POINT('',#136477) ;
#35344 = VERTEX_POINT('',#136481) ;
#35345 = VERTEX_POINT('',#136482) ;
#35346 = VERTEX_POINT('',#136484) ;
#35347 = VERTEX_POINT('',#136486) ;
#35348 = VERTEX_POINT('',#136490) ;
#35349 = VERTEX_POINT('',#136492) ;
#35350 = VERTEX_POINT('',#136494) ;
#35351 = VERTEX_POINT('',#136498) ;
#35352 = VERTEX_POINT('',#136500) ;
#35353 = VERTEX_POINT('',#136504) ;
#35354 = VERTEX_POINT('',#136506) ;
#35355 = VERTEX_POINT('',#136508) ;
#35356 = VERTEX_POINT('',#136512) ;
#35357 = VERTEX_POINT('',#136513) ;
#35358 = VERTEX_POINT('',#136515) ;
#35359 = VERTEX_POINT('',#136517) ;
#35360 = VERTEX_POINT('',#136521) ;
#35361 = VERTEX_POINT('',#136522) ;
#35362 = VERTEX_POINT('',#136524) ;
#35363 = VERTEX_POINT('',#136528) ;
#35364 = VERTEX_POINT('',#136530) ;
#35365 = VERTEX_POINT('',#136534) ;
#35366 = VERTEX_POINT('',#136535) ;
#35367 = VERTEX_POINT('',#136537) ;
#35368 = VERTEX_POINT('',#136541) ;
#35369 = VERTEX_POINT('',#136547) ;
#35370 = VERTEX_POINT('',#136548) ;
#35371 = VERTEX_POINT('',#136550) ;
#35372 = VERTEX_POINT('',#136561) ;
#35373 = VERTEX_POINT('',#136563) ;
#35374 = VERTEX_POINT('',#136574) ;
#35375 = VERTEX_POINT('',#136576) ;
#35376 = VERTEX_POINT('',#136587) ;
#35377 = VERTEX_POINT('',#136589) ;
#35378 = VERTEX_POINT('',#136621) ;
#35379 = VERTEX_POINT('',#136623) ;
#35380 = VERTEX_POINT('',#136634) ;
#35381 = VERTEX_POINT('',#136636) ;
#35382 = VERTEX_POINT('',#136647) ;
#35383 = VERTEX_POINT('',#136649) ;
#35384 = VERTEX_POINT('',#136660) ;
#35385 = VERTEX_POINT('',#136662) ;
#35386 = VERTEX_POINT('',#136697) ;
#35387 = VERTEX_POINT('',#136698) ;
#35388 = VERTEX_POINT('',#136700) ;
#35389 = VERTEX_POINT('',#136702) ;
#35390 = VERTEX_POINT('',#136705) ;
#35391 = VERTEX_POINT('',#136706) ;
#35392 = VERTEX_POINT('',#136708) ;
#35393 = VERTEX_POINT('',#136710) ;
#35394 = VERTEX_POINT('',#136715) ;
#35395 = VERTEX_POINT('',#136717) ;
#35396 = VERTEX_POINT('',#136722) ;
#35397 = VERTEX_POINT('',#136724) ;
#35398 = VERTEX_POINT('',#136728) ;
#35399 = VERTEX_POINT('',#136729) ;
#35400 = VERTEX_POINT('',#136731) ;
#35401 = VERTEX_POINT('',#136733) ;
#35402 = VERTEX_POINT('',#136737) ;
#35403 = VERTEX_POINT('',#136738) ;
#35404 = VERTEX_POINT('',#136740) ;
#35405 = VERTEX_POINT('',#136742) ;
#35406 = VERTEX_POINT('',#136746) ;
#35407 = VERTEX_POINT('',#136747) ;
#35408 = VERTEX_POINT('',#136749) ;
#35409 = VERTEX_POINT('',#136751) ;
#35410 = VERTEX_POINT('',#136755) ;
#35411 = VERTEX_POINT('',#136757) ;
#35412 = VERTEX_POINT('',#136767) ;
#35413 = VERTEX_POINT('',#136768) ;
#35414 = VERTEX_POINT('',#136770) ;
#35415 = VERTEX_POINT('',#136773) ;
#35416 = VERTEX_POINT('',#136777) ;
#35417 = VERTEX_POINT('',#136778) ;
#35418 = VERTEX_POINT('',#136780) ;
#35419 = VERTEX_POINT('',#136782) ;
#35420 = VERTEX_POINT('',#136786) ;
#35421 = VERTEX_POINT('',#136787) ;
#35422 = VERTEX_POINT('',#136789) ;
#35423 = VERTEX_POINT('',#136791) ;
#35424 = VERTEX_POINT('',#136795) ;
#35425 = VERTEX_POINT('',#136796) ;
#35426 = VERTEX_POINT('',#136798) ;
#35427 = VERTEX_POINT('',#136807) ;
#35428 = VERTEX_POINT('',#136809) ;
#35429 = VERTEX_POINT('',#136813) ;
#35430 = VERTEX_POINT('',#136815) ;
#35431 = VERTEX_POINT('',#136817) ;
#35432 = VERTEX_POINT('',#136819) ;
#35433 = VERTEX_POINT('',#136821) ;
#35434 = VERTEX_POINT('',#136823) ;
#35435 = VERTEX_POINT('',#136825) ;
#35436 = VERTEX_POINT('',#136827) ;
#35437 = VERTEX_POINT('',#136829) ;
#35438 = VERTEX_POINT('',#136831) ;
#35439 = VERTEX_POINT('',#136833) ;
#35440 = VERTEX_POINT('',#136835) ;
#35441 = VERTEX_POINT('',#136838) ;
#35442 = VERTEX_POINT('',#136840) ;
#35443 = VERTEX_POINT('',#136844) ;
#35444 = VERTEX_POINT('',#136846) ;
#35445 = VERTEX_POINT('',#136851) ;
#35446 = VERTEX_POINT('',#136852) ;
#35447 = VERTEX_POINT('',#136854) ;
#35448 = VERTEX_POINT('',#136856) ;
#35449 = VERTEX_POINT('',#136858) ;
#35450 = VERTEX_POINT('',#136860) ;
#35451 = VERTEX_POINT('',#136862) ;
#35452 = VERTEX_POINT('',#136864) ;
#35453 = VERTEX_POINT('',#136866) ;
#35454 = VERTEX_POINT('',#136868) ;
#35455 = VERTEX_POINT('',#136870) ;
#35456 = VERTEX_POINT('',#136872) ;
#35457 = VERTEX_POINT('',#136876) ;
#35458 = VERTEX_POINT('',#136878) ;
#35459 = VERTEX_POINT('',#136882) ;
#35460 = VERTEX_POINT('',#136884) ;
#35461 = VERTEX_POINT('',#136889) ;
#35462 = VERTEX_POINT('',#136890) ;
#35463 = VERTEX_POINT('',#136892) ;
#35464 = VERTEX_POINT('',#136894) ;
#35465 = VERTEX_POINT('',#136897) ;
#35466 = VERTEX_POINT('',#136898) ;
#35467 = VERTEX_POINT('',#136900) ;
#35468 = VERTEX_POINT('',#136902) ;
#35469 = VERTEX_POINT('',#136904) ;
#35470 = VERTEX_POINT('',#136906) ;
#35471 = VERTEX_POINT('',#136908) ;
#35472 = VERTEX_POINT('',#136910) ;
#35473 = VERTEX_POINT('',#136913) ;
#35474 = VERTEX_POINT('',#136914) ;
#35475 = VERTEX_POINT('',#136916) ;
#35476 = VERTEX_POINT('',#136918) ;
#35477 = VERTEX_POINT('',#136920) ;
#35478 = VERTEX_POINT('',#136922) ;
#35479 = VERTEX_POINT('',#136924) ;
#35480 = VERTEX_POINT('',#136926) ;
#35481 = VERTEX_POINT('',#136930) ;
#35482 = VERTEX_POINT('',#136931) ;
#35483 = VERTEX_POINT('',#136933) ;
#35484 = VERTEX_POINT('',#136935) ;
#35485 = VERTEX_POINT('',#136939) ;
#35486 = VERTEX_POINT('',#136941) ;
#35487 = VERTEX_POINT('',#136945) ;
#35488 = VERTEX_POINT('',#136947) ;
#35489 = VERTEX_POINT('',#136951) ;
#35490 = VERTEX_POINT('',#136952) ;
#35491 = VERTEX_POINT('',#136954) ;
#35492 = VERTEX_POINT('',#136956) ;
#35493 = VERTEX_POINT('',#136959) ;
#35494 = VERTEX_POINT('',#136960) ;
#35495 = VERTEX_POINT('',#136962) ;
#35496 = VERTEX_POINT('',#136969) ;
#35497 = VERTEX_POINT('',#136971) ;
#35498 = VERTEX_POINT('',#136978) ;
#35499 = VERTEX_POINT('',#136980) ;
#35500 = VERTEX_POINT('',#136987) ;
#35501 = VERTEX_POINT('',#136995) ;
#35502 = VERTEX_POINT('',#136996) ;
#35503 = VERTEX_POINT('',#136998) ;
#35504 = VERTEX_POINT('',#137005) ;
#35505 = VERTEX_POINT('',#137007) ;
#35506 = VERTEX_POINT('',#137014) ;
#35507 = VERTEX_POINT('',#137016) ;
#35508 = VERTEX_POINT('',#137023) ;
#35509 = VERTEX_POINT('',#137032) ;
#35510 = VERTEX_POINT('',#137033) ;
#35511 = VERTEX_POINT('',#137035) ;
#35512 = VERTEX_POINT('',#137037) ;
#35513 = VERTEX_POINT('',#137040) ;
#35514 = VERTEX_POINT('',#137041) ;
#35515 = VERTEX_POINT('',#137043) ;
#35516 = VERTEX_POINT('',#137045) ;
#35517 = VERTEX_POINT('',#137047) ;
#35518 = VERTEX_POINT('',#137049) ;
#35519 = VERTEX_POINT('',#137051) ;
#35520 = VERTEX_POINT('',#137053) ;
#35521 = VERTEX_POINT('',#137056) ;
#35522 = VERTEX_POINT('',#137057) ;
#35523 = VERTEX_POINT('',#137059) ;
#35524 = VERTEX_POINT('',#137061) ;
#35525 = VERTEX_POINT('',#137063) ;
#35526 = VERTEX_POINT('',#137065) ;
#35527 = VERTEX_POINT('',#137067) ;
#35528 = VERTEX_POINT('',#137069) ;
#35529 = VERTEX_POINT('',#137073) ;
#35530 = VERTEX_POINT('',#137074) ;
#35531 = VERTEX_POINT('',#137076) ;
#35532 = VERTEX_POINT('',#137078) ;
#35533 = VERTEX_POINT('',#137082) ;
#35534 = VERTEX_POINT('',#137083) ;
#35535 = VERTEX_POINT('',#137112) ;
#35536 = VERTEX_POINT('',#137123) ;
#35537 = VERTEX_POINT('',#137149) ;
#35538 = VERTEX_POINT('',#137166) ;
#35539 = VERTEX_POINT('',#137168) ;
#35540 = VERTEX_POINT('',#137197) ;
#35541 = VERTEX_POINT('',#137208) ;
#35542 = VERTEX_POINT('',#137234) ;
#35543 = VERTEX_POINT('',#137251) ;
#35544 = VERTEX_POINT('',#137253) ;
#35545 = VERTEX_POINT('',#137255) ;
#35546 = VERTEX_POINT('',#137257) ;
#35547 = VERTEX_POINT('',#137261) ;
#35548 = VERTEX_POINT('',#137262) ;
#35549 = VERTEX_POINT('',#137264) ;
#35550 = VERTEX_POINT('',#137266) ;
#35551 = VERTEX_POINT('',#137270) ;
#35552 = VERTEX_POINT('',#137271) ;
#35553 = VERTEX_POINT('',#137273) ;
#35554 = VERTEX_POINT('',#137275) ;
#35555 = VERTEX_POINT('',#137294) ;
#35556 = VERTEX_POINT('',#137295) ;
#35557 = VERTEX_POINT('',#137297) ;
#35558 = VERTEX_POINT('',#137299) ;
#35559 = VERTEX_POINT('',#137303) ;
#35560 = VERTEX_POINT('',#137304) ;
#35561 = VERTEX_POINT('',#137306) ;
#35562 = VERTEX_POINT('',#137308) ;
#35563 = VERTEX_POINT('',#137312) ;
#35564 = VERTEX_POINT('',#137313) ;
#35565 = VERTEX_POINT('',#137315) ;
#35566 = VERTEX_POINT('',#137317) ;
#35567 = VERTEX_POINT('',#137319) ;
#35568 = VERTEX_POINT('',#137321) ;
#35569 = VERTEX_POINT('',#137323) ;
#35570 = VERTEX_POINT('',#137325) ;
#35571 = VERTEX_POINT('',#137329) ;
#35572 = VERTEX_POINT('',#137330) ;
#35573 = VERTEX_POINT('',#137332) ;
#35574 = VERTEX_POINT('',#137334) ;
#35575 = VERTEX_POINT('',#137337) ;
#35576 = VERTEX_POINT('',#137339) ;
#35577 = VERTEX_POINT('',#137343) ;
#35578 = VERTEX_POINT('',#137344) ;
#35579 = VERTEX_POINT('',#137347) ;
#35580 = VERTEX_POINT('',#137349) ;
#35581 = VERTEX_POINT('',#137351) ;
#35582 = VERTEX_POINT('',#137353) ;
#35583 = VERTEX_POINT('',#137357) ;
#35584 = VERTEX_POINT('',#137359) ;
#35585 = VERTEX_POINT('',#137363) ;
#35586 = VERTEX_POINT('',#137365) ;
#35587 = VERTEX_POINT('',#137369) ;
#35588 = VERTEX_POINT('',#137370) ;
#35589 = VERTEX_POINT('',#137372) ;
#35590 = VERTEX_POINT('',#137374) ;
#35591 = VERTEX_POINT('',#137376) ;
#35592 = VERTEX_POINT('',#137378) ;
#35593 = VERTEX_POINT('',#137382) ;
#35594 = VERTEX_POINT('',#137383) ;
#35595 = VERTEX_POINT('',#137385) ;
#35596 = VERTEX_POINT('',#137387) ;
#35597 = VERTEX_POINT('',#137389) ;
#35598 = VERTEX_POINT('',#137391) ;
#35599 = VERTEX_POINT('',#137395) ;
#35600 = VERTEX_POINT('',#137396) ;
#35601 = VERTEX_POINT('',#137398) ;
#35602 = VERTEX_POINT('',#137400) ;
#35603 = VERTEX_POINT('',#137404) ;
#35604 = VERTEX_POINT('',#137405) ;
#35605 = VERTEX_POINT('',#137407) ;
#35606 = VERTEX_POINT('',#137409) ;
#35607 = VERTEX_POINT('',#137413) ;
#35608 = VERTEX_POINT('',#137414) ;
#35609 = VERTEX_POINT('',#137416) ;
#35610 = VERTEX_POINT('',#137418) ;
#35611 = VERTEX_POINT('',#137422) ;
#35612 = VERTEX_POINT('',#137423) ;
#35613 = VERTEX_POINT('',#137425) ;
#35614 = VERTEX_POINT('',#137427) ;
#35615 = VERTEX_POINT('',#137431) ;
#35616 = VERTEX_POINT('',#137432) ;
#35617 = VERTEX_POINT('',#137434) ;
#35618 = VERTEX_POINT('',#137436) ;
#35619 = VERTEX_POINT('',#137439) ;
#35620 = VERTEX_POINT('',#137440) ;
#35621 = VERTEX_POINT('',#137442) ;
#35622 = VERTEX_POINT('',#137444) ;
#35623 = VERTEX_POINT('',#137446) ;
#35624 = VERTEX_POINT('',#137448) ;
#35625 = VERTEX_POINT('',#137450) ;
#35626 = VERTEX_POINT('',#137452) ;
#35627 = VERTEX_POINT('',#137456) ;
#35628 = VERTEX_POINT('',#137457) ;
#35629 = VERTEX_POINT('',#137462) ;
#35630 = VERTEX_POINT('',#137466) ;
#35631 = VERTEX_POINT('',#137470) ;
#35632 = VERTEX_POINT('',#137474) ;
#35633 = VERTEX_POINT('',#137478) ;
#35634 = VERTEX_POINT('',#137482) ;
#35635 = VERTEX_POINT('',#137500) ;
#35636 = VERTEX_POINT('',#137501) ;
#35637 = VERTEX_POINT('',#137503) ;
#35638 = VERTEX_POINT('',#137505) ;
#35639 = VERTEX_POINT('',#137509) ;
#35640 = VERTEX_POINT('',#137510) ;
#35641 = VERTEX_POINT('',#137512) ;
#35642 = VERTEX_POINT('',#137514) ;
#35643 = VERTEX_POINT('',#137518) ;
#35644 = VERTEX_POINT('',#137519) ;
#35645 = VERTEX_POINT('',#137521) ;
#35646 = VERTEX_POINT('',#137523) ;
#35647 = VERTEX_POINT('',#137527) ;
#35648 = VERTEX_POINT('',#137528) ;
#35649 = VERTEX_POINT('',#137530) ;
#35650 = VERTEX_POINT('',#137532) ;
#35651 = VERTEX_POINT('',#137536) ;
#35652 = VERTEX_POINT('',#137537) ;
#35653 = VERTEX_POINT('',#137539) ;
#35654 = VERTEX_POINT('',#137541) ;
#35655 = VERTEX_POINT('',#137544) ;
#35656 = VERTEX_POINT('',#137545) ;
#35657 = VERTEX_POINT('',#137547) ;
#35658 = VERTEX_POINT('',#137549) ;
#35659 = VERTEX_POINT('',#137551) ;
#35660 = VERTEX_POINT('',#137553) ;
#35661 = VERTEX_POINT('',#137555) ;
#35662 = VERTEX_POINT('',#137557) ;
#35663 = VERTEX_POINT('',#137561) ;
#35664 = VERTEX_POINT('',#137563) ;
#35665 = VERTEX_POINT('',#137567) ;
#35666 = VERTEX_POINT('',#137571) ;
#35667 = VERTEX_POINT('',#137575) ;
#35668 = VERTEX_POINT('',#137579) ;
#35669 = VERTEX_POINT('',#137583) ;
#35670 = VERTEX_POINT('',#137587) ;
#35671 = VERTEX_POINT('',#137593) ;
#35672 = VERTEX_POINT('',#137594) ;
#35673 = VERTEX_POINT('',#137596) ;
#35674 = VERTEX_POINT('',#137598) ;
#35675 = VERTEX_POINT('',#137603) ;
#35676 = VERTEX_POINT('',#137605) ;
#35677 = VERTEX_POINT('',#137609) ;
#35678 = VERTEX_POINT('',#137611) ;
#35679 = VERTEX_POINT('',#137615) ;
#35680 = VERTEX_POINT('',#137620) ;
#35681 = VERTEX_POINT('',#137622) ;
#35682 = VERTEX_POINT('',#137624) ;
#35683 = VERTEX_POINT('',#137626) ;
#35684 = VERTEX_POINT('',#137631) ;
#35685 = VERTEX_POINT('',#137632) ;
#35686 = VERTEX_POINT('',#137634) ;
#35687 = VERTEX_POINT('',#137636) ;
#35688 = VERTEX_POINT('',#137638) ;
#35689 = VERTEX_POINT('',#137640) ;
#35690 = VERTEX_POINT('',#137835) ;
#35691 = VERTEX_POINT('',#137897) ;
#35692 = VERTEX_POINT('',#137898) ;
#35693 = VERTEX_POINT('',#138164) ;
#35694 = VERTEX_POINT('',#138165) ;
#35695 = VERTEX_POINT('',#138206) ;
#35696 = VERTEX_POINT('',#138541) ;
#35697 = VERTEX_POINT('',#138542) ;
#35698 = VERTEX_POINT('',#138544) ;
#35699 = VERTEX_POINT('',#138546) ;
#35700 = VERTEX_POINT('',#138550) ;
#35701 = VERTEX_POINT('',#138552) ;
#35702 = VERTEX_POINT('',#138556) ;
#35703 = VERTEX_POINT('',#138558) ;
#35704 = VERTEX_POINT('',#138562) ;
#35705 = VERTEX_POINT('',#138564) ;
#35706 = VERTEX_POINT('',#138568) ;
#35707 = VERTEX_POINT('',#138570) ;
#35708 = VERTEX_POINT('',#138574) ;
#35709 = VERTEX_POINT('',#138576) ;
#35710 = VERTEX_POINT('',#138580) ;
#35711 = VERTEX_POINT('',#138582) ;
#35712 = VERTEX_POINT('',#138586) ;
#35713 = VERTEX_POINT('',#138588) ;
#35714 = VERTEX_POINT('',#138592) ;
#35715 = VERTEX_POINT('',#138594) ;
#35716 = VERTEX_POINT('',#138598) ;
#35717 = VERTEX_POINT('',#138599) ;
#35718 = VERTEX_POINT('',#138601) ;
#35719 = VERTEX_POINT('',#138603) ;
#35720 = VERTEX_POINT('',#138605) ;
#35721 = VERTEX_POINT('',#138607) ;
#35722 = VERTEX_POINT('',#138609) ;
#35723 = VERTEX_POINT('',#138613) ;
#35724 = VERTEX_POINT('',#138614) ;
#35725 = VERTEX_POINT('',#138616) ;
#35726 = VERTEX_POINT('',#138618) ;
#35727 = VERTEX_POINT('',#138620) ;
#35728 = VERTEX_POINT('',#138622) ;
#35729 = VERTEX_POINT('',#138624) ;
#35730 = VERTEX_POINT('',#138628) ;
#35731 = VERTEX_POINT('',#138629) ;
#35732 = VERTEX_POINT('',#138631) ;
#35733 = VERTEX_POINT('',#138633) ;
#35734 = VERTEX_POINT('',#138639) ;
#35735 = VERTEX_POINT('',#138641) ;
#35736 = VERTEX_POINT('',#138643) ;
#35737 = VERTEX_POINT('',#138647) ;
#35738 = VERTEX_POINT('',#138648) ;
#35739 = VERTEX_POINT('',#138650) ;
#35740 = VERTEX_POINT('',#138652) ;
#35741 = VERTEX_POINT('',#138662) ;
#35742 = VERTEX_POINT('',#138663) ;
#35743 = VERTEX_POINT('',#138665) ;
#35744 = VERTEX_POINT('',#138667) ;
#35745 = VERTEX_POINT('',#138671) ;
#35746 = VERTEX_POINT('',#138672) ;
#35747 = VERTEX_POINT('',#138674) ;
#35748 = VERTEX_POINT('',#138676) ;
#35749 = VERTEX_POINT('',#138680) ;
#35750 = VERTEX_POINT('',#138681) ;
#35751 = VERTEX_POINT('',#138683) ;
#35752 = VERTEX_POINT('',#138685) ;
#35753 = VERTEX_POINT('',#138687) ;
#35754 = VERTEX_POINT('',#138689) ;
#35755 = VERTEX_POINT('',#138691) ;
#35756 = VERTEX_POINT('',#138693) ;
#35757 = VERTEX_POINT('',#138697) ;
#35758 = VERTEX_POINT('',#138698) ;
#35759 = VERTEX_POINT('',#138700) ;
#35760 = VERTEX_POINT('',#138702) ;
#35761 = VERTEX_POINT('',#138705) ;
#35762 = VERTEX_POINT('',#138707) ;
#35763 = VERTEX_POINT('',#138711) ;
#35764 = VERTEX_POINT('',#138712) ;
#35765 = VERTEX_POINT('',#138715) ;
#35766 = VERTEX_POINT('',#138717) ;
#35767 = VERTEX_POINT('',#138719) ;
#35768 = VERTEX_POINT('',#138721) ;
#35769 = VERTEX_POINT('',#138725) ;
#35770 = VERTEX_POINT('',#138727) ;
#35771 = VERTEX_POINT('',#138731) ;
#35772 = VERTEX_POINT('',#138733) ;
#35773 = VERTEX_POINT('',#138737) ;
#35774 = VERTEX_POINT('',#138738) ;
#35775 = VERTEX_POINT('',#138740) ;
#35776 = VERTEX_POINT('',#138742) ;
#35777 = VERTEX_POINT('',#138744) ;
#35778 = VERTEX_POINT('',#138746) ;
#35779 = VERTEX_POINT('',#138750) ;
#35780 = VERTEX_POINT('',#138751) ;
#35781 = VERTEX_POINT('',#138753) ;
#35782 = VERTEX_POINT('',#138755) ;
#35783 = VERTEX_POINT('',#138757) ;
#35784 = VERTEX_POINT('',#138759) ;
#35785 = VERTEX_POINT('',#138763) ;
#35786 = VERTEX_POINT('',#138764) ;
#35787 = VERTEX_POINT('',#138766) ;
#35788 = VERTEX_POINT('',#138768) ;
#35789 = VERTEX_POINT('',#138772) ;
#35790 = VERTEX_POINT('',#138773) ;
#35791 = VERTEX_POINT('',#138775) ;
#35792 = VERTEX_POINT('',#138777) ;
#35793 = VERTEX_POINT('',#138781) ;
#35794 = VERTEX_POINT('',#138782) ;
#35795 = VERTEX_POINT('',#138784) ;
#35796 = VERTEX_POINT('',#138786) ;
#35797 = VERTEX_POINT('',#138790) ;
#35798 = VERTEX_POINT('',#138791) ;
#35799 = VERTEX_POINT('',#138793) ;
#35800 = VERTEX_POINT('',#138795) ;
#35801 = VERTEX_POINT('',#138799) ;
#35802 = VERTEX_POINT('',#138800) ;
#35803 = VERTEX_POINT('',#138802) ;
#35804 = VERTEX_POINT('',#138804) ;
#35805 = VERTEX_POINT('',#138807) ;
#35806 = VERTEX_POINT('',#138808) ;
#35807 = VERTEX_POINT('',#138810) ;
#35808 = VERTEX_POINT('',#138812) ;
#35809 = VERTEX_POINT('',#138814) ;
#35810 = VERTEX_POINT('',#138816) ;
#35811 = VERTEX_POINT('',#138818) ;
#35812 = VERTEX_POINT('',#138820) ;
#35813 = VERTEX_POINT('',#138824) ;
#35814 = VERTEX_POINT('',#138825) ;
#35815 = VERTEX_POINT('',#138830) ;
#35816 = VERTEX_POINT('',#138834) ;
#35817 = VERTEX_POINT('',#138838) ;
#35818 = VERTEX_POINT('',#138842) ;
#35819 = VERTEX_POINT('',#138846) ;
#35820 = VERTEX_POINT('',#138850) ;
#35821 = VERTEX_POINT('',#138868) ;
#35822 = VERTEX_POINT('',#138869) ;
#35823 = VERTEX_POINT('',#138871) ;
#35824 = VERTEX_POINT('',#138873) ;
#35825 = VERTEX_POINT('',#138877) ;
#35826 = VERTEX_POINT('',#138878) ;
#35827 = VERTEX_POINT('',#138880) ;
#35828 = VERTEX_POINT('',#138882) ;
#35829 = VERTEX_POINT('',#138886) ;
#35830 = VERTEX_POINT('',#138887) ;
#35831 = VERTEX_POINT('',#138889) ;
#35832 = VERTEX_POINT('',#138891) ;
#35833 = VERTEX_POINT('',#138895) ;
#35834 = VERTEX_POINT('',#138896) ;
#35835 = VERTEX_POINT('',#138898) ;
#35836 = VERTEX_POINT('',#138900) ;
#35837 = VERTEX_POINT('',#138904) ;
#35838 = VERTEX_POINT('',#138905) ;
#35839 = VERTEX_POINT('',#138907) ;
#35840 = VERTEX_POINT('',#138909) ;
#35841 = VERTEX_POINT('',#138912) ;
#35842 = VERTEX_POINT('',#138913) ;
#35843 = VERTEX_POINT('',#138915) ;
#35844 = VERTEX_POINT('',#138917) ;
#35845 = VERTEX_POINT('',#138919) ;
#35846 = VERTEX_POINT('',#138921) ;
#35847 = VERTEX_POINT('',#138923) ;
#35848 = VERTEX_POINT('',#138925) ;
#35849 = VERTEX_POINT('',#138929) ;
#35850 = VERTEX_POINT('',#138931) ;
#35851 = VERTEX_POINT('',#138935) ;
#35852 = VERTEX_POINT('',#138939) ;
#35853 = VERTEX_POINT('',#138943) ;
#35854 = VERTEX_POINT('',#138947) ;
#35855 = VERTEX_POINT('',#138951) ;
#35856 = VERTEX_POINT('',#138955) ;
#35857 = VERTEX_POINT('',#138961) ;
#35858 = VERTEX_POINT('',#138962) ;
#35859 = VERTEX_POINT('',#138964) ;
#35860 = VERTEX_POINT('',#138966) ;
#35861 = VERTEX_POINT('',#138971) ;
#35862 = VERTEX_POINT('',#138973) ;
#35863 = VERTEX_POINT('',#138977) ;
#35864 = VERTEX_POINT('',#138979) ;
#35865 = VERTEX_POINT('',#138983) ;
#35866 = VERTEX_POINT('',#138988) ;
#35867 = VERTEX_POINT('',#138990) ;
#35868 = VERTEX_POINT('',#138992) ;
#35869 = VERTEX_POINT('',#138994) ;
#35870 = VERTEX_POINT('',#138999) ;
#35871 = VERTEX_POINT('',#139000) ;
#35872 = VERTEX_POINT('',#139002) ;
#35873 = VERTEX_POINT('',#139004) ;
#35874 = VERTEX_POINT('',#139006) ;
#35875 = VERTEX_POINT('',#139008) ;
#35876 = VERTEX_POINT('',#139202) ;
#35877 = VERTEX_POINT('',#139264) ;
#35878 = VERTEX_POINT('',#139265) ;
#35879 = VERTEX_POINT('',#139504) ;
#35880 = VERTEX_POINT('',#139505) ;
#35881 = VERTEX_POINT('',#139546) ;
#35882 = VERTEX_POINT('',#139959) ;
#35883 = VERTEX_POINT('',#139960) ;
#35884 = VERTEX_POINT('',#139962) ;
#35885 = VERTEX_POINT('',#139964) ;
#35886 = VERTEX_POINT('',#139968) ;
#35887 = VERTEX_POINT('',#139969) ;
#35888 = VERTEX_POINT('',#139971) ;
#35889 = VERTEX_POINT('',#139973) ;
#35890 = VERTEX_POINT('',#139977) ;
#35891 = VERTEX_POINT('',#139979) ;
#35892 = VERTEX_POINT('',#139981) ;
#35893 = VERTEX_POINT('',#139985) ;
#35894 = VERTEX_POINT('',#139987) ;
#35895 = VERTEX_POINT('',#139991) ;
#35896 = VERTEX_POINT('',#139993) ;
#35897 = VERTEX_POINT('',#139995) ;
#35898 = VERTEX_POINT('',#139999) ;
#35899 = VERTEX_POINT('',#140000) ;
#35900 = VERTEX_POINT('',#140002) ;
#35901 = VERTEX_POINT('',#140004) ;
#35902 = VERTEX_POINT('',#140008) ;
#35903 = VERTEX_POINT('',#140009) ;
#35904 = VERTEX_POINT('',#140011) ;
#35905 = VERTEX_POINT('',#140015) ;
#35906 = VERTEX_POINT('',#140017) ;
#35907 = VERTEX_POINT('',#140021) ;
#35908 = VERTEX_POINT('',#140022) ;
#35909 = VERTEX_POINT('',#140024) ;
#35910 = VERTEX_POINT('',#140028) ;
#35911 = VERTEX_POINT('',#140034) ;
#35912 = VERTEX_POINT('',#140035) ;
#35913 = VERTEX_POINT('',#140037) ;
#35914 = VERTEX_POINT('',#140048) ;
#35915 = VERTEX_POINT('',#140050) ;
#35916 = VERTEX_POINT('',#140061) ;
#35917 = VERTEX_POINT('',#140063) ;
#35918 = VERTEX_POINT('',#140074) ;
#35919 = VERTEX_POINT('',#140076) ;
#35920 = VERTEX_POINT('',#140108) ;
#35921 = VERTEX_POINT('',#140110) ;
#35922 = VERTEX_POINT('',#140121) ;
#35923 = VERTEX_POINT('',#140123) ;
#35924 = VERTEX_POINT('',#140134) ;
#35925 = VERTEX_POINT('',#140136) ;
#35926 = VERTEX_POINT('',#140147) ;
#35927 = VERTEX_POINT('',#140149) ;
#35928 = VERTEX_POINT('',#140184) ;
#35929 = VERTEX_POINT('',#140185) ;
#35930 = VERTEX_POINT('',#140187) ;
#35931 = VERTEX_POINT('',#140189) ;
#35932 = VERTEX_POINT('',#140193) ;
#35933 = VERTEX_POINT('',#140194) ;
#35934 = VERTEX_POINT('',#140196) ;
#35935 = VERTEX_POINT('',#140198) ;
#35936 = VERTEX_POINT('',#140202) ;
#35937 = VERTEX_POINT('',#140203) ;
#35938 = VERTEX_POINT('',#140205) ;
#35939 = VERTEX_POINT('',#140213) ;
#35940 = VERTEX_POINT('',#140215) ;
#35941 = VERTEX_POINT('',#140217) ;
#35942 = VERTEX_POINT('',#140219) ;
#35943 = VERTEX_POINT('',#140221) ;
#35944 = VERTEX_POINT('',#140223) ;
#35945 = VERTEX_POINT('',#140225) ;
#35946 = VERTEX_POINT('',#140227) ;
#35947 = VERTEX_POINT('',#140230) ;
#35948 = VERTEX_POINT('',#140232) ;
#35949 = VERTEX_POINT('',#140236) ;
#35950 = VERTEX_POINT('',#140238) ;
#35951 = VERTEX_POINT('',#140240) ;
#35952 = VERTEX_POINT('',#140244) ;
#35953 = VERTEX_POINT('',#140245) ;
#35954 = VERTEX_POINT('',#140247) ;
#35955 = VERTEX_POINT('',#140249) ;
#35956 = VERTEX_POINT('',#140251) ;
#35957 = VERTEX_POINT('',#140253) ;
#35958 = VERTEX_POINT('',#140255) ;
#35959 = VERTEX_POINT('',#140257) ;
#35960 = VERTEX_POINT('',#140261) ;
#35961 = VERTEX_POINT('',#140262) ;
#35962 = VERTEX_POINT('',#140264) ;
#35963 = VERTEX_POINT('',#140266) ;
#35964 = VERTEX_POINT('',#140270) ;
#35965 = VERTEX_POINT('',#140271) ;
#35966 = VERTEX_POINT('',#140273) ;
#35967 = VERTEX_POINT('',#140275) ;
#35968 = VERTEX_POINT('',#140279) ;
#35969 = VERTEX_POINT('',#140280) ;
#35970 = VERTEX_POINT('',#140282) ;
#35971 = VERTEX_POINT('',#140284) ;
#35972 = VERTEX_POINT('',#140288) ;
#35973 = VERTEX_POINT('',#140289) ;
#35974 = VERTEX_POINT('',#140291) ;
#35975 = VERTEX_POINT('',#140293) ;
#35976 = VERTEX_POINT('',#140297) ;
#35977 = VERTEX_POINT('',#140298) ;
#35978 = VERTEX_POINT('',#140300) ;
#35979 = VERTEX_POINT('',#140302) ;
#35980 = VERTEX_POINT('',#140306) ;
#35981 = VERTEX_POINT('',#140307) ;
#35982 = VERTEX_POINT('',#140309) ;
#35983 = VERTEX_POINT('',#140311) ;
#35984 = VERTEX_POINT('',#140315) ;
#35985 = VERTEX_POINT('',#140316) ;
#35986 = VERTEX_POINT('',#140318) ;
#35987 = VERTEX_POINT('',#140320) ;
#35988 = VERTEX_POINT('',#140323) ;
#35989 = VERTEX_POINT('',#140324) ;
#35990 = VERTEX_POINT('',#140326) ;
#35991 = VERTEX_POINT('',#140328) ;
#35992 = VERTEX_POINT('',#140330) ;
#35993 = VERTEX_POINT('',#140332) ;
#35994 = VERTEX_POINT('',#140334) ;
#35995 = VERTEX_POINT('',#140336) ;
#35996 = VERTEX_POINT('',#140340) ;
#35997 = VERTEX_POINT('',#140341) ;
#35998 = VERTEX_POINT('',#140343) ;
#35999 = VERTEX_POINT('',#140345) ;
#36000 = VERTEX_POINT('',#140349) ;
#36001 = VERTEX_POINT('',#140351) ;
#36002 = VERTEX_POINT('',#140355) ;
#36003 = VERTEX_POINT('',#140357) ;
#36004 = VERTEX_POINT('',#140361) ;
#36005 = VERTEX_POINT('',#140362) ;
#36006 = VERTEX_POINT('',#140364) ;
#36007 = VERTEX_POINT('',#140366) ;
#36008 = VERTEX_POINT('',#140369) ;
#36009 = VERTEX_POINT('',#140370) ;
#36010 = VERTEX_POINT('',#140372) ;
#36011 = VERTEX_POINT('',#140379) ;
#36012 = VERTEX_POINT('',#140381) ;
#36013 = VERTEX_POINT('',#140388) ;
#36014 = VERTEX_POINT('',#140390) ;
#36015 = VERTEX_POINT('',#140397) ;
#36016 = VERTEX_POINT('',#140406) ;
#36017 = VERTEX_POINT('',#140407) ;
#36018 = VERTEX_POINT('',#140409) ;
#36019 = VERTEX_POINT('',#140411) ;
#36020 = VERTEX_POINT('',#140414) ;
#36021 = VERTEX_POINT('',#140415) ;
#36022 = VERTEX_POINT('',#140417) ;
#36023 = VERTEX_POINT('',#140419) ;
#36024 = VERTEX_POINT('',#140421) ;
#36025 = VERTEX_POINT('',#140423) ;
#36026 = VERTEX_POINT('',#140425) ;
#36027 = VERTEX_POINT('',#140427) ;
#36028 = VERTEX_POINT('',#140431) ;
#36029 = VERTEX_POINT('',#140432) ;
#36030 = VERTEX_POINT('',#140434) ;
#36031 = VERTEX_POINT('',#140436) ;
#36032 = VERTEX_POINT('',#140440) ;
#36033 = VERTEX_POINT('',#140441) ;
#36034 = VERTEX_POINT('',#140470) ;
#36035 = VERTEX_POINT('',#140481) ;
#36036 = VERTEX_POINT('',#140507) ;
#36037 = VERTEX_POINT('',#140524) ;
#36038 = VERTEX_POINT('',#140526) ;
#36039 = VERTEX_POINT('',#140528) ;
#36040 = VERTEX_POINT('',#140530) ;
#36041 = VERTEX_POINT('',#140534) ;
#36042 = VERTEX_POINT('',#140535) ;
#36043 = VERTEX_POINT('',#140537) ;
#36044 = VERTEX_POINT('',#140539) ;
#36045 = VERTEX_POINT('',#140543) ;
#36046 = VERTEX_POINT('',#140544) ;
#36047 = VERTEX_POINT('',#140546) ;
#36048 = VERTEX_POINT('',#140548) ;
#36049 = VERTEX_POINT('',#140590) ;
#36050 = VERTEX_POINT('',#140591) ;
#36051 = VERTEX_POINT('',#140593) ;
#36052 = VERTEX_POINT('',#140595) ;
#36053 = VERTEX_POINT('',#140599) ;
#36054 = VERTEX_POINT('',#140600) ;
#36055 = VERTEX_POINT('',#140602) ;
#36056 = VERTEX_POINT('',#140604) ;
#36057 = VERTEX_POINT('',#140608) ;
#36058 = VERTEX_POINT('',#140609) ;
#36059 = VERTEX_POINT('',#140611) ;
#36060 = VERTEX_POINT('',#140613) ;
#36061 = VERTEX_POINT('',#140615) ;
#36062 = VERTEX_POINT('',#140617) ;
#36063 = VERTEX_POINT('',#140619) ;
#36064 = VERTEX_POINT('',#140621) ;
#36065 = VERTEX_POINT('',#140625) ;
#36066 = VERTEX_POINT('',#140626) ;
#36067 = VERTEX_POINT('',#140628) ;
#36068 = VERTEX_POINT('',#140630) ;
#36069 = VERTEX_POINT('',#140633) ;
#36070 = VERTEX_POINT('',#140635) ;
#36071 = VERTEX_POINT('',#140639) ;
#36072 = VERTEX_POINT('',#140640) ;
#36073 = VERTEX_POINT('',#140643) ;
#36074 = VERTEX_POINT('',#140645) ;
#36075 = VERTEX_POINT('',#140647) ;
#36076 = VERTEX_POINT('',#140649) ;
#36077 = VERTEX_POINT('',#140653) ;
#36078 = VERTEX_POINT('',#140655) ;
#36079 = VERTEX_POINT('',#140659) ;
#36080 = VERTEX_POINT('',#140661) ;
#36081 = VERTEX_POINT('',#140665) ;
#36082 = VERTEX_POINT('',#140666) ;
#36083 = VERTEX_POINT('',#140668) ;
#36084 = VERTEX_POINT('',#140670) ;
#36085 = VERTEX_POINT('',#140672) ;
#36086 = VERTEX_POINT('',#140674) ;
#36087 = VERTEX_POINT('',#140678) ;
#36088 = VERTEX_POINT('',#140679) ;
#36089 = VERTEX_POINT('',#140681) ;
#36090 = VERTEX_POINT('',#140683) ;
#36091 = VERTEX_POINT('',#140685) ;
#36092 = VERTEX_POINT('',#140687) ;
#36093 = VERTEX_POINT('',#140691) ;
#36094 = VERTEX_POINT('',#140692) ;
#36095 = VERTEX_POINT('',#140694) ;
#36096 = VERTEX_POINT('',#140696) ;
#36097 = VERTEX_POINT('',#140700) ;
#36098 = VERTEX_POINT('',#140701) ;
#36099 = VERTEX_POINT('',#140703) ;
#36100 = VERTEX_POINT('',#140705) ;
#36101 = VERTEX_POINT('',#140709) ;
#36102 = VERTEX_POINT('',#140710) ;
#36103 = VERTEX_POINT('',#140712) ;
#36104 = VERTEX_POINT('',#140714) ;
#36105 = VERTEX_POINT('',#140718) ;
#36106 = VERTEX_POINT('',#140719) ;
#36107 = VERTEX_POINT('',#140721) ;
#36108 = VERTEX_POINT('',#140723) ;
#36109 = VERTEX_POINT('',#140727) ;
#36110 = VERTEX_POINT('',#140728) ;
#36111 = VERTEX_POINT('',#140730) ;
#36112 = VERTEX_POINT('',#140732) ;
#36113 = VERTEX_POINT('',#140735) ;
#36114 = VERTEX_POINT('',#140736) ;
#36115 = VERTEX_POINT('',#140738) ;
#36116 = VERTEX_POINT('',#140740) ;
#36117 = VERTEX_POINT('',#140742) ;
#36118 = VERTEX_POINT('',#140744) ;
#36119 = VERTEX_POINT('',#140746) ;
#36120 = VERTEX_POINT('',#140748) ;
#36121 = VERTEX_POINT('',#140752) ;
#36122 = VERTEX_POINT('',#140753) ;
#36123 = VERTEX_POINT('',#140758) ;
#36124 = VERTEX_POINT('',#140762) ;
#36125 = VERTEX_POINT('',#140766) ;
#36126 = VERTEX_POINT('',#140770) ;
#36127 = VERTEX_POINT('',#140774) ;
#36128 = VERTEX_POINT('',#140778) ;
#36129 = VERTEX_POINT('',#140796) ;
#36130 = VERTEX_POINT('',#140797) ;
#36131 = VERTEX_POINT('',#140799) ;
#36132 = VERTEX_POINT('',#140801) ;
#36133 = VERTEX_POINT('',#140805) ;
#36134 = VERTEX_POINT('',#140806) ;
#36135 = VERTEX_POINT('',#140808) ;
#36136 = VERTEX_POINT('',#140810) ;
#36137 = VERTEX_POINT('',#140814) ;
#36138 = VERTEX_POINT('',#140815) ;
#36139 = VERTEX_POINT('',#140817) ;
#36140 = VERTEX_POINT('',#140819) ;
#36141 = VERTEX_POINT('',#140823) ;
#36142 = VERTEX_POINT('',#140824) ;
#36143 = VERTEX_POINT('',#140826) ;
#36144 = VERTEX_POINT('',#140828) ;
#36145 = VERTEX_POINT('',#140832) ;
#36146 = VERTEX_POINT('',#140833) ;
#36147 = VERTEX_POINT('',#140835) ;
#36148 = VERTEX_POINT('',#140837) ;
#36149 = VERTEX_POINT('',#140840) ;
#36150 = VERTEX_POINT('',#140841) ;
#36151 = VERTEX_POINT('',#140843) ;
#36152 = VERTEX_POINT('',#140845) ;
#36153 = VERTEX_POINT('',#140847) ;
#36154 = VERTEX_POINT('',#140849) ;
#36155 = VERTEX_POINT('',#140851) ;
#36156 = VERTEX_POINT('',#140853) ;
#36157 = VERTEX_POINT('',#140857) ;
#36158 = VERTEX_POINT('',#140859) ;
#36159 = VERTEX_POINT('',#140863) ;
#36160 = VERTEX_POINT('',#140867) ;
#36161 = VERTEX_POINT('',#140871) ;
#36162 = VERTEX_POINT('',#140875) ;
#36163 = VERTEX_POINT('',#140879) ;
#36164 = VERTEX_POINT('',#140883) ;
#36165 = VERTEX_POINT('',#140889) ;
#36166 = VERTEX_POINT('',#140890) ;
#36167 = VERTEX_POINT('',#140892) ;
#36168 = VERTEX_POINT('',#140894) ;
#36169 = VERTEX_POINT('',#140899) ;
#36170 = VERTEX_POINT('',#140901) ;
#36171 = VERTEX_POINT('',#140905) ;
#36172 = VERTEX_POINT('',#140907) ;
#36173 = VERTEX_POINT('',#140911) ;
#36174 = VERTEX_POINT('',#140916) ;
#36175 = VERTEX_POINT('',#140918) ;
#36176 = VERTEX_POINT('',#140920) ;
#36177 = VERTEX_POINT('',#140922) ;
#36178 = VERTEX_POINT('',#140927) ;
#36179 = VERTEX_POINT('',#140928) ;
#36180 = VERTEX_POINT('',#140930) ;
#36181 = VERTEX_POINT('',#140932) ;
#36182 = VERTEX_POINT('',#140934) ;
#36183 = VERTEX_POINT('',#140936) ;
#36184 = VERTEX_POINT('',#141131) ;
#36185 = VERTEX_POINT('',#141193) ;
#36186 = VERTEX_POINT('',#141194) ;
#36187 = VERTEX_POINT('',#141452) ;
#36188 = VERTEX_POINT('',#141453) ;
#36189 = VERTEX_POINT('',#141494) ;
#36190 = VERTEX_POINT('',#141828) ;
#36191 = VERTEX_POINT('',#141830) ;
#36192 = VERTEX_POINT('',#141832) ;
#36193 = VERTEX_POINT('',#141836) ;
#36194 = VERTEX_POINT('',#141838) ;
#36195 = VERTEX_POINT('',#141842) ;
#36196 = VERTEX_POINT('',#141843) ;
#36197 = VERTEX_POINT('',#141845) ;
#36198 = VERTEX_POINT('',#141849) ;
#36199 = VERTEX_POINT('',#141850) ;
#36200 = VERTEX_POINT('',#141852) ;
#36201 = VERTEX_POINT('',#141854) ;
#36202 = VERTEX_POINT('',#141856) ;
#36203 = VERTEX_POINT('',#141858) ;
#36204 = VERTEX_POINT('',#141860) ;
#36205 = VERTEX_POINT('',#141871) ;
#36206 = VERTEX_POINT('',#141873) ;
#36207 = VERTEX_POINT('',#141875) ;
#36208 = VERTEX_POINT('',#141879) ;
#36209 = VERTEX_POINT('',#141881) ;
#36210 = VERTEX_POINT('',#141885) ;
#36211 = VERTEX_POINT('',#141886) ;
#36212 = VERTEX_POINT('',#141888) ;
#36213 = VERTEX_POINT('',#141892) ;
#36214 = VERTEX_POINT('',#141893) ;
#36215 = VERTEX_POINT('',#141895) ;
#36216 = VERTEX_POINT('',#141897) ;
#36217 = VERTEX_POINT('',#141899) ;
#36218 = VERTEX_POINT('',#141901) ;
#36219 = VERTEX_POINT('',#141903) ;
#36220 = VERTEX_POINT('',#141914) ;
#36221 = VERTEX_POINT('',#141916) ;
#36222 = VERTEX_POINT('',#141918) ;
#36223 = VERTEX_POINT('',#141922) ;
#36224 = VERTEX_POINT('',#141924) ;
#36225 = VERTEX_POINT('',#141928) ;
#36226 = VERTEX_POINT('',#141929) ;
#36227 = VERTEX_POINT('',#141931) ;
#36228 = VERTEX_POINT('',#141935) ;
#36229 = VERTEX_POINT('',#141936) ;
#36230 = VERTEX_POINT('',#141938) ;
#36231 = VERTEX_POINT('',#141940) ;
#36232 = VERTEX_POINT('',#141942) ;
#36233 = VERTEX_POINT('',#141944) ;
#36234 = VERTEX_POINT('',#141946) ;
#36235 = VERTEX_POINT('',#141957) ;
#36236 = VERTEX_POINT('',#141959) ;
#36237 = VERTEX_POINT('',#141961) ;
#36238 = VERTEX_POINT('',#141965) ;
#36239 = VERTEX_POINT('',#141967) ;
#36240 = VERTEX_POINT('',#141971) ;
#36241 = VERTEX_POINT('',#141972) ;
#36242 = VERTEX_POINT('',#141974) ;
#36243 = VERTEX_POINT('',#141978) ;
#36244 = VERTEX_POINT('',#141979) ;
#36245 = VERTEX_POINT('',#141981) ;
#36246 = VERTEX_POINT('',#141983) ;
#36247 = VERTEX_POINT('',#141985) ;
#36248 = VERTEX_POINT('',#141987) ;
#36249 = VERTEX_POINT('',#141989) ;
#36250 = VERTEX_POINT('',#142000) ;
#36251 = VERTEX_POINT('',#142002) ;
#36252 = VERTEX_POINT('',#142004) ;
#36253 = VERTEX_POINT('',#142008) ;
#36254 = VERTEX_POINT('',#142010) ;
#36255 = VERTEX_POINT('',#142014) ;
#36256 = VERTEX_POINT('',#142015) ;
#36257 = VERTEX_POINT('',#142017) ;
#36258 = VERTEX_POINT('',#142021) ;
#36259 = VERTEX_POINT('',#142022) ;
#36260 = VERTEX_POINT('',#142024) ;
#36261 = VERTEX_POINT('',#142026) ;
#36262 = VERTEX_POINT('',#142028) ;
#36263 = VERTEX_POINT('',#142030) ;
#36264 = VERTEX_POINT('',#142032) ;
#36265 = VERTEX_POINT('',#142043) ;
#36266 = VERTEX_POINT('',#142045) ;
#36267 = VERTEX_POINT('',#142047) ;
#36268 = VERTEX_POINT('',#142051) ;
#36269 = VERTEX_POINT('',#142053) ;
#36270 = VERTEX_POINT('',#142057) ;
#36271 = VERTEX_POINT('',#142058) ;
#36272 = VERTEX_POINT('',#142060) ;
#36273 = VERTEX_POINT('',#142064) ;
#36274 = VERTEX_POINT('',#142065) ;
#36275 = VERTEX_POINT('',#142067) ;
#36276 = VERTEX_POINT('',#142069) ;
#36277 = VERTEX_POINT('',#142071) ;
#36278 = VERTEX_POINT('',#142073) ;
#36279 = VERTEX_POINT('',#142075) ;
#36280 = VERTEX_POINT('',#142086) ;
#36281 = VERTEX_POINT('',#142088) ;
#36282 = VERTEX_POINT('',#142090) ;
#36283 = VERTEX_POINT('',#142094) ;
#36284 = VERTEX_POINT('',#142096) ;
#36285 = VERTEX_POINT('',#142100) ;
#36286 = VERTEX_POINT('',#142101) ;
#36287 = VERTEX_POINT('',#142103) ;
#36288 = VERTEX_POINT('',#142107) ;
#36289 = VERTEX_POINT('',#142108) ;
#36290 = VERTEX_POINT('',#142110) ;
#36291 = VERTEX_POINT('',#142112) ;
#36292 = VERTEX_POINT('',#142114) ;
#36293 = VERTEX_POINT('',#142116) ;
#36294 = VERTEX_POINT('',#142118) ;
#36295 = VERTEX_POINT('',#142129) ;
#36296 = VERTEX_POINT('',#142131) ;
#36297 = VERTEX_POINT('',#142133) ;
#36298 = VERTEX_POINT('',#142137) ;
#36299 = VERTEX_POINT('',#142139) ;
#36300 = VERTEX_POINT('',#142143) ;
#36301 = VERTEX_POINT('',#142144) ;
#36302 = VERTEX_POINT('',#142146) ;
#36303 = VERTEX_POINT('',#142150) ;
#36304 = VERTEX_POINT('',#142151) ;
#36305 = VERTEX_POINT('',#142153) ;
#36306 = VERTEX_POINT('',#142155) ;
#36307 = VERTEX_POINT('',#142157) ;
#36308 = VERTEX_POINT('',#142159) ;
#36309 = VERTEX_POINT('',#142161) ;
#36310 = VERTEX_POINT('',#142172) ;
#36311 = VERTEX_POINT('',#142174) ;
#36312 = VERTEX_POINT('',#142176) ;
#36313 = VERTEX_POINT('',#142180) ;
#36314 = VERTEX_POINT('',#142181) ;
#36315 = VERTEX_POINT('',#142183) ;
#36316 = VERTEX_POINT('',#142185) ;
#36317 = VERTEX_POINT('',#142189) ;
#36318 = VERTEX_POINT('',#142190) ;
#36319 = VERTEX_POINT('',#142192) ;
#36320 = VERTEX_POINT('',#142194) ;
#36321 = VERTEX_POINT('',#142198) ;
#36322 = VERTEX_POINT('',#142199) ;
#36323 = VERTEX_POINT('',#142201) ;
#36324 = VERTEX_POINT('',#142203) ;
#36325 = VERTEX_POINT('',#142207) ;
#36326 = VERTEX_POINT('',#142208) ;
#36327 = VERTEX_POINT('',#142210) ;
#36328 = VERTEX_POINT('',#142212) ;
#36329 = VERTEX_POINT('',#142216) ;
#36330 = VERTEX_POINT('',#142217) ;
#36331 = VERTEX_POINT('',#142219) ;
#36332 = VERTEX_POINT('',#142221) ;
#36333 = VERTEX_POINT('',#142225) ;
#36334 = VERTEX_POINT('',#142226) ;
#36335 = VERTEX_POINT('',#142228) ;
#36336 = VERTEX_POINT('',#142230) ;
#36337 = VERTEX_POINT('',#142234) ;
#36338 = VERTEX_POINT('',#142235) ;
#36339 = VERTEX_POINT('',#142237) ;
#36340 = VERTEX_POINT('',#142239) ;
#36341 = VERTEX_POINT('',#142243) ;
#36342 = VERTEX_POINT('',#142244) ;
#36343 = VERTEX_POINT('',#142246) ;
#36344 = VERTEX_POINT('',#142248) ;
#36345 = VERTEX_POINT('',#142252) ;
#36346 = VERTEX_POINT('',#142253) ;
#36347 = VERTEX_POINT('',#142255) ;
#36348 = VERTEX_POINT('',#142257) ;
#36349 = VERTEX_POINT('',#142261) ;
#36350 = VERTEX_POINT('',#142263) ;
#36351 = VERTEX_POINT('',#142267) ;
#36352 = VERTEX_POINT('',#142268) ;
#36353 = VERTEX_POINT('',#142270) ;
#36354 = VERTEX_POINT('',#142274) ;
#36355 = VERTEX_POINT('',#142275) ;
#36356 = VERTEX_POINT('',#142277) ;
#36357 = VERTEX_POINT('',#142279) ;
#36358 = VERTEX_POINT('',#142281) ;
#36359 = VERTEX_POINT('',#142283) ;
#36360 = VERTEX_POINT('',#142285) ;
#36361 = VERTEX_POINT('',#142314) ;
#36362 = VERTEX_POINT('',#142315) ;
#36363 = VERTEX_POINT('',#142320) ;
#36364 = VERTEX_POINT('',#142321) ;
#36365 = VERTEX_POINT('',#142326) ;
#36366 = VERTEX_POINT('',#142327) ;
#36367 = VERTEX_POINT('',#142332) ;
#36368 = VERTEX_POINT('',#142333) ;
#36369 = VERTEX_POINT('',#142338) ;
#36370 = VERTEX_POINT('',#142339) ;
#36371 = VERTEX_POINT('',#142344) ;
#36372 = VERTEX_POINT('',#142345) ;
#36373 = VERTEX_POINT('',#142350) ;
#36374 = VERTEX_POINT('',#142351) ;
#36375 = VERTEX_POINT('',#142356) ;
#36376 = VERTEX_POINT('',#142357) ;
#36377 = VERTEX_POINT('',#142362) ;
#36378 = VERTEX_POINT('',#142363) ;
#36379 = VERTEX_POINT('',#142368) ;
#36380 = VERTEX_POINT('',#142370) ;
#36381 = VERTEX_POINT('',#142372) ;
#36382 = VERTEX_POINT('',#142376) ;
#36383 = VERTEX_POINT('',#142377) ;
#36384 = VERTEX_POINT('',#142379) ;
#36385 = VERTEX_POINT('',#142381) ;
#36386 = VERTEX_POINT('',#142385) ;
#36387 = VERTEX_POINT('',#142387) ;
#36388 = VERTEX_POINT('',#142391) ;
#36389 = VERTEX_POINT('',#142392) ;
#36390 = VERTEX_POINT('',#142394) ;
#36391 = VERTEX_POINT('',#142398) ;
#36392 = VERTEX_POINT('',#142399) ;
#36393 = VERTEX_POINT('',#142401) ;
#36394 = VERTEX_POINT('',#142403) ;
#36395 = VERTEX_POINT('',#142405) ;
#36396 = VERTEX_POINT('',#142407) ;
#36397 = VERTEX_POINT('',#142409) ;
#36398 = VERTEX_POINT('',#142422) ;
#36399 = VERTEX_POINT('',#142423) ;
#36400 = VERTEX_POINT('',#142428) ;
#36401 = VERTEX_POINT('',#142429) ;
#36402 = VERTEX_POINT('',#142431) ;
#36403 = VERTEX_POINT('',#142433) ;
#36404 = VERTEX_POINT('',#142436) ;
#36405 = VERTEX_POINT('',#142438) ;
#36406 = VERTEX_POINT('',#142440) ;
#36407 = VERTEX_POINT('',#142442) ;
#36408 = VERTEX_POINT('',#142444) ;
#36409 = VERTEX_POINT('',#142446) ;
#36410 = VERTEX_POINT('',#142450) ;
#36411 = VERTEX_POINT('',#142451) ;
#36412 = VERTEX_POINT('',#142453) ;
#36413 = VERTEX_POINT('',#142455) ;
#36414 = VERTEX_POINT('',#142458) ;
#36415 = VERTEX_POINT('',#142460) ;
#36416 = VERTEX_POINT('',#142462) ;
#36417 = VERTEX_POINT('',#142464) ;
#36418 = VERTEX_POINT('',#142466) ;
#36419 = VERTEX_POINT('',#142468) ;
#36420 = VERTEX_POINT('',#142472) ;
#36421 = VERTEX_POINT('',#142473) ;
#36422 = VERTEX_POINT('',#142475) ;
#36423 = VERTEX_POINT('',#142477) ;
#36424 = VERTEX_POINT('',#142480) ;
#36425 = VERTEX_POINT('',#142482) ;
#36426 = VERTEX_POINT('',#142484) ;
#36427 = VERTEX_POINT('',#142486) ;
#36428 = VERTEX_POINT('',#142488) ;
#36429 = VERTEX_POINT('',#142490) ;
#36430 = VERTEX_POINT('',#142494) ;
#36431 = VERTEX_POINT('',#142495) ;
#36432 = VERTEX_POINT('',#142497) ;
#36433 = VERTEX_POINT('',#142499) ;
#36434 = VERTEX_POINT('',#142502) ;
#36435 = VERTEX_POINT('',#142504) ;
#36436 = VERTEX_POINT('',#142506) ;
#36437 = VERTEX_POINT('',#142508) ;
#36438 = VERTEX_POINT('',#142510) ;
#36439 = VERTEX_POINT('',#142512) ;
#36440 = VERTEX_POINT('',#142516) ;
#36441 = VERTEX_POINT('',#142517) ;
#36442 = VERTEX_POINT('',#142519) ;
#36443 = VERTEX_POINT('',#142521) ;
#36444 = VERTEX_POINT('',#142524) ;
#36445 = VERTEX_POINT('',#142526) ;
#36446 = VERTEX_POINT('',#142528) ;
#36447 = VERTEX_POINT('',#142530) ;
#36448 = VERTEX_POINT('',#142532) ;
#36449 = VERTEX_POINT('',#142534) ;
#36450 = VERTEX_POINT('',#142538) ;
#36451 = VERTEX_POINT('',#142539) ;
#36452 = VERTEX_POINT('',#142541) ;
#36453 = VERTEX_POINT('',#142543) ;
#36454 = VERTEX_POINT('',#142546) ;
#36455 = VERTEX_POINT('',#142548) ;
#36456 = VERTEX_POINT('',#142550) ;
#36457 = VERTEX_POINT('',#142552) ;
#36458 = VERTEX_POINT('',#142554) ;
#36459 = VERTEX_POINT('',#142556) ;
#36460 = VERTEX_POINT('',#142560) ;
#36461 = VERTEX_POINT('',#142561) ;
#36462 = VERTEX_POINT('',#142563) ;
#36463 = VERTEX_POINT('',#142565) ;
#36464 = VERTEX_POINT('',#142568) ;
#36465 = VERTEX_POINT('',#142570) ;
#36466 = VERTEX_POINT('',#142572) ;
#36467 = VERTEX_POINT('',#142574) ;
#36468 = VERTEX_POINT('',#142576) ;
#36469 = VERTEX_POINT('',#142578) ;
#36470 = VERTEX_POINT('',#142582) ;
#36471 = VERTEX_POINT('',#142583) ;
#36472 = VERTEX_POINT('',#142585) ;
#36473 = VERTEX_POINT('',#142587) ;
#36474 = VERTEX_POINT('',#142590) ;
#36475 = VERTEX_POINT('',#142592) ;
#36476 = VERTEX_POINT('',#142594) ;
#36477 = VERTEX_POINT('',#142596) ;
#36478 = VERTEX_POINT('',#142598) ;
#36479 = VERTEX_POINT('',#142600) ;
#36480 = VERTEX_POINT('',#142604) ;
#36481 = VERTEX_POINT('',#142605) ;
#36482 = VERTEX_POINT('',#142607) ;
#36483 = VERTEX_POINT('',#142609) ;
#36484 = VERTEX_POINT('',#142612) ;
#36485 = VERTEX_POINT('',#142614) ;
#36486 = VERTEX_POINT('',#142616) ;
#36487 = VERTEX_POINT('',#142618) ;
#36488 = VERTEX_POINT('',#142620) ;
#36489 = VERTEX_POINT('',#142622) ;
#36490 = VERTEX_POINT('',#142626) ;
#36491 = VERTEX_POINT('',#142627) ;
#36492 = VERTEX_POINT('',#142629) ;
#36493 = VERTEX_POINT('',#142631) ;
#36494 = VERTEX_POINT('',#142633) ;
#36495 = VERTEX_POINT('',#142637) ;
#36496 = VERTEX_POINT('',#142638) ;
#36497 = VERTEX_POINT('',#142640) ;
#36498 = VERTEX_POINT('',#142642) ;
#36499 = VERTEX_POINT('',#142644) ;
#36500 = VERTEX_POINT('',#142648) ;
#36501 = VERTEX_POINT('',#142649) ;
#36502 = VERTEX_POINT('',#142651) ;
#36503 = VERTEX_POINT('',#142653) ;
#36504 = VERTEX_POINT('',#142655) ;
#36505 = VERTEX_POINT('',#142659) ;
#36506 = VERTEX_POINT('',#142660) ;
#36507 = VERTEX_POINT('',#142662) ;
#36508 = VERTEX_POINT('',#142664) ;
#36509 = VERTEX_POINT('',#142666) ;
#36510 = VERTEX_POINT('',#142670) ;
#36511 = VERTEX_POINT('',#142671) ;
#36512 = VERTEX_POINT('',#142673) ;
#36513 = VERTEX_POINT('',#142675) ;
#36514 = VERTEX_POINT('',#142677) ;
#36515 = VERTEX_POINT('',#142681) ;
#36516 = VERTEX_POINT('',#142682) ;
#36517 = VERTEX_POINT('',#142684) ;
#36518 = VERTEX_POINT('',#142686) ;
#36519 = VERTEX_POINT('',#142688) ;
#36520 = VERTEX_POINT('',#142692) ;
#36521 = VERTEX_POINT('',#142693) ;
#36522 = VERTEX_POINT('',#142695) ;
#36523 = VERTEX_POINT('',#142697) ;
#36524 = VERTEX_POINT('',#142699) ;
#36525 = VERTEX_POINT('',#142703) ;
#36526 = VERTEX_POINT('',#142704) ;
#36527 = VERTEX_POINT('',#142706) ;
#36528 = VERTEX_POINT('',#142708) ;
#36529 = VERTEX_POINT('',#142710) ;
#36530 = VERTEX_POINT('',#142714) ;
#36531 = VERTEX_POINT('',#142715) ;
#36532 = VERTEX_POINT('',#142717) ;
#36533 = VERTEX_POINT('',#142719) ;
#36534 = VERTEX_POINT('',#142721) ;
#36535 = VERTEX_POINT('',#142725) ;
#36536 = VERTEX_POINT('',#142726) ;
#36537 = VERTEX_POINT('',#142728) ;
#36538 = VERTEX_POINT('',#142730) ;
#36539 = VERTEX_POINT('',#142732) ;
#36540 = VERTEX_POINT('',#142736) ;
#36541 = VERTEX_POINT('',#142737) ;
#36542 = VERTEX_POINT('',#142739) ;
#36543 = VERTEX_POINT('',#142741) ;
#36544 = VERTEX_POINT('',#142743) ;
#36545 = VERTEX_POINT('',#142747) ;
#36546 = VERTEX_POINT('',#142748) ;
#36547 = VERTEX_POINT('',#142750) ;
#36548 = VERTEX_POINT('',#142752) ;
#36549 = VERTEX_POINT('',#142754) ;
#36550 = VERTEX_POINT('',#142758) ;
#36551 = VERTEX_POINT('',#142759) ;
#36552 = VERTEX_POINT('',#142761) ;
#36553 = VERTEX_POINT('',#142763) ;
#36554 = VERTEX_POINT('',#142765) ;
#36555 = VERTEX_POINT('',#142769) ;
#36556 = VERTEX_POINT('',#142770) ;
#36557 = VERTEX_POINT('',#142772) ;
#36558 = VERTEX_POINT('',#142774) ;
#36559 = VERTEX_POINT('',#142776) ;
#36560 = VERTEX_POINT('',#142780) ;
#36561 = VERTEX_POINT('',#142781) ;
#36562 = VERTEX_POINT('',#142783) ;
#36563 = VERTEX_POINT('',#142785) ;
#36564 = VERTEX_POINT('',#142787) ;
#36565 = VERTEX_POINT('',#142791) ;
#36566 = VERTEX_POINT('',#142792) ;
#36567 = VERTEX_POINT('',#142794) ;
#36568 = VERTEX_POINT('',#142796) ;
#36569 = VERTEX_POINT('',#142798) ;
#36570 = VERTEX_POINT('',#142802) ;
#36571 = VERTEX_POINT('',#142803) ;
#36572 = VERTEX_POINT('',#142805) ;
#36573 = VERTEX_POINT('',#142807) ;
#36574 = VERTEX_POINT('',#142809) ;
#36575 = VERTEX_POINT('',#142813) ;
#36576 = VERTEX_POINT('',#142814) ;
#36577 = VERTEX_POINT('',#142816) ;
#36578 = VERTEX_POINT('',#142818) ;
#36579 = VERTEX_POINT('',#142820) ;
#36580 = VERTEX_POINT('',#142824) ;
#36581 = VERTEX_POINT('',#142825) ;
#36582 = VERTEX_POINT('',#142827) ;
#36583 = VERTEX_POINT('',#142829) ;
#36584 = VERTEX_POINT('',#142833) ;
#36585 = VERTEX_POINT('',#142834) ;
#36586 = VERTEX_POINT('',#142836) ;
#36587 = VERTEX_POINT('',#142838) ;
#36588 = VERTEX_POINT('',#142842) ;
#36589 = VERTEX_POINT('',#142843) ;
#36590 = VERTEX_POINT('',#142845) ;
#36591 = VERTEX_POINT('',#142847) ;
#36592 = VERTEX_POINT('',#142851) ;
#36593 = VERTEX_POINT('',#142852) ;
#36594 = VERTEX_POINT('',#142854) ;
#36595 = VERTEX_POINT('',#142856) ;
#36596 = VERTEX_POINT('',#142860) ;
#36597 = VERTEX_POINT('',#142861) ;
#36598 = VERTEX_POINT('',#142863) ;
#36599 = VERTEX_POINT('',#142865) ;
#36600 = VERTEX_POINT('',#142869) ;
#36601 = VERTEX_POINT('',#142870) ;
#36602 = VERTEX_POINT('',#142872) ;
#36603 = VERTEX_POINT('',#142874) ;
#36604 = VERTEX_POINT('',#142878) ;
#36605 = VERTEX_POINT('',#142879) ;
#36606 = VERTEX_POINT('',#142881) ;
#36607 = VERTEX_POINT('',#142883) ;
#36608 = VERTEX_POINT('',#142887) ;
#36609 = VERTEX_POINT('',#142888) ;
#36610 = VERTEX_POINT('',#142890) ;
#36611 = VERTEX_POINT('',#142892) ;
#36612 = VERTEX_POINT('',#142896) ;
#36613 = VERTEX_POINT('',#142897) ;
#36614 = VERTEX_POINT('',#142899) ;
#36615 = VERTEX_POINT('',#142901) ;
#36616 = VERTEX_POINT('',#142905) ;
#36617 = VERTEX_POINT('',#142906) ;
#36618 = VERTEX_POINT('',#142908) ;
#36619 = VERTEX_POINT('',#142910) ;
#36620 = VERTEX_POINT('',#142913) ;
#36621 = VERTEX_POINT('',#142915) ;
#36622 = VERTEX_POINT('',#142917) ;
#36623 = VERTEX_POINT('',#142919) ;
#36624 = VERTEX_POINT('',#142921) ;
#36625 = VERTEX_POINT('',#142923) ;
#36626 = VERTEX_POINT('',#142927) ;
#36627 = VERTEX_POINT('',#142928) ;
#36628 = VERTEX_POINT('',#142930) ;
#36629 = VERTEX_POINT('',#142932) ;
#36630 = VERTEX_POINT('',#142934) ;
#36631 = VERTEX_POINT('',#142938) ;
#36632 = VERTEX_POINT('',#142939) ;
#36633 = VERTEX_POINT('',#142941) ;
#36634 = VERTEX_POINT('',#142943) ;
#36635 = VERTEX_POINT('',#142945) ;
#36636 = VERTEX_POINT('',#142949) ;
#36637 = VERTEX_POINT('',#142950) ;
#36638 = VERTEX_POINT('',#142952) ;
#36639 = VERTEX_POINT('',#142954) ;
#36640 = VERTEX_POINT('',#142958) ;
#36641 = VERTEX_POINT('',#142959) ;
#36642 = VERTEX_POINT('',#142961) ;
#36643 = VERTEX_POINT('',#142963) ;
#36644 = VERTEX_POINT('',#142967) ;
#36645 = VERTEX_POINT('',#142968) ;
#36646 = VERTEX_POINT('',#142970) ;
#36647 = VERTEX_POINT('',#142972) ;
#36648 = VERTEX_POINT('',#142976) ;
#36649 = VERTEX_POINT('',#142978) ;
#36650 = VERTEX_POINT('',#142980) ;
#36651 = VERTEX_POINT('',#142982) ;
#36652 = VERTEX_POINT('',#142985) ;
#36653 = VERTEX_POINT('',#142987) ;
#36654 = VERTEX_POINT('',#142989) ;
#36655 = VERTEX_POINT('',#142991) ;
#36656 = VERTEX_POINT('',#142994) ;
#36657 = VERTEX_POINT('',#142996) ;
#36658 = VERTEX_POINT('',#142998) ;
#36659 = VERTEX_POINT('',#143000) ;
#36660 = VERTEX_POINT('',#143003) ;
#36661 = VERTEX_POINT('',#143005) ;
#36662 = VERTEX_POINT('',#143007) ;
#36663 = VERTEX_POINT('',#143009) ;
#36664 = VERTEX_POINT('',#143012) ;
#36665 = VERTEX_POINT('',#143014) ;
#36666 = VERTEX_POINT('',#143016) ;
#36667 = VERTEX_POINT('',#143018) ;
#36668 = VERTEX_POINT('',#143021) ;
#36669 = VERTEX_POINT('',#143023) ;
#36670 = VERTEX_POINT('',#143025) ;
#36671 = VERTEX_POINT('',#143027) ;
#36672 = VERTEX_POINT('',#143030) ;
#36673 = VERTEX_POINT('',#143032) ;
#36674 = VERTEX_POINT('',#143034) ;
#36675 = VERTEX_POINT('',#143036) ;
#36676 = VERTEX_POINT('',#143039) ;
#36677 = VERTEX_POINT('',#143041) ;
#36678 = VERTEX_POINT('',#143043) ;
#36679 = VERTEX_POINT('',#143045) ;
#36680 = VERTEX_POINT('',#143048) ;
#36681 = VERTEX_POINT('',#143050) ;
#36682 = VERTEX_POINT('',#143052) ;
#36683 = VERTEX_POINT('',#143054) ;
#36684 = VERTEX_POINT('',#143057) ;
#36685 = VERTEX_POINT('',#143059) ;
#36686 = VERTEX_POINT('',#143063) ;
#36687 = VERTEX_POINT('',#143065) ;
#36688 = VERTEX_POINT('',#143069) ;
#36689 = VERTEX_POINT('',#143070) ;
#36690 = VERTEX_POINT('',#143073) ;
#36691 = VERTEX_POINT('',#143075) ;
#36692 = VERTEX_POINT('',#143077) ;
#36693 = VERTEX_POINT('',#143079) ;
#36694 = VERTEX_POINT('',#143082) ;
#36695 = VERTEX_POINT('',#143084) ;
#36696 = VERTEX_POINT('',#143086) ;
#36697 = VERTEX_POINT('',#143088) ;
#36698 = VERTEX_POINT('',#143091) ;
#36699 = VERTEX_POINT('',#143093) ;
#36700 = VERTEX_POINT('',#143095) ;
#36701 = VERTEX_POINT('',#143097) ;
#36702 = VERTEX_POINT('',#143100) ;
#36703 = VERTEX_POINT('',#143102) ;
#36704 = VERTEX_POINT('',#143104) ;
#36705 = VERTEX_POINT('',#143106) ;
#36706 = VERTEX_POINT('',#143109) ;
#36707 = VERTEX_POINT('',#143111) ;
#36708 = VERTEX_POINT('',#143113) ;
#36709 = VERTEX_POINT('',#143115) ;
#36710 = VERTEX_POINT('',#143118) ;
#36711 = VERTEX_POINT('',#143120) ;
#36712 = VERTEX_POINT('',#143122) ;
#36713 = VERTEX_POINT('',#143124) ;
#36714 = VERTEX_POINT('',#143127) ;
#36715 = VERTEX_POINT('',#143129) ;
#36716 = VERTEX_POINT('',#143131) ;
#36717 = VERTEX_POINT('',#143133) ;
#36718 = VERTEX_POINT('',#143136) ;
#36719 = VERTEX_POINT('',#143138) ;
#36720 = VERTEX_POINT('',#143140) ;
#36721 = VERTEX_POINT('',#143142) ;
#36722 = VERTEX_POINT('',#143145) ;
#36723 = VERTEX_POINT('',#143147) ;
#36724 = VERTEX_POINT('',#143149) ;
#36725 = VERTEX_POINT('',#143151) ;
#36726 = VERTEX_POINT('',#143154) ;
#36727 = VERTEX_POINT('',#143156) ;
#36728 = VERTEX_POINT('',#143159) ;
#36729 = VERTEX_POINT('',#143161) ;
#36730 = VERTEX_POINT('',#143165) ;
#36731 = VERTEX_POINT('',#143166) ;
#36732 = VERTEX_POINT('',#143171) ;
#36733 = VERTEX_POINT('',#143172) ;
#36734 = VERTEX_POINT('',#143177) ;
#36735 = VERTEX_POINT('',#143178) ;
#36736 = VERTEX_POINT('',#143183) ;
#36737 = VERTEX_POINT('',#143184) ;
#36738 = VERTEX_POINT('',#143189) ;
#36739 = VERTEX_POINT('',#143190) ;
#36740 = VERTEX_POINT('',#143195) ;
#36741 = VERTEX_POINT('',#143196) ;
#36742 = VERTEX_POINT('',#143201) ;
#36743 = VERTEX_POINT('',#143202) ;
#36744 = VERTEX_POINT('',#143207) ;
#36745 = VERTEX_POINT('',#143208) ;
#36746 = VERTEX_POINT('',#143213) ;
#36747 = VERTEX_POINT('',#143214) ;
#36748 = VERTEX_POINT('',#143219) ;
#36749 = VERTEX_POINT('',#143220) ;
#36750 = VERTEX_POINT('',#143225) ;
#36751 = VERTEX_POINT('',#143226) ;
#36752 = VERTEX_POINT('',#143233) ;
#36753 = VERTEX_POINT('',#143234) ;
#36754 = VERTEX_POINT('',#143236) ;
#36755 = VERTEX_POINT('',#143238) ;
#36756 = VERTEX_POINT('',#143240) ;
#36757 = VERTEX_POINT('',#143242) ;
#36758 = VERTEX_POINT('',#143244) ;
#36759 = VERTEX_POINT('',#143246) ;
#36760 = VERTEX_POINT('',#143249) ;
#36761 = VERTEX_POINT('',#143251) ;
#36762 = VERTEX_POINT('',#143253) ;
#36763 = VERTEX_POINT('',#143255) ;
#36764 = VERTEX_POINT('',#143257) ;
#36765 = VERTEX_POINT('',#143259) ;
#36766 = VERTEX_POINT('',#143261) ;
#36767 = VERTEX_POINT('',#143263) ;
#36768 = VERTEX_POINT('',#143265) ;
#36769 = VERTEX_POINT('',#143267) ;
#36770 = VERTEX_POINT('',#143269) ;
#36771 = VERTEX_POINT('',#143271) ;
#36772 = VERTEX_POINT('',#143273) ;
#36773 = VERTEX_POINT('',#143275) ;
#36774 = VERTEX_POINT('',#143278) ;
#36775 = VERTEX_POINT('',#143279) ;
#36776 = VERTEX_POINT('',#143281) ;
#36777 = VERTEX_POINT('',#143283) ;
#36778 = VERTEX_POINT('',#143285) ;
#36779 = VERTEX_POINT('',#143287) ;
#36780 = VERTEX_POINT('',#143289) ;
#36781 = VERTEX_POINT('',#143291) ;
#36782 = VERTEX_POINT('',#143294) ;
#36783 = VERTEX_POINT('',#143296) ;
#36784 = VERTEX_POINT('',#143298) ;
#36785 = VERTEX_POINT('',#143300) ;
#36786 = VERTEX_POINT('',#143302) ;
#36787 = VERTEX_POINT('',#143304) ;
#36788 = VERTEX_POINT('',#143306) ;
#36789 = VERTEX_POINT('',#143308) ;
#36790 = VERTEX_POINT('',#143310) ;
#36791 = VERTEX_POINT('',#143312) ;
#36792 = VERTEX_POINT('',#143314) ;
#36793 = VERTEX_POINT('',#143316) ;
#36794 = VERTEX_POINT('',#143318) ;
#36795 = VERTEX_POINT('',#143320) ;
#36796 = VERTEX_POINT('',#143323) ;
#36797 = VERTEX_POINT('',#143324) ;
#36798 = VERTEX_POINT('',#143326) ;
#36799 = VERTEX_POINT('',#143328) ;
#36800 = VERTEX_POINT('',#143330) ;
#36801 = VERTEX_POINT('',#143332) ;
#36802 = VERTEX_POINT('',#143334) ;
#36803 = VERTEX_POINT('',#143336) ;
#36804 = VERTEX_POINT('',#143339) ;
#36805 = VERTEX_POINT('',#143341) ;
#36806 = VERTEX_POINT('',#143343) ;
#36807 = VERTEX_POINT('',#143345) ;
#36808 = VERTEX_POINT('',#143347) ;
#36809 = VERTEX_POINT('',#143349) ;
#36810 = VERTEX_POINT('',#143351) ;
#36811 = VERTEX_POINT('',#143353) ;
#36812 = VERTEX_POINT('',#143355) ;
#36813 = VERTEX_POINT('',#143357) ;
#36814 = VERTEX_POINT('',#143359) ;
#36815 = VERTEX_POINT('',#143361) ;
#36816 = VERTEX_POINT('',#143363) ;
#36817 = VERTEX_POINT('',#143365) ;
#36818 = VERTEX_POINT('',#143368) ;
#36819 = VERTEX_POINT('',#143369) ;
#36820 = VERTEX_POINT('',#143371) ;
#36821 = VERTEX_POINT('',#143373) ;
#36822 = VERTEX_POINT('',#143375) ;
#36823 = VERTEX_POINT('',#143377) ;
#36824 = VERTEX_POINT('',#143379) ;
#36825 = VERTEX_POINT('',#143381) ;
#36826 = VERTEX_POINT('',#143384) ;
#36827 = VERTEX_POINT('',#143386) ;
#36828 = VERTEX_POINT('',#143388) ;
#36829 = VERTEX_POINT('',#143390) ;
#36830 = VERTEX_POINT('',#143392) ;
#36831 = VERTEX_POINT('',#143394) ;
#36832 = VERTEX_POINT('',#143396) ;
#36833 = VERTEX_POINT('',#143398) ;
#36834 = VERTEX_POINT('',#143400) ;
#36835 = VERTEX_POINT('',#143402) ;
#36836 = VERTEX_POINT('',#143404) ;
#36837 = VERTEX_POINT('',#143406) ;
#36838 = VERTEX_POINT('',#143408) ;
#36839 = VERTEX_POINT('',#143410) ;
#36840 = VERTEX_POINT('',#143413) ;
#36841 = VERTEX_POINT('',#143414) ;
#36842 = VERTEX_POINT('',#143416) ;
#36843 = VERTEX_POINT('',#143418) ;
#36844 = VERTEX_POINT('',#143420) ;
#36845 = VERTEX_POINT('',#143422) ;
#36846 = VERTEX_POINT('',#143424) ;
#36847 = VERTEX_POINT('',#143426) ;
#36848 = VERTEX_POINT('',#143429) ;
#36849 = VERTEX_POINT('',#143431) ;
#36850 = VERTEX_POINT('',#143433) ;
#36851 = VERTEX_POINT('',#143435) ;
#36852 = VERTEX_POINT('',#143437) ;
#36853 = VERTEX_POINT('',#143439) ;
#36854 = VERTEX_POINT('',#143441) ;
#36855 = VERTEX_POINT('',#143443) ;
#36856 = VERTEX_POINT('',#143445) ;
#36857 = VERTEX_POINT('',#143447) ;
#36858 = VERTEX_POINT('',#143449) ;
#36859 = VERTEX_POINT('',#143451) ;
#36860 = VERTEX_POINT('',#143453) ;
#36861 = VERTEX_POINT('',#143455) ;
#36862 = VERTEX_POINT('',#143458) ;
#36863 = VERTEX_POINT('',#143459) ;
#36864 = VERTEX_POINT('',#143461) ;
#36865 = VERTEX_POINT('',#143463) ;
#36866 = VERTEX_POINT('',#143465) ;
#36867 = VERTEX_POINT('',#143467) ;
#36868 = VERTEX_POINT('',#143469) ;
#36869 = VERTEX_POINT('',#143471) ;
#36870 = VERTEX_POINT('',#143474) ;
#36871 = VERTEX_POINT('',#143476) ;
#36872 = VERTEX_POINT('',#143478) ;
#36873 = VERTEX_POINT('',#143480) ;
#36874 = VERTEX_POINT('',#143482) ;
#36875 = VERTEX_POINT('',#143484) ;
#36876 = VERTEX_POINT('',#143486) ;
#36877 = VERTEX_POINT('',#143488) ;
#36878 = VERTEX_POINT('',#143490) ;
#36879 = VERTEX_POINT('',#143492) ;
#36880 = VERTEX_POINT('',#143494) ;
#36881 = VERTEX_POINT('',#143496) ;
#36882 = VERTEX_POINT('',#143498) ;
#36883 = VERTEX_POINT('',#143500) ;
#36884 = VERTEX_POINT('',#143503) ;
#36885 = VERTEX_POINT('',#143504) ;
#36886 = VERTEX_POINT('',#143506) ;
#36887 = VERTEX_POINT('',#143508) ;
#36888 = VERTEX_POINT('',#143510) ;
#36889 = VERTEX_POINT('',#143512) ;
#36890 = VERTEX_POINT('',#143514) ;
#36891 = VERTEX_POINT('',#143516) ;
#36892 = VERTEX_POINT('',#143519) ;
#36893 = VERTEX_POINT('',#143521) ;
#36894 = VERTEX_POINT('',#143523) ;
#36895 = VERTEX_POINT('',#143525) ;
#36896 = VERTEX_POINT('',#143527) ;
#36897 = VERTEX_POINT('',#143529) ;
#36898 = VERTEX_POINT('',#143531) ;
#36899 = VERTEX_POINT('',#143533) ;
#36900 = VERTEX_POINT('',#143535) ;
#36901 = VERTEX_POINT('',#143537) ;
#36902 = VERTEX_POINT('',#143539) ;
#36903 = VERTEX_POINT('',#143541) ;
#36904 = VERTEX_POINT('',#143543) ;
#36905 = VERTEX_POINT('',#143545) ;
#36906 = VERTEX_POINT('',#143548) ;
#36907 = VERTEX_POINT('',#143549) ;
#36908 = VERTEX_POINT('',#143551) ;
#36909 = VERTEX_POINT('',#143553) ;
#36910 = VERTEX_POINT('',#143555) ;
#36911 = VERTEX_POINT('',#143557) ;
#36912 = VERTEX_POINT('',#143559) ;
#36913 = VERTEX_POINT('',#143561) ;
#36914 = VERTEX_POINT('',#143564) ;
#36915 = VERTEX_POINT('',#143566) ;
#36916 = VERTEX_POINT('',#143568) ;
#36917 = VERTEX_POINT('',#143570) ;
#36918 = VERTEX_POINT('',#143572) ;
#36919 = VERTEX_POINT('',#143574) ;
#36920 = VERTEX_POINT('',#143576) ;
#36921 = VERTEX_POINT('',#143578) ;
#36922 = VERTEX_POINT('',#143580) ;
#36923 = VERTEX_POINT('',#143582) ;
#36924 = VERTEX_POINT('',#143584) ;
#36925 = VERTEX_POINT('',#143586) ;
#36926 = VERTEX_POINT('',#143588) ;
#36927 = VERTEX_POINT('',#143590) ;
#36928 = VERTEX_POINT('',#143593) ;
#36929 = VERTEX_POINT('',#143594) ;
#36930 = VERTEX_POINT('',#143596) ;
#36931 = VERTEX_POINT('',#143598) ;
#36932 = VERTEX_POINT('',#143600) ;
#36933 = VERTEX_POINT('',#143602) ;
#36934 = VERTEX_POINT('',#143604) ;
#36935 = VERTEX_POINT('',#143606) ;
#36936 = VERTEX_POINT('',#143609) ;
#36937 = VERTEX_POINT('',#143611) ;
#36938 = VERTEX_POINT('',#143613) ;
#36939 = VERTEX_POINT('',#143615) ;
#36940 = VERTEX_POINT('',#143617) ;
#36941 = VERTEX_POINT('',#143619) ;
#36942 = VERTEX_POINT('',#143621) ;
#36943 = VERTEX_POINT('',#143623) ;
#36944 = VERTEX_POINT('',#143625) ;
#36945 = VERTEX_POINT('',#143627) ;
#36946 = VERTEX_POINT('',#143629) ;
#36947 = VERTEX_POINT('',#143631) ;
#36948 = VERTEX_POINT('',#143633) ;
#36949 = VERTEX_POINT('',#143635) ;
#36950 = VERTEX_POINT('',#143638) ;
#36951 = VERTEX_POINT('',#143639) ;
#36952 = VERTEX_POINT('',#143641) ;
#36953 = VERTEX_POINT('',#143643) ;
#36954 = VERTEX_POINT('',#143645) ;
#36955 = VERTEX_POINT('',#143647) ;
#36956 = VERTEX_POINT('',#143649) ;
#36957 = VERTEX_POINT('',#143651) ;
#36958 = VERTEX_POINT('',#143654) ;
#36959 = VERTEX_POINT('',#143656) ;
#36960 = VERTEX_POINT('',#143658) ;
#36961 = VERTEX_POINT('',#143660) ;
#36962 = VERTEX_POINT('',#143662) ;
#36963 = VERTEX_POINT('',#143664) ;
#36964 = VERTEX_POINT('',#143666) ;
#36965 = VERTEX_POINT('',#143668) ;
#36966 = VERTEX_POINT('',#143670) ;
#36967 = VERTEX_POINT('',#143672) ;
#36968 = VERTEX_POINT('',#143674) ;
#36969 = VERTEX_POINT('',#143676) ;
#36970 = VERTEX_POINT('',#143678) ;
#36971 = VERTEX_POINT('',#143680) ;
#36972 = VERTEX_POINT('',#143684) ;
#36973 = VERTEX_POINT('',#143685) ;
#36974 = VERTEX_POINT('',#143687) ;
#36975 = VERTEX_POINT('',#143689) ;
#36976 = VERTEX_POINT('',#143691) ;
#36977 = VERTEX_POINT('',#143693) ;
#36978 = VERTEX_POINT('',#143695) ;
#36979 = VERTEX_POINT('',#143697) ;
#36980 = VERTEX_POINT('',#143699) ;
#36981 = VERTEX_POINT('',#143701) ;
#36982 = VERTEX_POINT('',#143705) ;
#36983 = VERTEX_POINT('',#143706) ;
#36984 = VERTEX_POINT('',#143708) ;
#36985 = VERTEX_POINT('',#143710) ;
#36986 = VERTEX_POINT('',#143712) ;
#36987 = VERTEX_POINT('',#143714) ;
#36988 = VERTEX_POINT('',#143716) ;
#36989 = VERTEX_POINT('',#143718) ;
#36990 = VERTEX_POINT('',#143720) ;
#36991 = VERTEX_POINT('',#143722) ;
#36992 = VERTEX_POINT('',#143726) ;
#36993 = VERTEX_POINT('',#143727) ;
#36994 = VERTEX_POINT('',#143729) ;
#36995 = VERTEX_POINT('',#143731) ;
#36996 = VERTEX_POINT('',#143733) ;
#36997 = VERTEX_POINT('',#143735) ;
#36998 = VERTEX_POINT('',#143737) ;
#36999 = VERTEX_POINT('',#143739) ;
#37000 = VERTEX_POINT('',#143741) ;
#37001 = VERTEX_POINT('',#143743) ;
#37002 = VERTEX_POINT('',#143747) ;
#37003 = VERTEX_POINT('',#143748) ;
#37004 = VERTEX_POINT('',#143750) ;
#37005 = VERTEX_POINT('',#143752) ;
#37006 = VERTEX_POINT('',#143756) ;
#37007 = VERTEX_POINT('',#143758) ;
#37008 = VERTEX_POINT('',#143762) ;
#37009 = VERTEX_POINT('',#143763) ;
#37010 = VERTEX_POINT('',#143765) ;
#37011 = VERTEX_POINT('',#143767) ;
#37012 = VERTEX_POINT('',#143771) ;
#37013 = VERTEX_POINT('',#143772) ;
#37014 = VERTEX_POINT('',#143774) ;
#37015 = VERTEX_POINT('',#143776) ;
#37016 = VERTEX_POINT('',#143780) ;
#37017 = VERTEX_POINT('',#143781) ;
#37018 = VERTEX_POINT('',#143783) ;
#37019 = VERTEX_POINT('',#143785) ;
#37020 = VERTEX_POINT('',#143789) ;
#37021 = VERTEX_POINT('',#143790) ;
#37022 = VERTEX_POINT('',#143792) ;
#37023 = VERTEX_POINT('',#143794) ;
#37024 = VERTEX_POINT('',#143798) ;
#37025 = VERTEX_POINT('',#143800) ;
#37026 = VERTEX_POINT('',#143804) ;
#37027 = VERTEX_POINT('',#143806) ;
#37028 = VERTEX_POINT('',#143810) ;
#37029 = VERTEX_POINT('',#143812) ;
#37030 = VERTEX_POINT('',#143816) ;
#37031 = VERTEX_POINT('',#143818) ;
#37032 = VERTEX_POINT('',#143823) ;
#37033 = VERTEX_POINT('',#143827) ;
#37034 = VERTEX_POINT('',#143834) ;
#37035 = VERTEX_POINT('',#143836) ;
#37036 = VERTEX_POINT('',#143840) ;
#37037 = VERTEX_POINT('',#143842) ;
#37038 = VERTEX_POINT('',#143846) ;
#37039 = VERTEX_POINT('',#143848) ;
#37040 = VERTEX_POINT('',#143852) ;
#37041 = VERTEX_POINT('',#143854) ;
#37042 = VERTEX_POINT('',#143858) ;
#37043 = VERTEX_POINT('',#143860) ;
#37044 = VERTEX_POINT('',#143864) ;
#37045 = VERTEX_POINT('',#143866) ;
#37046 = VERTEX_POINT('',#143870) ;
#37047 = VERTEX_POINT('',#143872) ;
#37048 = VERTEX_POINT('',#143876) ;
#37049 = VERTEX_POINT('',#143878) ;
#37050 = VERTEX_POINT('',#143882) ;
#37051 = VERTEX_POINT('',#143884) ;
#37052 = VERTEX_POINT('',#143888) ;
#37053 = VERTEX_POINT('',#143890) ;
#37054 = VERTEX_POINT('',#143894) ;
#37055 = VERTEX_POINT('',#143896) ;
#37056 = VERTEX_POINT('',#143900) ;
#37057 = VERTEX_POINT('',#143902) ;
#37058 = VERTEX_POINT('',#143906) ;
#37059 = VERTEX_POINT('',#143908) ;
#37060 = VERTEX_POINT('',#143912) ;
#37061 = VERTEX_POINT('',#143914) ;
#37062 = VERTEX_POINT('',#143918) ;
#37063 = VERTEX_POINT('',#143920) ;
#37064 = VERTEX_POINT('',#143924) ;
#37065 = VERTEX_POINT('',#143926) ;
#37066 = VERTEX_POINT('',#143930) ;
#37067 = VERTEX_POINT('',#143932) ;
#37068 = VERTEX_POINT('',#143936) ;
#37069 = VERTEX_POINT('',#143938) ;
#37070 = VERTEX_POINT('',#143945) ;
#37071 = VERTEX_POINT('',#143946) ;
#37072 = VERTEX_POINT('',#143948) ;
#37073 = VERTEX_POINT('',#143950) ;
#37074 = VERTEX_POINT('',#143952) ;
#37075 = VERTEX_POINT('',#143954) ;
#37076 = VERTEX_POINT('',#143956) ;
#37077 = VERTEX_POINT('',#143958) ;
#37078 = VERTEX_POINT('',#143960) ;
#37079 = VERTEX_POINT('',#143962) ;
#37080 = VERTEX_POINT('',#143964) ;
#37081 = VERTEX_POINT('',#143966) ;
#37082 = VERTEX_POINT('',#143968) ;
#37083 = VERTEX_POINT('',#143970) ;
#37084 = VERTEX_POINT('',#143972) ;
#37085 = VERTEX_POINT('',#143974) ;
#37086 = VERTEX_POINT('',#143977) ;
#37087 = VERTEX_POINT('',#143981) ;
#37088 = VERTEX_POINT('',#143982) ;
#37089 = VERTEX_POINT('',#143984) ;
#37090 = VERTEX_POINT('',#143986) ;
#37091 = VERTEX_POINT('',#143988) ;
#37092 = VERTEX_POINT('',#143990) ;
#37093 = VERTEX_POINT('',#143992) ;
#37094 = VERTEX_POINT('',#143994) ;
#37095 = VERTEX_POINT('',#144004) ;
#37096 = VERTEX_POINT('',#144014) ;
#37097 = VERTEX_POINT('',#144025) ;
#37098 = VERTEX_POINT('',#144057) ;
#37099 = VERTEX_POINT('',#144104) ;
#37100 = VERTEX_POINT('',#144122) ;
#37101 = VERTEX_POINT('',#144136) ;
#37102 = VERTEX_POINT('',#144151) ;
#37103 = VERTEX_POINT('',#144342) ;
#37104 = VERTEX_POINT('',#144343) ;
#37105 = VERTEX_POINT('',#144345) ;
#37106 = VERTEX_POINT('',#144347) ;
#37107 = VERTEX_POINT('',#144351) ;
#37108 = VERTEX_POINT('',#144352) ;
#37109 = VERTEX_POINT('',#144354) ;
#37110 = VERTEX_POINT('',#144356) ;
#37111 = VERTEX_POINT('',#144360) ;
#37112 = VERTEX_POINT('',#144361) ;
#37113 = VERTEX_POINT('',#144363) ;
#37114 = VERTEX_POINT('',#144365) ;
#37115 = VERTEX_POINT('',#144369) ;
#37116 = VERTEX_POINT('',#144370) ;
#37117 = VERTEX_POINT('',#144372) ;
#37118 = VERTEX_POINT('',#144374) ;
#37119 = VERTEX_POINT('',#144378) ;
#37120 = VERTEX_POINT('',#144379) ;
#37121 = VERTEX_POINT('',#144381) ;
#37122 = VERTEX_POINT('',#144383) ;
#37123 = VERTEX_POINT('',#144387) ;
#37124 = VERTEX_POINT('',#144388) ;
#37125 = VERTEX_POINT('',#144391) ;
#37126 = VERTEX_POINT('',#144393) ;
#37127 = VERTEX_POINT('',#144397) ;
#37128 = VERTEX_POINT('',#144398) ;
#37129 = VERTEX_POINT('',#144401) ;
#37130 = VERTEX_POINT('',#144403) ;
#37131 = VERTEX_POINT('',#144413) ;
#37132 = VERTEX_POINT('',#144414) ;
#37133 = VERTEX_POINT('',#144416) ;
#37134 = VERTEX_POINT('',#144418) ;
#37135 = VERTEX_POINT('',#144422) ;
#37136 = VERTEX_POINT('',#144423) ;
#37137 = VERTEX_POINT('',#144428) ;
#37138 = VERTEX_POINT('',#144430) ;
#37139 = VERTEX_POINT('',#144434) ;
#37140 = VERTEX_POINT('',#144435) ;
#37141 = VERTEX_POINT('',#144437) ;
#37142 = VERTEX_POINT('',#144439) ;
#37143 = VERTEX_POINT('',#144443) ;
#37144 = VERTEX_POINT('',#144444) ;
#37145 = VERTEX_POINT('',#144446) ;
#37146 = VERTEX_POINT('',#144448) ;
#37147 = VERTEX_POINT('',#144452) ;
#37148 = VERTEX_POINT('',#144453) ;
#37149 = VERTEX_POINT('',#144458) ;
#37150 = VERTEX_POINT('',#144460) ;
#37151 = VERTEX_POINT('',#144464) ;
#37152 = VERTEX_POINT('',#144465) ;
#37153 = VERTEX_POINT('',#144467) ;
#37154 = VERTEX_POINT('',#144469) ;
#37155 = VERTEX_POINT('',#144473) ;
#37156 = VERTEX_POINT('',#144474) ;
#37157 = VERTEX_POINT('',#144476) ;
#37158 = VERTEX_POINT('',#144478) ;
#37159 = VERTEX_POINT('',#144482) ;
#37160 = VERTEX_POINT('',#144483) ;
#37161 = VERTEX_POINT('',#144485) ;
#37162 = VERTEX_POINT('',#144487) ;
#37163 = VERTEX_POINT('',#144491) ;
#37164 = VERTEX_POINT('',#144492) ;
#37165 = VERTEX_POINT('',#144494) ;
#37166 = VERTEX_POINT('',#144496) ;
#37167 = VERTEX_POINT('',#144612) ;
#37168 = VERTEX_POINT('',#144613) ;
#37169 = VERTEX_POINT('',#144615) ;
#37170 = VERTEX_POINT('',#144617) ;
#37171 = VERTEX_POINT('',#144619) ;
#37172 = VERTEX_POINT('',#144621) ;
#37173 = VERTEX_POINT('',#144623) ;
#37174 = VERTEX_POINT('',#144625) ;
#37175 = VERTEX_POINT('',#144627) ;
#37176 = VERTEX_POINT('',#144629) ;
#37177 = VERTEX_POINT('',#144633) ;
#37178 = VERTEX_POINT('',#144634) ;
#37179 = VERTEX_POINT('',#144636) ;
#37180 = VERTEX_POINT('',#144638) ;
#37181 = VERTEX_POINT('',#144640) ;
#37182 = VERTEX_POINT('',#144642) ;
#37183 = VERTEX_POINT('',#144644) ;
#37184 = VERTEX_POINT('',#144646) ;
#37185 = VERTEX_POINT('',#144648) ;
#37186 = VERTEX_POINT('',#144650) ;
#37187 = VERTEX_POINT('',#144654) ;
#37188 = VERTEX_POINT('',#144655) ;
#37189 = VERTEX_POINT('',#144657) ;
#37190 = VERTEX_POINT('',#144659) ;
#37191 = VERTEX_POINT('',#144661) ;
#37192 = VERTEX_POINT('',#144663) ;
#37193 = VERTEX_POINT('',#144665) ;
#37194 = VERTEX_POINT('',#144667) ;
#37195 = VERTEX_POINT('',#144669) ;
#37196 = VERTEX_POINT('',#144671) ;
#37197 = VERTEX_POINT('',#144675) ;
#37198 = VERTEX_POINT('',#144676) ;
#37199 = VERTEX_POINT('',#144678) ;
#37200 = VERTEX_POINT('',#144680) ;
#37201 = VERTEX_POINT('',#144682) ;
#37202 = VERTEX_POINT('',#144684) ;
#37203 = VERTEX_POINT('',#144686) ;
#37204 = VERTEX_POINT('',#144688) ;
#37205 = VERTEX_POINT('',#144690) ;
#37206 = VERTEX_POINT('',#144692) ;
#37207 = VERTEX_POINT('',#144696) ;
#37208 = VERTEX_POINT('',#144697) ;
#37209 = VERTEX_POINT('',#144699) ;
#37210 = VERTEX_POINT('',#144701) ;
#37211 = VERTEX_POINT('',#144703) ;
#37212 = VERTEX_POINT('',#144705) ;
#37213 = VERTEX_POINT('',#144707) ;
#37214 = VERTEX_POINT('',#144709) ;
#37215 = VERTEX_POINT('',#144711) ;
#37216 = VERTEX_POINT('',#144713) ;
#37217 = VERTEX_POINT('',#144717) ;
#37218 = VERTEX_POINT('',#144718) ;
#37219 = VERTEX_POINT('',#144720) ;
#37220 = VERTEX_POINT('',#144722) ;
#37221 = VERTEX_POINT('',#144724) ;
#37222 = VERTEX_POINT('',#144726) ;
#37223 = VERTEX_POINT('',#144728) ;
#37224 = VERTEX_POINT('',#144730) ;
#37225 = VERTEX_POINT('',#144732) ;
#37226 = VERTEX_POINT('',#144734) ;
#37227 = VERTEX_POINT('',#144738) ;
#37228 = VERTEX_POINT('',#144739) ;
#37229 = VERTEX_POINT('',#144741) ;
#37230 = VERTEX_POINT('',#144743) ;
#37231 = VERTEX_POINT('',#144745) ;
#37232 = VERTEX_POINT('',#144747) ;
#37233 = VERTEX_POINT('',#144749) ;
#37234 = VERTEX_POINT('',#144751) ;
#37235 = VERTEX_POINT('',#144753) ;
#37236 = VERTEX_POINT('',#144755) ;
#37237 = VERTEX_POINT('',#144759) ;
#37238 = VERTEX_POINT('',#144760) ;
#37239 = VERTEX_POINT('',#144762) ;
#37240 = VERTEX_POINT('',#144764) ;
#37241 = VERTEX_POINT('',#144766) ;
#37242 = VERTEX_POINT('',#144768) ;
#37243 = VERTEX_POINT('',#144770) ;
#37244 = VERTEX_POINT('',#144772) ;
#37245 = VERTEX_POINT('',#144774) ;
#37246 = VERTEX_POINT('',#144776) ;
#37247 = VERTEX_POINT('',#144780) ;
#37248 = VERTEX_POINT('',#144781) ;
#37249 = VERTEX_POINT('',#144783) ;
#37250 = VERTEX_POINT('',#144785) ;
#37251 = VERTEX_POINT('',#144787) ;
#37252 = VERTEX_POINT('',#144789) ;
#37253 = VERTEX_POINT('',#144791) ;
#37254 = VERTEX_POINT('',#144793) ;
#37255 = VERTEX_POINT('',#144795) ;
#37256 = VERTEX_POINT('',#144797) ;
#37257 = VERTEX_POINT('',#144801) ;
#37258 = VERTEX_POINT('',#144802) ;
#37259 = VERTEX_POINT('',#144804) ;
#37260 = VERTEX_POINT('',#144806) ;
#37261 = VERTEX_POINT('',#144810) ;
#37262 = VERTEX_POINT('',#144812) ;
#37263 = VERTEX_POINT('',#144816) ;
#37264 = VERTEX_POINT('',#144817) ;
#37265 = VERTEX_POINT('',#144819) ;
#37266 = VERTEX_POINT('',#144821) ;
#37267 = VERTEX_POINT('',#144825) ;
#37268 = VERTEX_POINT('',#144826) ;
#37269 = VERTEX_POINT('',#144828) ;
#37270 = VERTEX_POINT('',#144830) ;
#37271 = VERTEX_POINT('',#144834) ;
#37272 = VERTEX_POINT('',#144835) ;
#37273 = VERTEX_POINT('',#144837) ;
#37274 = VERTEX_POINT('',#144839) ;
#37275 = VERTEX_POINT('',#144843) ;
#37276 = VERTEX_POINT('',#144844) ;
#37277 = VERTEX_POINT('',#144846) ;
#37278 = VERTEX_POINT('',#144848) ;
#37279 = VERTEX_POINT('',#144852) ;
#37280 = VERTEX_POINT('',#144854) ;
#37281 = VERTEX_POINT('',#144858) ;
#37282 = VERTEX_POINT('',#144859) ;
#37283 = VERTEX_POINT('',#144861) ;
#37284 = VERTEX_POINT('',#144863) ;
#37285 = VERTEX_POINT('',#144867) ;
#37286 = VERTEX_POINT('',#144868) ;
#37287 = VERTEX_POINT('',#144870) ;
#37288 = VERTEX_POINT('',#144872) ;
#37289 = VERTEX_POINT('',#144876) ;
#37290 = VERTEX_POINT('',#144877) ;
#37291 = VERTEX_POINT('',#144879) ;
#37292 = VERTEX_POINT('',#144881) ;
#37293 = VERTEX_POINT('',#144885) ;
#37294 = VERTEX_POINT('',#144886) ;
#37295 = VERTEX_POINT('',#144888) ;
#37296 = VERTEX_POINT('',#144890) ;
#37297 = VERTEX_POINT('',#144894) ;
#37298 = VERTEX_POINT('',#144896) ;
#37299 = VERTEX_POINT('',#144900) ;
#37300 = VERTEX_POINT('',#144901) ;
#37301 = VERTEX_POINT('',#144903) ;
#37302 = VERTEX_POINT('',#144905) ;
#37303 = VERTEX_POINT('',#144909) ;
#37304 = VERTEX_POINT('',#144910) ;
#37305 = VERTEX_POINT('',#144912) ;
#37306 = VERTEX_POINT('',#144914) ;
#37307 = VERTEX_POINT('',#144918) ;
#37308 = VERTEX_POINT('',#144919) ;
#37309 = VERTEX_POINT('',#144921) ;
#37310 = VERTEX_POINT('',#144923) ;
#37311 = VERTEX_POINT('',#144927) ;
#37312 = VERTEX_POINT('',#144928) ;
#37313 = VERTEX_POINT('',#144930) ;
#37314 = VERTEX_POINT('',#144932) ;
#37315 = VERTEX_POINT('',#144936) ;
#37316 = VERTEX_POINT('',#144938) ;
#37317 = VERTEX_POINT('',#144942) ;
#37318 = VERTEX_POINT('',#144943) ;
#37319 = VERTEX_POINT('',#144945) ;
#37320 = VERTEX_POINT('',#144947) ;
#37321 = VERTEX_POINT('',#144951) ;
#37322 = VERTEX_POINT('',#144952) ;
#37323 = VERTEX_POINT('',#144954) ;
#37324 = VERTEX_POINT('',#144956) ;
#37325 = VERTEX_POINT('',#144960) ;
#37326 = VERTEX_POINT('',#144961) ;
#37327 = VERTEX_POINT('',#144963) ;
#37328 = VERTEX_POINT('',#144965) ;
#37329 = VERTEX_POINT('',#144969) ;
#37330 = VERTEX_POINT('',#144970) ;
#37331 = VERTEX_POINT('',#144972) ;
#37332 = VERTEX_POINT('',#144974) ;
#37333 = VERTEX_POINT('',#144978) ;
#37334 = VERTEX_POINT('',#144980) ;
#37335 = VERTEX_POINT('',#144984) ;
#37336 = VERTEX_POINT('',#144985) ;
#37337 = VERTEX_POINT('',#144987) ;
#37338 = VERTEX_POINT('',#144989) ;
#37339 = VERTEX_POINT('',#144993) ;
#37340 = VERTEX_POINT('',#144994) ;
#37341 = VERTEX_POINT('',#144996) ;
#37342 = VERTEX_POINT('',#144998) ;
#37343 = VERTEX_POINT('',#145002) ;
#37344 = VERTEX_POINT('',#145003) ;
#37345 = VERTEX_POINT('',#145005) ;
#37346 = VERTEX_POINT('',#145007) ;
#37347 = VERTEX_POINT('',#145011) ;
#37348 = VERTEX_POINT('',#145012) ;
#37349 = VERTEX_POINT('',#145014) ;
#37350 = VERTEX_POINT('',#145016) ;
#37351 = VERTEX_POINT('',#145020) ;
#37352 = VERTEX_POINT('',#145022) ;
#37353 = VERTEX_POINT('',#145026) ;
#37354 = VERTEX_POINT('',#145027) ;
#37355 = VERTEX_POINT('',#145029) ;
#37356 = VERTEX_POINT('',#145031) ;
#37357 = VERTEX_POINT('',#145035) ;
#37358 = VERTEX_POINT('',#145036) ;
#37359 = VERTEX_POINT('',#145038) ;
#37360 = VERTEX_POINT('',#145040) ;
#37361 = VERTEX_POINT('',#145044) ;
#37362 = VERTEX_POINT('',#145045) ;
#37363 = VERTEX_POINT('',#145047) ;
#37364 = VERTEX_POINT('',#145049) ;
#37365 = VERTEX_POINT('',#145053) ;
#37366 = VERTEX_POINT('',#145054) ;
#37367 = VERTEX_POINT('',#145056) ;
#37368 = VERTEX_POINT('',#145058) ;
#37369 = VERTEX_POINT('',#145062) ;
#37370 = VERTEX_POINT('',#145064) ;
#37371 = VERTEX_POINT('',#145068) ;
#37372 = VERTEX_POINT('',#145069) ;
#37373 = VERTEX_POINT('',#145071) ;
#37374 = VERTEX_POINT('',#145073) ;
#37375 = VERTEX_POINT('',#145077) ;
#37376 = VERTEX_POINT('',#145078) ;
#37377 = VERTEX_POINT('',#145080) ;
#37378 = VERTEX_POINT('',#145082) ;
#37379 = VERTEX_POINT('',#145086) ;
#37380 = VERTEX_POINT('',#145087) ;
#37381 = VERTEX_POINT('',#145089) ;
#37382 = VERTEX_POINT('',#145091) ;
#37383 = VERTEX_POINT('',#145095) ;
#37384 = VERTEX_POINT('',#145096) ;
#37385 = VERTEX_POINT('',#145098) ;
#37386 = VERTEX_POINT('',#145100) ;
#37387 = VERTEX_POINT('',#145104) ;
#37388 = VERTEX_POINT('',#145106) ;
#37389 = VERTEX_POINT('',#145110) ;
#37390 = VERTEX_POINT('',#145111) ;
#37391 = VERTEX_POINT('',#145113) ;
#37392 = VERTEX_POINT('',#145115) ;
#37393 = VERTEX_POINT('',#145119) ;
#37394 = VERTEX_POINT('',#145120) ;
#37395 = VERTEX_POINT('',#145122) ;
#37396 = VERTEX_POINT('',#145124) ;
#37397 = VERTEX_POINT('',#145128) ;
#37398 = VERTEX_POINT('',#145129) ;
#37399 = VERTEX_POINT('',#145131) ;
#37400 = VERTEX_POINT('',#145133) ;
#37401 = VERTEX_POINT('',#145137) ;
#37402 = VERTEX_POINT('',#145138) ;
#37403 = VERTEX_POINT('',#145140) ;
#37404 = VERTEX_POINT('',#145142) ;
#37405 = VERTEX_POINT('',#145146) ;
#37406 = VERTEX_POINT('',#145148) ;
#37407 = VERTEX_POINT('',#145152) ;
#37408 = VERTEX_POINT('',#145153) ;
#37409 = VERTEX_POINT('',#145155) ;
#37410 = VERTEX_POINT('',#145157) ;
#37411 = VERTEX_POINT('',#145161) ;
#37412 = VERTEX_POINT('',#145162) ;
#37413 = VERTEX_POINT('',#145164) ;
#37414 = VERTEX_POINT('',#145166) ;
#37415 = VERTEX_POINT('',#145170) ;
#37416 = VERTEX_POINT('',#145171) ;
#37417 = VERTEX_POINT('',#145173) ;
#37418 = VERTEX_POINT('',#145175) ;
#37419 = VERTEX_POINT('',#145179) ;
#37420 = VERTEX_POINT('',#145180) ;
#37421 = VERTEX_POINT('',#145182) ;
#37422 = VERTEX_POINT('',#145184) ;
#37423 = VERTEX_POINT('',#145188) ;
#37424 = VERTEX_POINT('',#145190) ;
#37425 = VERTEX_POINT('',#145194) ;
#37426 = VERTEX_POINT('',#145196) ;
#37427 = VERTEX_POINT('',#145200) ;
#37428 = VERTEX_POINT('',#145202) ;
#37429 = VERTEX_POINT('',#145206) ;
#37430 = VERTEX_POINT('',#145208) ;
#37431 = VERTEX_POINT('',#145213) ;
#37432 = VERTEX_POINT('',#145217) ;
#37433 = VERTEX_POINT('',#145224) ;
#37434 = VERTEX_POINT('',#145226) ;
#37435 = VERTEX_POINT('',#145230) ;
#37436 = VERTEX_POINT('',#145232) ;
#37437 = VERTEX_POINT('',#145236) ;
#37438 = VERTEX_POINT('',#145238) ;
#37439 = VERTEX_POINT('',#145242) ;
#37440 = VERTEX_POINT('',#145244) ;
#37441 = VERTEX_POINT('',#145248) ;
#37442 = VERTEX_POINT('',#145250) ;
#37443 = VERTEX_POINT('',#145254) ;
#37444 = VERTEX_POINT('',#145256) ;
#37445 = VERTEX_POINT('',#145260) ;
#37446 = VERTEX_POINT('',#145262) ;
#37447 = VERTEX_POINT('',#145266) ;
#37448 = VERTEX_POINT('',#145268) ;
#37449 = VERTEX_POINT('',#145272) ;
#37450 = VERTEX_POINT('',#145274) ;
#37451 = VERTEX_POINT('',#145278) ;
#37452 = VERTEX_POINT('',#145280) ;
#37453 = VERTEX_POINT('',#145284) ;
#37454 = VERTEX_POINT('',#145286) ;
#37455 = VERTEX_POINT('',#145290) ;
#37456 = VERTEX_POINT('',#145292) ;
#37457 = VERTEX_POINT('',#145296) ;
#37458 = VERTEX_POINT('',#145298) ;
#37459 = VERTEX_POINT('',#145302) ;
#37460 = VERTEX_POINT('',#145304) ;
#37461 = VERTEX_POINT('',#145308) ;
#37462 = VERTEX_POINT('',#145310) ;
#37463 = VERTEX_POINT('',#145314) ;
#37464 = VERTEX_POINT('',#145316) ;
#37465 = VERTEX_POINT('',#145320) ;
#37466 = VERTEX_POINT('',#145322) ;
#37467 = VERTEX_POINT('',#145326) ;
#37468 = VERTEX_POINT('',#145328) ;
#37469 = VERTEX_POINT('',#145335) ;
#37470 = VERTEX_POINT('',#145336) ;
#37471 = VERTEX_POINT('',#145338) ;
#37472 = VERTEX_POINT('',#145340) ;
#37473 = VERTEX_POINT('',#145342) ;
#37474 = VERTEX_POINT('',#145344) ;
#37475 = VERTEX_POINT('',#145346) ;
#37476 = VERTEX_POINT('',#145348) ;
#37477 = VERTEX_POINT('',#145350) ;
#37478 = VERTEX_POINT('',#145352) ;
#37479 = VERTEX_POINT('',#145354) ;
#37480 = VERTEX_POINT('',#145356) ;
#37481 = VERTEX_POINT('',#145358) ;
#37482 = VERTEX_POINT('',#145360) ;
#37483 = VERTEX_POINT('',#145362) ;
#37484 = VERTEX_POINT('',#145364) ;
#37485 = VERTEX_POINT('',#145367) ;
#37486 = VERTEX_POINT('',#145371) ;
#37487 = VERTEX_POINT('',#145372) ;
#37488 = VERTEX_POINT('',#145374) ;
#37489 = VERTEX_POINT('',#145376) ;
#37490 = VERTEX_POINT('',#145380) ;
#37491 = VERTEX_POINT('',#145382) ;
#37492 = VERTEX_POINT('',#145386) ;
#37493 = VERTEX_POINT('',#145388) ;
#37494 = VERTEX_POINT('',#145392) ;
#37495 = VERTEX_POINT('',#145394) ;
#37496 = VERTEX_POINT('',#145398) ;
#37497 = VERTEX_POINT('',#145400) ;
#37498 = VERTEX_POINT('',#145405) ;
#37499 = VERTEX_POINT('',#145409) ;
#37500 = VERTEX_POINT('',#145416) ;
#37501 = VERTEX_POINT('',#145418) ;
#37502 = VERTEX_POINT('',#145422) ;
#37503 = VERTEX_POINT('',#145424) ;
#37504 = VERTEX_POINT('',#145428) ;
#37505 = VERTEX_POINT('',#145430) ;
#37506 = VERTEX_POINT('',#145434) ;
#37507 = VERTEX_POINT('',#145436) ;
#37508 = VERTEX_POINT('',#145440) ;
#37509 = VERTEX_POINT('',#145442) ;
#37510 = VERTEX_POINT('',#145446) ;
#37511 = VERTEX_POINT('',#145448) ;
#37512 = VERTEX_POINT('',#145452) ;
#37513 = VERTEX_POINT('',#145454) ;
#37514 = VERTEX_POINT('',#145458) ;
#37515 = VERTEX_POINT('',#145460) ;
#37516 = VERTEX_POINT('',#145464) ;
#37517 = VERTEX_POINT('',#145466) ;
#37518 = VERTEX_POINT('',#145470) ;
#37519 = VERTEX_POINT('',#145472) ;
#37520 = VERTEX_POINT('',#145476) ;
#37521 = VERTEX_POINT('',#145478) ;
#37522 = VERTEX_POINT('',#145482) ;
#37523 = VERTEX_POINT('',#145484) ;
#37524 = VERTEX_POINT('',#145488) ;
#37525 = VERTEX_POINT('',#145490) ;
#37526 = VERTEX_POINT('',#145494) ;
#37527 = VERTEX_POINT('',#145496) ;
#37528 = VERTEX_POINT('',#145500) ;
#37529 = VERTEX_POINT('',#145502) ;
#37530 = VERTEX_POINT('',#145506) ;
#37531 = VERTEX_POINT('',#145508) ;
#37532 = VERTEX_POINT('',#145512) ;
#37533 = VERTEX_POINT('',#145514) ;
#37534 = VERTEX_POINT('',#145518) ;
#37535 = VERTEX_POINT('',#145520) ;
#37536 = VERTEX_POINT('',#145527) ;
#37537 = VERTEX_POINT('',#145528) ;
#37538 = VERTEX_POINT('',#145530) ;
#37539 = VERTEX_POINT('',#145532) ;
#37540 = VERTEX_POINT('',#145534) ;
#37541 = VERTEX_POINT('',#145536) ;
#37542 = VERTEX_POINT('',#145538) ;
#37543 = VERTEX_POINT('',#145540) ;
#37544 = VERTEX_POINT('',#145542) ;
#37545 = VERTEX_POINT('',#145544) ;
#37546 = VERTEX_POINT('',#145546) ;
#37547 = VERTEX_POINT('',#145548) ;
#37548 = VERTEX_POINT('',#145550) ;
#37549 = VERTEX_POINT('',#145552) ;
#37550 = VERTEX_POINT('',#145554) ;
#37551 = VERTEX_POINT('',#145556) ;
#37552 = VERTEX_POINT('',#145559) ;
#37553 = VERTEX_POINT('',#145563) ;
#37554 = VERTEX_POINT('',#145564) ;
#37555 = VERTEX_POINT('',#145566) ;
#37556 = VERTEX_POINT('',#145568) ;
#37557 = VERTEX_POINT('',#145572) ;
#37558 = VERTEX_POINT('',#145574) ;
#37559 = VERTEX_POINT('',#145578) ;
#37560 = VERTEX_POINT('',#145580) ;
#37561 = VERTEX_POINT('',#145584) ;
#37562 = VERTEX_POINT('',#145586) ;
#37563 = VERTEX_POINT('',#145590) ;
#37564 = VERTEX_POINT('',#145592) ;
#37565 = VERTEX_POINT('',#145597) ;
#37566 = VERTEX_POINT('',#145601) ;
#37567 = VERTEX_POINT('',#145608) ;
#37568 = VERTEX_POINT('',#145610) ;
#37569 = VERTEX_POINT('',#145614) ;
#37570 = VERTEX_POINT('',#145616) ;
#37571 = VERTEX_POINT('',#145620) ;
#37572 = VERTEX_POINT('',#145622) ;
#37573 = VERTEX_POINT('',#145626) ;
#37574 = VERTEX_POINT('',#145628) ;
#37575 = VERTEX_POINT('',#145632) ;
#37576 = VERTEX_POINT('',#145634) ;
#37577 = VERTEX_POINT('',#145638) ;
#37578 = VERTEX_POINT('',#145640) ;
#37579 = VERTEX_POINT('',#145644) ;
#37580 = VERTEX_POINT('',#145646) ;
#37581 = VERTEX_POINT('',#145650) ;
#37582 = VERTEX_POINT('',#145652) ;
#37583 = VERTEX_POINT('',#145656) ;
#37584 = VERTEX_POINT('',#145658) ;
#37585 = VERTEX_POINT('',#145662) ;
#37586 = VERTEX_POINT('',#145664) ;
#37587 = VERTEX_POINT('',#145668) ;
#37588 = VERTEX_POINT('',#145670) ;
#37589 = VERTEX_POINT('',#145674) ;
#37590 = VERTEX_POINT('',#145676) ;
#37591 = VERTEX_POINT('',#145680) ;
#37592 = VERTEX_POINT('',#145682) ;
#37593 = VERTEX_POINT('',#145686) ;
#37594 = VERTEX_POINT('',#145688) ;
#37595 = VERTEX_POINT('',#145692) ;
#37596 = VERTEX_POINT('',#145694) ;
#37597 = VERTEX_POINT('',#145698) ;
#37598 = VERTEX_POINT('',#145700) ;
#37599 = VERTEX_POINT('',#145704) ;
#37600 = VERTEX_POINT('',#145706) ;
#37601 = VERTEX_POINT('',#145710) ;
#37602 = VERTEX_POINT('',#145712) ;
#37603 = VERTEX_POINT('',#145719) ;
#37604 = VERTEX_POINT('',#145720) ;
#37605 = VERTEX_POINT('',#145722) ;
#37606 = VERTEX_POINT('',#145724) ;
#37607 = VERTEX_POINT('',#145726) ;
#37608 = VERTEX_POINT('',#145728) ;
#37609 = VERTEX_POINT('',#145730) ;
#37610 = VERTEX_POINT('',#145732) ;
#37611 = VERTEX_POINT('',#145734) ;
#37612 = VERTEX_POINT('',#145736) ;
#37613 = VERTEX_POINT('',#145738) ;
#37614 = VERTEX_POINT('',#145740) ;
#37615 = VERTEX_POINT('',#145742) ;
#37616 = VERTEX_POINT('',#145744) ;
#37617 = VERTEX_POINT('',#145746) ;
#37618 = VERTEX_POINT('',#145748) ;
#37619 = VERTEX_POINT('',#145751) ;
#37620 = VERTEX_POINT('',#145755) ;
#37621 = VERTEX_POINT('',#145756) ;
#37622 = VERTEX_POINT('',#145758) ;
#37623 = VERTEX_POINT('',#145760) ;
#37624 = VERTEX_POINT('',#145764) ;
#37625 = VERTEX_POINT('',#145766) ;
#37626 = VERTEX_POINT('',#145770) ;
#37627 = VERTEX_POINT('',#145772) ;
#37628 = VERTEX_POINT('',#145776) ;
#37629 = VERTEX_POINT('',#145778) ;
#37630 = VERTEX_POINT('',#145782) ;
#37631 = VERTEX_POINT('',#145784) ;
#37632 = VERTEX_POINT('',#145789) ;
#37633 = VERTEX_POINT('',#145793) ;
#37634 = VERTEX_POINT('',#145800) ;
#37635 = VERTEX_POINT('',#145802) ;
#37636 = VERTEX_POINT('',#145806) ;
#37637 = VERTEX_POINT('',#145808) ;
#37638 = VERTEX_POINT('',#145812) ;
#37639 = VERTEX_POINT('',#145814) ;
#37640 = VERTEX_POINT('',#145818) ;
#37641 = VERTEX_POINT('',#145820) ;
#37642 = VERTEX_POINT('',#145824) ;
#37643 = VERTEX_POINT('',#145826) ;
#37644 = VERTEX_POINT('',#145830) ;
#37645 = VERTEX_POINT('',#145832) ;
#37646 = VERTEX_POINT('',#145836) ;
#37647 = VERTEX_POINT('',#145838) ;
#37648 = VERTEX_POINT('',#145842) ;
#37649 = VERTEX_POINT('',#145844) ;
#37650 = VERTEX_POINT('',#145848) ;
#37651 = VERTEX_POINT('',#145850) ;
#37652 = VERTEX_POINT('',#145854) ;
#37653 = VERTEX_POINT('',#145856) ;
#37654 = VERTEX_POINT('',#145860) ;
#37655 = VERTEX_POINT('',#145862) ;
#37656 = VERTEX_POINT('',#145866) ;
#37657 = VERTEX_POINT('',#145868) ;
#37658 = VERTEX_POINT('',#145872) ;
#37659 = VERTEX_POINT('',#145874) ;
#37660 = VERTEX_POINT('',#145878) ;
#37661 = VERTEX_POINT('',#145880) ;
#37662 = VERTEX_POINT('',#145884) ;
#37663 = VERTEX_POINT('',#145886) ;
#37664 = VERTEX_POINT('',#145890) ;
#37665 = VERTEX_POINT('',#145892) ;
#37666 = VERTEX_POINT('',#145896) ;
#37667 = VERTEX_POINT('',#145898) ;
#37668 = VERTEX_POINT('',#145902) ;
#37669 = VERTEX_POINT('',#145904) ;
#37670 = VERTEX_POINT('',#145911) ;
#37671 = VERTEX_POINT('',#145912) ;
#37672 = VERTEX_POINT('',#145914) ;
#37673 = VERTEX_POINT('',#145916) ;
#37674 = VERTEX_POINT('',#145918) ;
#37675 = VERTEX_POINT('',#145920) ;
#37676 = VERTEX_POINT('',#145922) ;
#37677 = VERTEX_POINT('',#145924) ;
#37678 = VERTEX_POINT('',#145926) ;
#37679 = VERTEX_POINT('',#145928) ;
#37680 = VERTEX_POINT('',#145930) ;
#37681 = VERTEX_POINT('',#145932) ;
#37682 = VERTEX_POINT('',#145934) ;
#37683 = VERTEX_POINT('',#145936) ;
#37684 = VERTEX_POINT('',#145938) ;
#37685 = VERTEX_POINT('',#145940) ;
#37686 = VERTEX_POINT('',#145943) ;
#37687 = VERTEX_POINT('',#145947) ;
#37688 = VERTEX_POINT('',#145948) ;
#37689 = VERTEX_POINT('',#145950) ;
#37690 = VERTEX_POINT('',#145952) ;
#37691 = VERTEX_POINT('',#145956) ;
#37692 = VERTEX_POINT('',#145958) ;
#37693 = VERTEX_POINT('',#145962) ;
#37694 = VERTEX_POINT('',#145964) ;
#37695 = VERTEX_POINT('',#145968) ;
#37696 = VERTEX_POINT('',#145970) ;
#37697 = VERTEX_POINT('',#145974) ;
#37698 = VERTEX_POINT('',#145976) ;
#37699 = VERTEX_POINT('',#145981) ;
#37700 = VERTEX_POINT('',#145985) ;
#37701 = VERTEX_POINT('',#145992) ;
#37702 = VERTEX_POINT('',#145994) ;
#37703 = VERTEX_POINT('',#145998) ;
#37704 = VERTEX_POINT('',#146000) ;
#37705 = VERTEX_POINT('',#146004) ;
#37706 = VERTEX_POINT('',#146006) ;
#37707 = VERTEX_POINT('',#146010) ;
#37708 = VERTEX_POINT('',#146012) ;
#37709 = VERTEX_POINT('',#146016) ;
#37710 = VERTEX_POINT('',#146018) ;
#37711 = VERTEX_POINT('',#146022) ;
#37712 = VERTEX_POINT('',#146024) ;
#37713 = VERTEX_POINT('',#146028) ;
#37714 = VERTEX_POINT('',#146030) ;
#37715 = VERTEX_POINT('',#146034) ;
#37716 = VERTEX_POINT('',#146036) ;
#37717 = VERTEX_POINT('',#146040) ;
#37718 = VERTEX_POINT('',#146042) ;
#37719 = VERTEX_POINT('',#146046) ;
#37720 = VERTEX_POINT('',#146048) ;
#37721 = VERTEX_POINT('',#146052) ;
#37722 = VERTEX_POINT('',#146054) ;
#37723 = VERTEX_POINT('',#146058) ;
#37724 = VERTEX_POINT('',#146060) ;
#37725 = VERTEX_POINT('',#146064) ;
#37726 = VERTEX_POINT('',#146066) ;
#37727 = VERTEX_POINT('',#146070) ;
#37728 = VERTEX_POINT('',#146072) ;
#37729 = VERTEX_POINT('',#146076) ;
#37730 = VERTEX_POINT('',#146078) ;
#37731 = VERTEX_POINT('',#146082) ;
#37732 = VERTEX_POINT('',#146084) ;
#37733 = VERTEX_POINT('',#146088) ;
#37734 = VERTEX_POINT('',#146090) ;
#37735 = VERTEX_POINT('',#146094) ;
#37736 = VERTEX_POINT('',#146096) ;
#37737 = VERTEX_POINT('',#146103) ;
#37738 = VERTEX_POINT('',#146104) ;
#37739 = VERTEX_POINT('',#146106) ;
#37740 = VERTEX_POINT('',#146108) ;
#37741 = VERTEX_POINT('',#146110) ;
#37742 = VERTEX_POINT('',#146112) ;
#37743 = VERTEX_POINT('',#146114) ;
#37744 = VERTEX_POINT('',#146116) ;
#37745 = VERTEX_POINT('',#146118) ;
#37746 = VERTEX_POINT('',#146120) ;
#37747 = VERTEX_POINT('',#146122) ;
#37748 = VERTEX_POINT('',#146124) ;
#37749 = VERTEX_POINT('',#146126) ;
#37750 = VERTEX_POINT('',#146128) ;
#37751 = VERTEX_POINT('',#146130) ;
#37752 = VERTEX_POINT('',#146132) ;
#37753 = VERTEX_POINT('',#146135) ;
#37754 = VERTEX_POINT('',#146139) ;
#37755 = VERTEX_POINT('',#146140) ;
#37756 = VERTEX_POINT('',#146142) ;
#37757 = VERTEX_POINT('',#146144) ;
#37758 = VERTEX_POINT('',#146148) ;
#37759 = VERTEX_POINT('',#146150) ;
#37760 = VERTEX_POINT('',#146154) ;
#37761 = VERTEX_POINT('',#146156) ;
#37762 = VERTEX_POINT('',#146160) ;
#37763 = VERTEX_POINT('',#146162) ;
#37764 = VERTEX_POINT('',#146166) ;
#37765 = VERTEX_POINT('',#146168) ;
#37766 = VERTEX_POINT('',#146173) ;
#37767 = VERTEX_POINT('',#146177) ;
#37768 = VERTEX_POINT('',#146184) ;
#37769 = VERTEX_POINT('',#146186) ;
#37770 = VERTEX_POINT('',#146190) ;
#37771 = VERTEX_POINT('',#146192) ;
#37772 = VERTEX_POINT('',#146196) ;
#37773 = VERTEX_POINT('',#146198) ;
#37774 = VERTEX_POINT('',#146202) ;
#37775 = VERTEX_POINT('',#146204) ;
#37776 = VERTEX_POINT('',#146208) ;
#37777 = VERTEX_POINT('',#146210) ;
#37778 = VERTEX_POINT('',#146214) ;
#37779 = VERTEX_POINT('',#146216) ;
#37780 = VERTEX_POINT('',#146220) ;
#37781 = VERTEX_POINT('',#146222) ;
#37782 = VERTEX_POINT('',#146226) ;
#37783 = VERTEX_POINT('',#146228) ;
#37784 = VERTEX_POINT('',#146232) ;
#37785 = VERTEX_POINT('',#146234) ;
#37786 = VERTEX_POINT('',#146238) ;
#37787 = VERTEX_POINT('',#146240) ;
#37788 = VERTEX_POINT('',#146244) ;
#37789 = VERTEX_POINT('',#146246) ;
#37790 = VERTEX_POINT('',#146250) ;
#37791 = VERTEX_POINT('',#146252) ;
#37792 = VERTEX_POINT('',#146256) ;
#37793 = VERTEX_POINT('',#146258) ;
#37794 = VERTEX_POINT('',#146262) ;
#37795 = VERTEX_POINT('',#146264) ;
#37796 = VERTEX_POINT('',#146268) ;
#37797 = VERTEX_POINT('',#146270) ;
#37798 = VERTEX_POINT('',#146274) ;
#37799 = VERTEX_POINT('',#146276) ;
#37800 = VERTEX_POINT('',#146280) ;
#37801 = VERTEX_POINT('',#146282) ;
#37802 = VERTEX_POINT('',#146286) ;
#37803 = VERTEX_POINT('',#146288) ;
#37804 = VERTEX_POINT('',#146295) ;
#37805 = VERTEX_POINT('',#146296) ;
#37806 = VERTEX_POINT('',#146298) ;
#37807 = VERTEX_POINT('',#146300) ;
#37808 = VERTEX_POINT('',#146302) ;
#37809 = VERTEX_POINT('',#146304) ;
#37810 = VERTEX_POINT('',#146306) ;
#37811 = VERTEX_POINT('',#146308) ;
#37812 = VERTEX_POINT('',#146310) ;
#37813 = VERTEX_POINT('',#146312) ;
#37814 = VERTEX_POINT('',#146314) ;
#37815 = VERTEX_POINT('',#146316) ;
#37816 = VERTEX_POINT('',#146318) ;
#37817 = VERTEX_POINT('',#146320) ;
#37818 = VERTEX_POINT('',#146322) ;
#37819 = VERTEX_POINT('',#146324) ;
#37820 = VERTEX_POINT('',#146327) ;
#37821 = VERTEX_POINT('',#146331) ;
#37822 = VERTEX_POINT('',#146332) ;
#37823 = VERTEX_POINT('',#146334) ;
#37824 = VERTEX_POINT('',#146336) ;
#37825 = VERTEX_POINT('',#146340) ;
#37826 = VERTEX_POINT('',#146342) ;
#37827 = VERTEX_POINT('',#146346) ;
#37828 = VERTEX_POINT('',#146348) ;
#37829 = VERTEX_POINT('',#146352) ;
#37830 = VERTEX_POINT('',#146354) ;
#37831 = VERTEX_POINT('',#146358) ;
#37832 = VERTEX_POINT('',#146360) ;
#37833 = VERTEX_POINT('',#146365) ;
#37834 = VERTEX_POINT('',#146369) ;
#37835 = VERTEX_POINT('',#146376) ;
#37836 = VERTEX_POINT('',#146378) ;
#37837 = VERTEX_POINT('',#146382) ;
#37838 = VERTEX_POINT('',#146384) ;
#37839 = VERTEX_POINT('',#146388) ;
#37840 = VERTEX_POINT('',#146390) ;
#37841 = VERTEX_POINT('',#146394) ;
#37842 = VERTEX_POINT('',#146396) ;
#37843 = VERTEX_POINT('',#146400) ;
#37844 = VERTEX_POINT('',#146402) ;
#37845 = VERTEX_POINT('',#146406) ;
#37846 = VERTEX_POINT('',#146408) ;
#37847 = VERTEX_POINT('',#146412) ;
#37848 = VERTEX_POINT('',#146414) ;
#37849 = VERTEX_POINT('',#146418) ;
#37850 = VERTEX_POINT('',#146420) ;
#37851 = VERTEX_POINT('',#146424) ;
#37852 = VERTEX_POINT('',#146426) ;
#37853 = VERTEX_POINT('',#146430) ;
#37854 = VERTEX_POINT('',#146432) ;
#37855 = VERTEX_POINT('',#146436) ;
#37856 = VERTEX_POINT('',#146438) ;
#37857 = VERTEX_POINT('',#146442) ;
#37858 = VERTEX_POINT('',#146444) ;
#37859 = VERTEX_POINT('',#146448) ;
#37860 = VERTEX_POINT('',#146450) ;
#37861 = VERTEX_POINT('',#146454) ;
#37862 = VERTEX_POINT('',#146456) ;
#37863 = VERTEX_POINT('',#146460) ;
#37864 = VERTEX_POINT('',#146462) ;
#37865 = VERTEX_POINT('',#146466) ;
#37866 = VERTEX_POINT('',#146468) ;
#37867 = VERTEX_POINT('',#146472) ;
#37868 = VERTEX_POINT('',#146474) ;
#37869 = VERTEX_POINT('',#146478) ;
#37870 = VERTEX_POINT('',#146480) ;
#37871 = VERTEX_POINT('',#146487) ;
#37872 = VERTEX_POINT('',#146488) ;
#37873 = VERTEX_POINT('',#146490) ;
#37874 = VERTEX_POINT('',#146492) ;
#37875 = VERTEX_POINT('',#146494) ;
#37876 = VERTEX_POINT('',#146496) ;
#37877 = VERTEX_POINT('',#146498) ;
#37878 = VERTEX_POINT('',#146500) ;
#37879 = VERTEX_POINT('',#146502) ;
#37880 = VERTEX_POINT('',#146504) ;
#37881 = VERTEX_POINT('',#146506) ;
#37882 = VERTEX_POINT('',#146508) ;
#37883 = VERTEX_POINT('',#146510) ;
#37884 = VERTEX_POINT('',#146512) ;
#37885 = VERTEX_POINT('',#146514) ;
#37886 = VERTEX_POINT('',#146516) ;
#37887 = VERTEX_POINT('',#146519) ;
#37888 = VERTEX_POINT('',#146523) ;
#37889 = VERTEX_POINT('',#146524) ;
#37890 = VERTEX_POINT('',#146526) ;
#37891 = VERTEX_POINT('',#146528) ;
#37892 = VERTEX_POINT('',#146532) ;
#37893 = VERTEX_POINT('',#146534) ;
#37894 = VERTEX_POINT('',#146538) ;
#37895 = VERTEX_POINT('',#146540) ;
#37896 = VERTEX_POINT('',#146544) ;
#37897 = VERTEX_POINT('',#146546) ;
#37898 = VERTEX_POINT('',#146550) ;
#37899 = VERTEX_POINT('',#146552) ;
#37900 = VERTEX_POINT('',#146557) ;
#37901 = VERTEX_POINT('',#146561) ;
#37902 = VERTEX_POINT('',#146568) ;
#37903 = VERTEX_POINT('',#146570) ;
#37904 = VERTEX_POINT('',#146574) ;
#37905 = VERTEX_POINT('',#146576) ;
#37906 = VERTEX_POINT('',#146580) ;
#37907 = VERTEX_POINT('',#146582) ;
#37908 = VERTEX_POINT('',#146586) ;
#37909 = VERTEX_POINT('',#146588) ;
#37910 = VERTEX_POINT('',#146592) ;
#37911 = VERTEX_POINT('',#146594) ;
#37912 = VERTEX_POINT('',#146598) ;
#37913 = VERTEX_POINT('',#146600) ;
#37914 = VERTEX_POINT('',#146604) ;
#37915 = VERTEX_POINT('',#146606) ;
#37916 = VERTEX_POINT('',#146610) ;
#37917 = VERTEX_POINT('',#146612) ;
#37918 = VERTEX_POINT('',#146616) ;
#37919 = VERTEX_POINT('',#146618) ;
#37920 = VERTEX_POINT('',#146622) ;
#37921 = VERTEX_POINT('',#146624) ;
#37922 = VERTEX_POINT('',#146628) ;
#37923 = VERTEX_POINT('',#146630) ;
#37924 = VERTEX_POINT('',#146634) ;
#37925 = VERTEX_POINT('',#146636) ;
#37926 = VERTEX_POINT('',#146640) ;
#37927 = VERTEX_POINT('',#146642) ;
#37928 = VERTEX_POINT('',#146646) ;
#37929 = VERTEX_POINT('',#146648) ;
#37930 = VERTEX_POINT('',#146652) ;
#37931 = VERTEX_POINT('',#146654) ;
#37932 = VERTEX_POINT('',#146658) ;
#37933 = VERTEX_POINT('',#146660) ;
#37934 = VERTEX_POINT('',#146664) ;
#37935 = VERTEX_POINT('',#146666) ;
#37936 = VERTEX_POINT('',#146670) ;
#37937 = VERTEX_POINT('',#146672) ;
#37938 = VERTEX_POINT('',#146679) ;
#37939 = VERTEX_POINT('',#146680) ;
#37940 = VERTEX_POINT('',#146682) ;
#37941 = VERTEX_POINT('',#146684) ;
#37942 = VERTEX_POINT('',#146686) ;
#37943 = VERTEX_POINT('',#146688) ;
#37944 = VERTEX_POINT('',#146690) ;
#37945 = VERTEX_POINT('',#146692) ;
#37946 = VERTEX_POINT('',#146694) ;
#37947 = VERTEX_POINT('',#146696) ;
#37948 = VERTEX_POINT('',#146698) ;
#37949 = VERTEX_POINT('',#146700) ;
#37950 = VERTEX_POINT('',#146702) ;
#37951 = VERTEX_POINT('',#146704) ;
#37952 = VERTEX_POINT('',#146706) ;
#37953 = VERTEX_POINT('',#146708) ;
#37954 = VERTEX_POINT('',#146711) ;
#37955 = VERTEX_POINT('',#146715) ;
#37956 = VERTEX_POINT('',#146716) ;
#37957 = VERTEX_POINT('',#146718) ;
#37958 = VERTEX_POINT('',#146720) ;
#37959 = VERTEX_POINT('',#146724) ;
#37960 = VERTEX_POINT('',#146726) ;
#37961 = VERTEX_POINT('',#146730) ;
#37962 = VERTEX_POINT('',#146732) ;
#37963 = VERTEX_POINT('',#146736) ;
#37964 = VERTEX_POINT('',#146738) ;
#37965 = VERTEX_POINT('',#146742) ;
#37966 = VERTEX_POINT('',#146744) ;
#37967 = VERTEX_POINT('',#146749) ;
#37968 = VERTEX_POINT('',#146753) ;
#37969 = VERTEX_POINT('',#146760) ;
#37970 = VERTEX_POINT('',#146762) ;
#37971 = VERTEX_POINT('',#146766) ;
#37972 = VERTEX_POINT('',#146768) ;
#37973 = VERTEX_POINT('',#146772) ;
#37974 = VERTEX_POINT('',#146774) ;
#37975 = VERTEX_POINT('',#146778) ;
#37976 = VERTEX_POINT('',#146780) ;
#37977 = VERTEX_POINT('',#146784) ;
#37978 = VERTEX_POINT('',#146786) ;
#37979 = VERTEX_POINT('',#146790) ;
#37980 = VERTEX_POINT('',#146792) ;
#37981 = VERTEX_POINT('',#146796) ;
#37982 = VERTEX_POINT('',#146798) ;
#37983 = VERTEX_POINT('',#146802) ;
#37984 = VERTEX_POINT('',#146804) ;
#37985 = VERTEX_POINT('',#146808) ;
#37986 = VERTEX_POINT('',#146810) ;
#37987 = VERTEX_POINT('',#146814) ;
#37988 = VERTEX_POINT('',#146816) ;
#37989 = VERTEX_POINT('',#146820) ;
#37990 = VERTEX_POINT('',#146822) ;
#37991 = VERTEX_POINT('',#146826) ;
#37992 = VERTEX_POINT('',#146828) ;
#37993 = VERTEX_POINT('',#146832) ;
#37994 = VERTEX_POINT('',#146834) ;
#37995 = VERTEX_POINT('',#146838) ;
#37996 = VERTEX_POINT('',#146840) ;
#37997 = VERTEX_POINT('',#146844) ;
#37998 = VERTEX_POINT('',#146846) ;
#37999 = VERTEX_POINT('',#146850) ;
#38000 = VERTEX_POINT('',#146852) ;
#38001 = VERTEX_POINT('',#146856) ;
#38002 = VERTEX_POINT('',#146858) ;
#38003 = VERTEX_POINT('',#146862) ;
#38004 = VERTEX_POINT('',#146864) ;
#38005 = VERTEX_POINT('',#146871) ;
#38006 = VERTEX_POINT('',#146872) ;
#38007 = VERTEX_POINT('',#146874) ;
#38008 = VERTEX_POINT('',#146876) ;
#38009 = VERTEX_POINT('',#146878) ;
#38010 = VERTEX_POINT('',#146880) ;
#38011 = VERTEX_POINT('',#146882) ;
#38012 = VERTEX_POINT('',#146884) ;
#38013 = VERTEX_POINT('',#146886) ;
#38014 = VERTEX_POINT('',#146888) ;
#38015 = VERTEX_POINT('',#146890) ;
#38016 = VERTEX_POINT('',#146892) ;
#38017 = VERTEX_POINT('',#146894) ;
#38018 = VERTEX_POINT('',#146896) ;
#38019 = VERTEX_POINT('',#146898) ;
#38020 = VERTEX_POINT('',#146900) ;
#38021 = VERTEX_POINT('',#146903) ;
#38022 = VERTEX_POINT('',#146907) ;
#38023 = VERTEX_POINT('',#146908) ;
#38024 = VERTEX_POINT('',#146910) ;
#38025 = VERTEX_POINT('',#146912) ;
#38026 = VERTEX_POINT('',#146914) ;
#38027 = VERTEX_POINT('',#146916) ;
#38028 = VERTEX_POINT('',#146918) ;
#38029 = VERTEX_POINT('',#146920) ;
#38030 = VERTEX_POINT('',#146924) ;
#38031 = VERTEX_POINT('',#146925) ;
#38032 = VERTEX_POINT('',#146927) ;
#38033 = VERTEX_POINT('',#146929) ;
#38034 = VERTEX_POINT('',#146931) ;
#38035 = VERTEX_POINT('',#146933) ;
#38036 = VERTEX_POINT('',#146935) ;
#38037 = VERTEX_POINT('',#146937) ;
#38038 = VERTEX_POINT('',#146941) ;
#38039 = VERTEX_POINT('',#146942) ;
#38040 = VERTEX_POINT('',#146944) ;
#38041 = VERTEX_POINT('',#146946) ;
#38042 = VERTEX_POINT('',#146948) ;
#38043 = VERTEX_POINT('',#146950) ;
#38044 = VERTEX_POINT('',#146952) ;
#38045 = VERTEX_POINT('',#146954) ;
#38046 = VERTEX_POINT('',#146958) ;
#38047 = VERTEX_POINT('',#146959) ;
#38048 = VERTEX_POINT('',#146961) ;
#38049 = VERTEX_POINT('',#146963) ;
#38050 = VERTEX_POINT('',#146965) ;
#38051 = VERTEX_POINT('',#146967) ;
#38052 = VERTEX_POINT('',#146969) ;
#38053 = VERTEX_POINT('',#146971) ;
#38054 = VERTEX_POINT('',#146975) ;
#38055 = VERTEX_POINT('',#146976) ;
#38056 = VERTEX_POINT('',#146978) ;
#38057 = VERTEX_POINT('',#146980) ;
#38058 = VERTEX_POINT('',#146982) ;
#38059 = VERTEX_POINT('',#146984) ;
#38060 = VERTEX_POINT('',#146986) ;
#38061 = VERTEX_POINT('',#146988) ;
#38062 = VERTEX_POINT('',#146992) ;
#38063 = VERTEX_POINT('',#146993) ;
#38064 = VERTEX_POINT('',#146995) ;
#38065 = VERTEX_POINT('',#146997) ;
#38066 = VERTEX_POINT('',#146999) ;
#38067 = VERTEX_POINT('',#147001) ;
#38068 = VERTEX_POINT('',#147003) ;
#38069 = VERTEX_POINT('',#147005) ;
#38070 = VERTEX_POINT('',#147009) ;
#38071 = VERTEX_POINT('',#147010) ;
#38072 = VERTEX_POINT('',#147012) ;
#38073 = VERTEX_POINT('',#147014) ;
#38074 = VERTEX_POINT('',#147016) ;
#38075 = VERTEX_POINT('',#147018) ;
#38076 = VERTEX_POINT('',#147020) ;
#38077 = VERTEX_POINT('',#147022) ;
#38078 = VERTEX_POINT('',#147026) ;
#38079 = VERTEX_POINT('',#147027) ;
#38080 = VERTEX_POINT('',#147029) ;
#38081 = VERTEX_POINT('',#147031) ;
#38082 = VERTEX_POINT('',#147033) ;
#38083 = VERTEX_POINT('',#147035) ;
#38084 = VERTEX_POINT('',#147037) ;
#38085 = VERTEX_POINT('',#147039) ;
#38086 = VERTEX_POINT('',#147043) ;
#38087 = VERTEX_POINT('',#147044) ;
#38088 = VERTEX_POINT('',#147046) ;
#38089 = VERTEX_POINT('',#147048) ;
#38090 = VERTEX_POINT('',#147050) ;
#38091 = VERTEX_POINT('',#147052) ;
#38092 = VERTEX_POINT('',#147054) ;
#38093 = VERTEX_POINT('',#147056) ;
#38094 = VERTEX_POINT('',#147066) ;
#38095 = VERTEX_POINT('',#147076) ;
#38096 = VERTEX_POINT('',#147087) ;
#38097 = VERTEX_POINT('',#147119) ;
#38098 = VERTEX_POINT('',#147166) ;
#38099 = VERTEX_POINT('',#147184) ;
#38100 = VERTEX_POINT('',#147198) ;
#38101 = VERTEX_POINT('',#147213) ;
#38102 = VERTEX_POINT('',#147770) ;
#38103 = VERTEX_POINT('',#147780) ;
#38104 = VERTEX_POINT('',#147791) ;
#38105 = VERTEX_POINT('',#147823) ;
#38106 = VERTEX_POINT('',#147870) ;
#38107 = VERTEX_POINT('',#147888) ;
#38108 = VERTEX_POINT('',#147902) ;
#38109 = VERTEX_POINT('',#147917) ;
#38110 = VERTEX_POINT('',#147997) ;
#38111 = VERTEX_POINT('',#148007) ;
#38112 = VERTEX_POINT('',#148018) ;
#38113 = VERTEX_POINT('',#148050) ;
#38114 = VERTEX_POINT('',#148097) ;
#38115 = VERTEX_POINT('',#148115) ;
#38116 = VERTEX_POINT('',#148129) ;
#38117 = VERTEX_POINT('',#148144) ;
#38118 = VERTEX_POINT('',#148224) ;
#38119 = VERTEX_POINT('',#148234) ;
#38120 = VERTEX_POINT('',#148245) ;
#38121 = VERTEX_POINT('',#148277) ;
#38122 = VERTEX_POINT('',#148324) ;
#38123 = VERTEX_POINT('',#148342) ;
#38124 = VERTEX_POINT('',#148356) ;
#38125 = VERTEX_POINT('',#148371) ;
#38126 = VERTEX_POINT('',#148451) ;
#38127 = VERTEX_POINT('',#148461) ;
#38128 = VERTEX_POINT('',#148472) ;
#38129 = VERTEX_POINT('',#148504) ;
#38130 = VERTEX_POINT('',#148551) ;
#38131 = VERTEX_POINT('',#148569) ;
#38132 = VERTEX_POINT('',#148583) ;
#38133 = VERTEX_POINT('',#148598) ;
#38134 = VERTEX_POINT('',#148678) ;
#38135 = VERTEX_POINT('',#148688) ;
#38136 = VERTEX_POINT('',#148699) ;
#38137 = VERTEX_POINT('',#148731) ;
#38138 = VERTEX_POINT('',#148778) ;
#38139 = VERTEX_POINT('',#148796) ;
#38140 = VERTEX_POINT('',#148810) ;
#38141 = VERTEX_POINT('',#148825) ;
#38142 = VERTEX_POINT('',#148905) ;
#38143 = VERTEX_POINT('',#148915) ;
#38144 = VERTEX_POINT('',#148926) ;
#38145 = VERTEX_POINT('',#148958) ;
#38146 = VERTEX_POINT('',#149005) ;
#38147 = VERTEX_POINT('',#149023) ;
#38148 = VERTEX_POINT('',#149037) ;
#38149 = VERTEX_POINT('',#149052) ;
#38150 = VERTEX_POINT('',#149132) ;
#38151 = VERTEX_POINT('',#149142) ;
#38152 = VERTEX_POINT('',#149153) ;
#38153 = VERTEX_POINT('',#149185) ;
#38154 = VERTEX_POINT('',#149232) ;
#38155 = VERTEX_POINT('',#149250) ;
#38156 = VERTEX_POINT('',#149264) ;
#38157 = VERTEX_POINT('',#149279) ;
#38158 = VERTEX_POINT('',#149359) ;
#38159 = VERTEX_POINT('',#149369) ;
#38160 = VERTEX_POINT('',#149380) ;
#38161 = VERTEX_POINT('',#149412) ;
#38162 = VERTEX_POINT('',#149459) ;
#38163 = VERTEX_POINT('',#149477) ;
#38164 = VERTEX_POINT('',#149491) ;
#38165 = VERTEX_POINT('',#149506) ;
#38166 = VERTEX_POINT('',#149580) ;
#38167 = VERTEX_POINT('',#149581) ;
#38168 = VERTEX_POINT('',#149583) ;
#38169 = VERTEX_POINT('',#149585) ;
#38170 = VERTEX_POINT('',#149589) ;
#38171 = VERTEX_POINT('',#149590) ;
#38172 = VERTEX_POINT('',#149592) ;
#38173 = VERTEX_POINT('',#149594) ;
#38174 = VERTEX_POINT('',#149598) ;
#38175 = VERTEX_POINT('',#149599) ;
#38176 = VERTEX_POINT('',#149601) ;
#38177 = VERTEX_POINT('',#149603) ;
#38178 = VERTEX_POINT('',#149607) ;
#38179 = VERTEX_POINT('',#149608) ;
#38180 = VERTEX_POINT('',#149610) ;
#38181 = VERTEX_POINT('',#149612) ;
#38182 = VERTEX_POINT('',#149616) ;
#38183 = VERTEX_POINT('',#149617) ;
#38184 = VERTEX_POINT('',#149619) ;
#38185 = VERTEX_POINT('',#149621) ;
#38186 = VERTEX_POINT('',#149625) ;
#38187 = VERTEX_POINT('',#149626) ;
#38188 = VERTEX_POINT('',#149629) ;
#38189 = VERTEX_POINT('',#149631) ;
#38190 = VERTEX_POINT('',#149635) ;
#38191 = VERTEX_POINT('',#149636) ;
#38192 = VERTEX_POINT('',#149639) ;
#38193 = VERTEX_POINT('',#149641) ;
#38194 = VERTEX_POINT('',#149651) ;
#38195 = VERTEX_POINT('',#149652) ;
#38196 = VERTEX_POINT('',#149654) ;
#38197 = VERTEX_POINT('',#149656) ;
#38198 = VERTEX_POINT('',#149660) ;
#38199 = VERTEX_POINT('',#149661) ;
#38200 = VERTEX_POINT('',#149666) ;
#38201 = VERTEX_POINT('',#149668) ;
#38202 = VERTEX_POINT('',#149672) ;
#38203 = VERTEX_POINT('',#149673) ;
#38204 = VERTEX_POINT('',#149675) ;
#38205 = VERTEX_POINT('',#149677) ;
#38206 = VERTEX_POINT('',#149681) ;
#38207 = VERTEX_POINT('',#149682) ;
#38208 = VERTEX_POINT('',#149684) ;
#38209 = VERTEX_POINT('',#149686) ;
#38210 = VERTEX_POINT('',#149690) ;
#38211 = VERTEX_POINT('',#149691) ;
#38212 = VERTEX_POINT('',#149696) ;
#38213 = VERTEX_POINT('',#149698) ;
#38214 = VERTEX_POINT('',#149702) ;
#38215 = VERTEX_POINT('',#149703) ;
#38216 = VERTEX_POINT('',#149705) ;
#38217 = VERTEX_POINT('',#149707) ;
#38218 = VERTEX_POINT('',#149711) ;
#38219 = VERTEX_POINT('',#149712) ;
#38220 = VERTEX_POINT('',#149714) ;
#38221 = VERTEX_POINT('',#149716) ;
#38222 = VERTEX_POINT('',#149720) ;
#38223 = VERTEX_POINT('',#149721) ;
#38224 = VERTEX_POINT('',#149723) ;
#38225 = VERTEX_POINT('',#149725) ;
#38226 = VERTEX_POINT('',#149729) ;
#38227 = VERTEX_POINT('',#149730) ;
#38228 = VERTEX_POINT('',#149732) ;
#38229 = VERTEX_POINT('',#149734) ;
#38230 = VERTEX_POINT('',#149738) ;
#38231 = VERTEX_POINT('',#149739) ;
#38232 = VERTEX_POINT('',#149741) ;
#38233 = VERTEX_POINT('',#149743) ;
#38234 = VERTEX_POINT('',#149747) ;
#38235 = VERTEX_POINT('',#149748) ;
#38236 = VERTEX_POINT('',#149751) ;
#38237 = VERTEX_POINT('',#149753) ;
#38238 = VERTEX_POINT('',#149757) ;
#38239 = VERTEX_POINT('',#149758) ;
#38240 = VERTEX_POINT('',#149761) ;
#38241 = VERTEX_POINT('',#149763) ;
#38242 = VERTEX_POINT('',#149773) ;
#38243 = VERTEX_POINT('',#149774) ;
#38244 = VERTEX_POINT('',#149776) ;
#38245 = VERTEX_POINT('',#149778) ;
#38246 = VERTEX_POINT('',#149782) ;
#38247 = VERTEX_POINT('',#149783) ;
#38248 = VERTEX_POINT('',#149788) ;
#38249 = VERTEX_POINT('',#149790) ;
#38250 = VERTEX_POINT('',#149794) ;
#38251 = VERTEX_POINT('',#149795) ;
#38252 = VERTEX_POINT('',#149797) ;
#38253 = VERTEX_POINT('',#149799) ;
#38254 = VERTEX_POINT('',#149803) ;
#38255 = VERTEX_POINT('',#149804) ;
#38256 = VERTEX_POINT('',#149806) ;
#38257 = VERTEX_POINT('',#149808) ;
#38258 = VERTEX_POINT('',#149812) ;
#38259 = VERTEX_POINT('',#149813) ;
#38260 = VERTEX_POINT('',#149818) ;
#38261 = VERTEX_POINT('',#149820) ;
#38262 = VERTEX_POINT('',#149824) ;
#38263 = VERTEX_POINT('',#149825) ;
#38264 = VERTEX_POINT('',#149827) ;
#38265 = VERTEX_POINT('',#149829) ;
#38266 = VERTEX_POINT('',#149833) ;
#38267 = VERTEX_POINT('',#149834) ;
#38268 = VERTEX_POINT('',#149836) ;
#38269 = VERTEX_POINT('',#149838) ;
#38270 = VERTEX_POINT('',#149842) ;
#38271 = VERTEX_POINT('',#149843) ;
#38272 = VERTEX_POINT('',#149845) ;
#38273 = VERTEX_POINT('',#149847) ;
#38274 = VERTEX_POINT('',#149851) ;
#38275 = VERTEX_POINT('',#149852) ;
#38276 = VERTEX_POINT('',#149854) ;
#38277 = VERTEX_POINT('',#149856) ;
#38278 = VERTEX_POINT('',#149860) ;
#38279 = VERTEX_POINT('',#149861) ;
#38280 = VERTEX_POINT('',#149863) ;
#38281 = VERTEX_POINT('',#149865) ;
#38282 = VERTEX_POINT('',#149869) ;
#38283 = VERTEX_POINT('',#149870) ;
#38284 = VERTEX_POINT('',#149873) ;
#38285 = VERTEX_POINT('',#149875) ;
#38286 = VERTEX_POINT('',#149879) ;
#38287 = VERTEX_POINT('',#149880) ;
#38288 = VERTEX_POINT('',#149883) ;
#38289 = VERTEX_POINT('',#149885) ;
#38290 = VERTEX_POINT('',#149895) ;
#38291 = VERTEX_POINT('',#149896) ;
#38292 = VERTEX_POINT('',#149898) ;
#38293 = VERTEX_POINT('',#149900) ;
#38294 = VERTEX_POINT('',#149904) ;
#38295 = VERTEX_POINT('',#149905) ;
#38296 = VERTEX_POINT('',#149910) ;
#38297 = VERTEX_POINT('',#149912) ;
#38298 = VERTEX_POINT('',#149916) ;
#38299 = VERTEX_POINT('',#149917) ;
#38300 = VERTEX_POINT('',#149919) ;
#38301 = VERTEX_POINT('',#149921) ;
#38302 = VERTEX_POINT('',#149925) ;
#38303 = VERTEX_POINT('',#149926) ;
#38304 = VERTEX_POINT('',#149928) ;
#38305 = VERTEX_POINT('',#149930) ;
#38306 = VERTEX_POINT('',#149934) ;
#38307 = VERTEX_POINT('',#149935) ;
#38308 = VERTEX_POINT('',#149940) ;
#38309 = VERTEX_POINT('',#149942) ;
#38310 = VERTEX_POINT('',#149946) ;
#38311 = VERTEX_POINT('',#149947) ;
#38312 = VERTEX_POINT('',#149949) ;
#38313 = VERTEX_POINT('',#149951) ;
#38314 = VERTEX_POINT('',#149955) ;
#38315 = VERTEX_POINT('',#149956) ;
#38316 = VERTEX_POINT('',#149958) ;
#38317 = VERTEX_POINT('',#149960) ;
#38318 = VERTEX_POINT('',#149964) ;
#38319 = VERTEX_POINT('',#149965) ;
#38320 = VERTEX_POINT('',#149967) ;
#38321 = VERTEX_POINT('',#149969) ;
#38322 = VERTEX_POINT('',#149973) ;
#38323 = VERTEX_POINT('',#149974) ;
#38324 = VERTEX_POINT('',#149976) ;
#38325 = VERTEX_POINT('',#149978) ;
#38326 = VERTEX_POINT('',#149982) ;
#38327 = VERTEX_POINT('',#149983) ;
#38328 = VERTEX_POINT('',#149985) ;
#38329 = VERTEX_POINT('',#149987) ;
#38330 = VERTEX_POINT('',#149991) ;
#38331 = VERTEX_POINT('',#149992) ;
#38332 = VERTEX_POINT('',#149995) ;
#38333 = VERTEX_POINT('',#149997) ;
#38334 = VERTEX_POINT('',#150001) ;
#38335 = VERTEX_POINT('',#150002) ;
#38336 = VERTEX_POINT('',#150005) ;
#38337 = VERTEX_POINT('',#150007) ;
#38338 = VERTEX_POINT('',#150017) ;
#38339 = VERTEX_POINT('',#150018) ;
#38340 = VERTEX_POINT('',#150020) ;
#38341 = VERTEX_POINT('',#150022) ;
#38342 = VERTEX_POINT('',#150026) ;
#38343 = VERTEX_POINT('',#150027) ;
#38344 = VERTEX_POINT('',#150032) ;
#38345 = VERTEX_POINT('',#150034) ;
#38346 = VERTEX_POINT('',#150038) ;
#38347 = VERTEX_POINT('',#150039) ;
#38348 = VERTEX_POINT('',#150041) ;
#38349 = VERTEX_POINT('',#150043) ;
#38350 = VERTEX_POINT('',#150047) ;
#38351 = VERTEX_POINT('',#150048) ;
#38352 = VERTEX_POINT('',#150050) ;
#38353 = VERTEX_POINT('',#150052) ;
#38354 = VERTEX_POINT('',#150056) ;
#38355 = VERTEX_POINT('',#150057) ;
#38356 = VERTEX_POINT('',#150062) ;
#38357 = VERTEX_POINT('',#150064) ;
#38358 = VERTEX_POINT('',#150068) ;
#38359 = VERTEX_POINT('',#150069) ;
#38360 = VERTEX_POINT('',#150071) ;
#38361 = VERTEX_POINT('',#150073) ;
#38362 = VERTEX_POINT('',#150077) ;
#38363 = VERTEX_POINT('',#150078) ;
#38364 = VERTEX_POINT('',#150080) ;
#38365 = VERTEX_POINT('',#150082) ;
#38366 = VERTEX_POINT('',#150086) ;
#38367 = VERTEX_POINT('',#150087) ;
#38368 = VERTEX_POINT('',#150089) ;
#38369 = VERTEX_POINT('',#150091) ;
#38370 = VERTEX_POINT('',#150095) ;
#38371 = VERTEX_POINT('',#150096) ;
#38372 = VERTEX_POINT('',#150098) ;
#38373 = VERTEX_POINT('',#150100) ;
#38374 = VERTEX_POINT('',#150104) ;
#38375 = VERTEX_POINT('',#150105) ;
#38376 = VERTEX_POINT('',#150107) ;
#38377 = VERTEX_POINT('',#150109) ;
#38378 = VERTEX_POINT('',#150113) ;
#38379 = VERTEX_POINT('',#150114) ;
#38380 = VERTEX_POINT('',#150117) ;
#38381 = VERTEX_POINT('',#150119) ;
#38382 = VERTEX_POINT('',#150123) ;
#38383 = VERTEX_POINT('',#150124) ;
#38384 = VERTEX_POINT('',#150127) ;
#38385 = VERTEX_POINT('',#150129) ;
#38386 = VERTEX_POINT('',#150139) ;
#38387 = VERTEX_POINT('',#150140) ;
#38388 = VERTEX_POINT('',#150142) ;
#38389 = VERTEX_POINT('',#150144) ;
#38390 = VERTEX_POINT('',#150148) ;
#38391 = VERTEX_POINT('',#150149) ;
#38392 = VERTEX_POINT('',#150154) ;
#38393 = VERTEX_POINT('',#150156) ;
#38394 = VERTEX_POINT('',#150160) ;
#38395 = VERTEX_POINT('',#150161) ;
#38396 = VERTEX_POINT('',#150163) ;
#38397 = VERTEX_POINT('',#150165) ;
#38398 = VERTEX_POINT('',#150169) ;
#38399 = VERTEX_POINT('',#150170) ;
#38400 = VERTEX_POINT('',#150172) ;
#38401 = VERTEX_POINT('',#150174) ;
#38402 = VERTEX_POINT('',#150178) ;
#38403 = VERTEX_POINT('',#150179) ;
#38404 = VERTEX_POINT('',#150184) ;
#38405 = VERTEX_POINT('',#150186) ;
#38406 = VERTEX_POINT('',#150190) ;
#38407 = VERTEX_POINT('',#150191) ;
#38408 = VERTEX_POINT('',#150193) ;
#38409 = VERTEX_POINT('',#150195) ;
#38410 = VERTEX_POINT('',#150199) ;
#38411 = VERTEX_POINT('',#150200) ;
#38412 = VERTEX_POINT('',#150202) ;
#38413 = VERTEX_POINT('',#150204) ;
#38414 = VERTEX_POINT('',#150208) ;
#38415 = VERTEX_POINT('',#150209) ;
#38416 = VERTEX_POINT('',#150211) ;
#38417 = VERTEX_POINT('',#150213) ;
#38418 = VERTEX_POINT('',#150217) ;
#38419 = VERTEX_POINT('',#150218) ;
#38420 = VERTEX_POINT('',#150220) ;
#38421 = VERTEX_POINT('',#150222) ;
#38422 = VERTEX_POINT('',#150226) ;
#38423 = VERTEX_POINT('',#150227) ;
#38424 = VERTEX_POINT('',#150229) ;
#38425 = VERTEX_POINT('',#150231) ;
#38426 = VERTEX_POINT('',#150235) ;
#38427 = VERTEX_POINT('',#150236) ;
#38428 = VERTEX_POINT('',#150239) ;
#38429 = VERTEX_POINT('',#150241) ;
#38430 = VERTEX_POINT('',#150245) ;
#38431 = VERTEX_POINT('',#150246) ;
#38432 = VERTEX_POINT('',#150249) ;
#38433 = VERTEX_POINT('',#150251) ;
#38434 = VERTEX_POINT('',#150261) ;
#38435 = VERTEX_POINT('',#150262) ;
#38436 = VERTEX_POINT('',#150264) ;
#38437 = VERTEX_POINT('',#150266) ;
#38438 = VERTEX_POINT('',#150270) ;
#38439 = VERTEX_POINT('',#150271) ;
#38440 = VERTEX_POINT('',#150276) ;
#38441 = VERTEX_POINT('',#150278) ;
#38442 = VERTEX_POINT('',#150282) ;
#38443 = VERTEX_POINT('',#150283) ;
#38444 = VERTEX_POINT('',#150285) ;
#38445 = VERTEX_POINT('',#150287) ;
#38446 = VERTEX_POINT('',#150291) ;
#38447 = VERTEX_POINT('',#150292) ;
#38448 = VERTEX_POINT('',#150294) ;
#38449 = VERTEX_POINT('',#150296) ;
#38450 = VERTEX_POINT('',#150300) ;
#38451 = VERTEX_POINT('',#150301) ;
#38452 = VERTEX_POINT('',#150306) ;
#38453 = VERTEX_POINT('',#150308) ;
#38454 = VERTEX_POINT('',#150312) ;
#38455 = VERTEX_POINT('',#150313) ;
#38456 = VERTEX_POINT('',#150315) ;
#38457 = VERTEX_POINT('',#150317) ;
#38458 = VERTEX_POINT('',#150321) ;
#38459 = VERTEX_POINT('',#150322) ;
#38460 = VERTEX_POINT('',#150324) ;
#38461 = VERTEX_POINT('',#150326) ;
#38462 = VERTEX_POINT('',#150330) ;
#38463 = VERTEX_POINT('',#150331) ;
#38464 = VERTEX_POINT('',#150333) ;
#38465 = VERTEX_POINT('',#150335) ;
#38466 = VERTEX_POINT('',#150339) ;
#38467 = VERTEX_POINT('',#150340) ;
#38468 = VERTEX_POINT('',#150342) ;
#38469 = VERTEX_POINT('',#150344) ;
#38470 = VERTEX_POINT('',#150348) ;
#38471 = VERTEX_POINT('',#150349) ;
#38472 = VERTEX_POINT('',#150351) ;
#38473 = VERTEX_POINT('',#150353) ;
#38474 = VERTEX_POINT('',#150357) ;
#38475 = VERTEX_POINT('',#150358) ;
#38476 = VERTEX_POINT('',#150361) ;
#38477 = VERTEX_POINT('',#150363) ;
#38478 = VERTEX_POINT('',#150367) ;
#38479 = VERTEX_POINT('',#150368) ;
#38480 = VERTEX_POINT('',#150371) ;
#38481 = VERTEX_POINT('',#150373) ;
#38482 = VERTEX_POINT('',#150383) ;
#38483 = VERTEX_POINT('',#150384) ;
#38484 = VERTEX_POINT('',#150386) ;
#38485 = VERTEX_POINT('',#150388) ;
#38486 = VERTEX_POINT('',#150392) ;
#38487 = VERTEX_POINT('',#150393) ;
#38488 = VERTEX_POINT('',#150398) ;
#38489 = VERTEX_POINT('',#150400) ;
#38490 = VERTEX_POINT('',#150404) ;
#38491 = VERTEX_POINT('',#150405) ;
#38492 = VERTEX_POINT('',#150407) ;
#38493 = VERTEX_POINT('',#150409) ;
#38494 = VERTEX_POINT('',#150413) ;
#38495 = VERTEX_POINT('',#150414) ;
#38496 = VERTEX_POINT('',#150416) ;
#38497 = VERTEX_POINT('',#150418) ;
#38498 = VERTEX_POINT('',#150422) ;
#38499 = VERTEX_POINT('',#150423) ;
#38500 = VERTEX_POINT('',#150428) ;
#38501 = VERTEX_POINT('',#150430) ;
#38502 = VERTEX_POINT('',#150434) ;
#38503 = VERTEX_POINT('',#150435) ;
#38504 = VERTEX_POINT('',#150437) ;
#38505 = VERTEX_POINT('',#150439) ;
#38506 = VERTEX_POINT('',#150443) ;
#38507 = VERTEX_POINT('',#150444) ;
#38508 = VERTEX_POINT('',#150446) ;
#38509 = VERTEX_POINT('',#150448) ;
#38510 = VERTEX_POINT('',#150452) ;
#38511 = VERTEX_POINT('',#150453) ;
#38512 = VERTEX_POINT('',#150455) ;
#38513 = VERTEX_POINT('',#150457) ;
#38514 = VERTEX_POINT('',#150461) ;
#38515 = VERTEX_POINT('',#150462) ;
#38516 = VERTEX_POINT('',#150464) ;
#38517 = VERTEX_POINT('',#150466) ;
#38518 = VERTEX_POINT('',#150470) ;
#38519 = VERTEX_POINT('',#150471) ;
#38520 = VERTEX_POINT('',#150473) ;
#38521 = VERTEX_POINT('',#150475) ;
#38522 = VERTEX_POINT('',#150479) ;
#38523 = VERTEX_POINT('',#150480) ;
#38524 = VERTEX_POINT('',#150483) ;
#38525 = VERTEX_POINT('',#150485) ;
#38526 = VERTEX_POINT('',#150489) ;
#38527 = VERTEX_POINT('',#150490) ;
#38528 = VERTEX_POINT('',#150493) ;
#38529 = VERTEX_POINT('',#150495) ;
#38530 = VERTEX_POINT('',#150505) ;
#38531 = VERTEX_POINT('',#150506) ;
#38532 = VERTEX_POINT('',#150508) ;
#38533 = VERTEX_POINT('',#150510) ;
#38534 = VERTEX_POINT('',#150514) ;
#38535 = VERTEX_POINT('',#150515) ;
#38536 = VERTEX_POINT('',#150520) ;
#38537 = VERTEX_POINT('',#150522) ;
#38538 = VERTEX_POINT('',#150526) ;
#38539 = VERTEX_POINT('',#150527) ;
#38540 = VERTEX_POINT('',#150529) ;
#38541 = VERTEX_POINT('',#150531) ;
#38542 = VERTEX_POINT('',#150535) ;
#38543 = VERTEX_POINT('',#150536) ;
#38544 = VERTEX_POINT('',#150538) ;
#38545 = VERTEX_POINT('',#150540) ;
#38546 = VERTEX_POINT('',#150544) ;
#38547 = VERTEX_POINT('',#150545) ;
#38548 = VERTEX_POINT('',#150550) ;
#38549 = VERTEX_POINT('',#150552) ;
#38550 = VERTEX_POINT('',#150556) ;
#38551 = VERTEX_POINT('',#150557) ;
#38552 = VERTEX_POINT('',#150559) ;
#38553 = VERTEX_POINT('',#150561) ;
#38554 = VERTEX_POINT('',#150565) ;
#38555 = VERTEX_POINT('',#150566) ;
#38556 = VERTEX_POINT('',#150568) ;
#38557 = VERTEX_POINT('',#150570) ;
#38558 = VERTEX_POINT('',#150574) ;
#38559 = VERTEX_POINT('',#150575) ;
#38560 = VERTEX_POINT('',#150577) ;
#38561 = VERTEX_POINT('',#150579) ;
#38562 = VERTEX_POINT('',#150583) ;
#38563 = VERTEX_POINT('',#150584) ;
#38564 = VERTEX_POINT('',#150586) ;
#38565 = VERTEX_POINT('',#150588) ;
#38566 = VERTEX_POINT('',#150592) ;
#38567 = VERTEX_POINT('',#150593) ;
#38568 = VERTEX_POINT('',#150595) ;
#38569 = VERTEX_POINT('',#150597) ;
#38570 = VERTEX_POINT('',#150601) ;
#38571 = VERTEX_POINT('',#150602) ;
#38572 = VERTEX_POINT('',#150605) ;
#38573 = VERTEX_POINT('',#150607) ;
#38574 = VERTEX_POINT('',#150611) ;
#38575 = VERTEX_POINT('',#150612) ;
#38576 = VERTEX_POINT('',#150615) ;
#38577 = VERTEX_POINT('',#150617) ;
#38578 = VERTEX_POINT('',#150627) ;
#38579 = VERTEX_POINT('',#150628) ;
#38580 = VERTEX_POINT('',#150630) ;
#38581 = VERTEX_POINT('',#150632) ;
#38582 = VERTEX_POINT('',#150636) ;
#38583 = VERTEX_POINT('',#150637) ;
#38584 = VERTEX_POINT('',#150642) ;
#38585 = VERTEX_POINT('',#150644) ;
#38586 = VERTEX_POINT('',#150648) ;
#38587 = VERTEX_POINT('',#150649) ;
#38588 = VERTEX_POINT('',#150651) ;
#38589 = VERTEX_POINT('',#150653) ;
#38590 = VERTEX_POINT('',#150657) ;
#38591 = VERTEX_POINT('',#150658) ;
#38592 = VERTEX_POINT('',#150660) ;
#38593 = VERTEX_POINT('',#150662) ;
#38594 = VERTEX_POINT('',#150666) ;
#38595 = VERTEX_POINT('',#150667) ;
#38596 = VERTEX_POINT('',#150672) ;
#38597 = VERTEX_POINT('',#150674) ;
#38598 = VERTEX_POINT('',#150678) ;
#38599 = VERTEX_POINT('',#150679) ;
#38600 = VERTEX_POINT('',#150681) ;
#38601 = VERTEX_POINT('',#150683) ;
#38602 = VERTEX_POINT('',#150687) ;
#38603 = VERTEX_POINT('',#150688) ;
#38604 = VERTEX_POINT('',#150690) ;
#38605 = VERTEX_POINT('',#150692) ;
#38606 = VERTEX_POINT('',#150696) ;
#38607 = VERTEX_POINT('',#150697) ;
#38608 = VERTEX_POINT('',#150699) ;
#38609 = VERTEX_POINT('',#150701) ;
#38610 = VERTEX_POINT('',#150705) ;
#38611 = VERTEX_POINT('',#150706) ;
#38612 = VERTEX_POINT('',#150708) ;
#38613 = VERTEX_POINT('',#150710) ;
#38614 = VERTEX_POINT('',#150714) ;
#38615 = VERTEX_POINT('',#150715) ;
#38616 = VERTEX_POINT('',#150717) ;
#38617 = VERTEX_POINT('',#150719) ;
#38618 = VERTEX_POINT('',#150723) ;
#38619 = VERTEX_POINT('',#150724) ;
#38620 = VERTEX_POINT('',#150726) ;
#38621 = VERTEX_POINT('',#150728) ;
#38622 = VERTEX_POINT('',#150732) ;
#38623 = VERTEX_POINT('',#150733) ;
#38624 = VERTEX_POINT('',#150735) ;
#38625 = VERTEX_POINT('',#150737) ;
#38626 = VERTEX_POINT('',#150741) ;
#38627 = VERTEX_POINT('',#150742) ;
#38628 = VERTEX_POINT('',#150744) ;
#38629 = VERTEX_POINT('',#150746) ;
#38630 = VERTEX_POINT('',#150750) ;
#38631 = VERTEX_POINT('',#150751) ;
#38632 = VERTEX_POINT('',#150753) ;
#38633 = VERTEX_POINT('',#150755) ;
#38634 = VERTEX_POINT('',#150759) ;
#38635 = VERTEX_POINT('',#150760) ;
#38636 = VERTEX_POINT('',#150762) ;
#38637 = VERTEX_POINT('',#150764) ;
#38638 = VERTEX_POINT('',#150768) ;
#38639 = VERTEX_POINT('',#150769) ;
#38640 = VERTEX_POINT('',#150771) ;
#38641 = VERTEX_POINT('',#150773) ;
#38642 = VERTEX_POINT('',#150777) ;
#38643 = VERTEX_POINT('',#150778) ;
#38644 = VERTEX_POINT('',#150780) ;
#38645 = VERTEX_POINT('',#150782) ;
#38646 = VERTEX_POINT('',#150786) ;
#38647 = VERTEX_POINT('',#150787) ;
#38648 = VERTEX_POINT('',#150789) ;
#38649 = VERTEX_POINT('',#150791) ;
#38650 = VERTEX_POINT('',#150795) ;
#38651 = VERTEX_POINT('',#150796) ;
#38652 = VERTEX_POINT('',#150798) ;
#38653 = VERTEX_POINT('',#150800) ;
#38654 = VERTEX_POINT('',#150804) ;
#38655 = VERTEX_POINT('',#150805) ;
#38656 = VERTEX_POINT('',#150807) ;
#38657 = VERTEX_POINT('',#150809) ;
#38658 = VERTEX_POINT('',#150813) ;
#38659 = VERTEX_POINT('',#150814) ;
#38660 = VERTEX_POINT('',#150816) ;
#38661 = VERTEX_POINT('',#150818) ;
#38662 = VERTEX_POINT('',#150822) ;
#38663 = VERTEX_POINT('',#150823) ;
#38664 = VERTEX_POINT('',#150825) ;
#38665 = VERTEX_POINT('',#150827) ;
#38666 = VERTEX_POINT('',#150831) ;
#38667 = VERTEX_POINT('',#150832) ;
#38668 = VERTEX_POINT('',#150834) ;
#38669 = VERTEX_POINT('',#150836) ;
#38670 = VERTEX_POINT('',#150840) ;
#38671 = VERTEX_POINT('',#150841) ;
#38672 = VERTEX_POINT('',#150843) ;
#38673 = VERTEX_POINT('',#150845) ;
#38674 = VERTEX_POINT('',#150849) ;
#38675 = VERTEX_POINT('',#150850) ;
#38676 = VERTEX_POINT('',#150852) ;
#38677 = VERTEX_POINT('',#150854) ;
#38678 = VERTEX_POINT('',#150858) ;
#38679 = VERTEX_POINT('',#150859) ;
#38680 = VERTEX_POINT('',#150861) ;
#38681 = VERTEX_POINT('',#150863) ;
#38682 = VERTEX_POINT('',#150867) ;
#38683 = VERTEX_POINT('',#150868) ;
#38684 = VERTEX_POINT('',#150870) ;
#38685 = VERTEX_POINT('',#150872) ;
#38686 = VERTEX_POINT('',#150876) ;
#38687 = VERTEX_POINT('',#150877) ;
#38688 = VERTEX_POINT('',#150879) ;
#38689 = VERTEX_POINT('',#150881) ;
#38690 = VERTEX_POINT('',#150885) ;
#38691 = VERTEX_POINT('',#150886) ;
#38692 = VERTEX_POINT('',#150888) ;
#38693 = VERTEX_POINT('',#150890) ;
#38694 = VERTEX_POINT('',#150894) ;
#38695 = VERTEX_POINT('',#150895) ;
#38696 = VERTEX_POINT('',#150897) ;
#38697 = VERTEX_POINT('',#150899) ;
#38698 = VERTEX_POINT('',#150903) ;
#38699 = VERTEX_POINT('',#150904) ;
#38700 = VERTEX_POINT('',#150906) ;
#38701 = VERTEX_POINT('',#150908) ;
#38702 = VERTEX_POINT('',#150912) ;
#38703 = VERTEX_POINT('',#150913) ;
#38704 = VERTEX_POINT('',#150915) ;
#38705 = VERTEX_POINT('',#150917) ;
#38706 = VERTEX_POINT('',#150921) ;
#38707 = VERTEX_POINT('',#150922) ;
#38708 = VERTEX_POINT('',#150924) ;
#38709 = VERTEX_POINT('',#150926) ;
#38710 = VERTEX_POINT('',#150930) ;
#38711 = VERTEX_POINT('',#150931) ;
#38712 = VERTEX_POINT('',#150933) ;
#38713 = VERTEX_POINT('',#150935) ;
#38714 = VERTEX_POINT('',#150939) ;
#38715 = VERTEX_POINT('',#150940) ;
#38716 = VERTEX_POINT('',#150942) ;
#38717 = VERTEX_POINT('',#150944) ;
#38718 = VERTEX_POINT('',#150948) ;
#38719 = VERTEX_POINT('',#150949) ;
#38720 = VERTEX_POINT('',#150951) ;
#38721 = VERTEX_POINT('',#150953) ;
#38722 = VERTEX_POINT('',#150957) ;
#38723 = VERTEX_POINT('',#150958) ;
#38724 = VERTEX_POINT('',#150960) ;
#38725 = VERTEX_POINT('',#150962) ;
#38726 = VERTEX_POINT('',#150966) ;
#38727 = VERTEX_POINT('',#150967) ;
#38728 = VERTEX_POINT('',#150969) ;
#38729 = VERTEX_POINT('',#150971) ;
#38730 = VERTEX_POINT('',#150975) ;
#38731 = VERTEX_POINT('',#150976) ;
#38732 = VERTEX_POINT('',#150978) ;
#38733 = VERTEX_POINT('',#150980) ;
#38734 = VERTEX_POINT('',#150984) ;
#38735 = VERTEX_POINT('',#150985) ;
#38736 = VERTEX_POINT('',#150987) ;
#38737 = VERTEX_POINT('',#150989) ;
#38738 = VERTEX_POINT('',#150993) ;
#38739 = VERTEX_POINT('',#150994) ;
#38740 = VERTEX_POINT('',#150996) ;
#38741 = VERTEX_POINT('',#150998) ;
#38742 = VERTEX_POINT('',#152011) ;
#38743 = VERTEX_POINT('',#152012) ;
#38744 = VERTEX_POINT('',#152014) ;
#38745 = VERTEX_POINT('',#152016) ;
#38746 = VERTEX_POINT('',#152020) ;
#38747 = VERTEX_POINT('',#152021) ;
#38748 = VERTEX_POINT('',#152023) ;
#38749 = VERTEX_POINT('',#152025) ;
#38750 = VERTEX_POINT('',#152029) ;
#38751 = VERTEX_POINT('',#152030) ;
#38752 = VERTEX_POINT('',#152032) ;
#38753 = VERTEX_POINT('',#152034) ;
#38754 = VERTEX_POINT('',#152038) ;
#38755 = VERTEX_POINT('',#152039) ;
#38756 = VERTEX_POINT('',#152041) ;
#38757 = VERTEX_POINT('',#152121) ;
#38758 = VERTEX_POINT('',#152174) ;
#38759 = VERTEX_POINT('',#152175) ;
#38760 = VERTEX_POINT('',#152177) ;
#38761 = VERTEX_POINT('',#152179) ;
#38762 = VERTEX_POINT('',#152183) ;
#38763 = VERTEX_POINT('',#152185) ;
#38764 = VERTEX_POINT('',#152265) ;
#38765 = VERTEX_POINT('',#152349) ;
#38766 = VERTEX_POINT('',#152350) ;
#38767 = VERTEX_POINT('',#152352) ;
#38768 = VERTEX_POINT('',#152354) ;
#38769 = VERTEX_POINT('',#152358) ;
#38770 = VERTEX_POINT('',#152360) ;
#38771 = VERTEX_POINT('',#152443) ;
#38772 = VERTEX_POINT('',#152525) ;
#38773 = VERTEX_POINT('',#152526) ;
#38774 = VERTEX_POINT('',#152528) ;
#38775 = VERTEX_POINT('',#152530) ;
#38776 = VERTEX_POINT('',#152534) ;
#38777 = VERTEX_POINT('',#152536) ;
#38778 = VERTEX_POINT('',#152617) ;
#38779 = VERTEX_POINT('',#152701) ;
#38780 = VERTEX_POINT('',#152702) ;
#38781 = VERTEX_POINT('',#152704) ;
#38782 = VERTEX_POINT('',#152706) ;
#38783 = VERTEX_POINT('',#152710) ;
#38784 = VERTEX_POINT('',#152712) ;
#38785 = VERTEX_POINT('',#152792) ;
#38786 = VERTEX_POINT('',#152876) ;
#38787 = VERTEX_POINT('',#152877) ;
#38788 = VERTEX_POINT('',#152879) ;
#38789 = VERTEX_POINT('',#152881) ;
#38790 = VERTEX_POINT('',#152885) ;
#38791 = VERTEX_POINT('',#152887) ;
#38792 = VERTEX_POINT('',#152967) ;
#38793 = VERTEX_POINT('',#153051) ;
#38794 = VERTEX_POINT('',#153052) ;
#38795 = VERTEX_POINT('',#153054) ;
#38796 = VERTEX_POINT('',#153056) ;
#38797 = VERTEX_POINT('',#153060) ;
#38798 = VERTEX_POINT('',#153062) ;
#38799 = VERTEX_POINT('',#153142) ;
#38800 = VERTEX_POINT('',#153226) ;
#38801 = VERTEX_POINT('',#153227) ;
#38802 = VERTEX_POINT('',#153229) ;
#38803 = VERTEX_POINT('',#153231) ;
#38804 = VERTEX_POINT('',#153235) ;
#38805 = VERTEX_POINT('',#153237) ;
#38806 = VERTEX_POINT('',#153319) ;
#38807 = VERTEX_POINT('',#153402) ;
#38808 = VERTEX_POINT('',#153403) ;
#38809 = VERTEX_POINT('',#153405) ;
#38810 = VERTEX_POINT('',#153407) ;
#38811 = VERTEX_POINT('',#153411) ;
#38812 = VERTEX_POINT('',#153413) ;
#38813 = VERTEX_POINT('',#153494) ;
#38814 = VERTEX_POINT('',#153576) ;
#38815 = VERTEX_POINT('',#153577) ;
#38816 = VERTEX_POINT('',#153579) ;
#38817 = VERTEX_POINT('',#153581) ;
#38818 = VERTEX_POINT('',#153585) ;
#38819 = VERTEX_POINT('',#153587) ;
#38820 = VERTEX_POINT('',#153638) ;
#38821 = VERTEX_POINT('',#153748) ;
#38822 = VERTEX_POINT('',#153750) ;
#38823 = VERTEX_POINT('',#153754) ;
#38824 = VERTEX_POINT('',#153756) ;
#38825 = VERTEX_POINT('',#153760) ;
#38826 = VERTEX_POINT('',#153762) ;
#38827 = VERTEX_POINT('',#153766) ;
#38828 = VERTEX_POINT('',#153768) ;
#38829 = VERTEX_POINT('',#153772) ;
#38830 = VERTEX_POINT('',#153774) ;
#38831 = VERTEX_POINT('',#153778) ;
#38832 = VERTEX_POINT('',#153780) ;
#38833 = VERTEX_POINT('',#153784) ;
#38834 = VERTEX_POINT('',#153786) ;
#38835 = VERTEX_POINT('',#153790) ;
#38836 = VERTEX_POINT('',#153792) ;
#38837 = VERTEX_POINT('',#153796) ;
#38838 = VERTEX_POINT('',#153798) ;
#38839 = VERTEX_POINT('',#153802) ;
#38840 = VERTEX_POINT('',#153804) ;
#38841 = VERTEX_POINT('',#153808) ;
#38842 = VERTEX_POINT('',#153810) ;
#38843 = VERTEX_POINT('',#153814) ;
#38844 = VERTEX_POINT('',#153816) ;
#38845 = VERTEX_POINT('',#153820) ;
#38846 = VERTEX_POINT('',#153822) ;
#38847 = VERTEX_POINT('',#153826) ;
#38848 = VERTEX_POINT('',#153828) ;
#38849 = VERTEX_POINT('',#153832) ;
#38850 = VERTEX_POINT('',#153834) ;
#38851 = VERTEX_POINT('',#153838) ;
#38852 = VERTEX_POINT('',#153840) ;
#38853 = VERTEX_POINT('',#153844) ;
#38854 = VERTEX_POINT('',#153846) ;
#38855 = VERTEX_POINT('',#153850) ;
#38856 = VERTEX_POINT('',#153852) ;
#38857 = VERTEX_POINT('',#153856) ;
#38858 = VERTEX_POINT('',#153858) ;
#38859 = VERTEX_POINT('',#153862) ;
#38860 = VERTEX_POINT('',#153864) ;
#38861 = VERTEX_POINT('',#153868) ;
#38862 = VERTEX_POINT('',#153870) ;
#38863 = VERTEX_POINT('',#153874) ;
#38864 = VERTEX_POINT('',#153876) ;
#38865 = VERTEX_POINT('',#153880) ;
#38866 = VERTEX_POINT('',#153882) ;
#38867 = VERTEX_POINT('',#153886) ;
#38868 = VERTEX_POINT('',#153888) ;
#38869 = VERTEX_POINT('',#153892) ;
#38870 = VERTEX_POINT('',#153894) ;
#38871 = VERTEX_POINT('',#153898) ;
#38872 = VERTEX_POINT('',#153900) ;
#38873 = VERTEX_POINT('',#153904) ;
#38874 = VERTEX_POINT('',#153906) ;
#38875 = VERTEX_POINT('',#153910) ;
#38876 = VERTEX_POINT('',#153911) ;
#38877 = VERTEX_POINT('',#153913) ;
#38878 = VERTEX_POINT('',#153924) ;
#38879 = VERTEX_POINT('',#153926) ;
#38880 = VERTEX_POINT('',#153937) ;
#38881 = VERTEX_POINT('',#153939) ;
#38882 = VERTEX_POINT('',#153950) ;
#38883 = VERTEX_POINT('',#153952) ;
#38884 = VERTEX_POINT('',#153984) ;
#38885 = VERTEX_POINT('',#153986) ;
#38886 = VERTEX_POINT('',#153997) ;
#38887 = VERTEX_POINT('',#153999) ;
#38888 = VERTEX_POINT('',#154010) ;
#38889 = VERTEX_POINT('',#154012) ;
#38890 = VERTEX_POINT('',#154023) ;
#38891 = VERTEX_POINT('',#154025) ;
#38892 = VERTEX_POINT('',#154060) ;
#38893 = VERTEX_POINT('',#154061) ;
#38894 = VERTEX_POINT('',#154063) ;
#38895 = VERTEX_POINT('',#154074) ;
#38896 = VERTEX_POINT('',#154076) ;
#38897 = VERTEX_POINT('',#154087) ;
#38898 = VERTEX_POINT('',#154089) ;
#38899 = VERTEX_POINT('',#154100) ;
#38900 = VERTEX_POINT('',#154102) ;
#38901 = VERTEX_POINT('',#154134) ;
#38902 = VERTEX_POINT('',#154136) ;
#38903 = VERTEX_POINT('',#154147) ;
#38904 = VERTEX_POINT('',#154149) ;
#38905 = VERTEX_POINT('',#154160) ;
#38906 = VERTEX_POINT('',#154162) ;
#38907 = VERTEX_POINT('',#154173) ;
#38908 = VERTEX_POINT('',#154175) ;
#38909 = VERTEX_POINT('',#154210) ;
#38910 = VERTEX_POINT('',#154211) ;
#38911 = VERTEX_POINT('',#154213) ;
#38912 = VERTEX_POINT('',#154224) ;
#38913 = VERTEX_POINT('',#154226) ;
#38914 = VERTEX_POINT('',#154237) ;
#38915 = VERTEX_POINT('',#154239) ;
#38916 = VERTEX_POINT('',#154250) ;
#38917 = VERTEX_POINT('',#154252) ;
#38918 = VERTEX_POINT('',#154284) ;
#38919 = VERTEX_POINT('',#154286) ;
#38920 = VERTEX_POINT('',#154297) ;
#38921 = VERTEX_POINT('',#154299) ;
#38922 = VERTEX_POINT('',#154310) ;
#38923 = VERTEX_POINT('',#154312) ;
#38924 = VERTEX_POINT('',#154323) ;
#38925 = VERTEX_POINT('',#154325) ;
#38926 = VERTEX_POINT('',#154360) ;
#38927 = VERTEX_POINT('',#154361) ;
#38928 = VERTEX_POINT('',#154363) ;
#38929 = VERTEX_POINT('',#154374) ;
#38930 = VERTEX_POINT('',#154376) ;
#38931 = VERTEX_POINT('',#154387) ;
#38932 = VERTEX_POINT('',#154389) ;
#38933 = VERTEX_POINT('',#154400) ;
#38934 = VERTEX_POINT('',#154402) ;
#38935 = VERTEX_POINT('',#154434) ;
#38936 = VERTEX_POINT('',#154436) ;
#38937 = VERTEX_POINT('',#154447) ;
#38938 = VERTEX_POINT('',#154449) ;
#38939 = VERTEX_POINT('',#154460) ;
#38940 = VERTEX_POINT('',#154462) ;
#38941 = VERTEX_POINT('',#154473) ;
#38942 = VERTEX_POINT('',#154475) ;
#38943 = VERTEX_POINT('',#154510) ;
#38944 = VERTEX_POINT('',#154511) ;
#38945 = VERTEX_POINT('',#154513) ;
#38946 = VERTEX_POINT('',#154524) ;
#38947 = VERTEX_POINT('',#154526) ;
#38948 = VERTEX_POINT('',#154537) ;
#38949 = VERTEX_POINT('',#154539) ;
#38950 = VERTEX_POINT('',#154550) ;
#38951 = VERTEX_POINT('',#154552) ;
#38952 = VERTEX_POINT('',#154584) ;
#38953 = VERTEX_POINT('',#154586) ;
#38954 = VERTEX_POINT('',#154597) ;
#38955 = VERTEX_POINT('',#154599) ;
#38956 = VERTEX_POINT('',#154610) ;
#38957 = VERTEX_POINT('',#154612) ;
#38958 = VERTEX_POINT('',#154623) ;
#38959 = VERTEX_POINT('',#154625) ;
#38960 = VERTEX_POINT('',#154660) ;
#38961 = VERTEX_POINT('',#154661) ;
#38962 = VERTEX_POINT('',#154663) ;
#38963 = VERTEX_POINT('',#154674) ;
#38964 = VERTEX_POINT('',#154676) ;
#38965 = VERTEX_POINT('',#154687) ;
#38966 = VERTEX_POINT('',#154689) ;
#38967 = VERTEX_POINT('',#154700) ;
#38968 = VERTEX_POINT('',#154702) ;
#38969 = VERTEX_POINT('',#154734) ;
#38970 = VERTEX_POINT('',#154736) ;
#38971 = VERTEX_POINT('',#154747) ;
#38972 = VERTEX_POINT('',#154749) ;
#38973 = VERTEX_POINT('',#154760) ;
#38974 = VERTEX_POINT('',#154762) ;
#38975 = VERTEX_POINT('',#154773) ;
#38976 = VERTEX_POINT('',#154775) ;
#38977 = VERTEX_POINT('',#154810) ;
#38978 = VERTEX_POINT('',#154811) ;
#38979 = VERTEX_POINT('',#154813) ;
#38980 = VERTEX_POINT('',#154824) ;
#38981 = VERTEX_POINT('',#154826) ;
#38982 = VERTEX_POINT('',#154837) ;
#38983 = VERTEX_POINT('',#154839) ;
#38984 = VERTEX_POINT('',#154850) ;
#38985 = VERTEX_POINT('',#154852) ;
#38986 = VERTEX_POINT('',#154884) ;
#38987 = VERTEX_POINT('',#154886) ;
#38988 = VERTEX_POINT('',#154897) ;
#38989 = VERTEX_POINT('',#154899) ;
#38990 = VERTEX_POINT('',#154910) ;
#38991 = VERTEX_POINT('',#154912) ;
#38992 = VERTEX_POINT('',#154923) ;
#38993 = VERTEX_POINT('',#154925) ;
#38994 = VERTEX_POINT('',#154960) ;
#38995 = VERTEX_POINT('',#154961) ;
#38996 = VERTEX_POINT('',#154963) ;
#38997 = VERTEX_POINT('',#154974) ;
#38998 = VERTEX_POINT('',#154976) ;
#38999 = VERTEX_POINT('',#154987) ;
#39000 = VERTEX_POINT('',#154989) ;
#39001 = VERTEX_POINT('',#155000) ;
#39002 = VERTEX_POINT('',#155002) ;
#39003 = VERTEX_POINT('',#155034) ;
#39004 = VERTEX_POINT('',#155036) ;
#39005 = VERTEX_POINT('',#155047) ;
#39006 = VERTEX_POINT('',#155049) ;
#39007 = VERTEX_POINT('',#155060) ;
#39008 = VERTEX_POINT('',#155062) ;
#39009 = VERTEX_POINT('',#155073) ;
#39010 = VERTEX_POINT('',#155075) ;
#39011 = VERTEX_POINT('',#155110) ;
#39012 = VERTEX_POINT('',#155111) ;
#39013 = VERTEX_POINT('',#155113) ;
#39014 = VERTEX_POINT('',#155124) ;
#39015 = VERTEX_POINT('',#155126) ;
#39016 = VERTEX_POINT('',#155137) ;
#39017 = VERTEX_POINT('',#155139) ;
#39018 = VERTEX_POINT('',#155150) ;
#39019 = VERTEX_POINT('',#155152) ;
#39020 = VERTEX_POINT('',#155184) ;
#39021 = VERTEX_POINT('',#155186) ;
#39022 = VERTEX_POINT('',#155197) ;
#39023 = VERTEX_POINT('',#155199) ;
#39024 = VERTEX_POINT('',#155210) ;
#39025 = VERTEX_POINT('',#155212) ;
#39026 = VERTEX_POINT('',#155223) ;
#39027 = VERTEX_POINT('',#155225) ;
#39028 = VERTEX_POINT('',#155260) ;
#39029 = VERTEX_POINT('',#155264) ;
#39030 = VERTEX_POINT('',#155268) ;
#39031 = VERTEX_POINT('',#155272) ;
#39032 = VERTEX_POINT('',#155276) ;
#39033 = VERTEX_POINT('',#155280) ;
#39034 = VERTEX_POINT('',#155284) ;
#39035 = VERTEX_POINT('',#155288) ;
#39036 = VERTEX_POINT('',#155292) ;
#39037 = VERTEX_POINT('',#155314) ;
#39038 = VERTEX_POINT('',#155316) ;
#39039 = VERTEX_POINT('',#155320) ;
#39040 = VERTEX_POINT('',#155322) ;
#39041 = VERTEX_POINT('',#155326) ;
#39042 = VERTEX_POINT('',#155328) ;
#39043 = VERTEX_POINT('',#155336) ;
#39044 = VERTEX_POINT('',#155341) ;
#39045 = VERTEX_POINT('',#155350) ;
#39046 = VERTEX_POINT('',#155351) ;
#39047 = VERTEX_POINT('',#155353) ;
#39048 = VERTEX_POINT('',#155364) ;
#39049 = VERTEX_POINT('',#155366) ;
#39050 = VERTEX_POINT('',#155377) ;
#39051 = VERTEX_POINT('',#155379) ;
#39052 = VERTEX_POINT('',#155390) ;
#39053 = VERTEX_POINT('',#155392) ;
#39054 = VERTEX_POINT('',#155424) ;
#39055 = VERTEX_POINT('',#155426) ;
#39056 = VERTEX_POINT('',#155437) ;
#39057 = VERTEX_POINT('',#155439) ;
#39058 = VERTEX_POINT('',#155450) ;
#39059 = VERTEX_POINT('',#155452) ;
#39060 = VERTEX_POINT('',#155463) ;
#39061 = VERTEX_POINT('',#155465) ;
#39062 = VERTEX_POINT('',#155500) ;
#39063 = VERTEX_POINT('',#155506) ;
#39064 = VERTEX_POINT('',#155507) ;
#39065 = VERTEX_POINT('',#155509) ;
#39066 = VERTEX_POINT('',#155511) ;
#39067 = VERTEX_POINT('',#155524) ;
#39068 = VERTEX_POINT('',#155526) ;
#39069 = VERTEX_POINT('',#155529) ;
#39070 = VERTEX_POINT('',#155530) ;
#39071 = VERTEX_POINT('',#155532) ;
#39072 = VERTEX_POINT('',#155534) ;
#39073 = VERTEX_POINT('',#155536) ;
#39074 = VERTEX_POINT('',#155538) ;
#39075 = VERTEX_POINT('',#155540) ;
#39076 = VERTEX_POINT('',#155542) ;
#39077 = VERTEX_POINT('',#155545) ;
#39078 = VERTEX_POINT('',#155546) ;
#39079 = VERTEX_POINT('',#155548) ;
#39080 = VERTEX_POINT('',#155550) ;
#39081 = VERTEX_POINT('',#155552) ;
#39082 = VERTEX_POINT('',#155554) ;
#39083 = VERTEX_POINT('',#155556) ;
#39084 = VERTEX_POINT('',#155558) ;
#39085 = VERTEX_POINT('',#155561) ;
#39086 = VERTEX_POINT('',#155562) ;
#39087 = VERTEX_POINT('',#155564) ;
#39088 = VERTEX_POINT('',#155566) ;
#39089 = VERTEX_POINT('',#155568) ;
#39090 = VERTEX_POINT('',#155570) ;
#39091 = VERTEX_POINT('',#155572) ;
#39092 = VERTEX_POINT('',#155574) ;
#39093 = VERTEX_POINT('',#155577) ;
#39094 = VERTEX_POINT('',#155578) ;
#39095 = VERTEX_POINT('',#155580) ;
#39096 = VERTEX_POINT('',#155582) ;
#39097 = VERTEX_POINT('',#155584) ;
#39098 = VERTEX_POINT('',#155586) ;
#39099 = VERTEX_POINT('',#155588) ;
#39100 = VERTEX_POINT('',#155590) ;
#39101 = VERTEX_POINT('',#155593) ;
#39102 = VERTEX_POINT('',#155594) ;
#39103 = VERTEX_POINT('',#155596) ;
#39104 = VERTEX_POINT('',#155598) ;
#39105 = VERTEX_POINT('',#155600) ;
#39106 = VERTEX_POINT('',#155602) ;
#39107 = VERTEX_POINT('',#155604) ;
#39108 = VERTEX_POINT('',#155606) ;
#39109 = VERTEX_POINT('',#155609) ;
#39110 = VERTEX_POINT('',#155610) ;
#39111 = VERTEX_POINT('',#155612) ;
#39112 = VERTEX_POINT('',#155614) ;
#39113 = VERTEX_POINT('',#155616) ;
#39114 = VERTEX_POINT('',#155618) ;
#39115 = VERTEX_POINT('',#155620) ;
#39116 = VERTEX_POINT('',#155622) ;
#39117 = VERTEX_POINT('',#155625) ;
#39118 = VERTEX_POINT('',#155626) ;
#39119 = VERTEX_POINT('',#155628) ;
#39120 = VERTEX_POINT('',#155630) ;
#39121 = VERTEX_POINT('',#155632) ;
#39122 = VERTEX_POINT('',#155634) ;
#39123 = VERTEX_POINT('',#155636) ;
#39124 = VERTEX_POINT('',#155638) ;
#39125 = VERTEX_POINT('',#155641) ;
#39126 = VERTEX_POINT('',#155642) ;
#39127 = VERTEX_POINT('',#155644) ;
#39128 = VERTEX_POINT('',#155646) ;
#39129 = VERTEX_POINT('',#155648) ;
#39130 = VERTEX_POINT('',#155650) ;
#39131 = VERTEX_POINT('',#155652) ;
#39132 = VERTEX_POINT('',#155654) ;
#39133 = VERTEX_POINT('',#155657) ;
#39134 = VERTEX_POINT('',#155658) ;
#39135 = VERTEX_POINT('',#155660) ;
#39136 = VERTEX_POINT('',#155662) ;
#39137 = VERTEX_POINT('',#155664) ;
#39138 = VERTEX_POINT('',#155666) ;
#39139 = VERTEX_POINT('',#155668) ;
#39140 = VERTEX_POINT('',#155670) ;
#39141 = VERTEX_POINT('',#155673) ;
#39142 = VERTEX_POINT('',#155674) ;
#39143 = VERTEX_POINT('',#155676) ;
#39144 = VERTEX_POINT('',#155678) ;
#39145 = VERTEX_POINT('',#155680) ;
#39146 = VERTEX_POINT('',#155682) ;
#39147 = VERTEX_POINT('',#155684) ;
#39148 = VERTEX_POINT('',#155686) ;
#39149 = VERTEX_POINT('',#155690) ;
#39150 = VERTEX_POINT('',#155691) ;
#39151 = VERTEX_POINT('',#155693) ;
#39152 = VERTEX_POINT('',#155695) ;
#39153 = VERTEX_POINT('',#155698) ;
#39154 = VERTEX_POINT('',#155699) ;
#39155 = VERTEX_POINT('',#155701) ;
#39156 = VERTEX_POINT('',#155703) ;
#39157 = VERTEX_POINT('',#155705) ;
#39158 = VERTEX_POINT('',#155707) ;
#39159 = VERTEX_POINT('',#155709) ;
#39160 = VERTEX_POINT('',#155711) ;
#39161 = VERTEX_POINT('',#155715) ;
#39162 = VERTEX_POINT('',#155716) ;
#39163 = VERTEX_POINT('',#155718) ;
#39164 = VERTEX_POINT('',#155720) ;
#39165 = VERTEX_POINT('',#155723) ;
#39166 = VERTEX_POINT('',#155724) ;
#39167 = VERTEX_POINT('',#155726) ;
#39168 = VERTEX_POINT('',#155728) ;
#39169 = VERTEX_POINT('',#155730) ;
#39170 = VERTEX_POINT('',#155732) ;
#39171 = VERTEX_POINT('',#155734) ;
#39172 = VERTEX_POINT('',#155736) ;
#39173 = VERTEX_POINT('',#155740) ;
#39174 = VERTEX_POINT('',#155741) ;
#39175 = VERTEX_POINT('',#155743) ;
#39176 = VERTEX_POINT('',#155745) ;
#39177 = VERTEX_POINT('',#155748) ;
#39178 = VERTEX_POINT('',#155749) ;
#39179 = VERTEX_POINT('',#155751) ;
#39180 = VERTEX_POINT('',#155753) ;
#39181 = VERTEX_POINT('',#155755) ;
#39182 = VERTEX_POINT('',#155757) ;
#39183 = VERTEX_POINT('',#155759) ;
#39184 = VERTEX_POINT('',#155761) ;
#39185 = VERTEX_POINT('',#155765) ;
#39186 = VERTEX_POINT('',#155766) ;
#39187 = VERTEX_POINT('',#155768) ;
#39188 = VERTEX_POINT('',#155770) ;
#39189 = VERTEX_POINT('',#155773) ;
#39190 = VERTEX_POINT('',#155774) ;
#39191 = VERTEX_POINT('',#155776) ;
#39192 = VERTEX_POINT('',#155778) ;
#39193 = VERTEX_POINT('',#155780) ;
#39194 = VERTEX_POINT('',#155782) ;
#39195 = VERTEX_POINT('',#155784) ;
#39196 = VERTEX_POINT('',#155786) ;
#39197 = VERTEX_POINT('',#155790) ;
#39198 = VERTEX_POINT('',#155791) ;
#39199 = VERTEX_POINT('',#155793) ;
#39200 = VERTEX_POINT('',#155795) ;
#39201 = VERTEX_POINT('',#155798) ;
#39202 = VERTEX_POINT('',#155799) ;
#39203 = VERTEX_POINT('',#155801) ;
#39204 = VERTEX_POINT('',#155803) ;
#39205 = VERTEX_POINT('',#155805) ;
#39206 = VERTEX_POINT('',#155807) ;
#39207 = VERTEX_POINT('',#155809) ;
#39208 = VERTEX_POINT('',#155811) ;
#39209 = VERTEX_POINT('',#155815) ;
#39210 = VERTEX_POINT('',#155816) ;
#39211 = VERTEX_POINT('',#155818) ;
#39212 = VERTEX_POINT('',#155820) ;
#39213 = VERTEX_POINT('',#155823) ;
#39214 = VERTEX_POINT('',#155824) ;
#39215 = VERTEX_POINT('',#155826) ;
#39216 = VERTEX_POINT('',#155828) ;
#39217 = VERTEX_POINT('',#155830) ;
#39218 = VERTEX_POINT('',#155832) ;
#39219 = VERTEX_POINT('',#155834) ;
#39220 = VERTEX_POINT('',#155836) ;
#39221 = VERTEX_POINT('',#155840) ;
#39222 = VERTEX_POINT('',#155841) ;
#39223 = VERTEX_POINT('',#155843) ;
#39224 = VERTEX_POINT('',#155845) ;
#39225 = VERTEX_POINT('',#155848) ;
#39226 = VERTEX_POINT('',#155849) ;
#39227 = VERTEX_POINT('',#155851) ;
#39228 = VERTEX_POINT('',#155853) ;
#39229 = VERTEX_POINT('',#155855) ;
#39230 = VERTEX_POINT('',#155857) ;
#39231 = VERTEX_POINT('',#155859) ;
#39232 = VERTEX_POINT('',#155861) ;
#39233 = VERTEX_POINT('',#155865) ;
#39234 = VERTEX_POINT('',#155866) ;
#39235 = VERTEX_POINT('',#155868) ;
#39236 = VERTEX_POINT('',#155870) ;
#39237 = VERTEX_POINT('',#155873) ;
#39238 = VERTEX_POINT('',#155874) ;
#39239 = VERTEX_POINT('',#155876) ;
#39240 = VERTEX_POINT('',#155878) ;
#39241 = VERTEX_POINT('',#155880) ;
#39242 = VERTEX_POINT('',#155882) ;
#39243 = VERTEX_POINT('',#155884) ;
#39244 = VERTEX_POINT('',#155886) ;
#39245 = VERTEX_POINT('',#155890) ;
#39246 = VERTEX_POINT('',#155891) ;
#39247 = VERTEX_POINT('',#155893) ;
#39248 = VERTEX_POINT('',#155895) ;
#39249 = VERTEX_POINT('',#155898) ;
#39250 = VERTEX_POINT('',#155899) ;
#39251 = VERTEX_POINT('',#155901) ;
#39252 = VERTEX_POINT('',#155903) ;
#39253 = VERTEX_POINT('',#155905) ;
#39254 = VERTEX_POINT('',#155907) ;
#39255 = VERTEX_POINT('',#155909) ;
#39256 = VERTEX_POINT('',#155911) ;
#39257 = VERTEX_POINT('',#155933) ;
#39258 = VERTEX_POINT('',#155934) ;
#39259 = VERTEX_POINT('',#155936) ;
#39260 = VERTEX_POINT('',#155938) ;
#39261 = VERTEX_POINT('',#155940) ;
#39262 = VERTEX_POINT('',#155942) ;
#39263 = VERTEX_POINT('',#155944) ;
#39264 = VERTEX_POINT('',#155946) ;
#39265 = VERTEX_POINT('',#155948) ;
#39266 = VERTEX_POINT('',#155950) ;
#39267 = VERTEX_POINT('',#155952) ;
#39268 = VERTEX_POINT('',#155954) ;
#39269 = VERTEX_POINT('',#155956) ;
#39270 = VERTEX_POINT('',#155958) ;
#39271 = VERTEX_POINT('',#155960) ;
#39272 = VERTEX_POINT('',#155962) ;
#39273 = VERTEX_POINT('',#155964) ;
#39274 = VERTEX_POINT('',#155966) ;
#39275 = VERTEX_POINT('',#155968) ;
#39276 = VERTEX_POINT('',#155970) ;
#39277 = VERTEX_POINT('',#155972) ;
#39278 = VERTEX_POINT('',#155974) ;
#39279 = VERTEX_POINT('',#155976) ;
#39280 = VERTEX_POINT('',#155978) ;
#39281 = VERTEX_POINT('',#155980) ;
#39282 = VERTEX_POINT('',#155982) ;
#39283 = VERTEX_POINT('',#155984) ;
#39284 = VERTEX_POINT('',#155986) ;
#39285 = VERTEX_POINT('',#155988) ;
#39286 = VERTEX_POINT('',#155990) ;
#39287 = VERTEX_POINT('',#155992) ;
#39288 = VERTEX_POINT('',#155994) ;
#39289 = VERTEX_POINT('',#155996) ;
#39290 = VERTEX_POINT('',#155998) ;
#39291 = VERTEX_POINT('',#156000) ;
#39292 = VERTEX_POINT('',#156002) ;
#39293 = VERTEX_POINT('',#156004) ;
#39294 = VERTEX_POINT('',#156006) ;
#39295 = VERTEX_POINT('',#156008) ;
#39296 = VERTEX_POINT('',#156010) ;
#39297 = VERTEX_POINT('',#156012) ;
#39298 = VERTEX_POINT('',#156014) ;
#39299 = VERTEX_POINT('',#156016) ;
#39300 = VERTEX_POINT('',#156018) ;
#39301 = VERTEX_POINT('',#156020) ;
#39302 = VERTEX_POINT('',#156022) ;
#39303 = VERTEX_POINT('',#156024) ;
#39304 = VERTEX_POINT('',#156026) ;
#39305 = VERTEX_POINT('',#156028) ;
#39306 = VERTEX_POINT('',#156030) ;
#39307 = VERTEX_POINT('',#156032) ;
#39308 = VERTEX_POINT('',#156034) ;
#39309 = VERTEX_POINT('',#156036) ;
#39310 = VERTEX_POINT('',#156038) ;
#39311 = VERTEX_POINT('',#156040) ;
#39312 = VERTEX_POINT('',#156042) ;
#39313 = VERTEX_POINT('',#156044) ;
#39314 = VERTEX_POINT('',#156046) ;
#39315 = VERTEX_POINT('',#156048) ;
#39316 = VERTEX_POINT('',#156050) ;
#39317 = VERTEX_POINT('',#156052) ;
#39318 = VERTEX_POINT('',#156054) ;
#39319 = VERTEX_POINT('',#156056) ;
#39320 = VERTEX_POINT('',#156058) ;
#39321 = VERTEX_POINT('',#156062) ;
#39322 = VERTEX_POINT('',#156063) ;
#39323 = VERTEX_POINT('',#156065) ;
#39324 = VERTEX_POINT('',#156067) ;
#39325 = VERTEX_POINT('',#156069) ;
#39326 = VERTEX_POINT('',#156071) ;
#39327 = VERTEX_POINT('',#156073) ;
#39328 = VERTEX_POINT('',#156075) ;
#39329 = VERTEX_POINT('',#156079) ;
#39330 = VERTEX_POINT('',#156080) ;
#39331 = VERTEX_POINT('',#156082) ;
#39332 = VERTEX_POINT('',#156084) ;
#39333 = VERTEX_POINT('',#156086) ;
#39334 = VERTEX_POINT('',#156088) ;
#39335 = VERTEX_POINT('',#156090) ;
#39336 = VERTEX_POINT('',#156092) ;
#39337 = VERTEX_POINT('',#156096) ;
#39338 = VERTEX_POINT('',#156097) ;
#39339 = VERTEX_POINT('',#156099) ;
#39340 = VERTEX_POINT('',#156101) ;
#39341 = VERTEX_POINT('',#156103) ;
#39342 = VERTEX_POINT('',#156105) ;
#39343 = VERTEX_POINT('',#156107) ;
#39344 = VERTEX_POINT('',#156109) ;
#39345 = VERTEX_POINT('',#156113) ;
#39346 = VERTEX_POINT('',#156114) ;
#39347 = VERTEX_POINT('',#156116) ;
#39348 = VERTEX_POINT('',#156118) ;
#39349 = VERTEX_POINT('',#156120) ;
#39350 = VERTEX_POINT('',#156122) ;
#39351 = VERTEX_POINT('',#156124) ;
#39352 = VERTEX_POINT('',#156126) ;
#39353 = VERTEX_POINT('',#156130) ;
#39354 = VERTEX_POINT('',#156131) ;
#39355 = VERTEX_POINT('',#156133) ;
#39356 = VERTEX_POINT('',#156135) ;
#39357 = VERTEX_POINT('',#156137) ;
#39358 = VERTEX_POINT('',#156139) ;
#39359 = VERTEX_POINT('',#156141) ;
#39360 = VERTEX_POINT('',#156143) ;
#39361 = VERTEX_POINT('',#156147) ;
#39362 = VERTEX_POINT('',#156148) ;
#39363 = VERTEX_POINT('',#156150) ;
#39364 = VERTEX_POINT('',#156152) ;
#39365 = VERTEX_POINT('',#156154) ;
#39366 = VERTEX_POINT('',#156156) ;
#39367 = VERTEX_POINT('',#156158) ;
#39368 = VERTEX_POINT('',#156160) ;
#39369 = VERTEX_POINT('',#156164) ;
#39370 = VERTEX_POINT('',#156165) ;
#39371 = VERTEX_POINT('',#156167) ;
#39372 = VERTEX_POINT('',#156169) ;
#39373 = VERTEX_POINT('',#156171) ;
#39374 = VERTEX_POINT('',#156173) ;
#39375 = VERTEX_POINT('',#156175) ;
#39376 = VERTEX_POINT('',#156177) ;
#39377 = VERTEX_POINT('',#156181) ;
#39378 = VERTEX_POINT('',#156182) ;
#39379 = VERTEX_POINT('',#156184) ;
#39380 = VERTEX_POINT('',#156186) ;
#39381 = VERTEX_POINT('',#156188) ;
#39382 = VERTEX_POINT('',#156190) ;
#39383 = VERTEX_POINT('',#156192) ;
#39384 = VERTEX_POINT('',#156194) ;
#39385 = VERTEX_POINT('',#156198) ;
#39386 = VERTEX_POINT('',#156199) ;
#39387 = VERTEX_POINT('',#156201) ;
#39388 = VERTEX_POINT('',#156203) ;
#39389 = VERTEX_POINT('',#156205) ;
#39390 = VERTEX_POINT('',#156207) ;
#39391 = VERTEX_POINT('',#156209) ;
#39392 = VERTEX_POINT('',#156211) ;
#39393 = VERTEX_POINT('',#156215) ;
#39394 = VERTEX_POINT('',#156216) ;
#39395 = VERTEX_POINT('',#156218) ;
#39396 = VERTEX_POINT('',#156220) ;
#39397 = VERTEX_POINT('',#156224) ;
#39398 = VERTEX_POINT('',#156225) ;
#39399 = VERTEX_POINT('',#156227) ;
#39400 = VERTEX_POINT('',#156229) ;
#39401 = VERTEX_POINT('',#156231) ;
#39402 = VERTEX_POINT('',#156233) ;
#39403 = VERTEX_POINT('',#156235) ;
#39404 = VERTEX_POINT('',#156237) ;
#39405 = VERTEX_POINT('',#156239) ;
#39406 = VERTEX_POINT('',#156241) ;
#39407 = VERTEX_POINT('',#156243) ;
#39408 = VERTEX_POINT('',#156245) ;
#39409 = VERTEX_POINT('',#156247) ;
#39410 = VERTEX_POINT('',#156249) ;
#39411 = VERTEX_POINT('',#156251) ;
#39412 = VERTEX_POINT('',#156253) ;
#39413 = VERTEX_POINT('',#156255) ;
#39414 = VERTEX_POINT('',#156257) ;
#39415 = VERTEX_POINT('',#156259) ;
#39416 = VERTEX_POINT('',#156261) ;
#39417 = VERTEX_POINT('',#156263) ;
#39418 = VERTEX_POINT('',#156265) ;
#39419 = VERTEX_POINT('',#156267) ;
#39420 = VERTEX_POINT('',#156269) ;
#39421 = VERTEX_POINT('',#156271) ;
#39422 = VERTEX_POINT('',#156273) ;
#39423 = VERTEX_POINT('',#156275) ;
#39424 = VERTEX_POINT('',#156277) ;
#39425 = VERTEX_POINT('',#156279) ;
#39426 = VERTEX_POINT('',#156281) ;
#39427 = VERTEX_POINT('',#156283) ;
#39428 = VERTEX_POINT('',#156285) ;
#39429 = VERTEX_POINT('',#156287) ;
#39430 = VERTEX_POINT('',#156289) ;
#39431 = VERTEX_POINT('',#156291) ;
#39432 = VERTEX_POINT('',#156293) ;
#39433 = VERTEX_POINT('',#156295) ;
#39434 = VERTEX_POINT('',#156297) ;
#39435 = VERTEX_POINT('',#156299) ;
#39436 = VERTEX_POINT('',#156301) ;
#39437 = VERTEX_POINT('',#156303) ;
#39438 = VERTEX_POINT('',#156305) ;
#39439 = VERTEX_POINT('',#156307) ;
#39440 = VERTEX_POINT('',#156309) ;
#39441 = VERTEX_POINT('',#156311) ;
#39442 = VERTEX_POINT('',#156313) ;
#39443 = VERTEX_POINT('',#156315) ;
#39444 = VERTEX_POINT('',#156317) ;
#39445 = VERTEX_POINT('',#156319) ;
#39446 = VERTEX_POINT('',#156321) ;
#39447 = VERTEX_POINT('',#156323) ;
#39448 = VERTEX_POINT('',#156325) ;
#39449 = VERTEX_POINT('',#156327) ;
#39450 = VERTEX_POINT('',#156329) ;
#39451 = VERTEX_POINT('',#156331) ;
#39452 = VERTEX_POINT('',#156333) ;
#39453 = VERTEX_POINT('',#156335) ;
#39454 = VERTEX_POINT('',#156337) ;
#39455 = VERTEX_POINT('',#156339) ;
#39456 = VERTEX_POINT('',#156341) ;
#39457 = VERTEX_POINT('',#156343) ;
#39458 = VERTEX_POINT('',#156345) ;
#39459 = VERTEX_POINT('',#156347) ;
#39460 = VERTEX_POINT('',#156349) ;
#39461 = VERTEX_POINT('',#156353) ;
#39462 = VERTEX_POINT('',#156354) ;
#39463 = VERTEX_POINT('',#156359) ;
#39464 = VERTEX_POINT('',#156360) ;
#39465 = VERTEX_POINT('',#156362) ;
#39466 = VERTEX_POINT('',#156365) ;
#39467 = VERTEX_POINT('',#156369) ;
#39468 = VERTEX_POINT('',#156370) ;
#39469 = VERTEX_POINT('',#156372) ;
#39470 = VERTEX_POINT('',#156374) ;
#39471 = VERTEX_POINT('',#156377) ;
#39472 = VERTEX_POINT('',#156378) ;
#39473 = VERTEX_POINT('',#156385) ;
#39474 = VERTEX_POINT('',#156387) ;
#39475 = VERTEX_POINT('',#156394) ;
#39476 = VERTEX_POINT('',#156396) ;
#39477 = VERTEX_POINT('',#156403) ;
#39478 = VERTEX_POINT('',#156405) ;
#39479 = VERTEX_POINT('',#156413) ;
#39480 = VERTEX_POINT('',#156414) ;
#39481 = VERTEX_POINT('',#156416) ;
#39482 = VERTEX_POINT('',#156418) ;
#39483 = VERTEX_POINT('',#156421) ;
#39484 = VERTEX_POINT('',#156422) ;
#39485 = VERTEX_POINT('',#156424) ;
#39486 = VERTEX_POINT('',#156426) ;
#39487 = VERTEX_POINT('',#156429) ;
#39488 = VERTEX_POINT('',#156430) ;
#39489 = VERTEX_POINT('',#156432) ;
#39490 = VERTEX_POINT('',#156434) ;
#39491 = VERTEX_POINT('',#156437) ;
#39492 = VERTEX_POINT('',#156438) ;
#39493 = VERTEX_POINT('',#156440) ;
#39494 = VERTEX_POINT('',#156442) ;
#39495 = VERTEX_POINT('',#156445) ;
#39496 = VERTEX_POINT('',#156446) ;
#39497 = VERTEX_POINT('',#156448) ;
#39498 = VERTEX_POINT('',#156450) ;
#39499 = VERTEX_POINT('',#156453) ;
#39500 = VERTEX_POINT('',#156454) ;
#39501 = VERTEX_POINT('',#156456) ;
#39502 = VERTEX_POINT('',#156458) ;
#39503 = VERTEX_POINT('',#156461) ;
#39504 = VERTEX_POINT('',#156462) ;
#39505 = VERTEX_POINT('',#156464) ;
#39506 = VERTEX_POINT('',#156466) ;
#39507 = VERTEX_POINT('',#156469) ;
#39508 = VERTEX_POINT('',#156470) ;
#39509 = VERTEX_POINT('',#156472) ;
#39510 = VERTEX_POINT('',#156474) ;
#39511 = VERTEX_POINT('',#156477) ;
#39512 = VERTEX_POINT('',#156478) ;
#39513 = VERTEX_POINT('',#156485) ;
#39514 = VERTEX_POINT('',#156487) ;
#39515 = VERTEX_POINT('',#156494) ;
#39516 = VERTEX_POINT('',#156496) ;
#39517 = VERTEX_POINT('',#156503) ;
#39518 = VERTEX_POINT('',#156505) ;
#39519 = VERTEX_POINT('',#156514) ;
#39520 = VERTEX_POINT('',#156515) ;
#39521 = VERTEX_POINT('',#156517) ;
#39522 = VERTEX_POINT('',#156519) ;
#39523 = VERTEX_POINT('',#156522) ;
#39524 = VERTEX_POINT('',#156523) ;
#39525 = VERTEX_POINT('',#156525) ;
#39526 = VERTEX_POINT('',#156527) ;
#39527 = VERTEX_POINT('',#156529) ;
#39528 = VERTEX_POINT('',#156531) ;
#39529 = VERTEX_POINT('',#156533) ;
#39530 = VERTEX_POINT('',#156535) ;
#39531 = VERTEX_POINT('',#156539) ;
#39532 = VERTEX_POINT('',#156540) ;
#39533 = VERTEX_POINT('',#156542) ;
#39534 = VERTEX_POINT('',#156544) ;
#39535 = VERTEX_POINT('',#156550) ;
#39536 = VERTEX_POINT('',#156551) ;
#39537 = VERTEX_POINT('',#156553) ;
#39538 = VERTEX_POINT('',#156555) ;
#39539 = VERTEX_POINT('',#156557) ;
#39540 = VERTEX_POINT('',#156559) ;
#39541 = VERTEX_POINT('',#156561) ;
#39542 = VERTEX_POINT('',#156563) ;
#39543 = VERTEX_POINT('',#156567) ;
#39544 = VERTEX_POINT('',#156568) ;
#39545 = VERTEX_POINT('',#156570) ;
#39546 = VERTEX_POINT('',#156572) ;
#39547 = VERTEX_POINT('',#156576) ;
#39548 = VERTEX_POINT('',#156578) ;
#39549 = VERTEX_POINT('',#156582) ;
#39550 = VERTEX_POINT('',#156583) ;
#39551 = VERTEX_POINT('',#156585) ;
#39552 = VERTEX_POINT('',#156587) ;
#39553 = VERTEX_POINT('',#156591) ;
#39554 = VERTEX_POINT('',#156592) ;
#39555 = VERTEX_POINT('',#156594) ;
#39556 = VERTEX_POINT('',#156596) ;
#39557 = VERTEX_POINT('',#156599) ;
#39558 = VERTEX_POINT('',#156600) ;
#39559 = VERTEX_POINT('',#156602) ;
#39560 = VERTEX_POINT('',#156604) ;
#39561 = VERTEX_POINT('',#156607) ;
#39562 = VERTEX_POINT('',#156608) ;
#39563 = VERTEX_POINT('',#156610) ;
#39564 = VERTEX_POINT('',#156612) ;
#39565 = VERTEX_POINT('',#156615) ;
#39566 = VERTEX_POINT('',#156616) ;
#39567 = VERTEX_POINT('',#156618) ;
#39568 = VERTEX_POINT('',#156620) ;
#39569 = VERTEX_POINT('',#156623) ;
#39570 = VERTEX_POINT('',#156624) ;
#39571 = VERTEX_POINT('',#156626) ;
#39572 = VERTEX_POINT('',#156628) ;
#39573 = VERTEX_POINT('',#156631) ;
#39574 = VERTEX_POINT('',#156632) ;
#39575 = VERTEX_POINT('',#156634) ;
#39576 = VERTEX_POINT('',#156636) ;
#39577 = VERTEX_POINT('',#156639) ;
#39578 = VERTEX_POINT('',#156640) ;
#39579 = VERTEX_POINT('',#156642) ;
#39580 = VERTEX_POINT('',#156644) ;
#39581 = VERTEX_POINT('',#156647) ;
#39582 = VERTEX_POINT('',#156648) ;
#39583 = VERTEX_POINT('',#156650) ;
#39584 = VERTEX_POINT('',#156652) ;
#39585 = VERTEX_POINT('',#156655) ;
#39586 = VERTEX_POINT('',#156656) ;
#39587 = VERTEX_POINT('',#156658) ;
#39588 = VERTEX_POINT('',#156660) ;
#39589 = VERTEX_POINT('',#156663) ;
#39590 = VERTEX_POINT('',#156664) ;
#39591 = VERTEX_POINT('',#156666) ;
#39592 = VERTEX_POINT('',#156668) ;
#39593 = VERTEX_POINT('',#156670) ;
#39594 = VERTEX_POINT('',#156672) ;
#39595 = VERTEX_POINT('',#156674) ;
#39596 = VERTEX_POINT('',#156676) ;
#39597 = VERTEX_POINT('',#156679) ;
#39598 = VERTEX_POINT('',#156680) ;
#39599 = VERTEX_POINT('',#156682) ;
#39600 = VERTEX_POINT('',#156684) ;
#39601 = VERTEX_POINT('',#156686) ;
#39602 = VERTEX_POINT('',#156688) ;
#39603 = VERTEX_POINT('',#156690) ;
#39604 = VERTEX_POINT('',#156692) ;
#39605 = VERTEX_POINT('',#156696) ;
#39606 = VERTEX_POINT('',#156697) ;
#39607 = VERTEX_POINT('',#156699) ;
#39608 = VERTEX_POINT('',#156701) ;
#39609 = VERTEX_POINT('',#156703) ;
#39610 = VERTEX_POINT('',#156705) ;
#39611 = VERTEX_POINT('',#156707) ;
#39612 = VERTEX_POINT('',#156709) ;
#39613 = VERTEX_POINT('',#156711) ;
#39614 = VERTEX_POINT('',#156713) ;
#39615 = VERTEX_POINT('',#156715) ;
#39616 = VERTEX_POINT('',#156717) ;
#39617 = VERTEX_POINT('',#156719) ;
#39618 = VERTEX_POINT('',#156721) ;
#39619 = VERTEX_POINT('',#156723) ;
#39620 = VERTEX_POINT('',#156727) ;
#39621 = VERTEX_POINT('',#156728) ;
#39622 = VERTEX_POINT('',#156730) ;
#39623 = VERTEX_POINT('',#156732) ;
#39624 = VERTEX_POINT('',#156734) ;
#39625 = VERTEX_POINT('',#156736) ;
#39626 = VERTEX_POINT('',#156738) ;
#39627 = VERTEX_POINT('',#156740) ;
#39628 = VERTEX_POINT('',#156742) ;
#39629 = VERTEX_POINT('',#156744) ;
#39630 = VERTEX_POINT('',#156746) ;
#39631 = VERTEX_POINT('',#156748) ;
#39632 = VERTEX_POINT('',#156750) ;
#39633 = VERTEX_POINT('',#156752) ;
#39634 = VERTEX_POINT('',#156754) ;
#39635 = VERTEX_POINT('',#156758) ;
#39636 = VERTEX_POINT('',#156759) ;
#39637 = VERTEX_POINT('',#156761) ;
#39638 = VERTEX_POINT('',#156763) ;
#39639 = VERTEX_POINT('',#156767) ;
#39640 = VERTEX_POINT('',#156768) ;
#39641 = VERTEX_POINT('',#156770) ;
#39642 = VERTEX_POINT('',#156772) ;
#39643 = VERTEX_POINT('',#156776) ;
#39644 = VERTEX_POINT('',#156777) ;
#39645 = VERTEX_POINT('',#156779) ;
#39646 = VERTEX_POINT('',#156781) ;
#39647 = VERTEX_POINT('',#156783) ;
#39648 = VERTEX_POINT('',#156785) ;
#39649 = VERTEX_POINT('',#156790) ;
#39650 = VERTEX_POINT('',#156792) ;
#39651 = VERTEX_POINT('',#156796) ;
#39652 = VERTEX_POINT('',#156797) ;
#39653 = VERTEX_POINT('',#156799) ;
#39654 = VERTEX_POINT('',#156801) ;
#39655 = VERTEX_POINT('',#156805) ;
#39656 = VERTEX_POINT('',#156806) ;
#39657 = VERTEX_POINT('',#156809) ;
#39658 = VERTEX_POINT('',#156811) ;
#39659 = VERTEX_POINT('',#156815) ;
#39660 = VERTEX_POINT('',#156816) ;
#39661 = VERTEX_POINT('',#156819) ;
#39662 = VERTEX_POINT('',#156821) ;
#39663 = VERTEX_POINT('',#156825) ;
#39664 = VERTEX_POINT('',#156826) ;
#39665 = VERTEX_POINT('',#156828) ;
#39666 = VERTEX_POINT('',#156830) ;
#39667 = VERTEX_POINT('',#156834) ;
#39668 = VERTEX_POINT('',#156835) ;
#39669 = VERTEX_POINT('',#156837) ;
#39670 = VERTEX_POINT('',#156839) ;
#39671 = VERTEX_POINT('',#156843) ;
#39672 = VERTEX_POINT('',#156844) ;
#39673 = VERTEX_POINT('',#156846) ;
#39674 = VERTEX_POINT('',#156848) ;
#39675 = VERTEX_POINT('',#156852) ;
#39676 = VERTEX_POINT('',#156853) ;
#39677 = VERTEX_POINT('',#156855) ;
#39678 = VERTEX_POINT('',#156857) ;
#39679 = VERTEX_POINT('',#156861) ;
#39680 = VERTEX_POINT('',#156862) ;
#39681 = VERTEX_POINT('',#156864) ;
#39682 = VERTEX_POINT('',#156866) ;
#39683 = VERTEX_POINT('',#156869) ;
#39684 = VERTEX_POINT('',#156870) ;
#39685 = VERTEX_POINT('',#156872) ;
#39686 = VERTEX_POINT('',#156874) ;
#39687 = VERTEX_POINT('',#156876) ;
#39688 = VERTEX_POINT('',#156878) ;
#39689 = VERTEX_POINT('',#156880) ;
#39690 = VERTEX_POINT('',#156882) ;
#39691 = VERTEX_POINT('',#156886) ;
#39692 = VERTEX_POINT('',#156888) ;
#39693 = VERTEX_POINT('',#156892) ;
#39694 = VERTEX_POINT('',#156894) ;
#39695 = VERTEX_POINT('',#156898) ;
#39696 = VERTEX_POINT('',#156899) ;
#39697 = VERTEX_POINT('',#156904) ;
#39698 = VERTEX_POINT('',#156906) ;
#39699 = VERTEX_POINT('',#156910) ;
#39700 = VERTEX_POINT('',#156911) ;
#39701 = VERTEX_POINT('',#156913) ;
#39702 = VERTEX_POINT('',#156915) ;
#39703 = VERTEX_POINT('',#156919) ;
#39704 = VERTEX_POINT('',#156921) ;
#39705 = VERTEX_POINT('',#156923) ;
#39706 = VERTEX_POINT('',#156926) ;
#39707 = VERTEX_POINT('',#156928) ;
#39708 = VERTEX_POINT('',#156930) ;
#39709 = VERTEX_POINT('',#156934) ;
#39710 = VERTEX_POINT('',#156935) ;
#39711 = VERTEX_POINT('',#156937) ;
#39712 = VERTEX_POINT('',#156939) ;
#39713 = VERTEX_POINT('',#156943) ;
#39714 = VERTEX_POINT('',#156944) ;
#39715 = VERTEX_POINT('',#156946) ;
#39716 = VERTEX_POINT('',#156948) ;
#39717 = VERTEX_POINT('',#156950) ;
#39718 = VERTEX_POINT('',#156952) ;
#39719 = VERTEX_POINT('',#156954) ;
#39720 = VERTEX_POINT('',#156956) ;
#39721 = VERTEX_POINT('',#156958) ;
#39722 = VERTEX_POINT('',#156960) ;
#39723 = VERTEX_POINT('',#156964) ;
#39724 = VERTEX_POINT('',#156965) ;
#39725 = VERTEX_POINT('',#156967) ;
#39726 = VERTEX_POINT('',#156969) ;
#39727 = VERTEX_POINT('',#156973) ;
#39728 = VERTEX_POINT('',#156974) ;
#39729 = VERTEX_POINT('',#156976) ;
#39730 = VERTEX_POINT('',#156978) ;
#39731 = VERTEX_POINT('',#156980) ;
#39732 = VERTEX_POINT('',#156982) ;
#39733 = VERTEX_POINT('',#156984) ;
#39734 = VERTEX_POINT('',#156986) ;
#39735 = VERTEX_POINT('',#156988) ;
#39736 = VERTEX_POINT('',#156990) ;
#39737 = VERTEX_POINT('',#156994) ;
#39738 = VERTEX_POINT('',#156996) ;
#39739 = VERTEX_POINT('',#157000) ;
#39740 = VERTEX_POINT('',#157001) ;
#39741 = VERTEX_POINT('',#157003) ;
#39742 = VERTEX_POINT('',#157005) ;
#39743 = VERTEX_POINT('',#157009) ;
#39744 = VERTEX_POINT('',#157010) ;
#39745 = VERTEX_POINT('',#157012) ;
#39746 = VERTEX_POINT('',#157014) ;
#39747 = VERTEX_POINT('',#157018) ;
#39748 = VERTEX_POINT('',#157019) ;
#39749 = VERTEX_POINT('',#157021) ;
#39750 = VERTEX_POINT('',#157023) ;
#39751 = VERTEX_POINT('',#157027) ;
#39752 = VERTEX_POINT('',#157028) ;
#39753 = VERTEX_POINT('',#157030) ;
#39754 = VERTEX_POINT('',#157032) ;
#39755 = VERTEX_POINT('',#157034) ;
#39756 = VERTEX_POINT('',#157036) ;
#39757 = VERTEX_POINT('',#157041) ;
#39758 = VERTEX_POINT('',#157042) ;
#39759 = VERTEX_POINT('',#157044) ;
#39760 = VERTEX_POINT('',#157046) ;
#39761 = VERTEX_POINT('',#157050) ;
#39762 = VERTEX_POINT('',#157051) ;
#39763 = VERTEX_POINT('',#157053) ;
#39764 = VERTEX_POINT('',#157055) ;
#39765 = VERTEX_POINT('',#157059) ;
#39766 = VERTEX_POINT('',#157060) ;
#39767 = VERTEX_POINT('',#157062) ;
#39768 = VERTEX_POINT('',#157064) ;
#39769 = VERTEX_POINT('',#157068) ;
#39770 = VERTEX_POINT('',#157069) ;
#39771 = VERTEX_POINT('',#157071) ;
#39772 = VERTEX_POINT('',#157073) ;
#39773 = VERTEX_POINT('',#157077) ;
#39774 = VERTEX_POINT('',#157078) ;
#39775 = VERTEX_POINT('',#157080) ;
#39776 = VERTEX_POINT('',#157082) ;
#39777 = VERTEX_POINT('',#157085) ;
#39778 = VERTEX_POINT('',#157086) ;
#39779 = VERTEX_POINT('',#157088) ;
#39780 = VERTEX_POINT('',#157090) ;
#39781 = VERTEX_POINT('',#157092) ;
#39782 = VERTEX_POINT('',#157094) ;
#39783 = VERTEX_POINT('',#157096) ;
#39784 = VERTEX_POINT('',#157098) ;
#39785 = VERTEX_POINT('',#157102) ;
#39786 = VERTEX_POINT('',#157103) ;
#39787 = VERTEX_POINT('',#157108) ;
#39788 = VERTEX_POINT('',#157109) ;
#39789 = VERTEX_POINT('',#157114) ;
#39790 = VERTEX_POINT('',#157116) ;
#39791 = VERTEX_POINT('',#157120) ;
#39792 = VERTEX_POINT('',#157121) ;
#39793 = VERTEX_POINT('',#157126) ;
#39794 = VERTEX_POINT('',#157127) ;
#39795 = VERTEX_POINT('',#157129) ;
#39796 = VERTEX_POINT('',#157131) ;
#39797 = VERTEX_POINT('',#157150) ;
#39798 = VERTEX_POINT('',#157152) ;
#39799 = VERTEX_POINT('',#157156) ;
#39800 = VERTEX_POINT('',#157157) ;
#39801 = VERTEX_POINT('',#157166) ;
#39802 = VERTEX_POINT('',#157167) ;
#39803 = VERTEX_POINT('',#157169) ;
#39804 = VERTEX_POINT('',#157171) ;
#39805 = VERTEX_POINT('',#157175) ;
#39806 = VERTEX_POINT('',#157177) ;
#39807 = VERTEX_POINT('',#157181) ;
#39808 = VERTEX_POINT('',#157183) ;
#39809 = VERTEX_POINT('',#157187) ;
#39810 = VERTEX_POINT('',#157189) ;
#39811 = VERTEX_POINT('',#157193) ;
#39812 = VERTEX_POINT('',#157195) ;
#39813 = VERTEX_POINT('',#157199) ;
#39814 = VERTEX_POINT('',#157201) ;
#39815 = VERTEX_POINT('',#157205) ;
#39816 = VERTEX_POINT('',#157207) ;
#39817 = VERTEX_POINT('',#157214) ;
#39818 = VERTEX_POINT('',#157215) ;
#39819 = VERTEX_POINT('',#157217) ;
#39820 = VERTEX_POINT('',#157219) ;
#39821 = VERTEX_POINT('',#157242) ;
#39822 = VERTEX_POINT('',#157244) ;
#39823 = VERTEX_POINT('',#157259) ;
#39824 = VERTEX_POINT('',#157261) ;
#39825 = VERTEX_POINT('',#157281) ;
#39826 = VERTEX_POINT('',#157289) ;
#39827 = VERTEX_POINT('',#157295) ;
#39828 = VERTEX_POINT('',#157297) ;
#39829 = VERTEX_POINT('',#157725) ;
#39830 = VERTEX_POINT('',#157756) ;
#39831 = VERTEX_POINT('',#157818) ;
#39832 = VERTEX_POINT('',#157919) ;
#39833 = VERTEX_POINT('',#157920) ;
#39834 = VERTEX_POINT('',#157922) ;
#39835 = VERTEX_POINT('',#157924) ;
#39836 = VERTEX_POINT('',#157928) ;
#39837 = VERTEX_POINT('',#157929) ;
#39838 = VERTEX_POINT('',#157931) ;
#39839 = VERTEX_POINT('',#157933) ;
#39840 = VERTEX_POINT('',#157937) ;
#39841 = VERTEX_POINT('',#157938) ;
#39842 = VERTEX_POINT('',#157940) ;
#39843 = VERTEX_POINT('',#157942) ;
#39844 = VERTEX_POINT('',#157944) ;
#39845 = VERTEX_POINT('',#157946) ;
#39846 = VERTEX_POINT('',#157951) ;
#39847 = VERTEX_POINT('',#157953) ;
#39848 = VERTEX_POINT('',#157957) ;
#39849 = VERTEX_POINT('',#157958) ;
#39850 = VERTEX_POINT('',#157960) ;
#39851 = VERTEX_POINT('',#157962) ;
#39852 = VERTEX_POINT('',#157966) ;
#39853 = VERTEX_POINT('',#157967) ;
#39854 = VERTEX_POINT('',#157969) ;
#39855 = VERTEX_POINT('',#157971) ;
#39856 = VERTEX_POINT('',#157975) ;
#39857 = VERTEX_POINT('',#157976) ;
#39858 = VERTEX_POINT('',#157978) ;
#39859 = VERTEX_POINT('',#157980) ;
#39860 = VERTEX_POINT('',#157984) ;
#39861 = VERTEX_POINT('',#157985) ;
#39862 = VERTEX_POINT('',#157987) ;
#39863 = VERTEX_POINT('',#157989) ;
#39864 = VERTEX_POINT('',#157991) ;
#39865 = VERTEX_POINT('',#157993) ;
#39866 = VERTEX_POINT('',#157998) ;
#39867 = VERTEX_POINT('',#158000) ;
#39868 = VERTEX_POINT('',#158004) ;
#39869 = VERTEX_POINT('',#158005) ;
#39870 = VERTEX_POINT('',#158007) ;
#39871 = VERTEX_POINT('',#158009) ;
#39872 = VERTEX_POINT('',#158013) ;
#39873 = VERTEX_POINT('',#158014) ;
#39874 = VERTEX_POINT('',#158016) ;
#39875 = VERTEX_POINT('',#158018) ;
#39876 = VERTEX_POINT('',#158022) ;
#39877 = VERTEX_POINT('',#158023) ;
#39878 = VERTEX_POINT('',#158025) ;
#39879 = VERTEX_POINT('',#158027) ;
#39880 = VERTEX_POINT('',#158031) ;
#39881 = VERTEX_POINT('',#158032) ;
#39882 = VERTEX_POINT('',#158034) ;
#39883 = VERTEX_POINT('',#158036) ;
#39884 = VERTEX_POINT('',#158038) ;
#39885 = VERTEX_POINT('',#158040) ;
#39886 = VERTEX_POINT('',#158045) ;
#39887 = VERTEX_POINT('',#158047) ;
#39888 = VERTEX_POINT('',#158051) ;
#39889 = VERTEX_POINT('',#158052) ;
#39890 = VERTEX_POINT('',#158054) ;
#39891 = VERTEX_POINT('',#158056) ;
#39892 = VERTEX_POINT('',#158060) ;
#39893 = VERTEX_POINT('',#158061) ;
#39894 = VERTEX_POINT('',#158063) ;
#39895 = VERTEX_POINT('',#158065) ;
#39896 = VERTEX_POINT('',#158069) ;
#39897 = VERTEX_POINT('',#158070) ;
#39898 = VERTEX_POINT('',#158072) ;
#39899 = VERTEX_POINT('',#158074) ;
#39900 = VERTEX_POINT('',#158078) ;
#39901 = VERTEX_POINT('',#158079) ;
#39902 = VERTEX_POINT('',#158081) ;
#39903 = VERTEX_POINT('',#158083) ;
#39904 = VERTEX_POINT('',#158085) ;
#39905 = VERTEX_POINT('',#158087) ;
#39906 = VERTEX_POINT('',#158092) ;
#39907 = VERTEX_POINT('',#158094) ;
#39908 = VERTEX_POINT('',#158098) ;
#39909 = VERTEX_POINT('',#158099) ;
#39910 = VERTEX_POINT('',#158101) ;
#39911 = VERTEX_POINT('',#158103) ;
#39912 = VERTEX_POINT('',#158107) ;
#39913 = VERTEX_POINT('',#158108) ;
#39914 = VERTEX_POINT('',#158110) ;
#39915 = VERTEX_POINT('',#158112) ;
#39916 = VERTEX_POINT('',#158116) ;
#39917 = VERTEX_POINT('',#158117) ;
#39918 = VERTEX_POINT('',#158119) ;
#39919 = VERTEX_POINT('',#158121) ;
#39920 = VERTEX_POINT('',#158125) ;
#39921 = VERTEX_POINT('',#158126) ;
#39922 = VERTEX_POINT('',#158128) ;
#39923 = VERTEX_POINT('',#158130) ;
#39924 = VERTEX_POINT('',#158132) ;
#39925 = VERTEX_POINT('',#158134) ;
#39926 = VERTEX_POINT('',#158139) ;
#39927 = VERTEX_POINT('',#158141) ;
#39928 = VERTEX_POINT('',#158145) ;
#39929 = VERTEX_POINT('',#158146) ;
#39930 = VERTEX_POINT('',#158148) ;
#39931 = VERTEX_POINT('',#158150) ;
#39932 = VERTEX_POINT('',#158154) ;
#39933 = VERTEX_POINT('',#158155) ;
#39934 = VERTEX_POINT('',#158157) ;
#39935 = VERTEX_POINT('',#158159) ;
#39936 = VERTEX_POINT('',#158163) ;
#39937 = VERTEX_POINT('',#158164) ;
#39938 = VERTEX_POINT('',#158166) ;
#39939 = VERTEX_POINT('',#158168) ;
#39940 = VERTEX_POINT('',#158172) ;
#39941 = VERTEX_POINT('',#158173) ;
#39942 = VERTEX_POINT('',#158175) ;
#39943 = VERTEX_POINT('',#158177) ;
#39944 = VERTEX_POINT('',#158179) ;
#39945 = VERTEX_POINT('',#158181) ;
#39946 = VERTEX_POINT('',#158186) ;
#39947 = VERTEX_POINT('',#158188) ;
#39948 = VERTEX_POINT('',#158192) ;
#39949 = VERTEX_POINT('',#158193) ;
#39950 = VERTEX_POINT('',#158195) ;
#39951 = VERTEX_POINT('',#158197) ;
#39952 = VERTEX_POINT('',#158201) ;
#39953 = VERTEX_POINT('',#158202) ;
#39954 = VERTEX_POINT('',#158204) ;
#39955 = VERTEX_POINT('',#158206) ;
#39956 = VERTEX_POINT('',#158210) ;
#39957 = VERTEX_POINT('',#158211) ;
#39958 = VERTEX_POINT('',#158213) ;
#39959 = VERTEX_POINT('',#158215) ;
#39960 = VERTEX_POINT('',#158219) ;
#39961 = VERTEX_POINT('',#158220) ;
#39962 = VERTEX_POINT('',#158222) ;
#39963 = VERTEX_POINT('',#158224) ;
#39964 = VERTEX_POINT('',#158226) ;
#39965 = VERTEX_POINT('',#158228) ;
#39966 = VERTEX_POINT('',#158233) ;
#39967 = VERTEX_POINT('',#158235) ;
#39968 = VERTEX_POINT('',#158239) ;
#39969 = VERTEX_POINT('',#158240) ;
#39970 = VERTEX_POINT('',#158242) ;
#39971 = VERTEX_POINT('',#158244) ;
#39972 = VERTEX_POINT('',#158248) ;
#39973 = VERTEX_POINT('',#158249) ;
#39974 = VERTEX_POINT('',#158251) ;
#39975 = VERTEX_POINT('',#158253) ;
#39976 = VERTEX_POINT('',#158257) ;
#39977 = VERTEX_POINT('',#158258) ;
#39978 = VERTEX_POINT('',#158260) ;
#39979 = VERTEX_POINT('',#158262) ;
#39980 = VERTEX_POINT('',#158266) ;
#39981 = VERTEX_POINT('',#158267) ;
#39982 = VERTEX_POINT('',#158269) ;
#39983 = VERTEX_POINT('',#158271) ;
#39984 = VERTEX_POINT('',#158273) ;
#39985 = VERTEX_POINT('',#158275) ;
#39986 = VERTEX_POINT('',#158280) ;
#39987 = VERTEX_POINT('',#158282) ;
#39988 = VERTEX_POINT('',#158286) ;
#39989 = VERTEX_POINT('',#158287) ;
#39990 = VERTEX_POINT('',#158289) ;
#39991 = VERTEX_POINT('',#158291) ;
#39992 = VERTEX_POINT('',#158295) ;
#39993 = VERTEX_POINT('',#158296) ;
#39994 = VERTEX_POINT('',#158298) ;
#39995 = VERTEX_POINT('',#158300) ;
#39996 = VERTEX_POINT('',#158304) ;
#39997 = VERTEX_POINT('',#158305) ;
#39998 = VERTEX_POINT('',#158307) ;
#39999 = VERTEX_POINT('',#158309) ;
#40000 = VERTEX_POINT('',#158313) ;
#40001 = VERTEX_POINT('',#158314) ;
#40002 = VERTEX_POINT('',#158316) ;
#40003 = VERTEX_POINT('',#158318) ;
#40004 = VERTEX_POINT('',#158320) ;
#40005 = VERTEX_POINT('',#158322) ;
#40006 = VERTEX_POINT('',#158327) ;
#40007 = VERTEX_POINT('',#158329) ;
#40008 = VERTEX_POINT('',#158333) ;
#40009 = VERTEX_POINT('',#158334) ;
#40010 = VERTEX_POINT('',#158336) ;
#40011 = VERTEX_POINT('',#158338) ;
#40012 = VERTEX_POINT('',#158342) ;
#40013 = VERTEX_POINT('',#158343) ;
#40014 = VERTEX_POINT('',#158346) ;
#40015 = VERTEX_POINT('',#158348) ;
#40016 = VERTEX_POINT('',#158352) ;
#40017 = VERTEX_POINT('',#158353) ;
#40018 = VERTEX_POINT('',#158355) ;
#40019 = VERTEX_POINT('',#158357) ;
#40020 = VERTEX_POINT('',#158360) ;
#40021 = VERTEX_POINT('',#158362) ;
#40022 = VERTEX_POINT('',#158366) ;
#40023 = VERTEX_POINT('',#158367) ;
#40024 = VERTEX_POINT('',#158369) ;
#40025 = VERTEX_POINT('',#158371) ;
#40026 = VERTEX_POINT('',#158374) ;
#40027 = VERTEX_POINT('',#158376) ;
#40028 = VERTEX_POINT('',#158380) ;
#40029 = VERTEX_POINT('',#158381) ;
#40030 = VERTEX_POINT('',#158383) ;
#40031 = VERTEX_POINT('',#158385) ;
#40032 = VERTEX_POINT('',#158388) ;
#40033 = VERTEX_POINT('',#158390) ;
#40034 = VERTEX_POINT('',#158394) ;
#40035 = VERTEX_POINT('',#158395) ;
#40036 = VERTEX_POINT('',#158397) ;
#40037 = VERTEX_POINT('',#158399) ;
#40038 = VERTEX_POINT('',#158402) ;
#40039 = VERTEX_POINT('',#158404) ;
#40040 = VERTEX_POINT('',#158408) ;
#40041 = VERTEX_POINT('',#158409) ;
#40042 = VERTEX_POINT('',#158411) ;
#40043 = VERTEX_POINT('',#158413) ;
#40044 = VERTEX_POINT('',#158416) ;
#40045 = VERTEX_POINT('',#158418) ;
#40046 = VERTEX_POINT('',#158422) ;
#40047 = VERTEX_POINT('',#158423) ;
#40048 = VERTEX_POINT('',#158425) ;
#40049 = VERTEX_POINT('',#158427) ;
#40050 = VERTEX_POINT('',#158430) ;
#40051 = VERTEX_POINT('',#158432) ;
#40052 = VERTEX_POINT('',#158436) ;
#40053 = VERTEX_POINT('',#158437) ;
#40054 = VERTEX_POINT('',#158439) ;
#40055 = VERTEX_POINT('',#158441) ;
#40056 = VERTEX_POINT('',#158444) ;
#40057 = VERTEX_POINT('',#158446) ;
#40058 = VERTEX_POINT('',#158450) ;
#40059 = VERTEX_POINT('',#158451) ;
#40060 = VERTEX_POINT('',#158453) ;
#40061 = VERTEX_POINT('',#158455) ;
#40062 = VERTEX_POINT('',#158458) ;
#40063 = VERTEX_POINT('',#158460) ;
#40064 = VERTEX_POINT('',#158464) ;
#40065 = VERTEX_POINT('',#158465) ;
#40066 = VERTEX_POINT('',#158468) ;
#40067 = VERTEX_POINT('',#158470) ;
#40068 = VERTEX_POINT('',#158474) ;
#40069 = VERTEX_POINT('',#158475) ;
#40070 = VERTEX_POINT('',#158477) ;
#40071 = VERTEX_POINT('',#158479) ;
#40072 = VERTEX_POINT('',#158482) ;
#40073 = VERTEX_POINT('',#158484) ;
#40074 = VERTEX_POINT('',#158488) ;
#40075 = VERTEX_POINT('',#158489) ;
#40076 = VERTEX_POINT('',#158491) ;
#40077 = VERTEX_POINT('',#158493) ;
#40078 = VERTEX_POINT('',#158496) ;
#40079 = VERTEX_POINT('',#158498) ;
#40080 = VERTEX_POINT('',#158502) ;
#40081 = VERTEX_POINT('',#158503) ;
#40082 = VERTEX_POINT('',#158505) ;
#40083 = VERTEX_POINT('',#158507) ;
#40084 = VERTEX_POINT('',#158510) ;
#40085 = VERTEX_POINT('',#158512) ;
#40086 = VERTEX_POINT('',#158516) ;
#40087 = VERTEX_POINT('',#158517) ;
#40088 = VERTEX_POINT('',#158519) ;
#40089 = VERTEX_POINT('',#158521) ;
#40090 = VERTEX_POINT('',#158524) ;
#40091 = VERTEX_POINT('',#158526) ;
#40092 = VERTEX_POINT('',#158530) ;
#40093 = VERTEX_POINT('',#158531) ;
#40094 = VERTEX_POINT('',#158533) ;
#40095 = VERTEX_POINT('',#158535) ;
#40096 = VERTEX_POINT('',#158538) ;
#40097 = VERTEX_POINT('',#158540) ;
#40098 = VERTEX_POINT('',#158544) ;
#40099 = VERTEX_POINT('',#158545) ;
#40100 = VERTEX_POINT('',#158547) ;
#40101 = VERTEX_POINT('',#158549) ;
#40102 = VERTEX_POINT('',#158552) ;
#40103 = VERTEX_POINT('',#158554) ;
#40104 = VERTEX_POINT('',#158558) ;
#40105 = VERTEX_POINT('',#158559) ;
#40106 = VERTEX_POINT('',#158561) ;
#40107 = VERTEX_POINT('',#158563) ;
#40108 = VERTEX_POINT('',#158566) ;
#40109 = VERTEX_POINT('',#158568) ;
#40110 = VERTEX_POINT('',#158572) ;
#40111 = VERTEX_POINT('',#158573) ;
#40112 = VERTEX_POINT('',#158575) ;
#40113 = VERTEX_POINT('',#158577) ;
#40114 = VERTEX_POINT('',#158580) ;
#40115 = VERTEX_POINT('',#158582) ;
#40116 = VERTEX_POINT('',#158586) ;
#40117 = VERTEX_POINT('',#158587) ;
#40118 = VERTEX_POINT('',#158589) ;
#40119 = VERTEX_POINT('',#158591) ;
#40120 = VERTEX_POINT('',#158595) ;
#40121 = VERTEX_POINT('',#158596) ;
#40122 = VERTEX_POINT('',#158598) ;
#40123 = VERTEX_POINT('',#158600) ;
#40124 = VERTEX_POINT('',#158604) ;
#40125 = VERTEX_POINT('',#158605) ;
#40126 = VERTEX_POINT('',#158607) ;
#40127 = VERTEX_POINT('',#158609) ;
#40128 = VERTEX_POINT('',#158613) ;
#40129 = VERTEX_POINT('',#158614) ;
#40130 = VERTEX_POINT('',#158616) ;
#40131 = VERTEX_POINT('',#158618) ;
#40132 = VERTEX_POINT('',#158622) ;
#40133 = VERTEX_POINT('',#158623) ;
#40134 = VERTEX_POINT('',#158625) ;
#40135 = VERTEX_POINT('',#158627) ;
#40136 = VERTEX_POINT('',#158631) ;
#40137 = VERTEX_POINT('',#158632) ;
#40138 = VERTEX_POINT('',#158634) ;
#40139 = VERTEX_POINT('',#158636) ;
#40140 = VERTEX_POINT('',#158640) ;
#40141 = VERTEX_POINT('',#158641) ;
#40142 = VERTEX_POINT('',#158643) ;
#40143 = VERTEX_POINT('',#158645) ;
#40144 = VERTEX_POINT('',#158649) ;
#40145 = VERTEX_POINT('',#158650) ;
#40146 = VERTEX_POINT('',#158652) ;
#40147 = VERTEX_POINT('',#158654) ;
#40148 = VERTEX_POINT('',#158658) ;
#40149 = VERTEX_POINT('',#158659) ;
#40150 = VERTEX_POINT('',#158661) ;
#40151 = VERTEX_POINT('',#158663) ;
#40152 = VERTEX_POINT('',#158667) ;
#40153 = VERTEX_POINT('',#158668) ;
#40154 = VERTEX_POINT('',#158670) ;
#40155 = VERTEX_POINT('',#158672) ;
#40156 = VERTEX_POINT('',#158676) ;
#40157 = VERTEX_POINT('',#158677) ;
#40158 = VERTEX_POINT('',#158679) ;
#40159 = VERTEX_POINT('',#158681) ;
#40160 = VERTEX_POINT('',#158685) ;
#40161 = VERTEX_POINT('',#158686) ;
#40162 = VERTEX_POINT('',#158688) ;
#40163 = VERTEX_POINT('',#158690) ;
#40164 = VERTEX_POINT('',#158694) ;
#40165 = VERTEX_POINT('',#158695) ;
#40166 = VERTEX_POINT('',#158697) ;
#40167 = VERTEX_POINT('',#158699) ;
#40168 = VERTEX_POINT('',#158703) ;
#40169 = VERTEX_POINT('',#158704) ;
#40170 = VERTEX_POINT('',#158706) ;
#40171 = VERTEX_POINT('',#158708) ;
#40172 = VERTEX_POINT('',#158712) ;
#40173 = VERTEX_POINT('',#158713) ;
#40174 = VERTEX_POINT('',#158715) ;
#40175 = VERTEX_POINT('',#158717) ;
#40176 = VERTEX_POINT('',#158721) ;
#40177 = VERTEX_POINT('',#158722) ;
#40178 = VERTEX_POINT('',#158724) ;
#40179 = VERTEX_POINT('',#158726) ;
#40180 = VERTEX_POINT('',#158730) ;
#40181 = VERTEX_POINT('',#158731) ;
#40182 = VERTEX_POINT('',#158733) ;
#40183 = VERTEX_POINT('',#158735) ;
#40184 = VERTEX_POINT('',#158739) ;
#40185 = VERTEX_POINT('',#158740) ;
#40186 = VERTEX_POINT('',#158742) ;
#40187 = VERTEX_POINT('',#158744) ;
#40188 = VERTEX_POINT('',#158748) ;
#40189 = VERTEX_POINT('',#158749) ;
#40190 = VERTEX_POINT('',#158751) ;
#40191 = VERTEX_POINT('',#158753) ;
#40192 = VERTEX_POINT('',#158757) ;
#40193 = VERTEX_POINT('',#158758) ;
#40194 = VERTEX_POINT('',#158760) ;
#40195 = VERTEX_POINT('',#158762) ;
#40196 = VERTEX_POINT('',#158766) ;
#40197 = VERTEX_POINT('',#158767) ;
#40198 = VERTEX_POINT('',#158769) ;
#40199 = VERTEX_POINT('',#158771) ;
#40200 = VERTEX_POINT('',#158775) ;
#40201 = VERTEX_POINT('',#158776) ;
#40202 = VERTEX_POINT('',#158778) ;
#40203 = VERTEX_POINT('',#158780) ;
#40204 = VERTEX_POINT('',#158784) ;
#40205 = VERTEX_POINT('',#158785) ;
#40206 = VERTEX_POINT('',#158787) ;
#40207 = VERTEX_POINT('',#158789) ;
#40208 = VERTEX_POINT('',#158793) ;
#40209 = VERTEX_POINT('',#158794) ;
#40210 = VERTEX_POINT('',#158796) ;
#40211 = VERTEX_POINT('',#158798) ;
#40212 = VERTEX_POINT('',#158802) ;
#40213 = VERTEX_POINT('',#158803) ;
#40214 = VERTEX_POINT('',#158805) ;
#40215 = VERTEX_POINT('',#158807) ;
#40216 = VERTEX_POINT('',#158811) ;
#40217 = VERTEX_POINT('',#158812) ;
#40218 = VERTEX_POINT('',#158814) ;
#40219 = VERTEX_POINT('',#158816) ;
#40220 = VERTEX_POINT('',#158820) ;
#40221 = VERTEX_POINT('',#158821) ;
#40222 = VERTEX_POINT('',#158823) ;
#40223 = VERTEX_POINT('',#158825) ;
#40224 = VERTEX_POINT('',#158829) ;
#40225 = VERTEX_POINT('',#158830) ;
#40226 = VERTEX_POINT('',#158832) ;
#40227 = VERTEX_POINT('',#158834) ;
#40228 = VERTEX_POINT('',#158838) ;
#40229 = VERTEX_POINT('',#158839) ;
#40230 = VERTEX_POINT('',#158841) ;
#40231 = VERTEX_POINT('',#158843) ;
#40232 = VERTEX_POINT('',#158847) ;
#40233 = VERTEX_POINT('',#158848) ;
#40234 = VERTEX_POINT('',#158850) ;
#40235 = VERTEX_POINT('',#158852) ;
#40236 = VERTEX_POINT('',#158856) ;
#40237 = VERTEX_POINT('',#158857) ;
#40238 = VERTEX_POINT('',#158859) ;
#40239 = VERTEX_POINT('',#158861) ;
#40240 = VERTEX_POINT('',#158865) ;
#40241 = VERTEX_POINT('',#158866) ;
#40242 = VERTEX_POINT('',#158868) ;
#40243 = VERTEX_POINT('',#158870) ;
#40244 = VERTEX_POINT('',#158874) ;
#40245 = VERTEX_POINT('',#158875) ;
#40246 = VERTEX_POINT('',#158877) ;
#40247 = VERTEX_POINT('',#158879) ;
#40248 = VERTEX_POINT('',#158883) ;
#40249 = VERTEX_POINT('',#158884) ;
#40250 = VERTEX_POINT('',#158886) ;
#40251 = VERTEX_POINT('',#158888) ;
#40252 = VERTEX_POINT('',#158892) ;
#40253 = VERTEX_POINT('',#158893) ;
#40254 = VERTEX_POINT('',#158895) ;
#40255 = VERTEX_POINT('',#158897) ;
#40256 = VERTEX_POINT('',#158901) ;
#40257 = VERTEX_POINT('',#158902) ;
#40258 = VERTEX_POINT('',#158904) ;
#40259 = VERTEX_POINT('',#158906) ;
#40260 = VERTEX_POINT('',#158910) ;
#40261 = VERTEX_POINT('',#158911) ;
#40262 = VERTEX_POINT('',#158913) ;
#40263 = VERTEX_POINT('',#158915) ;
#40264 = VERTEX_POINT('',#158918) ;
#40265 = VERTEX_POINT('',#158919) ;
#40266 = VERTEX_POINT('',#158921) ;
#40267 = VERTEX_POINT('',#158923) ;
#40268 = VERTEX_POINT('',#158925) ;
#40269 = VERTEX_POINT('',#158927) ;
#40270 = VERTEX_POINT('',#158929) ;
#40271 = VERTEX_POINT('',#158931) ;
#40272 = VERTEX_POINT('',#158935) ;
#40273 = VERTEX_POINT('',#158937) ;
#40274 = VERTEX_POINT('',#158941) ;
#40275 = VERTEX_POINT('',#158943) ;
#40276 = VERTEX_POINT('',#158947) ;
#40277 = VERTEX_POINT('',#158948) ;
#40278 = VERTEX_POINT('',#158953) ;
#40279 = VERTEX_POINT('',#158955) ;
#40280 = VERTEX_POINT('',#158959) ;
#40281 = VERTEX_POINT('',#158960) ;
#40282 = VERTEX_POINT('',#158962) ;
#40283 = VERTEX_POINT('',#158964) ;
#40284 = VERTEX_POINT('',#158967) ;
#40285 = VERTEX_POINT('',#158968) ;
#40286 = VERTEX_POINT('',#158970) ;
#40287 = VERTEX_POINT('',#158972) ;
#40288 = VERTEX_POINT('',#158974) ;
#40289 = VERTEX_POINT('',#158976) ;
#40290 = VERTEX_POINT('',#158978) ;
#40291 = VERTEX_POINT('',#158980) ;
#40292 = VERTEX_POINT('',#158984) ;
#40293 = VERTEX_POINT('',#158986) ;
#40294 = VERTEX_POINT('',#158990) ;
#40295 = VERTEX_POINT('',#158992) ;
#40296 = VERTEX_POINT('',#158996) ;
#40297 = VERTEX_POINT('',#158997) ;
#40298 = VERTEX_POINT('',#159002) ;
#40299 = VERTEX_POINT('',#159004) ;
#40300 = VERTEX_POINT('',#159008) ;
#40301 = VERTEX_POINT('',#159009) ;
#40302 = VERTEX_POINT('',#159011) ;
#40303 = VERTEX_POINT('',#159013) ;
#40304 = VERTEX_POINT('',#159016) ;
#40305 = VERTEX_POINT('',#159017) ;
#40306 = VERTEX_POINT('',#159019) ;
#40307 = VERTEX_POINT('',#159021) ;
#40308 = VERTEX_POINT('',#159023) ;
#40309 = VERTEX_POINT('',#159025) ;
#40310 = VERTEX_POINT('',#159027) ;
#40311 = VERTEX_POINT('',#159029) ;
#40312 = VERTEX_POINT('',#159033) ;
#40313 = VERTEX_POINT('',#159035) ;
#40314 = VERTEX_POINT('',#159039) ;
#40315 = VERTEX_POINT('',#159041) ;
#40316 = VERTEX_POINT('',#159045) ;
#40317 = VERTEX_POINT('',#159046) ;
#40318 = VERTEX_POINT('',#159051) ;
#40319 = VERTEX_POINT('',#159053) ;
#40320 = VERTEX_POINT('',#159057) ;
#40321 = VERTEX_POINT('',#159058) ;
#40322 = VERTEX_POINT('',#159060) ;
#40323 = VERTEX_POINT('',#159062) ;
#40324 = VERTEX_POINT('',#159065) ;
#40325 = VERTEX_POINT('',#159066) ;
#40326 = VERTEX_POINT('',#159068) ;
#40327 = VERTEX_POINT('',#159070) ;
#40328 = VERTEX_POINT('',#159072) ;
#40329 = VERTEX_POINT('',#159074) ;
#40330 = VERTEX_POINT('',#159076) ;
#40331 = VERTEX_POINT('',#159078) ;
#40332 = VERTEX_POINT('',#159082) ;
#40333 = VERTEX_POINT('',#159084) ;
#40334 = VERTEX_POINT('',#159088) ;
#40335 = VERTEX_POINT('',#159090) ;
#40336 = VERTEX_POINT('',#159094) ;
#40337 = VERTEX_POINT('',#159095) ;
#40338 = VERTEX_POINT('',#159100) ;
#40339 = VERTEX_POINT('',#159102) ;
#40340 = VERTEX_POINT('',#159106) ;
#40341 = VERTEX_POINT('',#159107) ;
#40342 = VERTEX_POINT('',#159109) ;
#40343 = VERTEX_POINT('',#159111) ;
#40344 = VERTEX_POINT('',#159114) ;
#40345 = VERTEX_POINT('',#159115) ;
#40346 = VERTEX_POINT('',#159117) ;
#40347 = VERTEX_POINT('',#159119) ;
#40348 = VERTEX_POINT('',#159121) ;
#40349 = VERTEX_POINT('',#159123) ;
#40350 = VERTEX_POINT('',#159125) ;
#40351 = VERTEX_POINT('',#159127) ;
#40352 = VERTEX_POINT('',#159131) ;
#40353 = VERTEX_POINT('',#159133) ;
#40354 = VERTEX_POINT('',#159137) ;
#40355 = VERTEX_POINT('',#159139) ;
#40356 = VERTEX_POINT('',#159143) ;
#40357 = VERTEX_POINT('',#159144) ;
#40358 = VERTEX_POINT('',#159149) ;
#40359 = VERTEX_POINT('',#159151) ;
#40360 = VERTEX_POINT('',#159155) ;
#40361 = VERTEX_POINT('',#159156) ;
#40362 = VERTEX_POINT('',#159158) ;
#40363 = VERTEX_POINT('',#159160) ;
#40364 = VERTEX_POINT('',#159163) ;
#40365 = VERTEX_POINT('',#159164) ;
#40366 = VERTEX_POINT('',#159166) ;
#40367 = VERTEX_POINT('',#159168) ;
#40368 = VERTEX_POINT('',#159170) ;
#40369 = VERTEX_POINT('',#159172) ;
#40370 = VERTEX_POINT('',#159174) ;
#40371 = VERTEX_POINT('',#159176) ;
#40372 = VERTEX_POINT('',#159180) ;
#40373 = VERTEX_POINT('',#159182) ;
#40374 = VERTEX_POINT('',#159186) ;
#40375 = VERTEX_POINT('',#159188) ;
#40376 = VERTEX_POINT('',#159192) ;
#40377 = VERTEX_POINT('',#159193) ;
#40378 = VERTEX_POINT('',#159198) ;
#40379 = VERTEX_POINT('',#159200) ;
#40380 = VERTEX_POINT('',#159204) ;
#40381 = VERTEX_POINT('',#159205) ;
#40382 = VERTEX_POINT('',#159207) ;
#40383 = VERTEX_POINT('',#159209) ;
#40384 = VERTEX_POINT('',#159212) ;
#40385 = VERTEX_POINT('',#159213) ;
#40386 = VERTEX_POINT('',#159215) ;
#40387 = VERTEX_POINT('',#159217) ;
#40388 = VERTEX_POINT('',#159219) ;
#40389 = VERTEX_POINT('',#159221) ;
#40390 = VERTEX_POINT('',#159223) ;
#40391 = VERTEX_POINT('',#159225) ;
#40392 = VERTEX_POINT('',#159229) ;
#40393 = VERTEX_POINT('',#159231) ;
#40394 = VERTEX_POINT('',#159235) ;
#40395 = VERTEX_POINT('',#159237) ;
#40396 = VERTEX_POINT('',#159241) ;
#40397 = VERTEX_POINT('',#159242) ;
#40398 = VERTEX_POINT('',#159247) ;
#40399 = VERTEX_POINT('',#159249) ;
#40400 = VERTEX_POINT('',#159253) ;
#40401 = VERTEX_POINT('',#159254) ;
#40402 = VERTEX_POINT('',#159256) ;
#40403 = VERTEX_POINT('',#159258) ;
#40404 = VERTEX_POINT('',#159261) ;
#40405 = VERTEX_POINT('',#159262) ;
#40406 = VERTEX_POINT('',#159264) ;
#40407 = VERTEX_POINT('',#159266) ;
#40408 = VERTEX_POINT('',#159268) ;
#40409 = VERTEX_POINT('',#159270) ;
#40410 = VERTEX_POINT('',#159272) ;
#40411 = VERTEX_POINT('',#159274) ;
#40412 = VERTEX_POINT('',#159278) ;
#40413 = VERTEX_POINT('',#159280) ;
#40414 = VERTEX_POINT('',#159284) ;
#40415 = VERTEX_POINT('',#159286) ;
#40416 = VERTEX_POINT('',#159290) ;
#40417 = VERTEX_POINT('',#159291) ;
#40418 = VERTEX_POINT('',#159296) ;
#40419 = VERTEX_POINT('',#159298) ;
#40420 = VERTEX_POINT('',#159302) ;
#40421 = VERTEX_POINT('',#159303) ;
#40422 = VERTEX_POINT('',#159305) ;
#40423 = VERTEX_POINT('',#159307) ;
#40424 = VERTEX_POINT('',#159310) ;
#40425 = VERTEX_POINT('',#159311) ;
#40426 = VERTEX_POINT('',#159313) ;
#40427 = VERTEX_POINT('',#159315) ;
#40428 = VERTEX_POINT('',#159317) ;
#40429 = VERTEX_POINT('',#159319) ;
#40430 = VERTEX_POINT('',#159321) ;
#40431 = VERTEX_POINT('',#159323) ;
#40432 = VERTEX_POINT('',#159327) ;
#40433 = VERTEX_POINT('',#159329) ;
#40434 = VERTEX_POINT('',#159333) ;
#40435 = VERTEX_POINT('',#159335) ;
#40436 = VERTEX_POINT('',#159339) ;
#40437 = VERTEX_POINT('',#159340) ;
#40438 = VERTEX_POINT('',#159345) ;
#40439 = VERTEX_POINT('',#159347) ;
#40440 = VERTEX_POINT('',#159351) ;
#40441 = VERTEX_POINT('',#159352) ;
#40442 = VERTEX_POINT('',#159354) ;
#40443 = VERTEX_POINT('',#159356) ;
#40444 = VERTEX_POINT('',#159360) ;
#40445 = VERTEX_POINT('',#159361) ;
#40446 = VERTEX_POINT('',#159363) ;
#40447 = VERTEX_POINT('',#159365) ;
#40448 = VERTEX_POINT('',#159369) ;
#40449 = VERTEX_POINT('',#159370) ;
#40450 = VERTEX_POINT('',#159372) ;
#40451 = VERTEX_POINT('',#159374) ;
#40452 = VERTEX_POINT('',#159378) ;
#40453 = VERTEX_POINT('',#159379) ;
#40454 = VERTEX_POINT('',#159381) ;
#40455 = VERTEX_POINT('',#159383) ;
#40456 = VERTEX_POINT('',#159387) ;
#40457 = VERTEX_POINT('',#159388) ;
#40458 = VERTEX_POINT('',#159390) ;
#40459 = VERTEX_POINT('',#159392) ;
#40460 = VERTEX_POINT('',#159396) ;
#40461 = VERTEX_POINT('',#159397) ;
#40462 = VERTEX_POINT('',#159399) ;
#40463 = VERTEX_POINT('',#159401) ;
#40464 = VERTEX_POINT('',#159405) ;
#40465 = VERTEX_POINT('',#159406) ;
#40466 = VERTEX_POINT('',#159408) ;
#40467 = VERTEX_POINT('',#159410) ;
#40468 = VERTEX_POINT('',#159414) ;
#40469 = VERTEX_POINT('',#159415) ;
#40470 = VERTEX_POINT('',#159417) ;
#40471 = VERTEX_POINT('',#159419) ;
#40472 = VERTEX_POINT('',#159423) ;
#40473 = VERTEX_POINT('',#159424) ;
#40474 = VERTEX_POINT('',#159426) ;
#40475 = VERTEX_POINT('',#159428) ;
#40476 = VERTEX_POINT('',#159432) ;
#40477 = VERTEX_POINT('',#159433) ;
#40478 = VERTEX_POINT('',#159435) ;
#40479 = VERTEX_POINT('',#159437) ;
#40480 = VERTEX_POINT('',#159439) ;
#40481 = VERTEX_POINT('',#159441) ;
#40482 = VERTEX_POINT('',#159443) ;
#40483 = VERTEX_POINT('',#159445) ;
#40484 = VERTEX_POINT('',#159447) ;
#40485 = VERTEX_POINT('',#159449) ;
#40486 = VERTEX_POINT('',#159453) ;
#40487 = VERTEX_POINT('',#159454) ;
#40488 = VERTEX_POINT('',#159456) ;
#40489 = VERTEX_POINT('',#159458) ;
#40490 = VERTEX_POINT('',#159462) ;
#40491 = VERTEX_POINT('',#159463) ;
#40492 = VERTEX_POINT('',#159465) ;
#40493 = VERTEX_POINT('',#159467) ;
#40494 = VERTEX_POINT('',#159469) ;
#40495 = VERTEX_POINT('',#159471) ;
#40496 = VERTEX_POINT('',#159473) ;
#40497 = VERTEX_POINT('',#159475) ;
#40498 = VERTEX_POINT('',#159477) ;
#40499 = VERTEX_POINT('',#159479) ;
#40500 = VERTEX_POINT('',#159483) ;
#40501 = VERTEX_POINT('',#159484) ;
#40502 = VERTEX_POINT('',#159486) ;
#40503 = VERTEX_POINT('',#159488) ;
#40504 = VERTEX_POINT('',#159492) ;
#40505 = VERTEX_POINT('',#159493) ;
#40506 = VERTEX_POINT('',#159495) ;
#40507 = VERTEX_POINT('',#159497) ;
#40508 = VERTEX_POINT('',#159499) ;
#40509 = VERTEX_POINT('',#159501) ;
#40510 = VERTEX_POINT('',#159503) ;
#40511 = VERTEX_POINT('',#159505) ;
#40512 = VERTEX_POINT('',#159507) ;
#40513 = VERTEX_POINT('',#159509) ;
#40514 = VERTEX_POINT('',#159513) ;
#40515 = VERTEX_POINT('',#159514) ;
#40516 = VERTEX_POINT('',#159516) ;
#40517 = VERTEX_POINT('',#159518) ;
#40518 = VERTEX_POINT('',#159522) ;
#40519 = VERTEX_POINT('',#159523) ;
#40520 = VERTEX_POINT('',#159525) ;
#40521 = VERTEX_POINT('',#159527) ;
#40522 = VERTEX_POINT('',#159529) ;
#40523 = VERTEX_POINT('',#159531) ;
#40524 = VERTEX_POINT('',#159533) ;
#40525 = VERTEX_POINT('',#159535) ;
#40526 = VERTEX_POINT('',#159537) ;
#40527 = VERTEX_POINT('',#159539) ;
#40528 = VERTEX_POINT('',#159543) ;
#40529 = VERTEX_POINT('',#159544) ;
#40530 = VERTEX_POINT('',#159546) ;
#40531 = VERTEX_POINT('',#159548) ;
#40532 = VERTEX_POINT('',#159552) ;
#40533 = VERTEX_POINT('',#159553) ;
#40534 = VERTEX_POINT('',#159555) ;
#40535 = VERTEX_POINT('',#159557) ;
#40536 = VERTEX_POINT('',#159559) ;
#40537 = VERTEX_POINT('',#159561) ;
#40538 = VERTEX_POINT('',#159563) ;
#40539 = VERTEX_POINT('',#159565) ;
#40540 = VERTEX_POINT('',#159567) ;
#40541 = VERTEX_POINT('',#159569) ;
#40542 = VERTEX_POINT('',#159573) ;
#40543 = VERTEX_POINT('',#159574) ;
#40544 = VERTEX_POINT('',#159576) ;
#40545 = VERTEX_POINT('',#159578) ;
#40546 = VERTEX_POINT('',#159582) ;
#40547 = VERTEX_POINT('',#159583) ;
#40548 = VERTEX_POINT('',#159585) ;
#40549 = VERTEX_POINT('',#159587) ;
#40550 = VERTEX_POINT('',#159589) ;
#40551 = VERTEX_POINT('',#159591) ;
#40552 = VERTEX_POINT('',#159593) ;
#40553 = VERTEX_POINT('',#159595) ;
#40554 = VERTEX_POINT('',#159597) ;
#40555 = VERTEX_POINT('',#159599) ;
#40556 = VERTEX_POINT('',#159603) ;
#40557 = VERTEX_POINT('',#159604) ;
#40558 = VERTEX_POINT('',#159606) ;
#40559 = VERTEX_POINT('',#159608) ;
#40560 = VERTEX_POINT('',#159612) ;
#40561 = VERTEX_POINT('',#159613) ;
#40562 = VERTEX_POINT('',#159615) ;
#40563 = VERTEX_POINT('',#159617) ;
#40564 = VERTEX_POINT('',#159619) ;
#40565 = VERTEX_POINT('',#159621) ;
#40566 = VERTEX_POINT('',#159623) ;
#40567 = VERTEX_POINT('',#159625) ;
#40568 = VERTEX_POINT('',#159627) ;
#40569 = VERTEX_POINT('',#159629) ;
#40570 = VERTEX_POINT('',#159633) ;
#40571 = VERTEX_POINT('',#159634) ;
#40572 = VERTEX_POINT('',#159636) ;
#40573 = VERTEX_POINT('',#159638) ;
#40574 = VERTEX_POINT('',#159642) ;
#40575 = VERTEX_POINT('',#159643) ;
#40576 = VERTEX_POINT('',#159645) ;
#40577 = VERTEX_POINT('',#159647) ;
#40578 = VERTEX_POINT('',#159649) ;
#40579 = VERTEX_POINT('',#159651) ;
#40580 = VERTEX_POINT('',#159653) ;
#40581 = VERTEX_POINT('',#159655) ;
#40582 = VERTEX_POINT('',#159657) ;
#40583 = VERTEX_POINT('',#159659) ;
#40584 = VERTEX_POINT('',#159663) ;
#40585 = VERTEX_POINT('',#159664) ;
#40586 = VERTEX_POINT('',#159666) ;
#40587 = VERTEX_POINT('',#159668) ;
#40588 = VERTEX_POINT('',#159672) ;
#40589 = VERTEX_POINT('',#159673) ;
#40590 = VERTEX_POINT('',#159675) ;
#40591 = VERTEX_POINT('',#159677) ;
#40592 = VERTEX_POINT('',#159679) ;
#40593 = VERTEX_POINT('',#159681) ;
#40594 = VERTEX_POINT('',#159683) ;
#40595 = VERTEX_POINT('',#159685) ;
#40596 = VERTEX_POINT('',#159687) ;
#40597 = VERTEX_POINT('',#159689) ;
#40598 = VERTEX_POINT('',#159693) ;
#40599 = VERTEX_POINT('',#159694) ;
#40600 = VERTEX_POINT('',#159696) ;
#40601 = VERTEX_POINT('',#159698) ;
#40602 = VERTEX_POINT('',#159702) ;
#40603 = VERTEX_POINT('',#159703) ;
#40604 = VERTEX_POINT('',#159705) ;
#40605 = VERTEX_POINT('',#159707) ;
#40606 = VERTEX_POINT('',#159709) ;
#40607 = VERTEX_POINT('',#159711) ;
#40608 = VERTEX_POINT('',#159713) ;
#40609 = VERTEX_POINT('',#159715) ;
#40610 = VERTEX_POINT('',#159717) ;
#40611 = VERTEX_POINT('',#159719) ;
#40612 = VERTEX_POINT('',#159723) ;
#40613 = VERTEX_POINT('',#159724) ;
#40614 = VERTEX_POINT('',#159726) ;
#40615 = VERTEX_POINT('',#159728) ;
#40616 = VERTEX_POINT('',#159732) ;
#40617 = VERTEX_POINT('',#159733) ;
#40618 = VERTEX_POINT('',#159735) ;
#40619 = VERTEX_POINT('',#159737) ;
#40620 = VERTEX_POINT('',#159739) ;
#40621 = VERTEX_POINT('',#159741) ;
#40622 = VERTEX_POINT('',#159743) ;
#40623 = VERTEX_POINT('',#159745) ;
#40624 = VERTEX_POINT('',#159747) ;
#40625 = VERTEX_POINT('',#159749) ;
#40626 = VERTEX_POINT('',#159753) ;
#40627 = VERTEX_POINT('',#159754) ;
#40628 = VERTEX_POINT('',#159756) ;
#40629 = VERTEX_POINT('',#159758) ;
#40630 = VERTEX_POINT('',#159762) ;
#40631 = VERTEX_POINT('',#159763) ;
#40632 = VERTEX_POINT('',#159765) ;
#40633 = VERTEX_POINT('',#159767) ;
#40634 = VERTEX_POINT('',#159769) ;
#40635 = VERTEX_POINT('',#159771) ;
#40636 = VERTEX_POINT('',#159773) ;
#40637 = VERTEX_POINT('',#159775) ;
#40638 = VERTEX_POINT('',#159777) ;
#40639 = VERTEX_POINT('',#159779) ;
#40640 = VERTEX_POINT('',#159783) ;
#40641 = VERTEX_POINT('',#159784) ;
#40642 = VERTEX_POINT('',#159786) ;
#40643 = VERTEX_POINT('',#159788) ;
#40644 = VERTEX_POINT('',#159792) ;
#40645 = VERTEX_POINT('',#159793) ;
#40646 = VERTEX_POINT('',#159795) ;
#40647 = VERTEX_POINT('',#159797) ;
#40648 = VERTEX_POINT('',#159799) ;
#40649 = VERTEX_POINT('',#159801) ;
#40650 = VERTEX_POINT('',#159803) ;
#40651 = VERTEX_POINT('',#159805) ;
#40652 = VERTEX_POINT('',#159807) ;
#40653 = VERTEX_POINT('',#159809) ;
#40654 = VERTEX_POINT('',#159813) ;
#40655 = VERTEX_POINT('',#159814) ;
#40656 = VERTEX_POINT('',#159816) ;
#40657 = VERTEX_POINT('',#159818) ;
#40658 = VERTEX_POINT('',#159822) ;
#40659 = VERTEX_POINT('',#159823) ;
#40660 = VERTEX_POINT('',#159825) ;
#40661 = VERTEX_POINT('',#159827) ;
#40662 = VERTEX_POINT('',#159829) ;
#40663 = VERTEX_POINT('',#159831) ;
#40664 = VERTEX_POINT('',#159833) ;
#40665 = VERTEX_POINT('',#159835) ;
#40666 = VERTEX_POINT('',#159837) ;
#40667 = VERTEX_POINT('',#159839) ;
#40668 = VERTEX_POINT('',#159843) ;
#40669 = VERTEX_POINT('',#159844) ;
#40670 = VERTEX_POINT('',#159846) ;
#40671 = VERTEX_POINT('',#159848) ;
#40672 = VERTEX_POINT('',#159852) ;
#40673 = VERTEX_POINT('',#159853) ;
#40674 = VERTEX_POINT('',#159855) ;
#40675 = VERTEX_POINT('',#159857) ;
#40676 = VERTEX_POINT('',#159859) ;
#40677 = VERTEX_POINT('',#159861) ;
#40678 = VERTEX_POINT('',#159863) ;
#40679 = VERTEX_POINT('',#159865) ;
#40680 = VERTEX_POINT('',#159867) ;
#40681 = VERTEX_POINT('',#159869) ;
#40682 = VERTEX_POINT('',#159873) ;
#40683 = VERTEX_POINT('',#159874) ;
#40684 = VERTEX_POINT('',#159876) ;
#40685 = VERTEX_POINT('',#159878) ;
#40686 = VERTEX_POINT('',#159882) ;
#40687 = VERTEX_POINT('',#159883) ;
#40688 = VERTEX_POINT('',#159885) ;
#40689 = VERTEX_POINT('',#159887) ;
#40690 = VERTEX_POINT('',#159889) ;
#40691 = VERTEX_POINT('',#159891) ;
#40692 = VERTEX_POINT('',#159893) ;
#40693 = VERTEX_POINT('',#159895) ;
#40694 = VERTEX_POINT('',#159897) ;
#40695 = VERTEX_POINT('',#159899) ;
#40696 = VERTEX_POINT('',#159903) ;
#40697 = VERTEX_POINT('',#159904) ;
#40698 = VERTEX_POINT('',#159906) ;
#40699 = VERTEX_POINT('',#159908) ;
#40700 = VERTEX_POINT('',#159912) ;
#40701 = VERTEX_POINT('',#159913) ;
#40702 = VERTEX_POINT('',#159915) ;
#40703 = VERTEX_POINT('',#159917) ;
#40704 = VERTEX_POINT('',#159919) ;
#40705 = VERTEX_POINT('',#159921) ;
#40706 = VERTEX_POINT('',#159923) ;
#40707 = VERTEX_POINT('',#159925) ;
#40708 = VERTEX_POINT('',#159927) ;
#40709 = VERTEX_POINT('',#159929) ;
#40710 = VERTEX_POINT('',#159933) ;
#40711 = VERTEX_POINT('',#159934) ;
#40712 = VERTEX_POINT('',#159936) ;
#40713 = VERTEX_POINT('',#159938) ;
#40714 = VERTEX_POINT('',#159942) ;
#40715 = VERTEX_POINT('',#159943) ;
#40716 = VERTEX_POINT('',#159945) ;
#40717 = VERTEX_POINT('',#159947) ;
#40718 = VERTEX_POINT('',#159949) ;
#40719 = VERTEX_POINT('',#159951) ;
#40720 = VERTEX_POINT('',#159953) ;
#40721 = VERTEX_POINT('',#159955) ;
#40722 = VERTEX_POINT('',#159957) ;
#40723 = VERTEX_POINT('',#159959) ;
#40724 = VERTEX_POINT('',#159963) ;
#40725 = VERTEX_POINT('',#159964) ;
#40726 = VERTEX_POINT('',#159966) ;
#40727 = VERTEX_POINT('',#159968) ;
#40728 = VERTEX_POINT('',#159972) ;
#40729 = VERTEX_POINT('',#159973) ;
#40730 = VERTEX_POINT('',#159975) ;
#40731 = VERTEX_POINT('',#159977) ;
#40732 = VERTEX_POINT('',#159981) ;
#40733 = VERTEX_POINT('',#159982) ;
#40734 = VERTEX_POINT('',#159984) ;
#40735 = VERTEX_POINT('',#159986) ;
#40736 = VERTEX_POINT('',#159990) ;
#40737 = VERTEX_POINT('',#159991) ;
#40738 = VERTEX_POINT('',#159993) ;
#40739 = VERTEX_POINT('',#159995) ;
#40740 = VERTEX_POINT('',#159999) ;
#40741 = VERTEX_POINT('',#160000) ;
#40742 = VERTEX_POINT('',#160002) ;
#40743 = VERTEX_POINT('',#160004) ;
#40744 = VERTEX_POINT('',#160006) ;
#40745 = VERTEX_POINT('',#160008) ;
#40746 = VERTEX_POINT('',#160012) ;
#40747 = VERTEX_POINT('',#160013) ;
#40748 = VERTEX_POINT('',#160015) ;
#40749 = VERTEX_POINT('',#160017) ;
#40750 = VERTEX_POINT('',#160021) ;
#40751 = VERTEX_POINT('',#160022) ;
#40752 = VERTEX_POINT('',#160024) ;
#40753 = VERTEX_POINT('',#160026) ;
#40754 = VERTEX_POINT('',#160030) ;
#40755 = VERTEX_POINT('',#160031) ;
#40756 = VERTEX_POINT('',#160033) ;
#40757 = VERTEX_POINT('',#160035) ;
#40758 = VERTEX_POINT('',#160039) ;
#40759 = VERTEX_POINT('',#160040) ;
#40760 = VERTEX_POINT('',#160042) ;
#40761 = VERTEX_POINT('',#160044) ;
#40762 = VERTEX_POINT('',#160046) ;
#40763 = VERTEX_POINT('',#160048) ;
#40764 = VERTEX_POINT('',#160052) ;
#40765 = VERTEX_POINT('',#160053) ;
#40766 = VERTEX_POINT('',#160055) ;
#40767 = VERTEX_POINT('',#160057) ;
#40768 = VERTEX_POINT('',#160061) ;
#40769 = VERTEX_POINT('',#160062) ;
#40770 = VERTEX_POINT('',#160064) ;
#40771 = VERTEX_POINT('',#160066) ;
#40772 = VERTEX_POINT('',#160070) ;
#40773 = VERTEX_POINT('',#160071) ;
#40774 = VERTEX_POINT('',#160073) ;
#40775 = VERTEX_POINT('',#160075) ;
#40776 = VERTEX_POINT('',#160079) ;
#40777 = VERTEX_POINT('',#160080) ;
#40778 = VERTEX_POINT('',#160082) ;
#40779 = VERTEX_POINT('',#160084) ;
#40780 = VERTEX_POINT('',#160086) ;
#40781 = VERTEX_POINT('',#160088) ;
#40782 = VERTEX_POINT('',#160092) ;
#40783 = VERTEX_POINT('',#160093) ;
#40784 = VERTEX_POINT('',#160095) ;
#40785 = VERTEX_POINT('',#160097) ;
#40786 = VERTEX_POINT('',#160101) ;
#40787 = VERTEX_POINT('',#160102) ;
#40788 = VERTEX_POINT('',#160104) ;
#40789 = VERTEX_POINT('',#160106) ;
#40790 = VERTEX_POINT('',#160110) ;
#40791 = VERTEX_POINT('',#160111) ;
#40792 = VERTEX_POINT('',#160113) ;
#40793 = VERTEX_POINT('',#160115) ;
#40794 = VERTEX_POINT('',#160119) ;
#40795 = VERTEX_POINT('',#160120) ;
#40796 = VERTEX_POINT('',#160122) ;
#40797 = VERTEX_POINT('',#160124) ;
#40798 = VERTEX_POINT('',#160126) ;
#40799 = VERTEX_POINT('',#160128) ;
#40800 = VERTEX_POINT('',#160132) ;
#40801 = VERTEX_POINT('',#160133) ;
#40802 = VERTEX_POINT('',#160135) ;
#40803 = VERTEX_POINT('',#160137) ;
#40804 = VERTEX_POINT('',#160141) ;
#40805 = VERTEX_POINT('',#160142) ;
#40806 = VERTEX_POINT('',#160144) ;
#40807 = VERTEX_POINT('',#160146) ;
#40808 = VERTEX_POINT('',#160150) ;
#40809 = VERTEX_POINT('',#160151) ;
#40810 = VERTEX_POINT('',#160153) ;
#40811 = VERTEX_POINT('',#160155) ;
#40812 = VERTEX_POINT('',#160159) ;
#40813 = VERTEX_POINT('',#160160) ;
#40814 = VERTEX_POINT('',#160162) ;
#40815 = VERTEX_POINT('',#160164) ;
#40816 = VERTEX_POINT('',#160166) ;
#40817 = VERTEX_POINT('',#160168) ;
#40818 = VERTEX_POINT('',#160172) ;
#40819 = VERTEX_POINT('',#160173) ;
#40820 = VERTEX_POINT('',#160175) ;
#40821 = VERTEX_POINT('',#160177) ;
#40822 = VERTEX_POINT('',#160181) ;
#40823 = VERTEX_POINT('',#160182) ;
#40824 = VERTEX_POINT('',#160184) ;
#40825 = VERTEX_POINT('',#160186) ;
#40826 = VERTEX_POINT('',#160190) ;
#40827 = VERTEX_POINT('',#160191) ;
#40828 = VERTEX_POINT('',#160193) ;
#40829 = VERTEX_POINT('',#160195) ;
#40830 = VERTEX_POINT('',#160199) ;
#40831 = VERTEX_POINT('',#160200) ;
#40832 = VERTEX_POINT('',#160202) ;
#40833 = VERTEX_POINT('',#160204) ;
#40834 = VERTEX_POINT('',#160206) ;
#40835 = VERTEX_POINT('',#160208) ;
#40836 = VERTEX_POINT('',#160212) ;
#40837 = VERTEX_POINT('',#160213) ;
#40838 = VERTEX_POINT('',#160215) ;
#40839 = VERTEX_POINT('',#160217) ;
#40840 = VERTEX_POINT('',#160221) ;
#40841 = VERTEX_POINT('',#160222) ;
#40842 = VERTEX_POINT('',#160224) ;
#40843 = VERTEX_POINT('',#160226) ;
#40844 = VERTEX_POINT('',#160230) ;
#40845 = VERTEX_POINT('',#160231) ;
#40846 = VERTEX_POINT('',#160233) ;
#40847 = VERTEX_POINT('',#160235) ;
#40848 = VERTEX_POINT('',#160239) ;
#40849 = VERTEX_POINT('',#160240) ;
#40850 = VERTEX_POINT('',#160242) ;
#40851 = VERTEX_POINT('',#160244) ;
#40852 = VERTEX_POINT('',#160246) ;
#40853 = VERTEX_POINT('',#160248) ;
#40854 = VERTEX_POINT('',#160252) ;
#40855 = VERTEX_POINT('',#160253) ;
#40856 = VERTEX_POINT('',#160255) ;
#40857 = VERTEX_POINT('',#160257) ;
#40858 = VERTEX_POINT('',#160261) ;
#40859 = VERTEX_POINT('',#160262) ;
#40860 = VERTEX_POINT('',#160264) ;
#40861 = VERTEX_POINT('',#160266) ;
#40862 = VERTEX_POINT('',#160270) ;
#40863 = VERTEX_POINT('',#160271) ;
#40864 = VERTEX_POINT('',#160273) ;
#40865 = VERTEX_POINT('',#160275) ;
#40866 = VERTEX_POINT('',#160279) ;
#40867 = VERTEX_POINT('',#160280) ;
#40868 = VERTEX_POINT('',#160282) ;
#40869 = VERTEX_POINT('',#160284) ;
#40870 = VERTEX_POINT('',#160286) ;
#40871 = VERTEX_POINT('',#160288) ;
#40872 = VERTEX_POINT('',#160292) ;
#40873 = VERTEX_POINT('',#160293) ;
#40874 = VERTEX_POINT('',#160295) ;
#40875 = VERTEX_POINT('',#160297) ;
#40876 = VERTEX_POINT('',#160301) ;
#40877 = VERTEX_POINT('',#160302) ;
#40878 = VERTEX_POINT('',#160304) ;
#40879 = VERTEX_POINT('',#160306) ;
#40880 = VERTEX_POINT('',#160310) ;
#40881 = VERTEX_POINT('',#160311) ;
#40882 = VERTEX_POINT('',#160313) ;
#40883 = VERTEX_POINT('',#160315) ;
#40884 = VERTEX_POINT('',#160319) ;
#40885 = VERTEX_POINT('',#160320) ;
#40886 = VERTEX_POINT('',#160322) ;
#40887 = VERTEX_POINT('',#160324) ;
#40888 = VERTEX_POINT('',#160326) ;
#40889 = VERTEX_POINT('',#160328) ;
#40890 = VERTEX_POINT('',#160341) ;
#40891 = VERTEX_POINT('',#160342) ;
#40892 = VERTEX_POINT('',#160344) ;
#40893 = VERTEX_POINT('',#160346) ;
#40894 = VERTEX_POINT('',#160350) ;
#40895 = VERTEX_POINT('',#160351) ;
#40896 = VERTEX_POINT('',#160353) ;
#40897 = VERTEX_POINT('',#160355) ;
#40898 = VERTEX_POINT('',#160359) ;
#40899 = VERTEX_POINT('',#160360) ;
#40900 = VERTEX_POINT('',#160362) ;
#40901 = VERTEX_POINT('',#160364) ;
#40902 = VERTEX_POINT('',#160368) ;
#40903 = VERTEX_POINT('',#160369) ;
#40904 = VERTEX_POINT('',#160371) ;
#40905 = VERTEX_POINT('',#160373) ;
#40906 = VERTEX_POINT('',#160377) ;
#40907 = VERTEX_POINT('',#160378) ;
#40908 = VERTEX_POINT('',#160380) ;
#40909 = VERTEX_POINT('',#160382) ;
#40910 = VERTEX_POINT('',#160386) ;
#40911 = VERTEX_POINT('',#160387) ;
#40912 = VERTEX_POINT('',#160389) ;
#40913 = VERTEX_POINT('',#160391) ;
#40914 = VERTEX_POINT('',#160395) ;
#40915 = VERTEX_POINT('',#160396) ;
#40916 = VERTEX_POINT('',#160398) ;
#40917 = VERTEX_POINT('',#160400) ;
#40918 = VERTEX_POINT('',#160404) ;
#40919 = VERTEX_POINT('',#160405) ;
#40920 = VERTEX_POINT('',#160407) ;
#40921 = VERTEX_POINT('',#160409) ;
#40922 = VERTEX_POINT('',#160413) ;
#40923 = VERTEX_POINT('',#160414) ;
#40924 = VERTEX_POINT('',#160416) ;
#40925 = VERTEX_POINT('',#160418) ;
#40926 = VERTEX_POINT('',#160422) ;
#40927 = VERTEX_POINT('',#160423) ;
#40928 = VERTEX_POINT('',#160425) ;
#40929 = VERTEX_POINT('',#160427) ;
#40930 = VERTEX_POINT('',#160431) ;
#40931 = VERTEX_POINT('',#160432) ;
#40932 = VERTEX_POINT('',#160434) ;
#40933 = VERTEX_POINT('',#160436) ;
#40934 = VERTEX_POINT('',#160440) ;
#40935 = VERTEX_POINT('',#160441) ;
#40936 = VERTEX_POINT('',#160443) ;
#40937 = VERTEX_POINT('',#160445) ;
#40938 = VERTEX_POINT('',#160449) ;
#40939 = VERTEX_POINT('',#160450) ;
#40940 = VERTEX_POINT('',#160452) ;
#40941 = VERTEX_POINT('',#160454) ;
#40942 = VERTEX_POINT('',#160458) ;
#40943 = VERTEX_POINT('',#160459) ;
#40944 = VERTEX_POINT('',#160461) ;
#40945 = VERTEX_POINT('',#160463) ;
#40946 = VERTEX_POINT('',#160467) ;
#40947 = VERTEX_POINT('',#160468) ;
#40948 = VERTEX_POINT('',#160470) ;
#40949 = VERTEX_POINT('',#160472) ;
#40950 = VERTEX_POINT('',#160476) ;
#40951 = VERTEX_POINT('',#160477) ;
#40952 = VERTEX_POINT('',#160479) ;
#40953 = VERTEX_POINT('',#160481) ;
#40954 = VERTEX_POINT('',#160485) ;
#40955 = VERTEX_POINT('',#160486) ;
#40956 = VERTEX_POINT('',#160488) ;
#40957 = VERTEX_POINT('',#160490) ;
#40958 = VERTEX_POINT('',#160494) ;
#40959 = VERTEX_POINT('',#160495) ;
#40960 = VERTEX_POINT('',#160497) ;
#40961 = VERTEX_POINT('',#160499) ;
#40962 = VERTEX_POINT('',#160503) ;
#40963 = VERTEX_POINT('',#160504) ;
#40964 = VERTEX_POINT('',#160506) ;
#40965 = VERTEX_POINT('',#160508) ;
#40966 = VERTEX_POINT('',#160512) ;
#40967 = VERTEX_POINT('',#160513) ;
#40968 = VERTEX_POINT('',#160515) ;
#40969 = VERTEX_POINT('',#160517) ;
#40970 = VERTEX_POINT('',#160521) ;
#40971 = VERTEX_POINT('',#160522) ;
#40972 = VERTEX_POINT('',#160524) ;
#40973 = VERTEX_POINT('',#160526) ;
#40974 = VERTEX_POINT('',#160530) ;
#40975 = VERTEX_POINT('',#160531) ;
#40976 = VERTEX_POINT('',#160533) ;
#40977 = VERTEX_POINT('',#160535) ;
#40978 = VERTEX_POINT('',#160539) ;
#40979 = VERTEX_POINT('',#160540) ;
#40980 = VERTEX_POINT('',#160542) ;
#40981 = VERTEX_POINT('',#160544) ;
#40982 = VERTEX_POINT('',#160548) ;
#40983 = VERTEX_POINT('',#160549) ;
#40984 = VERTEX_POINT('',#160551) ;
#40985 = VERTEX_POINT('',#160553) ;
#40986 = VERTEX_POINT('',#160557) ;
#40987 = VERTEX_POINT('',#160558) ;
#40988 = VERTEX_POINT('',#160560) ;
#40989 = VERTEX_POINT('',#160562) ;
#40990 = VERTEX_POINT('',#160566) ;
#40991 = VERTEX_POINT('',#160567) ;
#40992 = VERTEX_POINT('',#160569) ;
#40993 = VERTEX_POINT('',#160571) ;
#40994 = VERTEX_POINT('',#160575) ;
#40995 = VERTEX_POINT('',#160576) ;
#40996 = VERTEX_POINT('',#160578) ;
#40997 = VERTEX_POINT('',#160580) ;
#40998 = VERTEX_POINT('',#160584) ;
#40999 = VERTEX_POINT('',#160585) ;
#41000 = VERTEX_POINT('',#160587) ;
#41001 = VERTEX_POINT('',#160589) ;
#41002 = VERTEX_POINT('',#160593) ;
#41003 = VERTEX_POINT('',#160594) ;
#41004 = VERTEX_POINT('',#160596) ;
#41005 = VERTEX_POINT('',#160598) ;
#41006 = VERTEX_POINT('',#160602) ;
#41007 = VERTEX_POINT('',#160603) ;
#41008 = VERTEX_POINT('',#160605) ;
#41009 = VERTEX_POINT('',#160607) ;
#41010 = VERTEX_POINT('',#160611) ;
#41011 = VERTEX_POINT('',#160612) ;
#41012 = VERTEX_POINT('',#160614) ;
#41013 = VERTEX_POINT('',#160616) ;
#41014 = VERTEX_POINT('',#160620) ;
#41015 = VERTEX_POINT('',#160621) ;
#41016 = VERTEX_POINT('',#160623) ;
#41017 = VERTEX_POINT('',#160625) ;
#41018 = VERTEX_POINT('',#160629) ;
#41019 = VERTEX_POINT('',#160630) ;
#41020 = VERTEX_POINT('',#160632) ;
#41021 = VERTEX_POINT('',#160634) ;
#41022 = VERTEX_POINT('',#160638) ;
#41023 = VERTEX_POINT('',#160639) ;
#41024 = VERTEX_POINT('',#160641) ;
#41025 = VERTEX_POINT('',#160643) ;
#41026 = VERTEX_POINT('',#160647) ;
#41027 = VERTEX_POINT('',#160648) ;
#41028 = VERTEX_POINT('',#160650) ;
#41029 = VERTEX_POINT('',#160652) ;
#41030 = VERTEX_POINT('',#160656) ;
#41031 = VERTEX_POINT('',#160657) ;
#41032 = VERTEX_POINT('',#160659) ;
#41033 = VERTEX_POINT('',#160661) ;
#41034 = VERTEX_POINT('',#160665) ;
#41035 = VERTEX_POINT('',#160666) ;
#41036 = VERTEX_POINT('',#160668) ;
#41037 = VERTEX_POINT('',#160670) ;
#41038 = VERTEX_POINT('',#160673) ;
#41039 = VERTEX_POINT('',#160674) ;
#41040 = VERTEX_POINT('',#160676) ;
#41041 = VERTEX_POINT('',#160678) ;
#41042 = VERTEX_POINT('',#160680) ;
#41043 = VERTEX_POINT('',#160682) ;
#41044 = VERTEX_POINT('',#160684) ;
#41045 = VERTEX_POINT('',#160686) ;
#41046 = VERTEX_POINT('',#160690) ;
#41047 = VERTEX_POINT('',#160691) ;
#41048 = VERTEX_POINT('',#160696) ;
#41049 = VERTEX_POINT('',#160697) ;
#41050 = VERTEX_POINT('',#160702) ;
#41051 = VERTEX_POINT('',#160704) ;
#41052 = VERTEX_POINT('',#160708) ;
#41053 = VERTEX_POINT('',#160709) ;
#41054 = VERTEX_POINT('',#160714) ;
#41055 = VERTEX_POINT('',#160715) ;
#41056 = VERTEX_POINT('',#160717) ;
#41057 = VERTEX_POINT('',#160719) ;
#41058 = VERTEX_POINT('',#160722) ;
#41059 = VERTEX_POINT('',#160723) ;
#41060 = VERTEX_POINT('',#160725) ;
#41061 = VERTEX_POINT('',#160727) ;
#41062 = VERTEX_POINT('',#160729) ;
#41063 = VERTEX_POINT('',#160731) ;
#41064 = VERTEX_POINT('',#160733) ;
#41065 = VERTEX_POINT('',#160735) ;
#41066 = VERTEX_POINT('',#160739) ;
#41067 = VERTEX_POINT('',#160740) ;
#41068 = VERTEX_POINT('',#160745) ;
#41069 = VERTEX_POINT('',#160746) ;
#41070 = VERTEX_POINT('',#160751) ;
#41071 = VERTEX_POINT('',#160753) ;
#41072 = VERTEX_POINT('',#160757) ;
#41073 = VERTEX_POINT('',#160758) ;
#41074 = VERTEX_POINT('',#160763) ;
#41075 = VERTEX_POINT('',#160764) ;
#41076 = VERTEX_POINT('',#160766) ;
#41077 = VERTEX_POINT('',#160768) ;
#41078 = VERTEX_POINT('',#160771) ;
#41079 = VERTEX_POINT('',#160772) ;
#41080 = VERTEX_POINT('',#160774) ;
#41081 = VERTEX_POINT('',#160776) ;
#41082 = VERTEX_POINT('',#160778) ;
#41083 = VERTEX_POINT('',#160780) ;
#41084 = VERTEX_POINT('',#160782) ;
#41085 = VERTEX_POINT('',#160784) ;
#41086 = VERTEX_POINT('',#160788) ;
#41087 = VERTEX_POINT('',#160789) ;
#41088 = VERTEX_POINT('',#160794) ;
#41089 = VERTEX_POINT('',#160795) ;
#41090 = VERTEX_POINT('',#160800) ;
#41091 = VERTEX_POINT('',#160802) ;
#41092 = VERTEX_POINT('',#160806) ;
#41093 = VERTEX_POINT('',#160807) ;
#41094 = VERTEX_POINT('',#160812) ;
#41095 = VERTEX_POINT('',#160813) ;
#41096 = VERTEX_POINT('',#160815) ;
#41097 = VERTEX_POINT('',#160817) ;
#41098 = VERTEX_POINT('',#160820) ;
#41099 = VERTEX_POINT('',#160821) ;
#41100 = VERTEX_POINT('',#160823) ;
#41101 = VERTEX_POINT('',#160825) ;
#41102 = VERTEX_POINT('',#160827) ;
#41103 = VERTEX_POINT('',#160829) ;
#41104 = VERTEX_POINT('',#160831) ;
#41105 = VERTEX_POINT('',#160833) ;
#41106 = VERTEX_POINT('',#160837) ;
#41107 = VERTEX_POINT('',#160838) ;
#41108 = VERTEX_POINT('',#160843) ;
#41109 = VERTEX_POINT('',#160844) ;
#41110 = VERTEX_POINT('',#160849) ;
#41111 = VERTEX_POINT('',#160851) ;
#41112 = VERTEX_POINT('',#160855) ;
#41113 = VERTEX_POINT('',#160856) ;
#41114 = VERTEX_POINT('',#160861) ;
#41115 = VERTEX_POINT('',#160862) ;
#41116 = VERTEX_POINT('',#160864) ;
#41117 = VERTEX_POINT('',#160866) ;
#41118 = VERTEX_POINT('',#160869) ;
#41119 = VERTEX_POINT('',#160870) ;
#41120 = VERTEX_POINT('',#160872) ;
#41121 = VERTEX_POINT('',#160874) ;
#41122 = VERTEX_POINT('',#160876) ;
#41123 = VERTEX_POINT('',#160878) ;
#41124 = VERTEX_POINT('',#160880) ;
#41125 = VERTEX_POINT('',#160882) ;
#41126 = VERTEX_POINT('',#160886) ;
#41127 = VERTEX_POINT('',#160887) ;
#41128 = VERTEX_POINT('',#160892) ;
#41129 = VERTEX_POINT('',#160893) ;
#41130 = VERTEX_POINT('',#160898) ;
#41131 = VERTEX_POINT('',#160900) ;
#41132 = VERTEX_POINT('',#160904) ;
#41133 = VERTEX_POINT('',#160905) ;
#41134 = VERTEX_POINT('',#160910) ;
#41135 = VERTEX_POINT('',#160911) ;
#41136 = VERTEX_POINT('',#160913) ;
#41137 = VERTEX_POINT('',#160915) ;
#41138 = VERTEX_POINT('',#160918) ;
#41139 = VERTEX_POINT('',#160919) ;
#41140 = VERTEX_POINT('',#160921) ;
#41141 = VERTEX_POINT('',#160923) ;
#41142 = VERTEX_POINT('',#160925) ;
#41143 = VERTEX_POINT('',#160927) ;
#41144 = VERTEX_POINT('',#160929) ;
#41145 = VERTEX_POINT('',#160931) ;
#41146 = VERTEX_POINT('',#160935) ;
#41147 = VERTEX_POINT('',#160936) ;
#41148 = VERTEX_POINT('',#160941) ;
#41149 = VERTEX_POINT('',#160942) ;
#41150 = VERTEX_POINT('',#160947) ;
#41151 = VERTEX_POINT('',#160949) ;
#41152 = VERTEX_POINT('',#160953) ;
#41153 = VERTEX_POINT('',#160954) ;
#41154 = VERTEX_POINT('',#160959) ;
#41155 = VERTEX_POINT('',#160960) ;
#41156 = VERTEX_POINT('',#160962) ;
#41157 = VERTEX_POINT('',#160964) ;
#41158 = VERTEX_POINT('',#160967) ;
#41159 = VERTEX_POINT('',#160968) ;
#41160 = VERTEX_POINT('',#160970) ;
#41161 = VERTEX_POINT('',#160972) ;
#41162 = VERTEX_POINT('',#160974) ;
#41163 = VERTEX_POINT('',#160976) ;
#41164 = VERTEX_POINT('',#160978) ;
#41165 = VERTEX_POINT('',#160980) ;
#41166 = VERTEX_POINT('',#160984) ;
#41167 = VERTEX_POINT('',#160985) ;
#41168 = VERTEX_POINT('',#160990) ;
#41169 = VERTEX_POINT('',#160991) ;
#41170 = VERTEX_POINT('',#160996) ;
#41171 = VERTEX_POINT('',#160998) ;
#41172 = VERTEX_POINT('',#161002) ;
#41173 = VERTEX_POINT('',#161003) ;
#41174 = VERTEX_POINT('',#161008) ;
#41175 = VERTEX_POINT('',#161009) ;
#41176 = VERTEX_POINT('',#161011) ;
#41177 = VERTEX_POINT('',#161013) ;
#41178 = VERTEX_POINT('',#161016) ;
#41179 = VERTEX_POINT('',#161017) ;
#41180 = VERTEX_POINT('',#161019) ;
#41181 = VERTEX_POINT('',#161021) ;
#41182 = VERTEX_POINT('',#161023) ;
#41183 = VERTEX_POINT('',#161025) ;
#41184 = VERTEX_POINT('',#161027) ;
#41185 = VERTEX_POINT('',#161029) ;
#41186 = VERTEX_POINT('',#161033) ;
#41187 = VERTEX_POINT('',#161034) ;
#41188 = VERTEX_POINT('',#161039) ;
#41189 = VERTEX_POINT('',#161040) ;
#41190 = VERTEX_POINT('',#161045) ;
#41191 = VERTEX_POINT('',#161047) ;
#41192 = VERTEX_POINT('',#161051) ;
#41193 = VERTEX_POINT('',#161052) ;
#41194 = VERTEX_POINT('',#161057) ;
#41195 = VERTEX_POINT('',#161058) ;
#41196 = VERTEX_POINT('',#161060) ;
#41197 = VERTEX_POINT('',#161062) ;
#41198 = VERTEX_POINT('',#161065) ;
#41199 = VERTEX_POINT('',#161066) ;
#41200 = VERTEX_POINT('',#161068) ;
#41201 = VERTEX_POINT('',#161070) ;
#41202 = VERTEX_POINT('',#161072) ;
#41203 = VERTEX_POINT('',#161074) ;
#41204 = VERTEX_POINT('',#161076) ;
#41205 = VERTEX_POINT('',#161078) ;
#41206 = VERTEX_POINT('',#161082) ;
#41207 = VERTEX_POINT('',#161083) ;
#41208 = VERTEX_POINT('',#161088) ;
#41209 = VERTEX_POINT('',#161089) ;
#41210 = VERTEX_POINT('',#161094) ;
#41211 = VERTEX_POINT('',#161096) ;
#41212 = VERTEX_POINT('',#161100) ;
#41213 = VERTEX_POINT('',#161101) ;
#41214 = VERTEX_POINT('',#161106) ;
#41215 = VERTEX_POINT('',#161107) ;
#41216 = VERTEX_POINT('',#161109) ;
#41217 = VERTEX_POINT('',#161111) ;
#41218 = VERTEX_POINT('',#161115) ;
#41219 = VERTEX_POINT('',#161116) ;
#41220 = VERTEX_POINT('',#161118) ;
#41221 = VERTEX_POINT('',#161120) ;
#41222 = VERTEX_POINT('',#161124) ;
#41223 = VERTEX_POINT('',#161125) ;
#41224 = VERTEX_POINT('',#161127) ;
#41225 = VERTEX_POINT('',#161129) ;
#41226 = VERTEX_POINT('',#161133) ;
#41227 = VERTEX_POINT('',#161134) ;
#41228 = VERTEX_POINT('',#161136) ;
#41229 = VERTEX_POINT('',#161138) ;
#41230 = VERTEX_POINT('',#161142) ;
#41231 = VERTEX_POINT('',#161143) ;
#41232 = VERTEX_POINT('',#161145) ;
#41233 = VERTEX_POINT('',#161147) ;
#41234 = VERTEX_POINT('',#161151) ;
#41235 = VERTEX_POINT('',#161152) ;
#41236 = VERTEX_POINT('',#161154) ;
#41237 = VERTEX_POINT('',#161156) ;
#41238 = VERTEX_POINT('',#161160) ;
#41239 = VERTEX_POINT('',#161161) ;
#41240 = VERTEX_POINT('',#161163) ;
#41241 = VERTEX_POINT('',#161165) ;
#41242 = VERTEX_POINT('',#161169) ;
#41243 = VERTEX_POINT('',#161170) ;
#41244 = VERTEX_POINT('',#161172) ;
#41245 = VERTEX_POINT('',#161174) ;
#41246 = VERTEX_POINT('',#161178) ;
#41247 = VERTEX_POINT('',#161179) ;
#41248 = VERTEX_POINT('',#161181) ;
#41249 = VERTEX_POINT('',#161183) ;
#41250 = VERTEX_POINT('',#161286) ;
#41251 = VERTEX_POINT('',#161287) ;
#41252 = VERTEX_POINT('',#161289) ;
#41253 = VERTEX_POINT('',#161291) ;
#41254 = VERTEX_POINT('',#161295) ;
#41255 = VERTEX_POINT('',#161297) ;
#41256 = VERTEX_POINT('',#161301) ;
#41257 = VERTEX_POINT('',#161303) ;
#41258 = VERTEX_POINT('',#161307) ;
#41259 = VERTEX_POINT('',#161309) ;
#41260 = VERTEX_POINT('',#161313) ;
#41261 = VERTEX_POINT('',#161315) ;
#41262 = VERTEX_POINT('',#161319) ;
#41263 = VERTEX_POINT('',#161321) ;
#41264 = VERTEX_POINT('',#161325) ;
#41265 = VERTEX_POINT('',#161327) ;
#41266 = VERTEX_POINT('',#161334) ;
#41267 = VERTEX_POINT('',#161335) ;
#41268 = VERTEX_POINT('',#161337) ;
#41269 = VERTEX_POINT('',#161339) ;
#41270 = VERTEX_POINT('',#161343) ;
#41271 = VERTEX_POINT('',#161344) ;
#41272 = VERTEX_POINT('',#161346) ;
#41273 = VERTEX_POINT('',#161348) ;
#41274 = VERTEX_POINT('',#161352) ;
#41275 = VERTEX_POINT('',#161354) ;
#41276 = VERTEX_POINT('',#161358) ;
#41277 = VERTEX_POINT('',#161360) ;
#41278 = VERTEX_POINT('',#161364) ;
#41279 = VERTEX_POINT('',#161366) ;
#41280 = VERTEX_POINT('',#161370) ;
#41281 = VERTEX_POINT('',#161372) ;
#41282 = VERTEX_POINT('',#161376) ;
#41283 = VERTEX_POINT('',#161378) ;
#41284 = VERTEX_POINT('',#161382) ;
#41285 = VERTEX_POINT('',#161384) ;
#41286 = VERTEX_POINT('',#161391) ;
#41287 = VERTEX_POINT('',#161392) ;
#41288 = VERTEX_POINT('',#161394) ;
#41289 = VERTEX_POINT('',#161396) ;
#41290 = VERTEX_POINT('',#161400) ;
#41291 = VERTEX_POINT('',#161401) ;
#41292 = VERTEX_POINT('',#161403) ;
#41293 = VERTEX_POINT('',#161405) ;
#41294 = VERTEX_POINT('',#161409) ;
#41295 = VERTEX_POINT('',#161411) ;
#41296 = VERTEX_POINT('',#161415) ;
#41297 = VERTEX_POINT('',#161417) ;
#41298 = VERTEX_POINT('',#161421) ;
#41299 = VERTEX_POINT('',#161423) ;
#41300 = VERTEX_POINT('',#161427) ;
#41301 = VERTEX_POINT('',#161429) ;
#41302 = VERTEX_POINT('',#161433) ;
#41303 = VERTEX_POINT('',#161435) ;
#41304 = VERTEX_POINT('',#161439) ;
#41305 = VERTEX_POINT('',#161441) ;
#41306 = VERTEX_POINT('',#161448) ;
#41307 = VERTEX_POINT('',#161449) ;
#41308 = VERTEX_POINT('',#161451) ;
#41309 = VERTEX_POINT('',#161453) ;
#41310 = VERTEX_POINT('',#161457) ;
#41311 = VERTEX_POINT('',#161458) ;
#41312 = VERTEX_POINT('',#161460) ;
#41313 = VERTEX_POINT('',#161462) ;
#41314 = VERTEX_POINT('',#161466) ;
#41315 = VERTEX_POINT('',#161468) ;
#41316 = VERTEX_POINT('',#161472) ;
#41317 = VERTEX_POINT('',#161474) ;
#41318 = VERTEX_POINT('',#161478) ;
#41319 = VERTEX_POINT('',#161480) ;
#41320 = VERTEX_POINT('',#161484) ;
#41321 = VERTEX_POINT('',#161486) ;
#41322 = VERTEX_POINT('',#161490) ;
#41323 = VERTEX_POINT('',#161492) ;
#41324 = VERTEX_POINT('',#161496) ;
#41325 = VERTEX_POINT('',#161498) ;
#41326 = VERTEX_POINT('',#161505) ;
#41327 = VERTEX_POINT('',#161506) ;
#41328 = VERTEX_POINT('',#161508) ;
#41329 = VERTEX_POINT('',#161510) ;
#41330 = VERTEX_POINT('',#161514) ;
#41331 = VERTEX_POINT('',#161515) ;
#41332 = VERTEX_POINT('',#161517) ;
#41333 = VERTEX_POINT('',#161519) ;
#41334 = VERTEX_POINT('',#161523) ;
#41335 = VERTEX_POINT('',#161525) ;
#41336 = VERTEX_POINT('',#161529) ;
#41337 = VERTEX_POINT('',#161531) ;
#41338 = VERTEX_POINT('',#161535) ;
#41339 = VERTEX_POINT('',#161537) ;
#41340 = VERTEX_POINT('',#161541) ;
#41341 = VERTEX_POINT('',#161543) ;
#41342 = VERTEX_POINT('',#161547) ;
#41343 = VERTEX_POINT('',#161549) ;
#41344 = VERTEX_POINT('',#161553) ;
#41345 = VERTEX_POINT('',#161555) ;
#41346 = VERTEX_POINT('',#161562) ;
#41347 = VERTEX_POINT('',#161563) ;
#41348 = VERTEX_POINT('',#161565) ;
#41349 = VERTEX_POINT('',#161567) ;
#41350 = VERTEX_POINT('',#161571) ;
#41351 = VERTEX_POINT('',#161572) ;
#41352 = VERTEX_POINT('',#161574) ;
#41353 = VERTEX_POINT('',#161576) ;
#41354 = VERTEX_POINT('',#161580) ;
#41355 = VERTEX_POINT('',#161582) ;
#41356 = VERTEX_POINT('',#161586) ;
#41357 = VERTEX_POINT('',#161588) ;
#41358 = VERTEX_POINT('',#161592) ;
#41359 = VERTEX_POINT('',#161594) ;
#41360 = VERTEX_POINT('',#161598) ;
#41361 = VERTEX_POINT('',#161600) ;
#41362 = VERTEX_POINT('',#161604) ;
#41363 = VERTEX_POINT('',#161606) ;
#41364 = VERTEX_POINT('',#161610) ;
#41365 = VERTEX_POINT('',#161612) ;
#41366 = VERTEX_POINT('',#161619) ;
#41367 = VERTEX_POINT('',#161620) ;
#41368 = VERTEX_POINT('',#161622) ;
#41369 = VERTEX_POINT('',#161624) ;
#41370 = VERTEX_POINT('',#161628) ;
#41371 = VERTEX_POINT('',#161629) ;
#41372 = VERTEX_POINT('',#161631) ;
#41373 = VERTEX_POINT('',#161633) ;
#41374 = VERTEX_POINT('',#161637) ;
#41375 = VERTEX_POINT('',#161639) ;
#41376 = VERTEX_POINT('',#161643) ;
#41377 = VERTEX_POINT('',#161645) ;
#41378 = VERTEX_POINT('',#161649) ;
#41379 = VERTEX_POINT('',#161651) ;
#41380 = VERTEX_POINT('',#161655) ;
#41381 = VERTEX_POINT('',#161657) ;
#41382 = VERTEX_POINT('',#161661) ;
#41383 = VERTEX_POINT('',#161663) ;
#41384 = VERTEX_POINT('',#161667) ;
#41385 = VERTEX_POINT('',#161669) ;
#41386 = VERTEX_POINT('',#161676) ;
#41387 = VERTEX_POINT('',#161677) ;
#41388 = VERTEX_POINT('',#161679) ;
#41389 = VERTEX_POINT('',#161681) ;
#41390 = VERTEX_POINT('',#161685) ;
#41391 = VERTEX_POINT('',#161686) ;
#41392 = VERTEX_POINT('',#161688) ;
#41393 = VERTEX_POINT('',#161690) ;
#41394 = VERTEX_POINT('',#161694) ;
#41395 = VERTEX_POINT('',#161696) ;
#41396 = VERTEX_POINT('',#161700) ;
#41397 = VERTEX_POINT('',#161702) ;
#41398 = VERTEX_POINT('',#161706) ;
#41399 = VERTEX_POINT('',#161708) ;
#41400 = VERTEX_POINT('',#161712) ;
#41401 = VERTEX_POINT('',#161714) ;
#41402 = VERTEX_POINT('',#161718) ;
#41403 = VERTEX_POINT('',#161720) ;
#41404 = VERTEX_POINT('',#161724) ;
#41405 = VERTEX_POINT('',#161726) ;
#41406 = VERTEX_POINT('',#161733) ;
#41407 = VERTEX_POINT('',#161734) ;
#41408 = VERTEX_POINT('',#161736) ;
#41409 = VERTEX_POINT('',#161738) ;
#41410 = VERTEX_POINT('',#161742) ;
#41411 = VERTEX_POINT('',#161743) ;
#41412 = VERTEX_POINT('',#161745) ;
#41413 = VERTEX_POINT('',#161747) ;
#41414 = VERTEX_POINT('',#161751) ;
#41415 = VERTEX_POINT('',#161753) ;
#41416 = VERTEX_POINT('',#161757) ;
#41417 = VERTEX_POINT('',#161759) ;
#41418 = VERTEX_POINT('',#161763) ;
#41419 = VERTEX_POINT('',#161765) ;
#41420 = VERTEX_POINT('',#161769) ;
#41421 = VERTEX_POINT('',#161771) ;
#41422 = VERTEX_POINT('',#161775) ;
#41423 = VERTEX_POINT('',#161777) ;
#41424 = VERTEX_POINT('',#161781) ;
#41425 = VERTEX_POINT('',#161783) ;
#41426 = VERTEX_POINT('',#161790) ;
#41427 = VERTEX_POINT('',#161791) ;
#41428 = VERTEX_POINT('',#161793) ;
#41429 = VERTEX_POINT('',#161795) ;
#41430 = VERTEX_POINT('',#161901) ;
#41431 = VERTEX_POINT('',#161917) ;
#41432 = VERTEX_POINT('',#161934) ;
#41433 = VERTEX_POINT('',#161950) ;
#41434 = VERTEX_POINT('',#161967) ;
#41435 = VERTEX_POINT('',#161983) ;
#41436 = VERTEX_POINT('',#162000) ;
#41437 = VERTEX_POINT('',#162016) ;
#41438 = VERTEX_POINT('',#162033) ;
#41439 = VERTEX_POINT('',#162049) ;
#41440 = VERTEX_POINT('',#162066) ;
#41441 = VERTEX_POINT('',#162082) ;
#41442 = VERTEX_POINT('',#162099) ;
#41443 = VERTEX_POINT('',#162115) ;
#41444 = VERTEX_POINT('',#162132) ;
#41445 = VERTEX_POINT('',#162148) ;
#41446 = VERTEX_POINT('',#162165) ;
#41447 = VERTEX_POINT('',#162181) ;
#41448 = VERTEX_POINT('',#162198) ;
#41449 = VERTEX_POINT('',#162214) ;
#41450 = VERTEX_POINT('',#162231) ;
#41451 = VERTEX_POINT('',#162247) ;
#41452 = VERTEX_POINT('',#162264) ;
#41453 = VERTEX_POINT('',#162280) ;
#41454 = VERTEX_POINT('',#162297) ;
#41455 = VERTEX_POINT('',#162313) ;
#41456 = VERTEX_POINT('',#162330) ;
#41457 = VERTEX_POINT('',#162346) ;
#41458 = VERTEX_POINT('',#162363) ;
#41459 = VERTEX_POINT('',#162379) ;
#41460 = VERTEX_POINT('',#162396) ;
#41461 = VERTEX_POINT('',#162412) ;
#41462 = VERTEX_POINT('',#162429) ;
#41463 = VERTEX_POINT('',#162445) ;
#41464 = VERTEX_POINT('',#162462) ;
#41465 = VERTEX_POINT('',#162478) ;
#41466 = VERTEX_POINT('',#162495) ;
#41467 = VERTEX_POINT('',#162511) ;
#41468 = VERTEX_POINT('',#162528) ;
#41469 = VERTEX_POINT('',#162544) ;
#41470 = VERTEX_POINT('',#162561) ;
#41471 = VERTEX_POINT('',#162577) ;
#41472 = VERTEX_POINT('',#162594) ;
#41473 = VERTEX_POINT('',#162610) ;
#41474 = VERTEX_POINT('',#162627) ;
#41475 = VERTEX_POINT('',#162643) ;
#41476 = VERTEX_POINT('',#162660) ;
#41477 = VERTEX_POINT('',#162676) ;
#41478 = VERTEX_POINT('',#162693) ;
#41479 = VERTEX_POINT('',#162709) ;
#41480 = VERTEX_POINT('',#162726) ;
#41481 = VERTEX_POINT('',#162742) ;
#41482 = VERTEX_POINT('',#162759) ;
#41483 = VERTEX_POINT('',#162775) ;
#41484 = VERTEX_POINT('',#162792) ;
#41485 = VERTEX_POINT('',#162808) ;
#41486 = VERTEX_POINT('',#162825) ;
#41487 = VERTEX_POINT('',#162841) ;
#41488 = VERTEX_POINT('',#162858) ;
#41489 = VERTEX_POINT('',#162874) ;
#41490 = VERTEX_POINT('',#162891) ;
#41491 = VERTEX_POINT('',#162907) ;
#41492 = VERTEX_POINT('',#162924) ;
#41493 = VERTEX_POINT('',#162940) ;
#41494 = VERTEX_POINT('',#163149) ;
#41495 = VERTEX_POINT('',#163152) ;
#41496 = VERTEX_POINT('',#163154) ;
#41497 = VERTEX_POINT('',#163158) ;
#41498 = VERTEX_POINT('',#163161) ;
#41499 = VERTEX_POINT('',#163168) ;
#41500 = VERTEX_POINT('',#163170) ;
#41501 = VERTEX_POINT('',#163173) ;
#41502 = VERTEX_POINT('',#163177) ;
#41503 = VERTEX_POINT('',#163180) ;
#41504 = VERTEX_POINT('',#163182) ;
#41505 = VERTEX_POINT('',#163186) ;
#41506 = VERTEX_POINT('',#163189) ;
#41507 = VERTEX_POINT('',#163196) ;
#41508 = VERTEX_POINT('',#163198) ;
#41509 = VERTEX_POINT('',#163201) ;
#41510 = VERTEX_POINT('',#163205) ;
#41511 = VERTEX_POINT('',#163208) ;
#41512 = VERTEX_POINT('',#163210) ;
#41513 = VERTEX_POINT('',#163214) ;
#41514 = VERTEX_POINT('',#163217) ;
#41515 = VERTEX_POINT('',#163224) ;
#41516 = VERTEX_POINT('',#163226) ;
#41517 = VERTEX_POINT('',#163229) ;
#41518 = VERTEX_POINT('',#163233) ;
#41519 = VERTEX_POINT('',#163236) ;
#41520 = VERTEX_POINT('',#163238) ;
#41521 = VERTEX_POINT('',#163242) ;
#41522 = VERTEX_POINT('',#163245) ;
#41523 = VERTEX_POINT('',#163252) ;
#41524 = VERTEX_POINT('',#163254) ;
#41525 = VERTEX_POINT('',#163257) ;
#41526 = VERTEX_POINT('',#163261) ;
#41527 = VERTEX_POINT('',#163264) ;
#41528 = VERTEX_POINT('',#163266) ;
#41529 = VERTEX_POINT('',#163270) ;
#41530 = VERTEX_POINT('',#163273) ;
#41531 = VERTEX_POINT('',#163280) ;
#41532 = VERTEX_POINT('',#163282) ;
#41533 = VERTEX_POINT('',#163285) ;
#41534 = VERTEX_POINT('',#163289) ;
#41535 = VERTEX_POINT('',#163292) ;
#41536 = VERTEX_POINT('',#163294) ;
#41537 = VERTEX_POINT('',#163298) ;
#41538 = VERTEX_POINT('',#163301) ;
#41539 = VERTEX_POINT('',#163308) ;
#41540 = VERTEX_POINT('',#163310) ;
#41541 = VERTEX_POINT('',#163313) ;
#41542 = VERTEX_POINT('',#163317) ;
#41543 = VERTEX_POINT('',#163320) ;
#41544 = VERTEX_POINT('',#163322) ;
#41545 = VERTEX_POINT('',#163326) ;
#41546 = VERTEX_POINT('',#163329) ;
#41547 = VERTEX_POINT('',#163336) ;
#41548 = VERTEX_POINT('',#163338) ;
#41549 = VERTEX_POINT('',#163341) ;
#41550 = VERTEX_POINT('',#163345) ;
#41551 = VERTEX_POINT('',#163348) ;
#41552 = VERTEX_POINT('',#163350) ;
#41553 = VERTEX_POINT('',#163354) ;
#41554 = VERTEX_POINT('',#163357) ;
#41555 = VERTEX_POINT('',#163364) ;
#41556 = VERTEX_POINT('',#163366) ;
#41557 = VERTEX_POINT('',#163369) ;
#41558 = VERTEX_POINT('',#167424) ;
#41559 = VERTEX_POINT('',#167454) ;
#41560 = VERTEX_POINT('',#167520) ;
#41561 = VERTEX_POINT('',#167550) ;
#41562 = VERTEX_POINT('',#167589) ;
#41563 = VERTEX_POINT('',#167619) ;
#41564 = VERTEX_POINT('',#167658) ;
#41565 = VERTEX_POINT('',#167688) ;
#41566 = VERTEX_POINT('',#167727) ;
#41567 = VERTEX_POINT('',#167757) ;
#41568 = VERTEX_POINT('',#167796) ;
#41569 = VERTEX_POINT('',#167826) ;
#41570 = VERTEX_POINT('',#167865) ;
#41571 = VERTEX_POINT('',#167895) ;
#41572 = VERTEX_POINT('',#167934) ;
#41573 = VERTEX_POINT('',#167964) ;
#41574 = VERTEX_POINT('',#168004) ;
#41575 = VERTEX_POINT('',#168043) ;
#41576 = VERTEX_POINT('',#168105) ;
#41577 = VERTEX_POINT('',#168138) ;
#41578 = VERTEX_POINT('',#168200) ;
#41579 = VERTEX_POINT('',#168233) ;
#41580 = VERTEX_POINT('',#168295) ;
#41581 = VERTEX_POINT('',#168328) ;
#41582 = VERTEX_POINT('',#168390) ;
#41583 = VERTEX_POINT('',#168423) ;
#41584 = VERTEX_POINT('',#168485) ;
#41585 = VERTEX_POINT('',#168518) ;
#41586 = VERTEX_POINT('',#168580) ;
#41587 = VERTEX_POINT('',#168613) ;
#41588 = VERTEX_POINT('',#168675) ;
#41589 = VERTEX_POINT('',#168708) ;
#41590 = VERTEX_POINT('',#168770) ;
#41591 = VERTEX_POINT('',#168803) ;
#41592 = VERTEX_POINT('',#168865) ;
#41593 = EDGE_CURVE('',#34714,#34715,#28626,.T.) ;
#41594 = EDGE_CURVE('',#34716,#34714,#28627,.T.) ;
#41595 = EDGE_CURVE('',#34717,#34716,#28628,.T.) ;
#41596 = EDGE_CURVE('',#34717,#34715,#28629,.T.) ;
#41597 = EDGE_CURVE('',#34718,#34718,#28630,.T.) ;
#41598 = EDGE_CURVE('',#34718,#34719,#28631,.T.) ;
#41599 = EDGE_CURVE('',#34720,#34719,#28632,.T.) ;
#41600 = EDGE_CURVE('',#34719,#34720,#28633,.T.) ;
#41601 = EDGE_CURVE('',#34721,#34721,#28634,.T.) ;
#41602 = EDGE_CURVE('',#34721,#34722,#28635,.T.) ;
#41603 = EDGE_CURVE('',#34722,#34722,#28636,.T.) ;
#41604 = EDGE_CURVE('',#34723,#34723,#28637,.T.) ;
#41605 = EDGE_CURVE('',#34723,#34724,#28638,.T.) ;
#41606 = EDGE_CURVE('',#34725,#34724,#28639,.T.) ;
#41607 = EDGE_CURVE('',#34724,#34725,#28640,.T.) ;
#41608 = EDGE_CURVE('',#34726,#34727,#28641,.T.) ;
#41609 = EDGE_CURVE('',#34728,#34727,#28642,.T.) ;
#41610 = EDGE_CURVE('',#34728,#34729,#28643,.T.) ;
#41611 = EDGE_CURVE('',#34729,#34726,#28644,.T.) ;
#41612 = EDGE_CURVE('',#34730,#34731,#28645,.T.) ;
#41613 = EDGE_CURVE('',#34731,#34732,#28646,.T.) ;
#41614 = EDGE_CURVE('',#34730,#34732,#28647,.T.) ;
#41615 = EDGE_CURVE('',#34733,#34726,#2430,.T.) ;
#41616 = EDGE_CURVE('',#34733,#34734,#28648,.T.) ;
#41617 = EDGE_CURVE('',#34727,#34734,#2431,.T.) ;
#41618 = EDGE_CURVE('',#34735,#34736,#28649,.T.) ;
#41619 = EDGE_CURVE('',#34735,#34737,#28650,.T.) ;
#41620 = EDGE_CURVE('',#34736,#34737,#28651,.T.) ;
#41621 = EDGE_CURVE('',#34738,#34738,#28652,.T.) ;
#41622 = EDGE_CURVE('',#34738,#34721,#2432,.T.) ;
#41623 = EDGE_CURVE('',#34722,#34725,#2433,.T.) ;
#41624 = EDGE_CURVE('',#34739,#34740,#28653,.T.) ;
#41625 = EDGE_CURVE('',#34739,#34741,#1999,.T.) ;
#41626 = EDGE_CURVE('',#34742,#34741,#2434,.T.) ;
#41627 = EDGE_CURVE('',#34742,#34743,#2000,.T.) ;
#41628 = EDGE_CURVE('',#34744,#34743,#28654,.T.) ;
#41629 = EDGE_CURVE('',#34744,#34745,#2001,.T.) ;
#41630 = EDGE_CURVE('',#34745,#34746,#2435,.T.) ;
#41631 = EDGE_CURVE('',#34746,#34747,#2002,.T.) ;
#41632 = EDGE_CURVE('',#34748,#34747,#28655,.T.) ;
#41633 = EDGE_CURVE('',#34748,#34749,#2003,.T.) ;
#41634 = EDGE_CURVE('',#34750,#34749,#2436,.T.) ;
#41635 = EDGE_CURVE('',#34750,#34751,#2004,.T.) ;
#41636 = EDGE_CURVE('',#34752,#34751,#28656,.T.) ;
#41637 = EDGE_CURVE('',#34752,#34753,#2005,.T.) ;
#41638 = EDGE_CURVE('',#34753,#34754,#2437,.T.) ;
#41639 = EDGE_CURVE('',#34754,#34755,#2006,.T.) ;
#41640 = EDGE_CURVE('',#34740,#34755,#28657,.T.) ;
#41641 = EDGE_CURVE('',#34740,#34720,#2438,.T.) ;
#41642 = EDGE_CURVE('',#34756,#34757,#28658,.T.) ;
#41643 = EDGE_CURVE('',#34758,#34756,#28659,.T.) ;
#41644 = EDGE_CURVE('',#34759,#34758,#28660,.T.) ;
#41645 = EDGE_CURVE('',#34759,#34757,#28661,.T.) ;
#41646 = EDGE_CURVE('',#34760,#34761,#28662,.T.) ;
#41647 = EDGE_CURVE('',#34762,#34760,#2439,.T.) ;
#41648 = EDGE_CURVE('',#34763,#34762,#28663,.T.) ;
#41649 = EDGE_CURVE('',#34761,#34763,#2440,.T.) ;
#41650 = EDGE_CURVE('',#34764,#34764,#28664,.T.) ;
#41651 = EDGE_CURVE('',#34764,#34765,#28665,.T.) ;
#41652 = EDGE_CURVE('',#34766,#34765,#28666,.T.) ;
#41653 = EDGE_CURVE('',#34765,#34766,#28667,.T.) ;
#41654 = EDGE_CURVE('',#34767,#34767,#28668,.T.) ;
#41655 = EDGE_CURVE('',#34767,#34768,#28669,.T.) ;
#41656 = EDGE_CURVE('',#34768,#34768,#28670,.T.) ;
#41657 = EDGE_CURVE('',#34769,#34769,#28671,.T.) ;
#41658 = EDGE_CURVE('',#34769,#34770,#28672,.T.) ;
#41659 = EDGE_CURVE('',#34771,#34770,#28673,.T.) ;
#41660 = EDGE_CURVE('',#34770,#34771,#28674,.T.) ;
#41661 = EDGE_CURVE('',#34772,#34773,#28675,.T.) ;
#41662 = EDGE_CURVE('',#34774,#34773,#28676,.T.) ;
#41663 = EDGE_CURVE('',#34774,#34775,#28677,.T.) ;
#41664 = EDGE_CURVE('',#34775,#34772,#28678,.T.) ;
#41665 = EDGE_CURVE('',#34776,#34777,#28679,.T.) ;
#41666 = EDGE_CURVE('',#34777,#34778,#28680,.T.) ;
#41667 = EDGE_CURVE('',#34776,#34778,#28681,.T.) ;
#41668 = EDGE_CURVE('',#34779,#34772,#2441,.T.) ;
#41669 = EDGE_CURVE('',#34779,#34780,#28682,.T.) ;
#41670 = EDGE_CURVE('',#34773,#34780,#2442,.T.) ;
#41671 = EDGE_CURVE('',#34781,#34782,#28683,.T.) ;
#41672 = EDGE_CURVE('',#34781,#34783,#28684,.T.) ;
#41673 = EDGE_CURVE('',#34782,#34783,#28685,.T.) ;
#41674 = EDGE_CURVE('',#34784,#34784,#28686,.T.) ;
#41675 = EDGE_CURVE('',#34784,#34767,#2443,.T.) ;
#41676 = EDGE_CURVE('',#34768,#34771,#2444,.T.) ;
#41677 = EDGE_CURVE('',#34785,#34786,#28687,.T.) ;
#41678 = EDGE_CURVE('',#34785,#34787,#2007,.T.) ;
#41679 = EDGE_CURVE('',#34788,#34787,#2445,.T.) ;
#41680 = EDGE_CURVE('',#34788,#34789,#2008,.T.) ;
#41681 = EDGE_CURVE('',#34790,#34789,#28688,.T.) ;
#41682 = EDGE_CURVE('',#34790,#34791,#2009,.T.) ;
#41683 = EDGE_CURVE('',#34791,#34792,#2446,.T.) ;
#41684 = EDGE_CURVE('',#34792,#34793,#2010,.T.) ;
#41685 = EDGE_CURVE('',#34794,#34793,#28689,.T.) ;
#41686 = EDGE_CURVE('',#34794,#34795,#2011,.T.) ;
#41687 = EDGE_CURVE('',#34796,#34795,#2447,.T.) ;
#41688 = EDGE_CURVE('',#34796,#34797,#2012,.T.) ;
#41689 = EDGE_CURVE('',#34798,#34797,#28690,.T.) ;
#41690 = EDGE_CURVE('',#34798,#34799,#2013,.T.) ;
#41691 = EDGE_CURVE('',#34799,#34800,#2448,.T.) ;
#41692 = EDGE_CURVE('',#34800,#34801,#2014,.T.) ;
#41693 = EDGE_CURVE('',#34786,#34801,#28691,.T.) ;
#41694 = EDGE_CURVE('',#34786,#34766,#2449,.T.) ;
#41695 = EDGE_CURVE('',#34802,#34803,#2450,.T.) ;
#41696 = EDGE_CURVE('',#34803,#34804,#2451,.T.) ;
#41697 = EDGE_CURVE('',#34805,#34804,#2452,.T.) ;
#41698 = EDGE_CURVE('',#34805,#34802,#2453,.T.) ;
#41699 = EDGE_CURVE('',#34806,#34807,#28692,.T.) ;
#41700 = EDGE_CURVE('',#34806,#34808,#2454,.T.) ;
#41701 = EDGE_CURVE('',#34809,#34808,#2015,.T.) ;
#41702 = EDGE_CURVE('',#34809,#34810,#2455,.T.) ;
#41703 = EDGE_CURVE('',#34811,#34810,#2016,.T.) ;
#41704 = EDGE_CURVE('',#34811,#34812,#2456,.T.) ;
#41705 = EDGE_CURVE('',#34813,#34812,#28693,.T.) ;
#41706 = EDGE_CURVE('',#34813,#34807,#2457,.T.) ;
#41707 = EDGE_CURVE('',#34814,#34815,#2458,.T.) ;
#41708 = EDGE_CURVE('',#34814,#34816,#2459,.T.) ;
#41709 = EDGE_CURVE('',#34816,#34817,#2460,.T.) ;
#41710 = EDGE_CURVE('',#34817,#34815,#2461,.T.) ;
#41711 = EDGE_CURVE('',#34818,#34819,#2462,.T.) ;
#41712 = EDGE_CURVE('',#34818,#34820,#2463,.T.) ;
#41713 = EDGE_CURVE('',#34820,#34821,#2464,.T.) ;
#41714 = EDGE_CURVE('',#34821,#34819,#2465,.T.) ;
#41715 = EDGE_CURVE('',#34822,#34823,#2466,.T.) ;
#41716 = EDGE_CURVE('',#34822,#34824,#2467,.T.) ;
#41717 = EDGE_CURVE('',#34824,#34825,#2468,.T.) ;
#41718 = EDGE_CURVE('',#34825,#34823,#2469,.T.) ;
#41719 = EDGE_CURVE('',#34826,#34827,#2470,.T.) ;
#41720 = EDGE_CURVE('',#34826,#34823,#28694,.T.) ;
#41721 = EDGE_CURVE('',#34827,#34825,#28695,.T.) ;
#41722 = EDGE_CURVE('',#34819,#34822,#28696,.T.) ;
#41723 = EDGE_CURVE('',#34824,#34821,#28697,.T.) ;
#41724 = EDGE_CURVE('',#34815,#34818,#28698,.T.) ;
#41725 = EDGE_CURVE('',#34820,#34817,#28699,.T.) ;
#41726 = EDGE_CURVE('',#34814,#34828,#28700,.T.) ;
#41727 = EDGE_CURVE('',#34828,#34829,#2471,.T.) ;
#41728 = EDGE_CURVE('',#34830,#34829,#28701,.T.) ;
#41729 = EDGE_CURVE('',#34831,#34830,#2472,.T.) ;
#41730 = EDGE_CURVE('',#34816,#34831,#28702,.T.) ;
#41731 = EDGE_CURVE('',#34832,#34833,#28703,.T.) ;
#41732 = EDGE_CURVE('',#34833,#34834,#2473,.T.) ;
#41733 = EDGE_CURVE('',#34834,#34835,#28704,.T.) ;
#41734 = EDGE_CURVE('',#34835,#34832,#2474,.T.) ;
#41735 = EDGE_CURVE('',#34836,#34837,#2475,.T.) ;
#41736 = EDGE_CURVE('',#34836,#34838,#2476,.T.) ;
#41737 = EDGE_CURVE('',#34838,#34839,#2477,.T.) ;
#41738 = EDGE_CURVE('',#34839,#34837,#2478,.T.) ;
#41739 = EDGE_CURVE('',#34783,#34731,#2479,.T.) ;
#41740 = EDGE_CURVE('',#34731,#34840,#2480,.T.) ;
#41741 = EDGE_CURVE('',#34840,#34841,#2481,.T.) ;
#41742 = EDGE_CURVE('',#34841,#34783,#2482,.T.) ;
#41743 = EDGE_CURVE('',#34801,#34785,#2483,.T.) ;
#41744 = EDGE_CURVE('',#34774,#34778,#2484,.T.) ;
#41745 = EDGE_CURVE('',#34778,#34842,#2485,.T.) ;
#41746 = EDGE_CURVE('',#34843,#34842,#2486,.T.) ;
#41747 = EDGE_CURVE('',#34843,#34844,#2487,.T.) ;
#41748 = EDGE_CURVE('',#34845,#34844,#28705,.T.) ;
#41749 = EDGE_CURVE('',#34845,#34846,#28706,.T.) ;
#41750 = EDGE_CURVE('',#34847,#34846,#28707,.T.) ;
#41751 = EDGE_CURVE('',#34847,#34848,#2488,.T.) ;
#41752 = EDGE_CURVE('',#34849,#34848,#28708,.T.) ;
#41753 = EDGE_CURVE('',#34849,#34850,#28709,.T.) ;
#41754 = EDGE_CURVE('',#34851,#34850,#28710,.T.) ;
#41755 = EDGE_CURVE('',#34851,#34852,#2489,.T.) ;
#41756 = EDGE_CURVE('',#34852,#34853,#2490,.T.) ;
#41757 = EDGE_CURVE('',#34853,#34735,#2491,.T.) ;
#41758 = EDGE_CURVE('',#34735,#34854,#2492,.T.) ;
#41759 = EDGE_CURVE('',#34855,#34854,#28711,.T.) ;
#41760 = EDGE_CURVE('',#34855,#34729,#2493,.T.) ;
#41761 = EDGE_CURVE('',#34728,#34732,#2494,.T.) ;
#41762 = EDGE_CURVE('',#34732,#34781,#2495,.T.) ;
#41763 = EDGE_CURVE('',#34781,#34856,#2496,.T.) ;
#41764 = EDGE_CURVE('',#34857,#34856,#28712,.T.) ;
#41765 = EDGE_CURVE('',#34857,#34775,#2497,.T.) ;
#41766 = EDGE_CURVE('',#34777,#34858,#2498,.T.) ;
#41767 = EDGE_CURVE('',#34858,#34859,#2499,.T.) ;
#41768 = EDGE_CURVE('',#34860,#34859,#2500,.T.) ;
#41769 = EDGE_CURVE('',#34860,#34777,#2501,.T.) ;
#41770 = EDGE_CURVE('',#34861,#34862,#2502,.T.) ;
#41771 = EDGE_CURVE('',#34861,#34863,#2503,.T.) ;
#41772 = EDGE_CURVE('',#34863,#34864,#267,.T.) ;
#41773 = EDGE_CURVE('',#34864,#34865,#2504,.T.) ;
#41774 = EDGE_CURVE('',#34865,#34866,#268,.T.) ;
#41775 = EDGE_CURVE('',#34866,#34867,#2505,.T.) ;
#41776 = EDGE_CURVE('',#34867,#34868,#269,.T.) ;
#41777 = EDGE_CURVE('',#34868,#34869,#2506,.T.) ;
#41778 = EDGE_CURVE('',#34869,#34870,#270,.T.) ;
#41779 = EDGE_CURVE('',#34870,#34871,#2507,.T.) ;
#41780 = EDGE_CURVE('',#34871,#34872,#2508,.T.) ;
#41781 = EDGE_CURVE('',#34872,#34862,#2509,.T.) ;
#41782 = EDGE_CURVE('',#34873,#34874,#2510,.T.) ;
#41783 = EDGE_CURVE('',#34874,#34831,#2511,.T.) ;
#41784 = EDGE_CURVE('',#34873,#34830,#2512,.T.) ;
#41785 = EDGE_CURVE('',#34827,#34875,#2513,.T.) ;
#41786 = EDGE_CURVE('',#34875,#34876,#2514,.T.) ;
#41787 = EDGE_CURVE('',#34829,#34876,#2515,.T.) ;
#41788 = EDGE_CURVE('',#34826,#34828,#2516,.T.) ;
#41789 = EDGE_CURVE('',#34877,#34878,#2517,.T.) ;
#41790 = EDGE_CURVE('',#34878,#34879,#2518,.T.) ;
#41791 = EDGE_CURVE('',#34879,#34880,#2519,.T.) ;
#41792 = EDGE_CURVE('',#34877,#34880,#2520,.T.) ;
#41793 = EDGE_CURVE('',#34881,#34882,#28713,.T.) ;
#41794 = EDGE_CURVE('',#34881,#34883,#2521,.T.) ;
#41795 = EDGE_CURVE('',#34884,#34883,#28714,.T.) ;
#41796 = EDGE_CURVE('',#34884,#34885,#2522,.T.) ;
#41797 = EDGE_CURVE('',#34886,#34885,#28715,.T.) ;
#41798 = EDGE_CURVE('',#34886,#34887,#2523,.T.) ;
#41799 = EDGE_CURVE('',#34888,#34887,#28716,.T.) ;
#41800 = EDGE_CURVE('',#34888,#34882,#2524,.T.) ;
#41801 = EDGE_CURVE('',#34889,#34890,#28717,.T.) ;
#41802 = EDGE_CURVE('',#34889,#34891,#2525,.T.) ;
#41803 = EDGE_CURVE('',#34892,#34891,#28718,.T.) ;
#41804 = EDGE_CURVE('',#34892,#34893,#2526,.T.) ;
#41805 = EDGE_CURVE('',#34894,#34893,#28719,.T.) ;
#41806 = EDGE_CURVE('',#34894,#34895,#2527,.T.) ;
#41807 = EDGE_CURVE('',#34896,#34895,#28720,.T.) ;
#41808 = EDGE_CURVE('',#34896,#34890,#2528,.T.) ;
#41809 = EDGE_CURVE('',#34897,#34898,#2529,.T.) ;
#41810 = EDGE_CURVE('',#34898,#34899,#2530,.T.) ;
#41811 = EDGE_CURVE('',#34899,#34900,#2531,.T.) ;
#41812 = EDGE_CURVE('',#34897,#34900,#2532,.T.) ;
#41813 = EDGE_CURVE('',#34901,#34902,#2533,.T.) ;
#41814 = EDGE_CURVE('',#34902,#34761,#2534,.T.) ;
#41815 = EDGE_CURVE('',#34901,#34763,#2535,.T.) ;
#41816 = EDGE_CURVE('',#34760,#34903,#2536,.T.) ;
#41817 = EDGE_CURVE('',#34903,#34904,#2537,.T.) ;
#41818 = EDGE_CURVE('',#34762,#34904,#2538,.T.) ;
#41819 = EDGE_CURVE('',#34905,#34906,#2539,.T.) ;
#41820 = EDGE_CURVE('',#34906,#34907,#2540,.T.) ;
#41821 = EDGE_CURVE('',#34907,#34908,#2541,.T.) ;
#41822 = EDGE_CURVE('',#34905,#34908,#2542,.T.) ;
#41823 = EDGE_CURVE('',#34909,#34910,#2543,.T.) ;
#41824 = EDGE_CURVE('',#34910,#34911,#2017,.T.) ;
#41825 = EDGE_CURVE('',#34911,#34912,#2544,.T.) ;
#41826 = EDGE_CURVE('',#34913,#34912,#2018,.T.) ;
#41827 = EDGE_CURVE('',#34913,#34914,#2545,.T.) ;
#41828 = EDGE_CURVE('',#34915,#34914,#2019,.T.) ;
#41829 = EDGE_CURVE('',#34915,#34916,#2546,.T.) ;
#41830 = EDGE_CURVE('',#34916,#34909,#2020,.T.) ;
#41831 = EDGE_CURVE('',#34917,#34918,#2547,.T.) ;
#41832 = EDGE_CURVE('',#34918,#34919,#2021,.T.) ;
#41833 = EDGE_CURVE('',#34919,#34920,#2548,.T.) ;
#41834 = EDGE_CURVE('',#34921,#34920,#2022,.T.) ;
#41835 = EDGE_CURVE('',#34921,#34922,#2549,.T.) ;
#41836 = EDGE_CURVE('',#34923,#34922,#2023,.T.) ;
#41837 = EDGE_CURVE('',#34923,#34924,#2550,.T.) ;
#41838 = EDGE_CURVE('',#34924,#34917,#2024,.T.) ;
#41839 = EDGE_CURVE('',#34925,#34926,#2551,.T.) ;
#41840 = EDGE_CURVE('',#34926,#34927,#2552,.T.) ;
#41841 = EDGE_CURVE('',#34927,#34928,#2553,.T.) ;
#41842 = EDGE_CURVE('',#34925,#34928,#2554,.T.) ;
#41843 = EDGE_CURVE('',#34929,#34930,#28721,.T.) ;
#41844 = EDGE_CURVE('',#34929,#34931,#2555,.T.) ;
#41845 = EDGE_CURVE('',#34932,#34931,#28722,.T.) ;
#41846 = EDGE_CURVE('',#34932,#34933,#2556,.T.) ;
#41847 = EDGE_CURVE('',#34934,#34933,#28723,.T.) ;
#41848 = EDGE_CURVE('',#34934,#34935,#2557,.T.) ;
#41849 = EDGE_CURVE('',#34936,#34935,#28724,.T.) ;
#41850 = EDGE_CURVE('',#34936,#34930,#2558,.T.) ;
#41851 = EDGE_CURVE('',#34937,#34938,#28725,.T.) ;
#41852 = EDGE_CURVE('',#34937,#34939,#2559,.T.) ;
#41853 = EDGE_CURVE('',#34940,#34939,#28726,.T.) ;
#41854 = EDGE_CURVE('',#34940,#34941,#2560,.T.) ;
#41855 = EDGE_CURVE('',#34942,#34941,#28727,.T.) ;
#41856 = EDGE_CURVE('',#34942,#34943,#2561,.T.) ;
#41857 = EDGE_CURVE('',#34944,#34943,#28728,.T.) ;
#41858 = EDGE_CURVE('',#34944,#34938,#2562,.T.) ;
#41859 = EDGE_CURVE('',#34945,#34946,#2563,.T.) ;
#41860 = EDGE_CURVE('',#34946,#34947,#2564,.T.) ;
#41861 = EDGE_CURVE('',#34947,#34948,#2565,.T.) ;
#41862 = EDGE_CURVE('',#34945,#34948,#2566,.T.) ;
#41863 = EDGE_CURVE('',#34949,#34950,#2025,.T.) ;
#41864 = EDGE_CURVE('',#34950,#34951,#2026,.T.) ;
#41865 = EDGE_CURVE('',#34951,#34952,#2027,.T.) ;
#41866 = EDGE_CURVE('',#34952,#34953,#2028,.T.) ;
#41867 = EDGE_CURVE('',#34953,#34954,#2567,.T.) ;
#41868 = EDGE_CURVE('',#34955,#34954,#2568,.T.) ;
#41869 = EDGE_CURVE('',#34955,#34956,#2569,.T.) ;
#41870 = EDGE_CURVE('',#34956,#34957,#2570,.T.) ;
#41871 = EDGE_CURVE('',#34957,#34958,#2571,.T.) ;
#41872 = EDGE_CURVE('',#34958,#34959,#2029,.T.) ;
#41873 = EDGE_CURVE('',#34959,#34960,#2030,.T.) ;
#41874 = EDGE_CURVE('',#34960,#34961,#2031,.T.) ;
#41875 = EDGE_CURVE('',#34961,#34962,#2032,.T.) ;
#41876 = EDGE_CURVE('',#34962,#34949,#2572,.T.) ;
#41877 = EDGE_CURVE('',#34963,#34964,#2573,.T.) ;
#41878 = EDGE_CURVE('',#34963,#34965,#2574,.T.) ;
#41879 = EDGE_CURVE('',#34965,#34966,#28729,.T.) ;
#41880 = EDGE_CURVE('',#34966,#34964,#2575,.T.) ;
#41881 = EDGE_CURVE('',#34967,#34968,#2576,.T.) ;
#41882 = EDGE_CURVE('',#34968,#34969,#2577,.T.) ;
#41883 = EDGE_CURVE('',#34969,#34970,#2578,.T.) ;
#41884 = EDGE_CURVE('',#34970,#34967,#2579,.T.) ;
#41885 = EDGE_CURVE('',#34876,#34877,#28730,.T.) ;
#41886 = EDGE_CURVE('',#34880,#34897,#28731,.T.) ;
#41887 = EDGE_CURVE('',#34900,#34901,#28732,.T.) ;
#41888 = EDGE_CURVE('',#34904,#34905,#28733,.T.) ;
#41889 = EDGE_CURVE('',#34908,#34925,#28734,.T.) ;
#41890 = EDGE_CURVE('',#34928,#34945,#28735,.T.) ;
#41891 = EDGE_CURVE('',#34948,#34955,#28736,.T.) ;
#41892 = EDGE_CURVE('',#34954,#34963,#28737,.T.) ;
#41893 = EDGE_CURVE('',#34964,#34836,#28738,.T.) ;
#41894 = EDGE_CURVE('',#34837,#34843,#28739,.T.) ;
#41895 = EDGE_CURVE('',#34842,#34860,#28740,.T.) ;
#41896 = EDGE_CURVE('',#34859,#34861,#28741,.T.) ;
#41897 = EDGE_CURVE('',#34862,#34805,#28742,.T.) ;
#41898 = EDGE_CURVE('',#34804,#34873,#28743,.T.) ;
#41899 = EDGE_CURVE('',#34971,#34972,#2580,.T.) ;
#41900 = EDGE_CURVE('',#34972,#34973,#2581,.T.) ;
#41901 = EDGE_CURVE('',#34973,#34974,#2582,.T.) ;
#41902 = EDGE_CURVE('',#34974,#34971,#2583,.T.) ;
#41903 = EDGE_CURVE('',#34975,#34976,#2584,.T.) ;
#41904 = EDGE_CURVE('',#34976,#34977,#2585,.T.) ;
#41905 = EDGE_CURVE('',#34977,#34978,#2586,.T.) ;
#41906 = EDGE_CURVE('',#34978,#34975,#2587,.T.) ;
#41907 = EDGE_CURVE('',#34979,#34980,#271,.T.) ;
#41908 = EDGE_CURVE('',#34979,#34981,#2588,.T.) ;
#41909 = EDGE_CURVE('',#34981,#34982,#2589,.T.) ;
#41910 = EDGE_CURVE('',#34982,#34983,#2590,.T.) ;
#41911 = EDGE_CURVE('',#34984,#34983,#272,.T.) ;
#41912 = EDGE_CURVE('',#34984,#34985,#2591,.T.) ;
#41913 = EDGE_CURVE('',#34985,#34986,#2592,.T.) ;
#41914 = EDGE_CURVE('',#34986,#34980,#2593,.T.) ;
#41915 = EDGE_CURVE('',#34987,#34988,#2594,.T.) ;
#41916 = EDGE_CURVE('',#34988,#34989,#273,.T.) ;
#41917 = EDGE_CURVE('',#34990,#34989,#2595,.T.) ;
#41918 = EDGE_CURVE('',#34990,#34982,#274,.T.) ;
#41919 = EDGE_CURVE('',#34981,#34991,#275,.T.) ;
#41920 = EDGE_CURVE('',#34991,#34992,#2596,.T.) ;
#41921 = EDGE_CURVE('',#34992,#34987,#276,.T.) ;
#41922 = EDGE_CURVE('',#34993,#34994,#277,.T.) ;
#41923 = EDGE_CURVE('',#34993,#34988,#2597,.T.) ;
#41924 = EDGE_CURVE('',#34987,#34995,#2598,.T.) ;
#41925 = EDGE_CURVE('',#34996,#34995,#278,.T.) ;
#41926 = EDGE_CURVE('',#34996,#34997,#2599,.T.) ;
#41927 = EDGE_CURVE('',#34997,#34998,#2600,.T.) ;
#41928 = EDGE_CURVE('',#34998,#34994,#2601,.T.) ;
#41929 = EDGE_CURVE('',#34991,#34999,#2602,.T.) ;
#41930 = EDGE_CURVE('',#34999,#35000,#2603,.T.) ;
#41931 = EDGE_CURVE('',#35000,#34992,#2604,.T.) ;
#41932 = EDGE_CURVE('',#34989,#35001,#2605,.T.) ;
#41933 = EDGE_CURVE('',#35001,#35002,#2606,.T.) ;
#41934 = EDGE_CURVE('',#35002,#34990,#2607,.T.) ;
#41935 = EDGE_CURVE('',#35003,#35004,#2608,.T.) ;
#41936 = EDGE_CURVE('',#35004,#35005,#2609,.T.) ;
#41937 = EDGE_CURVE('',#35005,#35006,#2610,.T.) ;
#41938 = EDGE_CURVE('',#35006,#35007,#2611,.T.) ;
#41939 = EDGE_CURVE('',#35007,#35008,#2612,.T.) ;
#41940 = EDGE_CURVE('',#35008,#35003,#2613,.T.) ;
#41941 = EDGE_CURVE('',#35009,#35010,#2614,.T.) ;
#41942 = EDGE_CURVE('',#35010,#35011,#2615,.T.) ;
#41943 = EDGE_CURVE('',#35011,#35012,#2616,.T.) ;
#41944 = EDGE_CURVE('',#35012,#35013,#2617,.T.) ;
#41945 = EDGE_CURVE('',#35013,#35014,#2618,.T.) ;
#41946 = EDGE_CURVE('',#35014,#35009,#2619,.T.) ;
#41947 = EDGE_CURVE('',#35015,#35016,#2620,.T.) ;
#41948 = EDGE_CURVE('',#35016,#35017,#2621,.T.) ;
#41949 = EDGE_CURVE('',#35017,#35018,#2622,.T.) ;
#41950 = EDGE_CURVE('',#35018,#35015,#2623,.T.) ;
#41951 = EDGE_CURVE('',#35019,#35020,#2624,.T.) ;
#41952 = EDGE_CURVE('',#35020,#35021,#2625,.T.) ;
#41953 = EDGE_CURVE('',#35021,#35022,#2626,.T.) ;
#41954 = EDGE_CURVE('',#35022,#35019,#2627,.T.) ;
#41955 = EDGE_CURVE('',#35023,#35024,#2628,.T.) ;
#41956 = EDGE_CURVE('',#35024,#35025,#2629,.T.) ;
#41957 = EDGE_CURVE('',#35025,#35026,#2630,.T.) ;
#41958 = EDGE_CURVE('',#35026,#35023,#2631,.T.) ;
#41959 = EDGE_CURVE('',#35027,#35028,#2632,.T.) ;
#41960 = EDGE_CURVE('',#35028,#35029,#2633,.T.) ;
#41961 = EDGE_CURVE('',#35029,#35030,#2634,.T.) ;
#41962 = EDGE_CURVE('',#35030,#35027,#2635,.T.) ;
#41963 = EDGE_CURVE('',#35031,#35032,#2636,.T.) ;
#41964 = EDGE_CURVE('',#35032,#35033,#2637,.T.) ;
#41965 = EDGE_CURVE('',#35033,#35034,#2638,.T.) ;
#41966 = EDGE_CURVE('',#35034,#35031,#2639,.T.) ;
#41967 = EDGE_CURVE('',#35035,#35036,#2640,.T.) ;
#41968 = EDGE_CURVE('',#35037,#35035,#28744,.T.) ;
#41969 = EDGE_CURVE('',#35038,#35037,#2641,.T.) ;
#41970 = EDGE_CURVE('',#35039,#35038,#28745,.T.) ;
#41971 = EDGE_CURVE('',#35040,#35039,#2642,.T.) ;
#41972 = EDGE_CURVE('',#35041,#35040,#28746,.T.) ;
#41973 = EDGE_CURVE('',#35042,#35041,#2643,.T.) ;
#41974 = EDGE_CURVE('',#35036,#35042,#28747,.T.) ;
#41975 = EDGE_CURVE('',#35043,#35044,#28748,.T.) ;
#41976 = EDGE_CURVE('',#35036,#35043,#2644,.T.) ;
#41977 = EDGE_CURVE('',#35042,#35044,#2645,.T.) ;
#41978 = EDGE_CURVE('',#35045,#35043,#2646,.T.) ;
#41979 = EDGE_CURVE('',#35035,#35045,#2647,.T.) ;
#41980 = EDGE_CURVE('',#35046,#35045,#28749,.T.) ;
#41981 = EDGE_CURVE('',#35037,#35046,#2648,.T.) ;
#41982 = EDGE_CURVE('',#35047,#35046,#2649,.T.) ;
#41983 = EDGE_CURVE('',#35038,#35047,#2650,.T.) ;
#41984 = EDGE_CURVE('',#35048,#35047,#28750,.T.) ;
#41985 = EDGE_CURVE('',#35039,#35048,#2651,.T.) ;
#41986 = EDGE_CURVE('',#35049,#35048,#2652,.T.) ;
#41987 = EDGE_CURVE('',#35040,#35049,#2653,.T.) ;
#41988 = EDGE_CURVE('',#35050,#35049,#28751,.T.) ;
#41989 = EDGE_CURVE('',#35041,#35050,#2654,.T.) ;
#41990 = EDGE_CURVE('',#35044,#35050,#2655,.T.) ;
#41991 = EDGE_CURVE('',#34793,#34794,#2656,.T.) ;
#41992 = EDGE_CURVE('',#34791,#34796,#2657,.T.) ;
#41993 = EDGE_CURVE('',#34795,#34792,#2658,.T.) ;
#41994 = EDGE_CURVE('',#34799,#34788,#2659,.T.) ;
#41995 = EDGE_CURVE('',#34787,#34800,#2660,.T.) ;
#41996 = EDGE_CURVE('',#34789,#34798,#2661,.T.) ;
#41997 = EDGE_CURVE('',#34797,#34790,#2662,.T.) ;
#41998 = EDGE_CURVE('',#35051,#35052,#2663,.T.) ;
#41999 = EDGE_CURVE('',#35052,#35053,#2664,.T.) ;
#42000 = EDGE_CURVE('',#35053,#35054,#2665,.T.) ;
#42001 = EDGE_CURVE('',#35054,#35051,#2666,.T.) ;
#42002 = EDGE_CURVE('',#35055,#35056,#2667,.T.) ;
#42003 = EDGE_CURVE('',#35056,#35057,#2668,.T.) ;
#42004 = EDGE_CURVE('',#35057,#35058,#2669,.T.) ;
#42005 = EDGE_CURVE('',#35058,#35055,#2670,.T.) ;
#42006 = EDGE_CURVE('',#35059,#35060,#2671,.T.) ;
#42007 = EDGE_CURVE('',#35060,#35061,#2672,.T.) ;
#42008 = EDGE_CURVE('',#35061,#35062,#2673,.T.) ;
#42009 = EDGE_CURVE('',#35062,#35059,#2674,.T.) ;
#42010 = EDGE_CURVE('',#35063,#35064,#2675,.T.) ;
#42011 = EDGE_CURVE('',#35064,#35065,#2676,.T.) ;
#42012 = EDGE_CURVE('',#35065,#35066,#2677,.T.) ;
#42013 = EDGE_CURVE('',#35066,#35063,#2678,.T.) ;
#42014 = EDGE_CURVE('',#35067,#35068,#2679,.T.) ;
#42015 = EDGE_CURVE('',#35068,#35069,#2680,.T.) ;
#42016 = EDGE_CURVE('',#35069,#35070,#2681,.T.) ;
#42017 = EDGE_CURVE('',#35070,#35067,#2682,.T.) ;
#42018 = EDGE_CURVE('',#35071,#35072,#2683,.T.) ;
#42019 = EDGE_CURVE('',#35073,#35071,#28752,.T.) ;
#42020 = EDGE_CURVE('',#35074,#35073,#2684,.T.) ;
#42021 = EDGE_CURVE('',#35075,#35074,#28753,.T.) ;
#42022 = EDGE_CURVE('',#35076,#35075,#2685,.T.) ;
#42023 = EDGE_CURVE('',#35077,#35076,#28754,.T.) ;
#42024 = EDGE_CURVE('',#35078,#35077,#2686,.T.) ;
#42025 = EDGE_CURVE('',#35072,#35078,#28755,.T.) ;
#42026 = EDGE_CURVE('',#35078,#35079,#2687,.T.) ;
#42027 = EDGE_CURVE('',#35079,#35080,#28756,.T.) ;
#42028 = EDGE_CURVE('',#35072,#35080,#2688,.T.) ;
#42029 = EDGE_CURVE('',#35080,#35081,#2689,.T.) ;
#42030 = EDGE_CURVE('',#35071,#35081,#2690,.T.) ;
#42031 = EDGE_CURVE('',#35081,#35082,#28757,.T.) ;
#42032 = EDGE_CURVE('',#35073,#35082,#2691,.T.) ;
#42033 = EDGE_CURVE('',#35082,#35083,#2692,.T.) ;
#42034 = EDGE_CURVE('',#35074,#35083,#2693,.T.) ;
#42035 = EDGE_CURVE('',#35083,#35084,#28758,.T.) ;
#42036 = EDGE_CURVE('',#35075,#35084,#2694,.T.) ;
#42037 = EDGE_CURVE('',#35084,#35085,#2695,.T.) ;
#42038 = EDGE_CURVE('',#35076,#35085,#2696,.T.) ;
#42039 = EDGE_CURVE('',#35085,#35086,#28759,.T.) ;
#42040 = EDGE_CURVE('',#35077,#35086,#2697,.T.) ;
#42041 = EDGE_CURVE('',#35086,#35079,#2698,.T.) ;
#42042 = EDGE_CURVE('',#35087,#35088,#2699,.T.) ;
#42043 = EDGE_CURVE('',#35088,#35089,#2700,.T.) ;
#42044 = EDGE_CURVE('',#35089,#35090,#2701,.T.) ;
#42045 = EDGE_CURVE('',#35090,#35087,#2702,.T.) ;
#42046 = EDGE_CURVE('',#34782,#34758,#2703,.T.) ;
#42047 = EDGE_CURVE('',#34758,#35091,#2704,.T.) ;
#42048 = EDGE_CURVE('',#35091,#35092,#2705,.T.) ;
#42049 = EDGE_CURVE('',#35092,#34782,#2706,.T.) ;
#42050 = EDGE_CURVE('',#35093,#34779,#2707,.T.) ;
#42051 = EDGE_CURVE('',#34772,#35094,#2708,.T.) ;
#42052 = EDGE_CURVE('',#35094,#35093,#2709,.T.) ;
#42053 = EDGE_CURVE('',#34780,#35095,#2710,.T.) ;
#42054 = EDGE_CURVE('',#35095,#34776,#2711,.T.) ;
#42055 = EDGE_CURVE('',#34776,#34773,#2712,.T.) ;
#42056 = EDGE_CURVE('',#34757,#35096,#2713,.T.) ;
#42057 = EDGE_CURVE('',#35096,#35097,#28760,.T.) ;
#42058 = EDGE_CURVE('',#35097,#35098,#2714,.T.) ;
#42059 = EDGE_CURVE('',#35098,#35099,#2715,.T.) ;
#42060 = EDGE_CURVE('',#35099,#34756,#2716,.T.) ;
#42061 = EDGE_CURVE('',#35100,#35101,#28761,.T.) ;
#42062 = EDGE_CURVE('',#35101,#35102,#28762,.T.) ;
#42063 = EDGE_CURVE('',#35102,#35103,#28763,.T.) ;
#42064 = EDGE_CURVE('',#35103,#35104,#2717,.T.) ;
#42065 = EDGE_CURVE('',#35104,#35105,#28764,.T.) ;
#42066 = EDGE_CURVE('',#35105,#35100,#2718,.T.) ;
#42067 = EDGE_CURVE('',#35009,#34918,#28765,.T.) ;
#42068 = EDGE_CURVE('',#34977,#35009,#2033,.T.) ;
#42069 = EDGE_CURVE('',#34919,#34977,#28766,.T.) ;
#42070 = EDGE_CURVE('',#34999,#34979,#28767,.T.) ;
#42071 = EDGE_CURVE('',#35013,#34980,#28768,.T.) ;
#42072 = EDGE_CURVE('',#34999,#35013,#279,.T.) ;
#42073 = EDGE_CURVE('',#35014,#34986,#28769,.T.) ;
#42074 = EDGE_CURVE('',#34978,#35014,#28770,.T.) ;
#42075 = EDGE_CURVE('',#34920,#34976,#28771,.T.) ;
#42076 = EDGE_CURVE('',#35010,#34917,#28772,.T.) ;
#42077 = EDGE_CURVE('',#35000,#35012,#280,.T.) ;
#42078 = EDGE_CURVE('',#34995,#35000,#28773,.T.) ;
#42079 = EDGE_CURVE('',#34978,#34986,#28774,.T.) ;
#42080 = EDGE_CURVE('',#35007,#34976,#281,.T.) ;
#42081 = EDGE_CURVE('',#34921,#35007,#28775,.T.) ;
#42082 = EDGE_CURVE('',#34972,#34924,#28776,.T.) ;
#42083 = EDGE_CURVE('',#35010,#34972,#2034,.T.) ;
#42084 = EDGE_CURVE('',#34996,#35012,#28777,.T.) ;
#42085 = EDGE_CURVE('',#34975,#34985,#28778,.T.) ;
#42086 = EDGE_CURVE('',#35008,#34975,#28779,.T.) ;
#42087 = EDGE_CURVE('',#34922,#35006,#28780,.T.) ;
#42088 = EDGE_CURVE('',#34973,#34923,#28781,.T.) ;
#42089 = EDGE_CURVE('',#35011,#34971,#28782,.T.) ;
#42090 = EDGE_CURVE('',#34997,#35011,#28783,.T.) ;
#42091 = EDGE_CURVE('',#35008,#34985,#28784,.T.) ;
#42092 = EDGE_CURVE('',#34973,#35006,#282,.T.) ;
#42093 = EDGE_CURVE('',#34997,#34971,#28785,.T.) ;
#42094 = EDGE_CURVE('',#34983,#35002,#28786,.T.) ;
#42095 = EDGE_CURVE('',#35003,#34984,#28787,.T.) ;
#42096 = EDGE_CURVE('',#34974,#35005,#28788,.T.) ;
#42097 = EDGE_CURVE('',#34998,#34974,#28789,.T.) ;
#42098 = EDGE_CURVE('',#35003,#35002,#283,.T.) ;
#42099 = EDGE_CURVE('',#34998,#35005,#28790,.T.) ;
#42100 = EDGE_CURVE('',#35004,#35001,#284,.T.) ;
#42101 = EDGE_CURVE('',#34994,#35004,#28791,.T.) ;
#42102 = EDGE_CURVE('',#34993,#35001,#28792,.T.) ;
#42103 = EDGE_CURVE('',#34841,#35106,#285,.T.) ;
#42104 = EDGE_CURVE('',#35106,#34759,#2035,.T.) ;
#42105 = EDGE_CURVE('',#35091,#35093,#28793,.T.) ;
#42106 = EDGE_CURVE('',#35092,#35094,#28794,.T.) ;
#42107 = EDGE_CURVE('',#34856,#35092,#28795,.T.) ;
#42108 = EDGE_CURVE('',#34864,#35096,#2036,.T.) ;
#42109 = EDGE_CURVE('',#34757,#34865,#2037,.T.) ;
#42110 = EDGE_CURVE('',#35098,#34779,#28796,.T.) ;
#42111 = EDGE_CURVE('',#35093,#35099,#28797,.T.) ;
#42112 = EDGE_CURVE('',#34857,#35094,#28798,.T.) ;
#42113 = EDGE_CURVE('',#35107,#35108,#2038,.T.) ;
#42114 = EDGE_CURVE('',#35108,#34858,#286,.T.) ;
#42115 = EDGE_CURVE('',#35095,#35107,#28799,.T.) ;
#42116 = EDGE_CURVE('',#35082,#35087,#28800,.T.) ;
#42117 = EDGE_CURVE('',#35087,#35081,#28801,.T.) ;
#42118 = EDGE_CURVE('',#35088,#35080,#28802,.T.) ;
#42119 = EDGE_CURVE('',#35083,#35090,#28803,.T.) ;
#42120 = EDGE_CURVE('',#35088,#35079,#28804,.T.) ;
#42121 = EDGE_CURVE('',#35084,#35090,#28805,.T.) ;
#42122 = EDGE_CURVE('',#35089,#35086,#28806,.T.) ;
#42123 = EDGE_CURVE('',#35085,#35089,#28807,.T.) ;
#42124 = EDGE_CURVE('',#34943,#35018,#28808,.T.) ;
#42125 = EDGE_CURVE('',#35015,#34942,#28809,.T.) ;
#42126 = EDGE_CURVE('',#35030,#34941,#28810,.T.) ;
#42127 = EDGE_CURVE('',#35015,#35030,#28811,.T.) ;
#42128 = EDGE_CURVE('',#35022,#35018,#28812,.T.) ;
#42129 = EDGE_CURVE('',#34944,#35022,#28813,.T.) ;
#42130 = EDGE_CURVE('',#35027,#34940,#28814,.T.) ;
#42131 = EDGE_CURVE('',#35016,#35029,#28815,.T.) ;
#42132 = EDGE_CURVE('',#35017,#35034,#28816,.T.) ;
#42133 = EDGE_CURVE('',#35031,#35016,#28817,.T.) ;
#42134 = EDGE_CURVE('',#35019,#35017,#28818,.T.) ;
#42135 = EDGE_CURVE('',#34938,#35021,#28819,.T.) ;
#42136 = EDGE_CURVE('',#34939,#35025,#28820,.T.) ;
#42137 = EDGE_CURVE('',#35026,#34937,#28821,.T.) ;
#42138 = EDGE_CURVE('',#35027,#35025,#28822,.T.) ;
#42139 = EDGE_CURVE('',#35031,#35029,#28823,.T.) ;
#42140 = EDGE_CURVE('',#35019,#35034,#28824,.T.) ;
#42141 = EDGE_CURVE('',#35026,#35021,#28825,.T.) ;
#42142 = EDGE_CURVE('',#35028,#35024,#28826,.T.) ;
#42143 = EDGE_CURVE('',#35032,#35028,#28827,.T.) ;
#42144 = EDGE_CURVE('',#35020,#35033,#28828,.T.) ;
#42145 = EDGE_CURVE('',#35023,#35020,#28829,.T.) ;
#42146 = EDGE_CURVE('',#35032,#35024,#28830,.T.) ;
#42147 = EDGE_CURVE('',#35023,#35033,#28831,.T.) ;
#42148 = EDGE_CURVE('',#34895,#35062,#28832,.T.) ;
#42149 = EDGE_CURVE('',#35059,#34894,#28833,.T.) ;
#42150 = EDGE_CURVE('',#35058,#34893,#28834,.T.) ;
#42151 = EDGE_CURVE('',#35059,#35058,#28835,.T.) ;
#42152 = EDGE_CURVE('',#35066,#35062,#28836,.T.) ;
#42153 = EDGE_CURVE('',#34896,#35066,#28837,.T.) ;
#42154 = EDGE_CURVE('',#35055,#34892,#28838,.T.) ;
#42155 = EDGE_CURVE('',#35060,#35057,#28839,.T.) ;
#42156 = EDGE_CURVE('',#35061,#35070,#28840,.T.) ;
#42157 = EDGE_CURVE('',#35067,#35060,#28841,.T.) ;
#42158 = EDGE_CURVE('',#35063,#35061,#28842,.T.) ;
#42159 = EDGE_CURVE('',#34890,#35065,#28843,.T.) ;
#42160 = EDGE_CURVE('',#34891,#35053,#28844,.T.) ;
#42161 = EDGE_CURVE('',#35054,#34889,#28845,.T.) ;
#42162 = EDGE_CURVE('',#35055,#35053,#28846,.T.) ;
#42163 = EDGE_CURVE('',#35067,#35057,#28847,.T.) ;
#42164 = EDGE_CURVE('',#35063,#35070,#28848,.T.) ;
#42165 = EDGE_CURVE('',#35054,#35065,#28849,.T.) ;
#42166 = EDGE_CURVE('',#35056,#35052,#28850,.T.) ;
#42167 = EDGE_CURVE('',#35068,#35056,#28851,.T.) ;
#42168 = EDGE_CURVE('',#35064,#35069,#28852,.T.) ;
#42169 = EDGE_CURVE('',#35051,#35064,#28853,.T.) ;
#42170 = EDGE_CURVE('',#35068,#35052,#28854,.T.) ;
#42171 = EDGE_CURVE('',#35051,#35069,#28855,.T.) ;
#42172 = EDGE_CURVE('',#34965,#35101,#2039,.T.) ;
#42173 = EDGE_CURVE('',#34966,#35100,#28856,.T.) ;
#42174 = EDGE_CURVE('',#34838,#34966,#28857,.T.) ;
#42175 = EDGE_CURVE('',#34838,#35100,#28858,.T.) ;
#42176 = EDGE_CURVE('',#34839,#35105,#28859,.T.) ;
#42177 = EDGE_CURVE('',#34844,#34839,#28860,.T.) ;
#42178 = EDGE_CURVE('',#34845,#35105,#28861,.T.) ;
#42179 = EDGE_CURVE('',#34846,#35104,#28862,.T.) ;
#42180 = EDGE_CURVE('',#34848,#34970,#28863,.T.) ;
#42181 = EDGE_CURVE('',#34967,#34847,#28864,.T.) ;
#42182 = EDGE_CURVE('',#34967,#35104,#28865,.T.) ;
#42183 = EDGE_CURVE('',#34968,#35103,#28866,.T.) ;
#42184 = EDGE_CURVE('',#34969,#34835,#28867,.T.) ;
#42185 = EDGE_CURVE('',#34832,#34968,#28868,.T.) ;
#42186 = EDGE_CURVE('',#34832,#35103,#28869,.T.) ;
#42187 = EDGE_CURVE('',#35102,#34833,#2040,.T.) ;
#42188 = EDGE_CURVE('',#34956,#34947,#28870,.T.) ;
#42189 = EDGE_CURVE('',#34946,#34927,#28871,.T.) ;
#42190 = EDGE_CURVE('',#34926,#34907,#28872,.T.) ;
#42191 = EDGE_CURVE('',#34906,#34903,#28873,.T.) ;
#42192 = EDGE_CURVE('',#34902,#34899,#28874,.T.) ;
#42193 = EDGE_CURVE('',#34898,#34879,#28875,.T.) ;
#42194 = EDGE_CURVE('',#34878,#34875,#28876,.T.) ;
#42195 = EDGE_CURVE('',#34874,#34803,#28877,.T.) ;
#42196 = EDGE_CURVE('',#34802,#34872,#28878,.T.) ;
#42197 = EDGE_CURVE('',#34780,#35098,#28879,.T.) ;
#42198 = EDGE_CURVE('',#35095,#35097,#28880,.T.) ;
#42199 = EDGE_CURVE('',#35107,#35096,#28881,.T.) ;
#42200 = EDGE_CURVE('',#35108,#34864,#28882,.T.) ;
#42201 = EDGE_CURVE('',#34858,#34863,#28883,.T.) ;
#42202 = EDGE_CURVE('',#34840,#34867,#28884,.T.) ;
#42203 = EDGE_CURVE('',#34841,#34866,#28885,.T.) ;
#42204 = EDGE_CURVE('',#35106,#34865,#28886,.T.) ;
#42205 = EDGE_CURVE('',#35091,#35099,#28887,.T.) ;
#42206 = EDGE_CURVE('',#35109,#35110,#2041,.T.) ;
#42207 = EDGE_CURVE('',#35110,#35102,#2042,.T.) ;
#42208 = EDGE_CURVE('',#35101,#35111,#2043,.T.) ;
#42209 = EDGE_CURVE('',#35111,#35109,#2044,.T.) ;
#42210 = EDGE_CURVE('',#34965,#34953,#28888,.T.) ;
#42211 = EDGE_CURVE('',#34952,#35101,#2045,.T.) ;
#42212 = EDGE_CURVE('',#34834,#34962,#28889,.T.) ;
#42213 = EDGE_CURVE('',#34949,#34833,#28890,.T.) ;
#42214 = EDGE_CURVE('',#35102,#34950,#2046,.T.) ;
#42215 = EDGE_CURVE('',#35111,#34952,#28891,.T.) ;
#42216 = EDGE_CURVE('',#35109,#34951,#28892,.T.) ;
#42217 = EDGE_CURVE('',#35110,#34950,#28893,.T.) ;
#42218 = EDGE_CURVE('',#35112,#35113,#2719,.T.) ;
#42219 = EDGE_CURVE('',#35113,#35114,#2720,.T.) ;
#42220 = EDGE_CURVE('',#35115,#35114,#2721,.T.) ;
#42221 = EDGE_CURVE('',#35115,#35112,#2722,.T.) ;
#42222 = EDGE_CURVE('',#35114,#35116,#28894,.T.) ;
#42223 = EDGE_CURVE('',#35117,#35116,#2723,.T.) ;
#42224 = EDGE_CURVE('',#35117,#35115,#28895,.T.) ;
#42225 = EDGE_CURVE('',#35116,#35118,#2724,.T.) ;
#42226 = EDGE_CURVE('',#35119,#35118,#2725,.T.) ;
#42227 = EDGE_CURVE('',#35119,#35117,#2726,.T.) ;
#42228 = EDGE_CURVE('',#35118,#35120,#28896,.T.) ;
#42229 = EDGE_CURVE('',#35121,#35120,#2727,.T.) ;
#42230 = EDGE_CURVE('',#35121,#35119,#28897,.T.) ;
#42231 = EDGE_CURVE('',#35120,#35122,#2728,.T.) ;
#42232 = EDGE_CURVE('',#35123,#35122,#2729,.T.) ;
#42233 = EDGE_CURVE('',#35123,#35121,#2730,.T.) ;
#42234 = EDGE_CURVE('',#35122,#35124,#28898,.T.) ;
#42235 = EDGE_CURVE('',#35125,#35124,#2731,.T.) ;
#42236 = EDGE_CURVE('',#35125,#35123,#28899,.T.) ;
#42237 = EDGE_CURVE('',#35124,#35126,#2732,.T.) ;
#42238 = EDGE_CURVE('',#35127,#35126,#2733,.T.) ;
#42239 = EDGE_CURVE('',#35127,#35125,#2734,.T.) ;
#42240 = EDGE_CURVE('',#35126,#35128,#28900,.T.) ;
#42241 = EDGE_CURVE('',#35129,#35128,#2735,.T.) ;
#42242 = EDGE_CURVE('',#35129,#35127,#28901,.T.) ;
#42243 = EDGE_CURVE('',#35128,#35130,#2736,.T.) ;
#42244 = EDGE_CURVE('',#35130,#35131,#2737,.T.) ;
#42245 = EDGE_CURVE('',#35131,#35129,#2738,.T.) ;
#42246 = EDGE_CURVE('',#35132,#35133,#28902,.T.) ;
#42247 = EDGE_CURVE('',#35133,#35134,#2739,.T.) ;
#42248 = EDGE_CURVE('',#35134,#35135,#2740,.T.) ;
#42249 = EDGE_CURVE('',#35135,#35136,#2741,.T.) ;
#42250 = EDGE_CURVE('',#35136,#35137,#2742,.T.) ;
#42251 = EDGE_CURVE('',#35137,#35138,#2743,.T.) ;
#42252 = EDGE_CURVE('',#35138,#35132,#2744,.T.) ;
#42253 = EDGE_CURVE('',#35139,#35140,#2745,.T.) ;
#42254 = EDGE_CURVE('',#35140,#35141,#2746,.T.) ;
#42255 = EDGE_CURVE('',#35141,#35142,#2747,.T.) ;
#42256 = EDGE_CURVE('',#35142,#35143,#2748,.T.) ;
#42257 = EDGE_CURVE('',#35143,#35144,#28903,.T.) ;
#42258 = EDGE_CURVE('',#35144,#35145,#2749,.T.) ;
#42259 = EDGE_CURVE('',#35145,#35139,#2750,.T.) ;
#42260 = EDGE_CURVE('',#35146,#35147,#28904,.T.) ;
#42261 = EDGE_CURVE('',#35147,#35148,#2751,.T.) ;
#42262 = EDGE_CURVE('',#35148,#35149,#2752,.T.) ;
#42263 = EDGE_CURVE('',#35149,#35146,#2753,.T.) ;
#42264 = EDGE_CURVE('',#35150,#35151,#2754,.T.) ;
#42265 = EDGE_CURVE('',#35151,#35152,#2755,.T.) ;
#42266 = EDGE_CURVE('',#35152,#34737,#2756,.T.) ;
#42267 = EDGE_CURVE('',#34737,#35150,#2757,.T.) ;
#42268 = EDGE_CURVE('',#34755,#34739,#2758,.T.) ;
#42269 = EDGE_CURVE('',#35153,#35154,#2759,.T.) ;
#42270 = EDGE_CURVE('',#35154,#35155,#2760,.T.) ;
#42271 = EDGE_CURVE('',#35155,#35156,#2761,.T.) ;
#42272 = EDGE_CURVE('',#35156,#35153,#2762,.T.) ;
#42273 = EDGE_CURVE('',#35148,#34957,#28905,.T.) ;
#42274 = EDGE_CURVE('',#34871,#35151,#28906,.T.) ;
#42275 = EDGE_CURVE('',#35150,#34853,#28907,.T.) ;
#42276 = EDGE_CURVE('',#34852,#35156,#28908,.T.) ;
#42277 = EDGE_CURVE('',#35155,#35149,#28909,.T.) ;
#42278 = EDGE_CURVE('',#35157,#35158,#2763,.T.) ;
#42279 = EDGE_CURVE('',#35158,#35159,#2764,.T.) ;
#42280 = EDGE_CURVE('',#35159,#35160,#2765,.T.) ;
#42281 = EDGE_CURVE('',#35160,#35157,#2766,.T.) ;
#42282 = EDGE_CURVE('',#35161,#35162,#2767,.T.) ;
#42283 = EDGE_CURVE('',#35162,#35163,#2768,.T.) ;
#42284 = EDGE_CURVE('',#35163,#35164,#2769,.T.) ;
#42285 = EDGE_CURVE('',#35164,#35161,#2770,.T.) ;
#42286 = EDGE_CURVE('',#35165,#35166,#287,.T.) ;
#42287 = EDGE_CURVE('',#35165,#35167,#2771,.T.) ;
#42288 = EDGE_CURVE('',#35167,#35168,#2772,.T.) ;
#42289 = EDGE_CURVE('',#35168,#35169,#2773,.T.) ;
#42290 = EDGE_CURVE('',#35170,#35169,#288,.T.) ;
#42291 = EDGE_CURVE('',#35170,#35171,#2774,.T.) ;
#42292 = EDGE_CURVE('',#35171,#35172,#2775,.T.) ;
#42293 = EDGE_CURVE('',#35172,#35166,#2776,.T.) ;
#42294 = EDGE_CURVE('',#35173,#35174,#2777,.T.) ;
#42295 = EDGE_CURVE('',#35174,#35175,#289,.T.) ;
#42296 = EDGE_CURVE('',#35176,#35175,#2778,.T.) ;
#42297 = EDGE_CURVE('',#35176,#35168,#290,.T.) ;
#42298 = EDGE_CURVE('',#35167,#35177,#291,.T.) ;
#42299 = EDGE_CURVE('',#35177,#35178,#2779,.T.) ;
#42300 = EDGE_CURVE('',#35178,#35173,#292,.T.) ;
#42301 = EDGE_CURVE('',#35179,#35180,#293,.T.) ;
#42302 = EDGE_CURVE('',#35179,#35174,#2780,.T.) ;
#42303 = EDGE_CURVE('',#35173,#35181,#2781,.T.) ;
#42304 = EDGE_CURVE('',#35182,#35181,#294,.T.) ;
#42305 = EDGE_CURVE('',#35182,#35183,#2782,.T.) ;
#42306 = EDGE_CURVE('',#35183,#35184,#2783,.T.) ;
#42307 = EDGE_CURVE('',#35184,#35180,#2784,.T.) ;
#42308 = EDGE_CURVE('',#35177,#35185,#2785,.T.) ;
#42309 = EDGE_CURVE('',#35185,#35186,#2786,.T.) ;
#42310 = EDGE_CURVE('',#35186,#35178,#2787,.T.) ;
#42311 = EDGE_CURVE('',#35175,#35187,#2788,.T.) ;
#42312 = EDGE_CURVE('',#35187,#35188,#2789,.T.) ;
#42313 = EDGE_CURVE('',#35188,#35176,#2790,.T.) ;
#42314 = EDGE_CURVE('',#35189,#35190,#2791,.T.) ;
#42315 = EDGE_CURVE('',#35190,#35191,#2792,.T.) ;
#42316 = EDGE_CURVE('',#35191,#35192,#2793,.T.) ;
#42317 = EDGE_CURVE('',#35192,#35193,#2794,.T.) ;
#42318 = EDGE_CURVE('',#35193,#35194,#2795,.T.) ;
#42319 = EDGE_CURVE('',#35194,#35189,#2796,.T.) ;
#42320 = EDGE_CURVE('',#35195,#35196,#2797,.T.) ;
#42321 = EDGE_CURVE('',#35196,#35197,#2798,.T.) ;
#42322 = EDGE_CURVE('',#35197,#35198,#2799,.T.) ;
#42323 = EDGE_CURVE('',#35198,#35199,#2800,.T.) ;
#42324 = EDGE_CURVE('',#35199,#35200,#2801,.T.) ;
#42325 = EDGE_CURVE('',#35200,#35195,#2802,.T.) ;
#42326 = EDGE_CURVE('',#35201,#35202,#2803,.T.) ;
#42327 = EDGE_CURVE('',#35202,#35203,#2804,.T.) ;
#42328 = EDGE_CURVE('',#35203,#35204,#2805,.T.) ;
#42329 = EDGE_CURVE('',#35204,#35201,#2806,.T.) ;
#42330 = EDGE_CURVE('',#35205,#35206,#2807,.T.) ;
#42331 = EDGE_CURVE('',#35206,#35207,#2808,.T.) ;
#42332 = EDGE_CURVE('',#35207,#35208,#2809,.T.) ;
#42333 = EDGE_CURVE('',#35208,#35205,#2810,.T.) ;
#42334 = EDGE_CURVE('',#35209,#35210,#2811,.T.) ;
#42335 = EDGE_CURVE('',#35210,#35211,#2812,.T.) ;
#42336 = EDGE_CURVE('',#35211,#35212,#2813,.T.) ;
#42337 = EDGE_CURVE('',#35212,#35209,#2814,.T.) ;
#42338 = EDGE_CURVE('',#35213,#35214,#2815,.T.) ;
#42339 = EDGE_CURVE('',#35214,#35215,#2816,.T.) ;
#42340 = EDGE_CURVE('',#35215,#35216,#2817,.T.) ;
#42341 = EDGE_CURVE('',#35216,#35213,#2818,.T.) ;
#42342 = EDGE_CURVE('',#35217,#35218,#2819,.T.) ;
#42343 = EDGE_CURVE('',#35218,#35219,#2820,.T.) ;
#42344 = EDGE_CURVE('',#35219,#35220,#2821,.T.) ;
#42345 = EDGE_CURVE('',#35220,#35217,#2822,.T.) ;
#42346 = EDGE_CURVE('',#35221,#35222,#2823,.T.) ;
#42347 = EDGE_CURVE('',#35223,#35221,#28910,.T.) ;
#42348 = EDGE_CURVE('',#35224,#35223,#2824,.T.) ;
#42349 = EDGE_CURVE('',#35225,#35224,#28911,.T.) ;
#42350 = EDGE_CURVE('',#35226,#35225,#2825,.T.) ;
#42351 = EDGE_CURVE('',#35227,#35226,#28912,.T.) ;
#42352 = EDGE_CURVE('',#35228,#35227,#2826,.T.) ;
#42353 = EDGE_CURVE('',#35222,#35228,#28913,.T.) ;
#42354 = EDGE_CURVE('',#35229,#35230,#28914,.T.) ;
#42355 = EDGE_CURVE('',#35222,#35229,#2827,.T.) ;
#42356 = EDGE_CURVE('',#35228,#35230,#2828,.T.) ;
#42357 = EDGE_CURVE('',#35231,#35229,#2829,.T.) ;
#42358 = EDGE_CURVE('',#35221,#35231,#2830,.T.) ;
#42359 = EDGE_CURVE('',#35232,#35231,#28915,.T.) ;
#42360 = EDGE_CURVE('',#35223,#35232,#2831,.T.) ;
#42361 = EDGE_CURVE('',#35233,#35232,#2832,.T.) ;
#42362 = EDGE_CURVE('',#35224,#35233,#2833,.T.) ;
#42363 = EDGE_CURVE('',#35234,#35233,#28916,.T.) ;
#42364 = EDGE_CURVE('',#35225,#35234,#2834,.T.) ;
#42365 = EDGE_CURVE('',#35235,#35234,#2835,.T.) ;
#42366 = EDGE_CURVE('',#35226,#35235,#2836,.T.) ;
#42367 = EDGE_CURVE('',#35236,#35235,#28917,.T.) ;
#42368 = EDGE_CURVE('',#35227,#35236,#2837,.T.) ;
#42369 = EDGE_CURVE('',#35230,#35236,#2838,.T.) ;
#42370 = EDGE_CURVE('',#34747,#34748,#2839,.T.) ;
#42371 = EDGE_CURVE('',#34745,#34750,#2840,.T.) ;
#42372 = EDGE_CURVE('',#34749,#34746,#2841,.T.) ;
#42373 = EDGE_CURVE('',#34753,#34742,#2842,.T.) ;
#42374 = EDGE_CURVE('',#34741,#34754,#2843,.T.) ;
#42375 = EDGE_CURVE('',#34743,#34752,#2844,.T.) ;
#42376 = EDGE_CURVE('',#34751,#34744,#2845,.T.) ;
#42377 = EDGE_CURVE('',#35237,#35238,#2846,.T.) ;
#42378 = EDGE_CURVE('',#35238,#35239,#2847,.T.) ;
#42379 = EDGE_CURVE('',#35239,#35240,#2848,.T.) ;
#42380 = EDGE_CURVE('',#35240,#35237,#2849,.T.) ;
#42381 = EDGE_CURVE('',#35241,#35242,#2850,.T.) ;
#42382 = EDGE_CURVE('',#35242,#35243,#2851,.T.) ;
#42383 = EDGE_CURVE('',#35243,#35244,#2852,.T.) ;
#42384 = EDGE_CURVE('',#35244,#35241,#2853,.T.) ;
#42385 = EDGE_CURVE('',#35245,#35246,#2854,.T.) ;
#42386 = EDGE_CURVE('',#35246,#35247,#2855,.T.) ;
#42387 = EDGE_CURVE('',#35247,#35248,#2856,.T.) ;
#42388 = EDGE_CURVE('',#35248,#35245,#2857,.T.) ;
#42389 = EDGE_CURVE('',#35249,#35250,#2858,.T.) ;
#42390 = EDGE_CURVE('',#35250,#35251,#2859,.T.) ;
#42391 = EDGE_CURVE('',#35251,#35252,#2860,.T.) ;
#42392 = EDGE_CURVE('',#35252,#35249,#2861,.T.) ;
#42393 = EDGE_CURVE('',#35253,#35254,#2862,.T.) ;
#42394 = EDGE_CURVE('',#35254,#35255,#2863,.T.) ;
#42395 = EDGE_CURVE('',#35255,#35256,#2864,.T.) ;
#42396 = EDGE_CURVE('',#35256,#35253,#2865,.T.) ;
#42397 = EDGE_CURVE('',#35257,#35258,#2866,.T.) ;
#42398 = EDGE_CURVE('',#35259,#35257,#28918,.T.) ;
#42399 = EDGE_CURVE('',#35260,#35259,#2867,.T.) ;
#42400 = EDGE_CURVE('',#35261,#35260,#28919,.T.) ;
#42401 = EDGE_CURVE('',#35262,#35261,#2868,.T.) ;
#42402 = EDGE_CURVE('',#35263,#35262,#28920,.T.) ;
#42403 = EDGE_CURVE('',#35264,#35263,#2869,.T.) ;
#42404 = EDGE_CURVE('',#35258,#35264,#28921,.T.) ;
#42405 = EDGE_CURVE('',#35264,#35265,#2870,.T.) ;
#42406 = EDGE_CURVE('',#35265,#35266,#28922,.T.) ;
#42407 = EDGE_CURVE('',#35258,#35266,#2871,.T.) ;
#42408 = EDGE_CURVE('',#35266,#35267,#2872,.T.) ;
#42409 = EDGE_CURVE('',#35257,#35267,#2873,.T.) ;
#42410 = EDGE_CURVE('',#35267,#35268,#28923,.T.) ;
#42411 = EDGE_CURVE('',#35259,#35268,#2874,.T.) ;
#42412 = EDGE_CURVE('',#35268,#35269,#2875,.T.) ;
#42413 = EDGE_CURVE('',#35260,#35269,#2876,.T.) ;
#42414 = EDGE_CURVE('',#35269,#35270,#28924,.T.) ;
#42415 = EDGE_CURVE('',#35261,#35270,#2877,.T.) ;
#42416 = EDGE_CURVE('',#35270,#35271,#2878,.T.) ;
#42417 = EDGE_CURVE('',#35262,#35271,#2879,.T.) ;
#42418 = EDGE_CURVE('',#35271,#35272,#28925,.T.) ;
#42419 = EDGE_CURVE('',#35263,#35272,#2880,.T.) ;
#42420 = EDGE_CURVE('',#35272,#35265,#2881,.T.) ;
#42421 = EDGE_CURVE('',#35273,#35274,#2882,.T.) ;
#42422 = EDGE_CURVE('',#35274,#35275,#2883,.T.) ;
#42423 = EDGE_CURVE('',#35275,#35276,#2884,.T.) ;
#42424 = EDGE_CURVE('',#35276,#35273,#2885,.T.) ;
#42425 = EDGE_CURVE('',#34736,#34716,#2886,.T.) ;
#42426 = EDGE_CURVE('',#34716,#35277,#2887,.T.) ;
#42427 = EDGE_CURVE('',#35277,#35278,#2888,.T.) ;
#42428 = EDGE_CURVE('',#35278,#34736,#2889,.T.) ;
#42429 = EDGE_CURVE('',#35279,#34733,#2890,.T.) ;
#42430 = EDGE_CURVE('',#34726,#35280,#2891,.T.) ;
#42431 = EDGE_CURVE('',#35280,#35279,#2892,.T.) ;
#42432 = EDGE_CURVE('',#34734,#35281,#2893,.T.) ;
#42433 = EDGE_CURVE('',#35281,#34730,#2894,.T.) ;
#42434 = EDGE_CURVE('',#34730,#34727,#2895,.T.) ;
#42435 = EDGE_CURVE('',#34715,#35282,#2896,.T.) ;
#42436 = EDGE_CURVE('',#35282,#35283,#28926,.T.) ;
#42437 = EDGE_CURVE('',#35283,#35284,#2897,.T.) ;
#42438 = EDGE_CURVE('',#35284,#35285,#2898,.T.) ;
#42439 = EDGE_CURVE('',#35285,#34714,#2899,.T.) ;
#42440 = EDGE_CURVE('',#35286,#35287,#28927,.T.) ;
#42441 = EDGE_CURVE('',#35287,#35288,#28928,.T.) ;
#42442 = EDGE_CURVE('',#35288,#35289,#28929,.T.) ;
#42443 = EDGE_CURVE('',#35289,#35290,#2900,.T.) ;
#42444 = EDGE_CURVE('',#35290,#35291,#28930,.T.) ;
#42445 = EDGE_CURVE('',#35291,#35286,#2901,.T.) ;
#42446 = EDGE_CURVE('',#35195,#34910,#28931,.T.) ;
#42447 = EDGE_CURVE('',#35163,#35195,#2047,.T.) ;
#42448 = EDGE_CURVE('',#34911,#35163,#28932,.T.) ;
#42449 = EDGE_CURVE('',#35185,#35165,#28933,.T.) ;
#42450 = EDGE_CURVE('',#35199,#35166,#28934,.T.) ;
#42451 = EDGE_CURVE('',#35185,#35199,#295,.T.) ;
#42452 = EDGE_CURVE('',#35200,#35172,#28935,.T.) ;
#42453 = EDGE_CURVE('',#35164,#35200,#28936,.T.) ;
#42454 = EDGE_CURVE('',#34912,#35162,#28937,.T.) ;
#42455 = EDGE_CURVE('',#35196,#34909,#28938,.T.) ;
#42456 = EDGE_CURVE('',#35186,#35198,#296,.T.) ;
#42457 = EDGE_CURVE('',#35181,#35186,#28939,.T.) ;
#42458 = EDGE_CURVE('',#35164,#35172,#28940,.T.) ;
#42459 = EDGE_CURVE('',#35193,#35162,#297,.T.) ;
#42460 = EDGE_CURVE('',#34913,#35193,#28941,.T.) ;
#42461 = EDGE_CURVE('',#35158,#34916,#28942,.T.) ;
#42462 = EDGE_CURVE('',#35196,#35158,#2048,.T.) ;
#42463 = EDGE_CURVE('',#35182,#35198,#28943,.T.) ;
#42464 = EDGE_CURVE('',#35161,#35171,#28944,.T.) ;
#42465 = EDGE_CURVE('',#35194,#35161,#28945,.T.) ;
#42466 = EDGE_CURVE('',#34914,#35192,#28946,.T.) ;
#42467 = EDGE_CURVE('',#35159,#34915,#28947,.T.) ;
#42468 = EDGE_CURVE('',#35197,#35157,#28948,.T.) ;
#42469 = EDGE_CURVE('',#35183,#35197,#28949,.T.) ;
#42470 = EDGE_CURVE('',#35194,#35171,#28950,.T.) ;
#42471 = EDGE_CURVE('',#35159,#35192,#298,.T.) ;
#42472 = EDGE_CURVE('',#35183,#35157,#28951,.T.) ;
#42473 = EDGE_CURVE('',#35169,#35188,#28952,.T.) ;
#42474 = EDGE_CURVE('',#35189,#35170,#28953,.T.) ;
#42475 = EDGE_CURVE('',#35160,#35191,#28954,.T.) ;
#42476 = EDGE_CURVE('',#35184,#35160,#28955,.T.) ;
#42477 = EDGE_CURVE('',#35189,#35188,#299,.T.) ;
#42478 = EDGE_CURVE('',#35184,#35191,#28956,.T.) ;
#42479 = EDGE_CURVE('',#35190,#35187,#300,.T.) ;
#42480 = EDGE_CURVE('',#35180,#35190,#28957,.T.) ;
#42481 = EDGE_CURVE('',#35179,#35187,#28958,.T.) ;
#42482 = EDGE_CURVE('',#35152,#35292,#301,.T.) ;
#42483 = EDGE_CURVE('',#35292,#34717,#2049,.T.) ;
#42484 = EDGE_CURVE('',#35277,#35279,#28959,.T.) ;
#42485 = EDGE_CURVE('',#35278,#35280,#28960,.T.) ;
#42486 = EDGE_CURVE('',#34854,#35278,#28961,.T.) ;
#42487 = EDGE_CURVE('',#34868,#35282,#2050,.T.) ;
#42488 = EDGE_CURVE('',#34715,#34869,#2051,.T.) ;
#42489 = EDGE_CURVE('',#35284,#34733,#28962,.T.) ;
#42490 = EDGE_CURVE('',#35279,#35285,#28963,.T.) ;
#42491 = EDGE_CURVE('',#34855,#35280,#28964,.T.) ;
#42492 = EDGE_CURVE('',#35293,#35294,#2052,.T.) ;
#42493 = EDGE_CURVE('',#35294,#34840,#302,.T.) ;
#42494 = EDGE_CURVE('',#35281,#35293,#28965,.T.) ;
#42495 = EDGE_CURVE('',#35268,#35273,#28966,.T.) ;
#42496 = EDGE_CURVE('',#35273,#35267,#28967,.T.) ;
#42497 = EDGE_CURVE('',#35274,#35266,#28968,.T.) ;
#42498 = EDGE_CURVE('',#35269,#35276,#28969,.T.) ;
#42499 = EDGE_CURVE('',#35274,#35265,#28970,.T.) ;
#42500 = EDGE_CURVE('',#35270,#35276,#28971,.T.) ;
#42501 = EDGE_CURVE('',#35275,#35272,#28972,.T.) ;
#42502 = EDGE_CURVE('',#35271,#35275,#28973,.T.) ;
#42503 = EDGE_CURVE('',#34935,#35204,#28974,.T.) ;
#42504 = EDGE_CURVE('',#35201,#34934,#28975,.T.) ;
#42505 = EDGE_CURVE('',#35216,#34933,#28976,.T.) ;
#42506 = EDGE_CURVE('',#35201,#35216,#28977,.T.) ;
#42507 = EDGE_CURVE('',#35208,#35204,#28978,.T.) ;
#42508 = EDGE_CURVE('',#34936,#35208,#28979,.T.) ;
#42509 = EDGE_CURVE('',#35213,#34932,#28980,.T.) ;
#42510 = EDGE_CURVE('',#35202,#35215,#28981,.T.) ;
#42511 = EDGE_CURVE('',#35203,#35220,#28982,.T.) ;
#42512 = EDGE_CURVE('',#35217,#35202,#28983,.T.) ;
#42513 = EDGE_CURVE('',#35205,#35203,#28984,.T.) ;
#42514 = EDGE_CURVE('',#34930,#35207,#28985,.T.) ;
#42515 = EDGE_CURVE('',#34931,#35211,#28986,.T.) ;
#42516 = EDGE_CURVE('',#35212,#34929,#28987,.T.) ;
#42517 = EDGE_CURVE('',#35213,#35211,#28988,.T.) ;
#42518 = EDGE_CURVE('',#35217,#35215,#28989,.T.) ;
#42519 = EDGE_CURVE('',#35205,#35220,#28990,.T.) ;
#42520 = EDGE_CURVE('',#35212,#35207,#28991,.T.) ;
#42521 = EDGE_CURVE('',#35214,#35210,#28992,.T.) ;
#42522 = EDGE_CURVE('',#35218,#35214,#28993,.T.) ;
#42523 = EDGE_CURVE('',#35206,#35219,#28994,.T.) ;
#42524 = EDGE_CURVE('',#35209,#35206,#28995,.T.) ;
#42525 = EDGE_CURVE('',#35218,#35210,#28996,.T.) ;
#42526 = EDGE_CURVE('',#35209,#35219,#28997,.T.) ;
#42527 = EDGE_CURVE('',#34887,#35248,#28998,.T.) ;
#42528 = EDGE_CURVE('',#35245,#34886,#28999,.T.) ;
#42529 = EDGE_CURVE('',#35244,#34885,#29000,.T.) ;
#42530 = EDGE_CURVE('',#35245,#35244,#29001,.T.) ;
#42531 = EDGE_CURVE('',#35252,#35248,#29002,.T.) ;
#42532 = EDGE_CURVE('',#34888,#35252,#29003,.T.) ;
#42533 = EDGE_CURVE('',#35241,#34884,#29004,.T.) ;
#42534 = EDGE_CURVE('',#35246,#35243,#29005,.T.) ;
#42535 = EDGE_CURVE('',#35247,#35256,#29006,.T.) ;
#42536 = EDGE_CURVE('',#35253,#35246,#29007,.T.) ;
#42537 = EDGE_CURVE('',#35249,#35247,#29008,.T.) ;
#42538 = EDGE_CURVE('',#34882,#35251,#29009,.T.) ;
#42539 = EDGE_CURVE('',#34883,#35239,#29010,.T.) ;
#42540 = EDGE_CURVE('',#35240,#34881,#29011,.T.) ;
#42541 = EDGE_CURVE('',#35241,#35239,#29012,.T.) ;
#42542 = EDGE_CURVE('',#35253,#35243,#29013,.T.) ;
#42543 = EDGE_CURVE('',#35249,#35256,#29014,.T.) ;
#42544 = EDGE_CURVE('',#35240,#35251,#29015,.T.) ;
#42545 = EDGE_CURVE('',#35242,#35238,#29016,.T.) ;
#42546 = EDGE_CURVE('',#35254,#35242,#29017,.T.) ;
#42547 = EDGE_CURVE('',#35250,#35255,#29018,.T.) ;
#42548 = EDGE_CURVE('',#35237,#35250,#29019,.T.) ;
#42549 = EDGE_CURVE('',#35254,#35238,#29020,.T.) ;
#42550 = EDGE_CURVE('',#35237,#35255,#29021,.T.) ;
#42551 = EDGE_CURVE('',#34834,#35287,#2053,.T.) ;
#42552 = EDGE_CURVE('',#34835,#35286,#29022,.T.) ;
#42553 = EDGE_CURVE('',#34969,#35286,#29023,.T.) ;
#42554 = EDGE_CURVE('',#34970,#35291,#29024,.T.) ;
#42555 = EDGE_CURVE('',#34849,#35291,#29025,.T.) ;
#42556 = EDGE_CURVE('',#34850,#35290,#29026,.T.) ;
#42557 = EDGE_CURVE('',#35153,#34851,#29027,.T.) ;
#42558 = EDGE_CURVE('',#35153,#35290,#29028,.T.) ;
#42559 = EDGE_CURVE('',#35154,#35289,#29029,.T.) ;
#42560 = EDGE_CURVE('',#35146,#35154,#29030,.T.) ;
#42561 = EDGE_CURVE('',#35146,#35289,#29031,.T.) ;
#42562 = EDGE_CURVE('',#35288,#35147,#2054,.T.) ;
#42563 = EDGE_CURVE('',#34734,#35284,#29032,.T.) ;
#42564 = EDGE_CURVE('',#35281,#35283,#29033,.T.) ;
#42565 = EDGE_CURVE('',#35293,#35282,#29034,.T.) ;
#42566 = EDGE_CURVE('',#35294,#34868,#29035,.T.) ;
#42567 = EDGE_CURVE('',#35152,#34870,#29036,.T.) ;
#42568 = EDGE_CURVE('',#35292,#34869,#29037,.T.) ;
#42569 = EDGE_CURVE('',#35277,#35285,#29038,.T.) ;
#42570 = EDGE_CURVE('',#35295,#35296,#2055,.T.) ;
#42571 = EDGE_CURVE('',#35296,#35288,#2056,.T.) ;
#42572 = EDGE_CURVE('',#35287,#35297,#2057,.T.) ;
#42573 = EDGE_CURVE('',#35297,#35295,#2058,.T.) ;
#42574 = EDGE_CURVE('',#34961,#35287,#2059,.T.) ;
#42575 = EDGE_CURVE('',#34958,#35147,#29039,.T.) ;
#42576 = EDGE_CURVE('',#35288,#34959,#2060,.T.) ;
#42577 = EDGE_CURVE('',#35297,#34961,#29040,.T.) ;
#42578 = EDGE_CURVE('',#35295,#34960,#29041,.T.) ;
#42579 = EDGE_CURVE('',#35296,#34959,#29042,.T.) ;
#42580 = EDGE_CURVE('',#35119,#35137,#29043,.T.) ;
#42581 = EDGE_CURVE('',#35137,#35121,#29044,.T.) ;
#42582 = EDGE_CURVE('',#35120,#35139,#29045,.T.) ;
#42583 = EDGE_CURVE('',#35139,#35118,#29046,.T.) ;
#42584 = EDGE_CURVE('',#35138,#35123,#29047,.T.) ;
#42585 = EDGE_CURVE('',#35117,#35136,#29048,.T.) ;
#42586 = EDGE_CURVE('',#35140,#35116,#29049,.T.) ;
#42587 = EDGE_CURVE('',#35122,#35145,#29050,.T.) ;
#42588 = EDGE_CURVE('',#35138,#35125,#29051,.T.) ;
#42589 = EDGE_CURVE('',#35115,#35136,#29052,.T.) ;
#42590 = EDGE_CURVE('',#35140,#35114,#29053,.T.) ;
#42591 = EDGE_CURVE('',#35124,#35145,#29054,.T.) ;
#42592 = EDGE_CURVE('',#35132,#35127,#29055,.T.) ;
#42593 = EDGE_CURVE('',#35112,#35135,#2061,.T.) ;
#42594 = EDGE_CURVE('',#35113,#34809,#29056,.T.) ;
#42595 = EDGE_CURVE('',#34810,#35112,#29057,.T.) ;
#42596 = EDGE_CURVE('',#35141,#35113,#2062,.T.) ;
#42597 = EDGE_CURVE('',#35126,#35144,#29058,.T.) ;
#42598 = EDGE_CURVE('',#35133,#35129,#29059,.T.) ;
#42599 = EDGE_CURVE('',#34811,#35135,#29060,.T.) ;
#42600 = EDGE_CURVE('',#35141,#34808,#29061,.T.) ;
#42601 = EDGE_CURVE('',#35128,#35143,#29062,.T.) ;
#42602 = EDGE_CURVE('',#35134,#35131,#29063,.T.) ;
#42603 = EDGE_CURVE('',#34812,#35134,#29064,.T.) ;
#42604 = EDGE_CURVE('',#35142,#34806,#29065,.T.) ;
#42605 = EDGE_CURVE('',#35130,#35142,#29066,.T.) ;
#42606 = EDGE_CURVE('',#34813,#35131,#29067,.T.) ;
#42607 = EDGE_CURVE('',#35130,#34807,#29068,.T.) ;
#42608 = EDGE_CURVE('',#35298,#35299,#29069,.T.) ;
#42609 = EDGE_CURVE('',#35300,#35298,#29070,.T.) ;
#42610 = EDGE_CURVE('',#35301,#35300,#29071,.T.) ;
#42611 = EDGE_CURVE('',#35301,#35299,#29072,.T.) ;
#42612 = EDGE_CURVE('',#35302,#35302,#29073,.T.) ;
#42613 = EDGE_CURVE('',#35302,#35303,#29074,.T.) ;
#42614 = EDGE_CURVE('',#35304,#35303,#29075,.T.) ;
#42615 = EDGE_CURVE('',#35303,#35304,#29076,.T.) ;
#42616 = EDGE_CURVE('',#35305,#35305,#29077,.T.) ;
#42617 = EDGE_CURVE('',#35305,#35306,#29078,.T.) ;
#42618 = EDGE_CURVE('',#35306,#35306,#29079,.T.) ;
#42619 = EDGE_CURVE('',#35307,#35307,#29080,.T.) ;
#42620 = EDGE_CURVE('',#35307,#35308,#29081,.T.) ;
#42621 = EDGE_CURVE('',#35309,#35308,#29082,.T.) ;
#42622 = EDGE_CURVE('',#35308,#35309,#29083,.T.) ;
#42623 = EDGE_CURVE('',#35310,#35311,#29084,.T.) ;
#42624 = EDGE_CURVE('',#35312,#35311,#29085,.T.) ;
#42625 = EDGE_CURVE('',#35312,#35313,#29086,.T.) ;
#42626 = EDGE_CURVE('',#35313,#35310,#29087,.T.) ;
#42627 = EDGE_CURVE('',#35314,#35315,#29088,.T.) ;
#42628 = EDGE_CURVE('',#35315,#35316,#29089,.T.) ;
#42629 = EDGE_CURVE('',#35314,#35316,#29090,.T.) ;
#42630 = EDGE_CURVE('',#35317,#35310,#2902,.T.) ;
#42631 = EDGE_CURVE('',#35317,#35318,#29091,.T.) ;
#42632 = EDGE_CURVE('',#35311,#35318,#2903,.T.) ;
#42633 = EDGE_CURVE('',#35319,#35320,#29092,.T.) ;
#42634 = EDGE_CURVE('',#35319,#35321,#29093,.T.) ;
#42635 = EDGE_CURVE('',#35320,#35321,#29094,.T.) ;
#42636 = EDGE_CURVE('',#35322,#35322,#29095,.T.) ;
#42637 = EDGE_CURVE('',#35322,#35305,#2904,.T.) ;
#42638 = EDGE_CURVE('',#35306,#35309,#2905,.T.) ;
#42639 = EDGE_CURVE('',#35323,#35324,#29096,.T.) ;
#42640 = EDGE_CURVE('',#35323,#35325,#2063,.T.) ;
#42641 = EDGE_CURVE('',#35326,#35325,#2906,.T.) ;
#42642 = EDGE_CURVE('',#35326,#35327,#2064,.T.) ;
#42643 = EDGE_CURVE('',#35328,#35327,#29097,.T.) ;
#42644 = EDGE_CURVE('',#35328,#35329,#2065,.T.) ;
#42645 = EDGE_CURVE('',#35329,#35330,#2907,.T.) ;
#42646 = EDGE_CURVE('',#35330,#35331,#2066,.T.) ;
#42647 = EDGE_CURVE('',#35332,#35331,#29098,.T.) ;
#42648 = EDGE_CURVE('',#35332,#35333,#2067,.T.) ;
#42649 = EDGE_CURVE('',#35334,#35333,#2908,.T.) ;
#42650 = EDGE_CURVE('',#35334,#35335,#2068,.T.) ;
#42651 = EDGE_CURVE('',#35336,#35335,#29099,.T.) ;
#42652 = EDGE_CURVE('',#35336,#35337,#2069,.T.) ;
#42653 = EDGE_CURVE('',#35337,#35338,#2909,.T.) ;
#42654 = EDGE_CURVE('',#35338,#35339,#2070,.T.) ;
#42655 = EDGE_CURVE('',#35324,#35339,#29100,.T.) ;
#42656 = EDGE_CURVE('',#35324,#35304,#2910,.T.) ;
#42657 = EDGE_CURVE('',#35340,#35341,#29101,.T.) ;
#42658 = EDGE_CURVE('',#35342,#35340,#29102,.T.) ;
#42659 = EDGE_CURVE('',#35343,#35342,#29103,.T.) ;
#42660 = EDGE_CURVE('',#35343,#35341,#29104,.T.) ;
#42661 = EDGE_CURVE('',#35344,#35345,#29105,.T.) ;
#42662 = EDGE_CURVE('',#35346,#35344,#2911,.T.) ;
#42663 = EDGE_CURVE('',#35347,#35346,#29106,.T.) ;
#42664 = EDGE_CURVE('',#35345,#35347,#2912,.T.) ;
#42665 = EDGE_CURVE('',#35348,#35348,#29107,.T.) ;
#42666 = EDGE_CURVE('',#35348,#35349,#29108,.T.) ;
#42667 = EDGE_CURVE('',#35350,#35349,#29109,.T.) ;
#42668 = EDGE_CURVE('',#35349,#35350,#29110,.T.) ;
#42669 = EDGE_CURVE('',#35351,#35351,#29111,.T.) ;
#42670 = EDGE_CURVE('',#35351,#35352,#29112,.T.) ;
#42671 = EDGE_CURVE('',#35352,#35352,#29113,.T.) ;
#42672 = EDGE_CURVE('',#35353,#35353,#29114,.T.) ;
#42673 = EDGE_CURVE('',#35353,#35354,#29115,.T.) ;
#42674 = EDGE_CURVE('',#35355,#35354,#29116,.T.) ;
#42675 = EDGE_CURVE('',#35354,#35355,#29117,.T.) ;
#42676 = EDGE_CURVE('',#35356,#35357,#29118,.T.) ;
#42677 = EDGE_CURVE('',#35358,#35357,#29119,.T.) ;
#42678 = EDGE_CURVE('',#35358,#35359,#29120,.T.) ;
#42679 = EDGE_CURVE('',#35359,#35356,#29121,.T.) ;
#42680 = EDGE_CURVE('',#35360,#35361,#29122,.T.) ;
#42681 = EDGE_CURVE('',#35361,#35362,#29123,.T.) ;
#42682 = EDGE_CURVE('',#35360,#35362,#29124,.T.) ;
#42683 = EDGE_CURVE('',#35363,#35356,#2913,.T.) ;
#42684 = EDGE_CURVE('',#35363,#35364,#29125,.T.) ;
#42685 = EDGE_CURVE('',#35357,#35364,#2914,.T.) ;
#42686 = EDGE_CURVE('',#35365,#35366,#29126,.T.) ;
#42687 = EDGE_CURVE('',#35365,#35367,#29127,.T.) ;
#42688 = EDGE_CURVE('',#35366,#35367,#29128,.T.) ;
#42689 = EDGE_CURVE('',#35368,#35368,#29129,.T.) ;
#42690 = EDGE_CURVE('',#35368,#35351,#2915,.T.) ;
#42691 = EDGE_CURVE('',#35352,#35355,#2916,.T.) ;
#42692 = EDGE_CURVE('',#35369,#35370,#29130,.T.) ;
#42693 = EDGE_CURVE('',#35369,#35371,#2071,.T.) ;
#42694 = EDGE_CURVE('',#35372,#35371,#2917,.T.) ;
#42695 = EDGE_CURVE('',#35372,#35373,#2072,.T.) ;
#42696 = EDGE_CURVE('',#35374,#35373,#29131,.T.) ;
#42697 = EDGE_CURVE('',#35374,#35375,#2073,.T.) ;
#42698 = EDGE_CURVE('',#35375,#35376,#2918,.T.) ;
#42699 = EDGE_CURVE('',#35376,#35377,#2074,.T.) ;
#42700 = EDGE_CURVE('',#35378,#35377,#29132,.T.) ;
#42701 = EDGE_CURVE('',#35378,#35379,#2075,.T.) ;
#42702 = EDGE_CURVE('',#35380,#35379,#2919,.T.) ;
#42703 = EDGE_CURVE('',#35380,#35381,#2076,.T.) ;
#42704 = EDGE_CURVE('',#35382,#35381,#29133,.T.) ;
#42705 = EDGE_CURVE('',#35382,#35383,#2077,.T.) ;
#42706 = EDGE_CURVE('',#35383,#35384,#2920,.T.) ;
#42707 = EDGE_CURVE('',#35384,#35385,#2078,.T.) ;
#42708 = EDGE_CURVE('',#35370,#35385,#29134,.T.) ;
#42709 = EDGE_CURVE('',#35370,#35350,#2921,.T.) ;
#42710 = EDGE_CURVE('',#35386,#35387,#2922,.T.) ;
#42711 = EDGE_CURVE('',#35388,#35387,#2923,.T.) ;
#42712 = EDGE_CURVE('',#35388,#35389,#2924,.T.) ;
#42713 = EDGE_CURVE('',#35389,#35386,#2925,.T.) ;
#42714 = EDGE_CURVE('',#35390,#35391,#29135,.T.) ;
#42715 = EDGE_CURVE('',#35390,#35392,#2926,.T.) ;
#42716 = EDGE_CURVE('',#35393,#35392,#2079,.T.) ;
#42717 = EDGE_CURVE('',#35393,#35394,#2927,.T.) ;
#42718 = EDGE_CURVE('',#35395,#35394,#2080,.T.) ;
#42719 = EDGE_CURVE('',#35395,#35396,#2928,.T.) ;
#42720 = EDGE_CURVE('',#35397,#35396,#29136,.T.) ;
#42721 = EDGE_CURVE('',#35397,#35391,#2929,.T.) ;
#42722 = EDGE_CURVE('',#35398,#35399,#2930,.T.) ;
#42723 = EDGE_CURVE('',#35398,#35400,#2931,.T.) ;
#42724 = EDGE_CURVE('',#35401,#35400,#2932,.T.) ;
#42725 = EDGE_CURVE('',#35401,#35399,#2933,.T.) ;
#42726 = EDGE_CURVE('',#35402,#35403,#2934,.T.) ;
#42727 = EDGE_CURVE('',#35402,#35404,#2935,.T.) ;
#42728 = EDGE_CURVE('',#35405,#35404,#2936,.T.) ;
#42729 = EDGE_CURVE('',#35405,#35403,#2937,.T.) ;
#42730 = EDGE_CURVE('',#35406,#35407,#2938,.T.) ;
#42731 = EDGE_CURVE('',#35406,#35408,#2939,.T.) ;
#42732 = EDGE_CURVE('',#35409,#35408,#2940,.T.) ;
#42733 = EDGE_CURVE('',#35409,#35407,#2941,.T.) ;
#42734 = EDGE_CURVE('',#35406,#35410,#29137,.T.) ;
#42735 = EDGE_CURVE('',#35411,#35410,#2942,.T.) ;
#42736 = EDGE_CURVE('',#35408,#35411,#29138,.T.) ;
#42737 = EDGE_CURVE('',#35407,#35402,#29139,.T.) ;
#42738 = EDGE_CURVE('',#35404,#35409,#29140,.T.) ;
#42739 = EDGE_CURVE('',#35403,#35398,#29141,.T.) ;
#42740 = EDGE_CURVE('',#35400,#35405,#29142,.T.) ;
#42741 = EDGE_CURVE('',#35412,#35413,#29143,.T.) ;
#42742 = EDGE_CURVE('',#35412,#35414,#2943,.T.) ;
#42743 = EDGE_CURVE('',#35414,#35399,#29144,.T.) ;
#42744 = EDGE_CURVE('',#35415,#35401,#29145,.T.) ;
#42745 = EDGE_CURVE('',#35413,#35415,#2944,.T.) ;
#42746 = EDGE_CURVE('',#35416,#35417,#29146,.T.) ;
#42747 = EDGE_CURVE('',#35417,#35418,#2945,.T.) ;
#42748 = EDGE_CURVE('',#35418,#35419,#2946,.T.) ;
#42749 = EDGE_CURVE('',#35419,#35416,#2947,.T.) ;
#42750 = EDGE_CURVE('',#35420,#35421,#2948,.T.) ;
#42751 = EDGE_CURVE('',#35421,#35422,#2949,.T.) ;
#42752 = EDGE_CURVE('',#35422,#35423,#2950,.T.) ;
#42753 = EDGE_CURVE('',#35423,#35420,#2951,.T.) ;
#42754 = EDGE_CURVE('',#35424,#35425,#2952,.T.) ;
#42755 = EDGE_CURVE('',#35425,#35426,#2953,.T.) ;
#42756 = EDGE_CURVE('',#35426,#35367,#2954,.T.) ;
#42757 = EDGE_CURVE('',#35367,#35424,#2955,.T.) ;
#42758 = EDGE_CURVE('',#35385,#35369,#2956,.T.) ;
#42759 = EDGE_CURVE('',#35358,#35362,#2957,.T.) ;
#42760 = EDGE_CURVE('',#35362,#35319,#2958,.T.) ;
#42761 = EDGE_CURVE('',#35319,#35427,#2959,.T.) ;
#42762 = EDGE_CURVE('',#35428,#35427,#29147,.T.) ;
#42763 = EDGE_CURVE('',#35428,#35313,#2960,.T.) ;
#42764 = EDGE_CURVE('',#35312,#35316,#2961,.T.) ;
#42765 = EDGE_CURVE('',#35316,#35429,#2962,.T.) ;
#42766 = EDGE_CURVE('',#35430,#35429,#2963,.T.) ;
#42767 = EDGE_CURVE('',#35430,#35431,#2964,.T.) ;
#42768 = EDGE_CURVE('',#35432,#35431,#29148,.T.) ;
#42769 = EDGE_CURVE('',#35432,#35433,#29149,.T.) ;
#42770 = EDGE_CURVE('',#35434,#35433,#29150,.T.) ;
#42771 = EDGE_CURVE('',#35434,#35435,#2965,.T.) ;
#42772 = EDGE_CURVE('',#35436,#35435,#29151,.T.) ;
#42773 = EDGE_CURVE('',#35436,#35437,#29152,.T.) ;
#42774 = EDGE_CURVE('',#35438,#35437,#29153,.T.) ;
#42775 = EDGE_CURVE('',#35438,#35439,#2966,.T.) ;
#42776 = EDGE_CURVE('',#35439,#35440,#2967,.T.) ;
#42777 = EDGE_CURVE('',#35440,#35365,#2968,.T.) ;
#42778 = EDGE_CURVE('',#35365,#35441,#2969,.T.) ;
#42779 = EDGE_CURVE('',#35442,#35441,#29154,.T.) ;
#42780 = EDGE_CURVE('',#35442,#35359,#2970,.T.) ;
#42781 = EDGE_CURVE('',#35361,#35443,#2971,.T.) ;
#42782 = EDGE_CURVE('',#35443,#35444,#2972,.T.) ;
#42783 = EDGE_CURVE('',#35444,#35321,#2973,.T.) ;
#42784 = EDGE_CURVE('',#35321,#35361,#2974,.T.) ;
#42785 = EDGE_CURVE('',#35445,#35446,#2975,.T.) ;
#42786 = EDGE_CURVE('',#35447,#35446,#2976,.T.) ;
#42787 = EDGE_CURVE('',#35447,#35448,#2977,.T.) ;
#42788 = EDGE_CURVE('',#35448,#35449,#303,.T.) ;
#42789 = EDGE_CURVE('',#35449,#35450,#2978,.T.) ;
#42790 = EDGE_CURVE('',#35450,#35451,#304,.T.) ;
#42791 = EDGE_CURVE('',#35451,#35452,#2979,.T.) ;
#42792 = EDGE_CURVE('',#35452,#35453,#305,.T.) ;
#42793 = EDGE_CURVE('',#35453,#35454,#2980,.T.) ;
#42794 = EDGE_CURVE('',#35454,#35455,#306,.T.) ;
#42795 = EDGE_CURVE('',#35455,#35456,#2981,.T.) ;
#42796 = EDGE_CURVE('',#35456,#35445,#2982,.T.) ;
#42797 = EDGE_CURVE('',#35457,#35413,#2983,.T.) ;
#42798 = EDGE_CURVE('',#35458,#35415,#2984,.T.) ;
#42799 = EDGE_CURVE('',#35458,#35457,#2985,.T.) ;
#42800 = EDGE_CURVE('',#35412,#35459,#2986,.T.) ;
#42801 = EDGE_CURVE('',#35459,#35460,#2987,.T.) ;
#42802 = EDGE_CURVE('',#35411,#35460,#2988,.T.) ;
#42803 = EDGE_CURVE('',#35414,#35410,#2989,.T.) ;
#42804 = EDGE_CURVE('',#35461,#35462,#2990,.T.) ;
#42805 = EDGE_CURVE('',#35462,#35463,#2991,.T.) ;
#42806 = EDGE_CURVE('',#35464,#35463,#2992,.T.) ;
#42807 = EDGE_CURVE('',#35464,#35461,#2993,.T.) ;
#42808 = EDGE_CURVE('',#35465,#35466,#29155,.T.) ;
#42809 = EDGE_CURVE('',#35465,#35467,#2994,.T.) ;
#42810 = EDGE_CURVE('',#35468,#35467,#29156,.T.) ;
#42811 = EDGE_CURVE('',#35468,#35469,#2995,.T.) ;
#42812 = EDGE_CURVE('',#35470,#35469,#29157,.T.) ;
#42813 = EDGE_CURVE('',#35470,#35471,#2996,.T.) ;
#42814 = EDGE_CURVE('',#35472,#35471,#29158,.T.) ;
#42815 = EDGE_CURVE('',#35472,#35466,#2997,.T.) ;
#42816 = EDGE_CURVE('',#35473,#35474,#29159,.T.) ;
#42817 = EDGE_CURVE('',#35473,#35475,#2998,.T.) ;
#42818 = EDGE_CURVE('',#35476,#35475,#29160,.T.) ;
#42819 = EDGE_CURVE('',#35476,#35477,#2999,.T.) ;
#42820 = EDGE_CURVE('',#35478,#35477,#29161,.T.) ;
#42821 = EDGE_CURVE('',#35478,#35479,#3000,.T.) ;
#42822 = EDGE_CURVE('',#35480,#35479,#29162,.T.) ;
#42823 = EDGE_CURVE('',#35480,#35474,#3001,.T.) ;
#42824 = EDGE_CURVE('',#35481,#35482,#3002,.T.) ;
#42825 = EDGE_CURVE('',#35482,#35483,#3003,.T.) ;
#42826 = EDGE_CURVE('',#35484,#35483,#3004,.T.) ;
#42827 = EDGE_CURVE('',#35484,#35481,#3005,.T.) ;
#42828 = EDGE_CURVE('',#35485,#35345,#3006,.T.) ;
#42829 = EDGE_CURVE('',#35486,#35347,#3007,.T.) ;
#42830 = EDGE_CURVE('',#35486,#35485,#3008,.T.) ;
#42831 = EDGE_CURVE('',#35344,#35487,#3009,.T.) ;
#42832 = EDGE_CURVE('',#35487,#35488,#3010,.T.) ;
#42833 = EDGE_CURVE('',#35346,#35488,#3011,.T.) ;
#42834 = EDGE_CURVE('',#35489,#35490,#3012,.T.) ;
#42835 = EDGE_CURVE('',#35490,#35491,#3013,.T.) ;
#42836 = EDGE_CURVE('',#35492,#35491,#3014,.T.) ;
#42837 = EDGE_CURVE('',#35492,#35489,#3015,.T.) ;
#42838 = EDGE_CURVE('',#35493,#35494,#3016,.T.) ;
#42839 = EDGE_CURVE('',#35494,#35495,#2081,.T.) ;
#42840 = EDGE_CURVE('',#35495,#35496,#3017,.T.) ;
#42841 = EDGE_CURVE('',#35497,#35496,#2082,.T.) ;
#42842 = EDGE_CURVE('',#35497,#35498,#3018,.T.) ;
#42843 = EDGE_CURVE('',#35499,#35498,#2083,.T.) ;
#42844 = EDGE_CURVE('',#35499,#35500,#3019,.T.) ;
#42845 = EDGE_CURVE('',#35500,#35493,#2084,.T.) ;
#42846 = EDGE_CURVE('',#35501,#35502,#3020,.T.) ;
#42847 = EDGE_CURVE('',#35502,#35503,#2085,.T.) ;
#42848 = EDGE_CURVE('',#35503,#35504,#3021,.T.) ;
#42849 = EDGE_CURVE('',#35505,#35504,#2086,.T.) ;
#42850 = EDGE_CURVE('',#35505,#35506,#3022,.T.) ;
#42851 = EDGE_CURVE('',#35507,#35506,#2087,.T.) ;
#42852 = EDGE_CURVE('',#35507,#35508,#3023,.T.) ;
#42853 = EDGE_CURVE('',#35508,#35501,#2088,.T.) ;
#42854 = EDGE_CURVE('',#35509,#35510,#3024,.T.) ;
#42855 = EDGE_CURVE('',#35510,#35511,#3025,.T.) ;
#42856 = EDGE_CURVE('',#35512,#35511,#3026,.T.) ;
#42857 = EDGE_CURVE('',#35512,#35509,#3027,.T.) ;
#42858 = EDGE_CURVE('',#35513,#35514,#29163,.T.) ;
#42859 = EDGE_CURVE('',#35513,#35515,#3028,.T.) ;
#42860 = EDGE_CURVE('',#35516,#35515,#29164,.T.) ;
#42861 = EDGE_CURVE('',#35516,#35517,#3029,.T.) ;
#42862 = EDGE_CURVE('',#35518,#35517,#29165,.T.) ;
#42863 = EDGE_CURVE('',#35518,#35519,#3030,.T.) ;
#42864 = EDGE_CURVE('',#35520,#35519,#29166,.T.) ;
#42865 = EDGE_CURVE('',#35520,#35514,#3031,.T.) ;
#42866 = EDGE_CURVE('',#35521,#35522,#29167,.T.) ;
#42867 = EDGE_CURVE('',#35521,#35523,#3032,.T.) ;
#42868 = EDGE_CURVE('',#35524,#35523,#29168,.T.) ;
#42869 = EDGE_CURVE('',#35524,#35525,#3033,.T.) ;
#42870 = EDGE_CURVE('',#35526,#35525,#29169,.T.) ;
#42871 = EDGE_CURVE('',#35526,#35527,#3034,.T.) ;
#42872 = EDGE_CURVE('',#35528,#35527,#29170,.T.) ;
#42873 = EDGE_CURVE('',#35528,#35522,#3035,.T.) ;
#42874 = EDGE_CURVE('',#35529,#35530,#3036,.T.) ;
#42875 = EDGE_CURVE('',#35530,#35531,#3037,.T.) ;
#42876 = EDGE_CURVE('',#35532,#35531,#3038,.T.) ;
#42877 = EDGE_CURVE('',#35532,#35529,#3039,.T.) ;
#42878 = EDGE_CURVE('',#35533,#35534,#2089,.T.) ;
#42879 = EDGE_CURVE('',#35534,#35535,#2090,.T.) ;
#42880 = EDGE_CURVE('',#35535,#35536,#2091,.T.) ;
#42881 = EDGE_CURVE('',#35536,#35537,#2092,.T.) ;
#42882 = EDGE_CURVE('',#35537,#35538,#3040,.T.) ;
#42883 = EDGE_CURVE('',#35538,#35539,#2093,.T.) ;
#42884 = EDGE_CURVE('',#35539,#35540,#2094,.T.) ;
#42885 = EDGE_CURVE('',#35540,#35541,#2095,.T.) ;
#42886 = EDGE_CURVE('',#35541,#35542,#2096,.T.) ;
#42887 = EDGE_CURVE('',#35542,#35543,#3041,.T.) ;
#42888 = EDGE_CURVE('',#35544,#35543,#3042,.T.) ;
#42889 = EDGE_CURVE('',#35544,#35545,#3043,.T.) ;
#42890 = EDGE_CURVE('',#35545,#35546,#3044,.T.) ;
#42891 = EDGE_CURVE('',#35546,#35533,#3045,.T.) ;
#42892 = EDGE_CURVE('',#35547,#35548,#3046,.T.) ;
#42893 = EDGE_CURVE('',#35548,#35549,#29171,.T.) ;
#42894 = EDGE_CURVE('',#35549,#35550,#3047,.T.) ;
#42895 = EDGE_CURVE('',#35550,#35547,#29172,.T.) ;
#42896 = EDGE_CURVE('',#35551,#35552,#3048,.T.) ;
#42897 = EDGE_CURVE('',#35552,#35553,#3049,.T.) ;
#42898 = EDGE_CURVE('',#35553,#35554,#3050,.T.) ;
#42899 = EDGE_CURVE('',#35554,#35551,#3051,.T.) ;
#42900 = EDGE_CURVE('',#35461,#35459,#29173,.T.) ;
#42901 = EDGE_CURVE('',#35457,#35386,#29174,.T.) ;
#42902 = EDGE_CURVE('',#35389,#35445,#29175,.T.) ;
#42903 = EDGE_CURVE('',#35456,#35425,#29176,.T.) ;
#42904 = EDGE_CURVE('',#35424,#35440,#29177,.T.) ;
#42905 = EDGE_CURVE('',#35439,#35554,#29178,.T.) ;
#42906 = EDGE_CURVE('',#35553,#35419,#29179,.T.) ;
#42907 = EDGE_CURVE('',#35418,#35546,#29180,.T.) ;
#42908 = EDGE_CURVE('',#35545,#35530,#29181,.T.) ;
#42909 = EDGE_CURVE('',#35529,#35510,#29182,.T.) ;
#42910 = EDGE_CURVE('',#35509,#35490,#29183,.T.) ;
#42911 = EDGE_CURVE('',#35489,#35487,#29184,.T.) ;
#42912 = EDGE_CURVE('',#35485,#35482,#29185,.T.) ;
#42913 = EDGE_CURVE('',#35481,#35462,#29186,.T.) ;
#42914 = EDGE_CURVE('',#35555,#35556,#3052,.T.) ;
#42915 = EDGE_CURVE('',#35556,#35557,#3053,.T.) ;
#42916 = EDGE_CURVE('',#35557,#35558,#3054,.T.) ;
#42917 = EDGE_CURVE('',#35558,#35555,#3055,.T.) ;
#42918 = EDGE_CURVE('',#35559,#35560,#3056,.T.) ;
#42919 = EDGE_CURVE('',#35560,#35561,#3057,.T.) ;
#42920 = EDGE_CURVE('',#35561,#35562,#3058,.T.) ;
#42921 = EDGE_CURVE('',#35562,#35559,#3059,.T.) ;
#42922 = EDGE_CURVE('',#35563,#35564,#307,.T.) ;
#42923 = EDGE_CURVE('',#35563,#35565,#3060,.T.) ;
#42924 = EDGE_CURVE('',#35565,#35566,#3061,.T.) ;
#42925 = EDGE_CURVE('',#35566,#35567,#3062,.T.) ;
#42926 = EDGE_CURVE('',#35568,#35567,#308,.T.) ;
#42927 = EDGE_CURVE('',#35568,#35569,#3063,.T.) ;
#42928 = EDGE_CURVE('',#35569,#35570,#3064,.T.) ;
#42929 = EDGE_CURVE('',#35570,#35564,#3065,.T.) ;
#42930 = EDGE_CURVE('',#35571,#35572,#3066,.T.) ;
#42931 = EDGE_CURVE('',#35572,#35573,#309,.T.) ;
#42932 = EDGE_CURVE('',#35574,#35573,#3067,.T.) ;
#42933 = EDGE_CURVE('',#35574,#35566,#310,.T.) ;
#42934 = EDGE_CURVE('',#35565,#35575,#311,.T.) ;
#42935 = EDGE_CURVE('',#35575,#35576,#3068,.T.) ;
#42936 = EDGE_CURVE('',#35576,#35571,#312,.T.) ;
#42937 = EDGE_CURVE('',#35577,#35578,#313,.T.) ;
#42938 = EDGE_CURVE('',#35577,#35572,#3069,.T.) ;
#42939 = EDGE_CURVE('',#35571,#35579,#3070,.T.) ;
#42940 = EDGE_CURVE('',#35580,#35579,#314,.T.) ;
#42941 = EDGE_CURVE('',#35580,#35581,#3071,.T.) ;
#42942 = EDGE_CURVE('',#35581,#35582,#3072,.T.) ;
#42943 = EDGE_CURVE('',#35582,#35578,#3073,.T.) ;
#42944 = EDGE_CURVE('',#35575,#35583,#3074,.T.) ;
#42945 = EDGE_CURVE('',#35583,#35584,#3075,.T.) ;
#42946 = EDGE_CURVE('',#35584,#35576,#3076,.T.) ;
#42947 = EDGE_CURVE('',#35573,#35585,#3077,.T.) ;
#42948 = EDGE_CURVE('',#35585,#35586,#3078,.T.) ;
#42949 = EDGE_CURVE('',#35586,#35574,#3079,.T.) ;
#42950 = EDGE_CURVE('',#35587,#35588,#3080,.T.) ;
#42951 = EDGE_CURVE('',#35588,#35589,#3081,.T.) ;
#42952 = EDGE_CURVE('',#35589,#35590,#3082,.T.) ;
#42953 = EDGE_CURVE('',#35590,#35591,#3083,.T.) ;
#42954 = EDGE_CURVE('',#35591,#35592,#3084,.T.) ;
#42955 = EDGE_CURVE('',#35592,#35587,#3085,.T.) ;
#42956 = EDGE_CURVE('',#35593,#35594,#3086,.T.) ;
#42957 = EDGE_CURVE('',#35594,#35595,#3087,.T.) ;
#42958 = EDGE_CURVE('',#35595,#35596,#3088,.T.) ;
#42959 = EDGE_CURVE('',#35596,#35597,#3089,.T.) ;
#42960 = EDGE_CURVE('',#35597,#35598,#3090,.T.) ;
#42961 = EDGE_CURVE('',#35598,#35593,#3091,.T.) ;
#42962 = EDGE_CURVE('',#35599,#35600,#3092,.T.) ;
#42963 = EDGE_CURVE('',#35600,#35601,#3093,.T.) ;
#42964 = EDGE_CURVE('',#35601,#35602,#3094,.T.) ;
#42965 = EDGE_CURVE('',#35602,#35599,#3095,.T.) ;
#42966 = EDGE_CURVE('',#35603,#35604,#3096,.T.) ;
#42967 = EDGE_CURVE('',#35604,#35605,#3097,.T.) ;
#42968 = EDGE_CURVE('',#35605,#35606,#3098,.T.) ;
#42969 = EDGE_CURVE('',#35606,#35603,#3099,.T.) ;
#42970 = EDGE_CURVE('',#35607,#35608,#3100,.T.) ;
#42971 = EDGE_CURVE('',#35608,#35609,#3101,.T.) ;
#42972 = EDGE_CURVE('',#35609,#35610,#3102,.T.) ;
#42973 = EDGE_CURVE('',#35610,#35607,#3103,.T.) ;
#42974 = EDGE_CURVE('',#35611,#35612,#3104,.T.) ;
#42975 = EDGE_CURVE('',#35612,#35613,#3105,.T.) ;
#42976 = EDGE_CURVE('',#35613,#35614,#3106,.T.) ;
#42977 = EDGE_CURVE('',#35614,#35611,#3107,.T.) ;
#42978 = EDGE_CURVE('',#35615,#35616,#3108,.T.) ;
#42979 = EDGE_CURVE('',#35616,#35617,#3109,.T.) ;
#42980 = EDGE_CURVE('',#35617,#35618,#3110,.T.) ;
#42981 = EDGE_CURVE('',#35618,#35615,#3111,.T.) ;
#42982 = EDGE_CURVE('',#35619,#35620,#3112,.T.) ;
#42983 = EDGE_CURVE('',#35621,#35619,#29187,.T.) ;
#42984 = EDGE_CURVE('',#35622,#35621,#3113,.T.) ;
#42985 = EDGE_CURVE('',#35623,#35622,#29188,.T.) ;
#42986 = EDGE_CURVE('',#35624,#35623,#3114,.T.) ;
#42987 = EDGE_CURVE('',#35625,#35624,#29189,.T.) ;
#42988 = EDGE_CURVE('',#35626,#35625,#3115,.T.) ;
#42989 = EDGE_CURVE('',#35620,#35626,#29190,.T.) ;
#42990 = EDGE_CURVE('',#35627,#35628,#29191,.T.) ;
#42991 = EDGE_CURVE('',#35620,#35627,#3116,.T.) ;
#42992 = EDGE_CURVE('',#35626,#35628,#3117,.T.) ;
#42993 = EDGE_CURVE('',#35629,#35627,#3118,.T.) ;
#42994 = EDGE_CURVE('',#35619,#35629,#3119,.T.) ;
#42995 = EDGE_CURVE('',#35630,#35629,#29192,.T.) ;
#42996 = EDGE_CURVE('',#35621,#35630,#3120,.T.) ;
#42997 = EDGE_CURVE('',#35631,#35630,#3121,.T.) ;
#42998 = EDGE_CURVE('',#35622,#35631,#3122,.T.) ;
#42999 = EDGE_CURVE('',#35632,#35631,#29193,.T.) ;
#43000 = EDGE_CURVE('',#35623,#35632,#3123,.T.) ;
#43001 = EDGE_CURVE('',#35633,#35632,#3124,.T.) ;
#43002 = EDGE_CURVE('',#35624,#35633,#3125,.T.) ;
#43003 = EDGE_CURVE('',#35634,#35633,#29194,.T.) ;
#43004 = EDGE_CURVE('',#35625,#35634,#3126,.T.) ;
#43005 = EDGE_CURVE('',#35628,#35634,#3127,.T.) ;
#43006 = EDGE_CURVE('',#35377,#35378,#3128,.T.) ;
#43007 = EDGE_CURVE('',#35375,#35380,#3129,.T.) ;
#43008 = EDGE_CURVE('',#35379,#35376,#3130,.T.) ;
#43009 = EDGE_CURVE('',#35383,#35372,#3131,.T.) ;
#43010 = EDGE_CURVE('',#35371,#35384,#3132,.T.) ;
#43011 = EDGE_CURVE('',#35373,#35382,#3133,.T.) ;
#43012 = EDGE_CURVE('',#35381,#35374,#3134,.T.) ;
#43013 = EDGE_CURVE('',#35635,#35636,#3135,.T.) ;
#43014 = EDGE_CURVE('',#35636,#35637,#3136,.T.) ;
#43015 = EDGE_CURVE('',#35637,#35638,#3137,.T.) ;
#43016 = EDGE_CURVE('',#35638,#35635,#3138,.T.) ;
#43017 = EDGE_CURVE('',#35639,#35640,#3139,.T.) ;
#43018 = EDGE_CURVE('',#35640,#35641,#3140,.T.) ;
#43019 = EDGE_CURVE('',#35641,#35642,#3141,.T.) ;
#43020 = EDGE_CURVE('',#35642,#35639,#3142,.T.) ;
#43021 = EDGE_CURVE('',#35643,#35644,#3143,.T.) ;
#43022 = EDGE_CURVE('',#35644,#35645,#3144,.T.) ;
#43023 = EDGE_CURVE('',#35645,#35646,#3145,.T.) ;
#43024 = EDGE_CURVE('',#35646,#35643,#3146,.T.) ;
#43025 = EDGE_CURVE('',#35647,#35648,#3147,.T.) ;
#43026 = EDGE_CURVE('',#35648,#35649,#3148,.T.) ;
#43027 = EDGE_CURVE('',#35649,#35650,#3149,.T.) ;
#43028 = EDGE_CURVE('',#35650,#35647,#3150,.T.) ;
#43029 = EDGE_CURVE('',#35651,#35652,#3151,.T.) ;
#43030 = EDGE_CURVE('',#35652,#35653,#3152,.T.) ;
#43031 = EDGE_CURVE('',#35653,#35654,#3153,.T.) ;
#43032 = EDGE_CURVE('',#35654,#35651,#3154,.T.) ;
#43033 = EDGE_CURVE('',#35655,#35656,#3155,.T.) ;
#43034 = EDGE_CURVE('',#35657,#35655,#29195,.T.) ;
#43035 = EDGE_CURVE('',#35658,#35657,#3156,.T.) ;
#43036 = EDGE_CURVE('',#35659,#35658,#29196,.T.) ;
#43037 = EDGE_CURVE('',#35660,#35659,#3157,.T.) ;
#43038 = EDGE_CURVE('',#35661,#35660,#29197,.T.) ;
#43039 = EDGE_CURVE('',#35662,#35661,#3158,.T.) ;
#43040 = EDGE_CURVE('',#35656,#35662,#29198,.T.) ;
#43041 = EDGE_CURVE('',#35662,#35663,#3159,.T.) ;
#43042 = EDGE_CURVE('',#35663,#35664,#29199,.T.) ;
#43043 = EDGE_CURVE('',#35656,#35664,#3160,.T.) ;
#43044 = EDGE_CURVE('',#35664,#35665,#3161,.T.) ;
#43045 = EDGE_CURVE('',#35655,#35665,#3162,.T.) ;
#43046 = EDGE_CURVE('',#35665,#35666,#29200,.T.) ;
#43047 = EDGE_CURVE('',#35657,#35666,#3163,.T.) ;
#43048 = EDGE_CURVE('',#35666,#35667,#3164,.T.) ;
#43049 = EDGE_CURVE('',#35658,#35667,#3165,.T.) ;
#43050 = EDGE_CURVE('',#35667,#35668,#29201,.T.) ;
#43051 = EDGE_CURVE('',#35659,#35668,#3166,.T.) ;
#43052 = EDGE_CURVE('',#35668,#35669,#3167,.T.) ;
#43053 = EDGE_CURVE('',#35660,#35669,#3168,.T.) ;
#43054 = EDGE_CURVE('',#35669,#35670,#29202,.T.) ;
#43055 = EDGE_CURVE('',#35661,#35670,#3169,.T.) ;
#43056 = EDGE_CURVE('',#35670,#35663,#3170,.T.) ;
#43057 = EDGE_CURVE('',#35671,#35672,#3171,.T.) ;
#43058 = EDGE_CURVE('',#35672,#35673,#3172,.T.) ;
#43059 = EDGE_CURVE('',#35673,#35674,#3173,.T.) ;
#43060 = EDGE_CURVE('',#35674,#35671,#3174,.T.) ;
#43061 = EDGE_CURVE('',#35366,#35342,#3175,.T.) ;
#43062 = EDGE_CURVE('',#35342,#35675,#3176,.T.) ;
#43063 = EDGE_CURVE('',#35675,#35676,#3177,.T.) ;
#43064 = EDGE_CURVE('',#35676,#35366,#3178,.T.) ;
#43065 = EDGE_CURVE('',#35677,#35363,#3179,.T.) ;
#43066 = EDGE_CURVE('',#35356,#35678,#3180,.T.) ;
#43067 = EDGE_CURVE('',#35678,#35677,#3181,.T.) ;
#43068 = EDGE_CURVE('',#35364,#35679,#3182,.T.) ;
#43069 = EDGE_CURVE('',#35679,#35360,#3183,.T.) ;
#43070 = EDGE_CURVE('',#35360,#35357,#3184,.T.) ;
#43071 = EDGE_CURVE('',#35341,#35680,#3185,.T.) ;
#43072 = EDGE_CURVE('',#35680,#35681,#29203,.T.) ;
#43073 = EDGE_CURVE('',#35681,#35682,#3186,.T.) ;
#43074 = EDGE_CURVE('',#35682,#35683,#3187,.T.) ;
#43075 = EDGE_CURVE('',#35683,#35340,#3188,.T.) ;
#43076 = EDGE_CURVE('',#35684,#35685,#29204,.T.) ;
#43077 = EDGE_CURVE('',#35685,#35686,#29205,.T.) ;
#43078 = EDGE_CURVE('',#35686,#35687,#29206,.T.) ;
#43079 = EDGE_CURVE('',#35687,#35688,#3189,.T.) ;
#43080 = EDGE_CURVE('',#35688,#35689,#29207,.T.) ;
#43081 = EDGE_CURVE('',#35689,#35684,#3190,.T.) ;
#43082 = EDGE_CURVE('',#35593,#35502,#29208,.T.) ;
#43083 = EDGE_CURVE('',#35561,#35593,#2097,.T.) ;
#43084 = EDGE_CURVE('',#35503,#35561,#29209,.T.) ;
#43085 = EDGE_CURVE('',#35583,#35563,#29210,.T.) ;
#43086 = EDGE_CURVE('',#35597,#35564,#29211,.T.) ;
#43087 = EDGE_CURVE('',#35583,#35597,#315,.T.) ;
#43088 = EDGE_CURVE('',#35598,#35570,#29212,.T.) ;
#43089 = EDGE_CURVE('',#35562,#35598,#29213,.T.) ;
#43090 = EDGE_CURVE('',#35504,#35560,#29214,.T.) ;
#43091 = EDGE_CURVE('',#35594,#35501,#29215,.T.) ;
#43092 = EDGE_CURVE('',#35584,#35596,#316,.T.) ;
#43093 = EDGE_CURVE('',#35579,#35584,#29216,.T.) ;
#43094 = EDGE_CURVE('',#35562,#35570,#29217,.T.) ;
#43095 = EDGE_CURVE('',#35591,#35560,#317,.T.) ;
#43096 = EDGE_CURVE('',#35505,#35591,#29218,.T.) ;
#43097 = EDGE_CURVE('',#35556,#35508,#29219,.T.) ;
#43098 = EDGE_CURVE('',#35594,#35556,#2098,.T.) ;
#43099 = EDGE_CURVE('',#35580,#35596,#29220,.T.) ;
#43100 = EDGE_CURVE('',#35559,#35569,#29221,.T.) ;
#43101 = EDGE_CURVE('',#35592,#35559,#29222,.T.) ;
#43102 = EDGE_CURVE('',#35506,#35590,#29223,.T.) ;
#43103 = EDGE_CURVE('',#35557,#35507,#29224,.T.) ;
#43104 = EDGE_CURVE('',#35595,#35555,#29225,.T.) ;
#43105 = EDGE_CURVE('',#35581,#35595,#29226,.T.) ;
#43106 = EDGE_CURVE('',#35592,#35569,#29227,.T.) ;
#43107 = EDGE_CURVE('',#35557,#35590,#318,.T.) ;
#43108 = EDGE_CURVE('',#35581,#35555,#29228,.T.) ;
#43109 = EDGE_CURVE('',#35567,#35586,#29229,.T.) ;
#43110 = EDGE_CURVE('',#35587,#35568,#29230,.T.) ;
#43111 = EDGE_CURVE('',#35558,#35589,#29231,.T.) ;
#43112 = EDGE_CURVE('',#35582,#35558,#29232,.T.) ;
#43113 = EDGE_CURVE('',#35587,#35586,#319,.T.) ;
#43114 = EDGE_CURVE('',#35582,#35589,#29233,.T.) ;
#43115 = EDGE_CURVE('',#35588,#35585,#320,.T.) ;
#43116 = EDGE_CURVE('',#35578,#35588,#29234,.T.) ;
#43117 = EDGE_CURVE('',#35577,#35585,#29235,.T.) ;
#43118 = EDGE_CURVE('',#35426,#35690,#321,.T.) ;
#43119 = EDGE_CURVE('',#35690,#35343,#2099,.T.) ;
#43120 = EDGE_CURVE('',#35675,#35677,#29236,.T.) ;
#43121 = EDGE_CURVE('',#35676,#35678,#29237,.T.) ;
#43122 = EDGE_CURVE('',#35441,#35676,#29238,.T.) ;
#43123 = EDGE_CURVE('',#35453,#35680,#2100,.T.) ;
#43124 = EDGE_CURVE('',#35341,#35454,#2101,.T.) ;
#43125 = EDGE_CURVE('',#35682,#35363,#29239,.T.) ;
#43126 = EDGE_CURVE('',#35677,#35683,#29240,.T.) ;
#43127 = EDGE_CURVE('',#35442,#35678,#29241,.T.) ;
#43128 = EDGE_CURVE('',#35691,#35692,#2102,.T.) ;
#43129 = EDGE_CURVE('',#35692,#35443,#322,.T.) ;
#43130 = EDGE_CURVE('',#35679,#35691,#29242,.T.) ;
#43131 = EDGE_CURVE('',#35666,#35671,#29243,.T.) ;
#43132 = EDGE_CURVE('',#35671,#35665,#29244,.T.) ;
#43133 = EDGE_CURVE('',#35672,#35664,#29245,.T.) ;
#43134 = EDGE_CURVE('',#35667,#35674,#29246,.T.) ;
#43135 = EDGE_CURVE('',#35672,#35663,#29247,.T.) ;
#43136 = EDGE_CURVE('',#35668,#35674,#29248,.T.) ;
#43137 = EDGE_CURVE('',#35673,#35670,#29249,.T.) ;
#43138 = EDGE_CURVE('',#35669,#35673,#29250,.T.) ;
#43139 = EDGE_CURVE('',#35527,#35602,#29251,.T.) ;
#43140 = EDGE_CURVE('',#35599,#35526,#29252,.T.) ;
#43141 = EDGE_CURVE('',#35614,#35525,#29253,.T.) ;
#43142 = EDGE_CURVE('',#35599,#35614,#29254,.T.) ;
#43143 = EDGE_CURVE('',#35606,#35602,#29255,.T.) ;
#43144 = EDGE_CURVE('',#35528,#35606,#29256,.T.) ;
#43145 = EDGE_CURVE('',#35611,#35524,#29257,.T.) ;
#43146 = EDGE_CURVE('',#35600,#35613,#29258,.T.) ;
#43147 = EDGE_CURVE('',#35601,#35618,#29259,.T.) ;
#43148 = EDGE_CURVE('',#35615,#35600,#29260,.T.) ;
#43149 = EDGE_CURVE('',#35603,#35601,#29261,.T.) ;
#43150 = EDGE_CURVE('',#35522,#35605,#29262,.T.) ;
#43151 = EDGE_CURVE('',#35523,#35609,#29263,.T.) ;
#43152 = EDGE_CURVE('',#35610,#35521,#29264,.T.) ;
#43153 = EDGE_CURVE('',#35611,#35609,#29265,.T.) ;
#43154 = EDGE_CURVE('',#35615,#35613,#29266,.T.) ;
#43155 = EDGE_CURVE('',#35603,#35618,#29267,.T.) ;
#43156 = EDGE_CURVE('',#35610,#35605,#29268,.T.) ;
#43157 = EDGE_CURVE('',#35612,#35608,#29269,.T.) ;
#43158 = EDGE_CURVE('',#35616,#35612,#29270,.T.) ;
#43159 = EDGE_CURVE('',#35604,#35617,#29271,.T.) ;
#43160 = EDGE_CURVE('',#35607,#35604,#29272,.T.) ;
#43161 = EDGE_CURVE('',#35616,#35608,#29273,.T.) ;
#43162 = EDGE_CURVE('',#35607,#35617,#29274,.T.) ;
#43163 = EDGE_CURVE('',#35479,#35646,#29275,.T.) ;
#43164 = EDGE_CURVE('',#35643,#35478,#29276,.T.) ;
#43165 = EDGE_CURVE('',#35642,#35477,#29277,.T.) ;
#43166 = EDGE_CURVE('',#35643,#35642,#29278,.T.) ;
#43167 = EDGE_CURVE('',#35650,#35646,#29279,.T.) ;
#43168 = EDGE_CURVE('',#35480,#35650,#29280,.T.) ;
#43169 = EDGE_CURVE('',#35639,#35476,#29281,.T.) ;
#43170 = EDGE_CURVE('',#35644,#35641,#29282,.T.) ;
#43171 = EDGE_CURVE('',#35645,#35654,#29283,.T.) ;
#43172 = EDGE_CURVE('',#35651,#35644,#29284,.T.) ;
#43173 = EDGE_CURVE('',#35647,#35645,#29285,.T.) ;
#43174 = EDGE_CURVE('',#35474,#35649,#29286,.T.) ;
#43175 = EDGE_CURVE('',#35475,#35637,#29287,.T.) ;
#43176 = EDGE_CURVE('',#35638,#35473,#29288,.T.) ;
#43177 = EDGE_CURVE('',#35639,#35637,#29289,.T.) ;
#43178 = EDGE_CURVE('',#35651,#35641,#29290,.T.) ;
#43179 = EDGE_CURVE('',#35647,#35654,#29291,.T.) ;
#43180 = EDGE_CURVE('',#35638,#35649,#29292,.T.) ;
#43181 = EDGE_CURVE('',#35640,#35636,#29293,.T.) ;
#43182 = EDGE_CURVE('',#35652,#35640,#29294,.T.) ;
#43183 = EDGE_CURVE('',#35648,#35653,#29295,.T.) ;
#43184 = EDGE_CURVE('',#35635,#35648,#29296,.T.) ;
#43185 = EDGE_CURVE('',#35652,#35636,#29297,.T.) ;
#43186 = EDGE_CURVE('',#35635,#35653,#29298,.T.) ;
#43187 = EDGE_CURVE('',#35550,#35685,#2103,.T.) ;
#43188 = EDGE_CURVE('',#35547,#35684,#29299,.T.) ;
#43189 = EDGE_CURVE('',#35548,#35422,#29300,.T.) ;
#43190 = EDGE_CURVE('',#35423,#35547,#29301,.T.) ;
#43191 = EDGE_CURVE('',#35423,#35684,#29302,.T.) ;
#43192 = EDGE_CURVE('',#35420,#35689,#29303,.T.) ;
#43193 = EDGE_CURVE('',#35421,#35434,#29304,.T.) ;
#43194 = EDGE_CURVE('',#35435,#35420,#29305,.T.) ;
#43195 = EDGE_CURVE('',#35436,#35689,#29306,.T.) ;
#43196 = EDGE_CURVE('',#35437,#35688,#29307,.T.) ;
#43197 = EDGE_CURVE('',#35551,#35438,#29308,.T.) ;
#43198 = EDGE_CURVE('',#35551,#35688,#29309,.T.) ;
#43199 = EDGE_CURVE('',#35552,#35687,#29310,.T.) ;
#43200 = EDGE_CURVE('',#35416,#35552,#29311,.T.) ;
#43201 = EDGE_CURVE('',#35416,#35687,#29312,.T.) ;
#43202 = EDGE_CURVE('',#35686,#35417,#2104,.T.) ;
#43203 = EDGE_CURVE('',#35531,#35544,#29313,.T.) ;
#43204 = EDGE_CURVE('',#35511,#35532,#29314,.T.) ;
#43205 = EDGE_CURVE('',#35491,#35512,#29315,.T.) ;
#43206 = EDGE_CURVE('',#35488,#35492,#29316,.T.) ;
#43207 = EDGE_CURVE('',#35483,#35486,#29317,.T.) ;
#43208 = EDGE_CURVE('',#35463,#35484,#29318,.T.) ;
#43209 = EDGE_CURVE('',#35460,#35464,#29319,.T.) ;
#43210 = EDGE_CURVE('',#35387,#35458,#29320,.T.) ;
#43211 = EDGE_CURVE('',#35446,#35388,#29321,.T.) ;
#43212 = EDGE_CURVE('',#35364,#35682,#29322,.T.) ;
#43213 = EDGE_CURVE('',#35679,#35681,#29323,.T.) ;
#43214 = EDGE_CURVE('',#35691,#35680,#29324,.T.) ;
#43215 = EDGE_CURVE('',#35692,#35453,#29325,.T.) ;
#43216 = EDGE_CURVE('',#35443,#35452,#29326,.T.) ;
#43217 = EDGE_CURVE('',#35444,#35451,#29327,.T.) ;
#43218 = EDGE_CURVE('',#35426,#35455,#29328,.T.) ;
#43219 = EDGE_CURVE('',#35690,#35454,#29329,.T.) ;
#43220 = EDGE_CURVE('',#35675,#35683,#29330,.T.) ;
#43221 = EDGE_CURVE('',#35693,#35694,#2105,.T.) ;
#43222 = EDGE_CURVE('',#35694,#35686,#2106,.T.) ;
#43223 = EDGE_CURVE('',#35685,#35695,#2107,.T.) ;
#43224 = EDGE_CURVE('',#35695,#35693,#2108,.T.) ;
#43225 = EDGE_CURVE('',#35538,#35549,#29331,.T.) ;
#43226 = EDGE_CURVE('',#35550,#35537,#29332,.T.) ;
#43227 = EDGE_CURVE('',#35536,#35685,#2109,.T.) ;
#43228 = EDGE_CURVE('',#35533,#35417,#29333,.T.) ;
#43229 = EDGE_CURVE('',#35686,#35534,#2110,.T.) ;
#43230 = EDGE_CURVE('',#35695,#35536,#29334,.T.) ;
#43231 = EDGE_CURVE('',#35693,#35535,#29335,.T.) ;
#43232 = EDGE_CURVE('',#35694,#35534,#29336,.T.) ;
#43233 = EDGE_CURVE('',#35696,#35697,#3191,.T.) ;
#43234 = EDGE_CURVE('',#35697,#35698,#3192,.T.) ;
#43235 = EDGE_CURVE('',#35699,#35698,#3193,.T.) ;
#43236 = EDGE_CURVE('',#35699,#35696,#3194,.T.) ;
#43237 = EDGE_CURVE('',#35698,#35700,#29337,.T.) ;
#43238 = EDGE_CURVE('',#35701,#35700,#3195,.T.) ;
#43239 = EDGE_CURVE('',#35701,#35699,#29338,.T.) ;
#43240 = EDGE_CURVE('',#35700,#35702,#3196,.T.) ;
#43241 = EDGE_CURVE('',#35703,#35702,#3197,.T.) ;
#43242 = EDGE_CURVE('',#35703,#35701,#3198,.T.) ;
#43243 = EDGE_CURVE('',#35702,#35704,#29339,.T.) ;
#43244 = EDGE_CURVE('',#35705,#35704,#3199,.T.) ;
#43245 = EDGE_CURVE('',#35705,#35703,#29340,.T.) ;
#43246 = EDGE_CURVE('',#35704,#35706,#3200,.T.) ;
#43247 = EDGE_CURVE('',#35707,#35706,#3201,.T.) ;
#43248 = EDGE_CURVE('',#35707,#35705,#3202,.T.) ;
#43249 = EDGE_CURVE('',#35706,#35708,#29341,.T.) ;
#43250 = EDGE_CURVE('',#35709,#35708,#3203,.T.) ;
#43251 = EDGE_CURVE('',#35709,#35707,#29342,.T.) ;
#43252 = EDGE_CURVE('',#35708,#35710,#3204,.T.) ;
#43253 = EDGE_CURVE('',#35711,#35710,#3205,.T.) ;
#43254 = EDGE_CURVE('',#35711,#35709,#3206,.T.) ;
#43255 = EDGE_CURVE('',#35710,#35712,#29343,.T.) ;
#43256 = EDGE_CURVE('',#35713,#35712,#3207,.T.) ;
#43257 = EDGE_CURVE('',#35713,#35711,#29344,.T.) ;
#43258 = EDGE_CURVE('',#35712,#35714,#3208,.T.) ;
#43259 = EDGE_CURVE('',#35714,#35715,#3209,.T.) ;
#43260 = EDGE_CURVE('',#35715,#35713,#3210,.T.) ;
#43261 = EDGE_CURVE('',#35716,#35717,#29345,.T.) ;
#43262 = EDGE_CURVE('',#35717,#35718,#3211,.T.) ;
#43263 = EDGE_CURVE('',#35718,#35719,#3212,.T.) ;
#43264 = EDGE_CURVE('',#35719,#35720,#3213,.T.) ;
#43265 = EDGE_CURVE('',#35720,#35721,#3214,.T.) ;
#43266 = EDGE_CURVE('',#35721,#35722,#3215,.T.) ;
#43267 = EDGE_CURVE('',#35722,#35716,#3216,.T.) ;
#43268 = EDGE_CURVE('',#35723,#35724,#3217,.T.) ;
#43269 = EDGE_CURVE('',#35724,#35725,#3218,.T.) ;
#43270 = EDGE_CURVE('',#35725,#35726,#3219,.T.) ;
#43271 = EDGE_CURVE('',#35726,#35727,#3220,.T.) ;
#43272 = EDGE_CURVE('',#35727,#35728,#29346,.T.) ;
#43273 = EDGE_CURVE('',#35728,#35729,#3221,.T.) ;
#43274 = EDGE_CURVE('',#35729,#35723,#3222,.T.) ;
#43275 = EDGE_CURVE('',#35730,#35731,#3223,.T.) ;
#43276 = EDGE_CURVE('',#35730,#35732,#3224,.T.) ;
#43277 = EDGE_CURVE('',#35732,#35733,#3225,.T.) ;
#43278 = EDGE_CURVE('',#35733,#35731,#3226,.T.) ;
#43279 = EDGE_CURVE('',#35339,#35323,#3227,.T.) ;
#43280 = EDGE_CURVE('',#35315,#35734,#3228,.T.) ;
#43281 = EDGE_CURVE('',#35734,#35735,#3229,.T.) ;
#43282 = EDGE_CURVE('',#35736,#35735,#3230,.T.) ;
#43283 = EDGE_CURVE('',#35736,#35315,#3231,.T.) ;
#43284 = EDGE_CURVE('',#35737,#35738,#3232,.T.) ;
#43285 = EDGE_CURVE('',#35737,#35739,#3233,.T.) ;
#43286 = EDGE_CURVE('',#35739,#35740,#29347,.T.) ;
#43287 = EDGE_CURVE('',#35740,#35738,#3234,.T.) ;
#43288 = EDGE_CURVE('',#35543,#35737,#29348,.T.) ;
#43289 = EDGE_CURVE('',#35738,#35730,#29349,.T.) ;
#43290 = EDGE_CURVE('',#35731,#35430,#29350,.T.) ;
#43291 = EDGE_CURVE('',#35429,#35736,#29351,.T.) ;
#43292 = EDGE_CURVE('',#35735,#35447,#29352,.T.) ;
#43293 = EDGE_CURVE('',#35741,#35742,#3235,.T.) ;
#43294 = EDGE_CURVE('',#35742,#35743,#3236,.T.) ;
#43295 = EDGE_CURVE('',#35743,#35744,#3237,.T.) ;
#43296 = EDGE_CURVE('',#35744,#35741,#3238,.T.) ;
#43297 = EDGE_CURVE('',#35745,#35746,#3239,.T.) ;
#43298 = EDGE_CURVE('',#35746,#35747,#3240,.T.) ;
#43299 = EDGE_CURVE('',#35747,#35748,#3241,.T.) ;
#43300 = EDGE_CURVE('',#35748,#35745,#3242,.T.) ;
#43301 = EDGE_CURVE('',#35749,#35750,#323,.T.) ;
#43302 = EDGE_CURVE('',#35749,#35751,#3243,.T.) ;
#43303 = EDGE_CURVE('',#35751,#35752,#3244,.T.) ;
#43304 = EDGE_CURVE('',#35752,#35753,#3245,.T.) ;
#43305 = EDGE_CURVE('',#35754,#35753,#324,.T.) ;
#43306 = EDGE_CURVE('',#35754,#35755,#3246,.T.) ;
#43307 = EDGE_CURVE('',#35755,#35756,#3247,.T.) ;
#43308 = EDGE_CURVE('',#35756,#35750,#3248,.T.) ;
#43309 = EDGE_CURVE('',#35757,#35758,#3249,.T.) ;
#43310 = EDGE_CURVE('',#35758,#35759,#325,.T.) ;
#43311 = EDGE_CURVE('',#35760,#35759,#3250,.T.) ;
#43312 = EDGE_CURVE('',#35760,#35752,#326,.T.) ;
#43313 = EDGE_CURVE('',#35751,#35761,#327,.T.) ;
#43314 = EDGE_CURVE('',#35761,#35762,#3251,.T.) ;
#43315 = EDGE_CURVE('',#35762,#35757,#328,.T.) ;
#43316 = EDGE_CURVE('',#35763,#35764,#329,.T.) ;
#43317 = EDGE_CURVE('',#35763,#35758,#3252,.T.) ;
#43318 = EDGE_CURVE('',#35757,#35765,#3253,.T.) ;
#43319 = EDGE_CURVE('',#35766,#35765,#330,.T.) ;
#43320 = EDGE_CURVE('',#35766,#35767,#3254,.T.) ;
#43321 = EDGE_CURVE('',#35767,#35768,#3255,.T.) ;
#43322 = EDGE_CURVE('',#35768,#35764,#3256,.T.) ;
#43323 = EDGE_CURVE('',#35761,#35769,#3257,.T.) ;
#43324 = EDGE_CURVE('',#35769,#35770,#3258,.T.) ;
#43325 = EDGE_CURVE('',#35770,#35762,#3259,.T.) ;
#43326 = EDGE_CURVE('',#35759,#35771,#3260,.T.) ;
#43327 = EDGE_CURVE('',#35771,#35772,#3261,.T.) ;
#43328 = EDGE_CURVE('',#35772,#35760,#3262,.T.) ;
#43329 = EDGE_CURVE('',#35773,#35774,#3263,.T.) ;
#43330 = EDGE_CURVE('',#35774,#35775,#3264,.T.) ;
#43331 = EDGE_CURVE('',#35775,#35776,#3265,.T.) ;
#43332 = EDGE_CURVE('',#35776,#35777,#3266,.T.) ;
#43333 = EDGE_CURVE('',#35777,#35778,#3267,.T.) ;
#43334 = EDGE_CURVE('',#35778,#35773,#3268,.T.) ;
#43335 = EDGE_CURVE('',#35779,#35780,#3269,.T.) ;
#43336 = EDGE_CURVE('',#35780,#35781,#3270,.T.) ;
#43337 = EDGE_CURVE('',#35781,#35782,#3271,.T.) ;
#43338 = EDGE_CURVE('',#35782,#35783,#3272,.T.) ;
#43339 = EDGE_CURVE('',#35783,#35784,#3273,.T.) ;
#43340 = EDGE_CURVE('',#35784,#35779,#3274,.T.) ;
#43341 = EDGE_CURVE('',#35785,#35786,#3275,.T.) ;
#43342 = EDGE_CURVE('',#35786,#35787,#3276,.T.) ;
#43343 = EDGE_CURVE('',#35787,#35788,#3277,.T.) ;
#43344 = EDGE_CURVE('',#35788,#35785,#3278,.T.) ;
#43345 = EDGE_CURVE('',#35789,#35790,#3279,.T.) ;
#43346 = EDGE_CURVE('',#35790,#35791,#3280,.T.) ;
#43347 = EDGE_CURVE('',#35791,#35792,#3281,.T.) ;
#43348 = EDGE_CURVE('',#35792,#35789,#3282,.T.) ;
#43349 = EDGE_CURVE('',#35793,#35794,#3283,.T.) ;
#43350 = EDGE_CURVE('',#35794,#35795,#3284,.T.) ;
#43351 = EDGE_CURVE('',#35795,#35796,#3285,.T.) ;
#43352 = EDGE_CURVE('',#35796,#35793,#3286,.T.) ;
#43353 = EDGE_CURVE('',#35797,#35798,#3287,.T.) ;
#43354 = EDGE_CURVE('',#35798,#35799,#3288,.T.) ;
#43355 = EDGE_CURVE('',#35799,#35800,#3289,.T.) ;
#43356 = EDGE_CURVE('',#35800,#35797,#3290,.T.) ;
#43357 = EDGE_CURVE('',#35801,#35802,#3291,.T.) ;
#43358 = EDGE_CURVE('',#35802,#35803,#3292,.T.) ;
#43359 = EDGE_CURVE('',#35803,#35804,#3293,.T.) ;
#43360 = EDGE_CURVE('',#35804,#35801,#3294,.T.) ;
#43361 = EDGE_CURVE('',#35805,#35806,#3295,.T.) ;
#43362 = EDGE_CURVE('',#35807,#35805,#29353,.T.) ;
#43363 = EDGE_CURVE('',#35808,#35807,#3296,.T.) ;
#43364 = EDGE_CURVE('',#35809,#35808,#29354,.T.) ;
#43365 = EDGE_CURVE('',#35810,#35809,#3297,.T.) ;
#43366 = EDGE_CURVE('',#35811,#35810,#29355,.T.) ;
#43367 = EDGE_CURVE('',#35812,#35811,#3298,.T.) ;
#43368 = EDGE_CURVE('',#35806,#35812,#29356,.T.) ;
#43369 = EDGE_CURVE('',#35813,#35814,#29357,.T.) ;
#43370 = EDGE_CURVE('',#35806,#35813,#3299,.T.) ;
#43371 = EDGE_CURVE('',#35812,#35814,#3300,.T.) ;
#43372 = EDGE_CURVE('',#35815,#35813,#3301,.T.) ;
#43373 = EDGE_CURVE('',#35805,#35815,#3302,.T.) ;
#43374 = EDGE_CURVE('',#35816,#35815,#29358,.T.) ;
#43375 = EDGE_CURVE('',#35807,#35816,#3303,.T.) ;
#43376 = EDGE_CURVE('',#35817,#35816,#3304,.T.) ;
#43377 = EDGE_CURVE('',#35808,#35817,#3305,.T.) ;
#43378 = EDGE_CURVE('',#35818,#35817,#29359,.T.) ;
#43379 = EDGE_CURVE('',#35809,#35818,#3306,.T.) ;
#43380 = EDGE_CURVE('',#35819,#35818,#3307,.T.) ;
#43381 = EDGE_CURVE('',#35810,#35819,#3308,.T.) ;
#43382 = EDGE_CURVE('',#35820,#35819,#29360,.T.) ;
#43383 = EDGE_CURVE('',#35811,#35820,#3309,.T.) ;
#43384 = EDGE_CURVE('',#35814,#35820,#3310,.T.) ;
#43385 = EDGE_CURVE('',#35331,#35332,#3311,.T.) ;
#43386 = EDGE_CURVE('',#35329,#35334,#3312,.T.) ;
#43387 = EDGE_CURVE('',#35333,#35330,#3313,.T.) ;
#43388 = EDGE_CURVE('',#35337,#35326,#3314,.T.) ;
#43389 = EDGE_CURVE('',#35325,#35338,#3315,.T.) ;
#43390 = EDGE_CURVE('',#35327,#35336,#3316,.T.) ;
#43391 = EDGE_CURVE('',#35335,#35328,#3317,.T.) ;
#43392 = EDGE_CURVE('',#35821,#35822,#3318,.T.) ;
#43393 = EDGE_CURVE('',#35822,#35823,#3319,.T.) ;
#43394 = EDGE_CURVE('',#35823,#35824,#3320,.T.) ;
#43395 = EDGE_CURVE('',#35824,#35821,#3321,.T.) ;
#43396 = EDGE_CURVE('',#35825,#35826,#3322,.T.) ;
#43397 = EDGE_CURVE('',#35826,#35827,#3323,.T.) ;
#43398 = EDGE_CURVE('',#35827,#35828,#3324,.T.) ;
#43399 = EDGE_CURVE('',#35828,#35825,#3325,.T.) ;
#43400 = EDGE_CURVE('',#35829,#35830,#3326,.T.) ;
#43401 = EDGE_CURVE('',#35830,#35831,#3327,.T.) ;
#43402 = EDGE_CURVE('',#35831,#35832,#3328,.T.) ;
#43403 = EDGE_CURVE('',#35832,#35829,#3329,.T.) ;
#43404 = EDGE_CURVE('',#35833,#35834,#3330,.T.) ;
#43405 = EDGE_CURVE('',#35834,#35835,#3331,.T.) ;
#43406 = EDGE_CURVE('',#35835,#35836,#3332,.T.) ;
#43407 = EDGE_CURVE('',#35836,#35833,#3333,.T.) ;
#43408 = EDGE_CURVE('',#35837,#35838,#3334,.T.) ;
#43409 = EDGE_CURVE('',#35838,#35839,#3335,.T.) ;
#43410 = EDGE_CURVE('',#35839,#35840,#3336,.T.) ;
#43411 = EDGE_CURVE('',#35840,#35837,#3337,.T.) ;
#43412 = EDGE_CURVE('',#35841,#35842,#3338,.T.) ;
#43413 = EDGE_CURVE('',#35843,#35841,#29361,.T.) ;
#43414 = EDGE_CURVE('',#35844,#35843,#3339,.T.) ;
#43415 = EDGE_CURVE('',#35845,#35844,#29362,.T.) ;
#43416 = EDGE_CURVE('',#35846,#35845,#3340,.T.) ;
#43417 = EDGE_CURVE('',#35847,#35846,#29363,.T.) ;
#43418 = EDGE_CURVE('',#35848,#35847,#3341,.T.) ;
#43419 = EDGE_CURVE('',#35842,#35848,#29364,.T.) ;
#43420 = EDGE_CURVE('',#35848,#35849,#3342,.T.) ;
#43421 = EDGE_CURVE('',#35849,#35850,#29365,.T.) ;
#43422 = EDGE_CURVE('',#35842,#35850,#3343,.T.) ;
#43423 = EDGE_CURVE('',#35850,#35851,#3344,.T.) ;
#43424 = EDGE_CURVE('',#35841,#35851,#3345,.T.) ;
#43425 = EDGE_CURVE('',#35851,#35852,#29366,.T.) ;
#43426 = EDGE_CURVE('',#35843,#35852,#3346,.T.) ;
#43427 = EDGE_CURVE('',#35852,#35853,#3347,.T.) ;
#43428 = EDGE_CURVE('',#35844,#35853,#3348,.T.) ;
#43429 = EDGE_CURVE('',#35853,#35854,#29367,.T.) ;
#43430 = EDGE_CURVE('',#35845,#35854,#3349,.T.) ;
#43431 = EDGE_CURVE('',#35854,#35855,#3350,.T.) ;
#43432 = EDGE_CURVE('',#35846,#35855,#3351,.T.) ;
#43433 = EDGE_CURVE('',#35855,#35856,#29368,.T.) ;
#43434 = EDGE_CURVE('',#35847,#35856,#3352,.T.) ;
#43435 = EDGE_CURVE('',#35856,#35849,#3353,.T.) ;
#43436 = EDGE_CURVE('',#35857,#35858,#3354,.T.) ;
#43437 = EDGE_CURVE('',#35858,#35859,#3355,.T.) ;
#43438 = EDGE_CURVE('',#35859,#35860,#3356,.T.) ;
#43439 = EDGE_CURVE('',#35860,#35857,#3357,.T.) ;
#43440 = EDGE_CURVE('',#35320,#35300,#3358,.T.) ;
#43441 = EDGE_CURVE('',#35300,#35861,#3359,.T.) ;
#43442 = EDGE_CURVE('',#35861,#35862,#3360,.T.) ;
#43443 = EDGE_CURVE('',#35862,#35320,#3361,.T.) ;
#43444 = EDGE_CURVE('',#35863,#35317,#3362,.T.) ;
#43445 = EDGE_CURVE('',#35310,#35864,#3363,.T.) ;
#43446 = EDGE_CURVE('',#35864,#35863,#3364,.T.) ;
#43447 = EDGE_CURVE('',#35318,#35865,#3365,.T.) ;
#43448 = EDGE_CURVE('',#35865,#35314,#3366,.T.) ;
#43449 = EDGE_CURVE('',#35314,#35311,#3367,.T.) ;
#43450 = EDGE_CURVE('',#35299,#35866,#3368,.T.) ;
#43451 = EDGE_CURVE('',#35866,#35867,#29369,.T.) ;
#43452 = EDGE_CURVE('',#35867,#35868,#3369,.T.) ;
#43453 = EDGE_CURVE('',#35868,#35869,#3370,.T.) ;
#43454 = EDGE_CURVE('',#35869,#35298,#3371,.T.) ;
#43455 = EDGE_CURVE('',#35870,#35871,#29370,.T.) ;
#43456 = EDGE_CURVE('',#35871,#35872,#29371,.T.) ;
#43457 = EDGE_CURVE('',#35872,#35873,#29372,.T.) ;
#43458 = EDGE_CURVE('',#35873,#35874,#3372,.T.) ;
#43459 = EDGE_CURVE('',#35874,#35875,#29373,.T.) ;
#43460 = EDGE_CURVE('',#35875,#35870,#3373,.T.) ;
#43461 = EDGE_CURVE('',#35779,#35494,#29374,.T.) ;
#43462 = EDGE_CURVE('',#35747,#35779,#2111,.T.) ;
#43463 = EDGE_CURVE('',#35495,#35747,#29375,.T.) ;
#43464 = EDGE_CURVE('',#35769,#35749,#29376,.T.) ;
#43465 = EDGE_CURVE('',#35783,#35750,#29377,.T.) ;
#43466 = EDGE_CURVE('',#35769,#35783,#331,.T.) ;
#43467 = EDGE_CURVE('',#35784,#35756,#29378,.T.) ;
#43468 = EDGE_CURVE('',#35748,#35784,#29379,.T.) ;
#43469 = EDGE_CURVE('',#35496,#35746,#29380,.T.) ;
#43470 = EDGE_CURVE('',#35780,#35493,#29381,.T.) ;
#43471 = EDGE_CURVE('',#35770,#35782,#332,.T.) ;
#43472 = EDGE_CURVE('',#35765,#35770,#29382,.T.) ;
#43473 = EDGE_CURVE('',#35748,#35756,#29383,.T.) ;
#43474 = EDGE_CURVE('',#35777,#35746,#333,.T.) ;
#43475 = EDGE_CURVE('',#35497,#35777,#29384,.T.) ;
#43476 = EDGE_CURVE('',#35742,#35500,#29385,.T.) ;
#43477 = EDGE_CURVE('',#35780,#35742,#2112,.T.) ;
#43478 = EDGE_CURVE('',#35766,#35782,#29386,.T.) ;
#43479 = EDGE_CURVE('',#35745,#35755,#29387,.T.) ;
#43480 = EDGE_CURVE('',#35778,#35745,#29388,.T.) ;
#43481 = EDGE_CURVE('',#35498,#35776,#29389,.T.) ;
#43482 = EDGE_CURVE('',#35743,#35499,#29390,.T.) ;
#43483 = EDGE_CURVE('',#35781,#35741,#29391,.T.) ;
#43484 = EDGE_CURVE('',#35767,#35781,#29392,.T.) ;
#43485 = EDGE_CURVE('',#35778,#35755,#29393,.T.) ;
#43486 = EDGE_CURVE('',#35743,#35776,#334,.T.) ;
#43487 = EDGE_CURVE('',#35767,#35741,#29394,.T.) ;
#43488 = EDGE_CURVE('',#35753,#35772,#29395,.T.) ;
#43489 = EDGE_CURVE('',#35773,#35754,#29396,.T.) ;
#43490 = EDGE_CURVE('',#35744,#35775,#29397,.T.) ;
#43491 = EDGE_CURVE('',#35768,#35744,#29398,.T.) ;
#43492 = EDGE_CURVE('',#35773,#35772,#335,.T.) ;
#43493 = EDGE_CURVE('',#35768,#35775,#29399,.T.) ;
#43494 = EDGE_CURVE('',#35774,#35771,#336,.T.) ;
#43495 = EDGE_CURVE('',#35764,#35774,#29400,.T.) ;
#43496 = EDGE_CURVE('',#35763,#35771,#29401,.T.) ;
#43497 = EDGE_CURVE('',#35444,#35876,#337,.T.) ;
#43498 = EDGE_CURVE('',#35876,#35301,#2113,.T.) ;
#43499 = EDGE_CURVE('',#35861,#35863,#29402,.T.) ;
#43500 = EDGE_CURVE('',#35862,#35864,#29403,.T.) ;
#43501 = EDGE_CURVE('',#35427,#35862,#29404,.T.) ;
#43502 = EDGE_CURVE('',#35449,#35866,#2114,.T.) ;
#43503 = EDGE_CURVE('',#35299,#35450,#2115,.T.) ;
#43504 = EDGE_CURVE('',#35868,#35317,#29405,.T.) ;
#43505 = EDGE_CURVE('',#35863,#35869,#29406,.T.) ;
#43506 = EDGE_CURVE('',#35428,#35864,#29407,.T.) ;
#43507 = EDGE_CURVE('',#35877,#35878,#2116,.T.) ;
#43508 = EDGE_CURVE('',#35878,#35734,#338,.T.) ;
#43509 = EDGE_CURVE('',#35865,#35877,#29408,.T.) ;
#43510 = EDGE_CURVE('',#35852,#35857,#29409,.T.) ;
#43511 = EDGE_CURVE('',#35857,#35851,#29410,.T.) ;
#43512 = EDGE_CURVE('',#35858,#35850,#29411,.T.) ;
#43513 = EDGE_CURVE('',#35853,#35860,#29412,.T.) ;
#43514 = EDGE_CURVE('',#35858,#35849,#29413,.T.) ;
#43515 = EDGE_CURVE('',#35854,#35860,#29414,.T.) ;
#43516 = EDGE_CURVE('',#35859,#35856,#29415,.T.) ;
#43517 = EDGE_CURVE('',#35855,#35859,#29416,.T.) ;
#43518 = EDGE_CURVE('',#35519,#35788,#29417,.T.) ;
#43519 = EDGE_CURVE('',#35785,#35518,#29418,.T.) ;
#43520 = EDGE_CURVE('',#35800,#35517,#29419,.T.) ;
#43521 = EDGE_CURVE('',#35785,#35800,#29420,.T.) ;
#43522 = EDGE_CURVE('',#35792,#35788,#29421,.T.) ;
#43523 = EDGE_CURVE('',#35520,#35792,#29422,.T.) ;
#43524 = EDGE_CURVE('',#35797,#35516,#29423,.T.) ;
#43525 = EDGE_CURVE('',#35786,#35799,#29424,.T.) ;
#43526 = EDGE_CURVE('',#35787,#35804,#29425,.T.) ;
#43527 = EDGE_CURVE('',#35801,#35786,#29426,.T.) ;
#43528 = EDGE_CURVE('',#35789,#35787,#29427,.T.) ;
#43529 = EDGE_CURVE('',#35514,#35791,#29428,.T.) ;
#43530 = EDGE_CURVE('',#35515,#35795,#29429,.T.) ;
#43531 = EDGE_CURVE('',#35796,#35513,#29430,.T.) ;
#43532 = EDGE_CURVE('',#35797,#35795,#29431,.T.) ;
#43533 = EDGE_CURVE('',#35801,#35799,#29432,.T.) ;
#43534 = EDGE_CURVE('',#35789,#35804,#29433,.T.) ;
#43535 = EDGE_CURVE('',#35796,#35791,#29434,.T.) ;
#43536 = EDGE_CURVE('',#35798,#35794,#29435,.T.) ;
#43537 = EDGE_CURVE('',#35802,#35798,#29436,.T.) ;
#43538 = EDGE_CURVE('',#35790,#35803,#29437,.T.) ;
#43539 = EDGE_CURVE('',#35793,#35790,#29438,.T.) ;
#43540 = EDGE_CURVE('',#35802,#35794,#29439,.T.) ;
#43541 = EDGE_CURVE('',#35793,#35803,#29440,.T.) ;
#43542 = EDGE_CURVE('',#35471,#35832,#29441,.T.) ;
#43543 = EDGE_CURVE('',#35829,#35470,#29442,.T.) ;
#43544 = EDGE_CURVE('',#35828,#35469,#29443,.T.) ;
#43545 = EDGE_CURVE('',#35829,#35828,#29444,.T.) ;
#43546 = EDGE_CURVE('',#35836,#35832,#29445,.T.) ;
#43547 = EDGE_CURVE('',#35472,#35836,#29446,.T.) ;
#43548 = EDGE_CURVE('',#35825,#35468,#29447,.T.) ;
#43549 = EDGE_CURVE('',#35830,#35827,#29448,.T.) ;
#43550 = EDGE_CURVE('',#35831,#35840,#29449,.T.) ;
#43551 = EDGE_CURVE('',#35837,#35830,#29450,.T.) ;
#43552 = EDGE_CURVE('',#35833,#35831,#29451,.T.) ;
#43553 = EDGE_CURVE('',#35466,#35835,#29452,.T.) ;
#43554 = EDGE_CURVE('',#35467,#35823,#29453,.T.) ;
#43555 = EDGE_CURVE('',#35824,#35465,#29454,.T.) ;
#43556 = EDGE_CURVE('',#35825,#35823,#29455,.T.) ;
#43557 = EDGE_CURVE('',#35837,#35827,#29456,.T.) ;
#43558 = EDGE_CURVE('',#35833,#35840,#29457,.T.) ;
#43559 = EDGE_CURVE('',#35824,#35835,#29458,.T.) ;
#43560 = EDGE_CURVE('',#35826,#35822,#29459,.T.) ;
#43561 = EDGE_CURVE('',#35838,#35826,#29460,.T.) ;
#43562 = EDGE_CURVE('',#35834,#35839,#29461,.T.) ;
#43563 = EDGE_CURVE('',#35821,#35834,#29462,.T.) ;
#43564 = EDGE_CURVE('',#35838,#35822,#29463,.T.) ;
#43565 = EDGE_CURVE('',#35821,#35839,#29464,.T.) ;
#43566 = EDGE_CURVE('',#35739,#35871,#2117,.T.) ;
#43567 = EDGE_CURVE('',#35740,#35870,#29465,.T.) ;
#43568 = EDGE_CURVE('',#35732,#35740,#29466,.T.) ;
#43569 = EDGE_CURVE('',#35732,#35870,#29467,.T.) ;
#43570 = EDGE_CURVE('',#35733,#35875,#29468,.T.) ;
#43571 = EDGE_CURVE('',#35431,#35733,#29469,.T.) ;
#43572 = EDGE_CURVE('',#35432,#35875,#29470,.T.) ;
#43573 = EDGE_CURVE('',#35433,#35874,#29471,.T.) ;
#43574 = EDGE_CURVE('',#35421,#35874,#29472,.T.) ;
#43575 = EDGE_CURVE('',#35422,#35873,#29473,.T.) ;
#43576 = EDGE_CURVE('',#35548,#35873,#29474,.T.) ;
#43577 = EDGE_CURVE('',#35872,#35549,#2118,.T.) ;
#43578 = EDGE_CURVE('',#35318,#35868,#29475,.T.) ;
#43579 = EDGE_CURVE('',#35865,#35867,#29476,.T.) ;
#43580 = EDGE_CURVE('',#35877,#35866,#29477,.T.) ;
#43581 = EDGE_CURVE('',#35878,#35449,#29478,.T.) ;
#43582 = EDGE_CURVE('',#35734,#35448,#29479,.T.) ;
#43583 = EDGE_CURVE('',#35876,#35450,#29480,.T.) ;
#43584 = EDGE_CURVE('',#35861,#35869,#29481,.T.) ;
#43585 = EDGE_CURVE('',#35879,#35880,#2119,.T.) ;
#43586 = EDGE_CURVE('',#35880,#35872,#2120,.T.) ;
#43587 = EDGE_CURVE('',#35871,#35881,#2121,.T.) ;
#43588 = EDGE_CURVE('',#35881,#35879,#2122,.T.) ;
#43589 = EDGE_CURVE('',#35739,#35542,#29482,.T.) ;
#43590 = EDGE_CURVE('',#35541,#35871,#2123,.T.) ;
#43591 = EDGE_CURVE('',#35872,#35539,#2124,.T.) ;
#43592 = EDGE_CURVE('',#35881,#35541,#29483,.T.) ;
#43593 = EDGE_CURVE('',#35879,#35540,#29484,.T.) ;
#43594 = EDGE_CURVE('',#35880,#35539,#29485,.T.) ;
#43595 = EDGE_CURVE('',#35703,#35721,#29486,.T.) ;
#43596 = EDGE_CURVE('',#35721,#35705,#29487,.T.) ;
#43597 = EDGE_CURVE('',#35704,#35723,#29488,.T.) ;
#43598 = EDGE_CURVE('',#35723,#35702,#29489,.T.) ;
#43599 = EDGE_CURVE('',#35722,#35707,#29490,.T.) ;
#43600 = EDGE_CURVE('',#35701,#35720,#29491,.T.) ;
#43601 = EDGE_CURVE('',#35724,#35700,#29492,.T.) ;
#43602 = EDGE_CURVE('',#35706,#35729,#29493,.T.) ;
#43603 = EDGE_CURVE('',#35722,#35709,#29494,.T.) ;
#43604 = EDGE_CURVE('',#35699,#35720,#29495,.T.) ;
#43605 = EDGE_CURVE('',#35724,#35698,#29496,.T.) ;
#43606 = EDGE_CURVE('',#35708,#35729,#29497,.T.) ;
#43607 = EDGE_CURVE('',#35716,#35711,#29498,.T.) ;
#43608 = EDGE_CURVE('',#35696,#35719,#2125,.T.) ;
#43609 = EDGE_CURVE('',#35697,#35393,#29499,.T.) ;
#43610 = EDGE_CURVE('',#35394,#35696,#29500,.T.) ;
#43611 = EDGE_CURVE('',#35725,#35697,#2126,.T.) ;
#43612 = EDGE_CURVE('',#35710,#35728,#29501,.T.) ;
#43613 = EDGE_CURVE('',#35717,#35713,#29502,.T.) ;
#43614 = EDGE_CURVE('',#35395,#35719,#29503,.T.) ;
#43615 = EDGE_CURVE('',#35725,#35392,#29504,.T.) ;
#43616 = EDGE_CURVE('',#35712,#35727,#29505,.T.) ;
#43617 = EDGE_CURVE('',#35718,#35715,#29506,.T.) ;
#43618 = EDGE_CURVE('',#35396,#35718,#29507,.T.) ;
#43619 = EDGE_CURVE('',#35726,#35390,#29508,.T.) ;
#43620 = EDGE_CURVE('',#35714,#35726,#29509,.T.) ;
#43621 = EDGE_CURVE('',#35397,#35715,#29510,.T.) ;
#43622 = EDGE_CURVE('',#35714,#35391,#29511,.T.) ;
#43623 = EDGE_CURVE('',#35882,#35883,#29512,.T.) ;
#43624 = EDGE_CURVE('',#35884,#35882,#29513,.T.) ;
#43625 = EDGE_CURVE('',#35885,#35884,#29514,.T.) ;
#43626 = EDGE_CURVE('',#35885,#35883,#29515,.T.) ;
#43627 = EDGE_CURVE('',#35886,#35887,#29516,.T.) ;
#43628 = EDGE_CURVE('',#35888,#35886,#3374,.T.) ;
#43629 = EDGE_CURVE('',#35889,#35888,#29517,.T.) ;
#43630 = EDGE_CURVE('',#35887,#35889,#3375,.T.) ;
#43631 = EDGE_CURVE('',#35890,#35890,#29518,.T.) ;
#43632 = EDGE_CURVE('',#35890,#35891,#29519,.T.) ;
#43633 = EDGE_CURVE('',#35892,#35891,#29520,.T.) ;
#43634 = EDGE_CURVE('',#35891,#35892,#29521,.T.) ;
#43635 = EDGE_CURVE('',#35893,#35893,#29522,.T.) ;
#43636 = EDGE_CURVE('',#35893,#35894,#29523,.T.) ;
#43637 = EDGE_CURVE('',#35894,#35894,#29524,.T.) ;
#43638 = EDGE_CURVE('',#35895,#35895,#29525,.T.) ;
#43639 = EDGE_CURVE('',#35895,#35896,#29526,.T.) ;
#43640 = EDGE_CURVE('',#35897,#35896,#29527,.T.) ;
#43641 = EDGE_CURVE('',#35896,#35897,#29528,.T.) ;
#43642 = EDGE_CURVE('',#35898,#35899,#29529,.T.) ;
#43643 = EDGE_CURVE('',#35900,#35899,#29530,.T.) ;
#43644 = EDGE_CURVE('',#35900,#35901,#29531,.T.) ;
#43645 = EDGE_CURVE('',#35901,#35898,#29532,.T.) ;
#43646 = EDGE_CURVE('',#35902,#35903,#29533,.T.) ;
#43647 = EDGE_CURVE('',#35903,#35904,#29534,.T.) ;
#43648 = EDGE_CURVE('',#35902,#35904,#29535,.T.) ;
#43649 = EDGE_CURVE('',#35905,#35898,#3376,.T.) ;
#43650 = EDGE_CURVE('',#35905,#35906,#29536,.T.) ;
#43651 = EDGE_CURVE('',#35899,#35906,#3377,.T.) ;
#43652 = EDGE_CURVE('',#35907,#35908,#29537,.T.) ;
#43653 = EDGE_CURVE('',#35907,#35909,#29538,.T.) ;
#43654 = EDGE_CURVE('',#35908,#35909,#29539,.T.) ;
#43655 = EDGE_CURVE('',#35910,#35910,#29540,.T.) ;
#43656 = EDGE_CURVE('',#35910,#35893,#3378,.T.) ;
#43657 = EDGE_CURVE('',#35894,#35897,#3379,.T.) ;
#43658 = EDGE_CURVE('',#35911,#35912,#29541,.T.) ;
#43659 = EDGE_CURVE('',#35911,#35913,#2127,.T.) ;
#43660 = EDGE_CURVE('',#35914,#35913,#3380,.T.) ;
#43661 = EDGE_CURVE('',#35914,#35915,#2128,.T.) ;
#43662 = EDGE_CURVE('',#35916,#35915,#29542,.T.) ;
#43663 = EDGE_CURVE('',#35916,#35917,#2129,.T.) ;
#43664 = EDGE_CURVE('',#35917,#35918,#3381,.T.) ;
#43665 = EDGE_CURVE('',#35918,#35919,#2130,.T.) ;
#43666 = EDGE_CURVE('',#35920,#35919,#29543,.T.) ;
#43667 = EDGE_CURVE('',#35920,#35921,#2131,.T.) ;
#43668 = EDGE_CURVE('',#35922,#35921,#3382,.T.) ;
#43669 = EDGE_CURVE('',#35922,#35923,#2132,.T.) ;
#43670 = EDGE_CURVE('',#35924,#35923,#29544,.T.) ;
#43671 = EDGE_CURVE('',#35924,#35925,#2133,.T.) ;
#43672 = EDGE_CURVE('',#35925,#35926,#3383,.T.) ;
#43673 = EDGE_CURVE('',#35926,#35927,#2134,.T.) ;
#43674 = EDGE_CURVE('',#35912,#35927,#29545,.T.) ;
#43675 = EDGE_CURVE('',#35912,#35892,#3384,.T.) ;
#43676 = EDGE_CURVE('',#35928,#35929,#29546,.T.) ;
#43677 = EDGE_CURVE('',#35929,#35930,#3385,.T.) ;
#43678 = EDGE_CURVE('',#35930,#35931,#3386,.T.) ;
#43679 = EDGE_CURVE('',#35931,#35928,#3387,.T.) ;
#43680 = EDGE_CURVE('',#35932,#35933,#3388,.T.) ;
#43681 = EDGE_CURVE('',#35932,#35934,#3389,.T.) ;
#43682 = EDGE_CURVE('',#35934,#35935,#3390,.T.) ;
#43683 = EDGE_CURVE('',#35935,#35933,#3391,.T.) ;
#43684 = EDGE_CURVE('',#35936,#35937,#3392,.T.) ;
#43685 = EDGE_CURVE('',#35937,#35938,#3393,.T.) ;
#43686 = EDGE_CURVE('',#35938,#35909,#3394,.T.) ;
#43687 = EDGE_CURVE('',#35909,#35936,#3395,.T.) ;
#43688 = EDGE_CURVE('',#35927,#35911,#3396,.T.) ;
#43689 = EDGE_CURVE('',#35900,#35904,#3397,.T.) ;
#43690 = EDGE_CURVE('',#35904,#35939,#3398,.T.) ;
#43691 = EDGE_CURVE('',#35940,#35939,#3399,.T.) ;
#43692 = EDGE_CURVE('',#35940,#35941,#3400,.T.) ;
#43693 = EDGE_CURVE('',#35942,#35941,#29547,.T.) ;
#43694 = EDGE_CURVE('',#35942,#35943,#29548,.T.) ;
#43695 = EDGE_CURVE('',#35944,#35943,#29549,.T.) ;
#43696 = EDGE_CURVE('',#35944,#35945,#3401,.T.) ;
#43697 = EDGE_CURVE('',#35945,#35946,#3402,.T.) ;
#43698 = EDGE_CURVE('',#35946,#35907,#3403,.T.) ;
#43699 = EDGE_CURVE('',#35907,#35947,#3404,.T.) ;
#43700 = EDGE_CURVE('',#35948,#35947,#29550,.T.) ;
#43701 = EDGE_CURVE('',#35948,#35901,#3405,.T.) ;
#43702 = EDGE_CURVE('',#35903,#35949,#3406,.T.) ;
#43703 = EDGE_CURVE('',#35949,#35950,#3407,.T.) ;
#43704 = EDGE_CURVE('',#35951,#35950,#3408,.T.) ;
#43705 = EDGE_CURVE('',#35951,#35903,#3409,.T.) ;
#43706 = EDGE_CURVE('',#35952,#35953,#3410,.T.) ;
#43707 = EDGE_CURVE('',#35952,#35954,#3411,.T.) ;
#43708 = EDGE_CURVE('',#35954,#35955,#339,.T.) ;
#43709 = EDGE_CURVE('',#35955,#35956,#3412,.T.) ;
#43710 = EDGE_CURVE('',#35956,#35957,#340,.T.) ;
#43711 = EDGE_CURVE('',#35957,#35958,#3413,.T.) ;
#43712 = EDGE_CURVE('',#35958,#35959,#3414,.T.) ;
#43713 = EDGE_CURVE('',#35959,#35953,#3415,.T.) ;
#43714 = EDGE_CURVE('',#35960,#35961,#3416,.T.) ;
#43715 = EDGE_CURVE('',#35961,#35962,#3417,.T.) ;
#43716 = EDGE_CURVE('',#35963,#35962,#3418,.T.) ;
#43717 = EDGE_CURVE('',#35963,#35960,#3419,.T.) ;
#43718 = EDGE_CURVE('',#35964,#35965,#3420,.T.) ;
#43719 = EDGE_CURVE('',#35965,#35966,#3421,.T.) ;
#43720 = EDGE_CURVE('',#35967,#35966,#3422,.T.) ;
#43721 = EDGE_CURVE('',#35967,#35964,#3423,.T.) ;
#43722 = EDGE_CURVE('',#35968,#35969,#3424,.T.) ;
#43723 = EDGE_CURVE('',#35969,#35970,#3425,.T.) ;
#43724 = EDGE_CURVE('',#35971,#35970,#3426,.T.) ;
#43725 = EDGE_CURVE('',#35971,#35968,#3427,.T.) ;
#43726 = EDGE_CURVE('',#35972,#35973,#3428,.T.) ;
#43727 = EDGE_CURVE('',#35973,#35974,#3429,.T.) ;
#43728 = EDGE_CURVE('',#35975,#35974,#3430,.T.) ;
#43729 = EDGE_CURVE('',#35975,#35972,#3431,.T.) ;
#43730 = EDGE_CURVE('',#35976,#35977,#3432,.T.) ;
#43731 = EDGE_CURVE('',#35977,#35978,#3433,.T.) ;
#43732 = EDGE_CURVE('',#35979,#35978,#3434,.T.) ;
#43733 = EDGE_CURVE('',#35979,#35976,#3435,.T.) ;
#43734 = EDGE_CURVE('',#35980,#35981,#3436,.T.) ;
#43735 = EDGE_CURVE('',#35981,#35982,#3437,.T.) ;
#43736 = EDGE_CURVE('',#35983,#35982,#3438,.T.) ;
#43737 = EDGE_CURVE('',#35983,#35980,#3439,.T.) ;
#43738 = EDGE_CURVE('',#35984,#35985,#3440,.T.) ;
#43739 = EDGE_CURVE('',#35985,#35986,#3441,.T.) ;
#43740 = EDGE_CURVE('',#35987,#35986,#3442,.T.) ;
#43741 = EDGE_CURVE('',#35987,#35984,#3443,.T.) ;
#43742 = EDGE_CURVE('',#35988,#35989,#29551,.T.) ;
#43743 = EDGE_CURVE('',#35988,#35990,#3444,.T.) ;
#43744 = EDGE_CURVE('',#35991,#35990,#29552,.T.) ;
#43745 = EDGE_CURVE('',#35991,#35992,#3445,.T.) ;
#43746 = EDGE_CURVE('',#35993,#35992,#29553,.T.) ;
#43747 = EDGE_CURVE('',#35993,#35994,#3446,.T.) ;
#43748 = EDGE_CURVE('',#35995,#35994,#29554,.T.) ;
#43749 = EDGE_CURVE('',#35995,#35989,#3447,.T.) ;
#43750 = EDGE_CURVE('',#35996,#35997,#3448,.T.) ;
#43751 = EDGE_CURVE('',#35997,#35998,#3449,.T.) ;
#43752 = EDGE_CURVE('',#35999,#35998,#3450,.T.) ;
#43753 = EDGE_CURVE('',#35999,#35996,#3451,.T.) ;
#43754 = EDGE_CURVE('',#36000,#35887,#3452,.T.) ;
#43755 = EDGE_CURVE('',#36001,#35889,#3453,.T.) ;
#43756 = EDGE_CURVE('',#36001,#36000,#3454,.T.) ;
#43757 = EDGE_CURVE('',#35886,#36002,#3455,.T.) ;
#43758 = EDGE_CURVE('',#36002,#36003,#3456,.T.) ;
#43759 = EDGE_CURVE('',#35888,#36003,#3457,.T.) ;
#43760 = EDGE_CURVE('',#36004,#36005,#3458,.T.) ;
#43761 = EDGE_CURVE('',#36005,#36006,#3459,.T.) ;
#43762 = EDGE_CURVE('',#36007,#36006,#3460,.T.) ;
#43763 = EDGE_CURVE('',#36007,#36004,#3461,.T.) ;
#43764 = EDGE_CURVE('',#36008,#36009,#3462,.T.) ;
#43765 = EDGE_CURVE('',#36009,#36010,#2135,.T.) ;
#43766 = EDGE_CURVE('',#36010,#36011,#3463,.T.) ;
#43767 = EDGE_CURVE('',#36012,#36011,#2136,.T.) ;
#43768 = EDGE_CURVE('',#36012,#36013,#3464,.T.) ;
#43769 = EDGE_CURVE('',#36014,#36013,#2137,.T.) ;
#43770 = EDGE_CURVE('',#36014,#36015,#3465,.T.) ;
#43771 = EDGE_CURVE('',#36015,#36008,#2138,.T.) ;
#43772 = EDGE_CURVE('',#36016,#36017,#3466,.T.) ;
#43773 = EDGE_CURVE('',#36017,#36018,#3467,.T.) ;
#43774 = EDGE_CURVE('',#36019,#36018,#3468,.T.) ;
#43775 = EDGE_CURVE('',#36019,#36016,#3469,.T.) ;
#43776 = EDGE_CURVE('',#36020,#36021,#29555,.T.) ;
#43777 = EDGE_CURVE('',#36020,#36022,#3470,.T.) ;
#43778 = EDGE_CURVE('',#36023,#36022,#29556,.T.) ;
#43779 = EDGE_CURVE('',#36023,#36024,#3471,.T.) ;
#43780 = EDGE_CURVE('',#36025,#36024,#29557,.T.) ;
#43781 = EDGE_CURVE('',#36025,#36026,#3472,.T.) ;
#43782 = EDGE_CURVE('',#36027,#36026,#29558,.T.) ;
#43783 = EDGE_CURVE('',#36027,#36021,#3473,.T.) ;
#43784 = EDGE_CURVE('',#36028,#36029,#3474,.T.) ;
#43785 = EDGE_CURVE('',#36029,#36030,#3475,.T.) ;
#43786 = EDGE_CURVE('',#36031,#36030,#3476,.T.) ;
#43787 = EDGE_CURVE('',#36031,#36028,#3477,.T.) ;
#43788 = EDGE_CURVE('',#36032,#36033,#2139,.T.) ;
#43789 = EDGE_CURVE('',#36033,#36034,#2140,.T.) ;
#43790 = EDGE_CURVE('',#36034,#36035,#2141,.T.) ;
#43791 = EDGE_CURVE('',#36035,#36036,#2142,.T.) ;
#43792 = EDGE_CURVE('',#36036,#36037,#3478,.T.) ;
#43793 = EDGE_CURVE('',#36038,#36037,#3479,.T.) ;
#43794 = EDGE_CURVE('',#36038,#36039,#3480,.T.) ;
#43795 = EDGE_CURVE('',#36039,#36040,#3481,.T.) ;
#43796 = EDGE_CURVE('',#36040,#36032,#3482,.T.) ;
#43797 = EDGE_CURVE('',#36041,#36042,#3483,.T.) ;
#43798 = EDGE_CURVE('',#36041,#36043,#3484,.T.) ;
#43799 = EDGE_CURVE('',#36043,#36044,#29559,.T.) ;
#43800 = EDGE_CURVE('',#36044,#36042,#3485,.T.) ;
#43801 = EDGE_CURVE('',#36045,#36046,#3486,.T.) ;
#43802 = EDGE_CURVE('',#36046,#36047,#3487,.T.) ;
#43803 = EDGE_CURVE('',#36047,#36048,#3488,.T.) ;
#43804 = EDGE_CURVE('',#36048,#36045,#3489,.T.) ;
#43805 = EDGE_CURVE('',#36037,#36041,#29560,.T.) ;
#43806 = EDGE_CURVE('',#36042,#35932,#29561,.T.) ;
#43807 = EDGE_CURVE('',#35933,#35940,#29562,.T.) ;
#43808 = EDGE_CURVE('',#35939,#35951,#29563,.T.) ;
#43809 = EDGE_CURVE('',#35950,#35952,#29564,.T.) ;
#43810 = EDGE_CURVE('',#35953,#35963,#29565,.T.) ;
#43811 = EDGE_CURVE('',#35962,#35967,#29566,.T.) ;
#43812 = EDGE_CURVE('',#35966,#35971,#29567,.T.) ;
#43813 = EDGE_CURVE('',#35970,#35975,#29568,.T.) ;
#43814 = EDGE_CURVE('',#35974,#35979,#29569,.T.) ;
#43815 = EDGE_CURVE('',#35978,#35983,#29570,.T.) ;
#43816 = EDGE_CURVE('',#35982,#35987,#29571,.T.) ;
#43817 = EDGE_CURVE('',#35986,#35999,#29572,.T.) ;
#43818 = EDGE_CURVE('',#35998,#36001,#29573,.T.) ;
#43819 = EDGE_CURVE('',#36003,#36007,#29574,.T.) ;
#43820 = EDGE_CURVE('',#36006,#36019,#29575,.T.) ;
#43821 = EDGE_CURVE('',#36018,#36031,#29576,.T.) ;
#43822 = EDGE_CURVE('',#36030,#36038,#29577,.T.) ;
#43823 = EDGE_CURVE('',#35930,#36040,#29578,.T.) ;
#43824 = EDGE_CURVE('',#36039,#36029,#29579,.T.) ;
#43825 = EDGE_CURVE('',#36028,#36017,#29580,.T.) ;
#43826 = EDGE_CURVE('',#36016,#36005,#29581,.T.) ;
#43827 = EDGE_CURVE('',#36004,#36002,#29582,.T.) ;
#43828 = EDGE_CURVE('',#36000,#35997,#29583,.T.) ;
#43829 = EDGE_CURVE('',#35996,#35985,#29584,.T.) ;
#43830 = EDGE_CURVE('',#35984,#35981,#29585,.T.) ;
#43831 = EDGE_CURVE('',#35980,#35977,#29586,.T.) ;
#43832 = EDGE_CURVE('',#35976,#35973,#29587,.T.) ;
#43833 = EDGE_CURVE('',#35972,#35969,#29588,.T.) ;
#43834 = EDGE_CURVE('',#35968,#35965,#29589,.T.) ;
#43835 = EDGE_CURVE('',#35964,#35961,#29590,.T.) ;
#43836 = EDGE_CURVE('',#35960,#35959,#29591,.T.) ;
#43837 = EDGE_CURVE('',#35958,#35937,#29592,.T.) ;
#43838 = EDGE_CURVE('',#35936,#35946,#29593,.T.) ;
#43839 = EDGE_CURVE('',#35945,#36048,#29594,.T.) ;
#43840 = EDGE_CURVE('',#36047,#35931,#29595,.T.) ;
#43841 = EDGE_CURVE('',#36049,#36050,#3490,.T.) ;
#43842 = EDGE_CURVE('',#36050,#36051,#3491,.T.) ;
#43843 = EDGE_CURVE('',#36051,#36052,#3492,.T.) ;
#43844 = EDGE_CURVE('',#36052,#36049,#3493,.T.) ;
#43845 = EDGE_CURVE('',#36053,#36054,#3494,.T.) ;
#43846 = EDGE_CURVE('',#36054,#36055,#3495,.T.) ;
#43847 = EDGE_CURVE('',#36055,#36056,#3496,.T.) ;
#43848 = EDGE_CURVE('',#36056,#36053,#3497,.T.) ;
#43849 = EDGE_CURVE('',#36057,#36058,#341,.T.) ;
#43850 = EDGE_CURVE('',#36057,#36059,#3498,.T.) ;
#43851 = EDGE_CURVE('',#36059,#36060,#3499,.T.) ;
#43852 = EDGE_CURVE('',#36060,#36061,#3500,.T.) ;
#43853 = EDGE_CURVE('',#36062,#36061,#342,.T.) ;
#43854 = EDGE_CURVE('',#36062,#36063,#3501,.T.) ;
#43855 = EDGE_CURVE('',#36063,#36064,#3502,.T.) ;
#43856 = EDGE_CURVE('',#36064,#36058,#3503,.T.) ;
#43857 = EDGE_CURVE('',#36065,#36066,#3504,.T.) ;
#43858 = EDGE_CURVE('',#36066,#36067,#343,.T.) ;
#43859 = EDGE_CURVE('',#36068,#36067,#3505,.T.) ;
#43860 = EDGE_CURVE('',#36068,#36060,#344,.T.) ;
#43861 = EDGE_CURVE('',#36059,#36069,#345,.T.) ;
#43862 = EDGE_CURVE('',#36069,#36070,#3506,.T.) ;
#43863 = EDGE_CURVE('',#36070,#36065,#346,.T.) ;
#43864 = EDGE_CURVE('',#36071,#36072,#347,.T.) ;
#43865 = EDGE_CURVE('',#36071,#36066,#3507,.T.) ;
#43866 = EDGE_CURVE('',#36065,#36073,#3508,.T.) ;
#43867 = EDGE_CURVE('',#36074,#36073,#348,.T.) ;
#43868 = EDGE_CURVE('',#36074,#36075,#3509,.T.) ;
#43869 = EDGE_CURVE('',#36075,#36076,#3510,.T.) ;
#43870 = EDGE_CURVE('',#36076,#36072,#3511,.T.) ;
#43871 = EDGE_CURVE('',#36069,#36077,#3512,.T.) ;
#43872 = EDGE_CURVE('',#36077,#36078,#3513,.T.) ;
#43873 = EDGE_CURVE('',#36078,#36070,#3514,.T.) ;
#43874 = EDGE_CURVE('',#36067,#36079,#3515,.T.) ;
#43875 = EDGE_CURVE('',#36079,#36080,#3516,.T.) ;
#43876 = EDGE_CURVE('',#36080,#36068,#3517,.T.) ;
#43877 = EDGE_CURVE('',#36081,#36082,#3518,.T.) ;
#43878 = EDGE_CURVE('',#36082,#36083,#3519,.T.) ;
#43879 = EDGE_CURVE('',#36083,#36084,#3520,.T.) ;
#43880 = EDGE_CURVE('',#36084,#36085,#3521,.T.) ;
#43881 = EDGE_CURVE('',#36085,#36086,#3522,.T.) ;
#43882 = EDGE_CURVE('',#36086,#36081,#3523,.T.) ;
#43883 = EDGE_CURVE('',#36087,#36088,#3524,.T.) ;
#43884 = EDGE_CURVE('',#36088,#36089,#3525,.T.) ;
#43885 = EDGE_CURVE('',#36089,#36090,#3526,.T.) ;
#43886 = EDGE_CURVE('',#36090,#36091,#3527,.T.) ;
#43887 = EDGE_CURVE('',#36091,#36092,#3528,.T.) ;
#43888 = EDGE_CURVE('',#36092,#36087,#3529,.T.) ;
#43889 = EDGE_CURVE('',#36093,#36094,#3530,.T.) ;
#43890 = EDGE_CURVE('',#36094,#36095,#3531,.T.) ;
#43891 = EDGE_CURVE('',#36095,#36096,#3532,.T.) ;
#43892 = EDGE_CURVE('',#36096,#36093,#3533,.T.) ;
#43893 = EDGE_CURVE('',#36097,#36098,#3534,.T.) ;
#43894 = EDGE_CURVE('',#36098,#36099,#3535,.T.) ;
#43895 = EDGE_CURVE('',#36099,#36100,#3536,.T.) ;
#43896 = EDGE_CURVE('',#36100,#36097,#3537,.T.) ;
#43897 = EDGE_CURVE('',#36101,#36102,#3538,.T.) ;
#43898 = EDGE_CURVE('',#36102,#36103,#3539,.T.) ;
#43899 = EDGE_CURVE('',#36103,#36104,#3540,.T.) ;
#43900 = EDGE_CURVE('',#36104,#36101,#3541,.T.) ;
#43901 = EDGE_CURVE('',#36105,#36106,#3542,.T.) ;
#43902 = EDGE_CURVE('',#36106,#36107,#3543,.T.) ;
#43903 = EDGE_CURVE('',#36107,#36108,#3544,.T.) ;
#43904 = EDGE_CURVE('',#36108,#36105,#3545,.T.) ;
#43905 = EDGE_CURVE('',#36109,#36110,#3546,.T.) ;
#43906 = EDGE_CURVE('',#36110,#36111,#3547,.T.) ;
#43907 = EDGE_CURVE('',#36111,#36112,#3548,.T.) ;
#43908 = EDGE_CURVE('',#36112,#36109,#3549,.T.) ;
#43909 = EDGE_CURVE('',#36113,#36114,#3550,.T.) ;
#43910 = EDGE_CURVE('',#36115,#36113,#29596,.T.) ;
#43911 = EDGE_CURVE('',#36116,#36115,#3551,.T.) ;
#43912 = EDGE_CURVE('',#36117,#36116,#29597,.T.) ;
#43913 = EDGE_CURVE('',#36118,#36117,#3552,.T.) ;
#43914 = EDGE_CURVE('',#36119,#36118,#29598,.T.) ;
#43915 = EDGE_CURVE('',#36120,#36119,#3553,.T.) ;
#43916 = EDGE_CURVE('',#36114,#36120,#29599,.T.) ;
#43917 = EDGE_CURVE('',#36121,#36122,#29600,.T.) ;
#43918 = EDGE_CURVE('',#36114,#36121,#3554,.T.) ;
#43919 = EDGE_CURVE('',#36120,#36122,#3555,.T.) ;
#43920 = EDGE_CURVE('',#36123,#36121,#3556,.T.) ;
#43921 = EDGE_CURVE('',#36113,#36123,#3557,.T.) ;
#43922 = EDGE_CURVE('',#36124,#36123,#29601,.T.) ;
#43923 = EDGE_CURVE('',#36115,#36124,#3558,.T.) ;
#43924 = EDGE_CURVE('',#36125,#36124,#3559,.T.) ;
#43925 = EDGE_CURVE('',#36116,#36125,#3560,.T.) ;
#43926 = EDGE_CURVE('',#36126,#36125,#29602,.T.) ;
#43927 = EDGE_CURVE('',#36117,#36126,#3561,.T.) ;
#43928 = EDGE_CURVE('',#36127,#36126,#3562,.T.) ;
#43929 = EDGE_CURVE('',#36118,#36127,#3563,.T.) ;
#43930 = EDGE_CURVE('',#36128,#36127,#29603,.T.) ;
#43931 = EDGE_CURVE('',#36119,#36128,#3564,.T.) ;
#43932 = EDGE_CURVE('',#36122,#36128,#3565,.T.) ;
#43933 = EDGE_CURVE('',#35919,#35920,#3566,.T.) ;
#43934 = EDGE_CURVE('',#35917,#35922,#3567,.T.) ;
#43935 = EDGE_CURVE('',#35921,#35918,#3568,.T.) ;
#43936 = EDGE_CURVE('',#35925,#35914,#3569,.T.) ;
#43937 = EDGE_CURVE('',#35913,#35926,#3570,.T.) ;
#43938 = EDGE_CURVE('',#35915,#35924,#3571,.T.) ;
#43939 = EDGE_CURVE('',#35923,#35916,#3572,.T.) ;
#43940 = EDGE_CURVE('',#36129,#36130,#3573,.T.) ;
#43941 = EDGE_CURVE('',#36130,#36131,#3574,.T.) ;
#43942 = EDGE_CURVE('',#36131,#36132,#3575,.T.) ;
#43943 = EDGE_CURVE('',#36132,#36129,#3576,.T.) ;
#43944 = EDGE_CURVE('',#36133,#36134,#3577,.T.) ;
#43945 = EDGE_CURVE('',#36134,#36135,#3578,.T.) ;
#43946 = EDGE_CURVE('',#36135,#36136,#3579,.T.) ;
#43947 = EDGE_CURVE('',#36136,#36133,#3580,.T.) ;
#43948 = EDGE_CURVE('',#36137,#36138,#3581,.T.) ;
#43949 = EDGE_CURVE('',#36138,#36139,#3582,.T.) ;
#43950 = EDGE_CURVE('',#36139,#36140,#3583,.T.) ;
#43951 = EDGE_CURVE('',#36140,#36137,#3584,.T.) ;
#43952 = EDGE_CURVE('',#36141,#36142,#3585,.T.) ;
#43953 = EDGE_CURVE('',#36142,#36143,#3586,.T.) ;
#43954 = EDGE_CURVE('',#36143,#36144,#3587,.T.) ;
#43955 = EDGE_CURVE('',#36144,#36141,#3588,.T.) ;
#43956 = EDGE_CURVE('',#36145,#36146,#3589,.T.) ;
#43957 = EDGE_CURVE('',#36146,#36147,#3590,.T.) ;
#43958 = EDGE_CURVE('',#36147,#36148,#3591,.T.) ;
#43959 = EDGE_CURVE('',#36148,#36145,#3592,.T.) ;
#43960 = EDGE_CURVE('',#36149,#36150,#3593,.T.) ;
#43961 = EDGE_CURVE('',#36151,#36149,#29604,.T.) ;
#43962 = EDGE_CURVE('',#36152,#36151,#3594,.T.) ;
#43963 = EDGE_CURVE('',#36153,#36152,#29605,.T.) ;
#43964 = EDGE_CURVE('',#36154,#36153,#3595,.T.) ;
#43965 = EDGE_CURVE('',#36155,#36154,#29606,.T.) ;
#43966 = EDGE_CURVE('',#36156,#36155,#3596,.T.) ;
#43967 = EDGE_CURVE('',#36150,#36156,#29607,.T.) ;
#43968 = EDGE_CURVE('',#36156,#36157,#3597,.T.) ;
#43969 = EDGE_CURVE('',#36157,#36158,#29608,.T.) ;
#43970 = EDGE_CURVE('',#36150,#36158,#3598,.T.) ;
#43971 = EDGE_CURVE('',#36158,#36159,#3599,.T.) ;
#43972 = EDGE_CURVE('',#36149,#36159,#3600,.T.) ;
#43973 = EDGE_CURVE('',#36159,#36160,#29609,.T.) ;
#43974 = EDGE_CURVE('',#36151,#36160,#3601,.T.) ;
#43975 = EDGE_CURVE('',#36160,#36161,#3602,.T.) ;
#43976 = EDGE_CURVE('',#36152,#36161,#3603,.T.) ;
#43977 = EDGE_CURVE('',#36161,#36162,#29610,.T.) ;
#43978 = EDGE_CURVE('',#36153,#36162,#3604,.T.) ;
#43979 = EDGE_CURVE('',#36162,#36163,#3605,.T.) ;
#43980 = EDGE_CURVE('',#36154,#36163,#3606,.T.) ;
#43981 = EDGE_CURVE('',#36163,#36164,#29611,.T.) ;
#43982 = EDGE_CURVE('',#36155,#36164,#3607,.T.) ;
#43983 = EDGE_CURVE('',#36164,#36157,#3608,.T.) ;
#43984 = EDGE_CURVE('',#36165,#36166,#3609,.T.) ;
#43985 = EDGE_CURVE('',#36166,#36167,#3610,.T.) ;
#43986 = EDGE_CURVE('',#36167,#36168,#3611,.T.) ;
#43987 = EDGE_CURVE('',#36168,#36165,#3612,.T.) ;
#43988 = EDGE_CURVE('',#35908,#35884,#3613,.T.) ;
#43989 = EDGE_CURVE('',#35884,#36169,#3614,.T.) ;
#43990 = EDGE_CURVE('',#36169,#36170,#3615,.T.) ;
#43991 = EDGE_CURVE('',#36170,#35908,#3616,.T.) ;
#43992 = EDGE_CURVE('',#36171,#35905,#3617,.T.) ;
#43993 = EDGE_CURVE('',#35898,#36172,#3618,.T.) ;
#43994 = EDGE_CURVE('',#36172,#36171,#3619,.T.) ;
#43995 = EDGE_CURVE('',#35906,#36173,#3620,.T.) ;
#43996 = EDGE_CURVE('',#36173,#35902,#3621,.T.) ;
#43997 = EDGE_CURVE('',#35902,#35899,#3622,.T.) ;
#43998 = EDGE_CURVE('',#35883,#36174,#3623,.T.) ;
#43999 = EDGE_CURVE('',#36174,#36175,#29612,.T.) ;
#44000 = EDGE_CURVE('',#36175,#36176,#3624,.T.) ;
#44001 = EDGE_CURVE('',#36176,#36177,#3625,.T.) ;
#44002 = EDGE_CURVE('',#36177,#35882,#3626,.T.) ;
#44003 = EDGE_CURVE('',#36178,#36179,#29613,.T.) ;
#44004 = EDGE_CURVE('',#36179,#36180,#29614,.T.) ;
#44005 = EDGE_CURVE('',#36180,#36181,#29615,.T.) ;
#44006 = EDGE_CURVE('',#36181,#36182,#3627,.T.) ;
#44007 = EDGE_CURVE('',#36182,#36183,#29616,.T.) ;
#44008 = EDGE_CURVE('',#36183,#36178,#3628,.T.) ;
#44009 = EDGE_CURVE('',#36087,#36009,#29617,.T.) ;
#44010 = EDGE_CURVE('',#36055,#36087,#2143,.T.) ;
#44011 = EDGE_CURVE('',#36010,#36055,#29618,.T.) ;
#44012 = EDGE_CURVE('',#36077,#36057,#29619,.T.) ;
#44013 = EDGE_CURVE('',#36091,#36058,#29620,.T.) ;
#44014 = EDGE_CURVE('',#36077,#36091,#349,.T.) ;
#44015 = EDGE_CURVE('',#36092,#36064,#29621,.T.) ;
#44016 = EDGE_CURVE('',#36056,#36092,#29622,.T.) ;
#44017 = EDGE_CURVE('',#36011,#36054,#29623,.T.) ;
#44018 = EDGE_CURVE('',#36088,#36008,#29624,.T.) ;
#44019 = EDGE_CURVE('',#36078,#36090,#350,.T.) ;
#44020 = EDGE_CURVE('',#36073,#36078,#29625,.T.) ;
#44021 = EDGE_CURVE('',#36056,#36064,#29626,.T.) ;
#44022 = EDGE_CURVE('',#36085,#36054,#351,.T.) ;
#44023 = EDGE_CURVE('',#36012,#36085,#29627,.T.) ;
#44024 = EDGE_CURVE('',#36050,#36015,#29628,.T.) ;
#44025 = EDGE_CURVE('',#36088,#36050,#2144,.T.) ;
#44026 = EDGE_CURVE('',#36074,#36090,#29629,.T.) ;
#44027 = EDGE_CURVE('',#36053,#36063,#29630,.T.) ;
#44028 = EDGE_CURVE('',#36086,#36053,#29631,.T.) ;
#44029 = EDGE_CURVE('',#36013,#36084,#29632,.T.) ;
#44030 = EDGE_CURVE('',#36051,#36014,#29633,.T.) ;
#44031 = EDGE_CURVE('',#36089,#36049,#29634,.T.) ;
#44032 = EDGE_CURVE('',#36075,#36089,#29635,.T.) ;
#44033 = EDGE_CURVE('',#36086,#36063,#29636,.T.) ;
#44034 = EDGE_CURVE('',#36051,#36084,#352,.T.) ;
#44035 = EDGE_CURVE('',#36075,#36049,#29637,.T.) ;
#44036 = EDGE_CURVE('',#36061,#36080,#29638,.T.) ;
#44037 = EDGE_CURVE('',#36081,#36062,#29639,.T.) ;
#44038 = EDGE_CURVE('',#36052,#36083,#29640,.T.) ;
#44039 = EDGE_CURVE('',#36076,#36052,#29641,.T.) ;
#44040 = EDGE_CURVE('',#36081,#36080,#353,.T.) ;
#44041 = EDGE_CURVE('',#36076,#36083,#29642,.T.) ;
#44042 = EDGE_CURVE('',#36082,#36079,#354,.T.) ;
#44043 = EDGE_CURVE('',#36072,#36082,#29643,.T.) ;
#44044 = EDGE_CURVE('',#36071,#36079,#29644,.T.) ;
#44045 = EDGE_CURVE('',#35938,#36184,#355,.T.) ;
#44046 = EDGE_CURVE('',#36184,#35885,#2145,.T.) ;
#44047 = EDGE_CURVE('',#36169,#36171,#29645,.T.) ;
#44048 = EDGE_CURVE('',#36170,#36172,#29646,.T.) ;
#44049 = EDGE_CURVE('',#35947,#36170,#29647,.T.) ;
#44050 = EDGE_CURVE('',#35955,#36174,#2146,.T.) ;
#44051 = EDGE_CURVE('',#35883,#35956,#2147,.T.) ;
#44052 = EDGE_CURVE('',#36176,#35905,#29648,.T.) ;
#44053 = EDGE_CURVE('',#36171,#36177,#29649,.T.) ;
#44054 = EDGE_CURVE('',#35948,#36172,#29650,.T.) ;
#44055 = EDGE_CURVE('',#36185,#36186,#2148,.T.) ;
#44056 = EDGE_CURVE('',#36186,#35949,#356,.T.) ;
#44057 = EDGE_CURVE('',#36173,#36185,#29651,.T.) ;
#44058 = EDGE_CURVE('',#36160,#36165,#29652,.T.) ;
#44059 = EDGE_CURVE('',#36165,#36159,#29653,.T.) ;
#44060 = EDGE_CURVE('',#36166,#36158,#29654,.T.) ;
#44061 = EDGE_CURVE('',#36161,#36168,#29655,.T.) ;
#44062 = EDGE_CURVE('',#36166,#36157,#29656,.T.) ;
#44063 = EDGE_CURVE('',#36162,#36168,#29657,.T.) ;
#44064 = EDGE_CURVE('',#36167,#36164,#29658,.T.) ;
#44065 = EDGE_CURVE('',#36163,#36167,#29659,.T.) ;
#44066 = EDGE_CURVE('',#36026,#36096,#29660,.T.) ;
#44067 = EDGE_CURVE('',#36093,#36025,#29661,.T.) ;
#44068 = EDGE_CURVE('',#36108,#36024,#29662,.T.) ;
#44069 = EDGE_CURVE('',#36093,#36108,#29663,.T.) ;
#44070 = EDGE_CURVE('',#36100,#36096,#29664,.T.) ;
#44071 = EDGE_CURVE('',#36027,#36100,#29665,.T.) ;
#44072 = EDGE_CURVE('',#36105,#36023,#29666,.T.) ;
#44073 = EDGE_CURVE('',#36094,#36107,#29667,.T.) ;
#44074 = EDGE_CURVE('',#36095,#36112,#29668,.T.) ;
#44075 = EDGE_CURVE('',#36109,#36094,#29669,.T.) ;
#44076 = EDGE_CURVE('',#36097,#36095,#29670,.T.) ;
#44077 = EDGE_CURVE('',#36021,#36099,#29671,.T.) ;
#44078 = EDGE_CURVE('',#36022,#36103,#29672,.T.) ;
#44079 = EDGE_CURVE('',#36104,#36020,#29673,.T.) ;
#44080 = EDGE_CURVE('',#36105,#36103,#29674,.T.) ;
#44081 = EDGE_CURVE('',#36109,#36107,#29675,.T.) ;
#44082 = EDGE_CURVE('',#36097,#36112,#29676,.T.) ;
#44083 = EDGE_CURVE('',#36104,#36099,#29677,.T.) ;
#44084 = EDGE_CURVE('',#36106,#36102,#29678,.T.) ;
#44085 = EDGE_CURVE('',#36110,#36106,#29679,.T.) ;
#44086 = EDGE_CURVE('',#36098,#36111,#29680,.T.) ;
#44087 = EDGE_CURVE('',#36101,#36098,#29681,.T.) ;
#44088 = EDGE_CURVE('',#36110,#36102,#29682,.T.) ;
#44089 = EDGE_CURVE('',#36101,#36111,#29683,.T.) ;
#44090 = EDGE_CURVE('',#35994,#36140,#29684,.T.) ;
#44091 = EDGE_CURVE('',#36137,#35993,#29685,.T.) ;
#44092 = EDGE_CURVE('',#36136,#35992,#29686,.T.) ;
#44093 = EDGE_CURVE('',#36137,#36136,#29687,.T.) ;
#44094 = EDGE_CURVE('',#36144,#36140,#29688,.T.) ;
#44095 = EDGE_CURVE('',#35995,#36144,#29689,.T.) ;
#44096 = EDGE_CURVE('',#36133,#35991,#29690,.T.) ;
#44097 = EDGE_CURVE('',#36138,#36135,#29691,.T.) ;
#44098 = EDGE_CURVE('',#36139,#36148,#29692,.T.) ;
#44099 = EDGE_CURVE('',#36145,#36138,#29693,.T.) ;
#44100 = EDGE_CURVE('',#36141,#36139,#29694,.T.) ;
#44101 = EDGE_CURVE('',#35989,#36143,#29695,.T.) ;
#44102 = EDGE_CURVE('',#35990,#36131,#29696,.T.) ;
#44103 = EDGE_CURVE('',#36132,#35988,#29697,.T.) ;
#44104 = EDGE_CURVE('',#36133,#36131,#29698,.T.) ;
#44105 = EDGE_CURVE('',#36145,#36135,#29699,.T.) ;
#44106 = EDGE_CURVE('',#36141,#36148,#29700,.T.) ;
#44107 = EDGE_CURVE('',#36132,#36143,#29701,.T.) ;
#44108 = EDGE_CURVE('',#36134,#36130,#29702,.T.) ;
#44109 = EDGE_CURVE('',#36146,#36134,#29703,.T.) ;
#44110 = EDGE_CURVE('',#36142,#36147,#29704,.T.) ;
#44111 = EDGE_CURVE('',#36129,#36142,#29705,.T.) ;
#44112 = EDGE_CURVE('',#36146,#36130,#29706,.T.) ;
#44113 = EDGE_CURVE('',#36129,#36147,#29707,.T.) ;
#44114 = EDGE_CURVE('',#36043,#36179,#2149,.T.) ;
#44115 = EDGE_CURVE('',#36044,#36178,#29708,.T.) ;
#44116 = EDGE_CURVE('',#35934,#36044,#29709,.T.) ;
#44117 = EDGE_CURVE('',#35934,#36178,#29710,.T.) ;
#44118 = EDGE_CURVE('',#35935,#36183,#29711,.T.) ;
#44119 = EDGE_CURVE('',#35941,#35935,#29712,.T.) ;
#44120 = EDGE_CURVE('',#35942,#36183,#29713,.T.) ;
#44121 = EDGE_CURVE('',#35943,#36182,#29714,.T.) ;
#44122 = EDGE_CURVE('',#36045,#35944,#29715,.T.) ;
#44123 = EDGE_CURVE('',#36045,#36182,#29716,.T.) ;
#44124 = EDGE_CURVE('',#36046,#36181,#29717,.T.) ;
#44125 = EDGE_CURVE('',#35928,#36046,#29718,.T.) ;
#44126 = EDGE_CURVE('',#35928,#36181,#29719,.T.) ;
#44127 = EDGE_CURVE('',#36180,#35929,#2150,.T.) ;
#44128 = EDGE_CURVE('',#35906,#36176,#29720,.T.) ;
#44129 = EDGE_CURVE('',#36173,#36175,#29721,.T.) ;
#44130 = EDGE_CURVE('',#36185,#36174,#29722,.T.) ;
#44131 = EDGE_CURVE('',#36186,#35955,#29723,.T.) ;
#44132 = EDGE_CURVE('',#35949,#35954,#29724,.T.) ;
#44133 = EDGE_CURVE('',#35938,#35957,#29725,.T.) ;
#44134 = EDGE_CURVE('',#36184,#35956,#29726,.T.) ;
#44135 = EDGE_CURVE('',#36169,#36177,#29727,.T.) ;
#44136 = EDGE_CURVE('',#36187,#36188,#2151,.T.) ;
#44137 = EDGE_CURVE('',#36188,#36180,#2152,.T.) ;
#44138 = EDGE_CURVE('',#36179,#36189,#2153,.T.) ;
#44139 = EDGE_CURVE('',#36189,#36187,#2154,.T.) ;
#44140 = EDGE_CURVE('',#36043,#36036,#29728,.T.) ;
#44141 = EDGE_CURVE('',#36035,#36179,#2155,.T.) ;
#44142 = EDGE_CURVE('',#36032,#35929,#29729,.T.) ;
#44143 = EDGE_CURVE('',#36180,#36033,#2156,.T.) ;
#44144 = EDGE_CURVE('',#36189,#36035,#29730,.T.) ;
#44145 = EDGE_CURVE('',#36187,#36034,#29731,.T.) ;
#44146 = EDGE_CURVE('',#36188,#36033,#29732,.T.) ;
#44147 = EDGE_CURVE('',#36190,#36190,#29733,.T.) ;
#44148 = EDGE_CURVE('',#36190,#36191,#29734,.T.) ;
#44149 = EDGE_CURVE('',#36192,#36191,#29735,.T.) ;
#44150 = EDGE_CURVE('',#36191,#36192,#29736,.T.) ;
#44151 = EDGE_CURVE('',#36193,#36193,#29737,.T.) ;
#44152 = EDGE_CURVE('',#36193,#36194,#29738,.T.) ;
#44153 = EDGE_CURVE('',#36194,#36194,#29739,.T.) ;
#44154 = EDGE_CURVE('',#36195,#36196,#29740,.T.) ;
#44155 = EDGE_CURVE('',#36197,#36195,#29741,.T.) ;
#44156 = EDGE_CURVE('',#36197,#36196,#29742,.T.) ;
#44157 = EDGE_CURVE('',#36198,#36199,#357,.T.) ;
#44158 = EDGE_CURVE('',#36198,#36200,#29743,.T.) ;
#44159 = EDGE_CURVE('',#36201,#36200,#3629,.T.) ;
#44160 = EDGE_CURVE('',#36202,#36201,#29744,.T.) ;
#44161 = EDGE_CURVE('',#36203,#36202,#3630,.T.) ;
#44162 = EDGE_CURVE('',#36204,#36203,#3631,.T.) ;
#44163 = EDGE_CURVE('',#36204,#36199,#2157,.T.) ;
#44164 = EDGE_CURVE('',#36205,#36205,#29745,.T.) ;
#44165 = EDGE_CURVE('',#36205,#36206,#29746,.T.) ;
#44166 = EDGE_CURVE('',#36207,#36206,#29747,.T.) ;
#44167 = EDGE_CURVE('',#36206,#36207,#29748,.T.) ;
#44168 = EDGE_CURVE('',#36208,#36208,#29749,.T.) ;
#44169 = EDGE_CURVE('',#36208,#36209,#29750,.T.) ;
#44170 = EDGE_CURVE('',#36209,#36209,#29751,.T.) ;
#44171 = EDGE_CURVE('',#36210,#36211,#29752,.T.) ;
#44172 = EDGE_CURVE('',#36212,#36210,#29753,.T.) ;
#44173 = EDGE_CURVE('',#36212,#36211,#29754,.T.) ;
#44174 = EDGE_CURVE('',#36213,#36214,#358,.T.) ;
#44175 = EDGE_CURVE('',#36213,#36215,#29755,.T.) ;
#44176 = EDGE_CURVE('',#36216,#36215,#3632,.T.) ;
#44177 = EDGE_CURVE('',#36217,#36216,#29756,.T.) ;
#44178 = EDGE_CURVE('',#36218,#36217,#3633,.T.) ;
#44179 = EDGE_CURVE('',#36219,#36218,#3634,.T.) ;
#44180 = EDGE_CURVE('',#36219,#36214,#2158,.T.) ;
#44181 = EDGE_CURVE('',#36220,#36220,#29757,.T.) ;
#44182 = EDGE_CURVE('',#36220,#36221,#29758,.T.) ;
#44183 = EDGE_CURVE('',#36222,#36221,#29759,.T.) ;
#44184 = EDGE_CURVE('',#36221,#36222,#29760,.T.) ;
#44185 = EDGE_CURVE('',#36223,#36223,#29761,.T.) ;
#44186 = EDGE_CURVE('',#36223,#36224,#29762,.T.) ;
#44187 = EDGE_CURVE('',#36224,#36224,#29763,.T.) ;
#44188 = EDGE_CURVE('',#36225,#36226,#29764,.T.) ;
#44189 = EDGE_CURVE('',#36227,#36225,#29765,.T.) ;
#44190 = EDGE_CURVE('',#36227,#36226,#29766,.T.) ;
#44191 = EDGE_CURVE('',#36228,#36229,#359,.T.) ;
#44192 = EDGE_CURVE('',#36228,#36230,#29767,.T.) ;
#44193 = EDGE_CURVE('',#36231,#36230,#3635,.T.) ;
#44194 = EDGE_CURVE('',#36232,#36231,#29768,.T.) ;
#44195 = EDGE_CURVE('',#36233,#36232,#3636,.T.) ;
#44196 = EDGE_CURVE('',#36234,#36233,#3637,.T.) ;
#44197 = EDGE_CURVE('',#36234,#36229,#2159,.T.) ;
#44198 = EDGE_CURVE('',#36235,#36235,#29769,.T.) ;
#44199 = EDGE_CURVE('',#36235,#36236,#29770,.T.) ;
#44200 = EDGE_CURVE('',#36237,#36236,#29771,.T.) ;
#44201 = EDGE_CURVE('',#36236,#36237,#29772,.T.) ;
#44202 = EDGE_CURVE('',#36238,#36238,#29773,.T.) ;
#44203 = EDGE_CURVE('',#36238,#36239,#29774,.T.) ;
#44204 = EDGE_CURVE('',#36239,#36239,#29775,.T.) ;
#44205 = EDGE_CURVE('',#36240,#36241,#29776,.T.) ;
#44206 = EDGE_CURVE('',#36242,#36240,#29777,.T.) ;
#44207 = EDGE_CURVE('',#36242,#36241,#29778,.T.) ;
#44208 = EDGE_CURVE('',#36243,#36244,#360,.T.) ;
#44209 = EDGE_CURVE('',#36243,#36245,#29779,.T.) ;
#44210 = EDGE_CURVE('',#36246,#36245,#3638,.T.) ;
#44211 = EDGE_CURVE('',#36247,#36246,#29780,.T.) ;
#44212 = EDGE_CURVE('',#36248,#36247,#3639,.T.) ;
#44213 = EDGE_CURVE('',#36249,#36248,#3640,.T.) ;
#44214 = EDGE_CURVE('',#36249,#36244,#2160,.T.) ;
#44215 = EDGE_CURVE('',#36250,#36250,#29781,.T.) ;
#44216 = EDGE_CURVE('',#36250,#36251,#29782,.T.) ;
#44217 = EDGE_CURVE('',#36252,#36251,#29783,.T.) ;
#44218 = EDGE_CURVE('',#36251,#36252,#29784,.T.) ;
#44219 = EDGE_CURVE('',#36253,#36253,#29785,.T.) ;
#44220 = EDGE_CURVE('',#36253,#36254,#29786,.T.) ;
#44221 = EDGE_CURVE('',#36254,#36254,#29787,.T.) ;
#44222 = EDGE_CURVE('',#36255,#36256,#29788,.T.) ;
#44223 = EDGE_CURVE('',#36257,#36255,#29789,.T.) ;
#44224 = EDGE_CURVE('',#36257,#36256,#29790,.T.) ;
#44225 = EDGE_CURVE('',#36258,#36259,#361,.T.) ;
#44226 = EDGE_CURVE('',#36258,#36260,#29791,.T.) ;
#44227 = EDGE_CURVE('',#36261,#36260,#3641,.T.) ;
#44228 = EDGE_CURVE('',#36262,#36261,#29792,.T.) ;
#44229 = EDGE_CURVE('',#36263,#36262,#3642,.T.) ;
#44230 = EDGE_CURVE('',#36264,#36263,#3643,.T.) ;
#44231 = EDGE_CURVE('',#36264,#36259,#2161,.T.) ;
#44232 = EDGE_CURVE('',#36265,#36265,#29793,.T.) ;
#44233 = EDGE_CURVE('',#36265,#36266,#29794,.T.) ;
#44234 = EDGE_CURVE('',#36267,#36266,#29795,.T.) ;
#44235 = EDGE_CURVE('',#36266,#36267,#29796,.T.) ;
#44236 = EDGE_CURVE('',#36268,#36268,#29797,.T.) ;
#44237 = EDGE_CURVE('',#36268,#36269,#29798,.T.) ;
#44238 = EDGE_CURVE('',#36269,#36269,#29799,.T.) ;
#44239 = EDGE_CURVE('',#36270,#36271,#29800,.T.) ;
#44240 = EDGE_CURVE('',#36272,#36270,#29801,.T.) ;
#44241 = EDGE_CURVE('',#36272,#36271,#29802,.T.) ;
#44242 = EDGE_CURVE('',#36273,#36274,#362,.T.) ;
#44243 = EDGE_CURVE('',#36273,#36275,#29803,.T.) ;
#44244 = EDGE_CURVE('',#36276,#36275,#3644,.T.) ;
#44245 = EDGE_CURVE('',#36277,#36276,#29804,.T.) ;
#44246 = EDGE_CURVE('',#36278,#36277,#3645,.T.) ;
#44247 = EDGE_CURVE('',#36279,#36278,#3646,.T.) ;
#44248 = EDGE_CURVE('',#36279,#36274,#2162,.T.) ;
#44249 = EDGE_CURVE('',#36280,#36280,#29805,.T.) ;
#44250 = EDGE_CURVE('',#36280,#36281,#29806,.T.) ;
#44251 = EDGE_CURVE('',#36282,#36281,#29807,.T.) ;
#44252 = EDGE_CURVE('',#36281,#36282,#29808,.T.) ;
#44253 = EDGE_CURVE('',#36283,#36283,#29809,.T.) ;
#44254 = EDGE_CURVE('',#36283,#36284,#29810,.T.) ;
#44255 = EDGE_CURVE('',#36284,#36284,#29811,.T.) ;
#44256 = EDGE_CURVE('',#36285,#36286,#29812,.T.) ;
#44257 = EDGE_CURVE('',#36287,#36285,#29813,.T.) ;
#44258 = EDGE_CURVE('',#36287,#36286,#29814,.T.) ;
#44259 = EDGE_CURVE('',#36288,#36289,#363,.T.) ;
#44260 = EDGE_CURVE('',#36288,#36290,#29815,.T.) ;
#44261 = EDGE_CURVE('',#36291,#36290,#3647,.T.) ;
#44262 = EDGE_CURVE('',#36292,#36291,#29816,.T.) ;
#44263 = EDGE_CURVE('',#36293,#36292,#3648,.T.) ;
#44264 = EDGE_CURVE('',#36294,#36293,#3649,.T.) ;
#44265 = EDGE_CURVE('',#36294,#36289,#2163,.T.) ;
#44266 = EDGE_CURVE('',#36295,#36295,#29817,.T.) ;
#44267 = EDGE_CURVE('',#36295,#36296,#29818,.T.) ;
#44268 = EDGE_CURVE('',#36297,#36296,#29819,.T.) ;
#44269 = EDGE_CURVE('',#36296,#36297,#29820,.T.) ;
#44270 = EDGE_CURVE('',#36298,#36298,#29821,.T.) ;
#44271 = EDGE_CURVE('',#36298,#36299,#29822,.T.) ;
#44272 = EDGE_CURVE('',#36299,#36299,#29823,.T.) ;
#44273 = EDGE_CURVE('',#36300,#36301,#29824,.T.) ;
#44274 = EDGE_CURVE('',#36302,#36300,#29825,.T.) ;
#44275 = EDGE_CURVE('',#36302,#36301,#29826,.T.) ;
#44276 = EDGE_CURVE('',#36303,#36304,#364,.T.) ;
#44277 = EDGE_CURVE('',#36303,#36305,#29827,.T.) ;
#44278 = EDGE_CURVE('',#36306,#36305,#3650,.T.) ;
#44279 = EDGE_CURVE('',#36307,#36306,#29828,.T.) ;
#44280 = EDGE_CURVE('',#36308,#36307,#3651,.T.) ;
#44281 = EDGE_CURVE('',#36309,#36308,#3652,.T.) ;
#44282 = EDGE_CURVE('',#36309,#36304,#2164,.T.) ;
#44283 = EDGE_CURVE('',#36310,#36310,#29829,.T.) ;
#44284 = EDGE_CURVE('',#36310,#36311,#29830,.T.) ;
#44285 = EDGE_CURVE('',#36312,#36311,#29831,.T.) ;
#44286 = EDGE_CURVE('',#36311,#36312,#29832,.T.) ;
#44287 = EDGE_CURVE('',#36313,#36314,#29833,.T.) ;
#44288 = EDGE_CURVE('',#36315,#36313,#29834,.T.) ;
#44289 = EDGE_CURVE('',#36316,#36315,#29835,.T.) ;
#44290 = EDGE_CURVE('',#36316,#36314,#29836,.T.) ;
#44291 = EDGE_CURVE('',#36317,#36318,#29837,.T.) ;
#44292 = EDGE_CURVE('',#36319,#36317,#29838,.T.) ;
#44293 = EDGE_CURVE('',#36320,#36319,#29839,.T.) ;
#44294 = EDGE_CURVE('',#36320,#36318,#29840,.T.) ;
#44295 = EDGE_CURVE('',#36321,#36322,#29841,.T.) ;
#44296 = EDGE_CURVE('',#36323,#36321,#29842,.T.) ;
#44297 = EDGE_CURVE('',#36324,#36323,#29843,.T.) ;
#44298 = EDGE_CURVE('',#36324,#36322,#29844,.T.) ;
#44299 = EDGE_CURVE('',#36325,#36326,#29845,.T.) ;
#44300 = EDGE_CURVE('',#36327,#36325,#29846,.T.) ;
#44301 = EDGE_CURVE('',#36328,#36327,#29847,.T.) ;
#44302 = EDGE_CURVE('',#36328,#36326,#29848,.T.) ;
#44303 = EDGE_CURVE('',#36329,#36330,#29849,.T.) ;
#44304 = EDGE_CURVE('',#36331,#36329,#29850,.T.) ;
#44305 = EDGE_CURVE('',#36332,#36331,#29851,.T.) ;
#44306 = EDGE_CURVE('',#36332,#36330,#29852,.T.) ;
#44307 = EDGE_CURVE('',#36333,#36334,#29853,.T.) ;
#44308 = EDGE_CURVE('',#36335,#36333,#29854,.T.) ;
#44309 = EDGE_CURVE('',#36336,#36335,#29855,.T.) ;
#44310 = EDGE_CURVE('',#36336,#36334,#29856,.T.) ;
#44311 = EDGE_CURVE('',#36337,#36338,#29857,.T.) ;
#44312 = EDGE_CURVE('',#36339,#36337,#29858,.T.) ;
#44313 = EDGE_CURVE('',#36340,#36339,#29859,.T.) ;
#44314 = EDGE_CURVE('',#36340,#36338,#29860,.T.) ;
#44315 = EDGE_CURVE('',#36341,#36342,#29861,.T.) ;
#44316 = EDGE_CURVE('',#36343,#36341,#29862,.T.) ;
#44317 = EDGE_CURVE('',#36344,#36343,#29863,.T.) ;
#44318 = EDGE_CURVE('',#36344,#36342,#29864,.T.) ;
#44319 = EDGE_CURVE('',#36345,#36346,#29865,.T.) ;
#44320 = EDGE_CURVE('',#36347,#36345,#29866,.T.) ;
#44321 = EDGE_CURVE('',#36348,#36347,#29867,.T.) ;
#44322 = EDGE_CURVE('',#36348,#36346,#29868,.T.) ;
#44323 = EDGE_CURVE('',#36349,#36349,#29869,.T.) ;
#44324 = EDGE_CURVE('',#36349,#36350,#29870,.T.) ;
#44325 = EDGE_CURVE('',#36350,#36350,#29871,.T.) ;
#44326 = EDGE_CURVE('',#36351,#36352,#29872,.T.) ;
#44327 = EDGE_CURVE('',#36353,#36351,#29873,.T.) ;
#44328 = EDGE_CURVE('',#36353,#36352,#29874,.T.) ;
#44329 = EDGE_CURVE('',#36354,#36355,#365,.T.) ;
#44330 = EDGE_CURVE('',#36354,#36356,#29875,.T.) ;
#44331 = EDGE_CURVE('',#36357,#36356,#3653,.T.) ;
#44332 = EDGE_CURVE('',#36358,#36357,#29876,.T.) ;
#44333 = EDGE_CURVE('',#36359,#36358,#3654,.T.) ;
#44334 = EDGE_CURVE('',#36360,#36359,#3655,.T.) ;
#44335 = EDGE_CURVE('',#36360,#36355,#2165,.T.) ;
#44336 = EDGE_CURVE('',#36194,#36192,#3656,.T.) ;
#44337 = EDGE_CURVE('',#36209,#36207,#3657,.T.) ;
#44338 = EDGE_CURVE('',#36224,#36222,#3658,.T.) ;
#44339 = EDGE_CURVE('',#36239,#36237,#3659,.T.) ;
#44340 = EDGE_CURVE('',#36254,#36252,#3660,.T.) ;
#44341 = EDGE_CURVE('',#36269,#36267,#3661,.T.) ;
#44342 = EDGE_CURVE('',#36284,#36282,#3662,.T.) ;
#44343 = EDGE_CURVE('',#36299,#36297,#3663,.T.) ;
#44344 = EDGE_CURVE('',#36350,#36312,#3664,.T.) ;
#44345 = EDGE_CURVE('',#36361,#36362,#29877,.T.) ;
#44346 = EDGE_CURVE('',#36362,#36316,#3665,.T.) ;
#44347 = EDGE_CURVE('',#36361,#36315,#3666,.T.) ;
#44348 = EDGE_CURVE('',#36363,#36364,#29878,.T.) ;
#44349 = EDGE_CURVE('',#36364,#36320,#3667,.T.) ;
#44350 = EDGE_CURVE('',#36363,#36319,#3668,.T.) ;
#44351 = EDGE_CURVE('',#36365,#36366,#29879,.T.) ;
#44352 = EDGE_CURVE('',#36366,#36324,#3669,.T.) ;
#44353 = EDGE_CURVE('',#36365,#36323,#3670,.T.) ;
#44354 = EDGE_CURVE('',#36367,#36368,#29880,.T.) ;
#44355 = EDGE_CURVE('',#36368,#36328,#3671,.T.) ;
#44356 = EDGE_CURVE('',#36367,#36327,#3672,.T.) ;
#44357 = EDGE_CURVE('',#36369,#36370,#29881,.T.) ;
#44358 = EDGE_CURVE('',#36370,#36332,#3673,.T.) ;
#44359 = EDGE_CURVE('',#36369,#36331,#3674,.T.) ;
#44360 = EDGE_CURVE('',#36371,#36372,#29882,.T.) ;
#44361 = EDGE_CURVE('',#36372,#36336,#3675,.T.) ;
#44362 = EDGE_CURVE('',#36371,#36335,#3676,.T.) ;
#44363 = EDGE_CURVE('',#36373,#36374,#29883,.T.) ;
#44364 = EDGE_CURVE('',#36374,#36340,#3677,.T.) ;
#44365 = EDGE_CURVE('',#36373,#36339,#3678,.T.) ;
#44366 = EDGE_CURVE('',#36375,#36376,#29884,.T.) ;
#44367 = EDGE_CURVE('',#36376,#36344,#3679,.T.) ;
#44368 = EDGE_CURVE('',#36375,#36343,#3680,.T.) ;
#44369 = EDGE_CURVE('',#36377,#36378,#29885,.T.) ;
#44370 = EDGE_CURVE('',#36378,#36348,#3681,.T.) ;
#44371 = EDGE_CURVE('',#36377,#36347,#3682,.T.) ;
#44372 = EDGE_CURVE('',#36379,#36379,#29886,.T.) ;
#44373 = EDGE_CURVE('',#36379,#36380,#29887,.T.) ;
#44374 = EDGE_CURVE('',#36381,#36380,#29888,.T.) ;
#44375 = EDGE_CURVE('',#36380,#36381,#29889,.T.) ;
#44376 = EDGE_CURVE('',#36382,#36383,#29890,.T.) ;
#44377 = EDGE_CURVE('',#36384,#36382,#29891,.T.) ;
#44378 = EDGE_CURVE('',#36385,#36384,#29892,.T.) ;
#44379 = EDGE_CURVE('',#36385,#36383,#29893,.T.) ;
#44380 = EDGE_CURVE('',#36386,#36386,#29894,.T.) ;
#44381 = EDGE_CURVE('',#36386,#36387,#29895,.T.) ;
#44382 = EDGE_CURVE('',#36387,#36387,#29896,.T.) ;
#44383 = EDGE_CURVE('',#36388,#36389,#29897,.T.) ;
#44384 = EDGE_CURVE('',#36390,#36388,#29898,.T.) ;
#44385 = EDGE_CURVE('',#36390,#36389,#29899,.T.) ;
#44386 = EDGE_CURVE('',#36391,#36392,#366,.T.) ;
#44387 = EDGE_CURVE('',#36391,#36393,#29900,.T.) ;
#44388 = EDGE_CURVE('',#36394,#36393,#3683,.T.) ;
#44389 = EDGE_CURVE('',#36395,#36394,#29901,.T.) ;
#44390 = EDGE_CURVE('',#36396,#36395,#3684,.T.) ;
#44391 = EDGE_CURVE('',#36397,#36396,#3685,.T.) ;
#44392 = EDGE_CURVE('',#36397,#36392,#2166,.T.) ;
#44393 = EDGE_CURVE('',#36387,#36381,#3686,.T.) ;
#44394 = EDGE_CURVE('',#36398,#36399,#29902,.T.) ;
#44395 = EDGE_CURVE('',#36399,#36385,#3687,.T.) ;
#44396 = EDGE_CURVE('',#36398,#36384,#3688,.T.) ;
#44397 = EDGE_CURVE('',#36400,#36401,#3689,.T.) ;
#44398 = EDGE_CURVE('',#36401,#36402,#29903,.T.) ;
#44399 = EDGE_CURVE('',#36402,#36403,#3690,.T.) ;
#44400 = EDGE_CURVE('',#36403,#36203,#29904,.T.) ;
#44401 = EDGE_CURVE('',#36404,#36202,#29905,.T.) ;
#44402 = EDGE_CURVE('',#36404,#36405,#3691,.T.) ;
#44403 = EDGE_CURVE('',#36405,#36406,#3692,.T.) ;
#44404 = EDGE_CURVE('',#36406,#36407,#3693,.T.) ;
#44405 = EDGE_CURVE('',#36407,#36408,#3694,.T.) ;
#44406 = EDGE_CURVE('',#36408,#36409,#3695,.T.) ;
#44407 = EDGE_CURVE('',#36400,#36409,#29906,.T.) ;
#44408 = EDGE_CURVE('',#36410,#36411,#3696,.T.) ;
#44409 = EDGE_CURVE('',#36411,#36412,#29907,.T.) ;
#44410 = EDGE_CURVE('',#36412,#36413,#3697,.T.) ;
#44411 = EDGE_CURVE('',#36413,#36218,#29908,.T.) ;
#44412 = EDGE_CURVE('',#36414,#36217,#29909,.T.) ;
#44413 = EDGE_CURVE('',#36414,#36415,#3698,.T.) ;
#44414 = EDGE_CURVE('',#36415,#36416,#3699,.T.) ;
#44415 = EDGE_CURVE('',#36416,#36417,#3700,.T.) ;
#44416 = EDGE_CURVE('',#36417,#36418,#3701,.T.) ;
#44417 = EDGE_CURVE('',#36418,#36419,#3702,.T.) ;
#44418 = EDGE_CURVE('',#36410,#36419,#29910,.T.) ;
#44419 = EDGE_CURVE('',#36420,#36421,#3703,.T.) ;
#44420 = EDGE_CURVE('',#36421,#36422,#29911,.T.) ;
#44421 = EDGE_CURVE('',#36422,#36423,#3704,.T.) ;
#44422 = EDGE_CURVE('',#36423,#36233,#29912,.T.) ;
#44423 = EDGE_CURVE('',#36424,#36232,#29913,.T.) ;
#44424 = EDGE_CURVE('',#36424,#36425,#3705,.T.) ;
#44425 = EDGE_CURVE('',#36425,#36426,#3706,.T.) ;
#44426 = EDGE_CURVE('',#36426,#36427,#3707,.T.) ;
#44427 = EDGE_CURVE('',#36427,#36428,#3708,.T.) ;
#44428 = EDGE_CURVE('',#36428,#36429,#3709,.T.) ;
#44429 = EDGE_CURVE('',#36420,#36429,#29914,.T.) ;
#44430 = EDGE_CURVE('',#36430,#36431,#3710,.T.) ;
#44431 = EDGE_CURVE('',#36431,#36432,#29915,.T.) ;
#44432 = EDGE_CURVE('',#36432,#36433,#3711,.T.) ;
#44433 = EDGE_CURVE('',#36433,#36248,#29916,.T.) ;
#44434 = EDGE_CURVE('',#36434,#36247,#29917,.T.) ;
#44435 = EDGE_CURVE('',#36434,#36435,#3712,.T.) ;
#44436 = EDGE_CURVE('',#36435,#36436,#3713,.T.) ;
#44437 = EDGE_CURVE('',#36436,#36437,#3714,.T.) ;
#44438 = EDGE_CURVE('',#36437,#36438,#3715,.T.) ;
#44439 = EDGE_CURVE('',#36438,#36439,#3716,.T.) ;
#44440 = EDGE_CURVE('',#36430,#36439,#29918,.T.) ;
#44441 = EDGE_CURVE('',#36440,#36441,#3717,.T.) ;
#44442 = EDGE_CURVE('',#36441,#36442,#29919,.T.) ;
#44443 = EDGE_CURVE('',#36442,#36443,#3718,.T.) ;
#44444 = EDGE_CURVE('',#36443,#36263,#29920,.T.) ;
#44445 = EDGE_CURVE('',#36444,#36262,#29921,.T.) ;
#44446 = EDGE_CURVE('',#36444,#36445,#3719,.T.) ;
#44447 = EDGE_CURVE('',#36445,#36446,#3720,.T.) ;
#44448 = EDGE_CURVE('',#36446,#36447,#3721,.T.) ;
#44449 = EDGE_CURVE('',#36447,#36448,#3722,.T.) ;
#44450 = EDGE_CURVE('',#36448,#36449,#3723,.T.) ;
#44451 = EDGE_CURVE('',#36440,#36449,#29922,.T.) ;
#44452 = EDGE_CURVE('',#36450,#36451,#3724,.T.) ;
#44453 = EDGE_CURVE('',#36451,#36452,#29923,.T.) ;
#44454 = EDGE_CURVE('',#36452,#36453,#3725,.T.) ;
#44455 = EDGE_CURVE('',#36453,#36278,#29924,.T.) ;
#44456 = EDGE_CURVE('',#36454,#36277,#29925,.T.) ;
#44457 = EDGE_CURVE('',#36454,#36455,#3726,.T.) ;
#44458 = EDGE_CURVE('',#36455,#36456,#3727,.T.) ;
#44459 = EDGE_CURVE('',#36456,#36457,#3728,.T.) ;
#44460 = EDGE_CURVE('',#36457,#36458,#3729,.T.) ;
#44461 = EDGE_CURVE('',#36458,#36459,#3730,.T.) ;
#44462 = EDGE_CURVE('',#36450,#36459,#29926,.T.) ;
#44463 = EDGE_CURVE('',#36460,#36461,#3731,.T.) ;
#44464 = EDGE_CURVE('',#36461,#36462,#29927,.T.) ;
#44465 = EDGE_CURVE('',#36462,#36463,#3732,.T.) ;
#44466 = EDGE_CURVE('',#36463,#36293,#29928,.T.) ;
#44467 = EDGE_CURVE('',#36464,#36292,#29929,.T.) ;
#44468 = EDGE_CURVE('',#36464,#36465,#3733,.T.) ;
#44469 = EDGE_CURVE('',#36465,#36466,#3734,.T.) ;
#44470 = EDGE_CURVE('',#36466,#36467,#3735,.T.) ;
#44471 = EDGE_CURVE('',#36467,#36468,#3736,.T.) ;
#44472 = EDGE_CURVE('',#36468,#36469,#3737,.T.) ;
#44473 = EDGE_CURVE('',#36460,#36469,#29930,.T.) ;
#44474 = EDGE_CURVE('',#36470,#36471,#3738,.T.) ;
#44475 = EDGE_CURVE('',#36471,#36472,#29931,.T.) ;
#44476 = EDGE_CURVE('',#36472,#36473,#3739,.T.) ;
#44477 = EDGE_CURVE('',#36473,#36308,#29932,.T.) ;
#44478 = EDGE_CURVE('',#36474,#36307,#29933,.T.) ;
#44479 = EDGE_CURVE('',#36474,#36475,#3740,.T.) ;
#44480 = EDGE_CURVE('',#36475,#36476,#3741,.T.) ;
#44481 = EDGE_CURVE('',#36476,#36477,#3742,.T.) ;
#44482 = EDGE_CURVE('',#36477,#36478,#3743,.T.) ;
#44483 = EDGE_CURVE('',#36478,#36479,#3744,.T.) ;
#44484 = EDGE_CURVE('',#36470,#36479,#29934,.T.) ;
#44485 = EDGE_CURVE('',#36480,#36481,#3745,.T.) ;
#44486 = EDGE_CURVE('',#36481,#36482,#29935,.T.) ;
#44487 = EDGE_CURVE('',#36482,#36483,#3746,.T.) ;
#44488 = EDGE_CURVE('',#36483,#36359,#29936,.T.) ;
#44489 = EDGE_CURVE('',#36484,#36358,#29937,.T.) ;
#44490 = EDGE_CURVE('',#36484,#36485,#3747,.T.) ;
#44491 = EDGE_CURVE('',#36485,#36486,#3748,.T.) ;
#44492 = EDGE_CURVE('',#36486,#36487,#3749,.T.) ;
#44493 = EDGE_CURVE('',#36487,#36488,#3750,.T.) ;
#44494 = EDGE_CURVE('',#36488,#36489,#3751,.T.) ;
#44495 = EDGE_CURVE('',#36480,#36489,#29938,.T.) ;
#44496 = EDGE_CURVE('',#36490,#36491,#29939,.T.) ;
#44497 = EDGE_CURVE('',#36490,#36492,#3752,.T.) ;
#44498 = EDGE_CURVE('',#36492,#36493,#3753,.T.) ;
#44499 = EDGE_CURVE('',#36493,#36494,#3754,.T.) ;
#44500 = EDGE_CURVE('',#36494,#36491,#3755,.T.) ;
#44501 = EDGE_CURVE('',#36495,#36496,#29940,.T.) ;
#44502 = EDGE_CURVE('',#36495,#36497,#3756,.T.) ;
#44503 = EDGE_CURVE('',#36497,#36498,#3757,.T.) ;
#44504 = EDGE_CURVE('',#36498,#36499,#3758,.T.) ;
#44505 = EDGE_CURVE('',#36499,#36496,#3759,.T.) ;
#44506 = EDGE_CURVE('',#36500,#36501,#29941,.T.) ;
#44507 = EDGE_CURVE('',#36500,#36502,#3760,.T.) ;
#44508 = EDGE_CURVE('',#36502,#36503,#3761,.T.) ;
#44509 = EDGE_CURVE('',#36503,#36504,#3762,.T.) ;
#44510 = EDGE_CURVE('',#36504,#36501,#3763,.T.) ;
#44511 = EDGE_CURVE('',#36505,#36506,#29942,.T.) ;
#44512 = EDGE_CURVE('',#36505,#36507,#3764,.T.) ;
#44513 = EDGE_CURVE('',#36507,#36508,#3765,.T.) ;
#44514 = EDGE_CURVE('',#36508,#36509,#3766,.T.) ;
#44515 = EDGE_CURVE('',#36509,#36506,#3767,.T.) ;
#44516 = EDGE_CURVE('',#36510,#36511,#29943,.T.) ;
#44517 = EDGE_CURVE('',#36510,#36512,#3768,.T.) ;
#44518 = EDGE_CURVE('',#36512,#36513,#3769,.T.) ;
#44519 = EDGE_CURVE('',#36513,#36514,#3770,.T.) ;
#44520 = EDGE_CURVE('',#36514,#36511,#3771,.T.) ;
#44521 = EDGE_CURVE('',#36515,#36516,#29944,.T.) ;
#44522 = EDGE_CURVE('',#36515,#36517,#3772,.T.) ;
#44523 = EDGE_CURVE('',#36517,#36518,#3773,.T.) ;
#44524 = EDGE_CURVE('',#36518,#36519,#3774,.T.) ;
#44525 = EDGE_CURVE('',#36519,#36516,#3775,.T.) ;
#44526 = EDGE_CURVE('',#36520,#36521,#29945,.T.) ;
#44527 = EDGE_CURVE('',#36520,#36522,#3776,.T.) ;
#44528 = EDGE_CURVE('',#36522,#36523,#3777,.T.) ;
#44529 = EDGE_CURVE('',#36523,#36524,#3778,.T.) ;
#44530 = EDGE_CURVE('',#36524,#36521,#3779,.T.) ;
#44531 = EDGE_CURVE('',#36525,#36526,#29946,.T.) ;
#44532 = EDGE_CURVE('',#36525,#36527,#3780,.T.) ;
#44533 = EDGE_CURVE('',#36527,#36528,#3781,.T.) ;
#44534 = EDGE_CURVE('',#36528,#36529,#3782,.T.) ;
#44535 = EDGE_CURVE('',#36529,#36526,#3783,.T.) ;
#44536 = EDGE_CURVE('',#36530,#36531,#29947,.T.) ;
#44537 = EDGE_CURVE('',#36530,#36532,#3784,.T.) ;
#44538 = EDGE_CURVE('',#36532,#36533,#3785,.T.) ;
#44539 = EDGE_CURVE('',#36533,#36534,#3786,.T.) ;
#44540 = EDGE_CURVE('',#36534,#36531,#3787,.T.) ;
#44541 = EDGE_CURVE('',#36535,#36536,#29948,.T.) ;
#44542 = EDGE_CURVE('',#36535,#36537,#3788,.T.) ;
#44543 = EDGE_CURVE('',#36537,#36538,#3789,.T.) ;
#44544 = EDGE_CURVE('',#36538,#36539,#3790,.T.) ;
#44545 = EDGE_CURVE('',#36539,#36536,#3791,.T.) ;
#44546 = EDGE_CURVE('',#36540,#36541,#29949,.T.) ;
#44547 = EDGE_CURVE('',#36540,#36542,#3792,.T.) ;
#44548 = EDGE_CURVE('',#36542,#36543,#3793,.T.) ;
#44549 = EDGE_CURVE('',#36543,#36544,#3794,.T.) ;
#44550 = EDGE_CURVE('',#36544,#36541,#3795,.T.) ;
#44551 = EDGE_CURVE('',#36545,#36546,#29950,.T.) ;
#44552 = EDGE_CURVE('',#36545,#36547,#3796,.T.) ;
#44553 = EDGE_CURVE('',#36547,#36548,#3797,.T.) ;
#44554 = EDGE_CURVE('',#36548,#36549,#3798,.T.) ;
#44555 = EDGE_CURVE('',#36549,#36546,#3799,.T.) ;
#44556 = EDGE_CURVE('',#36550,#36551,#29951,.T.) ;
#44557 = EDGE_CURVE('',#36550,#36552,#3800,.T.) ;
#44558 = EDGE_CURVE('',#36552,#36553,#3801,.T.) ;
#44559 = EDGE_CURVE('',#36553,#36554,#3802,.T.) ;
#44560 = EDGE_CURVE('',#36554,#36551,#3803,.T.) ;
#44561 = EDGE_CURVE('',#36555,#36556,#29952,.T.) ;
#44562 = EDGE_CURVE('',#36555,#36557,#3804,.T.) ;
#44563 = EDGE_CURVE('',#36557,#36558,#3805,.T.) ;
#44564 = EDGE_CURVE('',#36558,#36559,#3806,.T.) ;
#44565 = EDGE_CURVE('',#36559,#36556,#3807,.T.) ;
#44566 = EDGE_CURVE('',#36560,#36561,#29953,.T.) ;
#44567 = EDGE_CURVE('',#36560,#36562,#3808,.T.) ;
#44568 = EDGE_CURVE('',#36562,#36563,#3809,.T.) ;
#44569 = EDGE_CURVE('',#36563,#36564,#3810,.T.) ;
#44570 = EDGE_CURVE('',#36564,#36561,#3811,.T.) ;
#44571 = EDGE_CURVE('',#36565,#36566,#29954,.T.) ;
#44572 = EDGE_CURVE('',#36565,#36567,#3812,.T.) ;
#44573 = EDGE_CURVE('',#36567,#36568,#3813,.T.) ;
#44574 = EDGE_CURVE('',#36568,#36569,#3814,.T.) ;
#44575 = EDGE_CURVE('',#36569,#36566,#3815,.T.) ;
#44576 = EDGE_CURVE('',#36570,#36571,#29955,.T.) ;
#44577 = EDGE_CURVE('',#36570,#36572,#3816,.T.) ;
#44578 = EDGE_CURVE('',#36572,#36573,#3817,.T.) ;
#44579 = EDGE_CURVE('',#36573,#36574,#3818,.T.) ;
#44580 = EDGE_CURVE('',#36574,#36571,#3819,.T.) ;
#44581 = EDGE_CURVE('',#36575,#36576,#29956,.T.) ;
#44582 = EDGE_CURVE('',#36575,#36577,#3820,.T.) ;
#44583 = EDGE_CURVE('',#36577,#36578,#3821,.T.) ;
#44584 = EDGE_CURVE('',#36578,#36579,#3822,.T.) ;
#44585 = EDGE_CURVE('',#36579,#36576,#3823,.T.) ;
#44586 = EDGE_CURVE('',#36580,#36581,#3824,.T.) ;
#44587 = EDGE_CURVE('',#36580,#36582,#29957,.T.) ;
#44588 = EDGE_CURVE('',#36582,#36583,#3825,.T.) ;
#44589 = EDGE_CURVE('',#36583,#36581,#29958,.T.) ;
#44590 = EDGE_CURVE('',#36584,#36585,#3826,.T.) ;
#44591 = EDGE_CURVE('',#36584,#36586,#29959,.T.) ;
#44592 = EDGE_CURVE('',#36586,#36587,#3827,.T.) ;
#44593 = EDGE_CURVE('',#36587,#36585,#29960,.T.) ;
#44594 = EDGE_CURVE('',#36588,#36589,#3828,.T.) ;
#44595 = EDGE_CURVE('',#36588,#36590,#29961,.T.) ;
#44596 = EDGE_CURVE('',#36590,#36591,#3829,.T.) ;
#44597 = EDGE_CURVE('',#36591,#36589,#29962,.T.) ;
#44598 = EDGE_CURVE('',#36592,#36593,#3830,.T.) ;
#44599 = EDGE_CURVE('',#36592,#36594,#29963,.T.) ;
#44600 = EDGE_CURVE('',#36594,#36595,#3831,.T.) ;
#44601 = EDGE_CURVE('',#36595,#36593,#29964,.T.) ;
#44602 = EDGE_CURVE('',#36596,#36597,#3832,.T.) ;
#44603 = EDGE_CURVE('',#36596,#36598,#29965,.T.) ;
#44604 = EDGE_CURVE('',#36598,#36599,#3833,.T.) ;
#44605 = EDGE_CURVE('',#36599,#36597,#29966,.T.) ;
#44606 = EDGE_CURVE('',#36600,#36601,#3834,.T.) ;
#44607 = EDGE_CURVE('',#36600,#36602,#29967,.T.) ;
#44608 = EDGE_CURVE('',#36602,#36603,#3835,.T.) ;
#44609 = EDGE_CURVE('',#36603,#36601,#29968,.T.) ;
#44610 = EDGE_CURVE('',#36604,#36605,#3836,.T.) ;
#44611 = EDGE_CURVE('',#36604,#36606,#29969,.T.) ;
#44612 = EDGE_CURVE('',#36606,#36607,#3837,.T.) ;
#44613 = EDGE_CURVE('',#36607,#36605,#29970,.T.) ;
#44614 = EDGE_CURVE('',#36608,#36609,#3838,.T.) ;
#44615 = EDGE_CURVE('',#36608,#36610,#29971,.T.) ;
#44616 = EDGE_CURVE('',#36610,#36611,#3839,.T.) ;
#44617 = EDGE_CURVE('',#36611,#36609,#29972,.T.) ;
#44618 = EDGE_CURVE('',#36612,#36613,#3840,.T.) ;
#44619 = EDGE_CURVE('',#36612,#36614,#29973,.T.) ;
#44620 = EDGE_CURVE('',#36614,#36615,#3841,.T.) ;
#44621 = EDGE_CURVE('',#36615,#36613,#29974,.T.) ;
#44622 = EDGE_CURVE('',#36616,#36617,#3842,.T.) ;
#44623 = EDGE_CURVE('',#36617,#36618,#29975,.T.) ;
#44624 = EDGE_CURVE('',#36618,#36619,#3843,.T.) ;
#44625 = EDGE_CURVE('',#36619,#36396,#29976,.T.) ;
#44626 = EDGE_CURVE('',#36620,#36395,#29977,.T.) ;
#44627 = EDGE_CURVE('',#36620,#36621,#3844,.T.) ;
#44628 = EDGE_CURVE('',#36621,#36622,#3845,.T.) ;
#44629 = EDGE_CURVE('',#36622,#36623,#3846,.T.) ;
#44630 = EDGE_CURVE('',#36623,#36624,#3847,.T.) ;
#44631 = EDGE_CURVE('',#36624,#36625,#3848,.T.) ;
#44632 = EDGE_CURVE('',#36616,#36625,#29978,.T.) ;
#44633 = EDGE_CURVE('',#36626,#36627,#29979,.T.) ;
#44634 = EDGE_CURVE('',#36626,#36628,#3849,.T.) ;
#44635 = EDGE_CURVE('',#36628,#36629,#3850,.T.) ;
#44636 = EDGE_CURVE('',#36629,#36630,#3851,.T.) ;
#44637 = EDGE_CURVE('',#36630,#36627,#3852,.T.) ;
#44638 = EDGE_CURVE('',#36631,#36632,#29980,.T.) ;
#44639 = EDGE_CURVE('',#36631,#36633,#3853,.T.) ;
#44640 = EDGE_CURVE('',#36633,#36634,#3854,.T.) ;
#44641 = EDGE_CURVE('',#36634,#36635,#3855,.T.) ;
#44642 = EDGE_CURVE('',#36635,#36632,#3856,.T.) ;
#44643 = EDGE_CURVE('',#36636,#36637,#3857,.T.) ;
#44644 = EDGE_CURVE('',#36636,#36638,#29981,.T.) ;
#44645 = EDGE_CURVE('',#36638,#36639,#3858,.T.) ;
#44646 = EDGE_CURVE('',#36639,#36637,#29982,.T.) ;
#44647 = EDGE_CURVE('',#36640,#36641,#3859,.T.) ;
#44648 = EDGE_CURVE('',#36640,#36642,#29983,.T.) ;
#44649 = EDGE_CURVE('',#36642,#36643,#3860,.T.) ;
#44650 = EDGE_CURVE('',#36643,#36641,#29984,.T.) ;
#44651 = EDGE_CURVE('',#36644,#36645,#29985,.T.) ;
#44652 = EDGE_CURVE('',#36644,#36646,#3861,.T.) ;
#44653 = EDGE_CURVE('',#36647,#36646,#3862,.T.) ;
#44654 = EDGE_CURVE('',#36647,#36640,#3863,.T.) ;
#44655 = EDGE_CURVE('',#36641,#36639,#3864,.T.) ;
#44656 = EDGE_CURVE('',#36638,#36648,#3865,.T.) ;
#44657 = EDGE_CURVE('',#36649,#36648,#29986,.T.) ;
#44658 = EDGE_CURVE('',#36649,#36650,#3866,.T.) ;
#44659 = EDGE_CURVE('',#36651,#36650,#29987,.T.) ;
#44660 = EDGE_CURVE('',#36651,#36583,#3867,.T.) ;
#44661 = EDGE_CURVE('',#36582,#36652,#3868,.T.) ;
#44662 = EDGE_CURVE('',#36653,#36652,#29988,.T.) ;
#44663 = EDGE_CURVE('',#36653,#36654,#3869,.T.) ;
#44664 = EDGE_CURVE('',#36655,#36654,#29989,.T.) ;
#44665 = EDGE_CURVE('',#36655,#36587,#3870,.T.) ;
#44666 = EDGE_CURVE('',#36586,#36656,#3871,.T.) ;
#44667 = EDGE_CURVE('',#36657,#36656,#29990,.T.) ;
#44668 = EDGE_CURVE('',#36657,#36658,#3872,.T.) ;
#44669 = EDGE_CURVE('',#36659,#36658,#29991,.T.) ;
#44670 = EDGE_CURVE('',#36659,#36591,#3873,.T.) ;
#44671 = EDGE_CURVE('',#36590,#36660,#3874,.T.) ;
#44672 = EDGE_CURVE('',#36661,#36660,#29992,.T.) ;
#44673 = EDGE_CURVE('',#36661,#36662,#3875,.T.) ;
#44674 = EDGE_CURVE('',#36663,#36662,#29993,.T.) ;
#44675 = EDGE_CURVE('',#36663,#36595,#3876,.T.) ;
#44676 = EDGE_CURVE('',#36594,#36664,#3877,.T.) ;
#44677 = EDGE_CURVE('',#36665,#36664,#29994,.T.) ;
#44678 = EDGE_CURVE('',#36665,#36666,#3878,.T.) ;
#44679 = EDGE_CURVE('',#36667,#36666,#29995,.T.) ;
#44680 = EDGE_CURVE('',#36667,#36599,#3879,.T.) ;
#44681 = EDGE_CURVE('',#36598,#36668,#3880,.T.) ;
#44682 = EDGE_CURVE('',#36669,#36668,#29996,.T.) ;
#44683 = EDGE_CURVE('',#36669,#36670,#3881,.T.) ;
#44684 = EDGE_CURVE('',#36671,#36670,#29997,.T.) ;
#44685 = EDGE_CURVE('',#36671,#36603,#3882,.T.) ;
#44686 = EDGE_CURVE('',#36602,#36672,#3883,.T.) ;
#44687 = EDGE_CURVE('',#36673,#36672,#29998,.T.) ;
#44688 = EDGE_CURVE('',#36673,#36674,#3884,.T.) ;
#44689 = EDGE_CURVE('',#36675,#36674,#29999,.T.) ;
#44690 = EDGE_CURVE('',#36675,#36607,#3885,.T.) ;
#44691 = EDGE_CURVE('',#36606,#36676,#3886,.T.) ;
#44692 = EDGE_CURVE('',#36677,#36676,#30000,.T.) ;
#44693 = EDGE_CURVE('',#36677,#36678,#3887,.T.) ;
#44694 = EDGE_CURVE('',#36679,#36678,#30001,.T.) ;
#44695 = EDGE_CURVE('',#36679,#36611,#3888,.T.) ;
#44696 = EDGE_CURVE('',#36610,#36680,#3889,.T.) ;
#44697 = EDGE_CURVE('',#36681,#36680,#30002,.T.) ;
#44698 = EDGE_CURVE('',#36681,#36682,#3890,.T.) ;
#44699 = EDGE_CURVE('',#36683,#36682,#30003,.T.) ;
#44700 = EDGE_CURVE('',#36683,#36615,#3891,.T.) ;
#44701 = EDGE_CURVE('',#36614,#36684,#3892,.T.) ;
#44702 = EDGE_CURVE('',#36685,#36684,#30004,.T.) ;
#44703 = EDGE_CURVE('',#36685,#36645,#3893,.T.) ;
#44704 = EDGE_CURVE('',#36646,#36686,#30005,.T.) ;
#44705 = EDGE_CURVE('',#36687,#36686,#3894,.T.) ;
#44706 = EDGE_CURVE('',#36687,#36647,#30006,.T.) ;
#44707 = EDGE_CURVE('',#36688,#36689,#30007,.T.) ;
#44708 = EDGE_CURVE('',#36688,#36612,#3895,.T.) ;
#44709 = EDGE_CURVE('',#36613,#36690,#3896,.T.) ;
#44710 = EDGE_CURVE('',#36691,#36690,#30008,.T.) ;
#44711 = EDGE_CURVE('',#36691,#36692,#3897,.T.) ;
#44712 = EDGE_CURVE('',#36693,#36692,#30009,.T.) ;
#44713 = EDGE_CURVE('',#36693,#36608,#3898,.T.) ;
#44714 = EDGE_CURVE('',#36609,#36694,#3899,.T.) ;
#44715 = EDGE_CURVE('',#36695,#36694,#30010,.T.) ;
#44716 = EDGE_CURVE('',#36695,#36696,#3900,.T.) ;
#44717 = EDGE_CURVE('',#36697,#36696,#30011,.T.) ;
#44718 = EDGE_CURVE('',#36697,#36604,#3901,.T.) ;
#44719 = EDGE_CURVE('',#36605,#36698,#3902,.T.) ;
#44720 = EDGE_CURVE('',#36699,#36698,#30012,.T.) ;
#44721 = EDGE_CURVE('',#36699,#36700,#3903,.T.) ;
#44722 = EDGE_CURVE('',#36701,#36700,#30013,.T.) ;
#44723 = EDGE_CURVE('',#36701,#36600,#3904,.T.) ;
#44724 = EDGE_CURVE('',#36601,#36702,#3905,.T.) ;
#44725 = EDGE_CURVE('',#36703,#36702,#30014,.T.) ;
#44726 = EDGE_CURVE('',#36703,#36704,#3906,.T.) ;
#44727 = EDGE_CURVE('',#36705,#36704,#30015,.T.) ;
#44728 = EDGE_CURVE('',#36705,#36596,#3907,.T.) ;
#44729 = EDGE_CURVE('',#36597,#36706,#3908,.T.) ;
#44730 = EDGE_CURVE('',#36707,#36706,#30016,.T.) ;
#44731 = EDGE_CURVE('',#36707,#36708,#3909,.T.) ;
#44732 = EDGE_CURVE('',#36709,#36708,#30017,.T.) ;
#44733 = EDGE_CURVE('',#36709,#36592,#3910,.T.) ;
#44734 = EDGE_CURVE('',#36593,#36710,#3911,.T.) ;
#44735 = EDGE_CURVE('',#36711,#36710,#30018,.T.) ;
#44736 = EDGE_CURVE('',#36711,#36712,#3912,.T.) ;
#44737 = EDGE_CURVE('',#36713,#36712,#30019,.T.) ;
#44738 = EDGE_CURVE('',#36713,#36588,#3913,.T.) ;
#44739 = EDGE_CURVE('',#36589,#36714,#3914,.T.) ;
#44740 = EDGE_CURVE('',#36715,#36714,#30020,.T.) ;
#44741 = EDGE_CURVE('',#36715,#36716,#3915,.T.) ;
#44742 = EDGE_CURVE('',#36717,#36716,#30021,.T.) ;
#44743 = EDGE_CURVE('',#36717,#36584,#3916,.T.) ;
#44744 = EDGE_CURVE('',#36585,#36718,#3917,.T.) ;
#44745 = EDGE_CURVE('',#36719,#36718,#30022,.T.) ;
#44746 = EDGE_CURVE('',#36719,#36720,#3918,.T.) ;
#44747 = EDGE_CURVE('',#36721,#36720,#30023,.T.) ;
#44748 = EDGE_CURVE('',#36721,#36580,#3919,.T.) ;
#44749 = EDGE_CURVE('',#36581,#36722,#3920,.T.) ;
#44750 = EDGE_CURVE('',#36723,#36722,#30024,.T.) ;
#44751 = EDGE_CURVE('',#36723,#36724,#3921,.T.) ;
#44752 = EDGE_CURVE('',#36725,#36724,#30025,.T.) ;
#44753 = EDGE_CURVE('',#36725,#36636,#3922,.T.) ;
#44754 = EDGE_CURVE('',#36637,#36726,#3923,.T.) ;
#44755 = EDGE_CURVE('',#36727,#36726,#3924,.T.) ;
#44756 = EDGE_CURVE('',#36727,#36687,#3925,.T.) ;
#44757 = EDGE_CURVE('',#36686,#36728,#3926,.T.) ;
#44758 = EDGE_CURVE('',#36729,#36728,#30026,.T.) ;
#44759 = EDGE_CURVE('',#36729,#36689,#3927,.T.) ;
#44760 = EDGE_CURVE('',#36730,#36731,#3928,.T.) ;
#44761 = EDGE_CURVE('',#36730,#36727,#30027,.T.) ;
#44762 = EDGE_CURVE('',#36726,#36731,#30028,.T.) ;
#44763 = EDGE_CURVE('',#36732,#36733,#3929,.T.) ;
#44764 = EDGE_CURVE('',#36732,#36730,#3930,.T.) ;
#44765 = EDGE_CURVE('',#36731,#36733,#3931,.T.) ;
#44766 = EDGE_CURVE('',#36734,#36735,#3932,.T.) ;
#44767 = EDGE_CURVE('',#36734,#36732,#30029,.T.) ;
#44768 = EDGE_CURVE('',#36733,#36735,#30030,.T.) ;
#44769 = EDGE_CURVE('',#36736,#36737,#3933,.T.) ;
#44770 = EDGE_CURVE('',#36736,#36734,#3934,.T.) ;
#44771 = EDGE_CURVE('',#36735,#36737,#3935,.T.) ;
#44772 = EDGE_CURVE('',#36738,#36739,#3936,.T.) ;
#44773 = EDGE_CURVE('',#36738,#36736,#30031,.T.) ;
#44774 = EDGE_CURVE('',#36737,#36739,#30032,.T.) ;
#44775 = EDGE_CURVE('',#36740,#36741,#3937,.T.) ;
#44776 = EDGE_CURVE('',#36740,#36738,#3938,.T.) ;
#44777 = EDGE_CURVE('',#36739,#36741,#3939,.T.) ;
#44778 = EDGE_CURVE('',#36742,#36743,#3940,.T.) ;
#44779 = EDGE_CURVE('',#36742,#36740,#30033,.T.) ;
#44780 = EDGE_CURVE('',#36741,#36743,#30034,.T.) ;
#44781 = EDGE_CURVE('',#36744,#36745,#3941,.T.) ;
#44782 = EDGE_CURVE('',#36744,#36742,#3942,.T.) ;
#44783 = EDGE_CURVE('',#36743,#36745,#3943,.T.) ;
#44784 = EDGE_CURVE('',#36746,#36747,#3944,.T.) ;
#44785 = EDGE_CURVE('',#36746,#36744,#30035,.T.) ;
#44786 = EDGE_CURVE('',#36745,#36747,#30036,.T.) ;
#44787 = EDGE_CURVE('',#36748,#36749,#3945,.T.) ;
#44788 = EDGE_CURVE('',#36748,#36746,#3946,.T.) ;
#44789 = EDGE_CURVE('',#36747,#36749,#3947,.T.) ;
#44790 = EDGE_CURVE('',#36750,#36751,#3948,.T.) ;
#44791 = EDGE_CURVE('',#36750,#36748,#30037,.T.) ;
#44792 = EDGE_CURVE('',#36749,#36751,#30038,.T.) ;
#44793 = EDGE_CURVE('',#36642,#36750,#3949,.T.) ;
#44794 = EDGE_CURVE('',#36751,#36643,#3950,.T.) ;
#44795 = EDGE_CURVE('',#36752,#36753,#30039,.T.) ;
#44796 = EDGE_CURVE('',#36753,#36754,#3951,.T.) ;
#44797 = EDGE_CURVE('',#36754,#36755,#3952,.T.) ;
#44798 = EDGE_CURVE('',#36755,#36756,#3953,.T.) ;
#44799 = EDGE_CURVE('',#36756,#36757,#30040,.T.) ;
#44800 = EDGE_CURVE('',#36757,#36758,#3954,.T.) ;
#44801 = EDGE_CURVE('',#36758,#36759,#30041,.T.) ;
#44802 = EDGE_CURVE('',#36759,#36345,#3955,.T.) ;
#44803 = EDGE_CURVE('',#36346,#36760,#3956,.T.) ;
#44804 = EDGE_CURVE('',#36760,#36761,#30042,.T.) ;
#44805 = EDGE_CURVE('',#36761,#36762,#3957,.T.) ;
#44806 = EDGE_CURVE('',#36762,#36763,#3958,.T.) ;
#44807 = EDGE_CURVE('',#36763,#36764,#3959,.T.) ;
#44808 = EDGE_CURVE('',#36764,#36765,#30043,.T.) ;
#44809 = EDGE_CURVE('',#36765,#36766,#3960,.T.) ;
#44810 = EDGE_CURVE('',#36766,#36767,#30044,.T.) ;
#44811 = EDGE_CURVE('',#36767,#36768,#3961,.T.) ;
#44812 = EDGE_CURVE('',#36768,#36769,#30045,.T.) ;
#44813 = EDGE_CURVE('',#36769,#36770,#30046,.T.) ;
#44814 = EDGE_CURVE('',#36770,#36771,#30047,.T.) ;
#44815 = EDGE_CURVE('',#36771,#36772,#3962,.T.) ;
#44816 = EDGE_CURVE('',#36772,#36773,#30048,.T.) ;
#44817 = EDGE_CURVE('',#36773,#36752,#3963,.T.) ;
#44818 = EDGE_CURVE('',#36774,#36775,#30049,.T.) ;
#44819 = EDGE_CURVE('',#36775,#36776,#3964,.T.) ;
#44820 = EDGE_CURVE('',#36776,#36777,#3965,.T.) ;
#44821 = EDGE_CURVE('',#36777,#36778,#3966,.T.) ;
#44822 = EDGE_CURVE('',#36778,#36779,#30050,.T.) ;
#44823 = EDGE_CURVE('',#36779,#36780,#3967,.T.) ;
#44824 = EDGE_CURVE('',#36780,#36781,#30051,.T.) ;
#44825 = EDGE_CURVE('',#36781,#36341,#3968,.T.) ;
#44826 = EDGE_CURVE('',#36342,#36782,#3969,.T.) ;
#44827 = EDGE_CURVE('',#36782,#36783,#30052,.T.) ;
#44828 = EDGE_CURVE('',#36783,#36784,#3970,.T.) ;
#44829 = EDGE_CURVE('',#36784,#36785,#3971,.T.) ;
#44830 = EDGE_CURVE('',#36785,#36786,#3972,.T.) ;
#44831 = EDGE_CURVE('',#36786,#36787,#30053,.T.) ;
#44832 = EDGE_CURVE('',#36787,#36788,#3973,.T.) ;
#44833 = EDGE_CURVE('',#36788,#36789,#30054,.T.) ;
#44834 = EDGE_CURVE('',#36789,#36790,#3974,.T.) ;
#44835 = EDGE_CURVE('',#36790,#36791,#30055,.T.) ;
#44836 = EDGE_CURVE('',#36791,#36792,#30056,.T.) ;
#44837 = EDGE_CURVE('',#36792,#36793,#30057,.T.) ;
#44838 = EDGE_CURVE('',#36793,#36794,#3975,.T.) ;
#44839 = EDGE_CURVE('',#36794,#36795,#30058,.T.) ;
#44840 = EDGE_CURVE('',#36795,#36774,#3976,.T.) ;
#44841 = EDGE_CURVE('',#36796,#36797,#30059,.T.) ;
#44842 = EDGE_CURVE('',#36797,#36798,#3977,.T.) ;
#44843 = EDGE_CURVE('',#36798,#36799,#3978,.T.) ;
#44844 = EDGE_CURVE('',#36799,#36800,#3979,.T.) ;
#44845 = EDGE_CURVE('',#36800,#36801,#30060,.T.) ;
#44846 = EDGE_CURVE('',#36801,#36802,#3980,.T.) ;
#44847 = EDGE_CURVE('',#36802,#36803,#30061,.T.) ;
#44848 = EDGE_CURVE('',#36803,#36337,#3981,.T.) ;
#44849 = EDGE_CURVE('',#36338,#36804,#3982,.T.) ;
#44850 = EDGE_CURVE('',#36804,#36805,#30062,.T.) ;
#44851 = EDGE_CURVE('',#36805,#36806,#3983,.T.) ;
#44852 = EDGE_CURVE('',#36806,#36807,#3984,.T.) ;
#44853 = EDGE_CURVE('',#36807,#36808,#3985,.T.) ;
#44854 = EDGE_CURVE('',#36808,#36809,#30063,.T.) ;
#44855 = EDGE_CURVE('',#36809,#36810,#3986,.T.) ;
#44856 = EDGE_CURVE('',#36810,#36811,#30064,.T.) ;
#44857 = EDGE_CURVE('',#36811,#36812,#3987,.T.) ;
#44858 = EDGE_CURVE('',#36812,#36813,#30065,.T.) ;
#44859 = EDGE_CURVE('',#36813,#36814,#30066,.T.) ;
#44860 = EDGE_CURVE('',#36814,#36815,#30067,.T.) ;
#44861 = EDGE_CURVE('',#36815,#36816,#3988,.T.) ;
#44862 = EDGE_CURVE('',#36816,#36817,#30068,.T.) ;
#44863 = EDGE_CURVE('',#36817,#36796,#3989,.T.) ;
#44864 = EDGE_CURVE('',#36818,#36819,#30069,.T.) ;
#44865 = EDGE_CURVE('',#36819,#36820,#3990,.T.) ;
#44866 = EDGE_CURVE('',#36820,#36821,#3991,.T.) ;
#44867 = EDGE_CURVE('',#36821,#36822,#3992,.T.) ;
#44868 = EDGE_CURVE('',#36822,#36823,#30070,.T.) ;
#44869 = EDGE_CURVE('',#36823,#36824,#3993,.T.) ;
#44870 = EDGE_CURVE('',#36824,#36825,#30071,.T.) ;
#44871 = EDGE_CURVE('',#36825,#36333,#3994,.T.) ;
#44872 = EDGE_CURVE('',#36334,#36826,#3995,.T.) ;
#44873 = EDGE_CURVE('',#36826,#36827,#30072,.T.) ;
#44874 = EDGE_CURVE('',#36827,#36828,#3996,.T.) ;
#44875 = EDGE_CURVE('',#36828,#36829,#3997,.T.) ;
#44876 = EDGE_CURVE('',#36829,#36830,#3998,.T.) ;
#44877 = EDGE_CURVE('',#36830,#36831,#30073,.T.) ;
#44878 = EDGE_CURVE('',#36831,#36832,#3999,.T.) ;
#44879 = EDGE_CURVE('',#36832,#36833,#30074,.T.) ;
#44880 = EDGE_CURVE('',#36833,#36834,#4000,.T.) ;
#44881 = EDGE_CURVE('',#36834,#36835,#30075,.T.) ;
#44882 = EDGE_CURVE('',#36835,#36836,#30076,.T.) ;
#44883 = EDGE_CURVE('',#36836,#36837,#30077,.T.) ;
#44884 = EDGE_CURVE('',#36837,#36838,#4001,.T.) ;
#44885 = EDGE_CURVE('',#36838,#36839,#30078,.T.) ;
#44886 = EDGE_CURVE('',#36839,#36818,#4002,.T.) ;
#44887 = EDGE_CURVE('',#36840,#36841,#30079,.T.) ;
#44888 = EDGE_CURVE('',#36841,#36842,#4003,.T.) ;
#44889 = EDGE_CURVE('',#36842,#36843,#4004,.T.) ;
#44890 = EDGE_CURVE('',#36843,#36844,#4005,.T.) ;
#44891 = EDGE_CURVE('',#36844,#36845,#30080,.T.) ;
#44892 = EDGE_CURVE('',#36845,#36846,#4006,.T.) ;
#44893 = EDGE_CURVE('',#36846,#36847,#30081,.T.) ;
#44894 = EDGE_CURVE('',#36847,#36329,#4007,.T.) ;
#44895 = EDGE_CURVE('',#36330,#36848,#4008,.T.) ;
#44896 = EDGE_CURVE('',#36848,#36849,#30082,.T.) ;
#44897 = EDGE_CURVE('',#36849,#36850,#4009,.T.) ;
#44898 = EDGE_CURVE('',#36850,#36851,#4010,.T.) ;
#44899 = EDGE_CURVE('',#36851,#36852,#4011,.T.) ;
#44900 = EDGE_CURVE('',#36852,#36853,#30083,.T.) ;
#44901 = EDGE_CURVE('',#36853,#36854,#4012,.T.) ;
#44902 = EDGE_CURVE('',#36854,#36855,#30084,.T.) ;
#44903 = EDGE_CURVE('',#36855,#36856,#4013,.T.) ;
#44904 = EDGE_CURVE('',#36856,#36857,#30085,.T.) ;
#44905 = EDGE_CURVE('',#36857,#36858,#30086,.T.) ;
#44906 = EDGE_CURVE('',#36858,#36859,#30087,.T.) ;
#44907 = EDGE_CURVE('',#36859,#36860,#4014,.T.) ;
#44908 = EDGE_CURVE('',#36860,#36861,#30088,.T.) ;
#44909 = EDGE_CURVE('',#36861,#36840,#4015,.T.) ;
#44910 = EDGE_CURVE('',#36862,#36863,#30089,.T.) ;
#44911 = EDGE_CURVE('',#36863,#36864,#4016,.T.) ;
#44912 = EDGE_CURVE('',#36864,#36865,#4017,.T.) ;
#44913 = EDGE_CURVE('',#36865,#36866,#4018,.T.) ;
#44914 = EDGE_CURVE('',#36866,#36867,#30090,.T.) ;
#44915 = EDGE_CURVE('',#36867,#36868,#4019,.T.) ;
#44916 = EDGE_CURVE('',#36868,#36869,#30091,.T.) ;
#44917 = EDGE_CURVE('',#36869,#36325,#4020,.T.) ;
#44918 = EDGE_CURVE('',#36326,#36870,#4021,.T.) ;
#44919 = EDGE_CURVE('',#36870,#36871,#30092,.T.) ;
#44920 = EDGE_CURVE('',#36871,#36872,#4022,.T.) ;
#44921 = EDGE_CURVE('',#36872,#36873,#4023,.T.) ;
#44922 = EDGE_CURVE('',#36873,#36874,#4024,.T.) ;
#44923 = EDGE_CURVE('',#36874,#36875,#30093,.T.) ;
#44924 = EDGE_CURVE('',#36875,#36876,#4025,.T.) ;
#44925 = EDGE_CURVE('',#36876,#36877,#30094,.T.) ;
#44926 = EDGE_CURVE('',#36877,#36878,#4026,.T.) ;
#44927 = EDGE_CURVE('',#36878,#36879,#30095,.T.) ;
#44928 = EDGE_CURVE('',#36879,#36880,#30096,.T.) ;
#44929 = EDGE_CURVE('',#36880,#36881,#30097,.T.) ;
#44930 = EDGE_CURVE('',#36881,#36882,#4027,.T.) ;
#44931 = EDGE_CURVE('',#36882,#36883,#30098,.T.) ;
#44932 = EDGE_CURVE('',#36883,#36862,#4028,.T.) ;
#44933 = EDGE_CURVE('',#36884,#36885,#30099,.T.) ;
#44934 = EDGE_CURVE('',#36885,#36886,#4029,.T.) ;
#44935 = EDGE_CURVE('',#36886,#36887,#4030,.T.) ;
#44936 = EDGE_CURVE('',#36887,#36888,#4031,.T.) ;
#44937 = EDGE_CURVE('',#36888,#36889,#30100,.T.) ;
#44938 = EDGE_CURVE('',#36889,#36890,#4032,.T.) ;
#44939 = EDGE_CURVE('',#36890,#36891,#30101,.T.) ;
#44940 = EDGE_CURVE('',#36891,#36321,#4033,.T.) ;
#44941 = EDGE_CURVE('',#36322,#36892,#4034,.T.) ;
#44942 = EDGE_CURVE('',#36892,#36893,#30102,.T.) ;
#44943 = EDGE_CURVE('',#36893,#36894,#4035,.T.) ;
#44944 = EDGE_CURVE('',#36894,#36895,#4036,.T.) ;
#44945 = EDGE_CURVE('',#36895,#36896,#4037,.T.) ;
#44946 = EDGE_CURVE('',#36896,#36897,#30103,.T.) ;
#44947 = EDGE_CURVE('',#36897,#36898,#4038,.T.) ;
#44948 = EDGE_CURVE('',#36898,#36899,#30104,.T.) ;
#44949 = EDGE_CURVE('',#36899,#36900,#4039,.T.) ;
#44950 = EDGE_CURVE('',#36900,#36901,#30105,.T.) ;
#44951 = EDGE_CURVE('',#36901,#36902,#30106,.T.) ;
#44952 = EDGE_CURVE('',#36902,#36903,#30107,.T.) ;
#44953 = EDGE_CURVE('',#36903,#36904,#4040,.T.) ;
#44954 = EDGE_CURVE('',#36904,#36905,#30108,.T.) ;
#44955 = EDGE_CURVE('',#36905,#36884,#4041,.T.) ;
#44956 = EDGE_CURVE('',#36906,#36907,#30109,.T.) ;
#44957 = EDGE_CURVE('',#36907,#36908,#4042,.T.) ;
#44958 = EDGE_CURVE('',#36908,#36909,#4043,.T.) ;
#44959 = EDGE_CURVE('',#36909,#36910,#4044,.T.) ;
#44960 = EDGE_CURVE('',#36910,#36911,#30110,.T.) ;
#44961 = EDGE_CURVE('',#36911,#36912,#4045,.T.) ;
#44962 = EDGE_CURVE('',#36912,#36913,#30111,.T.) ;
#44963 = EDGE_CURVE('',#36913,#36317,#4046,.T.) ;
#44964 = EDGE_CURVE('',#36318,#36914,#4047,.T.) ;
#44965 = EDGE_CURVE('',#36914,#36915,#30112,.T.) ;
#44966 = EDGE_CURVE('',#36915,#36916,#4048,.T.) ;
#44967 = EDGE_CURVE('',#36916,#36917,#4049,.T.) ;
#44968 = EDGE_CURVE('',#36917,#36918,#4050,.T.) ;
#44969 = EDGE_CURVE('',#36918,#36919,#30113,.T.) ;
#44970 = EDGE_CURVE('',#36919,#36920,#4051,.T.) ;
#44971 = EDGE_CURVE('',#36920,#36921,#30114,.T.) ;
#44972 = EDGE_CURVE('',#36921,#36922,#4052,.T.) ;
#44973 = EDGE_CURVE('',#36922,#36923,#30115,.T.) ;
#44974 = EDGE_CURVE('',#36923,#36924,#30116,.T.) ;
#44975 = EDGE_CURVE('',#36924,#36925,#30117,.T.) ;
#44976 = EDGE_CURVE('',#36925,#36926,#4053,.T.) ;
#44977 = EDGE_CURVE('',#36926,#36927,#30118,.T.) ;
#44978 = EDGE_CURVE('',#36927,#36906,#4054,.T.) ;
#44979 = EDGE_CURVE('',#36928,#36929,#30119,.T.) ;
#44980 = EDGE_CURVE('',#36929,#36930,#4055,.T.) ;
#44981 = EDGE_CURVE('',#36930,#36931,#4056,.T.) ;
#44982 = EDGE_CURVE('',#36931,#36932,#4057,.T.) ;
#44983 = EDGE_CURVE('',#36932,#36933,#30120,.T.) ;
#44984 = EDGE_CURVE('',#36933,#36934,#4058,.T.) ;
#44985 = EDGE_CURVE('',#36934,#36935,#30121,.T.) ;
#44986 = EDGE_CURVE('',#36935,#36313,#4059,.T.) ;
#44987 = EDGE_CURVE('',#36314,#36936,#4060,.T.) ;
#44988 = EDGE_CURVE('',#36936,#36937,#30122,.T.) ;
#44989 = EDGE_CURVE('',#36937,#36938,#4061,.T.) ;
#44990 = EDGE_CURVE('',#36938,#36939,#4062,.T.) ;
#44991 = EDGE_CURVE('',#36939,#36940,#4063,.T.) ;
#44992 = EDGE_CURVE('',#36940,#36941,#30123,.T.) ;
#44993 = EDGE_CURVE('',#36941,#36942,#4064,.T.) ;
#44994 = EDGE_CURVE('',#36942,#36943,#30124,.T.) ;
#44995 = EDGE_CURVE('',#36943,#36944,#4065,.T.) ;
#44996 = EDGE_CURVE('',#36944,#36945,#30125,.T.) ;
#44997 = EDGE_CURVE('',#36945,#36946,#30126,.T.) ;
#44998 = EDGE_CURVE('',#36946,#36947,#30127,.T.) ;
#44999 = EDGE_CURVE('',#36947,#36948,#4066,.T.) ;
#45000 = EDGE_CURVE('',#36948,#36949,#30128,.T.) ;
#45001 = EDGE_CURVE('',#36949,#36928,#4067,.T.) ;
#45002 = EDGE_CURVE('',#36950,#36951,#30129,.T.) ;
#45003 = EDGE_CURVE('',#36951,#36952,#4068,.T.) ;
#45004 = EDGE_CURVE('',#36952,#36953,#4069,.T.) ;
#45005 = EDGE_CURVE('',#36953,#36954,#4070,.T.) ;
#45006 = EDGE_CURVE('',#36954,#36955,#30130,.T.) ;
#45007 = EDGE_CURVE('',#36955,#36956,#4071,.T.) ;
#45008 = EDGE_CURVE('',#36956,#36957,#30131,.T.) ;
#45009 = EDGE_CURVE('',#36957,#36382,#4072,.T.) ;
#45010 = EDGE_CURVE('',#36383,#36958,#4073,.T.) ;
#45011 = EDGE_CURVE('',#36958,#36959,#30132,.T.) ;
#45012 = EDGE_CURVE('',#36959,#36960,#4074,.T.) ;
#45013 = EDGE_CURVE('',#36960,#36961,#4075,.T.) ;
#45014 = EDGE_CURVE('',#36961,#36962,#4076,.T.) ;
#45015 = EDGE_CURVE('',#36962,#36963,#30133,.T.) ;
#45016 = EDGE_CURVE('',#36963,#36964,#4077,.T.) ;
#45017 = EDGE_CURVE('',#36964,#36965,#30134,.T.) ;
#45018 = EDGE_CURVE('',#36965,#36966,#4078,.T.) ;
#45019 = EDGE_CURVE('',#36966,#36967,#30135,.T.) ;
#45020 = EDGE_CURVE('',#36967,#36968,#30136,.T.) ;
#45021 = EDGE_CURVE('',#36968,#36969,#30137,.T.) ;
#45022 = EDGE_CURVE('',#36969,#36970,#4079,.T.) ;
#45023 = EDGE_CURVE('',#36970,#36971,#30138,.T.) ;
#45024 = EDGE_CURVE('',#36971,#36950,#4080,.T.) ;
#45025 = EDGE_CURVE('',#36972,#36973,#4081,.T.) ;
#45026 = EDGE_CURVE('',#36973,#36974,#4082,.T.) ;
#45027 = EDGE_CURVE('',#36974,#36975,#4083,.T.) ;
#45028 = EDGE_CURVE('',#36975,#36976,#4084,.T.) ;
#45029 = EDGE_CURVE('',#36976,#36977,#30139,.T.) ;
#45030 = EDGE_CURVE('',#36977,#36978,#4085,.T.) ;
#45031 = EDGE_CURVE('',#36978,#36979,#4086,.T.) ;
#45032 = EDGE_CURVE('',#36979,#36980,#4087,.T.) ;
#45033 = EDGE_CURVE('',#36980,#36981,#30140,.T.) ;
#45034 = EDGE_CURVE('',#36981,#36972,#4088,.T.) ;
#45035 = EDGE_CURVE('',#36982,#36983,#4089,.T.) ;
#45036 = EDGE_CURVE('',#36983,#36984,#4090,.T.) ;
#45037 = EDGE_CURVE('',#36984,#36985,#4091,.T.) ;
#45038 = EDGE_CURVE('',#36985,#36986,#4092,.T.) ;
#45039 = EDGE_CURVE('',#36986,#36987,#30141,.T.) ;
#45040 = EDGE_CURVE('',#36987,#36988,#4093,.T.) ;
#45041 = EDGE_CURVE('',#36988,#36989,#4094,.T.) ;
#45042 = EDGE_CURVE('',#36989,#36990,#4095,.T.) ;
#45043 = EDGE_CURVE('',#36990,#36991,#30142,.T.) ;
#45044 = EDGE_CURVE('',#36991,#36982,#4096,.T.) ;
#45045 = EDGE_CURVE('',#36992,#36993,#4097,.T.) ;
#45046 = EDGE_CURVE('',#36993,#36994,#4098,.T.) ;
#45047 = EDGE_CURVE('',#36994,#36995,#4099,.T.) ;
#45048 = EDGE_CURVE('',#36995,#36996,#4100,.T.) ;
#45049 = EDGE_CURVE('',#36996,#36997,#4101,.T.) ;
#45050 = EDGE_CURVE('',#36997,#36998,#4102,.T.) ;
#45051 = EDGE_CURVE('',#36999,#36998,#30143,.T.) ;
#45052 = EDGE_CURVE('',#36999,#37000,#4103,.T.) ;
#45053 = EDGE_CURVE('',#37001,#37000,#30144,.T.) ;
#45054 = EDGE_CURVE('',#37001,#36992,#4104,.T.) ;
#45055 = EDGE_CURVE('',#37002,#37003,#4105,.T.) ;
#45056 = EDGE_CURVE('',#37003,#37004,#4106,.T.) ;
#45057 = EDGE_CURVE('',#37004,#37005,#4107,.T.) ;
#45058 = EDGE_CURVE('',#37005,#37002,#4108,.T.) ;
#45059 = EDGE_CURVE('',#36393,#37006,#4109,.T.) ;
#45060 = EDGE_CURVE('',#37006,#37007,#4110,.T.) ;
#45061 = EDGE_CURVE('',#37007,#36394,#4111,.T.) ;
#45062 = EDGE_CURVE('',#37008,#37009,#4112,.T.) ;
#45063 = EDGE_CURVE('',#37009,#37010,#4113,.T.) ;
#45064 = EDGE_CURVE('',#37010,#37011,#4114,.T.) ;
#45065 = EDGE_CURVE('',#37011,#37008,#4115,.T.) ;
#45066 = EDGE_CURVE('',#37012,#37013,#4116,.T.) ;
#45067 = EDGE_CURVE('',#37013,#37014,#4117,.T.) ;
#45068 = EDGE_CURVE('',#37014,#37015,#4118,.T.) ;
#45069 = EDGE_CURVE('',#37015,#37012,#4119,.T.) ;
#45070 = EDGE_CURVE('',#37016,#37017,#4120,.T.) ;
#45071 = EDGE_CURVE('',#37017,#37018,#4121,.T.) ;
#45072 = EDGE_CURVE('',#37018,#37019,#4122,.T.) ;
#45073 = EDGE_CURVE('',#37019,#37016,#4123,.T.) ;
#45074 = EDGE_CURVE('',#37020,#37021,#4124,.T.) ;
#45075 = EDGE_CURVE('',#37020,#37022,#30145,.T.) ;
#45076 = EDGE_CURVE('',#37022,#37023,#4125,.T.) ;
#45077 = EDGE_CURVE('',#37023,#37021,#30146,.T.) ;
#45078 = EDGE_CURVE('',#37022,#37024,#4126,.T.) ;
#45079 = EDGE_CURVE('',#37024,#37025,#4127,.T.) ;
#45080 = EDGE_CURVE('',#37025,#37023,#4128,.T.) ;
#45081 = EDGE_CURVE('',#37024,#37026,#30147,.T.) ;
#45082 = EDGE_CURVE('',#37026,#37027,#4129,.T.) ;
#45083 = EDGE_CURVE('',#37027,#37025,#30148,.T.) ;
#45084 = EDGE_CURVE('',#37026,#37028,#4130,.T.) ;
#45085 = EDGE_CURVE('',#37028,#37029,#4131,.T.) ;
#45086 = EDGE_CURVE('',#37029,#37027,#4132,.T.) ;
#45087 = EDGE_CURVE('',#37028,#37030,#30149,.T.) ;
#45088 = EDGE_CURVE('',#37030,#37031,#4133,.T.) ;
#45089 = EDGE_CURVE('',#37031,#37029,#30150,.T.) ;
#45090 = EDGE_CURVE('',#37030,#36388,#4134,.T.) ;
#45091 = EDGE_CURVE('',#36388,#37032,#4135,.T.) ;
#45092 = EDGE_CURVE('',#37032,#37031,#4136,.T.) ;
#45093 = EDGE_CURVE('',#36389,#37033,#4137,.T.) ;
#45094 = EDGE_CURVE('',#37033,#37032,#30151,.T.) ;
#45095 = EDGE_CURVE('',#36389,#36398,#4138,.T.) ;
#45096 = EDGE_CURVE('',#36384,#37033,#4139,.T.) ;
#45097 = EDGE_CURVE('',#36399,#37034,#4140,.T.) ;
#45098 = EDGE_CURVE('',#37034,#37035,#4141,.T.) ;
#45099 = EDGE_CURVE('',#37035,#36385,#4142,.T.) ;
#45100 = EDGE_CURVE('',#37034,#37036,#30152,.T.) ;
#45101 = EDGE_CURVE('',#37036,#37037,#4143,.T.) ;
#45102 = EDGE_CURVE('',#37037,#37035,#30153,.T.) ;
#45103 = EDGE_CURVE('',#37036,#37038,#4144,.T.) ;
#45104 = EDGE_CURVE('',#37038,#37039,#4145,.T.) ;
#45105 = EDGE_CURVE('',#37039,#37037,#4146,.T.) ;
#45106 = EDGE_CURVE('',#37038,#37040,#30154,.T.) ;
#45107 = EDGE_CURVE('',#37040,#37041,#4147,.T.) ;
#45108 = EDGE_CURVE('',#37041,#37039,#30155,.T.) ;
#45109 = EDGE_CURVE('',#37040,#37042,#4148,.T.) ;
#45110 = EDGE_CURVE('',#37042,#37043,#4149,.T.) ;
#45111 = EDGE_CURVE('',#37043,#37041,#4150,.T.) ;
#45112 = EDGE_CURVE('',#37042,#37044,#30156,.T.) ;
#45113 = EDGE_CURVE('',#37044,#37045,#4151,.T.) ;
#45114 = EDGE_CURVE('',#37045,#37043,#30157,.T.) ;
#45115 = EDGE_CURVE('',#37044,#37046,#4152,.T.) ;
#45116 = EDGE_CURVE('',#37046,#37047,#4153,.T.) ;
#45117 = EDGE_CURVE('',#37047,#37045,#4154,.T.) ;
#45118 = EDGE_CURVE('',#37046,#37048,#30158,.T.) ;
#45119 = EDGE_CURVE('',#37048,#37049,#4155,.T.) ;
#45120 = EDGE_CURVE('',#37049,#37047,#30159,.T.) ;
#45121 = EDGE_CURVE('',#37048,#37050,#4156,.T.) ;
#45122 = EDGE_CURVE('',#37050,#37051,#4157,.T.) ;
#45123 = EDGE_CURVE('',#37051,#37049,#4158,.T.) ;
#45124 = EDGE_CURVE('',#37050,#37052,#30160,.T.) ;
#45125 = EDGE_CURVE('',#37052,#37053,#4159,.T.) ;
#45126 = EDGE_CURVE('',#37053,#37051,#30161,.T.) ;
#45127 = EDGE_CURVE('',#37052,#37054,#4160,.T.) ;
#45128 = EDGE_CURVE('',#37054,#37055,#4161,.T.) ;
#45129 = EDGE_CURVE('',#37055,#37053,#4162,.T.) ;
#45130 = EDGE_CURVE('',#37054,#37056,#30162,.T.) ;
#45131 = EDGE_CURVE('',#37056,#37057,#4163,.T.) ;
#45132 = EDGE_CURVE('',#37057,#37055,#30163,.T.) ;
#45133 = EDGE_CURVE('',#37056,#37058,#30164,.T.) ;
#45134 = EDGE_CURVE('',#37058,#37059,#4164,.T.) ;
#45135 = EDGE_CURVE('',#37059,#37057,#30165,.T.) ;
#45136 = EDGE_CURVE('',#37058,#37060,#30166,.T.) ;
#45137 = EDGE_CURVE('',#37060,#37061,#4165,.T.) ;
#45138 = EDGE_CURVE('',#37061,#37059,#30167,.T.) ;
#45139 = EDGE_CURVE('',#37060,#37062,#4166,.T.) ;
#45140 = EDGE_CURVE('',#37062,#37063,#4167,.T.) ;
#45141 = EDGE_CURVE('',#37063,#37061,#4168,.T.) ;
#45142 = EDGE_CURVE('',#37062,#37064,#30168,.T.) ;
#45143 = EDGE_CURVE('',#37064,#37065,#4169,.T.) ;
#45144 = EDGE_CURVE('',#37065,#37063,#30169,.T.) ;
#45145 = EDGE_CURVE('',#37064,#37066,#4170,.T.) ;
#45146 = EDGE_CURVE('',#37066,#37067,#4171,.T.) ;
#45147 = EDGE_CURVE('',#37067,#37065,#4172,.T.) ;
#45148 = EDGE_CURVE('',#37066,#37068,#30170,.T.) ;
#45149 = EDGE_CURVE('',#37068,#37069,#4173,.T.) ;
#45150 = EDGE_CURVE('',#37069,#37067,#30171,.T.) ;
#45151 = EDGE_CURVE('',#37068,#37020,#4174,.T.) ;
#45152 = EDGE_CURVE('',#37021,#37069,#4175,.T.) ;
#45153 = EDGE_CURVE('',#37070,#37071,#30172,.T.) ;
#45154 = EDGE_CURVE('',#37071,#37072,#4176,.T.) ;
#45155 = EDGE_CURVE('',#37072,#37073,#30173,.T.) ;
#45156 = EDGE_CURVE('',#37073,#37074,#4177,.T.) ;
#45157 = EDGE_CURVE('',#37074,#37075,#4178,.T.) ;
#45158 = EDGE_CURVE('',#37075,#37076,#4179,.T.) ;
#45159 = EDGE_CURVE('',#37076,#37077,#30174,.T.) ;
#45160 = EDGE_CURVE('',#37077,#37078,#4180,.T.) ;
#45161 = EDGE_CURVE('',#37078,#37079,#4181,.T.) ;
#45162 = EDGE_CURVE('',#37079,#37080,#4182,.T.) ;
#45163 = EDGE_CURVE('',#37080,#37081,#30175,.T.) ;
#45164 = EDGE_CURVE('',#37081,#37082,#4183,.T.) ;
#45165 = EDGE_CURVE('',#37082,#37083,#30176,.T.) ;
#45166 = EDGE_CURVE('',#37083,#37084,#4184,.T.) ;
#45167 = EDGE_CURVE('',#37084,#37085,#4185,.T.) ;
#45168 = EDGE_CURVE('',#37085,#36390,#4186,.T.) ;
#45169 = EDGE_CURVE('',#36390,#37086,#4187,.T.) ;
#45170 = EDGE_CURVE('',#37086,#37070,#4188,.T.) ;
#45171 = EDGE_CURVE('',#37087,#37088,#4189,.T.) ;
#45172 = EDGE_CURVE('',#37087,#37089,#30177,.T.) ;
#45173 = EDGE_CURVE('',#37089,#37090,#4190,.T.) ;
#45174 = EDGE_CURVE('',#37090,#37091,#30178,.T.) ;
#45175 = EDGE_CURVE('',#37091,#37092,#4191,.T.) ;
#45176 = EDGE_CURVE('',#37092,#37093,#30179,.T.) ;
#45177 = EDGE_CURVE('',#37093,#37094,#4192,.T.) ;
#45178 = EDGE_CURVE('',#37094,#37088,#30180,.T.) ;
#45179 = EDGE_CURVE('',#37014,#37001,#30181,.T.) ;
#45180 = EDGE_CURVE('',#36992,#37013,#30182,.T.) ;
#45181 = EDGE_CURVE('',#37015,#37008,#30183,.T.) ;
#45182 = EDGE_CURVE('',#37009,#37014,#30184,.T.) ;
#45183 = EDGE_CURVE('',#37015,#37095,#30185,.T.) ;
#45184 = EDGE_CURVE('',#37095,#37008,#30186,.T.) ;
#45185 = EDGE_CURVE('',#36992,#37018,#30187,.T.) ;
#45186 = EDGE_CURVE('',#37018,#37013,#30188,.T.) ;
#45187 = EDGE_CURVE('',#37009,#37000,#30189,.T.) ;
#45188 = EDGE_CURVE('',#36391,#37011,#30190,.T.) ;
#45189 = EDGE_CURVE('',#36392,#37096,#2167,.T.) ;
#45190 = EDGE_CURVE('',#37095,#37096,#4193,.T.) ;
#45191 = EDGE_CURVE('',#37097,#37095,#2168,.T.) ;
#45192 = EDGE_CURVE('',#37097,#37098,#2169,.T.) ;
#45193 = EDGE_CURVE('',#36617,#37098,#4194,.T.) ;
#45194 = EDGE_CURVE('',#37012,#36616,#30191,.T.) ;
#45195 = EDGE_CURVE('',#37019,#37012,#30192,.T.) ;
#45196 = EDGE_CURVE('',#36993,#37017,#30193,.T.) ;
#45197 = EDGE_CURVE('',#37010,#36999,#30194,.T.) ;
#45198 = EDGE_CURVE('',#37011,#36393,#30195,.T.) ;
#45199 = EDGE_CURVE('',#37006,#37010,#30196,.T.) ;
#45200 = EDGE_CURVE('',#37019,#36625,#30197,.T.) ;
#45201 = EDGE_CURVE('',#36993,#36632,#30198,.T.) ;
#45202 = EDGE_CURVE('',#36631,#37017,#30199,.T.) ;
#45203 = EDGE_CURVE('',#37006,#36998,#30200,.T.) ;
#45204 = EDGE_CURVE('',#37016,#36624,#30201,.T.) ;
#45205 = EDGE_CURVE('',#36633,#37016,#30202,.T.) ;
#45206 = EDGE_CURVE('',#37099,#36632,#4195,.T.) ;
#45207 = EDGE_CURVE('',#36994,#37099,#30203,.T.) ;
#45208 = EDGE_CURVE('',#37007,#36997,#30204,.T.) ;
#45209 = EDGE_CURVE('',#36394,#37002,#30205,.T.) ;
#45210 = EDGE_CURVE('',#37003,#37007,#30206,.T.) ;
#45211 = EDGE_CURVE('',#36620,#37002,#30207,.T.) ;
#45212 = EDGE_CURVE('',#36633,#36624,#30208,.T.) ;
#45213 = EDGE_CURVE('',#36638,#36635,#30209,.T.) ;
#45214 = EDGE_CURVE('',#36635,#36636,#30210,.T.) ;
#45215 = EDGE_CURVE('',#37099,#36725,#30211,.T.) ;
#45216 = EDGE_CURVE('',#37100,#37099,#30212,.T.) ;
#45217 = EDGE_CURVE('',#36994,#37100,#30213,.T.) ;
#45218 = EDGE_CURVE('',#37003,#36997,#30214,.T.) ;
#45219 = EDGE_CURVE('',#36621,#37005,#30215,.T.) ;
#45220 = EDGE_CURVE('',#36634,#36623,#30216,.T.) ;
#45221 = EDGE_CURVE('',#36648,#36634,#30217,.T.) ;
#45222 = EDGE_CURVE('',#37100,#36724,#30218,.T.) ;
#45223 = EDGE_CURVE('',#37101,#37100,#4196,.T.) ;
#45224 = EDGE_CURVE('',#36995,#37101,#30219,.T.) ;
#45225 = EDGE_CURVE('',#37004,#36996,#30220,.T.) ;
#45226 = EDGE_CURVE('',#37005,#36630,#30221,.T.) ;
#45227 = EDGE_CURVE('',#36627,#37004,#30222,.T.) ;
#45228 = EDGE_CURVE('',#36621,#36630,#30223,.T.) ;
#45229 = EDGE_CURVE('',#36649,#36623,#30224,.T.) ;
#45230 = EDGE_CURVE('',#37101,#36723,#30225,.T.) ;
#45231 = EDGE_CURVE('',#37102,#37101,#30226,.T.) ;
#45232 = EDGE_CURVE('',#36995,#37102,#30227,.T.) ;
#45233 = EDGE_CURVE('',#36626,#36996,#30228,.T.) ;
#45234 = EDGE_CURVE('',#36622,#36629,#30229,.T.) ;
#45235 = EDGE_CURVE('',#36650,#36622,#30230,.T.) ;
#45236 = EDGE_CURVE('',#37102,#36722,#30231,.T.) ;
#45237 = EDGE_CURVE('',#36626,#37102,#4197,.T.) ;
#45238 = EDGE_CURVE('',#36651,#36629,#30232,.T.) ;
#45239 = EDGE_CURVE('',#36628,#36581,#30233,.T.) ;
#45240 = EDGE_CURVE('',#36583,#36628,#30234,.T.) ;
#45241 = EDGE_CURVE('',#36978,#36738,#30235,.T.) ;
#45242 = EDGE_CURVE('',#36736,#36978,#30236,.T.) ;
#45243 = EDGE_CURVE('',#36734,#36977,#30237,.T.) ;
#45244 = EDGE_CURVE('',#36979,#36740,#30238,.T.) ;
#45245 = EDGE_CURVE('',#36732,#36976,#30239,.T.) ;
#45246 = EDGE_CURVE('',#36979,#36742,#30240,.T.) ;
#45247 = EDGE_CURVE('',#36730,#36975,#30241,.T.) ;
#45248 = EDGE_CURVE('',#36980,#36744,#30242,.T.) ;
#45249 = EDGE_CURVE('',#36727,#36975,#30243,.T.) ;
#45250 = EDGE_CURVE('',#36981,#36746,#30244,.T.) ;
#45251 = EDGE_CURVE('',#36687,#36974,#30245,.T.) ;
#45252 = EDGE_CURVE('',#36972,#36748,#30246,.T.) ;
#45253 = EDGE_CURVE('',#36647,#36974,#30247,.T.) ;
#45254 = EDGE_CURVE('',#36972,#36750,#30248,.T.) ;
#45255 = EDGE_CURVE('',#36640,#36973,#30249,.T.) ;
#45256 = EDGE_CURVE('',#36973,#36642,#30250,.T.) ;
#45257 = EDGE_CURVE('',#36739,#36989,#30251,.T.) ;
#45258 = EDGE_CURVE('',#36989,#36737,#30252,.T.) ;
#45259 = EDGE_CURVE('',#36990,#36735,#30253,.T.) ;
#45260 = EDGE_CURVE('',#36741,#36988,#30254,.T.) ;
#45261 = EDGE_CURVE('',#36991,#36733,#30255,.T.) ;
#45262 = EDGE_CURVE('',#36743,#36988,#30256,.T.) ;
#45263 = EDGE_CURVE('',#36982,#36731,#30257,.T.) ;
#45264 = EDGE_CURVE('',#36745,#36987,#30258,.T.) ;
#45265 = EDGE_CURVE('',#36982,#36726,#30259,.T.) ;
#45266 = EDGE_CURVE('',#36747,#36986,#30260,.T.) ;
#45267 = EDGE_CURVE('',#36983,#36637,#30261,.T.) ;
#45268 = EDGE_CURVE('',#36749,#36985,#30262,.T.) ;
#45269 = EDGE_CURVE('',#36983,#36639,#30263,.T.) ;
#45270 = EDGE_CURVE('',#36751,#36985,#30264,.T.) ;
#45271 = EDGE_CURVE('',#36984,#36641,#30265,.T.) ;
#45272 = EDGE_CURVE('',#36643,#36984,#30266,.T.) ;
#45273 = EDGE_CURVE('',#37046,#37079,#30267,.T.) ;
#45274 = EDGE_CURVE('',#37080,#37044,#30268,.T.) ;
#45275 = EDGE_CURVE('',#37081,#37042,#30269,.T.) ;
#45276 = EDGE_CURVE('',#37048,#37079,#30270,.T.) ;
#45277 = EDGE_CURVE('',#37082,#37040,#30271,.T.) ;
#45278 = EDGE_CURVE('',#37050,#37078,#30272,.T.) ;
#45279 = EDGE_CURVE('',#37083,#37038,#30273,.T.) ;
#45280 = EDGE_CURVE('',#37052,#37078,#30274,.T.) ;
#45281 = EDGE_CURVE('',#37084,#37036,#30275,.T.) ;
#45282 = EDGE_CURVE('',#37054,#37077,#30276,.T.) ;
#45283 = EDGE_CURVE('',#37084,#37034,#30277,.T.) ;
#45284 = EDGE_CURVE('',#37056,#37077,#30278,.T.) ;
#45285 = EDGE_CURVE('',#37085,#36399,#30279,.T.) ;
#45286 = EDGE_CURVE('',#37058,#37076,#30280,.T.) ;
#45287 = EDGE_CURVE('',#37085,#36398,#30281,.T.) ;
#45288 = EDGE_CURVE('',#37060,#37076,#30282,.T.) ;
#45289 = EDGE_CURVE('',#37062,#37075,#30283,.T.) ;
#45290 = EDGE_CURVE('',#37064,#37075,#30284,.T.) ;
#45291 = EDGE_CURVE('',#37086,#37030,#30285,.T.) ;
#45292 = EDGE_CURVE('',#37066,#37074,#30286,.T.) ;
#45293 = EDGE_CURVE('',#37086,#37028,#30287,.T.) ;
#45294 = EDGE_CURVE('',#37068,#37074,#30288,.T.) ;
#45295 = EDGE_CURVE('',#37070,#37026,#30289,.T.) ;
#45296 = EDGE_CURVE('',#37020,#37073,#30290,.T.) ;
#45297 = EDGE_CURVE('',#37071,#37024,#30291,.T.) ;
#45298 = EDGE_CURVE('',#37022,#37072,#30292,.T.) ;
#45299 = EDGE_CURVE('',#37041,#36960,#30293,.T.) ;
#45300 = EDGE_CURVE('',#36961,#37043,#30294,.T.) ;
#45301 = EDGE_CURVE('',#37039,#36960,#30295,.T.) ;
#45302 = EDGE_CURVE('',#36961,#37045,#30296,.T.) ;
#45303 = EDGE_CURVE('',#37037,#36959,#30297,.T.) ;
#45304 = EDGE_CURVE('',#36962,#37047,#30298,.T.) ;
#45305 = EDGE_CURVE('',#37035,#36958,#30299,.T.) ;
#45306 = EDGE_CURVE('',#36963,#37049,#30300,.T.) ;
#45307 = EDGE_CURVE('',#36964,#37051,#30301,.T.) ;
#45308 = EDGE_CURVE('',#36965,#37053,#30302,.T.) ;
#45309 = EDGE_CURVE('',#37033,#36957,#30303,.T.) ;
#45310 = EDGE_CURVE('',#36966,#37055,#30304,.T.) ;
#45311 = EDGE_CURVE('',#37032,#36956,#30305,.T.) ;
#45312 = EDGE_CURVE('',#36967,#37057,#30306,.T.) ;
#45313 = EDGE_CURVE('',#37031,#36955,#30307,.T.) ;
#45314 = EDGE_CURVE('',#36968,#37059,#30308,.T.) ;
#45315 = EDGE_CURVE('',#37029,#36954,#30309,.T.) ;
#45316 = EDGE_CURVE('',#36969,#37061,#30310,.T.) ;
#45317 = EDGE_CURVE('',#37027,#36953,#30311,.T.) ;
#45318 = EDGE_CURVE('',#36970,#37063,#30312,.T.) ;
#45319 = EDGE_CURVE('',#37025,#36953,#30313,.T.) ;
#45320 = EDGE_CURVE('',#36971,#37065,#30314,.T.) ;
#45321 = EDGE_CURVE('',#37023,#36952,#30315,.T.) ;
#45322 = EDGE_CURVE('',#36950,#37067,#30316,.T.) ;
#45323 = EDGE_CURVE('',#37021,#36952,#30317,.T.) ;
#45324 = EDGE_CURVE('',#36951,#37069,#30318,.T.) ;
#45325 = EDGE_CURVE('',#37103,#37104,#4198,.T.) ;
#45326 = EDGE_CURVE('',#37104,#37105,#4199,.T.) ;
#45327 = EDGE_CURVE('',#37105,#37106,#4200,.T.) ;
#45328 = EDGE_CURVE('',#37106,#37103,#4201,.T.) ;
#45329 = EDGE_CURVE('',#37107,#37108,#4202,.T.) ;
#45330 = EDGE_CURVE('',#37108,#37109,#4203,.T.) ;
#45331 = EDGE_CURVE('',#37109,#37110,#4204,.T.) ;
#45332 = EDGE_CURVE('',#37110,#37107,#4205,.T.) ;
#45333 = EDGE_CURVE('',#37111,#37112,#4206,.T.) ;
#45334 = EDGE_CURVE('',#37112,#37113,#4207,.T.) ;
#45335 = EDGE_CURVE('',#37113,#37114,#4208,.T.) ;
#45336 = EDGE_CURVE('',#37114,#37111,#4209,.T.) ;
#45337 = EDGE_CURVE('',#37115,#37116,#4210,.T.) ;
#45338 = EDGE_CURVE('',#37116,#37117,#4211,.T.) ;
#45339 = EDGE_CURVE('',#37117,#37118,#4212,.T.) ;
#45340 = EDGE_CURVE('',#37118,#37115,#4213,.T.) ;
#45341 = EDGE_CURVE('',#37119,#37120,#4214,.T.) ;
#45342 = EDGE_CURVE('',#37120,#37121,#4215,.T.) ;
#45343 = EDGE_CURVE('',#37122,#37121,#4216,.T.) ;
#45344 = EDGE_CURVE('',#37122,#37119,#4217,.T.) ;
#45345 = EDGE_CURVE('',#37123,#37124,#4218,.T.) ;
#45346 = EDGE_CURVE('',#37124,#36617,#30319,.T.) ;
#45347 = EDGE_CURVE('',#37098,#37125,#30320,.T.) ;
#45348 = EDGE_CURVE('',#37125,#37126,#4219,.T.) ;
#45349 = EDGE_CURVE('',#37126,#37123,#4220,.T.) ;
#45350 = EDGE_CURVE('',#37127,#37128,#4221,.T.) ;
#45351 = EDGE_CURVE('',#37128,#36397,#30321,.T.) ;
#45352 = EDGE_CURVE('',#36396,#37129,#30322,.T.) ;
#45353 = EDGE_CURVE('',#37129,#37130,#4222,.T.) ;
#45354 = EDGE_CURVE('',#37130,#37127,#4223,.T.) ;
#45355 = EDGE_CURVE('',#37096,#37104,#30323,.T.) ;
#45356 = EDGE_CURVE('',#37103,#37097,#30324,.T.) ;
#45357 = EDGE_CURVE('',#37121,#36619,#30325,.T.) ;
#45358 = EDGE_CURVE('',#36618,#37122,#30326,.T.) ;
#45359 = EDGE_CURVE('',#37131,#37132,#4224,.T.) ;
#45360 = EDGE_CURVE('',#37132,#37133,#4225,.T.) ;
#45361 = EDGE_CURVE('',#37133,#37134,#4226,.T.) ;
#45362 = EDGE_CURVE('',#37134,#37131,#4227,.T.) ;
#45363 = EDGE_CURVE('',#37135,#37136,#4228,.T.) ;
#45364 = EDGE_CURVE('',#37136,#37090,#4229,.T.) ;
#45365 = EDGE_CURVE('',#37089,#37135,#4230,.T.) ;
#45366 = EDGE_CURVE('',#37093,#37137,#4231,.T.) ;
#45367 = EDGE_CURVE('',#37137,#37138,#4232,.T.) ;
#45368 = EDGE_CURVE('',#37138,#37094,#4233,.T.) ;
#45369 = EDGE_CURVE('',#37139,#37140,#4234,.T.) ;
#45370 = EDGE_CURVE('',#37140,#37141,#4235,.T.) ;
#45371 = EDGE_CURVE('',#37141,#37142,#4236,.T.) ;
#45372 = EDGE_CURVE('',#37142,#37139,#4237,.T.) ;
#45373 = EDGE_CURVE('',#37143,#37144,#4238,.T.) ;
#45374 = EDGE_CURVE('',#37144,#37145,#4239,.T.) ;
#45375 = EDGE_CURVE('',#37145,#37146,#4240,.T.) ;
#45376 = EDGE_CURVE('',#37146,#37143,#4241,.T.) ;
#45377 = EDGE_CURVE('',#37147,#37148,#4242,.T.) ;
#45378 = EDGE_CURVE('',#37148,#37087,#4243,.T.) ;
#45379 = EDGE_CURVE('',#37088,#37147,#4244,.T.) ;
#45380 = EDGE_CURVE('',#37091,#37149,#4245,.T.) ;
#45381 = EDGE_CURVE('',#37149,#37150,#4246,.T.) ;
#45382 = EDGE_CURVE('',#37150,#37092,#4247,.T.) ;
#45383 = EDGE_CURVE('',#37151,#37152,#4248,.T.) ;
#45384 = EDGE_CURVE('',#37152,#37153,#4249,.T.) ;
#45385 = EDGE_CURVE('',#37153,#37154,#4250,.T.) ;
#45386 = EDGE_CURVE('',#37154,#37151,#4251,.T.) ;
#45387 = EDGE_CURVE('',#37155,#37156,#4252,.T.) ;
#45388 = EDGE_CURVE('',#37156,#37157,#4253,.T.) ;
#45389 = EDGE_CURVE('',#37157,#37158,#4254,.T.) ;
#45390 = EDGE_CURVE('',#37158,#37155,#4255,.T.) ;
#45391 = EDGE_CURVE('',#37159,#37160,#4256,.T.) ;
#45392 = EDGE_CURVE('',#37160,#37161,#4257,.T.) ;
#45393 = EDGE_CURVE('',#37161,#37162,#4258,.T.) ;
#45394 = EDGE_CURVE('',#37162,#37159,#4259,.T.) ;
#45395 = EDGE_CURVE('',#37163,#37164,#4260,.T.) ;
#45396 = EDGE_CURVE('',#37164,#37165,#4261,.T.) ;
#45397 = EDGE_CURVE('',#37165,#37166,#4262,.T.) ;
#45398 = EDGE_CURVE('',#37166,#37163,#4263,.T.) ;
#45399 = EDGE_CURVE('',#37153,#37115,#30327,.T.) ;
#45400 = EDGE_CURVE('',#37154,#37118,#30328,.T.) ;
#45401 = EDGE_CURVE('',#37115,#37120,#30329,.T.) ;
#45402 = EDGE_CURVE('',#37119,#37116,#30330,.T.) ;
#45403 = EDGE_CURVE('',#37154,#37111,#30331,.T.) ;
#45404 = EDGE_CURVE('',#37111,#37118,#30332,.T.) ;
#45405 = EDGE_CURVE('',#37116,#37156,#30333,.T.) ;
#45406 = EDGE_CURVE('',#37117,#37155,#30334,.T.) ;
#45407 = EDGE_CURVE('',#37112,#37117,#30335,.T.) ;
#45408 = EDGE_CURVE('',#37151,#37114,#30336,.T.) ;
#45409 = EDGE_CURVE('',#37112,#37155,#30337,.T.) ;
#45410 = EDGE_CURVE('',#37151,#37107,#30338,.T.) ;
#45411 = EDGE_CURVE('',#37107,#37114,#30339,.T.) ;
#45412 = EDGE_CURVE('',#37113,#37158,#30340,.T.) ;
#45413 = EDGE_CURVE('',#37108,#37113,#30341,.T.) ;
#45414 = EDGE_CURVE('',#37110,#37152,#30342,.T.) ;
#45415 = EDGE_CURVE('',#37108,#37158,#30343,.T.) ;
#45416 = EDGE_CURVE('',#37105,#37110,#30344,.T.) ;
#45417 = EDGE_CURVE('',#37109,#37106,#30345,.T.) ;
#45418 = EDGE_CURVE('',#37157,#37109,#30346,.T.) ;
#45419 = EDGE_CURVE('',#37161,#37131,#30347,.T.) ;
#45420 = EDGE_CURVE('',#37162,#37134,#30348,.T.) ;
#45421 = EDGE_CURVE('',#37131,#37136,#30349,.T.) ;
#45422 = EDGE_CURVE('',#37135,#37132,#30350,.T.) ;
#45423 = EDGE_CURVE('',#37162,#37145,#30351,.T.) ;
#45424 = EDGE_CURVE('',#37145,#37134,#30352,.T.) ;
#45425 = EDGE_CURVE('',#37132,#37164,#30353,.T.) ;
#45426 = EDGE_CURVE('',#37133,#37163,#30354,.T.) ;
#45427 = EDGE_CURVE('',#37146,#37133,#30355,.T.) ;
#45428 = EDGE_CURVE('',#37159,#37144,#30356,.T.) ;
#45429 = EDGE_CURVE('',#37146,#37163,#30357,.T.) ;
#45430 = EDGE_CURVE('',#37159,#37139,#30358,.T.) ;
#45431 = EDGE_CURVE('',#37139,#37144,#30359,.T.) ;
#45432 = EDGE_CURVE('',#37143,#37166,#30360,.T.) ;
#45433 = EDGE_CURVE('',#37140,#37143,#30361,.T.) ;
#45434 = EDGE_CURVE('',#37142,#37160,#30362,.T.) ;
#45435 = EDGE_CURVE('',#37140,#37166,#30363,.T.) ;
#45436 = EDGE_CURVE('',#37137,#37142,#30364,.T.) ;
#45437 = EDGE_CURVE('',#37141,#37138,#30365,.T.) ;
#45438 = EDGE_CURVE('',#37165,#37141,#30366,.T.) ;
#45439 = EDGE_CURVE('',#37129,#37121,#30367,.T.) ;
#45440 = EDGE_CURVE('',#37130,#37120,#30368,.T.) ;
#45441 = EDGE_CURVE('',#37130,#37153,#30369,.T.) ;
#45442 = EDGE_CURVE('',#37127,#37152,#30370,.T.) ;
#45443 = EDGE_CURVE('',#37127,#37105,#30371,.T.) ;
#45444 = EDGE_CURVE('',#37128,#37104,#30372,.T.) ;
#45445 = EDGE_CURVE('',#37125,#37103,#30373,.T.) ;
#45446 = EDGE_CURVE('',#37126,#37106,#30374,.T.) ;
#45447 = EDGE_CURVE('',#37126,#37157,#30375,.T.) ;
#45448 = EDGE_CURVE('',#37123,#37156,#30376,.T.) ;
#45449 = EDGE_CURVE('',#37123,#37119,#30377,.T.) ;
#45450 = EDGE_CURVE('',#37124,#37122,#30378,.T.) ;
#45451 = EDGE_CURVE('',#37149,#37136,#30379,.T.) ;
#45452 = EDGE_CURVE('',#37149,#37161,#30380,.T.) ;
#45453 = EDGE_CURVE('',#37150,#37160,#30381,.T.) ;
#45454 = EDGE_CURVE('',#37150,#37137,#30382,.T.) ;
#45455 = EDGE_CURVE('',#37135,#37148,#30383,.T.) ;
#45456 = EDGE_CURVE('',#37164,#37148,#30384,.T.) ;
#45457 = EDGE_CURVE('',#37165,#37147,#30385,.T.) ;
#45458 = EDGE_CURVE('',#37147,#37138,#30386,.T.) ;
#45459 = EDGE_CURVE('',#37167,#37168,#4264,.T.) ;
#45460 = EDGE_CURVE('',#37168,#37169,#4265,.T.) ;
#45461 = EDGE_CURVE('',#37169,#37170,#4266,.T.) ;
#45462 = EDGE_CURVE('',#37170,#37171,#4267,.T.) ;
#45463 = EDGE_CURVE('',#37171,#37172,#4268,.T.) ;
#45464 = EDGE_CURVE('',#37172,#37173,#4269,.T.) ;
#45465 = EDGE_CURVE('',#37174,#37173,#30387,.T.) ;
#45466 = EDGE_CURVE('',#37174,#37175,#4270,.T.) ;
#45467 = EDGE_CURVE('',#37176,#37175,#30388,.T.) ;
#45468 = EDGE_CURVE('',#37176,#37167,#4271,.T.) ;
#45469 = EDGE_CURVE('',#37177,#37178,#4272,.T.) ;
#45470 = EDGE_CURVE('',#37178,#37179,#4273,.T.) ;
#45471 = EDGE_CURVE('',#37179,#37180,#4274,.T.) ;
#45472 = EDGE_CURVE('',#37180,#37181,#4275,.T.) ;
#45473 = EDGE_CURVE('',#37181,#37182,#4276,.T.) ;
#45474 = EDGE_CURVE('',#37182,#37183,#4277,.T.) ;
#45475 = EDGE_CURVE('',#37184,#37183,#30389,.T.) ;
#45476 = EDGE_CURVE('',#37184,#37185,#4278,.T.) ;
#45477 = EDGE_CURVE('',#37186,#37185,#30390,.T.) ;
#45478 = EDGE_CURVE('',#37186,#37177,#4279,.T.) ;
#45479 = EDGE_CURVE('',#37187,#37188,#4280,.T.) ;
#45480 = EDGE_CURVE('',#37188,#37189,#4281,.T.) ;
#45481 = EDGE_CURVE('',#37189,#37190,#4282,.T.) ;
#45482 = EDGE_CURVE('',#37190,#37191,#4283,.T.) ;
#45483 = EDGE_CURVE('',#37191,#37192,#4284,.T.) ;
#45484 = EDGE_CURVE('',#37192,#37193,#4285,.T.) ;
#45485 = EDGE_CURVE('',#37194,#37193,#30391,.T.) ;
#45486 = EDGE_CURVE('',#37194,#37195,#4286,.T.) ;
#45487 = EDGE_CURVE('',#37196,#37195,#30392,.T.) ;
#45488 = EDGE_CURVE('',#37196,#37187,#4287,.T.) ;
#45489 = EDGE_CURVE('',#37197,#37198,#4288,.T.) ;
#45490 = EDGE_CURVE('',#37198,#37199,#4289,.T.) ;
#45491 = EDGE_CURVE('',#37199,#37200,#4290,.T.) ;
#45492 = EDGE_CURVE('',#37200,#37201,#4291,.T.) ;
#45493 = EDGE_CURVE('',#37201,#37202,#4292,.T.) ;
#45494 = EDGE_CURVE('',#37202,#37203,#4293,.T.) ;
#45495 = EDGE_CURVE('',#37204,#37203,#30393,.T.) ;
#45496 = EDGE_CURVE('',#37204,#37205,#4294,.T.) ;
#45497 = EDGE_CURVE('',#37206,#37205,#30394,.T.) ;
#45498 = EDGE_CURVE('',#37206,#37197,#4295,.T.) ;
#45499 = EDGE_CURVE('',#37207,#37208,#4296,.T.) ;
#45500 = EDGE_CURVE('',#37208,#37209,#4297,.T.) ;
#45501 = EDGE_CURVE('',#37209,#37210,#4298,.T.) ;
#45502 = EDGE_CURVE('',#37210,#37211,#4299,.T.) ;
#45503 = EDGE_CURVE('',#37211,#37212,#4300,.T.) ;
#45504 = EDGE_CURVE('',#37212,#37213,#4301,.T.) ;
#45505 = EDGE_CURVE('',#37214,#37213,#30395,.T.) ;
#45506 = EDGE_CURVE('',#37214,#37215,#4302,.T.) ;
#45507 = EDGE_CURVE('',#37216,#37215,#30396,.T.) ;
#45508 = EDGE_CURVE('',#37216,#37207,#4303,.T.) ;
#45509 = EDGE_CURVE('',#37217,#37218,#4304,.T.) ;
#45510 = EDGE_CURVE('',#37218,#37219,#4305,.T.) ;
#45511 = EDGE_CURVE('',#37219,#37220,#4306,.T.) ;
#45512 = EDGE_CURVE('',#37220,#37221,#4307,.T.) ;
#45513 = EDGE_CURVE('',#37221,#37222,#4308,.T.) ;
#45514 = EDGE_CURVE('',#37222,#37223,#4309,.T.) ;
#45515 = EDGE_CURVE('',#37224,#37223,#30397,.T.) ;
#45516 = EDGE_CURVE('',#37224,#37225,#4310,.T.) ;
#45517 = EDGE_CURVE('',#37226,#37225,#30398,.T.) ;
#45518 = EDGE_CURVE('',#37226,#37217,#4311,.T.) ;
#45519 = EDGE_CURVE('',#37227,#37228,#4312,.T.) ;
#45520 = EDGE_CURVE('',#37228,#37229,#4313,.T.) ;
#45521 = EDGE_CURVE('',#37229,#37230,#4314,.T.) ;
#45522 = EDGE_CURVE('',#37230,#37231,#4315,.T.) ;
#45523 = EDGE_CURVE('',#37231,#37232,#4316,.T.) ;
#45524 = EDGE_CURVE('',#37232,#37233,#4317,.T.) ;
#45525 = EDGE_CURVE('',#37234,#37233,#30399,.T.) ;
#45526 = EDGE_CURVE('',#37234,#37235,#4318,.T.) ;
#45527 = EDGE_CURVE('',#37236,#37235,#30400,.T.) ;
#45528 = EDGE_CURVE('',#37236,#37227,#4319,.T.) ;
#45529 = EDGE_CURVE('',#37237,#37238,#4320,.T.) ;
#45530 = EDGE_CURVE('',#37238,#37239,#4321,.T.) ;
#45531 = EDGE_CURVE('',#37239,#37240,#4322,.T.) ;
#45532 = EDGE_CURVE('',#37240,#37241,#4323,.T.) ;
#45533 = EDGE_CURVE('',#37241,#37242,#4324,.T.) ;
#45534 = EDGE_CURVE('',#37242,#37243,#4325,.T.) ;
#45535 = EDGE_CURVE('',#37244,#37243,#30401,.T.) ;
#45536 = EDGE_CURVE('',#37244,#37245,#4326,.T.) ;
#45537 = EDGE_CURVE('',#37246,#37245,#30402,.T.) ;
#45538 = EDGE_CURVE('',#37246,#37237,#4327,.T.) ;
#45539 = EDGE_CURVE('',#37247,#37248,#4328,.T.) ;
#45540 = EDGE_CURVE('',#37248,#37249,#4329,.T.) ;
#45541 = EDGE_CURVE('',#37249,#37250,#4330,.T.) ;
#45542 = EDGE_CURVE('',#37250,#37251,#4331,.T.) ;
#45543 = EDGE_CURVE('',#37251,#37252,#4332,.T.) ;
#45544 = EDGE_CURVE('',#37252,#37253,#4333,.T.) ;
#45545 = EDGE_CURVE('',#37254,#37253,#30403,.T.) ;
#45546 = EDGE_CURVE('',#37254,#37255,#4334,.T.) ;
#45547 = EDGE_CURVE('',#37256,#37255,#30404,.T.) ;
#45548 = EDGE_CURVE('',#37256,#37247,#4335,.T.) ;
#45549 = EDGE_CURVE('',#37257,#37258,#4336,.T.) ;
#45550 = EDGE_CURVE('',#37258,#37259,#4337,.T.) ;
#45551 = EDGE_CURVE('',#37259,#37260,#4338,.T.) ;
#45552 = EDGE_CURVE('',#37260,#37257,#4339,.T.) ;
#45553 = EDGE_CURVE('',#36356,#37261,#4340,.T.) ;
#45554 = EDGE_CURVE('',#37261,#37262,#4341,.T.) ;
#45555 = EDGE_CURVE('',#37262,#36357,#4342,.T.) ;
#45556 = EDGE_CURVE('',#37263,#37264,#4343,.T.) ;
#45557 = EDGE_CURVE('',#37264,#37265,#4344,.T.) ;
#45558 = EDGE_CURVE('',#37265,#37266,#4345,.T.) ;
#45559 = EDGE_CURVE('',#37266,#37263,#4346,.T.) ;
#45560 = EDGE_CURVE('',#37267,#37268,#4347,.T.) ;
#45561 = EDGE_CURVE('',#37268,#37269,#4348,.T.) ;
#45562 = EDGE_CURVE('',#37269,#37270,#4349,.T.) ;
#45563 = EDGE_CURVE('',#37270,#37267,#4350,.T.) ;
#45564 = EDGE_CURVE('',#37271,#37272,#4351,.T.) ;
#45565 = EDGE_CURVE('',#37272,#37273,#4352,.T.) ;
#45566 = EDGE_CURVE('',#37273,#37274,#4353,.T.) ;
#45567 = EDGE_CURVE('',#37274,#37271,#4354,.T.) ;
#45568 = EDGE_CURVE('',#37275,#37276,#4355,.T.) ;
#45569 = EDGE_CURVE('',#37276,#37277,#4356,.T.) ;
#45570 = EDGE_CURVE('',#37277,#37278,#4357,.T.) ;
#45571 = EDGE_CURVE('',#37278,#37275,#4358,.T.) ;
#45572 = EDGE_CURVE('',#36305,#37279,#4359,.T.) ;
#45573 = EDGE_CURVE('',#37279,#37280,#4360,.T.) ;
#45574 = EDGE_CURVE('',#37280,#36306,#4361,.T.) ;
#45575 = EDGE_CURVE('',#37281,#37282,#4362,.T.) ;
#45576 = EDGE_CURVE('',#37282,#37283,#4363,.T.) ;
#45577 = EDGE_CURVE('',#37283,#37284,#4364,.T.) ;
#45578 = EDGE_CURVE('',#37284,#37281,#4365,.T.) ;
#45579 = EDGE_CURVE('',#37285,#37286,#4366,.T.) ;
#45580 = EDGE_CURVE('',#37286,#37287,#4367,.T.) ;
#45581 = EDGE_CURVE('',#37287,#37288,#4368,.T.) ;
#45582 = EDGE_CURVE('',#37288,#37285,#4369,.T.) ;
#45583 = EDGE_CURVE('',#37289,#37290,#4370,.T.) ;
#45584 = EDGE_CURVE('',#37290,#37291,#4371,.T.) ;
#45585 = EDGE_CURVE('',#37291,#37292,#4372,.T.) ;
#45586 = EDGE_CURVE('',#37292,#37289,#4373,.T.) ;
#45587 = EDGE_CURVE('',#37293,#37294,#4374,.T.) ;
#45588 = EDGE_CURVE('',#37294,#37295,#4375,.T.) ;
#45589 = EDGE_CURVE('',#37295,#37296,#4376,.T.) ;
#45590 = EDGE_CURVE('',#37296,#37293,#4377,.T.) ;
#45591 = EDGE_CURVE('',#36290,#37297,#4378,.T.) ;
#45592 = EDGE_CURVE('',#37297,#37298,#4379,.T.) ;
#45593 = EDGE_CURVE('',#37298,#36291,#4380,.T.) ;
#45594 = EDGE_CURVE('',#37299,#37300,#4381,.T.) ;
#45595 = EDGE_CURVE('',#37300,#37301,#4382,.T.) ;
#45596 = EDGE_CURVE('',#37301,#37302,#4383,.T.) ;
#45597 = EDGE_CURVE('',#37302,#37299,#4384,.T.) ;
#45598 = EDGE_CURVE('',#37303,#37304,#4385,.T.) ;
#45599 = EDGE_CURVE('',#37304,#37305,#4386,.T.) ;
#45600 = EDGE_CURVE('',#37305,#37306,#4387,.T.) ;
#45601 = EDGE_CURVE('',#37306,#37303,#4388,.T.) ;
#45602 = EDGE_CURVE('',#37307,#37308,#4389,.T.) ;
#45603 = EDGE_CURVE('',#37308,#37309,#4390,.T.) ;
#45604 = EDGE_CURVE('',#37309,#37310,#4391,.T.) ;
#45605 = EDGE_CURVE('',#37310,#37307,#4392,.T.) ;
#45606 = EDGE_CURVE('',#37311,#37312,#4393,.T.) ;
#45607 = EDGE_CURVE('',#37312,#37313,#4394,.T.) ;
#45608 = EDGE_CURVE('',#37313,#37314,#4395,.T.) ;
#45609 = EDGE_CURVE('',#37314,#37311,#4396,.T.) ;
#45610 = EDGE_CURVE('',#36275,#37315,#4397,.T.) ;
#45611 = EDGE_CURVE('',#37315,#37316,#4398,.T.) ;
#45612 = EDGE_CURVE('',#37316,#36276,#4399,.T.) ;
#45613 = EDGE_CURVE('',#37317,#37318,#4400,.T.) ;
#45614 = EDGE_CURVE('',#37318,#37319,#4401,.T.) ;
#45615 = EDGE_CURVE('',#37319,#37320,#4402,.T.) ;
#45616 = EDGE_CURVE('',#37320,#37317,#4403,.T.) ;
#45617 = EDGE_CURVE('',#37321,#37322,#4404,.T.) ;
#45618 = EDGE_CURVE('',#37322,#37323,#4405,.T.) ;
#45619 = EDGE_CURVE('',#37323,#37324,#4406,.T.) ;
#45620 = EDGE_CURVE('',#37324,#37321,#4407,.T.) ;
#45621 = EDGE_CURVE('',#37325,#37326,#4408,.T.) ;
#45622 = EDGE_CURVE('',#37326,#37327,#4409,.T.) ;
#45623 = EDGE_CURVE('',#37327,#37328,#4410,.T.) ;
#45624 = EDGE_CURVE('',#37328,#37325,#4411,.T.) ;
#45625 = EDGE_CURVE('',#37329,#37330,#4412,.T.) ;
#45626 = EDGE_CURVE('',#37330,#37331,#4413,.T.) ;
#45627 = EDGE_CURVE('',#37331,#37332,#4414,.T.) ;
#45628 = EDGE_CURVE('',#37332,#37329,#4415,.T.) ;
#45629 = EDGE_CURVE('',#36260,#37333,#4416,.T.) ;
#45630 = EDGE_CURVE('',#37333,#37334,#4417,.T.) ;
#45631 = EDGE_CURVE('',#37334,#36261,#4418,.T.) ;
#45632 = EDGE_CURVE('',#37335,#37336,#4419,.T.) ;
#45633 = EDGE_CURVE('',#37336,#37337,#4420,.T.) ;
#45634 = EDGE_CURVE('',#37337,#37338,#4421,.T.) ;
#45635 = EDGE_CURVE('',#37338,#37335,#4422,.T.) ;
#45636 = EDGE_CURVE('',#37339,#37340,#4423,.T.) ;
#45637 = EDGE_CURVE('',#37340,#37341,#4424,.T.) ;
#45638 = EDGE_CURVE('',#37341,#37342,#4425,.T.) ;
#45639 = EDGE_CURVE('',#37342,#37339,#4426,.T.) ;
#45640 = EDGE_CURVE('',#37343,#37344,#4427,.T.) ;
#45641 = EDGE_CURVE('',#37344,#37345,#4428,.T.) ;
#45642 = EDGE_CURVE('',#37345,#37346,#4429,.T.) ;
#45643 = EDGE_CURVE('',#37346,#37343,#4430,.T.) ;
#45644 = EDGE_CURVE('',#37347,#37348,#4431,.T.) ;
#45645 = EDGE_CURVE('',#37348,#37349,#4432,.T.) ;
#45646 = EDGE_CURVE('',#37349,#37350,#4433,.T.) ;
#45647 = EDGE_CURVE('',#37350,#37347,#4434,.T.) ;
#45648 = EDGE_CURVE('',#36245,#37351,#4435,.T.) ;
#45649 = EDGE_CURVE('',#37351,#37352,#4436,.T.) ;
#45650 = EDGE_CURVE('',#37352,#36246,#4437,.T.) ;
#45651 = EDGE_CURVE('',#37353,#37354,#4438,.T.) ;
#45652 = EDGE_CURVE('',#37354,#37355,#4439,.T.) ;
#45653 = EDGE_CURVE('',#37355,#37356,#4440,.T.) ;
#45654 = EDGE_CURVE('',#37356,#37353,#4441,.T.) ;
#45655 = EDGE_CURVE('',#37357,#37358,#4442,.T.) ;
#45656 = EDGE_CURVE('',#37358,#37359,#4443,.T.) ;
#45657 = EDGE_CURVE('',#37359,#37360,#4444,.T.) ;
#45658 = EDGE_CURVE('',#37360,#37357,#4445,.T.) ;
#45659 = EDGE_CURVE('',#37361,#37362,#4446,.T.) ;
#45660 = EDGE_CURVE('',#37362,#37363,#4447,.T.) ;
#45661 = EDGE_CURVE('',#37363,#37364,#4448,.T.) ;
#45662 = EDGE_CURVE('',#37364,#37361,#4449,.T.) ;
#45663 = EDGE_CURVE('',#37365,#37366,#4450,.T.) ;
#45664 = EDGE_CURVE('',#37366,#37367,#4451,.T.) ;
#45665 = EDGE_CURVE('',#37367,#37368,#4452,.T.) ;
#45666 = EDGE_CURVE('',#37368,#37365,#4453,.T.) ;
#45667 = EDGE_CURVE('',#36230,#37369,#4454,.T.) ;
#45668 = EDGE_CURVE('',#37369,#37370,#4455,.T.) ;
#45669 = EDGE_CURVE('',#37370,#36231,#4456,.T.) ;
#45670 = EDGE_CURVE('',#37371,#37372,#4457,.T.) ;
#45671 = EDGE_CURVE('',#37372,#37373,#4458,.T.) ;
#45672 = EDGE_CURVE('',#37373,#37374,#4459,.T.) ;
#45673 = EDGE_CURVE('',#37374,#37371,#4460,.T.) ;
#45674 = EDGE_CURVE('',#37375,#37376,#4461,.T.) ;
#45675 = EDGE_CURVE('',#37376,#37377,#4462,.T.) ;
#45676 = EDGE_CURVE('',#37377,#37378,#4463,.T.) ;
#45677 = EDGE_CURVE('',#37378,#37375,#4464,.T.) ;
#45678 = EDGE_CURVE('',#37379,#37380,#4465,.T.) ;
#45679 = EDGE_CURVE('',#37380,#37381,#4466,.T.) ;
#45680 = EDGE_CURVE('',#37381,#37382,#4467,.T.) ;
#45681 = EDGE_CURVE('',#37382,#37379,#4468,.T.) ;
#45682 = EDGE_CURVE('',#37383,#37384,#4469,.T.) ;
#45683 = EDGE_CURVE('',#37384,#37385,#4470,.T.) ;
#45684 = EDGE_CURVE('',#37385,#37386,#4471,.T.) ;
#45685 = EDGE_CURVE('',#37386,#37383,#4472,.T.) ;
#45686 = EDGE_CURVE('',#36215,#37387,#4473,.T.) ;
#45687 = EDGE_CURVE('',#37387,#37388,#4474,.T.) ;
#45688 = EDGE_CURVE('',#37388,#36216,#4475,.T.) ;
#45689 = EDGE_CURVE('',#37389,#37390,#4476,.T.) ;
#45690 = EDGE_CURVE('',#37390,#37391,#4477,.T.) ;
#45691 = EDGE_CURVE('',#37391,#37392,#4478,.T.) ;
#45692 = EDGE_CURVE('',#37392,#37389,#4479,.T.) ;
#45693 = EDGE_CURVE('',#37393,#37394,#4480,.T.) ;
#45694 = EDGE_CURVE('',#37394,#37395,#4481,.T.) ;
#45695 = EDGE_CURVE('',#37395,#37396,#4482,.T.) ;
#45696 = EDGE_CURVE('',#37396,#37393,#4483,.T.) ;
#45697 = EDGE_CURVE('',#37397,#37398,#4484,.T.) ;
#45698 = EDGE_CURVE('',#37398,#37399,#4485,.T.) ;
#45699 = EDGE_CURVE('',#37399,#37400,#4486,.T.) ;
#45700 = EDGE_CURVE('',#37400,#37397,#4487,.T.) ;
#45701 = EDGE_CURVE('',#37401,#37402,#4488,.T.) ;
#45702 = EDGE_CURVE('',#37402,#37403,#4489,.T.) ;
#45703 = EDGE_CURVE('',#37403,#37404,#4490,.T.) ;
#45704 = EDGE_CURVE('',#37404,#37401,#4491,.T.) ;
#45705 = EDGE_CURVE('',#36200,#37405,#4492,.T.) ;
#45706 = EDGE_CURVE('',#37405,#37406,#4493,.T.) ;
#45707 = EDGE_CURVE('',#37406,#36201,#4494,.T.) ;
#45708 = EDGE_CURVE('',#37407,#37408,#4495,.T.) ;
#45709 = EDGE_CURVE('',#37408,#37409,#4496,.T.) ;
#45710 = EDGE_CURVE('',#37409,#37410,#4497,.T.) ;
#45711 = EDGE_CURVE('',#37410,#37407,#4498,.T.) ;
#45712 = EDGE_CURVE('',#37411,#37412,#4499,.T.) ;
#45713 = EDGE_CURVE('',#37412,#37413,#4500,.T.) ;
#45714 = EDGE_CURVE('',#37413,#37414,#4501,.T.) ;
#45715 = EDGE_CURVE('',#37414,#37411,#4502,.T.) ;
#45716 = EDGE_CURVE('',#37415,#37416,#4503,.T.) ;
#45717 = EDGE_CURVE('',#37416,#37417,#4504,.T.) ;
#45718 = EDGE_CURVE('',#37417,#37418,#4505,.T.) ;
#45719 = EDGE_CURVE('',#37418,#37415,#4506,.T.) ;
#45720 = EDGE_CURVE('',#37419,#37420,#4507,.T.) ;
#45721 = EDGE_CURVE('',#37419,#37421,#30405,.T.) ;
#45722 = EDGE_CURVE('',#37421,#37422,#4508,.T.) ;
#45723 = EDGE_CURVE('',#37422,#37420,#30406,.T.) ;
#45724 = EDGE_CURVE('',#37421,#37423,#4509,.T.) ;
#45725 = EDGE_CURVE('',#37423,#37424,#4510,.T.) ;
#45726 = EDGE_CURVE('',#37424,#37422,#4511,.T.) ;
#45727 = EDGE_CURVE('',#37423,#37425,#30407,.T.) ;
#45728 = EDGE_CURVE('',#37425,#37426,#4512,.T.) ;
#45729 = EDGE_CURVE('',#37426,#37424,#30408,.T.) ;
#45730 = EDGE_CURVE('',#37425,#37427,#4513,.T.) ;
#45731 = EDGE_CURVE('',#37427,#37428,#4514,.T.) ;
#45732 = EDGE_CURVE('',#37428,#37426,#4515,.T.) ;
#45733 = EDGE_CURVE('',#37427,#37429,#30409,.T.) ;
#45734 = EDGE_CURVE('',#37429,#37430,#4516,.T.) ;
#45735 = EDGE_CURVE('',#37430,#37428,#30410,.T.) ;
#45736 = EDGE_CURVE('',#37429,#36195,#4517,.T.) ;
#45737 = EDGE_CURVE('',#36195,#37431,#4518,.T.) ;
#45738 = EDGE_CURVE('',#37431,#37430,#4519,.T.) ;
#45739 = EDGE_CURVE('',#36196,#37432,#4520,.T.) ;
#45740 = EDGE_CURVE('',#37432,#37431,#30411,.T.) ;
#45741 = EDGE_CURVE('',#36196,#36377,#4521,.T.) ;
#45742 = EDGE_CURVE('',#36347,#37432,#4522,.T.) ;
#45743 = EDGE_CURVE('',#36378,#37433,#4523,.T.) ;
#45744 = EDGE_CURVE('',#37433,#37434,#4524,.T.) ;
#45745 = EDGE_CURVE('',#37434,#36348,#4525,.T.) ;
#45746 = EDGE_CURVE('',#37433,#37435,#30412,.T.) ;
#45747 = EDGE_CURVE('',#37435,#37436,#4526,.T.) ;
#45748 = EDGE_CURVE('',#37436,#37434,#30413,.T.) ;
#45749 = EDGE_CURVE('',#37435,#37437,#4527,.T.) ;
#45750 = EDGE_CURVE('',#37437,#37438,#4528,.T.) ;
#45751 = EDGE_CURVE('',#37438,#37436,#4529,.T.) ;
#45752 = EDGE_CURVE('',#37437,#37439,#30414,.T.) ;
#45753 = EDGE_CURVE('',#37439,#37440,#4530,.T.) ;
#45754 = EDGE_CURVE('',#37440,#37438,#30415,.T.) ;
#45755 = EDGE_CURVE('',#37439,#37441,#4531,.T.) ;
#45756 = EDGE_CURVE('',#37441,#37442,#4532,.T.) ;
#45757 = EDGE_CURVE('',#37442,#37440,#4533,.T.) ;
#45758 = EDGE_CURVE('',#37441,#37443,#30416,.T.) ;
#45759 = EDGE_CURVE('',#37443,#37444,#4534,.T.) ;
#45760 = EDGE_CURVE('',#37444,#37442,#30417,.T.) ;
#45761 = EDGE_CURVE('',#37443,#37445,#4535,.T.) ;
#45762 = EDGE_CURVE('',#37445,#37446,#4536,.T.) ;
#45763 = EDGE_CURVE('',#37446,#37444,#4537,.T.) ;
#45764 = EDGE_CURVE('',#37445,#37447,#30418,.T.) ;
#45765 = EDGE_CURVE('',#37447,#37448,#4538,.T.) ;
#45766 = EDGE_CURVE('',#37448,#37446,#30419,.T.) ;
#45767 = EDGE_CURVE('',#37447,#37449,#4539,.T.) ;
#45768 = EDGE_CURVE('',#37449,#37450,#4540,.T.) ;
#45769 = EDGE_CURVE('',#37450,#37448,#4541,.T.) ;
#45770 = EDGE_CURVE('',#37449,#37451,#30420,.T.) ;
#45771 = EDGE_CURVE('',#37451,#37452,#4542,.T.) ;
#45772 = EDGE_CURVE('',#37452,#37450,#30421,.T.) ;
#45773 = EDGE_CURVE('',#37451,#37453,#4543,.T.) ;
#45774 = EDGE_CURVE('',#37453,#37454,#4544,.T.) ;
#45775 = EDGE_CURVE('',#37454,#37452,#4545,.T.) ;
#45776 = EDGE_CURVE('',#37453,#37455,#30422,.T.) ;
#45777 = EDGE_CURVE('',#37455,#37456,#4546,.T.) ;
#45778 = EDGE_CURVE('',#37456,#37454,#30423,.T.) ;
#45779 = EDGE_CURVE('',#37455,#37457,#30424,.T.) ;
#45780 = EDGE_CURVE('',#37457,#37458,#4547,.T.) ;
#45781 = EDGE_CURVE('',#37458,#37456,#30425,.T.) ;
#45782 = EDGE_CURVE('',#37457,#37459,#30426,.T.) ;
#45783 = EDGE_CURVE('',#37459,#37460,#4548,.T.) ;
#45784 = EDGE_CURVE('',#37460,#37458,#30427,.T.) ;
#45785 = EDGE_CURVE('',#37459,#37461,#4549,.T.) ;
#45786 = EDGE_CURVE('',#37461,#37462,#4550,.T.) ;
#45787 = EDGE_CURVE('',#37462,#37460,#4551,.T.) ;
#45788 = EDGE_CURVE('',#37461,#37463,#30428,.T.) ;
#45789 = EDGE_CURVE('',#37463,#37464,#4552,.T.) ;
#45790 = EDGE_CURVE('',#37464,#37462,#30429,.T.) ;
#45791 = EDGE_CURVE('',#37463,#37465,#4553,.T.) ;
#45792 = EDGE_CURVE('',#37465,#37466,#4554,.T.) ;
#45793 = EDGE_CURVE('',#37466,#37464,#4555,.T.) ;
#45794 = EDGE_CURVE('',#37465,#37467,#30430,.T.) ;
#45795 = EDGE_CURVE('',#37467,#37468,#4556,.T.) ;
#45796 = EDGE_CURVE('',#37468,#37466,#30431,.T.) ;
#45797 = EDGE_CURVE('',#37467,#37419,#4557,.T.) ;
#45798 = EDGE_CURVE('',#37420,#37468,#4558,.T.) ;
#45799 = EDGE_CURVE('',#37469,#37470,#30432,.T.) ;
#45800 = EDGE_CURVE('',#37470,#37471,#4559,.T.) ;
#45801 = EDGE_CURVE('',#37471,#37472,#30433,.T.) ;
#45802 = EDGE_CURVE('',#37472,#37473,#4560,.T.) ;
#45803 = EDGE_CURVE('',#37473,#37474,#4561,.T.) ;
#45804 = EDGE_CURVE('',#37474,#37475,#4562,.T.) ;
#45805 = EDGE_CURVE('',#37475,#37476,#30434,.T.) ;
#45806 = EDGE_CURVE('',#37476,#37477,#4563,.T.) ;
#45807 = EDGE_CURVE('',#37477,#37478,#4564,.T.) ;
#45808 = EDGE_CURVE('',#37478,#37479,#4565,.T.) ;
#45809 = EDGE_CURVE('',#37479,#37480,#30435,.T.) ;
#45810 = EDGE_CURVE('',#37480,#37481,#4566,.T.) ;
#45811 = EDGE_CURVE('',#37481,#37482,#30436,.T.) ;
#45812 = EDGE_CURVE('',#37482,#37483,#4567,.T.) ;
#45813 = EDGE_CURVE('',#37483,#37484,#4568,.T.) ;
#45814 = EDGE_CURVE('',#37484,#36197,#4569,.T.) ;
#45815 = EDGE_CURVE('',#36197,#37485,#4570,.T.) ;
#45816 = EDGE_CURVE('',#37485,#37469,#4571,.T.) ;
#45817 = EDGE_CURVE('',#37486,#37487,#4572,.T.) ;
#45818 = EDGE_CURVE('',#37486,#37488,#30437,.T.) ;
#45819 = EDGE_CURVE('',#37488,#37489,#4573,.T.) ;
#45820 = EDGE_CURVE('',#37489,#37487,#30438,.T.) ;
#45821 = EDGE_CURVE('',#37488,#37490,#4574,.T.) ;
#45822 = EDGE_CURVE('',#37490,#37491,#4575,.T.) ;
#45823 = EDGE_CURVE('',#37491,#37489,#4576,.T.) ;
#45824 = EDGE_CURVE('',#37490,#37492,#30439,.T.) ;
#45825 = EDGE_CURVE('',#37492,#37493,#4577,.T.) ;
#45826 = EDGE_CURVE('',#37493,#37491,#30440,.T.) ;
#45827 = EDGE_CURVE('',#37492,#37494,#4578,.T.) ;
#45828 = EDGE_CURVE('',#37494,#37495,#4579,.T.) ;
#45829 = EDGE_CURVE('',#37495,#37493,#4580,.T.) ;
#45830 = EDGE_CURVE('',#37494,#37496,#30441,.T.) ;
#45831 = EDGE_CURVE('',#37496,#37497,#4581,.T.) ;
#45832 = EDGE_CURVE('',#37497,#37495,#30442,.T.) ;
#45833 = EDGE_CURVE('',#37496,#36210,#4582,.T.) ;
#45834 = EDGE_CURVE('',#36210,#37498,#4583,.T.) ;
#45835 = EDGE_CURVE('',#37498,#37497,#4584,.T.) ;
#45836 = EDGE_CURVE('',#36211,#37499,#4585,.T.) ;
#45837 = EDGE_CURVE('',#37499,#37498,#30443,.T.) ;
#45838 = EDGE_CURVE('',#36211,#36375,#4586,.T.) ;
#45839 = EDGE_CURVE('',#36343,#37499,#4587,.T.) ;
#45840 = EDGE_CURVE('',#36376,#37500,#4588,.T.) ;
#45841 = EDGE_CURVE('',#37500,#37501,#4589,.T.) ;
#45842 = EDGE_CURVE('',#37501,#36344,#4590,.T.) ;
#45843 = EDGE_CURVE('',#37500,#37502,#30444,.T.) ;
#45844 = EDGE_CURVE('',#37502,#37503,#4591,.T.) ;
#45845 = EDGE_CURVE('',#37503,#37501,#30445,.T.) ;
#45846 = EDGE_CURVE('',#37502,#37504,#4592,.T.) ;
#45847 = EDGE_CURVE('',#37504,#37505,#4593,.T.) ;
#45848 = EDGE_CURVE('',#37505,#37503,#4594,.T.) ;
#45849 = EDGE_CURVE('',#37504,#37506,#30446,.T.) ;
#45850 = EDGE_CURVE('',#37506,#37507,#4595,.T.) ;
#45851 = EDGE_CURVE('',#37507,#37505,#30447,.T.) ;
#45852 = EDGE_CURVE('',#37506,#37508,#4596,.T.) ;
#45853 = EDGE_CURVE('',#37508,#37509,#4597,.T.) ;
#45854 = EDGE_CURVE('',#37509,#37507,#4598,.T.) ;
#45855 = EDGE_CURVE('',#37508,#37510,#30448,.T.) ;
#45856 = EDGE_CURVE('',#37510,#37511,#4599,.T.) ;
#45857 = EDGE_CURVE('',#37511,#37509,#30449,.T.) ;
#45858 = EDGE_CURVE('',#37510,#37512,#4600,.T.) ;
#45859 = EDGE_CURVE('',#37512,#37513,#4601,.T.) ;
#45860 = EDGE_CURVE('',#37513,#37511,#4602,.T.) ;
#45861 = EDGE_CURVE('',#37512,#37514,#30450,.T.) ;
#45862 = EDGE_CURVE('',#37514,#37515,#4603,.T.) ;
#45863 = EDGE_CURVE('',#37515,#37513,#30451,.T.) ;
#45864 = EDGE_CURVE('',#37514,#37516,#4604,.T.) ;
#45865 = EDGE_CURVE('',#37516,#37517,#4605,.T.) ;
#45866 = EDGE_CURVE('',#37517,#37515,#4606,.T.) ;
#45867 = EDGE_CURVE('',#37516,#37518,#30452,.T.) ;
#45868 = EDGE_CURVE('',#37518,#37519,#4607,.T.) ;
#45869 = EDGE_CURVE('',#37519,#37517,#30453,.T.) ;
#45870 = EDGE_CURVE('',#37518,#37520,#4608,.T.) ;
#45871 = EDGE_CURVE('',#37520,#37521,#4609,.T.) ;
#45872 = EDGE_CURVE('',#37521,#37519,#4610,.T.) ;
#45873 = EDGE_CURVE('',#37520,#37522,#30454,.T.) ;
#45874 = EDGE_CURVE('',#37522,#37523,#4611,.T.) ;
#45875 = EDGE_CURVE('',#37523,#37521,#30455,.T.) ;
#45876 = EDGE_CURVE('',#37522,#37524,#30456,.T.) ;
#45877 = EDGE_CURVE('',#37524,#37525,#4612,.T.) ;
#45878 = EDGE_CURVE('',#37525,#37523,#30457,.T.) ;
#45879 = EDGE_CURVE('',#37524,#37526,#30458,.T.) ;
#45880 = EDGE_CURVE('',#37526,#37527,#4613,.T.) ;
#45881 = EDGE_CURVE('',#37527,#37525,#30459,.T.) ;
#45882 = EDGE_CURVE('',#37526,#37528,#4614,.T.) ;
#45883 = EDGE_CURVE('',#37528,#37529,#4615,.T.) ;
#45884 = EDGE_CURVE('',#37529,#37527,#4616,.T.) ;
#45885 = EDGE_CURVE('',#37528,#37530,#30460,.T.) ;
#45886 = EDGE_CURVE('',#37530,#37531,#4617,.T.) ;
#45887 = EDGE_CURVE('',#37531,#37529,#30461,.T.) ;
#45888 = EDGE_CURVE('',#37530,#37532,#4618,.T.) ;
#45889 = EDGE_CURVE('',#37532,#37533,#4619,.T.) ;
#45890 = EDGE_CURVE('',#37533,#37531,#4620,.T.) ;
#45891 = EDGE_CURVE('',#37532,#37534,#30462,.T.) ;
#45892 = EDGE_CURVE('',#37534,#37535,#4621,.T.) ;
#45893 = EDGE_CURVE('',#37535,#37533,#30463,.T.) ;
#45894 = EDGE_CURVE('',#37534,#37486,#4622,.T.) ;
#45895 = EDGE_CURVE('',#37487,#37535,#4623,.T.) ;
#45896 = EDGE_CURVE('',#37536,#37537,#30464,.T.) ;
#45897 = EDGE_CURVE('',#37537,#37538,#4624,.T.) ;
#45898 = EDGE_CURVE('',#37538,#37539,#30465,.T.) ;
#45899 = EDGE_CURVE('',#37539,#37540,#4625,.T.) ;
#45900 = EDGE_CURVE('',#37540,#37541,#4626,.T.) ;
#45901 = EDGE_CURVE('',#37541,#37542,#4627,.T.) ;
#45902 = EDGE_CURVE('',#37542,#37543,#30466,.T.) ;
#45903 = EDGE_CURVE('',#37543,#37544,#4628,.T.) ;
#45904 = EDGE_CURVE('',#37544,#37545,#4629,.T.) ;
#45905 = EDGE_CURVE('',#37545,#37546,#4630,.T.) ;
#45906 = EDGE_CURVE('',#37546,#37547,#30467,.T.) ;
#45907 = EDGE_CURVE('',#37547,#37548,#4631,.T.) ;
#45908 = EDGE_CURVE('',#37548,#37549,#30468,.T.) ;
#45909 = EDGE_CURVE('',#37549,#37550,#4632,.T.) ;
#45910 = EDGE_CURVE('',#37550,#37551,#4633,.T.) ;
#45911 = EDGE_CURVE('',#37551,#36212,#4634,.T.) ;
#45912 = EDGE_CURVE('',#36212,#37552,#4635,.T.) ;
#45913 = EDGE_CURVE('',#37552,#37536,#4636,.T.) ;
#45914 = EDGE_CURVE('',#37553,#37554,#4637,.T.) ;
#45915 = EDGE_CURVE('',#37553,#37555,#30469,.T.) ;
#45916 = EDGE_CURVE('',#37555,#37556,#4638,.T.) ;
#45917 = EDGE_CURVE('',#37556,#37554,#30470,.T.) ;
#45918 = EDGE_CURVE('',#37555,#37557,#4639,.T.) ;
#45919 = EDGE_CURVE('',#37557,#37558,#4640,.T.) ;
#45920 = EDGE_CURVE('',#37558,#37556,#4641,.T.) ;
#45921 = EDGE_CURVE('',#37557,#37559,#30471,.T.) ;
#45922 = EDGE_CURVE('',#37559,#37560,#4642,.T.) ;
#45923 = EDGE_CURVE('',#37560,#37558,#30472,.T.) ;
#45924 = EDGE_CURVE('',#37559,#37561,#4643,.T.) ;
#45925 = EDGE_CURVE('',#37561,#37562,#4644,.T.) ;
#45926 = EDGE_CURVE('',#37562,#37560,#4645,.T.) ;
#45927 = EDGE_CURVE('',#37561,#37563,#30473,.T.) ;
#45928 = EDGE_CURVE('',#37563,#37564,#4646,.T.) ;
#45929 = EDGE_CURVE('',#37564,#37562,#30474,.T.) ;
#45930 = EDGE_CURVE('',#37563,#36225,#4647,.T.) ;
#45931 = EDGE_CURVE('',#36225,#37565,#4648,.T.) ;
#45932 = EDGE_CURVE('',#37565,#37564,#4649,.T.) ;
#45933 = EDGE_CURVE('',#36226,#37566,#4650,.T.) ;
#45934 = EDGE_CURVE('',#37566,#37565,#30475,.T.) ;
#45935 = EDGE_CURVE('',#36226,#36373,#4651,.T.) ;
#45936 = EDGE_CURVE('',#36339,#37566,#4652,.T.) ;
#45937 = EDGE_CURVE('',#36374,#37567,#4653,.T.) ;
#45938 = EDGE_CURVE('',#37567,#37568,#4654,.T.) ;
#45939 = EDGE_CURVE('',#37568,#36340,#4655,.T.) ;
#45940 = EDGE_CURVE('',#37567,#37569,#30476,.T.) ;
#45941 = EDGE_CURVE('',#37569,#37570,#4656,.T.) ;
#45942 = EDGE_CURVE('',#37570,#37568,#30477,.T.) ;
#45943 = EDGE_CURVE('',#37569,#37571,#4657,.T.) ;
#45944 = EDGE_CURVE('',#37571,#37572,#4658,.T.) ;
#45945 = EDGE_CURVE('',#37572,#37570,#4659,.T.) ;
#45946 = EDGE_CURVE('',#37571,#37573,#30478,.T.) ;
#45947 = EDGE_CURVE('',#37573,#37574,#4660,.T.) ;
#45948 = EDGE_CURVE('',#37574,#37572,#30479,.T.) ;
#45949 = EDGE_CURVE('',#37573,#37575,#4661,.T.) ;
#45950 = EDGE_CURVE('',#37575,#37576,#4662,.T.) ;
#45951 = EDGE_CURVE('',#37576,#37574,#4663,.T.) ;
#45952 = EDGE_CURVE('',#37575,#37577,#30480,.T.) ;
#45953 = EDGE_CURVE('',#37577,#37578,#4664,.T.) ;
#45954 = EDGE_CURVE('',#37578,#37576,#30481,.T.) ;
#45955 = EDGE_CURVE('',#37577,#37579,#4665,.T.) ;
#45956 = EDGE_CURVE('',#37579,#37580,#4666,.T.) ;
#45957 = EDGE_CURVE('',#37580,#37578,#4667,.T.) ;
#45958 = EDGE_CURVE('',#37579,#37581,#30482,.T.) ;
#45959 = EDGE_CURVE('',#37581,#37582,#4668,.T.) ;
#45960 = EDGE_CURVE('',#37582,#37580,#30483,.T.) ;
#45961 = EDGE_CURVE('',#37581,#37583,#4669,.T.) ;
#45962 = EDGE_CURVE('',#37583,#37584,#4670,.T.) ;
#45963 = EDGE_CURVE('',#37584,#37582,#4671,.T.) ;
#45964 = EDGE_CURVE('',#37583,#37585,#30484,.T.) ;
#45965 = EDGE_CURVE('',#37585,#37586,#4672,.T.) ;
#45966 = EDGE_CURVE('',#37586,#37584,#30485,.T.) ;
#45967 = EDGE_CURVE('',#37585,#37587,#4673,.T.) ;
#45968 = EDGE_CURVE('',#37587,#37588,#4674,.T.) ;
#45969 = EDGE_CURVE('',#37588,#37586,#4675,.T.) ;
#45970 = EDGE_CURVE('',#37587,#37589,#30486,.T.) ;
#45971 = EDGE_CURVE('',#37589,#37590,#4676,.T.) ;
#45972 = EDGE_CURVE('',#37590,#37588,#30487,.T.) ;
#45973 = EDGE_CURVE('',#37589,#37591,#30488,.T.) ;
#45974 = EDGE_CURVE('',#37591,#37592,#4677,.T.) ;
#45975 = EDGE_CURVE('',#37592,#37590,#30489,.T.) ;
#45976 = EDGE_CURVE('',#37591,#37593,#30490,.T.) ;
#45977 = EDGE_CURVE('',#37593,#37594,#4678,.T.) ;
#45978 = EDGE_CURVE('',#37594,#37592,#30491,.T.) ;
#45979 = EDGE_CURVE('',#37593,#37595,#4679,.T.) ;
#45980 = EDGE_CURVE('',#37595,#37596,#4680,.T.) ;
#45981 = EDGE_CURVE('',#37596,#37594,#4681,.T.) ;
#45982 = EDGE_CURVE('',#37595,#37597,#30492,.T.) ;
#45983 = EDGE_CURVE('',#37597,#37598,#4682,.T.) ;
#45984 = EDGE_CURVE('',#37598,#37596,#30493,.T.) ;
#45985 = EDGE_CURVE('',#37597,#37599,#4683,.T.) ;
#45986 = EDGE_CURVE('',#37599,#37600,#4684,.T.) ;
#45987 = EDGE_CURVE('',#37600,#37598,#4685,.T.) ;
#45988 = EDGE_CURVE('',#37599,#37601,#30494,.T.) ;
#45989 = EDGE_CURVE('',#37601,#37602,#4686,.T.) ;
#45990 = EDGE_CURVE('',#37602,#37600,#30495,.T.) ;
#45991 = EDGE_CURVE('',#37601,#37553,#4687,.T.) ;
#45992 = EDGE_CURVE('',#37554,#37602,#4688,.T.) ;
#45993 = EDGE_CURVE('',#37603,#37604,#30496,.T.) ;
#45994 = EDGE_CURVE('',#37604,#37605,#4689,.T.) ;
#45995 = EDGE_CURVE('',#37605,#37606,#30497,.T.) ;
#45996 = EDGE_CURVE('',#37606,#37607,#4690,.T.) ;
#45997 = EDGE_CURVE('',#37607,#37608,#4691,.T.) ;
#45998 = EDGE_CURVE('',#37608,#37609,#4692,.T.) ;
#45999 = EDGE_CURVE('',#37609,#37610,#30498,.T.) ;
#46000 = EDGE_CURVE('',#37610,#37611,#4693,.T.) ;
#46001 = EDGE_CURVE('',#37611,#37612,#4694,.T.) ;
#46002 = EDGE_CURVE('',#37612,#37613,#4695,.T.) ;
#46003 = EDGE_CURVE('',#37613,#37614,#30499,.T.) ;
#46004 = EDGE_CURVE('',#37614,#37615,#4696,.T.) ;
#46005 = EDGE_CURVE('',#37615,#37616,#30500,.T.) ;
#46006 = EDGE_CURVE('',#37616,#37617,#4697,.T.) ;
#46007 = EDGE_CURVE('',#37617,#37618,#4698,.T.) ;
#46008 = EDGE_CURVE('',#37618,#36227,#4699,.T.) ;
#46009 = EDGE_CURVE('',#36227,#37619,#4700,.T.) ;
#46010 = EDGE_CURVE('',#37619,#37603,#4701,.T.) ;
#46011 = EDGE_CURVE('',#37620,#37621,#4702,.T.) ;
#46012 = EDGE_CURVE('',#37620,#37622,#30501,.T.) ;
#46013 = EDGE_CURVE('',#37622,#37623,#4703,.T.) ;
#46014 = EDGE_CURVE('',#37623,#37621,#30502,.T.) ;
#46015 = EDGE_CURVE('',#37622,#37624,#4704,.T.) ;
#46016 = EDGE_CURVE('',#37624,#37625,#4705,.T.) ;
#46017 = EDGE_CURVE('',#37625,#37623,#4706,.T.) ;
#46018 = EDGE_CURVE('',#37624,#37626,#30503,.T.) ;
#46019 = EDGE_CURVE('',#37626,#37627,#4707,.T.) ;
#46020 = EDGE_CURVE('',#37627,#37625,#30504,.T.) ;
#46021 = EDGE_CURVE('',#37626,#37628,#4708,.T.) ;
#46022 = EDGE_CURVE('',#37628,#37629,#4709,.T.) ;
#46023 = EDGE_CURVE('',#37629,#37627,#4710,.T.) ;
#46024 = EDGE_CURVE('',#37628,#37630,#30505,.T.) ;
#46025 = EDGE_CURVE('',#37630,#37631,#4711,.T.) ;
#46026 = EDGE_CURVE('',#37631,#37629,#30506,.T.) ;
#46027 = EDGE_CURVE('',#37630,#36240,#4712,.T.) ;
#46028 = EDGE_CURVE('',#36240,#37632,#4713,.T.) ;
#46029 = EDGE_CURVE('',#37632,#37631,#4714,.T.) ;
#46030 = EDGE_CURVE('',#36241,#37633,#4715,.T.) ;
#46031 = EDGE_CURVE('',#37633,#37632,#30507,.T.) ;
#46032 = EDGE_CURVE('',#36241,#36371,#4716,.T.) ;
#46033 = EDGE_CURVE('',#36335,#37633,#4717,.T.) ;
#46034 = EDGE_CURVE('',#36372,#37634,#4718,.T.) ;
#46035 = EDGE_CURVE('',#37634,#37635,#4719,.T.) ;
#46036 = EDGE_CURVE('',#37635,#36336,#4720,.T.) ;
#46037 = EDGE_CURVE('',#37634,#37636,#30508,.T.) ;
#46038 = EDGE_CURVE('',#37636,#37637,#4721,.T.) ;
#46039 = EDGE_CURVE('',#37637,#37635,#30509,.T.) ;
#46040 = EDGE_CURVE('',#37636,#37638,#4722,.T.) ;
#46041 = EDGE_CURVE('',#37638,#37639,#4723,.T.) ;
#46042 = EDGE_CURVE('',#37639,#37637,#4724,.T.) ;
#46043 = EDGE_CURVE('',#37638,#37640,#30510,.T.) ;
#46044 = EDGE_CURVE('',#37640,#37641,#4725,.T.) ;
#46045 = EDGE_CURVE('',#37641,#37639,#30511,.T.) ;
#46046 = EDGE_CURVE('',#37640,#37642,#4726,.T.) ;
#46047 = EDGE_CURVE('',#37642,#37643,#4727,.T.) ;
#46048 = EDGE_CURVE('',#37643,#37641,#4728,.T.) ;
#46049 = EDGE_CURVE('',#37642,#37644,#30512,.T.) ;
#46050 = EDGE_CURVE('',#37644,#37645,#4729,.T.) ;
#46051 = EDGE_CURVE('',#37645,#37643,#30513,.T.) ;
#46052 = EDGE_CURVE('',#37644,#37646,#4730,.T.) ;
#46053 = EDGE_CURVE('',#37646,#37647,#4731,.T.) ;
#46054 = EDGE_CURVE('',#37647,#37645,#4732,.T.) ;
#46055 = EDGE_CURVE('',#37646,#37648,#30514,.T.) ;
#46056 = EDGE_CURVE('',#37648,#37649,#4733,.T.) ;
#46057 = EDGE_CURVE('',#37649,#37647,#30515,.T.) ;
#46058 = EDGE_CURVE('',#37648,#37650,#4734,.T.) ;
#46059 = EDGE_CURVE('',#37650,#37651,#4735,.T.) ;
#46060 = EDGE_CURVE('',#37651,#37649,#4736,.T.) ;
#46061 = EDGE_CURVE('',#37650,#37652,#30516,.T.) ;
#46062 = EDGE_CURVE('',#37652,#37653,#4737,.T.) ;
#46063 = EDGE_CURVE('',#37653,#37651,#30517,.T.) ;
#46064 = EDGE_CURVE('',#37652,#37654,#4738,.T.) ;
#46065 = EDGE_CURVE('',#37654,#37655,#4739,.T.) ;
#46066 = EDGE_CURVE('',#37655,#37653,#4740,.T.) ;
#46067 = EDGE_CURVE('',#37654,#37656,#30518,.T.) ;
#46068 = EDGE_CURVE('',#37656,#37657,#4741,.T.) ;
#46069 = EDGE_CURVE('',#37657,#37655,#30519,.T.) ;
#46070 = EDGE_CURVE('',#37656,#37658,#30520,.T.) ;
#46071 = EDGE_CURVE('',#37658,#37659,#4742,.T.) ;
#46072 = EDGE_CURVE('',#37659,#37657,#30521,.T.) ;
#46073 = EDGE_CURVE('',#37658,#37660,#30522,.T.) ;
#46074 = EDGE_CURVE('',#37660,#37661,#4743,.T.) ;
#46075 = EDGE_CURVE('',#37661,#37659,#30523,.T.) ;
#46076 = EDGE_CURVE('',#37660,#37662,#4744,.T.) ;
#46077 = EDGE_CURVE('',#37662,#37663,#4745,.T.) ;
#46078 = EDGE_CURVE('',#37663,#37661,#4746,.T.) ;
#46079 = EDGE_CURVE('',#37662,#37664,#30524,.T.) ;
#46080 = EDGE_CURVE('',#37664,#37665,#4747,.T.) ;
#46081 = EDGE_CURVE('',#37665,#37663,#30525,.T.) ;
#46082 = EDGE_CURVE('',#37664,#37666,#4748,.T.) ;
#46083 = EDGE_CURVE('',#37666,#37667,#4749,.T.) ;
#46084 = EDGE_CURVE('',#37667,#37665,#4750,.T.) ;
#46085 = EDGE_CURVE('',#37666,#37668,#30526,.T.) ;
#46086 = EDGE_CURVE('',#37668,#37669,#4751,.T.) ;
#46087 = EDGE_CURVE('',#37669,#37667,#30527,.T.) ;
#46088 = EDGE_CURVE('',#37668,#37620,#4752,.T.) ;
#46089 = EDGE_CURVE('',#37621,#37669,#4753,.T.) ;
#46090 = EDGE_CURVE('',#37670,#37671,#30528,.T.) ;
#46091 = EDGE_CURVE('',#37671,#37672,#4754,.T.) ;
#46092 = EDGE_CURVE('',#37672,#37673,#30529,.T.) ;
#46093 = EDGE_CURVE('',#37673,#37674,#4755,.T.) ;
#46094 = EDGE_CURVE('',#37674,#37675,#4756,.T.) ;
#46095 = EDGE_CURVE('',#37675,#37676,#4757,.T.) ;
#46096 = EDGE_CURVE('',#37676,#37677,#30530,.T.) ;
#46097 = EDGE_CURVE('',#37677,#37678,#4758,.T.) ;
#46098 = EDGE_CURVE('',#37678,#37679,#4759,.T.) ;
#46099 = EDGE_CURVE('',#37679,#37680,#4760,.T.) ;
#46100 = EDGE_CURVE('',#37680,#37681,#30531,.T.) ;
#46101 = EDGE_CURVE('',#37681,#37682,#4761,.T.) ;
#46102 = EDGE_CURVE('',#37682,#37683,#30532,.T.) ;
#46103 = EDGE_CURVE('',#37683,#37684,#4762,.T.) ;
#46104 = EDGE_CURVE('',#37684,#37685,#4763,.T.) ;
#46105 = EDGE_CURVE('',#37685,#36242,#4764,.T.) ;
#46106 = EDGE_CURVE('',#36242,#37686,#4765,.T.) ;
#46107 = EDGE_CURVE('',#37686,#37670,#4766,.T.) ;
#46108 = EDGE_CURVE('',#37687,#37688,#4767,.T.) ;
#46109 = EDGE_CURVE('',#37687,#37689,#30533,.T.) ;
#46110 = EDGE_CURVE('',#37689,#37690,#4768,.T.) ;
#46111 = EDGE_CURVE('',#37690,#37688,#30534,.T.) ;
#46112 = EDGE_CURVE('',#37689,#37691,#4769,.T.) ;
#46113 = EDGE_CURVE('',#37691,#37692,#4770,.T.) ;
#46114 = EDGE_CURVE('',#37692,#37690,#4771,.T.) ;
#46115 = EDGE_CURVE('',#37691,#37693,#30535,.T.) ;
#46116 = EDGE_CURVE('',#37693,#37694,#4772,.T.) ;
#46117 = EDGE_CURVE('',#37694,#37692,#30536,.T.) ;
#46118 = EDGE_CURVE('',#37693,#37695,#4773,.T.) ;
#46119 = EDGE_CURVE('',#37695,#37696,#4774,.T.) ;
#46120 = EDGE_CURVE('',#37696,#37694,#4775,.T.) ;
#46121 = EDGE_CURVE('',#37695,#37697,#30537,.T.) ;
#46122 = EDGE_CURVE('',#37697,#37698,#4776,.T.) ;
#46123 = EDGE_CURVE('',#37698,#37696,#30538,.T.) ;
#46124 = EDGE_CURVE('',#37697,#36255,#4777,.T.) ;
#46125 = EDGE_CURVE('',#36255,#37699,#4778,.T.) ;
#46126 = EDGE_CURVE('',#37699,#37698,#4779,.T.) ;
#46127 = EDGE_CURVE('',#36256,#37700,#4780,.T.) ;
#46128 = EDGE_CURVE('',#37700,#37699,#30539,.T.) ;
#46129 = EDGE_CURVE('',#36256,#36369,#4781,.T.) ;
#46130 = EDGE_CURVE('',#36331,#37700,#4782,.T.) ;
#46131 = EDGE_CURVE('',#36370,#37701,#4783,.T.) ;
#46132 = EDGE_CURVE('',#37701,#37702,#4784,.T.) ;
#46133 = EDGE_CURVE('',#37702,#36332,#4785,.T.) ;
#46134 = EDGE_CURVE('',#37701,#37703,#30540,.T.) ;
#46135 = EDGE_CURVE('',#37703,#37704,#4786,.T.) ;
#46136 = EDGE_CURVE('',#37704,#37702,#30541,.T.) ;
#46137 = EDGE_CURVE('',#37703,#37705,#4787,.T.) ;
#46138 = EDGE_CURVE('',#37705,#37706,#4788,.T.) ;
#46139 = EDGE_CURVE('',#37706,#37704,#4789,.T.) ;
#46140 = EDGE_CURVE('',#37705,#37707,#30542,.T.) ;
#46141 = EDGE_CURVE('',#37707,#37708,#4790,.T.) ;
#46142 = EDGE_CURVE('',#37708,#37706,#30543,.T.) ;
#46143 = EDGE_CURVE('',#37707,#37709,#4791,.T.) ;
#46144 = EDGE_CURVE('',#37709,#37710,#4792,.T.) ;
#46145 = EDGE_CURVE('',#37710,#37708,#4793,.T.) ;
#46146 = EDGE_CURVE('',#37709,#37711,#30544,.T.) ;
#46147 = EDGE_CURVE('',#37711,#37712,#4794,.T.) ;
#46148 = EDGE_CURVE('',#37712,#37710,#30545,.T.) ;
#46149 = EDGE_CURVE('',#37711,#37713,#4795,.T.) ;
#46150 = EDGE_CURVE('',#37713,#37714,#4796,.T.) ;
#46151 = EDGE_CURVE('',#37714,#37712,#4797,.T.) ;
#46152 = EDGE_CURVE('',#37713,#37715,#30546,.T.) ;
#46153 = EDGE_CURVE('',#37715,#37716,#4798,.T.) ;
#46154 = EDGE_CURVE('',#37716,#37714,#30547,.T.) ;
#46155 = EDGE_CURVE('',#37715,#37717,#4799,.T.) ;
#46156 = EDGE_CURVE('',#37717,#37718,#4800,.T.) ;
#46157 = EDGE_CURVE('',#37718,#37716,#4801,.T.) ;
#46158 = EDGE_CURVE('',#37717,#37719,#30548,.T.) ;
#46159 = EDGE_CURVE('',#37719,#37720,#4802,.T.) ;
#46160 = EDGE_CURVE('',#37720,#37718,#30549,.T.) ;
#46161 = EDGE_CURVE('',#37719,#37721,#4803,.T.) ;
#46162 = EDGE_CURVE('',#37721,#37722,#4804,.T.) ;
#46163 = EDGE_CURVE('',#37722,#37720,#4805,.T.) ;
#46164 = EDGE_CURVE('',#37721,#37723,#30550,.T.) ;
#46165 = EDGE_CURVE('',#37723,#37724,#4806,.T.) ;
#46166 = EDGE_CURVE('',#37724,#37722,#30551,.T.) ;
#46167 = EDGE_CURVE('',#37723,#37725,#30552,.T.) ;
#46168 = EDGE_CURVE('',#37725,#37726,#4807,.T.) ;
#46169 = EDGE_CURVE('',#37726,#37724,#30553,.T.) ;
#46170 = EDGE_CURVE('',#37725,#37727,#30554,.T.) ;
#46171 = EDGE_CURVE('',#37727,#37728,#4808,.T.) ;
#46172 = EDGE_CURVE('',#37728,#37726,#30555,.T.) ;
#46173 = EDGE_CURVE('',#37727,#37729,#4809,.T.) ;
#46174 = EDGE_CURVE('',#37729,#37730,#4810,.T.) ;
#46175 = EDGE_CURVE('',#37730,#37728,#4811,.T.) ;
#46176 = EDGE_CURVE('',#37729,#37731,#30556,.T.) ;
#46177 = EDGE_CURVE('',#37731,#37732,#4812,.T.) ;
#46178 = EDGE_CURVE('',#37732,#37730,#30557,.T.) ;
#46179 = EDGE_CURVE('',#37731,#37733,#4813,.T.) ;
#46180 = EDGE_CURVE('',#37733,#37734,#4814,.T.) ;
#46181 = EDGE_CURVE('',#37734,#37732,#4815,.T.) ;
#46182 = EDGE_CURVE('',#37733,#37735,#30558,.T.) ;
#46183 = EDGE_CURVE('',#37735,#37736,#4816,.T.) ;
#46184 = EDGE_CURVE('',#37736,#37734,#30559,.T.) ;
#46185 = EDGE_CURVE('',#37735,#37687,#4817,.T.) ;
#46186 = EDGE_CURVE('',#37688,#37736,#4818,.T.) ;
#46187 = EDGE_CURVE('',#37737,#37738,#30560,.T.) ;
#46188 = EDGE_CURVE('',#37738,#37739,#4819,.T.) ;
#46189 = EDGE_CURVE('',#37739,#37740,#30561,.T.) ;
#46190 = EDGE_CURVE('',#37740,#37741,#4820,.T.) ;
#46191 = EDGE_CURVE('',#37741,#37742,#4821,.T.) ;
#46192 = EDGE_CURVE('',#37742,#37743,#4822,.T.) ;
#46193 = EDGE_CURVE('',#37743,#37744,#30562,.T.) ;
#46194 = EDGE_CURVE('',#37744,#37745,#4823,.T.) ;
#46195 = EDGE_CURVE('',#37745,#37746,#4824,.T.) ;
#46196 = EDGE_CURVE('',#37746,#37747,#4825,.T.) ;
#46197 = EDGE_CURVE('',#37747,#37748,#30563,.T.) ;
#46198 = EDGE_CURVE('',#37748,#37749,#4826,.T.) ;
#46199 = EDGE_CURVE('',#37749,#37750,#30564,.T.) ;
#46200 = EDGE_CURVE('',#37750,#37751,#4827,.T.) ;
#46201 = EDGE_CURVE('',#37751,#37752,#4828,.T.) ;
#46202 = EDGE_CURVE('',#37752,#36257,#4829,.T.) ;
#46203 = EDGE_CURVE('',#36257,#37753,#4830,.T.) ;
#46204 = EDGE_CURVE('',#37753,#37737,#4831,.T.) ;
#46205 = EDGE_CURVE('',#37754,#37755,#4832,.T.) ;
#46206 = EDGE_CURVE('',#37754,#37756,#30565,.T.) ;
#46207 = EDGE_CURVE('',#37756,#37757,#4833,.T.) ;
#46208 = EDGE_CURVE('',#37757,#37755,#30566,.T.) ;
#46209 = EDGE_CURVE('',#37756,#37758,#4834,.T.) ;
#46210 = EDGE_CURVE('',#37758,#37759,#4835,.T.) ;
#46211 = EDGE_CURVE('',#37759,#37757,#4836,.T.) ;
#46212 = EDGE_CURVE('',#37758,#37760,#30567,.T.) ;
#46213 = EDGE_CURVE('',#37760,#37761,#4837,.T.) ;
#46214 = EDGE_CURVE('',#37761,#37759,#30568,.T.) ;
#46215 = EDGE_CURVE('',#37760,#37762,#4838,.T.) ;
#46216 = EDGE_CURVE('',#37762,#37763,#4839,.T.) ;
#46217 = EDGE_CURVE('',#37763,#37761,#4840,.T.) ;
#46218 = EDGE_CURVE('',#37762,#37764,#30569,.T.) ;
#46219 = EDGE_CURVE('',#37764,#37765,#4841,.T.) ;
#46220 = EDGE_CURVE('',#37765,#37763,#30570,.T.) ;
#46221 = EDGE_CURVE('',#37764,#36270,#4842,.T.) ;
#46222 = EDGE_CURVE('',#36270,#37766,#4843,.T.) ;
#46223 = EDGE_CURVE('',#37766,#37765,#4844,.T.) ;
#46224 = EDGE_CURVE('',#36271,#37767,#4845,.T.) ;
#46225 = EDGE_CURVE('',#37767,#37766,#30571,.T.) ;
#46226 = EDGE_CURVE('',#36271,#36367,#4846,.T.) ;
#46227 = EDGE_CURVE('',#36327,#37767,#4847,.T.) ;
#46228 = EDGE_CURVE('',#36368,#37768,#4848,.T.) ;
#46229 = EDGE_CURVE('',#37768,#37769,#4849,.T.) ;
#46230 = EDGE_CURVE('',#37769,#36328,#4850,.T.) ;
#46231 = EDGE_CURVE('',#37768,#37770,#30572,.T.) ;
#46232 = EDGE_CURVE('',#37770,#37771,#4851,.T.) ;
#46233 = EDGE_CURVE('',#37771,#37769,#30573,.T.) ;
#46234 = EDGE_CURVE('',#37770,#37772,#4852,.T.) ;
#46235 = EDGE_CURVE('',#37772,#37773,#4853,.T.) ;
#46236 = EDGE_CURVE('',#37773,#37771,#4854,.T.) ;
#46237 = EDGE_CURVE('',#37772,#37774,#30574,.T.) ;
#46238 = EDGE_CURVE('',#37774,#37775,#4855,.T.) ;
#46239 = EDGE_CURVE('',#37775,#37773,#30575,.T.) ;
#46240 = EDGE_CURVE('',#37774,#37776,#4856,.T.) ;
#46241 = EDGE_CURVE('',#37776,#37777,#4857,.T.) ;
#46242 = EDGE_CURVE('',#37777,#37775,#4858,.T.) ;
#46243 = EDGE_CURVE('',#37776,#37778,#30576,.T.) ;
#46244 = EDGE_CURVE('',#37778,#37779,#4859,.T.) ;
#46245 = EDGE_CURVE('',#37779,#37777,#30577,.T.) ;
#46246 = EDGE_CURVE('',#37778,#37780,#4860,.T.) ;
#46247 = EDGE_CURVE('',#37780,#37781,#4861,.T.) ;
#46248 = EDGE_CURVE('',#37781,#37779,#4862,.T.) ;
#46249 = EDGE_CURVE('',#37780,#37782,#30578,.T.) ;
#46250 = EDGE_CURVE('',#37782,#37783,#4863,.T.) ;
#46251 = EDGE_CURVE('',#37783,#37781,#30579,.T.) ;
#46252 = EDGE_CURVE('',#37782,#37784,#4864,.T.) ;
#46253 = EDGE_CURVE('',#37784,#37785,#4865,.T.) ;
#46254 = EDGE_CURVE('',#37785,#37783,#4866,.T.) ;
#46255 = EDGE_CURVE('',#37784,#37786,#30580,.T.) ;
#46256 = EDGE_CURVE('',#37786,#37787,#4867,.T.) ;
#46257 = EDGE_CURVE('',#37787,#37785,#30581,.T.) ;
#46258 = EDGE_CURVE('',#37786,#37788,#4868,.T.) ;
#46259 = EDGE_CURVE('',#37788,#37789,#4869,.T.) ;
#46260 = EDGE_CURVE('',#37789,#37787,#4870,.T.) ;
#46261 = EDGE_CURVE('',#37788,#37790,#30582,.T.) ;
#46262 = EDGE_CURVE('',#37790,#37791,#4871,.T.) ;
#46263 = EDGE_CURVE('',#37791,#37789,#30583,.T.) ;
#46264 = EDGE_CURVE('',#37790,#37792,#30584,.T.) ;
#46265 = EDGE_CURVE('',#37792,#37793,#4872,.T.) ;
#46266 = EDGE_CURVE('',#37793,#37791,#30585,.T.) ;
#46267 = EDGE_CURVE('',#37792,#37794,#30586,.T.) ;
#46268 = EDGE_CURVE('',#37794,#37795,#4873,.T.) ;
#46269 = EDGE_CURVE('',#37795,#37793,#30587,.T.) ;
#46270 = EDGE_CURVE('',#37794,#37796,#4874,.T.) ;
#46271 = EDGE_CURVE('',#37796,#37797,#4875,.T.) ;
#46272 = EDGE_CURVE('',#37797,#37795,#4876,.T.) ;
#46273 = EDGE_CURVE('',#37796,#37798,#30588,.T.) ;
#46274 = EDGE_CURVE('',#37798,#37799,#4877,.T.) ;
#46275 = EDGE_CURVE('',#37799,#37797,#30589,.T.) ;
#46276 = EDGE_CURVE('',#37798,#37800,#4878,.T.) ;
#46277 = EDGE_CURVE('',#37800,#37801,#4879,.T.) ;
#46278 = EDGE_CURVE('',#37801,#37799,#4880,.T.) ;
#46279 = EDGE_CURVE('',#37800,#37802,#30590,.T.) ;
#46280 = EDGE_CURVE('',#37802,#37803,#4881,.T.) ;
#46281 = EDGE_CURVE('',#37803,#37801,#30591,.T.) ;
#46282 = EDGE_CURVE('',#37802,#37754,#4882,.T.) ;
#46283 = EDGE_CURVE('',#37755,#37803,#4883,.T.) ;
#46284 = EDGE_CURVE('',#37804,#37805,#30592,.T.) ;
#46285 = EDGE_CURVE('',#37805,#37806,#4884,.T.) ;
#46286 = EDGE_CURVE('',#37806,#37807,#30593,.T.) ;
#46287 = EDGE_CURVE('',#37807,#37808,#4885,.T.) ;
#46288 = EDGE_CURVE('',#37808,#37809,#4886,.T.) ;
#46289 = EDGE_CURVE('',#37809,#37810,#4887,.T.) ;
#46290 = EDGE_CURVE('',#37810,#37811,#30594,.T.) ;
#46291 = EDGE_CURVE('',#37811,#37812,#4888,.T.) ;
#46292 = EDGE_CURVE('',#37812,#37813,#4889,.T.) ;
#46293 = EDGE_CURVE('',#37813,#37814,#4890,.T.) ;
#46294 = EDGE_CURVE('',#37814,#37815,#30595,.T.) ;
#46295 = EDGE_CURVE('',#37815,#37816,#4891,.T.) ;
#46296 = EDGE_CURVE('',#37816,#37817,#30596,.T.) ;
#46297 = EDGE_CURVE('',#37817,#37818,#4892,.T.) ;
#46298 = EDGE_CURVE('',#37818,#37819,#4893,.T.) ;
#46299 = EDGE_CURVE('',#37819,#36272,#4894,.T.) ;
#46300 = EDGE_CURVE('',#36272,#37820,#4895,.T.) ;
#46301 = EDGE_CURVE('',#37820,#37804,#4896,.T.) ;
#46302 = EDGE_CURVE('',#37821,#37822,#4897,.T.) ;
#46303 = EDGE_CURVE('',#37821,#37823,#30597,.T.) ;
#46304 = EDGE_CURVE('',#37823,#37824,#4898,.T.) ;
#46305 = EDGE_CURVE('',#37824,#37822,#30598,.T.) ;
#46306 = EDGE_CURVE('',#37823,#37825,#4899,.T.) ;
#46307 = EDGE_CURVE('',#37825,#37826,#4900,.T.) ;
#46308 = EDGE_CURVE('',#37826,#37824,#4901,.T.) ;
#46309 = EDGE_CURVE('',#37825,#37827,#30599,.T.) ;
#46310 = EDGE_CURVE('',#37827,#37828,#4902,.T.) ;
#46311 = EDGE_CURVE('',#37828,#37826,#30600,.T.) ;
#46312 = EDGE_CURVE('',#37827,#37829,#4903,.T.) ;
#46313 = EDGE_CURVE('',#37829,#37830,#4904,.T.) ;
#46314 = EDGE_CURVE('',#37830,#37828,#4905,.T.) ;
#46315 = EDGE_CURVE('',#37829,#37831,#30601,.T.) ;
#46316 = EDGE_CURVE('',#37831,#37832,#4906,.T.) ;
#46317 = EDGE_CURVE('',#37832,#37830,#30602,.T.) ;
#46318 = EDGE_CURVE('',#37831,#36285,#4907,.T.) ;
#46319 = EDGE_CURVE('',#36285,#37833,#4908,.T.) ;
#46320 = EDGE_CURVE('',#37833,#37832,#4909,.T.) ;
#46321 = EDGE_CURVE('',#36286,#37834,#4910,.T.) ;
#46322 = EDGE_CURVE('',#37834,#37833,#30603,.T.) ;
#46323 = EDGE_CURVE('',#36286,#36365,#4911,.T.) ;
#46324 = EDGE_CURVE('',#36323,#37834,#4912,.T.) ;
#46325 = EDGE_CURVE('',#36366,#37835,#4913,.T.) ;
#46326 = EDGE_CURVE('',#37835,#37836,#4914,.T.) ;
#46327 = EDGE_CURVE('',#37836,#36324,#4915,.T.) ;
#46328 = EDGE_CURVE('',#37835,#37837,#30604,.T.) ;
#46329 = EDGE_CURVE('',#37837,#37838,#4916,.T.) ;
#46330 = EDGE_CURVE('',#37838,#37836,#30605,.T.) ;
#46331 = EDGE_CURVE('',#37837,#37839,#4917,.T.) ;
#46332 = EDGE_CURVE('',#37839,#37840,#4918,.T.) ;
#46333 = EDGE_CURVE('',#37840,#37838,#4919,.T.) ;
#46334 = EDGE_CURVE('',#37839,#37841,#30606,.T.) ;
#46335 = EDGE_CURVE('',#37841,#37842,#4920,.T.) ;
#46336 = EDGE_CURVE('',#37842,#37840,#30607,.T.) ;
#46337 = EDGE_CURVE('',#37841,#37843,#4921,.T.) ;
#46338 = EDGE_CURVE('',#37843,#37844,#4922,.T.) ;
#46339 = EDGE_CURVE('',#37844,#37842,#4923,.T.) ;
#46340 = EDGE_CURVE('',#37843,#37845,#30608,.T.) ;
#46341 = EDGE_CURVE('',#37845,#37846,#4924,.T.) ;
#46342 = EDGE_CURVE('',#37846,#37844,#30609,.T.) ;
#46343 = EDGE_CURVE('',#37845,#37847,#4925,.T.) ;
#46344 = EDGE_CURVE('',#37847,#37848,#4926,.T.) ;
#46345 = EDGE_CURVE('',#37848,#37846,#4927,.T.) ;
#46346 = EDGE_CURVE('',#37847,#37849,#30610,.T.) ;
#46347 = EDGE_CURVE('',#37849,#37850,#4928,.T.) ;
#46348 = EDGE_CURVE('',#37850,#37848,#30611,.T.) ;
#46349 = EDGE_CURVE('',#37849,#37851,#4929,.T.) ;
#46350 = EDGE_CURVE('',#37851,#37852,#4930,.T.) ;
#46351 = EDGE_CURVE('',#37852,#37850,#4931,.T.) ;
#46352 = EDGE_CURVE('',#37851,#37853,#30612,.T.) ;
#46353 = EDGE_CURVE('',#37853,#37854,#4932,.T.) ;
#46354 = EDGE_CURVE('',#37854,#37852,#30613,.T.) ;
#46355 = EDGE_CURVE('',#37853,#37855,#4933,.T.) ;
#46356 = EDGE_CURVE('',#37855,#37856,#4934,.T.) ;
#46357 = EDGE_CURVE('',#37856,#37854,#4935,.T.) ;
#46358 = EDGE_CURVE('',#37855,#37857,#30614,.T.) ;
#46359 = EDGE_CURVE('',#37857,#37858,#4936,.T.) ;
#46360 = EDGE_CURVE('',#37858,#37856,#30615,.T.) ;
#46361 = EDGE_CURVE('',#37857,#37859,#30616,.T.) ;
#46362 = EDGE_CURVE('',#37859,#37860,#4937,.T.) ;
#46363 = EDGE_CURVE('',#37860,#37858,#30617,.T.) ;
#46364 = EDGE_CURVE('',#37859,#37861,#30618,.T.) ;
#46365 = EDGE_CURVE('',#37861,#37862,#4938,.T.) ;
#46366 = EDGE_CURVE('',#37862,#37860,#30619,.T.) ;
#46367 = EDGE_CURVE('',#37861,#37863,#4939,.T.) ;
#46368 = EDGE_CURVE('',#37863,#37864,#4940,.T.) ;
#46369 = EDGE_CURVE('',#37864,#37862,#4941,.T.) ;
#46370 = EDGE_CURVE('',#37863,#37865,#30620,.T.) ;
#46371 = EDGE_CURVE('',#37865,#37866,#4942,.T.) ;
#46372 = EDGE_CURVE('',#37866,#37864,#30621,.T.) ;
#46373 = EDGE_CURVE('',#37865,#37867,#4943,.T.) ;
#46374 = EDGE_CURVE('',#37867,#37868,#4944,.T.) ;
#46375 = EDGE_CURVE('',#37868,#37866,#4945,.T.) ;
#46376 = EDGE_CURVE('',#37867,#37869,#30622,.T.) ;
#46377 = EDGE_CURVE('',#37869,#37870,#4946,.T.) ;
#46378 = EDGE_CURVE('',#37870,#37868,#30623,.T.) ;
#46379 = EDGE_CURVE('',#37869,#37821,#4947,.T.) ;
#46380 = EDGE_CURVE('',#37822,#37870,#4948,.T.) ;
#46381 = EDGE_CURVE('',#37871,#37872,#30624,.T.) ;
#46382 = EDGE_CURVE('',#37872,#37873,#4949,.T.) ;
#46383 = EDGE_CURVE('',#37873,#37874,#30625,.T.) ;
#46384 = EDGE_CURVE('',#37874,#37875,#4950,.T.) ;
#46385 = EDGE_CURVE('',#37875,#37876,#4951,.T.) ;
#46386 = EDGE_CURVE('',#37876,#37877,#4952,.T.) ;
#46387 = EDGE_CURVE('',#37877,#37878,#30626,.T.) ;
#46388 = EDGE_CURVE('',#37878,#37879,#4953,.T.) ;
#46389 = EDGE_CURVE('',#37879,#37880,#4954,.T.) ;
#46390 = EDGE_CURVE('',#37880,#37881,#4955,.T.) ;
#46391 = EDGE_CURVE('',#37881,#37882,#30627,.T.) ;
#46392 = EDGE_CURVE('',#37882,#37883,#4956,.T.) ;
#46393 = EDGE_CURVE('',#37883,#37884,#30628,.T.) ;
#46394 = EDGE_CURVE('',#37884,#37885,#4957,.T.) ;
#46395 = EDGE_CURVE('',#37885,#37886,#4958,.T.) ;
#46396 = EDGE_CURVE('',#37886,#36287,#4959,.T.) ;
#46397 = EDGE_CURVE('',#36287,#37887,#4960,.T.) ;
#46398 = EDGE_CURVE('',#37887,#37871,#4961,.T.) ;
#46399 = EDGE_CURVE('',#37888,#37889,#4962,.T.) ;
#46400 = EDGE_CURVE('',#37888,#37890,#30629,.T.) ;
#46401 = EDGE_CURVE('',#37890,#37891,#4963,.T.) ;
#46402 = EDGE_CURVE('',#37891,#37889,#30630,.T.) ;
#46403 = EDGE_CURVE('',#37890,#37892,#4964,.T.) ;
#46404 = EDGE_CURVE('',#37892,#37893,#4965,.T.) ;
#46405 = EDGE_CURVE('',#37893,#37891,#4966,.T.) ;
#46406 = EDGE_CURVE('',#37892,#37894,#30631,.T.) ;
#46407 = EDGE_CURVE('',#37894,#37895,#4967,.T.) ;
#46408 = EDGE_CURVE('',#37895,#37893,#30632,.T.) ;
#46409 = EDGE_CURVE('',#37894,#37896,#4968,.T.) ;
#46410 = EDGE_CURVE('',#37896,#37897,#4969,.T.) ;
#46411 = EDGE_CURVE('',#37897,#37895,#4970,.T.) ;
#46412 = EDGE_CURVE('',#37896,#37898,#30633,.T.) ;
#46413 = EDGE_CURVE('',#37898,#37899,#4971,.T.) ;
#46414 = EDGE_CURVE('',#37899,#37897,#30634,.T.) ;
#46415 = EDGE_CURVE('',#37898,#36300,#4972,.T.) ;
#46416 = EDGE_CURVE('',#36300,#37900,#4973,.T.) ;
#46417 = EDGE_CURVE('',#37900,#37899,#4974,.T.) ;
#46418 = EDGE_CURVE('',#36301,#37901,#4975,.T.) ;
#46419 = EDGE_CURVE('',#37901,#37900,#30635,.T.) ;
#46420 = EDGE_CURVE('',#36301,#36363,#4976,.T.) ;
#46421 = EDGE_CURVE('',#36319,#37901,#4977,.T.) ;
#46422 = EDGE_CURVE('',#36364,#37902,#4978,.T.) ;
#46423 = EDGE_CURVE('',#37902,#37903,#4979,.T.) ;
#46424 = EDGE_CURVE('',#37903,#36320,#4980,.T.) ;
#46425 = EDGE_CURVE('',#37902,#37904,#30636,.T.) ;
#46426 = EDGE_CURVE('',#37904,#37905,#4981,.T.) ;
#46427 = EDGE_CURVE('',#37905,#37903,#30637,.T.) ;
#46428 = EDGE_CURVE('',#37904,#37906,#4982,.T.) ;
#46429 = EDGE_CURVE('',#37906,#37907,#4983,.T.) ;
#46430 = EDGE_CURVE('',#37907,#37905,#4984,.T.) ;
#46431 = EDGE_CURVE('',#37906,#37908,#30638,.T.) ;
#46432 = EDGE_CURVE('',#37908,#37909,#4985,.T.) ;
#46433 = EDGE_CURVE('',#37909,#37907,#30639,.T.) ;
#46434 = EDGE_CURVE('',#37908,#37910,#4986,.T.) ;
#46435 = EDGE_CURVE('',#37910,#37911,#4987,.T.) ;
#46436 = EDGE_CURVE('',#37911,#37909,#4988,.T.) ;
#46437 = EDGE_CURVE('',#37910,#37912,#30640,.T.) ;
#46438 = EDGE_CURVE('',#37912,#37913,#4989,.T.) ;
#46439 = EDGE_CURVE('',#37913,#37911,#30641,.T.) ;
#46440 = EDGE_CURVE('',#37912,#37914,#4990,.T.) ;
#46441 = EDGE_CURVE('',#37914,#37915,#4991,.T.) ;
#46442 = EDGE_CURVE('',#37915,#37913,#4992,.T.) ;
#46443 = EDGE_CURVE('',#37914,#37916,#30642,.T.) ;
#46444 = EDGE_CURVE('',#37916,#37917,#4993,.T.) ;
#46445 = EDGE_CURVE('',#37917,#37915,#30643,.T.) ;
#46446 = EDGE_CURVE('',#37916,#37918,#4994,.T.) ;
#46447 = EDGE_CURVE('',#37918,#37919,#4995,.T.) ;
#46448 = EDGE_CURVE('',#37919,#37917,#4996,.T.) ;
#46449 = EDGE_CURVE('',#37918,#37920,#30644,.T.) ;
#46450 = EDGE_CURVE('',#37920,#37921,#4997,.T.) ;
#46451 = EDGE_CURVE('',#37921,#37919,#30645,.T.) ;
#46452 = EDGE_CURVE('',#37920,#37922,#4998,.T.) ;
#46453 = EDGE_CURVE('',#37922,#37923,#4999,.T.) ;
#46454 = EDGE_CURVE('',#37923,#37921,#5000,.T.) ;
#46455 = EDGE_CURVE('',#37922,#37924,#30646,.T.) ;
#46456 = EDGE_CURVE('',#37924,#37925,#5001,.T.) ;
#46457 = EDGE_CURVE('',#37925,#37923,#30647,.T.) ;
#46458 = EDGE_CURVE('',#37924,#37926,#30648,.T.) ;
#46459 = EDGE_CURVE('',#37926,#37927,#5002,.T.) ;
#46460 = EDGE_CURVE('',#37927,#37925,#30649,.T.) ;
#46461 = EDGE_CURVE('',#37926,#37928,#30650,.T.) ;
#46462 = EDGE_CURVE('',#37928,#37929,#5003,.T.) ;
#46463 = EDGE_CURVE('',#37929,#37927,#30651,.T.) ;
#46464 = EDGE_CURVE('',#37928,#37930,#5004,.T.) ;
#46465 = EDGE_CURVE('',#37930,#37931,#5005,.T.) ;
#46466 = EDGE_CURVE('',#37931,#37929,#5006,.T.) ;
#46467 = EDGE_CURVE('',#37930,#37932,#30652,.T.) ;
#46468 = EDGE_CURVE('',#37932,#37933,#5007,.T.) ;
#46469 = EDGE_CURVE('',#37933,#37931,#30653,.T.) ;
#46470 = EDGE_CURVE('',#37932,#37934,#5008,.T.) ;
#46471 = EDGE_CURVE('',#37934,#37935,#5009,.T.) ;
#46472 = EDGE_CURVE('',#37935,#37933,#5010,.T.) ;
#46473 = EDGE_CURVE('',#37934,#37936,#30654,.T.) ;
#46474 = EDGE_CURVE('',#37936,#37937,#5011,.T.) ;
#46475 = EDGE_CURVE('',#37937,#37935,#30655,.T.) ;
#46476 = EDGE_CURVE('',#37936,#37888,#5012,.T.) ;
#46477 = EDGE_CURVE('',#37889,#37937,#5013,.T.) ;
#46478 = EDGE_CURVE('',#37938,#37939,#30656,.T.) ;
#46479 = EDGE_CURVE('',#37939,#37940,#5014,.T.) ;
#46480 = EDGE_CURVE('',#37940,#37941,#30657,.T.) ;
#46481 = EDGE_CURVE('',#37941,#37942,#5015,.T.) ;
#46482 = EDGE_CURVE('',#37942,#37943,#5016,.T.) ;
#46483 = EDGE_CURVE('',#37943,#37944,#5017,.T.) ;
#46484 = EDGE_CURVE('',#37944,#37945,#30658,.T.) ;
#46485 = EDGE_CURVE('',#37945,#37946,#5018,.T.) ;
#46486 = EDGE_CURVE('',#37946,#37947,#5019,.T.) ;
#46487 = EDGE_CURVE('',#37947,#37948,#5020,.T.) ;
#46488 = EDGE_CURVE('',#37948,#37949,#30659,.T.) ;
#46489 = EDGE_CURVE('',#37949,#37950,#5021,.T.) ;
#46490 = EDGE_CURVE('',#37950,#37951,#30660,.T.) ;
#46491 = EDGE_CURVE('',#37951,#37952,#5022,.T.) ;
#46492 = EDGE_CURVE('',#37952,#37953,#5023,.T.) ;
#46493 = EDGE_CURVE('',#37953,#36302,#5024,.T.) ;
#46494 = EDGE_CURVE('',#36302,#37954,#5025,.T.) ;
#46495 = EDGE_CURVE('',#37954,#37938,#5026,.T.) ;
#46496 = EDGE_CURVE('',#37955,#37956,#5027,.T.) ;
#46497 = EDGE_CURVE('',#37955,#37957,#30661,.T.) ;
#46498 = EDGE_CURVE('',#37957,#37958,#5028,.T.) ;
#46499 = EDGE_CURVE('',#37958,#37956,#30662,.T.) ;
#46500 = EDGE_CURVE('',#37957,#37959,#5029,.T.) ;
#46501 = EDGE_CURVE('',#37959,#37960,#5030,.T.) ;
#46502 = EDGE_CURVE('',#37960,#37958,#5031,.T.) ;
#46503 = EDGE_CURVE('',#37959,#37961,#30663,.T.) ;
#46504 = EDGE_CURVE('',#37961,#37962,#5032,.T.) ;
#46505 = EDGE_CURVE('',#37962,#37960,#30664,.T.) ;
#46506 = EDGE_CURVE('',#37961,#37963,#5033,.T.) ;
#46507 = EDGE_CURVE('',#37963,#37964,#5034,.T.) ;
#46508 = EDGE_CURVE('',#37964,#37962,#5035,.T.) ;
#46509 = EDGE_CURVE('',#37963,#37965,#30665,.T.) ;
#46510 = EDGE_CURVE('',#37965,#37966,#5036,.T.) ;
#46511 = EDGE_CURVE('',#37966,#37964,#30666,.T.) ;
#46512 = EDGE_CURVE('',#37965,#36351,#5037,.T.) ;
#46513 = EDGE_CURVE('',#36351,#37967,#5038,.T.) ;
#46514 = EDGE_CURVE('',#37967,#37966,#5039,.T.) ;
#46515 = EDGE_CURVE('',#36352,#37968,#5040,.T.) ;
#46516 = EDGE_CURVE('',#37968,#37967,#30667,.T.) ;
#46517 = EDGE_CURVE('',#36352,#36361,#5041,.T.) ;
#46518 = EDGE_CURVE('',#36315,#37968,#5042,.T.) ;
#46519 = EDGE_CURVE('',#36362,#37969,#5043,.T.) ;
#46520 = EDGE_CURVE('',#37969,#37970,#5044,.T.) ;
#46521 = EDGE_CURVE('',#37970,#36316,#5045,.T.) ;
#46522 = EDGE_CURVE('',#37969,#37971,#30668,.T.) ;
#46523 = EDGE_CURVE('',#37971,#37972,#5046,.T.) ;
#46524 = EDGE_CURVE('',#37972,#37970,#30669,.T.) ;
#46525 = EDGE_CURVE('',#37971,#37973,#5047,.T.) ;
#46526 = EDGE_CURVE('',#37973,#37974,#5048,.T.) ;
#46527 = EDGE_CURVE('',#37974,#37972,#5049,.T.) ;
#46528 = EDGE_CURVE('',#37973,#37975,#30670,.T.) ;
#46529 = EDGE_CURVE('',#37975,#37976,#5050,.T.) ;
#46530 = EDGE_CURVE('',#37976,#37974,#30671,.T.) ;
#46531 = EDGE_CURVE('',#37975,#37977,#5051,.T.) ;
#46532 = EDGE_CURVE('',#37977,#37978,#5052,.T.) ;
#46533 = EDGE_CURVE('',#37978,#37976,#5053,.T.) ;
#46534 = EDGE_CURVE('',#37977,#37979,#30672,.T.) ;
#46535 = EDGE_CURVE('',#37979,#37980,#5054,.T.) ;
#46536 = EDGE_CURVE('',#37980,#37978,#30673,.T.) ;
#46537 = EDGE_CURVE('',#37979,#37981,#5055,.T.) ;
#46538 = EDGE_CURVE('',#37981,#37982,#5056,.T.) ;
#46539 = EDGE_CURVE('',#37982,#37980,#5057,.T.) ;
#46540 = EDGE_CURVE('',#37981,#37983,#30674,.T.) ;
#46541 = EDGE_CURVE('',#37983,#37984,#5058,.T.) ;
#46542 = EDGE_CURVE('',#37984,#37982,#30675,.T.) ;
#46543 = EDGE_CURVE('',#37983,#37985,#5059,.T.) ;
#46544 = EDGE_CURVE('',#37985,#37986,#5060,.T.) ;
#46545 = EDGE_CURVE('',#37986,#37984,#5061,.T.) ;
#46546 = EDGE_CURVE('',#37985,#37987,#30676,.T.) ;
#46547 = EDGE_CURVE('',#37987,#37988,#5062,.T.) ;
#46548 = EDGE_CURVE('',#37988,#37986,#30677,.T.) ;
#46549 = EDGE_CURVE('',#37987,#37989,#5063,.T.) ;
#46550 = EDGE_CURVE('',#37989,#37990,#5064,.T.) ;
#46551 = EDGE_CURVE('',#37990,#37988,#5065,.T.) ;
#46552 = EDGE_CURVE('',#37989,#37991,#30678,.T.) ;
#46553 = EDGE_CURVE('',#37991,#37992,#5066,.T.) ;
#46554 = EDGE_CURVE('',#37992,#37990,#30679,.T.) ;
#46555 = EDGE_CURVE('',#37991,#37993,#30680,.T.) ;
#46556 = EDGE_CURVE('',#37993,#37994,#5067,.T.) ;
#46557 = EDGE_CURVE('',#37994,#37992,#30681,.T.) ;
#46558 = EDGE_CURVE('',#37993,#37995,#30682,.T.) ;
#46559 = EDGE_CURVE('',#37995,#37996,#5068,.T.) ;
#46560 = EDGE_CURVE('',#37996,#37994,#30683,.T.) ;
#46561 = EDGE_CURVE('',#37995,#37997,#5069,.T.) ;
#46562 = EDGE_CURVE('',#37997,#37998,#5070,.T.) ;
#46563 = EDGE_CURVE('',#37998,#37996,#5071,.T.) ;
#46564 = EDGE_CURVE('',#37997,#37999,#30684,.T.) ;
#46565 = EDGE_CURVE('',#37999,#38000,#5072,.T.) ;
#46566 = EDGE_CURVE('',#38000,#37998,#30685,.T.) ;
#46567 = EDGE_CURVE('',#37999,#38001,#5073,.T.) ;
#46568 = EDGE_CURVE('',#38001,#38002,#5074,.T.) ;
#46569 = EDGE_CURVE('',#38002,#38000,#5075,.T.) ;
#46570 = EDGE_CURVE('',#38001,#38003,#30686,.T.) ;
#46571 = EDGE_CURVE('',#38003,#38004,#5076,.T.) ;
#46572 = EDGE_CURVE('',#38004,#38002,#30687,.T.) ;
#46573 = EDGE_CURVE('',#38003,#37955,#5077,.T.) ;
#46574 = EDGE_CURVE('',#37956,#38004,#5078,.T.) ;
#46575 = EDGE_CURVE('',#38005,#38006,#30688,.T.) ;
#46576 = EDGE_CURVE('',#38006,#38007,#5079,.T.) ;
#46577 = EDGE_CURVE('',#38007,#38008,#30689,.T.) ;
#46578 = EDGE_CURVE('',#38008,#38009,#5080,.T.) ;
#46579 = EDGE_CURVE('',#38009,#38010,#5081,.T.) ;
#46580 = EDGE_CURVE('',#38010,#38011,#5082,.T.) ;
#46581 = EDGE_CURVE('',#38011,#38012,#30690,.T.) ;
#46582 = EDGE_CURVE('',#38012,#38013,#5083,.T.) ;
#46583 = EDGE_CURVE('',#38013,#38014,#5084,.T.) ;
#46584 = EDGE_CURVE('',#38014,#38015,#5085,.T.) ;
#46585 = EDGE_CURVE('',#38015,#38016,#30691,.T.) ;
#46586 = EDGE_CURVE('',#38016,#38017,#5086,.T.) ;
#46587 = EDGE_CURVE('',#38017,#38018,#30692,.T.) ;
#46588 = EDGE_CURVE('',#38018,#38019,#5087,.T.) ;
#46589 = EDGE_CURVE('',#38019,#38020,#5088,.T.) ;
#46590 = EDGE_CURVE('',#38020,#36353,#5089,.T.) ;
#46591 = EDGE_CURVE('',#36353,#38021,#5090,.T.) ;
#46592 = EDGE_CURVE('',#38021,#38005,#5091,.T.) ;
#46593 = EDGE_CURVE('',#38022,#38023,#5092,.T.) ;
#46594 = EDGE_CURVE('',#38022,#38024,#30693,.T.) ;
#46595 = EDGE_CURVE('',#38024,#38025,#5093,.T.) ;
#46596 = EDGE_CURVE('',#38025,#38026,#30694,.T.) ;
#46597 = EDGE_CURVE('',#38026,#38027,#5094,.T.) ;
#46598 = EDGE_CURVE('',#38027,#38028,#30695,.T.) ;
#46599 = EDGE_CURVE('',#38028,#38029,#5095,.T.) ;
#46600 = EDGE_CURVE('',#38029,#38023,#30696,.T.) ;
#46601 = EDGE_CURVE('',#38030,#38031,#5096,.T.) ;
#46602 = EDGE_CURVE('',#38030,#38032,#30697,.T.) ;
#46603 = EDGE_CURVE('',#38032,#38033,#5097,.T.) ;
#46604 = EDGE_CURVE('',#38033,#38034,#30698,.T.) ;
#46605 = EDGE_CURVE('',#38034,#38035,#5098,.T.) ;
#46606 = EDGE_CURVE('',#38035,#38036,#30699,.T.) ;
#46607 = EDGE_CURVE('',#38036,#38037,#5099,.T.) ;
#46608 = EDGE_CURVE('',#38037,#38031,#30700,.T.) ;
#46609 = EDGE_CURVE('',#38038,#38039,#5100,.T.) ;
#46610 = EDGE_CURVE('',#38038,#38040,#30701,.T.) ;
#46611 = EDGE_CURVE('',#38040,#38041,#5101,.T.) ;
#46612 = EDGE_CURVE('',#38041,#38042,#30702,.T.) ;
#46613 = EDGE_CURVE('',#38042,#38043,#5102,.T.) ;
#46614 = EDGE_CURVE('',#38043,#38044,#30703,.T.) ;
#46615 = EDGE_CURVE('',#38044,#38045,#5103,.T.) ;
#46616 = EDGE_CURVE('',#38045,#38039,#30704,.T.) ;
#46617 = EDGE_CURVE('',#38046,#38047,#5104,.T.) ;
#46618 = EDGE_CURVE('',#38046,#38048,#30705,.T.) ;
#46619 = EDGE_CURVE('',#38048,#38049,#5105,.T.) ;
#46620 = EDGE_CURVE('',#38049,#38050,#30706,.T.) ;
#46621 = EDGE_CURVE('',#38050,#38051,#5106,.T.) ;
#46622 = EDGE_CURVE('',#38051,#38052,#30707,.T.) ;
#46623 = EDGE_CURVE('',#38052,#38053,#5107,.T.) ;
#46624 = EDGE_CURVE('',#38053,#38047,#30708,.T.) ;
#46625 = EDGE_CURVE('',#38054,#38055,#5108,.T.) ;
#46626 = EDGE_CURVE('',#38054,#38056,#30709,.T.) ;
#46627 = EDGE_CURVE('',#38056,#38057,#5109,.T.) ;
#46628 = EDGE_CURVE('',#38057,#38058,#30710,.T.) ;
#46629 = EDGE_CURVE('',#38058,#38059,#5110,.T.) ;
#46630 = EDGE_CURVE('',#38059,#38060,#30711,.T.) ;
#46631 = EDGE_CURVE('',#38060,#38061,#5111,.T.) ;
#46632 = EDGE_CURVE('',#38061,#38055,#30712,.T.) ;
#46633 = EDGE_CURVE('',#38062,#38063,#5112,.T.) ;
#46634 = EDGE_CURVE('',#38062,#38064,#30713,.T.) ;
#46635 = EDGE_CURVE('',#38064,#38065,#5113,.T.) ;
#46636 = EDGE_CURVE('',#38065,#38066,#30714,.T.) ;
#46637 = EDGE_CURVE('',#38066,#38067,#5114,.T.) ;
#46638 = EDGE_CURVE('',#38067,#38068,#30715,.T.) ;
#46639 = EDGE_CURVE('',#38068,#38069,#5115,.T.) ;
#46640 = EDGE_CURVE('',#38069,#38063,#30716,.T.) ;
#46641 = EDGE_CURVE('',#38070,#38071,#5116,.T.) ;
#46642 = EDGE_CURVE('',#38070,#38072,#30717,.T.) ;
#46643 = EDGE_CURVE('',#38072,#38073,#5117,.T.) ;
#46644 = EDGE_CURVE('',#38073,#38074,#30718,.T.) ;
#46645 = EDGE_CURVE('',#38074,#38075,#5118,.T.) ;
#46646 = EDGE_CURVE('',#38075,#38076,#30719,.T.) ;
#46647 = EDGE_CURVE('',#38076,#38077,#5119,.T.) ;
#46648 = EDGE_CURVE('',#38077,#38071,#30720,.T.) ;
#46649 = EDGE_CURVE('',#38078,#38079,#5120,.T.) ;
#46650 = EDGE_CURVE('',#38078,#38080,#30721,.T.) ;
#46651 = EDGE_CURVE('',#38080,#38081,#5121,.T.) ;
#46652 = EDGE_CURVE('',#38081,#38082,#30722,.T.) ;
#46653 = EDGE_CURVE('',#38082,#38083,#5122,.T.) ;
#46654 = EDGE_CURVE('',#38083,#38084,#30723,.T.) ;
#46655 = EDGE_CURVE('',#38084,#38085,#5123,.T.) ;
#46656 = EDGE_CURVE('',#38085,#38079,#30724,.T.) ;
#46657 = EDGE_CURVE('',#38086,#38087,#5124,.T.) ;
#46658 = EDGE_CURVE('',#38086,#38088,#30725,.T.) ;
#46659 = EDGE_CURVE('',#38088,#38089,#5125,.T.) ;
#46660 = EDGE_CURVE('',#38089,#38090,#30726,.T.) ;
#46661 = EDGE_CURVE('',#38090,#38091,#5126,.T.) ;
#46662 = EDGE_CURVE('',#38091,#38092,#30727,.T.) ;
#46663 = EDGE_CURVE('',#38092,#38093,#5127,.T.) ;
#46664 = EDGE_CURVE('',#38093,#38087,#30728,.T.) ;
#46665 = EDGE_CURVE('',#37269,#37256,#30729,.T.) ;
#46666 = EDGE_CURVE('',#37247,#37268,#30730,.T.) ;
#46667 = EDGE_CURVE('',#37270,#37263,#30731,.T.) ;
#46668 = EDGE_CURVE('',#37264,#37269,#30732,.T.) ;
#46669 = EDGE_CURVE('',#37270,#38094,#30733,.T.) ;
#46670 = EDGE_CURVE('',#38094,#37263,#30734,.T.) ;
#46671 = EDGE_CURVE('',#37247,#37273,#30735,.T.) ;
#46672 = EDGE_CURVE('',#37273,#37268,#30736,.T.) ;
#46673 = EDGE_CURVE('',#37264,#37255,#30737,.T.) ;
#46674 = EDGE_CURVE('',#36354,#37266,#30738,.T.) ;
#46675 = EDGE_CURVE('',#36355,#38095,#2170,.T.) ;
#46676 = EDGE_CURVE('',#38094,#38095,#5128,.T.) ;
#46677 = EDGE_CURVE('',#38096,#38094,#2171,.T.) ;
#46678 = EDGE_CURVE('',#38096,#38097,#2172,.T.) ;
#46679 = EDGE_CURVE('',#36481,#38097,#5129,.T.) ;
#46680 = EDGE_CURVE('',#37267,#36480,#30739,.T.) ;
#46681 = EDGE_CURVE('',#37274,#37267,#30740,.T.) ;
#46682 = EDGE_CURVE('',#37248,#37272,#30741,.T.) ;
#46683 = EDGE_CURVE('',#37265,#37254,#30742,.T.) ;
#46684 = EDGE_CURVE('',#37266,#36356,#30743,.T.) ;
#46685 = EDGE_CURVE('',#37261,#37265,#30744,.T.) ;
#46686 = EDGE_CURVE('',#37274,#36489,#30745,.T.) ;
#46687 = EDGE_CURVE('',#37248,#36576,#30746,.T.) ;
#46688 = EDGE_CURVE('',#36575,#37272,#30747,.T.) ;
#46689 = EDGE_CURVE('',#37261,#37253,#30748,.T.) ;
#46690 = EDGE_CURVE('',#37271,#36488,#30749,.T.) ;
#46691 = EDGE_CURVE('',#36577,#37271,#30750,.T.) ;
#46692 = EDGE_CURVE('',#38098,#36576,#5130,.T.) ;
#46693 = EDGE_CURVE('',#37249,#38098,#30751,.T.) ;
#46694 = EDGE_CURVE('',#37262,#37252,#30752,.T.) ;
#46695 = EDGE_CURVE('',#36357,#37257,#30753,.T.) ;
#46696 = EDGE_CURVE('',#37258,#37262,#30754,.T.) ;
#46697 = EDGE_CURVE('',#36484,#37257,#30755,.T.) ;
#46698 = EDGE_CURVE('',#36577,#36488,#30756,.T.) ;
#46699 = EDGE_CURVE('',#36582,#36579,#30757,.T.) ;
#46700 = EDGE_CURVE('',#36579,#36580,#30758,.T.) ;
#46701 = EDGE_CURVE('',#38098,#36721,#30759,.T.) ;
#46702 = EDGE_CURVE('',#38099,#38098,#30760,.T.) ;
#46703 = EDGE_CURVE('',#37249,#38099,#30761,.T.) ;
#46704 = EDGE_CURVE('',#37258,#37252,#30762,.T.) ;
#46705 = EDGE_CURVE('',#36485,#37260,#30763,.T.) ;
#46706 = EDGE_CURVE('',#36578,#36487,#30764,.T.) ;
#46707 = EDGE_CURVE('',#36652,#36578,#30765,.T.) ;
#46708 = EDGE_CURVE('',#38099,#36720,#30766,.T.) ;
#46709 = EDGE_CURVE('',#38100,#38099,#5131,.T.) ;
#46710 = EDGE_CURVE('',#37250,#38100,#30767,.T.) ;
#46711 = EDGE_CURVE('',#37259,#37251,#30768,.T.) ;
#46712 = EDGE_CURVE('',#37260,#36574,#30769,.T.) ;
#46713 = EDGE_CURVE('',#36571,#37259,#30770,.T.) ;
#46714 = EDGE_CURVE('',#36485,#36574,#30771,.T.) ;
#46715 = EDGE_CURVE('',#36653,#36487,#30772,.T.) ;
#46716 = EDGE_CURVE('',#38100,#36719,#30773,.T.) ;
#46717 = EDGE_CURVE('',#38101,#38100,#30774,.T.) ;
#46718 = EDGE_CURVE('',#37250,#38101,#30775,.T.) ;
#46719 = EDGE_CURVE('',#36570,#37251,#30776,.T.) ;
#46720 = EDGE_CURVE('',#36486,#36573,#30777,.T.) ;
#46721 = EDGE_CURVE('',#36654,#36486,#30778,.T.) ;
#46722 = EDGE_CURVE('',#38101,#36718,#30779,.T.) ;
#46723 = EDGE_CURVE('',#36570,#38101,#5132,.T.) ;
#46724 = EDGE_CURVE('',#36655,#36573,#30780,.T.) ;
#46725 = EDGE_CURVE('',#36572,#36585,#30781,.T.) ;
#46726 = EDGE_CURVE('',#36587,#36572,#30782,.T.) ;
#46727 = EDGE_CURVE('',#37981,#38014,#30783,.T.) ;
#46728 = EDGE_CURVE('',#38015,#37979,#30784,.T.) ;
#46729 = EDGE_CURVE('',#38016,#37977,#30785,.T.) ;
#46730 = EDGE_CURVE('',#37983,#38014,#30786,.T.) ;
#46731 = EDGE_CURVE('',#38017,#37975,#30787,.T.) ;
#46732 = EDGE_CURVE('',#37985,#38013,#30788,.T.) ;
#46733 = EDGE_CURVE('',#38018,#37973,#30789,.T.) ;
#46734 = EDGE_CURVE('',#37987,#38013,#30790,.T.) ;
#46735 = EDGE_CURVE('',#38019,#37971,#30791,.T.) ;
#46736 = EDGE_CURVE('',#37989,#38012,#30792,.T.) ;
#46737 = EDGE_CURVE('',#38019,#37969,#30793,.T.) ;
#46738 = EDGE_CURVE('',#37991,#38012,#30794,.T.) ;
#46739 = EDGE_CURVE('',#38020,#36362,#30795,.T.) ;
#46740 = EDGE_CURVE('',#37993,#38011,#30796,.T.) ;
#46741 = EDGE_CURVE('',#38020,#36361,#30797,.T.) ;
#46742 = EDGE_CURVE('',#37995,#38011,#30798,.T.) ;
#46743 = EDGE_CURVE('',#37997,#38010,#30799,.T.) ;
#46744 = EDGE_CURVE('',#37999,#38010,#30800,.T.) ;
#46745 = EDGE_CURVE('',#38021,#37965,#30801,.T.) ;
#46746 = EDGE_CURVE('',#38001,#38009,#30802,.T.) ;
#46747 = EDGE_CURVE('',#38021,#37963,#30803,.T.) ;
#46748 = EDGE_CURVE('',#38003,#38009,#30804,.T.) ;
#46749 = EDGE_CURVE('',#38005,#37961,#30805,.T.) ;
#46750 = EDGE_CURVE('',#37955,#38008,#30806,.T.) ;
#46751 = EDGE_CURVE('',#38006,#37959,#30807,.T.) ;
#46752 = EDGE_CURVE('',#37957,#38007,#30808,.T.) ;
#46753 = EDGE_CURVE('',#37440,#36762,#30809,.T.) ;
#46754 = EDGE_CURVE('',#36763,#37442,#30810,.T.) ;
#46755 = EDGE_CURVE('',#37438,#36762,#30811,.T.) ;
#46756 = EDGE_CURVE('',#36763,#37444,#30812,.T.) ;
#46757 = EDGE_CURVE('',#37436,#36761,#30813,.T.) ;
#46758 = EDGE_CURVE('',#36764,#37446,#30814,.T.) ;
#46759 = EDGE_CURVE('',#37434,#36760,#30815,.T.) ;
#46760 = EDGE_CURVE('',#36765,#37448,#30816,.T.) ;
#46761 = EDGE_CURVE('',#36766,#37450,#30817,.T.) ;
#46762 = EDGE_CURVE('',#36767,#37452,#30818,.T.) ;
#46763 = EDGE_CURVE('',#37432,#36759,#30819,.T.) ;
#46764 = EDGE_CURVE('',#36768,#37454,#30820,.T.) ;
#46765 = EDGE_CURVE('',#37431,#36758,#30821,.T.) ;
#46766 = EDGE_CURVE('',#36769,#37456,#30822,.T.) ;
#46767 = EDGE_CURVE('',#37430,#36757,#30823,.T.) ;
#46768 = EDGE_CURVE('',#36770,#37458,#30824,.T.) ;
#46769 = EDGE_CURVE('',#37428,#36756,#30825,.T.) ;
#46770 = EDGE_CURVE('',#36771,#37460,#30826,.T.) ;
#46771 = EDGE_CURVE('',#37426,#36755,#30827,.T.) ;
#46772 = EDGE_CURVE('',#36772,#37462,#30828,.T.) ;
#46773 = EDGE_CURVE('',#37424,#36755,#30829,.T.) ;
#46774 = EDGE_CURVE('',#36773,#37464,#30830,.T.) ;
#46775 = EDGE_CURVE('',#37422,#36754,#30831,.T.) ;
#46776 = EDGE_CURVE('',#36752,#37466,#30832,.T.) ;
#46777 = EDGE_CURVE('',#37420,#36754,#30833,.T.) ;
#46778 = EDGE_CURVE('',#36753,#37468,#30834,.T.) ;
#46779 = EDGE_CURVE('',#37507,#36784,#30835,.T.) ;
#46780 = EDGE_CURVE('',#36785,#37509,#30836,.T.) ;
#46781 = EDGE_CURVE('',#37505,#36784,#30837,.T.) ;
#46782 = EDGE_CURVE('',#36785,#37511,#30838,.T.) ;
#46783 = EDGE_CURVE('',#37503,#36783,#30839,.T.) ;
#46784 = EDGE_CURVE('',#36786,#37513,#30840,.T.) ;
#46785 = EDGE_CURVE('',#37501,#36782,#30841,.T.) ;
#46786 = EDGE_CURVE('',#36787,#37515,#30842,.T.) ;
#46787 = EDGE_CURVE('',#36788,#37517,#30843,.T.) ;
#46788 = EDGE_CURVE('',#36789,#37519,#30844,.T.) ;
#46789 = EDGE_CURVE('',#37499,#36781,#30845,.T.) ;
#46790 = EDGE_CURVE('',#36790,#37521,#30846,.T.) ;
#46791 = EDGE_CURVE('',#37498,#36780,#30847,.T.) ;
#46792 = EDGE_CURVE('',#36791,#37523,#30848,.T.) ;
#46793 = EDGE_CURVE('',#37497,#36779,#30849,.T.) ;
#46794 = EDGE_CURVE('',#36792,#37525,#30850,.T.) ;
#46795 = EDGE_CURVE('',#37495,#36778,#30851,.T.) ;
#46796 = EDGE_CURVE('',#36793,#37527,#30852,.T.) ;
#46797 = EDGE_CURVE('',#37493,#36777,#30853,.T.) ;
#46798 = EDGE_CURVE('',#36794,#37529,#30854,.T.) ;
#46799 = EDGE_CURVE('',#37491,#36777,#30855,.T.) ;
#46800 = EDGE_CURVE('',#36795,#37531,#30856,.T.) ;
#46801 = EDGE_CURVE('',#37489,#36776,#30857,.T.) ;
#46802 = EDGE_CURVE('',#36774,#37533,#30858,.T.) ;
#46803 = EDGE_CURVE('',#37487,#36776,#30859,.T.) ;
#46804 = EDGE_CURVE('',#36775,#37535,#30860,.T.) ;
#46805 = EDGE_CURVE('',#37574,#36806,#30861,.T.) ;
#46806 = EDGE_CURVE('',#36807,#37576,#30862,.T.) ;
#46807 = EDGE_CURVE('',#37572,#36806,#30863,.T.) ;
#46808 = EDGE_CURVE('',#36807,#37578,#30864,.T.) ;
#46809 = EDGE_CURVE('',#37570,#36805,#30865,.T.) ;
#46810 = EDGE_CURVE('',#36808,#37580,#30866,.T.) ;
#46811 = EDGE_CURVE('',#37568,#36804,#30867,.T.) ;
#46812 = EDGE_CURVE('',#36809,#37582,#30868,.T.) ;
#46813 = EDGE_CURVE('',#36810,#37584,#30869,.T.) ;
#46814 = EDGE_CURVE('',#36811,#37586,#30870,.T.) ;
#46815 = EDGE_CURVE('',#37566,#36803,#30871,.T.) ;
#46816 = EDGE_CURVE('',#36812,#37588,#30872,.T.) ;
#46817 = EDGE_CURVE('',#37565,#36802,#30873,.T.) ;
#46818 = EDGE_CURVE('',#36813,#37590,#30874,.T.) ;
#46819 = EDGE_CURVE('',#37564,#36801,#30875,.T.) ;
#46820 = EDGE_CURVE('',#36814,#37592,#30876,.T.) ;
#46821 = EDGE_CURVE('',#37562,#36800,#30877,.T.) ;
#46822 = EDGE_CURVE('',#36815,#37594,#30878,.T.) ;
#46823 = EDGE_CURVE('',#37560,#36799,#30879,.T.) ;
#46824 = EDGE_CURVE('',#36816,#37596,#30880,.T.) ;
#46825 = EDGE_CURVE('',#37558,#36799,#30881,.T.) ;
#46826 = EDGE_CURVE('',#36817,#37598,#30882,.T.) ;
#46827 = EDGE_CURVE('',#37556,#36798,#30883,.T.) ;
#46828 = EDGE_CURVE('',#36796,#37600,#30884,.T.) ;
#46829 = EDGE_CURVE('',#37554,#36798,#30885,.T.) ;
#46830 = EDGE_CURVE('',#36797,#37602,#30886,.T.) ;
#46831 = EDGE_CURVE('',#37641,#36828,#30887,.T.) ;
#46832 = EDGE_CURVE('',#36829,#37643,#30888,.T.) ;
#46833 = EDGE_CURVE('',#37639,#36828,#30889,.T.) ;
#46834 = EDGE_CURVE('',#36829,#37645,#30890,.T.) ;
#46835 = EDGE_CURVE('',#37637,#36827,#30891,.T.) ;
#46836 = EDGE_CURVE('',#36830,#37647,#30892,.T.) ;
#46837 = EDGE_CURVE('',#37635,#36826,#30893,.T.) ;
#46838 = EDGE_CURVE('',#36831,#37649,#30894,.T.) ;
#46839 = EDGE_CURVE('',#36832,#37651,#30895,.T.) ;
#46840 = EDGE_CURVE('',#36833,#37653,#30896,.T.) ;
#46841 = EDGE_CURVE('',#37633,#36825,#30897,.T.) ;
#46842 = EDGE_CURVE('',#36834,#37655,#30898,.T.) ;
#46843 = EDGE_CURVE('',#37632,#36824,#30899,.T.) ;
#46844 = EDGE_CURVE('',#36835,#37657,#30900,.T.) ;
#46845 = EDGE_CURVE('',#37631,#36823,#30901,.T.) ;
#46846 = EDGE_CURVE('',#36836,#37659,#30902,.T.) ;
#46847 = EDGE_CURVE('',#37629,#36822,#30903,.T.) ;
#46848 = EDGE_CURVE('',#36837,#37661,#30904,.T.) ;
#46849 = EDGE_CURVE('',#37627,#36821,#30905,.T.) ;
#46850 = EDGE_CURVE('',#36838,#37663,#30906,.T.) ;
#46851 = EDGE_CURVE('',#37625,#36821,#30907,.T.) ;
#46852 = EDGE_CURVE('',#36839,#37665,#30908,.T.) ;
#46853 = EDGE_CURVE('',#37623,#36820,#30909,.T.) ;
#46854 = EDGE_CURVE('',#36818,#37667,#30910,.T.) ;
#46855 = EDGE_CURVE('',#37621,#36820,#30911,.T.) ;
#46856 = EDGE_CURVE('',#36819,#37669,#30912,.T.) ;
#46857 = EDGE_CURVE('',#37708,#36850,#30913,.T.) ;
#46858 = EDGE_CURVE('',#36851,#37710,#30914,.T.) ;
#46859 = EDGE_CURVE('',#37706,#36850,#30915,.T.) ;
#46860 = EDGE_CURVE('',#36851,#37712,#30916,.T.) ;
#46861 = EDGE_CURVE('',#37704,#36849,#30917,.T.) ;
#46862 = EDGE_CURVE('',#36852,#37714,#30918,.T.) ;
#46863 = EDGE_CURVE('',#37702,#36848,#30919,.T.) ;
#46864 = EDGE_CURVE('',#36853,#37716,#30920,.T.) ;
#46865 = EDGE_CURVE('',#36854,#37718,#30921,.T.) ;
#46866 = EDGE_CURVE('',#36855,#37720,#30922,.T.) ;
#46867 = EDGE_CURVE('',#37700,#36847,#30923,.T.) ;
#46868 = EDGE_CURVE('',#36856,#37722,#30924,.T.) ;
#46869 = EDGE_CURVE('',#37699,#36846,#30925,.T.) ;
#46870 = EDGE_CURVE('',#36857,#37724,#30926,.T.) ;
#46871 = EDGE_CURVE('',#37698,#36845,#30927,.T.) ;
#46872 = EDGE_CURVE('',#36858,#37726,#30928,.T.) ;
#46873 = EDGE_CURVE('',#37696,#36844,#30929,.T.) ;
#46874 = EDGE_CURVE('',#36859,#37728,#30930,.T.) ;
#46875 = EDGE_CURVE('',#37694,#36843,#30931,.T.) ;
#46876 = EDGE_CURVE('',#36860,#37730,#30932,.T.) ;
#46877 = EDGE_CURVE('',#37692,#36843,#30933,.T.) ;
#46878 = EDGE_CURVE('',#36861,#37732,#30934,.T.) ;
#46879 = EDGE_CURVE('',#37690,#36842,#30935,.T.) ;
#46880 = EDGE_CURVE('',#36840,#37734,#30936,.T.) ;
#46881 = EDGE_CURVE('',#37688,#36842,#30937,.T.) ;
#46882 = EDGE_CURVE('',#36841,#37736,#30938,.T.) ;
#46883 = EDGE_CURVE('',#37775,#36872,#30939,.T.) ;
#46884 = EDGE_CURVE('',#36873,#37777,#30940,.T.) ;
#46885 = EDGE_CURVE('',#37773,#36872,#30941,.T.) ;
#46886 = EDGE_CURVE('',#36873,#37779,#30942,.T.) ;
#46887 = EDGE_CURVE('',#37771,#36871,#30943,.T.) ;
#46888 = EDGE_CURVE('',#36874,#37781,#30944,.T.) ;
#46889 = EDGE_CURVE('',#37769,#36870,#30945,.T.) ;
#46890 = EDGE_CURVE('',#36875,#37783,#30946,.T.) ;
#46891 = EDGE_CURVE('',#36876,#37785,#30947,.T.) ;
#46892 = EDGE_CURVE('',#36877,#37787,#30948,.T.) ;
#46893 = EDGE_CURVE('',#37767,#36869,#30949,.T.) ;
#46894 = EDGE_CURVE('',#36878,#37789,#30950,.T.) ;
#46895 = EDGE_CURVE('',#37766,#36868,#30951,.T.) ;
#46896 = EDGE_CURVE('',#36879,#37791,#30952,.T.) ;
#46897 = EDGE_CURVE('',#37765,#36867,#30953,.T.) ;
#46898 = EDGE_CURVE('',#36880,#37793,#30954,.T.) ;
#46899 = EDGE_CURVE('',#37763,#36866,#30955,.T.) ;
#46900 = EDGE_CURVE('',#36881,#37795,#30956,.T.) ;
#46901 = EDGE_CURVE('',#37761,#36865,#30957,.T.) ;
#46902 = EDGE_CURVE('',#36882,#37797,#30958,.T.) ;
#46903 = EDGE_CURVE('',#37759,#36865,#30959,.T.) ;
#46904 = EDGE_CURVE('',#36883,#37799,#30960,.T.) ;
#46905 = EDGE_CURVE('',#37757,#36864,#30961,.T.) ;
#46906 = EDGE_CURVE('',#36862,#37801,#30962,.T.) ;
#46907 = EDGE_CURVE('',#37755,#36864,#30963,.T.) ;
#46908 = EDGE_CURVE('',#36863,#37803,#30964,.T.) ;
#46909 = EDGE_CURVE('',#37842,#36894,#30965,.T.) ;
#46910 = EDGE_CURVE('',#36895,#37844,#30966,.T.) ;
#46911 = EDGE_CURVE('',#37840,#36894,#30967,.T.) ;
#46912 = EDGE_CURVE('',#36895,#37846,#30968,.T.) ;
#46913 = EDGE_CURVE('',#37838,#36893,#30969,.T.) ;
#46914 = EDGE_CURVE('',#36896,#37848,#30970,.T.) ;
#46915 = EDGE_CURVE('',#37836,#36892,#30971,.T.) ;
#46916 = EDGE_CURVE('',#36897,#37850,#30972,.T.) ;
#46917 = EDGE_CURVE('',#36898,#37852,#30973,.T.) ;
#46918 = EDGE_CURVE('',#36899,#37854,#30974,.T.) ;
#46919 = EDGE_CURVE('',#37834,#36891,#30975,.T.) ;
#46920 = EDGE_CURVE('',#36900,#37856,#30976,.T.) ;
#46921 = EDGE_CURVE('',#37833,#36890,#30977,.T.) ;
#46922 = EDGE_CURVE('',#36901,#37858,#30978,.T.) ;
#46923 = EDGE_CURVE('',#37832,#36889,#30979,.T.) ;
#46924 = EDGE_CURVE('',#36902,#37860,#30980,.T.) ;
#46925 = EDGE_CURVE('',#37830,#36888,#30981,.T.) ;
#46926 = EDGE_CURVE('',#36903,#37862,#30982,.T.) ;
#46927 = EDGE_CURVE('',#37828,#36887,#30983,.T.) ;
#46928 = EDGE_CURVE('',#36904,#37864,#30984,.T.) ;
#46929 = EDGE_CURVE('',#37826,#36887,#30985,.T.) ;
#46930 = EDGE_CURVE('',#36905,#37866,#30986,.T.) ;
#46931 = EDGE_CURVE('',#37824,#36886,#30987,.T.) ;
#46932 = EDGE_CURVE('',#36884,#37868,#30988,.T.) ;
#46933 = EDGE_CURVE('',#37822,#36886,#30989,.T.) ;
#46934 = EDGE_CURVE('',#36885,#37870,#30990,.T.) ;
#46935 = EDGE_CURVE('',#37909,#36916,#30991,.T.) ;
#46936 = EDGE_CURVE('',#36917,#37911,#30992,.T.) ;
#46937 = EDGE_CURVE('',#37907,#36916,#30993,.T.) ;
#46938 = EDGE_CURVE('',#36917,#37913,#30994,.T.) ;
#46939 = EDGE_CURVE('',#37905,#36915,#30995,.T.) ;
#46940 = EDGE_CURVE('',#36918,#37915,#30996,.T.) ;
#46941 = EDGE_CURVE('',#37903,#36914,#30997,.T.) ;
#46942 = EDGE_CURVE('',#36919,#37917,#30998,.T.) ;
#46943 = EDGE_CURVE('',#36920,#37919,#30999,.T.) ;
#46944 = EDGE_CURVE('',#36921,#37921,#31000,.T.) ;
#46945 = EDGE_CURVE('',#37901,#36913,#31001,.T.) ;
#46946 = EDGE_CURVE('',#36922,#37923,#31002,.T.) ;
#46947 = EDGE_CURVE('',#37900,#36912,#31003,.T.) ;
#46948 = EDGE_CURVE('',#36923,#37925,#31004,.T.) ;
#46949 = EDGE_CURVE('',#37899,#36911,#31005,.T.) ;
#46950 = EDGE_CURVE('',#36924,#37927,#31006,.T.) ;
#46951 = EDGE_CURVE('',#37897,#36910,#31007,.T.) ;
#46952 = EDGE_CURVE('',#36925,#37929,#31008,.T.) ;
#46953 = EDGE_CURVE('',#37895,#36909,#31009,.T.) ;
#46954 = EDGE_CURVE('',#36926,#37931,#31010,.T.) ;
#46955 = EDGE_CURVE('',#37893,#36909,#31011,.T.) ;
#46956 = EDGE_CURVE('',#36927,#37933,#31012,.T.) ;
#46957 = EDGE_CURVE('',#37891,#36908,#31013,.T.) ;
#46958 = EDGE_CURVE('',#36906,#37935,#31014,.T.) ;
#46959 = EDGE_CURVE('',#37889,#36908,#31015,.T.) ;
#46960 = EDGE_CURVE('',#36907,#37937,#31016,.T.) ;
#46961 = EDGE_CURVE('',#37976,#36938,#31017,.T.) ;
#46962 = EDGE_CURVE('',#36939,#37978,#31018,.T.) ;
#46963 = EDGE_CURVE('',#37974,#36938,#31019,.T.) ;
#46964 = EDGE_CURVE('',#36939,#37980,#31020,.T.) ;
#46965 = EDGE_CURVE('',#37972,#36937,#31021,.T.) ;
#46966 = EDGE_CURVE('',#36940,#37982,#31022,.T.) ;
#46967 = EDGE_CURVE('',#37970,#36936,#31023,.T.) ;
#46968 = EDGE_CURVE('',#36941,#37984,#31024,.T.) ;
#46969 = EDGE_CURVE('',#36942,#37986,#31025,.T.) ;
#46970 = EDGE_CURVE('',#36943,#37988,#31026,.T.) ;
#46971 = EDGE_CURVE('',#37968,#36935,#31027,.T.) ;
#46972 = EDGE_CURVE('',#36944,#37990,#31028,.T.) ;
#46973 = EDGE_CURVE('',#37967,#36934,#31029,.T.) ;
#46974 = EDGE_CURVE('',#36945,#37992,#31030,.T.) ;
#46975 = EDGE_CURVE('',#37966,#36933,#31031,.T.) ;
#46976 = EDGE_CURVE('',#36946,#37994,#31032,.T.) ;
#46977 = EDGE_CURVE('',#37964,#36932,#31033,.T.) ;
#46978 = EDGE_CURVE('',#36947,#37996,#31034,.T.) ;
#46979 = EDGE_CURVE('',#37962,#36931,#31035,.T.) ;
#46980 = EDGE_CURVE('',#36948,#37998,#31036,.T.) ;
#46981 = EDGE_CURVE('',#37960,#36931,#31037,.T.) ;
#46982 = EDGE_CURVE('',#36949,#38000,#31038,.T.) ;
#46983 = EDGE_CURVE('',#37958,#36930,#31039,.T.) ;
#46984 = EDGE_CURVE('',#36928,#38002,#31040,.T.) ;
#46985 = EDGE_CURVE('',#37956,#36930,#31041,.T.) ;
#46986 = EDGE_CURVE('',#36929,#38004,#31042,.T.) ;
#46987 = EDGE_CURVE('',#37287,#37246,#31043,.T.) ;
#46988 = EDGE_CURVE('',#37237,#37286,#31044,.T.) ;
#46989 = EDGE_CURVE('',#37288,#37281,#31045,.T.) ;
#46990 = EDGE_CURVE('',#37282,#37287,#31046,.T.) ;
#46991 = EDGE_CURVE('',#37288,#38102,#31047,.T.) ;
#46992 = EDGE_CURVE('',#38102,#37281,#31048,.T.) ;
#46993 = EDGE_CURVE('',#37237,#37291,#31049,.T.) ;
#46994 = EDGE_CURVE('',#37291,#37286,#31050,.T.) ;
#46995 = EDGE_CURVE('',#37282,#37245,#31051,.T.) ;
#46996 = EDGE_CURVE('',#36303,#37284,#31052,.T.) ;
#46997 = EDGE_CURVE('',#36304,#38103,#2173,.T.) ;
#46998 = EDGE_CURVE('',#38102,#38103,#5133,.T.) ;
#46999 = EDGE_CURVE('',#38104,#38102,#2174,.T.) ;
#47000 = EDGE_CURVE('',#38104,#38105,#2175,.T.) ;
#47001 = EDGE_CURVE('',#36471,#38105,#5134,.T.) ;
#47002 = EDGE_CURVE('',#37285,#36470,#31053,.T.) ;
#47003 = EDGE_CURVE('',#37292,#37285,#31054,.T.) ;
#47004 = EDGE_CURVE('',#37238,#37290,#31055,.T.) ;
#47005 = EDGE_CURVE('',#37283,#37244,#31056,.T.) ;
#47006 = EDGE_CURVE('',#37284,#36305,#31057,.T.) ;
#47007 = EDGE_CURVE('',#37279,#37283,#31058,.T.) ;
#47008 = EDGE_CURVE('',#37292,#36479,#31059,.T.) ;
#47009 = EDGE_CURVE('',#37238,#36566,#31060,.T.) ;
#47010 = EDGE_CURVE('',#36565,#37290,#31061,.T.) ;
#47011 = EDGE_CURVE('',#37279,#37243,#31062,.T.) ;
#47012 = EDGE_CURVE('',#37289,#36478,#31063,.T.) ;
#47013 = EDGE_CURVE('',#36567,#37289,#31064,.T.) ;
#47014 = EDGE_CURVE('',#38106,#36566,#5135,.T.) ;
#47015 = EDGE_CURVE('',#37239,#38106,#31065,.T.) ;
#47016 = EDGE_CURVE('',#37280,#37242,#31066,.T.) ;
#47017 = EDGE_CURVE('',#36306,#37275,#31067,.T.) ;
#47018 = EDGE_CURVE('',#37276,#37280,#31068,.T.) ;
#47019 = EDGE_CURVE('',#36474,#37275,#31069,.T.) ;
#47020 = EDGE_CURVE('',#36567,#36478,#31070,.T.) ;
#47021 = EDGE_CURVE('',#36586,#36569,#31071,.T.) ;
#47022 = EDGE_CURVE('',#36569,#36584,#31072,.T.) ;
#47023 = EDGE_CURVE('',#38106,#36717,#31073,.T.) ;
#47024 = EDGE_CURVE('',#38107,#38106,#31074,.T.) ;
#47025 = EDGE_CURVE('',#37239,#38107,#31075,.T.) ;
#47026 = EDGE_CURVE('',#37276,#37242,#31076,.T.) ;
#47027 = EDGE_CURVE('',#36475,#37278,#31077,.T.) ;
#47028 = EDGE_CURVE('',#36568,#36477,#31078,.T.) ;
#47029 = EDGE_CURVE('',#36656,#36568,#31079,.T.) ;
#47030 = EDGE_CURVE('',#38107,#36716,#31080,.T.) ;
#47031 = EDGE_CURVE('',#38108,#38107,#5136,.T.) ;
#47032 = EDGE_CURVE('',#37240,#38108,#31081,.T.) ;
#47033 = EDGE_CURVE('',#37277,#37241,#31082,.T.) ;
#47034 = EDGE_CURVE('',#37278,#36564,#31083,.T.) ;
#47035 = EDGE_CURVE('',#36561,#37277,#31084,.T.) ;
#47036 = EDGE_CURVE('',#36475,#36564,#31085,.T.) ;
#47037 = EDGE_CURVE('',#36657,#36477,#31086,.T.) ;
#47038 = EDGE_CURVE('',#38108,#36715,#31087,.T.) ;
#47039 = EDGE_CURVE('',#38109,#38108,#31088,.T.) ;
#47040 = EDGE_CURVE('',#37240,#38109,#31089,.T.) ;
#47041 = EDGE_CURVE('',#36560,#37241,#31090,.T.) ;
#47042 = EDGE_CURVE('',#36476,#36563,#31091,.T.) ;
#47043 = EDGE_CURVE('',#36658,#36476,#31092,.T.) ;
#47044 = EDGE_CURVE('',#38109,#36714,#31093,.T.) ;
#47045 = EDGE_CURVE('',#36560,#38109,#5137,.T.) ;
#47046 = EDGE_CURVE('',#36659,#36563,#31094,.T.) ;
#47047 = EDGE_CURVE('',#36562,#36589,#31095,.T.) ;
#47048 = EDGE_CURVE('',#36591,#36562,#31096,.T.) ;
#47049 = EDGE_CURVE('',#37914,#37947,#31097,.T.) ;
#47050 = EDGE_CURVE('',#37948,#37912,#31098,.T.) ;
#47051 = EDGE_CURVE('',#37949,#37910,#31099,.T.) ;
#47052 = EDGE_CURVE('',#37916,#37947,#31100,.T.) ;
#47053 = EDGE_CURVE('',#37950,#37908,#31101,.T.) ;
#47054 = EDGE_CURVE('',#37918,#37946,#31102,.T.) ;
#47055 = EDGE_CURVE('',#37951,#37906,#31103,.T.) ;
#47056 = EDGE_CURVE('',#37920,#37946,#31104,.T.) ;
#47057 = EDGE_CURVE('',#37952,#37904,#31105,.T.) ;
#47058 = EDGE_CURVE('',#37922,#37945,#31106,.T.) ;
#47059 = EDGE_CURVE('',#37952,#37902,#31107,.T.) ;
#47060 = EDGE_CURVE('',#37924,#37945,#31108,.T.) ;
#47061 = EDGE_CURVE('',#37953,#36364,#31109,.T.) ;
#47062 = EDGE_CURVE('',#37926,#37944,#31110,.T.) ;
#47063 = EDGE_CURVE('',#37953,#36363,#31111,.T.) ;
#47064 = EDGE_CURVE('',#37928,#37944,#31112,.T.) ;
#47065 = EDGE_CURVE('',#37930,#37943,#31113,.T.) ;
#47066 = EDGE_CURVE('',#37932,#37943,#31114,.T.) ;
#47067 = EDGE_CURVE('',#37954,#37898,#31115,.T.) ;
#47068 = EDGE_CURVE('',#37934,#37942,#31116,.T.) ;
#47069 = EDGE_CURVE('',#37954,#37896,#31117,.T.) ;
#47070 = EDGE_CURVE('',#37936,#37942,#31118,.T.) ;
#47071 = EDGE_CURVE('',#37938,#37894,#31119,.T.) ;
#47072 = EDGE_CURVE('',#37888,#37941,#31120,.T.) ;
#47073 = EDGE_CURVE('',#37939,#37892,#31121,.T.) ;
#47074 = EDGE_CURVE('',#37890,#37940,#31122,.T.) ;
#47075 = EDGE_CURVE('',#37305,#37236,#31123,.T.) ;
#47076 = EDGE_CURVE('',#37227,#37304,#31124,.T.) ;
#47077 = EDGE_CURVE('',#37306,#37299,#31125,.T.) ;
#47078 = EDGE_CURVE('',#37300,#37305,#31126,.T.) ;
#47079 = EDGE_CURVE('',#37306,#38110,#31127,.T.) ;
#47080 = EDGE_CURVE('',#38110,#37299,#31128,.T.) ;
#47081 = EDGE_CURVE('',#37227,#37309,#31129,.T.) ;
#47082 = EDGE_CURVE('',#37309,#37304,#31130,.T.) ;
#47083 = EDGE_CURVE('',#37300,#37235,#31131,.T.) ;
#47084 = EDGE_CURVE('',#36288,#37302,#31132,.T.) ;
#47085 = EDGE_CURVE('',#36289,#38111,#2176,.T.) ;
#47086 = EDGE_CURVE('',#38110,#38111,#5138,.T.) ;
#47087 = EDGE_CURVE('',#38112,#38110,#2177,.T.) ;
#47088 = EDGE_CURVE('',#38112,#38113,#2178,.T.) ;
#47089 = EDGE_CURVE('',#36461,#38113,#5139,.T.) ;
#47090 = EDGE_CURVE('',#37303,#36460,#31133,.T.) ;
#47091 = EDGE_CURVE('',#37310,#37303,#31134,.T.) ;
#47092 = EDGE_CURVE('',#37228,#37308,#31135,.T.) ;
#47093 = EDGE_CURVE('',#37301,#37234,#31136,.T.) ;
#47094 = EDGE_CURVE('',#37302,#36290,#31137,.T.) ;
#47095 = EDGE_CURVE('',#37297,#37301,#31138,.T.) ;
#47096 = EDGE_CURVE('',#37310,#36469,#31139,.T.) ;
#47097 = EDGE_CURVE('',#37228,#36556,#31140,.T.) ;
#47098 = EDGE_CURVE('',#36555,#37308,#31141,.T.) ;
#47099 = EDGE_CURVE('',#37297,#37233,#31142,.T.) ;
#47100 = EDGE_CURVE('',#37307,#36468,#31143,.T.) ;
#47101 = EDGE_CURVE('',#36557,#37307,#31144,.T.) ;
#47102 = EDGE_CURVE('',#38114,#36556,#5140,.T.) ;
#47103 = EDGE_CURVE('',#37229,#38114,#31145,.T.) ;
#47104 = EDGE_CURVE('',#37298,#37232,#31146,.T.) ;
#47105 = EDGE_CURVE('',#36291,#37293,#31147,.T.) ;
#47106 = EDGE_CURVE('',#37294,#37298,#31148,.T.) ;
#47107 = EDGE_CURVE('',#36464,#37293,#31149,.T.) ;
#47108 = EDGE_CURVE('',#36557,#36468,#31150,.T.) ;
#47109 = EDGE_CURVE('',#36590,#36559,#31151,.T.) ;
#47110 = EDGE_CURVE('',#36559,#36588,#31152,.T.) ;
#47111 = EDGE_CURVE('',#38114,#36713,#31153,.T.) ;
#47112 = EDGE_CURVE('',#38115,#38114,#31154,.T.) ;
#47113 = EDGE_CURVE('',#37229,#38115,#31155,.T.) ;
#47114 = EDGE_CURVE('',#37294,#37232,#31156,.T.) ;
#47115 = EDGE_CURVE('',#36465,#37296,#31157,.T.) ;
#47116 = EDGE_CURVE('',#36558,#36467,#31158,.T.) ;
#47117 = EDGE_CURVE('',#36660,#36558,#31159,.T.) ;
#47118 = EDGE_CURVE('',#38115,#36712,#31160,.T.) ;
#47119 = EDGE_CURVE('',#38116,#38115,#5141,.T.) ;
#47120 = EDGE_CURVE('',#37230,#38116,#31161,.T.) ;
#47121 = EDGE_CURVE('',#37295,#37231,#31162,.T.) ;
#47122 = EDGE_CURVE('',#37296,#36554,#31163,.T.) ;
#47123 = EDGE_CURVE('',#36551,#37295,#31164,.T.) ;
#47124 = EDGE_CURVE('',#36465,#36554,#31165,.T.) ;
#47125 = EDGE_CURVE('',#36661,#36467,#31166,.T.) ;
#47126 = EDGE_CURVE('',#38116,#36711,#31167,.T.) ;
#47127 = EDGE_CURVE('',#38117,#38116,#31168,.T.) ;
#47128 = EDGE_CURVE('',#37230,#38117,#31169,.T.) ;
#47129 = EDGE_CURVE('',#36550,#37231,#31170,.T.) ;
#47130 = EDGE_CURVE('',#36466,#36553,#31171,.T.) ;
#47131 = EDGE_CURVE('',#36662,#36466,#31172,.T.) ;
#47132 = EDGE_CURVE('',#38117,#36710,#31173,.T.) ;
#47133 = EDGE_CURVE('',#36550,#38117,#5142,.T.) ;
#47134 = EDGE_CURVE('',#36663,#36553,#31174,.T.) ;
#47135 = EDGE_CURVE('',#36552,#36593,#31175,.T.) ;
#47136 = EDGE_CURVE('',#36595,#36552,#31176,.T.) ;
#47137 = EDGE_CURVE('',#37847,#37880,#31177,.T.) ;
#47138 = EDGE_CURVE('',#37881,#37845,#31178,.T.) ;
#47139 = EDGE_CURVE('',#37882,#37843,#31179,.T.) ;
#47140 = EDGE_CURVE('',#37849,#37880,#31180,.T.) ;
#47141 = EDGE_CURVE('',#37883,#37841,#31181,.T.) ;
#47142 = EDGE_CURVE('',#37851,#37879,#31182,.T.) ;
#47143 = EDGE_CURVE('',#37884,#37839,#31183,.T.) ;
#47144 = EDGE_CURVE('',#37853,#37879,#31184,.T.) ;
#47145 = EDGE_CURVE('',#37885,#37837,#31185,.T.) ;
#47146 = EDGE_CURVE('',#37855,#37878,#31186,.T.) ;
#47147 = EDGE_CURVE('',#37885,#37835,#31187,.T.) ;
#47148 = EDGE_CURVE('',#37857,#37878,#31188,.T.) ;
#47149 = EDGE_CURVE('',#37886,#36366,#31189,.T.) ;
#47150 = EDGE_CURVE('',#37859,#37877,#31190,.T.) ;
#47151 = EDGE_CURVE('',#37886,#36365,#31191,.T.) ;
#47152 = EDGE_CURVE('',#37861,#37877,#31192,.T.) ;
#47153 = EDGE_CURVE('',#37863,#37876,#31193,.T.) ;
#47154 = EDGE_CURVE('',#37865,#37876,#31194,.T.) ;
#47155 = EDGE_CURVE('',#37887,#37831,#31195,.T.) ;
#47156 = EDGE_CURVE('',#37867,#37875,#31196,.T.) ;
#47157 = EDGE_CURVE('',#37887,#37829,#31197,.T.) ;
#47158 = EDGE_CURVE('',#37869,#37875,#31198,.T.) ;
#47159 = EDGE_CURVE('',#37871,#37827,#31199,.T.) ;
#47160 = EDGE_CURVE('',#37821,#37874,#31200,.T.) ;
#47161 = EDGE_CURVE('',#37872,#37825,#31201,.T.) ;
#47162 = EDGE_CURVE('',#37823,#37873,#31202,.T.) ;
#47163 = EDGE_CURVE('',#37323,#37226,#31203,.T.) ;
#47164 = EDGE_CURVE('',#37217,#37322,#31204,.T.) ;
#47165 = EDGE_CURVE('',#37324,#37317,#31205,.T.) ;
#47166 = EDGE_CURVE('',#37318,#37323,#31206,.T.) ;
#47167 = EDGE_CURVE('',#37324,#38118,#31207,.T.) ;
#47168 = EDGE_CURVE('',#38118,#37317,#31208,.T.) ;
#47169 = EDGE_CURVE('',#37217,#37327,#31209,.T.) ;
#47170 = EDGE_CURVE('',#37327,#37322,#31210,.T.) ;
#47171 = EDGE_CURVE('',#37318,#37225,#31211,.T.) ;
#47172 = EDGE_CURVE('',#36273,#37320,#31212,.T.) ;
#47173 = EDGE_CURVE('',#36274,#38119,#2179,.T.) ;
#47174 = EDGE_CURVE('',#38118,#38119,#5143,.T.) ;
#47175 = EDGE_CURVE('',#38120,#38118,#2180,.T.) ;
#47176 = EDGE_CURVE('',#38120,#38121,#2181,.T.) ;
#47177 = EDGE_CURVE('',#36451,#38121,#5144,.T.) ;
#47178 = EDGE_CURVE('',#37321,#36450,#31213,.T.) ;
#47179 = EDGE_CURVE('',#37328,#37321,#31214,.T.) ;
#47180 = EDGE_CURVE('',#37218,#37326,#31215,.T.) ;
#47181 = EDGE_CURVE('',#37319,#37224,#31216,.T.) ;
#47182 = EDGE_CURVE('',#37320,#36275,#31217,.T.) ;
#47183 = EDGE_CURVE('',#37315,#37319,#31218,.T.) ;
#47184 = EDGE_CURVE('',#37328,#36459,#31219,.T.) ;
#47185 = EDGE_CURVE('',#37218,#36546,#31220,.T.) ;
#47186 = EDGE_CURVE('',#36545,#37326,#31221,.T.) ;
#47187 = EDGE_CURVE('',#37315,#37223,#31222,.T.) ;
#47188 = EDGE_CURVE('',#37325,#36458,#31223,.T.) ;
#47189 = EDGE_CURVE('',#36547,#37325,#31224,.T.) ;
#47190 = EDGE_CURVE('',#38122,#36546,#5145,.T.) ;
#47191 = EDGE_CURVE('',#37219,#38122,#31225,.T.) ;
#47192 = EDGE_CURVE('',#37316,#37222,#31226,.T.) ;
#47193 = EDGE_CURVE('',#36276,#37311,#31227,.T.) ;
#47194 = EDGE_CURVE('',#37312,#37316,#31228,.T.) ;
#47195 = EDGE_CURVE('',#36454,#37311,#31229,.T.) ;
#47196 = EDGE_CURVE('',#36547,#36458,#31230,.T.) ;
#47197 = EDGE_CURVE('',#36594,#36549,#31231,.T.) ;
#47198 = EDGE_CURVE('',#36549,#36592,#31232,.T.) ;
#47199 = EDGE_CURVE('',#38122,#36709,#31233,.T.) ;
#47200 = EDGE_CURVE('',#38123,#38122,#31234,.T.) ;
#47201 = EDGE_CURVE('',#37219,#38123,#31235,.T.) ;
#47202 = EDGE_CURVE('',#37312,#37222,#31236,.T.) ;
#47203 = EDGE_CURVE('',#36455,#37314,#31237,.T.) ;
#47204 = EDGE_CURVE('',#36548,#36457,#31238,.T.) ;
#47205 = EDGE_CURVE('',#36664,#36548,#31239,.T.) ;
#47206 = EDGE_CURVE('',#38123,#36708,#31240,.T.) ;
#47207 = EDGE_CURVE('',#38124,#38123,#5146,.T.) ;
#47208 = EDGE_CURVE('',#37220,#38124,#31241,.T.) ;
#47209 = EDGE_CURVE('',#37313,#37221,#31242,.T.) ;
#47210 = EDGE_CURVE('',#37314,#36544,#31243,.T.) ;
#47211 = EDGE_CURVE('',#36541,#37313,#31244,.T.) ;
#47212 = EDGE_CURVE('',#36455,#36544,#31245,.T.) ;
#47213 = EDGE_CURVE('',#36665,#36457,#31246,.T.) ;
#47214 = EDGE_CURVE('',#38124,#36707,#31247,.T.) ;
#47215 = EDGE_CURVE('',#38125,#38124,#31248,.T.) ;
#47216 = EDGE_CURVE('',#37220,#38125,#31249,.T.) ;
#47217 = EDGE_CURVE('',#36540,#37221,#31250,.T.) ;
#47218 = EDGE_CURVE('',#36456,#36543,#31251,.T.) ;
#47219 = EDGE_CURVE('',#36666,#36456,#31252,.T.) ;
#47220 = EDGE_CURVE('',#38125,#36706,#31253,.T.) ;
#47221 = EDGE_CURVE('',#36540,#38125,#5147,.T.) ;
#47222 = EDGE_CURVE('',#36667,#36543,#31254,.T.) ;
#47223 = EDGE_CURVE('',#36542,#36597,#31255,.T.) ;
#47224 = EDGE_CURVE('',#36599,#36542,#31256,.T.) ;
#47225 = EDGE_CURVE('',#37780,#37813,#31257,.T.) ;
#47226 = EDGE_CURVE('',#37814,#37778,#31258,.T.) ;
#47227 = EDGE_CURVE('',#37815,#37776,#31259,.T.) ;
#47228 = EDGE_CURVE('',#37782,#37813,#31260,.T.) ;
#47229 = EDGE_CURVE('',#37816,#37774,#31261,.T.) ;
#47230 = EDGE_CURVE('',#37784,#37812,#31262,.T.) ;
#47231 = EDGE_CURVE('',#37817,#37772,#31263,.T.) ;
#47232 = EDGE_CURVE('',#37786,#37812,#31264,.T.) ;
#47233 = EDGE_CURVE('',#37818,#37770,#31265,.T.) ;
#47234 = EDGE_CURVE('',#37788,#37811,#31266,.T.) ;
#47235 = EDGE_CURVE('',#37818,#37768,#31267,.T.) ;
#47236 = EDGE_CURVE('',#37790,#37811,#31268,.T.) ;
#47237 = EDGE_CURVE('',#37819,#36368,#31269,.T.) ;
#47238 = EDGE_CURVE('',#37792,#37810,#31270,.T.) ;
#47239 = EDGE_CURVE('',#37819,#36367,#31271,.T.) ;
#47240 = EDGE_CURVE('',#37794,#37810,#31272,.T.) ;
#47241 = EDGE_CURVE('',#37796,#37809,#31273,.T.) ;
#47242 = EDGE_CURVE('',#37798,#37809,#31274,.T.) ;
#47243 = EDGE_CURVE('',#37820,#37764,#31275,.T.) ;
#47244 = EDGE_CURVE('',#37800,#37808,#31276,.T.) ;
#47245 = EDGE_CURVE('',#37820,#37762,#31277,.T.) ;
#47246 = EDGE_CURVE('',#37802,#37808,#31278,.T.) ;
#47247 = EDGE_CURVE('',#37804,#37760,#31279,.T.) ;
#47248 = EDGE_CURVE('',#37754,#37807,#31280,.T.) ;
#47249 = EDGE_CURVE('',#37805,#37758,#31281,.T.) ;
#47250 = EDGE_CURVE('',#37756,#37806,#31282,.T.) ;
#47251 = EDGE_CURVE('',#37341,#37216,#31283,.T.) ;
#47252 = EDGE_CURVE('',#37207,#37340,#31284,.T.) ;
#47253 = EDGE_CURVE('',#37342,#37335,#31285,.T.) ;
#47254 = EDGE_CURVE('',#37336,#37341,#31286,.T.) ;
#47255 = EDGE_CURVE('',#37342,#38126,#31287,.T.) ;
#47256 = EDGE_CURVE('',#38126,#37335,#31288,.T.) ;
#47257 = EDGE_CURVE('',#37207,#37345,#31289,.T.) ;
#47258 = EDGE_CURVE('',#37345,#37340,#31290,.T.) ;
#47259 = EDGE_CURVE('',#37336,#37215,#31291,.T.) ;
#47260 = EDGE_CURVE('',#36258,#37338,#31292,.T.) ;
#47261 = EDGE_CURVE('',#36259,#38127,#2182,.T.) ;
#47262 = EDGE_CURVE('',#38126,#38127,#5148,.T.) ;
#47263 = EDGE_CURVE('',#38128,#38126,#2183,.T.) ;
#47264 = EDGE_CURVE('',#38128,#38129,#2184,.T.) ;
#47265 = EDGE_CURVE('',#36441,#38129,#5149,.T.) ;
#47266 = EDGE_CURVE('',#37339,#36440,#31293,.T.) ;
#47267 = EDGE_CURVE('',#37346,#37339,#31294,.T.) ;
#47268 = EDGE_CURVE('',#37208,#37344,#31295,.T.) ;
#47269 = EDGE_CURVE('',#37337,#37214,#31296,.T.) ;
#47270 = EDGE_CURVE('',#37338,#36260,#31297,.T.) ;
#47271 = EDGE_CURVE('',#37333,#37337,#31298,.T.) ;
#47272 = EDGE_CURVE('',#37346,#36449,#31299,.T.) ;
#47273 = EDGE_CURVE('',#37208,#36536,#31300,.T.) ;
#47274 = EDGE_CURVE('',#36535,#37344,#31301,.T.) ;
#47275 = EDGE_CURVE('',#37333,#37213,#31302,.T.) ;
#47276 = EDGE_CURVE('',#37343,#36448,#31303,.T.) ;
#47277 = EDGE_CURVE('',#36537,#37343,#31304,.T.) ;
#47278 = EDGE_CURVE('',#38130,#36536,#5150,.T.) ;
#47279 = EDGE_CURVE('',#37209,#38130,#31305,.T.) ;
#47280 = EDGE_CURVE('',#37334,#37212,#31306,.T.) ;
#47281 = EDGE_CURVE('',#36261,#37329,#31307,.T.) ;
#47282 = EDGE_CURVE('',#37330,#37334,#31308,.T.) ;
#47283 = EDGE_CURVE('',#36444,#37329,#31309,.T.) ;
#47284 = EDGE_CURVE('',#36537,#36448,#31310,.T.) ;
#47285 = EDGE_CURVE('',#36598,#36539,#31311,.T.) ;
#47286 = EDGE_CURVE('',#36539,#36596,#31312,.T.) ;
#47287 = EDGE_CURVE('',#38130,#36705,#31313,.T.) ;
#47288 = EDGE_CURVE('',#38131,#38130,#31314,.T.) ;
#47289 = EDGE_CURVE('',#37209,#38131,#31315,.T.) ;
#47290 = EDGE_CURVE('',#37330,#37212,#31316,.T.) ;
#47291 = EDGE_CURVE('',#36445,#37332,#31317,.T.) ;
#47292 = EDGE_CURVE('',#36538,#36447,#31318,.T.) ;
#47293 = EDGE_CURVE('',#36668,#36538,#31319,.T.) ;
#47294 = EDGE_CURVE('',#38131,#36704,#31320,.T.) ;
#47295 = EDGE_CURVE('',#38132,#38131,#5151,.T.) ;
#47296 = EDGE_CURVE('',#37210,#38132,#31321,.T.) ;
#47297 = EDGE_CURVE('',#37331,#37211,#31322,.T.) ;
#47298 = EDGE_CURVE('',#37332,#36534,#31323,.T.) ;
#47299 = EDGE_CURVE('',#36531,#37331,#31324,.T.) ;
#47300 = EDGE_CURVE('',#36445,#36534,#31325,.T.) ;
#47301 = EDGE_CURVE('',#36669,#36447,#31326,.T.) ;
#47302 = EDGE_CURVE('',#38132,#36703,#31327,.T.) ;
#47303 = EDGE_CURVE('',#38133,#38132,#31328,.T.) ;
#47304 = EDGE_CURVE('',#37210,#38133,#31329,.T.) ;
#47305 = EDGE_CURVE('',#36530,#37211,#31330,.T.) ;
#47306 = EDGE_CURVE('',#36446,#36533,#31331,.T.) ;
#47307 = EDGE_CURVE('',#36670,#36446,#31332,.T.) ;
#47308 = EDGE_CURVE('',#38133,#36702,#31333,.T.) ;
#47309 = EDGE_CURVE('',#36530,#38133,#5152,.T.) ;
#47310 = EDGE_CURVE('',#36671,#36533,#31334,.T.) ;
#47311 = EDGE_CURVE('',#36532,#36601,#31335,.T.) ;
#47312 = EDGE_CURVE('',#36603,#36532,#31336,.T.) ;
#47313 = EDGE_CURVE('',#37713,#37746,#31337,.T.) ;
#47314 = EDGE_CURVE('',#37747,#37711,#31338,.T.) ;
#47315 = EDGE_CURVE('',#37748,#37709,#31339,.T.) ;
#47316 = EDGE_CURVE('',#37715,#37746,#31340,.T.) ;
#47317 = EDGE_CURVE('',#37749,#37707,#31341,.T.) ;
#47318 = EDGE_CURVE('',#37717,#37745,#31342,.T.) ;
#47319 = EDGE_CURVE('',#37750,#37705,#31343,.T.) ;
#47320 = EDGE_CURVE('',#37719,#37745,#31344,.T.) ;
#47321 = EDGE_CURVE('',#37751,#37703,#31345,.T.) ;
#47322 = EDGE_CURVE('',#37721,#37744,#31346,.T.) ;
#47323 = EDGE_CURVE('',#37751,#37701,#31347,.T.) ;
#47324 = EDGE_CURVE('',#37723,#37744,#31348,.T.) ;
#47325 = EDGE_CURVE('',#37752,#36370,#31349,.T.) ;
#47326 = EDGE_CURVE('',#37725,#37743,#31350,.T.) ;
#47327 = EDGE_CURVE('',#37752,#36369,#31351,.T.) ;
#47328 = EDGE_CURVE('',#37727,#37743,#31352,.T.) ;
#47329 = EDGE_CURVE('',#37729,#37742,#31353,.T.) ;
#47330 = EDGE_CURVE('',#37731,#37742,#31354,.T.) ;
#47331 = EDGE_CURVE('',#37753,#37697,#31355,.T.) ;
#47332 = EDGE_CURVE('',#37733,#37741,#31356,.T.) ;
#47333 = EDGE_CURVE('',#37753,#37695,#31357,.T.) ;
#47334 = EDGE_CURVE('',#37735,#37741,#31358,.T.) ;
#47335 = EDGE_CURVE('',#37737,#37693,#31359,.T.) ;
#47336 = EDGE_CURVE('',#37687,#37740,#31360,.T.) ;
#47337 = EDGE_CURVE('',#37738,#37691,#31361,.T.) ;
#47338 = EDGE_CURVE('',#37689,#37739,#31362,.T.) ;
#47339 = EDGE_CURVE('',#37359,#37206,#31363,.T.) ;
#47340 = EDGE_CURVE('',#37197,#37358,#31364,.T.) ;
#47341 = EDGE_CURVE('',#37360,#37353,#31365,.T.) ;
#47342 = EDGE_CURVE('',#37354,#37359,#31366,.T.) ;
#47343 = EDGE_CURVE('',#37360,#38134,#31367,.T.) ;
#47344 = EDGE_CURVE('',#38134,#37353,#31368,.T.) ;
#47345 = EDGE_CURVE('',#37197,#37363,#31369,.T.) ;
#47346 = EDGE_CURVE('',#37363,#37358,#31370,.T.) ;
#47347 = EDGE_CURVE('',#37354,#37205,#31371,.T.) ;
#47348 = EDGE_CURVE('',#36243,#37356,#31372,.T.) ;
#47349 = EDGE_CURVE('',#36244,#38135,#2185,.T.) ;
#47350 = EDGE_CURVE('',#38134,#38135,#5153,.T.) ;
#47351 = EDGE_CURVE('',#38136,#38134,#2186,.T.) ;
#47352 = EDGE_CURVE('',#38136,#38137,#2187,.T.) ;
#47353 = EDGE_CURVE('',#36431,#38137,#5154,.T.) ;
#47354 = EDGE_CURVE('',#37357,#36430,#31373,.T.) ;
#47355 = EDGE_CURVE('',#37364,#37357,#31374,.T.) ;
#47356 = EDGE_CURVE('',#37198,#37362,#31375,.T.) ;
#47357 = EDGE_CURVE('',#37355,#37204,#31376,.T.) ;
#47358 = EDGE_CURVE('',#37356,#36245,#31377,.T.) ;
#47359 = EDGE_CURVE('',#37351,#37355,#31378,.T.) ;
#47360 = EDGE_CURVE('',#37364,#36439,#31379,.T.) ;
#47361 = EDGE_CURVE('',#37198,#36526,#31380,.T.) ;
#47362 = EDGE_CURVE('',#36525,#37362,#31381,.T.) ;
#47363 = EDGE_CURVE('',#37351,#37203,#31382,.T.) ;
#47364 = EDGE_CURVE('',#37361,#36438,#31383,.T.) ;
#47365 = EDGE_CURVE('',#36527,#37361,#31384,.T.) ;
#47366 = EDGE_CURVE('',#38138,#36526,#5155,.T.) ;
#47367 = EDGE_CURVE('',#37199,#38138,#31385,.T.) ;
#47368 = EDGE_CURVE('',#37352,#37202,#31386,.T.) ;
#47369 = EDGE_CURVE('',#36246,#37347,#31387,.T.) ;
#47370 = EDGE_CURVE('',#37348,#37352,#31388,.T.) ;
#47371 = EDGE_CURVE('',#36434,#37347,#31389,.T.) ;
#47372 = EDGE_CURVE('',#36527,#36438,#31390,.T.) ;
#47373 = EDGE_CURVE('',#36602,#36529,#31391,.T.) ;
#47374 = EDGE_CURVE('',#36529,#36600,#31392,.T.) ;
#47375 = EDGE_CURVE('',#38138,#36701,#31393,.T.) ;
#47376 = EDGE_CURVE('',#38139,#38138,#31394,.T.) ;
#47377 = EDGE_CURVE('',#37199,#38139,#31395,.T.) ;
#47378 = EDGE_CURVE('',#37348,#37202,#31396,.T.) ;
#47379 = EDGE_CURVE('',#36435,#37350,#31397,.T.) ;
#47380 = EDGE_CURVE('',#36528,#36437,#31398,.T.) ;
#47381 = EDGE_CURVE('',#36672,#36528,#31399,.T.) ;
#47382 = EDGE_CURVE('',#38139,#36700,#31400,.T.) ;
#47383 = EDGE_CURVE('',#38140,#38139,#5156,.T.) ;
#47384 = EDGE_CURVE('',#37200,#38140,#31401,.T.) ;
#47385 = EDGE_CURVE('',#37349,#37201,#31402,.T.) ;
#47386 = EDGE_CURVE('',#37350,#36524,#31403,.T.) ;
#47387 = EDGE_CURVE('',#36521,#37349,#31404,.T.) ;
#47388 = EDGE_CURVE('',#36435,#36524,#31405,.T.) ;
#47389 = EDGE_CURVE('',#36673,#36437,#31406,.T.) ;
#47390 = EDGE_CURVE('',#38140,#36699,#31407,.T.) ;
#47391 = EDGE_CURVE('',#38141,#38140,#31408,.T.) ;
#47392 = EDGE_CURVE('',#37200,#38141,#31409,.T.) ;
#47393 = EDGE_CURVE('',#36520,#37201,#31410,.T.) ;
#47394 = EDGE_CURVE('',#36436,#36523,#31411,.T.) ;
#47395 = EDGE_CURVE('',#36674,#36436,#31412,.T.) ;
#47396 = EDGE_CURVE('',#38141,#36698,#31413,.T.) ;
#47397 = EDGE_CURVE('',#36520,#38141,#5157,.T.) ;
#47398 = EDGE_CURVE('',#36675,#36523,#31414,.T.) ;
#47399 = EDGE_CURVE('',#36522,#36605,#31415,.T.) ;
#47400 = EDGE_CURVE('',#36607,#36522,#31416,.T.) ;
#47401 = EDGE_CURVE('',#37646,#37679,#31417,.T.) ;
#47402 = EDGE_CURVE('',#37680,#37644,#31418,.T.) ;
#47403 = EDGE_CURVE('',#37681,#37642,#31419,.T.) ;
#47404 = EDGE_CURVE('',#37648,#37679,#31420,.T.) ;
#47405 = EDGE_CURVE('',#37682,#37640,#31421,.T.) ;
#47406 = EDGE_CURVE('',#37650,#37678,#31422,.T.) ;
#47407 = EDGE_CURVE('',#37683,#37638,#31423,.T.) ;
#47408 = EDGE_CURVE('',#37652,#37678,#31424,.T.) ;
#47409 = EDGE_CURVE('',#37684,#37636,#31425,.T.) ;
#47410 = EDGE_CURVE('',#37654,#37677,#31426,.T.) ;
#47411 = EDGE_CURVE('',#37684,#37634,#31427,.T.) ;
#47412 = EDGE_CURVE('',#37656,#37677,#31428,.T.) ;
#47413 = EDGE_CURVE('',#37685,#36372,#31429,.T.) ;
#47414 = EDGE_CURVE('',#37658,#37676,#31430,.T.) ;
#47415 = EDGE_CURVE('',#37685,#36371,#31431,.T.) ;
#47416 = EDGE_CURVE('',#37660,#37676,#31432,.T.) ;
#47417 = EDGE_CURVE('',#37662,#37675,#31433,.T.) ;
#47418 = EDGE_CURVE('',#37664,#37675,#31434,.T.) ;
#47419 = EDGE_CURVE('',#37686,#37630,#31435,.T.) ;
#47420 = EDGE_CURVE('',#37666,#37674,#31436,.T.) ;
#47421 = EDGE_CURVE('',#37686,#37628,#31437,.T.) ;
#47422 = EDGE_CURVE('',#37668,#37674,#31438,.T.) ;
#47423 = EDGE_CURVE('',#37670,#37626,#31439,.T.) ;
#47424 = EDGE_CURVE('',#37620,#37673,#31440,.T.) ;
#47425 = EDGE_CURVE('',#37671,#37624,#31441,.T.) ;
#47426 = EDGE_CURVE('',#37622,#37672,#31442,.T.) ;
#47427 = EDGE_CURVE('',#37377,#37196,#31443,.T.) ;
#47428 = EDGE_CURVE('',#37187,#37376,#31444,.T.) ;
#47429 = EDGE_CURVE('',#37378,#37371,#31445,.T.) ;
#47430 = EDGE_CURVE('',#37372,#37377,#31446,.T.) ;
#47431 = EDGE_CURVE('',#37378,#38142,#31447,.T.) ;
#47432 = EDGE_CURVE('',#38142,#37371,#31448,.T.) ;
#47433 = EDGE_CURVE('',#37187,#37381,#31449,.T.) ;
#47434 = EDGE_CURVE('',#37381,#37376,#31450,.T.) ;
#47435 = EDGE_CURVE('',#37372,#37195,#31451,.T.) ;
#47436 = EDGE_CURVE('',#36228,#37374,#31452,.T.) ;
#47437 = EDGE_CURVE('',#36229,#38143,#2188,.T.) ;
#47438 = EDGE_CURVE('',#38142,#38143,#5158,.T.) ;
#47439 = EDGE_CURVE('',#38144,#38142,#2189,.T.) ;
#47440 = EDGE_CURVE('',#38144,#38145,#2190,.T.) ;
#47441 = EDGE_CURVE('',#36421,#38145,#5159,.T.) ;
#47442 = EDGE_CURVE('',#37375,#36420,#31453,.T.) ;
#47443 = EDGE_CURVE('',#37382,#37375,#31454,.T.) ;
#47444 = EDGE_CURVE('',#37188,#37380,#31455,.T.) ;
#47445 = EDGE_CURVE('',#37373,#37194,#31456,.T.) ;
#47446 = EDGE_CURVE('',#37374,#36230,#31457,.T.) ;
#47447 = EDGE_CURVE('',#37369,#37373,#31458,.T.) ;
#47448 = EDGE_CURVE('',#37382,#36429,#31459,.T.) ;
#47449 = EDGE_CURVE('',#37188,#36516,#31460,.T.) ;
#47450 = EDGE_CURVE('',#36515,#37380,#31461,.T.) ;
#47451 = EDGE_CURVE('',#37369,#37193,#31462,.T.) ;
#47452 = EDGE_CURVE('',#37379,#36428,#31463,.T.) ;
#47453 = EDGE_CURVE('',#36517,#37379,#31464,.T.) ;
#47454 = EDGE_CURVE('',#38146,#36516,#5160,.T.) ;
#47455 = EDGE_CURVE('',#37189,#38146,#31465,.T.) ;
#47456 = EDGE_CURVE('',#37370,#37192,#31466,.T.) ;
#47457 = EDGE_CURVE('',#36231,#37365,#31467,.T.) ;
#47458 = EDGE_CURVE('',#37366,#37370,#31468,.T.) ;
#47459 = EDGE_CURVE('',#36424,#37365,#31469,.T.) ;
#47460 = EDGE_CURVE('',#36517,#36428,#31470,.T.) ;
#47461 = EDGE_CURVE('',#36606,#36519,#31471,.T.) ;
#47462 = EDGE_CURVE('',#36519,#36604,#31472,.T.) ;
#47463 = EDGE_CURVE('',#38146,#36697,#31473,.T.) ;
#47464 = EDGE_CURVE('',#38147,#38146,#31474,.T.) ;
#47465 = EDGE_CURVE('',#37189,#38147,#31475,.T.) ;
#47466 = EDGE_CURVE('',#37366,#37192,#31476,.T.) ;
#47467 = EDGE_CURVE('',#36425,#37368,#31477,.T.) ;
#47468 = EDGE_CURVE('',#36518,#36427,#31478,.T.) ;
#47469 = EDGE_CURVE('',#36676,#36518,#31479,.T.) ;
#47470 = EDGE_CURVE('',#38147,#36696,#31480,.T.) ;
#47471 = EDGE_CURVE('',#38148,#38147,#5161,.T.) ;
#47472 = EDGE_CURVE('',#37190,#38148,#31481,.T.) ;
#47473 = EDGE_CURVE('',#37367,#37191,#31482,.T.) ;
#47474 = EDGE_CURVE('',#37368,#36514,#31483,.T.) ;
#47475 = EDGE_CURVE('',#36511,#37367,#31484,.T.) ;
#47476 = EDGE_CURVE('',#36425,#36514,#31485,.T.) ;
#47477 = EDGE_CURVE('',#36677,#36427,#31486,.T.) ;
#47478 = EDGE_CURVE('',#38148,#36695,#31487,.T.) ;
#47479 = EDGE_CURVE('',#38149,#38148,#31488,.T.) ;
#47480 = EDGE_CURVE('',#37190,#38149,#31489,.T.) ;
#47481 = EDGE_CURVE('',#36510,#37191,#31490,.T.) ;
#47482 = EDGE_CURVE('',#36426,#36513,#31491,.T.) ;
#47483 = EDGE_CURVE('',#36678,#36426,#31492,.T.) ;
#47484 = EDGE_CURVE('',#38149,#36694,#31493,.T.) ;
#47485 = EDGE_CURVE('',#36510,#38149,#5162,.T.) ;
#47486 = EDGE_CURVE('',#36679,#36513,#31494,.T.) ;
#47487 = EDGE_CURVE('',#36512,#36609,#31495,.T.) ;
#47488 = EDGE_CURVE('',#36611,#36512,#31496,.T.) ;
#47489 = EDGE_CURVE('',#37579,#37612,#31497,.T.) ;
#47490 = EDGE_CURVE('',#37613,#37577,#31498,.T.) ;
#47491 = EDGE_CURVE('',#37614,#37575,#31499,.T.) ;
#47492 = EDGE_CURVE('',#37581,#37612,#31500,.T.) ;
#47493 = EDGE_CURVE('',#37615,#37573,#31501,.T.) ;
#47494 = EDGE_CURVE('',#37583,#37611,#31502,.T.) ;
#47495 = EDGE_CURVE('',#37616,#37571,#31503,.T.) ;
#47496 = EDGE_CURVE('',#37585,#37611,#31504,.T.) ;
#47497 = EDGE_CURVE('',#37617,#37569,#31505,.T.) ;
#47498 = EDGE_CURVE('',#37587,#37610,#31506,.T.) ;
#47499 = EDGE_CURVE('',#37617,#37567,#31507,.T.) ;
#47500 = EDGE_CURVE('',#37589,#37610,#31508,.T.) ;
#47501 = EDGE_CURVE('',#37618,#36374,#31509,.T.) ;
#47502 = EDGE_CURVE('',#37591,#37609,#31510,.T.) ;
#47503 = EDGE_CURVE('',#37618,#36373,#31511,.T.) ;
#47504 = EDGE_CURVE('',#37593,#37609,#31512,.T.) ;
#47505 = EDGE_CURVE('',#37595,#37608,#31513,.T.) ;
#47506 = EDGE_CURVE('',#37597,#37608,#31514,.T.) ;
#47507 = EDGE_CURVE('',#37619,#37563,#31515,.T.) ;
#47508 = EDGE_CURVE('',#37599,#37607,#31516,.T.) ;
#47509 = EDGE_CURVE('',#37619,#37561,#31517,.T.) ;
#47510 = EDGE_CURVE('',#37601,#37607,#31518,.T.) ;
#47511 = EDGE_CURVE('',#37603,#37559,#31519,.T.) ;
#47512 = EDGE_CURVE('',#37553,#37606,#31520,.T.) ;
#47513 = EDGE_CURVE('',#37604,#37557,#31521,.T.) ;
#47514 = EDGE_CURVE('',#37555,#37605,#31522,.T.) ;
#47515 = EDGE_CURVE('',#37395,#37186,#31523,.T.) ;
#47516 = EDGE_CURVE('',#37177,#37394,#31524,.T.) ;
#47517 = EDGE_CURVE('',#37396,#37389,#31525,.T.) ;
#47518 = EDGE_CURVE('',#37390,#37395,#31526,.T.) ;
#47519 = EDGE_CURVE('',#37396,#38150,#31527,.T.) ;
#47520 = EDGE_CURVE('',#38150,#37389,#31528,.T.) ;
#47521 = EDGE_CURVE('',#37177,#37399,#31529,.T.) ;
#47522 = EDGE_CURVE('',#37399,#37394,#31530,.T.) ;
#47523 = EDGE_CURVE('',#37390,#37185,#31531,.T.) ;
#47524 = EDGE_CURVE('',#36213,#37392,#31532,.T.) ;
#47525 = EDGE_CURVE('',#36214,#38151,#2191,.T.) ;
#47526 = EDGE_CURVE('',#38150,#38151,#5163,.T.) ;
#47527 = EDGE_CURVE('',#38152,#38150,#2192,.T.) ;
#47528 = EDGE_CURVE('',#38152,#38153,#2193,.T.) ;
#47529 = EDGE_CURVE('',#36411,#38153,#5164,.T.) ;
#47530 = EDGE_CURVE('',#37393,#36410,#31533,.T.) ;
#47531 = EDGE_CURVE('',#37400,#37393,#31534,.T.) ;
#47532 = EDGE_CURVE('',#37178,#37398,#31535,.T.) ;
#47533 = EDGE_CURVE('',#37391,#37184,#31536,.T.) ;
#47534 = EDGE_CURVE('',#37392,#36215,#31537,.T.) ;
#47535 = EDGE_CURVE('',#37387,#37391,#31538,.T.) ;
#47536 = EDGE_CURVE('',#37400,#36419,#31539,.T.) ;
#47537 = EDGE_CURVE('',#37178,#36506,#31540,.T.) ;
#47538 = EDGE_CURVE('',#36505,#37398,#31541,.T.) ;
#47539 = EDGE_CURVE('',#37387,#37183,#31542,.T.) ;
#47540 = EDGE_CURVE('',#37397,#36418,#31543,.T.) ;
#47541 = EDGE_CURVE('',#36507,#37397,#31544,.T.) ;
#47542 = EDGE_CURVE('',#38154,#36506,#5165,.T.) ;
#47543 = EDGE_CURVE('',#37179,#38154,#31545,.T.) ;
#47544 = EDGE_CURVE('',#37388,#37182,#31546,.T.) ;
#47545 = EDGE_CURVE('',#36216,#37383,#31547,.T.) ;
#47546 = EDGE_CURVE('',#37384,#37388,#31548,.T.) ;
#47547 = EDGE_CURVE('',#36414,#37383,#31549,.T.) ;
#47548 = EDGE_CURVE('',#36507,#36418,#31550,.T.) ;
#47549 = EDGE_CURVE('',#36610,#36509,#31551,.T.) ;
#47550 = EDGE_CURVE('',#36509,#36608,#31552,.T.) ;
#47551 = EDGE_CURVE('',#38154,#36693,#31553,.T.) ;
#47552 = EDGE_CURVE('',#38155,#38154,#31554,.T.) ;
#47553 = EDGE_CURVE('',#37179,#38155,#31555,.T.) ;
#47554 = EDGE_CURVE('',#37384,#37182,#31556,.T.) ;
#47555 = EDGE_CURVE('',#36415,#37386,#31557,.T.) ;
#47556 = EDGE_CURVE('',#36508,#36417,#31558,.T.) ;
#47557 = EDGE_CURVE('',#36680,#36508,#31559,.T.) ;
#47558 = EDGE_CURVE('',#38155,#36692,#31560,.T.) ;
#47559 = EDGE_CURVE('',#38156,#38155,#5166,.T.) ;
#47560 = EDGE_CURVE('',#37180,#38156,#31561,.T.) ;
#47561 = EDGE_CURVE('',#37385,#37181,#31562,.T.) ;
#47562 = EDGE_CURVE('',#37386,#36504,#31563,.T.) ;
#47563 = EDGE_CURVE('',#36501,#37385,#31564,.T.) ;
#47564 = EDGE_CURVE('',#36415,#36504,#31565,.T.) ;
#47565 = EDGE_CURVE('',#36681,#36417,#31566,.T.) ;
#47566 = EDGE_CURVE('',#38156,#36691,#31567,.T.) ;
#47567 = EDGE_CURVE('',#38157,#38156,#31568,.T.) ;
#47568 = EDGE_CURVE('',#37180,#38157,#31569,.T.) ;
#47569 = EDGE_CURVE('',#36500,#37181,#31570,.T.) ;
#47570 = EDGE_CURVE('',#36416,#36503,#31571,.T.) ;
#47571 = EDGE_CURVE('',#36682,#36416,#31572,.T.) ;
#47572 = EDGE_CURVE('',#38157,#36690,#31573,.T.) ;
#47573 = EDGE_CURVE('',#36500,#38157,#5167,.T.) ;
#47574 = EDGE_CURVE('',#36683,#36503,#31574,.T.) ;
#47575 = EDGE_CURVE('',#36502,#36613,#31575,.T.) ;
#47576 = EDGE_CURVE('',#36615,#36502,#31576,.T.) ;
#47577 = EDGE_CURVE('',#37512,#37545,#31577,.T.) ;
#47578 = EDGE_CURVE('',#37546,#37510,#31578,.T.) ;
#47579 = EDGE_CURVE('',#37547,#37508,#31579,.T.) ;
#47580 = EDGE_CURVE('',#37514,#37545,#31580,.T.) ;
#47581 = EDGE_CURVE('',#37548,#37506,#31581,.T.) ;
#47582 = EDGE_CURVE('',#37516,#37544,#31582,.T.) ;
#47583 = EDGE_CURVE('',#37549,#37504,#31583,.T.) ;
#47584 = EDGE_CURVE('',#37518,#37544,#31584,.T.) ;
#47585 = EDGE_CURVE('',#37550,#37502,#31585,.T.) ;
#47586 = EDGE_CURVE('',#37520,#37543,#31586,.T.) ;
#47587 = EDGE_CURVE('',#37550,#37500,#31587,.T.) ;
#47588 = EDGE_CURVE('',#37522,#37543,#31588,.T.) ;
#47589 = EDGE_CURVE('',#37551,#36376,#31589,.T.) ;
#47590 = EDGE_CURVE('',#37524,#37542,#31590,.T.) ;
#47591 = EDGE_CURVE('',#37551,#36375,#31591,.T.) ;
#47592 = EDGE_CURVE('',#37526,#37542,#31592,.T.) ;
#47593 = EDGE_CURVE('',#37528,#37541,#31593,.T.) ;
#47594 = EDGE_CURVE('',#37530,#37541,#31594,.T.) ;
#47595 = EDGE_CURVE('',#37552,#37496,#31595,.T.) ;
#47596 = EDGE_CURVE('',#37532,#37540,#31596,.T.) ;
#47597 = EDGE_CURVE('',#37552,#37494,#31597,.T.) ;
#47598 = EDGE_CURVE('',#37534,#37540,#31598,.T.) ;
#47599 = EDGE_CURVE('',#37536,#37492,#31599,.T.) ;
#47600 = EDGE_CURVE('',#37486,#37539,#31600,.T.) ;
#47601 = EDGE_CURVE('',#37537,#37490,#31601,.T.) ;
#47602 = EDGE_CURVE('',#37488,#37538,#31602,.T.) ;
#47603 = EDGE_CURVE('',#37413,#37176,#31603,.T.) ;
#47604 = EDGE_CURVE('',#37167,#37412,#31604,.T.) ;
#47605 = EDGE_CURVE('',#37414,#37407,#31605,.T.) ;
#47606 = EDGE_CURVE('',#37408,#37413,#31606,.T.) ;
#47607 = EDGE_CURVE('',#37414,#38158,#31607,.T.) ;
#47608 = EDGE_CURVE('',#38158,#37407,#31608,.T.) ;
#47609 = EDGE_CURVE('',#37167,#37417,#31609,.T.) ;
#47610 = EDGE_CURVE('',#37417,#37412,#31610,.T.) ;
#47611 = EDGE_CURVE('',#37408,#37175,#31611,.T.) ;
#47612 = EDGE_CURVE('',#36198,#37410,#31612,.T.) ;
#47613 = EDGE_CURVE('',#36199,#38159,#2194,.T.) ;
#47614 = EDGE_CURVE('',#38158,#38159,#5168,.T.) ;
#47615 = EDGE_CURVE('',#38160,#38158,#2195,.T.) ;
#47616 = EDGE_CURVE('',#38160,#38161,#2196,.T.) ;
#47617 = EDGE_CURVE('',#36401,#38161,#5169,.T.) ;
#47618 = EDGE_CURVE('',#37411,#36400,#31613,.T.) ;
#47619 = EDGE_CURVE('',#37418,#37411,#31614,.T.) ;
#47620 = EDGE_CURVE('',#37168,#37416,#31615,.T.) ;
#47621 = EDGE_CURVE('',#37409,#37174,#31616,.T.) ;
#47622 = EDGE_CURVE('',#37410,#36200,#31617,.T.) ;
#47623 = EDGE_CURVE('',#37405,#37409,#31618,.T.) ;
#47624 = EDGE_CURVE('',#37418,#36409,#31619,.T.) ;
#47625 = EDGE_CURVE('',#37168,#36496,#31620,.T.) ;
#47626 = EDGE_CURVE('',#36495,#37416,#31621,.T.) ;
#47627 = EDGE_CURVE('',#37405,#37173,#31622,.T.) ;
#47628 = EDGE_CURVE('',#37415,#36408,#31623,.T.) ;
#47629 = EDGE_CURVE('',#36497,#37415,#31624,.T.) ;
#47630 = EDGE_CURVE('',#38162,#36496,#5170,.T.) ;
#47631 = EDGE_CURVE('',#37169,#38162,#31625,.T.) ;
#47632 = EDGE_CURVE('',#37406,#37172,#31626,.T.) ;
#47633 = EDGE_CURVE('',#36201,#37401,#31627,.T.) ;
#47634 = EDGE_CURVE('',#37402,#37406,#31628,.T.) ;
#47635 = EDGE_CURVE('',#36404,#37401,#31629,.T.) ;
#47636 = EDGE_CURVE('',#36497,#36408,#31630,.T.) ;
#47637 = EDGE_CURVE('',#36614,#36499,#31631,.T.) ;
#47638 = EDGE_CURVE('',#36499,#36612,#31632,.T.) ;
#47639 = EDGE_CURVE('',#38162,#36688,#31633,.T.) ;
#47640 = EDGE_CURVE('',#38163,#38162,#31634,.T.) ;
#47641 = EDGE_CURVE('',#37169,#38163,#31635,.T.) ;
#47642 = EDGE_CURVE('',#37402,#37172,#31636,.T.) ;
#47643 = EDGE_CURVE('',#36405,#37404,#31637,.T.) ;
#47644 = EDGE_CURVE('',#36498,#36407,#31638,.T.) ;
#47645 = EDGE_CURVE('',#36684,#36498,#31639,.T.) ;
#47646 = EDGE_CURVE('',#38163,#36689,#31640,.T.) ;
#47647 = EDGE_CURVE('',#38164,#38163,#5171,.T.) ;
#47648 = EDGE_CURVE('',#37170,#38164,#31641,.T.) ;
#47649 = EDGE_CURVE('',#37403,#37171,#31642,.T.) ;
#47650 = EDGE_CURVE('',#37404,#36494,#31643,.T.) ;
#47651 = EDGE_CURVE('',#36491,#37403,#31644,.T.) ;
#47652 = EDGE_CURVE('',#36405,#36494,#31645,.T.) ;
#47653 = EDGE_CURVE('',#36685,#36407,#31646,.T.) ;
#47654 = EDGE_CURVE('',#38164,#36729,#31647,.T.) ;
#47655 = EDGE_CURVE('',#38165,#38164,#31648,.T.) ;
#47656 = EDGE_CURVE('',#37170,#38165,#31649,.T.) ;
#47657 = EDGE_CURVE('',#36490,#37171,#31650,.T.) ;
#47658 = EDGE_CURVE('',#36406,#36493,#31651,.T.) ;
#47659 = EDGE_CURVE('',#36645,#36406,#31652,.T.) ;
#47660 = EDGE_CURVE('',#38165,#36728,#31653,.T.) ;
#47661 = EDGE_CURVE('',#36490,#38165,#5172,.T.) ;
#47662 = EDGE_CURVE('',#36644,#36493,#31654,.T.) ;
#47663 = EDGE_CURVE('',#36492,#36686,#31655,.T.) ;
#47664 = EDGE_CURVE('',#36646,#36492,#31656,.T.) ;
#47665 = EDGE_CURVE('',#37445,#37478,#31657,.T.) ;
#47666 = EDGE_CURVE('',#37479,#37443,#31658,.T.) ;
#47667 = EDGE_CURVE('',#37480,#37441,#31659,.T.) ;
#47668 = EDGE_CURVE('',#37447,#37478,#31660,.T.) ;
#47669 = EDGE_CURVE('',#37481,#37439,#31661,.T.) ;
#47670 = EDGE_CURVE('',#37449,#37477,#31662,.T.) ;
#47671 = EDGE_CURVE('',#37482,#37437,#31663,.T.) ;
#47672 = EDGE_CURVE('',#37451,#37477,#31664,.T.) ;
#47673 = EDGE_CURVE('',#37483,#37435,#31665,.T.) ;
#47674 = EDGE_CURVE('',#37453,#37476,#31666,.T.) ;
#47675 = EDGE_CURVE('',#37483,#37433,#31667,.T.) ;
#47676 = EDGE_CURVE('',#37455,#37476,#31668,.T.) ;
#47677 = EDGE_CURVE('',#37484,#36378,#31669,.T.) ;
#47678 = EDGE_CURVE('',#37457,#37475,#31670,.T.) ;
#47679 = EDGE_CURVE('',#37484,#36377,#31671,.T.) ;
#47680 = EDGE_CURVE('',#37459,#37475,#31672,.T.) ;
#47681 = EDGE_CURVE('',#37461,#37474,#31673,.T.) ;
#47682 = EDGE_CURVE('',#37463,#37474,#31674,.T.) ;
#47683 = EDGE_CURVE('',#37485,#37429,#31675,.T.) ;
#47684 = EDGE_CURVE('',#37465,#37473,#31676,.T.) ;
#47685 = EDGE_CURVE('',#37485,#37427,#31677,.T.) ;
#47686 = EDGE_CURVE('',#37467,#37473,#31678,.T.) ;
#47687 = EDGE_CURVE('',#37469,#37425,#31679,.T.) ;
#47688 = EDGE_CURVE('',#37419,#37472,#31680,.T.) ;
#47689 = EDGE_CURVE('',#37470,#37423,#31681,.T.) ;
#47690 = EDGE_CURVE('',#37421,#37471,#31682,.T.) ;
#47691 = EDGE_CURVE('',#38166,#38167,#5173,.T.) ;
#47692 = EDGE_CURVE('',#38167,#38168,#5174,.T.) ;
#47693 = EDGE_CURVE('',#38168,#38169,#5175,.T.) ;
#47694 = EDGE_CURVE('',#38169,#38166,#5176,.T.) ;
#47695 = EDGE_CURVE('',#38170,#38171,#5177,.T.) ;
#47696 = EDGE_CURVE('',#38171,#38172,#5178,.T.) ;
#47697 = EDGE_CURVE('',#38172,#38173,#5179,.T.) ;
#47698 = EDGE_CURVE('',#38173,#38170,#5180,.T.) ;
#47699 = EDGE_CURVE('',#38174,#38175,#5181,.T.) ;
#47700 = EDGE_CURVE('',#38175,#38176,#5182,.T.) ;
#47701 = EDGE_CURVE('',#38176,#38177,#5183,.T.) ;
#47702 = EDGE_CURVE('',#38177,#38174,#5184,.T.) ;
#47703 = EDGE_CURVE('',#38178,#38179,#5185,.T.) ;
#47704 = EDGE_CURVE('',#38179,#38180,#5186,.T.) ;
#47705 = EDGE_CURVE('',#38180,#38181,#5187,.T.) ;
#47706 = EDGE_CURVE('',#38181,#38178,#5188,.T.) ;
#47707 = EDGE_CURVE('',#38182,#38183,#5189,.T.) ;
#47708 = EDGE_CURVE('',#38183,#38184,#5190,.T.) ;
#47709 = EDGE_CURVE('',#38185,#38184,#5191,.T.) ;
#47710 = EDGE_CURVE('',#38185,#38182,#5192,.T.) ;
#47711 = EDGE_CURVE('',#38186,#38187,#5193,.T.) ;
#47712 = EDGE_CURVE('',#38187,#36481,#31683,.T.) ;
#47713 = EDGE_CURVE('',#38097,#38188,#31684,.T.) ;
#47714 = EDGE_CURVE('',#38188,#38189,#5194,.T.) ;
#47715 = EDGE_CURVE('',#38189,#38186,#5195,.T.) ;
#47716 = EDGE_CURVE('',#38190,#38191,#5196,.T.) ;
#47717 = EDGE_CURVE('',#38191,#36360,#31685,.T.) ;
#47718 = EDGE_CURVE('',#36359,#38192,#31686,.T.) ;
#47719 = EDGE_CURVE('',#38192,#38193,#5197,.T.) ;
#47720 = EDGE_CURVE('',#38193,#38190,#5198,.T.) ;
#47721 = EDGE_CURVE('',#38095,#38167,#31687,.T.) ;
#47722 = EDGE_CURVE('',#38166,#38096,#31688,.T.) ;
#47723 = EDGE_CURVE('',#38184,#36483,#31689,.T.) ;
#47724 = EDGE_CURVE('',#36482,#38185,#31690,.T.) ;
#47725 = EDGE_CURVE('',#38194,#38195,#5199,.T.) ;
#47726 = EDGE_CURVE('',#38195,#38196,#5200,.T.) ;
#47727 = EDGE_CURVE('',#38196,#38197,#5201,.T.) ;
#47728 = EDGE_CURVE('',#38197,#38194,#5202,.T.) ;
#47729 = EDGE_CURVE('',#38198,#38199,#5203,.T.) ;
#47730 = EDGE_CURVE('',#38199,#38025,#5204,.T.) ;
#47731 = EDGE_CURVE('',#38024,#38198,#5205,.T.) ;
#47732 = EDGE_CURVE('',#38028,#38200,#5206,.T.) ;
#47733 = EDGE_CURVE('',#38200,#38201,#5207,.T.) ;
#47734 = EDGE_CURVE('',#38201,#38029,#5208,.T.) ;
#47735 = EDGE_CURVE('',#38202,#38203,#5209,.T.) ;
#47736 = EDGE_CURVE('',#38203,#38204,#5210,.T.) ;
#47737 = EDGE_CURVE('',#38204,#38205,#5211,.T.) ;
#47738 = EDGE_CURVE('',#38205,#38202,#5212,.T.) ;
#47739 = EDGE_CURVE('',#38206,#38207,#5213,.T.) ;
#47740 = EDGE_CURVE('',#38207,#38208,#5214,.T.) ;
#47741 = EDGE_CURVE('',#38208,#38209,#5215,.T.) ;
#47742 = EDGE_CURVE('',#38209,#38206,#5216,.T.) ;
#47743 = EDGE_CURVE('',#38210,#38211,#5217,.T.) ;
#47744 = EDGE_CURVE('',#38211,#38022,#5218,.T.) ;
#47745 = EDGE_CURVE('',#38023,#38210,#5219,.T.) ;
#47746 = EDGE_CURVE('',#38026,#38212,#5220,.T.) ;
#47747 = EDGE_CURVE('',#38212,#38213,#5221,.T.) ;
#47748 = EDGE_CURVE('',#38213,#38027,#5222,.T.) ;
#47749 = EDGE_CURVE('',#38214,#38215,#5223,.T.) ;
#47750 = EDGE_CURVE('',#38215,#38216,#5224,.T.) ;
#47751 = EDGE_CURVE('',#38216,#38217,#5225,.T.) ;
#47752 = EDGE_CURVE('',#38217,#38214,#5226,.T.) ;
#47753 = EDGE_CURVE('',#38218,#38219,#5227,.T.) ;
#47754 = EDGE_CURVE('',#38219,#38220,#5228,.T.) ;
#47755 = EDGE_CURVE('',#38220,#38221,#5229,.T.) ;
#47756 = EDGE_CURVE('',#38221,#38218,#5230,.T.) ;
#47757 = EDGE_CURVE('',#38222,#38223,#5231,.T.) ;
#47758 = EDGE_CURVE('',#38223,#38224,#5232,.T.) ;
#47759 = EDGE_CURVE('',#38224,#38225,#5233,.T.) ;
#47760 = EDGE_CURVE('',#38225,#38222,#5234,.T.) ;
#47761 = EDGE_CURVE('',#38226,#38227,#5235,.T.) ;
#47762 = EDGE_CURVE('',#38227,#38228,#5236,.T.) ;
#47763 = EDGE_CURVE('',#38228,#38229,#5237,.T.) ;
#47764 = EDGE_CURVE('',#38229,#38226,#5238,.T.) ;
#47765 = EDGE_CURVE('',#38230,#38231,#5239,.T.) ;
#47766 = EDGE_CURVE('',#38231,#38232,#5240,.T.) ;
#47767 = EDGE_CURVE('',#38233,#38232,#5241,.T.) ;
#47768 = EDGE_CURVE('',#38233,#38230,#5242,.T.) ;
#47769 = EDGE_CURVE('',#38234,#38235,#5243,.T.) ;
#47770 = EDGE_CURVE('',#38235,#36471,#31691,.T.) ;
#47771 = EDGE_CURVE('',#38105,#38236,#31692,.T.) ;
#47772 = EDGE_CURVE('',#38236,#38237,#5244,.T.) ;
#47773 = EDGE_CURVE('',#38237,#38234,#5245,.T.) ;
#47774 = EDGE_CURVE('',#38238,#38239,#5246,.T.) ;
#47775 = EDGE_CURVE('',#38239,#36309,#31693,.T.) ;
#47776 = EDGE_CURVE('',#36308,#38240,#31694,.T.) ;
#47777 = EDGE_CURVE('',#38240,#38241,#5247,.T.) ;
#47778 = EDGE_CURVE('',#38241,#38238,#5248,.T.) ;
#47779 = EDGE_CURVE('',#38103,#38215,#31695,.T.) ;
#47780 = EDGE_CURVE('',#38214,#38104,#31696,.T.) ;
#47781 = EDGE_CURVE('',#38232,#36473,#31697,.T.) ;
#47782 = EDGE_CURVE('',#36472,#38233,#31698,.T.) ;
#47783 = EDGE_CURVE('',#38242,#38243,#5249,.T.) ;
#47784 = EDGE_CURVE('',#38243,#38244,#5250,.T.) ;
#47785 = EDGE_CURVE('',#38244,#38245,#5251,.T.) ;
#47786 = EDGE_CURVE('',#38245,#38242,#5252,.T.) ;
#47787 = EDGE_CURVE('',#38246,#38247,#5253,.T.) ;
#47788 = EDGE_CURVE('',#38247,#38033,#5254,.T.) ;
#47789 = EDGE_CURVE('',#38032,#38246,#5255,.T.) ;
#47790 = EDGE_CURVE('',#38036,#38248,#5256,.T.) ;
#47791 = EDGE_CURVE('',#38248,#38249,#5257,.T.) ;
#47792 = EDGE_CURVE('',#38249,#38037,#5258,.T.) ;
#47793 = EDGE_CURVE('',#38250,#38251,#5259,.T.) ;
#47794 = EDGE_CURVE('',#38251,#38252,#5260,.T.) ;
#47795 = EDGE_CURVE('',#38252,#38253,#5261,.T.) ;
#47796 = EDGE_CURVE('',#38253,#38250,#5262,.T.) ;
#47797 = EDGE_CURVE('',#38254,#38255,#5263,.T.) ;
#47798 = EDGE_CURVE('',#38255,#38256,#5264,.T.) ;
#47799 = EDGE_CURVE('',#38256,#38257,#5265,.T.) ;
#47800 = EDGE_CURVE('',#38257,#38254,#5266,.T.) ;
#47801 = EDGE_CURVE('',#38258,#38259,#5267,.T.) ;
#47802 = EDGE_CURVE('',#38259,#38030,#5268,.T.) ;
#47803 = EDGE_CURVE('',#38031,#38258,#5269,.T.) ;
#47804 = EDGE_CURVE('',#38034,#38260,#5270,.T.) ;
#47805 = EDGE_CURVE('',#38260,#38261,#5271,.T.) ;
#47806 = EDGE_CURVE('',#38261,#38035,#5272,.T.) ;
#47807 = EDGE_CURVE('',#38262,#38263,#5273,.T.) ;
#47808 = EDGE_CURVE('',#38263,#38264,#5274,.T.) ;
#47809 = EDGE_CURVE('',#38264,#38265,#5275,.T.) ;
#47810 = EDGE_CURVE('',#38265,#38262,#5276,.T.) ;
#47811 = EDGE_CURVE('',#38266,#38267,#5277,.T.) ;
#47812 = EDGE_CURVE('',#38267,#38268,#5278,.T.) ;
#47813 = EDGE_CURVE('',#38268,#38269,#5279,.T.) ;
#47814 = EDGE_CURVE('',#38269,#38266,#5280,.T.) ;
#47815 = EDGE_CURVE('',#38270,#38271,#5281,.T.) ;
#47816 = EDGE_CURVE('',#38271,#38272,#5282,.T.) ;
#47817 = EDGE_CURVE('',#38272,#38273,#5283,.T.) ;
#47818 = EDGE_CURVE('',#38273,#38270,#5284,.T.) ;
#47819 = EDGE_CURVE('',#38274,#38275,#5285,.T.) ;
#47820 = EDGE_CURVE('',#38275,#38276,#5286,.T.) ;
#47821 = EDGE_CURVE('',#38276,#38277,#5287,.T.) ;
#47822 = EDGE_CURVE('',#38277,#38274,#5288,.T.) ;
#47823 = EDGE_CURVE('',#38278,#38279,#5289,.T.) ;
#47824 = EDGE_CURVE('',#38279,#38280,#5290,.T.) ;
#47825 = EDGE_CURVE('',#38281,#38280,#5291,.T.) ;
#47826 = EDGE_CURVE('',#38281,#38278,#5292,.T.) ;
#47827 = EDGE_CURVE('',#38282,#38283,#5293,.T.) ;
#47828 = EDGE_CURVE('',#38283,#36461,#31699,.T.) ;
#47829 = EDGE_CURVE('',#38113,#38284,#31700,.T.) ;
#47830 = EDGE_CURVE('',#38284,#38285,#5294,.T.) ;
#47831 = EDGE_CURVE('',#38285,#38282,#5295,.T.) ;
#47832 = EDGE_CURVE('',#38286,#38287,#5296,.T.) ;
#47833 = EDGE_CURVE('',#38287,#36294,#31701,.T.) ;
#47834 = EDGE_CURVE('',#36293,#38288,#31702,.T.) ;
#47835 = EDGE_CURVE('',#38288,#38289,#5297,.T.) ;
#47836 = EDGE_CURVE('',#38289,#38286,#5298,.T.) ;
#47837 = EDGE_CURVE('',#38111,#38263,#31703,.T.) ;
#47838 = EDGE_CURVE('',#38262,#38112,#31704,.T.) ;
#47839 = EDGE_CURVE('',#38280,#36463,#31705,.T.) ;
#47840 = EDGE_CURVE('',#36462,#38281,#31706,.T.) ;
#47841 = EDGE_CURVE('',#38290,#38291,#5299,.T.) ;
#47842 = EDGE_CURVE('',#38291,#38292,#5300,.T.) ;
#47843 = EDGE_CURVE('',#38292,#38293,#5301,.T.) ;
#47844 = EDGE_CURVE('',#38293,#38290,#5302,.T.) ;
#47845 = EDGE_CURVE('',#38294,#38295,#5303,.T.) ;
#47846 = EDGE_CURVE('',#38295,#38041,#5304,.T.) ;
#47847 = EDGE_CURVE('',#38040,#38294,#5305,.T.) ;
#47848 = EDGE_CURVE('',#38044,#38296,#5306,.T.) ;
#47849 = EDGE_CURVE('',#38296,#38297,#5307,.T.) ;
#47850 = EDGE_CURVE('',#38297,#38045,#5308,.T.) ;
#47851 = EDGE_CURVE('',#38298,#38299,#5309,.T.) ;
#47852 = EDGE_CURVE('',#38299,#38300,#5310,.T.) ;
#47853 = EDGE_CURVE('',#38300,#38301,#5311,.T.) ;
#47854 = EDGE_CURVE('',#38301,#38298,#5312,.T.) ;
#47855 = EDGE_CURVE('',#38302,#38303,#5313,.T.) ;
#47856 = EDGE_CURVE('',#38303,#38304,#5314,.T.) ;
#47857 = EDGE_CURVE('',#38304,#38305,#5315,.T.) ;
#47858 = EDGE_CURVE('',#38305,#38302,#5316,.T.) ;
#47859 = EDGE_CURVE('',#38306,#38307,#5317,.T.) ;
#47860 = EDGE_CURVE('',#38307,#38038,#5318,.T.) ;
#47861 = EDGE_CURVE('',#38039,#38306,#5319,.T.) ;
#47862 = EDGE_CURVE('',#38042,#38308,#5320,.T.) ;
#47863 = EDGE_CURVE('',#38308,#38309,#5321,.T.) ;
#47864 = EDGE_CURVE('',#38309,#38043,#5322,.T.) ;
#47865 = EDGE_CURVE('',#38310,#38311,#5323,.T.) ;
#47866 = EDGE_CURVE('',#38311,#38312,#5324,.T.) ;
#47867 = EDGE_CURVE('',#38312,#38313,#5325,.T.) ;
#47868 = EDGE_CURVE('',#38313,#38310,#5326,.T.) ;
#47869 = EDGE_CURVE('',#38314,#38315,#5327,.T.) ;
#47870 = EDGE_CURVE('',#38315,#38316,#5328,.T.) ;
#47871 = EDGE_CURVE('',#38316,#38317,#5329,.T.) ;
#47872 = EDGE_CURVE('',#38317,#38314,#5330,.T.) ;
#47873 = EDGE_CURVE('',#38318,#38319,#5331,.T.) ;
#47874 = EDGE_CURVE('',#38319,#38320,#5332,.T.) ;
#47875 = EDGE_CURVE('',#38320,#38321,#5333,.T.) ;
#47876 = EDGE_CURVE('',#38321,#38318,#5334,.T.) ;
#47877 = EDGE_CURVE('',#38322,#38323,#5335,.T.) ;
#47878 = EDGE_CURVE('',#38323,#38324,#5336,.T.) ;
#47879 = EDGE_CURVE('',#38324,#38325,#5337,.T.) ;
#47880 = EDGE_CURVE('',#38325,#38322,#5338,.T.) ;
#47881 = EDGE_CURVE('',#38326,#38327,#5339,.T.) ;
#47882 = EDGE_CURVE('',#38327,#38328,#5340,.T.) ;
#47883 = EDGE_CURVE('',#38329,#38328,#5341,.T.) ;
#47884 = EDGE_CURVE('',#38329,#38326,#5342,.T.) ;
#47885 = EDGE_CURVE('',#38330,#38331,#5343,.T.) ;
#47886 = EDGE_CURVE('',#38331,#36451,#31707,.T.) ;
#47887 = EDGE_CURVE('',#38121,#38332,#31708,.T.) ;
#47888 = EDGE_CURVE('',#38332,#38333,#5344,.T.) ;
#47889 = EDGE_CURVE('',#38333,#38330,#5345,.T.) ;
#47890 = EDGE_CURVE('',#38334,#38335,#5346,.T.) ;
#47891 = EDGE_CURVE('',#38335,#36279,#31709,.T.) ;
#47892 = EDGE_CURVE('',#36278,#38336,#31710,.T.) ;
#47893 = EDGE_CURVE('',#38336,#38337,#5347,.T.) ;
#47894 = EDGE_CURVE('',#38337,#38334,#5348,.T.) ;
#47895 = EDGE_CURVE('',#38119,#38311,#31711,.T.) ;
#47896 = EDGE_CURVE('',#38310,#38120,#31712,.T.) ;
#47897 = EDGE_CURVE('',#38328,#36453,#31713,.T.) ;
#47898 = EDGE_CURVE('',#36452,#38329,#31714,.T.) ;
#47899 = EDGE_CURVE('',#38338,#38339,#5349,.T.) ;
#47900 = EDGE_CURVE('',#38339,#38340,#5350,.T.) ;
#47901 = EDGE_CURVE('',#38340,#38341,#5351,.T.) ;
#47902 = EDGE_CURVE('',#38341,#38338,#5352,.T.) ;
#47903 = EDGE_CURVE('',#38342,#38343,#5353,.T.) ;
#47904 = EDGE_CURVE('',#38343,#38049,#5354,.T.) ;
#47905 = EDGE_CURVE('',#38048,#38342,#5355,.T.) ;
#47906 = EDGE_CURVE('',#38052,#38344,#5356,.T.) ;
#47907 = EDGE_CURVE('',#38344,#38345,#5357,.T.) ;
#47908 = EDGE_CURVE('',#38345,#38053,#5358,.T.) ;
#47909 = EDGE_CURVE('',#38346,#38347,#5359,.T.) ;
#47910 = EDGE_CURVE('',#38347,#38348,#5360,.T.) ;
#47911 = EDGE_CURVE('',#38348,#38349,#5361,.T.) ;
#47912 = EDGE_CURVE('',#38349,#38346,#5362,.T.) ;
#47913 = EDGE_CURVE('',#38350,#38351,#5363,.T.) ;
#47914 = EDGE_CURVE('',#38351,#38352,#5364,.T.) ;
#47915 = EDGE_CURVE('',#38352,#38353,#5365,.T.) ;
#47916 = EDGE_CURVE('',#38353,#38350,#5366,.T.) ;
#47917 = EDGE_CURVE('',#38354,#38355,#5367,.T.) ;
#47918 = EDGE_CURVE('',#38355,#38046,#5368,.T.) ;
#47919 = EDGE_CURVE('',#38047,#38354,#5369,.T.) ;
#47920 = EDGE_CURVE('',#38050,#38356,#5370,.T.) ;
#47921 = EDGE_CURVE('',#38356,#38357,#5371,.T.) ;
#47922 = EDGE_CURVE('',#38357,#38051,#5372,.T.) ;
#47923 = EDGE_CURVE('',#38358,#38359,#5373,.T.) ;
#47924 = EDGE_CURVE('',#38359,#38360,#5374,.T.) ;
#47925 = EDGE_CURVE('',#38360,#38361,#5375,.T.) ;
#47926 = EDGE_CURVE('',#38361,#38358,#5376,.T.) ;
#47927 = EDGE_CURVE('',#38362,#38363,#5377,.T.) ;
#47928 = EDGE_CURVE('',#38363,#38364,#5378,.T.) ;
#47929 = EDGE_CURVE('',#38364,#38365,#5379,.T.) ;
#47930 = EDGE_CURVE('',#38365,#38362,#5380,.T.) ;
#47931 = EDGE_CURVE('',#38366,#38367,#5381,.T.) ;
#47932 = EDGE_CURVE('',#38367,#38368,#5382,.T.) ;
#47933 = EDGE_CURVE('',#38368,#38369,#5383,.T.) ;
#47934 = EDGE_CURVE('',#38369,#38366,#5384,.T.) ;
#47935 = EDGE_CURVE('',#38370,#38371,#5385,.T.) ;
#47936 = EDGE_CURVE('',#38371,#38372,#5386,.T.) ;
#47937 = EDGE_CURVE('',#38372,#38373,#5387,.T.) ;
#47938 = EDGE_CURVE('',#38373,#38370,#5388,.T.) ;
#47939 = EDGE_CURVE('',#38374,#38375,#5389,.T.) ;
#47940 = EDGE_CURVE('',#38375,#38376,#5390,.T.) ;
#47941 = EDGE_CURVE('',#38377,#38376,#5391,.T.) ;
#47942 = EDGE_CURVE('',#38377,#38374,#5392,.T.) ;
#47943 = EDGE_CURVE('',#38378,#38379,#5393,.T.) ;
#47944 = EDGE_CURVE('',#38379,#36441,#31715,.T.) ;
#47945 = EDGE_CURVE('',#38129,#38380,#31716,.T.) ;
#47946 = EDGE_CURVE('',#38380,#38381,#5394,.T.) ;
#47947 = EDGE_CURVE('',#38381,#38378,#5395,.T.) ;
#47948 = EDGE_CURVE('',#38382,#38383,#5396,.T.) ;
#47949 = EDGE_CURVE('',#38383,#36264,#31717,.T.) ;
#47950 = EDGE_CURVE('',#36263,#38384,#31718,.T.) ;
#47951 = EDGE_CURVE('',#38384,#38385,#5397,.T.) ;
#47952 = EDGE_CURVE('',#38385,#38382,#5398,.T.) ;
#47953 = EDGE_CURVE('',#38127,#38359,#31719,.T.) ;
#47954 = EDGE_CURVE('',#38358,#38128,#31720,.T.) ;
#47955 = EDGE_CURVE('',#38376,#36443,#31721,.T.) ;
#47956 = EDGE_CURVE('',#36442,#38377,#31722,.T.) ;
#47957 = EDGE_CURVE('',#38386,#38387,#5399,.T.) ;
#47958 = EDGE_CURVE('',#38387,#38388,#5400,.T.) ;
#47959 = EDGE_CURVE('',#38388,#38389,#5401,.T.) ;
#47960 = EDGE_CURVE('',#38389,#38386,#5402,.T.) ;
#47961 = EDGE_CURVE('',#38390,#38391,#5403,.T.) ;
#47962 = EDGE_CURVE('',#38391,#38057,#5404,.T.) ;
#47963 = EDGE_CURVE('',#38056,#38390,#5405,.T.) ;
#47964 = EDGE_CURVE('',#38060,#38392,#5406,.T.) ;
#47965 = EDGE_CURVE('',#38392,#38393,#5407,.T.) ;
#47966 = EDGE_CURVE('',#38393,#38061,#5408,.T.) ;
#47967 = EDGE_CURVE('',#38394,#38395,#5409,.T.) ;
#47968 = EDGE_CURVE('',#38395,#38396,#5410,.T.) ;
#47969 = EDGE_CURVE('',#38396,#38397,#5411,.T.) ;
#47970 = EDGE_CURVE('',#38397,#38394,#5412,.T.) ;
#47971 = EDGE_CURVE('',#38398,#38399,#5413,.T.) ;
#47972 = EDGE_CURVE('',#38399,#38400,#5414,.T.) ;
#47973 = EDGE_CURVE('',#38400,#38401,#5415,.T.) ;
#47974 = EDGE_CURVE('',#38401,#38398,#5416,.T.) ;
#47975 = EDGE_CURVE('',#38402,#38403,#5417,.T.) ;
#47976 = EDGE_CURVE('',#38403,#38054,#5418,.T.) ;
#47977 = EDGE_CURVE('',#38055,#38402,#5419,.T.) ;
#47978 = EDGE_CURVE('',#38058,#38404,#5420,.T.) ;
#47979 = EDGE_CURVE('',#38404,#38405,#5421,.T.) ;
#47980 = EDGE_CURVE('',#38405,#38059,#5422,.T.) ;
#47981 = EDGE_CURVE('',#38406,#38407,#5423,.T.) ;
#47982 = EDGE_CURVE('',#38407,#38408,#5424,.T.) ;
#47983 = EDGE_CURVE('',#38408,#38409,#5425,.T.) ;
#47984 = EDGE_CURVE('',#38409,#38406,#5426,.T.) ;
#47985 = EDGE_CURVE('',#38410,#38411,#5427,.T.) ;
#47986 = EDGE_CURVE('',#38411,#38412,#5428,.T.) ;
#47987 = EDGE_CURVE('',#38412,#38413,#5429,.T.) ;
#47988 = EDGE_CURVE('',#38413,#38410,#5430,.T.) ;
#47989 = EDGE_CURVE('',#38414,#38415,#5431,.T.) ;
#47990 = EDGE_CURVE('',#38415,#38416,#5432,.T.) ;
#47991 = EDGE_CURVE('',#38416,#38417,#5433,.T.) ;
#47992 = EDGE_CURVE('',#38417,#38414,#5434,.T.) ;
#47993 = EDGE_CURVE('',#38418,#38419,#5435,.T.) ;
#47994 = EDGE_CURVE('',#38419,#38420,#5436,.T.) ;
#47995 = EDGE_CURVE('',#38420,#38421,#5437,.T.) ;
#47996 = EDGE_CURVE('',#38421,#38418,#5438,.T.) ;
#47997 = EDGE_CURVE('',#38422,#38423,#5439,.T.) ;
#47998 = EDGE_CURVE('',#38423,#38424,#5440,.T.) ;
#47999 = EDGE_CURVE('',#38425,#38424,#5441,.T.) ;
#48000 = EDGE_CURVE('',#38425,#38422,#5442,.T.) ;
#48001 = EDGE_CURVE('',#38426,#38427,#5443,.T.) ;
#48002 = EDGE_CURVE('',#38427,#36431,#31723,.T.) ;
#48003 = EDGE_CURVE('',#38137,#38428,#31724,.T.) ;
#48004 = EDGE_CURVE('',#38428,#38429,#5444,.T.) ;
#48005 = EDGE_CURVE('',#38429,#38426,#5445,.T.) ;
#48006 = EDGE_CURVE('',#38430,#38431,#5446,.T.) ;
#48007 = EDGE_CURVE('',#38431,#36249,#31725,.T.) ;
#48008 = EDGE_CURVE('',#36248,#38432,#31726,.T.) ;
#48009 = EDGE_CURVE('',#38432,#38433,#5447,.T.) ;
#48010 = EDGE_CURVE('',#38433,#38430,#5448,.T.) ;
#48011 = EDGE_CURVE('',#38135,#38407,#31727,.T.) ;
#48012 = EDGE_CURVE('',#38406,#38136,#31728,.T.) ;
#48013 = EDGE_CURVE('',#38424,#36433,#31729,.T.) ;
#48014 = EDGE_CURVE('',#36432,#38425,#31730,.T.) ;
#48015 = EDGE_CURVE('',#38434,#38435,#5449,.T.) ;
#48016 = EDGE_CURVE('',#38435,#38436,#5450,.T.) ;
#48017 = EDGE_CURVE('',#38436,#38437,#5451,.T.) ;
#48018 = EDGE_CURVE('',#38437,#38434,#5452,.T.) ;
#48019 = EDGE_CURVE('',#38438,#38439,#5453,.T.) ;
#48020 = EDGE_CURVE('',#38439,#38065,#5454,.T.) ;
#48021 = EDGE_CURVE('',#38064,#38438,#5455,.T.) ;
#48022 = EDGE_CURVE('',#38068,#38440,#5456,.T.) ;
#48023 = EDGE_CURVE('',#38440,#38441,#5457,.T.) ;
#48024 = EDGE_CURVE('',#38441,#38069,#5458,.T.) ;
#48025 = EDGE_CURVE('',#38442,#38443,#5459,.T.) ;
#48026 = EDGE_CURVE('',#38443,#38444,#5460,.T.) ;
#48027 = EDGE_CURVE('',#38444,#38445,#5461,.T.) ;
#48028 = EDGE_CURVE('',#38445,#38442,#5462,.T.) ;
#48029 = EDGE_CURVE('',#38446,#38447,#5463,.T.) ;
#48030 = EDGE_CURVE('',#38447,#38448,#5464,.T.) ;
#48031 = EDGE_CURVE('',#38448,#38449,#5465,.T.) ;
#48032 = EDGE_CURVE('',#38449,#38446,#5466,.T.) ;
#48033 = EDGE_CURVE('',#38450,#38451,#5467,.T.) ;
#48034 = EDGE_CURVE('',#38451,#38062,#5468,.T.) ;
#48035 = EDGE_CURVE('',#38063,#38450,#5469,.T.) ;
#48036 = EDGE_CURVE('',#38066,#38452,#5470,.T.) ;
#48037 = EDGE_CURVE('',#38452,#38453,#5471,.T.) ;
#48038 = EDGE_CURVE('',#38453,#38067,#5472,.T.) ;
#48039 = EDGE_CURVE('',#38454,#38455,#5473,.T.) ;
#48040 = EDGE_CURVE('',#38455,#38456,#5474,.T.) ;
#48041 = EDGE_CURVE('',#38456,#38457,#5475,.T.) ;
#48042 = EDGE_CURVE('',#38457,#38454,#5476,.T.) ;
#48043 = EDGE_CURVE('',#38458,#38459,#5477,.T.) ;
#48044 = EDGE_CURVE('',#38459,#38460,#5478,.T.) ;
#48045 = EDGE_CURVE('',#38460,#38461,#5479,.T.) ;
#48046 = EDGE_CURVE('',#38461,#38458,#5480,.T.) ;
#48047 = EDGE_CURVE('',#38462,#38463,#5481,.T.) ;
#48048 = EDGE_CURVE('',#38463,#38464,#5482,.T.) ;
#48049 = EDGE_CURVE('',#38464,#38465,#5483,.T.) ;
#48050 = EDGE_CURVE('',#38465,#38462,#5484,.T.) ;
#48051 = EDGE_CURVE('',#38466,#38467,#5485,.T.) ;
#48052 = EDGE_CURVE('',#38467,#38468,#5486,.T.) ;
#48053 = EDGE_CURVE('',#38468,#38469,#5487,.T.) ;
#48054 = EDGE_CURVE('',#38469,#38466,#5488,.T.) ;
#48055 = EDGE_CURVE('',#38470,#38471,#5489,.T.) ;
#48056 = EDGE_CURVE('',#38471,#38472,#5490,.T.) ;
#48057 = EDGE_CURVE('',#38473,#38472,#5491,.T.) ;
#48058 = EDGE_CURVE('',#38473,#38470,#5492,.T.) ;
#48059 = EDGE_CURVE('',#38474,#38475,#5493,.T.) ;
#48060 = EDGE_CURVE('',#38475,#36421,#31731,.T.) ;
#48061 = EDGE_CURVE('',#38145,#38476,#31732,.T.) ;
#48062 = EDGE_CURVE('',#38476,#38477,#5494,.T.) ;
#48063 = EDGE_CURVE('',#38477,#38474,#5495,.T.) ;
#48064 = EDGE_CURVE('',#38478,#38479,#5496,.T.) ;
#48065 = EDGE_CURVE('',#38479,#36234,#31733,.T.) ;
#48066 = EDGE_CURVE('',#36233,#38480,#31734,.T.) ;
#48067 = EDGE_CURVE('',#38480,#38481,#5497,.T.) ;
#48068 = EDGE_CURVE('',#38481,#38478,#5498,.T.) ;
#48069 = EDGE_CURVE('',#38143,#38455,#31735,.T.) ;
#48070 = EDGE_CURVE('',#38454,#38144,#31736,.T.) ;
#48071 = EDGE_CURVE('',#38472,#36423,#31737,.T.) ;
#48072 = EDGE_CURVE('',#36422,#38473,#31738,.T.) ;
#48073 = EDGE_CURVE('',#38482,#38483,#5499,.T.) ;
#48074 = EDGE_CURVE('',#38483,#38484,#5500,.T.) ;
#48075 = EDGE_CURVE('',#38484,#38485,#5501,.T.) ;
#48076 = EDGE_CURVE('',#38485,#38482,#5502,.T.) ;
#48077 = EDGE_CURVE('',#38486,#38487,#5503,.T.) ;
#48078 = EDGE_CURVE('',#38487,#38073,#5504,.T.) ;
#48079 = EDGE_CURVE('',#38072,#38486,#5505,.T.) ;
#48080 = EDGE_CURVE('',#38076,#38488,#5506,.T.) ;
#48081 = EDGE_CURVE('',#38488,#38489,#5507,.T.) ;
#48082 = EDGE_CURVE('',#38489,#38077,#5508,.T.) ;
#48083 = EDGE_CURVE('',#38490,#38491,#5509,.T.) ;
#48084 = EDGE_CURVE('',#38491,#38492,#5510,.T.) ;
#48085 = EDGE_CURVE('',#38492,#38493,#5511,.T.) ;
#48086 = EDGE_CURVE('',#38493,#38490,#5512,.T.) ;
#48087 = EDGE_CURVE('',#38494,#38495,#5513,.T.) ;
#48088 = EDGE_CURVE('',#38495,#38496,#5514,.T.) ;
#48089 = EDGE_CURVE('',#38496,#38497,#5515,.T.) ;
#48090 = EDGE_CURVE('',#38497,#38494,#5516,.T.) ;
#48091 = EDGE_CURVE('',#38498,#38499,#5517,.T.) ;
#48092 = EDGE_CURVE('',#38499,#38070,#5518,.T.) ;
#48093 = EDGE_CURVE('',#38071,#38498,#5519,.T.) ;
#48094 = EDGE_CURVE('',#38074,#38500,#5520,.T.) ;
#48095 = EDGE_CURVE('',#38500,#38501,#5521,.T.) ;
#48096 = EDGE_CURVE('',#38501,#38075,#5522,.T.) ;
#48097 = EDGE_CURVE('',#38502,#38503,#5523,.T.) ;
#48098 = EDGE_CURVE('',#38503,#38504,#5524,.T.) ;
#48099 = EDGE_CURVE('',#38504,#38505,#5525,.T.) ;
#48100 = EDGE_CURVE('',#38505,#38502,#5526,.T.) ;
#48101 = EDGE_CURVE('',#38506,#38507,#5527,.T.) ;
#48102 = EDGE_CURVE('',#38507,#38508,#5528,.T.) ;
#48103 = EDGE_CURVE('',#38508,#38509,#5529,.T.) ;
#48104 = EDGE_CURVE('',#38509,#38506,#5530,.T.) ;
#48105 = EDGE_CURVE('',#38510,#38511,#5531,.T.) ;
#48106 = EDGE_CURVE('',#38511,#38512,#5532,.T.) ;
#48107 = EDGE_CURVE('',#38512,#38513,#5533,.T.) ;
#48108 = EDGE_CURVE('',#38513,#38510,#5534,.T.) ;
#48109 = EDGE_CURVE('',#38514,#38515,#5535,.T.) ;
#48110 = EDGE_CURVE('',#38515,#38516,#5536,.T.) ;
#48111 = EDGE_CURVE('',#38516,#38517,#5537,.T.) ;
#48112 = EDGE_CURVE('',#38517,#38514,#5538,.T.) ;
#48113 = EDGE_CURVE('',#38518,#38519,#5539,.T.) ;
#48114 = EDGE_CURVE('',#38519,#38520,#5540,.T.) ;
#48115 = EDGE_CURVE('',#38521,#38520,#5541,.T.) ;
#48116 = EDGE_CURVE('',#38521,#38518,#5542,.T.) ;
#48117 = EDGE_CURVE('',#38522,#38523,#5543,.T.) ;
#48118 = EDGE_CURVE('',#38523,#36411,#31739,.T.) ;
#48119 = EDGE_CURVE('',#38153,#38524,#31740,.T.) ;
#48120 = EDGE_CURVE('',#38524,#38525,#5544,.T.) ;
#48121 = EDGE_CURVE('',#38525,#38522,#5545,.T.) ;
#48122 = EDGE_CURVE('',#38526,#38527,#5546,.T.) ;
#48123 = EDGE_CURVE('',#38527,#36219,#31741,.T.) ;
#48124 = EDGE_CURVE('',#36218,#38528,#31742,.T.) ;
#48125 = EDGE_CURVE('',#38528,#38529,#5547,.T.) ;
#48126 = EDGE_CURVE('',#38529,#38526,#5548,.T.) ;
#48127 = EDGE_CURVE('',#38151,#38503,#31743,.T.) ;
#48128 = EDGE_CURVE('',#38502,#38152,#31744,.T.) ;
#48129 = EDGE_CURVE('',#38520,#36413,#31745,.T.) ;
#48130 = EDGE_CURVE('',#36412,#38521,#31746,.T.) ;
#48131 = EDGE_CURVE('',#38530,#38531,#5549,.T.) ;
#48132 = EDGE_CURVE('',#38531,#38532,#5550,.T.) ;
#48133 = EDGE_CURVE('',#38532,#38533,#5551,.T.) ;
#48134 = EDGE_CURVE('',#38533,#38530,#5552,.T.) ;
#48135 = EDGE_CURVE('',#38534,#38535,#5553,.T.) ;
#48136 = EDGE_CURVE('',#38535,#38081,#5554,.T.) ;
#48137 = EDGE_CURVE('',#38080,#38534,#5555,.T.) ;
#48138 = EDGE_CURVE('',#38084,#38536,#5556,.T.) ;
#48139 = EDGE_CURVE('',#38536,#38537,#5557,.T.) ;
#48140 = EDGE_CURVE('',#38537,#38085,#5558,.T.) ;
#48141 = EDGE_CURVE('',#38538,#38539,#5559,.T.) ;
#48142 = EDGE_CURVE('',#38539,#38540,#5560,.T.) ;
#48143 = EDGE_CURVE('',#38540,#38541,#5561,.T.) ;
#48144 = EDGE_CURVE('',#38541,#38538,#5562,.T.) ;
#48145 = EDGE_CURVE('',#38542,#38543,#5563,.T.) ;
#48146 = EDGE_CURVE('',#38543,#38544,#5564,.T.) ;
#48147 = EDGE_CURVE('',#38544,#38545,#5565,.T.) ;
#48148 = EDGE_CURVE('',#38545,#38542,#5566,.T.) ;
#48149 = EDGE_CURVE('',#38546,#38547,#5567,.T.) ;
#48150 = EDGE_CURVE('',#38547,#38078,#5568,.T.) ;
#48151 = EDGE_CURVE('',#38079,#38546,#5569,.T.) ;
#48152 = EDGE_CURVE('',#38082,#38548,#5570,.T.) ;
#48153 = EDGE_CURVE('',#38548,#38549,#5571,.T.) ;
#48154 = EDGE_CURVE('',#38549,#38083,#5572,.T.) ;
#48155 = EDGE_CURVE('',#38550,#38551,#5573,.T.) ;
#48156 = EDGE_CURVE('',#38551,#38552,#5574,.T.) ;
#48157 = EDGE_CURVE('',#38552,#38553,#5575,.T.) ;
#48158 = EDGE_CURVE('',#38553,#38550,#5576,.T.) ;
#48159 = EDGE_CURVE('',#38554,#38555,#5577,.T.) ;
#48160 = EDGE_CURVE('',#38555,#38556,#5578,.T.) ;
#48161 = EDGE_CURVE('',#38556,#38557,#5579,.T.) ;
#48162 = EDGE_CURVE('',#38557,#38554,#5580,.T.) ;
#48163 = EDGE_CURVE('',#38558,#38559,#5581,.T.) ;
#48164 = EDGE_CURVE('',#38559,#38560,#5582,.T.) ;
#48165 = EDGE_CURVE('',#38560,#38561,#5583,.T.) ;
#48166 = EDGE_CURVE('',#38561,#38558,#5584,.T.) ;
#48167 = EDGE_CURVE('',#38562,#38563,#5585,.T.) ;
#48168 = EDGE_CURVE('',#38563,#38564,#5586,.T.) ;
#48169 = EDGE_CURVE('',#38564,#38565,#5587,.T.) ;
#48170 = EDGE_CURVE('',#38565,#38562,#5588,.T.) ;
#48171 = EDGE_CURVE('',#38566,#38567,#5589,.T.) ;
#48172 = EDGE_CURVE('',#38567,#38568,#5590,.T.) ;
#48173 = EDGE_CURVE('',#38569,#38568,#5591,.T.) ;
#48174 = EDGE_CURVE('',#38569,#38566,#5592,.T.) ;
#48175 = EDGE_CURVE('',#38570,#38571,#5593,.T.) ;
#48176 = EDGE_CURVE('',#38571,#36401,#31747,.T.) ;
#48177 = EDGE_CURVE('',#38161,#38572,#31748,.T.) ;
#48178 = EDGE_CURVE('',#38572,#38573,#5594,.T.) ;
#48179 = EDGE_CURVE('',#38573,#38570,#5595,.T.) ;
#48180 = EDGE_CURVE('',#38574,#38575,#5596,.T.) ;
#48181 = EDGE_CURVE('',#38575,#36204,#31749,.T.) ;
#48182 = EDGE_CURVE('',#36203,#38576,#31750,.T.) ;
#48183 = EDGE_CURVE('',#38576,#38577,#5597,.T.) ;
#48184 = EDGE_CURVE('',#38577,#38574,#5598,.T.) ;
#48185 = EDGE_CURVE('',#38159,#38551,#31751,.T.) ;
#48186 = EDGE_CURVE('',#38550,#38160,#31752,.T.) ;
#48187 = EDGE_CURVE('',#38568,#36403,#31753,.T.) ;
#48188 = EDGE_CURVE('',#36402,#38569,#31754,.T.) ;
#48189 = EDGE_CURVE('',#38578,#38579,#5599,.T.) ;
#48190 = EDGE_CURVE('',#38579,#38580,#5600,.T.) ;
#48191 = EDGE_CURVE('',#38580,#38581,#5601,.T.) ;
#48192 = EDGE_CURVE('',#38581,#38578,#5602,.T.) ;
#48193 = EDGE_CURVE('',#38582,#38583,#5603,.T.) ;
#48194 = EDGE_CURVE('',#38583,#38089,#5604,.T.) ;
#48195 = EDGE_CURVE('',#38088,#38582,#5605,.T.) ;
#48196 = EDGE_CURVE('',#38092,#38584,#5606,.T.) ;
#48197 = EDGE_CURVE('',#38584,#38585,#5607,.T.) ;
#48198 = EDGE_CURVE('',#38585,#38093,#5608,.T.) ;
#48199 = EDGE_CURVE('',#38586,#38587,#5609,.T.) ;
#48200 = EDGE_CURVE('',#38587,#38588,#5610,.T.) ;
#48201 = EDGE_CURVE('',#38588,#38589,#5611,.T.) ;
#48202 = EDGE_CURVE('',#38589,#38586,#5612,.T.) ;
#48203 = EDGE_CURVE('',#38590,#38591,#5613,.T.) ;
#48204 = EDGE_CURVE('',#38591,#38592,#5614,.T.) ;
#48205 = EDGE_CURVE('',#38592,#38593,#5615,.T.) ;
#48206 = EDGE_CURVE('',#38593,#38590,#5616,.T.) ;
#48207 = EDGE_CURVE('',#38594,#38595,#5617,.T.) ;
#48208 = EDGE_CURVE('',#38595,#38086,#5618,.T.) ;
#48209 = EDGE_CURVE('',#38087,#38594,#5619,.T.) ;
#48210 = EDGE_CURVE('',#38090,#38596,#5620,.T.) ;
#48211 = EDGE_CURVE('',#38596,#38597,#5621,.T.) ;
#48212 = EDGE_CURVE('',#38597,#38091,#5622,.T.) ;
#48213 = EDGE_CURVE('',#38598,#38599,#5623,.T.) ;
#48214 = EDGE_CURVE('',#38599,#38600,#5624,.T.) ;
#48215 = EDGE_CURVE('',#38600,#38601,#5625,.T.) ;
#48216 = EDGE_CURVE('',#38601,#38598,#5626,.T.) ;
#48217 = EDGE_CURVE('',#38602,#38603,#5627,.T.) ;
#48218 = EDGE_CURVE('',#38603,#38604,#5628,.T.) ;
#48219 = EDGE_CURVE('',#38604,#38605,#5629,.T.) ;
#48220 = EDGE_CURVE('',#38605,#38602,#5630,.T.) ;
#48221 = EDGE_CURVE('',#38606,#38607,#5631,.T.) ;
#48222 = EDGE_CURVE('',#38607,#38608,#5632,.T.) ;
#48223 = EDGE_CURVE('',#38608,#38609,#5633,.T.) ;
#48224 = EDGE_CURVE('',#38609,#38606,#5634,.T.) ;
#48225 = EDGE_CURVE('',#38610,#38611,#5635,.T.) ;
#48226 = EDGE_CURVE('',#38611,#38612,#5636,.T.) ;
#48227 = EDGE_CURVE('',#38612,#38613,#5637,.T.) ;
#48228 = EDGE_CURVE('',#38613,#38610,#5638,.T.) ;
#48229 = EDGE_CURVE('',#38614,#38615,#5639,.T.) ;
#48230 = EDGE_CURVE('',#38615,#38616,#5640,.T.) ;
#48231 = EDGE_CURVE('',#38616,#38617,#5641,.T.) ;
#48232 = EDGE_CURVE('',#38617,#38614,#5642,.T.) ;
#48233 = EDGE_CURVE('',#38618,#38619,#5643,.T.) ;
#48234 = EDGE_CURVE('',#38619,#38620,#5644,.T.) ;
#48235 = EDGE_CURVE('',#38620,#38621,#5645,.T.) ;
#48236 = EDGE_CURVE('',#38621,#38618,#5646,.T.) ;
#48237 = EDGE_CURVE('',#38622,#38623,#5647,.T.) ;
#48238 = EDGE_CURVE('',#38623,#38624,#5648,.T.) ;
#48239 = EDGE_CURVE('',#38624,#38625,#5649,.T.) ;
#48240 = EDGE_CURVE('',#38625,#38622,#5650,.T.) ;
#48241 = EDGE_CURVE('',#38626,#38627,#5651,.T.) ;
#48242 = EDGE_CURVE('',#38627,#38628,#5652,.T.) ;
#48243 = EDGE_CURVE('',#38628,#38629,#5653,.T.) ;
#48244 = EDGE_CURVE('',#38629,#38626,#5654,.T.) ;
#48245 = EDGE_CURVE('',#38630,#38631,#5655,.T.) ;
#48246 = EDGE_CURVE('',#38631,#38632,#5656,.T.) ;
#48247 = EDGE_CURVE('',#38632,#38633,#5657,.T.) ;
#48248 = EDGE_CURVE('',#38633,#38630,#5658,.T.) ;
#48249 = EDGE_CURVE('',#38634,#38635,#5659,.T.) ;
#48250 = EDGE_CURVE('',#38635,#38636,#5660,.T.) ;
#48251 = EDGE_CURVE('',#38636,#38637,#5661,.T.) ;
#48252 = EDGE_CURVE('',#38637,#38634,#5662,.T.) ;
#48253 = EDGE_CURVE('',#38638,#38639,#5663,.T.) ;
#48254 = EDGE_CURVE('',#38639,#38640,#5664,.T.) ;
#48255 = EDGE_CURVE('',#38640,#38641,#5665,.T.) ;
#48256 = EDGE_CURVE('',#38641,#38638,#5666,.T.) ;
#48257 = EDGE_CURVE('',#38642,#38643,#5667,.T.) ;
#48258 = EDGE_CURVE('',#38643,#38644,#5668,.T.) ;
#48259 = EDGE_CURVE('',#38644,#38645,#5669,.T.) ;
#48260 = EDGE_CURVE('',#38645,#38642,#5670,.T.) ;
#48261 = EDGE_CURVE('',#38646,#38647,#5671,.T.) ;
#48262 = EDGE_CURVE('',#38647,#38648,#5672,.T.) ;
#48263 = EDGE_CURVE('',#38648,#38649,#5673,.T.) ;
#48264 = EDGE_CURVE('',#38649,#38646,#5674,.T.) ;
#48265 = EDGE_CURVE('',#38650,#38651,#5675,.T.) ;
#48266 = EDGE_CURVE('',#38651,#38652,#5676,.T.) ;
#48267 = EDGE_CURVE('',#38652,#38653,#5677,.T.) ;
#48268 = EDGE_CURVE('',#38653,#38650,#5678,.T.) ;
#48269 = EDGE_CURVE('',#38654,#38655,#5679,.T.) ;
#48270 = EDGE_CURVE('',#38655,#38656,#5680,.T.) ;
#48271 = EDGE_CURVE('',#38656,#38657,#5681,.T.) ;
#48272 = EDGE_CURVE('',#38657,#38654,#5682,.T.) ;
#48273 = EDGE_CURVE('',#38658,#38659,#5683,.T.) ;
#48274 = EDGE_CURVE('',#38659,#38660,#5684,.T.) ;
#48275 = EDGE_CURVE('',#38660,#38661,#5685,.T.) ;
#48276 = EDGE_CURVE('',#38661,#38658,#5686,.T.) ;
#48277 = EDGE_CURVE('',#38662,#38663,#5687,.T.) ;
#48278 = EDGE_CURVE('',#38663,#38664,#5688,.T.) ;
#48279 = EDGE_CURVE('',#38664,#38665,#5689,.T.) ;
#48280 = EDGE_CURVE('',#38665,#38662,#5690,.T.) ;
#48281 = EDGE_CURVE('',#38666,#38667,#5691,.T.) ;
#48282 = EDGE_CURVE('',#38667,#38668,#5692,.T.) ;
#48283 = EDGE_CURVE('',#38668,#38669,#5693,.T.) ;
#48284 = EDGE_CURVE('',#38669,#38666,#5694,.T.) ;
#48285 = EDGE_CURVE('',#38670,#38671,#5695,.T.) ;
#48286 = EDGE_CURVE('',#38671,#38672,#5696,.T.) ;
#48287 = EDGE_CURVE('',#38672,#38673,#5697,.T.) ;
#48288 = EDGE_CURVE('',#38673,#38670,#5698,.T.) ;
#48289 = EDGE_CURVE('',#38674,#38675,#5699,.T.) ;
#48290 = EDGE_CURVE('',#38675,#38676,#5700,.T.) ;
#48291 = EDGE_CURVE('',#38676,#38677,#5701,.T.) ;
#48292 = EDGE_CURVE('',#38677,#38674,#5702,.T.) ;
#48293 = EDGE_CURVE('',#38678,#38679,#5703,.T.) ;
#48294 = EDGE_CURVE('',#38679,#38680,#5704,.T.) ;
#48295 = EDGE_CURVE('',#38680,#38681,#5705,.T.) ;
#48296 = EDGE_CURVE('',#38681,#38678,#5706,.T.) ;
#48297 = EDGE_CURVE('',#38682,#38683,#5707,.T.) ;
#48298 = EDGE_CURVE('',#38683,#38684,#5708,.T.) ;
#48299 = EDGE_CURVE('',#38684,#38685,#5709,.T.) ;
#48300 = EDGE_CURVE('',#38685,#38682,#5710,.T.) ;
#48301 = EDGE_CURVE('',#38686,#38687,#5711,.T.) ;
#48302 = EDGE_CURVE('',#38687,#38688,#5712,.T.) ;
#48303 = EDGE_CURVE('',#38688,#38689,#5713,.T.) ;
#48304 = EDGE_CURVE('',#38689,#38686,#5714,.T.) ;
#48305 = EDGE_CURVE('',#38690,#38691,#5715,.T.) ;
#48306 = EDGE_CURVE('',#38691,#38692,#5716,.T.) ;
#48307 = EDGE_CURVE('',#38692,#38693,#5717,.T.) ;
#48308 = EDGE_CURVE('',#38693,#38690,#5718,.T.) ;
#48309 = EDGE_CURVE('',#38694,#38695,#5719,.T.) ;
#48310 = EDGE_CURVE('',#38695,#38696,#5720,.T.) ;
#48311 = EDGE_CURVE('',#38696,#38697,#5721,.T.) ;
#48312 = EDGE_CURVE('',#38697,#38694,#5722,.T.) ;
#48313 = EDGE_CURVE('',#38698,#38699,#5723,.T.) ;
#48314 = EDGE_CURVE('',#38699,#38700,#5724,.T.) ;
#48315 = EDGE_CURVE('',#38700,#38701,#5725,.T.) ;
#48316 = EDGE_CURVE('',#38701,#38698,#5726,.T.) ;
#48317 = EDGE_CURVE('',#38702,#38703,#5727,.T.) ;
#48318 = EDGE_CURVE('',#38703,#38704,#5728,.T.) ;
#48319 = EDGE_CURVE('',#38704,#38705,#5729,.T.) ;
#48320 = EDGE_CURVE('',#38705,#38702,#5730,.T.) ;
#48321 = EDGE_CURVE('',#38706,#38707,#5731,.T.) ;
#48322 = EDGE_CURVE('',#38707,#38708,#5732,.T.) ;
#48323 = EDGE_CURVE('',#38708,#38709,#5733,.T.) ;
#48324 = EDGE_CURVE('',#38709,#38706,#5734,.T.) ;
#48325 = EDGE_CURVE('',#38710,#38711,#5735,.T.) ;
#48326 = EDGE_CURVE('',#38711,#38712,#5736,.T.) ;
#48327 = EDGE_CURVE('',#38712,#38713,#5737,.T.) ;
#48328 = EDGE_CURVE('',#38713,#38710,#5738,.T.) ;
#48329 = EDGE_CURVE('',#38714,#38715,#5739,.T.) ;
#48330 = EDGE_CURVE('',#38715,#38716,#5740,.T.) ;
#48331 = EDGE_CURVE('',#38716,#38717,#5741,.T.) ;
#48332 = EDGE_CURVE('',#38717,#38714,#5742,.T.) ;
#48333 = EDGE_CURVE('',#38718,#38719,#5743,.T.) ;
#48334 = EDGE_CURVE('',#38719,#38720,#5744,.T.) ;
#48335 = EDGE_CURVE('',#38720,#38721,#5745,.T.) ;
#48336 = EDGE_CURVE('',#38721,#38718,#5746,.T.) ;
#48337 = EDGE_CURVE('',#38722,#38723,#5747,.T.) ;
#48338 = EDGE_CURVE('',#38723,#38724,#5748,.T.) ;
#48339 = EDGE_CURVE('',#38724,#38725,#5749,.T.) ;
#48340 = EDGE_CURVE('',#38725,#38722,#5750,.T.) ;
#48341 = EDGE_CURVE('',#38726,#38727,#5751,.T.) ;
#48342 = EDGE_CURVE('',#38727,#38728,#5752,.T.) ;
#48343 = EDGE_CURVE('',#38728,#38729,#5753,.T.) ;
#48344 = EDGE_CURVE('',#38729,#38726,#5754,.T.) ;
#48345 = EDGE_CURVE('',#38730,#38731,#5755,.T.) ;
#48346 = EDGE_CURVE('',#38731,#38732,#5756,.T.) ;
#48347 = EDGE_CURVE('',#38732,#38733,#5757,.T.) ;
#48348 = EDGE_CURVE('',#38733,#38730,#5758,.T.) ;
#48349 = EDGE_CURVE('',#38734,#38735,#5759,.T.) ;
#48350 = EDGE_CURVE('',#38735,#38736,#5760,.T.) ;
#48351 = EDGE_CURVE('',#38736,#38737,#5761,.T.) ;
#48352 = EDGE_CURVE('',#38737,#38734,#5762,.T.) ;
#48353 = EDGE_CURVE('',#38738,#38739,#5763,.T.) ;
#48354 = EDGE_CURVE('',#38739,#38740,#5764,.T.) ;
#48355 = EDGE_CURVE('',#38740,#38741,#5765,.T.) ;
#48356 = EDGE_CURVE('',#38741,#38738,#5766,.T.) ;
#48357 = EDGE_CURVE('',#38664,#38178,#31755,.T.) ;
#48358 = EDGE_CURVE('',#38665,#38181,#31756,.T.) ;
#48359 = EDGE_CURVE('',#38178,#38183,#31757,.T.) ;
#48360 = EDGE_CURVE('',#38182,#38179,#31758,.T.) ;
#48361 = EDGE_CURVE('',#38665,#38174,#31759,.T.) ;
#48362 = EDGE_CURVE('',#38174,#38181,#31760,.T.) ;
#48363 = EDGE_CURVE('',#38179,#38667,#31761,.T.) ;
#48364 = EDGE_CURVE('',#38180,#38666,#31762,.T.) ;
#48365 = EDGE_CURVE('',#38175,#38180,#31763,.T.) ;
#48366 = EDGE_CURVE('',#38662,#38177,#31764,.T.) ;
#48367 = EDGE_CURVE('',#38175,#38666,#31765,.T.) ;
#48368 = EDGE_CURVE('',#38662,#38170,#31766,.T.) ;
#48369 = EDGE_CURVE('',#38170,#38177,#31767,.T.) ;
#48370 = EDGE_CURVE('',#38176,#38669,#31768,.T.) ;
#48371 = EDGE_CURVE('',#38171,#38176,#31769,.T.) ;
#48372 = EDGE_CURVE('',#38173,#38663,#31770,.T.) ;
#48373 = EDGE_CURVE('',#38171,#38669,#31771,.T.) ;
#48374 = EDGE_CURVE('',#38168,#38173,#31772,.T.) ;
#48375 = EDGE_CURVE('',#38172,#38169,#31773,.T.) ;
#48376 = EDGE_CURVE('',#38668,#38172,#31774,.T.) ;
#48377 = EDGE_CURVE('',#38736,#38194,#31775,.T.) ;
#48378 = EDGE_CURVE('',#38737,#38197,#31776,.T.) ;
#48379 = EDGE_CURVE('',#38194,#38199,#31777,.T.) ;
#48380 = EDGE_CURVE('',#38198,#38195,#31778,.T.) ;
#48381 = EDGE_CURVE('',#38737,#38208,#31779,.T.) ;
#48382 = EDGE_CURVE('',#38208,#38197,#31780,.T.) ;
#48383 = EDGE_CURVE('',#38195,#38739,#31781,.T.) ;
#48384 = EDGE_CURVE('',#38196,#38738,#31782,.T.) ;
#48385 = EDGE_CURVE('',#38209,#38196,#31783,.T.) ;
#48386 = EDGE_CURVE('',#38734,#38207,#31784,.T.) ;
#48387 = EDGE_CURVE('',#38209,#38738,#31785,.T.) ;
#48388 = EDGE_CURVE('',#38734,#38202,#31786,.T.) ;
#48389 = EDGE_CURVE('',#38202,#38207,#31787,.T.) ;
#48390 = EDGE_CURVE('',#38206,#38741,#31788,.T.) ;
#48391 = EDGE_CURVE('',#38203,#38206,#31789,.T.) ;
#48392 = EDGE_CURVE('',#38205,#38735,#31790,.T.) ;
#48393 = EDGE_CURVE('',#38203,#38741,#31791,.T.) ;
#48394 = EDGE_CURVE('',#38200,#38205,#31792,.T.) ;
#48395 = EDGE_CURVE('',#38204,#38201,#31793,.T.) ;
#48396 = EDGE_CURVE('',#38740,#38204,#31794,.T.) ;
#48397 = EDGE_CURVE('',#38656,#38226,#31795,.T.) ;
#48398 = EDGE_CURVE('',#38657,#38229,#31796,.T.) ;
#48399 = EDGE_CURVE('',#38226,#38231,#31797,.T.) ;
#48400 = EDGE_CURVE('',#38230,#38227,#31798,.T.) ;
#48401 = EDGE_CURVE('',#38657,#38222,#31799,.T.) ;
#48402 = EDGE_CURVE('',#38222,#38229,#31800,.T.) ;
#48403 = EDGE_CURVE('',#38227,#38659,#31801,.T.) ;
#48404 = EDGE_CURVE('',#38228,#38658,#31802,.T.) ;
#48405 = EDGE_CURVE('',#38223,#38228,#31803,.T.) ;
#48406 = EDGE_CURVE('',#38654,#38225,#31804,.T.) ;
#48407 = EDGE_CURVE('',#38223,#38658,#31805,.T.) ;
#48408 = EDGE_CURVE('',#38654,#38218,#31806,.T.) ;
#48409 = EDGE_CURVE('',#38218,#38225,#31807,.T.) ;
#48410 = EDGE_CURVE('',#38224,#38661,#31808,.T.) ;
#48411 = EDGE_CURVE('',#38219,#38224,#31809,.T.) ;
#48412 = EDGE_CURVE('',#38221,#38655,#31810,.T.) ;
#48413 = EDGE_CURVE('',#38219,#38661,#31811,.T.) ;
#48414 = EDGE_CURVE('',#38216,#38221,#31812,.T.) ;
#48415 = EDGE_CURVE('',#38220,#38217,#31813,.T.) ;
#48416 = EDGE_CURVE('',#38660,#38220,#31814,.T.) ;
#48417 = EDGE_CURVE('',#38728,#38242,#31815,.T.) ;
#48418 = EDGE_CURVE('',#38729,#38245,#31816,.T.) ;
#48419 = EDGE_CURVE('',#38242,#38247,#31817,.T.) ;
#48420 = EDGE_CURVE('',#38246,#38243,#31818,.T.) ;
#48421 = EDGE_CURVE('',#38729,#38256,#31819,.T.) ;
#48422 = EDGE_CURVE('',#38256,#38245,#31820,.T.) ;
#48423 = EDGE_CURVE('',#38243,#38731,#31821,.T.) ;
#48424 = EDGE_CURVE('',#38244,#38730,#31822,.T.) ;
#48425 = EDGE_CURVE('',#38257,#38244,#31823,.T.) ;
#48426 = EDGE_CURVE('',#38726,#38255,#31824,.T.) ;
#48427 = EDGE_CURVE('',#38257,#38730,#31825,.T.) ;
#48428 = EDGE_CURVE('',#38726,#38250,#31826,.T.) ;
#48429 = EDGE_CURVE('',#38250,#38255,#31827,.T.) ;
#48430 = EDGE_CURVE('',#38254,#38733,#31828,.T.) ;
#48431 = EDGE_CURVE('',#38251,#38254,#31829,.T.) ;
#48432 = EDGE_CURVE('',#38253,#38727,#31830,.T.) ;
#48433 = EDGE_CURVE('',#38251,#38733,#31831,.T.) ;
#48434 = EDGE_CURVE('',#38248,#38253,#31832,.T.) ;
#48435 = EDGE_CURVE('',#38252,#38249,#31833,.T.) ;
#48436 = EDGE_CURVE('',#38732,#38252,#31834,.T.) ;
#48437 = EDGE_CURVE('',#38648,#38274,#31835,.T.) ;
#48438 = EDGE_CURVE('',#38649,#38277,#31836,.T.) ;
#48439 = EDGE_CURVE('',#38274,#38279,#31837,.T.) ;
#48440 = EDGE_CURVE('',#38278,#38275,#31838,.T.) ;
#48441 = EDGE_CURVE('',#38649,#38270,#31839,.T.) ;
#48442 = EDGE_CURVE('',#38270,#38277,#31840,.T.) ;
#48443 = EDGE_CURVE('',#38275,#38651,#31841,.T.) ;
#48444 = EDGE_CURVE('',#38276,#38650,#31842,.T.) ;
#48445 = EDGE_CURVE('',#38271,#38276,#31843,.T.) ;
#48446 = EDGE_CURVE('',#38646,#38273,#31844,.T.) ;
#48447 = EDGE_CURVE('',#38271,#38650,#31845,.T.) ;
#48448 = EDGE_CURVE('',#38646,#38266,#31846,.T.) ;
#48449 = EDGE_CURVE('',#38266,#38273,#31847,.T.) ;
#48450 = EDGE_CURVE('',#38272,#38653,#31848,.T.) ;
#48451 = EDGE_CURVE('',#38267,#38272,#31849,.T.) ;
#48452 = EDGE_CURVE('',#38269,#38647,#31850,.T.) ;
#48453 = EDGE_CURVE('',#38267,#38653,#31851,.T.) ;
#48454 = EDGE_CURVE('',#38264,#38269,#31852,.T.) ;
#48455 = EDGE_CURVE('',#38268,#38265,#31853,.T.) ;
#48456 = EDGE_CURVE('',#38652,#38268,#31854,.T.) ;
#48457 = EDGE_CURVE('',#38720,#38290,#31855,.T.) ;
#48458 = EDGE_CURVE('',#38721,#38293,#31856,.T.) ;
#48459 = EDGE_CURVE('',#38290,#38295,#31857,.T.) ;
#48460 = EDGE_CURVE('',#38294,#38291,#31858,.T.) ;
#48461 = EDGE_CURVE('',#38721,#38304,#31859,.T.) ;
#48462 = EDGE_CURVE('',#38304,#38293,#31860,.T.) ;
#48463 = EDGE_CURVE('',#38291,#38723,#31861,.T.) ;
#48464 = EDGE_CURVE('',#38292,#38722,#31862,.T.) ;
#48465 = EDGE_CURVE('',#38305,#38292,#31863,.T.) ;
#48466 = EDGE_CURVE('',#38718,#38303,#31864,.T.) ;
#48467 = EDGE_CURVE('',#38305,#38722,#31865,.T.) ;
#48468 = EDGE_CURVE('',#38718,#38298,#31866,.T.) ;
#48469 = EDGE_CURVE('',#38298,#38303,#31867,.T.) ;
#48470 = EDGE_CURVE('',#38302,#38725,#31868,.T.) ;
#48471 = EDGE_CURVE('',#38299,#38302,#31869,.T.) ;
#48472 = EDGE_CURVE('',#38301,#38719,#31870,.T.) ;
#48473 = EDGE_CURVE('',#38299,#38725,#31871,.T.) ;
#48474 = EDGE_CURVE('',#38296,#38301,#31872,.T.) ;
#48475 = EDGE_CURVE('',#38300,#38297,#31873,.T.) ;
#48476 = EDGE_CURVE('',#38724,#38300,#31874,.T.) ;
#48477 = EDGE_CURVE('',#38640,#38322,#31875,.T.) ;
#48478 = EDGE_CURVE('',#38641,#38325,#31876,.T.) ;
#48479 = EDGE_CURVE('',#38322,#38327,#31877,.T.) ;
#48480 = EDGE_CURVE('',#38326,#38323,#31878,.T.) ;
#48481 = EDGE_CURVE('',#38641,#38318,#31879,.T.) ;
#48482 = EDGE_CURVE('',#38318,#38325,#31880,.T.) ;
#48483 = EDGE_CURVE('',#38323,#38643,#31881,.T.) ;
#48484 = EDGE_CURVE('',#38324,#38642,#31882,.T.) ;
#48485 = EDGE_CURVE('',#38319,#38324,#31883,.T.) ;
#48486 = EDGE_CURVE('',#38638,#38321,#31884,.T.) ;
#48487 = EDGE_CURVE('',#38319,#38642,#31885,.T.) ;
#48488 = EDGE_CURVE('',#38638,#38314,#31886,.T.) ;
#48489 = EDGE_CURVE('',#38314,#38321,#31887,.T.) ;
#48490 = EDGE_CURVE('',#38320,#38645,#31888,.T.) ;
#48491 = EDGE_CURVE('',#38315,#38320,#31889,.T.) ;
#48492 = EDGE_CURVE('',#38317,#38639,#31890,.T.) ;
#48493 = EDGE_CURVE('',#38315,#38645,#31891,.T.) ;
#48494 = EDGE_CURVE('',#38312,#38317,#31892,.T.) ;
#48495 = EDGE_CURVE('',#38316,#38313,#31893,.T.) ;
#48496 = EDGE_CURVE('',#38644,#38316,#31894,.T.) ;
#48497 = EDGE_CURVE('',#38712,#38338,#31895,.T.) ;
#48498 = EDGE_CURVE('',#38713,#38341,#31896,.T.) ;
#48499 = EDGE_CURVE('',#38338,#38343,#31897,.T.) ;
#48500 = EDGE_CURVE('',#38342,#38339,#31898,.T.) ;
#48501 = EDGE_CURVE('',#38713,#38352,#31899,.T.) ;
#48502 = EDGE_CURVE('',#38352,#38341,#31900,.T.) ;
#48503 = EDGE_CURVE('',#38339,#38715,#31901,.T.) ;
#48504 = EDGE_CURVE('',#38340,#38714,#31902,.T.) ;
#48505 = EDGE_CURVE('',#38353,#38340,#31903,.T.) ;
#48506 = EDGE_CURVE('',#38710,#38351,#31904,.T.) ;
#48507 = EDGE_CURVE('',#38353,#38714,#31905,.T.) ;
#48508 = EDGE_CURVE('',#38710,#38346,#31906,.T.) ;
#48509 = EDGE_CURVE('',#38346,#38351,#31907,.T.) ;
#48510 = EDGE_CURVE('',#38350,#38717,#31908,.T.) ;
#48511 = EDGE_CURVE('',#38347,#38350,#31909,.T.) ;
#48512 = EDGE_CURVE('',#38349,#38711,#31910,.T.) ;
#48513 = EDGE_CURVE('',#38347,#38717,#31911,.T.) ;
#48514 = EDGE_CURVE('',#38344,#38349,#31912,.T.) ;
#48515 = EDGE_CURVE('',#38348,#38345,#31913,.T.) ;
#48516 = EDGE_CURVE('',#38716,#38348,#31914,.T.) ;
#48517 = EDGE_CURVE('',#38632,#38370,#31915,.T.) ;
#48518 = EDGE_CURVE('',#38633,#38373,#31916,.T.) ;
#48519 = EDGE_CURVE('',#38370,#38375,#31917,.T.) ;
#48520 = EDGE_CURVE('',#38374,#38371,#31918,.T.) ;
#48521 = EDGE_CURVE('',#38633,#38366,#31919,.T.) ;
#48522 = EDGE_CURVE('',#38366,#38373,#31920,.T.) ;
#48523 = EDGE_CURVE('',#38371,#38635,#31921,.T.) ;
#48524 = EDGE_CURVE('',#38372,#38634,#31922,.T.) ;
#48525 = EDGE_CURVE('',#38367,#38372,#31923,.T.) ;
#48526 = EDGE_CURVE('',#38630,#38369,#31924,.T.) ;
#48527 = EDGE_CURVE('',#38367,#38634,#31925,.T.) ;
#48528 = EDGE_CURVE('',#38630,#38362,#31926,.T.) ;
#48529 = EDGE_CURVE('',#38362,#38369,#31927,.T.) ;
#48530 = EDGE_CURVE('',#38368,#38637,#31928,.T.) ;
#48531 = EDGE_CURVE('',#38363,#38368,#31929,.T.) ;
#48532 = EDGE_CURVE('',#38365,#38631,#31930,.T.) ;
#48533 = EDGE_CURVE('',#38363,#38637,#31931,.T.) ;
#48534 = EDGE_CURVE('',#38360,#38365,#31932,.T.) ;
#48535 = EDGE_CURVE('',#38364,#38361,#31933,.T.) ;
#48536 = EDGE_CURVE('',#38636,#38364,#31934,.T.) ;
#48537 = EDGE_CURVE('',#38704,#38386,#31935,.T.) ;
#48538 = EDGE_CURVE('',#38705,#38389,#31936,.T.) ;
#48539 = EDGE_CURVE('',#38386,#38391,#31937,.T.) ;
#48540 = EDGE_CURVE('',#38390,#38387,#31938,.T.) ;
#48541 = EDGE_CURVE('',#38705,#38400,#31939,.T.) ;
#48542 = EDGE_CURVE('',#38400,#38389,#31940,.T.) ;
#48543 = EDGE_CURVE('',#38387,#38707,#31941,.T.) ;
#48544 = EDGE_CURVE('',#38388,#38706,#31942,.T.) ;
#48545 = EDGE_CURVE('',#38401,#38388,#31943,.T.) ;
#48546 = EDGE_CURVE('',#38702,#38399,#31944,.T.) ;
#48547 = EDGE_CURVE('',#38401,#38706,#31945,.T.) ;
#48548 = EDGE_CURVE('',#38702,#38394,#31946,.T.) ;
#48549 = EDGE_CURVE('',#38394,#38399,#31947,.T.) ;
#48550 = EDGE_CURVE('',#38398,#38709,#31948,.T.) ;
#48551 = EDGE_CURVE('',#38395,#38398,#31949,.T.) ;
#48552 = EDGE_CURVE('',#38397,#38703,#31950,.T.) ;
#48553 = EDGE_CURVE('',#38395,#38709,#31951,.T.) ;
#48554 = EDGE_CURVE('',#38392,#38397,#31952,.T.) ;
#48555 = EDGE_CURVE('',#38396,#38393,#31953,.T.) ;
#48556 = EDGE_CURVE('',#38708,#38396,#31954,.T.) ;
#48557 = EDGE_CURVE('',#38624,#38418,#31955,.T.) ;
#48558 = EDGE_CURVE('',#38625,#38421,#31956,.T.) ;
#48559 = EDGE_CURVE('',#38418,#38423,#31957,.T.) ;
#48560 = EDGE_CURVE('',#38422,#38419,#31958,.T.) ;
#48561 = EDGE_CURVE('',#38625,#38414,#31959,.T.) ;
#48562 = EDGE_CURVE('',#38414,#38421,#31960,.T.) ;
#48563 = EDGE_CURVE('',#38419,#38627,#31961,.T.) ;
#48564 = EDGE_CURVE('',#38420,#38626,#31962,.T.) ;
#48565 = EDGE_CURVE('',#38415,#38420,#31963,.T.) ;
#48566 = EDGE_CURVE('',#38622,#38417,#31964,.T.) ;
#48567 = EDGE_CURVE('',#38415,#38626,#31965,.T.) ;
#48568 = EDGE_CURVE('',#38622,#38410,#31966,.T.) ;
#48569 = EDGE_CURVE('',#38410,#38417,#31967,.T.) ;
#48570 = EDGE_CURVE('',#38416,#38629,#31968,.T.) ;
#48571 = EDGE_CURVE('',#38411,#38416,#31969,.T.) ;
#48572 = EDGE_CURVE('',#38413,#38623,#31970,.T.) ;
#48573 = EDGE_CURVE('',#38411,#38629,#31971,.T.) ;
#48574 = EDGE_CURVE('',#38408,#38413,#31972,.T.) ;
#48575 = EDGE_CURVE('',#38412,#38409,#31973,.T.) ;
#48576 = EDGE_CURVE('',#38628,#38412,#31974,.T.) ;
#48577 = EDGE_CURVE('',#38696,#38434,#31975,.T.) ;
#48578 = EDGE_CURVE('',#38697,#38437,#31976,.T.) ;
#48579 = EDGE_CURVE('',#38434,#38439,#31977,.T.) ;
#48580 = EDGE_CURVE('',#38438,#38435,#31978,.T.) ;
#48581 = EDGE_CURVE('',#38697,#38448,#31979,.T.) ;
#48582 = EDGE_CURVE('',#38448,#38437,#31980,.T.) ;
#48583 = EDGE_CURVE('',#38435,#38699,#31981,.T.) ;
#48584 = EDGE_CURVE('',#38436,#38698,#31982,.T.) ;
#48585 = EDGE_CURVE('',#38449,#38436,#31983,.T.) ;
#48586 = EDGE_CURVE('',#38694,#38447,#31984,.T.) ;
#48587 = EDGE_CURVE('',#38449,#38698,#31985,.T.) ;
#48588 = EDGE_CURVE('',#38694,#38442,#31986,.T.) ;
#48589 = EDGE_CURVE('',#38442,#38447,#31987,.T.) ;
#48590 = EDGE_CURVE('',#38446,#38701,#31988,.T.) ;
#48591 = EDGE_CURVE('',#38443,#38446,#31989,.T.) ;
#48592 = EDGE_CURVE('',#38445,#38695,#31990,.T.) ;
#48593 = EDGE_CURVE('',#38443,#38701,#31991,.T.) ;
#48594 = EDGE_CURVE('',#38440,#38445,#31992,.T.) ;
#48595 = EDGE_CURVE('',#38444,#38441,#31993,.T.) ;
#48596 = EDGE_CURVE('',#38700,#38444,#31994,.T.) ;
#48597 = EDGE_CURVE('',#38616,#38466,#31995,.T.) ;
#48598 = EDGE_CURVE('',#38617,#38469,#31996,.T.) ;
#48599 = EDGE_CURVE('',#38466,#38471,#31997,.T.) ;
#48600 = EDGE_CURVE('',#38470,#38467,#31998,.T.) ;
#48601 = EDGE_CURVE('',#38617,#38462,#31999,.T.) ;
#48602 = EDGE_CURVE('',#38462,#38469,#32000,.T.) ;
#48603 = EDGE_CURVE('',#38467,#38619,#32001,.T.) ;
#48604 = EDGE_CURVE('',#38468,#38618,#32002,.T.) ;
#48605 = EDGE_CURVE('',#38463,#38468,#32003,.T.) ;
#48606 = EDGE_CURVE('',#38614,#38465,#32004,.T.) ;
#48607 = EDGE_CURVE('',#38463,#38618,#32005,.T.) ;
#48608 = EDGE_CURVE('',#38614,#38458,#32006,.T.) ;
#48609 = EDGE_CURVE('',#38458,#38465,#32007,.T.) ;
#48610 = EDGE_CURVE('',#38464,#38621,#32008,.T.) ;
#48611 = EDGE_CURVE('',#38459,#38464,#32009,.T.) ;
#48612 = EDGE_CURVE('',#38461,#38615,#32010,.T.) ;
#48613 = EDGE_CURVE('',#38459,#38621,#32011,.T.) ;
#48614 = EDGE_CURVE('',#38456,#38461,#32012,.T.) ;
#48615 = EDGE_CURVE('',#38460,#38457,#32013,.T.) ;
#48616 = EDGE_CURVE('',#38620,#38460,#32014,.T.) ;
#48617 = EDGE_CURVE('',#38688,#38482,#32015,.T.) ;
#48618 = EDGE_CURVE('',#38689,#38485,#32016,.T.) ;
#48619 = EDGE_CURVE('',#38482,#38487,#32017,.T.) ;
#48620 = EDGE_CURVE('',#38486,#38483,#32018,.T.) ;
#48621 = EDGE_CURVE('',#38689,#38496,#32019,.T.) ;
#48622 = EDGE_CURVE('',#38496,#38485,#32020,.T.) ;
#48623 = EDGE_CURVE('',#38483,#38691,#32021,.T.) ;
#48624 = EDGE_CURVE('',#38484,#38690,#32022,.T.) ;
#48625 = EDGE_CURVE('',#38497,#38484,#32023,.T.) ;
#48626 = EDGE_CURVE('',#38686,#38495,#32024,.T.) ;
#48627 = EDGE_CURVE('',#38497,#38690,#32025,.T.) ;
#48628 = EDGE_CURVE('',#38686,#38490,#32026,.T.) ;
#48629 = EDGE_CURVE('',#38490,#38495,#32027,.T.) ;
#48630 = EDGE_CURVE('',#38494,#38693,#32028,.T.) ;
#48631 = EDGE_CURVE('',#38491,#38494,#32029,.T.) ;
#48632 = EDGE_CURVE('',#38493,#38687,#32030,.T.) ;
#48633 = EDGE_CURVE('',#38491,#38693,#32031,.T.) ;
#48634 = EDGE_CURVE('',#38488,#38493,#32032,.T.) ;
#48635 = EDGE_CURVE('',#38492,#38489,#32033,.T.) ;
#48636 = EDGE_CURVE('',#38692,#38492,#32034,.T.) ;
#48637 = EDGE_CURVE('',#38608,#38514,#32035,.T.) ;
#48638 = EDGE_CURVE('',#38609,#38517,#32036,.T.) ;
#48639 = EDGE_CURVE('',#38514,#38519,#32037,.T.) ;
#48640 = EDGE_CURVE('',#38518,#38515,#32038,.T.) ;
#48641 = EDGE_CURVE('',#38609,#38510,#32039,.T.) ;
#48642 = EDGE_CURVE('',#38510,#38517,#32040,.T.) ;
#48643 = EDGE_CURVE('',#38515,#38611,#32041,.T.) ;
#48644 = EDGE_CURVE('',#38516,#38610,#32042,.T.) ;
#48645 = EDGE_CURVE('',#38511,#38516,#32043,.T.) ;
#48646 = EDGE_CURVE('',#38606,#38513,#32044,.T.) ;
#48647 = EDGE_CURVE('',#38511,#38610,#32045,.T.) ;
#48648 = EDGE_CURVE('',#38606,#38506,#32046,.T.) ;
#48649 = EDGE_CURVE('',#38506,#38513,#32047,.T.) ;
#48650 = EDGE_CURVE('',#38512,#38613,#32048,.T.) ;
#48651 = EDGE_CURVE('',#38507,#38512,#32049,.T.) ;
#48652 = EDGE_CURVE('',#38509,#38607,#32050,.T.) ;
#48653 = EDGE_CURVE('',#38507,#38613,#32051,.T.) ;
#48654 = EDGE_CURVE('',#38504,#38509,#32052,.T.) ;
#48655 = EDGE_CURVE('',#38508,#38505,#32053,.T.) ;
#48656 = EDGE_CURVE('',#38612,#38508,#32054,.T.) ;
#48657 = EDGE_CURVE('',#38680,#38530,#32055,.T.) ;
#48658 = EDGE_CURVE('',#38681,#38533,#32056,.T.) ;
#48659 = EDGE_CURVE('',#38530,#38535,#32057,.T.) ;
#48660 = EDGE_CURVE('',#38534,#38531,#32058,.T.) ;
#48661 = EDGE_CURVE('',#38681,#38544,#32059,.T.) ;
#48662 = EDGE_CURVE('',#38544,#38533,#32060,.T.) ;
#48663 = EDGE_CURVE('',#38531,#38683,#32061,.T.) ;
#48664 = EDGE_CURVE('',#38532,#38682,#32062,.T.) ;
#48665 = EDGE_CURVE('',#38545,#38532,#32063,.T.) ;
#48666 = EDGE_CURVE('',#38678,#38543,#32064,.T.) ;
#48667 = EDGE_CURVE('',#38545,#38682,#32065,.T.) ;
#48668 = EDGE_CURVE('',#38678,#38538,#32066,.T.) ;
#48669 = EDGE_CURVE('',#38538,#38543,#32067,.T.) ;
#48670 = EDGE_CURVE('',#38542,#38685,#32068,.T.) ;
#48671 = EDGE_CURVE('',#38539,#38542,#32069,.T.) ;
#48672 = EDGE_CURVE('',#38541,#38679,#32070,.T.) ;
#48673 = EDGE_CURVE('',#38539,#38685,#32071,.T.) ;
#48674 = EDGE_CURVE('',#38536,#38541,#32072,.T.) ;
#48675 = EDGE_CURVE('',#38540,#38537,#32073,.T.) ;
#48676 = EDGE_CURVE('',#38684,#38540,#32074,.T.) ;
#48677 = EDGE_CURVE('',#38600,#38562,#32075,.T.) ;
#48678 = EDGE_CURVE('',#38601,#38565,#32076,.T.) ;
#48679 = EDGE_CURVE('',#38562,#38567,#32077,.T.) ;
#48680 = EDGE_CURVE('',#38566,#38563,#32078,.T.) ;
#48681 = EDGE_CURVE('',#38601,#38558,#32079,.T.) ;
#48682 = EDGE_CURVE('',#38558,#38565,#32080,.T.) ;
#48683 = EDGE_CURVE('',#38563,#38603,#32081,.T.) ;
#48684 = EDGE_CURVE('',#38564,#38602,#32082,.T.) ;
#48685 = EDGE_CURVE('',#38559,#38564,#32083,.T.) ;
#48686 = EDGE_CURVE('',#38598,#38561,#32084,.T.) ;
#48687 = EDGE_CURVE('',#38559,#38602,#32085,.T.) ;
#48688 = EDGE_CURVE('',#38598,#38554,#32086,.T.) ;
#48689 = EDGE_CURVE('',#38554,#38561,#32087,.T.) ;
#48690 = EDGE_CURVE('',#38560,#38605,#32088,.T.) ;
#48691 = EDGE_CURVE('',#38555,#38560,#32089,.T.) ;
#48692 = EDGE_CURVE('',#38557,#38599,#32090,.T.) ;
#48693 = EDGE_CURVE('',#38555,#38605,#32091,.T.) ;
#48694 = EDGE_CURVE('',#38552,#38557,#32092,.T.) ;
#48695 = EDGE_CURVE('',#38556,#38553,#32093,.T.) ;
#48696 = EDGE_CURVE('',#38604,#38556,#32094,.T.) ;
#48697 = EDGE_CURVE('',#38672,#38578,#32095,.T.) ;
#48698 = EDGE_CURVE('',#38673,#38581,#32096,.T.) ;
#48699 = EDGE_CURVE('',#38578,#38583,#32097,.T.) ;
#48700 = EDGE_CURVE('',#38582,#38579,#32098,.T.) ;
#48701 = EDGE_CURVE('',#38673,#38592,#32099,.T.) ;
#48702 = EDGE_CURVE('',#38592,#38581,#32100,.T.) ;
#48703 = EDGE_CURVE('',#38579,#38675,#32101,.T.) ;
#48704 = EDGE_CURVE('',#38580,#38674,#32102,.T.) ;
#48705 = EDGE_CURVE('',#38593,#38580,#32103,.T.) ;
#48706 = EDGE_CURVE('',#38670,#38591,#32104,.T.) ;
#48707 = EDGE_CURVE('',#38593,#38674,#32105,.T.) ;
#48708 = EDGE_CURVE('',#38670,#38586,#32106,.T.) ;
#48709 = EDGE_CURVE('',#38586,#38591,#32107,.T.) ;
#48710 = EDGE_CURVE('',#38590,#38677,#32108,.T.) ;
#48711 = EDGE_CURVE('',#38587,#38590,#32109,.T.) ;
#48712 = EDGE_CURVE('',#38589,#38671,#32110,.T.) ;
#48713 = EDGE_CURVE('',#38587,#38677,#32111,.T.) ;
#48714 = EDGE_CURVE('',#38584,#38589,#32112,.T.) ;
#48715 = EDGE_CURVE('',#38588,#38585,#32113,.T.) ;
#48716 = EDGE_CURVE('',#38676,#38588,#32114,.T.) ;
#48717 = EDGE_CURVE('',#38192,#38184,#32115,.T.) ;
#48718 = EDGE_CURVE('',#38193,#38183,#32116,.T.) ;
#48719 = EDGE_CURVE('',#38193,#38664,#32117,.T.) ;
#48720 = EDGE_CURVE('',#38190,#38663,#32118,.T.) ;
#48721 = EDGE_CURVE('',#38190,#38168,#32119,.T.) ;
#48722 = EDGE_CURVE('',#38191,#38167,#32120,.T.) ;
#48723 = EDGE_CURVE('',#38188,#38166,#32121,.T.) ;
#48724 = EDGE_CURVE('',#38189,#38169,#32122,.T.) ;
#48725 = EDGE_CURVE('',#38189,#38668,#32123,.T.) ;
#48726 = EDGE_CURVE('',#38186,#38667,#32124,.T.) ;
#48727 = EDGE_CURVE('',#38186,#38182,#32125,.T.) ;
#48728 = EDGE_CURVE('',#38187,#38185,#32126,.T.) ;
#48729 = EDGE_CURVE('',#38212,#38199,#32127,.T.) ;
#48730 = EDGE_CURVE('',#38212,#38736,#32128,.T.) ;
#48731 = EDGE_CURVE('',#38213,#38735,#32129,.T.) ;
#48732 = EDGE_CURVE('',#38213,#38200,#32130,.T.) ;
#48733 = EDGE_CURVE('',#38198,#38211,#32131,.T.) ;
#48734 = EDGE_CURVE('',#38739,#38211,#32132,.T.) ;
#48735 = EDGE_CURVE('',#38740,#38210,#32133,.T.) ;
#48736 = EDGE_CURVE('',#38210,#38201,#32134,.T.) ;
#48737 = EDGE_CURVE('',#38240,#38232,#32135,.T.) ;
#48738 = EDGE_CURVE('',#38241,#38231,#32136,.T.) ;
#48739 = EDGE_CURVE('',#38241,#38656,#32137,.T.) ;
#48740 = EDGE_CURVE('',#38238,#38655,#32138,.T.) ;
#48741 = EDGE_CURVE('',#38238,#38216,#32139,.T.) ;
#48742 = EDGE_CURVE('',#38239,#38215,#32140,.T.) ;
#48743 = EDGE_CURVE('',#38236,#38214,#32141,.T.) ;
#48744 = EDGE_CURVE('',#38237,#38217,#32142,.T.) ;
#48745 = EDGE_CURVE('',#38237,#38660,#32143,.T.) ;
#48746 = EDGE_CURVE('',#38234,#38659,#32144,.T.) ;
#48747 = EDGE_CURVE('',#38234,#38230,#32145,.T.) ;
#48748 = EDGE_CURVE('',#38235,#38233,#32146,.T.) ;
#48749 = EDGE_CURVE('',#38260,#38247,#32147,.T.) ;
#48750 = EDGE_CURVE('',#38260,#38728,#32148,.T.) ;
#48751 = EDGE_CURVE('',#38261,#38727,#32149,.T.) ;
#48752 = EDGE_CURVE('',#38261,#38248,#32150,.T.) ;
#48753 = EDGE_CURVE('',#38246,#38259,#32151,.T.) ;
#48754 = EDGE_CURVE('',#38731,#38259,#32152,.T.) ;
#48755 = EDGE_CURVE('',#38732,#38258,#32153,.T.) ;
#48756 = EDGE_CURVE('',#38258,#38249,#32154,.T.) ;
#48757 = EDGE_CURVE('',#38288,#38280,#32155,.T.) ;
#48758 = EDGE_CURVE('',#38289,#38279,#32156,.T.) ;
#48759 = EDGE_CURVE('',#38289,#38648,#32157,.T.) ;
#48760 = EDGE_CURVE('',#38286,#38647,#32158,.T.) ;
#48761 = EDGE_CURVE('',#38286,#38264,#32159,.T.) ;
#48762 = EDGE_CURVE('',#38287,#38263,#32160,.T.) ;
#48763 = EDGE_CURVE('',#38284,#38262,#32161,.T.) ;
#48764 = EDGE_CURVE('',#38285,#38265,#32162,.T.) ;
#48765 = EDGE_CURVE('',#38285,#38652,#32163,.T.) ;
#48766 = EDGE_CURVE('',#38282,#38651,#32164,.T.) ;
#48767 = EDGE_CURVE('',#38282,#38278,#32165,.T.) ;
#48768 = EDGE_CURVE('',#38283,#38281,#32166,.T.) ;
#48769 = EDGE_CURVE('',#38308,#38295,#32167,.T.) ;
#48770 = EDGE_CURVE('',#38308,#38720,#32168,.T.) ;
#48771 = EDGE_CURVE('',#38309,#38719,#32169,.T.) ;
#48772 = EDGE_CURVE('',#38309,#38296,#32170,.T.) ;
#48773 = EDGE_CURVE('',#38294,#38307,#32171,.T.) ;
#48774 = EDGE_CURVE('',#38723,#38307,#32172,.T.) ;
#48775 = EDGE_CURVE('',#38724,#38306,#32173,.T.) ;
#48776 = EDGE_CURVE('',#38306,#38297,#32174,.T.) ;
#48777 = EDGE_CURVE('',#38336,#38328,#32175,.T.) ;
#48778 = EDGE_CURVE('',#38337,#38327,#32176,.T.) ;
#48779 = EDGE_CURVE('',#38337,#38640,#32177,.T.) ;
#48780 = EDGE_CURVE('',#38334,#38639,#32178,.T.) ;
#48781 = EDGE_CURVE('',#38334,#38312,#32179,.T.) ;
#48782 = EDGE_CURVE('',#38335,#38311,#32180,.T.) ;
#48783 = EDGE_CURVE('',#38332,#38310,#32181,.T.) ;
#48784 = EDGE_CURVE('',#38333,#38313,#32182,.T.) ;
#48785 = EDGE_CURVE('',#38333,#38644,#32183,.T.) ;
#48786 = EDGE_CURVE('',#38330,#38643,#32184,.T.) ;
#48787 = EDGE_CURVE('',#38330,#38326,#32185,.T.) ;
#48788 = EDGE_CURVE('',#38331,#38329,#32186,.T.) ;
#48789 = EDGE_CURVE('',#38356,#38343,#32187,.T.) ;
#48790 = EDGE_CURVE('',#38356,#38712,#32188,.T.) ;
#48791 = EDGE_CURVE('',#38357,#38711,#32189,.T.) ;
#48792 = EDGE_CURVE('',#38357,#38344,#32190,.T.) ;
#48793 = EDGE_CURVE('',#38342,#38355,#32191,.T.) ;
#48794 = EDGE_CURVE('',#38715,#38355,#32192,.T.) ;
#48795 = EDGE_CURVE('',#38716,#38354,#32193,.T.) ;
#48796 = EDGE_CURVE('',#38354,#38345,#32194,.T.) ;
#48797 = EDGE_CURVE('',#38384,#38376,#32195,.T.) ;
#48798 = EDGE_CURVE('',#38385,#38375,#32196,.T.) ;
#48799 = EDGE_CURVE('',#38385,#38632,#32197,.T.) ;
#48800 = EDGE_CURVE('',#38382,#38631,#32198,.T.) ;
#48801 = EDGE_CURVE('',#38382,#38360,#32199,.T.) ;
#48802 = EDGE_CURVE('',#38383,#38359,#32200,.T.) ;
#48803 = EDGE_CURVE('',#38380,#38358,#32201,.T.) ;
#48804 = EDGE_CURVE('',#38381,#38361,#32202,.T.) ;
#48805 = EDGE_CURVE('',#38381,#38636,#32203,.T.) ;
#48806 = EDGE_CURVE('',#38378,#38635,#32204,.T.) ;
#48807 = EDGE_CURVE('',#38378,#38374,#32205,.T.) ;
#48808 = EDGE_CURVE('',#38379,#38377,#32206,.T.) ;
#48809 = EDGE_CURVE('',#38404,#38391,#32207,.T.) ;
#48810 = EDGE_CURVE('',#38404,#38704,#32208,.T.) ;
#48811 = EDGE_CURVE('',#38405,#38703,#32209,.T.) ;
#48812 = EDGE_CURVE('',#38405,#38392,#32210,.T.) ;
#48813 = EDGE_CURVE('',#38390,#38403,#32211,.T.) ;
#48814 = EDGE_CURVE('',#38707,#38403,#32212,.T.) ;
#48815 = EDGE_CURVE('',#38708,#38402,#32213,.T.) ;
#48816 = EDGE_CURVE('',#38402,#38393,#32214,.T.) ;
#48817 = EDGE_CURVE('',#38432,#38424,#32215,.T.) ;
#48818 = EDGE_CURVE('',#38433,#38423,#32216,.T.) ;
#48819 = EDGE_CURVE('',#38433,#38624,#32217,.T.) ;
#48820 = EDGE_CURVE('',#38430,#38623,#32218,.T.) ;
#48821 = EDGE_CURVE('',#38430,#38408,#32219,.T.) ;
#48822 = EDGE_CURVE('',#38431,#38407,#32220,.T.) ;
#48823 = EDGE_CURVE('',#38428,#38406,#32221,.T.) ;
#48824 = EDGE_CURVE('',#38429,#38409,#32222,.T.) ;
#48825 = EDGE_CURVE('',#38429,#38628,#32223,.T.) ;
#48826 = EDGE_CURVE('',#38426,#38627,#32224,.T.) ;
#48827 = EDGE_CURVE('',#38426,#38422,#32225,.T.) ;
#48828 = EDGE_CURVE('',#38427,#38425,#32226,.T.) ;
#48829 = EDGE_CURVE('',#38452,#38439,#32227,.T.) ;
#48830 = EDGE_CURVE('',#38452,#38696,#32228,.T.) ;
#48831 = EDGE_CURVE('',#38453,#38695,#32229,.T.) ;
#48832 = EDGE_CURVE('',#38453,#38440,#32230,.T.) ;
#48833 = EDGE_CURVE('',#38438,#38451,#32231,.T.) ;
#48834 = EDGE_CURVE('',#38699,#38451,#32232,.T.) ;
#48835 = EDGE_CURVE('',#38700,#38450,#32233,.T.) ;
#48836 = EDGE_CURVE('',#38450,#38441,#32234,.T.) ;
#48837 = EDGE_CURVE('',#38480,#38472,#32235,.T.) ;
#48838 = EDGE_CURVE('',#38481,#38471,#32236,.T.) ;
#48839 = EDGE_CURVE('',#38481,#38616,#32237,.T.) ;
#48840 = EDGE_CURVE('',#38478,#38615,#32238,.T.) ;
#48841 = EDGE_CURVE('',#38478,#38456,#32239,.T.) ;
#48842 = EDGE_CURVE('',#38479,#38455,#32240,.T.) ;
#48843 = EDGE_CURVE('',#38476,#38454,#32241,.T.) ;
#48844 = EDGE_CURVE('',#38477,#38457,#32242,.T.) ;
#48845 = EDGE_CURVE('',#38477,#38620,#32243,.T.) ;
#48846 = EDGE_CURVE('',#38474,#38619,#32244,.T.) ;
#48847 = EDGE_CURVE('',#38474,#38470,#32245,.T.) ;
#48848 = EDGE_CURVE('',#38475,#38473,#32246,.T.) ;
#48849 = EDGE_CURVE('',#38500,#38487,#32247,.T.) ;
#48850 = EDGE_CURVE('',#38500,#38688,#32248,.T.) ;
#48851 = EDGE_CURVE('',#38501,#38687,#32249,.T.) ;
#48852 = EDGE_CURVE('',#38501,#38488,#32250,.T.) ;
#48853 = EDGE_CURVE('',#38486,#38499,#32251,.T.) ;
#48854 = EDGE_CURVE('',#38691,#38499,#32252,.T.) ;
#48855 = EDGE_CURVE('',#38692,#38498,#32253,.T.) ;
#48856 = EDGE_CURVE('',#38498,#38489,#32254,.T.) ;
#48857 = EDGE_CURVE('',#38528,#38520,#32255,.T.) ;
#48858 = EDGE_CURVE('',#38529,#38519,#32256,.T.) ;
#48859 = EDGE_CURVE('',#38529,#38608,#32257,.T.) ;
#48860 = EDGE_CURVE('',#38526,#38607,#32258,.T.) ;
#48861 = EDGE_CURVE('',#38526,#38504,#32259,.T.) ;
#48862 = EDGE_CURVE('',#38527,#38503,#32260,.T.) ;
#48863 = EDGE_CURVE('',#38524,#38502,#32261,.T.) ;
#48864 = EDGE_CURVE('',#38525,#38505,#32262,.T.) ;
#48865 = EDGE_CURVE('',#38525,#38612,#32263,.T.) ;
#48866 = EDGE_CURVE('',#38522,#38611,#32264,.T.) ;
#48867 = EDGE_CURVE('',#38522,#38518,#32265,.T.) ;
#48868 = EDGE_CURVE('',#38523,#38521,#32266,.T.) ;
#48869 = EDGE_CURVE('',#38548,#38535,#32267,.T.) ;
#48870 = EDGE_CURVE('',#38548,#38680,#32268,.T.) ;
#48871 = EDGE_CURVE('',#38549,#38679,#32269,.T.) ;
#48872 = EDGE_CURVE('',#38549,#38536,#32270,.T.) ;
#48873 = EDGE_CURVE('',#38534,#38547,#32271,.T.) ;
#48874 = EDGE_CURVE('',#38683,#38547,#32272,.T.) ;
#48875 = EDGE_CURVE('',#38684,#38546,#32273,.T.) ;
#48876 = EDGE_CURVE('',#38546,#38537,#32274,.T.) ;
#48877 = EDGE_CURVE('',#38576,#38568,#32275,.T.) ;
#48878 = EDGE_CURVE('',#38577,#38567,#32276,.T.) ;
#48879 = EDGE_CURVE('',#38577,#38600,#32277,.T.) ;
#48880 = EDGE_CURVE('',#38574,#38599,#32278,.T.) ;
#48881 = EDGE_CURVE('',#38574,#38552,#32279,.T.) ;
#48882 = EDGE_CURVE('',#38575,#38551,#32280,.T.) ;
#48883 = EDGE_CURVE('',#38572,#38550,#32281,.T.) ;
#48884 = EDGE_CURVE('',#38573,#38553,#32282,.T.) ;
#48885 = EDGE_CURVE('',#38573,#38604,#32283,.T.) ;
#48886 = EDGE_CURVE('',#38570,#38603,#32284,.T.) ;
#48887 = EDGE_CURVE('',#38570,#38566,#32285,.T.) ;
#48888 = EDGE_CURVE('',#38571,#38569,#32286,.T.) ;
#48889 = EDGE_CURVE('',#38596,#38583,#32287,.T.) ;
#48890 = EDGE_CURVE('',#38596,#38672,#32288,.T.) ;
#48891 = EDGE_CURVE('',#38597,#38671,#32289,.T.) ;
#48892 = EDGE_CURVE('',#38597,#38584,#32290,.T.) ;
#48893 = EDGE_CURVE('',#38582,#38595,#32291,.T.) ;
#48894 = EDGE_CURVE('',#38675,#38595,#32292,.T.) ;
#48895 = EDGE_CURVE('',#38676,#38594,#32293,.T.) ;
#48896 = EDGE_CURVE('',#38594,#38585,#32294,.T.) ;
#48897 = EDGE_CURVE('',#38742,#38743,#32295,.T.) ;
#48898 = EDGE_CURVE('',#38744,#38742,#5767,.T.) ;
#48899 = EDGE_CURVE('',#38744,#38745,#32296,.T.) ;
#48900 = EDGE_CURVE('',#38743,#38745,#5768,.T.) ;
#48901 = EDGE_CURVE('',#38746,#38747,#32297,.T.) ;
#48902 = EDGE_CURVE('',#38748,#38746,#32298,.T.) ;
#48903 = EDGE_CURVE('',#38749,#38748,#32299,.T.) ;
#48904 = EDGE_CURVE('',#38749,#38747,#32300,.T.) ;
#48905 = EDGE_CURVE('',#38750,#38751,#32301,.T.) ;
#48906 = EDGE_CURVE('',#38752,#38750,#32302,.T.) ;
#48907 = EDGE_CURVE('',#38753,#38752,#32303,.T.) ;
#48908 = EDGE_CURVE('',#38753,#38751,#32304,.T.) ;
#48909 = EDGE_CURVE('',#38754,#38755,#32305,.T.) ;
#48910 = EDGE_CURVE('',#38754,#38756,#2197,.T.) ;
#48911 = EDGE_CURVE('',#38757,#38756,#32306,.T.) ;
#48912 = EDGE_CURVE('',#38755,#38757,#2198,.T.) ;
#48913 = EDGE_CURVE('',#38758,#38759,#32307,.T.) ;
#48914 = EDGE_CURVE('',#38760,#38758,#32308,.T.) ;
#48915 = EDGE_CURVE('',#38761,#38760,#32309,.T.) ;
#48916 = EDGE_CURVE('',#38761,#38759,#32310,.T.) ;
#48917 = EDGE_CURVE('',#38762,#38754,#32311,.T.) ;
#48918 = EDGE_CURVE('',#38762,#38763,#2199,.T.) ;
#48919 = EDGE_CURVE('',#38764,#38763,#32312,.T.) ;
#48920 = EDGE_CURVE('',#38754,#38764,#2200,.T.) ;
#48921 = EDGE_CURVE('',#38765,#38766,#32313,.T.) ;
#48922 = EDGE_CURVE('',#38767,#38765,#32314,.T.) ;
#48923 = EDGE_CURVE('',#38768,#38767,#32315,.T.) ;
#48924 = EDGE_CURVE('',#38768,#38766,#32316,.T.) ;
#48925 = EDGE_CURVE('',#38769,#38762,#32317,.T.) ;
#48926 = EDGE_CURVE('',#38769,#38770,#2201,.T.) ;
#48927 = EDGE_CURVE('',#38771,#38770,#32318,.T.) ;
#48928 = EDGE_CURVE('',#38762,#38771,#2202,.T.) ;
#48929 = EDGE_CURVE('',#38772,#38773,#32319,.T.) ;
#48930 = EDGE_CURVE('',#38774,#38772,#32320,.T.) ;
#48931 = EDGE_CURVE('',#38775,#38774,#32321,.T.) ;
#48932 = EDGE_CURVE('',#38775,#38773,#32322,.T.) ;
#48933 = EDGE_CURVE('',#38776,#38769,#32323,.T.) ;
#48934 = EDGE_CURVE('',#38776,#38777,#2203,.T.) ;
#48935 = EDGE_CURVE('',#38778,#38777,#32324,.T.) ;
#48936 = EDGE_CURVE('',#38769,#38778,#2204,.T.) ;
#48937 = EDGE_CURVE('',#38779,#38780,#32325,.T.) ;
#48938 = EDGE_CURVE('',#38781,#38779,#32326,.T.) ;
#48939 = EDGE_CURVE('',#38782,#38781,#32327,.T.) ;
#48940 = EDGE_CURVE('',#38782,#38780,#32328,.T.) ;
#48941 = EDGE_CURVE('',#38783,#38776,#32329,.T.) ;
#48942 = EDGE_CURVE('',#38783,#38784,#2205,.T.) ;
#48943 = EDGE_CURVE('',#38785,#38784,#32330,.T.) ;
#48944 = EDGE_CURVE('',#38776,#38785,#2206,.T.) ;
#48945 = EDGE_CURVE('',#38786,#38787,#32331,.T.) ;
#48946 = EDGE_CURVE('',#38788,#38786,#32332,.T.) ;
#48947 = EDGE_CURVE('',#38789,#38788,#32333,.T.) ;
#48948 = EDGE_CURVE('',#38789,#38787,#32334,.T.) ;
#48949 = EDGE_CURVE('',#38790,#38783,#32335,.T.) ;
#48950 = EDGE_CURVE('',#38790,#38791,#2207,.T.) ;
#48951 = EDGE_CURVE('',#38792,#38791,#32336,.T.) ;
#48952 = EDGE_CURVE('',#38783,#38792,#2208,.T.) ;
#48953 = EDGE_CURVE('',#38793,#38794,#32337,.T.) ;
#48954 = EDGE_CURVE('',#38795,#38793,#32338,.T.) ;
#48955 = EDGE_CURVE('',#38796,#38795,#32339,.T.) ;
#48956 = EDGE_CURVE('',#38796,#38794,#32340,.T.) ;
#48957 = EDGE_CURVE('',#38797,#38790,#32341,.T.) ;
#48958 = EDGE_CURVE('',#38797,#38798,#2209,.T.) ;
#48959 = EDGE_CURVE('',#38799,#38798,#32342,.T.) ;
#48960 = EDGE_CURVE('',#38790,#38799,#2210,.T.) ;
#48961 = EDGE_CURVE('',#38800,#38801,#32343,.T.) ;
#48962 = EDGE_CURVE('',#38802,#38800,#32344,.T.) ;
#48963 = EDGE_CURVE('',#38803,#38802,#32345,.T.) ;
#48964 = EDGE_CURVE('',#38803,#38801,#32346,.T.) ;
#48965 = EDGE_CURVE('',#38804,#38797,#32347,.T.) ;
#48966 = EDGE_CURVE('',#38804,#38805,#2211,.T.) ;
#48967 = EDGE_CURVE('',#38806,#38805,#32348,.T.) ;
#48968 = EDGE_CURVE('',#38797,#38806,#2212,.T.) ;
#48969 = EDGE_CURVE('',#38807,#38808,#32349,.T.) ;
#48970 = EDGE_CURVE('',#38809,#38807,#32350,.T.) ;
#48971 = EDGE_CURVE('',#38810,#38809,#32351,.T.) ;
#48972 = EDGE_CURVE('',#38810,#38808,#32352,.T.) ;
#48973 = EDGE_CURVE('',#38811,#38804,#32353,.T.) ;
#48974 = EDGE_CURVE('',#38811,#38812,#2213,.T.) ;
#48975 = EDGE_CURVE('',#38813,#38812,#32354,.T.) ;
#48976 = EDGE_CURVE('',#38804,#38813,#2214,.T.) ;
#48977 = EDGE_CURVE('',#38814,#38815,#32355,.T.) ;
#48978 = EDGE_CURVE('',#38816,#38814,#32356,.T.) ;
#48979 = EDGE_CURVE('',#38817,#38816,#32357,.T.) ;
#48980 = EDGE_CURVE('',#38817,#38815,#32358,.T.) ;
#48981 = EDGE_CURVE('',#38818,#38811,#32359,.T.) ;
#48982 = EDGE_CURVE('',#38818,#38819,#2215,.T.) ;
#48983 = EDGE_CURVE('',#38820,#38819,#32360,.T.) ;
#48984 = EDGE_CURVE('',#38811,#38820,#2216,.T.) ;
#48985 = EDGE_CURVE('',#38805,#38813,#32361,.T.) ;
#48986 = EDGE_CURVE('',#38813,#38803,#5769,.T.) ;
#48987 = EDGE_CURVE('',#38805,#38802,#5770,.T.) ;
#48988 = EDGE_CURVE('',#38798,#38806,#32362,.T.) ;
#48989 = EDGE_CURVE('',#38806,#38796,#5771,.T.) ;
#48990 = EDGE_CURVE('',#38798,#38795,#5772,.T.) ;
#48991 = EDGE_CURVE('',#38791,#38799,#32363,.T.) ;
#48992 = EDGE_CURVE('',#38799,#38789,#5773,.T.) ;
#48993 = EDGE_CURVE('',#38791,#38788,#5774,.T.) ;
#48994 = EDGE_CURVE('',#38784,#38792,#32364,.T.) ;
#48995 = EDGE_CURVE('',#38792,#38782,#5775,.T.) ;
#48996 = EDGE_CURVE('',#38784,#38781,#5776,.T.) ;
#48997 = EDGE_CURVE('',#38777,#38785,#32365,.T.) ;
#48998 = EDGE_CURVE('',#38785,#38775,#5777,.T.) ;
#48999 = EDGE_CURVE('',#38777,#38774,#5778,.T.) ;
#49000 = EDGE_CURVE('',#38770,#38778,#32366,.T.) ;
#49001 = EDGE_CURVE('',#38778,#38768,#5779,.T.) ;
#49002 = EDGE_CURVE('',#38770,#38767,#5780,.T.) ;
#49003 = EDGE_CURVE('',#38763,#38771,#32367,.T.) ;
#49004 = EDGE_CURVE('',#38771,#38761,#5781,.T.) ;
#49005 = EDGE_CURVE('',#38763,#38760,#5782,.T.) ;
#49006 = EDGE_CURVE('',#38821,#38821,#32368,.T.) ;
#49007 = EDGE_CURVE('',#38821,#38822,#32369,.T.) ;
#49008 = EDGE_CURVE('',#38822,#38822,#32370,.T.) ;
#49009 = EDGE_CURVE('',#38823,#38823,#32371,.T.) ;
#49010 = EDGE_CURVE('',#38823,#38824,#32372,.T.) ;
#49011 = EDGE_CURVE('',#38824,#38824,#32373,.T.) ;
#49012 = EDGE_CURVE('',#38825,#38825,#32374,.T.) ;
#49013 = EDGE_CURVE('',#38825,#38826,#32375,.T.) ;
#49014 = EDGE_CURVE('',#38826,#38826,#32376,.T.) ;
#49015 = EDGE_CURVE('',#38827,#38827,#32377,.T.) ;
#49016 = EDGE_CURVE('',#38827,#38828,#32378,.T.) ;
#49017 = EDGE_CURVE('',#38828,#38828,#32379,.T.) ;
#49018 = EDGE_CURVE('',#38829,#38829,#32380,.T.) ;
#49019 = EDGE_CURVE('',#38829,#38830,#32381,.T.) ;
#49020 = EDGE_CURVE('',#38830,#38830,#32382,.T.) ;
#49021 = EDGE_CURVE('',#38831,#38831,#32383,.T.) ;
#49022 = EDGE_CURVE('',#38831,#38832,#32384,.T.) ;
#49023 = EDGE_CURVE('',#38832,#38832,#32385,.T.) ;
#49024 = EDGE_CURVE('',#38833,#38833,#32386,.T.) ;
#49025 = EDGE_CURVE('',#38833,#38834,#32387,.T.) ;
#49026 = EDGE_CURVE('',#38834,#38834,#32388,.T.) ;
#49027 = EDGE_CURVE('',#38835,#38835,#32389,.T.) ;
#49028 = EDGE_CURVE('',#38835,#38836,#32390,.T.) ;
#49029 = EDGE_CURVE('',#38836,#38836,#32391,.T.) ;
#49030 = EDGE_CURVE('',#38837,#38837,#32392,.T.) ;
#49031 = EDGE_CURVE('',#38837,#38838,#32393,.T.) ;
#49032 = EDGE_CURVE('',#38838,#38838,#32394,.T.) ;
#49033 = EDGE_CURVE('',#38839,#38839,#32395,.T.) ;
#49034 = EDGE_CURVE('',#38839,#38840,#32396,.T.) ;
#49035 = EDGE_CURVE('',#38840,#38840,#32397,.T.) ;
#49036 = EDGE_CURVE('',#38841,#38841,#32398,.T.) ;
#49037 = EDGE_CURVE('',#38841,#38842,#32399,.T.) ;
#49038 = EDGE_CURVE('',#38842,#38842,#32400,.T.) ;
#49039 = EDGE_CURVE('',#38843,#38843,#32401,.T.) ;
#49040 = EDGE_CURVE('',#38843,#38844,#32402,.T.) ;
#49041 = EDGE_CURVE('',#38844,#38844,#32403,.T.) ;
#49042 = EDGE_CURVE('',#38845,#38845,#32404,.T.) ;
#49043 = EDGE_CURVE('',#38845,#38846,#32405,.T.) ;
#49044 = EDGE_CURVE('',#38846,#38846,#32406,.T.) ;
#49045 = EDGE_CURVE('',#38847,#38847,#32407,.T.) ;
#49046 = EDGE_CURVE('',#38847,#38848,#32408,.T.) ;
#49047 = EDGE_CURVE('',#38848,#38848,#32409,.T.) ;
#49048 = EDGE_CURVE('',#38849,#38849,#32410,.T.) ;
#49049 = EDGE_CURVE('',#38849,#38850,#32411,.T.) ;
#49050 = EDGE_CURVE('',#38850,#38850,#32412,.T.) ;
#49051 = EDGE_CURVE('',#38851,#38851,#32413,.T.) ;
#49052 = EDGE_CURVE('',#38851,#38852,#32414,.T.) ;
#49053 = EDGE_CURVE('',#38852,#38852,#32415,.T.) ;
#49054 = EDGE_CURVE('',#38853,#38853,#32416,.T.) ;
#49055 = EDGE_CURVE('',#38853,#38854,#32417,.T.) ;
#49056 = EDGE_CURVE('',#38854,#38854,#32418,.T.) ;
#49057 = EDGE_CURVE('',#38855,#38855,#32419,.T.) ;
#49058 = EDGE_CURVE('',#38855,#38856,#32420,.T.) ;
#49059 = EDGE_CURVE('',#38856,#38856,#32421,.T.) ;
#49060 = EDGE_CURVE('',#38857,#38857,#32422,.T.) ;
#49061 = EDGE_CURVE('',#38857,#38858,#32423,.T.) ;
#49062 = EDGE_CURVE('',#38858,#38858,#32424,.T.) ;
#49063 = EDGE_CURVE('',#38859,#38859,#32425,.T.) ;
#49064 = EDGE_CURVE('',#38859,#38860,#32426,.T.) ;
#49065 = EDGE_CURVE('',#38860,#38860,#32427,.T.) ;
#49066 = EDGE_CURVE('',#38861,#38861,#32428,.T.) ;
#49067 = EDGE_CURVE('',#38861,#38862,#32429,.T.) ;
#49068 = EDGE_CURVE('',#38862,#38862,#32430,.T.) ;
#49069 = EDGE_CURVE('',#38863,#38863,#32431,.T.) ;
#49070 = EDGE_CURVE('',#38863,#38864,#32432,.T.) ;
#49071 = EDGE_CURVE('',#38864,#38864,#32433,.T.) ;
#49072 = EDGE_CURVE('',#38865,#38865,#32434,.T.) ;
#49073 = EDGE_CURVE('',#38865,#38866,#32435,.T.) ;
#49074 = EDGE_CURVE('',#38866,#38866,#32436,.T.) ;
#49075 = EDGE_CURVE('',#38867,#38867,#32437,.T.) ;
#49076 = EDGE_CURVE('',#38867,#38868,#32438,.T.) ;
#49077 = EDGE_CURVE('',#38868,#38868,#32439,.T.) ;
#49078 = EDGE_CURVE('',#38869,#38869,#32440,.T.) ;
#49079 = EDGE_CURVE('',#38869,#38870,#32441,.T.) ;
#49080 = EDGE_CURVE('',#38870,#38870,#32442,.T.) ;
#49081 = EDGE_CURVE('',#38871,#38871,#32443,.T.) ;
#49082 = EDGE_CURVE('',#38871,#38872,#32444,.T.) ;
#49083 = EDGE_CURVE('',#38872,#38872,#32445,.T.) ;
#49084 = EDGE_CURVE('',#38873,#38873,#32446,.T.) ;
#49085 = EDGE_CURVE('',#38873,#38874,#32447,.T.) ;
#49086 = EDGE_CURVE('',#38874,#38874,#32448,.T.) ;
#49087 = EDGE_CURVE('',#38875,#38876,#32449,.T.) ;
#49088 = EDGE_CURVE('',#38875,#38877,#2217,.T.) ;
#49089 = EDGE_CURVE('',#38878,#38877,#5783,.T.) ;
#49090 = EDGE_CURVE('',#38878,#38879,#2218,.T.) ;
#49091 = EDGE_CURVE('',#38880,#38879,#32450,.T.) ;
#49092 = EDGE_CURVE('',#38880,#38881,#2219,.T.) ;
#49093 = EDGE_CURVE('',#38881,#38882,#5784,.T.) ;
#49094 = EDGE_CURVE('',#38882,#38883,#2220,.T.) ;
#49095 = EDGE_CURVE('',#38884,#38883,#32451,.T.) ;
#49096 = EDGE_CURVE('',#38884,#38885,#2221,.T.) ;
#49097 = EDGE_CURVE('',#38886,#38885,#5785,.T.) ;
#49098 = EDGE_CURVE('',#38886,#38887,#2222,.T.) ;
#49099 = EDGE_CURVE('',#38888,#38887,#32452,.T.) ;
#49100 = EDGE_CURVE('',#38888,#38889,#2223,.T.) ;
#49101 = EDGE_CURVE('',#38889,#38890,#5786,.T.) ;
#49102 = EDGE_CURVE('',#38890,#38891,#2224,.T.) ;
#49103 = EDGE_CURVE('',#38876,#38891,#32453,.T.) ;
#49104 = EDGE_CURVE('',#38876,#38871,#5787,.T.) ;
#49105 = EDGE_CURVE('',#38892,#38893,#32454,.T.) ;
#49106 = EDGE_CURVE('',#38892,#38894,#2225,.T.) ;
#49107 = EDGE_CURVE('',#38895,#38894,#5788,.T.) ;
#49108 = EDGE_CURVE('',#38895,#38896,#2226,.T.) ;
#49109 = EDGE_CURVE('',#38897,#38896,#32455,.T.) ;
#49110 = EDGE_CURVE('',#38897,#38898,#2227,.T.) ;
#49111 = EDGE_CURVE('',#38898,#38899,#5789,.T.) ;
#49112 = EDGE_CURVE('',#38899,#38900,#2228,.T.) ;
#49113 = EDGE_CURVE('',#38901,#38900,#32456,.T.) ;
#49114 = EDGE_CURVE('',#38901,#38902,#2229,.T.) ;
#49115 = EDGE_CURVE('',#38903,#38902,#5790,.T.) ;
#49116 = EDGE_CURVE('',#38903,#38904,#2230,.T.) ;
#49117 = EDGE_CURVE('',#38905,#38904,#32457,.T.) ;
#49118 = EDGE_CURVE('',#38905,#38906,#2231,.T.) ;
#49119 = EDGE_CURVE('',#38906,#38907,#5791,.T.) ;
#49120 = EDGE_CURVE('',#38907,#38908,#2232,.T.) ;
#49121 = EDGE_CURVE('',#38893,#38908,#32458,.T.) ;
#49122 = EDGE_CURVE('',#38893,#38865,#5792,.T.) ;
#49123 = EDGE_CURVE('',#38909,#38910,#32459,.T.) ;
#49124 = EDGE_CURVE('',#38909,#38911,#2233,.T.) ;
#49125 = EDGE_CURVE('',#38912,#38911,#5793,.T.) ;
#49126 = EDGE_CURVE('',#38912,#38913,#2234,.T.) ;
#49127 = EDGE_CURVE('',#38914,#38913,#32460,.T.) ;
#49128 = EDGE_CURVE('',#38914,#38915,#2235,.T.) ;
#49129 = EDGE_CURVE('',#38915,#38916,#5794,.T.) ;
#49130 = EDGE_CURVE('',#38916,#38917,#2236,.T.) ;
#49131 = EDGE_CURVE('',#38918,#38917,#32461,.T.) ;
#49132 = EDGE_CURVE('',#38918,#38919,#2237,.T.) ;
#49133 = EDGE_CURVE('',#38920,#38919,#5795,.T.) ;
#49134 = EDGE_CURVE('',#38920,#38921,#2238,.T.) ;
#49135 = EDGE_CURVE('',#38922,#38921,#32462,.T.) ;
#49136 = EDGE_CURVE('',#38922,#38923,#2239,.T.) ;
#49137 = EDGE_CURVE('',#38923,#38924,#5796,.T.) ;
#49138 = EDGE_CURVE('',#38924,#38925,#2240,.T.) ;
#49139 = EDGE_CURVE('',#38910,#38925,#32463,.T.) ;
#49140 = EDGE_CURVE('',#38910,#38859,#5797,.T.) ;
#49141 = EDGE_CURVE('',#38926,#38927,#32464,.T.) ;
#49142 = EDGE_CURVE('',#38926,#38928,#2241,.T.) ;
#49143 = EDGE_CURVE('',#38929,#38928,#5798,.T.) ;
#49144 = EDGE_CURVE('',#38929,#38930,#2242,.T.) ;
#49145 = EDGE_CURVE('',#38931,#38930,#32465,.T.) ;
#49146 = EDGE_CURVE('',#38931,#38932,#2243,.T.) ;
#49147 = EDGE_CURVE('',#38932,#38933,#5799,.T.) ;
#49148 = EDGE_CURVE('',#38933,#38934,#2244,.T.) ;
#49149 = EDGE_CURVE('',#38935,#38934,#32466,.T.) ;
#49150 = EDGE_CURVE('',#38935,#38936,#2245,.T.) ;
#49151 = EDGE_CURVE('',#38937,#38936,#5800,.T.) ;
#49152 = EDGE_CURVE('',#38937,#38938,#2246,.T.) ;
#49153 = EDGE_CURVE('',#38939,#38938,#32467,.T.) ;
#49154 = EDGE_CURVE('',#38939,#38940,#2247,.T.) ;
#49155 = EDGE_CURVE('',#38940,#38941,#5801,.T.) ;
#49156 = EDGE_CURVE('',#38941,#38942,#2248,.T.) ;
#49157 = EDGE_CURVE('',#38927,#38942,#32468,.T.) ;
#49158 = EDGE_CURVE('',#38927,#38853,#5802,.T.) ;
#49159 = EDGE_CURVE('',#38943,#38944,#32469,.T.) ;
#49160 = EDGE_CURVE('',#38943,#38945,#2249,.T.) ;
#49161 = EDGE_CURVE('',#38946,#38945,#5803,.T.) ;
#49162 = EDGE_CURVE('',#38946,#38947,#2250,.T.) ;
#49163 = EDGE_CURVE('',#38948,#38947,#32470,.T.) ;
#49164 = EDGE_CURVE('',#38948,#38949,#2251,.T.) ;
#49165 = EDGE_CURVE('',#38949,#38950,#5804,.T.) ;
#49166 = EDGE_CURVE('',#38950,#38951,#2252,.T.) ;
#49167 = EDGE_CURVE('',#38952,#38951,#32471,.T.) ;
#49168 = EDGE_CURVE('',#38952,#38953,#2253,.T.) ;
#49169 = EDGE_CURVE('',#38954,#38953,#5805,.T.) ;
#49170 = EDGE_CURVE('',#38954,#38955,#2254,.T.) ;
#49171 = EDGE_CURVE('',#38956,#38955,#32472,.T.) ;
#49172 = EDGE_CURVE('',#38956,#38957,#2255,.T.) ;
#49173 = EDGE_CURVE('',#38957,#38958,#5806,.T.) ;
#49174 = EDGE_CURVE('',#38958,#38959,#2256,.T.) ;
#49175 = EDGE_CURVE('',#38944,#38959,#32473,.T.) ;
#49176 = EDGE_CURVE('',#38944,#38847,#5807,.T.) ;
#49177 = EDGE_CURVE('',#38960,#38961,#32474,.T.) ;
#49178 = EDGE_CURVE('',#38960,#38962,#2257,.T.) ;
#49179 = EDGE_CURVE('',#38963,#38962,#5808,.T.) ;
#49180 = EDGE_CURVE('',#38963,#38964,#2258,.T.) ;
#49181 = EDGE_CURVE('',#38965,#38964,#32475,.T.) ;
#49182 = EDGE_CURVE('',#38965,#38966,#2259,.T.) ;
#49183 = EDGE_CURVE('',#38966,#38967,#5809,.T.) ;
#49184 = EDGE_CURVE('',#38967,#38968,#2260,.T.) ;
#49185 = EDGE_CURVE('',#38969,#38968,#32476,.T.) ;
#49186 = EDGE_CURVE('',#38969,#38970,#2261,.T.) ;
#49187 = EDGE_CURVE('',#38971,#38970,#5810,.T.) ;
#49188 = EDGE_CURVE('',#38971,#38972,#2262,.T.) ;
#49189 = EDGE_CURVE('',#38973,#38972,#32477,.T.) ;
#49190 = EDGE_CURVE('',#38973,#38974,#2263,.T.) ;
#49191 = EDGE_CURVE('',#38974,#38975,#5811,.T.) ;
#49192 = EDGE_CURVE('',#38975,#38976,#2264,.T.) ;
#49193 = EDGE_CURVE('',#38961,#38976,#32478,.T.) ;
#49194 = EDGE_CURVE('',#38961,#38841,#5812,.T.) ;
#49195 = EDGE_CURVE('',#38977,#38978,#32479,.T.) ;
#49196 = EDGE_CURVE('',#38977,#38979,#2265,.T.) ;
#49197 = EDGE_CURVE('',#38980,#38979,#5813,.T.) ;
#49198 = EDGE_CURVE('',#38980,#38981,#2266,.T.) ;
#49199 = EDGE_CURVE('',#38982,#38981,#32480,.T.) ;
#49200 = EDGE_CURVE('',#38982,#38983,#2267,.T.) ;
#49201 = EDGE_CURVE('',#38983,#38984,#5814,.T.) ;
#49202 = EDGE_CURVE('',#38984,#38985,#2268,.T.) ;
#49203 = EDGE_CURVE('',#38986,#38985,#32481,.T.) ;
#49204 = EDGE_CURVE('',#38986,#38987,#2269,.T.) ;
#49205 = EDGE_CURVE('',#38988,#38987,#5815,.T.) ;
#49206 = EDGE_CURVE('',#38988,#38989,#2270,.T.) ;
#49207 = EDGE_CURVE('',#38990,#38989,#32482,.T.) ;
#49208 = EDGE_CURVE('',#38990,#38991,#2271,.T.) ;
#49209 = EDGE_CURVE('',#38991,#38992,#5816,.T.) ;
#49210 = EDGE_CURVE('',#38992,#38993,#2272,.T.) ;
#49211 = EDGE_CURVE('',#38978,#38993,#32483,.T.) ;
#49212 = EDGE_CURVE('',#38978,#38835,#5817,.T.) ;
#49213 = EDGE_CURVE('',#38994,#38995,#32484,.T.) ;
#49214 = EDGE_CURVE('',#38994,#38996,#2273,.T.) ;
#49215 = EDGE_CURVE('',#38997,#38996,#5818,.T.) ;
#49216 = EDGE_CURVE('',#38997,#38998,#2274,.T.) ;
#49217 = EDGE_CURVE('',#38999,#38998,#32485,.T.) ;
#49218 = EDGE_CURVE('',#38999,#39000,#2275,.T.) ;
#49219 = EDGE_CURVE('',#39000,#39001,#5819,.T.) ;
#49220 = EDGE_CURVE('',#39001,#39002,#2276,.T.) ;
#49221 = EDGE_CURVE('',#39003,#39002,#32486,.T.) ;
#49222 = EDGE_CURVE('',#39003,#39004,#2277,.T.) ;
#49223 = EDGE_CURVE('',#39005,#39004,#5820,.T.) ;
#49224 = EDGE_CURVE('',#39005,#39006,#2278,.T.) ;
#49225 = EDGE_CURVE('',#39007,#39006,#32487,.T.) ;
#49226 = EDGE_CURVE('',#39007,#39008,#2279,.T.) ;
#49227 = EDGE_CURVE('',#39008,#39009,#5821,.T.) ;
#49228 = EDGE_CURVE('',#39009,#39010,#2280,.T.) ;
#49229 = EDGE_CURVE('',#38995,#39010,#32488,.T.) ;
#49230 = EDGE_CURVE('',#38995,#38829,#5822,.T.) ;
#49231 = EDGE_CURVE('',#39011,#39012,#32489,.T.) ;
#49232 = EDGE_CURVE('',#39011,#39013,#2281,.T.) ;
#49233 = EDGE_CURVE('',#39014,#39013,#5823,.T.) ;
#49234 = EDGE_CURVE('',#39014,#39015,#2282,.T.) ;
#49235 = EDGE_CURVE('',#39016,#39015,#32490,.T.) ;
#49236 = EDGE_CURVE('',#39016,#39017,#2283,.T.) ;
#49237 = EDGE_CURVE('',#39017,#39018,#5824,.T.) ;
#49238 = EDGE_CURVE('',#39018,#39019,#2284,.T.) ;
#49239 = EDGE_CURVE('',#39020,#39019,#32491,.T.) ;
#49240 = EDGE_CURVE('',#39020,#39021,#2285,.T.) ;
#49241 = EDGE_CURVE('',#39022,#39021,#5825,.T.) ;
#49242 = EDGE_CURVE('',#39022,#39023,#2286,.T.) ;
#49243 = EDGE_CURVE('',#39024,#39023,#32492,.T.) ;
#49244 = EDGE_CURVE('',#39024,#39025,#2287,.T.) ;
#49245 = EDGE_CURVE('',#39025,#39026,#5826,.T.) ;
#49246 = EDGE_CURVE('',#39026,#39027,#2288,.T.) ;
#49247 = EDGE_CURVE('',#39012,#39027,#32493,.T.) ;
#49248 = EDGE_CURVE('',#39012,#38823,#5827,.T.) ;
#49249 = EDGE_CURVE('',#39028,#39028,#32494,.T.) ;
#49250 = EDGE_CURVE('',#39028,#38821,#5828,.T.) ;
#49251 = EDGE_CURVE('',#39029,#39029,#32495,.T.) ;
#49252 = EDGE_CURVE('',#39029,#38827,#5829,.T.) ;
#49253 = EDGE_CURVE('',#39030,#39030,#32496,.T.) ;
#49254 = EDGE_CURVE('',#39030,#38833,#5830,.T.) ;
#49255 = EDGE_CURVE('',#39031,#39031,#32497,.T.) ;
#49256 = EDGE_CURVE('',#39031,#38839,#5831,.T.) ;
#49257 = EDGE_CURVE('',#39032,#39032,#32498,.T.) ;
#49258 = EDGE_CURVE('',#39032,#38845,#5832,.T.) ;
#49259 = EDGE_CURVE('',#39033,#39033,#32499,.T.) ;
#49260 = EDGE_CURVE('',#39033,#38851,#5833,.T.) ;
#49261 = EDGE_CURVE('',#39034,#39034,#32500,.T.) ;
#49262 = EDGE_CURVE('',#39034,#38857,#5834,.T.) ;
#49263 = EDGE_CURVE('',#39035,#39035,#32501,.T.) ;
#49264 = EDGE_CURVE('',#39035,#38863,#5835,.T.) ;
#49265 = EDGE_CURVE('',#39036,#39036,#32502,.T.) ;
#49266 = EDGE_CURVE('',#39036,#38869,#5836,.T.) ;
#49267 = EDGE_CURVE('',#38870,#38873,#5837,.T.) ;
#49268 = EDGE_CURVE('',#38864,#38867,#5838,.T.) ;
#49269 = EDGE_CURVE('',#38858,#38861,#5839,.T.) ;
#49270 = EDGE_CURVE('',#38852,#38855,#5840,.T.) ;
#49271 = EDGE_CURVE('',#38846,#38849,#5841,.T.) ;
#49272 = EDGE_CURVE('',#38840,#38843,#5842,.T.) ;
#49273 = EDGE_CURVE('',#38834,#38837,#5843,.T.) ;
#49274 = EDGE_CURVE('',#38828,#38831,#5844,.T.) ;
#49275 = EDGE_CURVE('',#38822,#38825,#5845,.T.) ;
#49276 = EDGE_CURVE('',#39037,#39037,#32503,.T.) ;
#49277 = EDGE_CURVE('',#39037,#39038,#32504,.T.) ;
#49278 = EDGE_CURVE('',#39038,#39038,#32505,.T.) ;
#49279 = EDGE_CURVE('',#39039,#39039,#32506,.T.) ;
#49280 = EDGE_CURVE('',#39039,#39040,#32507,.T.) ;
#49281 = EDGE_CURVE('',#39040,#39040,#32508,.T.) ;
#49282 = EDGE_CURVE('',#39041,#39041,#32509,.T.) ;
#49283 = EDGE_CURVE('',#39041,#39042,#32510,.T.) ;
#49284 = EDGE_CURVE('',#39042,#39042,#32511,.T.) ;
#49285 = EDGE_CURVE('',#38812,#38820,#32512,.T.) ;
#49286 = EDGE_CURVE('',#38820,#38810,#5846,.T.) ;
#49287 = EDGE_CURVE('',#38812,#38809,#5847,.T.) ;
#49288 = EDGE_CURVE('',#38819,#39043,#32513,.T.) ;
#49289 = EDGE_CURVE('',#39043,#38817,#5848,.T.) ;
#49290 = EDGE_CURVE('',#38819,#38816,#5849,.T.) ;
#49291 = EDGE_CURVE('',#39044,#38757,#32514,.T.) ;
#49292 = EDGE_CURVE('',#38757,#38749,#5850,.T.) ;
#49293 = EDGE_CURVE('',#39044,#38748,#5851,.T.) ;
#49294 = EDGE_CURVE('',#38756,#38764,#32515,.T.) ;
#49295 = EDGE_CURVE('',#38764,#38753,#5852,.T.) ;
#49296 = EDGE_CURVE('',#38756,#38752,#5853,.T.) ;
#49297 = EDGE_CURVE('',#39045,#39046,#32516,.T.) ;
#49298 = EDGE_CURVE('',#39045,#39047,#2289,.T.) ;
#49299 = EDGE_CURVE('',#39048,#39047,#5854,.T.) ;
#49300 = EDGE_CURVE('',#39048,#39049,#2290,.T.) ;
#49301 = EDGE_CURVE('',#39050,#39049,#32517,.T.) ;
#49302 = EDGE_CURVE('',#39050,#39051,#2291,.T.) ;
#49303 = EDGE_CURVE('',#39051,#39052,#5855,.T.) ;
#49304 = EDGE_CURVE('',#39052,#39053,#2292,.T.) ;
#49305 = EDGE_CURVE('',#39054,#39053,#32518,.T.) ;
#49306 = EDGE_CURVE('',#39054,#39055,#2293,.T.) ;
#49307 = EDGE_CURVE('',#39056,#39055,#5856,.T.) ;
#49308 = EDGE_CURVE('',#39056,#39057,#2294,.T.) ;
#49309 = EDGE_CURVE('',#39058,#39057,#32519,.T.) ;
#49310 = EDGE_CURVE('',#39058,#39059,#2295,.T.) ;
#49311 = EDGE_CURVE('',#39059,#39060,#5857,.T.) ;
#49312 = EDGE_CURVE('',#39060,#39061,#2296,.T.) ;
#49313 = EDGE_CURVE('',#39046,#39061,#32520,.T.) ;
#49314 = EDGE_CURVE('',#39046,#39039,#5858,.T.) ;
#49315 = EDGE_CURVE('',#39062,#39062,#32521,.T.) ;
#49316 = EDGE_CURVE('',#39062,#39037,#5859,.T.) ;
#49317 = EDGE_CURVE('',#39038,#39041,#5860,.T.) ;
#49318 = EDGE_CURVE('',#39063,#39064,#5861,.T.) ;
#49319 = EDGE_CURVE('',#39064,#39065,#5862,.T.) ;
#49320 = EDGE_CURVE('',#39065,#39066,#5863,.T.) ;
#49321 = EDGE_CURVE('',#39066,#38746,#5864,.T.) ;
#49322 = EDGE_CURVE('',#38747,#38750,#32522,.T.) ;
#49323 = EDGE_CURVE('',#38751,#38758,#32523,.T.) ;
#49324 = EDGE_CURVE('',#38759,#38765,#32524,.T.) ;
#49325 = EDGE_CURVE('',#38766,#38772,#32525,.T.) ;
#49326 = EDGE_CURVE('',#38773,#38779,#32526,.T.) ;
#49327 = EDGE_CURVE('',#38780,#38786,#32527,.T.) ;
#49328 = EDGE_CURVE('',#38787,#38793,#32528,.T.) ;
#49329 = EDGE_CURVE('',#38794,#38800,#32529,.T.) ;
#49330 = EDGE_CURVE('',#38801,#38807,#32530,.T.) ;
#49331 = EDGE_CURVE('',#38808,#38814,#32531,.T.) ;
#49332 = EDGE_CURVE('',#38815,#39067,#5865,.T.) ;
#49333 = EDGE_CURVE('',#39067,#39068,#5866,.T.) ;
#49334 = EDGE_CURVE('',#39068,#39063,#5867,.T.) ;
#49335 = EDGE_CURVE('',#39069,#39070,#32532,.T.) ;
#49336 = EDGE_CURVE('',#39069,#39071,#5868,.T.) ;
#49337 = EDGE_CURVE('',#39072,#39071,#32533,.T.) ;
#49338 = EDGE_CURVE('',#39072,#39073,#5869,.T.) ;
#49339 = EDGE_CURVE('',#39074,#39073,#32534,.T.) ;
#49340 = EDGE_CURVE('',#39074,#39075,#5870,.T.) ;
#49341 = EDGE_CURVE('',#39076,#39075,#32535,.T.) ;
#49342 = EDGE_CURVE('',#39076,#39070,#5871,.T.) ;
#49343 = EDGE_CURVE('',#39077,#39078,#32536,.T.) ;
#49344 = EDGE_CURVE('',#39077,#39079,#5872,.T.) ;
#49345 = EDGE_CURVE('',#39080,#39079,#32537,.T.) ;
#49346 = EDGE_CURVE('',#39080,#39081,#5873,.T.) ;
#49347 = EDGE_CURVE('',#39082,#39081,#32538,.T.) ;
#49348 = EDGE_CURVE('',#39082,#39083,#5874,.T.) ;
#49349 = EDGE_CURVE('',#39084,#39083,#32539,.T.) ;
#49350 = EDGE_CURVE('',#39084,#39078,#5875,.T.) ;
#49351 = EDGE_CURVE('',#39085,#39086,#32540,.T.) ;
#49352 = EDGE_CURVE('',#39085,#39087,#5876,.T.) ;
#49353 = EDGE_CURVE('',#39088,#39087,#32541,.T.) ;
#49354 = EDGE_CURVE('',#39088,#39089,#5877,.T.) ;
#49355 = EDGE_CURVE('',#39090,#39089,#32542,.T.) ;
#49356 = EDGE_CURVE('',#39090,#39091,#5878,.T.) ;
#49357 = EDGE_CURVE('',#39092,#39091,#32543,.T.) ;
#49358 = EDGE_CURVE('',#39092,#39086,#5879,.T.) ;
#49359 = EDGE_CURVE('',#39093,#39094,#32544,.T.) ;
#49360 = EDGE_CURVE('',#39093,#39095,#5880,.T.) ;
#49361 = EDGE_CURVE('',#39096,#39095,#32545,.T.) ;
#49362 = EDGE_CURVE('',#39096,#39097,#5881,.T.) ;
#49363 = EDGE_CURVE('',#39098,#39097,#32546,.T.) ;
#49364 = EDGE_CURVE('',#39098,#39099,#5882,.T.) ;
#49365 = EDGE_CURVE('',#39100,#39099,#32547,.T.) ;
#49366 = EDGE_CURVE('',#39100,#39094,#5883,.T.) ;
#49367 = EDGE_CURVE('',#39101,#39102,#32548,.T.) ;
#49368 = EDGE_CURVE('',#39101,#39103,#5884,.T.) ;
#49369 = EDGE_CURVE('',#39104,#39103,#32549,.T.) ;
#49370 = EDGE_CURVE('',#39104,#39105,#5885,.T.) ;
#49371 = EDGE_CURVE('',#39106,#39105,#32550,.T.) ;
#49372 = EDGE_CURVE('',#39106,#39107,#5886,.T.) ;
#49373 = EDGE_CURVE('',#39108,#39107,#32551,.T.) ;
#49374 = EDGE_CURVE('',#39108,#39102,#5887,.T.) ;
#49375 = EDGE_CURVE('',#39109,#39110,#32552,.T.) ;
#49376 = EDGE_CURVE('',#39109,#39111,#5888,.T.) ;
#49377 = EDGE_CURVE('',#39112,#39111,#32553,.T.) ;
#49378 = EDGE_CURVE('',#39112,#39113,#5889,.T.) ;
#49379 = EDGE_CURVE('',#39114,#39113,#32554,.T.) ;
#49380 = EDGE_CURVE('',#39114,#39115,#5890,.T.) ;
#49381 = EDGE_CURVE('',#39116,#39115,#32555,.T.) ;
#49382 = EDGE_CURVE('',#39116,#39110,#5891,.T.) ;
#49383 = EDGE_CURVE('',#39117,#39118,#32556,.T.) ;
#49384 = EDGE_CURVE('',#39117,#39119,#5892,.T.) ;
#49385 = EDGE_CURVE('',#39120,#39119,#32557,.T.) ;
#49386 = EDGE_CURVE('',#39120,#39121,#5893,.T.) ;
#49387 = EDGE_CURVE('',#39122,#39121,#32558,.T.) ;
#49388 = EDGE_CURVE('',#39122,#39123,#5894,.T.) ;
#49389 = EDGE_CURVE('',#39124,#39123,#32559,.T.) ;
#49390 = EDGE_CURVE('',#39124,#39118,#5895,.T.) ;
#49391 = EDGE_CURVE('',#39125,#39126,#32560,.T.) ;
#49392 = EDGE_CURVE('',#39125,#39127,#5896,.T.) ;
#49393 = EDGE_CURVE('',#39128,#39127,#32561,.T.) ;
#49394 = EDGE_CURVE('',#39128,#39129,#5897,.T.) ;
#49395 = EDGE_CURVE('',#39130,#39129,#32562,.T.) ;
#49396 = EDGE_CURVE('',#39130,#39131,#5898,.T.) ;
#49397 = EDGE_CURVE('',#39132,#39131,#32563,.T.) ;
#49398 = EDGE_CURVE('',#39132,#39126,#5899,.T.) ;
#49399 = EDGE_CURVE('',#39133,#39134,#32564,.T.) ;
#49400 = EDGE_CURVE('',#39133,#39135,#5900,.T.) ;
#49401 = EDGE_CURVE('',#39136,#39135,#32565,.T.) ;
#49402 = EDGE_CURVE('',#39136,#39137,#5901,.T.) ;
#49403 = EDGE_CURVE('',#39138,#39137,#32566,.T.) ;
#49404 = EDGE_CURVE('',#39138,#39139,#5902,.T.) ;
#49405 = EDGE_CURVE('',#39140,#39139,#32567,.T.) ;
#49406 = EDGE_CURVE('',#39140,#39134,#5903,.T.) ;
#49407 = EDGE_CURVE('',#39141,#39142,#32568,.T.) ;
#49408 = EDGE_CURVE('',#39141,#39143,#5904,.T.) ;
#49409 = EDGE_CURVE('',#39144,#39143,#32569,.T.) ;
#49410 = EDGE_CURVE('',#39144,#39145,#5905,.T.) ;
#49411 = EDGE_CURVE('',#39146,#39145,#32570,.T.) ;
#49412 = EDGE_CURVE('',#39146,#39147,#5906,.T.) ;
#49413 = EDGE_CURVE('',#39148,#39147,#32571,.T.) ;
#49414 = EDGE_CURVE('',#39148,#39142,#5907,.T.) ;
#49415 = EDGE_CURVE('',#39149,#39150,#5908,.T.) ;
#49416 = EDGE_CURVE('',#39150,#39151,#5909,.T.) ;
#49417 = EDGE_CURVE('',#39151,#39152,#5910,.T.) ;
#49418 = EDGE_CURVE('',#39152,#39149,#5911,.T.) ;
#49419 = EDGE_CURVE('',#39153,#39154,#5912,.T.) ;
#49420 = EDGE_CURVE('',#39154,#39155,#32572,.T.) ;
#49421 = EDGE_CURVE('',#39155,#39156,#5913,.T.) ;
#49422 = EDGE_CURVE('',#39156,#39157,#32573,.T.) ;
#49423 = EDGE_CURVE('',#39157,#39158,#5914,.T.) ;
#49424 = EDGE_CURVE('',#39158,#39159,#32574,.T.) ;
#49425 = EDGE_CURVE('',#39159,#39160,#5915,.T.) ;
#49426 = EDGE_CURVE('',#39160,#39153,#32575,.T.) ;
#49427 = EDGE_CURVE('',#39161,#39162,#5916,.T.) ;
#49428 = EDGE_CURVE('',#39162,#39163,#5917,.T.) ;
#49429 = EDGE_CURVE('',#39163,#39164,#5918,.T.) ;
#49430 = EDGE_CURVE('',#39164,#39161,#5919,.T.) ;
#49431 = EDGE_CURVE('',#39165,#39166,#5920,.T.) ;
#49432 = EDGE_CURVE('',#39166,#39167,#32576,.T.) ;
#49433 = EDGE_CURVE('',#39167,#39168,#5921,.T.) ;
#49434 = EDGE_CURVE('',#39168,#39169,#32577,.T.) ;
#49435 = EDGE_CURVE('',#39169,#39170,#5922,.T.) ;
#49436 = EDGE_CURVE('',#39170,#39171,#32578,.T.) ;
#49437 = EDGE_CURVE('',#39171,#39172,#5923,.T.) ;
#49438 = EDGE_CURVE('',#39172,#39165,#32579,.T.) ;
#49439 = EDGE_CURVE('',#39173,#39174,#5924,.T.) ;
#49440 = EDGE_CURVE('',#39174,#39175,#5925,.T.) ;
#49441 = EDGE_CURVE('',#39175,#39176,#5926,.T.) ;
#49442 = EDGE_CURVE('',#39176,#39173,#5927,.T.) ;
#49443 = EDGE_CURVE('',#39177,#39178,#5928,.T.) ;
#49444 = EDGE_CURVE('',#39178,#39179,#32580,.T.) ;
#49445 = EDGE_CURVE('',#39179,#39180,#5929,.T.) ;
#49446 = EDGE_CURVE('',#39180,#39181,#32581,.T.) ;
#49447 = EDGE_CURVE('',#39181,#39182,#5930,.T.) ;
#49448 = EDGE_CURVE('',#39182,#39183,#32582,.T.) ;
#49449 = EDGE_CURVE('',#39183,#39184,#5931,.T.) ;
#49450 = EDGE_CURVE('',#39184,#39177,#32583,.T.) ;
#49451 = EDGE_CURVE('',#39185,#39186,#5932,.T.) ;
#49452 = EDGE_CURVE('',#39186,#39187,#5933,.T.) ;
#49453 = EDGE_CURVE('',#39187,#39188,#5934,.T.) ;
#49454 = EDGE_CURVE('',#39188,#39185,#5935,.T.) ;
#49455 = EDGE_CURVE('',#39189,#39190,#5936,.T.) ;
#49456 = EDGE_CURVE('',#39190,#39191,#32584,.T.) ;
#49457 = EDGE_CURVE('',#39191,#39192,#5937,.T.) ;
#49458 = EDGE_CURVE('',#39192,#39193,#32585,.T.) ;
#49459 = EDGE_CURVE('',#39193,#39194,#5938,.T.) ;
#49460 = EDGE_CURVE('',#39194,#39195,#32586,.T.) ;
#49461 = EDGE_CURVE('',#39195,#39196,#5939,.T.) ;
#49462 = EDGE_CURVE('',#39196,#39189,#32587,.T.) ;
#49463 = EDGE_CURVE('',#39197,#39198,#5940,.T.) ;
#49464 = EDGE_CURVE('',#39198,#39199,#5941,.T.) ;
#49465 = EDGE_CURVE('',#39199,#39200,#5942,.T.) ;
#49466 = EDGE_CURVE('',#39200,#39197,#5943,.T.) ;
#49467 = EDGE_CURVE('',#39201,#39202,#5944,.T.) ;
#49468 = EDGE_CURVE('',#39202,#39203,#32588,.T.) ;
#49469 = EDGE_CURVE('',#39203,#39204,#5945,.T.) ;
#49470 = EDGE_CURVE('',#39204,#39205,#32589,.T.) ;
#49471 = EDGE_CURVE('',#39205,#39206,#5946,.T.) ;
#49472 = EDGE_CURVE('',#39206,#39207,#32590,.T.) ;
#49473 = EDGE_CURVE('',#39207,#39208,#5947,.T.) ;
#49474 = EDGE_CURVE('',#39208,#39201,#32591,.T.) ;
#49475 = EDGE_CURVE('',#39209,#39210,#5948,.T.) ;
#49476 = EDGE_CURVE('',#39210,#39211,#5949,.T.) ;
#49477 = EDGE_CURVE('',#39211,#39212,#5950,.T.) ;
#49478 = EDGE_CURVE('',#39212,#39209,#5951,.T.) ;
#49479 = EDGE_CURVE('',#39213,#39214,#5952,.T.) ;
#49480 = EDGE_CURVE('',#39214,#39215,#32592,.T.) ;
#49481 = EDGE_CURVE('',#39215,#39216,#5953,.T.) ;
#49482 = EDGE_CURVE('',#39216,#39217,#32593,.T.) ;
#49483 = EDGE_CURVE('',#39217,#39218,#5954,.T.) ;
#49484 = EDGE_CURVE('',#39218,#39219,#32594,.T.) ;
#49485 = EDGE_CURVE('',#39219,#39220,#5955,.T.) ;
#49486 = EDGE_CURVE('',#39220,#39213,#32595,.T.) ;
#49487 = EDGE_CURVE('',#39221,#39222,#5956,.T.) ;
#49488 = EDGE_CURVE('',#39222,#39223,#5957,.T.) ;
#49489 = EDGE_CURVE('',#39223,#39224,#5958,.T.) ;
#49490 = EDGE_CURVE('',#39224,#39221,#5959,.T.) ;
#49491 = EDGE_CURVE('',#39225,#39226,#5960,.T.) ;
#49492 = EDGE_CURVE('',#39226,#39227,#32596,.T.) ;
#49493 = EDGE_CURVE('',#39227,#39228,#5961,.T.) ;
#49494 = EDGE_CURVE('',#39228,#39229,#32597,.T.) ;
#49495 = EDGE_CURVE('',#39229,#39230,#5962,.T.) ;
#49496 = EDGE_CURVE('',#39230,#39231,#32598,.T.) ;
#49497 = EDGE_CURVE('',#39231,#39232,#5963,.T.) ;
#49498 = EDGE_CURVE('',#39232,#39225,#32599,.T.) ;
#49499 = EDGE_CURVE('',#39233,#39234,#5964,.T.) ;
#49500 = EDGE_CURVE('',#39234,#39235,#5965,.T.) ;
#49501 = EDGE_CURVE('',#39235,#39236,#5966,.T.) ;
#49502 = EDGE_CURVE('',#39236,#39233,#5967,.T.) ;
#49503 = EDGE_CURVE('',#39237,#39238,#5968,.T.) ;
#49504 = EDGE_CURVE('',#39238,#39239,#32600,.T.) ;
#49505 = EDGE_CURVE('',#39239,#39240,#5969,.T.) ;
#49506 = EDGE_CURVE('',#39240,#39241,#32601,.T.) ;
#49507 = EDGE_CURVE('',#39241,#39242,#5970,.T.) ;
#49508 = EDGE_CURVE('',#39242,#39243,#32602,.T.) ;
#49509 = EDGE_CURVE('',#39243,#39244,#5971,.T.) ;
#49510 = EDGE_CURVE('',#39244,#39237,#32603,.T.) ;
#49511 = EDGE_CURVE('',#39245,#39246,#5972,.T.) ;
#49512 = EDGE_CURVE('',#39246,#39247,#5973,.T.) ;
#49513 = EDGE_CURVE('',#39247,#39248,#5974,.T.) ;
#49514 = EDGE_CURVE('',#39248,#39245,#5975,.T.) ;
#49515 = EDGE_CURVE('',#39249,#39250,#5976,.T.) ;
#49516 = EDGE_CURVE('',#39250,#39251,#32604,.T.) ;
#49517 = EDGE_CURVE('',#39251,#39252,#5977,.T.) ;
#49518 = EDGE_CURVE('',#39252,#39253,#32605,.T.) ;
#49519 = EDGE_CURVE('',#39253,#39254,#5978,.T.) ;
#49520 = EDGE_CURVE('',#39254,#39255,#32606,.T.) ;
#49521 = EDGE_CURVE('',#39255,#39256,#5979,.T.) ;
#49522 = EDGE_CURVE('',#39256,#39249,#32607,.T.) ;
#49523 = EDGE_CURVE('',#39019,#39020,#5980,.T.) ;
#49524 = EDGE_CURVE('',#39002,#39003,#5981,.T.) ;
#49525 = EDGE_CURVE('',#38985,#38986,#5982,.T.) ;
#49526 = EDGE_CURVE('',#38968,#38969,#5983,.T.) ;
#49527 = EDGE_CURVE('',#38951,#38952,#5984,.T.) ;
#49528 = EDGE_CURVE('',#38934,#38935,#5985,.T.) ;
#49529 = EDGE_CURVE('',#38917,#38918,#5986,.T.) ;
#49530 = EDGE_CURVE('',#38900,#38901,#5987,.T.) ;
#49531 = EDGE_CURVE('',#38883,#38884,#5988,.T.) ;
#49532 = EDGE_CURVE('',#39257,#39258,#5989,.T.) ;
#49533 = EDGE_CURVE('',#39258,#39259,#5990,.T.) ;
#49534 = EDGE_CURVE('',#39259,#39260,#5991,.T.) ;
#49535 = EDGE_CURVE('',#39260,#39261,#5992,.T.) ;
#49536 = EDGE_CURVE('',#39261,#39262,#5993,.T.) ;
#49537 = EDGE_CURVE('',#39262,#39263,#32608,.T.) ;
#49538 = EDGE_CURVE('',#39263,#39264,#32609,.T.) ;
#49539 = EDGE_CURVE('',#39264,#39265,#5994,.T.) ;
#49540 = EDGE_CURVE('',#39265,#39266,#32610,.T.) ;
#49541 = EDGE_CURVE('',#39266,#39267,#32611,.T.) ;
#49542 = EDGE_CURVE('',#39267,#39268,#5995,.T.) ;
#49543 = EDGE_CURVE('',#39268,#39269,#32612,.T.) ;
#49544 = EDGE_CURVE('',#39269,#39270,#32613,.T.) ;
#49545 = EDGE_CURVE('',#39270,#39271,#5996,.T.) ;
#49546 = EDGE_CURVE('',#39271,#39272,#32614,.T.) ;
#49547 = EDGE_CURVE('',#39272,#39273,#32615,.T.) ;
#49548 = EDGE_CURVE('',#39273,#39274,#5997,.T.) ;
#49549 = EDGE_CURVE('',#39274,#39275,#32616,.T.) ;
#49550 = EDGE_CURVE('',#39275,#39276,#32617,.T.) ;
#49551 = EDGE_CURVE('',#39276,#39277,#5998,.T.) ;
#49552 = EDGE_CURVE('',#39277,#39278,#32618,.T.) ;
#49553 = EDGE_CURVE('',#39278,#39279,#32619,.T.) ;
#49554 = EDGE_CURVE('',#39279,#39280,#5999,.T.) ;
#49555 = EDGE_CURVE('',#39280,#39281,#32620,.T.) ;
#49556 = EDGE_CURVE('',#39281,#39282,#32621,.T.) ;
#49557 = EDGE_CURVE('',#39282,#39283,#6000,.T.) ;
#49558 = EDGE_CURVE('',#39283,#39284,#32622,.T.) ;
#49559 = EDGE_CURVE('',#39284,#39285,#32623,.T.) ;
#49560 = EDGE_CURVE('',#39285,#39286,#6001,.T.) ;
#49561 = EDGE_CURVE('',#39286,#39287,#32624,.T.) ;
#49562 = EDGE_CURVE('',#39287,#39288,#32625,.T.) ;
#49563 = EDGE_CURVE('',#39288,#39289,#6002,.T.) ;
#49564 = EDGE_CURVE('',#39289,#39290,#32626,.T.) ;
#49565 = EDGE_CURVE('',#39290,#39291,#32627,.T.) ;
#49566 = EDGE_CURVE('',#39291,#39292,#6003,.T.) ;
#49567 = EDGE_CURVE('',#39292,#39293,#32628,.T.) ;
#49568 = EDGE_CURVE('',#39293,#39294,#32629,.T.) ;
#49569 = EDGE_CURVE('',#39294,#39295,#6004,.T.) ;
#49570 = EDGE_CURVE('',#39295,#39296,#32630,.T.) ;
#49571 = EDGE_CURVE('',#39296,#39297,#32631,.T.) ;
#49572 = EDGE_CURVE('',#39297,#39298,#6005,.T.) ;
#49573 = EDGE_CURVE('',#39298,#39299,#32632,.T.) ;
#49574 = EDGE_CURVE('',#39299,#39300,#32633,.T.) ;
#49575 = EDGE_CURVE('',#39300,#39301,#6006,.T.) ;
#49576 = EDGE_CURVE('',#39301,#39302,#32634,.T.) ;
#49577 = EDGE_CURVE('',#39302,#39303,#32635,.T.) ;
#49578 = EDGE_CURVE('',#39303,#39304,#6007,.T.) ;
#49579 = EDGE_CURVE('',#39304,#39305,#32636,.T.) ;
#49580 = EDGE_CURVE('',#39305,#39306,#32637,.T.) ;
#49581 = EDGE_CURVE('',#39306,#39307,#6008,.T.) ;
#49582 = EDGE_CURVE('',#39307,#39308,#32638,.T.) ;
#49583 = EDGE_CURVE('',#39308,#39309,#32639,.T.) ;
#49584 = EDGE_CURVE('',#39309,#39310,#6009,.T.) ;
#49585 = EDGE_CURVE('',#39310,#39311,#32640,.T.) ;
#49586 = EDGE_CURVE('',#39311,#39312,#32641,.T.) ;
#49587 = EDGE_CURVE('',#39312,#39313,#6010,.T.) ;
#49588 = EDGE_CURVE('',#39313,#39314,#32642,.T.) ;
#49589 = EDGE_CURVE('',#39314,#39315,#32643,.T.) ;
#49590 = EDGE_CURVE('',#39315,#39316,#6011,.T.) ;
#49591 = EDGE_CURVE('',#39316,#39317,#32644,.T.) ;
#49592 = EDGE_CURVE('',#39317,#39318,#32645,.T.) ;
#49593 = EDGE_CURVE('',#39318,#39319,#6012,.T.) ;
#49594 = EDGE_CURVE('',#39319,#39320,#32646,.T.) ;
#49595 = EDGE_CURVE('',#39320,#39257,#32647,.T.) ;
#49596 = EDGE_CURVE('',#39321,#39322,#32648,.T.) ;
#49597 = EDGE_CURVE('',#39321,#39323,#6013,.T.) ;
#49598 = EDGE_CURVE('',#39323,#39324,#6014,.T.) ;
#49599 = EDGE_CURVE('',#39324,#39325,#6015,.T.) ;
#49600 = EDGE_CURVE('',#39325,#39326,#6016,.T.) ;
#49601 = EDGE_CURVE('',#39326,#39327,#6017,.T.) ;
#49602 = EDGE_CURVE('',#39328,#39327,#32649,.T.) ;
#49603 = EDGE_CURVE('',#39328,#39322,#32650,.T.) ;
#49604 = EDGE_CURVE('',#39329,#39330,#32651,.T.) ;
#49605 = EDGE_CURVE('',#39329,#39331,#6018,.T.) ;
#49606 = EDGE_CURVE('',#39331,#39332,#6019,.T.) ;
#49607 = EDGE_CURVE('',#39332,#39333,#6020,.T.) ;
#49608 = EDGE_CURVE('',#39333,#39334,#6021,.T.) ;
#49609 = EDGE_CURVE('',#39334,#39335,#6022,.T.) ;
#49610 = EDGE_CURVE('',#39336,#39335,#32652,.T.) ;
#49611 = EDGE_CURVE('',#39336,#39330,#32653,.T.) ;
#49612 = EDGE_CURVE('',#39337,#39338,#32654,.T.) ;
#49613 = EDGE_CURVE('',#39337,#39339,#6023,.T.) ;
#49614 = EDGE_CURVE('',#39339,#39340,#6024,.T.) ;
#49615 = EDGE_CURVE('',#39340,#39341,#6025,.T.) ;
#49616 = EDGE_CURVE('',#39341,#39342,#6026,.T.) ;
#49617 = EDGE_CURVE('',#39342,#39343,#6027,.T.) ;
#49618 = EDGE_CURVE('',#39344,#39343,#32655,.T.) ;
#49619 = EDGE_CURVE('',#39344,#39338,#32656,.T.) ;
#49620 = EDGE_CURVE('',#39345,#39346,#32657,.T.) ;
#49621 = EDGE_CURVE('',#39345,#39347,#6028,.T.) ;
#49622 = EDGE_CURVE('',#39347,#39348,#6029,.T.) ;
#49623 = EDGE_CURVE('',#39348,#39349,#6030,.T.) ;
#49624 = EDGE_CURVE('',#39349,#39350,#6031,.T.) ;
#49625 = EDGE_CURVE('',#39350,#39351,#6032,.T.) ;
#49626 = EDGE_CURVE('',#39352,#39351,#32658,.T.) ;
#49627 = EDGE_CURVE('',#39352,#39346,#32659,.T.) ;
#49628 = EDGE_CURVE('',#39353,#39354,#32660,.T.) ;
#49629 = EDGE_CURVE('',#39353,#39355,#6033,.T.) ;
#49630 = EDGE_CURVE('',#39355,#39356,#6034,.T.) ;
#49631 = EDGE_CURVE('',#39356,#39357,#6035,.T.) ;
#49632 = EDGE_CURVE('',#39357,#39358,#6036,.T.) ;
#49633 = EDGE_CURVE('',#39358,#39359,#6037,.T.) ;
#49634 = EDGE_CURVE('',#39360,#39359,#32661,.T.) ;
#49635 = EDGE_CURVE('',#39360,#39354,#32662,.T.) ;
#49636 = EDGE_CURVE('',#39361,#39362,#32663,.T.) ;
#49637 = EDGE_CURVE('',#39361,#39363,#6038,.T.) ;
#49638 = EDGE_CURVE('',#39363,#39364,#6039,.T.) ;
#49639 = EDGE_CURVE('',#39364,#39365,#6040,.T.) ;
#49640 = EDGE_CURVE('',#39365,#39366,#6041,.T.) ;
#49641 = EDGE_CURVE('',#39366,#39367,#6042,.T.) ;
#49642 = EDGE_CURVE('',#39368,#39367,#32664,.T.) ;
#49643 = EDGE_CURVE('',#39368,#39362,#32665,.T.) ;
#49644 = EDGE_CURVE('',#39369,#39370,#32666,.T.) ;
#49645 = EDGE_CURVE('',#39369,#39371,#6043,.T.) ;
#49646 = EDGE_CURVE('',#39371,#39372,#6044,.T.) ;
#49647 = EDGE_CURVE('',#39372,#39373,#6045,.T.) ;
#49648 = EDGE_CURVE('',#39373,#39374,#6046,.T.) ;
#49649 = EDGE_CURVE('',#39374,#39375,#6047,.T.) ;
#49650 = EDGE_CURVE('',#39376,#39375,#32667,.T.) ;
#49651 = EDGE_CURVE('',#39376,#39370,#32668,.T.) ;
#49652 = EDGE_CURVE('',#39377,#39378,#32669,.T.) ;
#49653 = EDGE_CURVE('',#39377,#39379,#6048,.T.) ;
#49654 = EDGE_CURVE('',#39379,#39380,#6049,.T.) ;
#49655 = EDGE_CURVE('',#39380,#39381,#6050,.T.) ;
#49656 = EDGE_CURVE('',#39381,#39382,#6051,.T.) ;
#49657 = EDGE_CURVE('',#39382,#39383,#6052,.T.) ;
#49658 = EDGE_CURVE('',#39384,#39383,#32670,.T.) ;
#49659 = EDGE_CURVE('',#39384,#39378,#32671,.T.) ;
#49660 = EDGE_CURVE('',#39385,#39386,#32672,.T.) ;
#49661 = EDGE_CURVE('',#39385,#39387,#6053,.T.) ;
#49662 = EDGE_CURVE('',#39387,#39388,#6054,.T.) ;
#49663 = EDGE_CURVE('',#39388,#39389,#6055,.T.) ;
#49664 = EDGE_CURVE('',#39389,#39390,#6056,.T.) ;
#49665 = EDGE_CURVE('',#39390,#39391,#6057,.T.) ;
#49666 = EDGE_CURVE('',#39392,#39391,#32673,.T.) ;
#49667 = EDGE_CURVE('',#39392,#39386,#32674,.T.) ;
#49668 = EDGE_CURVE('',#39393,#39394,#6058,.T.) ;
#49669 = EDGE_CURVE('',#39394,#39395,#6059,.T.) ;
#49670 = EDGE_CURVE('',#39395,#39396,#6060,.T.) ;
#49671 = EDGE_CURVE('',#39396,#39393,#6061,.T.) ;
#49672 = EDGE_CURVE('',#39397,#39398,#6062,.T.) ;
#49673 = EDGE_CURVE('',#39398,#39399,#6063,.T.) ;
#49674 = EDGE_CURVE('',#39399,#39400,#6064,.T.) ;
#49675 = EDGE_CURVE('',#39400,#39401,#6065,.T.) ;
#49676 = EDGE_CURVE('',#39402,#39401,#32675,.T.) ;
#49677 = EDGE_CURVE('',#39402,#39403,#6066,.T.) ;
#49678 = EDGE_CURVE('',#39404,#39403,#32676,.T.) ;
#49679 = EDGE_CURVE('',#39404,#39405,#6067,.T.) ;
#49680 = EDGE_CURVE('',#39405,#39406,#6068,.T.) ;
#49681 = EDGE_CURVE('',#39406,#39407,#6069,.T.) ;
#49682 = EDGE_CURVE('',#39408,#39407,#32677,.T.) ;
#49683 = EDGE_CURVE('',#39408,#39409,#6070,.T.) ;
#49684 = EDGE_CURVE('',#39410,#39409,#32678,.T.) ;
#49685 = EDGE_CURVE('',#39410,#39411,#6071,.T.) ;
#49686 = EDGE_CURVE('',#39411,#39412,#6072,.T.) ;
#49687 = EDGE_CURVE('',#39412,#39413,#6073,.T.) ;
#49688 = EDGE_CURVE('',#39414,#39413,#32679,.T.) ;
#49689 = EDGE_CURVE('',#39414,#39415,#6074,.T.) ;
#49690 = EDGE_CURVE('',#39416,#39415,#32680,.T.) ;
#49691 = EDGE_CURVE('',#39416,#39417,#6075,.T.) ;
#49692 = EDGE_CURVE('',#39417,#39418,#6076,.T.) ;
#49693 = EDGE_CURVE('',#39418,#39419,#6077,.T.) ;
#49694 = EDGE_CURVE('',#39420,#39419,#32681,.T.) ;
#49695 = EDGE_CURVE('',#39420,#39421,#6078,.T.) ;
#49696 = EDGE_CURVE('',#39422,#39421,#32682,.T.) ;
#49697 = EDGE_CURVE('',#39422,#39423,#6079,.T.) ;
#49698 = EDGE_CURVE('',#39423,#39424,#6080,.T.) ;
#49699 = EDGE_CURVE('',#39424,#39425,#6081,.T.) ;
#49700 = EDGE_CURVE('',#39426,#39425,#32683,.T.) ;
#49701 = EDGE_CURVE('',#39426,#39427,#6082,.T.) ;
#49702 = EDGE_CURVE('',#39428,#39427,#32684,.T.) ;
#49703 = EDGE_CURVE('',#39428,#39429,#6083,.T.) ;
#49704 = EDGE_CURVE('',#39429,#39430,#6084,.T.) ;
#49705 = EDGE_CURVE('',#39430,#39431,#6085,.T.) ;
#49706 = EDGE_CURVE('',#39432,#39431,#32685,.T.) ;
#49707 = EDGE_CURVE('',#39432,#39433,#6086,.T.) ;
#49708 = EDGE_CURVE('',#39434,#39433,#32686,.T.) ;
#49709 = EDGE_CURVE('',#39434,#39435,#6087,.T.) ;
#49710 = EDGE_CURVE('',#39435,#39436,#6088,.T.) ;
#49711 = EDGE_CURVE('',#39436,#39437,#6089,.T.) ;
#49712 = EDGE_CURVE('',#39438,#39437,#32687,.T.) ;
#49713 = EDGE_CURVE('',#39438,#39439,#6090,.T.) ;
#49714 = EDGE_CURVE('',#39440,#39439,#32688,.T.) ;
#49715 = EDGE_CURVE('',#39440,#39441,#6091,.T.) ;
#49716 = EDGE_CURVE('',#39441,#39442,#6092,.T.) ;
#49717 = EDGE_CURVE('',#39442,#39443,#6093,.T.) ;
#49718 = EDGE_CURVE('',#39444,#39443,#32689,.T.) ;
#49719 = EDGE_CURVE('',#39444,#39445,#6094,.T.) ;
#49720 = EDGE_CURVE('',#39446,#39445,#32690,.T.) ;
#49721 = EDGE_CURVE('',#39446,#39447,#6095,.T.) ;
#49722 = EDGE_CURVE('',#39447,#39448,#6096,.T.) ;
#49723 = EDGE_CURVE('',#39448,#39449,#6097,.T.) ;
#49724 = EDGE_CURVE('',#39450,#39449,#32691,.T.) ;
#49725 = EDGE_CURVE('',#39450,#39451,#6098,.T.) ;
#49726 = EDGE_CURVE('',#39452,#39451,#32692,.T.) ;
#49727 = EDGE_CURVE('',#39452,#39453,#6099,.T.) ;
#49728 = EDGE_CURVE('',#39453,#39454,#6100,.T.) ;
#49729 = EDGE_CURVE('',#39454,#39455,#6101,.T.) ;
#49730 = EDGE_CURVE('',#39456,#39455,#32693,.T.) ;
#49731 = EDGE_CURVE('',#39456,#39457,#6102,.T.) ;
#49732 = EDGE_CURVE('',#39458,#39457,#32694,.T.) ;
#49733 = EDGE_CURVE('',#39458,#39459,#6103,.T.) ;
#49734 = EDGE_CURVE('',#39459,#39460,#6104,.T.) ;
#49735 = EDGE_CURVE('',#39460,#39397,#6105,.T.) ;
#49736 = EDGE_CURVE('',#39461,#39462,#6106,.T.) ;
#49737 = EDGE_CURVE('',#39461,#39260,#32695,.T.) ;
#49738 = EDGE_CURVE('',#39259,#39462,#32696,.T.) ;
#49739 = EDGE_CURVE('',#39463,#39464,#6107,.T.) ;
#49740 = EDGE_CURVE('',#39465,#39463,#32697,.T.) ;
#49741 = EDGE_CURVE('',#39268,#39465,#32698,.T.) ;
#49742 = EDGE_CURVE('',#39466,#39267,#32699,.T.) ;
#49743 = EDGE_CURVE('',#39464,#39466,#32700,.T.) ;
#49744 = EDGE_CURVE('',#39467,#39468,#6108,.T.) ;
#49745 = EDGE_CURVE('',#39468,#39469,#6109,.T.) ;
#49746 = EDGE_CURVE('',#39469,#39470,#6110,.T.) ;
#49747 = EDGE_CURVE('',#39470,#39467,#6111,.T.) ;
#49748 = EDGE_CURVE('',#39471,#39472,#2297,.T.) ;
#49749 = EDGE_CURVE('',#39471,#39473,#6112,.T.) ;
#49750 = EDGE_CURVE('',#39474,#39473,#2298,.T.) ;
#49751 = EDGE_CURVE('',#39474,#39475,#6113,.T.) ;
#49752 = EDGE_CURVE('',#39476,#39475,#2299,.T.) ;
#49753 = EDGE_CURVE('',#39476,#39477,#6114,.T.) ;
#49754 = EDGE_CURVE('',#39478,#39477,#2300,.T.) ;
#49755 = EDGE_CURVE('',#39478,#39472,#6115,.T.) ;
#49756 = EDGE_CURVE('',#39479,#39480,#6116,.T.) ;
#49757 = EDGE_CURVE('',#39480,#39481,#6117,.T.) ;
#49758 = EDGE_CURVE('',#39481,#39482,#6118,.T.) ;
#49759 = EDGE_CURVE('',#39482,#39479,#6119,.T.) ;
#49760 = EDGE_CURVE('',#39483,#39484,#6120,.T.) ;
#49761 = EDGE_CURVE('',#39484,#39485,#6121,.T.) ;
#49762 = EDGE_CURVE('',#39485,#39486,#6122,.T.) ;
#49763 = EDGE_CURVE('',#39486,#39483,#6123,.T.) ;
#49764 = EDGE_CURVE('',#39487,#39488,#6124,.T.) ;
#49765 = EDGE_CURVE('',#39488,#39489,#6125,.T.) ;
#49766 = EDGE_CURVE('',#39489,#39490,#6126,.T.) ;
#49767 = EDGE_CURVE('',#39490,#39487,#6127,.T.) ;
#49768 = EDGE_CURVE('',#39491,#39492,#6128,.T.) ;
#49769 = EDGE_CURVE('',#39492,#39493,#6129,.T.) ;
#49770 = EDGE_CURVE('',#39493,#39494,#6130,.T.) ;
#49771 = EDGE_CURVE('',#39494,#39491,#6131,.T.) ;
#49772 = EDGE_CURVE('',#39495,#39496,#6132,.T.) ;
#49773 = EDGE_CURVE('',#39496,#39497,#6133,.T.) ;
#49774 = EDGE_CURVE('',#39497,#39498,#6134,.T.) ;
#49775 = EDGE_CURVE('',#39498,#39495,#6135,.T.) ;
#49776 = EDGE_CURVE('',#39499,#39500,#6136,.T.) ;
#49777 = EDGE_CURVE('',#39500,#39501,#6137,.T.) ;
#49778 = EDGE_CURVE('',#39501,#39502,#6138,.T.) ;
#49779 = EDGE_CURVE('',#39502,#39499,#6139,.T.) ;
#49780 = EDGE_CURVE('',#39503,#39504,#6140,.T.) ;
#49781 = EDGE_CURVE('',#39504,#39505,#6141,.T.) ;
#49782 = EDGE_CURVE('',#39505,#39506,#6142,.T.) ;
#49783 = EDGE_CURVE('',#39506,#39503,#6143,.T.) ;
#49784 = EDGE_CURVE('',#39507,#39508,#6144,.T.) ;
#49785 = EDGE_CURVE('',#39508,#39509,#6145,.T.) ;
#49786 = EDGE_CURVE('',#39509,#39510,#6146,.T.) ;
#49787 = EDGE_CURVE('',#39510,#39507,#6147,.T.) ;
#49788 = EDGE_CURVE('',#39511,#39512,#2301,.T.) ;
#49789 = EDGE_CURVE('',#39511,#39513,#6148,.T.) ;
#49790 = EDGE_CURVE('',#39514,#39513,#2302,.T.) ;
#49791 = EDGE_CURVE('',#39514,#39515,#6149,.T.) ;
#49792 = EDGE_CURVE('',#39516,#39515,#2303,.T.) ;
#49793 = EDGE_CURVE('',#39516,#39517,#6150,.T.) ;
#49794 = EDGE_CURVE('',#39518,#39517,#2304,.T.) ;
#49795 = EDGE_CURVE('',#39518,#39512,#6151,.T.) ;
#49796 = EDGE_CURVE('',#39519,#39520,#6152,.T.) ;
#49797 = EDGE_CURVE('',#39520,#39521,#6153,.T.) ;
#49798 = EDGE_CURVE('',#39521,#39522,#6154,.T.) ;
#49799 = EDGE_CURVE('',#39522,#39519,#6155,.T.) ;
#49800 = EDGE_CURVE('',#39523,#39524,#6156,.T.) ;
#49801 = EDGE_CURVE('',#39524,#39525,#32701,.T.) ;
#49802 = EDGE_CURVE('',#39525,#39526,#6157,.T.) ;
#49803 = EDGE_CURVE('',#39526,#39527,#32702,.T.) ;
#49804 = EDGE_CURVE('',#39527,#39528,#6158,.T.) ;
#49805 = EDGE_CURVE('',#39528,#39529,#32703,.T.) ;
#49806 = EDGE_CURVE('',#39529,#39530,#6159,.T.) ;
#49807 = EDGE_CURVE('',#39530,#39523,#32704,.T.) ;
#49808 = EDGE_CURVE('',#39531,#39532,#6160,.T.) ;
#49809 = EDGE_CURVE('',#39532,#39533,#6161,.T.) ;
#49810 = EDGE_CURVE('',#39533,#39534,#6162,.T.) ;
#49811 = EDGE_CURVE('',#39534,#39531,#6163,.T.) ;
#49812 = EDGE_CURVE('',#39053,#39054,#6164,.T.) ;
#49813 = EDGE_CURVE('',#39535,#39536,#6165,.T.) ;
#49814 = EDGE_CURVE('',#39536,#39537,#6166,.T.) ;
#49815 = EDGE_CURVE('',#39537,#39538,#6167,.T.) ;
#49816 = EDGE_CURVE('',#39538,#39539,#6168,.T.) ;
#49817 = EDGE_CURVE('',#39540,#39539,#32705,.T.) ;
#49818 = EDGE_CURVE('',#39540,#39541,#32706,.T.) ;
#49819 = EDGE_CURVE('',#39542,#39541,#32707,.T.) ;
#49820 = EDGE_CURVE('',#39542,#39535,#6169,.T.) ;
#49821 = EDGE_CURVE('',#39543,#39544,#6170,.T.) ;
#49822 = EDGE_CURVE('',#39544,#39545,#6171,.T.) ;
#49823 = EDGE_CURVE('',#39545,#39546,#6172,.T.) ;
#49824 = EDGE_CURVE('',#39546,#39543,#6173,.T.) ;
#49825 = EDGE_CURVE('',#39547,#38744,#6174,.T.) ;
#49826 = EDGE_CURVE('',#38742,#39548,#6175,.T.) ;
#49827 = EDGE_CURVE('',#39548,#39547,#6176,.T.) ;
#49828 = EDGE_CURVE('',#39549,#39550,#6177,.T.) ;
#49829 = EDGE_CURVE('',#39550,#39551,#6178,.T.) ;
#49830 = EDGE_CURVE('',#39551,#39552,#6179,.T.) ;
#49831 = EDGE_CURVE('',#39552,#39549,#6180,.T.) ;
#49832 = EDGE_CURVE('',#39553,#39554,#6181,.T.) ;
#49833 = EDGE_CURVE('',#39554,#39555,#6182,.T.) ;
#49834 = EDGE_CURVE('',#39555,#39556,#6183,.T.) ;
#49835 = EDGE_CURVE('',#39556,#39553,#6184,.T.) ;
#49836 = EDGE_CURVE('',#39557,#39558,#6185,.T.) ;
#49837 = EDGE_CURVE('',#39558,#39559,#6186,.T.) ;
#49838 = EDGE_CURVE('',#39559,#39560,#6187,.T.) ;
#49839 = EDGE_CURVE('',#39560,#39557,#6188,.T.) ;
#49840 = EDGE_CURVE('',#39561,#39562,#6189,.T.) ;
#49841 = EDGE_CURVE('',#39562,#39563,#6190,.T.) ;
#49842 = EDGE_CURVE('',#39563,#39564,#6191,.T.) ;
#49843 = EDGE_CURVE('',#39564,#39561,#6192,.T.) ;
#49844 = EDGE_CURVE('',#39565,#39566,#6193,.T.) ;
#49845 = EDGE_CURVE('',#39566,#39567,#6194,.T.) ;
#49846 = EDGE_CURVE('',#39567,#39568,#6195,.T.) ;
#49847 = EDGE_CURVE('',#39568,#39565,#6196,.T.) ;
#49848 = EDGE_CURVE('',#39569,#39570,#6197,.T.) ;
#49849 = EDGE_CURVE('',#39570,#39571,#6198,.T.) ;
#49850 = EDGE_CURVE('',#39571,#39572,#6199,.T.) ;
#49851 = EDGE_CURVE('',#39572,#39569,#6200,.T.) ;
#49852 = EDGE_CURVE('',#39573,#39574,#6201,.T.) ;
#49853 = EDGE_CURVE('',#39574,#39575,#6202,.T.) ;
#49854 = EDGE_CURVE('',#39575,#39576,#6203,.T.) ;
#49855 = EDGE_CURVE('',#39576,#39573,#6204,.T.) ;
#49856 = EDGE_CURVE('',#39577,#39578,#6205,.T.) ;
#49857 = EDGE_CURVE('',#39578,#39579,#6206,.T.) ;
#49858 = EDGE_CURVE('',#39579,#39580,#6207,.T.) ;
#49859 = EDGE_CURVE('',#39580,#39577,#6208,.T.) ;
#49860 = EDGE_CURVE('',#39581,#39582,#6209,.T.) ;
#49861 = EDGE_CURVE('',#39582,#39583,#6210,.T.) ;
#49862 = EDGE_CURVE('',#39583,#39584,#6211,.T.) ;
#49863 = EDGE_CURVE('',#39584,#39581,#6212,.T.) ;
#49864 = EDGE_CURVE('',#39585,#39586,#6213,.T.) ;
#49865 = EDGE_CURVE('',#39586,#39587,#6214,.T.) ;
#49866 = EDGE_CURVE('',#39587,#39588,#6215,.T.) ;
#49867 = EDGE_CURVE('',#39588,#39585,#6216,.T.) ;
#49868 = EDGE_CURVE('',#39589,#39590,#32708,.T.) ;
#49869 = EDGE_CURVE('',#39589,#39591,#6217,.T.) ;
#49870 = EDGE_CURVE('',#39592,#39591,#32709,.T.) ;
#49871 = EDGE_CURVE('',#39592,#39593,#6218,.T.) ;
#49872 = EDGE_CURVE('',#39594,#39593,#32710,.T.) ;
#49873 = EDGE_CURVE('',#39594,#39595,#6219,.T.) ;
#49874 = EDGE_CURVE('',#39596,#39595,#32711,.T.) ;
#49875 = EDGE_CURVE('',#39596,#39590,#6220,.T.) ;
#49876 = EDGE_CURVE('',#39597,#39598,#32712,.T.) ;
#49877 = EDGE_CURVE('',#39597,#39599,#6221,.T.) ;
#49878 = EDGE_CURVE('',#39600,#39599,#32713,.T.) ;
#49879 = EDGE_CURVE('',#39600,#39601,#6222,.T.) ;
#49880 = EDGE_CURVE('',#39602,#39601,#32714,.T.) ;
#49881 = EDGE_CURVE('',#39602,#39603,#6223,.T.) ;
#49882 = EDGE_CURVE('',#39604,#39603,#32715,.T.) ;
#49883 = EDGE_CURVE('',#39604,#39598,#6224,.T.) ;
#49884 = EDGE_CURVE('',#39605,#39606,#6225,.T.) ;
#49885 = EDGE_CURVE('',#39606,#39607,#6226,.T.) ;
#49886 = EDGE_CURVE('',#39607,#39608,#6227,.T.) ;
#49887 = EDGE_CURVE('',#39609,#39608,#32716,.T.) ;
#49888 = EDGE_CURVE('',#39609,#39610,#6228,.T.) ;
#49889 = EDGE_CURVE('',#39610,#39611,#6229,.T.) ;
#49890 = EDGE_CURVE('',#39611,#39612,#6230,.T.) ;
#49891 = EDGE_CURVE('',#39612,#39613,#32717,.T.) ;
#49892 = EDGE_CURVE('',#39613,#39614,#6231,.T.) ;
#49893 = EDGE_CURVE('',#39614,#39615,#6232,.T.) ;
#49894 = EDGE_CURVE('',#39615,#39616,#6233,.T.) ;
#49895 = EDGE_CURVE('',#39616,#39617,#6234,.T.) ;
#49896 = EDGE_CURVE('',#39618,#39617,#32718,.T.) ;
#49897 = EDGE_CURVE('',#39618,#39619,#6235,.T.) ;
#49898 = EDGE_CURVE('',#39619,#39605,#6236,.T.) ;
#49899 = EDGE_CURVE('',#39620,#39621,#6237,.T.) ;
#49900 = EDGE_CURVE('',#39621,#39622,#6238,.T.) ;
#49901 = EDGE_CURVE('',#39622,#39623,#6239,.T.) ;
#49902 = EDGE_CURVE('',#39623,#39624,#6240,.T.) ;
#49903 = EDGE_CURVE('',#39624,#39625,#6241,.T.) ;
#49904 = EDGE_CURVE('',#39626,#39625,#32719,.T.) ;
#49905 = EDGE_CURVE('',#39626,#39627,#6242,.T.) ;
#49906 = EDGE_CURVE('',#39627,#39628,#6243,.T.) ;
#49907 = EDGE_CURVE('',#39628,#39629,#6244,.T.) ;
#49908 = EDGE_CURVE('',#39629,#39630,#6245,.T.) ;
#49909 = EDGE_CURVE('',#39630,#39631,#32720,.T.) ;
#49910 = EDGE_CURVE('',#39631,#39632,#6246,.T.) ;
#49911 = EDGE_CURVE('',#39632,#39633,#6247,.T.) ;
#49912 = EDGE_CURVE('',#39633,#39634,#6248,.T.) ;
#49913 = EDGE_CURVE('',#39620,#39634,#32721,.T.) ;
#49914 = EDGE_CURVE('',#39635,#39636,#6249,.T.) ;
#49915 = EDGE_CURVE('',#39636,#39637,#6250,.T.) ;
#49916 = EDGE_CURVE('',#39637,#39638,#6251,.T.) ;
#49917 = EDGE_CURVE('',#39638,#39635,#6252,.T.) ;
#49918 = EDGE_CURVE('',#39639,#39640,#6253,.T.) ;
#49919 = EDGE_CURVE('',#39640,#39641,#6254,.T.) ;
#49920 = EDGE_CURVE('',#39641,#39642,#6255,.T.) ;
#49921 = EDGE_CURVE('',#39642,#39639,#6256,.T.) ;
#49922 = EDGE_CURVE('',#39643,#39644,#6257,.T.) ;
#49923 = EDGE_CURVE('',#39643,#39645,#367,.T.) ;
#49924 = EDGE_CURVE('',#39645,#39646,#6258,.T.) ;
#49925 = EDGE_CURVE('',#39646,#39647,#368,.T.) ;
#49926 = EDGE_CURVE('',#39647,#39648,#6259,.T.) ;
#49927 = EDGE_CURVE('',#39648,#39642,#369,.T.) ;
#49928 = EDGE_CURVE('',#39641,#39644,#370,.T.) ;
#49929 = EDGE_CURVE('',#39645,#39649,#6260,.T.) ;
#49930 = EDGE_CURVE('',#39649,#39650,#6261,.T.) ;
#49931 = EDGE_CURVE('',#39650,#39646,#6262,.T.) ;
#49932 = EDGE_CURVE('',#39651,#39652,#6263,.T.) ;
#49933 = EDGE_CURVE('',#39652,#39653,#6264,.T.) ;
#49934 = EDGE_CURVE('',#39653,#39654,#6265,.T.) ;
#49935 = EDGE_CURVE('',#39654,#39651,#6266,.T.) ;
#49936 = EDGE_CURVE('',#39655,#39656,#6267,.T.) ;
#49937 = EDGE_CURVE('',#39656,#39643,#6268,.T.) ;
#49938 = EDGE_CURVE('',#39644,#39657,#6269,.T.) ;
#49939 = EDGE_CURVE('',#39657,#39658,#6270,.T.) ;
#49940 = EDGE_CURVE('',#39658,#39655,#6271,.T.) ;
#49941 = EDGE_CURVE('',#39659,#39660,#6272,.T.) ;
#49942 = EDGE_CURVE('',#39660,#39648,#6273,.T.) ;
#49943 = EDGE_CURVE('',#39647,#39661,#6274,.T.) ;
#49944 = EDGE_CURVE('',#39661,#39662,#6275,.T.) ;
#49945 = EDGE_CURVE('',#39662,#39659,#6276,.T.) ;
#49946 = EDGE_CURVE('',#39663,#39664,#6277,.T.) ;
#49947 = EDGE_CURVE('',#39664,#39665,#6278,.T.) ;
#49948 = EDGE_CURVE('',#39665,#39666,#6279,.T.) ;
#49949 = EDGE_CURVE('',#39666,#39663,#6280,.T.) ;
#49950 = EDGE_CURVE('',#39667,#39668,#6281,.T.) ;
#49951 = EDGE_CURVE('',#39668,#39669,#6282,.T.) ;
#49952 = EDGE_CURVE('',#39669,#39670,#6283,.T.) ;
#49953 = EDGE_CURVE('',#39670,#39667,#6284,.T.) ;
#49954 = EDGE_CURVE('',#39671,#39672,#6285,.T.) ;
#49955 = EDGE_CURVE('',#39672,#39673,#6286,.T.) ;
#49956 = EDGE_CURVE('',#39673,#39674,#6287,.T.) ;
#49957 = EDGE_CURVE('',#39674,#39671,#6288,.T.) ;
#49958 = EDGE_CURVE('',#39675,#39676,#6289,.T.) ;
#49959 = EDGE_CURVE('',#39676,#39677,#6290,.T.) ;
#49960 = EDGE_CURVE('',#39677,#39678,#6291,.T.) ;
#49961 = EDGE_CURVE('',#39678,#39675,#6292,.T.) ;
#49962 = EDGE_CURVE('',#39679,#39680,#6293,.T.) ;
#49963 = EDGE_CURVE('',#39680,#39681,#6294,.T.) ;
#49964 = EDGE_CURVE('',#39681,#39682,#6295,.T.) ;
#49965 = EDGE_CURVE('',#39682,#39679,#6296,.T.) ;
#49966 = EDGE_CURVE('',#39683,#39684,#6297,.T.) ;
#49967 = EDGE_CURVE('',#39683,#39685,#32722,.T.) ;
#49968 = EDGE_CURVE('',#39686,#39685,#6298,.T.) ;
#49969 = EDGE_CURVE('',#39686,#39687,#32723,.T.) ;
#49970 = EDGE_CURVE('',#39688,#39687,#6299,.T.) ;
#49971 = EDGE_CURVE('',#39688,#39689,#32724,.T.) ;
#49972 = EDGE_CURVE('',#39690,#39689,#6300,.T.) ;
#49973 = EDGE_CURVE('',#39690,#39684,#32725,.T.) ;
#49974 = EDGE_CURVE('',#39689,#39691,#6301,.T.) ;
#49975 = EDGE_CURVE('',#39691,#39692,#6302,.T.) ;
#49976 = EDGE_CURVE('',#39692,#39690,#6303,.T.) ;
#49977 = EDGE_CURVE('',#39684,#39693,#6304,.T.) ;
#49978 = EDGE_CURVE('',#39693,#39694,#6305,.T.) ;
#49979 = EDGE_CURVE('',#39694,#39683,#6306,.T.) ;
#49980 = EDGE_CURVE('',#39695,#39696,#6307,.T.) ;
#49981 = EDGE_CURVE('',#39696,#39686,#6308,.T.) ;
#49982 = EDGE_CURVE('',#39685,#39695,#6309,.T.) ;
#49983 = EDGE_CURVE('',#39687,#39697,#6310,.T.) ;
#49984 = EDGE_CURVE('',#39697,#39698,#6311,.T.) ;
#49985 = EDGE_CURVE('',#39698,#39688,#6312,.T.) ;
#49986 = EDGE_CURVE('',#39699,#39700,#6313,.T.) ;
#49987 = EDGE_CURVE('',#39700,#39701,#6314,.T.) ;
#49988 = EDGE_CURVE('',#39701,#39702,#6315,.T.) ;
#49989 = EDGE_CURVE('',#39702,#39699,#6316,.T.) ;
#49990 = EDGE_CURVE('',#39462,#39703,#6317,.T.) ;
#49991 = EDGE_CURVE('',#39703,#39704,#6318,.T.) ;
#49992 = EDGE_CURVE('',#39705,#39704,#32726,.T.) ;
#49993 = EDGE_CURVE('',#39705,#38818,#6319,.T.) ;
#49994 = EDGE_CURVE('',#38755,#39706,#6320,.T.) ;
#49995 = EDGE_CURVE('',#39707,#39706,#32727,.T.) ;
#49996 = EDGE_CURVE('',#39707,#39708,#6321,.T.) ;
#49997 = EDGE_CURVE('',#39708,#39461,#6322,.T.) ;
#49998 = EDGE_CURVE('',#39709,#39710,#6323,.T.) ;
#49999 = EDGE_CURVE('',#39710,#39711,#6324,.T.) ;
#50000 = EDGE_CURVE('',#39711,#39712,#6325,.T.) ;
#50001 = EDGE_CURVE('',#39712,#39709,#6326,.T.) ;
#50002 = EDGE_CURVE('',#39713,#39714,#32728,.T.) ;
#50003 = EDGE_CURVE('',#39714,#39715,#32729,.T.) ;
#50004 = EDGE_CURVE('',#39715,#39716,#6327,.T.) ;
#50005 = EDGE_CURVE('',#39716,#39717,#6328,.T.) ;
#50006 = EDGE_CURVE('',#39717,#39718,#6329,.T.) ;
#50007 = EDGE_CURVE('',#39718,#39719,#6330,.T.) ;
#50008 = EDGE_CURVE('',#39720,#39719,#32730,.T.) ;
#50009 = EDGE_CURVE('',#39720,#39721,#6331,.T.) ;
#50010 = EDGE_CURVE('',#39721,#39722,#6332,.T.) ;
#50011 = EDGE_CURVE('',#39722,#39713,#6333,.T.) ;
#50012 = EDGE_CURVE('',#39723,#39724,#6334,.T.) ;
#50013 = EDGE_CURVE('',#39724,#39725,#6335,.T.) ;
#50014 = EDGE_CURVE('',#39725,#39726,#6336,.T.) ;
#50015 = EDGE_CURVE('',#39726,#39723,#6337,.T.) ;
#50016 = EDGE_CURVE('',#39727,#39728,#6338,.T.) ;
#50017 = EDGE_CURVE('',#39728,#39729,#32731,.T.) ;
#50018 = EDGE_CURVE('',#39729,#39730,#32732,.T.) ;
#50019 = EDGE_CURVE('',#39730,#39731,#6339,.T.) ;
#50020 = EDGE_CURVE('',#39731,#39732,#6340,.T.) ;
#50021 = EDGE_CURVE('',#39732,#39733,#6341,.T.) ;
#50022 = EDGE_CURVE('',#39734,#39733,#32733,.T.) ;
#50023 = EDGE_CURVE('',#39734,#39735,#6342,.T.) ;
#50024 = EDGE_CURVE('',#39735,#39736,#6343,.T.) ;
#50025 = EDGE_CURVE('',#39736,#39727,#6344,.T.) ;
#50026 = EDGE_CURVE('',#39737,#39463,#6345,.T.) ;
#50027 = EDGE_CURVE('',#39464,#39738,#6346,.T.) ;
#50028 = EDGE_CURVE('',#39738,#39737,#6347,.T.) ;
#50029 = EDGE_CURVE('',#39739,#39740,#6348,.T.) ;
#50030 = EDGE_CURVE('',#39740,#39741,#6349,.T.) ;
#50031 = EDGE_CURVE('',#39741,#39742,#6350,.T.) ;
#50032 = EDGE_CURVE('',#39742,#39739,#6351,.T.) ;
#50033 = EDGE_CURVE('',#39743,#39744,#6352,.T.) ;
#50034 = EDGE_CURVE('',#39744,#39745,#6353,.T.) ;
#50035 = EDGE_CURVE('',#39745,#39746,#6354,.T.) ;
#50036 = EDGE_CURVE('',#39746,#39743,#6355,.T.) ;
#50037 = EDGE_CURVE('',#39747,#39748,#6356,.T.) ;
#50038 = EDGE_CURVE('',#39748,#39749,#32734,.T.) ;
#50039 = EDGE_CURVE('',#39749,#39750,#6357,.T.) ;
#50040 = EDGE_CURVE('',#39750,#39747,#32735,.T.) ;
#50041 = EDGE_CURVE('',#39751,#39752,#6358,.T.) ;
#50042 = EDGE_CURVE('',#39752,#39753,#32736,.T.) ;
#50043 = EDGE_CURVE('',#39753,#39754,#6359,.T.) ;
#50044 = EDGE_CURVE('',#39754,#39755,#6360,.T.) ;
#50045 = EDGE_CURVE('',#39755,#39756,#6361,.T.) ;
#50046 = EDGE_CURVE('',#39756,#39751,#6362,.T.) ;
#50047 = EDGE_CURVE('',#39757,#39758,#6363,.T.) ;
#50048 = EDGE_CURVE('',#39758,#39759,#6364,.T.) ;
#50049 = EDGE_CURVE('',#39759,#39760,#6365,.T.) ;
#50050 = EDGE_CURVE('',#39760,#39757,#6366,.T.) ;
#50051 = EDGE_CURVE('',#39761,#39762,#6367,.T.) ;
#50052 = EDGE_CURVE('',#39762,#39763,#6368,.T.) ;
#50053 = EDGE_CURVE('',#39763,#39764,#6369,.T.) ;
#50054 = EDGE_CURVE('',#39764,#39761,#6370,.T.) ;
#50055 = EDGE_CURVE('',#39765,#39766,#6371,.T.) ;
#50056 = EDGE_CURVE('',#39766,#39767,#6372,.T.) ;
#50057 = EDGE_CURVE('',#39767,#39768,#6373,.T.) ;
#50058 = EDGE_CURVE('',#39768,#39765,#6374,.T.) ;
#50059 = EDGE_CURVE('',#39769,#39770,#6375,.T.) ;
#50060 = EDGE_CURVE('',#39770,#39771,#6376,.T.) ;
#50061 = EDGE_CURVE('',#39771,#39772,#6377,.T.) ;
#50062 = EDGE_CURVE('',#39772,#39769,#6378,.T.) ;
#50063 = EDGE_CURVE('',#39773,#39774,#6379,.T.) ;
#50064 = EDGE_CURVE('',#39774,#39775,#6380,.T.) ;
#50065 = EDGE_CURVE('',#39775,#39776,#6381,.T.) ;
#50066 = EDGE_CURVE('',#39776,#39773,#6382,.T.) ;
#50067 = EDGE_CURVE('',#39777,#39778,#6383,.T.) ;
#50068 = EDGE_CURVE('',#39777,#39779,#32737,.T.) ;
#50069 = EDGE_CURVE('',#39780,#39779,#6384,.T.) ;
#50070 = EDGE_CURVE('',#39780,#39781,#32738,.T.) ;
#50071 = EDGE_CURVE('',#39782,#39781,#6385,.T.) ;
#50072 = EDGE_CURVE('',#39782,#39783,#32739,.T.) ;
#50073 = EDGE_CURVE('',#39784,#39783,#6386,.T.) ;
#50074 = EDGE_CURVE('',#39784,#39778,#32740,.T.) ;
#50075 = EDGE_CURVE('',#39785,#39786,#6387,.T.) ;
#50076 = EDGE_CURVE('',#39786,#39784,#6388,.T.) ;
#50077 = EDGE_CURVE('',#39783,#39785,#6389,.T.) ;
#50078 = EDGE_CURVE('',#39787,#39788,#6390,.T.) ;
#50079 = EDGE_CURVE('',#39788,#39777,#6391,.T.) ;
#50080 = EDGE_CURVE('',#39778,#39787,#6392,.T.) ;
#50081 = EDGE_CURVE('',#39779,#39789,#6393,.T.) ;
#50082 = EDGE_CURVE('',#39789,#39790,#6394,.T.) ;
#50083 = EDGE_CURVE('',#39790,#39780,#6395,.T.) ;
#50084 = EDGE_CURVE('',#39791,#39792,#6396,.T.) ;
#50085 = EDGE_CURVE('',#39792,#39782,#6397,.T.) ;
#50086 = EDGE_CURVE('',#39781,#39791,#6398,.T.) ;
#50087 = EDGE_CURVE('',#39793,#39794,#6399,.T.) ;
#50088 = EDGE_CURVE('',#39794,#39795,#6400,.T.) ;
#50089 = EDGE_CURVE('',#39795,#39796,#6401,.T.) ;
#50090 = EDGE_CURVE('',#39796,#39793,#6402,.T.) ;
#50091 = EDGE_CURVE('',#39061,#39045,#6403,.T.) ;
#50092 = EDGE_CURVE('',#39047,#39060,#6404,.T.) ;
#50093 = EDGE_CURVE('',#39059,#39048,#6405,.T.) ;
#50094 = EDGE_CURVE('',#39051,#39056,#6406,.T.) ;
#50095 = EDGE_CURVE('',#39055,#39052,#6407,.T.) ;
#50096 = EDGE_CURVE('',#39049,#39058,#6408,.T.) ;
#50097 = EDGE_CURVE('',#39057,#39050,#6409,.T.) ;
#50098 = EDGE_CURVE('',#38760,#38753,#32741,.T.) ;
#50099 = EDGE_CURVE('',#38752,#38749,#32742,.T.) ;
#50100 = EDGE_CURVE('',#38748,#39797,#6410,.T.) ;
#50101 = EDGE_CURVE('',#39797,#39798,#6411,.T.) ;
#50102 = EDGE_CURVE('',#39798,#39044,#6412,.T.) ;
#50103 = EDGE_CURVE('',#39799,#39800,#6413,.T.) ;
#50104 = EDGE_CURVE('',#39800,#38817,#6414,.T.) ;
#50105 = EDGE_CURVE('',#39043,#39799,#6415,.T.) ;
#50106 = EDGE_CURVE('',#38816,#38810,#32743,.T.) ;
#50107 = EDGE_CURVE('',#38809,#38803,#32744,.T.) ;
#50108 = EDGE_CURVE('',#39801,#39802,#6416,.T.) ;
#50109 = EDGE_CURVE('',#39802,#39803,#32745,.T.) ;
#50110 = EDGE_CURVE('',#39804,#39803,#6417,.T.) ;
#50111 = EDGE_CURVE('',#39804,#39801,#32746,.T.) ;
#50112 = EDGE_CURVE('',#39803,#39805,#6418,.T.) ;
#50113 = EDGE_CURVE('',#39806,#39805,#6419,.T.) ;
#50114 = EDGE_CURVE('',#39806,#39804,#6420,.T.) ;
#50115 = EDGE_CURVE('',#39805,#39807,#32747,.T.) ;
#50116 = EDGE_CURVE('',#39808,#39807,#6421,.T.) ;
#50117 = EDGE_CURVE('',#39808,#39806,#32748,.T.) ;
#50118 = EDGE_CURVE('',#39807,#39809,#6422,.T.) ;
#50119 = EDGE_CURVE('',#39810,#39809,#6423,.T.) ;
#50120 = EDGE_CURVE('',#39810,#39808,#6424,.T.) ;
#50121 = EDGE_CURVE('',#39809,#39811,#32749,.T.) ;
#50122 = EDGE_CURVE('',#39812,#39811,#6425,.T.) ;
#50123 = EDGE_CURVE('',#39812,#39810,#32750,.T.) ;
#50124 = EDGE_CURVE('',#39811,#39813,#6426,.T.) ;
#50125 = EDGE_CURVE('',#39814,#39813,#6427,.T.) ;
#50126 = EDGE_CURVE('',#39814,#39812,#6428,.T.) ;
#50127 = EDGE_CURVE('',#39813,#39815,#32751,.T.) ;
#50128 = EDGE_CURVE('',#39816,#39815,#6429,.T.) ;
#50129 = EDGE_CURVE('',#39816,#39814,#32752,.T.) ;
#50130 = EDGE_CURVE('',#39801,#39816,#6430,.T.) ;
#50131 = EDGE_CURVE('',#39815,#39802,#6431,.T.) ;
#50132 = EDGE_CURVE('',#39817,#39818,#6432,.T.) ;
#50133 = EDGE_CURVE('',#39818,#39819,#6433,.T.) ;
#50134 = EDGE_CURVE('',#39819,#39820,#6434,.T.) ;
#50135 = EDGE_CURVE('',#39820,#39817,#6435,.T.) ;
#50136 = EDGE_CURVE('',#39555,#39629,#32753,.T.) ;
#50137 = EDGE_CURVE('',#39556,#39628,#32754,.T.) ;
#50138 = EDGE_CURVE('',#39556,#39469,#32755,.T.) ;
#50139 = EDGE_CURVE('',#39469,#39628,#32756,.T.) ;
#50140 = EDGE_CURVE('',#39554,#39398,#32757,.T.) ;
#50141 = EDGE_CURVE('',#39397,#39555,#32758,.T.) ;
#50142 = EDGE_CURVE('',#39470,#39627,#32759,.T.) ;
#50143 = EDGE_CURVE('',#39553,#39468,#32760,.T.) ;
#50144 = EDGE_CURVE('',#39614,#39554,#32761,.T.) ;
#50145 = EDGE_CURVE('',#39615,#39553,#32762,.T.) ;
#50146 = EDGE_CURVE('',#39622,#39552,#32763,.T.) ;
#50147 = EDGE_CURVE('',#39623,#39551,#32764,.T.) ;
#50148 = EDGE_CURVE('',#39821,#39623,#32765,.T.) ;
#50149 = EDGE_CURVE('',#39821,#39822,#371,.T.) ;
#50150 = EDGE_CURVE('',#39822,#39624,#372,.T.) ;
#50151 = EDGE_CURVE('',#39470,#39546,#32766,.T.) ;
#50152 = EDGE_CURVE('',#39546,#39627,#32767,.T.) ;
#50153 = EDGE_CURVE('',#39615,#39468,#32768,.T.) ;
#50154 = EDGE_CURVE('',#39552,#39064,#32769,.T.) ;
#50155 = EDGE_CURVE('',#39063,#39549,#32770,.T.) ;
#50156 = EDGE_CURVE('',#38745,#39551,#32771,.T.) ;
#50157 = EDGE_CURVE('',#38745,#39821,#373,.T.) ;
#50158 = EDGE_CURVE('',#39624,#39823,#374,.T.) ;
#50159 = EDGE_CURVE('',#39823,#39824,#375,.T.) ;
#50160 = EDGE_CURVE('',#39824,#38744,#376,.T.) ;
#50161 = EDGE_CURVE('',#39625,#39547,#32772,.T.) ;
#50162 = EDGE_CURVE('',#39543,#39626,#32773,.T.) ;
#50163 = EDGE_CURVE('',#39467,#39545,#32774,.T.) ;
#50164 = EDGE_CURVE('',#39616,#39467,#32775,.T.) ;
#50165 = EDGE_CURVE('',#39549,#39606,#32776,.T.) ;
#50166 = EDGE_CURVE('',#39550,#39605,#32777,.T.) ;
#50167 = EDGE_CURVE('',#38743,#39550,#32778,.T.) ;
#50168 = EDGE_CURVE('',#39543,#39547,#32779,.T.) ;
#50169 = EDGE_CURVE('',#39616,#39545,#32780,.T.) ;
#50170 = EDGE_CURVE('',#39825,#39605,#32781,.T.) ;
#50171 = EDGE_CURVE('',#39825,#38743,#377,.T.) ;
#50172 = EDGE_CURVE('',#39544,#39548,#32782,.T.) ;
#50173 = EDGE_CURVE('',#39617,#39544,#32783,.T.) ;
#50174 = EDGE_CURVE('',#39619,#39826,#378,.T.) ;
#50175 = EDGE_CURVE('',#39826,#39825,#379,.T.) ;
#50176 = EDGE_CURVE('',#39618,#39548,#32784,.T.) ;
#50177 = EDGE_CURVE('',#38742,#39827,#380,.T.) ;
#50178 = EDGE_CURVE('',#39827,#39828,#381,.T.) ;
#50179 = EDGE_CURVE('',#39828,#39619,#382,.T.) ;
#50180 = EDGE_CURVE('',#39753,#39739,#32785,.T.) ;
#50181 = EDGE_CURVE('',#39750,#39753,#32786,.T.) ;
#50182 = EDGE_CURVE('',#39739,#39750,#32787,.T.) ;
#50183 = EDGE_CURVE('',#39747,#39752,#32788,.T.) ;
#50184 = EDGE_CURVE('',#39740,#39749,#32789,.T.) ;
#50185 = EDGE_CURVE('',#39754,#39742,#32790,.T.) ;
#50186 = EDGE_CURVE('',#39731,#39755,#32791,.T.) ;
#50187 = EDGE_CURVE('',#39732,#39754,#32792,.T.) ;
#50188 = EDGE_CURVE('',#39755,#39520,#32793,.T.) ;
#50189 = EDGE_CURVE('',#39519,#39756,#32794,.T.) ;
#50190 = EDGE_CURVE('',#39747,#39746,#32795,.T.) ;
#50191 = EDGE_CURVE('',#39746,#39752,#32796,.T.) ;
#50192 = EDGE_CURVE('',#39740,#39539,#32797,.T.) ;
#50193 = EDGE_CURVE('',#39540,#39749,#32798,.T.) ;
#50194 = EDGE_CURVE('',#39732,#39742,#32799,.T.) ;
#50195 = EDGE_CURVE('',#39756,#39722,#32800,.T.) ;
#50196 = EDGE_CURVE('',#39751,#39721,#32801,.T.) ;
#50197 = EDGE_CURVE('',#39743,#39751,#32802,.T.) ;
#50198 = EDGE_CURVE('',#39748,#39745,#32803,.T.) ;
#50199 = EDGE_CURVE('',#39541,#39748,#32804,.T.) ;
#50200 = EDGE_CURVE('',#39741,#39538,#32805,.T.) ;
#50201 = EDGE_CURVE('',#39733,#39741,#32806,.T.) ;
#50202 = EDGE_CURVE('',#39743,#39721,#32807,.T.) ;
#50203 = EDGE_CURVE('',#39542,#39745,#32808,.T.) ;
#50204 = EDGE_CURVE('',#39734,#39538,#32809,.T.) ;
#50205 = EDGE_CURVE('',#39744,#39720,#32810,.T.) ;
#50206 = EDGE_CURVE('',#39535,#39744,#32811,.T.) ;
#50207 = EDGE_CURVE('',#39735,#39537,#32812,.T.) ;
#50208 = EDGE_CURVE('',#39464,#39728,#32813,.T.) ;
#50209 = EDGE_CURVE('',#39738,#39727,#32814,.T.) ;
#50210 = EDGE_CURVE('',#39454,#39738,#32815,.T.) ;
#50211 = EDGE_CURVE('',#39737,#39453,#32816,.T.) ;
#50212 = EDGE_CURVE('',#39535,#39719,#32817,.T.) ;
#50213 = EDGE_CURVE('',#39735,#39726,#32818,.T.) ;
#50214 = EDGE_CURVE('',#39726,#39537,#32819,.T.) ;
#50215 = EDGE_CURVE('',#39454,#39727,#32820,.T.) ;
#50216 = EDGE_CURVE('',#39536,#39718,#32821,.T.) ;
#50217 = EDGE_CURVE('',#39723,#39536,#32822,.T.) ;
#50218 = EDGE_CURVE('',#39736,#39725,#32823,.T.) ;
#50219 = EDGE_CURVE('',#39455,#39736,#32824,.T.) ;
#50220 = EDGE_CURVE('',#39723,#39718,#32825,.T.) ;
#50221 = EDGE_CURVE('',#39456,#39725,#32826,.T.) ;
#50222 = EDGE_CURVE('',#39711,#39460,#32827,.T.) ;
#50223 = EDGE_CURVE('',#39712,#39459,#32828,.T.) ;
#50224 = EDGE_CURVE('',#39715,#39709,#32829,.T.) ;
#50225 = EDGE_CURVE('',#39716,#39712,#32830,.T.) ;
#50226 = EDGE_CURVE('',#39724,#39717,#32831,.T.) ;
#50227 = EDGE_CURVE('',#39457,#39724,#32832,.T.) ;
#50228 = EDGE_CURVE('',#39716,#39459,#32833,.T.) ;
#50229 = EDGE_CURVE('',#39458,#39717,#32834,.T.) ;
#50230 = EDGE_CURVE('',#39529,#39805,#32835,.T.) ;
#50231 = EDGE_CURVE('',#39807,#39528,#32836,.T.) ;
#50232 = EDGE_CURVE('',#39809,#39527,#32837,.T.) ;
#50233 = EDGE_CURVE('',#39530,#39803,#32838,.T.) ;
#50234 = EDGE_CURVE('',#39811,#39526,#32839,.T.) ;
#50235 = EDGE_CURVE('',#39523,#39802,#32840,.T.) ;
#50236 = EDGE_CURVE('',#39813,#39525,#32841,.T.) ;
#50237 = EDGE_CURVE('',#39524,#39815,#32842,.T.) ;
#50238 = EDGE_CURVE('',#39603,#39678,#32843,.T.) ;
#50239 = EDGE_CURVE('',#39675,#39602,#32844,.T.) ;
#50240 = EDGE_CURVE('',#39674,#39601,#32845,.T.) ;
#50241 = EDGE_CURVE('',#39675,#39674,#32846,.T.) ;
#50242 = EDGE_CURVE('',#39666,#39678,#32847,.T.) ;
#50243 = EDGE_CURVE('',#39604,#39666,#32848,.T.) ;
#50244 = EDGE_CURVE('',#39671,#39600,#32849,.T.) ;
#50245 = EDGE_CURVE('',#39676,#39673,#32850,.T.) ;
#50246 = EDGE_CURVE('',#39677,#39682,#32851,.T.) ;
#50247 = EDGE_CURVE('',#39679,#39676,#32852,.T.) ;
#50248 = EDGE_CURVE('',#39663,#39677,#32853,.T.) ;
#50249 = EDGE_CURVE('',#39598,#39665,#32854,.T.) ;
#50250 = EDGE_CURVE('',#39599,#39669,#32855,.T.) ;
#50251 = EDGE_CURVE('',#39670,#39597,#32856,.T.) ;
#50252 = EDGE_CURVE('',#39671,#39669,#32857,.T.) ;
#50253 = EDGE_CURVE('',#39679,#39673,#32858,.T.) ;
#50254 = EDGE_CURVE('',#39663,#39682,#32859,.T.) ;
#50255 = EDGE_CURVE('',#39670,#39665,#32860,.T.) ;
#50256 = EDGE_CURVE('',#39672,#39668,#32861,.T.) ;
#50257 = EDGE_CURVE('',#39680,#39672,#32862,.T.) ;
#50258 = EDGE_CURVE('',#39664,#39681,#32863,.T.) ;
#50259 = EDGE_CURVE('',#39667,#39664,#32864,.T.) ;
#50260 = EDGE_CURVE('',#39680,#39668,#32865,.T.) ;
#50261 = EDGE_CURVE('',#39667,#39681,#32866,.T.) ;
#50262 = EDGE_CURVE('',#39691,#39698,#32867,.T.) ;
#50263 = EDGE_CURVE('',#39692,#39702,#32868,.T.) ;
#50264 = EDGE_CURVE('',#39699,#39691,#32869,.T.) ;
#50265 = EDGE_CURVE('',#39693,#39692,#32870,.T.) ;
#50266 = EDGE_CURVE('',#39699,#39698,#32871,.T.) ;
#50267 = EDGE_CURVE('',#39693,#39702,#32872,.T.) ;
#50268 = EDGE_CURVE('',#39697,#39696,#32873,.T.) ;
#50269 = EDGE_CURVE('',#39700,#39697,#32874,.T.) ;
#50270 = EDGE_CURVE('',#39694,#39701,#32875,.T.) ;
#50271 = EDGE_CURVE('',#39695,#39694,#32876,.T.) ;
#50272 = EDGE_CURVE('',#39700,#39696,#32877,.T.) ;
#50273 = EDGE_CURVE('',#39695,#39701,#32878,.T.) ;
#50274 = EDGE_CURVE('',#39639,#39660,#32879,.T.) ;
#50275 = EDGE_CURVE('',#39639,#39637,#32880,.T.) ;
#50276 = EDGE_CURVE('',#39637,#39660,#32881,.T.) ;
#50277 = EDGE_CURVE('',#39638,#39659,#2305,.T.) ;
#50278 = EDGE_CURVE('',#39640,#39636,#32882,.T.) ;
#50279 = EDGE_CURVE('',#39657,#39640,#32883,.T.) ;
#50280 = EDGE_CURVE('',#39638,#39515,#32884,.T.) ;
#50281 = EDGE_CURVE('',#39516,#39659,#32885,.T.) ;
#50282 = EDGE_CURVE('',#39657,#39636,#32886,.T.) ;
#50283 = EDGE_CURVE('',#39661,#39650,#32887,.T.) ;
#50284 = EDGE_CURVE('',#39662,#39654,#2306,.T.) ;
#50285 = EDGE_CURVE('',#39651,#39661,#32888,.T.) ;
#50286 = EDGE_CURVE('',#39517,#39662,#32889,.T.) ;
#50287 = EDGE_CURVE('',#39635,#39514,#32890,.T.) ;
#50288 = EDGE_CURVE('',#39658,#39635,#383,.T.) ;
#50289 = EDGE_CURVE('',#39651,#39650,#32891,.T.) ;
#50290 = EDGE_CURVE('',#39518,#39654,#32892,.T.) ;
#50291 = EDGE_CURVE('',#39658,#39513,#32893,.T.) ;
#50292 = EDGE_CURVE('',#39649,#39656,#32894,.T.) ;
#50293 = EDGE_CURVE('',#39652,#39649,#32895,.T.) ;
#50294 = EDGE_CURVE('',#39512,#39653,#32896,.T.) ;
#50295 = EDGE_CURVE('',#39655,#39511,#32897,.T.) ;
#50296 = EDGE_CURVE('',#39652,#39656,#32898,.T.) ;
#50297 = EDGE_CURVE('',#39655,#39653,#384,.T.) ;
#50298 = EDGE_CURVE('',#39107,#39771,#32899,.T.) ;
#50299 = EDGE_CURVE('',#39772,#39106,#32900,.T.) ;
#50300 = EDGE_CURVE('',#39768,#39105,#32901,.T.) ;
#50301 = EDGE_CURVE('',#39772,#39768,#32902,.T.) ;
#50302 = EDGE_CURVE('',#39760,#39771,#32903,.T.) ;
#50303 = EDGE_CURVE('',#39108,#39760,#32904,.T.) ;
#50304 = EDGE_CURVE('',#39765,#39104,#32905,.T.) ;
#50305 = EDGE_CURVE('',#39769,#39767,#32906,.T.) ;
#50306 = EDGE_CURVE('',#39770,#39776,#32907,.T.) ;
#50307 = EDGE_CURVE('',#39773,#39769,#32908,.T.) ;
#50308 = EDGE_CURVE('',#39757,#39770,#32909,.T.) ;
#50309 = EDGE_CURVE('',#39102,#39759,#32910,.T.) ;
#50310 = EDGE_CURVE('',#39103,#39761,#32911,.T.) ;
#50311 = EDGE_CURVE('',#39762,#39101,#32912,.T.) ;
#50312 = EDGE_CURVE('',#39765,#39761,#32913,.T.) ;
#50313 = EDGE_CURVE('',#39773,#39767,#32914,.T.) ;
#50314 = EDGE_CURVE('',#39757,#39776,#32915,.T.) ;
#50315 = EDGE_CURVE('',#39762,#39759,#32916,.T.) ;
#50316 = EDGE_CURVE('',#39766,#39764,#32917,.T.) ;
#50317 = EDGE_CURVE('',#39774,#39766,#32918,.T.) ;
#50318 = EDGE_CURVE('',#39758,#39775,#32919,.T.) ;
#50319 = EDGE_CURVE('',#39763,#39758,#32920,.T.) ;
#50320 = EDGE_CURVE('',#39774,#39764,#32921,.T.) ;
#50321 = EDGE_CURVE('',#39763,#39775,#32922,.T.) ;
#50322 = EDGE_CURVE('',#39785,#39792,#32923,.T.) ;
#50323 = EDGE_CURVE('',#39786,#39796,#32924,.T.) ;
#50324 = EDGE_CURVE('',#39793,#39785,#32925,.T.) ;
#50325 = EDGE_CURVE('',#39787,#39786,#32926,.T.) ;
#50326 = EDGE_CURVE('',#39793,#39792,#32927,.T.) ;
#50327 = EDGE_CURVE('',#39787,#39796,#32928,.T.) ;
#50328 = EDGE_CURVE('',#39791,#39790,#32929,.T.) ;
#50329 = EDGE_CURVE('',#39794,#39791,#32930,.T.) ;
#50330 = EDGE_CURVE('',#39788,#39795,#32931,.T.) ;
#50331 = EDGE_CURVE('',#39789,#39788,#32932,.T.) ;
#50332 = EDGE_CURVE('',#39794,#39790,#32933,.T.) ;
#50333 = EDGE_CURVE('',#39789,#39795,#32934,.T.) ;
#50334 = EDGE_CURVE('',#39808,#39820,#32935,.T.) ;
#50335 = EDGE_CURVE('',#39817,#39810,#32936,.T.) ;
#50336 = EDGE_CURVE('',#39817,#39812,#32937,.T.) ;
#50337 = EDGE_CURVE('',#39806,#39820,#32938,.T.) ;
#50338 = EDGE_CURVE('',#39818,#39814,#32939,.T.) ;
#50339 = EDGE_CURVE('',#39804,#39819,#32940,.T.) ;
#50340 = EDGE_CURVE('',#39818,#39816,#32941,.T.) ;
#50341 = EDGE_CURVE('',#39801,#39819,#32942,.T.) ;
#50342 = EDGE_CURVE('',#39521,#39265,#32943,.T.) ;
#50343 = EDGE_CURVE('',#39264,#39522,#32944,.T.) ;
#50344 = EDGE_CURVE('',#39266,#39466,#2307,.T.) ;
#50345 = EDGE_CURVE('',#39261,#39710,#32945,.T.) ;
#50346 = EDGE_CURVE('',#39829,#39709,#32946,.T.) ;
#50347 = EDGE_CURVE('',#39262,#39829,#32947,.T.) ;
#50348 = EDGE_CURVE('',#39829,#39263,#2308,.T.) ;
#50349 = EDGE_CURVE('',#39729,#39830,#2309,.T.) ;
#50350 = EDGE_CURVE('',#39730,#39830,#32948,.T.) ;
#50351 = EDGE_CURVE('',#39830,#39521,#32949,.T.) ;
#50352 = EDGE_CURVE('',#39731,#39520,#32950,.T.) ;
#50353 = EDGE_CURVE('',#39831,#39713,#32951,.T.) ;
#50354 = EDGE_CURVE('',#39831,#39714,#2310,.T.) ;
#50355 = EDGE_CURVE('',#39522,#39831,#32952,.T.) ;
#50356 = EDGE_CURVE('',#39519,#39722,#32953,.T.) ;
#50357 = EDGE_CURVE('',#39266,#39830,#32954,.T.) ;
#50358 = EDGE_CURVE('',#39466,#39729,#32955,.T.) ;
#50359 = EDGE_CURVE('',#39831,#39263,#32956,.T.) ;
#50360 = EDGE_CURVE('',#39714,#39829,#32957,.T.) ;
#50361 = EDGE_CURVE('',#39832,#39833,#6436,.T.) ;
#50362 = EDGE_CURVE('',#39833,#39834,#6437,.T.) ;
#50363 = EDGE_CURVE('',#39834,#39835,#6438,.T.) ;
#50364 = EDGE_CURVE('',#39835,#39832,#6439,.T.) ;
#50365 = EDGE_CURVE('',#39836,#39837,#6440,.T.) ;
#50366 = EDGE_CURVE('',#39837,#39838,#6441,.T.) ;
#50367 = EDGE_CURVE('',#39838,#39839,#6442,.T.) ;
#50368 = EDGE_CURVE('',#39839,#39836,#6443,.T.) ;
#50369 = EDGE_CURVE('',#39840,#39841,#6444,.T.) ;
#50370 = EDGE_CURVE('',#39840,#39842,#385,.T.) ;
#50371 = EDGE_CURVE('',#39842,#39843,#6445,.T.) ;
#50372 = EDGE_CURVE('',#39843,#39844,#386,.T.) ;
#50373 = EDGE_CURVE('',#39844,#39845,#6446,.T.) ;
#50374 = EDGE_CURVE('',#39845,#39839,#387,.T.) ;
#50375 = EDGE_CURVE('',#39838,#39841,#388,.T.) ;
#50376 = EDGE_CURVE('',#39842,#39846,#6447,.T.) ;
#50377 = EDGE_CURVE('',#39846,#39847,#6448,.T.) ;
#50378 = EDGE_CURVE('',#39847,#39843,#6449,.T.) ;
#50379 = EDGE_CURVE('',#39848,#39849,#6450,.T.) ;
#50380 = EDGE_CURVE('',#39849,#39850,#6451,.T.) ;
#50381 = EDGE_CURVE('',#39850,#39851,#6452,.T.) ;
#50382 = EDGE_CURVE('',#39851,#39848,#6453,.T.) ;
#50383 = EDGE_CURVE('',#39852,#39853,#6454,.T.) ;
#50384 = EDGE_CURVE('',#39853,#39854,#6455,.T.) ;
#50385 = EDGE_CURVE('',#39854,#39855,#6456,.T.) ;
#50386 = EDGE_CURVE('',#39855,#39852,#6457,.T.) ;
#50387 = EDGE_CURVE('',#39856,#39857,#6458,.T.) ;
#50388 = EDGE_CURVE('',#39857,#39858,#6459,.T.) ;
#50389 = EDGE_CURVE('',#39858,#39859,#6460,.T.) ;
#50390 = EDGE_CURVE('',#39859,#39856,#6461,.T.) ;
#50391 = EDGE_CURVE('',#39860,#39861,#6462,.T.) ;
#50392 = EDGE_CURVE('',#39860,#39862,#389,.T.) ;
#50393 = EDGE_CURVE('',#39862,#39863,#6463,.T.) ;
#50394 = EDGE_CURVE('',#39863,#39864,#390,.T.) ;
#50395 = EDGE_CURVE('',#39864,#39865,#6464,.T.) ;
#50396 = EDGE_CURVE('',#39865,#39859,#391,.T.) ;
#50397 = EDGE_CURVE('',#39858,#39861,#392,.T.) ;
#50398 = EDGE_CURVE('',#39862,#39866,#6465,.T.) ;
#50399 = EDGE_CURVE('',#39866,#39867,#6466,.T.) ;
#50400 = EDGE_CURVE('',#39867,#39863,#6467,.T.) ;
#50401 = EDGE_CURVE('',#39868,#39869,#6468,.T.) ;
#50402 = EDGE_CURVE('',#39869,#39870,#6469,.T.) ;
#50403 = EDGE_CURVE('',#39870,#39871,#6470,.T.) ;
#50404 = EDGE_CURVE('',#39871,#39868,#6471,.T.) ;
#50405 = EDGE_CURVE('',#39872,#39873,#6472,.T.) ;
#50406 = EDGE_CURVE('',#39873,#39874,#6473,.T.) ;
#50407 = EDGE_CURVE('',#39874,#39875,#6474,.T.) ;
#50408 = EDGE_CURVE('',#39875,#39872,#6475,.T.) ;
#50409 = EDGE_CURVE('',#39876,#39877,#6476,.T.) ;
#50410 = EDGE_CURVE('',#39877,#39878,#6477,.T.) ;
#50411 = EDGE_CURVE('',#39878,#39879,#6478,.T.) ;
#50412 = EDGE_CURVE('',#39879,#39876,#6479,.T.) ;
#50413 = EDGE_CURVE('',#39880,#39881,#6480,.T.) ;
#50414 = EDGE_CURVE('',#39880,#39882,#393,.T.) ;
#50415 = EDGE_CURVE('',#39882,#39883,#6481,.T.) ;
#50416 = EDGE_CURVE('',#39883,#39884,#394,.T.) ;
#50417 = EDGE_CURVE('',#39884,#39885,#6482,.T.) ;
#50418 = EDGE_CURVE('',#39885,#39879,#395,.T.) ;
#50419 = EDGE_CURVE('',#39878,#39881,#396,.T.) ;
#50420 = EDGE_CURVE('',#39882,#39886,#6483,.T.) ;
#50421 = EDGE_CURVE('',#39886,#39887,#6484,.T.) ;
#50422 = EDGE_CURVE('',#39887,#39883,#6485,.T.) ;
#50423 = EDGE_CURVE('',#39888,#39889,#6486,.T.) ;
#50424 = EDGE_CURVE('',#39889,#39890,#6487,.T.) ;
#50425 = EDGE_CURVE('',#39890,#39891,#6488,.T.) ;
#50426 = EDGE_CURVE('',#39891,#39888,#6489,.T.) ;
#50427 = EDGE_CURVE('',#39892,#39893,#6490,.T.) ;
#50428 = EDGE_CURVE('',#39893,#39894,#6491,.T.) ;
#50429 = EDGE_CURVE('',#39894,#39895,#6492,.T.) ;
#50430 = EDGE_CURVE('',#39895,#39892,#6493,.T.) ;
#50431 = EDGE_CURVE('',#39896,#39897,#6494,.T.) ;
#50432 = EDGE_CURVE('',#39897,#39898,#6495,.T.) ;
#50433 = EDGE_CURVE('',#39898,#39899,#6496,.T.) ;
#50434 = EDGE_CURVE('',#39899,#39896,#6497,.T.) ;
#50435 = EDGE_CURVE('',#39900,#39901,#6498,.T.) ;
#50436 = EDGE_CURVE('',#39900,#39902,#397,.T.) ;
#50437 = EDGE_CURVE('',#39902,#39903,#6499,.T.) ;
#50438 = EDGE_CURVE('',#39903,#39904,#398,.T.) ;
#50439 = EDGE_CURVE('',#39904,#39905,#6500,.T.) ;
#50440 = EDGE_CURVE('',#39905,#39899,#399,.T.) ;
#50441 = EDGE_CURVE('',#39898,#39901,#400,.T.) ;
#50442 = EDGE_CURVE('',#39902,#39906,#6501,.T.) ;
#50443 = EDGE_CURVE('',#39906,#39907,#6502,.T.) ;
#50444 = EDGE_CURVE('',#39907,#39903,#6503,.T.) ;
#50445 = EDGE_CURVE('',#39908,#39909,#6504,.T.) ;
#50446 = EDGE_CURVE('',#39909,#39910,#6505,.T.) ;
#50447 = EDGE_CURVE('',#39910,#39911,#6506,.T.) ;
#50448 = EDGE_CURVE('',#39911,#39908,#6507,.T.) ;
#50449 = EDGE_CURVE('',#39912,#39913,#6508,.T.) ;
#50450 = EDGE_CURVE('',#39913,#39914,#6509,.T.) ;
#50451 = EDGE_CURVE('',#39914,#39915,#6510,.T.) ;
#50452 = EDGE_CURVE('',#39915,#39912,#6511,.T.) ;
#50453 = EDGE_CURVE('',#39916,#39917,#6512,.T.) ;
#50454 = EDGE_CURVE('',#39917,#39918,#6513,.T.) ;
#50455 = EDGE_CURVE('',#39918,#39919,#6514,.T.) ;
#50456 = EDGE_CURVE('',#39919,#39916,#6515,.T.) ;
#50457 = EDGE_CURVE('',#39920,#39921,#6516,.T.) ;
#50458 = EDGE_CURVE('',#39920,#39922,#401,.T.) ;
#50459 = EDGE_CURVE('',#39922,#39923,#6517,.T.) ;
#50460 = EDGE_CURVE('',#39923,#39924,#402,.T.) ;
#50461 = EDGE_CURVE('',#39924,#39925,#6518,.T.) ;
#50462 = EDGE_CURVE('',#39925,#39919,#403,.T.) ;
#50463 = EDGE_CURVE('',#39918,#39921,#404,.T.) ;
#50464 = EDGE_CURVE('',#39922,#39926,#6519,.T.) ;
#50465 = EDGE_CURVE('',#39926,#39927,#6520,.T.) ;
#50466 = EDGE_CURVE('',#39927,#39923,#6521,.T.) ;
#50467 = EDGE_CURVE('',#39928,#39929,#6522,.T.) ;
#50468 = EDGE_CURVE('',#39929,#39930,#6523,.T.) ;
#50469 = EDGE_CURVE('',#39930,#39931,#6524,.T.) ;
#50470 = EDGE_CURVE('',#39931,#39928,#6525,.T.) ;
#50471 = EDGE_CURVE('',#39932,#39933,#6526,.T.) ;
#50472 = EDGE_CURVE('',#39933,#39934,#6527,.T.) ;
#50473 = EDGE_CURVE('',#39934,#39935,#6528,.T.) ;
#50474 = EDGE_CURVE('',#39935,#39932,#6529,.T.) ;
#50475 = EDGE_CURVE('',#39936,#39937,#6530,.T.) ;
#50476 = EDGE_CURVE('',#39937,#39938,#6531,.T.) ;
#50477 = EDGE_CURVE('',#39938,#39939,#6532,.T.) ;
#50478 = EDGE_CURVE('',#39939,#39936,#6533,.T.) ;
#50479 = EDGE_CURVE('',#39940,#39941,#6534,.T.) ;
#50480 = EDGE_CURVE('',#39940,#39942,#405,.T.) ;
#50481 = EDGE_CURVE('',#39942,#39943,#6535,.T.) ;
#50482 = EDGE_CURVE('',#39943,#39944,#406,.T.) ;
#50483 = EDGE_CURVE('',#39944,#39945,#6536,.T.) ;
#50484 = EDGE_CURVE('',#39945,#39939,#407,.T.) ;
#50485 = EDGE_CURVE('',#39938,#39941,#408,.T.) ;
#50486 = EDGE_CURVE('',#39942,#39946,#6537,.T.) ;
#50487 = EDGE_CURVE('',#39946,#39947,#6538,.T.) ;
#50488 = EDGE_CURVE('',#39947,#39943,#6539,.T.) ;
#50489 = EDGE_CURVE('',#39948,#39949,#6540,.T.) ;
#50490 = EDGE_CURVE('',#39949,#39950,#6541,.T.) ;
#50491 = EDGE_CURVE('',#39950,#39951,#6542,.T.) ;
#50492 = EDGE_CURVE('',#39951,#39948,#6543,.T.) ;
#50493 = EDGE_CURVE('',#39952,#39953,#6544,.T.) ;
#50494 = EDGE_CURVE('',#39953,#39954,#6545,.T.) ;
#50495 = EDGE_CURVE('',#39954,#39955,#6546,.T.) ;
#50496 = EDGE_CURVE('',#39955,#39952,#6547,.T.) ;
#50497 = EDGE_CURVE('',#39956,#39957,#6548,.T.) ;
#50498 = EDGE_CURVE('',#39957,#39958,#6549,.T.) ;
#50499 = EDGE_CURVE('',#39958,#39959,#6550,.T.) ;
#50500 = EDGE_CURVE('',#39959,#39956,#6551,.T.) ;
#50501 = EDGE_CURVE('',#39960,#39961,#6552,.T.) ;
#50502 = EDGE_CURVE('',#39960,#39962,#409,.T.) ;
#50503 = EDGE_CURVE('',#39962,#39963,#6553,.T.) ;
#50504 = EDGE_CURVE('',#39963,#39964,#410,.T.) ;
#50505 = EDGE_CURVE('',#39964,#39965,#6554,.T.) ;
#50506 = EDGE_CURVE('',#39965,#39959,#411,.T.) ;
#50507 = EDGE_CURVE('',#39958,#39961,#412,.T.) ;
#50508 = EDGE_CURVE('',#39962,#39966,#6555,.T.) ;
#50509 = EDGE_CURVE('',#39966,#39967,#6556,.T.) ;
#50510 = EDGE_CURVE('',#39967,#39963,#6557,.T.) ;
#50511 = EDGE_CURVE('',#39968,#39969,#6558,.T.) ;
#50512 = EDGE_CURVE('',#39969,#39970,#6559,.T.) ;
#50513 = EDGE_CURVE('',#39970,#39971,#6560,.T.) ;
#50514 = EDGE_CURVE('',#39971,#39968,#6561,.T.) ;
#50515 = EDGE_CURVE('',#39972,#39973,#6562,.T.) ;
#50516 = EDGE_CURVE('',#39973,#39974,#6563,.T.) ;
#50517 = EDGE_CURVE('',#39974,#39975,#6564,.T.) ;
#50518 = EDGE_CURVE('',#39975,#39972,#6565,.T.) ;
#50519 = EDGE_CURVE('',#39976,#39977,#6566,.T.) ;
#50520 = EDGE_CURVE('',#39977,#39978,#6567,.T.) ;
#50521 = EDGE_CURVE('',#39978,#39979,#6568,.T.) ;
#50522 = EDGE_CURVE('',#39979,#39976,#6569,.T.) ;
#50523 = EDGE_CURVE('',#39980,#39981,#6570,.T.) ;
#50524 = EDGE_CURVE('',#39980,#39982,#413,.T.) ;
#50525 = EDGE_CURVE('',#39982,#39983,#6571,.T.) ;
#50526 = EDGE_CURVE('',#39983,#39984,#414,.T.) ;
#50527 = EDGE_CURVE('',#39984,#39985,#6572,.T.) ;
#50528 = EDGE_CURVE('',#39985,#39979,#415,.T.) ;
#50529 = EDGE_CURVE('',#39978,#39981,#416,.T.) ;
#50530 = EDGE_CURVE('',#39982,#39986,#6573,.T.) ;
#50531 = EDGE_CURVE('',#39986,#39987,#6574,.T.) ;
#50532 = EDGE_CURVE('',#39987,#39983,#6575,.T.) ;
#50533 = EDGE_CURVE('',#39988,#39989,#6576,.T.) ;
#50534 = EDGE_CURVE('',#39989,#39990,#6577,.T.) ;
#50535 = EDGE_CURVE('',#39990,#39991,#6578,.T.) ;
#50536 = EDGE_CURVE('',#39991,#39988,#6579,.T.) ;
#50537 = EDGE_CURVE('',#39992,#39993,#6580,.T.) ;
#50538 = EDGE_CURVE('',#39993,#39994,#6581,.T.) ;
#50539 = EDGE_CURVE('',#39994,#39995,#6582,.T.) ;
#50540 = EDGE_CURVE('',#39995,#39992,#6583,.T.) ;
#50541 = EDGE_CURVE('',#39996,#39997,#6584,.T.) ;
#50542 = EDGE_CURVE('',#39997,#39998,#6585,.T.) ;
#50543 = EDGE_CURVE('',#39998,#39999,#6586,.T.) ;
#50544 = EDGE_CURVE('',#39999,#39996,#6587,.T.) ;
#50545 = EDGE_CURVE('',#40000,#40001,#6588,.T.) ;
#50546 = EDGE_CURVE('',#40000,#40002,#417,.T.) ;
#50547 = EDGE_CURVE('',#40002,#40003,#6589,.T.) ;
#50548 = EDGE_CURVE('',#40003,#40004,#418,.T.) ;
#50549 = EDGE_CURVE('',#40004,#40005,#6590,.T.) ;
#50550 = EDGE_CURVE('',#40005,#39999,#419,.T.) ;
#50551 = EDGE_CURVE('',#39998,#40001,#420,.T.) ;
#50552 = EDGE_CURVE('',#40002,#40006,#6591,.T.) ;
#50553 = EDGE_CURVE('',#40006,#40007,#6592,.T.) ;
#50554 = EDGE_CURVE('',#40007,#40003,#6593,.T.) ;
#50555 = EDGE_CURVE('',#40008,#40009,#6594,.T.) ;
#50556 = EDGE_CURVE('',#40009,#40010,#6595,.T.) ;
#50557 = EDGE_CURVE('',#40010,#40011,#6596,.T.) ;
#50558 = EDGE_CURVE('',#40011,#40008,#6597,.T.) ;
#50559 = EDGE_CURVE('',#40012,#40013,#6598,.T.) ;
#50560 = EDGE_CURVE('',#40013,#40000,#6599,.T.) ;
#50561 = EDGE_CURVE('',#40001,#40014,#6600,.T.) ;
#50562 = EDGE_CURVE('',#40014,#40015,#6601,.T.) ;
#50563 = EDGE_CURVE('',#40015,#40012,#6602,.T.) ;
#50564 = EDGE_CURVE('',#40016,#40017,#6603,.T.) ;
#50565 = EDGE_CURVE('',#40017,#40018,#421,.T.) ;
#50566 = EDGE_CURVE('',#40018,#40019,#6604,.T.) ;
#50567 = EDGE_CURVE('',#40019,#39980,#6605,.T.) ;
#50568 = EDGE_CURVE('',#39981,#40020,#6606,.T.) ;
#50569 = EDGE_CURVE('',#40020,#40021,#6607,.T.) ;
#50570 = EDGE_CURVE('',#40021,#40016,#422,.T.) ;
#50571 = EDGE_CURVE('',#40022,#40023,#6608,.T.) ;
#50572 = EDGE_CURVE('',#40023,#40024,#423,.T.) ;
#50573 = EDGE_CURVE('',#40024,#40025,#6609,.T.) ;
#50574 = EDGE_CURVE('',#40025,#39960,#6610,.T.) ;
#50575 = EDGE_CURVE('',#39961,#40026,#6611,.T.) ;
#50576 = EDGE_CURVE('',#40026,#40027,#6612,.T.) ;
#50577 = EDGE_CURVE('',#40027,#40022,#424,.T.) ;
#50578 = EDGE_CURVE('',#40028,#40029,#6613,.T.) ;
#50579 = EDGE_CURVE('',#40029,#40030,#425,.T.) ;
#50580 = EDGE_CURVE('',#40030,#40031,#6614,.T.) ;
#50581 = EDGE_CURVE('',#40031,#39940,#6615,.T.) ;
#50582 = EDGE_CURVE('',#39941,#40032,#6616,.T.) ;
#50583 = EDGE_CURVE('',#40032,#40033,#6617,.T.) ;
#50584 = EDGE_CURVE('',#40033,#40028,#426,.T.) ;
#50585 = EDGE_CURVE('',#40034,#40035,#6618,.T.) ;
#50586 = EDGE_CURVE('',#40035,#40036,#427,.T.) ;
#50587 = EDGE_CURVE('',#40036,#40037,#6619,.T.) ;
#50588 = EDGE_CURVE('',#40037,#39920,#6620,.T.) ;
#50589 = EDGE_CURVE('',#39921,#40038,#6621,.T.) ;
#50590 = EDGE_CURVE('',#40038,#40039,#6622,.T.) ;
#50591 = EDGE_CURVE('',#40039,#40034,#428,.T.) ;
#50592 = EDGE_CURVE('',#40040,#40041,#6623,.T.) ;
#50593 = EDGE_CURVE('',#40041,#40042,#429,.T.) ;
#50594 = EDGE_CURVE('',#40042,#40043,#6624,.T.) ;
#50595 = EDGE_CURVE('',#40043,#39900,#6625,.T.) ;
#50596 = EDGE_CURVE('',#39901,#40044,#6626,.T.) ;
#50597 = EDGE_CURVE('',#40044,#40045,#6627,.T.) ;
#50598 = EDGE_CURVE('',#40045,#40040,#430,.T.) ;
#50599 = EDGE_CURVE('',#40046,#40047,#6628,.T.) ;
#50600 = EDGE_CURVE('',#40047,#40048,#431,.T.) ;
#50601 = EDGE_CURVE('',#40048,#40049,#6629,.T.) ;
#50602 = EDGE_CURVE('',#40049,#39880,#6630,.T.) ;
#50603 = EDGE_CURVE('',#39881,#40050,#6631,.T.) ;
#50604 = EDGE_CURVE('',#40050,#40051,#6632,.T.) ;
#50605 = EDGE_CURVE('',#40051,#40046,#432,.T.) ;
#50606 = EDGE_CURVE('',#40052,#40053,#6633,.T.) ;
#50607 = EDGE_CURVE('',#40053,#40054,#433,.T.) ;
#50608 = EDGE_CURVE('',#40054,#40055,#6634,.T.) ;
#50609 = EDGE_CURVE('',#40055,#39860,#6635,.T.) ;
#50610 = EDGE_CURVE('',#39861,#40056,#6636,.T.) ;
#50611 = EDGE_CURVE('',#40056,#40057,#6637,.T.) ;
#50612 = EDGE_CURVE('',#40057,#40052,#434,.T.) ;
#50613 = EDGE_CURVE('',#40058,#40059,#6638,.T.) ;
#50614 = EDGE_CURVE('',#40059,#40060,#435,.T.) ;
#50615 = EDGE_CURVE('',#40060,#40061,#6639,.T.) ;
#50616 = EDGE_CURVE('',#40061,#39840,#6640,.T.) ;
#50617 = EDGE_CURVE('',#39841,#40062,#6641,.T.) ;
#50618 = EDGE_CURVE('',#40062,#40063,#6642,.T.) ;
#50619 = EDGE_CURVE('',#40063,#40058,#436,.T.) ;
#50620 = EDGE_CURVE('',#40064,#40065,#6643,.T.) ;
#50621 = EDGE_CURVE('',#40065,#40005,#6644,.T.) ;
#50622 = EDGE_CURVE('',#40004,#40066,#6645,.T.) ;
#50623 = EDGE_CURVE('',#40066,#40067,#6646,.T.) ;
#50624 = EDGE_CURVE('',#40067,#40064,#6647,.T.) ;
#50625 = EDGE_CURVE('',#40068,#40069,#6648,.T.) ;
#50626 = EDGE_CURVE('',#40069,#40070,#437,.T.) ;
#50627 = EDGE_CURVE('',#40070,#40071,#6649,.T.) ;
#50628 = EDGE_CURVE('',#40071,#39985,#6650,.T.) ;
#50629 = EDGE_CURVE('',#39984,#40072,#6651,.T.) ;
#50630 = EDGE_CURVE('',#40072,#40073,#6652,.T.) ;
#50631 = EDGE_CURVE('',#40073,#40068,#438,.T.) ;
#50632 = EDGE_CURVE('',#40074,#40075,#6653,.T.) ;
#50633 = EDGE_CURVE('',#40075,#40076,#439,.T.) ;
#50634 = EDGE_CURVE('',#40076,#40077,#6654,.T.) ;
#50635 = EDGE_CURVE('',#40077,#39965,#6655,.T.) ;
#50636 = EDGE_CURVE('',#39964,#40078,#6656,.T.) ;
#50637 = EDGE_CURVE('',#40078,#40079,#6657,.T.) ;
#50638 = EDGE_CURVE('',#40079,#40074,#440,.T.) ;
#50639 = EDGE_CURVE('',#40080,#40081,#6658,.T.) ;
#50640 = EDGE_CURVE('',#40081,#40082,#441,.T.) ;
#50641 = EDGE_CURVE('',#40082,#40083,#6659,.T.) ;
#50642 = EDGE_CURVE('',#40083,#39945,#6660,.T.) ;
#50643 = EDGE_CURVE('',#39944,#40084,#6661,.T.) ;
#50644 = EDGE_CURVE('',#40084,#40085,#6662,.T.) ;
#50645 = EDGE_CURVE('',#40085,#40080,#442,.T.) ;
#50646 = EDGE_CURVE('',#40086,#40087,#6663,.T.) ;
#50647 = EDGE_CURVE('',#40087,#40088,#443,.T.) ;
#50648 = EDGE_CURVE('',#40088,#40089,#6664,.T.) ;
#50649 = EDGE_CURVE('',#40089,#39925,#6665,.T.) ;
#50650 = EDGE_CURVE('',#39924,#40090,#6666,.T.) ;
#50651 = EDGE_CURVE('',#40090,#40091,#6667,.T.) ;
#50652 = EDGE_CURVE('',#40091,#40086,#444,.T.) ;
#50653 = EDGE_CURVE('',#40092,#40093,#6668,.T.) ;
#50654 = EDGE_CURVE('',#40093,#40094,#445,.T.) ;
#50655 = EDGE_CURVE('',#40094,#40095,#6669,.T.) ;
#50656 = EDGE_CURVE('',#40095,#39905,#6670,.T.) ;
#50657 = EDGE_CURVE('',#39904,#40096,#6671,.T.) ;
#50658 = EDGE_CURVE('',#40096,#40097,#6672,.T.) ;
#50659 = EDGE_CURVE('',#40097,#40092,#446,.T.) ;
#50660 = EDGE_CURVE('',#40098,#40099,#6673,.T.) ;
#50661 = EDGE_CURVE('',#40099,#40100,#447,.T.) ;
#50662 = EDGE_CURVE('',#40100,#40101,#6674,.T.) ;
#50663 = EDGE_CURVE('',#40101,#39885,#6675,.T.) ;
#50664 = EDGE_CURVE('',#39884,#40102,#6676,.T.) ;
#50665 = EDGE_CURVE('',#40102,#40103,#6677,.T.) ;
#50666 = EDGE_CURVE('',#40103,#40098,#448,.T.) ;
#50667 = EDGE_CURVE('',#40104,#40105,#6678,.T.) ;
#50668 = EDGE_CURVE('',#40105,#40106,#449,.T.) ;
#50669 = EDGE_CURVE('',#40106,#40107,#6679,.T.) ;
#50670 = EDGE_CURVE('',#40107,#39865,#6680,.T.) ;
#50671 = EDGE_CURVE('',#39864,#40108,#6681,.T.) ;
#50672 = EDGE_CURVE('',#40108,#40109,#6682,.T.) ;
#50673 = EDGE_CURVE('',#40109,#40104,#450,.T.) ;
#50674 = EDGE_CURVE('',#40110,#40111,#6683,.T.) ;
#50675 = EDGE_CURVE('',#40111,#40112,#451,.T.) ;
#50676 = EDGE_CURVE('',#40112,#40113,#6684,.T.) ;
#50677 = EDGE_CURVE('',#40113,#39845,#6685,.T.) ;
#50678 = EDGE_CURVE('',#39844,#40114,#6686,.T.) ;
#50679 = EDGE_CURVE('',#40114,#40115,#6687,.T.) ;
#50680 = EDGE_CURVE('',#40115,#40110,#452,.T.) ;
#50681 = EDGE_CURVE('',#40116,#40117,#6688,.T.) ;
#50682 = EDGE_CURVE('',#40117,#40118,#6689,.T.) ;
#50683 = EDGE_CURVE('',#40118,#40119,#6690,.T.) ;
#50684 = EDGE_CURVE('',#40119,#40116,#6691,.T.) ;
#50685 = EDGE_CURVE('',#40120,#40121,#6692,.T.) ;
#50686 = EDGE_CURVE('',#40121,#40122,#6693,.T.) ;
#50687 = EDGE_CURVE('',#40122,#40123,#6694,.T.) ;
#50688 = EDGE_CURVE('',#40123,#40120,#6695,.T.) ;
#50689 = EDGE_CURVE('',#40124,#40125,#6696,.T.) ;
#50690 = EDGE_CURVE('',#40125,#40126,#6697,.T.) ;
#50691 = EDGE_CURVE('',#40126,#40127,#6698,.T.) ;
#50692 = EDGE_CURVE('',#40127,#40124,#6699,.T.) ;
#50693 = EDGE_CURVE('',#40128,#40129,#6700,.T.) ;
#50694 = EDGE_CURVE('',#40129,#40130,#6701,.T.) ;
#50695 = EDGE_CURVE('',#40130,#40131,#6702,.T.) ;
#50696 = EDGE_CURVE('',#40131,#40128,#6703,.T.) ;
#50697 = EDGE_CURVE('',#40132,#40133,#6704,.T.) ;
#50698 = EDGE_CURVE('',#40133,#40134,#6705,.T.) ;
#50699 = EDGE_CURVE('',#40134,#40135,#6706,.T.) ;
#50700 = EDGE_CURVE('',#40135,#40132,#6707,.T.) ;
#50701 = EDGE_CURVE('',#40136,#40137,#6708,.T.) ;
#50702 = EDGE_CURVE('',#40137,#40138,#6709,.T.) ;
#50703 = EDGE_CURVE('',#40138,#40139,#6710,.T.) ;
#50704 = EDGE_CURVE('',#40139,#40136,#6711,.T.) ;
#50705 = EDGE_CURVE('',#40140,#40141,#6712,.T.) ;
#50706 = EDGE_CURVE('',#40141,#40142,#6713,.T.) ;
#50707 = EDGE_CURVE('',#40142,#40143,#6714,.T.) ;
#50708 = EDGE_CURVE('',#40143,#40140,#6715,.T.) ;
#50709 = EDGE_CURVE('',#40144,#40145,#6716,.T.) ;
#50710 = EDGE_CURVE('',#40145,#40146,#6717,.T.) ;
#50711 = EDGE_CURVE('',#40146,#40147,#6718,.T.) ;
#50712 = EDGE_CURVE('',#40147,#40144,#6719,.T.) ;
#50713 = EDGE_CURVE('',#40148,#40149,#6720,.T.) ;
#50714 = EDGE_CURVE('',#40149,#40150,#6721,.T.) ;
#50715 = EDGE_CURVE('',#40150,#40151,#6722,.T.) ;
#50716 = EDGE_CURVE('',#40151,#40148,#6723,.T.) ;
#50717 = EDGE_CURVE('',#40152,#40153,#6724,.T.) ;
#50718 = EDGE_CURVE('',#40153,#40154,#6725,.T.) ;
#50719 = EDGE_CURVE('',#40154,#40155,#6726,.T.) ;
#50720 = EDGE_CURVE('',#40155,#40152,#6727,.T.) ;
#50721 = EDGE_CURVE('',#40156,#40157,#6728,.T.) ;
#50722 = EDGE_CURVE('',#40157,#40158,#6729,.T.) ;
#50723 = EDGE_CURVE('',#40158,#40159,#6730,.T.) ;
#50724 = EDGE_CURVE('',#40159,#40156,#6731,.T.) ;
#50725 = EDGE_CURVE('',#40160,#40161,#6732,.T.) ;
#50726 = EDGE_CURVE('',#40161,#40162,#6733,.T.) ;
#50727 = EDGE_CURVE('',#40162,#40163,#6734,.T.) ;
#50728 = EDGE_CURVE('',#40163,#40160,#6735,.T.) ;
#50729 = EDGE_CURVE('',#40164,#40165,#6736,.T.) ;
#50730 = EDGE_CURVE('',#40165,#40166,#6737,.T.) ;
#50731 = EDGE_CURVE('',#40166,#40167,#6738,.T.) ;
#50732 = EDGE_CURVE('',#40167,#40164,#6739,.T.) ;
#50733 = EDGE_CURVE('',#40168,#40169,#6740,.T.) ;
#50734 = EDGE_CURVE('',#40169,#40170,#6741,.T.) ;
#50735 = EDGE_CURVE('',#40170,#40171,#6742,.T.) ;
#50736 = EDGE_CURVE('',#40171,#40168,#6743,.T.) ;
#50737 = EDGE_CURVE('',#40172,#40173,#6744,.T.) ;
#50738 = EDGE_CURVE('',#40173,#40174,#6745,.T.) ;
#50739 = EDGE_CURVE('',#40174,#40175,#6746,.T.) ;
#50740 = EDGE_CURVE('',#40175,#40172,#6747,.T.) ;
#50741 = EDGE_CURVE('',#40176,#40177,#6748,.T.) ;
#50742 = EDGE_CURVE('',#40177,#40178,#6749,.T.) ;
#50743 = EDGE_CURVE('',#40178,#40179,#6750,.T.) ;
#50744 = EDGE_CURVE('',#40179,#40176,#6751,.T.) ;
#50745 = EDGE_CURVE('',#40180,#40181,#6752,.T.) ;
#50746 = EDGE_CURVE('',#40181,#40182,#6753,.T.) ;
#50747 = EDGE_CURVE('',#40182,#40183,#6754,.T.) ;
#50748 = EDGE_CURVE('',#40183,#40180,#6755,.T.) ;
#50749 = EDGE_CURVE('',#40184,#40185,#6756,.T.) ;
#50750 = EDGE_CURVE('',#40185,#40186,#6757,.T.) ;
#50751 = EDGE_CURVE('',#40186,#40187,#6758,.T.) ;
#50752 = EDGE_CURVE('',#40187,#40184,#6759,.T.) ;
#50753 = EDGE_CURVE('',#40188,#40189,#6760,.T.) ;
#50754 = EDGE_CURVE('',#40189,#40190,#6761,.T.) ;
#50755 = EDGE_CURVE('',#40190,#40191,#6762,.T.) ;
#50756 = EDGE_CURVE('',#40191,#40188,#6763,.T.) ;
#50757 = EDGE_CURVE('',#40192,#40193,#6764,.T.) ;
#50758 = EDGE_CURVE('',#40193,#40194,#6765,.T.) ;
#50759 = EDGE_CURVE('',#40194,#40195,#6766,.T.) ;
#50760 = EDGE_CURVE('',#40195,#40192,#6767,.T.) ;
#50761 = EDGE_CURVE('',#40196,#40197,#6768,.T.) ;
#50762 = EDGE_CURVE('',#40197,#40198,#6769,.T.) ;
#50763 = EDGE_CURVE('',#40198,#40199,#6770,.T.) ;
#50764 = EDGE_CURVE('',#40199,#40196,#6771,.T.) ;
#50765 = EDGE_CURVE('',#40200,#40201,#6772,.T.) ;
#50766 = EDGE_CURVE('',#40201,#40202,#6773,.T.) ;
#50767 = EDGE_CURVE('',#40202,#40203,#6774,.T.) ;
#50768 = EDGE_CURVE('',#40203,#40200,#6775,.T.) ;
#50769 = EDGE_CURVE('',#40204,#40205,#6776,.T.) ;
#50770 = EDGE_CURVE('',#40205,#40206,#6777,.T.) ;
#50771 = EDGE_CURVE('',#40206,#40207,#6778,.T.) ;
#50772 = EDGE_CURVE('',#40207,#40204,#6779,.T.) ;
#50773 = EDGE_CURVE('',#40208,#40209,#6780,.T.) ;
#50774 = EDGE_CURVE('',#40209,#40210,#6781,.T.) ;
#50775 = EDGE_CURVE('',#40210,#40211,#6782,.T.) ;
#50776 = EDGE_CURVE('',#40211,#40208,#6783,.T.) ;
#50777 = EDGE_CURVE('',#40212,#40213,#6784,.T.) ;
#50778 = EDGE_CURVE('',#40213,#40214,#6785,.T.) ;
#50779 = EDGE_CURVE('',#40214,#40215,#6786,.T.) ;
#50780 = EDGE_CURVE('',#40215,#40212,#6787,.T.) ;
#50781 = EDGE_CURVE('',#40216,#40217,#6788,.T.) ;
#50782 = EDGE_CURVE('',#40217,#40218,#6789,.T.) ;
#50783 = EDGE_CURVE('',#40218,#40219,#6790,.T.) ;
#50784 = EDGE_CURVE('',#40219,#40216,#6791,.T.) ;
#50785 = EDGE_CURVE('',#40220,#40221,#6792,.T.) ;
#50786 = EDGE_CURVE('',#40221,#40222,#6793,.T.) ;
#50787 = EDGE_CURVE('',#40222,#40223,#6794,.T.) ;
#50788 = EDGE_CURVE('',#40223,#40220,#6795,.T.) ;
#50789 = EDGE_CURVE('',#40224,#40225,#6796,.T.) ;
#50790 = EDGE_CURVE('',#40225,#40226,#6797,.T.) ;
#50791 = EDGE_CURVE('',#40226,#40227,#6798,.T.) ;
#50792 = EDGE_CURVE('',#40227,#40224,#6799,.T.) ;
#50793 = EDGE_CURVE('',#40228,#40229,#6800,.T.) ;
#50794 = EDGE_CURVE('',#40229,#40230,#6801,.T.) ;
#50795 = EDGE_CURVE('',#40230,#40231,#6802,.T.) ;
#50796 = EDGE_CURVE('',#40231,#40228,#6803,.T.) ;
#50797 = EDGE_CURVE('',#40232,#40233,#6804,.T.) ;
#50798 = EDGE_CURVE('',#40233,#40234,#6805,.T.) ;
#50799 = EDGE_CURVE('',#40234,#40235,#6806,.T.) ;
#50800 = EDGE_CURVE('',#40235,#40232,#6807,.T.) ;
#50801 = EDGE_CURVE('',#40236,#40237,#6808,.T.) ;
#50802 = EDGE_CURVE('',#40237,#40238,#6809,.T.) ;
#50803 = EDGE_CURVE('',#40238,#40239,#6810,.T.) ;
#50804 = EDGE_CURVE('',#40239,#40236,#6811,.T.) ;
#50805 = EDGE_CURVE('',#40240,#40241,#6812,.T.) ;
#50806 = EDGE_CURVE('',#40241,#40242,#6813,.T.) ;
#50807 = EDGE_CURVE('',#40242,#40243,#6814,.T.) ;
#50808 = EDGE_CURVE('',#40243,#40240,#6815,.T.) ;
#50809 = EDGE_CURVE('',#40244,#40245,#6816,.T.) ;
#50810 = EDGE_CURVE('',#40245,#40246,#6817,.T.) ;
#50811 = EDGE_CURVE('',#40246,#40247,#6818,.T.) ;
#50812 = EDGE_CURVE('',#40247,#40244,#6819,.T.) ;
#50813 = EDGE_CURVE('',#40248,#40249,#6820,.T.) ;
#50814 = EDGE_CURVE('',#40249,#40250,#6821,.T.) ;
#50815 = EDGE_CURVE('',#40250,#40251,#6822,.T.) ;
#50816 = EDGE_CURVE('',#40251,#40248,#6823,.T.) ;
#50817 = EDGE_CURVE('',#40252,#40253,#6824,.T.) ;
#50818 = EDGE_CURVE('',#40253,#40254,#6825,.T.) ;
#50819 = EDGE_CURVE('',#40254,#40255,#6826,.T.) ;
#50820 = EDGE_CURVE('',#40255,#40252,#6827,.T.) ;
#50821 = EDGE_CURVE('',#40256,#40257,#6828,.T.) ;
#50822 = EDGE_CURVE('',#40257,#40258,#6829,.T.) ;
#50823 = EDGE_CURVE('',#40258,#40259,#6830,.T.) ;
#50824 = EDGE_CURVE('',#40259,#40256,#6831,.T.) ;
#50825 = EDGE_CURVE('',#40260,#40261,#6832,.T.) ;
#50826 = EDGE_CURVE('',#40261,#40262,#6833,.T.) ;
#50827 = EDGE_CURVE('',#40262,#40263,#6834,.T.) ;
#50828 = EDGE_CURVE('',#40263,#40260,#6835,.T.) ;
#50829 = EDGE_CURVE('',#40264,#40265,#6836,.T.) ;
#50830 = EDGE_CURVE('',#40264,#40266,#32958,.T.) ;
#50831 = EDGE_CURVE('',#40267,#40266,#6837,.T.) ;
#50832 = EDGE_CURVE('',#40267,#40268,#32959,.T.) ;
#50833 = EDGE_CURVE('',#40269,#40268,#6838,.T.) ;
#50834 = EDGE_CURVE('',#40269,#40270,#32960,.T.) ;
#50835 = EDGE_CURVE('',#40271,#40270,#6839,.T.) ;
#50836 = EDGE_CURVE('',#40271,#40265,#32961,.T.) ;
#50837 = EDGE_CURVE('',#40270,#40272,#6840,.T.) ;
#50838 = EDGE_CURVE('',#40272,#40273,#6841,.T.) ;
#50839 = EDGE_CURVE('',#40273,#40271,#6842,.T.) ;
#50840 = EDGE_CURVE('',#40265,#40274,#6843,.T.) ;
#50841 = EDGE_CURVE('',#40274,#40275,#6844,.T.) ;
#50842 = EDGE_CURVE('',#40275,#40264,#6845,.T.) ;
#50843 = EDGE_CURVE('',#40276,#40277,#6846,.T.) ;
#50844 = EDGE_CURVE('',#40277,#40267,#6847,.T.) ;
#50845 = EDGE_CURVE('',#40266,#40276,#6848,.T.) ;
#50846 = EDGE_CURVE('',#40268,#40278,#6849,.T.) ;
#50847 = EDGE_CURVE('',#40278,#40279,#6850,.T.) ;
#50848 = EDGE_CURVE('',#40279,#40269,#6851,.T.) ;
#50849 = EDGE_CURVE('',#40280,#40281,#6852,.T.) ;
#50850 = EDGE_CURVE('',#40281,#40282,#6853,.T.) ;
#50851 = EDGE_CURVE('',#40282,#40283,#6854,.T.) ;
#50852 = EDGE_CURVE('',#40283,#40280,#6855,.T.) ;
#50853 = EDGE_CURVE('',#40284,#40285,#6856,.T.) ;
#50854 = EDGE_CURVE('',#40284,#40286,#32962,.T.) ;
#50855 = EDGE_CURVE('',#40287,#40286,#6857,.T.) ;
#50856 = EDGE_CURVE('',#40287,#40288,#32963,.T.) ;
#50857 = EDGE_CURVE('',#40289,#40288,#6858,.T.) ;
#50858 = EDGE_CURVE('',#40289,#40290,#32964,.T.) ;
#50859 = EDGE_CURVE('',#40291,#40290,#6859,.T.) ;
#50860 = EDGE_CURVE('',#40291,#40285,#32965,.T.) ;
#50861 = EDGE_CURVE('',#40290,#40292,#6860,.T.) ;
#50862 = EDGE_CURVE('',#40292,#40293,#6861,.T.) ;
#50863 = EDGE_CURVE('',#40293,#40291,#6862,.T.) ;
#50864 = EDGE_CURVE('',#40285,#40294,#6863,.T.) ;
#50865 = EDGE_CURVE('',#40294,#40295,#6864,.T.) ;
#50866 = EDGE_CURVE('',#40295,#40284,#6865,.T.) ;
#50867 = EDGE_CURVE('',#40296,#40297,#6866,.T.) ;
#50868 = EDGE_CURVE('',#40297,#40287,#6867,.T.) ;
#50869 = EDGE_CURVE('',#40286,#40296,#6868,.T.) ;
#50870 = EDGE_CURVE('',#40288,#40298,#6869,.T.) ;
#50871 = EDGE_CURVE('',#40298,#40299,#6870,.T.) ;
#50872 = EDGE_CURVE('',#40299,#40289,#6871,.T.) ;
#50873 = EDGE_CURVE('',#40300,#40301,#6872,.T.) ;
#50874 = EDGE_CURVE('',#40301,#40302,#6873,.T.) ;
#50875 = EDGE_CURVE('',#40302,#40303,#6874,.T.) ;
#50876 = EDGE_CURVE('',#40303,#40300,#6875,.T.) ;
#50877 = EDGE_CURVE('',#40304,#40305,#6876,.T.) ;
#50878 = EDGE_CURVE('',#40304,#40306,#32966,.T.) ;
#50879 = EDGE_CURVE('',#40307,#40306,#6877,.T.) ;
#50880 = EDGE_CURVE('',#40307,#40308,#32967,.T.) ;
#50881 = EDGE_CURVE('',#40309,#40308,#6878,.T.) ;
#50882 = EDGE_CURVE('',#40309,#40310,#32968,.T.) ;
#50883 = EDGE_CURVE('',#40311,#40310,#6879,.T.) ;
#50884 = EDGE_CURVE('',#40311,#40305,#32969,.T.) ;
#50885 = EDGE_CURVE('',#40310,#40312,#6880,.T.) ;
#50886 = EDGE_CURVE('',#40312,#40313,#6881,.T.) ;
#50887 = EDGE_CURVE('',#40313,#40311,#6882,.T.) ;
#50888 = EDGE_CURVE('',#40305,#40314,#6883,.T.) ;
#50889 = EDGE_CURVE('',#40314,#40315,#6884,.T.) ;
#50890 = EDGE_CURVE('',#40315,#40304,#6885,.T.) ;
#50891 = EDGE_CURVE('',#40316,#40317,#6886,.T.) ;
#50892 = EDGE_CURVE('',#40317,#40307,#6887,.T.) ;
#50893 = EDGE_CURVE('',#40306,#40316,#6888,.T.) ;
#50894 = EDGE_CURVE('',#40308,#40318,#6889,.T.) ;
#50895 = EDGE_CURVE('',#40318,#40319,#6890,.T.) ;
#50896 = EDGE_CURVE('',#40319,#40309,#6891,.T.) ;
#50897 = EDGE_CURVE('',#40320,#40321,#6892,.T.) ;
#50898 = EDGE_CURVE('',#40321,#40322,#6893,.T.) ;
#50899 = EDGE_CURVE('',#40322,#40323,#6894,.T.) ;
#50900 = EDGE_CURVE('',#40323,#40320,#6895,.T.) ;
#50901 = EDGE_CURVE('',#40324,#40325,#6896,.T.) ;
#50902 = EDGE_CURVE('',#40324,#40326,#32970,.T.) ;
#50903 = EDGE_CURVE('',#40327,#40326,#6897,.T.) ;
#50904 = EDGE_CURVE('',#40327,#40328,#32971,.T.) ;
#50905 = EDGE_CURVE('',#40329,#40328,#6898,.T.) ;
#50906 = EDGE_CURVE('',#40329,#40330,#32972,.T.) ;
#50907 = EDGE_CURVE('',#40331,#40330,#6899,.T.) ;
#50908 = EDGE_CURVE('',#40331,#40325,#32973,.T.) ;
#50909 = EDGE_CURVE('',#40330,#40332,#6900,.T.) ;
#50910 = EDGE_CURVE('',#40332,#40333,#6901,.T.) ;
#50911 = EDGE_CURVE('',#40333,#40331,#6902,.T.) ;
#50912 = EDGE_CURVE('',#40325,#40334,#6903,.T.) ;
#50913 = EDGE_CURVE('',#40334,#40335,#6904,.T.) ;
#50914 = EDGE_CURVE('',#40335,#40324,#6905,.T.) ;
#50915 = EDGE_CURVE('',#40336,#40337,#6906,.T.) ;
#50916 = EDGE_CURVE('',#40337,#40327,#6907,.T.) ;
#50917 = EDGE_CURVE('',#40326,#40336,#6908,.T.) ;
#50918 = EDGE_CURVE('',#40328,#40338,#6909,.T.) ;
#50919 = EDGE_CURVE('',#40338,#40339,#6910,.T.) ;
#50920 = EDGE_CURVE('',#40339,#40329,#6911,.T.) ;
#50921 = EDGE_CURVE('',#40340,#40341,#6912,.T.) ;
#50922 = EDGE_CURVE('',#40341,#40342,#6913,.T.) ;
#50923 = EDGE_CURVE('',#40342,#40343,#6914,.T.) ;
#50924 = EDGE_CURVE('',#40343,#40340,#6915,.T.) ;
#50925 = EDGE_CURVE('',#40344,#40345,#6916,.T.) ;
#50926 = EDGE_CURVE('',#40344,#40346,#32974,.T.) ;
#50927 = EDGE_CURVE('',#40347,#40346,#6917,.T.) ;
#50928 = EDGE_CURVE('',#40347,#40348,#32975,.T.) ;
#50929 = EDGE_CURVE('',#40349,#40348,#6918,.T.) ;
#50930 = EDGE_CURVE('',#40349,#40350,#32976,.T.) ;
#50931 = EDGE_CURVE('',#40351,#40350,#6919,.T.) ;
#50932 = EDGE_CURVE('',#40351,#40345,#32977,.T.) ;
#50933 = EDGE_CURVE('',#40350,#40352,#6920,.T.) ;
#50934 = EDGE_CURVE('',#40352,#40353,#6921,.T.) ;
#50935 = EDGE_CURVE('',#40353,#40351,#6922,.T.) ;
#50936 = EDGE_CURVE('',#40345,#40354,#6923,.T.) ;
#50937 = EDGE_CURVE('',#40354,#40355,#6924,.T.) ;
#50938 = EDGE_CURVE('',#40355,#40344,#6925,.T.) ;
#50939 = EDGE_CURVE('',#40356,#40357,#6926,.T.) ;
#50940 = EDGE_CURVE('',#40357,#40347,#6927,.T.) ;
#50941 = EDGE_CURVE('',#40346,#40356,#6928,.T.) ;
#50942 = EDGE_CURVE('',#40348,#40358,#6929,.T.) ;
#50943 = EDGE_CURVE('',#40358,#40359,#6930,.T.) ;
#50944 = EDGE_CURVE('',#40359,#40349,#6931,.T.) ;
#50945 = EDGE_CURVE('',#40360,#40361,#6932,.T.) ;
#50946 = EDGE_CURVE('',#40361,#40362,#6933,.T.) ;
#50947 = EDGE_CURVE('',#40362,#40363,#6934,.T.) ;
#50948 = EDGE_CURVE('',#40363,#40360,#6935,.T.) ;
#50949 = EDGE_CURVE('',#40364,#40365,#6936,.T.) ;
#50950 = EDGE_CURVE('',#40364,#40366,#32978,.T.) ;
#50951 = EDGE_CURVE('',#40367,#40366,#6937,.T.) ;
#50952 = EDGE_CURVE('',#40367,#40368,#32979,.T.) ;
#50953 = EDGE_CURVE('',#40369,#40368,#6938,.T.) ;
#50954 = EDGE_CURVE('',#40369,#40370,#32980,.T.) ;
#50955 = EDGE_CURVE('',#40371,#40370,#6939,.T.) ;
#50956 = EDGE_CURVE('',#40371,#40365,#32981,.T.) ;
#50957 = EDGE_CURVE('',#40370,#40372,#6940,.T.) ;
#50958 = EDGE_CURVE('',#40372,#40373,#6941,.T.) ;
#50959 = EDGE_CURVE('',#40373,#40371,#6942,.T.) ;
#50960 = EDGE_CURVE('',#40365,#40374,#6943,.T.) ;
#50961 = EDGE_CURVE('',#40374,#40375,#6944,.T.) ;
#50962 = EDGE_CURVE('',#40375,#40364,#6945,.T.) ;
#50963 = EDGE_CURVE('',#40376,#40377,#6946,.T.) ;
#50964 = EDGE_CURVE('',#40377,#40367,#6947,.T.) ;
#50965 = EDGE_CURVE('',#40366,#40376,#6948,.T.) ;
#50966 = EDGE_CURVE('',#40368,#40378,#6949,.T.) ;
#50967 = EDGE_CURVE('',#40378,#40379,#6950,.T.) ;
#50968 = EDGE_CURVE('',#40379,#40369,#6951,.T.) ;
#50969 = EDGE_CURVE('',#40380,#40381,#6952,.T.) ;
#50970 = EDGE_CURVE('',#40381,#40382,#6953,.T.) ;
#50971 = EDGE_CURVE('',#40382,#40383,#6954,.T.) ;
#50972 = EDGE_CURVE('',#40383,#40380,#6955,.T.) ;
#50973 = EDGE_CURVE('',#40384,#40385,#6956,.T.) ;
#50974 = EDGE_CURVE('',#40384,#40386,#32982,.T.) ;
#50975 = EDGE_CURVE('',#40387,#40386,#6957,.T.) ;
#50976 = EDGE_CURVE('',#40387,#40388,#32983,.T.) ;
#50977 = EDGE_CURVE('',#40389,#40388,#6958,.T.) ;
#50978 = EDGE_CURVE('',#40389,#40390,#32984,.T.) ;
#50979 = EDGE_CURVE('',#40391,#40390,#6959,.T.) ;
#50980 = EDGE_CURVE('',#40391,#40385,#32985,.T.) ;
#50981 = EDGE_CURVE('',#40390,#40392,#6960,.T.) ;
#50982 = EDGE_CURVE('',#40392,#40393,#6961,.T.) ;
#50983 = EDGE_CURVE('',#40393,#40391,#6962,.T.) ;
#50984 = EDGE_CURVE('',#40385,#40394,#6963,.T.) ;
#50985 = EDGE_CURVE('',#40394,#40395,#6964,.T.) ;
#50986 = EDGE_CURVE('',#40395,#40384,#6965,.T.) ;
#50987 = EDGE_CURVE('',#40396,#40397,#6966,.T.) ;
#50988 = EDGE_CURVE('',#40397,#40387,#6967,.T.) ;
#50989 = EDGE_CURVE('',#40386,#40396,#6968,.T.) ;
#50990 = EDGE_CURVE('',#40388,#40398,#6969,.T.) ;
#50991 = EDGE_CURVE('',#40398,#40399,#6970,.T.) ;
#50992 = EDGE_CURVE('',#40399,#40389,#6971,.T.) ;
#50993 = EDGE_CURVE('',#40400,#40401,#6972,.T.) ;
#50994 = EDGE_CURVE('',#40401,#40402,#6973,.T.) ;
#50995 = EDGE_CURVE('',#40402,#40403,#6974,.T.) ;
#50996 = EDGE_CURVE('',#40403,#40400,#6975,.T.) ;
#50997 = EDGE_CURVE('',#40404,#40405,#6976,.T.) ;
#50998 = EDGE_CURVE('',#40404,#40406,#32986,.T.) ;
#50999 = EDGE_CURVE('',#40407,#40406,#6977,.T.) ;
#51000 = EDGE_CURVE('',#40407,#40408,#32987,.T.) ;
#51001 = EDGE_CURVE('',#40409,#40408,#6978,.T.) ;
#51002 = EDGE_CURVE('',#40409,#40410,#32988,.T.) ;
#51003 = EDGE_CURVE('',#40411,#40410,#6979,.T.) ;
#51004 = EDGE_CURVE('',#40411,#40405,#32989,.T.) ;
#51005 = EDGE_CURVE('',#40410,#40412,#6980,.T.) ;
#51006 = EDGE_CURVE('',#40412,#40413,#6981,.T.) ;
#51007 = EDGE_CURVE('',#40413,#40411,#6982,.T.) ;
#51008 = EDGE_CURVE('',#40405,#40414,#6983,.T.) ;
#51009 = EDGE_CURVE('',#40414,#40415,#6984,.T.) ;
#51010 = EDGE_CURVE('',#40415,#40404,#6985,.T.) ;
#51011 = EDGE_CURVE('',#40416,#40417,#6986,.T.) ;
#51012 = EDGE_CURVE('',#40417,#40407,#6987,.T.) ;
#51013 = EDGE_CURVE('',#40406,#40416,#6988,.T.) ;
#51014 = EDGE_CURVE('',#40408,#40418,#6989,.T.) ;
#51015 = EDGE_CURVE('',#40418,#40419,#6990,.T.) ;
#51016 = EDGE_CURVE('',#40419,#40409,#6991,.T.) ;
#51017 = EDGE_CURVE('',#40420,#40421,#6992,.T.) ;
#51018 = EDGE_CURVE('',#40421,#40422,#6993,.T.) ;
#51019 = EDGE_CURVE('',#40422,#40423,#6994,.T.) ;
#51020 = EDGE_CURVE('',#40423,#40420,#6995,.T.) ;
#51021 = EDGE_CURVE('',#40424,#40425,#6996,.T.) ;
#51022 = EDGE_CURVE('',#40424,#40426,#32990,.T.) ;
#51023 = EDGE_CURVE('',#40427,#40426,#6997,.T.) ;
#51024 = EDGE_CURVE('',#40427,#40428,#32991,.T.) ;
#51025 = EDGE_CURVE('',#40429,#40428,#6998,.T.) ;
#51026 = EDGE_CURVE('',#40429,#40430,#32992,.T.) ;
#51027 = EDGE_CURVE('',#40431,#40430,#6999,.T.) ;
#51028 = EDGE_CURVE('',#40431,#40425,#32993,.T.) ;
#51029 = EDGE_CURVE('',#40430,#40432,#7000,.T.) ;
#51030 = EDGE_CURVE('',#40432,#40433,#7001,.T.) ;
#51031 = EDGE_CURVE('',#40433,#40431,#7002,.T.) ;
#51032 = EDGE_CURVE('',#40425,#40434,#7003,.T.) ;
#51033 = EDGE_CURVE('',#40434,#40435,#7004,.T.) ;
#51034 = EDGE_CURVE('',#40435,#40424,#7005,.T.) ;
#51035 = EDGE_CURVE('',#40436,#40437,#7006,.T.) ;
#51036 = EDGE_CURVE('',#40437,#40427,#7007,.T.) ;
#51037 = EDGE_CURVE('',#40426,#40436,#7008,.T.) ;
#51038 = EDGE_CURVE('',#40428,#40438,#7009,.T.) ;
#51039 = EDGE_CURVE('',#40438,#40439,#7010,.T.) ;
#51040 = EDGE_CURVE('',#40439,#40429,#7011,.T.) ;
#51041 = EDGE_CURVE('',#40440,#40441,#7012,.T.) ;
#51042 = EDGE_CURVE('',#40441,#40442,#7013,.T.) ;
#51043 = EDGE_CURVE('',#40442,#40443,#7014,.T.) ;
#51044 = EDGE_CURVE('',#40443,#40440,#7015,.T.) ;
#51045 = EDGE_CURVE('',#40444,#40445,#7016,.T.) ;
#51046 = EDGE_CURVE('',#40445,#40446,#7017,.T.) ;
#51047 = EDGE_CURVE('',#40446,#40447,#7018,.T.) ;
#51048 = EDGE_CURVE('',#40447,#40444,#7019,.T.) ;
#51049 = EDGE_CURVE('',#40448,#40449,#7020,.T.) ;
#51050 = EDGE_CURVE('',#40449,#40450,#7021,.T.) ;
#51051 = EDGE_CURVE('',#40450,#40451,#7022,.T.) ;
#51052 = EDGE_CURVE('',#40451,#40448,#7023,.T.) ;
#51053 = EDGE_CURVE('',#40452,#40453,#7024,.T.) ;
#51054 = EDGE_CURVE('',#40453,#40454,#7025,.T.) ;
#51055 = EDGE_CURVE('',#40454,#40455,#7026,.T.) ;
#51056 = EDGE_CURVE('',#40455,#40452,#7027,.T.) ;
#51057 = EDGE_CURVE('',#40456,#40457,#7028,.T.) ;
#51058 = EDGE_CURVE('',#40457,#40458,#7029,.T.) ;
#51059 = EDGE_CURVE('',#40458,#40459,#7030,.T.) ;
#51060 = EDGE_CURVE('',#40459,#40456,#7031,.T.) ;
#51061 = EDGE_CURVE('',#40460,#40461,#7032,.T.) ;
#51062 = EDGE_CURVE('',#40461,#40462,#7033,.T.) ;
#51063 = EDGE_CURVE('',#40462,#40463,#7034,.T.) ;
#51064 = EDGE_CURVE('',#40463,#40460,#7035,.T.) ;
#51065 = EDGE_CURVE('',#40464,#40465,#7036,.T.) ;
#51066 = EDGE_CURVE('',#40465,#40466,#7037,.T.) ;
#51067 = EDGE_CURVE('',#40466,#40467,#7038,.T.) ;
#51068 = EDGE_CURVE('',#40467,#40464,#7039,.T.) ;
#51069 = EDGE_CURVE('',#40468,#40469,#7040,.T.) ;
#51070 = EDGE_CURVE('',#40469,#40470,#7041,.T.) ;
#51071 = EDGE_CURVE('',#40470,#40471,#7042,.T.) ;
#51072 = EDGE_CURVE('',#40471,#40468,#7043,.T.) ;
#51073 = EDGE_CURVE('',#40472,#40473,#7044,.T.) ;
#51074 = EDGE_CURVE('',#40473,#40474,#7045,.T.) ;
#51075 = EDGE_CURVE('',#40474,#40475,#7046,.T.) ;
#51076 = EDGE_CURVE('',#40475,#40472,#7047,.T.) ;
#51077 = EDGE_CURVE('',#40476,#40477,#32994,.T.) ;
#51078 = EDGE_CURVE('',#40477,#40478,#32995,.T.) ;
#51079 = EDGE_CURVE('',#40478,#40479,#7048,.T.) ;
#51080 = EDGE_CURVE('',#40479,#40480,#7049,.T.) ;
#51081 = EDGE_CURVE('',#40480,#40481,#7050,.T.) ;
#51082 = EDGE_CURVE('',#40481,#40482,#7051,.T.) ;
#51083 = EDGE_CURVE('',#40483,#40482,#32996,.T.) ;
#51084 = EDGE_CURVE('',#40483,#40484,#7052,.T.) ;
#51085 = EDGE_CURVE('',#40484,#40485,#7053,.T.) ;
#51086 = EDGE_CURVE('',#40485,#40476,#7054,.T.) ;
#51087 = EDGE_CURVE('',#40486,#40487,#7055,.T.) ;
#51088 = EDGE_CURVE('',#40487,#40488,#7056,.T.) ;
#51089 = EDGE_CURVE('',#40488,#40489,#7057,.T.) ;
#51090 = EDGE_CURVE('',#40489,#40486,#7058,.T.) ;
#51091 = EDGE_CURVE('',#40490,#40491,#7059,.T.) ;
#51092 = EDGE_CURVE('',#40491,#40492,#32997,.T.) ;
#51093 = EDGE_CURVE('',#40492,#40493,#32998,.T.) ;
#51094 = EDGE_CURVE('',#40493,#40494,#7060,.T.) ;
#51095 = EDGE_CURVE('',#40494,#40495,#7061,.T.) ;
#51096 = EDGE_CURVE('',#40495,#40496,#7062,.T.) ;
#51097 = EDGE_CURVE('',#40497,#40496,#32999,.T.) ;
#51098 = EDGE_CURVE('',#40497,#40498,#7063,.T.) ;
#51099 = EDGE_CURVE('',#40498,#40499,#7064,.T.) ;
#51100 = EDGE_CURVE('',#40499,#40490,#7065,.T.) ;
#51101 = EDGE_CURVE('',#40500,#40501,#7066,.T.) ;
#51102 = EDGE_CURVE('',#40501,#40502,#7067,.T.) ;
#51103 = EDGE_CURVE('',#40502,#40503,#7068,.T.) ;
#51104 = EDGE_CURVE('',#40503,#40500,#7069,.T.) ;
#51105 = EDGE_CURVE('',#40504,#40505,#33000,.T.) ;
#51106 = EDGE_CURVE('',#40505,#40506,#33001,.T.) ;
#51107 = EDGE_CURVE('',#40506,#40507,#7070,.T.) ;
#51108 = EDGE_CURVE('',#40507,#40508,#7071,.T.) ;
#51109 = EDGE_CURVE('',#40508,#40509,#7072,.T.) ;
#51110 = EDGE_CURVE('',#40509,#40510,#7073,.T.) ;
#51111 = EDGE_CURVE('',#40511,#40510,#33002,.T.) ;
#51112 = EDGE_CURVE('',#40511,#40512,#7074,.T.) ;
#51113 = EDGE_CURVE('',#40512,#40513,#7075,.T.) ;
#51114 = EDGE_CURVE('',#40513,#40504,#7076,.T.) ;
#51115 = EDGE_CURVE('',#40514,#40515,#7077,.T.) ;
#51116 = EDGE_CURVE('',#40515,#40516,#7078,.T.) ;
#51117 = EDGE_CURVE('',#40516,#40517,#7079,.T.) ;
#51118 = EDGE_CURVE('',#40517,#40514,#7080,.T.) ;
#51119 = EDGE_CURVE('',#40518,#40519,#7081,.T.) ;
#51120 = EDGE_CURVE('',#40519,#40520,#33003,.T.) ;
#51121 = EDGE_CURVE('',#40520,#40521,#33004,.T.) ;
#51122 = EDGE_CURVE('',#40521,#40522,#7082,.T.) ;
#51123 = EDGE_CURVE('',#40522,#40523,#7083,.T.) ;
#51124 = EDGE_CURVE('',#40523,#40524,#7084,.T.) ;
#51125 = EDGE_CURVE('',#40525,#40524,#33005,.T.) ;
#51126 = EDGE_CURVE('',#40525,#40526,#7085,.T.) ;
#51127 = EDGE_CURVE('',#40526,#40527,#7086,.T.) ;
#51128 = EDGE_CURVE('',#40527,#40518,#7087,.T.) ;
#51129 = EDGE_CURVE('',#40528,#40529,#7088,.T.) ;
#51130 = EDGE_CURVE('',#40529,#40530,#7089,.T.) ;
#51131 = EDGE_CURVE('',#40530,#40531,#7090,.T.) ;
#51132 = EDGE_CURVE('',#40531,#40528,#7091,.T.) ;
#51133 = EDGE_CURVE('',#40532,#40533,#33006,.T.) ;
#51134 = EDGE_CURVE('',#40533,#40534,#33007,.T.) ;
#51135 = EDGE_CURVE('',#40534,#40535,#7092,.T.) ;
#51136 = EDGE_CURVE('',#40535,#40536,#7093,.T.) ;
#51137 = EDGE_CURVE('',#40536,#40537,#7094,.T.) ;
#51138 = EDGE_CURVE('',#40537,#40538,#7095,.T.) ;
#51139 = EDGE_CURVE('',#40539,#40538,#33008,.T.) ;
#51140 = EDGE_CURVE('',#40539,#40540,#7096,.T.) ;
#51141 = EDGE_CURVE('',#40540,#40541,#7097,.T.) ;
#51142 = EDGE_CURVE('',#40541,#40532,#7098,.T.) ;
#51143 = EDGE_CURVE('',#40542,#40543,#7099,.T.) ;
#51144 = EDGE_CURVE('',#40543,#40544,#7100,.T.) ;
#51145 = EDGE_CURVE('',#40544,#40545,#7101,.T.) ;
#51146 = EDGE_CURVE('',#40545,#40542,#7102,.T.) ;
#51147 = EDGE_CURVE('',#40546,#40547,#7103,.T.) ;
#51148 = EDGE_CURVE('',#40547,#40548,#33009,.T.) ;
#51149 = EDGE_CURVE('',#40548,#40549,#33010,.T.) ;
#51150 = EDGE_CURVE('',#40549,#40550,#7104,.T.) ;
#51151 = EDGE_CURVE('',#40550,#40551,#7105,.T.) ;
#51152 = EDGE_CURVE('',#40551,#40552,#7106,.T.) ;
#51153 = EDGE_CURVE('',#40553,#40552,#33011,.T.) ;
#51154 = EDGE_CURVE('',#40553,#40554,#7107,.T.) ;
#51155 = EDGE_CURVE('',#40554,#40555,#7108,.T.) ;
#51156 = EDGE_CURVE('',#40555,#40546,#7109,.T.) ;
#51157 = EDGE_CURVE('',#40556,#40557,#7110,.T.) ;
#51158 = EDGE_CURVE('',#40557,#40558,#7111,.T.) ;
#51159 = EDGE_CURVE('',#40558,#40559,#7112,.T.) ;
#51160 = EDGE_CURVE('',#40559,#40556,#7113,.T.) ;
#51161 = EDGE_CURVE('',#40560,#40561,#33012,.T.) ;
#51162 = EDGE_CURVE('',#40561,#40562,#33013,.T.) ;
#51163 = EDGE_CURVE('',#40562,#40563,#7114,.T.) ;
#51164 = EDGE_CURVE('',#40563,#40564,#7115,.T.) ;
#51165 = EDGE_CURVE('',#40564,#40565,#7116,.T.) ;
#51166 = EDGE_CURVE('',#40565,#40566,#7117,.T.) ;
#51167 = EDGE_CURVE('',#40567,#40566,#33014,.T.) ;
#51168 = EDGE_CURVE('',#40567,#40568,#7118,.T.) ;
#51169 = EDGE_CURVE('',#40568,#40569,#7119,.T.) ;
#51170 = EDGE_CURVE('',#40569,#40560,#7120,.T.) ;
#51171 = EDGE_CURVE('',#40570,#40571,#7121,.T.) ;
#51172 = EDGE_CURVE('',#40571,#40572,#7122,.T.) ;
#51173 = EDGE_CURVE('',#40572,#40573,#7123,.T.) ;
#51174 = EDGE_CURVE('',#40573,#40570,#7124,.T.) ;
#51175 = EDGE_CURVE('',#40574,#40575,#7125,.T.) ;
#51176 = EDGE_CURVE('',#40575,#40576,#33015,.T.) ;
#51177 = EDGE_CURVE('',#40576,#40577,#33016,.T.) ;
#51178 = EDGE_CURVE('',#40577,#40578,#7126,.T.) ;
#51179 = EDGE_CURVE('',#40578,#40579,#7127,.T.) ;
#51180 = EDGE_CURVE('',#40579,#40580,#7128,.T.) ;
#51181 = EDGE_CURVE('',#40581,#40580,#33017,.T.) ;
#51182 = EDGE_CURVE('',#40581,#40582,#7129,.T.) ;
#51183 = EDGE_CURVE('',#40582,#40583,#7130,.T.) ;
#51184 = EDGE_CURVE('',#40583,#40574,#7131,.T.) ;
#51185 = EDGE_CURVE('',#40584,#40585,#7132,.T.) ;
#51186 = EDGE_CURVE('',#40585,#40586,#7133,.T.) ;
#51187 = EDGE_CURVE('',#40586,#40587,#7134,.T.) ;
#51188 = EDGE_CURVE('',#40587,#40584,#7135,.T.) ;
#51189 = EDGE_CURVE('',#40588,#40589,#33018,.T.) ;
#51190 = EDGE_CURVE('',#40589,#40590,#33019,.T.) ;
#51191 = EDGE_CURVE('',#40590,#40591,#7136,.T.) ;
#51192 = EDGE_CURVE('',#40591,#40592,#7137,.T.) ;
#51193 = EDGE_CURVE('',#40592,#40593,#7138,.T.) ;
#51194 = EDGE_CURVE('',#40593,#40594,#7139,.T.) ;
#51195 = EDGE_CURVE('',#40595,#40594,#33020,.T.) ;
#51196 = EDGE_CURVE('',#40595,#40596,#7140,.T.) ;
#51197 = EDGE_CURVE('',#40596,#40597,#7141,.T.) ;
#51198 = EDGE_CURVE('',#40597,#40588,#7142,.T.) ;
#51199 = EDGE_CURVE('',#40598,#40599,#7143,.T.) ;
#51200 = EDGE_CURVE('',#40599,#40600,#7144,.T.) ;
#51201 = EDGE_CURVE('',#40600,#40601,#7145,.T.) ;
#51202 = EDGE_CURVE('',#40601,#40598,#7146,.T.) ;
#51203 = EDGE_CURVE('',#40602,#40603,#7147,.T.) ;
#51204 = EDGE_CURVE('',#40603,#40604,#33021,.T.) ;
#51205 = EDGE_CURVE('',#40604,#40605,#33022,.T.) ;
#51206 = EDGE_CURVE('',#40605,#40606,#7148,.T.) ;
#51207 = EDGE_CURVE('',#40606,#40607,#7149,.T.) ;
#51208 = EDGE_CURVE('',#40607,#40608,#7150,.T.) ;
#51209 = EDGE_CURVE('',#40609,#40608,#33023,.T.) ;
#51210 = EDGE_CURVE('',#40609,#40610,#7151,.T.) ;
#51211 = EDGE_CURVE('',#40610,#40611,#7152,.T.) ;
#51212 = EDGE_CURVE('',#40611,#40602,#7153,.T.) ;
#51213 = EDGE_CURVE('',#40612,#40613,#7154,.T.) ;
#51214 = EDGE_CURVE('',#40613,#40614,#7155,.T.) ;
#51215 = EDGE_CURVE('',#40614,#40615,#7156,.T.) ;
#51216 = EDGE_CURVE('',#40615,#40612,#7157,.T.) ;
#51217 = EDGE_CURVE('',#40616,#40617,#33024,.T.) ;
#51218 = EDGE_CURVE('',#40617,#40618,#33025,.T.) ;
#51219 = EDGE_CURVE('',#40618,#40619,#7158,.T.) ;
#51220 = EDGE_CURVE('',#40619,#40620,#7159,.T.) ;
#51221 = EDGE_CURVE('',#40620,#40621,#7160,.T.) ;
#51222 = EDGE_CURVE('',#40621,#40622,#7161,.T.) ;
#51223 = EDGE_CURVE('',#40623,#40622,#33026,.T.) ;
#51224 = EDGE_CURVE('',#40623,#40624,#7162,.T.) ;
#51225 = EDGE_CURVE('',#40624,#40625,#7163,.T.) ;
#51226 = EDGE_CURVE('',#40625,#40616,#7164,.T.) ;
#51227 = EDGE_CURVE('',#40626,#40627,#7165,.T.) ;
#51228 = EDGE_CURVE('',#40627,#40628,#7166,.T.) ;
#51229 = EDGE_CURVE('',#40628,#40629,#7167,.T.) ;
#51230 = EDGE_CURVE('',#40629,#40626,#7168,.T.) ;
#51231 = EDGE_CURVE('',#40630,#40631,#7169,.T.) ;
#51232 = EDGE_CURVE('',#40631,#40632,#33027,.T.) ;
#51233 = EDGE_CURVE('',#40632,#40633,#33028,.T.) ;
#51234 = EDGE_CURVE('',#40633,#40634,#7170,.T.) ;
#51235 = EDGE_CURVE('',#40634,#40635,#7171,.T.) ;
#51236 = EDGE_CURVE('',#40635,#40636,#7172,.T.) ;
#51237 = EDGE_CURVE('',#40637,#40636,#33029,.T.) ;
#51238 = EDGE_CURVE('',#40637,#40638,#7173,.T.) ;
#51239 = EDGE_CURVE('',#40638,#40639,#7174,.T.) ;
#51240 = EDGE_CURVE('',#40639,#40630,#7175,.T.) ;
#51241 = EDGE_CURVE('',#40640,#40641,#7176,.T.) ;
#51242 = EDGE_CURVE('',#40641,#40642,#7177,.T.) ;
#51243 = EDGE_CURVE('',#40642,#40643,#7178,.T.) ;
#51244 = EDGE_CURVE('',#40643,#40640,#7179,.T.) ;
#51245 = EDGE_CURVE('',#40644,#40645,#33030,.T.) ;
#51246 = EDGE_CURVE('',#40645,#40646,#33031,.T.) ;
#51247 = EDGE_CURVE('',#40646,#40647,#7180,.T.) ;
#51248 = EDGE_CURVE('',#40647,#40648,#7181,.T.) ;
#51249 = EDGE_CURVE('',#40648,#40649,#7182,.T.) ;
#51250 = EDGE_CURVE('',#40649,#40650,#7183,.T.) ;
#51251 = EDGE_CURVE('',#40651,#40650,#33032,.T.) ;
#51252 = EDGE_CURVE('',#40651,#40652,#7184,.T.) ;
#51253 = EDGE_CURVE('',#40652,#40653,#7185,.T.) ;
#51254 = EDGE_CURVE('',#40653,#40644,#7186,.T.) ;
#51255 = EDGE_CURVE('',#40654,#40655,#7187,.T.) ;
#51256 = EDGE_CURVE('',#40655,#40656,#7188,.T.) ;
#51257 = EDGE_CURVE('',#40656,#40657,#7189,.T.) ;
#51258 = EDGE_CURVE('',#40657,#40654,#7190,.T.) ;
#51259 = EDGE_CURVE('',#40658,#40659,#7191,.T.) ;
#51260 = EDGE_CURVE('',#40659,#40660,#33033,.T.) ;
#51261 = EDGE_CURVE('',#40660,#40661,#33034,.T.) ;
#51262 = EDGE_CURVE('',#40661,#40662,#7192,.T.) ;
#51263 = EDGE_CURVE('',#40662,#40663,#7193,.T.) ;
#51264 = EDGE_CURVE('',#40663,#40664,#7194,.T.) ;
#51265 = EDGE_CURVE('',#40665,#40664,#33035,.T.) ;
#51266 = EDGE_CURVE('',#40665,#40666,#7195,.T.) ;
#51267 = EDGE_CURVE('',#40666,#40667,#7196,.T.) ;
#51268 = EDGE_CURVE('',#40667,#40658,#7197,.T.) ;
#51269 = EDGE_CURVE('',#40668,#40669,#7198,.T.) ;
#51270 = EDGE_CURVE('',#40669,#40670,#7199,.T.) ;
#51271 = EDGE_CURVE('',#40670,#40671,#7200,.T.) ;
#51272 = EDGE_CURVE('',#40671,#40668,#7201,.T.) ;
#51273 = EDGE_CURVE('',#40672,#40673,#33036,.T.) ;
#51274 = EDGE_CURVE('',#40673,#40674,#33037,.T.) ;
#51275 = EDGE_CURVE('',#40674,#40675,#7202,.T.) ;
#51276 = EDGE_CURVE('',#40675,#40676,#7203,.T.) ;
#51277 = EDGE_CURVE('',#40676,#40677,#7204,.T.) ;
#51278 = EDGE_CURVE('',#40677,#40678,#7205,.T.) ;
#51279 = EDGE_CURVE('',#40679,#40678,#33038,.T.) ;
#51280 = EDGE_CURVE('',#40679,#40680,#7206,.T.) ;
#51281 = EDGE_CURVE('',#40680,#40681,#7207,.T.) ;
#51282 = EDGE_CURVE('',#40681,#40672,#7208,.T.) ;
#51283 = EDGE_CURVE('',#40682,#40683,#7209,.T.) ;
#51284 = EDGE_CURVE('',#40683,#40684,#7210,.T.) ;
#51285 = EDGE_CURVE('',#40684,#40685,#7211,.T.) ;
#51286 = EDGE_CURVE('',#40685,#40682,#7212,.T.) ;
#51287 = EDGE_CURVE('',#40686,#40687,#7213,.T.) ;
#51288 = EDGE_CURVE('',#40687,#40688,#33039,.T.) ;
#51289 = EDGE_CURVE('',#40688,#40689,#33040,.T.) ;
#51290 = EDGE_CURVE('',#40689,#40690,#7214,.T.) ;
#51291 = EDGE_CURVE('',#40690,#40691,#7215,.T.) ;
#51292 = EDGE_CURVE('',#40691,#40692,#7216,.T.) ;
#51293 = EDGE_CURVE('',#40693,#40692,#33041,.T.) ;
#51294 = EDGE_CURVE('',#40693,#40694,#7217,.T.) ;
#51295 = EDGE_CURVE('',#40694,#40695,#7218,.T.) ;
#51296 = EDGE_CURVE('',#40695,#40686,#7219,.T.) ;
#51297 = EDGE_CURVE('',#40696,#40697,#7220,.T.) ;
#51298 = EDGE_CURVE('',#40697,#40698,#7221,.T.) ;
#51299 = EDGE_CURVE('',#40698,#40699,#7222,.T.) ;
#51300 = EDGE_CURVE('',#40699,#40696,#7223,.T.) ;
#51301 = EDGE_CURVE('',#40700,#40701,#33042,.T.) ;
#51302 = EDGE_CURVE('',#40701,#40702,#33043,.T.) ;
#51303 = EDGE_CURVE('',#40702,#40703,#7224,.T.) ;
#51304 = EDGE_CURVE('',#40703,#40704,#7225,.T.) ;
#51305 = EDGE_CURVE('',#40704,#40705,#7226,.T.) ;
#51306 = EDGE_CURVE('',#40705,#40706,#7227,.T.) ;
#51307 = EDGE_CURVE('',#40707,#40706,#33044,.T.) ;
#51308 = EDGE_CURVE('',#40707,#40708,#7228,.T.) ;
#51309 = EDGE_CURVE('',#40708,#40709,#7229,.T.) ;
#51310 = EDGE_CURVE('',#40709,#40700,#7230,.T.) ;
#51311 = EDGE_CURVE('',#40710,#40711,#7231,.T.) ;
#51312 = EDGE_CURVE('',#40711,#40712,#7232,.T.) ;
#51313 = EDGE_CURVE('',#40712,#40713,#7233,.T.) ;
#51314 = EDGE_CURVE('',#40713,#40710,#7234,.T.) ;
#51315 = EDGE_CURVE('',#40714,#40715,#7235,.T.) ;
#51316 = EDGE_CURVE('',#40715,#40716,#33045,.T.) ;
#51317 = EDGE_CURVE('',#40716,#40717,#33046,.T.) ;
#51318 = EDGE_CURVE('',#40717,#40718,#7236,.T.) ;
#51319 = EDGE_CURVE('',#40718,#40719,#7237,.T.) ;
#51320 = EDGE_CURVE('',#40719,#40720,#7238,.T.) ;
#51321 = EDGE_CURVE('',#40721,#40720,#33047,.T.) ;
#51322 = EDGE_CURVE('',#40721,#40722,#7239,.T.) ;
#51323 = EDGE_CURVE('',#40722,#40723,#7240,.T.) ;
#51324 = EDGE_CURVE('',#40723,#40714,#7241,.T.) ;
#51325 = EDGE_CURVE('',#40724,#40725,#7242,.T.) ;
#51326 = EDGE_CURVE('',#40725,#40726,#7243,.T.) ;
#51327 = EDGE_CURVE('',#40726,#40727,#7244,.T.) ;
#51328 = EDGE_CURVE('',#40727,#40724,#7245,.T.) ;
#51329 = EDGE_CURVE('',#40728,#40729,#7246,.T.) ;
#51330 = EDGE_CURVE('',#40729,#40730,#7247,.T.) ;
#51331 = EDGE_CURVE('',#40730,#40731,#7248,.T.) ;
#51332 = EDGE_CURVE('',#40731,#40728,#7249,.T.) ;
#51333 = EDGE_CURVE('',#40732,#40733,#7250,.T.) ;
#51334 = EDGE_CURVE('',#40733,#40734,#7251,.T.) ;
#51335 = EDGE_CURVE('',#40734,#40735,#7252,.T.) ;
#51336 = EDGE_CURVE('',#40735,#40732,#7253,.T.) ;
#51337 = EDGE_CURVE('',#40736,#40737,#7254,.T.) ;
#51338 = EDGE_CURVE('',#40737,#40738,#33048,.T.) ;
#51339 = EDGE_CURVE('',#40738,#40739,#7255,.T.) ;
#51340 = EDGE_CURVE('',#40739,#40736,#33049,.T.) ;
#51341 = EDGE_CURVE('',#40740,#40741,#7256,.T.) ;
#51342 = EDGE_CURVE('',#40741,#40742,#33050,.T.) ;
#51343 = EDGE_CURVE('',#40742,#40743,#7257,.T.) ;
#51344 = EDGE_CURVE('',#40743,#40744,#7258,.T.) ;
#51345 = EDGE_CURVE('',#40744,#40745,#7259,.T.) ;
#51346 = EDGE_CURVE('',#40745,#40740,#7260,.T.) ;
#51347 = EDGE_CURVE('',#40746,#40747,#7261,.T.) ;
#51348 = EDGE_CURVE('',#40747,#40748,#7262,.T.) ;
#51349 = EDGE_CURVE('',#40748,#40749,#7263,.T.) ;
#51350 = EDGE_CURVE('',#40749,#40746,#7264,.T.) ;
#51351 = EDGE_CURVE('',#40750,#40751,#7265,.T.) ;
#51352 = EDGE_CURVE('',#40751,#40752,#7266,.T.) ;
#51353 = EDGE_CURVE('',#40752,#40753,#7267,.T.) ;
#51354 = EDGE_CURVE('',#40753,#40750,#7268,.T.) ;
#51355 = EDGE_CURVE('',#40754,#40755,#7269,.T.) ;
#51356 = EDGE_CURVE('',#40755,#40756,#33051,.T.) ;
#51357 = EDGE_CURVE('',#40756,#40757,#7270,.T.) ;
#51358 = EDGE_CURVE('',#40757,#40754,#33052,.T.) ;
#51359 = EDGE_CURVE('',#40758,#40759,#7271,.T.) ;
#51360 = EDGE_CURVE('',#40759,#40760,#33053,.T.) ;
#51361 = EDGE_CURVE('',#40760,#40761,#7272,.T.) ;
#51362 = EDGE_CURVE('',#40761,#40762,#7273,.T.) ;
#51363 = EDGE_CURVE('',#40762,#40763,#7274,.T.) ;
#51364 = EDGE_CURVE('',#40763,#40758,#7275,.T.) ;
#51365 = EDGE_CURVE('',#40764,#40765,#7276,.T.) ;
#51366 = EDGE_CURVE('',#40765,#40766,#7277,.T.) ;
#51367 = EDGE_CURVE('',#40766,#40767,#7278,.T.) ;
#51368 = EDGE_CURVE('',#40767,#40764,#7279,.T.) ;
#51369 = EDGE_CURVE('',#40768,#40769,#7280,.T.) ;
#51370 = EDGE_CURVE('',#40769,#40770,#7281,.T.) ;
#51371 = EDGE_CURVE('',#40770,#40771,#7282,.T.) ;
#51372 = EDGE_CURVE('',#40771,#40768,#7283,.T.) ;
#51373 = EDGE_CURVE('',#40772,#40773,#7284,.T.) ;
#51374 = EDGE_CURVE('',#40773,#40774,#33054,.T.) ;
#51375 = EDGE_CURVE('',#40774,#40775,#7285,.T.) ;
#51376 = EDGE_CURVE('',#40775,#40772,#33055,.T.) ;
#51377 = EDGE_CURVE('',#40776,#40777,#7286,.T.) ;
#51378 = EDGE_CURVE('',#40777,#40778,#33056,.T.) ;
#51379 = EDGE_CURVE('',#40778,#40779,#7287,.T.) ;
#51380 = EDGE_CURVE('',#40779,#40780,#7288,.T.) ;
#51381 = EDGE_CURVE('',#40780,#40781,#7289,.T.) ;
#51382 = EDGE_CURVE('',#40781,#40776,#7290,.T.) ;
#51383 = EDGE_CURVE('',#40782,#40783,#7291,.T.) ;
#51384 = EDGE_CURVE('',#40783,#40784,#7292,.T.) ;
#51385 = EDGE_CURVE('',#40784,#40785,#7293,.T.) ;
#51386 = EDGE_CURVE('',#40785,#40782,#7294,.T.) ;
#51387 = EDGE_CURVE('',#40786,#40787,#7295,.T.) ;
#51388 = EDGE_CURVE('',#40787,#40788,#7296,.T.) ;
#51389 = EDGE_CURVE('',#40788,#40789,#7297,.T.) ;
#51390 = EDGE_CURVE('',#40789,#40786,#7298,.T.) ;
#51391 = EDGE_CURVE('',#40790,#40791,#7299,.T.) ;
#51392 = EDGE_CURVE('',#40791,#40792,#33057,.T.) ;
#51393 = EDGE_CURVE('',#40792,#40793,#7300,.T.) ;
#51394 = EDGE_CURVE('',#40793,#40790,#33058,.T.) ;
#51395 = EDGE_CURVE('',#40794,#40795,#7301,.T.) ;
#51396 = EDGE_CURVE('',#40795,#40796,#33059,.T.) ;
#51397 = EDGE_CURVE('',#40796,#40797,#7302,.T.) ;
#51398 = EDGE_CURVE('',#40797,#40798,#7303,.T.) ;
#51399 = EDGE_CURVE('',#40798,#40799,#7304,.T.) ;
#51400 = EDGE_CURVE('',#40799,#40794,#7305,.T.) ;
#51401 = EDGE_CURVE('',#40800,#40801,#7306,.T.) ;
#51402 = EDGE_CURVE('',#40801,#40802,#7307,.T.) ;
#51403 = EDGE_CURVE('',#40802,#40803,#7308,.T.) ;
#51404 = EDGE_CURVE('',#40803,#40800,#7309,.T.) ;
#51405 = EDGE_CURVE('',#40804,#40805,#7310,.T.) ;
#51406 = EDGE_CURVE('',#40805,#40806,#7311,.T.) ;
#51407 = EDGE_CURVE('',#40806,#40807,#7312,.T.) ;
#51408 = EDGE_CURVE('',#40807,#40804,#7313,.T.) ;
#51409 = EDGE_CURVE('',#40808,#40809,#7314,.T.) ;
#51410 = EDGE_CURVE('',#40809,#40810,#33060,.T.) ;
#51411 = EDGE_CURVE('',#40810,#40811,#7315,.T.) ;
#51412 = EDGE_CURVE('',#40811,#40808,#33061,.T.) ;
#51413 = EDGE_CURVE('',#40812,#40813,#7316,.T.) ;
#51414 = EDGE_CURVE('',#40813,#40814,#33062,.T.) ;
#51415 = EDGE_CURVE('',#40814,#40815,#7317,.T.) ;
#51416 = EDGE_CURVE('',#40815,#40816,#7318,.T.) ;
#51417 = EDGE_CURVE('',#40816,#40817,#7319,.T.) ;
#51418 = EDGE_CURVE('',#40817,#40812,#7320,.T.) ;
#51419 = EDGE_CURVE('',#40818,#40819,#7321,.T.) ;
#51420 = EDGE_CURVE('',#40819,#40820,#7322,.T.) ;
#51421 = EDGE_CURVE('',#40820,#40821,#7323,.T.) ;
#51422 = EDGE_CURVE('',#40821,#40818,#7324,.T.) ;
#51423 = EDGE_CURVE('',#40822,#40823,#7325,.T.) ;
#51424 = EDGE_CURVE('',#40823,#40824,#7326,.T.) ;
#51425 = EDGE_CURVE('',#40824,#40825,#7327,.T.) ;
#51426 = EDGE_CURVE('',#40825,#40822,#7328,.T.) ;
#51427 = EDGE_CURVE('',#40826,#40827,#7329,.T.) ;
#51428 = EDGE_CURVE('',#40827,#40828,#33063,.T.) ;
#51429 = EDGE_CURVE('',#40828,#40829,#7330,.T.) ;
#51430 = EDGE_CURVE('',#40829,#40826,#33064,.T.) ;
#51431 = EDGE_CURVE('',#40830,#40831,#7331,.T.) ;
#51432 = EDGE_CURVE('',#40831,#40832,#33065,.T.) ;
#51433 = EDGE_CURVE('',#40832,#40833,#7332,.T.) ;
#51434 = EDGE_CURVE('',#40833,#40834,#7333,.T.) ;
#51435 = EDGE_CURVE('',#40834,#40835,#7334,.T.) ;
#51436 = EDGE_CURVE('',#40835,#40830,#7335,.T.) ;
#51437 = EDGE_CURVE('',#40836,#40837,#7336,.T.) ;
#51438 = EDGE_CURVE('',#40837,#40838,#7337,.T.) ;
#51439 = EDGE_CURVE('',#40838,#40839,#7338,.T.) ;
#51440 = EDGE_CURVE('',#40839,#40836,#7339,.T.) ;
#51441 = EDGE_CURVE('',#40840,#40841,#7340,.T.) ;
#51442 = EDGE_CURVE('',#40841,#40842,#7341,.T.) ;
#51443 = EDGE_CURVE('',#40842,#40843,#7342,.T.) ;
#51444 = EDGE_CURVE('',#40843,#40840,#7343,.T.) ;
#51445 = EDGE_CURVE('',#40844,#40845,#7344,.T.) ;
#51446 = EDGE_CURVE('',#40845,#40846,#33066,.T.) ;
#51447 = EDGE_CURVE('',#40846,#40847,#7345,.T.) ;
#51448 = EDGE_CURVE('',#40847,#40844,#33067,.T.) ;
#51449 = EDGE_CURVE('',#40848,#40849,#7346,.T.) ;
#51450 = EDGE_CURVE('',#40849,#40850,#33068,.T.) ;
#51451 = EDGE_CURVE('',#40850,#40851,#7347,.T.) ;
#51452 = EDGE_CURVE('',#40851,#40852,#7348,.T.) ;
#51453 = EDGE_CURVE('',#40852,#40853,#7349,.T.) ;
#51454 = EDGE_CURVE('',#40853,#40848,#7350,.T.) ;
#51455 = EDGE_CURVE('',#40854,#40855,#7351,.T.) ;
#51456 = EDGE_CURVE('',#40855,#40856,#7352,.T.) ;
#51457 = EDGE_CURVE('',#40856,#40857,#7353,.T.) ;
#51458 = EDGE_CURVE('',#40857,#40854,#7354,.T.) ;
#51459 = EDGE_CURVE('',#40858,#40859,#7355,.T.) ;
#51460 = EDGE_CURVE('',#40859,#40860,#7356,.T.) ;
#51461 = EDGE_CURVE('',#40860,#40861,#7357,.T.) ;
#51462 = EDGE_CURVE('',#40861,#40858,#7358,.T.) ;
#51463 = EDGE_CURVE('',#40862,#40863,#7359,.T.) ;
#51464 = EDGE_CURVE('',#40863,#40864,#33069,.T.) ;
#51465 = EDGE_CURVE('',#40864,#40865,#7360,.T.) ;
#51466 = EDGE_CURVE('',#40865,#40862,#33070,.T.) ;
#51467 = EDGE_CURVE('',#40866,#40867,#7361,.T.) ;
#51468 = EDGE_CURVE('',#40867,#40868,#33071,.T.) ;
#51469 = EDGE_CURVE('',#40868,#40869,#7362,.T.) ;
#51470 = EDGE_CURVE('',#40869,#40870,#7363,.T.) ;
#51471 = EDGE_CURVE('',#40870,#40871,#7364,.T.) ;
#51472 = EDGE_CURVE('',#40871,#40866,#7365,.T.) ;
#51473 = EDGE_CURVE('',#40872,#40873,#7366,.T.) ;
#51474 = EDGE_CURVE('',#40873,#40874,#7367,.T.) ;
#51475 = EDGE_CURVE('',#40874,#40875,#7368,.T.) ;
#51476 = EDGE_CURVE('',#40875,#40872,#7369,.T.) ;
#51477 = EDGE_CURVE('',#40876,#40877,#7370,.T.) ;
#51478 = EDGE_CURVE('',#40877,#40878,#7371,.T.) ;
#51479 = EDGE_CURVE('',#40878,#40879,#7372,.T.) ;
#51480 = EDGE_CURVE('',#40879,#40876,#7373,.T.) ;
#51481 = EDGE_CURVE('',#40880,#40881,#7374,.T.) ;
#51482 = EDGE_CURVE('',#40881,#40882,#33072,.T.) ;
#51483 = EDGE_CURVE('',#40882,#40883,#7375,.T.) ;
#51484 = EDGE_CURVE('',#40883,#40880,#33073,.T.) ;
#51485 = EDGE_CURVE('',#40884,#40885,#7376,.T.) ;
#51486 = EDGE_CURVE('',#40885,#40886,#33074,.T.) ;
#51487 = EDGE_CURVE('',#40886,#40887,#7377,.T.) ;
#51488 = EDGE_CURVE('',#40887,#40888,#7378,.T.) ;
#51489 = EDGE_CURVE('',#40888,#40889,#7379,.T.) ;
#51490 = EDGE_CURVE('',#40889,#40884,#7380,.T.) ;
#51491 = EDGE_CURVE('',#40890,#40891,#7381,.T.) ;
#51492 = EDGE_CURVE('',#40891,#40892,#7382,.T.) ;
#51493 = EDGE_CURVE('',#40892,#40893,#7383,.T.) ;
#51494 = EDGE_CURVE('',#40893,#40890,#7384,.T.) ;
#51495 = EDGE_CURVE('',#40894,#40895,#7385,.T.) ;
#51496 = EDGE_CURVE('',#40895,#40896,#7386,.T.) ;
#51497 = EDGE_CURVE('',#40896,#40897,#7387,.T.) ;
#51498 = EDGE_CURVE('',#40897,#40894,#7388,.T.) ;
#51499 = EDGE_CURVE('',#40898,#40899,#7389,.T.) ;
#51500 = EDGE_CURVE('',#40899,#40900,#7390,.T.) ;
#51501 = EDGE_CURVE('',#40900,#40901,#7391,.T.) ;
#51502 = EDGE_CURVE('',#40901,#40898,#7392,.T.) ;
#51503 = EDGE_CURVE('',#40902,#40903,#7393,.T.) ;
#51504 = EDGE_CURVE('',#40903,#40904,#7394,.T.) ;
#51505 = EDGE_CURVE('',#40904,#40905,#7395,.T.) ;
#51506 = EDGE_CURVE('',#40905,#40902,#7396,.T.) ;
#51507 = EDGE_CURVE('',#40906,#40907,#7397,.T.) ;
#51508 = EDGE_CURVE('',#40907,#40908,#7398,.T.) ;
#51509 = EDGE_CURVE('',#40908,#40909,#7399,.T.) ;
#51510 = EDGE_CURVE('',#40909,#40906,#7400,.T.) ;
#51511 = EDGE_CURVE('',#40910,#40911,#7401,.T.) ;
#51512 = EDGE_CURVE('',#40911,#40912,#7402,.T.) ;
#51513 = EDGE_CURVE('',#40912,#40913,#7403,.T.) ;
#51514 = EDGE_CURVE('',#40913,#40910,#7404,.T.) ;
#51515 = EDGE_CURVE('',#40914,#40915,#7405,.T.) ;
#51516 = EDGE_CURVE('',#40915,#40916,#7406,.T.) ;
#51517 = EDGE_CURVE('',#40916,#40917,#7407,.T.) ;
#51518 = EDGE_CURVE('',#40917,#40914,#7408,.T.) ;
#51519 = EDGE_CURVE('',#40918,#40919,#7409,.T.) ;
#51520 = EDGE_CURVE('',#40919,#40920,#7410,.T.) ;
#51521 = EDGE_CURVE('',#40920,#40921,#7411,.T.) ;
#51522 = EDGE_CURVE('',#40921,#40918,#7412,.T.) ;
#51523 = EDGE_CURVE('',#40922,#40923,#7413,.T.) ;
#51524 = EDGE_CURVE('',#40923,#40924,#7414,.T.) ;
#51525 = EDGE_CURVE('',#40924,#40925,#7415,.T.) ;
#51526 = EDGE_CURVE('',#40925,#40922,#7416,.T.) ;
#51527 = EDGE_CURVE('',#40926,#40927,#7417,.T.) ;
#51528 = EDGE_CURVE('',#40927,#40928,#7418,.T.) ;
#51529 = EDGE_CURVE('',#40928,#40929,#7419,.T.) ;
#51530 = EDGE_CURVE('',#40929,#40926,#7420,.T.) ;
#51531 = EDGE_CURVE('',#40930,#40931,#7421,.T.) ;
#51532 = EDGE_CURVE('',#40931,#40932,#7422,.T.) ;
#51533 = EDGE_CURVE('',#40932,#40933,#7423,.T.) ;
#51534 = EDGE_CURVE('',#40933,#40930,#7424,.T.) ;
#51535 = EDGE_CURVE('',#40934,#40935,#7425,.T.) ;
#51536 = EDGE_CURVE('',#40935,#40936,#7426,.T.) ;
#51537 = EDGE_CURVE('',#40936,#40937,#7427,.T.) ;
#51538 = EDGE_CURVE('',#40937,#40934,#7428,.T.) ;
#51539 = EDGE_CURVE('',#40938,#40939,#7429,.T.) ;
#51540 = EDGE_CURVE('',#40939,#40940,#7430,.T.) ;
#51541 = EDGE_CURVE('',#40940,#40941,#7431,.T.) ;
#51542 = EDGE_CURVE('',#40941,#40938,#7432,.T.) ;
#51543 = EDGE_CURVE('',#40942,#40943,#7433,.T.) ;
#51544 = EDGE_CURVE('',#40943,#40944,#7434,.T.) ;
#51545 = EDGE_CURVE('',#40944,#40945,#7435,.T.) ;
#51546 = EDGE_CURVE('',#40945,#40942,#7436,.T.) ;
#51547 = EDGE_CURVE('',#40946,#40947,#7437,.T.) ;
#51548 = EDGE_CURVE('',#40947,#40948,#7438,.T.) ;
#51549 = EDGE_CURVE('',#40948,#40949,#7439,.T.) ;
#51550 = EDGE_CURVE('',#40949,#40946,#7440,.T.) ;
#51551 = EDGE_CURVE('',#40950,#40951,#7441,.T.) ;
#51552 = EDGE_CURVE('',#40951,#40952,#7442,.T.) ;
#51553 = EDGE_CURVE('',#40952,#40953,#7443,.T.) ;
#51554 = EDGE_CURVE('',#40953,#40950,#7444,.T.) ;
#51555 = EDGE_CURVE('',#40954,#40955,#7445,.T.) ;
#51556 = EDGE_CURVE('',#40955,#40956,#7446,.T.) ;
#51557 = EDGE_CURVE('',#40956,#40957,#7447,.T.) ;
#51558 = EDGE_CURVE('',#40957,#40954,#7448,.T.) ;
#51559 = EDGE_CURVE('',#40958,#40959,#7449,.T.) ;
#51560 = EDGE_CURVE('',#40959,#40960,#7450,.T.) ;
#51561 = EDGE_CURVE('',#40960,#40961,#7451,.T.) ;
#51562 = EDGE_CURVE('',#40961,#40958,#7452,.T.) ;
#51563 = EDGE_CURVE('',#40962,#40963,#7453,.T.) ;
#51564 = EDGE_CURVE('',#40963,#40964,#7454,.T.) ;
#51565 = EDGE_CURVE('',#40964,#40965,#7455,.T.) ;
#51566 = EDGE_CURVE('',#40965,#40962,#7456,.T.) ;
#51567 = EDGE_CURVE('',#40966,#40967,#7457,.T.) ;
#51568 = EDGE_CURVE('',#40967,#40968,#7458,.T.) ;
#51569 = EDGE_CURVE('',#40968,#40969,#7459,.T.) ;
#51570 = EDGE_CURVE('',#40969,#40966,#7460,.T.) ;
#51571 = EDGE_CURVE('',#40970,#40971,#7461,.T.) ;
#51572 = EDGE_CURVE('',#40971,#40972,#7462,.T.) ;
#51573 = EDGE_CURVE('',#40972,#40973,#7463,.T.) ;
#51574 = EDGE_CURVE('',#40973,#40970,#7464,.T.) ;
#51575 = EDGE_CURVE('',#40974,#40975,#7465,.T.) ;
#51576 = EDGE_CURVE('',#40975,#40976,#7466,.T.) ;
#51577 = EDGE_CURVE('',#40976,#40977,#7467,.T.) ;
#51578 = EDGE_CURVE('',#40977,#40974,#7468,.T.) ;
#51579 = EDGE_CURVE('',#40978,#40979,#7469,.T.) ;
#51580 = EDGE_CURVE('',#40979,#40980,#7470,.T.) ;
#51581 = EDGE_CURVE('',#40980,#40981,#7471,.T.) ;
#51582 = EDGE_CURVE('',#40981,#40978,#7472,.T.) ;
#51583 = EDGE_CURVE('',#40982,#40983,#7473,.T.) ;
#51584 = EDGE_CURVE('',#40983,#40984,#7474,.T.) ;
#51585 = EDGE_CURVE('',#40984,#40985,#7475,.T.) ;
#51586 = EDGE_CURVE('',#40985,#40982,#7476,.T.) ;
#51587 = EDGE_CURVE('',#40986,#40987,#7477,.T.) ;
#51588 = EDGE_CURVE('',#40987,#40988,#7478,.T.) ;
#51589 = EDGE_CURVE('',#40988,#40989,#7479,.T.) ;
#51590 = EDGE_CURVE('',#40989,#40986,#7480,.T.) ;
#51591 = EDGE_CURVE('',#40990,#40991,#7481,.T.) ;
#51592 = EDGE_CURVE('',#40991,#40992,#7482,.T.) ;
#51593 = EDGE_CURVE('',#40992,#40993,#7483,.T.) ;
#51594 = EDGE_CURVE('',#40993,#40990,#7484,.T.) ;
#51595 = EDGE_CURVE('',#40994,#40995,#7485,.T.) ;
#51596 = EDGE_CURVE('',#40995,#40996,#7486,.T.) ;
#51597 = EDGE_CURVE('',#40996,#40997,#7487,.T.) ;
#51598 = EDGE_CURVE('',#40997,#40994,#7488,.T.) ;
#51599 = EDGE_CURVE('',#40998,#40999,#7489,.T.) ;
#51600 = EDGE_CURVE('',#40999,#41000,#7490,.T.) ;
#51601 = EDGE_CURVE('',#41000,#41001,#7491,.T.) ;
#51602 = EDGE_CURVE('',#41001,#40998,#7492,.T.) ;
#51603 = EDGE_CURVE('',#41002,#41003,#7493,.T.) ;
#51604 = EDGE_CURVE('',#41003,#41004,#7494,.T.) ;
#51605 = EDGE_CURVE('',#41004,#41005,#7495,.T.) ;
#51606 = EDGE_CURVE('',#41005,#41002,#7496,.T.) ;
#51607 = EDGE_CURVE('',#41006,#41007,#7497,.T.) ;
#51608 = EDGE_CURVE('',#41007,#41008,#7498,.T.) ;
#51609 = EDGE_CURVE('',#41008,#41009,#7499,.T.) ;
#51610 = EDGE_CURVE('',#41009,#41006,#7500,.T.) ;
#51611 = EDGE_CURVE('',#41010,#41011,#7501,.T.) ;
#51612 = EDGE_CURVE('',#41011,#41012,#7502,.T.) ;
#51613 = EDGE_CURVE('',#41012,#41013,#7503,.T.) ;
#51614 = EDGE_CURVE('',#41013,#41010,#7504,.T.) ;
#51615 = EDGE_CURVE('',#41014,#41015,#7505,.T.) ;
#51616 = EDGE_CURVE('',#41015,#41016,#7506,.T.) ;
#51617 = EDGE_CURVE('',#41016,#41017,#7507,.T.) ;
#51618 = EDGE_CURVE('',#41017,#41014,#7508,.T.) ;
#51619 = EDGE_CURVE('',#41018,#41019,#7509,.T.) ;
#51620 = EDGE_CURVE('',#41019,#41020,#7510,.T.) ;
#51621 = EDGE_CURVE('',#41020,#41021,#7511,.T.) ;
#51622 = EDGE_CURVE('',#41021,#41018,#7512,.T.) ;
#51623 = EDGE_CURVE('',#41022,#41023,#7513,.T.) ;
#51624 = EDGE_CURVE('',#41023,#41024,#7514,.T.) ;
#51625 = EDGE_CURVE('',#41024,#41025,#7515,.T.) ;
#51626 = EDGE_CURVE('',#41025,#41022,#7516,.T.) ;
#51627 = EDGE_CURVE('',#41026,#41027,#7517,.T.) ;
#51628 = EDGE_CURVE('',#41027,#41028,#7518,.T.) ;
#51629 = EDGE_CURVE('',#41028,#41029,#7519,.T.) ;
#51630 = EDGE_CURVE('',#41029,#41026,#7520,.T.) ;
#51631 = EDGE_CURVE('',#41030,#41031,#7521,.T.) ;
#51632 = EDGE_CURVE('',#41031,#41032,#7522,.T.) ;
#51633 = EDGE_CURVE('',#41032,#41033,#7523,.T.) ;
#51634 = EDGE_CURVE('',#41033,#41030,#7524,.T.) ;
#51635 = EDGE_CURVE('',#41034,#41035,#7525,.T.) ;
#51636 = EDGE_CURVE('',#41035,#41036,#7526,.T.) ;
#51637 = EDGE_CURVE('',#41036,#41037,#7527,.T.) ;
#51638 = EDGE_CURVE('',#41037,#41034,#7528,.T.) ;
#51639 = EDGE_CURVE('',#41038,#41039,#7529,.T.) ;
#51640 = EDGE_CURVE('',#41038,#41040,#33075,.T.) ;
#51641 = EDGE_CURVE('',#41041,#41040,#7530,.T.) ;
#51642 = EDGE_CURVE('',#41041,#41042,#33076,.T.) ;
#51643 = EDGE_CURVE('',#41043,#41042,#7531,.T.) ;
#51644 = EDGE_CURVE('',#41043,#41044,#33077,.T.) ;
#51645 = EDGE_CURVE('',#41045,#41044,#7532,.T.) ;
#51646 = EDGE_CURVE('',#41045,#41039,#33078,.T.) ;
#51647 = EDGE_CURVE('',#41046,#41047,#7533,.T.) ;
#51648 = EDGE_CURVE('',#41047,#41045,#7534,.T.) ;
#51649 = EDGE_CURVE('',#41044,#41046,#7535,.T.) ;
#51650 = EDGE_CURVE('',#41048,#41049,#7536,.T.) ;
#51651 = EDGE_CURVE('',#41049,#41038,#7537,.T.) ;
#51652 = EDGE_CURVE('',#41039,#41048,#7538,.T.) ;
#51653 = EDGE_CURVE('',#41040,#41050,#7539,.T.) ;
#51654 = EDGE_CURVE('',#41050,#41051,#7540,.T.) ;
#51655 = EDGE_CURVE('',#41051,#41041,#7541,.T.) ;
#51656 = EDGE_CURVE('',#41052,#41053,#7542,.T.) ;
#51657 = EDGE_CURVE('',#41053,#41043,#7543,.T.) ;
#51658 = EDGE_CURVE('',#41042,#41052,#7544,.T.) ;
#51659 = EDGE_CURVE('',#41054,#41055,#7545,.T.) ;
#51660 = EDGE_CURVE('',#41055,#41056,#7546,.T.) ;
#51661 = EDGE_CURVE('',#41056,#41057,#7547,.T.) ;
#51662 = EDGE_CURVE('',#41057,#41054,#7548,.T.) ;
#51663 = EDGE_CURVE('',#41058,#41059,#7549,.T.) ;
#51664 = EDGE_CURVE('',#41058,#41060,#33079,.T.) ;
#51665 = EDGE_CURVE('',#41061,#41060,#7550,.T.) ;
#51666 = EDGE_CURVE('',#41061,#41062,#33080,.T.) ;
#51667 = EDGE_CURVE('',#41063,#41062,#7551,.T.) ;
#51668 = EDGE_CURVE('',#41063,#41064,#33081,.T.) ;
#51669 = EDGE_CURVE('',#41065,#41064,#7552,.T.) ;
#51670 = EDGE_CURVE('',#41065,#41059,#33082,.T.) ;
#51671 = EDGE_CURVE('',#41066,#41067,#7553,.T.) ;
#51672 = EDGE_CURVE('',#41067,#41065,#7554,.T.) ;
#51673 = EDGE_CURVE('',#41064,#41066,#7555,.T.) ;
#51674 = EDGE_CURVE('',#41068,#41069,#7556,.T.) ;
#51675 = EDGE_CURVE('',#41069,#41058,#7557,.T.) ;
#51676 = EDGE_CURVE('',#41059,#41068,#7558,.T.) ;
#51677 = EDGE_CURVE('',#41060,#41070,#7559,.T.) ;
#51678 = EDGE_CURVE('',#41070,#41071,#7560,.T.) ;
#51679 = EDGE_CURVE('',#41071,#41061,#7561,.T.) ;
#51680 = EDGE_CURVE('',#41072,#41073,#7562,.T.) ;
#51681 = EDGE_CURVE('',#41073,#41063,#7563,.T.) ;
#51682 = EDGE_CURVE('',#41062,#41072,#7564,.T.) ;
#51683 = EDGE_CURVE('',#41074,#41075,#7565,.T.) ;
#51684 = EDGE_CURVE('',#41075,#41076,#7566,.T.) ;
#51685 = EDGE_CURVE('',#41076,#41077,#7567,.T.) ;
#51686 = EDGE_CURVE('',#41077,#41074,#7568,.T.) ;
#51687 = EDGE_CURVE('',#41078,#41079,#7569,.T.) ;
#51688 = EDGE_CURVE('',#41078,#41080,#33083,.T.) ;
#51689 = EDGE_CURVE('',#41081,#41080,#7570,.T.) ;
#51690 = EDGE_CURVE('',#41081,#41082,#33084,.T.) ;
#51691 = EDGE_CURVE('',#41083,#41082,#7571,.T.) ;
#51692 = EDGE_CURVE('',#41083,#41084,#33085,.T.) ;
#51693 = EDGE_CURVE('',#41085,#41084,#7572,.T.) ;
#51694 = EDGE_CURVE('',#41085,#41079,#33086,.T.) ;
#51695 = EDGE_CURVE('',#41086,#41087,#7573,.T.) ;
#51696 = EDGE_CURVE('',#41087,#41085,#7574,.T.) ;
#51697 = EDGE_CURVE('',#41084,#41086,#7575,.T.) ;
#51698 = EDGE_CURVE('',#41088,#41089,#7576,.T.) ;
#51699 = EDGE_CURVE('',#41089,#41078,#7577,.T.) ;
#51700 = EDGE_CURVE('',#41079,#41088,#7578,.T.) ;
#51701 = EDGE_CURVE('',#41080,#41090,#7579,.T.) ;
#51702 = EDGE_CURVE('',#41090,#41091,#7580,.T.) ;
#51703 = EDGE_CURVE('',#41091,#41081,#7581,.T.) ;
#51704 = EDGE_CURVE('',#41092,#41093,#7582,.T.) ;
#51705 = EDGE_CURVE('',#41093,#41083,#7583,.T.) ;
#51706 = EDGE_CURVE('',#41082,#41092,#7584,.T.) ;
#51707 = EDGE_CURVE('',#41094,#41095,#7585,.T.) ;
#51708 = EDGE_CURVE('',#41095,#41096,#7586,.T.) ;
#51709 = EDGE_CURVE('',#41096,#41097,#7587,.T.) ;
#51710 = EDGE_CURVE('',#41097,#41094,#7588,.T.) ;
#51711 = EDGE_CURVE('',#41098,#41099,#7589,.T.) ;
#51712 = EDGE_CURVE('',#41098,#41100,#33087,.T.) ;
#51713 = EDGE_CURVE('',#41101,#41100,#7590,.T.) ;
#51714 = EDGE_CURVE('',#41101,#41102,#33088,.T.) ;
#51715 = EDGE_CURVE('',#41103,#41102,#7591,.T.) ;
#51716 = EDGE_CURVE('',#41103,#41104,#33089,.T.) ;
#51717 = EDGE_CURVE('',#41105,#41104,#7592,.T.) ;
#51718 = EDGE_CURVE('',#41105,#41099,#33090,.T.) ;
#51719 = EDGE_CURVE('',#41106,#41107,#7593,.T.) ;
#51720 = EDGE_CURVE('',#41107,#41105,#7594,.T.) ;
#51721 = EDGE_CURVE('',#41104,#41106,#7595,.T.) ;
#51722 = EDGE_CURVE('',#41108,#41109,#7596,.T.) ;
#51723 = EDGE_CURVE('',#41109,#41098,#7597,.T.) ;
#51724 = EDGE_CURVE('',#41099,#41108,#7598,.T.) ;
#51725 = EDGE_CURVE('',#41100,#41110,#7599,.T.) ;
#51726 = EDGE_CURVE('',#41110,#41111,#7600,.T.) ;
#51727 = EDGE_CURVE('',#41111,#41101,#7601,.T.) ;
#51728 = EDGE_CURVE('',#41112,#41113,#7602,.T.) ;
#51729 = EDGE_CURVE('',#41113,#41103,#7603,.T.) ;
#51730 = EDGE_CURVE('',#41102,#41112,#7604,.T.) ;
#51731 = EDGE_CURVE('',#41114,#41115,#7605,.T.) ;
#51732 = EDGE_CURVE('',#41115,#41116,#7606,.T.) ;
#51733 = EDGE_CURVE('',#41116,#41117,#7607,.T.) ;
#51734 = EDGE_CURVE('',#41117,#41114,#7608,.T.) ;
#51735 = EDGE_CURVE('',#41118,#41119,#7609,.T.) ;
#51736 = EDGE_CURVE('',#41118,#41120,#33091,.T.) ;
#51737 = EDGE_CURVE('',#41121,#41120,#7610,.T.) ;
#51738 = EDGE_CURVE('',#41121,#41122,#33092,.T.) ;
#51739 = EDGE_CURVE('',#41123,#41122,#7611,.T.) ;
#51740 = EDGE_CURVE('',#41123,#41124,#33093,.T.) ;
#51741 = EDGE_CURVE('',#41125,#41124,#7612,.T.) ;
#51742 = EDGE_CURVE('',#41125,#41119,#33094,.T.) ;
#51743 = EDGE_CURVE('',#41126,#41127,#7613,.T.) ;
#51744 = EDGE_CURVE('',#41127,#41125,#7614,.T.) ;
#51745 = EDGE_CURVE('',#41124,#41126,#7615,.T.) ;
#51746 = EDGE_CURVE('',#41128,#41129,#7616,.T.) ;
#51747 = EDGE_CURVE('',#41129,#41118,#7617,.T.) ;
#51748 = EDGE_CURVE('',#41119,#41128,#7618,.T.) ;
#51749 = EDGE_CURVE('',#41120,#41130,#7619,.T.) ;
#51750 = EDGE_CURVE('',#41130,#41131,#7620,.T.) ;
#51751 = EDGE_CURVE('',#41131,#41121,#7621,.T.) ;
#51752 = EDGE_CURVE('',#41132,#41133,#7622,.T.) ;
#51753 = EDGE_CURVE('',#41133,#41123,#7623,.T.) ;
#51754 = EDGE_CURVE('',#41122,#41132,#7624,.T.) ;
#51755 = EDGE_CURVE('',#41134,#41135,#7625,.T.) ;
#51756 = EDGE_CURVE('',#41135,#41136,#7626,.T.) ;
#51757 = EDGE_CURVE('',#41136,#41137,#7627,.T.) ;
#51758 = EDGE_CURVE('',#41137,#41134,#7628,.T.) ;
#51759 = EDGE_CURVE('',#41138,#41139,#7629,.T.) ;
#51760 = EDGE_CURVE('',#41138,#41140,#33095,.T.) ;
#51761 = EDGE_CURVE('',#41141,#41140,#7630,.T.) ;
#51762 = EDGE_CURVE('',#41141,#41142,#33096,.T.) ;
#51763 = EDGE_CURVE('',#41143,#41142,#7631,.T.) ;
#51764 = EDGE_CURVE('',#41143,#41144,#33097,.T.) ;
#51765 = EDGE_CURVE('',#41145,#41144,#7632,.T.) ;
#51766 = EDGE_CURVE('',#41145,#41139,#33098,.T.) ;
#51767 = EDGE_CURVE('',#41146,#41147,#7633,.T.) ;
#51768 = EDGE_CURVE('',#41147,#41145,#7634,.T.) ;
#51769 = EDGE_CURVE('',#41144,#41146,#7635,.T.) ;
#51770 = EDGE_CURVE('',#41148,#41149,#7636,.T.) ;
#51771 = EDGE_CURVE('',#41149,#41138,#7637,.T.) ;
#51772 = EDGE_CURVE('',#41139,#41148,#7638,.T.) ;
#51773 = EDGE_CURVE('',#41140,#41150,#7639,.T.) ;
#51774 = EDGE_CURVE('',#41150,#41151,#7640,.T.) ;
#51775 = EDGE_CURVE('',#41151,#41141,#7641,.T.) ;
#51776 = EDGE_CURVE('',#41152,#41153,#7642,.T.) ;
#51777 = EDGE_CURVE('',#41153,#41143,#7643,.T.) ;
#51778 = EDGE_CURVE('',#41142,#41152,#7644,.T.) ;
#51779 = EDGE_CURVE('',#41154,#41155,#7645,.T.) ;
#51780 = EDGE_CURVE('',#41155,#41156,#7646,.T.) ;
#51781 = EDGE_CURVE('',#41156,#41157,#7647,.T.) ;
#51782 = EDGE_CURVE('',#41157,#41154,#7648,.T.) ;
#51783 = EDGE_CURVE('',#41158,#41159,#7649,.T.) ;
#51784 = EDGE_CURVE('',#41158,#41160,#33099,.T.) ;
#51785 = EDGE_CURVE('',#41161,#41160,#7650,.T.) ;
#51786 = EDGE_CURVE('',#41161,#41162,#33100,.T.) ;
#51787 = EDGE_CURVE('',#41163,#41162,#7651,.T.) ;
#51788 = EDGE_CURVE('',#41163,#41164,#33101,.T.) ;
#51789 = EDGE_CURVE('',#41165,#41164,#7652,.T.) ;
#51790 = EDGE_CURVE('',#41165,#41159,#33102,.T.) ;
#51791 = EDGE_CURVE('',#41166,#41167,#7653,.T.) ;
#51792 = EDGE_CURVE('',#41167,#41165,#7654,.T.) ;
#51793 = EDGE_CURVE('',#41164,#41166,#7655,.T.) ;
#51794 = EDGE_CURVE('',#41168,#41169,#7656,.T.) ;
#51795 = EDGE_CURVE('',#41169,#41158,#7657,.T.) ;
#51796 = EDGE_CURVE('',#41159,#41168,#7658,.T.) ;
#51797 = EDGE_CURVE('',#41160,#41170,#7659,.T.) ;
#51798 = EDGE_CURVE('',#41170,#41171,#7660,.T.) ;
#51799 = EDGE_CURVE('',#41171,#41161,#7661,.T.) ;
#51800 = EDGE_CURVE('',#41172,#41173,#7662,.T.) ;
#51801 = EDGE_CURVE('',#41173,#41163,#7663,.T.) ;
#51802 = EDGE_CURVE('',#41162,#41172,#7664,.T.) ;
#51803 = EDGE_CURVE('',#41174,#41175,#7665,.T.) ;
#51804 = EDGE_CURVE('',#41175,#41176,#7666,.T.) ;
#51805 = EDGE_CURVE('',#41176,#41177,#7667,.T.) ;
#51806 = EDGE_CURVE('',#41177,#41174,#7668,.T.) ;
#51807 = EDGE_CURVE('',#41178,#41179,#7669,.T.) ;
#51808 = EDGE_CURVE('',#41178,#41180,#33103,.T.) ;
#51809 = EDGE_CURVE('',#41181,#41180,#7670,.T.) ;
#51810 = EDGE_CURVE('',#41181,#41182,#33104,.T.) ;
#51811 = EDGE_CURVE('',#41183,#41182,#7671,.T.) ;
#51812 = EDGE_CURVE('',#41183,#41184,#33105,.T.) ;
#51813 = EDGE_CURVE('',#41185,#41184,#7672,.T.) ;
#51814 = EDGE_CURVE('',#41185,#41179,#33106,.T.) ;
#51815 = EDGE_CURVE('',#41186,#41187,#7673,.T.) ;
#51816 = EDGE_CURVE('',#41187,#41185,#7674,.T.) ;
#51817 = EDGE_CURVE('',#41184,#41186,#7675,.T.) ;
#51818 = EDGE_CURVE('',#41188,#41189,#7676,.T.) ;
#51819 = EDGE_CURVE('',#41189,#41178,#7677,.T.) ;
#51820 = EDGE_CURVE('',#41179,#41188,#7678,.T.) ;
#51821 = EDGE_CURVE('',#41180,#41190,#7679,.T.) ;
#51822 = EDGE_CURVE('',#41190,#41191,#7680,.T.) ;
#51823 = EDGE_CURVE('',#41191,#41181,#7681,.T.) ;
#51824 = EDGE_CURVE('',#41192,#41193,#7682,.T.) ;
#51825 = EDGE_CURVE('',#41193,#41183,#7683,.T.) ;
#51826 = EDGE_CURVE('',#41182,#41192,#7684,.T.) ;
#51827 = EDGE_CURVE('',#41194,#41195,#7685,.T.) ;
#51828 = EDGE_CURVE('',#41195,#41196,#7686,.T.) ;
#51829 = EDGE_CURVE('',#41196,#41197,#7687,.T.) ;
#51830 = EDGE_CURVE('',#41197,#41194,#7688,.T.) ;
#51831 = EDGE_CURVE('',#41198,#41199,#7689,.T.) ;
#51832 = EDGE_CURVE('',#41198,#41200,#33107,.T.) ;
#51833 = EDGE_CURVE('',#41201,#41200,#7690,.T.) ;
#51834 = EDGE_CURVE('',#41201,#41202,#33108,.T.) ;
#51835 = EDGE_CURVE('',#41203,#41202,#7691,.T.) ;
#51836 = EDGE_CURVE('',#41203,#41204,#33109,.T.) ;
#51837 = EDGE_CURVE('',#41205,#41204,#7692,.T.) ;
#51838 = EDGE_CURVE('',#41205,#41199,#33110,.T.) ;
#51839 = EDGE_CURVE('',#41206,#41207,#7693,.T.) ;
#51840 = EDGE_CURVE('',#41207,#41205,#7694,.T.) ;
#51841 = EDGE_CURVE('',#41204,#41206,#7695,.T.) ;
#51842 = EDGE_CURVE('',#41208,#41209,#7696,.T.) ;
#51843 = EDGE_CURVE('',#41209,#41198,#7697,.T.) ;
#51844 = EDGE_CURVE('',#41199,#41208,#7698,.T.) ;
#51845 = EDGE_CURVE('',#41200,#41210,#7699,.T.) ;
#51846 = EDGE_CURVE('',#41210,#41211,#7700,.T.) ;
#51847 = EDGE_CURVE('',#41211,#41201,#7701,.T.) ;
#51848 = EDGE_CURVE('',#41212,#41213,#7702,.T.) ;
#51849 = EDGE_CURVE('',#41213,#41203,#7703,.T.) ;
#51850 = EDGE_CURVE('',#41202,#41212,#7704,.T.) ;
#51851 = EDGE_CURVE('',#41214,#41215,#7705,.T.) ;
#51852 = EDGE_CURVE('',#41215,#41216,#7706,.T.) ;
#51853 = EDGE_CURVE('',#41216,#41217,#7707,.T.) ;
#51854 = EDGE_CURVE('',#41217,#41214,#7708,.T.) ;
#51855 = EDGE_CURVE('',#41218,#41219,#7709,.T.) ;
#51856 = EDGE_CURVE('',#41219,#41220,#7710,.T.) ;
#51857 = EDGE_CURVE('',#41220,#41221,#7711,.T.) ;
#51858 = EDGE_CURVE('',#41221,#41218,#7712,.T.) ;
#51859 = EDGE_CURVE('',#41222,#41223,#7713,.T.) ;
#51860 = EDGE_CURVE('',#41223,#41224,#7714,.T.) ;
#51861 = EDGE_CURVE('',#41224,#41225,#7715,.T.) ;
#51862 = EDGE_CURVE('',#41225,#41222,#7716,.T.) ;
#51863 = EDGE_CURVE('',#41226,#41227,#7717,.T.) ;
#51864 = EDGE_CURVE('',#41227,#41228,#7718,.T.) ;
#51865 = EDGE_CURVE('',#41228,#41229,#7719,.T.) ;
#51866 = EDGE_CURVE('',#41229,#41226,#7720,.T.) ;
#51867 = EDGE_CURVE('',#41230,#41231,#7721,.T.) ;
#51868 = EDGE_CURVE('',#41231,#41232,#7722,.T.) ;
#51869 = EDGE_CURVE('',#41232,#41233,#7723,.T.) ;
#51870 = EDGE_CURVE('',#41233,#41230,#7724,.T.) ;
#51871 = EDGE_CURVE('',#41234,#41235,#7725,.T.) ;
#51872 = EDGE_CURVE('',#41235,#41236,#7726,.T.) ;
#51873 = EDGE_CURVE('',#41236,#41237,#7727,.T.) ;
#51874 = EDGE_CURVE('',#41237,#41234,#7728,.T.) ;
#51875 = EDGE_CURVE('',#41238,#41239,#7729,.T.) ;
#51876 = EDGE_CURVE('',#41239,#41240,#7730,.T.) ;
#51877 = EDGE_CURVE('',#41240,#41241,#7731,.T.) ;
#51878 = EDGE_CURVE('',#41241,#41238,#7732,.T.) ;
#51879 = EDGE_CURVE('',#41242,#41243,#7733,.T.) ;
#51880 = EDGE_CURVE('',#41243,#41244,#7734,.T.) ;
#51881 = EDGE_CURVE('',#41244,#41245,#7735,.T.) ;
#51882 = EDGE_CURVE('',#41245,#41242,#7736,.T.) ;
#51883 = EDGE_CURVE('',#41246,#41247,#7737,.T.) ;
#51884 = EDGE_CURVE('',#41247,#41248,#7738,.T.) ;
#51885 = EDGE_CURVE('',#41248,#41249,#7739,.T.) ;
#51886 = EDGE_CURVE('',#41249,#41246,#7740,.T.) ;
#51887 = EDGE_CURVE('',#39027,#39011,#7741,.T.) ;
#51888 = EDGE_CURVE('',#39010,#38994,#7742,.T.) ;
#51889 = EDGE_CURVE('',#38993,#38977,#7743,.T.) ;
#51890 = EDGE_CURVE('',#38976,#38960,#7744,.T.) ;
#51891 = EDGE_CURVE('',#38959,#38943,#7745,.T.) ;
#51892 = EDGE_CURVE('',#38942,#38926,#7746,.T.) ;
#51893 = EDGE_CURVE('',#38925,#38909,#7747,.T.) ;
#51894 = EDGE_CURVE('',#38908,#38892,#7748,.T.) ;
#51895 = EDGE_CURVE('',#38891,#38875,#7749,.T.) ;
#51896 = EDGE_CURVE('',#38877,#38890,#7750,.T.) ;
#51897 = EDGE_CURVE('',#38889,#38878,#7751,.T.) ;
#51898 = EDGE_CURVE('',#38881,#38886,#7752,.T.) ;
#51899 = EDGE_CURVE('',#38885,#38882,#7753,.T.) ;
#51900 = EDGE_CURVE('',#38879,#38888,#7754,.T.) ;
#51901 = EDGE_CURVE('',#38887,#38880,#7755,.T.) ;
#51902 = EDGE_CURVE('',#38894,#38907,#7756,.T.) ;
#51903 = EDGE_CURVE('',#38906,#38895,#7757,.T.) ;
#51904 = EDGE_CURVE('',#38898,#38903,#7758,.T.) ;
#51905 = EDGE_CURVE('',#38902,#38899,#7759,.T.) ;
#51906 = EDGE_CURVE('',#38896,#38905,#7760,.T.) ;
#51907 = EDGE_CURVE('',#38904,#38897,#7761,.T.) ;
#51908 = EDGE_CURVE('',#38911,#38924,#7762,.T.) ;
#51909 = EDGE_CURVE('',#38923,#38912,#7763,.T.) ;
#51910 = EDGE_CURVE('',#38915,#38920,#7764,.T.) ;
#51911 = EDGE_CURVE('',#38919,#38916,#7765,.T.) ;
#51912 = EDGE_CURVE('',#38913,#38922,#7766,.T.) ;
#51913 = EDGE_CURVE('',#38921,#38914,#7767,.T.) ;
#51914 = EDGE_CURVE('',#38928,#38941,#7768,.T.) ;
#51915 = EDGE_CURVE('',#38940,#38929,#7769,.T.) ;
#51916 = EDGE_CURVE('',#38932,#38937,#7770,.T.) ;
#51917 = EDGE_CURVE('',#38936,#38933,#7771,.T.) ;
#51918 = EDGE_CURVE('',#38930,#38939,#7772,.T.) ;
#51919 = EDGE_CURVE('',#38938,#38931,#7773,.T.) ;
#51920 = EDGE_CURVE('',#38945,#38958,#7774,.T.) ;
#51921 = EDGE_CURVE('',#38957,#38946,#7775,.T.) ;
#51922 = EDGE_CURVE('',#38949,#38954,#7776,.T.) ;
#51923 = EDGE_CURVE('',#38953,#38950,#7777,.T.) ;
#51924 = EDGE_CURVE('',#38947,#38956,#7778,.T.) ;
#51925 = EDGE_CURVE('',#38955,#38948,#7779,.T.) ;
#51926 = EDGE_CURVE('',#38962,#38975,#7780,.T.) ;
#51927 = EDGE_CURVE('',#38974,#38963,#7781,.T.) ;
#51928 = EDGE_CURVE('',#38966,#38971,#7782,.T.) ;
#51929 = EDGE_CURVE('',#38970,#38967,#7783,.T.) ;
#51930 = EDGE_CURVE('',#38964,#38973,#7784,.T.) ;
#51931 = EDGE_CURVE('',#38972,#38965,#7785,.T.) ;
#51932 = EDGE_CURVE('',#38979,#38992,#7786,.T.) ;
#51933 = EDGE_CURVE('',#38991,#38980,#7787,.T.) ;
#51934 = EDGE_CURVE('',#38983,#38988,#7788,.T.) ;
#51935 = EDGE_CURVE('',#38987,#38984,#7789,.T.) ;
#51936 = EDGE_CURVE('',#38981,#38990,#7790,.T.) ;
#51937 = EDGE_CURVE('',#38989,#38982,#7791,.T.) ;
#51938 = EDGE_CURVE('',#38996,#39009,#7792,.T.) ;
#51939 = EDGE_CURVE('',#39008,#38997,#7793,.T.) ;
#51940 = EDGE_CURVE('',#39000,#39005,#7794,.T.) ;
#51941 = EDGE_CURVE('',#39004,#39001,#7795,.T.) ;
#51942 = EDGE_CURVE('',#38998,#39007,#7796,.T.) ;
#51943 = EDGE_CURVE('',#39006,#38999,#7797,.T.) ;
#51944 = EDGE_CURVE('',#39013,#39026,#7798,.T.) ;
#51945 = EDGE_CURVE('',#39025,#39014,#7799,.T.) ;
#51946 = EDGE_CURVE('',#39017,#39022,#7800,.T.) ;
#51947 = EDGE_CURVE('',#39021,#39018,#7801,.T.) ;
#51948 = EDGE_CURVE('',#39015,#39024,#7802,.T.) ;
#51949 = EDGE_CURVE('',#39023,#39016,#7803,.T.) ;
#51950 = EDGE_CURVE('',#41250,#41251,#7804,.T.) ;
#51951 = EDGE_CURVE('',#41251,#41252,#33111,.T.) ;
#51952 = EDGE_CURVE('',#41253,#41252,#7805,.T.) ;
#51953 = EDGE_CURVE('',#41253,#41250,#33112,.T.) ;
#51954 = EDGE_CURVE('',#41252,#41254,#7806,.T.) ;
#51955 = EDGE_CURVE('',#41255,#41254,#7807,.T.) ;
#51956 = EDGE_CURVE('',#41255,#41253,#7808,.T.) ;
#51957 = EDGE_CURVE('',#41254,#41256,#33113,.T.) ;
#51958 = EDGE_CURVE('',#41257,#41256,#7809,.T.) ;
#51959 = EDGE_CURVE('',#41257,#41255,#33114,.T.) ;
#51960 = EDGE_CURVE('',#41256,#41258,#7810,.T.) ;
#51961 = EDGE_CURVE('',#41259,#41258,#7811,.T.) ;
#51962 = EDGE_CURVE('',#41259,#41257,#7812,.T.) ;
#51963 = EDGE_CURVE('',#41258,#41260,#33115,.T.) ;
#51964 = EDGE_CURVE('',#41261,#41260,#7813,.T.) ;
#51965 = EDGE_CURVE('',#41261,#41259,#33116,.T.) ;
#51966 = EDGE_CURVE('',#41260,#41262,#7814,.T.) ;
#51967 = EDGE_CURVE('',#41263,#41262,#7815,.T.) ;
#51968 = EDGE_CURVE('',#41263,#41261,#7816,.T.) ;
#51969 = EDGE_CURVE('',#41262,#41264,#33117,.T.) ;
#51970 = EDGE_CURVE('',#41265,#41264,#7817,.T.) ;
#51971 = EDGE_CURVE('',#41265,#41263,#33118,.T.) ;
#51972 = EDGE_CURVE('',#41250,#41265,#7818,.T.) ;
#51973 = EDGE_CURVE('',#41264,#41251,#7819,.T.) ;
#51974 = EDGE_CURVE('',#41266,#41267,#7820,.T.) ;
#51975 = EDGE_CURVE('',#41267,#41268,#7821,.T.) ;
#51976 = EDGE_CURVE('',#41268,#41269,#7822,.T.) ;
#51977 = EDGE_CURVE('',#41269,#41266,#7823,.T.) ;
#51978 = EDGE_CURVE('',#41270,#41271,#7824,.T.) ;
#51979 = EDGE_CURVE('',#41271,#41272,#33119,.T.) ;
#51980 = EDGE_CURVE('',#41273,#41272,#7825,.T.) ;
#51981 = EDGE_CURVE('',#41273,#41270,#33120,.T.) ;
#51982 = EDGE_CURVE('',#41272,#41274,#7826,.T.) ;
#51983 = EDGE_CURVE('',#41275,#41274,#7827,.T.) ;
#51984 = EDGE_CURVE('',#41275,#41273,#7828,.T.) ;
#51985 = EDGE_CURVE('',#41274,#41276,#33121,.T.) ;
#51986 = EDGE_CURVE('',#41277,#41276,#7829,.T.) ;
#51987 = EDGE_CURVE('',#41277,#41275,#33122,.T.) ;
#51988 = EDGE_CURVE('',#41276,#41278,#7830,.T.) ;
#51989 = EDGE_CURVE('',#41279,#41278,#7831,.T.) ;
#51990 = EDGE_CURVE('',#41279,#41277,#7832,.T.) ;
#51991 = EDGE_CURVE('',#41278,#41280,#33123,.T.) ;
#51992 = EDGE_CURVE('',#41281,#41280,#7833,.T.) ;
#51993 = EDGE_CURVE('',#41281,#41279,#33124,.T.) ;
#51994 = EDGE_CURVE('',#41280,#41282,#7834,.T.) ;
#51995 = EDGE_CURVE('',#41283,#41282,#7835,.T.) ;
#51996 = EDGE_CURVE('',#41283,#41281,#7836,.T.) ;
#51997 = EDGE_CURVE('',#41282,#41284,#33125,.T.) ;
#51998 = EDGE_CURVE('',#41285,#41284,#7837,.T.) ;
#51999 = EDGE_CURVE('',#41285,#41283,#33126,.T.) ;
#52000 = EDGE_CURVE('',#41270,#41285,#7838,.T.) ;
#52001 = EDGE_CURVE('',#41284,#41271,#7839,.T.) ;
#52002 = EDGE_CURVE('',#41286,#41287,#7840,.T.) ;
#52003 = EDGE_CURVE('',#41287,#41288,#7841,.T.) ;
#52004 = EDGE_CURVE('',#41288,#41289,#7842,.T.) ;
#52005 = EDGE_CURVE('',#41289,#41286,#7843,.T.) ;
#52006 = EDGE_CURVE('',#41290,#41291,#7844,.T.) ;
#52007 = EDGE_CURVE('',#41291,#41292,#33127,.T.) ;
#52008 = EDGE_CURVE('',#41293,#41292,#7845,.T.) ;
#52009 = EDGE_CURVE('',#41293,#41290,#33128,.T.) ;
#52010 = EDGE_CURVE('',#41292,#41294,#7846,.T.) ;
#52011 = EDGE_CURVE('',#41295,#41294,#7847,.T.) ;
#52012 = EDGE_CURVE('',#41295,#41293,#7848,.T.) ;
#52013 = EDGE_CURVE('',#41294,#41296,#33129,.T.) ;
#52014 = EDGE_CURVE('',#41297,#41296,#7849,.T.) ;
#52015 = EDGE_CURVE('',#41297,#41295,#33130,.T.) ;
#52016 = EDGE_CURVE('',#41296,#41298,#7850,.T.) ;
#52017 = EDGE_CURVE('',#41299,#41298,#7851,.T.) ;
#52018 = EDGE_CURVE('',#41299,#41297,#7852,.T.) ;
#52019 = EDGE_CURVE('',#41298,#41300,#33131,.T.) ;
#52020 = EDGE_CURVE('',#41301,#41300,#7853,.T.) ;
#52021 = EDGE_CURVE('',#41301,#41299,#33132,.T.) ;
#52022 = EDGE_CURVE('',#41300,#41302,#7854,.T.) ;
#52023 = EDGE_CURVE('',#41303,#41302,#7855,.T.) ;
#52024 = EDGE_CURVE('',#41303,#41301,#7856,.T.) ;
#52025 = EDGE_CURVE('',#41302,#41304,#33133,.T.) ;
#52026 = EDGE_CURVE('',#41305,#41304,#7857,.T.) ;
#52027 = EDGE_CURVE('',#41305,#41303,#33134,.T.) ;
#52028 = EDGE_CURVE('',#41290,#41305,#7858,.T.) ;
#52029 = EDGE_CURVE('',#41304,#41291,#7859,.T.) ;
#52030 = EDGE_CURVE('',#41306,#41307,#7860,.T.) ;
#52031 = EDGE_CURVE('',#41307,#41308,#7861,.T.) ;
#52032 = EDGE_CURVE('',#41308,#41309,#7862,.T.) ;
#52033 = EDGE_CURVE('',#41309,#41306,#7863,.T.) ;
#52034 = EDGE_CURVE('',#41310,#41311,#7864,.T.) ;
#52035 = EDGE_CURVE('',#41311,#41312,#33135,.T.) ;
#52036 = EDGE_CURVE('',#41313,#41312,#7865,.T.) ;
#52037 = EDGE_CURVE('',#41313,#41310,#33136,.T.) ;
#52038 = EDGE_CURVE('',#41312,#41314,#7866,.T.) ;
#52039 = EDGE_CURVE('',#41315,#41314,#7867,.T.) ;
#52040 = EDGE_CURVE('',#41315,#41313,#7868,.T.) ;
#52041 = EDGE_CURVE('',#41314,#41316,#33137,.T.) ;
#52042 = EDGE_CURVE('',#41317,#41316,#7869,.T.) ;
#52043 = EDGE_CURVE('',#41317,#41315,#33138,.T.) ;
#52044 = EDGE_CURVE('',#41316,#41318,#7870,.T.) ;
#52045 = EDGE_CURVE('',#41319,#41318,#7871,.T.) ;
#52046 = EDGE_CURVE('',#41319,#41317,#7872,.T.) ;
#52047 = EDGE_CURVE('',#41318,#41320,#33139,.T.) ;
#52048 = EDGE_CURVE('',#41321,#41320,#7873,.T.) ;
#52049 = EDGE_CURVE('',#41321,#41319,#33140,.T.) ;
#52050 = EDGE_CURVE('',#41320,#41322,#7874,.T.) ;
#52051 = EDGE_CURVE('',#41323,#41322,#7875,.T.) ;
#52052 = EDGE_CURVE('',#41323,#41321,#7876,.T.) ;
#52053 = EDGE_CURVE('',#41322,#41324,#33141,.T.) ;
#52054 = EDGE_CURVE('',#41325,#41324,#7877,.T.) ;
#52055 = EDGE_CURVE('',#41325,#41323,#33142,.T.) ;
#52056 = EDGE_CURVE('',#41310,#41325,#7878,.T.) ;
#52057 = EDGE_CURVE('',#41324,#41311,#7879,.T.) ;
#52058 = EDGE_CURVE('',#41326,#41327,#7880,.T.) ;
#52059 = EDGE_CURVE('',#41327,#41328,#7881,.T.) ;
#52060 = EDGE_CURVE('',#41328,#41329,#7882,.T.) ;
#52061 = EDGE_CURVE('',#41329,#41326,#7883,.T.) ;
#52062 = EDGE_CURVE('',#41330,#41331,#7884,.T.) ;
#52063 = EDGE_CURVE('',#41331,#41332,#33143,.T.) ;
#52064 = EDGE_CURVE('',#41333,#41332,#7885,.T.) ;
#52065 = EDGE_CURVE('',#41333,#41330,#33144,.T.) ;
#52066 = EDGE_CURVE('',#41332,#41334,#7886,.T.) ;
#52067 = EDGE_CURVE('',#41335,#41334,#7887,.T.) ;
#52068 = EDGE_CURVE('',#41335,#41333,#7888,.T.) ;
#52069 = EDGE_CURVE('',#41334,#41336,#33145,.T.) ;
#52070 = EDGE_CURVE('',#41337,#41336,#7889,.T.) ;
#52071 = EDGE_CURVE('',#41337,#41335,#33146,.T.) ;
#52072 = EDGE_CURVE('',#41336,#41338,#7890,.T.) ;
#52073 = EDGE_CURVE('',#41339,#41338,#7891,.T.) ;
#52074 = EDGE_CURVE('',#41339,#41337,#7892,.T.) ;
#52075 = EDGE_CURVE('',#41338,#41340,#33147,.T.) ;
#52076 = EDGE_CURVE('',#41341,#41340,#7893,.T.) ;
#52077 = EDGE_CURVE('',#41341,#41339,#33148,.T.) ;
#52078 = EDGE_CURVE('',#41340,#41342,#7894,.T.) ;
#52079 = EDGE_CURVE('',#41343,#41342,#7895,.T.) ;
#52080 = EDGE_CURVE('',#41343,#41341,#7896,.T.) ;
#52081 = EDGE_CURVE('',#41342,#41344,#33149,.T.) ;
#52082 = EDGE_CURVE('',#41345,#41344,#7897,.T.) ;
#52083 = EDGE_CURVE('',#41345,#41343,#33150,.T.) ;
#52084 = EDGE_CURVE('',#41330,#41345,#7898,.T.) ;
#52085 = EDGE_CURVE('',#41344,#41331,#7899,.T.) ;
#52086 = EDGE_CURVE('',#41346,#41347,#7900,.T.) ;
#52087 = EDGE_CURVE('',#41347,#41348,#7901,.T.) ;
#52088 = EDGE_CURVE('',#41348,#41349,#7902,.T.) ;
#52089 = EDGE_CURVE('',#41349,#41346,#7903,.T.) ;
#52090 = EDGE_CURVE('',#41350,#41351,#7904,.T.) ;
#52091 = EDGE_CURVE('',#41351,#41352,#33151,.T.) ;
#52092 = EDGE_CURVE('',#41353,#41352,#7905,.T.) ;
#52093 = EDGE_CURVE('',#41353,#41350,#33152,.T.) ;
#52094 = EDGE_CURVE('',#41352,#41354,#7906,.T.) ;
#52095 = EDGE_CURVE('',#41355,#41354,#7907,.T.) ;
#52096 = EDGE_CURVE('',#41355,#41353,#7908,.T.) ;
#52097 = EDGE_CURVE('',#41354,#41356,#33153,.T.) ;
#52098 = EDGE_CURVE('',#41357,#41356,#7909,.T.) ;
#52099 = EDGE_CURVE('',#41357,#41355,#33154,.T.) ;
#52100 = EDGE_CURVE('',#41356,#41358,#7910,.T.) ;
#52101 = EDGE_CURVE('',#41359,#41358,#7911,.T.) ;
#52102 = EDGE_CURVE('',#41359,#41357,#7912,.T.) ;
#52103 = EDGE_CURVE('',#41358,#41360,#33155,.T.) ;
#52104 = EDGE_CURVE('',#41361,#41360,#7913,.T.) ;
#52105 = EDGE_CURVE('',#41361,#41359,#33156,.T.) ;
#52106 = EDGE_CURVE('',#41360,#41362,#7914,.T.) ;
#52107 = EDGE_CURVE('',#41363,#41362,#7915,.T.) ;
#52108 = EDGE_CURVE('',#41363,#41361,#7916,.T.) ;
#52109 = EDGE_CURVE('',#41362,#41364,#33157,.T.) ;
#52110 = EDGE_CURVE('',#41365,#41364,#7917,.T.) ;
#52111 = EDGE_CURVE('',#41365,#41363,#33158,.T.) ;
#52112 = EDGE_CURVE('',#41350,#41365,#7918,.T.) ;
#52113 = EDGE_CURVE('',#41364,#41351,#7919,.T.) ;
#52114 = EDGE_CURVE('',#41366,#41367,#7920,.T.) ;
#52115 = EDGE_CURVE('',#41367,#41368,#7921,.T.) ;
#52116 = EDGE_CURVE('',#41368,#41369,#7922,.T.) ;
#52117 = EDGE_CURVE('',#41369,#41366,#7923,.T.) ;
#52118 = EDGE_CURVE('',#41370,#41371,#7924,.T.) ;
#52119 = EDGE_CURVE('',#41371,#41372,#33159,.T.) ;
#52120 = EDGE_CURVE('',#41373,#41372,#7925,.T.) ;
#52121 = EDGE_CURVE('',#41373,#41370,#33160,.T.) ;
#52122 = EDGE_CURVE('',#41372,#41374,#7926,.T.) ;
#52123 = EDGE_CURVE('',#41375,#41374,#7927,.T.) ;
#52124 = EDGE_CURVE('',#41375,#41373,#7928,.T.) ;
#52125 = EDGE_CURVE('',#41374,#41376,#33161,.T.) ;
#52126 = EDGE_CURVE('',#41377,#41376,#7929,.T.) ;
#52127 = EDGE_CURVE('',#41377,#41375,#33162,.T.) ;
#52128 = EDGE_CURVE('',#41376,#41378,#7930,.T.) ;
#52129 = EDGE_CURVE('',#41379,#41378,#7931,.T.) ;
#52130 = EDGE_CURVE('',#41379,#41377,#7932,.T.) ;
#52131 = EDGE_CURVE('',#41378,#41380,#33163,.T.) ;
#52132 = EDGE_CURVE('',#41381,#41380,#7933,.T.) ;
#52133 = EDGE_CURVE('',#41381,#41379,#33164,.T.) ;
#52134 = EDGE_CURVE('',#41380,#41382,#7934,.T.) ;
#52135 = EDGE_CURVE('',#41383,#41382,#7935,.T.) ;
#52136 = EDGE_CURVE('',#41383,#41381,#7936,.T.) ;
#52137 = EDGE_CURVE('',#41382,#41384,#33165,.T.) ;
#52138 = EDGE_CURVE('',#41385,#41384,#7937,.T.) ;
#52139 = EDGE_CURVE('',#41385,#41383,#33166,.T.) ;
#52140 = EDGE_CURVE('',#41370,#41385,#7938,.T.) ;
#52141 = EDGE_CURVE('',#41384,#41371,#7939,.T.) ;
#52142 = EDGE_CURVE('',#41386,#41387,#7940,.T.) ;
#52143 = EDGE_CURVE('',#41387,#41388,#7941,.T.) ;
#52144 = EDGE_CURVE('',#41388,#41389,#7942,.T.) ;
#52145 = EDGE_CURVE('',#41389,#41386,#7943,.T.) ;
#52146 = EDGE_CURVE('',#41390,#41391,#7944,.T.) ;
#52147 = EDGE_CURVE('',#41391,#41392,#33167,.T.) ;
#52148 = EDGE_CURVE('',#41393,#41392,#7945,.T.) ;
#52149 = EDGE_CURVE('',#41393,#41390,#33168,.T.) ;
#52150 = EDGE_CURVE('',#41392,#41394,#7946,.T.) ;
#52151 = EDGE_CURVE('',#41395,#41394,#7947,.T.) ;
#52152 = EDGE_CURVE('',#41395,#41393,#7948,.T.) ;
#52153 = EDGE_CURVE('',#41394,#41396,#33169,.T.) ;
#52154 = EDGE_CURVE('',#41397,#41396,#7949,.T.) ;
#52155 = EDGE_CURVE('',#41397,#41395,#33170,.T.) ;
#52156 = EDGE_CURVE('',#41396,#41398,#7950,.T.) ;
#52157 = EDGE_CURVE('',#41399,#41398,#7951,.T.) ;
#52158 = EDGE_CURVE('',#41399,#41397,#7952,.T.) ;
#52159 = EDGE_CURVE('',#41398,#41400,#33171,.T.) ;
#52160 = EDGE_CURVE('',#41401,#41400,#7953,.T.) ;
#52161 = EDGE_CURVE('',#41401,#41399,#33172,.T.) ;
#52162 = EDGE_CURVE('',#41400,#41402,#7954,.T.) ;
#52163 = EDGE_CURVE('',#41403,#41402,#7955,.T.) ;
#52164 = EDGE_CURVE('',#41403,#41401,#7956,.T.) ;
#52165 = EDGE_CURVE('',#41402,#41404,#33173,.T.) ;
#52166 = EDGE_CURVE('',#41405,#41404,#7957,.T.) ;
#52167 = EDGE_CURVE('',#41405,#41403,#33174,.T.) ;
#52168 = EDGE_CURVE('',#41390,#41405,#7958,.T.) ;
#52169 = EDGE_CURVE('',#41404,#41391,#7959,.T.) ;
#52170 = EDGE_CURVE('',#41406,#41407,#7960,.T.) ;
#52171 = EDGE_CURVE('',#41407,#41408,#7961,.T.) ;
#52172 = EDGE_CURVE('',#41408,#41409,#7962,.T.) ;
#52173 = EDGE_CURVE('',#41409,#41406,#7963,.T.) ;
#52174 = EDGE_CURVE('',#41410,#41411,#7964,.T.) ;
#52175 = EDGE_CURVE('',#41411,#41412,#33175,.T.) ;
#52176 = EDGE_CURVE('',#41413,#41412,#7965,.T.) ;
#52177 = EDGE_CURVE('',#41413,#41410,#33176,.T.) ;
#52178 = EDGE_CURVE('',#41412,#41414,#7966,.T.) ;
#52179 = EDGE_CURVE('',#41415,#41414,#7967,.T.) ;
#52180 = EDGE_CURVE('',#41415,#41413,#7968,.T.) ;
#52181 = EDGE_CURVE('',#41414,#41416,#33177,.T.) ;
#52182 = EDGE_CURVE('',#41417,#41416,#7969,.T.) ;
#52183 = EDGE_CURVE('',#41417,#41415,#33178,.T.) ;
#52184 = EDGE_CURVE('',#41416,#41418,#7970,.T.) ;
#52185 = EDGE_CURVE('',#41419,#41418,#7971,.T.) ;
#52186 = EDGE_CURVE('',#41419,#41417,#7972,.T.) ;
#52187 = EDGE_CURVE('',#41418,#41420,#33179,.T.) ;
#52188 = EDGE_CURVE('',#41421,#41420,#7973,.T.) ;
#52189 = EDGE_CURVE('',#41421,#41419,#33180,.T.) ;
#52190 = EDGE_CURVE('',#41420,#41422,#7974,.T.) ;
#52191 = EDGE_CURVE('',#41423,#41422,#7975,.T.) ;
#52192 = EDGE_CURVE('',#41423,#41421,#7976,.T.) ;
#52193 = EDGE_CURVE('',#41422,#41424,#33181,.T.) ;
#52194 = EDGE_CURVE('',#41425,#41424,#7977,.T.) ;
#52195 = EDGE_CURVE('',#41425,#41423,#33182,.T.) ;
#52196 = EDGE_CURVE('',#41410,#41425,#7978,.T.) ;
#52197 = EDGE_CURVE('',#41424,#41411,#7979,.T.) ;
#52198 = EDGE_CURVE('',#41426,#41427,#7980,.T.) ;
#52199 = EDGE_CURVE('',#41427,#41428,#7981,.T.) ;
#52200 = EDGE_CURVE('',#41428,#41429,#7982,.T.) ;
#52201 = EDGE_CURVE('',#41429,#41426,#7983,.T.) ;
#52202 = EDGE_CURVE('',#40742,#40728,#33183,.T.) ;
#52203 = EDGE_CURVE('',#40739,#40742,#33184,.T.) ;
#52204 = EDGE_CURVE('',#40728,#40739,#33185,.T.) ;
#52205 = EDGE_CURVE('',#40736,#40741,#33186,.T.) ;
#52206 = EDGE_CURVE('',#40729,#40738,#33187,.T.) ;
#52207 = EDGE_CURVE('',#40743,#40731,#33188,.T.) ;
#52208 = EDGE_CURVE('',#40494,#40744,#33189,.T.) ;
#52209 = EDGE_CURVE('',#40495,#40743,#33190,.T.) ;
#52210 = EDGE_CURVE('',#40744,#39246,#33191,.T.) ;
#52211 = EDGE_CURVE('',#39245,#40745,#33192,.T.) ;
#52212 = EDGE_CURVE('',#40736,#40735,#33193,.T.) ;
#52213 = EDGE_CURVE('',#40735,#40741,#33194,.T.) ;
#52214 = EDGE_CURVE('',#40729,#39391,#33195,.T.) ;
#52215 = EDGE_CURVE('',#39392,#40738,#33196,.T.) ;
#52216 = EDGE_CURVE('',#40495,#40731,#33197,.T.) ;
#52217 = EDGE_CURVE('',#40745,#40485,#33198,.T.) ;
#52218 = EDGE_CURVE('',#40740,#40484,#33199,.T.) ;
#52219 = EDGE_CURVE('',#40732,#40740,#33200,.T.) ;
#52220 = EDGE_CURVE('',#40737,#40734,#33201,.T.) ;
#52221 = EDGE_CURVE('',#39386,#40737,#33202,.T.) ;
#52222 = EDGE_CURVE('',#40730,#39390,#33203,.T.) ;
#52223 = EDGE_CURVE('',#40496,#40730,#33204,.T.) ;
#52224 = EDGE_CURVE('',#40732,#40484,#33205,.T.) ;
#52225 = EDGE_CURVE('',#39385,#40734,#33206,.T.) ;
#52226 = EDGE_CURVE('',#40497,#39390,#33207,.T.) ;
#52227 = EDGE_CURVE('',#40733,#40483,#33208,.T.) ;
#52228 = EDGE_CURVE('',#39387,#40733,#33209,.T.) ;
#52229 = EDGE_CURVE('',#40498,#39389,#33210,.T.) ;
#52230 = EDGE_CURVE('',#40502,#40491,#33211,.T.) ;
#52231 = EDGE_CURVE('',#40503,#40490,#33212,.T.) ;
#52232 = EDGE_CURVE('',#39447,#40500,#33213,.T.) ;
#52233 = EDGE_CURVE('',#39448,#40503,#33214,.T.) ;
#52234 = EDGE_CURVE('',#39387,#40482,#33215,.T.) ;
#52235 = EDGE_CURVE('',#40498,#40489,#33216,.T.) ;
#52236 = EDGE_CURVE('',#40489,#39389,#33217,.T.) ;
#52237 = EDGE_CURVE('',#39448,#40490,#33218,.T.) ;
#52238 = EDGE_CURVE('',#39388,#40481,#33219,.T.) ;
#52239 = EDGE_CURVE('',#40486,#39388,#33220,.T.) ;
#52240 = EDGE_CURVE('',#40499,#40488,#33221,.T.) ;
#52241 = EDGE_CURVE('',#39449,#40499,#33222,.T.) ;
#52242 = EDGE_CURVE('',#40486,#40481,#33223,.T.) ;
#52243 = EDGE_CURVE('',#39450,#40488,#33224,.T.) ;
#52244 = EDGE_CURVE('',#40478,#39463,#33225,.T.) ;
#52245 = EDGE_CURVE('',#40479,#39737,#33226,.T.) ;
#52246 = EDGE_CURVE('',#40487,#40480,#33227,.T.) ;
#52247 = EDGE_CURVE('',#39451,#40487,#33228,.T.) ;
#52248 = EDGE_CURVE('',#40479,#39453,#33229,.T.) ;
#52249 = EDGE_CURVE('',#39452,#40480,#33230,.T.) ;
#52250 = EDGE_CURVE('',#39255,#41254,#33231,.T.) ;
#52251 = EDGE_CURVE('',#41256,#39254,#33232,.T.) ;
#52252 = EDGE_CURVE('',#41258,#39253,#33233,.T.) ;
#52253 = EDGE_CURVE('',#39256,#41252,#33234,.T.) ;
#52254 = EDGE_CURVE('',#41260,#39252,#33235,.T.) ;
#52255 = EDGE_CURVE('',#39249,#41251,#33236,.T.) ;
#52256 = EDGE_CURVE('',#41262,#39251,#33237,.T.) ;
#52257 = EDGE_CURVE('',#39250,#41264,#33238,.T.) ;
#52258 = EDGE_CURVE('',#40122,#41430,#453,.T.) ;
#52259 = EDGE_CURVE('',#41430,#39557,#2311,.T.) ;
#52260 = EDGE_CURVE('',#39560,#41431,#2312,.T.) ;
#52261 = EDGE_CURVE('',#41431,#40123,#454,.T.) ;
#52262 = EDGE_CURVE('',#39559,#41432,#2313,.T.) ;
#52263 = EDGE_CURVE('',#41432,#40117,#455,.T.) ;
#52264 = EDGE_CURVE('',#40116,#41433,#456,.T.) ;
#52265 = EDGE_CURVE('',#41433,#39560,#2314,.T.) ;
#52266 = EDGE_CURVE('',#39557,#41434,#2315,.T.) ;
#52267 = EDGE_CURVE('',#41434,#40125,#457,.T.) ;
#52268 = EDGE_CURVE('',#40124,#41435,#458,.T.) ;
#52269 = EDGE_CURVE('',#41435,#39558,#2316,.T.) ;
#52270 = EDGE_CURVE('',#39558,#41436,#2317,.T.) ;
#52271 = EDGE_CURVE('',#41436,#40129,#459,.T.) ;
#52272 = EDGE_CURVE('',#40128,#41437,#460,.T.) ;
#52273 = EDGE_CURVE('',#41437,#39559,#2318,.T.) ;
#52274 = EDGE_CURVE('',#40138,#41438,#461,.T.) ;
#52275 = EDGE_CURVE('',#41438,#39561,#2319,.T.) ;
#52276 = EDGE_CURVE('',#39564,#41439,#2320,.T.) ;
#52277 = EDGE_CURVE('',#41439,#40139,#462,.T.) ;
#52278 = EDGE_CURVE('',#39563,#41440,#2321,.T.) ;
#52279 = EDGE_CURVE('',#41440,#40133,#463,.T.) ;
#52280 = EDGE_CURVE('',#40132,#41441,#464,.T.) ;
#52281 = EDGE_CURVE('',#41441,#39564,#2322,.T.) ;
#52282 = EDGE_CURVE('',#39561,#41442,#2323,.T.) ;
#52283 = EDGE_CURVE('',#41442,#40141,#465,.T.) ;
#52284 = EDGE_CURVE('',#40140,#41443,#466,.T.) ;
#52285 = EDGE_CURVE('',#41443,#39562,#2324,.T.) ;
#52286 = EDGE_CURVE('',#39562,#41444,#2325,.T.) ;
#52287 = EDGE_CURVE('',#41444,#40145,#467,.T.) ;
#52288 = EDGE_CURVE('',#40144,#41445,#468,.T.) ;
#52289 = EDGE_CURVE('',#41445,#39563,#2326,.T.) ;
#52290 = EDGE_CURVE('',#40154,#41446,#469,.T.) ;
#52291 = EDGE_CURVE('',#41446,#39565,#2327,.T.) ;
#52292 = EDGE_CURVE('',#39568,#41447,#2328,.T.) ;
#52293 = EDGE_CURVE('',#41447,#40155,#470,.T.) ;
#52294 = EDGE_CURVE('',#39567,#41448,#2329,.T.) ;
#52295 = EDGE_CURVE('',#41448,#40149,#471,.T.) ;
#52296 = EDGE_CURVE('',#40148,#41449,#472,.T.) ;
#52297 = EDGE_CURVE('',#41449,#39568,#2330,.T.) ;
#52298 = EDGE_CURVE('',#39565,#41450,#2331,.T.) ;
#52299 = EDGE_CURVE('',#41450,#40157,#473,.T.) ;
#52300 = EDGE_CURVE('',#40156,#41451,#474,.T.) ;
#52301 = EDGE_CURVE('',#41451,#39566,#2332,.T.) ;
#52302 = EDGE_CURVE('',#39566,#41452,#2333,.T.) ;
#52303 = EDGE_CURVE('',#41452,#40161,#475,.T.) ;
#52304 = EDGE_CURVE('',#40160,#41453,#476,.T.) ;
#52305 = EDGE_CURVE('',#41453,#39567,#2334,.T.) ;
#52306 = EDGE_CURVE('',#40170,#41454,#477,.T.) ;
#52307 = EDGE_CURVE('',#41454,#39569,#2335,.T.) ;
#52308 = EDGE_CURVE('',#39572,#41455,#2336,.T.) ;
#52309 = EDGE_CURVE('',#41455,#40171,#478,.T.) ;
#52310 = EDGE_CURVE('',#39571,#41456,#2337,.T.) ;
#52311 = EDGE_CURVE('',#41456,#40165,#479,.T.) ;
#52312 = EDGE_CURVE('',#40164,#41457,#480,.T.) ;
#52313 = EDGE_CURVE('',#41457,#39572,#2338,.T.) ;
#52314 = EDGE_CURVE('',#39569,#41458,#2339,.T.) ;
#52315 = EDGE_CURVE('',#41458,#40173,#481,.T.) ;
#52316 = EDGE_CURVE('',#40172,#41459,#482,.T.) ;
#52317 = EDGE_CURVE('',#41459,#39570,#2340,.T.) ;
#52318 = EDGE_CURVE('',#39570,#41460,#2341,.T.) ;
#52319 = EDGE_CURVE('',#41460,#40177,#483,.T.) ;
#52320 = EDGE_CURVE('',#40176,#41461,#484,.T.) ;
#52321 = EDGE_CURVE('',#41461,#39571,#2342,.T.) ;
#52322 = EDGE_CURVE('',#40186,#41462,#485,.T.) ;
#52323 = EDGE_CURVE('',#41462,#39573,#2343,.T.) ;
#52324 = EDGE_CURVE('',#39576,#41463,#2344,.T.) ;
#52325 = EDGE_CURVE('',#41463,#40187,#486,.T.) ;
#52326 = EDGE_CURVE('',#39575,#41464,#2345,.T.) ;
#52327 = EDGE_CURVE('',#41464,#40181,#487,.T.) ;
#52328 = EDGE_CURVE('',#40180,#41465,#488,.T.) ;
#52329 = EDGE_CURVE('',#41465,#39576,#2346,.T.) ;
#52330 = EDGE_CURVE('',#39573,#41466,#2347,.T.) ;
#52331 = EDGE_CURVE('',#41466,#40189,#489,.T.) ;
#52332 = EDGE_CURVE('',#40188,#41467,#490,.T.) ;
#52333 = EDGE_CURVE('',#41467,#39574,#2348,.T.) ;
#52334 = EDGE_CURVE('',#39574,#41468,#2349,.T.) ;
#52335 = EDGE_CURVE('',#41468,#40193,#491,.T.) ;
#52336 = EDGE_CURVE('',#40192,#41469,#492,.T.) ;
#52337 = EDGE_CURVE('',#41469,#39575,#2350,.T.) ;
#52338 = EDGE_CURVE('',#40202,#41470,#493,.T.) ;
#52339 = EDGE_CURVE('',#41470,#39577,#2351,.T.) ;
#52340 = EDGE_CURVE('',#39580,#41471,#2352,.T.) ;
#52341 = EDGE_CURVE('',#41471,#40203,#494,.T.) ;
#52342 = EDGE_CURVE('',#39579,#41472,#2353,.T.) ;
#52343 = EDGE_CURVE('',#41472,#40197,#495,.T.) ;
#52344 = EDGE_CURVE('',#40196,#41473,#496,.T.) ;
#52345 = EDGE_CURVE('',#41473,#39580,#2354,.T.) ;
#52346 = EDGE_CURVE('',#39577,#41474,#2355,.T.) ;
#52347 = EDGE_CURVE('',#41474,#40205,#497,.T.) ;
#52348 = EDGE_CURVE('',#40204,#41475,#498,.T.) ;
#52349 = EDGE_CURVE('',#41475,#39578,#2356,.T.) ;
#52350 = EDGE_CURVE('',#39578,#41476,#2357,.T.) ;
#52351 = EDGE_CURVE('',#41476,#40209,#499,.T.) ;
#52352 = EDGE_CURVE('',#40208,#41477,#500,.T.) ;
#52353 = EDGE_CURVE('',#41477,#39579,#2358,.T.) ;
#52354 = EDGE_CURVE('',#40218,#41478,#501,.T.) ;
#52355 = EDGE_CURVE('',#41478,#39581,#2359,.T.) ;
#52356 = EDGE_CURVE('',#39584,#41479,#2360,.T.) ;
#52357 = EDGE_CURVE('',#41479,#40219,#502,.T.) ;
#52358 = EDGE_CURVE('',#39583,#41480,#2361,.T.) ;
#52359 = EDGE_CURVE('',#41480,#40213,#503,.T.) ;
#52360 = EDGE_CURVE('',#40212,#41481,#504,.T.) ;
#52361 = EDGE_CURVE('',#41481,#39584,#2362,.T.) ;
#52362 = EDGE_CURVE('',#39581,#41482,#2363,.T.) ;
#52363 = EDGE_CURVE('',#41482,#40221,#505,.T.) ;
#52364 = EDGE_CURVE('',#40220,#41483,#506,.T.) ;
#52365 = EDGE_CURVE('',#41483,#39582,#2364,.T.) ;
#52366 = EDGE_CURVE('',#39582,#41484,#2365,.T.) ;
#52367 = EDGE_CURVE('',#41484,#40225,#507,.T.) ;
#52368 = EDGE_CURVE('',#40224,#41485,#508,.T.) ;
#52369 = EDGE_CURVE('',#41485,#39583,#2366,.T.) ;
#52370 = EDGE_CURVE('',#40234,#41486,#509,.T.) ;
#52371 = EDGE_CURVE('',#41486,#39585,#2367,.T.) ;
#52372 = EDGE_CURVE('',#39588,#41487,#2368,.T.) ;
#52373 = EDGE_CURVE('',#41487,#40235,#510,.T.) ;
#52374 = EDGE_CURVE('',#39587,#41488,#2369,.T.) ;
#52375 = EDGE_CURVE('',#41488,#40229,#511,.T.) ;
#52376 = EDGE_CURVE('',#40228,#41489,#512,.T.) ;
#52377 = EDGE_CURVE('',#41489,#39588,#2370,.T.) ;
#52378 = EDGE_CURVE('',#39585,#41490,#2371,.T.) ;
#52379 = EDGE_CURVE('',#41490,#40237,#513,.T.) ;
#52380 = EDGE_CURVE('',#40236,#41491,#514,.T.) ;
#52381 = EDGE_CURVE('',#41491,#39586,#2372,.T.) ;
#52382 = EDGE_CURVE('',#39586,#41492,#2373,.T.) ;
#52383 = EDGE_CURVE('',#41492,#40241,#515,.T.) ;
#52384 = EDGE_CURVE('',#40240,#41493,#516,.T.) ;
#52385 = EDGE_CURVE('',#41493,#39587,#2374,.T.) ;
#52386 = EDGE_CURVE('',#39595,#40259,#33239,.T.) ;
#52387 = EDGE_CURVE('',#40256,#39594,#33240,.T.) ;
#52388 = EDGE_CURVE('',#40255,#39593,#33241,.T.) ;
#52389 = EDGE_CURVE('',#40256,#40255,#33242,.T.) ;
#52390 = EDGE_CURVE('',#40247,#40259,#33243,.T.) ;
#52391 = EDGE_CURVE('',#39596,#40247,#33244,.T.) ;
#52392 = EDGE_CURVE('',#40252,#39592,#33245,.T.) ;
#52393 = EDGE_CURVE('',#40257,#40254,#33246,.T.) ;
#52394 = EDGE_CURVE('',#40258,#40263,#33247,.T.) ;
#52395 = EDGE_CURVE('',#40260,#40257,#33248,.T.) ;
#52396 = EDGE_CURVE('',#40244,#40258,#33249,.T.) ;
#52397 = EDGE_CURVE('',#39590,#40246,#33250,.T.) ;
#52398 = EDGE_CURVE('',#39591,#40250,#33251,.T.) ;
#52399 = EDGE_CURVE('',#40251,#39589,#33252,.T.) ;
#52400 = EDGE_CURVE('',#40252,#40250,#33253,.T.) ;
#52401 = EDGE_CURVE('',#40260,#40254,#33254,.T.) ;
#52402 = EDGE_CURVE('',#40244,#40263,#33255,.T.) ;
#52403 = EDGE_CURVE('',#40251,#40246,#33256,.T.) ;
#52404 = EDGE_CURVE('',#40253,#40249,#33257,.T.) ;
#52405 = EDGE_CURVE('',#40261,#40253,#33258,.T.) ;
#52406 = EDGE_CURVE('',#40245,#40262,#33259,.T.) ;
#52407 = EDGE_CURVE('',#40248,#40245,#33260,.T.) ;
#52408 = EDGE_CURVE('',#40261,#40249,#33261,.T.) ;
#52409 = EDGE_CURVE('',#40248,#40262,#33262,.T.) ;
#52410 = EDGE_CURVE('',#40272,#40279,#33263,.T.) ;
#52411 = EDGE_CURVE('',#40273,#40443,#33264,.T.) ;
#52412 = EDGE_CURVE('',#40440,#40272,#33265,.T.) ;
#52413 = EDGE_CURVE('',#40274,#40273,#33266,.T.) ;
#52414 = EDGE_CURVE('',#40440,#40279,#33267,.T.) ;
#52415 = EDGE_CURVE('',#40274,#40443,#33268,.T.) ;
#52416 = EDGE_CURVE('',#40278,#40277,#33269,.T.) ;
#52417 = EDGE_CURVE('',#40441,#40278,#33270,.T.) ;
#52418 = EDGE_CURVE('',#40275,#40442,#33271,.T.) ;
#52419 = EDGE_CURVE('',#40276,#40275,#33272,.T.) ;
#52420 = EDGE_CURVE('',#40441,#40277,#33273,.T.) ;
#52421 = EDGE_CURVE('',#40276,#40442,#33274,.T.) ;
#52422 = EDGE_CURVE('',#39996,#40065,#33275,.T.) ;
#52423 = EDGE_CURVE('',#39996,#39994,#33276,.T.) ;
#52424 = EDGE_CURVE('',#39994,#40065,#33277,.T.) ;
#52425 = EDGE_CURVE('',#39995,#40064,#2375,.T.) ;
#52426 = EDGE_CURVE('',#39997,#39993,#33278,.T.) ;
#52427 = EDGE_CURVE('',#40014,#39997,#33279,.T.) ;
#52428 = EDGE_CURVE('',#39995,#39475,#33280,.T.) ;
#52429 = EDGE_CURVE('',#39476,#40064,#33281,.T.) ;
#52430 = EDGE_CURVE('',#40014,#39993,#33282,.T.) ;
#52431 = EDGE_CURVE('',#40066,#40007,#33283,.T.) ;
#52432 = EDGE_CURVE('',#40067,#40011,#2376,.T.) ;
#52433 = EDGE_CURVE('',#40008,#40066,#33284,.T.) ;
#52434 = EDGE_CURVE('',#39477,#40067,#33285,.T.) ;
#52435 = EDGE_CURVE('',#39992,#39474,#33286,.T.) ;
#52436 = EDGE_CURVE('',#40015,#39992,#517,.T.) ;
#52437 = EDGE_CURVE('',#40008,#40007,#33287,.T.) ;
#52438 = EDGE_CURVE('',#39478,#40011,#33288,.T.) ;
#52439 = EDGE_CURVE('',#40015,#39473,#33289,.T.) ;
#52440 = EDGE_CURVE('',#40006,#40013,#33290,.T.) ;
#52441 = EDGE_CURVE('',#40009,#40006,#33291,.T.) ;
#52442 = EDGE_CURVE('',#39472,#40010,#33292,.T.) ;
#52443 = EDGE_CURVE('',#40012,#39471,#33293,.T.) ;
#52444 = EDGE_CURVE('',#40009,#40013,#33294,.T.) ;
#52445 = EDGE_CURVE('',#40012,#40010,#518,.T.) ;
#52446 = EDGE_CURVE('',#39482,#41494,#519,.T.) ;
#52447 = EDGE_CURVE('',#41494,#39989,#520,.T.) ;
#52448 = EDGE_CURVE('',#39988,#41495,#521,.T.) ;
#52449 = EDGE_CURVE('',#41495,#41496,#522,.T.) ;
#52450 = EDGE_CURVE('',#41496,#39479,#523,.T.) ;
#52451 = EDGE_CURVE('',#39479,#41497,#524,.T.) ;
#52452 = EDGE_CURVE('',#41497,#40017,#525,.T.) ;
#52453 = EDGE_CURVE('',#40016,#41498,#526,.T.) ;
#52454 = EDGE_CURVE('',#41498,#39480,#527,.T.) ;
#52455 = EDGE_CURVE('',#40068,#39482,#528,.T.) ;
#52456 = EDGE_CURVE('',#39481,#40069,#529,.T.) ;
#52457 = EDGE_CURVE('',#39480,#41499,#530,.T.) ;
#52458 = EDGE_CURVE('',#41499,#41500,#531,.T.) ;
#52459 = EDGE_CURVE('',#41500,#39973,#532,.T.) ;
#52460 = EDGE_CURVE('',#39972,#41501,#533,.T.) ;
#52461 = EDGE_CURVE('',#41501,#39481,#534,.T.) ;
#52462 = EDGE_CURVE('',#39486,#41502,#535,.T.) ;
#52463 = EDGE_CURVE('',#41502,#39969,#536,.T.) ;
#52464 = EDGE_CURVE('',#39968,#41503,#537,.T.) ;
#52465 = EDGE_CURVE('',#41503,#41504,#538,.T.) ;
#52466 = EDGE_CURVE('',#41504,#39483,#539,.T.) ;
#52467 = EDGE_CURVE('',#39483,#41505,#540,.T.) ;
#52468 = EDGE_CURVE('',#41505,#40023,#541,.T.) ;
#52469 = EDGE_CURVE('',#40022,#41506,#542,.T.) ;
#52470 = EDGE_CURVE('',#41506,#39484,#543,.T.) ;
#52471 = EDGE_CURVE('',#40074,#39486,#544,.T.) ;
#52472 = EDGE_CURVE('',#39485,#40075,#545,.T.) ;
#52473 = EDGE_CURVE('',#39484,#41507,#546,.T.) ;
#52474 = EDGE_CURVE('',#41507,#41508,#547,.T.) ;
#52475 = EDGE_CURVE('',#41508,#39953,#548,.T.) ;
#52476 = EDGE_CURVE('',#39952,#41509,#549,.T.) ;
#52477 = EDGE_CURVE('',#41509,#39485,#550,.T.) ;
#52478 = EDGE_CURVE('',#39490,#41510,#551,.T.) ;
#52479 = EDGE_CURVE('',#41510,#39949,#552,.T.) ;
#52480 = EDGE_CURVE('',#39948,#41511,#553,.T.) ;
#52481 = EDGE_CURVE('',#41511,#41512,#554,.T.) ;
#52482 = EDGE_CURVE('',#41512,#39487,#555,.T.) ;
#52483 = EDGE_CURVE('',#39487,#41513,#556,.T.) ;
#52484 = EDGE_CURVE('',#41513,#40029,#557,.T.) ;
#52485 = EDGE_CURVE('',#40028,#41514,#558,.T.) ;
#52486 = EDGE_CURVE('',#41514,#39488,#559,.T.) ;
#52487 = EDGE_CURVE('',#40080,#39490,#560,.T.) ;
#52488 = EDGE_CURVE('',#39489,#40081,#561,.T.) ;
#52489 = EDGE_CURVE('',#39488,#41515,#562,.T.) ;
#52490 = EDGE_CURVE('',#41515,#41516,#563,.T.) ;
#52491 = EDGE_CURVE('',#41516,#39933,#564,.T.) ;
#52492 = EDGE_CURVE('',#39932,#41517,#565,.T.) ;
#52493 = EDGE_CURVE('',#41517,#39489,#566,.T.) ;
#52494 = EDGE_CURVE('',#39494,#41518,#567,.T.) ;
#52495 = EDGE_CURVE('',#41518,#39929,#568,.T.) ;
#52496 = EDGE_CURVE('',#39928,#41519,#569,.T.) ;
#52497 = EDGE_CURVE('',#41519,#41520,#570,.T.) ;
#52498 = EDGE_CURVE('',#41520,#39491,#571,.T.) ;
#52499 = EDGE_CURVE('',#39491,#41521,#572,.T.) ;
#52500 = EDGE_CURVE('',#41521,#40035,#573,.T.) ;
#52501 = EDGE_CURVE('',#40034,#41522,#574,.T.) ;
#52502 = EDGE_CURVE('',#41522,#39492,#575,.T.) ;
#52503 = EDGE_CURVE('',#40086,#39494,#576,.T.) ;
#52504 = EDGE_CURVE('',#39493,#40087,#577,.T.) ;
#52505 = EDGE_CURVE('',#39492,#41523,#578,.T.) ;
#52506 = EDGE_CURVE('',#41523,#41524,#579,.T.) ;
#52507 = EDGE_CURVE('',#41524,#39913,#580,.T.) ;
#52508 = EDGE_CURVE('',#39912,#41525,#581,.T.) ;
#52509 = EDGE_CURVE('',#41525,#39493,#582,.T.) ;
#52510 = EDGE_CURVE('',#39498,#41526,#583,.T.) ;
#52511 = EDGE_CURVE('',#41526,#39909,#584,.T.) ;
#52512 = EDGE_CURVE('',#39908,#41527,#585,.T.) ;
#52513 = EDGE_CURVE('',#41527,#41528,#586,.T.) ;
#52514 = EDGE_CURVE('',#41528,#39495,#587,.T.) ;
#52515 = EDGE_CURVE('',#39495,#41529,#588,.T.) ;
#52516 = EDGE_CURVE('',#41529,#40041,#589,.T.) ;
#52517 = EDGE_CURVE('',#40040,#41530,#590,.T.) ;
#52518 = EDGE_CURVE('',#41530,#39496,#591,.T.) ;
#52519 = EDGE_CURVE('',#40092,#39498,#592,.T.) ;
#52520 = EDGE_CURVE('',#39497,#40093,#593,.T.) ;
#52521 = EDGE_CURVE('',#39496,#41531,#594,.T.) ;
#52522 = EDGE_CURVE('',#41531,#41532,#595,.T.) ;
#52523 = EDGE_CURVE('',#41532,#39893,#596,.T.) ;
#52524 = EDGE_CURVE('',#39892,#41533,#597,.T.) ;
#52525 = EDGE_CURVE('',#41533,#39497,#598,.T.) ;
#52526 = EDGE_CURVE('',#39502,#41534,#599,.T.) ;
#52527 = EDGE_CURVE('',#41534,#39889,#600,.T.) ;
#52528 = EDGE_CURVE('',#39888,#41535,#601,.T.) ;
#52529 = EDGE_CURVE('',#41535,#41536,#602,.T.) ;
#52530 = EDGE_CURVE('',#41536,#39499,#603,.T.) ;
#52531 = EDGE_CURVE('',#39499,#41537,#604,.T.) ;
#52532 = EDGE_CURVE('',#41537,#40047,#605,.T.) ;
#52533 = EDGE_CURVE('',#40046,#41538,#606,.T.) ;
#52534 = EDGE_CURVE('',#41538,#39500,#607,.T.) ;
#52535 = EDGE_CURVE('',#40098,#39502,#608,.T.) ;
#52536 = EDGE_CURVE('',#39501,#40099,#609,.T.) ;
#52537 = EDGE_CURVE('',#39500,#41539,#610,.T.) ;
#52538 = EDGE_CURVE('',#41539,#41540,#611,.T.) ;
#52539 = EDGE_CURVE('',#41540,#39873,#612,.T.) ;
#52540 = EDGE_CURVE('',#39872,#41541,#613,.T.) ;
#52541 = EDGE_CURVE('',#41541,#39501,#614,.T.) ;
#52542 = EDGE_CURVE('',#39506,#41542,#615,.T.) ;
#52543 = EDGE_CURVE('',#41542,#39869,#616,.T.) ;
#52544 = EDGE_CURVE('',#39868,#41543,#617,.T.) ;
#52545 = EDGE_CURVE('',#41543,#41544,#618,.T.) ;
#52546 = EDGE_CURVE('',#41544,#39503,#619,.T.) ;
#52547 = EDGE_CURVE('',#39503,#41545,#620,.T.) ;
#52548 = EDGE_CURVE('',#41545,#40053,#621,.T.) ;
#52549 = EDGE_CURVE('',#40052,#41546,#622,.T.) ;
#52550 = EDGE_CURVE('',#41546,#39504,#623,.T.) ;
#52551 = EDGE_CURVE('',#40104,#39506,#624,.T.) ;
#52552 = EDGE_CURVE('',#39505,#40105,#625,.T.) ;
#52553 = EDGE_CURVE('',#39504,#41547,#626,.T.) ;
#52554 = EDGE_CURVE('',#41547,#41548,#627,.T.) ;
#52555 = EDGE_CURVE('',#41548,#39853,#628,.T.) ;
#52556 = EDGE_CURVE('',#39852,#41549,#629,.T.) ;
#52557 = EDGE_CURVE('',#41549,#39505,#630,.T.) ;
#52558 = EDGE_CURVE('',#39510,#41550,#631,.T.) ;
#52559 = EDGE_CURVE('',#41550,#39849,#632,.T.) ;
#52560 = EDGE_CURVE('',#39848,#41551,#633,.T.) ;
#52561 = EDGE_CURVE('',#41551,#41552,#634,.T.) ;
#52562 = EDGE_CURVE('',#41552,#39507,#635,.T.) ;
#52563 = EDGE_CURVE('',#39507,#41553,#636,.T.) ;
#52564 = EDGE_CURVE('',#41553,#40059,#637,.T.) ;
#52565 = EDGE_CURVE('',#40058,#41554,#638,.T.) ;
#52566 = EDGE_CURVE('',#41554,#39508,#639,.T.) ;
#52567 = EDGE_CURVE('',#40110,#39510,#640,.T.) ;
#52568 = EDGE_CURVE('',#39509,#40111,#641,.T.) ;
#52569 = EDGE_CURVE('',#39508,#41555,#642,.T.) ;
#52570 = EDGE_CURVE('',#41555,#41556,#643,.T.) ;
#52571 = EDGE_CURVE('',#41556,#39833,#644,.T.) ;
#52572 = EDGE_CURVE('',#39832,#41557,#645,.T.) ;
#52573 = EDGE_CURVE('',#41557,#39509,#646,.T.) ;
#52574 = EDGE_CURVE('',#39115,#41032,#33295,.T.) ;
#52575 = EDGE_CURVE('',#41033,#39114,#33296,.T.) ;
#52576 = EDGE_CURVE('',#41029,#39113,#33297,.T.) ;
#52577 = EDGE_CURVE('',#41033,#41029,#33298,.T.) ;
#52578 = EDGE_CURVE('',#41021,#41032,#33299,.T.) ;
#52579 = EDGE_CURVE('',#39116,#41021,#33300,.T.) ;
#52580 = EDGE_CURVE('',#41026,#39112,#33301,.T.) ;
#52581 = EDGE_CURVE('',#41030,#41028,#33302,.T.) ;
#52582 = EDGE_CURVE('',#41031,#41037,#33303,.T.) ;
#52583 = EDGE_CURVE('',#41034,#41030,#33304,.T.) ;
#52584 = EDGE_CURVE('',#41018,#41031,#33305,.T.) ;
#52585 = EDGE_CURVE('',#39110,#41020,#33306,.T.) ;
#52586 = EDGE_CURVE('',#39111,#41022,#33307,.T.) ;
#52587 = EDGE_CURVE('',#41023,#39109,#33308,.T.) ;
#52588 = EDGE_CURVE('',#41026,#41022,#33309,.T.) ;
#52589 = EDGE_CURVE('',#41034,#41028,#33310,.T.) ;
#52590 = EDGE_CURVE('',#41018,#41037,#33311,.T.) ;
#52591 = EDGE_CURVE('',#41023,#41020,#33312,.T.) ;
#52592 = EDGE_CURVE('',#41027,#41025,#33313,.T.) ;
#52593 = EDGE_CURVE('',#41035,#41027,#33314,.T.) ;
#52594 = EDGE_CURVE('',#41019,#41036,#33315,.T.) ;
#52595 = EDGE_CURVE('',#41024,#41019,#33316,.T.) ;
#52596 = EDGE_CURVE('',#41035,#41025,#33317,.T.) ;
#52597 = EDGE_CURVE('',#41024,#41036,#33318,.T.) ;
#52598 = EDGE_CURVE('',#41046,#41053,#33319,.T.) ;
#52599 = EDGE_CURVE('',#41047,#41217,#33320,.T.) ;
#52600 = EDGE_CURVE('',#41214,#41046,#33321,.T.) ;
#52601 = EDGE_CURVE('',#41048,#41047,#33322,.T.) ;
#52602 = EDGE_CURVE('',#41214,#41053,#33323,.T.) ;
#52603 = EDGE_CURVE('',#41048,#41217,#33324,.T.) ;
#52604 = EDGE_CURVE('',#41052,#41051,#33325,.T.) ;
#52605 = EDGE_CURVE('',#41215,#41052,#33326,.T.) ;
#52606 = EDGE_CURVE('',#41049,#41216,#33327,.T.) ;
#52607 = EDGE_CURVE('',#41050,#41049,#33328,.T.) ;
#52608 = EDGE_CURVE('',#41215,#41051,#33329,.T.) ;
#52609 = EDGE_CURVE('',#41050,#41216,#33330,.T.) ;
#52610 = EDGE_CURVE('',#41257,#41269,#33331,.T.) ;
#52611 = EDGE_CURVE('',#41266,#41259,#33332,.T.) ;
#52612 = EDGE_CURVE('',#41266,#41261,#33333,.T.) ;
#52613 = EDGE_CURVE('',#41255,#41269,#33334,.T.) ;
#52614 = EDGE_CURVE('',#41267,#41263,#33335,.T.) ;
#52615 = EDGE_CURVE('',#41253,#41268,#33336,.T.) ;
#52616 = EDGE_CURVE('',#41267,#41265,#33337,.T.) ;
#52617 = EDGE_CURVE('',#41250,#41268,#33338,.T.) ;
#52618 = EDGE_CURVE('',#40759,#40754,#33339,.T.) ;
#52619 = EDGE_CURVE('',#40753,#40759,#33340,.T.) ;
#52620 = EDGE_CURVE('',#40754,#40753,#33341,.T.) ;
#52621 = EDGE_CURVE('',#40750,#40758,#33342,.T.) ;
#52622 = EDGE_CURVE('',#40755,#40752,#33343,.T.) ;
#52623 = EDGE_CURVE('',#40760,#40757,#33344,.T.) ;
#52624 = EDGE_CURVE('',#40763,#40513,#33345,.T.) ;
#52625 = EDGE_CURVE('',#40758,#40512,#33346,.T.) ;
#52626 = EDGE_CURVE('',#40750,#40512,#33347,.T.) ;
#52627 = EDGE_CURVE('',#40755,#39378,#33348,.T.) ;
#52628 = EDGE_CURVE('',#39377,#40752,#33349,.T.) ;
#52629 = EDGE_CURVE('',#40760,#40746,#33350,.T.) ;
#52630 = EDGE_CURVE('',#40746,#40757,#33351,.T.) ;
#52631 = EDGE_CURVE('',#40762,#39234,#33352,.T.) ;
#52632 = EDGE_CURVE('',#39233,#40763,#33353,.T.) ;
#52633 = EDGE_CURVE('',#40751,#40511,#33354,.T.) ;
#52634 = EDGE_CURVE('',#39379,#40751,#33355,.T.) ;
#52635 = EDGE_CURVE('',#40756,#39384,#33356,.T.) ;
#52636 = EDGE_CURVE('',#40747,#40756,#33357,.T.) ;
#52637 = EDGE_CURVE('',#40761,#40749,#33358,.T.) ;
#52638 = EDGE_CURVE('',#40522,#40762,#33359,.T.) ;
#52639 = EDGE_CURVE('',#40523,#40761,#33360,.T.) ;
#52640 = EDGE_CURVE('',#39379,#40510,#33361,.T.) ;
#52641 = EDGE_CURVE('',#40747,#39383,#33362,.T.) ;
#52642 = EDGE_CURVE('',#40523,#40749,#33363,.T.) ;
#52643 = EDGE_CURVE('',#40506,#40501,#33364,.T.) ;
#52644 = EDGE_CURVE('',#40507,#40500,#33365,.T.) ;
#52645 = EDGE_CURVE('',#39380,#40509,#33366,.T.) ;
#52646 = EDGE_CURVE('',#40748,#39382,#33367,.T.) ;
#52647 = EDGE_CURVE('',#40524,#40748,#33368,.T.) ;
#52648 = EDGE_CURVE('',#40507,#39447,#33369,.T.) ;
#52649 = EDGE_CURVE('',#39380,#40514,#33370,.T.) ;
#52650 = EDGE_CURVE('',#40514,#40509,#33371,.T.) ;
#52651 = EDGE_CURVE('',#40525,#39382,#33372,.T.) ;
#52652 = EDGE_CURVE('',#40508,#39446,#33373,.T.) ;
#52653 = EDGE_CURVE('',#40515,#40508,#33374,.T.) ;
#52654 = EDGE_CURVE('',#39381,#40517,#33375,.T.) ;
#52655 = EDGE_CURVE('',#40526,#39381,#33376,.T.) ;
#52656 = EDGE_CURVE('',#40515,#39445,#33377,.T.) ;
#52657 = EDGE_CURVE('',#40526,#40517,#33378,.T.) ;
#52658 = EDGE_CURVE('',#40516,#39444,#33379,.T.) ;
#52659 = EDGE_CURVE('',#40527,#40516,#33380,.T.) ;
#52660 = EDGE_CURVE('',#40530,#40519,#33381,.T.) ;
#52661 = EDGE_CURVE('',#40531,#40518,#33382,.T.) ;
#52662 = EDGE_CURVE('',#39441,#40528,#33383,.T.) ;
#52663 = EDGE_CURVE('',#39442,#40531,#33384,.T.) ;
#52664 = EDGE_CURVE('',#40527,#39443,#33385,.T.) ;
#52665 = EDGE_CURVE('',#39442,#40518,#33386,.T.) ;
#52666 = EDGE_CURVE('',#40229,#40240,#33387,.T.) ;
#52667 = EDGE_CURVE('',#40230,#40243,#33388,.T.) ;
#52668 = EDGE_CURVE('',#40241,#40236,#33389,.T.) ;
#52669 = EDGE_CURVE('',#40230,#40283,#33390,.T.) ;
#52670 = EDGE_CURVE('',#40283,#40243,#33391,.T.) ;
#52671 = EDGE_CURVE('',#40235,#40228,#33392,.T.) ;
#52672 = EDGE_CURVE('',#40242,#40239,#33393,.T.) ;
#52673 = EDGE_CURVE('',#40280,#40242,#33394,.T.) ;
#52674 = EDGE_CURVE('',#40231,#40282,#33395,.T.) ;
#52675 = EDGE_CURVE('',#40232,#40231,#33396,.T.) ;
#52676 = EDGE_CURVE('',#40280,#40239,#33397,.T.) ;
#52677 = EDGE_CURVE('',#40232,#40282,#33398,.T.) ;
#52678 = EDGE_CURVE('',#40281,#40238,#33399,.T.) ;
#52679 = EDGE_CURVE('',#40233,#40281,#33400,.T.) ;
#52680 = EDGE_CURVE('',#40233,#40238,#33401,.T.) ;
#52681 = EDGE_CURVE('',#40234,#40237,#33402,.T.) ;
#52682 = EDGE_CURVE('',#40017,#41495,#33403,.T.) ;
#52683 = EDGE_CURVE('',#40018,#39988,#33404,.T.) ;
#52684 = EDGE_CURVE('',#40019,#39991,#33405,.T.) ;
#52685 = EDGE_CURVE('',#39986,#40019,#33406,.T.) ;
#52686 = EDGE_CURVE('',#39986,#39991,#33407,.T.) ;
#52687 = EDGE_CURVE('',#39987,#39990,#33408,.T.) ;
#52688 = EDGE_CURVE('',#40072,#39987,#33409,.T.) ;
#52689 = EDGE_CURVE('',#40072,#39990,#33410,.T.) ;
#52690 = EDGE_CURVE('',#40073,#39989,#33411,.T.) ;
#52691 = EDGE_CURVE('',#40068,#41494,#33412,.T.) ;
#52692 = EDGE_CURVE('',#40069,#41501,#33413,.T.) ;
#52693 = EDGE_CURVE('',#40070,#39972,#33414,.T.) ;
#52694 = EDGE_CURVE('',#40071,#39975,#33415,.T.) ;
#52695 = EDGE_CURVE('',#39976,#40071,#33416,.T.) ;
#52696 = EDGE_CURVE('',#39976,#39975,#33417,.T.) ;
#52697 = EDGE_CURVE('',#39977,#39974,#33418,.T.) ;
#52698 = EDGE_CURVE('',#40020,#39977,#33419,.T.) ;
#52699 = EDGE_CURVE('',#40020,#39974,#33420,.T.) ;
#52700 = EDGE_CURVE('',#40021,#39973,#33421,.T.) ;
#52701 = EDGE_CURVE('',#40016,#41500,#33422,.T.) ;
#52702 = EDGE_CURVE('',#39243,#41274,#33423,.T.) ;
#52703 = EDGE_CURVE('',#41276,#39242,#33424,.T.) ;
#52704 = EDGE_CURVE('',#41278,#39241,#33425,.T.) ;
#52705 = EDGE_CURVE('',#39244,#41272,#33426,.T.) ;
#52706 = EDGE_CURVE('',#41280,#39240,#33427,.T.) ;
#52707 = EDGE_CURVE('',#39237,#41271,#33428,.T.) ;
#52708 = EDGE_CURVE('',#41282,#39239,#33429,.T.) ;
#52709 = EDGE_CURVE('',#39238,#41284,#33430,.T.) ;
#52710 = EDGE_CURVE('',#40292,#40299,#33431,.T.) ;
#52711 = EDGE_CURVE('',#40293,#40447,#33432,.T.) ;
#52712 = EDGE_CURVE('',#40444,#40292,#33433,.T.) ;
#52713 = EDGE_CURVE('',#40294,#40293,#33434,.T.) ;
#52714 = EDGE_CURVE('',#40444,#40299,#33435,.T.) ;
#52715 = EDGE_CURVE('',#40294,#40447,#33436,.T.) ;
#52716 = EDGE_CURVE('',#40298,#40297,#33437,.T.) ;
#52717 = EDGE_CURVE('',#40445,#40298,#33438,.T.) ;
#52718 = EDGE_CURVE('',#40295,#40446,#33439,.T.) ;
#52719 = EDGE_CURVE('',#40296,#40295,#33440,.T.) ;
#52720 = EDGE_CURVE('',#40445,#40297,#33441,.T.) ;
#52721 = EDGE_CURVE('',#40296,#40446,#33442,.T.) ;
#52722 = EDGE_CURVE('',#39099,#41016,#33443,.T.) ;
#52723 = EDGE_CURVE('',#41017,#39098,#33444,.T.) ;
#52724 = EDGE_CURVE('',#41013,#39097,#33445,.T.) ;
#52725 = EDGE_CURVE('',#41017,#41013,#33446,.T.) ;
#52726 = EDGE_CURVE('',#41005,#41016,#33447,.T.) ;
#52727 = EDGE_CURVE('',#39100,#41005,#33448,.T.) ;
#52728 = EDGE_CURVE('',#41010,#39096,#33449,.T.) ;
#52729 = EDGE_CURVE('',#41014,#41012,#33450,.T.) ;
#52730 = EDGE_CURVE('',#41015,#41057,#33451,.T.) ;
#52731 = EDGE_CURVE('',#41054,#41014,#33452,.T.) ;
#52732 = EDGE_CURVE('',#41002,#41015,#33453,.T.) ;
#52733 = EDGE_CURVE('',#39094,#41004,#33454,.T.) ;
#52734 = EDGE_CURVE('',#39095,#41006,#33455,.T.) ;
#52735 = EDGE_CURVE('',#41007,#39093,#33456,.T.) ;
#52736 = EDGE_CURVE('',#41010,#41006,#33457,.T.) ;
#52737 = EDGE_CURVE('',#41054,#41012,#33458,.T.) ;
#52738 = EDGE_CURVE('',#41002,#41057,#33459,.T.) ;
#52739 = EDGE_CURVE('',#41007,#41004,#33460,.T.) ;
#52740 = EDGE_CURVE('',#41011,#41009,#33461,.T.) ;
#52741 = EDGE_CURVE('',#41055,#41011,#33462,.T.) ;
#52742 = EDGE_CURVE('',#41003,#41056,#33463,.T.) ;
#52743 = EDGE_CURVE('',#41008,#41003,#33464,.T.) ;
#52744 = EDGE_CURVE('',#41055,#41009,#33465,.T.) ;
#52745 = EDGE_CURVE('',#41008,#41056,#33466,.T.) ;
#52746 = EDGE_CURVE('',#41066,#41073,#33467,.T.) ;
#52747 = EDGE_CURVE('',#41067,#41221,#33468,.T.) ;
#52748 = EDGE_CURVE('',#41218,#41066,#33469,.T.) ;
#52749 = EDGE_CURVE('',#41068,#41067,#33470,.T.) ;
#52750 = EDGE_CURVE('',#41218,#41073,#33471,.T.) ;
#52751 = EDGE_CURVE('',#41068,#41221,#33472,.T.) ;
#52752 = EDGE_CURVE('',#41072,#41071,#33473,.T.) ;
#52753 = EDGE_CURVE('',#41219,#41072,#33474,.T.) ;
#52754 = EDGE_CURVE('',#41069,#41220,#33475,.T.) ;
#52755 = EDGE_CURVE('',#41070,#41069,#33476,.T.) ;
#52756 = EDGE_CURVE('',#41219,#41071,#33477,.T.) ;
#52757 = EDGE_CURVE('',#41070,#41220,#33478,.T.) ;
#52758 = EDGE_CURVE('',#41277,#41289,#33479,.T.) ;
#52759 = EDGE_CURVE('',#41286,#41279,#33480,.T.) ;
#52760 = EDGE_CURVE('',#41286,#41281,#33481,.T.) ;
#52761 = EDGE_CURVE('',#41275,#41289,#33482,.T.) ;
#52762 = EDGE_CURVE('',#41287,#41283,#33483,.T.) ;
#52763 = EDGE_CURVE('',#41273,#41288,#33484,.T.) ;
#52764 = EDGE_CURVE('',#41287,#41285,#33485,.T.) ;
#52765 = EDGE_CURVE('',#41270,#41288,#33486,.T.) ;
#52766 = EDGE_CURVE('',#40777,#40772,#33487,.T.) ;
#52767 = EDGE_CURVE('',#40771,#40777,#33488,.T.) ;
#52768 = EDGE_CURVE('',#40772,#40771,#33489,.T.) ;
#52769 = EDGE_CURVE('',#40768,#40776,#33490,.T.) ;
#52770 = EDGE_CURVE('',#40773,#40770,#33491,.T.) ;
#52771 = EDGE_CURVE('',#40778,#40775,#33492,.T.) ;
#52772 = EDGE_CURVE('',#40781,#40541,#33493,.T.) ;
#52773 = EDGE_CURVE('',#40776,#40540,#33494,.T.) ;
#52774 = EDGE_CURVE('',#40768,#40540,#33495,.T.) ;
#52775 = EDGE_CURVE('',#40773,#39370,#33496,.T.) ;
#52776 = EDGE_CURVE('',#39369,#40770,#33497,.T.) ;
#52777 = EDGE_CURVE('',#40778,#40764,#33498,.T.) ;
#52778 = EDGE_CURVE('',#40764,#40775,#33499,.T.) ;
#52779 = EDGE_CURVE('',#40780,#39222,#33500,.T.) ;
#52780 = EDGE_CURVE('',#39221,#40781,#33501,.T.) ;
#52781 = EDGE_CURVE('',#40769,#40539,#33502,.T.) ;
#52782 = EDGE_CURVE('',#39371,#40769,#33503,.T.) ;
#52783 = EDGE_CURVE('',#40774,#39376,#33504,.T.) ;
#52784 = EDGE_CURVE('',#40765,#40774,#33505,.T.) ;
#52785 = EDGE_CURVE('',#40779,#40767,#33506,.T.) ;
#52786 = EDGE_CURVE('',#40550,#40780,#33507,.T.) ;
#52787 = EDGE_CURVE('',#40551,#40779,#33508,.T.) ;
#52788 = EDGE_CURVE('',#39371,#40538,#33509,.T.) ;
#52789 = EDGE_CURVE('',#40765,#39375,#33510,.T.) ;
#52790 = EDGE_CURVE('',#40551,#40767,#33511,.T.) ;
#52791 = EDGE_CURVE('',#40534,#40529,#33512,.T.) ;
#52792 = EDGE_CURVE('',#40535,#40528,#33513,.T.) ;
#52793 = EDGE_CURVE('',#39372,#40537,#33514,.T.) ;
#52794 = EDGE_CURVE('',#40766,#39374,#33515,.T.) ;
#52795 = EDGE_CURVE('',#40552,#40766,#33516,.T.) ;
#52796 = EDGE_CURVE('',#40535,#39441,#33517,.T.) ;
#52797 = EDGE_CURVE('',#39372,#40542,#33518,.T.) ;
#52798 = EDGE_CURVE('',#40542,#40537,#33519,.T.) ;
#52799 = EDGE_CURVE('',#40553,#39374,#33520,.T.) ;
#52800 = EDGE_CURVE('',#40536,#39440,#33521,.T.) ;
#52801 = EDGE_CURVE('',#40543,#40536,#33522,.T.) ;
#52802 = EDGE_CURVE('',#39373,#40545,#33523,.T.) ;
#52803 = EDGE_CURVE('',#40554,#39373,#33524,.T.) ;
#52804 = EDGE_CURVE('',#40543,#39439,#33525,.T.) ;
#52805 = EDGE_CURVE('',#40554,#40545,#33526,.T.) ;
#52806 = EDGE_CURVE('',#40544,#39438,#33527,.T.) ;
#52807 = EDGE_CURVE('',#40555,#40544,#33528,.T.) ;
#52808 = EDGE_CURVE('',#40558,#40547,#33529,.T.) ;
#52809 = EDGE_CURVE('',#40559,#40546,#33530,.T.) ;
#52810 = EDGE_CURVE('',#39435,#40556,#33531,.T.) ;
#52811 = EDGE_CURVE('',#39436,#40559,#33532,.T.) ;
#52812 = EDGE_CURVE('',#40555,#39437,#33533,.T.) ;
#52813 = EDGE_CURVE('',#39436,#40546,#33534,.T.) ;
#52814 = EDGE_CURVE('',#40213,#40224,#33535,.T.) ;
#52815 = EDGE_CURVE('',#40214,#40227,#33536,.T.) ;
#52816 = EDGE_CURVE('',#40225,#40220,#33537,.T.) ;
#52817 = EDGE_CURVE('',#40214,#40303,#33538,.T.) ;
#52818 = EDGE_CURVE('',#40303,#40227,#33539,.T.) ;
#52819 = EDGE_CURVE('',#40219,#40212,#33540,.T.) ;
#52820 = EDGE_CURVE('',#40226,#40223,#33541,.T.) ;
#52821 = EDGE_CURVE('',#40300,#40226,#33542,.T.) ;
#52822 = EDGE_CURVE('',#40215,#40302,#33543,.T.) ;
#52823 = EDGE_CURVE('',#40216,#40215,#33544,.T.) ;
#52824 = EDGE_CURVE('',#40300,#40223,#33545,.T.) ;
#52825 = EDGE_CURVE('',#40216,#40302,#33546,.T.) ;
#52826 = EDGE_CURVE('',#40301,#40222,#33547,.T.) ;
#52827 = EDGE_CURVE('',#40217,#40301,#33548,.T.) ;
#52828 = EDGE_CURVE('',#40217,#40222,#33549,.T.) ;
#52829 = EDGE_CURVE('',#40218,#40221,#33550,.T.) ;
#52830 = EDGE_CURVE('',#40023,#41503,#33551,.T.) ;
#52831 = EDGE_CURVE('',#40024,#39968,#33552,.T.) ;
#52832 = EDGE_CURVE('',#40025,#39971,#33553,.T.) ;
#52833 = EDGE_CURVE('',#39966,#40025,#33554,.T.) ;
#52834 = EDGE_CURVE('',#39966,#39971,#33555,.T.) ;
#52835 = EDGE_CURVE('',#39967,#39970,#33556,.T.) ;
#52836 = EDGE_CURVE('',#40078,#39967,#33557,.T.) ;
#52837 = EDGE_CURVE('',#40078,#39970,#33558,.T.) ;
#52838 = EDGE_CURVE('',#40079,#39969,#33559,.T.) ;
#52839 = EDGE_CURVE('',#40074,#41502,#33560,.T.) ;
#52840 = EDGE_CURVE('',#40075,#41509,#33561,.T.) ;
#52841 = EDGE_CURVE('',#40076,#39952,#33562,.T.) ;
#52842 = EDGE_CURVE('',#40077,#39955,#33563,.T.) ;
#52843 = EDGE_CURVE('',#39956,#40077,#33564,.T.) ;
#52844 = EDGE_CURVE('',#39956,#39955,#33565,.T.) ;
#52845 = EDGE_CURVE('',#39957,#39954,#33566,.T.) ;
#52846 = EDGE_CURVE('',#40026,#39957,#33567,.T.) ;
#52847 = EDGE_CURVE('',#40026,#39954,#33568,.T.) ;
#52848 = EDGE_CURVE('',#40027,#39953,#33569,.T.) ;
#52849 = EDGE_CURVE('',#40022,#41508,#33570,.T.) ;
#52850 = EDGE_CURVE('',#39231,#41294,#33571,.T.) ;
#52851 = EDGE_CURVE('',#41296,#39230,#33572,.T.) ;
#52852 = EDGE_CURVE('',#41298,#39229,#33573,.T.) ;
#52853 = EDGE_CURVE('',#39232,#41292,#33574,.T.) ;
#52854 = EDGE_CURVE('',#41300,#39228,#33575,.T.) ;
#52855 = EDGE_CURVE('',#39225,#41291,#33576,.T.) ;
#52856 = EDGE_CURVE('',#41302,#39227,#33577,.T.) ;
#52857 = EDGE_CURVE('',#39226,#41304,#33578,.T.) ;
#52858 = EDGE_CURVE('',#40312,#40319,#33579,.T.) ;
#52859 = EDGE_CURVE('',#40313,#40451,#33580,.T.) ;
#52860 = EDGE_CURVE('',#40448,#40312,#33581,.T.) ;
#52861 = EDGE_CURVE('',#40314,#40313,#33582,.T.) ;
#52862 = EDGE_CURVE('',#40448,#40319,#33583,.T.) ;
#52863 = EDGE_CURVE('',#40314,#40451,#33584,.T.) ;
#52864 = EDGE_CURVE('',#40318,#40317,#33585,.T.) ;
#52865 = EDGE_CURVE('',#40449,#40318,#33586,.T.) ;
#52866 = EDGE_CURVE('',#40315,#40450,#33587,.T.) ;
#52867 = EDGE_CURVE('',#40316,#40315,#33588,.T.) ;
#52868 = EDGE_CURVE('',#40449,#40317,#33589,.T.) ;
#52869 = EDGE_CURVE('',#40316,#40450,#33590,.T.) ;
#52870 = EDGE_CURVE('',#39123,#41000,#33591,.T.) ;
#52871 = EDGE_CURVE('',#41001,#39122,#33592,.T.) ;
#52872 = EDGE_CURVE('',#40997,#39121,#33593,.T.) ;
#52873 = EDGE_CURVE('',#41001,#40997,#33594,.T.) ;
#52874 = EDGE_CURVE('',#40989,#41000,#33595,.T.) ;
#52875 = EDGE_CURVE('',#39124,#40989,#33596,.T.) ;
#52876 = EDGE_CURVE('',#40994,#39120,#33597,.T.) ;
#52877 = EDGE_CURVE('',#40998,#40996,#33598,.T.) ;
#52878 = EDGE_CURVE('',#40999,#41077,#33599,.T.) ;
#52879 = EDGE_CURVE('',#41074,#40998,#33600,.T.) ;
#52880 = EDGE_CURVE('',#40986,#40999,#33601,.T.) ;
#52881 = EDGE_CURVE('',#39118,#40988,#33602,.T.) ;
#52882 = EDGE_CURVE('',#39119,#40990,#33603,.T.) ;
#52883 = EDGE_CURVE('',#40991,#39117,#33604,.T.) ;
#52884 = EDGE_CURVE('',#40994,#40990,#33605,.T.) ;
#52885 = EDGE_CURVE('',#41074,#40996,#33606,.T.) ;
#52886 = EDGE_CURVE('',#40986,#41077,#33607,.T.) ;
#52887 = EDGE_CURVE('',#40991,#40988,#33608,.T.) ;
#52888 = EDGE_CURVE('',#40995,#40993,#33609,.T.) ;
#52889 = EDGE_CURVE('',#41075,#40995,#33610,.T.) ;
#52890 = EDGE_CURVE('',#40987,#41076,#33611,.T.) ;
#52891 = EDGE_CURVE('',#40992,#40987,#33612,.T.) ;
#52892 = EDGE_CURVE('',#41075,#40993,#33613,.T.) ;
#52893 = EDGE_CURVE('',#40992,#41076,#33614,.T.) ;
#52894 = EDGE_CURVE('',#41086,#41093,#33615,.T.) ;
#52895 = EDGE_CURVE('',#41087,#41225,#33616,.T.) ;
#52896 = EDGE_CURVE('',#41222,#41086,#33617,.T.) ;
#52897 = EDGE_CURVE('',#41088,#41087,#33618,.T.) ;
#52898 = EDGE_CURVE('',#41222,#41093,#33619,.T.) ;
#52899 = EDGE_CURVE('',#41088,#41225,#33620,.T.) ;
#52900 = EDGE_CURVE('',#41092,#41091,#33621,.T.) ;
#52901 = EDGE_CURVE('',#41223,#41092,#33622,.T.) ;
#52902 = EDGE_CURVE('',#41089,#41224,#33623,.T.) ;
#52903 = EDGE_CURVE('',#41090,#41089,#33624,.T.) ;
#52904 = EDGE_CURVE('',#41223,#41091,#33625,.T.) ;
#52905 = EDGE_CURVE('',#41090,#41224,#33626,.T.) ;
#52906 = EDGE_CURVE('',#41297,#41309,#33627,.T.) ;
#52907 = EDGE_CURVE('',#41306,#41299,#33628,.T.) ;
#52908 = EDGE_CURVE('',#41306,#41301,#33629,.T.) ;
#52909 = EDGE_CURVE('',#41295,#41309,#33630,.T.) ;
#52910 = EDGE_CURVE('',#41307,#41303,#33631,.T.) ;
#52911 = EDGE_CURVE('',#41293,#41308,#33632,.T.) ;
#52912 = EDGE_CURVE('',#41307,#41305,#33633,.T.) ;
#52913 = EDGE_CURVE('',#41290,#41308,#33634,.T.) ;
#52914 = EDGE_CURVE('',#40795,#40790,#33635,.T.) ;
#52915 = EDGE_CURVE('',#40789,#40795,#33636,.T.) ;
#52916 = EDGE_CURVE('',#40790,#40789,#33637,.T.) ;
#52917 = EDGE_CURVE('',#40786,#40794,#33638,.T.) ;
#52918 = EDGE_CURVE('',#40791,#40788,#33639,.T.) ;
#52919 = EDGE_CURVE('',#40796,#40793,#33640,.T.) ;
#52920 = EDGE_CURVE('',#40799,#40569,#33641,.T.) ;
#52921 = EDGE_CURVE('',#40794,#40568,#33642,.T.) ;
#52922 = EDGE_CURVE('',#40786,#40568,#33643,.T.) ;
#52923 = EDGE_CURVE('',#40791,#39362,#33644,.T.) ;
#52924 = EDGE_CURVE('',#39361,#40788,#33645,.T.) ;
#52925 = EDGE_CURVE('',#40796,#40782,#33646,.T.) ;
#52926 = EDGE_CURVE('',#40782,#40793,#33647,.T.) ;
#52927 = EDGE_CURVE('',#40798,#39210,#33648,.T.) ;
#52928 = EDGE_CURVE('',#39209,#40799,#33649,.T.) ;
#52929 = EDGE_CURVE('',#40787,#40567,#33650,.T.) ;
#52930 = EDGE_CURVE('',#39363,#40787,#33651,.T.) ;
#52931 = EDGE_CURVE('',#40792,#39368,#33652,.T.) ;
#52932 = EDGE_CURVE('',#40783,#40792,#33653,.T.) ;
#52933 = EDGE_CURVE('',#40797,#40785,#33654,.T.) ;
#52934 = EDGE_CURVE('',#40578,#40798,#33655,.T.) ;
#52935 = EDGE_CURVE('',#40579,#40797,#33656,.T.) ;
#52936 = EDGE_CURVE('',#39363,#40566,#33657,.T.) ;
#52937 = EDGE_CURVE('',#40783,#39367,#33658,.T.) ;
#52938 = EDGE_CURVE('',#40579,#40785,#33659,.T.) ;
#52939 = EDGE_CURVE('',#40562,#40557,#33660,.T.) ;
#52940 = EDGE_CURVE('',#40563,#40556,#33661,.T.) ;
#52941 = EDGE_CURVE('',#39364,#40565,#33662,.T.) ;
#52942 = EDGE_CURVE('',#40784,#39366,#33663,.T.) ;
#52943 = EDGE_CURVE('',#40580,#40784,#33664,.T.) ;
#52944 = EDGE_CURVE('',#40563,#39435,#33665,.T.) ;
#52945 = EDGE_CURVE('',#39364,#40570,#33666,.T.) ;
#52946 = EDGE_CURVE('',#40570,#40565,#33667,.T.) ;
#52947 = EDGE_CURVE('',#40581,#39366,#33668,.T.) ;
#52948 = EDGE_CURVE('',#40564,#39434,#33669,.T.) ;
#52949 = EDGE_CURVE('',#40571,#40564,#33670,.T.) ;
#52950 = EDGE_CURVE('',#39365,#40573,#33671,.T.) ;
#52951 = EDGE_CURVE('',#40582,#39365,#33672,.T.) ;
#52952 = EDGE_CURVE('',#40571,#39433,#33673,.T.) ;
#52953 = EDGE_CURVE('',#40582,#40573,#33674,.T.) ;
#52954 = EDGE_CURVE('',#40572,#39432,#33675,.T.) ;
#52955 = EDGE_CURVE('',#40583,#40572,#33676,.T.) ;
#52956 = EDGE_CURVE('',#40586,#40575,#33677,.T.) ;
#52957 = EDGE_CURVE('',#40587,#40574,#33678,.T.) ;
#52958 = EDGE_CURVE('',#39429,#40584,#33679,.T.) ;
#52959 = EDGE_CURVE('',#39430,#40587,#33680,.T.) ;
#52960 = EDGE_CURVE('',#40583,#39431,#33681,.T.) ;
#52961 = EDGE_CURVE('',#39430,#40574,#33682,.T.) ;
#52962 = EDGE_CURVE('',#40197,#40208,#33683,.T.) ;
#52963 = EDGE_CURVE('',#40198,#40211,#33684,.T.) ;
#52964 = EDGE_CURVE('',#40209,#40204,#33685,.T.) ;
#52965 = EDGE_CURVE('',#40198,#40323,#33686,.T.) ;
#52966 = EDGE_CURVE('',#40323,#40211,#33687,.T.) ;
#52967 = EDGE_CURVE('',#40203,#40196,#33688,.T.) ;
#52968 = EDGE_CURVE('',#40210,#40207,#33689,.T.) ;
#52969 = EDGE_CURVE('',#40320,#40210,#33690,.T.) ;
#52970 = EDGE_CURVE('',#40199,#40322,#33691,.T.) ;
#52971 = EDGE_CURVE('',#40200,#40199,#33692,.T.) ;
#52972 = EDGE_CURVE('',#40320,#40207,#33693,.T.) ;
#52973 = EDGE_CURVE('',#40200,#40322,#33694,.T.) ;
#52974 = EDGE_CURVE('',#40321,#40206,#33695,.T.) ;
#52975 = EDGE_CURVE('',#40201,#40321,#33696,.T.) ;
#52976 = EDGE_CURVE('',#40201,#40206,#33697,.T.) ;
#52977 = EDGE_CURVE('',#40202,#40205,#33698,.T.) ;
#52978 = EDGE_CURVE('',#40029,#41511,#33699,.T.) ;
#52979 = EDGE_CURVE('',#40030,#39948,#33700,.T.) ;
#52980 = EDGE_CURVE('',#40031,#39951,#33701,.T.) ;
#52981 = EDGE_CURVE('',#39946,#40031,#33702,.T.) ;
#52982 = EDGE_CURVE('',#39946,#39951,#33703,.T.) ;
#52983 = EDGE_CURVE('',#39947,#39950,#33704,.T.) ;
#52984 = EDGE_CURVE('',#40084,#39947,#33705,.T.) ;
#52985 = EDGE_CURVE('',#40084,#39950,#33706,.T.) ;
#52986 = EDGE_CURVE('',#40085,#39949,#33707,.T.) ;
#52987 = EDGE_CURVE('',#40080,#41510,#33708,.T.) ;
#52988 = EDGE_CURVE('',#40081,#41517,#33709,.T.) ;
#52989 = EDGE_CURVE('',#40082,#39932,#33710,.T.) ;
#52990 = EDGE_CURVE('',#40083,#39935,#33711,.T.) ;
#52991 = EDGE_CURVE('',#39936,#40083,#33712,.T.) ;
#52992 = EDGE_CURVE('',#39936,#39935,#33713,.T.) ;
#52993 = EDGE_CURVE('',#39937,#39934,#33714,.T.) ;
#52994 = EDGE_CURVE('',#40032,#39937,#33715,.T.) ;
#52995 = EDGE_CURVE('',#40032,#39934,#33716,.T.) ;
#52996 = EDGE_CURVE('',#40033,#39933,#33717,.T.) ;
#52997 = EDGE_CURVE('',#40028,#41516,#33718,.T.) ;
#52998 = EDGE_CURVE('',#39219,#41314,#33719,.T.) ;
#52999 = EDGE_CURVE('',#41316,#39218,#33720,.T.) ;
#53000 = EDGE_CURVE('',#41318,#39217,#33721,.T.) ;
#53001 = EDGE_CURVE('',#39220,#41312,#33722,.T.) ;
#53002 = EDGE_CURVE('',#41320,#39216,#33723,.T.) ;
#53003 = EDGE_CURVE('',#39213,#41311,#33724,.T.) ;
#53004 = EDGE_CURVE('',#41322,#39215,#33725,.T.) ;
#53005 = EDGE_CURVE('',#39214,#41324,#33726,.T.) ;
#53006 = EDGE_CURVE('',#40332,#40339,#33727,.T.) ;
#53007 = EDGE_CURVE('',#40333,#40455,#33728,.T.) ;
#53008 = EDGE_CURVE('',#40452,#40332,#33729,.T.) ;
#53009 = EDGE_CURVE('',#40334,#40333,#33730,.T.) ;
#53010 = EDGE_CURVE('',#40452,#40339,#33731,.T.) ;
#53011 = EDGE_CURVE('',#40334,#40455,#33732,.T.) ;
#53012 = EDGE_CURVE('',#40338,#40337,#33733,.T.) ;
#53013 = EDGE_CURVE('',#40453,#40338,#33734,.T.) ;
#53014 = EDGE_CURVE('',#40335,#40454,#33735,.T.) ;
#53015 = EDGE_CURVE('',#40336,#40335,#33736,.T.) ;
#53016 = EDGE_CURVE('',#40453,#40337,#33737,.T.) ;
#53017 = EDGE_CURVE('',#40336,#40454,#33738,.T.) ;
#53018 = EDGE_CURVE('',#39091,#40984,#33739,.T.) ;
#53019 = EDGE_CURVE('',#40985,#39090,#33740,.T.) ;
#53020 = EDGE_CURVE('',#40981,#39089,#33741,.T.) ;
#53021 = EDGE_CURVE('',#40985,#40981,#33742,.T.) ;
#53022 = EDGE_CURVE('',#40973,#40984,#33743,.T.) ;
#53023 = EDGE_CURVE('',#39092,#40973,#33744,.T.) ;
#53024 = EDGE_CURVE('',#40978,#39088,#33745,.T.) ;
#53025 = EDGE_CURVE('',#40982,#40980,#33746,.T.) ;
#53026 = EDGE_CURVE('',#40983,#41097,#33747,.T.) ;
#53027 = EDGE_CURVE('',#41094,#40982,#33748,.T.) ;
#53028 = EDGE_CURVE('',#40970,#40983,#33749,.T.) ;
#53029 = EDGE_CURVE('',#39086,#40972,#33750,.T.) ;
#53030 = EDGE_CURVE('',#39087,#40974,#33751,.T.) ;
#53031 = EDGE_CURVE('',#40975,#39085,#33752,.T.) ;
#53032 = EDGE_CURVE('',#40978,#40974,#33753,.T.) ;
#53033 = EDGE_CURVE('',#41094,#40980,#33754,.T.) ;
#53034 = EDGE_CURVE('',#40970,#41097,#33755,.T.) ;
#53035 = EDGE_CURVE('',#40975,#40972,#33756,.T.) ;
#53036 = EDGE_CURVE('',#40979,#40977,#33757,.T.) ;
#53037 = EDGE_CURVE('',#41095,#40979,#33758,.T.) ;
#53038 = EDGE_CURVE('',#40971,#41096,#33759,.T.) ;
#53039 = EDGE_CURVE('',#40976,#40971,#33760,.T.) ;
#53040 = EDGE_CURVE('',#41095,#40977,#33761,.T.) ;
#53041 = EDGE_CURVE('',#40976,#41096,#33762,.T.) ;
#53042 = EDGE_CURVE('',#41106,#41113,#33763,.T.) ;
#53043 = EDGE_CURVE('',#41107,#41229,#33764,.T.) ;
#53044 = EDGE_CURVE('',#41226,#41106,#33765,.T.) ;
#53045 = EDGE_CURVE('',#41108,#41107,#33766,.T.) ;
#53046 = EDGE_CURVE('',#41226,#41113,#33767,.T.) ;
#53047 = EDGE_CURVE('',#41108,#41229,#33768,.T.) ;
#53048 = EDGE_CURVE('',#41112,#41111,#33769,.T.) ;
#53049 = EDGE_CURVE('',#41227,#41112,#33770,.T.) ;
#53050 = EDGE_CURVE('',#41109,#41228,#33771,.T.) ;
#53051 = EDGE_CURVE('',#41110,#41109,#33772,.T.) ;
#53052 = EDGE_CURVE('',#41227,#41111,#33773,.T.) ;
#53053 = EDGE_CURVE('',#41110,#41228,#33774,.T.) ;
#53054 = EDGE_CURVE('',#41317,#41329,#33775,.T.) ;
#53055 = EDGE_CURVE('',#41326,#41319,#33776,.T.) ;
#53056 = EDGE_CURVE('',#41326,#41321,#33777,.T.) ;
#53057 = EDGE_CURVE('',#41315,#41329,#33778,.T.) ;
#53058 = EDGE_CURVE('',#41327,#41323,#33779,.T.) ;
#53059 = EDGE_CURVE('',#41313,#41328,#33780,.T.) ;
#53060 = EDGE_CURVE('',#41327,#41325,#33781,.T.) ;
#53061 = EDGE_CURVE('',#41310,#41328,#33782,.T.) ;
#53062 = EDGE_CURVE('',#40813,#40808,#33783,.T.) ;
#53063 = EDGE_CURVE('',#40807,#40813,#33784,.T.) ;
#53064 = EDGE_CURVE('',#40808,#40807,#33785,.T.) ;
#53065 = EDGE_CURVE('',#40804,#40812,#33786,.T.) ;
#53066 = EDGE_CURVE('',#40809,#40806,#33787,.T.) ;
#53067 = EDGE_CURVE('',#40814,#40811,#33788,.T.) ;
#53068 = EDGE_CURVE('',#40817,#40597,#33789,.T.) ;
#53069 = EDGE_CURVE('',#40812,#40596,#33790,.T.) ;
#53070 = EDGE_CURVE('',#40804,#40596,#33791,.T.) ;
#53071 = EDGE_CURVE('',#40809,#39354,#33792,.T.) ;
#53072 = EDGE_CURVE('',#39353,#40806,#33793,.T.) ;
#53073 = EDGE_CURVE('',#40814,#40800,#33794,.T.) ;
#53074 = EDGE_CURVE('',#40800,#40811,#33795,.T.) ;
#53075 = EDGE_CURVE('',#40816,#39198,#33796,.T.) ;
#53076 = EDGE_CURVE('',#39197,#40817,#33797,.T.) ;
#53077 = EDGE_CURVE('',#40805,#40595,#33798,.T.) ;
#53078 = EDGE_CURVE('',#39355,#40805,#33799,.T.) ;
#53079 = EDGE_CURVE('',#40810,#39360,#33800,.T.) ;
#53080 = EDGE_CURVE('',#40801,#40810,#33801,.T.) ;
#53081 = EDGE_CURVE('',#40815,#40803,#33802,.T.) ;
#53082 = EDGE_CURVE('',#40606,#40816,#33803,.T.) ;
#53083 = EDGE_CURVE('',#40607,#40815,#33804,.T.) ;
#53084 = EDGE_CURVE('',#39355,#40594,#33805,.T.) ;
#53085 = EDGE_CURVE('',#40801,#39359,#33806,.T.) ;
#53086 = EDGE_CURVE('',#40607,#40803,#33807,.T.) ;
#53087 = EDGE_CURVE('',#40590,#40585,#33808,.T.) ;
#53088 = EDGE_CURVE('',#40591,#40584,#33809,.T.) ;
#53089 = EDGE_CURVE('',#39356,#40593,#33810,.T.) ;
#53090 = EDGE_CURVE('',#40802,#39358,#33811,.T.) ;
#53091 = EDGE_CURVE('',#40608,#40802,#33812,.T.) ;
#53092 = EDGE_CURVE('',#40591,#39429,#33813,.T.) ;
#53093 = EDGE_CURVE('',#39356,#40598,#33814,.T.) ;
#53094 = EDGE_CURVE('',#40598,#40593,#33815,.T.) ;
#53095 = EDGE_CURVE('',#40609,#39358,#33816,.T.) ;
#53096 = EDGE_CURVE('',#40592,#39428,#33817,.T.) ;
#53097 = EDGE_CURVE('',#40599,#40592,#33818,.T.) ;
#53098 = EDGE_CURVE('',#39357,#40601,#33819,.T.) ;
#53099 = EDGE_CURVE('',#40610,#39357,#33820,.T.) ;
#53100 = EDGE_CURVE('',#40599,#39427,#33821,.T.) ;
#53101 = EDGE_CURVE('',#40610,#40601,#33822,.T.) ;
#53102 = EDGE_CURVE('',#40600,#39426,#33823,.T.) ;
#53103 = EDGE_CURVE('',#40611,#40600,#33824,.T.) ;
#53104 = EDGE_CURVE('',#40614,#40603,#33825,.T.) ;
#53105 = EDGE_CURVE('',#40615,#40602,#33826,.T.) ;
#53106 = EDGE_CURVE('',#39423,#40612,#33827,.T.) ;
#53107 = EDGE_CURVE('',#39424,#40615,#33828,.T.) ;
#53108 = EDGE_CURVE('',#40611,#39425,#33829,.T.) ;
#53109 = EDGE_CURVE('',#39424,#40602,#33830,.T.) ;
#53110 = EDGE_CURVE('',#40181,#40192,#33831,.T.) ;
#53111 = EDGE_CURVE('',#40182,#40195,#33832,.T.) ;
#53112 = EDGE_CURVE('',#40193,#40188,#33833,.T.) ;
#53113 = EDGE_CURVE('',#40182,#40343,#33834,.T.) ;
#53114 = EDGE_CURVE('',#40343,#40195,#33835,.T.) ;
#53115 = EDGE_CURVE('',#40187,#40180,#33836,.T.) ;
#53116 = EDGE_CURVE('',#40194,#40191,#33837,.T.) ;
#53117 = EDGE_CURVE('',#40340,#40194,#33838,.T.) ;
#53118 = EDGE_CURVE('',#40183,#40342,#33839,.T.) ;
#53119 = EDGE_CURVE('',#40184,#40183,#33840,.T.) ;
#53120 = EDGE_CURVE('',#40340,#40191,#33841,.T.) ;
#53121 = EDGE_CURVE('',#40184,#40342,#33842,.T.) ;
#53122 = EDGE_CURVE('',#40341,#40190,#33843,.T.) ;
#53123 = EDGE_CURVE('',#40185,#40341,#33844,.T.) ;
#53124 = EDGE_CURVE('',#40185,#40190,#33845,.T.) ;
#53125 = EDGE_CURVE('',#40186,#40189,#33846,.T.) ;
#53126 = EDGE_CURVE('',#40035,#41519,#33847,.T.) ;
#53127 = EDGE_CURVE('',#40036,#39928,#33848,.T.) ;
#53128 = EDGE_CURVE('',#40037,#39931,#33849,.T.) ;
#53129 = EDGE_CURVE('',#39926,#40037,#33850,.T.) ;
#53130 = EDGE_CURVE('',#39926,#39931,#33851,.T.) ;
#53131 = EDGE_CURVE('',#39927,#39930,#33852,.T.) ;
#53132 = EDGE_CURVE('',#40090,#39927,#33853,.T.) ;
#53133 = EDGE_CURVE('',#40090,#39930,#33854,.T.) ;
#53134 = EDGE_CURVE('',#40091,#39929,#33855,.T.) ;
#53135 = EDGE_CURVE('',#40086,#41518,#33856,.T.) ;
#53136 = EDGE_CURVE('',#40087,#41525,#33857,.T.) ;
#53137 = EDGE_CURVE('',#40088,#39912,#33858,.T.) ;
#53138 = EDGE_CURVE('',#40089,#39915,#33859,.T.) ;
#53139 = EDGE_CURVE('',#39916,#40089,#33860,.T.) ;
#53140 = EDGE_CURVE('',#39916,#39915,#33861,.T.) ;
#53141 = EDGE_CURVE('',#39917,#39914,#33862,.T.) ;
#53142 = EDGE_CURVE('',#40038,#39917,#33863,.T.) ;
#53143 = EDGE_CURVE('',#40038,#39914,#33864,.T.) ;
#53144 = EDGE_CURVE('',#40039,#39913,#33865,.T.) ;
#53145 = EDGE_CURVE('',#40034,#41524,#33866,.T.) ;
#53146 = EDGE_CURVE('',#39207,#41334,#33867,.T.) ;
#53147 = EDGE_CURVE('',#41336,#39206,#33868,.T.) ;
#53148 = EDGE_CURVE('',#41338,#39205,#33869,.T.) ;
#53149 = EDGE_CURVE('',#39208,#41332,#33870,.T.) ;
#53150 = EDGE_CURVE('',#41340,#39204,#33871,.T.) ;
#53151 = EDGE_CURVE('',#39201,#41331,#33872,.T.) ;
#53152 = EDGE_CURVE('',#41342,#39203,#33873,.T.) ;
#53153 = EDGE_CURVE('',#39202,#41344,#33874,.T.) ;
#53154 = EDGE_CURVE('',#40352,#40359,#33875,.T.) ;
#53155 = EDGE_CURVE('',#40353,#40459,#33876,.T.) ;
#53156 = EDGE_CURVE('',#40456,#40352,#33877,.T.) ;
#53157 = EDGE_CURVE('',#40354,#40353,#33878,.T.) ;
#53158 = EDGE_CURVE('',#40456,#40359,#33879,.T.) ;
#53159 = EDGE_CURVE('',#40354,#40459,#33880,.T.) ;
#53160 = EDGE_CURVE('',#40358,#40357,#33881,.T.) ;
#53161 = EDGE_CURVE('',#40457,#40358,#33882,.T.) ;
#53162 = EDGE_CURVE('',#40355,#40458,#33883,.T.) ;
#53163 = EDGE_CURVE('',#40356,#40355,#33884,.T.) ;
#53164 = EDGE_CURVE('',#40457,#40357,#33885,.T.) ;
#53165 = EDGE_CURVE('',#40356,#40458,#33886,.T.) ;
#53166 = EDGE_CURVE('',#39131,#40968,#33887,.T.) ;
#53167 = EDGE_CURVE('',#40969,#39130,#33888,.T.) ;
#53168 = EDGE_CURVE('',#40965,#39129,#33889,.T.) ;
#53169 = EDGE_CURVE('',#40969,#40965,#33890,.T.) ;
#53170 = EDGE_CURVE('',#40957,#40968,#33891,.T.) ;
#53171 = EDGE_CURVE('',#39132,#40957,#33892,.T.) ;
#53172 = EDGE_CURVE('',#40962,#39128,#33893,.T.) ;
#53173 = EDGE_CURVE('',#40966,#40964,#33894,.T.) ;
#53174 = EDGE_CURVE('',#40967,#41117,#33895,.T.) ;
#53175 = EDGE_CURVE('',#41114,#40966,#33896,.T.) ;
#53176 = EDGE_CURVE('',#40954,#40967,#33897,.T.) ;
#53177 = EDGE_CURVE('',#39126,#40956,#33898,.T.) ;
#53178 = EDGE_CURVE('',#39127,#40958,#33899,.T.) ;
#53179 = EDGE_CURVE('',#40959,#39125,#33900,.T.) ;
#53180 = EDGE_CURVE('',#40962,#40958,#33901,.T.) ;
#53181 = EDGE_CURVE('',#41114,#40964,#33902,.T.) ;
#53182 = EDGE_CURVE('',#40954,#41117,#33903,.T.) ;
#53183 = EDGE_CURVE('',#40959,#40956,#33904,.T.) ;
#53184 = EDGE_CURVE('',#40963,#40961,#33905,.T.) ;
#53185 = EDGE_CURVE('',#41115,#40963,#33906,.T.) ;
#53186 = EDGE_CURVE('',#40955,#41116,#33907,.T.) ;
#53187 = EDGE_CURVE('',#40960,#40955,#33908,.T.) ;
#53188 = EDGE_CURVE('',#41115,#40961,#33909,.T.) ;
#53189 = EDGE_CURVE('',#40960,#41116,#33910,.T.) ;
#53190 = EDGE_CURVE('',#41126,#41133,#33911,.T.) ;
#53191 = EDGE_CURVE('',#41127,#41233,#33912,.T.) ;
#53192 = EDGE_CURVE('',#41230,#41126,#33913,.T.) ;
#53193 = EDGE_CURVE('',#41128,#41127,#33914,.T.) ;
#53194 = EDGE_CURVE('',#41230,#41133,#33915,.T.) ;
#53195 = EDGE_CURVE('',#41128,#41233,#33916,.T.) ;
#53196 = EDGE_CURVE('',#41132,#41131,#33917,.T.) ;
#53197 = EDGE_CURVE('',#41231,#41132,#33918,.T.) ;
#53198 = EDGE_CURVE('',#41129,#41232,#33919,.T.) ;
#53199 = EDGE_CURVE('',#41130,#41129,#33920,.T.) ;
#53200 = EDGE_CURVE('',#41231,#41131,#33921,.T.) ;
#53201 = EDGE_CURVE('',#41130,#41232,#33922,.T.) ;
#53202 = EDGE_CURVE('',#41337,#41349,#33923,.T.) ;
#53203 = EDGE_CURVE('',#41346,#41339,#33924,.T.) ;
#53204 = EDGE_CURVE('',#41346,#41341,#33925,.T.) ;
#53205 = EDGE_CURVE('',#41335,#41349,#33926,.T.) ;
#53206 = EDGE_CURVE('',#41347,#41343,#33927,.T.) ;
#53207 = EDGE_CURVE('',#41333,#41348,#33928,.T.) ;
#53208 = EDGE_CURVE('',#41347,#41345,#33929,.T.) ;
#53209 = EDGE_CURVE('',#41330,#41348,#33930,.T.) ;
#53210 = EDGE_CURVE('',#40831,#40826,#33931,.T.) ;
#53211 = EDGE_CURVE('',#40825,#40831,#33932,.T.) ;
#53212 = EDGE_CURVE('',#40826,#40825,#33933,.T.) ;
#53213 = EDGE_CURVE('',#40822,#40830,#33934,.T.) ;
#53214 = EDGE_CURVE('',#40827,#40824,#33935,.T.) ;
#53215 = EDGE_CURVE('',#40832,#40829,#33936,.T.) ;
#53216 = EDGE_CURVE('',#40835,#40625,#33937,.T.) ;
#53217 = EDGE_CURVE('',#40830,#40624,#33938,.T.) ;
#53218 = EDGE_CURVE('',#40822,#40624,#33939,.T.) ;
#53219 = EDGE_CURVE('',#40827,#39346,#33940,.T.) ;
#53220 = EDGE_CURVE('',#39345,#40824,#33941,.T.) ;
#53221 = EDGE_CURVE('',#40832,#40818,#33942,.T.) ;
#53222 = EDGE_CURVE('',#40818,#40829,#33943,.T.) ;
#53223 = EDGE_CURVE('',#40834,#39186,#33944,.T.) ;
#53224 = EDGE_CURVE('',#39185,#40835,#33945,.T.) ;
#53225 = EDGE_CURVE('',#40823,#40623,#33946,.T.) ;
#53226 = EDGE_CURVE('',#39347,#40823,#33947,.T.) ;
#53227 = EDGE_CURVE('',#40828,#39352,#33948,.T.) ;
#53228 = EDGE_CURVE('',#40819,#40828,#33949,.T.) ;
#53229 = EDGE_CURVE('',#40833,#40821,#33950,.T.) ;
#53230 = EDGE_CURVE('',#40634,#40834,#33951,.T.) ;
#53231 = EDGE_CURVE('',#40635,#40833,#33952,.T.) ;
#53232 = EDGE_CURVE('',#39347,#40622,#33953,.T.) ;
#53233 = EDGE_CURVE('',#40819,#39351,#33954,.T.) ;
#53234 = EDGE_CURVE('',#40635,#40821,#33955,.T.) ;
#53235 = EDGE_CURVE('',#40618,#40613,#33956,.T.) ;
#53236 = EDGE_CURVE('',#40619,#40612,#33957,.T.) ;
#53237 = EDGE_CURVE('',#39348,#40621,#33958,.T.) ;
#53238 = EDGE_CURVE('',#40820,#39350,#33959,.T.) ;
#53239 = EDGE_CURVE('',#40636,#40820,#33960,.T.) ;
#53240 = EDGE_CURVE('',#40619,#39423,#33961,.T.) ;
#53241 = EDGE_CURVE('',#39348,#40626,#33962,.T.) ;
#53242 = EDGE_CURVE('',#40626,#40621,#33963,.T.) ;
#53243 = EDGE_CURVE('',#40637,#39350,#33964,.T.) ;
#53244 = EDGE_CURVE('',#40620,#39422,#33965,.T.) ;
#53245 = EDGE_CURVE('',#40627,#40620,#33966,.T.) ;
#53246 = EDGE_CURVE('',#39349,#40629,#33967,.T.) ;
#53247 = EDGE_CURVE('',#40638,#39349,#33968,.T.) ;
#53248 = EDGE_CURVE('',#40627,#39421,#33969,.T.) ;
#53249 = EDGE_CURVE('',#40638,#40629,#33970,.T.) ;
#53250 = EDGE_CURVE('',#40628,#39420,#33971,.T.) ;
#53251 = EDGE_CURVE('',#40639,#40628,#33972,.T.) ;
#53252 = EDGE_CURVE('',#40642,#40631,#33973,.T.) ;
#53253 = EDGE_CURVE('',#40643,#40630,#33974,.T.) ;
#53254 = EDGE_CURVE('',#39417,#40640,#33975,.T.) ;
#53255 = EDGE_CURVE('',#39418,#40643,#33976,.T.) ;
#53256 = EDGE_CURVE('',#40639,#39419,#33977,.T.) ;
#53257 = EDGE_CURVE('',#39418,#40630,#33978,.T.) ;
#53258 = EDGE_CURVE('',#40165,#40176,#33979,.T.) ;
#53259 = EDGE_CURVE('',#40166,#40179,#33980,.T.) ;
#53260 = EDGE_CURVE('',#40177,#40172,#33981,.T.) ;
#53261 = EDGE_CURVE('',#40166,#40363,#33982,.T.) ;
#53262 = EDGE_CURVE('',#40363,#40179,#33983,.T.) ;
#53263 = EDGE_CURVE('',#40171,#40164,#33984,.T.) ;
#53264 = EDGE_CURVE('',#40178,#40175,#33985,.T.) ;
#53265 = EDGE_CURVE('',#40360,#40178,#33986,.T.) ;
#53266 = EDGE_CURVE('',#40167,#40362,#33987,.T.) ;
#53267 = EDGE_CURVE('',#40168,#40167,#33988,.T.) ;
#53268 = EDGE_CURVE('',#40360,#40175,#33989,.T.) ;
#53269 = EDGE_CURVE('',#40168,#40362,#33990,.T.) ;
#53270 = EDGE_CURVE('',#40361,#40174,#33991,.T.) ;
#53271 = EDGE_CURVE('',#40169,#40361,#33992,.T.) ;
#53272 = EDGE_CURVE('',#40169,#40174,#33993,.T.) ;
#53273 = EDGE_CURVE('',#40170,#40173,#33994,.T.) ;
#53274 = EDGE_CURVE('',#40041,#41527,#33995,.T.) ;
#53275 = EDGE_CURVE('',#40042,#39908,#33996,.T.) ;
#53276 = EDGE_CURVE('',#40043,#39911,#33997,.T.) ;
#53277 = EDGE_CURVE('',#39906,#40043,#33998,.T.) ;
#53278 = EDGE_CURVE('',#39906,#39911,#33999,.T.) ;
#53279 = EDGE_CURVE('',#39907,#39910,#34000,.T.) ;
#53280 = EDGE_CURVE('',#40096,#39907,#34001,.T.) ;
#53281 = EDGE_CURVE('',#40096,#39910,#34002,.T.) ;
#53282 = EDGE_CURVE('',#40097,#39909,#34003,.T.) ;
#53283 = EDGE_CURVE('',#40092,#41526,#34004,.T.) ;
#53284 = EDGE_CURVE('',#40093,#41533,#34005,.T.) ;
#53285 = EDGE_CURVE('',#40094,#39892,#34006,.T.) ;
#53286 = EDGE_CURVE('',#40095,#39895,#34007,.T.) ;
#53287 = EDGE_CURVE('',#39896,#40095,#34008,.T.) ;
#53288 = EDGE_CURVE('',#39896,#39895,#34009,.T.) ;
#53289 = EDGE_CURVE('',#39897,#39894,#34010,.T.) ;
#53290 = EDGE_CURVE('',#40044,#39897,#34011,.T.) ;
#53291 = EDGE_CURVE('',#40044,#39894,#34012,.T.) ;
#53292 = EDGE_CURVE('',#40045,#39893,#34013,.T.) ;
#53293 = EDGE_CURVE('',#40040,#41532,#34014,.T.) ;
#53294 = EDGE_CURVE('',#39195,#41354,#34015,.T.) ;
#53295 = EDGE_CURVE('',#41356,#39194,#34016,.T.) ;
#53296 = EDGE_CURVE('',#41358,#39193,#34017,.T.) ;
#53297 = EDGE_CURVE('',#39196,#41352,#34018,.T.) ;
#53298 = EDGE_CURVE('',#41360,#39192,#34019,.T.) ;
#53299 = EDGE_CURVE('',#39189,#41351,#34020,.T.) ;
#53300 = EDGE_CURVE('',#41362,#39191,#34021,.T.) ;
#53301 = EDGE_CURVE('',#39190,#41364,#34022,.T.) ;
#53302 = EDGE_CURVE('',#40372,#40379,#34023,.T.) ;
#53303 = EDGE_CURVE('',#40373,#40463,#34024,.T.) ;
#53304 = EDGE_CURVE('',#40460,#40372,#34025,.T.) ;
#53305 = EDGE_CURVE('',#40374,#40373,#34026,.T.) ;
#53306 = EDGE_CURVE('',#40460,#40379,#34027,.T.) ;
#53307 = EDGE_CURVE('',#40374,#40463,#34028,.T.) ;
#53308 = EDGE_CURVE('',#40378,#40377,#34029,.T.) ;
#53309 = EDGE_CURVE('',#40461,#40378,#34030,.T.) ;
#53310 = EDGE_CURVE('',#40375,#40462,#34031,.T.) ;
#53311 = EDGE_CURVE('',#40376,#40375,#34032,.T.) ;
#53312 = EDGE_CURVE('',#40461,#40377,#34033,.T.) ;
#53313 = EDGE_CURVE('',#40376,#40462,#34034,.T.) ;
#53314 = EDGE_CURVE('',#39083,#40952,#34035,.T.) ;
#53315 = EDGE_CURVE('',#40953,#39082,#34036,.T.) ;
#53316 = EDGE_CURVE('',#40949,#39081,#34037,.T.) ;
#53317 = EDGE_CURVE('',#40953,#40949,#34038,.T.) ;
#53318 = EDGE_CURVE('',#40941,#40952,#34039,.T.) ;
#53319 = EDGE_CURVE('',#39084,#40941,#34040,.T.) ;
#53320 = EDGE_CURVE('',#40946,#39080,#34041,.T.) ;
#53321 = EDGE_CURVE('',#40950,#40948,#34042,.T.) ;
#53322 = EDGE_CURVE('',#40951,#41137,#34043,.T.) ;
#53323 = EDGE_CURVE('',#41134,#40950,#34044,.T.) ;
#53324 = EDGE_CURVE('',#40938,#40951,#34045,.T.) ;
#53325 = EDGE_CURVE('',#39078,#40940,#34046,.T.) ;
#53326 = EDGE_CURVE('',#39079,#40942,#34047,.T.) ;
#53327 = EDGE_CURVE('',#40943,#39077,#34048,.T.) ;
#53328 = EDGE_CURVE('',#40946,#40942,#34049,.T.) ;
#53329 = EDGE_CURVE('',#41134,#40948,#34050,.T.) ;
#53330 = EDGE_CURVE('',#40938,#41137,#34051,.T.) ;
#53331 = EDGE_CURVE('',#40943,#40940,#34052,.T.) ;
#53332 = EDGE_CURVE('',#40947,#40945,#34053,.T.) ;
#53333 = EDGE_CURVE('',#41135,#40947,#34054,.T.) ;
#53334 = EDGE_CURVE('',#40939,#41136,#34055,.T.) ;
#53335 = EDGE_CURVE('',#40944,#40939,#34056,.T.) ;
#53336 = EDGE_CURVE('',#41135,#40945,#34057,.T.) ;
#53337 = EDGE_CURVE('',#40944,#41136,#34058,.T.) ;
#53338 = EDGE_CURVE('',#41146,#41153,#34059,.T.) ;
#53339 = EDGE_CURVE('',#41147,#41237,#34060,.T.) ;
#53340 = EDGE_CURVE('',#41234,#41146,#34061,.T.) ;
#53341 = EDGE_CURVE('',#41148,#41147,#34062,.T.) ;
#53342 = EDGE_CURVE('',#41234,#41153,#34063,.T.) ;
#53343 = EDGE_CURVE('',#41148,#41237,#34064,.T.) ;
#53344 = EDGE_CURVE('',#41152,#41151,#34065,.T.) ;
#53345 = EDGE_CURVE('',#41235,#41152,#34066,.T.) ;
#53346 = EDGE_CURVE('',#41149,#41236,#34067,.T.) ;
#53347 = EDGE_CURVE('',#41150,#41149,#34068,.T.) ;
#53348 = EDGE_CURVE('',#41235,#41151,#34069,.T.) ;
#53349 = EDGE_CURVE('',#41150,#41236,#34070,.T.) ;
#53350 = EDGE_CURVE('',#41357,#41369,#34071,.T.) ;
#53351 = EDGE_CURVE('',#41366,#41359,#34072,.T.) ;
#53352 = EDGE_CURVE('',#41366,#41361,#34073,.T.) ;
#53353 = EDGE_CURVE('',#41355,#41369,#34074,.T.) ;
#53354 = EDGE_CURVE('',#41367,#41363,#34075,.T.) ;
#53355 = EDGE_CURVE('',#41353,#41368,#34076,.T.) ;
#53356 = EDGE_CURVE('',#41367,#41365,#34077,.T.) ;
#53357 = EDGE_CURVE('',#41350,#41368,#34078,.T.) ;
#53358 = EDGE_CURVE('',#40849,#40844,#34079,.T.) ;
#53359 = EDGE_CURVE('',#40843,#40849,#34080,.T.) ;
#53360 = EDGE_CURVE('',#40844,#40843,#34081,.T.) ;
#53361 = EDGE_CURVE('',#40840,#40848,#34082,.T.) ;
#53362 = EDGE_CURVE('',#40845,#40842,#34083,.T.) ;
#53363 = EDGE_CURVE('',#40850,#40847,#34084,.T.) ;
#53364 = EDGE_CURVE('',#40853,#40653,#34085,.T.) ;
#53365 = EDGE_CURVE('',#40848,#40652,#34086,.T.) ;
#53366 = EDGE_CURVE('',#40840,#40652,#34087,.T.) ;
#53367 = EDGE_CURVE('',#40845,#39338,#34088,.T.) ;
#53368 = EDGE_CURVE('',#39337,#40842,#34089,.T.) ;
#53369 = EDGE_CURVE('',#40850,#40836,#34090,.T.) ;
#53370 = EDGE_CURVE('',#40836,#40847,#34091,.T.) ;
#53371 = EDGE_CURVE('',#40852,#39174,#34092,.T.) ;
#53372 = EDGE_CURVE('',#39173,#40853,#34093,.T.) ;
#53373 = EDGE_CURVE('',#40841,#40651,#34094,.T.) ;
#53374 = EDGE_CURVE('',#39339,#40841,#34095,.T.) ;
#53375 = EDGE_CURVE('',#40846,#39344,#34096,.T.) ;
#53376 = EDGE_CURVE('',#40837,#40846,#34097,.T.) ;
#53377 = EDGE_CURVE('',#40851,#40839,#34098,.T.) ;
#53378 = EDGE_CURVE('',#40662,#40852,#34099,.T.) ;
#53379 = EDGE_CURVE('',#40663,#40851,#34100,.T.) ;
#53380 = EDGE_CURVE('',#39339,#40650,#34101,.T.) ;
#53381 = EDGE_CURVE('',#40837,#39343,#34102,.T.) ;
#53382 = EDGE_CURVE('',#40663,#40839,#34103,.T.) ;
#53383 = EDGE_CURVE('',#40646,#40641,#34104,.T.) ;
#53384 = EDGE_CURVE('',#40647,#40640,#34105,.T.) ;
#53385 = EDGE_CURVE('',#39340,#40649,#34106,.T.) ;
#53386 = EDGE_CURVE('',#40838,#39342,#34107,.T.) ;
#53387 = EDGE_CURVE('',#40664,#40838,#34108,.T.) ;
#53388 = EDGE_CURVE('',#40647,#39417,#34109,.T.) ;
#53389 = EDGE_CURVE('',#39340,#40654,#34110,.T.) ;
#53390 = EDGE_CURVE('',#40654,#40649,#34111,.T.) ;
#53391 = EDGE_CURVE('',#40665,#39342,#34112,.T.) ;
#53392 = EDGE_CURVE('',#40648,#39416,#34113,.T.) ;
#53393 = EDGE_CURVE('',#40655,#40648,#34114,.T.) ;
#53394 = EDGE_CURVE('',#39341,#40657,#34115,.T.) ;
#53395 = EDGE_CURVE('',#40666,#39341,#34116,.T.) ;
#53396 = EDGE_CURVE('',#40655,#39415,#34117,.T.) ;
#53397 = EDGE_CURVE('',#40666,#40657,#34118,.T.) ;
#53398 = EDGE_CURVE('',#40656,#39414,#34119,.T.) ;
#53399 = EDGE_CURVE('',#40667,#40656,#34120,.T.) ;
#53400 = EDGE_CURVE('',#40670,#40659,#34121,.T.) ;
#53401 = EDGE_CURVE('',#40671,#40658,#34122,.T.) ;
#53402 = EDGE_CURVE('',#39411,#40668,#34123,.T.) ;
#53403 = EDGE_CURVE('',#39412,#40671,#34124,.T.) ;
#53404 = EDGE_CURVE('',#40667,#39413,#34125,.T.) ;
#53405 = EDGE_CURVE('',#39412,#40658,#34126,.T.) ;
#53406 = EDGE_CURVE('',#40149,#40160,#34127,.T.) ;
#53407 = EDGE_CURVE('',#40150,#40163,#34128,.T.) ;
#53408 = EDGE_CURVE('',#40161,#40156,#34129,.T.) ;
#53409 = EDGE_CURVE('',#40150,#40383,#34130,.T.) ;
#53410 = EDGE_CURVE('',#40383,#40163,#34131,.T.) ;
#53411 = EDGE_CURVE('',#40155,#40148,#34132,.T.) ;
#53412 = EDGE_CURVE('',#40162,#40159,#34133,.T.) ;
#53413 = EDGE_CURVE('',#40380,#40162,#34134,.T.) ;
#53414 = EDGE_CURVE('',#40151,#40382,#34135,.T.) ;
#53415 = EDGE_CURVE('',#40152,#40151,#34136,.T.) ;
#53416 = EDGE_CURVE('',#40380,#40159,#34137,.T.) ;
#53417 = EDGE_CURVE('',#40152,#40382,#34138,.T.) ;
#53418 = EDGE_CURVE('',#40381,#40158,#34139,.T.) ;
#53419 = EDGE_CURVE('',#40153,#40381,#34140,.T.) ;
#53420 = EDGE_CURVE('',#40153,#40158,#34141,.T.) ;
#53421 = EDGE_CURVE('',#40154,#40157,#34142,.T.) ;
#53422 = EDGE_CURVE('',#40047,#41535,#34143,.T.) ;
#53423 = EDGE_CURVE('',#40048,#39888,#34144,.T.) ;
#53424 = EDGE_CURVE('',#40049,#39891,#34145,.T.) ;
#53425 = EDGE_CURVE('',#39886,#40049,#34146,.T.) ;
#53426 = EDGE_CURVE('',#39886,#39891,#34147,.T.) ;
#53427 = EDGE_CURVE('',#39887,#39890,#34148,.T.) ;
#53428 = EDGE_CURVE('',#40102,#39887,#34149,.T.) ;
#53429 = EDGE_CURVE('',#40102,#39890,#34150,.T.) ;
#53430 = EDGE_CURVE('',#40103,#39889,#34151,.T.) ;
#53431 = EDGE_CURVE('',#40098,#41534,#34152,.T.) ;
#53432 = EDGE_CURVE('',#40099,#41541,#34153,.T.) ;
#53433 = EDGE_CURVE('',#40100,#39872,#34154,.T.) ;
#53434 = EDGE_CURVE('',#40101,#39875,#34155,.T.) ;
#53435 = EDGE_CURVE('',#39876,#40101,#34156,.T.) ;
#53436 = EDGE_CURVE('',#39876,#39875,#34157,.T.) ;
#53437 = EDGE_CURVE('',#39877,#39874,#34158,.T.) ;
#53438 = EDGE_CURVE('',#40050,#39877,#34159,.T.) ;
#53439 = EDGE_CURVE('',#40050,#39874,#34160,.T.) ;
#53440 = EDGE_CURVE('',#40051,#39873,#34161,.T.) ;
#53441 = EDGE_CURVE('',#40046,#41540,#34162,.T.) ;
#53442 = EDGE_CURVE('',#39183,#41374,#34163,.T.) ;
#53443 = EDGE_CURVE('',#41376,#39182,#34164,.T.) ;
#53444 = EDGE_CURVE('',#41378,#39181,#34165,.T.) ;
#53445 = EDGE_CURVE('',#39184,#41372,#34166,.T.) ;
#53446 = EDGE_CURVE('',#41380,#39180,#34167,.T.) ;
#53447 = EDGE_CURVE('',#39177,#41371,#34168,.T.) ;
#53448 = EDGE_CURVE('',#41382,#39179,#34169,.T.) ;
#53449 = EDGE_CURVE('',#39178,#41384,#34170,.T.) ;
#53450 = EDGE_CURVE('',#40392,#40399,#34171,.T.) ;
#53451 = EDGE_CURVE('',#40393,#40467,#34172,.T.) ;
#53452 = EDGE_CURVE('',#40464,#40392,#34173,.T.) ;
#53453 = EDGE_CURVE('',#40394,#40393,#34174,.T.) ;
#53454 = EDGE_CURVE('',#40464,#40399,#34175,.T.) ;
#53455 = EDGE_CURVE('',#40394,#40467,#34176,.T.) ;
#53456 = EDGE_CURVE('',#40398,#40397,#34177,.T.) ;
#53457 = EDGE_CURVE('',#40465,#40398,#34178,.T.) ;
#53458 = EDGE_CURVE('',#40395,#40466,#34179,.T.) ;
#53459 = EDGE_CURVE('',#40396,#40395,#34180,.T.) ;
#53460 = EDGE_CURVE('',#40465,#40397,#34181,.T.) ;
#53461 = EDGE_CURVE('',#40396,#40466,#34182,.T.) ;
#53462 = EDGE_CURVE('',#39139,#40936,#34183,.T.) ;
#53463 = EDGE_CURVE('',#40937,#39138,#34184,.T.) ;
#53464 = EDGE_CURVE('',#40933,#39137,#34185,.T.) ;
#53465 = EDGE_CURVE('',#40937,#40933,#34186,.T.) ;
#53466 = EDGE_CURVE('',#40925,#40936,#34187,.T.) ;
#53467 = EDGE_CURVE('',#39140,#40925,#34188,.T.) ;
#53468 = EDGE_CURVE('',#40930,#39136,#34189,.T.) ;
#53469 = EDGE_CURVE('',#40934,#40932,#34190,.T.) ;
#53470 = EDGE_CURVE('',#40935,#41157,#34191,.T.) ;
#53471 = EDGE_CURVE('',#41154,#40934,#34192,.T.) ;
#53472 = EDGE_CURVE('',#40922,#40935,#34193,.T.) ;
#53473 = EDGE_CURVE('',#39134,#40924,#34194,.T.) ;
#53474 = EDGE_CURVE('',#39135,#40926,#34195,.T.) ;
#53475 = EDGE_CURVE('',#40927,#39133,#34196,.T.) ;
#53476 = EDGE_CURVE('',#40930,#40926,#34197,.T.) ;
#53477 = EDGE_CURVE('',#41154,#40932,#34198,.T.) ;
#53478 = EDGE_CURVE('',#40922,#41157,#34199,.T.) ;
#53479 = EDGE_CURVE('',#40927,#40924,#34200,.T.) ;
#53480 = EDGE_CURVE('',#40931,#40929,#34201,.T.) ;
#53481 = EDGE_CURVE('',#41155,#40931,#34202,.T.) ;
#53482 = EDGE_CURVE('',#40923,#41156,#34203,.T.) ;
#53483 = EDGE_CURVE('',#40928,#40923,#34204,.T.) ;
#53484 = EDGE_CURVE('',#41155,#40929,#34205,.T.) ;
#53485 = EDGE_CURVE('',#40928,#41156,#34206,.T.) ;
#53486 = EDGE_CURVE('',#41166,#41173,#34207,.T.) ;
#53487 = EDGE_CURVE('',#41167,#41241,#34208,.T.) ;
#53488 = EDGE_CURVE('',#41238,#41166,#34209,.T.) ;
#53489 = EDGE_CURVE('',#41168,#41167,#34210,.T.) ;
#53490 = EDGE_CURVE('',#41238,#41173,#34211,.T.) ;
#53491 = EDGE_CURVE('',#41168,#41241,#34212,.T.) ;
#53492 = EDGE_CURVE('',#41172,#41171,#34213,.T.) ;
#53493 = EDGE_CURVE('',#41239,#41172,#34214,.T.) ;
#53494 = EDGE_CURVE('',#41169,#41240,#34215,.T.) ;
#53495 = EDGE_CURVE('',#41170,#41169,#34216,.T.) ;
#53496 = EDGE_CURVE('',#41239,#41171,#34217,.T.) ;
#53497 = EDGE_CURVE('',#41170,#41240,#34218,.T.) ;
#53498 = EDGE_CURVE('',#41377,#41389,#34219,.T.) ;
#53499 = EDGE_CURVE('',#41386,#41379,#34220,.T.) ;
#53500 = EDGE_CURVE('',#41386,#41381,#34221,.T.) ;
#53501 = EDGE_CURVE('',#41375,#41389,#34222,.T.) ;
#53502 = EDGE_CURVE('',#41387,#41383,#34223,.T.) ;
#53503 = EDGE_CURVE('',#41373,#41388,#34224,.T.) ;
#53504 = EDGE_CURVE('',#41387,#41385,#34225,.T.) ;
#53505 = EDGE_CURVE('',#41370,#41388,#34226,.T.) ;
#53506 = EDGE_CURVE('',#40867,#40862,#34227,.T.) ;
#53507 = EDGE_CURVE('',#40861,#40867,#34228,.T.) ;
#53508 = EDGE_CURVE('',#40862,#40861,#34229,.T.) ;
#53509 = EDGE_CURVE('',#40858,#40866,#34230,.T.) ;
#53510 = EDGE_CURVE('',#40863,#40860,#34231,.T.) ;
#53511 = EDGE_CURVE('',#40868,#40865,#34232,.T.) ;
#53512 = EDGE_CURVE('',#40871,#40681,#34233,.T.) ;
#53513 = EDGE_CURVE('',#40866,#40680,#34234,.T.) ;
#53514 = EDGE_CURVE('',#40858,#40680,#34235,.T.) ;
#53515 = EDGE_CURVE('',#40863,#39330,#34236,.T.) ;
#53516 = EDGE_CURVE('',#39329,#40860,#34237,.T.) ;
#53517 = EDGE_CURVE('',#40868,#40854,#34238,.T.) ;
#53518 = EDGE_CURVE('',#40854,#40865,#34239,.T.) ;
#53519 = EDGE_CURVE('',#40870,#39162,#34240,.T.) ;
#53520 = EDGE_CURVE('',#39161,#40871,#34241,.T.) ;
#53521 = EDGE_CURVE('',#40859,#40679,#34242,.T.) ;
#53522 = EDGE_CURVE('',#39331,#40859,#34243,.T.) ;
#53523 = EDGE_CURVE('',#40864,#39336,#34244,.T.) ;
#53524 = EDGE_CURVE('',#40855,#40864,#34245,.T.) ;
#53525 = EDGE_CURVE('',#40869,#40857,#34246,.T.) ;
#53526 = EDGE_CURVE('',#40690,#40870,#34247,.T.) ;
#53527 = EDGE_CURVE('',#40691,#40869,#34248,.T.) ;
#53528 = EDGE_CURVE('',#39331,#40678,#34249,.T.) ;
#53529 = EDGE_CURVE('',#40855,#39335,#34250,.T.) ;
#53530 = EDGE_CURVE('',#40691,#40857,#34251,.T.) ;
#53531 = EDGE_CURVE('',#40674,#40669,#34252,.T.) ;
#53532 = EDGE_CURVE('',#40675,#40668,#34253,.T.) ;
#53533 = EDGE_CURVE('',#39332,#40677,#34254,.T.) ;
#53534 = EDGE_CURVE('',#40856,#39334,#34255,.T.) ;
#53535 = EDGE_CURVE('',#40692,#40856,#34256,.T.) ;
#53536 = EDGE_CURVE('',#40675,#39411,#34257,.T.) ;
#53537 = EDGE_CURVE('',#39332,#40682,#34258,.T.) ;
#53538 = EDGE_CURVE('',#40682,#40677,#34259,.T.) ;
#53539 = EDGE_CURVE('',#40693,#39334,#34260,.T.) ;
#53540 = EDGE_CURVE('',#40676,#39410,#34261,.T.) ;
#53541 = EDGE_CURVE('',#40683,#40676,#34262,.T.) ;
#53542 = EDGE_CURVE('',#39333,#40685,#34263,.T.) ;
#53543 = EDGE_CURVE('',#40694,#39333,#34264,.T.) ;
#53544 = EDGE_CURVE('',#40683,#39409,#34265,.T.) ;
#53545 = EDGE_CURVE('',#40694,#40685,#34266,.T.) ;
#53546 = EDGE_CURVE('',#40684,#39408,#34267,.T.) ;
#53547 = EDGE_CURVE('',#40695,#40684,#34268,.T.) ;
#53548 = EDGE_CURVE('',#40698,#40687,#34269,.T.) ;
#53549 = EDGE_CURVE('',#40699,#40686,#34270,.T.) ;
#53550 = EDGE_CURVE('',#39405,#40696,#34271,.T.) ;
#53551 = EDGE_CURVE('',#39406,#40699,#34272,.T.) ;
#53552 = EDGE_CURVE('',#40695,#39407,#34273,.T.) ;
#53553 = EDGE_CURVE('',#39406,#40686,#34274,.T.) ;
#53554 = EDGE_CURVE('',#40133,#40144,#34275,.T.) ;
#53555 = EDGE_CURVE('',#40134,#40147,#34276,.T.) ;
#53556 = EDGE_CURVE('',#40145,#40140,#34277,.T.) ;
#53557 = EDGE_CURVE('',#40134,#40403,#34278,.T.) ;
#53558 = EDGE_CURVE('',#40403,#40147,#34279,.T.) ;
#53559 = EDGE_CURVE('',#40139,#40132,#34280,.T.) ;
#53560 = EDGE_CURVE('',#40146,#40143,#34281,.T.) ;
#53561 = EDGE_CURVE('',#40400,#40146,#34282,.T.) ;
#53562 = EDGE_CURVE('',#40135,#40402,#34283,.T.) ;
#53563 = EDGE_CURVE('',#40136,#40135,#34284,.T.) ;
#53564 = EDGE_CURVE('',#40400,#40143,#34285,.T.) ;
#53565 = EDGE_CURVE('',#40136,#40402,#34286,.T.) ;
#53566 = EDGE_CURVE('',#40401,#40142,#34287,.T.) ;
#53567 = EDGE_CURVE('',#40137,#40401,#34288,.T.) ;
#53568 = EDGE_CURVE('',#40137,#40142,#34289,.T.) ;
#53569 = EDGE_CURVE('',#40138,#40141,#34290,.T.) ;
#53570 = EDGE_CURVE('',#40053,#41543,#34291,.T.) ;
#53571 = EDGE_CURVE('',#40054,#39868,#34292,.T.) ;
#53572 = EDGE_CURVE('',#40055,#39871,#34293,.T.) ;
#53573 = EDGE_CURVE('',#39866,#40055,#34294,.T.) ;
#53574 = EDGE_CURVE('',#39866,#39871,#34295,.T.) ;
#53575 = EDGE_CURVE('',#39867,#39870,#34296,.T.) ;
#53576 = EDGE_CURVE('',#40108,#39867,#34297,.T.) ;
#53577 = EDGE_CURVE('',#40108,#39870,#34298,.T.) ;
#53578 = EDGE_CURVE('',#40109,#39869,#34299,.T.) ;
#53579 = EDGE_CURVE('',#40104,#41542,#34300,.T.) ;
#53580 = EDGE_CURVE('',#40105,#41549,#34301,.T.) ;
#53581 = EDGE_CURVE('',#40106,#39852,#34302,.T.) ;
#53582 = EDGE_CURVE('',#40107,#39855,#34303,.T.) ;
#53583 = EDGE_CURVE('',#39856,#40107,#34304,.T.) ;
#53584 = EDGE_CURVE('',#39856,#39855,#34305,.T.) ;
#53585 = EDGE_CURVE('',#39857,#39854,#34306,.T.) ;
#53586 = EDGE_CURVE('',#40056,#39857,#34307,.T.) ;
#53587 = EDGE_CURVE('',#40056,#39854,#34308,.T.) ;
#53588 = EDGE_CURVE('',#40057,#39853,#34309,.T.) ;
#53589 = EDGE_CURVE('',#40052,#41548,#34310,.T.) ;
#53590 = EDGE_CURVE('',#39171,#41394,#34311,.T.) ;
#53591 = EDGE_CURVE('',#41396,#39170,#34312,.T.) ;
#53592 = EDGE_CURVE('',#41398,#39169,#34313,.T.) ;
#53593 = EDGE_CURVE('',#39172,#41392,#34314,.T.) ;
#53594 = EDGE_CURVE('',#41400,#39168,#34315,.T.) ;
#53595 = EDGE_CURVE('',#39165,#41391,#34316,.T.) ;
#53596 = EDGE_CURVE('',#41402,#39167,#34317,.T.) ;
#53597 = EDGE_CURVE('',#39166,#41404,#34318,.T.) ;
#53598 = EDGE_CURVE('',#40412,#40419,#34319,.T.) ;
#53599 = EDGE_CURVE('',#40413,#40471,#34320,.T.) ;
#53600 = EDGE_CURVE('',#40468,#40412,#34321,.T.) ;
#53601 = EDGE_CURVE('',#40414,#40413,#34322,.T.) ;
#53602 = EDGE_CURVE('',#40468,#40419,#34323,.T.) ;
#53603 = EDGE_CURVE('',#40414,#40471,#34324,.T.) ;
#53604 = EDGE_CURVE('',#40418,#40417,#34325,.T.) ;
#53605 = EDGE_CURVE('',#40469,#40418,#34326,.T.) ;
#53606 = EDGE_CURVE('',#40415,#40470,#34327,.T.) ;
#53607 = EDGE_CURVE('',#40416,#40415,#34328,.T.) ;
#53608 = EDGE_CURVE('',#40469,#40417,#34329,.T.) ;
#53609 = EDGE_CURVE('',#40416,#40470,#34330,.T.) ;
#53610 = EDGE_CURVE('',#39075,#40920,#34331,.T.) ;
#53611 = EDGE_CURVE('',#40921,#39074,#34332,.T.) ;
#53612 = EDGE_CURVE('',#40917,#39073,#34333,.T.) ;
#53613 = EDGE_CURVE('',#40921,#40917,#34334,.T.) ;
#53614 = EDGE_CURVE('',#40909,#40920,#34335,.T.) ;
#53615 = EDGE_CURVE('',#39076,#40909,#34336,.T.) ;
#53616 = EDGE_CURVE('',#40914,#39072,#34337,.T.) ;
#53617 = EDGE_CURVE('',#40918,#40916,#34338,.T.) ;
#53618 = EDGE_CURVE('',#40919,#41177,#34339,.T.) ;
#53619 = EDGE_CURVE('',#41174,#40918,#34340,.T.) ;
#53620 = EDGE_CURVE('',#40906,#40919,#34341,.T.) ;
#53621 = EDGE_CURVE('',#39070,#40908,#34342,.T.) ;
#53622 = EDGE_CURVE('',#39071,#40910,#34343,.T.) ;
#53623 = EDGE_CURVE('',#40911,#39069,#34344,.T.) ;
#53624 = EDGE_CURVE('',#40914,#40910,#34345,.T.) ;
#53625 = EDGE_CURVE('',#41174,#40916,#34346,.T.) ;
#53626 = EDGE_CURVE('',#40906,#41177,#34347,.T.) ;
#53627 = EDGE_CURVE('',#40911,#40908,#34348,.T.) ;
#53628 = EDGE_CURVE('',#40915,#40913,#34349,.T.) ;
#53629 = EDGE_CURVE('',#41175,#40915,#34350,.T.) ;
#53630 = EDGE_CURVE('',#40907,#41176,#34351,.T.) ;
#53631 = EDGE_CURVE('',#40912,#40907,#34352,.T.) ;
#53632 = EDGE_CURVE('',#41175,#40913,#34353,.T.) ;
#53633 = EDGE_CURVE('',#40912,#41176,#34354,.T.) ;
#53634 = EDGE_CURVE('',#41186,#41193,#34355,.T.) ;
#53635 = EDGE_CURVE('',#41187,#41245,#34356,.T.) ;
#53636 = EDGE_CURVE('',#41242,#41186,#34357,.T.) ;
#53637 = EDGE_CURVE('',#41188,#41187,#34358,.T.) ;
#53638 = EDGE_CURVE('',#41242,#41193,#34359,.T.) ;
#53639 = EDGE_CURVE('',#41188,#41245,#34360,.T.) ;
#53640 = EDGE_CURVE('',#41192,#41191,#34361,.T.) ;
#53641 = EDGE_CURVE('',#41243,#41192,#34362,.T.) ;
#53642 = EDGE_CURVE('',#41189,#41244,#34363,.T.) ;
#53643 = EDGE_CURVE('',#41190,#41189,#34364,.T.) ;
#53644 = EDGE_CURVE('',#41243,#41191,#34365,.T.) ;
#53645 = EDGE_CURVE('',#41190,#41244,#34366,.T.) ;
#53646 = EDGE_CURVE('',#41397,#41409,#34367,.T.) ;
#53647 = EDGE_CURVE('',#41406,#41399,#34368,.T.) ;
#53648 = EDGE_CURVE('',#41406,#41401,#34369,.T.) ;
#53649 = EDGE_CURVE('',#41395,#41409,#34370,.T.) ;
#53650 = EDGE_CURVE('',#41407,#41403,#34371,.T.) ;
#53651 = EDGE_CURVE('',#41393,#41408,#34372,.T.) ;
#53652 = EDGE_CURVE('',#41407,#41405,#34373,.T.) ;
#53653 = EDGE_CURVE('',#41390,#41408,#34374,.T.) ;
#53654 = EDGE_CURVE('',#40885,#40880,#34375,.T.) ;
#53655 = EDGE_CURVE('',#40879,#40885,#34376,.T.) ;
#53656 = EDGE_CURVE('',#40880,#40879,#34377,.T.) ;
#53657 = EDGE_CURVE('',#40876,#40884,#34378,.T.) ;
#53658 = EDGE_CURVE('',#40881,#40878,#34379,.T.) ;
#53659 = EDGE_CURVE('',#40886,#40883,#34380,.T.) ;
#53660 = EDGE_CURVE('',#40889,#40709,#34381,.T.) ;
#53661 = EDGE_CURVE('',#40884,#40708,#34382,.T.) ;
#53662 = EDGE_CURVE('',#40876,#40708,#34383,.T.) ;
#53663 = EDGE_CURVE('',#40881,#39322,#34384,.T.) ;
#53664 = EDGE_CURVE('',#39321,#40878,#34385,.T.) ;
#53665 = EDGE_CURVE('',#40886,#40872,#34386,.T.) ;
#53666 = EDGE_CURVE('',#40872,#40883,#34387,.T.) ;
#53667 = EDGE_CURVE('',#40888,#39150,#34388,.T.) ;
#53668 = EDGE_CURVE('',#39149,#40889,#34389,.T.) ;
#53669 = EDGE_CURVE('',#40877,#40707,#34390,.T.) ;
#53670 = EDGE_CURVE('',#39323,#40877,#34391,.T.) ;
#53671 = EDGE_CURVE('',#40882,#39328,#34392,.T.) ;
#53672 = EDGE_CURVE('',#40873,#40882,#34393,.T.) ;
#53673 = EDGE_CURVE('',#40887,#40875,#34394,.T.) ;
#53674 = EDGE_CURVE('',#40718,#40888,#34395,.T.) ;
#53675 = EDGE_CURVE('',#40719,#40887,#34396,.T.) ;
#53676 = EDGE_CURVE('',#39323,#40706,#34397,.T.) ;
#53677 = EDGE_CURVE('',#40873,#39327,#34398,.T.) ;
#53678 = EDGE_CURVE('',#40719,#40875,#34399,.T.) ;
#53679 = EDGE_CURVE('',#40702,#40697,#34400,.T.) ;
#53680 = EDGE_CURVE('',#40703,#40696,#34401,.T.) ;
#53681 = EDGE_CURVE('',#39324,#40705,#34402,.T.) ;
#53682 = EDGE_CURVE('',#40874,#39326,#34403,.T.) ;
#53683 = EDGE_CURVE('',#40720,#40874,#34404,.T.) ;
#53684 = EDGE_CURVE('',#40703,#39405,#34405,.T.) ;
#53685 = EDGE_CURVE('',#39324,#40710,#34406,.T.) ;
#53686 = EDGE_CURVE('',#40710,#40705,#34407,.T.) ;
#53687 = EDGE_CURVE('',#40721,#39326,#34408,.T.) ;
#53688 = EDGE_CURVE('',#40704,#39404,#34409,.T.) ;
#53689 = EDGE_CURVE('',#40711,#40704,#34410,.T.) ;
#53690 = EDGE_CURVE('',#39325,#40713,#34411,.T.) ;
#53691 = EDGE_CURVE('',#40722,#39325,#34412,.T.) ;
#53692 = EDGE_CURVE('',#40711,#39403,#34413,.T.) ;
#53693 = EDGE_CURVE('',#40722,#40713,#34414,.T.) ;
#53694 = EDGE_CURVE('',#40712,#39402,#34415,.T.) ;
#53695 = EDGE_CURVE('',#40723,#40712,#34416,.T.) ;
#53696 = EDGE_CURVE('',#40727,#40715,#34417,.T.) ;
#53697 = EDGE_CURVE('',#40724,#40714,#34418,.T.) ;
#53698 = EDGE_CURVE('',#39399,#40725,#34419,.T.) ;
#53699 = EDGE_CURVE('',#39400,#40724,#34420,.T.) ;
#53700 = EDGE_CURVE('',#40723,#39401,#34421,.T.) ;
#53701 = EDGE_CURVE('',#39400,#40714,#34422,.T.) ;
#53702 = EDGE_CURVE('',#40117,#40128,#34423,.T.) ;
#53703 = EDGE_CURVE('',#40118,#40131,#34424,.T.) ;
#53704 = EDGE_CURVE('',#40129,#40124,#34425,.T.) ;
#53705 = EDGE_CURVE('',#40118,#40423,#34426,.T.) ;
#53706 = EDGE_CURVE('',#40423,#40131,#34427,.T.) ;
#53707 = EDGE_CURVE('',#40123,#40116,#34428,.T.) ;
#53708 = EDGE_CURVE('',#40130,#40127,#34429,.T.) ;
#53709 = EDGE_CURVE('',#40420,#40130,#34430,.T.) ;
#53710 = EDGE_CURVE('',#40119,#40422,#34431,.T.) ;
#53711 = EDGE_CURVE('',#40120,#40119,#34432,.T.) ;
#53712 = EDGE_CURVE('',#40420,#40127,#34433,.T.) ;
#53713 = EDGE_CURVE('',#40120,#40422,#34434,.T.) ;
#53714 = EDGE_CURVE('',#40421,#40126,#34435,.T.) ;
#53715 = EDGE_CURVE('',#40121,#40421,#34436,.T.) ;
#53716 = EDGE_CURVE('',#40121,#40126,#34437,.T.) ;
#53717 = EDGE_CURVE('',#40122,#40125,#34438,.T.) ;
#53718 = EDGE_CURVE('',#40059,#41551,#34439,.T.) ;
#53719 = EDGE_CURVE('',#40060,#39848,#34440,.T.) ;
#53720 = EDGE_CURVE('',#40061,#39851,#34441,.T.) ;
#53721 = EDGE_CURVE('',#39846,#40061,#34442,.T.) ;
#53722 = EDGE_CURVE('',#39846,#39851,#34443,.T.) ;
#53723 = EDGE_CURVE('',#39847,#39850,#34444,.T.) ;
#53724 = EDGE_CURVE('',#40114,#39847,#34445,.T.) ;
#53725 = EDGE_CURVE('',#40114,#39850,#34446,.T.) ;
#53726 = EDGE_CURVE('',#40115,#39849,#34447,.T.) ;
#53727 = EDGE_CURVE('',#40110,#41550,#34448,.T.) ;
#53728 = EDGE_CURVE('',#40111,#41557,#34449,.T.) ;
#53729 = EDGE_CURVE('',#40112,#39832,#34450,.T.) ;
#53730 = EDGE_CURVE('',#40113,#39835,#34451,.T.) ;
#53731 = EDGE_CURVE('',#39836,#40113,#34452,.T.) ;
#53732 = EDGE_CURVE('',#39836,#39835,#34453,.T.) ;
#53733 = EDGE_CURVE('',#39837,#39834,#34454,.T.) ;
#53734 = EDGE_CURVE('',#40062,#39837,#34455,.T.) ;
#53735 = EDGE_CURVE('',#40062,#39834,#34456,.T.) ;
#53736 = EDGE_CURVE('',#40063,#39833,#34457,.T.) ;
#53737 = EDGE_CURVE('',#40058,#41556,#34458,.T.) ;
#53738 = EDGE_CURVE('',#39159,#41414,#34459,.T.) ;
#53739 = EDGE_CURVE('',#41416,#39158,#34460,.T.) ;
#53740 = EDGE_CURVE('',#41418,#39157,#34461,.T.) ;
#53741 = EDGE_CURVE('',#39160,#41412,#34462,.T.) ;
#53742 = EDGE_CURVE('',#41420,#39156,#34463,.T.) ;
#53743 = EDGE_CURVE('',#39153,#41411,#34464,.T.) ;
#53744 = EDGE_CURVE('',#41422,#39155,#34465,.T.) ;
#53745 = EDGE_CURVE('',#39154,#41424,#34466,.T.) ;
#53746 = EDGE_CURVE('',#40432,#40439,#34467,.T.) ;
#53747 = EDGE_CURVE('',#40433,#40475,#34468,.T.) ;
#53748 = EDGE_CURVE('',#40472,#40432,#34469,.T.) ;
#53749 = EDGE_CURVE('',#40434,#40433,#34470,.T.) ;
#53750 = EDGE_CURVE('',#40472,#40439,#34471,.T.) ;
#53751 = EDGE_CURVE('',#40434,#40475,#34472,.T.) ;
#53752 = EDGE_CURVE('',#40438,#40437,#34473,.T.) ;
#53753 = EDGE_CURVE('',#40473,#40438,#34474,.T.) ;
#53754 = EDGE_CURVE('',#40435,#40474,#34475,.T.) ;
#53755 = EDGE_CURVE('',#40436,#40435,#34476,.T.) ;
#53756 = EDGE_CURVE('',#40473,#40437,#34477,.T.) ;
#53757 = EDGE_CURVE('',#40436,#40474,#34478,.T.) ;
#53758 = EDGE_CURVE('',#39147,#40904,#34479,.T.) ;
#53759 = EDGE_CURVE('',#40905,#39146,#34480,.T.) ;
#53760 = EDGE_CURVE('',#40901,#39145,#34481,.T.) ;
#53761 = EDGE_CURVE('',#40905,#40901,#34482,.T.) ;
#53762 = EDGE_CURVE('',#40893,#40904,#34483,.T.) ;
#53763 = EDGE_CURVE('',#39148,#40893,#34484,.T.) ;
#53764 = EDGE_CURVE('',#40898,#39144,#34485,.T.) ;
#53765 = EDGE_CURVE('',#40902,#40900,#34486,.T.) ;
#53766 = EDGE_CURVE('',#40903,#41197,#34487,.T.) ;
#53767 = EDGE_CURVE('',#41194,#40902,#34488,.T.) ;
#53768 = EDGE_CURVE('',#40890,#40903,#34489,.T.) ;
#53769 = EDGE_CURVE('',#39142,#40892,#34490,.T.) ;
#53770 = EDGE_CURVE('',#39143,#40894,#34491,.T.) ;
#53771 = EDGE_CURVE('',#40895,#39141,#34492,.T.) ;
#53772 = EDGE_CURVE('',#40898,#40894,#34493,.T.) ;
#53773 = EDGE_CURVE('',#41194,#40900,#34494,.T.) ;
#53774 = EDGE_CURVE('',#40890,#41197,#34495,.T.) ;
#53775 = EDGE_CURVE('',#40895,#40892,#34496,.T.) ;
#53776 = EDGE_CURVE('',#40899,#40897,#34497,.T.) ;
#53777 = EDGE_CURVE('',#41195,#40899,#34498,.T.) ;
#53778 = EDGE_CURVE('',#40891,#41196,#34499,.T.) ;
#53779 = EDGE_CURVE('',#40896,#40891,#34500,.T.) ;
#53780 = EDGE_CURVE('',#41195,#40897,#34501,.T.) ;
#53781 = EDGE_CURVE('',#40896,#41196,#34502,.T.) ;
#53782 = EDGE_CURVE('',#41206,#41213,#34503,.T.) ;
#53783 = EDGE_CURVE('',#41207,#41249,#34504,.T.) ;
#53784 = EDGE_CURVE('',#41246,#41206,#34505,.T.) ;
#53785 = EDGE_CURVE('',#41208,#41207,#34506,.T.) ;
#53786 = EDGE_CURVE('',#41246,#41213,#34507,.T.) ;
#53787 = EDGE_CURVE('',#41208,#41249,#34508,.T.) ;
#53788 = EDGE_CURVE('',#41212,#41211,#34509,.T.) ;
#53789 = EDGE_CURVE('',#41247,#41212,#34510,.T.) ;
#53790 = EDGE_CURVE('',#41209,#41248,#34511,.T.) ;
#53791 = EDGE_CURVE('',#41210,#41209,#34512,.T.) ;
#53792 = EDGE_CURVE('',#41247,#41211,#34513,.T.) ;
#53793 = EDGE_CURVE('',#41210,#41248,#34514,.T.) ;
#53794 = EDGE_CURVE('',#41417,#41429,#34515,.T.) ;
#53795 = EDGE_CURVE('',#41426,#41419,#34516,.T.) ;
#53796 = EDGE_CURVE('',#41426,#41421,#34517,.T.) ;
#53797 = EDGE_CURVE('',#41415,#41429,#34518,.T.) ;
#53798 = EDGE_CURVE('',#41427,#41423,#34519,.T.) ;
#53799 = EDGE_CURVE('',#41413,#41428,#34520,.T.) ;
#53800 = EDGE_CURVE('',#41427,#41425,#34521,.T.) ;
#53801 = EDGE_CURVE('',#41410,#41428,#34522,.T.) ;
#53802 = EDGE_CURVE('',#39247,#39271,#34523,.T.) ;
#53803 = EDGE_CURVE('',#39270,#39248,#34524,.T.) ;
#53804 = EDGE_CURVE('',#39235,#39277,#34525,.T.) ;
#53805 = EDGE_CURVE('',#39276,#39236,#34526,.T.) ;
#53806 = EDGE_CURVE('',#39223,#39283,#34527,.T.) ;
#53807 = EDGE_CURVE('',#39282,#39224,#34528,.T.) ;
#53808 = EDGE_CURVE('',#39211,#39289,#34529,.T.) ;
#53809 = EDGE_CURVE('',#39288,#39212,#34530,.T.) ;
#53810 = EDGE_CURVE('',#39199,#39295,#34531,.T.) ;
#53811 = EDGE_CURVE('',#39294,#39200,#34532,.T.) ;
#53812 = EDGE_CURVE('',#39187,#39301,#34533,.T.) ;
#53813 = EDGE_CURVE('',#39300,#39188,#34534,.T.) ;
#53814 = EDGE_CURVE('',#39175,#39307,#34535,.T.) ;
#53815 = EDGE_CURVE('',#39306,#39176,#34536,.T.) ;
#53816 = EDGE_CURVE('',#39163,#39313,#34537,.T.) ;
#53817 = EDGE_CURVE('',#39312,#39164,#34538,.T.) ;
#53818 = EDGE_CURVE('',#39151,#39319,#34539,.T.) ;
#53819 = EDGE_CURVE('',#39318,#39152,#34540,.T.) ;
#53820 = EDGE_CURVE('',#41558,#39274,#34541,.T.) ;
#53821 = EDGE_CURVE('',#41558,#39275,#2377,.T.) ;
#53822 = EDGE_CURVE('',#40501,#41558,#34542,.T.) ;
#53823 = EDGE_CURVE('',#41559,#39273,#34543,.T.) ;
#53824 = EDGE_CURVE('',#40502,#41559,#34544,.T.) ;
#53825 = EDGE_CURVE('',#39272,#41559,#2378,.T.) ;
#53826 = EDGE_CURVE('',#39465,#39269,#2379,.T.) ;
#53827 = EDGE_CURVE('',#41560,#39280,#34545,.T.) ;
#53828 = EDGE_CURVE('',#41560,#39281,#2380,.T.) ;
#53829 = EDGE_CURVE('',#40529,#41560,#34546,.T.) ;
#53830 = EDGE_CURVE('',#41561,#39279,#34547,.T.) ;
#53831 = EDGE_CURVE('',#40530,#41561,#34548,.T.) ;
#53832 = EDGE_CURVE('',#39278,#41561,#2381,.T.) ;
#53833 = EDGE_CURVE('',#41562,#39286,#34549,.T.) ;
#53834 = EDGE_CURVE('',#41562,#39287,#2382,.T.) ;
#53835 = EDGE_CURVE('',#40557,#41562,#34550,.T.) ;
#53836 = EDGE_CURVE('',#41563,#39285,#34551,.T.) ;
#53837 = EDGE_CURVE('',#40558,#41563,#34552,.T.) ;
#53838 = EDGE_CURVE('',#39284,#41563,#2383,.T.) ;
#53839 = EDGE_CURVE('',#41564,#39292,#34553,.T.) ;
#53840 = EDGE_CURVE('',#41564,#39293,#2384,.T.) ;
#53841 = EDGE_CURVE('',#40585,#41564,#34554,.T.) ;
#53842 = EDGE_CURVE('',#41565,#39291,#34555,.T.) ;
#53843 = EDGE_CURVE('',#40586,#41565,#34556,.T.) ;
#53844 = EDGE_CURVE('',#39290,#41565,#2385,.T.) ;
#53845 = EDGE_CURVE('',#41566,#39298,#34557,.T.) ;
#53846 = EDGE_CURVE('',#41566,#39299,#2386,.T.) ;
#53847 = EDGE_CURVE('',#40613,#41566,#34558,.T.) ;
#53848 = EDGE_CURVE('',#41567,#39297,#34559,.T.) ;
#53849 = EDGE_CURVE('',#40614,#41567,#34560,.T.) ;
#53850 = EDGE_CURVE('',#39296,#41567,#2387,.T.) ;
#53851 = EDGE_CURVE('',#41568,#39304,#34561,.T.) ;
#53852 = EDGE_CURVE('',#41568,#39305,#2388,.T.) ;
#53853 = EDGE_CURVE('',#40641,#41568,#34562,.T.) ;
#53854 = EDGE_CURVE('',#41569,#39303,#34563,.T.) ;
#53855 = EDGE_CURVE('',#40642,#41569,#34564,.T.) ;
#53856 = EDGE_CURVE('',#39302,#41569,#2389,.T.) ;
#53857 = EDGE_CURVE('',#41570,#39310,#34565,.T.) ;
#53858 = EDGE_CURVE('',#41570,#39311,#2390,.T.) ;
#53859 = EDGE_CURVE('',#40669,#41570,#34566,.T.) ;
#53860 = EDGE_CURVE('',#41571,#39309,#34567,.T.) ;
#53861 = EDGE_CURVE('',#40670,#41571,#34568,.T.) ;
#53862 = EDGE_CURVE('',#39308,#41571,#2391,.T.) ;
#53863 = EDGE_CURVE('',#41572,#39316,#34569,.T.) ;
#53864 = EDGE_CURVE('',#41572,#39317,#2392,.T.) ;
#53865 = EDGE_CURVE('',#40697,#41572,#34570,.T.) ;
#53866 = EDGE_CURVE('',#41573,#39315,#34571,.T.) ;
#53867 = EDGE_CURVE('',#40698,#41573,#34572,.T.) ;
#53868 = EDGE_CURVE('',#39314,#41573,#2393,.T.) ;
#53869 = EDGE_CURVE('',#40726,#39258,#34573,.T.) ;
#53870 = EDGE_CURVE('',#41574,#39257,#34574,.T.) ;
#53871 = EDGE_CURVE('',#40727,#41574,#34575,.T.) ;
#53872 = EDGE_CURVE('',#39320,#41574,#2394,.T.) ;
#53873 = EDGE_CURVE('',#40492,#41575,#2395,.T.) ;
#53874 = EDGE_CURVE('',#40493,#41575,#34576,.T.) ;
#53875 = EDGE_CURVE('',#41575,#39247,#34577,.T.) ;
#53876 = EDGE_CURVE('',#40494,#39246,#34578,.T.) ;
#53877 = EDGE_CURVE('',#41576,#40476,#34579,.T.) ;
#53878 = EDGE_CURVE('',#41576,#40477,#2396,.T.) ;
#53879 = EDGE_CURVE('',#39248,#41576,#34580,.T.) ;
#53880 = EDGE_CURVE('',#39245,#40485,#34581,.T.) ;
#53881 = EDGE_CURVE('',#40520,#41577,#2397,.T.) ;
#53882 = EDGE_CURVE('',#40521,#41577,#34582,.T.) ;
#53883 = EDGE_CURVE('',#41577,#39235,#34583,.T.) ;
#53884 = EDGE_CURVE('',#40522,#39234,#34584,.T.) ;
#53885 = EDGE_CURVE('',#41578,#40504,#34585,.T.) ;
#53886 = EDGE_CURVE('',#41578,#40505,#2398,.T.) ;
#53887 = EDGE_CURVE('',#39236,#41578,#34586,.T.) ;
#53888 = EDGE_CURVE('',#39233,#40513,#34587,.T.) ;
#53889 = EDGE_CURVE('',#40548,#41579,#2399,.T.) ;
#53890 = EDGE_CURVE('',#40549,#41579,#34588,.T.) ;
#53891 = EDGE_CURVE('',#41579,#39223,#34589,.T.) ;
#53892 = EDGE_CURVE('',#40550,#39222,#34590,.T.) ;
#53893 = EDGE_CURVE('',#41580,#40532,#34591,.T.) ;
#53894 = EDGE_CURVE('',#41580,#40533,#2400,.T.) ;
#53895 = EDGE_CURVE('',#39224,#41580,#34592,.T.) ;
#53896 = EDGE_CURVE('',#39221,#40541,#34593,.T.) ;
#53897 = EDGE_CURVE('',#40576,#41581,#2401,.T.) ;
#53898 = EDGE_CURVE('',#40577,#41581,#34594,.T.) ;
#53899 = EDGE_CURVE('',#41581,#39211,#34595,.T.) ;
#53900 = EDGE_CURVE('',#40578,#39210,#34596,.T.) ;
#53901 = EDGE_CURVE('',#41582,#40560,#34597,.T.) ;
#53902 = EDGE_CURVE('',#41582,#40561,#2402,.T.) ;
#53903 = EDGE_CURVE('',#39212,#41582,#34598,.T.) ;
#53904 = EDGE_CURVE('',#39209,#40569,#34599,.T.) ;
#53905 = EDGE_CURVE('',#40604,#41583,#2403,.T.) ;
#53906 = EDGE_CURVE('',#40605,#41583,#34600,.T.) ;
#53907 = EDGE_CURVE('',#41583,#39199,#34601,.T.) ;
#53908 = EDGE_CURVE('',#40606,#39198,#34602,.T.) ;
#53909 = EDGE_CURVE('',#41584,#40588,#34603,.T.) ;
#53910 = EDGE_CURVE('',#41584,#40589,#2404,.T.) ;
#53911 = EDGE_CURVE('',#39200,#41584,#34604,.T.) ;
#53912 = EDGE_CURVE('',#39197,#40597,#34605,.T.) ;
#53913 = EDGE_CURVE('',#40632,#41585,#2405,.T.) ;
#53914 = EDGE_CURVE('',#40633,#41585,#34606,.T.) ;
#53915 = EDGE_CURVE('',#41585,#39187,#34607,.T.) ;
#53916 = EDGE_CURVE('',#40634,#39186,#34608,.T.) ;
#53917 = EDGE_CURVE('',#41586,#40616,#34609,.T.) ;
#53918 = EDGE_CURVE('',#41586,#40617,#2406,.T.) ;
#53919 = EDGE_CURVE('',#39188,#41586,#34610,.T.) ;
#53920 = EDGE_CURVE('',#39185,#40625,#34611,.T.) ;
#53921 = EDGE_CURVE('',#40660,#41587,#2407,.T.) ;
#53922 = EDGE_CURVE('',#40661,#41587,#34612,.T.) ;
#53923 = EDGE_CURVE('',#41587,#39175,#34613,.T.) ;
#53924 = EDGE_CURVE('',#40662,#39174,#34614,.T.) ;
#53925 = EDGE_CURVE('',#41588,#40644,#34615,.T.) ;
#53926 = EDGE_CURVE('',#41588,#40645,#2408,.T.) ;
#53927 = EDGE_CURVE('',#39176,#41588,#34616,.T.) ;
#53928 = EDGE_CURVE('',#39173,#40653,#34617,.T.) ;
#53929 = EDGE_CURVE('',#40688,#41589,#2409,.T.) ;
#53930 = EDGE_CURVE('',#40689,#41589,#34618,.T.) ;
#53931 = EDGE_CURVE('',#41589,#39163,#34619,.T.) ;
#53932 = EDGE_CURVE('',#40690,#39162,#34620,.T.) ;
#53933 = EDGE_CURVE('',#41590,#40672,#34621,.T.) ;
#53934 = EDGE_CURVE('',#41590,#40673,#2410,.T.) ;
#53935 = EDGE_CURVE('',#39164,#41590,#34622,.T.) ;
#53936 = EDGE_CURVE('',#39161,#40681,#34623,.T.) ;
#53937 = EDGE_CURVE('',#40716,#41591,#2411,.T.) ;
#53938 = EDGE_CURVE('',#40717,#41591,#34624,.T.) ;
#53939 = EDGE_CURVE('',#41591,#39151,#34625,.T.) ;
#53940 = EDGE_CURVE('',#40718,#39150,#34626,.T.) ;
#53941 = EDGE_CURVE('',#41592,#40700,#34627,.T.) ;
#53942 = EDGE_CURVE('',#41592,#40701,#2412,.T.) ;
#53943 = EDGE_CURVE('',#39152,#41592,#34628,.T.) ;
#53944 = EDGE_CURVE('',#39149,#40709,#34629,.T.) ;
#53945 = EDGE_CURVE('',#39272,#41575,#34630,.T.) ;
#53946 = EDGE_CURVE('',#41559,#40492,#34631,.T.) ;
#53947 = EDGE_CURVE('',#41576,#39269,#34632,.T.) ;
#53948 = EDGE_CURVE('',#40477,#39465,#34633,.T.) ;
#53949 = EDGE_CURVE('',#39278,#41577,#34634,.T.) ;
#53950 = EDGE_CURVE('',#41561,#40520,#34635,.T.) ;
#53951 = EDGE_CURVE('',#41578,#39275,#34636,.T.) ;
#53952 = EDGE_CURVE('',#40505,#41558,#34637,.T.) ;
#53953 = EDGE_CURVE('',#39284,#41579,#34638,.T.) ;
#53954 = EDGE_CURVE('',#41563,#40548,#34639,.T.) ;
#53955 = EDGE_CURVE('',#41580,#39281,#34640,.T.) ;
#53956 = EDGE_CURVE('',#40533,#41560,#34641,.T.) ;
#53957 = EDGE_CURVE('',#39290,#41581,#34642,.T.) ;
#53958 = EDGE_CURVE('',#41565,#40576,#34643,.T.) ;
#53959 = EDGE_CURVE('',#41582,#39287,#34644,.T.) ;
#53960 = EDGE_CURVE('',#40561,#41562,#34645,.T.) ;
#53961 = EDGE_CURVE('',#39296,#41583,#34646,.T.) ;
#53962 = EDGE_CURVE('',#41567,#40604,#34647,.T.) ;
#53963 = EDGE_CURVE('',#41584,#39293,#34648,.T.) ;
#53964 = EDGE_CURVE('',#40589,#41564,#34649,.T.) ;
#53965 = EDGE_CURVE('',#39302,#41585,#34650,.T.) ;
#53966 = EDGE_CURVE('',#41569,#40632,#34651,.T.) ;
#53967 = EDGE_CURVE('',#41586,#39299,#34652,.T.) ;
#53968 = EDGE_CURVE('',#40617,#41566,#34653,.T.) ;
#53969 = EDGE_CURVE('',#39308,#41587,#34654,.T.) ;
#53970 = EDGE_CURVE('',#41571,#40660,#34655,.T.) ;
#53971 = EDGE_CURVE('',#41588,#39305,#34656,.T.) ;
#53972 = EDGE_CURVE('',#40645,#41568,#34657,.T.) ;
#53973 = EDGE_CURVE('',#39314,#41589,#34658,.T.) ;
#53974 = EDGE_CURVE('',#41573,#40688,#34659,.T.) ;
#53975 = EDGE_CURVE('',#41590,#39311,#34660,.T.) ;
#53976 = EDGE_CURVE('',#40673,#41570,#34661,.T.) ;
#53977 = EDGE_CURVE('',#39320,#41591,#34662,.T.) ;
#53978 = EDGE_CURVE('',#41574,#40716,#34663,.T.) ;
#53979 = EDGE_CURVE('',#41592,#39317,#34664,.T.) ;
#53980 = EDGE_CURVE('',#40701,#41572,#34665,.T.) ;
#53981 = EDGE_CURVE('',#38767,#38761,#34666,.T.) ;
#53982 = EDGE_CURVE('',#38774,#38768,#34667,.T.) ;
#53983 = EDGE_CURVE('',#38781,#38775,#34668,.T.) ;
#53984 = EDGE_CURVE('',#38788,#38782,#34669,.T.) ;
#53985 = EDGE_CURVE('',#38795,#38789,#34670,.T.) ;
#53986 = EDGE_CURVE('',#38802,#38796,#34671,.T.) ;
#53987 = EDGE_CURVE('',#39398,#39614,#34672,.T.) ;
#53988 = EDGE_CURVE('',#39399,#39613,#34673,.T.) ;
#53989 = EDGE_CURVE('',#40725,#39612,#34674,.T.) ;
#53990 = EDGE_CURVE('',#40726,#39611,#34675,.T.) ;
#53991 = EDGE_CURVE('',#39258,#39611,#34676,.T.) ;
#53992 = EDGE_CURVE('',#39259,#39610,#34677,.T.) ;
#53993 = EDGE_CURVE('',#39462,#39610,#34678,.T.) ;
#53994 = EDGE_CURVE('',#39703,#39609,#34679,.T.) ;
#53995 = EDGE_CURVE('',#39606,#39063,#34680,.T.) ;
#53996 = EDGE_CURVE('',#39393,#39608,#34681,.T.) ;
#53997 = EDGE_CURVE('',#39703,#39393,#34682,.T.) ;
#53998 = EDGE_CURVE('',#39607,#39068,#34683,.T.) ;
#53999 = EDGE_CURVE('',#39394,#39607,#34684,.T.) ;
#54000 = EDGE_CURVE('',#39704,#39396,#34685,.T.) ;
#54001 = EDGE_CURVE('',#39394,#39068,#34686,.T.) ;
#54002 = EDGE_CURVE('',#39799,#39396,#34687,.T.) ;
#54003 = EDGE_CURVE('',#39705,#39799,#34688,.T.) ;
#54004 = EDGE_CURVE('',#39395,#39067,#34689,.T.) ;
#54005 = EDGE_CURVE('',#39800,#39395,#34690,.T.) ;
#54006 = EDGE_CURVE('',#38818,#39043,#2413,.T.) ;
#54007 = EDGE_CURVE('',#39800,#39067,#34691,.T.) ;
#54008 = EDGE_CURVE('',#39629,#39397,#34692,.T.) ;
#54009 = EDGE_CURVE('',#39630,#39460,#34693,.T.) ;
#54010 = EDGE_CURVE('',#39631,#39711,#34694,.T.) ;
#54011 = EDGE_CURVE('',#39632,#39710,#34695,.T.) ;
#54012 = EDGE_CURVE('',#38755,#39044,#2414,.T.) ;
#54013 = EDGE_CURVE('',#39632,#39261,#34696,.T.) ;
#54014 = EDGE_CURVE('',#39706,#39798,#34697,.T.) ;
#54015 = EDGE_CURVE('',#39633,#39260,#34698,.T.) ;
#54016 = EDGE_CURVE('',#39531,#39798,#34699,.T.) ;
#54017 = EDGE_CURVE('',#39707,#39531,#34700,.T.) ;
#54018 = EDGE_CURVE('',#39633,#39461,#34701,.T.) ;
#54019 = EDGE_CURVE('',#39797,#39066,#34702,.T.) ;
#54020 = EDGE_CURVE('',#39532,#39797,#34703,.T.) ;
#54021 = EDGE_CURVE('',#39708,#39534,#34704,.T.) ;
#54022 = EDGE_CURVE('',#39634,#39708,#34705,.T.) ;
#54023 = EDGE_CURVE('',#39532,#39066,#34706,.T.) ;
#54024 = EDGE_CURVE('',#39620,#39534,#34707,.T.) ;
#54025 = EDGE_CURVE('',#39533,#39065,#34708,.T.) ;
#54026 = EDGE_CURVE('',#39621,#39533,#34709,.T.) ;
#54027 = EDGE_CURVE('',#39621,#39065,#34710,.T.) ;
#54028 = EDGE_CURVE('',#39622,#39064,#34711,.T.) ;
#54029 = EDGE_CURVE('',#39824,#39821,#34712,.T.) ;
#54030 = EDGE_CURVE('',#39825,#39827,#34713,.T.) ;
#54031 = ORIENTED_EDGE('',*,*,#41593,.F.) ;
#54032 = ORIENTED_EDGE('',*,*,#41594,.F.) ;
#54033 = ORIENTED_EDGE('',*,*,#41595,.F.) ;
#54034 = ORIENTED_EDGE('',*,*,#41596,.T.) ;
#54035 = ORIENTED_EDGE('',*,*,#41597,.F.) ;
#54036 = ORIENTED_EDGE('',*,*,#41598,.T.) ;
#54037 = ORIENTED_EDGE('',*,*,#41599,.F.) ;
#54038 = ORIENTED_EDGE('',*,*,#41600,.F.) ;
#54039 = ORIENTED_EDGE('',*,*,#41598,.F.) ;
#54040 = ORIENTED_EDGE('',*,*,#41601,.F.) ;
#54041 = ORIENTED_EDGE('',*,*,#41602,.T.) ;
#54042 = ORIENTED_EDGE('',*,*,#41603,.F.) ;
#54043 = ORIENTED_EDGE('',*,*,#41602,.F.) ;
#54044 = ORIENTED_EDGE('',*,*,#41604,.F.) ;
#54045 = ORIENTED_EDGE('',*,*,#41605,.T.) ;
#54046 = ORIENTED_EDGE('',*,*,#41606,.F.) ;
#54047 = ORIENTED_EDGE('',*,*,#41607,.F.) ;
#54048 = ORIENTED_EDGE('',*,*,#41605,.F.) ;
#54049 = ORIENTED_EDGE('',*,*,#41608,.T.) ;
#54050 = ORIENTED_EDGE('',*,*,#41609,.F.) ;
#54051 = ORIENTED_EDGE('',*,*,#41610,.T.) ;
#54052 = ORIENTED_EDGE('',*,*,#41611,.T.) ;
#54053 = ORIENTED_EDGE('',*,*,#41612,.T.) ;
#54054 = ORIENTED_EDGE('',*,*,#41613,.T.) ;
#54055 = ORIENTED_EDGE('',*,*,#41614,.F.) ;
#54056 = ORIENTED_EDGE('',*,*,#41608,.F.) ;
#54057 = ORIENTED_EDGE('',*,*,#41615,.F.) ;
#54058 = ORIENTED_EDGE('',*,*,#41616,.T.) ;
#54059 = ORIENTED_EDGE('',*,*,#41617,.F.) ;
#54060 = ORIENTED_EDGE('',*,*,#41618,.F.) ;
#54061 = ORIENTED_EDGE('',*,*,#41619,.T.) ;
#54062 = ORIENTED_EDGE('',*,*,#41620,.F.) ;
#54063 = ORIENTED_EDGE('',*,*,#41621,.F.) ;
#54064 = ORIENTED_EDGE('',*,*,#41622,.T.) ;
#54065 = ORIENTED_EDGE('',*,*,#41601,.T.) ;
#54066 = ORIENTED_EDGE('',*,*,#41622,.F.) ;
#54067 = ORIENTED_EDGE('',*,*,#41603,.T.) ;
#54068 = ORIENTED_EDGE('',*,*,#41623,.T.) ;
#54069 = ORIENTED_EDGE('',*,*,#41606,.T.) ;
#54070 = ORIENTED_EDGE('',*,*,#41607,.T.) ;
#54071 = ORIENTED_EDGE('',*,*,#41623,.F.) ;
#54072 = ORIENTED_EDGE('',*,*,#41624,.F.) ;
#54073 = ORIENTED_EDGE('',*,*,#41625,.T.) ;
#54074 = ORIENTED_EDGE('',*,*,#41626,.F.) ;
#54075 = ORIENTED_EDGE('',*,*,#41627,.T.) ;
#54076 = ORIENTED_EDGE('',*,*,#41628,.F.) ;
#54077 = ORIENTED_EDGE('',*,*,#41629,.T.) ;
#54078 = ORIENTED_EDGE('',*,*,#41630,.T.) ;
#54079 = ORIENTED_EDGE('',*,*,#41631,.T.) ;
#54080 = ORIENTED_EDGE('',*,*,#41632,.F.) ;
#54081 = ORIENTED_EDGE('',*,*,#41633,.T.) ;
#54082 = ORIENTED_EDGE('',*,*,#41634,.F.) ;
#54083 = ORIENTED_EDGE('',*,*,#41635,.T.) ;
#54084 = ORIENTED_EDGE('',*,*,#41636,.F.) ;
#54085 = ORIENTED_EDGE('',*,*,#41637,.T.) ;
#54086 = ORIENTED_EDGE('',*,*,#41638,.T.) ;
#54087 = ORIENTED_EDGE('',*,*,#41639,.T.) ;
#54088 = ORIENTED_EDGE('',*,*,#41640,.F.) ;
#54089 = ORIENTED_EDGE('',*,*,#41641,.T.) ;
#54090 = ORIENTED_EDGE('',*,*,#41599,.T.) ;
#54091 = ORIENTED_EDGE('',*,*,#41600,.T.) ;
#54092 = ORIENTED_EDGE('',*,*,#41641,.F.) ;
#54093 = ORIENTED_EDGE('',*,*,#41642,.F.) ;
#54094 = ORIENTED_EDGE('',*,*,#41643,.F.) ;
#54095 = ORIENTED_EDGE('',*,*,#41644,.F.) ;
#54096 = ORIENTED_EDGE('',*,*,#41645,.T.) ;
#54097 = ORIENTED_EDGE('',*,*,#41646,.F.) ;
#54098 = ORIENTED_EDGE('',*,*,#41647,.F.) ;
#54099 = ORIENTED_EDGE('',*,*,#41648,.F.) ;
#54100 = ORIENTED_EDGE('',*,*,#41649,.F.) ;
#54101 = ORIENTED_EDGE('',*,*,#41650,.F.) ;
#54102 = ORIENTED_EDGE('',*,*,#41651,.T.) ;
#54103 = ORIENTED_EDGE('',*,*,#41652,.F.) ;
#54104 = ORIENTED_EDGE('',*,*,#41653,.F.) ;
#54105 = ORIENTED_EDGE('',*,*,#41651,.F.) ;
#54106 = ORIENTED_EDGE('',*,*,#41654,.F.) ;
#54107 = ORIENTED_EDGE('',*,*,#41655,.T.) ;
#54108 = ORIENTED_EDGE('',*,*,#41656,.F.) ;
#54109 = ORIENTED_EDGE('',*,*,#41655,.F.) ;
#54110 = ORIENTED_EDGE('',*,*,#41657,.F.) ;
#54111 = ORIENTED_EDGE('',*,*,#41658,.T.) ;
#54112 = ORIENTED_EDGE('',*,*,#41659,.F.) ;
#54113 = ORIENTED_EDGE('',*,*,#41660,.F.) ;
#54114 = ORIENTED_EDGE('',*,*,#41658,.F.) ;
#54115 = ORIENTED_EDGE('',*,*,#41661,.T.) ;
#54116 = ORIENTED_EDGE('',*,*,#41662,.F.) ;
#54117 = ORIENTED_EDGE('',*,*,#41663,.T.) ;
#54118 = ORIENTED_EDGE('',*,*,#41664,.T.) ;
#54119 = ORIENTED_EDGE('',*,*,#41665,.T.) ;
#54120 = ORIENTED_EDGE('',*,*,#41666,.T.) ;
#54121 = ORIENTED_EDGE('',*,*,#41667,.F.) ;
#54122 = ORIENTED_EDGE('',*,*,#41661,.F.) ;
#54123 = ORIENTED_EDGE('',*,*,#41668,.F.) ;
#54124 = ORIENTED_EDGE('',*,*,#41669,.T.) ;
#54125 = ORIENTED_EDGE('',*,*,#41670,.F.) ;
#54126 = ORIENTED_EDGE('',*,*,#41671,.F.) ;
#54127 = ORIENTED_EDGE('',*,*,#41672,.T.) ;
#54128 = ORIENTED_EDGE('',*,*,#41673,.F.) ;
#54129 = ORIENTED_EDGE('',*,*,#41674,.F.) ;
#54130 = ORIENTED_EDGE('',*,*,#41675,.T.) ;
#54131 = ORIENTED_EDGE('',*,*,#41654,.T.) ;
#54132 = ORIENTED_EDGE('',*,*,#41675,.F.) ;
#54133 = ORIENTED_EDGE('',*,*,#41656,.T.) ;
#54134 = ORIENTED_EDGE('',*,*,#41676,.T.) ;
#54135 = ORIENTED_EDGE('',*,*,#41659,.T.) ;
#54136 = ORIENTED_EDGE('',*,*,#41660,.T.) ;
#54137 = ORIENTED_EDGE('',*,*,#41676,.F.) ;
#54138 = ORIENTED_EDGE('',*,*,#41677,.F.) ;
#54139 = ORIENTED_EDGE('',*,*,#41678,.T.) ;
#54140 = ORIENTED_EDGE('',*,*,#41679,.F.) ;
#54141 = ORIENTED_EDGE('',*,*,#41680,.T.) ;
#54142 = ORIENTED_EDGE('',*,*,#41681,.F.) ;
#54143 = ORIENTED_EDGE('',*,*,#41682,.T.) ;
#54144 = ORIENTED_EDGE('',*,*,#41683,.T.) ;
#54145 = ORIENTED_EDGE('',*,*,#41684,.T.) ;
#54146 = ORIENTED_EDGE('',*,*,#41685,.F.) ;
#54147 = ORIENTED_EDGE('',*,*,#41686,.T.) ;
#54148 = ORIENTED_EDGE('',*,*,#41687,.F.) ;
#54149 = ORIENTED_EDGE('',*,*,#41688,.T.) ;
#54150 = ORIENTED_EDGE('',*,*,#41689,.F.) ;
#54151 = ORIENTED_EDGE('',*,*,#41690,.T.) ;
#54152 = ORIENTED_EDGE('',*,*,#41691,.T.) ;
#54153 = ORIENTED_EDGE('',*,*,#41692,.T.) ;
#54154 = ORIENTED_EDGE('',*,*,#41693,.F.) ;
#54155 = ORIENTED_EDGE('',*,*,#41694,.T.) ;
#54156 = ORIENTED_EDGE('',*,*,#41652,.T.) ;
#54157 = ORIENTED_EDGE('',*,*,#41653,.T.) ;
#54158 = ORIENTED_EDGE('',*,*,#41694,.F.) ;
#54159 = ORIENTED_EDGE('',*,*,#41695,.T.) ;
#54160 = ORIENTED_EDGE('',*,*,#41696,.T.) ;
#54161 = ORIENTED_EDGE('',*,*,#41697,.F.) ;
#54162 = ORIENTED_EDGE('',*,*,#41698,.T.) ;
#54163 = ORIENTED_EDGE('',*,*,#41699,.F.) ;
#54164 = ORIENTED_EDGE('',*,*,#41700,.T.) ;
#54165 = ORIENTED_EDGE('',*,*,#41701,.F.) ;
#54166 = ORIENTED_EDGE('',*,*,#41702,.T.) ;
#54167 = ORIENTED_EDGE('',*,*,#41703,.F.) ;
#54168 = ORIENTED_EDGE('',*,*,#41704,.T.) ;
#54169 = ORIENTED_EDGE('',*,*,#41705,.F.) ;
#54170 = ORIENTED_EDGE('',*,*,#41706,.T.) ;
#54171 = ORIENTED_EDGE('',*,*,#41707,.F.) ;
#54172 = ORIENTED_EDGE('',*,*,#41708,.T.) ;
#54173 = ORIENTED_EDGE('',*,*,#41709,.T.) ;
#54174 = ORIENTED_EDGE('',*,*,#41710,.T.) ;
#54175 = ORIENTED_EDGE('',*,*,#41711,.F.) ;
#54176 = ORIENTED_EDGE('',*,*,#41712,.T.) ;
#54177 = ORIENTED_EDGE('',*,*,#41713,.T.) ;
#54178 = ORIENTED_EDGE('',*,*,#41714,.T.) ;
#54179 = ORIENTED_EDGE('',*,*,#41715,.F.) ;
#54180 = ORIENTED_EDGE('',*,*,#41716,.T.) ;
#54181 = ORIENTED_EDGE('',*,*,#41717,.T.) ;
#54182 = ORIENTED_EDGE('',*,*,#41718,.T.) ;
#54183 = ORIENTED_EDGE('',*,*,#41719,.F.) ;
#54184 = ORIENTED_EDGE('',*,*,#41720,.T.) ;
#54185 = ORIENTED_EDGE('',*,*,#41718,.F.) ;
#54186 = ORIENTED_EDGE('',*,*,#41721,.F.) ;
#54187 = ORIENTED_EDGE('',*,*,#41722,.F.) ;
#54188 = ORIENTED_EDGE('',*,*,#41714,.F.) ;
#54189 = ORIENTED_EDGE('',*,*,#41723,.F.) ;
#54190 = ORIENTED_EDGE('',*,*,#41716,.F.) ;
#54191 = ORIENTED_EDGE('',*,*,#41724,.F.) ;
#54192 = ORIENTED_EDGE('',*,*,#41710,.F.) ;
#54193 = ORIENTED_EDGE('',*,*,#41725,.F.) ;
#54194 = ORIENTED_EDGE('',*,*,#41712,.F.) ;
#54195 = ORIENTED_EDGE('',*,*,#41708,.F.) ;
#54196 = ORIENTED_EDGE('',*,*,#41726,.T.) ;
#54197 = ORIENTED_EDGE('',*,*,#41727,.T.) ;
#54198 = ORIENTED_EDGE('',*,*,#41728,.F.) ;
#54199 = ORIENTED_EDGE('',*,*,#41729,.F.) ;
#54200 = ORIENTED_EDGE('',*,*,#41730,.F.) ;
#54201 = ORIENTED_EDGE('',*,*,#41731,.T.) ;
#54202 = ORIENTED_EDGE('',*,*,#41732,.T.) ;
#54203 = ORIENTED_EDGE('',*,*,#41733,.T.) ;
#54204 = ORIENTED_EDGE('',*,*,#41734,.T.) ;
#54205 = ORIENTED_EDGE('',*,*,#41735,.F.) ;
#54206 = ORIENTED_EDGE('',*,*,#41736,.T.) ;
#54207 = ORIENTED_EDGE('',*,*,#41737,.T.) ;
#54208 = ORIENTED_EDGE('',*,*,#41738,.T.) ;
#54209 = ORIENTED_EDGE('',*,*,#41739,.T.) ;
#54210 = ORIENTED_EDGE('',*,*,#41740,.T.) ;
#54211 = ORIENTED_EDGE('',*,*,#41741,.T.) ;
#54212 = ORIENTED_EDGE('',*,*,#41742,.T.) ;
#54213 = ORIENTED_EDGE('',*,*,#41677,.T.) ;
#54214 = ORIENTED_EDGE('',*,*,#41693,.T.) ;
#54215 = ORIENTED_EDGE('',*,*,#41743,.T.) ;
#54216 = ORIENTED_EDGE('',*,*,#41744,.T.) ;
#54217 = ORIENTED_EDGE('',*,*,#41745,.T.) ;
#54218 = ORIENTED_EDGE('',*,*,#41746,.F.) ;
#54219 = ORIENTED_EDGE('',*,*,#41747,.T.) ;
#54220 = ORIENTED_EDGE('',*,*,#41748,.F.) ;
#54221 = ORIENTED_EDGE('',*,*,#41749,.T.) ;
#54222 = ORIENTED_EDGE('',*,*,#41750,.F.) ;
#54223 = ORIENTED_EDGE('',*,*,#41751,.T.) ;
#54224 = ORIENTED_EDGE('',*,*,#41752,.F.) ;
#54225 = ORIENTED_EDGE('',*,*,#41753,.T.) ;
#54226 = ORIENTED_EDGE('',*,*,#41754,.F.) ;
#54227 = ORIENTED_EDGE('',*,*,#41755,.T.) ;
#54228 = ORIENTED_EDGE('',*,*,#41756,.T.) ;
#54229 = ORIENTED_EDGE('',*,*,#41757,.T.) ;
#54230 = ORIENTED_EDGE('',*,*,#41758,.T.) ;
#54231 = ORIENTED_EDGE('',*,*,#41759,.F.) ;
#54232 = ORIENTED_EDGE('',*,*,#41760,.T.) ;
#54233 = ORIENTED_EDGE('',*,*,#41610,.F.) ;
#54234 = ORIENTED_EDGE('',*,*,#41761,.T.) ;
#54235 = ORIENTED_EDGE('',*,*,#41762,.T.) ;
#54236 = ORIENTED_EDGE('',*,*,#41763,.T.) ;
#54237 = ORIENTED_EDGE('',*,*,#41764,.F.) ;
#54238 = ORIENTED_EDGE('',*,*,#41765,.T.) ;
#54239 = ORIENTED_EDGE('',*,*,#41663,.F.) ;
#54240 = ORIENTED_EDGE('',*,*,#41604,.T.) ;
#54241 = ORIENTED_EDGE('',*,*,#41657,.T.) ;
#54242 = ORIENTED_EDGE('',*,*,#41766,.T.) ;
#54243 = ORIENTED_EDGE('',*,*,#41767,.T.) ;
#54244 = ORIENTED_EDGE('',*,*,#41768,.F.) ;
#54245 = ORIENTED_EDGE('',*,*,#41769,.T.) ;
#54246 = ORIENTED_EDGE('',*,*,#41770,.F.) ;
#54247 = ORIENTED_EDGE('',*,*,#41771,.T.) ;
#54248 = ORIENTED_EDGE('',*,*,#41772,.T.) ;
#54249 = ORIENTED_EDGE('',*,*,#41773,.T.) ;
#54250 = ORIENTED_EDGE('',*,*,#41774,.T.) ;
#54251 = ORIENTED_EDGE('',*,*,#41775,.T.) ;
#54252 = ORIENTED_EDGE('',*,*,#41776,.T.) ;
#54253 = ORIENTED_EDGE('',*,*,#41777,.T.) ;
#54254 = ORIENTED_EDGE('',*,*,#41778,.T.) ;
#54255 = ORIENTED_EDGE('',*,*,#41779,.T.) ;
#54256 = ORIENTED_EDGE('',*,*,#41780,.T.) ;
#54257 = ORIENTED_EDGE('',*,*,#41781,.T.) ;
#54258 = ORIENTED_EDGE('',*,*,#41782,.T.) ;
#54259 = ORIENTED_EDGE('',*,*,#41783,.T.) ;
#54260 = ORIENTED_EDGE('',*,*,#41729,.T.) ;
#54261 = ORIENTED_EDGE('',*,*,#41784,.F.) ;
#54262 = ORIENTED_EDGE('',*,*,#41719,.T.) ;
#54263 = ORIENTED_EDGE('',*,*,#41785,.T.) ;
#54264 = ORIENTED_EDGE('',*,*,#41786,.T.) ;
#54265 = ORIENTED_EDGE('',*,*,#41787,.F.) ;
#54266 = ORIENTED_EDGE('',*,*,#41727,.F.) ;
#54267 = ORIENTED_EDGE('',*,*,#41788,.F.) ;
#54268 = ORIENTED_EDGE('',*,*,#41789,.T.) ;
#54269 = ORIENTED_EDGE('',*,*,#41790,.T.) ;
#54270 = ORIENTED_EDGE('',*,*,#41791,.T.) ;
#54271 = ORIENTED_EDGE('',*,*,#41792,.F.) ;
#54272 = ORIENTED_EDGE('',*,*,#41793,.F.) ;
#54273 = ORIENTED_EDGE('',*,*,#41794,.T.) ;
#54274 = ORIENTED_EDGE('',*,*,#41795,.F.) ;
#54275 = ORIENTED_EDGE('',*,*,#41796,.T.) ;
#54276 = ORIENTED_EDGE('',*,*,#41797,.F.) ;
#54277 = ORIENTED_EDGE('',*,*,#41798,.T.) ;
#54278 = ORIENTED_EDGE('',*,*,#41799,.F.) ;
#54279 = ORIENTED_EDGE('',*,*,#41800,.T.) ;
#54280 = ORIENTED_EDGE('',*,*,#41597,.T.) ;
#54281 = ORIENTED_EDGE('',*,*,#41801,.F.) ;
#54282 = ORIENTED_EDGE('',*,*,#41802,.T.) ;
#54283 = ORIENTED_EDGE('',*,*,#41803,.F.) ;
#54284 = ORIENTED_EDGE('',*,*,#41804,.T.) ;
#54285 = ORIENTED_EDGE('',*,*,#41805,.F.) ;
#54286 = ORIENTED_EDGE('',*,*,#41806,.T.) ;
#54287 = ORIENTED_EDGE('',*,*,#41807,.F.) ;
#54288 = ORIENTED_EDGE('',*,*,#41808,.T.) ;
#54289 = ORIENTED_EDGE('',*,*,#41650,.T.) ;
#54290 = ORIENTED_EDGE('',*,*,#41809,.T.) ;
#54291 = ORIENTED_EDGE('',*,*,#41810,.T.) ;
#54292 = ORIENTED_EDGE('',*,*,#41811,.T.) ;
#54293 = ORIENTED_EDGE('',*,*,#41812,.F.) ;
#54294 = ORIENTED_EDGE('',*,*,#41813,.T.) ;
#54295 = ORIENTED_EDGE('',*,*,#41814,.T.) ;
#54296 = ORIENTED_EDGE('',*,*,#41649,.T.) ;
#54297 = ORIENTED_EDGE('',*,*,#41815,.F.) ;
#54298 = ORIENTED_EDGE('',*,*,#41647,.T.) ;
#54299 = ORIENTED_EDGE('',*,*,#41816,.T.) ;
#54300 = ORIENTED_EDGE('',*,*,#41817,.T.) ;
#54301 = ORIENTED_EDGE('',*,*,#41818,.F.) ;
#54302 = ORIENTED_EDGE('',*,*,#41819,.T.) ;
#54303 = ORIENTED_EDGE('',*,*,#41820,.T.) ;
#54304 = ORIENTED_EDGE('',*,*,#41821,.T.) ;
#54305 = ORIENTED_EDGE('',*,*,#41822,.F.) ;
#54306 = ORIENTED_EDGE('',*,*,#41823,.T.) ;
#54307 = ORIENTED_EDGE('',*,*,#41824,.T.) ;
#54308 = ORIENTED_EDGE('',*,*,#41825,.T.) ;
#54309 = ORIENTED_EDGE('',*,*,#41826,.F.) ;
#54310 = ORIENTED_EDGE('',*,*,#41827,.T.) ;
#54311 = ORIENTED_EDGE('',*,*,#41828,.F.) ;
#54312 = ORIENTED_EDGE('',*,*,#41829,.T.) ;
#54313 = ORIENTED_EDGE('',*,*,#41830,.T.) ;
#54314 = ORIENTED_EDGE('',*,*,#41831,.T.) ;
#54315 = ORIENTED_EDGE('',*,*,#41832,.T.) ;
#54316 = ORIENTED_EDGE('',*,*,#41833,.T.) ;
#54317 = ORIENTED_EDGE('',*,*,#41834,.F.) ;
#54318 = ORIENTED_EDGE('',*,*,#41835,.T.) ;
#54319 = ORIENTED_EDGE('',*,*,#41836,.F.) ;
#54320 = ORIENTED_EDGE('',*,*,#41837,.T.) ;
#54321 = ORIENTED_EDGE('',*,*,#41838,.T.) ;
#54322 = ORIENTED_EDGE('',*,*,#41839,.T.) ;
#54323 = ORIENTED_EDGE('',*,*,#41840,.T.) ;
#54324 = ORIENTED_EDGE('',*,*,#41841,.T.) ;
#54325 = ORIENTED_EDGE('',*,*,#41842,.F.) ;
#54326 = ORIENTED_EDGE('',*,*,#41843,.F.) ;
#54327 = ORIENTED_EDGE('',*,*,#41844,.T.) ;
#54328 = ORIENTED_EDGE('',*,*,#41845,.F.) ;
#54329 = ORIENTED_EDGE('',*,*,#41846,.T.) ;
#54330 = ORIENTED_EDGE('',*,*,#41847,.F.) ;
#54331 = ORIENTED_EDGE('',*,*,#41848,.T.) ;
#54332 = ORIENTED_EDGE('',*,*,#41849,.F.) ;
#54333 = ORIENTED_EDGE('',*,*,#41850,.T.) ;
#54334 = ORIENTED_EDGE('',*,*,#41851,.F.) ;
#54335 = ORIENTED_EDGE('',*,*,#41852,.T.) ;
#54336 = ORIENTED_EDGE('',*,*,#41853,.F.) ;
#54337 = ORIENTED_EDGE('',*,*,#41854,.T.) ;
#54338 = ORIENTED_EDGE('',*,*,#41855,.F.) ;
#54339 = ORIENTED_EDGE('',*,*,#41856,.T.) ;
#54340 = ORIENTED_EDGE('',*,*,#41857,.F.) ;
#54341 = ORIENTED_EDGE('',*,*,#41858,.T.) ;
#54342 = ORIENTED_EDGE('',*,*,#41859,.T.) ;
#54343 = ORIENTED_EDGE('',*,*,#41860,.T.) ;
#54344 = ORIENTED_EDGE('',*,*,#41861,.T.) ;
#54345 = ORIENTED_EDGE('',*,*,#41862,.F.) ;
#54346 = ORIENTED_EDGE('',*,*,#41863,.T.) ;
#54347 = ORIENTED_EDGE('',*,*,#41864,.T.) ;
#54348 = ORIENTED_EDGE('',*,*,#41865,.T.) ;
#54349 = ORIENTED_EDGE('',*,*,#41866,.T.) ;
#54350 = ORIENTED_EDGE('',*,*,#41867,.T.) ;
#54351 = ORIENTED_EDGE('',*,*,#41868,.F.) ;
#54352 = ORIENTED_EDGE('',*,*,#41869,.T.) ;
#54353 = ORIENTED_EDGE('',*,*,#41870,.T.) ;
#54354 = ORIENTED_EDGE('',*,*,#41871,.T.) ;
#54355 = ORIENTED_EDGE('',*,*,#41872,.T.) ;
#54356 = ORIENTED_EDGE('',*,*,#41873,.T.) ;
#54357 = ORIENTED_EDGE('',*,*,#41874,.T.) ;
#54358 = ORIENTED_EDGE('',*,*,#41875,.T.) ;
#54359 = ORIENTED_EDGE('',*,*,#41876,.T.) ;
#54360 = ORIENTED_EDGE('',*,*,#41877,.F.) ;
#54361 = ORIENTED_EDGE('',*,*,#41878,.T.) ;
#54362 = ORIENTED_EDGE('',*,*,#41879,.T.) ;
#54363 = ORIENTED_EDGE('',*,*,#41880,.T.) ;
#54364 = ORIENTED_EDGE('',*,*,#41881,.T.) ;
#54365 = ORIENTED_EDGE('',*,*,#41882,.T.) ;
#54366 = ORIENTED_EDGE('',*,*,#41883,.T.) ;
#54367 = ORIENTED_EDGE('',*,*,#41884,.T.) ;
#54368 = ORIENTED_EDGE('',*,*,#41728,.T.) ;
#54369 = ORIENTED_EDGE('',*,*,#41787,.T.) ;
#54370 = ORIENTED_EDGE('',*,*,#41885,.T.) ;
#54371 = ORIENTED_EDGE('',*,*,#41792,.T.) ;
#54372 = ORIENTED_EDGE('',*,*,#41886,.T.) ;
#54373 = ORIENTED_EDGE('',*,*,#41812,.T.) ;
#54374 = ORIENTED_EDGE('',*,*,#41887,.T.) ;
#54375 = ORIENTED_EDGE('',*,*,#41815,.T.) ;
#54376 = ORIENTED_EDGE('',*,*,#41648,.T.) ;
#54377 = ORIENTED_EDGE('',*,*,#41818,.T.) ;
#54378 = ORIENTED_EDGE('',*,*,#41888,.T.) ;
#54379 = ORIENTED_EDGE('',*,*,#41822,.T.) ;
#54380 = ORIENTED_EDGE('',*,*,#41889,.T.) ;
#54381 = ORIENTED_EDGE('',*,*,#41842,.T.) ;
#54382 = ORIENTED_EDGE('',*,*,#41890,.T.) ;
#54383 = ORIENTED_EDGE('',*,*,#41862,.T.) ;
#54384 = ORIENTED_EDGE('',*,*,#41891,.T.) ;
#54385 = ORIENTED_EDGE('',*,*,#41868,.T.) ;
#54386 = ORIENTED_EDGE('',*,*,#41892,.T.) ;
#54387 = ORIENTED_EDGE('',*,*,#41877,.T.) ;
#54388 = ORIENTED_EDGE('',*,*,#41893,.T.) ;
#54389 = ORIENTED_EDGE('',*,*,#41735,.T.) ;
#54390 = ORIENTED_EDGE('',*,*,#41894,.T.) ;
#54391 = ORIENTED_EDGE('',*,*,#41746,.T.) ;
#54392 = ORIENTED_EDGE('',*,*,#41895,.T.) ;
#54393 = ORIENTED_EDGE('',*,*,#41768,.T.) ;
#54394 = ORIENTED_EDGE('',*,*,#41896,.T.) ;
#54395 = ORIENTED_EDGE('',*,*,#41770,.T.) ;
#54396 = ORIENTED_EDGE('',*,*,#41897,.T.) ;
#54397 = ORIENTED_EDGE('',*,*,#41697,.T.) ;
#54398 = ORIENTED_EDGE('',*,*,#41898,.T.) ;
#54399 = ORIENTED_EDGE('',*,*,#41784,.T.) ;
#54400 = ORIENTED_EDGE('',*,*,#41899,.T.) ;
#54401 = ORIENTED_EDGE('',*,*,#41900,.T.) ;
#54402 = ORIENTED_EDGE('',*,*,#41901,.T.) ;
#54403 = ORIENTED_EDGE('',*,*,#41902,.T.) ;
#54404 = ORIENTED_EDGE('',*,*,#41903,.T.) ;
#54405 = ORIENTED_EDGE('',*,*,#41904,.T.) ;
#54406 = ORIENTED_EDGE('',*,*,#41905,.T.) ;
#54407 = ORIENTED_EDGE('',*,*,#41906,.T.) ;
#54408 = ORIENTED_EDGE('',*,*,#41907,.F.) ;
#54409 = ORIENTED_EDGE('',*,*,#41908,.T.) ;
#54410 = ORIENTED_EDGE('',*,*,#41909,.T.) ;
#54411 = ORIENTED_EDGE('',*,*,#41910,.T.) ;
#54412 = ORIENTED_EDGE('',*,*,#41911,.F.) ;
#54413 = ORIENTED_EDGE('',*,*,#41912,.T.) ;
#54414 = ORIENTED_EDGE('',*,*,#41913,.T.) ;
#54415 = ORIENTED_EDGE('',*,*,#41914,.T.) ;
#54416 = ORIENTED_EDGE('',*,*,#41915,.T.) ;
#54417 = ORIENTED_EDGE('',*,*,#41916,.T.) ;
#54418 = ORIENTED_EDGE('',*,*,#41917,.F.) ;
#54419 = ORIENTED_EDGE('',*,*,#41918,.T.) ;
#54420 = ORIENTED_EDGE('',*,*,#41909,.F.) ;
#54421 = ORIENTED_EDGE('',*,*,#41919,.T.) ;
#54422 = ORIENTED_EDGE('',*,*,#41920,.T.) ;
#54423 = ORIENTED_EDGE('',*,*,#41921,.T.) ;
#54424 = ORIENTED_EDGE('',*,*,#41922,.F.) ;
#54425 = ORIENTED_EDGE('',*,*,#41923,.T.) ;
#54426 = ORIENTED_EDGE('',*,*,#41915,.F.) ;
#54427 = ORIENTED_EDGE('',*,*,#41924,.T.) ;
#54428 = ORIENTED_EDGE('',*,*,#41925,.F.) ;
#54429 = ORIENTED_EDGE('',*,*,#41926,.T.) ;
#54430 = ORIENTED_EDGE('',*,*,#41927,.T.) ;
#54431 = ORIENTED_EDGE('',*,*,#41928,.T.) ;
#54432 = ORIENTED_EDGE('',*,*,#41920,.F.) ;
#54433 = ORIENTED_EDGE('',*,*,#41929,.T.) ;
#54434 = ORIENTED_EDGE('',*,*,#41930,.T.) ;
#54435 = ORIENTED_EDGE('',*,*,#41931,.T.) ;
#54436 = ORIENTED_EDGE('',*,*,#41917,.T.) ;
#54437 = ORIENTED_EDGE('',*,*,#41932,.T.) ;
#54438 = ORIENTED_EDGE('',*,*,#41933,.T.) ;
#54439 = ORIENTED_EDGE('',*,*,#41934,.T.) ;
#54440 = ORIENTED_EDGE('',*,*,#41935,.T.) ;
#54441 = ORIENTED_EDGE('',*,*,#41936,.T.) ;
#54442 = ORIENTED_EDGE('',*,*,#41937,.T.) ;
#54443 = ORIENTED_EDGE('',*,*,#41938,.T.) ;
#54444 = ORIENTED_EDGE('',*,*,#41939,.T.) ;
#54445 = ORIENTED_EDGE('',*,*,#41940,.T.) ;
#54446 = ORIENTED_EDGE('',*,*,#41941,.T.) ;
#54447 = ORIENTED_EDGE('',*,*,#41942,.T.) ;
#54448 = ORIENTED_EDGE('',*,*,#41943,.T.) ;
#54449 = ORIENTED_EDGE('',*,*,#41944,.T.) ;
#54450 = ORIENTED_EDGE('',*,*,#41945,.T.) ;
#54451 = ORIENTED_EDGE('',*,*,#41946,.T.) ;
#54452 = ORIENTED_EDGE('',*,*,#41947,.T.) ;
#54453 = ORIENTED_EDGE('',*,*,#41948,.T.) ;
#54454 = ORIENTED_EDGE('',*,*,#41949,.T.) ;
#54455 = ORIENTED_EDGE('',*,*,#41950,.T.) ;
#54456 = ORIENTED_EDGE('',*,*,#41951,.T.) ;
#54457 = ORIENTED_EDGE('',*,*,#41952,.T.) ;
#54458 = ORIENTED_EDGE('',*,*,#41953,.T.) ;
#54459 = ORIENTED_EDGE('',*,*,#41954,.T.) ;
#54460 = ORIENTED_EDGE('',*,*,#41955,.T.) ;
#54461 = ORIENTED_EDGE('',*,*,#41956,.T.) ;
#54462 = ORIENTED_EDGE('',*,*,#41957,.T.) ;
#54463 = ORIENTED_EDGE('',*,*,#41958,.T.) ;
#54464 = ORIENTED_EDGE('',*,*,#41959,.T.) ;
#54465 = ORIENTED_EDGE('',*,*,#41960,.T.) ;
#54466 = ORIENTED_EDGE('',*,*,#41961,.T.) ;
#54467 = ORIENTED_EDGE('',*,*,#41962,.T.) ;
#54468 = ORIENTED_EDGE('',*,*,#41963,.T.) ;
#54469 = ORIENTED_EDGE('',*,*,#41964,.T.) ;
#54470 = ORIENTED_EDGE('',*,*,#41965,.T.) ;
#54471 = ORIENTED_EDGE('',*,*,#41966,.T.) ;
#54472 = ORIENTED_EDGE('',*,*,#41967,.F.) ;
#54473 = ORIENTED_EDGE('',*,*,#41968,.F.) ;
#54474 = ORIENTED_EDGE('',*,*,#41969,.F.) ;
#54475 = ORIENTED_EDGE('',*,*,#41970,.F.) ;
#54476 = ORIENTED_EDGE('',*,*,#41971,.F.) ;
#54477 = ORIENTED_EDGE('',*,*,#41972,.F.) ;
#54478 = ORIENTED_EDGE('',*,*,#41973,.F.) ;
#54479 = ORIENTED_EDGE('',*,*,#41974,.F.) ;
#54480 = ORIENTED_EDGE('',*,*,#41975,.F.) ;
#54481 = ORIENTED_EDGE('',*,*,#41976,.F.) ;
#54482 = ORIENTED_EDGE('',*,*,#41974,.T.) ;
#54483 = ORIENTED_EDGE('',*,*,#41977,.T.) ;
#54484 = ORIENTED_EDGE('',*,*,#41978,.F.) ;
#54485 = ORIENTED_EDGE('',*,*,#41979,.F.) ;
#54486 = ORIENTED_EDGE('',*,*,#41967,.T.) ;
#54487 = ORIENTED_EDGE('',*,*,#41976,.T.) ;
#54488 = ORIENTED_EDGE('',*,*,#41980,.F.) ;
#54489 = ORIENTED_EDGE('',*,*,#41981,.F.) ;
#54490 = ORIENTED_EDGE('',*,*,#41968,.T.) ;
#54491 = ORIENTED_EDGE('',*,*,#41979,.T.) ;
#54492 = ORIENTED_EDGE('',*,*,#41982,.F.) ;
#54493 = ORIENTED_EDGE('',*,*,#41983,.F.) ;
#54494 = ORIENTED_EDGE('',*,*,#41969,.T.) ;
#54495 = ORIENTED_EDGE('',*,*,#41981,.T.) ;
#54496 = ORIENTED_EDGE('',*,*,#41984,.F.) ;
#54497 = ORIENTED_EDGE('',*,*,#41985,.F.) ;
#54498 = ORIENTED_EDGE('',*,*,#41970,.T.) ;
#54499 = ORIENTED_EDGE('',*,*,#41983,.T.) ;
#54500 = ORIENTED_EDGE('',*,*,#41986,.F.) ;
#54501 = ORIENTED_EDGE('',*,*,#41987,.F.) ;
#54502 = ORIENTED_EDGE('',*,*,#41971,.T.) ;
#54503 = ORIENTED_EDGE('',*,*,#41985,.T.) ;
#54504 = ORIENTED_EDGE('',*,*,#41988,.F.) ;
#54505 = ORIENTED_EDGE('',*,*,#41989,.F.) ;
#54506 = ORIENTED_EDGE('',*,*,#41972,.T.) ;
#54507 = ORIENTED_EDGE('',*,*,#41987,.T.) ;
#54508 = ORIENTED_EDGE('',*,*,#41990,.F.) ;
#54509 = ORIENTED_EDGE('',*,*,#41977,.F.) ;
#54510 = ORIENTED_EDGE('',*,*,#41973,.T.) ;
#54511 = ORIENTED_EDGE('',*,*,#41989,.T.) ;
#54512 = ORIENTED_EDGE('',*,*,#41978,.T.) ;
#54513 = ORIENTED_EDGE('',*,*,#41975,.T.) ;
#54514 = ORIENTED_EDGE('',*,*,#41990,.T.) ;
#54515 = ORIENTED_EDGE('',*,*,#41988,.T.) ;
#54516 = ORIENTED_EDGE('',*,*,#41986,.T.) ;
#54517 = ORIENTED_EDGE('',*,*,#41984,.T.) ;
#54518 = ORIENTED_EDGE('',*,*,#41982,.T.) ;
#54519 = ORIENTED_EDGE('',*,*,#41980,.T.) ;
#54520 = ORIENTED_EDGE('',*,*,#41685,.T.) ;
#54521 = ORIENTED_EDGE('',*,*,#41991,.T.) ;
#54522 = ORIENTED_EDGE('',*,*,#41683,.F.) ;
#54523 = ORIENTED_EDGE('',*,*,#41992,.T.) ;
#54524 = ORIENTED_EDGE('',*,*,#41687,.T.) ;
#54525 = ORIENTED_EDGE('',*,*,#41993,.T.) ;
#54526 = ORIENTED_EDGE('',*,*,#41691,.F.) ;
#54527 = ORIENTED_EDGE('',*,*,#41994,.T.) ;
#54528 = ORIENTED_EDGE('',*,*,#41679,.T.) ;
#54529 = ORIENTED_EDGE('',*,*,#41995,.T.) ;
#54530 = ORIENTED_EDGE('',*,*,#41681,.T.) ;
#54531 = ORIENTED_EDGE('',*,*,#41996,.T.) ;
#54532 = ORIENTED_EDGE('',*,*,#41689,.T.) ;
#54533 = ORIENTED_EDGE('',*,*,#41997,.T.) ;
#54534 = ORIENTED_EDGE('',*,*,#41998,.T.) ;
#54535 = ORIENTED_EDGE('',*,*,#41999,.T.) ;
#54536 = ORIENTED_EDGE('',*,*,#42000,.T.) ;
#54537 = ORIENTED_EDGE('',*,*,#42001,.T.) ;
#54538 = ORIENTED_EDGE('',*,*,#42002,.T.) ;
#54539 = ORIENTED_EDGE('',*,*,#42003,.T.) ;
#54540 = ORIENTED_EDGE('',*,*,#42004,.T.) ;
#54541 = ORIENTED_EDGE('',*,*,#42005,.T.) ;
#54542 = ORIENTED_EDGE('',*,*,#42006,.T.) ;
#54543 = ORIENTED_EDGE('',*,*,#42007,.T.) ;
#54544 = ORIENTED_EDGE('',*,*,#42008,.T.) ;
#54545 = ORIENTED_EDGE('',*,*,#42009,.T.) ;
#54546 = ORIENTED_EDGE('',*,*,#42010,.T.) ;
#54547 = ORIENTED_EDGE('',*,*,#42011,.T.) ;
#54548 = ORIENTED_EDGE('',*,*,#42012,.T.) ;
#54549 = ORIENTED_EDGE('',*,*,#42013,.T.) ;
#54550 = ORIENTED_EDGE('',*,*,#42014,.T.) ;
#54551 = ORIENTED_EDGE('',*,*,#42015,.T.) ;
#54552 = ORIENTED_EDGE('',*,*,#42016,.T.) ;
#54553 = ORIENTED_EDGE('',*,*,#42017,.T.) ;
#54554 = ORIENTED_EDGE('',*,*,#42018,.F.) ;
#54555 = ORIENTED_EDGE('',*,*,#42019,.F.) ;
#54556 = ORIENTED_EDGE('',*,*,#42020,.F.) ;
#54557 = ORIENTED_EDGE('',*,*,#42021,.F.) ;
#54558 = ORIENTED_EDGE('',*,*,#42022,.F.) ;
#54559 = ORIENTED_EDGE('',*,*,#42023,.F.) ;
#54560 = ORIENTED_EDGE('',*,*,#42024,.F.) ;
#54561 = ORIENTED_EDGE('',*,*,#42025,.F.) ;
#54562 = ORIENTED_EDGE('',*,*,#42026,.T.) ;
#54563 = ORIENTED_EDGE('',*,*,#42027,.T.) ;
#54564 = ORIENTED_EDGE('',*,*,#42028,.F.) ;
#54565 = ORIENTED_EDGE('',*,*,#42025,.T.) ;
#54566 = ORIENTED_EDGE('',*,*,#42028,.T.) ;
#54567 = ORIENTED_EDGE('',*,*,#42029,.T.) ;
#54568 = ORIENTED_EDGE('',*,*,#42030,.F.) ;
#54569 = ORIENTED_EDGE('',*,*,#42018,.T.) ;
#54570 = ORIENTED_EDGE('',*,*,#42030,.T.) ;
#54571 = ORIENTED_EDGE('',*,*,#42031,.T.) ;
#54572 = ORIENTED_EDGE('',*,*,#42032,.F.) ;
#54573 = ORIENTED_EDGE('',*,*,#42019,.T.) ;
#54574 = ORIENTED_EDGE('',*,*,#42032,.T.) ;
#54575 = ORIENTED_EDGE('',*,*,#42033,.T.) ;
#54576 = ORIENTED_EDGE('',*,*,#42034,.F.) ;
#54577 = ORIENTED_EDGE('',*,*,#42020,.T.) ;
#54578 = ORIENTED_EDGE('',*,*,#42034,.T.) ;
#54579 = ORIENTED_EDGE('',*,*,#42035,.T.) ;
#54580 = ORIENTED_EDGE('',*,*,#42036,.F.) ;
#54581 = ORIENTED_EDGE('',*,*,#42021,.T.) ;
#54582 = ORIENTED_EDGE('',*,*,#42036,.T.) ;
#54583 = ORIENTED_EDGE('',*,*,#42037,.T.) ;
#54584 = ORIENTED_EDGE('',*,*,#42038,.F.) ;
#54585 = ORIENTED_EDGE('',*,*,#42022,.T.) ;
#54586 = ORIENTED_EDGE('',*,*,#42038,.T.) ;
#54587 = ORIENTED_EDGE('',*,*,#42039,.T.) ;
#54588 = ORIENTED_EDGE('',*,*,#42040,.F.) ;
#54589 = ORIENTED_EDGE('',*,*,#42023,.T.) ;
#54590 = ORIENTED_EDGE('',*,*,#42040,.T.) ;
#54591 = ORIENTED_EDGE('',*,*,#42041,.T.) ;
#54592 = ORIENTED_EDGE('',*,*,#42026,.F.) ;
#54593 = ORIENTED_EDGE('',*,*,#42024,.T.) ;
#54594 = ORIENTED_EDGE('',*,*,#42042,.T.) ;
#54595 = ORIENTED_EDGE('',*,*,#42043,.T.) ;
#54596 = ORIENTED_EDGE('',*,*,#42044,.T.) ;
#54597 = ORIENTED_EDGE('',*,*,#42045,.T.) ;
#54598 = ORIENTED_EDGE('',*,*,#42046,.T.) ;
#54599 = ORIENTED_EDGE('',*,*,#42047,.T.) ;
#54600 = ORIENTED_EDGE('',*,*,#42048,.T.) ;
#54601 = ORIENTED_EDGE('',*,*,#42049,.T.) ;
#54602 = ORIENTED_EDGE('',*,*,#42050,.T.) ;
#54603 = ORIENTED_EDGE('',*,*,#41668,.T.) ;
#54604 = ORIENTED_EDGE('',*,*,#42051,.T.) ;
#54605 = ORIENTED_EDGE('',*,*,#42052,.T.) ;
#54606 = ORIENTED_EDGE('',*,*,#41670,.T.) ;
#54607 = ORIENTED_EDGE('',*,*,#42053,.T.) ;
#54608 = ORIENTED_EDGE('',*,*,#42054,.T.) ;
#54609 = ORIENTED_EDGE('',*,*,#42055,.T.) ;
#54610 = ORIENTED_EDGE('',*,*,#42056,.T.) ;
#54611 = ORIENTED_EDGE('',*,*,#42057,.T.) ;
#54612 = ORIENTED_EDGE('',*,*,#42058,.T.) ;
#54613 = ORIENTED_EDGE('',*,*,#42059,.T.) ;
#54614 = ORIENTED_EDGE('',*,*,#42060,.T.) ;
#54615 = ORIENTED_EDGE('',*,*,#41642,.T.) ;
#54616 = ORIENTED_EDGE('',*,*,#41674,.T.) ;
#54617 = ORIENTED_EDGE('',*,*,#42061,.T.) ;
#54618 = ORIENTED_EDGE('',*,*,#42062,.T.) ;
#54619 = ORIENTED_EDGE('',*,*,#42063,.T.) ;
#54620 = ORIENTED_EDGE('',*,*,#42064,.T.) ;
#54621 = ORIENTED_EDGE('',*,*,#42065,.T.) ;
#54622 = ORIENTED_EDGE('',*,*,#42066,.T.) ;
#54623 = ORIENTED_EDGE('',*,*,#42067,.F.) ;
#54624 = ORIENTED_EDGE('',*,*,#42068,.F.) ;
#54625 = ORIENTED_EDGE('',*,*,#42069,.F.) ;
#54626 = ORIENTED_EDGE('',*,*,#41832,.F.) ;
#54627 = ORIENTED_EDGE('',*,*,#41919,.F.) ;
#54628 = ORIENTED_EDGE('',*,*,#41908,.F.) ;
#54629 = ORIENTED_EDGE('',*,*,#42070,.F.) ;
#54630 = ORIENTED_EDGE('',*,*,#41929,.F.) ;
#54631 = ORIENTED_EDGE('',*,*,#42070,.T.) ;
#54632 = ORIENTED_EDGE('',*,*,#41907,.T.) ;
#54633 = ORIENTED_EDGE('',*,*,#42071,.F.) ;
#54634 = ORIENTED_EDGE('',*,*,#42072,.F.) ;
#54635 = ORIENTED_EDGE('',*,*,#42071,.T.) ;
#54636 = ORIENTED_EDGE('',*,*,#41914,.F.) ;
#54637 = ORIENTED_EDGE('',*,*,#42073,.F.) ;
#54638 = ORIENTED_EDGE('',*,*,#41945,.F.) ;
#54639 = ORIENTED_EDGE('',*,*,#42068,.T.) ;
#54640 = ORIENTED_EDGE('',*,*,#41946,.F.) ;
#54641 = ORIENTED_EDGE('',*,*,#42074,.F.) ;
#54642 = ORIENTED_EDGE('',*,*,#41905,.F.) ;
#54643 = ORIENTED_EDGE('',*,*,#42069,.T.) ;
#54644 = ORIENTED_EDGE('',*,*,#41904,.F.) ;
#54645 = ORIENTED_EDGE('',*,*,#42075,.F.) ;
#54646 = ORIENTED_EDGE('',*,*,#41833,.F.) ;
#54647 = ORIENTED_EDGE('',*,*,#42067,.T.) ;
#54648 = ORIENTED_EDGE('',*,*,#41831,.F.) ;
#54649 = ORIENTED_EDGE('',*,*,#42076,.F.) ;
#54650 = ORIENTED_EDGE('',*,*,#41941,.F.) ;
#54651 = ORIENTED_EDGE('',*,*,#42072,.T.) ;
#54652 = ORIENTED_EDGE('',*,*,#41944,.F.) ;
#54653 = ORIENTED_EDGE('',*,*,#42077,.F.) ;
#54654 = ORIENTED_EDGE('',*,*,#41930,.F.) ;
#54655 = ORIENTED_EDGE('',*,*,#41921,.F.) ;
#54656 = ORIENTED_EDGE('',*,*,#41931,.F.) ;
#54657 = ORIENTED_EDGE('',*,*,#42078,.F.) ;
#54658 = ORIENTED_EDGE('',*,*,#41924,.F.) ;
#54659 = ORIENTED_EDGE('',*,*,#42074,.T.) ;
#54660 = ORIENTED_EDGE('',*,*,#42073,.T.) ;
#54661 = ORIENTED_EDGE('',*,*,#42079,.F.) ;
#54662 = ORIENTED_EDGE('',*,*,#41834,.T.) ;
#54663 = ORIENTED_EDGE('',*,*,#42075,.T.) ;
#54664 = ORIENTED_EDGE('',*,*,#42080,.F.) ;
#54665 = ORIENTED_EDGE('',*,*,#42081,.F.) ;
#54666 = ORIENTED_EDGE('',*,*,#42076,.T.) ;
#54667 = ORIENTED_EDGE('',*,*,#41838,.F.) ;
#54668 = ORIENTED_EDGE('',*,*,#42082,.F.) ;
#54669 = ORIENTED_EDGE('',*,*,#42083,.F.) ;
#54670 = ORIENTED_EDGE('',*,*,#42078,.T.) ;
#54671 = ORIENTED_EDGE('',*,*,#42077,.T.) ;
#54672 = ORIENTED_EDGE('',*,*,#42084,.F.) ;
#54673 = ORIENTED_EDGE('',*,*,#41925,.T.) ;
#54674 = ORIENTED_EDGE('',*,*,#42079,.T.) ;
#54675 = ORIENTED_EDGE('',*,*,#41913,.F.) ;
#54676 = ORIENTED_EDGE('',*,*,#42085,.F.) ;
#54677 = ORIENTED_EDGE('',*,*,#41906,.F.) ;
#54678 = ORIENTED_EDGE('',*,*,#42080,.T.) ;
#54679 = ORIENTED_EDGE('',*,*,#41903,.F.) ;
#54680 = ORIENTED_EDGE('',*,*,#42086,.F.) ;
#54681 = ORIENTED_EDGE('',*,*,#41939,.F.) ;
#54682 = ORIENTED_EDGE('',*,*,#42081,.T.) ;
#54683 = ORIENTED_EDGE('',*,*,#41938,.F.) ;
#54684 = ORIENTED_EDGE('',*,*,#42087,.F.) ;
#54685 = ORIENTED_EDGE('',*,*,#41835,.F.) ;
#54686 = ORIENTED_EDGE('',*,*,#42082,.T.) ;
#54687 = ORIENTED_EDGE('',*,*,#41837,.F.) ;
#54688 = ORIENTED_EDGE('',*,*,#42088,.F.) ;
#54689 = ORIENTED_EDGE('',*,*,#41900,.F.) ;
#54690 = ORIENTED_EDGE('',*,*,#42083,.T.) ;
#54691 = ORIENTED_EDGE('',*,*,#41899,.F.) ;
#54692 = ORIENTED_EDGE('',*,*,#42089,.F.) ;
#54693 = ORIENTED_EDGE('',*,*,#41942,.F.) ;
#54694 = ORIENTED_EDGE('',*,*,#42084,.T.) ;
#54695 = ORIENTED_EDGE('',*,*,#41943,.F.) ;
#54696 = ORIENTED_EDGE('',*,*,#42090,.F.) ;
#54697 = ORIENTED_EDGE('',*,*,#41926,.F.) ;
#54698 = ORIENTED_EDGE('',*,*,#42086,.T.) ;
#54699 = ORIENTED_EDGE('',*,*,#42085,.T.) ;
#54700 = ORIENTED_EDGE('',*,*,#42091,.F.) ;
#54701 = ORIENTED_EDGE('',*,*,#41836,.T.) ;
#54702 = ORIENTED_EDGE('',*,*,#42087,.T.) ;
#54703 = ORIENTED_EDGE('',*,*,#42092,.F.) ;
#54704 = ORIENTED_EDGE('',*,*,#42088,.T.) ;
#54705 = ORIENTED_EDGE('',*,*,#42090,.T.) ;
#54706 = ORIENTED_EDGE('',*,*,#42089,.T.) ;
#54707 = ORIENTED_EDGE('',*,*,#42093,.F.) ;
#54708 = ORIENTED_EDGE('',*,*,#41918,.F.) ;
#54709 = ORIENTED_EDGE('',*,*,#41934,.F.) ;
#54710 = ORIENTED_EDGE('',*,*,#42094,.F.) ;
#54711 = ORIENTED_EDGE('',*,*,#41910,.F.) ;
#54712 = ORIENTED_EDGE('',*,*,#42091,.T.) ;
#54713 = ORIENTED_EDGE('',*,*,#41912,.F.) ;
#54714 = ORIENTED_EDGE('',*,*,#42095,.F.) ;
#54715 = ORIENTED_EDGE('',*,*,#41940,.F.) ;
#54716 = ORIENTED_EDGE('',*,*,#42092,.T.) ;
#54717 = ORIENTED_EDGE('',*,*,#41937,.F.) ;
#54718 = ORIENTED_EDGE('',*,*,#42096,.F.) ;
#54719 = ORIENTED_EDGE('',*,*,#41901,.F.) ;
#54720 = ORIENTED_EDGE('',*,*,#42093,.T.) ;
#54721 = ORIENTED_EDGE('',*,*,#41902,.F.) ;
#54722 = ORIENTED_EDGE('',*,*,#42097,.F.) ;
#54723 = ORIENTED_EDGE('',*,*,#41927,.F.) ;
#54724 = ORIENTED_EDGE('',*,*,#41911,.T.) ;
#54725 = ORIENTED_EDGE('',*,*,#42094,.T.) ;
#54726 = ORIENTED_EDGE('',*,*,#42098,.F.) ;
#54727 = ORIENTED_EDGE('',*,*,#42095,.T.) ;
#54728 = ORIENTED_EDGE('',*,*,#42097,.T.) ;
#54729 = ORIENTED_EDGE('',*,*,#42096,.T.) ;
#54730 = ORIENTED_EDGE('',*,*,#42099,.F.) ;
#54731 = ORIENTED_EDGE('',*,*,#42098,.T.) ;
#54732 = ORIENTED_EDGE('',*,*,#41933,.F.) ;
#54733 = ORIENTED_EDGE('',*,*,#42100,.F.) ;
#54734 = ORIENTED_EDGE('',*,*,#41935,.F.) ;
#54735 = ORIENTED_EDGE('',*,*,#42099,.T.) ;
#54736 = ORIENTED_EDGE('',*,*,#41936,.F.) ;
#54737 = ORIENTED_EDGE('',*,*,#42101,.F.) ;
#54738 = ORIENTED_EDGE('',*,*,#41928,.F.) ;
#54739 = ORIENTED_EDGE('',*,*,#42101,.T.) ;
#54740 = ORIENTED_EDGE('',*,*,#42100,.T.) ;
#54741 = ORIENTED_EDGE('',*,*,#42102,.F.) ;
#54742 = ORIENTED_EDGE('',*,*,#41922,.T.) ;
#54743 = ORIENTED_EDGE('',*,*,#41916,.F.) ;
#54744 = ORIENTED_EDGE('',*,*,#41923,.F.) ;
#54745 = ORIENTED_EDGE('',*,*,#42102,.T.) ;
#54746 = ORIENTED_EDGE('',*,*,#41932,.F.) ;
#54747 = ORIENTED_EDGE('',*,*,#41672,.F.) ;
#54748 = ORIENTED_EDGE('',*,*,#41762,.F.) ;
#54749 = ORIENTED_EDGE('',*,*,#41613,.F.) ;
#54750 = ORIENTED_EDGE('',*,*,#41739,.F.) ;
#54751 = ORIENTED_EDGE('',*,*,#41742,.F.) ;
#54752 = ORIENTED_EDGE('',*,*,#42103,.T.) ;
#54753 = ORIENTED_EDGE('',*,*,#42104,.T.) ;
#54754 = ORIENTED_EDGE('',*,*,#41644,.T.) ;
#54755 = ORIENTED_EDGE('',*,*,#42046,.F.) ;
#54756 = ORIENTED_EDGE('',*,*,#41673,.T.) ;
#54757 = ORIENTED_EDGE('',*,*,#42048,.F.) ;
#54758 = ORIENTED_EDGE('',*,*,#42105,.T.) ;
#54759 = ORIENTED_EDGE('',*,*,#42052,.F.) ;
#54760 = ORIENTED_EDGE('',*,*,#42106,.F.) ;
#54761 = ORIENTED_EDGE('',*,*,#41671,.T.) ;
#54762 = ORIENTED_EDGE('',*,*,#42049,.F.) ;
#54763 = ORIENTED_EDGE('',*,*,#42107,.F.) ;
#54764 = ORIENTED_EDGE('',*,*,#41763,.F.) ;
#54765 = ORIENTED_EDGE('',*,*,#41773,.F.) ;
#54766 = ORIENTED_EDGE('',*,*,#42108,.T.) ;
#54767 = ORIENTED_EDGE('',*,*,#42056,.F.) ;
#54768 = ORIENTED_EDGE('',*,*,#42109,.T.) ;
#54769 = ORIENTED_EDGE('',*,*,#42059,.F.) ;
#54770 = ORIENTED_EDGE('',*,*,#42110,.T.) ;
#54771 = ORIENTED_EDGE('',*,*,#42050,.F.) ;
#54772 = ORIENTED_EDGE('',*,*,#42111,.T.) ;
#54773 = ORIENTED_EDGE('',*,*,#42107,.T.) ;
#54774 = ORIENTED_EDGE('',*,*,#42106,.T.) ;
#54775 = ORIENTED_EDGE('',*,*,#42112,.F.) ;
#54776 = ORIENTED_EDGE('',*,*,#41764,.T.) ;
#54777 = ORIENTED_EDGE('',*,*,#41895,.F.) ;
#54778 = ORIENTED_EDGE('',*,*,#41745,.F.) ;
#54779 = ORIENTED_EDGE('',*,*,#41666,.F.) ;
#54780 = ORIENTED_EDGE('',*,*,#41769,.F.) ;
#54781 = ORIENTED_EDGE('',*,*,#42113,.T.) ;
#54782 = ORIENTED_EDGE('',*,*,#42114,.T.) ;
#54783 = ORIENTED_EDGE('',*,*,#41766,.F.) ;
#54784 = ORIENTED_EDGE('',*,*,#41665,.F.) ;
#54785 = ORIENTED_EDGE('',*,*,#42054,.F.) ;
#54786 = ORIENTED_EDGE('',*,*,#42115,.T.) ;
#54787 = ORIENTED_EDGE('',*,*,#42112,.T.) ;
#54788 = ORIENTED_EDGE('',*,*,#42051,.F.) ;
#54789 = ORIENTED_EDGE('',*,*,#41664,.F.) ;
#54790 = ORIENTED_EDGE('',*,*,#41765,.F.) ;
#54791 = ORIENTED_EDGE('',*,*,#41667,.T.) ;
#54792 = ORIENTED_EDGE('',*,*,#41744,.F.) ;
#54793 = ORIENTED_EDGE('',*,*,#41662,.T.) ;
#54794 = ORIENTED_EDGE('',*,*,#42055,.F.) ;
#54795 = ORIENTED_EDGE('',*,*,#42116,.F.) ;
#54796 = ORIENTED_EDGE('',*,*,#42031,.F.) ;
#54797 = ORIENTED_EDGE('',*,*,#42117,.F.) ;
#54798 = ORIENTED_EDGE('',*,*,#42117,.T.) ;
#54799 = ORIENTED_EDGE('',*,*,#42029,.F.) ;
#54800 = ORIENTED_EDGE('',*,*,#42118,.F.) ;
#54801 = ORIENTED_EDGE('',*,*,#42042,.F.) ;
#54802 = ORIENTED_EDGE('',*,*,#42116,.T.) ;
#54803 = ORIENTED_EDGE('',*,*,#42045,.F.) ;
#54804 = ORIENTED_EDGE('',*,*,#42119,.F.) ;
#54805 = ORIENTED_EDGE('',*,*,#42033,.F.) ;
#54806 = ORIENTED_EDGE('',*,*,#42118,.T.) ;
#54807 = ORIENTED_EDGE('',*,*,#42027,.F.) ;
#54808 = ORIENTED_EDGE('',*,*,#42120,.F.) ;
#54809 = ORIENTED_EDGE('',*,*,#42035,.F.) ;
#54810 = ORIENTED_EDGE('',*,*,#42119,.T.) ;
#54811 = ORIENTED_EDGE('',*,*,#42121,.F.) ;
#54812 = ORIENTED_EDGE('',*,*,#42120,.T.) ;
#54813 = ORIENTED_EDGE('',*,*,#42041,.F.) ;
#54814 = ORIENTED_EDGE('',*,*,#42122,.F.) ;
#54815 = ORIENTED_EDGE('',*,*,#42043,.F.) ;
#54816 = ORIENTED_EDGE('',*,*,#42121,.T.) ;
#54817 = ORIENTED_EDGE('',*,*,#42044,.F.) ;
#54818 = ORIENTED_EDGE('',*,*,#42123,.F.) ;
#54819 = ORIENTED_EDGE('',*,*,#42037,.F.) ;
#54820 = ORIENTED_EDGE('',*,*,#42122,.T.) ;
#54821 = ORIENTED_EDGE('',*,*,#42039,.F.) ;
#54822 = ORIENTED_EDGE('',*,*,#42123,.T.) ;
#54823 = ORIENTED_EDGE('',*,*,#42124,.F.) ;
#54824 = ORIENTED_EDGE('',*,*,#41856,.F.) ;
#54825 = ORIENTED_EDGE('',*,*,#42125,.F.) ;
#54826 = ORIENTED_EDGE('',*,*,#41950,.F.) ;
#54827 = ORIENTED_EDGE('',*,*,#42125,.T.) ;
#54828 = ORIENTED_EDGE('',*,*,#41855,.T.) ;
#54829 = ORIENTED_EDGE('',*,*,#42126,.F.) ;
#54830 = ORIENTED_EDGE('',*,*,#42127,.F.) ;
#54831 = ORIENTED_EDGE('',*,*,#41857,.T.) ;
#54832 = ORIENTED_EDGE('',*,*,#42124,.T.) ;
#54833 = ORIENTED_EDGE('',*,*,#42128,.F.) ;
#54834 = ORIENTED_EDGE('',*,*,#42129,.F.) ;
#54835 = ORIENTED_EDGE('',*,*,#42126,.T.) ;
#54836 = ORIENTED_EDGE('',*,*,#41854,.F.) ;
#54837 = ORIENTED_EDGE('',*,*,#42130,.F.) ;
#54838 = ORIENTED_EDGE('',*,*,#41962,.F.) ;
#54839 = ORIENTED_EDGE('',*,*,#42127,.T.) ;
#54840 = ORIENTED_EDGE('',*,*,#41961,.F.) ;
#54841 = ORIENTED_EDGE('',*,*,#42131,.F.) ;
#54842 = ORIENTED_EDGE('',*,*,#41947,.F.) ;
#54843 = ORIENTED_EDGE('',*,*,#42132,.F.) ;
#54844 = ORIENTED_EDGE('',*,*,#41948,.F.) ;
#54845 = ORIENTED_EDGE('',*,*,#42133,.F.) ;
#54846 = ORIENTED_EDGE('',*,*,#41966,.F.) ;
#54847 = ORIENTED_EDGE('',*,*,#42128,.T.) ;
#54848 = ORIENTED_EDGE('',*,*,#41949,.F.) ;
#54849 = ORIENTED_EDGE('',*,*,#42134,.F.) ;
#54850 = ORIENTED_EDGE('',*,*,#41954,.F.) ;
#54851 = ORIENTED_EDGE('',*,*,#42129,.T.) ;
#54852 = ORIENTED_EDGE('',*,*,#41953,.F.) ;
#54853 = ORIENTED_EDGE('',*,*,#42135,.F.) ;
#54854 = ORIENTED_EDGE('',*,*,#41858,.F.) ;
#54855 = ORIENTED_EDGE('',*,*,#42136,.F.) ;
#54856 = ORIENTED_EDGE('',*,*,#41852,.F.) ;
#54857 = ORIENTED_EDGE('',*,*,#42137,.F.) ;
#54858 = ORIENTED_EDGE('',*,*,#41957,.F.) ;
#54859 = ORIENTED_EDGE('',*,*,#41853,.T.) ;
#54860 = ORIENTED_EDGE('',*,*,#42136,.T.) ;
#54861 = ORIENTED_EDGE('',*,*,#42138,.F.) ;
#54862 = ORIENTED_EDGE('',*,*,#42130,.T.) ;
#54863 = ORIENTED_EDGE('',*,*,#42133,.T.) ;
#54864 = ORIENTED_EDGE('',*,*,#42131,.T.) ;
#54865 = ORIENTED_EDGE('',*,*,#42139,.F.) ;
#54866 = ORIENTED_EDGE('',*,*,#42134,.T.) ;
#54867 = ORIENTED_EDGE('',*,*,#42132,.T.) ;
#54868 = ORIENTED_EDGE('',*,*,#42140,.F.) ;
#54869 = ORIENTED_EDGE('',*,*,#41851,.T.) ;
#54870 = ORIENTED_EDGE('',*,*,#42135,.T.) ;
#54871 = ORIENTED_EDGE('',*,*,#42141,.F.) ;
#54872 = ORIENTED_EDGE('',*,*,#42137,.T.) ;
#54873 = ORIENTED_EDGE('',*,*,#42138,.T.) ;
#54874 = ORIENTED_EDGE('',*,*,#41956,.F.) ;
#54875 = ORIENTED_EDGE('',*,*,#42142,.F.) ;
#54876 = ORIENTED_EDGE('',*,*,#41959,.F.) ;
#54877 = ORIENTED_EDGE('',*,*,#42139,.T.) ;
#54878 = ORIENTED_EDGE('',*,*,#41960,.F.) ;
#54879 = ORIENTED_EDGE('',*,*,#42143,.F.) ;
#54880 = ORIENTED_EDGE('',*,*,#41963,.F.) ;
#54881 = ORIENTED_EDGE('',*,*,#42140,.T.) ;
#54882 = ORIENTED_EDGE('',*,*,#41965,.F.) ;
#54883 = ORIENTED_EDGE('',*,*,#42144,.F.) ;
#54884 = ORIENTED_EDGE('',*,*,#41951,.F.) ;
#54885 = ORIENTED_EDGE('',*,*,#42141,.T.) ;
#54886 = ORIENTED_EDGE('',*,*,#41952,.F.) ;
#54887 = ORIENTED_EDGE('',*,*,#42145,.F.) ;
#54888 = ORIENTED_EDGE('',*,*,#41958,.F.) ;
#54889 = ORIENTED_EDGE('',*,*,#42143,.T.) ;
#54890 = ORIENTED_EDGE('',*,*,#42142,.T.) ;
#54891 = ORIENTED_EDGE('',*,*,#42146,.F.) ;
#54892 = ORIENTED_EDGE('',*,*,#42145,.T.) ;
#54893 = ORIENTED_EDGE('',*,*,#42144,.T.) ;
#54894 = ORIENTED_EDGE('',*,*,#42147,.F.) ;
#54895 = ORIENTED_EDGE('',*,*,#42146,.T.) ;
#54896 = ORIENTED_EDGE('',*,*,#41955,.F.) ;
#54897 = ORIENTED_EDGE('',*,*,#42147,.T.) ;
#54898 = ORIENTED_EDGE('',*,*,#41964,.F.) ;
#54899 = ORIENTED_EDGE('',*,*,#42148,.F.) ;
#54900 = ORIENTED_EDGE('',*,*,#41806,.F.) ;
#54901 = ORIENTED_EDGE('',*,*,#42149,.F.) ;
#54902 = ORIENTED_EDGE('',*,*,#42009,.F.) ;
#54903 = ORIENTED_EDGE('',*,*,#42149,.T.) ;
#54904 = ORIENTED_EDGE('',*,*,#41805,.T.) ;
#54905 = ORIENTED_EDGE('',*,*,#42150,.F.) ;
#54906 = ORIENTED_EDGE('',*,*,#42151,.F.) ;
#54907 = ORIENTED_EDGE('',*,*,#41807,.T.) ;
#54908 = ORIENTED_EDGE('',*,*,#42148,.T.) ;
#54909 = ORIENTED_EDGE('',*,*,#42152,.F.) ;
#54910 = ORIENTED_EDGE('',*,*,#42153,.F.) ;
#54911 = ORIENTED_EDGE('',*,*,#42150,.T.) ;
#54912 = ORIENTED_EDGE('',*,*,#41804,.F.) ;
#54913 = ORIENTED_EDGE('',*,*,#42154,.F.) ;
#54914 = ORIENTED_EDGE('',*,*,#42005,.F.) ;
#54915 = ORIENTED_EDGE('',*,*,#42151,.T.) ;
#54916 = ORIENTED_EDGE('',*,*,#42004,.F.) ;
#54917 = ORIENTED_EDGE('',*,*,#42155,.F.) ;
#54918 = ORIENTED_EDGE('',*,*,#42006,.F.) ;
#54919 = ORIENTED_EDGE('',*,*,#42156,.F.) ;
#54920 = ORIENTED_EDGE('',*,*,#42007,.F.) ;
#54921 = ORIENTED_EDGE('',*,*,#42157,.F.) ;
#54922 = ORIENTED_EDGE('',*,*,#42017,.F.) ;
#54923 = ORIENTED_EDGE('',*,*,#42152,.T.) ;
#54924 = ORIENTED_EDGE('',*,*,#42008,.F.) ;
#54925 = ORIENTED_EDGE('',*,*,#42158,.F.) ;
#54926 = ORIENTED_EDGE('',*,*,#42013,.F.) ;
#54927 = ORIENTED_EDGE('',*,*,#42153,.T.) ;
#54928 = ORIENTED_EDGE('',*,*,#42012,.F.) ;
#54929 = ORIENTED_EDGE('',*,*,#42159,.F.) ;
#54930 = ORIENTED_EDGE('',*,*,#41808,.F.) ;
#54931 = ORIENTED_EDGE('',*,*,#42160,.F.) ;
#54932 = ORIENTED_EDGE('',*,*,#41802,.F.) ;
#54933 = ORIENTED_EDGE('',*,*,#42161,.F.) ;
#54934 = ORIENTED_EDGE('',*,*,#42000,.F.) ;
#54935 = ORIENTED_EDGE('',*,*,#41803,.T.) ;
#54936 = ORIENTED_EDGE('',*,*,#42160,.T.) ;
#54937 = ORIENTED_EDGE('',*,*,#42162,.F.) ;
#54938 = ORIENTED_EDGE('',*,*,#42154,.T.) ;
#54939 = ORIENTED_EDGE('',*,*,#42157,.T.) ;
#54940 = ORIENTED_EDGE('',*,*,#42155,.T.) ;
#54941 = ORIENTED_EDGE('',*,*,#42163,.F.) ;
#54942 = ORIENTED_EDGE('',*,*,#42158,.T.) ;
#54943 = ORIENTED_EDGE('',*,*,#42156,.T.) ;
#54944 = ORIENTED_EDGE('',*,*,#42164,.F.) ;
#54945 = ORIENTED_EDGE('',*,*,#41801,.T.) ;
#54946 = ORIENTED_EDGE('',*,*,#42159,.T.) ;
#54947 = ORIENTED_EDGE('',*,*,#42165,.F.) ;
#54948 = ORIENTED_EDGE('',*,*,#42161,.T.) ;
#54949 = ORIENTED_EDGE('',*,*,#42162,.T.) ;
#54950 = ORIENTED_EDGE('',*,*,#41999,.F.) ;
#54951 = ORIENTED_EDGE('',*,*,#42166,.F.) ;
#54952 = ORIENTED_EDGE('',*,*,#42002,.F.) ;
#54953 = ORIENTED_EDGE('',*,*,#42163,.T.) ;
#54954 = ORIENTED_EDGE('',*,*,#42003,.F.) ;
#54955 = ORIENTED_EDGE('',*,*,#42167,.F.) ;
#54956 = ORIENTED_EDGE('',*,*,#42014,.F.) ;
#54957 = ORIENTED_EDGE('',*,*,#42164,.T.) ;
#54958 = ORIENTED_EDGE('',*,*,#42016,.F.) ;
#54959 = ORIENTED_EDGE('',*,*,#42168,.F.) ;
#54960 = ORIENTED_EDGE('',*,*,#42010,.F.) ;
#54961 = ORIENTED_EDGE('',*,*,#42165,.T.) ;
#54962 = ORIENTED_EDGE('',*,*,#42011,.F.) ;
#54963 = ORIENTED_EDGE('',*,*,#42169,.F.) ;
#54964 = ORIENTED_EDGE('',*,*,#42001,.F.) ;
#54965 = ORIENTED_EDGE('',*,*,#42167,.T.) ;
#54966 = ORIENTED_EDGE('',*,*,#42166,.T.) ;
#54967 = ORIENTED_EDGE('',*,*,#42170,.F.) ;
#54968 = ORIENTED_EDGE('',*,*,#42169,.T.) ;
#54969 = ORIENTED_EDGE('',*,*,#42168,.T.) ;
#54970 = ORIENTED_EDGE('',*,*,#42171,.F.) ;
#54971 = ORIENTED_EDGE('',*,*,#42170,.T.) ;
#54972 = ORIENTED_EDGE('',*,*,#41998,.F.) ;
#54973 = ORIENTED_EDGE('',*,*,#42171,.T.) ;
#54974 = ORIENTED_EDGE('',*,*,#42015,.F.) ;
#54975 = ORIENTED_EDGE('',*,*,#41879,.F.) ;
#54976 = ORIENTED_EDGE('',*,*,#42172,.T.) ;
#54977 = ORIENTED_EDGE('',*,*,#42061,.F.) ;
#54978 = ORIENTED_EDGE('',*,*,#42173,.F.) ;
#54979 = ORIENTED_EDGE('',*,*,#41893,.F.) ;
#54980 = ORIENTED_EDGE('',*,*,#41880,.F.) ;
#54981 = ORIENTED_EDGE('',*,*,#42174,.F.) ;
#54982 = ORIENTED_EDGE('',*,*,#41736,.F.) ;
#54983 = ORIENTED_EDGE('',*,*,#42174,.T.) ;
#54984 = ORIENTED_EDGE('',*,*,#42173,.T.) ;
#54985 = ORIENTED_EDGE('',*,*,#42175,.F.) ;
#54986 = ORIENTED_EDGE('',*,*,#42175,.T.) ;
#54987 = ORIENTED_EDGE('',*,*,#42066,.F.) ;
#54988 = ORIENTED_EDGE('',*,*,#42176,.F.) ;
#54989 = ORIENTED_EDGE('',*,*,#41737,.F.) ;
#54990 = ORIENTED_EDGE('',*,*,#41894,.F.) ;
#54991 = ORIENTED_EDGE('',*,*,#41738,.F.) ;
#54992 = ORIENTED_EDGE('',*,*,#42177,.F.) ;
#54993 = ORIENTED_EDGE('',*,*,#41747,.F.) ;
#54994 = ORIENTED_EDGE('',*,*,#42177,.T.) ;
#54995 = ORIENTED_EDGE('',*,*,#42176,.T.) ;
#54996 = ORIENTED_EDGE('',*,*,#42178,.F.) ;
#54997 = ORIENTED_EDGE('',*,*,#41748,.T.) ;
#54998 = ORIENTED_EDGE('',*,*,#42178,.T.) ;
#54999 = ORIENTED_EDGE('',*,*,#42065,.F.) ;
#55000 = ORIENTED_EDGE('',*,*,#42179,.F.) ;
#55001 = ORIENTED_EDGE('',*,*,#41749,.F.) ;
#55002 = ORIENTED_EDGE('',*,*,#41884,.F.) ;
#55003 = ORIENTED_EDGE('',*,*,#42180,.F.) ;
#55004 = ORIENTED_EDGE('',*,*,#41751,.F.) ;
#55005 = ORIENTED_EDGE('',*,*,#42181,.F.) ;
#55006 = ORIENTED_EDGE('',*,*,#41750,.T.) ;
#55007 = ORIENTED_EDGE('',*,*,#42179,.T.) ;
#55008 = ORIENTED_EDGE('',*,*,#42182,.F.) ;
#55009 = ORIENTED_EDGE('',*,*,#42181,.T.) ;
#55010 = ORIENTED_EDGE('',*,*,#42182,.T.) ;
#55011 = ORIENTED_EDGE('',*,*,#42064,.F.) ;
#55012 = ORIENTED_EDGE('',*,*,#42183,.F.) ;
#55013 = ORIENTED_EDGE('',*,*,#41881,.F.) ;
#55014 = ORIENTED_EDGE('',*,*,#41734,.F.) ;
#55015 = ORIENTED_EDGE('',*,*,#42184,.F.) ;
#55016 = ORIENTED_EDGE('',*,*,#41882,.F.) ;
#55017 = ORIENTED_EDGE('',*,*,#42185,.F.) ;
#55018 = ORIENTED_EDGE('',*,*,#42185,.T.) ;
#55019 = ORIENTED_EDGE('',*,*,#42183,.T.) ;
#55020 = ORIENTED_EDGE('',*,*,#42186,.F.) ;
#55021 = ORIENTED_EDGE('',*,*,#42063,.F.) ;
#55022 = ORIENTED_EDGE('',*,*,#42187,.T.) ;
#55023 = ORIENTED_EDGE('',*,*,#41731,.F.) ;
#55024 = ORIENTED_EDGE('',*,*,#42186,.T.) ;
#55025 = ORIENTED_EDGE('',*,*,#41891,.F.) ;
#55026 = ORIENTED_EDGE('',*,*,#41861,.F.) ;
#55027 = ORIENTED_EDGE('',*,*,#42188,.F.) ;
#55028 = ORIENTED_EDGE('',*,*,#41869,.F.) ;
#55029 = ORIENTED_EDGE('',*,*,#41890,.F.) ;
#55030 = ORIENTED_EDGE('',*,*,#41841,.F.) ;
#55031 = ORIENTED_EDGE('',*,*,#42189,.F.) ;
#55032 = ORIENTED_EDGE('',*,*,#41859,.F.) ;
#55033 = ORIENTED_EDGE('',*,*,#41889,.F.) ;
#55034 = ORIENTED_EDGE('',*,*,#41821,.F.) ;
#55035 = ORIENTED_EDGE('',*,*,#42190,.F.) ;
#55036 = ORIENTED_EDGE('',*,*,#41839,.F.) ;
#55037 = ORIENTED_EDGE('',*,*,#41888,.F.) ;
#55038 = ORIENTED_EDGE('',*,*,#41817,.F.) ;
#55039 = ORIENTED_EDGE('',*,*,#42191,.F.) ;
#55040 = ORIENTED_EDGE('',*,*,#41819,.F.) ;
#55041 = ORIENTED_EDGE('',*,*,#41887,.F.) ;
#55042 = ORIENTED_EDGE('',*,*,#41811,.F.) ;
#55043 = ORIENTED_EDGE('',*,*,#42192,.F.) ;
#55044 = ORIENTED_EDGE('',*,*,#41813,.F.) ;
#55045 = ORIENTED_EDGE('',*,*,#41886,.F.) ;
#55046 = ORIENTED_EDGE('',*,*,#41791,.F.) ;
#55047 = ORIENTED_EDGE('',*,*,#42193,.F.) ;
#55048 = ORIENTED_EDGE('',*,*,#41809,.F.) ;
#55049 = ORIENTED_EDGE('',*,*,#41680,.F.) ;
#55050 = ORIENTED_EDGE('',*,*,#41994,.F.) ;
#55051 = ORIENTED_EDGE('',*,*,#41690,.F.) ;
#55052 = ORIENTED_EDGE('',*,*,#41996,.F.) ;
#55053 = ORIENTED_EDGE('',*,*,#41688,.F.) ;
#55054 = ORIENTED_EDGE('',*,*,#41992,.F.) ;
#55055 = ORIENTED_EDGE('',*,*,#41682,.F.) ;
#55056 = ORIENTED_EDGE('',*,*,#41997,.F.) ;
#55057 = ORIENTED_EDGE('',*,*,#41678,.F.) ;
#55058 = ORIENTED_EDGE('',*,*,#41743,.F.) ;
#55059 = ORIENTED_EDGE('',*,*,#41692,.F.) ;
#55060 = ORIENTED_EDGE('',*,*,#41995,.F.) ;
#55061 = ORIENTED_EDGE('',*,*,#41686,.F.) ;
#55062 = ORIENTED_EDGE('',*,*,#41991,.F.) ;
#55063 = ORIENTED_EDGE('',*,*,#41684,.F.) ;
#55064 = ORIENTED_EDGE('',*,*,#41993,.F.) ;
#55065 = ORIENTED_EDGE('',*,*,#41885,.F.) ;
#55066 = ORIENTED_EDGE('',*,*,#41786,.F.) ;
#55067 = ORIENTED_EDGE('',*,*,#42194,.F.) ;
#55068 = ORIENTED_EDGE('',*,*,#41789,.F.) ;
#55069 = ORIENTED_EDGE('',*,*,#41898,.F.) ;
#55070 = ORIENTED_EDGE('',*,*,#41696,.F.) ;
#55071 = ORIENTED_EDGE('',*,*,#42195,.F.) ;
#55072 = ORIENTED_EDGE('',*,*,#41782,.F.) ;
#55073 = ORIENTED_EDGE('',*,*,#41897,.F.) ;
#55074 = ORIENTED_EDGE('',*,*,#41781,.F.) ;
#55075 = ORIENTED_EDGE('',*,*,#42196,.F.) ;
#55076 = ORIENTED_EDGE('',*,*,#41698,.F.) ;
#55077 = ORIENTED_EDGE('',*,*,#42197,.F.) ;
#55078 = ORIENTED_EDGE('',*,*,#41669,.F.) ;
#55079 = ORIENTED_EDGE('',*,*,#42110,.F.) ;
#55080 = ORIENTED_EDGE('',*,*,#42197,.T.) ;
#55081 = ORIENTED_EDGE('',*,*,#42058,.F.) ;
#55082 = ORIENTED_EDGE('',*,*,#42198,.F.) ;
#55083 = ORIENTED_EDGE('',*,*,#42053,.F.) ;
#55084 = ORIENTED_EDGE('',*,*,#42198,.T.) ;
#55085 = ORIENTED_EDGE('',*,*,#42057,.F.) ;
#55086 = ORIENTED_EDGE('',*,*,#42199,.F.) ;
#55087 = ORIENTED_EDGE('',*,*,#42115,.F.) ;
#55088 = ORIENTED_EDGE('',*,*,#42199,.T.) ;
#55089 = ORIENTED_EDGE('',*,*,#42108,.F.) ;
#55090 = ORIENTED_EDGE('',*,*,#42200,.F.) ;
#55091 = ORIENTED_EDGE('',*,*,#42113,.F.) ;
#55092 = ORIENTED_EDGE('',*,*,#42200,.T.) ;
#55093 = ORIENTED_EDGE('',*,*,#41772,.F.) ;
#55094 = ORIENTED_EDGE('',*,*,#42201,.F.) ;
#55095 = ORIENTED_EDGE('',*,*,#42114,.F.) ;
#55096 = ORIENTED_EDGE('',*,*,#42201,.T.) ;
#55097 = ORIENTED_EDGE('',*,*,#41771,.F.) ;
#55098 = ORIENTED_EDGE('',*,*,#41896,.F.) ;
#55099 = ORIENTED_EDGE('',*,*,#41767,.F.) ;
#55100 = ORIENTED_EDGE('',*,*,#41741,.F.) ;
#55101 = ORIENTED_EDGE('',*,*,#42202,.T.) ;
#55102 = ORIENTED_EDGE('',*,*,#41775,.F.) ;
#55103 = ORIENTED_EDGE('',*,*,#42203,.F.) ;
#55104 = ORIENTED_EDGE('',*,*,#42203,.T.) ;
#55105 = ORIENTED_EDGE('',*,*,#41774,.F.) ;
#55106 = ORIENTED_EDGE('',*,*,#42204,.F.) ;
#55107 = ORIENTED_EDGE('',*,*,#42103,.F.) ;
#55108 = ORIENTED_EDGE('',*,*,#42204,.T.) ;
#55109 = ORIENTED_EDGE('',*,*,#42109,.F.) ;
#55110 = ORIENTED_EDGE('',*,*,#41645,.F.) ;
#55111 = ORIENTED_EDGE('',*,*,#42104,.F.) ;
#55112 = ORIENTED_EDGE('',*,*,#42205,.F.) ;
#55113 = ORIENTED_EDGE('',*,*,#42047,.F.) ;
#55114 = ORIENTED_EDGE('',*,*,#41643,.T.) ;
#55115 = ORIENTED_EDGE('',*,*,#42060,.F.) ;
#55116 = ORIENTED_EDGE('',*,*,#42111,.F.) ;
#55117 = ORIENTED_EDGE('',*,*,#42105,.F.) ;
#55118 = ORIENTED_EDGE('',*,*,#42205,.T.) ;
#55119 = ORIENTED_EDGE('',*,*,#42206,.T.) ;
#55120 = ORIENTED_EDGE('',*,*,#42207,.T.) ;
#55121 = ORIENTED_EDGE('',*,*,#42062,.F.) ;
#55122 = ORIENTED_EDGE('',*,*,#42208,.T.) ;
#55123 = ORIENTED_EDGE('',*,*,#42209,.T.) ;
#55124 = ORIENTED_EDGE('',*,*,#41892,.F.) ;
#55125 = ORIENTED_EDGE('',*,*,#41867,.F.) ;
#55126 = ORIENTED_EDGE('',*,*,#42210,.F.) ;
#55127 = ORIENTED_EDGE('',*,*,#41878,.F.) ;
#55128 = ORIENTED_EDGE('',*,*,#41866,.F.) ;
#55129 = ORIENTED_EDGE('',*,*,#42211,.T.) ;
#55130 = ORIENTED_EDGE('',*,*,#42172,.F.) ;
#55131 = ORIENTED_EDGE('',*,*,#42210,.T.) ;
#55132 = ORIENTED_EDGE('',*,*,#41876,.F.) ;
#55133 = ORIENTED_EDGE('',*,*,#42212,.F.) ;
#55134 = ORIENTED_EDGE('',*,*,#41732,.F.) ;
#55135 = ORIENTED_EDGE('',*,*,#42213,.F.) ;
#55136 = ORIENTED_EDGE('',*,*,#42187,.F.) ;
#55137 = ORIENTED_EDGE('',*,*,#42214,.T.) ;
#55138 = ORIENTED_EDGE('',*,*,#41863,.F.) ;
#55139 = ORIENTED_EDGE('',*,*,#42213,.T.) ;
#55140 = ORIENTED_EDGE('',*,*,#42208,.F.) ;
#55141 = ORIENTED_EDGE('',*,*,#42211,.F.) ;
#55142 = ORIENTED_EDGE('',*,*,#42215,.F.) ;
#55143 = ORIENTED_EDGE('',*,*,#42216,.F.) ;
#55144 = ORIENTED_EDGE('',*,*,#42209,.F.) ;
#55145 = ORIENTED_EDGE('',*,*,#42215,.T.) ;
#55146 = ORIENTED_EDGE('',*,*,#41865,.F.) ;
#55147 = ORIENTED_EDGE('',*,*,#42216,.T.) ;
#55148 = ORIENTED_EDGE('',*,*,#41864,.F.) ;
#55149 = ORIENTED_EDGE('',*,*,#42217,.F.) ;
#55150 = ORIENTED_EDGE('',*,*,#42206,.F.) ;
#55151 = ORIENTED_EDGE('',*,*,#42217,.T.) ;
#55152 = ORIENTED_EDGE('',*,*,#42214,.F.) ;
#55153 = ORIENTED_EDGE('',*,*,#42207,.F.) ;
#55154 = ORIENTED_EDGE('',*,*,#41720,.F.) ;
#55155 = ORIENTED_EDGE('',*,*,#41788,.T.) ;
#55156 = ORIENTED_EDGE('',*,*,#41726,.F.) ;
#55157 = ORIENTED_EDGE('',*,*,#41707,.T.) ;
#55158 = ORIENTED_EDGE('',*,*,#41724,.T.) ;
#55159 = ORIENTED_EDGE('',*,*,#41711,.T.) ;
#55160 = ORIENTED_EDGE('',*,*,#41722,.T.) ;
#55161 = ORIENTED_EDGE('',*,*,#41715,.T.) ;
#55162 = ORIENTED_EDGE('',*,*,#42218,.T.) ;
#55163 = ORIENTED_EDGE('',*,*,#42219,.T.) ;
#55164 = ORIENTED_EDGE('',*,*,#42220,.F.) ;
#55165 = ORIENTED_EDGE('',*,*,#42221,.T.) ;
#55166 = ORIENTED_EDGE('',*,*,#42220,.T.) ;
#55167 = ORIENTED_EDGE('',*,*,#42222,.T.) ;
#55168 = ORIENTED_EDGE('',*,*,#42223,.F.) ;
#55169 = ORIENTED_EDGE('',*,*,#42224,.T.) ;
#55170 = ORIENTED_EDGE('',*,*,#42223,.T.) ;
#55171 = ORIENTED_EDGE('',*,*,#42225,.T.) ;
#55172 = ORIENTED_EDGE('',*,*,#42226,.F.) ;
#55173 = ORIENTED_EDGE('',*,*,#42227,.T.) ;
#55174 = ORIENTED_EDGE('',*,*,#42226,.T.) ;
#55175 = ORIENTED_EDGE('',*,*,#42228,.T.) ;
#55176 = ORIENTED_EDGE('',*,*,#42229,.F.) ;
#55177 = ORIENTED_EDGE('',*,*,#42230,.T.) ;
#55178 = ORIENTED_EDGE('',*,*,#42229,.T.) ;
#55179 = ORIENTED_EDGE('',*,*,#42231,.T.) ;
#55180 = ORIENTED_EDGE('',*,*,#42232,.F.) ;
#55181 = ORIENTED_EDGE('',*,*,#42233,.T.) ;
#55182 = ORIENTED_EDGE('',*,*,#42232,.T.) ;
#55183 = ORIENTED_EDGE('',*,*,#42234,.T.) ;
#55184 = ORIENTED_EDGE('',*,*,#42235,.F.) ;
#55185 = ORIENTED_EDGE('',*,*,#42236,.T.) ;
#55186 = ORIENTED_EDGE('',*,*,#42235,.T.) ;
#55187 = ORIENTED_EDGE('',*,*,#42237,.T.) ;
#55188 = ORIENTED_EDGE('',*,*,#42238,.F.) ;
#55189 = ORIENTED_EDGE('',*,*,#42239,.T.) ;
#55190 = ORIENTED_EDGE('',*,*,#42238,.T.) ;
#55191 = ORIENTED_EDGE('',*,*,#42240,.T.) ;
#55192 = ORIENTED_EDGE('',*,*,#42241,.F.) ;
#55193 = ORIENTED_EDGE('',*,*,#42242,.T.) ;
#55194 = ORIENTED_EDGE('',*,*,#42241,.T.) ;
#55195 = ORIENTED_EDGE('',*,*,#42243,.T.) ;
#55196 = ORIENTED_EDGE('',*,*,#42244,.T.) ;
#55197 = ORIENTED_EDGE('',*,*,#42245,.T.) ;
#55198 = ORIENTED_EDGE('',*,*,#42246,.T.) ;
#55199 = ORIENTED_EDGE('',*,*,#42247,.T.) ;
#55200 = ORIENTED_EDGE('',*,*,#42248,.T.) ;
#55201 = ORIENTED_EDGE('',*,*,#42249,.T.) ;
#55202 = ORIENTED_EDGE('',*,*,#42250,.T.) ;
#55203 = ORIENTED_EDGE('',*,*,#42251,.T.) ;
#55204 = ORIENTED_EDGE('',*,*,#42252,.T.) ;
#55205 = ORIENTED_EDGE('',*,*,#42253,.T.) ;
#55206 = ORIENTED_EDGE('',*,*,#42254,.T.) ;
#55207 = ORIENTED_EDGE('',*,*,#42255,.T.) ;
#55208 = ORIENTED_EDGE('',*,*,#42256,.T.) ;
#55209 = ORIENTED_EDGE('',*,*,#42257,.T.) ;
#55210 = ORIENTED_EDGE('',*,*,#42258,.T.) ;
#55211 = ORIENTED_EDGE('',*,*,#42259,.T.) ;
#55212 = ORIENTED_EDGE('',*,*,#42260,.T.) ;
#55213 = ORIENTED_EDGE('',*,*,#42261,.T.) ;
#55214 = ORIENTED_EDGE('',*,*,#42262,.T.) ;
#55215 = ORIENTED_EDGE('',*,*,#42263,.T.) ;
#55216 = ORIENTED_EDGE('',*,*,#42264,.T.) ;
#55217 = ORIENTED_EDGE('',*,*,#42265,.T.) ;
#55218 = ORIENTED_EDGE('',*,*,#42266,.T.) ;
#55219 = ORIENTED_EDGE('',*,*,#42267,.T.) ;
#55220 = ORIENTED_EDGE('',*,*,#41624,.T.) ;
#55221 = ORIENTED_EDGE('',*,*,#41640,.T.) ;
#55222 = ORIENTED_EDGE('',*,*,#42268,.T.) ;
#55223 = ORIENTED_EDGE('',*,*,#42269,.T.) ;
#55224 = ORIENTED_EDGE('',*,*,#42270,.T.) ;
#55225 = ORIENTED_EDGE('',*,*,#42271,.T.) ;
#55226 = ORIENTED_EDGE('',*,*,#42272,.T.) ;
#55227 = ORIENTED_EDGE('',*,*,#42262,.F.) ;
#55228 = ORIENTED_EDGE('',*,*,#42273,.T.) ;
#55229 = ORIENTED_EDGE('',*,*,#41870,.F.) ;
#55230 = ORIENTED_EDGE('',*,*,#42188,.T.) ;
#55231 = ORIENTED_EDGE('',*,*,#41860,.F.) ;
#55232 = ORIENTED_EDGE('',*,*,#42189,.T.) ;
#55233 = ORIENTED_EDGE('',*,*,#41840,.F.) ;
#55234 = ORIENTED_EDGE('',*,*,#42190,.T.) ;
#55235 = ORIENTED_EDGE('',*,*,#41820,.F.) ;
#55236 = ORIENTED_EDGE('',*,*,#42191,.T.) ;
#55237 = ORIENTED_EDGE('',*,*,#41816,.F.) ;
#55238 = ORIENTED_EDGE('',*,*,#41646,.T.) ;
#55239 = ORIENTED_EDGE('',*,*,#41814,.F.) ;
#55240 = ORIENTED_EDGE('',*,*,#42192,.T.) ;
#55241 = ORIENTED_EDGE('',*,*,#41810,.F.) ;
#55242 = ORIENTED_EDGE('',*,*,#42193,.T.) ;
#55243 = ORIENTED_EDGE('',*,*,#41790,.F.) ;
#55244 = ORIENTED_EDGE('',*,*,#42194,.T.) ;
#55245 = ORIENTED_EDGE('',*,*,#41785,.F.) ;
#55246 = ORIENTED_EDGE('',*,*,#41721,.T.) ;
#55247 = ORIENTED_EDGE('',*,*,#41717,.F.) ;
#55248 = ORIENTED_EDGE('',*,*,#41723,.T.) ;
#55249 = ORIENTED_EDGE('',*,*,#41713,.F.) ;
#55250 = ORIENTED_EDGE('',*,*,#41725,.T.) ;
#55251 = ORIENTED_EDGE('',*,*,#41709,.F.) ;
#55252 = ORIENTED_EDGE('',*,*,#41730,.T.) ;
#55253 = ORIENTED_EDGE('',*,*,#41783,.F.) ;
#55254 = ORIENTED_EDGE('',*,*,#42195,.T.) ;
#55255 = ORIENTED_EDGE('',*,*,#41695,.F.) ;
#55256 = ORIENTED_EDGE('',*,*,#42196,.T.) ;
#55257 = ORIENTED_EDGE('',*,*,#41780,.F.) ;
#55258 = ORIENTED_EDGE('',*,*,#42274,.T.) ;
#55259 = ORIENTED_EDGE('',*,*,#42264,.F.) ;
#55260 = ORIENTED_EDGE('',*,*,#42275,.T.) ;
#55261 = ORIENTED_EDGE('',*,*,#41756,.F.) ;
#55262 = ORIENTED_EDGE('',*,*,#42276,.T.) ;
#55263 = ORIENTED_EDGE('',*,*,#42271,.F.) ;
#55264 = ORIENTED_EDGE('',*,*,#42277,.T.) ;
#55265 = ORIENTED_EDGE('',*,*,#42278,.T.) ;
#55266 = ORIENTED_EDGE('',*,*,#42279,.T.) ;
#55267 = ORIENTED_EDGE('',*,*,#42280,.T.) ;
#55268 = ORIENTED_EDGE('',*,*,#42281,.T.) ;
#55269 = ORIENTED_EDGE('',*,*,#42282,.T.) ;
#55270 = ORIENTED_EDGE('',*,*,#42283,.T.) ;
#55271 = ORIENTED_EDGE('',*,*,#42284,.T.) ;
#55272 = ORIENTED_EDGE('',*,*,#42285,.T.) ;
#55273 = ORIENTED_EDGE('',*,*,#42286,.F.) ;
#55274 = ORIENTED_EDGE('',*,*,#42287,.T.) ;
#55275 = ORIENTED_EDGE('',*,*,#42288,.T.) ;
#55276 = ORIENTED_EDGE('',*,*,#42289,.T.) ;
#55277 = ORIENTED_EDGE('',*,*,#42290,.F.) ;
#55278 = ORIENTED_EDGE('',*,*,#42291,.T.) ;
#55279 = ORIENTED_EDGE('',*,*,#42292,.T.) ;
#55280 = ORIENTED_EDGE('',*,*,#42293,.T.) ;
#55281 = ORIENTED_EDGE('',*,*,#42294,.T.) ;
#55282 = ORIENTED_EDGE('',*,*,#42295,.T.) ;
#55283 = ORIENTED_EDGE('',*,*,#42296,.F.) ;
#55284 = ORIENTED_EDGE('',*,*,#42297,.T.) ;
#55285 = ORIENTED_EDGE('',*,*,#42288,.F.) ;
#55286 = ORIENTED_EDGE('',*,*,#42298,.T.) ;
#55287 = ORIENTED_EDGE('',*,*,#42299,.T.) ;
#55288 = ORIENTED_EDGE('',*,*,#42300,.T.) ;
#55289 = ORIENTED_EDGE('',*,*,#42301,.F.) ;
#55290 = ORIENTED_EDGE('',*,*,#42302,.T.) ;
#55291 = ORIENTED_EDGE('',*,*,#42294,.F.) ;
#55292 = ORIENTED_EDGE('',*,*,#42303,.T.) ;
#55293 = ORIENTED_EDGE('',*,*,#42304,.F.) ;
#55294 = ORIENTED_EDGE('',*,*,#42305,.T.) ;
#55295 = ORIENTED_EDGE('',*,*,#42306,.T.) ;
#55296 = ORIENTED_EDGE('',*,*,#42307,.T.) ;
#55297 = ORIENTED_EDGE('',*,*,#42299,.F.) ;
#55298 = ORIENTED_EDGE('',*,*,#42308,.T.) ;
#55299 = ORIENTED_EDGE('',*,*,#42309,.T.) ;
#55300 = ORIENTED_EDGE('',*,*,#42310,.T.) ;
#55301 = ORIENTED_EDGE('',*,*,#42296,.T.) ;
#55302 = ORIENTED_EDGE('',*,*,#42311,.T.) ;
#55303 = ORIENTED_EDGE('',*,*,#42312,.T.) ;
#55304 = ORIENTED_EDGE('',*,*,#42313,.T.) ;
#55305 = ORIENTED_EDGE('',*,*,#42314,.T.) ;
#55306 = ORIENTED_EDGE('',*,*,#42315,.T.) ;
#55307 = ORIENTED_EDGE('',*,*,#42316,.T.) ;
#55308 = ORIENTED_EDGE('',*,*,#42317,.T.) ;
#55309 = ORIENTED_EDGE('',*,*,#42318,.T.) ;
#55310 = ORIENTED_EDGE('',*,*,#42319,.T.) ;
#55311 = ORIENTED_EDGE('',*,*,#42320,.T.) ;
#55312 = ORIENTED_EDGE('',*,*,#42321,.T.) ;
#55313 = ORIENTED_EDGE('',*,*,#42322,.T.) ;
#55314 = ORIENTED_EDGE('',*,*,#42323,.T.) ;
#55315 = ORIENTED_EDGE('',*,*,#42324,.T.) ;
#55316 = ORIENTED_EDGE('',*,*,#42325,.T.) ;
#55317 = ORIENTED_EDGE('',*,*,#42326,.T.) ;
#55318 = ORIENTED_EDGE('',*,*,#42327,.T.) ;
#55319 = ORIENTED_EDGE('',*,*,#42328,.T.) ;
#55320 = ORIENTED_EDGE('',*,*,#42329,.T.) ;
#55321 = ORIENTED_EDGE('',*,*,#42330,.T.) ;
#55322 = ORIENTED_EDGE('',*,*,#42331,.T.) ;
#55323 = ORIENTED_EDGE('',*,*,#42332,.T.) ;
#55324 = ORIENTED_EDGE('',*,*,#42333,.T.) ;
#55325 = ORIENTED_EDGE('',*,*,#42334,.T.) ;
#55326 = ORIENTED_EDGE('',*,*,#42335,.T.) ;
#55327 = ORIENTED_EDGE('',*,*,#42336,.T.) ;
#55328 = ORIENTED_EDGE('',*,*,#42337,.T.) ;
#55329 = ORIENTED_EDGE('',*,*,#42338,.T.) ;
#55330 = ORIENTED_EDGE('',*,*,#42339,.T.) ;
#55331 = ORIENTED_EDGE('',*,*,#42340,.T.) ;
#55332 = ORIENTED_EDGE('',*,*,#42341,.T.) ;
#55333 = ORIENTED_EDGE('',*,*,#42342,.T.) ;
#55334 = ORIENTED_EDGE('',*,*,#42343,.T.) ;
#55335 = ORIENTED_EDGE('',*,*,#42344,.T.) ;
#55336 = ORIENTED_EDGE('',*,*,#42345,.T.) ;
#55337 = ORIENTED_EDGE('',*,*,#42346,.F.) ;
#55338 = ORIENTED_EDGE('',*,*,#42347,.F.) ;
#55339 = ORIENTED_EDGE('',*,*,#42348,.F.) ;
#55340 = ORIENTED_EDGE('',*,*,#42349,.F.) ;
#55341 = ORIENTED_EDGE('',*,*,#42350,.F.) ;
#55342 = ORIENTED_EDGE('',*,*,#42351,.F.) ;
#55343 = ORIENTED_EDGE('',*,*,#42352,.F.) ;
#55344 = ORIENTED_EDGE('',*,*,#42353,.F.) ;
#55345 = ORIENTED_EDGE('',*,*,#42354,.F.) ;
#55346 = ORIENTED_EDGE('',*,*,#42355,.F.) ;
#55347 = ORIENTED_EDGE('',*,*,#42353,.T.) ;
#55348 = ORIENTED_EDGE('',*,*,#42356,.T.) ;
#55349 = ORIENTED_EDGE('',*,*,#42357,.F.) ;
#55350 = ORIENTED_EDGE('',*,*,#42358,.F.) ;
#55351 = ORIENTED_EDGE('',*,*,#42346,.T.) ;
#55352 = ORIENTED_EDGE('',*,*,#42355,.T.) ;
#55353 = ORIENTED_EDGE('',*,*,#42359,.F.) ;
#55354 = ORIENTED_EDGE('',*,*,#42360,.F.) ;
#55355 = ORIENTED_EDGE('',*,*,#42347,.T.) ;
#55356 = ORIENTED_EDGE('',*,*,#42358,.T.) ;
#55357 = ORIENTED_EDGE('',*,*,#42361,.F.) ;
#55358 = ORIENTED_EDGE('',*,*,#42362,.F.) ;
#55359 = ORIENTED_EDGE('',*,*,#42348,.T.) ;
#55360 = ORIENTED_EDGE('',*,*,#42360,.T.) ;
#55361 = ORIENTED_EDGE('',*,*,#42363,.F.) ;
#55362 = ORIENTED_EDGE('',*,*,#42364,.F.) ;
#55363 = ORIENTED_EDGE('',*,*,#42349,.T.) ;
#55364 = ORIENTED_EDGE('',*,*,#42362,.T.) ;
#55365 = ORIENTED_EDGE('',*,*,#42365,.F.) ;
#55366 = ORIENTED_EDGE('',*,*,#42366,.F.) ;
#55367 = ORIENTED_EDGE('',*,*,#42350,.T.) ;
#55368 = ORIENTED_EDGE('',*,*,#42364,.T.) ;
#55369 = ORIENTED_EDGE('',*,*,#42367,.F.) ;
#55370 = ORIENTED_EDGE('',*,*,#42368,.F.) ;
#55371 = ORIENTED_EDGE('',*,*,#42351,.T.) ;
#55372 = ORIENTED_EDGE('',*,*,#42366,.T.) ;
#55373 = ORIENTED_EDGE('',*,*,#42369,.F.) ;
#55374 = ORIENTED_EDGE('',*,*,#42356,.F.) ;
#55375 = ORIENTED_EDGE('',*,*,#42352,.T.) ;
#55376 = ORIENTED_EDGE('',*,*,#42368,.T.) ;
#55377 = ORIENTED_EDGE('',*,*,#42357,.T.) ;
#55378 = ORIENTED_EDGE('',*,*,#42354,.T.) ;
#55379 = ORIENTED_EDGE('',*,*,#42369,.T.) ;
#55380 = ORIENTED_EDGE('',*,*,#42367,.T.) ;
#55381 = ORIENTED_EDGE('',*,*,#42365,.T.) ;
#55382 = ORIENTED_EDGE('',*,*,#42363,.T.) ;
#55383 = ORIENTED_EDGE('',*,*,#42361,.T.) ;
#55384 = ORIENTED_EDGE('',*,*,#42359,.T.) ;
#55385 = ORIENTED_EDGE('',*,*,#41632,.T.) ;
#55386 = ORIENTED_EDGE('',*,*,#42370,.T.) ;
#55387 = ORIENTED_EDGE('',*,*,#41630,.F.) ;
#55388 = ORIENTED_EDGE('',*,*,#42371,.T.) ;
#55389 = ORIENTED_EDGE('',*,*,#41634,.T.) ;
#55390 = ORIENTED_EDGE('',*,*,#42372,.T.) ;
#55391 = ORIENTED_EDGE('',*,*,#41638,.F.) ;
#55392 = ORIENTED_EDGE('',*,*,#42373,.T.) ;
#55393 = ORIENTED_EDGE('',*,*,#41626,.T.) ;
#55394 = ORIENTED_EDGE('',*,*,#42374,.T.) ;
#55395 = ORIENTED_EDGE('',*,*,#41628,.T.) ;
#55396 = ORIENTED_EDGE('',*,*,#42375,.T.) ;
#55397 = ORIENTED_EDGE('',*,*,#41636,.T.) ;
#55398 = ORIENTED_EDGE('',*,*,#42376,.T.) ;
#55399 = ORIENTED_EDGE('',*,*,#42377,.T.) ;
#55400 = ORIENTED_EDGE('',*,*,#42378,.T.) ;
#55401 = ORIENTED_EDGE('',*,*,#42379,.T.) ;
#55402 = ORIENTED_EDGE('',*,*,#42380,.T.) ;
#55403 = ORIENTED_EDGE('',*,*,#42381,.T.) ;
#55404 = ORIENTED_EDGE('',*,*,#42382,.T.) ;
#55405 = ORIENTED_EDGE('',*,*,#42383,.T.) ;
#55406 = ORIENTED_EDGE('',*,*,#42384,.T.) ;
#55407 = ORIENTED_EDGE('',*,*,#42385,.T.) ;
#55408 = ORIENTED_EDGE('',*,*,#42386,.T.) ;
#55409 = ORIENTED_EDGE('',*,*,#42387,.T.) ;
#55410 = ORIENTED_EDGE('',*,*,#42388,.T.) ;
#55411 = ORIENTED_EDGE('',*,*,#42389,.T.) ;
#55412 = ORIENTED_EDGE('',*,*,#42390,.T.) ;
#55413 = ORIENTED_EDGE('',*,*,#42391,.T.) ;
#55414 = ORIENTED_EDGE('',*,*,#42392,.T.) ;
#55415 = ORIENTED_EDGE('',*,*,#42393,.T.) ;
#55416 = ORIENTED_EDGE('',*,*,#42394,.T.) ;
#55417 = ORIENTED_EDGE('',*,*,#42395,.T.) ;
#55418 = ORIENTED_EDGE('',*,*,#42396,.T.) ;
#55419 = ORIENTED_EDGE('',*,*,#42397,.F.) ;
#55420 = ORIENTED_EDGE('',*,*,#42398,.F.) ;
#55421 = ORIENTED_EDGE('',*,*,#42399,.F.) ;
#55422 = ORIENTED_EDGE('',*,*,#42400,.F.) ;
#55423 = ORIENTED_EDGE('',*,*,#42401,.F.) ;
#55424 = ORIENTED_EDGE('',*,*,#42402,.F.) ;
#55425 = ORIENTED_EDGE('',*,*,#42403,.F.) ;
#55426 = ORIENTED_EDGE('',*,*,#42404,.F.) ;
#55427 = ORIENTED_EDGE('',*,*,#42405,.T.) ;
#55428 = ORIENTED_EDGE('',*,*,#42406,.T.) ;
#55429 = ORIENTED_EDGE('',*,*,#42407,.F.) ;
#55430 = ORIENTED_EDGE('',*,*,#42404,.T.) ;
#55431 = ORIENTED_EDGE('',*,*,#42407,.T.) ;
#55432 = ORIENTED_EDGE('',*,*,#42408,.T.) ;
#55433 = ORIENTED_EDGE('',*,*,#42409,.F.) ;
#55434 = ORIENTED_EDGE('',*,*,#42397,.T.) ;
#55435 = ORIENTED_EDGE('',*,*,#42409,.T.) ;
#55436 = ORIENTED_EDGE('',*,*,#42410,.T.) ;
#55437 = ORIENTED_EDGE('',*,*,#42411,.F.) ;
#55438 = ORIENTED_EDGE('',*,*,#42398,.T.) ;
#55439 = ORIENTED_EDGE('',*,*,#42411,.T.) ;
#55440 = ORIENTED_EDGE('',*,*,#42412,.T.) ;
#55441 = ORIENTED_EDGE('',*,*,#42413,.F.) ;
#55442 = ORIENTED_EDGE('',*,*,#42399,.T.) ;
#55443 = ORIENTED_EDGE('',*,*,#42413,.T.) ;
#55444 = ORIENTED_EDGE('',*,*,#42414,.T.) ;
#55445 = ORIENTED_EDGE('',*,*,#42415,.F.) ;
#55446 = ORIENTED_EDGE('',*,*,#42400,.T.) ;
#55447 = ORIENTED_EDGE('',*,*,#42415,.T.) ;
#55448 = ORIENTED_EDGE('',*,*,#42416,.T.) ;
#55449 = ORIENTED_EDGE('',*,*,#42417,.F.) ;
#55450 = ORIENTED_EDGE('',*,*,#42401,.T.) ;
#55451 = ORIENTED_EDGE('',*,*,#42417,.T.) ;
#55452 = ORIENTED_EDGE('',*,*,#42418,.T.) ;
#55453 = ORIENTED_EDGE('',*,*,#42419,.F.) ;
#55454 = ORIENTED_EDGE('',*,*,#42402,.T.) ;
#55455 = ORIENTED_EDGE('',*,*,#42419,.T.) ;
#55456 = ORIENTED_EDGE('',*,*,#42420,.T.) ;
#55457 = ORIENTED_EDGE('',*,*,#42405,.F.) ;
#55458 = ORIENTED_EDGE('',*,*,#42403,.T.) ;
#55459 = ORIENTED_EDGE('',*,*,#42421,.T.) ;
#55460 = ORIENTED_EDGE('',*,*,#42422,.T.) ;
#55461 = ORIENTED_EDGE('',*,*,#42423,.T.) ;
#55462 = ORIENTED_EDGE('',*,*,#42424,.T.) ;
#55463 = ORIENTED_EDGE('',*,*,#42425,.T.) ;
#55464 = ORIENTED_EDGE('',*,*,#42426,.T.) ;
#55465 = ORIENTED_EDGE('',*,*,#42427,.T.) ;
#55466 = ORIENTED_EDGE('',*,*,#42428,.T.) ;
#55467 = ORIENTED_EDGE('',*,*,#42429,.T.) ;
#55468 = ORIENTED_EDGE('',*,*,#41615,.T.) ;
#55469 = ORIENTED_EDGE('',*,*,#42430,.T.) ;
#55470 = ORIENTED_EDGE('',*,*,#42431,.T.) ;
#55471 = ORIENTED_EDGE('',*,*,#41617,.T.) ;
#55472 = ORIENTED_EDGE('',*,*,#42432,.T.) ;
#55473 = ORIENTED_EDGE('',*,*,#42433,.T.) ;
#55474 = ORIENTED_EDGE('',*,*,#42434,.T.) ;
#55475 = ORIENTED_EDGE('',*,*,#42435,.T.) ;
#55476 = ORIENTED_EDGE('',*,*,#42436,.T.) ;
#55477 = ORIENTED_EDGE('',*,*,#42437,.T.) ;
#55478 = ORIENTED_EDGE('',*,*,#42438,.T.) ;
#55479 = ORIENTED_EDGE('',*,*,#42439,.T.) ;
#55480 = ORIENTED_EDGE('',*,*,#41593,.T.) ;
#55481 = ORIENTED_EDGE('',*,*,#41621,.T.) ;
#55482 = ORIENTED_EDGE('',*,*,#42440,.T.) ;
#55483 = ORIENTED_EDGE('',*,*,#42441,.T.) ;
#55484 = ORIENTED_EDGE('',*,*,#42442,.T.) ;
#55485 = ORIENTED_EDGE('',*,*,#42443,.T.) ;
#55486 = ORIENTED_EDGE('',*,*,#42444,.T.) ;
#55487 = ORIENTED_EDGE('',*,*,#42445,.T.) ;
#55488 = ORIENTED_EDGE('',*,*,#42446,.F.) ;
#55489 = ORIENTED_EDGE('',*,*,#42447,.F.) ;
#55490 = ORIENTED_EDGE('',*,*,#42448,.F.) ;
#55491 = ORIENTED_EDGE('',*,*,#41824,.F.) ;
#55492 = ORIENTED_EDGE('',*,*,#42298,.F.) ;
#55493 = ORIENTED_EDGE('',*,*,#42287,.F.) ;
#55494 = ORIENTED_EDGE('',*,*,#42449,.F.) ;
#55495 = ORIENTED_EDGE('',*,*,#42308,.F.) ;
#55496 = ORIENTED_EDGE('',*,*,#42449,.T.) ;
#55497 = ORIENTED_EDGE('',*,*,#42286,.T.) ;
#55498 = ORIENTED_EDGE('',*,*,#42450,.F.) ;
#55499 = ORIENTED_EDGE('',*,*,#42451,.F.) ;
#55500 = ORIENTED_EDGE('',*,*,#42450,.T.) ;
#55501 = ORIENTED_EDGE('',*,*,#42293,.F.) ;
#55502 = ORIENTED_EDGE('',*,*,#42452,.F.) ;
#55503 = ORIENTED_EDGE('',*,*,#42324,.F.) ;
#55504 = ORIENTED_EDGE('',*,*,#42447,.T.) ;
#55505 = ORIENTED_EDGE('',*,*,#42325,.F.) ;
#55506 = ORIENTED_EDGE('',*,*,#42453,.F.) ;
#55507 = ORIENTED_EDGE('',*,*,#42284,.F.) ;
#55508 = ORIENTED_EDGE('',*,*,#42448,.T.) ;
#55509 = ORIENTED_EDGE('',*,*,#42283,.F.) ;
#55510 = ORIENTED_EDGE('',*,*,#42454,.F.) ;
#55511 = ORIENTED_EDGE('',*,*,#41825,.F.) ;
#55512 = ORIENTED_EDGE('',*,*,#42446,.T.) ;
#55513 = ORIENTED_EDGE('',*,*,#41823,.F.) ;
#55514 = ORIENTED_EDGE('',*,*,#42455,.F.) ;
#55515 = ORIENTED_EDGE('',*,*,#42320,.F.) ;
#55516 = ORIENTED_EDGE('',*,*,#42451,.T.) ;
#55517 = ORIENTED_EDGE('',*,*,#42323,.F.) ;
#55518 = ORIENTED_EDGE('',*,*,#42456,.F.) ;
#55519 = ORIENTED_EDGE('',*,*,#42309,.F.) ;
#55520 = ORIENTED_EDGE('',*,*,#42300,.F.) ;
#55521 = ORIENTED_EDGE('',*,*,#42310,.F.) ;
#55522 = ORIENTED_EDGE('',*,*,#42457,.F.) ;
#55523 = ORIENTED_EDGE('',*,*,#42303,.F.) ;
#55524 = ORIENTED_EDGE('',*,*,#42453,.T.) ;
#55525 = ORIENTED_EDGE('',*,*,#42452,.T.) ;
#55526 = ORIENTED_EDGE('',*,*,#42458,.F.) ;
#55527 = ORIENTED_EDGE('',*,*,#41826,.T.) ;
#55528 = ORIENTED_EDGE('',*,*,#42454,.T.) ;
#55529 = ORIENTED_EDGE('',*,*,#42459,.F.) ;
#55530 = ORIENTED_EDGE('',*,*,#42460,.F.) ;
#55531 = ORIENTED_EDGE('',*,*,#42455,.T.) ;
#55532 = ORIENTED_EDGE('',*,*,#41830,.F.) ;
#55533 = ORIENTED_EDGE('',*,*,#42461,.F.) ;
#55534 = ORIENTED_EDGE('',*,*,#42462,.F.) ;
#55535 = ORIENTED_EDGE('',*,*,#42457,.T.) ;
#55536 = ORIENTED_EDGE('',*,*,#42456,.T.) ;
#55537 = ORIENTED_EDGE('',*,*,#42463,.F.) ;
#55538 = ORIENTED_EDGE('',*,*,#42304,.T.) ;
#55539 = ORIENTED_EDGE('',*,*,#42458,.T.) ;
#55540 = ORIENTED_EDGE('',*,*,#42292,.F.) ;
#55541 = ORIENTED_EDGE('',*,*,#42464,.F.) ;
#55542 = ORIENTED_EDGE('',*,*,#42285,.F.) ;
#55543 = ORIENTED_EDGE('',*,*,#42459,.T.) ;
#55544 = ORIENTED_EDGE('',*,*,#42282,.F.) ;
#55545 = ORIENTED_EDGE('',*,*,#42465,.F.) ;
#55546 = ORIENTED_EDGE('',*,*,#42318,.F.) ;
#55547 = ORIENTED_EDGE('',*,*,#42460,.T.) ;
#55548 = ORIENTED_EDGE('',*,*,#42317,.F.) ;
#55549 = ORIENTED_EDGE('',*,*,#42466,.F.) ;
#55550 = ORIENTED_EDGE('',*,*,#41827,.F.) ;
#55551 = ORIENTED_EDGE('',*,*,#42461,.T.) ;
#55552 = ORIENTED_EDGE('',*,*,#41829,.F.) ;
#55553 = ORIENTED_EDGE('',*,*,#42467,.F.) ;
#55554 = ORIENTED_EDGE('',*,*,#42279,.F.) ;
#55555 = ORIENTED_EDGE('',*,*,#42462,.T.) ;
#55556 = ORIENTED_EDGE('',*,*,#42278,.F.) ;
#55557 = ORIENTED_EDGE('',*,*,#42468,.F.) ;
#55558 = ORIENTED_EDGE('',*,*,#42321,.F.) ;
#55559 = ORIENTED_EDGE('',*,*,#42463,.T.) ;
#55560 = ORIENTED_EDGE('',*,*,#42322,.F.) ;
#55561 = ORIENTED_EDGE('',*,*,#42469,.F.) ;
#55562 = ORIENTED_EDGE('',*,*,#42305,.F.) ;
#55563 = ORIENTED_EDGE('',*,*,#42465,.T.) ;
#55564 = ORIENTED_EDGE('',*,*,#42464,.T.) ;
#55565 = ORIENTED_EDGE('',*,*,#42470,.F.) ;
#55566 = ORIENTED_EDGE('',*,*,#41828,.T.) ;
#55567 = ORIENTED_EDGE('',*,*,#42466,.T.) ;
#55568 = ORIENTED_EDGE('',*,*,#42471,.F.) ;
#55569 = ORIENTED_EDGE('',*,*,#42467,.T.) ;
#55570 = ORIENTED_EDGE('',*,*,#42469,.T.) ;
#55571 = ORIENTED_EDGE('',*,*,#42468,.T.) ;
#55572 = ORIENTED_EDGE('',*,*,#42472,.F.) ;
#55573 = ORIENTED_EDGE('',*,*,#42297,.F.) ;
#55574 = ORIENTED_EDGE('',*,*,#42313,.F.) ;
#55575 = ORIENTED_EDGE('',*,*,#42473,.F.) ;
#55576 = ORIENTED_EDGE('',*,*,#42289,.F.) ;
#55577 = ORIENTED_EDGE('',*,*,#42470,.T.) ;
#55578 = ORIENTED_EDGE('',*,*,#42291,.F.) ;
#55579 = ORIENTED_EDGE('',*,*,#42474,.F.) ;
#55580 = ORIENTED_EDGE('',*,*,#42319,.F.) ;
#55581 = ORIENTED_EDGE('',*,*,#42471,.T.) ;
#55582 = ORIENTED_EDGE('',*,*,#42316,.F.) ;
#55583 = ORIENTED_EDGE('',*,*,#42475,.F.) ;
#55584 = ORIENTED_EDGE('',*,*,#42280,.F.) ;
#55585 = ORIENTED_EDGE('',*,*,#42472,.T.) ;
#55586 = ORIENTED_EDGE('',*,*,#42281,.F.) ;
#55587 = ORIENTED_EDGE('',*,*,#42476,.F.) ;
#55588 = ORIENTED_EDGE('',*,*,#42306,.F.) ;
#55589 = ORIENTED_EDGE('',*,*,#42290,.T.) ;
#55590 = ORIENTED_EDGE('',*,*,#42473,.T.) ;
#55591 = ORIENTED_EDGE('',*,*,#42477,.F.) ;
#55592 = ORIENTED_EDGE('',*,*,#42474,.T.) ;
#55593 = ORIENTED_EDGE('',*,*,#42476,.T.) ;
#55594 = ORIENTED_EDGE('',*,*,#42475,.T.) ;
#55595 = ORIENTED_EDGE('',*,*,#42478,.F.) ;
#55596 = ORIENTED_EDGE('',*,*,#42477,.T.) ;
#55597 = ORIENTED_EDGE('',*,*,#42312,.F.) ;
#55598 = ORIENTED_EDGE('',*,*,#42479,.F.) ;
#55599 = ORIENTED_EDGE('',*,*,#42314,.F.) ;
#55600 = ORIENTED_EDGE('',*,*,#42478,.T.) ;
#55601 = ORIENTED_EDGE('',*,*,#42315,.F.) ;
#55602 = ORIENTED_EDGE('',*,*,#42480,.F.) ;
#55603 = ORIENTED_EDGE('',*,*,#42307,.F.) ;
#55604 = ORIENTED_EDGE('',*,*,#42480,.T.) ;
#55605 = ORIENTED_EDGE('',*,*,#42479,.T.) ;
#55606 = ORIENTED_EDGE('',*,*,#42481,.F.) ;
#55607 = ORIENTED_EDGE('',*,*,#42301,.T.) ;
#55608 = ORIENTED_EDGE('',*,*,#42295,.F.) ;
#55609 = ORIENTED_EDGE('',*,*,#42302,.F.) ;
#55610 = ORIENTED_EDGE('',*,*,#42481,.T.) ;
#55611 = ORIENTED_EDGE('',*,*,#42311,.F.) ;
#55612 = ORIENTED_EDGE('',*,*,#41619,.F.) ;
#55613 = ORIENTED_EDGE('',*,*,#41757,.F.) ;
#55614 = ORIENTED_EDGE('',*,*,#42275,.F.) ;
#55615 = ORIENTED_EDGE('',*,*,#42267,.F.) ;
#55616 = ORIENTED_EDGE('',*,*,#42266,.F.) ;
#55617 = ORIENTED_EDGE('',*,*,#42482,.T.) ;
#55618 = ORIENTED_EDGE('',*,*,#42483,.T.) ;
#55619 = ORIENTED_EDGE('',*,*,#41595,.T.) ;
#55620 = ORIENTED_EDGE('',*,*,#42425,.F.) ;
#55621 = ORIENTED_EDGE('',*,*,#41620,.T.) ;
#55622 = ORIENTED_EDGE('',*,*,#42427,.F.) ;
#55623 = ORIENTED_EDGE('',*,*,#42484,.T.) ;
#55624 = ORIENTED_EDGE('',*,*,#42431,.F.) ;
#55625 = ORIENTED_EDGE('',*,*,#42485,.F.) ;
#55626 = ORIENTED_EDGE('',*,*,#41618,.T.) ;
#55627 = ORIENTED_EDGE('',*,*,#42428,.F.) ;
#55628 = ORIENTED_EDGE('',*,*,#42486,.F.) ;
#55629 = ORIENTED_EDGE('',*,*,#41758,.F.) ;
#55630 = ORIENTED_EDGE('',*,*,#41777,.F.) ;
#55631 = ORIENTED_EDGE('',*,*,#42487,.T.) ;
#55632 = ORIENTED_EDGE('',*,*,#42435,.F.) ;
#55633 = ORIENTED_EDGE('',*,*,#42488,.T.) ;
#55634 = ORIENTED_EDGE('',*,*,#42438,.F.) ;
#55635 = ORIENTED_EDGE('',*,*,#42489,.T.) ;
#55636 = ORIENTED_EDGE('',*,*,#42429,.F.) ;
#55637 = ORIENTED_EDGE('',*,*,#42490,.T.) ;
#55638 = ORIENTED_EDGE('',*,*,#42486,.T.) ;
#55639 = ORIENTED_EDGE('',*,*,#42485,.T.) ;
#55640 = ORIENTED_EDGE('',*,*,#42491,.F.) ;
#55641 = ORIENTED_EDGE('',*,*,#41759,.T.) ;
#55642 = ORIENTED_EDGE('',*,*,#42492,.T.) ;
#55643 = ORIENTED_EDGE('',*,*,#42493,.T.) ;
#55644 = ORIENTED_EDGE('',*,*,#41740,.F.) ;
#55645 = ORIENTED_EDGE('',*,*,#41612,.F.) ;
#55646 = ORIENTED_EDGE('',*,*,#42433,.F.) ;
#55647 = ORIENTED_EDGE('',*,*,#42494,.T.) ;
#55648 = ORIENTED_EDGE('',*,*,#42491,.T.) ;
#55649 = ORIENTED_EDGE('',*,*,#42430,.F.) ;
#55650 = ORIENTED_EDGE('',*,*,#41611,.F.) ;
#55651 = ORIENTED_EDGE('',*,*,#41760,.F.) ;
#55652 = ORIENTED_EDGE('',*,*,#41614,.T.) ;
#55653 = ORIENTED_EDGE('',*,*,#41761,.F.) ;
#55654 = ORIENTED_EDGE('',*,*,#41609,.T.) ;
#55655 = ORIENTED_EDGE('',*,*,#42434,.F.) ;
#55656 = ORIENTED_EDGE('',*,*,#42495,.F.) ;
#55657 = ORIENTED_EDGE('',*,*,#42410,.F.) ;
#55658 = ORIENTED_EDGE('',*,*,#42496,.F.) ;
#55659 = ORIENTED_EDGE('',*,*,#42496,.T.) ;
#55660 = ORIENTED_EDGE('',*,*,#42408,.F.) ;
#55661 = ORIENTED_EDGE('',*,*,#42497,.F.) ;
#55662 = ORIENTED_EDGE('',*,*,#42421,.F.) ;
#55663 = ORIENTED_EDGE('',*,*,#42495,.T.) ;
#55664 = ORIENTED_EDGE('',*,*,#42424,.F.) ;
#55665 = ORIENTED_EDGE('',*,*,#42498,.F.) ;
#55666 = ORIENTED_EDGE('',*,*,#42412,.F.) ;
#55667 = ORIENTED_EDGE('',*,*,#42497,.T.) ;
#55668 = ORIENTED_EDGE('',*,*,#42406,.F.) ;
#55669 = ORIENTED_EDGE('',*,*,#42499,.F.) ;
#55670 = ORIENTED_EDGE('',*,*,#42414,.F.) ;
#55671 = ORIENTED_EDGE('',*,*,#42498,.T.) ;
#55672 = ORIENTED_EDGE('',*,*,#42500,.F.) ;
#55673 = ORIENTED_EDGE('',*,*,#42499,.T.) ;
#55674 = ORIENTED_EDGE('',*,*,#42420,.F.) ;
#55675 = ORIENTED_EDGE('',*,*,#42501,.F.) ;
#55676 = ORIENTED_EDGE('',*,*,#42422,.F.) ;
#55677 = ORIENTED_EDGE('',*,*,#42500,.T.) ;
#55678 = ORIENTED_EDGE('',*,*,#42423,.F.) ;
#55679 = ORIENTED_EDGE('',*,*,#42502,.F.) ;
#55680 = ORIENTED_EDGE('',*,*,#42416,.F.) ;
#55681 = ORIENTED_EDGE('',*,*,#42501,.T.) ;
#55682 = ORIENTED_EDGE('',*,*,#42418,.F.) ;
#55683 = ORIENTED_EDGE('',*,*,#42502,.T.) ;
#55684 = ORIENTED_EDGE('',*,*,#42503,.F.) ;
#55685 = ORIENTED_EDGE('',*,*,#41848,.F.) ;
#55686 = ORIENTED_EDGE('',*,*,#42504,.F.) ;
#55687 = ORIENTED_EDGE('',*,*,#42329,.F.) ;
#55688 = ORIENTED_EDGE('',*,*,#42504,.T.) ;
#55689 = ORIENTED_EDGE('',*,*,#41847,.T.) ;
#55690 = ORIENTED_EDGE('',*,*,#42505,.F.) ;
#55691 = ORIENTED_EDGE('',*,*,#42506,.F.) ;
#55692 = ORIENTED_EDGE('',*,*,#41849,.T.) ;
#55693 = ORIENTED_EDGE('',*,*,#42503,.T.) ;
#55694 = ORIENTED_EDGE('',*,*,#42507,.F.) ;
#55695 = ORIENTED_EDGE('',*,*,#42508,.F.) ;
#55696 = ORIENTED_EDGE('',*,*,#42505,.T.) ;
#55697 = ORIENTED_EDGE('',*,*,#41846,.F.) ;
#55698 = ORIENTED_EDGE('',*,*,#42509,.F.) ;
#55699 = ORIENTED_EDGE('',*,*,#42341,.F.) ;
#55700 = ORIENTED_EDGE('',*,*,#42506,.T.) ;
#55701 = ORIENTED_EDGE('',*,*,#42340,.F.) ;
#55702 = ORIENTED_EDGE('',*,*,#42510,.F.) ;
#55703 = ORIENTED_EDGE('',*,*,#42326,.F.) ;
#55704 = ORIENTED_EDGE('',*,*,#42511,.F.) ;
#55705 = ORIENTED_EDGE('',*,*,#42327,.F.) ;
#55706 = ORIENTED_EDGE('',*,*,#42512,.F.) ;
#55707 = ORIENTED_EDGE('',*,*,#42345,.F.) ;
#55708 = ORIENTED_EDGE('',*,*,#42507,.T.) ;
#55709 = ORIENTED_EDGE('',*,*,#42328,.F.) ;
#55710 = ORIENTED_EDGE('',*,*,#42513,.F.) ;
#55711 = ORIENTED_EDGE('',*,*,#42333,.F.) ;
#55712 = ORIENTED_EDGE('',*,*,#42508,.T.) ;
#55713 = ORIENTED_EDGE('',*,*,#42332,.F.) ;
#55714 = ORIENTED_EDGE('',*,*,#42514,.F.) ;
#55715 = ORIENTED_EDGE('',*,*,#41850,.F.) ;
#55716 = ORIENTED_EDGE('',*,*,#42515,.F.) ;
#55717 = ORIENTED_EDGE('',*,*,#41844,.F.) ;
#55718 = ORIENTED_EDGE('',*,*,#42516,.F.) ;
#55719 = ORIENTED_EDGE('',*,*,#42336,.F.) ;
#55720 = ORIENTED_EDGE('',*,*,#41845,.T.) ;
#55721 = ORIENTED_EDGE('',*,*,#42515,.T.) ;
#55722 = ORIENTED_EDGE('',*,*,#42517,.F.) ;
#55723 = ORIENTED_EDGE('',*,*,#42509,.T.) ;
#55724 = ORIENTED_EDGE('',*,*,#42512,.T.) ;
#55725 = ORIENTED_EDGE('',*,*,#42510,.T.) ;
#55726 = ORIENTED_EDGE('',*,*,#42518,.F.) ;
#55727 = ORIENTED_EDGE('',*,*,#42513,.T.) ;
#55728 = ORIENTED_EDGE('',*,*,#42511,.T.) ;
#55729 = ORIENTED_EDGE('',*,*,#42519,.F.) ;
#55730 = ORIENTED_EDGE('',*,*,#41843,.T.) ;
#55731 = ORIENTED_EDGE('',*,*,#42514,.T.) ;
#55732 = ORIENTED_EDGE('',*,*,#42520,.F.) ;
#55733 = ORIENTED_EDGE('',*,*,#42516,.T.) ;
#55734 = ORIENTED_EDGE('',*,*,#42517,.T.) ;
#55735 = ORIENTED_EDGE('',*,*,#42335,.F.) ;
#55736 = ORIENTED_EDGE('',*,*,#42521,.F.) ;
#55737 = ORIENTED_EDGE('',*,*,#42338,.F.) ;
#55738 = ORIENTED_EDGE('',*,*,#42518,.T.) ;
#55739 = ORIENTED_EDGE('',*,*,#42339,.F.) ;
#55740 = ORIENTED_EDGE('',*,*,#42522,.F.) ;
#55741 = ORIENTED_EDGE('',*,*,#42342,.F.) ;
#55742 = ORIENTED_EDGE('',*,*,#42519,.T.) ;
#55743 = ORIENTED_EDGE('',*,*,#42344,.F.) ;
#55744 = ORIENTED_EDGE('',*,*,#42523,.F.) ;
#55745 = ORIENTED_EDGE('',*,*,#42330,.F.) ;
#55746 = ORIENTED_EDGE('',*,*,#42520,.T.) ;
#55747 = ORIENTED_EDGE('',*,*,#42331,.F.) ;
#55748 = ORIENTED_EDGE('',*,*,#42524,.F.) ;
#55749 = ORIENTED_EDGE('',*,*,#42337,.F.) ;
#55750 = ORIENTED_EDGE('',*,*,#42522,.T.) ;
#55751 = ORIENTED_EDGE('',*,*,#42521,.T.) ;
#55752 = ORIENTED_EDGE('',*,*,#42525,.F.) ;
#55753 = ORIENTED_EDGE('',*,*,#42524,.T.) ;
#55754 = ORIENTED_EDGE('',*,*,#42523,.T.) ;
#55755 = ORIENTED_EDGE('',*,*,#42526,.F.) ;
#55756 = ORIENTED_EDGE('',*,*,#42525,.T.) ;
#55757 = ORIENTED_EDGE('',*,*,#42334,.F.) ;
#55758 = ORIENTED_EDGE('',*,*,#42526,.T.) ;
#55759 = ORIENTED_EDGE('',*,*,#42343,.F.) ;
#55760 = ORIENTED_EDGE('',*,*,#42527,.F.) ;
#55761 = ORIENTED_EDGE('',*,*,#41798,.F.) ;
#55762 = ORIENTED_EDGE('',*,*,#42528,.F.) ;
#55763 = ORIENTED_EDGE('',*,*,#42388,.F.) ;
#55764 = ORIENTED_EDGE('',*,*,#42528,.T.) ;
#55765 = ORIENTED_EDGE('',*,*,#41797,.T.) ;
#55766 = ORIENTED_EDGE('',*,*,#42529,.F.) ;
#55767 = ORIENTED_EDGE('',*,*,#42530,.F.) ;
#55768 = ORIENTED_EDGE('',*,*,#41799,.T.) ;
#55769 = ORIENTED_EDGE('',*,*,#42527,.T.) ;
#55770 = ORIENTED_EDGE('',*,*,#42531,.F.) ;
#55771 = ORIENTED_EDGE('',*,*,#42532,.F.) ;
#55772 = ORIENTED_EDGE('',*,*,#42529,.T.) ;
#55773 = ORIENTED_EDGE('',*,*,#41796,.F.) ;
#55774 = ORIENTED_EDGE('',*,*,#42533,.F.) ;
#55775 = ORIENTED_EDGE('',*,*,#42384,.F.) ;
#55776 = ORIENTED_EDGE('',*,*,#42530,.T.) ;
#55777 = ORIENTED_EDGE('',*,*,#42383,.F.) ;
#55778 = ORIENTED_EDGE('',*,*,#42534,.F.) ;
#55779 = ORIENTED_EDGE('',*,*,#42385,.F.) ;
#55780 = ORIENTED_EDGE('',*,*,#42535,.F.) ;
#55781 = ORIENTED_EDGE('',*,*,#42386,.F.) ;
#55782 = ORIENTED_EDGE('',*,*,#42536,.F.) ;
#55783 = ORIENTED_EDGE('',*,*,#42396,.F.) ;
#55784 = ORIENTED_EDGE('',*,*,#42531,.T.) ;
#55785 = ORIENTED_EDGE('',*,*,#42387,.F.) ;
#55786 = ORIENTED_EDGE('',*,*,#42537,.F.) ;
#55787 = ORIENTED_EDGE('',*,*,#42392,.F.) ;
#55788 = ORIENTED_EDGE('',*,*,#42532,.T.) ;
#55789 = ORIENTED_EDGE('',*,*,#42391,.F.) ;
#55790 = ORIENTED_EDGE('',*,*,#42538,.F.) ;
#55791 = ORIENTED_EDGE('',*,*,#41800,.F.) ;
#55792 = ORIENTED_EDGE('',*,*,#42539,.F.) ;
#55793 = ORIENTED_EDGE('',*,*,#41794,.F.) ;
#55794 = ORIENTED_EDGE('',*,*,#42540,.F.) ;
#55795 = ORIENTED_EDGE('',*,*,#42379,.F.) ;
#55796 = ORIENTED_EDGE('',*,*,#41795,.T.) ;
#55797 = ORIENTED_EDGE('',*,*,#42539,.T.) ;
#55798 = ORIENTED_EDGE('',*,*,#42541,.F.) ;
#55799 = ORIENTED_EDGE('',*,*,#42533,.T.) ;
#55800 = ORIENTED_EDGE('',*,*,#42536,.T.) ;
#55801 = ORIENTED_EDGE('',*,*,#42534,.T.) ;
#55802 = ORIENTED_EDGE('',*,*,#42542,.F.) ;
#55803 = ORIENTED_EDGE('',*,*,#42537,.T.) ;
#55804 = ORIENTED_EDGE('',*,*,#42535,.T.) ;
#55805 = ORIENTED_EDGE('',*,*,#42543,.F.) ;
#55806 = ORIENTED_EDGE('',*,*,#41793,.T.) ;
#55807 = ORIENTED_EDGE('',*,*,#42538,.T.) ;
#55808 = ORIENTED_EDGE('',*,*,#42544,.F.) ;
#55809 = ORIENTED_EDGE('',*,*,#42540,.T.) ;
#55810 = ORIENTED_EDGE('',*,*,#42541,.T.) ;
#55811 = ORIENTED_EDGE('',*,*,#42378,.F.) ;
#55812 = ORIENTED_EDGE('',*,*,#42545,.F.) ;
#55813 = ORIENTED_EDGE('',*,*,#42381,.F.) ;
#55814 = ORIENTED_EDGE('',*,*,#42542,.T.) ;
#55815 = ORIENTED_EDGE('',*,*,#42382,.F.) ;
#55816 = ORIENTED_EDGE('',*,*,#42546,.F.) ;
#55817 = ORIENTED_EDGE('',*,*,#42393,.F.) ;
#55818 = ORIENTED_EDGE('',*,*,#42543,.T.) ;
#55819 = ORIENTED_EDGE('',*,*,#42395,.F.) ;
#55820 = ORIENTED_EDGE('',*,*,#42547,.F.) ;
#55821 = ORIENTED_EDGE('',*,*,#42389,.F.) ;
#55822 = ORIENTED_EDGE('',*,*,#42544,.T.) ;
#55823 = ORIENTED_EDGE('',*,*,#42390,.F.) ;
#55824 = ORIENTED_EDGE('',*,*,#42548,.F.) ;
#55825 = ORIENTED_EDGE('',*,*,#42380,.F.) ;
#55826 = ORIENTED_EDGE('',*,*,#42546,.T.) ;
#55827 = ORIENTED_EDGE('',*,*,#42545,.T.) ;
#55828 = ORIENTED_EDGE('',*,*,#42549,.F.) ;
#55829 = ORIENTED_EDGE('',*,*,#42548,.T.) ;
#55830 = ORIENTED_EDGE('',*,*,#42547,.T.) ;
#55831 = ORIENTED_EDGE('',*,*,#42550,.F.) ;
#55832 = ORIENTED_EDGE('',*,*,#42549,.T.) ;
#55833 = ORIENTED_EDGE('',*,*,#42377,.F.) ;
#55834 = ORIENTED_EDGE('',*,*,#42550,.T.) ;
#55835 = ORIENTED_EDGE('',*,*,#42394,.F.) ;
#55836 = ORIENTED_EDGE('',*,*,#41733,.F.) ;
#55837 = ORIENTED_EDGE('',*,*,#42551,.T.) ;
#55838 = ORIENTED_EDGE('',*,*,#42440,.F.) ;
#55839 = ORIENTED_EDGE('',*,*,#42552,.F.) ;
#55840 = ORIENTED_EDGE('',*,*,#42184,.T.) ;
#55841 = ORIENTED_EDGE('',*,*,#42552,.T.) ;
#55842 = ORIENTED_EDGE('',*,*,#42553,.F.) ;
#55843 = ORIENTED_EDGE('',*,*,#42553,.T.) ;
#55844 = ORIENTED_EDGE('',*,*,#42445,.F.) ;
#55845 = ORIENTED_EDGE('',*,*,#42554,.F.) ;
#55846 = ORIENTED_EDGE('',*,*,#41883,.F.) ;
#55847 = ORIENTED_EDGE('',*,*,#42180,.T.) ;
#55848 = ORIENTED_EDGE('',*,*,#42554,.T.) ;
#55849 = ORIENTED_EDGE('',*,*,#42555,.F.) ;
#55850 = ORIENTED_EDGE('',*,*,#41752,.T.) ;
#55851 = ORIENTED_EDGE('',*,*,#42555,.T.) ;
#55852 = ORIENTED_EDGE('',*,*,#42444,.F.) ;
#55853 = ORIENTED_EDGE('',*,*,#42556,.F.) ;
#55854 = ORIENTED_EDGE('',*,*,#41753,.F.) ;
#55855 = ORIENTED_EDGE('',*,*,#42276,.F.) ;
#55856 = ORIENTED_EDGE('',*,*,#41755,.F.) ;
#55857 = ORIENTED_EDGE('',*,*,#42557,.F.) ;
#55858 = ORIENTED_EDGE('',*,*,#42272,.F.) ;
#55859 = ORIENTED_EDGE('',*,*,#41754,.T.) ;
#55860 = ORIENTED_EDGE('',*,*,#42556,.T.) ;
#55861 = ORIENTED_EDGE('',*,*,#42558,.F.) ;
#55862 = ORIENTED_EDGE('',*,*,#42557,.T.) ;
#55863 = ORIENTED_EDGE('',*,*,#42558,.T.) ;
#55864 = ORIENTED_EDGE('',*,*,#42443,.F.) ;
#55865 = ORIENTED_EDGE('',*,*,#42559,.F.) ;
#55866 = ORIENTED_EDGE('',*,*,#42269,.F.) ;
#55867 = ORIENTED_EDGE('',*,*,#42277,.F.) ;
#55868 = ORIENTED_EDGE('',*,*,#42270,.F.) ;
#55869 = ORIENTED_EDGE('',*,*,#42560,.F.) ;
#55870 = ORIENTED_EDGE('',*,*,#42263,.F.) ;
#55871 = ORIENTED_EDGE('',*,*,#42560,.T.) ;
#55872 = ORIENTED_EDGE('',*,*,#42559,.T.) ;
#55873 = ORIENTED_EDGE('',*,*,#42561,.F.) ;
#55874 = ORIENTED_EDGE('',*,*,#42442,.F.) ;
#55875 = ORIENTED_EDGE('',*,*,#42562,.T.) ;
#55876 = ORIENTED_EDGE('',*,*,#42260,.F.) ;
#55877 = ORIENTED_EDGE('',*,*,#42561,.T.) ;
#55878 = ORIENTED_EDGE('',*,*,#41627,.F.) ;
#55879 = ORIENTED_EDGE('',*,*,#42373,.F.) ;
#55880 = ORIENTED_EDGE('',*,*,#41637,.F.) ;
#55881 = ORIENTED_EDGE('',*,*,#42375,.F.) ;
#55882 = ORIENTED_EDGE('',*,*,#41635,.F.) ;
#55883 = ORIENTED_EDGE('',*,*,#42371,.F.) ;
#55884 = ORIENTED_EDGE('',*,*,#41629,.F.) ;
#55885 = ORIENTED_EDGE('',*,*,#42376,.F.) ;
#55886 = ORIENTED_EDGE('',*,*,#41625,.F.) ;
#55887 = ORIENTED_EDGE('',*,*,#42268,.F.) ;
#55888 = ORIENTED_EDGE('',*,*,#41639,.F.) ;
#55889 = ORIENTED_EDGE('',*,*,#42374,.F.) ;
#55890 = ORIENTED_EDGE('',*,*,#41633,.F.) ;
#55891 = ORIENTED_EDGE('',*,*,#42370,.F.) ;
#55892 = ORIENTED_EDGE('',*,*,#41631,.F.) ;
#55893 = ORIENTED_EDGE('',*,*,#42372,.F.) ;
#55894 = ORIENTED_EDGE('',*,*,#42563,.F.) ;
#55895 = ORIENTED_EDGE('',*,*,#41616,.F.) ;
#55896 = ORIENTED_EDGE('',*,*,#42489,.F.) ;
#55897 = ORIENTED_EDGE('',*,*,#42563,.T.) ;
#55898 = ORIENTED_EDGE('',*,*,#42437,.F.) ;
#55899 = ORIENTED_EDGE('',*,*,#42564,.F.) ;
#55900 = ORIENTED_EDGE('',*,*,#42432,.F.) ;
#55901 = ORIENTED_EDGE('',*,*,#42564,.T.) ;
#55902 = ORIENTED_EDGE('',*,*,#42436,.F.) ;
#55903 = ORIENTED_EDGE('',*,*,#42565,.F.) ;
#55904 = ORIENTED_EDGE('',*,*,#42494,.F.) ;
#55905 = ORIENTED_EDGE('',*,*,#42565,.T.) ;
#55906 = ORIENTED_EDGE('',*,*,#42487,.F.) ;
#55907 = ORIENTED_EDGE('',*,*,#42566,.F.) ;
#55908 = ORIENTED_EDGE('',*,*,#42492,.F.) ;
#55909 = ORIENTED_EDGE('',*,*,#42566,.T.) ;
#55910 = ORIENTED_EDGE('',*,*,#41776,.F.) ;
#55911 = ORIENTED_EDGE('',*,*,#42202,.F.) ;
#55912 = ORIENTED_EDGE('',*,*,#42493,.F.) ;
#55913 = ORIENTED_EDGE('',*,*,#42274,.F.) ;
#55914 = ORIENTED_EDGE('',*,*,#41779,.F.) ;
#55915 = ORIENTED_EDGE('',*,*,#42567,.F.) ;
#55916 = ORIENTED_EDGE('',*,*,#42265,.F.) ;
#55917 = ORIENTED_EDGE('',*,*,#42567,.T.) ;
#55918 = ORIENTED_EDGE('',*,*,#41778,.F.) ;
#55919 = ORIENTED_EDGE('',*,*,#42568,.F.) ;
#55920 = ORIENTED_EDGE('',*,*,#42482,.F.) ;
#55921 = ORIENTED_EDGE('',*,*,#42568,.T.) ;
#55922 = ORIENTED_EDGE('',*,*,#42488,.F.) ;
#55923 = ORIENTED_EDGE('',*,*,#41596,.F.) ;
#55924 = ORIENTED_EDGE('',*,*,#42483,.F.) ;
#55925 = ORIENTED_EDGE('',*,*,#42569,.F.) ;
#55926 = ORIENTED_EDGE('',*,*,#42426,.F.) ;
#55927 = ORIENTED_EDGE('',*,*,#41594,.T.) ;
#55928 = ORIENTED_EDGE('',*,*,#42439,.F.) ;
#55929 = ORIENTED_EDGE('',*,*,#42490,.F.) ;
#55930 = ORIENTED_EDGE('',*,*,#42484,.F.) ;
#55931 = ORIENTED_EDGE('',*,*,#42569,.T.) ;
#55932 = ORIENTED_EDGE('',*,*,#42570,.T.) ;
#55933 = ORIENTED_EDGE('',*,*,#42571,.T.) ;
#55934 = ORIENTED_EDGE('',*,*,#42441,.F.) ;
#55935 = ORIENTED_EDGE('',*,*,#42572,.T.) ;
#55936 = ORIENTED_EDGE('',*,*,#42573,.T.) ;
#55937 = ORIENTED_EDGE('',*,*,#41875,.F.) ;
#55938 = ORIENTED_EDGE('',*,*,#42574,.T.) ;
#55939 = ORIENTED_EDGE('',*,*,#42551,.F.) ;
#55940 = ORIENTED_EDGE('',*,*,#42212,.T.) ;
#55941 = ORIENTED_EDGE('',*,*,#42273,.F.) ;
#55942 = ORIENTED_EDGE('',*,*,#42261,.F.) ;
#55943 = ORIENTED_EDGE('',*,*,#42575,.F.) ;
#55944 = ORIENTED_EDGE('',*,*,#41871,.F.) ;
#55945 = ORIENTED_EDGE('',*,*,#42562,.F.) ;
#55946 = ORIENTED_EDGE('',*,*,#42576,.T.) ;
#55947 = ORIENTED_EDGE('',*,*,#41872,.F.) ;
#55948 = ORIENTED_EDGE('',*,*,#42575,.T.) ;
#55949 = ORIENTED_EDGE('',*,*,#42572,.F.) ;
#55950 = ORIENTED_EDGE('',*,*,#42574,.F.) ;
#55951 = ORIENTED_EDGE('',*,*,#42577,.F.) ;
#55952 = ORIENTED_EDGE('',*,*,#42578,.F.) ;
#55953 = ORIENTED_EDGE('',*,*,#42573,.F.) ;
#55954 = ORIENTED_EDGE('',*,*,#42577,.T.) ;
#55955 = ORIENTED_EDGE('',*,*,#41874,.F.) ;
#55956 = ORIENTED_EDGE('',*,*,#42578,.T.) ;
#55957 = ORIENTED_EDGE('',*,*,#41873,.F.) ;
#55958 = ORIENTED_EDGE('',*,*,#42579,.F.) ;
#55959 = ORIENTED_EDGE('',*,*,#42570,.F.) ;
#55960 = ORIENTED_EDGE('',*,*,#42579,.T.) ;
#55961 = ORIENTED_EDGE('',*,*,#42576,.F.) ;
#55962 = ORIENTED_EDGE('',*,*,#42571,.F.) ;
#55963 = ORIENTED_EDGE('',*,*,#42580,.F.) ;
#55964 = ORIENTED_EDGE('',*,*,#42230,.F.) ;
#55965 = ORIENTED_EDGE('',*,*,#42581,.F.) ;
#55966 = ORIENTED_EDGE('',*,*,#42582,.F.) ;
#55967 = ORIENTED_EDGE('',*,*,#42228,.F.) ;
#55968 = ORIENTED_EDGE('',*,*,#42583,.F.) ;
#55969 = ORIENTED_EDGE('',*,*,#42581,.T.) ;
#55970 = ORIENTED_EDGE('',*,*,#42233,.F.) ;
#55971 = ORIENTED_EDGE('',*,*,#42584,.F.) ;
#55972 = ORIENTED_EDGE('',*,*,#42251,.F.) ;
#55973 = ORIENTED_EDGE('',*,*,#42580,.T.) ;
#55974 = ORIENTED_EDGE('',*,*,#42250,.F.) ;
#55975 = ORIENTED_EDGE('',*,*,#42585,.F.) ;
#55976 = ORIENTED_EDGE('',*,*,#42227,.F.) ;
#55977 = ORIENTED_EDGE('',*,*,#42583,.T.) ;
#55978 = ORIENTED_EDGE('',*,*,#42225,.F.) ;
#55979 = ORIENTED_EDGE('',*,*,#42586,.F.) ;
#55980 = ORIENTED_EDGE('',*,*,#42253,.F.) ;
#55981 = ORIENTED_EDGE('',*,*,#42582,.T.) ;
#55982 = ORIENTED_EDGE('',*,*,#42259,.F.) ;
#55983 = ORIENTED_EDGE('',*,*,#42587,.F.) ;
#55984 = ORIENTED_EDGE('',*,*,#42231,.F.) ;
#55985 = ORIENTED_EDGE('',*,*,#42584,.T.) ;
#55986 = ORIENTED_EDGE('',*,*,#42236,.F.) ;
#55987 = ORIENTED_EDGE('',*,*,#42588,.F.) ;
#55988 = ORIENTED_EDGE('',*,*,#42224,.F.) ;
#55989 = ORIENTED_EDGE('',*,*,#42585,.T.) ;
#55990 = ORIENTED_EDGE('',*,*,#42589,.F.) ;
#55991 = ORIENTED_EDGE('',*,*,#42586,.T.) ;
#55992 = ORIENTED_EDGE('',*,*,#42222,.F.) ;
#55993 = ORIENTED_EDGE('',*,*,#42590,.F.) ;
#55994 = ORIENTED_EDGE('',*,*,#42234,.F.) ;
#55995 = ORIENTED_EDGE('',*,*,#42587,.T.) ;
#55996 = ORIENTED_EDGE('',*,*,#42591,.F.) ;
#55997 = ORIENTED_EDGE('',*,*,#42588,.T.) ;
#55998 = ORIENTED_EDGE('',*,*,#42239,.F.) ;
#55999 = ORIENTED_EDGE('',*,*,#42592,.F.) ;
#56000 = ORIENTED_EDGE('',*,*,#42252,.F.) ;
#56001 = ORIENTED_EDGE('',*,*,#42589,.T.) ;
#56002 = ORIENTED_EDGE('',*,*,#42249,.F.) ;
#56003 = ORIENTED_EDGE('',*,*,#42593,.F.) ;
#56004 = ORIENTED_EDGE('',*,*,#42221,.F.) ;
#56005 = ORIENTED_EDGE('',*,*,#42594,.F.) ;
#56006 = ORIENTED_EDGE('',*,*,#42218,.F.) ;
#56007 = ORIENTED_EDGE('',*,*,#42595,.F.) ;
#56008 = ORIENTED_EDGE('',*,*,#41702,.F.) ;
#56009 = ORIENTED_EDGE('',*,*,#42590,.T.) ;
#56010 = ORIENTED_EDGE('',*,*,#42219,.F.) ;
#56011 = ORIENTED_EDGE('',*,*,#42596,.F.) ;
#56012 = ORIENTED_EDGE('',*,*,#42254,.F.) ;
#56013 = ORIENTED_EDGE('',*,*,#42591,.T.) ;
#56014 = ORIENTED_EDGE('',*,*,#42258,.F.) ;
#56015 = ORIENTED_EDGE('',*,*,#42597,.F.) ;
#56016 = ORIENTED_EDGE('',*,*,#42237,.F.) ;
#56017 = ORIENTED_EDGE('',*,*,#42592,.T.) ;
#56018 = ORIENTED_EDGE('',*,*,#42242,.F.) ;
#56019 = ORIENTED_EDGE('',*,*,#42598,.F.) ;
#56020 = ORIENTED_EDGE('',*,*,#42246,.F.) ;
#56021 = ORIENTED_EDGE('',*,*,#42595,.T.) ;
#56022 = ORIENTED_EDGE('',*,*,#42593,.T.) ;
#56023 = ORIENTED_EDGE('',*,*,#42599,.F.) ;
#56024 = ORIENTED_EDGE('',*,*,#41703,.T.) ;
#56025 = ORIENTED_EDGE('',*,*,#42594,.T.) ;
#56026 = ORIENTED_EDGE('',*,*,#41701,.T.) ;
#56027 = ORIENTED_EDGE('',*,*,#42600,.F.) ;
#56028 = ORIENTED_EDGE('',*,*,#42596,.T.) ;
#56029 = ORIENTED_EDGE('',*,*,#42597,.T.) ;
#56030 = ORIENTED_EDGE('',*,*,#42257,.F.) ;
#56031 = ORIENTED_EDGE('',*,*,#42601,.F.) ;
#56032 = ORIENTED_EDGE('',*,*,#42240,.F.) ;
#56033 = ORIENTED_EDGE('',*,*,#42598,.T.) ;
#56034 = ORIENTED_EDGE('',*,*,#42245,.F.) ;
#56035 = ORIENTED_EDGE('',*,*,#42602,.F.) ;
#56036 = ORIENTED_EDGE('',*,*,#42247,.F.) ;
#56037 = ORIENTED_EDGE('',*,*,#42599,.T.) ;
#56038 = ORIENTED_EDGE('',*,*,#42248,.F.) ;
#56039 = ORIENTED_EDGE('',*,*,#42603,.F.) ;
#56040 = ORIENTED_EDGE('',*,*,#41704,.F.) ;
#56041 = ORIENTED_EDGE('',*,*,#42600,.T.) ;
#56042 = ORIENTED_EDGE('',*,*,#41700,.F.) ;
#56043 = ORIENTED_EDGE('',*,*,#42604,.F.) ;
#56044 = ORIENTED_EDGE('',*,*,#42255,.F.) ;
#56045 = ORIENTED_EDGE('',*,*,#42601,.T.) ;
#56046 = ORIENTED_EDGE('',*,*,#42256,.F.) ;
#56047 = ORIENTED_EDGE('',*,*,#42605,.F.) ;
#56048 = ORIENTED_EDGE('',*,*,#42243,.F.) ;
#56049 = ORIENTED_EDGE('',*,*,#42603,.T.) ;
#56050 = ORIENTED_EDGE('',*,*,#42602,.T.) ;
#56051 = ORIENTED_EDGE('',*,*,#42606,.F.) ;
#56052 = ORIENTED_EDGE('',*,*,#41705,.T.) ;
#56053 = ORIENTED_EDGE('',*,*,#42604,.T.) ;
#56054 = ORIENTED_EDGE('',*,*,#41699,.T.) ;
#56055 = ORIENTED_EDGE('',*,*,#42607,.F.) ;
#56056 = ORIENTED_EDGE('',*,*,#42605,.T.) ;
#56057 = ORIENTED_EDGE('',*,*,#42606,.T.) ;
#56058 = ORIENTED_EDGE('',*,*,#42244,.F.) ;
#56059 = ORIENTED_EDGE('',*,*,#42607,.T.) ;
#56060 = ORIENTED_EDGE('',*,*,#41706,.F.) ;
#56061 = ORIENTED_EDGE('',*,*,#42608,.F.) ;
#56062 = ORIENTED_EDGE('',*,*,#42609,.F.) ;
#56063 = ORIENTED_EDGE('',*,*,#42610,.F.) ;
#56064 = ORIENTED_EDGE('',*,*,#42611,.T.) ;
#56065 = ORIENTED_EDGE('',*,*,#42612,.F.) ;
#56066 = ORIENTED_EDGE('',*,*,#42613,.T.) ;
#56067 = ORIENTED_EDGE('',*,*,#42614,.F.) ;
#56068 = ORIENTED_EDGE('',*,*,#42615,.F.) ;
#56069 = ORIENTED_EDGE('',*,*,#42613,.F.) ;
#56070 = ORIENTED_EDGE('',*,*,#42616,.F.) ;
#56071 = ORIENTED_EDGE('',*,*,#42617,.T.) ;
#56072 = ORIENTED_EDGE('',*,*,#42618,.F.) ;
#56073 = ORIENTED_EDGE('',*,*,#42617,.F.) ;
#56074 = ORIENTED_EDGE('',*,*,#42619,.F.) ;
#56075 = ORIENTED_EDGE('',*,*,#42620,.T.) ;
#56076 = ORIENTED_EDGE('',*,*,#42621,.F.) ;
#56077 = ORIENTED_EDGE('',*,*,#42622,.F.) ;
#56078 = ORIENTED_EDGE('',*,*,#42620,.F.) ;
#56079 = ORIENTED_EDGE('',*,*,#42623,.T.) ;
#56080 = ORIENTED_EDGE('',*,*,#42624,.F.) ;
#56081 = ORIENTED_EDGE('',*,*,#42625,.T.) ;
#56082 = ORIENTED_EDGE('',*,*,#42626,.T.) ;
#56083 = ORIENTED_EDGE('',*,*,#42627,.T.) ;
#56084 = ORIENTED_EDGE('',*,*,#42628,.T.) ;
#56085 = ORIENTED_EDGE('',*,*,#42629,.F.) ;
#56086 = ORIENTED_EDGE('',*,*,#42623,.F.) ;
#56087 = ORIENTED_EDGE('',*,*,#42630,.F.) ;
#56088 = ORIENTED_EDGE('',*,*,#42631,.T.) ;
#56089 = ORIENTED_EDGE('',*,*,#42632,.F.) ;
#56090 = ORIENTED_EDGE('',*,*,#42633,.F.) ;
#56091 = ORIENTED_EDGE('',*,*,#42634,.T.) ;
#56092 = ORIENTED_EDGE('',*,*,#42635,.F.) ;
#56093 = ORIENTED_EDGE('',*,*,#42636,.F.) ;
#56094 = ORIENTED_EDGE('',*,*,#42637,.T.) ;
#56095 = ORIENTED_EDGE('',*,*,#42616,.T.) ;
#56096 = ORIENTED_EDGE('',*,*,#42637,.F.) ;
#56097 = ORIENTED_EDGE('',*,*,#42618,.T.) ;
#56098 = ORIENTED_EDGE('',*,*,#42638,.T.) ;
#56099 = ORIENTED_EDGE('',*,*,#42621,.T.) ;
#56100 = ORIENTED_EDGE('',*,*,#42622,.T.) ;
#56101 = ORIENTED_EDGE('',*,*,#42638,.F.) ;
#56102 = ORIENTED_EDGE('',*,*,#42639,.F.) ;
#56103 = ORIENTED_EDGE('',*,*,#42640,.T.) ;
#56104 = ORIENTED_EDGE('',*,*,#42641,.F.) ;
#56105 = ORIENTED_EDGE('',*,*,#42642,.T.) ;
#56106 = ORIENTED_EDGE('',*,*,#42643,.F.) ;
#56107 = ORIENTED_EDGE('',*,*,#42644,.T.) ;
#56108 = ORIENTED_EDGE('',*,*,#42645,.T.) ;
#56109 = ORIENTED_EDGE('',*,*,#42646,.T.) ;
#56110 = ORIENTED_EDGE('',*,*,#42647,.F.) ;
#56111 = ORIENTED_EDGE('',*,*,#42648,.T.) ;
#56112 = ORIENTED_EDGE('',*,*,#42649,.F.) ;
#56113 = ORIENTED_EDGE('',*,*,#42650,.T.) ;
#56114 = ORIENTED_EDGE('',*,*,#42651,.F.) ;
#56115 = ORIENTED_EDGE('',*,*,#42652,.T.) ;
#56116 = ORIENTED_EDGE('',*,*,#42653,.T.) ;
#56117 = ORIENTED_EDGE('',*,*,#42654,.T.) ;
#56118 = ORIENTED_EDGE('',*,*,#42655,.F.) ;
#56119 = ORIENTED_EDGE('',*,*,#42656,.T.) ;
#56120 = ORIENTED_EDGE('',*,*,#42614,.T.) ;
#56121 = ORIENTED_EDGE('',*,*,#42615,.T.) ;
#56122 = ORIENTED_EDGE('',*,*,#42656,.F.) ;
#56123 = ORIENTED_EDGE('',*,*,#42657,.F.) ;
#56124 = ORIENTED_EDGE('',*,*,#42658,.F.) ;
#56125 = ORIENTED_EDGE('',*,*,#42659,.F.) ;
#56126 = ORIENTED_EDGE('',*,*,#42660,.T.) ;
#56127 = ORIENTED_EDGE('',*,*,#42661,.F.) ;
#56128 = ORIENTED_EDGE('',*,*,#42662,.F.) ;
#56129 = ORIENTED_EDGE('',*,*,#42663,.F.) ;
#56130 = ORIENTED_EDGE('',*,*,#42664,.F.) ;
#56131 = ORIENTED_EDGE('',*,*,#42665,.F.) ;
#56132 = ORIENTED_EDGE('',*,*,#42666,.T.) ;
#56133 = ORIENTED_EDGE('',*,*,#42667,.F.) ;
#56134 = ORIENTED_EDGE('',*,*,#42668,.F.) ;
#56135 = ORIENTED_EDGE('',*,*,#42666,.F.) ;
#56136 = ORIENTED_EDGE('',*,*,#42669,.F.) ;
#56137 = ORIENTED_EDGE('',*,*,#42670,.T.) ;
#56138 = ORIENTED_EDGE('',*,*,#42671,.F.) ;
#56139 = ORIENTED_EDGE('',*,*,#42670,.F.) ;
#56140 = ORIENTED_EDGE('',*,*,#42672,.F.) ;
#56141 = ORIENTED_EDGE('',*,*,#42673,.T.) ;
#56142 = ORIENTED_EDGE('',*,*,#42674,.F.) ;
#56143 = ORIENTED_EDGE('',*,*,#42675,.F.) ;
#56144 = ORIENTED_EDGE('',*,*,#42673,.F.) ;
#56145 = ORIENTED_EDGE('',*,*,#42676,.T.) ;
#56146 = ORIENTED_EDGE('',*,*,#42677,.F.) ;
#56147 = ORIENTED_EDGE('',*,*,#42678,.T.) ;
#56148 = ORIENTED_EDGE('',*,*,#42679,.T.) ;
#56149 = ORIENTED_EDGE('',*,*,#42680,.T.) ;
#56150 = ORIENTED_EDGE('',*,*,#42681,.T.) ;
#56151 = ORIENTED_EDGE('',*,*,#42682,.F.) ;
#56152 = ORIENTED_EDGE('',*,*,#42676,.F.) ;
#56153 = ORIENTED_EDGE('',*,*,#42683,.F.) ;
#56154 = ORIENTED_EDGE('',*,*,#42684,.T.) ;
#56155 = ORIENTED_EDGE('',*,*,#42685,.F.) ;
#56156 = ORIENTED_EDGE('',*,*,#42686,.F.) ;
#56157 = ORIENTED_EDGE('',*,*,#42687,.T.) ;
#56158 = ORIENTED_EDGE('',*,*,#42688,.F.) ;
#56159 = ORIENTED_EDGE('',*,*,#42689,.F.) ;
#56160 = ORIENTED_EDGE('',*,*,#42690,.T.) ;
#56161 = ORIENTED_EDGE('',*,*,#42669,.T.) ;
#56162 = ORIENTED_EDGE('',*,*,#42690,.F.) ;
#56163 = ORIENTED_EDGE('',*,*,#42671,.T.) ;
#56164 = ORIENTED_EDGE('',*,*,#42691,.T.) ;
#56165 = ORIENTED_EDGE('',*,*,#42674,.T.) ;
#56166 = ORIENTED_EDGE('',*,*,#42675,.T.) ;
#56167 = ORIENTED_EDGE('',*,*,#42691,.F.) ;
#56168 = ORIENTED_EDGE('',*,*,#42692,.F.) ;
#56169 = ORIENTED_EDGE('',*,*,#42693,.T.) ;
#56170 = ORIENTED_EDGE('',*,*,#42694,.F.) ;
#56171 = ORIENTED_EDGE('',*,*,#42695,.T.) ;
#56172 = ORIENTED_EDGE('',*,*,#42696,.F.) ;
#56173 = ORIENTED_EDGE('',*,*,#42697,.T.) ;
#56174 = ORIENTED_EDGE('',*,*,#42698,.T.) ;
#56175 = ORIENTED_EDGE('',*,*,#42699,.T.) ;
#56176 = ORIENTED_EDGE('',*,*,#42700,.F.) ;
#56177 = ORIENTED_EDGE('',*,*,#42701,.T.) ;
#56178 = ORIENTED_EDGE('',*,*,#42702,.F.) ;
#56179 = ORIENTED_EDGE('',*,*,#42703,.T.) ;
#56180 = ORIENTED_EDGE('',*,*,#42704,.F.) ;
#56181 = ORIENTED_EDGE('',*,*,#42705,.T.) ;
#56182 = ORIENTED_EDGE('',*,*,#42706,.T.) ;
#56183 = ORIENTED_EDGE('',*,*,#42707,.T.) ;
#56184 = ORIENTED_EDGE('',*,*,#42708,.F.) ;
#56185 = ORIENTED_EDGE('',*,*,#42709,.T.) ;
#56186 = ORIENTED_EDGE('',*,*,#42667,.T.) ;
#56187 = ORIENTED_EDGE('',*,*,#42668,.T.) ;
#56188 = ORIENTED_EDGE('',*,*,#42709,.F.) ;
#56189 = ORIENTED_EDGE('',*,*,#42710,.T.) ;
#56190 = ORIENTED_EDGE('',*,*,#42711,.F.) ;
#56191 = ORIENTED_EDGE('',*,*,#42712,.T.) ;
#56192 = ORIENTED_EDGE('',*,*,#42713,.T.) ;
#56193 = ORIENTED_EDGE('',*,*,#42714,.F.) ;
#56194 = ORIENTED_EDGE('',*,*,#42715,.T.) ;
#56195 = ORIENTED_EDGE('',*,*,#42716,.F.) ;
#56196 = ORIENTED_EDGE('',*,*,#42717,.T.) ;
#56197 = ORIENTED_EDGE('',*,*,#42718,.F.) ;
#56198 = ORIENTED_EDGE('',*,*,#42719,.T.) ;
#56199 = ORIENTED_EDGE('',*,*,#42720,.F.) ;
#56200 = ORIENTED_EDGE('',*,*,#42721,.T.) ;
#56201 = ORIENTED_EDGE('',*,*,#42722,.F.) ;
#56202 = ORIENTED_EDGE('',*,*,#42723,.T.) ;
#56203 = ORIENTED_EDGE('',*,*,#42724,.F.) ;
#56204 = ORIENTED_EDGE('',*,*,#42725,.T.) ;
#56205 = ORIENTED_EDGE('',*,*,#42726,.F.) ;
#56206 = ORIENTED_EDGE('',*,*,#42727,.T.) ;
#56207 = ORIENTED_EDGE('',*,*,#42728,.F.) ;
#56208 = ORIENTED_EDGE('',*,*,#42729,.T.) ;
#56209 = ORIENTED_EDGE('',*,*,#42730,.F.) ;
#56210 = ORIENTED_EDGE('',*,*,#42731,.T.) ;
#56211 = ORIENTED_EDGE('',*,*,#42732,.F.) ;
#56212 = ORIENTED_EDGE('',*,*,#42733,.T.) ;
#56213 = ORIENTED_EDGE('',*,*,#42731,.F.) ;
#56214 = ORIENTED_EDGE('',*,*,#42734,.T.) ;
#56215 = ORIENTED_EDGE('',*,*,#42735,.F.) ;
#56216 = ORIENTED_EDGE('',*,*,#42736,.F.) ;
#56217 = ORIENTED_EDGE('',*,*,#42737,.F.) ;
#56218 = ORIENTED_EDGE('',*,*,#42733,.F.) ;
#56219 = ORIENTED_EDGE('',*,*,#42738,.F.) ;
#56220 = ORIENTED_EDGE('',*,*,#42727,.F.) ;
#56221 = ORIENTED_EDGE('',*,*,#42739,.F.) ;
#56222 = ORIENTED_EDGE('',*,*,#42729,.F.) ;
#56223 = ORIENTED_EDGE('',*,*,#42740,.F.) ;
#56224 = ORIENTED_EDGE('',*,*,#42723,.F.) ;
#56225 = ORIENTED_EDGE('',*,*,#42741,.F.) ;
#56226 = ORIENTED_EDGE('',*,*,#42742,.T.) ;
#56227 = ORIENTED_EDGE('',*,*,#42743,.T.) ;
#56228 = ORIENTED_EDGE('',*,*,#42725,.F.) ;
#56229 = ORIENTED_EDGE('',*,*,#42744,.F.) ;
#56230 = ORIENTED_EDGE('',*,*,#42745,.F.) ;
#56231 = ORIENTED_EDGE('',*,*,#42746,.T.) ;
#56232 = ORIENTED_EDGE('',*,*,#42747,.T.) ;
#56233 = ORIENTED_EDGE('',*,*,#42748,.T.) ;
#56234 = ORIENTED_EDGE('',*,*,#42749,.T.) ;
#56235 = ORIENTED_EDGE('',*,*,#42750,.T.) ;
#56236 = ORIENTED_EDGE('',*,*,#42751,.T.) ;
#56237 = ORIENTED_EDGE('',*,*,#42752,.T.) ;
#56238 = ORIENTED_EDGE('',*,*,#42753,.T.) ;
#56239 = ORIENTED_EDGE('',*,*,#42754,.T.) ;
#56240 = ORIENTED_EDGE('',*,*,#42755,.T.) ;
#56241 = ORIENTED_EDGE('',*,*,#42756,.T.) ;
#56242 = ORIENTED_EDGE('',*,*,#42757,.T.) ;
#56243 = ORIENTED_EDGE('',*,*,#42692,.T.) ;
#56244 = ORIENTED_EDGE('',*,*,#42708,.T.) ;
#56245 = ORIENTED_EDGE('',*,*,#42758,.T.) ;
#56246 = ORIENTED_EDGE('',*,*,#42759,.T.) ;
#56247 = ORIENTED_EDGE('',*,*,#42760,.T.) ;
#56248 = ORIENTED_EDGE('',*,*,#42761,.T.) ;
#56249 = ORIENTED_EDGE('',*,*,#42762,.F.) ;
#56250 = ORIENTED_EDGE('',*,*,#42763,.T.) ;
#56251 = ORIENTED_EDGE('',*,*,#42625,.F.) ;
#56252 = ORIENTED_EDGE('',*,*,#42764,.T.) ;
#56253 = ORIENTED_EDGE('',*,*,#42765,.T.) ;
#56254 = ORIENTED_EDGE('',*,*,#42766,.F.) ;
#56255 = ORIENTED_EDGE('',*,*,#42767,.T.) ;
#56256 = ORIENTED_EDGE('',*,*,#42768,.F.) ;
#56257 = ORIENTED_EDGE('',*,*,#42769,.T.) ;
#56258 = ORIENTED_EDGE('',*,*,#42770,.F.) ;
#56259 = ORIENTED_EDGE('',*,*,#42771,.T.) ;
#56260 = ORIENTED_EDGE('',*,*,#42772,.F.) ;
#56261 = ORIENTED_EDGE('',*,*,#42773,.T.) ;
#56262 = ORIENTED_EDGE('',*,*,#42774,.F.) ;
#56263 = ORIENTED_EDGE('',*,*,#42775,.T.) ;
#56264 = ORIENTED_EDGE('',*,*,#42776,.T.) ;
#56265 = ORIENTED_EDGE('',*,*,#42777,.T.) ;
#56266 = ORIENTED_EDGE('',*,*,#42778,.T.) ;
#56267 = ORIENTED_EDGE('',*,*,#42779,.F.) ;
#56268 = ORIENTED_EDGE('',*,*,#42780,.T.) ;
#56269 = ORIENTED_EDGE('',*,*,#42678,.F.) ;
#56270 = ORIENTED_EDGE('',*,*,#42619,.T.) ;
#56271 = ORIENTED_EDGE('',*,*,#42672,.T.) ;
#56272 = ORIENTED_EDGE('',*,*,#42781,.T.) ;
#56273 = ORIENTED_EDGE('',*,*,#42782,.T.) ;
#56274 = ORIENTED_EDGE('',*,*,#42783,.T.) ;
#56275 = ORIENTED_EDGE('',*,*,#42784,.T.) ;
#56276 = ORIENTED_EDGE('',*,*,#42785,.T.) ;
#56277 = ORIENTED_EDGE('',*,*,#42786,.F.) ;
#56278 = ORIENTED_EDGE('',*,*,#42787,.T.) ;
#56279 = ORIENTED_EDGE('',*,*,#42788,.T.) ;
#56280 = ORIENTED_EDGE('',*,*,#42789,.T.) ;
#56281 = ORIENTED_EDGE('',*,*,#42790,.T.) ;
#56282 = ORIENTED_EDGE('',*,*,#42791,.T.) ;
#56283 = ORIENTED_EDGE('',*,*,#42792,.T.) ;
#56284 = ORIENTED_EDGE('',*,*,#42793,.T.) ;
#56285 = ORIENTED_EDGE('',*,*,#42794,.T.) ;
#56286 = ORIENTED_EDGE('',*,*,#42795,.T.) ;
#56287 = ORIENTED_EDGE('',*,*,#42796,.T.) ;
#56288 = ORIENTED_EDGE('',*,*,#42797,.T.) ;
#56289 = ORIENTED_EDGE('',*,*,#42745,.T.) ;
#56290 = ORIENTED_EDGE('',*,*,#42798,.F.) ;
#56291 = ORIENTED_EDGE('',*,*,#42799,.T.) ;
#56292 = ORIENTED_EDGE('',*,*,#42800,.T.) ;
#56293 = ORIENTED_EDGE('',*,*,#42801,.T.) ;
#56294 = ORIENTED_EDGE('',*,*,#42802,.F.) ;
#56295 = ORIENTED_EDGE('',*,*,#42735,.T.) ;
#56296 = ORIENTED_EDGE('',*,*,#42803,.F.) ;
#56297 = ORIENTED_EDGE('',*,*,#42742,.F.) ;
#56298 = ORIENTED_EDGE('',*,*,#42804,.T.) ;
#56299 = ORIENTED_EDGE('',*,*,#42805,.T.) ;
#56300 = ORIENTED_EDGE('',*,*,#42806,.F.) ;
#56301 = ORIENTED_EDGE('',*,*,#42807,.T.) ;
#56302 = ORIENTED_EDGE('',*,*,#42808,.F.) ;
#56303 = ORIENTED_EDGE('',*,*,#42809,.T.) ;
#56304 = ORIENTED_EDGE('',*,*,#42810,.F.) ;
#56305 = ORIENTED_EDGE('',*,*,#42811,.T.) ;
#56306 = ORIENTED_EDGE('',*,*,#42812,.F.) ;
#56307 = ORIENTED_EDGE('',*,*,#42813,.T.) ;
#56308 = ORIENTED_EDGE('',*,*,#42814,.F.) ;
#56309 = ORIENTED_EDGE('',*,*,#42815,.T.) ;
#56310 = ORIENTED_EDGE('',*,*,#42612,.T.) ;
#56311 = ORIENTED_EDGE('',*,*,#42816,.F.) ;
#56312 = ORIENTED_EDGE('',*,*,#42817,.T.) ;
#56313 = ORIENTED_EDGE('',*,*,#42818,.F.) ;
#56314 = ORIENTED_EDGE('',*,*,#42819,.T.) ;
#56315 = ORIENTED_EDGE('',*,*,#42820,.F.) ;
#56316 = ORIENTED_EDGE('',*,*,#42821,.T.) ;
#56317 = ORIENTED_EDGE('',*,*,#42822,.F.) ;
#56318 = ORIENTED_EDGE('',*,*,#42823,.T.) ;
#56319 = ORIENTED_EDGE('',*,*,#42665,.T.) ;
#56320 = ORIENTED_EDGE('',*,*,#42824,.T.) ;
#56321 = ORIENTED_EDGE('',*,*,#42825,.T.) ;
#56322 = ORIENTED_EDGE('',*,*,#42826,.F.) ;
#56323 = ORIENTED_EDGE('',*,*,#42827,.T.) ;
#56324 = ORIENTED_EDGE('',*,*,#42828,.T.) ;
#56325 = ORIENTED_EDGE('',*,*,#42664,.T.) ;
#56326 = ORIENTED_EDGE('',*,*,#42829,.F.) ;
#56327 = ORIENTED_EDGE('',*,*,#42830,.T.) ;
#56328 = ORIENTED_EDGE('',*,*,#42831,.T.) ;
#56329 = ORIENTED_EDGE('',*,*,#42832,.T.) ;
#56330 = ORIENTED_EDGE('',*,*,#42833,.F.) ;
#56331 = ORIENTED_EDGE('',*,*,#42662,.T.) ;
#56332 = ORIENTED_EDGE('',*,*,#42834,.T.) ;
#56333 = ORIENTED_EDGE('',*,*,#42835,.T.) ;
#56334 = ORIENTED_EDGE('',*,*,#42836,.F.) ;
#56335 = ORIENTED_EDGE('',*,*,#42837,.T.) ;
#56336 = ORIENTED_EDGE('',*,*,#42838,.T.) ;
#56337 = ORIENTED_EDGE('',*,*,#42839,.T.) ;
#56338 = ORIENTED_EDGE('',*,*,#42840,.T.) ;
#56339 = ORIENTED_EDGE('',*,*,#42841,.F.) ;
#56340 = ORIENTED_EDGE('',*,*,#42842,.T.) ;
#56341 = ORIENTED_EDGE('',*,*,#42843,.F.) ;
#56342 = ORIENTED_EDGE('',*,*,#42844,.T.) ;
#56343 = ORIENTED_EDGE('',*,*,#42845,.T.) ;
#56344 = ORIENTED_EDGE('',*,*,#42846,.T.) ;
#56345 = ORIENTED_EDGE('',*,*,#42847,.T.) ;
#56346 = ORIENTED_EDGE('',*,*,#42848,.T.) ;
#56347 = ORIENTED_EDGE('',*,*,#42849,.F.) ;
#56348 = ORIENTED_EDGE('',*,*,#42850,.T.) ;
#56349 = ORIENTED_EDGE('',*,*,#42851,.F.) ;
#56350 = ORIENTED_EDGE('',*,*,#42852,.T.) ;
#56351 = ORIENTED_EDGE('',*,*,#42853,.T.) ;
#56352 = ORIENTED_EDGE('',*,*,#42854,.T.) ;
#56353 = ORIENTED_EDGE('',*,*,#42855,.T.) ;
#56354 = ORIENTED_EDGE('',*,*,#42856,.F.) ;
#56355 = ORIENTED_EDGE('',*,*,#42857,.T.) ;
#56356 = ORIENTED_EDGE('',*,*,#42858,.F.) ;
#56357 = ORIENTED_EDGE('',*,*,#42859,.T.) ;
#56358 = ORIENTED_EDGE('',*,*,#42860,.F.) ;
#56359 = ORIENTED_EDGE('',*,*,#42861,.T.) ;
#56360 = ORIENTED_EDGE('',*,*,#42862,.F.) ;
#56361 = ORIENTED_EDGE('',*,*,#42863,.T.) ;
#56362 = ORIENTED_EDGE('',*,*,#42864,.F.) ;
#56363 = ORIENTED_EDGE('',*,*,#42865,.T.) ;
#56364 = ORIENTED_EDGE('',*,*,#42866,.F.) ;
#56365 = ORIENTED_EDGE('',*,*,#42867,.T.) ;
#56366 = ORIENTED_EDGE('',*,*,#42868,.F.) ;
#56367 = ORIENTED_EDGE('',*,*,#42869,.T.) ;
#56368 = ORIENTED_EDGE('',*,*,#42870,.F.) ;
#56369 = ORIENTED_EDGE('',*,*,#42871,.T.) ;
#56370 = ORIENTED_EDGE('',*,*,#42872,.F.) ;
#56371 = ORIENTED_EDGE('',*,*,#42873,.T.) ;
#56372 = ORIENTED_EDGE('',*,*,#42874,.T.) ;
#56373 = ORIENTED_EDGE('',*,*,#42875,.T.) ;
#56374 = ORIENTED_EDGE('',*,*,#42876,.F.) ;
#56375 = ORIENTED_EDGE('',*,*,#42877,.T.) ;
#56376 = ORIENTED_EDGE('',*,*,#42878,.T.) ;
#56377 = ORIENTED_EDGE('',*,*,#42879,.T.) ;
#56378 = ORIENTED_EDGE('',*,*,#42880,.T.) ;
#56379 = ORIENTED_EDGE('',*,*,#42881,.T.) ;
#56380 = ORIENTED_EDGE('',*,*,#42882,.T.) ;
#56381 = ORIENTED_EDGE('',*,*,#42883,.T.) ;
#56382 = ORIENTED_EDGE('',*,*,#42884,.T.) ;
#56383 = ORIENTED_EDGE('',*,*,#42885,.T.) ;
#56384 = ORIENTED_EDGE('',*,*,#42886,.T.) ;
#56385 = ORIENTED_EDGE('',*,*,#42887,.T.) ;
#56386 = ORIENTED_EDGE('',*,*,#42888,.F.) ;
#56387 = ORIENTED_EDGE('',*,*,#42889,.T.) ;
#56388 = ORIENTED_EDGE('',*,*,#42890,.T.) ;
#56389 = ORIENTED_EDGE('',*,*,#42891,.T.) ;
#56390 = ORIENTED_EDGE('',*,*,#42892,.T.) ;
#56391 = ORIENTED_EDGE('',*,*,#42893,.T.) ;
#56392 = ORIENTED_EDGE('',*,*,#42894,.T.) ;
#56393 = ORIENTED_EDGE('',*,*,#42895,.T.) ;
#56394 = ORIENTED_EDGE('',*,*,#42896,.T.) ;
#56395 = ORIENTED_EDGE('',*,*,#42897,.T.) ;
#56396 = ORIENTED_EDGE('',*,*,#42898,.T.) ;
#56397 = ORIENTED_EDGE('',*,*,#42899,.T.) ;
#56398 = ORIENTED_EDGE('',*,*,#42900,.T.) ;
#56399 = ORIENTED_EDGE('',*,*,#42800,.F.) ;
#56400 = ORIENTED_EDGE('',*,*,#42741,.T.) ;
#56401 = ORIENTED_EDGE('',*,*,#42797,.F.) ;
#56402 = ORIENTED_EDGE('',*,*,#42901,.T.) ;
#56403 = ORIENTED_EDGE('',*,*,#42713,.F.) ;
#56404 = ORIENTED_EDGE('',*,*,#42902,.T.) ;
#56405 = ORIENTED_EDGE('',*,*,#42796,.F.) ;
#56406 = ORIENTED_EDGE('',*,*,#42903,.T.) ;
#56407 = ORIENTED_EDGE('',*,*,#42754,.F.) ;
#56408 = ORIENTED_EDGE('',*,*,#42904,.T.) ;
#56409 = ORIENTED_EDGE('',*,*,#42776,.F.) ;
#56410 = ORIENTED_EDGE('',*,*,#42905,.T.) ;
#56411 = ORIENTED_EDGE('',*,*,#42898,.F.) ;
#56412 = ORIENTED_EDGE('',*,*,#42906,.T.) ;
#56413 = ORIENTED_EDGE('',*,*,#42748,.F.) ;
#56414 = ORIENTED_EDGE('',*,*,#42907,.T.) ;
#56415 = ORIENTED_EDGE('',*,*,#42890,.F.) ;
#56416 = ORIENTED_EDGE('',*,*,#42908,.T.) ;
#56417 = ORIENTED_EDGE('',*,*,#42874,.F.) ;
#56418 = ORIENTED_EDGE('',*,*,#42909,.T.) ;
#56419 = ORIENTED_EDGE('',*,*,#42854,.F.) ;
#56420 = ORIENTED_EDGE('',*,*,#42910,.T.) ;
#56421 = ORIENTED_EDGE('',*,*,#42834,.F.) ;
#56422 = ORIENTED_EDGE('',*,*,#42911,.T.) ;
#56423 = ORIENTED_EDGE('',*,*,#42831,.F.) ;
#56424 = ORIENTED_EDGE('',*,*,#42661,.T.) ;
#56425 = ORIENTED_EDGE('',*,*,#42828,.F.) ;
#56426 = ORIENTED_EDGE('',*,*,#42912,.T.) ;
#56427 = ORIENTED_EDGE('',*,*,#42824,.F.) ;
#56428 = ORIENTED_EDGE('',*,*,#42913,.T.) ;
#56429 = ORIENTED_EDGE('',*,*,#42804,.F.) ;
#56430 = ORIENTED_EDGE('',*,*,#42914,.T.) ;
#56431 = ORIENTED_EDGE('',*,*,#42915,.T.) ;
#56432 = ORIENTED_EDGE('',*,*,#42916,.T.) ;
#56433 = ORIENTED_EDGE('',*,*,#42917,.T.) ;
#56434 = ORIENTED_EDGE('',*,*,#42918,.T.) ;
#56435 = ORIENTED_EDGE('',*,*,#42919,.T.) ;
#56436 = ORIENTED_EDGE('',*,*,#42920,.T.) ;
#56437 = ORIENTED_EDGE('',*,*,#42921,.T.) ;
#56438 = ORIENTED_EDGE('',*,*,#42922,.F.) ;
#56439 = ORIENTED_EDGE('',*,*,#42923,.T.) ;
#56440 = ORIENTED_EDGE('',*,*,#42924,.T.) ;
#56441 = ORIENTED_EDGE('',*,*,#42925,.T.) ;
#56442 = ORIENTED_EDGE('',*,*,#42926,.F.) ;
#56443 = ORIENTED_EDGE('',*,*,#42927,.T.) ;
#56444 = ORIENTED_EDGE('',*,*,#42928,.T.) ;
#56445 = ORIENTED_EDGE('',*,*,#42929,.T.) ;
#56446 = ORIENTED_EDGE('',*,*,#42930,.T.) ;
#56447 = ORIENTED_EDGE('',*,*,#42931,.T.) ;
#56448 = ORIENTED_EDGE('',*,*,#42932,.F.) ;
#56449 = ORIENTED_EDGE('',*,*,#42933,.T.) ;
#56450 = ORIENTED_EDGE('',*,*,#42924,.F.) ;
#56451 = ORIENTED_EDGE('',*,*,#42934,.T.) ;
#56452 = ORIENTED_EDGE('',*,*,#42935,.T.) ;
#56453 = ORIENTED_EDGE('',*,*,#42936,.T.) ;
#56454 = ORIENTED_EDGE('',*,*,#42937,.F.) ;
#56455 = ORIENTED_EDGE('',*,*,#42938,.T.) ;
#56456 = ORIENTED_EDGE('',*,*,#42930,.F.) ;
#56457 = ORIENTED_EDGE('',*,*,#42939,.T.) ;
#56458 = ORIENTED_EDGE('',*,*,#42940,.F.) ;
#56459 = ORIENTED_EDGE('',*,*,#42941,.T.) ;
#56460 = ORIENTED_EDGE('',*,*,#42942,.T.) ;
#56461 = ORIENTED_EDGE('',*,*,#42943,.T.) ;
#56462 = ORIENTED_EDGE('',*,*,#42935,.F.) ;
#56463 = ORIENTED_EDGE('',*,*,#42944,.T.) ;
#56464 = ORIENTED_EDGE('',*,*,#42945,.T.) ;
#56465 = ORIENTED_EDGE('',*,*,#42946,.T.) ;
#56466 = ORIENTED_EDGE('',*,*,#42932,.T.) ;
#56467 = ORIENTED_EDGE('',*,*,#42947,.T.) ;
#56468 = ORIENTED_EDGE('',*,*,#42948,.T.) ;
#56469 = ORIENTED_EDGE('',*,*,#42949,.T.) ;
#56470 = ORIENTED_EDGE('',*,*,#42950,.T.) ;
#56471 = ORIENTED_EDGE('',*,*,#42951,.T.) ;
#56472 = ORIENTED_EDGE('',*,*,#42952,.T.) ;
#56473 = ORIENTED_EDGE('',*,*,#42953,.T.) ;
#56474 = ORIENTED_EDGE('',*,*,#42954,.T.) ;
#56475 = ORIENTED_EDGE('',*,*,#42955,.T.) ;
#56476 = ORIENTED_EDGE('',*,*,#42956,.T.) ;
#56477 = ORIENTED_EDGE('',*,*,#42957,.T.) ;
#56478 = ORIENTED_EDGE('',*,*,#42958,.T.) ;
#56479 = ORIENTED_EDGE('',*,*,#42959,.T.) ;
#56480 = ORIENTED_EDGE('',*,*,#42960,.T.) ;
#56481 = ORIENTED_EDGE('',*,*,#42961,.T.) ;
#56482 = ORIENTED_EDGE('',*,*,#42962,.T.) ;
#56483 = ORIENTED_EDGE('',*,*,#42963,.T.) ;
#56484 = ORIENTED_EDGE('',*,*,#42964,.T.) ;
#56485 = ORIENTED_EDGE('',*,*,#42965,.T.) ;
#56486 = ORIENTED_EDGE('',*,*,#42966,.T.) ;
#56487 = ORIENTED_EDGE('',*,*,#42967,.T.) ;
#56488 = ORIENTED_EDGE('',*,*,#42968,.T.) ;
#56489 = ORIENTED_EDGE('',*,*,#42969,.T.) ;
#56490 = ORIENTED_EDGE('',*,*,#42970,.T.) ;
#56491 = ORIENTED_EDGE('',*,*,#42971,.T.) ;
#56492 = ORIENTED_EDGE('',*,*,#42972,.T.) ;
#56493 = ORIENTED_EDGE('',*,*,#42973,.T.) ;
#56494 = ORIENTED_EDGE('',*,*,#42974,.T.) ;
#56495 = ORIENTED_EDGE('',*,*,#42975,.T.) ;
#56496 = ORIENTED_EDGE('',*,*,#42976,.T.) ;
#56497 = ORIENTED_EDGE('',*,*,#42977,.T.) ;
#56498 = ORIENTED_EDGE('',*,*,#42978,.T.) ;
#56499 = ORIENTED_EDGE('',*,*,#42979,.T.) ;
#56500 = ORIENTED_EDGE('',*,*,#42980,.T.) ;
#56501 = ORIENTED_EDGE('',*,*,#42981,.T.) ;
#56502 = ORIENTED_EDGE('',*,*,#42982,.F.) ;
#56503 = ORIENTED_EDGE('',*,*,#42983,.F.) ;
#56504 = ORIENTED_EDGE('',*,*,#42984,.F.) ;
#56505 = ORIENTED_EDGE('',*,*,#42985,.F.) ;
#56506 = ORIENTED_EDGE('',*,*,#42986,.F.) ;
#56507 = ORIENTED_EDGE('',*,*,#42987,.F.) ;
#56508 = ORIENTED_EDGE('',*,*,#42988,.F.) ;
#56509 = ORIENTED_EDGE('',*,*,#42989,.F.) ;
#56510 = ORIENTED_EDGE('',*,*,#42990,.F.) ;
#56511 = ORIENTED_EDGE('',*,*,#42991,.F.) ;
#56512 = ORIENTED_EDGE('',*,*,#42989,.T.) ;
#56513 = ORIENTED_EDGE('',*,*,#42992,.T.) ;
#56514 = ORIENTED_EDGE('',*,*,#42993,.F.) ;
#56515 = ORIENTED_EDGE('',*,*,#42994,.F.) ;
#56516 = ORIENTED_EDGE('',*,*,#42982,.T.) ;
#56517 = ORIENTED_EDGE('',*,*,#42991,.T.) ;
#56518 = ORIENTED_EDGE('',*,*,#42995,.F.) ;
#56519 = ORIENTED_EDGE('',*,*,#42996,.F.) ;
#56520 = ORIENTED_EDGE('',*,*,#42983,.T.) ;
#56521 = ORIENTED_EDGE('',*,*,#42994,.T.) ;
#56522 = ORIENTED_EDGE('',*,*,#42997,.F.) ;
#56523 = ORIENTED_EDGE('',*,*,#42998,.F.) ;
#56524 = ORIENTED_EDGE('',*,*,#42984,.T.) ;
#56525 = ORIENTED_EDGE('',*,*,#42996,.T.) ;
#56526 = ORIENTED_EDGE('',*,*,#42999,.F.) ;
#56527 = ORIENTED_EDGE('',*,*,#43000,.F.) ;
#56528 = ORIENTED_EDGE('',*,*,#42985,.T.) ;
#56529 = ORIENTED_EDGE('',*,*,#42998,.T.) ;
#56530 = ORIENTED_EDGE('',*,*,#43001,.F.) ;
#56531 = ORIENTED_EDGE('',*,*,#43002,.F.) ;
#56532 = ORIENTED_EDGE('',*,*,#42986,.T.) ;
#56533 = ORIENTED_EDGE('',*,*,#43000,.T.) ;
#56534 = ORIENTED_EDGE('',*,*,#43003,.F.) ;
#56535 = ORIENTED_EDGE('',*,*,#43004,.F.) ;
#56536 = ORIENTED_EDGE('',*,*,#42987,.T.) ;
#56537 = ORIENTED_EDGE('',*,*,#43002,.T.) ;
#56538 = ORIENTED_EDGE('',*,*,#43005,.F.) ;
#56539 = ORIENTED_EDGE('',*,*,#42992,.F.) ;
#56540 = ORIENTED_EDGE('',*,*,#42988,.T.) ;
#56541 = ORIENTED_EDGE('',*,*,#43004,.T.) ;
#56542 = ORIENTED_EDGE('',*,*,#42993,.T.) ;
#56543 = ORIENTED_EDGE('',*,*,#42990,.T.) ;
#56544 = ORIENTED_EDGE('',*,*,#43005,.T.) ;
#56545 = ORIENTED_EDGE('',*,*,#43003,.T.) ;
#56546 = ORIENTED_EDGE('',*,*,#43001,.T.) ;
#56547 = ORIENTED_EDGE('',*,*,#42999,.T.) ;
#56548 = ORIENTED_EDGE('',*,*,#42997,.T.) ;
#56549 = ORIENTED_EDGE('',*,*,#42995,.T.) ;
#56550 = ORIENTED_EDGE('',*,*,#42700,.T.) ;
#56551 = ORIENTED_EDGE('',*,*,#43006,.T.) ;
#56552 = ORIENTED_EDGE('',*,*,#42698,.F.) ;
#56553 = ORIENTED_EDGE('',*,*,#43007,.T.) ;
#56554 = ORIENTED_EDGE('',*,*,#42702,.T.) ;
#56555 = ORIENTED_EDGE('',*,*,#43008,.T.) ;
#56556 = ORIENTED_EDGE('',*,*,#42706,.F.) ;
#56557 = ORIENTED_EDGE('',*,*,#43009,.T.) ;
#56558 = ORIENTED_EDGE('',*,*,#42694,.T.) ;
#56559 = ORIENTED_EDGE('',*,*,#43010,.T.) ;
#56560 = ORIENTED_EDGE('',*,*,#42696,.T.) ;
#56561 = ORIENTED_EDGE('',*,*,#43011,.T.) ;
#56562 = ORIENTED_EDGE('',*,*,#42704,.T.) ;
#56563 = ORIENTED_EDGE('',*,*,#43012,.T.) ;
#56564 = ORIENTED_EDGE('',*,*,#43013,.T.) ;
#56565 = ORIENTED_EDGE('',*,*,#43014,.T.) ;
#56566 = ORIENTED_EDGE('',*,*,#43015,.T.) ;
#56567 = ORIENTED_EDGE('',*,*,#43016,.T.) ;
#56568 = ORIENTED_EDGE('',*,*,#43017,.T.) ;
#56569 = ORIENTED_EDGE('',*,*,#43018,.T.) ;
#56570 = ORIENTED_EDGE('',*,*,#43019,.T.) ;
#56571 = ORIENTED_EDGE('',*,*,#43020,.T.) ;
#56572 = ORIENTED_EDGE('',*,*,#43021,.T.) ;
#56573 = ORIENTED_EDGE('',*,*,#43022,.T.) ;
#56574 = ORIENTED_EDGE('',*,*,#43023,.T.) ;
#56575 = ORIENTED_EDGE('',*,*,#43024,.T.) ;
#56576 = ORIENTED_EDGE('',*,*,#43025,.T.) ;
#56577 = ORIENTED_EDGE('',*,*,#43026,.T.) ;
#56578 = ORIENTED_EDGE('',*,*,#43027,.T.) ;
#56579 = ORIENTED_EDGE('',*,*,#43028,.T.) ;
#56580 = ORIENTED_EDGE('',*,*,#43029,.T.) ;
#56581 = ORIENTED_EDGE('',*,*,#43030,.T.) ;
#56582 = ORIENTED_EDGE('',*,*,#43031,.T.) ;
#56583 = ORIENTED_EDGE('',*,*,#43032,.T.) ;
#56584 = ORIENTED_EDGE('',*,*,#43033,.F.) ;
#56585 = ORIENTED_EDGE('',*,*,#43034,.F.) ;
#56586 = ORIENTED_EDGE('',*,*,#43035,.F.) ;
#56587 = ORIENTED_EDGE('',*,*,#43036,.F.) ;
#56588 = ORIENTED_EDGE('',*,*,#43037,.F.) ;
#56589 = ORIENTED_EDGE('',*,*,#43038,.F.) ;
#56590 = ORIENTED_EDGE('',*,*,#43039,.F.) ;
#56591 = ORIENTED_EDGE('',*,*,#43040,.F.) ;
#56592 = ORIENTED_EDGE('',*,*,#43041,.T.) ;
#56593 = ORIENTED_EDGE('',*,*,#43042,.T.) ;
#56594 = ORIENTED_EDGE('',*,*,#43043,.F.) ;
#56595 = ORIENTED_EDGE('',*,*,#43040,.T.) ;
#56596 = ORIENTED_EDGE('',*,*,#43043,.T.) ;
#56597 = ORIENTED_EDGE('',*,*,#43044,.T.) ;
#56598 = ORIENTED_EDGE('',*,*,#43045,.F.) ;
#56599 = ORIENTED_EDGE('',*,*,#43033,.T.) ;
#56600 = ORIENTED_EDGE('',*,*,#43045,.T.) ;
#56601 = ORIENTED_EDGE('',*,*,#43046,.T.) ;
#56602 = ORIENTED_EDGE('',*,*,#43047,.F.) ;
#56603 = ORIENTED_EDGE('',*,*,#43034,.T.) ;
#56604 = ORIENTED_EDGE('',*,*,#43047,.T.) ;
#56605 = ORIENTED_EDGE('',*,*,#43048,.T.) ;
#56606 = ORIENTED_EDGE('',*,*,#43049,.F.) ;
#56607 = ORIENTED_EDGE('',*,*,#43035,.T.) ;
#56608 = ORIENTED_EDGE('',*,*,#43049,.T.) ;
#56609 = ORIENTED_EDGE('',*,*,#43050,.T.) ;
#56610 = ORIENTED_EDGE('',*,*,#43051,.F.) ;
#56611 = ORIENTED_EDGE('',*,*,#43036,.T.) ;
#56612 = ORIENTED_EDGE('',*,*,#43051,.T.) ;
#56613 = ORIENTED_EDGE('',*,*,#43052,.T.) ;
#56614 = ORIENTED_EDGE('',*,*,#43053,.F.) ;
#56615 = ORIENTED_EDGE('',*,*,#43037,.T.) ;
#56616 = ORIENTED_EDGE('',*,*,#43053,.T.) ;
#56617 = ORIENTED_EDGE('',*,*,#43054,.T.) ;
#56618 = ORIENTED_EDGE('',*,*,#43055,.F.) ;
#56619 = ORIENTED_EDGE('',*,*,#43038,.T.) ;
#56620 = ORIENTED_EDGE('',*,*,#43055,.T.) ;
#56621 = ORIENTED_EDGE('',*,*,#43056,.T.) ;
#56622 = ORIENTED_EDGE('',*,*,#43041,.F.) ;
#56623 = ORIENTED_EDGE('',*,*,#43039,.T.) ;
#56624 = ORIENTED_EDGE('',*,*,#43057,.T.) ;
#56625 = ORIENTED_EDGE('',*,*,#43058,.T.) ;
#56626 = ORIENTED_EDGE('',*,*,#43059,.T.) ;
#56627 = ORIENTED_EDGE('',*,*,#43060,.T.) ;
#56628 = ORIENTED_EDGE('',*,*,#43061,.T.) ;
#56629 = ORIENTED_EDGE('',*,*,#43062,.T.) ;
#56630 = ORIENTED_EDGE('',*,*,#43063,.T.) ;
#56631 = ORIENTED_EDGE('',*,*,#43064,.T.) ;
#56632 = ORIENTED_EDGE('',*,*,#43065,.T.) ;
#56633 = ORIENTED_EDGE('',*,*,#42683,.T.) ;
#56634 = ORIENTED_EDGE('',*,*,#43066,.T.) ;
#56635 = ORIENTED_EDGE('',*,*,#43067,.T.) ;
#56636 = ORIENTED_EDGE('',*,*,#42685,.T.) ;
#56637 = ORIENTED_EDGE('',*,*,#43068,.T.) ;
#56638 = ORIENTED_EDGE('',*,*,#43069,.T.) ;
#56639 = ORIENTED_EDGE('',*,*,#43070,.T.) ;
#56640 = ORIENTED_EDGE('',*,*,#43071,.T.) ;
#56641 = ORIENTED_EDGE('',*,*,#43072,.T.) ;
#56642 = ORIENTED_EDGE('',*,*,#43073,.T.) ;
#56643 = ORIENTED_EDGE('',*,*,#43074,.T.) ;
#56644 = ORIENTED_EDGE('',*,*,#43075,.T.) ;
#56645 = ORIENTED_EDGE('',*,*,#42657,.T.) ;
#56646 = ORIENTED_EDGE('',*,*,#42689,.T.) ;
#56647 = ORIENTED_EDGE('',*,*,#43076,.T.) ;
#56648 = ORIENTED_EDGE('',*,*,#43077,.T.) ;
#56649 = ORIENTED_EDGE('',*,*,#43078,.T.) ;
#56650 = ORIENTED_EDGE('',*,*,#43079,.T.) ;
#56651 = ORIENTED_EDGE('',*,*,#43080,.T.) ;
#56652 = ORIENTED_EDGE('',*,*,#43081,.T.) ;
#56653 = ORIENTED_EDGE('',*,*,#43082,.F.) ;
#56654 = ORIENTED_EDGE('',*,*,#43083,.F.) ;
#56655 = ORIENTED_EDGE('',*,*,#43084,.F.) ;
#56656 = ORIENTED_EDGE('',*,*,#42847,.F.) ;
#56657 = ORIENTED_EDGE('',*,*,#42934,.F.) ;
#56658 = ORIENTED_EDGE('',*,*,#42923,.F.) ;
#56659 = ORIENTED_EDGE('',*,*,#43085,.F.) ;
#56660 = ORIENTED_EDGE('',*,*,#42944,.F.) ;
#56661 = ORIENTED_EDGE('',*,*,#43085,.T.) ;
#56662 = ORIENTED_EDGE('',*,*,#42922,.T.) ;
#56663 = ORIENTED_EDGE('',*,*,#43086,.F.) ;
#56664 = ORIENTED_EDGE('',*,*,#43087,.F.) ;
#56665 = ORIENTED_EDGE('',*,*,#43086,.T.) ;
#56666 = ORIENTED_EDGE('',*,*,#42929,.F.) ;
#56667 = ORIENTED_EDGE('',*,*,#43088,.F.) ;
#56668 = ORIENTED_EDGE('',*,*,#42960,.F.) ;
#56669 = ORIENTED_EDGE('',*,*,#43083,.T.) ;
#56670 = ORIENTED_EDGE('',*,*,#42961,.F.) ;
#56671 = ORIENTED_EDGE('',*,*,#43089,.F.) ;
#56672 = ORIENTED_EDGE('',*,*,#42920,.F.) ;
#56673 = ORIENTED_EDGE('',*,*,#43084,.T.) ;
#56674 = ORIENTED_EDGE('',*,*,#42919,.F.) ;
#56675 = ORIENTED_EDGE('',*,*,#43090,.F.) ;
#56676 = ORIENTED_EDGE('',*,*,#42848,.F.) ;
#56677 = ORIENTED_EDGE('',*,*,#43082,.T.) ;
#56678 = ORIENTED_EDGE('',*,*,#42846,.F.) ;
#56679 = ORIENTED_EDGE('',*,*,#43091,.F.) ;
#56680 = ORIENTED_EDGE('',*,*,#42956,.F.) ;
#56681 = ORIENTED_EDGE('',*,*,#43087,.T.) ;
#56682 = ORIENTED_EDGE('',*,*,#42959,.F.) ;
#56683 = ORIENTED_EDGE('',*,*,#43092,.F.) ;
#56684 = ORIENTED_EDGE('',*,*,#42945,.F.) ;
#56685 = ORIENTED_EDGE('',*,*,#42936,.F.) ;
#56686 = ORIENTED_EDGE('',*,*,#42946,.F.) ;
#56687 = ORIENTED_EDGE('',*,*,#43093,.F.) ;
#56688 = ORIENTED_EDGE('',*,*,#42939,.F.) ;
#56689 = ORIENTED_EDGE('',*,*,#43089,.T.) ;
#56690 = ORIENTED_EDGE('',*,*,#43088,.T.) ;
#56691 = ORIENTED_EDGE('',*,*,#43094,.F.) ;
#56692 = ORIENTED_EDGE('',*,*,#42849,.T.) ;
#56693 = ORIENTED_EDGE('',*,*,#43090,.T.) ;
#56694 = ORIENTED_EDGE('',*,*,#43095,.F.) ;
#56695 = ORIENTED_EDGE('',*,*,#43096,.F.) ;
#56696 = ORIENTED_EDGE('',*,*,#43091,.T.) ;
#56697 = ORIENTED_EDGE('',*,*,#42853,.F.) ;
#56698 = ORIENTED_EDGE('',*,*,#43097,.F.) ;
#56699 = ORIENTED_EDGE('',*,*,#43098,.F.) ;
#56700 = ORIENTED_EDGE('',*,*,#43093,.T.) ;
#56701 = ORIENTED_EDGE('',*,*,#43092,.T.) ;
#56702 = ORIENTED_EDGE('',*,*,#43099,.F.) ;
#56703 = ORIENTED_EDGE('',*,*,#42940,.T.) ;
#56704 = ORIENTED_EDGE('',*,*,#43094,.T.) ;
#56705 = ORIENTED_EDGE('',*,*,#42928,.F.) ;
#56706 = ORIENTED_EDGE('',*,*,#43100,.F.) ;
#56707 = ORIENTED_EDGE('',*,*,#42921,.F.) ;
#56708 = ORIENTED_EDGE('',*,*,#43095,.T.) ;
#56709 = ORIENTED_EDGE('',*,*,#42918,.F.) ;
#56710 = ORIENTED_EDGE('',*,*,#43101,.F.) ;
#56711 = ORIENTED_EDGE('',*,*,#42954,.F.) ;
#56712 = ORIENTED_EDGE('',*,*,#43096,.T.) ;
#56713 = ORIENTED_EDGE('',*,*,#42953,.F.) ;
#56714 = ORIENTED_EDGE('',*,*,#43102,.F.) ;
#56715 = ORIENTED_EDGE('',*,*,#42850,.F.) ;
#56716 = ORIENTED_EDGE('',*,*,#43097,.T.) ;
#56717 = ORIENTED_EDGE('',*,*,#42852,.F.) ;
#56718 = ORIENTED_EDGE('',*,*,#43103,.F.) ;
#56719 = ORIENTED_EDGE('',*,*,#42915,.F.) ;
#56720 = ORIENTED_EDGE('',*,*,#43098,.T.) ;
#56721 = ORIENTED_EDGE('',*,*,#42914,.F.) ;
#56722 = ORIENTED_EDGE('',*,*,#43104,.F.) ;
#56723 = ORIENTED_EDGE('',*,*,#42957,.F.) ;
#56724 = ORIENTED_EDGE('',*,*,#43099,.T.) ;
#56725 = ORIENTED_EDGE('',*,*,#42958,.F.) ;
#56726 = ORIENTED_EDGE('',*,*,#43105,.F.) ;
#56727 = ORIENTED_EDGE('',*,*,#42941,.F.) ;
#56728 = ORIENTED_EDGE('',*,*,#43101,.T.) ;
#56729 = ORIENTED_EDGE('',*,*,#43100,.T.) ;
#56730 = ORIENTED_EDGE('',*,*,#43106,.F.) ;
#56731 = ORIENTED_EDGE('',*,*,#42851,.T.) ;
#56732 = ORIENTED_EDGE('',*,*,#43102,.T.) ;
#56733 = ORIENTED_EDGE('',*,*,#43107,.F.) ;
#56734 = ORIENTED_EDGE('',*,*,#43103,.T.) ;
#56735 = ORIENTED_EDGE('',*,*,#43105,.T.) ;
#56736 = ORIENTED_EDGE('',*,*,#43104,.T.) ;
#56737 = ORIENTED_EDGE('',*,*,#43108,.F.) ;
#56738 = ORIENTED_EDGE('',*,*,#42933,.F.) ;
#56739 = ORIENTED_EDGE('',*,*,#42949,.F.) ;
#56740 = ORIENTED_EDGE('',*,*,#43109,.F.) ;
#56741 = ORIENTED_EDGE('',*,*,#42925,.F.) ;
#56742 = ORIENTED_EDGE('',*,*,#43106,.T.) ;
#56743 = ORIENTED_EDGE('',*,*,#42927,.F.) ;
#56744 = ORIENTED_EDGE('',*,*,#43110,.F.) ;
#56745 = ORIENTED_EDGE('',*,*,#42955,.F.) ;
#56746 = ORIENTED_EDGE('',*,*,#43107,.T.) ;
#56747 = ORIENTED_EDGE('',*,*,#42952,.F.) ;
#56748 = ORIENTED_EDGE('',*,*,#43111,.F.) ;
#56749 = ORIENTED_EDGE('',*,*,#42916,.F.) ;
#56750 = ORIENTED_EDGE('',*,*,#43108,.T.) ;
#56751 = ORIENTED_EDGE('',*,*,#42917,.F.) ;
#56752 = ORIENTED_EDGE('',*,*,#43112,.F.) ;
#56753 = ORIENTED_EDGE('',*,*,#42942,.F.) ;
#56754 = ORIENTED_EDGE('',*,*,#42926,.T.) ;
#56755 = ORIENTED_EDGE('',*,*,#43109,.T.) ;
#56756 = ORIENTED_EDGE('',*,*,#43113,.F.) ;
#56757 = ORIENTED_EDGE('',*,*,#43110,.T.) ;
#56758 = ORIENTED_EDGE('',*,*,#43112,.T.) ;
#56759 = ORIENTED_EDGE('',*,*,#43111,.T.) ;
#56760 = ORIENTED_EDGE('',*,*,#43114,.F.) ;
#56761 = ORIENTED_EDGE('',*,*,#43113,.T.) ;
#56762 = ORIENTED_EDGE('',*,*,#42948,.F.) ;
#56763 = ORIENTED_EDGE('',*,*,#43115,.F.) ;
#56764 = ORIENTED_EDGE('',*,*,#42950,.F.) ;
#56765 = ORIENTED_EDGE('',*,*,#43114,.T.) ;
#56766 = ORIENTED_EDGE('',*,*,#42951,.F.) ;
#56767 = ORIENTED_EDGE('',*,*,#43116,.F.) ;
#56768 = ORIENTED_EDGE('',*,*,#42943,.F.) ;
#56769 = ORIENTED_EDGE('',*,*,#43116,.T.) ;
#56770 = ORIENTED_EDGE('',*,*,#43115,.T.) ;
#56771 = ORIENTED_EDGE('',*,*,#43117,.F.) ;
#56772 = ORIENTED_EDGE('',*,*,#42937,.T.) ;
#56773 = ORIENTED_EDGE('',*,*,#42931,.F.) ;
#56774 = ORIENTED_EDGE('',*,*,#42938,.F.) ;
#56775 = ORIENTED_EDGE('',*,*,#43117,.T.) ;
#56776 = ORIENTED_EDGE('',*,*,#42947,.F.) ;
#56777 = ORIENTED_EDGE('',*,*,#42687,.F.) ;
#56778 = ORIENTED_EDGE('',*,*,#42777,.F.) ;
#56779 = ORIENTED_EDGE('',*,*,#42904,.F.) ;
#56780 = ORIENTED_EDGE('',*,*,#42757,.F.) ;
#56781 = ORIENTED_EDGE('',*,*,#42756,.F.) ;
#56782 = ORIENTED_EDGE('',*,*,#43118,.T.) ;
#56783 = ORIENTED_EDGE('',*,*,#43119,.T.) ;
#56784 = ORIENTED_EDGE('',*,*,#42659,.T.) ;
#56785 = ORIENTED_EDGE('',*,*,#43061,.F.) ;
#56786 = ORIENTED_EDGE('',*,*,#42688,.T.) ;
#56787 = ORIENTED_EDGE('',*,*,#43063,.F.) ;
#56788 = ORIENTED_EDGE('',*,*,#43120,.T.) ;
#56789 = ORIENTED_EDGE('',*,*,#43067,.F.) ;
#56790 = ORIENTED_EDGE('',*,*,#43121,.F.) ;
#56791 = ORIENTED_EDGE('',*,*,#42686,.T.) ;
#56792 = ORIENTED_EDGE('',*,*,#43064,.F.) ;
#56793 = ORIENTED_EDGE('',*,*,#43122,.F.) ;
#56794 = ORIENTED_EDGE('',*,*,#42778,.F.) ;
#56795 = ORIENTED_EDGE('',*,*,#42793,.F.) ;
#56796 = ORIENTED_EDGE('',*,*,#43123,.T.) ;
#56797 = ORIENTED_EDGE('',*,*,#43071,.F.) ;
#56798 = ORIENTED_EDGE('',*,*,#43124,.T.) ;
#56799 = ORIENTED_EDGE('',*,*,#43074,.F.) ;
#56800 = ORIENTED_EDGE('',*,*,#43125,.T.) ;
#56801 = ORIENTED_EDGE('',*,*,#43065,.F.) ;
#56802 = ORIENTED_EDGE('',*,*,#43126,.T.) ;
#56803 = ORIENTED_EDGE('',*,*,#43122,.T.) ;
#56804 = ORIENTED_EDGE('',*,*,#43121,.T.) ;
#56805 = ORIENTED_EDGE('',*,*,#43127,.F.) ;
#56806 = ORIENTED_EDGE('',*,*,#42779,.T.) ;
#56807 = ORIENTED_EDGE('',*,*,#42784,.F.) ;
#56808 = ORIENTED_EDGE('',*,*,#42634,.F.) ;
#56809 = ORIENTED_EDGE('',*,*,#42760,.F.) ;
#56810 = ORIENTED_EDGE('',*,*,#42681,.F.) ;
#56811 = ORIENTED_EDGE('',*,*,#43128,.T.) ;
#56812 = ORIENTED_EDGE('',*,*,#43129,.T.) ;
#56813 = ORIENTED_EDGE('',*,*,#42781,.F.) ;
#56814 = ORIENTED_EDGE('',*,*,#42680,.F.) ;
#56815 = ORIENTED_EDGE('',*,*,#43069,.F.) ;
#56816 = ORIENTED_EDGE('',*,*,#43130,.T.) ;
#56817 = ORIENTED_EDGE('',*,*,#43127,.T.) ;
#56818 = ORIENTED_EDGE('',*,*,#43066,.F.) ;
#56819 = ORIENTED_EDGE('',*,*,#42679,.F.) ;
#56820 = ORIENTED_EDGE('',*,*,#42780,.F.) ;
#56821 = ORIENTED_EDGE('',*,*,#42682,.T.) ;
#56822 = ORIENTED_EDGE('',*,*,#42759,.F.) ;
#56823 = ORIENTED_EDGE('',*,*,#42677,.T.) ;
#56824 = ORIENTED_EDGE('',*,*,#43070,.F.) ;
#56825 = ORIENTED_EDGE('',*,*,#43131,.F.) ;
#56826 = ORIENTED_EDGE('',*,*,#43046,.F.) ;
#56827 = ORIENTED_EDGE('',*,*,#43132,.F.) ;
#56828 = ORIENTED_EDGE('',*,*,#43132,.T.) ;
#56829 = ORIENTED_EDGE('',*,*,#43044,.F.) ;
#56830 = ORIENTED_EDGE('',*,*,#43133,.F.) ;
#56831 = ORIENTED_EDGE('',*,*,#43057,.F.) ;
#56832 = ORIENTED_EDGE('',*,*,#43131,.T.) ;
#56833 = ORIENTED_EDGE('',*,*,#43060,.F.) ;
#56834 = ORIENTED_EDGE('',*,*,#43134,.F.) ;
#56835 = ORIENTED_EDGE('',*,*,#43048,.F.) ;
#56836 = ORIENTED_EDGE('',*,*,#43133,.T.) ;
#56837 = ORIENTED_EDGE('',*,*,#43042,.F.) ;
#56838 = ORIENTED_EDGE('',*,*,#43135,.F.) ;
#56839 = ORIENTED_EDGE('',*,*,#43050,.F.) ;
#56840 = ORIENTED_EDGE('',*,*,#43134,.T.) ;
#56841 = ORIENTED_EDGE('',*,*,#43136,.F.) ;
#56842 = ORIENTED_EDGE('',*,*,#43135,.T.) ;
#56843 = ORIENTED_EDGE('',*,*,#43056,.F.) ;
#56844 = ORIENTED_EDGE('',*,*,#43137,.F.) ;
#56845 = ORIENTED_EDGE('',*,*,#43058,.F.) ;
#56846 = ORIENTED_EDGE('',*,*,#43136,.T.) ;
#56847 = ORIENTED_EDGE('',*,*,#43059,.F.) ;
#56848 = ORIENTED_EDGE('',*,*,#43138,.F.) ;
#56849 = ORIENTED_EDGE('',*,*,#43052,.F.) ;
#56850 = ORIENTED_EDGE('',*,*,#43137,.T.) ;
#56851 = ORIENTED_EDGE('',*,*,#43054,.F.) ;
#56852 = ORIENTED_EDGE('',*,*,#43138,.T.) ;
#56853 = ORIENTED_EDGE('',*,*,#43139,.F.) ;
#56854 = ORIENTED_EDGE('',*,*,#42871,.F.) ;
#56855 = ORIENTED_EDGE('',*,*,#43140,.F.) ;
#56856 = ORIENTED_EDGE('',*,*,#42965,.F.) ;
#56857 = ORIENTED_EDGE('',*,*,#43140,.T.) ;
#56858 = ORIENTED_EDGE('',*,*,#42870,.T.) ;
#56859 = ORIENTED_EDGE('',*,*,#43141,.F.) ;
#56860 = ORIENTED_EDGE('',*,*,#43142,.F.) ;
#56861 = ORIENTED_EDGE('',*,*,#42872,.T.) ;
#56862 = ORIENTED_EDGE('',*,*,#43139,.T.) ;
#56863 = ORIENTED_EDGE('',*,*,#43143,.F.) ;
#56864 = ORIENTED_EDGE('',*,*,#43144,.F.) ;
#56865 = ORIENTED_EDGE('',*,*,#43141,.T.) ;
#56866 = ORIENTED_EDGE('',*,*,#42869,.F.) ;
#56867 = ORIENTED_EDGE('',*,*,#43145,.F.) ;
#56868 = ORIENTED_EDGE('',*,*,#42977,.F.) ;
#56869 = ORIENTED_EDGE('',*,*,#43142,.T.) ;
#56870 = ORIENTED_EDGE('',*,*,#42976,.F.) ;
#56871 = ORIENTED_EDGE('',*,*,#43146,.F.) ;
#56872 = ORIENTED_EDGE('',*,*,#42962,.F.) ;
#56873 = ORIENTED_EDGE('',*,*,#43147,.F.) ;
#56874 = ORIENTED_EDGE('',*,*,#42963,.F.) ;
#56875 = ORIENTED_EDGE('',*,*,#43148,.F.) ;
#56876 = ORIENTED_EDGE('',*,*,#42981,.F.) ;
#56877 = ORIENTED_EDGE('',*,*,#43143,.T.) ;
#56878 = ORIENTED_EDGE('',*,*,#42964,.F.) ;
#56879 = ORIENTED_EDGE('',*,*,#43149,.F.) ;
#56880 = ORIENTED_EDGE('',*,*,#42969,.F.) ;
#56881 = ORIENTED_EDGE('',*,*,#43144,.T.) ;
#56882 = ORIENTED_EDGE('',*,*,#42968,.F.) ;
#56883 = ORIENTED_EDGE('',*,*,#43150,.F.) ;
#56884 = ORIENTED_EDGE('',*,*,#42873,.F.) ;
#56885 = ORIENTED_EDGE('',*,*,#43151,.F.) ;
#56886 = ORIENTED_EDGE('',*,*,#42867,.F.) ;
#56887 = ORIENTED_EDGE('',*,*,#43152,.F.) ;
#56888 = ORIENTED_EDGE('',*,*,#42972,.F.) ;
#56889 = ORIENTED_EDGE('',*,*,#42868,.T.) ;
#56890 = ORIENTED_EDGE('',*,*,#43151,.T.) ;
#56891 = ORIENTED_EDGE('',*,*,#43153,.F.) ;
#56892 = ORIENTED_EDGE('',*,*,#43145,.T.) ;
#56893 = ORIENTED_EDGE('',*,*,#43148,.T.) ;
#56894 = ORIENTED_EDGE('',*,*,#43146,.T.) ;
#56895 = ORIENTED_EDGE('',*,*,#43154,.F.) ;
#56896 = ORIENTED_EDGE('',*,*,#43149,.T.) ;
#56897 = ORIENTED_EDGE('',*,*,#43147,.T.) ;
#56898 = ORIENTED_EDGE('',*,*,#43155,.F.) ;
#56899 = ORIENTED_EDGE('',*,*,#42866,.T.) ;
#56900 = ORIENTED_EDGE('',*,*,#43150,.T.) ;
#56901 = ORIENTED_EDGE('',*,*,#43156,.F.) ;
#56902 = ORIENTED_EDGE('',*,*,#43152,.T.) ;
#56903 = ORIENTED_EDGE('',*,*,#43153,.T.) ;
#56904 = ORIENTED_EDGE('',*,*,#42971,.F.) ;
#56905 = ORIENTED_EDGE('',*,*,#43157,.F.) ;
#56906 = ORIENTED_EDGE('',*,*,#42974,.F.) ;
#56907 = ORIENTED_EDGE('',*,*,#43154,.T.) ;
#56908 = ORIENTED_EDGE('',*,*,#42975,.F.) ;
#56909 = ORIENTED_EDGE('',*,*,#43158,.F.) ;
#56910 = ORIENTED_EDGE('',*,*,#42978,.F.) ;
#56911 = ORIENTED_EDGE('',*,*,#43155,.T.) ;
#56912 = ORIENTED_EDGE('',*,*,#42980,.F.) ;
#56913 = ORIENTED_EDGE('',*,*,#43159,.F.) ;
#56914 = ORIENTED_EDGE('',*,*,#42966,.F.) ;
#56915 = ORIENTED_EDGE('',*,*,#43156,.T.) ;
#56916 = ORIENTED_EDGE('',*,*,#42967,.F.) ;
#56917 = ORIENTED_EDGE('',*,*,#43160,.F.) ;
#56918 = ORIENTED_EDGE('',*,*,#42973,.F.) ;
#56919 = ORIENTED_EDGE('',*,*,#43158,.T.) ;
#56920 = ORIENTED_EDGE('',*,*,#43157,.T.) ;
#56921 = ORIENTED_EDGE('',*,*,#43161,.F.) ;
#56922 = ORIENTED_EDGE('',*,*,#43160,.T.) ;
#56923 = ORIENTED_EDGE('',*,*,#43159,.T.) ;
#56924 = ORIENTED_EDGE('',*,*,#43162,.F.) ;
#56925 = ORIENTED_EDGE('',*,*,#43161,.T.) ;
#56926 = ORIENTED_EDGE('',*,*,#42970,.F.) ;
#56927 = ORIENTED_EDGE('',*,*,#43162,.T.) ;
#56928 = ORIENTED_EDGE('',*,*,#42979,.F.) ;
#56929 = ORIENTED_EDGE('',*,*,#43163,.F.) ;
#56930 = ORIENTED_EDGE('',*,*,#42821,.F.) ;
#56931 = ORIENTED_EDGE('',*,*,#43164,.F.) ;
#56932 = ORIENTED_EDGE('',*,*,#43024,.F.) ;
#56933 = ORIENTED_EDGE('',*,*,#43164,.T.) ;
#56934 = ORIENTED_EDGE('',*,*,#42820,.T.) ;
#56935 = ORIENTED_EDGE('',*,*,#43165,.F.) ;
#56936 = ORIENTED_EDGE('',*,*,#43166,.F.) ;
#56937 = ORIENTED_EDGE('',*,*,#42822,.T.) ;
#56938 = ORIENTED_EDGE('',*,*,#43163,.T.) ;
#56939 = ORIENTED_EDGE('',*,*,#43167,.F.) ;
#56940 = ORIENTED_EDGE('',*,*,#43168,.F.) ;
#56941 = ORIENTED_EDGE('',*,*,#43165,.T.) ;
#56942 = ORIENTED_EDGE('',*,*,#42819,.F.) ;
#56943 = ORIENTED_EDGE('',*,*,#43169,.F.) ;
#56944 = ORIENTED_EDGE('',*,*,#43020,.F.) ;
#56945 = ORIENTED_EDGE('',*,*,#43166,.T.) ;
#56946 = ORIENTED_EDGE('',*,*,#43019,.F.) ;
#56947 = ORIENTED_EDGE('',*,*,#43170,.F.) ;
#56948 = ORIENTED_EDGE('',*,*,#43021,.F.) ;
#56949 = ORIENTED_EDGE('',*,*,#43171,.F.) ;
#56950 = ORIENTED_EDGE('',*,*,#43022,.F.) ;
#56951 = ORIENTED_EDGE('',*,*,#43172,.F.) ;
#56952 = ORIENTED_EDGE('',*,*,#43032,.F.) ;
#56953 = ORIENTED_EDGE('',*,*,#43167,.T.) ;
#56954 = ORIENTED_EDGE('',*,*,#43023,.F.) ;
#56955 = ORIENTED_EDGE('',*,*,#43173,.F.) ;
#56956 = ORIENTED_EDGE('',*,*,#43028,.F.) ;
#56957 = ORIENTED_EDGE('',*,*,#43168,.T.) ;
#56958 = ORIENTED_EDGE('',*,*,#43027,.F.) ;
#56959 = ORIENTED_EDGE('',*,*,#43174,.F.) ;
#56960 = ORIENTED_EDGE('',*,*,#42823,.F.) ;
#56961 = ORIENTED_EDGE('',*,*,#43175,.F.) ;
#56962 = ORIENTED_EDGE('',*,*,#42817,.F.) ;
#56963 = ORIENTED_EDGE('',*,*,#43176,.F.) ;
#56964 = ORIENTED_EDGE('',*,*,#43015,.F.) ;
#56965 = ORIENTED_EDGE('',*,*,#42818,.T.) ;
#56966 = ORIENTED_EDGE('',*,*,#43175,.T.) ;
#56967 = ORIENTED_EDGE('',*,*,#43177,.F.) ;
#56968 = ORIENTED_EDGE('',*,*,#43169,.T.) ;
#56969 = ORIENTED_EDGE('',*,*,#43172,.T.) ;
#56970 = ORIENTED_EDGE('',*,*,#43170,.T.) ;
#56971 = ORIENTED_EDGE('',*,*,#43178,.F.) ;
#56972 = ORIENTED_EDGE('',*,*,#43173,.T.) ;
#56973 = ORIENTED_EDGE('',*,*,#43171,.T.) ;
#56974 = ORIENTED_EDGE('',*,*,#43179,.F.) ;
#56975 = ORIENTED_EDGE('',*,*,#42816,.T.) ;
#56976 = ORIENTED_EDGE('',*,*,#43174,.T.) ;
#56977 = ORIENTED_EDGE('',*,*,#43180,.F.) ;
#56978 = ORIENTED_EDGE('',*,*,#43176,.T.) ;
#56979 = ORIENTED_EDGE('',*,*,#43177,.T.) ;
#56980 = ORIENTED_EDGE('',*,*,#43014,.F.) ;
#56981 = ORIENTED_EDGE('',*,*,#43181,.F.) ;
#56982 = ORIENTED_EDGE('',*,*,#43017,.F.) ;
#56983 = ORIENTED_EDGE('',*,*,#43178,.T.) ;
#56984 = ORIENTED_EDGE('',*,*,#43018,.F.) ;
#56985 = ORIENTED_EDGE('',*,*,#43182,.F.) ;
#56986 = ORIENTED_EDGE('',*,*,#43029,.F.) ;
#56987 = ORIENTED_EDGE('',*,*,#43179,.T.) ;
#56988 = ORIENTED_EDGE('',*,*,#43031,.F.) ;
#56989 = ORIENTED_EDGE('',*,*,#43183,.F.) ;
#56990 = ORIENTED_EDGE('',*,*,#43025,.F.) ;
#56991 = ORIENTED_EDGE('',*,*,#43180,.T.) ;
#56992 = ORIENTED_EDGE('',*,*,#43026,.F.) ;
#56993 = ORIENTED_EDGE('',*,*,#43184,.F.) ;
#56994 = ORIENTED_EDGE('',*,*,#43016,.F.) ;
#56995 = ORIENTED_EDGE('',*,*,#43182,.T.) ;
#56996 = ORIENTED_EDGE('',*,*,#43181,.T.) ;
#56997 = ORIENTED_EDGE('',*,*,#43185,.F.) ;
#56998 = ORIENTED_EDGE('',*,*,#43184,.T.) ;
#56999 = ORIENTED_EDGE('',*,*,#43183,.T.) ;
#57000 = ORIENTED_EDGE('',*,*,#43186,.F.) ;
#57001 = ORIENTED_EDGE('',*,*,#43185,.T.) ;
#57002 = ORIENTED_EDGE('',*,*,#43013,.F.) ;
#57003 = ORIENTED_EDGE('',*,*,#43186,.T.) ;
#57004 = ORIENTED_EDGE('',*,*,#43030,.F.) ;
#57005 = ORIENTED_EDGE('',*,*,#42895,.F.) ;
#57006 = ORIENTED_EDGE('',*,*,#43187,.T.) ;
#57007 = ORIENTED_EDGE('',*,*,#43076,.F.) ;
#57008 = ORIENTED_EDGE('',*,*,#43188,.F.) ;
#57009 = ORIENTED_EDGE('',*,*,#42752,.F.) ;
#57010 = ORIENTED_EDGE('',*,*,#43189,.F.) ;
#57011 = ORIENTED_EDGE('',*,*,#42892,.F.) ;
#57012 = ORIENTED_EDGE('',*,*,#43190,.F.) ;
#57013 = ORIENTED_EDGE('',*,*,#43190,.T.) ;
#57014 = ORIENTED_EDGE('',*,*,#43188,.T.) ;
#57015 = ORIENTED_EDGE('',*,*,#43191,.F.) ;
#57016 = ORIENTED_EDGE('',*,*,#43191,.T.) ;
#57017 = ORIENTED_EDGE('',*,*,#43081,.F.) ;
#57018 = ORIENTED_EDGE('',*,*,#43192,.F.) ;
#57019 = ORIENTED_EDGE('',*,*,#42753,.F.) ;
#57020 = ORIENTED_EDGE('',*,*,#42771,.F.) ;
#57021 = ORIENTED_EDGE('',*,*,#43193,.F.) ;
#57022 = ORIENTED_EDGE('',*,*,#42750,.F.) ;
#57023 = ORIENTED_EDGE('',*,*,#43194,.F.) ;
#57024 = ORIENTED_EDGE('',*,*,#43194,.T.) ;
#57025 = ORIENTED_EDGE('',*,*,#43192,.T.) ;
#57026 = ORIENTED_EDGE('',*,*,#43195,.F.) ;
#57027 = ORIENTED_EDGE('',*,*,#42772,.T.) ;
#57028 = ORIENTED_EDGE('',*,*,#43195,.T.) ;
#57029 = ORIENTED_EDGE('',*,*,#43080,.F.) ;
#57030 = ORIENTED_EDGE('',*,*,#43196,.F.) ;
#57031 = ORIENTED_EDGE('',*,*,#42773,.F.) ;
#57032 = ORIENTED_EDGE('',*,*,#42905,.F.) ;
#57033 = ORIENTED_EDGE('',*,*,#42775,.F.) ;
#57034 = ORIENTED_EDGE('',*,*,#43197,.F.) ;
#57035 = ORIENTED_EDGE('',*,*,#42899,.F.) ;
#57036 = ORIENTED_EDGE('',*,*,#42774,.T.) ;
#57037 = ORIENTED_EDGE('',*,*,#43196,.T.) ;
#57038 = ORIENTED_EDGE('',*,*,#43198,.F.) ;
#57039 = ORIENTED_EDGE('',*,*,#43197,.T.) ;
#57040 = ORIENTED_EDGE('',*,*,#43198,.T.) ;
#57041 = ORIENTED_EDGE('',*,*,#43079,.F.) ;
#57042 = ORIENTED_EDGE('',*,*,#43199,.F.) ;
#57043 = ORIENTED_EDGE('',*,*,#42896,.F.) ;
#57044 = ORIENTED_EDGE('',*,*,#42906,.F.) ;
#57045 = ORIENTED_EDGE('',*,*,#42897,.F.) ;
#57046 = ORIENTED_EDGE('',*,*,#43200,.F.) ;
#57047 = ORIENTED_EDGE('',*,*,#42749,.F.) ;
#57048 = ORIENTED_EDGE('',*,*,#43200,.T.) ;
#57049 = ORIENTED_EDGE('',*,*,#43199,.T.) ;
#57050 = ORIENTED_EDGE('',*,*,#43201,.F.) ;
#57051 = ORIENTED_EDGE('',*,*,#43078,.F.) ;
#57052 = ORIENTED_EDGE('',*,*,#43202,.T.) ;
#57053 = ORIENTED_EDGE('',*,*,#42746,.F.) ;
#57054 = ORIENTED_EDGE('',*,*,#43201,.T.) ;
#57055 = ORIENTED_EDGE('',*,*,#42889,.F.) ;
#57056 = ORIENTED_EDGE('',*,*,#43203,.F.) ;
#57057 = ORIENTED_EDGE('',*,*,#42875,.F.) ;
#57058 = ORIENTED_EDGE('',*,*,#42908,.F.) ;
#57059 = ORIENTED_EDGE('',*,*,#42877,.F.) ;
#57060 = ORIENTED_EDGE('',*,*,#43204,.F.) ;
#57061 = ORIENTED_EDGE('',*,*,#42855,.F.) ;
#57062 = ORIENTED_EDGE('',*,*,#42909,.F.) ;
#57063 = ORIENTED_EDGE('',*,*,#42857,.F.) ;
#57064 = ORIENTED_EDGE('',*,*,#43205,.F.) ;
#57065 = ORIENTED_EDGE('',*,*,#42835,.F.) ;
#57066 = ORIENTED_EDGE('',*,*,#42910,.F.) ;
#57067 = ORIENTED_EDGE('',*,*,#42837,.F.) ;
#57068 = ORIENTED_EDGE('',*,*,#43206,.F.) ;
#57069 = ORIENTED_EDGE('',*,*,#42832,.F.) ;
#57070 = ORIENTED_EDGE('',*,*,#42911,.F.) ;
#57071 = ORIENTED_EDGE('',*,*,#42830,.F.) ;
#57072 = ORIENTED_EDGE('',*,*,#43207,.F.) ;
#57073 = ORIENTED_EDGE('',*,*,#42825,.F.) ;
#57074 = ORIENTED_EDGE('',*,*,#42912,.F.) ;
#57075 = ORIENTED_EDGE('',*,*,#42827,.F.) ;
#57076 = ORIENTED_EDGE('',*,*,#43208,.F.) ;
#57077 = ORIENTED_EDGE('',*,*,#42805,.F.) ;
#57078 = ORIENTED_EDGE('',*,*,#42913,.F.) ;
#57079 = ORIENTED_EDGE('',*,*,#42695,.F.) ;
#57080 = ORIENTED_EDGE('',*,*,#43009,.F.) ;
#57081 = ORIENTED_EDGE('',*,*,#42705,.F.) ;
#57082 = ORIENTED_EDGE('',*,*,#43011,.F.) ;
#57083 = ORIENTED_EDGE('',*,*,#42703,.F.) ;
#57084 = ORIENTED_EDGE('',*,*,#43007,.F.) ;
#57085 = ORIENTED_EDGE('',*,*,#42697,.F.) ;
#57086 = ORIENTED_EDGE('',*,*,#43012,.F.) ;
#57087 = ORIENTED_EDGE('',*,*,#42693,.F.) ;
#57088 = ORIENTED_EDGE('',*,*,#42758,.F.) ;
#57089 = ORIENTED_EDGE('',*,*,#42707,.F.) ;
#57090 = ORIENTED_EDGE('',*,*,#43010,.F.) ;
#57091 = ORIENTED_EDGE('',*,*,#42701,.F.) ;
#57092 = ORIENTED_EDGE('',*,*,#43006,.F.) ;
#57093 = ORIENTED_EDGE('',*,*,#42699,.F.) ;
#57094 = ORIENTED_EDGE('',*,*,#43008,.F.) ;
#57095 = ORIENTED_EDGE('',*,*,#42807,.F.) ;
#57096 = ORIENTED_EDGE('',*,*,#43209,.F.) ;
#57097 = ORIENTED_EDGE('',*,*,#42801,.F.) ;
#57098 = ORIENTED_EDGE('',*,*,#42900,.F.) ;
#57099 = ORIENTED_EDGE('',*,*,#42799,.F.) ;
#57100 = ORIENTED_EDGE('',*,*,#43210,.F.) ;
#57101 = ORIENTED_EDGE('',*,*,#42710,.F.) ;
#57102 = ORIENTED_EDGE('',*,*,#42901,.F.) ;
#57103 = ORIENTED_EDGE('',*,*,#42712,.F.) ;
#57104 = ORIENTED_EDGE('',*,*,#43211,.F.) ;
#57105 = ORIENTED_EDGE('',*,*,#42785,.F.) ;
#57106 = ORIENTED_EDGE('',*,*,#42902,.F.) ;
#57107 = ORIENTED_EDGE('',*,*,#43212,.F.) ;
#57108 = ORIENTED_EDGE('',*,*,#42684,.F.) ;
#57109 = ORIENTED_EDGE('',*,*,#43125,.F.) ;
#57110 = ORIENTED_EDGE('',*,*,#43212,.T.) ;
#57111 = ORIENTED_EDGE('',*,*,#43073,.F.) ;
#57112 = ORIENTED_EDGE('',*,*,#43213,.F.) ;
#57113 = ORIENTED_EDGE('',*,*,#43068,.F.) ;
#57114 = ORIENTED_EDGE('',*,*,#43213,.T.) ;
#57115 = ORIENTED_EDGE('',*,*,#43072,.F.) ;
#57116 = ORIENTED_EDGE('',*,*,#43214,.F.) ;
#57117 = ORIENTED_EDGE('',*,*,#43130,.F.) ;
#57118 = ORIENTED_EDGE('',*,*,#43214,.T.) ;
#57119 = ORIENTED_EDGE('',*,*,#43123,.F.) ;
#57120 = ORIENTED_EDGE('',*,*,#43215,.F.) ;
#57121 = ORIENTED_EDGE('',*,*,#43128,.F.) ;
#57122 = ORIENTED_EDGE('',*,*,#43215,.T.) ;
#57123 = ORIENTED_EDGE('',*,*,#42792,.F.) ;
#57124 = ORIENTED_EDGE('',*,*,#43216,.F.) ;
#57125 = ORIENTED_EDGE('',*,*,#43129,.F.) ;
#57126 = ORIENTED_EDGE('',*,*,#43216,.T.) ;
#57127 = ORIENTED_EDGE('',*,*,#42791,.F.) ;
#57128 = ORIENTED_EDGE('',*,*,#43217,.F.) ;
#57129 = ORIENTED_EDGE('',*,*,#42782,.F.) ;
#57130 = ORIENTED_EDGE('',*,*,#42903,.F.) ;
#57131 = ORIENTED_EDGE('',*,*,#42795,.F.) ;
#57132 = ORIENTED_EDGE('',*,*,#43218,.F.) ;
#57133 = ORIENTED_EDGE('',*,*,#42755,.F.) ;
#57134 = ORIENTED_EDGE('',*,*,#43218,.T.) ;
#57135 = ORIENTED_EDGE('',*,*,#42794,.F.) ;
#57136 = ORIENTED_EDGE('',*,*,#43219,.F.) ;
#57137 = ORIENTED_EDGE('',*,*,#43118,.F.) ;
#57138 = ORIENTED_EDGE('',*,*,#43219,.T.) ;
#57139 = ORIENTED_EDGE('',*,*,#43124,.F.) ;
#57140 = ORIENTED_EDGE('',*,*,#42660,.F.) ;
#57141 = ORIENTED_EDGE('',*,*,#43119,.F.) ;
#57142 = ORIENTED_EDGE('',*,*,#43220,.F.) ;
#57143 = ORIENTED_EDGE('',*,*,#43062,.F.) ;
#57144 = ORIENTED_EDGE('',*,*,#42658,.T.) ;
#57145 = ORIENTED_EDGE('',*,*,#43075,.F.) ;
#57146 = ORIENTED_EDGE('',*,*,#43126,.F.) ;
#57147 = ORIENTED_EDGE('',*,*,#43120,.F.) ;
#57148 = ORIENTED_EDGE('',*,*,#43220,.T.) ;
#57149 = ORIENTED_EDGE('',*,*,#43221,.T.) ;
#57150 = ORIENTED_EDGE('',*,*,#43222,.T.) ;
#57151 = ORIENTED_EDGE('',*,*,#43077,.F.) ;
#57152 = ORIENTED_EDGE('',*,*,#43223,.T.) ;
#57153 = ORIENTED_EDGE('',*,*,#43224,.T.) ;
#57154 = ORIENTED_EDGE('',*,*,#42894,.F.) ;
#57155 = ORIENTED_EDGE('',*,*,#43225,.F.) ;
#57156 = ORIENTED_EDGE('',*,*,#42882,.F.) ;
#57157 = ORIENTED_EDGE('',*,*,#43226,.F.) ;
#57158 = ORIENTED_EDGE('',*,*,#42881,.F.) ;
#57159 = ORIENTED_EDGE('',*,*,#43227,.T.) ;
#57160 = ORIENTED_EDGE('',*,*,#43187,.F.) ;
#57161 = ORIENTED_EDGE('',*,*,#43226,.T.) ;
#57162 = ORIENTED_EDGE('',*,*,#42907,.F.) ;
#57163 = ORIENTED_EDGE('',*,*,#42747,.F.) ;
#57164 = ORIENTED_EDGE('',*,*,#43228,.F.) ;
#57165 = ORIENTED_EDGE('',*,*,#42891,.F.) ;
#57166 = ORIENTED_EDGE('',*,*,#43202,.F.) ;
#57167 = ORIENTED_EDGE('',*,*,#43229,.T.) ;
#57168 = ORIENTED_EDGE('',*,*,#42878,.F.) ;
#57169 = ORIENTED_EDGE('',*,*,#43228,.T.) ;
#57170 = ORIENTED_EDGE('',*,*,#43223,.F.) ;
#57171 = ORIENTED_EDGE('',*,*,#43227,.F.) ;
#57172 = ORIENTED_EDGE('',*,*,#43230,.F.) ;
#57173 = ORIENTED_EDGE('',*,*,#43231,.F.) ;
#57174 = ORIENTED_EDGE('',*,*,#43224,.F.) ;
#57175 = ORIENTED_EDGE('',*,*,#43230,.T.) ;
#57176 = ORIENTED_EDGE('',*,*,#42880,.F.) ;
#57177 = ORIENTED_EDGE('',*,*,#43231,.T.) ;
#57178 = ORIENTED_EDGE('',*,*,#42879,.F.) ;
#57179 = ORIENTED_EDGE('',*,*,#43232,.F.) ;
#57180 = ORIENTED_EDGE('',*,*,#43221,.F.) ;
#57181 = ORIENTED_EDGE('',*,*,#43232,.T.) ;
#57182 = ORIENTED_EDGE('',*,*,#43229,.F.) ;
#57183 = ORIENTED_EDGE('',*,*,#43222,.F.) ;
#57184 = ORIENTED_EDGE('',*,*,#42734,.F.) ;
#57185 = ORIENTED_EDGE('',*,*,#42730,.T.) ;
#57186 = ORIENTED_EDGE('',*,*,#42737,.T.) ;
#57187 = ORIENTED_EDGE('',*,*,#42726,.T.) ;
#57188 = ORIENTED_EDGE('',*,*,#42739,.T.) ;
#57189 = ORIENTED_EDGE('',*,*,#42722,.T.) ;
#57190 = ORIENTED_EDGE('',*,*,#42743,.F.) ;
#57191 = ORIENTED_EDGE('',*,*,#42803,.T.) ;
#57192 = ORIENTED_EDGE('',*,*,#43233,.T.) ;
#57193 = ORIENTED_EDGE('',*,*,#43234,.T.) ;
#57194 = ORIENTED_EDGE('',*,*,#43235,.F.) ;
#57195 = ORIENTED_EDGE('',*,*,#43236,.T.) ;
#57196 = ORIENTED_EDGE('',*,*,#43235,.T.) ;
#57197 = ORIENTED_EDGE('',*,*,#43237,.T.) ;
#57198 = ORIENTED_EDGE('',*,*,#43238,.F.) ;
#57199 = ORIENTED_EDGE('',*,*,#43239,.T.) ;
#57200 = ORIENTED_EDGE('',*,*,#43238,.T.) ;
#57201 = ORIENTED_EDGE('',*,*,#43240,.T.) ;
#57202 = ORIENTED_EDGE('',*,*,#43241,.F.) ;
#57203 = ORIENTED_EDGE('',*,*,#43242,.T.) ;
#57204 = ORIENTED_EDGE('',*,*,#43241,.T.) ;
#57205 = ORIENTED_EDGE('',*,*,#43243,.T.) ;
#57206 = ORIENTED_EDGE('',*,*,#43244,.F.) ;
#57207 = ORIENTED_EDGE('',*,*,#43245,.T.) ;
#57208 = ORIENTED_EDGE('',*,*,#43244,.T.) ;
#57209 = ORIENTED_EDGE('',*,*,#43246,.T.) ;
#57210 = ORIENTED_EDGE('',*,*,#43247,.F.) ;
#57211 = ORIENTED_EDGE('',*,*,#43248,.T.) ;
#57212 = ORIENTED_EDGE('',*,*,#43247,.T.) ;
#57213 = ORIENTED_EDGE('',*,*,#43249,.T.) ;
#57214 = ORIENTED_EDGE('',*,*,#43250,.F.) ;
#57215 = ORIENTED_EDGE('',*,*,#43251,.T.) ;
#57216 = ORIENTED_EDGE('',*,*,#43250,.T.) ;
#57217 = ORIENTED_EDGE('',*,*,#43252,.T.) ;
#57218 = ORIENTED_EDGE('',*,*,#43253,.F.) ;
#57219 = ORIENTED_EDGE('',*,*,#43254,.T.) ;
#57220 = ORIENTED_EDGE('',*,*,#43253,.T.) ;
#57221 = ORIENTED_EDGE('',*,*,#43255,.T.) ;
#57222 = ORIENTED_EDGE('',*,*,#43256,.F.) ;
#57223 = ORIENTED_EDGE('',*,*,#43257,.T.) ;
#57224 = ORIENTED_EDGE('',*,*,#43256,.T.) ;
#57225 = ORIENTED_EDGE('',*,*,#43258,.T.) ;
#57226 = ORIENTED_EDGE('',*,*,#43259,.T.) ;
#57227 = ORIENTED_EDGE('',*,*,#43260,.T.) ;
#57228 = ORIENTED_EDGE('',*,*,#43261,.T.) ;
#57229 = ORIENTED_EDGE('',*,*,#43262,.T.) ;
#57230 = ORIENTED_EDGE('',*,*,#43263,.T.) ;
#57231 = ORIENTED_EDGE('',*,*,#43264,.T.) ;
#57232 = ORIENTED_EDGE('',*,*,#43265,.T.) ;
#57233 = ORIENTED_EDGE('',*,*,#43266,.T.) ;
#57234 = ORIENTED_EDGE('',*,*,#43267,.T.) ;
#57235 = ORIENTED_EDGE('',*,*,#43268,.T.) ;
#57236 = ORIENTED_EDGE('',*,*,#43269,.T.) ;
#57237 = ORIENTED_EDGE('',*,*,#43270,.T.) ;
#57238 = ORIENTED_EDGE('',*,*,#43271,.T.) ;
#57239 = ORIENTED_EDGE('',*,*,#43272,.T.) ;
#57240 = ORIENTED_EDGE('',*,*,#43273,.T.) ;
#57241 = ORIENTED_EDGE('',*,*,#43274,.T.) ;
#57242 = ORIENTED_EDGE('',*,*,#43275,.F.) ;
#57243 = ORIENTED_EDGE('',*,*,#43276,.T.) ;
#57244 = ORIENTED_EDGE('',*,*,#43277,.T.) ;
#57245 = ORIENTED_EDGE('',*,*,#43278,.T.) ;
#57246 = ORIENTED_EDGE('',*,*,#42639,.T.) ;
#57247 = ORIENTED_EDGE('',*,*,#42655,.T.) ;
#57248 = ORIENTED_EDGE('',*,*,#43279,.T.) ;
#57249 = ORIENTED_EDGE('',*,*,#43280,.T.) ;
#57250 = ORIENTED_EDGE('',*,*,#43281,.T.) ;
#57251 = ORIENTED_EDGE('',*,*,#43282,.F.) ;
#57252 = ORIENTED_EDGE('',*,*,#43283,.T.) ;
#57253 = ORIENTED_EDGE('',*,*,#43284,.F.) ;
#57254 = ORIENTED_EDGE('',*,*,#43285,.T.) ;
#57255 = ORIENTED_EDGE('',*,*,#43286,.T.) ;
#57256 = ORIENTED_EDGE('',*,*,#43287,.T.) ;
#57257 = ORIENTED_EDGE('',*,*,#42888,.T.) ;
#57258 = ORIENTED_EDGE('',*,*,#43288,.T.) ;
#57259 = ORIENTED_EDGE('',*,*,#43284,.T.) ;
#57260 = ORIENTED_EDGE('',*,*,#43289,.T.) ;
#57261 = ORIENTED_EDGE('',*,*,#43275,.T.) ;
#57262 = ORIENTED_EDGE('',*,*,#43290,.T.) ;
#57263 = ORIENTED_EDGE('',*,*,#42766,.T.) ;
#57264 = ORIENTED_EDGE('',*,*,#43291,.T.) ;
#57265 = ORIENTED_EDGE('',*,*,#43282,.T.) ;
#57266 = ORIENTED_EDGE('',*,*,#43292,.T.) ;
#57267 = ORIENTED_EDGE('',*,*,#42786,.T.) ;
#57268 = ORIENTED_EDGE('',*,*,#43211,.T.) ;
#57269 = ORIENTED_EDGE('',*,*,#42711,.T.) ;
#57270 = ORIENTED_EDGE('',*,*,#43210,.T.) ;
#57271 = ORIENTED_EDGE('',*,*,#42798,.T.) ;
#57272 = ORIENTED_EDGE('',*,*,#42744,.T.) ;
#57273 = ORIENTED_EDGE('',*,*,#42724,.T.) ;
#57274 = ORIENTED_EDGE('',*,*,#42740,.T.) ;
#57275 = ORIENTED_EDGE('',*,*,#42728,.T.) ;
#57276 = ORIENTED_EDGE('',*,*,#42738,.T.) ;
#57277 = ORIENTED_EDGE('',*,*,#42732,.T.) ;
#57278 = ORIENTED_EDGE('',*,*,#42736,.T.) ;
#57279 = ORIENTED_EDGE('',*,*,#42802,.T.) ;
#57280 = ORIENTED_EDGE('',*,*,#43209,.T.) ;
#57281 = ORIENTED_EDGE('',*,*,#42806,.T.) ;
#57282 = ORIENTED_EDGE('',*,*,#43208,.T.) ;
#57283 = ORIENTED_EDGE('',*,*,#42826,.T.) ;
#57284 = ORIENTED_EDGE('',*,*,#43207,.T.) ;
#57285 = ORIENTED_EDGE('',*,*,#42829,.T.) ;
#57286 = ORIENTED_EDGE('',*,*,#42663,.T.) ;
#57287 = ORIENTED_EDGE('',*,*,#42833,.T.) ;
#57288 = ORIENTED_EDGE('',*,*,#43206,.T.) ;
#57289 = ORIENTED_EDGE('',*,*,#42836,.T.) ;
#57290 = ORIENTED_EDGE('',*,*,#43205,.T.) ;
#57291 = ORIENTED_EDGE('',*,*,#42856,.T.) ;
#57292 = ORIENTED_EDGE('',*,*,#43204,.T.) ;
#57293 = ORIENTED_EDGE('',*,*,#42876,.T.) ;
#57294 = ORIENTED_EDGE('',*,*,#43203,.T.) ;
#57295 = ORIENTED_EDGE('',*,*,#43293,.T.) ;
#57296 = ORIENTED_EDGE('',*,*,#43294,.T.) ;
#57297 = ORIENTED_EDGE('',*,*,#43295,.T.) ;
#57298 = ORIENTED_EDGE('',*,*,#43296,.T.) ;
#57299 = ORIENTED_EDGE('',*,*,#43297,.T.) ;
#57300 = ORIENTED_EDGE('',*,*,#43298,.T.) ;
#57301 = ORIENTED_EDGE('',*,*,#43299,.T.) ;
#57302 = ORIENTED_EDGE('',*,*,#43300,.T.) ;
#57303 = ORIENTED_EDGE('',*,*,#43301,.F.) ;
#57304 = ORIENTED_EDGE('',*,*,#43302,.T.) ;
#57305 = ORIENTED_EDGE('',*,*,#43303,.T.) ;
#57306 = ORIENTED_EDGE('',*,*,#43304,.T.) ;
#57307 = ORIENTED_EDGE('',*,*,#43305,.F.) ;
#57308 = ORIENTED_EDGE('',*,*,#43306,.T.) ;
#57309 = ORIENTED_EDGE('',*,*,#43307,.T.) ;
#57310 = ORIENTED_EDGE('',*,*,#43308,.T.) ;
#57311 = ORIENTED_EDGE('',*,*,#43309,.T.) ;
#57312 = ORIENTED_EDGE('',*,*,#43310,.T.) ;
#57313 = ORIENTED_EDGE('',*,*,#43311,.F.) ;
#57314 = ORIENTED_EDGE('',*,*,#43312,.T.) ;
#57315 = ORIENTED_EDGE('',*,*,#43303,.F.) ;
#57316 = ORIENTED_EDGE('',*,*,#43313,.T.) ;
#57317 = ORIENTED_EDGE('',*,*,#43314,.T.) ;
#57318 = ORIENTED_EDGE('',*,*,#43315,.T.) ;
#57319 = ORIENTED_EDGE('',*,*,#43316,.F.) ;
#57320 = ORIENTED_EDGE('',*,*,#43317,.T.) ;
#57321 = ORIENTED_EDGE('',*,*,#43309,.F.) ;
#57322 = ORIENTED_EDGE('',*,*,#43318,.T.) ;
#57323 = ORIENTED_EDGE('',*,*,#43319,.F.) ;
#57324 = ORIENTED_EDGE('',*,*,#43320,.T.) ;
#57325 = ORIENTED_EDGE('',*,*,#43321,.T.) ;
#57326 = ORIENTED_EDGE('',*,*,#43322,.T.) ;
#57327 = ORIENTED_EDGE('',*,*,#43314,.F.) ;
#57328 = ORIENTED_EDGE('',*,*,#43323,.T.) ;
#57329 = ORIENTED_EDGE('',*,*,#43324,.T.) ;
#57330 = ORIENTED_EDGE('',*,*,#43325,.T.) ;
#57331 = ORIENTED_EDGE('',*,*,#43311,.T.) ;
#57332 = ORIENTED_EDGE('',*,*,#43326,.T.) ;
#57333 = ORIENTED_EDGE('',*,*,#43327,.T.) ;
#57334 = ORIENTED_EDGE('',*,*,#43328,.T.) ;
#57335 = ORIENTED_EDGE('',*,*,#43329,.T.) ;
#57336 = ORIENTED_EDGE('',*,*,#43330,.T.) ;
#57337 = ORIENTED_EDGE('',*,*,#43331,.T.) ;
#57338 = ORIENTED_EDGE('',*,*,#43332,.T.) ;
#57339 = ORIENTED_EDGE('',*,*,#43333,.T.) ;
#57340 = ORIENTED_EDGE('',*,*,#43334,.T.) ;
#57341 = ORIENTED_EDGE('',*,*,#43335,.T.) ;
#57342 = ORIENTED_EDGE('',*,*,#43336,.T.) ;
#57343 = ORIENTED_EDGE('',*,*,#43337,.T.) ;
#57344 = ORIENTED_EDGE('',*,*,#43338,.T.) ;
#57345 = ORIENTED_EDGE('',*,*,#43339,.T.) ;
#57346 = ORIENTED_EDGE('',*,*,#43340,.T.) ;
#57347 = ORIENTED_EDGE('',*,*,#43341,.T.) ;
#57348 = ORIENTED_EDGE('',*,*,#43342,.T.) ;
#57349 = ORIENTED_EDGE('',*,*,#43343,.T.) ;
#57350 = ORIENTED_EDGE('',*,*,#43344,.T.) ;
#57351 = ORIENTED_EDGE('',*,*,#43345,.T.) ;
#57352 = ORIENTED_EDGE('',*,*,#43346,.T.) ;
#57353 = ORIENTED_EDGE('',*,*,#43347,.T.) ;
#57354 = ORIENTED_EDGE('',*,*,#43348,.T.) ;
#57355 = ORIENTED_EDGE('',*,*,#43349,.T.) ;
#57356 = ORIENTED_EDGE('',*,*,#43350,.T.) ;
#57357 = ORIENTED_EDGE('',*,*,#43351,.T.) ;
#57358 = ORIENTED_EDGE('',*,*,#43352,.T.) ;
#57359 = ORIENTED_EDGE('',*,*,#43353,.T.) ;
#57360 = ORIENTED_EDGE('',*,*,#43354,.T.) ;
#57361 = ORIENTED_EDGE('',*,*,#43355,.T.) ;
#57362 = ORIENTED_EDGE('',*,*,#43356,.T.) ;
#57363 = ORIENTED_EDGE('',*,*,#43357,.T.) ;
#57364 = ORIENTED_EDGE('',*,*,#43358,.T.) ;
#57365 = ORIENTED_EDGE('',*,*,#43359,.T.) ;
#57366 = ORIENTED_EDGE('',*,*,#43360,.T.) ;
#57367 = ORIENTED_EDGE('',*,*,#43361,.F.) ;
#57368 = ORIENTED_EDGE('',*,*,#43362,.F.) ;
#57369 = ORIENTED_EDGE('',*,*,#43363,.F.) ;
#57370 = ORIENTED_EDGE('',*,*,#43364,.F.) ;
#57371 = ORIENTED_EDGE('',*,*,#43365,.F.) ;
#57372 = ORIENTED_EDGE('',*,*,#43366,.F.) ;
#57373 = ORIENTED_EDGE('',*,*,#43367,.F.) ;
#57374 = ORIENTED_EDGE('',*,*,#43368,.F.) ;
#57375 = ORIENTED_EDGE('',*,*,#43369,.F.) ;
#57376 = ORIENTED_EDGE('',*,*,#43370,.F.) ;
#57377 = ORIENTED_EDGE('',*,*,#43368,.T.) ;
#57378 = ORIENTED_EDGE('',*,*,#43371,.T.) ;
#57379 = ORIENTED_EDGE('',*,*,#43372,.F.) ;
#57380 = ORIENTED_EDGE('',*,*,#43373,.F.) ;
#57381 = ORIENTED_EDGE('',*,*,#43361,.T.) ;
#57382 = ORIENTED_EDGE('',*,*,#43370,.T.) ;
#57383 = ORIENTED_EDGE('',*,*,#43374,.F.) ;
#57384 = ORIENTED_EDGE('',*,*,#43375,.F.) ;
#57385 = ORIENTED_EDGE('',*,*,#43362,.T.) ;
#57386 = ORIENTED_EDGE('',*,*,#43373,.T.) ;
#57387 = ORIENTED_EDGE('',*,*,#43376,.F.) ;
#57388 = ORIENTED_EDGE('',*,*,#43377,.F.) ;
#57389 = ORIENTED_EDGE('',*,*,#43363,.T.) ;
#57390 = ORIENTED_EDGE('',*,*,#43375,.T.) ;
#57391 = ORIENTED_EDGE('',*,*,#43378,.F.) ;
#57392 = ORIENTED_EDGE('',*,*,#43379,.F.) ;
#57393 = ORIENTED_EDGE('',*,*,#43364,.T.) ;
#57394 = ORIENTED_EDGE('',*,*,#43377,.T.) ;
#57395 = ORIENTED_EDGE('',*,*,#43380,.F.) ;
#57396 = ORIENTED_EDGE('',*,*,#43381,.F.) ;
#57397 = ORIENTED_EDGE('',*,*,#43365,.T.) ;
#57398 = ORIENTED_EDGE('',*,*,#43379,.T.) ;
#57399 = ORIENTED_EDGE('',*,*,#43382,.F.) ;
#57400 = ORIENTED_EDGE('',*,*,#43383,.F.) ;
#57401 = ORIENTED_EDGE('',*,*,#43366,.T.) ;
#57402 = ORIENTED_EDGE('',*,*,#43381,.T.) ;
#57403 = ORIENTED_EDGE('',*,*,#43384,.F.) ;
#57404 = ORIENTED_EDGE('',*,*,#43371,.F.) ;
#57405 = ORIENTED_EDGE('',*,*,#43367,.T.) ;
#57406 = ORIENTED_EDGE('',*,*,#43383,.T.) ;
#57407 = ORIENTED_EDGE('',*,*,#43372,.T.) ;
#57408 = ORIENTED_EDGE('',*,*,#43369,.T.) ;
#57409 = ORIENTED_EDGE('',*,*,#43384,.T.) ;
#57410 = ORIENTED_EDGE('',*,*,#43382,.T.) ;
#57411 = ORIENTED_EDGE('',*,*,#43380,.T.) ;
#57412 = ORIENTED_EDGE('',*,*,#43378,.T.) ;
#57413 = ORIENTED_EDGE('',*,*,#43376,.T.) ;
#57414 = ORIENTED_EDGE('',*,*,#43374,.T.) ;
#57415 = ORIENTED_EDGE('',*,*,#42647,.T.) ;
#57416 = ORIENTED_EDGE('',*,*,#43385,.T.) ;
#57417 = ORIENTED_EDGE('',*,*,#42645,.F.) ;
#57418 = ORIENTED_EDGE('',*,*,#43386,.T.) ;
#57419 = ORIENTED_EDGE('',*,*,#42649,.T.) ;
#57420 = ORIENTED_EDGE('',*,*,#43387,.T.) ;
#57421 = ORIENTED_EDGE('',*,*,#42653,.F.) ;
#57422 = ORIENTED_EDGE('',*,*,#43388,.T.) ;
#57423 = ORIENTED_EDGE('',*,*,#42641,.T.) ;
#57424 = ORIENTED_EDGE('',*,*,#43389,.T.) ;
#57425 = ORIENTED_EDGE('',*,*,#42643,.T.) ;
#57426 = ORIENTED_EDGE('',*,*,#43390,.T.) ;
#57427 = ORIENTED_EDGE('',*,*,#42651,.T.) ;
#57428 = ORIENTED_EDGE('',*,*,#43391,.T.) ;
#57429 = ORIENTED_EDGE('',*,*,#43392,.T.) ;
#57430 = ORIENTED_EDGE('',*,*,#43393,.T.) ;
#57431 = ORIENTED_EDGE('',*,*,#43394,.T.) ;
#57432 = ORIENTED_EDGE('',*,*,#43395,.T.) ;
#57433 = ORIENTED_EDGE('',*,*,#43396,.T.) ;
#57434 = ORIENTED_EDGE('',*,*,#43397,.T.) ;
#57435 = ORIENTED_EDGE('',*,*,#43398,.T.) ;
#57436 = ORIENTED_EDGE('',*,*,#43399,.T.) ;
#57437 = ORIENTED_EDGE('',*,*,#43400,.T.) ;
#57438 = ORIENTED_EDGE('',*,*,#43401,.T.) ;
#57439 = ORIENTED_EDGE('',*,*,#43402,.T.) ;
#57440 = ORIENTED_EDGE('',*,*,#43403,.T.) ;
#57441 = ORIENTED_EDGE('',*,*,#43404,.T.) ;
#57442 = ORIENTED_EDGE('',*,*,#43405,.T.) ;
#57443 = ORIENTED_EDGE('',*,*,#43406,.T.) ;
#57444 = ORIENTED_EDGE('',*,*,#43407,.T.) ;
#57445 = ORIENTED_EDGE('',*,*,#43408,.T.) ;
#57446 = ORIENTED_EDGE('',*,*,#43409,.T.) ;
#57447 = ORIENTED_EDGE('',*,*,#43410,.T.) ;
#57448 = ORIENTED_EDGE('',*,*,#43411,.T.) ;
#57449 = ORIENTED_EDGE('',*,*,#43412,.F.) ;
#57450 = ORIENTED_EDGE('',*,*,#43413,.F.) ;
#57451 = ORIENTED_EDGE('',*,*,#43414,.F.) ;
#57452 = ORIENTED_EDGE('',*,*,#43415,.F.) ;
#57453 = ORIENTED_EDGE('',*,*,#43416,.F.) ;
#57454 = ORIENTED_EDGE('',*,*,#43417,.F.) ;
#57455 = ORIENTED_EDGE('',*,*,#43418,.F.) ;
#57456 = ORIENTED_EDGE('',*,*,#43419,.F.) ;
#57457 = ORIENTED_EDGE('',*,*,#43420,.T.) ;
#57458 = ORIENTED_EDGE('',*,*,#43421,.T.) ;
#57459 = ORIENTED_EDGE('',*,*,#43422,.F.) ;
#57460 = ORIENTED_EDGE('',*,*,#43419,.T.) ;
#57461 = ORIENTED_EDGE('',*,*,#43422,.T.) ;
#57462 = ORIENTED_EDGE('',*,*,#43423,.T.) ;
#57463 = ORIENTED_EDGE('',*,*,#43424,.F.) ;
#57464 = ORIENTED_EDGE('',*,*,#43412,.T.) ;
#57465 = ORIENTED_EDGE('',*,*,#43424,.T.) ;
#57466 = ORIENTED_EDGE('',*,*,#43425,.T.) ;
#57467 = ORIENTED_EDGE('',*,*,#43426,.F.) ;
#57468 = ORIENTED_EDGE('',*,*,#43413,.T.) ;
#57469 = ORIENTED_EDGE('',*,*,#43426,.T.) ;
#57470 = ORIENTED_EDGE('',*,*,#43427,.T.) ;
#57471 = ORIENTED_EDGE('',*,*,#43428,.F.) ;
#57472 = ORIENTED_EDGE('',*,*,#43414,.T.) ;
#57473 = ORIENTED_EDGE('',*,*,#43428,.T.) ;
#57474 = ORIENTED_EDGE('',*,*,#43429,.T.) ;
#57475 = ORIENTED_EDGE('',*,*,#43430,.F.) ;
#57476 = ORIENTED_EDGE('',*,*,#43415,.T.) ;
#57477 = ORIENTED_EDGE('',*,*,#43430,.T.) ;
#57478 = ORIENTED_EDGE('',*,*,#43431,.T.) ;
#57479 = ORIENTED_EDGE('',*,*,#43432,.F.) ;
#57480 = ORIENTED_EDGE('',*,*,#43416,.T.) ;
#57481 = ORIENTED_EDGE('',*,*,#43432,.T.) ;
#57482 = ORIENTED_EDGE('',*,*,#43433,.T.) ;
#57483 = ORIENTED_EDGE('',*,*,#43434,.F.) ;
#57484 = ORIENTED_EDGE('',*,*,#43417,.T.) ;
#57485 = ORIENTED_EDGE('',*,*,#43434,.T.) ;
#57486 = ORIENTED_EDGE('',*,*,#43435,.T.) ;
#57487 = ORIENTED_EDGE('',*,*,#43420,.F.) ;
#57488 = ORIENTED_EDGE('',*,*,#43418,.T.) ;
#57489 = ORIENTED_EDGE('',*,*,#43436,.T.) ;
#57490 = ORIENTED_EDGE('',*,*,#43437,.T.) ;
#57491 = ORIENTED_EDGE('',*,*,#43438,.T.) ;
#57492 = ORIENTED_EDGE('',*,*,#43439,.T.) ;
#57493 = ORIENTED_EDGE('',*,*,#43440,.T.) ;
#57494 = ORIENTED_EDGE('',*,*,#43441,.T.) ;
#57495 = ORIENTED_EDGE('',*,*,#43442,.T.) ;
#57496 = ORIENTED_EDGE('',*,*,#43443,.T.) ;
#57497 = ORIENTED_EDGE('',*,*,#43444,.T.) ;
#57498 = ORIENTED_EDGE('',*,*,#42630,.T.) ;
#57499 = ORIENTED_EDGE('',*,*,#43445,.T.) ;
#57500 = ORIENTED_EDGE('',*,*,#43446,.T.) ;
#57501 = ORIENTED_EDGE('',*,*,#42632,.T.) ;
#57502 = ORIENTED_EDGE('',*,*,#43447,.T.) ;
#57503 = ORIENTED_EDGE('',*,*,#43448,.T.) ;
#57504 = ORIENTED_EDGE('',*,*,#43449,.T.) ;
#57505 = ORIENTED_EDGE('',*,*,#43450,.T.) ;
#57506 = ORIENTED_EDGE('',*,*,#43451,.T.) ;
#57507 = ORIENTED_EDGE('',*,*,#43452,.T.) ;
#57508 = ORIENTED_EDGE('',*,*,#43453,.T.) ;
#57509 = ORIENTED_EDGE('',*,*,#43454,.T.) ;
#57510 = ORIENTED_EDGE('',*,*,#42608,.T.) ;
#57511 = ORIENTED_EDGE('',*,*,#42636,.T.) ;
#57512 = ORIENTED_EDGE('',*,*,#43455,.T.) ;
#57513 = ORIENTED_EDGE('',*,*,#43456,.T.) ;
#57514 = ORIENTED_EDGE('',*,*,#43457,.T.) ;
#57515 = ORIENTED_EDGE('',*,*,#43458,.T.) ;
#57516 = ORIENTED_EDGE('',*,*,#43459,.T.) ;
#57517 = ORIENTED_EDGE('',*,*,#43460,.T.) ;
#57518 = ORIENTED_EDGE('',*,*,#43461,.F.) ;
#57519 = ORIENTED_EDGE('',*,*,#43462,.F.) ;
#57520 = ORIENTED_EDGE('',*,*,#43463,.F.) ;
#57521 = ORIENTED_EDGE('',*,*,#42839,.F.) ;
#57522 = ORIENTED_EDGE('',*,*,#43313,.F.) ;
#57523 = ORIENTED_EDGE('',*,*,#43302,.F.) ;
#57524 = ORIENTED_EDGE('',*,*,#43464,.F.) ;
#57525 = ORIENTED_EDGE('',*,*,#43323,.F.) ;
#57526 = ORIENTED_EDGE('',*,*,#43464,.T.) ;
#57527 = ORIENTED_EDGE('',*,*,#43301,.T.) ;
#57528 = ORIENTED_EDGE('',*,*,#43465,.F.) ;
#57529 = ORIENTED_EDGE('',*,*,#43466,.F.) ;
#57530 = ORIENTED_EDGE('',*,*,#43465,.T.) ;
#57531 = ORIENTED_EDGE('',*,*,#43308,.F.) ;
#57532 = ORIENTED_EDGE('',*,*,#43467,.F.) ;
#57533 = ORIENTED_EDGE('',*,*,#43339,.F.) ;
#57534 = ORIENTED_EDGE('',*,*,#43462,.T.) ;
#57535 = ORIENTED_EDGE('',*,*,#43340,.F.) ;
#57536 = ORIENTED_EDGE('',*,*,#43468,.F.) ;
#57537 = ORIENTED_EDGE('',*,*,#43299,.F.) ;
#57538 = ORIENTED_EDGE('',*,*,#43463,.T.) ;
#57539 = ORIENTED_EDGE('',*,*,#43298,.F.) ;
#57540 = ORIENTED_EDGE('',*,*,#43469,.F.) ;
#57541 = ORIENTED_EDGE('',*,*,#42840,.F.) ;
#57542 = ORIENTED_EDGE('',*,*,#43461,.T.) ;
#57543 = ORIENTED_EDGE('',*,*,#42838,.F.) ;
#57544 = ORIENTED_EDGE('',*,*,#43470,.F.) ;
#57545 = ORIENTED_EDGE('',*,*,#43335,.F.) ;
#57546 = ORIENTED_EDGE('',*,*,#43466,.T.) ;
#57547 = ORIENTED_EDGE('',*,*,#43338,.F.) ;
#57548 = ORIENTED_EDGE('',*,*,#43471,.F.) ;
#57549 = ORIENTED_EDGE('',*,*,#43324,.F.) ;
#57550 = ORIENTED_EDGE('',*,*,#43315,.F.) ;
#57551 = ORIENTED_EDGE('',*,*,#43325,.F.) ;
#57552 = ORIENTED_EDGE('',*,*,#43472,.F.) ;
#57553 = ORIENTED_EDGE('',*,*,#43318,.F.) ;
#57554 = ORIENTED_EDGE('',*,*,#43468,.T.) ;
#57555 = ORIENTED_EDGE('',*,*,#43467,.T.) ;
#57556 = ORIENTED_EDGE('',*,*,#43473,.F.) ;
#57557 = ORIENTED_EDGE('',*,*,#42841,.T.) ;
#57558 = ORIENTED_EDGE('',*,*,#43469,.T.) ;
#57559 = ORIENTED_EDGE('',*,*,#43474,.F.) ;
#57560 = ORIENTED_EDGE('',*,*,#43475,.F.) ;
#57561 = ORIENTED_EDGE('',*,*,#43470,.T.) ;
#57562 = ORIENTED_EDGE('',*,*,#42845,.F.) ;
#57563 = ORIENTED_EDGE('',*,*,#43476,.F.) ;
#57564 = ORIENTED_EDGE('',*,*,#43477,.F.) ;
#57565 = ORIENTED_EDGE('',*,*,#43472,.T.) ;
#57566 = ORIENTED_EDGE('',*,*,#43471,.T.) ;
#57567 = ORIENTED_EDGE('',*,*,#43478,.F.) ;
#57568 = ORIENTED_EDGE('',*,*,#43319,.T.) ;
#57569 = ORIENTED_EDGE('',*,*,#43473,.T.) ;
#57570 = ORIENTED_EDGE('',*,*,#43307,.F.) ;
#57571 = ORIENTED_EDGE('',*,*,#43479,.F.) ;
#57572 = ORIENTED_EDGE('',*,*,#43300,.F.) ;
#57573 = ORIENTED_EDGE('',*,*,#43474,.T.) ;
#57574 = ORIENTED_EDGE('',*,*,#43297,.F.) ;
#57575 = ORIENTED_EDGE('',*,*,#43480,.F.) ;
#57576 = ORIENTED_EDGE('',*,*,#43333,.F.) ;
#57577 = ORIENTED_EDGE('',*,*,#43475,.T.) ;
#57578 = ORIENTED_EDGE('',*,*,#43332,.F.) ;
#57579 = ORIENTED_EDGE('',*,*,#43481,.F.) ;
#57580 = ORIENTED_EDGE('',*,*,#42842,.F.) ;
#57581 = ORIENTED_EDGE('',*,*,#43476,.T.) ;
#57582 = ORIENTED_EDGE('',*,*,#42844,.F.) ;
#57583 = ORIENTED_EDGE('',*,*,#43482,.F.) ;
#57584 = ORIENTED_EDGE('',*,*,#43294,.F.) ;
#57585 = ORIENTED_EDGE('',*,*,#43477,.T.) ;
#57586 = ORIENTED_EDGE('',*,*,#43293,.F.) ;
#57587 = ORIENTED_EDGE('',*,*,#43483,.F.) ;
#57588 = ORIENTED_EDGE('',*,*,#43336,.F.) ;
#57589 = ORIENTED_EDGE('',*,*,#43478,.T.) ;
#57590 = ORIENTED_EDGE('',*,*,#43337,.F.) ;
#57591 = ORIENTED_EDGE('',*,*,#43484,.F.) ;
#57592 = ORIENTED_EDGE('',*,*,#43320,.F.) ;
#57593 = ORIENTED_EDGE('',*,*,#43480,.T.) ;
#57594 = ORIENTED_EDGE('',*,*,#43479,.T.) ;
#57595 = ORIENTED_EDGE('',*,*,#43485,.F.) ;
#57596 = ORIENTED_EDGE('',*,*,#42843,.T.) ;
#57597 = ORIENTED_EDGE('',*,*,#43481,.T.) ;
#57598 = ORIENTED_EDGE('',*,*,#43486,.F.) ;
#57599 = ORIENTED_EDGE('',*,*,#43482,.T.) ;
#57600 = ORIENTED_EDGE('',*,*,#43484,.T.) ;
#57601 = ORIENTED_EDGE('',*,*,#43483,.T.) ;
#57602 = ORIENTED_EDGE('',*,*,#43487,.F.) ;
#57603 = ORIENTED_EDGE('',*,*,#43312,.F.) ;
#57604 = ORIENTED_EDGE('',*,*,#43328,.F.) ;
#57605 = ORIENTED_EDGE('',*,*,#43488,.F.) ;
#57606 = ORIENTED_EDGE('',*,*,#43304,.F.) ;
#57607 = ORIENTED_EDGE('',*,*,#43485,.T.) ;
#57608 = ORIENTED_EDGE('',*,*,#43306,.F.) ;
#57609 = ORIENTED_EDGE('',*,*,#43489,.F.) ;
#57610 = ORIENTED_EDGE('',*,*,#43334,.F.) ;
#57611 = ORIENTED_EDGE('',*,*,#43486,.T.) ;
#57612 = ORIENTED_EDGE('',*,*,#43331,.F.) ;
#57613 = ORIENTED_EDGE('',*,*,#43490,.F.) ;
#57614 = ORIENTED_EDGE('',*,*,#43295,.F.) ;
#57615 = ORIENTED_EDGE('',*,*,#43487,.T.) ;
#57616 = ORIENTED_EDGE('',*,*,#43296,.F.) ;
#57617 = ORIENTED_EDGE('',*,*,#43491,.F.) ;
#57618 = ORIENTED_EDGE('',*,*,#43321,.F.) ;
#57619 = ORIENTED_EDGE('',*,*,#43305,.T.) ;
#57620 = ORIENTED_EDGE('',*,*,#43488,.T.) ;
#57621 = ORIENTED_EDGE('',*,*,#43492,.F.) ;
#57622 = ORIENTED_EDGE('',*,*,#43489,.T.) ;
#57623 = ORIENTED_EDGE('',*,*,#43491,.T.) ;
#57624 = ORIENTED_EDGE('',*,*,#43490,.T.) ;
#57625 = ORIENTED_EDGE('',*,*,#43493,.F.) ;
#57626 = ORIENTED_EDGE('',*,*,#43492,.T.) ;
#57627 = ORIENTED_EDGE('',*,*,#43327,.F.) ;
#57628 = ORIENTED_EDGE('',*,*,#43494,.F.) ;
#57629 = ORIENTED_EDGE('',*,*,#43329,.F.) ;
#57630 = ORIENTED_EDGE('',*,*,#43493,.T.) ;
#57631 = ORIENTED_EDGE('',*,*,#43330,.F.) ;
#57632 = ORIENTED_EDGE('',*,*,#43495,.F.) ;
#57633 = ORIENTED_EDGE('',*,*,#43322,.F.) ;
#57634 = ORIENTED_EDGE('',*,*,#43495,.T.) ;
#57635 = ORIENTED_EDGE('',*,*,#43494,.T.) ;
#57636 = ORIENTED_EDGE('',*,*,#43496,.F.) ;
#57637 = ORIENTED_EDGE('',*,*,#43316,.T.) ;
#57638 = ORIENTED_EDGE('',*,*,#43310,.F.) ;
#57639 = ORIENTED_EDGE('',*,*,#43317,.F.) ;
#57640 = ORIENTED_EDGE('',*,*,#43496,.T.) ;
#57641 = ORIENTED_EDGE('',*,*,#43326,.F.) ;
#57642 = ORIENTED_EDGE('',*,*,#42783,.F.) ;
#57643 = ORIENTED_EDGE('',*,*,#43497,.T.) ;
#57644 = ORIENTED_EDGE('',*,*,#43498,.T.) ;
#57645 = ORIENTED_EDGE('',*,*,#42610,.T.) ;
#57646 = ORIENTED_EDGE('',*,*,#43440,.F.) ;
#57647 = ORIENTED_EDGE('',*,*,#42635,.T.) ;
#57648 = ORIENTED_EDGE('',*,*,#43442,.F.) ;
#57649 = ORIENTED_EDGE('',*,*,#43499,.T.) ;
#57650 = ORIENTED_EDGE('',*,*,#43446,.F.) ;
#57651 = ORIENTED_EDGE('',*,*,#43500,.F.) ;
#57652 = ORIENTED_EDGE('',*,*,#42633,.T.) ;
#57653 = ORIENTED_EDGE('',*,*,#43443,.F.) ;
#57654 = ORIENTED_EDGE('',*,*,#43501,.F.) ;
#57655 = ORIENTED_EDGE('',*,*,#42761,.F.) ;
#57656 = ORIENTED_EDGE('',*,*,#42789,.F.) ;
#57657 = ORIENTED_EDGE('',*,*,#43502,.T.) ;
#57658 = ORIENTED_EDGE('',*,*,#43450,.F.) ;
#57659 = ORIENTED_EDGE('',*,*,#43503,.T.) ;
#57660 = ORIENTED_EDGE('',*,*,#43453,.F.) ;
#57661 = ORIENTED_EDGE('',*,*,#43504,.T.) ;
#57662 = ORIENTED_EDGE('',*,*,#43444,.F.) ;
#57663 = ORIENTED_EDGE('',*,*,#43505,.T.) ;
#57664 = ORIENTED_EDGE('',*,*,#43501,.T.) ;
#57665 = ORIENTED_EDGE('',*,*,#43500,.T.) ;
#57666 = ORIENTED_EDGE('',*,*,#43506,.F.) ;
#57667 = ORIENTED_EDGE('',*,*,#42762,.T.) ;
#57668 = ORIENTED_EDGE('',*,*,#43291,.F.) ;
#57669 = ORIENTED_EDGE('',*,*,#42765,.F.) ;
#57670 = ORIENTED_EDGE('',*,*,#42628,.F.) ;
#57671 = ORIENTED_EDGE('',*,*,#43283,.F.) ;
#57672 = ORIENTED_EDGE('',*,*,#43507,.T.) ;
#57673 = ORIENTED_EDGE('',*,*,#43508,.T.) ;
#57674 = ORIENTED_EDGE('',*,*,#43280,.F.) ;
#57675 = ORIENTED_EDGE('',*,*,#42627,.F.) ;
#57676 = ORIENTED_EDGE('',*,*,#43448,.F.) ;
#57677 = ORIENTED_EDGE('',*,*,#43509,.T.) ;
#57678 = ORIENTED_EDGE('',*,*,#43506,.T.) ;
#57679 = ORIENTED_EDGE('',*,*,#43445,.F.) ;
#57680 = ORIENTED_EDGE('',*,*,#42626,.F.) ;
#57681 = ORIENTED_EDGE('',*,*,#42763,.F.) ;
#57682 = ORIENTED_EDGE('',*,*,#42629,.T.) ;
#57683 = ORIENTED_EDGE('',*,*,#42764,.F.) ;
#57684 = ORIENTED_EDGE('',*,*,#42624,.T.) ;
#57685 = ORIENTED_EDGE('',*,*,#43449,.F.) ;
#57686 = ORIENTED_EDGE('',*,*,#43510,.F.) ;
#57687 = ORIENTED_EDGE('',*,*,#43425,.F.) ;
#57688 = ORIENTED_EDGE('',*,*,#43511,.F.) ;
#57689 = ORIENTED_EDGE('',*,*,#43511,.T.) ;
#57690 = ORIENTED_EDGE('',*,*,#43423,.F.) ;
#57691 = ORIENTED_EDGE('',*,*,#43512,.F.) ;
#57692 = ORIENTED_EDGE('',*,*,#43436,.F.) ;
#57693 = ORIENTED_EDGE('',*,*,#43510,.T.) ;
#57694 = ORIENTED_EDGE('',*,*,#43439,.F.) ;
#57695 = ORIENTED_EDGE('',*,*,#43513,.F.) ;
#57696 = ORIENTED_EDGE('',*,*,#43427,.F.) ;
#57697 = ORIENTED_EDGE('',*,*,#43512,.T.) ;
#57698 = ORIENTED_EDGE('',*,*,#43421,.F.) ;
#57699 = ORIENTED_EDGE('',*,*,#43514,.F.) ;
#57700 = ORIENTED_EDGE('',*,*,#43429,.F.) ;
#57701 = ORIENTED_EDGE('',*,*,#43513,.T.) ;
#57702 = ORIENTED_EDGE('',*,*,#43515,.F.) ;
#57703 = ORIENTED_EDGE('',*,*,#43514,.T.) ;
#57704 = ORIENTED_EDGE('',*,*,#43435,.F.) ;
#57705 = ORIENTED_EDGE('',*,*,#43516,.F.) ;
#57706 = ORIENTED_EDGE('',*,*,#43437,.F.) ;
#57707 = ORIENTED_EDGE('',*,*,#43515,.T.) ;
#57708 = ORIENTED_EDGE('',*,*,#43438,.F.) ;
#57709 = ORIENTED_EDGE('',*,*,#43517,.F.) ;
#57710 = ORIENTED_EDGE('',*,*,#43431,.F.) ;
#57711 = ORIENTED_EDGE('',*,*,#43516,.T.) ;
#57712 = ORIENTED_EDGE('',*,*,#43433,.F.) ;
#57713 = ORIENTED_EDGE('',*,*,#43517,.T.) ;
#57714 = ORIENTED_EDGE('',*,*,#43518,.F.) ;
#57715 = ORIENTED_EDGE('',*,*,#42863,.F.) ;
#57716 = ORIENTED_EDGE('',*,*,#43519,.F.) ;
#57717 = ORIENTED_EDGE('',*,*,#43344,.F.) ;
#57718 = ORIENTED_EDGE('',*,*,#43519,.T.) ;
#57719 = ORIENTED_EDGE('',*,*,#42862,.T.) ;
#57720 = ORIENTED_EDGE('',*,*,#43520,.F.) ;
#57721 = ORIENTED_EDGE('',*,*,#43521,.F.) ;
#57722 = ORIENTED_EDGE('',*,*,#42864,.T.) ;
#57723 = ORIENTED_EDGE('',*,*,#43518,.T.) ;
#57724 = ORIENTED_EDGE('',*,*,#43522,.F.) ;
#57725 = ORIENTED_EDGE('',*,*,#43523,.F.) ;
#57726 = ORIENTED_EDGE('',*,*,#43520,.T.) ;
#57727 = ORIENTED_EDGE('',*,*,#42861,.F.) ;
#57728 = ORIENTED_EDGE('',*,*,#43524,.F.) ;
#57729 = ORIENTED_EDGE('',*,*,#43356,.F.) ;
#57730 = ORIENTED_EDGE('',*,*,#43521,.T.) ;
#57731 = ORIENTED_EDGE('',*,*,#43355,.F.) ;
#57732 = ORIENTED_EDGE('',*,*,#43525,.F.) ;
#57733 = ORIENTED_EDGE('',*,*,#43341,.F.) ;
#57734 = ORIENTED_EDGE('',*,*,#43526,.F.) ;
#57735 = ORIENTED_EDGE('',*,*,#43342,.F.) ;
#57736 = ORIENTED_EDGE('',*,*,#43527,.F.) ;
#57737 = ORIENTED_EDGE('',*,*,#43360,.F.) ;
#57738 = ORIENTED_EDGE('',*,*,#43522,.T.) ;
#57739 = ORIENTED_EDGE('',*,*,#43343,.F.) ;
#57740 = ORIENTED_EDGE('',*,*,#43528,.F.) ;
#57741 = ORIENTED_EDGE('',*,*,#43348,.F.) ;
#57742 = ORIENTED_EDGE('',*,*,#43523,.T.) ;
#57743 = ORIENTED_EDGE('',*,*,#43347,.F.) ;
#57744 = ORIENTED_EDGE('',*,*,#43529,.F.) ;
#57745 = ORIENTED_EDGE('',*,*,#42865,.F.) ;
#57746 = ORIENTED_EDGE('',*,*,#43530,.F.) ;
#57747 = ORIENTED_EDGE('',*,*,#42859,.F.) ;
#57748 = ORIENTED_EDGE('',*,*,#43531,.F.) ;
#57749 = ORIENTED_EDGE('',*,*,#43351,.F.) ;
#57750 = ORIENTED_EDGE('',*,*,#42860,.T.) ;
#57751 = ORIENTED_EDGE('',*,*,#43530,.T.) ;
#57752 = ORIENTED_EDGE('',*,*,#43532,.F.) ;
#57753 = ORIENTED_EDGE('',*,*,#43524,.T.) ;
#57754 = ORIENTED_EDGE('',*,*,#43527,.T.) ;
#57755 = ORIENTED_EDGE('',*,*,#43525,.T.) ;
#57756 = ORIENTED_EDGE('',*,*,#43533,.F.) ;
#57757 = ORIENTED_EDGE('',*,*,#43528,.T.) ;
#57758 = ORIENTED_EDGE('',*,*,#43526,.T.) ;
#57759 = ORIENTED_EDGE('',*,*,#43534,.F.) ;
#57760 = ORIENTED_EDGE('',*,*,#42858,.T.) ;
#57761 = ORIENTED_EDGE('',*,*,#43529,.T.) ;
#57762 = ORIENTED_EDGE('',*,*,#43535,.F.) ;
#57763 = ORIENTED_EDGE('',*,*,#43531,.T.) ;
#57764 = ORIENTED_EDGE('',*,*,#43532,.T.) ;
#57765 = ORIENTED_EDGE('',*,*,#43350,.F.) ;
#57766 = ORIENTED_EDGE('',*,*,#43536,.F.) ;
#57767 = ORIENTED_EDGE('',*,*,#43353,.F.) ;
#57768 = ORIENTED_EDGE('',*,*,#43533,.T.) ;
#57769 = ORIENTED_EDGE('',*,*,#43354,.F.) ;
#57770 = ORIENTED_EDGE('',*,*,#43537,.F.) ;
#57771 = ORIENTED_EDGE('',*,*,#43357,.F.) ;
#57772 = ORIENTED_EDGE('',*,*,#43534,.T.) ;
#57773 = ORIENTED_EDGE('',*,*,#43359,.F.) ;
#57774 = ORIENTED_EDGE('',*,*,#43538,.F.) ;
#57775 = ORIENTED_EDGE('',*,*,#43345,.F.) ;
#57776 = ORIENTED_EDGE('',*,*,#43535,.T.) ;
#57777 = ORIENTED_EDGE('',*,*,#43346,.F.) ;
#57778 = ORIENTED_EDGE('',*,*,#43539,.F.) ;
#57779 = ORIENTED_EDGE('',*,*,#43352,.F.) ;
#57780 = ORIENTED_EDGE('',*,*,#43537,.T.) ;
#57781 = ORIENTED_EDGE('',*,*,#43536,.T.) ;
#57782 = ORIENTED_EDGE('',*,*,#43540,.F.) ;
#57783 = ORIENTED_EDGE('',*,*,#43539,.T.) ;
#57784 = ORIENTED_EDGE('',*,*,#43538,.T.) ;
#57785 = ORIENTED_EDGE('',*,*,#43541,.F.) ;
#57786 = ORIENTED_EDGE('',*,*,#43540,.T.) ;
#57787 = ORIENTED_EDGE('',*,*,#43349,.F.) ;
#57788 = ORIENTED_EDGE('',*,*,#43541,.T.) ;
#57789 = ORIENTED_EDGE('',*,*,#43358,.F.) ;
#57790 = ORIENTED_EDGE('',*,*,#43542,.F.) ;
#57791 = ORIENTED_EDGE('',*,*,#42813,.F.) ;
#57792 = ORIENTED_EDGE('',*,*,#43543,.F.) ;
#57793 = ORIENTED_EDGE('',*,*,#43403,.F.) ;
#57794 = ORIENTED_EDGE('',*,*,#43543,.T.) ;
#57795 = ORIENTED_EDGE('',*,*,#42812,.T.) ;
#57796 = ORIENTED_EDGE('',*,*,#43544,.F.) ;
#57797 = ORIENTED_EDGE('',*,*,#43545,.F.) ;
#57798 = ORIENTED_EDGE('',*,*,#42814,.T.) ;
#57799 = ORIENTED_EDGE('',*,*,#43542,.T.) ;
#57800 = ORIENTED_EDGE('',*,*,#43546,.F.) ;
#57801 = ORIENTED_EDGE('',*,*,#43547,.F.) ;
#57802 = ORIENTED_EDGE('',*,*,#43544,.T.) ;
#57803 = ORIENTED_EDGE('',*,*,#42811,.F.) ;
#57804 = ORIENTED_EDGE('',*,*,#43548,.F.) ;
#57805 = ORIENTED_EDGE('',*,*,#43399,.F.) ;
#57806 = ORIENTED_EDGE('',*,*,#43545,.T.) ;
#57807 = ORIENTED_EDGE('',*,*,#43398,.F.) ;
#57808 = ORIENTED_EDGE('',*,*,#43549,.F.) ;
#57809 = ORIENTED_EDGE('',*,*,#43400,.F.) ;
#57810 = ORIENTED_EDGE('',*,*,#43550,.F.) ;
#57811 = ORIENTED_EDGE('',*,*,#43401,.F.) ;
#57812 = ORIENTED_EDGE('',*,*,#43551,.F.) ;
#57813 = ORIENTED_EDGE('',*,*,#43411,.F.) ;
#57814 = ORIENTED_EDGE('',*,*,#43546,.T.) ;
#57815 = ORIENTED_EDGE('',*,*,#43402,.F.) ;
#57816 = ORIENTED_EDGE('',*,*,#43552,.F.) ;
#57817 = ORIENTED_EDGE('',*,*,#43407,.F.) ;
#57818 = ORIENTED_EDGE('',*,*,#43547,.T.) ;
#57819 = ORIENTED_EDGE('',*,*,#43406,.F.) ;
#57820 = ORIENTED_EDGE('',*,*,#43553,.F.) ;
#57821 = ORIENTED_EDGE('',*,*,#42815,.F.) ;
#57822 = ORIENTED_EDGE('',*,*,#43554,.F.) ;
#57823 = ORIENTED_EDGE('',*,*,#42809,.F.) ;
#57824 = ORIENTED_EDGE('',*,*,#43555,.F.) ;
#57825 = ORIENTED_EDGE('',*,*,#43394,.F.) ;
#57826 = ORIENTED_EDGE('',*,*,#42810,.T.) ;
#57827 = ORIENTED_EDGE('',*,*,#43554,.T.) ;
#57828 = ORIENTED_EDGE('',*,*,#43556,.F.) ;
#57829 = ORIENTED_EDGE('',*,*,#43548,.T.) ;
#57830 = ORIENTED_EDGE('',*,*,#43551,.T.) ;
#57831 = ORIENTED_EDGE('',*,*,#43549,.T.) ;
#57832 = ORIENTED_EDGE('',*,*,#43557,.F.) ;
#57833 = ORIENTED_EDGE('',*,*,#43552,.T.) ;
#57834 = ORIENTED_EDGE('',*,*,#43550,.T.) ;
#57835 = ORIENTED_EDGE('',*,*,#43558,.F.) ;
#57836 = ORIENTED_EDGE('',*,*,#42808,.T.) ;
#57837 = ORIENTED_EDGE('',*,*,#43553,.T.) ;
#57838 = ORIENTED_EDGE('',*,*,#43559,.F.) ;
#57839 = ORIENTED_EDGE('',*,*,#43555,.T.) ;
#57840 = ORIENTED_EDGE('',*,*,#43556,.T.) ;
#57841 = ORIENTED_EDGE('',*,*,#43393,.F.) ;
#57842 = ORIENTED_EDGE('',*,*,#43560,.F.) ;
#57843 = ORIENTED_EDGE('',*,*,#43396,.F.) ;
#57844 = ORIENTED_EDGE('',*,*,#43557,.T.) ;
#57845 = ORIENTED_EDGE('',*,*,#43397,.F.) ;
#57846 = ORIENTED_EDGE('',*,*,#43561,.F.) ;
#57847 = ORIENTED_EDGE('',*,*,#43408,.F.) ;
#57848 = ORIENTED_EDGE('',*,*,#43558,.T.) ;
#57849 = ORIENTED_EDGE('',*,*,#43410,.F.) ;
#57850 = ORIENTED_EDGE('',*,*,#43562,.F.) ;
#57851 = ORIENTED_EDGE('',*,*,#43404,.F.) ;
#57852 = ORIENTED_EDGE('',*,*,#43559,.T.) ;
#57853 = ORIENTED_EDGE('',*,*,#43405,.F.) ;
#57854 = ORIENTED_EDGE('',*,*,#43563,.F.) ;
#57855 = ORIENTED_EDGE('',*,*,#43395,.F.) ;
#57856 = ORIENTED_EDGE('',*,*,#43561,.T.) ;
#57857 = ORIENTED_EDGE('',*,*,#43560,.T.) ;
#57858 = ORIENTED_EDGE('',*,*,#43564,.F.) ;
#57859 = ORIENTED_EDGE('',*,*,#43563,.T.) ;
#57860 = ORIENTED_EDGE('',*,*,#43562,.T.) ;
#57861 = ORIENTED_EDGE('',*,*,#43565,.F.) ;
#57862 = ORIENTED_EDGE('',*,*,#43564,.T.) ;
#57863 = ORIENTED_EDGE('',*,*,#43392,.F.) ;
#57864 = ORIENTED_EDGE('',*,*,#43565,.T.) ;
#57865 = ORIENTED_EDGE('',*,*,#43409,.F.) ;
#57866 = ORIENTED_EDGE('',*,*,#43286,.F.) ;
#57867 = ORIENTED_EDGE('',*,*,#43566,.T.) ;
#57868 = ORIENTED_EDGE('',*,*,#43455,.F.) ;
#57869 = ORIENTED_EDGE('',*,*,#43567,.F.) ;
#57870 = ORIENTED_EDGE('',*,*,#43289,.F.) ;
#57871 = ORIENTED_EDGE('',*,*,#43287,.F.) ;
#57872 = ORIENTED_EDGE('',*,*,#43568,.F.) ;
#57873 = ORIENTED_EDGE('',*,*,#43276,.F.) ;
#57874 = ORIENTED_EDGE('',*,*,#43568,.T.) ;
#57875 = ORIENTED_EDGE('',*,*,#43567,.T.) ;
#57876 = ORIENTED_EDGE('',*,*,#43569,.F.) ;
#57877 = ORIENTED_EDGE('',*,*,#43569,.T.) ;
#57878 = ORIENTED_EDGE('',*,*,#43460,.F.) ;
#57879 = ORIENTED_EDGE('',*,*,#43570,.F.) ;
#57880 = ORIENTED_EDGE('',*,*,#43277,.F.) ;
#57881 = ORIENTED_EDGE('',*,*,#43290,.F.) ;
#57882 = ORIENTED_EDGE('',*,*,#43278,.F.) ;
#57883 = ORIENTED_EDGE('',*,*,#43571,.F.) ;
#57884 = ORIENTED_EDGE('',*,*,#42767,.F.) ;
#57885 = ORIENTED_EDGE('',*,*,#43571,.T.) ;
#57886 = ORIENTED_EDGE('',*,*,#43570,.T.) ;
#57887 = ORIENTED_EDGE('',*,*,#43572,.F.) ;
#57888 = ORIENTED_EDGE('',*,*,#42768,.T.) ;
#57889 = ORIENTED_EDGE('',*,*,#43572,.T.) ;
#57890 = ORIENTED_EDGE('',*,*,#43459,.F.) ;
#57891 = ORIENTED_EDGE('',*,*,#43573,.F.) ;
#57892 = ORIENTED_EDGE('',*,*,#42769,.F.) ;
#57893 = ORIENTED_EDGE('',*,*,#42770,.T.) ;
#57894 = ORIENTED_EDGE('',*,*,#43573,.T.) ;
#57895 = ORIENTED_EDGE('',*,*,#43574,.F.) ;
#57896 = ORIENTED_EDGE('',*,*,#43193,.T.) ;
#57897 = ORIENTED_EDGE('',*,*,#43574,.T.) ;
#57898 = ORIENTED_EDGE('',*,*,#43458,.F.) ;
#57899 = ORIENTED_EDGE('',*,*,#43575,.F.) ;
#57900 = ORIENTED_EDGE('',*,*,#42751,.F.) ;
#57901 = ORIENTED_EDGE('',*,*,#43189,.T.) ;
#57902 = ORIENTED_EDGE('',*,*,#43575,.T.) ;
#57903 = ORIENTED_EDGE('',*,*,#43576,.F.) ;
#57904 = ORIENTED_EDGE('',*,*,#43457,.F.) ;
#57905 = ORIENTED_EDGE('',*,*,#43577,.T.) ;
#57906 = ORIENTED_EDGE('',*,*,#42893,.F.) ;
#57907 = ORIENTED_EDGE('',*,*,#43576,.T.) ;
#57908 = ORIENTED_EDGE('',*,*,#42642,.F.) ;
#57909 = ORIENTED_EDGE('',*,*,#43388,.F.) ;
#57910 = ORIENTED_EDGE('',*,*,#42652,.F.) ;
#57911 = ORIENTED_EDGE('',*,*,#43390,.F.) ;
#57912 = ORIENTED_EDGE('',*,*,#42650,.F.) ;
#57913 = ORIENTED_EDGE('',*,*,#43386,.F.) ;
#57914 = ORIENTED_EDGE('',*,*,#42644,.F.) ;
#57915 = ORIENTED_EDGE('',*,*,#43391,.F.) ;
#57916 = ORIENTED_EDGE('',*,*,#42640,.F.) ;
#57917 = ORIENTED_EDGE('',*,*,#43279,.F.) ;
#57918 = ORIENTED_EDGE('',*,*,#42654,.F.) ;
#57919 = ORIENTED_EDGE('',*,*,#43389,.F.) ;
#57920 = ORIENTED_EDGE('',*,*,#42648,.F.) ;
#57921 = ORIENTED_EDGE('',*,*,#43385,.F.) ;
#57922 = ORIENTED_EDGE('',*,*,#42646,.F.) ;
#57923 = ORIENTED_EDGE('',*,*,#43387,.F.) ;
#57924 = ORIENTED_EDGE('',*,*,#43578,.F.) ;
#57925 = ORIENTED_EDGE('',*,*,#42631,.F.) ;
#57926 = ORIENTED_EDGE('',*,*,#43504,.F.) ;
#57927 = ORIENTED_EDGE('',*,*,#43578,.T.) ;
#57928 = ORIENTED_EDGE('',*,*,#43452,.F.) ;
#57929 = ORIENTED_EDGE('',*,*,#43579,.F.) ;
#57930 = ORIENTED_EDGE('',*,*,#43447,.F.) ;
#57931 = ORIENTED_EDGE('',*,*,#43579,.T.) ;
#57932 = ORIENTED_EDGE('',*,*,#43451,.F.) ;
#57933 = ORIENTED_EDGE('',*,*,#43580,.F.) ;
#57934 = ORIENTED_EDGE('',*,*,#43509,.F.) ;
#57935 = ORIENTED_EDGE('',*,*,#43580,.T.) ;
#57936 = ORIENTED_EDGE('',*,*,#43502,.F.) ;
#57937 = ORIENTED_EDGE('',*,*,#43581,.F.) ;
#57938 = ORIENTED_EDGE('',*,*,#43507,.F.) ;
#57939 = ORIENTED_EDGE('',*,*,#43581,.T.) ;
#57940 = ORIENTED_EDGE('',*,*,#42788,.F.) ;
#57941 = ORIENTED_EDGE('',*,*,#43582,.F.) ;
#57942 = ORIENTED_EDGE('',*,*,#43508,.F.) ;
#57943 = ORIENTED_EDGE('',*,*,#43582,.T.) ;
#57944 = ORIENTED_EDGE('',*,*,#42787,.F.) ;
#57945 = ORIENTED_EDGE('',*,*,#43292,.F.) ;
#57946 = ORIENTED_EDGE('',*,*,#43281,.F.) ;
#57947 = ORIENTED_EDGE('',*,*,#43217,.T.) ;
#57948 = ORIENTED_EDGE('',*,*,#42790,.F.) ;
#57949 = ORIENTED_EDGE('',*,*,#43583,.F.) ;
#57950 = ORIENTED_EDGE('',*,*,#43497,.F.) ;
#57951 = ORIENTED_EDGE('',*,*,#43583,.T.) ;
#57952 = ORIENTED_EDGE('',*,*,#43503,.F.) ;
#57953 = ORIENTED_EDGE('',*,*,#42611,.F.) ;
#57954 = ORIENTED_EDGE('',*,*,#43498,.F.) ;
#57955 = ORIENTED_EDGE('',*,*,#43584,.F.) ;
#57956 = ORIENTED_EDGE('',*,*,#43441,.F.) ;
#57957 = ORIENTED_EDGE('',*,*,#42609,.T.) ;
#57958 = ORIENTED_EDGE('',*,*,#43454,.F.) ;
#57959 = ORIENTED_EDGE('',*,*,#43505,.F.) ;
#57960 = ORIENTED_EDGE('',*,*,#43499,.F.) ;
#57961 = ORIENTED_EDGE('',*,*,#43584,.T.) ;
#57962 = ORIENTED_EDGE('',*,*,#43585,.T.) ;
#57963 = ORIENTED_EDGE('',*,*,#43586,.T.) ;
#57964 = ORIENTED_EDGE('',*,*,#43456,.F.) ;
#57965 = ORIENTED_EDGE('',*,*,#43587,.T.) ;
#57966 = ORIENTED_EDGE('',*,*,#43588,.T.) ;
#57967 = ORIENTED_EDGE('',*,*,#43288,.F.) ;
#57968 = ORIENTED_EDGE('',*,*,#42887,.F.) ;
#57969 = ORIENTED_EDGE('',*,*,#43589,.F.) ;
#57970 = ORIENTED_EDGE('',*,*,#43285,.F.) ;
#57971 = ORIENTED_EDGE('',*,*,#42886,.F.) ;
#57972 = ORIENTED_EDGE('',*,*,#43590,.T.) ;
#57973 = ORIENTED_EDGE('',*,*,#43566,.F.) ;
#57974 = ORIENTED_EDGE('',*,*,#43589,.T.) ;
#57975 = ORIENTED_EDGE('',*,*,#43577,.F.) ;
#57976 = ORIENTED_EDGE('',*,*,#43591,.T.) ;
#57977 = ORIENTED_EDGE('',*,*,#42883,.F.) ;
#57978 = ORIENTED_EDGE('',*,*,#43225,.T.) ;
#57979 = ORIENTED_EDGE('',*,*,#43587,.F.) ;
#57980 = ORIENTED_EDGE('',*,*,#43590,.F.) ;
#57981 = ORIENTED_EDGE('',*,*,#43592,.F.) ;
#57982 = ORIENTED_EDGE('',*,*,#43593,.F.) ;
#57983 = ORIENTED_EDGE('',*,*,#43588,.F.) ;
#57984 = ORIENTED_EDGE('',*,*,#43592,.T.) ;
#57985 = ORIENTED_EDGE('',*,*,#42885,.F.) ;
#57986 = ORIENTED_EDGE('',*,*,#43593,.T.) ;
#57987 = ORIENTED_EDGE('',*,*,#42884,.F.) ;
#57988 = ORIENTED_EDGE('',*,*,#43594,.F.) ;
#57989 = ORIENTED_EDGE('',*,*,#43585,.F.) ;
#57990 = ORIENTED_EDGE('',*,*,#43594,.T.) ;
#57991 = ORIENTED_EDGE('',*,*,#43591,.F.) ;
#57992 = ORIENTED_EDGE('',*,*,#43586,.F.) ;
#57993 = ORIENTED_EDGE('',*,*,#43595,.F.) ;
#57994 = ORIENTED_EDGE('',*,*,#43245,.F.) ;
#57995 = ORIENTED_EDGE('',*,*,#43596,.F.) ;
#57996 = ORIENTED_EDGE('',*,*,#43597,.F.) ;
#57997 = ORIENTED_EDGE('',*,*,#43243,.F.) ;
#57998 = ORIENTED_EDGE('',*,*,#43598,.F.) ;
#57999 = ORIENTED_EDGE('',*,*,#43596,.T.) ;
#58000 = ORIENTED_EDGE('',*,*,#43248,.F.) ;
#58001 = ORIENTED_EDGE('',*,*,#43599,.F.) ;
#58002 = ORIENTED_EDGE('',*,*,#43266,.F.) ;
#58003 = ORIENTED_EDGE('',*,*,#43595,.T.) ;
#58004 = ORIENTED_EDGE('',*,*,#43265,.F.) ;
#58005 = ORIENTED_EDGE('',*,*,#43600,.F.) ;
#58006 = ORIENTED_EDGE('',*,*,#43242,.F.) ;
#58007 = ORIENTED_EDGE('',*,*,#43598,.T.) ;
#58008 = ORIENTED_EDGE('',*,*,#43240,.F.) ;
#58009 = ORIENTED_EDGE('',*,*,#43601,.F.) ;
#58010 = ORIENTED_EDGE('',*,*,#43268,.F.) ;
#58011 = ORIENTED_EDGE('',*,*,#43597,.T.) ;
#58012 = ORIENTED_EDGE('',*,*,#43274,.F.) ;
#58013 = ORIENTED_EDGE('',*,*,#43602,.F.) ;
#58014 = ORIENTED_EDGE('',*,*,#43246,.F.) ;
#58015 = ORIENTED_EDGE('',*,*,#43599,.T.) ;
#58016 = ORIENTED_EDGE('',*,*,#43251,.F.) ;
#58017 = ORIENTED_EDGE('',*,*,#43603,.F.) ;
#58018 = ORIENTED_EDGE('',*,*,#43239,.F.) ;
#58019 = ORIENTED_EDGE('',*,*,#43600,.T.) ;
#58020 = ORIENTED_EDGE('',*,*,#43604,.F.) ;
#58021 = ORIENTED_EDGE('',*,*,#43601,.T.) ;
#58022 = ORIENTED_EDGE('',*,*,#43237,.F.) ;
#58023 = ORIENTED_EDGE('',*,*,#43605,.F.) ;
#58024 = ORIENTED_EDGE('',*,*,#43249,.F.) ;
#58025 = ORIENTED_EDGE('',*,*,#43602,.T.) ;
#58026 = ORIENTED_EDGE('',*,*,#43606,.F.) ;
#58027 = ORIENTED_EDGE('',*,*,#43603,.T.) ;
#58028 = ORIENTED_EDGE('',*,*,#43254,.F.) ;
#58029 = ORIENTED_EDGE('',*,*,#43607,.F.) ;
#58030 = ORIENTED_EDGE('',*,*,#43267,.F.) ;
#58031 = ORIENTED_EDGE('',*,*,#43604,.T.) ;
#58032 = ORIENTED_EDGE('',*,*,#43264,.F.) ;
#58033 = ORIENTED_EDGE('',*,*,#43608,.F.) ;
#58034 = ORIENTED_EDGE('',*,*,#43236,.F.) ;
#58035 = ORIENTED_EDGE('',*,*,#43609,.F.) ;
#58036 = ORIENTED_EDGE('',*,*,#43233,.F.) ;
#58037 = ORIENTED_EDGE('',*,*,#43610,.F.) ;
#58038 = ORIENTED_EDGE('',*,*,#42717,.F.) ;
#58039 = ORIENTED_EDGE('',*,*,#43605,.T.) ;
#58040 = ORIENTED_EDGE('',*,*,#43234,.F.) ;
#58041 = ORIENTED_EDGE('',*,*,#43611,.F.) ;
#58042 = ORIENTED_EDGE('',*,*,#43269,.F.) ;
#58043 = ORIENTED_EDGE('',*,*,#43606,.T.) ;
#58044 = ORIENTED_EDGE('',*,*,#43273,.F.) ;
#58045 = ORIENTED_EDGE('',*,*,#43612,.F.) ;
#58046 = ORIENTED_EDGE('',*,*,#43252,.F.) ;
#58047 = ORIENTED_EDGE('',*,*,#43607,.T.) ;
#58048 = ORIENTED_EDGE('',*,*,#43257,.F.) ;
#58049 = ORIENTED_EDGE('',*,*,#43613,.F.) ;
#58050 = ORIENTED_EDGE('',*,*,#43261,.F.) ;
#58051 = ORIENTED_EDGE('',*,*,#43610,.T.) ;
#58052 = ORIENTED_EDGE('',*,*,#43608,.T.) ;
#58053 = ORIENTED_EDGE('',*,*,#43614,.F.) ;
#58054 = ORIENTED_EDGE('',*,*,#42718,.T.) ;
#58055 = ORIENTED_EDGE('',*,*,#43609,.T.) ;
#58056 = ORIENTED_EDGE('',*,*,#42716,.T.) ;
#58057 = ORIENTED_EDGE('',*,*,#43615,.F.) ;
#58058 = ORIENTED_EDGE('',*,*,#43611,.T.) ;
#58059 = ORIENTED_EDGE('',*,*,#43612,.T.) ;
#58060 = ORIENTED_EDGE('',*,*,#43272,.F.) ;
#58061 = ORIENTED_EDGE('',*,*,#43616,.F.) ;
#58062 = ORIENTED_EDGE('',*,*,#43255,.F.) ;
#58063 = ORIENTED_EDGE('',*,*,#43613,.T.) ;
#58064 = ORIENTED_EDGE('',*,*,#43260,.F.) ;
#58065 = ORIENTED_EDGE('',*,*,#43617,.F.) ;
#58066 = ORIENTED_EDGE('',*,*,#43262,.F.) ;
#58067 = ORIENTED_EDGE('',*,*,#43614,.T.) ;
#58068 = ORIENTED_EDGE('',*,*,#43263,.F.) ;
#58069 = ORIENTED_EDGE('',*,*,#43618,.F.) ;
#58070 = ORIENTED_EDGE('',*,*,#42719,.F.) ;
#58071 = ORIENTED_EDGE('',*,*,#43615,.T.) ;
#58072 = ORIENTED_EDGE('',*,*,#42715,.F.) ;
#58073 = ORIENTED_EDGE('',*,*,#43619,.F.) ;
#58074 = ORIENTED_EDGE('',*,*,#43270,.F.) ;
#58075 = ORIENTED_EDGE('',*,*,#43616,.T.) ;
#58076 = ORIENTED_EDGE('',*,*,#43271,.F.) ;
#58077 = ORIENTED_EDGE('',*,*,#43620,.F.) ;
#58078 = ORIENTED_EDGE('',*,*,#43258,.F.) ;
#58079 = ORIENTED_EDGE('',*,*,#43618,.T.) ;
#58080 = ORIENTED_EDGE('',*,*,#43617,.T.) ;
#58081 = ORIENTED_EDGE('',*,*,#43621,.F.) ;
#58082 = ORIENTED_EDGE('',*,*,#42720,.T.) ;
#58083 = ORIENTED_EDGE('',*,*,#43619,.T.) ;
#58084 = ORIENTED_EDGE('',*,*,#42714,.T.) ;
#58085 = ORIENTED_EDGE('',*,*,#43622,.F.) ;
#58086 = ORIENTED_EDGE('',*,*,#43620,.T.) ;
#58087 = ORIENTED_EDGE('',*,*,#43621,.T.) ;
#58088 = ORIENTED_EDGE('',*,*,#43259,.F.) ;
#58089 = ORIENTED_EDGE('',*,*,#43622,.T.) ;
#58090 = ORIENTED_EDGE('',*,*,#42721,.F.) ;
#58091 = ORIENTED_EDGE('',*,*,#43623,.F.) ;
#58092 = ORIENTED_EDGE('',*,*,#43624,.F.) ;
#58093 = ORIENTED_EDGE('',*,*,#43625,.F.) ;
#58094 = ORIENTED_EDGE('',*,*,#43626,.T.) ;
#58095 = ORIENTED_EDGE('',*,*,#43627,.F.) ;
#58096 = ORIENTED_EDGE('',*,*,#43628,.F.) ;
#58097 = ORIENTED_EDGE('',*,*,#43629,.F.) ;
#58098 = ORIENTED_EDGE('',*,*,#43630,.F.) ;
#58099 = ORIENTED_EDGE('',*,*,#43631,.F.) ;
#58100 = ORIENTED_EDGE('',*,*,#43632,.T.) ;
#58101 = ORIENTED_EDGE('',*,*,#43633,.F.) ;
#58102 = ORIENTED_EDGE('',*,*,#43634,.F.) ;
#58103 = ORIENTED_EDGE('',*,*,#43632,.F.) ;
#58104 = ORIENTED_EDGE('',*,*,#43635,.F.) ;
#58105 = ORIENTED_EDGE('',*,*,#43636,.T.) ;
#58106 = ORIENTED_EDGE('',*,*,#43637,.F.) ;
#58107 = ORIENTED_EDGE('',*,*,#43636,.F.) ;
#58108 = ORIENTED_EDGE('',*,*,#43638,.F.) ;
#58109 = ORIENTED_EDGE('',*,*,#43639,.T.) ;
#58110 = ORIENTED_EDGE('',*,*,#43640,.F.) ;
#58111 = ORIENTED_EDGE('',*,*,#43641,.F.) ;
#58112 = ORIENTED_EDGE('',*,*,#43639,.F.) ;
#58113 = ORIENTED_EDGE('',*,*,#43642,.T.) ;
#58114 = ORIENTED_EDGE('',*,*,#43643,.F.) ;
#58115 = ORIENTED_EDGE('',*,*,#43644,.T.) ;
#58116 = ORIENTED_EDGE('',*,*,#43645,.T.) ;
#58117 = ORIENTED_EDGE('',*,*,#43646,.T.) ;
#58118 = ORIENTED_EDGE('',*,*,#43647,.T.) ;
#58119 = ORIENTED_EDGE('',*,*,#43648,.F.) ;
#58120 = ORIENTED_EDGE('',*,*,#43642,.F.) ;
#58121 = ORIENTED_EDGE('',*,*,#43649,.F.) ;
#58122 = ORIENTED_EDGE('',*,*,#43650,.T.) ;
#58123 = ORIENTED_EDGE('',*,*,#43651,.F.) ;
#58124 = ORIENTED_EDGE('',*,*,#43652,.F.) ;
#58125 = ORIENTED_EDGE('',*,*,#43653,.T.) ;
#58126 = ORIENTED_EDGE('',*,*,#43654,.F.) ;
#58127 = ORIENTED_EDGE('',*,*,#43655,.F.) ;
#58128 = ORIENTED_EDGE('',*,*,#43656,.T.) ;
#58129 = ORIENTED_EDGE('',*,*,#43635,.T.) ;
#58130 = ORIENTED_EDGE('',*,*,#43656,.F.) ;
#58131 = ORIENTED_EDGE('',*,*,#43637,.T.) ;
#58132 = ORIENTED_EDGE('',*,*,#43657,.T.) ;
#58133 = ORIENTED_EDGE('',*,*,#43640,.T.) ;
#58134 = ORIENTED_EDGE('',*,*,#43641,.T.) ;
#58135 = ORIENTED_EDGE('',*,*,#43657,.F.) ;
#58136 = ORIENTED_EDGE('',*,*,#43658,.F.) ;
#58137 = ORIENTED_EDGE('',*,*,#43659,.T.) ;
#58138 = ORIENTED_EDGE('',*,*,#43660,.F.) ;
#58139 = ORIENTED_EDGE('',*,*,#43661,.T.) ;
#58140 = ORIENTED_EDGE('',*,*,#43662,.F.) ;
#58141 = ORIENTED_EDGE('',*,*,#43663,.T.) ;
#58142 = ORIENTED_EDGE('',*,*,#43664,.T.) ;
#58143 = ORIENTED_EDGE('',*,*,#43665,.T.) ;
#58144 = ORIENTED_EDGE('',*,*,#43666,.F.) ;
#58145 = ORIENTED_EDGE('',*,*,#43667,.T.) ;
#58146 = ORIENTED_EDGE('',*,*,#43668,.F.) ;
#58147 = ORIENTED_EDGE('',*,*,#43669,.T.) ;
#58148 = ORIENTED_EDGE('',*,*,#43670,.F.) ;
#58149 = ORIENTED_EDGE('',*,*,#43671,.T.) ;
#58150 = ORIENTED_EDGE('',*,*,#43672,.T.) ;
#58151 = ORIENTED_EDGE('',*,*,#43673,.T.) ;
#58152 = ORIENTED_EDGE('',*,*,#43674,.F.) ;
#58153 = ORIENTED_EDGE('',*,*,#43675,.T.) ;
#58154 = ORIENTED_EDGE('',*,*,#43633,.T.) ;
#58155 = ORIENTED_EDGE('',*,*,#43634,.T.) ;
#58156 = ORIENTED_EDGE('',*,*,#43675,.F.) ;
#58157 = ORIENTED_EDGE('',*,*,#43676,.T.) ;
#58158 = ORIENTED_EDGE('',*,*,#43677,.T.) ;
#58159 = ORIENTED_EDGE('',*,*,#43678,.T.) ;
#58160 = ORIENTED_EDGE('',*,*,#43679,.T.) ;
#58161 = ORIENTED_EDGE('',*,*,#43680,.F.) ;
#58162 = ORIENTED_EDGE('',*,*,#43681,.T.) ;
#58163 = ORIENTED_EDGE('',*,*,#43682,.T.) ;
#58164 = ORIENTED_EDGE('',*,*,#43683,.T.) ;
#58165 = ORIENTED_EDGE('',*,*,#43684,.T.) ;
#58166 = ORIENTED_EDGE('',*,*,#43685,.T.) ;
#58167 = ORIENTED_EDGE('',*,*,#43686,.T.) ;
#58168 = ORIENTED_EDGE('',*,*,#43687,.T.) ;
#58169 = ORIENTED_EDGE('',*,*,#43658,.T.) ;
#58170 = ORIENTED_EDGE('',*,*,#43674,.T.) ;
#58171 = ORIENTED_EDGE('',*,*,#43688,.T.) ;
#58172 = ORIENTED_EDGE('',*,*,#43689,.T.) ;
#58173 = ORIENTED_EDGE('',*,*,#43690,.T.) ;
#58174 = ORIENTED_EDGE('',*,*,#43691,.F.) ;
#58175 = ORIENTED_EDGE('',*,*,#43692,.T.) ;
#58176 = ORIENTED_EDGE('',*,*,#43693,.F.) ;
#58177 = ORIENTED_EDGE('',*,*,#43694,.T.) ;
#58178 = ORIENTED_EDGE('',*,*,#43695,.F.) ;
#58179 = ORIENTED_EDGE('',*,*,#43696,.T.) ;
#58180 = ORIENTED_EDGE('',*,*,#43697,.T.) ;
#58181 = ORIENTED_EDGE('',*,*,#43698,.T.) ;
#58182 = ORIENTED_EDGE('',*,*,#43699,.T.) ;
#58183 = ORIENTED_EDGE('',*,*,#43700,.F.) ;
#58184 = ORIENTED_EDGE('',*,*,#43701,.T.) ;
#58185 = ORIENTED_EDGE('',*,*,#43644,.F.) ;
#58186 = ORIENTED_EDGE('',*,*,#43638,.T.) ;
#58187 = ORIENTED_EDGE('',*,*,#43702,.T.) ;
#58188 = ORIENTED_EDGE('',*,*,#43703,.T.) ;
#58189 = ORIENTED_EDGE('',*,*,#43704,.F.) ;
#58190 = ORIENTED_EDGE('',*,*,#43705,.T.) ;
#58191 = ORIENTED_EDGE('',*,*,#43706,.F.) ;
#58192 = ORIENTED_EDGE('',*,*,#43707,.T.) ;
#58193 = ORIENTED_EDGE('',*,*,#43708,.T.) ;
#58194 = ORIENTED_EDGE('',*,*,#43709,.T.) ;
#58195 = ORIENTED_EDGE('',*,*,#43710,.T.) ;
#58196 = ORIENTED_EDGE('',*,*,#43711,.T.) ;
#58197 = ORIENTED_EDGE('',*,*,#43712,.T.) ;
#58198 = ORIENTED_EDGE('',*,*,#43713,.T.) ;
#58199 = ORIENTED_EDGE('',*,*,#43714,.T.) ;
#58200 = ORIENTED_EDGE('',*,*,#43715,.T.) ;
#58201 = ORIENTED_EDGE('',*,*,#43716,.F.) ;
#58202 = ORIENTED_EDGE('',*,*,#43717,.T.) ;
#58203 = ORIENTED_EDGE('',*,*,#43718,.T.) ;
#58204 = ORIENTED_EDGE('',*,*,#43719,.T.) ;
#58205 = ORIENTED_EDGE('',*,*,#43720,.F.) ;
#58206 = ORIENTED_EDGE('',*,*,#43721,.T.) ;
#58207 = ORIENTED_EDGE('',*,*,#43722,.T.) ;
#58208 = ORIENTED_EDGE('',*,*,#43723,.T.) ;
#58209 = ORIENTED_EDGE('',*,*,#43724,.F.) ;
#58210 = ORIENTED_EDGE('',*,*,#43725,.T.) ;
#58211 = ORIENTED_EDGE('',*,*,#43726,.T.) ;
#58212 = ORIENTED_EDGE('',*,*,#43727,.T.) ;
#58213 = ORIENTED_EDGE('',*,*,#43728,.F.) ;
#58214 = ORIENTED_EDGE('',*,*,#43729,.T.) ;
#58215 = ORIENTED_EDGE('',*,*,#43730,.T.) ;
#58216 = ORIENTED_EDGE('',*,*,#43731,.T.) ;
#58217 = ORIENTED_EDGE('',*,*,#43732,.F.) ;
#58218 = ORIENTED_EDGE('',*,*,#43733,.T.) ;
#58219 = ORIENTED_EDGE('',*,*,#43734,.T.) ;
#58220 = ORIENTED_EDGE('',*,*,#43735,.T.) ;
#58221 = ORIENTED_EDGE('',*,*,#43736,.F.) ;
#58222 = ORIENTED_EDGE('',*,*,#43737,.T.) ;
#58223 = ORIENTED_EDGE('',*,*,#43738,.T.) ;
#58224 = ORIENTED_EDGE('',*,*,#43739,.T.) ;
#58225 = ORIENTED_EDGE('',*,*,#43740,.F.) ;
#58226 = ORIENTED_EDGE('',*,*,#43741,.T.) ;
#58227 = ORIENTED_EDGE('',*,*,#43742,.F.) ;
#58228 = ORIENTED_EDGE('',*,*,#43743,.T.) ;
#58229 = ORIENTED_EDGE('',*,*,#43744,.F.) ;
#58230 = ORIENTED_EDGE('',*,*,#43745,.T.) ;
#58231 = ORIENTED_EDGE('',*,*,#43746,.F.) ;
#58232 = ORIENTED_EDGE('',*,*,#43747,.T.) ;
#58233 = ORIENTED_EDGE('',*,*,#43748,.F.) ;
#58234 = ORIENTED_EDGE('',*,*,#43749,.T.) ;
#58235 = ORIENTED_EDGE('',*,*,#43631,.T.) ;
#58236 = ORIENTED_EDGE('',*,*,#43750,.T.) ;
#58237 = ORIENTED_EDGE('',*,*,#43751,.T.) ;
#58238 = ORIENTED_EDGE('',*,*,#43752,.F.) ;
#58239 = ORIENTED_EDGE('',*,*,#43753,.T.) ;
#58240 = ORIENTED_EDGE('',*,*,#43754,.T.) ;
#58241 = ORIENTED_EDGE('',*,*,#43630,.T.) ;
#58242 = ORIENTED_EDGE('',*,*,#43755,.F.) ;
#58243 = ORIENTED_EDGE('',*,*,#43756,.T.) ;
#58244 = ORIENTED_EDGE('',*,*,#43757,.T.) ;
#58245 = ORIENTED_EDGE('',*,*,#43758,.T.) ;
#58246 = ORIENTED_EDGE('',*,*,#43759,.F.) ;
#58247 = ORIENTED_EDGE('',*,*,#43628,.T.) ;
#58248 = ORIENTED_EDGE('',*,*,#43760,.T.) ;
#58249 = ORIENTED_EDGE('',*,*,#43761,.T.) ;
#58250 = ORIENTED_EDGE('',*,*,#43762,.F.) ;
#58251 = ORIENTED_EDGE('',*,*,#43763,.T.) ;
#58252 = ORIENTED_EDGE('',*,*,#43764,.T.) ;
#58253 = ORIENTED_EDGE('',*,*,#43765,.T.) ;
#58254 = ORIENTED_EDGE('',*,*,#43766,.T.) ;
#58255 = ORIENTED_EDGE('',*,*,#43767,.F.) ;
#58256 = ORIENTED_EDGE('',*,*,#43768,.T.) ;
#58257 = ORIENTED_EDGE('',*,*,#43769,.F.) ;
#58258 = ORIENTED_EDGE('',*,*,#43770,.T.) ;
#58259 = ORIENTED_EDGE('',*,*,#43771,.T.) ;
#58260 = ORIENTED_EDGE('',*,*,#43772,.T.) ;
#58261 = ORIENTED_EDGE('',*,*,#43773,.T.) ;
#58262 = ORIENTED_EDGE('',*,*,#43774,.F.) ;
#58263 = ORIENTED_EDGE('',*,*,#43775,.T.) ;
#58264 = ORIENTED_EDGE('',*,*,#43776,.F.) ;
#58265 = ORIENTED_EDGE('',*,*,#43777,.T.) ;
#58266 = ORIENTED_EDGE('',*,*,#43778,.F.) ;
#58267 = ORIENTED_EDGE('',*,*,#43779,.T.) ;
#58268 = ORIENTED_EDGE('',*,*,#43780,.F.) ;
#58269 = ORIENTED_EDGE('',*,*,#43781,.T.) ;
#58270 = ORIENTED_EDGE('',*,*,#43782,.F.) ;
#58271 = ORIENTED_EDGE('',*,*,#43783,.T.) ;
#58272 = ORIENTED_EDGE('',*,*,#43784,.T.) ;
#58273 = ORIENTED_EDGE('',*,*,#43785,.T.) ;
#58274 = ORIENTED_EDGE('',*,*,#43786,.F.) ;
#58275 = ORIENTED_EDGE('',*,*,#43787,.T.) ;
#58276 = ORIENTED_EDGE('',*,*,#43788,.T.) ;
#58277 = ORIENTED_EDGE('',*,*,#43789,.T.) ;
#58278 = ORIENTED_EDGE('',*,*,#43790,.T.) ;
#58279 = ORIENTED_EDGE('',*,*,#43791,.T.) ;
#58280 = ORIENTED_EDGE('',*,*,#43792,.T.) ;
#58281 = ORIENTED_EDGE('',*,*,#43793,.F.) ;
#58282 = ORIENTED_EDGE('',*,*,#43794,.T.) ;
#58283 = ORIENTED_EDGE('',*,*,#43795,.T.) ;
#58284 = ORIENTED_EDGE('',*,*,#43796,.T.) ;
#58285 = ORIENTED_EDGE('',*,*,#43797,.F.) ;
#58286 = ORIENTED_EDGE('',*,*,#43798,.T.) ;
#58287 = ORIENTED_EDGE('',*,*,#43799,.T.) ;
#58288 = ORIENTED_EDGE('',*,*,#43800,.T.) ;
#58289 = ORIENTED_EDGE('',*,*,#43801,.T.) ;
#58290 = ORIENTED_EDGE('',*,*,#43802,.T.) ;
#58291 = ORIENTED_EDGE('',*,*,#43803,.T.) ;
#58292 = ORIENTED_EDGE('',*,*,#43804,.T.) ;
#58293 = ORIENTED_EDGE('',*,*,#43793,.T.) ;
#58294 = ORIENTED_EDGE('',*,*,#43805,.T.) ;
#58295 = ORIENTED_EDGE('',*,*,#43797,.T.) ;
#58296 = ORIENTED_EDGE('',*,*,#43806,.T.) ;
#58297 = ORIENTED_EDGE('',*,*,#43680,.T.) ;
#58298 = ORIENTED_EDGE('',*,*,#43807,.T.) ;
#58299 = ORIENTED_EDGE('',*,*,#43691,.T.) ;
#58300 = ORIENTED_EDGE('',*,*,#43808,.T.) ;
#58301 = ORIENTED_EDGE('',*,*,#43704,.T.) ;
#58302 = ORIENTED_EDGE('',*,*,#43809,.T.) ;
#58303 = ORIENTED_EDGE('',*,*,#43706,.T.) ;
#58304 = ORIENTED_EDGE('',*,*,#43810,.T.) ;
#58305 = ORIENTED_EDGE('',*,*,#43716,.T.) ;
#58306 = ORIENTED_EDGE('',*,*,#43811,.T.) ;
#58307 = ORIENTED_EDGE('',*,*,#43720,.T.) ;
#58308 = ORIENTED_EDGE('',*,*,#43812,.T.) ;
#58309 = ORIENTED_EDGE('',*,*,#43724,.T.) ;
#58310 = ORIENTED_EDGE('',*,*,#43813,.T.) ;
#58311 = ORIENTED_EDGE('',*,*,#43728,.T.) ;
#58312 = ORIENTED_EDGE('',*,*,#43814,.T.) ;
#58313 = ORIENTED_EDGE('',*,*,#43732,.T.) ;
#58314 = ORIENTED_EDGE('',*,*,#43815,.T.) ;
#58315 = ORIENTED_EDGE('',*,*,#43736,.T.) ;
#58316 = ORIENTED_EDGE('',*,*,#43816,.T.) ;
#58317 = ORIENTED_EDGE('',*,*,#43740,.T.) ;
#58318 = ORIENTED_EDGE('',*,*,#43817,.T.) ;
#58319 = ORIENTED_EDGE('',*,*,#43752,.T.) ;
#58320 = ORIENTED_EDGE('',*,*,#43818,.T.) ;
#58321 = ORIENTED_EDGE('',*,*,#43755,.T.) ;
#58322 = ORIENTED_EDGE('',*,*,#43629,.T.) ;
#58323 = ORIENTED_EDGE('',*,*,#43759,.T.) ;
#58324 = ORIENTED_EDGE('',*,*,#43819,.T.) ;
#58325 = ORIENTED_EDGE('',*,*,#43762,.T.) ;
#58326 = ORIENTED_EDGE('',*,*,#43820,.T.) ;
#58327 = ORIENTED_EDGE('',*,*,#43774,.T.) ;
#58328 = ORIENTED_EDGE('',*,*,#43821,.T.) ;
#58329 = ORIENTED_EDGE('',*,*,#43786,.T.) ;
#58330 = ORIENTED_EDGE('',*,*,#43822,.T.) ;
#58331 = ORIENTED_EDGE('',*,*,#43678,.F.) ;
#58332 = ORIENTED_EDGE('',*,*,#43823,.T.) ;
#58333 = ORIENTED_EDGE('',*,*,#43795,.F.) ;
#58334 = ORIENTED_EDGE('',*,*,#43824,.T.) ;
#58335 = ORIENTED_EDGE('',*,*,#43784,.F.) ;
#58336 = ORIENTED_EDGE('',*,*,#43825,.T.) ;
#58337 = ORIENTED_EDGE('',*,*,#43772,.F.) ;
#58338 = ORIENTED_EDGE('',*,*,#43826,.T.) ;
#58339 = ORIENTED_EDGE('',*,*,#43760,.F.) ;
#58340 = ORIENTED_EDGE('',*,*,#43827,.T.) ;
#58341 = ORIENTED_EDGE('',*,*,#43757,.F.) ;
#58342 = ORIENTED_EDGE('',*,*,#43627,.T.) ;
#58343 = ORIENTED_EDGE('',*,*,#43754,.F.) ;
#58344 = ORIENTED_EDGE('',*,*,#43828,.T.) ;
#58345 = ORIENTED_EDGE('',*,*,#43750,.F.) ;
#58346 = ORIENTED_EDGE('',*,*,#43829,.T.) ;
#58347 = ORIENTED_EDGE('',*,*,#43738,.F.) ;
#58348 = ORIENTED_EDGE('',*,*,#43830,.T.) ;
#58349 = ORIENTED_EDGE('',*,*,#43734,.F.) ;
#58350 = ORIENTED_EDGE('',*,*,#43831,.T.) ;
#58351 = ORIENTED_EDGE('',*,*,#43730,.F.) ;
#58352 = ORIENTED_EDGE('',*,*,#43832,.T.) ;
#58353 = ORIENTED_EDGE('',*,*,#43726,.F.) ;
#58354 = ORIENTED_EDGE('',*,*,#43833,.T.) ;
#58355 = ORIENTED_EDGE('',*,*,#43722,.F.) ;
#58356 = ORIENTED_EDGE('',*,*,#43834,.T.) ;
#58357 = ORIENTED_EDGE('',*,*,#43718,.F.) ;
#58358 = ORIENTED_EDGE('',*,*,#43835,.T.) ;
#58359 = ORIENTED_EDGE('',*,*,#43714,.F.) ;
#58360 = ORIENTED_EDGE('',*,*,#43836,.T.) ;
#58361 = ORIENTED_EDGE('',*,*,#43712,.F.) ;
#58362 = ORIENTED_EDGE('',*,*,#43837,.T.) ;
#58363 = ORIENTED_EDGE('',*,*,#43684,.F.) ;
#58364 = ORIENTED_EDGE('',*,*,#43838,.T.) ;
#58365 = ORIENTED_EDGE('',*,*,#43697,.F.) ;
#58366 = ORIENTED_EDGE('',*,*,#43839,.T.) ;
#58367 = ORIENTED_EDGE('',*,*,#43803,.F.) ;
#58368 = ORIENTED_EDGE('',*,*,#43840,.T.) ;
#58369 = ORIENTED_EDGE('',*,*,#43841,.T.) ;
#58370 = ORIENTED_EDGE('',*,*,#43842,.T.) ;
#58371 = ORIENTED_EDGE('',*,*,#43843,.T.) ;
#58372 = ORIENTED_EDGE('',*,*,#43844,.T.) ;
#58373 = ORIENTED_EDGE('',*,*,#43845,.T.) ;
#58374 = ORIENTED_EDGE('',*,*,#43846,.T.) ;
#58375 = ORIENTED_EDGE('',*,*,#43847,.T.) ;
#58376 = ORIENTED_EDGE('',*,*,#43848,.T.) ;
#58377 = ORIENTED_EDGE('',*,*,#43849,.F.) ;
#58378 = ORIENTED_EDGE('',*,*,#43850,.T.) ;
#58379 = ORIENTED_EDGE('',*,*,#43851,.T.) ;
#58380 = ORIENTED_EDGE('',*,*,#43852,.T.) ;
#58381 = ORIENTED_EDGE('',*,*,#43853,.F.) ;
#58382 = ORIENTED_EDGE('',*,*,#43854,.T.) ;
#58383 = ORIENTED_EDGE('',*,*,#43855,.T.) ;
#58384 = ORIENTED_EDGE('',*,*,#43856,.T.) ;
#58385 = ORIENTED_EDGE('',*,*,#43857,.T.) ;
#58386 = ORIENTED_EDGE('',*,*,#43858,.T.) ;
#58387 = ORIENTED_EDGE('',*,*,#43859,.F.) ;
#58388 = ORIENTED_EDGE('',*,*,#43860,.T.) ;
#58389 = ORIENTED_EDGE('',*,*,#43851,.F.) ;
#58390 = ORIENTED_EDGE('',*,*,#43861,.T.) ;
#58391 = ORIENTED_EDGE('',*,*,#43862,.T.) ;
#58392 = ORIENTED_EDGE('',*,*,#43863,.T.) ;
#58393 = ORIENTED_EDGE('',*,*,#43864,.F.) ;
#58394 = ORIENTED_EDGE('',*,*,#43865,.T.) ;
#58395 = ORIENTED_EDGE('',*,*,#43857,.F.) ;
#58396 = ORIENTED_EDGE('',*,*,#43866,.T.) ;
#58397 = ORIENTED_EDGE('',*,*,#43867,.F.) ;
#58398 = ORIENTED_EDGE('',*,*,#43868,.T.) ;
#58399 = ORIENTED_EDGE('',*,*,#43869,.T.) ;
#58400 = ORIENTED_EDGE('',*,*,#43870,.T.) ;
#58401 = ORIENTED_EDGE('',*,*,#43862,.F.) ;
#58402 = ORIENTED_EDGE('',*,*,#43871,.T.) ;
#58403 = ORIENTED_EDGE('',*,*,#43872,.T.) ;
#58404 = ORIENTED_EDGE('',*,*,#43873,.T.) ;
#58405 = ORIENTED_EDGE('',*,*,#43859,.T.) ;
#58406 = ORIENTED_EDGE('',*,*,#43874,.T.) ;
#58407 = ORIENTED_EDGE('',*,*,#43875,.T.) ;
#58408 = ORIENTED_EDGE('',*,*,#43876,.T.) ;
#58409 = ORIENTED_EDGE('',*,*,#43877,.T.) ;
#58410 = ORIENTED_EDGE('',*,*,#43878,.T.) ;
#58411 = ORIENTED_EDGE('',*,*,#43879,.T.) ;
#58412 = ORIENTED_EDGE('',*,*,#43880,.T.) ;
#58413 = ORIENTED_EDGE('',*,*,#43881,.T.) ;
#58414 = ORIENTED_EDGE('',*,*,#43882,.T.) ;
#58415 = ORIENTED_EDGE('',*,*,#43883,.T.) ;
#58416 = ORIENTED_EDGE('',*,*,#43884,.T.) ;
#58417 = ORIENTED_EDGE('',*,*,#43885,.T.) ;
#58418 = ORIENTED_EDGE('',*,*,#43886,.T.) ;
#58419 = ORIENTED_EDGE('',*,*,#43887,.T.) ;
#58420 = ORIENTED_EDGE('',*,*,#43888,.T.) ;
#58421 = ORIENTED_EDGE('',*,*,#43889,.T.) ;
#58422 = ORIENTED_EDGE('',*,*,#43890,.T.) ;
#58423 = ORIENTED_EDGE('',*,*,#43891,.T.) ;
#58424 = ORIENTED_EDGE('',*,*,#43892,.T.) ;
#58425 = ORIENTED_EDGE('',*,*,#43893,.T.) ;
#58426 = ORIENTED_EDGE('',*,*,#43894,.T.) ;
#58427 = ORIENTED_EDGE('',*,*,#43895,.T.) ;
#58428 = ORIENTED_EDGE('',*,*,#43896,.T.) ;
#58429 = ORIENTED_EDGE('',*,*,#43897,.T.) ;
#58430 = ORIENTED_EDGE('',*,*,#43898,.T.) ;
#58431 = ORIENTED_EDGE('',*,*,#43899,.T.) ;
#58432 = ORIENTED_EDGE('',*,*,#43900,.T.) ;
#58433 = ORIENTED_EDGE('',*,*,#43901,.T.) ;
#58434 = ORIENTED_EDGE('',*,*,#43902,.T.) ;
#58435 = ORIENTED_EDGE('',*,*,#43903,.T.) ;
#58436 = ORIENTED_EDGE('',*,*,#43904,.T.) ;
#58437 = ORIENTED_EDGE('',*,*,#43905,.T.) ;
#58438 = ORIENTED_EDGE('',*,*,#43906,.T.) ;
#58439 = ORIENTED_EDGE('',*,*,#43907,.T.) ;
#58440 = ORIENTED_EDGE('',*,*,#43908,.T.) ;
#58441 = ORIENTED_EDGE('',*,*,#43909,.F.) ;
#58442 = ORIENTED_EDGE('',*,*,#43910,.F.) ;
#58443 = ORIENTED_EDGE('',*,*,#43911,.F.) ;
#58444 = ORIENTED_EDGE('',*,*,#43912,.F.) ;
#58445 = ORIENTED_EDGE('',*,*,#43913,.F.) ;
#58446 = ORIENTED_EDGE('',*,*,#43914,.F.) ;
#58447 = ORIENTED_EDGE('',*,*,#43915,.F.) ;
#58448 = ORIENTED_EDGE('',*,*,#43916,.F.) ;
#58449 = ORIENTED_EDGE('',*,*,#43917,.F.) ;
#58450 = ORIENTED_EDGE('',*,*,#43918,.F.) ;
#58451 = ORIENTED_EDGE('',*,*,#43916,.T.) ;
#58452 = ORIENTED_EDGE('',*,*,#43919,.T.) ;
#58453 = ORIENTED_EDGE('',*,*,#43920,.F.) ;
#58454 = ORIENTED_EDGE('',*,*,#43921,.F.) ;
#58455 = ORIENTED_EDGE('',*,*,#43909,.T.) ;
#58456 = ORIENTED_EDGE('',*,*,#43918,.T.) ;
#58457 = ORIENTED_EDGE('',*,*,#43922,.F.) ;
#58458 = ORIENTED_EDGE('',*,*,#43923,.F.) ;
#58459 = ORIENTED_EDGE('',*,*,#43910,.T.) ;
#58460 = ORIENTED_EDGE('',*,*,#43921,.T.) ;
#58461 = ORIENTED_EDGE('',*,*,#43924,.F.) ;
#58462 = ORIENTED_EDGE('',*,*,#43925,.F.) ;
#58463 = ORIENTED_EDGE('',*,*,#43911,.T.) ;
#58464 = ORIENTED_EDGE('',*,*,#43923,.T.) ;
#58465 = ORIENTED_EDGE('',*,*,#43926,.F.) ;
#58466 = ORIENTED_EDGE('',*,*,#43927,.F.) ;
#58467 = ORIENTED_EDGE('',*,*,#43912,.T.) ;
#58468 = ORIENTED_EDGE('',*,*,#43925,.T.) ;
#58469 = ORIENTED_EDGE('',*,*,#43928,.F.) ;
#58470 = ORIENTED_EDGE('',*,*,#43929,.F.) ;
#58471 = ORIENTED_EDGE('',*,*,#43913,.T.) ;
#58472 = ORIENTED_EDGE('',*,*,#43927,.T.) ;
#58473 = ORIENTED_EDGE('',*,*,#43930,.F.) ;
#58474 = ORIENTED_EDGE('',*,*,#43931,.F.) ;
#58475 = ORIENTED_EDGE('',*,*,#43914,.T.) ;
#58476 = ORIENTED_EDGE('',*,*,#43929,.T.) ;
#58477 = ORIENTED_EDGE('',*,*,#43932,.F.) ;
#58478 = ORIENTED_EDGE('',*,*,#43919,.F.) ;
#58479 = ORIENTED_EDGE('',*,*,#43915,.T.) ;
#58480 = ORIENTED_EDGE('',*,*,#43931,.T.) ;
#58481 = ORIENTED_EDGE('',*,*,#43920,.T.) ;
#58482 = ORIENTED_EDGE('',*,*,#43917,.T.) ;
#58483 = ORIENTED_EDGE('',*,*,#43932,.T.) ;
#58484 = ORIENTED_EDGE('',*,*,#43930,.T.) ;
#58485 = ORIENTED_EDGE('',*,*,#43928,.T.) ;
#58486 = ORIENTED_EDGE('',*,*,#43926,.T.) ;
#58487 = ORIENTED_EDGE('',*,*,#43924,.T.) ;
#58488 = ORIENTED_EDGE('',*,*,#43922,.T.) ;
#58489 = ORIENTED_EDGE('',*,*,#43666,.T.) ;
#58490 = ORIENTED_EDGE('',*,*,#43933,.T.) ;
#58491 = ORIENTED_EDGE('',*,*,#43664,.F.) ;
#58492 = ORIENTED_EDGE('',*,*,#43934,.T.) ;
#58493 = ORIENTED_EDGE('',*,*,#43668,.T.) ;
#58494 = ORIENTED_EDGE('',*,*,#43935,.T.) ;
#58495 = ORIENTED_EDGE('',*,*,#43672,.F.) ;
#58496 = ORIENTED_EDGE('',*,*,#43936,.T.) ;
#58497 = ORIENTED_EDGE('',*,*,#43660,.T.) ;
#58498 = ORIENTED_EDGE('',*,*,#43937,.T.) ;
#58499 = ORIENTED_EDGE('',*,*,#43662,.T.) ;
#58500 = ORIENTED_EDGE('',*,*,#43938,.T.) ;
#58501 = ORIENTED_EDGE('',*,*,#43670,.T.) ;
#58502 = ORIENTED_EDGE('',*,*,#43939,.T.) ;
#58503 = ORIENTED_EDGE('',*,*,#43940,.T.) ;
#58504 = ORIENTED_EDGE('',*,*,#43941,.T.) ;
#58505 = ORIENTED_EDGE('',*,*,#43942,.T.) ;
#58506 = ORIENTED_EDGE('',*,*,#43943,.T.) ;
#58507 = ORIENTED_EDGE('',*,*,#43944,.T.) ;
#58508 = ORIENTED_EDGE('',*,*,#43945,.T.) ;
#58509 = ORIENTED_EDGE('',*,*,#43946,.T.) ;
#58510 = ORIENTED_EDGE('',*,*,#43947,.T.) ;
#58511 = ORIENTED_EDGE('',*,*,#43948,.T.) ;
#58512 = ORIENTED_EDGE('',*,*,#43949,.T.) ;
#58513 = ORIENTED_EDGE('',*,*,#43950,.T.) ;
#58514 = ORIENTED_EDGE('',*,*,#43951,.T.) ;
#58515 = ORIENTED_EDGE('',*,*,#43952,.T.) ;
#58516 = ORIENTED_EDGE('',*,*,#43953,.T.) ;
#58517 = ORIENTED_EDGE('',*,*,#43954,.T.) ;
#58518 = ORIENTED_EDGE('',*,*,#43955,.T.) ;
#58519 = ORIENTED_EDGE('',*,*,#43956,.T.) ;
#58520 = ORIENTED_EDGE('',*,*,#43957,.T.) ;
#58521 = ORIENTED_EDGE('',*,*,#43958,.T.) ;
#58522 = ORIENTED_EDGE('',*,*,#43959,.T.) ;
#58523 = ORIENTED_EDGE('',*,*,#43960,.F.) ;
#58524 = ORIENTED_EDGE('',*,*,#43961,.F.) ;
#58525 = ORIENTED_EDGE('',*,*,#43962,.F.) ;
#58526 = ORIENTED_EDGE('',*,*,#43963,.F.) ;
#58527 = ORIENTED_EDGE('',*,*,#43964,.F.) ;
#58528 = ORIENTED_EDGE('',*,*,#43965,.F.) ;
#58529 = ORIENTED_EDGE('',*,*,#43966,.F.) ;
#58530 = ORIENTED_EDGE('',*,*,#43967,.F.) ;
#58531 = ORIENTED_EDGE('',*,*,#43968,.T.) ;
#58532 = ORIENTED_EDGE('',*,*,#43969,.T.) ;
#58533 = ORIENTED_EDGE('',*,*,#43970,.F.) ;
#58534 = ORIENTED_EDGE('',*,*,#43967,.T.) ;
#58535 = ORIENTED_EDGE('',*,*,#43970,.T.) ;
#58536 = ORIENTED_EDGE('',*,*,#43971,.T.) ;
#58537 = ORIENTED_EDGE('',*,*,#43972,.F.) ;
#58538 = ORIENTED_EDGE('',*,*,#43960,.T.) ;
#58539 = ORIENTED_EDGE('',*,*,#43972,.T.) ;
#58540 = ORIENTED_EDGE('',*,*,#43973,.T.) ;
#58541 = ORIENTED_EDGE('',*,*,#43974,.F.) ;
#58542 = ORIENTED_EDGE('',*,*,#43961,.T.) ;
#58543 = ORIENTED_EDGE('',*,*,#43974,.T.) ;
#58544 = ORIENTED_EDGE('',*,*,#43975,.T.) ;
#58545 = ORIENTED_EDGE('',*,*,#43976,.F.) ;
#58546 = ORIENTED_EDGE('',*,*,#43962,.T.) ;
#58547 = ORIENTED_EDGE('',*,*,#43976,.T.) ;
#58548 = ORIENTED_EDGE('',*,*,#43977,.T.) ;
#58549 = ORIENTED_EDGE('',*,*,#43978,.F.) ;
#58550 = ORIENTED_EDGE('',*,*,#43963,.T.) ;
#58551 = ORIENTED_EDGE('',*,*,#43978,.T.) ;
#58552 = ORIENTED_EDGE('',*,*,#43979,.T.) ;
#58553 = ORIENTED_EDGE('',*,*,#43980,.F.) ;
#58554 = ORIENTED_EDGE('',*,*,#43964,.T.) ;
#58555 = ORIENTED_EDGE('',*,*,#43980,.T.) ;
#58556 = ORIENTED_EDGE('',*,*,#43981,.T.) ;
#58557 = ORIENTED_EDGE('',*,*,#43982,.F.) ;
#58558 = ORIENTED_EDGE('',*,*,#43965,.T.) ;
#58559 = ORIENTED_EDGE('',*,*,#43982,.T.) ;
#58560 = ORIENTED_EDGE('',*,*,#43983,.T.) ;
#58561 = ORIENTED_EDGE('',*,*,#43968,.F.) ;
#58562 = ORIENTED_EDGE('',*,*,#43966,.T.) ;
#58563 = ORIENTED_EDGE('',*,*,#43984,.T.) ;
#58564 = ORIENTED_EDGE('',*,*,#43985,.T.) ;
#58565 = ORIENTED_EDGE('',*,*,#43986,.T.) ;
#58566 = ORIENTED_EDGE('',*,*,#43987,.T.) ;
#58567 = ORIENTED_EDGE('',*,*,#43988,.T.) ;
#58568 = ORIENTED_EDGE('',*,*,#43989,.T.) ;
#58569 = ORIENTED_EDGE('',*,*,#43990,.T.) ;
#58570 = ORIENTED_EDGE('',*,*,#43991,.T.) ;
#58571 = ORIENTED_EDGE('',*,*,#43992,.T.) ;
#58572 = ORIENTED_EDGE('',*,*,#43649,.T.) ;
#58573 = ORIENTED_EDGE('',*,*,#43993,.T.) ;
#58574 = ORIENTED_EDGE('',*,*,#43994,.T.) ;
#58575 = ORIENTED_EDGE('',*,*,#43651,.T.) ;
#58576 = ORIENTED_EDGE('',*,*,#43995,.T.) ;
#58577 = ORIENTED_EDGE('',*,*,#43996,.T.) ;
#58578 = ORIENTED_EDGE('',*,*,#43997,.T.) ;
#58579 = ORIENTED_EDGE('',*,*,#43998,.T.) ;
#58580 = ORIENTED_EDGE('',*,*,#43999,.T.) ;
#58581 = ORIENTED_EDGE('',*,*,#44000,.T.) ;
#58582 = ORIENTED_EDGE('',*,*,#44001,.T.) ;
#58583 = ORIENTED_EDGE('',*,*,#44002,.T.) ;
#58584 = ORIENTED_EDGE('',*,*,#43623,.T.) ;
#58585 = ORIENTED_EDGE('',*,*,#43655,.T.) ;
#58586 = ORIENTED_EDGE('',*,*,#44003,.T.) ;
#58587 = ORIENTED_EDGE('',*,*,#44004,.T.) ;
#58588 = ORIENTED_EDGE('',*,*,#44005,.T.) ;
#58589 = ORIENTED_EDGE('',*,*,#44006,.T.) ;
#58590 = ORIENTED_EDGE('',*,*,#44007,.T.) ;
#58591 = ORIENTED_EDGE('',*,*,#44008,.T.) ;
#58592 = ORIENTED_EDGE('',*,*,#44009,.F.) ;
#58593 = ORIENTED_EDGE('',*,*,#44010,.F.) ;
#58594 = ORIENTED_EDGE('',*,*,#44011,.F.) ;
#58595 = ORIENTED_EDGE('',*,*,#43765,.F.) ;
#58596 = ORIENTED_EDGE('',*,*,#43861,.F.) ;
#58597 = ORIENTED_EDGE('',*,*,#43850,.F.) ;
#58598 = ORIENTED_EDGE('',*,*,#44012,.F.) ;
#58599 = ORIENTED_EDGE('',*,*,#43871,.F.) ;
#58600 = ORIENTED_EDGE('',*,*,#44012,.T.) ;
#58601 = ORIENTED_EDGE('',*,*,#43849,.T.) ;
#58602 = ORIENTED_EDGE('',*,*,#44013,.F.) ;
#58603 = ORIENTED_EDGE('',*,*,#44014,.F.) ;
#58604 = ORIENTED_EDGE('',*,*,#44013,.T.) ;
#58605 = ORIENTED_EDGE('',*,*,#43856,.F.) ;
#58606 = ORIENTED_EDGE('',*,*,#44015,.F.) ;
#58607 = ORIENTED_EDGE('',*,*,#43887,.F.) ;
#58608 = ORIENTED_EDGE('',*,*,#44010,.T.) ;
#58609 = ORIENTED_EDGE('',*,*,#43888,.F.) ;
#58610 = ORIENTED_EDGE('',*,*,#44016,.F.) ;
#58611 = ORIENTED_EDGE('',*,*,#43847,.F.) ;
#58612 = ORIENTED_EDGE('',*,*,#44011,.T.) ;
#58613 = ORIENTED_EDGE('',*,*,#43846,.F.) ;
#58614 = ORIENTED_EDGE('',*,*,#44017,.F.) ;
#58615 = ORIENTED_EDGE('',*,*,#43766,.F.) ;
#58616 = ORIENTED_EDGE('',*,*,#44009,.T.) ;
#58617 = ORIENTED_EDGE('',*,*,#43764,.F.) ;
#58618 = ORIENTED_EDGE('',*,*,#44018,.F.) ;
#58619 = ORIENTED_EDGE('',*,*,#43883,.F.) ;
#58620 = ORIENTED_EDGE('',*,*,#44014,.T.) ;
#58621 = ORIENTED_EDGE('',*,*,#43886,.F.) ;
#58622 = ORIENTED_EDGE('',*,*,#44019,.F.) ;
#58623 = ORIENTED_EDGE('',*,*,#43872,.F.) ;
#58624 = ORIENTED_EDGE('',*,*,#43863,.F.) ;
#58625 = ORIENTED_EDGE('',*,*,#43873,.F.) ;
#58626 = ORIENTED_EDGE('',*,*,#44020,.F.) ;
#58627 = ORIENTED_EDGE('',*,*,#43866,.F.) ;
#58628 = ORIENTED_EDGE('',*,*,#44016,.T.) ;
#58629 = ORIENTED_EDGE('',*,*,#44015,.T.) ;
#58630 = ORIENTED_EDGE('',*,*,#44021,.F.) ;
#58631 = ORIENTED_EDGE('',*,*,#43767,.T.) ;
#58632 = ORIENTED_EDGE('',*,*,#44017,.T.) ;
#58633 = ORIENTED_EDGE('',*,*,#44022,.F.) ;
#58634 = ORIENTED_EDGE('',*,*,#44023,.F.) ;
#58635 = ORIENTED_EDGE('',*,*,#44018,.T.) ;
#58636 = ORIENTED_EDGE('',*,*,#43771,.F.) ;
#58637 = ORIENTED_EDGE('',*,*,#44024,.F.) ;
#58638 = ORIENTED_EDGE('',*,*,#44025,.F.) ;
#58639 = ORIENTED_EDGE('',*,*,#44020,.T.) ;
#58640 = ORIENTED_EDGE('',*,*,#44019,.T.) ;
#58641 = ORIENTED_EDGE('',*,*,#44026,.F.) ;
#58642 = ORIENTED_EDGE('',*,*,#43867,.T.) ;
#58643 = ORIENTED_EDGE('',*,*,#44021,.T.) ;
#58644 = ORIENTED_EDGE('',*,*,#43855,.F.) ;
#58645 = ORIENTED_EDGE('',*,*,#44027,.F.) ;
#58646 = ORIENTED_EDGE('',*,*,#43848,.F.) ;
#58647 = ORIENTED_EDGE('',*,*,#44022,.T.) ;
#58648 = ORIENTED_EDGE('',*,*,#43845,.F.) ;
#58649 = ORIENTED_EDGE('',*,*,#44028,.F.) ;
#58650 = ORIENTED_EDGE('',*,*,#43881,.F.) ;
#58651 = ORIENTED_EDGE('',*,*,#44023,.T.) ;
#58652 = ORIENTED_EDGE('',*,*,#43880,.F.) ;
#58653 = ORIENTED_EDGE('',*,*,#44029,.F.) ;
#58654 = ORIENTED_EDGE('',*,*,#43768,.F.) ;
#58655 = ORIENTED_EDGE('',*,*,#44024,.T.) ;
#58656 = ORIENTED_EDGE('',*,*,#43770,.F.) ;
#58657 = ORIENTED_EDGE('',*,*,#44030,.F.) ;
#58658 = ORIENTED_EDGE('',*,*,#43842,.F.) ;
#58659 = ORIENTED_EDGE('',*,*,#44025,.T.) ;
#58660 = ORIENTED_EDGE('',*,*,#43841,.F.) ;
#58661 = ORIENTED_EDGE('',*,*,#44031,.F.) ;
#58662 = ORIENTED_EDGE('',*,*,#43884,.F.) ;
#58663 = ORIENTED_EDGE('',*,*,#44026,.T.) ;
#58664 = ORIENTED_EDGE('',*,*,#43885,.F.) ;
#58665 = ORIENTED_EDGE('',*,*,#44032,.F.) ;
#58666 = ORIENTED_EDGE('',*,*,#43868,.F.) ;
#58667 = ORIENTED_EDGE('',*,*,#44028,.T.) ;
#58668 = ORIENTED_EDGE('',*,*,#44027,.T.) ;
#58669 = ORIENTED_EDGE('',*,*,#44033,.F.) ;
#58670 = ORIENTED_EDGE('',*,*,#43769,.T.) ;
#58671 = ORIENTED_EDGE('',*,*,#44029,.T.) ;
#58672 = ORIENTED_EDGE('',*,*,#44034,.F.) ;
#58673 = ORIENTED_EDGE('',*,*,#44030,.T.) ;
#58674 = ORIENTED_EDGE('',*,*,#44032,.T.) ;
#58675 = ORIENTED_EDGE('',*,*,#44031,.T.) ;
#58676 = ORIENTED_EDGE('',*,*,#44035,.F.) ;
#58677 = ORIENTED_EDGE('',*,*,#43860,.F.) ;
#58678 = ORIENTED_EDGE('',*,*,#43876,.F.) ;
#58679 = ORIENTED_EDGE('',*,*,#44036,.F.) ;
#58680 = ORIENTED_EDGE('',*,*,#43852,.F.) ;
#58681 = ORIENTED_EDGE('',*,*,#44033,.T.) ;
#58682 = ORIENTED_EDGE('',*,*,#43854,.F.) ;
#58683 = ORIENTED_EDGE('',*,*,#44037,.F.) ;
#58684 = ORIENTED_EDGE('',*,*,#43882,.F.) ;
#58685 = ORIENTED_EDGE('',*,*,#44034,.T.) ;
#58686 = ORIENTED_EDGE('',*,*,#43879,.F.) ;
#58687 = ORIENTED_EDGE('',*,*,#44038,.F.) ;
#58688 = ORIENTED_EDGE('',*,*,#43843,.F.) ;
#58689 = ORIENTED_EDGE('',*,*,#44035,.T.) ;
#58690 = ORIENTED_EDGE('',*,*,#43844,.F.) ;
#58691 = ORIENTED_EDGE('',*,*,#44039,.F.) ;
#58692 = ORIENTED_EDGE('',*,*,#43869,.F.) ;
#58693 = ORIENTED_EDGE('',*,*,#43853,.T.) ;
#58694 = ORIENTED_EDGE('',*,*,#44036,.T.) ;
#58695 = ORIENTED_EDGE('',*,*,#44040,.F.) ;
#58696 = ORIENTED_EDGE('',*,*,#44037,.T.) ;
#58697 = ORIENTED_EDGE('',*,*,#44039,.T.) ;
#58698 = ORIENTED_EDGE('',*,*,#44038,.T.) ;
#58699 = ORIENTED_EDGE('',*,*,#44041,.F.) ;
#58700 = ORIENTED_EDGE('',*,*,#44040,.T.) ;
#58701 = ORIENTED_EDGE('',*,*,#43875,.F.) ;
#58702 = ORIENTED_EDGE('',*,*,#44042,.F.) ;
#58703 = ORIENTED_EDGE('',*,*,#43877,.F.) ;
#58704 = ORIENTED_EDGE('',*,*,#44041,.T.) ;
#58705 = ORIENTED_EDGE('',*,*,#43878,.F.) ;
#58706 = ORIENTED_EDGE('',*,*,#44043,.F.) ;
#58707 = ORIENTED_EDGE('',*,*,#43870,.F.) ;
#58708 = ORIENTED_EDGE('',*,*,#44043,.T.) ;
#58709 = ORIENTED_EDGE('',*,*,#44042,.T.) ;
#58710 = ORIENTED_EDGE('',*,*,#44044,.F.) ;
#58711 = ORIENTED_EDGE('',*,*,#43864,.T.) ;
#58712 = ORIENTED_EDGE('',*,*,#43858,.F.) ;
#58713 = ORIENTED_EDGE('',*,*,#43865,.F.) ;
#58714 = ORIENTED_EDGE('',*,*,#44044,.T.) ;
#58715 = ORIENTED_EDGE('',*,*,#43874,.F.) ;
#58716 = ORIENTED_EDGE('',*,*,#43653,.F.) ;
#58717 = ORIENTED_EDGE('',*,*,#43698,.F.) ;
#58718 = ORIENTED_EDGE('',*,*,#43838,.F.) ;
#58719 = ORIENTED_EDGE('',*,*,#43687,.F.) ;
#58720 = ORIENTED_EDGE('',*,*,#43686,.F.) ;
#58721 = ORIENTED_EDGE('',*,*,#44045,.T.) ;
#58722 = ORIENTED_EDGE('',*,*,#44046,.T.) ;
#58723 = ORIENTED_EDGE('',*,*,#43625,.T.) ;
#58724 = ORIENTED_EDGE('',*,*,#43988,.F.) ;
#58725 = ORIENTED_EDGE('',*,*,#43654,.T.) ;
#58726 = ORIENTED_EDGE('',*,*,#43990,.F.) ;
#58727 = ORIENTED_EDGE('',*,*,#44047,.T.) ;
#58728 = ORIENTED_EDGE('',*,*,#43994,.F.) ;
#58729 = ORIENTED_EDGE('',*,*,#44048,.F.) ;
#58730 = ORIENTED_EDGE('',*,*,#43652,.T.) ;
#58731 = ORIENTED_EDGE('',*,*,#43991,.F.) ;
#58732 = ORIENTED_EDGE('',*,*,#44049,.F.) ;
#58733 = ORIENTED_EDGE('',*,*,#43699,.F.) ;
#58734 = ORIENTED_EDGE('',*,*,#43709,.F.) ;
#58735 = ORIENTED_EDGE('',*,*,#44050,.T.) ;
#58736 = ORIENTED_EDGE('',*,*,#43998,.F.) ;
#58737 = ORIENTED_EDGE('',*,*,#44051,.T.) ;
#58738 = ORIENTED_EDGE('',*,*,#44001,.F.) ;
#58739 = ORIENTED_EDGE('',*,*,#44052,.T.) ;
#58740 = ORIENTED_EDGE('',*,*,#43992,.F.) ;
#58741 = ORIENTED_EDGE('',*,*,#44053,.T.) ;
#58742 = ORIENTED_EDGE('',*,*,#44049,.T.) ;
#58743 = ORIENTED_EDGE('',*,*,#44048,.T.) ;
#58744 = ORIENTED_EDGE('',*,*,#44054,.F.) ;
#58745 = ORIENTED_EDGE('',*,*,#43700,.T.) ;
#58746 = ORIENTED_EDGE('',*,*,#43808,.F.) ;
#58747 = ORIENTED_EDGE('',*,*,#43690,.F.) ;
#58748 = ORIENTED_EDGE('',*,*,#43647,.F.) ;
#58749 = ORIENTED_EDGE('',*,*,#43705,.F.) ;
#58750 = ORIENTED_EDGE('',*,*,#44055,.T.) ;
#58751 = ORIENTED_EDGE('',*,*,#44056,.T.) ;
#58752 = ORIENTED_EDGE('',*,*,#43702,.F.) ;
#58753 = ORIENTED_EDGE('',*,*,#43646,.F.) ;
#58754 = ORIENTED_EDGE('',*,*,#43996,.F.) ;
#58755 = ORIENTED_EDGE('',*,*,#44057,.T.) ;
#58756 = ORIENTED_EDGE('',*,*,#44054,.T.) ;
#58757 = ORIENTED_EDGE('',*,*,#43993,.F.) ;
#58758 = ORIENTED_EDGE('',*,*,#43645,.F.) ;
#58759 = ORIENTED_EDGE('',*,*,#43701,.F.) ;
#58760 = ORIENTED_EDGE('',*,*,#43648,.T.) ;
#58761 = ORIENTED_EDGE('',*,*,#43689,.F.) ;
#58762 = ORIENTED_EDGE('',*,*,#43643,.T.) ;
#58763 = ORIENTED_EDGE('',*,*,#43997,.F.) ;
#58764 = ORIENTED_EDGE('',*,*,#44058,.F.) ;
#58765 = ORIENTED_EDGE('',*,*,#43973,.F.) ;
#58766 = ORIENTED_EDGE('',*,*,#44059,.F.) ;
#58767 = ORIENTED_EDGE('',*,*,#44059,.T.) ;
#58768 = ORIENTED_EDGE('',*,*,#43971,.F.) ;
#58769 = ORIENTED_EDGE('',*,*,#44060,.F.) ;
#58770 = ORIENTED_EDGE('',*,*,#43984,.F.) ;
#58771 = ORIENTED_EDGE('',*,*,#44058,.T.) ;
#58772 = ORIENTED_EDGE('',*,*,#43987,.F.) ;
#58773 = ORIENTED_EDGE('',*,*,#44061,.F.) ;
#58774 = ORIENTED_EDGE('',*,*,#43975,.F.) ;
#58775 = ORIENTED_EDGE('',*,*,#44060,.T.) ;
#58776 = ORIENTED_EDGE('',*,*,#43969,.F.) ;
#58777 = ORIENTED_EDGE('',*,*,#44062,.F.) ;
#58778 = ORIENTED_EDGE('',*,*,#43977,.F.) ;
#58779 = ORIENTED_EDGE('',*,*,#44061,.T.) ;
#58780 = ORIENTED_EDGE('',*,*,#44063,.F.) ;
#58781 = ORIENTED_EDGE('',*,*,#44062,.T.) ;
#58782 = ORIENTED_EDGE('',*,*,#43983,.F.) ;
#58783 = ORIENTED_EDGE('',*,*,#44064,.F.) ;
#58784 = ORIENTED_EDGE('',*,*,#43985,.F.) ;
#58785 = ORIENTED_EDGE('',*,*,#44063,.T.) ;
#58786 = ORIENTED_EDGE('',*,*,#43986,.F.) ;
#58787 = ORIENTED_EDGE('',*,*,#44065,.F.) ;
#58788 = ORIENTED_EDGE('',*,*,#43979,.F.) ;
#58789 = ORIENTED_EDGE('',*,*,#44064,.T.) ;
#58790 = ORIENTED_EDGE('',*,*,#43981,.F.) ;
#58791 = ORIENTED_EDGE('',*,*,#44065,.T.) ;
#58792 = ORIENTED_EDGE('',*,*,#44066,.F.) ;
#58793 = ORIENTED_EDGE('',*,*,#43781,.F.) ;
#58794 = ORIENTED_EDGE('',*,*,#44067,.F.) ;
#58795 = ORIENTED_EDGE('',*,*,#43892,.F.) ;
#58796 = ORIENTED_EDGE('',*,*,#44067,.T.) ;
#58797 = ORIENTED_EDGE('',*,*,#43780,.T.) ;
#58798 = ORIENTED_EDGE('',*,*,#44068,.F.) ;
#58799 = ORIENTED_EDGE('',*,*,#44069,.F.) ;
#58800 = ORIENTED_EDGE('',*,*,#43782,.T.) ;
#58801 = ORIENTED_EDGE('',*,*,#44066,.T.) ;
#58802 = ORIENTED_EDGE('',*,*,#44070,.F.) ;
#58803 = ORIENTED_EDGE('',*,*,#44071,.F.) ;
#58804 = ORIENTED_EDGE('',*,*,#44068,.T.) ;
#58805 = ORIENTED_EDGE('',*,*,#43779,.F.) ;
#58806 = ORIENTED_EDGE('',*,*,#44072,.F.) ;
#58807 = ORIENTED_EDGE('',*,*,#43904,.F.) ;
#58808 = ORIENTED_EDGE('',*,*,#44069,.T.) ;
#58809 = ORIENTED_EDGE('',*,*,#43903,.F.) ;
#58810 = ORIENTED_EDGE('',*,*,#44073,.F.) ;
#58811 = ORIENTED_EDGE('',*,*,#43889,.F.) ;
#58812 = ORIENTED_EDGE('',*,*,#44074,.F.) ;
#58813 = ORIENTED_EDGE('',*,*,#43890,.F.) ;
#58814 = ORIENTED_EDGE('',*,*,#44075,.F.) ;
#58815 = ORIENTED_EDGE('',*,*,#43908,.F.) ;
#58816 = ORIENTED_EDGE('',*,*,#44070,.T.) ;
#58817 = ORIENTED_EDGE('',*,*,#43891,.F.) ;
#58818 = ORIENTED_EDGE('',*,*,#44076,.F.) ;
#58819 = ORIENTED_EDGE('',*,*,#43896,.F.) ;
#58820 = ORIENTED_EDGE('',*,*,#44071,.T.) ;
#58821 = ORIENTED_EDGE('',*,*,#43895,.F.) ;
#58822 = ORIENTED_EDGE('',*,*,#44077,.F.) ;
#58823 = ORIENTED_EDGE('',*,*,#43783,.F.) ;
#58824 = ORIENTED_EDGE('',*,*,#44078,.F.) ;
#58825 = ORIENTED_EDGE('',*,*,#43777,.F.) ;
#58826 = ORIENTED_EDGE('',*,*,#44079,.F.) ;
#58827 = ORIENTED_EDGE('',*,*,#43899,.F.) ;
#58828 = ORIENTED_EDGE('',*,*,#43778,.T.) ;
#58829 = ORIENTED_EDGE('',*,*,#44078,.T.) ;
#58830 = ORIENTED_EDGE('',*,*,#44080,.F.) ;
#58831 = ORIENTED_EDGE('',*,*,#44072,.T.) ;
#58832 = ORIENTED_EDGE('',*,*,#44075,.T.) ;
#58833 = ORIENTED_EDGE('',*,*,#44073,.T.) ;
#58834 = ORIENTED_EDGE('',*,*,#44081,.F.) ;
#58835 = ORIENTED_EDGE('',*,*,#44076,.T.) ;
#58836 = ORIENTED_EDGE('',*,*,#44074,.T.) ;
#58837 = ORIENTED_EDGE('',*,*,#44082,.F.) ;
#58838 = ORIENTED_EDGE('',*,*,#43776,.T.) ;
#58839 = ORIENTED_EDGE('',*,*,#44077,.T.) ;
#58840 = ORIENTED_EDGE('',*,*,#44083,.F.) ;
#58841 = ORIENTED_EDGE('',*,*,#44079,.T.) ;
#58842 = ORIENTED_EDGE('',*,*,#44080,.T.) ;
#58843 = ORIENTED_EDGE('',*,*,#43898,.F.) ;
#58844 = ORIENTED_EDGE('',*,*,#44084,.F.) ;
#58845 = ORIENTED_EDGE('',*,*,#43901,.F.) ;
#58846 = ORIENTED_EDGE('',*,*,#44081,.T.) ;
#58847 = ORIENTED_EDGE('',*,*,#43902,.F.) ;
#58848 = ORIENTED_EDGE('',*,*,#44085,.F.) ;
#58849 = ORIENTED_EDGE('',*,*,#43905,.F.) ;
#58850 = ORIENTED_EDGE('',*,*,#44082,.T.) ;
#58851 = ORIENTED_EDGE('',*,*,#43907,.F.) ;
#58852 = ORIENTED_EDGE('',*,*,#44086,.F.) ;
#58853 = ORIENTED_EDGE('',*,*,#43893,.F.) ;
#58854 = ORIENTED_EDGE('',*,*,#44083,.T.) ;
#58855 = ORIENTED_EDGE('',*,*,#43894,.F.) ;
#58856 = ORIENTED_EDGE('',*,*,#44087,.F.) ;
#58857 = ORIENTED_EDGE('',*,*,#43900,.F.) ;
#58858 = ORIENTED_EDGE('',*,*,#44085,.T.) ;
#58859 = ORIENTED_EDGE('',*,*,#44084,.T.) ;
#58860 = ORIENTED_EDGE('',*,*,#44088,.F.) ;
#58861 = ORIENTED_EDGE('',*,*,#44087,.T.) ;
#58862 = ORIENTED_EDGE('',*,*,#44086,.T.) ;
#58863 = ORIENTED_EDGE('',*,*,#44089,.F.) ;
#58864 = ORIENTED_EDGE('',*,*,#44088,.T.) ;
#58865 = ORIENTED_EDGE('',*,*,#43897,.F.) ;
#58866 = ORIENTED_EDGE('',*,*,#44089,.T.) ;
#58867 = ORIENTED_EDGE('',*,*,#43906,.F.) ;
#58868 = ORIENTED_EDGE('',*,*,#44090,.F.) ;
#58869 = ORIENTED_EDGE('',*,*,#43747,.F.) ;
#58870 = ORIENTED_EDGE('',*,*,#44091,.F.) ;
#58871 = ORIENTED_EDGE('',*,*,#43951,.F.) ;
#58872 = ORIENTED_EDGE('',*,*,#44091,.T.) ;
#58873 = ORIENTED_EDGE('',*,*,#43746,.T.) ;
#58874 = ORIENTED_EDGE('',*,*,#44092,.F.) ;
#58875 = ORIENTED_EDGE('',*,*,#44093,.F.) ;
#58876 = ORIENTED_EDGE('',*,*,#43748,.T.) ;
#58877 = ORIENTED_EDGE('',*,*,#44090,.T.) ;
#58878 = ORIENTED_EDGE('',*,*,#44094,.F.) ;
#58879 = ORIENTED_EDGE('',*,*,#44095,.F.) ;
#58880 = ORIENTED_EDGE('',*,*,#44092,.T.) ;
#58881 = ORIENTED_EDGE('',*,*,#43745,.F.) ;
#58882 = ORIENTED_EDGE('',*,*,#44096,.F.) ;
#58883 = ORIENTED_EDGE('',*,*,#43947,.F.) ;
#58884 = ORIENTED_EDGE('',*,*,#44093,.T.) ;
#58885 = ORIENTED_EDGE('',*,*,#43946,.F.) ;
#58886 = ORIENTED_EDGE('',*,*,#44097,.F.) ;
#58887 = ORIENTED_EDGE('',*,*,#43948,.F.) ;
#58888 = ORIENTED_EDGE('',*,*,#44098,.F.) ;
#58889 = ORIENTED_EDGE('',*,*,#43949,.F.) ;
#58890 = ORIENTED_EDGE('',*,*,#44099,.F.) ;
#58891 = ORIENTED_EDGE('',*,*,#43959,.F.) ;
#58892 = ORIENTED_EDGE('',*,*,#44094,.T.) ;
#58893 = ORIENTED_EDGE('',*,*,#43950,.F.) ;
#58894 = ORIENTED_EDGE('',*,*,#44100,.F.) ;
#58895 = ORIENTED_EDGE('',*,*,#43955,.F.) ;
#58896 = ORIENTED_EDGE('',*,*,#44095,.T.) ;
#58897 = ORIENTED_EDGE('',*,*,#43954,.F.) ;
#58898 = ORIENTED_EDGE('',*,*,#44101,.F.) ;
#58899 = ORIENTED_EDGE('',*,*,#43749,.F.) ;
#58900 = ORIENTED_EDGE('',*,*,#44102,.F.) ;
#58901 = ORIENTED_EDGE('',*,*,#43743,.F.) ;
#58902 = ORIENTED_EDGE('',*,*,#44103,.F.) ;
#58903 = ORIENTED_EDGE('',*,*,#43942,.F.) ;
#58904 = ORIENTED_EDGE('',*,*,#43744,.T.) ;
#58905 = ORIENTED_EDGE('',*,*,#44102,.T.) ;
#58906 = ORIENTED_EDGE('',*,*,#44104,.F.) ;
#58907 = ORIENTED_EDGE('',*,*,#44096,.T.) ;
#58908 = ORIENTED_EDGE('',*,*,#44099,.T.) ;
#58909 = ORIENTED_EDGE('',*,*,#44097,.T.) ;
#58910 = ORIENTED_EDGE('',*,*,#44105,.F.) ;
#58911 = ORIENTED_EDGE('',*,*,#44100,.T.) ;
#58912 = ORIENTED_EDGE('',*,*,#44098,.T.) ;
#58913 = ORIENTED_EDGE('',*,*,#44106,.F.) ;
#58914 = ORIENTED_EDGE('',*,*,#43742,.T.) ;
#58915 = ORIENTED_EDGE('',*,*,#44101,.T.) ;
#58916 = ORIENTED_EDGE('',*,*,#44107,.F.) ;
#58917 = ORIENTED_EDGE('',*,*,#44103,.T.) ;
#58918 = ORIENTED_EDGE('',*,*,#44104,.T.) ;
#58919 = ORIENTED_EDGE('',*,*,#43941,.F.) ;
#58920 = ORIENTED_EDGE('',*,*,#44108,.F.) ;
#58921 = ORIENTED_EDGE('',*,*,#43944,.F.) ;
#58922 = ORIENTED_EDGE('',*,*,#44105,.T.) ;
#58923 = ORIENTED_EDGE('',*,*,#43945,.F.) ;
#58924 = ORIENTED_EDGE('',*,*,#44109,.F.) ;
#58925 = ORIENTED_EDGE('',*,*,#43956,.F.) ;
#58926 = ORIENTED_EDGE('',*,*,#44106,.T.) ;
#58927 = ORIENTED_EDGE('',*,*,#43958,.F.) ;
#58928 = ORIENTED_EDGE('',*,*,#44110,.F.) ;
#58929 = ORIENTED_EDGE('',*,*,#43952,.F.) ;
#58930 = ORIENTED_EDGE('',*,*,#44107,.T.) ;
#58931 = ORIENTED_EDGE('',*,*,#43953,.F.) ;
#58932 = ORIENTED_EDGE('',*,*,#44111,.F.) ;
#58933 = ORIENTED_EDGE('',*,*,#43943,.F.) ;
#58934 = ORIENTED_EDGE('',*,*,#44109,.T.) ;
#58935 = ORIENTED_EDGE('',*,*,#44108,.T.) ;
#58936 = ORIENTED_EDGE('',*,*,#44112,.F.) ;
#58937 = ORIENTED_EDGE('',*,*,#44111,.T.) ;
#58938 = ORIENTED_EDGE('',*,*,#44110,.T.) ;
#58939 = ORIENTED_EDGE('',*,*,#44113,.F.) ;
#58940 = ORIENTED_EDGE('',*,*,#44112,.T.) ;
#58941 = ORIENTED_EDGE('',*,*,#43940,.F.) ;
#58942 = ORIENTED_EDGE('',*,*,#44113,.T.) ;
#58943 = ORIENTED_EDGE('',*,*,#43957,.F.) ;
#58944 = ORIENTED_EDGE('',*,*,#43799,.F.) ;
#58945 = ORIENTED_EDGE('',*,*,#44114,.T.) ;
#58946 = ORIENTED_EDGE('',*,*,#44003,.F.) ;
#58947 = ORIENTED_EDGE('',*,*,#44115,.F.) ;
#58948 = ORIENTED_EDGE('',*,*,#43806,.F.) ;
#58949 = ORIENTED_EDGE('',*,*,#43800,.F.) ;
#58950 = ORIENTED_EDGE('',*,*,#44116,.F.) ;
#58951 = ORIENTED_EDGE('',*,*,#43681,.F.) ;
#58952 = ORIENTED_EDGE('',*,*,#44116,.T.) ;
#58953 = ORIENTED_EDGE('',*,*,#44115,.T.) ;
#58954 = ORIENTED_EDGE('',*,*,#44117,.F.) ;
#58955 = ORIENTED_EDGE('',*,*,#44117,.T.) ;
#58956 = ORIENTED_EDGE('',*,*,#44008,.F.) ;
#58957 = ORIENTED_EDGE('',*,*,#44118,.F.) ;
#58958 = ORIENTED_EDGE('',*,*,#43682,.F.) ;
#58959 = ORIENTED_EDGE('',*,*,#43807,.F.) ;
#58960 = ORIENTED_EDGE('',*,*,#43683,.F.) ;
#58961 = ORIENTED_EDGE('',*,*,#44119,.F.) ;
#58962 = ORIENTED_EDGE('',*,*,#43692,.F.) ;
#58963 = ORIENTED_EDGE('',*,*,#44119,.T.) ;
#58964 = ORIENTED_EDGE('',*,*,#44118,.T.) ;
#58965 = ORIENTED_EDGE('',*,*,#44120,.F.) ;
#58966 = ORIENTED_EDGE('',*,*,#43693,.T.) ;
#58967 = ORIENTED_EDGE('',*,*,#44120,.T.) ;
#58968 = ORIENTED_EDGE('',*,*,#44007,.F.) ;
#58969 = ORIENTED_EDGE('',*,*,#44121,.F.) ;
#58970 = ORIENTED_EDGE('',*,*,#43694,.F.) ;
#58971 = ORIENTED_EDGE('',*,*,#43839,.F.) ;
#58972 = ORIENTED_EDGE('',*,*,#43696,.F.) ;
#58973 = ORIENTED_EDGE('',*,*,#44122,.F.) ;
#58974 = ORIENTED_EDGE('',*,*,#43804,.F.) ;
#58975 = ORIENTED_EDGE('',*,*,#43695,.T.) ;
#58976 = ORIENTED_EDGE('',*,*,#44121,.T.) ;
#58977 = ORIENTED_EDGE('',*,*,#44123,.F.) ;
#58978 = ORIENTED_EDGE('',*,*,#44122,.T.) ;
#58979 = ORIENTED_EDGE('',*,*,#44123,.T.) ;
#58980 = ORIENTED_EDGE('',*,*,#44006,.F.) ;
#58981 = ORIENTED_EDGE('',*,*,#44124,.F.) ;
#58982 = ORIENTED_EDGE('',*,*,#43801,.F.) ;
#58983 = ORIENTED_EDGE('',*,*,#43840,.F.) ;
#58984 = ORIENTED_EDGE('',*,*,#43802,.F.) ;
#58985 = ORIENTED_EDGE('',*,*,#44125,.F.) ;
#58986 = ORIENTED_EDGE('',*,*,#43679,.F.) ;
#58987 = ORIENTED_EDGE('',*,*,#44125,.T.) ;
#58988 = ORIENTED_EDGE('',*,*,#44124,.T.) ;
#58989 = ORIENTED_EDGE('',*,*,#44126,.F.) ;
#58990 = ORIENTED_EDGE('',*,*,#44005,.F.) ;
#58991 = ORIENTED_EDGE('',*,*,#44127,.T.) ;
#58992 = ORIENTED_EDGE('',*,*,#43676,.F.) ;
#58993 = ORIENTED_EDGE('',*,*,#44126,.T.) ;
#58994 = ORIENTED_EDGE('',*,*,#43822,.F.) ;
#58995 = ORIENTED_EDGE('',*,*,#43785,.F.) ;
#58996 = ORIENTED_EDGE('',*,*,#43824,.F.) ;
#58997 = ORIENTED_EDGE('',*,*,#43794,.F.) ;
#58998 = ORIENTED_EDGE('',*,*,#43821,.F.) ;
#58999 = ORIENTED_EDGE('',*,*,#43773,.F.) ;
#59000 = ORIENTED_EDGE('',*,*,#43825,.F.) ;
#59001 = ORIENTED_EDGE('',*,*,#43787,.F.) ;
#59002 = ORIENTED_EDGE('',*,*,#43820,.F.) ;
#59003 = ORIENTED_EDGE('',*,*,#43761,.F.) ;
#59004 = ORIENTED_EDGE('',*,*,#43826,.F.) ;
#59005 = ORIENTED_EDGE('',*,*,#43775,.F.) ;
#59006 = ORIENTED_EDGE('',*,*,#43819,.F.) ;
#59007 = ORIENTED_EDGE('',*,*,#43758,.F.) ;
#59008 = ORIENTED_EDGE('',*,*,#43827,.F.) ;
#59009 = ORIENTED_EDGE('',*,*,#43763,.F.) ;
#59010 = ORIENTED_EDGE('',*,*,#43818,.F.) ;
#59011 = ORIENTED_EDGE('',*,*,#43751,.F.) ;
#59012 = ORIENTED_EDGE('',*,*,#43828,.F.) ;
#59013 = ORIENTED_EDGE('',*,*,#43756,.F.) ;
#59014 = ORIENTED_EDGE('',*,*,#43817,.F.) ;
#59015 = ORIENTED_EDGE('',*,*,#43739,.F.) ;
#59016 = ORIENTED_EDGE('',*,*,#43829,.F.) ;
#59017 = ORIENTED_EDGE('',*,*,#43753,.F.) ;
#59018 = ORIENTED_EDGE('',*,*,#43661,.F.) ;
#59019 = ORIENTED_EDGE('',*,*,#43936,.F.) ;
#59020 = ORIENTED_EDGE('',*,*,#43671,.F.) ;
#59021 = ORIENTED_EDGE('',*,*,#43938,.F.) ;
#59022 = ORIENTED_EDGE('',*,*,#43669,.F.) ;
#59023 = ORIENTED_EDGE('',*,*,#43934,.F.) ;
#59024 = ORIENTED_EDGE('',*,*,#43663,.F.) ;
#59025 = ORIENTED_EDGE('',*,*,#43939,.F.) ;
#59026 = ORIENTED_EDGE('',*,*,#43659,.F.) ;
#59027 = ORIENTED_EDGE('',*,*,#43688,.F.) ;
#59028 = ORIENTED_EDGE('',*,*,#43673,.F.) ;
#59029 = ORIENTED_EDGE('',*,*,#43937,.F.) ;
#59030 = ORIENTED_EDGE('',*,*,#43667,.F.) ;
#59031 = ORIENTED_EDGE('',*,*,#43933,.F.) ;
#59032 = ORIENTED_EDGE('',*,*,#43665,.F.) ;
#59033 = ORIENTED_EDGE('',*,*,#43935,.F.) ;
#59034 = ORIENTED_EDGE('',*,*,#43816,.F.) ;
#59035 = ORIENTED_EDGE('',*,*,#43735,.F.) ;
#59036 = ORIENTED_EDGE('',*,*,#43830,.F.) ;
#59037 = ORIENTED_EDGE('',*,*,#43741,.F.) ;
#59038 = ORIENTED_EDGE('',*,*,#43815,.F.) ;
#59039 = ORIENTED_EDGE('',*,*,#43731,.F.) ;
#59040 = ORIENTED_EDGE('',*,*,#43831,.F.) ;
#59041 = ORIENTED_EDGE('',*,*,#43737,.F.) ;
#59042 = ORIENTED_EDGE('',*,*,#43814,.F.) ;
#59043 = ORIENTED_EDGE('',*,*,#43727,.F.) ;
#59044 = ORIENTED_EDGE('',*,*,#43832,.F.) ;
#59045 = ORIENTED_EDGE('',*,*,#43733,.F.) ;
#59046 = ORIENTED_EDGE('',*,*,#43813,.F.) ;
#59047 = ORIENTED_EDGE('',*,*,#43723,.F.) ;
#59048 = ORIENTED_EDGE('',*,*,#43833,.F.) ;
#59049 = ORIENTED_EDGE('',*,*,#43729,.F.) ;
#59050 = ORIENTED_EDGE('',*,*,#43812,.F.) ;
#59051 = ORIENTED_EDGE('',*,*,#43719,.F.) ;
#59052 = ORIENTED_EDGE('',*,*,#43834,.F.) ;
#59053 = ORIENTED_EDGE('',*,*,#43725,.F.) ;
#59054 = ORIENTED_EDGE('',*,*,#43811,.F.) ;
#59055 = ORIENTED_EDGE('',*,*,#43715,.F.) ;
#59056 = ORIENTED_EDGE('',*,*,#43835,.F.) ;
#59057 = ORIENTED_EDGE('',*,*,#43721,.F.) ;
#59058 = ORIENTED_EDGE('',*,*,#43810,.F.) ;
#59059 = ORIENTED_EDGE('',*,*,#43713,.F.) ;
#59060 = ORIENTED_EDGE('',*,*,#43836,.F.) ;
#59061 = ORIENTED_EDGE('',*,*,#43717,.F.) ;
#59062 = ORIENTED_EDGE('',*,*,#44128,.F.) ;
#59063 = ORIENTED_EDGE('',*,*,#43650,.F.) ;
#59064 = ORIENTED_EDGE('',*,*,#44052,.F.) ;
#59065 = ORIENTED_EDGE('',*,*,#44128,.T.) ;
#59066 = ORIENTED_EDGE('',*,*,#44000,.F.) ;
#59067 = ORIENTED_EDGE('',*,*,#44129,.F.) ;
#59068 = ORIENTED_EDGE('',*,*,#43995,.F.) ;
#59069 = ORIENTED_EDGE('',*,*,#44129,.T.) ;
#59070 = ORIENTED_EDGE('',*,*,#43999,.F.) ;
#59071 = ORIENTED_EDGE('',*,*,#44130,.F.) ;
#59072 = ORIENTED_EDGE('',*,*,#44057,.F.) ;
#59073 = ORIENTED_EDGE('',*,*,#44130,.T.) ;
#59074 = ORIENTED_EDGE('',*,*,#44050,.F.) ;
#59075 = ORIENTED_EDGE('',*,*,#44131,.F.) ;
#59076 = ORIENTED_EDGE('',*,*,#44055,.F.) ;
#59077 = ORIENTED_EDGE('',*,*,#44131,.T.) ;
#59078 = ORIENTED_EDGE('',*,*,#43708,.F.) ;
#59079 = ORIENTED_EDGE('',*,*,#44132,.F.) ;
#59080 = ORIENTED_EDGE('',*,*,#44056,.F.) ;
#59081 = ORIENTED_EDGE('',*,*,#44132,.T.) ;
#59082 = ORIENTED_EDGE('',*,*,#43707,.F.) ;
#59083 = ORIENTED_EDGE('',*,*,#43809,.F.) ;
#59084 = ORIENTED_EDGE('',*,*,#43703,.F.) ;
#59085 = ORIENTED_EDGE('',*,*,#43837,.F.) ;
#59086 = ORIENTED_EDGE('',*,*,#43711,.F.) ;
#59087 = ORIENTED_EDGE('',*,*,#44133,.F.) ;
#59088 = ORIENTED_EDGE('',*,*,#43685,.F.) ;
#59089 = ORIENTED_EDGE('',*,*,#44133,.T.) ;
#59090 = ORIENTED_EDGE('',*,*,#43710,.F.) ;
#59091 = ORIENTED_EDGE('',*,*,#44134,.F.) ;
#59092 = ORIENTED_EDGE('',*,*,#44045,.F.) ;
#59093 = ORIENTED_EDGE('',*,*,#44134,.T.) ;
#59094 = ORIENTED_EDGE('',*,*,#44051,.F.) ;
#59095 = ORIENTED_EDGE('',*,*,#43626,.F.) ;
#59096 = ORIENTED_EDGE('',*,*,#44046,.F.) ;
#59097 = ORIENTED_EDGE('',*,*,#44135,.F.) ;
#59098 = ORIENTED_EDGE('',*,*,#43989,.F.) ;
#59099 = ORIENTED_EDGE('',*,*,#43624,.T.) ;
#59100 = ORIENTED_EDGE('',*,*,#44002,.F.) ;
#59101 = ORIENTED_EDGE('',*,*,#44053,.F.) ;
#59102 = ORIENTED_EDGE('',*,*,#44047,.F.) ;
#59103 = ORIENTED_EDGE('',*,*,#44135,.T.) ;
#59104 = ORIENTED_EDGE('',*,*,#44136,.T.) ;
#59105 = ORIENTED_EDGE('',*,*,#44137,.T.) ;
#59106 = ORIENTED_EDGE('',*,*,#44004,.F.) ;
#59107 = ORIENTED_EDGE('',*,*,#44138,.T.) ;
#59108 = ORIENTED_EDGE('',*,*,#44139,.T.) ;
#59109 = ORIENTED_EDGE('',*,*,#43805,.F.) ;
#59110 = ORIENTED_EDGE('',*,*,#43792,.F.) ;
#59111 = ORIENTED_EDGE('',*,*,#44140,.F.) ;
#59112 = ORIENTED_EDGE('',*,*,#43798,.F.) ;
#59113 = ORIENTED_EDGE('',*,*,#43791,.F.) ;
#59114 = ORIENTED_EDGE('',*,*,#44141,.T.) ;
#59115 = ORIENTED_EDGE('',*,*,#44114,.F.) ;
#59116 = ORIENTED_EDGE('',*,*,#44140,.T.) ;
#59117 = ORIENTED_EDGE('',*,*,#43823,.F.) ;
#59118 = ORIENTED_EDGE('',*,*,#43677,.F.) ;
#59119 = ORIENTED_EDGE('',*,*,#44142,.F.) ;
#59120 = ORIENTED_EDGE('',*,*,#43796,.F.) ;
#59121 = ORIENTED_EDGE('',*,*,#44127,.F.) ;
#59122 = ORIENTED_EDGE('',*,*,#44143,.T.) ;
#59123 = ORIENTED_EDGE('',*,*,#43788,.F.) ;
#59124 = ORIENTED_EDGE('',*,*,#44142,.T.) ;
#59125 = ORIENTED_EDGE('',*,*,#44138,.F.) ;
#59126 = ORIENTED_EDGE('',*,*,#44141,.F.) ;
#59127 = ORIENTED_EDGE('',*,*,#44144,.F.) ;
#59128 = ORIENTED_EDGE('',*,*,#44145,.F.) ;
#59129 = ORIENTED_EDGE('',*,*,#44139,.F.) ;
#59130 = ORIENTED_EDGE('',*,*,#44144,.T.) ;
#59131 = ORIENTED_EDGE('',*,*,#43790,.F.) ;
#59132 = ORIENTED_EDGE('',*,*,#44145,.T.) ;
#59133 = ORIENTED_EDGE('',*,*,#43789,.F.) ;
#59134 = ORIENTED_EDGE('',*,*,#44146,.F.) ;
#59135 = ORIENTED_EDGE('',*,*,#44136,.F.) ;
#59136 = ORIENTED_EDGE('',*,*,#44146,.T.) ;
#59137 = ORIENTED_EDGE('',*,*,#44143,.F.) ;
#59138 = ORIENTED_EDGE('',*,*,#44137,.F.) ;
#59139 = ORIENTED_EDGE('',*,*,#44147,.F.) ;
#59140 = ORIENTED_EDGE('',*,*,#44148,.T.) ;
#59141 = ORIENTED_EDGE('',*,*,#44149,.F.) ;
#59142 = ORIENTED_EDGE('',*,*,#44150,.F.) ;
#59143 = ORIENTED_EDGE('',*,*,#44148,.F.) ;
#59144 = ORIENTED_EDGE('',*,*,#44151,.F.) ;
#59145 = ORIENTED_EDGE('',*,*,#44152,.T.) ;
#59146 = ORIENTED_EDGE('',*,*,#44153,.F.) ;
#59147 = ORIENTED_EDGE('',*,*,#44152,.F.) ;
#59148 = ORIENTED_EDGE('',*,*,#44154,.F.) ;
#59149 = ORIENTED_EDGE('',*,*,#44155,.F.) ;
#59150 = ORIENTED_EDGE('',*,*,#44156,.T.) ;
#59151 = ORIENTED_EDGE('',*,*,#44157,.F.) ;
#59152 = ORIENTED_EDGE('',*,*,#44158,.T.) ;
#59153 = ORIENTED_EDGE('',*,*,#44159,.F.) ;
#59154 = ORIENTED_EDGE('',*,*,#44160,.F.) ;
#59155 = ORIENTED_EDGE('',*,*,#44161,.F.) ;
#59156 = ORIENTED_EDGE('',*,*,#44162,.F.) ;
#59157 = ORIENTED_EDGE('',*,*,#44163,.T.) ;
#59158 = ORIENTED_EDGE('',*,*,#44164,.F.) ;
#59159 = ORIENTED_EDGE('',*,*,#44165,.T.) ;
#59160 = ORIENTED_EDGE('',*,*,#44166,.F.) ;
#59161 = ORIENTED_EDGE('',*,*,#44167,.F.) ;
#59162 = ORIENTED_EDGE('',*,*,#44165,.F.) ;
#59163 = ORIENTED_EDGE('',*,*,#44168,.F.) ;
#59164 = ORIENTED_EDGE('',*,*,#44169,.T.) ;
#59165 = ORIENTED_EDGE('',*,*,#44170,.F.) ;
#59166 = ORIENTED_EDGE('',*,*,#44169,.F.) ;
#59167 = ORIENTED_EDGE('',*,*,#44171,.F.) ;
#59168 = ORIENTED_EDGE('',*,*,#44172,.F.) ;
#59169 = ORIENTED_EDGE('',*,*,#44173,.T.) ;
#59170 = ORIENTED_EDGE('',*,*,#44174,.F.) ;
#59171 = ORIENTED_EDGE('',*,*,#44175,.T.) ;
#59172 = ORIENTED_EDGE('',*,*,#44176,.F.) ;
#59173 = ORIENTED_EDGE('',*,*,#44177,.F.) ;
#59174 = ORIENTED_EDGE('',*,*,#44178,.F.) ;
#59175 = ORIENTED_EDGE('',*,*,#44179,.F.) ;
#59176 = ORIENTED_EDGE('',*,*,#44180,.T.) ;
#59177 = ORIENTED_EDGE('',*,*,#44181,.F.) ;
#59178 = ORIENTED_EDGE('',*,*,#44182,.T.) ;
#59179 = ORIENTED_EDGE('',*,*,#44183,.F.) ;
#59180 = ORIENTED_EDGE('',*,*,#44184,.F.) ;
#59181 = ORIENTED_EDGE('',*,*,#44182,.F.) ;
#59182 = ORIENTED_EDGE('',*,*,#44185,.F.) ;
#59183 = ORIENTED_EDGE('',*,*,#44186,.T.) ;
#59184 = ORIENTED_EDGE('',*,*,#44187,.F.) ;
#59185 = ORIENTED_EDGE('',*,*,#44186,.F.) ;
#59186 = ORIENTED_EDGE('',*,*,#44188,.F.) ;
#59187 = ORIENTED_EDGE('',*,*,#44189,.F.) ;
#59188 = ORIENTED_EDGE('',*,*,#44190,.T.) ;
#59189 = ORIENTED_EDGE('',*,*,#44191,.F.) ;
#59190 = ORIENTED_EDGE('',*,*,#44192,.T.) ;
#59191 = ORIENTED_EDGE('',*,*,#44193,.F.) ;
#59192 = ORIENTED_EDGE('',*,*,#44194,.F.) ;
#59193 = ORIENTED_EDGE('',*,*,#44195,.F.) ;
#59194 = ORIENTED_EDGE('',*,*,#44196,.F.) ;
#59195 = ORIENTED_EDGE('',*,*,#44197,.T.) ;
#59196 = ORIENTED_EDGE('',*,*,#44198,.F.) ;
#59197 = ORIENTED_EDGE('',*,*,#44199,.T.) ;
#59198 = ORIENTED_EDGE('',*,*,#44200,.F.) ;
#59199 = ORIENTED_EDGE('',*,*,#44201,.F.) ;
#59200 = ORIENTED_EDGE('',*,*,#44199,.F.) ;
#59201 = ORIENTED_EDGE('',*,*,#44202,.F.) ;
#59202 = ORIENTED_EDGE('',*,*,#44203,.T.) ;
#59203 = ORIENTED_EDGE('',*,*,#44204,.F.) ;
#59204 = ORIENTED_EDGE('',*,*,#44203,.F.) ;
#59205 = ORIENTED_EDGE('',*,*,#44205,.F.) ;
#59206 = ORIENTED_EDGE('',*,*,#44206,.F.) ;
#59207 = ORIENTED_EDGE('',*,*,#44207,.T.) ;
#59208 = ORIENTED_EDGE('',*,*,#44208,.F.) ;
#59209 = ORIENTED_EDGE('',*,*,#44209,.T.) ;
#59210 = ORIENTED_EDGE('',*,*,#44210,.F.) ;
#59211 = ORIENTED_EDGE('',*,*,#44211,.F.) ;
#59212 = ORIENTED_EDGE('',*,*,#44212,.F.) ;
#59213 = ORIENTED_EDGE('',*,*,#44213,.F.) ;
#59214 = ORIENTED_EDGE('',*,*,#44214,.T.) ;
#59215 = ORIENTED_EDGE('',*,*,#44215,.F.) ;
#59216 = ORIENTED_EDGE('',*,*,#44216,.T.) ;
#59217 = ORIENTED_EDGE('',*,*,#44217,.F.) ;
#59218 = ORIENTED_EDGE('',*,*,#44218,.F.) ;
#59219 = ORIENTED_EDGE('',*,*,#44216,.F.) ;
#59220 = ORIENTED_EDGE('',*,*,#44219,.F.) ;
#59221 = ORIENTED_EDGE('',*,*,#44220,.T.) ;
#59222 = ORIENTED_EDGE('',*,*,#44221,.F.) ;
#59223 = ORIENTED_EDGE('',*,*,#44220,.F.) ;
#59224 = ORIENTED_EDGE('',*,*,#44222,.F.) ;
#59225 = ORIENTED_EDGE('',*,*,#44223,.F.) ;
#59226 = ORIENTED_EDGE('',*,*,#44224,.T.) ;
#59227 = ORIENTED_EDGE('',*,*,#44225,.F.) ;
#59228 = ORIENTED_EDGE('',*,*,#44226,.T.) ;
#59229 = ORIENTED_EDGE('',*,*,#44227,.F.) ;
#59230 = ORIENTED_EDGE('',*,*,#44228,.F.) ;
#59231 = ORIENTED_EDGE('',*,*,#44229,.F.) ;
#59232 = ORIENTED_EDGE('',*,*,#44230,.F.) ;
#59233 = ORIENTED_EDGE('',*,*,#44231,.T.) ;
#59234 = ORIENTED_EDGE('',*,*,#44232,.F.) ;
#59235 = ORIENTED_EDGE('',*,*,#44233,.T.) ;
#59236 = ORIENTED_EDGE('',*,*,#44234,.F.) ;
#59237 = ORIENTED_EDGE('',*,*,#44235,.F.) ;
#59238 = ORIENTED_EDGE('',*,*,#44233,.F.) ;
#59239 = ORIENTED_EDGE('',*,*,#44236,.F.) ;
#59240 = ORIENTED_EDGE('',*,*,#44237,.T.) ;
#59241 = ORIENTED_EDGE('',*,*,#44238,.F.) ;
#59242 = ORIENTED_EDGE('',*,*,#44237,.F.) ;
#59243 = ORIENTED_EDGE('',*,*,#44239,.F.) ;
#59244 = ORIENTED_EDGE('',*,*,#44240,.F.) ;
#59245 = ORIENTED_EDGE('',*,*,#44241,.T.) ;
#59246 = ORIENTED_EDGE('',*,*,#44242,.F.) ;
#59247 = ORIENTED_EDGE('',*,*,#44243,.T.) ;
#59248 = ORIENTED_EDGE('',*,*,#44244,.F.) ;
#59249 = ORIENTED_EDGE('',*,*,#44245,.F.) ;
#59250 = ORIENTED_EDGE('',*,*,#44246,.F.) ;
#59251 = ORIENTED_EDGE('',*,*,#44247,.F.) ;
#59252 = ORIENTED_EDGE('',*,*,#44248,.T.) ;
#59253 = ORIENTED_EDGE('',*,*,#44249,.F.) ;
#59254 = ORIENTED_EDGE('',*,*,#44250,.T.) ;
#59255 = ORIENTED_EDGE('',*,*,#44251,.F.) ;
#59256 = ORIENTED_EDGE('',*,*,#44252,.F.) ;
#59257 = ORIENTED_EDGE('',*,*,#44250,.F.) ;
#59258 = ORIENTED_EDGE('',*,*,#44253,.F.) ;
#59259 = ORIENTED_EDGE('',*,*,#44254,.T.) ;
#59260 = ORIENTED_EDGE('',*,*,#44255,.F.) ;
#59261 = ORIENTED_EDGE('',*,*,#44254,.F.) ;
#59262 = ORIENTED_EDGE('',*,*,#44256,.F.) ;
#59263 = ORIENTED_EDGE('',*,*,#44257,.F.) ;
#59264 = ORIENTED_EDGE('',*,*,#44258,.T.) ;
#59265 = ORIENTED_EDGE('',*,*,#44259,.F.) ;
#59266 = ORIENTED_EDGE('',*,*,#44260,.T.) ;
#59267 = ORIENTED_EDGE('',*,*,#44261,.F.) ;
#59268 = ORIENTED_EDGE('',*,*,#44262,.F.) ;
#59269 = ORIENTED_EDGE('',*,*,#44263,.F.) ;
#59270 = ORIENTED_EDGE('',*,*,#44264,.F.) ;
#59271 = ORIENTED_EDGE('',*,*,#44265,.T.) ;
#59272 = ORIENTED_EDGE('',*,*,#44266,.F.) ;
#59273 = ORIENTED_EDGE('',*,*,#44267,.T.) ;
#59274 = ORIENTED_EDGE('',*,*,#44268,.F.) ;
#59275 = ORIENTED_EDGE('',*,*,#44269,.F.) ;
#59276 = ORIENTED_EDGE('',*,*,#44267,.F.) ;
#59277 = ORIENTED_EDGE('',*,*,#44270,.F.) ;
#59278 = ORIENTED_EDGE('',*,*,#44271,.T.) ;
#59279 = ORIENTED_EDGE('',*,*,#44272,.F.) ;
#59280 = ORIENTED_EDGE('',*,*,#44271,.F.) ;
#59281 = ORIENTED_EDGE('',*,*,#44273,.F.) ;
#59282 = ORIENTED_EDGE('',*,*,#44274,.F.) ;
#59283 = ORIENTED_EDGE('',*,*,#44275,.T.) ;
#59284 = ORIENTED_EDGE('',*,*,#44276,.F.) ;
#59285 = ORIENTED_EDGE('',*,*,#44277,.T.) ;
#59286 = ORIENTED_EDGE('',*,*,#44278,.F.) ;
#59287 = ORIENTED_EDGE('',*,*,#44279,.F.) ;
#59288 = ORIENTED_EDGE('',*,*,#44280,.F.) ;
#59289 = ORIENTED_EDGE('',*,*,#44281,.F.) ;
#59290 = ORIENTED_EDGE('',*,*,#44282,.T.) ;
#59291 = ORIENTED_EDGE('',*,*,#44283,.F.) ;
#59292 = ORIENTED_EDGE('',*,*,#44284,.T.) ;
#59293 = ORIENTED_EDGE('',*,*,#44285,.F.) ;
#59294 = ORIENTED_EDGE('',*,*,#44286,.F.) ;
#59295 = ORIENTED_EDGE('',*,*,#44284,.F.) ;
#59296 = ORIENTED_EDGE('',*,*,#44287,.F.) ;
#59297 = ORIENTED_EDGE('',*,*,#44288,.F.) ;
#59298 = ORIENTED_EDGE('',*,*,#44289,.F.) ;
#59299 = ORIENTED_EDGE('',*,*,#44290,.T.) ;
#59300 = ORIENTED_EDGE('',*,*,#44291,.F.) ;
#59301 = ORIENTED_EDGE('',*,*,#44292,.F.) ;
#59302 = ORIENTED_EDGE('',*,*,#44293,.F.) ;
#59303 = ORIENTED_EDGE('',*,*,#44294,.T.) ;
#59304 = ORIENTED_EDGE('',*,*,#44295,.F.) ;
#59305 = ORIENTED_EDGE('',*,*,#44296,.F.) ;
#59306 = ORIENTED_EDGE('',*,*,#44297,.F.) ;
#59307 = ORIENTED_EDGE('',*,*,#44298,.T.) ;
#59308 = ORIENTED_EDGE('',*,*,#44299,.F.) ;
#59309 = ORIENTED_EDGE('',*,*,#44300,.F.) ;
#59310 = ORIENTED_EDGE('',*,*,#44301,.F.) ;
#59311 = ORIENTED_EDGE('',*,*,#44302,.T.) ;
#59312 = ORIENTED_EDGE('',*,*,#44303,.F.) ;
#59313 = ORIENTED_EDGE('',*,*,#44304,.F.) ;
#59314 = ORIENTED_EDGE('',*,*,#44305,.F.) ;
#59315 = ORIENTED_EDGE('',*,*,#44306,.T.) ;
#59316 = ORIENTED_EDGE('',*,*,#44307,.F.) ;
#59317 = ORIENTED_EDGE('',*,*,#44308,.F.) ;
#59318 = ORIENTED_EDGE('',*,*,#44309,.F.) ;
#59319 = ORIENTED_EDGE('',*,*,#44310,.T.) ;
#59320 = ORIENTED_EDGE('',*,*,#44311,.F.) ;
#59321 = ORIENTED_EDGE('',*,*,#44312,.F.) ;
#59322 = ORIENTED_EDGE('',*,*,#44313,.F.) ;
#59323 = ORIENTED_EDGE('',*,*,#44314,.T.) ;
#59324 = ORIENTED_EDGE('',*,*,#44315,.F.) ;
#59325 = ORIENTED_EDGE('',*,*,#44316,.F.) ;
#59326 = ORIENTED_EDGE('',*,*,#44317,.F.) ;
#59327 = ORIENTED_EDGE('',*,*,#44318,.T.) ;
#59328 = ORIENTED_EDGE('',*,*,#44319,.F.) ;
#59329 = ORIENTED_EDGE('',*,*,#44320,.F.) ;
#59330 = ORIENTED_EDGE('',*,*,#44321,.F.) ;
#59331 = ORIENTED_EDGE('',*,*,#44322,.T.) ;
#59332 = ORIENTED_EDGE('',*,*,#44323,.F.) ;
#59333 = ORIENTED_EDGE('',*,*,#44324,.T.) ;
#59334 = ORIENTED_EDGE('',*,*,#44325,.F.) ;
#59335 = ORIENTED_EDGE('',*,*,#44324,.F.) ;
#59336 = ORIENTED_EDGE('',*,*,#44326,.F.) ;
#59337 = ORIENTED_EDGE('',*,*,#44327,.F.) ;
#59338 = ORIENTED_EDGE('',*,*,#44328,.T.) ;
#59339 = ORIENTED_EDGE('',*,*,#44329,.F.) ;
#59340 = ORIENTED_EDGE('',*,*,#44330,.T.) ;
#59341 = ORIENTED_EDGE('',*,*,#44331,.F.) ;
#59342 = ORIENTED_EDGE('',*,*,#44332,.F.) ;
#59343 = ORIENTED_EDGE('',*,*,#44333,.F.) ;
#59344 = ORIENTED_EDGE('',*,*,#44334,.F.) ;
#59345 = ORIENTED_EDGE('',*,*,#44335,.T.) ;
#59346 = ORIENTED_EDGE('',*,*,#44153,.T.) ;
#59347 = ORIENTED_EDGE('',*,*,#44336,.T.) ;
#59348 = ORIENTED_EDGE('',*,*,#44149,.T.) ;
#59349 = ORIENTED_EDGE('',*,*,#44150,.T.) ;
#59350 = ORIENTED_EDGE('',*,*,#44336,.F.) ;
#59351 = ORIENTED_EDGE('',*,*,#44170,.T.) ;
#59352 = ORIENTED_EDGE('',*,*,#44337,.T.) ;
#59353 = ORIENTED_EDGE('',*,*,#44166,.T.) ;
#59354 = ORIENTED_EDGE('',*,*,#44167,.T.) ;
#59355 = ORIENTED_EDGE('',*,*,#44337,.F.) ;
#59356 = ORIENTED_EDGE('',*,*,#44187,.T.) ;
#59357 = ORIENTED_EDGE('',*,*,#44338,.T.) ;
#59358 = ORIENTED_EDGE('',*,*,#44183,.T.) ;
#59359 = ORIENTED_EDGE('',*,*,#44184,.T.) ;
#59360 = ORIENTED_EDGE('',*,*,#44338,.F.) ;
#59361 = ORIENTED_EDGE('',*,*,#44204,.T.) ;
#59362 = ORIENTED_EDGE('',*,*,#44339,.T.) ;
#59363 = ORIENTED_EDGE('',*,*,#44200,.T.) ;
#59364 = ORIENTED_EDGE('',*,*,#44201,.T.) ;
#59365 = ORIENTED_EDGE('',*,*,#44339,.F.) ;
#59366 = ORIENTED_EDGE('',*,*,#44221,.T.) ;
#59367 = ORIENTED_EDGE('',*,*,#44340,.T.) ;
#59368 = ORIENTED_EDGE('',*,*,#44217,.T.) ;
#59369 = ORIENTED_EDGE('',*,*,#44218,.T.) ;
#59370 = ORIENTED_EDGE('',*,*,#44340,.F.) ;
#59371 = ORIENTED_EDGE('',*,*,#44238,.T.) ;
#59372 = ORIENTED_EDGE('',*,*,#44341,.T.) ;
#59373 = ORIENTED_EDGE('',*,*,#44234,.T.) ;
#59374 = ORIENTED_EDGE('',*,*,#44235,.T.) ;
#59375 = ORIENTED_EDGE('',*,*,#44341,.F.) ;
#59376 = ORIENTED_EDGE('',*,*,#44255,.T.) ;
#59377 = ORIENTED_EDGE('',*,*,#44342,.T.) ;
#59378 = ORIENTED_EDGE('',*,*,#44251,.T.) ;
#59379 = ORIENTED_EDGE('',*,*,#44252,.T.) ;
#59380 = ORIENTED_EDGE('',*,*,#44342,.F.) ;
#59381 = ORIENTED_EDGE('',*,*,#44272,.T.) ;
#59382 = ORIENTED_EDGE('',*,*,#44343,.T.) ;
#59383 = ORIENTED_EDGE('',*,*,#44268,.T.) ;
#59384 = ORIENTED_EDGE('',*,*,#44269,.T.) ;
#59385 = ORIENTED_EDGE('',*,*,#44343,.F.) ;
#59386 = ORIENTED_EDGE('',*,*,#44325,.T.) ;
#59387 = ORIENTED_EDGE('',*,*,#44344,.T.) ;
#59388 = ORIENTED_EDGE('',*,*,#44285,.T.) ;
#59389 = ORIENTED_EDGE('',*,*,#44286,.T.) ;
#59390 = ORIENTED_EDGE('',*,*,#44344,.F.) ;
#59391 = ORIENTED_EDGE('',*,*,#44345,.T.) ;
#59392 = ORIENTED_EDGE('',*,*,#44346,.T.) ;
#59393 = ORIENTED_EDGE('',*,*,#44289,.T.) ;
#59394 = ORIENTED_EDGE('',*,*,#44347,.F.) ;
#59395 = ORIENTED_EDGE('',*,*,#44348,.T.) ;
#59396 = ORIENTED_EDGE('',*,*,#44349,.T.) ;
#59397 = ORIENTED_EDGE('',*,*,#44293,.T.) ;
#59398 = ORIENTED_EDGE('',*,*,#44350,.F.) ;
#59399 = ORIENTED_EDGE('',*,*,#44351,.T.) ;
#59400 = ORIENTED_EDGE('',*,*,#44352,.T.) ;
#59401 = ORIENTED_EDGE('',*,*,#44297,.T.) ;
#59402 = ORIENTED_EDGE('',*,*,#44353,.F.) ;
#59403 = ORIENTED_EDGE('',*,*,#44354,.T.) ;
#59404 = ORIENTED_EDGE('',*,*,#44355,.T.) ;
#59405 = ORIENTED_EDGE('',*,*,#44301,.T.) ;
#59406 = ORIENTED_EDGE('',*,*,#44356,.F.) ;
#59407 = ORIENTED_EDGE('',*,*,#44357,.T.) ;
#59408 = ORIENTED_EDGE('',*,*,#44358,.T.) ;
#59409 = ORIENTED_EDGE('',*,*,#44305,.T.) ;
#59410 = ORIENTED_EDGE('',*,*,#44359,.F.) ;
#59411 = ORIENTED_EDGE('',*,*,#44360,.T.) ;
#59412 = ORIENTED_EDGE('',*,*,#44361,.T.) ;
#59413 = ORIENTED_EDGE('',*,*,#44309,.T.) ;
#59414 = ORIENTED_EDGE('',*,*,#44362,.F.) ;
#59415 = ORIENTED_EDGE('',*,*,#44363,.T.) ;
#59416 = ORIENTED_EDGE('',*,*,#44364,.T.) ;
#59417 = ORIENTED_EDGE('',*,*,#44313,.T.) ;
#59418 = ORIENTED_EDGE('',*,*,#44365,.F.) ;
#59419 = ORIENTED_EDGE('',*,*,#44366,.T.) ;
#59420 = ORIENTED_EDGE('',*,*,#44367,.T.) ;
#59421 = ORIENTED_EDGE('',*,*,#44317,.T.) ;
#59422 = ORIENTED_EDGE('',*,*,#44368,.F.) ;
#59423 = ORIENTED_EDGE('',*,*,#44369,.T.) ;
#59424 = ORIENTED_EDGE('',*,*,#44370,.T.) ;
#59425 = ORIENTED_EDGE('',*,*,#44321,.T.) ;
#59426 = ORIENTED_EDGE('',*,*,#44371,.F.) ;
#59427 = ORIENTED_EDGE('',*,*,#44372,.F.) ;
#59428 = ORIENTED_EDGE('',*,*,#44373,.T.) ;
#59429 = ORIENTED_EDGE('',*,*,#44374,.F.) ;
#59430 = ORIENTED_EDGE('',*,*,#44375,.F.) ;
#59431 = ORIENTED_EDGE('',*,*,#44373,.F.) ;
#59432 = ORIENTED_EDGE('',*,*,#44376,.F.) ;
#59433 = ORIENTED_EDGE('',*,*,#44377,.F.) ;
#59434 = ORIENTED_EDGE('',*,*,#44378,.F.) ;
#59435 = ORIENTED_EDGE('',*,*,#44379,.T.) ;
#59436 = ORIENTED_EDGE('',*,*,#44380,.F.) ;
#59437 = ORIENTED_EDGE('',*,*,#44381,.T.) ;
#59438 = ORIENTED_EDGE('',*,*,#44382,.F.) ;
#59439 = ORIENTED_EDGE('',*,*,#44381,.F.) ;
#59440 = ORIENTED_EDGE('',*,*,#44383,.F.) ;
#59441 = ORIENTED_EDGE('',*,*,#44384,.F.) ;
#59442 = ORIENTED_EDGE('',*,*,#44385,.T.) ;
#59443 = ORIENTED_EDGE('',*,*,#44386,.F.) ;
#59444 = ORIENTED_EDGE('',*,*,#44387,.T.) ;
#59445 = ORIENTED_EDGE('',*,*,#44388,.F.) ;
#59446 = ORIENTED_EDGE('',*,*,#44389,.F.) ;
#59447 = ORIENTED_EDGE('',*,*,#44390,.F.) ;
#59448 = ORIENTED_EDGE('',*,*,#44391,.F.) ;
#59449 = ORIENTED_EDGE('',*,*,#44392,.T.) ;
#59450 = ORIENTED_EDGE('',*,*,#44382,.T.) ;
#59451 = ORIENTED_EDGE('',*,*,#44393,.T.) ;
#59452 = ORIENTED_EDGE('',*,*,#44374,.T.) ;
#59453 = ORIENTED_EDGE('',*,*,#44375,.T.) ;
#59454 = ORIENTED_EDGE('',*,*,#44393,.F.) ;
#59455 = ORIENTED_EDGE('',*,*,#44394,.T.) ;
#59456 = ORIENTED_EDGE('',*,*,#44395,.T.) ;
#59457 = ORIENTED_EDGE('',*,*,#44378,.T.) ;
#59458 = ORIENTED_EDGE('',*,*,#44396,.F.) ;
#59459 = ORIENTED_EDGE('',*,*,#44397,.T.) ;
#59460 = ORIENTED_EDGE('',*,*,#44398,.T.) ;
#59461 = ORIENTED_EDGE('',*,*,#44399,.T.) ;
#59462 = ORIENTED_EDGE('',*,*,#44400,.T.) ;
#59463 = ORIENTED_EDGE('',*,*,#44161,.T.) ;
#59464 = ORIENTED_EDGE('',*,*,#44401,.F.) ;
#59465 = ORIENTED_EDGE('',*,*,#44402,.T.) ;
#59466 = ORIENTED_EDGE('',*,*,#44403,.T.) ;
#59467 = ORIENTED_EDGE('',*,*,#44404,.T.) ;
#59468 = ORIENTED_EDGE('',*,*,#44405,.T.) ;
#59469 = ORIENTED_EDGE('',*,*,#44406,.T.) ;
#59470 = ORIENTED_EDGE('',*,*,#44407,.F.) ;
#59471 = ORIENTED_EDGE('',*,*,#44408,.T.) ;
#59472 = ORIENTED_EDGE('',*,*,#44409,.T.) ;
#59473 = ORIENTED_EDGE('',*,*,#44410,.T.) ;
#59474 = ORIENTED_EDGE('',*,*,#44411,.T.) ;
#59475 = ORIENTED_EDGE('',*,*,#44178,.T.) ;
#59476 = ORIENTED_EDGE('',*,*,#44412,.F.) ;
#59477 = ORIENTED_EDGE('',*,*,#44413,.T.) ;
#59478 = ORIENTED_EDGE('',*,*,#44414,.T.) ;
#59479 = ORIENTED_EDGE('',*,*,#44415,.T.) ;
#59480 = ORIENTED_EDGE('',*,*,#44416,.T.) ;
#59481 = ORIENTED_EDGE('',*,*,#44417,.T.) ;
#59482 = ORIENTED_EDGE('',*,*,#44418,.F.) ;
#59483 = ORIENTED_EDGE('',*,*,#44419,.T.) ;
#59484 = ORIENTED_EDGE('',*,*,#44420,.T.) ;
#59485 = ORIENTED_EDGE('',*,*,#44421,.T.) ;
#59486 = ORIENTED_EDGE('',*,*,#44422,.T.) ;
#59487 = ORIENTED_EDGE('',*,*,#44195,.T.) ;
#59488 = ORIENTED_EDGE('',*,*,#44423,.F.) ;
#59489 = ORIENTED_EDGE('',*,*,#44424,.T.) ;
#59490 = ORIENTED_EDGE('',*,*,#44425,.T.) ;
#59491 = ORIENTED_EDGE('',*,*,#44426,.T.) ;
#59492 = ORIENTED_EDGE('',*,*,#44427,.T.) ;
#59493 = ORIENTED_EDGE('',*,*,#44428,.T.) ;
#59494 = ORIENTED_EDGE('',*,*,#44429,.F.) ;
#59495 = ORIENTED_EDGE('',*,*,#44430,.T.) ;
#59496 = ORIENTED_EDGE('',*,*,#44431,.T.) ;
#59497 = ORIENTED_EDGE('',*,*,#44432,.T.) ;
#59498 = ORIENTED_EDGE('',*,*,#44433,.T.) ;
#59499 = ORIENTED_EDGE('',*,*,#44212,.T.) ;
#59500 = ORIENTED_EDGE('',*,*,#44434,.F.) ;
#59501 = ORIENTED_EDGE('',*,*,#44435,.T.) ;
#59502 = ORIENTED_EDGE('',*,*,#44436,.T.) ;
#59503 = ORIENTED_EDGE('',*,*,#44437,.T.) ;
#59504 = ORIENTED_EDGE('',*,*,#44438,.T.) ;
#59505 = ORIENTED_EDGE('',*,*,#44439,.T.) ;
#59506 = ORIENTED_EDGE('',*,*,#44440,.F.) ;
#59507 = ORIENTED_EDGE('',*,*,#44441,.T.) ;
#59508 = ORIENTED_EDGE('',*,*,#44442,.T.) ;
#59509 = ORIENTED_EDGE('',*,*,#44443,.T.) ;
#59510 = ORIENTED_EDGE('',*,*,#44444,.T.) ;
#59511 = ORIENTED_EDGE('',*,*,#44229,.T.) ;
#59512 = ORIENTED_EDGE('',*,*,#44445,.F.) ;
#59513 = ORIENTED_EDGE('',*,*,#44446,.T.) ;
#59514 = ORIENTED_EDGE('',*,*,#44447,.T.) ;
#59515 = ORIENTED_EDGE('',*,*,#44448,.T.) ;
#59516 = ORIENTED_EDGE('',*,*,#44449,.T.) ;
#59517 = ORIENTED_EDGE('',*,*,#44450,.T.) ;
#59518 = ORIENTED_EDGE('',*,*,#44451,.F.) ;
#59519 = ORIENTED_EDGE('',*,*,#44452,.T.) ;
#59520 = ORIENTED_EDGE('',*,*,#44453,.T.) ;
#59521 = ORIENTED_EDGE('',*,*,#44454,.T.) ;
#59522 = ORIENTED_EDGE('',*,*,#44455,.T.) ;
#59523 = ORIENTED_EDGE('',*,*,#44246,.T.) ;
#59524 = ORIENTED_EDGE('',*,*,#44456,.F.) ;
#59525 = ORIENTED_EDGE('',*,*,#44457,.T.) ;
#59526 = ORIENTED_EDGE('',*,*,#44458,.T.) ;
#59527 = ORIENTED_EDGE('',*,*,#44459,.T.) ;
#59528 = ORIENTED_EDGE('',*,*,#44460,.T.) ;
#59529 = ORIENTED_EDGE('',*,*,#44461,.T.) ;
#59530 = ORIENTED_EDGE('',*,*,#44462,.F.) ;
#59531 = ORIENTED_EDGE('',*,*,#44463,.T.) ;
#59532 = ORIENTED_EDGE('',*,*,#44464,.T.) ;
#59533 = ORIENTED_EDGE('',*,*,#44465,.T.) ;
#59534 = ORIENTED_EDGE('',*,*,#44466,.T.) ;
#59535 = ORIENTED_EDGE('',*,*,#44263,.T.) ;
#59536 = ORIENTED_EDGE('',*,*,#44467,.F.) ;
#59537 = ORIENTED_EDGE('',*,*,#44468,.T.) ;
#59538 = ORIENTED_EDGE('',*,*,#44469,.T.) ;
#59539 = ORIENTED_EDGE('',*,*,#44470,.T.) ;
#59540 = ORIENTED_EDGE('',*,*,#44471,.T.) ;
#59541 = ORIENTED_EDGE('',*,*,#44472,.T.) ;
#59542 = ORIENTED_EDGE('',*,*,#44473,.F.) ;
#59543 = ORIENTED_EDGE('',*,*,#44474,.T.) ;
#59544 = ORIENTED_EDGE('',*,*,#44475,.T.) ;
#59545 = ORIENTED_EDGE('',*,*,#44476,.T.) ;
#59546 = ORIENTED_EDGE('',*,*,#44477,.T.) ;
#59547 = ORIENTED_EDGE('',*,*,#44280,.T.) ;
#59548 = ORIENTED_EDGE('',*,*,#44478,.F.) ;
#59549 = ORIENTED_EDGE('',*,*,#44479,.T.) ;
#59550 = ORIENTED_EDGE('',*,*,#44480,.T.) ;
#59551 = ORIENTED_EDGE('',*,*,#44481,.T.) ;
#59552 = ORIENTED_EDGE('',*,*,#44482,.T.) ;
#59553 = ORIENTED_EDGE('',*,*,#44483,.T.) ;
#59554 = ORIENTED_EDGE('',*,*,#44484,.F.) ;
#59555 = ORIENTED_EDGE('',*,*,#44485,.T.) ;
#59556 = ORIENTED_EDGE('',*,*,#44486,.T.) ;
#59557 = ORIENTED_EDGE('',*,*,#44487,.T.) ;
#59558 = ORIENTED_EDGE('',*,*,#44488,.T.) ;
#59559 = ORIENTED_EDGE('',*,*,#44333,.T.) ;
#59560 = ORIENTED_EDGE('',*,*,#44489,.F.) ;
#59561 = ORIENTED_EDGE('',*,*,#44490,.T.) ;
#59562 = ORIENTED_EDGE('',*,*,#44491,.T.) ;
#59563 = ORIENTED_EDGE('',*,*,#44492,.T.) ;
#59564 = ORIENTED_EDGE('',*,*,#44493,.T.) ;
#59565 = ORIENTED_EDGE('',*,*,#44494,.T.) ;
#59566 = ORIENTED_EDGE('',*,*,#44495,.F.) ;
#59567 = ORIENTED_EDGE('',*,*,#44496,.F.) ;
#59568 = ORIENTED_EDGE('',*,*,#44497,.T.) ;
#59569 = ORIENTED_EDGE('',*,*,#44498,.T.) ;
#59570 = ORIENTED_EDGE('',*,*,#44499,.T.) ;
#59571 = ORIENTED_EDGE('',*,*,#44500,.T.) ;
#59572 = ORIENTED_EDGE('',*,*,#44501,.F.) ;
#59573 = ORIENTED_EDGE('',*,*,#44502,.T.) ;
#59574 = ORIENTED_EDGE('',*,*,#44503,.T.) ;
#59575 = ORIENTED_EDGE('',*,*,#44504,.T.) ;
#59576 = ORIENTED_EDGE('',*,*,#44505,.T.) ;
#59577 = ORIENTED_EDGE('',*,*,#44506,.F.) ;
#59578 = ORIENTED_EDGE('',*,*,#44507,.T.) ;
#59579 = ORIENTED_EDGE('',*,*,#44508,.T.) ;
#59580 = ORIENTED_EDGE('',*,*,#44509,.T.) ;
#59581 = ORIENTED_EDGE('',*,*,#44510,.T.) ;
#59582 = ORIENTED_EDGE('',*,*,#44511,.F.) ;
#59583 = ORIENTED_EDGE('',*,*,#44512,.T.) ;
#59584 = ORIENTED_EDGE('',*,*,#44513,.T.) ;
#59585 = ORIENTED_EDGE('',*,*,#44514,.T.) ;
#59586 = ORIENTED_EDGE('',*,*,#44515,.T.) ;
#59587 = ORIENTED_EDGE('',*,*,#44516,.F.) ;
#59588 = ORIENTED_EDGE('',*,*,#44517,.T.) ;
#59589 = ORIENTED_EDGE('',*,*,#44518,.T.) ;
#59590 = ORIENTED_EDGE('',*,*,#44519,.T.) ;
#59591 = ORIENTED_EDGE('',*,*,#44520,.T.) ;
#59592 = ORIENTED_EDGE('',*,*,#44521,.F.) ;
#59593 = ORIENTED_EDGE('',*,*,#44522,.T.) ;
#59594 = ORIENTED_EDGE('',*,*,#44523,.T.) ;
#59595 = ORIENTED_EDGE('',*,*,#44524,.T.) ;
#59596 = ORIENTED_EDGE('',*,*,#44525,.T.) ;
#59597 = ORIENTED_EDGE('',*,*,#44526,.F.) ;
#59598 = ORIENTED_EDGE('',*,*,#44527,.T.) ;
#59599 = ORIENTED_EDGE('',*,*,#44528,.T.) ;
#59600 = ORIENTED_EDGE('',*,*,#44529,.T.) ;
#59601 = ORIENTED_EDGE('',*,*,#44530,.T.) ;
#59602 = ORIENTED_EDGE('',*,*,#44531,.F.) ;
#59603 = ORIENTED_EDGE('',*,*,#44532,.T.) ;
#59604 = ORIENTED_EDGE('',*,*,#44533,.T.) ;
#59605 = ORIENTED_EDGE('',*,*,#44534,.T.) ;
#59606 = ORIENTED_EDGE('',*,*,#44535,.T.) ;
#59607 = ORIENTED_EDGE('',*,*,#44536,.F.) ;
#59608 = ORIENTED_EDGE('',*,*,#44537,.T.) ;
#59609 = ORIENTED_EDGE('',*,*,#44538,.T.) ;
#59610 = ORIENTED_EDGE('',*,*,#44539,.T.) ;
#59611 = ORIENTED_EDGE('',*,*,#44540,.T.) ;
#59612 = ORIENTED_EDGE('',*,*,#44541,.F.) ;
#59613 = ORIENTED_EDGE('',*,*,#44542,.T.) ;
#59614 = ORIENTED_EDGE('',*,*,#44543,.T.) ;
#59615 = ORIENTED_EDGE('',*,*,#44544,.T.) ;
#59616 = ORIENTED_EDGE('',*,*,#44545,.T.) ;
#59617 = ORIENTED_EDGE('',*,*,#44546,.F.) ;
#59618 = ORIENTED_EDGE('',*,*,#44547,.T.) ;
#59619 = ORIENTED_EDGE('',*,*,#44548,.T.) ;
#59620 = ORIENTED_EDGE('',*,*,#44549,.T.) ;
#59621 = ORIENTED_EDGE('',*,*,#44550,.T.) ;
#59622 = ORIENTED_EDGE('',*,*,#44551,.F.) ;
#59623 = ORIENTED_EDGE('',*,*,#44552,.T.) ;
#59624 = ORIENTED_EDGE('',*,*,#44553,.T.) ;
#59625 = ORIENTED_EDGE('',*,*,#44554,.T.) ;
#59626 = ORIENTED_EDGE('',*,*,#44555,.T.) ;
#59627 = ORIENTED_EDGE('',*,*,#44556,.F.) ;
#59628 = ORIENTED_EDGE('',*,*,#44557,.T.) ;
#59629 = ORIENTED_EDGE('',*,*,#44558,.T.) ;
#59630 = ORIENTED_EDGE('',*,*,#44559,.T.) ;
#59631 = ORIENTED_EDGE('',*,*,#44560,.T.) ;
#59632 = ORIENTED_EDGE('',*,*,#44561,.F.) ;
#59633 = ORIENTED_EDGE('',*,*,#44562,.T.) ;
#59634 = ORIENTED_EDGE('',*,*,#44563,.T.) ;
#59635 = ORIENTED_EDGE('',*,*,#44564,.T.) ;
#59636 = ORIENTED_EDGE('',*,*,#44565,.T.) ;
#59637 = ORIENTED_EDGE('',*,*,#44566,.F.) ;
#59638 = ORIENTED_EDGE('',*,*,#44567,.T.) ;
#59639 = ORIENTED_EDGE('',*,*,#44568,.T.) ;
#59640 = ORIENTED_EDGE('',*,*,#44569,.T.) ;
#59641 = ORIENTED_EDGE('',*,*,#44570,.T.) ;
#59642 = ORIENTED_EDGE('',*,*,#44571,.F.) ;
#59643 = ORIENTED_EDGE('',*,*,#44572,.T.) ;
#59644 = ORIENTED_EDGE('',*,*,#44573,.T.) ;
#59645 = ORIENTED_EDGE('',*,*,#44574,.T.) ;
#59646 = ORIENTED_EDGE('',*,*,#44575,.T.) ;
#59647 = ORIENTED_EDGE('',*,*,#44576,.F.) ;
#59648 = ORIENTED_EDGE('',*,*,#44577,.T.) ;
#59649 = ORIENTED_EDGE('',*,*,#44578,.T.) ;
#59650 = ORIENTED_EDGE('',*,*,#44579,.T.) ;
#59651 = ORIENTED_EDGE('',*,*,#44580,.T.) ;
#59652 = ORIENTED_EDGE('',*,*,#44581,.F.) ;
#59653 = ORIENTED_EDGE('',*,*,#44582,.T.) ;
#59654 = ORIENTED_EDGE('',*,*,#44583,.T.) ;
#59655 = ORIENTED_EDGE('',*,*,#44584,.T.) ;
#59656 = ORIENTED_EDGE('',*,*,#44585,.T.) ;
#59657 = ORIENTED_EDGE('',*,*,#44586,.F.) ;
#59658 = ORIENTED_EDGE('',*,*,#44587,.T.) ;
#59659 = ORIENTED_EDGE('',*,*,#44588,.T.) ;
#59660 = ORIENTED_EDGE('',*,*,#44589,.T.) ;
#59661 = ORIENTED_EDGE('',*,*,#44590,.F.) ;
#59662 = ORIENTED_EDGE('',*,*,#44591,.T.) ;
#59663 = ORIENTED_EDGE('',*,*,#44592,.T.) ;
#59664 = ORIENTED_EDGE('',*,*,#44593,.T.) ;
#59665 = ORIENTED_EDGE('',*,*,#44594,.F.) ;
#59666 = ORIENTED_EDGE('',*,*,#44595,.T.) ;
#59667 = ORIENTED_EDGE('',*,*,#44596,.T.) ;
#59668 = ORIENTED_EDGE('',*,*,#44597,.T.) ;
#59669 = ORIENTED_EDGE('',*,*,#44598,.F.) ;
#59670 = ORIENTED_EDGE('',*,*,#44599,.T.) ;
#59671 = ORIENTED_EDGE('',*,*,#44600,.T.) ;
#59672 = ORIENTED_EDGE('',*,*,#44601,.T.) ;
#59673 = ORIENTED_EDGE('',*,*,#44602,.F.) ;
#59674 = ORIENTED_EDGE('',*,*,#44603,.T.) ;
#59675 = ORIENTED_EDGE('',*,*,#44604,.T.) ;
#59676 = ORIENTED_EDGE('',*,*,#44605,.T.) ;
#59677 = ORIENTED_EDGE('',*,*,#44606,.F.) ;
#59678 = ORIENTED_EDGE('',*,*,#44607,.T.) ;
#59679 = ORIENTED_EDGE('',*,*,#44608,.T.) ;
#59680 = ORIENTED_EDGE('',*,*,#44609,.T.) ;
#59681 = ORIENTED_EDGE('',*,*,#44610,.F.) ;
#59682 = ORIENTED_EDGE('',*,*,#44611,.T.) ;
#59683 = ORIENTED_EDGE('',*,*,#44612,.T.) ;
#59684 = ORIENTED_EDGE('',*,*,#44613,.T.) ;
#59685 = ORIENTED_EDGE('',*,*,#44614,.F.) ;
#59686 = ORIENTED_EDGE('',*,*,#44615,.T.) ;
#59687 = ORIENTED_EDGE('',*,*,#44616,.T.) ;
#59688 = ORIENTED_EDGE('',*,*,#44617,.T.) ;
#59689 = ORIENTED_EDGE('',*,*,#44618,.F.) ;
#59690 = ORIENTED_EDGE('',*,*,#44619,.T.) ;
#59691 = ORIENTED_EDGE('',*,*,#44620,.T.) ;
#59692 = ORIENTED_EDGE('',*,*,#44621,.T.) ;
#59693 = ORIENTED_EDGE('',*,*,#44622,.T.) ;
#59694 = ORIENTED_EDGE('',*,*,#44623,.T.) ;
#59695 = ORIENTED_EDGE('',*,*,#44624,.T.) ;
#59696 = ORIENTED_EDGE('',*,*,#44625,.T.) ;
#59697 = ORIENTED_EDGE('',*,*,#44390,.T.) ;
#59698 = ORIENTED_EDGE('',*,*,#44626,.F.) ;
#59699 = ORIENTED_EDGE('',*,*,#44627,.T.) ;
#59700 = ORIENTED_EDGE('',*,*,#44628,.T.) ;
#59701 = ORIENTED_EDGE('',*,*,#44629,.T.) ;
#59702 = ORIENTED_EDGE('',*,*,#44630,.T.) ;
#59703 = ORIENTED_EDGE('',*,*,#44631,.T.) ;
#59704 = ORIENTED_EDGE('',*,*,#44632,.F.) ;
#59705 = ORIENTED_EDGE('',*,*,#44633,.F.) ;
#59706 = ORIENTED_EDGE('',*,*,#44634,.T.) ;
#59707 = ORIENTED_EDGE('',*,*,#44635,.T.) ;
#59708 = ORIENTED_EDGE('',*,*,#44636,.T.) ;
#59709 = ORIENTED_EDGE('',*,*,#44637,.T.) ;
#59710 = ORIENTED_EDGE('',*,*,#44638,.F.) ;
#59711 = ORIENTED_EDGE('',*,*,#44639,.T.) ;
#59712 = ORIENTED_EDGE('',*,*,#44640,.T.) ;
#59713 = ORIENTED_EDGE('',*,*,#44641,.T.) ;
#59714 = ORIENTED_EDGE('',*,*,#44642,.T.) ;
#59715 = ORIENTED_EDGE('',*,*,#44643,.F.) ;
#59716 = ORIENTED_EDGE('',*,*,#44644,.T.) ;
#59717 = ORIENTED_EDGE('',*,*,#44645,.T.) ;
#59718 = ORIENTED_EDGE('',*,*,#44646,.T.) ;
#59719 = ORIENTED_EDGE('',*,*,#44647,.F.) ;
#59720 = ORIENTED_EDGE('',*,*,#44648,.T.) ;
#59721 = ORIENTED_EDGE('',*,*,#44649,.T.) ;
#59722 = ORIENTED_EDGE('',*,*,#44650,.T.) ;
#59723 = ORIENTED_EDGE('',*,*,#44651,.F.) ;
#59724 = ORIENTED_EDGE('',*,*,#44652,.T.) ;
#59725 = ORIENTED_EDGE('',*,*,#44653,.F.) ;
#59726 = ORIENTED_EDGE('',*,*,#44654,.T.) ;
#59727 = ORIENTED_EDGE('',*,*,#44647,.T.) ;
#59728 = ORIENTED_EDGE('',*,*,#44655,.T.) ;
#59729 = ORIENTED_EDGE('',*,*,#44645,.F.) ;
#59730 = ORIENTED_EDGE('',*,*,#44656,.T.) ;
#59731 = ORIENTED_EDGE('',*,*,#44657,.F.) ;
#59732 = ORIENTED_EDGE('',*,*,#44658,.T.) ;
#59733 = ORIENTED_EDGE('',*,*,#44659,.F.) ;
#59734 = ORIENTED_EDGE('',*,*,#44660,.T.) ;
#59735 = ORIENTED_EDGE('',*,*,#44588,.F.) ;
#59736 = ORIENTED_EDGE('',*,*,#44661,.T.) ;
#59737 = ORIENTED_EDGE('',*,*,#44662,.F.) ;
#59738 = ORIENTED_EDGE('',*,*,#44663,.T.) ;
#59739 = ORIENTED_EDGE('',*,*,#44664,.F.) ;
#59740 = ORIENTED_EDGE('',*,*,#44665,.T.) ;
#59741 = ORIENTED_EDGE('',*,*,#44592,.F.) ;
#59742 = ORIENTED_EDGE('',*,*,#44666,.T.) ;
#59743 = ORIENTED_EDGE('',*,*,#44667,.F.) ;
#59744 = ORIENTED_EDGE('',*,*,#44668,.T.) ;
#59745 = ORIENTED_EDGE('',*,*,#44669,.F.) ;
#59746 = ORIENTED_EDGE('',*,*,#44670,.T.) ;
#59747 = ORIENTED_EDGE('',*,*,#44596,.F.) ;
#59748 = ORIENTED_EDGE('',*,*,#44671,.T.) ;
#59749 = ORIENTED_EDGE('',*,*,#44672,.F.) ;
#59750 = ORIENTED_EDGE('',*,*,#44673,.T.) ;
#59751 = ORIENTED_EDGE('',*,*,#44674,.F.) ;
#59752 = ORIENTED_EDGE('',*,*,#44675,.T.) ;
#59753 = ORIENTED_EDGE('',*,*,#44600,.F.) ;
#59754 = ORIENTED_EDGE('',*,*,#44676,.T.) ;
#59755 = ORIENTED_EDGE('',*,*,#44677,.F.) ;
#59756 = ORIENTED_EDGE('',*,*,#44678,.T.) ;
#59757 = ORIENTED_EDGE('',*,*,#44679,.F.) ;
#59758 = ORIENTED_EDGE('',*,*,#44680,.T.) ;
#59759 = ORIENTED_EDGE('',*,*,#44604,.F.) ;
#59760 = ORIENTED_EDGE('',*,*,#44681,.T.) ;
#59761 = ORIENTED_EDGE('',*,*,#44682,.F.) ;
#59762 = ORIENTED_EDGE('',*,*,#44683,.T.) ;
#59763 = ORIENTED_EDGE('',*,*,#44684,.F.) ;
#59764 = ORIENTED_EDGE('',*,*,#44685,.T.) ;
#59765 = ORIENTED_EDGE('',*,*,#44608,.F.) ;
#59766 = ORIENTED_EDGE('',*,*,#44686,.T.) ;
#59767 = ORIENTED_EDGE('',*,*,#44687,.F.) ;
#59768 = ORIENTED_EDGE('',*,*,#44688,.T.) ;
#59769 = ORIENTED_EDGE('',*,*,#44689,.F.) ;
#59770 = ORIENTED_EDGE('',*,*,#44690,.T.) ;
#59771 = ORIENTED_EDGE('',*,*,#44612,.F.) ;
#59772 = ORIENTED_EDGE('',*,*,#44691,.T.) ;
#59773 = ORIENTED_EDGE('',*,*,#44692,.F.) ;
#59774 = ORIENTED_EDGE('',*,*,#44693,.T.) ;
#59775 = ORIENTED_EDGE('',*,*,#44694,.F.) ;
#59776 = ORIENTED_EDGE('',*,*,#44695,.T.) ;
#59777 = ORIENTED_EDGE('',*,*,#44616,.F.) ;
#59778 = ORIENTED_EDGE('',*,*,#44696,.T.) ;
#59779 = ORIENTED_EDGE('',*,*,#44697,.F.) ;
#59780 = ORIENTED_EDGE('',*,*,#44698,.T.) ;
#59781 = ORIENTED_EDGE('',*,*,#44699,.F.) ;
#59782 = ORIENTED_EDGE('',*,*,#44700,.T.) ;
#59783 = ORIENTED_EDGE('',*,*,#44620,.F.) ;
#59784 = ORIENTED_EDGE('',*,*,#44701,.T.) ;
#59785 = ORIENTED_EDGE('',*,*,#44702,.F.) ;
#59786 = ORIENTED_EDGE('',*,*,#44703,.T.) ;
#59787 = ORIENTED_EDGE('',*,*,#44653,.T.) ;
#59788 = ORIENTED_EDGE('',*,*,#44704,.T.) ;
#59789 = ORIENTED_EDGE('',*,*,#44705,.F.) ;
#59790 = ORIENTED_EDGE('',*,*,#44706,.T.) ;
#59791 = ORIENTED_EDGE('',*,*,#44707,.F.) ;
#59792 = ORIENTED_EDGE('',*,*,#44708,.T.) ;
#59793 = ORIENTED_EDGE('',*,*,#44618,.T.) ;
#59794 = ORIENTED_EDGE('',*,*,#44709,.T.) ;
#59795 = ORIENTED_EDGE('',*,*,#44710,.F.) ;
#59796 = ORIENTED_EDGE('',*,*,#44711,.T.) ;
#59797 = ORIENTED_EDGE('',*,*,#44712,.F.) ;
#59798 = ORIENTED_EDGE('',*,*,#44713,.T.) ;
#59799 = ORIENTED_EDGE('',*,*,#44614,.T.) ;
#59800 = ORIENTED_EDGE('',*,*,#44714,.T.) ;
#59801 = ORIENTED_EDGE('',*,*,#44715,.F.) ;
#59802 = ORIENTED_EDGE('',*,*,#44716,.T.) ;
#59803 = ORIENTED_EDGE('',*,*,#44717,.F.) ;
#59804 = ORIENTED_EDGE('',*,*,#44718,.T.) ;
#59805 = ORIENTED_EDGE('',*,*,#44610,.T.) ;
#59806 = ORIENTED_EDGE('',*,*,#44719,.T.) ;
#59807 = ORIENTED_EDGE('',*,*,#44720,.F.) ;
#59808 = ORIENTED_EDGE('',*,*,#44721,.T.) ;
#59809 = ORIENTED_EDGE('',*,*,#44722,.F.) ;
#59810 = ORIENTED_EDGE('',*,*,#44723,.T.) ;
#59811 = ORIENTED_EDGE('',*,*,#44606,.T.) ;
#59812 = ORIENTED_EDGE('',*,*,#44724,.T.) ;
#59813 = ORIENTED_EDGE('',*,*,#44725,.F.) ;
#59814 = ORIENTED_EDGE('',*,*,#44726,.T.) ;
#59815 = ORIENTED_EDGE('',*,*,#44727,.F.) ;
#59816 = ORIENTED_EDGE('',*,*,#44728,.T.) ;
#59817 = ORIENTED_EDGE('',*,*,#44602,.T.) ;
#59818 = ORIENTED_EDGE('',*,*,#44729,.T.) ;
#59819 = ORIENTED_EDGE('',*,*,#44730,.F.) ;
#59820 = ORIENTED_EDGE('',*,*,#44731,.T.) ;
#59821 = ORIENTED_EDGE('',*,*,#44732,.F.) ;
#59822 = ORIENTED_EDGE('',*,*,#44733,.T.) ;
#59823 = ORIENTED_EDGE('',*,*,#44598,.T.) ;
#59824 = ORIENTED_EDGE('',*,*,#44734,.T.) ;
#59825 = ORIENTED_EDGE('',*,*,#44735,.F.) ;
#59826 = ORIENTED_EDGE('',*,*,#44736,.T.) ;
#59827 = ORIENTED_EDGE('',*,*,#44737,.F.) ;
#59828 = ORIENTED_EDGE('',*,*,#44738,.T.) ;
#59829 = ORIENTED_EDGE('',*,*,#44594,.T.) ;
#59830 = ORIENTED_EDGE('',*,*,#44739,.T.) ;
#59831 = ORIENTED_EDGE('',*,*,#44740,.F.) ;
#59832 = ORIENTED_EDGE('',*,*,#44741,.T.) ;
#59833 = ORIENTED_EDGE('',*,*,#44742,.F.) ;
#59834 = ORIENTED_EDGE('',*,*,#44743,.T.) ;
#59835 = ORIENTED_EDGE('',*,*,#44590,.T.) ;
#59836 = ORIENTED_EDGE('',*,*,#44744,.T.) ;
#59837 = ORIENTED_EDGE('',*,*,#44745,.F.) ;
#59838 = ORIENTED_EDGE('',*,*,#44746,.T.) ;
#59839 = ORIENTED_EDGE('',*,*,#44747,.F.) ;
#59840 = ORIENTED_EDGE('',*,*,#44748,.T.) ;
#59841 = ORIENTED_EDGE('',*,*,#44586,.T.) ;
#59842 = ORIENTED_EDGE('',*,*,#44749,.T.) ;
#59843 = ORIENTED_EDGE('',*,*,#44750,.F.) ;
#59844 = ORIENTED_EDGE('',*,*,#44751,.T.) ;
#59845 = ORIENTED_EDGE('',*,*,#44752,.F.) ;
#59846 = ORIENTED_EDGE('',*,*,#44753,.T.) ;
#59847 = ORIENTED_EDGE('',*,*,#44643,.T.) ;
#59848 = ORIENTED_EDGE('',*,*,#44754,.T.) ;
#59849 = ORIENTED_EDGE('',*,*,#44755,.F.) ;
#59850 = ORIENTED_EDGE('',*,*,#44756,.T.) ;
#59851 = ORIENTED_EDGE('',*,*,#44705,.T.) ;
#59852 = ORIENTED_EDGE('',*,*,#44757,.T.) ;
#59853 = ORIENTED_EDGE('',*,*,#44758,.F.) ;
#59854 = ORIENTED_EDGE('',*,*,#44759,.T.) ;
#59855 = ORIENTED_EDGE('',*,*,#44760,.F.) ;
#59856 = ORIENTED_EDGE('',*,*,#44761,.T.) ;
#59857 = ORIENTED_EDGE('',*,*,#44755,.T.) ;
#59858 = ORIENTED_EDGE('',*,*,#44762,.T.) ;
#59859 = ORIENTED_EDGE('',*,*,#44763,.F.) ;
#59860 = ORIENTED_EDGE('',*,*,#44764,.T.) ;
#59861 = ORIENTED_EDGE('',*,*,#44760,.T.) ;
#59862 = ORIENTED_EDGE('',*,*,#44765,.T.) ;
#59863 = ORIENTED_EDGE('',*,*,#44766,.F.) ;
#59864 = ORIENTED_EDGE('',*,*,#44767,.T.) ;
#59865 = ORIENTED_EDGE('',*,*,#44763,.T.) ;
#59866 = ORIENTED_EDGE('',*,*,#44768,.T.) ;
#59867 = ORIENTED_EDGE('',*,*,#44769,.F.) ;
#59868 = ORIENTED_EDGE('',*,*,#44770,.T.) ;
#59869 = ORIENTED_EDGE('',*,*,#44766,.T.) ;
#59870 = ORIENTED_EDGE('',*,*,#44771,.T.) ;
#59871 = ORIENTED_EDGE('',*,*,#44772,.F.) ;
#59872 = ORIENTED_EDGE('',*,*,#44773,.T.) ;
#59873 = ORIENTED_EDGE('',*,*,#44769,.T.) ;
#59874 = ORIENTED_EDGE('',*,*,#44774,.T.) ;
#59875 = ORIENTED_EDGE('',*,*,#44775,.F.) ;
#59876 = ORIENTED_EDGE('',*,*,#44776,.T.) ;
#59877 = ORIENTED_EDGE('',*,*,#44772,.T.) ;
#59878 = ORIENTED_EDGE('',*,*,#44777,.T.) ;
#59879 = ORIENTED_EDGE('',*,*,#44778,.F.) ;
#59880 = ORIENTED_EDGE('',*,*,#44779,.T.) ;
#59881 = ORIENTED_EDGE('',*,*,#44775,.T.) ;
#59882 = ORIENTED_EDGE('',*,*,#44780,.T.) ;
#59883 = ORIENTED_EDGE('',*,*,#44781,.F.) ;
#59884 = ORIENTED_EDGE('',*,*,#44782,.T.) ;
#59885 = ORIENTED_EDGE('',*,*,#44778,.T.) ;
#59886 = ORIENTED_EDGE('',*,*,#44783,.T.) ;
#59887 = ORIENTED_EDGE('',*,*,#44784,.F.) ;
#59888 = ORIENTED_EDGE('',*,*,#44785,.T.) ;
#59889 = ORIENTED_EDGE('',*,*,#44781,.T.) ;
#59890 = ORIENTED_EDGE('',*,*,#44786,.T.) ;
#59891 = ORIENTED_EDGE('',*,*,#44787,.F.) ;
#59892 = ORIENTED_EDGE('',*,*,#44788,.T.) ;
#59893 = ORIENTED_EDGE('',*,*,#44784,.T.) ;
#59894 = ORIENTED_EDGE('',*,*,#44789,.T.) ;
#59895 = ORIENTED_EDGE('',*,*,#44790,.F.) ;
#59896 = ORIENTED_EDGE('',*,*,#44791,.T.) ;
#59897 = ORIENTED_EDGE('',*,*,#44787,.T.) ;
#59898 = ORIENTED_EDGE('',*,*,#44792,.T.) ;
#59899 = ORIENTED_EDGE('',*,*,#44649,.F.) ;
#59900 = ORIENTED_EDGE('',*,*,#44793,.T.) ;
#59901 = ORIENTED_EDGE('',*,*,#44790,.T.) ;
#59902 = ORIENTED_EDGE('',*,*,#44794,.T.) ;
#59903 = ORIENTED_EDGE('',*,*,#44795,.T.) ;
#59904 = ORIENTED_EDGE('',*,*,#44796,.T.) ;
#59905 = ORIENTED_EDGE('',*,*,#44797,.T.) ;
#59906 = ORIENTED_EDGE('',*,*,#44798,.T.) ;
#59907 = ORIENTED_EDGE('',*,*,#44799,.T.) ;
#59908 = ORIENTED_EDGE('',*,*,#44800,.T.) ;
#59909 = ORIENTED_EDGE('',*,*,#44801,.T.) ;
#59910 = ORIENTED_EDGE('',*,*,#44802,.T.) ;
#59911 = ORIENTED_EDGE('',*,*,#44319,.T.) ;
#59912 = ORIENTED_EDGE('',*,*,#44803,.T.) ;
#59913 = ORIENTED_EDGE('',*,*,#44804,.T.) ;
#59914 = ORIENTED_EDGE('',*,*,#44805,.T.) ;
#59915 = ORIENTED_EDGE('',*,*,#44806,.T.) ;
#59916 = ORIENTED_EDGE('',*,*,#44807,.T.) ;
#59917 = ORIENTED_EDGE('',*,*,#44808,.T.) ;
#59918 = ORIENTED_EDGE('',*,*,#44809,.T.) ;
#59919 = ORIENTED_EDGE('',*,*,#44810,.T.) ;
#59920 = ORIENTED_EDGE('',*,*,#44811,.T.) ;
#59921 = ORIENTED_EDGE('',*,*,#44812,.T.) ;
#59922 = ORIENTED_EDGE('',*,*,#44813,.T.) ;
#59923 = ORIENTED_EDGE('',*,*,#44814,.T.) ;
#59924 = ORIENTED_EDGE('',*,*,#44815,.T.) ;
#59925 = ORIENTED_EDGE('',*,*,#44816,.T.) ;
#59926 = ORIENTED_EDGE('',*,*,#44817,.T.) ;
#59927 = ORIENTED_EDGE('',*,*,#44818,.T.) ;
#59928 = ORIENTED_EDGE('',*,*,#44819,.T.) ;
#59929 = ORIENTED_EDGE('',*,*,#44820,.T.) ;
#59930 = ORIENTED_EDGE('',*,*,#44821,.T.) ;
#59931 = ORIENTED_EDGE('',*,*,#44822,.T.) ;
#59932 = ORIENTED_EDGE('',*,*,#44823,.T.) ;
#59933 = ORIENTED_EDGE('',*,*,#44824,.T.) ;
#59934 = ORIENTED_EDGE('',*,*,#44825,.T.) ;
#59935 = ORIENTED_EDGE('',*,*,#44315,.T.) ;
#59936 = ORIENTED_EDGE('',*,*,#44826,.T.) ;
#59937 = ORIENTED_EDGE('',*,*,#44827,.T.) ;
#59938 = ORIENTED_EDGE('',*,*,#44828,.T.) ;
#59939 = ORIENTED_EDGE('',*,*,#44829,.T.) ;
#59940 = ORIENTED_EDGE('',*,*,#44830,.T.) ;
#59941 = ORIENTED_EDGE('',*,*,#44831,.T.) ;
#59942 = ORIENTED_EDGE('',*,*,#44832,.T.) ;
#59943 = ORIENTED_EDGE('',*,*,#44833,.T.) ;
#59944 = ORIENTED_EDGE('',*,*,#44834,.T.) ;
#59945 = ORIENTED_EDGE('',*,*,#44835,.T.) ;
#59946 = ORIENTED_EDGE('',*,*,#44836,.T.) ;
#59947 = ORIENTED_EDGE('',*,*,#44837,.T.) ;
#59948 = ORIENTED_EDGE('',*,*,#44838,.T.) ;
#59949 = ORIENTED_EDGE('',*,*,#44839,.T.) ;
#59950 = ORIENTED_EDGE('',*,*,#44840,.T.) ;
#59951 = ORIENTED_EDGE('',*,*,#44841,.T.) ;
#59952 = ORIENTED_EDGE('',*,*,#44842,.T.) ;
#59953 = ORIENTED_EDGE('',*,*,#44843,.T.) ;
#59954 = ORIENTED_EDGE('',*,*,#44844,.T.) ;
#59955 = ORIENTED_EDGE('',*,*,#44845,.T.) ;
#59956 = ORIENTED_EDGE('',*,*,#44846,.T.) ;
#59957 = ORIENTED_EDGE('',*,*,#44847,.T.) ;
#59958 = ORIENTED_EDGE('',*,*,#44848,.T.) ;
#59959 = ORIENTED_EDGE('',*,*,#44311,.T.) ;
#59960 = ORIENTED_EDGE('',*,*,#44849,.T.) ;
#59961 = ORIENTED_EDGE('',*,*,#44850,.T.) ;
#59962 = ORIENTED_EDGE('',*,*,#44851,.T.) ;
#59963 = ORIENTED_EDGE('',*,*,#44852,.T.) ;
#59964 = ORIENTED_EDGE('',*,*,#44853,.T.) ;
#59965 = ORIENTED_EDGE('',*,*,#44854,.T.) ;
#59966 = ORIENTED_EDGE('',*,*,#44855,.T.) ;
#59967 = ORIENTED_EDGE('',*,*,#44856,.T.) ;
#59968 = ORIENTED_EDGE('',*,*,#44857,.T.) ;
#59969 = ORIENTED_EDGE('',*,*,#44858,.T.) ;
#59970 = ORIENTED_EDGE('',*,*,#44859,.T.) ;
#59971 = ORIENTED_EDGE('',*,*,#44860,.T.) ;
#59972 = ORIENTED_EDGE('',*,*,#44861,.T.) ;
#59973 = ORIENTED_EDGE('',*,*,#44862,.T.) ;
#59974 = ORIENTED_EDGE('',*,*,#44863,.T.) ;
#59975 = ORIENTED_EDGE('',*,*,#44864,.T.) ;
#59976 = ORIENTED_EDGE('',*,*,#44865,.T.) ;
#59977 = ORIENTED_EDGE('',*,*,#44866,.T.) ;
#59978 = ORIENTED_EDGE('',*,*,#44867,.T.) ;
#59979 = ORIENTED_EDGE('',*,*,#44868,.T.) ;
#59980 = ORIENTED_EDGE('',*,*,#44869,.T.) ;
#59981 = ORIENTED_EDGE('',*,*,#44870,.T.) ;
#59982 = ORIENTED_EDGE('',*,*,#44871,.T.) ;
#59983 = ORIENTED_EDGE('',*,*,#44307,.T.) ;
#59984 = ORIENTED_EDGE('',*,*,#44872,.T.) ;
#59985 = ORIENTED_EDGE('',*,*,#44873,.T.) ;
#59986 = ORIENTED_EDGE('',*,*,#44874,.T.) ;
#59987 = ORIENTED_EDGE('',*,*,#44875,.T.) ;
#59988 = ORIENTED_EDGE('',*,*,#44876,.T.) ;
#59989 = ORIENTED_EDGE('',*,*,#44877,.T.) ;
#59990 = ORIENTED_EDGE('',*,*,#44878,.T.) ;
#59991 = ORIENTED_EDGE('',*,*,#44879,.T.) ;
#59992 = ORIENTED_EDGE('',*,*,#44880,.T.) ;
#59993 = ORIENTED_EDGE('',*,*,#44881,.T.) ;
#59994 = ORIENTED_EDGE('',*,*,#44882,.T.) ;
#59995 = ORIENTED_EDGE('',*,*,#44883,.T.) ;
#59996 = ORIENTED_EDGE('',*,*,#44884,.T.) ;
#59997 = ORIENTED_EDGE('',*,*,#44885,.T.) ;
#59998 = ORIENTED_EDGE('',*,*,#44886,.T.) ;
#59999 = ORIENTED_EDGE('',*,*,#44887,.T.) ;
#60000 = ORIENTED_EDGE('',*,*,#44888,.T.) ;
#60001 = ORIENTED_EDGE('',*,*,#44889,.T.) ;
#60002 = ORIENTED_EDGE('',*,*,#44890,.T.) ;
#60003 = ORIENTED_EDGE('',*,*,#44891,.T.) ;
#60004 = ORIENTED_EDGE('',*,*,#44892,.T.) ;
#60005 = ORIENTED_EDGE('',*,*,#44893,.T.) ;
#60006 = ORIENTED_EDGE('',*,*,#44894,.T.) ;
#60007 = ORIENTED_EDGE('',*,*,#44303,.T.) ;
#60008 = ORIENTED_EDGE('',*,*,#44895,.T.) ;
#60009 = ORIENTED_EDGE('',*,*,#44896,.T.) ;
#60010 = ORIENTED_EDGE('',*,*,#44897,.T.) ;
#60011 = ORIENTED_EDGE('',*,*,#44898,.T.) ;
#60012 = ORIENTED_EDGE('',*,*,#44899,.T.) ;
#60013 = ORIENTED_EDGE('',*,*,#44900,.T.) ;
#60014 = ORIENTED_EDGE('',*,*,#44901,.T.) ;
#60015 = ORIENTED_EDGE('',*,*,#44902,.T.) ;
#60016 = ORIENTED_EDGE('',*,*,#44903,.T.) ;
#60017 = ORIENTED_EDGE('',*,*,#44904,.T.) ;
#60018 = ORIENTED_EDGE('',*,*,#44905,.T.) ;
#60019 = ORIENTED_EDGE('',*,*,#44906,.T.) ;
#60020 = ORIENTED_EDGE('',*,*,#44907,.T.) ;
#60021 = ORIENTED_EDGE('',*,*,#44908,.T.) ;
#60022 = ORIENTED_EDGE('',*,*,#44909,.T.) ;
#60023 = ORIENTED_EDGE('',*,*,#44910,.T.) ;
#60024 = ORIENTED_EDGE('',*,*,#44911,.T.) ;
#60025 = ORIENTED_EDGE('',*,*,#44912,.T.) ;
#60026 = ORIENTED_EDGE('',*,*,#44913,.T.) ;
#60027 = ORIENTED_EDGE('',*,*,#44914,.T.) ;
#60028 = ORIENTED_EDGE('',*,*,#44915,.T.) ;
#60029 = ORIENTED_EDGE('',*,*,#44916,.T.) ;
#60030 = ORIENTED_EDGE('',*,*,#44917,.T.) ;
#60031 = ORIENTED_EDGE('',*,*,#44299,.T.) ;
#60032 = ORIENTED_EDGE('',*,*,#44918,.T.) ;
#60033 = ORIENTED_EDGE('',*,*,#44919,.T.) ;
#60034 = ORIENTED_EDGE('',*,*,#44920,.T.) ;
#60035 = ORIENTED_EDGE('',*,*,#44921,.T.) ;
#60036 = ORIENTED_EDGE('',*,*,#44922,.T.) ;
#60037 = ORIENTED_EDGE('',*,*,#44923,.T.) ;
#60038 = ORIENTED_EDGE('',*,*,#44924,.T.) ;
#60039 = ORIENTED_EDGE('',*,*,#44925,.T.) ;
#60040 = ORIENTED_EDGE('',*,*,#44926,.T.) ;
#60041 = ORIENTED_EDGE('',*,*,#44927,.T.) ;
#60042 = ORIENTED_EDGE('',*,*,#44928,.T.) ;
#60043 = ORIENTED_EDGE('',*,*,#44929,.T.) ;
#60044 = ORIENTED_EDGE('',*,*,#44930,.T.) ;
#60045 = ORIENTED_EDGE('',*,*,#44931,.T.) ;
#60046 = ORIENTED_EDGE('',*,*,#44932,.T.) ;
#60047 = ORIENTED_EDGE('',*,*,#44933,.T.) ;
#60048 = ORIENTED_EDGE('',*,*,#44934,.T.) ;
#60049 = ORIENTED_EDGE('',*,*,#44935,.T.) ;
#60050 = ORIENTED_EDGE('',*,*,#44936,.T.) ;
#60051 = ORIENTED_EDGE('',*,*,#44937,.T.) ;
#60052 = ORIENTED_EDGE('',*,*,#44938,.T.) ;
#60053 = ORIENTED_EDGE('',*,*,#44939,.T.) ;
#60054 = ORIENTED_EDGE('',*,*,#44940,.T.) ;
#60055 = ORIENTED_EDGE('',*,*,#44295,.T.) ;
#60056 = ORIENTED_EDGE('',*,*,#44941,.T.) ;
#60057 = ORIENTED_EDGE('',*,*,#44942,.T.) ;
#60058 = ORIENTED_EDGE('',*,*,#44943,.T.) ;
#60059 = ORIENTED_EDGE('',*,*,#44944,.T.) ;
#60060 = ORIENTED_EDGE('',*,*,#44945,.T.) ;
#60061 = ORIENTED_EDGE('',*,*,#44946,.T.) ;
#60062 = ORIENTED_EDGE('',*,*,#44947,.T.) ;
#60063 = ORIENTED_EDGE('',*,*,#44948,.T.) ;
#60064 = ORIENTED_EDGE('',*,*,#44949,.T.) ;
#60065 = ORIENTED_EDGE('',*,*,#44950,.T.) ;
#60066 = ORIENTED_EDGE('',*,*,#44951,.T.) ;
#60067 = ORIENTED_EDGE('',*,*,#44952,.T.) ;
#60068 = ORIENTED_EDGE('',*,*,#44953,.T.) ;
#60069 = ORIENTED_EDGE('',*,*,#44954,.T.) ;
#60070 = ORIENTED_EDGE('',*,*,#44955,.T.) ;
#60071 = ORIENTED_EDGE('',*,*,#44956,.T.) ;
#60072 = ORIENTED_EDGE('',*,*,#44957,.T.) ;
#60073 = ORIENTED_EDGE('',*,*,#44958,.T.) ;
#60074 = ORIENTED_EDGE('',*,*,#44959,.T.) ;
#60075 = ORIENTED_EDGE('',*,*,#44960,.T.) ;
#60076 = ORIENTED_EDGE('',*,*,#44961,.T.) ;
#60077 = ORIENTED_EDGE('',*,*,#44962,.T.) ;
#60078 = ORIENTED_EDGE('',*,*,#44963,.T.) ;
#60079 = ORIENTED_EDGE('',*,*,#44291,.T.) ;
#60080 = ORIENTED_EDGE('',*,*,#44964,.T.) ;
#60081 = ORIENTED_EDGE('',*,*,#44965,.T.) ;
#60082 = ORIENTED_EDGE('',*,*,#44966,.T.) ;
#60083 = ORIENTED_EDGE('',*,*,#44967,.T.) ;
#60084 = ORIENTED_EDGE('',*,*,#44968,.T.) ;
#60085 = ORIENTED_EDGE('',*,*,#44969,.T.) ;
#60086 = ORIENTED_EDGE('',*,*,#44970,.T.) ;
#60087 = ORIENTED_EDGE('',*,*,#44971,.T.) ;
#60088 = ORIENTED_EDGE('',*,*,#44972,.T.) ;
#60089 = ORIENTED_EDGE('',*,*,#44973,.T.) ;
#60090 = ORIENTED_EDGE('',*,*,#44974,.T.) ;
#60091 = ORIENTED_EDGE('',*,*,#44975,.T.) ;
#60092 = ORIENTED_EDGE('',*,*,#44976,.T.) ;
#60093 = ORIENTED_EDGE('',*,*,#44977,.T.) ;
#60094 = ORIENTED_EDGE('',*,*,#44978,.T.) ;
#60095 = ORIENTED_EDGE('',*,*,#44979,.T.) ;
#60096 = ORIENTED_EDGE('',*,*,#44980,.T.) ;
#60097 = ORIENTED_EDGE('',*,*,#44981,.T.) ;
#60098 = ORIENTED_EDGE('',*,*,#44982,.T.) ;
#60099 = ORIENTED_EDGE('',*,*,#44983,.T.) ;
#60100 = ORIENTED_EDGE('',*,*,#44984,.T.) ;
#60101 = ORIENTED_EDGE('',*,*,#44985,.T.) ;
#60102 = ORIENTED_EDGE('',*,*,#44986,.T.) ;
#60103 = ORIENTED_EDGE('',*,*,#44287,.T.) ;
#60104 = ORIENTED_EDGE('',*,*,#44987,.T.) ;
#60105 = ORIENTED_EDGE('',*,*,#44988,.T.) ;
#60106 = ORIENTED_EDGE('',*,*,#44989,.T.) ;
#60107 = ORIENTED_EDGE('',*,*,#44990,.T.) ;
#60108 = ORIENTED_EDGE('',*,*,#44991,.T.) ;
#60109 = ORIENTED_EDGE('',*,*,#44992,.T.) ;
#60110 = ORIENTED_EDGE('',*,*,#44993,.T.) ;
#60111 = ORIENTED_EDGE('',*,*,#44994,.T.) ;
#60112 = ORIENTED_EDGE('',*,*,#44995,.T.) ;
#60113 = ORIENTED_EDGE('',*,*,#44996,.T.) ;
#60114 = ORIENTED_EDGE('',*,*,#44997,.T.) ;
#60115 = ORIENTED_EDGE('',*,*,#44998,.T.) ;
#60116 = ORIENTED_EDGE('',*,*,#44999,.T.) ;
#60117 = ORIENTED_EDGE('',*,*,#45000,.T.) ;
#60118 = ORIENTED_EDGE('',*,*,#45001,.T.) ;
#60119 = ORIENTED_EDGE('',*,*,#45002,.T.) ;
#60120 = ORIENTED_EDGE('',*,*,#45003,.T.) ;
#60121 = ORIENTED_EDGE('',*,*,#45004,.T.) ;
#60122 = ORIENTED_EDGE('',*,*,#45005,.T.) ;
#60123 = ORIENTED_EDGE('',*,*,#45006,.T.) ;
#60124 = ORIENTED_EDGE('',*,*,#45007,.T.) ;
#60125 = ORIENTED_EDGE('',*,*,#45008,.T.) ;
#60126 = ORIENTED_EDGE('',*,*,#45009,.T.) ;
#60127 = ORIENTED_EDGE('',*,*,#44376,.T.) ;
#60128 = ORIENTED_EDGE('',*,*,#45010,.T.) ;
#60129 = ORIENTED_EDGE('',*,*,#45011,.T.) ;
#60130 = ORIENTED_EDGE('',*,*,#45012,.T.) ;
#60131 = ORIENTED_EDGE('',*,*,#45013,.T.) ;
#60132 = ORIENTED_EDGE('',*,*,#45014,.T.) ;
#60133 = ORIENTED_EDGE('',*,*,#45015,.T.) ;
#60134 = ORIENTED_EDGE('',*,*,#45016,.T.) ;
#60135 = ORIENTED_EDGE('',*,*,#45017,.T.) ;
#60136 = ORIENTED_EDGE('',*,*,#45018,.T.) ;
#60137 = ORIENTED_EDGE('',*,*,#45019,.T.) ;
#60138 = ORIENTED_EDGE('',*,*,#45020,.T.) ;
#60139 = ORIENTED_EDGE('',*,*,#45021,.T.) ;
#60140 = ORIENTED_EDGE('',*,*,#45022,.T.) ;
#60141 = ORIENTED_EDGE('',*,*,#45023,.T.) ;
#60142 = ORIENTED_EDGE('',*,*,#45024,.T.) ;
#60143 = ORIENTED_EDGE('',*,*,#45025,.T.) ;
#60144 = ORIENTED_EDGE('',*,*,#45026,.T.) ;
#60145 = ORIENTED_EDGE('',*,*,#45027,.T.) ;
#60146 = ORIENTED_EDGE('',*,*,#45028,.T.) ;
#60147 = ORIENTED_EDGE('',*,*,#45029,.T.) ;
#60148 = ORIENTED_EDGE('',*,*,#45030,.T.) ;
#60149 = ORIENTED_EDGE('',*,*,#45031,.T.) ;
#60150 = ORIENTED_EDGE('',*,*,#45032,.T.) ;
#60151 = ORIENTED_EDGE('',*,*,#45033,.T.) ;
#60152 = ORIENTED_EDGE('',*,*,#45034,.T.) ;
#60153 = ORIENTED_EDGE('',*,*,#45035,.T.) ;
#60154 = ORIENTED_EDGE('',*,*,#45036,.T.) ;
#60155 = ORIENTED_EDGE('',*,*,#45037,.T.) ;
#60156 = ORIENTED_EDGE('',*,*,#45038,.T.) ;
#60157 = ORIENTED_EDGE('',*,*,#45039,.T.) ;
#60158 = ORIENTED_EDGE('',*,*,#45040,.T.) ;
#60159 = ORIENTED_EDGE('',*,*,#45041,.T.) ;
#60160 = ORIENTED_EDGE('',*,*,#45042,.T.) ;
#60161 = ORIENTED_EDGE('',*,*,#45043,.T.) ;
#60162 = ORIENTED_EDGE('',*,*,#45044,.T.) ;
#60163 = ORIENTED_EDGE('',*,*,#45045,.T.) ;
#60164 = ORIENTED_EDGE('',*,*,#45046,.T.) ;
#60165 = ORIENTED_EDGE('',*,*,#45047,.T.) ;
#60166 = ORIENTED_EDGE('',*,*,#45048,.T.) ;
#60167 = ORIENTED_EDGE('',*,*,#45049,.T.) ;
#60168 = ORIENTED_EDGE('',*,*,#45050,.T.) ;
#60169 = ORIENTED_EDGE('',*,*,#45051,.F.) ;
#60170 = ORIENTED_EDGE('',*,*,#45052,.T.) ;
#60171 = ORIENTED_EDGE('',*,*,#45053,.F.) ;
#60172 = ORIENTED_EDGE('',*,*,#45054,.T.) ;
#60173 = ORIENTED_EDGE('',*,*,#45055,.T.) ;
#60174 = ORIENTED_EDGE('',*,*,#45056,.T.) ;
#60175 = ORIENTED_EDGE('',*,*,#45057,.T.) ;
#60176 = ORIENTED_EDGE('',*,*,#45058,.T.) ;
#60177 = ORIENTED_EDGE('',*,*,#45059,.T.) ;
#60178 = ORIENTED_EDGE('',*,*,#45060,.T.) ;
#60179 = ORIENTED_EDGE('',*,*,#45061,.T.) ;
#60180 = ORIENTED_EDGE('',*,*,#44388,.T.) ;
#60181 = ORIENTED_EDGE('',*,*,#45062,.T.) ;
#60182 = ORIENTED_EDGE('',*,*,#45063,.T.) ;
#60183 = ORIENTED_EDGE('',*,*,#45064,.T.) ;
#60184 = ORIENTED_EDGE('',*,*,#45065,.T.) ;
#60185 = ORIENTED_EDGE('',*,*,#45066,.T.) ;
#60186 = ORIENTED_EDGE('',*,*,#45067,.T.) ;
#60187 = ORIENTED_EDGE('',*,*,#45068,.T.) ;
#60188 = ORIENTED_EDGE('',*,*,#45069,.T.) ;
#60189 = ORIENTED_EDGE('',*,*,#45070,.T.) ;
#60190 = ORIENTED_EDGE('',*,*,#45071,.T.) ;
#60191 = ORIENTED_EDGE('',*,*,#45072,.T.) ;
#60192 = ORIENTED_EDGE('',*,*,#45073,.T.) ;
#60193 = ORIENTED_EDGE('',*,*,#45074,.F.) ;
#60194 = ORIENTED_EDGE('',*,*,#45075,.T.) ;
#60195 = ORIENTED_EDGE('',*,*,#45076,.T.) ;
#60196 = ORIENTED_EDGE('',*,*,#45077,.T.) ;
#60197 = ORIENTED_EDGE('',*,*,#45076,.F.) ;
#60198 = ORIENTED_EDGE('',*,*,#45078,.T.) ;
#60199 = ORIENTED_EDGE('',*,*,#45079,.T.) ;
#60200 = ORIENTED_EDGE('',*,*,#45080,.T.) ;
#60201 = ORIENTED_EDGE('',*,*,#45079,.F.) ;
#60202 = ORIENTED_EDGE('',*,*,#45081,.T.) ;
#60203 = ORIENTED_EDGE('',*,*,#45082,.T.) ;
#60204 = ORIENTED_EDGE('',*,*,#45083,.T.) ;
#60205 = ORIENTED_EDGE('',*,*,#45082,.F.) ;
#60206 = ORIENTED_EDGE('',*,*,#45084,.T.) ;
#60207 = ORIENTED_EDGE('',*,*,#45085,.T.) ;
#60208 = ORIENTED_EDGE('',*,*,#45086,.T.) ;
#60209 = ORIENTED_EDGE('',*,*,#45085,.F.) ;
#60210 = ORIENTED_EDGE('',*,*,#45087,.T.) ;
#60211 = ORIENTED_EDGE('',*,*,#45088,.T.) ;
#60212 = ORIENTED_EDGE('',*,*,#45089,.T.) ;
#60213 = ORIENTED_EDGE('',*,*,#45088,.F.) ;
#60214 = ORIENTED_EDGE('',*,*,#45090,.T.) ;
#60215 = ORIENTED_EDGE('',*,*,#45091,.T.) ;
#60216 = ORIENTED_EDGE('',*,*,#45092,.T.) ;
#60217 = ORIENTED_EDGE('',*,*,#45091,.F.) ;
#60218 = ORIENTED_EDGE('',*,*,#44383,.T.) ;
#60219 = ORIENTED_EDGE('',*,*,#45093,.T.) ;
#60220 = ORIENTED_EDGE('',*,*,#45094,.T.) ;
#60221 = ORIENTED_EDGE('',*,*,#45093,.F.) ;
#60222 = ORIENTED_EDGE('',*,*,#45095,.T.) ;
#60223 = ORIENTED_EDGE('',*,*,#44396,.T.) ;
#60224 = ORIENTED_EDGE('',*,*,#45096,.T.) ;
#60225 = ORIENTED_EDGE('',*,*,#44395,.F.) ;
#60226 = ORIENTED_EDGE('',*,*,#45097,.T.) ;
#60227 = ORIENTED_EDGE('',*,*,#45098,.T.) ;
#60228 = ORIENTED_EDGE('',*,*,#45099,.T.) ;
#60229 = ORIENTED_EDGE('',*,*,#45098,.F.) ;
#60230 = ORIENTED_EDGE('',*,*,#45100,.T.) ;
#60231 = ORIENTED_EDGE('',*,*,#45101,.T.) ;
#60232 = ORIENTED_EDGE('',*,*,#45102,.T.) ;
#60233 = ORIENTED_EDGE('',*,*,#45101,.F.) ;
#60234 = ORIENTED_EDGE('',*,*,#45103,.T.) ;
#60235 = ORIENTED_EDGE('',*,*,#45104,.T.) ;
#60236 = ORIENTED_EDGE('',*,*,#45105,.T.) ;
#60237 = ORIENTED_EDGE('',*,*,#45104,.F.) ;
#60238 = ORIENTED_EDGE('',*,*,#45106,.T.) ;
#60239 = ORIENTED_EDGE('',*,*,#45107,.T.) ;
#60240 = ORIENTED_EDGE('',*,*,#45108,.T.) ;
#60241 = ORIENTED_EDGE('',*,*,#45107,.F.) ;
#60242 = ORIENTED_EDGE('',*,*,#45109,.T.) ;
#60243 = ORIENTED_EDGE('',*,*,#45110,.T.) ;
#60244 = ORIENTED_EDGE('',*,*,#45111,.T.) ;
#60245 = ORIENTED_EDGE('',*,*,#45110,.F.) ;
#60246 = ORIENTED_EDGE('',*,*,#45112,.T.) ;
#60247 = ORIENTED_EDGE('',*,*,#45113,.T.) ;
#60248 = ORIENTED_EDGE('',*,*,#45114,.T.) ;
#60249 = ORIENTED_EDGE('',*,*,#45113,.F.) ;
#60250 = ORIENTED_EDGE('',*,*,#45115,.T.) ;
#60251 = ORIENTED_EDGE('',*,*,#45116,.T.) ;
#60252 = ORIENTED_EDGE('',*,*,#45117,.T.) ;
#60253 = ORIENTED_EDGE('',*,*,#45116,.F.) ;
#60254 = ORIENTED_EDGE('',*,*,#45118,.T.) ;
#60255 = ORIENTED_EDGE('',*,*,#45119,.T.) ;
#60256 = ORIENTED_EDGE('',*,*,#45120,.T.) ;
#60257 = ORIENTED_EDGE('',*,*,#45119,.F.) ;
#60258 = ORIENTED_EDGE('',*,*,#45121,.T.) ;
#60259 = ORIENTED_EDGE('',*,*,#45122,.T.) ;
#60260 = ORIENTED_EDGE('',*,*,#45123,.T.) ;
#60261 = ORIENTED_EDGE('',*,*,#45122,.F.) ;
#60262 = ORIENTED_EDGE('',*,*,#45124,.T.) ;
#60263 = ORIENTED_EDGE('',*,*,#45125,.T.) ;
#60264 = ORIENTED_EDGE('',*,*,#45126,.T.) ;
#60265 = ORIENTED_EDGE('',*,*,#45125,.F.) ;
#60266 = ORIENTED_EDGE('',*,*,#45127,.T.) ;
#60267 = ORIENTED_EDGE('',*,*,#45128,.T.) ;
#60268 = ORIENTED_EDGE('',*,*,#45129,.T.) ;
#60269 = ORIENTED_EDGE('',*,*,#45128,.F.) ;
#60270 = ORIENTED_EDGE('',*,*,#45130,.T.) ;
#60271 = ORIENTED_EDGE('',*,*,#45131,.T.) ;
#60272 = ORIENTED_EDGE('',*,*,#45132,.T.) ;
#60273 = ORIENTED_EDGE('',*,*,#45131,.F.) ;
#60274 = ORIENTED_EDGE('',*,*,#45133,.T.) ;
#60275 = ORIENTED_EDGE('',*,*,#45134,.T.) ;
#60276 = ORIENTED_EDGE('',*,*,#45135,.T.) ;
#60277 = ORIENTED_EDGE('',*,*,#45134,.F.) ;
#60278 = ORIENTED_EDGE('',*,*,#45136,.T.) ;
#60279 = ORIENTED_EDGE('',*,*,#45137,.T.) ;
#60280 = ORIENTED_EDGE('',*,*,#45138,.T.) ;
#60281 = ORIENTED_EDGE('',*,*,#45137,.F.) ;
#60282 = ORIENTED_EDGE('',*,*,#45139,.T.) ;
#60283 = ORIENTED_EDGE('',*,*,#45140,.T.) ;
#60284 = ORIENTED_EDGE('',*,*,#45141,.T.) ;
#60285 = ORIENTED_EDGE('',*,*,#45140,.F.) ;
#60286 = ORIENTED_EDGE('',*,*,#45142,.T.) ;
#60287 = ORIENTED_EDGE('',*,*,#45143,.T.) ;
#60288 = ORIENTED_EDGE('',*,*,#45144,.T.) ;
#60289 = ORIENTED_EDGE('',*,*,#45143,.F.) ;
#60290 = ORIENTED_EDGE('',*,*,#45145,.T.) ;
#60291 = ORIENTED_EDGE('',*,*,#45146,.T.) ;
#60292 = ORIENTED_EDGE('',*,*,#45147,.T.) ;
#60293 = ORIENTED_EDGE('',*,*,#45146,.F.) ;
#60294 = ORIENTED_EDGE('',*,*,#45148,.T.) ;
#60295 = ORIENTED_EDGE('',*,*,#45149,.T.) ;
#60296 = ORIENTED_EDGE('',*,*,#45150,.T.) ;
#60297 = ORIENTED_EDGE('',*,*,#45149,.F.) ;
#60298 = ORIENTED_EDGE('',*,*,#45151,.T.) ;
#60299 = ORIENTED_EDGE('',*,*,#45074,.T.) ;
#60300 = ORIENTED_EDGE('',*,*,#45152,.T.) ;
#60301 = ORIENTED_EDGE('',*,*,#45153,.T.) ;
#60302 = ORIENTED_EDGE('',*,*,#45154,.T.) ;
#60303 = ORIENTED_EDGE('',*,*,#45155,.T.) ;
#60304 = ORIENTED_EDGE('',*,*,#45156,.T.) ;
#60305 = ORIENTED_EDGE('',*,*,#45157,.T.) ;
#60306 = ORIENTED_EDGE('',*,*,#45158,.T.) ;
#60307 = ORIENTED_EDGE('',*,*,#45159,.T.) ;
#60308 = ORIENTED_EDGE('',*,*,#45160,.T.) ;
#60309 = ORIENTED_EDGE('',*,*,#45161,.T.) ;
#60310 = ORIENTED_EDGE('',*,*,#45162,.T.) ;
#60311 = ORIENTED_EDGE('',*,*,#45163,.T.) ;
#60312 = ORIENTED_EDGE('',*,*,#45164,.T.) ;
#60313 = ORIENTED_EDGE('',*,*,#45165,.T.) ;
#60314 = ORIENTED_EDGE('',*,*,#45166,.T.) ;
#60315 = ORIENTED_EDGE('',*,*,#45167,.T.) ;
#60316 = ORIENTED_EDGE('',*,*,#45168,.T.) ;
#60317 = ORIENTED_EDGE('',*,*,#45169,.T.) ;
#60318 = ORIENTED_EDGE('',*,*,#45170,.T.) ;
#60319 = ORIENTED_EDGE('',*,*,#44380,.T.) ;
#60320 = ORIENTED_EDGE('',*,*,#44372,.T.) ;
#60321 = ORIENTED_EDGE('',*,*,#45171,.F.) ;
#60322 = ORIENTED_EDGE('',*,*,#45172,.T.) ;
#60323 = ORIENTED_EDGE('',*,*,#45173,.T.) ;
#60324 = ORIENTED_EDGE('',*,*,#45174,.T.) ;
#60325 = ORIENTED_EDGE('',*,*,#45175,.T.) ;
#60326 = ORIENTED_EDGE('',*,*,#45176,.T.) ;
#60327 = ORIENTED_EDGE('',*,*,#45177,.T.) ;
#60328 = ORIENTED_EDGE('',*,*,#45178,.T.) ;
#60329 = ORIENTED_EDGE('',*,*,#45179,.F.) ;
#60330 = ORIENTED_EDGE('',*,*,#45067,.F.) ;
#60331 = ORIENTED_EDGE('',*,*,#45180,.F.) ;
#60332 = ORIENTED_EDGE('',*,*,#45054,.F.) ;
#60333 = ORIENTED_EDGE('',*,*,#45181,.F.) ;
#60334 = ORIENTED_EDGE('',*,*,#45068,.F.) ;
#60335 = ORIENTED_EDGE('',*,*,#45182,.F.) ;
#60336 = ORIENTED_EDGE('',*,*,#45062,.F.) ;
#60337 = ORIENTED_EDGE('',*,*,#45183,.F.) ;
#60338 = ORIENTED_EDGE('',*,*,#45181,.T.) ;
#60339 = ORIENTED_EDGE('',*,*,#45184,.F.) ;
#60340 = ORIENTED_EDGE('',*,*,#45185,.F.) ;
#60341 = ORIENTED_EDGE('',*,*,#45180,.T.) ;
#60342 = ORIENTED_EDGE('',*,*,#45186,.F.) ;
#60343 = ORIENTED_EDGE('',*,*,#45179,.T.) ;
#60344 = ORIENTED_EDGE('',*,*,#45053,.T.) ;
#60345 = ORIENTED_EDGE('',*,*,#45187,.F.) ;
#60346 = ORIENTED_EDGE('',*,*,#45182,.T.) ;
#60347 = ORIENTED_EDGE('',*,*,#45184,.T.) ;
#60348 = ORIENTED_EDGE('',*,*,#45065,.F.) ;
#60349 = ORIENTED_EDGE('',*,*,#45188,.F.) ;
#60350 = ORIENTED_EDGE('',*,*,#44386,.T.) ;
#60351 = ORIENTED_EDGE('',*,*,#45189,.T.) ;
#60352 = ORIENTED_EDGE('',*,*,#45190,.F.) ;
#60353 = ORIENTED_EDGE('',*,*,#45183,.T.) ;
#60354 = ORIENTED_EDGE('',*,*,#45191,.F.) ;
#60355 = ORIENTED_EDGE('',*,*,#45192,.T.) ;
#60356 = ORIENTED_EDGE('',*,*,#45193,.F.) ;
#60357 = ORIENTED_EDGE('',*,*,#44622,.F.) ;
#60358 = ORIENTED_EDGE('',*,*,#45194,.F.) ;
#60359 = ORIENTED_EDGE('',*,*,#45069,.F.) ;
#60360 = ORIENTED_EDGE('',*,*,#45186,.T.) ;
#60361 = ORIENTED_EDGE('',*,*,#45066,.F.) ;
#60362 = ORIENTED_EDGE('',*,*,#45195,.F.) ;
#60363 = ORIENTED_EDGE('',*,*,#45072,.F.) ;
#60364 = ORIENTED_EDGE('',*,*,#45185,.T.) ;
#60365 = ORIENTED_EDGE('',*,*,#45071,.F.) ;
#60366 = ORIENTED_EDGE('',*,*,#45196,.F.) ;
#60367 = ORIENTED_EDGE('',*,*,#45045,.F.) ;
#60368 = ORIENTED_EDGE('',*,*,#45187,.T.) ;
#60369 = ORIENTED_EDGE('',*,*,#45052,.F.) ;
#60370 = ORIENTED_EDGE('',*,*,#45197,.F.) ;
#60371 = ORIENTED_EDGE('',*,*,#45063,.F.) ;
#60372 = ORIENTED_EDGE('',*,*,#45198,.F.) ;
#60373 = ORIENTED_EDGE('',*,*,#45064,.F.) ;
#60374 = ORIENTED_EDGE('',*,*,#45199,.F.) ;
#60375 = ORIENTED_EDGE('',*,*,#45059,.F.) ;
#60376 = ORIENTED_EDGE('',*,*,#45188,.T.) ;
#60377 = ORIENTED_EDGE('',*,*,#45198,.T.) ;
#60378 = ORIENTED_EDGE('',*,*,#44387,.F.) ;
#60379 = ORIENTED_EDGE('',*,*,#45194,.T.) ;
#60380 = ORIENTED_EDGE('',*,*,#44632,.T.) ;
#60381 = ORIENTED_EDGE('',*,*,#45200,.F.) ;
#60382 = ORIENTED_EDGE('',*,*,#45195,.T.) ;
#60383 = ORIENTED_EDGE('',*,*,#45201,.F.) ;
#60384 = ORIENTED_EDGE('',*,*,#45196,.T.) ;
#60385 = ORIENTED_EDGE('',*,*,#45202,.F.) ;
#60386 = ORIENTED_EDGE('',*,*,#44638,.T.) ;
#60387 = ORIENTED_EDGE('',*,*,#45197,.T.) ;
#60388 = ORIENTED_EDGE('',*,*,#45051,.T.) ;
#60389 = ORIENTED_EDGE('',*,*,#45203,.F.) ;
#60390 = ORIENTED_EDGE('',*,*,#45199,.T.) ;
#60391 = ORIENTED_EDGE('',*,*,#45200,.T.) ;
#60392 = ORIENTED_EDGE('',*,*,#44631,.F.) ;
#60393 = ORIENTED_EDGE('',*,*,#45204,.F.) ;
#60394 = ORIENTED_EDGE('',*,*,#45073,.F.) ;
#60395 = ORIENTED_EDGE('',*,*,#45202,.T.) ;
#60396 = ORIENTED_EDGE('',*,*,#45070,.F.) ;
#60397 = ORIENTED_EDGE('',*,*,#45205,.F.) ;
#60398 = ORIENTED_EDGE('',*,*,#44639,.F.) ;
#60399 = ORIENTED_EDGE('',*,*,#45046,.F.) ;
#60400 = ORIENTED_EDGE('',*,*,#45201,.T.) ;
#60401 = ORIENTED_EDGE('',*,*,#45206,.F.) ;
#60402 = ORIENTED_EDGE('',*,*,#45207,.F.) ;
#60403 = ORIENTED_EDGE('',*,*,#45203,.T.) ;
#60404 = ORIENTED_EDGE('',*,*,#45050,.F.) ;
#60405 = ORIENTED_EDGE('',*,*,#45208,.F.) ;
#60406 = ORIENTED_EDGE('',*,*,#45060,.F.) ;
#60407 = ORIENTED_EDGE('',*,*,#45209,.F.) ;
#60408 = ORIENTED_EDGE('',*,*,#45061,.F.) ;
#60409 = ORIENTED_EDGE('',*,*,#45210,.F.) ;
#60410 = ORIENTED_EDGE('',*,*,#45055,.F.) ;
#60411 = ORIENTED_EDGE('',*,*,#44389,.T.) ;
#60412 = ORIENTED_EDGE('',*,*,#45209,.T.) ;
#60413 = ORIENTED_EDGE('',*,*,#45211,.F.) ;
#60414 = ORIENTED_EDGE('',*,*,#44626,.T.) ;
#60415 = ORIENTED_EDGE('',*,*,#45205,.T.) ;
#60416 = ORIENTED_EDGE('',*,*,#45204,.T.) ;
#60417 = ORIENTED_EDGE('',*,*,#45212,.F.) ;
#60418 = ORIENTED_EDGE('',*,*,#45213,.F.) ;
#60419 = ORIENTED_EDGE('',*,*,#44644,.F.) ;
#60420 = ORIENTED_EDGE('',*,*,#45214,.F.) ;
#60421 = ORIENTED_EDGE('',*,*,#45215,.F.) ;
#60422 = ORIENTED_EDGE('',*,*,#45206,.T.) ;
#60423 = ORIENTED_EDGE('',*,*,#44642,.F.) ;
#60424 = ORIENTED_EDGE('',*,*,#45214,.T.) ;
#60425 = ORIENTED_EDGE('',*,*,#44753,.F.) ;
#60426 = ORIENTED_EDGE('',*,*,#45207,.T.) ;
#60427 = ORIENTED_EDGE('',*,*,#45216,.F.) ;
#60428 = ORIENTED_EDGE('',*,*,#45217,.F.) ;
#60429 = ORIENTED_EDGE('',*,*,#45210,.T.) ;
#60430 = ORIENTED_EDGE('',*,*,#45208,.T.) ;
#60431 = ORIENTED_EDGE('',*,*,#45218,.F.) ;
#60432 = ORIENTED_EDGE('',*,*,#45211,.T.) ;
#60433 = ORIENTED_EDGE('',*,*,#45058,.F.) ;
#60434 = ORIENTED_EDGE('',*,*,#45219,.F.) ;
#60435 = ORIENTED_EDGE('',*,*,#44627,.F.) ;
#60436 = ORIENTED_EDGE('',*,*,#45212,.T.) ;
#60437 = ORIENTED_EDGE('',*,*,#44630,.F.) ;
#60438 = ORIENTED_EDGE('',*,*,#45220,.F.) ;
#60439 = ORIENTED_EDGE('',*,*,#44640,.F.) ;
#60440 = ORIENTED_EDGE('',*,*,#45213,.T.) ;
#60441 = ORIENTED_EDGE('',*,*,#44641,.F.) ;
#60442 = ORIENTED_EDGE('',*,*,#45221,.F.) ;
#60443 = ORIENTED_EDGE('',*,*,#44656,.F.) ;
#60444 = ORIENTED_EDGE('',*,*,#45215,.T.) ;
#60445 = ORIENTED_EDGE('',*,*,#44752,.T.) ;
#60446 = ORIENTED_EDGE('',*,*,#45222,.F.) ;
#60447 = ORIENTED_EDGE('',*,*,#45216,.T.) ;
#60448 = ORIENTED_EDGE('',*,*,#45047,.F.) ;
#60449 = ORIENTED_EDGE('',*,*,#45217,.T.) ;
#60450 = ORIENTED_EDGE('',*,*,#45223,.F.) ;
#60451 = ORIENTED_EDGE('',*,*,#45224,.F.) ;
#60452 = ORIENTED_EDGE('',*,*,#45218,.T.) ;
#60453 = ORIENTED_EDGE('',*,*,#45049,.F.) ;
#60454 = ORIENTED_EDGE('',*,*,#45225,.F.) ;
#60455 = ORIENTED_EDGE('',*,*,#45056,.F.) ;
#60456 = ORIENTED_EDGE('',*,*,#45226,.F.) ;
#60457 = ORIENTED_EDGE('',*,*,#45057,.F.) ;
#60458 = ORIENTED_EDGE('',*,*,#45227,.F.) ;
#60459 = ORIENTED_EDGE('',*,*,#44637,.F.) ;
#60460 = ORIENTED_EDGE('',*,*,#45219,.T.) ;
#60461 = ORIENTED_EDGE('',*,*,#45226,.T.) ;
#60462 = ORIENTED_EDGE('',*,*,#45228,.F.) ;
#60463 = ORIENTED_EDGE('',*,*,#45221,.T.) ;
#60464 = ORIENTED_EDGE('',*,*,#45220,.T.) ;
#60465 = ORIENTED_EDGE('',*,*,#45229,.F.) ;
#60466 = ORIENTED_EDGE('',*,*,#44657,.T.) ;
#60467 = ORIENTED_EDGE('',*,*,#45230,.F.) ;
#60468 = ORIENTED_EDGE('',*,*,#45223,.T.) ;
#60469 = ORIENTED_EDGE('',*,*,#45222,.T.) ;
#60470 = ORIENTED_EDGE('',*,*,#44751,.F.) ;
#60471 = ORIENTED_EDGE('',*,*,#45224,.T.) ;
#60472 = ORIENTED_EDGE('',*,*,#45231,.F.) ;
#60473 = ORIENTED_EDGE('',*,*,#45232,.F.) ;
#60474 = ORIENTED_EDGE('',*,*,#45227,.T.) ;
#60475 = ORIENTED_EDGE('',*,*,#45225,.T.) ;
#60476 = ORIENTED_EDGE('',*,*,#45233,.F.) ;
#60477 = ORIENTED_EDGE('',*,*,#44633,.T.) ;
#60478 = ORIENTED_EDGE('',*,*,#45228,.T.) ;
#60479 = ORIENTED_EDGE('',*,*,#44636,.F.) ;
#60480 = ORIENTED_EDGE('',*,*,#45234,.F.) ;
#60481 = ORIENTED_EDGE('',*,*,#44628,.F.) ;
#60482 = ORIENTED_EDGE('',*,*,#45229,.T.) ;
#60483 = ORIENTED_EDGE('',*,*,#44629,.F.) ;
#60484 = ORIENTED_EDGE('',*,*,#45235,.F.) ;
#60485 = ORIENTED_EDGE('',*,*,#44658,.F.) ;
#60486 = ORIENTED_EDGE('',*,*,#45230,.T.) ;
#60487 = ORIENTED_EDGE('',*,*,#44750,.T.) ;
#60488 = ORIENTED_EDGE('',*,*,#45236,.F.) ;
#60489 = ORIENTED_EDGE('',*,*,#45231,.T.) ;
#60490 = ORIENTED_EDGE('',*,*,#45048,.F.) ;
#60491 = ORIENTED_EDGE('',*,*,#45232,.T.) ;
#60492 = ORIENTED_EDGE('',*,*,#45237,.F.) ;
#60493 = ORIENTED_EDGE('',*,*,#45233,.T.) ;
#60494 = ORIENTED_EDGE('',*,*,#45235,.T.) ;
#60495 = ORIENTED_EDGE('',*,*,#45234,.T.) ;
#60496 = ORIENTED_EDGE('',*,*,#45238,.F.) ;
#60497 = ORIENTED_EDGE('',*,*,#44659,.T.) ;
#60498 = ORIENTED_EDGE('',*,*,#45236,.T.) ;
#60499 = ORIENTED_EDGE('',*,*,#44749,.F.) ;
#60500 = ORIENTED_EDGE('',*,*,#45239,.F.) ;
#60501 = ORIENTED_EDGE('',*,*,#44634,.F.) ;
#60502 = ORIENTED_EDGE('',*,*,#45237,.T.) ;
#60503 = ORIENTED_EDGE('',*,*,#45238,.T.) ;
#60504 = ORIENTED_EDGE('',*,*,#44635,.F.) ;
#60505 = ORIENTED_EDGE('',*,*,#45240,.F.) ;
#60506 = ORIENTED_EDGE('',*,*,#44660,.F.) ;
#60507 = ORIENTED_EDGE('',*,*,#45239,.T.) ;
#60508 = ORIENTED_EDGE('',*,*,#44589,.F.) ;
#60509 = ORIENTED_EDGE('',*,*,#45240,.T.) ;
#60510 = ORIENTED_EDGE('',*,*,#45241,.F.) ;
#60511 = ORIENTED_EDGE('',*,*,#45242,.F.) ;
#60512 = ORIENTED_EDGE('',*,*,#44773,.F.) ;
#60513 = ORIENTED_EDGE('',*,*,#45242,.T.) ;
#60514 = ORIENTED_EDGE('',*,*,#45030,.F.) ;
#60515 = ORIENTED_EDGE('',*,*,#45243,.F.) ;
#60516 = ORIENTED_EDGE('',*,*,#44770,.F.) ;
#60517 = ORIENTED_EDGE('',*,*,#45241,.T.) ;
#60518 = ORIENTED_EDGE('',*,*,#44776,.F.) ;
#60519 = ORIENTED_EDGE('',*,*,#45244,.F.) ;
#60520 = ORIENTED_EDGE('',*,*,#45031,.F.) ;
#60521 = ORIENTED_EDGE('',*,*,#45243,.T.) ;
#60522 = ORIENTED_EDGE('',*,*,#45029,.F.) ;
#60523 = ORIENTED_EDGE('',*,*,#45245,.F.) ;
#60524 = ORIENTED_EDGE('',*,*,#44767,.F.) ;
#60525 = ORIENTED_EDGE('',*,*,#45244,.T.) ;
#60526 = ORIENTED_EDGE('',*,*,#44779,.F.) ;
#60527 = ORIENTED_EDGE('',*,*,#45246,.F.) ;
#60528 = ORIENTED_EDGE('',*,*,#45245,.T.) ;
#60529 = ORIENTED_EDGE('',*,*,#45028,.F.) ;
#60530 = ORIENTED_EDGE('',*,*,#45247,.F.) ;
#60531 = ORIENTED_EDGE('',*,*,#44764,.F.) ;
#60532 = ORIENTED_EDGE('',*,*,#45246,.T.) ;
#60533 = ORIENTED_EDGE('',*,*,#44782,.F.) ;
#60534 = ORIENTED_EDGE('',*,*,#45248,.F.) ;
#60535 = ORIENTED_EDGE('',*,*,#45032,.F.) ;
#60536 = ORIENTED_EDGE('',*,*,#44761,.F.) ;
#60537 = ORIENTED_EDGE('',*,*,#45247,.T.) ;
#60538 = ORIENTED_EDGE('',*,*,#45249,.F.) ;
#60539 = ORIENTED_EDGE('',*,*,#45248,.T.) ;
#60540 = ORIENTED_EDGE('',*,*,#44785,.F.) ;
#60541 = ORIENTED_EDGE('',*,*,#45250,.F.) ;
#60542 = ORIENTED_EDGE('',*,*,#45033,.F.) ;
#60543 = ORIENTED_EDGE('',*,*,#45249,.T.) ;
#60544 = ORIENTED_EDGE('',*,*,#45027,.F.) ;
#60545 = ORIENTED_EDGE('',*,*,#45251,.F.) ;
#60546 = ORIENTED_EDGE('',*,*,#44756,.F.) ;
#60547 = ORIENTED_EDGE('',*,*,#45250,.T.) ;
#60548 = ORIENTED_EDGE('',*,*,#44788,.F.) ;
#60549 = ORIENTED_EDGE('',*,*,#45252,.F.) ;
#60550 = ORIENTED_EDGE('',*,*,#45034,.F.) ;
#60551 = ORIENTED_EDGE('',*,*,#44706,.F.) ;
#60552 = ORIENTED_EDGE('',*,*,#45251,.T.) ;
#60553 = ORIENTED_EDGE('',*,*,#45253,.F.) ;
#60554 = ORIENTED_EDGE('',*,*,#45252,.T.) ;
#60555 = ORIENTED_EDGE('',*,*,#44791,.F.) ;
#60556 = ORIENTED_EDGE('',*,*,#45254,.F.) ;
#60557 = ORIENTED_EDGE('',*,*,#45253,.T.) ;
#60558 = ORIENTED_EDGE('',*,*,#45026,.F.) ;
#60559 = ORIENTED_EDGE('',*,*,#45255,.F.) ;
#60560 = ORIENTED_EDGE('',*,*,#44654,.F.) ;
#60561 = ORIENTED_EDGE('',*,*,#45254,.T.) ;
#60562 = ORIENTED_EDGE('',*,*,#44793,.F.) ;
#60563 = ORIENTED_EDGE('',*,*,#45256,.F.) ;
#60564 = ORIENTED_EDGE('',*,*,#45025,.F.) ;
#60565 = ORIENTED_EDGE('',*,*,#44648,.F.) ;
#60566 = ORIENTED_EDGE('',*,*,#45255,.T.) ;
#60567 = ORIENTED_EDGE('',*,*,#45256,.T.) ;
#60568 = ORIENTED_EDGE('',*,*,#45257,.F.) ;
#60569 = ORIENTED_EDGE('',*,*,#44774,.F.) ;
#60570 = ORIENTED_EDGE('',*,*,#45258,.F.) ;
#60571 = ORIENTED_EDGE('',*,*,#45258,.T.) ;
#60572 = ORIENTED_EDGE('',*,*,#44771,.F.) ;
#60573 = ORIENTED_EDGE('',*,*,#45259,.F.) ;
#60574 = ORIENTED_EDGE('',*,*,#45042,.F.) ;
#60575 = ORIENTED_EDGE('',*,*,#45257,.T.) ;
#60576 = ORIENTED_EDGE('',*,*,#45041,.F.) ;
#60577 = ORIENTED_EDGE('',*,*,#45260,.F.) ;
#60578 = ORIENTED_EDGE('',*,*,#44777,.F.) ;
#60579 = ORIENTED_EDGE('',*,*,#45259,.T.) ;
#60580 = ORIENTED_EDGE('',*,*,#44768,.F.) ;
#60581 = ORIENTED_EDGE('',*,*,#45261,.F.) ;
#60582 = ORIENTED_EDGE('',*,*,#45043,.F.) ;
#60583 = ORIENTED_EDGE('',*,*,#44780,.F.) ;
#60584 = ORIENTED_EDGE('',*,*,#45260,.T.) ;
#60585 = ORIENTED_EDGE('',*,*,#45262,.F.) ;
#60586 = ORIENTED_EDGE('',*,*,#45261,.T.) ;
#60587 = ORIENTED_EDGE('',*,*,#44765,.F.) ;
#60588 = ORIENTED_EDGE('',*,*,#45263,.F.) ;
#60589 = ORIENTED_EDGE('',*,*,#45044,.F.) ;
#60590 = ORIENTED_EDGE('',*,*,#45262,.T.) ;
#60591 = ORIENTED_EDGE('',*,*,#45040,.F.) ;
#60592 = ORIENTED_EDGE('',*,*,#45264,.F.) ;
#60593 = ORIENTED_EDGE('',*,*,#44783,.F.) ;
#60594 = ORIENTED_EDGE('',*,*,#45263,.T.) ;
#60595 = ORIENTED_EDGE('',*,*,#44762,.F.) ;
#60596 = ORIENTED_EDGE('',*,*,#45265,.F.) ;
#60597 = ORIENTED_EDGE('',*,*,#45264,.T.) ;
#60598 = ORIENTED_EDGE('',*,*,#45039,.F.) ;
#60599 = ORIENTED_EDGE('',*,*,#45266,.F.) ;
#60600 = ORIENTED_EDGE('',*,*,#44786,.F.) ;
#60601 = ORIENTED_EDGE('',*,*,#45265,.T.) ;
#60602 = ORIENTED_EDGE('',*,*,#44754,.F.) ;
#60603 = ORIENTED_EDGE('',*,*,#45267,.F.) ;
#60604 = ORIENTED_EDGE('',*,*,#45035,.F.) ;
#60605 = ORIENTED_EDGE('',*,*,#45266,.T.) ;
#60606 = ORIENTED_EDGE('',*,*,#45038,.F.) ;
#60607 = ORIENTED_EDGE('',*,*,#45268,.F.) ;
#60608 = ORIENTED_EDGE('',*,*,#44789,.F.) ;
#60609 = ORIENTED_EDGE('',*,*,#45267,.T.) ;
#60610 = ORIENTED_EDGE('',*,*,#44646,.F.) ;
#60611 = ORIENTED_EDGE('',*,*,#45269,.F.) ;
#60612 = ORIENTED_EDGE('',*,*,#44792,.F.) ;
#60613 = ORIENTED_EDGE('',*,*,#45268,.T.) ;
#60614 = ORIENTED_EDGE('',*,*,#45270,.F.) ;
#60615 = ORIENTED_EDGE('',*,*,#45269,.T.) ;
#60616 = ORIENTED_EDGE('',*,*,#44655,.F.) ;
#60617 = ORIENTED_EDGE('',*,*,#45271,.F.) ;
#60618 = ORIENTED_EDGE('',*,*,#45036,.F.) ;
#60619 = ORIENTED_EDGE('',*,*,#45270,.T.) ;
#60620 = ORIENTED_EDGE('',*,*,#45037,.F.) ;
#60621 = ORIENTED_EDGE('',*,*,#45272,.F.) ;
#60622 = ORIENTED_EDGE('',*,*,#44794,.F.) ;
#60623 = ORIENTED_EDGE('',*,*,#45271,.T.) ;
#60624 = ORIENTED_EDGE('',*,*,#44650,.F.) ;
#60625 = ORIENTED_EDGE('',*,*,#45272,.T.) ;
#60626 = ORIENTED_EDGE('',*,*,#45273,.F.) ;
#60627 = ORIENTED_EDGE('',*,*,#45115,.F.) ;
#60628 = ORIENTED_EDGE('',*,*,#45274,.F.) ;
#60629 = ORIENTED_EDGE('',*,*,#45162,.F.) ;
#60630 = ORIENTED_EDGE('',*,*,#45274,.T.) ;
#60631 = ORIENTED_EDGE('',*,*,#45112,.F.) ;
#60632 = ORIENTED_EDGE('',*,*,#45275,.F.) ;
#60633 = ORIENTED_EDGE('',*,*,#45163,.F.) ;
#60634 = ORIENTED_EDGE('',*,*,#45118,.F.) ;
#60635 = ORIENTED_EDGE('',*,*,#45273,.T.) ;
#60636 = ORIENTED_EDGE('',*,*,#45276,.F.) ;
#60637 = ORIENTED_EDGE('',*,*,#45275,.T.) ;
#60638 = ORIENTED_EDGE('',*,*,#45109,.F.) ;
#60639 = ORIENTED_EDGE('',*,*,#45277,.F.) ;
#60640 = ORIENTED_EDGE('',*,*,#45164,.F.) ;
#60641 = ORIENTED_EDGE('',*,*,#45276,.T.) ;
#60642 = ORIENTED_EDGE('',*,*,#45161,.F.) ;
#60643 = ORIENTED_EDGE('',*,*,#45278,.F.) ;
#60644 = ORIENTED_EDGE('',*,*,#45121,.F.) ;
#60645 = ORIENTED_EDGE('',*,*,#45277,.T.) ;
#60646 = ORIENTED_EDGE('',*,*,#45106,.F.) ;
#60647 = ORIENTED_EDGE('',*,*,#45279,.F.) ;
#60648 = ORIENTED_EDGE('',*,*,#45165,.F.) ;
#60649 = ORIENTED_EDGE('',*,*,#45124,.F.) ;
#60650 = ORIENTED_EDGE('',*,*,#45278,.T.) ;
#60651 = ORIENTED_EDGE('',*,*,#45280,.F.) ;
#60652 = ORIENTED_EDGE('',*,*,#45279,.T.) ;
#60653 = ORIENTED_EDGE('',*,*,#45103,.F.) ;
#60654 = ORIENTED_EDGE('',*,*,#45281,.F.) ;
#60655 = ORIENTED_EDGE('',*,*,#45166,.F.) ;
#60656 = ORIENTED_EDGE('',*,*,#45280,.T.) ;
#60657 = ORIENTED_EDGE('',*,*,#45160,.F.) ;
#60658 = ORIENTED_EDGE('',*,*,#45282,.F.) ;
#60659 = ORIENTED_EDGE('',*,*,#45127,.F.) ;
#60660 = ORIENTED_EDGE('',*,*,#45281,.T.) ;
#60661 = ORIENTED_EDGE('',*,*,#45100,.F.) ;
#60662 = ORIENTED_EDGE('',*,*,#45283,.F.) ;
#60663 = ORIENTED_EDGE('',*,*,#45130,.F.) ;
#60664 = ORIENTED_EDGE('',*,*,#45282,.T.) ;
#60665 = ORIENTED_EDGE('',*,*,#45284,.F.) ;
#60666 = ORIENTED_EDGE('',*,*,#45283,.T.) ;
#60667 = ORIENTED_EDGE('',*,*,#45097,.F.) ;
#60668 = ORIENTED_EDGE('',*,*,#45285,.F.) ;
#60669 = ORIENTED_EDGE('',*,*,#45167,.F.) ;
#60670 = ORIENTED_EDGE('',*,*,#45284,.T.) ;
#60671 = ORIENTED_EDGE('',*,*,#45159,.F.) ;
#60672 = ORIENTED_EDGE('',*,*,#45286,.F.) ;
#60673 = ORIENTED_EDGE('',*,*,#45133,.F.) ;
#60674 = ORIENTED_EDGE('',*,*,#45285,.T.) ;
#60675 = ORIENTED_EDGE('',*,*,#44394,.F.) ;
#60676 = ORIENTED_EDGE('',*,*,#45287,.F.) ;
#60677 = ORIENTED_EDGE('',*,*,#45136,.F.) ;
#60678 = ORIENTED_EDGE('',*,*,#45286,.T.) ;
#60679 = ORIENTED_EDGE('',*,*,#45288,.F.) ;
#60680 = ORIENTED_EDGE('',*,*,#45287,.T.) ;
#60681 = ORIENTED_EDGE('',*,*,#45095,.F.) ;
#60682 = ORIENTED_EDGE('',*,*,#44385,.F.) ;
#60683 = ORIENTED_EDGE('',*,*,#45168,.F.) ;
#60684 = ORIENTED_EDGE('',*,*,#45288,.T.) ;
#60685 = ORIENTED_EDGE('',*,*,#45158,.F.) ;
#60686 = ORIENTED_EDGE('',*,*,#45289,.F.) ;
#60687 = ORIENTED_EDGE('',*,*,#45139,.F.) ;
#60688 = ORIENTED_EDGE('',*,*,#45142,.F.) ;
#60689 = ORIENTED_EDGE('',*,*,#45289,.T.) ;
#60690 = ORIENTED_EDGE('',*,*,#45290,.F.) ;
#60691 = ORIENTED_EDGE('',*,*,#44384,.T.) ;
#60692 = ORIENTED_EDGE('',*,*,#45090,.F.) ;
#60693 = ORIENTED_EDGE('',*,*,#45291,.F.) ;
#60694 = ORIENTED_EDGE('',*,*,#45169,.F.) ;
#60695 = ORIENTED_EDGE('',*,*,#45290,.T.) ;
#60696 = ORIENTED_EDGE('',*,*,#45157,.F.) ;
#60697 = ORIENTED_EDGE('',*,*,#45292,.F.) ;
#60698 = ORIENTED_EDGE('',*,*,#45145,.F.) ;
#60699 = ORIENTED_EDGE('',*,*,#45291,.T.) ;
#60700 = ORIENTED_EDGE('',*,*,#45087,.F.) ;
#60701 = ORIENTED_EDGE('',*,*,#45293,.F.) ;
#60702 = ORIENTED_EDGE('',*,*,#45148,.F.) ;
#60703 = ORIENTED_EDGE('',*,*,#45292,.T.) ;
#60704 = ORIENTED_EDGE('',*,*,#45294,.F.) ;
#60705 = ORIENTED_EDGE('',*,*,#45293,.T.) ;
#60706 = ORIENTED_EDGE('',*,*,#45084,.F.) ;
#60707 = ORIENTED_EDGE('',*,*,#45295,.F.) ;
#60708 = ORIENTED_EDGE('',*,*,#45170,.F.) ;
#60709 = ORIENTED_EDGE('',*,*,#45294,.T.) ;
#60710 = ORIENTED_EDGE('',*,*,#45156,.F.) ;
#60711 = ORIENTED_EDGE('',*,*,#45296,.F.) ;
#60712 = ORIENTED_EDGE('',*,*,#45151,.F.) ;
#60713 = ORIENTED_EDGE('',*,*,#45295,.T.) ;
#60714 = ORIENTED_EDGE('',*,*,#45081,.F.) ;
#60715 = ORIENTED_EDGE('',*,*,#45297,.F.) ;
#60716 = ORIENTED_EDGE('',*,*,#45153,.F.) ;
#60717 = ORIENTED_EDGE('',*,*,#45296,.T.) ;
#60718 = ORIENTED_EDGE('',*,*,#45155,.F.) ;
#60719 = ORIENTED_EDGE('',*,*,#45298,.F.) ;
#60720 = ORIENTED_EDGE('',*,*,#45075,.F.) ;
#60721 = ORIENTED_EDGE('',*,*,#45297,.T.) ;
#60722 = ORIENTED_EDGE('',*,*,#45078,.F.) ;
#60723 = ORIENTED_EDGE('',*,*,#45298,.T.) ;
#60724 = ORIENTED_EDGE('',*,*,#45154,.F.) ;
#60725 = ORIENTED_EDGE('',*,*,#45299,.F.) ;
#60726 = ORIENTED_EDGE('',*,*,#45111,.F.) ;
#60727 = ORIENTED_EDGE('',*,*,#45300,.F.) ;
#60728 = ORIENTED_EDGE('',*,*,#45013,.F.) ;
#60729 = ORIENTED_EDGE('',*,*,#45108,.F.) ;
#60730 = ORIENTED_EDGE('',*,*,#45299,.T.) ;
#60731 = ORIENTED_EDGE('',*,*,#45301,.F.) ;
#60732 = ORIENTED_EDGE('',*,*,#45300,.T.) ;
#60733 = ORIENTED_EDGE('',*,*,#45114,.F.) ;
#60734 = ORIENTED_EDGE('',*,*,#45302,.F.) ;
#60735 = ORIENTED_EDGE('',*,*,#45301,.T.) ;
#60736 = ORIENTED_EDGE('',*,*,#45012,.F.) ;
#60737 = ORIENTED_EDGE('',*,*,#45303,.F.) ;
#60738 = ORIENTED_EDGE('',*,*,#45105,.F.) ;
#60739 = ORIENTED_EDGE('',*,*,#45302,.T.) ;
#60740 = ORIENTED_EDGE('',*,*,#45117,.F.) ;
#60741 = ORIENTED_EDGE('',*,*,#45304,.F.) ;
#60742 = ORIENTED_EDGE('',*,*,#45014,.F.) ;
#60743 = ORIENTED_EDGE('',*,*,#45303,.T.) ;
#60744 = ORIENTED_EDGE('',*,*,#45011,.F.) ;
#60745 = ORIENTED_EDGE('',*,*,#45305,.F.) ;
#60746 = ORIENTED_EDGE('',*,*,#45102,.F.) ;
#60747 = ORIENTED_EDGE('',*,*,#45304,.T.) ;
#60748 = ORIENTED_EDGE('',*,*,#45120,.F.) ;
#60749 = ORIENTED_EDGE('',*,*,#45306,.F.) ;
#60750 = ORIENTED_EDGE('',*,*,#45015,.F.) ;
#60751 = ORIENTED_EDGE('',*,*,#45305,.T.) ;
#60752 = ORIENTED_EDGE('',*,*,#45010,.F.) ;
#60753 = ORIENTED_EDGE('',*,*,#44379,.F.) ;
#60754 = ORIENTED_EDGE('',*,*,#45099,.F.) ;
#60755 = ORIENTED_EDGE('',*,*,#45306,.T.) ;
#60756 = ORIENTED_EDGE('',*,*,#45123,.F.) ;
#60757 = ORIENTED_EDGE('',*,*,#45307,.F.) ;
#60758 = ORIENTED_EDGE('',*,*,#45016,.F.) ;
#60759 = ORIENTED_EDGE('',*,*,#45307,.T.) ;
#60760 = ORIENTED_EDGE('',*,*,#45126,.F.) ;
#60761 = ORIENTED_EDGE('',*,*,#45308,.F.) ;
#60762 = ORIENTED_EDGE('',*,*,#45017,.F.) ;
#60763 = ORIENTED_EDGE('',*,*,#44377,.T.) ;
#60764 = ORIENTED_EDGE('',*,*,#45009,.F.) ;
#60765 = ORIENTED_EDGE('',*,*,#45309,.F.) ;
#60766 = ORIENTED_EDGE('',*,*,#45096,.F.) ;
#60767 = ORIENTED_EDGE('',*,*,#45308,.T.) ;
#60768 = ORIENTED_EDGE('',*,*,#45129,.F.) ;
#60769 = ORIENTED_EDGE('',*,*,#45310,.F.) ;
#60770 = ORIENTED_EDGE('',*,*,#45018,.F.) ;
#60771 = ORIENTED_EDGE('',*,*,#45309,.T.) ;
#60772 = ORIENTED_EDGE('',*,*,#45008,.F.) ;
#60773 = ORIENTED_EDGE('',*,*,#45311,.F.) ;
#60774 = ORIENTED_EDGE('',*,*,#45094,.F.) ;
#60775 = ORIENTED_EDGE('',*,*,#45310,.T.) ;
#60776 = ORIENTED_EDGE('',*,*,#45132,.F.) ;
#60777 = ORIENTED_EDGE('',*,*,#45312,.F.) ;
#60778 = ORIENTED_EDGE('',*,*,#45019,.F.) ;
#60779 = ORIENTED_EDGE('',*,*,#45311,.T.) ;
#60780 = ORIENTED_EDGE('',*,*,#45007,.F.) ;
#60781 = ORIENTED_EDGE('',*,*,#45313,.F.) ;
#60782 = ORIENTED_EDGE('',*,*,#45092,.F.) ;
#60783 = ORIENTED_EDGE('',*,*,#45312,.T.) ;
#60784 = ORIENTED_EDGE('',*,*,#45135,.F.) ;
#60785 = ORIENTED_EDGE('',*,*,#45314,.F.) ;
#60786 = ORIENTED_EDGE('',*,*,#45020,.F.) ;
#60787 = ORIENTED_EDGE('',*,*,#45313,.T.) ;
#60788 = ORIENTED_EDGE('',*,*,#45006,.F.) ;
#60789 = ORIENTED_EDGE('',*,*,#45315,.F.) ;
#60790 = ORIENTED_EDGE('',*,*,#45089,.F.) ;
#60791 = ORIENTED_EDGE('',*,*,#45314,.T.) ;
#60792 = ORIENTED_EDGE('',*,*,#45138,.F.) ;
#60793 = ORIENTED_EDGE('',*,*,#45316,.F.) ;
#60794 = ORIENTED_EDGE('',*,*,#45021,.F.) ;
#60795 = ORIENTED_EDGE('',*,*,#45315,.T.) ;
#60796 = ORIENTED_EDGE('',*,*,#45005,.F.) ;
#60797 = ORIENTED_EDGE('',*,*,#45317,.F.) ;
#60798 = ORIENTED_EDGE('',*,*,#45086,.F.) ;
#60799 = ORIENTED_EDGE('',*,*,#45316,.T.) ;
#60800 = ORIENTED_EDGE('',*,*,#45141,.F.) ;
#60801 = ORIENTED_EDGE('',*,*,#45318,.F.) ;
#60802 = ORIENTED_EDGE('',*,*,#45022,.F.) ;
#60803 = ORIENTED_EDGE('',*,*,#45083,.F.) ;
#60804 = ORIENTED_EDGE('',*,*,#45317,.T.) ;
#60805 = ORIENTED_EDGE('',*,*,#45319,.F.) ;
#60806 = ORIENTED_EDGE('',*,*,#45318,.T.) ;
#60807 = ORIENTED_EDGE('',*,*,#45144,.F.) ;
#60808 = ORIENTED_EDGE('',*,*,#45320,.F.) ;
#60809 = ORIENTED_EDGE('',*,*,#45023,.F.) ;
#60810 = ORIENTED_EDGE('',*,*,#45319,.T.) ;
#60811 = ORIENTED_EDGE('',*,*,#45004,.F.) ;
#60812 = ORIENTED_EDGE('',*,*,#45321,.F.) ;
#60813 = ORIENTED_EDGE('',*,*,#45080,.F.) ;
#60814 = ORIENTED_EDGE('',*,*,#45320,.T.) ;
#60815 = ORIENTED_EDGE('',*,*,#45147,.F.) ;
#60816 = ORIENTED_EDGE('',*,*,#45322,.F.) ;
#60817 = ORIENTED_EDGE('',*,*,#45024,.F.) ;
#60818 = ORIENTED_EDGE('',*,*,#45077,.F.) ;
#60819 = ORIENTED_EDGE('',*,*,#45321,.T.) ;
#60820 = ORIENTED_EDGE('',*,*,#45323,.F.) ;
#60821 = ORIENTED_EDGE('',*,*,#45322,.T.) ;
#60822 = ORIENTED_EDGE('',*,*,#45150,.F.) ;
#60823 = ORIENTED_EDGE('',*,*,#45324,.F.) ;
#60824 = ORIENTED_EDGE('',*,*,#45002,.F.) ;
#60825 = ORIENTED_EDGE('',*,*,#45323,.T.) ;
#60826 = ORIENTED_EDGE('',*,*,#45003,.F.) ;
#60827 = ORIENTED_EDGE('',*,*,#45324,.T.) ;
#60828 = ORIENTED_EDGE('',*,*,#45152,.F.) ;
#60829 = ORIENTED_EDGE('',*,*,#45325,.T.) ;
#60830 = ORIENTED_EDGE('',*,*,#45326,.T.) ;
#60831 = ORIENTED_EDGE('',*,*,#45327,.T.) ;
#60832 = ORIENTED_EDGE('',*,*,#45328,.T.) ;
#60833 = ORIENTED_EDGE('',*,*,#45329,.T.) ;
#60834 = ORIENTED_EDGE('',*,*,#45330,.T.) ;
#60835 = ORIENTED_EDGE('',*,*,#45331,.T.) ;
#60836 = ORIENTED_EDGE('',*,*,#45332,.T.) ;
#60837 = ORIENTED_EDGE('',*,*,#45333,.T.) ;
#60838 = ORIENTED_EDGE('',*,*,#45334,.T.) ;
#60839 = ORIENTED_EDGE('',*,*,#45335,.T.) ;
#60840 = ORIENTED_EDGE('',*,*,#45336,.T.) ;
#60841 = ORIENTED_EDGE('',*,*,#45337,.T.) ;
#60842 = ORIENTED_EDGE('',*,*,#45338,.T.) ;
#60843 = ORIENTED_EDGE('',*,*,#45339,.T.) ;
#60844 = ORIENTED_EDGE('',*,*,#45340,.T.) ;
#60845 = ORIENTED_EDGE('',*,*,#45341,.T.) ;
#60846 = ORIENTED_EDGE('',*,*,#45342,.T.) ;
#60847 = ORIENTED_EDGE('',*,*,#45343,.F.) ;
#60848 = ORIENTED_EDGE('',*,*,#45344,.T.) ;
#60849 = ORIENTED_EDGE('',*,*,#45345,.T.) ;
#60850 = ORIENTED_EDGE('',*,*,#45346,.T.) ;
#60851 = ORIENTED_EDGE('',*,*,#45193,.T.) ;
#60852 = ORIENTED_EDGE('',*,*,#45347,.T.) ;
#60853 = ORIENTED_EDGE('',*,*,#45348,.T.) ;
#60854 = ORIENTED_EDGE('',*,*,#45349,.T.) ;
#60855 = ORIENTED_EDGE('',*,*,#45350,.T.) ;
#60856 = ORIENTED_EDGE('',*,*,#45351,.T.) ;
#60857 = ORIENTED_EDGE('',*,*,#44391,.T.) ;
#60858 = ORIENTED_EDGE('',*,*,#45352,.T.) ;
#60859 = ORIENTED_EDGE('',*,*,#45353,.T.) ;
#60860 = ORIENTED_EDGE('',*,*,#45354,.T.) ;
#60861 = ORIENTED_EDGE('',*,*,#45190,.T.) ;
#60862 = ORIENTED_EDGE('',*,*,#45355,.T.) ;
#60863 = ORIENTED_EDGE('',*,*,#45325,.F.) ;
#60864 = ORIENTED_EDGE('',*,*,#45356,.T.) ;
#60865 = ORIENTED_EDGE('',*,*,#45191,.T.) ;
#60866 = ORIENTED_EDGE('',*,*,#45343,.T.) ;
#60867 = ORIENTED_EDGE('',*,*,#45357,.T.) ;
#60868 = ORIENTED_EDGE('',*,*,#44624,.F.) ;
#60869 = ORIENTED_EDGE('',*,*,#45358,.T.) ;
#60870 = ORIENTED_EDGE('',*,*,#45359,.T.) ;
#60871 = ORIENTED_EDGE('',*,*,#45360,.T.) ;
#60872 = ORIENTED_EDGE('',*,*,#45361,.T.) ;
#60873 = ORIENTED_EDGE('',*,*,#45362,.T.) ;
#60874 = ORIENTED_EDGE('',*,*,#45363,.T.) ;
#60875 = ORIENTED_EDGE('',*,*,#45364,.T.) ;
#60876 = ORIENTED_EDGE('',*,*,#45173,.F.) ;
#60877 = ORIENTED_EDGE('',*,*,#45365,.T.) ;
#60878 = ORIENTED_EDGE('',*,*,#45177,.F.) ;
#60879 = ORIENTED_EDGE('',*,*,#45366,.T.) ;
#60880 = ORIENTED_EDGE('',*,*,#45367,.T.) ;
#60881 = ORIENTED_EDGE('',*,*,#45368,.T.) ;
#60882 = ORIENTED_EDGE('',*,*,#45369,.T.) ;
#60883 = ORIENTED_EDGE('',*,*,#45370,.T.) ;
#60884 = ORIENTED_EDGE('',*,*,#45371,.T.) ;
#60885 = ORIENTED_EDGE('',*,*,#45372,.T.) ;
#60886 = ORIENTED_EDGE('',*,*,#45373,.T.) ;
#60887 = ORIENTED_EDGE('',*,*,#45374,.T.) ;
#60888 = ORIENTED_EDGE('',*,*,#45375,.T.) ;
#60889 = ORIENTED_EDGE('',*,*,#45376,.T.) ;
#60890 = ORIENTED_EDGE('',*,*,#45377,.T.) ;
#60891 = ORIENTED_EDGE('',*,*,#45378,.T.) ;
#60892 = ORIENTED_EDGE('',*,*,#45171,.T.) ;
#60893 = ORIENTED_EDGE('',*,*,#45379,.T.) ;
#60894 = ORIENTED_EDGE('',*,*,#45175,.F.) ;
#60895 = ORIENTED_EDGE('',*,*,#45380,.T.) ;
#60896 = ORIENTED_EDGE('',*,*,#45381,.T.) ;
#60897 = ORIENTED_EDGE('',*,*,#45382,.T.) ;
#60898 = ORIENTED_EDGE('',*,*,#45383,.T.) ;
#60899 = ORIENTED_EDGE('',*,*,#45384,.T.) ;
#60900 = ORIENTED_EDGE('',*,*,#45385,.T.) ;
#60901 = ORIENTED_EDGE('',*,*,#45386,.T.) ;
#60902 = ORIENTED_EDGE('',*,*,#45387,.T.) ;
#60903 = ORIENTED_EDGE('',*,*,#45388,.T.) ;
#60904 = ORIENTED_EDGE('',*,*,#45389,.T.) ;
#60905 = ORIENTED_EDGE('',*,*,#45390,.T.) ;
#60906 = ORIENTED_EDGE('',*,*,#45391,.T.) ;
#60907 = ORIENTED_EDGE('',*,*,#45392,.T.) ;
#60908 = ORIENTED_EDGE('',*,*,#45393,.T.) ;
#60909 = ORIENTED_EDGE('',*,*,#45394,.T.) ;
#60910 = ORIENTED_EDGE('',*,*,#45395,.T.) ;
#60911 = ORIENTED_EDGE('',*,*,#45396,.T.) ;
#60912 = ORIENTED_EDGE('',*,*,#45397,.T.) ;
#60913 = ORIENTED_EDGE('',*,*,#45398,.T.) ;
#60914 = ORIENTED_EDGE('',*,*,#45385,.F.) ;
#60915 = ORIENTED_EDGE('',*,*,#45399,.T.) ;
#60916 = ORIENTED_EDGE('',*,*,#45340,.F.) ;
#60917 = ORIENTED_EDGE('',*,*,#45400,.F.) ;
#60918 = ORIENTED_EDGE('',*,*,#45337,.F.) ;
#60919 = ORIENTED_EDGE('',*,*,#45401,.T.) ;
#60920 = ORIENTED_EDGE('',*,*,#45341,.F.) ;
#60921 = ORIENTED_EDGE('',*,*,#45402,.T.) ;
#60922 = ORIENTED_EDGE('',*,*,#45403,.F.) ;
#60923 = ORIENTED_EDGE('',*,*,#45400,.T.) ;
#60924 = ORIENTED_EDGE('',*,*,#45404,.F.) ;
#60925 = ORIENTED_EDGE('',*,*,#45338,.F.) ;
#60926 = ORIENTED_EDGE('',*,*,#45405,.T.) ;
#60927 = ORIENTED_EDGE('',*,*,#45387,.F.) ;
#60928 = ORIENTED_EDGE('',*,*,#45406,.F.) ;
#60929 = ORIENTED_EDGE('',*,*,#45404,.T.) ;
#60930 = ORIENTED_EDGE('',*,*,#45339,.F.) ;
#60931 = ORIENTED_EDGE('',*,*,#45407,.F.) ;
#60932 = ORIENTED_EDGE('',*,*,#45333,.F.) ;
#60933 = ORIENTED_EDGE('',*,*,#45403,.T.) ;
#60934 = ORIENTED_EDGE('',*,*,#45336,.F.) ;
#60935 = ORIENTED_EDGE('',*,*,#45408,.F.) ;
#60936 = ORIENTED_EDGE('',*,*,#45386,.F.) ;
#60937 = ORIENTED_EDGE('',*,*,#45407,.T.) ;
#60938 = ORIENTED_EDGE('',*,*,#45406,.T.) ;
#60939 = ORIENTED_EDGE('',*,*,#45409,.F.) ;
#60940 = ORIENTED_EDGE('',*,*,#45410,.F.) ;
#60941 = ORIENTED_EDGE('',*,*,#45408,.T.) ;
#60942 = ORIENTED_EDGE('',*,*,#45411,.F.) ;
#60943 = ORIENTED_EDGE('',*,*,#45409,.T.) ;
#60944 = ORIENTED_EDGE('',*,*,#45390,.F.) ;
#60945 = ORIENTED_EDGE('',*,*,#45412,.F.) ;
#60946 = ORIENTED_EDGE('',*,*,#45334,.F.) ;
#60947 = ORIENTED_EDGE('',*,*,#45411,.T.) ;
#60948 = ORIENTED_EDGE('',*,*,#45335,.F.) ;
#60949 = ORIENTED_EDGE('',*,*,#45413,.F.) ;
#60950 = ORIENTED_EDGE('',*,*,#45329,.F.) ;
#60951 = ORIENTED_EDGE('',*,*,#45332,.F.) ;
#60952 = ORIENTED_EDGE('',*,*,#45414,.T.) ;
#60953 = ORIENTED_EDGE('',*,*,#45383,.F.) ;
#60954 = ORIENTED_EDGE('',*,*,#45410,.T.) ;
#60955 = ORIENTED_EDGE('',*,*,#45413,.T.) ;
#60956 = ORIENTED_EDGE('',*,*,#45412,.T.) ;
#60957 = ORIENTED_EDGE('',*,*,#45415,.F.) ;
#60958 = ORIENTED_EDGE('',*,*,#45327,.F.) ;
#60959 = ORIENTED_EDGE('',*,*,#45416,.T.) ;
#60960 = ORIENTED_EDGE('',*,*,#45331,.F.) ;
#60961 = ORIENTED_EDGE('',*,*,#45417,.T.) ;
#60962 = ORIENTED_EDGE('',*,*,#45389,.F.) ;
#60963 = ORIENTED_EDGE('',*,*,#45418,.T.) ;
#60964 = ORIENTED_EDGE('',*,*,#45330,.F.) ;
#60965 = ORIENTED_EDGE('',*,*,#45415,.T.) ;
#60966 = ORIENTED_EDGE('',*,*,#45393,.F.) ;
#60967 = ORIENTED_EDGE('',*,*,#45419,.T.) ;
#60968 = ORIENTED_EDGE('',*,*,#45362,.F.) ;
#60969 = ORIENTED_EDGE('',*,*,#45420,.F.) ;
#60970 = ORIENTED_EDGE('',*,*,#45359,.F.) ;
#60971 = ORIENTED_EDGE('',*,*,#45421,.T.) ;
#60972 = ORIENTED_EDGE('',*,*,#45363,.F.) ;
#60973 = ORIENTED_EDGE('',*,*,#45422,.T.) ;
#60974 = ORIENTED_EDGE('',*,*,#45423,.F.) ;
#60975 = ORIENTED_EDGE('',*,*,#45420,.T.) ;
#60976 = ORIENTED_EDGE('',*,*,#45424,.F.) ;
#60977 = ORIENTED_EDGE('',*,*,#45360,.F.) ;
#60978 = ORIENTED_EDGE('',*,*,#45425,.T.) ;
#60979 = ORIENTED_EDGE('',*,*,#45395,.F.) ;
#60980 = ORIENTED_EDGE('',*,*,#45426,.F.) ;
#60981 = ORIENTED_EDGE('',*,*,#45424,.T.) ;
#60982 = ORIENTED_EDGE('',*,*,#45361,.F.) ;
#60983 = ORIENTED_EDGE('',*,*,#45427,.F.) ;
#60984 = ORIENTED_EDGE('',*,*,#45375,.F.) ;
#60985 = ORIENTED_EDGE('',*,*,#45423,.T.) ;
#60986 = ORIENTED_EDGE('',*,*,#45374,.F.) ;
#60987 = ORIENTED_EDGE('',*,*,#45428,.F.) ;
#60988 = ORIENTED_EDGE('',*,*,#45394,.F.) ;
#60989 = ORIENTED_EDGE('',*,*,#45427,.T.) ;
#60990 = ORIENTED_EDGE('',*,*,#45426,.T.) ;
#60991 = ORIENTED_EDGE('',*,*,#45429,.F.) ;
#60992 = ORIENTED_EDGE('',*,*,#45430,.F.) ;
#60993 = ORIENTED_EDGE('',*,*,#45428,.T.) ;
#60994 = ORIENTED_EDGE('',*,*,#45431,.F.) ;
#60995 = ORIENTED_EDGE('',*,*,#45429,.T.) ;
#60996 = ORIENTED_EDGE('',*,*,#45398,.F.) ;
#60997 = ORIENTED_EDGE('',*,*,#45432,.F.) ;
#60998 = ORIENTED_EDGE('',*,*,#45376,.F.) ;
#60999 = ORIENTED_EDGE('',*,*,#45431,.T.) ;
#61000 = ORIENTED_EDGE('',*,*,#45373,.F.) ;
#61001 = ORIENTED_EDGE('',*,*,#45433,.F.) ;
#61002 = ORIENTED_EDGE('',*,*,#45369,.F.) ;
#61003 = ORIENTED_EDGE('',*,*,#45372,.F.) ;
#61004 = ORIENTED_EDGE('',*,*,#45434,.T.) ;
#61005 = ORIENTED_EDGE('',*,*,#45391,.F.) ;
#61006 = ORIENTED_EDGE('',*,*,#45430,.T.) ;
#61007 = ORIENTED_EDGE('',*,*,#45433,.T.) ;
#61008 = ORIENTED_EDGE('',*,*,#45432,.T.) ;
#61009 = ORIENTED_EDGE('',*,*,#45435,.F.) ;
#61010 = ORIENTED_EDGE('',*,*,#45367,.F.) ;
#61011 = ORIENTED_EDGE('',*,*,#45436,.T.) ;
#61012 = ORIENTED_EDGE('',*,*,#45371,.F.) ;
#61013 = ORIENTED_EDGE('',*,*,#45437,.T.) ;
#61014 = ORIENTED_EDGE('',*,*,#45397,.F.) ;
#61015 = ORIENTED_EDGE('',*,*,#45438,.T.) ;
#61016 = ORIENTED_EDGE('',*,*,#45370,.F.) ;
#61017 = ORIENTED_EDGE('',*,*,#45435,.T.) ;
#61018 = ORIENTED_EDGE('',*,*,#44625,.F.) ;
#61019 = ORIENTED_EDGE('',*,*,#45357,.F.) ;
#61020 = ORIENTED_EDGE('',*,*,#45439,.F.) ;
#61021 = ORIENTED_EDGE('',*,*,#45352,.F.) ;
#61022 = ORIENTED_EDGE('',*,*,#45439,.T.) ;
#61023 = ORIENTED_EDGE('',*,*,#45342,.F.) ;
#61024 = ORIENTED_EDGE('',*,*,#45440,.F.) ;
#61025 = ORIENTED_EDGE('',*,*,#45353,.F.) ;
#61026 = ORIENTED_EDGE('',*,*,#45440,.T.) ;
#61027 = ORIENTED_EDGE('',*,*,#45401,.F.) ;
#61028 = ORIENTED_EDGE('',*,*,#45399,.F.) ;
#61029 = ORIENTED_EDGE('',*,*,#45441,.F.) ;
#61030 = ORIENTED_EDGE('',*,*,#45441,.T.) ;
#61031 = ORIENTED_EDGE('',*,*,#45384,.F.) ;
#61032 = ORIENTED_EDGE('',*,*,#45442,.F.) ;
#61033 = ORIENTED_EDGE('',*,*,#45354,.F.) ;
#61034 = ORIENTED_EDGE('',*,*,#45442,.T.) ;
#61035 = ORIENTED_EDGE('',*,*,#45414,.F.) ;
#61036 = ORIENTED_EDGE('',*,*,#45416,.F.) ;
#61037 = ORIENTED_EDGE('',*,*,#45443,.F.) ;
#61038 = ORIENTED_EDGE('',*,*,#45443,.T.) ;
#61039 = ORIENTED_EDGE('',*,*,#45326,.F.) ;
#61040 = ORIENTED_EDGE('',*,*,#45444,.F.) ;
#61041 = ORIENTED_EDGE('',*,*,#45350,.F.) ;
#61042 = ORIENTED_EDGE('',*,*,#44392,.F.) ;
#61043 = ORIENTED_EDGE('',*,*,#45351,.F.) ;
#61044 = ORIENTED_EDGE('',*,*,#45444,.T.) ;
#61045 = ORIENTED_EDGE('',*,*,#45355,.F.) ;
#61046 = ORIENTED_EDGE('',*,*,#45189,.F.) ;
#61047 = ORIENTED_EDGE('',*,*,#45192,.F.) ;
#61048 = ORIENTED_EDGE('',*,*,#45356,.F.) ;
#61049 = ORIENTED_EDGE('',*,*,#45445,.F.) ;
#61050 = ORIENTED_EDGE('',*,*,#45347,.F.) ;
#61051 = ORIENTED_EDGE('',*,*,#45445,.T.) ;
#61052 = ORIENTED_EDGE('',*,*,#45328,.F.) ;
#61053 = ORIENTED_EDGE('',*,*,#45446,.F.) ;
#61054 = ORIENTED_EDGE('',*,*,#45348,.F.) ;
#61055 = ORIENTED_EDGE('',*,*,#45446,.T.) ;
#61056 = ORIENTED_EDGE('',*,*,#45417,.F.) ;
#61057 = ORIENTED_EDGE('',*,*,#45418,.F.) ;
#61058 = ORIENTED_EDGE('',*,*,#45447,.F.) ;
#61059 = ORIENTED_EDGE('',*,*,#45447,.T.) ;
#61060 = ORIENTED_EDGE('',*,*,#45388,.F.) ;
#61061 = ORIENTED_EDGE('',*,*,#45448,.F.) ;
#61062 = ORIENTED_EDGE('',*,*,#45349,.F.) ;
#61063 = ORIENTED_EDGE('',*,*,#45448,.T.) ;
#61064 = ORIENTED_EDGE('',*,*,#45405,.F.) ;
#61065 = ORIENTED_EDGE('',*,*,#45402,.F.) ;
#61066 = ORIENTED_EDGE('',*,*,#45449,.F.) ;
#61067 = ORIENTED_EDGE('',*,*,#45449,.T.) ;
#61068 = ORIENTED_EDGE('',*,*,#45344,.F.) ;
#61069 = ORIENTED_EDGE('',*,*,#45450,.F.) ;
#61070 = ORIENTED_EDGE('',*,*,#45345,.F.) ;
#61071 = ORIENTED_EDGE('',*,*,#45450,.T.) ;
#61072 = ORIENTED_EDGE('',*,*,#45358,.F.) ;
#61073 = ORIENTED_EDGE('',*,*,#44623,.F.) ;
#61074 = ORIENTED_EDGE('',*,*,#45346,.F.) ;
#61075 = ORIENTED_EDGE('',*,*,#45174,.F.) ;
#61076 = ORIENTED_EDGE('',*,*,#45364,.F.) ;
#61077 = ORIENTED_EDGE('',*,*,#45451,.F.) ;
#61078 = ORIENTED_EDGE('',*,*,#45380,.F.) ;
#61079 = ORIENTED_EDGE('',*,*,#45451,.T.) ;
#61080 = ORIENTED_EDGE('',*,*,#45421,.F.) ;
#61081 = ORIENTED_EDGE('',*,*,#45419,.F.) ;
#61082 = ORIENTED_EDGE('',*,*,#45452,.F.) ;
#61083 = ORIENTED_EDGE('',*,*,#45452,.T.) ;
#61084 = ORIENTED_EDGE('',*,*,#45392,.F.) ;
#61085 = ORIENTED_EDGE('',*,*,#45453,.F.) ;
#61086 = ORIENTED_EDGE('',*,*,#45381,.F.) ;
#61087 = ORIENTED_EDGE('',*,*,#45453,.T.) ;
#61088 = ORIENTED_EDGE('',*,*,#45434,.F.) ;
#61089 = ORIENTED_EDGE('',*,*,#45436,.F.) ;
#61090 = ORIENTED_EDGE('',*,*,#45454,.F.) ;
#61091 = ORIENTED_EDGE('',*,*,#45176,.F.) ;
#61092 = ORIENTED_EDGE('',*,*,#45382,.F.) ;
#61093 = ORIENTED_EDGE('',*,*,#45454,.T.) ;
#61094 = ORIENTED_EDGE('',*,*,#45366,.F.) ;
#61095 = ORIENTED_EDGE('',*,*,#45455,.F.) ;
#61096 = ORIENTED_EDGE('',*,*,#45365,.F.) ;
#61097 = ORIENTED_EDGE('',*,*,#45172,.F.) ;
#61098 = ORIENTED_EDGE('',*,*,#45378,.F.) ;
#61099 = ORIENTED_EDGE('',*,*,#45422,.F.) ;
#61100 = ORIENTED_EDGE('',*,*,#45455,.T.) ;
#61101 = ORIENTED_EDGE('',*,*,#45456,.F.) ;
#61102 = ORIENTED_EDGE('',*,*,#45425,.F.) ;
#61103 = ORIENTED_EDGE('',*,*,#45456,.T.) ;
#61104 = ORIENTED_EDGE('',*,*,#45377,.F.) ;
#61105 = ORIENTED_EDGE('',*,*,#45457,.F.) ;
#61106 = ORIENTED_EDGE('',*,*,#45396,.F.) ;
#61107 = ORIENTED_EDGE('',*,*,#45178,.F.) ;
#61108 = ORIENTED_EDGE('',*,*,#45368,.F.) ;
#61109 = ORIENTED_EDGE('',*,*,#45458,.F.) ;
#61110 = ORIENTED_EDGE('',*,*,#45379,.F.) ;
#61111 = ORIENTED_EDGE('',*,*,#45438,.F.) ;
#61112 = ORIENTED_EDGE('',*,*,#45457,.T.) ;
#61113 = ORIENTED_EDGE('',*,*,#45458,.T.) ;
#61114 = ORIENTED_EDGE('',*,*,#45437,.F.) ;
#61115 = ORIENTED_EDGE('',*,*,#45459,.T.) ;
#61116 = ORIENTED_EDGE('',*,*,#45460,.T.) ;
#61117 = ORIENTED_EDGE('',*,*,#45461,.T.) ;
#61118 = ORIENTED_EDGE('',*,*,#45462,.T.) ;
#61119 = ORIENTED_EDGE('',*,*,#45463,.T.) ;
#61120 = ORIENTED_EDGE('',*,*,#45464,.T.) ;
#61121 = ORIENTED_EDGE('',*,*,#45465,.F.) ;
#61122 = ORIENTED_EDGE('',*,*,#45466,.T.) ;
#61123 = ORIENTED_EDGE('',*,*,#45467,.F.) ;
#61124 = ORIENTED_EDGE('',*,*,#45468,.T.) ;
#61125 = ORIENTED_EDGE('',*,*,#45469,.T.) ;
#61126 = ORIENTED_EDGE('',*,*,#45470,.T.) ;
#61127 = ORIENTED_EDGE('',*,*,#45471,.T.) ;
#61128 = ORIENTED_EDGE('',*,*,#45472,.T.) ;
#61129 = ORIENTED_EDGE('',*,*,#45473,.T.) ;
#61130 = ORIENTED_EDGE('',*,*,#45474,.T.) ;
#61131 = ORIENTED_EDGE('',*,*,#45475,.F.) ;
#61132 = ORIENTED_EDGE('',*,*,#45476,.T.) ;
#61133 = ORIENTED_EDGE('',*,*,#45477,.F.) ;
#61134 = ORIENTED_EDGE('',*,*,#45478,.T.) ;
#61135 = ORIENTED_EDGE('',*,*,#45479,.T.) ;
#61136 = ORIENTED_EDGE('',*,*,#45480,.T.) ;
#61137 = ORIENTED_EDGE('',*,*,#45481,.T.) ;
#61138 = ORIENTED_EDGE('',*,*,#45482,.T.) ;
#61139 = ORIENTED_EDGE('',*,*,#45483,.T.) ;
#61140 = ORIENTED_EDGE('',*,*,#45484,.T.) ;
#61141 = ORIENTED_EDGE('',*,*,#45485,.F.) ;
#61142 = ORIENTED_EDGE('',*,*,#45486,.T.) ;
#61143 = ORIENTED_EDGE('',*,*,#45487,.F.) ;
#61144 = ORIENTED_EDGE('',*,*,#45488,.T.) ;
#61145 = ORIENTED_EDGE('',*,*,#45489,.T.) ;
#61146 = ORIENTED_EDGE('',*,*,#45490,.T.) ;
#61147 = ORIENTED_EDGE('',*,*,#45491,.T.) ;
#61148 = ORIENTED_EDGE('',*,*,#45492,.T.) ;
#61149 = ORIENTED_EDGE('',*,*,#45493,.T.) ;
#61150 = ORIENTED_EDGE('',*,*,#45494,.T.) ;
#61151 = ORIENTED_EDGE('',*,*,#45495,.F.) ;
#61152 = ORIENTED_EDGE('',*,*,#45496,.T.) ;
#61153 = ORIENTED_EDGE('',*,*,#45497,.F.) ;
#61154 = ORIENTED_EDGE('',*,*,#45498,.T.) ;
#61155 = ORIENTED_EDGE('',*,*,#45499,.T.) ;
#61156 = ORIENTED_EDGE('',*,*,#45500,.T.) ;
#61157 = ORIENTED_EDGE('',*,*,#45501,.T.) ;
#61158 = ORIENTED_EDGE('',*,*,#45502,.T.) ;
#61159 = ORIENTED_EDGE('',*,*,#45503,.T.) ;
#61160 = ORIENTED_EDGE('',*,*,#45504,.T.) ;
#61161 = ORIENTED_EDGE('',*,*,#45505,.F.) ;
#61162 = ORIENTED_EDGE('',*,*,#45506,.T.) ;
#61163 = ORIENTED_EDGE('',*,*,#45507,.F.) ;
#61164 = ORIENTED_EDGE('',*,*,#45508,.T.) ;
#61165 = ORIENTED_EDGE('',*,*,#45509,.T.) ;
#61166 = ORIENTED_EDGE('',*,*,#45510,.T.) ;
#61167 = ORIENTED_EDGE('',*,*,#45511,.T.) ;
#61168 = ORIENTED_EDGE('',*,*,#45512,.T.) ;
#61169 = ORIENTED_EDGE('',*,*,#45513,.T.) ;
#61170 = ORIENTED_EDGE('',*,*,#45514,.T.) ;
#61171 = ORIENTED_EDGE('',*,*,#45515,.F.) ;
#61172 = ORIENTED_EDGE('',*,*,#45516,.T.) ;
#61173 = ORIENTED_EDGE('',*,*,#45517,.F.) ;
#61174 = ORIENTED_EDGE('',*,*,#45518,.T.) ;
#61175 = ORIENTED_EDGE('',*,*,#45519,.T.) ;
#61176 = ORIENTED_EDGE('',*,*,#45520,.T.) ;
#61177 = ORIENTED_EDGE('',*,*,#45521,.T.) ;
#61178 = ORIENTED_EDGE('',*,*,#45522,.T.) ;
#61179 = ORIENTED_EDGE('',*,*,#45523,.T.) ;
#61180 = ORIENTED_EDGE('',*,*,#45524,.T.) ;
#61181 = ORIENTED_EDGE('',*,*,#45525,.F.) ;
#61182 = ORIENTED_EDGE('',*,*,#45526,.T.) ;
#61183 = ORIENTED_EDGE('',*,*,#45527,.F.) ;
#61184 = ORIENTED_EDGE('',*,*,#45528,.T.) ;
#61185 = ORIENTED_EDGE('',*,*,#45529,.T.) ;
#61186 = ORIENTED_EDGE('',*,*,#45530,.T.) ;
#61187 = ORIENTED_EDGE('',*,*,#45531,.T.) ;
#61188 = ORIENTED_EDGE('',*,*,#45532,.T.) ;
#61189 = ORIENTED_EDGE('',*,*,#45533,.T.) ;
#61190 = ORIENTED_EDGE('',*,*,#45534,.T.) ;
#61191 = ORIENTED_EDGE('',*,*,#45535,.F.) ;
#61192 = ORIENTED_EDGE('',*,*,#45536,.T.) ;
#61193 = ORIENTED_EDGE('',*,*,#45537,.F.) ;
#61194 = ORIENTED_EDGE('',*,*,#45538,.T.) ;
#61195 = ORIENTED_EDGE('',*,*,#45539,.T.) ;
#61196 = ORIENTED_EDGE('',*,*,#45540,.T.) ;
#61197 = ORIENTED_EDGE('',*,*,#45541,.T.) ;
#61198 = ORIENTED_EDGE('',*,*,#45542,.T.) ;
#61199 = ORIENTED_EDGE('',*,*,#45543,.T.) ;
#61200 = ORIENTED_EDGE('',*,*,#45544,.T.) ;
#61201 = ORIENTED_EDGE('',*,*,#45545,.F.) ;
#61202 = ORIENTED_EDGE('',*,*,#45546,.T.) ;
#61203 = ORIENTED_EDGE('',*,*,#45547,.F.) ;
#61204 = ORIENTED_EDGE('',*,*,#45548,.T.) ;
#61205 = ORIENTED_EDGE('',*,*,#45549,.T.) ;
#61206 = ORIENTED_EDGE('',*,*,#45550,.T.) ;
#61207 = ORIENTED_EDGE('',*,*,#45551,.T.) ;
#61208 = ORIENTED_EDGE('',*,*,#45552,.T.) ;
#61209 = ORIENTED_EDGE('',*,*,#45553,.T.) ;
#61210 = ORIENTED_EDGE('',*,*,#45554,.T.) ;
#61211 = ORIENTED_EDGE('',*,*,#45555,.T.) ;
#61212 = ORIENTED_EDGE('',*,*,#44331,.T.) ;
#61213 = ORIENTED_EDGE('',*,*,#45556,.T.) ;
#61214 = ORIENTED_EDGE('',*,*,#45557,.T.) ;
#61215 = ORIENTED_EDGE('',*,*,#45558,.T.) ;
#61216 = ORIENTED_EDGE('',*,*,#45559,.T.) ;
#61217 = ORIENTED_EDGE('',*,*,#45560,.T.) ;
#61218 = ORIENTED_EDGE('',*,*,#45561,.T.) ;
#61219 = ORIENTED_EDGE('',*,*,#45562,.T.) ;
#61220 = ORIENTED_EDGE('',*,*,#45563,.T.) ;
#61221 = ORIENTED_EDGE('',*,*,#45564,.T.) ;
#61222 = ORIENTED_EDGE('',*,*,#45565,.T.) ;
#61223 = ORIENTED_EDGE('',*,*,#45566,.T.) ;
#61224 = ORIENTED_EDGE('',*,*,#45567,.T.) ;
#61225 = ORIENTED_EDGE('',*,*,#45568,.T.) ;
#61226 = ORIENTED_EDGE('',*,*,#45569,.T.) ;
#61227 = ORIENTED_EDGE('',*,*,#45570,.T.) ;
#61228 = ORIENTED_EDGE('',*,*,#45571,.T.) ;
#61229 = ORIENTED_EDGE('',*,*,#45572,.T.) ;
#61230 = ORIENTED_EDGE('',*,*,#45573,.T.) ;
#61231 = ORIENTED_EDGE('',*,*,#45574,.T.) ;
#61232 = ORIENTED_EDGE('',*,*,#44278,.T.) ;
#61233 = ORIENTED_EDGE('',*,*,#45575,.T.) ;
#61234 = ORIENTED_EDGE('',*,*,#45576,.T.) ;
#61235 = ORIENTED_EDGE('',*,*,#45577,.T.) ;
#61236 = ORIENTED_EDGE('',*,*,#45578,.T.) ;
#61237 = ORIENTED_EDGE('',*,*,#45579,.T.) ;
#61238 = ORIENTED_EDGE('',*,*,#45580,.T.) ;
#61239 = ORIENTED_EDGE('',*,*,#45581,.T.) ;
#61240 = ORIENTED_EDGE('',*,*,#45582,.T.) ;
#61241 = ORIENTED_EDGE('',*,*,#45583,.T.) ;
#61242 = ORIENTED_EDGE('',*,*,#45584,.T.) ;
#61243 = ORIENTED_EDGE('',*,*,#45585,.T.) ;
#61244 = ORIENTED_EDGE('',*,*,#45586,.T.) ;
#61245 = ORIENTED_EDGE('',*,*,#45587,.T.) ;
#61246 = ORIENTED_EDGE('',*,*,#45588,.T.) ;
#61247 = ORIENTED_EDGE('',*,*,#45589,.T.) ;
#61248 = ORIENTED_EDGE('',*,*,#45590,.T.) ;
#61249 = ORIENTED_EDGE('',*,*,#45591,.T.) ;
#61250 = ORIENTED_EDGE('',*,*,#45592,.T.) ;
#61251 = ORIENTED_EDGE('',*,*,#45593,.T.) ;
#61252 = ORIENTED_EDGE('',*,*,#44261,.T.) ;
#61253 = ORIENTED_EDGE('',*,*,#45594,.T.) ;
#61254 = ORIENTED_EDGE('',*,*,#45595,.T.) ;
#61255 = ORIENTED_EDGE('',*,*,#45596,.T.) ;
#61256 = ORIENTED_EDGE('',*,*,#45597,.T.) ;
#61257 = ORIENTED_EDGE('',*,*,#45598,.T.) ;
#61258 = ORIENTED_EDGE('',*,*,#45599,.T.) ;
#61259 = ORIENTED_EDGE('',*,*,#45600,.T.) ;
#61260 = ORIENTED_EDGE('',*,*,#45601,.T.) ;
#61261 = ORIENTED_EDGE('',*,*,#45602,.T.) ;
#61262 = ORIENTED_EDGE('',*,*,#45603,.T.) ;
#61263 = ORIENTED_EDGE('',*,*,#45604,.T.) ;
#61264 = ORIENTED_EDGE('',*,*,#45605,.T.) ;
#61265 = ORIENTED_EDGE('',*,*,#45606,.T.) ;
#61266 = ORIENTED_EDGE('',*,*,#45607,.T.) ;
#61267 = ORIENTED_EDGE('',*,*,#45608,.T.) ;
#61268 = ORIENTED_EDGE('',*,*,#45609,.T.) ;
#61269 = ORIENTED_EDGE('',*,*,#45610,.T.) ;
#61270 = ORIENTED_EDGE('',*,*,#45611,.T.) ;
#61271 = ORIENTED_EDGE('',*,*,#45612,.T.) ;
#61272 = ORIENTED_EDGE('',*,*,#44244,.T.) ;
#61273 = ORIENTED_EDGE('',*,*,#45613,.T.) ;
#61274 = ORIENTED_EDGE('',*,*,#45614,.T.) ;
#61275 = ORIENTED_EDGE('',*,*,#45615,.T.) ;
#61276 = ORIENTED_EDGE('',*,*,#45616,.T.) ;
#61277 = ORIENTED_EDGE('',*,*,#45617,.T.) ;
#61278 = ORIENTED_EDGE('',*,*,#45618,.T.) ;
#61279 = ORIENTED_EDGE('',*,*,#45619,.T.) ;
#61280 = ORIENTED_EDGE('',*,*,#45620,.T.) ;
#61281 = ORIENTED_EDGE('',*,*,#45621,.T.) ;
#61282 = ORIENTED_EDGE('',*,*,#45622,.T.) ;
#61283 = ORIENTED_EDGE('',*,*,#45623,.T.) ;
#61284 = ORIENTED_EDGE('',*,*,#45624,.T.) ;
#61285 = ORIENTED_EDGE('',*,*,#45625,.T.) ;
#61286 = ORIENTED_EDGE('',*,*,#45626,.T.) ;
#61287 = ORIENTED_EDGE('',*,*,#45627,.T.) ;
#61288 = ORIENTED_EDGE('',*,*,#45628,.T.) ;
#61289 = ORIENTED_EDGE('',*,*,#45629,.T.) ;
#61290 = ORIENTED_EDGE('',*,*,#45630,.T.) ;
#61291 = ORIENTED_EDGE('',*,*,#45631,.T.) ;
#61292 = ORIENTED_EDGE('',*,*,#44227,.T.) ;
#61293 = ORIENTED_EDGE('',*,*,#45632,.T.) ;
#61294 = ORIENTED_EDGE('',*,*,#45633,.T.) ;
#61295 = ORIENTED_EDGE('',*,*,#45634,.T.) ;
#61296 = ORIENTED_EDGE('',*,*,#45635,.T.) ;
#61297 = ORIENTED_EDGE('',*,*,#45636,.T.) ;
#61298 = ORIENTED_EDGE('',*,*,#45637,.T.) ;
#61299 = ORIENTED_EDGE('',*,*,#45638,.T.) ;
#61300 = ORIENTED_EDGE('',*,*,#45639,.T.) ;
#61301 = ORIENTED_EDGE('',*,*,#45640,.T.) ;
#61302 = ORIENTED_EDGE('',*,*,#45641,.T.) ;
#61303 = ORIENTED_EDGE('',*,*,#45642,.T.) ;
#61304 = ORIENTED_EDGE('',*,*,#45643,.T.) ;
#61305 = ORIENTED_EDGE('',*,*,#45644,.T.) ;
#61306 = ORIENTED_EDGE('',*,*,#45645,.T.) ;
#61307 = ORIENTED_EDGE('',*,*,#45646,.T.) ;
#61308 = ORIENTED_EDGE('',*,*,#45647,.T.) ;
#61309 = ORIENTED_EDGE('',*,*,#45648,.T.) ;
#61310 = ORIENTED_EDGE('',*,*,#45649,.T.) ;
#61311 = ORIENTED_EDGE('',*,*,#45650,.T.) ;
#61312 = ORIENTED_EDGE('',*,*,#44210,.T.) ;
#61313 = ORIENTED_EDGE('',*,*,#45651,.T.) ;
#61314 = ORIENTED_EDGE('',*,*,#45652,.T.) ;
#61315 = ORIENTED_EDGE('',*,*,#45653,.T.) ;
#61316 = ORIENTED_EDGE('',*,*,#45654,.T.) ;
#61317 = ORIENTED_EDGE('',*,*,#45655,.T.) ;
#61318 = ORIENTED_EDGE('',*,*,#45656,.T.) ;
#61319 = ORIENTED_EDGE('',*,*,#45657,.T.) ;
#61320 = ORIENTED_EDGE('',*,*,#45658,.T.) ;
#61321 = ORIENTED_EDGE('',*,*,#45659,.T.) ;
#61322 = ORIENTED_EDGE('',*,*,#45660,.T.) ;
#61323 = ORIENTED_EDGE('',*,*,#45661,.T.) ;
#61324 = ORIENTED_EDGE('',*,*,#45662,.T.) ;
#61325 = ORIENTED_EDGE('',*,*,#45663,.T.) ;
#61326 = ORIENTED_EDGE('',*,*,#45664,.T.) ;
#61327 = ORIENTED_EDGE('',*,*,#45665,.T.) ;
#61328 = ORIENTED_EDGE('',*,*,#45666,.T.) ;
#61329 = ORIENTED_EDGE('',*,*,#45667,.T.) ;
#61330 = ORIENTED_EDGE('',*,*,#45668,.T.) ;
#61331 = ORIENTED_EDGE('',*,*,#45669,.T.) ;
#61332 = ORIENTED_EDGE('',*,*,#44193,.T.) ;
#61333 = ORIENTED_EDGE('',*,*,#45670,.T.) ;
#61334 = ORIENTED_EDGE('',*,*,#45671,.T.) ;
#61335 = ORIENTED_EDGE('',*,*,#45672,.T.) ;
#61336 = ORIENTED_EDGE('',*,*,#45673,.T.) ;
#61337 = ORIENTED_EDGE('',*,*,#45674,.T.) ;
#61338 = ORIENTED_EDGE('',*,*,#45675,.T.) ;
#61339 = ORIENTED_EDGE('',*,*,#45676,.T.) ;
#61340 = ORIENTED_EDGE('',*,*,#45677,.T.) ;
#61341 = ORIENTED_EDGE('',*,*,#45678,.T.) ;
#61342 = ORIENTED_EDGE('',*,*,#45679,.T.) ;
#61343 = ORIENTED_EDGE('',*,*,#45680,.T.) ;
#61344 = ORIENTED_EDGE('',*,*,#45681,.T.) ;
#61345 = ORIENTED_EDGE('',*,*,#45682,.T.) ;
#61346 = ORIENTED_EDGE('',*,*,#45683,.T.) ;
#61347 = ORIENTED_EDGE('',*,*,#45684,.T.) ;
#61348 = ORIENTED_EDGE('',*,*,#45685,.T.) ;
#61349 = ORIENTED_EDGE('',*,*,#45686,.T.) ;
#61350 = ORIENTED_EDGE('',*,*,#45687,.T.) ;
#61351 = ORIENTED_EDGE('',*,*,#45688,.T.) ;
#61352 = ORIENTED_EDGE('',*,*,#44176,.T.) ;
#61353 = ORIENTED_EDGE('',*,*,#45689,.T.) ;
#61354 = ORIENTED_EDGE('',*,*,#45690,.T.) ;
#61355 = ORIENTED_EDGE('',*,*,#45691,.T.) ;
#61356 = ORIENTED_EDGE('',*,*,#45692,.T.) ;
#61357 = ORIENTED_EDGE('',*,*,#45693,.T.) ;
#61358 = ORIENTED_EDGE('',*,*,#45694,.T.) ;
#61359 = ORIENTED_EDGE('',*,*,#45695,.T.) ;
#61360 = ORIENTED_EDGE('',*,*,#45696,.T.) ;
#61361 = ORIENTED_EDGE('',*,*,#45697,.T.) ;
#61362 = ORIENTED_EDGE('',*,*,#45698,.T.) ;
#61363 = ORIENTED_EDGE('',*,*,#45699,.T.) ;
#61364 = ORIENTED_EDGE('',*,*,#45700,.T.) ;
#61365 = ORIENTED_EDGE('',*,*,#45701,.T.) ;
#61366 = ORIENTED_EDGE('',*,*,#45702,.T.) ;
#61367 = ORIENTED_EDGE('',*,*,#45703,.T.) ;
#61368 = ORIENTED_EDGE('',*,*,#45704,.T.) ;
#61369 = ORIENTED_EDGE('',*,*,#45705,.T.) ;
#61370 = ORIENTED_EDGE('',*,*,#45706,.T.) ;
#61371 = ORIENTED_EDGE('',*,*,#45707,.T.) ;
#61372 = ORIENTED_EDGE('',*,*,#44159,.T.) ;
#61373 = ORIENTED_EDGE('',*,*,#45708,.T.) ;
#61374 = ORIENTED_EDGE('',*,*,#45709,.T.) ;
#61375 = ORIENTED_EDGE('',*,*,#45710,.T.) ;
#61376 = ORIENTED_EDGE('',*,*,#45711,.T.) ;
#61377 = ORIENTED_EDGE('',*,*,#45712,.T.) ;
#61378 = ORIENTED_EDGE('',*,*,#45713,.T.) ;
#61379 = ORIENTED_EDGE('',*,*,#45714,.T.) ;
#61380 = ORIENTED_EDGE('',*,*,#45715,.T.) ;
#61381 = ORIENTED_EDGE('',*,*,#45716,.T.) ;
#61382 = ORIENTED_EDGE('',*,*,#45717,.T.) ;
#61383 = ORIENTED_EDGE('',*,*,#45718,.T.) ;
#61384 = ORIENTED_EDGE('',*,*,#45719,.T.) ;
#61385 = ORIENTED_EDGE('',*,*,#45720,.F.) ;
#61386 = ORIENTED_EDGE('',*,*,#45721,.T.) ;
#61387 = ORIENTED_EDGE('',*,*,#45722,.T.) ;
#61388 = ORIENTED_EDGE('',*,*,#45723,.T.) ;
#61389 = ORIENTED_EDGE('',*,*,#45722,.F.) ;
#61390 = ORIENTED_EDGE('',*,*,#45724,.T.) ;
#61391 = ORIENTED_EDGE('',*,*,#45725,.T.) ;
#61392 = ORIENTED_EDGE('',*,*,#45726,.T.) ;
#61393 = ORIENTED_EDGE('',*,*,#45725,.F.) ;
#61394 = ORIENTED_EDGE('',*,*,#45727,.T.) ;
#61395 = ORIENTED_EDGE('',*,*,#45728,.T.) ;
#61396 = ORIENTED_EDGE('',*,*,#45729,.T.) ;
#61397 = ORIENTED_EDGE('',*,*,#45728,.F.) ;
#61398 = ORIENTED_EDGE('',*,*,#45730,.T.) ;
#61399 = ORIENTED_EDGE('',*,*,#45731,.T.) ;
#61400 = ORIENTED_EDGE('',*,*,#45732,.T.) ;
#61401 = ORIENTED_EDGE('',*,*,#45731,.F.) ;
#61402 = ORIENTED_EDGE('',*,*,#45733,.T.) ;
#61403 = ORIENTED_EDGE('',*,*,#45734,.T.) ;
#61404 = ORIENTED_EDGE('',*,*,#45735,.T.) ;
#61405 = ORIENTED_EDGE('',*,*,#45734,.F.) ;
#61406 = ORIENTED_EDGE('',*,*,#45736,.T.) ;
#61407 = ORIENTED_EDGE('',*,*,#45737,.T.) ;
#61408 = ORIENTED_EDGE('',*,*,#45738,.T.) ;
#61409 = ORIENTED_EDGE('',*,*,#45737,.F.) ;
#61410 = ORIENTED_EDGE('',*,*,#44154,.T.) ;
#61411 = ORIENTED_EDGE('',*,*,#45739,.T.) ;
#61412 = ORIENTED_EDGE('',*,*,#45740,.T.) ;
#61413 = ORIENTED_EDGE('',*,*,#45739,.F.) ;
#61414 = ORIENTED_EDGE('',*,*,#45741,.T.) ;
#61415 = ORIENTED_EDGE('',*,*,#44371,.T.) ;
#61416 = ORIENTED_EDGE('',*,*,#45742,.T.) ;
#61417 = ORIENTED_EDGE('',*,*,#44370,.F.) ;
#61418 = ORIENTED_EDGE('',*,*,#45743,.T.) ;
#61419 = ORIENTED_EDGE('',*,*,#45744,.T.) ;
#61420 = ORIENTED_EDGE('',*,*,#45745,.T.) ;
#61421 = ORIENTED_EDGE('',*,*,#45744,.F.) ;
#61422 = ORIENTED_EDGE('',*,*,#45746,.T.) ;
#61423 = ORIENTED_EDGE('',*,*,#45747,.T.) ;
#61424 = ORIENTED_EDGE('',*,*,#45748,.T.) ;
#61425 = ORIENTED_EDGE('',*,*,#45747,.F.) ;
#61426 = ORIENTED_EDGE('',*,*,#45749,.T.) ;
#61427 = ORIENTED_EDGE('',*,*,#45750,.T.) ;
#61428 = ORIENTED_EDGE('',*,*,#45751,.T.) ;
#61429 = ORIENTED_EDGE('',*,*,#45750,.F.) ;
#61430 = ORIENTED_EDGE('',*,*,#45752,.T.) ;
#61431 = ORIENTED_EDGE('',*,*,#45753,.T.) ;
#61432 = ORIENTED_EDGE('',*,*,#45754,.T.) ;
#61433 = ORIENTED_EDGE('',*,*,#45753,.F.) ;
#61434 = ORIENTED_EDGE('',*,*,#45755,.T.) ;
#61435 = ORIENTED_EDGE('',*,*,#45756,.T.) ;
#61436 = ORIENTED_EDGE('',*,*,#45757,.T.) ;
#61437 = ORIENTED_EDGE('',*,*,#45756,.F.) ;
#61438 = ORIENTED_EDGE('',*,*,#45758,.T.) ;
#61439 = ORIENTED_EDGE('',*,*,#45759,.T.) ;
#61440 = ORIENTED_EDGE('',*,*,#45760,.T.) ;
#61441 = ORIENTED_EDGE('',*,*,#45759,.F.) ;
#61442 = ORIENTED_EDGE('',*,*,#45761,.T.) ;
#61443 = ORIENTED_EDGE('',*,*,#45762,.T.) ;
#61444 = ORIENTED_EDGE('',*,*,#45763,.T.) ;
#61445 = ORIENTED_EDGE('',*,*,#45762,.F.) ;
#61446 = ORIENTED_EDGE('',*,*,#45764,.T.) ;
#61447 = ORIENTED_EDGE('',*,*,#45765,.T.) ;
#61448 = ORIENTED_EDGE('',*,*,#45766,.T.) ;
#61449 = ORIENTED_EDGE('',*,*,#45765,.F.) ;
#61450 = ORIENTED_EDGE('',*,*,#45767,.T.) ;
#61451 = ORIENTED_EDGE('',*,*,#45768,.T.) ;
#61452 = ORIENTED_EDGE('',*,*,#45769,.T.) ;
#61453 = ORIENTED_EDGE('',*,*,#45768,.F.) ;
#61454 = ORIENTED_EDGE('',*,*,#45770,.T.) ;
#61455 = ORIENTED_EDGE('',*,*,#45771,.T.) ;
#61456 = ORIENTED_EDGE('',*,*,#45772,.T.) ;
#61457 = ORIENTED_EDGE('',*,*,#45771,.F.) ;
#61458 = ORIENTED_EDGE('',*,*,#45773,.T.) ;
#61459 = ORIENTED_EDGE('',*,*,#45774,.T.) ;
#61460 = ORIENTED_EDGE('',*,*,#45775,.T.) ;
#61461 = ORIENTED_EDGE('',*,*,#45774,.F.) ;
#61462 = ORIENTED_EDGE('',*,*,#45776,.T.) ;
#61463 = ORIENTED_EDGE('',*,*,#45777,.T.) ;
#61464 = ORIENTED_EDGE('',*,*,#45778,.T.) ;
#61465 = ORIENTED_EDGE('',*,*,#45777,.F.) ;
#61466 = ORIENTED_EDGE('',*,*,#45779,.T.) ;
#61467 = ORIENTED_EDGE('',*,*,#45780,.T.) ;
#61468 = ORIENTED_EDGE('',*,*,#45781,.T.) ;
#61469 = ORIENTED_EDGE('',*,*,#45780,.F.) ;
#61470 = ORIENTED_EDGE('',*,*,#45782,.T.) ;
#61471 = ORIENTED_EDGE('',*,*,#45783,.T.) ;
#61472 = ORIENTED_EDGE('',*,*,#45784,.T.) ;
#61473 = ORIENTED_EDGE('',*,*,#45783,.F.) ;
#61474 = ORIENTED_EDGE('',*,*,#45785,.T.) ;
#61475 = ORIENTED_EDGE('',*,*,#45786,.T.) ;
#61476 = ORIENTED_EDGE('',*,*,#45787,.T.) ;
#61477 = ORIENTED_EDGE('',*,*,#45786,.F.) ;
#61478 = ORIENTED_EDGE('',*,*,#45788,.T.) ;
#61479 = ORIENTED_EDGE('',*,*,#45789,.T.) ;
#61480 = ORIENTED_EDGE('',*,*,#45790,.T.) ;
#61481 = ORIENTED_EDGE('',*,*,#45789,.F.) ;
#61482 = ORIENTED_EDGE('',*,*,#45791,.T.) ;
#61483 = ORIENTED_EDGE('',*,*,#45792,.T.) ;
#61484 = ORIENTED_EDGE('',*,*,#45793,.T.) ;
#61485 = ORIENTED_EDGE('',*,*,#45792,.F.) ;
#61486 = ORIENTED_EDGE('',*,*,#45794,.T.) ;
#61487 = ORIENTED_EDGE('',*,*,#45795,.T.) ;
#61488 = ORIENTED_EDGE('',*,*,#45796,.T.) ;
#61489 = ORIENTED_EDGE('',*,*,#45795,.F.) ;
#61490 = ORIENTED_EDGE('',*,*,#45797,.T.) ;
#61491 = ORIENTED_EDGE('',*,*,#45720,.T.) ;
#61492 = ORIENTED_EDGE('',*,*,#45798,.T.) ;
#61493 = ORIENTED_EDGE('',*,*,#45799,.T.) ;
#61494 = ORIENTED_EDGE('',*,*,#45800,.T.) ;
#61495 = ORIENTED_EDGE('',*,*,#45801,.T.) ;
#61496 = ORIENTED_EDGE('',*,*,#45802,.T.) ;
#61497 = ORIENTED_EDGE('',*,*,#45803,.T.) ;
#61498 = ORIENTED_EDGE('',*,*,#45804,.T.) ;
#61499 = ORIENTED_EDGE('',*,*,#45805,.T.) ;
#61500 = ORIENTED_EDGE('',*,*,#45806,.T.) ;
#61501 = ORIENTED_EDGE('',*,*,#45807,.T.) ;
#61502 = ORIENTED_EDGE('',*,*,#45808,.T.) ;
#61503 = ORIENTED_EDGE('',*,*,#45809,.T.) ;
#61504 = ORIENTED_EDGE('',*,*,#45810,.T.) ;
#61505 = ORIENTED_EDGE('',*,*,#45811,.T.) ;
#61506 = ORIENTED_EDGE('',*,*,#45812,.T.) ;
#61507 = ORIENTED_EDGE('',*,*,#45813,.T.) ;
#61508 = ORIENTED_EDGE('',*,*,#45814,.T.) ;
#61509 = ORIENTED_EDGE('',*,*,#45815,.T.) ;
#61510 = ORIENTED_EDGE('',*,*,#45816,.T.) ;
#61511 = ORIENTED_EDGE('',*,*,#44151,.T.) ;
#61512 = ORIENTED_EDGE('',*,*,#45817,.F.) ;
#61513 = ORIENTED_EDGE('',*,*,#45818,.T.) ;
#61514 = ORIENTED_EDGE('',*,*,#45819,.T.) ;
#61515 = ORIENTED_EDGE('',*,*,#45820,.T.) ;
#61516 = ORIENTED_EDGE('',*,*,#45819,.F.) ;
#61517 = ORIENTED_EDGE('',*,*,#45821,.T.) ;
#61518 = ORIENTED_EDGE('',*,*,#45822,.T.) ;
#61519 = ORIENTED_EDGE('',*,*,#45823,.T.) ;
#61520 = ORIENTED_EDGE('',*,*,#45822,.F.) ;
#61521 = ORIENTED_EDGE('',*,*,#45824,.T.) ;
#61522 = ORIENTED_EDGE('',*,*,#45825,.T.) ;
#61523 = ORIENTED_EDGE('',*,*,#45826,.T.) ;
#61524 = ORIENTED_EDGE('',*,*,#45825,.F.) ;
#61525 = ORIENTED_EDGE('',*,*,#45827,.T.) ;
#61526 = ORIENTED_EDGE('',*,*,#45828,.T.) ;
#61527 = ORIENTED_EDGE('',*,*,#45829,.T.) ;
#61528 = ORIENTED_EDGE('',*,*,#45828,.F.) ;
#61529 = ORIENTED_EDGE('',*,*,#45830,.T.) ;
#61530 = ORIENTED_EDGE('',*,*,#45831,.T.) ;
#61531 = ORIENTED_EDGE('',*,*,#45832,.T.) ;
#61532 = ORIENTED_EDGE('',*,*,#45831,.F.) ;
#61533 = ORIENTED_EDGE('',*,*,#45833,.T.) ;
#61534 = ORIENTED_EDGE('',*,*,#45834,.T.) ;
#61535 = ORIENTED_EDGE('',*,*,#45835,.T.) ;
#61536 = ORIENTED_EDGE('',*,*,#45834,.F.) ;
#61537 = ORIENTED_EDGE('',*,*,#44171,.T.) ;
#61538 = ORIENTED_EDGE('',*,*,#45836,.T.) ;
#61539 = ORIENTED_EDGE('',*,*,#45837,.T.) ;
#61540 = ORIENTED_EDGE('',*,*,#45836,.F.) ;
#61541 = ORIENTED_EDGE('',*,*,#45838,.T.) ;
#61542 = ORIENTED_EDGE('',*,*,#44368,.T.) ;
#61543 = ORIENTED_EDGE('',*,*,#45839,.T.) ;
#61544 = ORIENTED_EDGE('',*,*,#44367,.F.) ;
#61545 = ORIENTED_EDGE('',*,*,#45840,.T.) ;
#61546 = ORIENTED_EDGE('',*,*,#45841,.T.) ;
#61547 = ORIENTED_EDGE('',*,*,#45842,.T.) ;
#61548 = ORIENTED_EDGE('',*,*,#45841,.F.) ;
#61549 = ORIENTED_EDGE('',*,*,#45843,.T.) ;
#61550 = ORIENTED_EDGE('',*,*,#45844,.T.) ;
#61551 = ORIENTED_EDGE('',*,*,#45845,.T.) ;
#61552 = ORIENTED_EDGE('',*,*,#45844,.F.) ;
#61553 = ORIENTED_EDGE('',*,*,#45846,.T.) ;
#61554 = ORIENTED_EDGE('',*,*,#45847,.T.) ;
#61555 = ORIENTED_EDGE('',*,*,#45848,.T.) ;
#61556 = ORIENTED_EDGE('',*,*,#45847,.F.) ;
#61557 = ORIENTED_EDGE('',*,*,#45849,.T.) ;
#61558 = ORIENTED_EDGE('',*,*,#45850,.T.) ;
#61559 = ORIENTED_EDGE('',*,*,#45851,.T.) ;
#61560 = ORIENTED_EDGE('',*,*,#45850,.F.) ;
#61561 = ORIENTED_EDGE('',*,*,#45852,.T.) ;
#61562 = ORIENTED_EDGE('',*,*,#45853,.T.) ;
#61563 = ORIENTED_EDGE('',*,*,#45854,.T.) ;
#61564 = ORIENTED_EDGE('',*,*,#45853,.F.) ;
#61565 = ORIENTED_EDGE('',*,*,#45855,.T.) ;
#61566 = ORIENTED_EDGE('',*,*,#45856,.T.) ;
#61567 = ORIENTED_EDGE('',*,*,#45857,.T.) ;
#61568 = ORIENTED_EDGE('',*,*,#45856,.F.) ;
#61569 = ORIENTED_EDGE('',*,*,#45858,.T.) ;
#61570 = ORIENTED_EDGE('',*,*,#45859,.T.) ;
#61571 = ORIENTED_EDGE('',*,*,#45860,.T.) ;
#61572 = ORIENTED_EDGE('',*,*,#45859,.F.) ;
#61573 = ORIENTED_EDGE('',*,*,#45861,.T.) ;
#61574 = ORIENTED_EDGE('',*,*,#45862,.T.) ;
#61575 = ORIENTED_EDGE('',*,*,#45863,.T.) ;
#61576 = ORIENTED_EDGE('',*,*,#45862,.F.) ;
#61577 = ORIENTED_EDGE('',*,*,#45864,.T.) ;
#61578 = ORIENTED_EDGE('',*,*,#45865,.T.) ;
#61579 = ORIENTED_EDGE('',*,*,#45866,.T.) ;
#61580 = ORIENTED_EDGE('',*,*,#45865,.F.) ;
#61581 = ORIENTED_EDGE('',*,*,#45867,.T.) ;
#61582 = ORIENTED_EDGE('',*,*,#45868,.T.) ;
#61583 = ORIENTED_EDGE('',*,*,#45869,.T.) ;
#61584 = ORIENTED_EDGE('',*,*,#45868,.F.) ;
#61585 = ORIENTED_EDGE('',*,*,#45870,.T.) ;
#61586 = ORIENTED_EDGE('',*,*,#45871,.T.) ;
#61587 = ORIENTED_EDGE('',*,*,#45872,.T.) ;
#61588 = ORIENTED_EDGE('',*,*,#45871,.F.) ;
#61589 = ORIENTED_EDGE('',*,*,#45873,.T.) ;
#61590 = ORIENTED_EDGE('',*,*,#45874,.T.) ;
#61591 = ORIENTED_EDGE('',*,*,#45875,.T.) ;
#61592 = ORIENTED_EDGE('',*,*,#45874,.F.) ;
#61593 = ORIENTED_EDGE('',*,*,#45876,.T.) ;
#61594 = ORIENTED_EDGE('',*,*,#45877,.T.) ;
#61595 = ORIENTED_EDGE('',*,*,#45878,.T.) ;
#61596 = ORIENTED_EDGE('',*,*,#45877,.F.) ;
#61597 = ORIENTED_EDGE('',*,*,#45879,.T.) ;
#61598 = ORIENTED_EDGE('',*,*,#45880,.T.) ;
#61599 = ORIENTED_EDGE('',*,*,#45881,.T.) ;
#61600 = ORIENTED_EDGE('',*,*,#45880,.F.) ;
#61601 = ORIENTED_EDGE('',*,*,#45882,.T.) ;
#61602 = ORIENTED_EDGE('',*,*,#45883,.T.) ;
#61603 = ORIENTED_EDGE('',*,*,#45884,.T.) ;
#61604 = ORIENTED_EDGE('',*,*,#45883,.F.) ;
#61605 = ORIENTED_EDGE('',*,*,#45885,.T.) ;
#61606 = ORIENTED_EDGE('',*,*,#45886,.T.) ;
#61607 = ORIENTED_EDGE('',*,*,#45887,.T.) ;
#61608 = ORIENTED_EDGE('',*,*,#45886,.F.) ;
#61609 = ORIENTED_EDGE('',*,*,#45888,.T.) ;
#61610 = ORIENTED_EDGE('',*,*,#45889,.T.) ;
#61611 = ORIENTED_EDGE('',*,*,#45890,.T.) ;
#61612 = ORIENTED_EDGE('',*,*,#45889,.F.) ;
#61613 = ORIENTED_EDGE('',*,*,#45891,.T.) ;
#61614 = ORIENTED_EDGE('',*,*,#45892,.T.) ;
#61615 = ORIENTED_EDGE('',*,*,#45893,.T.) ;
#61616 = ORIENTED_EDGE('',*,*,#45892,.F.) ;
#61617 = ORIENTED_EDGE('',*,*,#45894,.T.) ;
#61618 = ORIENTED_EDGE('',*,*,#45817,.T.) ;
#61619 = ORIENTED_EDGE('',*,*,#45895,.T.) ;
#61620 = ORIENTED_EDGE('',*,*,#45896,.T.) ;
#61621 = ORIENTED_EDGE('',*,*,#45897,.T.) ;
#61622 = ORIENTED_EDGE('',*,*,#45898,.T.) ;
#61623 = ORIENTED_EDGE('',*,*,#45899,.T.) ;
#61624 = ORIENTED_EDGE('',*,*,#45900,.T.) ;
#61625 = ORIENTED_EDGE('',*,*,#45901,.T.) ;
#61626 = ORIENTED_EDGE('',*,*,#45902,.T.) ;
#61627 = ORIENTED_EDGE('',*,*,#45903,.T.) ;
#61628 = ORIENTED_EDGE('',*,*,#45904,.T.) ;
#61629 = ORIENTED_EDGE('',*,*,#45905,.T.) ;
#61630 = ORIENTED_EDGE('',*,*,#45906,.T.) ;
#61631 = ORIENTED_EDGE('',*,*,#45907,.T.) ;
#61632 = ORIENTED_EDGE('',*,*,#45908,.T.) ;
#61633 = ORIENTED_EDGE('',*,*,#45909,.T.) ;
#61634 = ORIENTED_EDGE('',*,*,#45910,.T.) ;
#61635 = ORIENTED_EDGE('',*,*,#45911,.T.) ;
#61636 = ORIENTED_EDGE('',*,*,#45912,.T.) ;
#61637 = ORIENTED_EDGE('',*,*,#45913,.T.) ;
#61638 = ORIENTED_EDGE('',*,*,#44168,.T.) ;
#61639 = ORIENTED_EDGE('',*,*,#45914,.F.) ;
#61640 = ORIENTED_EDGE('',*,*,#45915,.T.) ;
#61641 = ORIENTED_EDGE('',*,*,#45916,.T.) ;
#61642 = ORIENTED_EDGE('',*,*,#45917,.T.) ;
#61643 = ORIENTED_EDGE('',*,*,#45916,.F.) ;
#61644 = ORIENTED_EDGE('',*,*,#45918,.T.) ;
#61645 = ORIENTED_EDGE('',*,*,#45919,.T.) ;
#61646 = ORIENTED_EDGE('',*,*,#45920,.T.) ;
#61647 = ORIENTED_EDGE('',*,*,#45919,.F.) ;
#61648 = ORIENTED_EDGE('',*,*,#45921,.T.) ;
#61649 = ORIENTED_EDGE('',*,*,#45922,.T.) ;
#61650 = ORIENTED_EDGE('',*,*,#45923,.T.) ;
#61651 = ORIENTED_EDGE('',*,*,#45922,.F.) ;
#61652 = ORIENTED_EDGE('',*,*,#45924,.T.) ;
#61653 = ORIENTED_EDGE('',*,*,#45925,.T.) ;
#61654 = ORIENTED_EDGE('',*,*,#45926,.T.) ;
#61655 = ORIENTED_EDGE('',*,*,#45925,.F.) ;
#61656 = ORIENTED_EDGE('',*,*,#45927,.T.) ;
#61657 = ORIENTED_EDGE('',*,*,#45928,.T.) ;
#61658 = ORIENTED_EDGE('',*,*,#45929,.T.) ;
#61659 = ORIENTED_EDGE('',*,*,#45928,.F.) ;
#61660 = ORIENTED_EDGE('',*,*,#45930,.T.) ;
#61661 = ORIENTED_EDGE('',*,*,#45931,.T.) ;
#61662 = ORIENTED_EDGE('',*,*,#45932,.T.) ;
#61663 = ORIENTED_EDGE('',*,*,#45931,.F.) ;
#61664 = ORIENTED_EDGE('',*,*,#44188,.T.) ;
#61665 = ORIENTED_EDGE('',*,*,#45933,.T.) ;
#61666 = ORIENTED_EDGE('',*,*,#45934,.T.) ;
#61667 = ORIENTED_EDGE('',*,*,#45933,.F.) ;
#61668 = ORIENTED_EDGE('',*,*,#45935,.T.) ;
#61669 = ORIENTED_EDGE('',*,*,#44365,.T.) ;
#61670 = ORIENTED_EDGE('',*,*,#45936,.T.) ;
#61671 = ORIENTED_EDGE('',*,*,#44364,.F.) ;
#61672 = ORIENTED_EDGE('',*,*,#45937,.T.) ;
#61673 = ORIENTED_EDGE('',*,*,#45938,.T.) ;
#61674 = ORIENTED_EDGE('',*,*,#45939,.T.) ;
#61675 = ORIENTED_EDGE('',*,*,#45938,.F.) ;
#61676 = ORIENTED_EDGE('',*,*,#45940,.T.) ;
#61677 = ORIENTED_EDGE('',*,*,#45941,.T.) ;
#61678 = ORIENTED_EDGE('',*,*,#45942,.T.) ;
#61679 = ORIENTED_EDGE('',*,*,#45941,.F.) ;
#61680 = ORIENTED_EDGE('',*,*,#45943,.T.) ;
#61681 = ORIENTED_EDGE('',*,*,#45944,.T.) ;
#61682 = ORIENTED_EDGE('',*,*,#45945,.T.) ;
#61683 = ORIENTED_EDGE('',*,*,#45944,.F.) ;
#61684 = ORIENTED_EDGE('',*,*,#45946,.T.) ;
#61685 = ORIENTED_EDGE('',*,*,#45947,.T.) ;
#61686 = ORIENTED_EDGE('',*,*,#45948,.T.) ;
#61687 = ORIENTED_EDGE('',*,*,#45947,.F.) ;
#61688 = ORIENTED_EDGE('',*,*,#45949,.T.) ;
#61689 = ORIENTED_EDGE('',*,*,#45950,.T.) ;
#61690 = ORIENTED_EDGE('',*,*,#45951,.T.) ;
#61691 = ORIENTED_EDGE('',*,*,#45950,.F.) ;
#61692 = ORIENTED_EDGE('',*,*,#45952,.T.) ;
#61693 = ORIENTED_EDGE('',*,*,#45953,.T.) ;
#61694 = ORIENTED_EDGE('',*,*,#45954,.T.) ;
#61695 = ORIENTED_EDGE('',*,*,#45953,.F.) ;
#61696 = ORIENTED_EDGE('',*,*,#45955,.T.) ;
#61697 = ORIENTED_EDGE('',*,*,#45956,.T.) ;
#61698 = ORIENTED_EDGE('',*,*,#45957,.T.) ;
#61699 = ORIENTED_EDGE('',*,*,#45956,.F.) ;
#61700 = ORIENTED_EDGE('',*,*,#45958,.T.) ;
#61701 = ORIENTED_EDGE('',*,*,#45959,.T.) ;
#61702 = ORIENTED_EDGE('',*,*,#45960,.T.) ;
#61703 = ORIENTED_EDGE('',*,*,#45959,.F.) ;
#61704 = ORIENTED_EDGE('',*,*,#45961,.T.) ;
#61705 = ORIENTED_EDGE('',*,*,#45962,.T.) ;
#61706 = ORIENTED_EDGE('',*,*,#45963,.T.) ;
#61707 = ORIENTED_EDGE('',*,*,#45962,.F.) ;
#61708 = ORIENTED_EDGE('',*,*,#45964,.T.) ;
#61709 = ORIENTED_EDGE('',*,*,#45965,.T.) ;
#61710 = ORIENTED_EDGE('',*,*,#45966,.T.) ;
#61711 = ORIENTED_EDGE('',*,*,#45965,.F.) ;
#61712 = ORIENTED_EDGE('',*,*,#45967,.T.) ;
#61713 = ORIENTED_EDGE('',*,*,#45968,.T.) ;
#61714 = ORIENTED_EDGE('',*,*,#45969,.T.) ;
#61715 = ORIENTED_EDGE('',*,*,#45968,.F.) ;
#61716 = ORIENTED_EDGE('',*,*,#45970,.T.) ;
#61717 = ORIENTED_EDGE('',*,*,#45971,.T.) ;
#61718 = ORIENTED_EDGE('',*,*,#45972,.T.) ;
#61719 = ORIENTED_EDGE('',*,*,#45971,.F.) ;
#61720 = ORIENTED_EDGE('',*,*,#45973,.T.) ;
#61721 = ORIENTED_EDGE('',*,*,#45974,.T.) ;
#61722 = ORIENTED_EDGE('',*,*,#45975,.T.) ;
#61723 = ORIENTED_EDGE('',*,*,#45974,.F.) ;
#61724 = ORIENTED_EDGE('',*,*,#45976,.T.) ;
#61725 = ORIENTED_EDGE('',*,*,#45977,.T.) ;
#61726 = ORIENTED_EDGE('',*,*,#45978,.T.) ;
#61727 = ORIENTED_EDGE('',*,*,#45977,.F.) ;
#61728 = ORIENTED_EDGE('',*,*,#45979,.T.) ;
#61729 = ORIENTED_EDGE('',*,*,#45980,.T.) ;
#61730 = ORIENTED_EDGE('',*,*,#45981,.T.) ;
#61731 = ORIENTED_EDGE('',*,*,#45980,.F.) ;
#61732 = ORIENTED_EDGE('',*,*,#45982,.T.) ;
#61733 = ORIENTED_EDGE('',*,*,#45983,.T.) ;
#61734 = ORIENTED_EDGE('',*,*,#45984,.T.) ;
#61735 = ORIENTED_EDGE('',*,*,#45983,.F.) ;
#61736 = ORIENTED_EDGE('',*,*,#45985,.T.) ;
#61737 = ORIENTED_EDGE('',*,*,#45986,.T.) ;
#61738 = ORIENTED_EDGE('',*,*,#45987,.T.) ;
#61739 = ORIENTED_EDGE('',*,*,#45986,.F.) ;
#61740 = ORIENTED_EDGE('',*,*,#45988,.T.) ;
#61741 = ORIENTED_EDGE('',*,*,#45989,.T.) ;
#61742 = ORIENTED_EDGE('',*,*,#45990,.T.) ;
#61743 = ORIENTED_EDGE('',*,*,#45989,.F.) ;
#61744 = ORIENTED_EDGE('',*,*,#45991,.T.) ;
#61745 = ORIENTED_EDGE('',*,*,#45914,.T.) ;
#61746 = ORIENTED_EDGE('',*,*,#45992,.T.) ;
#61747 = ORIENTED_EDGE('',*,*,#45993,.T.) ;
#61748 = ORIENTED_EDGE('',*,*,#45994,.T.) ;
#61749 = ORIENTED_EDGE('',*,*,#45995,.T.) ;
#61750 = ORIENTED_EDGE('',*,*,#45996,.T.) ;
#61751 = ORIENTED_EDGE('',*,*,#45997,.T.) ;
#61752 = ORIENTED_EDGE('',*,*,#45998,.T.) ;
#61753 = ORIENTED_EDGE('',*,*,#45999,.T.) ;
#61754 = ORIENTED_EDGE('',*,*,#46000,.T.) ;
#61755 = ORIENTED_EDGE('',*,*,#46001,.T.) ;
#61756 = ORIENTED_EDGE('',*,*,#46002,.T.) ;
#61757 = ORIENTED_EDGE('',*,*,#46003,.T.) ;
#61758 = ORIENTED_EDGE('',*,*,#46004,.T.) ;
#61759 = ORIENTED_EDGE('',*,*,#46005,.T.) ;
#61760 = ORIENTED_EDGE('',*,*,#46006,.T.) ;
#61761 = ORIENTED_EDGE('',*,*,#46007,.T.) ;
#61762 = ORIENTED_EDGE('',*,*,#46008,.T.) ;
#61763 = ORIENTED_EDGE('',*,*,#46009,.T.) ;
#61764 = ORIENTED_EDGE('',*,*,#46010,.T.) ;
#61765 = ORIENTED_EDGE('',*,*,#44185,.T.) ;
#61766 = ORIENTED_EDGE('',*,*,#46011,.F.) ;
#61767 = ORIENTED_EDGE('',*,*,#46012,.T.) ;
#61768 = ORIENTED_EDGE('',*,*,#46013,.T.) ;
#61769 = ORIENTED_EDGE('',*,*,#46014,.T.) ;
#61770 = ORIENTED_EDGE('',*,*,#46013,.F.) ;
#61771 = ORIENTED_EDGE('',*,*,#46015,.T.) ;
#61772 = ORIENTED_EDGE('',*,*,#46016,.T.) ;
#61773 = ORIENTED_EDGE('',*,*,#46017,.T.) ;
#61774 = ORIENTED_EDGE('',*,*,#46016,.F.) ;
#61775 = ORIENTED_EDGE('',*,*,#46018,.T.) ;
#61776 = ORIENTED_EDGE('',*,*,#46019,.T.) ;
#61777 = ORIENTED_EDGE('',*,*,#46020,.T.) ;
#61778 = ORIENTED_EDGE('',*,*,#46019,.F.) ;
#61779 = ORIENTED_EDGE('',*,*,#46021,.T.) ;
#61780 = ORIENTED_EDGE('',*,*,#46022,.T.) ;
#61781 = ORIENTED_EDGE('',*,*,#46023,.T.) ;
#61782 = ORIENTED_EDGE('',*,*,#46022,.F.) ;
#61783 = ORIENTED_EDGE('',*,*,#46024,.T.) ;
#61784 = ORIENTED_EDGE('',*,*,#46025,.T.) ;
#61785 = ORIENTED_EDGE('',*,*,#46026,.T.) ;
#61786 = ORIENTED_EDGE('',*,*,#46025,.F.) ;
#61787 = ORIENTED_EDGE('',*,*,#46027,.T.) ;
#61788 = ORIENTED_EDGE('',*,*,#46028,.T.) ;
#61789 = ORIENTED_EDGE('',*,*,#46029,.T.) ;
#61790 = ORIENTED_EDGE('',*,*,#46028,.F.) ;
#61791 = ORIENTED_EDGE('',*,*,#44205,.T.) ;
#61792 = ORIENTED_EDGE('',*,*,#46030,.T.) ;
#61793 = ORIENTED_EDGE('',*,*,#46031,.T.) ;
#61794 = ORIENTED_EDGE('',*,*,#46030,.F.) ;
#61795 = ORIENTED_EDGE('',*,*,#46032,.T.) ;
#61796 = ORIENTED_EDGE('',*,*,#44362,.T.) ;
#61797 = ORIENTED_EDGE('',*,*,#46033,.T.) ;
#61798 = ORIENTED_EDGE('',*,*,#44361,.F.) ;
#61799 = ORIENTED_EDGE('',*,*,#46034,.T.) ;
#61800 = ORIENTED_EDGE('',*,*,#46035,.T.) ;
#61801 = ORIENTED_EDGE('',*,*,#46036,.T.) ;
#61802 = ORIENTED_EDGE('',*,*,#46035,.F.) ;
#61803 = ORIENTED_EDGE('',*,*,#46037,.T.) ;
#61804 = ORIENTED_EDGE('',*,*,#46038,.T.) ;
#61805 = ORIENTED_EDGE('',*,*,#46039,.T.) ;
#61806 = ORIENTED_EDGE('',*,*,#46038,.F.) ;
#61807 = ORIENTED_EDGE('',*,*,#46040,.T.) ;
#61808 = ORIENTED_EDGE('',*,*,#46041,.T.) ;
#61809 = ORIENTED_EDGE('',*,*,#46042,.T.) ;
#61810 = ORIENTED_EDGE('',*,*,#46041,.F.) ;
#61811 = ORIENTED_EDGE('',*,*,#46043,.T.) ;
#61812 = ORIENTED_EDGE('',*,*,#46044,.T.) ;
#61813 = ORIENTED_EDGE('',*,*,#46045,.T.) ;
#61814 = ORIENTED_EDGE('',*,*,#46044,.F.) ;
#61815 = ORIENTED_EDGE('',*,*,#46046,.T.) ;
#61816 = ORIENTED_EDGE('',*,*,#46047,.T.) ;
#61817 = ORIENTED_EDGE('',*,*,#46048,.T.) ;
#61818 = ORIENTED_EDGE('',*,*,#46047,.F.) ;
#61819 = ORIENTED_EDGE('',*,*,#46049,.T.) ;
#61820 = ORIENTED_EDGE('',*,*,#46050,.T.) ;
#61821 = ORIENTED_EDGE('',*,*,#46051,.T.) ;
#61822 = ORIENTED_EDGE('',*,*,#46050,.F.) ;
#61823 = ORIENTED_EDGE('',*,*,#46052,.T.) ;
#61824 = ORIENTED_EDGE('',*,*,#46053,.T.) ;
#61825 = ORIENTED_EDGE('',*,*,#46054,.T.) ;
#61826 = ORIENTED_EDGE('',*,*,#46053,.F.) ;
#61827 = ORIENTED_EDGE('',*,*,#46055,.T.) ;
#61828 = ORIENTED_EDGE('',*,*,#46056,.T.) ;
#61829 = ORIENTED_EDGE('',*,*,#46057,.T.) ;
#61830 = ORIENTED_EDGE('',*,*,#46056,.F.) ;
#61831 = ORIENTED_EDGE('',*,*,#46058,.T.) ;
#61832 = ORIENTED_EDGE('',*,*,#46059,.T.) ;
#61833 = ORIENTED_EDGE('',*,*,#46060,.T.) ;
#61834 = ORIENTED_EDGE('',*,*,#46059,.F.) ;
#61835 = ORIENTED_EDGE('',*,*,#46061,.T.) ;
#61836 = ORIENTED_EDGE('',*,*,#46062,.T.) ;
#61837 = ORIENTED_EDGE('',*,*,#46063,.T.) ;
#61838 = ORIENTED_EDGE('',*,*,#46062,.F.) ;
#61839 = ORIENTED_EDGE('',*,*,#46064,.T.) ;
#61840 = ORIENTED_EDGE('',*,*,#46065,.T.) ;
#61841 = ORIENTED_EDGE('',*,*,#46066,.T.) ;
#61842 = ORIENTED_EDGE('',*,*,#46065,.F.) ;
#61843 = ORIENTED_EDGE('',*,*,#46067,.T.) ;
#61844 = ORIENTED_EDGE('',*,*,#46068,.T.) ;
#61845 = ORIENTED_EDGE('',*,*,#46069,.T.) ;
#61846 = ORIENTED_EDGE('',*,*,#46068,.F.) ;
#61847 = ORIENTED_EDGE('',*,*,#46070,.T.) ;
#61848 = ORIENTED_EDGE('',*,*,#46071,.T.) ;
#61849 = ORIENTED_EDGE('',*,*,#46072,.T.) ;
#61850 = ORIENTED_EDGE('',*,*,#46071,.F.) ;
#61851 = ORIENTED_EDGE('',*,*,#46073,.T.) ;
#61852 = ORIENTED_EDGE('',*,*,#46074,.T.) ;
#61853 = ORIENTED_EDGE('',*,*,#46075,.T.) ;
#61854 = ORIENTED_EDGE('',*,*,#46074,.F.) ;
#61855 = ORIENTED_EDGE('',*,*,#46076,.T.) ;
#61856 = ORIENTED_EDGE('',*,*,#46077,.T.) ;
#61857 = ORIENTED_EDGE('',*,*,#46078,.T.) ;
#61858 = ORIENTED_EDGE('',*,*,#46077,.F.) ;
#61859 = ORIENTED_EDGE('',*,*,#46079,.T.) ;
#61860 = ORIENTED_EDGE('',*,*,#46080,.T.) ;
#61861 = ORIENTED_EDGE('',*,*,#46081,.T.) ;
#61862 = ORIENTED_EDGE('',*,*,#46080,.F.) ;
#61863 = ORIENTED_EDGE('',*,*,#46082,.T.) ;
#61864 = ORIENTED_EDGE('',*,*,#46083,.T.) ;
#61865 = ORIENTED_EDGE('',*,*,#46084,.T.) ;
#61866 = ORIENTED_EDGE('',*,*,#46083,.F.) ;
#61867 = ORIENTED_EDGE('',*,*,#46085,.T.) ;
#61868 = ORIENTED_EDGE('',*,*,#46086,.T.) ;
#61869 = ORIENTED_EDGE('',*,*,#46087,.T.) ;
#61870 = ORIENTED_EDGE('',*,*,#46086,.F.) ;
#61871 = ORIENTED_EDGE('',*,*,#46088,.T.) ;
#61872 = ORIENTED_EDGE('',*,*,#46011,.T.) ;
#61873 = ORIENTED_EDGE('',*,*,#46089,.T.) ;
#61874 = ORIENTED_EDGE('',*,*,#46090,.T.) ;
#61875 = ORIENTED_EDGE('',*,*,#46091,.T.) ;
#61876 = ORIENTED_EDGE('',*,*,#46092,.T.) ;
#61877 = ORIENTED_EDGE('',*,*,#46093,.T.) ;
#61878 = ORIENTED_EDGE('',*,*,#46094,.T.) ;
#61879 = ORIENTED_EDGE('',*,*,#46095,.T.) ;
#61880 = ORIENTED_EDGE('',*,*,#46096,.T.) ;
#61881 = ORIENTED_EDGE('',*,*,#46097,.T.) ;
#61882 = ORIENTED_EDGE('',*,*,#46098,.T.) ;
#61883 = ORIENTED_EDGE('',*,*,#46099,.T.) ;
#61884 = ORIENTED_EDGE('',*,*,#46100,.T.) ;
#61885 = ORIENTED_EDGE('',*,*,#46101,.T.) ;
#61886 = ORIENTED_EDGE('',*,*,#46102,.T.) ;
#61887 = ORIENTED_EDGE('',*,*,#46103,.T.) ;
#61888 = ORIENTED_EDGE('',*,*,#46104,.T.) ;
#61889 = ORIENTED_EDGE('',*,*,#46105,.T.) ;
#61890 = ORIENTED_EDGE('',*,*,#46106,.T.) ;
#61891 = ORIENTED_EDGE('',*,*,#46107,.T.) ;
#61892 = ORIENTED_EDGE('',*,*,#44202,.T.) ;
#61893 = ORIENTED_EDGE('',*,*,#46108,.F.) ;
#61894 = ORIENTED_EDGE('',*,*,#46109,.T.) ;
#61895 = ORIENTED_EDGE('',*,*,#46110,.T.) ;
#61896 = ORIENTED_EDGE('',*,*,#46111,.T.) ;
#61897 = ORIENTED_EDGE('',*,*,#46110,.F.) ;
#61898 = ORIENTED_EDGE('',*,*,#46112,.T.) ;
#61899 = ORIENTED_EDGE('',*,*,#46113,.T.) ;
#61900 = ORIENTED_EDGE('',*,*,#46114,.T.) ;
#61901 = ORIENTED_EDGE('',*,*,#46113,.F.) ;
#61902 = ORIENTED_EDGE('',*,*,#46115,.T.) ;
#61903 = ORIENTED_EDGE('',*,*,#46116,.T.) ;
#61904 = ORIENTED_EDGE('',*,*,#46117,.T.) ;
#61905 = ORIENTED_EDGE('',*,*,#46116,.F.) ;
#61906 = ORIENTED_EDGE('',*,*,#46118,.T.) ;
#61907 = ORIENTED_EDGE('',*,*,#46119,.T.) ;
#61908 = ORIENTED_EDGE('',*,*,#46120,.T.) ;
#61909 = ORIENTED_EDGE('',*,*,#46119,.F.) ;
#61910 = ORIENTED_EDGE('',*,*,#46121,.T.) ;
#61911 = ORIENTED_EDGE('',*,*,#46122,.T.) ;
#61912 = ORIENTED_EDGE('',*,*,#46123,.T.) ;
#61913 = ORIENTED_EDGE('',*,*,#46122,.F.) ;
#61914 = ORIENTED_EDGE('',*,*,#46124,.T.) ;
#61915 = ORIENTED_EDGE('',*,*,#46125,.T.) ;
#61916 = ORIENTED_EDGE('',*,*,#46126,.T.) ;
#61917 = ORIENTED_EDGE('',*,*,#46125,.F.) ;
#61918 = ORIENTED_EDGE('',*,*,#44222,.T.) ;
#61919 = ORIENTED_EDGE('',*,*,#46127,.T.) ;
#61920 = ORIENTED_EDGE('',*,*,#46128,.T.) ;
#61921 = ORIENTED_EDGE('',*,*,#46127,.F.) ;
#61922 = ORIENTED_EDGE('',*,*,#46129,.T.) ;
#61923 = ORIENTED_EDGE('',*,*,#44359,.T.) ;
#61924 = ORIENTED_EDGE('',*,*,#46130,.T.) ;
#61925 = ORIENTED_EDGE('',*,*,#44358,.F.) ;
#61926 = ORIENTED_EDGE('',*,*,#46131,.T.) ;
#61927 = ORIENTED_EDGE('',*,*,#46132,.T.) ;
#61928 = ORIENTED_EDGE('',*,*,#46133,.T.) ;
#61929 = ORIENTED_EDGE('',*,*,#46132,.F.) ;
#61930 = ORIENTED_EDGE('',*,*,#46134,.T.) ;
#61931 = ORIENTED_EDGE('',*,*,#46135,.T.) ;
#61932 = ORIENTED_EDGE('',*,*,#46136,.T.) ;
#61933 = ORIENTED_EDGE('',*,*,#46135,.F.) ;
#61934 = ORIENTED_EDGE('',*,*,#46137,.T.) ;
#61935 = ORIENTED_EDGE('',*,*,#46138,.T.) ;
#61936 = ORIENTED_EDGE('',*,*,#46139,.T.) ;
#61937 = ORIENTED_EDGE('',*,*,#46138,.F.) ;
#61938 = ORIENTED_EDGE('',*,*,#46140,.T.) ;
#61939 = ORIENTED_EDGE('',*,*,#46141,.T.) ;
#61940 = ORIENTED_EDGE('',*,*,#46142,.T.) ;
#61941 = ORIENTED_EDGE('',*,*,#46141,.F.) ;
#61942 = ORIENTED_EDGE('',*,*,#46143,.T.) ;
#61943 = ORIENTED_EDGE('',*,*,#46144,.T.) ;
#61944 = ORIENTED_EDGE('',*,*,#46145,.T.) ;
#61945 = ORIENTED_EDGE('',*,*,#46144,.F.) ;
#61946 = ORIENTED_EDGE('',*,*,#46146,.T.) ;
#61947 = ORIENTED_EDGE('',*,*,#46147,.T.) ;
#61948 = ORIENTED_EDGE('',*,*,#46148,.T.) ;
#61949 = ORIENTED_EDGE('',*,*,#46147,.F.) ;
#61950 = ORIENTED_EDGE('',*,*,#46149,.T.) ;
#61951 = ORIENTED_EDGE('',*,*,#46150,.T.) ;
#61952 = ORIENTED_EDGE('',*,*,#46151,.T.) ;
#61953 = ORIENTED_EDGE('',*,*,#46150,.F.) ;
#61954 = ORIENTED_EDGE('',*,*,#46152,.T.) ;
#61955 = ORIENTED_EDGE('',*,*,#46153,.T.) ;
#61956 = ORIENTED_EDGE('',*,*,#46154,.T.) ;
#61957 = ORIENTED_EDGE('',*,*,#46153,.F.) ;
#61958 = ORIENTED_EDGE('',*,*,#46155,.T.) ;
#61959 = ORIENTED_EDGE('',*,*,#46156,.T.) ;
#61960 = ORIENTED_EDGE('',*,*,#46157,.T.) ;
#61961 = ORIENTED_EDGE('',*,*,#46156,.F.) ;
#61962 = ORIENTED_EDGE('',*,*,#46158,.T.) ;
#61963 = ORIENTED_EDGE('',*,*,#46159,.T.) ;
#61964 = ORIENTED_EDGE('',*,*,#46160,.T.) ;
#61965 = ORIENTED_EDGE('',*,*,#46159,.F.) ;
#61966 = ORIENTED_EDGE('',*,*,#46161,.T.) ;
#61967 = ORIENTED_EDGE('',*,*,#46162,.T.) ;
#61968 = ORIENTED_EDGE('',*,*,#46163,.T.) ;
#61969 = ORIENTED_EDGE('',*,*,#46162,.F.) ;
#61970 = ORIENTED_EDGE('',*,*,#46164,.T.) ;
#61971 = ORIENTED_EDGE('',*,*,#46165,.T.) ;
#61972 = ORIENTED_EDGE('',*,*,#46166,.T.) ;
#61973 = ORIENTED_EDGE('',*,*,#46165,.F.) ;
#61974 = ORIENTED_EDGE('',*,*,#46167,.T.) ;
#61975 = ORIENTED_EDGE('',*,*,#46168,.T.) ;
#61976 = ORIENTED_EDGE('',*,*,#46169,.T.) ;
#61977 = ORIENTED_EDGE('',*,*,#46168,.F.) ;
#61978 = ORIENTED_EDGE('',*,*,#46170,.T.) ;
#61979 = ORIENTED_EDGE('',*,*,#46171,.T.) ;
#61980 = ORIENTED_EDGE('',*,*,#46172,.T.) ;
#61981 = ORIENTED_EDGE('',*,*,#46171,.F.) ;
#61982 = ORIENTED_EDGE('',*,*,#46173,.T.) ;
#61983 = ORIENTED_EDGE('',*,*,#46174,.T.) ;
#61984 = ORIENTED_EDGE('',*,*,#46175,.T.) ;
#61985 = ORIENTED_EDGE('',*,*,#46174,.F.) ;
#61986 = ORIENTED_EDGE('',*,*,#46176,.T.) ;
#61987 = ORIENTED_EDGE('',*,*,#46177,.T.) ;
#61988 = ORIENTED_EDGE('',*,*,#46178,.T.) ;
#61989 = ORIENTED_EDGE('',*,*,#46177,.F.) ;
#61990 = ORIENTED_EDGE('',*,*,#46179,.T.) ;
#61991 = ORIENTED_EDGE('',*,*,#46180,.T.) ;
#61992 = ORIENTED_EDGE('',*,*,#46181,.T.) ;
#61993 = ORIENTED_EDGE('',*,*,#46180,.F.) ;
#61994 = ORIENTED_EDGE('',*,*,#46182,.T.) ;
#61995 = ORIENTED_EDGE('',*,*,#46183,.T.) ;
#61996 = ORIENTED_EDGE('',*,*,#46184,.T.) ;
#61997 = ORIENTED_EDGE('',*,*,#46183,.F.) ;
#61998 = ORIENTED_EDGE('',*,*,#46185,.T.) ;
#61999 = ORIENTED_EDGE('',*,*,#46108,.T.) ;
#62000 = ORIENTED_EDGE('',*,*,#46186,.T.) ;
#62001 = ORIENTED_EDGE('',*,*,#46187,.T.) ;
#62002 = ORIENTED_EDGE('',*,*,#46188,.T.) ;
#62003 = ORIENTED_EDGE('',*,*,#46189,.T.) ;
#62004 = ORIENTED_EDGE('',*,*,#46190,.T.) ;
#62005 = ORIENTED_EDGE('',*,*,#46191,.T.) ;
#62006 = ORIENTED_EDGE('',*,*,#46192,.T.) ;
#62007 = ORIENTED_EDGE('',*,*,#46193,.T.) ;
#62008 = ORIENTED_EDGE('',*,*,#46194,.T.) ;
#62009 = ORIENTED_EDGE('',*,*,#46195,.T.) ;
#62010 = ORIENTED_EDGE('',*,*,#46196,.T.) ;
#62011 = ORIENTED_EDGE('',*,*,#46197,.T.) ;
#62012 = ORIENTED_EDGE('',*,*,#46198,.T.) ;
#62013 = ORIENTED_EDGE('',*,*,#46199,.T.) ;
#62014 = ORIENTED_EDGE('',*,*,#46200,.T.) ;
#62015 = ORIENTED_EDGE('',*,*,#46201,.T.) ;
#62016 = ORIENTED_EDGE('',*,*,#46202,.T.) ;
#62017 = ORIENTED_EDGE('',*,*,#46203,.T.) ;
#62018 = ORIENTED_EDGE('',*,*,#46204,.T.) ;
#62019 = ORIENTED_EDGE('',*,*,#44219,.T.) ;
#62020 = ORIENTED_EDGE('',*,*,#46205,.F.) ;
#62021 = ORIENTED_EDGE('',*,*,#46206,.T.) ;
#62022 = ORIENTED_EDGE('',*,*,#46207,.T.) ;
#62023 = ORIENTED_EDGE('',*,*,#46208,.T.) ;
#62024 = ORIENTED_EDGE('',*,*,#46207,.F.) ;
#62025 = ORIENTED_EDGE('',*,*,#46209,.T.) ;
#62026 = ORIENTED_EDGE('',*,*,#46210,.T.) ;
#62027 = ORIENTED_EDGE('',*,*,#46211,.T.) ;
#62028 = ORIENTED_EDGE('',*,*,#46210,.F.) ;
#62029 = ORIENTED_EDGE('',*,*,#46212,.T.) ;
#62030 = ORIENTED_EDGE('',*,*,#46213,.T.) ;
#62031 = ORIENTED_EDGE('',*,*,#46214,.T.) ;
#62032 = ORIENTED_EDGE('',*,*,#46213,.F.) ;
#62033 = ORIENTED_EDGE('',*,*,#46215,.T.) ;
#62034 = ORIENTED_EDGE('',*,*,#46216,.T.) ;
#62035 = ORIENTED_EDGE('',*,*,#46217,.T.) ;
#62036 = ORIENTED_EDGE('',*,*,#46216,.F.) ;
#62037 = ORIENTED_EDGE('',*,*,#46218,.T.) ;
#62038 = ORIENTED_EDGE('',*,*,#46219,.T.) ;
#62039 = ORIENTED_EDGE('',*,*,#46220,.T.) ;
#62040 = ORIENTED_EDGE('',*,*,#46219,.F.) ;
#62041 = ORIENTED_EDGE('',*,*,#46221,.T.) ;
#62042 = ORIENTED_EDGE('',*,*,#46222,.T.) ;
#62043 = ORIENTED_EDGE('',*,*,#46223,.T.) ;
#62044 = ORIENTED_EDGE('',*,*,#46222,.F.) ;
#62045 = ORIENTED_EDGE('',*,*,#44239,.T.) ;
#62046 = ORIENTED_EDGE('',*,*,#46224,.T.) ;
#62047 = ORIENTED_EDGE('',*,*,#46225,.T.) ;
#62048 = ORIENTED_EDGE('',*,*,#46224,.F.) ;
#62049 = ORIENTED_EDGE('',*,*,#46226,.T.) ;
#62050 = ORIENTED_EDGE('',*,*,#44356,.T.) ;
#62051 = ORIENTED_EDGE('',*,*,#46227,.T.) ;
#62052 = ORIENTED_EDGE('',*,*,#44355,.F.) ;
#62053 = ORIENTED_EDGE('',*,*,#46228,.T.) ;
#62054 = ORIENTED_EDGE('',*,*,#46229,.T.) ;
#62055 = ORIENTED_EDGE('',*,*,#46230,.T.) ;
#62056 = ORIENTED_EDGE('',*,*,#46229,.F.) ;
#62057 = ORIENTED_EDGE('',*,*,#46231,.T.) ;
#62058 = ORIENTED_EDGE('',*,*,#46232,.T.) ;
#62059 = ORIENTED_EDGE('',*,*,#46233,.T.) ;
#62060 = ORIENTED_EDGE('',*,*,#46232,.F.) ;
#62061 = ORIENTED_EDGE('',*,*,#46234,.T.) ;
#62062 = ORIENTED_EDGE('',*,*,#46235,.T.) ;
#62063 = ORIENTED_EDGE('',*,*,#46236,.T.) ;
#62064 = ORIENTED_EDGE('',*,*,#46235,.F.) ;
#62065 = ORIENTED_EDGE('',*,*,#46237,.T.) ;
#62066 = ORIENTED_EDGE('',*,*,#46238,.T.) ;
#62067 = ORIENTED_EDGE('',*,*,#46239,.T.) ;
#62068 = ORIENTED_EDGE('',*,*,#46238,.F.) ;
#62069 = ORIENTED_EDGE('',*,*,#46240,.T.) ;
#62070 = ORIENTED_EDGE('',*,*,#46241,.T.) ;
#62071 = ORIENTED_EDGE('',*,*,#46242,.T.) ;
#62072 = ORIENTED_EDGE('',*,*,#46241,.F.) ;
#62073 = ORIENTED_EDGE('',*,*,#46243,.T.) ;
#62074 = ORIENTED_EDGE('',*,*,#46244,.T.) ;
#62075 = ORIENTED_EDGE('',*,*,#46245,.T.) ;
#62076 = ORIENTED_EDGE('',*,*,#46244,.F.) ;
#62077 = ORIENTED_EDGE('',*,*,#46246,.T.) ;
#62078 = ORIENTED_EDGE('',*,*,#46247,.T.) ;
#62079 = ORIENTED_EDGE('',*,*,#46248,.T.) ;
#62080 = ORIENTED_EDGE('',*,*,#46247,.F.) ;
#62081 = ORIENTED_EDGE('',*,*,#46249,.T.) ;
#62082 = ORIENTED_EDGE('',*,*,#46250,.T.) ;
#62083 = ORIENTED_EDGE('',*,*,#46251,.T.) ;
#62084 = ORIENTED_EDGE('',*,*,#46250,.F.) ;
#62085 = ORIENTED_EDGE('',*,*,#46252,.T.) ;
#62086 = ORIENTED_EDGE('',*,*,#46253,.T.) ;
#62087 = ORIENTED_EDGE('',*,*,#46254,.T.) ;
#62088 = ORIENTED_EDGE('',*,*,#46253,.F.) ;
#62089 = ORIENTED_EDGE('',*,*,#46255,.T.) ;
#62090 = ORIENTED_EDGE('',*,*,#46256,.T.) ;
#62091 = ORIENTED_EDGE('',*,*,#46257,.T.) ;
#62092 = ORIENTED_EDGE('',*,*,#46256,.F.) ;
#62093 = ORIENTED_EDGE('',*,*,#46258,.T.) ;
#62094 = ORIENTED_EDGE('',*,*,#46259,.T.) ;
#62095 = ORIENTED_EDGE('',*,*,#46260,.T.) ;
#62096 = ORIENTED_EDGE('',*,*,#46259,.F.) ;
#62097 = ORIENTED_EDGE('',*,*,#46261,.T.) ;
#62098 = ORIENTED_EDGE('',*,*,#46262,.T.) ;
#62099 = ORIENTED_EDGE('',*,*,#46263,.T.) ;
#62100 = ORIENTED_EDGE('',*,*,#46262,.F.) ;
#62101 = ORIENTED_EDGE('',*,*,#46264,.T.) ;
#62102 = ORIENTED_EDGE('',*,*,#46265,.T.) ;
#62103 = ORIENTED_EDGE('',*,*,#46266,.T.) ;
#62104 = ORIENTED_EDGE('',*,*,#46265,.F.) ;
#62105 = ORIENTED_EDGE('',*,*,#46267,.T.) ;
#62106 = ORIENTED_EDGE('',*,*,#46268,.T.) ;
#62107 = ORIENTED_EDGE('',*,*,#46269,.T.) ;
#62108 = ORIENTED_EDGE('',*,*,#46268,.F.) ;
#62109 = ORIENTED_EDGE('',*,*,#46270,.T.) ;
#62110 = ORIENTED_EDGE('',*,*,#46271,.T.) ;
#62111 = ORIENTED_EDGE('',*,*,#46272,.T.) ;
#62112 = ORIENTED_EDGE('',*,*,#46271,.F.) ;
#62113 = ORIENTED_EDGE('',*,*,#46273,.T.) ;
#62114 = ORIENTED_EDGE('',*,*,#46274,.T.) ;
#62115 = ORIENTED_EDGE('',*,*,#46275,.T.) ;
#62116 = ORIENTED_EDGE('',*,*,#46274,.F.) ;
#62117 = ORIENTED_EDGE('',*,*,#46276,.T.) ;
#62118 = ORIENTED_EDGE('',*,*,#46277,.T.) ;
#62119 = ORIENTED_EDGE('',*,*,#46278,.T.) ;
#62120 = ORIENTED_EDGE('',*,*,#46277,.F.) ;
#62121 = ORIENTED_EDGE('',*,*,#46279,.T.) ;
#62122 = ORIENTED_EDGE('',*,*,#46280,.T.) ;
#62123 = ORIENTED_EDGE('',*,*,#46281,.T.) ;
#62124 = ORIENTED_EDGE('',*,*,#46280,.F.) ;
#62125 = ORIENTED_EDGE('',*,*,#46282,.T.) ;
#62126 = ORIENTED_EDGE('',*,*,#46205,.T.) ;
#62127 = ORIENTED_EDGE('',*,*,#46283,.T.) ;
#62128 = ORIENTED_EDGE('',*,*,#46284,.T.) ;
#62129 = ORIENTED_EDGE('',*,*,#46285,.T.) ;
#62130 = ORIENTED_EDGE('',*,*,#46286,.T.) ;
#62131 = ORIENTED_EDGE('',*,*,#46287,.T.) ;
#62132 = ORIENTED_EDGE('',*,*,#46288,.T.) ;
#62133 = ORIENTED_EDGE('',*,*,#46289,.T.) ;
#62134 = ORIENTED_EDGE('',*,*,#46290,.T.) ;
#62135 = ORIENTED_EDGE('',*,*,#46291,.T.) ;
#62136 = ORIENTED_EDGE('',*,*,#46292,.T.) ;
#62137 = ORIENTED_EDGE('',*,*,#46293,.T.) ;
#62138 = ORIENTED_EDGE('',*,*,#46294,.T.) ;
#62139 = ORIENTED_EDGE('',*,*,#46295,.T.) ;
#62140 = ORIENTED_EDGE('',*,*,#46296,.T.) ;
#62141 = ORIENTED_EDGE('',*,*,#46297,.T.) ;
#62142 = ORIENTED_EDGE('',*,*,#46298,.T.) ;
#62143 = ORIENTED_EDGE('',*,*,#46299,.T.) ;
#62144 = ORIENTED_EDGE('',*,*,#46300,.T.) ;
#62145 = ORIENTED_EDGE('',*,*,#46301,.T.) ;
#62146 = ORIENTED_EDGE('',*,*,#44236,.T.) ;
#62147 = ORIENTED_EDGE('',*,*,#46302,.F.) ;
#62148 = ORIENTED_EDGE('',*,*,#46303,.T.) ;
#62149 = ORIENTED_EDGE('',*,*,#46304,.T.) ;
#62150 = ORIENTED_EDGE('',*,*,#46305,.T.) ;
#62151 = ORIENTED_EDGE('',*,*,#46304,.F.) ;
#62152 = ORIENTED_EDGE('',*,*,#46306,.T.) ;
#62153 = ORIENTED_EDGE('',*,*,#46307,.T.) ;
#62154 = ORIENTED_EDGE('',*,*,#46308,.T.) ;
#62155 = ORIENTED_EDGE('',*,*,#46307,.F.) ;
#62156 = ORIENTED_EDGE('',*,*,#46309,.T.) ;
#62157 = ORIENTED_EDGE('',*,*,#46310,.T.) ;
#62158 = ORIENTED_EDGE('',*,*,#46311,.T.) ;
#62159 = ORIENTED_EDGE('',*,*,#46310,.F.) ;
#62160 = ORIENTED_EDGE('',*,*,#46312,.T.) ;
#62161 = ORIENTED_EDGE('',*,*,#46313,.T.) ;
#62162 = ORIENTED_EDGE('',*,*,#46314,.T.) ;
#62163 = ORIENTED_EDGE('',*,*,#46313,.F.) ;
#62164 = ORIENTED_EDGE('',*,*,#46315,.T.) ;
#62165 = ORIENTED_EDGE('',*,*,#46316,.T.) ;
#62166 = ORIENTED_EDGE('',*,*,#46317,.T.) ;
#62167 = ORIENTED_EDGE('',*,*,#46316,.F.) ;
#62168 = ORIENTED_EDGE('',*,*,#46318,.T.) ;
#62169 = ORIENTED_EDGE('',*,*,#46319,.T.) ;
#62170 = ORIENTED_EDGE('',*,*,#46320,.T.) ;
#62171 = ORIENTED_EDGE('',*,*,#46319,.F.) ;
#62172 = ORIENTED_EDGE('',*,*,#44256,.T.) ;
#62173 = ORIENTED_EDGE('',*,*,#46321,.T.) ;
#62174 = ORIENTED_EDGE('',*,*,#46322,.T.) ;
#62175 = ORIENTED_EDGE('',*,*,#46321,.F.) ;
#62176 = ORIENTED_EDGE('',*,*,#46323,.T.) ;
#62177 = ORIENTED_EDGE('',*,*,#44353,.T.) ;
#62178 = ORIENTED_EDGE('',*,*,#46324,.T.) ;
#62179 = ORIENTED_EDGE('',*,*,#44352,.F.) ;
#62180 = ORIENTED_EDGE('',*,*,#46325,.T.) ;
#62181 = ORIENTED_EDGE('',*,*,#46326,.T.) ;
#62182 = ORIENTED_EDGE('',*,*,#46327,.T.) ;
#62183 = ORIENTED_EDGE('',*,*,#46326,.F.) ;
#62184 = ORIENTED_EDGE('',*,*,#46328,.T.) ;
#62185 = ORIENTED_EDGE('',*,*,#46329,.T.) ;
#62186 = ORIENTED_EDGE('',*,*,#46330,.T.) ;
#62187 = ORIENTED_EDGE('',*,*,#46329,.F.) ;
#62188 = ORIENTED_EDGE('',*,*,#46331,.T.) ;
#62189 = ORIENTED_EDGE('',*,*,#46332,.T.) ;
#62190 = ORIENTED_EDGE('',*,*,#46333,.T.) ;
#62191 = ORIENTED_EDGE('',*,*,#46332,.F.) ;
#62192 = ORIENTED_EDGE('',*,*,#46334,.T.) ;
#62193 = ORIENTED_EDGE('',*,*,#46335,.T.) ;
#62194 = ORIENTED_EDGE('',*,*,#46336,.T.) ;
#62195 = ORIENTED_EDGE('',*,*,#46335,.F.) ;
#62196 = ORIENTED_EDGE('',*,*,#46337,.T.) ;
#62197 = ORIENTED_EDGE('',*,*,#46338,.T.) ;
#62198 = ORIENTED_EDGE('',*,*,#46339,.T.) ;
#62199 = ORIENTED_EDGE('',*,*,#46338,.F.) ;
#62200 = ORIENTED_EDGE('',*,*,#46340,.T.) ;
#62201 = ORIENTED_EDGE('',*,*,#46341,.T.) ;
#62202 = ORIENTED_EDGE('',*,*,#46342,.T.) ;
#62203 = ORIENTED_EDGE('',*,*,#46341,.F.) ;
#62204 = ORIENTED_EDGE('',*,*,#46343,.T.) ;
#62205 = ORIENTED_EDGE('',*,*,#46344,.T.) ;
#62206 = ORIENTED_EDGE('',*,*,#46345,.T.) ;
#62207 = ORIENTED_EDGE('',*,*,#46344,.F.) ;
#62208 = ORIENTED_EDGE('',*,*,#46346,.T.) ;
#62209 = ORIENTED_EDGE('',*,*,#46347,.T.) ;
#62210 = ORIENTED_EDGE('',*,*,#46348,.T.) ;
#62211 = ORIENTED_EDGE('',*,*,#46347,.F.) ;
#62212 = ORIENTED_EDGE('',*,*,#46349,.T.) ;
#62213 = ORIENTED_EDGE('',*,*,#46350,.T.) ;
#62214 = ORIENTED_EDGE('',*,*,#46351,.T.) ;
#62215 = ORIENTED_EDGE('',*,*,#46350,.F.) ;
#62216 = ORIENTED_EDGE('',*,*,#46352,.T.) ;
#62217 = ORIENTED_EDGE('',*,*,#46353,.T.) ;
#62218 = ORIENTED_EDGE('',*,*,#46354,.T.) ;
#62219 = ORIENTED_EDGE('',*,*,#46353,.F.) ;
#62220 = ORIENTED_EDGE('',*,*,#46355,.T.) ;
#62221 = ORIENTED_EDGE('',*,*,#46356,.T.) ;
#62222 = ORIENTED_EDGE('',*,*,#46357,.T.) ;
#62223 = ORIENTED_EDGE('',*,*,#46356,.F.) ;
#62224 = ORIENTED_EDGE('',*,*,#46358,.T.) ;
#62225 = ORIENTED_EDGE('',*,*,#46359,.T.) ;
#62226 = ORIENTED_EDGE('',*,*,#46360,.T.) ;
#62227 = ORIENTED_EDGE('',*,*,#46359,.F.) ;
#62228 = ORIENTED_EDGE('',*,*,#46361,.T.) ;
#62229 = ORIENTED_EDGE('',*,*,#46362,.T.) ;
#62230 = ORIENTED_EDGE('',*,*,#46363,.T.) ;
#62231 = ORIENTED_EDGE('',*,*,#46362,.F.) ;
#62232 = ORIENTED_EDGE('',*,*,#46364,.T.) ;
#62233 = ORIENTED_EDGE('',*,*,#46365,.T.) ;
#62234 = ORIENTED_EDGE('',*,*,#46366,.T.) ;
#62235 = ORIENTED_EDGE('',*,*,#46365,.F.) ;
#62236 = ORIENTED_EDGE('',*,*,#46367,.T.) ;
#62237 = ORIENTED_EDGE('',*,*,#46368,.T.) ;
#62238 = ORIENTED_EDGE('',*,*,#46369,.T.) ;
#62239 = ORIENTED_EDGE('',*,*,#46368,.F.) ;
#62240 = ORIENTED_EDGE('',*,*,#46370,.T.) ;
#62241 = ORIENTED_EDGE('',*,*,#46371,.T.) ;
#62242 = ORIENTED_EDGE('',*,*,#46372,.T.) ;
#62243 = ORIENTED_EDGE('',*,*,#46371,.F.) ;
#62244 = ORIENTED_EDGE('',*,*,#46373,.T.) ;
#62245 = ORIENTED_EDGE('',*,*,#46374,.T.) ;
#62246 = ORIENTED_EDGE('',*,*,#46375,.T.) ;
#62247 = ORIENTED_EDGE('',*,*,#46374,.F.) ;
#62248 = ORIENTED_EDGE('',*,*,#46376,.T.) ;
#62249 = ORIENTED_EDGE('',*,*,#46377,.T.) ;
#62250 = ORIENTED_EDGE('',*,*,#46378,.T.) ;
#62251 = ORIENTED_EDGE('',*,*,#46377,.F.) ;
#62252 = ORIENTED_EDGE('',*,*,#46379,.T.) ;
#62253 = ORIENTED_EDGE('',*,*,#46302,.T.) ;
#62254 = ORIENTED_EDGE('',*,*,#46380,.T.) ;
#62255 = ORIENTED_EDGE('',*,*,#46381,.T.) ;
#62256 = ORIENTED_EDGE('',*,*,#46382,.T.) ;
#62257 = ORIENTED_EDGE('',*,*,#46383,.T.) ;
#62258 = ORIENTED_EDGE('',*,*,#46384,.T.) ;
#62259 = ORIENTED_EDGE('',*,*,#46385,.T.) ;
#62260 = ORIENTED_EDGE('',*,*,#46386,.T.) ;
#62261 = ORIENTED_EDGE('',*,*,#46387,.T.) ;
#62262 = ORIENTED_EDGE('',*,*,#46388,.T.) ;
#62263 = ORIENTED_EDGE('',*,*,#46389,.T.) ;
#62264 = ORIENTED_EDGE('',*,*,#46390,.T.) ;
#62265 = ORIENTED_EDGE('',*,*,#46391,.T.) ;
#62266 = ORIENTED_EDGE('',*,*,#46392,.T.) ;
#62267 = ORIENTED_EDGE('',*,*,#46393,.T.) ;
#62268 = ORIENTED_EDGE('',*,*,#46394,.T.) ;
#62269 = ORIENTED_EDGE('',*,*,#46395,.T.) ;
#62270 = ORIENTED_EDGE('',*,*,#46396,.T.) ;
#62271 = ORIENTED_EDGE('',*,*,#46397,.T.) ;
#62272 = ORIENTED_EDGE('',*,*,#46398,.T.) ;
#62273 = ORIENTED_EDGE('',*,*,#44253,.T.) ;
#62274 = ORIENTED_EDGE('',*,*,#46399,.F.) ;
#62275 = ORIENTED_EDGE('',*,*,#46400,.T.) ;
#62276 = ORIENTED_EDGE('',*,*,#46401,.T.) ;
#62277 = ORIENTED_EDGE('',*,*,#46402,.T.) ;
#62278 = ORIENTED_EDGE('',*,*,#46401,.F.) ;
#62279 = ORIENTED_EDGE('',*,*,#46403,.T.) ;
#62280 = ORIENTED_EDGE('',*,*,#46404,.T.) ;
#62281 = ORIENTED_EDGE('',*,*,#46405,.T.) ;
#62282 = ORIENTED_EDGE('',*,*,#46404,.F.) ;
#62283 = ORIENTED_EDGE('',*,*,#46406,.T.) ;
#62284 = ORIENTED_EDGE('',*,*,#46407,.T.) ;
#62285 = ORIENTED_EDGE('',*,*,#46408,.T.) ;
#62286 = ORIENTED_EDGE('',*,*,#46407,.F.) ;
#62287 = ORIENTED_EDGE('',*,*,#46409,.T.) ;
#62288 = ORIENTED_EDGE('',*,*,#46410,.T.) ;
#62289 = ORIENTED_EDGE('',*,*,#46411,.T.) ;
#62290 = ORIENTED_EDGE('',*,*,#46410,.F.) ;
#62291 = ORIENTED_EDGE('',*,*,#46412,.T.) ;
#62292 = ORIENTED_EDGE('',*,*,#46413,.T.) ;
#62293 = ORIENTED_EDGE('',*,*,#46414,.T.) ;
#62294 = ORIENTED_EDGE('',*,*,#46413,.F.) ;
#62295 = ORIENTED_EDGE('',*,*,#46415,.T.) ;
#62296 = ORIENTED_EDGE('',*,*,#46416,.T.) ;
#62297 = ORIENTED_EDGE('',*,*,#46417,.T.) ;
#62298 = ORIENTED_EDGE('',*,*,#46416,.F.) ;
#62299 = ORIENTED_EDGE('',*,*,#44273,.T.) ;
#62300 = ORIENTED_EDGE('',*,*,#46418,.T.) ;
#62301 = ORIENTED_EDGE('',*,*,#46419,.T.) ;
#62302 = ORIENTED_EDGE('',*,*,#46418,.F.) ;
#62303 = ORIENTED_EDGE('',*,*,#46420,.T.) ;
#62304 = ORIENTED_EDGE('',*,*,#44350,.T.) ;
#62305 = ORIENTED_EDGE('',*,*,#46421,.T.) ;
#62306 = ORIENTED_EDGE('',*,*,#44349,.F.) ;
#62307 = ORIENTED_EDGE('',*,*,#46422,.T.) ;
#62308 = ORIENTED_EDGE('',*,*,#46423,.T.) ;
#62309 = ORIENTED_EDGE('',*,*,#46424,.T.) ;
#62310 = ORIENTED_EDGE('',*,*,#46423,.F.) ;
#62311 = ORIENTED_EDGE('',*,*,#46425,.T.) ;
#62312 = ORIENTED_EDGE('',*,*,#46426,.T.) ;
#62313 = ORIENTED_EDGE('',*,*,#46427,.T.) ;
#62314 = ORIENTED_EDGE('',*,*,#46426,.F.) ;
#62315 = ORIENTED_EDGE('',*,*,#46428,.T.) ;
#62316 = ORIENTED_EDGE('',*,*,#46429,.T.) ;
#62317 = ORIENTED_EDGE('',*,*,#46430,.T.) ;
#62318 = ORIENTED_EDGE('',*,*,#46429,.F.) ;
#62319 = ORIENTED_EDGE('',*,*,#46431,.T.) ;
#62320 = ORIENTED_EDGE('',*,*,#46432,.T.) ;
#62321 = ORIENTED_EDGE('',*,*,#46433,.T.) ;
#62322 = ORIENTED_EDGE('',*,*,#46432,.F.) ;
#62323 = ORIENTED_EDGE('',*,*,#46434,.T.) ;
#62324 = ORIENTED_EDGE('',*,*,#46435,.T.) ;
#62325 = ORIENTED_EDGE('',*,*,#46436,.T.) ;
#62326 = ORIENTED_EDGE('',*,*,#46435,.F.) ;
#62327 = ORIENTED_EDGE('',*,*,#46437,.T.) ;
#62328 = ORIENTED_EDGE('',*,*,#46438,.T.) ;
#62329 = ORIENTED_EDGE('',*,*,#46439,.T.) ;
#62330 = ORIENTED_EDGE('',*,*,#46438,.F.) ;
#62331 = ORIENTED_EDGE('',*,*,#46440,.T.) ;
#62332 = ORIENTED_EDGE('',*,*,#46441,.T.) ;
#62333 = ORIENTED_EDGE('',*,*,#46442,.T.) ;
#62334 = ORIENTED_EDGE('',*,*,#46441,.F.) ;
#62335 = ORIENTED_EDGE('',*,*,#46443,.T.) ;
#62336 = ORIENTED_EDGE('',*,*,#46444,.T.) ;
#62337 = ORIENTED_EDGE('',*,*,#46445,.T.) ;
#62338 = ORIENTED_EDGE('',*,*,#46444,.F.) ;
#62339 = ORIENTED_EDGE('',*,*,#46446,.T.) ;
#62340 = ORIENTED_EDGE('',*,*,#46447,.T.) ;
#62341 = ORIENTED_EDGE('',*,*,#46448,.T.) ;
#62342 = ORIENTED_EDGE('',*,*,#46447,.F.) ;
#62343 = ORIENTED_EDGE('',*,*,#46449,.T.) ;
#62344 = ORIENTED_EDGE('',*,*,#46450,.T.) ;
#62345 = ORIENTED_EDGE('',*,*,#46451,.T.) ;
#62346 = ORIENTED_EDGE('',*,*,#46450,.F.) ;
#62347 = ORIENTED_EDGE('',*,*,#46452,.T.) ;
#62348 = ORIENTED_EDGE('',*,*,#46453,.T.) ;
#62349 = ORIENTED_EDGE('',*,*,#46454,.T.) ;
#62350 = ORIENTED_EDGE('',*,*,#46453,.F.) ;
#62351 = ORIENTED_EDGE('',*,*,#46455,.T.) ;
#62352 = ORIENTED_EDGE('',*,*,#46456,.T.) ;
#62353 = ORIENTED_EDGE('',*,*,#46457,.T.) ;
#62354 = ORIENTED_EDGE('',*,*,#46456,.F.) ;
#62355 = ORIENTED_EDGE('',*,*,#46458,.T.) ;
#62356 = ORIENTED_EDGE('',*,*,#46459,.T.) ;
#62357 = ORIENTED_EDGE('',*,*,#46460,.T.) ;
#62358 = ORIENTED_EDGE('',*,*,#46459,.F.) ;
#62359 = ORIENTED_EDGE('',*,*,#46461,.T.) ;
#62360 = ORIENTED_EDGE('',*,*,#46462,.T.) ;
#62361 = ORIENTED_EDGE('',*,*,#46463,.T.) ;
#62362 = ORIENTED_EDGE('',*,*,#46462,.F.) ;
#62363 = ORIENTED_EDGE('',*,*,#46464,.T.) ;
#62364 = ORIENTED_EDGE('',*,*,#46465,.T.) ;
#62365 = ORIENTED_EDGE('',*,*,#46466,.T.) ;
#62366 = ORIENTED_EDGE('',*,*,#46465,.F.) ;
#62367 = ORIENTED_EDGE('',*,*,#46467,.T.) ;
#62368 = ORIENTED_EDGE('',*,*,#46468,.T.) ;
#62369 = ORIENTED_EDGE('',*,*,#46469,.T.) ;
#62370 = ORIENTED_EDGE('',*,*,#46468,.F.) ;
#62371 = ORIENTED_EDGE('',*,*,#46470,.T.) ;
#62372 = ORIENTED_EDGE('',*,*,#46471,.T.) ;
#62373 = ORIENTED_EDGE('',*,*,#46472,.T.) ;
#62374 = ORIENTED_EDGE('',*,*,#46471,.F.) ;
#62375 = ORIENTED_EDGE('',*,*,#46473,.T.) ;
#62376 = ORIENTED_EDGE('',*,*,#46474,.T.) ;
#62377 = ORIENTED_EDGE('',*,*,#46475,.T.) ;
#62378 = ORIENTED_EDGE('',*,*,#46474,.F.) ;
#62379 = ORIENTED_EDGE('',*,*,#46476,.T.) ;
#62380 = ORIENTED_EDGE('',*,*,#46399,.T.) ;
#62381 = ORIENTED_EDGE('',*,*,#46477,.T.) ;
#62382 = ORIENTED_EDGE('',*,*,#46478,.T.) ;
#62383 = ORIENTED_EDGE('',*,*,#46479,.T.) ;
#62384 = ORIENTED_EDGE('',*,*,#46480,.T.) ;
#62385 = ORIENTED_EDGE('',*,*,#46481,.T.) ;
#62386 = ORIENTED_EDGE('',*,*,#46482,.T.) ;
#62387 = ORIENTED_EDGE('',*,*,#46483,.T.) ;
#62388 = ORIENTED_EDGE('',*,*,#46484,.T.) ;
#62389 = ORIENTED_EDGE('',*,*,#46485,.T.) ;
#62390 = ORIENTED_EDGE('',*,*,#46486,.T.) ;
#62391 = ORIENTED_EDGE('',*,*,#46487,.T.) ;
#62392 = ORIENTED_EDGE('',*,*,#46488,.T.) ;
#62393 = ORIENTED_EDGE('',*,*,#46489,.T.) ;
#62394 = ORIENTED_EDGE('',*,*,#46490,.T.) ;
#62395 = ORIENTED_EDGE('',*,*,#46491,.T.) ;
#62396 = ORIENTED_EDGE('',*,*,#46492,.T.) ;
#62397 = ORIENTED_EDGE('',*,*,#46493,.T.) ;
#62398 = ORIENTED_EDGE('',*,*,#46494,.T.) ;
#62399 = ORIENTED_EDGE('',*,*,#46495,.T.) ;
#62400 = ORIENTED_EDGE('',*,*,#44270,.T.) ;
#62401 = ORIENTED_EDGE('',*,*,#46496,.F.) ;
#62402 = ORIENTED_EDGE('',*,*,#46497,.T.) ;
#62403 = ORIENTED_EDGE('',*,*,#46498,.T.) ;
#62404 = ORIENTED_EDGE('',*,*,#46499,.T.) ;
#62405 = ORIENTED_EDGE('',*,*,#46498,.F.) ;
#62406 = ORIENTED_EDGE('',*,*,#46500,.T.) ;
#62407 = ORIENTED_EDGE('',*,*,#46501,.T.) ;
#62408 = ORIENTED_EDGE('',*,*,#46502,.T.) ;
#62409 = ORIENTED_EDGE('',*,*,#46501,.F.) ;
#62410 = ORIENTED_EDGE('',*,*,#46503,.T.) ;
#62411 = ORIENTED_EDGE('',*,*,#46504,.T.) ;
#62412 = ORIENTED_EDGE('',*,*,#46505,.T.) ;
#62413 = ORIENTED_EDGE('',*,*,#46504,.F.) ;
#62414 = ORIENTED_EDGE('',*,*,#46506,.T.) ;
#62415 = ORIENTED_EDGE('',*,*,#46507,.T.) ;
#62416 = ORIENTED_EDGE('',*,*,#46508,.T.) ;
#62417 = ORIENTED_EDGE('',*,*,#46507,.F.) ;
#62418 = ORIENTED_EDGE('',*,*,#46509,.T.) ;
#62419 = ORIENTED_EDGE('',*,*,#46510,.T.) ;
#62420 = ORIENTED_EDGE('',*,*,#46511,.T.) ;
#62421 = ORIENTED_EDGE('',*,*,#46510,.F.) ;
#62422 = ORIENTED_EDGE('',*,*,#46512,.T.) ;
#62423 = ORIENTED_EDGE('',*,*,#46513,.T.) ;
#62424 = ORIENTED_EDGE('',*,*,#46514,.T.) ;
#62425 = ORIENTED_EDGE('',*,*,#46513,.F.) ;
#62426 = ORIENTED_EDGE('',*,*,#44326,.T.) ;
#62427 = ORIENTED_EDGE('',*,*,#46515,.T.) ;
#62428 = ORIENTED_EDGE('',*,*,#46516,.T.) ;
#62429 = ORIENTED_EDGE('',*,*,#46515,.F.) ;
#62430 = ORIENTED_EDGE('',*,*,#46517,.T.) ;
#62431 = ORIENTED_EDGE('',*,*,#44347,.T.) ;
#62432 = ORIENTED_EDGE('',*,*,#46518,.T.) ;
#62433 = ORIENTED_EDGE('',*,*,#44346,.F.) ;
#62434 = ORIENTED_EDGE('',*,*,#46519,.T.) ;
#62435 = ORIENTED_EDGE('',*,*,#46520,.T.) ;
#62436 = ORIENTED_EDGE('',*,*,#46521,.T.) ;
#62437 = ORIENTED_EDGE('',*,*,#46520,.F.) ;
#62438 = ORIENTED_EDGE('',*,*,#46522,.T.) ;
#62439 = ORIENTED_EDGE('',*,*,#46523,.T.) ;
#62440 = ORIENTED_EDGE('',*,*,#46524,.T.) ;
#62441 = ORIENTED_EDGE('',*,*,#46523,.F.) ;
#62442 = ORIENTED_EDGE('',*,*,#46525,.T.) ;
#62443 = ORIENTED_EDGE('',*,*,#46526,.T.) ;
#62444 = ORIENTED_EDGE('',*,*,#46527,.T.) ;
#62445 = ORIENTED_EDGE('',*,*,#46526,.F.) ;
#62446 = ORIENTED_EDGE('',*,*,#46528,.T.) ;
#62447 = ORIENTED_EDGE('',*,*,#46529,.T.) ;
#62448 = ORIENTED_EDGE('',*,*,#46530,.T.) ;
#62449 = ORIENTED_EDGE('',*,*,#46529,.F.) ;
#62450 = ORIENTED_EDGE('',*,*,#46531,.T.) ;
#62451 = ORIENTED_EDGE('',*,*,#46532,.T.) ;
#62452 = ORIENTED_EDGE('',*,*,#46533,.T.) ;
#62453 = ORIENTED_EDGE('',*,*,#46532,.F.) ;
#62454 = ORIENTED_EDGE('',*,*,#46534,.T.) ;
#62455 = ORIENTED_EDGE('',*,*,#46535,.T.) ;
#62456 = ORIENTED_EDGE('',*,*,#46536,.T.) ;
#62457 = ORIENTED_EDGE('',*,*,#46535,.F.) ;
#62458 = ORIENTED_EDGE('',*,*,#46537,.T.) ;
#62459 = ORIENTED_EDGE('',*,*,#46538,.T.) ;
#62460 = ORIENTED_EDGE('',*,*,#46539,.T.) ;
#62461 = ORIENTED_EDGE('',*,*,#46538,.F.) ;
#62462 = ORIENTED_EDGE('',*,*,#46540,.T.) ;
#62463 = ORIENTED_EDGE('',*,*,#46541,.T.) ;
#62464 = ORIENTED_EDGE('',*,*,#46542,.T.) ;
#62465 = ORIENTED_EDGE('',*,*,#46541,.F.) ;
#62466 = ORIENTED_EDGE('',*,*,#46543,.T.) ;
#62467 = ORIENTED_EDGE('',*,*,#46544,.T.) ;
#62468 = ORIENTED_EDGE('',*,*,#46545,.T.) ;
#62469 = ORIENTED_EDGE('',*,*,#46544,.F.) ;
#62470 = ORIENTED_EDGE('',*,*,#46546,.T.) ;
#62471 = ORIENTED_EDGE('',*,*,#46547,.T.) ;
#62472 = ORIENTED_EDGE('',*,*,#46548,.T.) ;
#62473 = ORIENTED_EDGE('',*,*,#46547,.F.) ;
#62474 = ORIENTED_EDGE('',*,*,#46549,.T.) ;
#62475 = ORIENTED_EDGE('',*,*,#46550,.T.) ;
#62476 = ORIENTED_EDGE('',*,*,#46551,.T.) ;
#62477 = ORIENTED_EDGE('',*,*,#46550,.F.) ;
#62478 = ORIENTED_EDGE('',*,*,#46552,.T.) ;
#62479 = ORIENTED_EDGE('',*,*,#46553,.T.) ;
#62480 = ORIENTED_EDGE('',*,*,#46554,.T.) ;
#62481 = ORIENTED_EDGE('',*,*,#46553,.F.) ;
#62482 = ORIENTED_EDGE('',*,*,#46555,.T.) ;
#62483 = ORIENTED_EDGE('',*,*,#46556,.T.) ;
#62484 = ORIENTED_EDGE('',*,*,#46557,.T.) ;
#62485 = ORIENTED_EDGE('',*,*,#46556,.F.) ;
#62486 = ORIENTED_EDGE('',*,*,#46558,.T.) ;
#62487 = ORIENTED_EDGE('',*,*,#46559,.T.) ;
#62488 = ORIENTED_EDGE('',*,*,#46560,.T.) ;
#62489 = ORIENTED_EDGE('',*,*,#46559,.F.) ;
#62490 = ORIENTED_EDGE('',*,*,#46561,.T.) ;
#62491 = ORIENTED_EDGE('',*,*,#46562,.T.) ;
#62492 = ORIENTED_EDGE('',*,*,#46563,.T.) ;
#62493 = ORIENTED_EDGE('',*,*,#46562,.F.) ;
#62494 = ORIENTED_EDGE('',*,*,#46564,.T.) ;
#62495 = ORIENTED_EDGE('',*,*,#46565,.T.) ;
#62496 = ORIENTED_EDGE('',*,*,#46566,.T.) ;
#62497 = ORIENTED_EDGE('',*,*,#46565,.F.) ;
#62498 = ORIENTED_EDGE('',*,*,#46567,.T.) ;
#62499 = ORIENTED_EDGE('',*,*,#46568,.T.) ;
#62500 = ORIENTED_EDGE('',*,*,#46569,.T.) ;
#62501 = ORIENTED_EDGE('',*,*,#46568,.F.) ;
#62502 = ORIENTED_EDGE('',*,*,#46570,.T.) ;
#62503 = ORIENTED_EDGE('',*,*,#46571,.T.) ;
#62504 = ORIENTED_EDGE('',*,*,#46572,.T.) ;
#62505 = ORIENTED_EDGE('',*,*,#46571,.F.) ;
#62506 = ORIENTED_EDGE('',*,*,#46573,.T.) ;
#62507 = ORIENTED_EDGE('',*,*,#46496,.T.) ;
#62508 = ORIENTED_EDGE('',*,*,#46574,.T.) ;
#62509 = ORIENTED_EDGE('',*,*,#46575,.T.) ;
#62510 = ORIENTED_EDGE('',*,*,#46576,.T.) ;
#62511 = ORIENTED_EDGE('',*,*,#46577,.T.) ;
#62512 = ORIENTED_EDGE('',*,*,#46578,.T.) ;
#62513 = ORIENTED_EDGE('',*,*,#46579,.T.) ;
#62514 = ORIENTED_EDGE('',*,*,#46580,.T.) ;
#62515 = ORIENTED_EDGE('',*,*,#46581,.T.) ;
#62516 = ORIENTED_EDGE('',*,*,#46582,.T.) ;
#62517 = ORIENTED_EDGE('',*,*,#46583,.T.) ;
#62518 = ORIENTED_EDGE('',*,*,#46584,.T.) ;
#62519 = ORIENTED_EDGE('',*,*,#46585,.T.) ;
#62520 = ORIENTED_EDGE('',*,*,#46586,.T.) ;
#62521 = ORIENTED_EDGE('',*,*,#46587,.T.) ;
#62522 = ORIENTED_EDGE('',*,*,#46588,.T.) ;
#62523 = ORIENTED_EDGE('',*,*,#46589,.T.) ;
#62524 = ORIENTED_EDGE('',*,*,#46590,.T.) ;
#62525 = ORIENTED_EDGE('',*,*,#46591,.T.) ;
#62526 = ORIENTED_EDGE('',*,*,#46592,.T.) ;
#62527 = ORIENTED_EDGE('',*,*,#44323,.T.) ;
#62528 = ORIENTED_EDGE('',*,*,#44283,.T.) ;
#62529 = ORIENTED_EDGE('',*,*,#46593,.F.) ;
#62530 = ORIENTED_EDGE('',*,*,#46594,.T.) ;
#62531 = ORIENTED_EDGE('',*,*,#46595,.T.) ;
#62532 = ORIENTED_EDGE('',*,*,#46596,.T.) ;
#62533 = ORIENTED_EDGE('',*,*,#46597,.T.) ;
#62534 = ORIENTED_EDGE('',*,*,#46598,.T.) ;
#62535 = ORIENTED_EDGE('',*,*,#46599,.T.) ;
#62536 = ORIENTED_EDGE('',*,*,#46600,.T.) ;
#62537 = ORIENTED_EDGE('',*,*,#44266,.T.) ;
#62538 = ORIENTED_EDGE('',*,*,#46601,.F.) ;
#62539 = ORIENTED_EDGE('',*,*,#46602,.T.) ;
#62540 = ORIENTED_EDGE('',*,*,#46603,.T.) ;
#62541 = ORIENTED_EDGE('',*,*,#46604,.T.) ;
#62542 = ORIENTED_EDGE('',*,*,#46605,.T.) ;
#62543 = ORIENTED_EDGE('',*,*,#46606,.T.) ;
#62544 = ORIENTED_EDGE('',*,*,#46607,.T.) ;
#62545 = ORIENTED_EDGE('',*,*,#46608,.T.) ;
#62546 = ORIENTED_EDGE('',*,*,#44249,.T.) ;
#62547 = ORIENTED_EDGE('',*,*,#46609,.F.) ;
#62548 = ORIENTED_EDGE('',*,*,#46610,.T.) ;
#62549 = ORIENTED_EDGE('',*,*,#46611,.T.) ;
#62550 = ORIENTED_EDGE('',*,*,#46612,.T.) ;
#62551 = ORIENTED_EDGE('',*,*,#46613,.T.) ;
#62552 = ORIENTED_EDGE('',*,*,#46614,.T.) ;
#62553 = ORIENTED_EDGE('',*,*,#46615,.T.) ;
#62554 = ORIENTED_EDGE('',*,*,#46616,.T.) ;
#62555 = ORIENTED_EDGE('',*,*,#44232,.T.) ;
#62556 = ORIENTED_EDGE('',*,*,#46617,.F.) ;
#62557 = ORIENTED_EDGE('',*,*,#46618,.T.) ;
#62558 = ORIENTED_EDGE('',*,*,#46619,.T.) ;
#62559 = ORIENTED_EDGE('',*,*,#46620,.T.) ;
#62560 = ORIENTED_EDGE('',*,*,#46621,.T.) ;
#62561 = ORIENTED_EDGE('',*,*,#46622,.T.) ;
#62562 = ORIENTED_EDGE('',*,*,#46623,.T.) ;
#62563 = ORIENTED_EDGE('',*,*,#46624,.T.) ;
#62564 = ORIENTED_EDGE('',*,*,#44215,.T.) ;
#62565 = ORIENTED_EDGE('',*,*,#46625,.F.) ;
#62566 = ORIENTED_EDGE('',*,*,#46626,.T.) ;
#62567 = ORIENTED_EDGE('',*,*,#46627,.T.) ;
#62568 = ORIENTED_EDGE('',*,*,#46628,.T.) ;
#62569 = ORIENTED_EDGE('',*,*,#46629,.T.) ;
#62570 = ORIENTED_EDGE('',*,*,#46630,.T.) ;
#62571 = ORIENTED_EDGE('',*,*,#46631,.T.) ;
#62572 = ORIENTED_EDGE('',*,*,#46632,.T.) ;
#62573 = ORIENTED_EDGE('',*,*,#44198,.T.) ;
#62574 = ORIENTED_EDGE('',*,*,#46633,.F.) ;
#62575 = ORIENTED_EDGE('',*,*,#46634,.T.) ;
#62576 = ORIENTED_EDGE('',*,*,#46635,.T.) ;
#62577 = ORIENTED_EDGE('',*,*,#46636,.T.) ;
#62578 = ORIENTED_EDGE('',*,*,#46637,.T.) ;
#62579 = ORIENTED_EDGE('',*,*,#46638,.T.) ;
#62580 = ORIENTED_EDGE('',*,*,#46639,.T.) ;
#62581 = ORIENTED_EDGE('',*,*,#46640,.T.) ;
#62582 = ORIENTED_EDGE('',*,*,#44181,.T.) ;
#62583 = ORIENTED_EDGE('',*,*,#46641,.F.) ;
#62584 = ORIENTED_EDGE('',*,*,#46642,.T.) ;
#62585 = ORIENTED_EDGE('',*,*,#46643,.T.) ;
#62586 = ORIENTED_EDGE('',*,*,#46644,.T.) ;
#62587 = ORIENTED_EDGE('',*,*,#46645,.T.) ;
#62588 = ORIENTED_EDGE('',*,*,#46646,.T.) ;
#62589 = ORIENTED_EDGE('',*,*,#46647,.T.) ;
#62590 = ORIENTED_EDGE('',*,*,#46648,.T.) ;
#62591 = ORIENTED_EDGE('',*,*,#44164,.T.) ;
#62592 = ORIENTED_EDGE('',*,*,#46649,.F.) ;
#62593 = ORIENTED_EDGE('',*,*,#46650,.T.) ;
#62594 = ORIENTED_EDGE('',*,*,#46651,.T.) ;
#62595 = ORIENTED_EDGE('',*,*,#46652,.T.) ;
#62596 = ORIENTED_EDGE('',*,*,#46653,.T.) ;
#62597 = ORIENTED_EDGE('',*,*,#46654,.T.) ;
#62598 = ORIENTED_EDGE('',*,*,#46655,.T.) ;
#62599 = ORIENTED_EDGE('',*,*,#46656,.T.) ;
#62600 = ORIENTED_EDGE('',*,*,#44147,.T.) ;
#62601 = ORIENTED_EDGE('',*,*,#46657,.F.) ;
#62602 = ORIENTED_EDGE('',*,*,#46658,.T.) ;
#62603 = ORIENTED_EDGE('',*,*,#46659,.T.) ;
#62604 = ORIENTED_EDGE('',*,*,#46660,.T.) ;
#62605 = ORIENTED_EDGE('',*,*,#46661,.T.) ;
#62606 = ORIENTED_EDGE('',*,*,#46662,.T.) ;
#62607 = ORIENTED_EDGE('',*,*,#46663,.T.) ;
#62608 = ORIENTED_EDGE('',*,*,#46664,.T.) ;
#62609 = ORIENTED_EDGE('',*,*,#46665,.F.) ;
#62610 = ORIENTED_EDGE('',*,*,#45561,.F.) ;
#62611 = ORIENTED_EDGE('',*,*,#46666,.F.) ;
#62612 = ORIENTED_EDGE('',*,*,#45548,.F.) ;
#62613 = ORIENTED_EDGE('',*,*,#46667,.F.) ;
#62614 = ORIENTED_EDGE('',*,*,#45562,.F.) ;
#62615 = ORIENTED_EDGE('',*,*,#46668,.F.) ;
#62616 = ORIENTED_EDGE('',*,*,#45556,.F.) ;
#62617 = ORIENTED_EDGE('',*,*,#46669,.F.) ;
#62618 = ORIENTED_EDGE('',*,*,#46667,.T.) ;
#62619 = ORIENTED_EDGE('',*,*,#46670,.F.) ;
#62620 = ORIENTED_EDGE('',*,*,#46671,.F.) ;
#62621 = ORIENTED_EDGE('',*,*,#46666,.T.) ;
#62622 = ORIENTED_EDGE('',*,*,#46672,.F.) ;
#62623 = ORIENTED_EDGE('',*,*,#46665,.T.) ;
#62624 = ORIENTED_EDGE('',*,*,#45547,.T.) ;
#62625 = ORIENTED_EDGE('',*,*,#46673,.F.) ;
#62626 = ORIENTED_EDGE('',*,*,#46668,.T.) ;
#62627 = ORIENTED_EDGE('',*,*,#46670,.T.) ;
#62628 = ORIENTED_EDGE('',*,*,#45559,.F.) ;
#62629 = ORIENTED_EDGE('',*,*,#46674,.F.) ;
#62630 = ORIENTED_EDGE('',*,*,#44329,.T.) ;
#62631 = ORIENTED_EDGE('',*,*,#46675,.T.) ;
#62632 = ORIENTED_EDGE('',*,*,#46676,.F.) ;
#62633 = ORIENTED_EDGE('',*,*,#46669,.T.) ;
#62634 = ORIENTED_EDGE('',*,*,#46677,.F.) ;
#62635 = ORIENTED_EDGE('',*,*,#46678,.T.) ;
#62636 = ORIENTED_EDGE('',*,*,#46679,.F.) ;
#62637 = ORIENTED_EDGE('',*,*,#44485,.F.) ;
#62638 = ORIENTED_EDGE('',*,*,#46680,.F.) ;
#62639 = ORIENTED_EDGE('',*,*,#45563,.F.) ;
#62640 = ORIENTED_EDGE('',*,*,#46672,.T.) ;
#62641 = ORIENTED_EDGE('',*,*,#45560,.F.) ;
#62642 = ORIENTED_EDGE('',*,*,#46681,.F.) ;
#62643 = ORIENTED_EDGE('',*,*,#45566,.F.) ;
#62644 = ORIENTED_EDGE('',*,*,#46671,.T.) ;
#62645 = ORIENTED_EDGE('',*,*,#45565,.F.) ;
#62646 = ORIENTED_EDGE('',*,*,#46682,.F.) ;
#62647 = ORIENTED_EDGE('',*,*,#45539,.F.) ;
#62648 = ORIENTED_EDGE('',*,*,#46673,.T.) ;
#62649 = ORIENTED_EDGE('',*,*,#45546,.F.) ;
#62650 = ORIENTED_EDGE('',*,*,#46683,.F.) ;
#62651 = ORIENTED_EDGE('',*,*,#45557,.F.) ;
#62652 = ORIENTED_EDGE('',*,*,#46684,.F.) ;
#62653 = ORIENTED_EDGE('',*,*,#45558,.F.) ;
#62654 = ORIENTED_EDGE('',*,*,#46685,.F.) ;
#62655 = ORIENTED_EDGE('',*,*,#45553,.F.) ;
#62656 = ORIENTED_EDGE('',*,*,#46674,.T.) ;
#62657 = ORIENTED_EDGE('',*,*,#46684,.T.) ;
#62658 = ORIENTED_EDGE('',*,*,#44330,.F.) ;
#62659 = ORIENTED_EDGE('',*,*,#46680,.T.) ;
#62660 = ORIENTED_EDGE('',*,*,#44495,.T.) ;
#62661 = ORIENTED_EDGE('',*,*,#46686,.F.) ;
#62662 = ORIENTED_EDGE('',*,*,#46681,.T.) ;
#62663 = ORIENTED_EDGE('',*,*,#46687,.F.) ;
#62664 = ORIENTED_EDGE('',*,*,#46682,.T.) ;
#62665 = ORIENTED_EDGE('',*,*,#46688,.F.) ;
#62666 = ORIENTED_EDGE('',*,*,#44581,.T.) ;
#62667 = ORIENTED_EDGE('',*,*,#46683,.T.) ;
#62668 = ORIENTED_EDGE('',*,*,#45545,.T.) ;
#62669 = ORIENTED_EDGE('',*,*,#46689,.F.) ;
#62670 = ORIENTED_EDGE('',*,*,#46685,.T.) ;
#62671 = ORIENTED_EDGE('',*,*,#46686,.T.) ;
#62672 = ORIENTED_EDGE('',*,*,#44494,.F.) ;
#62673 = ORIENTED_EDGE('',*,*,#46690,.F.) ;
#62674 = ORIENTED_EDGE('',*,*,#45567,.F.) ;
#62675 = ORIENTED_EDGE('',*,*,#46688,.T.) ;
#62676 = ORIENTED_EDGE('',*,*,#45564,.F.) ;
#62677 = ORIENTED_EDGE('',*,*,#46691,.F.) ;
#62678 = ORIENTED_EDGE('',*,*,#44582,.F.) ;
#62679 = ORIENTED_EDGE('',*,*,#45540,.F.) ;
#62680 = ORIENTED_EDGE('',*,*,#46687,.T.) ;
#62681 = ORIENTED_EDGE('',*,*,#46692,.F.) ;
#62682 = ORIENTED_EDGE('',*,*,#46693,.F.) ;
#62683 = ORIENTED_EDGE('',*,*,#46689,.T.) ;
#62684 = ORIENTED_EDGE('',*,*,#45544,.F.) ;
#62685 = ORIENTED_EDGE('',*,*,#46694,.F.) ;
#62686 = ORIENTED_EDGE('',*,*,#45554,.F.) ;
#62687 = ORIENTED_EDGE('',*,*,#46695,.F.) ;
#62688 = ORIENTED_EDGE('',*,*,#45555,.F.) ;
#62689 = ORIENTED_EDGE('',*,*,#46696,.F.) ;
#62690 = ORIENTED_EDGE('',*,*,#45549,.F.) ;
#62691 = ORIENTED_EDGE('',*,*,#44332,.T.) ;
#62692 = ORIENTED_EDGE('',*,*,#46695,.T.) ;
#62693 = ORIENTED_EDGE('',*,*,#46697,.F.) ;
#62694 = ORIENTED_EDGE('',*,*,#44489,.T.) ;
#62695 = ORIENTED_EDGE('',*,*,#46691,.T.) ;
#62696 = ORIENTED_EDGE('',*,*,#46690,.T.) ;
#62697 = ORIENTED_EDGE('',*,*,#46698,.F.) ;
#62698 = ORIENTED_EDGE('',*,*,#46699,.F.) ;
#62699 = ORIENTED_EDGE('',*,*,#44587,.F.) ;
#62700 = ORIENTED_EDGE('',*,*,#46700,.F.) ;
#62701 = ORIENTED_EDGE('',*,*,#46701,.F.) ;
#62702 = ORIENTED_EDGE('',*,*,#46692,.T.) ;
#62703 = ORIENTED_EDGE('',*,*,#44585,.F.) ;
#62704 = ORIENTED_EDGE('',*,*,#46700,.T.) ;
#62705 = ORIENTED_EDGE('',*,*,#44748,.F.) ;
#62706 = ORIENTED_EDGE('',*,*,#46693,.T.) ;
#62707 = ORIENTED_EDGE('',*,*,#46702,.F.) ;
#62708 = ORIENTED_EDGE('',*,*,#46703,.F.) ;
#62709 = ORIENTED_EDGE('',*,*,#46696,.T.) ;
#62710 = ORIENTED_EDGE('',*,*,#46694,.T.) ;
#62711 = ORIENTED_EDGE('',*,*,#46704,.F.) ;
#62712 = ORIENTED_EDGE('',*,*,#46697,.T.) ;
#62713 = ORIENTED_EDGE('',*,*,#45552,.F.) ;
#62714 = ORIENTED_EDGE('',*,*,#46705,.F.) ;
#62715 = ORIENTED_EDGE('',*,*,#44490,.F.) ;
#62716 = ORIENTED_EDGE('',*,*,#46698,.T.) ;
#62717 = ORIENTED_EDGE('',*,*,#44493,.F.) ;
#62718 = ORIENTED_EDGE('',*,*,#46706,.F.) ;
#62719 = ORIENTED_EDGE('',*,*,#44583,.F.) ;
#62720 = ORIENTED_EDGE('',*,*,#46699,.T.) ;
#62721 = ORIENTED_EDGE('',*,*,#44584,.F.) ;
#62722 = ORIENTED_EDGE('',*,*,#46707,.F.) ;
#62723 = ORIENTED_EDGE('',*,*,#44661,.F.) ;
#62724 = ORIENTED_EDGE('',*,*,#46701,.T.) ;
#62725 = ORIENTED_EDGE('',*,*,#44747,.T.) ;
#62726 = ORIENTED_EDGE('',*,*,#46708,.F.) ;
#62727 = ORIENTED_EDGE('',*,*,#46702,.T.) ;
#62728 = ORIENTED_EDGE('',*,*,#45541,.F.) ;
#62729 = ORIENTED_EDGE('',*,*,#46703,.T.) ;
#62730 = ORIENTED_EDGE('',*,*,#46709,.F.) ;
#62731 = ORIENTED_EDGE('',*,*,#46710,.F.) ;
#62732 = ORIENTED_EDGE('',*,*,#46704,.T.) ;
#62733 = ORIENTED_EDGE('',*,*,#45543,.F.) ;
#62734 = ORIENTED_EDGE('',*,*,#46711,.F.) ;
#62735 = ORIENTED_EDGE('',*,*,#45550,.F.) ;
#62736 = ORIENTED_EDGE('',*,*,#46712,.F.) ;
#62737 = ORIENTED_EDGE('',*,*,#45551,.F.) ;
#62738 = ORIENTED_EDGE('',*,*,#46713,.F.) ;
#62739 = ORIENTED_EDGE('',*,*,#44580,.F.) ;
#62740 = ORIENTED_EDGE('',*,*,#46705,.T.) ;
#62741 = ORIENTED_EDGE('',*,*,#46712,.T.) ;
#62742 = ORIENTED_EDGE('',*,*,#46714,.F.) ;
#62743 = ORIENTED_EDGE('',*,*,#46707,.T.) ;
#62744 = ORIENTED_EDGE('',*,*,#46706,.T.) ;
#62745 = ORIENTED_EDGE('',*,*,#46715,.F.) ;
#62746 = ORIENTED_EDGE('',*,*,#44662,.T.) ;
#62747 = ORIENTED_EDGE('',*,*,#46716,.F.) ;
#62748 = ORIENTED_EDGE('',*,*,#46709,.T.) ;
#62749 = ORIENTED_EDGE('',*,*,#46708,.T.) ;
#62750 = ORIENTED_EDGE('',*,*,#44746,.F.) ;
#62751 = ORIENTED_EDGE('',*,*,#46710,.T.) ;
#62752 = ORIENTED_EDGE('',*,*,#46717,.F.) ;
#62753 = ORIENTED_EDGE('',*,*,#46718,.F.) ;
#62754 = ORIENTED_EDGE('',*,*,#46713,.T.) ;
#62755 = ORIENTED_EDGE('',*,*,#46711,.T.) ;
#62756 = ORIENTED_EDGE('',*,*,#46719,.F.) ;
#62757 = ORIENTED_EDGE('',*,*,#44576,.T.) ;
#62758 = ORIENTED_EDGE('',*,*,#46714,.T.) ;
#62759 = ORIENTED_EDGE('',*,*,#44579,.F.) ;
#62760 = ORIENTED_EDGE('',*,*,#46720,.F.) ;
#62761 = ORIENTED_EDGE('',*,*,#44491,.F.) ;
#62762 = ORIENTED_EDGE('',*,*,#46715,.T.) ;
#62763 = ORIENTED_EDGE('',*,*,#44492,.F.) ;
#62764 = ORIENTED_EDGE('',*,*,#46721,.F.) ;
#62765 = ORIENTED_EDGE('',*,*,#44663,.F.) ;
#62766 = ORIENTED_EDGE('',*,*,#46716,.T.) ;
#62767 = ORIENTED_EDGE('',*,*,#44745,.T.) ;
#62768 = ORIENTED_EDGE('',*,*,#46722,.F.) ;
#62769 = ORIENTED_EDGE('',*,*,#46717,.T.) ;
#62770 = ORIENTED_EDGE('',*,*,#45542,.F.) ;
#62771 = ORIENTED_EDGE('',*,*,#46718,.T.) ;
#62772 = ORIENTED_EDGE('',*,*,#46723,.F.) ;
#62773 = ORIENTED_EDGE('',*,*,#46719,.T.) ;
#62774 = ORIENTED_EDGE('',*,*,#46721,.T.) ;
#62775 = ORIENTED_EDGE('',*,*,#46720,.T.) ;
#62776 = ORIENTED_EDGE('',*,*,#46724,.F.) ;
#62777 = ORIENTED_EDGE('',*,*,#44664,.T.) ;
#62778 = ORIENTED_EDGE('',*,*,#46722,.T.) ;
#62779 = ORIENTED_EDGE('',*,*,#44744,.F.) ;
#62780 = ORIENTED_EDGE('',*,*,#46725,.F.) ;
#62781 = ORIENTED_EDGE('',*,*,#44577,.F.) ;
#62782 = ORIENTED_EDGE('',*,*,#46723,.T.) ;
#62783 = ORIENTED_EDGE('',*,*,#46724,.T.) ;
#62784 = ORIENTED_EDGE('',*,*,#44578,.F.) ;
#62785 = ORIENTED_EDGE('',*,*,#46726,.F.) ;
#62786 = ORIENTED_EDGE('',*,*,#44665,.F.) ;
#62787 = ORIENTED_EDGE('',*,*,#46725,.T.) ;
#62788 = ORIENTED_EDGE('',*,*,#44593,.F.) ;
#62789 = ORIENTED_EDGE('',*,*,#46726,.T.) ;
#62790 = ORIENTED_EDGE('',*,*,#46727,.F.) ;
#62791 = ORIENTED_EDGE('',*,*,#46537,.F.) ;
#62792 = ORIENTED_EDGE('',*,*,#46728,.F.) ;
#62793 = ORIENTED_EDGE('',*,*,#46584,.F.) ;
#62794 = ORIENTED_EDGE('',*,*,#46728,.T.) ;
#62795 = ORIENTED_EDGE('',*,*,#46534,.F.) ;
#62796 = ORIENTED_EDGE('',*,*,#46729,.F.) ;
#62797 = ORIENTED_EDGE('',*,*,#46585,.F.) ;
#62798 = ORIENTED_EDGE('',*,*,#46540,.F.) ;
#62799 = ORIENTED_EDGE('',*,*,#46727,.T.) ;
#62800 = ORIENTED_EDGE('',*,*,#46730,.F.) ;
#62801 = ORIENTED_EDGE('',*,*,#46729,.T.) ;
#62802 = ORIENTED_EDGE('',*,*,#46531,.F.) ;
#62803 = ORIENTED_EDGE('',*,*,#46731,.F.) ;
#62804 = ORIENTED_EDGE('',*,*,#46586,.F.) ;
#62805 = ORIENTED_EDGE('',*,*,#46730,.T.) ;
#62806 = ORIENTED_EDGE('',*,*,#46583,.F.) ;
#62807 = ORIENTED_EDGE('',*,*,#46732,.F.) ;
#62808 = ORIENTED_EDGE('',*,*,#46543,.F.) ;
#62809 = ORIENTED_EDGE('',*,*,#46731,.T.) ;
#62810 = ORIENTED_EDGE('',*,*,#46528,.F.) ;
#62811 = ORIENTED_EDGE('',*,*,#46733,.F.) ;
#62812 = ORIENTED_EDGE('',*,*,#46587,.F.) ;
#62813 = ORIENTED_EDGE('',*,*,#46546,.F.) ;
#62814 = ORIENTED_EDGE('',*,*,#46732,.T.) ;
#62815 = ORIENTED_EDGE('',*,*,#46734,.F.) ;
#62816 = ORIENTED_EDGE('',*,*,#46733,.T.) ;
#62817 = ORIENTED_EDGE('',*,*,#46525,.F.) ;
#62818 = ORIENTED_EDGE('',*,*,#46735,.F.) ;
#62819 = ORIENTED_EDGE('',*,*,#46588,.F.) ;
#62820 = ORIENTED_EDGE('',*,*,#46734,.T.) ;
#62821 = ORIENTED_EDGE('',*,*,#46582,.F.) ;
#62822 = ORIENTED_EDGE('',*,*,#46736,.F.) ;
#62823 = ORIENTED_EDGE('',*,*,#46549,.F.) ;
#62824 = ORIENTED_EDGE('',*,*,#46735,.T.) ;
#62825 = ORIENTED_EDGE('',*,*,#46522,.F.) ;
#62826 = ORIENTED_EDGE('',*,*,#46737,.F.) ;
#62827 = ORIENTED_EDGE('',*,*,#46552,.F.) ;
#62828 = ORIENTED_EDGE('',*,*,#46736,.T.) ;
#62829 = ORIENTED_EDGE('',*,*,#46738,.F.) ;
#62830 = ORIENTED_EDGE('',*,*,#46737,.T.) ;
#62831 = ORIENTED_EDGE('',*,*,#46519,.F.) ;
#62832 = ORIENTED_EDGE('',*,*,#46739,.F.) ;
#62833 = ORIENTED_EDGE('',*,*,#46589,.F.) ;
#62834 = ORIENTED_EDGE('',*,*,#46738,.T.) ;
#62835 = ORIENTED_EDGE('',*,*,#46581,.F.) ;
#62836 = ORIENTED_EDGE('',*,*,#46740,.F.) ;
#62837 = ORIENTED_EDGE('',*,*,#46555,.F.) ;
#62838 = ORIENTED_EDGE('',*,*,#46739,.T.) ;
#62839 = ORIENTED_EDGE('',*,*,#44345,.F.) ;
#62840 = ORIENTED_EDGE('',*,*,#46741,.F.) ;
#62841 = ORIENTED_EDGE('',*,*,#46558,.F.) ;
#62842 = ORIENTED_EDGE('',*,*,#46740,.T.) ;
#62843 = ORIENTED_EDGE('',*,*,#46742,.F.) ;
#62844 = ORIENTED_EDGE('',*,*,#46741,.T.) ;
#62845 = ORIENTED_EDGE('',*,*,#46517,.F.) ;
#62846 = ORIENTED_EDGE('',*,*,#44328,.F.) ;
#62847 = ORIENTED_EDGE('',*,*,#46590,.F.) ;
#62848 = ORIENTED_EDGE('',*,*,#46742,.T.) ;
#62849 = ORIENTED_EDGE('',*,*,#46580,.F.) ;
#62850 = ORIENTED_EDGE('',*,*,#46743,.F.) ;
#62851 = ORIENTED_EDGE('',*,*,#46561,.F.) ;
#62852 = ORIENTED_EDGE('',*,*,#46564,.F.) ;
#62853 = ORIENTED_EDGE('',*,*,#46743,.T.) ;
#62854 = ORIENTED_EDGE('',*,*,#46744,.F.) ;
#62855 = ORIENTED_EDGE('',*,*,#44327,.T.) ;
#62856 = ORIENTED_EDGE('',*,*,#46512,.F.) ;
#62857 = ORIENTED_EDGE('',*,*,#46745,.F.) ;
#62858 = ORIENTED_EDGE('',*,*,#46591,.F.) ;
#62859 = ORIENTED_EDGE('',*,*,#46744,.T.) ;
#62860 = ORIENTED_EDGE('',*,*,#46579,.F.) ;
#62861 = ORIENTED_EDGE('',*,*,#46746,.F.) ;
#62862 = ORIENTED_EDGE('',*,*,#46567,.F.) ;
#62863 = ORIENTED_EDGE('',*,*,#46745,.T.) ;
#62864 = ORIENTED_EDGE('',*,*,#46509,.F.) ;
#62865 = ORIENTED_EDGE('',*,*,#46747,.F.) ;
#62866 = ORIENTED_EDGE('',*,*,#46570,.F.) ;
#62867 = ORIENTED_EDGE('',*,*,#46746,.T.) ;
#62868 = ORIENTED_EDGE('',*,*,#46748,.F.) ;
#62869 = ORIENTED_EDGE('',*,*,#46747,.T.) ;
#62870 = ORIENTED_EDGE('',*,*,#46506,.F.) ;
#62871 = ORIENTED_EDGE('',*,*,#46749,.F.) ;
#62872 = ORIENTED_EDGE('',*,*,#46592,.F.) ;
#62873 = ORIENTED_EDGE('',*,*,#46748,.T.) ;
#62874 = ORIENTED_EDGE('',*,*,#46578,.F.) ;
#62875 = ORIENTED_EDGE('',*,*,#46750,.F.) ;
#62876 = ORIENTED_EDGE('',*,*,#46573,.F.) ;
#62877 = ORIENTED_EDGE('',*,*,#46749,.T.) ;
#62878 = ORIENTED_EDGE('',*,*,#46503,.F.) ;
#62879 = ORIENTED_EDGE('',*,*,#46751,.F.) ;
#62880 = ORIENTED_EDGE('',*,*,#46575,.F.) ;
#62881 = ORIENTED_EDGE('',*,*,#46750,.T.) ;
#62882 = ORIENTED_EDGE('',*,*,#46577,.F.) ;
#62883 = ORIENTED_EDGE('',*,*,#46752,.F.) ;
#62884 = ORIENTED_EDGE('',*,*,#46497,.F.) ;
#62885 = ORIENTED_EDGE('',*,*,#46751,.T.) ;
#62886 = ORIENTED_EDGE('',*,*,#46500,.F.) ;
#62887 = ORIENTED_EDGE('',*,*,#46752,.T.) ;
#62888 = ORIENTED_EDGE('',*,*,#46576,.F.) ;
#62889 = ORIENTED_EDGE('',*,*,#46753,.F.) ;
#62890 = ORIENTED_EDGE('',*,*,#45757,.F.) ;
#62891 = ORIENTED_EDGE('',*,*,#46754,.F.) ;
#62892 = ORIENTED_EDGE('',*,*,#44806,.F.) ;
#62893 = ORIENTED_EDGE('',*,*,#45754,.F.) ;
#62894 = ORIENTED_EDGE('',*,*,#46753,.T.) ;
#62895 = ORIENTED_EDGE('',*,*,#46755,.F.) ;
#62896 = ORIENTED_EDGE('',*,*,#46754,.T.) ;
#62897 = ORIENTED_EDGE('',*,*,#45760,.F.) ;
#62898 = ORIENTED_EDGE('',*,*,#46756,.F.) ;
#62899 = ORIENTED_EDGE('',*,*,#46755,.T.) ;
#62900 = ORIENTED_EDGE('',*,*,#44805,.F.) ;
#62901 = ORIENTED_EDGE('',*,*,#46757,.F.) ;
#62902 = ORIENTED_EDGE('',*,*,#45751,.F.) ;
#62903 = ORIENTED_EDGE('',*,*,#46756,.T.) ;
#62904 = ORIENTED_EDGE('',*,*,#45763,.F.) ;
#62905 = ORIENTED_EDGE('',*,*,#46758,.F.) ;
#62906 = ORIENTED_EDGE('',*,*,#44807,.F.) ;
#62907 = ORIENTED_EDGE('',*,*,#46757,.T.) ;
#62908 = ORIENTED_EDGE('',*,*,#44804,.F.) ;
#62909 = ORIENTED_EDGE('',*,*,#46759,.F.) ;
#62910 = ORIENTED_EDGE('',*,*,#45748,.F.) ;
#62911 = ORIENTED_EDGE('',*,*,#46758,.T.) ;
#62912 = ORIENTED_EDGE('',*,*,#45766,.F.) ;
#62913 = ORIENTED_EDGE('',*,*,#46760,.F.) ;
#62914 = ORIENTED_EDGE('',*,*,#44808,.F.) ;
#62915 = ORIENTED_EDGE('',*,*,#46759,.T.) ;
#62916 = ORIENTED_EDGE('',*,*,#44803,.F.) ;
#62917 = ORIENTED_EDGE('',*,*,#44322,.F.) ;
#62918 = ORIENTED_EDGE('',*,*,#45745,.F.) ;
#62919 = ORIENTED_EDGE('',*,*,#46760,.T.) ;
#62920 = ORIENTED_EDGE('',*,*,#45769,.F.) ;
#62921 = ORIENTED_EDGE('',*,*,#46761,.F.) ;
#62922 = ORIENTED_EDGE('',*,*,#44809,.F.) ;
#62923 = ORIENTED_EDGE('',*,*,#46761,.T.) ;
#62924 = ORIENTED_EDGE('',*,*,#45772,.F.) ;
#62925 = ORIENTED_EDGE('',*,*,#46762,.F.) ;
#62926 = ORIENTED_EDGE('',*,*,#44810,.F.) ;
#62927 = ORIENTED_EDGE('',*,*,#44320,.T.) ;
#62928 = ORIENTED_EDGE('',*,*,#44802,.F.) ;
#62929 = ORIENTED_EDGE('',*,*,#46763,.F.) ;
#62930 = ORIENTED_EDGE('',*,*,#45742,.F.) ;
#62931 = ORIENTED_EDGE('',*,*,#46762,.T.) ;
#62932 = ORIENTED_EDGE('',*,*,#45775,.F.) ;
#62933 = ORIENTED_EDGE('',*,*,#46764,.F.) ;
#62934 = ORIENTED_EDGE('',*,*,#44811,.F.) ;
#62935 = ORIENTED_EDGE('',*,*,#46763,.T.) ;
#62936 = ORIENTED_EDGE('',*,*,#44801,.F.) ;
#62937 = ORIENTED_EDGE('',*,*,#46765,.F.) ;
#62938 = ORIENTED_EDGE('',*,*,#45740,.F.) ;
#62939 = ORIENTED_EDGE('',*,*,#46764,.T.) ;
#62940 = ORIENTED_EDGE('',*,*,#45778,.F.) ;
#62941 = ORIENTED_EDGE('',*,*,#46766,.F.) ;
#62942 = ORIENTED_EDGE('',*,*,#44812,.F.) ;
#62943 = ORIENTED_EDGE('',*,*,#46765,.T.) ;
#62944 = ORIENTED_EDGE('',*,*,#44800,.F.) ;
#62945 = ORIENTED_EDGE('',*,*,#46767,.F.) ;
#62946 = ORIENTED_EDGE('',*,*,#45738,.F.) ;
#62947 = ORIENTED_EDGE('',*,*,#46766,.T.) ;
#62948 = ORIENTED_EDGE('',*,*,#45781,.F.) ;
#62949 = ORIENTED_EDGE('',*,*,#46768,.F.) ;
#62950 = ORIENTED_EDGE('',*,*,#44813,.F.) ;
#62951 = ORIENTED_EDGE('',*,*,#46767,.T.) ;
#62952 = ORIENTED_EDGE('',*,*,#44799,.F.) ;
#62953 = ORIENTED_EDGE('',*,*,#46769,.F.) ;
#62954 = ORIENTED_EDGE('',*,*,#45735,.F.) ;
#62955 = ORIENTED_EDGE('',*,*,#46768,.T.) ;
#62956 = ORIENTED_EDGE('',*,*,#45784,.F.) ;
#62957 = ORIENTED_EDGE('',*,*,#46770,.F.) ;
#62958 = ORIENTED_EDGE('',*,*,#44814,.F.) ;
#62959 = ORIENTED_EDGE('',*,*,#46769,.T.) ;
#62960 = ORIENTED_EDGE('',*,*,#44798,.F.) ;
#62961 = ORIENTED_EDGE('',*,*,#46771,.F.) ;
#62962 = ORIENTED_EDGE('',*,*,#45732,.F.) ;
#62963 = ORIENTED_EDGE('',*,*,#46770,.T.) ;
#62964 = ORIENTED_EDGE('',*,*,#45787,.F.) ;
#62965 = ORIENTED_EDGE('',*,*,#46772,.F.) ;
#62966 = ORIENTED_EDGE('',*,*,#44815,.F.) ;
#62967 = ORIENTED_EDGE('',*,*,#45729,.F.) ;
#62968 = ORIENTED_EDGE('',*,*,#46771,.T.) ;
#62969 = ORIENTED_EDGE('',*,*,#46773,.F.) ;
#62970 = ORIENTED_EDGE('',*,*,#46772,.T.) ;
#62971 = ORIENTED_EDGE('',*,*,#45790,.F.) ;
#62972 = ORIENTED_EDGE('',*,*,#46774,.F.) ;
#62973 = ORIENTED_EDGE('',*,*,#44816,.F.) ;
#62974 = ORIENTED_EDGE('',*,*,#46773,.T.) ;
#62975 = ORIENTED_EDGE('',*,*,#44797,.F.) ;
#62976 = ORIENTED_EDGE('',*,*,#46775,.F.) ;
#62977 = ORIENTED_EDGE('',*,*,#45726,.F.) ;
#62978 = ORIENTED_EDGE('',*,*,#46774,.T.) ;
#62979 = ORIENTED_EDGE('',*,*,#45793,.F.) ;
#62980 = ORIENTED_EDGE('',*,*,#46776,.F.) ;
#62981 = ORIENTED_EDGE('',*,*,#44817,.F.) ;
#62982 = ORIENTED_EDGE('',*,*,#45723,.F.) ;
#62983 = ORIENTED_EDGE('',*,*,#46775,.T.) ;
#62984 = ORIENTED_EDGE('',*,*,#46777,.F.) ;
#62985 = ORIENTED_EDGE('',*,*,#46776,.T.) ;
#62986 = ORIENTED_EDGE('',*,*,#45796,.F.) ;
#62987 = ORIENTED_EDGE('',*,*,#46778,.F.) ;
#62988 = ORIENTED_EDGE('',*,*,#44795,.F.) ;
#62989 = ORIENTED_EDGE('',*,*,#46777,.T.) ;
#62990 = ORIENTED_EDGE('',*,*,#44796,.F.) ;
#62991 = ORIENTED_EDGE('',*,*,#46778,.T.) ;
#62992 = ORIENTED_EDGE('',*,*,#45798,.F.) ;
#62993 = ORIENTED_EDGE('',*,*,#46779,.F.) ;
#62994 = ORIENTED_EDGE('',*,*,#45854,.F.) ;
#62995 = ORIENTED_EDGE('',*,*,#46780,.F.) ;
#62996 = ORIENTED_EDGE('',*,*,#44829,.F.) ;
#62997 = ORIENTED_EDGE('',*,*,#45851,.F.) ;
#62998 = ORIENTED_EDGE('',*,*,#46779,.T.) ;
#62999 = ORIENTED_EDGE('',*,*,#46781,.F.) ;
#63000 = ORIENTED_EDGE('',*,*,#46780,.T.) ;
#63001 = ORIENTED_EDGE('',*,*,#45857,.F.) ;
#63002 = ORIENTED_EDGE('',*,*,#46782,.F.) ;
#63003 = ORIENTED_EDGE('',*,*,#46781,.T.) ;
#63004 = ORIENTED_EDGE('',*,*,#44828,.F.) ;
#63005 = ORIENTED_EDGE('',*,*,#46783,.F.) ;
#63006 = ORIENTED_EDGE('',*,*,#45848,.F.) ;
#63007 = ORIENTED_EDGE('',*,*,#46782,.T.) ;
#63008 = ORIENTED_EDGE('',*,*,#45860,.F.) ;
#63009 = ORIENTED_EDGE('',*,*,#46784,.F.) ;
#63010 = ORIENTED_EDGE('',*,*,#44830,.F.) ;
#63011 = ORIENTED_EDGE('',*,*,#46783,.T.) ;
#63012 = ORIENTED_EDGE('',*,*,#44827,.F.) ;
#63013 = ORIENTED_EDGE('',*,*,#46785,.F.) ;
#63014 = ORIENTED_EDGE('',*,*,#45845,.F.) ;
#63015 = ORIENTED_EDGE('',*,*,#46784,.T.) ;
#63016 = ORIENTED_EDGE('',*,*,#45863,.F.) ;
#63017 = ORIENTED_EDGE('',*,*,#46786,.F.) ;
#63018 = ORIENTED_EDGE('',*,*,#44831,.F.) ;
#63019 = ORIENTED_EDGE('',*,*,#46785,.T.) ;
#63020 = ORIENTED_EDGE('',*,*,#44826,.F.) ;
#63021 = ORIENTED_EDGE('',*,*,#44318,.F.) ;
#63022 = ORIENTED_EDGE('',*,*,#45842,.F.) ;
#63023 = ORIENTED_EDGE('',*,*,#46786,.T.) ;
#63024 = ORIENTED_EDGE('',*,*,#45866,.F.) ;
#63025 = ORIENTED_EDGE('',*,*,#46787,.F.) ;
#63026 = ORIENTED_EDGE('',*,*,#44832,.F.) ;
#63027 = ORIENTED_EDGE('',*,*,#46787,.T.) ;
#63028 = ORIENTED_EDGE('',*,*,#45869,.F.) ;
#63029 = ORIENTED_EDGE('',*,*,#46788,.F.) ;
#63030 = ORIENTED_EDGE('',*,*,#44833,.F.) ;
#63031 = ORIENTED_EDGE('',*,*,#44316,.T.) ;
#63032 = ORIENTED_EDGE('',*,*,#44825,.F.) ;
#63033 = ORIENTED_EDGE('',*,*,#46789,.F.) ;
#63034 = ORIENTED_EDGE('',*,*,#45839,.F.) ;
#63035 = ORIENTED_EDGE('',*,*,#46788,.T.) ;
#63036 = ORIENTED_EDGE('',*,*,#45872,.F.) ;
#63037 = ORIENTED_EDGE('',*,*,#46790,.F.) ;
#63038 = ORIENTED_EDGE('',*,*,#44834,.F.) ;
#63039 = ORIENTED_EDGE('',*,*,#46789,.T.) ;
#63040 = ORIENTED_EDGE('',*,*,#44824,.F.) ;
#63041 = ORIENTED_EDGE('',*,*,#46791,.F.) ;
#63042 = ORIENTED_EDGE('',*,*,#45837,.F.) ;
#63043 = ORIENTED_EDGE('',*,*,#46790,.T.) ;
#63044 = ORIENTED_EDGE('',*,*,#45875,.F.) ;
#63045 = ORIENTED_EDGE('',*,*,#46792,.F.) ;
#63046 = ORIENTED_EDGE('',*,*,#44835,.F.) ;
#63047 = ORIENTED_EDGE('',*,*,#46791,.T.) ;
#63048 = ORIENTED_EDGE('',*,*,#44823,.F.) ;
#63049 = ORIENTED_EDGE('',*,*,#46793,.F.) ;
#63050 = ORIENTED_EDGE('',*,*,#45835,.F.) ;
#63051 = ORIENTED_EDGE('',*,*,#46792,.T.) ;
#63052 = ORIENTED_EDGE('',*,*,#45878,.F.) ;
#63053 = ORIENTED_EDGE('',*,*,#46794,.F.) ;
#63054 = ORIENTED_EDGE('',*,*,#44836,.F.) ;
#63055 = ORIENTED_EDGE('',*,*,#46793,.T.) ;
#63056 = ORIENTED_EDGE('',*,*,#44822,.F.) ;
#63057 = ORIENTED_EDGE('',*,*,#46795,.F.) ;
#63058 = ORIENTED_EDGE('',*,*,#45832,.F.) ;
#63059 = ORIENTED_EDGE('',*,*,#46794,.T.) ;
#63060 = ORIENTED_EDGE('',*,*,#45881,.F.) ;
#63061 = ORIENTED_EDGE('',*,*,#46796,.F.) ;
#63062 = ORIENTED_EDGE('',*,*,#44837,.F.) ;
#63063 = ORIENTED_EDGE('',*,*,#46795,.T.) ;
#63064 = ORIENTED_EDGE('',*,*,#44821,.F.) ;
#63065 = ORIENTED_EDGE('',*,*,#46797,.F.) ;
#63066 = ORIENTED_EDGE('',*,*,#45829,.F.) ;
#63067 = ORIENTED_EDGE('',*,*,#46796,.T.) ;
#63068 = ORIENTED_EDGE('',*,*,#45884,.F.) ;
#63069 = ORIENTED_EDGE('',*,*,#46798,.F.) ;
#63070 = ORIENTED_EDGE('',*,*,#44838,.F.) ;
#63071 = ORIENTED_EDGE('',*,*,#45826,.F.) ;
#63072 = ORIENTED_EDGE('',*,*,#46797,.T.) ;
#63073 = ORIENTED_EDGE('',*,*,#46799,.F.) ;
#63074 = ORIENTED_EDGE('',*,*,#46798,.T.) ;
#63075 = ORIENTED_EDGE('',*,*,#45887,.F.) ;
#63076 = ORIENTED_EDGE('',*,*,#46800,.F.) ;
#63077 = ORIENTED_EDGE('',*,*,#44839,.F.) ;
#63078 = ORIENTED_EDGE('',*,*,#46799,.T.) ;
#63079 = ORIENTED_EDGE('',*,*,#44820,.F.) ;
#63080 = ORIENTED_EDGE('',*,*,#46801,.F.) ;
#63081 = ORIENTED_EDGE('',*,*,#45823,.F.) ;
#63082 = ORIENTED_EDGE('',*,*,#46800,.T.) ;
#63083 = ORIENTED_EDGE('',*,*,#45890,.F.) ;
#63084 = ORIENTED_EDGE('',*,*,#46802,.F.) ;
#63085 = ORIENTED_EDGE('',*,*,#44840,.F.) ;
#63086 = ORIENTED_EDGE('',*,*,#45820,.F.) ;
#63087 = ORIENTED_EDGE('',*,*,#46801,.T.) ;
#63088 = ORIENTED_EDGE('',*,*,#46803,.F.) ;
#63089 = ORIENTED_EDGE('',*,*,#46802,.T.) ;
#63090 = ORIENTED_EDGE('',*,*,#45893,.F.) ;
#63091 = ORIENTED_EDGE('',*,*,#46804,.F.) ;
#63092 = ORIENTED_EDGE('',*,*,#44818,.F.) ;
#63093 = ORIENTED_EDGE('',*,*,#46803,.T.) ;
#63094 = ORIENTED_EDGE('',*,*,#44819,.F.) ;
#63095 = ORIENTED_EDGE('',*,*,#46804,.T.) ;
#63096 = ORIENTED_EDGE('',*,*,#45895,.F.) ;
#63097 = ORIENTED_EDGE('',*,*,#46805,.F.) ;
#63098 = ORIENTED_EDGE('',*,*,#45951,.F.) ;
#63099 = ORIENTED_EDGE('',*,*,#46806,.F.) ;
#63100 = ORIENTED_EDGE('',*,*,#44852,.F.) ;
#63101 = ORIENTED_EDGE('',*,*,#45948,.F.) ;
#63102 = ORIENTED_EDGE('',*,*,#46805,.T.) ;
#63103 = ORIENTED_EDGE('',*,*,#46807,.F.) ;
#63104 = ORIENTED_EDGE('',*,*,#46806,.T.) ;
#63105 = ORIENTED_EDGE('',*,*,#45954,.F.) ;
#63106 = ORIENTED_EDGE('',*,*,#46808,.F.) ;
#63107 = ORIENTED_EDGE('',*,*,#46807,.T.) ;
#63108 = ORIENTED_EDGE('',*,*,#44851,.F.) ;
#63109 = ORIENTED_EDGE('',*,*,#46809,.F.) ;
#63110 = ORIENTED_EDGE('',*,*,#45945,.F.) ;
#63111 = ORIENTED_EDGE('',*,*,#46808,.T.) ;
#63112 = ORIENTED_EDGE('',*,*,#45957,.F.) ;
#63113 = ORIENTED_EDGE('',*,*,#46810,.F.) ;
#63114 = ORIENTED_EDGE('',*,*,#44853,.F.) ;
#63115 = ORIENTED_EDGE('',*,*,#46809,.T.) ;
#63116 = ORIENTED_EDGE('',*,*,#44850,.F.) ;
#63117 = ORIENTED_EDGE('',*,*,#46811,.F.) ;
#63118 = ORIENTED_EDGE('',*,*,#45942,.F.) ;
#63119 = ORIENTED_EDGE('',*,*,#46810,.T.) ;
#63120 = ORIENTED_EDGE('',*,*,#45960,.F.) ;
#63121 = ORIENTED_EDGE('',*,*,#46812,.F.) ;
#63122 = ORIENTED_EDGE('',*,*,#44854,.F.) ;
#63123 = ORIENTED_EDGE('',*,*,#46811,.T.) ;
#63124 = ORIENTED_EDGE('',*,*,#44849,.F.) ;
#63125 = ORIENTED_EDGE('',*,*,#44314,.F.) ;
#63126 = ORIENTED_EDGE('',*,*,#45939,.F.) ;
#63127 = ORIENTED_EDGE('',*,*,#46812,.T.) ;
#63128 = ORIENTED_EDGE('',*,*,#45963,.F.) ;
#63129 = ORIENTED_EDGE('',*,*,#46813,.F.) ;
#63130 = ORIENTED_EDGE('',*,*,#44855,.F.) ;
#63131 = ORIENTED_EDGE('',*,*,#46813,.T.) ;
#63132 = ORIENTED_EDGE('',*,*,#45966,.F.) ;
#63133 = ORIENTED_EDGE('',*,*,#46814,.F.) ;
#63134 = ORIENTED_EDGE('',*,*,#44856,.F.) ;
#63135 = ORIENTED_EDGE('',*,*,#44312,.T.) ;
#63136 = ORIENTED_EDGE('',*,*,#44848,.F.) ;
#63137 = ORIENTED_EDGE('',*,*,#46815,.F.) ;
#63138 = ORIENTED_EDGE('',*,*,#45936,.F.) ;
#63139 = ORIENTED_EDGE('',*,*,#46814,.T.) ;
#63140 = ORIENTED_EDGE('',*,*,#45969,.F.) ;
#63141 = ORIENTED_EDGE('',*,*,#46816,.F.) ;
#63142 = ORIENTED_EDGE('',*,*,#44857,.F.) ;
#63143 = ORIENTED_EDGE('',*,*,#46815,.T.) ;
#63144 = ORIENTED_EDGE('',*,*,#44847,.F.) ;
#63145 = ORIENTED_EDGE('',*,*,#46817,.F.) ;
#63146 = ORIENTED_EDGE('',*,*,#45934,.F.) ;
#63147 = ORIENTED_EDGE('',*,*,#46816,.T.) ;
#63148 = ORIENTED_EDGE('',*,*,#45972,.F.) ;
#63149 = ORIENTED_EDGE('',*,*,#46818,.F.) ;
#63150 = ORIENTED_EDGE('',*,*,#44858,.F.) ;
#63151 = ORIENTED_EDGE('',*,*,#46817,.T.) ;
#63152 = ORIENTED_EDGE('',*,*,#44846,.F.) ;
#63153 = ORIENTED_EDGE('',*,*,#46819,.F.) ;
#63154 = ORIENTED_EDGE('',*,*,#45932,.F.) ;
#63155 = ORIENTED_EDGE('',*,*,#46818,.T.) ;
#63156 = ORIENTED_EDGE('',*,*,#45975,.F.) ;
#63157 = ORIENTED_EDGE('',*,*,#46820,.F.) ;
#63158 = ORIENTED_EDGE('',*,*,#44859,.F.) ;
#63159 = ORIENTED_EDGE('',*,*,#46819,.T.) ;
#63160 = ORIENTED_EDGE('',*,*,#44845,.F.) ;
#63161 = ORIENTED_EDGE('',*,*,#46821,.F.) ;
#63162 = ORIENTED_EDGE('',*,*,#45929,.F.) ;
#63163 = ORIENTED_EDGE('',*,*,#46820,.T.) ;
#63164 = ORIENTED_EDGE('',*,*,#45978,.F.) ;
#63165 = ORIENTED_EDGE('',*,*,#46822,.F.) ;
#63166 = ORIENTED_EDGE('',*,*,#44860,.F.) ;
#63167 = ORIENTED_EDGE('',*,*,#46821,.T.) ;
#63168 = ORIENTED_EDGE('',*,*,#44844,.F.) ;
#63169 = ORIENTED_EDGE('',*,*,#46823,.F.) ;
#63170 = ORIENTED_EDGE('',*,*,#45926,.F.) ;
#63171 = ORIENTED_EDGE('',*,*,#46822,.T.) ;
#63172 = ORIENTED_EDGE('',*,*,#45981,.F.) ;
#63173 = ORIENTED_EDGE('',*,*,#46824,.F.) ;
#63174 = ORIENTED_EDGE('',*,*,#44861,.F.) ;
#63175 = ORIENTED_EDGE('',*,*,#45923,.F.) ;
#63176 = ORIENTED_EDGE('',*,*,#46823,.T.) ;
#63177 = ORIENTED_EDGE('',*,*,#46825,.F.) ;
#63178 = ORIENTED_EDGE('',*,*,#46824,.T.) ;
#63179 = ORIENTED_EDGE('',*,*,#45984,.F.) ;
#63180 = ORIENTED_EDGE('',*,*,#46826,.F.) ;
#63181 = ORIENTED_EDGE('',*,*,#44862,.F.) ;
#63182 = ORIENTED_EDGE('',*,*,#46825,.T.) ;
#63183 = ORIENTED_EDGE('',*,*,#44843,.F.) ;
#63184 = ORIENTED_EDGE('',*,*,#46827,.F.) ;
#63185 = ORIENTED_EDGE('',*,*,#45920,.F.) ;
#63186 = ORIENTED_EDGE('',*,*,#46826,.T.) ;
#63187 = ORIENTED_EDGE('',*,*,#45987,.F.) ;
#63188 = ORIENTED_EDGE('',*,*,#46828,.F.) ;
#63189 = ORIENTED_EDGE('',*,*,#44863,.F.) ;
#63190 = ORIENTED_EDGE('',*,*,#45917,.F.) ;
#63191 = ORIENTED_EDGE('',*,*,#46827,.T.) ;
#63192 = ORIENTED_EDGE('',*,*,#46829,.F.) ;
#63193 = ORIENTED_EDGE('',*,*,#46828,.T.) ;
#63194 = ORIENTED_EDGE('',*,*,#45990,.F.) ;
#63195 = ORIENTED_EDGE('',*,*,#46830,.F.) ;
#63196 = ORIENTED_EDGE('',*,*,#44841,.F.) ;
#63197 = ORIENTED_EDGE('',*,*,#46829,.T.) ;
#63198 = ORIENTED_EDGE('',*,*,#44842,.F.) ;
#63199 = ORIENTED_EDGE('',*,*,#46830,.T.) ;
#63200 = ORIENTED_EDGE('',*,*,#45992,.F.) ;
#63201 = ORIENTED_EDGE('',*,*,#46831,.F.) ;
#63202 = ORIENTED_EDGE('',*,*,#46048,.F.) ;
#63203 = ORIENTED_EDGE('',*,*,#46832,.F.) ;
#63204 = ORIENTED_EDGE('',*,*,#44875,.F.) ;
#63205 = ORIENTED_EDGE('',*,*,#46045,.F.) ;
#63206 = ORIENTED_EDGE('',*,*,#46831,.T.) ;
#63207 = ORIENTED_EDGE('',*,*,#46833,.F.) ;
#63208 = ORIENTED_EDGE('',*,*,#46832,.T.) ;
#63209 = ORIENTED_EDGE('',*,*,#46051,.F.) ;
#63210 = ORIENTED_EDGE('',*,*,#46834,.F.) ;
#63211 = ORIENTED_EDGE('',*,*,#46833,.T.) ;
#63212 = ORIENTED_EDGE('',*,*,#44874,.F.) ;
#63213 = ORIENTED_EDGE('',*,*,#46835,.F.) ;
#63214 = ORIENTED_EDGE('',*,*,#46042,.F.) ;
#63215 = ORIENTED_EDGE('',*,*,#46834,.T.) ;
#63216 = ORIENTED_EDGE('',*,*,#46054,.F.) ;
#63217 = ORIENTED_EDGE('',*,*,#46836,.F.) ;
#63218 = ORIENTED_EDGE('',*,*,#44876,.F.) ;
#63219 = ORIENTED_EDGE('',*,*,#46835,.T.) ;
#63220 = ORIENTED_EDGE('',*,*,#44873,.F.) ;
#63221 = ORIENTED_EDGE('',*,*,#46837,.F.) ;
#63222 = ORIENTED_EDGE('',*,*,#46039,.F.) ;
#63223 = ORIENTED_EDGE('',*,*,#46836,.T.) ;
#63224 = ORIENTED_EDGE('',*,*,#46057,.F.) ;
#63225 = ORIENTED_EDGE('',*,*,#46838,.F.) ;
#63226 = ORIENTED_EDGE('',*,*,#44877,.F.) ;
#63227 = ORIENTED_EDGE('',*,*,#46837,.T.) ;
#63228 = ORIENTED_EDGE('',*,*,#44872,.F.) ;
#63229 = ORIENTED_EDGE('',*,*,#44310,.F.) ;
#63230 = ORIENTED_EDGE('',*,*,#46036,.F.) ;
#63231 = ORIENTED_EDGE('',*,*,#46838,.T.) ;
#63232 = ORIENTED_EDGE('',*,*,#46060,.F.) ;
#63233 = ORIENTED_EDGE('',*,*,#46839,.F.) ;
#63234 = ORIENTED_EDGE('',*,*,#44878,.F.) ;
#63235 = ORIENTED_EDGE('',*,*,#46839,.T.) ;
#63236 = ORIENTED_EDGE('',*,*,#46063,.F.) ;
#63237 = ORIENTED_EDGE('',*,*,#46840,.F.) ;
#63238 = ORIENTED_EDGE('',*,*,#44879,.F.) ;
#63239 = ORIENTED_EDGE('',*,*,#44308,.T.) ;
#63240 = ORIENTED_EDGE('',*,*,#44871,.F.) ;
#63241 = ORIENTED_EDGE('',*,*,#46841,.F.) ;
#63242 = ORIENTED_EDGE('',*,*,#46033,.F.) ;
#63243 = ORIENTED_EDGE('',*,*,#46840,.T.) ;
#63244 = ORIENTED_EDGE('',*,*,#46066,.F.) ;
#63245 = ORIENTED_EDGE('',*,*,#46842,.F.) ;
#63246 = ORIENTED_EDGE('',*,*,#44880,.F.) ;
#63247 = ORIENTED_EDGE('',*,*,#46841,.T.) ;
#63248 = ORIENTED_EDGE('',*,*,#44870,.F.) ;
#63249 = ORIENTED_EDGE('',*,*,#46843,.F.) ;
#63250 = ORIENTED_EDGE('',*,*,#46031,.F.) ;
#63251 = ORIENTED_EDGE('',*,*,#46842,.T.) ;
#63252 = ORIENTED_EDGE('',*,*,#46069,.F.) ;
#63253 = ORIENTED_EDGE('',*,*,#46844,.F.) ;
#63254 = ORIENTED_EDGE('',*,*,#44881,.F.) ;
#63255 = ORIENTED_EDGE('',*,*,#46843,.T.) ;
#63256 = ORIENTED_EDGE('',*,*,#44869,.F.) ;
#63257 = ORIENTED_EDGE('',*,*,#46845,.F.) ;
#63258 = ORIENTED_EDGE('',*,*,#46029,.F.) ;
#63259 = ORIENTED_EDGE('',*,*,#46844,.T.) ;
#63260 = ORIENTED_EDGE('',*,*,#46072,.F.) ;
#63261 = ORIENTED_EDGE('',*,*,#46846,.F.) ;
#63262 = ORIENTED_EDGE('',*,*,#44882,.F.) ;
#63263 = ORIENTED_EDGE('',*,*,#46845,.T.) ;
#63264 = ORIENTED_EDGE('',*,*,#44868,.F.) ;
#63265 = ORIENTED_EDGE('',*,*,#46847,.F.) ;
#63266 = ORIENTED_EDGE('',*,*,#46026,.F.) ;
#63267 = ORIENTED_EDGE('',*,*,#46846,.T.) ;
#63268 = ORIENTED_EDGE('',*,*,#46075,.F.) ;
#63269 = ORIENTED_EDGE('',*,*,#46848,.F.) ;
#63270 = ORIENTED_EDGE('',*,*,#44883,.F.) ;
#63271 = ORIENTED_EDGE('',*,*,#46847,.T.) ;
#63272 = ORIENTED_EDGE('',*,*,#44867,.F.) ;
#63273 = ORIENTED_EDGE('',*,*,#46849,.F.) ;
#63274 = ORIENTED_EDGE('',*,*,#46023,.F.) ;
#63275 = ORIENTED_EDGE('',*,*,#46848,.T.) ;
#63276 = ORIENTED_EDGE('',*,*,#46078,.F.) ;
#63277 = ORIENTED_EDGE('',*,*,#46850,.F.) ;
#63278 = ORIENTED_EDGE('',*,*,#44884,.F.) ;
#63279 = ORIENTED_EDGE('',*,*,#46020,.F.) ;
#63280 = ORIENTED_EDGE('',*,*,#46849,.T.) ;
#63281 = ORIENTED_EDGE('',*,*,#46851,.F.) ;
#63282 = ORIENTED_EDGE('',*,*,#46850,.T.) ;
#63283 = ORIENTED_EDGE('',*,*,#46081,.F.) ;
#63284 = ORIENTED_EDGE('',*,*,#46852,.F.) ;
#63285 = ORIENTED_EDGE('',*,*,#44885,.F.) ;
#63286 = ORIENTED_EDGE('',*,*,#46851,.T.) ;
#63287 = ORIENTED_EDGE('',*,*,#44866,.F.) ;
#63288 = ORIENTED_EDGE('',*,*,#46853,.F.) ;
#63289 = ORIENTED_EDGE('',*,*,#46017,.F.) ;
#63290 = ORIENTED_EDGE('',*,*,#46852,.T.) ;
#63291 = ORIENTED_EDGE('',*,*,#46084,.F.) ;
#63292 = ORIENTED_EDGE('',*,*,#46854,.F.) ;
#63293 = ORIENTED_EDGE('',*,*,#44886,.F.) ;
#63294 = ORIENTED_EDGE('',*,*,#46014,.F.) ;
#63295 = ORIENTED_EDGE('',*,*,#46853,.T.) ;
#63296 = ORIENTED_EDGE('',*,*,#46855,.F.) ;
#63297 = ORIENTED_EDGE('',*,*,#46854,.T.) ;
#63298 = ORIENTED_EDGE('',*,*,#46087,.F.) ;
#63299 = ORIENTED_EDGE('',*,*,#46856,.F.) ;
#63300 = ORIENTED_EDGE('',*,*,#44864,.F.) ;
#63301 = ORIENTED_EDGE('',*,*,#46855,.T.) ;
#63302 = ORIENTED_EDGE('',*,*,#44865,.F.) ;
#63303 = ORIENTED_EDGE('',*,*,#46856,.T.) ;
#63304 = ORIENTED_EDGE('',*,*,#46089,.F.) ;
#63305 = ORIENTED_EDGE('',*,*,#46857,.F.) ;
#63306 = ORIENTED_EDGE('',*,*,#46145,.F.) ;
#63307 = ORIENTED_EDGE('',*,*,#46858,.F.) ;
#63308 = ORIENTED_EDGE('',*,*,#44898,.F.) ;
#63309 = ORIENTED_EDGE('',*,*,#46142,.F.) ;
#63310 = ORIENTED_EDGE('',*,*,#46857,.T.) ;
#63311 = ORIENTED_EDGE('',*,*,#46859,.F.) ;
#63312 = ORIENTED_EDGE('',*,*,#46858,.T.) ;
#63313 = ORIENTED_EDGE('',*,*,#46148,.F.) ;
#63314 = ORIENTED_EDGE('',*,*,#46860,.F.) ;
#63315 = ORIENTED_EDGE('',*,*,#46859,.T.) ;
#63316 = ORIENTED_EDGE('',*,*,#44897,.F.) ;
#63317 = ORIENTED_EDGE('',*,*,#46861,.F.) ;
#63318 = ORIENTED_EDGE('',*,*,#46139,.F.) ;
#63319 = ORIENTED_EDGE('',*,*,#46860,.T.) ;
#63320 = ORIENTED_EDGE('',*,*,#46151,.F.) ;
#63321 = ORIENTED_EDGE('',*,*,#46862,.F.) ;
#63322 = ORIENTED_EDGE('',*,*,#44899,.F.) ;
#63323 = ORIENTED_EDGE('',*,*,#46861,.T.) ;
#63324 = ORIENTED_EDGE('',*,*,#44896,.F.) ;
#63325 = ORIENTED_EDGE('',*,*,#46863,.F.) ;
#63326 = ORIENTED_EDGE('',*,*,#46136,.F.) ;
#63327 = ORIENTED_EDGE('',*,*,#46862,.T.) ;
#63328 = ORIENTED_EDGE('',*,*,#46154,.F.) ;
#63329 = ORIENTED_EDGE('',*,*,#46864,.F.) ;
#63330 = ORIENTED_EDGE('',*,*,#44900,.F.) ;
#63331 = ORIENTED_EDGE('',*,*,#46863,.T.) ;
#63332 = ORIENTED_EDGE('',*,*,#44895,.F.) ;
#63333 = ORIENTED_EDGE('',*,*,#44306,.F.) ;
#63334 = ORIENTED_EDGE('',*,*,#46133,.F.) ;
#63335 = ORIENTED_EDGE('',*,*,#46864,.T.) ;
#63336 = ORIENTED_EDGE('',*,*,#46157,.F.) ;
#63337 = ORIENTED_EDGE('',*,*,#46865,.F.) ;
#63338 = ORIENTED_EDGE('',*,*,#44901,.F.) ;
#63339 = ORIENTED_EDGE('',*,*,#46865,.T.) ;
#63340 = ORIENTED_EDGE('',*,*,#46160,.F.) ;
#63341 = ORIENTED_EDGE('',*,*,#46866,.F.) ;
#63342 = ORIENTED_EDGE('',*,*,#44902,.F.) ;
#63343 = ORIENTED_EDGE('',*,*,#44304,.T.) ;
#63344 = ORIENTED_EDGE('',*,*,#44894,.F.) ;
#63345 = ORIENTED_EDGE('',*,*,#46867,.F.) ;
#63346 = ORIENTED_EDGE('',*,*,#46130,.F.) ;
#63347 = ORIENTED_EDGE('',*,*,#46866,.T.) ;
#63348 = ORIENTED_EDGE('',*,*,#46163,.F.) ;
#63349 = ORIENTED_EDGE('',*,*,#46868,.F.) ;
#63350 = ORIENTED_EDGE('',*,*,#44903,.F.) ;
#63351 = ORIENTED_EDGE('',*,*,#46867,.T.) ;
#63352 = ORIENTED_EDGE('',*,*,#44893,.F.) ;
#63353 = ORIENTED_EDGE('',*,*,#46869,.F.) ;
#63354 = ORIENTED_EDGE('',*,*,#46128,.F.) ;
#63355 = ORIENTED_EDGE('',*,*,#46868,.T.) ;
#63356 = ORIENTED_EDGE('',*,*,#46166,.F.) ;
#63357 = ORIENTED_EDGE('',*,*,#46870,.F.) ;
#63358 = ORIENTED_EDGE('',*,*,#44904,.F.) ;
#63359 = ORIENTED_EDGE('',*,*,#46869,.T.) ;
#63360 = ORIENTED_EDGE('',*,*,#44892,.F.) ;
#63361 = ORIENTED_EDGE('',*,*,#46871,.F.) ;
#63362 = ORIENTED_EDGE('',*,*,#46126,.F.) ;
#63363 = ORIENTED_EDGE('',*,*,#46870,.T.) ;
#63364 = ORIENTED_EDGE('',*,*,#46169,.F.) ;
#63365 = ORIENTED_EDGE('',*,*,#46872,.F.) ;
#63366 = ORIENTED_EDGE('',*,*,#44905,.F.) ;
#63367 = ORIENTED_EDGE('',*,*,#46871,.T.) ;
#63368 = ORIENTED_EDGE('',*,*,#44891,.F.) ;
#63369 = ORIENTED_EDGE('',*,*,#46873,.F.) ;
#63370 = ORIENTED_EDGE('',*,*,#46123,.F.) ;
#63371 = ORIENTED_EDGE('',*,*,#46872,.T.) ;
#63372 = ORIENTED_EDGE('',*,*,#46172,.F.) ;
#63373 = ORIENTED_EDGE('',*,*,#46874,.F.) ;
#63374 = ORIENTED_EDGE('',*,*,#44906,.F.) ;
#63375 = ORIENTED_EDGE('',*,*,#46873,.T.) ;
#63376 = ORIENTED_EDGE('',*,*,#44890,.F.) ;
#63377 = ORIENTED_EDGE('',*,*,#46875,.F.) ;
#63378 = ORIENTED_EDGE('',*,*,#46120,.F.) ;
#63379 = ORIENTED_EDGE('',*,*,#46874,.T.) ;
#63380 = ORIENTED_EDGE('',*,*,#46175,.F.) ;
#63381 = ORIENTED_EDGE('',*,*,#46876,.F.) ;
#63382 = ORIENTED_EDGE('',*,*,#44907,.F.) ;
#63383 = ORIENTED_EDGE('',*,*,#46117,.F.) ;
#63384 = ORIENTED_EDGE('',*,*,#46875,.T.) ;
#63385 = ORIENTED_EDGE('',*,*,#46877,.F.) ;
#63386 = ORIENTED_EDGE('',*,*,#46876,.T.) ;
#63387 = ORIENTED_EDGE('',*,*,#46178,.F.) ;
#63388 = ORIENTED_EDGE('',*,*,#46878,.F.) ;
#63389 = ORIENTED_EDGE('',*,*,#44908,.F.) ;
#63390 = ORIENTED_EDGE('',*,*,#46877,.T.) ;
#63391 = ORIENTED_EDGE('',*,*,#44889,.F.) ;
#63392 = ORIENTED_EDGE('',*,*,#46879,.F.) ;
#63393 = ORIENTED_EDGE('',*,*,#46114,.F.) ;
#63394 = ORIENTED_EDGE('',*,*,#46878,.T.) ;
#63395 = ORIENTED_EDGE('',*,*,#46181,.F.) ;
#63396 = ORIENTED_EDGE('',*,*,#46880,.F.) ;
#63397 = ORIENTED_EDGE('',*,*,#44909,.F.) ;
#63398 = ORIENTED_EDGE('',*,*,#46111,.F.) ;
#63399 = ORIENTED_EDGE('',*,*,#46879,.T.) ;
#63400 = ORIENTED_EDGE('',*,*,#46881,.F.) ;
#63401 = ORIENTED_EDGE('',*,*,#46880,.T.) ;
#63402 = ORIENTED_EDGE('',*,*,#46184,.F.) ;
#63403 = ORIENTED_EDGE('',*,*,#46882,.F.) ;
#63404 = ORIENTED_EDGE('',*,*,#44887,.F.) ;
#63405 = ORIENTED_EDGE('',*,*,#46881,.T.) ;
#63406 = ORIENTED_EDGE('',*,*,#44888,.F.) ;
#63407 = ORIENTED_EDGE('',*,*,#46882,.T.) ;
#63408 = ORIENTED_EDGE('',*,*,#46186,.F.) ;
#63409 = ORIENTED_EDGE('',*,*,#46883,.F.) ;
#63410 = ORIENTED_EDGE('',*,*,#46242,.F.) ;
#63411 = ORIENTED_EDGE('',*,*,#46884,.F.) ;
#63412 = ORIENTED_EDGE('',*,*,#44921,.F.) ;
#63413 = ORIENTED_EDGE('',*,*,#46239,.F.) ;
#63414 = ORIENTED_EDGE('',*,*,#46883,.T.) ;
#63415 = ORIENTED_EDGE('',*,*,#46885,.F.) ;
#63416 = ORIENTED_EDGE('',*,*,#46884,.T.) ;
#63417 = ORIENTED_EDGE('',*,*,#46245,.F.) ;
#63418 = ORIENTED_EDGE('',*,*,#46886,.F.) ;
#63419 = ORIENTED_EDGE('',*,*,#46885,.T.) ;
#63420 = ORIENTED_EDGE('',*,*,#44920,.F.) ;
#63421 = ORIENTED_EDGE('',*,*,#46887,.F.) ;
#63422 = ORIENTED_EDGE('',*,*,#46236,.F.) ;
#63423 = ORIENTED_EDGE('',*,*,#46886,.T.) ;
#63424 = ORIENTED_EDGE('',*,*,#46248,.F.) ;
#63425 = ORIENTED_EDGE('',*,*,#46888,.F.) ;
#63426 = ORIENTED_EDGE('',*,*,#44922,.F.) ;
#63427 = ORIENTED_EDGE('',*,*,#46887,.T.) ;
#63428 = ORIENTED_EDGE('',*,*,#44919,.F.) ;
#63429 = ORIENTED_EDGE('',*,*,#46889,.F.) ;
#63430 = ORIENTED_EDGE('',*,*,#46233,.F.) ;
#63431 = ORIENTED_EDGE('',*,*,#46888,.T.) ;
#63432 = ORIENTED_EDGE('',*,*,#46251,.F.) ;
#63433 = ORIENTED_EDGE('',*,*,#46890,.F.) ;
#63434 = ORIENTED_EDGE('',*,*,#44923,.F.) ;
#63435 = ORIENTED_EDGE('',*,*,#46889,.T.) ;
#63436 = ORIENTED_EDGE('',*,*,#44918,.F.) ;
#63437 = ORIENTED_EDGE('',*,*,#44302,.F.) ;
#63438 = ORIENTED_EDGE('',*,*,#46230,.F.) ;
#63439 = ORIENTED_EDGE('',*,*,#46890,.T.) ;
#63440 = ORIENTED_EDGE('',*,*,#46254,.F.) ;
#63441 = ORIENTED_EDGE('',*,*,#46891,.F.) ;
#63442 = ORIENTED_EDGE('',*,*,#44924,.F.) ;
#63443 = ORIENTED_EDGE('',*,*,#46891,.T.) ;
#63444 = ORIENTED_EDGE('',*,*,#46257,.F.) ;
#63445 = ORIENTED_EDGE('',*,*,#46892,.F.) ;
#63446 = ORIENTED_EDGE('',*,*,#44925,.F.) ;
#63447 = ORIENTED_EDGE('',*,*,#44300,.T.) ;
#63448 = ORIENTED_EDGE('',*,*,#44917,.F.) ;
#63449 = ORIENTED_EDGE('',*,*,#46893,.F.) ;
#63450 = ORIENTED_EDGE('',*,*,#46227,.F.) ;
#63451 = ORIENTED_EDGE('',*,*,#46892,.T.) ;
#63452 = ORIENTED_EDGE('',*,*,#46260,.F.) ;
#63453 = ORIENTED_EDGE('',*,*,#46894,.F.) ;
#63454 = ORIENTED_EDGE('',*,*,#44926,.F.) ;
#63455 = ORIENTED_EDGE('',*,*,#46893,.T.) ;
#63456 = ORIENTED_EDGE('',*,*,#44916,.F.) ;
#63457 = ORIENTED_EDGE('',*,*,#46895,.F.) ;
#63458 = ORIENTED_EDGE('',*,*,#46225,.F.) ;
#63459 = ORIENTED_EDGE('',*,*,#46894,.T.) ;
#63460 = ORIENTED_EDGE('',*,*,#46263,.F.) ;
#63461 = ORIENTED_EDGE('',*,*,#46896,.F.) ;
#63462 = ORIENTED_EDGE('',*,*,#44927,.F.) ;
#63463 = ORIENTED_EDGE('',*,*,#46895,.T.) ;
#63464 = ORIENTED_EDGE('',*,*,#44915,.F.) ;
#63465 = ORIENTED_EDGE('',*,*,#46897,.F.) ;
#63466 = ORIENTED_EDGE('',*,*,#46223,.F.) ;
#63467 = ORIENTED_EDGE('',*,*,#46896,.T.) ;
#63468 = ORIENTED_EDGE('',*,*,#46266,.F.) ;
#63469 = ORIENTED_EDGE('',*,*,#46898,.F.) ;
#63470 = ORIENTED_EDGE('',*,*,#44928,.F.) ;
#63471 = ORIENTED_EDGE('',*,*,#46897,.T.) ;
#63472 = ORIENTED_EDGE('',*,*,#44914,.F.) ;
#63473 = ORIENTED_EDGE('',*,*,#46899,.F.) ;
#63474 = ORIENTED_EDGE('',*,*,#46220,.F.) ;
#63475 = ORIENTED_EDGE('',*,*,#46898,.T.) ;
#63476 = ORIENTED_EDGE('',*,*,#46269,.F.) ;
#63477 = ORIENTED_EDGE('',*,*,#46900,.F.) ;
#63478 = ORIENTED_EDGE('',*,*,#44929,.F.) ;
#63479 = ORIENTED_EDGE('',*,*,#46899,.T.) ;
#63480 = ORIENTED_EDGE('',*,*,#44913,.F.) ;
#63481 = ORIENTED_EDGE('',*,*,#46901,.F.) ;
#63482 = ORIENTED_EDGE('',*,*,#46217,.F.) ;
#63483 = ORIENTED_EDGE('',*,*,#46900,.T.) ;
#63484 = ORIENTED_EDGE('',*,*,#46272,.F.) ;
#63485 = ORIENTED_EDGE('',*,*,#46902,.F.) ;
#63486 = ORIENTED_EDGE('',*,*,#44930,.F.) ;
#63487 = ORIENTED_EDGE('',*,*,#46214,.F.) ;
#63488 = ORIENTED_EDGE('',*,*,#46901,.T.) ;
#63489 = ORIENTED_EDGE('',*,*,#46903,.F.) ;
#63490 = ORIENTED_EDGE('',*,*,#46902,.T.) ;
#63491 = ORIENTED_EDGE('',*,*,#46275,.F.) ;
#63492 = ORIENTED_EDGE('',*,*,#46904,.F.) ;
#63493 = ORIENTED_EDGE('',*,*,#44931,.F.) ;
#63494 = ORIENTED_EDGE('',*,*,#46903,.T.) ;
#63495 = ORIENTED_EDGE('',*,*,#44912,.F.) ;
#63496 = ORIENTED_EDGE('',*,*,#46905,.F.) ;
#63497 = ORIENTED_EDGE('',*,*,#46211,.F.) ;
#63498 = ORIENTED_EDGE('',*,*,#46904,.T.) ;
#63499 = ORIENTED_EDGE('',*,*,#46278,.F.) ;
#63500 = ORIENTED_EDGE('',*,*,#46906,.F.) ;
#63501 = ORIENTED_EDGE('',*,*,#44932,.F.) ;
#63502 = ORIENTED_EDGE('',*,*,#46208,.F.) ;
#63503 = ORIENTED_EDGE('',*,*,#46905,.T.) ;
#63504 = ORIENTED_EDGE('',*,*,#46907,.F.) ;
#63505 = ORIENTED_EDGE('',*,*,#46906,.T.) ;
#63506 = ORIENTED_EDGE('',*,*,#46281,.F.) ;
#63507 = ORIENTED_EDGE('',*,*,#46908,.F.) ;
#63508 = ORIENTED_EDGE('',*,*,#44910,.F.) ;
#63509 = ORIENTED_EDGE('',*,*,#46907,.T.) ;
#63510 = ORIENTED_EDGE('',*,*,#44911,.F.) ;
#63511 = ORIENTED_EDGE('',*,*,#46908,.T.) ;
#63512 = ORIENTED_EDGE('',*,*,#46283,.F.) ;
#63513 = ORIENTED_EDGE('',*,*,#46909,.F.) ;
#63514 = ORIENTED_EDGE('',*,*,#46339,.F.) ;
#63515 = ORIENTED_EDGE('',*,*,#46910,.F.) ;
#63516 = ORIENTED_EDGE('',*,*,#44944,.F.) ;
#63517 = ORIENTED_EDGE('',*,*,#46336,.F.) ;
#63518 = ORIENTED_EDGE('',*,*,#46909,.T.) ;
#63519 = ORIENTED_EDGE('',*,*,#46911,.F.) ;
#63520 = ORIENTED_EDGE('',*,*,#46910,.T.) ;
#63521 = ORIENTED_EDGE('',*,*,#46342,.F.) ;
#63522 = ORIENTED_EDGE('',*,*,#46912,.F.) ;
#63523 = ORIENTED_EDGE('',*,*,#46911,.T.) ;
#63524 = ORIENTED_EDGE('',*,*,#44943,.F.) ;
#63525 = ORIENTED_EDGE('',*,*,#46913,.F.) ;
#63526 = ORIENTED_EDGE('',*,*,#46333,.F.) ;
#63527 = ORIENTED_EDGE('',*,*,#46912,.T.) ;
#63528 = ORIENTED_EDGE('',*,*,#46345,.F.) ;
#63529 = ORIENTED_EDGE('',*,*,#46914,.F.) ;
#63530 = ORIENTED_EDGE('',*,*,#44945,.F.) ;
#63531 = ORIENTED_EDGE('',*,*,#46913,.T.) ;
#63532 = ORIENTED_EDGE('',*,*,#44942,.F.) ;
#63533 = ORIENTED_EDGE('',*,*,#46915,.F.) ;
#63534 = ORIENTED_EDGE('',*,*,#46330,.F.) ;
#63535 = ORIENTED_EDGE('',*,*,#46914,.T.) ;
#63536 = ORIENTED_EDGE('',*,*,#46348,.F.) ;
#63537 = ORIENTED_EDGE('',*,*,#46916,.F.) ;
#63538 = ORIENTED_EDGE('',*,*,#44946,.F.) ;
#63539 = ORIENTED_EDGE('',*,*,#46915,.T.) ;
#63540 = ORIENTED_EDGE('',*,*,#44941,.F.) ;
#63541 = ORIENTED_EDGE('',*,*,#44298,.F.) ;
#63542 = ORIENTED_EDGE('',*,*,#46327,.F.) ;
#63543 = ORIENTED_EDGE('',*,*,#46916,.T.) ;
#63544 = ORIENTED_EDGE('',*,*,#46351,.F.) ;
#63545 = ORIENTED_EDGE('',*,*,#46917,.F.) ;
#63546 = ORIENTED_EDGE('',*,*,#44947,.F.) ;
#63547 = ORIENTED_EDGE('',*,*,#46917,.T.) ;
#63548 = ORIENTED_EDGE('',*,*,#46354,.F.) ;
#63549 = ORIENTED_EDGE('',*,*,#46918,.F.) ;
#63550 = ORIENTED_EDGE('',*,*,#44948,.F.) ;
#63551 = ORIENTED_EDGE('',*,*,#44296,.T.) ;
#63552 = ORIENTED_EDGE('',*,*,#44940,.F.) ;
#63553 = ORIENTED_EDGE('',*,*,#46919,.F.) ;
#63554 = ORIENTED_EDGE('',*,*,#46324,.F.) ;
#63555 = ORIENTED_EDGE('',*,*,#46918,.T.) ;
#63556 = ORIENTED_EDGE('',*,*,#46357,.F.) ;
#63557 = ORIENTED_EDGE('',*,*,#46920,.F.) ;
#63558 = ORIENTED_EDGE('',*,*,#44949,.F.) ;
#63559 = ORIENTED_EDGE('',*,*,#46919,.T.) ;
#63560 = ORIENTED_EDGE('',*,*,#44939,.F.) ;
#63561 = ORIENTED_EDGE('',*,*,#46921,.F.) ;
#63562 = ORIENTED_EDGE('',*,*,#46322,.F.) ;
#63563 = ORIENTED_EDGE('',*,*,#46920,.T.) ;
#63564 = ORIENTED_EDGE('',*,*,#46360,.F.) ;
#63565 = ORIENTED_EDGE('',*,*,#46922,.F.) ;
#63566 = ORIENTED_EDGE('',*,*,#44950,.F.) ;
#63567 = ORIENTED_EDGE('',*,*,#46921,.T.) ;
#63568 = ORIENTED_EDGE('',*,*,#44938,.F.) ;
#63569 = ORIENTED_EDGE('',*,*,#46923,.F.) ;
#63570 = ORIENTED_EDGE('',*,*,#46320,.F.) ;
#63571 = ORIENTED_EDGE('',*,*,#46922,.T.) ;
#63572 = ORIENTED_EDGE('',*,*,#46363,.F.) ;
#63573 = ORIENTED_EDGE('',*,*,#46924,.F.) ;
#63574 = ORIENTED_EDGE('',*,*,#44951,.F.) ;
#63575 = ORIENTED_EDGE('',*,*,#46923,.T.) ;
#63576 = ORIENTED_EDGE('',*,*,#44937,.F.) ;
#63577 = ORIENTED_EDGE('',*,*,#46925,.F.) ;
#63578 = ORIENTED_EDGE('',*,*,#46317,.F.) ;
#63579 = ORIENTED_EDGE('',*,*,#46924,.T.) ;
#63580 = ORIENTED_EDGE('',*,*,#46366,.F.) ;
#63581 = ORIENTED_EDGE('',*,*,#46926,.F.) ;
#63582 = ORIENTED_EDGE('',*,*,#44952,.F.) ;
#63583 = ORIENTED_EDGE('',*,*,#46925,.T.) ;
#63584 = ORIENTED_EDGE('',*,*,#44936,.F.) ;
#63585 = ORIENTED_EDGE('',*,*,#46927,.F.) ;
#63586 = ORIENTED_EDGE('',*,*,#46314,.F.) ;
#63587 = ORIENTED_EDGE('',*,*,#46926,.T.) ;
#63588 = ORIENTED_EDGE('',*,*,#46369,.F.) ;
#63589 = ORIENTED_EDGE('',*,*,#46928,.F.) ;
#63590 = ORIENTED_EDGE('',*,*,#44953,.F.) ;
#63591 = ORIENTED_EDGE('',*,*,#46311,.F.) ;
#63592 = ORIENTED_EDGE('',*,*,#46927,.T.) ;
#63593 = ORIENTED_EDGE('',*,*,#46929,.F.) ;
#63594 = ORIENTED_EDGE('',*,*,#46928,.T.) ;
#63595 = ORIENTED_EDGE('',*,*,#46372,.F.) ;
#63596 = ORIENTED_EDGE('',*,*,#46930,.F.) ;
#63597 = ORIENTED_EDGE('',*,*,#44954,.F.) ;
#63598 = ORIENTED_EDGE('',*,*,#46929,.T.) ;
#63599 = ORIENTED_EDGE('',*,*,#44935,.F.) ;
#63600 = ORIENTED_EDGE('',*,*,#46931,.F.) ;
#63601 = ORIENTED_EDGE('',*,*,#46308,.F.) ;
#63602 = ORIENTED_EDGE('',*,*,#46930,.T.) ;
#63603 = ORIENTED_EDGE('',*,*,#46375,.F.) ;
#63604 = ORIENTED_EDGE('',*,*,#46932,.F.) ;
#63605 = ORIENTED_EDGE('',*,*,#44955,.F.) ;
#63606 = ORIENTED_EDGE('',*,*,#46305,.F.) ;
#63607 = ORIENTED_EDGE('',*,*,#46931,.T.) ;
#63608 = ORIENTED_EDGE('',*,*,#46933,.F.) ;
#63609 = ORIENTED_EDGE('',*,*,#46932,.T.) ;
#63610 = ORIENTED_EDGE('',*,*,#46378,.F.) ;
#63611 = ORIENTED_EDGE('',*,*,#46934,.F.) ;
#63612 = ORIENTED_EDGE('',*,*,#44933,.F.) ;
#63613 = ORIENTED_EDGE('',*,*,#46933,.T.) ;
#63614 = ORIENTED_EDGE('',*,*,#44934,.F.) ;
#63615 = ORIENTED_EDGE('',*,*,#46934,.T.) ;
#63616 = ORIENTED_EDGE('',*,*,#46380,.F.) ;
#63617 = ORIENTED_EDGE('',*,*,#46935,.F.) ;
#63618 = ORIENTED_EDGE('',*,*,#46436,.F.) ;
#63619 = ORIENTED_EDGE('',*,*,#46936,.F.) ;
#63620 = ORIENTED_EDGE('',*,*,#44967,.F.) ;
#63621 = ORIENTED_EDGE('',*,*,#46433,.F.) ;
#63622 = ORIENTED_EDGE('',*,*,#46935,.T.) ;
#63623 = ORIENTED_EDGE('',*,*,#46937,.F.) ;
#63624 = ORIENTED_EDGE('',*,*,#46936,.T.) ;
#63625 = ORIENTED_EDGE('',*,*,#46439,.F.) ;
#63626 = ORIENTED_EDGE('',*,*,#46938,.F.) ;
#63627 = ORIENTED_EDGE('',*,*,#46937,.T.) ;
#63628 = ORIENTED_EDGE('',*,*,#44966,.F.) ;
#63629 = ORIENTED_EDGE('',*,*,#46939,.F.) ;
#63630 = ORIENTED_EDGE('',*,*,#46430,.F.) ;
#63631 = ORIENTED_EDGE('',*,*,#46938,.T.) ;
#63632 = ORIENTED_EDGE('',*,*,#46442,.F.) ;
#63633 = ORIENTED_EDGE('',*,*,#46940,.F.) ;
#63634 = ORIENTED_EDGE('',*,*,#44968,.F.) ;
#63635 = ORIENTED_EDGE('',*,*,#46939,.T.) ;
#63636 = ORIENTED_EDGE('',*,*,#44965,.F.) ;
#63637 = ORIENTED_EDGE('',*,*,#46941,.F.) ;
#63638 = ORIENTED_EDGE('',*,*,#46427,.F.) ;
#63639 = ORIENTED_EDGE('',*,*,#46940,.T.) ;
#63640 = ORIENTED_EDGE('',*,*,#46445,.F.) ;
#63641 = ORIENTED_EDGE('',*,*,#46942,.F.) ;
#63642 = ORIENTED_EDGE('',*,*,#44969,.F.) ;
#63643 = ORIENTED_EDGE('',*,*,#46941,.T.) ;
#63644 = ORIENTED_EDGE('',*,*,#44964,.F.) ;
#63645 = ORIENTED_EDGE('',*,*,#44294,.F.) ;
#63646 = ORIENTED_EDGE('',*,*,#46424,.F.) ;
#63647 = ORIENTED_EDGE('',*,*,#46942,.T.) ;
#63648 = ORIENTED_EDGE('',*,*,#46448,.F.) ;
#63649 = ORIENTED_EDGE('',*,*,#46943,.F.) ;
#63650 = ORIENTED_EDGE('',*,*,#44970,.F.) ;
#63651 = ORIENTED_EDGE('',*,*,#46943,.T.) ;
#63652 = ORIENTED_EDGE('',*,*,#46451,.F.) ;
#63653 = ORIENTED_EDGE('',*,*,#46944,.F.) ;
#63654 = ORIENTED_EDGE('',*,*,#44971,.F.) ;
#63655 = ORIENTED_EDGE('',*,*,#44292,.T.) ;
#63656 = ORIENTED_EDGE('',*,*,#44963,.F.) ;
#63657 = ORIENTED_EDGE('',*,*,#46945,.F.) ;
#63658 = ORIENTED_EDGE('',*,*,#46421,.F.) ;
#63659 = ORIENTED_EDGE('',*,*,#46944,.T.) ;
#63660 = ORIENTED_EDGE('',*,*,#46454,.F.) ;
#63661 = ORIENTED_EDGE('',*,*,#46946,.F.) ;
#63662 = ORIENTED_EDGE('',*,*,#44972,.F.) ;
#63663 = ORIENTED_EDGE('',*,*,#46945,.T.) ;
#63664 = ORIENTED_EDGE('',*,*,#44962,.F.) ;
#63665 = ORIENTED_EDGE('',*,*,#46947,.F.) ;
#63666 = ORIENTED_EDGE('',*,*,#46419,.F.) ;
#63667 = ORIENTED_EDGE('',*,*,#46946,.T.) ;
#63668 = ORIENTED_EDGE('',*,*,#46457,.F.) ;
#63669 = ORIENTED_EDGE('',*,*,#46948,.F.) ;
#63670 = ORIENTED_EDGE('',*,*,#44973,.F.) ;
#63671 = ORIENTED_EDGE('',*,*,#46947,.T.) ;
#63672 = ORIENTED_EDGE('',*,*,#44961,.F.) ;
#63673 = ORIENTED_EDGE('',*,*,#46949,.F.) ;
#63674 = ORIENTED_EDGE('',*,*,#46417,.F.) ;
#63675 = ORIENTED_EDGE('',*,*,#46948,.T.) ;
#63676 = ORIENTED_EDGE('',*,*,#46460,.F.) ;
#63677 = ORIENTED_EDGE('',*,*,#46950,.F.) ;
#63678 = ORIENTED_EDGE('',*,*,#44974,.F.) ;
#63679 = ORIENTED_EDGE('',*,*,#46949,.T.) ;
#63680 = ORIENTED_EDGE('',*,*,#44960,.F.) ;
#63681 = ORIENTED_EDGE('',*,*,#46951,.F.) ;
#63682 = ORIENTED_EDGE('',*,*,#46414,.F.) ;
#63683 = ORIENTED_EDGE('',*,*,#46950,.T.) ;
#63684 = ORIENTED_EDGE('',*,*,#46463,.F.) ;
#63685 = ORIENTED_EDGE('',*,*,#46952,.F.) ;
#63686 = ORIENTED_EDGE('',*,*,#44975,.F.) ;
#63687 = ORIENTED_EDGE('',*,*,#46951,.T.) ;
#63688 = ORIENTED_EDGE('',*,*,#44959,.F.) ;
#63689 = ORIENTED_EDGE('',*,*,#46953,.F.) ;
#63690 = ORIENTED_EDGE('',*,*,#46411,.F.) ;
#63691 = ORIENTED_EDGE('',*,*,#46952,.T.) ;
#63692 = ORIENTED_EDGE('',*,*,#46466,.F.) ;
#63693 = ORIENTED_EDGE('',*,*,#46954,.F.) ;
#63694 = ORIENTED_EDGE('',*,*,#44976,.F.) ;
#63695 = ORIENTED_EDGE('',*,*,#46408,.F.) ;
#63696 = ORIENTED_EDGE('',*,*,#46953,.T.) ;
#63697 = ORIENTED_EDGE('',*,*,#46955,.F.) ;
#63698 = ORIENTED_EDGE('',*,*,#46954,.T.) ;
#63699 = ORIENTED_EDGE('',*,*,#46469,.F.) ;
#63700 = ORIENTED_EDGE('',*,*,#46956,.F.) ;
#63701 = ORIENTED_EDGE('',*,*,#44977,.F.) ;
#63702 = ORIENTED_EDGE('',*,*,#46955,.T.) ;
#63703 = ORIENTED_EDGE('',*,*,#44958,.F.) ;
#63704 = ORIENTED_EDGE('',*,*,#46957,.F.) ;
#63705 = ORIENTED_EDGE('',*,*,#46405,.F.) ;
#63706 = ORIENTED_EDGE('',*,*,#46956,.T.) ;
#63707 = ORIENTED_EDGE('',*,*,#46472,.F.) ;
#63708 = ORIENTED_EDGE('',*,*,#46958,.F.) ;
#63709 = ORIENTED_EDGE('',*,*,#44978,.F.) ;
#63710 = ORIENTED_EDGE('',*,*,#46402,.F.) ;
#63711 = ORIENTED_EDGE('',*,*,#46957,.T.) ;
#63712 = ORIENTED_EDGE('',*,*,#46959,.F.) ;
#63713 = ORIENTED_EDGE('',*,*,#46958,.T.) ;
#63714 = ORIENTED_EDGE('',*,*,#46475,.F.) ;
#63715 = ORIENTED_EDGE('',*,*,#46960,.F.) ;
#63716 = ORIENTED_EDGE('',*,*,#44956,.F.) ;
#63717 = ORIENTED_EDGE('',*,*,#46959,.T.) ;
#63718 = ORIENTED_EDGE('',*,*,#44957,.F.) ;
#63719 = ORIENTED_EDGE('',*,*,#46960,.T.) ;
#63720 = ORIENTED_EDGE('',*,*,#46477,.F.) ;
#63721 = ORIENTED_EDGE('',*,*,#46961,.F.) ;
#63722 = ORIENTED_EDGE('',*,*,#46533,.F.) ;
#63723 = ORIENTED_EDGE('',*,*,#46962,.F.) ;
#63724 = ORIENTED_EDGE('',*,*,#44990,.F.) ;
#63725 = ORIENTED_EDGE('',*,*,#46530,.F.) ;
#63726 = ORIENTED_EDGE('',*,*,#46961,.T.) ;
#63727 = ORIENTED_EDGE('',*,*,#46963,.F.) ;
#63728 = ORIENTED_EDGE('',*,*,#46962,.T.) ;
#63729 = ORIENTED_EDGE('',*,*,#46536,.F.) ;
#63730 = ORIENTED_EDGE('',*,*,#46964,.F.) ;
#63731 = ORIENTED_EDGE('',*,*,#46963,.T.) ;
#63732 = ORIENTED_EDGE('',*,*,#44989,.F.) ;
#63733 = ORIENTED_EDGE('',*,*,#46965,.F.) ;
#63734 = ORIENTED_EDGE('',*,*,#46527,.F.) ;
#63735 = ORIENTED_EDGE('',*,*,#46964,.T.) ;
#63736 = ORIENTED_EDGE('',*,*,#46539,.F.) ;
#63737 = ORIENTED_EDGE('',*,*,#46966,.F.) ;
#63738 = ORIENTED_EDGE('',*,*,#44991,.F.) ;
#63739 = ORIENTED_EDGE('',*,*,#46965,.T.) ;
#63740 = ORIENTED_EDGE('',*,*,#44988,.F.) ;
#63741 = ORIENTED_EDGE('',*,*,#46967,.F.) ;
#63742 = ORIENTED_EDGE('',*,*,#46524,.F.) ;
#63743 = ORIENTED_EDGE('',*,*,#46966,.T.) ;
#63744 = ORIENTED_EDGE('',*,*,#46542,.F.) ;
#63745 = ORIENTED_EDGE('',*,*,#46968,.F.) ;
#63746 = ORIENTED_EDGE('',*,*,#44992,.F.) ;
#63747 = ORIENTED_EDGE('',*,*,#46967,.T.) ;
#63748 = ORIENTED_EDGE('',*,*,#44987,.F.) ;
#63749 = ORIENTED_EDGE('',*,*,#44290,.F.) ;
#63750 = ORIENTED_EDGE('',*,*,#46521,.F.) ;
#63751 = ORIENTED_EDGE('',*,*,#46968,.T.) ;
#63752 = ORIENTED_EDGE('',*,*,#46545,.F.) ;
#63753 = ORIENTED_EDGE('',*,*,#46969,.F.) ;
#63754 = ORIENTED_EDGE('',*,*,#44993,.F.) ;
#63755 = ORIENTED_EDGE('',*,*,#46969,.T.) ;
#63756 = ORIENTED_EDGE('',*,*,#46548,.F.) ;
#63757 = ORIENTED_EDGE('',*,*,#46970,.F.) ;
#63758 = ORIENTED_EDGE('',*,*,#44994,.F.) ;
#63759 = ORIENTED_EDGE('',*,*,#44288,.T.) ;
#63760 = ORIENTED_EDGE('',*,*,#44986,.F.) ;
#63761 = ORIENTED_EDGE('',*,*,#46971,.F.) ;
#63762 = ORIENTED_EDGE('',*,*,#46518,.F.) ;
#63763 = ORIENTED_EDGE('',*,*,#46970,.T.) ;
#63764 = ORIENTED_EDGE('',*,*,#46551,.F.) ;
#63765 = ORIENTED_EDGE('',*,*,#46972,.F.) ;
#63766 = ORIENTED_EDGE('',*,*,#44995,.F.) ;
#63767 = ORIENTED_EDGE('',*,*,#46971,.T.) ;
#63768 = ORIENTED_EDGE('',*,*,#44985,.F.) ;
#63769 = ORIENTED_EDGE('',*,*,#46973,.F.) ;
#63770 = ORIENTED_EDGE('',*,*,#46516,.F.) ;
#63771 = ORIENTED_EDGE('',*,*,#46972,.T.) ;
#63772 = ORIENTED_EDGE('',*,*,#46554,.F.) ;
#63773 = ORIENTED_EDGE('',*,*,#46974,.F.) ;
#63774 = ORIENTED_EDGE('',*,*,#44996,.F.) ;
#63775 = ORIENTED_EDGE('',*,*,#46973,.T.) ;
#63776 = ORIENTED_EDGE('',*,*,#44984,.F.) ;
#63777 = ORIENTED_EDGE('',*,*,#46975,.F.) ;
#63778 = ORIENTED_EDGE('',*,*,#46514,.F.) ;
#63779 = ORIENTED_EDGE('',*,*,#46974,.T.) ;
#63780 = ORIENTED_EDGE('',*,*,#46557,.F.) ;
#63781 = ORIENTED_EDGE('',*,*,#46976,.F.) ;
#63782 = ORIENTED_EDGE('',*,*,#44997,.F.) ;
#63783 = ORIENTED_EDGE('',*,*,#46975,.T.) ;
#63784 = ORIENTED_EDGE('',*,*,#44983,.F.) ;
#63785 = ORIENTED_EDGE('',*,*,#46977,.F.) ;
#63786 = ORIENTED_EDGE('',*,*,#46511,.F.) ;
#63787 = ORIENTED_EDGE('',*,*,#46976,.T.) ;
#63788 = ORIENTED_EDGE('',*,*,#46560,.F.) ;
#63789 = ORIENTED_EDGE('',*,*,#46978,.F.) ;
#63790 = ORIENTED_EDGE('',*,*,#44998,.F.) ;
#63791 = ORIENTED_EDGE('',*,*,#46977,.T.) ;
#63792 = ORIENTED_EDGE('',*,*,#44982,.F.) ;
#63793 = ORIENTED_EDGE('',*,*,#46979,.F.) ;
#63794 = ORIENTED_EDGE('',*,*,#46508,.F.) ;
#63795 = ORIENTED_EDGE('',*,*,#46978,.T.) ;
#63796 = ORIENTED_EDGE('',*,*,#46563,.F.) ;
#63797 = ORIENTED_EDGE('',*,*,#46980,.F.) ;
#63798 = ORIENTED_EDGE('',*,*,#44999,.F.) ;
#63799 = ORIENTED_EDGE('',*,*,#46505,.F.) ;
#63800 = ORIENTED_EDGE('',*,*,#46979,.T.) ;
#63801 = ORIENTED_EDGE('',*,*,#46981,.F.) ;
#63802 = ORIENTED_EDGE('',*,*,#46980,.T.) ;
#63803 = ORIENTED_EDGE('',*,*,#46566,.F.) ;
#63804 = ORIENTED_EDGE('',*,*,#46982,.F.) ;
#63805 = ORIENTED_EDGE('',*,*,#45000,.F.) ;
#63806 = ORIENTED_EDGE('',*,*,#46981,.T.) ;
#63807 = ORIENTED_EDGE('',*,*,#44981,.F.) ;
#63808 = ORIENTED_EDGE('',*,*,#46983,.F.) ;
#63809 = ORIENTED_EDGE('',*,*,#46502,.F.) ;
#63810 = ORIENTED_EDGE('',*,*,#46982,.T.) ;
#63811 = ORIENTED_EDGE('',*,*,#46569,.F.) ;
#63812 = ORIENTED_EDGE('',*,*,#46984,.F.) ;
#63813 = ORIENTED_EDGE('',*,*,#45001,.F.) ;
#63814 = ORIENTED_EDGE('',*,*,#46499,.F.) ;
#63815 = ORIENTED_EDGE('',*,*,#46983,.T.) ;
#63816 = ORIENTED_EDGE('',*,*,#46985,.F.) ;
#63817 = ORIENTED_EDGE('',*,*,#46984,.T.) ;
#63818 = ORIENTED_EDGE('',*,*,#46572,.F.) ;
#63819 = ORIENTED_EDGE('',*,*,#46986,.F.) ;
#63820 = ORIENTED_EDGE('',*,*,#44979,.F.) ;
#63821 = ORIENTED_EDGE('',*,*,#46985,.T.) ;
#63822 = ORIENTED_EDGE('',*,*,#44980,.F.) ;
#63823 = ORIENTED_EDGE('',*,*,#46986,.T.) ;
#63824 = ORIENTED_EDGE('',*,*,#46574,.F.) ;
#63825 = ORIENTED_EDGE('',*,*,#46987,.F.) ;
#63826 = ORIENTED_EDGE('',*,*,#45580,.F.) ;
#63827 = ORIENTED_EDGE('',*,*,#46988,.F.) ;
#63828 = ORIENTED_EDGE('',*,*,#45538,.F.) ;
#63829 = ORIENTED_EDGE('',*,*,#46989,.F.) ;
#63830 = ORIENTED_EDGE('',*,*,#45581,.F.) ;
#63831 = ORIENTED_EDGE('',*,*,#46990,.F.) ;
#63832 = ORIENTED_EDGE('',*,*,#45575,.F.) ;
#63833 = ORIENTED_EDGE('',*,*,#46991,.F.) ;
#63834 = ORIENTED_EDGE('',*,*,#46989,.T.) ;
#63835 = ORIENTED_EDGE('',*,*,#46992,.F.) ;
#63836 = ORIENTED_EDGE('',*,*,#46993,.F.) ;
#63837 = ORIENTED_EDGE('',*,*,#46988,.T.) ;
#63838 = ORIENTED_EDGE('',*,*,#46994,.F.) ;
#63839 = ORIENTED_EDGE('',*,*,#46987,.T.) ;
#63840 = ORIENTED_EDGE('',*,*,#45537,.T.) ;
#63841 = ORIENTED_EDGE('',*,*,#46995,.F.) ;
#63842 = ORIENTED_EDGE('',*,*,#46990,.T.) ;
#63843 = ORIENTED_EDGE('',*,*,#46992,.T.) ;
#63844 = ORIENTED_EDGE('',*,*,#45578,.F.) ;
#63845 = ORIENTED_EDGE('',*,*,#46996,.F.) ;
#63846 = ORIENTED_EDGE('',*,*,#44276,.T.) ;
#63847 = ORIENTED_EDGE('',*,*,#46997,.T.) ;
#63848 = ORIENTED_EDGE('',*,*,#46998,.F.) ;
#63849 = ORIENTED_EDGE('',*,*,#46991,.T.) ;
#63850 = ORIENTED_EDGE('',*,*,#46999,.F.) ;
#63851 = ORIENTED_EDGE('',*,*,#47000,.T.) ;
#63852 = ORIENTED_EDGE('',*,*,#47001,.F.) ;
#63853 = ORIENTED_EDGE('',*,*,#44474,.F.) ;
#63854 = ORIENTED_EDGE('',*,*,#47002,.F.) ;
#63855 = ORIENTED_EDGE('',*,*,#45582,.F.) ;
#63856 = ORIENTED_EDGE('',*,*,#46994,.T.) ;
#63857 = ORIENTED_EDGE('',*,*,#45579,.F.) ;
#63858 = ORIENTED_EDGE('',*,*,#47003,.F.) ;
#63859 = ORIENTED_EDGE('',*,*,#45585,.F.) ;
#63860 = ORIENTED_EDGE('',*,*,#46993,.T.) ;
#63861 = ORIENTED_EDGE('',*,*,#45584,.F.) ;
#63862 = ORIENTED_EDGE('',*,*,#47004,.F.) ;
#63863 = ORIENTED_EDGE('',*,*,#45529,.F.) ;
#63864 = ORIENTED_EDGE('',*,*,#46995,.T.) ;
#63865 = ORIENTED_EDGE('',*,*,#45536,.F.) ;
#63866 = ORIENTED_EDGE('',*,*,#47005,.F.) ;
#63867 = ORIENTED_EDGE('',*,*,#45576,.F.) ;
#63868 = ORIENTED_EDGE('',*,*,#47006,.F.) ;
#63869 = ORIENTED_EDGE('',*,*,#45577,.F.) ;
#63870 = ORIENTED_EDGE('',*,*,#47007,.F.) ;
#63871 = ORIENTED_EDGE('',*,*,#45572,.F.) ;
#63872 = ORIENTED_EDGE('',*,*,#46996,.T.) ;
#63873 = ORIENTED_EDGE('',*,*,#47006,.T.) ;
#63874 = ORIENTED_EDGE('',*,*,#44277,.F.) ;
#63875 = ORIENTED_EDGE('',*,*,#47002,.T.) ;
#63876 = ORIENTED_EDGE('',*,*,#44484,.T.) ;
#63877 = ORIENTED_EDGE('',*,*,#47008,.F.) ;
#63878 = ORIENTED_EDGE('',*,*,#47003,.T.) ;
#63879 = ORIENTED_EDGE('',*,*,#47009,.F.) ;
#63880 = ORIENTED_EDGE('',*,*,#47004,.T.) ;
#63881 = ORIENTED_EDGE('',*,*,#47010,.F.) ;
#63882 = ORIENTED_EDGE('',*,*,#44571,.T.) ;
#63883 = ORIENTED_EDGE('',*,*,#47005,.T.) ;
#63884 = ORIENTED_EDGE('',*,*,#45535,.T.) ;
#63885 = ORIENTED_EDGE('',*,*,#47011,.F.) ;
#63886 = ORIENTED_EDGE('',*,*,#47007,.T.) ;
#63887 = ORIENTED_EDGE('',*,*,#47008,.T.) ;
#63888 = ORIENTED_EDGE('',*,*,#44483,.F.) ;
#63889 = ORIENTED_EDGE('',*,*,#47012,.F.) ;
#63890 = ORIENTED_EDGE('',*,*,#45586,.F.) ;
#63891 = ORIENTED_EDGE('',*,*,#47010,.T.) ;
#63892 = ORIENTED_EDGE('',*,*,#45583,.F.) ;
#63893 = ORIENTED_EDGE('',*,*,#47013,.F.) ;
#63894 = ORIENTED_EDGE('',*,*,#44572,.F.) ;
#63895 = ORIENTED_EDGE('',*,*,#45530,.F.) ;
#63896 = ORIENTED_EDGE('',*,*,#47009,.T.) ;
#63897 = ORIENTED_EDGE('',*,*,#47014,.F.) ;
#63898 = ORIENTED_EDGE('',*,*,#47015,.F.) ;
#63899 = ORIENTED_EDGE('',*,*,#47011,.T.) ;
#63900 = ORIENTED_EDGE('',*,*,#45534,.F.) ;
#63901 = ORIENTED_EDGE('',*,*,#47016,.F.) ;
#63902 = ORIENTED_EDGE('',*,*,#45573,.F.) ;
#63903 = ORIENTED_EDGE('',*,*,#47017,.F.) ;
#63904 = ORIENTED_EDGE('',*,*,#45574,.F.) ;
#63905 = ORIENTED_EDGE('',*,*,#47018,.F.) ;
#63906 = ORIENTED_EDGE('',*,*,#45568,.F.) ;
#63907 = ORIENTED_EDGE('',*,*,#44279,.T.) ;
#63908 = ORIENTED_EDGE('',*,*,#47017,.T.) ;
#63909 = ORIENTED_EDGE('',*,*,#47019,.F.) ;
#63910 = ORIENTED_EDGE('',*,*,#44478,.T.) ;
#63911 = ORIENTED_EDGE('',*,*,#47013,.T.) ;
#63912 = ORIENTED_EDGE('',*,*,#47012,.T.) ;
#63913 = ORIENTED_EDGE('',*,*,#47020,.F.) ;
#63914 = ORIENTED_EDGE('',*,*,#47021,.F.) ;
#63915 = ORIENTED_EDGE('',*,*,#44591,.F.) ;
#63916 = ORIENTED_EDGE('',*,*,#47022,.F.) ;
#63917 = ORIENTED_EDGE('',*,*,#47023,.F.) ;
#63918 = ORIENTED_EDGE('',*,*,#47014,.T.) ;
#63919 = ORIENTED_EDGE('',*,*,#44575,.F.) ;
#63920 = ORIENTED_EDGE('',*,*,#47022,.T.) ;
#63921 = ORIENTED_EDGE('',*,*,#44743,.F.) ;
#63922 = ORIENTED_EDGE('',*,*,#47015,.T.) ;
#63923 = ORIENTED_EDGE('',*,*,#47024,.F.) ;
#63924 = ORIENTED_EDGE('',*,*,#47025,.F.) ;
#63925 = ORIENTED_EDGE('',*,*,#47018,.T.) ;
#63926 = ORIENTED_EDGE('',*,*,#47016,.T.) ;
#63927 = ORIENTED_EDGE('',*,*,#47026,.F.) ;
#63928 = ORIENTED_EDGE('',*,*,#47019,.T.) ;
#63929 = ORIENTED_EDGE('',*,*,#45571,.F.) ;
#63930 = ORIENTED_EDGE('',*,*,#47027,.F.) ;
#63931 = ORIENTED_EDGE('',*,*,#44479,.F.) ;
#63932 = ORIENTED_EDGE('',*,*,#47020,.T.) ;
#63933 = ORIENTED_EDGE('',*,*,#44482,.F.) ;
#63934 = ORIENTED_EDGE('',*,*,#47028,.F.) ;
#63935 = ORIENTED_EDGE('',*,*,#44573,.F.) ;
#63936 = ORIENTED_EDGE('',*,*,#47021,.T.) ;
#63937 = ORIENTED_EDGE('',*,*,#44574,.F.) ;
#63938 = ORIENTED_EDGE('',*,*,#47029,.F.) ;
#63939 = ORIENTED_EDGE('',*,*,#44666,.F.) ;
#63940 = ORIENTED_EDGE('',*,*,#47023,.T.) ;
#63941 = ORIENTED_EDGE('',*,*,#44742,.T.) ;
#63942 = ORIENTED_EDGE('',*,*,#47030,.F.) ;
#63943 = ORIENTED_EDGE('',*,*,#47024,.T.) ;
#63944 = ORIENTED_EDGE('',*,*,#45531,.F.) ;
#63945 = ORIENTED_EDGE('',*,*,#47025,.T.) ;
#63946 = ORIENTED_EDGE('',*,*,#47031,.F.) ;
#63947 = ORIENTED_EDGE('',*,*,#47032,.F.) ;
#63948 = ORIENTED_EDGE('',*,*,#47026,.T.) ;
#63949 = ORIENTED_EDGE('',*,*,#45533,.F.) ;
#63950 = ORIENTED_EDGE('',*,*,#47033,.F.) ;
#63951 = ORIENTED_EDGE('',*,*,#45569,.F.) ;
#63952 = ORIENTED_EDGE('',*,*,#47034,.F.) ;
#63953 = ORIENTED_EDGE('',*,*,#45570,.F.) ;
#63954 = ORIENTED_EDGE('',*,*,#47035,.F.) ;
#63955 = ORIENTED_EDGE('',*,*,#44570,.F.) ;
#63956 = ORIENTED_EDGE('',*,*,#47027,.T.) ;
#63957 = ORIENTED_EDGE('',*,*,#47034,.T.) ;
#63958 = ORIENTED_EDGE('',*,*,#47036,.F.) ;
#63959 = ORIENTED_EDGE('',*,*,#47029,.T.) ;
#63960 = ORIENTED_EDGE('',*,*,#47028,.T.) ;
#63961 = ORIENTED_EDGE('',*,*,#47037,.F.) ;
#63962 = ORIENTED_EDGE('',*,*,#44667,.T.) ;
#63963 = ORIENTED_EDGE('',*,*,#47038,.F.) ;
#63964 = ORIENTED_EDGE('',*,*,#47031,.T.) ;
#63965 = ORIENTED_EDGE('',*,*,#47030,.T.) ;
#63966 = ORIENTED_EDGE('',*,*,#44741,.F.) ;
#63967 = ORIENTED_EDGE('',*,*,#47032,.T.) ;
#63968 = ORIENTED_EDGE('',*,*,#47039,.F.) ;
#63969 = ORIENTED_EDGE('',*,*,#47040,.F.) ;
#63970 = ORIENTED_EDGE('',*,*,#47035,.T.) ;
#63971 = ORIENTED_EDGE('',*,*,#47033,.T.) ;
#63972 = ORIENTED_EDGE('',*,*,#47041,.F.) ;
#63973 = ORIENTED_EDGE('',*,*,#44566,.T.) ;
#63974 = ORIENTED_EDGE('',*,*,#47036,.T.) ;
#63975 = ORIENTED_EDGE('',*,*,#44569,.F.) ;
#63976 = ORIENTED_EDGE('',*,*,#47042,.F.) ;
#63977 = ORIENTED_EDGE('',*,*,#44480,.F.) ;
#63978 = ORIENTED_EDGE('',*,*,#47037,.T.) ;
#63979 = ORIENTED_EDGE('',*,*,#44481,.F.) ;
#63980 = ORIENTED_EDGE('',*,*,#47043,.F.) ;
#63981 = ORIENTED_EDGE('',*,*,#44668,.F.) ;
#63982 = ORIENTED_EDGE('',*,*,#47038,.T.) ;
#63983 = ORIENTED_EDGE('',*,*,#44740,.T.) ;
#63984 = ORIENTED_EDGE('',*,*,#47044,.F.) ;
#63985 = ORIENTED_EDGE('',*,*,#47039,.T.) ;
#63986 = ORIENTED_EDGE('',*,*,#45532,.F.) ;
#63987 = ORIENTED_EDGE('',*,*,#47040,.T.) ;
#63988 = ORIENTED_EDGE('',*,*,#47045,.F.) ;
#63989 = ORIENTED_EDGE('',*,*,#47041,.T.) ;
#63990 = ORIENTED_EDGE('',*,*,#47043,.T.) ;
#63991 = ORIENTED_EDGE('',*,*,#47042,.T.) ;
#63992 = ORIENTED_EDGE('',*,*,#47046,.F.) ;
#63993 = ORIENTED_EDGE('',*,*,#44669,.T.) ;
#63994 = ORIENTED_EDGE('',*,*,#47044,.T.) ;
#63995 = ORIENTED_EDGE('',*,*,#44739,.F.) ;
#63996 = ORIENTED_EDGE('',*,*,#47047,.F.) ;
#63997 = ORIENTED_EDGE('',*,*,#44567,.F.) ;
#63998 = ORIENTED_EDGE('',*,*,#47045,.T.) ;
#63999 = ORIENTED_EDGE('',*,*,#47046,.T.) ;
#64000 = ORIENTED_EDGE('',*,*,#44568,.F.) ;
#64001 = ORIENTED_EDGE('',*,*,#47048,.F.) ;
#64002 = ORIENTED_EDGE('',*,*,#44670,.F.) ;
#64003 = ORIENTED_EDGE('',*,*,#47047,.T.) ;
#64004 = ORIENTED_EDGE('',*,*,#44597,.F.) ;
#64005 = ORIENTED_EDGE('',*,*,#47048,.T.) ;
#64006 = ORIENTED_EDGE('',*,*,#47049,.F.) ;
#64007 = ORIENTED_EDGE('',*,*,#46440,.F.) ;
#64008 = ORIENTED_EDGE('',*,*,#47050,.F.) ;
#64009 = ORIENTED_EDGE('',*,*,#46487,.F.) ;
#64010 = ORIENTED_EDGE('',*,*,#47050,.T.) ;
#64011 = ORIENTED_EDGE('',*,*,#46437,.F.) ;
#64012 = ORIENTED_EDGE('',*,*,#47051,.F.) ;
#64013 = ORIENTED_EDGE('',*,*,#46488,.F.) ;
#64014 = ORIENTED_EDGE('',*,*,#46443,.F.) ;
#64015 = ORIENTED_EDGE('',*,*,#47049,.T.) ;
#64016 = ORIENTED_EDGE('',*,*,#47052,.F.) ;
#64017 = ORIENTED_EDGE('',*,*,#47051,.T.) ;
#64018 = ORIENTED_EDGE('',*,*,#46434,.F.) ;
#64019 = ORIENTED_EDGE('',*,*,#47053,.F.) ;
#64020 = ORIENTED_EDGE('',*,*,#46489,.F.) ;
#64021 = ORIENTED_EDGE('',*,*,#47052,.T.) ;
#64022 = ORIENTED_EDGE('',*,*,#46486,.F.) ;
#64023 = ORIENTED_EDGE('',*,*,#47054,.F.) ;
#64024 = ORIENTED_EDGE('',*,*,#46446,.F.) ;
#64025 = ORIENTED_EDGE('',*,*,#47053,.T.) ;
#64026 = ORIENTED_EDGE('',*,*,#46431,.F.) ;
#64027 = ORIENTED_EDGE('',*,*,#47055,.F.) ;
#64028 = ORIENTED_EDGE('',*,*,#46490,.F.) ;
#64029 = ORIENTED_EDGE('',*,*,#46449,.F.) ;
#64030 = ORIENTED_EDGE('',*,*,#47054,.T.) ;
#64031 = ORIENTED_EDGE('',*,*,#47056,.F.) ;
#64032 = ORIENTED_EDGE('',*,*,#47055,.T.) ;
#64033 = ORIENTED_EDGE('',*,*,#46428,.F.) ;
#64034 = ORIENTED_EDGE('',*,*,#47057,.F.) ;
#64035 = ORIENTED_EDGE('',*,*,#46491,.F.) ;
#64036 = ORIENTED_EDGE('',*,*,#47056,.T.) ;
#64037 = ORIENTED_EDGE('',*,*,#46485,.F.) ;
#64038 = ORIENTED_EDGE('',*,*,#47058,.F.) ;
#64039 = ORIENTED_EDGE('',*,*,#46452,.F.) ;
#64040 = ORIENTED_EDGE('',*,*,#47057,.T.) ;
#64041 = ORIENTED_EDGE('',*,*,#46425,.F.) ;
#64042 = ORIENTED_EDGE('',*,*,#47059,.F.) ;
#64043 = ORIENTED_EDGE('',*,*,#46455,.F.) ;
#64044 = ORIENTED_EDGE('',*,*,#47058,.T.) ;
#64045 = ORIENTED_EDGE('',*,*,#47060,.F.) ;
#64046 = ORIENTED_EDGE('',*,*,#47059,.T.) ;
#64047 = ORIENTED_EDGE('',*,*,#46422,.F.) ;
#64048 = ORIENTED_EDGE('',*,*,#47061,.F.) ;
#64049 = ORIENTED_EDGE('',*,*,#46492,.F.) ;
#64050 = ORIENTED_EDGE('',*,*,#47060,.T.) ;
#64051 = ORIENTED_EDGE('',*,*,#46484,.F.) ;
#64052 = ORIENTED_EDGE('',*,*,#47062,.F.) ;
#64053 = ORIENTED_EDGE('',*,*,#46458,.F.) ;
#64054 = ORIENTED_EDGE('',*,*,#47061,.T.) ;
#64055 = ORIENTED_EDGE('',*,*,#44348,.F.) ;
#64056 = ORIENTED_EDGE('',*,*,#47063,.F.) ;
#64057 = ORIENTED_EDGE('',*,*,#46461,.F.) ;
#64058 = ORIENTED_EDGE('',*,*,#47062,.T.) ;
#64059 = ORIENTED_EDGE('',*,*,#47064,.F.) ;
#64060 = ORIENTED_EDGE('',*,*,#47063,.T.) ;
#64061 = ORIENTED_EDGE('',*,*,#46420,.F.) ;
#64062 = ORIENTED_EDGE('',*,*,#44275,.F.) ;
#64063 = ORIENTED_EDGE('',*,*,#46493,.F.) ;
#64064 = ORIENTED_EDGE('',*,*,#47064,.T.) ;
#64065 = ORIENTED_EDGE('',*,*,#46483,.F.) ;
#64066 = ORIENTED_EDGE('',*,*,#47065,.F.) ;
#64067 = ORIENTED_EDGE('',*,*,#46464,.F.) ;
#64068 = ORIENTED_EDGE('',*,*,#46467,.F.) ;
#64069 = ORIENTED_EDGE('',*,*,#47065,.T.) ;
#64070 = ORIENTED_EDGE('',*,*,#47066,.F.) ;
#64071 = ORIENTED_EDGE('',*,*,#44274,.T.) ;
#64072 = ORIENTED_EDGE('',*,*,#46415,.F.) ;
#64073 = ORIENTED_EDGE('',*,*,#47067,.F.) ;
#64074 = ORIENTED_EDGE('',*,*,#46494,.F.) ;
#64075 = ORIENTED_EDGE('',*,*,#47066,.T.) ;
#64076 = ORIENTED_EDGE('',*,*,#46482,.F.) ;
#64077 = ORIENTED_EDGE('',*,*,#47068,.F.) ;
#64078 = ORIENTED_EDGE('',*,*,#46470,.F.) ;
#64079 = ORIENTED_EDGE('',*,*,#47067,.T.) ;
#64080 = ORIENTED_EDGE('',*,*,#46412,.F.) ;
#64081 = ORIENTED_EDGE('',*,*,#47069,.F.) ;
#64082 = ORIENTED_EDGE('',*,*,#46473,.F.) ;
#64083 = ORIENTED_EDGE('',*,*,#47068,.T.) ;
#64084 = ORIENTED_EDGE('',*,*,#47070,.F.) ;
#64085 = ORIENTED_EDGE('',*,*,#47069,.T.) ;
#64086 = ORIENTED_EDGE('',*,*,#46409,.F.) ;
#64087 = ORIENTED_EDGE('',*,*,#47071,.F.) ;
#64088 = ORIENTED_EDGE('',*,*,#46495,.F.) ;
#64089 = ORIENTED_EDGE('',*,*,#47070,.T.) ;
#64090 = ORIENTED_EDGE('',*,*,#46481,.F.) ;
#64091 = ORIENTED_EDGE('',*,*,#47072,.F.) ;
#64092 = ORIENTED_EDGE('',*,*,#46476,.F.) ;
#64093 = ORIENTED_EDGE('',*,*,#47071,.T.) ;
#64094 = ORIENTED_EDGE('',*,*,#46406,.F.) ;
#64095 = ORIENTED_EDGE('',*,*,#47073,.F.) ;
#64096 = ORIENTED_EDGE('',*,*,#46478,.F.) ;
#64097 = ORIENTED_EDGE('',*,*,#47072,.T.) ;
#64098 = ORIENTED_EDGE('',*,*,#46480,.F.) ;
#64099 = ORIENTED_EDGE('',*,*,#47074,.F.) ;
#64100 = ORIENTED_EDGE('',*,*,#46400,.F.) ;
#64101 = ORIENTED_EDGE('',*,*,#47073,.T.) ;
#64102 = ORIENTED_EDGE('',*,*,#46403,.F.) ;
#64103 = ORIENTED_EDGE('',*,*,#47074,.T.) ;
#64104 = ORIENTED_EDGE('',*,*,#46479,.F.) ;
#64105 = ORIENTED_EDGE('',*,*,#47075,.F.) ;
#64106 = ORIENTED_EDGE('',*,*,#45599,.F.) ;
#64107 = ORIENTED_EDGE('',*,*,#47076,.F.) ;
#64108 = ORIENTED_EDGE('',*,*,#45528,.F.) ;
#64109 = ORIENTED_EDGE('',*,*,#47077,.F.) ;
#64110 = ORIENTED_EDGE('',*,*,#45600,.F.) ;
#64111 = ORIENTED_EDGE('',*,*,#47078,.F.) ;
#64112 = ORIENTED_EDGE('',*,*,#45594,.F.) ;
#64113 = ORIENTED_EDGE('',*,*,#47079,.F.) ;
#64114 = ORIENTED_EDGE('',*,*,#47077,.T.) ;
#64115 = ORIENTED_EDGE('',*,*,#47080,.F.) ;
#64116 = ORIENTED_EDGE('',*,*,#47081,.F.) ;
#64117 = ORIENTED_EDGE('',*,*,#47076,.T.) ;
#64118 = ORIENTED_EDGE('',*,*,#47082,.F.) ;
#64119 = ORIENTED_EDGE('',*,*,#47075,.T.) ;
#64120 = ORIENTED_EDGE('',*,*,#45527,.T.) ;
#64121 = ORIENTED_EDGE('',*,*,#47083,.F.) ;
#64122 = ORIENTED_EDGE('',*,*,#47078,.T.) ;
#64123 = ORIENTED_EDGE('',*,*,#47080,.T.) ;
#64124 = ORIENTED_EDGE('',*,*,#45597,.F.) ;
#64125 = ORIENTED_EDGE('',*,*,#47084,.F.) ;
#64126 = ORIENTED_EDGE('',*,*,#44259,.T.) ;
#64127 = ORIENTED_EDGE('',*,*,#47085,.T.) ;
#64128 = ORIENTED_EDGE('',*,*,#47086,.F.) ;
#64129 = ORIENTED_EDGE('',*,*,#47079,.T.) ;
#64130 = ORIENTED_EDGE('',*,*,#47087,.F.) ;
#64131 = ORIENTED_EDGE('',*,*,#47088,.T.) ;
#64132 = ORIENTED_EDGE('',*,*,#47089,.F.) ;
#64133 = ORIENTED_EDGE('',*,*,#44463,.F.) ;
#64134 = ORIENTED_EDGE('',*,*,#47090,.F.) ;
#64135 = ORIENTED_EDGE('',*,*,#45601,.F.) ;
#64136 = ORIENTED_EDGE('',*,*,#47082,.T.) ;
#64137 = ORIENTED_EDGE('',*,*,#45598,.F.) ;
#64138 = ORIENTED_EDGE('',*,*,#47091,.F.) ;
#64139 = ORIENTED_EDGE('',*,*,#45604,.F.) ;
#64140 = ORIENTED_EDGE('',*,*,#47081,.T.) ;
#64141 = ORIENTED_EDGE('',*,*,#45603,.F.) ;
#64142 = ORIENTED_EDGE('',*,*,#47092,.F.) ;
#64143 = ORIENTED_EDGE('',*,*,#45519,.F.) ;
#64144 = ORIENTED_EDGE('',*,*,#47083,.T.) ;
#64145 = ORIENTED_EDGE('',*,*,#45526,.F.) ;
#64146 = ORIENTED_EDGE('',*,*,#47093,.F.) ;
#64147 = ORIENTED_EDGE('',*,*,#45595,.F.) ;
#64148 = ORIENTED_EDGE('',*,*,#47094,.F.) ;
#64149 = ORIENTED_EDGE('',*,*,#45596,.F.) ;
#64150 = ORIENTED_EDGE('',*,*,#47095,.F.) ;
#64151 = ORIENTED_EDGE('',*,*,#45591,.F.) ;
#64152 = ORIENTED_EDGE('',*,*,#47084,.T.) ;
#64153 = ORIENTED_EDGE('',*,*,#47094,.T.) ;
#64154 = ORIENTED_EDGE('',*,*,#44260,.F.) ;
#64155 = ORIENTED_EDGE('',*,*,#47090,.T.) ;
#64156 = ORIENTED_EDGE('',*,*,#44473,.T.) ;
#64157 = ORIENTED_EDGE('',*,*,#47096,.F.) ;
#64158 = ORIENTED_EDGE('',*,*,#47091,.T.) ;
#64159 = ORIENTED_EDGE('',*,*,#47097,.F.) ;
#64160 = ORIENTED_EDGE('',*,*,#47092,.T.) ;
#64161 = ORIENTED_EDGE('',*,*,#47098,.F.) ;
#64162 = ORIENTED_EDGE('',*,*,#44561,.T.) ;
#64163 = ORIENTED_EDGE('',*,*,#47093,.T.) ;
#64164 = ORIENTED_EDGE('',*,*,#45525,.T.) ;
#64165 = ORIENTED_EDGE('',*,*,#47099,.F.) ;
#64166 = ORIENTED_EDGE('',*,*,#47095,.T.) ;
#64167 = ORIENTED_EDGE('',*,*,#47096,.T.) ;
#64168 = ORIENTED_EDGE('',*,*,#44472,.F.) ;
#64169 = ORIENTED_EDGE('',*,*,#47100,.F.) ;
#64170 = ORIENTED_EDGE('',*,*,#45605,.F.) ;
#64171 = ORIENTED_EDGE('',*,*,#47098,.T.) ;
#64172 = ORIENTED_EDGE('',*,*,#45602,.F.) ;
#64173 = ORIENTED_EDGE('',*,*,#47101,.F.) ;
#64174 = ORIENTED_EDGE('',*,*,#44562,.F.) ;
#64175 = ORIENTED_EDGE('',*,*,#45520,.F.) ;
#64176 = ORIENTED_EDGE('',*,*,#47097,.T.) ;
#64177 = ORIENTED_EDGE('',*,*,#47102,.F.) ;
#64178 = ORIENTED_EDGE('',*,*,#47103,.F.) ;
#64179 = ORIENTED_EDGE('',*,*,#47099,.T.) ;
#64180 = ORIENTED_EDGE('',*,*,#45524,.F.) ;
#64181 = ORIENTED_EDGE('',*,*,#47104,.F.) ;
#64182 = ORIENTED_EDGE('',*,*,#45592,.F.) ;
#64183 = ORIENTED_EDGE('',*,*,#47105,.F.) ;
#64184 = ORIENTED_EDGE('',*,*,#45593,.F.) ;
#64185 = ORIENTED_EDGE('',*,*,#47106,.F.) ;
#64186 = ORIENTED_EDGE('',*,*,#45587,.F.) ;
#64187 = ORIENTED_EDGE('',*,*,#44262,.T.) ;
#64188 = ORIENTED_EDGE('',*,*,#47105,.T.) ;
#64189 = ORIENTED_EDGE('',*,*,#47107,.F.) ;
#64190 = ORIENTED_EDGE('',*,*,#44467,.T.) ;
#64191 = ORIENTED_EDGE('',*,*,#47101,.T.) ;
#64192 = ORIENTED_EDGE('',*,*,#47100,.T.) ;
#64193 = ORIENTED_EDGE('',*,*,#47108,.F.) ;
#64194 = ORIENTED_EDGE('',*,*,#47109,.F.) ;
#64195 = ORIENTED_EDGE('',*,*,#44595,.F.) ;
#64196 = ORIENTED_EDGE('',*,*,#47110,.F.) ;
#64197 = ORIENTED_EDGE('',*,*,#47111,.F.) ;
#64198 = ORIENTED_EDGE('',*,*,#47102,.T.) ;
#64199 = ORIENTED_EDGE('',*,*,#44565,.F.) ;
#64200 = ORIENTED_EDGE('',*,*,#47110,.T.) ;
#64201 = ORIENTED_EDGE('',*,*,#44738,.F.) ;
#64202 = ORIENTED_EDGE('',*,*,#47103,.T.) ;
#64203 = ORIENTED_EDGE('',*,*,#47112,.F.) ;
#64204 = ORIENTED_EDGE('',*,*,#47113,.F.) ;
#64205 = ORIENTED_EDGE('',*,*,#47106,.T.) ;
#64206 = ORIENTED_EDGE('',*,*,#47104,.T.) ;
#64207 = ORIENTED_EDGE('',*,*,#47114,.F.) ;
#64208 = ORIENTED_EDGE('',*,*,#47107,.T.) ;
#64209 = ORIENTED_EDGE('',*,*,#45590,.F.) ;
#64210 = ORIENTED_EDGE('',*,*,#47115,.F.) ;
#64211 = ORIENTED_EDGE('',*,*,#44468,.F.) ;
#64212 = ORIENTED_EDGE('',*,*,#47108,.T.) ;
#64213 = ORIENTED_EDGE('',*,*,#44471,.F.) ;
#64214 = ORIENTED_EDGE('',*,*,#47116,.F.) ;
#64215 = ORIENTED_EDGE('',*,*,#44563,.F.) ;
#64216 = ORIENTED_EDGE('',*,*,#47109,.T.) ;
#64217 = ORIENTED_EDGE('',*,*,#44564,.F.) ;
#64218 = ORIENTED_EDGE('',*,*,#47117,.F.) ;
#64219 = ORIENTED_EDGE('',*,*,#44671,.F.) ;
#64220 = ORIENTED_EDGE('',*,*,#47111,.T.) ;
#64221 = ORIENTED_EDGE('',*,*,#44737,.T.) ;
#64222 = ORIENTED_EDGE('',*,*,#47118,.F.) ;
#64223 = ORIENTED_EDGE('',*,*,#47112,.T.) ;
#64224 = ORIENTED_EDGE('',*,*,#45521,.F.) ;
#64225 = ORIENTED_EDGE('',*,*,#47113,.T.) ;
#64226 = ORIENTED_EDGE('',*,*,#47119,.F.) ;
#64227 = ORIENTED_EDGE('',*,*,#47120,.F.) ;
#64228 = ORIENTED_EDGE('',*,*,#47114,.T.) ;
#64229 = ORIENTED_EDGE('',*,*,#45523,.F.) ;
#64230 = ORIENTED_EDGE('',*,*,#47121,.F.) ;
#64231 = ORIENTED_EDGE('',*,*,#45588,.F.) ;
#64232 = ORIENTED_EDGE('',*,*,#47122,.F.) ;
#64233 = ORIENTED_EDGE('',*,*,#45589,.F.) ;
#64234 = ORIENTED_EDGE('',*,*,#47123,.F.) ;
#64235 = ORIENTED_EDGE('',*,*,#44560,.F.) ;
#64236 = ORIENTED_EDGE('',*,*,#47115,.T.) ;
#64237 = ORIENTED_EDGE('',*,*,#47122,.T.) ;
#64238 = ORIENTED_EDGE('',*,*,#47124,.F.) ;
#64239 = ORIENTED_EDGE('',*,*,#47117,.T.) ;
#64240 = ORIENTED_EDGE('',*,*,#47116,.T.) ;
#64241 = ORIENTED_EDGE('',*,*,#47125,.F.) ;
#64242 = ORIENTED_EDGE('',*,*,#44672,.T.) ;
#64243 = ORIENTED_EDGE('',*,*,#47126,.F.) ;
#64244 = ORIENTED_EDGE('',*,*,#47119,.T.) ;
#64245 = ORIENTED_EDGE('',*,*,#47118,.T.) ;
#64246 = ORIENTED_EDGE('',*,*,#44736,.F.) ;
#64247 = ORIENTED_EDGE('',*,*,#47120,.T.) ;
#64248 = ORIENTED_EDGE('',*,*,#47127,.F.) ;
#64249 = ORIENTED_EDGE('',*,*,#47128,.F.) ;
#64250 = ORIENTED_EDGE('',*,*,#47123,.T.) ;
#64251 = ORIENTED_EDGE('',*,*,#47121,.T.) ;
#64252 = ORIENTED_EDGE('',*,*,#47129,.F.) ;
#64253 = ORIENTED_EDGE('',*,*,#44556,.T.) ;
#64254 = ORIENTED_EDGE('',*,*,#47124,.T.) ;
#64255 = ORIENTED_EDGE('',*,*,#44559,.F.) ;
#64256 = ORIENTED_EDGE('',*,*,#47130,.F.) ;
#64257 = ORIENTED_EDGE('',*,*,#44469,.F.) ;
#64258 = ORIENTED_EDGE('',*,*,#47125,.T.) ;
#64259 = ORIENTED_EDGE('',*,*,#44470,.F.) ;
#64260 = ORIENTED_EDGE('',*,*,#47131,.F.) ;
#64261 = ORIENTED_EDGE('',*,*,#44673,.F.) ;
#64262 = ORIENTED_EDGE('',*,*,#47126,.T.) ;
#64263 = ORIENTED_EDGE('',*,*,#44735,.T.) ;
#64264 = ORIENTED_EDGE('',*,*,#47132,.F.) ;
#64265 = ORIENTED_EDGE('',*,*,#47127,.T.) ;
#64266 = ORIENTED_EDGE('',*,*,#45522,.F.) ;
#64267 = ORIENTED_EDGE('',*,*,#47128,.T.) ;
#64268 = ORIENTED_EDGE('',*,*,#47133,.F.) ;
#64269 = ORIENTED_EDGE('',*,*,#47129,.T.) ;
#64270 = ORIENTED_EDGE('',*,*,#47131,.T.) ;
#64271 = ORIENTED_EDGE('',*,*,#47130,.T.) ;
#64272 = ORIENTED_EDGE('',*,*,#47134,.F.) ;
#64273 = ORIENTED_EDGE('',*,*,#44674,.T.) ;
#64274 = ORIENTED_EDGE('',*,*,#47132,.T.) ;
#64275 = ORIENTED_EDGE('',*,*,#44734,.F.) ;
#64276 = ORIENTED_EDGE('',*,*,#47135,.F.) ;
#64277 = ORIENTED_EDGE('',*,*,#44557,.F.) ;
#64278 = ORIENTED_EDGE('',*,*,#47133,.T.) ;
#64279 = ORIENTED_EDGE('',*,*,#47134,.T.) ;
#64280 = ORIENTED_EDGE('',*,*,#44558,.F.) ;
#64281 = ORIENTED_EDGE('',*,*,#47136,.F.) ;
#64282 = ORIENTED_EDGE('',*,*,#44675,.F.) ;
#64283 = ORIENTED_EDGE('',*,*,#47135,.T.) ;
#64284 = ORIENTED_EDGE('',*,*,#44601,.F.) ;
#64285 = ORIENTED_EDGE('',*,*,#47136,.T.) ;
#64286 = ORIENTED_EDGE('',*,*,#47137,.F.) ;
#64287 = ORIENTED_EDGE('',*,*,#46343,.F.) ;
#64288 = ORIENTED_EDGE('',*,*,#47138,.F.) ;
#64289 = ORIENTED_EDGE('',*,*,#46390,.F.) ;
#64290 = ORIENTED_EDGE('',*,*,#47138,.T.) ;
#64291 = ORIENTED_EDGE('',*,*,#46340,.F.) ;
#64292 = ORIENTED_EDGE('',*,*,#47139,.F.) ;
#64293 = ORIENTED_EDGE('',*,*,#46391,.F.) ;
#64294 = ORIENTED_EDGE('',*,*,#46346,.F.) ;
#64295 = ORIENTED_EDGE('',*,*,#47137,.T.) ;
#64296 = ORIENTED_EDGE('',*,*,#47140,.F.) ;
#64297 = ORIENTED_EDGE('',*,*,#47139,.T.) ;
#64298 = ORIENTED_EDGE('',*,*,#46337,.F.) ;
#64299 = ORIENTED_EDGE('',*,*,#47141,.F.) ;
#64300 = ORIENTED_EDGE('',*,*,#46392,.F.) ;
#64301 = ORIENTED_EDGE('',*,*,#47140,.T.) ;
#64302 = ORIENTED_EDGE('',*,*,#46389,.F.) ;
#64303 = ORIENTED_EDGE('',*,*,#47142,.F.) ;
#64304 = ORIENTED_EDGE('',*,*,#46349,.F.) ;
#64305 = ORIENTED_EDGE('',*,*,#47141,.T.) ;
#64306 = ORIENTED_EDGE('',*,*,#46334,.F.) ;
#64307 = ORIENTED_EDGE('',*,*,#47143,.F.) ;
#64308 = ORIENTED_EDGE('',*,*,#46393,.F.) ;
#64309 = ORIENTED_EDGE('',*,*,#46352,.F.) ;
#64310 = ORIENTED_EDGE('',*,*,#47142,.T.) ;
#64311 = ORIENTED_EDGE('',*,*,#47144,.F.) ;
#64312 = ORIENTED_EDGE('',*,*,#47143,.T.) ;
#64313 = ORIENTED_EDGE('',*,*,#46331,.F.) ;
#64314 = ORIENTED_EDGE('',*,*,#47145,.F.) ;
#64315 = ORIENTED_EDGE('',*,*,#46394,.F.) ;
#64316 = ORIENTED_EDGE('',*,*,#47144,.T.) ;
#64317 = ORIENTED_EDGE('',*,*,#46388,.F.) ;
#64318 = ORIENTED_EDGE('',*,*,#47146,.F.) ;
#64319 = ORIENTED_EDGE('',*,*,#46355,.F.) ;
#64320 = ORIENTED_EDGE('',*,*,#47145,.T.) ;
#64321 = ORIENTED_EDGE('',*,*,#46328,.F.) ;
#64322 = ORIENTED_EDGE('',*,*,#47147,.F.) ;
#64323 = ORIENTED_EDGE('',*,*,#46358,.F.) ;
#64324 = ORIENTED_EDGE('',*,*,#47146,.T.) ;
#64325 = ORIENTED_EDGE('',*,*,#47148,.F.) ;
#64326 = ORIENTED_EDGE('',*,*,#47147,.T.) ;
#64327 = ORIENTED_EDGE('',*,*,#46325,.F.) ;
#64328 = ORIENTED_EDGE('',*,*,#47149,.F.) ;
#64329 = ORIENTED_EDGE('',*,*,#46395,.F.) ;
#64330 = ORIENTED_EDGE('',*,*,#47148,.T.) ;
#64331 = ORIENTED_EDGE('',*,*,#46387,.F.) ;
#64332 = ORIENTED_EDGE('',*,*,#47150,.F.) ;
#64333 = ORIENTED_EDGE('',*,*,#46361,.F.) ;
#64334 = ORIENTED_EDGE('',*,*,#47149,.T.) ;
#64335 = ORIENTED_EDGE('',*,*,#44351,.F.) ;
#64336 = ORIENTED_EDGE('',*,*,#47151,.F.) ;
#64337 = ORIENTED_EDGE('',*,*,#46364,.F.) ;
#64338 = ORIENTED_EDGE('',*,*,#47150,.T.) ;
#64339 = ORIENTED_EDGE('',*,*,#47152,.F.) ;
#64340 = ORIENTED_EDGE('',*,*,#47151,.T.) ;
#64341 = ORIENTED_EDGE('',*,*,#46323,.F.) ;
#64342 = ORIENTED_EDGE('',*,*,#44258,.F.) ;
#64343 = ORIENTED_EDGE('',*,*,#46396,.F.) ;
#64344 = ORIENTED_EDGE('',*,*,#47152,.T.) ;
#64345 = ORIENTED_EDGE('',*,*,#46386,.F.) ;
#64346 = ORIENTED_EDGE('',*,*,#47153,.F.) ;
#64347 = ORIENTED_EDGE('',*,*,#46367,.F.) ;
#64348 = ORIENTED_EDGE('',*,*,#46370,.F.) ;
#64349 = ORIENTED_EDGE('',*,*,#47153,.T.) ;
#64350 = ORIENTED_EDGE('',*,*,#47154,.F.) ;
#64351 = ORIENTED_EDGE('',*,*,#44257,.T.) ;
#64352 = ORIENTED_EDGE('',*,*,#46318,.F.) ;
#64353 = ORIENTED_EDGE('',*,*,#47155,.F.) ;
#64354 = ORIENTED_EDGE('',*,*,#46397,.F.) ;
#64355 = ORIENTED_EDGE('',*,*,#47154,.T.) ;
#64356 = ORIENTED_EDGE('',*,*,#46385,.F.) ;
#64357 = ORIENTED_EDGE('',*,*,#47156,.F.) ;
#64358 = ORIENTED_EDGE('',*,*,#46373,.F.) ;
#64359 = ORIENTED_EDGE('',*,*,#47155,.T.) ;
#64360 = ORIENTED_EDGE('',*,*,#46315,.F.) ;
#64361 = ORIENTED_EDGE('',*,*,#47157,.F.) ;
#64362 = ORIENTED_EDGE('',*,*,#46376,.F.) ;
#64363 = ORIENTED_EDGE('',*,*,#47156,.T.) ;
#64364 = ORIENTED_EDGE('',*,*,#47158,.F.) ;
#64365 = ORIENTED_EDGE('',*,*,#47157,.T.) ;
#64366 = ORIENTED_EDGE('',*,*,#46312,.F.) ;
#64367 = ORIENTED_EDGE('',*,*,#47159,.F.) ;
#64368 = ORIENTED_EDGE('',*,*,#46398,.F.) ;
#64369 = ORIENTED_EDGE('',*,*,#47158,.T.) ;
#64370 = ORIENTED_EDGE('',*,*,#46384,.F.) ;
#64371 = ORIENTED_EDGE('',*,*,#47160,.F.) ;
#64372 = ORIENTED_EDGE('',*,*,#46379,.F.) ;
#64373 = ORIENTED_EDGE('',*,*,#47159,.T.) ;
#64374 = ORIENTED_EDGE('',*,*,#46309,.F.) ;
#64375 = ORIENTED_EDGE('',*,*,#47161,.F.) ;
#64376 = ORIENTED_EDGE('',*,*,#46381,.F.) ;
#64377 = ORIENTED_EDGE('',*,*,#47160,.T.) ;
#64378 = ORIENTED_EDGE('',*,*,#46383,.F.) ;
#64379 = ORIENTED_EDGE('',*,*,#47162,.F.) ;
#64380 = ORIENTED_EDGE('',*,*,#46303,.F.) ;
#64381 = ORIENTED_EDGE('',*,*,#47161,.T.) ;
#64382 = ORIENTED_EDGE('',*,*,#46306,.F.) ;
#64383 = ORIENTED_EDGE('',*,*,#47162,.T.) ;
#64384 = ORIENTED_EDGE('',*,*,#46382,.F.) ;
#64385 = ORIENTED_EDGE('',*,*,#47163,.F.) ;
#64386 = ORIENTED_EDGE('',*,*,#45618,.F.) ;
#64387 = ORIENTED_EDGE('',*,*,#47164,.F.) ;
#64388 = ORIENTED_EDGE('',*,*,#45518,.F.) ;
#64389 = ORIENTED_EDGE('',*,*,#47165,.F.) ;
#64390 = ORIENTED_EDGE('',*,*,#45619,.F.) ;
#64391 = ORIENTED_EDGE('',*,*,#47166,.F.) ;
#64392 = ORIENTED_EDGE('',*,*,#45613,.F.) ;
#64393 = ORIENTED_EDGE('',*,*,#47167,.F.) ;
#64394 = ORIENTED_EDGE('',*,*,#47165,.T.) ;
#64395 = ORIENTED_EDGE('',*,*,#47168,.F.) ;
#64396 = ORIENTED_EDGE('',*,*,#47169,.F.) ;
#64397 = ORIENTED_EDGE('',*,*,#47164,.T.) ;
#64398 = ORIENTED_EDGE('',*,*,#47170,.F.) ;
#64399 = ORIENTED_EDGE('',*,*,#47163,.T.) ;
#64400 = ORIENTED_EDGE('',*,*,#45517,.T.) ;
#64401 = ORIENTED_EDGE('',*,*,#47171,.F.) ;
#64402 = ORIENTED_EDGE('',*,*,#47166,.T.) ;
#64403 = ORIENTED_EDGE('',*,*,#47168,.T.) ;
#64404 = ORIENTED_EDGE('',*,*,#45616,.F.) ;
#64405 = ORIENTED_EDGE('',*,*,#47172,.F.) ;
#64406 = ORIENTED_EDGE('',*,*,#44242,.T.) ;
#64407 = ORIENTED_EDGE('',*,*,#47173,.T.) ;
#64408 = ORIENTED_EDGE('',*,*,#47174,.F.) ;
#64409 = ORIENTED_EDGE('',*,*,#47167,.T.) ;
#64410 = ORIENTED_EDGE('',*,*,#47175,.F.) ;
#64411 = ORIENTED_EDGE('',*,*,#47176,.T.) ;
#64412 = ORIENTED_EDGE('',*,*,#47177,.F.) ;
#64413 = ORIENTED_EDGE('',*,*,#44452,.F.) ;
#64414 = ORIENTED_EDGE('',*,*,#47178,.F.) ;
#64415 = ORIENTED_EDGE('',*,*,#45620,.F.) ;
#64416 = ORIENTED_EDGE('',*,*,#47170,.T.) ;
#64417 = ORIENTED_EDGE('',*,*,#45617,.F.) ;
#64418 = ORIENTED_EDGE('',*,*,#47179,.F.) ;
#64419 = ORIENTED_EDGE('',*,*,#45623,.F.) ;
#64420 = ORIENTED_EDGE('',*,*,#47169,.T.) ;
#64421 = ORIENTED_EDGE('',*,*,#45622,.F.) ;
#64422 = ORIENTED_EDGE('',*,*,#47180,.F.) ;
#64423 = ORIENTED_EDGE('',*,*,#45509,.F.) ;
#64424 = ORIENTED_EDGE('',*,*,#47171,.T.) ;
#64425 = ORIENTED_EDGE('',*,*,#45516,.F.) ;
#64426 = ORIENTED_EDGE('',*,*,#47181,.F.) ;
#64427 = ORIENTED_EDGE('',*,*,#45614,.F.) ;
#64428 = ORIENTED_EDGE('',*,*,#47182,.F.) ;
#64429 = ORIENTED_EDGE('',*,*,#45615,.F.) ;
#64430 = ORIENTED_EDGE('',*,*,#47183,.F.) ;
#64431 = ORIENTED_EDGE('',*,*,#45610,.F.) ;
#64432 = ORIENTED_EDGE('',*,*,#47172,.T.) ;
#64433 = ORIENTED_EDGE('',*,*,#47182,.T.) ;
#64434 = ORIENTED_EDGE('',*,*,#44243,.F.) ;
#64435 = ORIENTED_EDGE('',*,*,#47178,.T.) ;
#64436 = ORIENTED_EDGE('',*,*,#44462,.T.) ;
#64437 = ORIENTED_EDGE('',*,*,#47184,.F.) ;
#64438 = ORIENTED_EDGE('',*,*,#47179,.T.) ;
#64439 = ORIENTED_EDGE('',*,*,#47185,.F.) ;
#64440 = ORIENTED_EDGE('',*,*,#47180,.T.) ;
#64441 = ORIENTED_EDGE('',*,*,#47186,.F.) ;
#64442 = ORIENTED_EDGE('',*,*,#44551,.T.) ;
#64443 = ORIENTED_EDGE('',*,*,#47181,.T.) ;
#64444 = ORIENTED_EDGE('',*,*,#45515,.T.) ;
#64445 = ORIENTED_EDGE('',*,*,#47187,.F.) ;
#64446 = ORIENTED_EDGE('',*,*,#47183,.T.) ;
#64447 = ORIENTED_EDGE('',*,*,#47184,.T.) ;
#64448 = ORIENTED_EDGE('',*,*,#44461,.F.) ;
#64449 = ORIENTED_EDGE('',*,*,#47188,.F.) ;
#64450 = ORIENTED_EDGE('',*,*,#45624,.F.) ;
#64451 = ORIENTED_EDGE('',*,*,#47186,.T.) ;
#64452 = ORIENTED_EDGE('',*,*,#45621,.F.) ;
#64453 = ORIENTED_EDGE('',*,*,#47189,.F.) ;
#64454 = ORIENTED_EDGE('',*,*,#44552,.F.) ;
#64455 = ORIENTED_EDGE('',*,*,#45510,.F.) ;
#64456 = ORIENTED_EDGE('',*,*,#47185,.T.) ;
#64457 = ORIENTED_EDGE('',*,*,#47190,.F.) ;
#64458 = ORIENTED_EDGE('',*,*,#47191,.F.) ;
#64459 = ORIENTED_EDGE('',*,*,#47187,.T.) ;
#64460 = ORIENTED_EDGE('',*,*,#45514,.F.) ;
#64461 = ORIENTED_EDGE('',*,*,#47192,.F.) ;
#64462 = ORIENTED_EDGE('',*,*,#45611,.F.) ;
#64463 = ORIENTED_EDGE('',*,*,#47193,.F.) ;
#64464 = ORIENTED_EDGE('',*,*,#45612,.F.) ;
#64465 = ORIENTED_EDGE('',*,*,#47194,.F.) ;
#64466 = ORIENTED_EDGE('',*,*,#45606,.F.) ;
#64467 = ORIENTED_EDGE('',*,*,#44245,.T.) ;
#64468 = ORIENTED_EDGE('',*,*,#47193,.T.) ;
#64469 = ORIENTED_EDGE('',*,*,#47195,.F.) ;
#64470 = ORIENTED_EDGE('',*,*,#44456,.T.) ;
#64471 = ORIENTED_EDGE('',*,*,#47189,.T.) ;
#64472 = ORIENTED_EDGE('',*,*,#47188,.T.) ;
#64473 = ORIENTED_EDGE('',*,*,#47196,.F.) ;
#64474 = ORIENTED_EDGE('',*,*,#47197,.F.) ;
#64475 = ORIENTED_EDGE('',*,*,#44599,.F.) ;
#64476 = ORIENTED_EDGE('',*,*,#47198,.F.) ;
#64477 = ORIENTED_EDGE('',*,*,#47199,.F.) ;
#64478 = ORIENTED_EDGE('',*,*,#47190,.T.) ;
#64479 = ORIENTED_EDGE('',*,*,#44555,.F.) ;
#64480 = ORIENTED_EDGE('',*,*,#47198,.T.) ;
#64481 = ORIENTED_EDGE('',*,*,#44733,.F.) ;
#64482 = ORIENTED_EDGE('',*,*,#47191,.T.) ;
#64483 = ORIENTED_EDGE('',*,*,#47200,.F.) ;
#64484 = ORIENTED_EDGE('',*,*,#47201,.F.) ;
#64485 = ORIENTED_EDGE('',*,*,#47194,.T.) ;
#64486 = ORIENTED_EDGE('',*,*,#47192,.T.) ;
#64487 = ORIENTED_EDGE('',*,*,#47202,.F.) ;
#64488 = ORIENTED_EDGE('',*,*,#47195,.T.) ;
#64489 = ORIENTED_EDGE('',*,*,#45609,.F.) ;
#64490 = ORIENTED_EDGE('',*,*,#47203,.F.) ;
#64491 = ORIENTED_EDGE('',*,*,#44457,.F.) ;
#64492 = ORIENTED_EDGE('',*,*,#47196,.T.) ;
#64493 = ORIENTED_EDGE('',*,*,#44460,.F.) ;
#64494 = ORIENTED_EDGE('',*,*,#47204,.F.) ;
#64495 = ORIENTED_EDGE('',*,*,#44553,.F.) ;
#64496 = ORIENTED_EDGE('',*,*,#47197,.T.) ;
#64497 = ORIENTED_EDGE('',*,*,#44554,.F.) ;
#64498 = ORIENTED_EDGE('',*,*,#47205,.F.) ;
#64499 = ORIENTED_EDGE('',*,*,#44676,.F.) ;
#64500 = ORIENTED_EDGE('',*,*,#47199,.T.) ;
#64501 = ORIENTED_EDGE('',*,*,#44732,.T.) ;
#64502 = ORIENTED_EDGE('',*,*,#47206,.F.) ;
#64503 = ORIENTED_EDGE('',*,*,#47200,.T.) ;
#64504 = ORIENTED_EDGE('',*,*,#45511,.F.) ;
#64505 = ORIENTED_EDGE('',*,*,#47201,.T.) ;
#64506 = ORIENTED_EDGE('',*,*,#47207,.F.) ;
#64507 = ORIENTED_EDGE('',*,*,#47208,.F.) ;
#64508 = ORIENTED_EDGE('',*,*,#47202,.T.) ;
#64509 = ORIENTED_EDGE('',*,*,#45513,.F.) ;
#64510 = ORIENTED_EDGE('',*,*,#47209,.F.) ;
#64511 = ORIENTED_EDGE('',*,*,#45607,.F.) ;
#64512 = ORIENTED_EDGE('',*,*,#47210,.F.) ;
#64513 = ORIENTED_EDGE('',*,*,#45608,.F.) ;
#64514 = ORIENTED_EDGE('',*,*,#47211,.F.) ;
#64515 = ORIENTED_EDGE('',*,*,#44550,.F.) ;
#64516 = ORIENTED_EDGE('',*,*,#47203,.T.) ;
#64517 = ORIENTED_EDGE('',*,*,#47210,.T.) ;
#64518 = ORIENTED_EDGE('',*,*,#47212,.F.) ;
#64519 = ORIENTED_EDGE('',*,*,#47205,.T.) ;
#64520 = ORIENTED_EDGE('',*,*,#47204,.T.) ;
#64521 = ORIENTED_EDGE('',*,*,#47213,.F.) ;
#64522 = ORIENTED_EDGE('',*,*,#44677,.T.) ;
#64523 = ORIENTED_EDGE('',*,*,#47214,.F.) ;
#64524 = ORIENTED_EDGE('',*,*,#47207,.T.) ;
#64525 = ORIENTED_EDGE('',*,*,#47206,.T.) ;
#64526 = ORIENTED_EDGE('',*,*,#44731,.F.) ;
#64527 = ORIENTED_EDGE('',*,*,#47208,.T.) ;
#64528 = ORIENTED_EDGE('',*,*,#47215,.F.) ;
#64529 = ORIENTED_EDGE('',*,*,#47216,.F.) ;
#64530 = ORIENTED_EDGE('',*,*,#47211,.T.) ;
#64531 = ORIENTED_EDGE('',*,*,#47209,.T.) ;
#64532 = ORIENTED_EDGE('',*,*,#47217,.F.) ;
#64533 = ORIENTED_EDGE('',*,*,#44546,.T.) ;
#64534 = ORIENTED_EDGE('',*,*,#47212,.T.) ;
#64535 = ORIENTED_EDGE('',*,*,#44549,.F.) ;
#64536 = ORIENTED_EDGE('',*,*,#47218,.F.) ;
#64537 = ORIENTED_EDGE('',*,*,#44458,.F.) ;
#64538 = ORIENTED_EDGE('',*,*,#47213,.T.) ;
#64539 = ORIENTED_EDGE('',*,*,#44459,.F.) ;
#64540 = ORIENTED_EDGE('',*,*,#47219,.F.) ;
#64541 = ORIENTED_EDGE('',*,*,#44678,.F.) ;
#64542 = ORIENTED_EDGE('',*,*,#47214,.T.) ;
#64543 = ORIENTED_EDGE('',*,*,#44730,.T.) ;
#64544 = ORIENTED_EDGE('',*,*,#47220,.F.) ;
#64545 = ORIENTED_EDGE('',*,*,#47215,.T.) ;
#64546 = ORIENTED_EDGE('',*,*,#45512,.F.) ;
#64547 = ORIENTED_EDGE('',*,*,#47216,.T.) ;
#64548 = ORIENTED_EDGE('',*,*,#47221,.F.) ;
#64549 = ORIENTED_EDGE('',*,*,#47217,.T.) ;
#64550 = ORIENTED_EDGE('',*,*,#47219,.T.) ;
#64551 = ORIENTED_EDGE('',*,*,#47218,.T.) ;
#64552 = ORIENTED_EDGE('',*,*,#47222,.F.) ;
#64553 = ORIENTED_EDGE('',*,*,#44679,.T.) ;
#64554 = ORIENTED_EDGE('',*,*,#47220,.T.) ;
#64555 = ORIENTED_EDGE('',*,*,#44729,.F.) ;
#64556 = ORIENTED_EDGE('',*,*,#47223,.F.) ;
#64557 = ORIENTED_EDGE('',*,*,#44547,.F.) ;
#64558 = ORIENTED_EDGE('',*,*,#47221,.T.) ;
#64559 = ORIENTED_EDGE('',*,*,#47222,.T.) ;
#64560 = ORIENTED_EDGE('',*,*,#44548,.F.) ;
#64561 = ORIENTED_EDGE('',*,*,#47224,.F.) ;
#64562 = ORIENTED_EDGE('',*,*,#44680,.F.) ;
#64563 = ORIENTED_EDGE('',*,*,#47223,.T.) ;
#64564 = ORIENTED_EDGE('',*,*,#44605,.F.) ;
#64565 = ORIENTED_EDGE('',*,*,#47224,.T.) ;
#64566 = ORIENTED_EDGE('',*,*,#47225,.F.) ;
#64567 = ORIENTED_EDGE('',*,*,#46246,.F.) ;
#64568 = ORIENTED_EDGE('',*,*,#47226,.F.) ;
#64569 = ORIENTED_EDGE('',*,*,#46293,.F.) ;
#64570 = ORIENTED_EDGE('',*,*,#47226,.T.) ;
#64571 = ORIENTED_EDGE('',*,*,#46243,.F.) ;
#64572 = ORIENTED_EDGE('',*,*,#47227,.F.) ;
#64573 = ORIENTED_EDGE('',*,*,#46294,.F.) ;
#64574 = ORIENTED_EDGE('',*,*,#46249,.F.) ;
#64575 = ORIENTED_EDGE('',*,*,#47225,.T.) ;
#64576 = ORIENTED_EDGE('',*,*,#47228,.F.) ;
#64577 = ORIENTED_EDGE('',*,*,#47227,.T.) ;
#64578 = ORIENTED_EDGE('',*,*,#46240,.F.) ;
#64579 = ORIENTED_EDGE('',*,*,#47229,.F.) ;
#64580 = ORIENTED_EDGE('',*,*,#46295,.F.) ;
#64581 = ORIENTED_EDGE('',*,*,#47228,.T.) ;
#64582 = ORIENTED_EDGE('',*,*,#46292,.F.) ;
#64583 = ORIENTED_EDGE('',*,*,#47230,.F.) ;
#64584 = ORIENTED_EDGE('',*,*,#46252,.F.) ;
#64585 = ORIENTED_EDGE('',*,*,#47229,.T.) ;
#64586 = ORIENTED_EDGE('',*,*,#46237,.F.) ;
#64587 = ORIENTED_EDGE('',*,*,#47231,.F.) ;
#64588 = ORIENTED_EDGE('',*,*,#46296,.F.) ;
#64589 = ORIENTED_EDGE('',*,*,#46255,.F.) ;
#64590 = ORIENTED_EDGE('',*,*,#47230,.T.) ;
#64591 = ORIENTED_EDGE('',*,*,#47232,.F.) ;
#64592 = ORIENTED_EDGE('',*,*,#47231,.T.) ;
#64593 = ORIENTED_EDGE('',*,*,#46234,.F.) ;
#64594 = ORIENTED_EDGE('',*,*,#47233,.F.) ;
#64595 = ORIENTED_EDGE('',*,*,#46297,.F.) ;
#64596 = ORIENTED_EDGE('',*,*,#47232,.T.) ;
#64597 = ORIENTED_EDGE('',*,*,#46291,.F.) ;
#64598 = ORIENTED_EDGE('',*,*,#47234,.F.) ;
#64599 = ORIENTED_EDGE('',*,*,#46258,.F.) ;
#64600 = ORIENTED_EDGE('',*,*,#47233,.T.) ;
#64601 = ORIENTED_EDGE('',*,*,#46231,.F.) ;
#64602 = ORIENTED_EDGE('',*,*,#47235,.F.) ;
#64603 = ORIENTED_EDGE('',*,*,#46261,.F.) ;
#64604 = ORIENTED_EDGE('',*,*,#47234,.T.) ;
#64605 = ORIENTED_EDGE('',*,*,#47236,.F.) ;
#64606 = ORIENTED_EDGE('',*,*,#47235,.T.) ;
#64607 = ORIENTED_EDGE('',*,*,#46228,.F.) ;
#64608 = ORIENTED_EDGE('',*,*,#47237,.F.) ;
#64609 = ORIENTED_EDGE('',*,*,#46298,.F.) ;
#64610 = ORIENTED_EDGE('',*,*,#47236,.T.) ;
#64611 = ORIENTED_EDGE('',*,*,#46290,.F.) ;
#64612 = ORIENTED_EDGE('',*,*,#47238,.F.) ;
#64613 = ORIENTED_EDGE('',*,*,#46264,.F.) ;
#64614 = ORIENTED_EDGE('',*,*,#47237,.T.) ;
#64615 = ORIENTED_EDGE('',*,*,#44354,.F.) ;
#64616 = ORIENTED_EDGE('',*,*,#47239,.F.) ;
#64617 = ORIENTED_EDGE('',*,*,#46267,.F.) ;
#64618 = ORIENTED_EDGE('',*,*,#47238,.T.) ;
#64619 = ORIENTED_EDGE('',*,*,#47240,.F.) ;
#64620 = ORIENTED_EDGE('',*,*,#47239,.T.) ;
#64621 = ORIENTED_EDGE('',*,*,#46226,.F.) ;
#64622 = ORIENTED_EDGE('',*,*,#44241,.F.) ;
#64623 = ORIENTED_EDGE('',*,*,#46299,.F.) ;
#64624 = ORIENTED_EDGE('',*,*,#47240,.T.) ;
#64625 = ORIENTED_EDGE('',*,*,#46289,.F.) ;
#64626 = ORIENTED_EDGE('',*,*,#47241,.F.) ;
#64627 = ORIENTED_EDGE('',*,*,#46270,.F.) ;
#64628 = ORIENTED_EDGE('',*,*,#46273,.F.) ;
#64629 = ORIENTED_EDGE('',*,*,#47241,.T.) ;
#64630 = ORIENTED_EDGE('',*,*,#47242,.F.) ;
#64631 = ORIENTED_EDGE('',*,*,#44240,.T.) ;
#64632 = ORIENTED_EDGE('',*,*,#46221,.F.) ;
#64633 = ORIENTED_EDGE('',*,*,#47243,.F.) ;
#64634 = ORIENTED_EDGE('',*,*,#46300,.F.) ;
#64635 = ORIENTED_EDGE('',*,*,#47242,.T.) ;
#64636 = ORIENTED_EDGE('',*,*,#46288,.F.) ;
#64637 = ORIENTED_EDGE('',*,*,#47244,.F.) ;
#64638 = ORIENTED_EDGE('',*,*,#46276,.F.) ;
#64639 = ORIENTED_EDGE('',*,*,#47243,.T.) ;
#64640 = ORIENTED_EDGE('',*,*,#46218,.F.) ;
#64641 = ORIENTED_EDGE('',*,*,#47245,.F.) ;
#64642 = ORIENTED_EDGE('',*,*,#46279,.F.) ;
#64643 = ORIENTED_EDGE('',*,*,#47244,.T.) ;
#64644 = ORIENTED_EDGE('',*,*,#47246,.F.) ;
#64645 = ORIENTED_EDGE('',*,*,#47245,.T.) ;
#64646 = ORIENTED_EDGE('',*,*,#46215,.F.) ;
#64647 = ORIENTED_EDGE('',*,*,#47247,.F.) ;
#64648 = ORIENTED_EDGE('',*,*,#46301,.F.) ;
#64649 = ORIENTED_EDGE('',*,*,#47246,.T.) ;
#64650 = ORIENTED_EDGE('',*,*,#46287,.F.) ;
#64651 = ORIENTED_EDGE('',*,*,#47248,.F.) ;
#64652 = ORIENTED_EDGE('',*,*,#46282,.F.) ;
#64653 = ORIENTED_EDGE('',*,*,#47247,.T.) ;
#64654 = ORIENTED_EDGE('',*,*,#46212,.F.) ;
#64655 = ORIENTED_EDGE('',*,*,#47249,.F.) ;
#64656 = ORIENTED_EDGE('',*,*,#46284,.F.) ;
#64657 = ORIENTED_EDGE('',*,*,#47248,.T.) ;
#64658 = ORIENTED_EDGE('',*,*,#46286,.F.) ;
#64659 = ORIENTED_EDGE('',*,*,#47250,.F.) ;
#64660 = ORIENTED_EDGE('',*,*,#46206,.F.) ;
#64661 = ORIENTED_EDGE('',*,*,#47249,.T.) ;
#64662 = ORIENTED_EDGE('',*,*,#46209,.F.) ;
#64663 = ORIENTED_EDGE('',*,*,#47250,.T.) ;
#64664 = ORIENTED_EDGE('',*,*,#46285,.F.) ;
#64665 = ORIENTED_EDGE('',*,*,#47251,.F.) ;
#64666 = ORIENTED_EDGE('',*,*,#45637,.F.) ;
#64667 = ORIENTED_EDGE('',*,*,#47252,.F.) ;
#64668 = ORIENTED_EDGE('',*,*,#45508,.F.) ;
#64669 = ORIENTED_EDGE('',*,*,#47253,.F.) ;
#64670 = ORIENTED_EDGE('',*,*,#45638,.F.) ;
#64671 = ORIENTED_EDGE('',*,*,#47254,.F.) ;
#64672 = ORIENTED_EDGE('',*,*,#45632,.F.) ;
#64673 = ORIENTED_EDGE('',*,*,#47255,.F.) ;
#64674 = ORIENTED_EDGE('',*,*,#47253,.T.) ;
#64675 = ORIENTED_EDGE('',*,*,#47256,.F.) ;
#64676 = ORIENTED_EDGE('',*,*,#47257,.F.) ;
#64677 = ORIENTED_EDGE('',*,*,#47252,.T.) ;
#64678 = ORIENTED_EDGE('',*,*,#47258,.F.) ;
#64679 = ORIENTED_EDGE('',*,*,#47251,.T.) ;
#64680 = ORIENTED_EDGE('',*,*,#45507,.T.) ;
#64681 = ORIENTED_EDGE('',*,*,#47259,.F.) ;
#64682 = ORIENTED_EDGE('',*,*,#47254,.T.) ;
#64683 = ORIENTED_EDGE('',*,*,#47256,.T.) ;
#64684 = ORIENTED_EDGE('',*,*,#45635,.F.) ;
#64685 = ORIENTED_EDGE('',*,*,#47260,.F.) ;
#64686 = ORIENTED_EDGE('',*,*,#44225,.T.) ;
#64687 = ORIENTED_EDGE('',*,*,#47261,.T.) ;
#64688 = ORIENTED_EDGE('',*,*,#47262,.F.) ;
#64689 = ORIENTED_EDGE('',*,*,#47255,.T.) ;
#64690 = ORIENTED_EDGE('',*,*,#47263,.F.) ;
#64691 = ORIENTED_EDGE('',*,*,#47264,.T.) ;
#64692 = ORIENTED_EDGE('',*,*,#47265,.F.) ;
#64693 = ORIENTED_EDGE('',*,*,#44441,.F.) ;
#64694 = ORIENTED_EDGE('',*,*,#47266,.F.) ;
#64695 = ORIENTED_EDGE('',*,*,#45639,.F.) ;
#64696 = ORIENTED_EDGE('',*,*,#47258,.T.) ;
#64697 = ORIENTED_EDGE('',*,*,#45636,.F.) ;
#64698 = ORIENTED_EDGE('',*,*,#47267,.F.) ;
#64699 = ORIENTED_EDGE('',*,*,#45642,.F.) ;
#64700 = ORIENTED_EDGE('',*,*,#47257,.T.) ;
#64701 = ORIENTED_EDGE('',*,*,#45641,.F.) ;
#64702 = ORIENTED_EDGE('',*,*,#47268,.F.) ;
#64703 = ORIENTED_EDGE('',*,*,#45499,.F.) ;
#64704 = ORIENTED_EDGE('',*,*,#47259,.T.) ;
#64705 = ORIENTED_EDGE('',*,*,#45506,.F.) ;
#64706 = ORIENTED_EDGE('',*,*,#47269,.F.) ;
#64707 = ORIENTED_EDGE('',*,*,#45633,.F.) ;
#64708 = ORIENTED_EDGE('',*,*,#47270,.F.) ;
#64709 = ORIENTED_EDGE('',*,*,#45634,.F.) ;
#64710 = ORIENTED_EDGE('',*,*,#47271,.F.) ;
#64711 = ORIENTED_EDGE('',*,*,#45629,.F.) ;
#64712 = ORIENTED_EDGE('',*,*,#47260,.T.) ;
#64713 = ORIENTED_EDGE('',*,*,#47270,.T.) ;
#64714 = ORIENTED_EDGE('',*,*,#44226,.F.) ;
#64715 = ORIENTED_EDGE('',*,*,#47266,.T.) ;
#64716 = ORIENTED_EDGE('',*,*,#44451,.T.) ;
#64717 = ORIENTED_EDGE('',*,*,#47272,.F.) ;
#64718 = ORIENTED_EDGE('',*,*,#47267,.T.) ;
#64719 = ORIENTED_EDGE('',*,*,#47273,.F.) ;
#64720 = ORIENTED_EDGE('',*,*,#47268,.T.) ;
#64721 = ORIENTED_EDGE('',*,*,#47274,.F.) ;
#64722 = ORIENTED_EDGE('',*,*,#44541,.T.) ;
#64723 = ORIENTED_EDGE('',*,*,#47269,.T.) ;
#64724 = ORIENTED_EDGE('',*,*,#45505,.T.) ;
#64725 = ORIENTED_EDGE('',*,*,#47275,.F.) ;
#64726 = ORIENTED_EDGE('',*,*,#47271,.T.) ;
#64727 = ORIENTED_EDGE('',*,*,#47272,.T.) ;
#64728 = ORIENTED_EDGE('',*,*,#44450,.F.) ;
#64729 = ORIENTED_EDGE('',*,*,#47276,.F.) ;
#64730 = ORIENTED_EDGE('',*,*,#45643,.F.) ;
#64731 = ORIENTED_EDGE('',*,*,#47274,.T.) ;
#64732 = ORIENTED_EDGE('',*,*,#45640,.F.) ;
#64733 = ORIENTED_EDGE('',*,*,#47277,.F.) ;
#64734 = ORIENTED_EDGE('',*,*,#44542,.F.) ;
#64735 = ORIENTED_EDGE('',*,*,#45500,.F.) ;
#64736 = ORIENTED_EDGE('',*,*,#47273,.T.) ;
#64737 = ORIENTED_EDGE('',*,*,#47278,.F.) ;
#64738 = ORIENTED_EDGE('',*,*,#47279,.F.) ;
#64739 = ORIENTED_EDGE('',*,*,#47275,.T.) ;
#64740 = ORIENTED_EDGE('',*,*,#45504,.F.) ;
#64741 = ORIENTED_EDGE('',*,*,#47280,.F.) ;
#64742 = ORIENTED_EDGE('',*,*,#45630,.F.) ;
#64743 = ORIENTED_EDGE('',*,*,#47281,.F.) ;
#64744 = ORIENTED_EDGE('',*,*,#45631,.F.) ;
#64745 = ORIENTED_EDGE('',*,*,#47282,.F.) ;
#64746 = ORIENTED_EDGE('',*,*,#45625,.F.) ;
#64747 = ORIENTED_EDGE('',*,*,#44228,.T.) ;
#64748 = ORIENTED_EDGE('',*,*,#47281,.T.) ;
#64749 = ORIENTED_EDGE('',*,*,#47283,.F.) ;
#64750 = ORIENTED_EDGE('',*,*,#44445,.T.) ;
#64751 = ORIENTED_EDGE('',*,*,#47277,.T.) ;
#64752 = ORIENTED_EDGE('',*,*,#47276,.T.) ;
#64753 = ORIENTED_EDGE('',*,*,#47284,.F.) ;
#64754 = ORIENTED_EDGE('',*,*,#47285,.F.) ;
#64755 = ORIENTED_EDGE('',*,*,#44603,.F.) ;
#64756 = ORIENTED_EDGE('',*,*,#47286,.F.) ;
#64757 = ORIENTED_EDGE('',*,*,#47287,.F.) ;
#64758 = ORIENTED_EDGE('',*,*,#47278,.T.) ;
#64759 = ORIENTED_EDGE('',*,*,#44545,.F.) ;
#64760 = ORIENTED_EDGE('',*,*,#47286,.T.) ;
#64761 = ORIENTED_EDGE('',*,*,#44728,.F.) ;
#64762 = ORIENTED_EDGE('',*,*,#47279,.T.) ;
#64763 = ORIENTED_EDGE('',*,*,#47288,.F.) ;
#64764 = ORIENTED_EDGE('',*,*,#47289,.F.) ;
#64765 = ORIENTED_EDGE('',*,*,#47282,.T.) ;
#64766 = ORIENTED_EDGE('',*,*,#47280,.T.) ;
#64767 = ORIENTED_EDGE('',*,*,#47290,.F.) ;
#64768 = ORIENTED_EDGE('',*,*,#47283,.T.) ;
#64769 = ORIENTED_EDGE('',*,*,#45628,.F.) ;
#64770 = ORIENTED_EDGE('',*,*,#47291,.F.) ;
#64771 = ORIENTED_EDGE('',*,*,#44446,.F.) ;
#64772 = ORIENTED_EDGE('',*,*,#47284,.T.) ;
#64773 = ORIENTED_EDGE('',*,*,#44449,.F.) ;
#64774 = ORIENTED_EDGE('',*,*,#47292,.F.) ;
#64775 = ORIENTED_EDGE('',*,*,#44543,.F.) ;
#64776 = ORIENTED_EDGE('',*,*,#47285,.T.) ;
#64777 = ORIENTED_EDGE('',*,*,#44544,.F.) ;
#64778 = ORIENTED_EDGE('',*,*,#47293,.F.) ;
#64779 = ORIENTED_EDGE('',*,*,#44681,.F.) ;
#64780 = ORIENTED_EDGE('',*,*,#47287,.T.) ;
#64781 = ORIENTED_EDGE('',*,*,#44727,.T.) ;
#64782 = ORIENTED_EDGE('',*,*,#47294,.F.) ;
#64783 = ORIENTED_EDGE('',*,*,#47288,.T.) ;
#64784 = ORIENTED_EDGE('',*,*,#45501,.F.) ;
#64785 = ORIENTED_EDGE('',*,*,#47289,.T.) ;
#64786 = ORIENTED_EDGE('',*,*,#47295,.F.) ;
#64787 = ORIENTED_EDGE('',*,*,#47296,.F.) ;
#64788 = ORIENTED_EDGE('',*,*,#47290,.T.) ;
#64789 = ORIENTED_EDGE('',*,*,#45503,.F.) ;
#64790 = ORIENTED_EDGE('',*,*,#47297,.F.) ;
#64791 = ORIENTED_EDGE('',*,*,#45626,.F.) ;
#64792 = ORIENTED_EDGE('',*,*,#47298,.F.) ;
#64793 = ORIENTED_EDGE('',*,*,#45627,.F.) ;
#64794 = ORIENTED_EDGE('',*,*,#47299,.F.) ;
#64795 = ORIENTED_EDGE('',*,*,#44540,.F.) ;
#64796 = ORIENTED_EDGE('',*,*,#47291,.T.) ;
#64797 = ORIENTED_EDGE('',*,*,#47298,.T.) ;
#64798 = ORIENTED_EDGE('',*,*,#47300,.F.) ;
#64799 = ORIENTED_EDGE('',*,*,#47293,.T.) ;
#64800 = ORIENTED_EDGE('',*,*,#47292,.T.) ;
#64801 = ORIENTED_EDGE('',*,*,#47301,.F.) ;
#64802 = ORIENTED_EDGE('',*,*,#44682,.T.) ;
#64803 = ORIENTED_EDGE('',*,*,#47302,.F.) ;
#64804 = ORIENTED_EDGE('',*,*,#47295,.T.) ;
#64805 = ORIENTED_EDGE('',*,*,#47294,.T.) ;
#64806 = ORIENTED_EDGE('',*,*,#44726,.F.) ;
#64807 = ORIENTED_EDGE('',*,*,#47296,.T.) ;
#64808 = ORIENTED_EDGE('',*,*,#47303,.F.) ;
#64809 = ORIENTED_EDGE('',*,*,#47304,.F.) ;
#64810 = ORIENTED_EDGE('',*,*,#47299,.T.) ;
#64811 = ORIENTED_EDGE('',*,*,#47297,.T.) ;
#64812 = ORIENTED_EDGE('',*,*,#47305,.F.) ;
#64813 = ORIENTED_EDGE('',*,*,#44536,.T.) ;
#64814 = ORIENTED_EDGE('',*,*,#47300,.T.) ;
#64815 = ORIENTED_EDGE('',*,*,#44539,.F.) ;
#64816 = ORIENTED_EDGE('',*,*,#47306,.F.) ;
#64817 = ORIENTED_EDGE('',*,*,#44447,.F.) ;
#64818 = ORIENTED_EDGE('',*,*,#47301,.T.) ;
#64819 = ORIENTED_EDGE('',*,*,#44448,.F.) ;
#64820 = ORIENTED_EDGE('',*,*,#47307,.F.) ;
#64821 = ORIENTED_EDGE('',*,*,#44683,.F.) ;
#64822 = ORIENTED_EDGE('',*,*,#47302,.T.) ;
#64823 = ORIENTED_EDGE('',*,*,#44725,.T.) ;
#64824 = ORIENTED_EDGE('',*,*,#47308,.F.) ;
#64825 = ORIENTED_EDGE('',*,*,#47303,.T.) ;
#64826 = ORIENTED_EDGE('',*,*,#45502,.F.) ;
#64827 = ORIENTED_EDGE('',*,*,#47304,.T.) ;
#64828 = ORIENTED_EDGE('',*,*,#47309,.F.) ;
#64829 = ORIENTED_EDGE('',*,*,#47305,.T.) ;
#64830 = ORIENTED_EDGE('',*,*,#47307,.T.) ;
#64831 = ORIENTED_EDGE('',*,*,#47306,.T.) ;
#64832 = ORIENTED_EDGE('',*,*,#47310,.F.) ;
#64833 = ORIENTED_EDGE('',*,*,#44684,.T.) ;
#64834 = ORIENTED_EDGE('',*,*,#47308,.T.) ;
#64835 = ORIENTED_EDGE('',*,*,#44724,.F.) ;
#64836 = ORIENTED_EDGE('',*,*,#47311,.F.) ;
#64837 = ORIENTED_EDGE('',*,*,#44537,.F.) ;
#64838 = ORIENTED_EDGE('',*,*,#47309,.T.) ;
#64839 = ORIENTED_EDGE('',*,*,#47310,.T.) ;
#64840 = ORIENTED_EDGE('',*,*,#44538,.F.) ;
#64841 = ORIENTED_EDGE('',*,*,#47312,.F.) ;
#64842 = ORIENTED_EDGE('',*,*,#44685,.F.) ;
#64843 = ORIENTED_EDGE('',*,*,#47311,.T.) ;
#64844 = ORIENTED_EDGE('',*,*,#44609,.F.) ;
#64845 = ORIENTED_EDGE('',*,*,#47312,.T.) ;
#64846 = ORIENTED_EDGE('',*,*,#47313,.F.) ;
#64847 = ORIENTED_EDGE('',*,*,#46149,.F.) ;
#64848 = ORIENTED_EDGE('',*,*,#47314,.F.) ;
#64849 = ORIENTED_EDGE('',*,*,#46196,.F.) ;
#64850 = ORIENTED_EDGE('',*,*,#47314,.T.) ;
#64851 = ORIENTED_EDGE('',*,*,#46146,.F.) ;
#64852 = ORIENTED_EDGE('',*,*,#47315,.F.) ;
#64853 = ORIENTED_EDGE('',*,*,#46197,.F.) ;
#64854 = ORIENTED_EDGE('',*,*,#46152,.F.) ;
#64855 = ORIENTED_EDGE('',*,*,#47313,.T.) ;
#64856 = ORIENTED_EDGE('',*,*,#47316,.F.) ;
#64857 = ORIENTED_EDGE('',*,*,#47315,.T.) ;
#64858 = ORIENTED_EDGE('',*,*,#46143,.F.) ;
#64859 = ORIENTED_EDGE('',*,*,#47317,.F.) ;
#64860 = ORIENTED_EDGE('',*,*,#46198,.F.) ;
#64861 = ORIENTED_EDGE('',*,*,#47316,.T.) ;
#64862 = ORIENTED_EDGE('',*,*,#46195,.F.) ;
#64863 = ORIENTED_EDGE('',*,*,#47318,.F.) ;
#64864 = ORIENTED_EDGE('',*,*,#46155,.F.) ;
#64865 = ORIENTED_EDGE('',*,*,#47317,.T.) ;
#64866 = ORIENTED_EDGE('',*,*,#46140,.F.) ;
#64867 = ORIENTED_EDGE('',*,*,#47319,.F.) ;
#64868 = ORIENTED_EDGE('',*,*,#46199,.F.) ;
#64869 = ORIENTED_EDGE('',*,*,#46158,.F.) ;
#64870 = ORIENTED_EDGE('',*,*,#47318,.T.) ;
#64871 = ORIENTED_EDGE('',*,*,#47320,.F.) ;
#64872 = ORIENTED_EDGE('',*,*,#47319,.T.) ;
#64873 = ORIENTED_EDGE('',*,*,#46137,.F.) ;
#64874 = ORIENTED_EDGE('',*,*,#47321,.F.) ;
#64875 = ORIENTED_EDGE('',*,*,#46200,.F.) ;
#64876 = ORIENTED_EDGE('',*,*,#47320,.T.) ;
#64877 = ORIENTED_EDGE('',*,*,#46194,.F.) ;
#64878 = ORIENTED_EDGE('',*,*,#47322,.F.) ;
#64879 = ORIENTED_EDGE('',*,*,#46161,.F.) ;
#64880 = ORIENTED_EDGE('',*,*,#47321,.T.) ;
#64881 = ORIENTED_EDGE('',*,*,#46134,.F.) ;
#64882 = ORIENTED_EDGE('',*,*,#47323,.F.) ;
#64883 = ORIENTED_EDGE('',*,*,#46164,.F.) ;
#64884 = ORIENTED_EDGE('',*,*,#47322,.T.) ;
#64885 = ORIENTED_EDGE('',*,*,#47324,.F.) ;
#64886 = ORIENTED_EDGE('',*,*,#47323,.T.) ;
#64887 = ORIENTED_EDGE('',*,*,#46131,.F.) ;
#64888 = ORIENTED_EDGE('',*,*,#47325,.F.) ;
#64889 = ORIENTED_EDGE('',*,*,#46201,.F.) ;
#64890 = ORIENTED_EDGE('',*,*,#47324,.T.) ;
#64891 = ORIENTED_EDGE('',*,*,#46193,.F.) ;
#64892 = ORIENTED_EDGE('',*,*,#47326,.F.) ;
#64893 = ORIENTED_EDGE('',*,*,#46167,.F.) ;
#64894 = ORIENTED_EDGE('',*,*,#47325,.T.) ;
#64895 = ORIENTED_EDGE('',*,*,#44357,.F.) ;
#64896 = ORIENTED_EDGE('',*,*,#47327,.F.) ;
#64897 = ORIENTED_EDGE('',*,*,#46170,.F.) ;
#64898 = ORIENTED_EDGE('',*,*,#47326,.T.) ;
#64899 = ORIENTED_EDGE('',*,*,#47328,.F.) ;
#64900 = ORIENTED_EDGE('',*,*,#47327,.T.) ;
#64901 = ORIENTED_EDGE('',*,*,#46129,.F.) ;
#64902 = ORIENTED_EDGE('',*,*,#44224,.F.) ;
#64903 = ORIENTED_EDGE('',*,*,#46202,.F.) ;
#64904 = ORIENTED_EDGE('',*,*,#47328,.T.) ;
#64905 = ORIENTED_EDGE('',*,*,#46192,.F.) ;
#64906 = ORIENTED_EDGE('',*,*,#47329,.F.) ;
#64907 = ORIENTED_EDGE('',*,*,#46173,.F.) ;
#64908 = ORIENTED_EDGE('',*,*,#46176,.F.) ;
#64909 = ORIENTED_EDGE('',*,*,#47329,.T.) ;
#64910 = ORIENTED_EDGE('',*,*,#47330,.F.) ;
#64911 = ORIENTED_EDGE('',*,*,#44223,.T.) ;
#64912 = ORIENTED_EDGE('',*,*,#46124,.F.) ;
#64913 = ORIENTED_EDGE('',*,*,#47331,.F.) ;
#64914 = ORIENTED_EDGE('',*,*,#46203,.F.) ;
#64915 = ORIENTED_EDGE('',*,*,#47330,.T.) ;
#64916 = ORIENTED_EDGE('',*,*,#46191,.F.) ;
#64917 = ORIENTED_EDGE('',*,*,#47332,.F.) ;
#64918 = ORIENTED_EDGE('',*,*,#46179,.F.) ;
#64919 = ORIENTED_EDGE('',*,*,#47331,.T.) ;
#64920 = ORIENTED_EDGE('',*,*,#46121,.F.) ;
#64921 = ORIENTED_EDGE('',*,*,#47333,.F.) ;
#64922 = ORIENTED_EDGE('',*,*,#46182,.F.) ;
#64923 = ORIENTED_EDGE('',*,*,#47332,.T.) ;
#64924 = ORIENTED_EDGE('',*,*,#47334,.F.) ;
#64925 = ORIENTED_EDGE('',*,*,#47333,.T.) ;
#64926 = ORIENTED_EDGE('',*,*,#46118,.F.) ;
#64927 = ORIENTED_EDGE('',*,*,#47335,.F.) ;
#64928 = ORIENTED_EDGE('',*,*,#46204,.F.) ;
#64929 = ORIENTED_EDGE('',*,*,#47334,.T.) ;
#64930 = ORIENTED_EDGE('',*,*,#46190,.F.) ;
#64931 = ORIENTED_EDGE('',*,*,#47336,.F.) ;
#64932 = ORIENTED_EDGE('',*,*,#46185,.F.) ;
#64933 = ORIENTED_EDGE('',*,*,#47335,.T.) ;
#64934 = ORIENTED_EDGE('',*,*,#46115,.F.) ;
#64935 = ORIENTED_EDGE('',*,*,#47337,.F.) ;
#64936 = ORIENTED_EDGE('',*,*,#46187,.F.) ;
#64937 = ORIENTED_EDGE('',*,*,#47336,.T.) ;
#64938 = ORIENTED_EDGE('',*,*,#46189,.F.) ;
#64939 = ORIENTED_EDGE('',*,*,#47338,.F.) ;
#64940 = ORIENTED_EDGE('',*,*,#46109,.F.) ;
#64941 = ORIENTED_EDGE('',*,*,#47337,.T.) ;
#64942 = ORIENTED_EDGE('',*,*,#46112,.F.) ;
#64943 = ORIENTED_EDGE('',*,*,#47338,.T.) ;
#64944 = ORIENTED_EDGE('',*,*,#46188,.F.) ;
#64945 = ORIENTED_EDGE('',*,*,#47339,.F.) ;
#64946 = ORIENTED_EDGE('',*,*,#45656,.F.) ;
#64947 = ORIENTED_EDGE('',*,*,#47340,.F.) ;
#64948 = ORIENTED_EDGE('',*,*,#45498,.F.) ;
#64949 = ORIENTED_EDGE('',*,*,#47341,.F.) ;
#64950 = ORIENTED_EDGE('',*,*,#45657,.F.) ;
#64951 = ORIENTED_EDGE('',*,*,#47342,.F.) ;
#64952 = ORIENTED_EDGE('',*,*,#45651,.F.) ;
#64953 = ORIENTED_EDGE('',*,*,#47343,.F.) ;
#64954 = ORIENTED_EDGE('',*,*,#47341,.T.) ;
#64955 = ORIENTED_EDGE('',*,*,#47344,.F.) ;
#64956 = ORIENTED_EDGE('',*,*,#47345,.F.) ;
#64957 = ORIENTED_EDGE('',*,*,#47340,.T.) ;
#64958 = ORIENTED_EDGE('',*,*,#47346,.F.) ;
#64959 = ORIENTED_EDGE('',*,*,#47339,.T.) ;
#64960 = ORIENTED_EDGE('',*,*,#45497,.T.) ;
#64961 = ORIENTED_EDGE('',*,*,#47347,.F.) ;
#64962 = ORIENTED_EDGE('',*,*,#47342,.T.) ;
#64963 = ORIENTED_EDGE('',*,*,#47344,.T.) ;
#64964 = ORIENTED_EDGE('',*,*,#45654,.F.) ;
#64965 = ORIENTED_EDGE('',*,*,#47348,.F.) ;
#64966 = ORIENTED_EDGE('',*,*,#44208,.T.) ;
#64967 = ORIENTED_EDGE('',*,*,#47349,.T.) ;
#64968 = ORIENTED_EDGE('',*,*,#47350,.F.) ;
#64969 = ORIENTED_EDGE('',*,*,#47343,.T.) ;
#64970 = ORIENTED_EDGE('',*,*,#47351,.F.) ;
#64971 = ORIENTED_EDGE('',*,*,#47352,.T.) ;
#64972 = ORIENTED_EDGE('',*,*,#47353,.F.) ;
#64973 = ORIENTED_EDGE('',*,*,#44430,.F.) ;
#64974 = ORIENTED_EDGE('',*,*,#47354,.F.) ;
#64975 = ORIENTED_EDGE('',*,*,#45658,.F.) ;
#64976 = ORIENTED_EDGE('',*,*,#47346,.T.) ;
#64977 = ORIENTED_EDGE('',*,*,#45655,.F.) ;
#64978 = ORIENTED_EDGE('',*,*,#47355,.F.) ;
#64979 = ORIENTED_EDGE('',*,*,#45661,.F.) ;
#64980 = ORIENTED_EDGE('',*,*,#47345,.T.) ;
#64981 = ORIENTED_EDGE('',*,*,#45660,.F.) ;
#64982 = ORIENTED_EDGE('',*,*,#47356,.F.) ;
#64983 = ORIENTED_EDGE('',*,*,#45489,.F.) ;
#64984 = ORIENTED_EDGE('',*,*,#47347,.T.) ;
#64985 = ORIENTED_EDGE('',*,*,#45496,.F.) ;
#64986 = ORIENTED_EDGE('',*,*,#47357,.F.) ;
#64987 = ORIENTED_EDGE('',*,*,#45652,.F.) ;
#64988 = ORIENTED_EDGE('',*,*,#47358,.F.) ;
#64989 = ORIENTED_EDGE('',*,*,#45653,.F.) ;
#64990 = ORIENTED_EDGE('',*,*,#47359,.F.) ;
#64991 = ORIENTED_EDGE('',*,*,#45648,.F.) ;
#64992 = ORIENTED_EDGE('',*,*,#47348,.T.) ;
#64993 = ORIENTED_EDGE('',*,*,#47358,.T.) ;
#64994 = ORIENTED_EDGE('',*,*,#44209,.F.) ;
#64995 = ORIENTED_EDGE('',*,*,#47354,.T.) ;
#64996 = ORIENTED_EDGE('',*,*,#44440,.T.) ;
#64997 = ORIENTED_EDGE('',*,*,#47360,.F.) ;
#64998 = ORIENTED_EDGE('',*,*,#47355,.T.) ;
#64999 = ORIENTED_EDGE('',*,*,#47361,.F.) ;
#65000 = ORIENTED_EDGE('',*,*,#47356,.T.) ;
#65001 = ORIENTED_EDGE('',*,*,#47362,.F.) ;
#65002 = ORIENTED_EDGE('',*,*,#44531,.T.) ;
#65003 = ORIENTED_EDGE('',*,*,#47357,.T.) ;
#65004 = ORIENTED_EDGE('',*,*,#45495,.T.) ;
#65005 = ORIENTED_EDGE('',*,*,#47363,.F.) ;
#65006 = ORIENTED_EDGE('',*,*,#47359,.T.) ;
#65007 = ORIENTED_EDGE('',*,*,#47360,.T.) ;
#65008 = ORIENTED_EDGE('',*,*,#44439,.F.) ;
#65009 = ORIENTED_EDGE('',*,*,#47364,.F.) ;
#65010 = ORIENTED_EDGE('',*,*,#45662,.F.) ;
#65011 = ORIENTED_EDGE('',*,*,#47362,.T.) ;
#65012 = ORIENTED_EDGE('',*,*,#45659,.F.) ;
#65013 = ORIENTED_EDGE('',*,*,#47365,.F.) ;
#65014 = ORIENTED_EDGE('',*,*,#44532,.F.) ;
#65015 = ORIENTED_EDGE('',*,*,#45490,.F.) ;
#65016 = ORIENTED_EDGE('',*,*,#47361,.T.) ;
#65017 = ORIENTED_EDGE('',*,*,#47366,.F.) ;
#65018 = ORIENTED_EDGE('',*,*,#47367,.F.) ;
#65019 = ORIENTED_EDGE('',*,*,#47363,.T.) ;
#65020 = ORIENTED_EDGE('',*,*,#45494,.F.) ;
#65021 = ORIENTED_EDGE('',*,*,#47368,.F.) ;
#65022 = ORIENTED_EDGE('',*,*,#45649,.F.) ;
#65023 = ORIENTED_EDGE('',*,*,#47369,.F.) ;
#65024 = ORIENTED_EDGE('',*,*,#45650,.F.) ;
#65025 = ORIENTED_EDGE('',*,*,#47370,.F.) ;
#65026 = ORIENTED_EDGE('',*,*,#45644,.F.) ;
#65027 = ORIENTED_EDGE('',*,*,#44211,.T.) ;
#65028 = ORIENTED_EDGE('',*,*,#47369,.T.) ;
#65029 = ORIENTED_EDGE('',*,*,#47371,.F.) ;
#65030 = ORIENTED_EDGE('',*,*,#44434,.T.) ;
#65031 = ORIENTED_EDGE('',*,*,#47365,.T.) ;
#65032 = ORIENTED_EDGE('',*,*,#47364,.T.) ;
#65033 = ORIENTED_EDGE('',*,*,#47372,.F.) ;
#65034 = ORIENTED_EDGE('',*,*,#47373,.F.) ;
#65035 = ORIENTED_EDGE('',*,*,#44607,.F.) ;
#65036 = ORIENTED_EDGE('',*,*,#47374,.F.) ;
#65037 = ORIENTED_EDGE('',*,*,#47375,.F.) ;
#65038 = ORIENTED_EDGE('',*,*,#47366,.T.) ;
#65039 = ORIENTED_EDGE('',*,*,#44535,.F.) ;
#65040 = ORIENTED_EDGE('',*,*,#47374,.T.) ;
#65041 = ORIENTED_EDGE('',*,*,#44723,.F.) ;
#65042 = ORIENTED_EDGE('',*,*,#47367,.T.) ;
#65043 = ORIENTED_EDGE('',*,*,#47376,.F.) ;
#65044 = ORIENTED_EDGE('',*,*,#47377,.F.) ;
#65045 = ORIENTED_EDGE('',*,*,#47370,.T.) ;
#65046 = ORIENTED_EDGE('',*,*,#47368,.T.) ;
#65047 = ORIENTED_EDGE('',*,*,#47378,.F.) ;
#65048 = ORIENTED_EDGE('',*,*,#47371,.T.) ;
#65049 = ORIENTED_EDGE('',*,*,#45647,.F.) ;
#65050 = ORIENTED_EDGE('',*,*,#47379,.F.) ;
#65051 = ORIENTED_EDGE('',*,*,#44435,.F.) ;
#65052 = ORIENTED_EDGE('',*,*,#47372,.T.) ;
#65053 = ORIENTED_EDGE('',*,*,#44438,.F.) ;
#65054 = ORIENTED_EDGE('',*,*,#47380,.F.) ;
#65055 = ORIENTED_EDGE('',*,*,#44533,.F.) ;
#65056 = ORIENTED_EDGE('',*,*,#47373,.T.) ;
#65057 = ORIENTED_EDGE('',*,*,#44534,.F.) ;
#65058 = ORIENTED_EDGE('',*,*,#47381,.F.) ;
#65059 = ORIENTED_EDGE('',*,*,#44686,.F.) ;
#65060 = ORIENTED_EDGE('',*,*,#47375,.T.) ;
#65061 = ORIENTED_EDGE('',*,*,#44722,.T.) ;
#65062 = ORIENTED_EDGE('',*,*,#47382,.F.) ;
#65063 = ORIENTED_EDGE('',*,*,#47376,.T.) ;
#65064 = ORIENTED_EDGE('',*,*,#45491,.F.) ;
#65065 = ORIENTED_EDGE('',*,*,#47377,.T.) ;
#65066 = ORIENTED_EDGE('',*,*,#47383,.F.) ;
#65067 = ORIENTED_EDGE('',*,*,#47384,.F.) ;
#65068 = ORIENTED_EDGE('',*,*,#47378,.T.) ;
#65069 = ORIENTED_EDGE('',*,*,#45493,.F.) ;
#65070 = ORIENTED_EDGE('',*,*,#47385,.F.) ;
#65071 = ORIENTED_EDGE('',*,*,#45645,.F.) ;
#65072 = ORIENTED_EDGE('',*,*,#47386,.F.) ;
#65073 = ORIENTED_EDGE('',*,*,#45646,.F.) ;
#65074 = ORIENTED_EDGE('',*,*,#47387,.F.) ;
#65075 = ORIENTED_EDGE('',*,*,#44530,.F.) ;
#65076 = ORIENTED_EDGE('',*,*,#47379,.T.) ;
#65077 = ORIENTED_EDGE('',*,*,#47386,.T.) ;
#65078 = ORIENTED_EDGE('',*,*,#47388,.F.) ;
#65079 = ORIENTED_EDGE('',*,*,#47381,.T.) ;
#65080 = ORIENTED_EDGE('',*,*,#47380,.T.) ;
#65081 = ORIENTED_EDGE('',*,*,#47389,.F.) ;
#65082 = ORIENTED_EDGE('',*,*,#44687,.T.) ;
#65083 = ORIENTED_EDGE('',*,*,#47390,.F.) ;
#65084 = ORIENTED_EDGE('',*,*,#47383,.T.) ;
#65085 = ORIENTED_EDGE('',*,*,#47382,.T.) ;
#65086 = ORIENTED_EDGE('',*,*,#44721,.F.) ;
#65087 = ORIENTED_EDGE('',*,*,#47384,.T.) ;
#65088 = ORIENTED_EDGE('',*,*,#47391,.F.) ;
#65089 = ORIENTED_EDGE('',*,*,#47392,.F.) ;
#65090 = ORIENTED_EDGE('',*,*,#47387,.T.) ;
#65091 = ORIENTED_EDGE('',*,*,#47385,.T.) ;
#65092 = ORIENTED_EDGE('',*,*,#47393,.F.) ;
#65093 = ORIENTED_EDGE('',*,*,#44526,.T.) ;
#65094 = ORIENTED_EDGE('',*,*,#47388,.T.) ;
#65095 = ORIENTED_EDGE('',*,*,#44529,.F.) ;
#65096 = ORIENTED_EDGE('',*,*,#47394,.F.) ;
#65097 = ORIENTED_EDGE('',*,*,#44436,.F.) ;
#65098 = ORIENTED_EDGE('',*,*,#47389,.T.) ;
#65099 = ORIENTED_EDGE('',*,*,#44437,.F.) ;
#65100 = ORIENTED_EDGE('',*,*,#47395,.F.) ;
#65101 = ORIENTED_EDGE('',*,*,#44688,.F.) ;
#65102 = ORIENTED_EDGE('',*,*,#47390,.T.) ;
#65103 = ORIENTED_EDGE('',*,*,#44720,.T.) ;
#65104 = ORIENTED_EDGE('',*,*,#47396,.F.) ;
#65105 = ORIENTED_EDGE('',*,*,#47391,.T.) ;
#65106 = ORIENTED_EDGE('',*,*,#45492,.F.) ;
#65107 = ORIENTED_EDGE('',*,*,#47392,.T.) ;
#65108 = ORIENTED_EDGE('',*,*,#47397,.F.) ;
#65109 = ORIENTED_EDGE('',*,*,#47393,.T.) ;
#65110 = ORIENTED_EDGE('',*,*,#47395,.T.) ;
#65111 = ORIENTED_EDGE('',*,*,#47394,.T.) ;
#65112 = ORIENTED_EDGE('',*,*,#47398,.F.) ;
#65113 = ORIENTED_EDGE('',*,*,#44689,.T.) ;
#65114 = ORIENTED_EDGE('',*,*,#47396,.T.) ;
#65115 = ORIENTED_EDGE('',*,*,#44719,.F.) ;
#65116 = ORIENTED_EDGE('',*,*,#47399,.F.) ;
#65117 = ORIENTED_EDGE('',*,*,#44527,.F.) ;
#65118 = ORIENTED_EDGE('',*,*,#47397,.T.) ;
#65119 = ORIENTED_EDGE('',*,*,#47398,.T.) ;
#65120 = ORIENTED_EDGE('',*,*,#44528,.F.) ;
#65121 = ORIENTED_EDGE('',*,*,#47400,.F.) ;
#65122 = ORIENTED_EDGE('',*,*,#44690,.F.) ;
#65123 = ORIENTED_EDGE('',*,*,#47399,.T.) ;
#65124 = ORIENTED_EDGE('',*,*,#44613,.F.) ;
#65125 = ORIENTED_EDGE('',*,*,#47400,.T.) ;
#65126 = ORIENTED_EDGE('',*,*,#47401,.F.) ;
#65127 = ORIENTED_EDGE('',*,*,#46052,.F.) ;
#65128 = ORIENTED_EDGE('',*,*,#47402,.F.) ;
#65129 = ORIENTED_EDGE('',*,*,#46099,.F.) ;
#65130 = ORIENTED_EDGE('',*,*,#47402,.T.) ;
#65131 = ORIENTED_EDGE('',*,*,#46049,.F.) ;
#65132 = ORIENTED_EDGE('',*,*,#47403,.F.) ;
#65133 = ORIENTED_EDGE('',*,*,#46100,.F.) ;
#65134 = ORIENTED_EDGE('',*,*,#46055,.F.) ;
#65135 = ORIENTED_EDGE('',*,*,#47401,.T.) ;
#65136 = ORIENTED_EDGE('',*,*,#47404,.F.) ;
#65137 = ORIENTED_EDGE('',*,*,#47403,.T.) ;
#65138 = ORIENTED_EDGE('',*,*,#46046,.F.) ;
#65139 = ORIENTED_EDGE('',*,*,#47405,.F.) ;
#65140 = ORIENTED_EDGE('',*,*,#46101,.F.) ;
#65141 = ORIENTED_EDGE('',*,*,#47404,.T.) ;
#65142 = ORIENTED_EDGE('',*,*,#46098,.F.) ;
#65143 = ORIENTED_EDGE('',*,*,#47406,.F.) ;
#65144 = ORIENTED_EDGE('',*,*,#46058,.F.) ;
#65145 = ORIENTED_EDGE('',*,*,#47405,.T.) ;
#65146 = ORIENTED_EDGE('',*,*,#46043,.F.) ;
#65147 = ORIENTED_EDGE('',*,*,#47407,.F.) ;
#65148 = ORIENTED_EDGE('',*,*,#46102,.F.) ;
#65149 = ORIENTED_EDGE('',*,*,#46061,.F.) ;
#65150 = ORIENTED_EDGE('',*,*,#47406,.T.) ;
#65151 = ORIENTED_EDGE('',*,*,#47408,.F.) ;
#65152 = ORIENTED_EDGE('',*,*,#47407,.T.) ;
#65153 = ORIENTED_EDGE('',*,*,#46040,.F.) ;
#65154 = ORIENTED_EDGE('',*,*,#47409,.F.) ;
#65155 = ORIENTED_EDGE('',*,*,#46103,.F.) ;
#65156 = ORIENTED_EDGE('',*,*,#47408,.T.) ;
#65157 = ORIENTED_EDGE('',*,*,#46097,.F.) ;
#65158 = ORIENTED_EDGE('',*,*,#47410,.F.) ;
#65159 = ORIENTED_EDGE('',*,*,#46064,.F.) ;
#65160 = ORIENTED_EDGE('',*,*,#47409,.T.) ;
#65161 = ORIENTED_EDGE('',*,*,#46037,.F.) ;
#65162 = ORIENTED_EDGE('',*,*,#47411,.F.) ;
#65163 = ORIENTED_EDGE('',*,*,#46067,.F.) ;
#65164 = ORIENTED_EDGE('',*,*,#47410,.T.) ;
#65165 = ORIENTED_EDGE('',*,*,#47412,.F.) ;
#65166 = ORIENTED_EDGE('',*,*,#47411,.T.) ;
#65167 = ORIENTED_EDGE('',*,*,#46034,.F.) ;
#65168 = ORIENTED_EDGE('',*,*,#47413,.F.) ;
#65169 = ORIENTED_EDGE('',*,*,#46104,.F.) ;
#65170 = ORIENTED_EDGE('',*,*,#47412,.T.) ;
#65171 = ORIENTED_EDGE('',*,*,#46096,.F.) ;
#65172 = ORIENTED_EDGE('',*,*,#47414,.F.) ;
#65173 = ORIENTED_EDGE('',*,*,#46070,.F.) ;
#65174 = ORIENTED_EDGE('',*,*,#47413,.T.) ;
#65175 = ORIENTED_EDGE('',*,*,#44360,.F.) ;
#65176 = ORIENTED_EDGE('',*,*,#47415,.F.) ;
#65177 = ORIENTED_EDGE('',*,*,#46073,.F.) ;
#65178 = ORIENTED_EDGE('',*,*,#47414,.T.) ;
#65179 = ORIENTED_EDGE('',*,*,#47416,.F.) ;
#65180 = ORIENTED_EDGE('',*,*,#47415,.T.) ;
#65181 = ORIENTED_EDGE('',*,*,#46032,.F.) ;
#65182 = ORIENTED_EDGE('',*,*,#44207,.F.) ;
#65183 = ORIENTED_EDGE('',*,*,#46105,.F.) ;
#65184 = ORIENTED_EDGE('',*,*,#47416,.T.) ;
#65185 = ORIENTED_EDGE('',*,*,#46095,.F.) ;
#65186 = ORIENTED_EDGE('',*,*,#47417,.F.) ;
#65187 = ORIENTED_EDGE('',*,*,#46076,.F.) ;
#65188 = ORIENTED_EDGE('',*,*,#46079,.F.) ;
#65189 = ORIENTED_EDGE('',*,*,#47417,.T.) ;
#65190 = ORIENTED_EDGE('',*,*,#47418,.F.) ;
#65191 = ORIENTED_EDGE('',*,*,#44206,.T.) ;
#65192 = ORIENTED_EDGE('',*,*,#46027,.F.) ;
#65193 = ORIENTED_EDGE('',*,*,#47419,.F.) ;
#65194 = ORIENTED_EDGE('',*,*,#46106,.F.) ;
#65195 = ORIENTED_EDGE('',*,*,#47418,.T.) ;
#65196 = ORIENTED_EDGE('',*,*,#46094,.F.) ;
#65197 = ORIENTED_EDGE('',*,*,#47420,.F.) ;
#65198 = ORIENTED_EDGE('',*,*,#46082,.F.) ;
#65199 = ORIENTED_EDGE('',*,*,#47419,.T.) ;
#65200 = ORIENTED_EDGE('',*,*,#46024,.F.) ;
#65201 = ORIENTED_EDGE('',*,*,#47421,.F.) ;
#65202 = ORIENTED_EDGE('',*,*,#46085,.F.) ;
#65203 = ORIENTED_EDGE('',*,*,#47420,.T.) ;
#65204 = ORIENTED_EDGE('',*,*,#47422,.F.) ;
#65205 = ORIENTED_EDGE('',*,*,#47421,.T.) ;
#65206 = ORIENTED_EDGE('',*,*,#46021,.F.) ;
#65207 = ORIENTED_EDGE('',*,*,#47423,.F.) ;
#65208 = ORIENTED_EDGE('',*,*,#46107,.F.) ;
#65209 = ORIENTED_EDGE('',*,*,#47422,.T.) ;
#65210 = ORIENTED_EDGE('',*,*,#46093,.F.) ;
#65211 = ORIENTED_EDGE('',*,*,#47424,.F.) ;
#65212 = ORIENTED_EDGE('',*,*,#46088,.F.) ;
#65213 = ORIENTED_EDGE('',*,*,#47423,.T.) ;
#65214 = ORIENTED_EDGE('',*,*,#46018,.F.) ;
#65215 = ORIENTED_EDGE('',*,*,#47425,.F.) ;
#65216 = ORIENTED_EDGE('',*,*,#46090,.F.) ;
#65217 = ORIENTED_EDGE('',*,*,#47424,.T.) ;
#65218 = ORIENTED_EDGE('',*,*,#46092,.F.) ;
#65219 = ORIENTED_EDGE('',*,*,#47426,.F.) ;
#65220 = ORIENTED_EDGE('',*,*,#46012,.F.) ;
#65221 = ORIENTED_EDGE('',*,*,#47425,.T.) ;
#65222 = ORIENTED_EDGE('',*,*,#46015,.F.) ;
#65223 = ORIENTED_EDGE('',*,*,#47426,.T.) ;
#65224 = ORIENTED_EDGE('',*,*,#46091,.F.) ;
#65225 = ORIENTED_EDGE('',*,*,#47427,.F.) ;
#65226 = ORIENTED_EDGE('',*,*,#45675,.F.) ;
#65227 = ORIENTED_EDGE('',*,*,#47428,.F.) ;
#65228 = ORIENTED_EDGE('',*,*,#45488,.F.) ;
#65229 = ORIENTED_EDGE('',*,*,#47429,.F.) ;
#65230 = ORIENTED_EDGE('',*,*,#45676,.F.) ;
#65231 = ORIENTED_EDGE('',*,*,#47430,.F.) ;
#65232 = ORIENTED_EDGE('',*,*,#45670,.F.) ;
#65233 = ORIENTED_EDGE('',*,*,#47431,.F.) ;
#65234 = ORIENTED_EDGE('',*,*,#47429,.T.) ;
#65235 = ORIENTED_EDGE('',*,*,#47432,.F.) ;
#65236 = ORIENTED_EDGE('',*,*,#47433,.F.) ;
#65237 = ORIENTED_EDGE('',*,*,#47428,.T.) ;
#65238 = ORIENTED_EDGE('',*,*,#47434,.F.) ;
#65239 = ORIENTED_EDGE('',*,*,#47427,.T.) ;
#65240 = ORIENTED_EDGE('',*,*,#45487,.T.) ;
#65241 = ORIENTED_EDGE('',*,*,#47435,.F.) ;
#65242 = ORIENTED_EDGE('',*,*,#47430,.T.) ;
#65243 = ORIENTED_EDGE('',*,*,#47432,.T.) ;
#65244 = ORIENTED_EDGE('',*,*,#45673,.F.) ;
#65245 = ORIENTED_EDGE('',*,*,#47436,.F.) ;
#65246 = ORIENTED_EDGE('',*,*,#44191,.T.) ;
#65247 = ORIENTED_EDGE('',*,*,#47437,.T.) ;
#65248 = ORIENTED_EDGE('',*,*,#47438,.F.) ;
#65249 = ORIENTED_EDGE('',*,*,#47431,.T.) ;
#65250 = ORIENTED_EDGE('',*,*,#47439,.F.) ;
#65251 = ORIENTED_EDGE('',*,*,#47440,.T.) ;
#65252 = ORIENTED_EDGE('',*,*,#47441,.F.) ;
#65253 = ORIENTED_EDGE('',*,*,#44419,.F.) ;
#65254 = ORIENTED_EDGE('',*,*,#47442,.F.) ;
#65255 = ORIENTED_EDGE('',*,*,#45677,.F.) ;
#65256 = ORIENTED_EDGE('',*,*,#47434,.T.) ;
#65257 = ORIENTED_EDGE('',*,*,#45674,.F.) ;
#65258 = ORIENTED_EDGE('',*,*,#47443,.F.) ;
#65259 = ORIENTED_EDGE('',*,*,#45680,.F.) ;
#65260 = ORIENTED_EDGE('',*,*,#47433,.T.) ;
#65261 = ORIENTED_EDGE('',*,*,#45679,.F.) ;
#65262 = ORIENTED_EDGE('',*,*,#47444,.F.) ;
#65263 = ORIENTED_EDGE('',*,*,#45479,.F.) ;
#65264 = ORIENTED_EDGE('',*,*,#47435,.T.) ;
#65265 = ORIENTED_EDGE('',*,*,#45486,.F.) ;
#65266 = ORIENTED_EDGE('',*,*,#47445,.F.) ;
#65267 = ORIENTED_EDGE('',*,*,#45671,.F.) ;
#65268 = ORIENTED_EDGE('',*,*,#47446,.F.) ;
#65269 = ORIENTED_EDGE('',*,*,#45672,.F.) ;
#65270 = ORIENTED_EDGE('',*,*,#47447,.F.) ;
#65271 = ORIENTED_EDGE('',*,*,#45667,.F.) ;
#65272 = ORIENTED_EDGE('',*,*,#47436,.T.) ;
#65273 = ORIENTED_EDGE('',*,*,#47446,.T.) ;
#65274 = ORIENTED_EDGE('',*,*,#44192,.F.) ;
#65275 = ORIENTED_EDGE('',*,*,#47442,.T.) ;
#65276 = ORIENTED_EDGE('',*,*,#44429,.T.) ;
#65277 = ORIENTED_EDGE('',*,*,#47448,.F.) ;
#65278 = ORIENTED_EDGE('',*,*,#47443,.T.) ;
#65279 = ORIENTED_EDGE('',*,*,#47449,.F.) ;
#65280 = ORIENTED_EDGE('',*,*,#47444,.T.) ;
#65281 = ORIENTED_EDGE('',*,*,#47450,.F.) ;
#65282 = ORIENTED_EDGE('',*,*,#44521,.T.) ;
#65283 = ORIENTED_EDGE('',*,*,#47445,.T.) ;
#65284 = ORIENTED_EDGE('',*,*,#45485,.T.) ;
#65285 = ORIENTED_EDGE('',*,*,#47451,.F.) ;
#65286 = ORIENTED_EDGE('',*,*,#47447,.T.) ;
#65287 = ORIENTED_EDGE('',*,*,#47448,.T.) ;
#65288 = ORIENTED_EDGE('',*,*,#44428,.F.) ;
#65289 = ORIENTED_EDGE('',*,*,#47452,.F.) ;
#65290 = ORIENTED_EDGE('',*,*,#45681,.F.) ;
#65291 = ORIENTED_EDGE('',*,*,#47450,.T.) ;
#65292 = ORIENTED_EDGE('',*,*,#45678,.F.) ;
#65293 = ORIENTED_EDGE('',*,*,#47453,.F.) ;
#65294 = ORIENTED_EDGE('',*,*,#44522,.F.) ;
#65295 = ORIENTED_EDGE('',*,*,#45480,.F.) ;
#65296 = ORIENTED_EDGE('',*,*,#47449,.T.) ;
#65297 = ORIENTED_EDGE('',*,*,#47454,.F.) ;
#65298 = ORIENTED_EDGE('',*,*,#47455,.F.) ;
#65299 = ORIENTED_EDGE('',*,*,#47451,.T.) ;
#65300 = ORIENTED_EDGE('',*,*,#45484,.F.) ;
#65301 = ORIENTED_EDGE('',*,*,#47456,.F.) ;
#65302 = ORIENTED_EDGE('',*,*,#45668,.F.) ;
#65303 = ORIENTED_EDGE('',*,*,#47457,.F.) ;
#65304 = ORIENTED_EDGE('',*,*,#45669,.F.) ;
#65305 = ORIENTED_EDGE('',*,*,#47458,.F.) ;
#65306 = ORIENTED_EDGE('',*,*,#45663,.F.) ;
#65307 = ORIENTED_EDGE('',*,*,#44194,.T.) ;
#65308 = ORIENTED_EDGE('',*,*,#47457,.T.) ;
#65309 = ORIENTED_EDGE('',*,*,#47459,.F.) ;
#65310 = ORIENTED_EDGE('',*,*,#44423,.T.) ;
#65311 = ORIENTED_EDGE('',*,*,#47453,.T.) ;
#65312 = ORIENTED_EDGE('',*,*,#47452,.T.) ;
#65313 = ORIENTED_EDGE('',*,*,#47460,.F.) ;
#65314 = ORIENTED_EDGE('',*,*,#47461,.F.) ;
#65315 = ORIENTED_EDGE('',*,*,#44611,.F.) ;
#65316 = ORIENTED_EDGE('',*,*,#47462,.F.) ;
#65317 = ORIENTED_EDGE('',*,*,#47463,.F.) ;
#65318 = ORIENTED_EDGE('',*,*,#47454,.T.) ;
#65319 = ORIENTED_EDGE('',*,*,#44525,.F.) ;
#65320 = ORIENTED_EDGE('',*,*,#47462,.T.) ;
#65321 = ORIENTED_EDGE('',*,*,#44718,.F.) ;
#65322 = ORIENTED_EDGE('',*,*,#47455,.T.) ;
#65323 = ORIENTED_EDGE('',*,*,#47464,.F.) ;
#65324 = ORIENTED_EDGE('',*,*,#47465,.F.) ;
#65325 = ORIENTED_EDGE('',*,*,#47458,.T.) ;
#65326 = ORIENTED_EDGE('',*,*,#47456,.T.) ;
#65327 = ORIENTED_EDGE('',*,*,#47466,.F.) ;
#65328 = ORIENTED_EDGE('',*,*,#47459,.T.) ;
#65329 = ORIENTED_EDGE('',*,*,#45666,.F.) ;
#65330 = ORIENTED_EDGE('',*,*,#47467,.F.) ;
#65331 = ORIENTED_EDGE('',*,*,#44424,.F.) ;
#65332 = ORIENTED_EDGE('',*,*,#47460,.T.) ;
#65333 = ORIENTED_EDGE('',*,*,#44427,.F.) ;
#65334 = ORIENTED_EDGE('',*,*,#47468,.F.) ;
#65335 = ORIENTED_EDGE('',*,*,#44523,.F.) ;
#65336 = ORIENTED_EDGE('',*,*,#47461,.T.) ;
#65337 = ORIENTED_EDGE('',*,*,#44524,.F.) ;
#65338 = ORIENTED_EDGE('',*,*,#47469,.F.) ;
#65339 = ORIENTED_EDGE('',*,*,#44691,.F.) ;
#65340 = ORIENTED_EDGE('',*,*,#47463,.T.) ;
#65341 = ORIENTED_EDGE('',*,*,#44717,.T.) ;
#65342 = ORIENTED_EDGE('',*,*,#47470,.F.) ;
#65343 = ORIENTED_EDGE('',*,*,#47464,.T.) ;
#65344 = ORIENTED_EDGE('',*,*,#45481,.F.) ;
#65345 = ORIENTED_EDGE('',*,*,#47465,.T.) ;
#65346 = ORIENTED_EDGE('',*,*,#47471,.F.) ;
#65347 = ORIENTED_EDGE('',*,*,#47472,.F.) ;
#65348 = ORIENTED_EDGE('',*,*,#47466,.T.) ;
#65349 = ORIENTED_EDGE('',*,*,#45483,.F.) ;
#65350 = ORIENTED_EDGE('',*,*,#47473,.F.) ;
#65351 = ORIENTED_EDGE('',*,*,#45664,.F.) ;
#65352 = ORIENTED_EDGE('',*,*,#47474,.F.) ;
#65353 = ORIENTED_EDGE('',*,*,#45665,.F.) ;
#65354 = ORIENTED_EDGE('',*,*,#47475,.F.) ;
#65355 = ORIENTED_EDGE('',*,*,#44520,.F.) ;
#65356 = ORIENTED_EDGE('',*,*,#47467,.T.) ;
#65357 = ORIENTED_EDGE('',*,*,#47474,.T.) ;
#65358 = ORIENTED_EDGE('',*,*,#47476,.F.) ;
#65359 = ORIENTED_EDGE('',*,*,#47469,.T.) ;
#65360 = ORIENTED_EDGE('',*,*,#47468,.T.) ;
#65361 = ORIENTED_EDGE('',*,*,#47477,.F.) ;
#65362 = ORIENTED_EDGE('',*,*,#44692,.T.) ;
#65363 = ORIENTED_EDGE('',*,*,#47478,.F.) ;
#65364 = ORIENTED_EDGE('',*,*,#47471,.T.) ;
#65365 = ORIENTED_EDGE('',*,*,#47470,.T.) ;
#65366 = ORIENTED_EDGE('',*,*,#44716,.F.) ;
#65367 = ORIENTED_EDGE('',*,*,#47472,.T.) ;
#65368 = ORIENTED_EDGE('',*,*,#47479,.F.) ;
#65369 = ORIENTED_EDGE('',*,*,#47480,.F.) ;
#65370 = ORIENTED_EDGE('',*,*,#47475,.T.) ;
#65371 = ORIENTED_EDGE('',*,*,#47473,.T.) ;
#65372 = ORIENTED_EDGE('',*,*,#47481,.F.) ;
#65373 = ORIENTED_EDGE('',*,*,#44516,.T.) ;
#65374 = ORIENTED_EDGE('',*,*,#47476,.T.) ;
#65375 = ORIENTED_EDGE('',*,*,#44519,.F.) ;
#65376 = ORIENTED_EDGE('',*,*,#47482,.F.) ;
#65377 = ORIENTED_EDGE('',*,*,#44425,.F.) ;
#65378 = ORIENTED_EDGE('',*,*,#47477,.T.) ;
#65379 = ORIENTED_EDGE('',*,*,#44426,.F.) ;
#65380 = ORIENTED_EDGE('',*,*,#47483,.F.) ;
#65381 = ORIENTED_EDGE('',*,*,#44693,.F.) ;
#65382 = ORIENTED_EDGE('',*,*,#47478,.T.) ;
#65383 = ORIENTED_EDGE('',*,*,#44715,.T.) ;
#65384 = ORIENTED_EDGE('',*,*,#47484,.F.) ;
#65385 = ORIENTED_EDGE('',*,*,#47479,.T.) ;
#65386 = ORIENTED_EDGE('',*,*,#45482,.F.) ;
#65387 = ORIENTED_EDGE('',*,*,#47480,.T.) ;
#65388 = ORIENTED_EDGE('',*,*,#47485,.F.) ;
#65389 = ORIENTED_EDGE('',*,*,#47481,.T.) ;
#65390 = ORIENTED_EDGE('',*,*,#47483,.T.) ;
#65391 = ORIENTED_EDGE('',*,*,#47482,.T.) ;
#65392 = ORIENTED_EDGE('',*,*,#47486,.F.) ;
#65393 = ORIENTED_EDGE('',*,*,#44694,.T.) ;
#65394 = ORIENTED_EDGE('',*,*,#47484,.T.) ;
#65395 = ORIENTED_EDGE('',*,*,#44714,.F.) ;
#65396 = ORIENTED_EDGE('',*,*,#47487,.F.) ;
#65397 = ORIENTED_EDGE('',*,*,#44517,.F.) ;
#65398 = ORIENTED_EDGE('',*,*,#47485,.T.) ;
#65399 = ORIENTED_EDGE('',*,*,#47486,.T.) ;
#65400 = ORIENTED_EDGE('',*,*,#44518,.F.) ;
#65401 = ORIENTED_EDGE('',*,*,#47488,.F.) ;
#65402 = ORIENTED_EDGE('',*,*,#44695,.F.) ;
#65403 = ORIENTED_EDGE('',*,*,#47487,.T.) ;
#65404 = ORIENTED_EDGE('',*,*,#44617,.F.) ;
#65405 = ORIENTED_EDGE('',*,*,#47488,.T.) ;
#65406 = ORIENTED_EDGE('',*,*,#47489,.F.) ;
#65407 = ORIENTED_EDGE('',*,*,#45955,.F.) ;
#65408 = ORIENTED_EDGE('',*,*,#47490,.F.) ;
#65409 = ORIENTED_EDGE('',*,*,#46002,.F.) ;
#65410 = ORIENTED_EDGE('',*,*,#47490,.T.) ;
#65411 = ORIENTED_EDGE('',*,*,#45952,.F.) ;
#65412 = ORIENTED_EDGE('',*,*,#47491,.F.) ;
#65413 = ORIENTED_EDGE('',*,*,#46003,.F.) ;
#65414 = ORIENTED_EDGE('',*,*,#45958,.F.) ;
#65415 = ORIENTED_EDGE('',*,*,#47489,.T.) ;
#65416 = ORIENTED_EDGE('',*,*,#47492,.F.) ;
#65417 = ORIENTED_EDGE('',*,*,#47491,.T.) ;
#65418 = ORIENTED_EDGE('',*,*,#45949,.F.) ;
#65419 = ORIENTED_EDGE('',*,*,#47493,.F.) ;
#65420 = ORIENTED_EDGE('',*,*,#46004,.F.) ;
#65421 = ORIENTED_EDGE('',*,*,#47492,.T.) ;
#65422 = ORIENTED_EDGE('',*,*,#46001,.F.) ;
#65423 = ORIENTED_EDGE('',*,*,#47494,.F.) ;
#65424 = ORIENTED_EDGE('',*,*,#45961,.F.) ;
#65425 = ORIENTED_EDGE('',*,*,#47493,.T.) ;
#65426 = ORIENTED_EDGE('',*,*,#45946,.F.) ;
#65427 = ORIENTED_EDGE('',*,*,#47495,.F.) ;
#65428 = ORIENTED_EDGE('',*,*,#46005,.F.) ;
#65429 = ORIENTED_EDGE('',*,*,#45964,.F.) ;
#65430 = ORIENTED_EDGE('',*,*,#47494,.T.) ;
#65431 = ORIENTED_EDGE('',*,*,#47496,.F.) ;
#65432 = ORIENTED_EDGE('',*,*,#47495,.T.) ;
#65433 = ORIENTED_EDGE('',*,*,#45943,.F.) ;
#65434 = ORIENTED_EDGE('',*,*,#47497,.F.) ;
#65435 = ORIENTED_EDGE('',*,*,#46006,.F.) ;
#65436 = ORIENTED_EDGE('',*,*,#47496,.T.) ;
#65437 = ORIENTED_EDGE('',*,*,#46000,.F.) ;
#65438 = ORIENTED_EDGE('',*,*,#47498,.F.) ;
#65439 = ORIENTED_EDGE('',*,*,#45967,.F.) ;
#65440 = ORIENTED_EDGE('',*,*,#47497,.T.) ;
#65441 = ORIENTED_EDGE('',*,*,#45940,.F.) ;
#65442 = ORIENTED_EDGE('',*,*,#47499,.F.) ;
#65443 = ORIENTED_EDGE('',*,*,#45970,.F.) ;
#65444 = ORIENTED_EDGE('',*,*,#47498,.T.) ;
#65445 = ORIENTED_EDGE('',*,*,#47500,.F.) ;
#65446 = ORIENTED_EDGE('',*,*,#47499,.T.) ;
#65447 = ORIENTED_EDGE('',*,*,#45937,.F.) ;
#65448 = ORIENTED_EDGE('',*,*,#47501,.F.) ;
#65449 = ORIENTED_EDGE('',*,*,#46007,.F.) ;
#65450 = ORIENTED_EDGE('',*,*,#47500,.T.) ;
#65451 = ORIENTED_EDGE('',*,*,#45999,.F.) ;
#65452 = ORIENTED_EDGE('',*,*,#47502,.F.) ;
#65453 = ORIENTED_EDGE('',*,*,#45973,.F.) ;
#65454 = ORIENTED_EDGE('',*,*,#47501,.T.) ;
#65455 = ORIENTED_EDGE('',*,*,#44363,.F.) ;
#65456 = ORIENTED_EDGE('',*,*,#47503,.F.) ;
#65457 = ORIENTED_EDGE('',*,*,#45976,.F.) ;
#65458 = ORIENTED_EDGE('',*,*,#47502,.T.) ;
#65459 = ORIENTED_EDGE('',*,*,#47504,.F.) ;
#65460 = ORIENTED_EDGE('',*,*,#47503,.T.) ;
#65461 = ORIENTED_EDGE('',*,*,#45935,.F.) ;
#65462 = ORIENTED_EDGE('',*,*,#44190,.F.) ;
#65463 = ORIENTED_EDGE('',*,*,#46008,.F.) ;
#65464 = ORIENTED_EDGE('',*,*,#47504,.T.) ;
#65465 = ORIENTED_EDGE('',*,*,#45998,.F.) ;
#65466 = ORIENTED_EDGE('',*,*,#47505,.F.) ;
#65467 = ORIENTED_EDGE('',*,*,#45979,.F.) ;
#65468 = ORIENTED_EDGE('',*,*,#45982,.F.) ;
#65469 = ORIENTED_EDGE('',*,*,#47505,.T.) ;
#65470 = ORIENTED_EDGE('',*,*,#47506,.F.) ;
#65471 = ORIENTED_EDGE('',*,*,#44189,.T.) ;
#65472 = ORIENTED_EDGE('',*,*,#45930,.F.) ;
#65473 = ORIENTED_EDGE('',*,*,#47507,.F.) ;
#65474 = ORIENTED_EDGE('',*,*,#46009,.F.) ;
#65475 = ORIENTED_EDGE('',*,*,#47506,.T.) ;
#65476 = ORIENTED_EDGE('',*,*,#45997,.F.) ;
#65477 = ORIENTED_EDGE('',*,*,#47508,.F.) ;
#65478 = ORIENTED_EDGE('',*,*,#45985,.F.) ;
#65479 = ORIENTED_EDGE('',*,*,#47507,.T.) ;
#65480 = ORIENTED_EDGE('',*,*,#45927,.F.) ;
#65481 = ORIENTED_EDGE('',*,*,#47509,.F.) ;
#65482 = ORIENTED_EDGE('',*,*,#45988,.F.) ;
#65483 = ORIENTED_EDGE('',*,*,#47508,.T.) ;
#65484 = ORIENTED_EDGE('',*,*,#47510,.F.) ;
#65485 = ORIENTED_EDGE('',*,*,#47509,.T.) ;
#65486 = ORIENTED_EDGE('',*,*,#45924,.F.) ;
#65487 = ORIENTED_EDGE('',*,*,#47511,.F.) ;
#65488 = ORIENTED_EDGE('',*,*,#46010,.F.) ;
#65489 = ORIENTED_EDGE('',*,*,#47510,.T.) ;
#65490 = ORIENTED_EDGE('',*,*,#45996,.F.) ;
#65491 = ORIENTED_EDGE('',*,*,#47512,.F.) ;
#65492 = ORIENTED_EDGE('',*,*,#45991,.F.) ;
#65493 = ORIENTED_EDGE('',*,*,#47511,.T.) ;
#65494 = ORIENTED_EDGE('',*,*,#45921,.F.) ;
#65495 = ORIENTED_EDGE('',*,*,#47513,.F.) ;
#65496 = ORIENTED_EDGE('',*,*,#45993,.F.) ;
#65497 = ORIENTED_EDGE('',*,*,#47512,.T.) ;
#65498 = ORIENTED_EDGE('',*,*,#45995,.F.) ;
#65499 = ORIENTED_EDGE('',*,*,#47514,.F.) ;
#65500 = ORIENTED_EDGE('',*,*,#45915,.F.) ;
#65501 = ORIENTED_EDGE('',*,*,#47513,.T.) ;
#65502 = ORIENTED_EDGE('',*,*,#45918,.F.) ;
#65503 = ORIENTED_EDGE('',*,*,#47514,.T.) ;
#65504 = ORIENTED_EDGE('',*,*,#45994,.F.) ;
#65505 = ORIENTED_EDGE('',*,*,#47515,.F.) ;
#65506 = ORIENTED_EDGE('',*,*,#45694,.F.) ;
#65507 = ORIENTED_EDGE('',*,*,#47516,.F.) ;
#65508 = ORIENTED_EDGE('',*,*,#45478,.F.) ;
#65509 = ORIENTED_EDGE('',*,*,#47517,.F.) ;
#65510 = ORIENTED_EDGE('',*,*,#45695,.F.) ;
#65511 = ORIENTED_EDGE('',*,*,#47518,.F.) ;
#65512 = ORIENTED_EDGE('',*,*,#45689,.F.) ;
#65513 = ORIENTED_EDGE('',*,*,#47519,.F.) ;
#65514 = ORIENTED_EDGE('',*,*,#47517,.T.) ;
#65515 = ORIENTED_EDGE('',*,*,#47520,.F.) ;
#65516 = ORIENTED_EDGE('',*,*,#47521,.F.) ;
#65517 = ORIENTED_EDGE('',*,*,#47516,.T.) ;
#65518 = ORIENTED_EDGE('',*,*,#47522,.F.) ;
#65519 = ORIENTED_EDGE('',*,*,#47515,.T.) ;
#65520 = ORIENTED_EDGE('',*,*,#45477,.T.) ;
#65521 = ORIENTED_EDGE('',*,*,#47523,.F.) ;
#65522 = ORIENTED_EDGE('',*,*,#47518,.T.) ;
#65523 = ORIENTED_EDGE('',*,*,#47520,.T.) ;
#65524 = ORIENTED_EDGE('',*,*,#45692,.F.) ;
#65525 = ORIENTED_EDGE('',*,*,#47524,.F.) ;
#65526 = ORIENTED_EDGE('',*,*,#44174,.T.) ;
#65527 = ORIENTED_EDGE('',*,*,#47525,.T.) ;
#65528 = ORIENTED_EDGE('',*,*,#47526,.F.) ;
#65529 = ORIENTED_EDGE('',*,*,#47519,.T.) ;
#65530 = ORIENTED_EDGE('',*,*,#47527,.F.) ;
#65531 = ORIENTED_EDGE('',*,*,#47528,.T.) ;
#65532 = ORIENTED_EDGE('',*,*,#47529,.F.) ;
#65533 = ORIENTED_EDGE('',*,*,#44408,.F.) ;
#65534 = ORIENTED_EDGE('',*,*,#47530,.F.) ;
#65535 = ORIENTED_EDGE('',*,*,#45696,.F.) ;
#65536 = ORIENTED_EDGE('',*,*,#47522,.T.) ;
#65537 = ORIENTED_EDGE('',*,*,#45693,.F.) ;
#65538 = ORIENTED_EDGE('',*,*,#47531,.F.) ;
#65539 = ORIENTED_EDGE('',*,*,#45699,.F.) ;
#65540 = ORIENTED_EDGE('',*,*,#47521,.T.) ;
#65541 = ORIENTED_EDGE('',*,*,#45698,.F.) ;
#65542 = ORIENTED_EDGE('',*,*,#47532,.F.) ;
#65543 = ORIENTED_EDGE('',*,*,#45469,.F.) ;
#65544 = ORIENTED_EDGE('',*,*,#47523,.T.) ;
#65545 = ORIENTED_EDGE('',*,*,#45476,.F.) ;
#65546 = ORIENTED_EDGE('',*,*,#47533,.F.) ;
#65547 = ORIENTED_EDGE('',*,*,#45690,.F.) ;
#65548 = ORIENTED_EDGE('',*,*,#47534,.F.) ;
#65549 = ORIENTED_EDGE('',*,*,#45691,.F.) ;
#65550 = ORIENTED_EDGE('',*,*,#47535,.F.) ;
#65551 = ORIENTED_EDGE('',*,*,#45686,.F.) ;
#65552 = ORIENTED_EDGE('',*,*,#47524,.T.) ;
#65553 = ORIENTED_EDGE('',*,*,#47534,.T.) ;
#65554 = ORIENTED_EDGE('',*,*,#44175,.F.) ;
#65555 = ORIENTED_EDGE('',*,*,#47530,.T.) ;
#65556 = ORIENTED_EDGE('',*,*,#44418,.T.) ;
#65557 = ORIENTED_EDGE('',*,*,#47536,.F.) ;
#65558 = ORIENTED_EDGE('',*,*,#47531,.T.) ;
#65559 = ORIENTED_EDGE('',*,*,#47537,.F.) ;
#65560 = ORIENTED_EDGE('',*,*,#47532,.T.) ;
#65561 = ORIENTED_EDGE('',*,*,#47538,.F.) ;
#65562 = ORIENTED_EDGE('',*,*,#44511,.T.) ;
#65563 = ORIENTED_EDGE('',*,*,#47533,.T.) ;
#65564 = ORIENTED_EDGE('',*,*,#45475,.T.) ;
#65565 = ORIENTED_EDGE('',*,*,#47539,.F.) ;
#65566 = ORIENTED_EDGE('',*,*,#47535,.T.) ;
#65567 = ORIENTED_EDGE('',*,*,#47536,.T.) ;
#65568 = ORIENTED_EDGE('',*,*,#44417,.F.) ;
#65569 = ORIENTED_EDGE('',*,*,#47540,.F.) ;
#65570 = ORIENTED_EDGE('',*,*,#45700,.F.) ;
#65571 = ORIENTED_EDGE('',*,*,#47538,.T.) ;
#65572 = ORIENTED_EDGE('',*,*,#45697,.F.) ;
#65573 = ORIENTED_EDGE('',*,*,#47541,.F.) ;
#65574 = ORIENTED_EDGE('',*,*,#44512,.F.) ;
#65575 = ORIENTED_EDGE('',*,*,#45470,.F.) ;
#65576 = ORIENTED_EDGE('',*,*,#47537,.T.) ;
#65577 = ORIENTED_EDGE('',*,*,#47542,.F.) ;
#65578 = ORIENTED_EDGE('',*,*,#47543,.F.) ;
#65579 = ORIENTED_EDGE('',*,*,#47539,.T.) ;
#65580 = ORIENTED_EDGE('',*,*,#45474,.F.) ;
#65581 = ORIENTED_EDGE('',*,*,#47544,.F.) ;
#65582 = ORIENTED_EDGE('',*,*,#45687,.F.) ;
#65583 = ORIENTED_EDGE('',*,*,#47545,.F.) ;
#65584 = ORIENTED_EDGE('',*,*,#45688,.F.) ;
#65585 = ORIENTED_EDGE('',*,*,#47546,.F.) ;
#65586 = ORIENTED_EDGE('',*,*,#45682,.F.) ;
#65587 = ORIENTED_EDGE('',*,*,#44177,.T.) ;
#65588 = ORIENTED_EDGE('',*,*,#47545,.T.) ;
#65589 = ORIENTED_EDGE('',*,*,#47547,.F.) ;
#65590 = ORIENTED_EDGE('',*,*,#44412,.T.) ;
#65591 = ORIENTED_EDGE('',*,*,#47541,.T.) ;
#65592 = ORIENTED_EDGE('',*,*,#47540,.T.) ;
#65593 = ORIENTED_EDGE('',*,*,#47548,.F.) ;
#65594 = ORIENTED_EDGE('',*,*,#47549,.F.) ;
#65595 = ORIENTED_EDGE('',*,*,#44615,.F.) ;
#65596 = ORIENTED_EDGE('',*,*,#47550,.F.) ;
#65597 = ORIENTED_EDGE('',*,*,#47551,.F.) ;
#65598 = ORIENTED_EDGE('',*,*,#47542,.T.) ;
#65599 = ORIENTED_EDGE('',*,*,#44515,.F.) ;
#65600 = ORIENTED_EDGE('',*,*,#47550,.T.) ;
#65601 = ORIENTED_EDGE('',*,*,#44713,.F.) ;
#65602 = ORIENTED_EDGE('',*,*,#47543,.T.) ;
#65603 = ORIENTED_EDGE('',*,*,#47552,.F.) ;
#65604 = ORIENTED_EDGE('',*,*,#47553,.F.) ;
#65605 = ORIENTED_EDGE('',*,*,#47546,.T.) ;
#65606 = ORIENTED_EDGE('',*,*,#47544,.T.) ;
#65607 = ORIENTED_EDGE('',*,*,#47554,.F.) ;
#65608 = ORIENTED_EDGE('',*,*,#47547,.T.) ;
#65609 = ORIENTED_EDGE('',*,*,#45685,.F.) ;
#65610 = ORIENTED_EDGE('',*,*,#47555,.F.) ;
#65611 = ORIENTED_EDGE('',*,*,#44413,.F.) ;
#65612 = ORIENTED_EDGE('',*,*,#47548,.T.) ;
#65613 = ORIENTED_EDGE('',*,*,#44416,.F.) ;
#65614 = ORIENTED_EDGE('',*,*,#47556,.F.) ;
#65615 = ORIENTED_EDGE('',*,*,#44513,.F.) ;
#65616 = ORIENTED_EDGE('',*,*,#47549,.T.) ;
#65617 = ORIENTED_EDGE('',*,*,#44514,.F.) ;
#65618 = ORIENTED_EDGE('',*,*,#47557,.F.) ;
#65619 = ORIENTED_EDGE('',*,*,#44696,.F.) ;
#65620 = ORIENTED_EDGE('',*,*,#47551,.T.) ;
#65621 = ORIENTED_EDGE('',*,*,#44712,.T.) ;
#65622 = ORIENTED_EDGE('',*,*,#47558,.F.) ;
#65623 = ORIENTED_EDGE('',*,*,#47552,.T.) ;
#65624 = ORIENTED_EDGE('',*,*,#45471,.F.) ;
#65625 = ORIENTED_EDGE('',*,*,#47553,.T.) ;
#65626 = ORIENTED_EDGE('',*,*,#47559,.F.) ;
#65627 = ORIENTED_EDGE('',*,*,#47560,.F.) ;
#65628 = ORIENTED_EDGE('',*,*,#47554,.T.) ;
#65629 = ORIENTED_EDGE('',*,*,#45473,.F.) ;
#65630 = ORIENTED_EDGE('',*,*,#47561,.F.) ;
#65631 = ORIENTED_EDGE('',*,*,#45683,.F.) ;
#65632 = ORIENTED_EDGE('',*,*,#47562,.F.) ;
#65633 = ORIENTED_EDGE('',*,*,#45684,.F.) ;
#65634 = ORIENTED_EDGE('',*,*,#47563,.F.) ;
#65635 = ORIENTED_EDGE('',*,*,#44510,.F.) ;
#65636 = ORIENTED_EDGE('',*,*,#47555,.T.) ;
#65637 = ORIENTED_EDGE('',*,*,#47562,.T.) ;
#65638 = ORIENTED_EDGE('',*,*,#47564,.F.) ;
#65639 = ORIENTED_EDGE('',*,*,#47557,.T.) ;
#65640 = ORIENTED_EDGE('',*,*,#47556,.T.) ;
#65641 = ORIENTED_EDGE('',*,*,#47565,.F.) ;
#65642 = ORIENTED_EDGE('',*,*,#44697,.T.) ;
#65643 = ORIENTED_EDGE('',*,*,#47566,.F.) ;
#65644 = ORIENTED_EDGE('',*,*,#47559,.T.) ;
#65645 = ORIENTED_EDGE('',*,*,#47558,.T.) ;
#65646 = ORIENTED_EDGE('',*,*,#44711,.F.) ;
#65647 = ORIENTED_EDGE('',*,*,#47560,.T.) ;
#65648 = ORIENTED_EDGE('',*,*,#47567,.F.) ;
#65649 = ORIENTED_EDGE('',*,*,#47568,.F.) ;
#65650 = ORIENTED_EDGE('',*,*,#47563,.T.) ;
#65651 = ORIENTED_EDGE('',*,*,#47561,.T.) ;
#65652 = ORIENTED_EDGE('',*,*,#47569,.F.) ;
#65653 = ORIENTED_EDGE('',*,*,#44506,.T.) ;
#65654 = ORIENTED_EDGE('',*,*,#47564,.T.) ;
#65655 = ORIENTED_EDGE('',*,*,#44509,.F.) ;
#65656 = ORIENTED_EDGE('',*,*,#47570,.F.) ;
#65657 = ORIENTED_EDGE('',*,*,#44414,.F.) ;
#65658 = ORIENTED_EDGE('',*,*,#47565,.T.) ;
#65659 = ORIENTED_EDGE('',*,*,#44415,.F.) ;
#65660 = ORIENTED_EDGE('',*,*,#47571,.F.) ;
#65661 = ORIENTED_EDGE('',*,*,#44698,.F.) ;
#65662 = ORIENTED_EDGE('',*,*,#47566,.T.) ;
#65663 = ORIENTED_EDGE('',*,*,#44710,.T.) ;
#65664 = ORIENTED_EDGE('',*,*,#47572,.F.) ;
#65665 = ORIENTED_EDGE('',*,*,#47567,.T.) ;
#65666 = ORIENTED_EDGE('',*,*,#45472,.F.) ;
#65667 = ORIENTED_EDGE('',*,*,#47568,.T.) ;
#65668 = ORIENTED_EDGE('',*,*,#47573,.F.) ;
#65669 = ORIENTED_EDGE('',*,*,#47569,.T.) ;
#65670 = ORIENTED_EDGE('',*,*,#47571,.T.) ;
#65671 = ORIENTED_EDGE('',*,*,#47570,.T.) ;
#65672 = ORIENTED_EDGE('',*,*,#47574,.F.) ;
#65673 = ORIENTED_EDGE('',*,*,#44699,.T.) ;
#65674 = ORIENTED_EDGE('',*,*,#47572,.T.) ;
#65675 = ORIENTED_EDGE('',*,*,#44709,.F.) ;
#65676 = ORIENTED_EDGE('',*,*,#47575,.F.) ;
#65677 = ORIENTED_EDGE('',*,*,#44507,.F.) ;
#65678 = ORIENTED_EDGE('',*,*,#47573,.T.) ;
#65679 = ORIENTED_EDGE('',*,*,#47574,.T.) ;
#65680 = ORIENTED_EDGE('',*,*,#44508,.F.) ;
#65681 = ORIENTED_EDGE('',*,*,#47576,.F.) ;
#65682 = ORIENTED_EDGE('',*,*,#44700,.F.) ;
#65683 = ORIENTED_EDGE('',*,*,#47575,.T.) ;
#65684 = ORIENTED_EDGE('',*,*,#44621,.F.) ;
#65685 = ORIENTED_EDGE('',*,*,#47576,.T.) ;
#65686 = ORIENTED_EDGE('',*,*,#47577,.F.) ;
#65687 = ORIENTED_EDGE('',*,*,#45858,.F.) ;
#65688 = ORIENTED_EDGE('',*,*,#47578,.F.) ;
#65689 = ORIENTED_EDGE('',*,*,#45905,.F.) ;
#65690 = ORIENTED_EDGE('',*,*,#47578,.T.) ;
#65691 = ORIENTED_EDGE('',*,*,#45855,.F.) ;
#65692 = ORIENTED_EDGE('',*,*,#47579,.F.) ;
#65693 = ORIENTED_EDGE('',*,*,#45906,.F.) ;
#65694 = ORIENTED_EDGE('',*,*,#45861,.F.) ;
#65695 = ORIENTED_EDGE('',*,*,#47577,.T.) ;
#65696 = ORIENTED_EDGE('',*,*,#47580,.F.) ;
#65697 = ORIENTED_EDGE('',*,*,#47579,.T.) ;
#65698 = ORIENTED_EDGE('',*,*,#45852,.F.) ;
#65699 = ORIENTED_EDGE('',*,*,#47581,.F.) ;
#65700 = ORIENTED_EDGE('',*,*,#45907,.F.) ;
#65701 = ORIENTED_EDGE('',*,*,#47580,.T.) ;
#65702 = ORIENTED_EDGE('',*,*,#45904,.F.) ;
#65703 = ORIENTED_EDGE('',*,*,#47582,.F.) ;
#65704 = ORIENTED_EDGE('',*,*,#45864,.F.) ;
#65705 = ORIENTED_EDGE('',*,*,#47581,.T.) ;
#65706 = ORIENTED_EDGE('',*,*,#45849,.F.) ;
#65707 = ORIENTED_EDGE('',*,*,#47583,.F.) ;
#65708 = ORIENTED_EDGE('',*,*,#45908,.F.) ;
#65709 = ORIENTED_EDGE('',*,*,#45867,.F.) ;
#65710 = ORIENTED_EDGE('',*,*,#47582,.T.) ;
#65711 = ORIENTED_EDGE('',*,*,#47584,.F.) ;
#65712 = ORIENTED_EDGE('',*,*,#47583,.T.) ;
#65713 = ORIENTED_EDGE('',*,*,#45846,.F.) ;
#65714 = ORIENTED_EDGE('',*,*,#47585,.F.) ;
#65715 = ORIENTED_EDGE('',*,*,#45909,.F.) ;
#65716 = ORIENTED_EDGE('',*,*,#47584,.T.) ;
#65717 = ORIENTED_EDGE('',*,*,#45903,.F.) ;
#65718 = ORIENTED_EDGE('',*,*,#47586,.F.) ;
#65719 = ORIENTED_EDGE('',*,*,#45870,.F.) ;
#65720 = ORIENTED_EDGE('',*,*,#47585,.T.) ;
#65721 = ORIENTED_EDGE('',*,*,#45843,.F.) ;
#65722 = ORIENTED_EDGE('',*,*,#47587,.F.) ;
#65723 = ORIENTED_EDGE('',*,*,#45873,.F.) ;
#65724 = ORIENTED_EDGE('',*,*,#47586,.T.) ;
#65725 = ORIENTED_EDGE('',*,*,#47588,.F.) ;
#65726 = ORIENTED_EDGE('',*,*,#47587,.T.) ;
#65727 = ORIENTED_EDGE('',*,*,#45840,.F.) ;
#65728 = ORIENTED_EDGE('',*,*,#47589,.F.) ;
#65729 = ORIENTED_EDGE('',*,*,#45910,.F.) ;
#65730 = ORIENTED_EDGE('',*,*,#47588,.T.) ;
#65731 = ORIENTED_EDGE('',*,*,#45902,.F.) ;
#65732 = ORIENTED_EDGE('',*,*,#47590,.F.) ;
#65733 = ORIENTED_EDGE('',*,*,#45876,.F.) ;
#65734 = ORIENTED_EDGE('',*,*,#47589,.T.) ;
#65735 = ORIENTED_EDGE('',*,*,#44366,.F.) ;
#65736 = ORIENTED_EDGE('',*,*,#47591,.F.) ;
#65737 = ORIENTED_EDGE('',*,*,#45879,.F.) ;
#65738 = ORIENTED_EDGE('',*,*,#47590,.T.) ;
#65739 = ORIENTED_EDGE('',*,*,#47592,.F.) ;
#65740 = ORIENTED_EDGE('',*,*,#47591,.T.) ;
#65741 = ORIENTED_EDGE('',*,*,#45838,.F.) ;
#65742 = ORIENTED_EDGE('',*,*,#44173,.F.) ;
#65743 = ORIENTED_EDGE('',*,*,#45911,.F.) ;
#65744 = ORIENTED_EDGE('',*,*,#47592,.T.) ;
#65745 = ORIENTED_EDGE('',*,*,#45901,.F.) ;
#65746 = ORIENTED_EDGE('',*,*,#47593,.F.) ;
#65747 = ORIENTED_EDGE('',*,*,#45882,.F.) ;
#65748 = ORIENTED_EDGE('',*,*,#45885,.F.) ;
#65749 = ORIENTED_EDGE('',*,*,#47593,.T.) ;
#65750 = ORIENTED_EDGE('',*,*,#47594,.F.) ;
#65751 = ORIENTED_EDGE('',*,*,#44172,.T.) ;
#65752 = ORIENTED_EDGE('',*,*,#45833,.F.) ;
#65753 = ORIENTED_EDGE('',*,*,#47595,.F.) ;
#65754 = ORIENTED_EDGE('',*,*,#45912,.F.) ;
#65755 = ORIENTED_EDGE('',*,*,#47594,.T.) ;
#65756 = ORIENTED_EDGE('',*,*,#45900,.F.) ;
#65757 = ORIENTED_EDGE('',*,*,#47596,.F.) ;
#65758 = ORIENTED_EDGE('',*,*,#45888,.F.) ;
#65759 = ORIENTED_EDGE('',*,*,#47595,.T.) ;
#65760 = ORIENTED_EDGE('',*,*,#45830,.F.) ;
#65761 = ORIENTED_EDGE('',*,*,#47597,.F.) ;
#65762 = ORIENTED_EDGE('',*,*,#45891,.F.) ;
#65763 = ORIENTED_EDGE('',*,*,#47596,.T.) ;
#65764 = ORIENTED_EDGE('',*,*,#47598,.F.) ;
#65765 = ORIENTED_EDGE('',*,*,#47597,.T.) ;
#65766 = ORIENTED_EDGE('',*,*,#45827,.F.) ;
#65767 = ORIENTED_EDGE('',*,*,#47599,.F.) ;
#65768 = ORIENTED_EDGE('',*,*,#45913,.F.) ;
#65769 = ORIENTED_EDGE('',*,*,#47598,.T.) ;
#65770 = ORIENTED_EDGE('',*,*,#45899,.F.) ;
#65771 = ORIENTED_EDGE('',*,*,#47600,.F.) ;
#65772 = ORIENTED_EDGE('',*,*,#45894,.F.) ;
#65773 = ORIENTED_EDGE('',*,*,#47599,.T.) ;
#65774 = ORIENTED_EDGE('',*,*,#45824,.F.) ;
#65775 = ORIENTED_EDGE('',*,*,#47601,.F.) ;
#65776 = ORIENTED_EDGE('',*,*,#45896,.F.) ;
#65777 = ORIENTED_EDGE('',*,*,#47600,.T.) ;
#65778 = ORIENTED_EDGE('',*,*,#45898,.F.) ;
#65779 = ORIENTED_EDGE('',*,*,#47602,.F.) ;
#65780 = ORIENTED_EDGE('',*,*,#45818,.F.) ;
#65781 = ORIENTED_EDGE('',*,*,#47601,.T.) ;
#65782 = ORIENTED_EDGE('',*,*,#45821,.F.) ;
#65783 = ORIENTED_EDGE('',*,*,#47602,.T.) ;
#65784 = ORIENTED_EDGE('',*,*,#45897,.F.) ;
#65785 = ORIENTED_EDGE('',*,*,#47603,.F.) ;
#65786 = ORIENTED_EDGE('',*,*,#45713,.F.) ;
#65787 = ORIENTED_EDGE('',*,*,#47604,.F.) ;
#65788 = ORIENTED_EDGE('',*,*,#45468,.F.) ;
#65789 = ORIENTED_EDGE('',*,*,#47605,.F.) ;
#65790 = ORIENTED_EDGE('',*,*,#45714,.F.) ;
#65791 = ORIENTED_EDGE('',*,*,#47606,.F.) ;
#65792 = ORIENTED_EDGE('',*,*,#45708,.F.) ;
#65793 = ORIENTED_EDGE('',*,*,#47607,.F.) ;
#65794 = ORIENTED_EDGE('',*,*,#47605,.T.) ;
#65795 = ORIENTED_EDGE('',*,*,#47608,.F.) ;
#65796 = ORIENTED_EDGE('',*,*,#47609,.F.) ;
#65797 = ORIENTED_EDGE('',*,*,#47604,.T.) ;
#65798 = ORIENTED_EDGE('',*,*,#47610,.F.) ;
#65799 = ORIENTED_EDGE('',*,*,#47603,.T.) ;
#65800 = ORIENTED_EDGE('',*,*,#45467,.T.) ;
#65801 = ORIENTED_EDGE('',*,*,#47611,.F.) ;
#65802 = ORIENTED_EDGE('',*,*,#47606,.T.) ;
#65803 = ORIENTED_EDGE('',*,*,#47608,.T.) ;
#65804 = ORIENTED_EDGE('',*,*,#45711,.F.) ;
#65805 = ORIENTED_EDGE('',*,*,#47612,.F.) ;
#65806 = ORIENTED_EDGE('',*,*,#44157,.T.) ;
#65807 = ORIENTED_EDGE('',*,*,#47613,.T.) ;
#65808 = ORIENTED_EDGE('',*,*,#47614,.F.) ;
#65809 = ORIENTED_EDGE('',*,*,#47607,.T.) ;
#65810 = ORIENTED_EDGE('',*,*,#47615,.F.) ;
#65811 = ORIENTED_EDGE('',*,*,#47616,.T.) ;
#65812 = ORIENTED_EDGE('',*,*,#47617,.F.) ;
#65813 = ORIENTED_EDGE('',*,*,#44397,.F.) ;
#65814 = ORIENTED_EDGE('',*,*,#47618,.F.) ;
#65815 = ORIENTED_EDGE('',*,*,#45715,.F.) ;
#65816 = ORIENTED_EDGE('',*,*,#47610,.T.) ;
#65817 = ORIENTED_EDGE('',*,*,#45712,.F.) ;
#65818 = ORIENTED_EDGE('',*,*,#47619,.F.) ;
#65819 = ORIENTED_EDGE('',*,*,#45718,.F.) ;
#65820 = ORIENTED_EDGE('',*,*,#47609,.T.) ;
#65821 = ORIENTED_EDGE('',*,*,#45717,.F.) ;
#65822 = ORIENTED_EDGE('',*,*,#47620,.F.) ;
#65823 = ORIENTED_EDGE('',*,*,#45459,.F.) ;
#65824 = ORIENTED_EDGE('',*,*,#47611,.T.) ;
#65825 = ORIENTED_EDGE('',*,*,#45466,.F.) ;
#65826 = ORIENTED_EDGE('',*,*,#47621,.F.) ;
#65827 = ORIENTED_EDGE('',*,*,#45709,.F.) ;
#65828 = ORIENTED_EDGE('',*,*,#47622,.F.) ;
#65829 = ORIENTED_EDGE('',*,*,#45710,.F.) ;
#65830 = ORIENTED_EDGE('',*,*,#47623,.F.) ;
#65831 = ORIENTED_EDGE('',*,*,#45705,.F.) ;
#65832 = ORIENTED_EDGE('',*,*,#47612,.T.) ;
#65833 = ORIENTED_EDGE('',*,*,#47622,.T.) ;
#65834 = ORIENTED_EDGE('',*,*,#44158,.F.) ;
#65835 = ORIENTED_EDGE('',*,*,#47618,.T.) ;
#65836 = ORIENTED_EDGE('',*,*,#44407,.T.) ;
#65837 = ORIENTED_EDGE('',*,*,#47624,.F.) ;
#65838 = ORIENTED_EDGE('',*,*,#47619,.T.) ;
#65839 = ORIENTED_EDGE('',*,*,#47625,.F.) ;
#65840 = ORIENTED_EDGE('',*,*,#47620,.T.) ;
#65841 = ORIENTED_EDGE('',*,*,#47626,.F.) ;
#65842 = ORIENTED_EDGE('',*,*,#44501,.T.) ;
#65843 = ORIENTED_EDGE('',*,*,#47621,.T.) ;
#65844 = ORIENTED_EDGE('',*,*,#45465,.T.) ;
#65845 = ORIENTED_EDGE('',*,*,#47627,.F.) ;
#65846 = ORIENTED_EDGE('',*,*,#47623,.T.) ;
#65847 = ORIENTED_EDGE('',*,*,#47624,.T.) ;
#65848 = ORIENTED_EDGE('',*,*,#44406,.F.) ;
#65849 = ORIENTED_EDGE('',*,*,#47628,.F.) ;
#65850 = ORIENTED_EDGE('',*,*,#45719,.F.) ;
#65851 = ORIENTED_EDGE('',*,*,#47626,.T.) ;
#65852 = ORIENTED_EDGE('',*,*,#45716,.F.) ;
#65853 = ORIENTED_EDGE('',*,*,#47629,.F.) ;
#65854 = ORIENTED_EDGE('',*,*,#44502,.F.) ;
#65855 = ORIENTED_EDGE('',*,*,#45460,.F.) ;
#65856 = ORIENTED_EDGE('',*,*,#47625,.T.) ;
#65857 = ORIENTED_EDGE('',*,*,#47630,.F.) ;
#65858 = ORIENTED_EDGE('',*,*,#47631,.F.) ;
#65859 = ORIENTED_EDGE('',*,*,#47627,.T.) ;
#65860 = ORIENTED_EDGE('',*,*,#45464,.F.) ;
#65861 = ORIENTED_EDGE('',*,*,#47632,.F.) ;
#65862 = ORIENTED_EDGE('',*,*,#45706,.F.) ;
#65863 = ORIENTED_EDGE('',*,*,#47633,.F.) ;
#65864 = ORIENTED_EDGE('',*,*,#45707,.F.) ;
#65865 = ORIENTED_EDGE('',*,*,#47634,.F.) ;
#65866 = ORIENTED_EDGE('',*,*,#45701,.F.) ;
#65867 = ORIENTED_EDGE('',*,*,#44160,.T.) ;
#65868 = ORIENTED_EDGE('',*,*,#47633,.T.) ;
#65869 = ORIENTED_EDGE('',*,*,#47635,.F.) ;
#65870 = ORIENTED_EDGE('',*,*,#44401,.T.) ;
#65871 = ORIENTED_EDGE('',*,*,#47629,.T.) ;
#65872 = ORIENTED_EDGE('',*,*,#47628,.T.) ;
#65873 = ORIENTED_EDGE('',*,*,#47636,.F.) ;
#65874 = ORIENTED_EDGE('',*,*,#47637,.F.) ;
#65875 = ORIENTED_EDGE('',*,*,#44619,.F.) ;
#65876 = ORIENTED_EDGE('',*,*,#47638,.F.) ;
#65877 = ORIENTED_EDGE('',*,*,#47639,.F.) ;
#65878 = ORIENTED_EDGE('',*,*,#47630,.T.) ;
#65879 = ORIENTED_EDGE('',*,*,#44505,.F.) ;
#65880 = ORIENTED_EDGE('',*,*,#47638,.T.) ;
#65881 = ORIENTED_EDGE('',*,*,#44708,.F.) ;
#65882 = ORIENTED_EDGE('',*,*,#47631,.T.) ;
#65883 = ORIENTED_EDGE('',*,*,#47640,.F.) ;
#65884 = ORIENTED_EDGE('',*,*,#47641,.F.) ;
#65885 = ORIENTED_EDGE('',*,*,#47634,.T.) ;
#65886 = ORIENTED_EDGE('',*,*,#47632,.T.) ;
#65887 = ORIENTED_EDGE('',*,*,#47642,.F.) ;
#65888 = ORIENTED_EDGE('',*,*,#47635,.T.) ;
#65889 = ORIENTED_EDGE('',*,*,#45704,.F.) ;
#65890 = ORIENTED_EDGE('',*,*,#47643,.F.) ;
#65891 = ORIENTED_EDGE('',*,*,#44402,.F.) ;
#65892 = ORIENTED_EDGE('',*,*,#47636,.T.) ;
#65893 = ORIENTED_EDGE('',*,*,#44405,.F.) ;
#65894 = ORIENTED_EDGE('',*,*,#47644,.F.) ;
#65895 = ORIENTED_EDGE('',*,*,#44503,.F.) ;
#65896 = ORIENTED_EDGE('',*,*,#47637,.T.) ;
#65897 = ORIENTED_EDGE('',*,*,#44504,.F.) ;
#65898 = ORIENTED_EDGE('',*,*,#47645,.F.) ;
#65899 = ORIENTED_EDGE('',*,*,#44701,.F.) ;
#65900 = ORIENTED_EDGE('',*,*,#47639,.T.) ;
#65901 = ORIENTED_EDGE('',*,*,#44707,.T.) ;
#65902 = ORIENTED_EDGE('',*,*,#47646,.F.) ;
#65903 = ORIENTED_EDGE('',*,*,#47640,.T.) ;
#65904 = ORIENTED_EDGE('',*,*,#45461,.F.) ;
#65905 = ORIENTED_EDGE('',*,*,#47641,.T.) ;
#65906 = ORIENTED_EDGE('',*,*,#47647,.F.) ;
#65907 = ORIENTED_EDGE('',*,*,#47648,.F.) ;
#65908 = ORIENTED_EDGE('',*,*,#47642,.T.) ;
#65909 = ORIENTED_EDGE('',*,*,#45463,.F.) ;
#65910 = ORIENTED_EDGE('',*,*,#47649,.F.) ;
#65911 = ORIENTED_EDGE('',*,*,#45702,.F.) ;
#65912 = ORIENTED_EDGE('',*,*,#47650,.F.) ;
#65913 = ORIENTED_EDGE('',*,*,#45703,.F.) ;
#65914 = ORIENTED_EDGE('',*,*,#47651,.F.) ;
#65915 = ORIENTED_EDGE('',*,*,#44500,.F.) ;
#65916 = ORIENTED_EDGE('',*,*,#47643,.T.) ;
#65917 = ORIENTED_EDGE('',*,*,#47650,.T.) ;
#65918 = ORIENTED_EDGE('',*,*,#47652,.F.) ;
#65919 = ORIENTED_EDGE('',*,*,#47645,.T.) ;
#65920 = ORIENTED_EDGE('',*,*,#47644,.T.) ;
#65921 = ORIENTED_EDGE('',*,*,#47653,.F.) ;
#65922 = ORIENTED_EDGE('',*,*,#44702,.T.) ;
#65923 = ORIENTED_EDGE('',*,*,#47654,.F.) ;
#65924 = ORIENTED_EDGE('',*,*,#47647,.T.) ;
#65925 = ORIENTED_EDGE('',*,*,#47646,.T.) ;
#65926 = ORIENTED_EDGE('',*,*,#44759,.F.) ;
#65927 = ORIENTED_EDGE('',*,*,#47648,.T.) ;
#65928 = ORIENTED_EDGE('',*,*,#47655,.F.) ;
#65929 = ORIENTED_EDGE('',*,*,#47656,.F.) ;
#65930 = ORIENTED_EDGE('',*,*,#47651,.T.) ;
#65931 = ORIENTED_EDGE('',*,*,#47649,.T.) ;
#65932 = ORIENTED_EDGE('',*,*,#47657,.F.) ;
#65933 = ORIENTED_EDGE('',*,*,#44496,.T.) ;
#65934 = ORIENTED_EDGE('',*,*,#47652,.T.) ;
#65935 = ORIENTED_EDGE('',*,*,#44499,.F.) ;
#65936 = ORIENTED_EDGE('',*,*,#47658,.F.) ;
#65937 = ORIENTED_EDGE('',*,*,#44403,.F.) ;
#65938 = ORIENTED_EDGE('',*,*,#47653,.T.) ;
#65939 = ORIENTED_EDGE('',*,*,#44404,.F.) ;
#65940 = ORIENTED_EDGE('',*,*,#47659,.F.) ;
#65941 = ORIENTED_EDGE('',*,*,#44703,.F.) ;
#65942 = ORIENTED_EDGE('',*,*,#47654,.T.) ;
#65943 = ORIENTED_EDGE('',*,*,#44758,.T.) ;
#65944 = ORIENTED_EDGE('',*,*,#47660,.F.) ;
#65945 = ORIENTED_EDGE('',*,*,#47655,.T.) ;
#65946 = ORIENTED_EDGE('',*,*,#45462,.F.) ;
#65947 = ORIENTED_EDGE('',*,*,#47656,.T.) ;
#65948 = ORIENTED_EDGE('',*,*,#47661,.F.) ;
#65949 = ORIENTED_EDGE('',*,*,#47657,.T.) ;
#65950 = ORIENTED_EDGE('',*,*,#47659,.T.) ;
#65951 = ORIENTED_EDGE('',*,*,#47658,.T.) ;
#65952 = ORIENTED_EDGE('',*,*,#47662,.F.) ;
#65953 = ORIENTED_EDGE('',*,*,#44651,.T.) ;
#65954 = ORIENTED_EDGE('',*,*,#47660,.T.) ;
#65955 = ORIENTED_EDGE('',*,*,#44757,.F.) ;
#65956 = ORIENTED_EDGE('',*,*,#47663,.F.) ;
#65957 = ORIENTED_EDGE('',*,*,#44497,.F.) ;
#65958 = ORIENTED_EDGE('',*,*,#47661,.T.) ;
#65959 = ORIENTED_EDGE('',*,*,#47662,.T.) ;
#65960 = ORIENTED_EDGE('',*,*,#44498,.F.) ;
#65961 = ORIENTED_EDGE('',*,*,#47664,.F.) ;
#65962 = ORIENTED_EDGE('',*,*,#44652,.F.) ;
#65963 = ORIENTED_EDGE('',*,*,#47663,.T.) ;
#65964 = ORIENTED_EDGE('',*,*,#44704,.F.) ;
#65965 = ORIENTED_EDGE('',*,*,#47664,.T.) ;
#65966 = ORIENTED_EDGE('',*,*,#47665,.F.) ;
#65967 = ORIENTED_EDGE('',*,*,#45761,.F.) ;
#65968 = ORIENTED_EDGE('',*,*,#47666,.F.) ;
#65969 = ORIENTED_EDGE('',*,*,#45808,.F.) ;
#65970 = ORIENTED_EDGE('',*,*,#47666,.T.) ;
#65971 = ORIENTED_EDGE('',*,*,#45758,.F.) ;
#65972 = ORIENTED_EDGE('',*,*,#47667,.F.) ;
#65973 = ORIENTED_EDGE('',*,*,#45809,.F.) ;
#65974 = ORIENTED_EDGE('',*,*,#45764,.F.) ;
#65975 = ORIENTED_EDGE('',*,*,#47665,.T.) ;
#65976 = ORIENTED_EDGE('',*,*,#47668,.F.) ;
#65977 = ORIENTED_EDGE('',*,*,#47667,.T.) ;
#65978 = ORIENTED_EDGE('',*,*,#45755,.F.) ;
#65979 = ORIENTED_EDGE('',*,*,#47669,.F.) ;
#65980 = ORIENTED_EDGE('',*,*,#45810,.F.) ;
#65981 = ORIENTED_EDGE('',*,*,#47668,.T.) ;
#65982 = ORIENTED_EDGE('',*,*,#45807,.F.) ;
#65983 = ORIENTED_EDGE('',*,*,#47670,.F.) ;
#65984 = ORIENTED_EDGE('',*,*,#45767,.F.) ;
#65985 = ORIENTED_EDGE('',*,*,#47669,.T.) ;
#65986 = ORIENTED_EDGE('',*,*,#45752,.F.) ;
#65987 = ORIENTED_EDGE('',*,*,#47671,.F.) ;
#65988 = ORIENTED_EDGE('',*,*,#45811,.F.) ;
#65989 = ORIENTED_EDGE('',*,*,#45770,.F.) ;
#65990 = ORIENTED_EDGE('',*,*,#47670,.T.) ;
#65991 = ORIENTED_EDGE('',*,*,#47672,.F.) ;
#65992 = ORIENTED_EDGE('',*,*,#47671,.T.) ;
#65993 = ORIENTED_EDGE('',*,*,#45749,.F.) ;
#65994 = ORIENTED_EDGE('',*,*,#47673,.F.) ;
#65995 = ORIENTED_EDGE('',*,*,#45812,.F.) ;
#65996 = ORIENTED_EDGE('',*,*,#47672,.T.) ;
#65997 = ORIENTED_EDGE('',*,*,#45806,.F.) ;
#65998 = ORIENTED_EDGE('',*,*,#47674,.F.) ;
#65999 = ORIENTED_EDGE('',*,*,#45773,.F.) ;
#66000 = ORIENTED_EDGE('',*,*,#47673,.T.) ;
#66001 = ORIENTED_EDGE('',*,*,#45746,.F.) ;
#66002 = ORIENTED_EDGE('',*,*,#47675,.F.) ;
#66003 = ORIENTED_EDGE('',*,*,#45776,.F.) ;
#66004 = ORIENTED_EDGE('',*,*,#47674,.T.) ;
#66005 = ORIENTED_EDGE('',*,*,#47676,.F.) ;
#66006 = ORIENTED_EDGE('',*,*,#47675,.T.) ;
#66007 = ORIENTED_EDGE('',*,*,#45743,.F.) ;
#66008 = ORIENTED_EDGE('',*,*,#47677,.F.) ;
#66009 = ORIENTED_EDGE('',*,*,#45813,.F.) ;
#66010 = ORIENTED_EDGE('',*,*,#47676,.T.) ;
#66011 = ORIENTED_EDGE('',*,*,#45805,.F.) ;
#66012 = ORIENTED_EDGE('',*,*,#47678,.F.) ;
#66013 = ORIENTED_EDGE('',*,*,#45779,.F.) ;
#66014 = ORIENTED_EDGE('',*,*,#47677,.T.) ;
#66015 = ORIENTED_EDGE('',*,*,#44369,.F.) ;
#66016 = ORIENTED_EDGE('',*,*,#47679,.F.) ;
#66017 = ORIENTED_EDGE('',*,*,#45782,.F.) ;
#66018 = ORIENTED_EDGE('',*,*,#47678,.T.) ;
#66019 = ORIENTED_EDGE('',*,*,#47680,.F.) ;
#66020 = ORIENTED_EDGE('',*,*,#47679,.T.) ;
#66021 = ORIENTED_EDGE('',*,*,#45741,.F.) ;
#66022 = ORIENTED_EDGE('',*,*,#44156,.F.) ;
#66023 = ORIENTED_EDGE('',*,*,#45814,.F.) ;
#66024 = ORIENTED_EDGE('',*,*,#47680,.T.) ;
#66025 = ORIENTED_EDGE('',*,*,#45804,.F.) ;
#66026 = ORIENTED_EDGE('',*,*,#47681,.F.) ;
#66027 = ORIENTED_EDGE('',*,*,#45785,.F.) ;
#66028 = ORIENTED_EDGE('',*,*,#45788,.F.) ;
#66029 = ORIENTED_EDGE('',*,*,#47681,.T.) ;
#66030 = ORIENTED_EDGE('',*,*,#47682,.F.) ;
#66031 = ORIENTED_EDGE('',*,*,#44155,.T.) ;
#66032 = ORIENTED_EDGE('',*,*,#45736,.F.) ;
#66033 = ORIENTED_EDGE('',*,*,#47683,.F.) ;
#66034 = ORIENTED_EDGE('',*,*,#45815,.F.) ;
#66035 = ORIENTED_EDGE('',*,*,#47682,.T.) ;
#66036 = ORIENTED_EDGE('',*,*,#45803,.F.) ;
#66037 = ORIENTED_EDGE('',*,*,#47684,.F.) ;
#66038 = ORIENTED_EDGE('',*,*,#45791,.F.) ;
#66039 = ORIENTED_EDGE('',*,*,#47683,.T.) ;
#66040 = ORIENTED_EDGE('',*,*,#45733,.F.) ;
#66041 = ORIENTED_EDGE('',*,*,#47685,.F.) ;
#66042 = ORIENTED_EDGE('',*,*,#45794,.F.) ;
#66043 = ORIENTED_EDGE('',*,*,#47684,.T.) ;
#66044 = ORIENTED_EDGE('',*,*,#47686,.F.) ;
#66045 = ORIENTED_EDGE('',*,*,#47685,.T.) ;
#66046 = ORIENTED_EDGE('',*,*,#45730,.F.) ;
#66047 = ORIENTED_EDGE('',*,*,#47687,.F.) ;
#66048 = ORIENTED_EDGE('',*,*,#45816,.F.) ;
#66049 = ORIENTED_EDGE('',*,*,#47686,.T.) ;
#66050 = ORIENTED_EDGE('',*,*,#45802,.F.) ;
#66051 = ORIENTED_EDGE('',*,*,#47688,.F.) ;
#66052 = ORIENTED_EDGE('',*,*,#45797,.F.) ;
#66053 = ORIENTED_EDGE('',*,*,#47687,.T.) ;
#66054 = ORIENTED_EDGE('',*,*,#45727,.F.) ;
#66055 = ORIENTED_EDGE('',*,*,#47689,.F.) ;
#66056 = ORIENTED_EDGE('',*,*,#45799,.F.) ;
#66057 = ORIENTED_EDGE('',*,*,#47688,.T.) ;
#66058 = ORIENTED_EDGE('',*,*,#45801,.F.) ;
#66059 = ORIENTED_EDGE('',*,*,#47690,.F.) ;
#66060 = ORIENTED_EDGE('',*,*,#45721,.F.) ;
#66061 = ORIENTED_EDGE('',*,*,#47689,.T.) ;
#66062 = ORIENTED_EDGE('',*,*,#45724,.F.) ;
#66063 = ORIENTED_EDGE('',*,*,#47690,.T.) ;
#66064 = ORIENTED_EDGE('',*,*,#45800,.F.) ;
#66065 = ORIENTED_EDGE('',*,*,#47691,.T.) ;
#66066 = ORIENTED_EDGE('',*,*,#47692,.T.) ;
#66067 = ORIENTED_EDGE('',*,*,#47693,.T.) ;
#66068 = ORIENTED_EDGE('',*,*,#47694,.T.) ;
#66069 = ORIENTED_EDGE('',*,*,#47695,.T.) ;
#66070 = ORIENTED_EDGE('',*,*,#47696,.T.) ;
#66071 = ORIENTED_EDGE('',*,*,#47697,.T.) ;
#66072 = ORIENTED_EDGE('',*,*,#47698,.T.) ;
#66073 = ORIENTED_EDGE('',*,*,#47699,.T.) ;
#66074 = ORIENTED_EDGE('',*,*,#47700,.T.) ;
#66075 = ORIENTED_EDGE('',*,*,#47701,.T.) ;
#66076 = ORIENTED_EDGE('',*,*,#47702,.T.) ;
#66077 = ORIENTED_EDGE('',*,*,#47703,.T.) ;
#66078 = ORIENTED_EDGE('',*,*,#47704,.T.) ;
#66079 = ORIENTED_EDGE('',*,*,#47705,.T.) ;
#66080 = ORIENTED_EDGE('',*,*,#47706,.T.) ;
#66081 = ORIENTED_EDGE('',*,*,#47707,.T.) ;
#66082 = ORIENTED_EDGE('',*,*,#47708,.T.) ;
#66083 = ORIENTED_EDGE('',*,*,#47709,.F.) ;
#66084 = ORIENTED_EDGE('',*,*,#47710,.T.) ;
#66085 = ORIENTED_EDGE('',*,*,#47711,.T.) ;
#66086 = ORIENTED_EDGE('',*,*,#47712,.T.) ;
#66087 = ORIENTED_EDGE('',*,*,#46679,.T.) ;
#66088 = ORIENTED_EDGE('',*,*,#47713,.T.) ;
#66089 = ORIENTED_EDGE('',*,*,#47714,.T.) ;
#66090 = ORIENTED_EDGE('',*,*,#47715,.T.) ;
#66091 = ORIENTED_EDGE('',*,*,#47716,.T.) ;
#66092 = ORIENTED_EDGE('',*,*,#47717,.T.) ;
#66093 = ORIENTED_EDGE('',*,*,#44334,.T.) ;
#66094 = ORIENTED_EDGE('',*,*,#47718,.T.) ;
#66095 = ORIENTED_EDGE('',*,*,#47719,.T.) ;
#66096 = ORIENTED_EDGE('',*,*,#47720,.T.) ;
#66097 = ORIENTED_EDGE('',*,*,#46676,.T.) ;
#66098 = ORIENTED_EDGE('',*,*,#47721,.T.) ;
#66099 = ORIENTED_EDGE('',*,*,#47691,.F.) ;
#66100 = ORIENTED_EDGE('',*,*,#47722,.T.) ;
#66101 = ORIENTED_EDGE('',*,*,#46677,.T.) ;
#66102 = ORIENTED_EDGE('',*,*,#47709,.T.) ;
#66103 = ORIENTED_EDGE('',*,*,#47723,.T.) ;
#66104 = ORIENTED_EDGE('',*,*,#44487,.F.) ;
#66105 = ORIENTED_EDGE('',*,*,#47724,.T.) ;
#66106 = ORIENTED_EDGE('',*,*,#47725,.T.) ;
#66107 = ORIENTED_EDGE('',*,*,#47726,.T.) ;
#66108 = ORIENTED_EDGE('',*,*,#47727,.T.) ;
#66109 = ORIENTED_EDGE('',*,*,#47728,.T.) ;
#66110 = ORIENTED_EDGE('',*,*,#47729,.T.) ;
#66111 = ORIENTED_EDGE('',*,*,#47730,.T.) ;
#66112 = ORIENTED_EDGE('',*,*,#46595,.F.) ;
#66113 = ORIENTED_EDGE('',*,*,#47731,.T.) ;
#66114 = ORIENTED_EDGE('',*,*,#46599,.F.) ;
#66115 = ORIENTED_EDGE('',*,*,#47732,.T.) ;
#66116 = ORIENTED_EDGE('',*,*,#47733,.T.) ;
#66117 = ORIENTED_EDGE('',*,*,#47734,.T.) ;
#66118 = ORIENTED_EDGE('',*,*,#47735,.T.) ;
#66119 = ORIENTED_EDGE('',*,*,#47736,.T.) ;
#66120 = ORIENTED_EDGE('',*,*,#47737,.T.) ;
#66121 = ORIENTED_EDGE('',*,*,#47738,.T.) ;
#66122 = ORIENTED_EDGE('',*,*,#47739,.T.) ;
#66123 = ORIENTED_EDGE('',*,*,#47740,.T.) ;
#66124 = ORIENTED_EDGE('',*,*,#47741,.T.) ;
#66125 = ORIENTED_EDGE('',*,*,#47742,.T.) ;
#66126 = ORIENTED_EDGE('',*,*,#47743,.T.) ;
#66127 = ORIENTED_EDGE('',*,*,#47744,.T.) ;
#66128 = ORIENTED_EDGE('',*,*,#46593,.T.) ;
#66129 = ORIENTED_EDGE('',*,*,#47745,.T.) ;
#66130 = ORIENTED_EDGE('',*,*,#46597,.F.) ;
#66131 = ORIENTED_EDGE('',*,*,#47746,.T.) ;
#66132 = ORIENTED_EDGE('',*,*,#47747,.T.) ;
#66133 = ORIENTED_EDGE('',*,*,#47748,.T.) ;
#66134 = ORIENTED_EDGE('',*,*,#47749,.T.) ;
#66135 = ORIENTED_EDGE('',*,*,#47750,.T.) ;
#66136 = ORIENTED_EDGE('',*,*,#47751,.T.) ;
#66137 = ORIENTED_EDGE('',*,*,#47752,.T.) ;
#66138 = ORIENTED_EDGE('',*,*,#47753,.T.) ;
#66139 = ORIENTED_EDGE('',*,*,#47754,.T.) ;
#66140 = ORIENTED_EDGE('',*,*,#47755,.T.) ;
#66141 = ORIENTED_EDGE('',*,*,#47756,.T.) ;
#66142 = ORIENTED_EDGE('',*,*,#47757,.T.) ;
#66143 = ORIENTED_EDGE('',*,*,#47758,.T.) ;
#66144 = ORIENTED_EDGE('',*,*,#47759,.T.) ;
#66145 = ORIENTED_EDGE('',*,*,#47760,.T.) ;
#66146 = ORIENTED_EDGE('',*,*,#47761,.T.) ;
#66147 = ORIENTED_EDGE('',*,*,#47762,.T.) ;
#66148 = ORIENTED_EDGE('',*,*,#47763,.T.) ;
#66149 = ORIENTED_EDGE('',*,*,#47764,.T.) ;
#66150 = ORIENTED_EDGE('',*,*,#47765,.T.) ;
#66151 = ORIENTED_EDGE('',*,*,#47766,.T.) ;
#66152 = ORIENTED_EDGE('',*,*,#47767,.F.) ;
#66153 = ORIENTED_EDGE('',*,*,#47768,.T.) ;
#66154 = ORIENTED_EDGE('',*,*,#47769,.T.) ;
#66155 = ORIENTED_EDGE('',*,*,#47770,.T.) ;
#66156 = ORIENTED_EDGE('',*,*,#47001,.T.) ;
#66157 = ORIENTED_EDGE('',*,*,#47771,.T.) ;
#66158 = ORIENTED_EDGE('',*,*,#47772,.T.) ;
#66159 = ORIENTED_EDGE('',*,*,#47773,.T.) ;
#66160 = ORIENTED_EDGE('',*,*,#47774,.T.) ;
#66161 = ORIENTED_EDGE('',*,*,#47775,.T.) ;
#66162 = ORIENTED_EDGE('',*,*,#44281,.T.) ;
#66163 = ORIENTED_EDGE('',*,*,#47776,.T.) ;
#66164 = ORIENTED_EDGE('',*,*,#47777,.T.) ;
#66165 = ORIENTED_EDGE('',*,*,#47778,.T.) ;
#66166 = ORIENTED_EDGE('',*,*,#46998,.T.) ;
#66167 = ORIENTED_EDGE('',*,*,#47779,.T.) ;
#66168 = ORIENTED_EDGE('',*,*,#47749,.F.) ;
#66169 = ORIENTED_EDGE('',*,*,#47780,.T.) ;
#66170 = ORIENTED_EDGE('',*,*,#46999,.T.) ;
#66171 = ORIENTED_EDGE('',*,*,#47767,.T.) ;
#66172 = ORIENTED_EDGE('',*,*,#47781,.T.) ;
#66173 = ORIENTED_EDGE('',*,*,#44476,.F.) ;
#66174 = ORIENTED_EDGE('',*,*,#47782,.T.) ;
#66175 = ORIENTED_EDGE('',*,*,#47783,.T.) ;
#66176 = ORIENTED_EDGE('',*,*,#47784,.T.) ;
#66177 = ORIENTED_EDGE('',*,*,#47785,.T.) ;
#66178 = ORIENTED_EDGE('',*,*,#47786,.T.) ;
#66179 = ORIENTED_EDGE('',*,*,#47787,.T.) ;
#66180 = ORIENTED_EDGE('',*,*,#47788,.T.) ;
#66181 = ORIENTED_EDGE('',*,*,#46603,.F.) ;
#66182 = ORIENTED_EDGE('',*,*,#47789,.T.) ;
#66183 = ORIENTED_EDGE('',*,*,#46607,.F.) ;
#66184 = ORIENTED_EDGE('',*,*,#47790,.T.) ;
#66185 = ORIENTED_EDGE('',*,*,#47791,.T.) ;
#66186 = ORIENTED_EDGE('',*,*,#47792,.T.) ;
#66187 = ORIENTED_EDGE('',*,*,#47793,.T.) ;
#66188 = ORIENTED_EDGE('',*,*,#47794,.T.) ;
#66189 = ORIENTED_EDGE('',*,*,#47795,.T.) ;
#66190 = ORIENTED_EDGE('',*,*,#47796,.T.) ;
#66191 = ORIENTED_EDGE('',*,*,#47797,.T.) ;
#66192 = ORIENTED_EDGE('',*,*,#47798,.T.) ;
#66193 = ORIENTED_EDGE('',*,*,#47799,.T.) ;
#66194 = ORIENTED_EDGE('',*,*,#47800,.T.) ;
#66195 = ORIENTED_EDGE('',*,*,#47801,.T.) ;
#66196 = ORIENTED_EDGE('',*,*,#47802,.T.) ;
#66197 = ORIENTED_EDGE('',*,*,#46601,.T.) ;
#66198 = ORIENTED_EDGE('',*,*,#47803,.T.) ;
#66199 = ORIENTED_EDGE('',*,*,#46605,.F.) ;
#66200 = ORIENTED_EDGE('',*,*,#47804,.T.) ;
#66201 = ORIENTED_EDGE('',*,*,#47805,.T.) ;
#66202 = ORIENTED_EDGE('',*,*,#47806,.T.) ;
#66203 = ORIENTED_EDGE('',*,*,#47807,.T.) ;
#66204 = ORIENTED_EDGE('',*,*,#47808,.T.) ;
#66205 = ORIENTED_EDGE('',*,*,#47809,.T.) ;
#66206 = ORIENTED_EDGE('',*,*,#47810,.T.) ;
#66207 = ORIENTED_EDGE('',*,*,#47811,.T.) ;
#66208 = ORIENTED_EDGE('',*,*,#47812,.T.) ;
#66209 = ORIENTED_EDGE('',*,*,#47813,.T.) ;
#66210 = ORIENTED_EDGE('',*,*,#47814,.T.) ;
#66211 = ORIENTED_EDGE('',*,*,#47815,.T.) ;
#66212 = ORIENTED_EDGE('',*,*,#47816,.T.) ;
#66213 = ORIENTED_EDGE('',*,*,#47817,.T.) ;
#66214 = ORIENTED_EDGE('',*,*,#47818,.T.) ;
#66215 = ORIENTED_EDGE('',*,*,#47819,.T.) ;
#66216 = ORIENTED_EDGE('',*,*,#47820,.T.) ;
#66217 = ORIENTED_EDGE('',*,*,#47821,.T.) ;
#66218 = ORIENTED_EDGE('',*,*,#47822,.T.) ;
#66219 = ORIENTED_EDGE('',*,*,#47823,.T.) ;
#66220 = ORIENTED_EDGE('',*,*,#47824,.T.) ;
#66221 = ORIENTED_EDGE('',*,*,#47825,.F.) ;
#66222 = ORIENTED_EDGE('',*,*,#47826,.T.) ;
#66223 = ORIENTED_EDGE('',*,*,#47827,.T.) ;
#66224 = ORIENTED_EDGE('',*,*,#47828,.T.) ;
#66225 = ORIENTED_EDGE('',*,*,#47089,.T.) ;
#66226 = ORIENTED_EDGE('',*,*,#47829,.T.) ;
#66227 = ORIENTED_EDGE('',*,*,#47830,.T.) ;
#66228 = ORIENTED_EDGE('',*,*,#47831,.T.) ;
#66229 = ORIENTED_EDGE('',*,*,#47832,.T.) ;
#66230 = ORIENTED_EDGE('',*,*,#47833,.T.) ;
#66231 = ORIENTED_EDGE('',*,*,#44264,.T.) ;
#66232 = ORIENTED_EDGE('',*,*,#47834,.T.) ;
#66233 = ORIENTED_EDGE('',*,*,#47835,.T.) ;
#66234 = ORIENTED_EDGE('',*,*,#47836,.T.) ;
#66235 = ORIENTED_EDGE('',*,*,#47086,.T.) ;
#66236 = ORIENTED_EDGE('',*,*,#47837,.T.) ;
#66237 = ORIENTED_EDGE('',*,*,#47807,.F.) ;
#66238 = ORIENTED_EDGE('',*,*,#47838,.T.) ;
#66239 = ORIENTED_EDGE('',*,*,#47087,.T.) ;
#66240 = ORIENTED_EDGE('',*,*,#47825,.T.) ;
#66241 = ORIENTED_EDGE('',*,*,#47839,.T.) ;
#66242 = ORIENTED_EDGE('',*,*,#44465,.F.) ;
#66243 = ORIENTED_EDGE('',*,*,#47840,.T.) ;
#66244 = ORIENTED_EDGE('',*,*,#47841,.T.) ;
#66245 = ORIENTED_EDGE('',*,*,#47842,.T.) ;
#66246 = ORIENTED_EDGE('',*,*,#47843,.T.) ;
#66247 = ORIENTED_EDGE('',*,*,#47844,.T.) ;
#66248 = ORIENTED_EDGE('',*,*,#47845,.T.) ;
#66249 = ORIENTED_EDGE('',*,*,#47846,.T.) ;
#66250 = ORIENTED_EDGE('',*,*,#46611,.F.) ;
#66251 = ORIENTED_EDGE('',*,*,#47847,.T.) ;
#66252 = ORIENTED_EDGE('',*,*,#46615,.F.) ;
#66253 = ORIENTED_EDGE('',*,*,#47848,.T.) ;
#66254 = ORIENTED_EDGE('',*,*,#47849,.T.) ;
#66255 = ORIENTED_EDGE('',*,*,#47850,.T.) ;
#66256 = ORIENTED_EDGE('',*,*,#47851,.T.) ;
#66257 = ORIENTED_EDGE('',*,*,#47852,.T.) ;
#66258 = ORIENTED_EDGE('',*,*,#47853,.T.) ;
#66259 = ORIENTED_EDGE('',*,*,#47854,.T.) ;
#66260 = ORIENTED_EDGE('',*,*,#47855,.T.) ;
#66261 = ORIENTED_EDGE('',*,*,#47856,.T.) ;
#66262 = ORIENTED_EDGE('',*,*,#47857,.T.) ;
#66263 = ORIENTED_EDGE('',*,*,#47858,.T.) ;
#66264 = ORIENTED_EDGE('',*,*,#47859,.T.) ;
#66265 = ORIENTED_EDGE('',*,*,#47860,.T.) ;
#66266 = ORIENTED_EDGE('',*,*,#46609,.T.) ;
#66267 = ORIENTED_EDGE('',*,*,#47861,.T.) ;
#66268 = ORIENTED_EDGE('',*,*,#46613,.F.) ;
#66269 = ORIENTED_EDGE('',*,*,#47862,.T.) ;
#66270 = ORIENTED_EDGE('',*,*,#47863,.T.) ;
#66271 = ORIENTED_EDGE('',*,*,#47864,.T.) ;
#66272 = ORIENTED_EDGE('',*,*,#47865,.T.) ;
#66273 = ORIENTED_EDGE('',*,*,#47866,.T.) ;
#66274 = ORIENTED_EDGE('',*,*,#47867,.T.) ;
#66275 = ORIENTED_EDGE('',*,*,#47868,.T.) ;
#66276 = ORIENTED_EDGE('',*,*,#47869,.T.) ;
#66277 = ORIENTED_EDGE('',*,*,#47870,.T.) ;
#66278 = ORIENTED_EDGE('',*,*,#47871,.T.) ;
#66279 = ORIENTED_EDGE('',*,*,#47872,.T.) ;
#66280 = ORIENTED_EDGE('',*,*,#47873,.T.) ;
#66281 = ORIENTED_EDGE('',*,*,#47874,.T.) ;
#66282 = ORIENTED_EDGE('',*,*,#47875,.T.) ;
#66283 = ORIENTED_EDGE('',*,*,#47876,.T.) ;
#66284 = ORIENTED_EDGE('',*,*,#47877,.T.) ;
#66285 = ORIENTED_EDGE('',*,*,#47878,.T.) ;
#66286 = ORIENTED_EDGE('',*,*,#47879,.T.) ;
#66287 = ORIENTED_EDGE('',*,*,#47880,.T.) ;
#66288 = ORIENTED_EDGE('',*,*,#47881,.T.) ;
#66289 = ORIENTED_EDGE('',*,*,#47882,.T.) ;
#66290 = ORIENTED_EDGE('',*,*,#47883,.F.) ;
#66291 = ORIENTED_EDGE('',*,*,#47884,.T.) ;
#66292 = ORIENTED_EDGE('',*,*,#47885,.T.) ;
#66293 = ORIENTED_EDGE('',*,*,#47886,.T.) ;
#66294 = ORIENTED_EDGE('',*,*,#47177,.T.) ;
#66295 = ORIENTED_EDGE('',*,*,#47887,.T.) ;
#66296 = ORIENTED_EDGE('',*,*,#47888,.T.) ;
#66297 = ORIENTED_EDGE('',*,*,#47889,.T.) ;
#66298 = ORIENTED_EDGE('',*,*,#47890,.T.) ;
#66299 = ORIENTED_EDGE('',*,*,#47891,.T.) ;
#66300 = ORIENTED_EDGE('',*,*,#44247,.T.) ;
#66301 = ORIENTED_EDGE('',*,*,#47892,.T.) ;
#66302 = ORIENTED_EDGE('',*,*,#47893,.T.) ;
#66303 = ORIENTED_EDGE('',*,*,#47894,.T.) ;
#66304 = ORIENTED_EDGE('',*,*,#47174,.T.) ;
#66305 = ORIENTED_EDGE('',*,*,#47895,.T.) ;
#66306 = ORIENTED_EDGE('',*,*,#47865,.F.) ;
#66307 = ORIENTED_EDGE('',*,*,#47896,.T.) ;
#66308 = ORIENTED_EDGE('',*,*,#47175,.T.) ;
#66309 = ORIENTED_EDGE('',*,*,#47883,.T.) ;
#66310 = ORIENTED_EDGE('',*,*,#47897,.T.) ;
#66311 = ORIENTED_EDGE('',*,*,#44454,.F.) ;
#66312 = ORIENTED_EDGE('',*,*,#47898,.T.) ;
#66313 = ORIENTED_EDGE('',*,*,#47899,.T.) ;
#66314 = ORIENTED_EDGE('',*,*,#47900,.T.) ;
#66315 = ORIENTED_EDGE('',*,*,#47901,.T.) ;
#66316 = ORIENTED_EDGE('',*,*,#47902,.T.) ;
#66317 = ORIENTED_EDGE('',*,*,#47903,.T.) ;
#66318 = ORIENTED_EDGE('',*,*,#47904,.T.) ;
#66319 = ORIENTED_EDGE('',*,*,#46619,.F.) ;
#66320 = ORIENTED_EDGE('',*,*,#47905,.T.) ;
#66321 = ORIENTED_EDGE('',*,*,#46623,.F.) ;
#66322 = ORIENTED_EDGE('',*,*,#47906,.T.) ;
#66323 = ORIENTED_EDGE('',*,*,#47907,.T.) ;
#66324 = ORIENTED_EDGE('',*,*,#47908,.T.) ;
#66325 = ORIENTED_EDGE('',*,*,#47909,.T.) ;
#66326 = ORIENTED_EDGE('',*,*,#47910,.T.) ;
#66327 = ORIENTED_EDGE('',*,*,#47911,.T.) ;
#66328 = ORIENTED_EDGE('',*,*,#47912,.T.) ;
#66329 = ORIENTED_EDGE('',*,*,#47913,.T.) ;
#66330 = ORIENTED_EDGE('',*,*,#47914,.T.) ;
#66331 = ORIENTED_EDGE('',*,*,#47915,.T.) ;
#66332 = ORIENTED_EDGE('',*,*,#47916,.T.) ;
#66333 = ORIENTED_EDGE('',*,*,#47917,.T.) ;
#66334 = ORIENTED_EDGE('',*,*,#47918,.T.) ;
#66335 = ORIENTED_EDGE('',*,*,#46617,.T.) ;
#66336 = ORIENTED_EDGE('',*,*,#47919,.T.) ;
#66337 = ORIENTED_EDGE('',*,*,#46621,.F.) ;
#66338 = ORIENTED_EDGE('',*,*,#47920,.T.) ;
#66339 = ORIENTED_EDGE('',*,*,#47921,.T.) ;
#66340 = ORIENTED_EDGE('',*,*,#47922,.T.) ;
#66341 = ORIENTED_EDGE('',*,*,#47923,.T.) ;
#66342 = ORIENTED_EDGE('',*,*,#47924,.T.) ;
#66343 = ORIENTED_EDGE('',*,*,#47925,.T.) ;
#66344 = ORIENTED_EDGE('',*,*,#47926,.T.) ;
#66345 = ORIENTED_EDGE('',*,*,#47927,.T.) ;
#66346 = ORIENTED_EDGE('',*,*,#47928,.T.) ;
#66347 = ORIENTED_EDGE('',*,*,#47929,.T.) ;
#66348 = ORIENTED_EDGE('',*,*,#47930,.T.) ;
#66349 = ORIENTED_EDGE('',*,*,#47931,.T.) ;
#66350 = ORIENTED_EDGE('',*,*,#47932,.T.) ;
#66351 = ORIENTED_EDGE('',*,*,#47933,.T.) ;
#66352 = ORIENTED_EDGE('',*,*,#47934,.T.) ;
#66353 = ORIENTED_EDGE('',*,*,#47935,.T.) ;
#66354 = ORIENTED_EDGE('',*,*,#47936,.T.) ;
#66355 = ORIENTED_EDGE('',*,*,#47937,.T.) ;
#66356 = ORIENTED_EDGE('',*,*,#47938,.T.) ;
#66357 = ORIENTED_EDGE('',*,*,#47939,.T.) ;
#66358 = ORIENTED_EDGE('',*,*,#47940,.T.) ;
#66359 = ORIENTED_EDGE('',*,*,#47941,.F.) ;
#66360 = ORIENTED_EDGE('',*,*,#47942,.T.) ;
#66361 = ORIENTED_EDGE('',*,*,#47943,.T.) ;
#66362 = ORIENTED_EDGE('',*,*,#47944,.T.) ;
#66363 = ORIENTED_EDGE('',*,*,#47265,.T.) ;
#66364 = ORIENTED_EDGE('',*,*,#47945,.T.) ;
#66365 = ORIENTED_EDGE('',*,*,#47946,.T.) ;
#66366 = ORIENTED_EDGE('',*,*,#47947,.T.) ;
#66367 = ORIENTED_EDGE('',*,*,#47948,.T.) ;
#66368 = ORIENTED_EDGE('',*,*,#47949,.T.) ;
#66369 = ORIENTED_EDGE('',*,*,#44230,.T.) ;
#66370 = ORIENTED_EDGE('',*,*,#47950,.T.) ;
#66371 = ORIENTED_EDGE('',*,*,#47951,.T.) ;
#66372 = ORIENTED_EDGE('',*,*,#47952,.T.) ;
#66373 = ORIENTED_EDGE('',*,*,#47262,.T.) ;
#66374 = ORIENTED_EDGE('',*,*,#47953,.T.) ;
#66375 = ORIENTED_EDGE('',*,*,#47923,.F.) ;
#66376 = ORIENTED_EDGE('',*,*,#47954,.T.) ;
#66377 = ORIENTED_EDGE('',*,*,#47263,.T.) ;
#66378 = ORIENTED_EDGE('',*,*,#47941,.T.) ;
#66379 = ORIENTED_EDGE('',*,*,#47955,.T.) ;
#66380 = ORIENTED_EDGE('',*,*,#44443,.F.) ;
#66381 = ORIENTED_EDGE('',*,*,#47956,.T.) ;
#66382 = ORIENTED_EDGE('',*,*,#47957,.T.) ;
#66383 = ORIENTED_EDGE('',*,*,#47958,.T.) ;
#66384 = ORIENTED_EDGE('',*,*,#47959,.T.) ;
#66385 = ORIENTED_EDGE('',*,*,#47960,.T.) ;
#66386 = ORIENTED_EDGE('',*,*,#47961,.T.) ;
#66387 = ORIENTED_EDGE('',*,*,#47962,.T.) ;
#66388 = ORIENTED_EDGE('',*,*,#46627,.F.) ;
#66389 = ORIENTED_EDGE('',*,*,#47963,.T.) ;
#66390 = ORIENTED_EDGE('',*,*,#46631,.F.) ;
#66391 = ORIENTED_EDGE('',*,*,#47964,.T.) ;
#66392 = ORIENTED_EDGE('',*,*,#47965,.T.) ;
#66393 = ORIENTED_EDGE('',*,*,#47966,.T.) ;
#66394 = ORIENTED_EDGE('',*,*,#47967,.T.) ;
#66395 = ORIENTED_EDGE('',*,*,#47968,.T.) ;
#66396 = ORIENTED_EDGE('',*,*,#47969,.T.) ;
#66397 = ORIENTED_EDGE('',*,*,#47970,.T.) ;
#66398 = ORIENTED_EDGE('',*,*,#47971,.T.) ;
#66399 = ORIENTED_EDGE('',*,*,#47972,.T.) ;
#66400 = ORIENTED_EDGE('',*,*,#47973,.T.) ;
#66401 = ORIENTED_EDGE('',*,*,#47974,.T.) ;
#66402 = ORIENTED_EDGE('',*,*,#47975,.T.) ;
#66403 = ORIENTED_EDGE('',*,*,#47976,.T.) ;
#66404 = ORIENTED_EDGE('',*,*,#46625,.T.) ;
#66405 = ORIENTED_EDGE('',*,*,#47977,.T.) ;
#66406 = ORIENTED_EDGE('',*,*,#46629,.F.) ;
#66407 = ORIENTED_EDGE('',*,*,#47978,.T.) ;
#66408 = ORIENTED_EDGE('',*,*,#47979,.T.) ;
#66409 = ORIENTED_EDGE('',*,*,#47980,.T.) ;
#66410 = ORIENTED_EDGE('',*,*,#47981,.T.) ;
#66411 = ORIENTED_EDGE('',*,*,#47982,.T.) ;
#66412 = ORIENTED_EDGE('',*,*,#47983,.T.) ;
#66413 = ORIENTED_EDGE('',*,*,#47984,.T.) ;
#66414 = ORIENTED_EDGE('',*,*,#47985,.T.) ;
#66415 = ORIENTED_EDGE('',*,*,#47986,.T.) ;
#66416 = ORIENTED_EDGE('',*,*,#47987,.T.) ;
#66417 = ORIENTED_EDGE('',*,*,#47988,.T.) ;
#66418 = ORIENTED_EDGE('',*,*,#47989,.T.) ;
#66419 = ORIENTED_EDGE('',*,*,#47990,.T.) ;
#66420 = ORIENTED_EDGE('',*,*,#47991,.T.) ;
#66421 = ORIENTED_EDGE('',*,*,#47992,.T.) ;
#66422 = ORIENTED_EDGE('',*,*,#47993,.T.) ;
#66423 = ORIENTED_EDGE('',*,*,#47994,.T.) ;
#66424 = ORIENTED_EDGE('',*,*,#47995,.T.) ;
#66425 = ORIENTED_EDGE('',*,*,#47996,.T.) ;
#66426 = ORIENTED_EDGE('',*,*,#47997,.T.) ;
#66427 = ORIENTED_EDGE('',*,*,#47998,.T.) ;
#66428 = ORIENTED_EDGE('',*,*,#47999,.F.) ;
#66429 = ORIENTED_EDGE('',*,*,#48000,.T.) ;
#66430 = ORIENTED_EDGE('',*,*,#48001,.T.) ;
#66431 = ORIENTED_EDGE('',*,*,#48002,.T.) ;
#66432 = ORIENTED_EDGE('',*,*,#47353,.T.) ;
#66433 = ORIENTED_EDGE('',*,*,#48003,.T.) ;
#66434 = ORIENTED_EDGE('',*,*,#48004,.T.) ;
#66435 = ORIENTED_EDGE('',*,*,#48005,.T.) ;
#66436 = ORIENTED_EDGE('',*,*,#48006,.T.) ;
#66437 = ORIENTED_EDGE('',*,*,#48007,.T.) ;
#66438 = ORIENTED_EDGE('',*,*,#44213,.T.) ;
#66439 = ORIENTED_EDGE('',*,*,#48008,.T.) ;
#66440 = ORIENTED_EDGE('',*,*,#48009,.T.) ;
#66441 = ORIENTED_EDGE('',*,*,#48010,.T.) ;
#66442 = ORIENTED_EDGE('',*,*,#47350,.T.) ;
#66443 = ORIENTED_EDGE('',*,*,#48011,.T.) ;
#66444 = ORIENTED_EDGE('',*,*,#47981,.F.) ;
#66445 = ORIENTED_EDGE('',*,*,#48012,.T.) ;
#66446 = ORIENTED_EDGE('',*,*,#47351,.T.) ;
#66447 = ORIENTED_EDGE('',*,*,#47999,.T.) ;
#66448 = ORIENTED_EDGE('',*,*,#48013,.T.) ;
#66449 = ORIENTED_EDGE('',*,*,#44432,.F.) ;
#66450 = ORIENTED_EDGE('',*,*,#48014,.T.) ;
#66451 = ORIENTED_EDGE('',*,*,#48015,.T.) ;
#66452 = ORIENTED_EDGE('',*,*,#48016,.T.) ;
#66453 = ORIENTED_EDGE('',*,*,#48017,.T.) ;
#66454 = ORIENTED_EDGE('',*,*,#48018,.T.) ;
#66455 = ORIENTED_EDGE('',*,*,#48019,.T.) ;
#66456 = ORIENTED_EDGE('',*,*,#48020,.T.) ;
#66457 = ORIENTED_EDGE('',*,*,#46635,.F.) ;
#66458 = ORIENTED_EDGE('',*,*,#48021,.T.) ;
#66459 = ORIENTED_EDGE('',*,*,#46639,.F.) ;
#66460 = ORIENTED_EDGE('',*,*,#48022,.T.) ;
#66461 = ORIENTED_EDGE('',*,*,#48023,.T.) ;
#66462 = ORIENTED_EDGE('',*,*,#48024,.T.) ;
#66463 = ORIENTED_EDGE('',*,*,#48025,.T.) ;
#66464 = ORIENTED_EDGE('',*,*,#48026,.T.) ;
#66465 = ORIENTED_EDGE('',*,*,#48027,.T.) ;
#66466 = ORIENTED_EDGE('',*,*,#48028,.T.) ;
#66467 = ORIENTED_EDGE('',*,*,#48029,.T.) ;
#66468 = ORIENTED_EDGE('',*,*,#48030,.T.) ;
#66469 = ORIENTED_EDGE('',*,*,#48031,.T.) ;
#66470 = ORIENTED_EDGE('',*,*,#48032,.T.) ;
#66471 = ORIENTED_EDGE('',*,*,#48033,.T.) ;
#66472 = ORIENTED_EDGE('',*,*,#48034,.T.) ;
#66473 = ORIENTED_EDGE('',*,*,#46633,.T.) ;
#66474 = ORIENTED_EDGE('',*,*,#48035,.T.) ;
#66475 = ORIENTED_EDGE('',*,*,#46637,.F.) ;
#66476 = ORIENTED_EDGE('',*,*,#48036,.T.) ;
#66477 = ORIENTED_EDGE('',*,*,#48037,.T.) ;
#66478 = ORIENTED_EDGE('',*,*,#48038,.T.) ;
#66479 = ORIENTED_EDGE('',*,*,#48039,.T.) ;
#66480 = ORIENTED_EDGE('',*,*,#48040,.T.) ;
#66481 = ORIENTED_EDGE('',*,*,#48041,.T.) ;
#66482 = ORIENTED_EDGE('',*,*,#48042,.T.) ;
#66483 = ORIENTED_EDGE('',*,*,#48043,.T.) ;
#66484 = ORIENTED_EDGE('',*,*,#48044,.T.) ;
#66485 = ORIENTED_EDGE('',*,*,#48045,.T.) ;
#66486 = ORIENTED_EDGE('',*,*,#48046,.T.) ;
#66487 = ORIENTED_EDGE('',*,*,#48047,.T.) ;
#66488 = ORIENTED_EDGE('',*,*,#48048,.T.) ;
#66489 = ORIENTED_EDGE('',*,*,#48049,.T.) ;
#66490 = ORIENTED_EDGE('',*,*,#48050,.T.) ;
#66491 = ORIENTED_EDGE('',*,*,#48051,.T.) ;
#66492 = ORIENTED_EDGE('',*,*,#48052,.T.) ;
#66493 = ORIENTED_EDGE('',*,*,#48053,.T.) ;
#66494 = ORIENTED_EDGE('',*,*,#48054,.T.) ;
#66495 = ORIENTED_EDGE('',*,*,#48055,.T.) ;
#66496 = ORIENTED_EDGE('',*,*,#48056,.T.) ;
#66497 = ORIENTED_EDGE('',*,*,#48057,.F.) ;
#66498 = ORIENTED_EDGE('',*,*,#48058,.T.) ;
#66499 = ORIENTED_EDGE('',*,*,#48059,.T.) ;
#66500 = ORIENTED_EDGE('',*,*,#48060,.T.) ;
#66501 = ORIENTED_EDGE('',*,*,#47441,.T.) ;
#66502 = ORIENTED_EDGE('',*,*,#48061,.T.) ;
#66503 = ORIENTED_EDGE('',*,*,#48062,.T.) ;
#66504 = ORIENTED_EDGE('',*,*,#48063,.T.) ;
#66505 = ORIENTED_EDGE('',*,*,#48064,.T.) ;
#66506 = ORIENTED_EDGE('',*,*,#48065,.T.) ;
#66507 = ORIENTED_EDGE('',*,*,#44196,.T.) ;
#66508 = ORIENTED_EDGE('',*,*,#48066,.T.) ;
#66509 = ORIENTED_EDGE('',*,*,#48067,.T.) ;
#66510 = ORIENTED_EDGE('',*,*,#48068,.T.) ;
#66511 = ORIENTED_EDGE('',*,*,#47438,.T.) ;
#66512 = ORIENTED_EDGE('',*,*,#48069,.T.) ;
#66513 = ORIENTED_EDGE('',*,*,#48039,.F.) ;
#66514 = ORIENTED_EDGE('',*,*,#48070,.T.) ;
#66515 = ORIENTED_EDGE('',*,*,#47439,.T.) ;
#66516 = ORIENTED_EDGE('',*,*,#48057,.T.) ;
#66517 = ORIENTED_EDGE('',*,*,#48071,.T.) ;
#66518 = ORIENTED_EDGE('',*,*,#44421,.F.) ;
#66519 = ORIENTED_EDGE('',*,*,#48072,.T.) ;
#66520 = ORIENTED_EDGE('',*,*,#48073,.T.) ;
#66521 = ORIENTED_EDGE('',*,*,#48074,.T.) ;
#66522 = ORIENTED_EDGE('',*,*,#48075,.T.) ;
#66523 = ORIENTED_EDGE('',*,*,#48076,.T.) ;
#66524 = ORIENTED_EDGE('',*,*,#48077,.T.) ;
#66525 = ORIENTED_EDGE('',*,*,#48078,.T.) ;
#66526 = ORIENTED_EDGE('',*,*,#46643,.F.) ;
#66527 = ORIENTED_EDGE('',*,*,#48079,.T.) ;
#66528 = ORIENTED_EDGE('',*,*,#46647,.F.) ;
#66529 = ORIENTED_EDGE('',*,*,#48080,.T.) ;
#66530 = ORIENTED_EDGE('',*,*,#48081,.T.) ;
#66531 = ORIENTED_EDGE('',*,*,#48082,.T.) ;
#66532 = ORIENTED_EDGE('',*,*,#48083,.T.) ;
#66533 = ORIENTED_EDGE('',*,*,#48084,.T.) ;
#66534 = ORIENTED_EDGE('',*,*,#48085,.T.) ;
#66535 = ORIENTED_EDGE('',*,*,#48086,.T.) ;
#66536 = ORIENTED_EDGE('',*,*,#48087,.T.) ;
#66537 = ORIENTED_EDGE('',*,*,#48088,.T.) ;
#66538 = ORIENTED_EDGE('',*,*,#48089,.T.) ;
#66539 = ORIENTED_EDGE('',*,*,#48090,.T.) ;
#66540 = ORIENTED_EDGE('',*,*,#48091,.T.) ;
#66541 = ORIENTED_EDGE('',*,*,#48092,.T.) ;
#66542 = ORIENTED_EDGE('',*,*,#46641,.T.) ;
#66543 = ORIENTED_EDGE('',*,*,#48093,.T.) ;
#66544 = ORIENTED_EDGE('',*,*,#46645,.F.) ;
#66545 = ORIENTED_EDGE('',*,*,#48094,.T.) ;
#66546 = ORIENTED_EDGE('',*,*,#48095,.T.) ;
#66547 = ORIENTED_EDGE('',*,*,#48096,.T.) ;
#66548 = ORIENTED_EDGE('',*,*,#48097,.T.) ;
#66549 = ORIENTED_EDGE('',*,*,#48098,.T.) ;
#66550 = ORIENTED_EDGE('',*,*,#48099,.T.) ;
#66551 = ORIENTED_EDGE('',*,*,#48100,.T.) ;
#66552 = ORIENTED_EDGE('',*,*,#48101,.T.) ;
#66553 = ORIENTED_EDGE('',*,*,#48102,.T.) ;
#66554 = ORIENTED_EDGE('',*,*,#48103,.T.) ;
#66555 = ORIENTED_EDGE('',*,*,#48104,.T.) ;
#66556 = ORIENTED_EDGE('',*,*,#48105,.T.) ;
#66557 = ORIENTED_EDGE('',*,*,#48106,.T.) ;
#66558 = ORIENTED_EDGE('',*,*,#48107,.T.) ;
#66559 = ORIENTED_EDGE('',*,*,#48108,.T.) ;
#66560 = ORIENTED_EDGE('',*,*,#48109,.T.) ;
#66561 = ORIENTED_EDGE('',*,*,#48110,.T.) ;
#66562 = ORIENTED_EDGE('',*,*,#48111,.T.) ;
#66563 = ORIENTED_EDGE('',*,*,#48112,.T.) ;
#66564 = ORIENTED_EDGE('',*,*,#48113,.T.) ;
#66565 = ORIENTED_EDGE('',*,*,#48114,.T.) ;
#66566 = ORIENTED_EDGE('',*,*,#48115,.F.) ;
#66567 = ORIENTED_EDGE('',*,*,#48116,.T.) ;
#66568 = ORIENTED_EDGE('',*,*,#48117,.T.) ;
#66569 = ORIENTED_EDGE('',*,*,#48118,.T.) ;
#66570 = ORIENTED_EDGE('',*,*,#47529,.T.) ;
#66571 = ORIENTED_EDGE('',*,*,#48119,.T.) ;
#66572 = ORIENTED_EDGE('',*,*,#48120,.T.) ;
#66573 = ORIENTED_EDGE('',*,*,#48121,.T.) ;
#66574 = ORIENTED_EDGE('',*,*,#48122,.T.) ;
#66575 = ORIENTED_EDGE('',*,*,#48123,.T.) ;
#66576 = ORIENTED_EDGE('',*,*,#44179,.T.) ;
#66577 = ORIENTED_EDGE('',*,*,#48124,.T.) ;
#66578 = ORIENTED_EDGE('',*,*,#48125,.T.) ;
#66579 = ORIENTED_EDGE('',*,*,#48126,.T.) ;
#66580 = ORIENTED_EDGE('',*,*,#47526,.T.) ;
#66581 = ORIENTED_EDGE('',*,*,#48127,.T.) ;
#66582 = ORIENTED_EDGE('',*,*,#48097,.F.) ;
#66583 = ORIENTED_EDGE('',*,*,#48128,.T.) ;
#66584 = ORIENTED_EDGE('',*,*,#47527,.T.) ;
#66585 = ORIENTED_EDGE('',*,*,#48115,.T.) ;
#66586 = ORIENTED_EDGE('',*,*,#48129,.T.) ;
#66587 = ORIENTED_EDGE('',*,*,#44410,.F.) ;
#66588 = ORIENTED_EDGE('',*,*,#48130,.T.) ;
#66589 = ORIENTED_EDGE('',*,*,#48131,.T.) ;
#66590 = ORIENTED_EDGE('',*,*,#48132,.T.) ;
#66591 = ORIENTED_EDGE('',*,*,#48133,.T.) ;
#66592 = ORIENTED_EDGE('',*,*,#48134,.T.) ;
#66593 = ORIENTED_EDGE('',*,*,#48135,.T.) ;
#66594 = ORIENTED_EDGE('',*,*,#48136,.T.) ;
#66595 = ORIENTED_EDGE('',*,*,#46651,.F.) ;
#66596 = ORIENTED_EDGE('',*,*,#48137,.T.) ;
#66597 = ORIENTED_EDGE('',*,*,#46655,.F.) ;
#66598 = ORIENTED_EDGE('',*,*,#48138,.T.) ;
#66599 = ORIENTED_EDGE('',*,*,#48139,.T.) ;
#66600 = ORIENTED_EDGE('',*,*,#48140,.T.) ;
#66601 = ORIENTED_EDGE('',*,*,#48141,.T.) ;
#66602 = ORIENTED_EDGE('',*,*,#48142,.T.) ;
#66603 = ORIENTED_EDGE('',*,*,#48143,.T.) ;
#66604 = ORIENTED_EDGE('',*,*,#48144,.T.) ;
#66605 = ORIENTED_EDGE('',*,*,#48145,.T.) ;
#66606 = ORIENTED_EDGE('',*,*,#48146,.T.) ;
#66607 = ORIENTED_EDGE('',*,*,#48147,.T.) ;
#66608 = ORIENTED_EDGE('',*,*,#48148,.T.) ;
#66609 = ORIENTED_EDGE('',*,*,#48149,.T.) ;
#66610 = ORIENTED_EDGE('',*,*,#48150,.T.) ;
#66611 = ORIENTED_EDGE('',*,*,#46649,.T.) ;
#66612 = ORIENTED_EDGE('',*,*,#48151,.T.) ;
#66613 = ORIENTED_EDGE('',*,*,#46653,.F.) ;
#66614 = ORIENTED_EDGE('',*,*,#48152,.T.) ;
#66615 = ORIENTED_EDGE('',*,*,#48153,.T.) ;
#66616 = ORIENTED_EDGE('',*,*,#48154,.T.) ;
#66617 = ORIENTED_EDGE('',*,*,#48155,.T.) ;
#66618 = ORIENTED_EDGE('',*,*,#48156,.T.) ;
#66619 = ORIENTED_EDGE('',*,*,#48157,.T.) ;
#66620 = ORIENTED_EDGE('',*,*,#48158,.T.) ;
#66621 = ORIENTED_EDGE('',*,*,#48159,.T.) ;
#66622 = ORIENTED_EDGE('',*,*,#48160,.T.) ;
#66623 = ORIENTED_EDGE('',*,*,#48161,.T.) ;
#66624 = ORIENTED_EDGE('',*,*,#48162,.T.) ;
#66625 = ORIENTED_EDGE('',*,*,#48163,.T.) ;
#66626 = ORIENTED_EDGE('',*,*,#48164,.T.) ;
#66627 = ORIENTED_EDGE('',*,*,#48165,.T.) ;
#66628 = ORIENTED_EDGE('',*,*,#48166,.T.) ;
#66629 = ORIENTED_EDGE('',*,*,#48167,.T.) ;
#66630 = ORIENTED_EDGE('',*,*,#48168,.T.) ;
#66631 = ORIENTED_EDGE('',*,*,#48169,.T.) ;
#66632 = ORIENTED_EDGE('',*,*,#48170,.T.) ;
#66633 = ORIENTED_EDGE('',*,*,#48171,.T.) ;
#66634 = ORIENTED_EDGE('',*,*,#48172,.T.) ;
#66635 = ORIENTED_EDGE('',*,*,#48173,.F.) ;
#66636 = ORIENTED_EDGE('',*,*,#48174,.T.) ;
#66637 = ORIENTED_EDGE('',*,*,#48175,.T.) ;
#66638 = ORIENTED_EDGE('',*,*,#48176,.T.) ;
#66639 = ORIENTED_EDGE('',*,*,#47617,.T.) ;
#66640 = ORIENTED_EDGE('',*,*,#48177,.T.) ;
#66641 = ORIENTED_EDGE('',*,*,#48178,.T.) ;
#66642 = ORIENTED_EDGE('',*,*,#48179,.T.) ;
#66643 = ORIENTED_EDGE('',*,*,#48180,.T.) ;
#66644 = ORIENTED_EDGE('',*,*,#48181,.T.) ;
#66645 = ORIENTED_EDGE('',*,*,#44162,.T.) ;
#66646 = ORIENTED_EDGE('',*,*,#48182,.T.) ;
#66647 = ORIENTED_EDGE('',*,*,#48183,.T.) ;
#66648 = ORIENTED_EDGE('',*,*,#48184,.T.) ;
#66649 = ORIENTED_EDGE('',*,*,#47614,.T.) ;
#66650 = ORIENTED_EDGE('',*,*,#48185,.T.) ;
#66651 = ORIENTED_EDGE('',*,*,#48155,.F.) ;
#66652 = ORIENTED_EDGE('',*,*,#48186,.T.) ;
#66653 = ORIENTED_EDGE('',*,*,#47615,.T.) ;
#66654 = ORIENTED_EDGE('',*,*,#48173,.T.) ;
#66655 = ORIENTED_EDGE('',*,*,#48187,.T.) ;
#66656 = ORIENTED_EDGE('',*,*,#44399,.F.) ;
#66657 = ORIENTED_EDGE('',*,*,#48188,.T.) ;
#66658 = ORIENTED_EDGE('',*,*,#48189,.T.) ;
#66659 = ORIENTED_EDGE('',*,*,#48190,.T.) ;
#66660 = ORIENTED_EDGE('',*,*,#48191,.T.) ;
#66661 = ORIENTED_EDGE('',*,*,#48192,.T.) ;
#66662 = ORIENTED_EDGE('',*,*,#48193,.T.) ;
#66663 = ORIENTED_EDGE('',*,*,#48194,.T.) ;
#66664 = ORIENTED_EDGE('',*,*,#46659,.F.) ;
#66665 = ORIENTED_EDGE('',*,*,#48195,.T.) ;
#66666 = ORIENTED_EDGE('',*,*,#46663,.F.) ;
#66667 = ORIENTED_EDGE('',*,*,#48196,.T.) ;
#66668 = ORIENTED_EDGE('',*,*,#48197,.T.) ;
#66669 = ORIENTED_EDGE('',*,*,#48198,.T.) ;
#66670 = ORIENTED_EDGE('',*,*,#48199,.T.) ;
#66671 = ORIENTED_EDGE('',*,*,#48200,.T.) ;
#66672 = ORIENTED_EDGE('',*,*,#48201,.T.) ;
#66673 = ORIENTED_EDGE('',*,*,#48202,.T.) ;
#66674 = ORIENTED_EDGE('',*,*,#48203,.T.) ;
#66675 = ORIENTED_EDGE('',*,*,#48204,.T.) ;
#66676 = ORIENTED_EDGE('',*,*,#48205,.T.) ;
#66677 = ORIENTED_EDGE('',*,*,#48206,.T.) ;
#66678 = ORIENTED_EDGE('',*,*,#48207,.T.) ;
#66679 = ORIENTED_EDGE('',*,*,#48208,.T.) ;
#66680 = ORIENTED_EDGE('',*,*,#46657,.T.) ;
#66681 = ORIENTED_EDGE('',*,*,#48209,.T.) ;
#66682 = ORIENTED_EDGE('',*,*,#46661,.F.) ;
#66683 = ORIENTED_EDGE('',*,*,#48210,.T.) ;
#66684 = ORIENTED_EDGE('',*,*,#48211,.T.) ;
#66685 = ORIENTED_EDGE('',*,*,#48212,.T.) ;
#66686 = ORIENTED_EDGE('',*,*,#48213,.T.) ;
#66687 = ORIENTED_EDGE('',*,*,#48214,.T.) ;
#66688 = ORIENTED_EDGE('',*,*,#48215,.T.) ;
#66689 = ORIENTED_EDGE('',*,*,#48216,.T.) ;
#66690 = ORIENTED_EDGE('',*,*,#48217,.T.) ;
#66691 = ORIENTED_EDGE('',*,*,#48218,.T.) ;
#66692 = ORIENTED_EDGE('',*,*,#48219,.T.) ;
#66693 = ORIENTED_EDGE('',*,*,#48220,.T.) ;
#66694 = ORIENTED_EDGE('',*,*,#48221,.T.) ;
#66695 = ORIENTED_EDGE('',*,*,#48222,.T.) ;
#66696 = ORIENTED_EDGE('',*,*,#48223,.T.) ;
#66697 = ORIENTED_EDGE('',*,*,#48224,.T.) ;
#66698 = ORIENTED_EDGE('',*,*,#48225,.T.) ;
#66699 = ORIENTED_EDGE('',*,*,#48226,.T.) ;
#66700 = ORIENTED_EDGE('',*,*,#48227,.T.) ;
#66701 = ORIENTED_EDGE('',*,*,#48228,.T.) ;
#66702 = ORIENTED_EDGE('',*,*,#48229,.T.) ;
#66703 = ORIENTED_EDGE('',*,*,#48230,.T.) ;
#66704 = ORIENTED_EDGE('',*,*,#48231,.T.) ;
#66705 = ORIENTED_EDGE('',*,*,#48232,.T.) ;
#66706 = ORIENTED_EDGE('',*,*,#48233,.T.) ;
#66707 = ORIENTED_EDGE('',*,*,#48234,.T.) ;
#66708 = ORIENTED_EDGE('',*,*,#48235,.T.) ;
#66709 = ORIENTED_EDGE('',*,*,#48236,.T.) ;
#66710 = ORIENTED_EDGE('',*,*,#48237,.T.) ;
#66711 = ORIENTED_EDGE('',*,*,#48238,.T.) ;
#66712 = ORIENTED_EDGE('',*,*,#48239,.T.) ;
#66713 = ORIENTED_EDGE('',*,*,#48240,.T.) ;
#66714 = ORIENTED_EDGE('',*,*,#48241,.T.) ;
#66715 = ORIENTED_EDGE('',*,*,#48242,.T.) ;
#66716 = ORIENTED_EDGE('',*,*,#48243,.T.) ;
#66717 = ORIENTED_EDGE('',*,*,#48244,.T.) ;
#66718 = ORIENTED_EDGE('',*,*,#48245,.T.) ;
#66719 = ORIENTED_EDGE('',*,*,#48246,.T.) ;
#66720 = ORIENTED_EDGE('',*,*,#48247,.T.) ;
#66721 = ORIENTED_EDGE('',*,*,#48248,.T.) ;
#66722 = ORIENTED_EDGE('',*,*,#48249,.T.) ;
#66723 = ORIENTED_EDGE('',*,*,#48250,.T.) ;
#66724 = ORIENTED_EDGE('',*,*,#48251,.T.) ;
#66725 = ORIENTED_EDGE('',*,*,#48252,.T.) ;
#66726 = ORIENTED_EDGE('',*,*,#48253,.T.) ;
#66727 = ORIENTED_EDGE('',*,*,#48254,.T.) ;
#66728 = ORIENTED_EDGE('',*,*,#48255,.T.) ;
#66729 = ORIENTED_EDGE('',*,*,#48256,.T.) ;
#66730 = ORIENTED_EDGE('',*,*,#48257,.T.) ;
#66731 = ORIENTED_EDGE('',*,*,#48258,.T.) ;
#66732 = ORIENTED_EDGE('',*,*,#48259,.T.) ;
#66733 = ORIENTED_EDGE('',*,*,#48260,.T.) ;
#66734 = ORIENTED_EDGE('',*,*,#48261,.T.) ;
#66735 = ORIENTED_EDGE('',*,*,#48262,.T.) ;
#66736 = ORIENTED_EDGE('',*,*,#48263,.T.) ;
#66737 = ORIENTED_EDGE('',*,*,#48264,.T.) ;
#66738 = ORIENTED_EDGE('',*,*,#48265,.T.) ;
#66739 = ORIENTED_EDGE('',*,*,#48266,.T.) ;
#66740 = ORIENTED_EDGE('',*,*,#48267,.T.) ;
#66741 = ORIENTED_EDGE('',*,*,#48268,.T.) ;
#66742 = ORIENTED_EDGE('',*,*,#48269,.T.) ;
#66743 = ORIENTED_EDGE('',*,*,#48270,.T.) ;
#66744 = ORIENTED_EDGE('',*,*,#48271,.T.) ;
#66745 = ORIENTED_EDGE('',*,*,#48272,.T.) ;
#66746 = ORIENTED_EDGE('',*,*,#48273,.T.) ;
#66747 = ORIENTED_EDGE('',*,*,#48274,.T.) ;
#66748 = ORIENTED_EDGE('',*,*,#48275,.T.) ;
#66749 = ORIENTED_EDGE('',*,*,#48276,.T.) ;
#66750 = ORIENTED_EDGE('',*,*,#48277,.T.) ;
#66751 = ORIENTED_EDGE('',*,*,#48278,.T.) ;
#66752 = ORIENTED_EDGE('',*,*,#48279,.T.) ;
#66753 = ORIENTED_EDGE('',*,*,#48280,.T.) ;
#66754 = ORIENTED_EDGE('',*,*,#48281,.T.) ;
#66755 = ORIENTED_EDGE('',*,*,#48282,.T.) ;
#66756 = ORIENTED_EDGE('',*,*,#48283,.T.) ;
#66757 = ORIENTED_EDGE('',*,*,#48284,.T.) ;
#66758 = ORIENTED_EDGE('',*,*,#48285,.T.) ;
#66759 = ORIENTED_EDGE('',*,*,#48286,.T.) ;
#66760 = ORIENTED_EDGE('',*,*,#48287,.T.) ;
#66761 = ORIENTED_EDGE('',*,*,#48288,.T.) ;
#66762 = ORIENTED_EDGE('',*,*,#48289,.T.) ;
#66763 = ORIENTED_EDGE('',*,*,#48290,.T.) ;
#66764 = ORIENTED_EDGE('',*,*,#48291,.T.) ;
#66765 = ORIENTED_EDGE('',*,*,#48292,.T.) ;
#66766 = ORIENTED_EDGE('',*,*,#48293,.T.) ;
#66767 = ORIENTED_EDGE('',*,*,#48294,.T.) ;
#66768 = ORIENTED_EDGE('',*,*,#48295,.T.) ;
#66769 = ORIENTED_EDGE('',*,*,#48296,.T.) ;
#66770 = ORIENTED_EDGE('',*,*,#48297,.T.) ;
#66771 = ORIENTED_EDGE('',*,*,#48298,.T.) ;
#66772 = ORIENTED_EDGE('',*,*,#48299,.T.) ;
#66773 = ORIENTED_EDGE('',*,*,#48300,.T.) ;
#66774 = ORIENTED_EDGE('',*,*,#48301,.T.) ;
#66775 = ORIENTED_EDGE('',*,*,#48302,.T.) ;
#66776 = ORIENTED_EDGE('',*,*,#48303,.T.) ;
#66777 = ORIENTED_EDGE('',*,*,#48304,.T.) ;
#66778 = ORIENTED_EDGE('',*,*,#48305,.T.) ;
#66779 = ORIENTED_EDGE('',*,*,#48306,.T.) ;
#66780 = ORIENTED_EDGE('',*,*,#48307,.T.) ;
#66781 = ORIENTED_EDGE('',*,*,#48308,.T.) ;
#66782 = ORIENTED_EDGE('',*,*,#48309,.T.) ;
#66783 = ORIENTED_EDGE('',*,*,#48310,.T.) ;
#66784 = ORIENTED_EDGE('',*,*,#48311,.T.) ;
#66785 = ORIENTED_EDGE('',*,*,#48312,.T.) ;
#66786 = ORIENTED_EDGE('',*,*,#48313,.T.) ;
#66787 = ORIENTED_EDGE('',*,*,#48314,.T.) ;
#66788 = ORIENTED_EDGE('',*,*,#48315,.T.) ;
#66789 = ORIENTED_EDGE('',*,*,#48316,.T.) ;
#66790 = ORIENTED_EDGE('',*,*,#48317,.T.) ;
#66791 = ORIENTED_EDGE('',*,*,#48318,.T.) ;
#66792 = ORIENTED_EDGE('',*,*,#48319,.T.) ;
#66793 = ORIENTED_EDGE('',*,*,#48320,.T.) ;
#66794 = ORIENTED_EDGE('',*,*,#48321,.T.) ;
#66795 = ORIENTED_EDGE('',*,*,#48322,.T.) ;
#66796 = ORIENTED_EDGE('',*,*,#48323,.T.) ;
#66797 = ORIENTED_EDGE('',*,*,#48324,.T.) ;
#66798 = ORIENTED_EDGE('',*,*,#48325,.T.) ;
#66799 = ORIENTED_EDGE('',*,*,#48326,.T.) ;
#66800 = ORIENTED_EDGE('',*,*,#48327,.T.) ;
#66801 = ORIENTED_EDGE('',*,*,#48328,.T.) ;
#66802 = ORIENTED_EDGE('',*,*,#48329,.T.) ;
#66803 = ORIENTED_EDGE('',*,*,#48330,.T.) ;
#66804 = ORIENTED_EDGE('',*,*,#48331,.T.) ;
#66805 = ORIENTED_EDGE('',*,*,#48332,.T.) ;
#66806 = ORIENTED_EDGE('',*,*,#48333,.T.) ;
#66807 = ORIENTED_EDGE('',*,*,#48334,.T.) ;
#66808 = ORIENTED_EDGE('',*,*,#48335,.T.) ;
#66809 = ORIENTED_EDGE('',*,*,#48336,.T.) ;
#66810 = ORIENTED_EDGE('',*,*,#48337,.T.) ;
#66811 = ORIENTED_EDGE('',*,*,#48338,.T.) ;
#66812 = ORIENTED_EDGE('',*,*,#48339,.T.) ;
#66813 = ORIENTED_EDGE('',*,*,#48340,.T.) ;
#66814 = ORIENTED_EDGE('',*,*,#48341,.T.) ;
#66815 = ORIENTED_EDGE('',*,*,#48342,.T.) ;
#66816 = ORIENTED_EDGE('',*,*,#48343,.T.) ;
#66817 = ORIENTED_EDGE('',*,*,#48344,.T.) ;
#66818 = ORIENTED_EDGE('',*,*,#48345,.T.) ;
#66819 = ORIENTED_EDGE('',*,*,#48346,.T.) ;
#66820 = ORIENTED_EDGE('',*,*,#48347,.T.) ;
#66821 = ORIENTED_EDGE('',*,*,#48348,.T.) ;
#66822 = ORIENTED_EDGE('',*,*,#48349,.T.) ;
#66823 = ORIENTED_EDGE('',*,*,#48350,.T.) ;
#66824 = ORIENTED_EDGE('',*,*,#48351,.T.) ;
#66825 = ORIENTED_EDGE('',*,*,#48352,.T.) ;
#66826 = ORIENTED_EDGE('',*,*,#48353,.T.) ;
#66827 = ORIENTED_EDGE('',*,*,#48354,.T.) ;
#66828 = ORIENTED_EDGE('',*,*,#48355,.T.) ;
#66829 = ORIENTED_EDGE('',*,*,#48356,.T.) ;
#66830 = ORIENTED_EDGE('',*,*,#48279,.F.) ;
#66831 = ORIENTED_EDGE('',*,*,#48357,.T.) ;
#66832 = ORIENTED_EDGE('',*,*,#47706,.F.) ;
#66833 = ORIENTED_EDGE('',*,*,#48358,.F.) ;
#66834 = ORIENTED_EDGE('',*,*,#47703,.F.) ;
#66835 = ORIENTED_EDGE('',*,*,#48359,.T.) ;
#66836 = ORIENTED_EDGE('',*,*,#47707,.F.) ;
#66837 = ORIENTED_EDGE('',*,*,#48360,.T.) ;
#66838 = ORIENTED_EDGE('',*,*,#48361,.F.) ;
#66839 = ORIENTED_EDGE('',*,*,#48358,.T.) ;
#66840 = ORIENTED_EDGE('',*,*,#48362,.F.) ;
#66841 = ORIENTED_EDGE('',*,*,#47704,.F.) ;
#66842 = ORIENTED_EDGE('',*,*,#48363,.T.) ;
#66843 = ORIENTED_EDGE('',*,*,#48281,.F.) ;
#66844 = ORIENTED_EDGE('',*,*,#48364,.F.) ;
#66845 = ORIENTED_EDGE('',*,*,#48362,.T.) ;
#66846 = ORIENTED_EDGE('',*,*,#47705,.F.) ;
#66847 = ORIENTED_EDGE('',*,*,#48365,.F.) ;
#66848 = ORIENTED_EDGE('',*,*,#47699,.F.) ;
#66849 = ORIENTED_EDGE('',*,*,#48361,.T.) ;
#66850 = ORIENTED_EDGE('',*,*,#47702,.F.) ;
#66851 = ORIENTED_EDGE('',*,*,#48366,.F.) ;
#66852 = ORIENTED_EDGE('',*,*,#48280,.F.) ;
#66853 = ORIENTED_EDGE('',*,*,#48365,.T.) ;
#66854 = ORIENTED_EDGE('',*,*,#48364,.T.) ;
#66855 = ORIENTED_EDGE('',*,*,#48367,.F.) ;
#66856 = ORIENTED_EDGE('',*,*,#48368,.F.) ;
#66857 = ORIENTED_EDGE('',*,*,#48366,.T.) ;
#66858 = ORIENTED_EDGE('',*,*,#48369,.F.) ;
#66859 = ORIENTED_EDGE('',*,*,#48367,.T.) ;
#66860 = ORIENTED_EDGE('',*,*,#48284,.F.) ;
#66861 = ORIENTED_EDGE('',*,*,#48370,.F.) ;
#66862 = ORIENTED_EDGE('',*,*,#47700,.F.) ;
#66863 = ORIENTED_EDGE('',*,*,#48369,.T.) ;
#66864 = ORIENTED_EDGE('',*,*,#47701,.F.) ;
#66865 = ORIENTED_EDGE('',*,*,#48371,.F.) ;
#66866 = ORIENTED_EDGE('',*,*,#47695,.F.) ;
#66867 = ORIENTED_EDGE('',*,*,#47698,.F.) ;
#66868 = ORIENTED_EDGE('',*,*,#48372,.T.) ;
#66869 = ORIENTED_EDGE('',*,*,#48277,.F.) ;
#66870 = ORIENTED_EDGE('',*,*,#48368,.T.) ;
#66871 = ORIENTED_EDGE('',*,*,#48371,.T.) ;
#66872 = ORIENTED_EDGE('',*,*,#48370,.T.) ;
#66873 = ORIENTED_EDGE('',*,*,#48373,.F.) ;
#66874 = ORIENTED_EDGE('',*,*,#47693,.F.) ;
#66875 = ORIENTED_EDGE('',*,*,#48374,.T.) ;
#66876 = ORIENTED_EDGE('',*,*,#47697,.F.) ;
#66877 = ORIENTED_EDGE('',*,*,#48375,.T.) ;
#66878 = ORIENTED_EDGE('',*,*,#48283,.F.) ;
#66879 = ORIENTED_EDGE('',*,*,#48376,.T.) ;
#66880 = ORIENTED_EDGE('',*,*,#47696,.F.) ;
#66881 = ORIENTED_EDGE('',*,*,#48373,.T.) ;
#66882 = ORIENTED_EDGE('',*,*,#48351,.F.) ;
#66883 = ORIENTED_EDGE('',*,*,#48377,.T.) ;
#66884 = ORIENTED_EDGE('',*,*,#47728,.F.) ;
#66885 = ORIENTED_EDGE('',*,*,#48378,.F.) ;
#66886 = ORIENTED_EDGE('',*,*,#47725,.F.) ;
#66887 = ORIENTED_EDGE('',*,*,#48379,.T.) ;
#66888 = ORIENTED_EDGE('',*,*,#47729,.F.) ;
#66889 = ORIENTED_EDGE('',*,*,#48380,.T.) ;
#66890 = ORIENTED_EDGE('',*,*,#48381,.F.) ;
#66891 = ORIENTED_EDGE('',*,*,#48378,.T.) ;
#66892 = ORIENTED_EDGE('',*,*,#48382,.F.) ;
#66893 = ORIENTED_EDGE('',*,*,#47726,.F.) ;
#66894 = ORIENTED_EDGE('',*,*,#48383,.T.) ;
#66895 = ORIENTED_EDGE('',*,*,#48353,.F.) ;
#66896 = ORIENTED_EDGE('',*,*,#48384,.F.) ;
#66897 = ORIENTED_EDGE('',*,*,#48382,.T.) ;
#66898 = ORIENTED_EDGE('',*,*,#47727,.F.) ;
#66899 = ORIENTED_EDGE('',*,*,#48385,.F.) ;
#66900 = ORIENTED_EDGE('',*,*,#47741,.F.) ;
#66901 = ORIENTED_EDGE('',*,*,#48381,.T.) ;
#66902 = ORIENTED_EDGE('',*,*,#47740,.F.) ;
#66903 = ORIENTED_EDGE('',*,*,#48386,.F.) ;
#66904 = ORIENTED_EDGE('',*,*,#48352,.F.) ;
#66905 = ORIENTED_EDGE('',*,*,#48385,.T.) ;
#66906 = ORIENTED_EDGE('',*,*,#48384,.T.) ;
#66907 = ORIENTED_EDGE('',*,*,#48387,.F.) ;
#66908 = ORIENTED_EDGE('',*,*,#48388,.F.) ;
#66909 = ORIENTED_EDGE('',*,*,#48386,.T.) ;
#66910 = ORIENTED_EDGE('',*,*,#48389,.F.) ;
#66911 = ORIENTED_EDGE('',*,*,#48387,.T.) ;
#66912 = ORIENTED_EDGE('',*,*,#48356,.F.) ;
#66913 = ORIENTED_EDGE('',*,*,#48390,.F.) ;
#66914 = ORIENTED_EDGE('',*,*,#47742,.F.) ;
#66915 = ORIENTED_EDGE('',*,*,#48389,.T.) ;
#66916 = ORIENTED_EDGE('',*,*,#47739,.F.) ;
#66917 = ORIENTED_EDGE('',*,*,#48391,.F.) ;
#66918 = ORIENTED_EDGE('',*,*,#47735,.F.) ;
#66919 = ORIENTED_EDGE('',*,*,#47738,.F.) ;
#66920 = ORIENTED_EDGE('',*,*,#48392,.T.) ;
#66921 = ORIENTED_EDGE('',*,*,#48349,.F.) ;
#66922 = ORIENTED_EDGE('',*,*,#48388,.T.) ;
#66923 = ORIENTED_EDGE('',*,*,#48391,.T.) ;
#66924 = ORIENTED_EDGE('',*,*,#48390,.T.) ;
#66925 = ORIENTED_EDGE('',*,*,#48393,.F.) ;
#66926 = ORIENTED_EDGE('',*,*,#47733,.F.) ;
#66927 = ORIENTED_EDGE('',*,*,#48394,.T.) ;
#66928 = ORIENTED_EDGE('',*,*,#47737,.F.) ;
#66929 = ORIENTED_EDGE('',*,*,#48395,.T.) ;
#66930 = ORIENTED_EDGE('',*,*,#48355,.F.) ;
#66931 = ORIENTED_EDGE('',*,*,#48396,.T.) ;
#66932 = ORIENTED_EDGE('',*,*,#47736,.F.) ;
#66933 = ORIENTED_EDGE('',*,*,#48393,.T.) ;
#66934 = ORIENTED_EDGE('',*,*,#48271,.F.) ;
#66935 = ORIENTED_EDGE('',*,*,#48397,.T.) ;
#66936 = ORIENTED_EDGE('',*,*,#47764,.F.) ;
#66937 = ORIENTED_EDGE('',*,*,#48398,.F.) ;
#66938 = ORIENTED_EDGE('',*,*,#47761,.F.) ;
#66939 = ORIENTED_EDGE('',*,*,#48399,.T.) ;
#66940 = ORIENTED_EDGE('',*,*,#47765,.F.) ;
#66941 = ORIENTED_EDGE('',*,*,#48400,.T.) ;
#66942 = ORIENTED_EDGE('',*,*,#48401,.F.) ;
#66943 = ORIENTED_EDGE('',*,*,#48398,.T.) ;
#66944 = ORIENTED_EDGE('',*,*,#48402,.F.) ;
#66945 = ORIENTED_EDGE('',*,*,#47762,.F.) ;
#66946 = ORIENTED_EDGE('',*,*,#48403,.T.) ;
#66947 = ORIENTED_EDGE('',*,*,#48273,.F.) ;
#66948 = ORIENTED_EDGE('',*,*,#48404,.F.) ;
#66949 = ORIENTED_EDGE('',*,*,#48402,.T.) ;
#66950 = ORIENTED_EDGE('',*,*,#47763,.F.) ;
#66951 = ORIENTED_EDGE('',*,*,#48405,.F.) ;
#66952 = ORIENTED_EDGE('',*,*,#47757,.F.) ;
#66953 = ORIENTED_EDGE('',*,*,#48401,.T.) ;
#66954 = ORIENTED_EDGE('',*,*,#47760,.F.) ;
#66955 = ORIENTED_EDGE('',*,*,#48406,.F.) ;
#66956 = ORIENTED_EDGE('',*,*,#48272,.F.) ;
#66957 = ORIENTED_EDGE('',*,*,#48405,.T.) ;
#66958 = ORIENTED_EDGE('',*,*,#48404,.T.) ;
#66959 = ORIENTED_EDGE('',*,*,#48407,.F.) ;
#66960 = ORIENTED_EDGE('',*,*,#48408,.F.) ;
#66961 = ORIENTED_EDGE('',*,*,#48406,.T.) ;
#66962 = ORIENTED_EDGE('',*,*,#48409,.F.) ;
#66963 = ORIENTED_EDGE('',*,*,#48407,.T.) ;
#66964 = ORIENTED_EDGE('',*,*,#48276,.F.) ;
#66965 = ORIENTED_EDGE('',*,*,#48410,.F.) ;
#66966 = ORIENTED_EDGE('',*,*,#47758,.F.) ;
#66967 = ORIENTED_EDGE('',*,*,#48409,.T.) ;
#66968 = ORIENTED_EDGE('',*,*,#47759,.F.) ;
#66969 = ORIENTED_EDGE('',*,*,#48411,.F.) ;
#66970 = ORIENTED_EDGE('',*,*,#47753,.F.) ;
#66971 = ORIENTED_EDGE('',*,*,#47756,.F.) ;
#66972 = ORIENTED_EDGE('',*,*,#48412,.T.) ;
#66973 = ORIENTED_EDGE('',*,*,#48269,.F.) ;
#66974 = ORIENTED_EDGE('',*,*,#48408,.T.) ;
#66975 = ORIENTED_EDGE('',*,*,#48411,.T.) ;
#66976 = ORIENTED_EDGE('',*,*,#48410,.T.) ;
#66977 = ORIENTED_EDGE('',*,*,#48413,.F.) ;
#66978 = ORIENTED_EDGE('',*,*,#47751,.F.) ;
#66979 = ORIENTED_EDGE('',*,*,#48414,.T.) ;
#66980 = ORIENTED_EDGE('',*,*,#47755,.F.) ;
#66981 = ORIENTED_EDGE('',*,*,#48415,.T.) ;
#66982 = ORIENTED_EDGE('',*,*,#48275,.F.) ;
#66983 = ORIENTED_EDGE('',*,*,#48416,.T.) ;
#66984 = ORIENTED_EDGE('',*,*,#47754,.F.) ;
#66985 = ORIENTED_EDGE('',*,*,#48413,.T.) ;
#66986 = ORIENTED_EDGE('',*,*,#48343,.F.) ;
#66987 = ORIENTED_EDGE('',*,*,#48417,.T.) ;
#66988 = ORIENTED_EDGE('',*,*,#47786,.F.) ;
#66989 = ORIENTED_EDGE('',*,*,#48418,.F.) ;
#66990 = ORIENTED_EDGE('',*,*,#47783,.F.) ;
#66991 = ORIENTED_EDGE('',*,*,#48419,.T.) ;
#66992 = ORIENTED_EDGE('',*,*,#47787,.F.) ;
#66993 = ORIENTED_EDGE('',*,*,#48420,.T.) ;
#66994 = ORIENTED_EDGE('',*,*,#48421,.F.) ;
#66995 = ORIENTED_EDGE('',*,*,#48418,.T.) ;
#66996 = ORIENTED_EDGE('',*,*,#48422,.F.) ;
#66997 = ORIENTED_EDGE('',*,*,#47784,.F.) ;
#66998 = ORIENTED_EDGE('',*,*,#48423,.T.) ;
#66999 = ORIENTED_EDGE('',*,*,#48345,.F.) ;
#67000 = ORIENTED_EDGE('',*,*,#48424,.F.) ;
#67001 = ORIENTED_EDGE('',*,*,#48422,.T.) ;
#67002 = ORIENTED_EDGE('',*,*,#47785,.F.) ;
#67003 = ORIENTED_EDGE('',*,*,#48425,.F.) ;
#67004 = ORIENTED_EDGE('',*,*,#47799,.F.) ;
#67005 = ORIENTED_EDGE('',*,*,#48421,.T.) ;
#67006 = ORIENTED_EDGE('',*,*,#47798,.F.) ;
#67007 = ORIENTED_EDGE('',*,*,#48426,.F.) ;
#67008 = ORIENTED_EDGE('',*,*,#48344,.F.) ;
#67009 = ORIENTED_EDGE('',*,*,#48425,.T.) ;
#67010 = ORIENTED_EDGE('',*,*,#48424,.T.) ;
#67011 = ORIENTED_EDGE('',*,*,#48427,.F.) ;
#67012 = ORIENTED_EDGE('',*,*,#48428,.F.) ;
#67013 = ORIENTED_EDGE('',*,*,#48426,.T.) ;
#67014 = ORIENTED_EDGE('',*,*,#48429,.F.) ;
#67015 = ORIENTED_EDGE('',*,*,#48427,.T.) ;
#67016 = ORIENTED_EDGE('',*,*,#48348,.F.) ;
#67017 = ORIENTED_EDGE('',*,*,#48430,.F.) ;
#67018 = ORIENTED_EDGE('',*,*,#47800,.F.) ;
#67019 = ORIENTED_EDGE('',*,*,#48429,.T.) ;
#67020 = ORIENTED_EDGE('',*,*,#47797,.F.) ;
#67021 = ORIENTED_EDGE('',*,*,#48431,.F.) ;
#67022 = ORIENTED_EDGE('',*,*,#47793,.F.) ;
#67023 = ORIENTED_EDGE('',*,*,#47796,.F.) ;
#67024 = ORIENTED_EDGE('',*,*,#48432,.T.) ;
#67025 = ORIENTED_EDGE('',*,*,#48341,.F.) ;
#67026 = ORIENTED_EDGE('',*,*,#48428,.T.) ;
#67027 = ORIENTED_EDGE('',*,*,#48431,.T.) ;
#67028 = ORIENTED_EDGE('',*,*,#48430,.T.) ;
#67029 = ORIENTED_EDGE('',*,*,#48433,.F.) ;
#67030 = ORIENTED_EDGE('',*,*,#47791,.F.) ;
#67031 = ORIENTED_EDGE('',*,*,#48434,.T.) ;
#67032 = ORIENTED_EDGE('',*,*,#47795,.F.) ;
#67033 = ORIENTED_EDGE('',*,*,#48435,.T.) ;
#67034 = ORIENTED_EDGE('',*,*,#48347,.F.) ;
#67035 = ORIENTED_EDGE('',*,*,#48436,.T.) ;
#67036 = ORIENTED_EDGE('',*,*,#47794,.F.) ;
#67037 = ORIENTED_EDGE('',*,*,#48433,.T.) ;
#67038 = ORIENTED_EDGE('',*,*,#48263,.F.) ;
#67039 = ORIENTED_EDGE('',*,*,#48437,.T.) ;
#67040 = ORIENTED_EDGE('',*,*,#47822,.F.) ;
#67041 = ORIENTED_EDGE('',*,*,#48438,.F.) ;
#67042 = ORIENTED_EDGE('',*,*,#47819,.F.) ;
#67043 = ORIENTED_EDGE('',*,*,#48439,.T.) ;
#67044 = ORIENTED_EDGE('',*,*,#47823,.F.) ;
#67045 = ORIENTED_EDGE('',*,*,#48440,.T.) ;
#67046 = ORIENTED_EDGE('',*,*,#48441,.F.) ;
#67047 = ORIENTED_EDGE('',*,*,#48438,.T.) ;
#67048 = ORIENTED_EDGE('',*,*,#48442,.F.) ;
#67049 = ORIENTED_EDGE('',*,*,#47820,.F.) ;
#67050 = ORIENTED_EDGE('',*,*,#48443,.T.) ;
#67051 = ORIENTED_EDGE('',*,*,#48265,.F.) ;
#67052 = ORIENTED_EDGE('',*,*,#48444,.F.) ;
#67053 = ORIENTED_EDGE('',*,*,#48442,.T.) ;
#67054 = ORIENTED_EDGE('',*,*,#47821,.F.) ;
#67055 = ORIENTED_EDGE('',*,*,#48445,.F.) ;
#67056 = ORIENTED_EDGE('',*,*,#47815,.F.) ;
#67057 = ORIENTED_EDGE('',*,*,#48441,.T.) ;
#67058 = ORIENTED_EDGE('',*,*,#47818,.F.) ;
#67059 = ORIENTED_EDGE('',*,*,#48446,.F.) ;
#67060 = ORIENTED_EDGE('',*,*,#48264,.F.) ;
#67061 = ORIENTED_EDGE('',*,*,#48445,.T.) ;
#67062 = ORIENTED_EDGE('',*,*,#48444,.T.) ;
#67063 = ORIENTED_EDGE('',*,*,#48447,.F.) ;
#67064 = ORIENTED_EDGE('',*,*,#48448,.F.) ;
#67065 = ORIENTED_EDGE('',*,*,#48446,.T.) ;
#67066 = ORIENTED_EDGE('',*,*,#48449,.F.) ;
#67067 = ORIENTED_EDGE('',*,*,#48447,.T.) ;
#67068 = ORIENTED_EDGE('',*,*,#48268,.F.) ;
#67069 = ORIENTED_EDGE('',*,*,#48450,.F.) ;
#67070 = ORIENTED_EDGE('',*,*,#47816,.F.) ;
#67071 = ORIENTED_EDGE('',*,*,#48449,.T.) ;
#67072 = ORIENTED_EDGE('',*,*,#47817,.F.) ;
#67073 = ORIENTED_EDGE('',*,*,#48451,.F.) ;
#67074 = ORIENTED_EDGE('',*,*,#47811,.F.) ;
#67075 = ORIENTED_EDGE('',*,*,#47814,.F.) ;
#67076 = ORIENTED_EDGE('',*,*,#48452,.T.) ;
#67077 = ORIENTED_EDGE('',*,*,#48261,.F.) ;
#67078 = ORIENTED_EDGE('',*,*,#48448,.T.) ;
#67079 = ORIENTED_EDGE('',*,*,#48451,.T.) ;
#67080 = ORIENTED_EDGE('',*,*,#48450,.T.) ;
#67081 = ORIENTED_EDGE('',*,*,#48453,.F.) ;
#67082 = ORIENTED_EDGE('',*,*,#47809,.F.) ;
#67083 = ORIENTED_EDGE('',*,*,#48454,.T.) ;
#67084 = ORIENTED_EDGE('',*,*,#47813,.F.) ;
#67085 = ORIENTED_EDGE('',*,*,#48455,.T.) ;
#67086 = ORIENTED_EDGE('',*,*,#48267,.F.) ;
#67087 = ORIENTED_EDGE('',*,*,#48456,.T.) ;
#67088 = ORIENTED_EDGE('',*,*,#47812,.F.) ;
#67089 = ORIENTED_EDGE('',*,*,#48453,.T.) ;
#67090 = ORIENTED_EDGE('',*,*,#48335,.F.) ;
#67091 = ORIENTED_EDGE('',*,*,#48457,.T.) ;
#67092 = ORIENTED_EDGE('',*,*,#47844,.F.) ;
#67093 = ORIENTED_EDGE('',*,*,#48458,.F.) ;
#67094 = ORIENTED_EDGE('',*,*,#47841,.F.) ;
#67095 = ORIENTED_EDGE('',*,*,#48459,.T.) ;
#67096 = ORIENTED_EDGE('',*,*,#47845,.F.) ;
#67097 = ORIENTED_EDGE('',*,*,#48460,.T.) ;
#67098 = ORIENTED_EDGE('',*,*,#48461,.F.) ;
#67099 = ORIENTED_EDGE('',*,*,#48458,.T.) ;
#67100 = ORIENTED_EDGE('',*,*,#48462,.F.) ;
#67101 = ORIENTED_EDGE('',*,*,#47842,.F.) ;
#67102 = ORIENTED_EDGE('',*,*,#48463,.T.) ;
#67103 = ORIENTED_EDGE('',*,*,#48337,.F.) ;
#67104 = ORIENTED_EDGE('',*,*,#48464,.F.) ;
#67105 = ORIENTED_EDGE('',*,*,#48462,.T.) ;
#67106 = ORIENTED_EDGE('',*,*,#47843,.F.) ;
#67107 = ORIENTED_EDGE('',*,*,#48465,.F.) ;
#67108 = ORIENTED_EDGE('',*,*,#47857,.F.) ;
#67109 = ORIENTED_EDGE('',*,*,#48461,.T.) ;
#67110 = ORIENTED_EDGE('',*,*,#47856,.F.) ;
#67111 = ORIENTED_EDGE('',*,*,#48466,.F.) ;
#67112 = ORIENTED_EDGE('',*,*,#48336,.F.) ;
#67113 = ORIENTED_EDGE('',*,*,#48465,.T.) ;
#67114 = ORIENTED_EDGE('',*,*,#48464,.T.) ;
#67115 = ORIENTED_EDGE('',*,*,#48467,.F.) ;
#67116 = ORIENTED_EDGE('',*,*,#48468,.F.) ;
#67117 = ORIENTED_EDGE('',*,*,#48466,.T.) ;
#67118 = ORIENTED_EDGE('',*,*,#48469,.F.) ;
#67119 = ORIENTED_EDGE('',*,*,#48467,.T.) ;
#67120 = ORIENTED_EDGE('',*,*,#48340,.F.) ;
#67121 = ORIENTED_EDGE('',*,*,#48470,.F.) ;
#67122 = ORIENTED_EDGE('',*,*,#47858,.F.) ;
#67123 = ORIENTED_EDGE('',*,*,#48469,.T.) ;
#67124 = ORIENTED_EDGE('',*,*,#47855,.F.) ;
#67125 = ORIENTED_EDGE('',*,*,#48471,.F.) ;
#67126 = ORIENTED_EDGE('',*,*,#47851,.F.) ;
#67127 = ORIENTED_EDGE('',*,*,#47854,.F.) ;
#67128 = ORIENTED_EDGE('',*,*,#48472,.T.) ;
#67129 = ORIENTED_EDGE('',*,*,#48333,.F.) ;
#67130 = ORIENTED_EDGE('',*,*,#48468,.T.) ;
#67131 = ORIENTED_EDGE('',*,*,#48471,.T.) ;
#67132 = ORIENTED_EDGE('',*,*,#48470,.T.) ;
#67133 = ORIENTED_EDGE('',*,*,#48473,.F.) ;
#67134 = ORIENTED_EDGE('',*,*,#47849,.F.) ;
#67135 = ORIENTED_EDGE('',*,*,#48474,.T.) ;
#67136 = ORIENTED_EDGE('',*,*,#47853,.F.) ;
#67137 = ORIENTED_EDGE('',*,*,#48475,.T.) ;
#67138 = ORIENTED_EDGE('',*,*,#48339,.F.) ;
#67139 = ORIENTED_EDGE('',*,*,#48476,.T.) ;
#67140 = ORIENTED_EDGE('',*,*,#47852,.F.) ;
#67141 = ORIENTED_EDGE('',*,*,#48473,.T.) ;
#67142 = ORIENTED_EDGE('',*,*,#48255,.F.) ;
#67143 = ORIENTED_EDGE('',*,*,#48477,.T.) ;
#67144 = ORIENTED_EDGE('',*,*,#47880,.F.) ;
#67145 = ORIENTED_EDGE('',*,*,#48478,.F.) ;
#67146 = ORIENTED_EDGE('',*,*,#47877,.F.) ;
#67147 = ORIENTED_EDGE('',*,*,#48479,.T.) ;
#67148 = ORIENTED_EDGE('',*,*,#47881,.F.) ;
#67149 = ORIENTED_EDGE('',*,*,#48480,.T.) ;
#67150 = ORIENTED_EDGE('',*,*,#48481,.F.) ;
#67151 = ORIENTED_EDGE('',*,*,#48478,.T.) ;
#67152 = ORIENTED_EDGE('',*,*,#48482,.F.) ;
#67153 = ORIENTED_EDGE('',*,*,#47878,.F.) ;
#67154 = ORIENTED_EDGE('',*,*,#48483,.T.) ;
#67155 = ORIENTED_EDGE('',*,*,#48257,.F.) ;
#67156 = ORIENTED_EDGE('',*,*,#48484,.F.) ;
#67157 = ORIENTED_EDGE('',*,*,#48482,.T.) ;
#67158 = ORIENTED_EDGE('',*,*,#47879,.F.) ;
#67159 = ORIENTED_EDGE('',*,*,#48485,.F.) ;
#67160 = ORIENTED_EDGE('',*,*,#47873,.F.) ;
#67161 = ORIENTED_EDGE('',*,*,#48481,.T.) ;
#67162 = ORIENTED_EDGE('',*,*,#47876,.F.) ;
#67163 = ORIENTED_EDGE('',*,*,#48486,.F.) ;
#67164 = ORIENTED_EDGE('',*,*,#48256,.F.) ;
#67165 = ORIENTED_EDGE('',*,*,#48485,.T.) ;
#67166 = ORIENTED_EDGE('',*,*,#48484,.T.) ;
#67167 = ORIENTED_EDGE('',*,*,#48487,.F.) ;
#67168 = ORIENTED_EDGE('',*,*,#48488,.F.) ;
#67169 = ORIENTED_EDGE('',*,*,#48486,.T.) ;
#67170 = ORIENTED_EDGE('',*,*,#48489,.F.) ;
#67171 = ORIENTED_EDGE('',*,*,#48487,.T.) ;
#67172 = ORIENTED_EDGE('',*,*,#48260,.F.) ;
#67173 = ORIENTED_EDGE('',*,*,#48490,.F.) ;
#67174 = ORIENTED_EDGE('',*,*,#47874,.F.) ;
#67175 = ORIENTED_EDGE('',*,*,#48489,.T.) ;
#67176 = ORIENTED_EDGE('',*,*,#47875,.F.) ;
#67177 = ORIENTED_EDGE('',*,*,#48491,.F.) ;
#67178 = ORIENTED_EDGE('',*,*,#47869,.F.) ;
#67179 = ORIENTED_EDGE('',*,*,#47872,.F.) ;
#67180 = ORIENTED_EDGE('',*,*,#48492,.T.) ;
#67181 = ORIENTED_EDGE('',*,*,#48253,.F.) ;
#67182 = ORIENTED_EDGE('',*,*,#48488,.T.) ;
#67183 = ORIENTED_EDGE('',*,*,#48491,.T.) ;
#67184 = ORIENTED_EDGE('',*,*,#48490,.T.) ;
#67185 = ORIENTED_EDGE('',*,*,#48493,.F.) ;
#67186 = ORIENTED_EDGE('',*,*,#47867,.F.) ;
#67187 = ORIENTED_EDGE('',*,*,#48494,.T.) ;
#67188 = ORIENTED_EDGE('',*,*,#47871,.F.) ;
#67189 = ORIENTED_EDGE('',*,*,#48495,.T.) ;
#67190 = ORIENTED_EDGE('',*,*,#48259,.F.) ;
#67191 = ORIENTED_EDGE('',*,*,#48496,.T.) ;
#67192 = ORIENTED_EDGE('',*,*,#47870,.F.) ;
#67193 = ORIENTED_EDGE('',*,*,#48493,.T.) ;
#67194 = ORIENTED_EDGE('',*,*,#48327,.F.) ;
#67195 = ORIENTED_EDGE('',*,*,#48497,.T.) ;
#67196 = ORIENTED_EDGE('',*,*,#47902,.F.) ;
#67197 = ORIENTED_EDGE('',*,*,#48498,.F.) ;
#67198 = ORIENTED_EDGE('',*,*,#47899,.F.) ;
#67199 = ORIENTED_EDGE('',*,*,#48499,.T.) ;
#67200 = ORIENTED_EDGE('',*,*,#47903,.F.) ;
#67201 = ORIENTED_EDGE('',*,*,#48500,.T.) ;
#67202 = ORIENTED_EDGE('',*,*,#48501,.F.) ;
#67203 = ORIENTED_EDGE('',*,*,#48498,.T.) ;
#67204 = ORIENTED_EDGE('',*,*,#48502,.F.) ;
#67205 = ORIENTED_EDGE('',*,*,#47900,.F.) ;
#67206 = ORIENTED_EDGE('',*,*,#48503,.T.) ;
#67207 = ORIENTED_EDGE('',*,*,#48329,.F.) ;
#67208 = ORIENTED_EDGE('',*,*,#48504,.F.) ;
#67209 = ORIENTED_EDGE('',*,*,#48502,.T.) ;
#67210 = ORIENTED_EDGE('',*,*,#47901,.F.) ;
#67211 = ORIENTED_EDGE('',*,*,#48505,.F.) ;
#67212 = ORIENTED_EDGE('',*,*,#47915,.F.) ;
#67213 = ORIENTED_EDGE('',*,*,#48501,.T.) ;
#67214 = ORIENTED_EDGE('',*,*,#47914,.F.) ;
#67215 = ORIENTED_EDGE('',*,*,#48506,.F.) ;
#67216 = ORIENTED_EDGE('',*,*,#48328,.F.) ;
#67217 = ORIENTED_EDGE('',*,*,#48505,.T.) ;
#67218 = ORIENTED_EDGE('',*,*,#48504,.T.) ;
#67219 = ORIENTED_EDGE('',*,*,#48507,.F.) ;
#67220 = ORIENTED_EDGE('',*,*,#48508,.F.) ;
#67221 = ORIENTED_EDGE('',*,*,#48506,.T.) ;
#67222 = ORIENTED_EDGE('',*,*,#48509,.F.) ;
#67223 = ORIENTED_EDGE('',*,*,#48507,.T.) ;
#67224 = ORIENTED_EDGE('',*,*,#48332,.F.) ;
#67225 = ORIENTED_EDGE('',*,*,#48510,.F.) ;
#67226 = ORIENTED_EDGE('',*,*,#47916,.F.) ;
#67227 = ORIENTED_EDGE('',*,*,#48509,.T.) ;
#67228 = ORIENTED_EDGE('',*,*,#47913,.F.) ;
#67229 = ORIENTED_EDGE('',*,*,#48511,.F.) ;
#67230 = ORIENTED_EDGE('',*,*,#47909,.F.) ;
#67231 = ORIENTED_EDGE('',*,*,#47912,.F.) ;
#67232 = ORIENTED_EDGE('',*,*,#48512,.T.) ;
#67233 = ORIENTED_EDGE('',*,*,#48325,.F.) ;
#67234 = ORIENTED_EDGE('',*,*,#48508,.T.) ;
#67235 = ORIENTED_EDGE('',*,*,#48511,.T.) ;
#67236 = ORIENTED_EDGE('',*,*,#48510,.T.) ;
#67237 = ORIENTED_EDGE('',*,*,#48513,.F.) ;
#67238 = ORIENTED_EDGE('',*,*,#47907,.F.) ;
#67239 = ORIENTED_EDGE('',*,*,#48514,.T.) ;
#67240 = ORIENTED_EDGE('',*,*,#47911,.F.) ;
#67241 = ORIENTED_EDGE('',*,*,#48515,.T.) ;
#67242 = ORIENTED_EDGE('',*,*,#48331,.F.) ;
#67243 = ORIENTED_EDGE('',*,*,#48516,.T.) ;
#67244 = ORIENTED_EDGE('',*,*,#47910,.F.) ;
#67245 = ORIENTED_EDGE('',*,*,#48513,.T.) ;
#67246 = ORIENTED_EDGE('',*,*,#48247,.F.) ;
#67247 = ORIENTED_EDGE('',*,*,#48517,.T.) ;
#67248 = ORIENTED_EDGE('',*,*,#47938,.F.) ;
#67249 = ORIENTED_EDGE('',*,*,#48518,.F.) ;
#67250 = ORIENTED_EDGE('',*,*,#47935,.F.) ;
#67251 = ORIENTED_EDGE('',*,*,#48519,.T.) ;
#67252 = ORIENTED_EDGE('',*,*,#47939,.F.) ;
#67253 = ORIENTED_EDGE('',*,*,#48520,.T.) ;
#67254 = ORIENTED_EDGE('',*,*,#48521,.F.) ;
#67255 = ORIENTED_EDGE('',*,*,#48518,.T.) ;
#67256 = ORIENTED_EDGE('',*,*,#48522,.F.) ;
#67257 = ORIENTED_EDGE('',*,*,#47936,.F.) ;
#67258 = ORIENTED_EDGE('',*,*,#48523,.T.) ;
#67259 = ORIENTED_EDGE('',*,*,#48249,.F.) ;
#67260 = ORIENTED_EDGE('',*,*,#48524,.F.) ;
#67261 = ORIENTED_EDGE('',*,*,#48522,.T.) ;
#67262 = ORIENTED_EDGE('',*,*,#47937,.F.) ;
#67263 = ORIENTED_EDGE('',*,*,#48525,.F.) ;
#67264 = ORIENTED_EDGE('',*,*,#47931,.F.) ;
#67265 = ORIENTED_EDGE('',*,*,#48521,.T.) ;
#67266 = ORIENTED_EDGE('',*,*,#47934,.F.) ;
#67267 = ORIENTED_EDGE('',*,*,#48526,.F.) ;
#67268 = ORIENTED_EDGE('',*,*,#48248,.F.) ;
#67269 = ORIENTED_EDGE('',*,*,#48525,.T.) ;
#67270 = ORIENTED_EDGE('',*,*,#48524,.T.) ;
#67271 = ORIENTED_EDGE('',*,*,#48527,.F.) ;
#67272 = ORIENTED_EDGE('',*,*,#48528,.F.) ;
#67273 = ORIENTED_EDGE('',*,*,#48526,.T.) ;
#67274 = ORIENTED_EDGE('',*,*,#48529,.F.) ;
#67275 = ORIENTED_EDGE('',*,*,#48527,.T.) ;
#67276 = ORIENTED_EDGE('',*,*,#48252,.F.) ;
#67277 = ORIENTED_EDGE('',*,*,#48530,.F.) ;
#67278 = ORIENTED_EDGE('',*,*,#47932,.F.) ;
#67279 = ORIENTED_EDGE('',*,*,#48529,.T.) ;
#67280 = ORIENTED_EDGE('',*,*,#47933,.F.) ;
#67281 = ORIENTED_EDGE('',*,*,#48531,.F.) ;
#67282 = ORIENTED_EDGE('',*,*,#47927,.F.) ;
#67283 = ORIENTED_EDGE('',*,*,#47930,.F.) ;
#67284 = ORIENTED_EDGE('',*,*,#48532,.T.) ;
#67285 = ORIENTED_EDGE('',*,*,#48245,.F.) ;
#67286 = ORIENTED_EDGE('',*,*,#48528,.T.) ;
#67287 = ORIENTED_EDGE('',*,*,#48531,.T.) ;
#67288 = ORIENTED_EDGE('',*,*,#48530,.T.) ;
#67289 = ORIENTED_EDGE('',*,*,#48533,.F.) ;
#67290 = ORIENTED_EDGE('',*,*,#47925,.F.) ;
#67291 = ORIENTED_EDGE('',*,*,#48534,.T.) ;
#67292 = ORIENTED_EDGE('',*,*,#47929,.F.) ;
#67293 = ORIENTED_EDGE('',*,*,#48535,.T.) ;
#67294 = ORIENTED_EDGE('',*,*,#48251,.F.) ;
#67295 = ORIENTED_EDGE('',*,*,#48536,.T.) ;
#67296 = ORIENTED_EDGE('',*,*,#47928,.F.) ;
#67297 = ORIENTED_EDGE('',*,*,#48533,.T.) ;
#67298 = ORIENTED_EDGE('',*,*,#48319,.F.) ;
#67299 = ORIENTED_EDGE('',*,*,#48537,.T.) ;
#67300 = ORIENTED_EDGE('',*,*,#47960,.F.) ;
#67301 = ORIENTED_EDGE('',*,*,#48538,.F.) ;
#67302 = ORIENTED_EDGE('',*,*,#47957,.F.) ;
#67303 = ORIENTED_EDGE('',*,*,#48539,.T.) ;
#67304 = ORIENTED_EDGE('',*,*,#47961,.F.) ;
#67305 = ORIENTED_EDGE('',*,*,#48540,.T.) ;
#67306 = ORIENTED_EDGE('',*,*,#48541,.F.) ;
#67307 = ORIENTED_EDGE('',*,*,#48538,.T.) ;
#67308 = ORIENTED_EDGE('',*,*,#48542,.F.) ;
#67309 = ORIENTED_EDGE('',*,*,#47958,.F.) ;
#67310 = ORIENTED_EDGE('',*,*,#48543,.T.) ;
#67311 = ORIENTED_EDGE('',*,*,#48321,.F.) ;
#67312 = ORIENTED_EDGE('',*,*,#48544,.F.) ;
#67313 = ORIENTED_EDGE('',*,*,#48542,.T.) ;
#67314 = ORIENTED_EDGE('',*,*,#47959,.F.) ;
#67315 = ORIENTED_EDGE('',*,*,#48545,.F.) ;
#67316 = ORIENTED_EDGE('',*,*,#47973,.F.) ;
#67317 = ORIENTED_EDGE('',*,*,#48541,.T.) ;
#67318 = ORIENTED_EDGE('',*,*,#47972,.F.) ;
#67319 = ORIENTED_EDGE('',*,*,#48546,.F.) ;
#67320 = ORIENTED_EDGE('',*,*,#48320,.F.) ;
#67321 = ORIENTED_EDGE('',*,*,#48545,.T.) ;
#67322 = ORIENTED_EDGE('',*,*,#48544,.T.) ;
#67323 = ORIENTED_EDGE('',*,*,#48547,.F.) ;
#67324 = ORIENTED_EDGE('',*,*,#48548,.F.) ;
#67325 = ORIENTED_EDGE('',*,*,#48546,.T.) ;
#67326 = ORIENTED_EDGE('',*,*,#48549,.F.) ;
#67327 = ORIENTED_EDGE('',*,*,#48547,.T.) ;
#67328 = ORIENTED_EDGE('',*,*,#48324,.F.) ;
#67329 = ORIENTED_EDGE('',*,*,#48550,.F.) ;
#67330 = ORIENTED_EDGE('',*,*,#47974,.F.) ;
#67331 = ORIENTED_EDGE('',*,*,#48549,.T.) ;
#67332 = ORIENTED_EDGE('',*,*,#47971,.F.) ;
#67333 = ORIENTED_EDGE('',*,*,#48551,.F.) ;
#67334 = ORIENTED_EDGE('',*,*,#47967,.F.) ;
#67335 = ORIENTED_EDGE('',*,*,#47970,.F.) ;
#67336 = ORIENTED_EDGE('',*,*,#48552,.T.) ;
#67337 = ORIENTED_EDGE('',*,*,#48317,.F.) ;
#67338 = ORIENTED_EDGE('',*,*,#48548,.T.) ;
#67339 = ORIENTED_EDGE('',*,*,#48551,.T.) ;
#67340 = ORIENTED_EDGE('',*,*,#48550,.T.) ;
#67341 = ORIENTED_EDGE('',*,*,#48553,.F.) ;
#67342 = ORIENTED_EDGE('',*,*,#47965,.F.) ;
#67343 = ORIENTED_EDGE('',*,*,#48554,.T.) ;
#67344 = ORIENTED_EDGE('',*,*,#47969,.F.) ;
#67345 = ORIENTED_EDGE('',*,*,#48555,.T.) ;
#67346 = ORIENTED_EDGE('',*,*,#48323,.F.) ;
#67347 = ORIENTED_EDGE('',*,*,#48556,.T.) ;
#67348 = ORIENTED_EDGE('',*,*,#47968,.F.) ;
#67349 = ORIENTED_EDGE('',*,*,#48553,.T.) ;
#67350 = ORIENTED_EDGE('',*,*,#48239,.F.) ;
#67351 = ORIENTED_EDGE('',*,*,#48557,.T.) ;
#67352 = ORIENTED_EDGE('',*,*,#47996,.F.) ;
#67353 = ORIENTED_EDGE('',*,*,#48558,.F.) ;
#67354 = ORIENTED_EDGE('',*,*,#47993,.F.) ;
#67355 = ORIENTED_EDGE('',*,*,#48559,.T.) ;
#67356 = ORIENTED_EDGE('',*,*,#47997,.F.) ;
#67357 = ORIENTED_EDGE('',*,*,#48560,.T.) ;
#67358 = ORIENTED_EDGE('',*,*,#48561,.F.) ;
#67359 = ORIENTED_EDGE('',*,*,#48558,.T.) ;
#67360 = ORIENTED_EDGE('',*,*,#48562,.F.) ;
#67361 = ORIENTED_EDGE('',*,*,#47994,.F.) ;
#67362 = ORIENTED_EDGE('',*,*,#48563,.T.) ;
#67363 = ORIENTED_EDGE('',*,*,#48241,.F.) ;
#67364 = ORIENTED_EDGE('',*,*,#48564,.F.) ;
#67365 = ORIENTED_EDGE('',*,*,#48562,.T.) ;
#67366 = ORIENTED_EDGE('',*,*,#47995,.F.) ;
#67367 = ORIENTED_EDGE('',*,*,#48565,.F.) ;
#67368 = ORIENTED_EDGE('',*,*,#47989,.F.) ;
#67369 = ORIENTED_EDGE('',*,*,#48561,.T.) ;
#67370 = ORIENTED_EDGE('',*,*,#47992,.F.) ;
#67371 = ORIENTED_EDGE('',*,*,#48566,.F.) ;
#67372 = ORIENTED_EDGE('',*,*,#48240,.F.) ;
#67373 = ORIENTED_EDGE('',*,*,#48565,.T.) ;
#67374 = ORIENTED_EDGE('',*,*,#48564,.T.) ;
#67375 = ORIENTED_EDGE('',*,*,#48567,.F.) ;
#67376 = ORIENTED_EDGE('',*,*,#48568,.F.) ;
#67377 = ORIENTED_EDGE('',*,*,#48566,.T.) ;
#67378 = ORIENTED_EDGE('',*,*,#48569,.F.) ;
#67379 = ORIENTED_EDGE('',*,*,#48567,.T.) ;
#67380 = ORIENTED_EDGE('',*,*,#48244,.F.) ;
#67381 = ORIENTED_EDGE('',*,*,#48570,.F.) ;
#67382 = ORIENTED_EDGE('',*,*,#47990,.F.) ;
#67383 = ORIENTED_EDGE('',*,*,#48569,.T.) ;
#67384 = ORIENTED_EDGE('',*,*,#47991,.F.) ;
#67385 = ORIENTED_EDGE('',*,*,#48571,.F.) ;
#67386 = ORIENTED_EDGE('',*,*,#47985,.F.) ;
#67387 = ORIENTED_EDGE('',*,*,#47988,.F.) ;
#67388 = ORIENTED_EDGE('',*,*,#48572,.T.) ;
#67389 = ORIENTED_EDGE('',*,*,#48237,.F.) ;
#67390 = ORIENTED_EDGE('',*,*,#48568,.T.) ;
#67391 = ORIENTED_EDGE('',*,*,#48571,.T.) ;
#67392 = ORIENTED_EDGE('',*,*,#48570,.T.) ;
#67393 = ORIENTED_EDGE('',*,*,#48573,.F.) ;
#67394 = ORIENTED_EDGE('',*,*,#47983,.F.) ;
#67395 = ORIENTED_EDGE('',*,*,#48574,.T.) ;
#67396 = ORIENTED_EDGE('',*,*,#47987,.F.) ;
#67397 = ORIENTED_EDGE('',*,*,#48575,.T.) ;
#67398 = ORIENTED_EDGE('',*,*,#48243,.F.) ;
#67399 = ORIENTED_EDGE('',*,*,#48576,.T.) ;
#67400 = ORIENTED_EDGE('',*,*,#47986,.F.) ;
#67401 = ORIENTED_EDGE('',*,*,#48573,.T.) ;
#67402 = ORIENTED_EDGE('',*,*,#48311,.F.) ;
#67403 = ORIENTED_EDGE('',*,*,#48577,.T.) ;
#67404 = ORIENTED_EDGE('',*,*,#48018,.F.) ;
#67405 = ORIENTED_EDGE('',*,*,#48578,.F.) ;
#67406 = ORIENTED_EDGE('',*,*,#48015,.F.) ;
#67407 = ORIENTED_EDGE('',*,*,#48579,.T.) ;
#67408 = ORIENTED_EDGE('',*,*,#48019,.F.) ;
#67409 = ORIENTED_EDGE('',*,*,#48580,.T.) ;
#67410 = ORIENTED_EDGE('',*,*,#48581,.F.) ;
#67411 = ORIENTED_EDGE('',*,*,#48578,.T.) ;
#67412 = ORIENTED_EDGE('',*,*,#48582,.F.) ;
#67413 = ORIENTED_EDGE('',*,*,#48016,.F.) ;
#67414 = ORIENTED_EDGE('',*,*,#48583,.T.) ;
#67415 = ORIENTED_EDGE('',*,*,#48313,.F.) ;
#67416 = ORIENTED_EDGE('',*,*,#48584,.F.) ;
#67417 = ORIENTED_EDGE('',*,*,#48582,.T.) ;
#67418 = ORIENTED_EDGE('',*,*,#48017,.F.) ;
#67419 = ORIENTED_EDGE('',*,*,#48585,.F.) ;
#67420 = ORIENTED_EDGE('',*,*,#48031,.F.) ;
#67421 = ORIENTED_EDGE('',*,*,#48581,.T.) ;
#67422 = ORIENTED_EDGE('',*,*,#48030,.F.) ;
#67423 = ORIENTED_EDGE('',*,*,#48586,.F.) ;
#67424 = ORIENTED_EDGE('',*,*,#48312,.F.) ;
#67425 = ORIENTED_EDGE('',*,*,#48585,.T.) ;
#67426 = ORIENTED_EDGE('',*,*,#48584,.T.) ;
#67427 = ORIENTED_EDGE('',*,*,#48587,.F.) ;
#67428 = ORIENTED_EDGE('',*,*,#48588,.F.) ;
#67429 = ORIENTED_EDGE('',*,*,#48586,.T.) ;
#67430 = ORIENTED_EDGE('',*,*,#48589,.F.) ;
#67431 = ORIENTED_EDGE('',*,*,#48587,.T.) ;
#67432 = ORIENTED_EDGE('',*,*,#48316,.F.) ;
#67433 = ORIENTED_EDGE('',*,*,#48590,.F.) ;
#67434 = ORIENTED_EDGE('',*,*,#48032,.F.) ;
#67435 = ORIENTED_EDGE('',*,*,#48589,.T.) ;
#67436 = ORIENTED_EDGE('',*,*,#48029,.F.) ;
#67437 = ORIENTED_EDGE('',*,*,#48591,.F.) ;
#67438 = ORIENTED_EDGE('',*,*,#48025,.F.) ;
#67439 = ORIENTED_EDGE('',*,*,#48028,.F.) ;
#67440 = ORIENTED_EDGE('',*,*,#48592,.T.) ;
#67441 = ORIENTED_EDGE('',*,*,#48309,.F.) ;
#67442 = ORIENTED_EDGE('',*,*,#48588,.T.) ;
#67443 = ORIENTED_EDGE('',*,*,#48591,.T.) ;
#67444 = ORIENTED_EDGE('',*,*,#48590,.T.) ;
#67445 = ORIENTED_EDGE('',*,*,#48593,.F.) ;
#67446 = ORIENTED_EDGE('',*,*,#48023,.F.) ;
#67447 = ORIENTED_EDGE('',*,*,#48594,.T.) ;
#67448 = ORIENTED_EDGE('',*,*,#48027,.F.) ;
#67449 = ORIENTED_EDGE('',*,*,#48595,.T.) ;
#67450 = ORIENTED_EDGE('',*,*,#48315,.F.) ;
#67451 = ORIENTED_EDGE('',*,*,#48596,.T.) ;
#67452 = ORIENTED_EDGE('',*,*,#48026,.F.) ;
#67453 = ORIENTED_EDGE('',*,*,#48593,.T.) ;
#67454 = ORIENTED_EDGE('',*,*,#48231,.F.) ;
#67455 = ORIENTED_EDGE('',*,*,#48597,.T.) ;
#67456 = ORIENTED_EDGE('',*,*,#48054,.F.) ;
#67457 = ORIENTED_EDGE('',*,*,#48598,.F.) ;
#67458 = ORIENTED_EDGE('',*,*,#48051,.F.) ;
#67459 = ORIENTED_EDGE('',*,*,#48599,.T.) ;
#67460 = ORIENTED_EDGE('',*,*,#48055,.F.) ;
#67461 = ORIENTED_EDGE('',*,*,#48600,.T.) ;
#67462 = ORIENTED_EDGE('',*,*,#48601,.F.) ;
#67463 = ORIENTED_EDGE('',*,*,#48598,.T.) ;
#67464 = ORIENTED_EDGE('',*,*,#48602,.F.) ;
#67465 = ORIENTED_EDGE('',*,*,#48052,.F.) ;
#67466 = ORIENTED_EDGE('',*,*,#48603,.T.) ;
#67467 = ORIENTED_EDGE('',*,*,#48233,.F.) ;
#67468 = ORIENTED_EDGE('',*,*,#48604,.F.) ;
#67469 = ORIENTED_EDGE('',*,*,#48602,.T.) ;
#67470 = ORIENTED_EDGE('',*,*,#48053,.F.) ;
#67471 = ORIENTED_EDGE('',*,*,#48605,.F.) ;
#67472 = ORIENTED_EDGE('',*,*,#48047,.F.) ;
#67473 = ORIENTED_EDGE('',*,*,#48601,.T.) ;
#67474 = ORIENTED_EDGE('',*,*,#48050,.F.) ;
#67475 = ORIENTED_EDGE('',*,*,#48606,.F.) ;
#67476 = ORIENTED_EDGE('',*,*,#48232,.F.) ;
#67477 = ORIENTED_EDGE('',*,*,#48605,.T.) ;
#67478 = ORIENTED_EDGE('',*,*,#48604,.T.) ;
#67479 = ORIENTED_EDGE('',*,*,#48607,.F.) ;
#67480 = ORIENTED_EDGE('',*,*,#48608,.F.) ;
#67481 = ORIENTED_EDGE('',*,*,#48606,.T.) ;
#67482 = ORIENTED_EDGE('',*,*,#48609,.F.) ;
#67483 = ORIENTED_EDGE('',*,*,#48607,.T.) ;
#67484 = ORIENTED_EDGE('',*,*,#48236,.F.) ;
#67485 = ORIENTED_EDGE('',*,*,#48610,.F.) ;
#67486 = ORIENTED_EDGE('',*,*,#48048,.F.) ;
#67487 = ORIENTED_EDGE('',*,*,#48609,.T.) ;
#67488 = ORIENTED_EDGE('',*,*,#48049,.F.) ;
#67489 = ORIENTED_EDGE('',*,*,#48611,.F.) ;
#67490 = ORIENTED_EDGE('',*,*,#48043,.F.) ;
#67491 = ORIENTED_EDGE('',*,*,#48046,.F.) ;
#67492 = ORIENTED_EDGE('',*,*,#48612,.T.) ;
#67493 = ORIENTED_EDGE('',*,*,#48229,.F.) ;
#67494 = ORIENTED_EDGE('',*,*,#48608,.T.) ;
#67495 = ORIENTED_EDGE('',*,*,#48611,.T.) ;
#67496 = ORIENTED_EDGE('',*,*,#48610,.T.) ;
#67497 = ORIENTED_EDGE('',*,*,#48613,.F.) ;
#67498 = ORIENTED_EDGE('',*,*,#48041,.F.) ;
#67499 = ORIENTED_EDGE('',*,*,#48614,.T.) ;
#67500 = ORIENTED_EDGE('',*,*,#48045,.F.) ;
#67501 = ORIENTED_EDGE('',*,*,#48615,.T.) ;
#67502 = ORIENTED_EDGE('',*,*,#48235,.F.) ;
#67503 = ORIENTED_EDGE('',*,*,#48616,.T.) ;
#67504 = ORIENTED_EDGE('',*,*,#48044,.F.) ;
#67505 = ORIENTED_EDGE('',*,*,#48613,.T.) ;
#67506 = ORIENTED_EDGE('',*,*,#48303,.F.) ;
#67507 = ORIENTED_EDGE('',*,*,#48617,.T.) ;
#67508 = ORIENTED_EDGE('',*,*,#48076,.F.) ;
#67509 = ORIENTED_EDGE('',*,*,#48618,.F.) ;
#67510 = ORIENTED_EDGE('',*,*,#48073,.F.) ;
#67511 = ORIENTED_EDGE('',*,*,#48619,.T.) ;
#67512 = ORIENTED_EDGE('',*,*,#48077,.F.) ;
#67513 = ORIENTED_EDGE('',*,*,#48620,.T.) ;
#67514 = ORIENTED_EDGE('',*,*,#48621,.F.) ;
#67515 = ORIENTED_EDGE('',*,*,#48618,.T.) ;
#67516 = ORIENTED_EDGE('',*,*,#48622,.F.) ;
#67517 = ORIENTED_EDGE('',*,*,#48074,.F.) ;
#67518 = ORIENTED_EDGE('',*,*,#48623,.T.) ;
#67519 = ORIENTED_EDGE('',*,*,#48305,.F.) ;
#67520 = ORIENTED_EDGE('',*,*,#48624,.F.) ;
#67521 = ORIENTED_EDGE('',*,*,#48622,.T.) ;
#67522 = ORIENTED_EDGE('',*,*,#48075,.F.) ;
#67523 = ORIENTED_EDGE('',*,*,#48625,.F.) ;
#67524 = ORIENTED_EDGE('',*,*,#48089,.F.) ;
#67525 = ORIENTED_EDGE('',*,*,#48621,.T.) ;
#67526 = ORIENTED_EDGE('',*,*,#48088,.F.) ;
#67527 = ORIENTED_EDGE('',*,*,#48626,.F.) ;
#67528 = ORIENTED_EDGE('',*,*,#48304,.F.) ;
#67529 = ORIENTED_EDGE('',*,*,#48625,.T.) ;
#67530 = ORIENTED_EDGE('',*,*,#48624,.T.) ;
#67531 = ORIENTED_EDGE('',*,*,#48627,.F.) ;
#67532 = ORIENTED_EDGE('',*,*,#48628,.F.) ;
#67533 = ORIENTED_EDGE('',*,*,#48626,.T.) ;
#67534 = ORIENTED_EDGE('',*,*,#48629,.F.) ;
#67535 = ORIENTED_EDGE('',*,*,#48627,.T.) ;
#67536 = ORIENTED_EDGE('',*,*,#48308,.F.) ;
#67537 = ORIENTED_EDGE('',*,*,#48630,.F.) ;
#67538 = ORIENTED_EDGE('',*,*,#48090,.F.) ;
#67539 = ORIENTED_EDGE('',*,*,#48629,.T.) ;
#67540 = ORIENTED_EDGE('',*,*,#48087,.F.) ;
#67541 = ORIENTED_EDGE('',*,*,#48631,.F.) ;
#67542 = ORIENTED_EDGE('',*,*,#48083,.F.) ;
#67543 = ORIENTED_EDGE('',*,*,#48086,.F.) ;
#67544 = ORIENTED_EDGE('',*,*,#48632,.T.) ;
#67545 = ORIENTED_EDGE('',*,*,#48301,.F.) ;
#67546 = ORIENTED_EDGE('',*,*,#48628,.T.) ;
#67547 = ORIENTED_EDGE('',*,*,#48631,.T.) ;
#67548 = ORIENTED_EDGE('',*,*,#48630,.T.) ;
#67549 = ORIENTED_EDGE('',*,*,#48633,.F.) ;
#67550 = ORIENTED_EDGE('',*,*,#48081,.F.) ;
#67551 = ORIENTED_EDGE('',*,*,#48634,.T.) ;
#67552 = ORIENTED_EDGE('',*,*,#48085,.F.) ;
#67553 = ORIENTED_EDGE('',*,*,#48635,.T.) ;
#67554 = ORIENTED_EDGE('',*,*,#48307,.F.) ;
#67555 = ORIENTED_EDGE('',*,*,#48636,.T.) ;
#67556 = ORIENTED_EDGE('',*,*,#48084,.F.) ;
#67557 = ORIENTED_EDGE('',*,*,#48633,.T.) ;
#67558 = ORIENTED_EDGE('',*,*,#48223,.F.) ;
#67559 = ORIENTED_EDGE('',*,*,#48637,.T.) ;
#67560 = ORIENTED_EDGE('',*,*,#48112,.F.) ;
#67561 = ORIENTED_EDGE('',*,*,#48638,.F.) ;
#67562 = ORIENTED_EDGE('',*,*,#48109,.F.) ;
#67563 = ORIENTED_EDGE('',*,*,#48639,.T.) ;
#67564 = ORIENTED_EDGE('',*,*,#48113,.F.) ;
#67565 = ORIENTED_EDGE('',*,*,#48640,.T.) ;
#67566 = ORIENTED_EDGE('',*,*,#48641,.F.) ;
#67567 = ORIENTED_EDGE('',*,*,#48638,.T.) ;
#67568 = ORIENTED_EDGE('',*,*,#48642,.F.) ;
#67569 = ORIENTED_EDGE('',*,*,#48110,.F.) ;
#67570 = ORIENTED_EDGE('',*,*,#48643,.T.) ;
#67571 = ORIENTED_EDGE('',*,*,#48225,.F.) ;
#67572 = ORIENTED_EDGE('',*,*,#48644,.F.) ;
#67573 = ORIENTED_EDGE('',*,*,#48642,.T.) ;
#67574 = ORIENTED_EDGE('',*,*,#48111,.F.) ;
#67575 = ORIENTED_EDGE('',*,*,#48645,.F.) ;
#67576 = ORIENTED_EDGE('',*,*,#48105,.F.) ;
#67577 = ORIENTED_EDGE('',*,*,#48641,.T.) ;
#67578 = ORIENTED_EDGE('',*,*,#48108,.F.) ;
#67579 = ORIENTED_EDGE('',*,*,#48646,.F.) ;
#67580 = ORIENTED_EDGE('',*,*,#48224,.F.) ;
#67581 = ORIENTED_EDGE('',*,*,#48645,.T.) ;
#67582 = ORIENTED_EDGE('',*,*,#48644,.T.) ;
#67583 = ORIENTED_EDGE('',*,*,#48647,.F.) ;
#67584 = ORIENTED_EDGE('',*,*,#48648,.F.) ;
#67585 = ORIENTED_EDGE('',*,*,#48646,.T.) ;
#67586 = ORIENTED_EDGE('',*,*,#48649,.F.) ;
#67587 = ORIENTED_EDGE('',*,*,#48647,.T.) ;
#67588 = ORIENTED_EDGE('',*,*,#48228,.F.) ;
#67589 = ORIENTED_EDGE('',*,*,#48650,.F.) ;
#67590 = ORIENTED_EDGE('',*,*,#48106,.F.) ;
#67591 = ORIENTED_EDGE('',*,*,#48649,.T.) ;
#67592 = ORIENTED_EDGE('',*,*,#48107,.F.) ;
#67593 = ORIENTED_EDGE('',*,*,#48651,.F.) ;
#67594 = ORIENTED_EDGE('',*,*,#48101,.F.) ;
#67595 = ORIENTED_EDGE('',*,*,#48104,.F.) ;
#67596 = ORIENTED_EDGE('',*,*,#48652,.T.) ;
#67597 = ORIENTED_EDGE('',*,*,#48221,.F.) ;
#67598 = ORIENTED_EDGE('',*,*,#48648,.T.) ;
#67599 = ORIENTED_EDGE('',*,*,#48651,.T.) ;
#67600 = ORIENTED_EDGE('',*,*,#48650,.T.) ;
#67601 = ORIENTED_EDGE('',*,*,#48653,.F.) ;
#67602 = ORIENTED_EDGE('',*,*,#48099,.F.) ;
#67603 = ORIENTED_EDGE('',*,*,#48654,.T.) ;
#67604 = ORIENTED_EDGE('',*,*,#48103,.F.) ;
#67605 = ORIENTED_EDGE('',*,*,#48655,.T.) ;
#67606 = ORIENTED_EDGE('',*,*,#48227,.F.) ;
#67607 = ORIENTED_EDGE('',*,*,#48656,.T.) ;
#67608 = ORIENTED_EDGE('',*,*,#48102,.F.) ;
#67609 = ORIENTED_EDGE('',*,*,#48653,.T.) ;
#67610 = ORIENTED_EDGE('',*,*,#48295,.F.) ;
#67611 = ORIENTED_EDGE('',*,*,#48657,.T.) ;
#67612 = ORIENTED_EDGE('',*,*,#48134,.F.) ;
#67613 = ORIENTED_EDGE('',*,*,#48658,.F.) ;
#67614 = ORIENTED_EDGE('',*,*,#48131,.F.) ;
#67615 = ORIENTED_EDGE('',*,*,#48659,.T.) ;
#67616 = ORIENTED_EDGE('',*,*,#48135,.F.) ;
#67617 = ORIENTED_EDGE('',*,*,#48660,.T.) ;
#67618 = ORIENTED_EDGE('',*,*,#48661,.F.) ;
#67619 = ORIENTED_EDGE('',*,*,#48658,.T.) ;
#67620 = ORIENTED_EDGE('',*,*,#48662,.F.) ;
#67621 = ORIENTED_EDGE('',*,*,#48132,.F.) ;
#67622 = ORIENTED_EDGE('',*,*,#48663,.T.) ;
#67623 = ORIENTED_EDGE('',*,*,#48297,.F.) ;
#67624 = ORIENTED_EDGE('',*,*,#48664,.F.) ;
#67625 = ORIENTED_EDGE('',*,*,#48662,.T.) ;
#67626 = ORIENTED_EDGE('',*,*,#48133,.F.) ;
#67627 = ORIENTED_EDGE('',*,*,#48665,.F.) ;
#67628 = ORIENTED_EDGE('',*,*,#48147,.F.) ;
#67629 = ORIENTED_EDGE('',*,*,#48661,.T.) ;
#67630 = ORIENTED_EDGE('',*,*,#48146,.F.) ;
#67631 = ORIENTED_EDGE('',*,*,#48666,.F.) ;
#67632 = ORIENTED_EDGE('',*,*,#48296,.F.) ;
#67633 = ORIENTED_EDGE('',*,*,#48665,.T.) ;
#67634 = ORIENTED_EDGE('',*,*,#48664,.T.) ;
#67635 = ORIENTED_EDGE('',*,*,#48667,.F.) ;
#67636 = ORIENTED_EDGE('',*,*,#48668,.F.) ;
#67637 = ORIENTED_EDGE('',*,*,#48666,.T.) ;
#67638 = ORIENTED_EDGE('',*,*,#48669,.F.) ;
#67639 = ORIENTED_EDGE('',*,*,#48667,.T.) ;
#67640 = ORIENTED_EDGE('',*,*,#48300,.F.) ;
#67641 = ORIENTED_EDGE('',*,*,#48670,.F.) ;
#67642 = ORIENTED_EDGE('',*,*,#48148,.F.) ;
#67643 = ORIENTED_EDGE('',*,*,#48669,.T.) ;
#67644 = ORIENTED_EDGE('',*,*,#48145,.F.) ;
#67645 = ORIENTED_EDGE('',*,*,#48671,.F.) ;
#67646 = ORIENTED_EDGE('',*,*,#48141,.F.) ;
#67647 = ORIENTED_EDGE('',*,*,#48144,.F.) ;
#67648 = ORIENTED_EDGE('',*,*,#48672,.T.) ;
#67649 = ORIENTED_EDGE('',*,*,#48293,.F.) ;
#67650 = ORIENTED_EDGE('',*,*,#48668,.T.) ;
#67651 = ORIENTED_EDGE('',*,*,#48671,.T.) ;
#67652 = ORIENTED_EDGE('',*,*,#48670,.T.) ;
#67653 = ORIENTED_EDGE('',*,*,#48673,.F.) ;
#67654 = ORIENTED_EDGE('',*,*,#48139,.F.) ;
#67655 = ORIENTED_EDGE('',*,*,#48674,.T.) ;
#67656 = ORIENTED_EDGE('',*,*,#48143,.F.) ;
#67657 = ORIENTED_EDGE('',*,*,#48675,.T.) ;
#67658 = ORIENTED_EDGE('',*,*,#48299,.F.) ;
#67659 = ORIENTED_EDGE('',*,*,#48676,.T.) ;
#67660 = ORIENTED_EDGE('',*,*,#48142,.F.) ;
#67661 = ORIENTED_EDGE('',*,*,#48673,.T.) ;
#67662 = ORIENTED_EDGE('',*,*,#48215,.F.) ;
#67663 = ORIENTED_EDGE('',*,*,#48677,.T.) ;
#67664 = ORIENTED_EDGE('',*,*,#48170,.F.) ;
#67665 = ORIENTED_EDGE('',*,*,#48678,.F.) ;
#67666 = ORIENTED_EDGE('',*,*,#48167,.F.) ;
#67667 = ORIENTED_EDGE('',*,*,#48679,.T.) ;
#67668 = ORIENTED_EDGE('',*,*,#48171,.F.) ;
#67669 = ORIENTED_EDGE('',*,*,#48680,.T.) ;
#67670 = ORIENTED_EDGE('',*,*,#48681,.F.) ;
#67671 = ORIENTED_EDGE('',*,*,#48678,.T.) ;
#67672 = ORIENTED_EDGE('',*,*,#48682,.F.) ;
#67673 = ORIENTED_EDGE('',*,*,#48168,.F.) ;
#67674 = ORIENTED_EDGE('',*,*,#48683,.T.) ;
#67675 = ORIENTED_EDGE('',*,*,#48217,.F.) ;
#67676 = ORIENTED_EDGE('',*,*,#48684,.F.) ;
#67677 = ORIENTED_EDGE('',*,*,#48682,.T.) ;
#67678 = ORIENTED_EDGE('',*,*,#48169,.F.) ;
#67679 = ORIENTED_EDGE('',*,*,#48685,.F.) ;
#67680 = ORIENTED_EDGE('',*,*,#48163,.F.) ;
#67681 = ORIENTED_EDGE('',*,*,#48681,.T.) ;
#67682 = ORIENTED_EDGE('',*,*,#48166,.F.) ;
#67683 = ORIENTED_EDGE('',*,*,#48686,.F.) ;
#67684 = ORIENTED_EDGE('',*,*,#48216,.F.) ;
#67685 = ORIENTED_EDGE('',*,*,#48685,.T.) ;
#67686 = ORIENTED_EDGE('',*,*,#48684,.T.) ;
#67687 = ORIENTED_EDGE('',*,*,#48687,.F.) ;
#67688 = ORIENTED_EDGE('',*,*,#48688,.F.) ;
#67689 = ORIENTED_EDGE('',*,*,#48686,.T.) ;
#67690 = ORIENTED_EDGE('',*,*,#48689,.F.) ;
#67691 = ORIENTED_EDGE('',*,*,#48687,.T.) ;
#67692 = ORIENTED_EDGE('',*,*,#48220,.F.) ;
#67693 = ORIENTED_EDGE('',*,*,#48690,.F.) ;
#67694 = ORIENTED_EDGE('',*,*,#48164,.F.) ;
#67695 = ORIENTED_EDGE('',*,*,#48689,.T.) ;
#67696 = ORIENTED_EDGE('',*,*,#48165,.F.) ;
#67697 = ORIENTED_EDGE('',*,*,#48691,.F.) ;
#67698 = ORIENTED_EDGE('',*,*,#48159,.F.) ;
#67699 = ORIENTED_EDGE('',*,*,#48162,.F.) ;
#67700 = ORIENTED_EDGE('',*,*,#48692,.T.) ;
#67701 = ORIENTED_EDGE('',*,*,#48213,.F.) ;
#67702 = ORIENTED_EDGE('',*,*,#48688,.T.) ;
#67703 = ORIENTED_EDGE('',*,*,#48691,.T.) ;
#67704 = ORIENTED_EDGE('',*,*,#48690,.T.) ;
#67705 = ORIENTED_EDGE('',*,*,#48693,.F.) ;
#67706 = ORIENTED_EDGE('',*,*,#48157,.F.) ;
#67707 = ORIENTED_EDGE('',*,*,#48694,.T.) ;
#67708 = ORIENTED_EDGE('',*,*,#48161,.F.) ;
#67709 = ORIENTED_EDGE('',*,*,#48695,.T.) ;
#67710 = ORIENTED_EDGE('',*,*,#48219,.F.) ;
#67711 = ORIENTED_EDGE('',*,*,#48696,.T.) ;
#67712 = ORIENTED_EDGE('',*,*,#48160,.F.) ;
#67713 = ORIENTED_EDGE('',*,*,#48693,.T.) ;
#67714 = ORIENTED_EDGE('',*,*,#48287,.F.) ;
#67715 = ORIENTED_EDGE('',*,*,#48697,.T.) ;
#67716 = ORIENTED_EDGE('',*,*,#48192,.F.) ;
#67717 = ORIENTED_EDGE('',*,*,#48698,.F.) ;
#67718 = ORIENTED_EDGE('',*,*,#48189,.F.) ;
#67719 = ORIENTED_EDGE('',*,*,#48699,.T.) ;
#67720 = ORIENTED_EDGE('',*,*,#48193,.F.) ;
#67721 = ORIENTED_EDGE('',*,*,#48700,.T.) ;
#67722 = ORIENTED_EDGE('',*,*,#48701,.F.) ;
#67723 = ORIENTED_EDGE('',*,*,#48698,.T.) ;
#67724 = ORIENTED_EDGE('',*,*,#48702,.F.) ;
#67725 = ORIENTED_EDGE('',*,*,#48190,.F.) ;
#67726 = ORIENTED_EDGE('',*,*,#48703,.T.) ;
#67727 = ORIENTED_EDGE('',*,*,#48289,.F.) ;
#67728 = ORIENTED_EDGE('',*,*,#48704,.F.) ;
#67729 = ORIENTED_EDGE('',*,*,#48702,.T.) ;
#67730 = ORIENTED_EDGE('',*,*,#48191,.F.) ;
#67731 = ORIENTED_EDGE('',*,*,#48705,.F.) ;
#67732 = ORIENTED_EDGE('',*,*,#48205,.F.) ;
#67733 = ORIENTED_EDGE('',*,*,#48701,.T.) ;
#67734 = ORIENTED_EDGE('',*,*,#48204,.F.) ;
#67735 = ORIENTED_EDGE('',*,*,#48706,.F.) ;
#67736 = ORIENTED_EDGE('',*,*,#48288,.F.) ;
#67737 = ORIENTED_EDGE('',*,*,#48705,.T.) ;
#67738 = ORIENTED_EDGE('',*,*,#48704,.T.) ;
#67739 = ORIENTED_EDGE('',*,*,#48707,.F.) ;
#67740 = ORIENTED_EDGE('',*,*,#48708,.F.) ;
#67741 = ORIENTED_EDGE('',*,*,#48706,.T.) ;
#67742 = ORIENTED_EDGE('',*,*,#48709,.F.) ;
#67743 = ORIENTED_EDGE('',*,*,#48707,.T.) ;
#67744 = ORIENTED_EDGE('',*,*,#48292,.F.) ;
#67745 = ORIENTED_EDGE('',*,*,#48710,.F.) ;
#67746 = ORIENTED_EDGE('',*,*,#48206,.F.) ;
#67747 = ORIENTED_EDGE('',*,*,#48709,.T.) ;
#67748 = ORIENTED_EDGE('',*,*,#48203,.F.) ;
#67749 = ORIENTED_EDGE('',*,*,#48711,.F.) ;
#67750 = ORIENTED_EDGE('',*,*,#48199,.F.) ;
#67751 = ORIENTED_EDGE('',*,*,#48202,.F.) ;
#67752 = ORIENTED_EDGE('',*,*,#48712,.T.) ;
#67753 = ORIENTED_EDGE('',*,*,#48285,.F.) ;
#67754 = ORIENTED_EDGE('',*,*,#48708,.T.) ;
#67755 = ORIENTED_EDGE('',*,*,#48711,.T.) ;
#67756 = ORIENTED_EDGE('',*,*,#48710,.T.) ;
#67757 = ORIENTED_EDGE('',*,*,#48713,.F.) ;
#67758 = ORIENTED_EDGE('',*,*,#48197,.F.) ;
#67759 = ORIENTED_EDGE('',*,*,#48714,.T.) ;
#67760 = ORIENTED_EDGE('',*,*,#48201,.F.) ;
#67761 = ORIENTED_EDGE('',*,*,#48715,.T.) ;
#67762 = ORIENTED_EDGE('',*,*,#48291,.F.) ;
#67763 = ORIENTED_EDGE('',*,*,#48716,.T.) ;
#67764 = ORIENTED_EDGE('',*,*,#48200,.F.) ;
#67765 = ORIENTED_EDGE('',*,*,#48713,.T.) ;
#67766 = ORIENTED_EDGE('',*,*,#44488,.F.) ;
#67767 = ORIENTED_EDGE('',*,*,#47723,.F.) ;
#67768 = ORIENTED_EDGE('',*,*,#48717,.F.) ;
#67769 = ORIENTED_EDGE('',*,*,#47718,.F.) ;
#67770 = ORIENTED_EDGE('',*,*,#48717,.T.) ;
#67771 = ORIENTED_EDGE('',*,*,#47708,.F.) ;
#67772 = ORIENTED_EDGE('',*,*,#48718,.F.) ;
#67773 = ORIENTED_EDGE('',*,*,#47719,.F.) ;
#67774 = ORIENTED_EDGE('',*,*,#48718,.T.) ;
#67775 = ORIENTED_EDGE('',*,*,#48359,.F.) ;
#67776 = ORIENTED_EDGE('',*,*,#48357,.F.) ;
#67777 = ORIENTED_EDGE('',*,*,#48719,.F.) ;
#67778 = ORIENTED_EDGE('',*,*,#48719,.T.) ;
#67779 = ORIENTED_EDGE('',*,*,#48278,.F.) ;
#67780 = ORIENTED_EDGE('',*,*,#48720,.F.) ;
#67781 = ORIENTED_EDGE('',*,*,#47720,.F.) ;
#67782 = ORIENTED_EDGE('',*,*,#48720,.T.) ;
#67783 = ORIENTED_EDGE('',*,*,#48372,.F.) ;
#67784 = ORIENTED_EDGE('',*,*,#48374,.F.) ;
#67785 = ORIENTED_EDGE('',*,*,#48721,.F.) ;
#67786 = ORIENTED_EDGE('',*,*,#48721,.T.) ;
#67787 = ORIENTED_EDGE('',*,*,#47692,.F.) ;
#67788 = ORIENTED_EDGE('',*,*,#48722,.F.) ;
#67789 = ORIENTED_EDGE('',*,*,#47716,.F.) ;
#67790 = ORIENTED_EDGE('',*,*,#44335,.F.) ;
#67791 = ORIENTED_EDGE('',*,*,#47717,.F.) ;
#67792 = ORIENTED_EDGE('',*,*,#48722,.T.) ;
#67793 = ORIENTED_EDGE('',*,*,#47721,.F.) ;
#67794 = ORIENTED_EDGE('',*,*,#46675,.F.) ;
#67795 = ORIENTED_EDGE('',*,*,#46678,.F.) ;
#67796 = ORIENTED_EDGE('',*,*,#47722,.F.) ;
#67797 = ORIENTED_EDGE('',*,*,#48723,.F.) ;
#67798 = ORIENTED_EDGE('',*,*,#47713,.F.) ;
#67799 = ORIENTED_EDGE('',*,*,#48723,.T.) ;
#67800 = ORIENTED_EDGE('',*,*,#47694,.F.) ;
#67801 = ORIENTED_EDGE('',*,*,#48724,.F.) ;
#67802 = ORIENTED_EDGE('',*,*,#47714,.F.) ;
#67803 = ORIENTED_EDGE('',*,*,#48724,.T.) ;
#67804 = ORIENTED_EDGE('',*,*,#48375,.F.) ;
#67805 = ORIENTED_EDGE('',*,*,#48376,.F.) ;
#67806 = ORIENTED_EDGE('',*,*,#48725,.F.) ;
#67807 = ORIENTED_EDGE('',*,*,#48725,.T.) ;
#67808 = ORIENTED_EDGE('',*,*,#48282,.F.) ;
#67809 = ORIENTED_EDGE('',*,*,#48726,.F.) ;
#67810 = ORIENTED_EDGE('',*,*,#47715,.F.) ;
#67811 = ORIENTED_EDGE('',*,*,#48726,.T.) ;
#67812 = ORIENTED_EDGE('',*,*,#48363,.F.) ;
#67813 = ORIENTED_EDGE('',*,*,#48360,.F.) ;
#67814 = ORIENTED_EDGE('',*,*,#48727,.F.) ;
#67815 = ORIENTED_EDGE('',*,*,#48727,.T.) ;
#67816 = ORIENTED_EDGE('',*,*,#47710,.F.) ;
#67817 = ORIENTED_EDGE('',*,*,#48728,.F.) ;
#67818 = ORIENTED_EDGE('',*,*,#47711,.F.) ;
#67819 = ORIENTED_EDGE('',*,*,#48728,.T.) ;
#67820 = ORIENTED_EDGE('',*,*,#47724,.F.) ;
#67821 = ORIENTED_EDGE('',*,*,#44486,.F.) ;
#67822 = ORIENTED_EDGE('',*,*,#47712,.F.) ;
#67823 = ORIENTED_EDGE('',*,*,#46596,.F.) ;
#67824 = ORIENTED_EDGE('',*,*,#47730,.F.) ;
#67825 = ORIENTED_EDGE('',*,*,#48729,.F.) ;
#67826 = ORIENTED_EDGE('',*,*,#47746,.F.) ;
#67827 = ORIENTED_EDGE('',*,*,#48729,.T.) ;
#67828 = ORIENTED_EDGE('',*,*,#48379,.F.) ;
#67829 = ORIENTED_EDGE('',*,*,#48377,.F.) ;
#67830 = ORIENTED_EDGE('',*,*,#48730,.F.) ;
#67831 = ORIENTED_EDGE('',*,*,#48730,.T.) ;
#67832 = ORIENTED_EDGE('',*,*,#48350,.F.) ;
#67833 = ORIENTED_EDGE('',*,*,#48731,.F.) ;
#67834 = ORIENTED_EDGE('',*,*,#47747,.F.) ;
#67835 = ORIENTED_EDGE('',*,*,#48731,.T.) ;
#67836 = ORIENTED_EDGE('',*,*,#48392,.F.) ;
#67837 = ORIENTED_EDGE('',*,*,#48394,.F.) ;
#67838 = ORIENTED_EDGE('',*,*,#48732,.F.) ;
#67839 = ORIENTED_EDGE('',*,*,#46598,.F.) ;
#67840 = ORIENTED_EDGE('',*,*,#47748,.F.) ;
#67841 = ORIENTED_EDGE('',*,*,#48732,.T.) ;
#67842 = ORIENTED_EDGE('',*,*,#47732,.F.) ;
#67843 = ORIENTED_EDGE('',*,*,#48733,.F.) ;
#67844 = ORIENTED_EDGE('',*,*,#47731,.F.) ;
#67845 = ORIENTED_EDGE('',*,*,#46594,.F.) ;
#67846 = ORIENTED_EDGE('',*,*,#47744,.F.) ;
#67847 = ORIENTED_EDGE('',*,*,#48380,.F.) ;
#67848 = ORIENTED_EDGE('',*,*,#48733,.T.) ;
#67849 = ORIENTED_EDGE('',*,*,#48734,.F.) ;
#67850 = ORIENTED_EDGE('',*,*,#48383,.F.) ;
#67851 = ORIENTED_EDGE('',*,*,#48734,.T.) ;
#67852 = ORIENTED_EDGE('',*,*,#47743,.F.) ;
#67853 = ORIENTED_EDGE('',*,*,#48735,.F.) ;
#67854 = ORIENTED_EDGE('',*,*,#48354,.F.) ;
#67855 = ORIENTED_EDGE('',*,*,#46600,.F.) ;
#67856 = ORIENTED_EDGE('',*,*,#47734,.F.) ;
#67857 = ORIENTED_EDGE('',*,*,#48736,.F.) ;
#67858 = ORIENTED_EDGE('',*,*,#47745,.F.) ;
#67859 = ORIENTED_EDGE('',*,*,#48396,.F.) ;
#67860 = ORIENTED_EDGE('',*,*,#48735,.T.) ;
#67861 = ORIENTED_EDGE('',*,*,#48736,.T.) ;
#67862 = ORIENTED_EDGE('',*,*,#48395,.F.) ;
#67863 = ORIENTED_EDGE('',*,*,#44477,.F.) ;
#67864 = ORIENTED_EDGE('',*,*,#47781,.F.) ;
#67865 = ORIENTED_EDGE('',*,*,#48737,.F.) ;
#67866 = ORIENTED_EDGE('',*,*,#47776,.F.) ;
#67867 = ORIENTED_EDGE('',*,*,#48737,.T.) ;
#67868 = ORIENTED_EDGE('',*,*,#47766,.F.) ;
#67869 = ORIENTED_EDGE('',*,*,#48738,.F.) ;
#67870 = ORIENTED_EDGE('',*,*,#47777,.F.) ;
#67871 = ORIENTED_EDGE('',*,*,#48738,.T.) ;
#67872 = ORIENTED_EDGE('',*,*,#48399,.F.) ;
#67873 = ORIENTED_EDGE('',*,*,#48397,.F.) ;
#67874 = ORIENTED_EDGE('',*,*,#48739,.F.) ;
#67875 = ORIENTED_EDGE('',*,*,#48739,.T.) ;
#67876 = ORIENTED_EDGE('',*,*,#48270,.F.) ;
#67877 = ORIENTED_EDGE('',*,*,#48740,.F.) ;
#67878 = ORIENTED_EDGE('',*,*,#47778,.F.) ;
#67879 = ORIENTED_EDGE('',*,*,#48740,.T.) ;
#67880 = ORIENTED_EDGE('',*,*,#48412,.F.) ;
#67881 = ORIENTED_EDGE('',*,*,#48414,.F.) ;
#67882 = ORIENTED_EDGE('',*,*,#48741,.F.) ;
#67883 = ORIENTED_EDGE('',*,*,#48741,.T.) ;
#67884 = ORIENTED_EDGE('',*,*,#47750,.F.) ;
#67885 = ORIENTED_EDGE('',*,*,#48742,.F.) ;
#67886 = ORIENTED_EDGE('',*,*,#47774,.F.) ;
#67887 = ORIENTED_EDGE('',*,*,#44282,.F.) ;
#67888 = ORIENTED_EDGE('',*,*,#47775,.F.) ;
#67889 = ORIENTED_EDGE('',*,*,#48742,.T.) ;
#67890 = ORIENTED_EDGE('',*,*,#47779,.F.) ;
#67891 = ORIENTED_EDGE('',*,*,#46997,.F.) ;
#67892 = ORIENTED_EDGE('',*,*,#47000,.F.) ;
#67893 = ORIENTED_EDGE('',*,*,#47780,.F.) ;
#67894 = ORIENTED_EDGE('',*,*,#48743,.F.) ;
#67895 = ORIENTED_EDGE('',*,*,#47771,.F.) ;
#67896 = ORIENTED_EDGE('',*,*,#48743,.T.) ;
#67897 = ORIENTED_EDGE('',*,*,#47752,.F.) ;
#67898 = ORIENTED_EDGE('',*,*,#48744,.F.) ;
#67899 = ORIENTED_EDGE('',*,*,#47772,.F.) ;
#67900 = ORIENTED_EDGE('',*,*,#48744,.T.) ;
#67901 = ORIENTED_EDGE('',*,*,#48415,.F.) ;
#67902 = ORIENTED_EDGE('',*,*,#48416,.F.) ;
#67903 = ORIENTED_EDGE('',*,*,#48745,.F.) ;
#67904 = ORIENTED_EDGE('',*,*,#48745,.T.) ;
#67905 = ORIENTED_EDGE('',*,*,#48274,.F.) ;
#67906 = ORIENTED_EDGE('',*,*,#48746,.F.) ;
#67907 = ORIENTED_EDGE('',*,*,#47773,.F.) ;
#67908 = ORIENTED_EDGE('',*,*,#48746,.T.) ;
#67909 = ORIENTED_EDGE('',*,*,#48403,.F.) ;
#67910 = ORIENTED_EDGE('',*,*,#48400,.F.) ;
#67911 = ORIENTED_EDGE('',*,*,#48747,.F.) ;
#67912 = ORIENTED_EDGE('',*,*,#48747,.T.) ;
#67913 = ORIENTED_EDGE('',*,*,#47768,.F.) ;
#67914 = ORIENTED_EDGE('',*,*,#48748,.F.) ;
#67915 = ORIENTED_EDGE('',*,*,#47769,.F.) ;
#67916 = ORIENTED_EDGE('',*,*,#48748,.T.) ;
#67917 = ORIENTED_EDGE('',*,*,#47782,.F.) ;
#67918 = ORIENTED_EDGE('',*,*,#44475,.F.) ;
#67919 = ORIENTED_EDGE('',*,*,#47770,.F.) ;
#67920 = ORIENTED_EDGE('',*,*,#46604,.F.) ;
#67921 = ORIENTED_EDGE('',*,*,#47788,.F.) ;
#67922 = ORIENTED_EDGE('',*,*,#48749,.F.) ;
#67923 = ORIENTED_EDGE('',*,*,#47804,.F.) ;
#67924 = ORIENTED_EDGE('',*,*,#48749,.T.) ;
#67925 = ORIENTED_EDGE('',*,*,#48419,.F.) ;
#67926 = ORIENTED_EDGE('',*,*,#48417,.F.) ;
#67927 = ORIENTED_EDGE('',*,*,#48750,.F.) ;
#67928 = ORIENTED_EDGE('',*,*,#48750,.T.) ;
#67929 = ORIENTED_EDGE('',*,*,#48342,.F.) ;
#67930 = ORIENTED_EDGE('',*,*,#48751,.F.) ;
#67931 = ORIENTED_EDGE('',*,*,#47805,.F.) ;
#67932 = ORIENTED_EDGE('',*,*,#48751,.T.) ;
#67933 = ORIENTED_EDGE('',*,*,#48432,.F.) ;
#67934 = ORIENTED_EDGE('',*,*,#48434,.F.) ;
#67935 = ORIENTED_EDGE('',*,*,#48752,.F.) ;
#67936 = ORIENTED_EDGE('',*,*,#46606,.F.) ;
#67937 = ORIENTED_EDGE('',*,*,#47806,.F.) ;
#67938 = ORIENTED_EDGE('',*,*,#48752,.T.) ;
#67939 = ORIENTED_EDGE('',*,*,#47790,.F.) ;
#67940 = ORIENTED_EDGE('',*,*,#48753,.F.) ;
#67941 = ORIENTED_EDGE('',*,*,#47789,.F.) ;
#67942 = ORIENTED_EDGE('',*,*,#46602,.F.) ;
#67943 = ORIENTED_EDGE('',*,*,#47802,.F.) ;
#67944 = ORIENTED_EDGE('',*,*,#48420,.F.) ;
#67945 = ORIENTED_EDGE('',*,*,#48753,.T.) ;
#67946 = ORIENTED_EDGE('',*,*,#48754,.F.) ;
#67947 = ORIENTED_EDGE('',*,*,#48423,.F.) ;
#67948 = ORIENTED_EDGE('',*,*,#48754,.T.) ;
#67949 = ORIENTED_EDGE('',*,*,#47801,.F.) ;
#67950 = ORIENTED_EDGE('',*,*,#48755,.F.) ;
#67951 = ORIENTED_EDGE('',*,*,#48346,.F.) ;
#67952 = ORIENTED_EDGE('',*,*,#46608,.F.) ;
#67953 = ORIENTED_EDGE('',*,*,#47792,.F.) ;
#67954 = ORIENTED_EDGE('',*,*,#48756,.F.) ;
#67955 = ORIENTED_EDGE('',*,*,#47803,.F.) ;
#67956 = ORIENTED_EDGE('',*,*,#48436,.F.) ;
#67957 = ORIENTED_EDGE('',*,*,#48755,.T.) ;
#67958 = ORIENTED_EDGE('',*,*,#48756,.T.) ;
#67959 = ORIENTED_EDGE('',*,*,#48435,.F.) ;
#67960 = ORIENTED_EDGE('',*,*,#44466,.F.) ;
#67961 = ORIENTED_EDGE('',*,*,#47839,.F.) ;
#67962 = ORIENTED_EDGE('',*,*,#48757,.F.) ;
#67963 = ORIENTED_EDGE('',*,*,#47834,.F.) ;
#67964 = ORIENTED_EDGE('',*,*,#48757,.T.) ;
#67965 = ORIENTED_EDGE('',*,*,#47824,.F.) ;
#67966 = ORIENTED_EDGE('',*,*,#48758,.F.) ;
#67967 = ORIENTED_EDGE('',*,*,#47835,.F.) ;
#67968 = ORIENTED_EDGE('',*,*,#48758,.T.) ;
#67969 = ORIENTED_EDGE('',*,*,#48439,.F.) ;
#67970 = ORIENTED_EDGE('',*,*,#48437,.F.) ;
#67971 = ORIENTED_EDGE('',*,*,#48759,.F.) ;
#67972 = ORIENTED_EDGE('',*,*,#48759,.T.) ;
#67973 = ORIENTED_EDGE('',*,*,#48262,.F.) ;
#67974 = ORIENTED_EDGE('',*,*,#48760,.F.) ;
#67975 = ORIENTED_EDGE('',*,*,#47836,.F.) ;
#67976 = ORIENTED_EDGE('',*,*,#48760,.T.) ;
#67977 = ORIENTED_EDGE('',*,*,#48452,.F.) ;
#67978 = ORIENTED_EDGE('',*,*,#48454,.F.) ;
#67979 = ORIENTED_EDGE('',*,*,#48761,.F.) ;
#67980 = ORIENTED_EDGE('',*,*,#48761,.T.) ;
#67981 = ORIENTED_EDGE('',*,*,#47808,.F.) ;
#67982 = ORIENTED_EDGE('',*,*,#48762,.F.) ;
#67983 = ORIENTED_EDGE('',*,*,#47832,.F.) ;
#67984 = ORIENTED_EDGE('',*,*,#44265,.F.) ;
#67985 = ORIENTED_EDGE('',*,*,#47833,.F.) ;
#67986 = ORIENTED_EDGE('',*,*,#48762,.T.) ;
#67987 = ORIENTED_EDGE('',*,*,#47837,.F.) ;
#67988 = ORIENTED_EDGE('',*,*,#47085,.F.) ;
#67989 = ORIENTED_EDGE('',*,*,#47088,.F.) ;
#67990 = ORIENTED_EDGE('',*,*,#47838,.F.) ;
#67991 = ORIENTED_EDGE('',*,*,#48763,.F.) ;
#67992 = ORIENTED_EDGE('',*,*,#47829,.F.) ;
#67993 = ORIENTED_EDGE('',*,*,#48763,.T.) ;
#67994 = ORIENTED_EDGE('',*,*,#47810,.F.) ;
#67995 = ORIENTED_EDGE('',*,*,#48764,.F.) ;
#67996 = ORIENTED_EDGE('',*,*,#47830,.F.) ;
#67997 = ORIENTED_EDGE('',*,*,#48764,.T.) ;
#67998 = ORIENTED_EDGE('',*,*,#48455,.F.) ;
#67999 = ORIENTED_EDGE('',*,*,#48456,.F.) ;
#68000 = ORIENTED_EDGE('',*,*,#48765,.F.) ;
#68001 = ORIENTED_EDGE('',*,*,#48765,.T.) ;
#68002 = ORIENTED_EDGE('',*,*,#48266,.F.) ;
#68003 = ORIENTED_EDGE('',*,*,#48766,.F.) ;
#68004 = ORIENTED_EDGE('',*,*,#47831,.F.) ;
#68005 = ORIENTED_EDGE('',*,*,#48766,.T.) ;
#68006 = ORIENTED_EDGE('',*,*,#48443,.F.) ;
#68007 = ORIENTED_EDGE('',*,*,#48440,.F.) ;
#68008 = ORIENTED_EDGE('',*,*,#48767,.F.) ;
#68009 = ORIENTED_EDGE('',*,*,#48767,.T.) ;
#68010 = ORIENTED_EDGE('',*,*,#47826,.F.) ;
#68011 = ORIENTED_EDGE('',*,*,#48768,.F.) ;
#68012 = ORIENTED_EDGE('',*,*,#47827,.F.) ;
#68013 = ORIENTED_EDGE('',*,*,#48768,.T.) ;
#68014 = ORIENTED_EDGE('',*,*,#47840,.F.) ;
#68015 = ORIENTED_EDGE('',*,*,#44464,.F.) ;
#68016 = ORIENTED_EDGE('',*,*,#47828,.F.) ;
#68017 = ORIENTED_EDGE('',*,*,#46612,.F.) ;
#68018 = ORIENTED_EDGE('',*,*,#47846,.F.) ;
#68019 = ORIENTED_EDGE('',*,*,#48769,.F.) ;
#68020 = ORIENTED_EDGE('',*,*,#47862,.F.) ;
#68021 = ORIENTED_EDGE('',*,*,#48769,.T.) ;
#68022 = ORIENTED_EDGE('',*,*,#48459,.F.) ;
#68023 = ORIENTED_EDGE('',*,*,#48457,.F.) ;
#68024 = ORIENTED_EDGE('',*,*,#48770,.F.) ;
#68025 = ORIENTED_EDGE('',*,*,#48770,.T.) ;
#68026 = ORIENTED_EDGE('',*,*,#48334,.F.) ;
#68027 = ORIENTED_EDGE('',*,*,#48771,.F.) ;
#68028 = ORIENTED_EDGE('',*,*,#47863,.F.) ;
#68029 = ORIENTED_EDGE('',*,*,#48771,.T.) ;
#68030 = ORIENTED_EDGE('',*,*,#48472,.F.) ;
#68031 = ORIENTED_EDGE('',*,*,#48474,.F.) ;
#68032 = ORIENTED_EDGE('',*,*,#48772,.F.) ;
#68033 = ORIENTED_EDGE('',*,*,#46614,.F.) ;
#68034 = ORIENTED_EDGE('',*,*,#47864,.F.) ;
#68035 = ORIENTED_EDGE('',*,*,#48772,.T.) ;
#68036 = ORIENTED_EDGE('',*,*,#47848,.F.) ;
#68037 = ORIENTED_EDGE('',*,*,#48773,.F.) ;
#68038 = ORIENTED_EDGE('',*,*,#47847,.F.) ;
#68039 = ORIENTED_EDGE('',*,*,#46610,.F.) ;
#68040 = ORIENTED_EDGE('',*,*,#47860,.F.) ;
#68041 = ORIENTED_EDGE('',*,*,#48460,.F.) ;
#68042 = ORIENTED_EDGE('',*,*,#48773,.T.) ;
#68043 = ORIENTED_EDGE('',*,*,#48774,.F.) ;
#68044 = ORIENTED_EDGE('',*,*,#48463,.F.) ;
#68045 = ORIENTED_EDGE('',*,*,#48774,.T.) ;
#68046 = ORIENTED_EDGE('',*,*,#47859,.F.) ;
#68047 = ORIENTED_EDGE('',*,*,#48775,.F.) ;
#68048 = ORIENTED_EDGE('',*,*,#48338,.F.) ;
#68049 = ORIENTED_EDGE('',*,*,#46616,.F.) ;
#68050 = ORIENTED_EDGE('',*,*,#47850,.F.) ;
#68051 = ORIENTED_EDGE('',*,*,#48776,.F.) ;
#68052 = ORIENTED_EDGE('',*,*,#47861,.F.) ;
#68053 = ORIENTED_EDGE('',*,*,#48476,.F.) ;
#68054 = ORIENTED_EDGE('',*,*,#48775,.T.) ;
#68055 = ORIENTED_EDGE('',*,*,#48776,.T.) ;
#68056 = ORIENTED_EDGE('',*,*,#48475,.F.) ;
#68057 = ORIENTED_EDGE('',*,*,#44455,.F.) ;
#68058 = ORIENTED_EDGE('',*,*,#47897,.F.) ;
#68059 = ORIENTED_EDGE('',*,*,#48777,.F.) ;
#68060 = ORIENTED_EDGE('',*,*,#47892,.F.) ;
#68061 = ORIENTED_EDGE('',*,*,#48777,.T.) ;
#68062 = ORIENTED_EDGE('',*,*,#47882,.F.) ;
#68063 = ORIENTED_EDGE('',*,*,#48778,.F.) ;
#68064 = ORIENTED_EDGE('',*,*,#47893,.F.) ;
#68065 = ORIENTED_EDGE('',*,*,#48778,.T.) ;
#68066 = ORIENTED_EDGE('',*,*,#48479,.F.) ;
#68067 = ORIENTED_EDGE('',*,*,#48477,.F.) ;
#68068 = ORIENTED_EDGE('',*,*,#48779,.F.) ;
#68069 = ORIENTED_EDGE('',*,*,#48779,.T.) ;
#68070 = ORIENTED_EDGE('',*,*,#48254,.F.) ;
#68071 = ORIENTED_EDGE('',*,*,#48780,.F.) ;
#68072 = ORIENTED_EDGE('',*,*,#47894,.F.) ;
#68073 = ORIENTED_EDGE('',*,*,#48780,.T.) ;
#68074 = ORIENTED_EDGE('',*,*,#48492,.F.) ;
#68075 = ORIENTED_EDGE('',*,*,#48494,.F.) ;
#68076 = ORIENTED_EDGE('',*,*,#48781,.F.) ;
#68077 = ORIENTED_EDGE('',*,*,#48781,.T.) ;
#68078 = ORIENTED_EDGE('',*,*,#47866,.F.) ;
#68079 = ORIENTED_EDGE('',*,*,#48782,.F.) ;
#68080 = ORIENTED_EDGE('',*,*,#47890,.F.) ;
#68081 = ORIENTED_EDGE('',*,*,#44248,.F.) ;
#68082 = ORIENTED_EDGE('',*,*,#47891,.F.) ;
#68083 = ORIENTED_EDGE('',*,*,#48782,.T.) ;
#68084 = ORIENTED_EDGE('',*,*,#47895,.F.) ;
#68085 = ORIENTED_EDGE('',*,*,#47173,.F.) ;
#68086 = ORIENTED_EDGE('',*,*,#47176,.F.) ;
#68087 = ORIENTED_EDGE('',*,*,#47896,.F.) ;
#68088 = ORIENTED_EDGE('',*,*,#48783,.F.) ;
#68089 = ORIENTED_EDGE('',*,*,#47887,.F.) ;
#68090 = ORIENTED_EDGE('',*,*,#48783,.T.) ;
#68091 = ORIENTED_EDGE('',*,*,#47868,.F.) ;
#68092 = ORIENTED_EDGE('',*,*,#48784,.F.) ;
#68093 = ORIENTED_EDGE('',*,*,#47888,.F.) ;
#68094 = ORIENTED_EDGE('',*,*,#48784,.T.) ;
#68095 = ORIENTED_EDGE('',*,*,#48495,.F.) ;
#68096 = ORIENTED_EDGE('',*,*,#48496,.F.) ;
#68097 = ORIENTED_EDGE('',*,*,#48785,.F.) ;
#68098 = ORIENTED_EDGE('',*,*,#48785,.T.) ;
#68099 = ORIENTED_EDGE('',*,*,#48258,.F.) ;
#68100 = ORIENTED_EDGE('',*,*,#48786,.F.) ;
#68101 = ORIENTED_EDGE('',*,*,#47889,.F.) ;
#68102 = ORIENTED_EDGE('',*,*,#48786,.T.) ;
#68103 = ORIENTED_EDGE('',*,*,#48483,.F.) ;
#68104 = ORIENTED_EDGE('',*,*,#48480,.F.) ;
#68105 = ORIENTED_EDGE('',*,*,#48787,.F.) ;
#68106 = ORIENTED_EDGE('',*,*,#48787,.T.) ;
#68107 = ORIENTED_EDGE('',*,*,#47884,.F.) ;
#68108 = ORIENTED_EDGE('',*,*,#48788,.F.) ;
#68109 = ORIENTED_EDGE('',*,*,#47885,.F.) ;
#68110 = ORIENTED_EDGE('',*,*,#48788,.T.) ;
#68111 = ORIENTED_EDGE('',*,*,#47898,.F.) ;
#68112 = ORIENTED_EDGE('',*,*,#44453,.F.) ;
#68113 = ORIENTED_EDGE('',*,*,#47886,.F.) ;
#68114 = ORIENTED_EDGE('',*,*,#46620,.F.) ;
#68115 = ORIENTED_EDGE('',*,*,#47904,.F.) ;
#68116 = ORIENTED_EDGE('',*,*,#48789,.F.) ;
#68117 = ORIENTED_EDGE('',*,*,#47920,.F.) ;
#68118 = ORIENTED_EDGE('',*,*,#48789,.T.) ;
#68119 = ORIENTED_EDGE('',*,*,#48499,.F.) ;
#68120 = ORIENTED_EDGE('',*,*,#48497,.F.) ;
#68121 = ORIENTED_EDGE('',*,*,#48790,.F.) ;
#68122 = ORIENTED_EDGE('',*,*,#48790,.T.) ;
#68123 = ORIENTED_EDGE('',*,*,#48326,.F.) ;
#68124 = ORIENTED_EDGE('',*,*,#48791,.F.) ;
#68125 = ORIENTED_EDGE('',*,*,#47921,.F.) ;
#68126 = ORIENTED_EDGE('',*,*,#48791,.T.) ;
#68127 = ORIENTED_EDGE('',*,*,#48512,.F.) ;
#68128 = ORIENTED_EDGE('',*,*,#48514,.F.) ;
#68129 = ORIENTED_EDGE('',*,*,#48792,.F.) ;
#68130 = ORIENTED_EDGE('',*,*,#46622,.F.) ;
#68131 = ORIENTED_EDGE('',*,*,#47922,.F.) ;
#68132 = ORIENTED_EDGE('',*,*,#48792,.T.) ;
#68133 = ORIENTED_EDGE('',*,*,#47906,.F.) ;
#68134 = ORIENTED_EDGE('',*,*,#48793,.F.) ;
#68135 = ORIENTED_EDGE('',*,*,#47905,.F.) ;
#68136 = ORIENTED_EDGE('',*,*,#46618,.F.) ;
#68137 = ORIENTED_EDGE('',*,*,#47918,.F.) ;
#68138 = ORIENTED_EDGE('',*,*,#48500,.F.) ;
#68139 = ORIENTED_EDGE('',*,*,#48793,.T.) ;
#68140 = ORIENTED_EDGE('',*,*,#48794,.F.) ;
#68141 = ORIENTED_EDGE('',*,*,#48503,.F.) ;
#68142 = ORIENTED_EDGE('',*,*,#48794,.T.) ;
#68143 = ORIENTED_EDGE('',*,*,#47917,.F.) ;
#68144 = ORIENTED_EDGE('',*,*,#48795,.F.) ;
#68145 = ORIENTED_EDGE('',*,*,#48330,.F.) ;
#68146 = ORIENTED_EDGE('',*,*,#46624,.F.) ;
#68147 = ORIENTED_EDGE('',*,*,#47908,.F.) ;
#68148 = ORIENTED_EDGE('',*,*,#48796,.F.) ;
#68149 = ORIENTED_EDGE('',*,*,#47919,.F.) ;
#68150 = ORIENTED_EDGE('',*,*,#48516,.F.) ;
#68151 = ORIENTED_EDGE('',*,*,#48795,.T.) ;
#68152 = ORIENTED_EDGE('',*,*,#48796,.T.) ;
#68153 = ORIENTED_EDGE('',*,*,#48515,.F.) ;
#68154 = ORIENTED_EDGE('',*,*,#44444,.F.) ;
#68155 = ORIENTED_EDGE('',*,*,#47955,.F.) ;
#68156 = ORIENTED_EDGE('',*,*,#48797,.F.) ;
#68157 = ORIENTED_EDGE('',*,*,#47950,.F.) ;
#68158 = ORIENTED_EDGE('',*,*,#48797,.T.) ;
#68159 = ORIENTED_EDGE('',*,*,#47940,.F.) ;
#68160 = ORIENTED_EDGE('',*,*,#48798,.F.) ;
#68161 = ORIENTED_EDGE('',*,*,#47951,.F.) ;
#68162 = ORIENTED_EDGE('',*,*,#48798,.T.) ;
#68163 = ORIENTED_EDGE('',*,*,#48519,.F.) ;
#68164 = ORIENTED_EDGE('',*,*,#48517,.F.) ;
#68165 = ORIENTED_EDGE('',*,*,#48799,.F.) ;
#68166 = ORIENTED_EDGE('',*,*,#48799,.T.) ;
#68167 = ORIENTED_EDGE('',*,*,#48246,.F.) ;
#68168 = ORIENTED_EDGE('',*,*,#48800,.F.) ;
#68169 = ORIENTED_EDGE('',*,*,#47952,.F.) ;
#68170 = ORIENTED_EDGE('',*,*,#48800,.T.) ;
#68171 = ORIENTED_EDGE('',*,*,#48532,.F.) ;
#68172 = ORIENTED_EDGE('',*,*,#48534,.F.) ;
#68173 = ORIENTED_EDGE('',*,*,#48801,.F.) ;
#68174 = ORIENTED_EDGE('',*,*,#48801,.T.) ;
#68175 = ORIENTED_EDGE('',*,*,#47924,.F.) ;
#68176 = ORIENTED_EDGE('',*,*,#48802,.F.) ;
#68177 = ORIENTED_EDGE('',*,*,#47948,.F.) ;
#68178 = ORIENTED_EDGE('',*,*,#44231,.F.) ;
#68179 = ORIENTED_EDGE('',*,*,#47949,.F.) ;
#68180 = ORIENTED_EDGE('',*,*,#48802,.T.) ;
#68181 = ORIENTED_EDGE('',*,*,#47953,.F.) ;
#68182 = ORIENTED_EDGE('',*,*,#47261,.F.) ;
#68183 = ORIENTED_EDGE('',*,*,#47264,.F.) ;
#68184 = ORIENTED_EDGE('',*,*,#47954,.F.) ;
#68185 = ORIENTED_EDGE('',*,*,#48803,.F.) ;
#68186 = ORIENTED_EDGE('',*,*,#47945,.F.) ;
#68187 = ORIENTED_EDGE('',*,*,#48803,.T.) ;
#68188 = ORIENTED_EDGE('',*,*,#47926,.F.) ;
#68189 = ORIENTED_EDGE('',*,*,#48804,.F.) ;
#68190 = ORIENTED_EDGE('',*,*,#47946,.F.) ;
#68191 = ORIENTED_EDGE('',*,*,#48804,.T.) ;
#68192 = ORIENTED_EDGE('',*,*,#48535,.F.) ;
#68193 = ORIENTED_EDGE('',*,*,#48536,.F.) ;
#68194 = ORIENTED_EDGE('',*,*,#48805,.F.) ;
#68195 = ORIENTED_EDGE('',*,*,#48805,.T.) ;
#68196 = ORIENTED_EDGE('',*,*,#48250,.F.) ;
#68197 = ORIENTED_EDGE('',*,*,#48806,.F.) ;
#68198 = ORIENTED_EDGE('',*,*,#47947,.F.) ;
#68199 = ORIENTED_EDGE('',*,*,#48806,.T.) ;
#68200 = ORIENTED_EDGE('',*,*,#48523,.F.) ;
#68201 = ORIENTED_EDGE('',*,*,#48520,.F.) ;
#68202 = ORIENTED_EDGE('',*,*,#48807,.F.) ;
#68203 = ORIENTED_EDGE('',*,*,#48807,.T.) ;
#68204 = ORIENTED_EDGE('',*,*,#47942,.F.) ;
#68205 = ORIENTED_EDGE('',*,*,#48808,.F.) ;
#68206 = ORIENTED_EDGE('',*,*,#47943,.F.) ;
#68207 = ORIENTED_EDGE('',*,*,#48808,.T.) ;
#68208 = ORIENTED_EDGE('',*,*,#47956,.F.) ;
#68209 = ORIENTED_EDGE('',*,*,#44442,.F.) ;
#68210 = ORIENTED_EDGE('',*,*,#47944,.F.) ;
#68211 = ORIENTED_EDGE('',*,*,#46628,.F.) ;
#68212 = ORIENTED_EDGE('',*,*,#47962,.F.) ;
#68213 = ORIENTED_EDGE('',*,*,#48809,.F.) ;
#68214 = ORIENTED_EDGE('',*,*,#47978,.F.) ;
#68215 = ORIENTED_EDGE('',*,*,#48809,.T.) ;
#68216 = ORIENTED_EDGE('',*,*,#48539,.F.) ;
#68217 = ORIENTED_EDGE('',*,*,#48537,.F.) ;
#68218 = ORIENTED_EDGE('',*,*,#48810,.F.) ;
#68219 = ORIENTED_EDGE('',*,*,#48810,.T.) ;
#68220 = ORIENTED_EDGE('',*,*,#48318,.F.) ;
#68221 = ORIENTED_EDGE('',*,*,#48811,.F.) ;
#68222 = ORIENTED_EDGE('',*,*,#47979,.F.) ;
#68223 = ORIENTED_EDGE('',*,*,#48811,.T.) ;
#68224 = ORIENTED_EDGE('',*,*,#48552,.F.) ;
#68225 = ORIENTED_EDGE('',*,*,#48554,.F.) ;
#68226 = ORIENTED_EDGE('',*,*,#48812,.F.) ;
#68227 = ORIENTED_EDGE('',*,*,#46630,.F.) ;
#68228 = ORIENTED_EDGE('',*,*,#47980,.F.) ;
#68229 = ORIENTED_EDGE('',*,*,#48812,.T.) ;
#68230 = ORIENTED_EDGE('',*,*,#47964,.F.) ;
#68231 = ORIENTED_EDGE('',*,*,#48813,.F.) ;
#68232 = ORIENTED_EDGE('',*,*,#47963,.F.) ;
#68233 = ORIENTED_EDGE('',*,*,#46626,.F.) ;
#68234 = ORIENTED_EDGE('',*,*,#47976,.F.) ;
#68235 = ORIENTED_EDGE('',*,*,#48540,.F.) ;
#68236 = ORIENTED_EDGE('',*,*,#48813,.T.) ;
#68237 = ORIENTED_EDGE('',*,*,#48814,.F.) ;
#68238 = ORIENTED_EDGE('',*,*,#48543,.F.) ;
#68239 = ORIENTED_EDGE('',*,*,#48814,.T.) ;
#68240 = ORIENTED_EDGE('',*,*,#47975,.F.) ;
#68241 = ORIENTED_EDGE('',*,*,#48815,.F.) ;
#68242 = ORIENTED_EDGE('',*,*,#48322,.F.) ;
#68243 = ORIENTED_EDGE('',*,*,#46632,.F.) ;
#68244 = ORIENTED_EDGE('',*,*,#47966,.F.) ;
#68245 = ORIENTED_EDGE('',*,*,#48816,.F.) ;
#68246 = ORIENTED_EDGE('',*,*,#47977,.F.) ;
#68247 = ORIENTED_EDGE('',*,*,#48556,.F.) ;
#68248 = ORIENTED_EDGE('',*,*,#48815,.T.) ;
#68249 = ORIENTED_EDGE('',*,*,#48816,.T.) ;
#68250 = ORIENTED_EDGE('',*,*,#48555,.F.) ;
#68251 = ORIENTED_EDGE('',*,*,#44433,.F.) ;
#68252 = ORIENTED_EDGE('',*,*,#48013,.F.) ;
#68253 = ORIENTED_EDGE('',*,*,#48817,.F.) ;
#68254 = ORIENTED_EDGE('',*,*,#48008,.F.) ;
#68255 = ORIENTED_EDGE('',*,*,#48817,.T.) ;
#68256 = ORIENTED_EDGE('',*,*,#47998,.F.) ;
#68257 = ORIENTED_EDGE('',*,*,#48818,.F.) ;
#68258 = ORIENTED_EDGE('',*,*,#48009,.F.) ;
#68259 = ORIENTED_EDGE('',*,*,#48818,.T.) ;
#68260 = ORIENTED_EDGE('',*,*,#48559,.F.) ;
#68261 = ORIENTED_EDGE('',*,*,#48557,.F.) ;
#68262 = ORIENTED_EDGE('',*,*,#48819,.F.) ;
#68263 = ORIENTED_EDGE('',*,*,#48819,.T.) ;
#68264 = ORIENTED_EDGE('',*,*,#48238,.F.) ;
#68265 = ORIENTED_EDGE('',*,*,#48820,.F.) ;
#68266 = ORIENTED_EDGE('',*,*,#48010,.F.) ;
#68267 = ORIENTED_EDGE('',*,*,#48820,.T.) ;
#68268 = ORIENTED_EDGE('',*,*,#48572,.F.) ;
#68269 = ORIENTED_EDGE('',*,*,#48574,.F.) ;
#68270 = ORIENTED_EDGE('',*,*,#48821,.F.) ;
#68271 = ORIENTED_EDGE('',*,*,#48821,.T.) ;
#68272 = ORIENTED_EDGE('',*,*,#47982,.F.) ;
#68273 = ORIENTED_EDGE('',*,*,#48822,.F.) ;
#68274 = ORIENTED_EDGE('',*,*,#48006,.F.) ;
#68275 = ORIENTED_EDGE('',*,*,#44214,.F.) ;
#68276 = ORIENTED_EDGE('',*,*,#48007,.F.) ;
#68277 = ORIENTED_EDGE('',*,*,#48822,.T.) ;
#68278 = ORIENTED_EDGE('',*,*,#48011,.F.) ;
#68279 = ORIENTED_EDGE('',*,*,#47349,.F.) ;
#68280 = ORIENTED_EDGE('',*,*,#47352,.F.) ;
#68281 = ORIENTED_EDGE('',*,*,#48012,.F.) ;
#68282 = ORIENTED_EDGE('',*,*,#48823,.F.) ;
#68283 = ORIENTED_EDGE('',*,*,#48003,.F.) ;
#68284 = ORIENTED_EDGE('',*,*,#48823,.T.) ;
#68285 = ORIENTED_EDGE('',*,*,#47984,.F.) ;
#68286 = ORIENTED_EDGE('',*,*,#48824,.F.) ;
#68287 = ORIENTED_EDGE('',*,*,#48004,.F.) ;
#68288 = ORIENTED_EDGE('',*,*,#48824,.T.) ;
#68289 = ORIENTED_EDGE('',*,*,#48575,.F.) ;
#68290 = ORIENTED_EDGE('',*,*,#48576,.F.) ;
#68291 = ORIENTED_EDGE('',*,*,#48825,.F.) ;
#68292 = ORIENTED_EDGE('',*,*,#48825,.T.) ;
#68293 = ORIENTED_EDGE('',*,*,#48242,.F.) ;
#68294 = ORIENTED_EDGE('',*,*,#48826,.F.) ;
#68295 = ORIENTED_EDGE('',*,*,#48005,.F.) ;
#68296 = ORIENTED_EDGE('',*,*,#48826,.T.) ;
#68297 = ORIENTED_EDGE('',*,*,#48563,.F.) ;
#68298 = ORIENTED_EDGE('',*,*,#48560,.F.) ;
#68299 = ORIENTED_EDGE('',*,*,#48827,.F.) ;
#68300 = ORIENTED_EDGE('',*,*,#48827,.T.) ;
#68301 = ORIENTED_EDGE('',*,*,#48000,.F.) ;
#68302 = ORIENTED_EDGE('',*,*,#48828,.F.) ;
#68303 = ORIENTED_EDGE('',*,*,#48001,.F.) ;
#68304 = ORIENTED_EDGE('',*,*,#48828,.T.) ;
#68305 = ORIENTED_EDGE('',*,*,#48014,.F.) ;
#68306 = ORIENTED_EDGE('',*,*,#44431,.F.) ;
#68307 = ORIENTED_EDGE('',*,*,#48002,.F.) ;
#68308 = ORIENTED_EDGE('',*,*,#46636,.F.) ;
#68309 = ORIENTED_EDGE('',*,*,#48020,.F.) ;
#68310 = ORIENTED_EDGE('',*,*,#48829,.F.) ;
#68311 = ORIENTED_EDGE('',*,*,#48036,.F.) ;
#68312 = ORIENTED_EDGE('',*,*,#48829,.T.) ;
#68313 = ORIENTED_EDGE('',*,*,#48579,.F.) ;
#68314 = ORIENTED_EDGE('',*,*,#48577,.F.) ;
#68315 = ORIENTED_EDGE('',*,*,#48830,.F.) ;
#68316 = ORIENTED_EDGE('',*,*,#48830,.T.) ;
#68317 = ORIENTED_EDGE('',*,*,#48310,.F.) ;
#68318 = ORIENTED_EDGE('',*,*,#48831,.F.) ;
#68319 = ORIENTED_EDGE('',*,*,#48037,.F.) ;
#68320 = ORIENTED_EDGE('',*,*,#48831,.T.) ;
#68321 = ORIENTED_EDGE('',*,*,#48592,.F.) ;
#68322 = ORIENTED_EDGE('',*,*,#48594,.F.) ;
#68323 = ORIENTED_EDGE('',*,*,#48832,.F.) ;
#68324 = ORIENTED_EDGE('',*,*,#46638,.F.) ;
#68325 = ORIENTED_EDGE('',*,*,#48038,.F.) ;
#68326 = ORIENTED_EDGE('',*,*,#48832,.T.) ;
#68327 = ORIENTED_EDGE('',*,*,#48022,.F.) ;
#68328 = ORIENTED_EDGE('',*,*,#48833,.F.) ;
#68329 = ORIENTED_EDGE('',*,*,#48021,.F.) ;
#68330 = ORIENTED_EDGE('',*,*,#46634,.F.) ;
#68331 = ORIENTED_EDGE('',*,*,#48034,.F.) ;
#68332 = ORIENTED_EDGE('',*,*,#48580,.F.) ;
#68333 = ORIENTED_EDGE('',*,*,#48833,.T.) ;
#68334 = ORIENTED_EDGE('',*,*,#48834,.F.) ;
#68335 = ORIENTED_EDGE('',*,*,#48583,.F.) ;
#68336 = ORIENTED_EDGE('',*,*,#48834,.T.) ;
#68337 = ORIENTED_EDGE('',*,*,#48033,.F.) ;
#68338 = ORIENTED_EDGE('',*,*,#48835,.F.) ;
#68339 = ORIENTED_EDGE('',*,*,#48314,.F.) ;
#68340 = ORIENTED_EDGE('',*,*,#46640,.F.) ;
#68341 = ORIENTED_EDGE('',*,*,#48024,.F.) ;
#68342 = ORIENTED_EDGE('',*,*,#48836,.F.) ;
#68343 = ORIENTED_EDGE('',*,*,#48035,.F.) ;
#68344 = ORIENTED_EDGE('',*,*,#48596,.F.) ;
#68345 = ORIENTED_EDGE('',*,*,#48835,.T.) ;
#68346 = ORIENTED_EDGE('',*,*,#48836,.T.) ;
#68347 = ORIENTED_EDGE('',*,*,#48595,.F.) ;
#68348 = ORIENTED_EDGE('',*,*,#44422,.F.) ;
#68349 = ORIENTED_EDGE('',*,*,#48071,.F.) ;
#68350 = ORIENTED_EDGE('',*,*,#48837,.F.) ;
#68351 = ORIENTED_EDGE('',*,*,#48066,.F.) ;
#68352 = ORIENTED_EDGE('',*,*,#48837,.T.) ;
#68353 = ORIENTED_EDGE('',*,*,#48056,.F.) ;
#68354 = ORIENTED_EDGE('',*,*,#48838,.F.) ;
#68355 = ORIENTED_EDGE('',*,*,#48067,.F.) ;
#68356 = ORIENTED_EDGE('',*,*,#48838,.T.) ;
#68357 = ORIENTED_EDGE('',*,*,#48599,.F.) ;
#68358 = ORIENTED_EDGE('',*,*,#48597,.F.) ;
#68359 = ORIENTED_EDGE('',*,*,#48839,.F.) ;
#68360 = ORIENTED_EDGE('',*,*,#48839,.T.) ;
#68361 = ORIENTED_EDGE('',*,*,#48230,.F.) ;
#68362 = ORIENTED_EDGE('',*,*,#48840,.F.) ;
#68363 = ORIENTED_EDGE('',*,*,#48068,.F.) ;
#68364 = ORIENTED_EDGE('',*,*,#48840,.T.) ;
#68365 = ORIENTED_EDGE('',*,*,#48612,.F.) ;
#68366 = ORIENTED_EDGE('',*,*,#48614,.F.) ;
#68367 = ORIENTED_EDGE('',*,*,#48841,.F.) ;
#68368 = ORIENTED_EDGE('',*,*,#48841,.T.) ;
#68369 = ORIENTED_EDGE('',*,*,#48040,.F.) ;
#68370 = ORIENTED_EDGE('',*,*,#48842,.F.) ;
#68371 = ORIENTED_EDGE('',*,*,#48064,.F.) ;
#68372 = ORIENTED_EDGE('',*,*,#44197,.F.) ;
#68373 = ORIENTED_EDGE('',*,*,#48065,.F.) ;
#68374 = ORIENTED_EDGE('',*,*,#48842,.T.) ;
#68375 = ORIENTED_EDGE('',*,*,#48069,.F.) ;
#68376 = ORIENTED_EDGE('',*,*,#47437,.F.) ;
#68377 = ORIENTED_EDGE('',*,*,#47440,.F.) ;
#68378 = ORIENTED_EDGE('',*,*,#48070,.F.) ;
#68379 = ORIENTED_EDGE('',*,*,#48843,.F.) ;
#68380 = ORIENTED_EDGE('',*,*,#48061,.F.) ;
#68381 = ORIENTED_EDGE('',*,*,#48843,.T.) ;
#68382 = ORIENTED_EDGE('',*,*,#48042,.F.) ;
#68383 = ORIENTED_EDGE('',*,*,#48844,.F.) ;
#68384 = ORIENTED_EDGE('',*,*,#48062,.F.) ;
#68385 = ORIENTED_EDGE('',*,*,#48844,.T.) ;
#68386 = ORIENTED_EDGE('',*,*,#48615,.F.) ;
#68387 = ORIENTED_EDGE('',*,*,#48616,.F.) ;
#68388 = ORIENTED_EDGE('',*,*,#48845,.F.) ;
#68389 = ORIENTED_EDGE('',*,*,#48845,.T.) ;
#68390 = ORIENTED_EDGE('',*,*,#48234,.F.) ;
#68391 = ORIENTED_EDGE('',*,*,#48846,.F.) ;
#68392 = ORIENTED_EDGE('',*,*,#48063,.F.) ;
#68393 = ORIENTED_EDGE('',*,*,#48846,.T.) ;
#68394 = ORIENTED_EDGE('',*,*,#48603,.F.) ;
#68395 = ORIENTED_EDGE('',*,*,#48600,.F.) ;
#68396 = ORIENTED_EDGE('',*,*,#48847,.F.) ;
#68397 = ORIENTED_EDGE('',*,*,#48847,.T.) ;
#68398 = ORIENTED_EDGE('',*,*,#48058,.F.) ;
#68399 = ORIENTED_EDGE('',*,*,#48848,.F.) ;
#68400 = ORIENTED_EDGE('',*,*,#48059,.F.) ;
#68401 = ORIENTED_EDGE('',*,*,#48848,.T.) ;
#68402 = ORIENTED_EDGE('',*,*,#48072,.F.) ;
#68403 = ORIENTED_EDGE('',*,*,#44420,.F.) ;
#68404 = ORIENTED_EDGE('',*,*,#48060,.F.) ;
#68405 = ORIENTED_EDGE('',*,*,#46644,.F.) ;
#68406 = ORIENTED_EDGE('',*,*,#48078,.F.) ;
#68407 = ORIENTED_EDGE('',*,*,#48849,.F.) ;
#68408 = ORIENTED_EDGE('',*,*,#48094,.F.) ;
#68409 = ORIENTED_EDGE('',*,*,#48849,.T.) ;
#68410 = ORIENTED_EDGE('',*,*,#48619,.F.) ;
#68411 = ORIENTED_EDGE('',*,*,#48617,.F.) ;
#68412 = ORIENTED_EDGE('',*,*,#48850,.F.) ;
#68413 = ORIENTED_EDGE('',*,*,#48850,.T.) ;
#68414 = ORIENTED_EDGE('',*,*,#48302,.F.) ;
#68415 = ORIENTED_EDGE('',*,*,#48851,.F.) ;
#68416 = ORIENTED_EDGE('',*,*,#48095,.F.) ;
#68417 = ORIENTED_EDGE('',*,*,#48851,.T.) ;
#68418 = ORIENTED_EDGE('',*,*,#48632,.F.) ;
#68419 = ORIENTED_EDGE('',*,*,#48634,.F.) ;
#68420 = ORIENTED_EDGE('',*,*,#48852,.F.) ;
#68421 = ORIENTED_EDGE('',*,*,#46646,.F.) ;
#68422 = ORIENTED_EDGE('',*,*,#48096,.F.) ;
#68423 = ORIENTED_EDGE('',*,*,#48852,.T.) ;
#68424 = ORIENTED_EDGE('',*,*,#48080,.F.) ;
#68425 = ORIENTED_EDGE('',*,*,#48853,.F.) ;
#68426 = ORIENTED_EDGE('',*,*,#48079,.F.) ;
#68427 = ORIENTED_EDGE('',*,*,#46642,.F.) ;
#68428 = ORIENTED_EDGE('',*,*,#48092,.F.) ;
#68429 = ORIENTED_EDGE('',*,*,#48620,.F.) ;
#68430 = ORIENTED_EDGE('',*,*,#48853,.T.) ;
#68431 = ORIENTED_EDGE('',*,*,#48854,.F.) ;
#68432 = ORIENTED_EDGE('',*,*,#48623,.F.) ;
#68433 = ORIENTED_EDGE('',*,*,#48854,.T.) ;
#68434 = ORIENTED_EDGE('',*,*,#48091,.F.) ;
#68435 = ORIENTED_EDGE('',*,*,#48855,.F.) ;
#68436 = ORIENTED_EDGE('',*,*,#48306,.F.) ;
#68437 = ORIENTED_EDGE('',*,*,#46648,.F.) ;
#68438 = ORIENTED_EDGE('',*,*,#48082,.F.) ;
#68439 = ORIENTED_EDGE('',*,*,#48856,.F.) ;
#68440 = ORIENTED_EDGE('',*,*,#48093,.F.) ;
#68441 = ORIENTED_EDGE('',*,*,#48636,.F.) ;
#68442 = ORIENTED_EDGE('',*,*,#48855,.T.) ;
#68443 = ORIENTED_EDGE('',*,*,#48856,.T.) ;
#68444 = ORIENTED_EDGE('',*,*,#48635,.F.) ;
#68445 = ORIENTED_EDGE('',*,*,#44411,.F.) ;
#68446 = ORIENTED_EDGE('',*,*,#48129,.F.) ;
#68447 = ORIENTED_EDGE('',*,*,#48857,.F.) ;
#68448 = ORIENTED_EDGE('',*,*,#48124,.F.) ;
#68449 = ORIENTED_EDGE('',*,*,#48857,.T.) ;
#68450 = ORIENTED_EDGE('',*,*,#48114,.F.) ;
#68451 = ORIENTED_EDGE('',*,*,#48858,.F.) ;
#68452 = ORIENTED_EDGE('',*,*,#48125,.F.) ;
#68453 = ORIENTED_EDGE('',*,*,#48858,.T.) ;
#68454 = ORIENTED_EDGE('',*,*,#48639,.F.) ;
#68455 = ORIENTED_EDGE('',*,*,#48637,.F.) ;
#68456 = ORIENTED_EDGE('',*,*,#48859,.F.) ;
#68457 = ORIENTED_EDGE('',*,*,#48859,.T.) ;
#68458 = ORIENTED_EDGE('',*,*,#48222,.F.) ;
#68459 = ORIENTED_EDGE('',*,*,#48860,.F.) ;
#68460 = ORIENTED_EDGE('',*,*,#48126,.F.) ;
#68461 = ORIENTED_EDGE('',*,*,#48860,.T.) ;
#68462 = ORIENTED_EDGE('',*,*,#48652,.F.) ;
#68463 = ORIENTED_EDGE('',*,*,#48654,.F.) ;
#68464 = ORIENTED_EDGE('',*,*,#48861,.F.) ;
#68465 = ORIENTED_EDGE('',*,*,#48861,.T.) ;
#68466 = ORIENTED_EDGE('',*,*,#48098,.F.) ;
#68467 = ORIENTED_EDGE('',*,*,#48862,.F.) ;
#68468 = ORIENTED_EDGE('',*,*,#48122,.F.) ;
#68469 = ORIENTED_EDGE('',*,*,#44180,.F.) ;
#68470 = ORIENTED_EDGE('',*,*,#48123,.F.) ;
#68471 = ORIENTED_EDGE('',*,*,#48862,.T.) ;
#68472 = ORIENTED_EDGE('',*,*,#48127,.F.) ;
#68473 = ORIENTED_EDGE('',*,*,#47525,.F.) ;
#68474 = ORIENTED_EDGE('',*,*,#47528,.F.) ;
#68475 = ORIENTED_EDGE('',*,*,#48128,.F.) ;
#68476 = ORIENTED_EDGE('',*,*,#48863,.F.) ;
#68477 = ORIENTED_EDGE('',*,*,#48119,.F.) ;
#68478 = ORIENTED_EDGE('',*,*,#48863,.T.) ;
#68479 = ORIENTED_EDGE('',*,*,#48100,.F.) ;
#68480 = ORIENTED_EDGE('',*,*,#48864,.F.) ;
#68481 = ORIENTED_EDGE('',*,*,#48120,.F.) ;
#68482 = ORIENTED_EDGE('',*,*,#48864,.T.) ;
#68483 = ORIENTED_EDGE('',*,*,#48655,.F.) ;
#68484 = ORIENTED_EDGE('',*,*,#48656,.F.) ;
#68485 = ORIENTED_EDGE('',*,*,#48865,.F.) ;
#68486 = ORIENTED_EDGE('',*,*,#48865,.T.) ;
#68487 = ORIENTED_EDGE('',*,*,#48226,.F.) ;
#68488 = ORIENTED_EDGE('',*,*,#48866,.F.) ;
#68489 = ORIENTED_EDGE('',*,*,#48121,.F.) ;
#68490 = ORIENTED_EDGE('',*,*,#48866,.T.) ;
#68491 = ORIENTED_EDGE('',*,*,#48643,.F.) ;
#68492 = ORIENTED_EDGE('',*,*,#48640,.F.) ;
#68493 = ORIENTED_EDGE('',*,*,#48867,.F.) ;
#68494 = ORIENTED_EDGE('',*,*,#48867,.T.) ;
#68495 = ORIENTED_EDGE('',*,*,#48116,.F.) ;
#68496 = ORIENTED_EDGE('',*,*,#48868,.F.) ;
#68497 = ORIENTED_EDGE('',*,*,#48117,.F.) ;
#68498 = ORIENTED_EDGE('',*,*,#48868,.T.) ;
#68499 = ORIENTED_EDGE('',*,*,#48130,.F.) ;
#68500 = ORIENTED_EDGE('',*,*,#44409,.F.) ;
#68501 = ORIENTED_EDGE('',*,*,#48118,.F.) ;
#68502 = ORIENTED_EDGE('',*,*,#46652,.F.) ;
#68503 = ORIENTED_EDGE('',*,*,#48136,.F.) ;
#68504 = ORIENTED_EDGE('',*,*,#48869,.F.) ;
#68505 = ORIENTED_EDGE('',*,*,#48152,.F.) ;
#68506 = ORIENTED_EDGE('',*,*,#48869,.T.) ;
#68507 = ORIENTED_EDGE('',*,*,#48659,.F.) ;
#68508 = ORIENTED_EDGE('',*,*,#48657,.F.) ;
#68509 = ORIENTED_EDGE('',*,*,#48870,.F.) ;
#68510 = ORIENTED_EDGE('',*,*,#48870,.T.) ;
#68511 = ORIENTED_EDGE('',*,*,#48294,.F.) ;
#68512 = ORIENTED_EDGE('',*,*,#48871,.F.) ;
#68513 = ORIENTED_EDGE('',*,*,#48153,.F.) ;
#68514 = ORIENTED_EDGE('',*,*,#48871,.T.) ;
#68515 = ORIENTED_EDGE('',*,*,#48672,.F.) ;
#68516 = ORIENTED_EDGE('',*,*,#48674,.F.) ;
#68517 = ORIENTED_EDGE('',*,*,#48872,.F.) ;
#68518 = ORIENTED_EDGE('',*,*,#46654,.F.) ;
#68519 = ORIENTED_EDGE('',*,*,#48154,.F.) ;
#68520 = ORIENTED_EDGE('',*,*,#48872,.T.) ;
#68521 = ORIENTED_EDGE('',*,*,#48138,.F.) ;
#68522 = ORIENTED_EDGE('',*,*,#48873,.F.) ;
#68523 = ORIENTED_EDGE('',*,*,#48137,.F.) ;
#68524 = ORIENTED_EDGE('',*,*,#46650,.F.) ;
#68525 = ORIENTED_EDGE('',*,*,#48150,.F.) ;
#68526 = ORIENTED_EDGE('',*,*,#48660,.F.) ;
#68527 = ORIENTED_EDGE('',*,*,#48873,.T.) ;
#68528 = ORIENTED_EDGE('',*,*,#48874,.F.) ;
#68529 = ORIENTED_EDGE('',*,*,#48663,.F.) ;
#68530 = ORIENTED_EDGE('',*,*,#48874,.T.) ;
#68531 = ORIENTED_EDGE('',*,*,#48149,.F.) ;
#68532 = ORIENTED_EDGE('',*,*,#48875,.F.) ;
#68533 = ORIENTED_EDGE('',*,*,#48298,.F.) ;
#68534 = ORIENTED_EDGE('',*,*,#46656,.F.) ;
#68535 = ORIENTED_EDGE('',*,*,#48140,.F.) ;
#68536 = ORIENTED_EDGE('',*,*,#48876,.F.) ;
#68537 = ORIENTED_EDGE('',*,*,#48151,.F.) ;
#68538 = ORIENTED_EDGE('',*,*,#48676,.F.) ;
#68539 = ORIENTED_EDGE('',*,*,#48875,.T.) ;
#68540 = ORIENTED_EDGE('',*,*,#48876,.T.) ;
#68541 = ORIENTED_EDGE('',*,*,#48675,.F.) ;
#68542 = ORIENTED_EDGE('',*,*,#44400,.F.) ;
#68543 = ORIENTED_EDGE('',*,*,#48187,.F.) ;
#68544 = ORIENTED_EDGE('',*,*,#48877,.F.) ;
#68545 = ORIENTED_EDGE('',*,*,#48182,.F.) ;
#68546 = ORIENTED_EDGE('',*,*,#48877,.T.) ;
#68547 = ORIENTED_EDGE('',*,*,#48172,.F.) ;
#68548 = ORIENTED_EDGE('',*,*,#48878,.F.) ;
#68549 = ORIENTED_EDGE('',*,*,#48183,.F.) ;
#68550 = ORIENTED_EDGE('',*,*,#48878,.T.) ;
#68551 = ORIENTED_EDGE('',*,*,#48679,.F.) ;
#68552 = ORIENTED_EDGE('',*,*,#48677,.F.) ;
#68553 = ORIENTED_EDGE('',*,*,#48879,.F.) ;
#68554 = ORIENTED_EDGE('',*,*,#48879,.T.) ;
#68555 = ORIENTED_EDGE('',*,*,#48214,.F.) ;
#68556 = ORIENTED_EDGE('',*,*,#48880,.F.) ;
#68557 = ORIENTED_EDGE('',*,*,#48184,.F.) ;
#68558 = ORIENTED_EDGE('',*,*,#48880,.T.) ;
#68559 = ORIENTED_EDGE('',*,*,#48692,.F.) ;
#68560 = ORIENTED_EDGE('',*,*,#48694,.F.) ;
#68561 = ORIENTED_EDGE('',*,*,#48881,.F.) ;
#68562 = ORIENTED_EDGE('',*,*,#48881,.T.) ;
#68563 = ORIENTED_EDGE('',*,*,#48156,.F.) ;
#68564 = ORIENTED_EDGE('',*,*,#48882,.F.) ;
#68565 = ORIENTED_EDGE('',*,*,#48180,.F.) ;
#68566 = ORIENTED_EDGE('',*,*,#44163,.F.) ;
#68567 = ORIENTED_EDGE('',*,*,#48181,.F.) ;
#68568 = ORIENTED_EDGE('',*,*,#48882,.T.) ;
#68569 = ORIENTED_EDGE('',*,*,#48185,.F.) ;
#68570 = ORIENTED_EDGE('',*,*,#47613,.F.) ;
#68571 = ORIENTED_EDGE('',*,*,#47616,.F.) ;
#68572 = ORIENTED_EDGE('',*,*,#48186,.F.) ;
#68573 = ORIENTED_EDGE('',*,*,#48883,.F.) ;
#68574 = ORIENTED_EDGE('',*,*,#48177,.F.) ;
#68575 = ORIENTED_EDGE('',*,*,#48883,.T.) ;
#68576 = ORIENTED_EDGE('',*,*,#48158,.F.) ;
#68577 = ORIENTED_EDGE('',*,*,#48884,.F.) ;
#68578 = ORIENTED_EDGE('',*,*,#48178,.F.) ;
#68579 = ORIENTED_EDGE('',*,*,#48884,.T.) ;
#68580 = ORIENTED_EDGE('',*,*,#48695,.F.) ;
#68581 = ORIENTED_EDGE('',*,*,#48696,.F.) ;
#68582 = ORIENTED_EDGE('',*,*,#48885,.F.) ;
#68583 = ORIENTED_EDGE('',*,*,#48885,.T.) ;
#68584 = ORIENTED_EDGE('',*,*,#48218,.F.) ;
#68585 = ORIENTED_EDGE('',*,*,#48886,.F.) ;
#68586 = ORIENTED_EDGE('',*,*,#48179,.F.) ;
#68587 = ORIENTED_EDGE('',*,*,#48886,.T.) ;
#68588 = ORIENTED_EDGE('',*,*,#48683,.F.) ;
#68589 = ORIENTED_EDGE('',*,*,#48680,.F.) ;
#68590 = ORIENTED_EDGE('',*,*,#48887,.F.) ;
#68591 = ORIENTED_EDGE('',*,*,#48887,.T.) ;
#68592 = ORIENTED_EDGE('',*,*,#48174,.F.) ;
#68593 = ORIENTED_EDGE('',*,*,#48888,.F.) ;
#68594 = ORIENTED_EDGE('',*,*,#48175,.F.) ;
#68595 = ORIENTED_EDGE('',*,*,#48888,.T.) ;
#68596 = ORIENTED_EDGE('',*,*,#48188,.F.) ;
#68597 = ORIENTED_EDGE('',*,*,#44398,.F.) ;
#68598 = ORIENTED_EDGE('',*,*,#48176,.F.) ;
#68599 = ORIENTED_EDGE('',*,*,#46660,.F.) ;
#68600 = ORIENTED_EDGE('',*,*,#48194,.F.) ;
#68601 = ORIENTED_EDGE('',*,*,#48889,.F.) ;
#68602 = ORIENTED_EDGE('',*,*,#48210,.F.) ;
#68603 = ORIENTED_EDGE('',*,*,#48889,.T.) ;
#68604 = ORIENTED_EDGE('',*,*,#48699,.F.) ;
#68605 = ORIENTED_EDGE('',*,*,#48697,.F.) ;
#68606 = ORIENTED_EDGE('',*,*,#48890,.F.) ;
#68607 = ORIENTED_EDGE('',*,*,#48890,.T.) ;
#68608 = ORIENTED_EDGE('',*,*,#48286,.F.) ;
#68609 = ORIENTED_EDGE('',*,*,#48891,.F.) ;
#68610 = ORIENTED_EDGE('',*,*,#48211,.F.) ;
#68611 = ORIENTED_EDGE('',*,*,#48891,.T.) ;
#68612 = ORIENTED_EDGE('',*,*,#48712,.F.) ;
#68613 = ORIENTED_EDGE('',*,*,#48714,.F.) ;
#68614 = ORIENTED_EDGE('',*,*,#48892,.F.) ;
#68615 = ORIENTED_EDGE('',*,*,#46662,.F.) ;
#68616 = ORIENTED_EDGE('',*,*,#48212,.F.) ;
#68617 = ORIENTED_EDGE('',*,*,#48892,.T.) ;
#68618 = ORIENTED_EDGE('',*,*,#48196,.F.) ;
#68619 = ORIENTED_EDGE('',*,*,#48893,.F.) ;
#68620 = ORIENTED_EDGE('',*,*,#48195,.F.) ;
#68621 = ORIENTED_EDGE('',*,*,#46658,.F.) ;
#68622 = ORIENTED_EDGE('',*,*,#48208,.F.) ;
#68623 = ORIENTED_EDGE('',*,*,#48700,.F.) ;
#68624 = ORIENTED_EDGE('',*,*,#48893,.T.) ;
#68625 = ORIENTED_EDGE('',*,*,#48894,.F.) ;
#68626 = ORIENTED_EDGE('',*,*,#48703,.F.) ;
#68627 = ORIENTED_EDGE('',*,*,#48894,.T.) ;
#68628 = ORIENTED_EDGE('',*,*,#48207,.F.) ;
#68629 = ORIENTED_EDGE('',*,*,#48895,.F.) ;
#68630 = ORIENTED_EDGE('',*,*,#48290,.F.) ;
#68631 = ORIENTED_EDGE('',*,*,#46664,.F.) ;
#68632 = ORIENTED_EDGE('',*,*,#48198,.F.) ;
#68633 = ORIENTED_EDGE('',*,*,#48896,.F.) ;
#68634 = ORIENTED_EDGE('',*,*,#48209,.F.) ;
#68635 = ORIENTED_EDGE('',*,*,#48716,.F.) ;
#68636 = ORIENTED_EDGE('',*,*,#48895,.T.) ;
#68637 = ORIENTED_EDGE('',*,*,#48896,.T.) ;
#68638 = ORIENTED_EDGE('',*,*,#48715,.F.) ;
#68639 = ORIENTED_EDGE('',*,*,#48897,.F.) ;
#68640 = ORIENTED_EDGE('',*,*,#48898,.F.) ;
#68641 = ORIENTED_EDGE('',*,*,#48899,.T.) ;
#68642 = ORIENTED_EDGE('',*,*,#48900,.F.) ;
#68643 = ORIENTED_EDGE('',*,*,#48901,.F.) ;
#68644 = ORIENTED_EDGE('',*,*,#48902,.F.) ;
#68645 = ORIENTED_EDGE('',*,*,#48903,.F.) ;
#68646 = ORIENTED_EDGE('',*,*,#48904,.T.) ;
#68647 = ORIENTED_EDGE('',*,*,#48905,.F.) ;
#68648 = ORIENTED_EDGE('',*,*,#48906,.F.) ;
#68649 = ORIENTED_EDGE('',*,*,#48907,.F.) ;
#68650 = ORIENTED_EDGE('',*,*,#48908,.T.) ;
#68651 = ORIENTED_EDGE('',*,*,#48909,.F.) ;
#68652 = ORIENTED_EDGE('',*,*,#48910,.T.) ;
#68653 = ORIENTED_EDGE('',*,*,#48911,.F.) ;
#68654 = ORIENTED_EDGE('',*,*,#48912,.F.) ;
#68655 = ORIENTED_EDGE('',*,*,#48913,.F.) ;
#68656 = ORIENTED_EDGE('',*,*,#48914,.F.) ;
#68657 = ORIENTED_EDGE('',*,*,#48915,.F.) ;
#68658 = ORIENTED_EDGE('',*,*,#48916,.T.) ;
#68659 = ORIENTED_EDGE('',*,*,#48917,.F.) ;
#68660 = ORIENTED_EDGE('',*,*,#48918,.T.) ;
#68661 = ORIENTED_EDGE('',*,*,#48919,.F.) ;
#68662 = ORIENTED_EDGE('',*,*,#48920,.F.) ;
#68663 = ORIENTED_EDGE('',*,*,#48921,.F.) ;
#68664 = ORIENTED_EDGE('',*,*,#48922,.F.) ;
#68665 = ORIENTED_EDGE('',*,*,#48923,.F.) ;
#68666 = ORIENTED_EDGE('',*,*,#48924,.T.) ;
#68667 = ORIENTED_EDGE('',*,*,#48925,.F.) ;
#68668 = ORIENTED_EDGE('',*,*,#48926,.T.) ;
#68669 = ORIENTED_EDGE('',*,*,#48927,.F.) ;
#68670 = ORIENTED_EDGE('',*,*,#48928,.F.) ;
#68671 = ORIENTED_EDGE('',*,*,#48929,.F.) ;
#68672 = ORIENTED_EDGE('',*,*,#48930,.F.) ;
#68673 = ORIENTED_EDGE('',*,*,#48931,.F.) ;
#68674 = ORIENTED_EDGE('',*,*,#48932,.T.) ;
#68675 = ORIENTED_EDGE('',*,*,#48933,.F.) ;
#68676 = ORIENTED_EDGE('',*,*,#48934,.T.) ;
#68677 = ORIENTED_EDGE('',*,*,#48935,.F.) ;
#68678 = ORIENTED_EDGE('',*,*,#48936,.F.) ;
#68679 = ORIENTED_EDGE('',*,*,#48937,.F.) ;
#68680 = ORIENTED_EDGE('',*,*,#48938,.F.) ;
#68681 = ORIENTED_EDGE('',*,*,#48939,.F.) ;
#68682 = ORIENTED_EDGE('',*,*,#48940,.T.) ;
#68683 = ORIENTED_EDGE('',*,*,#48941,.F.) ;
#68684 = ORIENTED_EDGE('',*,*,#48942,.T.) ;
#68685 = ORIENTED_EDGE('',*,*,#48943,.F.) ;
#68686 = ORIENTED_EDGE('',*,*,#48944,.F.) ;
#68687 = ORIENTED_EDGE('',*,*,#48945,.F.) ;
#68688 = ORIENTED_EDGE('',*,*,#48946,.F.) ;
#68689 = ORIENTED_EDGE('',*,*,#48947,.F.) ;
#68690 = ORIENTED_EDGE('',*,*,#48948,.T.) ;
#68691 = ORIENTED_EDGE('',*,*,#48949,.F.) ;
#68692 = ORIENTED_EDGE('',*,*,#48950,.T.) ;
#68693 = ORIENTED_EDGE('',*,*,#48951,.F.) ;
#68694 = ORIENTED_EDGE('',*,*,#48952,.F.) ;
#68695 = ORIENTED_EDGE('',*,*,#48953,.F.) ;
#68696 = ORIENTED_EDGE('',*,*,#48954,.F.) ;
#68697 = ORIENTED_EDGE('',*,*,#48955,.F.) ;
#68698 = ORIENTED_EDGE('',*,*,#48956,.T.) ;
#68699 = ORIENTED_EDGE('',*,*,#48957,.F.) ;
#68700 = ORIENTED_EDGE('',*,*,#48958,.T.) ;
#68701 = ORIENTED_EDGE('',*,*,#48959,.F.) ;
#68702 = ORIENTED_EDGE('',*,*,#48960,.F.) ;
#68703 = ORIENTED_EDGE('',*,*,#48961,.F.) ;
#68704 = ORIENTED_EDGE('',*,*,#48962,.F.) ;
#68705 = ORIENTED_EDGE('',*,*,#48963,.F.) ;
#68706 = ORIENTED_EDGE('',*,*,#48964,.T.) ;
#68707 = ORIENTED_EDGE('',*,*,#48965,.F.) ;
#68708 = ORIENTED_EDGE('',*,*,#48966,.T.) ;
#68709 = ORIENTED_EDGE('',*,*,#48967,.F.) ;
#68710 = ORIENTED_EDGE('',*,*,#48968,.F.) ;
#68711 = ORIENTED_EDGE('',*,*,#48969,.F.) ;
#68712 = ORIENTED_EDGE('',*,*,#48970,.F.) ;
#68713 = ORIENTED_EDGE('',*,*,#48971,.F.) ;
#68714 = ORIENTED_EDGE('',*,*,#48972,.T.) ;
#68715 = ORIENTED_EDGE('',*,*,#48973,.F.) ;
#68716 = ORIENTED_EDGE('',*,*,#48974,.T.) ;
#68717 = ORIENTED_EDGE('',*,*,#48975,.F.) ;
#68718 = ORIENTED_EDGE('',*,*,#48976,.F.) ;
#68719 = ORIENTED_EDGE('',*,*,#48977,.F.) ;
#68720 = ORIENTED_EDGE('',*,*,#48978,.F.) ;
#68721 = ORIENTED_EDGE('',*,*,#48979,.F.) ;
#68722 = ORIENTED_EDGE('',*,*,#48980,.T.) ;
#68723 = ORIENTED_EDGE('',*,*,#48981,.F.) ;
#68724 = ORIENTED_EDGE('',*,*,#48982,.T.) ;
#68725 = ORIENTED_EDGE('',*,*,#48983,.F.) ;
#68726 = ORIENTED_EDGE('',*,*,#48984,.F.) ;
#68727 = ORIENTED_EDGE('',*,*,#48985,.T.) ;
#68728 = ORIENTED_EDGE('',*,*,#48986,.T.) ;
#68729 = ORIENTED_EDGE('',*,*,#48963,.T.) ;
#68730 = ORIENTED_EDGE('',*,*,#48987,.F.) ;
#68731 = ORIENTED_EDGE('',*,*,#48988,.T.) ;
#68732 = ORIENTED_EDGE('',*,*,#48989,.T.) ;
#68733 = ORIENTED_EDGE('',*,*,#48955,.T.) ;
#68734 = ORIENTED_EDGE('',*,*,#48990,.F.) ;
#68735 = ORIENTED_EDGE('',*,*,#48991,.T.) ;
#68736 = ORIENTED_EDGE('',*,*,#48992,.T.) ;
#68737 = ORIENTED_EDGE('',*,*,#48947,.T.) ;
#68738 = ORIENTED_EDGE('',*,*,#48993,.F.) ;
#68739 = ORIENTED_EDGE('',*,*,#48994,.T.) ;
#68740 = ORIENTED_EDGE('',*,*,#48995,.T.) ;
#68741 = ORIENTED_EDGE('',*,*,#48939,.T.) ;
#68742 = ORIENTED_EDGE('',*,*,#48996,.F.) ;
#68743 = ORIENTED_EDGE('',*,*,#48997,.T.) ;
#68744 = ORIENTED_EDGE('',*,*,#48998,.T.) ;
#68745 = ORIENTED_EDGE('',*,*,#48931,.T.) ;
#68746 = ORIENTED_EDGE('',*,*,#48999,.F.) ;
#68747 = ORIENTED_EDGE('',*,*,#49000,.T.) ;
#68748 = ORIENTED_EDGE('',*,*,#49001,.T.) ;
#68749 = ORIENTED_EDGE('',*,*,#48923,.T.) ;
#68750 = ORIENTED_EDGE('',*,*,#49002,.F.) ;
#68751 = ORIENTED_EDGE('',*,*,#49003,.T.) ;
#68752 = ORIENTED_EDGE('',*,*,#49004,.T.) ;
#68753 = ORIENTED_EDGE('',*,*,#48915,.T.) ;
#68754 = ORIENTED_EDGE('',*,*,#49005,.F.) ;
#68755 = ORIENTED_EDGE('',*,*,#49006,.F.) ;
#68756 = ORIENTED_EDGE('',*,*,#49007,.T.) ;
#68757 = ORIENTED_EDGE('',*,*,#49008,.F.) ;
#68758 = ORIENTED_EDGE('',*,*,#49007,.F.) ;
#68759 = ORIENTED_EDGE('',*,*,#49009,.F.) ;
#68760 = ORIENTED_EDGE('',*,*,#49010,.T.) ;
#68761 = ORIENTED_EDGE('',*,*,#49011,.F.) ;
#68762 = ORIENTED_EDGE('',*,*,#49010,.F.) ;
#68763 = ORIENTED_EDGE('',*,*,#49012,.F.) ;
#68764 = ORIENTED_EDGE('',*,*,#49013,.T.) ;
#68765 = ORIENTED_EDGE('',*,*,#49014,.F.) ;
#68766 = ORIENTED_EDGE('',*,*,#49013,.F.) ;
#68767 = ORIENTED_EDGE('',*,*,#49015,.F.) ;
#68768 = ORIENTED_EDGE('',*,*,#49016,.T.) ;
#68769 = ORIENTED_EDGE('',*,*,#49017,.F.) ;
#68770 = ORIENTED_EDGE('',*,*,#49016,.F.) ;
#68771 = ORIENTED_EDGE('',*,*,#49018,.F.) ;
#68772 = ORIENTED_EDGE('',*,*,#49019,.T.) ;
#68773 = ORIENTED_EDGE('',*,*,#49020,.F.) ;
#68774 = ORIENTED_EDGE('',*,*,#49019,.F.) ;
#68775 = ORIENTED_EDGE('',*,*,#49021,.F.) ;
#68776 = ORIENTED_EDGE('',*,*,#49022,.T.) ;
#68777 = ORIENTED_EDGE('',*,*,#49023,.F.) ;
#68778 = ORIENTED_EDGE('',*,*,#49022,.F.) ;
#68779 = ORIENTED_EDGE('',*,*,#49024,.F.) ;
#68780 = ORIENTED_EDGE('',*,*,#49025,.T.) ;
#68781 = ORIENTED_EDGE('',*,*,#49026,.F.) ;
#68782 = ORIENTED_EDGE('',*,*,#49025,.F.) ;
#68783 = ORIENTED_EDGE('',*,*,#49027,.F.) ;
#68784 = ORIENTED_EDGE('',*,*,#49028,.T.) ;
#68785 = ORIENTED_EDGE('',*,*,#49029,.F.) ;
#68786 = ORIENTED_EDGE('',*,*,#49028,.F.) ;
#68787 = ORIENTED_EDGE('',*,*,#49030,.F.) ;
#68788 = ORIENTED_EDGE('',*,*,#49031,.T.) ;
#68789 = ORIENTED_EDGE('',*,*,#49032,.F.) ;
#68790 = ORIENTED_EDGE('',*,*,#49031,.F.) ;
#68791 = ORIENTED_EDGE('',*,*,#49033,.F.) ;
#68792 = ORIENTED_EDGE('',*,*,#49034,.T.) ;
#68793 = ORIENTED_EDGE('',*,*,#49035,.F.) ;
#68794 = ORIENTED_EDGE('',*,*,#49034,.F.) ;
#68795 = ORIENTED_EDGE('',*,*,#49036,.F.) ;
#68796 = ORIENTED_EDGE('',*,*,#49037,.T.) ;
#68797 = ORIENTED_EDGE('',*,*,#49038,.F.) ;
#68798 = ORIENTED_EDGE('',*,*,#49037,.F.) ;
#68799 = ORIENTED_EDGE('',*,*,#49039,.F.) ;
#68800 = ORIENTED_EDGE('',*,*,#49040,.T.) ;
#68801 = ORIENTED_EDGE('',*,*,#49041,.F.) ;
#68802 = ORIENTED_EDGE('',*,*,#49040,.F.) ;
#68803 = ORIENTED_EDGE('',*,*,#49042,.F.) ;
#68804 = ORIENTED_EDGE('',*,*,#49043,.T.) ;
#68805 = ORIENTED_EDGE('',*,*,#49044,.F.) ;
#68806 = ORIENTED_EDGE('',*,*,#49043,.F.) ;
#68807 = ORIENTED_EDGE('',*,*,#49045,.F.) ;
#68808 = ORIENTED_EDGE('',*,*,#49046,.T.) ;
#68809 = ORIENTED_EDGE('',*,*,#49047,.F.) ;
#68810 = ORIENTED_EDGE('',*,*,#49046,.F.) ;
#68811 = ORIENTED_EDGE('',*,*,#49048,.F.) ;
#68812 = ORIENTED_EDGE('',*,*,#49049,.T.) ;
#68813 = ORIENTED_EDGE('',*,*,#49050,.F.) ;
#68814 = ORIENTED_EDGE('',*,*,#49049,.F.) ;
#68815 = ORIENTED_EDGE('',*,*,#49051,.F.) ;
#68816 = ORIENTED_EDGE('',*,*,#49052,.T.) ;
#68817 = ORIENTED_EDGE('',*,*,#49053,.F.) ;
#68818 = ORIENTED_EDGE('',*,*,#49052,.F.) ;
#68819 = ORIENTED_EDGE('',*,*,#49054,.F.) ;
#68820 = ORIENTED_EDGE('',*,*,#49055,.T.) ;
#68821 = ORIENTED_EDGE('',*,*,#49056,.F.) ;
#68822 = ORIENTED_EDGE('',*,*,#49055,.F.) ;
#68823 = ORIENTED_EDGE('',*,*,#49057,.F.) ;
#68824 = ORIENTED_EDGE('',*,*,#49058,.T.) ;
#68825 = ORIENTED_EDGE('',*,*,#49059,.F.) ;
#68826 = ORIENTED_EDGE('',*,*,#49058,.F.) ;
#68827 = ORIENTED_EDGE('',*,*,#49060,.F.) ;
#68828 = ORIENTED_EDGE('',*,*,#49061,.T.) ;
#68829 = ORIENTED_EDGE('',*,*,#49062,.F.) ;
#68830 = ORIENTED_EDGE('',*,*,#49061,.F.) ;
#68831 = ORIENTED_EDGE('',*,*,#49063,.F.) ;
#68832 = ORIENTED_EDGE('',*,*,#49064,.T.) ;
#68833 = ORIENTED_EDGE('',*,*,#49065,.F.) ;
#68834 = ORIENTED_EDGE('',*,*,#49064,.F.) ;
#68835 = ORIENTED_EDGE('',*,*,#49066,.F.) ;
#68836 = ORIENTED_EDGE('',*,*,#49067,.T.) ;
#68837 = ORIENTED_EDGE('',*,*,#49068,.F.) ;
#68838 = ORIENTED_EDGE('',*,*,#49067,.F.) ;
#68839 = ORIENTED_EDGE('',*,*,#49069,.F.) ;
#68840 = ORIENTED_EDGE('',*,*,#49070,.T.) ;
#68841 = ORIENTED_EDGE('',*,*,#49071,.F.) ;
#68842 = ORIENTED_EDGE('',*,*,#49070,.F.) ;
#68843 = ORIENTED_EDGE('',*,*,#49072,.F.) ;
#68844 = ORIENTED_EDGE('',*,*,#49073,.T.) ;
#68845 = ORIENTED_EDGE('',*,*,#49074,.F.) ;
#68846 = ORIENTED_EDGE('',*,*,#49073,.F.) ;
#68847 = ORIENTED_EDGE('',*,*,#49075,.F.) ;
#68848 = ORIENTED_EDGE('',*,*,#49076,.T.) ;
#68849 = ORIENTED_EDGE('',*,*,#49077,.F.) ;
#68850 = ORIENTED_EDGE('',*,*,#49076,.F.) ;
#68851 = ORIENTED_EDGE('',*,*,#49078,.F.) ;
#68852 = ORIENTED_EDGE('',*,*,#49079,.T.) ;
#68853 = ORIENTED_EDGE('',*,*,#49080,.F.) ;
#68854 = ORIENTED_EDGE('',*,*,#49079,.F.) ;
#68855 = ORIENTED_EDGE('',*,*,#49081,.F.) ;
#68856 = ORIENTED_EDGE('',*,*,#49082,.T.) ;
#68857 = ORIENTED_EDGE('',*,*,#49083,.F.) ;
#68858 = ORIENTED_EDGE('',*,*,#49082,.F.) ;
#68859 = ORIENTED_EDGE('',*,*,#49084,.F.) ;
#68860 = ORIENTED_EDGE('',*,*,#49085,.T.) ;
#68861 = ORIENTED_EDGE('',*,*,#49086,.F.) ;
#68862 = ORIENTED_EDGE('',*,*,#49085,.F.) ;
#68863 = ORIENTED_EDGE('',*,*,#49087,.F.) ;
#68864 = ORIENTED_EDGE('',*,*,#49088,.T.) ;
#68865 = ORIENTED_EDGE('',*,*,#49089,.F.) ;
#68866 = ORIENTED_EDGE('',*,*,#49090,.T.) ;
#68867 = ORIENTED_EDGE('',*,*,#49091,.F.) ;
#68868 = ORIENTED_EDGE('',*,*,#49092,.T.) ;
#68869 = ORIENTED_EDGE('',*,*,#49093,.T.) ;
#68870 = ORIENTED_EDGE('',*,*,#49094,.T.) ;
#68871 = ORIENTED_EDGE('',*,*,#49095,.F.) ;
#68872 = ORIENTED_EDGE('',*,*,#49096,.T.) ;
#68873 = ORIENTED_EDGE('',*,*,#49097,.F.) ;
#68874 = ORIENTED_EDGE('',*,*,#49098,.T.) ;
#68875 = ORIENTED_EDGE('',*,*,#49099,.F.) ;
#68876 = ORIENTED_EDGE('',*,*,#49100,.T.) ;
#68877 = ORIENTED_EDGE('',*,*,#49101,.T.) ;
#68878 = ORIENTED_EDGE('',*,*,#49102,.T.) ;
#68879 = ORIENTED_EDGE('',*,*,#49103,.F.) ;
#68880 = ORIENTED_EDGE('',*,*,#49104,.T.) ;
#68881 = ORIENTED_EDGE('',*,*,#49081,.T.) ;
#68882 = ORIENTED_EDGE('',*,*,#49104,.F.) ;
#68883 = ORIENTED_EDGE('',*,*,#49105,.F.) ;
#68884 = ORIENTED_EDGE('',*,*,#49106,.T.) ;
#68885 = ORIENTED_EDGE('',*,*,#49107,.F.) ;
#68886 = ORIENTED_EDGE('',*,*,#49108,.T.) ;
#68887 = ORIENTED_EDGE('',*,*,#49109,.F.) ;
#68888 = ORIENTED_EDGE('',*,*,#49110,.T.) ;
#68889 = ORIENTED_EDGE('',*,*,#49111,.T.) ;
#68890 = ORIENTED_EDGE('',*,*,#49112,.T.) ;
#68891 = ORIENTED_EDGE('',*,*,#49113,.F.) ;
#68892 = ORIENTED_EDGE('',*,*,#49114,.T.) ;
#68893 = ORIENTED_EDGE('',*,*,#49115,.F.) ;
#68894 = ORIENTED_EDGE('',*,*,#49116,.T.) ;
#68895 = ORIENTED_EDGE('',*,*,#49117,.F.) ;
#68896 = ORIENTED_EDGE('',*,*,#49118,.T.) ;
#68897 = ORIENTED_EDGE('',*,*,#49119,.T.) ;
#68898 = ORIENTED_EDGE('',*,*,#49120,.T.) ;
#68899 = ORIENTED_EDGE('',*,*,#49121,.F.) ;
#68900 = ORIENTED_EDGE('',*,*,#49122,.T.) ;
#68901 = ORIENTED_EDGE('',*,*,#49072,.T.) ;
#68902 = ORIENTED_EDGE('',*,*,#49122,.F.) ;
#68903 = ORIENTED_EDGE('',*,*,#49123,.F.) ;
#68904 = ORIENTED_EDGE('',*,*,#49124,.T.) ;
#68905 = ORIENTED_EDGE('',*,*,#49125,.F.) ;
#68906 = ORIENTED_EDGE('',*,*,#49126,.T.) ;
#68907 = ORIENTED_EDGE('',*,*,#49127,.F.) ;
#68908 = ORIENTED_EDGE('',*,*,#49128,.T.) ;
#68909 = ORIENTED_EDGE('',*,*,#49129,.T.) ;
#68910 = ORIENTED_EDGE('',*,*,#49130,.T.) ;
#68911 = ORIENTED_EDGE('',*,*,#49131,.F.) ;
#68912 = ORIENTED_EDGE('',*,*,#49132,.T.) ;
#68913 = ORIENTED_EDGE('',*,*,#49133,.F.) ;
#68914 = ORIENTED_EDGE('',*,*,#49134,.T.) ;
#68915 = ORIENTED_EDGE('',*,*,#49135,.F.) ;
#68916 = ORIENTED_EDGE('',*,*,#49136,.T.) ;
#68917 = ORIENTED_EDGE('',*,*,#49137,.T.) ;
#68918 = ORIENTED_EDGE('',*,*,#49138,.T.) ;
#68919 = ORIENTED_EDGE('',*,*,#49139,.F.) ;
#68920 = ORIENTED_EDGE('',*,*,#49140,.T.) ;
#68921 = ORIENTED_EDGE('',*,*,#49063,.T.) ;
#68922 = ORIENTED_EDGE('',*,*,#49140,.F.) ;
#68923 = ORIENTED_EDGE('',*,*,#49141,.F.) ;
#68924 = ORIENTED_EDGE('',*,*,#49142,.T.) ;
#68925 = ORIENTED_EDGE('',*,*,#49143,.F.) ;
#68926 = ORIENTED_EDGE('',*,*,#49144,.T.) ;
#68927 = ORIENTED_EDGE('',*,*,#49145,.F.) ;
#68928 = ORIENTED_EDGE('',*,*,#49146,.T.) ;
#68929 = ORIENTED_EDGE('',*,*,#49147,.T.) ;
#68930 = ORIENTED_EDGE('',*,*,#49148,.T.) ;
#68931 = ORIENTED_EDGE('',*,*,#49149,.F.) ;
#68932 = ORIENTED_EDGE('',*,*,#49150,.T.) ;
#68933 = ORIENTED_EDGE('',*,*,#49151,.F.) ;
#68934 = ORIENTED_EDGE('',*,*,#49152,.T.) ;
#68935 = ORIENTED_EDGE('',*,*,#49153,.F.) ;
#68936 = ORIENTED_EDGE('',*,*,#49154,.T.) ;
#68937 = ORIENTED_EDGE('',*,*,#49155,.T.) ;
#68938 = ORIENTED_EDGE('',*,*,#49156,.T.) ;
#68939 = ORIENTED_EDGE('',*,*,#49157,.F.) ;
#68940 = ORIENTED_EDGE('',*,*,#49158,.T.) ;
#68941 = ORIENTED_EDGE('',*,*,#49054,.T.) ;
#68942 = ORIENTED_EDGE('',*,*,#49158,.F.) ;
#68943 = ORIENTED_EDGE('',*,*,#49159,.F.) ;
#68944 = ORIENTED_EDGE('',*,*,#49160,.T.) ;
#68945 = ORIENTED_EDGE('',*,*,#49161,.F.) ;
#68946 = ORIENTED_EDGE('',*,*,#49162,.T.) ;
#68947 = ORIENTED_EDGE('',*,*,#49163,.F.) ;
#68948 = ORIENTED_EDGE('',*,*,#49164,.T.) ;
#68949 = ORIENTED_EDGE('',*,*,#49165,.T.) ;
#68950 = ORIENTED_EDGE('',*,*,#49166,.T.) ;
#68951 = ORIENTED_EDGE('',*,*,#49167,.F.) ;
#68952 = ORIENTED_EDGE('',*,*,#49168,.T.) ;
#68953 = ORIENTED_EDGE('',*,*,#49169,.F.) ;
#68954 = ORIENTED_EDGE('',*,*,#49170,.T.) ;
#68955 = ORIENTED_EDGE('',*,*,#49171,.F.) ;
#68956 = ORIENTED_EDGE('',*,*,#49172,.T.) ;
#68957 = ORIENTED_EDGE('',*,*,#49173,.T.) ;
#68958 = ORIENTED_EDGE('',*,*,#49174,.T.) ;
#68959 = ORIENTED_EDGE('',*,*,#49175,.F.) ;
#68960 = ORIENTED_EDGE('',*,*,#49176,.T.) ;
#68961 = ORIENTED_EDGE('',*,*,#49045,.T.) ;
#68962 = ORIENTED_EDGE('',*,*,#49176,.F.) ;
#68963 = ORIENTED_EDGE('',*,*,#49177,.F.) ;
#68964 = ORIENTED_EDGE('',*,*,#49178,.T.) ;
#68965 = ORIENTED_EDGE('',*,*,#49179,.F.) ;
#68966 = ORIENTED_EDGE('',*,*,#49180,.T.) ;
#68967 = ORIENTED_EDGE('',*,*,#49181,.F.) ;
#68968 = ORIENTED_EDGE('',*,*,#49182,.T.) ;
#68969 = ORIENTED_EDGE('',*,*,#49183,.T.) ;
#68970 = ORIENTED_EDGE('',*,*,#49184,.T.) ;
#68971 = ORIENTED_EDGE('',*,*,#49185,.F.) ;
#68972 = ORIENTED_EDGE('',*,*,#49186,.T.) ;
#68973 = ORIENTED_EDGE('',*,*,#49187,.F.) ;
#68974 = ORIENTED_EDGE('',*,*,#49188,.T.) ;
#68975 = ORIENTED_EDGE('',*,*,#49189,.F.) ;
#68976 = ORIENTED_EDGE('',*,*,#49190,.T.) ;
#68977 = ORIENTED_EDGE('',*,*,#49191,.T.) ;
#68978 = ORIENTED_EDGE('',*,*,#49192,.T.) ;
#68979 = ORIENTED_EDGE('',*,*,#49193,.F.) ;
#68980 = ORIENTED_EDGE('',*,*,#49194,.T.) ;
#68981 = ORIENTED_EDGE('',*,*,#49036,.T.) ;
#68982 = ORIENTED_EDGE('',*,*,#49194,.F.) ;
#68983 = ORIENTED_EDGE('',*,*,#49195,.F.) ;
#68984 = ORIENTED_EDGE('',*,*,#49196,.T.) ;
#68985 = ORIENTED_EDGE('',*,*,#49197,.F.) ;
#68986 = ORIENTED_EDGE('',*,*,#49198,.T.) ;
#68987 = ORIENTED_EDGE('',*,*,#49199,.F.) ;
#68988 = ORIENTED_EDGE('',*,*,#49200,.T.) ;
#68989 = ORIENTED_EDGE('',*,*,#49201,.T.) ;
#68990 = ORIENTED_EDGE('',*,*,#49202,.T.) ;
#68991 = ORIENTED_EDGE('',*,*,#49203,.F.) ;
#68992 = ORIENTED_EDGE('',*,*,#49204,.T.) ;
#68993 = ORIENTED_EDGE('',*,*,#49205,.F.) ;
#68994 = ORIENTED_EDGE('',*,*,#49206,.T.) ;
#68995 = ORIENTED_EDGE('',*,*,#49207,.F.) ;
#68996 = ORIENTED_EDGE('',*,*,#49208,.T.) ;
#68997 = ORIENTED_EDGE('',*,*,#49209,.T.) ;
#68998 = ORIENTED_EDGE('',*,*,#49210,.T.) ;
#68999 = ORIENTED_EDGE('',*,*,#49211,.F.) ;
#69000 = ORIENTED_EDGE('',*,*,#49212,.T.) ;
#69001 = ORIENTED_EDGE('',*,*,#49027,.T.) ;
#69002 = ORIENTED_EDGE('',*,*,#49212,.F.) ;
#69003 = ORIENTED_EDGE('',*,*,#49213,.F.) ;
#69004 = ORIENTED_EDGE('',*,*,#49214,.T.) ;
#69005 = ORIENTED_EDGE('',*,*,#49215,.F.) ;
#69006 = ORIENTED_EDGE('',*,*,#49216,.T.) ;
#69007 = ORIENTED_EDGE('',*,*,#49217,.F.) ;
#69008 = ORIENTED_EDGE('',*,*,#49218,.T.) ;
#69009 = ORIENTED_EDGE('',*,*,#49219,.T.) ;
#69010 = ORIENTED_EDGE('',*,*,#49220,.T.) ;
#69011 = ORIENTED_EDGE('',*,*,#49221,.F.) ;
#69012 = ORIENTED_EDGE('',*,*,#49222,.T.) ;
#69013 = ORIENTED_EDGE('',*,*,#49223,.F.) ;
#69014 = ORIENTED_EDGE('',*,*,#49224,.T.) ;
#69015 = ORIENTED_EDGE('',*,*,#49225,.F.) ;
#69016 = ORIENTED_EDGE('',*,*,#49226,.T.) ;
#69017 = ORIENTED_EDGE('',*,*,#49227,.T.) ;
#69018 = ORIENTED_EDGE('',*,*,#49228,.T.) ;
#69019 = ORIENTED_EDGE('',*,*,#49229,.F.) ;
#69020 = ORIENTED_EDGE('',*,*,#49230,.T.) ;
#69021 = ORIENTED_EDGE('',*,*,#49018,.T.) ;
#69022 = ORIENTED_EDGE('',*,*,#49230,.F.) ;
#69023 = ORIENTED_EDGE('',*,*,#49231,.F.) ;
#69024 = ORIENTED_EDGE('',*,*,#49232,.T.) ;
#69025 = ORIENTED_EDGE('',*,*,#49233,.F.) ;
#69026 = ORIENTED_EDGE('',*,*,#49234,.T.) ;
#69027 = ORIENTED_EDGE('',*,*,#49235,.F.) ;
#69028 = ORIENTED_EDGE('',*,*,#49236,.T.) ;
#69029 = ORIENTED_EDGE('',*,*,#49237,.T.) ;
#69030 = ORIENTED_EDGE('',*,*,#49238,.T.) ;
#69031 = ORIENTED_EDGE('',*,*,#49239,.F.) ;
#69032 = ORIENTED_EDGE('',*,*,#49240,.T.) ;
#69033 = ORIENTED_EDGE('',*,*,#49241,.F.) ;
#69034 = ORIENTED_EDGE('',*,*,#49242,.T.) ;
#69035 = ORIENTED_EDGE('',*,*,#49243,.F.) ;
#69036 = ORIENTED_EDGE('',*,*,#49244,.T.) ;
#69037 = ORIENTED_EDGE('',*,*,#49245,.T.) ;
#69038 = ORIENTED_EDGE('',*,*,#49246,.T.) ;
#69039 = ORIENTED_EDGE('',*,*,#49247,.F.) ;
#69040 = ORIENTED_EDGE('',*,*,#49248,.T.) ;
#69041 = ORIENTED_EDGE('',*,*,#49009,.T.) ;
#69042 = ORIENTED_EDGE('',*,*,#49248,.F.) ;
#69043 = ORIENTED_EDGE('',*,*,#49249,.F.) ;
#69044 = ORIENTED_EDGE('',*,*,#49250,.T.) ;
#69045 = ORIENTED_EDGE('',*,*,#49006,.T.) ;
#69046 = ORIENTED_EDGE('',*,*,#49250,.F.) ;
#69047 = ORIENTED_EDGE('',*,*,#49251,.F.) ;
#69048 = ORIENTED_EDGE('',*,*,#49252,.T.) ;
#69049 = ORIENTED_EDGE('',*,*,#49015,.T.) ;
#69050 = ORIENTED_EDGE('',*,*,#49252,.F.) ;
#69051 = ORIENTED_EDGE('',*,*,#49253,.F.) ;
#69052 = ORIENTED_EDGE('',*,*,#49254,.T.) ;
#69053 = ORIENTED_EDGE('',*,*,#49024,.T.) ;
#69054 = ORIENTED_EDGE('',*,*,#49254,.F.) ;
#69055 = ORIENTED_EDGE('',*,*,#49255,.F.) ;
#69056 = ORIENTED_EDGE('',*,*,#49256,.T.) ;
#69057 = ORIENTED_EDGE('',*,*,#49033,.T.) ;
#69058 = ORIENTED_EDGE('',*,*,#49256,.F.) ;
#69059 = ORIENTED_EDGE('',*,*,#49257,.F.) ;
#69060 = ORIENTED_EDGE('',*,*,#49258,.T.) ;
#69061 = ORIENTED_EDGE('',*,*,#49042,.T.) ;
#69062 = ORIENTED_EDGE('',*,*,#49258,.F.) ;
#69063 = ORIENTED_EDGE('',*,*,#49259,.F.) ;
#69064 = ORIENTED_EDGE('',*,*,#49260,.T.) ;
#69065 = ORIENTED_EDGE('',*,*,#49051,.T.) ;
#69066 = ORIENTED_EDGE('',*,*,#49260,.F.) ;
#69067 = ORIENTED_EDGE('',*,*,#49261,.F.) ;
#69068 = ORIENTED_EDGE('',*,*,#49262,.T.) ;
#69069 = ORIENTED_EDGE('',*,*,#49060,.T.) ;
#69070 = ORIENTED_EDGE('',*,*,#49262,.F.) ;
#69071 = ORIENTED_EDGE('',*,*,#49263,.F.) ;
#69072 = ORIENTED_EDGE('',*,*,#49264,.T.) ;
#69073 = ORIENTED_EDGE('',*,*,#49069,.T.) ;
#69074 = ORIENTED_EDGE('',*,*,#49264,.F.) ;
#69075 = ORIENTED_EDGE('',*,*,#49265,.F.) ;
#69076 = ORIENTED_EDGE('',*,*,#49266,.T.) ;
#69077 = ORIENTED_EDGE('',*,*,#49078,.T.) ;
#69078 = ORIENTED_EDGE('',*,*,#49266,.F.) ;
#69079 = ORIENTED_EDGE('',*,*,#49080,.T.) ;
#69080 = ORIENTED_EDGE('',*,*,#49267,.T.) ;
#69081 = ORIENTED_EDGE('',*,*,#49084,.T.) ;
#69082 = ORIENTED_EDGE('',*,*,#49267,.F.) ;
#69083 = ORIENTED_EDGE('',*,*,#49071,.T.) ;
#69084 = ORIENTED_EDGE('',*,*,#49268,.T.) ;
#69085 = ORIENTED_EDGE('',*,*,#49075,.T.) ;
#69086 = ORIENTED_EDGE('',*,*,#49268,.F.) ;
#69087 = ORIENTED_EDGE('',*,*,#49062,.T.) ;
#69088 = ORIENTED_EDGE('',*,*,#49269,.T.) ;
#69089 = ORIENTED_EDGE('',*,*,#49066,.T.) ;
#69090 = ORIENTED_EDGE('',*,*,#49269,.F.) ;
#69091 = ORIENTED_EDGE('',*,*,#49053,.T.) ;
#69092 = ORIENTED_EDGE('',*,*,#49270,.T.) ;
#69093 = ORIENTED_EDGE('',*,*,#49057,.T.) ;
#69094 = ORIENTED_EDGE('',*,*,#49270,.F.) ;
#69095 = ORIENTED_EDGE('',*,*,#49044,.T.) ;
#69096 = ORIENTED_EDGE('',*,*,#49271,.T.) ;
#69097 = ORIENTED_EDGE('',*,*,#49048,.T.) ;
#69098 = ORIENTED_EDGE('',*,*,#49271,.F.) ;
#69099 = ORIENTED_EDGE('',*,*,#49035,.T.) ;
#69100 = ORIENTED_EDGE('',*,*,#49272,.T.) ;
#69101 = ORIENTED_EDGE('',*,*,#49039,.T.) ;
#69102 = ORIENTED_EDGE('',*,*,#49272,.F.) ;
#69103 = ORIENTED_EDGE('',*,*,#49026,.T.) ;
#69104 = ORIENTED_EDGE('',*,*,#49273,.T.) ;
#69105 = ORIENTED_EDGE('',*,*,#49030,.T.) ;
#69106 = ORIENTED_EDGE('',*,*,#49273,.F.) ;
#69107 = ORIENTED_EDGE('',*,*,#49017,.T.) ;
#69108 = ORIENTED_EDGE('',*,*,#49274,.T.) ;
#69109 = ORIENTED_EDGE('',*,*,#49021,.T.) ;
#69110 = ORIENTED_EDGE('',*,*,#49274,.F.) ;
#69111 = ORIENTED_EDGE('',*,*,#49008,.T.) ;
#69112 = ORIENTED_EDGE('',*,*,#49275,.T.) ;
#69113 = ORIENTED_EDGE('',*,*,#49012,.T.) ;
#69114 = ORIENTED_EDGE('',*,*,#49275,.F.) ;
#69115 = ORIENTED_EDGE('',*,*,#49276,.F.) ;
#69116 = ORIENTED_EDGE('',*,*,#49277,.T.) ;
#69117 = ORIENTED_EDGE('',*,*,#49278,.F.) ;
#69118 = ORIENTED_EDGE('',*,*,#49277,.F.) ;
#69119 = ORIENTED_EDGE('',*,*,#49279,.F.) ;
#69120 = ORIENTED_EDGE('',*,*,#49280,.T.) ;
#69121 = ORIENTED_EDGE('',*,*,#49281,.F.) ;
#69122 = ORIENTED_EDGE('',*,*,#49280,.F.) ;
#69123 = ORIENTED_EDGE('',*,*,#49282,.F.) ;
#69124 = ORIENTED_EDGE('',*,*,#49283,.T.) ;
#69125 = ORIENTED_EDGE('',*,*,#49284,.F.) ;
#69126 = ORIENTED_EDGE('',*,*,#49283,.F.) ;
#69127 = ORIENTED_EDGE('',*,*,#49285,.T.) ;
#69128 = ORIENTED_EDGE('',*,*,#49286,.T.) ;
#69129 = ORIENTED_EDGE('',*,*,#48971,.T.) ;
#69130 = ORIENTED_EDGE('',*,*,#49287,.F.) ;
#69131 = ORIENTED_EDGE('',*,*,#49288,.T.) ;
#69132 = ORIENTED_EDGE('',*,*,#49289,.T.) ;
#69133 = ORIENTED_EDGE('',*,*,#48979,.T.) ;
#69134 = ORIENTED_EDGE('',*,*,#49290,.F.) ;
#69135 = ORIENTED_EDGE('',*,*,#49291,.T.) ;
#69136 = ORIENTED_EDGE('',*,*,#49292,.T.) ;
#69137 = ORIENTED_EDGE('',*,*,#48903,.T.) ;
#69138 = ORIENTED_EDGE('',*,*,#49293,.F.) ;
#69139 = ORIENTED_EDGE('',*,*,#49294,.T.) ;
#69140 = ORIENTED_EDGE('',*,*,#49295,.T.) ;
#69141 = ORIENTED_EDGE('',*,*,#48907,.T.) ;
#69142 = ORIENTED_EDGE('',*,*,#49296,.F.) ;
#69143 = ORIENTED_EDGE('',*,*,#49297,.F.) ;
#69144 = ORIENTED_EDGE('',*,*,#49298,.T.) ;
#69145 = ORIENTED_EDGE('',*,*,#49299,.F.) ;
#69146 = ORIENTED_EDGE('',*,*,#49300,.T.) ;
#69147 = ORIENTED_EDGE('',*,*,#49301,.F.) ;
#69148 = ORIENTED_EDGE('',*,*,#49302,.T.) ;
#69149 = ORIENTED_EDGE('',*,*,#49303,.T.) ;
#69150 = ORIENTED_EDGE('',*,*,#49304,.T.) ;
#69151 = ORIENTED_EDGE('',*,*,#49305,.F.) ;
#69152 = ORIENTED_EDGE('',*,*,#49306,.T.) ;
#69153 = ORIENTED_EDGE('',*,*,#49307,.F.) ;
#69154 = ORIENTED_EDGE('',*,*,#49308,.T.) ;
#69155 = ORIENTED_EDGE('',*,*,#49309,.F.) ;
#69156 = ORIENTED_EDGE('',*,*,#49310,.T.) ;
#69157 = ORIENTED_EDGE('',*,*,#49311,.T.) ;
#69158 = ORIENTED_EDGE('',*,*,#49312,.T.) ;
#69159 = ORIENTED_EDGE('',*,*,#49313,.F.) ;
#69160 = ORIENTED_EDGE('',*,*,#49314,.T.) ;
#69161 = ORIENTED_EDGE('',*,*,#49279,.T.) ;
#69162 = ORIENTED_EDGE('',*,*,#49314,.F.) ;
#69163 = ORIENTED_EDGE('',*,*,#49315,.F.) ;
#69164 = ORIENTED_EDGE('',*,*,#49316,.T.) ;
#69165 = ORIENTED_EDGE('',*,*,#49276,.T.) ;
#69166 = ORIENTED_EDGE('',*,*,#49316,.F.) ;
#69167 = ORIENTED_EDGE('',*,*,#49278,.T.) ;
#69168 = ORIENTED_EDGE('',*,*,#49317,.T.) ;
#69169 = ORIENTED_EDGE('',*,*,#49282,.T.) ;
#69170 = ORIENTED_EDGE('',*,*,#49317,.F.) ;
#69171 = ORIENTED_EDGE('',*,*,#49318,.T.) ;
#69172 = ORIENTED_EDGE('',*,*,#49319,.T.) ;
#69173 = ORIENTED_EDGE('',*,*,#49320,.T.) ;
#69174 = ORIENTED_EDGE('',*,*,#49321,.T.) ;
#69175 = ORIENTED_EDGE('',*,*,#48901,.T.) ;
#69176 = ORIENTED_EDGE('',*,*,#49322,.T.) ;
#69177 = ORIENTED_EDGE('',*,*,#48905,.T.) ;
#69178 = ORIENTED_EDGE('',*,*,#49323,.T.) ;
#69179 = ORIENTED_EDGE('',*,*,#48913,.T.) ;
#69180 = ORIENTED_EDGE('',*,*,#49324,.T.) ;
#69181 = ORIENTED_EDGE('',*,*,#48921,.T.) ;
#69182 = ORIENTED_EDGE('',*,*,#49325,.T.) ;
#69183 = ORIENTED_EDGE('',*,*,#48929,.T.) ;
#69184 = ORIENTED_EDGE('',*,*,#49326,.T.) ;
#69185 = ORIENTED_EDGE('',*,*,#48937,.T.) ;
#69186 = ORIENTED_EDGE('',*,*,#49327,.T.) ;
#69187 = ORIENTED_EDGE('',*,*,#48945,.T.) ;
#69188 = ORIENTED_EDGE('',*,*,#49328,.T.) ;
#69189 = ORIENTED_EDGE('',*,*,#48953,.T.) ;
#69190 = ORIENTED_EDGE('',*,*,#49329,.T.) ;
#69191 = ORIENTED_EDGE('',*,*,#48961,.T.) ;
#69192 = ORIENTED_EDGE('',*,*,#49330,.T.) ;
#69193 = ORIENTED_EDGE('',*,*,#48969,.T.) ;
#69194 = ORIENTED_EDGE('',*,*,#49331,.T.) ;
#69195 = ORIENTED_EDGE('',*,*,#48977,.T.) ;
#69196 = ORIENTED_EDGE('',*,*,#49332,.T.) ;
#69197 = ORIENTED_EDGE('',*,*,#49333,.T.) ;
#69198 = ORIENTED_EDGE('',*,*,#49334,.T.) ;
#69199 = ORIENTED_EDGE('',*,*,#49335,.F.) ;
#69200 = ORIENTED_EDGE('',*,*,#49336,.T.) ;
#69201 = ORIENTED_EDGE('',*,*,#49337,.F.) ;
#69202 = ORIENTED_EDGE('',*,*,#49338,.T.) ;
#69203 = ORIENTED_EDGE('',*,*,#49339,.F.) ;
#69204 = ORIENTED_EDGE('',*,*,#49340,.T.) ;
#69205 = ORIENTED_EDGE('',*,*,#49341,.F.) ;
#69206 = ORIENTED_EDGE('',*,*,#49342,.T.) ;
#69207 = ORIENTED_EDGE('',*,*,#49020,.T.) ;
#69208 = ORIENTED_EDGE('',*,*,#49343,.F.) ;
#69209 = ORIENTED_EDGE('',*,*,#49344,.T.) ;
#69210 = ORIENTED_EDGE('',*,*,#49345,.F.) ;
#69211 = ORIENTED_EDGE('',*,*,#49346,.T.) ;
#69212 = ORIENTED_EDGE('',*,*,#49347,.F.) ;
#69213 = ORIENTED_EDGE('',*,*,#49348,.T.) ;
#69214 = ORIENTED_EDGE('',*,*,#49349,.F.) ;
#69215 = ORIENTED_EDGE('',*,*,#49350,.T.) ;
#69216 = ORIENTED_EDGE('',*,*,#49038,.T.) ;
#69217 = ORIENTED_EDGE('',*,*,#49351,.F.) ;
#69218 = ORIENTED_EDGE('',*,*,#49352,.T.) ;
#69219 = ORIENTED_EDGE('',*,*,#49353,.F.) ;
#69220 = ORIENTED_EDGE('',*,*,#49354,.T.) ;
#69221 = ORIENTED_EDGE('',*,*,#49355,.F.) ;
#69222 = ORIENTED_EDGE('',*,*,#49356,.T.) ;
#69223 = ORIENTED_EDGE('',*,*,#49357,.F.) ;
#69224 = ORIENTED_EDGE('',*,*,#49358,.T.) ;
#69225 = ORIENTED_EDGE('',*,*,#49056,.T.) ;
#69226 = ORIENTED_EDGE('',*,*,#49359,.F.) ;
#69227 = ORIENTED_EDGE('',*,*,#49360,.T.) ;
#69228 = ORIENTED_EDGE('',*,*,#49361,.F.) ;
#69229 = ORIENTED_EDGE('',*,*,#49362,.T.) ;
#69230 = ORIENTED_EDGE('',*,*,#49363,.F.) ;
#69231 = ORIENTED_EDGE('',*,*,#49364,.T.) ;
#69232 = ORIENTED_EDGE('',*,*,#49365,.F.) ;
#69233 = ORIENTED_EDGE('',*,*,#49366,.T.) ;
#69234 = ORIENTED_EDGE('',*,*,#49074,.T.) ;
#69235 = ORIENTED_EDGE('',*,*,#49367,.F.) ;
#69236 = ORIENTED_EDGE('',*,*,#49368,.T.) ;
#69237 = ORIENTED_EDGE('',*,*,#49369,.F.) ;
#69238 = ORIENTED_EDGE('',*,*,#49370,.T.) ;
#69239 = ORIENTED_EDGE('',*,*,#49371,.F.) ;
#69240 = ORIENTED_EDGE('',*,*,#49372,.T.) ;
#69241 = ORIENTED_EDGE('',*,*,#49373,.F.) ;
#69242 = ORIENTED_EDGE('',*,*,#49374,.T.) ;
#69243 = ORIENTED_EDGE('',*,*,#49281,.T.) ;
#69244 = ORIENTED_EDGE('',*,*,#49083,.T.) ;
#69245 = ORIENTED_EDGE('',*,*,#49375,.F.) ;
#69246 = ORIENTED_EDGE('',*,*,#49376,.T.) ;
#69247 = ORIENTED_EDGE('',*,*,#49377,.F.) ;
#69248 = ORIENTED_EDGE('',*,*,#49378,.T.) ;
#69249 = ORIENTED_EDGE('',*,*,#49379,.F.) ;
#69250 = ORIENTED_EDGE('',*,*,#49380,.T.) ;
#69251 = ORIENTED_EDGE('',*,*,#49381,.F.) ;
#69252 = ORIENTED_EDGE('',*,*,#49382,.T.) ;
#69253 = ORIENTED_EDGE('',*,*,#49065,.T.) ;
#69254 = ORIENTED_EDGE('',*,*,#49383,.F.) ;
#69255 = ORIENTED_EDGE('',*,*,#49384,.T.) ;
#69256 = ORIENTED_EDGE('',*,*,#49385,.F.) ;
#69257 = ORIENTED_EDGE('',*,*,#49386,.T.) ;
#69258 = ORIENTED_EDGE('',*,*,#49387,.F.) ;
#69259 = ORIENTED_EDGE('',*,*,#49388,.T.) ;
#69260 = ORIENTED_EDGE('',*,*,#49389,.F.) ;
#69261 = ORIENTED_EDGE('',*,*,#49390,.T.) ;
#69262 = ORIENTED_EDGE('',*,*,#49047,.T.) ;
#69263 = ORIENTED_EDGE('',*,*,#49391,.F.) ;
#69264 = ORIENTED_EDGE('',*,*,#49392,.T.) ;
#69265 = ORIENTED_EDGE('',*,*,#49393,.F.) ;
#69266 = ORIENTED_EDGE('',*,*,#49394,.T.) ;
#69267 = ORIENTED_EDGE('',*,*,#49395,.F.) ;
#69268 = ORIENTED_EDGE('',*,*,#49396,.T.) ;
#69269 = ORIENTED_EDGE('',*,*,#49397,.F.) ;
#69270 = ORIENTED_EDGE('',*,*,#49398,.T.) ;
#69271 = ORIENTED_EDGE('',*,*,#49029,.T.) ;
#69272 = ORIENTED_EDGE('',*,*,#49399,.F.) ;
#69273 = ORIENTED_EDGE('',*,*,#49400,.T.) ;
#69274 = ORIENTED_EDGE('',*,*,#49401,.F.) ;
#69275 = ORIENTED_EDGE('',*,*,#49402,.T.) ;
#69276 = ORIENTED_EDGE('',*,*,#49403,.F.) ;
#69277 = ORIENTED_EDGE('',*,*,#49404,.T.) ;
#69278 = ORIENTED_EDGE('',*,*,#49405,.F.) ;
#69279 = ORIENTED_EDGE('',*,*,#49406,.T.) ;
#69280 = ORIENTED_EDGE('',*,*,#49011,.T.) ;
#69281 = ORIENTED_EDGE('',*,*,#49407,.F.) ;
#69282 = ORIENTED_EDGE('',*,*,#49408,.T.) ;
#69283 = ORIENTED_EDGE('',*,*,#49409,.F.) ;
#69284 = ORIENTED_EDGE('',*,*,#49410,.T.) ;
#69285 = ORIENTED_EDGE('',*,*,#49411,.F.) ;
#69286 = ORIENTED_EDGE('',*,*,#49412,.T.) ;
#69287 = ORIENTED_EDGE('',*,*,#49413,.F.) ;
#69288 = ORIENTED_EDGE('',*,*,#49414,.T.) ;
#69289 = ORIENTED_EDGE('',*,*,#49415,.T.) ;
#69290 = ORIENTED_EDGE('',*,*,#49416,.T.) ;
#69291 = ORIENTED_EDGE('',*,*,#49417,.T.) ;
#69292 = ORIENTED_EDGE('',*,*,#49418,.T.) ;
#69293 = ORIENTED_EDGE('',*,*,#49419,.T.) ;
#69294 = ORIENTED_EDGE('',*,*,#49420,.T.) ;
#69295 = ORIENTED_EDGE('',*,*,#49421,.T.) ;
#69296 = ORIENTED_EDGE('',*,*,#49422,.T.) ;
#69297 = ORIENTED_EDGE('',*,*,#49423,.T.) ;
#69298 = ORIENTED_EDGE('',*,*,#49424,.T.) ;
#69299 = ORIENTED_EDGE('',*,*,#49425,.T.) ;
#69300 = ORIENTED_EDGE('',*,*,#49426,.T.) ;
#69301 = ORIENTED_EDGE('',*,*,#49427,.T.) ;
#69302 = ORIENTED_EDGE('',*,*,#49428,.T.) ;
#69303 = ORIENTED_EDGE('',*,*,#49429,.T.) ;
#69304 = ORIENTED_EDGE('',*,*,#49430,.T.) ;
#69305 = ORIENTED_EDGE('',*,*,#49431,.T.) ;
#69306 = ORIENTED_EDGE('',*,*,#49432,.T.) ;
#69307 = ORIENTED_EDGE('',*,*,#49433,.T.) ;
#69308 = ORIENTED_EDGE('',*,*,#49434,.T.) ;
#69309 = ORIENTED_EDGE('',*,*,#49435,.T.) ;
#69310 = ORIENTED_EDGE('',*,*,#49436,.T.) ;
#69311 = ORIENTED_EDGE('',*,*,#49437,.T.) ;
#69312 = ORIENTED_EDGE('',*,*,#49438,.T.) ;
#69313 = ORIENTED_EDGE('',*,*,#49439,.T.) ;
#69314 = ORIENTED_EDGE('',*,*,#49440,.T.) ;
#69315 = ORIENTED_EDGE('',*,*,#49441,.T.) ;
#69316 = ORIENTED_EDGE('',*,*,#49442,.T.) ;
#69317 = ORIENTED_EDGE('',*,*,#49443,.T.) ;
#69318 = ORIENTED_EDGE('',*,*,#49444,.T.) ;
#69319 = ORIENTED_EDGE('',*,*,#49445,.T.) ;
#69320 = ORIENTED_EDGE('',*,*,#49446,.T.) ;
#69321 = ORIENTED_EDGE('',*,*,#49447,.T.) ;
#69322 = ORIENTED_EDGE('',*,*,#49448,.T.) ;
#69323 = ORIENTED_EDGE('',*,*,#49449,.T.) ;
#69324 = ORIENTED_EDGE('',*,*,#49450,.T.) ;
#69325 = ORIENTED_EDGE('',*,*,#49451,.T.) ;
#69326 = ORIENTED_EDGE('',*,*,#49452,.T.) ;
#69327 = ORIENTED_EDGE('',*,*,#49453,.T.) ;
#69328 = ORIENTED_EDGE('',*,*,#49454,.T.) ;
#69329 = ORIENTED_EDGE('',*,*,#49455,.T.) ;
#69330 = ORIENTED_EDGE('',*,*,#49456,.T.) ;
#69331 = ORIENTED_EDGE('',*,*,#49457,.T.) ;
#69332 = ORIENTED_EDGE('',*,*,#49458,.T.) ;
#69333 = ORIENTED_EDGE('',*,*,#49459,.T.) ;
#69334 = ORIENTED_EDGE('',*,*,#49460,.T.) ;
#69335 = ORIENTED_EDGE('',*,*,#49461,.T.) ;
#69336 = ORIENTED_EDGE('',*,*,#49462,.T.) ;
#69337 = ORIENTED_EDGE('',*,*,#49463,.T.) ;
#69338 = ORIENTED_EDGE('',*,*,#49464,.T.) ;
#69339 = ORIENTED_EDGE('',*,*,#49465,.T.) ;
#69340 = ORIENTED_EDGE('',*,*,#49466,.T.) ;
#69341 = ORIENTED_EDGE('',*,*,#49467,.T.) ;
#69342 = ORIENTED_EDGE('',*,*,#49468,.T.) ;
#69343 = ORIENTED_EDGE('',*,*,#49469,.T.) ;
#69344 = ORIENTED_EDGE('',*,*,#49470,.T.) ;
#69345 = ORIENTED_EDGE('',*,*,#49471,.T.) ;
#69346 = ORIENTED_EDGE('',*,*,#49472,.T.) ;
#69347 = ORIENTED_EDGE('',*,*,#49473,.T.) ;
#69348 = ORIENTED_EDGE('',*,*,#49474,.T.) ;
#69349 = ORIENTED_EDGE('',*,*,#49475,.T.) ;
#69350 = ORIENTED_EDGE('',*,*,#49476,.T.) ;
#69351 = ORIENTED_EDGE('',*,*,#49477,.T.) ;
#69352 = ORIENTED_EDGE('',*,*,#49478,.T.) ;
#69353 = ORIENTED_EDGE('',*,*,#49479,.T.) ;
#69354 = ORIENTED_EDGE('',*,*,#49480,.T.) ;
#69355 = ORIENTED_EDGE('',*,*,#49481,.T.) ;
#69356 = ORIENTED_EDGE('',*,*,#49482,.T.) ;
#69357 = ORIENTED_EDGE('',*,*,#49483,.T.) ;
#69358 = ORIENTED_EDGE('',*,*,#49484,.T.) ;
#69359 = ORIENTED_EDGE('',*,*,#49485,.T.) ;
#69360 = ORIENTED_EDGE('',*,*,#49486,.T.) ;
#69361 = ORIENTED_EDGE('',*,*,#49487,.T.) ;
#69362 = ORIENTED_EDGE('',*,*,#49488,.T.) ;
#69363 = ORIENTED_EDGE('',*,*,#49489,.T.) ;
#69364 = ORIENTED_EDGE('',*,*,#49490,.T.) ;
#69365 = ORIENTED_EDGE('',*,*,#49491,.T.) ;
#69366 = ORIENTED_EDGE('',*,*,#49492,.T.) ;
#69367 = ORIENTED_EDGE('',*,*,#49493,.T.) ;
#69368 = ORIENTED_EDGE('',*,*,#49494,.T.) ;
#69369 = ORIENTED_EDGE('',*,*,#49495,.T.) ;
#69370 = ORIENTED_EDGE('',*,*,#49496,.T.) ;
#69371 = ORIENTED_EDGE('',*,*,#49497,.T.) ;
#69372 = ORIENTED_EDGE('',*,*,#49498,.T.) ;
#69373 = ORIENTED_EDGE('',*,*,#49499,.T.) ;
#69374 = ORIENTED_EDGE('',*,*,#49500,.T.) ;
#69375 = ORIENTED_EDGE('',*,*,#49501,.T.) ;
#69376 = ORIENTED_EDGE('',*,*,#49502,.T.) ;
#69377 = ORIENTED_EDGE('',*,*,#49503,.T.) ;
#69378 = ORIENTED_EDGE('',*,*,#49504,.T.) ;
#69379 = ORIENTED_EDGE('',*,*,#49505,.T.) ;
#69380 = ORIENTED_EDGE('',*,*,#49506,.T.) ;
#69381 = ORIENTED_EDGE('',*,*,#49507,.T.) ;
#69382 = ORIENTED_EDGE('',*,*,#49508,.T.) ;
#69383 = ORIENTED_EDGE('',*,*,#49509,.T.) ;
#69384 = ORIENTED_EDGE('',*,*,#49510,.T.) ;
#69385 = ORIENTED_EDGE('',*,*,#49511,.T.) ;
#69386 = ORIENTED_EDGE('',*,*,#49512,.T.) ;
#69387 = ORIENTED_EDGE('',*,*,#49513,.T.) ;
#69388 = ORIENTED_EDGE('',*,*,#49514,.T.) ;
#69389 = ORIENTED_EDGE('',*,*,#49515,.T.) ;
#69390 = ORIENTED_EDGE('',*,*,#49516,.T.) ;
#69391 = ORIENTED_EDGE('',*,*,#49517,.T.) ;
#69392 = ORIENTED_EDGE('',*,*,#49518,.T.) ;
#69393 = ORIENTED_EDGE('',*,*,#49519,.T.) ;
#69394 = ORIENTED_EDGE('',*,*,#49520,.T.) ;
#69395 = ORIENTED_EDGE('',*,*,#49521,.T.) ;
#69396 = ORIENTED_EDGE('',*,*,#49522,.T.) ;
#69397 = ORIENTED_EDGE('',*,*,#49239,.T.) ;
#69398 = ORIENTED_EDGE('',*,*,#49523,.T.) ;
#69399 = ORIENTED_EDGE('',*,*,#49221,.T.) ;
#69400 = ORIENTED_EDGE('',*,*,#49524,.T.) ;
#69401 = ORIENTED_EDGE('',*,*,#49203,.T.) ;
#69402 = ORIENTED_EDGE('',*,*,#49525,.T.) ;
#69403 = ORIENTED_EDGE('',*,*,#49185,.T.) ;
#69404 = ORIENTED_EDGE('',*,*,#49526,.T.) ;
#69405 = ORIENTED_EDGE('',*,*,#49167,.T.) ;
#69406 = ORIENTED_EDGE('',*,*,#49527,.T.) ;
#69407 = ORIENTED_EDGE('',*,*,#49149,.T.) ;
#69408 = ORIENTED_EDGE('',*,*,#49528,.T.) ;
#69409 = ORIENTED_EDGE('',*,*,#49131,.T.) ;
#69410 = ORIENTED_EDGE('',*,*,#49529,.T.) ;
#69411 = ORIENTED_EDGE('',*,*,#49113,.T.) ;
#69412 = ORIENTED_EDGE('',*,*,#49530,.T.) ;
#69413 = ORIENTED_EDGE('',*,*,#49095,.T.) ;
#69414 = ORIENTED_EDGE('',*,*,#49531,.T.) ;
#69415 = ORIENTED_EDGE('',*,*,#49532,.T.) ;
#69416 = ORIENTED_EDGE('',*,*,#49533,.T.) ;
#69417 = ORIENTED_EDGE('',*,*,#49534,.T.) ;
#69418 = ORIENTED_EDGE('',*,*,#49535,.T.) ;
#69419 = ORIENTED_EDGE('',*,*,#49536,.T.) ;
#69420 = ORIENTED_EDGE('',*,*,#49537,.T.) ;
#69421 = ORIENTED_EDGE('',*,*,#49538,.T.) ;
#69422 = ORIENTED_EDGE('',*,*,#49539,.T.) ;
#69423 = ORIENTED_EDGE('',*,*,#49540,.T.) ;
#69424 = ORIENTED_EDGE('',*,*,#49541,.T.) ;
#69425 = ORIENTED_EDGE('',*,*,#49542,.T.) ;
#69426 = ORIENTED_EDGE('',*,*,#49543,.T.) ;
#69427 = ORIENTED_EDGE('',*,*,#49544,.T.) ;
#69428 = ORIENTED_EDGE('',*,*,#49545,.T.) ;
#69429 = ORIENTED_EDGE('',*,*,#49546,.T.) ;
#69430 = ORIENTED_EDGE('',*,*,#49547,.T.) ;
#69431 = ORIENTED_EDGE('',*,*,#49548,.T.) ;
#69432 = ORIENTED_EDGE('',*,*,#49549,.T.) ;
#69433 = ORIENTED_EDGE('',*,*,#49550,.T.) ;
#69434 = ORIENTED_EDGE('',*,*,#49551,.T.) ;
#69435 = ORIENTED_EDGE('',*,*,#49552,.T.) ;
#69436 = ORIENTED_EDGE('',*,*,#49553,.T.) ;
#69437 = ORIENTED_EDGE('',*,*,#49554,.T.) ;
#69438 = ORIENTED_EDGE('',*,*,#49555,.T.) ;
#69439 = ORIENTED_EDGE('',*,*,#49556,.T.) ;
#69440 = ORIENTED_EDGE('',*,*,#49557,.T.) ;
#69441 = ORIENTED_EDGE('',*,*,#49558,.T.) ;
#69442 = ORIENTED_EDGE('',*,*,#49559,.T.) ;
#69443 = ORIENTED_EDGE('',*,*,#49560,.T.) ;
#69444 = ORIENTED_EDGE('',*,*,#49561,.T.) ;
#69445 = ORIENTED_EDGE('',*,*,#49562,.T.) ;
#69446 = ORIENTED_EDGE('',*,*,#49563,.T.) ;
#69447 = ORIENTED_EDGE('',*,*,#49564,.T.) ;
#69448 = ORIENTED_EDGE('',*,*,#49565,.T.) ;
#69449 = ORIENTED_EDGE('',*,*,#49566,.T.) ;
#69450 = ORIENTED_EDGE('',*,*,#49567,.T.) ;
#69451 = ORIENTED_EDGE('',*,*,#49568,.T.) ;
#69452 = ORIENTED_EDGE('',*,*,#49569,.T.) ;
#69453 = ORIENTED_EDGE('',*,*,#49570,.T.) ;
#69454 = ORIENTED_EDGE('',*,*,#49571,.T.) ;
#69455 = ORIENTED_EDGE('',*,*,#49572,.T.) ;
#69456 = ORIENTED_EDGE('',*,*,#49573,.T.) ;
#69457 = ORIENTED_EDGE('',*,*,#49574,.T.) ;
#69458 = ORIENTED_EDGE('',*,*,#49575,.T.) ;
#69459 = ORIENTED_EDGE('',*,*,#49576,.T.) ;
#69460 = ORIENTED_EDGE('',*,*,#49577,.T.) ;
#69461 = ORIENTED_EDGE('',*,*,#49578,.T.) ;
#69462 = ORIENTED_EDGE('',*,*,#49579,.T.) ;
#69463 = ORIENTED_EDGE('',*,*,#49580,.T.) ;
#69464 = ORIENTED_EDGE('',*,*,#49581,.T.) ;
#69465 = ORIENTED_EDGE('',*,*,#49582,.T.) ;
#69466 = ORIENTED_EDGE('',*,*,#49583,.T.) ;
#69467 = ORIENTED_EDGE('',*,*,#49584,.T.) ;
#69468 = ORIENTED_EDGE('',*,*,#49585,.T.) ;
#69469 = ORIENTED_EDGE('',*,*,#49586,.T.) ;
#69470 = ORIENTED_EDGE('',*,*,#49587,.T.) ;
#69471 = ORIENTED_EDGE('',*,*,#49588,.T.) ;
#69472 = ORIENTED_EDGE('',*,*,#49589,.T.) ;
#69473 = ORIENTED_EDGE('',*,*,#49590,.T.) ;
#69474 = ORIENTED_EDGE('',*,*,#49591,.T.) ;
#69475 = ORIENTED_EDGE('',*,*,#49592,.T.) ;
#69476 = ORIENTED_EDGE('',*,*,#49593,.T.) ;
#69477 = ORIENTED_EDGE('',*,*,#49594,.T.) ;
#69478 = ORIENTED_EDGE('',*,*,#49595,.T.) ;
#69479 = ORIENTED_EDGE('',*,*,#49596,.F.) ;
#69480 = ORIENTED_EDGE('',*,*,#49597,.T.) ;
#69481 = ORIENTED_EDGE('',*,*,#49598,.T.) ;
#69482 = ORIENTED_EDGE('',*,*,#49599,.T.) ;
#69483 = ORIENTED_EDGE('',*,*,#49600,.T.) ;
#69484 = ORIENTED_EDGE('',*,*,#49601,.T.) ;
#69485 = ORIENTED_EDGE('',*,*,#49602,.F.) ;
#69486 = ORIENTED_EDGE('',*,*,#49603,.T.) ;
#69487 = ORIENTED_EDGE('',*,*,#49604,.F.) ;
#69488 = ORIENTED_EDGE('',*,*,#49605,.T.) ;
#69489 = ORIENTED_EDGE('',*,*,#49606,.T.) ;
#69490 = ORIENTED_EDGE('',*,*,#49607,.T.) ;
#69491 = ORIENTED_EDGE('',*,*,#49608,.T.) ;
#69492 = ORIENTED_EDGE('',*,*,#49609,.T.) ;
#69493 = ORIENTED_EDGE('',*,*,#49610,.F.) ;
#69494 = ORIENTED_EDGE('',*,*,#49611,.T.) ;
#69495 = ORIENTED_EDGE('',*,*,#49612,.F.) ;
#69496 = ORIENTED_EDGE('',*,*,#49613,.T.) ;
#69497 = ORIENTED_EDGE('',*,*,#49614,.T.) ;
#69498 = ORIENTED_EDGE('',*,*,#49615,.T.) ;
#69499 = ORIENTED_EDGE('',*,*,#49616,.T.) ;
#69500 = ORIENTED_EDGE('',*,*,#49617,.T.) ;
#69501 = ORIENTED_EDGE('',*,*,#49618,.F.) ;
#69502 = ORIENTED_EDGE('',*,*,#49619,.T.) ;
#69503 = ORIENTED_EDGE('',*,*,#49620,.F.) ;
#69504 = ORIENTED_EDGE('',*,*,#49621,.T.) ;
#69505 = ORIENTED_EDGE('',*,*,#49622,.T.) ;
#69506 = ORIENTED_EDGE('',*,*,#49623,.T.) ;
#69507 = ORIENTED_EDGE('',*,*,#49624,.T.) ;
#69508 = ORIENTED_EDGE('',*,*,#49625,.T.) ;
#69509 = ORIENTED_EDGE('',*,*,#49626,.F.) ;
#69510 = ORIENTED_EDGE('',*,*,#49627,.T.) ;
#69511 = ORIENTED_EDGE('',*,*,#49628,.F.) ;
#69512 = ORIENTED_EDGE('',*,*,#49629,.T.) ;
#69513 = ORIENTED_EDGE('',*,*,#49630,.T.) ;
#69514 = ORIENTED_EDGE('',*,*,#49631,.T.) ;
#69515 = ORIENTED_EDGE('',*,*,#49632,.T.) ;
#69516 = ORIENTED_EDGE('',*,*,#49633,.T.) ;
#69517 = ORIENTED_EDGE('',*,*,#49634,.F.) ;
#69518 = ORIENTED_EDGE('',*,*,#49635,.T.) ;
#69519 = ORIENTED_EDGE('',*,*,#49636,.F.) ;
#69520 = ORIENTED_EDGE('',*,*,#49637,.T.) ;
#69521 = ORIENTED_EDGE('',*,*,#49638,.T.) ;
#69522 = ORIENTED_EDGE('',*,*,#49639,.T.) ;
#69523 = ORIENTED_EDGE('',*,*,#49640,.T.) ;
#69524 = ORIENTED_EDGE('',*,*,#49641,.T.) ;
#69525 = ORIENTED_EDGE('',*,*,#49642,.F.) ;
#69526 = ORIENTED_EDGE('',*,*,#49643,.T.) ;
#69527 = ORIENTED_EDGE('',*,*,#49644,.F.) ;
#69528 = ORIENTED_EDGE('',*,*,#49645,.T.) ;
#69529 = ORIENTED_EDGE('',*,*,#49646,.T.) ;
#69530 = ORIENTED_EDGE('',*,*,#49647,.T.) ;
#69531 = ORIENTED_EDGE('',*,*,#49648,.T.) ;
#69532 = ORIENTED_EDGE('',*,*,#49649,.T.) ;
#69533 = ORIENTED_EDGE('',*,*,#49650,.F.) ;
#69534 = ORIENTED_EDGE('',*,*,#49651,.T.) ;
#69535 = ORIENTED_EDGE('',*,*,#49652,.F.) ;
#69536 = ORIENTED_EDGE('',*,*,#49653,.T.) ;
#69537 = ORIENTED_EDGE('',*,*,#49654,.T.) ;
#69538 = ORIENTED_EDGE('',*,*,#49655,.T.) ;
#69539 = ORIENTED_EDGE('',*,*,#49656,.T.) ;
#69540 = ORIENTED_EDGE('',*,*,#49657,.T.) ;
#69541 = ORIENTED_EDGE('',*,*,#49658,.F.) ;
#69542 = ORIENTED_EDGE('',*,*,#49659,.T.) ;
#69543 = ORIENTED_EDGE('',*,*,#49660,.F.) ;
#69544 = ORIENTED_EDGE('',*,*,#49661,.T.) ;
#69545 = ORIENTED_EDGE('',*,*,#49662,.T.) ;
#69546 = ORIENTED_EDGE('',*,*,#49663,.T.) ;
#69547 = ORIENTED_EDGE('',*,*,#49664,.T.) ;
#69548 = ORIENTED_EDGE('',*,*,#49665,.T.) ;
#69549 = ORIENTED_EDGE('',*,*,#49666,.F.) ;
#69550 = ORIENTED_EDGE('',*,*,#49667,.T.) ;
#69551 = ORIENTED_EDGE('',*,*,#49668,.T.) ;
#69552 = ORIENTED_EDGE('',*,*,#49669,.T.) ;
#69553 = ORIENTED_EDGE('',*,*,#49670,.T.) ;
#69554 = ORIENTED_EDGE('',*,*,#49671,.T.) ;
#69555 = ORIENTED_EDGE('',*,*,#49672,.T.) ;
#69556 = ORIENTED_EDGE('',*,*,#49673,.T.) ;
#69557 = ORIENTED_EDGE('',*,*,#49674,.T.) ;
#69558 = ORIENTED_EDGE('',*,*,#49675,.T.) ;
#69559 = ORIENTED_EDGE('',*,*,#49676,.F.) ;
#69560 = ORIENTED_EDGE('',*,*,#49677,.T.) ;
#69561 = ORIENTED_EDGE('',*,*,#49678,.F.) ;
#69562 = ORIENTED_EDGE('',*,*,#49679,.T.) ;
#69563 = ORIENTED_EDGE('',*,*,#49680,.T.) ;
#69564 = ORIENTED_EDGE('',*,*,#49681,.T.) ;
#69565 = ORIENTED_EDGE('',*,*,#49682,.F.) ;
#69566 = ORIENTED_EDGE('',*,*,#49683,.T.) ;
#69567 = ORIENTED_EDGE('',*,*,#49684,.F.) ;
#69568 = ORIENTED_EDGE('',*,*,#49685,.T.) ;
#69569 = ORIENTED_EDGE('',*,*,#49686,.T.) ;
#69570 = ORIENTED_EDGE('',*,*,#49687,.T.) ;
#69571 = ORIENTED_EDGE('',*,*,#49688,.F.) ;
#69572 = ORIENTED_EDGE('',*,*,#49689,.T.) ;
#69573 = ORIENTED_EDGE('',*,*,#49690,.F.) ;
#69574 = ORIENTED_EDGE('',*,*,#49691,.T.) ;
#69575 = ORIENTED_EDGE('',*,*,#49692,.T.) ;
#69576 = ORIENTED_EDGE('',*,*,#49693,.T.) ;
#69577 = ORIENTED_EDGE('',*,*,#49694,.F.) ;
#69578 = ORIENTED_EDGE('',*,*,#49695,.T.) ;
#69579 = ORIENTED_EDGE('',*,*,#49696,.F.) ;
#69580 = ORIENTED_EDGE('',*,*,#49697,.T.) ;
#69581 = ORIENTED_EDGE('',*,*,#49698,.T.) ;
#69582 = ORIENTED_EDGE('',*,*,#49699,.T.) ;
#69583 = ORIENTED_EDGE('',*,*,#49700,.F.) ;
#69584 = ORIENTED_EDGE('',*,*,#49701,.T.) ;
#69585 = ORIENTED_EDGE('',*,*,#49702,.F.) ;
#69586 = ORIENTED_EDGE('',*,*,#49703,.T.) ;
#69587 = ORIENTED_EDGE('',*,*,#49704,.T.) ;
#69588 = ORIENTED_EDGE('',*,*,#49705,.T.) ;
#69589 = ORIENTED_EDGE('',*,*,#49706,.F.) ;
#69590 = ORIENTED_EDGE('',*,*,#49707,.T.) ;
#69591 = ORIENTED_EDGE('',*,*,#49708,.F.) ;
#69592 = ORIENTED_EDGE('',*,*,#49709,.T.) ;
#69593 = ORIENTED_EDGE('',*,*,#49710,.T.) ;
#69594 = ORIENTED_EDGE('',*,*,#49711,.T.) ;
#69595 = ORIENTED_EDGE('',*,*,#49712,.F.) ;
#69596 = ORIENTED_EDGE('',*,*,#49713,.T.) ;
#69597 = ORIENTED_EDGE('',*,*,#49714,.F.) ;
#69598 = ORIENTED_EDGE('',*,*,#49715,.T.) ;
#69599 = ORIENTED_EDGE('',*,*,#49716,.T.) ;
#69600 = ORIENTED_EDGE('',*,*,#49717,.T.) ;
#69601 = ORIENTED_EDGE('',*,*,#49718,.F.) ;
#69602 = ORIENTED_EDGE('',*,*,#49719,.T.) ;
#69603 = ORIENTED_EDGE('',*,*,#49720,.F.) ;
#69604 = ORIENTED_EDGE('',*,*,#49721,.T.) ;
#69605 = ORIENTED_EDGE('',*,*,#49722,.T.) ;
#69606 = ORIENTED_EDGE('',*,*,#49723,.T.) ;
#69607 = ORIENTED_EDGE('',*,*,#49724,.F.) ;
#69608 = ORIENTED_EDGE('',*,*,#49725,.T.) ;
#69609 = ORIENTED_EDGE('',*,*,#49726,.F.) ;
#69610 = ORIENTED_EDGE('',*,*,#49727,.T.) ;
#69611 = ORIENTED_EDGE('',*,*,#49728,.T.) ;
#69612 = ORIENTED_EDGE('',*,*,#49729,.T.) ;
#69613 = ORIENTED_EDGE('',*,*,#49730,.F.) ;
#69614 = ORIENTED_EDGE('',*,*,#49731,.T.) ;
#69615 = ORIENTED_EDGE('',*,*,#49732,.F.) ;
#69616 = ORIENTED_EDGE('',*,*,#49733,.T.) ;
#69617 = ORIENTED_EDGE('',*,*,#49734,.T.) ;
#69618 = ORIENTED_EDGE('',*,*,#49735,.T.) ;
#69619 = ORIENTED_EDGE('',*,*,#49736,.F.) ;
#69620 = ORIENTED_EDGE('',*,*,#49737,.T.) ;
#69621 = ORIENTED_EDGE('',*,*,#49534,.F.) ;
#69622 = ORIENTED_EDGE('',*,*,#49738,.T.) ;
#69623 = ORIENTED_EDGE('',*,*,#49739,.F.) ;
#69624 = ORIENTED_EDGE('',*,*,#49740,.F.) ;
#69625 = ORIENTED_EDGE('',*,*,#49741,.F.) ;
#69626 = ORIENTED_EDGE('',*,*,#49542,.F.) ;
#69627 = ORIENTED_EDGE('',*,*,#49742,.F.) ;
#69628 = ORIENTED_EDGE('',*,*,#49743,.F.) ;
#69629 = ORIENTED_EDGE('',*,*,#49744,.T.) ;
#69630 = ORIENTED_EDGE('',*,*,#49745,.T.) ;
#69631 = ORIENTED_EDGE('',*,*,#49746,.T.) ;
#69632 = ORIENTED_EDGE('',*,*,#49747,.T.) ;
#69633 = ORIENTED_EDGE('',*,*,#49748,.F.) ;
#69634 = ORIENTED_EDGE('',*,*,#49749,.T.) ;
#69635 = ORIENTED_EDGE('',*,*,#49750,.F.) ;
#69636 = ORIENTED_EDGE('',*,*,#49751,.T.) ;
#69637 = ORIENTED_EDGE('',*,*,#49752,.F.) ;
#69638 = ORIENTED_EDGE('',*,*,#49753,.T.) ;
#69639 = ORIENTED_EDGE('',*,*,#49754,.F.) ;
#69640 = ORIENTED_EDGE('',*,*,#49755,.T.) ;
#69641 = ORIENTED_EDGE('',*,*,#49756,.T.) ;
#69642 = ORIENTED_EDGE('',*,*,#49757,.T.) ;
#69643 = ORIENTED_EDGE('',*,*,#49758,.T.) ;
#69644 = ORIENTED_EDGE('',*,*,#49759,.T.) ;
#69645 = ORIENTED_EDGE('',*,*,#49760,.T.) ;
#69646 = ORIENTED_EDGE('',*,*,#49761,.T.) ;
#69647 = ORIENTED_EDGE('',*,*,#49762,.T.) ;
#69648 = ORIENTED_EDGE('',*,*,#49763,.T.) ;
#69649 = ORIENTED_EDGE('',*,*,#49764,.T.) ;
#69650 = ORIENTED_EDGE('',*,*,#49765,.T.) ;
#69651 = ORIENTED_EDGE('',*,*,#49766,.T.) ;
#69652 = ORIENTED_EDGE('',*,*,#49767,.T.) ;
#69653 = ORIENTED_EDGE('',*,*,#49768,.T.) ;
#69654 = ORIENTED_EDGE('',*,*,#49769,.T.) ;
#69655 = ORIENTED_EDGE('',*,*,#49770,.T.) ;
#69656 = ORIENTED_EDGE('',*,*,#49771,.T.) ;
#69657 = ORIENTED_EDGE('',*,*,#49772,.T.) ;
#69658 = ORIENTED_EDGE('',*,*,#49773,.T.) ;
#69659 = ORIENTED_EDGE('',*,*,#49774,.T.) ;
#69660 = ORIENTED_EDGE('',*,*,#49775,.T.) ;
#69661 = ORIENTED_EDGE('',*,*,#49776,.T.) ;
#69662 = ORIENTED_EDGE('',*,*,#49777,.T.) ;
#69663 = ORIENTED_EDGE('',*,*,#49778,.T.) ;
#69664 = ORIENTED_EDGE('',*,*,#49779,.T.) ;
#69665 = ORIENTED_EDGE('',*,*,#49780,.T.) ;
#69666 = ORIENTED_EDGE('',*,*,#49781,.T.) ;
#69667 = ORIENTED_EDGE('',*,*,#49782,.T.) ;
#69668 = ORIENTED_EDGE('',*,*,#49783,.T.) ;
#69669 = ORIENTED_EDGE('',*,*,#49784,.T.) ;
#69670 = ORIENTED_EDGE('',*,*,#49785,.T.) ;
#69671 = ORIENTED_EDGE('',*,*,#49786,.T.) ;
#69672 = ORIENTED_EDGE('',*,*,#49787,.T.) ;
#69673 = ORIENTED_EDGE('',*,*,#49788,.F.) ;
#69674 = ORIENTED_EDGE('',*,*,#49789,.T.) ;
#69675 = ORIENTED_EDGE('',*,*,#49790,.F.) ;
#69676 = ORIENTED_EDGE('',*,*,#49791,.T.) ;
#69677 = ORIENTED_EDGE('',*,*,#49792,.F.) ;
#69678 = ORIENTED_EDGE('',*,*,#49793,.T.) ;
#69679 = ORIENTED_EDGE('',*,*,#49794,.F.) ;
#69680 = ORIENTED_EDGE('',*,*,#49795,.T.) ;
#69681 = ORIENTED_EDGE('',*,*,#49796,.T.) ;
#69682 = ORIENTED_EDGE('',*,*,#49797,.T.) ;
#69683 = ORIENTED_EDGE('',*,*,#49798,.T.) ;
#69684 = ORIENTED_EDGE('',*,*,#49799,.T.) ;
#69685 = ORIENTED_EDGE('',*,*,#49800,.T.) ;
#69686 = ORIENTED_EDGE('',*,*,#49801,.T.) ;
#69687 = ORIENTED_EDGE('',*,*,#49802,.T.) ;
#69688 = ORIENTED_EDGE('',*,*,#49803,.T.) ;
#69689 = ORIENTED_EDGE('',*,*,#49804,.T.) ;
#69690 = ORIENTED_EDGE('',*,*,#49805,.T.) ;
#69691 = ORIENTED_EDGE('',*,*,#49806,.T.) ;
#69692 = ORIENTED_EDGE('',*,*,#49807,.T.) ;
#69693 = ORIENTED_EDGE('',*,*,#49808,.T.) ;
#69694 = ORIENTED_EDGE('',*,*,#49809,.T.) ;
#69695 = ORIENTED_EDGE('',*,*,#49810,.T.) ;
#69696 = ORIENTED_EDGE('',*,*,#49811,.T.) ;
#69697 = ORIENTED_EDGE('',*,*,#49305,.T.) ;
#69698 = ORIENTED_EDGE('',*,*,#49812,.T.) ;
#69699 = ORIENTED_EDGE('',*,*,#49813,.T.) ;
#69700 = ORIENTED_EDGE('',*,*,#49814,.T.) ;
#69701 = ORIENTED_EDGE('',*,*,#49815,.T.) ;
#69702 = ORIENTED_EDGE('',*,*,#49816,.T.) ;
#69703 = ORIENTED_EDGE('',*,*,#49817,.F.) ;
#69704 = ORIENTED_EDGE('',*,*,#49818,.T.) ;
#69705 = ORIENTED_EDGE('',*,*,#49819,.F.) ;
#69706 = ORIENTED_EDGE('',*,*,#49820,.T.) ;
#69707 = ORIENTED_EDGE('',*,*,#49821,.T.) ;
#69708 = ORIENTED_EDGE('',*,*,#49822,.T.) ;
#69709 = ORIENTED_EDGE('',*,*,#49823,.T.) ;
#69710 = ORIENTED_EDGE('',*,*,#49824,.T.) ;
#69711 = ORIENTED_EDGE('',*,*,#49825,.T.) ;
#69712 = ORIENTED_EDGE('',*,*,#48898,.T.) ;
#69713 = ORIENTED_EDGE('',*,*,#49826,.T.) ;
#69714 = ORIENTED_EDGE('',*,*,#49827,.T.) ;
#69715 = ORIENTED_EDGE('',*,*,#49828,.T.) ;
#69716 = ORIENTED_EDGE('',*,*,#49829,.T.) ;
#69717 = ORIENTED_EDGE('',*,*,#49830,.T.) ;
#69718 = ORIENTED_EDGE('',*,*,#49831,.T.) ;
#69719 = ORIENTED_EDGE('',*,*,#49832,.T.) ;
#69720 = ORIENTED_EDGE('',*,*,#49833,.T.) ;
#69721 = ORIENTED_EDGE('',*,*,#49834,.T.) ;
#69722 = ORIENTED_EDGE('',*,*,#49835,.T.) ;
#69723 = ORIENTED_EDGE('',*,*,#49836,.T.) ;
#69724 = ORIENTED_EDGE('',*,*,#49837,.T.) ;
#69725 = ORIENTED_EDGE('',*,*,#49838,.T.) ;
#69726 = ORIENTED_EDGE('',*,*,#49839,.T.) ;
#69727 = ORIENTED_EDGE('',*,*,#49840,.T.) ;
#69728 = ORIENTED_EDGE('',*,*,#49841,.T.) ;
#69729 = ORIENTED_EDGE('',*,*,#49842,.T.) ;
#69730 = ORIENTED_EDGE('',*,*,#49843,.T.) ;
#69731 = ORIENTED_EDGE('',*,*,#49844,.T.) ;
#69732 = ORIENTED_EDGE('',*,*,#49845,.T.) ;
#69733 = ORIENTED_EDGE('',*,*,#49846,.T.) ;
#69734 = ORIENTED_EDGE('',*,*,#49847,.T.) ;
#69735 = ORIENTED_EDGE('',*,*,#49848,.T.) ;
#69736 = ORIENTED_EDGE('',*,*,#49849,.T.) ;
#69737 = ORIENTED_EDGE('',*,*,#49850,.T.) ;
#69738 = ORIENTED_EDGE('',*,*,#49851,.T.) ;
#69739 = ORIENTED_EDGE('',*,*,#49852,.T.) ;
#69740 = ORIENTED_EDGE('',*,*,#49853,.T.) ;
#69741 = ORIENTED_EDGE('',*,*,#49854,.T.) ;
#69742 = ORIENTED_EDGE('',*,*,#49855,.T.) ;
#69743 = ORIENTED_EDGE('',*,*,#49856,.T.) ;
#69744 = ORIENTED_EDGE('',*,*,#49857,.T.) ;
#69745 = ORIENTED_EDGE('',*,*,#49858,.T.) ;
#69746 = ORIENTED_EDGE('',*,*,#49859,.T.) ;
#69747 = ORIENTED_EDGE('',*,*,#49860,.T.) ;
#69748 = ORIENTED_EDGE('',*,*,#49861,.T.) ;
#69749 = ORIENTED_EDGE('',*,*,#49862,.T.) ;
#69750 = ORIENTED_EDGE('',*,*,#49863,.T.) ;
#69751 = ORIENTED_EDGE('',*,*,#49864,.T.) ;
#69752 = ORIENTED_EDGE('',*,*,#49865,.T.) ;
#69753 = ORIENTED_EDGE('',*,*,#49866,.T.) ;
#69754 = ORIENTED_EDGE('',*,*,#49867,.T.) ;
#69755 = ORIENTED_EDGE('',*,*,#49868,.F.) ;
#69756 = ORIENTED_EDGE('',*,*,#49869,.T.) ;
#69757 = ORIENTED_EDGE('',*,*,#49870,.F.) ;
#69758 = ORIENTED_EDGE('',*,*,#49871,.T.) ;
#69759 = ORIENTED_EDGE('',*,*,#49872,.F.) ;
#69760 = ORIENTED_EDGE('',*,*,#49873,.T.) ;
#69761 = ORIENTED_EDGE('',*,*,#49874,.F.) ;
#69762 = ORIENTED_EDGE('',*,*,#49875,.T.) ;
#69763 = ORIENTED_EDGE('',*,*,#49876,.F.) ;
#69764 = ORIENTED_EDGE('',*,*,#49877,.T.) ;
#69765 = ORIENTED_EDGE('',*,*,#49878,.F.) ;
#69766 = ORIENTED_EDGE('',*,*,#49879,.T.) ;
#69767 = ORIENTED_EDGE('',*,*,#49880,.F.) ;
#69768 = ORIENTED_EDGE('',*,*,#49881,.T.) ;
#69769 = ORIENTED_EDGE('',*,*,#49882,.F.) ;
#69770 = ORIENTED_EDGE('',*,*,#49883,.T.) ;
#69771 = ORIENTED_EDGE('',*,*,#49884,.T.) ;
#69772 = ORIENTED_EDGE('',*,*,#49885,.T.) ;
#69773 = ORIENTED_EDGE('',*,*,#49886,.T.) ;
#69774 = ORIENTED_EDGE('',*,*,#49887,.F.) ;
#69775 = ORIENTED_EDGE('',*,*,#49888,.T.) ;
#69776 = ORIENTED_EDGE('',*,*,#49889,.T.) ;
#69777 = ORIENTED_EDGE('',*,*,#49890,.T.) ;
#69778 = ORIENTED_EDGE('',*,*,#49891,.T.) ;
#69779 = ORIENTED_EDGE('',*,*,#49892,.T.) ;
#69780 = ORIENTED_EDGE('',*,*,#49893,.T.) ;
#69781 = ORIENTED_EDGE('',*,*,#49894,.T.) ;
#69782 = ORIENTED_EDGE('',*,*,#49895,.T.) ;
#69783 = ORIENTED_EDGE('',*,*,#49896,.F.) ;
#69784 = ORIENTED_EDGE('',*,*,#49897,.T.) ;
#69785 = ORIENTED_EDGE('',*,*,#49898,.T.) ;
#69786 = ORIENTED_EDGE('',*,*,#49899,.T.) ;
#69787 = ORIENTED_EDGE('',*,*,#49900,.T.) ;
#69788 = ORIENTED_EDGE('',*,*,#49901,.T.) ;
#69789 = ORIENTED_EDGE('',*,*,#49902,.T.) ;
#69790 = ORIENTED_EDGE('',*,*,#49903,.T.) ;
#69791 = ORIENTED_EDGE('',*,*,#49904,.F.) ;
#69792 = ORIENTED_EDGE('',*,*,#49905,.T.) ;
#69793 = ORIENTED_EDGE('',*,*,#49906,.T.) ;
#69794 = ORIENTED_EDGE('',*,*,#49907,.T.) ;
#69795 = ORIENTED_EDGE('',*,*,#49908,.T.) ;
#69796 = ORIENTED_EDGE('',*,*,#49909,.T.) ;
#69797 = ORIENTED_EDGE('',*,*,#49910,.T.) ;
#69798 = ORIENTED_EDGE('',*,*,#49911,.T.) ;
#69799 = ORIENTED_EDGE('',*,*,#49912,.T.) ;
#69800 = ORIENTED_EDGE('',*,*,#49913,.F.) ;
#69801 = ORIENTED_EDGE('',*,*,#49914,.T.) ;
#69802 = ORIENTED_EDGE('',*,*,#49915,.T.) ;
#69803 = ORIENTED_EDGE('',*,*,#49916,.T.) ;
#69804 = ORIENTED_EDGE('',*,*,#49917,.T.) ;
#69805 = ORIENTED_EDGE('',*,*,#49918,.T.) ;
#69806 = ORIENTED_EDGE('',*,*,#49919,.T.) ;
#69807 = ORIENTED_EDGE('',*,*,#49920,.T.) ;
#69808 = ORIENTED_EDGE('',*,*,#49921,.T.) ;
#69809 = ORIENTED_EDGE('',*,*,#49922,.F.) ;
#69810 = ORIENTED_EDGE('',*,*,#49923,.T.) ;
#69811 = ORIENTED_EDGE('',*,*,#49924,.T.) ;
#69812 = ORIENTED_EDGE('',*,*,#49925,.T.) ;
#69813 = ORIENTED_EDGE('',*,*,#49926,.T.) ;
#69814 = ORIENTED_EDGE('',*,*,#49927,.T.) ;
#69815 = ORIENTED_EDGE('',*,*,#49920,.F.) ;
#69816 = ORIENTED_EDGE('',*,*,#49928,.T.) ;
#69817 = ORIENTED_EDGE('',*,*,#49924,.F.) ;
#69818 = ORIENTED_EDGE('',*,*,#49929,.T.) ;
#69819 = ORIENTED_EDGE('',*,*,#49930,.T.) ;
#69820 = ORIENTED_EDGE('',*,*,#49931,.T.) ;
#69821 = ORIENTED_EDGE('',*,*,#49932,.T.) ;
#69822 = ORIENTED_EDGE('',*,*,#49933,.T.) ;
#69823 = ORIENTED_EDGE('',*,*,#49934,.T.) ;
#69824 = ORIENTED_EDGE('',*,*,#49935,.T.) ;
#69825 = ORIENTED_EDGE('',*,*,#49936,.T.) ;
#69826 = ORIENTED_EDGE('',*,*,#49937,.T.) ;
#69827 = ORIENTED_EDGE('',*,*,#49922,.T.) ;
#69828 = ORIENTED_EDGE('',*,*,#49938,.T.) ;
#69829 = ORIENTED_EDGE('',*,*,#49939,.T.) ;
#69830 = ORIENTED_EDGE('',*,*,#49940,.T.) ;
#69831 = ORIENTED_EDGE('',*,*,#49941,.T.) ;
#69832 = ORIENTED_EDGE('',*,*,#49942,.T.) ;
#69833 = ORIENTED_EDGE('',*,*,#49926,.F.) ;
#69834 = ORIENTED_EDGE('',*,*,#49943,.T.) ;
#69835 = ORIENTED_EDGE('',*,*,#49944,.T.) ;
#69836 = ORIENTED_EDGE('',*,*,#49945,.T.) ;
#69837 = ORIENTED_EDGE('',*,*,#49946,.T.) ;
#69838 = ORIENTED_EDGE('',*,*,#49947,.T.) ;
#69839 = ORIENTED_EDGE('',*,*,#49948,.T.) ;
#69840 = ORIENTED_EDGE('',*,*,#49949,.T.) ;
#69841 = ORIENTED_EDGE('',*,*,#49950,.T.) ;
#69842 = ORIENTED_EDGE('',*,*,#49951,.T.) ;
#69843 = ORIENTED_EDGE('',*,*,#49952,.T.) ;
#69844 = ORIENTED_EDGE('',*,*,#49953,.T.) ;
#69845 = ORIENTED_EDGE('',*,*,#49954,.T.) ;
#69846 = ORIENTED_EDGE('',*,*,#49955,.T.) ;
#69847 = ORIENTED_EDGE('',*,*,#49956,.T.) ;
#69848 = ORIENTED_EDGE('',*,*,#49957,.T.) ;
#69849 = ORIENTED_EDGE('',*,*,#49958,.T.) ;
#69850 = ORIENTED_EDGE('',*,*,#49959,.T.) ;
#69851 = ORIENTED_EDGE('',*,*,#49960,.T.) ;
#69852 = ORIENTED_EDGE('',*,*,#49961,.T.) ;
#69853 = ORIENTED_EDGE('',*,*,#49962,.T.) ;
#69854 = ORIENTED_EDGE('',*,*,#49963,.T.) ;
#69855 = ORIENTED_EDGE('',*,*,#49964,.T.) ;
#69856 = ORIENTED_EDGE('',*,*,#49965,.T.) ;
#69857 = ORIENTED_EDGE('',*,*,#49966,.F.) ;
#69858 = ORIENTED_EDGE('',*,*,#49967,.T.) ;
#69859 = ORIENTED_EDGE('',*,*,#49968,.F.) ;
#69860 = ORIENTED_EDGE('',*,*,#49969,.T.) ;
#69861 = ORIENTED_EDGE('',*,*,#49970,.F.) ;
#69862 = ORIENTED_EDGE('',*,*,#49971,.T.) ;
#69863 = ORIENTED_EDGE('',*,*,#49972,.F.) ;
#69864 = ORIENTED_EDGE('',*,*,#49973,.T.) ;
#69865 = ORIENTED_EDGE('',*,*,#49972,.T.) ;
#69866 = ORIENTED_EDGE('',*,*,#49974,.T.) ;
#69867 = ORIENTED_EDGE('',*,*,#49975,.T.) ;
#69868 = ORIENTED_EDGE('',*,*,#49976,.T.) ;
#69869 = ORIENTED_EDGE('',*,*,#49966,.T.) ;
#69870 = ORIENTED_EDGE('',*,*,#49977,.T.) ;
#69871 = ORIENTED_EDGE('',*,*,#49978,.T.) ;
#69872 = ORIENTED_EDGE('',*,*,#49979,.T.) ;
#69873 = ORIENTED_EDGE('',*,*,#49980,.T.) ;
#69874 = ORIENTED_EDGE('',*,*,#49981,.T.) ;
#69875 = ORIENTED_EDGE('',*,*,#49968,.T.) ;
#69876 = ORIENTED_EDGE('',*,*,#49982,.T.) ;
#69877 = ORIENTED_EDGE('',*,*,#49970,.T.) ;
#69878 = ORIENTED_EDGE('',*,*,#49983,.T.) ;
#69879 = ORIENTED_EDGE('',*,*,#49984,.T.) ;
#69880 = ORIENTED_EDGE('',*,*,#49985,.T.) ;
#69881 = ORIENTED_EDGE('',*,*,#49986,.T.) ;
#69882 = ORIENTED_EDGE('',*,*,#49987,.T.) ;
#69883 = ORIENTED_EDGE('',*,*,#49988,.T.) ;
#69884 = ORIENTED_EDGE('',*,*,#49989,.T.) ;
#69885 = ORIENTED_EDGE('',*,*,#49736,.T.) ;
#69886 = ORIENTED_EDGE('',*,*,#49990,.T.) ;
#69887 = ORIENTED_EDGE('',*,*,#49991,.T.) ;
#69888 = ORIENTED_EDGE('',*,*,#49992,.F.) ;
#69889 = ORIENTED_EDGE('',*,*,#49993,.T.) ;
#69890 = ORIENTED_EDGE('',*,*,#48981,.T.) ;
#69891 = ORIENTED_EDGE('',*,*,#48973,.T.) ;
#69892 = ORIENTED_EDGE('',*,*,#48965,.T.) ;
#69893 = ORIENTED_EDGE('',*,*,#48957,.T.) ;
#69894 = ORIENTED_EDGE('',*,*,#48949,.T.) ;
#69895 = ORIENTED_EDGE('',*,*,#48941,.T.) ;
#69896 = ORIENTED_EDGE('',*,*,#48933,.T.) ;
#69897 = ORIENTED_EDGE('',*,*,#48925,.T.) ;
#69898 = ORIENTED_EDGE('',*,*,#48917,.T.) ;
#69899 = ORIENTED_EDGE('',*,*,#48909,.T.) ;
#69900 = ORIENTED_EDGE('',*,*,#49994,.T.) ;
#69901 = ORIENTED_EDGE('',*,*,#49995,.F.) ;
#69902 = ORIENTED_EDGE('',*,*,#49996,.T.) ;
#69903 = ORIENTED_EDGE('',*,*,#49997,.T.) ;
#69904 = ORIENTED_EDGE('',*,*,#49998,.T.) ;
#69905 = ORIENTED_EDGE('',*,*,#49999,.T.) ;
#69906 = ORIENTED_EDGE('',*,*,#50000,.T.) ;
#69907 = ORIENTED_EDGE('',*,*,#50001,.T.) ;
#69908 = ORIENTED_EDGE('',*,*,#50002,.T.) ;
#69909 = ORIENTED_EDGE('',*,*,#50003,.T.) ;
#69910 = ORIENTED_EDGE('',*,*,#50004,.T.) ;
#69911 = ORIENTED_EDGE('',*,*,#50005,.T.) ;
#69912 = ORIENTED_EDGE('',*,*,#50006,.T.) ;
#69913 = ORIENTED_EDGE('',*,*,#50007,.T.) ;
#69914 = ORIENTED_EDGE('',*,*,#50008,.F.) ;
#69915 = ORIENTED_EDGE('',*,*,#50009,.T.) ;
#69916 = ORIENTED_EDGE('',*,*,#50010,.T.) ;
#69917 = ORIENTED_EDGE('',*,*,#50011,.T.) ;
#69918 = ORIENTED_EDGE('',*,*,#50012,.T.) ;
#69919 = ORIENTED_EDGE('',*,*,#50013,.T.) ;
#69920 = ORIENTED_EDGE('',*,*,#50014,.T.) ;
#69921 = ORIENTED_EDGE('',*,*,#50015,.T.) ;
#69922 = ORIENTED_EDGE('',*,*,#50016,.T.) ;
#69923 = ORIENTED_EDGE('',*,*,#50017,.T.) ;
#69924 = ORIENTED_EDGE('',*,*,#50018,.T.) ;
#69925 = ORIENTED_EDGE('',*,*,#50019,.T.) ;
#69926 = ORIENTED_EDGE('',*,*,#50020,.T.) ;
#69927 = ORIENTED_EDGE('',*,*,#50021,.T.) ;
#69928 = ORIENTED_EDGE('',*,*,#50022,.F.) ;
#69929 = ORIENTED_EDGE('',*,*,#50023,.T.) ;
#69930 = ORIENTED_EDGE('',*,*,#50024,.T.) ;
#69931 = ORIENTED_EDGE('',*,*,#50025,.T.) ;
#69932 = ORIENTED_EDGE('',*,*,#50026,.T.) ;
#69933 = ORIENTED_EDGE('',*,*,#49739,.T.) ;
#69934 = ORIENTED_EDGE('',*,*,#50027,.T.) ;
#69935 = ORIENTED_EDGE('',*,*,#50028,.T.) ;
#69936 = ORIENTED_EDGE('',*,*,#50029,.T.) ;
#69937 = ORIENTED_EDGE('',*,*,#50030,.T.) ;
#69938 = ORIENTED_EDGE('',*,*,#50031,.T.) ;
#69939 = ORIENTED_EDGE('',*,*,#50032,.T.) ;
#69940 = ORIENTED_EDGE('',*,*,#50033,.T.) ;
#69941 = ORIENTED_EDGE('',*,*,#50034,.T.) ;
#69942 = ORIENTED_EDGE('',*,*,#50035,.T.) ;
#69943 = ORIENTED_EDGE('',*,*,#50036,.T.) ;
#69944 = ORIENTED_EDGE('',*,*,#50037,.T.) ;
#69945 = ORIENTED_EDGE('',*,*,#50038,.T.) ;
#69946 = ORIENTED_EDGE('',*,*,#50039,.T.) ;
#69947 = ORIENTED_EDGE('',*,*,#50040,.T.) ;
#69948 = ORIENTED_EDGE('',*,*,#50041,.T.) ;
#69949 = ORIENTED_EDGE('',*,*,#50042,.T.) ;
#69950 = ORIENTED_EDGE('',*,*,#50043,.T.) ;
#69951 = ORIENTED_EDGE('',*,*,#50044,.T.) ;
#69952 = ORIENTED_EDGE('',*,*,#50045,.T.) ;
#69953 = ORIENTED_EDGE('',*,*,#50046,.T.) ;
#69954 = ORIENTED_EDGE('',*,*,#49284,.T.) ;
#69955 = ORIENTED_EDGE('',*,*,#49315,.T.) ;
#69956 = ORIENTED_EDGE('',*,*,#50047,.T.) ;
#69957 = ORIENTED_EDGE('',*,*,#50048,.T.) ;
#69958 = ORIENTED_EDGE('',*,*,#50049,.T.) ;
#69959 = ORIENTED_EDGE('',*,*,#50050,.T.) ;
#69960 = ORIENTED_EDGE('',*,*,#50051,.T.) ;
#69961 = ORIENTED_EDGE('',*,*,#50052,.T.) ;
#69962 = ORIENTED_EDGE('',*,*,#50053,.T.) ;
#69963 = ORIENTED_EDGE('',*,*,#50054,.T.) ;
#69964 = ORIENTED_EDGE('',*,*,#50055,.T.) ;
#69965 = ORIENTED_EDGE('',*,*,#50056,.T.) ;
#69966 = ORIENTED_EDGE('',*,*,#50057,.T.) ;
#69967 = ORIENTED_EDGE('',*,*,#50058,.T.) ;
#69968 = ORIENTED_EDGE('',*,*,#50059,.T.) ;
#69969 = ORIENTED_EDGE('',*,*,#50060,.T.) ;
#69970 = ORIENTED_EDGE('',*,*,#50061,.T.) ;
#69971 = ORIENTED_EDGE('',*,*,#50062,.T.) ;
#69972 = ORIENTED_EDGE('',*,*,#50063,.T.) ;
#69973 = ORIENTED_EDGE('',*,*,#50064,.T.) ;
#69974 = ORIENTED_EDGE('',*,*,#50065,.T.) ;
#69975 = ORIENTED_EDGE('',*,*,#50066,.T.) ;
#69976 = ORIENTED_EDGE('',*,*,#50067,.F.) ;
#69977 = ORIENTED_EDGE('',*,*,#50068,.T.) ;
#69978 = ORIENTED_EDGE('',*,*,#50069,.F.) ;
#69979 = ORIENTED_EDGE('',*,*,#50070,.T.) ;
#69980 = ORIENTED_EDGE('',*,*,#50071,.F.) ;
#69981 = ORIENTED_EDGE('',*,*,#50072,.T.) ;
#69982 = ORIENTED_EDGE('',*,*,#50073,.F.) ;
#69983 = ORIENTED_EDGE('',*,*,#50074,.T.) ;
#69984 = ORIENTED_EDGE('',*,*,#50075,.T.) ;
#69985 = ORIENTED_EDGE('',*,*,#50076,.T.) ;
#69986 = ORIENTED_EDGE('',*,*,#50073,.T.) ;
#69987 = ORIENTED_EDGE('',*,*,#50077,.T.) ;
#69988 = ORIENTED_EDGE('',*,*,#50078,.T.) ;
#69989 = ORIENTED_EDGE('',*,*,#50079,.T.) ;
#69990 = ORIENTED_EDGE('',*,*,#50067,.T.) ;
#69991 = ORIENTED_EDGE('',*,*,#50080,.T.) ;
#69992 = ORIENTED_EDGE('',*,*,#50069,.T.) ;
#69993 = ORIENTED_EDGE('',*,*,#50081,.T.) ;
#69994 = ORIENTED_EDGE('',*,*,#50082,.T.) ;
#69995 = ORIENTED_EDGE('',*,*,#50083,.T.) ;
#69996 = ORIENTED_EDGE('',*,*,#50084,.T.) ;
#69997 = ORIENTED_EDGE('',*,*,#50085,.T.) ;
#69998 = ORIENTED_EDGE('',*,*,#50071,.T.) ;
#69999 = ORIENTED_EDGE('',*,*,#50086,.T.) ;
#70000 = ORIENTED_EDGE('',*,*,#50087,.T.) ;
#70001 = ORIENTED_EDGE('',*,*,#50088,.T.) ;
#70002 = ORIENTED_EDGE('',*,*,#50089,.T.) ;
#70003 = ORIENTED_EDGE('',*,*,#50090,.T.) ;
#70004 = ORIENTED_EDGE('',*,*,#49297,.T.) ;
#70005 = ORIENTED_EDGE('',*,*,#49313,.T.) ;
#70006 = ORIENTED_EDGE('',*,*,#50091,.T.) ;
#70007 = ORIENTED_EDGE('',*,*,#49299,.T.) ;
#70008 = ORIENTED_EDGE('',*,*,#50092,.T.) ;
#70009 = ORIENTED_EDGE('',*,*,#49311,.F.) ;
#70010 = ORIENTED_EDGE('',*,*,#50093,.T.) ;
#70011 = ORIENTED_EDGE('',*,*,#49303,.F.) ;
#70012 = ORIENTED_EDGE('',*,*,#50094,.T.) ;
#70013 = ORIENTED_EDGE('',*,*,#49307,.T.) ;
#70014 = ORIENTED_EDGE('',*,*,#50095,.T.) ;
#70015 = ORIENTED_EDGE('',*,*,#49301,.T.) ;
#70016 = ORIENTED_EDGE('',*,*,#50096,.T.) ;
#70017 = ORIENTED_EDGE('',*,*,#49309,.T.) ;
#70018 = ORIENTED_EDGE('',*,*,#50097,.T.) ;
#70019 = ORIENTED_EDGE('',*,*,#49005,.T.) ;
#70020 = ORIENTED_EDGE('',*,*,#50098,.T.) ;
#70021 = ORIENTED_EDGE('',*,*,#49295,.F.) ;
#70022 = ORIENTED_EDGE('',*,*,#48919,.T.) ;
#70023 = ORIENTED_EDGE('',*,*,#49296,.T.) ;
#70024 = ORIENTED_EDGE('',*,*,#50099,.T.) ;
#70025 = ORIENTED_EDGE('',*,*,#49292,.F.) ;
#70026 = ORIENTED_EDGE('',*,*,#48911,.T.) ;
#70027 = ORIENTED_EDGE('',*,*,#49293,.T.) ;
#70028 = ORIENTED_EDGE('',*,*,#50100,.T.) ;
#70029 = ORIENTED_EDGE('',*,*,#50101,.T.) ;
#70030 = ORIENTED_EDGE('',*,*,#50102,.T.) ;
#70031 = ORIENTED_EDGE('',*,*,#50103,.T.) ;
#70032 = ORIENTED_EDGE('',*,*,#50104,.T.) ;
#70033 = ORIENTED_EDGE('',*,*,#49289,.F.) ;
#70034 = ORIENTED_EDGE('',*,*,#50105,.T.) ;
#70035 = ORIENTED_EDGE('',*,*,#49290,.T.) ;
#70036 = ORIENTED_EDGE('',*,*,#50106,.T.) ;
#70037 = ORIENTED_EDGE('',*,*,#49286,.F.) ;
#70038 = ORIENTED_EDGE('',*,*,#48983,.T.) ;
#70039 = ORIENTED_EDGE('',*,*,#49287,.T.) ;
#70040 = ORIENTED_EDGE('',*,*,#50107,.T.) ;
#70041 = ORIENTED_EDGE('',*,*,#48986,.F.) ;
#70042 = ORIENTED_EDGE('',*,*,#48975,.T.) ;
#70043 = ORIENTED_EDGE('',*,*,#50108,.T.) ;
#70044 = ORIENTED_EDGE('',*,*,#50109,.T.) ;
#70045 = ORIENTED_EDGE('',*,*,#50110,.F.) ;
#70046 = ORIENTED_EDGE('',*,*,#50111,.T.) ;
#70047 = ORIENTED_EDGE('',*,*,#50110,.T.) ;
#70048 = ORIENTED_EDGE('',*,*,#50112,.T.) ;
#70049 = ORIENTED_EDGE('',*,*,#50113,.F.) ;
#70050 = ORIENTED_EDGE('',*,*,#50114,.T.) ;
#70051 = ORIENTED_EDGE('',*,*,#50113,.T.) ;
#70052 = ORIENTED_EDGE('',*,*,#50115,.T.) ;
#70053 = ORIENTED_EDGE('',*,*,#50116,.F.) ;
#70054 = ORIENTED_EDGE('',*,*,#50117,.T.) ;
#70055 = ORIENTED_EDGE('',*,*,#50116,.T.) ;
#70056 = ORIENTED_EDGE('',*,*,#50118,.T.) ;
#70057 = ORIENTED_EDGE('',*,*,#50119,.F.) ;
#70058 = ORIENTED_EDGE('',*,*,#50120,.T.) ;
#70059 = ORIENTED_EDGE('',*,*,#50119,.T.) ;
#70060 = ORIENTED_EDGE('',*,*,#50121,.T.) ;
#70061 = ORIENTED_EDGE('',*,*,#50122,.F.) ;
#70062 = ORIENTED_EDGE('',*,*,#50123,.T.) ;
#70063 = ORIENTED_EDGE('',*,*,#50122,.T.) ;
#70064 = ORIENTED_EDGE('',*,*,#50124,.T.) ;
#70065 = ORIENTED_EDGE('',*,*,#50125,.F.) ;
#70066 = ORIENTED_EDGE('',*,*,#50126,.T.) ;
#70067 = ORIENTED_EDGE('',*,*,#50125,.T.) ;
#70068 = ORIENTED_EDGE('',*,*,#50127,.T.) ;
#70069 = ORIENTED_EDGE('',*,*,#50128,.F.) ;
#70070 = ORIENTED_EDGE('',*,*,#50129,.T.) ;
#70071 = ORIENTED_EDGE('',*,*,#50108,.F.) ;
#70072 = ORIENTED_EDGE('',*,*,#50130,.T.) ;
#70073 = ORIENTED_EDGE('',*,*,#50128,.T.) ;
#70074 = ORIENTED_EDGE('',*,*,#50131,.T.) ;
#70075 = ORIENTED_EDGE('',*,*,#50132,.T.) ;
#70076 = ORIENTED_EDGE('',*,*,#50133,.T.) ;
#70077 = ORIENTED_EDGE('',*,*,#50134,.T.) ;
#70078 = ORIENTED_EDGE('',*,*,#50135,.T.) ;
#70079 = ORIENTED_EDGE('',*,*,#49834,.F.) ;
#70080 = ORIENTED_EDGE('',*,*,#50136,.T.) ;
#70081 = ORIENTED_EDGE('',*,*,#49907,.F.) ;
#70082 = ORIENTED_EDGE('',*,*,#50137,.F.) ;
#70083 = ORIENTED_EDGE('',*,*,#50138,.F.) ;
#70084 = ORIENTED_EDGE('',*,*,#50137,.T.) ;
#70085 = ORIENTED_EDGE('',*,*,#50139,.F.) ;
#70086 = ORIENTED_EDGE('',*,*,#49833,.F.) ;
#70087 = ORIENTED_EDGE('',*,*,#50140,.T.) ;
#70088 = ORIENTED_EDGE('',*,*,#49672,.F.) ;
#70089 = ORIENTED_EDGE('',*,*,#50141,.T.) ;
#70090 = ORIENTED_EDGE('',*,*,#50139,.T.) ;
#70091 = ORIENTED_EDGE('',*,*,#49906,.F.) ;
#70092 = ORIENTED_EDGE('',*,*,#50142,.F.) ;
#70093 = ORIENTED_EDGE('',*,*,#49746,.F.) ;
#70094 = ORIENTED_EDGE('',*,*,#50138,.T.) ;
#70095 = ORIENTED_EDGE('',*,*,#49745,.F.) ;
#70096 = ORIENTED_EDGE('',*,*,#50143,.F.) ;
#70097 = ORIENTED_EDGE('',*,*,#49835,.F.) ;
#70098 = ORIENTED_EDGE('',*,*,#49893,.F.) ;
#70099 = ORIENTED_EDGE('',*,*,#50144,.T.) ;
#70100 = ORIENTED_EDGE('',*,*,#49832,.F.) ;
#70101 = ORIENTED_EDGE('',*,*,#50145,.F.) ;
#70102 = ORIENTED_EDGE('',*,*,#49901,.F.) ;
#70103 = ORIENTED_EDGE('',*,*,#50146,.T.) ;
#70104 = ORIENTED_EDGE('',*,*,#49830,.F.) ;
#70105 = ORIENTED_EDGE('',*,*,#50147,.F.) ;
#70106 = ORIENTED_EDGE('',*,*,#50148,.F.) ;
#70107 = ORIENTED_EDGE('',*,*,#50149,.T.) ;
#70108 = ORIENTED_EDGE('',*,*,#50150,.T.) ;
#70109 = ORIENTED_EDGE('',*,*,#49902,.F.) ;
#70110 = ORIENTED_EDGE('',*,*,#50151,.F.) ;
#70111 = ORIENTED_EDGE('',*,*,#50142,.T.) ;
#70112 = ORIENTED_EDGE('',*,*,#50152,.F.) ;
#70113 = ORIENTED_EDGE('',*,*,#50145,.T.) ;
#70114 = ORIENTED_EDGE('',*,*,#50143,.T.) ;
#70115 = ORIENTED_EDGE('',*,*,#50153,.F.) ;
#70116 = ORIENTED_EDGE('',*,*,#49831,.F.) ;
#70117 = ORIENTED_EDGE('',*,*,#50154,.T.) ;
#70118 = ORIENTED_EDGE('',*,*,#49318,.F.) ;
#70119 = ORIENTED_EDGE('',*,*,#50155,.T.) ;
#70120 = ORIENTED_EDGE('',*,*,#50156,.F.) ;
#70121 = ORIENTED_EDGE('',*,*,#50157,.T.) ;
#70122 = ORIENTED_EDGE('',*,*,#50148,.T.) ;
#70123 = ORIENTED_EDGE('',*,*,#50147,.T.) ;
#70124 = ORIENTED_EDGE('',*,*,#49903,.F.) ;
#70125 = ORIENTED_EDGE('',*,*,#50158,.T.) ;
#70126 = ORIENTED_EDGE('',*,*,#50159,.T.) ;
#70127 = ORIENTED_EDGE('',*,*,#50160,.T.) ;
#70128 = ORIENTED_EDGE('',*,*,#49825,.F.) ;
#70129 = ORIENTED_EDGE('',*,*,#50161,.F.) ;
#70130 = ORIENTED_EDGE('',*,*,#50152,.T.) ;
#70131 = ORIENTED_EDGE('',*,*,#49905,.F.) ;
#70132 = ORIENTED_EDGE('',*,*,#50162,.F.) ;
#70133 = ORIENTED_EDGE('',*,*,#49824,.F.) ;
#70134 = ORIENTED_EDGE('',*,*,#50151,.T.) ;
#70135 = ORIENTED_EDGE('',*,*,#49823,.F.) ;
#70136 = ORIENTED_EDGE('',*,*,#50163,.F.) ;
#70137 = ORIENTED_EDGE('',*,*,#49747,.F.) ;
#70138 = ORIENTED_EDGE('',*,*,#50153,.T.) ;
#70139 = ORIENTED_EDGE('',*,*,#49744,.F.) ;
#70140 = ORIENTED_EDGE('',*,*,#50164,.F.) ;
#70141 = ORIENTED_EDGE('',*,*,#49894,.F.) ;
#70142 = ORIENTED_EDGE('',*,*,#49828,.F.) ;
#70143 = ORIENTED_EDGE('',*,*,#50165,.T.) ;
#70144 = ORIENTED_EDGE('',*,*,#49884,.F.) ;
#70145 = ORIENTED_EDGE('',*,*,#50166,.F.) ;
#70146 = ORIENTED_EDGE('',*,*,#50167,.F.) ;
#70147 = ORIENTED_EDGE('',*,*,#48900,.T.) ;
#70148 = ORIENTED_EDGE('',*,*,#50156,.T.) ;
#70149 = ORIENTED_EDGE('',*,*,#49829,.F.) ;
#70150 = ORIENTED_EDGE('',*,*,#49904,.T.) ;
#70151 = ORIENTED_EDGE('',*,*,#50161,.T.) ;
#70152 = ORIENTED_EDGE('',*,*,#50168,.F.) ;
#70153 = ORIENTED_EDGE('',*,*,#50162,.T.) ;
#70154 = ORIENTED_EDGE('',*,*,#50164,.T.) ;
#70155 = ORIENTED_EDGE('',*,*,#50163,.T.) ;
#70156 = ORIENTED_EDGE('',*,*,#50169,.F.) ;
#70157 = ORIENTED_EDGE('',*,*,#50170,.F.) ;
#70158 = ORIENTED_EDGE('',*,*,#50171,.T.) ;
#70159 = ORIENTED_EDGE('',*,*,#50167,.T.) ;
#70160 = ORIENTED_EDGE('',*,*,#50166,.T.) ;
#70161 = ORIENTED_EDGE('',*,*,#50168,.T.) ;
#70162 = ORIENTED_EDGE('',*,*,#49827,.F.) ;
#70163 = ORIENTED_EDGE('',*,*,#50172,.F.) ;
#70164 = ORIENTED_EDGE('',*,*,#49821,.F.) ;
#70165 = ORIENTED_EDGE('',*,*,#50169,.T.) ;
#70166 = ORIENTED_EDGE('',*,*,#49822,.F.) ;
#70167 = ORIENTED_EDGE('',*,*,#50173,.F.) ;
#70168 = ORIENTED_EDGE('',*,*,#49895,.F.) ;
#70169 = ORIENTED_EDGE('',*,*,#49898,.F.) ;
#70170 = ORIENTED_EDGE('',*,*,#50174,.T.) ;
#70171 = ORIENTED_EDGE('',*,*,#50175,.T.) ;
#70172 = ORIENTED_EDGE('',*,*,#50170,.T.) ;
#70173 = ORIENTED_EDGE('',*,*,#50173,.T.) ;
#70174 = ORIENTED_EDGE('',*,*,#50172,.T.) ;
#70175 = ORIENTED_EDGE('',*,*,#50176,.F.) ;
#70176 = ORIENTED_EDGE('',*,*,#49896,.T.) ;
#70177 = ORIENTED_EDGE('',*,*,#49826,.F.) ;
#70178 = ORIENTED_EDGE('',*,*,#50177,.T.) ;
#70179 = ORIENTED_EDGE('',*,*,#50178,.T.) ;
#70180 = ORIENTED_EDGE('',*,*,#50179,.T.) ;
#70181 = ORIENTED_EDGE('',*,*,#49897,.F.) ;
#70182 = ORIENTED_EDGE('',*,*,#50176,.T.) ;
#70183 = ORIENTED_EDGE('',*,*,#50180,.F.) ;
#70184 = ORIENTED_EDGE('',*,*,#50181,.F.) ;
#70185 = ORIENTED_EDGE('',*,*,#50182,.F.) ;
#70186 = ORIENTED_EDGE('',*,*,#50181,.T.) ;
#70187 = ORIENTED_EDGE('',*,*,#50042,.F.) ;
#70188 = ORIENTED_EDGE('',*,*,#50183,.F.) ;
#70189 = ORIENTED_EDGE('',*,*,#50040,.F.) ;
#70190 = ORIENTED_EDGE('',*,*,#50182,.T.) ;
#70191 = ORIENTED_EDGE('',*,*,#50039,.F.) ;
#70192 = ORIENTED_EDGE('',*,*,#50184,.F.) ;
#70193 = ORIENTED_EDGE('',*,*,#50029,.F.) ;
#70194 = ORIENTED_EDGE('',*,*,#50180,.T.) ;
#70195 = ORIENTED_EDGE('',*,*,#50032,.F.) ;
#70196 = ORIENTED_EDGE('',*,*,#50185,.F.) ;
#70197 = ORIENTED_EDGE('',*,*,#50043,.F.) ;
#70198 = ORIENTED_EDGE('',*,*,#50020,.F.) ;
#70199 = ORIENTED_EDGE('',*,*,#50186,.T.) ;
#70200 = ORIENTED_EDGE('',*,*,#50044,.F.) ;
#70201 = ORIENTED_EDGE('',*,*,#50187,.F.) ;
#70202 = ORIENTED_EDGE('',*,*,#50045,.F.) ;
#70203 = ORIENTED_EDGE('',*,*,#50188,.T.) ;
#70204 = ORIENTED_EDGE('',*,*,#49796,.F.) ;
#70205 = ORIENTED_EDGE('',*,*,#50189,.T.) ;
#70206 = ORIENTED_EDGE('',*,*,#50190,.F.) ;
#70207 = ORIENTED_EDGE('',*,*,#50183,.T.) ;
#70208 = ORIENTED_EDGE('',*,*,#50191,.F.) ;
#70209 = ORIENTED_EDGE('',*,*,#50192,.F.) ;
#70210 = ORIENTED_EDGE('',*,*,#50184,.T.) ;
#70211 = ORIENTED_EDGE('',*,*,#50193,.F.) ;
#70212 = ORIENTED_EDGE('',*,*,#49817,.T.) ;
#70213 = ORIENTED_EDGE('',*,*,#50187,.T.) ;
#70214 = ORIENTED_EDGE('',*,*,#50185,.T.) ;
#70215 = ORIENTED_EDGE('',*,*,#50194,.F.) ;
#70216 = ORIENTED_EDGE('',*,*,#50046,.F.) ;
#70217 = ORIENTED_EDGE('',*,*,#50195,.T.) ;
#70218 = ORIENTED_EDGE('',*,*,#50010,.F.) ;
#70219 = ORIENTED_EDGE('',*,*,#50196,.F.) ;
#70220 = ORIENTED_EDGE('',*,*,#50191,.T.) ;
#70221 = ORIENTED_EDGE('',*,*,#50041,.F.) ;
#70222 = ORIENTED_EDGE('',*,*,#50197,.F.) ;
#70223 = ORIENTED_EDGE('',*,*,#50036,.F.) ;
#70224 = ORIENTED_EDGE('',*,*,#50190,.T.) ;
#70225 = ORIENTED_EDGE('',*,*,#50035,.F.) ;
#70226 = ORIENTED_EDGE('',*,*,#50198,.F.) ;
#70227 = ORIENTED_EDGE('',*,*,#50037,.F.) ;
#70228 = ORIENTED_EDGE('',*,*,#50193,.T.) ;
#70229 = ORIENTED_EDGE('',*,*,#50038,.F.) ;
#70230 = ORIENTED_EDGE('',*,*,#50199,.F.) ;
#70231 = ORIENTED_EDGE('',*,*,#49818,.F.) ;
#70232 = ORIENTED_EDGE('',*,*,#50192,.T.) ;
#70233 = ORIENTED_EDGE('',*,*,#49816,.F.) ;
#70234 = ORIENTED_EDGE('',*,*,#50200,.F.) ;
#70235 = ORIENTED_EDGE('',*,*,#50030,.F.) ;
#70236 = ORIENTED_EDGE('',*,*,#50194,.T.) ;
#70237 = ORIENTED_EDGE('',*,*,#50031,.F.) ;
#70238 = ORIENTED_EDGE('',*,*,#50201,.F.) ;
#70239 = ORIENTED_EDGE('',*,*,#50021,.F.) ;
#70240 = ORIENTED_EDGE('',*,*,#50197,.T.) ;
#70241 = ORIENTED_EDGE('',*,*,#50196,.T.) ;
#70242 = ORIENTED_EDGE('',*,*,#50202,.F.) ;
#70243 = ORIENTED_EDGE('',*,*,#50199,.T.) ;
#70244 = ORIENTED_EDGE('',*,*,#50198,.T.) ;
#70245 = ORIENTED_EDGE('',*,*,#50203,.F.) ;
#70246 = ORIENTED_EDGE('',*,*,#49819,.T.) ;
#70247 = ORIENTED_EDGE('',*,*,#50201,.T.) ;
#70248 = ORIENTED_EDGE('',*,*,#50200,.T.) ;
#70249 = ORIENTED_EDGE('',*,*,#50204,.F.) ;
#70250 = ORIENTED_EDGE('',*,*,#50022,.T.) ;
#70251 = ORIENTED_EDGE('',*,*,#50202,.T.) ;
#70252 = ORIENTED_EDGE('',*,*,#50009,.F.) ;
#70253 = ORIENTED_EDGE('',*,*,#50205,.F.) ;
#70254 = ORIENTED_EDGE('',*,*,#50033,.F.) ;
#70255 = ORIENTED_EDGE('',*,*,#50203,.T.) ;
#70256 = ORIENTED_EDGE('',*,*,#50034,.F.) ;
#70257 = ORIENTED_EDGE('',*,*,#50206,.F.) ;
#70258 = ORIENTED_EDGE('',*,*,#49820,.F.) ;
#70259 = ORIENTED_EDGE('',*,*,#50204,.T.) ;
#70260 = ORIENTED_EDGE('',*,*,#49815,.F.) ;
#70261 = ORIENTED_EDGE('',*,*,#50207,.F.) ;
#70262 = ORIENTED_EDGE('',*,*,#50023,.F.) ;
#70263 = ORIENTED_EDGE('',*,*,#50027,.F.) ;
#70264 = ORIENTED_EDGE('',*,*,#50208,.T.) ;
#70265 = ORIENTED_EDGE('',*,*,#50016,.F.) ;
#70266 = ORIENTED_EDGE('',*,*,#50209,.F.) ;
#70267 = ORIENTED_EDGE('',*,*,#50028,.F.) ;
#70268 = ORIENTED_EDGE('',*,*,#50210,.F.) ;
#70269 = ORIENTED_EDGE('',*,*,#49728,.F.) ;
#70270 = ORIENTED_EDGE('',*,*,#50211,.F.) ;
#70271 = ORIENTED_EDGE('',*,*,#50205,.T.) ;
#70272 = ORIENTED_EDGE('',*,*,#50008,.T.) ;
#70273 = ORIENTED_EDGE('',*,*,#50212,.F.) ;
#70274 = ORIENTED_EDGE('',*,*,#50206,.T.) ;
#70275 = ORIENTED_EDGE('',*,*,#50213,.F.) ;
#70276 = ORIENTED_EDGE('',*,*,#50207,.T.) ;
#70277 = ORIENTED_EDGE('',*,*,#50214,.F.) ;
#70278 = ORIENTED_EDGE('',*,*,#50210,.T.) ;
#70279 = ORIENTED_EDGE('',*,*,#50209,.T.) ;
#70280 = ORIENTED_EDGE('',*,*,#50215,.F.) ;
#70281 = ORIENTED_EDGE('',*,*,#50212,.T.) ;
#70282 = ORIENTED_EDGE('',*,*,#50007,.F.) ;
#70283 = ORIENTED_EDGE('',*,*,#50216,.F.) ;
#70284 = ORIENTED_EDGE('',*,*,#49813,.F.) ;
#70285 = ORIENTED_EDGE('',*,*,#50214,.T.) ;
#70286 = ORIENTED_EDGE('',*,*,#49814,.F.) ;
#70287 = ORIENTED_EDGE('',*,*,#50217,.F.) ;
#70288 = ORIENTED_EDGE('',*,*,#50015,.F.) ;
#70289 = ORIENTED_EDGE('',*,*,#50213,.T.) ;
#70290 = ORIENTED_EDGE('',*,*,#50014,.F.) ;
#70291 = ORIENTED_EDGE('',*,*,#50218,.F.) ;
#70292 = ORIENTED_EDGE('',*,*,#50024,.F.) ;
#70293 = ORIENTED_EDGE('',*,*,#50215,.T.) ;
#70294 = ORIENTED_EDGE('',*,*,#50025,.F.) ;
#70295 = ORIENTED_EDGE('',*,*,#50219,.F.) ;
#70296 = ORIENTED_EDGE('',*,*,#49729,.F.) ;
#70297 = ORIENTED_EDGE('',*,*,#50217,.T.) ;
#70298 = ORIENTED_EDGE('',*,*,#50216,.T.) ;
#70299 = ORIENTED_EDGE('',*,*,#50220,.F.) ;
#70300 = ORIENTED_EDGE('',*,*,#50219,.T.) ;
#70301 = ORIENTED_EDGE('',*,*,#50218,.T.) ;
#70302 = ORIENTED_EDGE('',*,*,#50221,.F.) ;
#70303 = ORIENTED_EDGE('',*,*,#49730,.T.) ;
#70304 = ORIENTED_EDGE('',*,*,#50000,.F.) ;
#70305 = ORIENTED_EDGE('',*,*,#50222,.T.) ;
#70306 = ORIENTED_EDGE('',*,*,#49734,.F.) ;
#70307 = ORIENTED_EDGE('',*,*,#50223,.F.) ;
#70308 = ORIENTED_EDGE('',*,*,#50004,.F.) ;
#70309 = ORIENTED_EDGE('',*,*,#50224,.T.) ;
#70310 = ORIENTED_EDGE('',*,*,#50001,.F.) ;
#70311 = ORIENTED_EDGE('',*,*,#50225,.F.) ;
#70312 = ORIENTED_EDGE('',*,*,#50220,.T.) ;
#70313 = ORIENTED_EDGE('',*,*,#50006,.F.) ;
#70314 = ORIENTED_EDGE('',*,*,#50226,.F.) ;
#70315 = ORIENTED_EDGE('',*,*,#50012,.F.) ;
#70316 = ORIENTED_EDGE('',*,*,#50221,.T.) ;
#70317 = ORIENTED_EDGE('',*,*,#50013,.F.) ;
#70318 = ORIENTED_EDGE('',*,*,#50227,.F.) ;
#70319 = ORIENTED_EDGE('',*,*,#49731,.F.) ;
#70320 = ORIENTED_EDGE('',*,*,#50225,.T.) ;
#70321 = ORIENTED_EDGE('',*,*,#50223,.T.) ;
#70322 = ORIENTED_EDGE('',*,*,#50228,.F.) ;
#70323 = ORIENTED_EDGE('',*,*,#50227,.T.) ;
#70324 = ORIENTED_EDGE('',*,*,#50226,.T.) ;
#70325 = ORIENTED_EDGE('',*,*,#50229,.F.) ;
#70326 = ORIENTED_EDGE('',*,*,#49732,.T.) ;
#70327 = ORIENTED_EDGE('',*,*,#50228,.T.) ;
#70328 = ORIENTED_EDGE('',*,*,#49733,.F.) ;
#70329 = ORIENTED_EDGE('',*,*,#50229,.T.) ;
#70330 = ORIENTED_EDGE('',*,*,#50005,.F.) ;
#70331 = ORIENTED_EDGE('',*,*,#50230,.F.) ;
#70332 = ORIENTED_EDGE('',*,*,#49805,.F.) ;
#70333 = ORIENTED_EDGE('',*,*,#50231,.F.) ;
#70334 = ORIENTED_EDGE('',*,*,#50115,.F.) ;
#70335 = ORIENTED_EDGE('',*,*,#50231,.T.) ;
#70336 = ORIENTED_EDGE('',*,*,#49804,.F.) ;
#70337 = ORIENTED_EDGE('',*,*,#50232,.F.) ;
#70338 = ORIENTED_EDGE('',*,*,#50118,.F.) ;
#70339 = ORIENTED_EDGE('',*,*,#50230,.T.) ;
#70340 = ORIENTED_EDGE('',*,*,#50112,.F.) ;
#70341 = ORIENTED_EDGE('',*,*,#50233,.F.) ;
#70342 = ORIENTED_EDGE('',*,*,#49806,.F.) ;
#70343 = ORIENTED_EDGE('',*,*,#50232,.T.) ;
#70344 = ORIENTED_EDGE('',*,*,#49803,.F.) ;
#70345 = ORIENTED_EDGE('',*,*,#50234,.F.) ;
#70346 = ORIENTED_EDGE('',*,*,#50121,.F.) ;
#70347 = ORIENTED_EDGE('',*,*,#50233,.T.) ;
#70348 = ORIENTED_EDGE('',*,*,#50109,.F.) ;
#70349 = ORIENTED_EDGE('',*,*,#50235,.F.) ;
#70350 = ORIENTED_EDGE('',*,*,#49807,.F.) ;
#70351 = ORIENTED_EDGE('',*,*,#50234,.T.) ;
#70352 = ORIENTED_EDGE('',*,*,#49802,.F.) ;
#70353 = ORIENTED_EDGE('',*,*,#50236,.F.) ;
#70354 = ORIENTED_EDGE('',*,*,#50124,.F.) ;
#70355 = ORIENTED_EDGE('',*,*,#50235,.T.) ;
#70356 = ORIENTED_EDGE('',*,*,#50131,.F.) ;
#70357 = ORIENTED_EDGE('',*,*,#50237,.F.) ;
#70358 = ORIENTED_EDGE('',*,*,#49800,.F.) ;
#70359 = ORIENTED_EDGE('',*,*,#50236,.T.) ;
#70360 = ORIENTED_EDGE('',*,*,#49801,.F.) ;
#70361 = ORIENTED_EDGE('',*,*,#50237,.T.) ;
#70362 = ORIENTED_EDGE('',*,*,#50127,.F.) ;
#70363 = ORIENTED_EDGE('',*,*,#50238,.F.) ;
#70364 = ORIENTED_EDGE('',*,*,#49881,.F.) ;
#70365 = ORIENTED_EDGE('',*,*,#50239,.F.) ;
#70366 = ORIENTED_EDGE('',*,*,#49961,.F.) ;
#70367 = ORIENTED_EDGE('',*,*,#50239,.T.) ;
#70368 = ORIENTED_EDGE('',*,*,#49880,.T.) ;
#70369 = ORIENTED_EDGE('',*,*,#50240,.F.) ;
#70370 = ORIENTED_EDGE('',*,*,#50241,.F.) ;
#70371 = ORIENTED_EDGE('',*,*,#49882,.T.) ;
#70372 = ORIENTED_EDGE('',*,*,#50238,.T.) ;
#70373 = ORIENTED_EDGE('',*,*,#50242,.F.) ;
#70374 = ORIENTED_EDGE('',*,*,#50243,.F.) ;
#70375 = ORIENTED_EDGE('',*,*,#50240,.T.) ;
#70376 = ORIENTED_EDGE('',*,*,#49879,.F.) ;
#70377 = ORIENTED_EDGE('',*,*,#50244,.F.) ;
#70378 = ORIENTED_EDGE('',*,*,#49957,.F.) ;
#70379 = ORIENTED_EDGE('',*,*,#50241,.T.) ;
#70380 = ORIENTED_EDGE('',*,*,#49956,.F.) ;
#70381 = ORIENTED_EDGE('',*,*,#50245,.F.) ;
#70382 = ORIENTED_EDGE('',*,*,#49958,.F.) ;
#70383 = ORIENTED_EDGE('',*,*,#50246,.F.) ;
#70384 = ORIENTED_EDGE('',*,*,#49959,.F.) ;
#70385 = ORIENTED_EDGE('',*,*,#50247,.F.) ;
#70386 = ORIENTED_EDGE('',*,*,#49965,.F.) ;
#70387 = ORIENTED_EDGE('',*,*,#50242,.T.) ;
#70388 = ORIENTED_EDGE('',*,*,#49960,.F.) ;
#70389 = ORIENTED_EDGE('',*,*,#50248,.F.) ;
#70390 = ORIENTED_EDGE('',*,*,#49949,.F.) ;
#70391 = ORIENTED_EDGE('',*,*,#50243,.T.) ;
#70392 = ORIENTED_EDGE('',*,*,#49948,.F.) ;
#70393 = ORIENTED_EDGE('',*,*,#50249,.F.) ;
#70394 = ORIENTED_EDGE('',*,*,#49883,.F.) ;
#70395 = ORIENTED_EDGE('',*,*,#50250,.F.) ;
#70396 = ORIENTED_EDGE('',*,*,#49877,.F.) ;
#70397 = ORIENTED_EDGE('',*,*,#50251,.F.) ;
#70398 = ORIENTED_EDGE('',*,*,#49952,.F.) ;
#70399 = ORIENTED_EDGE('',*,*,#49878,.T.) ;
#70400 = ORIENTED_EDGE('',*,*,#50250,.T.) ;
#70401 = ORIENTED_EDGE('',*,*,#50252,.F.) ;
#70402 = ORIENTED_EDGE('',*,*,#50244,.T.) ;
#70403 = ORIENTED_EDGE('',*,*,#50247,.T.) ;
#70404 = ORIENTED_EDGE('',*,*,#50245,.T.) ;
#70405 = ORIENTED_EDGE('',*,*,#50253,.F.) ;
#70406 = ORIENTED_EDGE('',*,*,#50248,.T.) ;
#70407 = ORIENTED_EDGE('',*,*,#50246,.T.) ;
#70408 = ORIENTED_EDGE('',*,*,#50254,.F.) ;
#70409 = ORIENTED_EDGE('',*,*,#49876,.T.) ;
#70410 = ORIENTED_EDGE('',*,*,#50249,.T.) ;
#70411 = ORIENTED_EDGE('',*,*,#50255,.F.) ;
#70412 = ORIENTED_EDGE('',*,*,#50251,.T.) ;
#70413 = ORIENTED_EDGE('',*,*,#50252,.T.) ;
#70414 = ORIENTED_EDGE('',*,*,#49951,.F.) ;
#70415 = ORIENTED_EDGE('',*,*,#50256,.F.) ;
#70416 = ORIENTED_EDGE('',*,*,#49954,.F.) ;
#70417 = ORIENTED_EDGE('',*,*,#50253,.T.) ;
#70418 = ORIENTED_EDGE('',*,*,#49955,.F.) ;
#70419 = ORIENTED_EDGE('',*,*,#50257,.F.) ;
#70420 = ORIENTED_EDGE('',*,*,#49962,.F.) ;
#70421 = ORIENTED_EDGE('',*,*,#50254,.T.) ;
#70422 = ORIENTED_EDGE('',*,*,#49964,.F.) ;
#70423 = ORIENTED_EDGE('',*,*,#50258,.F.) ;
#70424 = ORIENTED_EDGE('',*,*,#49946,.F.) ;
#70425 = ORIENTED_EDGE('',*,*,#50255,.T.) ;
#70426 = ORIENTED_EDGE('',*,*,#49947,.F.) ;
#70427 = ORIENTED_EDGE('',*,*,#50259,.F.) ;
#70428 = ORIENTED_EDGE('',*,*,#49953,.F.) ;
#70429 = ORIENTED_EDGE('',*,*,#50257,.T.) ;
#70430 = ORIENTED_EDGE('',*,*,#50256,.T.) ;
#70431 = ORIENTED_EDGE('',*,*,#50260,.F.) ;
#70432 = ORIENTED_EDGE('',*,*,#50259,.T.) ;
#70433 = ORIENTED_EDGE('',*,*,#50258,.T.) ;
#70434 = ORIENTED_EDGE('',*,*,#50261,.F.) ;
#70435 = ORIENTED_EDGE('',*,*,#50260,.T.) ;
#70436 = ORIENTED_EDGE('',*,*,#49950,.F.) ;
#70437 = ORIENTED_EDGE('',*,*,#50261,.T.) ;
#70438 = ORIENTED_EDGE('',*,*,#49963,.F.) ;
#70439 = ORIENTED_EDGE('',*,*,#49971,.F.) ;
#70440 = ORIENTED_EDGE('',*,*,#49985,.F.) ;
#70441 = ORIENTED_EDGE('',*,*,#50262,.F.) ;
#70442 = ORIENTED_EDGE('',*,*,#49974,.F.) ;
#70443 = ORIENTED_EDGE('',*,*,#50263,.F.) ;
#70444 = ORIENTED_EDGE('',*,*,#49975,.F.) ;
#70445 = ORIENTED_EDGE('',*,*,#50264,.F.) ;
#70446 = ORIENTED_EDGE('',*,*,#49989,.F.) ;
#70447 = ORIENTED_EDGE('',*,*,#49973,.F.) ;
#70448 = ORIENTED_EDGE('',*,*,#49976,.F.) ;
#70449 = ORIENTED_EDGE('',*,*,#50265,.F.) ;
#70450 = ORIENTED_EDGE('',*,*,#49977,.F.) ;
#70451 = ORIENTED_EDGE('',*,*,#50264,.T.) ;
#70452 = ORIENTED_EDGE('',*,*,#50262,.T.) ;
#70453 = ORIENTED_EDGE('',*,*,#50266,.F.) ;
#70454 = ORIENTED_EDGE('',*,*,#50265,.T.) ;
#70455 = ORIENTED_EDGE('',*,*,#50263,.T.) ;
#70456 = ORIENTED_EDGE('',*,*,#50267,.F.) ;
#70457 = ORIENTED_EDGE('',*,*,#49969,.F.) ;
#70458 = ORIENTED_EDGE('',*,*,#49981,.F.) ;
#70459 = ORIENTED_EDGE('',*,*,#50268,.F.) ;
#70460 = ORIENTED_EDGE('',*,*,#49983,.F.) ;
#70461 = ORIENTED_EDGE('',*,*,#50266,.T.) ;
#70462 = ORIENTED_EDGE('',*,*,#49984,.F.) ;
#70463 = ORIENTED_EDGE('',*,*,#50269,.F.) ;
#70464 = ORIENTED_EDGE('',*,*,#49986,.F.) ;
#70465 = ORIENTED_EDGE('',*,*,#50267,.T.) ;
#70466 = ORIENTED_EDGE('',*,*,#49988,.F.) ;
#70467 = ORIENTED_EDGE('',*,*,#50270,.F.) ;
#70468 = ORIENTED_EDGE('',*,*,#49978,.F.) ;
#70469 = ORIENTED_EDGE('',*,*,#49967,.F.) ;
#70470 = ORIENTED_EDGE('',*,*,#49979,.F.) ;
#70471 = ORIENTED_EDGE('',*,*,#50271,.F.) ;
#70472 = ORIENTED_EDGE('',*,*,#49982,.F.) ;
#70473 = ORIENTED_EDGE('',*,*,#50269,.T.) ;
#70474 = ORIENTED_EDGE('',*,*,#50268,.T.) ;
#70475 = ORIENTED_EDGE('',*,*,#50272,.F.) ;
#70476 = ORIENTED_EDGE('',*,*,#50271,.T.) ;
#70477 = ORIENTED_EDGE('',*,*,#50270,.T.) ;
#70478 = ORIENTED_EDGE('',*,*,#50273,.F.) ;
#70479 = ORIENTED_EDGE('',*,*,#50272,.T.) ;
#70480 = ORIENTED_EDGE('',*,*,#49980,.F.) ;
#70481 = ORIENTED_EDGE('',*,*,#50273,.T.) ;
#70482 = ORIENTED_EDGE('',*,*,#49987,.F.) ;
#70483 = ORIENTED_EDGE('',*,*,#50274,.F.) ;
#70484 = ORIENTED_EDGE('',*,*,#49921,.F.) ;
#70485 = ORIENTED_EDGE('',*,*,#49927,.F.) ;
#70486 = ORIENTED_EDGE('',*,*,#49942,.F.) ;
#70487 = ORIENTED_EDGE('',*,*,#50275,.F.) ;
#70488 = ORIENTED_EDGE('',*,*,#50274,.T.) ;
#70489 = ORIENTED_EDGE('',*,*,#50276,.F.) ;
#70490 = ORIENTED_EDGE('',*,*,#50276,.T.) ;
#70491 = ORIENTED_EDGE('',*,*,#49941,.F.) ;
#70492 = ORIENTED_EDGE('',*,*,#50277,.F.) ;
#70493 = ORIENTED_EDGE('',*,*,#49916,.F.) ;
#70494 = ORIENTED_EDGE('',*,*,#50275,.T.) ;
#70495 = ORIENTED_EDGE('',*,*,#49915,.F.) ;
#70496 = ORIENTED_EDGE('',*,*,#50278,.F.) ;
#70497 = ORIENTED_EDGE('',*,*,#49918,.F.) ;
#70498 = ORIENTED_EDGE('',*,*,#49928,.F.) ;
#70499 = ORIENTED_EDGE('',*,*,#49919,.F.) ;
#70500 = ORIENTED_EDGE('',*,*,#50279,.F.) ;
#70501 = ORIENTED_EDGE('',*,*,#49938,.F.) ;
#70502 = ORIENTED_EDGE('',*,*,#50280,.F.) ;
#70503 = ORIENTED_EDGE('',*,*,#50277,.T.) ;
#70504 = ORIENTED_EDGE('',*,*,#50281,.F.) ;
#70505 = ORIENTED_EDGE('',*,*,#49792,.T.) ;
#70506 = ORIENTED_EDGE('',*,*,#50279,.T.) ;
#70507 = ORIENTED_EDGE('',*,*,#50278,.T.) ;
#70508 = ORIENTED_EDGE('',*,*,#50282,.F.) ;
#70509 = ORIENTED_EDGE('',*,*,#49925,.F.) ;
#70510 = ORIENTED_EDGE('',*,*,#49931,.F.) ;
#70511 = ORIENTED_EDGE('',*,*,#50283,.F.) ;
#70512 = ORIENTED_EDGE('',*,*,#49943,.F.) ;
#70513 = ORIENTED_EDGE('',*,*,#50284,.F.) ;
#70514 = ORIENTED_EDGE('',*,*,#49944,.F.) ;
#70515 = ORIENTED_EDGE('',*,*,#50285,.F.) ;
#70516 = ORIENTED_EDGE('',*,*,#49935,.F.) ;
#70517 = ORIENTED_EDGE('',*,*,#50281,.T.) ;
#70518 = ORIENTED_EDGE('',*,*,#49945,.F.) ;
#70519 = ORIENTED_EDGE('',*,*,#50286,.F.) ;
#70520 = ORIENTED_EDGE('',*,*,#49793,.F.) ;
#70521 = ORIENTED_EDGE('',*,*,#50280,.T.) ;
#70522 = ORIENTED_EDGE('',*,*,#49791,.F.) ;
#70523 = ORIENTED_EDGE('',*,*,#50287,.F.) ;
#70524 = ORIENTED_EDGE('',*,*,#49917,.F.) ;
#70525 = ORIENTED_EDGE('',*,*,#50282,.T.) ;
#70526 = ORIENTED_EDGE('',*,*,#49914,.F.) ;
#70527 = ORIENTED_EDGE('',*,*,#50288,.F.) ;
#70528 = ORIENTED_EDGE('',*,*,#49939,.F.) ;
#70529 = ORIENTED_EDGE('',*,*,#50285,.T.) ;
#70530 = ORIENTED_EDGE('',*,*,#50283,.T.) ;
#70531 = ORIENTED_EDGE('',*,*,#50289,.F.) ;
#70532 = ORIENTED_EDGE('',*,*,#50286,.T.) ;
#70533 = ORIENTED_EDGE('',*,*,#50284,.T.) ;
#70534 = ORIENTED_EDGE('',*,*,#50290,.F.) ;
#70535 = ORIENTED_EDGE('',*,*,#49794,.T.) ;
#70536 = ORIENTED_EDGE('',*,*,#50287,.T.) ;
#70537 = ORIENTED_EDGE('',*,*,#49790,.T.) ;
#70538 = ORIENTED_EDGE('',*,*,#50291,.F.) ;
#70539 = ORIENTED_EDGE('',*,*,#50288,.T.) ;
#70540 = ORIENTED_EDGE('',*,*,#49923,.F.) ;
#70541 = ORIENTED_EDGE('',*,*,#49937,.F.) ;
#70542 = ORIENTED_EDGE('',*,*,#50292,.F.) ;
#70543 = ORIENTED_EDGE('',*,*,#49929,.F.) ;
#70544 = ORIENTED_EDGE('',*,*,#50289,.T.) ;
#70545 = ORIENTED_EDGE('',*,*,#49930,.F.) ;
#70546 = ORIENTED_EDGE('',*,*,#50293,.F.) ;
#70547 = ORIENTED_EDGE('',*,*,#49932,.F.) ;
#70548 = ORIENTED_EDGE('',*,*,#50290,.T.) ;
#70549 = ORIENTED_EDGE('',*,*,#49934,.F.) ;
#70550 = ORIENTED_EDGE('',*,*,#50294,.F.) ;
#70551 = ORIENTED_EDGE('',*,*,#49795,.F.) ;
#70552 = ORIENTED_EDGE('',*,*,#50291,.T.) ;
#70553 = ORIENTED_EDGE('',*,*,#49789,.F.) ;
#70554 = ORIENTED_EDGE('',*,*,#50295,.F.) ;
#70555 = ORIENTED_EDGE('',*,*,#49940,.F.) ;
#70556 = ORIENTED_EDGE('',*,*,#50293,.T.) ;
#70557 = ORIENTED_EDGE('',*,*,#50292,.T.) ;
#70558 = ORIENTED_EDGE('',*,*,#50296,.F.) ;
#70559 = ORIENTED_EDGE('',*,*,#49788,.T.) ;
#70560 = ORIENTED_EDGE('',*,*,#50294,.T.) ;
#70561 = ORIENTED_EDGE('',*,*,#50297,.F.) ;
#70562 = ORIENTED_EDGE('',*,*,#50295,.T.) ;
#70563 = ORIENTED_EDGE('',*,*,#50296,.T.) ;
#70564 = ORIENTED_EDGE('',*,*,#49936,.F.) ;
#70565 = ORIENTED_EDGE('',*,*,#50297,.T.) ;
#70566 = ORIENTED_EDGE('',*,*,#49933,.F.) ;
#70567 = ORIENTED_EDGE('',*,*,#50298,.F.) ;
#70568 = ORIENTED_EDGE('',*,*,#49372,.F.) ;
#70569 = ORIENTED_EDGE('',*,*,#50299,.F.) ;
#70570 = ORIENTED_EDGE('',*,*,#50061,.F.) ;
#70571 = ORIENTED_EDGE('',*,*,#50299,.T.) ;
#70572 = ORIENTED_EDGE('',*,*,#49371,.T.) ;
#70573 = ORIENTED_EDGE('',*,*,#50300,.F.) ;
#70574 = ORIENTED_EDGE('',*,*,#50301,.F.) ;
#70575 = ORIENTED_EDGE('',*,*,#49373,.T.) ;
#70576 = ORIENTED_EDGE('',*,*,#50298,.T.) ;
#70577 = ORIENTED_EDGE('',*,*,#50302,.F.) ;
#70578 = ORIENTED_EDGE('',*,*,#50303,.F.) ;
#70579 = ORIENTED_EDGE('',*,*,#50300,.T.) ;
#70580 = ORIENTED_EDGE('',*,*,#49370,.F.) ;
#70581 = ORIENTED_EDGE('',*,*,#50304,.F.) ;
#70582 = ORIENTED_EDGE('',*,*,#50058,.F.) ;
#70583 = ORIENTED_EDGE('',*,*,#50301,.T.) ;
#70584 = ORIENTED_EDGE('',*,*,#50057,.F.) ;
#70585 = ORIENTED_EDGE('',*,*,#50305,.F.) ;
#70586 = ORIENTED_EDGE('',*,*,#50062,.F.) ;
#70587 = ORIENTED_EDGE('',*,*,#50306,.F.) ;
#70588 = ORIENTED_EDGE('',*,*,#50059,.F.) ;
#70589 = ORIENTED_EDGE('',*,*,#50307,.F.) ;
#70590 = ORIENTED_EDGE('',*,*,#50066,.F.) ;
#70591 = ORIENTED_EDGE('',*,*,#50302,.T.) ;
#70592 = ORIENTED_EDGE('',*,*,#50060,.F.) ;
#70593 = ORIENTED_EDGE('',*,*,#50308,.F.) ;
#70594 = ORIENTED_EDGE('',*,*,#50050,.F.) ;
#70595 = ORIENTED_EDGE('',*,*,#50303,.T.) ;
#70596 = ORIENTED_EDGE('',*,*,#50049,.F.) ;
#70597 = ORIENTED_EDGE('',*,*,#50309,.F.) ;
#70598 = ORIENTED_EDGE('',*,*,#49374,.F.) ;
#70599 = ORIENTED_EDGE('',*,*,#50310,.F.) ;
#70600 = ORIENTED_EDGE('',*,*,#49368,.F.) ;
#70601 = ORIENTED_EDGE('',*,*,#50311,.F.) ;
#70602 = ORIENTED_EDGE('',*,*,#50051,.F.) ;
#70603 = ORIENTED_EDGE('',*,*,#49369,.T.) ;
#70604 = ORIENTED_EDGE('',*,*,#50310,.T.) ;
#70605 = ORIENTED_EDGE('',*,*,#50312,.F.) ;
#70606 = ORIENTED_EDGE('',*,*,#50304,.T.) ;
#70607 = ORIENTED_EDGE('',*,*,#50307,.T.) ;
#70608 = ORIENTED_EDGE('',*,*,#50305,.T.) ;
#70609 = ORIENTED_EDGE('',*,*,#50313,.F.) ;
#70610 = ORIENTED_EDGE('',*,*,#50308,.T.) ;
#70611 = ORIENTED_EDGE('',*,*,#50306,.T.) ;
#70612 = ORIENTED_EDGE('',*,*,#50314,.F.) ;
#70613 = ORIENTED_EDGE('',*,*,#49367,.T.) ;
#70614 = ORIENTED_EDGE('',*,*,#50309,.T.) ;
#70615 = ORIENTED_EDGE('',*,*,#50315,.F.) ;
#70616 = ORIENTED_EDGE('',*,*,#50311,.T.) ;
#70617 = ORIENTED_EDGE('',*,*,#50312,.T.) ;
#70618 = ORIENTED_EDGE('',*,*,#50054,.F.) ;
#70619 = ORIENTED_EDGE('',*,*,#50316,.F.) ;
#70620 = ORIENTED_EDGE('',*,*,#50055,.F.) ;
#70621 = ORIENTED_EDGE('',*,*,#50313,.T.) ;
#70622 = ORIENTED_EDGE('',*,*,#50056,.F.) ;
#70623 = ORIENTED_EDGE('',*,*,#50317,.F.) ;
#70624 = ORIENTED_EDGE('',*,*,#50063,.F.) ;
#70625 = ORIENTED_EDGE('',*,*,#50314,.T.) ;
#70626 = ORIENTED_EDGE('',*,*,#50065,.F.) ;
#70627 = ORIENTED_EDGE('',*,*,#50318,.F.) ;
#70628 = ORIENTED_EDGE('',*,*,#50047,.F.) ;
#70629 = ORIENTED_EDGE('',*,*,#50315,.T.) ;
#70630 = ORIENTED_EDGE('',*,*,#50048,.F.) ;
#70631 = ORIENTED_EDGE('',*,*,#50319,.F.) ;
#70632 = ORIENTED_EDGE('',*,*,#50052,.F.) ;
#70633 = ORIENTED_EDGE('',*,*,#50317,.T.) ;
#70634 = ORIENTED_EDGE('',*,*,#50316,.T.) ;
#70635 = ORIENTED_EDGE('',*,*,#50320,.F.) ;
#70636 = ORIENTED_EDGE('',*,*,#50319,.T.) ;
#70637 = ORIENTED_EDGE('',*,*,#50318,.T.) ;
#70638 = ORIENTED_EDGE('',*,*,#50321,.F.) ;
#70639 = ORIENTED_EDGE('',*,*,#50320,.T.) ;
#70640 = ORIENTED_EDGE('',*,*,#50053,.F.) ;
#70641 = ORIENTED_EDGE('',*,*,#50321,.T.) ;
#70642 = ORIENTED_EDGE('',*,*,#50064,.F.) ;
#70643 = ORIENTED_EDGE('',*,*,#50072,.F.) ;
#70644 = ORIENTED_EDGE('',*,*,#50085,.F.) ;
#70645 = ORIENTED_EDGE('',*,*,#50322,.F.) ;
#70646 = ORIENTED_EDGE('',*,*,#50077,.F.) ;
#70647 = ORIENTED_EDGE('',*,*,#50323,.F.) ;
#70648 = ORIENTED_EDGE('',*,*,#50075,.F.) ;
#70649 = ORIENTED_EDGE('',*,*,#50324,.F.) ;
#70650 = ORIENTED_EDGE('',*,*,#50090,.F.) ;
#70651 = ORIENTED_EDGE('',*,*,#50074,.F.) ;
#70652 = ORIENTED_EDGE('',*,*,#50076,.F.) ;
#70653 = ORIENTED_EDGE('',*,*,#50325,.F.) ;
#70654 = ORIENTED_EDGE('',*,*,#50080,.F.) ;
#70655 = ORIENTED_EDGE('',*,*,#50324,.T.) ;
#70656 = ORIENTED_EDGE('',*,*,#50322,.T.) ;
#70657 = ORIENTED_EDGE('',*,*,#50326,.F.) ;
#70658 = ORIENTED_EDGE('',*,*,#50325,.T.) ;
#70659 = ORIENTED_EDGE('',*,*,#50323,.T.) ;
#70660 = ORIENTED_EDGE('',*,*,#50327,.F.) ;
#70661 = ORIENTED_EDGE('',*,*,#50070,.F.) ;
#70662 = ORIENTED_EDGE('',*,*,#50083,.F.) ;
#70663 = ORIENTED_EDGE('',*,*,#50328,.F.) ;
#70664 = ORIENTED_EDGE('',*,*,#50086,.F.) ;
#70665 = ORIENTED_EDGE('',*,*,#50326,.T.) ;
#70666 = ORIENTED_EDGE('',*,*,#50084,.F.) ;
#70667 = ORIENTED_EDGE('',*,*,#50329,.F.) ;
#70668 = ORIENTED_EDGE('',*,*,#50087,.F.) ;
#70669 = ORIENTED_EDGE('',*,*,#50327,.T.) ;
#70670 = ORIENTED_EDGE('',*,*,#50089,.F.) ;
#70671 = ORIENTED_EDGE('',*,*,#50330,.F.) ;
#70672 = ORIENTED_EDGE('',*,*,#50078,.F.) ;
#70673 = ORIENTED_EDGE('',*,*,#50068,.F.) ;
#70674 = ORIENTED_EDGE('',*,*,#50079,.F.) ;
#70675 = ORIENTED_EDGE('',*,*,#50331,.F.) ;
#70676 = ORIENTED_EDGE('',*,*,#50081,.F.) ;
#70677 = ORIENTED_EDGE('',*,*,#50329,.T.) ;
#70678 = ORIENTED_EDGE('',*,*,#50328,.T.) ;
#70679 = ORIENTED_EDGE('',*,*,#50332,.F.) ;
#70680 = ORIENTED_EDGE('',*,*,#50331,.T.) ;
#70681 = ORIENTED_EDGE('',*,*,#50330,.T.) ;
#70682 = ORIENTED_EDGE('',*,*,#50333,.F.) ;
#70683 = ORIENTED_EDGE('',*,*,#50332,.T.) ;
#70684 = ORIENTED_EDGE('',*,*,#50082,.F.) ;
#70685 = ORIENTED_EDGE('',*,*,#50333,.T.) ;
#70686 = ORIENTED_EDGE('',*,*,#50088,.F.) ;
#70687 = ORIENTED_EDGE('',*,*,#50334,.F.) ;
#70688 = ORIENTED_EDGE('',*,*,#50120,.F.) ;
#70689 = ORIENTED_EDGE('',*,*,#50335,.F.) ;
#70690 = ORIENTED_EDGE('',*,*,#50135,.F.) ;
#70691 = ORIENTED_EDGE('',*,*,#50335,.T.) ;
#70692 = ORIENTED_EDGE('',*,*,#50123,.F.) ;
#70693 = ORIENTED_EDGE('',*,*,#50336,.F.) ;
#70694 = ORIENTED_EDGE('',*,*,#50117,.F.) ;
#70695 = ORIENTED_EDGE('',*,*,#50334,.T.) ;
#70696 = ORIENTED_EDGE('',*,*,#50337,.F.) ;
#70697 = ORIENTED_EDGE('',*,*,#50336,.T.) ;
#70698 = ORIENTED_EDGE('',*,*,#50126,.F.) ;
#70699 = ORIENTED_EDGE('',*,*,#50338,.F.) ;
#70700 = ORIENTED_EDGE('',*,*,#50132,.F.) ;
#70701 = ORIENTED_EDGE('',*,*,#50337,.T.) ;
#70702 = ORIENTED_EDGE('',*,*,#50134,.F.) ;
#70703 = ORIENTED_EDGE('',*,*,#50339,.F.) ;
#70704 = ORIENTED_EDGE('',*,*,#50114,.F.) ;
#70705 = ORIENTED_EDGE('',*,*,#50338,.T.) ;
#70706 = ORIENTED_EDGE('',*,*,#50129,.F.) ;
#70707 = ORIENTED_EDGE('',*,*,#50340,.F.) ;
#70708 = ORIENTED_EDGE('',*,*,#50111,.F.) ;
#70709 = ORIENTED_EDGE('',*,*,#50339,.T.) ;
#70710 = ORIENTED_EDGE('',*,*,#50341,.F.) ;
#70711 = ORIENTED_EDGE('',*,*,#50340,.T.) ;
#70712 = ORIENTED_EDGE('',*,*,#50130,.F.) ;
#70713 = ORIENTED_EDGE('',*,*,#50341,.T.) ;
#70714 = ORIENTED_EDGE('',*,*,#50133,.F.) ;
#70715 = ORIENTED_EDGE('',*,*,#49298,.F.) ;
#70716 = ORIENTED_EDGE('',*,*,#50091,.F.) ;
#70717 = ORIENTED_EDGE('',*,*,#49312,.F.) ;
#70718 = ORIENTED_EDGE('',*,*,#50092,.F.) ;
#70719 = ORIENTED_EDGE('',*,*,#49300,.F.) ;
#70720 = ORIENTED_EDGE('',*,*,#50093,.F.) ;
#70721 = ORIENTED_EDGE('',*,*,#49310,.F.) ;
#70722 = ORIENTED_EDGE('',*,*,#50096,.F.) ;
#70723 = ORIENTED_EDGE('',*,*,#49308,.F.) ;
#70724 = ORIENTED_EDGE('',*,*,#50094,.F.) ;
#70725 = ORIENTED_EDGE('',*,*,#49302,.F.) ;
#70726 = ORIENTED_EDGE('',*,*,#50097,.F.) ;
#70727 = ORIENTED_EDGE('',*,*,#49306,.F.) ;
#70728 = ORIENTED_EDGE('',*,*,#49812,.F.) ;
#70729 = ORIENTED_EDGE('',*,*,#49304,.F.) ;
#70730 = ORIENTED_EDGE('',*,*,#50095,.F.) ;
#70731 = ORIENTED_EDGE('',*,*,#49798,.F.) ;
#70732 = ORIENTED_EDGE('',*,*,#50342,.T.) ;
#70733 = ORIENTED_EDGE('',*,*,#49539,.F.) ;
#70734 = ORIENTED_EDGE('',*,*,#50343,.T.) ;
#70735 = ORIENTED_EDGE('',*,*,#49541,.F.) ;
#70736 = ORIENTED_EDGE('',*,*,#50344,.T.) ;
#70737 = ORIENTED_EDGE('',*,*,#49742,.T.) ;
#70738 = ORIENTED_EDGE('',*,*,#49536,.F.) ;
#70739 = ORIENTED_EDGE('',*,*,#50345,.T.) ;
#70740 = ORIENTED_EDGE('',*,*,#49998,.F.) ;
#70741 = ORIENTED_EDGE('',*,*,#50346,.F.) ;
#70742 = ORIENTED_EDGE('',*,*,#50347,.F.) ;
#70743 = ORIENTED_EDGE('',*,*,#50347,.T.) ;
#70744 = ORIENTED_EDGE('',*,*,#50348,.T.) ;
#70745 = ORIENTED_EDGE('',*,*,#49537,.F.) ;
#70746 = ORIENTED_EDGE('',*,*,#50018,.F.) ;
#70747 = ORIENTED_EDGE('',*,*,#50349,.T.) ;
#70748 = ORIENTED_EDGE('',*,*,#50350,.F.) ;
#70749 = ORIENTED_EDGE('',*,*,#50350,.T.) ;
#70750 = ORIENTED_EDGE('',*,*,#50351,.T.) ;
#70751 = ORIENTED_EDGE('',*,*,#49797,.F.) ;
#70752 = ORIENTED_EDGE('',*,*,#50352,.F.) ;
#70753 = ORIENTED_EDGE('',*,*,#50019,.F.) ;
#70754 = ORIENTED_EDGE('',*,*,#50188,.F.) ;
#70755 = ORIENTED_EDGE('',*,*,#50186,.F.) ;
#70756 = ORIENTED_EDGE('',*,*,#50352,.T.) ;
#70757 = ORIENTED_EDGE('',*,*,#50353,.F.) ;
#70758 = ORIENTED_EDGE('',*,*,#50354,.T.) ;
#70759 = ORIENTED_EDGE('',*,*,#50002,.F.) ;
#70760 = ORIENTED_EDGE('',*,*,#50355,.T.) ;
#70761 = ORIENTED_EDGE('',*,*,#50353,.T.) ;
#70762 = ORIENTED_EDGE('',*,*,#50011,.F.) ;
#70763 = ORIENTED_EDGE('',*,*,#50356,.F.) ;
#70764 = ORIENTED_EDGE('',*,*,#49799,.F.) ;
#70765 = ORIENTED_EDGE('',*,*,#50195,.F.) ;
#70766 = ORIENTED_EDGE('',*,*,#50189,.F.) ;
#70767 = ORIENTED_EDGE('',*,*,#50356,.T.) ;
#70768 = ORIENTED_EDGE('',*,*,#50342,.F.) ;
#70769 = ORIENTED_EDGE('',*,*,#50351,.F.) ;
#70770 = ORIENTED_EDGE('',*,*,#50357,.F.) ;
#70771 = ORIENTED_EDGE('',*,*,#49540,.F.) ;
#70772 = ORIENTED_EDGE('',*,*,#50357,.T.) ;
#70773 = ORIENTED_EDGE('',*,*,#50349,.F.) ;
#70774 = ORIENTED_EDGE('',*,*,#50358,.F.) ;
#70775 = ORIENTED_EDGE('',*,*,#50344,.F.) ;
#70776 = ORIENTED_EDGE('',*,*,#50208,.F.) ;
#70777 = ORIENTED_EDGE('',*,*,#49743,.T.) ;
#70778 = ORIENTED_EDGE('',*,*,#50358,.T.) ;
#70779 = ORIENTED_EDGE('',*,*,#50017,.F.) ;
#70780 = ORIENTED_EDGE('',*,*,#50343,.F.) ;
#70781 = ORIENTED_EDGE('',*,*,#49538,.F.) ;
#70782 = ORIENTED_EDGE('',*,*,#50359,.F.) ;
#70783 = ORIENTED_EDGE('',*,*,#50355,.F.) ;
#70784 = ORIENTED_EDGE('',*,*,#50359,.T.) ;
#70785 = ORIENTED_EDGE('',*,*,#50348,.F.) ;
#70786 = ORIENTED_EDGE('',*,*,#50360,.F.) ;
#70787 = ORIENTED_EDGE('',*,*,#50354,.F.) ;
#70788 = ORIENTED_EDGE('',*,*,#50360,.T.) ;
#70789 = ORIENTED_EDGE('',*,*,#50346,.T.) ;
#70790 = ORIENTED_EDGE('',*,*,#50224,.F.) ;
#70791 = ORIENTED_EDGE('',*,*,#50003,.F.) ;
#70792 = ORIENTED_EDGE('',*,*,#50361,.T.) ;
#70793 = ORIENTED_EDGE('',*,*,#50362,.T.) ;
#70794 = ORIENTED_EDGE('',*,*,#50363,.T.) ;
#70795 = ORIENTED_EDGE('',*,*,#50364,.T.) ;
#70796 = ORIENTED_EDGE('',*,*,#50365,.T.) ;
#70797 = ORIENTED_EDGE('',*,*,#50366,.T.) ;
#70798 = ORIENTED_EDGE('',*,*,#50367,.T.) ;
#70799 = ORIENTED_EDGE('',*,*,#50368,.T.) ;
#70800 = ORIENTED_EDGE('',*,*,#50369,.F.) ;
#70801 = ORIENTED_EDGE('',*,*,#50370,.T.) ;
#70802 = ORIENTED_EDGE('',*,*,#50371,.T.) ;
#70803 = ORIENTED_EDGE('',*,*,#50372,.T.) ;
#70804 = ORIENTED_EDGE('',*,*,#50373,.T.) ;
#70805 = ORIENTED_EDGE('',*,*,#50374,.T.) ;
#70806 = ORIENTED_EDGE('',*,*,#50367,.F.) ;
#70807 = ORIENTED_EDGE('',*,*,#50375,.T.) ;
#70808 = ORIENTED_EDGE('',*,*,#50371,.F.) ;
#70809 = ORIENTED_EDGE('',*,*,#50376,.T.) ;
#70810 = ORIENTED_EDGE('',*,*,#50377,.T.) ;
#70811 = ORIENTED_EDGE('',*,*,#50378,.T.) ;
#70812 = ORIENTED_EDGE('',*,*,#50379,.T.) ;
#70813 = ORIENTED_EDGE('',*,*,#50380,.T.) ;
#70814 = ORIENTED_EDGE('',*,*,#50381,.T.) ;
#70815 = ORIENTED_EDGE('',*,*,#50382,.T.) ;
#70816 = ORIENTED_EDGE('',*,*,#50383,.T.) ;
#70817 = ORIENTED_EDGE('',*,*,#50384,.T.) ;
#70818 = ORIENTED_EDGE('',*,*,#50385,.T.) ;
#70819 = ORIENTED_EDGE('',*,*,#50386,.T.) ;
#70820 = ORIENTED_EDGE('',*,*,#50387,.T.) ;
#70821 = ORIENTED_EDGE('',*,*,#50388,.T.) ;
#70822 = ORIENTED_EDGE('',*,*,#50389,.T.) ;
#70823 = ORIENTED_EDGE('',*,*,#50390,.T.) ;
#70824 = ORIENTED_EDGE('',*,*,#50391,.F.) ;
#70825 = ORIENTED_EDGE('',*,*,#50392,.T.) ;
#70826 = ORIENTED_EDGE('',*,*,#50393,.T.) ;
#70827 = ORIENTED_EDGE('',*,*,#50394,.T.) ;
#70828 = ORIENTED_EDGE('',*,*,#50395,.T.) ;
#70829 = ORIENTED_EDGE('',*,*,#50396,.T.) ;
#70830 = ORIENTED_EDGE('',*,*,#50389,.F.) ;
#70831 = ORIENTED_EDGE('',*,*,#50397,.T.) ;
#70832 = ORIENTED_EDGE('',*,*,#50393,.F.) ;
#70833 = ORIENTED_EDGE('',*,*,#50398,.T.) ;
#70834 = ORIENTED_EDGE('',*,*,#50399,.T.) ;
#70835 = ORIENTED_EDGE('',*,*,#50400,.T.) ;
#70836 = ORIENTED_EDGE('',*,*,#50401,.T.) ;
#70837 = ORIENTED_EDGE('',*,*,#50402,.T.) ;
#70838 = ORIENTED_EDGE('',*,*,#50403,.T.) ;
#70839 = ORIENTED_EDGE('',*,*,#50404,.T.) ;
#70840 = ORIENTED_EDGE('',*,*,#50405,.T.) ;
#70841 = ORIENTED_EDGE('',*,*,#50406,.T.) ;
#70842 = ORIENTED_EDGE('',*,*,#50407,.T.) ;
#70843 = ORIENTED_EDGE('',*,*,#50408,.T.) ;
#70844 = ORIENTED_EDGE('',*,*,#50409,.T.) ;
#70845 = ORIENTED_EDGE('',*,*,#50410,.T.) ;
#70846 = ORIENTED_EDGE('',*,*,#50411,.T.) ;
#70847 = ORIENTED_EDGE('',*,*,#50412,.T.) ;
#70848 = ORIENTED_EDGE('',*,*,#50413,.F.) ;
#70849 = ORIENTED_EDGE('',*,*,#50414,.T.) ;
#70850 = ORIENTED_EDGE('',*,*,#50415,.T.) ;
#70851 = ORIENTED_EDGE('',*,*,#50416,.T.) ;
#70852 = ORIENTED_EDGE('',*,*,#50417,.T.) ;
#70853 = ORIENTED_EDGE('',*,*,#50418,.T.) ;
#70854 = ORIENTED_EDGE('',*,*,#50411,.F.) ;
#70855 = ORIENTED_EDGE('',*,*,#50419,.T.) ;
#70856 = ORIENTED_EDGE('',*,*,#50415,.F.) ;
#70857 = ORIENTED_EDGE('',*,*,#50420,.T.) ;
#70858 = ORIENTED_EDGE('',*,*,#50421,.T.) ;
#70859 = ORIENTED_EDGE('',*,*,#50422,.T.) ;
#70860 = ORIENTED_EDGE('',*,*,#50423,.T.) ;
#70861 = ORIENTED_EDGE('',*,*,#50424,.T.) ;
#70862 = ORIENTED_EDGE('',*,*,#50425,.T.) ;
#70863 = ORIENTED_EDGE('',*,*,#50426,.T.) ;
#70864 = ORIENTED_EDGE('',*,*,#50427,.T.) ;
#70865 = ORIENTED_EDGE('',*,*,#50428,.T.) ;
#70866 = ORIENTED_EDGE('',*,*,#50429,.T.) ;
#70867 = ORIENTED_EDGE('',*,*,#50430,.T.) ;
#70868 = ORIENTED_EDGE('',*,*,#50431,.T.) ;
#70869 = ORIENTED_EDGE('',*,*,#50432,.T.) ;
#70870 = ORIENTED_EDGE('',*,*,#50433,.T.) ;
#70871 = ORIENTED_EDGE('',*,*,#50434,.T.) ;
#70872 = ORIENTED_EDGE('',*,*,#50435,.F.) ;
#70873 = ORIENTED_EDGE('',*,*,#50436,.T.) ;
#70874 = ORIENTED_EDGE('',*,*,#50437,.T.) ;
#70875 = ORIENTED_EDGE('',*,*,#50438,.T.) ;
#70876 = ORIENTED_EDGE('',*,*,#50439,.T.) ;
#70877 = ORIENTED_EDGE('',*,*,#50440,.T.) ;
#70878 = ORIENTED_EDGE('',*,*,#50433,.F.) ;
#70879 = ORIENTED_EDGE('',*,*,#50441,.T.) ;
#70880 = ORIENTED_EDGE('',*,*,#50437,.F.) ;
#70881 = ORIENTED_EDGE('',*,*,#50442,.T.) ;
#70882 = ORIENTED_EDGE('',*,*,#50443,.T.) ;
#70883 = ORIENTED_EDGE('',*,*,#50444,.T.) ;
#70884 = ORIENTED_EDGE('',*,*,#50445,.T.) ;
#70885 = ORIENTED_EDGE('',*,*,#50446,.T.) ;
#70886 = ORIENTED_EDGE('',*,*,#50447,.T.) ;
#70887 = ORIENTED_EDGE('',*,*,#50448,.T.) ;
#70888 = ORIENTED_EDGE('',*,*,#50449,.T.) ;
#70889 = ORIENTED_EDGE('',*,*,#50450,.T.) ;
#70890 = ORIENTED_EDGE('',*,*,#50451,.T.) ;
#70891 = ORIENTED_EDGE('',*,*,#50452,.T.) ;
#70892 = ORIENTED_EDGE('',*,*,#50453,.T.) ;
#70893 = ORIENTED_EDGE('',*,*,#50454,.T.) ;
#70894 = ORIENTED_EDGE('',*,*,#50455,.T.) ;
#70895 = ORIENTED_EDGE('',*,*,#50456,.T.) ;
#70896 = ORIENTED_EDGE('',*,*,#50457,.F.) ;
#70897 = ORIENTED_EDGE('',*,*,#50458,.T.) ;
#70898 = ORIENTED_EDGE('',*,*,#50459,.T.) ;
#70899 = ORIENTED_EDGE('',*,*,#50460,.T.) ;
#70900 = ORIENTED_EDGE('',*,*,#50461,.T.) ;
#70901 = ORIENTED_EDGE('',*,*,#50462,.T.) ;
#70902 = ORIENTED_EDGE('',*,*,#50455,.F.) ;
#70903 = ORIENTED_EDGE('',*,*,#50463,.T.) ;
#70904 = ORIENTED_EDGE('',*,*,#50459,.F.) ;
#70905 = ORIENTED_EDGE('',*,*,#50464,.T.) ;
#70906 = ORIENTED_EDGE('',*,*,#50465,.T.) ;
#70907 = ORIENTED_EDGE('',*,*,#50466,.T.) ;
#70908 = ORIENTED_EDGE('',*,*,#50467,.T.) ;
#70909 = ORIENTED_EDGE('',*,*,#50468,.T.) ;
#70910 = ORIENTED_EDGE('',*,*,#50469,.T.) ;
#70911 = ORIENTED_EDGE('',*,*,#50470,.T.) ;
#70912 = ORIENTED_EDGE('',*,*,#50471,.T.) ;
#70913 = ORIENTED_EDGE('',*,*,#50472,.T.) ;
#70914 = ORIENTED_EDGE('',*,*,#50473,.T.) ;
#70915 = ORIENTED_EDGE('',*,*,#50474,.T.) ;
#70916 = ORIENTED_EDGE('',*,*,#50475,.T.) ;
#70917 = ORIENTED_EDGE('',*,*,#50476,.T.) ;
#70918 = ORIENTED_EDGE('',*,*,#50477,.T.) ;
#70919 = ORIENTED_EDGE('',*,*,#50478,.T.) ;
#70920 = ORIENTED_EDGE('',*,*,#50479,.F.) ;
#70921 = ORIENTED_EDGE('',*,*,#50480,.T.) ;
#70922 = ORIENTED_EDGE('',*,*,#50481,.T.) ;
#70923 = ORIENTED_EDGE('',*,*,#50482,.T.) ;
#70924 = ORIENTED_EDGE('',*,*,#50483,.T.) ;
#70925 = ORIENTED_EDGE('',*,*,#50484,.T.) ;
#70926 = ORIENTED_EDGE('',*,*,#50477,.F.) ;
#70927 = ORIENTED_EDGE('',*,*,#50485,.T.) ;
#70928 = ORIENTED_EDGE('',*,*,#50481,.F.) ;
#70929 = ORIENTED_EDGE('',*,*,#50486,.T.) ;
#70930 = ORIENTED_EDGE('',*,*,#50487,.T.) ;
#70931 = ORIENTED_EDGE('',*,*,#50488,.T.) ;
#70932 = ORIENTED_EDGE('',*,*,#50489,.T.) ;
#70933 = ORIENTED_EDGE('',*,*,#50490,.T.) ;
#70934 = ORIENTED_EDGE('',*,*,#50491,.T.) ;
#70935 = ORIENTED_EDGE('',*,*,#50492,.T.) ;
#70936 = ORIENTED_EDGE('',*,*,#50493,.T.) ;
#70937 = ORIENTED_EDGE('',*,*,#50494,.T.) ;
#70938 = ORIENTED_EDGE('',*,*,#50495,.T.) ;
#70939 = ORIENTED_EDGE('',*,*,#50496,.T.) ;
#70940 = ORIENTED_EDGE('',*,*,#50497,.T.) ;
#70941 = ORIENTED_EDGE('',*,*,#50498,.T.) ;
#70942 = ORIENTED_EDGE('',*,*,#50499,.T.) ;
#70943 = ORIENTED_EDGE('',*,*,#50500,.T.) ;
#70944 = ORIENTED_EDGE('',*,*,#50501,.F.) ;
#70945 = ORIENTED_EDGE('',*,*,#50502,.T.) ;
#70946 = ORIENTED_EDGE('',*,*,#50503,.T.) ;
#70947 = ORIENTED_EDGE('',*,*,#50504,.T.) ;
#70948 = ORIENTED_EDGE('',*,*,#50505,.T.) ;
#70949 = ORIENTED_EDGE('',*,*,#50506,.T.) ;
#70950 = ORIENTED_EDGE('',*,*,#50499,.F.) ;
#70951 = ORIENTED_EDGE('',*,*,#50507,.T.) ;
#70952 = ORIENTED_EDGE('',*,*,#50503,.F.) ;
#70953 = ORIENTED_EDGE('',*,*,#50508,.T.) ;
#70954 = ORIENTED_EDGE('',*,*,#50509,.T.) ;
#70955 = ORIENTED_EDGE('',*,*,#50510,.T.) ;
#70956 = ORIENTED_EDGE('',*,*,#50511,.T.) ;
#70957 = ORIENTED_EDGE('',*,*,#50512,.T.) ;
#70958 = ORIENTED_EDGE('',*,*,#50513,.T.) ;
#70959 = ORIENTED_EDGE('',*,*,#50514,.T.) ;
#70960 = ORIENTED_EDGE('',*,*,#50515,.T.) ;
#70961 = ORIENTED_EDGE('',*,*,#50516,.T.) ;
#70962 = ORIENTED_EDGE('',*,*,#50517,.T.) ;
#70963 = ORIENTED_EDGE('',*,*,#50518,.T.) ;
#70964 = ORIENTED_EDGE('',*,*,#50519,.T.) ;
#70965 = ORIENTED_EDGE('',*,*,#50520,.T.) ;
#70966 = ORIENTED_EDGE('',*,*,#50521,.T.) ;
#70967 = ORIENTED_EDGE('',*,*,#50522,.T.) ;
#70968 = ORIENTED_EDGE('',*,*,#50523,.F.) ;
#70969 = ORIENTED_EDGE('',*,*,#50524,.T.) ;
#70970 = ORIENTED_EDGE('',*,*,#50525,.T.) ;
#70971 = ORIENTED_EDGE('',*,*,#50526,.T.) ;
#70972 = ORIENTED_EDGE('',*,*,#50527,.T.) ;
#70973 = ORIENTED_EDGE('',*,*,#50528,.T.) ;
#70974 = ORIENTED_EDGE('',*,*,#50521,.F.) ;
#70975 = ORIENTED_EDGE('',*,*,#50529,.T.) ;
#70976 = ORIENTED_EDGE('',*,*,#50525,.F.) ;
#70977 = ORIENTED_EDGE('',*,*,#50530,.T.) ;
#70978 = ORIENTED_EDGE('',*,*,#50531,.T.) ;
#70979 = ORIENTED_EDGE('',*,*,#50532,.T.) ;
#70980 = ORIENTED_EDGE('',*,*,#50533,.T.) ;
#70981 = ORIENTED_EDGE('',*,*,#50534,.T.) ;
#70982 = ORIENTED_EDGE('',*,*,#50535,.T.) ;
#70983 = ORIENTED_EDGE('',*,*,#50536,.T.) ;
#70984 = ORIENTED_EDGE('',*,*,#50537,.T.) ;
#70985 = ORIENTED_EDGE('',*,*,#50538,.T.) ;
#70986 = ORIENTED_EDGE('',*,*,#50539,.T.) ;
#70987 = ORIENTED_EDGE('',*,*,#50540,.T.) ;
#70988 = ORIENTED_EDGE('',*,*,#50541,.T.) ;
#70989 = ORIENTED_EDGE('',*,*,#50542,.T.) ;
#70990 = ORIENTED_EDGE('',*,*,#50543,.T.) ;
#70991 = ORIENTED_EDGE('',*,*,#50544,.T.) ;
#70992 = ORIENTED_EDGE('',*,*,#50545,.F.) ;
#70993 = ORIENTED_EDGE('',*,*,#50546,.T.) ;
#70994 = ORIENTED_EDGE('',*,*,#50547,.T.) ;
#70995 = ORIENTED_EDGE('',*,*,#50548,.T.) ;
#70996 = ORIENTED_EDGE('',*,*,#50549,.T.) ;
#70997 = ORIENTED_EDGE('',*,*,#50550,.T.) ;
#70998 = ORIENTED_EDGE('',*,*,#50543,.F.) ;
#70999 = ORIENTED_EDGE('',*,*,#50551,.T.) ;
#71000 = ORIENTED_EDGE('',*,*,#50547,.F.) ;
#71001 = ORIENTED_EDGE('',*,*,#50552,.T.) ;
#71002 = ORIENTED_EDGE('',*,*,#50553,.T.) ;
#71003 = ORIENTED_EDGE('',*,*,#50554,.T.) ;
#71004 = ORIENTED_EDGE('',*,*,#50555,.T.) ;
#71005 = ORIENTED_EDGE('',*,*,#50556,.T.) ;
#71006 = ORIENTED_EDGE('',*,*,#50557,.T.) ;
#71007 = ORIENTED_EDGE('',*,*,#50558,.T.) ;
#71008 = ORIENTED_EDGE('',*,*,#50559,.T.) ;
#71009 = ORIENTED_EDGE('',*,*,#50560,.T.) ;
#71010 = ORIENTED_EDGE('',*,*,#50545,.T.) ;
#71011 = ORIENTED_EDGE('',*,*,#50561,.T.) ;
#71012 = ORIENTED_EDGE('',*,*,#50562,.T.) ;
#71013 = ORIENTED_EDGE('',*,*,#50563,.T.) ;
#71014 = ORIENTED_EDGE('',*,*,#50564,.T.) ;
#71015 = ORIENTED_EDGE('',*,*,#50565,.T.) ;
#71016 = ORIENTED_EDGE('',*,*,#50566,.T.) ;
#71017 = ORIENTED_EDGE('',*,*,#50567,.T.) ;
#71018 = ORIENTED_EDGE('',*,*,#50523,.T.) ;
#71019 = ORIENTED_EDGE('',*,*,#50568,.T.) ;
#71020 = ORIENTED_EDGE('',*,*,#50569,.T.) ;
#71021 = ORIENTED_EDGE('',*,*,#50570,.T.) ;
#71022 = ORIENTED_EDGE('',*,*,#50571,.T.) ;
#71023 = ORIENTED_EDGE('',*,*,#50572,.T.) ;
#71024 = ORIENTED_EDGE('',*,*,#50573,.T.) ;
#71025 = ORIENTED_EDGE('',*,*,#50574,.T.) ;
#71026 = ORIENTED_EDGE('',*,*,#50501,.T.) ;
#71027 = ORIENTED_EDGE('',*,*,#50575,.T.) ;
#71028 = ORIENTED_EDGE('',*,*,#50576,.T.) ;
#71029 = ORIENTED_EDGE('',*,*,#50577,.T.) ;
#71030 = ORIENTED_EDGE('',*,*,#50578,.T.) ;
#71031 = ORIENTED_EDGE('',*,*,#50579,.T.) ;
#71032 = ORIENTED_EDGE('',*,*,#50580,.T.) ;
#71033 = ORIENTED_EDGE('',*,*,#50581,.T.) ;
#71034 = ORIENTED_EDGE('',*,*,#50479,.T.) ;
#71035 = ORIENTED_EDGE('',*,*,#50582,.T.) ;
#71036 = ORIENTED_EDGE('',*,*,#50583,.T.) ;
#71037 = ORIENTED_EDGE('',*,*,#50584,.T.) ;
#71038 = ORIENTED_EDGE('',*,*,#50585,.T.) ;
#71039 = ORIENTED_EDGE('',*,*,#50586,.T.) ;
#71040 = ORIENTED_EDGE('',*,*,#50587,.T.) ;
#71041 = ORIENTED_EDGE('',*,*,#50588,.T.) ;
#71042 = ORIENTED_EDGE('',*,*,#50457,.T.) ;
#71043 = ORIENTED_EDGE('',*,*,#50589,.T.) ;
#71044 = ORIENTED_EDGE('',*,*,#50590,.T.) ;
#71045 = ORIENTED_EDGE('',*,*,#50591,.T.) ;
#71046 = ORIENTED_EDGE('',*,*,#50592,.T.) ;
#71047 = ORIENTED_EDGE('',*,*,#50593,.T.) ;
#71048 = ORIENTED_EDGE('',*,*,#50594,.T.) ;
#71049 = ORIENTED_EDGE('',*,*,#50595,.T.) ;
#71050 = ORIENTED_EDGE('',*,*,#50435,.T.) ;
#71051 = ORIENTED_EDGE('',*,*,#50596,.T.) ;
#71052 = ORIENTED_EDGE('',*,*,#50597,.T.) ;
#71053 = ORIENTED_EDGE('',*,*,#50598,.T.) ;
#71054 = ORIENTED_EDGE('',*,*,#50599,.T.) ;
#71055 = ORIENTED_EDGE('',*,*,#50600,.T.) ;
#71056 = ORIENTED_EDGE('',*,*,#50601,.T.) ;
#71057 = ORIENTED_EDGE('',*,*,#50602,.T.) ;
#71058 = ORIENTED_EDGE('',*,*,#50413,.T.) ;
#71059 = ORIENTED_EDGE('',*,*,#50603,.T.) ;
#71060 = ORIENTED_EDGE('',*,*,#50604,.T.) ;
#71061 = ORIENTED_EDGE('',*,*,#50605,.T.) ;
#71062 = ORIENTED_EDGE('',*,*,#50606,.T.) ;
#71063 = ORIENTED_EDGE('',*,*,#50607,.T.) ;
#71064 = ORIENTED_EDGE('',*,*,#50608,.T.) ;
#71065 = ORIENTED_EDGE('',*,*,#50609,.T.) ;
#71066 = ORIENTED_EDGE('',*,*,#50391,.T.) ;
#71067 = ORIENTED_EDGE('',*,*,#50610,.T.) ;
#71068 = ORIENTED_EDGE('',*,*,#50611,.T.) ;
#71069 = ORIENTED_EDGE('',*,*,#50612,.T.) ;
#71070 = ORIENTED_EDGE('',*,*,#50613,.T.) ;
#71071 = ORIENTED_EDGE('',*,*,#50614,.T.) ;
#71072 = ORIENTED_EDGE('',*,*,#50615,.T.) ;
#71073 = ORIENTED_EDGE('',*,*,#50616,.T.) ;
#71074 = ORIENTED_EDGE('',*,*,#50369,.T.) ;
#71075 = ORIENTED_EDGE('',*,*,#50617,.T.) ;
#71076 = ORIENTED_EDGE('',*,*,#50618,.T.) ;
#71077 = ORIENTED_EDGE('',*,*,#50619,.T.) ;
#71078 = ORIENTED_EDGE('',*,*,#50620,.T.) ;
#71079 = ORIENTED_EDGE('',*,*,#50621,.T.) ;
#71080 = ORIENTED_EDGE('',*,*,#50549,.F.) ;
#71081 = ORIENTED_EDGE('',*,*,#50622,.T.) ;
#71082 = ORIENTED_EDGE('',*,*,#50623,.T.) ;
#71083 = ORIENTED_EDGE('',*,*,#50624,.T.) ;
#71084 = ORIENTED_EDGE('',*,*,#50625,.T.) ;
#71085 = ORIENTED_EDGE('',*,*,#50626,.T.) ;
#71086 = ORIENTED_EDGE('',*,*,#50627,.T.) ;
#71087 = ORIENTED_EDGE('',*,*,#50628,.T.) ;
#71088 = ORIENTED_EDGE('',*,*,#50527,.F.) ;
#71089 = ORIENTED_EDGE('',*,*,#50629,.T.) ;
#71090 = ORIENTED_EDGE('',*,*,#50630,.T.) ;
#71091 = ORIENTED_EDGE('',*,*,#50631,.T.) ;
#71092 = ORIENTED_EDGE('',*,*,#50632,.T.) ;
#71093 = ORIENTED_EDGE('',*,*,#50633,.T.) ;
#71094 = ORIENTED_EDGE('',*,*,#50634,.T.) ;
#71095 = ORIENTED_EDGE('',*,*,#50635,.T.) ;
#71096 = ORIENTED_EDGE('',*,*,#50505,.F.) ;
#71097 = ORIENTED_EDGE('',*,*,#50636,.T.) ;
#71098 = ORIENTED_EDGE('',*,*,#50637,.T.) ;
#71099 = ORIENTED_EDGE('',*,*,#50638,.T.) ;
#71100 = ORIENTED_EDGE('',*,*,#50639,.T.) ;
#71101 = ORIENTED_EDGE('',*,*,#50640,.T.) ;
#71102 = ORIENTED_EDGE('',*,*,#50641,.T.) ;
#71103 = ORIENTED_EDGE('',*,*,#50642,.T.) ;
#71104 = ORIENTED_EDGE('',*,*,#50483,.F.) ;
#71105 = ORIENTED_EDGE('',*,*,#50643,.T.) ;
#71106 = ORIENTED_EDGE('',*,*,#50644,.T.) ;
#71107 = ORIENTED_EDGE('',*,*,#50645,.T.) ;
#71108 = ORIENTED_EDGE('',*,*,#50646,.T.) ;
#71109 = ORIENTED_EDGE('',*,*,#50647,.T.) ;
#71110 = ORIENTED_EDGE('',*,*,#50648,.T.) ;
#71111 = ORIENTED_EDGE('',*,*,#50649,.T.) ;
#71112 = ORIENTED_EDGE('',*,*,#50461,.F.) ;
#71113 = ORIENTED_EDGE('',*,*,#50650,.T.) ;
#71114 = ORIENTED_EDGE('',*,*,#50651,.T.) ;
#71115 = ORIENTED_EDGE('',*,*,#50652,.T.) ;
#71116 = ORIENTED_EDGE('',*,*,#50653,.T.) ;
#71117 = ORIENTED_EDGE('',*,*,#50654,.T.) ;
#71118 = ORIENTED_EDGE('',*,*,#50655,.T.) ;
#71119 = ORIENTED_EDGE('',*,*,#50656,.T.) ;
#71120 = ORIENTED_EDGE('',*,*,#50439,.F.) ;
#71121 = ORIENTED_EDGE('',*,*,#50657,.T.) ;
#71122 = ORIENTED_EDGE('',*,*,#50658,.T.) ;
#71123 = ORIENTED_EDGE('',*,*,#50659,.T.) ;
#71124 = ORIENTED_EDGE('',*,*,#50660,.T.) ;
#71125 = ORIENTED_EDGE('',*,*,#50661,.T.) ;
#71126 = ORIENTED_EDGE('',*,*,#50662,.T.) ;
#71127 = ORIENTED_EDGE('',*,*,#50663,.T.) ;
#71128 = ORIENTED_EDGE('',*,*,#50417,.F.) ;
#71129 = ORIENTED_EDGE('',*,*,#50664,.T.) ;
#71130 = ORIENTED_EDGE('',*,*,#50665,.T.) ;
#71131 = ORIENTED_EDGE('',*,*,#50666,.T.) ;
#71132 = ORIENTED_EDGE('',*,*,#50667,.T.) ;
#71133 = ORIENTED_EDGE('',*,*,#50668,.T.) ;
#71134 = ORIENTED_EDGE('',*,*,#50669,.T.) ;
#71135 = ORIENTED_EDGE('',*,*,#50670,.T.) ;
#71136 = ORIENTED_EDGE('',*,*,#50395,.F.) ;
#71137 = ORIENTED_EDGE('',*,*,#50671,.T.) ;
#71138 = ORIENTED_EDGE('',*,*,#50672,.T.) ;
#71139 = ORIENTED_EDGE('',*,*,#50673,.T.) ;
#71140 = ORIENTED_EDGE('',*,*,#50674,.T.) ;
#71141 = ORIENTED_EDGE('',*,*,#50675,.T.) ;
#71142 = ORIENTED_EDGE('',*,*,#50676,.T.) ;
#71143 = ORIENTED_EDGE('',*,*,#50677,.T.) ;
#71144 = ORIENTED_EDGE('',*,*,#50373,.F.) ;
#71145 = ORIENTED_EDGE('',*,*,#50678,.T.) ;
#71146 = ORIENTED_EDGE('',*,*,#50679,.T.) ;
#71147 = ORIENTED_EDGE('',*,*,#50680,.T.) ;
#71148 = ORIENTED_EDGE('',*,*,#50681,.T.) ;
#71149 = ORIENTED_EDGE('',*,*,#50682,.T.) ;
#71150 = ORIENTED_EDGE('',*,*,#50683,.T.) ;
#71151 = ORIENTED_EDGE('',*,*,#50684,.T.) ;
#71152 = ORIENTED_EDGE('',*,*,#50685,.T.) ;
#71153 = ORIENTED_EDGE('',*,*,#50686,.T.) ;
#71154 = ORIENTED_EDGE('',*,*,#50687,.T.) ;
#71155 = ORIENTED_EDGE('',*,*,#50688,.T.) ;
#71156 = ORIENTED_EDGE('',*,*,#50689,.T.) ;
#71157 = ORIENTED_EDGE('',*,*,#50690,.T.) ;
#71158 = ORIENTED_EDGE('',*,*,#50691,.T.) ;
#71159 = ORIENTED_EDGE('',*,*,#50692,.T.) ;
#71160 = ORIENTED_EDGE('',*,*,#50693,.T.) ;
#71161 = ORIENTED_EDGE('',*,*,#50694,.T.) ;
#71162 = ORIENTED_EDGE('',*,*,#50695,.T.) ;
#71163 = ORIENTED_EDGE('',*,*,#50696,.T.) ;
#71164 = ORIENTED_EDGE('',*,*,#50697,.T.) ;
#71165 = ORIENTED_EDGE('',*,*,#50698,.T.) ;
#71166 = ORIENTED_EDGE('',*,*,#50699,.T.) ;
#71167 = ORIENTED_EDGE('',*,*,#50700,.T.) ;
#71168 = ORIENTED_EDGE('',*,*,#50701,.T.) ;
#71169 = ORIENTED_EDGE('',*,*,#50702,.T.) ;
#71170 = ORIENTED_EDGE('',*,*,#50703,.T.) ;
#71171 = ORIENTED_EDGE('',*,*,#50704,.T.) ;
#71172 = ORIENTED_EDGE('',*,*,#50705,.T.) ;
#71173 = ORIENTED_EDGE('',*,*,#50706,.T.) ;
#71174 = ORIENTED_EDGE('',*,*,#50707,.T.) ;
#71175 = ORIENTED_EDGE('',*,*,#50708,.T.) ;
#71176 = ORIENTED_EDGE('',*,*,#50709,.T.) ;
#71177 = ORIENTED_EDGE('',*,*,#50710,.T.) ;
#71178 = ORIENTED_EDGE('',*,*,#50711,.T.) ;
#71179 = ORIENTED_EDGE('',*,*,#50712,.T.) ;
#71180 = ORIENTED_EDGE('',*,*,#50713,.T.) ;
#71181 = ORIENTED_EDGE('',*,*,#50714,.T.) ;
#71182 = ORIENTED_EDGE('',*,*,#50715,.T.) ;
#71183 = ORIENTED_EDGE('',*,*,#50716,.T.) ;
#71184 = ORIENTED_EDGE('',*,*,#50717,.T.) ;
#71185 = ORIENTED_EDGE('',*,*,#50718,.T.) ;
#71186 = ORIENTED_EDGE('',*,*,#50719,.T.) ;
#71187 = ORIENTED_EDGE('',*,*,#50720,.T.) ;
#71188 = ORIENTED_EDGE('',*,*,#50721,.T.) ;
#71189 = ORIENTED_EDGE('',*,*,#50722,.T.) ;
#71190 = ORIENTED_EDGE('',*,*,#50723,.T.) ;
#71191 = ORIENTED_EDGE('',*,*,#50724,.T.) ;
#71192 = ORIENTED_EDGE('',*,*,#50725,.T.) ;
#71193 = ORIENTED_EDGE('',*,*,#50726,.T.) ;
#71194 = ORIENTED_EDGE('',*,*,#50727,.T.) ;
#71195 = ORIENTED_EDGE('',*,*,#50728,.T.) ;
#71196 = ORIENTED_EDGE('',*,*,#50729,.T.) ;
#71197 = ORIENTED_EDGE('',*,*,#50730,.T.) ;
#71198 = ORIENTED_EDGE('',*,*,#50731,.T.) ;
#71199 = ORIENTED_EDGE('',*,*,#50732,.T.) ;
#71200 = ORIENTED_EDGE('',*,*,#50733,.T.) ;
#71201 = ORIENTED_EDGE('',*,*,#50734,.T.) ;
#71202 = ORIENTED_EDGE('',*,*,#50735,.T.) ;
#71203 = ORIENTED_EDGE('',*,*,#50736,.T.) ;
#71204 = ORIENTED_EDGE('',*,*,#50737,.T.) ;
#71205 = ORIENTED_EDGE('',*,*,#50738,.T.) ;
#71206 = ORIENTED_EDGE('',*,*,#50739,.T.) ;
#71207 = ORIENTED_EDGE('',*,*,#50740,.T.) ;
#71208 = ORIENTED_EDGE('',*,*,#50741,.T.) ;
#71209 = ORIENTED_EDGE('',*,*,#50742,.T.) ;
#71210 = ORIENTED_EDGE('',*,*,#50743,.T.) ;
#71211 = ORIENTED_EDGE('',*,*,#50744,.T.) ;
#71212 = ORIENTED_EDGE('',*,*,#50745,.T.) ;
#71213 = ORIENTED_EDGE('',*,*,#50746,.T.) ;
#71214 = ORIENTED_EDGE('',*,*,#50747,.T.) ;
#71215 = ORIENTED_EDGE('',*,*,#50748,.T.) ;
#71216 = ORIENTED_EDGE('',*,*,#50749,.T.) ;
#71217 = ORIENTED_EDGE('',*,*,#50750,.T.) ;
#71218 = ORIENTED_EDGE('',*,*,#50751,.T.) ;
#71219 = ORIENTED_EDGE('',*,*,#50752,.T.) ;
#71220 = ORIENTED_EDGE('',*,*,#50753,.T.) ;
#71221 = ORIENTED_EDGE('',*,*,#50754,.T.) ;
#71222 = ORIENTED_EDGE('',*,*,#50755,.T.) ;
#71223 = ORIENTED_EDGE('',*,*,#50756,.T.) ;
#71224 = ORIENTED_EDGE('',*,*,#50757,.T.) ;
#71225 = ORIENTED_EDGE('',*,*,#50758,.T.) ;
#71226 = ORIENTED_EDGE('',*,*,#50759,.T.) ;
#71227 = ORIENTED_EDGE('',*,*,#50760,.T.) ;
#71228 = ORIENTED_EDGE('',*,*,#50761,.T.) ;
#71229 = ORIENTED_EDGE('',*,*,#50762,.T.) ;
#71230 = ORIENTED_EDGE('',*,*,#50763,.T.) ;
#71231 = ORIENTED_EDGE('',*,*,#50764,.T.) ;
#71232 = ORIENTED_EDGE('',*,*,#50765,.T.) ;
#71233 = ORIENTED_EDGE('',*,*,#50766,.T.) ;
#71234 = ORIENTED_EDGE('',*,*,#50767,.T.) ;
#71235 = ORIENTED_EDGE('',*,*,#50768,.T.) ;
#71236 = ORIENTED_EDGE('',*,*,#50769,.T.) ;
#71237 = ORIENTED_EDGE('',*,*,#50770,.T.) ;
#71238 = ORIENTED_EDGE('',*,*,#50771,.T.) ;
#71239 = ORIENTED_EDGE('',*,*,#50772,.T.) ;
#71240 = ORIENTED_EDGE('',*,*,#50773,.T.) ;
#71241 = ORIENTED_EDGE('',*,*,#50774,.T.) ;
#71242 = ORIENTED_EDGE('',*,*,#50775,.T.) ;
#71243 = ORIENTED_EDGE('',*,*,#50776,.T.) ;
#71244 = ORIENTED_EDGE('',*,*,#50777,.T.) ;
#71245 = ORIENTED_EDGE('',*,*,#50778,.T.) ;
#71246 = ORIENTED_EDGE('',*,*,#50779,.T.) ;
#71247 = ORIENTED_EDGE('',*,*,#50780,.T.) ;
#71248 = ORIENTED_EDGE('',*,*,#50781,.T.) ;
#71249 = ORIENTED_EDGE('',*,*,#50782,.T.) ;
#71250 = ORIENTED_EDGE('',*,*,#50783,.T.) ;
#71251 = ORIENTED_EDGE('',*,*,#50784,.T.) ;
#71252 = ORIENTED_EDGE('',*,*,#50785,.T.) ;
#71253 = ORIENTED_EDGE('',*,*,#50786,.T.) ;
#71254 = ORIENTED_EDGE('',*,*,#50787,.T.) ;
#71255 = ORIENTED_EDGE('',*,*,#50788,.T.) ;
#71256 = ORIENTED_EDGE('',*,*,#50789,.T.) ;
#71257 = ORIENTED_EDGE('',*,*,#50790,.T.) ;
#71258 = ORIENTED_EDGE('',*,*,#50791,.T.) ;
#71259 = ORIENTED_EDGE('',*,*,#50792,.T.) ;
#71260 = ORIENTED_EDGE('',*,*,#50793,.T.) ;
#71261 = ORIENTED_EDGE('',*,*,#50794,.T.) ;
#71262 = ORIENTED_EDGE('',*,*,#50795,.T.) ;
#71263 = ORIENTED_EDGE('',*,*,#50796,.T.) ;
#71264 = ORIENTED_EDGE('',*,*,#50797,.T.) ;
#71265 = ORIENTED_EDGE('',*,*,#50798,.T.) ;
#71266 = ORIENTED_EDGE('',*,*,#50799,.T.) ;
#71267 = ORIENTED_EDGE('',*,*,#50800,.T.) ;
#71268 = ORIENTED_EDGE('',*,*,#50801,.T.) ;
#71269 = ORIENTED_EDGE('',*,*,#50802,.T.) ;
#71270 = ORIENTED_EDGE('',*,*,#50803,.T.) ;
#71271 = ORIENTED_EDGE('',*,*,#50804,.T.) ;
#71272 = ORIENTED_EDGE('',*,*,#50805,.T.) ;
#71273 = ORIENTED_EDGE('',*,*,#50806,.T.) ;
#71274 = ORIENTED_EDGE('',*,*,#50807,.T.) ;
#71275 = ORIENTED_EDGE('',*,*,#50808,.T.) ;
#71276 = ORIENTED_EDGE('',*,*,#50809,.T.) ;
#71277 = ORIENTED_EDGE('',*,*,#50810,.T.) ;
#71278 = ORIENTED_EDGE('',*,*,#50811,.T.) ;
#71279 = ORIENTED_EDGE('',*,*,#50812,.T.) ;
#71280 = ORIENTED_EDGE('',*,*,#50813,.T.) ;
#71281 = ORIENTED_EDGE('',*,*,#50814,.T.) ;
#71282 = ORIENTED_EDGE('',*,*,#50815,.T.) ;
#71283 = ORIENTED_EDGE('',*,*,#50816,.T.) ;
#71284 = ORIENTED_EDGE('',*,*,#50817,.T.) ;
#71285 = ORIENTED_EDGE('',*,*,#50818,.T.) ;
#71286 = ORIENTED_EDGE('',*,*,#50819,.T.) ;
#71287 = ORIENTED_EDGE('',*,*,#50820,.T.) ;
#71288 = ORIENTED_EDGE('',*,*,#50821,.T.) ;
#71289 = ORIENTED_EDGE('',*,*,#50822,.T.) ;
#71290 = ORIENTED_EDGE('',*,*,#50823,.T.) ;
#71291 = ORIENTED_EDGE('',*,*,#50824,.T.) ;
#71292 = ORIENTED_EDGE('',*,*,#50825,.T.) ;
#71293 = ORIENTED_EDGE('',*,*,#50826,.T.) ;
#71294 = ORIENTED_EDGE('',*,*,#50827,.T.) ;
#71295 = ORIENTED_EDGE('',*,*,#50828,.T.) ;
#71296 = ORIENTED_EDGE('',*,*,#50829,.F.) ;
#71297 = ORIENTED_EDGE('',*,*,#50830,.T.) ;
#71298 = ORIENTED_EDGE('',*,*,#50831,.F.) ;
#71299 = ORIENTED_EDGE('',*,*,#50832,.T.) ;
#71300 = ORIENTED_EDGE('',*,*,#50833,.F.) ;
#71301 = ORIENTED_EDGE('',*,*,#50834,.T.) ;
#71302 = ORIENTED_EDGE('',*,*,#50835,.F.) ;
#71303 = ORIENTED_EDGE('',*,*,#50836,.T.) ;
#71304 = ORIENTED_EDGE('',*,*,#50835,.T.) ;
#71305 = ORIENTED_EDGE('',*,*,#50837,.T.) ;
#71306 = ORIENTED_EDGE('',*,*,#50838,.T.) ;
#71307 = ORIENTED_EDGE('',*,*,#50839,.T.) ;
#71308 = ORIENTED_EDGE('',*,*,#50829,.T.) ;
#71309 = ORIENTED_EDGE('',*,*,#50840,.T.) ;
#71310 = ORIENTED_EDGE('',*,*,#50841,.T.) ;
#71311 = ORIENTED_EDGE('',*,*,#50842,.T.) ;
#71312 = ORIENTED_EDGE('',*,*,#50843,.T.) ;
#71313 = ORIENTED_EDGE('',*,*,#50844,.T.) ;
#71314 = ORIENTED_EDGE('',*,*,#50831,.T.) ;
#71315 = ORIENTED_EDGE('',*,*,#50845,.T.) ;
#71316 = ORIENTED_EDGE('',*,*,#50833,.T.) ;
#71317 = ORIENTED_EDGE('',*,*,#50846,.T.) ;
#71318 = ORIENTED_EDGE('',*,*,#50847,.T.) ;
#71319 = ORIENTED_EDGE('',*,*,#50848,.T.) ;
#71320 = ORIENTED_EDGE('',*,*,#50849,.T.) ;
#71321 = ORIENTED_EDGE('',*,*,#50850,.T.) ;
#71322 = ORIENTED_EDGE('',*,*,#50851,.T.) ;
#71323 = ORIENTED_EDGE('',*,*,#50852,.T.) ;
#71324 = ORIENTED_EDGE('',*,*,#50853,.F.) ;
#71325 = ORIENTED_EDGE('',*,*,#50854,.T.) ;
#71326 = ORIENTED_EDGE('',*,*,#50855,.F.) ;
#71327 = ORIENTED_EDGE('',*,*,#50856,.T.) ;
#71328 = ORIENTED_EDGE('',*,*,#50857,.F.) ;
#71329 = ORIENTED_EDGE('',*,*,#50858,.T.) ;
#71330 = ORIENTED_EDGE('',*,*,#50859,.F.) ;
#71331 = ORIENTED_EDGE('',*,*,#50860,.T.) ;
#71332 = ORIENTED_EDGE('',*,*,#50859,.T.) ;
#71333 = ORIENTED_EDGE('',*,*,#50861,.T.) ;
#71334 = ORIENTED_EDGE('',*,*,#50862,.T.) ;
#71335 = ORIENTED_EDGE('',*,*,#50863,.T.) ;
#71336 = ORIENTED_EDGE('',*,*,#50853,.T.) ;
#71337 = ORIENTED_EDGE('',*,*,#50864,.T.) ;
#71338 = ORIENTED_EDGE('',*,*,#50865,.T.) ;
#71339 = ORIENTED_EDGE('',*,*,#50866,.T.) ;
#71340 = ORIENTED_EDGE('',*,*,#50867,.T.) ;
#71341 = ORIENTED_EDGE('',*,*,#50868,.T.) ;
#71342 = ORIENTED_EDGE('',*,*,#50855,.T.) ;
#71343 = ORIENTED_EDGE('',*,*,#50869,.T.) ;
#71344 = ORIENTED_EDGE('',*,*,#50857,.T.) ;
#71345 = ORIENTED_EDGE('',*,*,#50870,.T.) ;
#71346 = ORIENTED_EDGE('',*,*,#50871,.T.) ;
#71347 = ORIENTED_EDGE('',*,*,#50872,.T.) ;
#71348 = ORIENTED_EDGE('',*,*,#50873,.T.) ;
#71349 = ORIENTED_EDGE('',*,*,#50874,.T.) ;
#71350 = ORIENTED_EDGE('',*,*,#50875,.T.) ;
#71351 = ORIENTED_EDGE('',*,*,#50876,.T.) ;
#71352 = ORIENTED_EDGE('',*,*,#50877,.F.) ;
#71353 = ORIENTED_EDGE('',*,*,#50878,.T.) ;
#71354 = ORIENTED_EDGE('',*,*,#50879,.F.) ;
#71355 = ORIENTED_EDGE('',*,*,#50880,.T.) ;
#71356 = ORIENTED_EDGE('',*,*,#50881,.F.) ;
#71357 = ORIENTED_EDGE('',*,*,#50882,.T.) ;
#71358 = ORIENTED_EDGE('',*,*,#50883,.F.) ;
#71359 = ORIENTED_EDGE('',*,*,#50884,.T.) ;
#71360 = ORIENTED_EDGE('',*,*,#50883,.T.) ;
#71361 = ORIENTED_EDGE('',*,*,#50885,.T.) ;
#71362 = ORIENTED_EDGE('',*,*,#50886,.T.) ;
#71363 = ORIENTED_EDGE('',*,*,#50887,.T.) ;
#71364 = ORIENTED_EDGE('',*,*,#50877,.T.) ;
#71365 = ORIENTED_EDGE('',*,*,#50888,.T.) ;
#71366 = ORIENTED_EDGE('',*,*,#50889,.T.) ;
#71367 = ORIENTED_EDGE('',*,*,#50890,.T.) ;
#71368 = ORIENTED_EDGE('',*,*,#50891,.T.) ;
#71369 = ORIENTED_EDGE('',*,*,#50892,.T.) ;
#71370 = ORIENTED_EDGE('',*,*,#50879,.T.) ;
#71371 = ORIENTED_EDGE('',*,*,#50893,.T.) ;
#71372 = ORIENTED_EDGE('',*,*,#50881,.T.) ;
#71373 = ORIENTED_EDGE('',*,*,#50894,.T.) ;
#71374 = ORIENTED_EDGE('',*,*,#50895,.T.) ;
#71375 = ORIENTED_EDGE('',*,*,#50896,.T.) ;
#71376 = ORIENTED_EDGE('',*,*,#50897,.T.) ;
#71377 = ORIENTED_EDGE('',*,*,#50898,.T.) ;
#71378 = ORIENTED_EDGE('',*,*,#50899,.T.) ;
#71379 = ORIENTED_EDGE('',*,*,#50900,.T.) ;
#71380 = ORIENTED_EDGE('',*,*,#50901,.F.) ;
#71381 = ORIENTED_EDGE('',*,*,#50902,.T.) ;
#71382 = ORIENTED_EDGE('',*,*,#50903,.F.) ;
#71383 = ORIENTED_EDGE('',*,*,#50904,.T.) ;
#71384 = ORIENTED_EDGE('',*,*,#50905,.F.) ;
#71385 = ORIENTED_EDGE('',*,*,#50906,.T.) ;
#71386 = ORIENTED_EDGE('',*,*,#50907,.F.) ;
#71387 = ORIENTED_EDGE('',*,*,#50908,.T.) ;
#71388 = ORIENTED_EDGE('',*,*,#50907,.T.) ;
#71389 = ORIENTED_EDGE('',*,*,#50909,.T.) ;
#71390 = ORIENTED_EDGE('',*,*,#50910,.T.) ;
#71391 = ORIENTED_EDGE('',*,*,#50911,.T.) ;
#71392 = ORIENTED_EDGE('',*,*,#50901,.T.) ;
#71393 = ORIENTED_EDGE('',*,*,#50912,.T.) ;
#71394 = ORIENTED_EDGE('',*,*,#50913,.T.) ;
#71395 = ORIENTED_EDGE('',*,*,#50914,.T.) ;
#71396 = ORIENTED_EDGE('',*,*,#50915,.T.) ;
#71397 = ORIENTED_EDGE('',*,*,#50916,.T.) ;
#71398 = ORIENTED_EDGE('',*,*,#50903,.T.) ;
#71399 = ORIENTED_EDGE('',*,*,#50917,.T.) ;
#71400 = ORIENTED_EDGE('',*,*,#50905,.T.) ;
#71401 = ORIENTED_EDGE('',*,*,#50918,.T.) ;
#71402 = ORIENTED_EDGE('',*,*,#50919,.T.) ;
#71403 = ORIENTED_EDGE('',*,*,#50920,.T.) ;
#71404 = ORIENTED_EDGE('',*,*,#50921,.T.) ;
#71405 = ORIENTED_EDGE('',*,*,#50922,.T.) ;
#71406 = ORIENTED_EDGE('',*,*,#50923,.T.) ;
#71407 = ORIENTED_EDGE('',*,*,#50924,.T.) ;
#71408 = ORIENTED_EDGE('',*,*,#50925,.F.) ;
#71409 = ORIENTED_EDGE('',*,*,#50926,.T.) ;
#71410 = ORIENTED_EDGE('',*,*,#50927,.F.) ;
#71411 = ORIENTED_EDGE('',*,*,#50928,.T.) ;
#71412 = ORIENTED_EDGE('',*,*,#50929,.F.) ;
#71413 = ORIENTED_EDGE('',*,*,#50930,.T.) ;
#71414 = ORIENTED_EDGE('',*,*,#50931,.F.) ;
#71415 = ORIENTED_EDGE('',*,*,#50932,.T.) ;
#71416 = ORIENTED_EDGE('',*,*,#50931,.T.) ;
#71417 = ORIENTED_EDGE('',*,*,#50933,.T.) ;
#71418 = ORIENTED_EDGE('',*,*,#50934,.T.) ;
#71419 = ORIENTED_EDGE('',*,*,#50935,.T.) ;
#71420 = ORIENTED_EDGE('',*,*,#50925,.T.) ;
#71421 = ORIENTED_EDGE('',*,*,#50936,.T.) ;
#71422 = ORIENTED_EDGE('',*,*,#50937,.T.) ;
#71423 = ORIENTED_EDGE('',*,*,#50938,.T.) ;
#71424 = ORIENTED_EDGE('',*,*,#50939,.T.) ;
#71425 = ORIENTED_EDGE('',*,*,#50940,.T.) ;
#71426 = ORIENTED_EDGE('',*,*,#50927,.T.) ;
#71427 = ORIENTED_EDGE('',*,*,#50941,.T.) ;
#71428 = ORIENTED_EDGE('',*,*,#50929,.T.) ;
#71429 = ORIENTED_EDGE('',*,*,#50942,.T.) ;
#71430 = ORIENTED_EDGE('',*,*,#50943,.T.) ;
#71431 = ORIENTED_EDGE('',*,*,#50944,.T.) ;
#71432 = ORIENTED_EDGE('',*,*,#50945,.T.) ;
#71433 = ORIENTED_EDGE('',*,*,#50946,.T.) ;
#71434 = ORIENTED_EDGE('',*,*,#50947,.T.) ;
#71435 = ORIENTED_EDGE('',*,*,#50948,.T.) ;
#71436 = ORIENTED_EDGE('',*,*,#50949,.F.) ;
#71437 = ORIENTED_EDGE('',*,*,#50950,.T.) ;
#71438 = ORIENTED_EDGE('',*,*,#50951,.F.) ;
#71439 = ORIENTED_EDGE('',*,*,#50952,.T.) ;
#71440 = ORIENTED_EDGE('',*,*,#50953,.F.) ;
#71441 = ORIENTED_EDGE('',*,*,#50954,.T.) ;
#71442 = ORIENTED_EDGE('',*,*,#50955,.F.) ;
#71443 = ORIENTED_EDGE('',*,*,#50956,.T.) ;
#71444 = ORIENTED_EDGE('',*,*,#50955,.T.) ;
#71445 = ORIENTED_EDGE('',*,*,#50957,.T.) ;
#71446 = ORIENTED_EDGE('',*,*,#50958,.T.) ;
#71447 = ORIENTED_EDGE('',*,*,#50959,.T.) ;
#71448 = ORIENTED_EDGE('',*,*,#50949,.T.) ;
#71449 = ORIENTED_EDGE('',*,*,#50960,.T.) ;
#71450 = ORIENTED_EDGE('',*,*,#50961,.T.) ;
#71451 = ORIENTED_EDGE('',*,*,#50962,.T.) ;
#71452 = ORIENTED_EDGE('',*,*,#50963,.T.) ;
#71453 = ORIENTED_EDGE('',*,*,#50964,.T.) ;
#71454 = ORIENTED_EDGE('',*,*,#50951,.T.) ;
#71455 = ORIENTED_EDGE('',*,*,#50965,.T.) ;
#71456 = ORIENTED_EDGE('',*,*,#50953,.T.) ;
#71457 = ORIENTED_EDGE('',*,*,#50966,.T.) ;
#71458 = ORIENTED_EDGE('',*,*,#50967,.T.) ;
#71459 = ORIENTED_EDGE('',*,*,#50968,.T.) ;
#71460 = ORIENTED_EDGE('',*,*,#50969,.T.) ;
#71461 = ORIENTED_EDGE('',*,*,#50970,.T.) ;
#71462 = ORIENTED_EDGE('',*,*,#50971,.T.) ;
#71463 = ORIENTED_EDGE('',*,*,#50972,.T.) ;
#71464 = ORIENTED_EDGE('',*,*,#50973,.F.) ;
#71465 = ORIENTED_EDGE('',*,*,#50974,.T.) ;
#71466 = ORIENTED_EDGE('',*,*,#50975,.F.) ;
#71467 = ORIENTED_EDGE('',*,*,#50976,.T.) ;
#71468 = ORIENTED_EDGE('',*,*,#50977,.F.) ;
#71469 = ORIENTED_EDGE('',*,*,#50978,.T.) ;
#71470 = ORIENTED_EDGE('',*,*,#50979,.F.) ;
#71471 = ORIENTED_EDGE('',*,*,#50980,.T.) ;
#71472 = ORIENTED_EDGE('',*,*,#50979,.T.) ;
#71473 = ORIENTED_EDGE('',*,*,#50981,.T.) ;
#71474 = ORIENTED_EDGE('',*,*,#50982,.T.) ;
#71475 = ORIENTED_EDGE('',*,*,#50983,.T.) ;
#71476 = ORIENTED_EDGE('',*,*,#50973,.T.) ;
#71477 = ORIENTED_EDGE('',*,*,#50984,.T.) ;
#71478 = ORIENTED_EDGE('',*,*,#50985,.T.) ;
#71479 = ORIENTED_EDGE('',*,*,#50986,.T.) ;
#71480 = ORIENTED_EDGE('',*,*,#50987,.T.) ;
#71481 = ORIENTED_EDGE('',*,*,#50988,.T.) ;
#71482 = ORIENTED_EDGE('',*,*,#50975,.T.) ;
#71483 = ORIENTED_EDGE('',*,*,#50989,.T.) ;
#71484 = ORIENTED_EDGE('',*,*,#50977,.T.) ;
#71485 = ORIENTED_EDGE('',*,*,#50990,.T.) ;
#71486 = ORIENTED_EDGE('',*,*,#50991,.T.) ;
#71487 = ORIENTED_EDGE('',*,*,#50992,.T.) ;
#71488 = ORIENTED_EDGE('',*,*,#50993,.T.) ;
#71489 = ORIENTED_EDGE('',*,*,#50994,.T.) ;
#71490 = ORIENTED_EDGE('',*,*,#50995,.T.) ;
#71491 = ORIENTED_EDGE('',*,*,#50996,.T.) ;
#71492 = ORIENTED_EDGE('',*,*,#50997,.F.) ;
#71493 = ORIENTED_EDGE('',*,*,#50998,.T.) ;
#71494 = ORIENTED_EDGE('',*,*,#50999,.F.) ;
#71495 = ORIENTED_EDGE('',*,*,#51000,.T.) ;
#71496 = ORIENTED_EDGE('',*,*,#51001,.F.) ;
#71497 = ORIENTED_EDGE('',*,*,#51002,.T.) ;
#71498 = ORIENTED_EDGE('',*,*,#51003,.F.) ;
#71499 = ORIENTED_EDGE('',*,*,#51004,.T.) ;
#71500 = ORIENTED_EDGE('',*,*,#51003,.T.) ;
#71501 = ORIENTED_EDGE('',*,*,#51005,.T.) ;
#71502 = ORIENTED_EDGE('',*,*,#51006,.T.) ;
#71503 = ORIENTED_EDGE('',*,*,#51007,.T.) ;
#71504 = ORIENTED_EDGE('',*,*,#50997,.T.) ;
#71505 = ORIENTED_EDGE('',*,*,#51008,.T.) ;
#71506 = ORIENTED_EDGE('',*,*,#51009,.T.) ;
#71507 = ORIENTED_EDGE('',*,*,#51010,.T.) ;
#71508 = ORIENTED_EDGE('',*,*,#51011,.T.) ;
#71509 = ORIENTED_EDGE('',*,*,#51012,.T.) ;
#71510 = ORIENTED_EDGE('',*,*,#50999,.T.) ;
#71511 = ORIENTED_EDGE('',*,*,#51013,.T.) ;
#71512 = ORIENTED_EDGE('',*,*,#51001,.T.) ;
#71513 = ORIENTED_EDGE('',*,*,#51014,.T.) ;
#71514 = ORIENTED_EDGE('',*,*,#51015,.T.) ;
#71515 = ORIENTED_EDGE('',*,*,#51016,.T.) ;
#71516 = ORIENTED_EDGE('',*,*,#51017,.T.) ;
#71517 = ORIENTED_EDGE('',*,*,#51018,.T.) ;
#71518 = ORIENTED_EDGE('',*,*,#51019,.T.) ;
#71519 = ORIENTED_EDGE('',*,*,#51020,.T.) ;
#71520 = ORIENTED_EDGE('',*,*,#51021,.F.) ;
#71521 = ORIENTED_EDGE('',*,*,#51022,.T.) ;
#71522 = ORIENTED_EDGE('',*,*,#51023,.F.) ;
#71523 = ORIENTED_EDGE('',*,*,#51024,.T.) ;
#71524 = ORIENTED_EDGE('',*,*,#51025,.F.) ;
#71525 = ORIENTED_EDGE('',*,*,#51026,.T.) ;
#71526 = ORIENTED_EDGE('',*,*,#51027,.F.) ;
#71527 = ORIENTED_EDGE('',*,*,#51028,.T.) ;
#71528 = ORIENTED_EDGE('',*,*,#51027,.T.) ;
#71529 = ORIENTED_EDGE('',*,*,#51029,.T.) ;
#71530 = ORIENTED_EDGE('',*,*,#51030,.T.) ;
#71531 = ORIENTED_EDGE('',*,*,#51031,.T.) ;
#71532 = ORIENTED_EDGE('',*,*,#51021,.T.) ;
#71533 = ORIENTED_EDGE('',*,*,#51032,.T.) ;
#71534 = ORIENTED_EDGE('',*,*,#51033,.T.) ;
#71535 = ORIENTED_EDGE('',*,*,#51034,.T.) ;
#71536 = ORIENTED_EDGE('',*,*,#51035,.T.) ;
#71537 = ORIENTED_EDGE('',*,*,#51036,.T.) ;
#71538 = ORIENTED_EDGE('',*,*,#51023,.T.) ;
#71539 = ORIENTED_EDGE('',*,*,#51037,.T.) ;
#71540 = ORIENTED_EDGE('',*,*,#51025,.T.) ;
#71541 = ORIENTED_EDGE('',*,*,#51038,.T.) ;
#71542 = ORIENTED_EDGE('',*,*,#51039,.T.) ;
#71543 = ORIENTED_EDGE('',*,*,#51040,.T.) ;
#71544 = ORIENTED_EDGE('',*,*,#51041,.T.) ;
#71545 = ORIENTED_EDGE('',*,*,#51042,.T.) ;
#71546 = ORIENTED_EDGE('',*,*,#51043,.T.) ;
#71547 = ORIENTED_EDGE('',*,*,#51044,.T.) ;
#71548 = ORIENTED_EDGE('',*,*,#51045,.T.) ;
#71549 = ORIENTED_EDGE('',*,*,#51046,.T.) ;
#71550 = ORIENTED_EDGE('',*,*,#51047,.T.) ;
#71551 = ORIENTED_EDGE('',*,*,#51048,.T.) ;
#71552 = ORIENTED_EDGE('',*,*,#51049,.T.) ;
#71553 = ORIENTED_EDGE('',*,*,#51050,.T.) ;
#71554 = ORIENTED_EDGE('',*,*,#51051,.T.) ;
#71555 = ORIENTED_EDGE('',*,*,#51052,.T.) ;
#71556 = ORIENTED_EDGE('',*,*,#51053,.T.) ;
#71557 = ORIENTED_EDGE('',*,*,#51054,.T.) ;
#71558 = ORIENTED_EDGE('',*,*,#51055,.T.) ;
#71559 = ORIENTED_EDGE('',*,*,#51056,.T.) ;
#71560 = ORIENTED_EDGE('',*,*,#51057,.T.) ;
#71561 = ORIENTED_EDGE('',*,*,#51058,.T.) ;
#71562 = ORIENTED_EDGE('',*,*,#51059,.T.) ;
#71563 = ORIENTED_EDGE('',*,*,#51060,.T.) ;
#71564 = ORIENTED_EDGE('',*,*,#51061,.T.) ;
#71565 = ORIENTED_EDGE('',*,*,#51062,.T.) ;
#71566 = ORIENTED_EDGE('',*,*,#51063,.T.) ;
#71567 = ORIENTED_EDGE('',*,*,#51064,.T.) ;
#71568 = ORIENTED_EDGE('',*,*,#51065,.T.) ;
#71569 = ORIENTED_EDGE('',*,*,#51066,.T.) ;
#71570 = ORIENTED_EDGE('',*,*,#51067,.T.) ;
#71571 = ORIENTED_EDGE('',*,*,#51068,.T.) ;
#71572 = ORIENTED_EDGE('',*,*,#51069,.T.) ;
#71573 = ORIENTED_EDGE('',*,*,#51070,.T.) ;
#71574 = ORIENTED_EDGE('',*,*,#51071,.T.) ;
#71575 = ORIENTED_EDGE('',*,*,#51072,.T.) ;
#71576 = ORIENTED_EDGE('',*,*,#51073,.T.) ;
#71577 = ORIENTED_EDGE('',*,*,#51074,.T.) ;
#71578 = ORIENTED_EDGE('',*,*,#51075,.T.) ;
#71579 = ORIENTED_EDGE('',*,*,#51076,.T.) ;
#71580 = ORIENTED_EDGE('',*,*,#51077,.T.) ;
#71581 = ORIENTED_EDGE('',*,*,#51078,.T.) ;
#71582 = ORIENTED_EDGE('',*,*,#51079,.T.) ;
#71583 = ORIENTED_EDGE('',*,*,#51080,.T.) ;
#71584 = ORIENTED_EDGE('',*,*,#51081,.T.) ;
#71585 = ORIENTED_EDGE('',*,*,#51082,.T.) ;
#71586 = ORIENTED_EDGE('',*,*,#51083,.F.) ;
#71587 = ORIENTED_EDGE('',*,*,#51084,.T.) ;
#71588 = ORIENTED_EDGE('',*,*,#51085,.T.) ;
#71589 = ORIENTED_EDGE('',*,*,#51086,.T.) ;
#71590 = ORIENTED_EDGE('',*,*,#51087,.T.) ;
#71591 = ORIENTED_EDGE('',*,*,#51088,.T.) ;
#71592 = ORIENTED_EDGE('',*,*,#51089,.T.) ;
#71593 = ORIENTED_EDGE('',*,*,#51090,.T.) ;
#71594 = ORIENTED_EDGE('',*,*,#51091,.T.) ;
#71595 = ORIENTED_EDGE('',*,*,#51092,.T.) ;
#71596 = ORIENTED_EDGE('',*,*,#51093,.T.) ;
#71597 = ORIENTED_EDGE('',*,*,#51094,.T.) ;
#71598 = ORIENTED_EDGE('',*,*,#51095,.T.) ;
#71599 = ORIENTED_EDGE('',*,*,#51096,.T.) ;
#71600 = ORIENTED_EDGE('',*,*,#51097,.F.) ;
#71601 = ORIENTED_EDGE('',*,*,#51098,.T.) ;
#71602 = ORIENTED_EDGE('',*,*,#51099,.T.) ;
#71603 = ORIENTED_EDGE('',*,*,#51100,.T.) ;
#71604 = ORIENTED_EDGE('',*,*,#51101,.T.) ;
#71605 = ORIENTED_EDGE('',*,*,#51102,.T.) ;
#71606 = ORIENTED_EDGE('',*,*,#51103,.T.) ;
#71607 = ORIENTED_EDGE('',*,*,#51104,.T.) ;
#71608 = ORIENTED_EDGE('',*,*,#51105,.T.) ;
#71609 = ORIENTED_EDGE('',*,*,#51106,.T.) ;
#71610 = ORIENTED_EDGE('',*,*,#51107,.T.) ;
#71611 = ORIENTED_EDGE('',*,*,#51108,.T.) ;
#71612 = ORIENTED_EDGE('',*,*,#51109,.T.) ;
#71613 = ORIENTED_EDGE('',*,*,#51110,.T.) ;
#71614 = ORIENTED_EDGE('',*,*,#51111,.F.) ;
#71615 = ORIENTED_EDGE('',*,*,#51112,.T.) ;
#71616 = ORIENTED_EDGE('',*,*,#51113,.T.) ;
#71617 = ORIENTED_EDGE('',*,*,#51114,.T.) ;
#71618 = ORIENTED_EDGE('',*,*,#51115,.T.) ;
#71619 = ORIENTED_EDGE('',*,*,#51116,.T.) ;
#71620 = ORIENTED_EDGE('',*,*,#51117,.T.) ;
#71621 = ORIENTED_EDGE('',*,*,#51118,.T.) ;
#71622 = ORIENTED_EDGE('',*,*,#51119,.T.) ;
#71623 = ORIENTED_EDGE('',*,*,#51120,.T.) ;
#71624 = ORIENTED_EDGE('',*,*,#51121,.T.) ;
#71625 = ORIENTED_EDGE('',*,*,#51122,.T.) ;
#71626 = ORIENTED_EDGE('',*,*,#51123,.T.) ;
#71627 = ORIENTED_EDGE('',*,*,#51124,.T.) ;
#71628 = ORIENTED_EDGE('',*,*,#51125,.F.) ;
#71629 = ORIENTED_EDGE('',*,*,#51126,.T.) ;
#71630 = ORIENTED_EDGE('',*,*,#51127,.T.) ;
#71631 = ORIENTED_EDGE('',*,*,#51128,.T.) ;
#71632 = ORIENTED_EDGE('',*,*,#51129,.T.) ;
#71633 = ORIENTED_EDGE('',*,*,#51130,.T.) ;
#71634 = ORIENTED_EDGE('',*,*,#51131,.T.) ;
#71635 = ORIENTED_EDGE('',*,*,#51132,.T.) ;
#71636 = ORIENTED_EDGE('',*,*,#51133,.T.) ;
#71637 = ORIENTED_EDGE('',*,*,#51134,.T.) ;
#71638 = ORIENTED_EDGE('',*,*,#51135,.T.) ;
#71639 = ORIENTED_EDGE('',*,*,#51136,.T.) ;
#71640 = ORIENTED_EDGE('',*,*,#51137,.T.) ;
#71641 = ORIENTED_EDGE('',*,*,#51138,.T.) ;
#71642 = ORIENTED_EDGE('',*,*,#51139,.F.) ;
#71643 = ORIENTED_EDGE('',*,*,#51140,.T.) ;
#71644 = ORIENTED_EDGE('',*,*,#51141,.T.) ;
#71645 = ORIENTED_EDGE('',*,*,#51142,.T.) ;
#71646 = ORIENTED_EDGE('',*,*,#51143,.T.) ;
#71647 = ORIENTED_EDGE('',*,*,#51144,.T.) ;
#71648 = ORIENTED_EDGE('',*,*,#51145,.T.) ;
#71649 = ORIENTED_EDGE('',*,*,#51146,.T.) ;
#71650 = ORIENTED_EDGE('',*,*,#51147,.T.) ;
#71651 = ORIENTED_EDGE('',*,*,#51148,.T.) ;
#71652 = ORIENTED_EDGE('',*,*,#51149,.T.) ;
#71653 = ORIENTED_EDGE('',*,*,#51150,.T.) ;
#71654 = ORIENTED_EDGE('',*,*,#51151,.T.) ;
#71655 = ORIENTED_EDGE('',*,*,#51152,.T.) ;
#71656 = ORIENTED_EDGE('',*,*,#51153,.F.) ;
#71657 = ORIENTED_EDGE('',*,*,#51154,.T.) ;
#71658 = ORIENTED_EDGE('',*,*,#51155,.T.) ;
#71659 = ORIENTED_EDGE('',*,*,#51156,.T.) ;
#71660 = ORIENTED_EDGE('',*,*,#51157,.T.) ;
#71661 = ORIENTED_EDGE('',*,*,#51158,.T.) ;
#71662 = ORIENTED_EDGE('',*,*,#51159,.T.) ;
#71663 = ORIENTED_EDGE('',*,*,#51160,.T.) ;
#71664 = ORIENTED_EDGE('',*,*,#51161,.T.) ;
#71665 = ORIENTED_EDGE('',*,*,#51162,.T.) ;
#71666 = ORIENTED_EDGE('',*,*,#51163,.T.) ;
#71667 = ORIENTED_EDGE('',*,*,#51164,.T.) ;
#71668 = ORIENTED_EDGE('',*,*,#51165,.T.) ;
#71669 = ORIENTED_EDGE('',*,*,#51166,.T.) ;
#71670 = ORIENTED_EDGE('',*,*,#51167,.F.) ;
#71671 = ORIENTED_EDGE('',*,*,#51168,.T.) ;
#71672 = ORIENTED_EDGE('',*,*,#51169,.T.) ;
#71673 = ORIENTED_EDGE('',*,*,#51170,.T.) ;
#71674 = ORIENTED_EDGE('',*,*,#51171,.T.) ;
#71675 = ORIENTED_EDGE('',*,*,#51172,.T.) ;
#71676 = ORIENTED_EDGE('',*,*,#51173,.T.) ;
#71677 = ORIENTED_EDGE('',*,*,#51174,.T.) ;
#71678 = ORIENTED_EDGE('',*,*,#51175,.T.) ;
#71679 = ORIENTED_EDGE('',*,*,#51176,.T.) ;
#71680 = ORIENTED_EDGE('',*,*,#51177,.T.) ;
#71681 = ORIENTED_EDGE('',*,*,#51178,.T.) ;
#71682 = ORIENTED_EDGE('',*,*,#51179,.T.) ;
#71683 = ORIENTED_EDGE('',*,*,#51180,.T.) ;
#71684 = ORIENTED_EDGE('',*,*,#51181,.F.) ;
#71685 = ORIENTED_EDGE('',*,*,#51182,.T.) ;
#71686 = ORIENTED_EDGE('',*,*,#51183,.T.) ;
#71687 = ORIENTED_EDGE('',*,*,#51184,.T.) ;
#71688 = ORIENTED_EDGE('',*,*,#51185,.T.) ;
#71689 = ORIENTED_EDGE('',*,*,#51186,.T.) ;
#71690 = ORIENTED_EDGE('',*,*,#51187,.T.) ;
#71691 = ORIENTED_EDGE('',*,*,#51188,.T.) ;
#71692 = ORIENTED_EDGE('',*,*,#51189,.T.) ;
#71693 = ORIENTED_EDGE('',*,*,#51190,.T.) ;
#71694 = ORIENTED_EDGE('',*,*,#51191,.T.) ;
#71695 = ORIENTED_EDGE('',*,*,#51192,.T.) ;
#71696 = ORIENTED_EDGE('',*,*,#51193,.T.) ;
#71697 = ORIENTED_EDGE('',*,*,#51194,.T.) ;
#71698 = ORIENTED_EDGE('',*,*,#51195,.F.) ;
#71699 = ORIENTED_EDGE('',*,*,#51196,.T.) ;
#71700 = ORIENTED_EDGE('',*,*,#51197,.T.) ;
#71701 = ORIENTED_EDGE('',*,*,#51198,.T.) ;
#71702 = ORIENTED_EDGE('',*,*,#51199,.T.) ;
#71703 = ORIENTED_EDGE('',*,*,#51200,.T.) ;
#71704 = ORIENTED_EDGE('',*,*,#51201,.T.) ;
#71705 = ORIENTED_EDGE('',*,*,#51202,.T.) ;
#71706 = ORIENTED_EDGE('',*,*,#51203,.T.) ;
#71707 = ORIENTED_EDGE('',*,*,#51204,.T.) ;
#71708 = ORIENTED_EDGE('',*,*,#51205,.T.) ;
#71709 = ORIENTED_EDGE('',*,*,#51206,.T.) ;
#71710 = ORIENTED_EDGE('',*,*,#51207,.T.) ;
#71711 = ORIENTED_EDGE('',*,*,#51208,.T.) ;
#71712 = ORIENTED_EDGE('',*,*,#51209,.F.) ;
#71713 = ORIENTED_EDGE('',*,*,#51210,.T.) ;
#71714 = ORIENTED_EDGE('',*,*,#51211,.T.) ;
#71715 = ORIENTED_EDGE('',*,*,#51212,.T.) ;
#71716 = ORIENTED_EDGE('',*,*,#51213,.T.) ;
#71717 = ORIENTED_EDGE('',*,*,#51214,.T.) ;
#71718 = ORIENTED_EDGE('',*,*,#51215,.T.) ;
#71719 = ORIENTED_EDGE('',*,*,#51216,.T.) ;
#71720 = ORIENTED_EDGE('',*,*,#51217,.T.) ;
#71721 = ORIENTED_EDGE('',*,*,#51218,.T.) ;
#71722 = ORIENTED_EDGE('',*,*,#51219,.T.) ;
#71723 = ORIENTED_EDGE('',*,*,#51220,.T.) ;
#71724 = ORIENTED_EDGE('',*,*,#51221,.T.) ;
#71725 = ORIENTED_EDGE('',*,*,#51222,.T.) ;
#71726 = ORIENTED_EDGE('',*,*,#51223,.F.) ;
#71727 = ORIENTED_EDGE('',*,*,#51224,.T.) ;
#71728 = ORIENTED_EDGE('',*,*,#51225,.T.) ;
#71729 = ORIENTED_EDGE('',*,*,#51226,.T.) ;
#71730 = ORIENTED_EDGE('',*,*,#51227,.T.) ;
#71731 = ORIENTED_EDGE('',*,*,#51228,.T.) ;
#71732 = ORIENTED_EDGE('',*,*,#51229,.T.) ;
#71733 = ORIENTED_EDGE('',*,*,#51230,.T.) ;
#71734 = ORIENTED_EDGE('',*,*,#51231,.T.) ;
#71735 = ORIENTED_EDGE('',*,*,#51232,.T.) ;
#71736 = ORIENTED_EDGE('',*,*,#51233,.T.) ;
#71737 = ORIENTED_EDGE('',*,*,#51234,.T.) ;
#71738 = ORIENTED_EDGE('',*,*,#51235,.T.) ;
#71739 = ORIENTED_EDGE('',*,*,#51236,.T.) ;
#71740 = ORIENTED_EDGE('',*,*,#51237,.F.) ;
#71741 = ORIENTED_EDGE('',*,*,#51238,.T.) ;
#71742 = ORIENTED_EDGE('',*,*,#51239,.T.) ;
#71743 = ORIENTED_EDGE('',*,*,#51240,.T.) ;
#71744 = ORIENTED_EDGE('',*,*,#51241,.T.) ;
#71745 = ORIENTED_EDGE('',*,*,#51242,.T.) ;
#71746 = ORIENTED_EDGE('',*,*,#51243,.T.) ;
#71747 = ORIENTED_EDGE('',*,*,#51244,.T.) ;
#71748 = ORIENTED_EDGE('',*,*,#51245,.T.) ;
#71749 = ORIENTED_EDGE('',*,*,#51246,.T.) ;
#71750 = ORIENTED_EDGE('',*,*,#51247,.T.) ;
#71751 = ORIENTED_EDGE('',*,*,#51248,.T.) ;
#71752 = ORIENTED_EDGE('',*,*,#51249,.T.) ;
#71753 = ORIENTED_EDGE('',*,*,#51250,.T.) ;
#71754 = ORIENTED_EDGE('',*,*,#51251,.F.) ;
#71755 = ORIENTED_EDGE('',*,*,#51252,.T.) ;
#71756 = ORIENTED_EDGE('',*,*,#51253,.T.) ;
#71757 = ORIENTED_EDGE('',*,*,#51254,.T.) ;
#71758 = ORIENTED_EDGE('',*,*,#51255,.T.) ;
#71759 = ORIENTED_EDGE('',*,*,#51256,.T.) ;
#71760 = ORIENTED_EDGE('',*,*,#51257,.T.) ;
#71761 = ORIENTED_EDGE('',*,*,#51258,.T.) ;
#71762 = ORIENTED_EDGE('',*,*,#51259,.T.) ;
#71763 = ORIENTED_EDGE('',*,*,#51260,.T.) ;
#71764 = ORIENTED_EDGE('',*,*,#51261,.T.) ;
#71765 = ORIENTED_EDGE('',*,*,#51262,.T.) ;
#71766 = ORIENTED_EDGE('',*,*,#51263,.T.) ;
#71767 = ORIENTED_EDGE('',*,*,#51264,.T.) ;
#71768 = ORIENTED_EDGE('',*,*,#51265,.F.) ;
#71769 = ORIENTED_EDGE('',*,*,#51266,.T.) ;
#71770 = ORIENTED_EDGE('',*,*,#51267,.T.) ;
#71771 = ORIENTED_EDGE('',*,*,#51268,.T.) ;
#71772 = ORIENTED_EDGE('',*,*,#51269,.T.) ;
#71773 = ORIENTED_EDGE('',*,*,#51270,.T.) ;
#71774 = ORIENTED_EDGE('',*,*,#51271,.T.) ;
#71775 = ORIENTED_EDGE('',*,*,#51272,.T.) ;
#71776 = ORIENTED_EDGE('',*,*,#51273,.T.) ;
#71777 = ORIENTED_EDGE('',*,*,#51274,.T.) ;
#71778 = ORIENTED_EDGE('',*,*,#51275,.T.) ;
#71779 = ORIENTED_EDGE('',*,*,#51276,.T.) ;
#71780 = ORIENTED_EDGE('',*,*,#51277,.T.) ;
#71781 = ORIENTED_EDGE('',*,*,#51278,.T.) ;
#71782 = ORIENTED_EDGE('',*,*,#51279,.F.) ;
#71783 = ORIENTED_EDGE('',*,*,#51280,.T.) ;
#71784 = ORIENTED_EDGE('',*,*,#51281,.T.) ;
#71785 = ORIENTED_EDGE('',*,*,#51282,.T.) ;
#71786 = ORIENTED_EDGE('',*,*,#51283,.T.) ;
#71787 = ORIENTED_EDGE('',*,*,#51284,.T.) ;
#71788 = ORIENTED_EDGE('',*,*,#51285,.T.) ;
#71789 = ORIENTED_EDGE('',*,*,#51286,.T.) ;
#71790 = ORIENTED_EDGE('',*,*,#51287,.T.) ;
#71791 = ORIENTED_EDGE('',*,*,#51288,.T.) ;
#71792 = ORIENTED_EDGE('',*,*,#51289,.T.) ;
#71793 = ORIENTED_EDGE('',*,*,#51290,.T.) ;
#71794 = ORIENTED_EDGE('',*,*,#51291,.T.) ;
#71795 = ORIENTED_EDGE('',*,*,#51292,.T.) ;
#71796 = ORIENTED_EDGE('',*,*,#51293,.F.) ;
#71797 = ORIENTED_EDGE('',*,*,#51294,.T.) ;
#71798 = ORIENTED_EDGE('',*,*,#51295,.T.) ;
#71799 = ORIENTED_EDGE('',*,*,#51296,.T.) ;
#71800 = ORIENTED_EDGE('',*,*,#51297,.T.) ;
#71801 = ORIENTED_EDGE('',*,*,#51298,.T.) ;
#71802 = ORIENTED_EDGE('',*,*,#51299,.T.) ;
#71803 = ORIENTED_EDGE('',*,*,#51300,.T.) ;
#71804 = ORIENTED_EDGE('',*,*,#51301,.T.) ;
#71805 = ORIENTED_EDGE('',*,*,#51302,.T.) ;
#71806 = ORIENTED_EDGE('',*,*,#51303,.T.) ;
#71807 = ORIENTED_EDGE('',*,*,#51304,.T.) ;
#71808 = ORIENTED_EDGE('',*,*,#51305,.T.) ;
#71809 = ORIENTED_EDGE('',*,*,#51306,.T.) ;
#71810 = ORIENTED_EDGE('',*,*,#51307,.F.) ;
#71811 = ORIENTED_EDGE('',*,*,#51308,.T.) ;
#71812 = ORIENTED_EDGE('',*,*,#51309,.T.) ;
#71813 = ORIENTED_EDGE('',*,*,#51310,.T.) ;
#71814 = ORIENTED_EDGE('',*,*,#51311,.T.) ;
#71815 = ORIENTED_EDGE('',*,*,#51312,.T.) ;
#71816 = ORIENTED_EDGE('',*,*,#51313,.T.) ;
#71817 = ORIENTED_EDGE('',*,*,#51314,.T.) ;
#71818 = ORIENTED_EDGE('',*,*,#51315,.T.) ;
#71819 = ORIENTED_EDGE('',*,*,#51316,.T.) ;
#71820 = ORIENTED_EDGE('',*,*,#51317,.T.) ;
#71821 = ORIENTED_EDGE('',*,*,#51318,.T.) ;
#71822 = ORIENTED_EDGE('',*,*,#51319,.T.) ;
#71823 = ORIENTED_EDGE('',*,*,#51320,.T.) ;
#71824 = ORIENTED_EDGE('',*,*,#51321,.F.) ;
#71825 = ORIENTED_EDGE('',*,*,#51322,.T.) ;
#71826 = ORIENTED_EDGE('',*,*,#51323,.T.) ;
#71827 = ORIENTED_EDGE('',*,*,#51324,.T.) ;
#71828 = ORIENTED_EDGE('',*,*,#51325,.T.) ;
#71829 = ORIENTED_EDGE('',*,*,#51326,.T.) ;
#71830 = ORIENTED_EDGE('',*,*,#51327,.T.) ;
#71831 = ORIENTED_EDGE('',*,*,#51328,.T.) ;
#71832 = ORIENTED_EDGE('',*,*,#51329,.T.) ;
#71833 = ORIENTED_EDGE('',*,*,#51330,.T.) ;
#71834 = ORIENTED_EDGE('',*,*,#51331,.T.) ;
#71835 = ORIENTED_EDGE('',*,*,#51332,.T.) ;
#71836 = ORIENTED_EDGE('',*,*,#51333,.T.) ;
#71837 = ORIENTED_EDGE('',*,*,#51334,.T.) ;
#71838 = ORIENTED_EDGE('',*,*,#51335,.T.) ;
#71839 = ORIENTED_EDGE('',*,*,#51336,.T.) ;
#71840 = ORIENTED_EDGE('',*,*,#51337,.T.) ;
#71841 = ORIENTED_EDGE('',*,*,#51338,.T.) ;
#71842 = ORIENTED_EDGE('',*,*,#51339,.T.) ;
#71843 = ORIENTED_EDGE('',*,*,#51340,.T.) ;
#71844 = ORIENTED_EDGE('',*,*,#51341,.T.) ;
#71845 = ORIENTED_EDGE('',*,*,#51342,.T.) ;
#71846 = ORIENTED_EDGE('',*,*,#51343,.T.) ;
#71847 = ORIENTED_EDGE('',*,*,#51344,.T.) ;
#71848 = ORIENTED_EDGE('',*,*,#51345,.T.) ;
#71849 = ORIENTED_EDGE('',*,*,#51346,.T.) ;
#71850 = ORIENTED_EDGE('',*,*,#49086,.T.) ;
#71851 = ORIENTED_EDGE('',*,*,#51347,.T.) ;
#71852 = ORIENTED_EDGE('',*,*,#51348,.T.) ;
#71853 = ORIENTED_EDGE('',*,*,#51349,.T.) ;
#71854 = ORIENTED_EDGE('',*,*,#51350,.T.) ;
#71855 = ORIENTED_EDGE('',*,*,#51351,.T.) ;
#71856 = ORIENTED_EDGE('',*,*,#51352,.T.) ;
#71857 = ORIENTED_EDGE('',*,*,#51353,.T.) ;
#71858 = ORIENTED_EDGE('',*,*,#51354,.T.) ;
#71859 = ORIENTED_EDGE('',*,*,#51355,.T.) ;
#71860 = ORIENTED_EDGE('',*,*,#51356,.T.) ;
#71861 = ORIENTED_EDGE('',*,*,#51357,.T.) ;
#71862 = ORIENTED_EDGE('',*,*,#51358,.T.) ;
#71863 = ORIENTED_EDGE('',*,*,#51359,.T.) ;
#71864 = ORIENTED_EDGE('',*,*,#51360,.T.) ;
#71865 = ORIENTED_EDGE('',*,*,#51361,.T.) ;
#71866 = ORIENTED_EDGE('',*,*,#51362,.T.) ;
#71867 = ORIENTED_EDGE('',*,*,#51363,.T.) ;
#71868 = ORIENTED_EDGE('',*,*,#51364,.T.) ;
#71869 = ORIENTED_EDGE('',*,*,#49077,.T.) ;
#71870 = ORIENTED_EDGE('',*,*,#51365,.T.) ;
#71871 = ORIENTED_EDGE('',*,*,#51366,.T.) ;
#71872 = ORIENTED_EDGE('',*,*,#51367,.T.) ;
#71873 = ORIENTED_EDGE('',*,*,#51368,.T.) ;
#71874 = ORIENTED_EDGE('',*,*,#51369,.T.) ;
#71875 = ORIENTED_EDGE('',*,*,#51370,.T.) ;
#71876 = ORIENTED_EDGE('',*,*,#51371,.T.) ;
#71877 = ORIENTED_EDGE('',*,*,#51372,.T.) ;
#71878 = ORIENTED_EDGE('',*,*,#51373,.T.) ;
#71879 = ORIENTED_EDGE('',*,*,#51374,.T.) ;
#71880 = ORIENTED_EDGE('',*,*,#51375,.T.) ;
#71881 = ORIENTED_EDGE('',*,*,#51376,.T.) ;
#71882 = ORIENTED_EDGE('',*,*,#51377,.T.) ;
#71883 = ORIENTED_EDGE('',*,*,#51378,.T.) ;
#71884 = ORIENTED_EDGE('',*,*,#51379,.T.) ;
#71885 = ORIENTED_EDGE('',*,*,#51380,.T.) ;
#71886 = ORIENTED_EDGE('',*,*,#51381,.T.) ;
#71887 = ORIENTED_EDGE('',*,*,#51382,.T.) ;
#71888 = ORIENTED_EDGE('',*,*,#49068,.T.) ;
#71889 = ORIENTED_EDGE('',*,*,#51383,.T.) ;
#71890 = ORIENTED_EDGE('',*,*,#51384,.T.) ;
#71891 = ORIENTED_EDGE('',*,*,#51385,.T.) ;
#71892 = ORIENTED_EDGE('',*,*,#51386,.T.) ;
#71893 = ORIENTED_EDGE('',*,*,#51387,.T.) ;
#71894 = ORIENTED_EDGE('',*,*,#51388,.T.) ;
#71895 = ORIENTED_EDGE('',*,*,#51389,.T.) ;
#71896 = ORIENTED_EDGE('',*,*,#51390,.T.) ;
#71897 = ORIENTED_EDGE('',*,*,#51391,.T.) ;
#71898 = ORIENTED_EDGE('',*,*,#51392,.T.) ;
#71899 = ORIENTED_EDGE('',*,*,#51393,.T.) ;
#71900 = ORIENTED_EDGE('',*,*,#51394,.T.) ;
#71901 = ORIENTED_EDGE('',*,*,#51395,.T.) ;
#71902 = ORIENTED_EDGE('',*,*,#51396,.T.) ;
#71903 = ORIENTED_EDGE('',*,*,#51397,.T.) ;
#71904 = ORIENTED_EDGE('',*,*,#51398,.T.) ;
#71905 = ORIENTED_EDGE('',*,*,#51399,.T.) ;
#71906 = ORIENTED_EDGE('',*,*,#51400,.T.) ;
#71907 = ORIENTED_EDGE('',*,*,#49059,.T.) ;
#71908 = ORIENTED_EDGE('',*,*,#51401,.T.) ;
#71909 = ORIENTED_EDGE('',*,*,#51402,.T.) ;
#71910 = ORIENTED_EDGE('',*,*,#51403,.T.) ;
#71911 = ORIENTED_EDGE('',*,*,#51404,.T.) ;
#71912 = ORIENTED_EDGE('',*,*,#51405,.T.) ;
#71913 = ORIENTED_EDGE('',*,*,#51406,.T.) ;
#71914 = ORIENTED_EDGE('',*,*,#51407,.T.) ;
#71915 = ORIENTED_EDGE('',*,*,#51408,.T.) ;
#71916 = ORIENTED_EDGE('',*,*,#51409,.T.) ;
#71917 = ORIENTED_EDGE('',*,*,#51410,.T.) ;
#71918 = ORIENTED_EDGE('',*,*,#51411,.T.) ;
#71919 = ORIENTED_EDGE('',*,*,#51412,.T.) ;
#71920 = ORIENTED_EDGE('',*,*,#51413,.T.) ;
#71921 = ORIENTED_EDGE('',*,*,#51414,.T.) ;
#71922 = ORIENTED_EDGE('',*,*,#51415,.T.) ;
#71923 = ORIENTED_EDGE('',*,*,#51416,.T.) ;
#71924 = ORIENTED_EDGE('',*,*,#51417,.T.) ;
#71925 = ORIENTED_EDGE('',*,*,#51418,.T.) ;
#71926 = ORIENTED_EDGE('',*,*,#49050,.T.) ;
#71927 = ORIENTED_EDGE('',*,*,#51419,.T.) ;
#71928 = ORIENTED_EDGE('',*,*,#51420,.T.) ;
#71929 = ORIENTED_EDGE('',*,*,#51421,.T.) ;
#71930 = ORIENTED_EDGE('',*,*,#51422,.T.) ;
#71931 = ORIENTED_EDGE('',*,*,#51423,.T.) ;
#71932 = ORIENTED_EDGE('',*,*,#51424,.T.) ;
#71933 = ORIENTED_EDGE('',*,*,#51425,.T.) ;
#71934 = ORIENTED_EDGE('',*,*,#51426,.T.) ;
#71935 = ORIENTED_EDGE('',*,*,#51427,.T.) ;
#71936 = ORIENTED_EDGE('',*,*,#51428,.T.) ;
#71937 = ORIENTED_EDGE('',*,*,#51429,.T.) ;
#71938 = ORIENTED_EDGE('',*,*,#51430,.T.) ;
#71939 = ORIENTED_EDGE('',*,*,#51431,.T.) ;
#71940 = ORIENTED_EDGE('',*,*,#51432,.T.) ;
#71941 = ORIENTED_EDGE('',*,*,#51433,.T.) ;
#71942 = ORIENTED_EDGE('',*,*,#51434,.T.) ;
#71943 = ORIENTED_EDGE('',*,*,#51435,.T.) ;
#71944 = ORIENTED_EDGE('',*,*,#51436,.T.) ;
#71945 = ORIENTED_EDGE('',*,*,#49041,.T.) ;
#71946 = ORIENTED_EDGE('',*,*,#51437,.T.) ;
#71947 = ORIENTED_EDGE('',*,*,#51438,.T.) ;
#71948 = ORIENTED_EDGE('',*,*,#51439,.T.) ;
#71949 = ORIENTED_EDGE('',*,*,#51440,.T.) ;
#71950 = ORIENTED_EDGE('',*,*,#51441,.T.) ;
#71951 = ORIENTED_EDGE('',*,*,#51442,.T.) ;
#71952 = ORIENTED_EDGE('',*,*,#51443,.T.) ;
#71953 = ORIENTED_EDGE('',*,*,#51444,.T.) ;
#71954 = ORIENTED_EDGE('',*,*,#51445,.T.) ;
#71955 = ORIENTED_EDGE('',*,*,#51446,.T.) ;
#71956 = ORIENTED_EDGE('',*,*,#51447,.T.) ;
#71957 = ORIENTED_EDGE('',*,*,#51448,.T.) ;
#71958 = ORIENTED_EDGE('',*,*,#51449,.T.) ;
#71959 = ORIENTED_EDGE('',*,*,#51450,.T.) ;
#71960 = ORIENTED_EDGE('',*,*,#51451,.T.) ;
#71961 = ORIENTED_EDGE('',*,*,#51452,.T.) ;
#71962 = ORIENTED_EDGE('',*,*,#51453,.T.) ;
#71963 = ORIENTED_EDGE('',*,*,#51454,.T.) ;
#71964 = ORIENTED_EDGE('',*,*,#49032,.T.) ;
#71965 = ORIENTED_EDGE('',*,*,#51455,.T.) ;
#71966 = ORIENTED_EDGE('',*,*,#51456,.T.) ;
#71967 = ORIENTED_EDGE('',*,*,#51457,.T.) ;
#71968 = ORIENTED_EDGE('',*,*,#51458,.T.) ;
#71969 = ORIENTED_EDGE('',*,*,#51459,.T.) ;
#71970 = ORIENTED_EDGE('',*,*,#51460,.T.) ;
#71971 = ORIENTED_EDGE('',*,*,#51461,.T.) ;
#71972 = ORIENTED_EDGE('',*,*,#51462,.T.) ;
#71973 = ORIENTED_EDGE('',*,*,#51463,.T.) ;
#71974 = ORIENTED_EDGE('',*,*,#51464,.T.) ;
#71975 = ORIENTED_EDGE('',*,*,#51465,.T.) ;
#71976 = ORIENTED_EDGE('',*,*,#51466,.T.) ;
#71977 = ORIENTED_EDGE('',*,*,#51467,.T.) ;
#71978 = ORIENTED_EDGE('',*,*,#51468,.T.) ;
#71979 = ORIENTED_EDGE('',*,*,#51469,.T.) ;
#71980 = ORIENTED_EDGE('',*,*,#51470,.T.) ;
#71981 = ORIENTED_EDGE('',*,*,#51471,.T.) ;
#71982 = ORIENTED_EDGE('',*,*,#51472,.T.) ;
#71983 = ORIENTED_EDGE('',*,*,#49023,.T.) ;
#71984 = ORIENTED_EDGE('',*,*,#51473,.T.) ;
#71985 = ORIENTED_EDGE('',*,*,#51474,.T.) ;
#71986 = ORIENTED_EDGE('',*,*,#51475,.T.) ;
#71987 = ORIENTED_EDGE('',*,*,#51476,.T.) ;
#71988 = ORIENTED_EDGE('',*,*,#51477,.T.) ;
#71989 = ORIENTED_EDGE('',*,*,#51478,.T.) ;
#71990 = ORIENTED_EDGE('',*,*,#51479,.T.) ;
#71991 = ORIENTED_EDGE('',*,*,#51480,.T.) ;
#71992 = ORIENTED_EDGE('',*,*,#51481,.T.) ;
#71993 = ORIENTED_EDGE('',*,*,#51482,.T.) ;
#71994 = ORIENTED_EDGE('',*,*,#51483,.T.) ;
#71995 = ORIENTED_EDGE('',*,*,#51484,.T.) ;
#71996 = ORIENTED_EDGE('',*,*,#51485,.T.) ;
#71997 = ORIENTED_EDGE('',*,*,#51486,.T.) ;
#71998 = ORIENTED_EDGE('',*,*,#51487,.T.) ;
#71999 = ORIENTED_EDGE('',*,*,#51488,.T.) ;
#72000 = ORIENTED_EDGE('',*,*,#51489,.T.) ;
#72001 = ORIENTED_EDGE('',*,*,#51490,.T.) ;
#72002 = ORIENTED_EDGE('',*,*,#49014,.T.) ;
#72003 = ORIENTED_EDGE('',*,*,#49265,.T.) ;
#72004 = ORIENTED_EDGE('',*,*,#49263,.T.) ;
#72005 = ORIENTED_EDGE('',*,*,#49261,.T.) ;
#72006 = ORIENTED_EDGE('',*,*,#49259,.T.) ;
#72007 = ORIENTED_EDGE('',*,*,#49257,.T.) ;
#72008 = ORIENTED_EDGE('',*,*,#49255,.T.) ;
#72009 = ORIENTED_EDGE('',*,*,#49253,.T.) ;
#72010 = ORIENTED_EDGE('',*,*,#49251,.T.) ;
#72011 = ORIENTED_EDGE('',*,*,#49249,.T.) ;
#72012 = ORIENTED_EDGE('',*,*,#51491,.T.) ;
#72013 = ORIENTED_EDGE('',*,*,#51492,.T.) ;
#72014 = ORIENTED_EDGE('',*,*,#51493,.T.) ;
#72015 = ORIENTED_EDGE('',*,*,#51494,.T.) ;
#72016 = ORIENTED_EDGE('',*,*,#51495,.T.) ;
#72017 = ORIENTED_EDGE('',*,*,#51496,.T.) ;
#72018 = ORIENTED_EDGE('',*,*,#51497,.T.) ;
#72019 = ORIENTED_EDGE('',*,*,#51498,.T.) ;
#72020 = ORIENTED_EDGE('',*,*,#51499,.T.) ;
#72021 = ORIENTED_EDGE('',*,*,#51500,.T.) ;
#72022 = ORIENTED_EDGE('',*,*,#51501,.T.) ;
#72023 = ORIENTED_EDGE('',*,*,#51502,.T.) ;
#72024 = ORIENTED_EDGE('',*,*,#51503,.T.) ;
#72025 = ORIENTED_EDGE('',*,*,#51504,.T.) ;
#72026 = ORIENTED_EDGE('',*,*,#51505,.T.) ;
#72027 = ORIENTED_EDGE('',*,*,#51506,.T.) ;
#72028 = ORIENTED_EDGE('',*,*,#51507,.T.) ;
#72029 = ORIENTED_EDGE('',*,*,#51508,.T.) ;
#72030 = ORIENTED_EDGE('',*,*,#51509,.T.) ;
#72031 = ORIENTED_EDGE('',*,*,#51510,.T.) ;
#72032 = ORIENTED_EDGE('',*,*,#51511,.T.) ;
#72033 = ORIENTED_EDGE('',*,*,#51512,.T.) ;
#72034 = ORIENTED_EDGE('',*,*,#51513,.T.) ;
#72035 = ORIENTED_EDGE('',*,*,#51514,.T.) ;
#72036 = ORIENTED_EDGE('',*,*,#51515,.T.) ;
#72037 = ORIENTED_EDGE('',*,*,#51516,.T.) ;
#72038 = ORIENTED_EDGE('',*,*,#51517,.T.) ;
#72039 = ORIENTED_EDGE('',*,*,#51518,.T.) ;
#72040 = ORIENTED_EDGE('',*,*,#51519,.T.) ;
#72041 = ORIENTED_EDGE('',*,*,#51520,.T.) ;
#72042 = ORIENTED_EDGE('',*,*,#51521,.T.) ;
#72043 = ORIENTED_EDGE('',*,*,#51522,.T.) ;
#72044 = ORIENTED_EDGE('',*,*,#51523,.T.) ;
#72045 = ORIENTED_EDGE('',*,*,#51524,.T.) ;
#72046 = ORIENTED_EDGE('',*,*,#51525,.T.) ;
#72047 = ORIENTED_EDGE('',*,*,#51526,.T.) ;
#72048 = ORIENTED_EDGE('',*,*,#51527,.T.) ;
#72049 = ORIENTED_EDGE('',*,*,#51528,.T.) ;
#72050 = ORIENTED_EDGE('',*,*,#51529,.T.) ;
#72051 = ORIENTED_EDGE('',*,*,#51530,.T.) ;
#72052 = ORIENTED_EDGE('',*,*,#51531,.T.) ;
#72053 = ORIENTED_EDGE('',*,*,#51532,.T.) ;
#72054 = ORIENTED_EDGE('',*,*,#51533,.T.) ;
#72055 = ORIENTED_EDGE('',*,*,#51534,.T.) ;
#72056 = ORIENTED_EDGE('',*,*,#51535,.T.) ;
#72057 = ORIENTED_EDGE('',*,*,#51536,.T.) ;
#72058 = ORIENTED_EDGE('',*,*,#51537,.T.) ;
#72059 = ORIENTED_EDGE('',*,*,#51538,.T.) ;
#72060 = ORIENTED_EDGE('',*,*,#51539,.T.) ;
#72061 = ORIENTED_EDGE('',*,*,#51540,.T.) ;
#72062 = ORIENTED_EDGE('',*,*,#51541,.T.) ;
#72063 = ORIENTED_EDGE('',*,*,#51542,.T.) ;
#72064 = ORIENTED_EDGE('',*,*,#51543,.T.) ;
#72065 = ORIENTED_EDGE('',*,*,#51544,.T.) ;
#72066 = ORIENTED_EDGE('',*,*,#51545,.T.) ;
#72067 = ORIENTED_EDGE('',*,*,#51546,.T.) ;
#72068 = ORIENTED_EDGE('',*,*,#51547,.T.) ;
#72069 = ORIENTED_EDGE('',*,*,#51548,.T.) ;
#72070 = ORIENTED_EDGE('',*,*,#51549,.T.) ;
#72071 = ORIENTED_EDGE('',*,*,#51550,.T.) ;
#72072 = ORIENTED_EDGE('',*,*,#51551,.T.) ;
#72073 = ORIENTED_EDGE('',*,*,#51552,.T.) ;
#72074 = ORIENTED_EDGE('',*,*,#51553,.T.) ;
#72075 = ORIENTED_EDGE('',*,*,#51554,.T.) ;
#72076 = ORIENTED_EDGE('',*,*,#51555,.T.) ;
#72077 = ORIENTED_EDGE('',*,*,#51556,.T.) ;
#72078 = ORIENTED_EDGE('',*,*,#51557,.T.) ;
#72079 = ORIENTED_EDGE('',*,*,#51558,.T.) ;
#72080 = ORIENTED_EDGE('',*,*,#51559,.T.) ;
#72081 = ORIENTED_EDGE('',*,*,#51560,.T.) ;
#72082 = ORIENTED_EDGE('',*,*,#51561,.T.) ;
#72083 = ORIENTED_EDGE('',*,*,#51562,.T.) ;
#72084 = ORIENTED_EDGE('',*,*,#51563,.T.) ;
#72085 = ORIENTED_EDGE('',*,*,#51564,.T.) ;
#72086 = ORIENTED_EDGE('',*,*,#51565,.T.) ;
#72087 = ORIENTED_EDGE('',*,*,#51566,.T.) ;
#72088 = ORIENTED_EDGE('',*,*,#51567,.T.) ;
#72089 = ORIENTED_EDGE('',*,*,#51568,.T.) ;
#72090 = ORIENTED_EDGE('',*,*,#51569,.T.) ;
#72091 = ORIENTED_EDGE('',*,*,#51570,.T.) ;
#72092 = ORIENTED_EDGE('',*,*,#51571,.T.) ;
#72093 = ORIENTED_EDGE('',*,*,#51572,.T.) ;
#72094 = ORIENTED_EDGE('',*,*,#51573,.T.) ;
#72095 = ORIENTED_EDGE('',*,*,#51574,.T.) ;
#72096 = ORIENTED_EDGE('',*,*,#51575,.T.) ;
#72097 = ORIENTED_EDGE('',*,*,#51576,.T.) ;
#72098 = ORIENTED_EDGE('',*,*,#51577,.T.) ;
#72099 = ORIENTED_EDGE('',*,*,#51578,.T.) ;
#72100 = ORIENTED_EDGE('',*,*,#51579,.T.) ;
#72101 = ORIENTED_EDGE('',*,*,#51580,.T.) ;
#72102 = ORIENTED_EDGE('',*,*,#51581,.T.) ;
#72103 = ORIENTED_EDGE('',*,*,#51582,.T.) ;
#72104 = ORIENTED_EDGE('',*,*,#51583,.T.) ;
#72105 = ORIENTED_EDGE('',*,*,#51584,.T.) ;
#72106 = ORIENTED_EDGE('',*,*,#51585,.T.) ;
#72107 = ORIENTED_EDGE('',*,*,#51586,.T.) ;
#72108 = ORIENTED_EDGE('',*,*,#51587,.T.) ;
#72109 = ORIENTED_EDGE('',*,*,#51588,.T.) ;
#72110 = ORIENTED_EDGE('',*,*,#51589,.T.) ;
#72111 = ORIENTED_EDGE('',*,*,#51590,.T.) ;
#72112 = ORIENTED_EDGE('',*,*,#51591,.T.) ;
#72113 = ORIENTED_EDGE('',*,*,#51592,.T.) ;
#72114 = ORIENTED_EDGE('',*,*,#51593,.T.) ;
#72115 = ORIENTED_EDGE('',*,*,#51594,.T.) ;
#72116 = ORIENTED_EDGE('',*,*,#51595,.T.) ;
#72117 = ORIENTED_EDGE('',*,*,#51596,.T.) ;
#72118 = ORIENTED_EDGE('',*,*,#51597,.T.) ;
#72119 = ORIENTED_EDGE('',*,*,#51598,.T.) ;
#72120 = ORIENTED_EDGE('',*,*,#51599,.T.) ;
#72121 = ORIENTED_EDGE('',*,*,#51600,.T.) ;
#72122 = ORIENTED_EDGE('',*,*,#51601,.T.) ;
#72123 = ORIENTED_EDGE('',*,*,#51602,.T.) ;
#72124 = ORIENTED_EDGE('',*,*,#51603,.T.) ;
#72125 = ORIENTED_EDGE('',*,*,#51604,.T.) ;
#72126 = ORIENTED_EDGE('',*,*,#51605,.T.) ;
#72127 = ORIENTED_EDGE('',*,*,#51606,.T.) ;
#72128 = ORIENTED_EDGE('',*,*,#51607,.T.) ;
#72129 = ORIENTED_EDGE('',*,*,#51608,.T.) ;
#72130 = ORIENTED_EDGE('',*,*,#51609,.T.) ;
#72131 = ORIENTED_EDGE('',*,*,#51610,.T.) ;
#72132 = ORIENTED_EDGE('',*,*,#51611,.T.) ;
#72133 = ORIENTED_EDGE('',*,*,#51612,.T.) ;
#72134 = ORIENTED_EDGE('',*,*,#51613,.T.) ;
#72135 = ORIENTED_EDGE('',*,*,#51614,.T.) ;
#72136 = ORIENTED_EDGE('',*,*,#51615,.T.) ;
#72137 = ORIENTED_EDGE('',*,*,#51616,.T.) ;
#72138 = ORIENTED_EDGE('',*,*,#51617,.T.) ;
#72139 = ORIENTED_EDGE('',*,*,#51618,.T.) ;
#72140 = ORIENTED_EDGE('',*,*,#51619,.T.) ;
#72141 = ORIENTED_EDGE('',*,*,#51620,.T.) ;
#72142 = ORIENTED_EDGE('',*,*,#51621,.T.) ;
#72143 = ORIENTED_EDGE('',*,*,#51622,.T.) ;
#72144 = ORIENTED_EDGE('',*,*,#51623,.T.) ;
#72145 = ORIENTED_EDGE('',*,*,#51624,.T.) ;
#72146 = ORIENTED_EDGE('',*,*,#51625,.T.) ;
#72147 = ORIENTED_EDGE('',*,*,#51626,.T.) ;
#72148 = ORIENTED_EDGE('',*,*,#51627,.T.) ;
#72149 = ORIENTED_EDGE('',*,*,#51628,.T.) ;
#72150 = ORIENTED_EDGE('',*,*,#51629,.T.) ;
#72151 = ORIENTED_EDGE('',*,*,#51630,.T.) ;
#72152 = ORIENTED_EDGE('',*,*,#51631,.T.) ;
#72153 = ORIENTED_EDGE('',*,*,#51632,.T.) ;
#72154 = ORIENTED_EDGE('',*,*,#51633,.T.) ;
#72155 = ORIENTED_EDGE('',*,*,#51634,.T.) ;
#72156 = ORIENTED_EDGE('',*,*,#51635,.T.) ;
#72157 = ORIENTED_EDGE('',*,*,#51636,.T.) ;
#72158 = ORIENTED_EDGE('',*,*,#51637,.T.) ;
#72159 = ORIENTED_EDGE('',*,*,#51638,.T.) ;
#72160 = ORIENTED_EDGE('',*,*,#51639,.F.) ;
#72161 = ORIENTED_EDGE('',*,*,#51640,.T.) ;
#72162 = ORIENTED_EDGE('',*,*,#51641,.F.) ;
#72163 = ORIENTED_EDGE('',*,*,#51642,.T.) ;
#72164 = ORIENTED_EDGE('',*,*,#51643,.F.) ;
#72165 = ORIENTED_EDGE('',*,*,#51644,.T.) ;
#72166 = ORIENTED_EDGE('',*,*,#51645,.F.) ;
#72167 = ORIENTED_EDGE('',*,*,#51646,.T.) ;
#72168 = ORIENTED_EDGE('',*,*,#51647,.T.) ;
#72169 = ORIENTED_EDGE('',*,*,#51648,.T.) ;
#72170 = ORIENTED_EDGE('',*,*,#51645,.T.) ;
#72171 = ORIENTED_EDGE('',*,*,#51649,.T.) ;
#72172 = ORIENTED_EDGE('',*,*,#51650,.T.) ;
#72173 = ORIENTED_EDGE('',*,*,#51651,.T.) ;
#72174 = ORIENTED_EDGE('',*,*,#51639,.T.) ;
#72175 = ORIENTED_EDGE('',*,*,#51652,.T.) ;
#72176 = ORIENTED_EDGE('',*,*,#51641,.T.) ;
#72177 = ORIENTED_EDGE('',*,*,#51653,.T.) ;
#72178 = ORIENTED_EDGE('',*,*,#51654,.T.) ;
#72179 = ORIENTED_EDGE('',*,*,#51655,.T.) ;
#72180 = ORIENTED_EDGE('',*,*,#51656,.T.) ;
#72181 = ORIENTED_EDGE('',*,*,#51657,.T.) ;
#72182 = ORIENTED_EDGE('',*,*,#51643,.T.) ;
#72183 = ORIENTED_EDGE('',*,*,#51658,.T.) ;
#72184 = ORIENTED_EDGE('',*,*,#51659,.T.) ;
#72185 = ORIENTED_EDGE('',*,*,#51660,.T.) ;
#72186 = ORIENTED_EDGE('',*,*,#51661,.T.) ;
#72187 = ORIENTED_EDGE('',*,*,#51662,.T.) ;
#72188 = ORIENTED_EDGE('',*,*,#51663,.F.) ;
#72189 = ORIENTED_EDGE('',*,*,#51664,.T.) ;
#72190 = ORIENTED_EDGE('',*,*,#51665,.F.) ;
#72191 = ORIENTED_EDGE('',*,*,#51666,.T.) ;
#72192 = ORIENTED_EDGE('',*,*,#51667,.F.) ;
#72193 = ORIENTED_EDGE('',*,*,#51668,.T.) ;
#72194 = ORIENTED_EDGE('',*,*,#51669,.F.) ;
#72195 = ORIENTED_EDGE('',*,*,#51670,.T.) ;
#72196 = ORIENTED_EDGE('',*,*,#51671,.T.) ;
#72197 = ORIENTED_EDGE('',*,*,#51672,.T.) ;
#72198 = ORIENTED_EDGE('',*,*,#51669,.T.) ;
#72199 = ORIENTED_EDGE('',*,*,#51673,.T.) ;
#72200 = ORIENTED_EDGE('',*,*,#51674,.T.) ;
#72201 = ORIENTED_EDGE('',*,*,#51675,.T.) ;
#72202 = ORIENTED_EDGE('',*,*,#51663,.T.) ;
#72203 = ORIENTED_EDGE('',*,*,#51676,.T.) ;
#72204 = ORIENTED_EDGE('',*,*,#51665,.T.) ;
#72205 = ORIENTED_EDGE('',*,*,#51677,.T.) ;
#72206 = ORIENTED_EDGE('',*,*,#51678,.T.) ;
#72207 = ORIENTED_EDGE('',*,*,#51679,.T.) ;
#72208 = ORIENTED_EDGE('',*,*,#51680,.T.) ;
#72209 = ORIENTED_EDGE('',*,*,#51681,.T.) ;
#72210 = ORIENTED_EDGE('',*,*,#51667,.T.) ;
#72211 = ORIENTED_EDGE('',*,*,#51682,.T.) ;
#72212 = ORIENTED_EDGE('',*,*,#51683,.T.) ;
#72213 = ORIENTED_EDGE('',*,*,#51684,.T.) ;
#72214 = ORIENTED_EDGE('',*,*,#51685,.T.) ;
#72215 = ORIENTED_EDGE('',*,*,#51686,.T.) ;
#72216 = ORIENTED_EDGE('',*,*,#51687,.F.) ;
#72217 = ORIENTED_EDGE('',*,*,#51688,.T.) ;
#72218 = ORIENTED_EDGE('',*,*,#51689,.F.) ;
#72219 = ORIENTED_EDGE('',*,*,#51690,.T.) ;
#72220 = ORIENTED_EDGE('',*,*,#51691,.F.) ;
#72221 = ORIENTED_EDGE('',*,*,#51692,.T.) ;
#72222 = ORIENTED_EDGE('',*,*,#51693,.F.) ;
#72223 = ORIENTED_EDGE('',*,*,#51694,.T.) ;
#72224 = ORIENTED_EDGE('',*,*,#51695,.T.) ;
#72225 = ORIENTED_EDGE('',*,*,#51696,.T.) ;
#72226 = ORIENTED_EDGE('',*,*,#51693,.T.) ;
#72227 = ORIENTED_EDGE('',*,*,#51697,.T.) ;
#72228 = ORIENTED_EDGE('',*,*,#51698,.T.) ;
#72229 = ORIENTED_EDGE('',*,*,#51699,.T.) ;
#72230 = ORIENTED_EDGE('',*,*,#51687,.T.) ;
#72231 = ORIENTED_EDGE('',*,*,#51700,.T.) ;
#72232 = ORIENTED_EDGE('',*,*,#51689,.T.) ;
#72233 = ORIENTED_EDGE('',*,*,#51701,.T.) ;
#72234 = ORIENTED_EDGE('',*,*,#51702,.T.) ;
#72235 = ORIENTED_EDGE('',*,*,#51703,.T.) ;
#72236 = ORIENTED_EDGE('',*,*,#51704,.T.) ;
#72237 = ORIENTED_EDGE('',*,*,#51705,.T.) ;
#72238 = ORIENTED_EDGE('',*,*,#51691,.T.) ;
#72239 = ORIENTED_EDGE('',*,*,#51706,.T.) ;
#72240 = ORIENTED_EDGE('',*,*,#51707,.T.) ;
#72241 = ORIENTED_EDGE('',*,*,#51708,.T.) ;
#72242 = ORIENTED_EDGE('',*,*,#51709,.T.) ;
#72243 = ORIENTED_EDGE('',*,*,#51710,.T.) ;
#72244 = ORIENTED_EDGE('',*,*,#51711,.F.) ;
#72245 = ORIENTED_EDGE('',*,*,#51712,.T.) ;
#72246 = ORIENTED_EDGE('',*,*,#51713,.F.) ;
#72247 = ORIENTED_EDGE('',*,*,#51714,.T.) ;
#72248 = ORIENTED_EDGE('',*,*,#51715,.F.) ;
#72249 = ORIENTED_EDGE('',*,*,#51716,.T.) ;
#72250 = ORIENTED_EDGE('',*,*,#51717,.F.) ;
#72251 = ORIENTED_EDGE('',*,*,#51718,.T.) ;
#72252 = ORIENTED_EDGE('',*,*,#51719,.T.) ;
#72253 = ORIENTED_EDGE('',*,*,#51720,.T.) ;
#72254 = ORIENTED_EDGE('',*,*,#51717,.T.) ;
#72255 = ORIENTED_EDGE('',*,*,#51721,.T.) ;
#72256 = ORIENTED_EDGE('',*,*,#51722,.T.) ;
#72257 = ORIENTED_EDGE('',*,*,#51723,.T.) ;
#72258 = ORIENTED_EDGE('',*,*,#51711,.T.) ;
#72259 = ORIENTED_EDGE('',*,*,#51724,.T.) ;
#72260 = ORIENTED_EDGE('',*,*,#51713,.T.) ;
#72261 = ORIENTED_EDGE('',*,*,#51725,.T.) ;
#72262 = ORIENTED_EDGE('',*,*,#51726,.T.) ;
#72263 = ORIENTED_EDGE('',*,*,#51727,.T.) ;
#72264 = ORIENTED_EDGE('',*,*,#51728,.T.) ;
#72265 = ORIENTED_EDGE('',*,*,#51729,.T.) ;
#72266 = ORIENTED_EDGE('',*,*,#51715,.T.) ;
#72267 = ORIENTED_EDGE('',*,*,#51730,.T.) ;
#72268 = ORIENTED_EDGE('',*,*,#51731,.T.) ;
#72269 = ORIENTED_EDGE('',*,*,#51732,.T.) ;
#72270 = ORIENTED_EDGE('',*,*,#51733,.T.) ;
#72271 = ORIENTED_EDGE('',*,*,#51734,.T.) ;
#72272 = ORIENTED_EDGE('',*,*,#51735,.F.) ;
#72273 = ORIENTED_EDGE('',*,*,#51736,.T.) ;
#72274 = ORIENTED_EDGE('',*,*,#51737,.F.) ;
#72275 = ORIENTED_EDGE('',*,*,#51738,.T.) ;
#72276 = ORIENTED_EDGE('',*,*,#51739,.F.) ;
#72277 = ORIENTED_EDGE('',*,*,#51740,.T.) ;
#72278 = ORIENTED_EDGE('',*,*,#51741,.F.) ;
#72279 = ORIENTED_EDGE('',*,*,#51742,.T.) ;
#72280 = ORIENTED_EDGE('',*,*,#51743,.T.) ;
#72281 = ORIENTED_EDGE('',*,*,#51744,.T.) ;
#72282 = ORIENTED_EDGE('',*,*,#51741,.T.) ;
#72283 = ORIENTED_EDGE('',*,*,#51745,.T.) ;
#72284 = ORIENTED_EDGE('',*,*,#51746,.T.) ;
#72285 = ORIENTED_EDGE('',*,*,#51747,.T.) ;
#72286 = ORIENTED_EDGE('',*,*,#51735,.T.) ;
#72287 = ORIENTED_EDGE('',*,*,#51748,.T.) ;
#72288 = ORIENTED_EDGE('',*,*,#51737,.T.) ;
#72289 = ORIENTED_EDGE('',*,*,#51749,.T.) ;
#72290 = ORIENTED_EDGE('',*,*,#51750,.T.) ;
#72291 = ORIENTED_EDGE('',*,*,#51751,.T.) ;
#72292 = ORIENTED_EDGE('',*,*,#51752,.T.) ;
#72293 = ORIENTED_EDGE('',*,*,#51753,.T.) ;
#72294 = ORIENTED_EDGE('',*,*,#51739,.T.) ;
#72295 = ORIENTED_EDGE('',*,*,#51754,.T.) ;
#72296 = ORIENTED_EDGE('',*,*,#51755,.T.) ;
#72297 = ORIENTED_EDGE('',*,*,#51756,.T.) ;
#72298 = ORIENTED_EDGE('',*,*,#51757,.T.) ;
#72299 = ORIENTED_EDGE('',*,*,#51758,.T.) ;
#72300 = ORIENTED_EDGE('',*,*,#51759,.F.) ;
#72301 = ORIENTED_EDGE('',*,*,#51760,.T.) ;
#72302 = ORIENTED_EDGE('',*,*,#51761,.F.) ;
#72303 = ORIENTED_EDGE('',*,*,#51762,.T.) ;
#72304 = ORIENTED_EDGE('',*,*,#51763,.F.) ;
#72305 = ORIENTED_EDGE('',*,*,#51764,.T.) ;
#72306 = ORIENTED_EDGE('',*,*,#51765,.F.) ;
#72307 = ORIENTED_EDGE('',*,*,#51766,.T.) ;
#72308 = ORIENTED_EDGE('',*,*,#51767,.T.) ;
#72309 = ORIENTED_EDGE('',*,*,#51768,.T.) ;
#72310 = ORIENTED_EDGE('',*,*,#51765,.T.) ;
#72311 = ORIENTED_EDGE('',*,*,#51769,.T.) ;
#72312 = ORIENTED_EDGE('',*,*,#51770,.T.) ;
#72313 = ORIENTED_EDGE('',*,*,#51771,.T.) ;
#72314 = ORIENTED_EDGE('',*,*,#51759,.T.) ;
#72315 = ORIENTED_EDGE('',*,*,#51772,.T.) ;
#72316 = ORIENTED_EDGE('',*,*,#51761,.T.) ;
#72317 = ORIENTED_EDGE('',*,*,#51773,.T.) ;
#72318 = ORIENTED_EDGE('',*,*,#51774,.T.) ;
#72319 = ORIENTED_EDGE('',*,*,#51775,.T.) ;
#72320 = ORIENTED_EDGE('',*,*,#51776,.T.) ;
#72321 = ORIENTED_EDGE('',*,*,#51777,.T.) ;
#72322 = ORIENTED_EDGE('',*,*,#51763,.T.) ;
#72323 = ORIENTED_EDGE('',*,*,#51778,.T.) ;
#72324 = ORIENTED_EDGE('',*,*,#51779,.T.) ;
#72325 = ORIENTED_EDGE('',*,*,#51780,.T.) ;
#72326 = ORIENTED_EDGE('',*,*,#51781,.T.) ;
#72327 = ORIENTED_EDGE('',*,*,#51782,.T.) ;
#72328 = ORIENTED_EDGE('',*,*,#51783,.F.) ;
#72329 = ORIENTED_EDGE('',*,*,#51784,.T.) ;
#72330 = ORIENTED_EDGE('',*,*,#51785,.F.) ;
#72331 = ORIENTED_EDGE('',*,*,#51786,.T.) ;
#72332 = ORIENTED_EDGE('',*,*,#51787,.F.) ;
#72333 = ORIENTED_EDGE('',*,*,#51788,.T.) ;
#72334 = ORIENTED_EDGE('',*,*,#51789,.F.) ;
#72335 = ORIENTED_EDGE('',*,*,#51790,.T.) ;
#72336 = ORIENTED_EDGE('',*,*,#51791,.T.) ;
#72337 = ORIENTED_EDGE('',*,*,#51792,.T.) ;
#72338 = ORIENTED_EDGE('',*,*,#51789,.T.) ;
#72339 = ORIENTED_EDGE('',*,*,#51793,.T.) ;
#72340 = ORIENTED_EDGE('',*,*,#51794,.T.) ;
#72341 = ORIENTED_EDGE('',*,*,#51795,.T.) ;
#72342 = ORIENTED_EDGE('',*,*,#51783,.T.) ;
#72343 = ORIENTED_EDGE('',*,*,#51796,.T.) ;
#72344 = ORIENTED_EDGE('',*,*,#51785,.T.) ;
#72345 = ORIENTED_EDGE('',*,*,#51797,.T.) ;
#72346 = ORIENTED_EDGE('',*,*,#51798,.T.) ;
#72347 = ORIENTED_EDGE('',*,*,#51799,.T.) ;
#72348 = ORIENTED_EDGE('',*,*,#51800,.T.) ;
#72349 = ORIENTED_EDGE('',*,*,#51801,.T.) ;
#72350 = ORIENTED_EDGE('',*,*,#51787,.T.) ;
#72351 = ORIENTED_EDGE('',*,*,#51802,.T.) ;
#72352 = ORIENTED_EDGE('',*,*,#51803,.T.) ;
#72353 = ORIENTED_EDGE('',*,*,#51804,.T.) ;
#72354 = ORIENTED_EDGE('',*,*,#51805,.T.) ;
#72355 = ORIENTED_EDGE('',*,*,#51806,.T.) ;
#72356 = ORIENTED_EDGE('',*,*,#51807,.F.) ;
#72357 = ORIENTED_EDGE('',*,*,#51808,.T.) ;
#72358 = ORIENTED_EDGE('',*,*,#51809,.F.) ;
#72359 = ORIENTED_EDGE('',*,*,#51810,.T.) ;
#72360 = ORIENTED_EDGE('',*,*,#51811,.F.) ;
#72361 = ORIENTED_EDGE('',*,*,#51812,.T.) ;
#72362 = ORIENTED_EDGE('',*,*,#51813,.F.) ;
#72363 = ORIENTED_EDGE('',*,*,#51814,.T.) ;
#72364 = ORIENTED_EDGE('',*,*,#51815,.T.) ;
#72365 = ORIENTED_EDGE('',*,*,#51816,.T.) ;
#72366 = ORIENTED_EDGE('',*,*,#51813,.T.) ;
#72367 = ORIENTED_EDGE('',*,*,#51817,.T.) ;
#72368 = ORIENTED_EDGE('',*,*,#51818,.T.) ;
#72369 = ORIENTED_EDGE('',*,*,#51819,.T.) ;
#72370 = ORIENTED_EDGE('',*,*,#51807,.T.) ;
#72371 = ORIENTED_EDGE('',*,*,#51820,.T.) ;
#72372 = ORIENTED_EDGE('',*,*,#51809,.T.) ;
#72373 = ORIENTED_EDGE('',*,*,#51821,.T.) ;
#72374 = ORIENTED_EDGE('',*,*,#51822,.T.) ;
#72375 = ORIENTED_EDGE('',*,*,#51823,.T.) ;
#72376 = ORIENTED_EDGE('',*,*,#51824,.T.) ;
#72377 = ORIENTED_EDGE('',*,*,#51825,.T.) ;
#72378 = ORIENTED_EDGE('',*,*,#51811,.T.) ;
#72379 = ORIENTED_EDGE('',*,*,#51826,.T.) ;
#72380 = ORIENTED_EDGE('',*,*,#51827,.T.) ;
#72381 = ORIENTED_EDGE('',*,*,#51828,.T.) ;
#72382 = ORIENTED_EDGE('',*,*,#51829,.T.) ;
#72383 = ORIENTED_EDGE('',*,*,#51830,.T.) ;
#72384 = ORIENTED_EDGE('',*,*,#51831,.F.) ;
#72385 = ORIENTED_EDGE('',*,*,#51832,.T.) ;
#72386 = ORIENTED_EDGE('',*,*,#51833,.F.) ;
#72387 = ORIENTED_EDGE('',*,*,#51834,.T.) ;
#72388 = ORIENTED_EDGE('',*,*,#51835,.F.) ;
#72389 = ORIENTED_EDGE('',*,*,#51836,.T.) ;
#72390 = ORIENTED_EDGE('',*,*,#51837,.F.) ;
#72391 = ORIENTED_EDGE('',*,*,#51838,.T.) ;
#72392 = ORIENTED_EDGE('',*,*,#51839,.T.) ;
#72393 = ORIENTED_EDGE('',*,*,#51840,.T.) ;
#72394 = ORIENTED_EDGE('',*,*,#51837,.T.) ;
#72395 = ORIENTED_EDGE('',*,*,#51841,.T.) ;
#72396 = ORIENTED_EDGE('',*,*,#51842,.T.) ;
#72397 = ORIENTED_EDGE('',*,*,#51843,.T.) ;
#72398 = ORIENTED_EDGE('',*,*,#51831,.T.) ;
#72399 = ORIENTED_EDGE('',*,*,#51844,.T.) ;
#72400 = ORIENTED_EDGE('',*,*,#51833,.T.) ;
#72401 = ORIENTED_EDGE('',*,*,#51845,.T.) ;
#72402 = ORIENTED_EDGE('',*,*,#51846,.T.) ;
#72403 = ORIENTED_EDGE('',*,*,#51847,.T.) ;
#72404 = ORIENTED_EDGE('',*,*,#51848,.T.) ;
#72405 = ORIENTED_EDGE('',*,*,#51849,.T.) ;
#72406 = ORIENTED_EDGE('',*,*,#51835,.T.) ;
#72407 = ORIENTED_EDGE('',*,*,#51850,.T.) ;
#72408 = ORIENTED_EDGE('',*,*,#51851,.T.) ;
#72409 = ORIENTED_EDGE('',*,*,#51852,.T.) ;
#72410 = ORIENTED_EDGE('',*,*,#51853,.T.) ;
#72411 = ORIENTED_EDGE('',*,*,#51854,.T.) ;
#72412 = ORIENTED_EDGE('',*,*,#51855,.T.) ;
#72413 = ORIENTED_EDGE('',*,*,#51856,.T.) ;
#72414 = ORIENTED_EDGE('',*,*,#51857,.T.) ;
#72415 = ORIENTED_EDGE('',*,*,#51858,.T.) ;
#72416 = ORIENTED_EDGE('',*,*,#51859,.T.) ;
#72417 = ORIENTED_EDGE('',*,*,#51860,.T.) ;
#72418 = ORIENTED_EDGE('',*,*,#51861,.T.) ;
#72419 = ORIENTED_EDGE('',*,*,#51862,.T.) ;
#72420 = ORIENTED_EDGE('',*,*,#51863,.T.) ;
#72421 = ORIENTED_EDGE('',*,*,#51864,.T.) ;
#72422 = ORIENTED_EDGE('',*,*,#51865,.T.) ;
#72423 = ORIENTED_EDGE('',*,*,#51866,.T.) ;
#72424 = ORIENTED_EDGE('',*,*,#51867,.T.) ;
#72425 = ORIENTED_EDGE('',*,*,#51868,.T.) ;
#72426 = ORIENTED_EDGE('',*,*,#51869,.T.) ;
#72427 = ORIENTED_EDGE('',*,*,#51870,.T.) ;
#72428 = ORIENTED_EDGE('',*,*,#51871,.T.) ;
#72429 = ORIENTED_EDGE('',*,*,#51872,.T.) ;
#72430 = ORIENTED_EDGE('',*,*,#51873,.T.) ;
#72431 = ORIENTED_EDGE('',*,*,#51874,.T.) ;
#72432 = ORIENTED_EDGE('',*,*,#51875,.T.) ;
#72433 = ORIENTED_EDGE('',*,*,#51876,.T.) ;
#72434 = ORIENTED_EDGE('',*,*,#51877,.T.) ;
#72435 = ORIENTED_EDGE('',*,*,#51878,.T.) ;
#72436 = ORIENTED_EDGE('',*,*,#51879,.T.) ;
#72437 = ORIENTED_EDGE('',*,*,#51880,.T.) ;
#72438 = ORIENTED_EDGE('',*,*,#51881,.T.) ;
#72439 = ORIENTED_EDGE('',*,*,#51882,.T.) ;
#72440 = ORIENTED_EDGE('',*,*,#51883,.T.) ;
#72441 = ORIENTED_EDGE('',*,*,#51884,.T.) ;
#72442 = ORIENTED_EDGE('',*,*,#51885,.T.) ;
#72443 = ORIENTED_EDGE('',*,*,#51886,.T.) ;
#72444 = ORIENTED_EDGE('',*,*,#49231,.T.) ;
#72445 = ORIENTED_EDGE('',*,*,#49247,.T.) ;
#72446 = ORIENTED_EDGE('',*,*,#51887,.T.) ;
#72447 = ORIENTED_EDGE('',*,*,#49213,.T.) ;
#72448 = ORIENTED_EDGE('',*,*,#49229,.T.) ;
#72449 = ORIENTED_EDGE('',*,*,#51888,.T.) ;
#72450 = ORIENTED_EDGE('',*,*,#49195,.T.) ;
#72451 = ORIENTED_EDGE('',*,*,#49211,.T.) ;
#72452 = ORIENTED_EDGE('',*,*,#51889,.T.) ;
#72453 = ORIENTED_EDGE('',*,*,#49177,.T.) ;
#72454 = ORIENTED_EDGE('',*,*,#49193,.T.) ;
#72455 = ORIENTED_EDGE('',*,*,#51890,.T.) ;
#72456 = ORIENTED_EDGE('',*,*,#49159,.T.) ;
#72457 = ORIENTED_EDGE('',*,*,#49175,.T.) ;
#72458 = ORIENTED_EDGE('',*,*,#51891,.T.) ;
#72459 = ORIENTED_EDGE('',*,*,#49141,.T.) ;
#72460 = ORIENTED_EDGE('',*,*,#49157,.T.) ;
#72461 = ORIENTED_EDGE('',*,*,#51892,.T.) ;
#72462 = ORIENTED_EDGE('',*,*,#49123,.T.) ;
#72463 = ORIENTED_EDGE('',*,*,#49139,.T.) ;
#72464 = ORIENTED_EDGE('',*,*,#51893,.T.) ;
#72465 = ORIENTED_EDGE('',*,*,#49105,.T.) ;
#72466 = ORIENTED_EDGE('',*,*,#49121,.T.) ;
#72467 = ORIENTED_EDGE('',*,*,#51894,.T.) ;
#72468 = ORIENTED_EDGE('',*,*,#49087,.T.) ;
#72469 = ORIENTED_EDGE('',*,*,#49103,.T.) ;
#72470 = ORIENTED_EDGE('',*,*,#51895,.T.) ;
#72471 = ORIENTED_EDGE('',*,*,#49089,.T.) ;
#72472 = ORIENTED_EDGE('',*,*,#51896,.T.) ;
#72473 = ORIENTED_EDGE('',*,*,#49101,.F.) ;
#72474 = ORIENTED_EDGE('',*,*,#51897,.T.) ;
#72475 = ORIENTED_EDGE('',*,*,#49093,.F.) ;
#72476 = ORIENTED_EDGE('',*,*,#51898,.T.) ;
#72477 = ORIENTED_EDGE('',*,*,#49097,.T.) ;
#72478 = ORIENTED_EDGE('',*,*,#51899,.T.) ;
#72479 = ORIENTED_EDGE('',*,*,#49091,.T.) ;
#72480 = ORIENTED_EDGE('',*,*,#51900,.T.) ;
#72481 = ORIENTED_EDGE('',*,*,#49099,.T.) ;
#72482 = ORIENTED_EDGE('',*,*,#51901,.T.) ;
#72483 = ORIENTED_EDGE('',*,*,#49107,.T.) ;
#72484 = ORIENTED_EDGE('',*,*,#51902,.T.) ;
#72485 = ORIENTED_EDGE('',*,*,#49119,.F.) ;
#72486 = ORIENTED_EDGE('',*,*,#51903,.T.) ;
#72487 = ORIENTED_EDGE('',*,*,#49111,.F.) ;
#72488 = ORIENTED_EDGE('',*,*,#51904,.T.) ;
#72489 = ORIENTED_EDGE('',*,*,#49115,.T.) ;
#72490 = ORIENTED_EDGE('',*,*,#51905,.T.) ;
#72491 = ORIENTED_EDGE('',*,*,#49109,.T.) ;
#72492 = ORIENTED_EDGE('',*,*,#51906,.T.) ;
#72493 = ORIENTED_EDGE('',*,*,#49117,.T.) ;
#72494 = ORIENTED_EDGE('',*,*,#51907,.T.) ;
#72495 = ORIENTED_EDGE('',*,*,#49125,.T.) ;
#72496 = ORIENTED_EDGE('',*,*,#51908,.T.) ;
#72497 = ORIENTED_EDGE('',*,*,#49137,.F.) ;
#72498 = ORIENTED_EDGE('',*,*,#51909,.T.) ;
#72499 = ORIENTED_EDGE('',*,*,#49129,.F.) ;
#72500 = ORIENTED_EDGE('',*,*,#51910,.T.) ;
#72501 = ORIENTED_EDGE('',*,*,#49133,.T.) ;
#72502 = ORIENTED_EDGE('',*,*,#51911,.T.) ;
#72503 = ORIENTED_EDGE('',*,*,#49127,.T.) ;
#72504 = ORIENTED_EDGE('',*,*,#51912,.T.) ;
#72505 = ORIENTED_EDGE('',*,*,#49135,.T.) ;
#72506 = ORIENTED_EDGE('',*,*,#51913,.T.) ;
#72507 = ORIENTED_EDGE('',*,*,#49143,.T.) ;
#72508 = ORIENTED_EDGE('',*,*,#51914,.T.) ;
#72509 = ORIENTED_EDGE('',*,*,#49155,.F.) ;
#72510 = ORIENTED_EDGE('',*,*,#51915,.T.) ;
#72511 = ORIENTED_EDGE('',*,*,#49147,.F.) ;
#72512 = ORIENTED_EDGE('',*,*,#51916,.T.) ;
#72513 = ORIENTED_EDGE('',*,*,#49151,.T.) ;
#72514 = ORIENTED_EDGE('',*,*,#51917,.T.) ;
#72515 = ORIENTED_EDGE('',*,*,#49145,.T.) ;
#72516 = ORIENTED_EDGE('',*,*,#51918,.T.) ;
#72517 = ORIENTED_EDGE('',*,*,#49153,.T.) ;
#72518 = ORIENTED_EDGE('',*,*,#51919,.T.) ;
#72519 = ORIENTED_EDGE('',*,*,#49161,.T.) ;
#72520 = ORIENTED_EDGE('',*,*,#51920,.T.) ;
#72521 = ORIENTED_EDGE('',*,*,#49173,.F.) ;
#72522 = ORIENTED_EDGE('',*,*,#51921,.T.) ;
#72523 = ORIENTED_EDGE('',*,*,#49165,.F.) ;
#72524 = ORIENTED_EDGE('',*,*,#51922,.T.) ;
#72525 = ORIENTED_EDGE('',*,*,#49169,.T.) ;
#72526 = ORIENTED_EDGE('',*,*,#51923,.T.) ;
#72527 = ORIENTED_EDGE('',*,*,#49163,.T.) ;
#72528 = ORIENTED_EDGE('',*,*,#51924,.T.) ;
#72529 = ORIENTED_EDGE('',*,*,#49171,.T.) ;
#72530 = ORIENTED_EDGE('',*,*,#51925,.T.) ;
#72531 = ORIENTED_EDGE('',*,*,#49179,.T.) ;
#72532 = ORIENTED_EDGE('',*,*,#51926,.T.) ;
#72533 = ORIENTED_EDGE('',*,*,#49191,.F.) ;
#72534 = ORIENTED_EDGE('',*,*,#51927,.T.) ;
#72535 = ORIENTED_EDGE('',*,*,#49183,.F.) ;
#72536 = ORIENTED_EDGE('',*,*,#51928,.T.) ;
#72537 = ORIENTED_EDGE('',*,*,#49187,.T.) ;
#72538 = ORIENTED_EDGE('',*,*,#51929,.T.) ;
#72539 = ORIENTED_EDGE('',*,*,#49181,.T.) ;
#72540 = ORIENTED_EDGE('',*,*,#51930,.T.) ;
#72541 = ORIENTED_EDGE('',*,*,#49189,.T.) ;
#72542 = ORIENTED_EDGE('',*,*,#51931,.T.) ;
#72543 = ORIENTED_EDGE('',*,*,#49197,.T.) ;
#72544 = ORIENTED_EDGE('',*,*,#51932,.T.) ;
#72545 = ORIENTED_EDGE('',*,*,#49209,.F.) ;
#72546 = ORIENTED_EDGE('',*,*,#51933,.T.) ;
#72547 = ORIENTED_EDGE('',*,*,#49201,.F.) ;
#72548 = ORIENTED_EDGE('',*,*,#51934,.T.) ;
#72549 = ORIENTED_EDGE('',*,*,#49205,.T.) ;
#72550 = ORIENTED_EDGE('',*,*,#51935,.T.) ;
#72551 = ORIENTED_EDGE('',*,*,#49199,.T.) ;
#72552 = ORIENTED_EDGE('',*,*,#51936,.T.) ;
#72553 = ORIENTED_EDGE('',*,*,#49207,.T.) ;
#72554 = ORIENTED_EDGE('',*,*,#51937,.T.) ;
#72555 = ORIENTED_EDGE('',*,*,#49215,.T.) ;
#72556 = ORIENTED_EDGE('',*,*,#51938,.T.) ;
#72557 = ORIENTED_EDGE('',*,*,#49227,.F.) ;
#72558 = ORIENTED_EDGE('',*,*,#51939,.T.) ;
#72559 = ORIENTED_EDGE('',*,*,#49219,.F.) ;
#72560 = ORIENTED_EDGE('',*,*,#51940,.T.) ;
#72561 = ORIENTED_EDGE('',*,*,#49223,.T.) ;
#72562 = ORIENTED_EDGE('',*,*,#51941,.T.) ;
#72563 = ORIENTED_EDGE('',*,*,#49217,.T.) ;
#72564 = ORIENTED_EDGE('',*,*,#51942,.T.) ;
#72565 = ORIENTED_EDGE('',*,*,#49225,.T.) ;
#72566 = ORIENTED_EDGE('',*,*,#51943,.T.) ;
#72567 = ORIENTED_EDGE('',*,*,#49233,.T.) ;
#72568 = ORIENTED_EDGE('',*,*,#51944,.T.) ;
#72569 = ORIENTED_EDGE('',*,*,#49245,.F.) ;
#72570 = ORIENTED_EDGE('',*,*,#51945,.T.) ;
#72571 = ORIENTED_EDGE('',*,*,#49237,.F.) ;
#72572 = ORIENTED_EDGE('',*,*,#51946,.T.) ;
#72573 = ORIENTED_EDGE('',*,*,#49241,.T.) ;
#72574 = ORIENTED_EDGE('',*,*,#51947,.T.) ;
#72575 = ORIENTED_EDGE('',*,*,#49235,.T.) ;
#72576 = ORIENTED_EDGE('',*,*,#51948,.T.) ;
#72577 = ORIENTED_EDGE('',*,*,#49243,.T.) ;
#72578 = ORIENTED_EDGE('',*,*,#51949,.T.) ;
#72579 = ORIENTED_EDGE('',*,*,#51950,.T.) ;
#72580 = ORIENTED_EDGE('',*,*,#51951,.T.) ;
#72581 = ORIENTED_EDGE('',*,*,#51952,.F.) ;
#72582 = ORIENTED_EDGE('',*,*,#51953,.T.) ;
#72583 = ORIENTED_EDGE('',*,*,#51952,.T.) ;
#72584 = ORIENTED_EDGE('',*,*,#51954,.T.) ;
#72585 = ORIENTED_EDGE('',*,*,#51955,.F.) ;
#72586 = ORIENTED_EDGE('',*,*,#51956,.T.) ;
#72587 = ORIENTED_EDGE('',*,*,#51955,.T.) ;
#72588 = ORIENTED_EDGE('',*,*,#51957,.T.) ;
#72589 = ORIENTED_EDGE('',*,*,#51958,.F.) ;
#72590 = ORIENTED_EDGE('',*,*,#51959,.T.) ;
#72591 = ORIENTED_EDGE('',*,*,#51958,.T.) ;
#72592 = ORIENTED_EDGE('',*,*,#51960,.T.) ;
#72593 = ORIENTED_EDGE('',*,*,#51961,.F.) ;
#72594 = ORIENTED_EDGE('',*,*,#51962,.T.) ;
#72595 = ORIENTED_EDGE('',*,*,#51961,.T.) ;
#72596 = ORIENTED_EDGE('',*,*,#51963,.T.) ;
#72597 = ORIENTED_EDGE('',*,*,#51964,.F.) ;
#72598 = ORIENTED_EDGE('',*,*,#51965,.T.) ;
#72599 = ORIENTED_EDGE('',*,*,#51964,.T.) ;
#72600 = ORIENTED_EDGE('',*,*,#51966,.T.) ;
#72601 = ORIENTED_EDGE('',*,*,#51967,.F.) ;
#72602 = ORIENTED_EDGE('',*,*,#51968,.T.) ;
#72603 = ORIENTED_EDGE('',*,*,#51967,.T.) ;
#72604 = ORIENTED_EDGE('',*,*,#51969,.T.) ;
#72605 = ORIENTED_EDGE('',*,*,#51970,.F.) ;
#72606 = ORIENTED_EDGE('',*,*,#51971,.T.) ;
#72607 = ORIENTED_EDGE('',*,*,#51950,.F.) ;
#72608 = ORIENTED_EDGE('',*,*,#51972,.T.) ;
#72609 = ORIENTED_EDGE('',*,*,#51970,.T.) ;
#72610 = ORIENTED_EDGE('',*,*,#51973,.T.) ;
#72611 = ORIENTED_EDGE('',*,*,#51974,.T.) ;
#72612 = ORIENTED_EDGE('',*,*,#51975,.T.) ;
#72613 = ORIENTED_EDGE('',*,*,#51976,.T.) ;
#72614 = ORIENTED_EDGE('',*,*,#51977,.T.) ;
#72615 = ORIENTED_EDGE('',*,*,#51978,.T.) ;
#72616 = ORIENTED_EDGE('',*,*,#51979,.T.) ;
#72617 = ORIENTED_EDGE('',*,*,#51980,.F.) ;
#72618 = ORIENTED_EDGE('',*,*,#51981,.T.) ;
#72619 = ORIENTED_EDGE('',*,*,#51980,.T.) ;
#72620 = ORIENTED_EDGE('',*,*,#51982,.T.) ;
#72621 = ORIENTED_EDGE('',*,*,#51983,.F.) ;
#72622 = ORIENTED_EDGE('',*,*,#51984,.T.) ;
#72623 = ORIENTED_EDGE('',*,*,#51983,.T.) ;
#72624 = ORIENTED_EDGE('',*,*,#51985,.T.) ;
#72625 = ORIENTED_EDGE('',*,*,#51986,.F.) ;
#72626 = ORIENTED_EDGE('',*,*,#51987,.T.) ;
#72627 = ORIENTED_EDGE('',*,*,#51986,.T.) ;
#72628 = ORIENTED_EDGE('',*,*,#51988,.T.) ;
#72629 = ORIENTED_EDGE('',*,*,#51989,.F.) ;
#72630 = ORIENTED_EDGE('',*,*,#51990,.T.) ;
#72631 = ORIENTED_EDGE('',*,*,#51989,.T.) ;
#72632 = ORIENTED_EDGE('',*,*,#51991,.T.) ;
#72633 = ORIENTED_EDGE('',*,*,#51992,.F.) ;
#72634 = ORIENTED_EDGE('',*,*,#51993,.T.) ;
#72635 = ORIENTED_EDGE('',*,*,#51992,.T.) ;
#72636 = ORIENTED_EDGE('',*,*,#51994,.T.) ;
#72637 = ORIENTED_EDGE('',*,*,#51995,.F.) ;
#72638 = ORIENTED_EDGE('',*,*,#51996,.T.) ;
#72639 = ORIENTED_EDGE('',*,*,#51995,.T.) ;
#72640 = ORIENTED_EDGE('',*,*,#51997,.T.) ;
#72641 = ORIENTED_EDGE('',*,*,#51998,.F.) ;
#72642 = ORIENTED_EDGE('',*,*,#51999,.T.) ;
#72643 = ORIENTED_EDGE('',*,*,#51978,.F.) ;
#72644 = ORIENTED_EDGE('',*,*,#52000,.T.) ;
#72645 = ORIENTED_EDGE('',*,*,#51998,.T.) ;
#72646 = ORIENTED_EDGE('',*,*,#52001,.T.) ;
#72647 = ORIENTED_EDGE('',*,*,#52002,.T.) ;
#72648 = ORIENTED_EDGE('',*,*,#52003,.T.) ;
#72649 = ORIENTED_EDGE('',*,*,#52004,.T.) ;
#72650 = ORIENTED_EDGE('',*,*,#52005,.T.) ;
#72651 = ORIENTED_EDGE('',*,*,#52006,.T.) ;
#72652 = ORIENTED_EDGE('',*,*,#52007,.T.) ;
#72653 = ORIENTED_EDGE('',*,*,#52008,.F.) ;
#72654 = ORIENTED_EDGE('',*,*,#52009,.T.) ;
#72655 = ORIENTED_EDGE('',*,*,#52008,.T.) ;
#72656 = ORIENTED_EDGE('',*,*,#52010,.T.) ;
#72657 = ORIENTED_EDGE('',*,*,#52011,.F.) ;
#72658 = ORIENTED_EDGE('',*,*,#52012,.T.) ;
#72659 = ORIENTED_EDGE('',*,*,#52011,.T.) ;
#72660 = ORIENTED_EDGE('',*,*,#52013,.T.) ;
#72661 = ORIENTED_EDGE('',*,*,#52014,.F.) ;
#72662 = ORIENTED_EDGE('',*,*,#52015,.T.) ;
#72663 = ORIENTED_EDGE('',*,*,#52014,.T.) ;
#72664 = ORIENTED_EDGE('',*,*,#52016,.T.) ;
#72665 = ORIENTED_EDGE('',*,*,#52017,.F.) ;
#72666 = ORIENTED_EDGE('',*,*,#52018,.T.) ;
#72667 = ORIENTED_EDGE('',*,*,#52017,.T.) ;
#72668 = ORIENTED_EDGE('',*,*,#52019,.T.) ;
#72669 = ORIENTED_EDGE('',*,*,#52020,.F.) ;
#72670 = ORIENTED_EDGE('',*,*,#52021,.T.) ;
#72671 = ORIENTED_EDGE('',*,*,#52020,.T.) ;
#72672 = ORIENTED_EDGE('',*,*,#52022,.T.) ;
#72673 = ORIENTED_EDGE('',*,*,#52023,.F.) ;
#72674 = ORIENTED_EDGE('',*,*,#52024,.T.) ;
#72675 = ORIENTED_EDGE('',*,*,#52023,.T.) ;
#72676 = ORIENTED_EDGE('',*,*,#52025,.T.) ;
#72677 = ORIENTED_EDGE('',*,*,#52026,.F.) ;
#72678 = ORIENTED_EDGE('',*,*,#52027,.T.) ;
#72679 = ORIENTED_EDGE('',*,*,#52006,.F.) ;
#72680 = ORIENTED_EDGE('',*,*,#52028,.T.) ;
#72681 = ORIENTED_EDGE('',*,*,#52026,.T.) ;
#72682 = ORIENTED_EDGE('',*,*,#52029,.T.) ;
#72683 = ORIENTED_EDGE('',*,*,#52030,.T.) ;
#72684 = ORIENTED_EDGE('',*,*,#52031,.T.) ;
#72685 = ORIENTED_EDGE('',*,*,#52032,.T.) ;
#72686 = ORIENTED_EDGE('',*,*,#52033,.T.) ;
#72687 = ORIENTED_EDGE('',*,*,#52034,.T.) ;
#72688 = ORIENTED_EDGE('',*,*,#52035,.T.) ;
#72689 = ORIENTED_EDGE('',*,*,#52036,.F.) ;
#72690 = ORIENTED_EDGE('',*,*,#52037,.T.) ;
#72691 = ORIENTED_EDGE('',*,*,#52036,.T.) ;
#72692 = ORIENTED_EDGE('',*,*,#52038,.T.) ;
#72693 = ORIENTED_EDGE('',*,*,#52039,.F.) ;
#72694 = ORIENTED_EDGE('',*,*,#52040,.T.) ;
#72695 = ORIENTED_EDGE('',*,*,#52039,.T.) ;
#72696 = ORIENTED_EDGE('',*,*,#52041,.T.) ;
#72697 = ORIENTED_EDGE('',*,*,#52042,.F.) ;
#72698 = ORIENTED_EDGE('',*,*,#52043,.T.) ;
#72699 = ORIENTED_EDGE('',*,*,#52042,.T.) ;
#72700 = ORIENTED_EDGE('',*,*,#52044,.T.) ;
#72701 = ORIENTED_EDGE('',*,*,#52045,.F.) ;
#72702 = ORIENTED_EDGE('',*,*,#52046,.T.) ;
#72703 = ORIENTED_EDGE('',*,*,#52045,.T.) ;
#72704 = ORIENTED_EDGE('',*,*,#52047,.T.) ;
#72705 = ORIENTED_EDGE('',*,*,#52048,.F.) ;
#72706 = ORIENTED_EDGE('',*,*,#52049,.T.) ;
#72707 = ORIENTED_EDGE('',*,*,#52048,.T.) ;
#72708 = ORIENTED_EDGE('',*,*,#52050,.T.) ;
#72709 = ORIENTED_EDGE('',*,*,#52051,.F.) ;
#72710 = ORIENTED_EDGE('',*,*,#52052,.T.) ;
#72711 = ORIENTED_EDGE('',*,*,#52051,.T.) ;
#72712 = ORIENTED_EDGE('',*,*,#52053,.T.) ;
#72713 = ORIENTED_EDGE('',*,*,#52054,.F.) ;
#72714 = ORIENTED_EDGE('',*,*,#52055,.T.) ;
#72715 = ORIENTED_EDGE('',*,*,#52034,.F.) ;
#72716 = ORIENTED_EDGE('',*,*,#52056,.T.) ;
#72717 = ORIENTED_EDGE('',*,*,#52054,.T.) ;
#72718 = ORIENTED_EDGE('',*,*,#52057,.T.) ;
#72719 = ORIENTED_EDGE('',*,*,#52058,.T.) ;
#72720 = ORIENTED_EDGE('',*,*,#52059,.T.) ;
#72721 = ORIENTED_EDGE('',*,*,#52060,.T.) ;
#72722 = ORIENTED_EDGE('',*,*,#52061,.T.) ;
#72723 = ORIENTED_EDGE('',*,*,#52062,.T.) ;
#72724 = ORIENTED_EDGE('',*,*,#52063,.T.) ;
#72725 = ORIENTED_EDGE('',*,*,#52064,.F.) ;
#72726 = ORIENTED_EDGE('',*,*,#52065,.T.) ;
#72727 = ORIENTED_EDGE('',*,*,#52064,.T.) ;
#72728 = ORIENTED_EDGE('',*,*,#52066,.T.) ;
#72729 = ORIENTED_EDGE('',*,*,#52067,.F.) ;
#72730 = ORIENTED_EDGE('',*,*,#52068,.T.) ;
#72731 = ORIENTED_EDGE('',*,*,#52067,.T.) ;
#72732 = ORIENTED_EDGE('',*,*,#52069,.T.) ;
#72733 = ORIENTED_EDGE('',*,*,#52070,.F.) ;
#72734 = ORIENTED_EDGE('',*,*,#52071,.T.) ;
#72735 = ORIENTED_EDGE('',*,*,#52070,.T.) ;
#72736 = ORIENTED_EDGE('',*,*,#52072,.T.) ;
#72737 = ORIENTED_EDGE('',*,*,#52073,.F.) ;
#72738 = ORIENTED_EDGE('',*,*,#52074,.T.) ;
#72739 = ORIENTED_EDGE('',*,*,#52073,.T.) ;
#72740 = ORIENTED_EDGE('',*,*,#52075,.T.) ;
#72741 = ORIENTED_EDGE('',*,*,#52076,.F.) ;
#72742 = ORIENTED_EDGE('',*,*,#52077,.T.) ;
#72743 = ORIENTED_EDGE('',*,*,#52076,.T.) ;
#72744 = ORIENTED_EDGE('',*,*,#52078,.T.) ;
#72745 = ORIENTED_EDGE('',*,*,#52079,.F.) ;
#72746 = ORIENTED_EDGE('',*,*,#52080,.T.) ;
#72747 = ORIENTED_EDGE('',*,*,#52079,.T.) ;
#72748 = ORIENTED_EDGE('',*,*,#52081,.T.) ;
#72749 = ORIENTED_EDGE('',*,*,#52082,.F.) ;
#72750 = ORIENTED_EDGE('',*,*,#52083,.T.) ;
#72751 = ORIENTED_EDGE('',*,*,#52062,.F.) ;
#72752 = ORIENTED_EDGE('',*,*,#52084,.T.) ;
#72753 = ORIENTED_EDGE('',*,*,#52082,.T.) ;
#72754 = ORIENTED_EDGE('',*,*,#52085,.T.) ;
#72755 = ORIENTED_EDGE('',*,*,#52086,.T.) ;
#72756 = ORIENTED_EDGE('',*,*,#52087,.T.) ;
#72757 = ORIENTED_EDGE('',*,*,#52088,.T.) ;
#72758 = ORIENTED_EDGE('',*,*,#52089,.T.) ;
#72759 = ORIENTED_EDGE('',*,*,#52090,.T.) ;
#72760 = ORIENTED_EDGE('',*,*,#52091,.T.) ;
#72761 = ORIENTED_EDGE('',*,*,#52092,.F.) ;
#72762 = ORIENTED_EDGE('',*,*,#52093,.T.) ;
#72763 = ORIENTED_EDGE('',*,*,#52092,.T.) ;
#72764 = ORIENTED_EDGE('',*,*,#52094,.T.) ;
#72765 = ORIENTED_EDGE('',*,*,#52095,.F.) ;
#72766 = ORIENTED_EDGE('',*,*,#52096,.T.) ;
#72767 = ORIENTED_EDGE('',*,*,#52095,.T.) ;
#72768 = ORIENTED_EDGE('',*,*,#52097,.T.) ;
#72769 = ORIENTED_EDGE('',*,*,#52098,.F.) ;
#72770 = ORIENTED_EDGE('',*,*,#52099,.T.) ;
#72771 = ORIENTED_EDGE('',*,*,#52098,.T.) ;
#72772 = ORIENTED_EDGE('',*,*,#52100,.T.) ;
#72773 = ORIENTED_EDGE('',*,*,#52101,.F.) ;
#72774 = ORIENTED_EDGE('',*,*,#52102,.T.) ;
#72775 = ORIENTED_EDGE('',*,*,#52101,.T.) ;
#72776 = ORIENTED_EDGE('',*,*,#52103,.T.) ;
#72777 = ORIENTED_EDGE('',*,*,#52104,.F.) ;
#72778 = ORIENTED_EDGE('',*,*,#52105,.T.) ;
#72779 = ORIENTED_EDGE('',*,*,#52104,.T.) ;
#72780 = ORIENTED_EDGE('',*,*,#52106,.T.) ;
#72781 = ORIENTED_EDGE('',*,*,#52107,.F.) ;
#72782 = ORIENTED_EDGE('',*,*,#52108,.T.) ;
#72783 = ORIENTED_EDGE('',*,*,#52107,.T.) ;
#72784 = ORIENTED_EDGE('',*,*,#52109,.T.) ;
#72785 = ORIENTED_EDGE('',*,*,#52110,.F.) ;
#72786 = ORIENTED_EDGE('',*,*,#52111,.T.) ;
#72787 = ORIENTED_EDGE('',*,*,#52090,.F.) ;
#72788 = ORIENTED_EDGE('',*,*,#52112,.T.) ;
#72789 = ORIENTED_EDGE('',*,*,#52110,.T.) ;
#72790 = ORIENTED_EDGE('',*,*,#52113,.T.) ;
#72791 = ORIENTED_EDGE('',*,*,#52114,.T.) ;
#72792 = ORIENTED_EDGE('',*,*,#52115,.T.) ;
#72793 = ORIENTED_EDGE('',*,*,#52116,.T.) ;
#72794 = ORIENTED_EDGE('',*,*,#52117,.T.) ;
#72795 = ORIENTED_EDGE('',*,*,#52118,.T.) ;
#72796 = ORIENTED_EDGE('',*,*,#52119,.T.) ;
#72797 = ORIENTED_EDGE('',*,*,#52120,.F.) ;
#72798 = ORIENTED_EDGE('',*,*,#52121,.T.) ;
#72799 = ORIENTED_EDGE('',*,*,#52120,.T.) ;
#72800 = ORIENTED_EDGE('',*,*,#52122,.T.) ;
#72801 = ORIENTED_EDGE('',*,*,#52123,.F.) ;
#72802 = ORIENTED_EDGE('',*,*,#52124,.T.) ;
#72803 = ORIENTED_EDGE('',*,*,#52123,.T.) ;
#72804 = ORIENTED_EDGE('',*,*,#52125,.T.) ;
#72805 = ORIENTED_EDGE('',*,*,#52126,.F.) ;
#72806 = ORIENTED_EDGE('',*,*,#52127,.T.) ;
#72807 = ORIENTED_EDGE('',*,*,#52126,.T.) ;
#72808 = ORIENTED_EDGE('',*,*,#52128,.T.) ;
#72809 = ORIENTED_EDGE('',*,*,#52129,.F.) ;
#72810 = ORIENTED_EDGE('',*,*,#52130,.T.) ;
#72811 = ORIENTED_EDGE('',*,*,#52129,.T.) ;
#72812 = ORIENTED_EDGE('',*,*,#52131,.T.) ;
#72813 = ORIENTED_EDGE('',*,*,#52132,.F.) ;
#72814 = ORIENTED_EDGE('',*,*,#52133,.T.) ;
#72815 = ORIENTED_EDGE('',*,*,#52132,.T.) ;
#72816 = ORIENTED_EDGE('',*,*,#52134,.T.) ;
#72817 = ORIENTED_EDGE('',*,*,#52135,.F.) ;
#72818 = ORIENTED_EDGE('',*,*,#52136,.T.) ;
#72819 = ORIENTED_EDGE('',*,*,#52135,.T.) ;
#72820 = ORIENTED_EDGE('',*,*,#52137,.T.) ;
#72821 = ORIENTED_EDGE('',*,*,#52138,.F.) ;
#72822 = ORIENTED_EDGE('',*,*,#52139,.T.) ;
#72823 = ORIENTED_EDGE('',*,*,#52118,.F.) ;
#72824 = ORIENTED_EDGE('',*,*,#52140,.T.) ;
#72825 = ORIENTED_EDGE('',*,*,#52138,.T.) ;
#72826 = ORIENTED_EDGE('',*,*,#52141,.T.) ;
#72827 = ORIENTED_EDGE('',*,*,#52142,.T.) ;
#72828 = ORIENTED_EDGE('',*,*,#52143,.T.) ;
#72829 = ORIENTED_EDGE('',*,*,#52144,.T.) ;
#72830 = ORIENTED_EDGE('',*,*,#52145,.T.) ;
#72831 = ORIENTED_EDGE('',*,*,#52146,.T.) ;
#72832 = ORIENTED_EDGE('',*,*,#52147,.T.) ;
#72833 = ORIENTED_EDGE('',*,*,#52148,.F.) ;
#72834 = ORIENTED_EDGE('',*,*,#52149,.T.) ;
#72835 = ORIENTED_EDGE('',*,*,#52148,.T.) ;
#72836 = ORIENTED_EDGE('',*,*,#52150,.T.) ;
#72837 = ORIENTED_EDGE('',*,*,#52151,.F.) ;
#72838 = ORIENTED_EDGE('',*,*,#52152,.T.) ;
#72839 = ORIENTED_EDGE('',*,*,#52151,.T.) ;
#72840 = ORIENTED_EDGE('',*,*,#52153,.T.) ;
#72841 = ORIENTED_EDGE('',*,*,#52154,.F.) ;
#72842 = ORIENTED_EDGE('',*,*,#52155,.T.) ;
#72843 = ORIENTED_EDGE('',*,*,#52154,.T.) ;
#72844 = ORIENTED_EDGE('',*,*,#52156,.T.) ;
#72845 = ORIENTED_EDGE('',*,*,#52157,.F.) ;
#72846 = ORIENTED_EDGE('',*,*,#52158,.T.) ;
#72847 = ORIENTED_EDGE('',*,*,#52157,.T.) ;
#72848 = ORIENTED_EDGE('',*,*,#52159,.T.) ;
#72849 = ORIENTED_EDGE('',*,*,#52160,.F.) ;
#72850 = ORIENTED_EDGE('',*,*,#52161,.T.) ;
#72851 = ORIENTED_EDGE('',*,*,#52160,.T.) ;
#72852 = ORIENTED_EDGE('',*,*,#52162,.T.) ;
#72853 = ORIENTED_EDGE('',*,*,#52163,.F.) ;
#72854 = ORIENTED_EDGE('',*,*,#52164,.T.) ;
#72855 = ORIENTED_EDGE('',*,*,#52163,.T.) ;
#72856 = ORIENTED_EDGE('',*,*,#52165,.T.) ;
#72857 = ORIENTED_EDGE('',*,*,#52166,.F.) ;
#72858 = ORIENTED_EDGE('',*,*,#52167,.T.) ;
#72859 = ORIENTED_EDGE('',*,*,#52146,.F.) ;
#72860 = ORIENTED_EDGE('',*,*,#52168,.T.) ;
#72861 = ORIENTED_EDGE('',*,*,#52166,.T.) ;
#72862 = ORIENTED_EDGE('',*,*,#52169,.T.) ;
#72863 = ORIENTED_EDGE('',*,*,#52170,.T.) ;
#72864 = ORIENTED_EDGE('',*,*,#52171,.T.) ;
#72865 = ORIENTED_EDGE('',*,*,#52172,.T.) ;
#72866 = ORIENTED_EDGE('',*,*,#52173,.T.) ;
#72867 = ORIENTED_EDGE('',*,*,#52174,.T.) ;
#72868 = ORIENTED_EDGE('',*,*,#52175,.T.) ;
#72869 = ORIENTED_EDGE('',*,*,#52176,.F.) ;
#72870 = ORIENTED_EDGE('',*,*,#52177,.T.) ;
#72871 = ORIENTED_EDGE('',*,*,#52176,.T.) ;
#72872 = ORIENTED_EDGE('',*,*,#52178,.T.) ;
#72873 = ORIENTED_EDGE('',*,*,#52179,.F.) ;
#72874 = ORIENTED_EDGE('',*,*,#52180,.T.) ;
#72875 = ORIENTED_EDGE('',*,*,#52179,.T.) ;
#72876 = ORIENTED_EDGE('',*,*,#52181,.T.) ;
#72877 = ORIENTED_EDGE('',*,*,#52182,.F.) ;
#72878 = ORIENTED_EDGE('',*,*,#52183,.T.) ;
#72879 = ORIENTED_EDGE('',*,*,#52182,.T.) ;
#72880 = ORIENTED_EDGE('',*,*,#52184,.T.) ;
#72881 = ORIENTED_EDGE('',*,*,#52185,.F.) ;
#72882 = ORIENTED_EDGE('',*,*,#52186,.T.) ;
#72883 = ORIENTED_EDGE('',*,*,#52185,.T.) ;
#72884 = ORIENTED_EDGE('',*,*,#52187,.T.) ;
#72885 = ORIENTED_EDGE('',*,*,#52188,.F.) ;
#72886 = ORIENTED_EDGE('',*,*,#52189,.T.) ;
#72887 = ORIENTED_EDGE('',*,*,#52188,.T.) ;
#72888 = ORIENTED_EDGE('',*,*,#52190,.T.) ;
#72889 = ORIENTED_EDGE('',*,*,#52191,.F.) ;
#72890 = ORIENTED_EDGE('',*,*,#52192,.T.) ;
#72891 = ORIENTED_EDGE('',*,*,#52191,.T.) ;
#72892 = ORIENTED_EDGE('',*,*,#52193,.T.) ;
#72893 = ORIENTED_EDGE('',*,*,#52194,.F.) ;
#72894 = ORIENTED_EDGE('',*,*,#52195,.T.) ;
#72895 = ORIENTED_EDGE('',*,*,#52174,.F.) ;
#72896 = ORIENTED_EDGE('',*,*,#52196,.T.) ;
#72897 = ORIENTED_EDGE('',*,*,#52194,.T.) ;
#72898 = ORIENTED_EDGE('',*,*,#52197,.T.) ;
#72899 = ORIENTED_EDGE('',*,*,#52198,.T.) ;
#72900 = ORIENTED_EDGE('',*,*,#52199,.T.) ;
#72901 = ORIENTED_EDGE('',*,*,#52200,.T.) ;
#72902 = ORIENTED_EDGE('',*,*,#52201,.T.) ;
#72903 = ORIENTED_EDGE('',*,*,#52202,.F.) ;
#72904 = ORIENTED_EDGE('',*,*,#52203,.F.) ;
#72905 = ORIENTED_EDGE('',*,*,#52204,.F.) ;
#72906 = ORIENTED_EDGE('',*,*,#52203,.T.) ;
#72907 = ORIENTED_EDGE('',*,*,#51342,.F.) ;
#72908 = ORIENTED_EDGE('',*,*,#52205,.F.) ;
#72909 = ORIENTED_EDGE('',*,*,#51340,.F.) ;
#72910 = ORIENTED_EDGE('',*,*,#52204,.T.) ;
#72911 = ORIENTED_EDGE('',*,*,#51339,.F.) ;
#72912 = ORIENTED_EDGE('',*,*,#52206,.F.) ;
#72913 = ORIENTED_EDGE('',*,*,#51329,.F.) ;
#72914 = ORIENTED_EDGE('',*,*,#52202,.T.) ;
#72915 = ORIENTED_EDGE('',*,*,#51332,.F.) ;
#72916 = ORIENTED_EDGE('',*,*,#52207,.F.) ;
#72917 = ORIENTED_EDGE('',*,*,#51343,.F.) ;
#72918 = ORIENTED_EDGE('',*,*,#51095,.F.) ;
#72919 = ORIENTED_EDGE('',*,*,#52208,.T.) ;
#72920 = ORIENTED_EDGE('',*,*,#51344,.F.) ;
#72921 = ORIENTED_EDGE('',*,*,#52209,.F.) ;
#72922 = ORIENTED_EDGE('',*,*,#51345,.F.) ;
#72923 = ORIENTED_EDGE('',*,*,#52210,.T.) ;
#72924 = ORIENTED_EDGE('',*,*,#49511,.F.) ;
#72925 = ORIENTED_EDGE('',*,*,#52211,.T.) ;
#72926 = ORIENTED_EDGE('',*,*,#52212,.F.) ;
#72927 = ORIENTED_EDGE('',*,*,#52205,.T.) ;
#72928 = ORIENTED_EDGE('',*,*,#52213,.F.) ;
#72929 = ORIENTED_EDGE('',*,*,#52214,.F.) ;
#72930 = ORIENTED_EDGE('',*,*,#52206,.T.) ;
#72931 = ORIENTED_EDGE('',*,*,#52215,.F.) ;
#72932 = ORIENTED_EDGE('',*,*,#49666,.T.) ;
#72933 = ORIENTED_EDGE('',*,*,#52209,.T.) ;
#72934 = ORIENTED_EDGE('',*,*,#52207,.T.) ;
#72935 = ORIENTED_EDGE('',*,*,#52216,.F.) ;
#72936 = ORIENTED_EDGE('',*,*,#51346,.F.) ;
#72937 = ORIENTED_EDGE('',*,*,#52217,.T.) ;
#72938 = ORIENTED_EDGE('',*,*,#51085,.F.) ;
#72939 = ORIENTED_EDGE('',*,*,#52218,.F.) ;
#72940 = ORIENTED_EDGE('',*,*,#52213,.T.) ;
#72941 = ORIENTED_EDGE('',*,*,#51341,.F.) ;
#72942 = ORIENTED_EDGE('',*,*,#52219,.F.) ;
#72943 = ORIENTED_EDGE('',*,*,#51336,.F.) ;
#72944 = ORIENTED_EDGE('',*,*,#52212,.T.) ;
#72945 = ORIENTED_EDGE('',*,*,#51335,.F.) ;
#72946 = ORIENTED_EDGE('',*,*,#52220,.F.) ;
#72947 = ORIENTED_EDGE('',*,*,#51337,.F.) ;
#72948 = ORIENTED_EDGE('',*,*,#52215,.T.) ;
#72949 = ORIENTED_EDGE('',*,*,#51338,.F.) ;
#72950 = ORIENTED_EDGE('',*,*,#52221,.F.) ;
#72951 = ORIENTED_EDGE('',*,*,#49667,.F.) ;
#72952 = ORIENTED_EDGE('',*,*,#52214,.T.) ;
#72953 = ORIENTED_EDGE('',*,*,#49665,.F.) ;
#72954 = ORIENTED_EDGE('',*,*,#52222,.F.) ;
#72955 = ORIENTED_EDGE('',*,*,#51330,.F.) ;
#72956 = ORIENTED_EDGE('',*,*,#52216,.T.) ;
#72957 = ORIENTED_EDGE('',*,*,#51331,.F.) ;
#72958 = ORIENTED_EDGE('',*,*,#52223,.F.) ;
#72959 = ORIENTED_EDGE('',*,*,#51096,.F.) ;
#72960 = ORIENTED_EDGE('',*,*,#52219,.T.) ;
#72961 = ORIENTED_EDGE('',*,*,#52218,.T.) ;
#72962 = ORIENTED_EDGE('',*,*,#52224,.F.) ;
#72963 = ORIENTED_EDGE('',*,*,#52221,.T.) ;
#72964 = ORIENTED_EDGE('',*,*,#52220,.T.) ;
#72965 = ORIENTED_EDGE('',*,*,#52225,.F.) ;
#72966 = ORIENTED_EDGE('',*,*,#49660,.T.) ;
#72967 = ORIENTED_EDGE('',*,*,#52223,.T.) ;
#72968 = ORIENTED_EDGE('',*,*,#52222,.T.) ;
#72969 = ORIENTED_EDGE('',*,*,#52226,.F.) ;
#72970 = ORIENTED_EDGE('',*,*,#51097,.T.) ;
#72971 = ORIENTED_EDGE('',*,*,#52224,.T.) ;
#72972 = ORIENTED_EDGE('',*,*,#51084,.F.) ;
#72973 = ORIENTED_EDGE('',*,*,#52227,.F.) ;
#72974 = ORIENTED_EDGE('',*,*,#51333,.F.) ;
#72975 = ORIENTED_EDGE('',*,*,#52225,.T.) ;
#72976 = ORIENTED_EDGE('',*,*,#51334,.F.) ;
#72977 = ORIENTED_EDGE('',*,*,#52228,.F.) ;
#72978 = ORIENTED_EDGE('',*,*,#49661,.F.) ;
#72979 = ORIENTED_EDGE('',*,*,#52226,.T.) ;
#72980 = ORIENTED_EDGE('',*,*,#49664,.F.) ;
#72981 = ORIENTED_EDGE('',*,*,#52229,.F.) ;
#72982 = ORIENTED_EDGE('',*,*,#51098,.F.) ;
#72983 = ORIENTED_EDGE('',*,*,#51103,.F.) ;
#72984 = ORIENTED_EDGE('',*,*,#52230,.T.) ;
#72985 = ORIENTED_EDGE('',*,*,#51091,.F.) ;
#72986 = ORIENTED_EDGE('',*,*,#52231,.F.) ;
#72987 = ORIENTED_EDGE('',*,*,#49722,.F.) ;
#72988 = ORIENTED_EDGE('',*,*,#52232,.T.) ;
#72989 = ORIENTED_EDGE('',*,*,#51104,.F.) ;
#72990 = ORIENTED_EDGE('',*,*,#52233,.F.) ;
#72991 = ORIENTED_EDGE('',*,*,#52227,.T.) ;
#72992 = ORIENTED_EDGE('',*,*,#51083,.T.) ;
#72993 = ORIENTED_EDGE('',*,*,#52234,.F.) ;
#72994 = ORIENTED_EDGE('',*,*,#52228,.T.) ;
#72995 = ORIENTED_EDGE('',*,*,#52235,.F.) ;
#72996 = ORIENTED_EDGE('',*,*,#52229,.T.) ;
#72997 = ORIENTED_EDGE('',*,*,#52236,.F.) ;
#72998 = ORIENTED_EDGE('',*,*,#52233,.T.) ;
#72999 = ORIENTED_EDGE('',*,*,#52231,.T.) ;
#73000 = ORIENTED_EDGE('',*,*,#52237,.F.) ;
#73001 = ORIENTED_EDGE('',*,*,#52234,.T.) ;
#73002 = ORIENTED_EDGE('',*,*,#51082,.F.) ;
#73003 = ORIENTED_EDGE('',*,*,#52238,.F.) ;
#73004 = ORIENTED_EDGE('',*,*,#49662,.F.) ;
#73005 = ORIENTED_EDGE('',*,*,#52236,.T.) ;
#73006 = ORIENTED_EDGE('',*,*,#49663,.F.) ;
#73007 = ORIENTED_EDGE('',*,*,#52239,.F.) ;
#73008 = ORIENTED_EDGE('',*,*,#51090,.F.) ;
#73009 = ORIENTED_EDGE('',*,*,#52235,.T.) ;
#73010 = ORIENTED_EDGE('',*,*,#51089,.F.) ;
#73011 = ORIENTED_EDGE('',*,*,#52240,.F.) ;
#73012 = ORIENTED_EDGE('',*,*,#51099,.F.) ;
#73013 = ORIENTED_EDGE('',*,*,#52237,.T.) ;
#73014 = ORIENTED_EDGE('',*,*,#51100,.F.) ;
#73015 = ORIENTED_EDGE('',*,*,#52241,.F.) ;
#73016 = ORIENTED_EDGE('',*,*,#49723,.F.) ;
#73017 = ORIENTED_EDGE('',*,*,#52239,.T.) ;
#73018 = ORIENTED_EDGE('',*,*,#52238,.T.) ;
#73019 = ORIENTED_EDGE('',*,*,#52242,.F.) ;
#73020 = ORIENTED_EDGE('',*,*,#52241,.T.) ;
#73021 = ORIENTED_EDGE('',*,*,#52240,.T.) ;
#73022 = ORIENTED_EDGE('',*,*,#52243,.F.) ;
#73023 = ORIENTED_EDGE('',*,*,#49724,.T.) ;
#73024 = ORIENTED_EDGE('',*,*,#51079,.F.) ;
#73025 = ORIENTED_EDGE('',*,*,#52244,.T.) ;
#73026 = ORIENTED_EDGE('',*,*,#50026,.F.) ;
#73027 = ORIENTED_EDGE('',*,*,#52245,.F.) ;
#73028 = ORIENTED_EDGE('',*,*,#52242,.T.) ;
#73029 = ORIENTED_EDGE('',*,*,#51081,.F.) ;
#73030 = ORIENTED_EDGE('',*,*,#52246,.F.) ;
#73031 = ORIENTED_EDGE('',*,*,#51087,.F.) ;
#73032 = ORIENTED_EDGE('',*,*,#52243,.T.) ;
#73033 = ORIENTED_EDGE('',*,*,#51088,.F.) ;
#73034 = ORIENTED_EDGE('',*,*,#52247,.F.) ;
#73035 = ORIENTED_EDGE('',*,*,#49725,.F.) ;
#73036 = ORIENTED_EDGE('',*,*,#52245,.T.) ;
#73037 = ORIENTED_EDGE('',*,*,#50211,.T.) ;
#73038 = ORIENTED_EDGE('',*,*,#52248,.F.) ;
#73039 = ORIENTED_EDGE('',*,*,#52247,.T.) ;
#73040 = ORIENTED_EDGE('',*,*,#52246,.T.) ;
#73041 = ORIENTED_EDGE('',*,*,#52249,.F.) ;
#73042 = ORIENTED_EDGE('',*,*,#49726,.T.) ;
#73043 = ORIENTED_EDGE('',*,*,#52248,.T.) ;
#73044 = ORIENTED_EDGE('',*,*,#49727,.F.) ;
#73045 = ORIENTED_EDGE('',*,*,#52249,.T.) ;
#73046 = ORIENTED_EDGE('',*,*,#51080,.F.) ;
#73047 = ORIENTED_EDGE('',*,*,#52250,.F.) ;
#73048 = ORIENTED_EDGE('',*,*,#49520,.F.) ;
#73049 = ORIENTED_EDGE('',*,*,#52251,.F.) ;
#73050 = ORIENTED_EDGE('',*,*,#51957,.F.) ;
#73051 = ORIENTED_EDGE('',*,*,#52251,.T.) ;
#73052 = ORIENTED_EDGE('',*,*,#49519,.F.) ;
#73053 = ORIENTED_EDGE('',*,*,#52252,.F.) ;
#73054 = ORIENTED_EDGE('',*,*,#51960,.F.) ;
#73055 = ORIENTED_EDGE('',*,*,#52250,.T.) ;
#73056 = ORIENTED_EDGE('',*,*,#51954,.F.) ;
#73057 = ORIENTED_EDGE('',*,*,#52253,.F.) ;
#73058 = ORIENTED_EDGE('',*,*,#49521,.F.) ;
#73059 = ORIENTED_EDGE('',*,*,#52252,.T.) ;
#73060 = ORIENTED_EDGE('',*,*,#49518,.F.) ;
#73061 = ORIENTED_EDGE('',*,*,#52254,.F.) ;
#73062 = ORIENTED_EDGE('',*,*,#51963,.F.) ;
#73063 = ORIENTED_EDGE('',*,*,#52253,.T.) ;
#73064 = ORIENTED_EDGE('',*,*,#51951,.F.) ;
#73065 = ORIENTED_EDGE('',*,*,#52255,.F.) ;
#73066 = ORIENTED_EDGE('',*,*,#49522,.F.) ;
#73067 = ORIENTED_EDGE('',*,*,#52254,.T.) ;
#73068 = ORIENTED_EDGE('',*,*,#49517,.F.) ;
#73069 = ORIENTED_EDGE('',*,*,#52256,.F.) ;
#73070 = ORIENTED_EDGE('',*,*,#51966,.F.) ;
#73071 = ORIENTED_EDGE('',*,*,#52255,.T.) ;
#73072 = ORIENTED_EDGE('',*,*,#51973,.F.) ;
#73073 = ORIENTED_EDGE('',*,*,#52257,.F.) ;
#73074 = ORIENTED_EDGE('',*,*,#49515,.F.) ;
#73075 = ORIENTED_EDGE('',*,*,#52256,.T.) ;
#73076 = ORIENTED_EDGE('',*,*,#49516,.F.) ;
#73077 = ORIENTED_EDGE('',*,*,#52257,.T.) ;
#73078 = ORIENTED_EDGE('',*,*,#51969,.F.) ;
#73079 = ORIENTED_EDGE('',*,*,#50687,.F.) ;
#73080 = ORIENTED_EDGE('',*,*,#52258,.T.) ;
#73081 = ORIENTED_EDGE('',*,*,#52259,.T.) ;
#73082 = ORIENTED_EDGE('',*,*,#49839,.F.) ;
#73083 = ORIENTED_EDGE('',*,*,#52260,.T.) ;
#73084 = ORIENTED_EDGE('',*,*,#52261,.T.) ;
#73085 = ORIENTED_EDGE('',*,*,#49838,.F.) ;
#73086 = ORIENTED_EDGE('',*,*,#52262,.T.) ;
#73087 = ORIENTED_EDGE('',*,*,#52263,.T.) ;
#73088 = ORIENTED_EDGE('',*,*,#50681,.F.) ;
#73089 = ORIENTED_EDGE('',*,*,#52264,.T.) ;
#73090 = ORIENTED_EDGE('',*,*,#52265,.T.) ;
#73091 = ORIENTED_EDGE('',*,*,#49836,.F.) ;
#73092 = ORIENTED_EDGE('',*,*,#52266,.T.) ;
#73093 = ORIENTED_EDGE('',*,*,#52267,.T.) ;
#73094 = ORIENTED_EDGE('',*,*,#50689,.F.) ;
#73095 = ORIENTED_EDGE('',*,*,#52268,.T.) ;
#73096 = ORIENTED_EDGE('',*,*,#52269,.T.) ;
#73097 = ORIENTED_EDGE('',*,*,#49837,.F.) ;
#73098 = ORIENTED_EDGE('',*,*,#52270,.T.) ;
#73099 = ORIENTED_EDGE('',*,*,#52271,.T.) ;
#73100 = ORIENTED_EDGE('',*,*,#50693,.F.) ;
#73101 = ORIENTED_EDGE('',*,*,#52272,.T.) ;
#73102 = ORIENTED_EDGE('',*,*,#52273,.T.) ;
#73103 = ORIENTED_EDGE('',*,*,#50703,.F.) ;
#73104 = ORIENTED_EDGE('',*,*,#52274,.T.) ;
#73105 = ORIENTED_EDGE('',*,*,#52275,.T.) ;
#73106 = ORIENTED_EDGE('',*,*,#49843,.F.) ;
#73107 = ORIENTED_EDGE('',*,*,#52276,.T.) ;
#73108 = ORIENTED_EDGE('',*,*,#52277,.T.) ;
#73109 = ORIENTED_EDGE('',*,*,#49842,.F.) ;
#73110 = ORIENTED_EDGE('',*,*,#52278,.T.) ;
#73111 = ORIENTED_EDGE('',*,*,#52279,.T.) ;
#73112 = ORIENTED_EDGE('',*,*,#50697,.F.) ;
#73113 = ORIENTED_EDGE('',*,*,#52280,.T.) ;
#73114 = ORIENTED_EDGE('',*,*,#52281,.T.) ;
#73115 = ORIENTED_EDGE('',*,*,#49840,.F.) ;
#73116 = ORIENTED_EDGE('',*,*,#52282,.T.) ;
#73117 = ORIENTED_EDGE('',*,*,#52283,.T.) ;
#73118 = ORIENTED_EDGE('',*,*,#50705,.F.) ;
#73119 = ORIENTED_EDGE('',*,*,#52284,.T.) ;
#73120 = ORIENTED_EDGE('',*,*,#52285,.T.) ;
#73121 = ORIENTED_EDGE('',*,*,#49841,.F.) ;
#73122 = ORIENTED_EDGE('',*,*,#52286,.T.) ;
#73123 = ORIENTED_EDGE('',*,*,#52287,.T.) ;
#73124 = ORIENTED_EDGE('',*,*,#50709,.F.) ;
#73125 = ORIENTED_EDGE('',*,*,#52288,.T.) ;
#73126 = ORIENTED_EDGE('',*,*,#52289,.T.) ;
#73127 = ORIENTED_EDGE('',*,*,#50719,.F.) ;
#73128 = ORIENTED_EDGE('',*,*,#52290,.T.) ;
#73129 = ORIENTED_EDGE('',*,*,#52291,.T.) ;
#73130 = ORIENTED_EDGE('',*,*,#49847,.F.) ;
#73131 = ORIENTED_EDGE('',*,*,#52292,.T.) ;
#73132 = ORIENTED_EDGE('',*,*,#52293,.T.) ;
#73133 = ORIENTED_EDGE('',*,*,#49846,.F.) ;
#73134 = ORIENTED_EDGE('',*,*,#52294,.T.) ;
#73135 = ORIENTED_EDGE('',*,*,#52295,.T.) ;
#73136 = ORIENTED_EDGE('',*,*,#50713,.F.) ;
#73137 = ORIENTED_EDGE('',*,*,#52296,.T.) ;
#73138 = ORIENTED_EDGE('',*,*,#52297,.T.) ;
#73139 = ORIENTED_EDGE('',*,*,#49844,.F.) ;
#73140 = ORIENTED_EDGE('',*,*,#52298,.T.) ;
#73141 = ORIENTED_EDGE('',*,*,#52299,.T.) ;
#73142 = ORIENTED_EDGE('',*,*,#50721,.F.) ;
#73143 = ORIENTED_EDGE('',*,*,#52300,.T.) ;
#73144 = ORIENTED_EDGE('',*,*,#52301,.T.) ;
#73145 = ORIENTED_EDGE('',*,*,#49845,.F.) ;
#73146 = ORIENTED_EDGE('',*,*,#52302,.T.) ;
#73147 = ORIENTED_EDGE('',*,*,#52303,.T.) ;
#73148 = ORIENTED_EDGE('',*,*,#50725,.F.) ;
#73149 = ORIENTED_EDGE('',*,*,#52304,.T.) ;
#73150 = ORIENTED_EDGE('',*,*,#52305,.T.) ;
#73151 = ORIENTED_EDGE('',*,*,#50735,.F.) ;
#73152 = ORIENTED_EDGE('',*,*,#52306,.T.) ;
#73153 = ORIENTED_EDGE('',*,*,#52307,.T.) ;
#73154 = ORIENTED_EDGE('',*,*,#49851,.F.) ;
#73155 = ORIENTED_EDGE('',*,*,#52308,.T.) ;
#73156 = ORIENTED_EDGE('',*,*,#52309,.T.) ;
#73157 = ORIENTED_EDGE('',*,*,#49850,.F.) ;
#73158 = ORIENTED_EDGE('',*,*,#52310,.T.) ;
#73159 = ORIENTED_EDGE('',*,*,#52311,.T.) ;
#73160 = ORIENTED_EDGE('',*,*,#50729,.F.) ;
#73161 = ORIENTED_EDGE('',*,*,#52312,.T.) ;
#73162 = ORIENTED_EDGE('',*,*,#52313,.T.) ;
#73163 = ORIENTED_EDGE('',*,*,#49848,.F.) ;
#73164 = ORIENTED_EDGE('',*,*,#52314,.T.) ;
#73165 = ORIENTED_EDGE('',*,*,#52315,.T.) ;
#73166 = ORIENTED_EDGE('',*,*,#50737,.F.) ;
#73167 = ORIENTED_EDGE('',*,*,#52316,.T.) ;
#73168 = ORIENTED_EDGE('',*,*,#52317,.T.) ;
#73169 = ORIENTED_EDGE('',*,*,#49849,.F.) ;
#73170 = ORIENTED_EDGE('',*,*,#52318,.T.) ;
#73171 = ORIENTED_EDGE('',*,*,#52319,.T.) ;
#73172 = ORIENTED_EDGE('',*,*,#50741,.F.) ;
#73173 = ORIENTED_EDGE('',*,*,#52320,.T.) ;
#73174 = ORIENTED_EDGE('',*,*,#52321,.T.) ;
#73175 = ORIENTED_EDGE('',*,*,#50751,.F.) ;
#73176 = ORIENTED_EDGE('',*,*,#52322,.T.) ;
#73177 = ORIENTED_EDGE('',*,*,#52323,.T.) ;
#73178 = ORIENTED_EDGE('',*,*,#49855,.F.) ;
#73179 = ORIENTED_EDGE('',*,*,#52324,.T.) ;
#73180 = ORIENTED_EDGE('',*,*,#52325,.T.) ;
#73181 = ORIENTED_EDGE('',*,*,#49854,.F.) ;
#73182 = ORIENTED_EDGE('',*,*,#52326,.T.) ;
#73183 = ORIENTED_EDGE('',*,*,#52327,.T.) ;
#73184 = ORIENTED_EDGE('',*,*,#50745,.F.) ;
#73185 = ORIENTED_EDGE('',*,*,#52328,.T.) ;
#73186 = ORIENTED_EDGE('',*,*,#52329,.T.) ;
#73187 = ORIENTED_EDGE('',*,*,#49852,.F.) ;
#73188 = ORIENTED_EDGE('',*,*,#52330,.T.) ;
#73189 = ORIENTED_EDGE('',*,*,#52331,.T.) ;
#73190 = ORIENTED_EDGE('',*,*,#50753,.F.) ;
#73191 = ORIENTED_EDGE('',*,*,#52332,.T.) ;
#73192 = ORIENTED_EDGE('',*,*,#52333,.T.) ;
#73193 = ORIENTED_EDGE('',*,*,#49853,.F.) ;
#73194 = ORIENTED_EDGE('',*,*,#52334,.T.) ;
#73195 = ORIENTED_EDGE('',*,*,#52335,.T.) ;
#73196 = ORIENTED_EDGE('',*,*,#50757,.F.) ;
#73197 = ORIENTED_EDGE('',*,*,#52336,.T.) ;
#73198 = ORIENTED_EDGE('',*,*,#52337,.T.) ;
#73199 = ORIENTED_EDGE('',*,*,#50767,.F.) ;
#73200 = ORIENTED_EDGE('',*,*,#52338,.T.) ;
#73201 = ORIENTED_EDGE('',*,*,#52339,.T.) ;
#73202 = ORIENTED_EDGE('',*,*,#49859,.F.) ;
#73203 = ORIENTED_EDGE('',*,*,#52340,.T.) ;
#73204 = ORIENTED_EDGE('',*,*,#52341,.T.) ;
#73205 = ORIENTED_EDGE('',*,*,#49858,.F.) ;
#73206 = ORIENTED_EDGE('',*,*,#52342,.T.) ;
#73207 = ORIENTED_EDGE('',*,*,#52343,.T.) ;
#73208 = ORIENTED_EDGE('',*,*,#50761,.F.) ;
#73209 = ORIENTED_EDGE('',*,*,#52344,.T.) ;
#73210 = ORIENTED_EDGE('',*,*,#52345,.T.) ;
#73211 = ORIENTED_EDGE('',*,*,#49856,.F.) ;
#73212 = ORIENTED_EDGE('',*,*,#52346,.T.) ;
#73213 = ORIENTED_EDGE('',*,*,#52347,.T.) ;
#73214 = ORIENTED_EDGE('',*,*,#50769,.F.) ;
#73215 = ORIENTED_EDGE('',*,*,#52348,.T.) ;
#73216 = ORIENTED_EDGE('',*,*,#52349,.T.) ;
#73217 = ORIENTED_EDGE('',*,*,#49857,.F.) ;
#73218 = ORIENTED_EDGE('',*,*,#52350,.T.) ;
#73219 = ORIENTED_EDGE('',*,*,#52351,.T.) ;
#73220 = ORIENTED_EDGE('',*,*,#50773,.F.) ;
#73221 = ORIENTED_EDGE('',*,*,#52352,.T.) ;
#73222 = ORIENTED_EDGE('',*,*,#52353,.T.) ;
#73223 = ORIENTED_EDGE('',*,*,#50783,.F.) ;
#73224 = ORIENTED_EDGE('',*,*,#52354,.T.) ;
#73225 = ORIENTED_EDGE('',*,*,#52355,.T.) ;
#73226 = ORIENTED_EDGE('',*,*,#49863,.F.) ;
#73227 = ORIENTED_EDGE('',*,*,#52356,.T.) ;
#73228 = ORIENTED_EDGE('',*,*,#52357,.T.) ;
#73229 = ORIENTED_EDGE('',*,*,#49862,.F.) ;
#73230 = ORIENTED_EDGE('',*,*,#52358,.T.) ;
#73231 = ORIENTED_EDGE('',*,*,#52359,.T.) ;
#73232 = ORIENTED_EDGE('',*,*,#50777,.F.) ;
#73233 = ORIENTED_EDGE('',*,*,#52360,.T.) ;
#73234 = ORIENTED_EDGE('',*,*,#52361,.T.) ;
#73235 = ORIENTED_EDGE('',*,*,#49860,.F.) ;
#73236 = ORIENTED_EDGE('',*,*,#52362,.T.) ;
#73237 = ORIENTED_EDGE('',*,*,#52363,.T.) ;
#73238 = ORIENTED_EDGE('',*,*,#50785,.F.) ;
#73239 = ORIENTED_EDGE('',*,*,#52364,.T.) ;
#73240 = ORIENTED_EDGE('',*,*,#52365,.T.) ;
#73241 = ORIENTED_EDGE('',*,*,#49861,.F.) ;
#73242 = ORIENTED_EDGE('',*,*,#52366,.T.) ;
#73243 = ORIENTED_EDGE('',*,*,#52367,.T.) ;
#73244 = ORIENTED_EDGE('',*,*,#50789,.F.) ;
#73245 = ORIENTED_EDGE('',*,*,#52368,.T.) ;
#73246 = ORIENTED_EDGE('',*,*,#52369,.T.) ;
#73247 = ORIENTED_EDGE('',*,*,#50799,.F.) ;
#73248 = ORIENTED_EDGE('',*,*,#52370,.T.) ;
#73249 = ORIENTED_EDGE('',*,*,#52371,.T.) ;
#73250 = ORIENTED_EDGE('',*,*,#49867,.F.) ;
#73251 = ORIENTED_EDGE('',*,*,#52372,.T.) ;
#73252 = ORIENTED_EDGE('',*,*,#52373,.T.) ;
#73253 = ORIENTED_EDGE('',*,*,#49866,.F.) ;
#73254 = ORIENTED_EDGE('',*,*,#52374,.T.) ;
#73255 = ORIENTED_EDGE('',*,*,#52375,.T.) ;
#73256 = ORIENTED_EDGE('',*,*,#50793,.F.) ;
#73257 = ORIENTED_EDGE('',*,*,#52376,.T.) ;
#73258 = ORIENTED_EDGE('',*,*,#52377,.T.) ;
#73259 = ORIENTED_EDGE('',*,*,#49864,.F.) ;
#73260 = ORIENTED_EDGE('',*,*,#52378,.T.) ;
#73261 = ORIENTED_EDGE('',*,*,#52379,.T.) ;
#73262 = ORIENTED_EDGE('',*,*,#50801,.F.) ;
#73263 = ORIENTED_EDGE('',*,*,#52380,.T.) ;
#73264 = ORIENTED_EDGE('',*,*,#52381,.T.) ;
#73265 = ORIENTED_EDGE('',*,*,#49865,.F.) ;
#73266 = ORIENTED_EDGE('',*,*,#52382,.T.) ;
#73267 = ORIENTED_EDGE('',*,*,#52383,.T.) ;
#73268 = ORIENTED_EDGE('',*,*,#50805,.F.) ;
#73269 = ORIENTED_EDGE('',*,*,#52384,.T.) ;
#73270 = ORIENTED_EDGE('',*,*,#52385,.T.) ;
#73271 = ORIENTED_EDGE('',*,*,#52386,.F.) ;
#73272 = ORIENTED_EDGE('',*,*,#49873,.F.) ;
#73273 = ORIENTED_EDGE('',*,*,#52387,.F.) ;
#73274 = ORIENTED_EDGE('',*,*,#50824,.F.) ;
#73275 = ORIENTED_EDGE('',*,*,#52387,.T.) ;
#73276 = ORIENTED_EDGE('',*,*,#49872,.T.) ;
#73277 = ORIENTED_EDGE('',*,*,#52388,.F.) ;
#73278 = ORIENTED_EDGE('',*,*,#52389,.F.) ;
#73279 = ORIENTED_EDGE('',*,*,#49874,.T.) ;
#73280 = ORIENTED_EDGE('',*,*,#52386,.T.) ;
#73281 = ORIENTED_EDGE('',*,*,#52390,.F.) ;
#73282 = ORIENTED_EDGE('',*,*,#52391,.F.) ;
#73283 = ORIENTED_EDGE('',*,*,#52388,.T.) ;
#73284 = ORIENTED_EDGE('',*,*,#49871,.F.) ;
#73285 = ORIENTED_EDGE('',*,*,#52392,.F.) ;
#73286 = ORIENTED_EDGE('',*,*,#50820,.F.) ;
#73287 = ORIENTED_EDGE('',*,*,#52389,.T.) ;
#73288 = ORIENTED_EDGE('',*,*,#50819,.F.) ;
#73289 = ORIENTED_EDGE('',*,*,#52393,.F.) ;
#73290 = ORIENTED_EDGE('',*,*,#50821,.F.) ;
#73291 = ORIENTED_EDGE('',*,*,#52394,.F.) ;
#73292 = ORIENTED_EDGE('',*,*,#50822,.F.) ;
#73293 = ORIENTED_EDGE('',*,*,#52395,.F.) ;
#73294 = ORIENTED_EDGE('',*,*,#50828,.F.) ;
#73295 = ORIENTED_EDGE('',*,*,#52390,.T.) ;
#73296 = ORIENTED_EDGE('',*,*,#50823,.F.) ;
#73297 = ORIENTED_EDGE('',*,*,#52396,.F.) ;
#73298 = ORIENTED_EDGE('',*,*,#50812,.F.) ;
#73299 = ORIENTED_EDGE('',*,*,#52391,.T.) ;
#73300 = ORIENTED_EDGE('',*,*,#50811,.F.) ;
#73301 = ORIENTED_EDGE('',*,*,#52397,.F.) ;
#73302 = ORIENTED_EDGE('',*,*,#49875,.F.) ;
#73303 = ORIENTED_EDGE('',*,*,#52398,.F.) ;
#73304 = ORIENTED_EDGE('',*,*,#49869,.F.) ;
#73305 = ORIENTED_EDGE('',*,*,#52399,.F.) ;
#73306 = ORIENTED_EDGE('',*,*,#50815,.F.) ;
#73307 = ORIENTED_EDGE('',*,*,#49870,.T.) ;
#73308 = ORIENTED_EDGE('',*,*,#52398,.T.) ;
#73309 = ORIENTED_EDGE('',*,*,#52400,.F.) ;
#73310 = ORIENTED_EDGE('',*,*,#52392,.T.) ;
#73311 = ORIENTED_EDGE('',*,*,#52395,.T.) ;
#73312 = ORIENTED_EDGE('',*,*,#52393,.T.) ;
#73313 = ORIENTED_EDGE('',*,*,#52401,.F.) ;
#73314 = ORIENTED_EDGE('',*,*,#52396,.T.) ;
#73315 = ORIENTED_EDGE('',*,*,#52394,.T.) ;
#73316 = ORIENTED_EDGE('',*,*,#52402,.F.) ;
#73317 = ORIENTED_EDGE('',*,*,#49868,.T.) ;
#73318 = ORIENTED_EDGE('',*,*,#52397,.T.) ;
#73319 = ORIENTED_EDGE('',*,*,#52403,.F.) ;
#73320 = ORIENTED_EDGE('',*,*,#52399,.T.) ;
#73321 = ORIENTED_EDGE('',*,*,#52400,.T.) ;
#73322 = ORIENTED_EDGE('',*,*,#50814,.F.) ;
#73323 = ORIENTED_EDGE('',*,*,#52404,.F.) ;
#73324 = ORIENTED_EDGE('',*,*,#50817,.F.) ;
#73325 = ORIENTED_EDGE('',*,*,#52401,.T.) ;
#73326 = ORIENTED_EDGE('',*,*,#50818,.F.) ;
#73327 = ORIENTED_EDGE('',*,*,#52405,.F.) ;
#73328 = ORIENTED_EDGE('',*,*,#50825,.F.) ;
#73329 = ORIENTED_EDGE('',*,*,#52402,.T.) ;
#73330 = ORIENTED_EDGE('',*,*,#50827,.F.) ;
#73331 = ORIENTED_EDGE('',*,*,#52406,.F.) ;
#73332 = ORIENTED_EDGE('',*,*,#50809,.F.) ;
#73333 = ORIENTED_EDGE('',*,*,#52403,.T.) ;
#73334 = ORIENTED_EDGE('',*,*,#50810,.F.) ;
#73335 = ORIENTED_EDGE('',*,*,#52407,.F.) ;
#73336 = ORIENTED_EDGE('',*,*,#50816,.F.) ;
#73337 = ORIENTED_EDGE('',*,*,#52405,.T.) ;
#73338 = ORIENTED_EDGE('',*,*,#52404,.T.) ;
#73339 = ORIENTED_EDGE('',*,*,#52408,.F.) ;
#73340 = ORIENTED_EDGE('',*,*,#52407,.T.) ;
#73341 = ORIENTED_EDGE('',*,*,#52406,.T.) ;
#73342 = ORIENTED_EDGE('',*,*,#52409,.F.) ;
#73343 = ORIENTED_EDGE('',*,*,#52408,.T.) ;
#73344 = ORIENTED_EDGE('',*,*,#50813,.F.) ;
#73345 = ORIENTED_EDGE('',*,*,#52409,.T.) ;
#73346 = ORIENTED_EDGE('',*,*,#50826,.F.) ;
#73347 = ORIENTED_EDGE('',*,*,#50834,.F.) ;
#73348 = ORIENTED_EDGE('',*,*,#50848,.F.) ;
#73349 = ORIENTED_EDGE('',*,*,#52410,.F.) ;
#73350 = ORIENTED_EDGE('',*,*,#50837,.F.) ;
#73351 = ORIENTED_EDGE('',*,*,#52411,.F.) ;
#73352 = ORIENTED_EDGE('',*,*,#50838,.F.) ;
#73353 = ORIENTED_EDGE('',*,*,#52412,.F.) ;
#73354 = ORIENTED_EDGE('',*,*,#51044,.F.) ;
#73355 = ORIENTED_EDGE('',*,*,#50836,.F.) ;
#73356 = ORIENTED_EDGE('',*,*,#50839,.F.) ;
#73357 = ORIENTED_EDGE('',*,*,#52413,.F.) ;
#73358 = ORIENTED_EDGE('',*,*,#50840,.F.) ;
#73359 = ORIENTED_EDGE('',*,*,#52412,.T.) ;
#73360 = ORIENTED_EDGE('',*,*,#52410,.T.) ;
#73361 = ORIENTED_EDGE('',*,*,#52414,.F.) ;
#73362 = ORIENTED_EDGE('',*,*,#52413,.T.) ;
#73363 = ORIENTED_EDGE('',*,*,#52411,.T.) ;
#73364 = ORIENTED_EDGE('',*,*,#52415,.F.) ;
#73365 = ORIENTED_EDGE('',*,*,#50832,.F.) ;
#73366 = ORIENTED_EDGE('',*,*,#50844,.F.) ;
#73367 = ORIENTED_EDGE('',*,*,#52416,.F.) ;
#73368 = ORIENTED_EDGE('',*,*,#50846,.F.) ;
#73369 = ORIENTED_EDGE('',*,*,#52414,.T.) ;
#73370 = ORIENTED_EDGE('',*,*,#50847,.F.) ;
#73371 = ORIENTED_EDGE('',*,*,#52417,.F.) ;
#73372 = ORIENTED_EDGE('',*,*,#51041,.F.) ;
#73373 = ORIENTED_EDGE('',*,*,#52415,.T.) ;
#73374 = ORIENTED_EDGE('',*,*,#51043,.F.) ;
#73375 = ORIENTED_EDGE('',*,*,#52418,.F.) ;
#73376 = ORIENTED_EDGE('',*,*,#50841,.F.) ;
#73377 = ORIENTED_EDGE('',*,*,#50830,.F.) ;
#73378 = ORIENTED_EDGE('',*,*,#50842,.F.) ;
#73379 = ORIENTED_EDGE('',*,*,#52419,.F.) ;
#73380 = ORIENTED_EDGE('',*,*,#50845,.F.) ;
#73381 = ORIENTED_EDGE('',*,*,#52417,.T.) ;
#73382 = ORIENTED_EDGE('',*,*,#52416,.T.) ;
#73383 = ORIENTED_EDGE('',*,*,#52420,.F.) ;
#73384 = ORIENTED_EDGE('',*,*,#52419,.T.) ;
#73385 = ORIENTED_EDGE('',*,*,#52418,.T.) ;
#73386 = ORIENTED_EDGE('',*,*,#52421,.F.) ;
#73387 = ORIENTED_EDGE('',*,*,#52420,.T.) ;
#73388 = ORIENTED_EDGE('',*,*,#50843,.F.) ;
#73389 = ORIENTED_EDGE('',*,*,#52421,.T.) ;
#73390 = ORIENTED_EDGE('',*,*,#51042,.F.) ;
#73391 = ORIENTED_EDGE('',*,*,#52422,.F.) ;
#73392 = ORIENTED_EDGE('',*,*,#50544,.F.) ;
#73393 = ORIENTED_EDGE('',*,*,#50550,.F.) ;
#73394 = ORIENTED_EDGE('',*,*,#50621,.F.) ;
#73395 = ORIENTED_EDGE('',*,*,#52423,.F.) ;
#73396 = ORIENTED_EDGE('',*,*,#52422,.T.) ;
#73397 = ORIENTED_EDGE('',*,*,#52424,.F.) ;
#73398 = ORIENTED_EDGE('',*,*,#52424,.T.) ;
#73399 = ORIENTED_EDGE('',*,*,#50620,.F.) ;
#73400 = ORIENTED_EDGE('',*,*,#52425,.F.) ;
#73401 = ORIENTED_EDGE('',*,*,#50539,.F.) ;
#73402 = ORIENTED_EDGE('',*,*,#52423,.T.) ;
#73403 = ORIENTED_EDGE('',*,*,#50538,.F.) ;
#73404 = ORIENTED_EDGE('',*,*,#52426,.F.) ;
#73405 = ORIENTED_EDGE('',*,*,#50541,.F.) ;
#73406 = ORIENTED_EDGE('',*,*,#50551,.F.) ;
#73407 = ORIENTED_EDGE('',*,*,#50542,.F.) ;
#73408 = ORIENTED_EDGE('',*,*,#52427,.F.) ;
#73409 = ORIENTED_EDGE('',*,*,#50561,.F.) ;
#73410 = ORIENTED_EDGE('',*,*,#52428,.F.) ;
#73411 = ORIENTED_EDGE('',*,*,#52425,.T.) ;
#73412 = ORIENTED_EDGE('',*,*,#52429,.F.) ;
#73413 = ORIENTED_EDGE('',*,*,#49752,.T.) ;
#73414 = ORIENTED_EDGE('',*,*,#52427,.T.) ;
#73415 = ORIENTED_EDGE('',*,*,#52426,.T.) ;
#73416 = ORIENTED_EDGE('',*,*,#52430,.F.) ;
#73417 = ORIENTED_EDGE('',*,*,#50548,.F.) ;
#73418 = ORIENTED_EDGE('',*,*,#50554,.F.) ;
#73419 = ORIENTED_EDGE('',*,*,#52431,.F.) ;
#73420 = ORIENTED_EDGE('',*,*,#50622,.F.) ;
#73421 = ORIENTED_EDGE('',*,*,#52432,.F.) ;
#73422 = ORIENTED_EDGE('',*,*,#50623,.F.) ;
#73423 = ORIENTED_EDGE('',*,*,#52433,.F.) ;
#73424 = ORIENTED_EDGE('',*,*,#50558,.F.) ;
#73425 = ORIENTED_EDGE('',*,*,#52429,.T.) ;
#73426 = ORIENTED_EDGE('',*,*,#50624,.F.) ;
#73427 = ORIENTED_EDGE('',*,*,#52434,.F.) ;
#73428 = ORIENTED_EDGE('',*,*,#49753,.F.) ;
#73429 = ORIENTED_EDGE('',*,*,#52428,.T.) ;
#73430 = ORIENTED_EDGE('',*,*,#49751,.F.) ;
#73431 = ORIENTED_EDGE('',*,*,#52435,.F.) ;
#73432 = ORIENTED_EDGE('',*,*,#50540,.F.) ;
#73433 = ORIENTED_EDGE('',*,*,#52430,.T.) ;
#73434 = ORIENTED_EDGE('',*,*,#50537,.F.) ;
#73435 = ORIENTED_EDGE('',*,*,#52436,.F.) ;
#73436 = ORIENTED_EDGE('',*,*,#50562,.F.) ;
#73437 = ORIENTED_EDGE('',*,*,#52433,.T.) ;
#73438 = ORIENTED_EDGE('',*,*,#52431,.T.) ;
#73439 = ORIENTED_EDGE('',*,*,#52437,.F.) ;
#73440 = ORIENTED_EDGE('',*,*,#52434,.T.) ;
#73441 = ORIENTED_EDGE('',*,*,#52432,.T.) ;
#73442 = ORIENTED_EDGE('',*,*,#52438,.F.) ;
#73443 = ORIENTED_EDGE('',*,*,#49754,.T.) ;
#73444 = ORIENTED_EDGE('',*,*,#52435,.T.) ;
#73445 = ORIENTED_EDGE('',*,*,#49750,.T.) ;
#73446 = ORIENTED_EDGE('',*,*,#52439,.F.) ;
#73447 = ORIENTED_EDGE('',*,*,#52436,.T.) ;
#73448 = ORIENTED_EDGE('',*,*,#50546,.F.) ;
#73449 = ORIENTED_EDGE('',*,*,#50560,.F.) ;
#73450 = ORIENTED_EDGE('',*,*,#52440,.F.) ;
#73451 = ORIENTED_EDGE('',*,*,#50552,.F.) ;
#73452 = ORIENTED_EDGE('',*,*,#52437,.T.) ;
#73453 = ORIENTED_EDGE('',*,*,#50553,.F.) ;
#73454 = ORIENTED_EDGE('',*,*,#52441,.F.) ;
#73455 = ORIENTED_EDGE('',*,*,#50555,.F.) ;
#73456 = ORIENTED_EDGE('',*,*,#52438,.T.) ;
#73457 = ORIENTED_EDGE('',*,*,#50557,.F.) ;
#73458 = ORIENTED_EDGE('',*,*,#52442,.F.) ;
#73459 = ORIENTED_EDGE('',*,*,#49755,.F.) ;
#73460 = ORIENTED_EDGE('',*,*,#52439,.T.) ;
#73461 = ORIENTED_EDGE('',*,*,#49749,.F.) ;
#73462 = ORIENTED_EDGE('',*,*,#52443,.F.) ;
#73463 = ORIENTED_EDGE('',*,*,#50563,.F.) ;
#73464 = ORIENTED_EDGE('',*,*,#52441,.T.) ;
#73465 = ORIENTED_EDGE('',*,*,#52440,.T.) ;
#73466 = ORIENTED_EDGE('',*,*,#52444,.F.) ;
#73467 = ORIENTED_EDGE('',*,*,#49748,.T.) ;
#73468 = ORIENTED_EDGE('',*,*,#52442,.T.) ;
#73469 = ORIENTED_EDGE('',*,*,#52445,.F.) ;
#73470 = ORIENTED_EDGE('',*,*,#52443,.T.) ;
#73471 = ORIENTED_EDGE('',*,*,#52444,.T.) ;
#73472 = ORIENTED_EDGE('',*,*,#50559,.F.) ;
#73473 = ORIENTED_EDGE('',*,*,#52445,.T.) ;
#73474 = ORIENTED_EDGE('',*,*,#50556,.F.) ;
#73475 = ORIENTED_EDGE('',*,*,#49759,.F.) ;
#73476 = ORIENTED_EDGE('',*,*,#52446,.T.) ;
#73477 = ORIENTED_EDGE('',*,*,#52447,.T.) ;
#73478 = ORIENTED_EDGE('',*,*,#50533,.F.) ;
#73479 = ORIENTED_EDGE('',*,*,#52448,.T.) ;
#73480 = ORIENTED_EDGE('',*,*,#52449,.T.) ;
#73481 = ORIENTED_EDGE('',*,*,#52450,.T.) ;
#73482 = ORIENTED_EDGE('',*,*,#49756,.F.) ;
#73483 = ORIENTED_EDGE('',*,*,#52451,.T.) ;
#73484 = ORIENTED_EDGE('',*,*,#52452,.T.) ;
#73485 = ORIENTED_EDGE('',*,*,#50564,.F.) ;
#73486 = ORIENTED_EDGE('',*,*,#52453,.T.) ;
#73487 = ORIENTED_EDGE('',*,*,#52454,.T.) ;
#73488 = ORIENTED_EDGE('',*,*,#50625,.F.) ;
#73489 = ORIENTED_EDGE('',*,*,#52455,.T.) ;
#73490 = ORIENTED_EDGE('',*,*,#49758,.F.) ;
#73491 = ORIENTED_EDGE('',*,*,#52456,.T.) ;
#73492 = ORIENTED_EDGE('',*,*,#49757,.F.) ;
#73493 = ORIENTED_EDGE('',*,*,#52457,.T.) ;
#73494 = ORIENTED_EDGE('',*,*,#52458,.T.) ;
#73495 = ORIENTED_EDGE('',*,*,#52459,.T.) ;
#73496 = ORIENTED_EDGE('',*,*,#50515,.F.) ;
#73497 = ORIENTED_EDGE('',*,*,#52460,.T.) ;
#73498 = ORIENTED_EDGE('',*,*,#52461,.T.) ;
#73499 = ORIENTED_EDGE('',*,*,#49763,.F.) ;
#73500 = ORIENTED_EDGE('',*,*,#52462,.T.) ;
#73501 = ORIENTED_EDGE('',*,*,#52463,.T.) ;
#73502 = ORIENTED_EDGE('',*,*,#50511,.F.) ;
#73503 = ORIENTED_EDGE('',*,*,#52464,.T.) ;
#73504 = ORIENTED_EDGE('',*,*,#52465,.T.) ;
#73505 = ORIENTED_EDGE('',*,*,#52466,.T.) ;
#73506 = ORIENTED_EDGE('',*,*,#49760,.F.) ;
#73507 = ORIENTED_EDGE('',*,*,#52467,.T.) ;
#73508 = ORIENTED_EDGE('',*,*,#52468,.T.) ;
#73509 = ORIENTED_EDGE('',*,*,#50571,.F.) ;
#73510 = ORIENTED_EDGE('',*,*,#52469,.T.) ;
#73511 = ORIENTED_EDGE('',*,*,#52470,.T.) ;
#73512 = ORIENTED_EDGE('',*,*,#50632,.F.) ;
#73513 = ORIENTED_EDGE('',*,*,#52471,.T.) ;
#73514 = ORIENTED_EDGE('',*,*,#49762,.F.) ;
#73515 = ORIENTED_EDGE('',*,*,#52472,.T.) ;
#73516 = ORIENTED_EDGE('',*,*,#49761,.F.) ;
#73517 = ORIENTED_EDGE('',*,*,#52473,.T.) ;
#73518 = ORIENTED_EDGE('',*,*,#52474,.T.) ;
#73519 = ORIENTED_EDGE('',*,*,#52475,.T.) ;
#73520 = ORIENTED_EDGE('',*,*,#50493,.F.) ;
#73521 = ORIENTED_EDGE('',*,*,#52476,.T.) ;
#73522 = ORIENTED_EDGE('',*,*,#52477,.T.) ;
#73523 = ORIENTED_EDGE('',*,*,#49767,.F.) ;
#73524 = ORIENTED_EDGE('',*,*,#52478,.T.) ;
#73525 = ORIENTED_EDGE('',*,*,#52479,.T.) ;
#73526 = ORIENTED_EDGE('',*,*,#50489,.F.) ;
#73527 = ORIENTED_EDGE('',*,*,#52480,.T.) ;
#73528 = ORIENTED_EDGE('',*,*,#52481,.T.) ;
#73529 = ORIENTED_EDGE('',*,*,#52482,.T.) ;
#73530 = ORIENTED_EDGE('',*,*,#49764,.F.) ;
#73531 = ORIENTED_EDGE('',*,*,#52483,.T.) ;
#73532 = ORIENTED_EDGE('',*,*,#52484,.T.) ;
#73533 = ORIENTED_EDGE('',*,*,#50578,.F.) ;
#73534 = ORIENTED_EDGE('',*,*,#52485,.T.) ;
#73535 = ORIENTED_EDGE('',*,*,#52486,.T.) ;
#73536 = ORIENTED_EDGE('',*,*,#50639,.F.) ;
#73537 = ORIENTED_EDGE('',*,*,#52487,.T.) ;
#73538 = ORIENTED_EDGE('',*,*,#49766,.F.) ;
#73539 = ORIENTED_EDGE('',*,*,#52488,.T.) ;
#73540 = ORIENTED_EDGE('',*,*,#49765,.F.) ;
#73541 = ORIENTED_EDGE('',*,*,#52489,.T.) ;
#73542 = ORIENTED_EDGE('',*,*,#52490,.T.) ;
#73543 = ORIENTED_EDGE('',*,*,#52491,.T.) ;
#73544 = ORIENTED_EDGE('',*,*,#50471,.F.) ;
#73545 = ORIENTED_EDGE('',*,*,#52492,.T.) ;
#73546 = ORIENTED_EDGE('',*,*,#52493,.T.) ;
#73547 = ORIENTED_EDGE('',*,*,#49771,.F.) ;
#73548 = ORIENTED_EDGE('',*,*,#52494,.T.) ;
#73549 = ORIENTED_EDGE('',*,*,#52495,.T.) ;
#73550 = ORIENTED_EDGE('',*,*,#50467,.F.) ;
#73551 = ORIENTED_EDGE('',*,*,#52496,.T.) ;
#73552 = ORIENTED_EDGE('',*,*,#52497,.T.) ;
#73553 = ORIENTED_EDGE('',*,*,#52498,.T.) ;
#73554 = ORIENTED_EDGE('',*,*,#49768,.F.) ;
#73555 = ORIENTED_EDGE('',*,*,#52499,.T.) ;
#73556 = ORIENTED_EDGE('',*,*,#52500,.T.) ;
#73557 = ORIENTED_EDGE('',*,*,#50585,.F.) ;
#73558 = ORIENTED_EDGE('',*,*,#52501,.T.) ;
#73559 = ORIENTED_EDGE('',*,*,#52502,.T.) ;
#73560 = ORIENTED_EDGE('',*,*,#50646,.F.) ;
#73561 = ORIENTED_EDGE('',*,*,#52503,.T.) ;
#73562 = ORIENTED_EDGE('',*,*,#49770,.F.) ;
#73563 = ORIENTED_EDGE('',*,*,#52504,.T.) ;
#73564 = ORIENTED_EDGE('',*,*,#49769,.F.) ;
#73565 = ORIENTED_EDGE('',*,*,#52505,.T.) ;
#73566 = ORIENTED_EDGE('',*,*,#52506,.T.) ;
#73567 = ORIENTED_EDGE('',*,*,#52507,.T.) ;
#73568 = ORIENTED_EDGE('',*,*,#50449,.F.) ;
#73569 = ORIENTED_EDGE('',*,*,#52508,.T.) ;
#73570 = ORIENTED_EDGE('',*,*,#52509,.T.) ;
#73571 = ORIENTED_EDGE('',*,*,#49775,.F.) ;
#73572 = ORIENTED_EDGE('',*,*,#52510,.T.) ;
#73573 = ORIENTED_EDGE('',*,*,#52511,.T.) ;
#73574 = ORIENTED_EDGE('',*,*,#50445,.F.) ;
#73575 = ORIENTED_EDGE('',*,*,#52512,.T.) ;
#73576 = ORIENTED_EDGE('',*,*,#52513,.T.) ;
#73577 = ORIENTED_EDGE('',*,*,#52514,.T.) ;
#73578 = ORIENTED_EDGE('',*,*,#49772,.F.) ;
#73579 = ORIENTED_EDGE('',*,*,#52515,.T.) ;
#73580 = ORIENTED_EDGE('',*,*,#52516,.T.) ;
#73581 = ORIENTED_EDGE('',*,*,#50592,.F.) ;
#73582 = ORIENTED_EDGE('',*,*,#52517,.T.) ;
#73583 = ORIENTED_EDGE('',*,*,#52518,.T.) ;
#73584 = ORIENTED_EDGE('',*,*,#50653,.F.) ;
#73585 = ORIENTED_EDGE('',*,*,#52519,.T.) ;
#73586 = ORIENTED_EDGE('',*,*,#49774,.F.) ;
#73587 = ORIENTED_EDGE('',*,*,#52520,.T.) ;
#73588 = ORIENTED_EDGE('',*,*,#49773,.F.) ;
#73589 = ORIENTED_EDGE('',*,*,#52521,.T.) ;
#73590 = ORIENTED_EDGE('',*,*,#52522,.T.) ;
#73591 = ORIENTED_EDGE('',*,*,#52523,.T.) ;
#73592 = ORIENTED_EDGE('',*,*,#50427,.F.) ;
#73593 = ORIENTED_EDGE('',*,*,#52524,.T.) ;
#73594 = ORIENTED_EDGE('',*,*,#52525,.T.) ;
#73595 = ORIENTED_EDGE('',*,*,#49779,.F.) ;
#73596 = ORIENTED_EDGE('',*,*,#52526,.T.) ;
#73597 = ORIENTED_EDGE('',*,*,#52527,.T.) ;
#73598 = ORIENTED_EDGE('',*,*,#50423,.F.) ;
#73599 = ORIENTED_EDGE('',*,*,#52528,.T.) ;
#73600 = ORIENTED_EDGE('',*,*,#52529,.T.) ;
#73601 = ORIENTED_EDGE('',*,*,#52530,.T.) ;
#73602 = ORIENTED_EDGE('',*,*,#49776,.F.) ;
#73603 = ORIENTED_EDGE('',*,*,#52531,.T.) ;
#73604 = ORIENTED_EDGE('',*,*,#52532,.T.) ;
#73605 = ORIENTED_EDGE('',*,*,#50599,.F.) ;
#73606 = ORIENTED_EDGE('',*,*,#52533,.T.) ;
#73607 = ORIENTED_EDGE('',*,*,#52534,.T.) ;
#73608 = ORIENTED_EDGE('',*,*,#50660,.F.) ;
#73609 = ORIENTED_EDGE('',*,*,#52535,.T.) ;
#73610 = ORIENTED_EDGE('',*,*,#49778,.F.) ;
#73611 = ORIENTED_EDGE('',*,*,#52536,.T.) ;
#73612 = ORIENTED_EDGE('',*,*,#49777,.F.) ;
#73613 = ORIENTED_EDGE('',*,*,#52537,.T.) ;
#73614 = ORIENTED_EDGE('',*,*,#52538,.T.) ;
#73615 = ORIENTED_EDGE('',*,*,#52539,.T.) ;
#73616 = ORIENTED_EDGE('',*,*,#50405,.F.) ;
#73617 = ORIENTED_EDGE('',*,*,#52540,.T.) ;
#73618 = ORIENTED_EDGE('',*,*,#52541,.T.) ;
#73619 = ORIENTED_EDGE('',*,*,#49783,.F.) ;
#73620 = ORIENTED_EDGE('',*,*,#52542,.T.) ;
#73621 = ORIENTED_EDGE('',*,*,#52543,.T.) ;
#73622 = ORIENTED_EDGE('',*,*,#50401,.F.) ;
#73623 = ORIENTED_EDGE('',*,*,#52544,.T.) ;
#73624 = ORIENTED_EDGE('',*,*,#52545,.T.) ;
#73625 = ORIENTED_EDGE('',*,*,#52546,.T.) ;
#73626 = ORIENTED_EDGE('',*,*,#49780,.F.) ;
#73627 = ORIENTED_EDGE('',*,*,#52547,.T.) ;
#73628 = ORIENTED_EDGE('',*,*,#52548,.T.) ;
#73629 = ORIENTED_EDGE('',*,*,#50606,.F.) ;
#73630 = ORIENTED_EDGE('',*,*,#52549,.T.) ;
#73631 = ORIENTED_EDGE('',*,*,#52550,.T.) ;
#73632 = ORIENTED_EDGE('',*,*,#50667,.F.) ;
#73633 = ORIENTED_EDGE('',*,*,#52551,.T.) ;
#73634 = ORIENTED_EDGE('',*,*,#49782,.F.) ;
#73635 = ORIENTED_EDGE('',*,*,#52552,.T.) ;
#73636 = ORIENTED_EDGE('',*,*,#49781,.F.) ;
#73637 = ORIENTED_EDGE('',*,*,#52553,.T.) ;
#73638 = ORIENTED_EDGE('',*,*,#52554,.T.) ;
#73639 = ORIENTED_EDGE('',*,*,#52555,.T.) ;
#73640 = ORIENTED_EDGE('',*,*,#50383,.F.) ;
#73641 = ORIENTED_EDGE('',*,*,#52556,.T.) ;
#73642 = ORIENTED_EDGE('',*,*,#52557,.T.) ;
#73643 = ORIENTED_EDGE('',*,*,#49787,.F.) ;
#73644 = ORIENTED_EDGE('',*,*,#52558,.T.) ;
#73645 = ORIENTED_EDGE('',*,*,#52559,.T.) ;
#73646 = ORIENTED_EDGE('',*,*,#50379,.F.) ;
#73647 = ORIENTED_EDGE('',*,*,#52560,.T.) ;
#73648 = ORIENTED_EDGE('',*,*,#52561,.T.) ;
#73649 = ORIENTED_EDGE('',*,*,#52562,.T.) ;
#73650 = ORIENTED_EDGE('',*,*,#49784,.F.) ;
#73651 = ORIENTED_EDGE('',*,*,#52563,.T.) ;
#73652 = ORIENTED_EDGE('',*,*,#52564,.T.) ;
#73653 = ORIENTED_EDGE('',*,*,#50613,.F.) ;
#73654 = ORIENTED_EDGE('',*,*,#52565,.T.) ;
#73655 = ORIENTED_EDGE('',*,*,#52566,.T.) ;
#73656 = ORIENTED_EDGE('',*,*,#50674,.F.) ;
#73657 = ORIENTED_EDGE('',*,*,#52567,.T.) ;
#73658 = ORIENTED_EDGE('',*,*,#49786,.F.) ;
#73659 = ORIENTED_EDGE('',*,*,#52568,.T.) ;
#73660 = ORIENTED_EDGE('',*,*,#49785,.F.) ;
#73661 = ORIENTED_EDGE('',*,*,#52569,.T.) ;
#73662 = ORIENTED_EDGE('',*,*,#52570,.T.) ;
#73663 = ORIENTED_EDGE('',*,*,#52571,.T.) ;
#73664 = ORIENTED_EDGE('',*,*,#50361,.F.) ;
#73665 = ORIENTED_EDGE('',*,*,#52572,.T.) ;
#73666 = ORIENTED_EDGE('',*,*,#52573,.T.) ;
#73667 = ORIENTED_EDGE('',*,*,#52574,.F.) ;
#73668 = ORIENTED_EDGE('',*,*,#49380,.F.) ;
#73669 = ORIENTED_EDGE('',*,*,#52575,.F.) ;
#73670 = ORIENTED_EDGE('',*,*,#51633,.F.) ;
#73671 = ORIENTED_EDGE('',*,*,#52575,.T.) ;
#73672 = ORIENTED_EDGE('',*,*,#49379,.T.) ;
#73673 = ORIENTED_EDGE('',*,*,#52576,.F.) ;
#73674 = ORIENTED_EDGE('',*,*,#52577,.F.) ;
#73675 = ORIENTED_EDGE('',*,*,#49381,.T.) ;
#73676 = ORIENTED_EDGE('',*,*,#52574,.T.) ;
#73677 = ORIENTED_EDGE('',*,*,#52578,.F.) ;
#73678 = ORIENTED_EDGE('',*,*,#52579,.F.) ;
#73679 = ORIENTED_EDGE('',*,*,#52576,.T.) ;
#73680 = ORIENTED_EDGE('',*,*,#49378,.F.) ;
#73681 = ORIENTED_EDGE('',*,*,#52580,.F.) ;
#73682 = ORIENTED_EDGE('',*,*,#51630,.F.) ;
#73683 = ORIENTED_EDGE('',*,*,#52577,.T.) ;
#73684 = ORIENTED_EDGE('',*,*,#51629,.F.) ;
#73685 = ORIENTED_EDGE('',*,*,#52581,.F.) ;
#73686 = ORIENTED_EDGE('',*,*,#51634,.F.) ;
#73687 = ORIENTED_EDGE('',*,*,#52582,.F.) ;
#73688 = ORIENTED_EDGE('',*,*,#51631,.F.) ;
#73689 = ORIENTED_EDGE('',*,*,#52583,.F.) ;
#73690 = ORIENTED_EDGE('',*,*,#51638,.F.) ;
#73691 = ORIENTED_EDGE('',*,*,#52578,.T.) ;
#73692 = ORIENTED_EDGE('',*,*,#51632,.F.) ;
#73693 = ORIENTED_EDGE('',*,*,#52584,.F.) ;
#73694 = ORIENTED_EDGE('',*,*,#51622,.F.) ;
#73695 = ORIENTED_EDGE('',*,*,#52579,.T.) ;
#73696 = ORIENTED_EDGE('',*,*,#51621,.F.) ;
#73697 = ORIENTED_EDGE('',*,*,#52585,.F.) ;
#73698 = ORIENTED_EDGE('',*,*,#49382,.F.) ;
#73699 = ORIENTED_EDGE('',*,*,#52586,.F.) ;
#73700 = ORIENTED_EDGE('',*,*,#49376,.F.) ;
#73701 = ORIENTED_EDGE('',*,*,#52587,.F.) ;
#73702 = ORIENTED_EDGE('',*,*,#51623,.F.) ;
#73703 = ORIENTED_EDGE('',*,*,#49377,.T.) ;
#73704 = ORIENTED_EDGE('',*,*,#52586,.T.) ;
#73705 = ORIENTED_EDGE('',*,*,#52588,.F.) ;
#73706 = ORIENTED_EDGE('',*,*,#52580,.T.) ;
#73707 = ORIENTED_EDGE('',*,*,#52583,.T.) ;
#73708 = ORIENTED_EDGE('',*,*,#52581,.T.) ;
#73709 = ORIENTED_EDGE('',*,*,#52589,.F.) ;
#73710 = ORIENTED_EDGE('',*,*,#52584,.T.) ;
#73711 = ORIENTED_EDGE('',*,*,#52582,.T.) ;
#73712 = ORIENTED_EDGE('',*,*,#52590,.F.) ;
#73713 = ORIENTED_EDGE('',*,*,#49375,.T.) ;
#73714 = ORIENTED_EDGE('',*,*,#52585,.T.) ;
#73715 = ORIENTED_EDGE('',*,*,#52591,.F.) ;
#73716 = ORIENTED_EDGE('',*,*,#52587,.T.) ;
#73717 = ORIENTED_EDGE('',*,*,#52588,.T.) ;
#73718 = ORIENTED_EDGE('',*,*,#51626,.F.) ;
#73719 = ORIENTED_EDGE('',*,*,#52592,.F.) ;
#73720 = ORIENTED_EDGE('',*,*,#51627,.F.) ;
#73721 = ORIENTED_EDGE('',*,*,#52589,.T.) ;
#73722 = ORIENTED_EDGE('',*,*,#51628,.F.) ;
#73723 = ORIENTED_EDGE('',*,*,#52593,.F.) ;
#73724 = ORIENTED_EDGE('',*,*,#51635,.F.) ;
#73725 = ORIENTED_EDGE('',*,*,#52590,.T.) ;
#73726 = ORIENTED_EDGE('',*,*,#51637,.F.) ;
#73727 = ORIENTED_EDGE('',*,*,#52594,.F.) ;
#73728 = ORIENTED_EDGE('',*,*,#51619,.F.) ;
#73729 = ORIENTED_EDGE('',*,*,#52591,.T.) ;
#73730 = ORIENTED_EDGE('',*,*,#51620,.F.) ;
#73731 = ORIENTED_EDGE('',*,*,#52595,.F.) ;
#73732 = ORIENTED_EDGE('',*,*,#51624,.F.) ;
#73733 = ORIENTED_EDGE('',*,*,#52593,.T.) ;
#73734 = ORIENTED_EDGE('',*,*,#52592,.T.) ;
#73735 = ORIENTED_EDGE('',*,*,#52596,.F.) ;
#73736 = ORIENTED_EDGE('',*,*,#52595,.T.) ;
#73737 = ORIENTED_EDGE('',*,*,#52594,.T.) ;
#73738 = ORIENTED_EDGE('',*,*,#52597,.F.) ;
#73739 = ORIENTED_EDGE('',*,*,#52596,.T.) ;
#73740 = ORIENTED_EDGE('',*,*,#51625,.F.) ;
#73741 = ORIENTED_EDGE('',*,*,#52597,.T.) ;
#73742 = ORIENTED_EDGE('',*,*,#51636,.F.) ;
#73743 = ORIENTED_EDGE('',*,*,#51644,.F.) ;
#73744 = ORIENTED_EDGE('',*,*,#51657,.F.) ;
#73745 = ORIENTED_EDGE('',*,*,#52598,.F.) ;
#73746 = ORIENTED_EDGE('',*,*,#51649,.F.) ;
#73747 = ORIENTED_EDGE('',*,*,#52599,.F.) ;
#73748 = ORIENTED_EDGE('',*,*,#51647,.F.) ;
#73749 = ORIENTED_EDGE('',*,*,#52600,.F.) ;
#73750 = ORIENTED_EDGE('',*,*,#51854,.F.) ;
#73751 = ORIENTED_EDGE('',*,*,#51646,.F.) ;
#73752 = ORIENTED_EDGE('',*,*,#51648,.F.) ;
#73753 = ORIENTED_EDGE('',*,*,#52601,.F.) ;
#73754 = ORIENTED_EDGE('',*,*,#51652,.F.) ;
#73755 = ORIENTED_EDGE('',*,*,#52600,.T.) ;
#73756 = ORIENTED_EDGE('',*,*,#52598,.T.) ;
#73757 = ORIENTED_EDGE('',*,*,#52602,.F.) ;
#73758 = ORIENTED_EDGE('',*,*,#52601,.T.) ;
#73759 = ORIENTED_EDGE('',*,*,#52599,.T.) ;
#73760 = ORIENTED_EDGE('',*,*,#52603,.F.) ;
#73761 = ORIENTED_EDGE('',*,*,#51642,.F.) ;
#73762 = ORIENTED_EDGE('',*,*,#51655,.F.) ;
#73763 = ORIENTED_EDGE('',*,*,#52604,.F.) ;
#73764 = ORIENTED_EDGE('',*,*,#51658,.F.) ;
#73765 = ORIENTED_EDGE('',*,*,#52602,.T.) ;
#73766 = ORIENTED_EDGE('',*,*,#51656,.F.) ;
#73767 = ORIENTED_EDGE('',*,*,#52605,.F.) ;
#73768 = ORIENTED_EDGE('',*,*,#51851,.F.) ;
#73769 = ORIENTED_EDGE('',*,*,#52603,.T.) ;
#73770 = ORIENTED_EDGE('',*,*,#51853,.F.) ;
#73771 = ORIENTED_EDGE('',*,*,#52606,.F.) ;
#73772 = ORIENTED_EDGE('',*,*,#51650,.F.) ;
#73773 = ORIENTED_EDGE('',*,*,#51640,.F.) ;
#73774 = ORIENTED_EDGE('',*,*,#51651,.F.) ;
#73775 = ORIENTED_EDGE('',*,*,#52607,.F.) ;
#73776 = ORIENTED_EDGE('',*,*,#51653,.F.) ;
#73777 = ORIENTED_EDGE('',*,*,#52605,.T.) ;
#73778 = ORIENTED_EDGE('',*,*,#52604,.T.) ;
#73779 = ORIENTED_EDGE('',*,*,#52608,.F.) ;
#73780 = ORIENTED_EDGE('',*,*,#52607,.T.) ;
#73781 = ORIENTED_EDGE('',*,*,#52606,.T.) ;
#73782 = ORIENTED_EDGE('',*,*,#52609,.F.) ;
#73783 = ORIENTED_EDGE('',*,*,#52608,.T.) ;
#73784 = ORIENTED_EDGE('',*,*,#51654,.F.) ;
#73785 = ORIENTED_EDGE('',*,*,#52609,.T.) ;
#73786 = ORIENTED_EDGE('',*,*,#51852,.F.) ;
#73787 = ORIENTED_EDGE('',*,*,#52610,.F.) ;
#73788 = ORIENTED_EDGE('',*,*,#51962,.F.) ;
#73789 = ORIENTED_EDGE('',*,*,#52611,.F.) ;
#73790 = ORIENTED_EDGE('',*,*,#51977,.F.) ;
#73791 = ORIENTED_EDGE('',*,*,#52611,.T.) ;
#73792 = ORIENTED_EDGE('',*,*,#51965,.F.) ;
#73793 = ORIENTED_EDGE('',*,*,#52612,.F.) ;
#73794 = ORIENTED_EDGE('',*,*,#51959,.F.) ;
#73795 = ORIENTED_EDGE('',*,*,#52610,.T.) ;
#73796 = ORIENTED_EDGE('',*,*,#52613,.F.) ;
#73797 = ORIENTED_EDGE('',*,*,#52612,.T.) ;
#73798 = ORIENTED_EDGE('',*,*,#51968,.F.) ;
#73799 = ORIENTED_EDGE('',*,*,#52614,.F.) ;
#73800 = ORIENTED_EDGE('',*,*,#51974,.F.) ;
#73801 = ORIENTED_EDGE('',*,*,#52613,.T.) ;
#73802 = ORIENTED_EDGE('',*,*,#51976,.F.) ;
#73803 = ORIENTED_EDGE('',*,*,#52615,.F.) ;
#73804 = ORIENTED_EDGE('',*,*,#51956,.F.) ;
#73805 = ORIENTED_EDGE('',*,*,#52614,.T.) ;
#73806 = ORIENTED_EDGE('',*,*,#51971,.F.) ;
#73807 = ORIENTED_EDGE('',*,*,#52616,.F.) ;
#73808 = ORIENTED_EDGE('',*,*,#51953,.F.) ;
#73809 = ORIENTED_EDGE('',*,*,#52615,.T.) ;
#73810 = ORIENTED_EDGE('',*,*,#52617,.F.) ;
#73811 = ORIENTED_EDGE('',*,*,#52616,.T.) ;
#73812 = ORIENTED_EDGE('',*,*,#51972,.F.) ;
#73813 = ORIENTED_EDGE('',*,*,#52617,.T.) ;
#73814 = ORIENTED_EDGE('',*,*,#51975,.F.) ;
#73815 = ORIENTED_EDGE('',*,*,#49088,.F.) ;
#73816 = ORIENTED_EDGE('',*,*,#51895,.F.) ;
#73817 = ORIENTED_EDGE('',*,*,#49102,.F.) ;
#73818 = ORIENTED_EDGE('',*,*,#51896,.F.) ;
#73819 = ORIENTED_EDGE('',*,*,#49090,.F.) ;
#73820 = ORIENTED_EDGE('',*,*,#51897,.F.) ;
#73821 = ORIENTED_EDGE('',*,*,#49100,.F.) ;
#73822 = ORIENTED_EDGE('',*,*,#51900,.F.) ;
#73823 = ORIENTED_EDGE('',*,*,#49098,.F.) ;
#73824 = ORIENTED_EDGE('',*,*,#51898,.F.) ;
#73825 = ORIENTED_EDGE('',*,*,#49092,.F.) ;
#73826 = ORIENTED_EDGE('',*,*,#51901,.F.) ;
#73827 = ORIENTED_EDGE('',*,*,#49096,.F.) ;
#73828 = ORIENTED_EDGE('',*,*,#49531,.F.) ;
#73829 = ORIENTED_EDGE('',*,*,#49094,.F.) ;
#73830 = ORIENTED_EDGE('',*,*,#51899,.F.) ;
#73831 = ORIENTED_EDGE('',*,*,#52618,.F.) ;
#73832 = ORIENTED_EDGE('',*,*,#52619,.F.) ;
#73833 = ORIENTED_EDGE('',*,*,#52620,.F.) ;
#73834 = ORIENTED_EDGE('',*,*,#52619,.T.) ;
#73835 = ORIENTED_EDGE('',*,*,#51359,.F.) ;
#73836 = ORIENTED_EDGE('',*,*,#52621,.F.) ;
#73837 = ORIENTED_EDGE('',*,*,#51354,.F.) ;
#73838 = ORIENTED_EDGE('',*,*,#52620,.T.) ;
#73839 = ORIENTED_EDGE('',*,*,#51353,.F.) ;
#73840 = ORIENTED_EDGE('',*,*,#52622,.F.) ;
#73841 = ORIENTED_EDGE('',*,*,#51355,.F.) ;
#73842 = ORIENTED_EDGE('',*,*,#52618,.T.) ;
#73843 = ORIENTED_EDGE('',*,*,#51358,.F.) ;
#73844 = ORIENTED_EDGE('',*,*,#52623,.F.) ;
#73845 = ORIENTED_EDGE('',*,*,#51360,.F.) ;
#73846 = ORIENTED_EDGE('',*,*,#51364,.F.) ;
#73847 = ORIENTED_EDGE('',*,*,#52624,.T.) ;
#73848 = ORIENTED_EDGE('',*,*,#51113,.F.) ;
#73849 = ORIENTED_EDGE('',*,*,#52625,.F.) ;
#73850 = ORIENTED_EDGE('',*,*,#52621,.T.) ;
#73851 = ORIENTED_EDGE('',*,*,#52625,.T.) ;
#73852 = ORIENTED_EDGE('',*,*,#52626,.F.) ;
#73853 = ORIENTED_EDGE('',*,*,#52627,.F.) ;
#73854 = ORIENTED_EDGE('',*,*,#52622,.T.) ;
#73855 = ORIENTED_EDGE('',*,*,#52628,.F.) ;
#73856 = ORIENTED_EDGE('',*,*,#49652,.T.) ;
#73857 = ORIENTED_EDGE('',*,*,#52629,.F.) ;
#73858 = ORIENTED_EDGE('',*,*,#52623,.T.) ;
#73859 = ORIENTED_EDGE('',*,*,#52630,.F.) ;
#73860 = ORIENTED_EDGE('',*,*,#51363,.F.) ;
#73861 = ORIENTED_EDGE('',*,*,#52631,.T.) ;
#73862 = ORIENTED_EDGE('',*,*,#49499,.F.) ;
#73863 = ORIENTED_EDGE('',*,*,#52632,.T.) ;
#73864 = ORIENTED_EDGE('',*,*,#52626,.T.) ;
#73865 = ORIENTED_EDGE('',*,*,#51112,.F.) ;
#73866 = ORIENTED_EDGE('',*,*,#52633,.F.) ;
#73867 = ORIENTED_EDGE('',*,*,#51351,.F.) ;
#73868 = ORIENTED_EDGE('',*,*,#52628,.T.) ;
#73869 = ORIENTED_EDGE('',*,*,#51352,.F.) ;
#73870 = ORIENTED_EDGE('',*,*,#52634,.F.) ;
#73871 = ORIENTED_EDGE('',*,*,#49653,.F.) ;
#73872 = ORIENTED_EDGE('',*,*,#52627,.T.) ;
#73873 = ORIENTED_EDGE('',*,*,#49659,.F.) ;
#73874 = ORIENTED_EDGE('',*,*,#52635,.F.) ;
#73875 = ORIENTED_EDGE('',*,*,#51356,.F.) ;
#73876 = ORIENTED_EDGE('',*,*,#52630,.T.) ;
#73877 = ORIENTED_EDGE('',*,*,#51357,.F.) ;
#73878 = ORIENTED_EDGE('',*,*,#52636,.F.) ;
#73879 = ORIENTED_EDGE('',*,*,#51347,.F.) ;
#73880 = ORIENTED_EDGE('',*,*,#52629,.T.) ;
#73881 = ORIENTED_EDGE('',*,*,#51350,.F.) ;
#73882 = ORIENTED_EDGE('',*,*,#52637,.F.) ;
#73883 = ORIENTED_EDGE('',*,*,#51361,.F.) ;
#73884 = ORIENTED_EDGE('',*,*,#51123,.F.) ;
#73885 = ORIENTED_EDGE('',*,*,#52638,.T.) ;
#73886 = ORIENTED_EDGE('',*,*,#51362,.F.) ;
#73887 = ORIENTED_EDGE('',*,*,#52639,.F.) ;
#73888 = ORIENTED_EDGE('',*,*,#52633,.T.) ;
#73889 = ORIENTED_EDGE('',*,*,#51111,.T.) ;
#73890 = ORIENTED_EDGE('',*,*,#52640,.F.) ;
#73891 = ORIENTED_EDGE('',*,*,#52634,.T.) ;
#73892 = ORIENTED_EDGE('',*,*,#52635,.T.) ;
#73893 = ORIENTED_EDGE('',*,*,#49658,.T.) ;
#73894 = ORIENTED_EDGE('',*,*,#52641,.F.) ;
#73895 = ORIENTED_EDGE('',*,*,#52636,.T.) ;
#73896 = ORIENTED_EDGE('',*,*,#52639,.T.) ;
#73897 = ORIENTED_EDGE('',*,*,#52637,.T.) ;
#73898 = ORIENTED_EDGE('',*,*,#52642,.F.) ;
#73899 = ORIENTED_EDGE('',*,*,#51107,.F.) ;
#73900 = ORIENTED_EDGE('',*,*,#52643,.T.) ;
#73901 = ORIENTED_EDGE('',*,*,#51101,.F.) ;
#73902 = ORIENTED_EDGE('',*,*,#52644,.F.) ;
#73903 = ORIENTED_EDGE('',*,*,#52640,.T.) ;
#73904 = ORIENTED_EDGE('',*,*,#51110,.F.) ;
#73905 = ORIENTED_EDGE('',*,*,#52645,.F.) ;
#73906 = ORIENTED_EDGE('',*,*,#49654,.F.) ;
#73907 = ORIENTED_EDGE('',*,*,#52641,.T.) ;
#73908 = ORIENTED_EDGE('',*,*,#49657,.F.) ;
#73909 = ORIENTED_EDGE('',*,*,#52646,.F.) ;
#73910 = ORIENTED_EDGE('',*,*,#51348,.F.) ;
#73911 = ORIENTED_EDGE('',*,*,#52642,.T.) ;
#73912 = ORIENTED_EDGE('',*,*,#51349,.F.) ;
#73913 = ORIENTED_EDGE('',*,*,#52647,.F.) ;
#73914 = ORIENTED_EDGE('',*,*,#51124,.F.) ;
#73915 = ORIENTED_EDGE('',*,*,#52644,.T.) ;
#73916 = ORIENTED_EDGE('',*,*,#52232,.F.) ;
#73917 = ORIENTED_EDGE('',*,*,#52648,.F.) ;
#73918 = ORIENTED_EDGE('',*,*,#52649,.F.) ;
#73919 = ORIENTED_EDGE('',*,*,#52645,.T.) ;
#73920 = ORIENTED_EDGE('',*,*,#52650,.F.) ;
#73921 = ORIENTED_EDGE('',*,*,#52647,.T.) ;
#73922 = ORIENTED_EDGE('',*,*,#52646,.T.) ;
#73923 = ORIENTED_EDGE('',*,*,#52651,.F.) ;
#73924 = ORIENTED_EDGE('',*,*,#51125,.T.) ;
#73925 = ORIENTED_EDGE('',*,*,#52648,.T.) ;
#73926 = ORIENTED_EDGE('',*,*,#49721,.F.) ;
#73927 = ORIENTED_EDGE('',*,*,#52652,.F.) ;
#73928 = ORIENTED_EDGE('',*,*,#51108,.F.) ;
#73929 = ORIENTED_EDGE('',*,*,#52650,.T.) ;
#73930 = ORIENTED_EDGE('',*,*,#51109,.F.) ;
#73931 = ORIENTED_EDGE('',*,*,#52653,.F.) ;
#73932 = ORIENTED_EDGE('',*,*,#51115,.F.) ;
#73933 = ORIENTED_EDGE('',*,*,#52649,.T.) ;
#73934 = ORIENTED_EDGE('',*,*,#51118,.F.) ;
#73935 = ORIENTED_EDGE('',*,*,#52654,.F.) ;
#73936 = ORIENTED_EDGE('',*,*,#49655,.F.) ;
#73937 = ORIENTED_EDGE('',*,*,#52651,.T.) ;
#73938 = ORIENTED_EDGE('',*,*,#49656,.F.) ;
#73939 = ORIENTED_EDGE('',*,*,#52655,.F.) ;
#73940 = ORIENTED_EDGE('',*,*,#51126,.F.) ;
#73941 = ORIENTED_EDGE('',*,*,#52652,.T.) ;
#73942 = ORIENTED_EDGE('',*,*,#49720,.T.) ;
#73943 = ORIENTED_EDGE('',*,*,#52656,.F.) ;
#73944 = ORIENTED_EDGE('',*,*,#52653,.T.) ;
#73945 = ORIENTED_EDGE('',*,*,#52655,.T.) ;
#73946 = ORIENTED_EDGE('',*,*,#52654,.T.) ;
#73947 = ORIENTED_EDGE('',*,*,#52657,.F.) ;
#73948 = ORIENTED_EDGE('',*,*,#52656,.T.) ;
#73949 = ORIENTED_EDGE('',*,*,#49719,.F.) ;
#73950 = ORIENTED_EDGE('',*,*,#52658,.F.) ;
#73951 = ORIENTED_EDGE('',*,*,#51116,.F.) ;
#73952 = ORIENTED_EDGE('',*,*,#52657,.T.) ;
#73953 = ORIENTED_EDGE('',*,*,#51117,.F.) ;
#73954 = ORIENTED_EDGE('',*,*,#52659,.F.) ;
#73955 = ORIENTED_EDGE('',*,*,#51127,.F.) ;
#73956 = ORIENTED_EDGE('',*,*,#51131,.F.) ;
#73957 = ORIENTED_EDGE('',*,*,#52660,.T.) ;
#73958 = ORIENTED_EDGE('',*,*,#51119,.F.) ;
#73959 = ORIENTED_EDGE('',*,*,#52661,.F.) ;
#73960 = ORIENTED_EDGE('',*,*,#49716,.F.) ;
#73961 = ORIENTED_EDGE('',*,*,#52662,.T.) ;
#73962 = ORIENTED_EDGE('',*,*,#51132,.F.) ;
#73963 = ORIENTED_EDGE('',*,*,#52663,.F.) ;
#73964 = ORIENTED_EDGE('',*,*,#52658,.T.) ;
#73965 = ORIENTED_EDGE('',*,*,#49718,.T.) ;
#73966 = ORIENTED_EDGE('',*,*,#52664,.F.) ;
#73967 = ORIENTED_EDGE('',*,*,#52659,.T.) ;
#73968 = ORIENTED_EDGE('',*,*,#52663,.T.) ;
#73969 = ORIENTED_EDGE('',*,*,#52661,.T.) ;
#73970 = ORIENTED_EDGE('',*,*,#52665,.F.) ;
#73971 = ORIENTED_EDGE('',*,*,#52664,.T.) ;
#73972 = ORIENTED_EDGE('',*,*,#49717,.F.) ;
#73973 = ORIENTED_EDGE('',*,*,#52665,.T.) ;
#73974 = ORIENTED_EDGE('',*,*,#51128,.F.) ;
#73975 = ORIENTED_EDGE('',*,*,#52374,.F.) ;
#73976 = ORIENTED_EDGE('',*,*,#52385,.F.) ;
#73977 = ORIENTED_EDGE('',*,*,#52384,.F.) ;
#73978 = ORIENTED_EDGE('',*,*,#52666,.F.) ;
#73979 = ORIENTED_EDGE('',*,*,#52375,.F.) ;
#73980 = ORIENTED_EDGE('',*,*,#52666,.T.) ;
#73981 = ORIENTED_EDGE('',*,*,#50808,.F.) ;
#73982 = ORIENTED_EDGE('',*,*,#52667,.F.) ;
#73983 = ORIENTED_EDGE('',*,*,#50794,.F.) ;
#73984 = ORIENTED_EDGE('',*,*,#52382,.F.) ;
#73985 = ORIENTED_EDGE('',*,*,#52381,.F.) ;
#73986 = ORIENTED_EDGE('',*,*,#52380,.F.) ;
#73987 = ORIENTED_EDGE('',*,*,#52668,.F.) ;
#73988 = ORIENTED_EDGE('',*,*,#52383,.F.) ;
#73989 = ORIENTED_EDGE('',*,*,#52669,.F.) ;
#73990 = ORIENTED_EDGE('',*,*,#52667,.T.) ;
#73991 = ORIENTED_EDGE('',*,*,#52670,.F.) ;
#73992 = ORIENTED_EDGE('',*,*,#52372,.F.) ;
#73993 = ORIENTED_EDGE('',*,*,#52377,.F.) ;
#73994 = ORIENTED_EDGE('',*,*,#52376,.F.) ;
#73995 = ORIENTED_EDGE('',*,*,#52671,.F.) ;
#73996 = ORIENTED_EDGE('',*,*,#52373,.F.) ;
#73997 = ORIENTED_EDGE('',*,*,#52668,.T.) ;
#73998 = ORIENTED_EDGE('',*,*,#50804,.F.) ;
#73999 = ORIENTED_EDGE('',*,*,#52672,.F.) ;
#74000 = ORIENTED_EDGE('',*,*,#50806,.F.) ;
#74001 = ORIENTED_EDGE('',*,*,#52670,.T.) ;
#74002 = ORIENTED_EDGE('',*,*,#50807,.F.) ;
#74003 = ORIENTED_EDGE('',*,*,#52673,.F.) ;
#74004 = ORIENTED_EDGE('',*,*,#50852,.F.) ;
#74005 = ORIENTED_EDGE('',*,*,#52669,.T.) ;
#74006 = ORIENTED_EDGE('',*,*,#50851,.F.) ;
#74007 = ORIENTED_EDGE('',*,*,#52674,.F.) ;
#74008 = ORIENTED_EDGE('',*,*,#50795,.F.) ;
#74009 = ORIENTED_EDGE('',*,*,#52671,.T.) ;
#74010 = ORIENTED_EDGE('',*,*,#50796,.F.) ;
#74011 = ORIENTED_EDGE('',*,*,#52675,.F.) ;
#74012 = ORIENTED_EDGE('',*,*,#50800,.F.) ;
#74013 = ORIENTED_EDGE('',*,*,#52673,.T.) ;
#74014 = ORIENTED_EDGE('',*,*,#52672,.T.) ;
#74015 = ORIENTED_EDGE('',*,*,#52676,.F.) ;
#74016 = ORIENTED_EDGE('',*,*,#52675,.T.) ;
#74017 = ORIENTED_EDGE('',*,*,#52674,.T.) ;
#74018 = ORIENTED_EDGE('',*,*,#52677,.F.) ;
#74019 = ORIENTED_EDGE('',*,*,#52676,.T.) ;
#74020 = ORIENTED_EDGE('',*,*,#50803,.F.) ;
#74021 = ORIENTED_EDGE('',*,*,#52678,.F.) ;
#74022 = ORIENTED_EDGE('',*,*,#50849,.F.) ;
#74023 = ORIENTED_EDGE('',*,*,#52677,.T.) ;
#74024 = ORIENTED_EDGE('',*,*,#50850,.F.) ;
#74025 = ORIENTED_EDGE('',*,*,#52679,.F.) ;
#74026 = ORIENTED_EDGE('',*,*,#50797,.F.) ;
#74027 = ORIENTED_EDGE('',*,*,#52679,.T.) ;
#74028 = ORIENTED_EDGE('',*,*,#52678,.T.) ;
#74029 = ORIENTED_EDGE('',*,*,#52680,.F.) ;
#74030 = ORIENTED_EDGE('',*,*,#52680,.T.) ;
#74031 = ORIENTED_EDGE('',*,*,#50802,.F.) ;
#74032 = ORIENTED_EDGE('',*,*,#52681,.F.) ;
#74033 = ORIENTED_EDGE('',*,*,#50798,.F.) ;
#74034 = ORIENTED_EDGE('',*,*,#52378,.F.) ;
#74035 = ORIENTED_EDGE('',*,*,#52371,.F.) ;
#74036 = ORIENTED_EDGE('',*,*,#52370,.F.) ;
#74037 = ORIENTED_EDGE('',*,*,#52681,.T.) ;
#74038 = ORIENTED_EDGE('',*,*,#52379,.F.) ;
#74039 = ORIENTED_EDGE('',*,*,#52451,.F.) ;
#74040 = ORIENTED_EDGE('',*,*,#52450,.F.) ;
#74041 = ORIENTED_EDGE('',*,*,#52449,.F.) ;
#74042 = ORIENTED_EDGE('',*,*,#52682,.F.) ;
#74043 = ORIENTED_EDGE('',*,*,#52452,.F.) ;
#74044 = ORIENTED_EDGE('',*,*,#52682,.T.) ;
#74045 = ORIENTED_EDGE('',*,*,#52448,.F.) ;
#74046 = ORIENTED_EDGE('',*,*,#52683,.F.) ;
#74047 = ORIENTED_EDGE('',*,*,#50565,.F.) ;
#74048 = ORIENTED_EDGE('',*,*,#52683,.T.) ;
#74049 = ORIENTED_EDGE('',*,*,#50536,.F.) ;
#74050 = ORIENTED_EDGE('',*,*,#52684,.F.) ;
#74051 = ORIENTED_EDGE('',*,*,#50566,.F.) ;
#74052 = ORIENTED_EDGE('',*,*,#50524,.F.) ;
#74053 = ORIENTED_EDGE('',*,*,#50567,.F.) ;
#74054 = ORIENTED_EDGE('',*,*,#52685,.F.) ;
#74055 = ORIENTED_EDGE('',*,*,#50530,.F.) ;
#74056 = ORIENTED_EDGE('',*,*,#52685,.T.) ;
#74057 = ORIENTED_EDGE('',*,*,#52684,.T.) ;
#74058 = ORIENTED_EDGE('',*,*,#52686,.F.) ;
#74059 = ORIENTED_EDGE('',*,*,#52686,.T.) ;
#74060 = ORIENTED_EDGE('',*,*,#50535,.F.) ;
#74061 = ORIENTED_EDGE('',*,*,#52687,.F.) ;
#74062 = ORIENTED_EDGE('',*,*,#50531,.F.) ;
#74063 = ORIENTED_EDGE('',*,*,#50526,.F.) ;
#74064 = ORIENTED_EDGE('',*,*,#50532,.F.) ;
#74065 = ORIENTED_EDGE('',*,*,#52688,.F.) ;
#74066 = ORIENTED_EDGE('',*,*,#50629,.F.) ;
#74067 = ORIENTED_EDGE('',*,*,#52688,.T.) ;
#74068 = ORIENTED_EDGE('',*,*,#52687,.T.) ;
#74069 = ORIENTED_EDGE('',*,*,#52689,.F.) ;
#74070 = ORIENTED_EDGE('',*,*,#52689,.T.) ;
#74071 = ORIENTED_EDGE('',*,*,#50534,.F.) ;
#74072 = ORIENTED_EDGE('',*,*,#52690,.F.) ;
#74073 = ORIENTED_EDGE('',*,*,#50630,.F.) ;
#74074 = ORIENTED_EDGE('',*,*,#52690,.T.) ;
#74075 = ORIENTED_EDGE('',*,*,#52447,.F.) ;
#74076 = ORIENTED_EDGE('',*,*,#52691,.F.) ;
#74077 = ORIENTED_EDGE('',*,*,#50631,.F.) ;
#74078 = ORIENTED_EDGE('',*,*,#52691,.T.) ;
#74079 = ORIENTED_EDGE('',*,*,#52446,.F.) ;
#74080 = ORIENTED_EDGE('',*,*,#52455,.F.) ;
#74081 = ORIENTED_EDGE('',*,*,#52456,.F.) ;
#74082 = ORIENTED_EDGE('',*,*,#52461,.F.) ;
#74083 = ORIENTED_EDGE('',*,*,#52692,.F.) ;
#74084 = ORIENTED_EDGE('',*,*,#52692,.T.) ;
#74085 = ORIENTED_EDGE('',*,*,#52460,.F.) ;
#74086 = ORIENTED_EDGE('',*,*,#52693,.F.) ;
#74087 = ORIENTED_EDGE('',*,*,#50626,.F.) ;
#74088 = ORIENTED_EDGE('',*,*,#52693,.T.) ;
#74089 = ORIENTED_EDGE('',*,*,#50518,.F.) ;
#74090 = ORIENTED_EDGE('',*,*,#52694,.F.) ;
#74091 = ORIENTED_EDGE('',*,*,#50627,.F.) ;
#74092 = ORIENTED_EDGE('',*,*,#50528,.F.) ;
#74093 = ORIENTED_EDGE('',*,*,#50628,.F.) ;
#74094 = ORIENTED_EDGE('',*,*,#52695,.F.) ;
#74095 = ORIENTED_EDGE('',*,*,#50522,.F.) ;
#74096 = ORIENTED_EDGE('',*,*,#52695,.T.) ;
#74097 = ORIENTED_EDGE('',*,*,#52694,.T.) ;
#74098 = ORIENTED_EDGE('',*,*,#52696,.F.) ;
#74099 = ORIENTED_EDGE('',*,*,#52696,.T.) ;
#74100 = ORIENTED_EDGE('',*,*,#50517,.F.) ;
#74101 = ORIENTED_EDGE('',*,*,#52697,.F.) ;
#74102 = ORIENTED_EDGE('',*,*,#50519,.F.) ;
#74103 = ORIENTED_EDGE('',*,*,#50529,.F.) ;
#74104 = ORIENTED_EDGE('',*,*,#50520,.F.) ;
#74105 = ORIENTED_EDGE('',*,*,#52698,.F.) ;
#74106 = ORIENTED_EDGE('',*,*,#50568,.F.) ;
#74107 = ORIENTED_EDGE('',*,*,#52698,.T.) ;
#74108 = ORIENTED_EDGE('',*,*,#52697,.T.) ;
#74109 = ORIENTED_EDGE('',*,*,#52699,.F.) ;
#74110 = ORIENTED_EDGE('',*,*,#52699,.T.) ;
#74111 = ORIENTED_EDGE('',*,*,#50516,.F.) ;
#74112 = ORIENTED_EDGE('',*,*,#52700,.F.) ;
#74113 = ORIENTED_EDGE('',*,*,#50569,.F.) ;
#74114 = ORIENTED_EDGE('',*,*,#52700,.T.) ;
#74115 = ORIENTED_EDGE('',*,*,#52459,.F.) ;
#74116 = ORIENTED_EDGE('',*,*,#52701,.F.) ;
#74117 = ORIENTED_EDGE('',*,*,#50570,.F.) ;
#74118 = ORIENTED_EDGE('',*,*,#52457,.F.) ;
#74119 = ORIENTED_EDGE('',*,*,#52454,.F.) ;
#74120 = ORIENTED_EDGE('',*,*,#52453,.F.) ;
#74121 = ORIENTED_EDGE('',*,*,#52701,.T.) ;
#74122 = ORIENTED_EDGE('',*,*,#52458,.F.) ;
#74123 = ORIENTED_EDGE('',*,*,#52702,.F.) ;
#74124 = ORIENTED_EDGE('',*,*,#49508,.F.) ;
#74125 = ORIENTED_EDGE('',*,*,#52703,.F.) ;
#74126 = ORIENTED_EDGE('',*,*,#51985,.F.) ;
#74127 = ORIENTED_EDGE('',*,*,#52703,.T.) ;
#74128 = ORIENTED_EDGE('',*,*,#49507,.F.) ;
#74129 = ORIENTED_EDGE('',*,*,#52704,.F.) ;
#74130 = ORIENTED_EDGE('',*,*,#51988,.F.) ;
#74131 = ORIENTED_EDGE('',*,*,#52702,.T.) ;
#74132 = ORIENTED_EDGE('',*,*,#51982,.F.) ;
#74133 = ORIENTED_EDGE('',*,*,#52705,.F.) ;
#74134 = ORIENTED_EDGE('',*,*,#49509,.F.) ;
#74135 = ORIENTED_EDGE('',*,*,#52704,.T.) ;
#74136 = ORIENTED_EDGE('',*,*,#49506,.F.) ;
#74137 = ORIENTED_EDGE('',*,*,#52706,.F.) ;
#74138 = ORIENTED_EDGE('',*,*,#51991,.F.) ;
#74139 = ORIENTED_EDGE('',*,*,#52705,.T.) ;
#74140 = ORIENTED_EDGE('',*,*,#51979,.F.) ;
#74141 = ORIENTED_EDGE('',*,*,#52707,.F.) ;
#74142 = ORIENTED_EDGE('',*,*,#49510,.F.) ;
#74143 = ORIENTED_EDGE('',*,*,#52706,.T.) ;
#74144 = ORIENTED_EDGE('',*,*,#49505,.F.) ;
#74145 = ORIENTED_EDGE('',*,*,#52708,.F.) ;
#74146 = ORIENTED_EDGE('',*,*,#51994,.F.) ;
#74147 = ORIENTED_EDGE('',*,*,#52707,.T.) ;
#74148 = ORIENTED_EDGE('',*,*,#52001,.F.) ;
#74149 = ORIENTED_EDGE('',*,*,#52709,.F.) ;
#74150 = ORIENTED_EDGE('',*,*,#49503,.F.) ;
#74151 = ORIENTED_EDGE('',*,*,#52708,.T.) ;
#74152 = ORIENTED_EDGE('',*,*,#49504,.F.) ;
#74153 = ORIENTED_EDGE('',*,*,#52709,.T.) ;
#74154 = ORIENTED_EDGE('',*,*,#51997,.F.) ;
#74155 = ORIENTED_EDGE('',*,*,#50858,.F.) ;
#74156 = ORIENTED_EDGE('',*,*,#50872,.F.) ;
#74157 = ORIENTED_EDGE('',*,*,#52710,.F.) ;
#74158 = ORIENTED_EDGE('',*,*,#50861,.F.) ;
#74159 = ORIENTED_EDGE('',*,*,#52711,.F.) ;
#74160 = ORIENTED_EDGE('',*,*,#50862,.F.) ;
#74161 = ORIENTED_EDGE('',*,*,#52712,.F.) ;
#74162 = ORIENTED_EDGE('',*,*,#51048,.F.) ;
#74163 = ORIENTED_EDGE('',*,*,#50860,.F.) ;
#74164 = ORIENTED_EDGE('',*,*,#50863,.F.) ;
#74165 = ORIENTED_EDGE('',*,*,#52713,.F.) ;
#74166 = ORIENTED_EDGE('',*,*,#50864,.F.) ;
#74167 = ORIENTED_EDGE('',*,*,#52712,.T.) ;
#74168 = ORIENTED_EDGE('',*,*,#52710,.T.) ;
#74169 = ORIENTED_EDGE('',*,*,#52714,.F.) ;
#74170 = ORIENTED_EDGE('',*,*,#52713,.T.) ;
#74171 = ORIENTED_EDGE('',*,*,#52711,.T.) ;
#74172 = ORIENTED_EDGE('',*,*,#52715,.F.) ;
#74173 = ORIENTED_EDGE('',*,*,#50856,.F.) ;
#74174 = ORIENTED_EDGE('',*,*,#50868,.F.) ;
#74175 = ORIENTED_EDGE('',*,*,#52716,.F.) ;
#74176 = ORIENTED_EDGE('',*,*,#50870,.F.) ;
#74177 = ORIENTED_EDGE('',*,*,#52714,.T.) ;
#74178 = ORIENTED_EDGE('',*,*,#50871,.F.) ;
#74179 = ORIENTED_EDGE('',*,*,#52717,.F.) ;
#74180 = ORIENTED_EDGE('',*,*,#51045,.F.) ;
#74181 = ORIENTED_EDGE('',*,*,#52715,.T.) ;
#74182 = ORIENTED_EDGE('',*,*,#51047,.F.) ;
#74183 = ORIENTED_EDGE('',*,*,#52718,.F.) ;
#74184 = ORIENTED_EDGE('',*,*,#50865,.F.) ;
#74185 = ORIENTED_EDGE('',*,*,#50854,.F.) ;
#74186 = ORIENTED_EDGE('',*,*,#50866,.F.) ;
#74187 = ORIENTED_EDGE('',*,*,#52719,.F.) ;
#74188 = ORIENTED_EDGE('',*,*,#50869,.F.) ;
#74189 = ORIENTED_EDGE('',*,*,#52717,.T.) ;
#74190 = ORIENTED_EDGE('',*,*,#52716,.T.) ;
#74191 = ORIENTED_EDGE('',*,*,#52720,.F.) ;
#74192 = ORIENTED_EDGE('',*,*,#52719,.T.) ;
#74193 = ORIENTED_EDGE('',*,*,#52718,.T.) ;
#74194 = ORIENTED_EDGE('',*,*,#52721,.F.) ;
#74195 = ORIENTED_EDGE('',*,*,#52720,.T.) ;
#74196 = ORIENTED_EDGE('',*,*,#50867,.F.) ;
#74197 = ORIENTED_EDGE('',*,*,#52721,.T.) ;
#74198 = ORIENTED_EDGE('',*,*,#51046,.F.) ;
#74199 = ORIENTED_EDGE('',*,*,#52722,.F.) ;
#74200 = ORIENTED_EDGE('',*,*,#49364,.F.) ;
#74201 = ORIENTED_EDGE('',*,*,#52723,.F.) ;
#74202 = ORIENTED_EDGE('',*,*,#51617,.F.) ;
#74203 = ORIENTED_EDGE('',*,*,#52723,.T.) ;
#74204 = ORIENTED_EDGE('',*,*,#49363,.T.) ;
#74205 = ORIENTED_EDGE('',*,*,#52724,.F.) ;
#74206 = ORIENTED_EDGE('',*,*,#52725,.F.) ;
#74207 = ORIENTED_EDGE('',*,*,#49365,.T.) ;
#74208 = ORIENTED_EDGE('',*,*,#52722,.T.) ;
#74209 = ORIENTED_EDGE('',*,*,#52726,.F.) ;
#74210 = ORIENTED_EDGE('',*,*,#52727,.F.) ;
#74211 = ORIENTED_EDGE('',*,*,#52724,.T.) ;
#74212 = ORIENTED_EDGE('',*,*,#49362,.F.) ;
#74213 = ORIENTED_EDGE('',*,*,#52728,.F.) ;
#74214 = ORIENTED_EDGE('',*,*,#51614,.F.) ;
#74215 = ORIENTED_EDGE('',*,*,#52725,.T.) ;
#74216 = ORIENTED_EDGE('',*,*,#51613,.F.) ;
#74217 = ORIENTED_EDGE('',*,*,#52729,.F.) ;
#74218 = ORIENTED_EDGE('',*,*,#51618,.F.) ;
#74219 = ORIENTED_EDGE('',*,*,#52730,.F.) ;
#74220 = ORIENTED_EDGE('',*,*,#51615,.F.) ;
#74221 = ORIENTED_EDGE('',*,*,#52731,.F.) ;
#74222 = ORIENTED_EDGE('',*,*,#51662,.F.) ;
#74223 = ORIENTED_EDGE('',*,*,#52726,.T.) ;
#74224 = ORIENTED_EDGE('',*,*,#51616,.F.) ;
#74225 = ORIENTED_EDGE('',*,*,#52732,.F.) ;
#74226 = ORIENTED_EDGE('',*,*,#51606,.F.) ;
#74227 = ORIENTED_EDGE('',*,*,#52727,.T.) ;
#74228 = ORIENTED_EDGE('',*,*,#51605,.F.) ;
#74229 = ORIENTED_EDGE('',*,*,#52733,.F.) ;
#74230 = ORIENTED_EDGE('',*,*,#49366,.F.) ;
#74231 = ORIENTED_EDGE('',*,*,#52734,.F.) ;
#74232 = ORIENTED_EDGE('',*,*,#49360,.F.) ;
#74233 = ORIENTED_EDGE('',*,*,#52735,.F.) ;
#74234 = ORIENTED_EDGE('',*,*,#51607,.F.) ;
#74235 = ORIENTED_EDGE('',*,*,#49361,.T.) ;
#74236 = ORIENTED_EDGE('',*,*,#52734,.T.) ;
#74237 = ORIENTED_EDGE('',*,*,#52736,.F.) ;
#74238 = ORIENTED_EDGE('',*,*,#52728,.T.) ;
#74239 = ORIENTED_EDGE('',*,*,#52731,.T.) ;
#74240 = ORIENTED_EDGE('',*,*,#52729,.T.) ;
#74241 = ORIENTED_EDGE('',*,*,#52737,.F.) ;
#74242 = ORIENTED_EDGE('',*,*,#52732,.T.) ;
#74243 = ORIENTED_EDGE('',*,*,#52730,.T.) ;
#74244 = ORIENTED_EDGE('',*,*,#52738,.F.) ;
#74245 = ORIENTED_EDGE('',*,*,#49359,.T.) ;
#74246 = ORIENTED_EDGE('',*,*,#52733,.T.) ;
#74247 = ORIENTED_EDGE('',*,*,#52739,.F.) ;
#74248 = ORIENTED_EDGE('',*,*,#52735,.T.) ;
#74249 = ORIENTED_EDGE('',*,*,#52736,.T.) ;
#74250 = ORIENTED_EDGE('',*,*,#51610,.F.) ;
#74251 = ORIENTED_EDGE('',*,*,#52740,.F.) ;
#74252 = ORIENTED_EDGE('',*,*,#51611,.F.) ;
#74253 = ORIENTED_EDGE('',*,*,#52737,.T.) ;
#74254 = ORIENTED_EDGE('',*,*,#51612,.F.) ;
#74255 = ORIENTED_EDGE('',*,*,#52741,.F.) ;
#74256 = ORIENTED_EDGE('',*,*,#51659,.F.) ;
#74257 = ORIENTED_EDGE('',*,*,#52738,.T.) ;
#74258 = ORIENTED_EDGE('',*,*,#51661,.F.) ;
#74259 = ORIENTED_EDGE('',*,*,#52742,.F.) ;
#74260 = ORIENTED_EDGE('',*,*,#51603,.F.) ;
#74261 = ORIENTED_EDGE('',*,*,#52739,.T.) ;
#74262 = ORIENTED_EDGE('',*,*,#51604,.F.) ;
#74263 = ORIENTED_EDGE('',*,*,#52743,.F.) ;
#74264 = ORIENTED_EDGE('',*,*,#51608,.F.) ;
#74265 = ORIENTED_EDGE('',*,*,#52741,.T.) ;
#74266 = ORIENTED_EDGE('',*,*,#52740,.T.) ;
#74267 = ORIENTED_EDGE('',*,*,#52744,.F.) ;
#74268 = ORIENTED_EDGE('',*,*,#52743,.T.) ;
#74269 = ORIENTED_EDGE('',*,*,#52742,.T.) ;
#74270 = ORIENTED_EDGE('',*,*,#52745,.F.) ;
#74271 = ORIENTED_EDGE('',*,*,#52744,.T.) ;
#74272 = ORIENTED_EDGE('',*,*,#51609,.F.) ;
#74273 = ORIENTED_EDGE('',*,*,#52745,.T.) ;
#74274 = ORIENTED_EDGE('',*,*,#51660,.F.) ;
#74275 = ORIENTED_EDGE('',*,*,#51668,.F.) ;
#74276 = ORIENTED_EDGE('',*,*,#51681,.F.) ;
#74277 = ORIENTED_EDGE('',*,*,#52746,.F.) ;
#74278 = ORIENTED_EDGE('',*,*,#51673,.F.) ;
#74279 = ORIENTED_EDGE('',*,*,#52747,.F.) ;
#74280 = ORIENTED_EDGE('',*,*,#51671,.F.) ;
#74281 = ORIENTED_EDGE('',*,*,#52748,.F.) ;
#74282 = ORIENTED_EDGE('',*,*,#51858,.F.) ;
#74283 = ORIENTED_EDGE('',*,*,#51670,.F.) ;
#74284 = ORIENTED_EDGE('',*,*,#51672,.F.) ;
#74285 = ORIENTED_EDGE('',*,*,#52749,.F.) ;
#74286 = ORIENTED_EDGE('',*,*,#51676,.F.) ;
#74287 = ORIENTED_EDGE('',*,*,#52748,.T.) ;
#74288 = ORIENTED_EDGE('',*,*,#52746,.T.) ;
#74289 = ORIENTED_EDGE('',*,*,#52750,.F.) ;
#74290 = ORIENTED_EDGE('',*,*,#52749,.T.) ;
#74291 = ORIENTED_EDGE('',*,*,#52747,.T.) ;
#74292 = ORIENTED_EDGE('',*,*,#52751,.F.) ;
#74293 = ORIENTED_EDGE('',*,*,#51666,.F.) ;
#74294 = ORIENTED_EDGE('',*,*,#51679,.F.) ;
#74295 = ORIENTED_EDGE('',*,*,#52752,.F.) ;
#74296 = ORIENTED_EDGE('',*,*,#51682,.F.) ;
#74297 = ORIENTED_EDGE('',*,*,#52750,.T.) ;
#74298 = ORIENTED_EDGE('',*,*,#51680,.F.) ;
#74299 = ORIENTED_EDGE('',*,*,#52753,.F.) ;
#74300 = ORIENTED_EDGE('',*,*,#51855,.F.) ;
#74301 = ORIENTED_EDGE('',*,*,#52751,.T.) ;
#74302 = ORIENTED_EDGE('',*,*,#51857,.F.) ;
#74303 = ORIENTED_EDGE('',*,*,#52754,.F.) ;
#74304 = ORIENTED_EDGE('',*,*,#51674,.F.) ;
#74305 = ORIENTED_EDGE('',*,*,#51664,.F.) ;
#74306 = ORIENTED_EDGE('',*,*,#51675,.F.) ;
#74307 = ORIENTED_EDGE('',*,*,#52755,.F.) ;
#74308 = ORIENTED_EDGE('',*,*,#51677,.F.) ;
#74309 = ORIENTED_EDGE('',*,*,#52753,.T.) ;
#74310 = ORIENTED_EDGE('',*,*,#52752,.T.) ;
#74311 = ORIENTED_EDGE('',*,*,#52756,.F.) ;
#74312 = ORIENTED_EDGE('',*,*,#52755,.T.) ;
#74313 = ORIENTED_EDGE('',*,*,#52754,.T.) ;
#74314 = ORIENTED_EDGE('',*,*,#52757,.F.) ;
#74315 = ORIENTED_EDGE('',*,*,#52756,.T.) ;
#74316 = ORIENTED_EDGE('',*,*,#51678,.F.) ;
#74317 = ORIENTED_EDGE('',*,*,#52757,.T.) ;
#74318 = ORIENTED_EDGE('',*,*,#51856,.F.) ;
#74319 = ORIENTED_EDGE('',*,*,#52758,.F.) ;
#74320 = ORIENTED_EDGE('',*,*,#51990,.F.) ;
#74321 = ORIENTED_EDGE('',*,*,#52759,.F.) ;
#74322 = ORIENTED_EDGE('',*,*,#52005,.F.) ;
#74323 = ORIENTED_EDGE('',*,*,#52759,.T.) ;
#74324 = ORIENTED_EDGE('',*,*,#51993,.F.) ;
#74325 = ORIENTED_EDGE('',*,*,#52760,.F.) ;
#74326 = ORIENTED_EDGE('',*,*,#51987,.F.) ;
#74327 = ORIENTED_EDGE('',*,*,#52758,.T.) ;
#74328 = ORIENTED_EDGE('',*,*,#52761,.F.) ;
#74329 = ORIENTED_EDGE('',*,*,#52760,.T.) ;
#74330 = ORIENTED_EDGE('',*,*,#51996,.F.) ;
#74331 = ORIENTED_EDGE('',*,*,#52762,.F.) ;
#74332 = ORIENTED_EDGE('',*,*,#52002,.F.) ;
#74333 = ORIENTED_EDGE('',*,*,#52761,.T.) ;
#74334 = ORIENTED_EDGE('',*,*,#52004,.F.) ;
#74335 = ORIENTED_EDGE('',*,*,#52763,.F.) ;
#74336 = ORIENTED_EDGE('',*,*,#51984,.F.) ;
#74337 = ORIENTED_EDGE('',*,*,#52762,.T.) ;
#74338 = ORIENTED_EDGE('',*,*,#51999,.F.) ;
#74339 = ORIENTED_EDGE('',*,*,#52764,.F.) ;
#74340 = ORIENTED_EDGE('',*,*,#51981,.F.) ;
#74341 = ORIENTED_EDGE('',*,*,#52763,.T.) ;
#74342 = ORIENTED_EDGE('',*,*,#52765,.F.) ;
#74343 = ORIENTED_EDGE('',*,*,#52764,.T.) ;
#74344 = ORIENTED_EDGE('',*,*,#52000,.F.) ;
#74345 = ORIENTED_EDGE('',*,*,#52765,.T.) ;
#74346 = ORIENTED_EDGE('',*,*,#52003,.F.) ;
#74347 = ORIENTED_EDGE('',*,*,#49106,.F.) ;
#74348 = ORIENTED_EDGE('',*,*,#51894,.F.) ;
#74349 = ORIENTED_EDGE('',*,*,#49120,.F.) ;
#74350 = ORIENTED_EDGE('',*,*,#51902,.F.) ;
#74351 = ORIENTED_EDGE('',*,*,#49108,.F.) ;
#74352 = ORIENTED_EDGE('',*,*,#51903,.F.) ;
#74353 = ORIENTED_EDGE('',*,*,#49118,.F.) ;
#74354 = ORIENTED_EDGE('',*,*,#51906,.F.) ;
#74355 = ORIENTED_EDGE('',*,*,#49116,.F.) ;
#74356 = ORIENTED_EDGE('',*,*,#51904,.F.) ;
#74357 = ORIENTED_EDGE('',*,*,#49110,.F.) ;
#74358 = ORIENTED_EDGE('',*,*,#51907,.F.) ;
#74359 = ORIENTED_EDGE('',*,*,#49114,.F.) ;
#74360 = ORIENTED_EDGE('',*,*,#49530,.F.) ;
#74361 = ORIENTED_EDGE('',*,*,#49112,.F.) ;
#74362 = ORIENTED_EDGE('',*,*,#51905,.F.) ;
#74363 = ORIENTED_EDGE('',*,*,#52766,.F.) ;
#74364 = ORIENTED_EDGE('',*,*,#52767,.F.) ;
#74365 = ORIENTED_EDGE('',*,*,#52768,.F.) ;
#74366 = ORIENTED_EDGE('',*,*,#52767,.T.) ;
#74367 = ORIENTED_EDGE('',*,*,#51377,.F.) ;
#74368 = ORIENTED_EDGE('',*,*,#52769,.F.) ;
#74369 = ORIENTED_EDGE('',*,*,#51372,.F.) ;
#74370 = ORIENTED_EDGE('',*,*,#52768,.T.) ;
#74371 = ORIENTED_EDGE('',*,*,#51371,.F.) ;
#74372 = ORIENTED_EDGE('',*,*,#52770,.F.) ;
#74373 = ORIENTED_EDGE('',*,*,#51373,.F.) ;
#74374 = ORIENTED_EDGE('',*,*,#52766,.T.) ;
#74375 = ORIENTED_EDGE('',*,*,#51376,.F.) ;
#74376 = ORIENTED_EDGE('',*,*,#52771,.F.) ;
#74377 = ORIENTED_EDGE('',*,*,#51378,.F.) ;
#74378 = ORIENTED_EDGE('',*,*,#51382,.F.) ;
#74379 = ORIENTED_EDGE('',*,*,#52772,.T.) ;
#74380 = ORIENTED_EDGE('',*,*,#51141,.F.) ;
#74381 = ORIENTED_EDGE('',*,*,#52773,.F.) ;
#74382 = ORIENTED_EDGE('',*,*,#52769,.T.) ;
#74383 = ORIENTED_EDGE('',*,*,#52773,.T.) ;
#74384 = ORIENTED_EDGE('',*,*,#52774,.F.) ;
#74385 = ORIENTED_EDGE('',*,*,#52775,.F.) ;
#74386 = ORIENTED_EDGE('',*,*,#52770,.T.) ;
#74387 = ORIENTED_EDGE('',*,*,#52776,.F.) ;
#74388 = ORIENTED_EDGE('',*,*,#49644,.T.) ;
#74389 = ORIENTED_EDGE('',*,*,#52777,.F.) ;
#74390 = ORIENTED_EDGE('',*,*,#52771,.T.) ;
#74391 = ORIENTED_EDGE('',*,*,#52778,.F.) ;
#74392 = ORIENTED_EDGE('',*,*,#51381,.F.) ;
#74393 = ORIENTED_EDGE('',*,*,#52779,.T.) ;
#74394 = ORIENTED_EDGE('',*,*,#49487,.F.) ;
#74395 = ORIENTED_EDGE('',*,*,#52780,.T.) ;
#74396 = ORIENTED_EDGE('',*,*,#52774,.T.) ;
#74397 = ORIENTED_EDGE('',*,*,#51140,.F.) ;
#74398 = ORIENTED_EDGE('',*,*,#52781,.F.) ;
#74399 = ORIENTED_EDGE('',*,*,#51369,.F.) ;
#74400 = ORIENTED_EDGE('',*,*,#52776,.T.) ;
#74401 = ORIENTED_EDGE('',*,*,#51370,.F.) ;
#74402 = ORIENTED_EDGE('',*,*,#52782,.F.) ;
#74403 = ORIENTED_EDGE('',*,*,#49645,.F.) ;
#74404 = ORIENTED_EDGE('',*,*,#52775,.T.) ;
#74405 = ORIENTED_EDGE('',*,*,#49651,.F.) ;
#74406 = ORIENTED_EDGE('',*,*,#52783,.F.) ;
#74407 = ORIENTED_EDGE('',*,*,#51374,.F.) ;
#74408 = ORIENTED_EDGE('',*,*,#52778,.T.) ;
#74409 = ORIENTED_EDGE('',*,*,#51375,.F.) ;
#74410 = ORIENTED_EDGE('',*,*,#52784,.F.) ;
#74411 = ORIENTED_EDGE('',*,*,#51365,.F.) ;
#74412 = ORIENTED_EDGE('',*,*,#52777,.T.) ;
#74413 = ORIENTED_EDGE('',*,*,#51368,.F.) ;
#74414 = ORIENTED_EDGE('',*,*,#52785,.F.) ;
#74415 = ORIENTED_EDGE('',*,*,#51379,.F.) ;
#74416 = ORIENTED_EDGE('',*,*,#51151,.F.) ;
#74417 = ORIENTED_EDGE('',*,*,#52786,.T.) ;
#74418 = ORIENTED_EDGE('',*,*,#51380,.F.) ;
#74419 = ORIENTED_EDGE('',*,*,#52787,.F.) ;
#74420 = ORIENTED_EDGE('',*,*,#52781,.T.) ;
#74421 = ORIENTED_EDGE('',*,*,#51139,.T.) ;
#74422 = ORIENTED_EDGE('',*,*,#52788,.F.) ;
#74423 = ORIENTED_EDGE('',*,*,#52782,.T.) ;
#74424 = ORIENTED_EDGE('',*,*,#52783,.T.) ;
#74425 = ORIENTED_EDGE('',*,*,#49650,.T.) ;
#74426 = ORIENTED_EDGE('',*,*,#52789,.F.) ;
#74427 = ORIENTED_EDGE('',*,*,#52784,.T.) ;
#74428 = ORIENTED_EDGE('',*,*,#52787,.T.) ;
#74429 = ORIENTED_EDGE('',*,*,#52785,.T.) ;
#74430 = ORIENTED_EDGE('',*,*,#52790,.F.) ;
#74431 = ORIENTED_EDGE('',*,*,#51135,.F.) ;
#74432 = ORIENTED_EDGE('',*,*,#52791,.T.) ;
#74433 = ORIENTED_EDGE('',*,*,#51129,.F.) ;
#74434 = ORIENTED_EDGE('',*,*,#52792,.F.) ;
#74435 = ORIENTED_EDGE('',*,*,#52788,.T.) ;
#74436 = ORIENTED_EDGE('',*,*,#51138,.F.) ;
#74437 = ORIENTED_EDGE('',*,*,#52793,.F.) ;
#74438 = ORIENTED_EDGE('',*,*,#49646,.F.) ;
#74439 = ORIENTED_EDGE('',*,*,#52789,.T.) ;
#74440 = ORIENTED_EDGE('',*,*,#49649,.F.) ;
#74441 = ORIENTED_EDGE('',*,*,#52794,.F.) ;
#74442 = ORIENTED_EDGE('',*,*,#51366,.F.) ;
#74443 = ORIENTED_EDGE('',*,*,#52790,.T.) ;
#74444 = ORIENTED_EDGE('',*,*,#51367,.F.) ;
#74445 = ORIENTED_EDGE('',*,*,#52795,.F.) ;
#74446 = ORIENTED_EDGE('',*,*,#51152,.F.) ;
#74447 = ORIENTED_EDGE('',*,*,#52792,.T.) ;
#74448 = ORIENTED_EDGE('',*,*,#52662,.F.) ;
#74449 = ORIENTED_EDGE('',*,*,#52796,.F.) ;
#74450 = ORIENTED_EDGE('',*,*,#52797,.F.) ;
#74451 = ORIENTED_EDGE('',*,*,#52793,.T.) ;
#74452 = ORIENTED_EDGE('',*,*,#52798,.F.) ;
#74453 = ORIENTED_EDGE('',*,*,#52795,.T.) ;
#74454 = ORIENTED_EDGE('',*,*,#52794,.T.) ;
#74455 = ORIENTED_EDGE('',*,*,#52799,.F.) ;
#74456 = ORIENTED_EDGE('',*,*,#51153,.T.) ;
#74457 = ORIENTED_EDGE('',*,*,#52796,.T.) ;
#74458 = ORIENTED_EDGE('',*,*,#49715,.F.) ;
#74459 = ORIENTED_EDGE('',*,*,#52800,.F.) ;
#74460 = ORIENTED_EDGE('',*,*,#51136,.F.) ;
#74461 = ORIENTED_EDGE('',*,*,#52798,.T.) ;
#74462 = ORIENTED_EDGE('',*,*,#51137,.F.) ;
#74463 = ORIENTED_EDGE('',*,*,#52801,.F.) ;
#74464 = ORIENTED_EDGE('',*,*,#51143,.F.) ;
#74465 = ORIENTED_EDGE('',*,*,#52797,.T.) ;
#74466 = ORIENTED_EDGE('',*,*,#51146,.F.) ;
#74467 = ORIENTED_EDGE('',*,*,#52802,.F.) ;
#74468 = ORIENTED_EDGE('',*,*,#49647,.F.) ;
#74469 = ORIENTED_EDGE('',*,*,#52799,.T.) ;
#74470 = ORIENTED_EDGE('',*,*,#49648,.F.) ;
#74471 = ORIENTED_EDGE('',*,*,#52803,.F.) ;
#74472 = ORIENTED_EDGE('',*,*,#51154,.F.) ;
#74473 = ORIENTED_EDGE('',*,*,#52800,.T.) ;
#74474 = ORIENTED_EDGE('',*,*,#49714,.T.) ;
#74475 = ORIENTED_EDGE('',*,*,#52804,.F.) ;
#74476 = ORIENTED_EDGE('',*,*,#52801,.T.) ;
#74477 = ORIENTED_EDGE('',*,*,#52803,.T.) ;
#74478 = ORIENTED_EDGE('',*,*,#52802,.T.) ;
#74479 = ORIENTED_EDGE('',*,*,#52805,.F.) ;
#74480 = ORIENTED_EDGE('',*,*,#52804,.T.) ;
#74481 = ORIENTED_EDGE('',*,*,#49713,.F.) ;
#74482 = ORIENTED_EDGE('',*,*,#52806,.F.) ;
#74483 = ORIENTED_EDGE('',*,*,#51144,.F.) ;
#74484 = ORIENTED_EDGE('',*,*,#52805,.T.) ;
#74485 = ORIENTED_EDGE('',*,*,#51145,.F.) ;
#74486 = ORIENTED_EDGE('',*,*,#52807,.F.) ;
#74487 = ORIENTED_EDGE('',*,*,#51155,.F.) ;
#74488 = ORIENTED_EDGE('',*,*,#51159,.F.) ;
#74489 = ORIENTED_EDGE('',*,*,#52808,.T.) ;
#74490 = ORIENTED_EDGE('',*,*,#51147,.F.) ;
#74491 = ORIENTED_EDGE('',*,*,#52809,.F.) ;
#74492 = ORIENTED_EDGE('',*,*,#49710,.F.) ;
#74493 = ORIENTED_EDGE('',*,*,#52810,.T.) ;
#74494 = ORIENTED_EDGE('',*,*,#51160,.F.) ;
#74495 = ORIENTED_EDGE('',*,*,#52811,.F.) ;
#74496 = ORIENTED_EDGE('',*,*,#52806,.T.) ;
#74497 = ORIENTED_EDGE('',*,*,#49712,.T.) ;
#74498 = ORIENTED_EDGE('',*,*,#52812,.F.) ;
#74499 = ORIENTED_EDGE('',*,*,#52807,.T.) ;
#74500 = ORIENTED_EDGE('',*,*,#52811,.T.) ;
#74501 = ORIENTED_EDGE('',*,*,#52809,.T.) ;
#74502 = ORIENTED_EDGE('',*,*,#52813,.F.) ;
#74503 = ORIENTED_EDGE('',*,*,#52812,.T.) ;
#74504 = ORIENTED_EDGE('',*,*,#49711,.F.) ;
#74505 = ORIENTED_EDGE('',*,*,#52813,.T.) ;
#74506 = ORIENTED_EDGE('',*,*,#51156,.F.) ;
#74507 = ORIENTED_EDGE('',*,*,#52358,.F.) ;
#74508 = ORIENTED_EDGE('',*,*,#52369,.F.) ;
#74509 = ORIENTED_EDGE('',*,*,#52368,.F.) ;
#74510 = ORIENTED_EDGE('',*,*,#52814,.F.) ;
#74511 = ORIENTED_EDGE('',*,*,#52359,.F.) ;
#74512 = ORIENTED_EDGE('',*,*,#52814,.T.) ;
#74513 = ORIENTED_EDGE('',*,*,#50792,.F.) ;
#74514 = ORIENTED_EDGE('',*,*,#52815,.F.) ;
#74515 = ORIENTED_EDGE('',*,*,#50778,.F.) ;
#74516 = ORIENTED_EDGE('',*,*,#52366,.F.) ;
#74517 = ORIENTED_EDGE('',*,*,#52365,.F.) ;
#74518 = ORIENTED_EDGE('',*,*,#52364,.F.) ;
#74519 = ORIENTED_EDGE('',*,*,#52816,.F.) ;
#74520 = ORIENTED_EDGE('',*,*,#52367,.F.) ;
#74521 = ORIENTED_EDGE('',*,*,#52817,.F.) ;
#74522 = ORIENTED_EDGE('',*,*,#52815,.T.) ;
#74523 = ORIENTED_EDGE('',*,*,#52818,.F.) ;
#74524 = ORIENTED_EDGE('',*,*,#52356,.F.) ;
#74525 = ORIENTED_EDGE('',*,*,#52361,.F.) ;
#74526 = ORIENTED_EDGE('',*,*,#52360,.F.) ;
#74527 = ORIENTED_EDGE('',*,*,#52819,.F.) ;
#74528 = ORIENTED_EDGE('',*,*,#52357,.F.) ;
#74529 = ORIENTED_EDGE('',*,*,#52816,.T.) ;
#74530 = ORIENTED_EDGE('',*,*,#50788,.F.) ;
#74531 = ORIENTED_EDGE('',*,*,#52820,.F.) ;
#74532 = ORIENTED_EDGE('',*,*,#50790,.F.) ;
#74533 = ORIENTED_EDGE('',*,*,#52818,.T.) ;
#74534 = ORIENTED_EDGE('',*,*,#50791,.F.) ;
#74535 = ORIENTED_EDGE('',*,*,#52821,.F.) ;
#74536 = ORIENTED_EDGE('',*,*,#50876,.F.) ;
#74537 = ORIENTED_EDGE('',*,*,#52817,.T.) ;
#74538 = ORIENTED_EDGE('',*,*,#50875,.F.) ;
#74539 = ORIENTED_EDGE('',*,*,#52822,.F.) ;
#74540 = ORIENTED_EDGE('',*,*,#50779,.F.) ;
#74541 = ORIENTED_EDGE('',*,*,#52819,.T.) ;
#74542 = ORIENTED_EDGE('',*,*,#50780,.F.) ;
#74543 = ORIENTED_EDGE('',*,*,#52823,.F.) ;
#74544 = ORIENTED_EDGE('',*,*,#50784,.F.) ;
#74545 = ORIENTED_EDGE('',*,*,#52821,.T.) ;
#74546 = ORIENTED_EDGE('',*,*,#52820,.T.) ;
#74547 = ORIENTED_EDGE('',*,*,#52824,.F.) ;
#74548 = ORIENTED_EDGE('',*,*,#52823,.T.) ;
#74549 = ORIENTED_EDGE('',*,*,#52822,.T.) ;
#74550 = ORIENTED_EDGE('',*,*,#52825,.F.) ;
#74551 = ORIENTED_EDGE('',*,*,#52824,.T.) ;
#74552 = ORIENTED_EDGE('',*,*,#50787,.F.) ;
#74553 = ORIENTED_EDGE('',*,*,#52826,.F.) ;
#74554 = ORIENTED_EDGE('',*,*,#50873,.F.) ;
#74555 = ORIENTED_EDGE('',*,*,#52825,.T.) ;
#74556 = ORIENTED_EDGE('',*,*,#50874,.F.) ;
#74557 = ORIENTED_EDGE('',*,*,#52827,.F.) ;
#74558 = ORIENTED_EDGE('',*,*,#50781,.F.) ;
#74559 = ORIENTED_EDGE('',*,*,#52827,.T.) ;
#74560 = ORIENTED_EDGE('',*,*,#52826,.T.) ;
#74561 = ORIENTED_EDGE('',*,*,#52828,.F.) ;
#74562 = ORIENTED_EDGE('',*,*,#52828,.T.) ;
#74563 = ORIENTED_EDGE('',*,*,#50786,.F.) ;
#74564 = ORIENTED_EDGE('',*,*,#52829,.F.) ;
#74565 = ORIENTED_EDGE('',*,*,#50782,.F.) ;
#74566 = ORIENTED_EDGE('',*,*,#52362,.F.) ;
#74567 = ORIENTED_EDGE('',*,*,#52355,.F.) ;
#74568 = ORIENTED_EDGE('',*,*,#52354,.F.) ;
#74569 = ORIENTED_EDGE('',*,*,#52829,.T.) ;
#74570 = ORIENTED_EDGE('',*,*,#52363,.F.) ;
#74571 = ORIENTED_EDGE('',*,*,#52467,.F.) ;
#74572 = ORIENTED_EDGE('',*,*,#52466,.F.) ;
#74573 = ORIENTED_EDGE('',*,*,#52465,.F.) ;
#74574 = ORIENTED_EDGE('',*,*,#52830,.F.) ;
#74575 = ORIENTED_EDGE('',*,*,#52468,.F.) ;
#74576 = ORIENTED_EDGE('',*,*,#52830,.T.) ;
#74577 = ORIENTED_EDGE('',*,*,#52464,.F.) ;
#74578 = ORIENTED_EDGE('',*,*,#52831,.F.) ;
#74579 = ORIENTED_EDGE('',*,*,#50572,.F.) ;
#74580 = ORIENTED_EDGE('',*,*,#52831,.T.) ;
#74581 = ORIENTED_EDGE('',*,*,#50514,.F.) ;
#74582 = ORIENTED_EDGE('',*,*,#52832,.F.) ;
#74583 = ORIENTED_EDGE('',*,*,#50573,.F.) ;
#74584 = ORIENTED_EDGE('',*,*,#50502,.F.) ;
#74585 = ORIENTED_EDGE('',*,*,#50574,.F.) ;
#74586 = ORIENTED_EDGE('',*,*,#52833,.F.) ;
#74587 = ORIENTED_EDGE('',*,*,#50508,.F.) ;
#74588 = ORIENTED_EDGE('',*,*,#52833,.T.) ;
#74589 = ORIENTED_EDGE('',*,*,#52832,.T.) ;
#74590 = ORIENTED_EDGE('',*,*,#52834,.F.) ;
#74591 = ORIENTED_EDGE('',*,*,#52834,.T.) ;
#74592 = ORIENTED_EDGE('',*,*,#50513,.F.) ;
#74593 = ORIENTED_EDGE('',*,*,#52835,.F.) ;
#74594 = ORIENTED_EDGE('',*,*,#50509,.F.) ;
#74595 = ORIENTED_EDGE('',*,*,#50504,.F.) ;
#74596 = ORIENTED_EDGE('',*,*,#50510,.F.) ;
#74597 = ORIENTED_EDGE('',*,*,#52836,.F.) ;
#74598 = ORIENTED_EDGE('',*,*,#50636,.F.) ;
#74599 = ORIENTED_EDGE('',*,*,#52836,.T.) ;
#74600 = ORIENTED_EDGE('',*,*,#52835,.T.) ;
#74601 = ORIENTED_EDGE('',*,*,#52837,.F.) ;
#74602 = ORIENTED_EDGE('',*,*,#52837,.T.) ;
#74603 = ORIENTED_EDGE('',*,*,#50512,.F.) ;
#74604 = ORIENTED_EDGE('',*,*,#52838,.F.) ;
#74605 = ORIENTED_EDGE('',*,*,#50637,.F.) ;
#74606 = ORIENTED_EDGE('',*,*,#52838,.T.) ;
#74607 = ORIENTED_EDGE('',*,*,#52463,.F.) ;
#74608 = ORIENTED_EDGE('',*,*,#52839,.F.) ;
#74609 = ORIENTED_EDGE('',*,*,#50638,.F.) ;
#74610 = ORIENTED_EDGE('',*,*,#52839,.T.) ;
#74611 = ORIENTED_EDGE('',*,*,#52462,.F.) ;
#74612 = ORIENTED_EDGE('',*,*,#52471,.F.) ;
#74613 = ORIENTED_EDGE('',*,*,#52472,.F.) ;
#74614 = ORIENTED_EDGE('',*,*,#52477,.F.) ;
#74615 = ORIENTED_EDGE('',*,*,#52840,.F.) ;
#74616 = ORIENTED_EDGE('',*,*,#52840,.T.) ;
#74617 = ORIENTED_EDGE('',*,*,#52476,.F.) ;
#74618 = ORIENTED_EDGE('',*,*,#52841,.F.) ;
#74619 = ORIENTED_EDGE('',*,*,#50633,.F.) ;
#74620 = ORIENTED_EDGE('',*,*,#52841,.T.) ;
#74621 = ORIENTED_EDGE('',*,*,#50496,.F.) ;
#74622 = ORIENTED_EDGE('',*,*,#52842,.F.) ;
#74623 = ORIENTED_EDGE('',*,*,#50634,.F.) ;
#74624 = ORIENTED_EDGE('',*,*,#50506,.F.) ;
#74625 = ORIENTED_EDGE('',*,*,#50635,.F.) ;
#74626 = ORIENTED_EDGE('',*,*,#52843,.F.) ;
#74627 = ORIENTED_EDGE('',*,*,#50500,.F.) ;
#74628 = ORIENTED_EDGE('',*,*,#52843,.T.) ;
#74629 = ORIENTED_EDGE('',*,*,#52842,.T.) ;
#74630 = ORIENTED_EDGE('',*,*,#52844,.F.) ;
#74631 = ORIENTED_EDGE('',*,*,#52844,.T.) ;
#74632 = ORIENTED_EDGE('',*,*,#50495,.F.) ;
#74633 = ORIENTED_EDGE('',*,*,#52845,.F.) ;
#74634 = ORIENTED_EDGE('',*,*,#50497,.F.) ;
#74635 = ORIENTED_EDGE('',*,*,#50507,.F.) ;
#74636 = ORIENTED_EDGE('',*,*,#50498,.F.) ;
#74637 = ORIENTED_EDGE('',*,*,#52846,.F.) ;
#74638 = ORIENTED_EDGE('',*,*,#50575,.F.) ;
#74639 = ORIENTED_EDGE('',*,*,#52846,.T.) ;
#74640 = ORIENTED_EDGE('',*,*,#52845,.T.) ;
#74641 = ORIENTED_EDGE('',*,*,#52847,.F.) ;
#74642 = ORIENTED_EDGE('',*,*,#52847,.T.) ;
#74643 = ORIENTED_EDGE('',*,*,#50494,.F.) ;
#74644 = ORIENTED_EDGE('',*,*,#52848,.F.) ;
#74645 = ORIENTED_EDGE('',*,*,#50576,.F.) ;
#74646 = ORIENTED_EDGE('',*,*,#52848,.T.) ;
#74647 = ORIENTED_EDGE('',*,*,#52475,.F.) ;
#74648 = ORIENTED_EDGE('',*,*,#52849,.F.) ;
#74649 = ORIENTED_EDGE('',*,*,#50577,.F.) ;
#74650 = ORIENTED_EDGE('',*,*,#52473,.F.) ;
#74651 = ORIENTED_EDGE('',*,*,#52470,.F.) ;
#74652 = ORIENTED_EDGE('',*,*,#52469,.F.) ;
#74653 = ORIENTED_EDGE('',*,*,#52849,.T.) ;
#74654 = ORIENTED_EDGE('',*,*,#52474,.F.) ;
#74655 = ORIENTED_EDGE('',*,*,#52850,.F.) ;
#74656 = ORIENTED_EDGE('',*,*,#49496,.F.) ;
#74657 = ORIENTED_EDGE('',*,*,#52851,.F.) ;
#74658 = ORIENTED_EDGE('',*,*,#52013,.F.) ;
#74659 = ORIENTED_EDGE('',*,*,#52851,.T.) ;
#74660 = ORIENTED_EDGE('',*,*,#49495,.F.) ;
#74661 = ORIENTED_EDGE('',*,*,#52852,.F.) ;
#74662 = ORIENTED_EDGE('',*,*,#52016,.F.) ;
#74663 = ORIENTED_EDGE('',*,*,#52850,.T.) ;
#74664 = ORIENTED_EDGE('',*,*,#52010,.F.) ;
#74665 = ORIENTED_EDGE('',*,*,#52853,.F.) ;
#74666 = ORIENTED_EDGE('',*,*,#49497,.F.) ;
#74667 = ORIENTED_EDGE('',*,*,#52852,.T.) ;
#74668 = ORIENTED_EDGE('',*,*,#49494,.F.) ;
#74669 = ORIENTED_EDGE('',*,*,#52854,.F.) ;
#74670 = ORIENTED_EDGE('',*,*,#52019,.F.) ;
#74671 = ORIENTED_EDGE('',*,*,#52853,.T.) ;
#74672 = ORIENTED_EDGE('',*,*,#52007,.F.) ;
#74673 = ORIENTED_EDGE('',*,*,#52855,.F.) ;
#74674 = ORIENTED_EDGE('',*,*,#49498,.F.) ;
#74675 = ORIENTED_EDGE('',*,*,#52854,.T.) ;
#74676 = ORIENTED_EDGE('',*,*,#49493,.F.) ;
#74677 = ORIENTED_EDGE('',*,*,#52856,.F.) ;
#74678 = ORIENTED_EDGE('',*,*,#52022,.F.) ;
#74679 = ORIENTED_EDGE('',*,*,#52855,.T.) ;
#74680 = ORIENTED_EDGE('',*,*,#52029,.F.) ;
#74681 = ORIENTED_EDGE('',*,*,#52857,.F.) ;
#74682 = ORIENTED_EDGE('',*,*,#49491,.F.) ;
#74683 = ORIENTED_EDGE('',*,*,#52856,.T.) ;
#74684 = ORIENTED_EDGE('',*,*,#49492,.F.) ;
#74685 = ORIENTED_EDGE('',*,*,#52857,.T.) ;
#74686 = ORIENTED_EDGE('',*,*,#52025,.F.) ;
#74687 = ORIENTED_EDGE('',*,*,#50882,.F.) ;
#74688 = ORIENTED_EDGE('',*,*,#50896,.F.) ;
#74689 = ORIENTED_EDGE('',*,*,#52858,.F.) ;
#74690 = ORIENTED_EDGE('',*,*,#50885,.F.) ;
#74691 = ORIENTED_EDGE('',*,*,#52859,.F.) ;
#74692 = ORIENTED_EDGE('',*,*,#50886,.F.) ;
#74693 = ORIENTED_EDGE('',*,*,#52860,.F.) ;
#74694 = ORIENTED_EDGE('',*,*,#51052,.F.) ;
#74695 = ORIENTED_EDGE('',*,*,#50884,.F.) ;
#74696 = ORIENTED_EDGE('',*,*,#50887,.F.) ;
#74697 = ORIENTED_EDGE('',*,*,#52861,.F.) ;
#74698 = ORIENTED_EDGE('',*,*,#50888,.F.) ;
#74699 = ORIENTED_EDGE('',*,*,#52860,.T.) ;
#74700 = ORIENTED_EDGE('',*,*,#52858,.T.) ;
#74701 = ORIENTED_EDGE('',*,*,#52862,.F.) ;
#74702 = ORIENTED_EDGE('',*,*,#52861,.T.) ;
#74703 = ORIENTED_EDGE('',*,*,#52859,.T.) ;
#74704 = ORIENTED_EDGE('',*,*,#52863,.F.) ;
#74705 = ORIENTED_EDGE('',*,*,#50880,.F.) ;
#74706 = ORIENTED_EDGE('',*,*,#50892,.F.) ;
#74707 = ORIENTED_EDGE('',*,*,#52864,.F.) ;
#74708 = ORIENTED_EDGE('',*,*,#50894,.F.) ;
#74709 = ORIENTED_EDGE('',*,*,#52862,.T.) ;
#74710 = ORIENTED_EDGE('',*,*,#50895,.F.) ;
#74711 = ORIENTED_EDGE('',*,*,#52865,.F.) ;
#74712 = ORIENTED_EDGE('',*,*,#51049,.F.) ;
#74713 = ORIENTED_EDGE('',*,*,#52863,.T.) ;
#74714 = ORIENTED_EDGE('',*,*,#51051,.F.) ;
#74715 = ORIENTED_EDGE('',*,*,#52866,.F.) ;
#74716 = ORIENTED_EDGE('',*,*,#50889,.F.) ;
#74717 = ORIENTED_EDGE('',*,*,#50878,.F.) ;
#74718 = ORIENTED_EDGE('',*,*,#50890,.F.) ;
#74719 = ORIENTED_EDGE('',*,*,#52867,.F.) ;
#74720 = ORIENTED_EDGE('',*,*,#50893,.F.) ;
#74721 = ORIENTED_EDGE('',*,*,#52865,.T.) ;
#74722 = ORIENTED_EDGE('',*,*,#52864,.T.) ;
#74723 = ORIENTED_EDGE('',*,*,#52868,.F.) ;
#74724 = ORIENTED_EDGE('',*,*,#52867,.T.) ;
#74725 = ORIENTED_EDGE('',*,*,#52866,.T.) ;
#74726 = ORIENTED_EDGE('',*,*,#52869,.F.) ;
#74727 = ORIENTED_EDGE('',*,*,#52868,.T.) ;
#74728 = ORIENTED_EDGE('',*,*,#50891,.F.) ;
#74729 = ORIENTED_EDGE('',*,*,#52869,.T.) ;
#74730 = ORIENTED_EDGE('',*,*,#51050,.F.) ;
#74731 = ORIENTED_EDGE('',*,*,#52870,.F.) ;
#74732 = ORIENTED_EDGE('',*,*,#49388,.F.) ;
#74733 = ORIENTED_EDGE('',*,*,#52871,.F.) ;
#74734 = ORIENTED_EDGE('',*,*,#51601,.F.) ;
#74735 = ORIENTED_EDGE('',*,*,#52871,.T.) ;
#74736 = ORIENTED_EDGE('',*,*,#49387,.T.) ;
#74737 = ORIENTED_EDGE('',*,*,#52872,.F.) ;
#74738 = ORIENTED_EDGE('',*,*,#52873,.F.) ;
#74739 = ORIENTED_EDGE('',*,*,#49389,.T.) ;
#74740 = ORIENTED_EDGE('',*,*,#52870,.T.) ;
#74741 = ORIENTED_EDGE('',*,*,#52874,.F.) ;
#74742 = ORIENTED_EDGE('',*,*,#52875,.F.) ;
#74743 = ORIENTED_EDGE('',*,*,#52872,.T.) ;
#74744 = ORIENTED_EDGE('',*,*,#49386,.F.) ;
#74745 = ORIENTED_EDGE('',*,*,#52876,.F.) ;
#74746 = ORIENTED_EDGE('',*,*,#51598,.F.) ;
#74747 = ORIENTED_EDGE('',*,*,#52873,.T.) ;
#74748 = ORIENTED_EDGE('',*,*,#51597,.F.) ;
#74749 = ORIENTED_EDGE('',*,*,#52877,.F.) ;
#74750 = ORIENTED_EDGE('',*,*,#51602,.F.) ;
#74751 = ORIENTED_EDGE('',*,*,#52878,.F.) ;
#74752 = ORIENTED_EDGE('',*,*,#51599,.F.) ;
#74753 = ORIENTED_EDGE('',*,*,#52879,.F.) ;
#74754 = ORIENTED_EDGE('',*,*,#51686,.F.) ;
#74755 = ORIENTED_EDGE('',*,*,#52874,.T.) ;
#74756 = ORIENTED_EDGE('',*,*,#51600,.F.) ;
#74757 = ORIENTED_EDGE('',*,*,#52880,.F.) ;
#74758 = ORIENTED_EDGE('',*,*,#51590,.F.) ;
#74759 = ORIENTED_EDGE('',*,*,#52875,.T.) ;
#74760 = ORIENTED_EDGE('',*,*,#51589,.F.) ;
#74761 = ORIENTED_EDGE('',*,*,#52881,.F.) ;
#74762 = ORIENTED_EDGE('',*,*,#49390,.F.) ;
#74763 = ORIENTED_EDGE('',*,*,#52882,.F.) ;
#74764 = ORIENTED_EDGE('',*,*,#49384,.F.) ;
#74765 = ORIENTED_EDGE('',*,*,#52883,.F.) ;
#74766 = ORIENTED_EDGE('',*,*,#51591,.F.) ;
#74767 = ORIENTED_EDGE('',*,*,#49385,.T.) ;
#74768 = ORIENTED_EDGE('',*,*,#52882,.T.) ;
#74769 = ORIENTED_EDGE('',*,*,#52884,.F.) ;
#74770 = ORIENTED_EDGE('',*,*,#52876,.T.) ;
#74771 = ORIENTED_EDGE('',*,*,#52879,.T.) ;
#74772 = ORIENTED_EDGE('',*,*,#52877,.T.) ;
#74773 = ORIENTED_EDGE('',*,*,#52885,.F.) ;
#74774 = ORIENTED_EDGE('',*,*,#52880,.T.) ;
#74775 = ORIENTED_EDGE('',*,*,#52878,.T.) ;
#74776 = ORIENTED_EDGE('',*,*,#52886,.F.) ;
#74777 = ORIENTED_EDGE('',*,*,#49383,.T.) ;
#74778 = ORIENTED_EDGE('',*,*,#52881,.T.) ;
#74779 = ORIENTED_EDGE('',*,*,#52887,.F.) ;
#74780 = ORIENTED_EDGE('',*,*,#52883,.T.) ;
#74781 = ORIENTED_EDGE('',*,*,#52884,.T.) ;
#74782 = ORIENTED_EDGE('',*,*,#51594,.F.) ;
#74783 = ORIENTED_EDGE('',*,*,#52888,.F.) ;
#74784 = ORIENTED_EDGE('',*,*,#51595,.F.) ;
#74785 = ORIENTED_EDGE('',*,*,#52885,.T.) ;
#74786 = ORIENTED_EDGE('',*,*,#51596,.F.) ;
#74787 = ORIENTED_EDGE('',*,*,#52889,.F.) ;
#74788 = ORIENTED_EDGE('',*,*,#51683,.F.) ;
#74789 = ORIENTED_EDGE('',*,*,#52886,.T.) ;
#74790 = ORIENTED_EDGE('',*,*,#51685,.F.) ;
#74791 = ORIENTED_EDGE('',*,*,#52890,.F.) ;
#74792 = ORIENTED_EDGE('',*,*,#51587,.F.) ;
#74793 = ORIENTED_EDGE('',*,*,#52887,.T.) ;
#74794 = ORIENTED_EDGE('',*,*,#51588,.F.) ;
#74795 = ORIENTED_EDGE('',*,*,#52891,.F.) ;
#74796 = ORIENTED_EDGE('',*,*,#51592,.F.) ;
#74797 = ORIENTED_EDGE('',*,*,#52889,.T.) ;
#74798 = ORIENTED_EDGE('',*,*,#52888,.T.) ;
#74799 = ORIENTED_EDGE('',*,*,#52892,.F.) ;
#74800 = ORIENTED_EDGE('',*,*,#52891,.T.) ;
#74801 = ORIENTED_EDGE('',*,*,#52890,.T.) ;
#74802 = ORIENTED_EDGE('',*,*,#52893,.F.) ;
#74803 = ORIENTED_EDGE('',*,*,#52892,.T.) ;
#74804 = ORIENTED_EDGE('',*,*,#51593,.F.) ;
#74805 = ORIENTED_EDGE('',*,*,#52893,.T.) ;
#74806 = ORIENTED_EDGE('',*,*,#51684,.F.) ;
#74807 = ORIENTED_EDGE('',*,*,#51692,.F.) ;
#74808 = ORIENTED_EDGE('',*,*,#51705,.F.) ;
#74809 = ORIENTED_EDGE('',*,*,#52894,.F.) ;
#74810 = ORIENTED_EDGE('',*,*,#51697,.F.) ;
#74811 = ORIENTED_EDGE('',*,*,#52895,.F.) ;
#74812 = ORIENTED_EDGE('',*,*,#51695,.F.) ;
#74813 = ORIENTED_EDGE('',*,*,#52896,.F.) ;
#74814 = ORIENTED_EDGE('',*,*,#51862,.F.) ;
#74815 = ORIENTED_EDGE('',*,*,#51694,.F.) ;
#74816 = ORIENTED_EDGE('',*,*,#51696,.F.) ;
#74817 = ORIENTED_EDGE('',*,*,#52897,.F.) ;
#74818 = ORIENTED_EDGE('',*,*,#51700,.F.) ;
#74819 = ORIENTED_EDGE('',*,*,#52896,.T.) ;
#74820 = ORIENTED_EDGE('',*,*,#52894,.T.) ;
#74821 = ORIENTED_EDGE('',*,*,#52898,.F.) ;
#74822 = ORIENTED_EDGE('',*,*,#52897,.T.) ;
#74823 = ORIENTED_EDGE('',*,*,#52895,.T.) ;
#74824 = ORIENTED_EDGE('',*,*,#52899,.F.) ;
#74825 = ORIENTED_EDGE('',*,*,#51690,.F.) ;
#74826 = ORIENTED_EDGE('',*,*,#51703,.F.) ;
#74827 = ORIENTED_EDGE('',*,*,#52900,.F.) ;
#74828 = ORIENTED_EDGE('',*,*,#51706,.F.) ;
#74829 = ORIENTED_EDGE('',*,*,#52898,.T.) ;
#74830 = ORIENTED_EDGE('',*,*,#51704,.F.) ;
#74831 = ORIENTED_EDGE('',*,*,#52901,.F.) ;
#74832 = ORIENTED_EDGE('',*,*,#51859,.F.) ;
#74833 = ORIENTED_EDGE('',*,*,#52899,.T.) ;
#74834 = ORIENTED_EDGE('',*,*,#51861,.F.) ;
#74835 = ORIENTED_EDGE('',*,*,#52902,.F.) ;
#74836 = ORIENTED_EDGE('',*,*,#51698,.F.) ;
#74837 = ORIENTED_EDGE('',*,*,#51688,.F.) ;
#74838 = ORIENTED_EDGE('',*,*,#51699,.F.) ;
#74839 = ORIENTED_EDGE('',*,*,#52903,.F.) ;
#74840 = ORIENTED_EDGE('',*,*,#51701,.F.) ;
#74841 = ORIENTED_EDGE('',*,*,#52901,.T.) ;
#74842 = ORIENTED_EDGE('',*,*,#52900,.T.) ;
#74843 = ORIENTED_EDGE('',*,*,#52904,.F.) ;
#74844 = ORIENTED_EDGE('',*,*,#52903,.T.) ;
#74845 = ORIENTED_EDGE('',*,*,#52902,.T.) ;
#74846 = ORIENTED_EDGE('',*,*,#52905,.F.) ;
#74847 = ORIENTED_EDGE('',*,*,#52904,.T.) ;
#74848 = ORIENTED_EDGE('',*,*,#51702,.F.) ;
#74849 = ORIENTED_EDGE('',*,*,#52905,.T.) ;
#74850 = ORIENTED_EDGE('',*,*,#51860,.F.) ;
#74851 = ORIENTED_EDGE('',*,*,#52906,.F.) ;
#74852 = ORIENTED_EDGE('',*,*,#52018,.F.) ;
#74853 = ORIENTED_EDGE('',*,*,#52907,.F.) ;
#74854 = ORIENTED_EDGE('',*,*,#52033,.F.) ;
#74855 = ORIENTED_EDGE('',*,*,#52907,.T.) ;
#74856 = ORIENTED_EDGE('',*,*,#52021,.F.) ;
#74857 = ORIENTED_EDGE('',*,*,#52908,.F.) ;
#74858 = ORIENTED_EDGE('',*,*,#52015,.F.) ;
#74859 = ORIENTED_EDGE('',*,*,#52906,.T.) ;
#74860 = ORIENTED_EDGE('',*,*,#52909,.F.) ;
#74861 = ORIENTED_EDGE('',*,*,#52908,.T.) ;
#74862 = ORIENTED_EDGE('',*,*,#52024,.F.) ;
#74863 = ORIENTED_EDGE('',*,*,#52910,.F.) ;
#74864 = ORIENTED_EDGE('',*,*,#52030,.F.) ;
#74865 = ORIENTED_EDGE('',*,*,#52909,.T.) ;
#74866 = ORIENTED_EDGE('',*,*,#52032,.F.) ;
#74867 = ORIENTED_EDGE('',*,*,#52911,.F.) ;
#74868 = ORIENTED_EDGE('',*,*,#52012,.F.) ;
#74869 = ORIENTED_EDGE('',*,*,#52910,.T.) ;
#74870 = ORIENTED_EDGE('',*,*,#52027,.F.) ;
#74871 = ORIENTED_EDGE('',*,*,#52912,.F.) ;
#74872 = ORIENTED_EDGE('',*,*,#52009,.F.) ;
#74873 = ORIENTED_EDGE('',*,*,#52911,.T.) ;
#74874 = ORIENTED_EDGE('',*,*,#52913,.F.) ;
#74875 = ORIENTED_EDGE('',*,*,#52912,.T.) ;
#74876 = ORIENTED_EDGE('',*,*,#52028,.F.) ;
#74877 = ORIENTED_EDGE('',*,*,#52913,.T.) ;
#74878 = ORIENTED_EDGE('',*,*,#52031,.F.) ;
#74879 = ORIENTED_EDGE('',*,*,#49124,.F.) ;
#74880 = ORIENTED_EDGE('',*,*,#51893,.F.) ;
#74881 = ORIENTED_EDGE('',*,*,#49138,.F.) ;
#74882 = ORIENTED_EDGE('',*,*,#51908,.F.) ;
#74883 = ORIENTED_EDGE('',*,*,#49126,.F.) ;
#74884 = ORIENTED_EDGE('',*,*,#51909,.F.) ;
#74885 = ORIENTED_EDGE('',*,*,#49136,.F.) ;
#74886 = ORIENTED_EDGE('',*,*,#51912,.F.) ;
#74887 = ORIENTED_EDGE('',*,*,#49134,.F.) ;
#74888 = ORIENTED_EDGE('',*,*,#51910,.F.) ;
#74889 = ORIENTED_EDGE('',*,*,#49128,.F.) ;
#74890 = ORIENTED_EDGE('',*,*,#51913,.F.) ;
#74891 = ORIENTED_EDGE('',*,*,#49132,.F.) ;
#74892 = ORIENTED_EDGE('',*,*,#49529,.F.) ;
#74893 = ORIENTED_EDGE('',*,*,#49130,.F.) ;
#74894 = ORIENTED_EDGE('',*,*,#51911,.F.) ;
#74895 = ORIENTED_EDGE('',*,*,#52914,.F.) ;
#74896 = ORIENTED_EDGE('',*,*,#52915,.F.) ;
#74897 = ORIENTED_EDGE('',*,*,#52916,.F.) ;
#74898 = ORIENTED_EDGE('',*,*,#52915,.T.) ;
#74899 = ORIENTED_EDGE('',*,*,#51395,.F.) ;
#74900 = ORIENTED_EDGE('',*,*,#52917,.F.) ;
#74901 = ORIENTED_EDGE('',*,*,#51390,.F.) ;
#74902 = ORIENTED_EDGE('',*,*,#52916,.T.) ;
#74903 = ORIENTED_EDGE('',*,*,#51389,.F.) ;
#74904 = ORIENTED_EDGE('',*,*,#52918,.F.) ;
#74905 = ORIENTED_EDGE('',*,*,#51391,.F.) ;
#74906 = ORIENTED_EDGE('',*,*,#52914,.T.) ;
#74907 = ORIENTED_EDGE('',*,*,#51394,.F.) ;
#74908 = ORIENTED_EDGE('',*,*,#52919,.F.) ;
#74909 = ORIENTED_EDGE('',*,*,#51396,.F.) ;
#74910 = ORIENTED_EDGE('',*,*,#51400,.F.) ;
#74911 = ORIENTED_EDGE('',*,*,#52920,.T.) ;
#74912 = ORIENTED_EDGE('',*,*,#51169,.F.) ;
#74913 = ORIENTED_EDGE('',*,*,#52921,.F.) ;
#74914 = ORIENTED_EDGE('',*,*,#52917,.T.) ;
#74915 = ORIENTED_EDGE('',*,*,#52921,.T.) ;
#74916 = ORIENTED_EDGE('',*,*,#52922,.F.) ;
#74917 = ORIENTED_EDGE('',*,*,#52923,.F.) ;
#74918 = ORIENTED_EDGE('',*,*,#52918,.T.) ;
#74919 = ORIENTED_EDGE('',*,*,#52924,.F.) ;
#74920 = ORIENTED_EDGE('',*,*,#49636,.T.) ;
#74921 = ORIENTED_EDGE('',*,*,#52925,.F.) ;
#74922 = ORIENTED_EDGE('',*,*,#52919,.T.) ;
#74923 = ORIENTED_EDGE('',*,*,#52926,.F.) ;
#74924 = ORIENTED_EDGE('',*,*,#51399,.F.) ;
#74925 = ORIENTED_EDGE('',*,*,#52927,.T.) ;
#74926 = ORIENTED_EDGE('',*,*,#49475,.F.) ;
#74927 = ORIENTED_EDGE('',*,*,#52928,.T.) ;
#74928 = ORIENTED_EDGE('',*,*,#52922,.T.) ;
#74929 = ORIENTED_EDGE('',*,*,#51168,.F.) ;
#74930 = ORIENTED_EDGE('',*,*,#52929,.F.) ;
#74931 = ORIENTED_EDGE('',*,*,#51387,.F.) ;
#74932 = ORIENTED_EDGE('',*,*,#52924,.T.) ;
#74933 = ORIENTED_EDGE('',*,*,#51388,.F.) ;
#74934 = ORIENTED_EDGE('',*,*,#52930,.F.) ;
#74935 = ORIENTED_EDGE('',*,*,#49637,.F.) ;
#74936 = ORIENTED_EDGE('',*,*,#52923,.T.) ;
#74937 = ORIENTED_EDGE('',*,*,#49643,.F.) ;
#74938 = ORIENTED_EDGE('',*,*,#52931,.F.) ;
#74939 = ORIENTED_EDGE('',*,*,#51392,.F.) ;
#74940 = ORIENTED_EDGE('',*,*,#52926,.T.) ;
#74941 = ORIENTED_EDGE('',*,*,#51393,.F.) ;
#74942 = ORIENTED_EDGE('',*,*,#52932,.F.) ;
#74943 = ORIENTED_EDGE('',*,*,#51383,.F.) ;
#74944 = ORIENTED_EDGE('',*,*,#52925,.T.) ;
#74945 = ORIENTED_EDGE('',*,*,#51386,.F.) ;
#74946 = ORIENTED_EDGE('',*,*,#52933,.F.) ;
#74947 = ORIENTED_EDGE('',*,*,#51397,.F.) ;
#74948 = ORIENTED_EDGE('',*,*,#51179,.F.) ;
#74949 = ORIENTED_EDGE('',*,*,#52934,.T.) ;
#74950 = ORIENTED_EDGE('',*,*,#51398,.F.) ;
#74951 = ORIENTED_EDGE('',*,*,#52935,.F.) ;
#74952 = ORIENTED_EDGE('',*,*,#52929,.T.) ;
#74953 = ORIENTED_EDGE('',*,*,#51167,.T.) ;
#74954 = ORIENTED_EDGE('',*,*,#52936,.F.) ;
#74955 = ORIENTED_EDGE('',*,*,#52930,.T.) ;
#74956 = ORIENTED_EDGE('',*,*,#52931,.T.) ;
#74957 = ORIENTED_EDGE('',*,*,#49642,.T.) ;
#74958 = ORIENTED_EDGE('',*,*,#52937,.F.) ;
#74959 = ORIENTED_EDGE('',*,*,#52932,.T.) ;
#74960 = ORIENTED_EDGE('',*,*,#52935,.T.) ;
#74961 = ORIENTED_EDGE('',*,*,#52933,.T.) ;
#74962 = ORIENTED_EDGE('',*,*,#52938,.F.) ;
#74963 = ORIENTED_EDGE('',*,*,#51163,.F.) ;
#74964 = ORIENTED_EDGE('',*,*,#52939,.T.) ;
#74965 = ORIENTED_EDGE('',*,*,#51157,.F.) ;
#74966 = ORIENTED_EDGE('',*,*,#52940,.F.) ;
#74967 = ORIENTED_EDGE('',*,*,#52936,.T.) ;
#74968 = ORIENTED_EDGE('',*,*,#51166,.F.) ;
#74969 = ORIENTED_EDGE('',*,*,#52941,.F.) ;
#74970 = ORIENTED_EDGE('',*,*,#49638,.F.) ;
#74971 = ORIENTED_EDGE('',*,*,#52937,.T.) ;
#74972 = ORIENTED_EDGE('',*,*,#49641,.F.) ;
#74973 = ORIENTED_EDGE('',*,*,#52942,.F.) ;
#74974 = ORIENTED_EDGE('',*,*,#51384,.F.) ;
#74975 = ORIENTED_EDGE('',*,*,#52938,.T.) ;
#74976 = ORIENTED_EDGE('',*,*,#51385,.F.) ;
#74977 = ORIENTED_EDGE('',*,*,#52943,.F.) ;
#74978 = ORIENTED_EDGE('',*,*,#51180,.F.) ;
#74979 = ORIENTED_EDGE('',*,*,#52940,.T.) ;
#74980 = ORIENTED_EDGE('',*,*,#52810,.F.) ;
#74981 = ORIENTED_EDGE('',*,*,#52944,.F.) ;
#74982 = ORIENTED_EDGE('',*,*,#52945,.F.) ;
#74983 = ORIENTED_EDGE('',*,*,#52941,.T.) ;
#74984 = ORIENTED_EDGE('',*,*,#52946,.F.) ;
#74985 = ORIENTED_EDGE('',*,*,#52943,.T.) ;
#74986 = ORIENTED_EDGE('',*,*,#52942,.T.) ;
#74987 = ORIENTED_EDGE('',*,*,#52947,.F.) ;
#74988 = ORIENTED_EDGE('',*,*,#51181,.T.) ;
#74989 = ORIENTED_EDGE('',*,*,#52944,.T.) ;
#74990 = ORIENTED_EDGE('',*,*,#49709,.F.) ;
#74991 = ORIENTED_EDGE('',*,*,#52948,.F.) ;
#74992 = ORIENTED_EDGE('',*,*,#51164,.F.) ;
#74993 = ORIENTED_EDGE('',*,*,#52946,.T.) ;
#74994 = ORIENTED_EDGE('',*,*,#51165,.F.) ;
#74995 = ORIENTED_EDGE('',*,*,#52949,.F.) ;
#74996 = ORIENTED_EDGE('',*,*,#51171,.F.) ;
#74997 = ORIENTED_EDGE('',*,*,#52945,.T.) ;
#74998 = ORIENTED_EDGE('',*,*,#51174,.F.) ;
#74999 = ORIENTED_EDGE('',*,*,#52950,.F.) ;
#75000 = ORIENTED_EDGE('',*,*,#49639,.F.) ;
#75001 = ORIENTED_EDGE('',*,*,#52947,.T.) ;
#75002 = ORIENTED_EDGE('',*,*,#49640,.F.) ;
#75003 = ORIENTED_EDGE('',*,*,#52951,.F.) ;
#75004 = ORIENTED_EDGE('',*,*,#51182,.F.) ;
#75005 = ORIENTED_EDGE('',*,*,#52948,.T.) ;
#75006 = ORIENTED_EDGE('',*,*,#49708,.T.) ;
#75007 = ORIENTED_EDGE('',*,*,#52952,.F.) ;
#75008 = ORIENTED_EDGE('',*,*,#52949,.T.) ;
#75009 = ORIENTED_EDGE('',*,*,#52951,.T.) ;
#75010 = ORIENTED_EDGE('',*,*,#52950,.T.) ;
#75011 = ORIENTED_EDGE('',*,*,#52953,.F.) ;
#75012 = ORIENTED_EDGE('',*,*,#52952,.T.) ;
#75013 = ORIENTED_EDGE('',*,*,#49707,.F.) ;
#75014 = ORIENTED_EDGE('',*,*,#52954,.F.) ;
#75015 = ORIENTED_EDGE('',*,*,#51172,.F.) ;
#75016 = ORIENTED_EDGE('',*,*,#52953,.T.) ;
#75017 = ORIENTED_EDGE('',*,*,#51173,.F.) ;
#75018 = ORIENTED_EDGE('',*,*,#52955,.F.) ;
#75019 = ORIENTED_EDGE('',*,*,#51183,.F.) ;
#75020 = ORIENTED_EDGE('',*,*,#51187,.F.) ;
#75021 = ORIENTED_EDGE('',*,*,#52956,.T.) ;
#75022 = ORIENTED_EDGE('',*,*,#51175,.F.) ;
#75023 = ORIENTED_EDGE('',*,*,#52957,.F.) ;
#75024 = ORIENTED_EDGE('',*,*,#49704,.F.) ;
#75025 = ORIENTED_EDGE('',*,*,#52958,.T.) ;
#75026 = ORIENTED_EDGE('',*,*,#51188,.F.) ;
#75027 = ORIENTED_EDGE('',*,*,#52959,.F.) ;
#75028 = ORIENTED_EDGE('',*,*,#52954,.T.) ;
#75029 = ORIENTED_EDGE('',*,*,#49706,.T.) ;
#75030 = ORIENTED_EDGE('',*,*,#52960,.F.) ;
#75031 = ORIENTED_EDGE('',*,*,#52955,.T.) ;
#75032 = ORIENTED_EDGE('',*,*,#52959,.T.) ;
#75033 = ORIENTED_EDGE('',*,*,#52957,.T.) ;
#75034 = ORIENTED_EDGE('',*,*,#52961,.F.) ;
#75035 = ORIENTED_EDGE('',*,*,#52960,.T.) ;
#75036 = ORIENTED_EDGE('',*,*,#49705,.F.) ;
#75037 = ORIENTED_EDGE('',*,*,#52961,.T.) ;
#75038 = ORIENTED_EDGE('',*,*,#51184,.F.) ;
#75039 = ORIENTED_EDGE('',*,*,#52342,.F.) ;
#75040 = ORIENTED_EDGE('',*,*,#52353,.F.) ;
#75041 = ORIENTED_EDGE('',*,*,#52352,.F.) ;
#75042 = ORIENTED_EDGE('',*,*,#52962,.F.) ;
#75043 = ORIENTED_EDGE('',*,*,#52343,.F.) ;
#75044 = ORIENTED_EDGE('',*,*,#52962,.T.) ;
#75045 = ORIENTED_EDGE('',*,*,#50776,.F.) ;
#75046 = ORIENTED_EDGE('',*,*,#52963,.F.) ;
#75047 = ORIENTED_EDGE('',*,*,#50762,.F.) ;
#75048 = ORIENTED_EDGE('',*,*,#52350,.F.) ;
#75049 = ORIENTED_EDGE('',*,*,#52349,.F.) ;
#75050 = ORIENTED_EDGE('',*,*,#52348,.F.) ;
#75051 = ORIENTED_EDGE('',*,*,#52964,.F.) ;
#75052 = ORIENTED_EDGE('',*,*,#52351,.F.) ;
#75053 = ORIENTED_EDGE('',*,*,#52965,.F.) ;
#75054 = ORIENTED_EDGE('',*,*,#52963,.T.) ;
#75055 = ORIENTED_EDGE('',*,*,#52966,.F.) ;
#75056 = ORIENTED_EDGE('',*,*,#52340,.F.) ;
#75057 = ORIENTED_EDGE('',*,*,#52345,.F.) ;
#75058 = ORIENTED_EDGE('',*,*,#52344,.F.) ;
#75059 = ORIENTED_EDGE('',*,*,#52967,.F.) ;
#75060 = ORIENTED_EDGE('',*,*,#52341,.F.) ;
#75061 = ORIENTED_EDGE('',*,*,#52964,.T.) ;
#75062 = ORIENTED_EDGE('',*,*,#50772,.F.) ;
#75063 = ORIENTED_EDGE('',*,*,#52968,.F.) ;
#75064 = ORIENTED_EDGE('',*,*,#50774,.F.) ;
#75065 = ORIENTED_EDGE('',*,*,#52966,.T.) ;
#75066 = ORIENTED_EDGE('',*,*,#50775,.F.) ;
#75067 = ORIENTED_EDGE('',*,*,#52969,.F.) ;
#75068 = ORIENTED_EDGE('',*,*,#50900,.F.) ;
#75069 = ORIENTED_EDGE('',*,*,#52965,.T.) ;
#75070 = ORIENTED_EDGE('',*,*,#50899,.F.) ;
#75071 = ORIENTED_EDGE('',*,*,#52970,.F.) ;
#75072 = ORIENTED_EDGE('',*,*,#50763,.F.) ;
#75073 = ORIENTED_EDGE('',*,*,#52967,.T.) ;
#75074 = ORIENTED_EDGE('',*,*,#50764,.F.) ;
#75075 = ORIENTED_EDGE('',*,*,#52971,.F.) ;
#75076 = ORIENTED_EDGE('',*,*,#50768,.F.) ;
#75077 = ORIENTED_EDGE('',*,*,#52969,.T.) ;
#75078 = ORIENTED_EDGE('',*,*,#52968,.T.) ;
#75079 = ORIENTED_EDGE('',*,*,#52972,.F.) ;
#75080 = ORIENTED_EDGE('',*,*,#52971,.T.) ;
#75081 = ORIENTED_EDGE('',*,*,#52970,.T.) ;
#75082 = ORIENTED_EDGE('',*,*,#52973,.F.) ;
#75083 = ORIENTED_EDGE('',*,*,#52972,.T.) ;
#75084 = ORIENTED_EDGE('',*,*,#50771,.F.) ;
#75085 = ORIENTED_EDGE('',*,*,#52974,.F.) ;
#75086 = ORIENTED_EDGE('',*,*,#50897,.F.) ;
#75087 = ORIENTED_EDGE('',*,*,#52973,.T.) ;
#75088 = ORIENTED_EDGE('',*,*,#50898,.F.) ;
#75089 = ORIENTED_EDGE('',*,*,#52975,.F.) ;
#75090 = ORIENTED_EDGE('',*,*,#50765,.F.) ;
#75091 = ORIENTED_EDGE('',*,*,#52975,.T.) ;
#75092 = ORIENTED_EDGE('',*,*,#52974,.T.) ;
#75093 = ORIENTED_EDGE('',*,*,#52976,.F.) ;
#75094 = ORIENTED_EDGE('',*,*,#52976,.T.) ;
#75095 = ORIENTED_EDGE('',*,*,#50770,.F.) ;
#75096 = ORIENTED_EDGE('',*,*,#52977,.F.) ;
#75097 = ORIENTED_EDGE('',*,*,#50766,.F.) ;
#75098 = ORIENTED_EDGE('',*,*,#52346,.F.) ;
#75099 = ORIENTED_EDGE('',*,*,#52339,.F.) ;
#75100 = ORIENTED_EDGE('',*,*,#52338,.F.) ;
#75101 = ORIENTED_EDGE('',*,*,#52977,.T.) ;
#75102 = ORIENTED_EDGE('',*,*,#52347,.F.) ;
#75103 = ORIENTED_EDGE('',*,*,#52483,.F.) ;
#75104 = ORIENTED_EDGE('',*,*,#52482,.F.) ;
#75105 = ORIENTED_EDGE('',*,*,#52481,.F.) ;
#75106 = ORIENTED_EDGE('',*,*,#52978,.F.) ;
#75107 = ORIENTED_EDGE('',*,*,#52484,.F.) ;
#75108 = ORIENTED_EDGE('',*,*,#52978,.T.) ;
#75109 = ORIENTED_EDGE('',*,*,#52480,.F.) ;
#75110 = ORIENTED_EDGE('',*,*,#52979,.F.) ;
#75111 = ORIENTED_EDGE('',*,*,#50579,.F.) ;
#75112 = ORIENTED_EDGE('',*,*,#52979,.T.) ;
#75113 = ORIENTED_EDGE('',*,*,#50492,.F.) ;
#75114 = ORIENTED_EDGE('',*,*,#52980,.F.) ;
#75115 = ORIENTED_EDGE('',*,*,#50580,.F.) ;
#75116 = ORIENTED_EDGE('',*,*,#50480,.F.) ;
#75117 = ORIENTED_EDGE('',*,*,#50581,.F.) ;
#75118 = ORIENTED_EDGE('',*,*,#52981,.F.) ;
#75119 = ORIENTED_EDGE('',*,*,#50486,.F.) ;
#75120 = ORIENTED_EDGE('',*,*,#52981,.T.) ;
#75121 = ORIENTED_EDGE('',*,*,#52980,.T.) ;
#75122 = ORIENTED_EDGE('',*,*,#52982,.F.) ;
#75123 = ORIENTED_EDGE('',*,*,#52982,.T.) ;
#75124 = ORIENTED_EDGE('',*,*,#50491,.F.) ;
#75125 = ORIENTED_EDGE('',*,*,#52983,.F.) ;
#75126 = ORIENTED_EDGE('',*,*,#50487,.F.) ;
#75127 = ORIENTED_EDGE('',*,*,#50482,.F.) ;
#75128 = ORIENTED_EDGE('',*,*,#50488,.F.) ;
#75129 = ORIENTED_EDGE('',*,*,#52984,.F.) ;
#75130 = ORIENTED_EDGE('',*,*,#50643,.F.) ;
#75131 = ORIENTED_EDGE('',*,*,#52984,.T.) ;
#75132 = ORIENTED_EDGE('',*,*,#52983,.T.) ;
#75133 = ORIENTED_EDGE('',*,*,#52985,.F.) ;
#75134 = ORIENTED_EDGE('',*,*,#52985,.T.) ;
#75135 = ORIENTED_EDGE('',*,*,#50490,.F.) ;
#75136 = ORIENTED_EDGE('',*,*,#52986,.F.) ;
#75137 = ORIENTED_EDGE('',*,*,#50644,.F.) ;
#75138 = ORIENTED_EDGE('',*,*,#52986,.T.) ;
#75139 = ORIENTED_EDGE('',*,*,#52479,.F.) ;
#75140 = ORIENTED_EDGE('',*,*,#52987,.F.) ;
#75141 = ORIENTED_EDGE('',*,*,#50645,.F.) ;
#75142 = ORIENTED_EDGE('',*,*,#52987,.T.) ;
#75143 = ORIENTED_EDGE('',*,*,#52478,.F.) ;
#75144 = ORIENTED_EDGE('',*,*,#52487,.F.) ;
#75145 = ORIENTED_EDGE('',*,*,#52488,.F.) ;
#75146 = ORIENTED_EDGE('',*,*,#52493,.F.) ;
#75147 = ORIENTED_EDGE('',*,*,#52988,.F.) ;
#75148 = ORIENTED_EDGE('',*,*,#52988,.T.) ;
#75149 = ORIENTED_EDGE('',*,*,#52492,.F.) ;
#75150 = ORIENTED_EDGE('',*,*,#52989,.F.) ;
#75151 = ORIENTED_EDGE('',*,*,#50640,.F.) ;
#75152 = ORIENTED_EDGE('',*,*,#52989,.T.) ;
#75153 = ORIENTED_EDGE('',*,*,#50474,.F.) ;
#75154 = ORIENTED_EDGE('',*,*,#52990,.F.) ;
#75155 = ORIENTED_EDGE('',*,*,#50641,.F.) ;
#75156 = ORIENTED_EDGE('',*,*,#50484,.F.) ;
#75157 = ORIENTED_EDGE('',*,*,#50642,.F.) ;
#75158 = ORIENTED_EDGE('',*,*,#52991,.F.) ;
#75159 = ORIENTED_EDGE('',*,*,#50478,.F.) ;
#75160 = ORIENTED_EDGE('',*,*,#52991,.T.) ;
#75161 = ORIENTED_EDGE('',*,*,#52990,.T.) ;
#75162 = ORIENTED_EDGE('',*,*,#52992,.F.) ;
#75163 = ORIENTED_EDGE('',*,*,#52992,.T.) ;
#75164 = ORIENTED_EDGE('',*,*,#50473,.F.) ;
#75165 = ORIENTED_EDGE('',*,*,#52993,.F.) ;
#75166 = ORIENTED_EDGE('',*,*,#50475,.F.) ;
#75167 = ORIENTED_EDGE('',*,*,#50485,.F.) ;
#75168 = ORIENTED_EDGE('',*,*,#50476,.F.) ;
#75169 = ORIENTED_EDGE('',*,*,#52994,.F.) ;
#75170 = ORIENTED_EDGE('',*,*,#50582,.F.) ;
#75171 = ORIENTED_EDGE('',*,*,#52994,.T.) ;
#75172 = ORIENTED_EDGE('',*,*,#52993,.T.) ;
#75173 = ORIENTED_EDGE('',*,*,#52995,.F.) ;
#75174 = ORIENTED_EDGE('',*,*,#52995,.T.) ;
#75175 = ORIENTED_EDGE('',*,*,#50472,.F.) ;
#75176 = ORIENTED_EDGE('',*,*,#52996,.F.) ;
#75177 = ORIENTED_EDGE('',*,*,#50583,.F.) ;
#75178 = ORIENTED_EDGE('',*,*,#52996,.T.) ;
#75179 = ORIENTED_EDGE('',*,*,#52491,.F.) ;
#75180 = ORIENTED_EDGE('',*,*,#52997,.F.) ;
#75181 = ORIENTED_EDGE('',*,*,#50584,.F.) ;
#75182 = ORIENTED_EDGE('',*,*,#52489,.F.) ;
#75183 = ORIENTED_EDGE('',*,*,#52486,.F.) ;
#75184 = ORIENTED_EDGE('',*,*,#52485,.F.) ;
#75185 = ORIENTED_EDGE('',*,*,#52997,.T.) ;
#75186 = ORIENTED_EDGE('',*,*,#52490,.F.) ;
#75187 = ORIENTED_EDGE('',*,*,#52998,.F.) ;
#75188 = ORIENTED_EDGE('',*,*,#49484,.F.) ;
#75189 = ORIENTED_EDGE('',*,*,#52999,.F.) ;
#75190 = ORIENTED_EDGE('',*,*,#52041,.F.) ;
#75191 = ORIENTED_EDGE('',*,*,#52999,.T.) ;
#75192 = ORIENTED_EDGE('',*,*,#49483,.F.) ;
#75193 = ORIENTED_EDGE('',*,*,#53000,.F.) ;
#75194 = ORIENTED_EDGE('',*,*,#52044,.F.) ;
#75195 = ORIENTED_EDGE('',*,*,#52998,.T.) ;
#75196 = ORIENTED_EDGE('',*,*,#52038,.F.) ;
#75197 = ORIENTED_EDGE('',*,*,#53001,.F.) ;
#75198 = ORIENTED_EDGE('',*,*,#49485,.F.) ;
#75199 = ORIENTED_EDGE('',*,*,#53000,.T.) ;
#75200 = ORIENTED_EDGE('',*,*,#49482,.F.) ;
#75201 = ORIENTED_EDGE('',*,*,#53002,.F.) ;
#75202 = ORIENTED_EDGE('',*,*,#52047,.F.) ;
#75203 = ORIENTED_EDGE('',*,*,#53001,.T.) ;
#75204 = ORIENTED_EDGE('',*,*,#52035,.F.) ;
#75205 = ORIENTED_EDGE('',*,*,#53003,.F.) ;
#75206 = ORIENTED_EDGE('',*,*,#49486,.F.) ;
#75207 = ORIENTED_EDGE('',*,*,#53002,.T.) ;
#75208 = ORIENTED_EDGE('',*,*,#49481,.F.) ;
#75209 = ORIENTED_EDGE('',*,*,#53004,.F.) ;
#75210 = ORIENTED_EDGE('',*,*,#52050,.F.) ;
#75211 = ORIENTED_EDGE('',*,*,#53003,.T.) ;
#75212 = ORIENTED_EDGE('',*,*,#52057,.F.) ;
#75213 = ORIENTED_EDGE('',*,*,#53005,.F.) ;
#75214 = ORIENTED_EDGE('',*,*,#49479,.F.) ;
#75215 = ORIENTED_EDGE('',*,*,#53004,.T.) ;
#75216 = ORIENTED_EDGE('',*,*,#49480,.F.) ;
#75217 = ORIENTED_EDGE('',*,*,#53005,.T.) ;
#75218 = ORIENTED_EDGE('',*,*,#52053,.F.) ;
#75219 = ORIENTED_EDGE('',*,*,#50906,.F.) ;
#75220 = ORIENTED_EDGE('',*,*,#50920,.F.) ;
#75221 = ORIENTED_EDGE('',*,*,#53006,.F.) ;
#75222 = ORIENTED_EDGE('',*,*,#50909,.F.) ;
#75223 = ORIENTED_EDGE('',*,*,#53007,.F.) ;
#75224 = ORIENTED_EDGE('',*,*,#50910,.F.) ;
#75225 = ORIENTED_EDGE('',*,*,#53008,.F.) ;
#75226 = ORIENTED_EDGE('',*,*,#51056,.F.) ;
#75227 = ORIENTED_EDGE('',*,*,#50908,.F.) ;
#75228 = ORIENTED_EDGE('',*,*,#50911,.F.) ;
#75229 = ORIENTED_EDGE('',*,*,#53009,.F.) ;
#75230 = ORIENTED_EDGE('',*,*,#50912,.F.) ;
#75231 = ORIENTED_EDGE('',*,*,#53008,.T.) ;
#75232 = ORIENTED_EDGE('',*,*,#53006,.T.) ;
#75233 = ORIENTED_EDGE('',*,*,#53010,.F.) ;
#75234 = ORIENTED_EDGE('',*,*,#53009,.T.) ;
#75235 = ORIENTED_EDGE('',*,*,#53007,.T.) ;
#75236 = ORIENTED_EDGE('',*,*,#53011,.F.) ;
#75237 = ORIENTED_EDGE('',*,*,#50904,.F.) ;
#75238 = ORIENTED_EDGE('',*,*,#50916,.F.) ;
#75239 = ORIENTED_EDGE('',*,*,#53012,.F.) ;
#75240 = ORIENTED_EDGE('',*,*,#50918,.F.) ;
#75241 = ORIENTED_EDGE('',*,*,#53010,.T.) ;
#75242 = ORIENTED_EDGE('',*,*,#50919,.F.) ;
#75243 = ORIENTED_EDGE('',*,*,#53013,.F.) ;
#75244 = ORIENTED_EDGE('',*,*,#51053,.F.) ;
#75245 = ORIENTED_EDGE('',*,*,#53011,.T.) ;
#75246 = ORIENTED_EDGE('',*,*,#51055,.F.) ;
#75247 = ORIENTED_EDGE('',*,*,#53014,.F.) ;
#75248 = ORIENTED_EDGE('',*,*,#50913,.F.) ;
#75249 = ORIENTED_EDGE('',*,*,#50902,.F.) ;
#75250 = ORIENTED_EDGE('',*,*,#50914,.F.) ;
#75251 = ORIENTED_EDGE('',*,*,#53015,.F.) ;
#75252 = ORIENTED_EDGE('',*,*,#50917,.F.) ;
#75253 = ORIENTED_EDGE('',*,*,#53013,.T.) ;
#75254 = ORIENTED_EDGE('',*,*,#53012,.T.) ;
#75255 = ORIENTED_EDGE('',*,*,#53016,.F.) ;
#75256 = ORIENTED_EDGE('',*,*,#53015,.T.) ;
#75257 = ORIENTED_EDGE('',*,*,#53014,.T.) ;
#75258 = ORIENTED_EDGE('',*,*,#53017,.F.) ;
#75259 = ORIENTED_EDGE('',*,*,#53016,.T.) ;
#75260 = ORIENTED_EDGE('',*,*,#50915,.F.) ;
#75261 = ORIENTED_EDGE('',*,*,#53017,.T.) ;
#75262 = ORIENTED_EDGE('',*,*,#51054,.F.) ;
#75263 = ORIENTED_EDGE('',*,*,#53018,.F.) ;
#75264 = ORIENTED_EDGE('',*,*,#49356,.F.) ;
#75265 = ORIENTED_EDGE('',*,*,#53019,.F.) ;
#75266 = ORIENTED_EDGE('',*,*,#51585,.F.) ;
#75267 = ORIENTED_EDGE('',*,*,#53019,.T.) ;
#75268 = ORIENTED_EDGE('',*,*,#49355,.T.) ;
#75269 = ORIENTED_EDGE('',*,*,#53020,.F.) ;
#75270 = ORIENTED_EDGE('',*,*,#53021,.F.) ;
#75271 = ORIENTED_EDGE('',*,*,#49357,.T.) ;
#75272 = ORIENTED_EDGE('',*,*,#53018,.T.) ;
#75273 = ORIENTED_EDGE('',*,*,#53022,.F.) ;
#75274 = ORIENTED_EDGE('',*,*,#53023,.F.) ;
#75275 = ORIENTED_EDGE('',*,*,#53020,.T.) ;
#75276 = ORIENTED_EDGE('',*,*,#49354,.F.) ;
#75277 = ORIENTED_EDGE('',*,*,#53024,.F.) ;
#75278 = ORIENTED_EDGE('',*,*,#51582,.F.) ;
#75279 = ORIENTED_EDGE('',*,*,#53021,.T.) ;
#75280 = ORIENTED_EDGE('',*,*,#51581,.F.) ;
#75281 = ORIENTED_EDGE('',*,*,#53025,.F.) ;
#75282 = ORIENTED_EDGE('',*,*,#51586,.F.) ;
#75283 = ORIENTED_EDGE('',*,*,#53026,.F.) ;
#75284 = ORIENTED_EDGE('',*,*,#51583,.F.) ;
#75285 = ORIENTED_EDGE('',*,*,#53027,.F.) ;
#75286 = ORIENTED_EDGE('',*,*,#51710,.F.) ;
#75287 = ORIENTED_EDGE('',*,*,#53022,.T.) ;
#75288 = ORIENTED_EDGE('',*,*,#51584,.F.) ;
#75289 = ORIENTED_EDGE('',*,*,#53028,.F.) ;
#75290 = ORIENTED_EDGE('',*,*,#51574,.F.) ;
#75291 = ORIENTED_EDGE('',*,*,#53023,.T.) ;
#75292 = ORIENTED_EDGE('',*,*,#51573,.F.) ;
#75293 = ORIENTED_EDGE('',*,*,#53029,.F.) ;
#75294 = ORIENTED_EDGE('',*,*,#49358,.F.) ;
#75295 = ORIENTED_EDGE('',*,*,#53030,.F.) ;
#75296 = ORIENTED_EDGE('',*,*,#49352,.F.) ;
#75297 = ORIENTED_EDGE('',*,*,#53031,.F.) ;
#75298 = ORIENTED_EDGE('',*,*,#51575,.F.) ;
#75299 = ORIENTED_EDGE('',*,*,#49353,.T.) ;
#75300 = ORIENTED_EDGE('',*,*,#53030,.T.) ;
#75301 = ORIENTED_EDGE('',*,*,#53032,.F.) ;
#75302 = ORIENTED_EDGE('',*,*,#53024,.T.) ;
#75303 = ORIENTED_EDGE('',*,*,#53027,.T.) ;
#75304 = ORIENTED_EDGE('',*,*,#53025,.T.) ;
#75305 = ORIENTED_EDGE('',*,*,#53033,.F.) ;
#75306 = ORIENTED_EDGE('',*,*,#53028,.T.) ;
#75307 = ORIENTED_EDGE('',*,*,#53026,.T.) ;
#75308 = ORIENTED_EDGE('',*,*,#53034,.F.) ;
#75309 = ORIENTED_EDGE('',*,*,#49351,.T.) ;
#75310 = ORIENTED_EDGE('',*,*,#53029,.T.) ;
#75311 = ORIENTED_EDGE('',*,*,#53035,.F.) ;
#75312 = ORIENTED_EDGE('',*,*,#53031,.T.) ;
#75313 = ORIENTED_EDGE('',*,*,#53032,.T.) ;
#75314 = ORIENTED_EDGE('',*,*,#51578,.F.) ;
#75315 = ORIENTED_EDGE('',*,*,#53036,.F.) ;
#75316 = ORIENTED_EDGE('',*,*,#51579,.F.) ;
#75317 = ORIENTED_EDGE('',*,*,#53033,.T.) ;
#75318 = ORIENTED_EDGE('',*,*,#51580,.F.) ;
#75319 = ORIENTED_EDGE('',*,*,#53037,.F.) ;
#75320 = ORIENTED_EDGE('',*,*,#51707,.F.) ;
#75321 = ORIENTED_EDGE('',*,*,#53034,.T.) ;
#75322 = ORIENTED_EDGE('',*,*,#51709,.F.) ;
#75323 = ORIENTED_EDGE('',*,*,#53038,.F.) ;
#75324 = ORIENTED_EDGE('',*,*,#51571,.F.) ;
#75325 = ORIENTED_EDGE('',*,*,#53035,.T.) ;
#75326 = ORIENTED_EDGE('',*,*,#51572,.F.) ;
#75327 = ORIENTED_EDGE('',*,*,#53039,.F.) ;
#75328 = ORIENTED_EDGE('',*,*,#51576,.F.) ;
#75329 = ORIENTED_EDGE('',*,*,#53037,.T.) ;
#75330 = ORIENTED_EDGE('',*,*,#53036,.T.) ;
#75331 = ORIENTED_EDGE('',*,*,#53040,.F.) ;
#75332 = ORIENTED_EDGE('',*,*,#53039,.T.) ;
#75333 = ORIENTED_EDGE('',*,*,#53038,.T.) ;
#75334 = ORIENTED_EDGE('',*,*,#53041,.F.) ;
#75335 = ORIENTED_EDGE('',*,*,#53040,.T.) ;
#75336 = ORIENTED_EDGE('',*,*,#51577,.F.) ;
#75337 = ORIENTED_EDGE('',*,*,#53041,.T.) ;
#75338 = ORIENTED_EDGE('',*,*,#51708,.F.) ;
#75339 = ORIENTED_EDGE('',*,*,#51716,.F.) ;
#75340 = ORIENTED_EDGE('',*,*,#51729,.F.) ;
#75341 = ORIENTED_EDGE('',*,*,#53042,.F.) ;
#75342 = ORIENTED_EDGE('',*,*,#51721,.F.) ;
#75343 = ORIENTED_EDGE('',*,*,#53043,.F.) ;
#75344 = ORIENTED_EDGE('',*,*,#51719,.F.) ;
#75345 = ORIENTED_EDGE('',*,*,#53044,.F.) ;
#75346 = ORIENTED_EDGE('',*,*,#51866,.F.) ;
#75347 = ORIENTED_EDGE('',*,*,#51718,.F.) ;
#75348 = ORIENTED_EDGE('',*,*,#51720,.F.) ;
#75349 = ORIENTED_EDGE('',*,*,#53045,.F.) ;
#75350 = ORIENTED_EDGE('',*,*,#51724,.F.) ;
#75351 = ORIENTED_EDGE('',*,*,#53044,.T.) ;
#75352 = ORIENTED_EDGE('',*,*,#53042,.T.) ;
#75353 = ORIENTED_EDGE('',*,*,#53046,.F.) ;
#75354 = ORIENTED_EDGE('',*,*,#53045,.T.) ;
#75355 = ORIENTED_EDGE('',*,*,#53043,.T.) ;
#75356 = ORIENTED_EDGE('',*,*,#53047,.F.) ;
#75357 = ORIENTED_EDGE('',*,*,#51714,.F.) ;
#75358 = ORIENTED_EDGE('',*,*,#51727,.F.) ;
#75359 = ORIENTED_EDGE('',*,*,#53048,.F.) ;
#75360 = ORIENTED_EDGE('',*,*,#51730,.F.) ;
#75361 = ORIENTED_EDGE('',*,*,#53046,.T.) ;
#75362 = ORIENTED_EDGE('',*,*,#51728,.F.) ;
#75363 = ORIENTED_EDGE('',*,*,#53049,.F.) ;
#75364 = ORIENTED_EDGE('',*,*,#51863,.F.) ;
#75365 = ORIENTED_EDGE('',*,*,#53047,.T.) ;
#75366 = ORIENTED_EDGE('',*,*,#51865,.F.) ;
#75367 = ORIENTED_EDGE('',*,*,#53050,.F.) ;
#75368 = ORIENTED_EDGE('',*,*,#51722,.F.) ;
#75369 = ORIENTED_EDGE('',*,*,#51712,.F.) ;
#75370 = ORIENTED_EDGE('',*,*,#51723,.F.) ;
#75371 = ORIENTED_EDGE('',*,*,#53051,.F.) ;
#75372 = ORIENTED_EDGE('',*,*,#51725,.F.) ;
#75373 = ORIENTED_EDGE('',*,*,#53049,.T.) ;
#75374 = ORIENTED_EDGE('',*,*,#53048,.T.) ;
#75375 = ORIENTED_EDGE('',*,*,#53052,.F.) ;
#75376 = ORIENTED_EDGE('',*,*,#53051,.T.) ;
#75377 = ORIENTED_EDGE('',*,*,#53050,.T.) ;
#75378 = ORIENTED_EDGE('',*,*,#53053,.F.) ;
#75379 = ORIENTED_EDGE('',*,*,#53052,.T.) ;
#75380 = ORIENTED_EDGE('',*,*,#51726,.F.) ;
#75381 = ORIENTED_EDGE('',*,*,#53053,.T.) ;
#75382 = ORIENTED_EDGE('',*,*,#51864,.F.) ;
#75383 = ORIENTED_EDGE('',*,*,#53054,.F.) ;
#75384 = ORIENTED_EDGE('',*,*,#52046,.F.) ;
#75385 = ORIENTED_EDGE('',*,*,#53055,.F.) ;
#75386 = ORIENTED_EDGE('',*,*,#52061,.F.) ;
#75387 = ORIENTED_EDGE('',*,*,#53055,.T.) ;
#75388 = ORIENTED_EDGE('',*,*,#52049,.F.) ;
#75389 = ORIENTED_EDGE('',*,*,#53056,.F.) ;
#75390 = ORIENTED_EDGE('',*,*,#52043,.F.) ;
#75391 = ORIENTED_EDGE('',*,*,#53054,.T.) ;
#75392 = ORIENTED_EDGE('',*,*,#53057,.F.) ;
#75393 = ORIENTED_EDGE('',*,*,#53056,.T.) ;
#75394 = ORIENTED_EDGE('',*,*,#52052,.F.) ;
#75395 = ORIENTED_EDGE('',*,*,#53058,.F.) ;
#75396 = ORIENTED_EDGE('',*,*,#52058,.F.) ;
#75397 = ORIENTED_EDGE('',*,*,#53057,.T.) ;
#75398 = ORIENTED_EDGE('',*,*,#52060,.F.) ;
#75399 = ORIENTED_EDGE('',*,*,#53059,.F.) ;
#75400 = ORIENTED_EDGE('',*,*,#52040,.F.) ;
#75401 = ORIENTED_EDGE('',*,*,#53058,.T.) ;
#75402 = ORIENTED_EDGE('',*,*,#52055,.F.) ;
#75403 = ORIENTED_EDGE('',*,*,#53060,.F.) ;
#75404 = ORIENTED_EDGE('',*,*,#52037,.F.) ;
#75405 = ORIENTED_EDGE('',*,*,#53059,.T.) ;
#75406 = ORIENTED_EDGE('',*,*,#53061,.F.) ;
#75407 = ORIENTED_EDGE('',*,*,#53060,.T.) ;
#75408 = ORIENTED_EDGE('',*,*,#52056,.F.) ;
#75409 = ORIENTED_EDGE('',*,*,#53061,.T.) ;
#75410 = ORIENTED_EDGE('',*,*,#52059,.F.) ;
#75411 = ORIENTED_EDGE('',*,*,#49142,.F.) ;
#75412 = ORIENTED_EDGE('',*,*,#51892,.F.) ;
#75413 = ORIENTED_EDGE('',*,*,#49156,.F.) ;
#75414 = ORIENTED_EDGE('',*,*,#51914,.F.) ;
#75415 = ORIENTED_EDGE('',*,*,#49144,.F.) ;
#75416 = ORIENTED_EDGE('',*,*,#51915,.F.) ;
#75417 = ORIENTED_EDGE('',*,*,#49154,.F.) ;
#75418 = ORIENTED_EDGE('',*,*,#51918,.F.) ;
#75419 = ORIENTED_EDGE('',*,*,#49152,.F.) ;
#75420 = ORIENTED_EDGE('',*,*,#51916,.F.) ;
#75421 = ORIENTED_EDGE('',*,*,#49146,.F.) ;
#75422 = ORIENTED_EDGE('',*,*,#51919,.F.) ;
#75423 = ORIENTED_EDGE('',*,*,#49150,.F.) ;
#75424 = ORIENTED_EDGE('',*,*,#49528,.F.) ;
#75425 = ORIENTED_EDGE('',*,*,#49148,.F.) ;
#75426 = ORIENTED_EDGE('',*,*,#51917,.F.) ;
#75427 = ORIENTED_EDGE('',*,*,#53062,.F.) ;
#75428 = ORIENTED_EDGE('',*,*,#53063,.F.) ;
#75429 = ORIENTED_EDGE('',*,*,#53064,.F.) ;
#75430 = ORIENTED_EDGE('',*,*,#53063,.T.) ;
#75431 = ORIENTED_EDGE('',*,*,#51413,.F.) ;
#75432 = ORIENTED_EDGE('',*,*,#53065,.F.) ;
#75433 = ORIENTED_EDGE('',*,*,#51408,.F.) ;
#75434 = ORIENTED_EDGE('',*,*,#53064,.T.) ;
#75435 = ORIENTED_EDGE('',*,*,#51407,.F.) ;
#75436 = ORIENTED_EDGE('',*,*,#53066,.F.) ;
#75437 = ORIENTED_EDGE('',*,*,#51409,.F.) ;
#75438 = ORIENTED_EDGE('',*,*,#53062,.T.) ;
#75439 = ORIENTED_EDGE('',*,*,#51412,.F.) ;
#75440 = ORIENTED_EDGE('',*,*,#53067,.F.) ;
#75441 = ORIENTED_EDGE('',*,*,#51414,.F.) ;
#75442 = ORIENTED_EDGE('',*,*,#51418,.F.) ;
#75443 = ORIENTED_EDGE('',*,*,#53068,.T.) ;
#75444 = ORIENTED_EDGE('',*,*,#51197,.F.) ;
#75445 = ORIENTED_EDGE('',*,*,#53069,.F.) ;
#75446 = ORIENTED_EDGE('',*,*,#53065,.T.) ;
#75447 = ORIENTED_EDGE('',*,*,#53069,.T.) ;
#75448 = ORIENTED_EDGE('',*,*,#53070,.F.) ;
#75449 = ORIENTED_EDGE('',*,*,#53071,.F.) ;
#75450 = ORIENTED_EDGE('',*,*,#53066,.T.) ;
#75451 = ORIENTED_EDGE('',*,*,#53072,.F.) ;
#75452 = ORIENTED_EDGE('',*,*,#49628,.T.) ;
#75453 = ORIENTED_EDGE('',*,*,#53073,.F.) ;
#75454 = ORIENTED_EDGE('',*,*,#53067,.T.) ;
#75455 = ORIENTED_EDGE('',*,*,#53074,.F.) ;
#75456 = ORIENTED_EDGE('',*,*,#51417,.F.) ;
#75457 = ORIENTED_EDGE('',*,*,#53075,.T.) ;
#75458 = ORIENTED_EDGE('',*,*,#49463,.F.) ;
#75459 = ORIENTED_EDGE('',*,*,#53076,.T.) ;
#75460 = ORIENTED_EDGE('',*,*,#53070,.T.) ;
#75461 = ORIENTED_EDGE('',*,*,#51196,.F.) ;
#75462 = ORIENTED_EDGE('',*,*,#53077,.F.) ;
#75463 = ORIENTED_EDGE('',*,*,#51405,.F.) ;
#75464 = ORIENTED_EDGE('',*,*,#53072,.T.) ;
#75465 = ORIENTED_EDGE('',*,*,#51406,.F.) ;
#75466 = ORIENTED_EDGE('',*,*,#53078,.F.) ;
#75467 = ORIENTED_EDGE('',*,*,#49629,.F.) ;
#75468 = ORIENTED_EDGE('',*,*,#53071,.T.) ;
#75469 = ORIENTED_EDGE('',*,*,#49635,.F.) ;
#75470 = ORIENTED_EDGE('',*,*,#53079,.F.) ;
#75471 = ORIENTED_EDGE('',*,*,#51410,.F.) ;
#75472 = ORIENTED_EDGE('',*,*,#53074,.T.) ;
#75473 = ORIENTED_EDGE('',*,*,#51411,.F.) ;
#75474 = ORIENTED_EDGE('',*,*,#53080,.F.) ;
#75475 = ORIENTED_EDGE('',*,*,#51401,.F.) ;
#75476 = ORIENTED_EDGE('',*,*,#53073,.T.) ;
#75477 = ORIENTED_EDGE('',*,*,#51404,.F.) ;
#75478 = ORIENTED_EDGE('',*,*,#53081,.F.) ;
#75479 = ORIENTED_EDGE('',*,*,#51415,.F.) ;
#75480 = ORIENTED_EDGE('',*,*,#51207,.F.) ;
#75481 = ORIENTED_EDGE('',*,*,#53082,.T.) ;
#75482 = ORIENTED_EDGE('',*,*,#51416,.F.) ;
#75483 = ORIENTED_EDGE('',*,*,#53083,.F.) ;
#75484 = ORIENTED_EDGE('',*,*,#53077,.T.) ;
#75485 = ORIENTED_EDGE('',*,*,#51195,.T.) ;
#75486 = ORIENTED_EDGE('',*,*,#53084,.F.) ;
#75487 = ORIENTED_EDGE('',*,*,#53078,.T.) ;
#75488 = ORIENTED_EDGE('',*,*,#53079,.T.) ;
#75489 = ORIENTED_EDGE('',*,*,#49634,.T.) ;
#75490 = ORIENTED_EDGE('',*,*,#53085,.F.) ;
#75491 = ORIENTED_EDGE('',*,*,#53080,.T.) ;
#75492 = ORIENTED_EDGE('',*,*,#53083,.T.) ;
#75493 = ORIENTED_EDGE('',*,*,#53081,.T.) ;
#75494 = ORIENTED_EDGE('',*,*,#53086,.F.) ;
#75495 = ORIENTED_EDGE('',*,*,#51191,.F.) ;
#75496 = ORIENTED_EDGE('',*,*,#53087,.T.) ;
#75497 = ORIENTED_EDGE('',*,*,#51185,.F.) ;
#75498 = ORIENTED_EDGE('',*,*,#53088,.F.) ;
#75499 = ORIENTED_EDGE('',*,*,#53084,.T.) ;
#75500 = ORIENTED_EDGE('',*,*,#51194,.F.) ;
#75501 = ORIENTED_EDGE('',*,*,#53089,.F.) ;
#75502 = ORIENTED_EDGE('',*,*,#49630,.F.) ;
#75503 = ORIENTED_EDGE('',*,*,#53085,.T.) ;
#75504 = ORIENTED_EDGE('',*,*,#49633,.F.) ;
#75505 = ORIENTED_EDGE('',*,*,#53090,.F.) ;
#75506 = ORIENTED_EDGE('',*,*,#51402,.F.) ;
#75507 = ORIENTED_EDGE('',*,*,#53086,.T.) ;
#75508 = ORIENTED_EDGE('',*,*,#51403,.F.) ;
#75509 = ORIENTED_EDGE('',*,*,#53091,.F.) ;
#75510 = ORIENTED_EDGE('',*,*,#51208,.F.) ;
#75511 = ORIENTED_EDGE('',*,*,#53088,.T.) ;
#75512 = ORIENTED_EDGE('',*,*,#52958,.F.) ;
#75513 = ORIENTED_EDGE('',*,*,#53092,.F.) ;
#75514 = ORIENTED_EDGE('',*,*,#53093,.F.) ;
#75515 = ORIENTED_EDGE('',*,*,#53089,.T.) ;
#75516 = ORIENTED_EDGE('',*,*,#53094,.F.) ;
#75517 = ORIENTED_EDGE('',*,*,#53091,.T.) ;
#75518 = ORIENTED_EDGE('',*,*,#53090,.T.) ;
#75519 = ORIENTED_EDGE('',*,*,#53095,.F.) ;
#75520 = ORIENTED_EDGE('',*,*,#51209,.T.) ;
#75521 = ORIENTED_EDGE('',*,*,#53092,.T.) ;
#75522 = ORIENTED_EDGE('',*,*,#49703,.F.) ;
#75523 = ORIENTED_EDGE('',*,*,#53096,.F.) ;
#75524 = ORIENTED_EDGE('',*,*,#51192,.F.) ;
#75525 = ORIENTED_EDGE('',*,*,#53094,.T.) ;
#75526 = ORIENTED_EDGE('',*,*,#51193,.F.) ;
#75527 = ORIENTED_EDGE('',*,*,#53097,.F.) ;
#75528 = ORIENTED_EDGE('',*,*,#51199,.F.) ;
#75529 = ORIENTED_EDGE('',*,*,#53093,.T.) ;
#75530 = ORIENTED_EDGE('',*,*,#51202,.F.) ;
#75531 = ORIENTED_EDGE('',*,*,#53098,.F.) ;
#75532 = ORIENTED_EDGE('',*,*,#49631,.F.) ;
#75533 = ORIENTED_EDGE('',*,*,#53095,.T.) ;
#75534 = ORIENTED_EDGE('',*,*,#49632,.F.) ;
#75535 = ORIENTED_EDGE('',*,*,#53099,.F.) ;
#75536 = ORIENTED_EDGE('',*,*,#51210,.F.) ;
#75537 = ORIENTED_EDGE('',*,*,#53096,.T.) ;
#75538 = ORIENTED_EDGE('',*,*,#49702,.T.) ;
#75539 = ORIENTED_EDGE('',*,*,#53100,.F.) ;
#75540 = ORIENTED_EDGE('',*,*,#53097,.T.) ;
#75541 = ORIENTED_EDGE('',*,*,#53099,.T.) ;
#75542 = ORIENTED_EDGE('',*,*,#53098,.T.) ;
#75543 = ORIENTED_EDGE('',*,*,#53101,.F.) ;
#75544 = ORIENTED_EDGE('',*,*,#53100,.T.) ;
#75545 = ORIENTED_EDGE('',*,*,#49701,.F.) ;
#75546 = ORIENTED_EDGE('',*,*,#53102,.F.) ;
#75547 = ORIENTED_EDGE('',*,*,#51200,.F.) ;
#75548 = ORIENTED_EDGE('',*,*,#53101,.T.) ;
#75549 = ORIENTED_EDGE('',*,*,#51201,.F.) ;
#75550 = ORIENTED_EDGE('',*,*,#53103,.F.) ;
#75551 = ORIENTED_EDGE('',*,*,#51211,.F.) ;
#75552 = ORIENTED_EDGE('',*,*,#51215,.F.) ;
#75553 = ORIENTED_EDGE('',*,*,#53104,.T.) ;
#75554 = ORIENTED_EDGE('',*,*,#51203,.F.) ;
#75555 = ORIENTED_EDGE('',*,*,#53105,.F.) ;
#75556 = ORIENTED_EDGE('',*,*,#49698,.F.) ;
#75557 = ORIENTED_EDGE('',*,*,#53106,.T.) ;
#75558 = ORIENTED_EDGE('',*,*,#51216,.F.) ;
#75559 = ORIENTED_EDGE('',*,*,#53107,.F.) ;
#75560 = ORIENTED_EDGE('',*,*,#53102,.T.) ;
#75561 = ORIENTED_EDGE('',*,*,#49700,.T.) ;
#75562 = ORIENTED_EDGE('',*,*,#53108,.F.) ;
#75563 = ORIENTED_EDGE('',*,*,#53103,.T.) ;
#75564 = ORIENTED_EDGE('',*,*,#53107,.T.) ;
#75565 = ORIENTED_EDGE('',*,*,#53105,.T.) ;
#75566 = ORIENTED_EDGE('',*,*,#53109,.F.) ;
#75567 = ORIENTED_EDGE('',*,*,#53108,.T.) ;
#75568 = ORIENTED_EDGE('',*,*,#49699,.F.) ;
#75569 = ORIENTED_EDGE('',*,*,#53109,.T.) ;
#75570 = ORIENTED_EDGE('',*,*,#51212,.F.) ;
#75571 = ORIENTED_EDGE('',*,*,#52326,.F.) ;
#75572 = ORIENTED_EDGE('',*,*,#52337,.F.) ;
#75573 = ORIENTED_EDGE('',*,*,#52336,.F.) ;
#75574 = ORIENTED_EDGE('',*,*,#53110,.F.) ;
#75575 = ORIENTED_EDGE('',*,*,#52327,.F.) ;
#75576 = ORIENTED_EDGE('',*,*,#53110,.T.) ;
#75577 = ORIENTED_EDGE('',*,*,#50760,.F.) ;
#75578 = ORIENTED_EDGE('',*,*,#53111,.F.) ;
#75579 = ORIENTED_EDGE('',*,*,#50746,.F.) ;
#75580 = ORIENTED_EDGE('',*,*,#52334,.F.) ;
#75581 = ORIENTED_EDGE('',*,*,#52333,.F.) ;
#75582 = ORIENTED_EDGE('',*,*,#52332,.F.) ;
#75583 = ORIENTED_EDGE('',*,*,#53112,.F.) ;
#75584 = ORIENTED_EDGE('',*,*,#52335,.F.) ;
#75585 = ORIENTED_EDGE('',*,*,#53113,.F.) ;
#75586 = ORIENTED_EDGE('',*,*,#53111,.T.) ;
#75587 = ORIENTED_EDGE('',*,*,#53114,.F.) ;
#75588 = ORIENTED_EDGE('',*,*,#52324,.F.) ;
#75589 = ORIENTED_EDGE('',*,*,#52329,.F.) ;
#75590 = ORIENTED_EDGE('',*,*,#52328,.F.) ;
#75591 = ORIENTED_EDGE('',*,*,#53115,.F.) ;
#75592 = ORIENTED_EDGE('',*,*,#52325,.F.) ;
#75593 = ORIENTED_EDGE('',*,*,#53112,.T.) ;
#75594 = ORIENTED_EDGE('',*,*,#50756,.F.) ;
#75595 = ORIENTED_EDGE('',*,*,#53116,.F.) ;
#75596 = ORIENTED_EDGE('',*,*,#50758,.F.) ;
#75597 = ORIENTED_EDGE('',*,*,#53114,.T.) ;
#75598 = ORIENTED_EDGE('',*,*,#50759,.F.) ;
#75599 = ORIENTED_EDGE('',*,*,#53117,.F.) ;
#75600 = ORIENTED_EDGE('',*,*,#50924,.F.) ;
#75601 = ORIENTED_EDGE('',*,*,#53113,.T.) ;
#75602 = ORIENTED_EDGE('',*,*,#50923,.F.) ;
#75603 = ORIENTED_EDGE('',*,*,#53118,.F.) ;
#75604 = ORIENTED_EDGE('',*,*,#50747,.F.) ;
#75605 = ORIENTED_EDGE('',*,*,#53115,.T.) ;
#75606 = ORIENTED_EDGE('',*,*,#50748,.F.) ;
#75607 = ORIENTED_EDGE('',*,*,#53119,.F.) ;
#75608 = ORIENTED_EDGE('',*,*,#50752,.F.) ;
#75609 = ORIENTED_EDGE('',*,*,#53117,.T.) ;
#75610 = ORIENTED_EDGE('',*,*,#53116,.T.) ;
#75611 = ORIENTED_EDGE('',*,*,#53120,.F.) ;
#75612 = ORIENTED_EDGE('',*,*,#53119,.T.) ;
#75613 = ORIENTED_EDGE('',*,*,#53118,.T.) ;
#75614 = ORIENTED_EDGE('',*,*,#53121,.F.) ;
#75615 = ORIENTED_EDGE('',*,*,#53120,.T.) ;
#75616 = ORIENTED_EDGE('',*,*,#50755,.F.) ;
#75617 = ORIENTED_EDGE('',*,*,#53122,.F.) ;
#75618 = ORIENTED_EDGE('',*,*,#50921,.F.) ;
#75619 = ORIENTED_EDGE('',*,*,#53121,.T.) ;
#75620 = ORIENTED_EDGE('',*,*,#50922,.F.) ;
#75621 = ORIENTED_EDGE('',*,*,#53123,.F.) ;
#75622 = ORIENTED_EDGE('',*,*,#50749,.F.) ;
#75623 = ORIENTED_EDGE('',*,*,#53123,.T.) ;
#75624 = ORIENTED_EDGE('',*,*,#53122,.T.) ;
#75625 = ORIENTED_EDGE('',*,*,#53124,.F.) ;
#75626 = ORIENTED_EDGE('',*,*,#53124,.T.) ;
#75627 = ORIENTED_EDGE('',*,*,#50754,.F.) ;
#75628 = ORIENTED_EDGE('',*,*,#53125,.F.) ;
#75629 = ORIENTED_EDGE('',*,*,#50750,.F.) ;
#75630 = ORIENTED_EDGE('',*,*,#52330,.F.) ;
#75631 = ORIENTED_EDGE('',*,*,#52323,.F.) ;
#75632 = ORIENTED_EDGE('',*,*,#52322,.F.) ;
#75633 = ORIENTED_EDGE('',*,*,#53125,.T.) ;
#75634 = ORIENTED_EDGE('',*,*,#52331,.F.) ;
#75635 = ORIENTED_EDGE('',*,*,#52499,.F.) ;
#75636 = ORIENTED_EDGE('',*,*,#52498,.F.) ;
#75637 = ORIENTED_EDGE('',*,*,#52497,.F.) ;
#75638 = ORIENTED_EDGE('',*,*,#53126,.F.) ;
#75639 = ORIENTED_EDGE('',*,*,#52500,.F.) ;
#75640 = ORIENTED_EDGE('',*,*,#53126,.T.) ;
#75641 = ORIENTED_EDGE('',*,*,#52496,.F.) ;
#75642 = ORIENTED_EDGE('',*,*,#53127,.F.) ;
#75643 = ORIENTED_EDGE('',*,*,#50586,.F.) ;
#75644 = ORIENTED_EDGE('',*,*,#53127,.T.) ;
#75645 = ORIENTED_EDGE('',*,*,#50470,.F.) ;
#75646 = ORIENTED_EDGE('',*,*,#53128,.F.) ;
#75647 = ORIENTED_EDGE('',*,*,#50587,.F.) ;
#75648 = ORIENTED_EDGE('',*,*,#50458,.F.) ;
#75649 = ORIENTED_EDGE('',*,*,#50588,.F.) ;
#75650 = ORIENTED_EDGE('',*,*,#53129,.F.) ;
#75651 = ORIENTED_EDGE('',*,*,#50464,.F.) ;
#75652 = ORIENTED_EDGE('',*,*,#53129,.T.) ;
#75653 = ORIENTED_EDGE('',*,*,#53128,.T.) ;
#75654 = ORIENTED_EDGE('',*,*,#53130,.F.) ;
#75655 = ORIENTED_EDGE('',*,*,#53130,.T.) ;
#75656 = ORIENTED_EDGE('',*,*,#50469,.F.) ;
#75657 = ORIENTED_EDGE('',*,*,#53131,.F.) ;
#75658 = ORIENTED_EDGE('',*,*,#50465,.F.) ;
#75659 = ORIENTED_EDGE('',*,*,#50460,.F.) ;
#75660 = ORIENTED_EDGE('',*,*,#50466,.F.) ;
#75661 = ORIENTED_EDGE('',*,*,#53132,.F.) ;
#75662 = ORIENTED_EDGE('',*,*,#50650,.F.) ;
#75663 = ORIENTED_EDGE('',*,*,#53132,.T.) ;
#75664 = ORIENTED_EDGE('',*,*,#53131,.T.) ;
#75665 = ORIENTED_EDGE('',*,*,#53133,.F.) ;
#75666 = ORIENTED_EDGE('',*,*,#53133,.T.) ;
#75667 = ORIENTED_EDGE('',*,*,#50468,.F.) ;
#75668 = ORIENTED_EDGE('',*,*,#53134,.F.) ;
#75669 = ORIENTED_EDGE('',*,*,#50651,.F.) ;
#75670 = ORIENTED_EDGE('',*,*,#53134,.T.) ;
#75671 = ORIENTED_EDGE('',*,*,#52495,.F.) ;
#75672 = ORIENTED_EDGE('',*,*,#53135,.F.) ;
#75673 = ORIENTED_EDGE('',*,*,#50652,.F.) ;
#75674 = ORIENTED_EDGE('',*,*,#53135,.T.) ;
#75675 = ORIENTED_EDGE('',*,*,#52494,.F.) ;
#75676 = ORIENTED_EDGE('',*,*,#52503,.F.) ;
#75677 = ORIENTED_EDGE('',*,*,#52504,.F.) ;
#75678 = ORIENTED_EDGE('',*,*,#52509,.F.) ;
#75679 = ORIENTED_EDGE('',*,*,#53136,.F.) ;
#75680 = ORIENTED_EDGE('',*,*,#53136,.T.) ;
#75681 = ORIENTED_EDGE('',*,*,#52508,.F.) ;
#75682 = ORIENTED_EDGE('',*,*,#53137,.F.) ;
#75683 = ORIENTED_EDGE('',*,*,#50647,.F.) ;
#75684 = ORIENTED_EDGE('',*,*,#53137,.T.) ;
#75685 = ORIENTED_EDGE('',*,*,#50452,.F.) ;
#75686 = ORIENTED_EDGE('',*,*,#53138,.F.) ;
#75687 = ORIENTED_EDGE('',*,*,#50648,.F.) ;
#75688 = ORIENTED_EDGE('',*,*,#50462,.F.) ;
#75689 = ORIENTED_EDGE('',*,*,#50649,.F.) ;
#75690 = ORIENTED_EDGE('',*,*,#53139,.F.) ;
#75691 = ORIENTED_EDGE('',*,*,#50456,.F.) ;
#75692 = ORIENTED_EDGE('',*,*,#53139,.T.) ;
#75693 = ORIENTED_EDGE('',*,*,#53138,.T.) ;
#75694 = ORIENTED_EDGE('',*,*,#53140,.F.) ;
#75695 = ORIENTED_EDGE('',*,*,#53140,.T.) ;
#75696 = ORIENTED_EDGE('',*,*,#50451,.F.) ;
#75697 = ORIENTED_EDGE('',*,*,#53141,.F.) ;
#75698 = ORIENTED_EDGE('',*,*,#50453,.F.) ;
#75699 = ORIENTED_EDGE('',*,*,#50463,.F.) ;
#75700 = ORIENTED_EDGE('',*,*,#50454,.F.) ;
#75701 = ORIENTED_EDGE('',*,*,#53142,.F.) ;
#75702 = ORIENTED_EDGE('',*,*,#50589,.F.) ;
#75703 = ORIENTED_EDGE('',*,*,#53142,.T.) ;
#75704 = ORIENTED_EDGE('',*,*,#53141,.T.) ;
#75705 = ORIENTED_EDGE('',*,*,#53143,.F.) ;
#75706 = ORIENTED_EDGE('',*,*,#53143,.T.) ;
#75707 = ORIENTED_EDGE('',*,*,#50450,.F.) ;
#75708 = ORIENTED_EDGE('',*,*,#53144,.F.) ;
#75709 = ORIENTED_EDGE('',*,*,#50590,.F.) ;
#75710 = ORIENTED_EDGE('',*,*,#53144,.T.) ;
#75711 = ORIENTED_EDGE('',*,*,#52507,.F.) ;
#75712 = ORIENTED_EDGE('',*,*,#53145,.F.) ;
#75713 = ORIENTED_EDGE('',*,*,#50591,.F.) ;
#75714 = ORIENTED_EDGE('',*,*,#52505,.F.) ;
#75715 = ORIENTED_EDGE('',*,*,#52502,.F.) ;
#75716 = ORIENTED_EDGE('',*,*,#52501,.F.) ;
#75717 = ORIENTED_EDGE('',*,*,#53145,.T.) ;
#75718 = ORIENTED_EDGE('',*,*,#52506,.F.) ;
#75719 = ORIENTED_EDGE('',*,*,#53146,.F.) ;
#75720 = ORIENTED_EDGE('',*,*,#49472,.F.) ;
#75721 = ORIENTED_EDGE('',*,*,#53147,.F.) ;
#75722 = ORIENTED_EDGE('',*,*,#52069,.F.) ;
#75723 = ORIENTED_EDGE('',*,*,#53147,.T.) ;
#75724 = ORIENTED_EDGE('',*,*,#49471,.F.) ;
#75725 = ORIENTED_EDGE('',*,*,#53148,.F.) ;
#75726 = ORIENTED_EDGE('',*,*,#52072,.F.) ;
#75727 = ORIENTED_EDGE('',*,*,#53146,.T.) ;
#75728 = ORIENTED_EDGE('',*,*,#52066,.F.) ;
#75729 = ORIENTED_EDGE('',*,*,#53149,.F.) ;
#75730 = ORIENTED_EDGE('',*,*,#49473,.F.) ;
#75731 = ORIENTED_EDGE('',*,*,#53148,.T.) ;
#75732 = ORIENTED_EDGE('',*,*,#49470,.F.) ;
#75733 = ORIENTED_EDGE('',*,*,#53150,.F.) ;
#75734 = ORIENTED_EDGE('',*,*,#52075,.F.) ;
#75735 = ORIENTED_EDGE('',*,*,#53149,.T.) ;
#75736 = ORIENTED_EDGE('',*,*,#52063,.F.) ;
#75737 = ORIENTED_EDGE('',*,*,#53151,.F.) ;
#75738 = ORIENTED_EDGE('',*,*,#49474,.F.) ;
#75739 = ORIENTED_EDGE('',*,*,#53150,.T.) ;
#75740 = ORIENTED_EDGE('',*,*,#49469,.F.) ;
#75741 = ORIENTED_EDGE('',*,*,#53152,.F.) ;
#75742 = ORIENTED_EDGE('',*,*,#52078,.F.) ;
#75743 = ORIENTED_EDGE('',*,*,#53151,.T.) ;
#75744 = ORIENTED_EDGE('',*,*,#52085,.F.) ;
#75745 = ORIENTED_EDGE('',*,*,#53153,.F.) ;
#75746 = ORIENTED_EDGE('',*,*,#49467,.F.) ;
#75747 = ORIENTED_EDGE('',*,*,#53152,.T.) ;
#75748 = ORIENTED_EDGE('',*,*,#49468,.F.) ;
#75749 = ORIENTED_EDGE('',*,*,#53153,.T.) ;
#75750 = ORIENTED_EDGE('',*,*,#52081,.F.) ;
#75751 = ORIENTED_EDGE('',*,*,#50930,.F.) ;
#75752 = ORIENTED_EDGE('',*,*,#50944,.F.) ;
#75753 = ORIENTED_EDGE('',*,*,#53154,.F.) ;
#75754 = ORIENTED_EDGE('',*,*,#50933,.F.) ;
#75755 = ORIENTED_EDGE('',*,*,#53155,.F.) ;
#75756 = ORIENTED_EDGE('',*,*,#50934,.F.) ;
#75757 = ORIENTED_EDGE('',*,*,#53156,.F.) ;
#75758 = ORIENTED_EDGE('',*,*,#51060,.F.) ;
#75759 = ORIENTED_EDGE('',*,*,#50932,.F.) ;
#75760 = ORIENTED_EDGE('',*,*,#50935,.F.) ;
#75761 = ORIENTED_EDGE('',*,*,#53157,.F.) ;
#75762 = ORIENTED_EDGE('',*,*,#50936,.F.) ;
#75763 = ORIENTED_EDGE('',*,*,#53156,.T.) ;
#75764 = ORIENTED_EDGE('',*,*,#53154,.T.) ;
#75765 = ORIENTED_EDGE('',*,*,#53158,.F.) ;
#75766 = ORIENTED_EDGE('',*,*,#53157,.T.) ;
#75767 = ORIENTED_EDGE('',*,*,#53155,.T.) ;
#75768 = ORIENTED_EDGE('',*,*,#53159,.F.) ;
#75769 = ORIENTED_EDGE('',*,*,#50928,.F.) ;
#75770 = ORIENTED_EDGE('',*,*,#50940,.F.) ;
#75771 = ORIENTED_EDGE('',*,*,#53160,.F.) ;
#75772 = ORIENTED_EDGE('',*,*,#50942,.F.) ;
#75773 = ORIENTED_EDGE('',*,*,#53158,.T.) ;
#75774 = ORIENTED_EDGE('',*,*,#50943,.F.) ;
#75775 = ORIENTED_EDGE('',*,*,#53161,.F.) ;
#75776 = ORIENTED_EDGE('',*,*,#51057,.F.) ;
#75777 = ORIENTED_EDGE('',*,*,#53159,.T.) ;
#75778 = ORIENTED_EDGE('',*,*,#51059,.F.) ;
#75779 = ORIENTED_EDGE('',*,*,#53162,.F.) ;
#75780 = ORIENTED_EDGE('',*,*,#50937,.F.) ;
#75781 = ORIENTED_EDGE('',*,*,#50926,.F.) ;
#75782 = ORIENTED_EDGE('',*,*,#50938,.F.) ;
#75783 = ORIENTED_EDGE('',*,*,#53163,.F.) ;
#75784 = ORIENTED_EDGE('',*,*,#50941,.F.) ;
#75785 = ORIENTED_EDGE('',*,*,#53161,.T.) ;
#75786 = ORIENTED_EDGE('',*,*,#53160,.T.) ;
#75787 = ORIENTED_EDGE('',*,*,#53164,.F.) ;
#75788 = ORIENTED_EDGE('',*,*,#53163,.T.) ;
#75789 = ORIENTED_EDGE('',*,*,#53162,.T.) ;
#75790 = ORIENTED_EDGE('',*,*,#53165,.F.) ;
#75791 = ORIENTED_EDGE('',*,*,#53164,.T.) ;
#75792 = ORIENTED_EDGE('',*,*,#50939,.F.) ;
#75793 = ORIENTED_EDGE('',*,*,#53165,.T.) ;
#75794 = ORIENTED_EDGE('',*,*,#51058,.F.) ;
#75795 = ORIENTED_EDGE('',*,*,#53166,.F.) ;
#75796 = ORIENTED_EDGE('',*,*,#49396,.F.) ;
#75797 = ORIENTED_EDGE('',*,*,#53167,.F.) ;
#75798 = ORIENTED_EDGE('',*,*,#51569,.F.) ;
#75799 = ORIENTED_EDGE('',*,*,#53167,.T.) ;
#75800 = ORIENTED_EDGE('',*,*,#49395,.T.) ;
#75801 = ORIENTED_EDGE('',*,*,#53168,.F.) ;
#75802 = ORIENTED_EDGE('',*,*,#53169,.F.) ;
#75803 = ORIENTED_EDGE('',*,*,#49397,.T.) ;
#75804 = ORIENTED_EDGE('',*,*,#53166,.T.) ;
#75805 = ORIENTED_EDGE('',*,*,#53170,.F.) ;
#75806 = ORIENTED_EDGE('',*,*,#53171,.F.) ;
#75807 = ORIENTED_EDGE('',*,*,#53168,.T.) ;
#75808 = ORIENTED_EDGE('',*,*,#49394,.F.) ;
#75809 = ORIENTED_EDGE('',*,*,#53172,.F.) ;
#75810 = ORIENTED_EDGE('',*,*,#51566,.F.) ;
#75811 = ORIENTED_EDGE('',*,*,#53169,.T.) ;
#75812 = ORIENTED_EDGE('',*,*,#51565,.F.) ;
#75813 = ORIENTED_EDGE('',*,*,#53173,.F.) ;
#75814 = ORIENTED_EDGE('',*,*,#51570,.F.) ;
#75815 = ORIENTED_EDGE('',*,*,#53174,.F.) ;
#75816 = ORIENTED_EDGE('',*,*,#51567,.F.) ;
#75817 = ORIENTED_EDGE('',*,*,#53175,.F.) ;
#75818 = ORIENTED_EDGE('',*,*,#51734,.F.) ;
#75819 = ORIENTED_EDGE('',*,*,#53170,.T.) ;
#75820 = ORIENTED_EDGE('',*,*,#51568,.F.) ;
#75821 = ORIENTED_EDGE('',*,*,#53176,.F.) ;
#75822 = ORIENTED_EDGE('',*,*,#51558,.F.) ;
#75823 = ORIENTED_EDGE('',*,*,#53171,.T.) ;
#75824 = ORIENTED_EDGE('',*,*,#51557,.F.) ;
#75825 = ORIENTED_EDGE('',*,*,#53177,.F.) ;
#75826 = ORIENTED_EDGE('',*,*,#49398,.F.) ;
#75827 = ORIENTED_EDGE('',*,*,#53178,.F.) ;
#75828 = ORIENTED_EDGE('',*,*,#49392,.F.) ;
#75829 = ORIENTED_EDGE('',*,*,#53179,.F.) ;
#75830 = ORIENTED_EDGE('',*,*,#51559,.F.) ;
#75831 = ORIENTED_EDGE('',*,*,#49393,.T.) ;
#75832 = ORIENTED_EDGE('',*,*,#53178,.T.) ;
#75833 = ORIENTED_EDGE('',*,*,#53180,.F.) ;
#75834 = ORIENTED_EDGE('',*,*,#53172,.T.) ;
#75835 = ORIENTED_EDGE('',*,*,#53175,.T.) ;
#75836 = ORIENTED_EDGE('',*,*,#53173,.T.) ;
#75837 = ORIENTED_EDGE('',*,*,#53181,.F.) ;
#75838 = ORIENTED_EDGE('',*,*,#53176,.T.) ;
#75839 = ORIENTED_EDGE('',*,*,#53174,.T.) ;
#75840 = ORIENTED_EDGE('',*,*,#53182,.F.) ;
#75841 = ORIENTED_EDGE('',*,*,#49391,.T.) ;
#75842 = ORIENTED_EDGE('',*,*,#53177,.T.) ;
#75843 = ORIENTED_EDGE('',*,*,#53183,.F.) ;
#75844 = ORIENTED_EDGE('',*,*,#53179,.T.) ;
#75845 = ORIENTED_EDGE('',*,*,#53180,.T.) ;
#75846 = ORIENTED_EDGE('',*,*,#51562,.F.) ;
#75847 = ORIENTED_EDGE('',*,*,#53184,.F.) ;
#75848 = ORIENTED_EDGE('',*,*,#51563,.F.) ;
#75849 = ORIENTED_EDGE('',*,*,#53181,.T.) ;
#75850 = ORIENTED_EDGE('',*,*,#51564,.F.) ;
#75851 = ORIENTED_EDGE('',*,*,#53185,.F.) ;
#75852 = ORIENTED_EDGE('',*,*,#51731,.F.) ;
#75853 = ORIENTED_EDGE('',*,*,#53182,.T.) ;
#75854 = ORIENTED_EDGE('',*,*,#51733,.F.) ;
#75855 = ORIENTED_EDGE('',*,*,#53186,.F.) ;
#75856 = ORIENTED_EDGE('',*,*,#51555,.F.) ;
#75857 = ORIENTED_EDGE('',*,*,#53183,.T.) ;
#75858 = ORIENTED_EDGE('',*,*,#51556,.F.) ;
#75859 = ORIENTED_EDGE('',*,*,#53187,.F.) ;
#75860 = ORIENTED_EDGE('',*,*,#51560,.F.) ;
#75861 = ORIENTED_EDGE('',*,*,#53185,.T.) ;
#75862 = ORIENTED_EDGE('',*,*,#53184,.T.) ;
#75863 = ORIENTED_EDGE('',*,*,#53188,.F.) ;
#75864 = ORIENTED_EDGE('',*,*,#53187,.T.) ;
#75865 = ORIENTED_EDGE('',*,*,#53186,.T.) ;
#75866 = ORIENTED_EDGE('',*,*,#53189,.F.) ;
#75867 = ORIENTED_EDGE('',*,*,#53188,.T.) ;
#75868 = ORIENTED_EDGE('',*,*,#51561,.F.) ;
#75869 = ORIENTED_EDGE('',*,*,#53189,.T.) ;
#75870 = ORIENTED_EDGE('',*,*,#51732,.F.) ;
#75871 = ORIENTED_EDGE('',*,*,#51740,.F.) ;
#75872 = ORIENTED_EDGE('',*,*,#51753,.F.) ;
#75873 = ORIENTED_EDGE('',*,*,#53190,.F.) ;
#75874 = ORIENTED_EDGE('',*,*,#51745,.F.) ;
#75875 = ORIENTED_EDGE('',*,*,#53191,.F.) ;
#75876 = ORIENTED_EDGE('',*,*,#51743,.F.) ;
#75877 = ORIENTED_EDGE('',*,*,#53192,.F.) ;
#75878 = ORIENTED_EDGE('',*,*,#51870,.F.) ;
#75879 = ORIENTED_EDGE('',*,*,#51742,.F.) ;
#75880 = ORIENTED_EDGE('',*,*,#51744,.F.) ;
#75881 = ORIENTED_EDGE('',*,*,#53193,.F.) ;
#75882 = ORIENTED_EDGE('',*,*,#51748,.F.) ;
#75883 = ORIENTED_EDGE('',*,*,#53192,.T.) ;
#75884 = ORIENTED_EDGE('',*,*,#53190,.T.) ;
#75885 = ORIENTED_EDGE('',*,*,#53194,.F.) ;
#75886 = ORIENTED_EDGE('',*,*,#53193,.T.) ;
#75887 = ORIENTED_EDGE('',*,*,#53191,.T.) ;
#75888 = ORIENTED_EDGE('',*,*,#53195,.F.) ;
#75889 = ORIENTED_EDGE('',*,*,#51738,.F.) ;
#75890 = ORIENTED_EDGE('',*,*,#51751,.F.) ;
#75891 = ORIENTED_EDGE('',*,*,#53196,.F.) ;
#75892 = ORIENTED_EDGE('',*,*,#51754,.F.) ;
#75893 = ORIENTED_EDGE('',*,*,#53194,.T.) ;
#75894 = ORIENTED_EDGE('',*,*,#51752,.F.) ;
#75895 = ORIENTED_EDGE('',*,*,#53197,.F.) ;
#75896 = ORIENTED_EDGE('',*,*,#51867,.F.) ;
#75897 = ORIENTED_EDGE('',*,*,#53195,.T.) ;
#75898 = ORIENTED_EDGE('',*,*,#51869,.F.) ;
#75899 = ORIENTED_EDGE('',*,*,#53198,.F.) ;
#75900 = ORIENTED_EDGE('',*,*,#51746,.F.) ;
#75901 = ORIENTED_EDGE('',*,*,#51736,.F.) ;
#75902 = ORIENTED_EDGE('',*,*,#51747,.F.) ;
#75903 = ORIENTED_EDGE('',*,*,#53199,.F.) ;
#75904 = ORIENTED_EDGE('',*,*,#51749,.F.) ;
#75905 = ORIENTED_EDGE('',*,*,#53197,.T.) ;
#75906 = ORIENTED_EDGE('',*,*,#53196,.T.) ;
#75907 = ORIENTED_EDGE('',*,*,#53200,.F.) ;
#75908 = ORIENTED_EDGE('',*,*,#53199,.T.) ;
#75909 = ORIENTED_EDGE('',*,*,#53198,.T.) ;
#75910 = ORIENTED_EDGE('',*,*,#53201,.F.) ;
#75911 = ORIENTED_EDGE('',*,*,#53200,.T.) ;
#75912 = ORIENTED_EDGE('',*,*,#51750,.F.) ;
#75913 = ORIENTED_EDGE('',*,*,#53201,.T.) ;
#75914 = ORIENTED_EDGE('',*,*,#51868,.F.) ;
#75915 = ORIENTED_EDGE('',*,*,#53202,.F.) ;
#75916 = ORIENTED_EDGE('',*,*,#52074,.F.) ;
#75917 = ORIENTED_EDGE('',*,*,#53203,.F.) ;
#75918 = ORIENTED_EDGE('',*,*,#52089,.F.) ;
#75919 = ORIENTED_EDGE('',*,*,#53203,.T.) ;
#75920 = ORIENTED_EDGE('',*,*,#52077,.F.) ;
#75921 = ORIENTED_EDGE('',*,*,#53204,.F.) ;
#75922 = ORIENTED_EDGE('',*,*,#52071,.F.) ;
#75923 = ORIENTED_EDGE('',*,*,#53202,.T.) ;
#75924 = ORIENTED_EDGE('',*,*,#53205,.F.) ;
#75925 = ORIENTED_EDGE('',*,*,#53204,.T.) ;
#75926 = ORIENTED_EDGE('',*,*,#52080,.F.) ;
#75927 = ORIENTED_EDGE('',*,*,#53206,.F.) ;
#75928 = ORIENTED_EDGE('',*,*,#52086,.F.) ;
#75929 = ORIENTED_EDGE('',*,*,#53205,.T.) ;
#75930 = ORIENTED_EDGE('',*,*,#52088,.F.) ;
#75931 = ORIENTED_EDGE('',*,*,#53207,.F.) ;
#75932 = ORIENTED_EDGE('',*,*,#52068,.F.) ;
#75933 = ORIENTED_EDGE('',*,*,#53206,.T.) ;
#75934 = ORIENTED_EDGE('',*,*,#52083,.F.) ;
#75935 = ORIENTED_EDGE('',*,*,#53208,.F.) ;
#75936 = ORIENTED_EDGE('',*,*,#52065,.F.) ;
#75937 = ORIENTED_EDGE('',*,*,#53207,.T.) ;
#75938 = ORIENTED_EDGE('',*,*,#53209,.F.) ;
#75939 = ORIENTED_EDGE('',*,*,#53208,.T.) ;
#75940 = ORIENTED_EDGE('',*,*,#52084,.F.) ;
#75941 = ORIENTED_EDGE('',*,*,#53209,.T.) ;
#75942 = ORIENTED_EDGE('',*,*,#52087,.F.) ;
#75943 = ORIENTED_EDGE('',*,*,#49160,.F.) ;
#75944 = ORIENTED_EDGE('',*,*,#51891,.F.) ;
#75945 = ORIENTED_EDGE('',*,*,#49174,.F.) ;
#75946 = ORIENTED_EDGE('',*,*,#51920,.F.) ;
#75947 = ORIENTED_EDGE('',*,*,#49162,.F.) ;
#75948 = ORIENTED_EDGE('',*,*,#51921,.F.) ;
#75949 = ORIENTED_EDGE('',*,*,#49172,.F.) ;
#75950 = ORIENTED_EDGE('',*,*,#51924,.F.) ;
#75951 = ORIENTED_EDGE('',*,*,#49170,.F.) ;
#75952 = ORIENTED_EDGE('',*,*,#51922,.F.) ;
#75953 = ORIENTED_EDGE('',*,*,#49164,.F.) ;
#75954 = ORIENTED_EDGE('',*,*,#51925,.F.) ;
#75955 = ORIENTED_EDGE('',*,*,#49168,.F.) ;
#75956 = ORIENTED_EDGE('',*,*,#49527,.F.) ;
#75957 = ORIENTED_EDGE('',*,*,#49166,.F.) ;
#75958 = ORIENTED_EDGE('',*,*,#51923,.F.) ;
#75959 = ORIENTED_EDGE('',*,*,#53210,.F.) ;
#75960 = ORIENTED_EDGE('',*,*,#53211,.F.) ;
#75961 = ORIENTED_EDGE('',*,*,#53212,.F.) ;
#75962 = ORIENTED_EDGE('',*,*,#53211,.T.) ;
#75963 = ORIENTED_EDGE('',*,*,#51431,.F.) ;
#75964 = ORIENTED_EDGE('',*,*,#53213,.F.) ;
#75965 = ORIENTED_EDGE('',*,*,#51426,.F.) ;
#75966 = ORIENTED_EDGE('',*,*,#53212,.T.) ;
#75967 = ORIENTED_EDGE('',*,*,#51425,.F.) ;
#75968 = ORIENTED_EDGE('',*,*,#53214,.F.) ;
#75969 = ORIENTED_EDGE('',*,*,#51427,.F.) ;
#75970 = ORIENTED_EDGE('',*,*,#53210,.T.) ;
#75971 = ORIENTED_EDGE('',*,*,#51430,.F.) ;
#75972 = ORIENTED_EDGE('',*,*,#53215,.F.) ;
#75973 = ORIENTED_EDGE('',*,*,#51432,.F.) ;
#75974 = ORIENTED_EDGE('',*,*,#51436,.F.) ;
#75975 = ORIENTED_EDGE('',*,*,#53216,.T.) ;
#75976 = ORIENTED_EDGE('',*,*,#51225,.F.) ;
#75977 = ORIENTED_EDGE('',*,*,#53217,.F.) ;
#75978 = ORIENTED_EDGE('',*,*,#53213,.T.) ;
#75979 = ORIENTED_EDGE('',*,*,#53217,.T.) ;
#75980 = ORIENTED_EDGE('',*,*,#53218,.F.) ;
#75981 = ORIENTED_EDGE('',*,*,#53219,.F.) ;
#75982 = ORIENTED_EDGE('',*,*,#53214,.T.) ;
#75983 = ORIENTED_EDGE('',*,*,#53220,.F.) ;
#75984 = ORIENTED_EDGE('',*,*,#49620,.T.) ;
#75985 = ORIENTED_EDGE('',*,*,#53221,.F.) ;
#75986 = ORIENTED_EDGE('',*,*,#53215,.T.) ;
#75987 = ORIENTED_EDGE('',*,*,#53222,.F.) ;
#75988 = ORIENTED_EDGE('',*,*,#51435,.F.) ;
#75989 = ORIENTED_EDGE('',*,*,#53223,.T.) ;
#75990 = ORIENTED_EDGE('',*,*,#49451,.F.) ;
#75991 = ORIENTED_EDGE('',*,*,#53224,.T.) ;
#75992 = ORIENTED_EDGE('',*,*,#53218,.T.) ;
#75993 = ORIENTED_EDGE('',*,*,#51224,.F.) ;
#75994 = ORIENTED_EDGE('',*,*,#53225,.F.) ;
#75995 = ORIENTED_EDGE('',*,*,#51423,.F.) ;
#75996 = ORIENTED_EDGE('',*,*,#53220,.T.) ;
#75997 = ORIENTED_EDGE('',*,*,#51424,.F.) ;
#75998 = ORIENTED_EDGE('',*,*,#53226,.F.) ;
#75999 = ORIENTED_EDGE('',*,*,#49621,.F.) ;
#76000 = ORIENTED_EDGE('',*,*,#53219,.T.) ;
#76001 = ORIENTED_EDGE('',*,*,#49627,.F.) ;
#76002 = ORIENTED_EDGE('',*,*,#53227,.F.) ;
#76003 = ORIENTED_EDGE('',*,*,#51428,.F.) ;
#76004 = ORIENTED_EDGE('',*,*,#53222,.T.) ;
#76005 = ORIENTED_EDGE('',*,*,#51429,.F.) ;
#76006 = ORIENTED_EDGE('',*,*,#53228,.F.) ;
#76007 = ORIENTED_EDGE('',*,*,#51419,.F.) ;
#76008 = ORIENTED_EDGE('',*,*,#53221,.T.) ;
#76009 = ORIENTED_EDGE('',*,*,#51422,.F.) ;
#76010 = ORIENTED_EDGE('',*,*,#53229,.F.) ;
#76011 = ORIENTED_EDGE('',*,*,#51433,.F.) ;
#76012 = ORIENTED_EDGE('',*,*,#51235,.F.) ;
#76013 = ORIENTED_EDGE('',*,*,#53230,.T.) ;
#76014 = ORIENTED_EDGE('',*,*,#51434,.F.) ;
#76015 = ORIENTED_EDGE('',*,*,#53231,.F.) ;
#76016 = ORIENTED_EDGE('',*,*,#53225,.T.) ;
#76017 = ORIENTED_EDGE('',*,*,#51223,.T.) ;
#76018 = ORIENTED_EDGE('',*,*,#53232,.F.) ;
#76019 = ORIENTED_EDGE('',*,*,#53226,.T.) ;
#76020 = ORIENTED_EDGE('',*,*,#53227,.T.) ;
#76021 = ORIENTED_EDGE('',*,*,#49626,.T.) ;
#76022 = ORIENTED_EDGE('',*,*,#53233,.F.) ;
#76023 = ORIENTED_EDGE('',*,*,#53228,.T.) ;
#76024 = ORIENTED_EDGE('',*,*,#53231,.T.) ;
#76025 = ORIENTED_EDGE('',*,*,#53229,.T.) ;
#76026 = ORIENTED_EDGE('',*,*,#53234,.F.) ;
#76027 = ORIENTED_EDGE('',*,*,#51219,.F.) ;
#76028 = ORIENTED_EDGE('',*,*,#53235,.T.) ;
#76029 = ORIENTED_EDGE('',*,*,#51213,.F.) ;
#76030 = ORIENTED_EDGE('',*,*,#53236,.F.) ;
#76031 = ORIENTED_EDGE('',*,*,#53232,.T.) ;
#76032 = ORIENTED_EDGE('',*,*,#51222,.F.) ;
#76033 = ORIENTED_EDGE('',*,*,#53237,.F.) ;
#76034 = ORIENTED_EDGE('',*,*,#49622,.F.) ;
#76035 = ORIENTED_EDGE('',*,*,#53233,.T.) ;
#76036 = ORIENTED_EDGE('',*,*,#49625,.F.) ;
#76037 = ORIENTED_EDGE('',*,*,#53238,.F.) ;
#76038 = ORIENTED_EDGE('',*,*,#51420,.F.) ;
#76039 = ORIENTED_EDGE('',*,*,#53234,.T.) ;
#76040 = ORIENTED_EDGE('',*,*,#51421,.F.) ;
#76041 = ORIENTED_EDGE('',*,*,#53239,.F.) ;
#76042 = ORIENTED_EDGE('',*,*,#51236,.F.) ;
#76043 = ORIENTED_EDGE('',*,*,#53236,.T.) ;
#76044 = ORIENTED_EDGE('',*,*,#53106,.F.) ;
#76045 = ORIENTED_EDGE('',*,*,#53240,.F.) ;
#76046 = ORIENTED_EDGE('',*,*,#53241,.F.) ;
#76047 = ORIENTED_EDGE('',*,*,#53237,.T.) ;
#76048 = ORIENTED_EDGE('',*,*,#53242,.F.) ;
#76049 = ORIENTED_EDGE('',*,*,#53239,.T.) ;
#76050 = ORIENTED_EDGE('',*,*,#53238,.T.) ;
#76051 = ORIENTED_EDGE('',*,*,#53243,.F.) ;
#76052 = ORIENTED_EDGE('',*,*,#51237,.T.) ;
#76053 = ORIENTED_EDGE('',*,*,#53240,.T.) ;
#76054 = ORIENTED_EDGE('',*,*,#49697,.F.) ;
#76055 = ORIENTED_EDGE('',*,*,#53244,.F.) ;
#76056 = ORIENTED_EDGE('',*,*,#51220,.F.) ;
#76057 = ORIENTED_EDGE('',*,*,#53242,.T.) ;
#76058 = ORIENTED_EDGE('',*,*,#51221,.F.) ;
#76059 = ORIENTED_EDGE('',*,*,#53245,.F.) ;
#76060 = ORIENTED_EDGE('',*,*,#51227,.F.) ;
#76061 = ORIENTED_EDGE('',*,*,#53241,.T.) ;
#76062 = ORIENTED_EDGE('',*,*,#51230,.F.) ;
#76063 = ORIENTED_EDGE('',*,*,#53246,.F.) ;
#76064 = ORIENTED_EDGE('',*,*,#49623,.F.) ;
#76065 = ORIENTED_EDGE('',*,*,#53243,.T.) ;
#76066 = ORIENTED_EDGE('',*,*,#49624,.F.) ;
#76067 = ORIENTED_EDGE('',*,*,#53247,.F.) ;
#76068 = ORIENTED_EDGE('',*,*,#51238,.F.) ;
#76069 = ORIENTED_EDGE('',*,*,#53244,.T.) ;
#76070 = ORIENTED_EDGE('',*,*,#49696,.T.) ;
#76071 = ORIENTED_EDGE('',*,*,#53248,.F.) ;
#76072 = ORIENTED_EDGE('',*,*,#53245,.T.) ;
#76073 = ORIENTED_EDGE('',*,*,#53247,.T.) ;
#76074 = ORIENTED_EDGE('',*,*,#53246,.T.) ;
#76075 = ORIENTED_EDGE('',*,*,#53249,.F.) ;
#76076 = ORIENTED_EDGE('',*,*,#53248,.T.) ;
#76077 = ORIENTED_EDGE('',*,*,#49695,.F.) ;
#76078 = ORIENTED_EDGE('',*,*,#53250,.F.) ;
#76079 = ORIENTED_EDGE('',*,*,#51228,.F.) ;
#76080 = ORIENTED_EDGE('',*,*,#53249,.T.) ;
#76081 = ORIENTED_EDGE('',*,*,#51229,.F.) ;
#76082 = ORIENTED_EDGE('',*,*,#53251,.F.) ;
#76083 = ORIENTED_EDGE('',*,*,#51239,.F.) ;
#76084 = ORIENTED_EDGE('',*,*,#51243,.F.) ;
#76085 = ORIENTED_EDGE('',*,*,#53252,.T.) ;
#76086 = ORIENTED_EDGE('',*,*,#51231,.F.) ;
#76087 = ORIENTED_EDGE('',*,*,#53253,.F.) ;
#76088 = ORIENTED_EDGE('',*,*,#49692,.F.) ;
#76089 = ORIENTED_EDGE('',*,*,#53254,.T.) ;
#76090 = ORIENTED_EDGE('',*,*,#51244,.F.) ;
#76091 = ORIENTED_EDGE('',*,*,#53255,.F.) ;
#76092 = ORIENTED_EDGE('',*,*,#53250,.T.) ;
#76093 = ORIENTED_EDGE('',*,*,#49694,.T.) ;
#76094 = ORIENTED_EDGE('',*,*,#53256,.F.) ;
#76095 = ORIENTED_EDGE('',*,*,#53251,.T.) ;
#76096 = ORIENTED_EDGE('',*,*,#53255,.T.) ;
#76097 = ORIENTED_EDGE('',*,*,#53253,.T.) ;
#76098 = ORIENTED_EDGE('',*,*,#53257,.F.) ;
#76099 = ORIENTED_EDGE('',*,*,#53256,.T.) ;
#76100 = ORIENTED_EDGE('',*,*,#49693,.F.) ;
#76101 = ORIENTED_EDGE('',*,*,#53257,.T.) ;
#76102 = ORIENTED_EDGE('',*,*,#51240,.F.) ;
#76103 = ORIENTED_EDGE('',*,*,#52310,.F.) ;
#76104 = ORIENTED_EDGE('',*,*,#52321,.F.) ;
#76105 = ORIENTED_EDGE('',*,*,#52320,.F.) ;
#76106 = ORIENTED_EDGE('',*,*,#53258,.F.) ;
#76107 = ORIENTED_EDGE('',*,*,#52311,.F.) ;
#76108 = ORIENTED_EDGE('',*,*,#53258,.T.) ;
#76109 = ORIENTED_EDGE('',*,*,#50744,.F.) ;
#76110 = ORIENTED_EDGE('',*,*,#53259,.F.) ;
#76111 = ORIENTED_EDGE('',*,*,#50730,.F.) ;
#76112 = ORIENTED_EDGE('',*,*,#52318,.F.) ;
#76113 = ORIENTED_EDGE('',*,*,#52317,.F.) ;
#76114 = ORIENTED_EDGE('',*,*,#52316,.F.) ;
#76115 = ORIENTED_EDGE('',*,*,#53260,.F.) ;
#76116 = ORIENTED_EDGE('',*,*,#52319,.F.) ;
#76117 = ORIENTED_EDGE('',*,*,#53261,.F.) ;
#76118 = ORIENTED_EDGE('',*,*,#53259,.T.) ;
#76119 = ORIENTED_EDGE('',*,*,#53262,.F.) ;
#76120 = ORIENTED_EDGE('',*,*,#52308,.F.) ;
#76121 = ORIENTED_EDGE('',*,*,#52313,.F.) ;
#76122 = ORIENTED_EDGE('',*,*,#52312,.F.) ;
#76123 = ORIENTED_EDGE('',*,*,#53263,.F.) ;
#76124 = ORIENTED_EDGE('',*,*,#52309,.F.) ;
#76125 = ORIENTED_EDGE('',*,*,#53260,.T.) ;
#76126 = ORIENTED_EDGE('',*,*,#50740,.F.) ;
#76127 = ORIENTED_EDGE('',*,*,#53264,.F.) ;
#76128 = ORIENTED_EDGE('',*,*,#50742,.F.) ;
#76129 = ORIENTED_EDGE('',*,*,#53262,.T.) ;
#76130 = ORIENTED_EDGE('',*,*,#50743,.F.) ;
#76131 = ORIENTED_EDGE('',*,*,#53265,.F.) ;
#76132 = ORIENTED_EDGE('',*,*,#50948,.F.) ;
#76133 = ORIENTED_EDGE('',*,*,#53261,.T.) ;
#76134 = ORIENTED_EDGE('',*,*,#50947,.F.) ;
#76135 = ORIENTED_EDGE('',*,*,#53266,.F.) ;
#76136 = ORIENTED_EDGE('',*,*,#50731,.F.) ;
#76137 = ORIENTED_EDGE('',*,*,#53263,.T.) ;
#76138 = ORIENTED_EDGE('',*,*,#50732,.F.) ;
#76139 = ORIENTED_EDGE('',*,*,#53267,.F.) ;
#76140 = ORIENTED_EDGE('',*,*,#50736,.F.) ;
#76141 = ORIENTED_EDGE('',*,*,#53265,.T.) ;
#76142 = ORIENTED_EDGE('',*,*,#53264,.T.) ;
#76143 = ORIENTED_EDGE('',*,*,#53268,.F.) ;
#76144 = ORIENTED_EDGE('',*,*,#53267,.T.) ;
#76145 = ORIENTED_EDGE('',*,*,#53266,.T.) ;
#76146 = ORIENTED_EDGE('',*,*,#53269,.F.) ;
#76147 = ORIENTED_EDGE('',*,*,#53268,.T.) ;
#76148 = ORIENTED_EDGE('',*,*,#50739,.F.) ;
#76149 = ORIENTED_EDGE('',*,*,#53270,.F.) ;
#76150 = ORIENTED_EDGE('',*,*,#50945,.F.) ;
#76151 = ORIENTED_EDGE('',*,*,#53269,.T.) ;
#76152 = ORIENTED_EDGE('',*,*,#50946,.F.) ;
#76153 = ORIENTED_EDGE('',*,*,#53271,.F.) ;
#76154 = ORIENTED_EDGE('',*,*,#50733,.F.) ;
#76155 = ORIENTED_EDGE('',*,*,#53271,.T.) ;
#76156 = ORIENTED_EDGE('',*,*,#53270,.T.) ;
#76157 = ORIENTED_EDGE('',*,*,#53272,.F.) ;
#76158 = ORIENTED_EDGE('',*,*,#53272,.T.) ;
#76159 = ORIENTED_EDGE('',*,*,#50738,.F.) ;
#76160 = ORIENTED_EDGE('',*,*,#53273,.F.) ;
#76161 = ORIENTED_EDGE('',*,*,#50734,.F.) ;
#76162 = ORIENTED_EDGE('',*,*,#52314,.F.) ;
#76163 = ORIENTED_EDGE('',*,*,#52307,.F.) ;
#76164 = ORIENTED_EDGE('',*,*,#52306,.F.) ;
#76165 = ORIENTED_EDGE('',*,*,#53273,.T.) ;
#76166 = ORIENTED_EDGE('',*,*,#52315,.F.) ;
#76167 = ORIENTED_EDGE('',*,*,#52515,.F.) ;
#76168 = ORIENTED_EDGE('',*,*,#52514,.F.) ;
#76169 = ORIENTED_EDGE('',*,*,#52513,.F.) ;
#76170 = ORIENTED_EDGE('',*,*,#53274,.F.) ;
#76171 = ORIENTED_EDGE('',*,*,#52516,.F.) ;
#76172 = ORIENTED_EDGE('',*,*,#53274,.T.) ;
#76173 = ORIENTED_EDGE('',*,*,#52512,.F.) ;
#76174 = ORIENTED_EDGE('',*,*,#53275,.F.) ;
#76175 = ORIENTED_EDGE('',*,*,#50593,.F.) ;
#76176 = ORIENTED_EDGE('',*,*,#53275,.T.) ;
#76177 = ORIENTED_EDGE('',*,*,#50448,.F.) ;
#76178 = ORIENTED_EDGE('',*,*,#53276,.F.) ;
#76179 = ORIENTED_EDGE('',*,*,#50594,.F.) ;
#76180 = ORIENTED_EDGE('',*,*,#50436,.F.) ;
#76181 = ORIENTED_EDGE('',*,*,#50595,.F.) ;
#76182 = ORIENTED_EDGE('',*,*,#53277,.F.) ;
#76183 = ORIENTED_EDGE('',*,*,#50442,.F.) ;
#76184 = ORIENTED_EDGE('',*,*,#53277,.T.) ;
#76185 = ORIENTED_EDGE('',*,*,#53276,.T.) ;
#76186 = ORIENTED_EDGE('',*,*,#53278,.F.) ;
#76187 = ORIENTED_EDGE('',*,*,#53278,.T.) ;
#76188 = ORIENTED_EDGE('',*,*,#50447,.F.) ;
#76189 = ORIENTED_EDGE('',*,*,#53279,.F.) ;
#76190 = ORIENTED_EDGE('',*,*,#50443,.F.) ;
#76191 = ORIENTED_EDGE('',*,*,#50438,.F.) ;
#76192 = ORIENTED_EDGE('',*,*,#50444,.F.) ;
#76193 = ORIENTED_EDGE('',*,*,#53280,.F.) ;
#76194 = ORIENTED_EDGE('',*,*,#50657,.F.) ;
#76195 = ORIENTED_EDGE('',*,*,#53280,.T.) ;
#76196 = ORIENTED_EDGE('',*,*,#53279,.T.) ;
#76197 = ORIENTED_EDGE('',*,*,#53281,.F.) ;
#76198 = ORIENTED_EDGE('',*,*,#53281,.T.) ;
#76199 = ORIENTED_EDGE('',*,*,#50446,.F.) ;
#76200 = ORIENTED_EDGE('',*,*,#53282,.F.) ;
#76201 = ORIENTED_EDGE('',*,*,#50658,.F.) ;
#76202 = ORIENTED_EDGE('',*,*,#53282,.T.) ;
#76203 = ORIENTED_EDGE('',*,*,#52511,.F.) ;
#76204 = ORIENTED_EDGE('',*,*,#53283,.F.) ;
#76205 = ORIENTED_EDGE('',*,*,#50659,.F.) ;
#76206 = ORIENTED_EDGE('',*,*,#53283,.T.) ;
#76207 = ORIENTED_EDGE('',*,*,#52510,.F.) ;
#76208 = ORIENTED_EDGE('',*,*,#52519,.F.) ;
#76209 = ORIENTED_EDGE('',*,*,#52520,.F.) ;
#76210 = ORIENTED_EDGE('',*,*,#52525,.F.) ;
#76211 = ORIENTED_EDGE('',*,*,#53284,.F.) ;
#76212 = ORIENTED_EDGE('',*,*,#53284,.T.) ;
#76213 = ORIENTED_EDGE('',*,*,#52524,.F.) ;
#76214 = ORIENTED_EDGE('',*,*,#53285,.F.) ;
#76215 = ORIENTED_EDGE('',*,*,#50654,.F.) ;
#76216 = ORIENTED_EDGE('',*,*,#53285,.T.) ;
#76217 = ORIENTED_EDGE('',*,*,#50430,.F.) ;
#76218 = ORIENTED_EDGE('',*,*,#53286,.F.) ;
#76219 = ORIENTED_EDGE('',*,*,#50655,.F.) ;
#76220 = ORIENTED_EDGE('',*,*,#50440,.F.) ;
#76221 = ORIENTED_EDGE('',*,*,#50656,.F.) ;
#76222 = ORIENTED_EDGE('',*,*,#53287,.F.) ;
#76223 = ORIENTED_EDGE('',*,*,#50434,.F.) ;
#76224 = ORIENTED_EDGE('',*,*,#53287,.T.) ;
#76225 = ORIENTED_EDGE('',*,*,#53286,.T.) ;
#76226 = ORIENTED_EDGE('',*,*,#53288,.F.) ;
#76227 = ORIENTED_EDGE('',*,*,#53288,.T.) ;
#76228 = ORIENTED_EDGE('',*,*,#50429,.F.) ;
#76229 = ORIENTED_EDGE('',*,*,#53289,.F.) ;
#76230 = ORIENTED_EDGE('',*,*,#50431,.F.) ;
#76231 = ORIENTED_EDGE('',*,*,#50441,.F.) ;
#76232 = ORIENTED_EDGE('',*,*,#50432,.F.) ;
#76233 = ORIENTED_EDGE('',*,*,#53290,.F.) ;
#76234 = ORIENTED_EDGE('',*,*,#50596,.F.) ;
#76235 = ORIENTED_EDGE('',*,*,#53290,.T.) ;
#76236 = ORIENTED_EDGE('',*,*,#53289,.T.) ;
#76237 = ORIENTED_EDGE('',*,*,#53291,.F.) ;
#76238 = ORIENTED_EDGE('',*,*,#53291,.T.) ;
#76239 = ORIENTED_EDGE('',*,*,#50428,.F.) ;
#76240 = ORIENTED_EDGE('',*,*,#53292,.F.) ;
#76241 = ORIENTED_EDGE('',*,*,#50597,.F.) ;
#76242 = ORIENTED_EDGE('',*,*,#53292,.T.) ;
#76243 = ORIENTED_EDGE('',*,*,#52523,.F.) ;
#76244 = ORIENTED_EDGE('',*,*,#53293,.F.) ;
#76245 = ORIENTED_EDGE('',*,*,#50598,.F.) ;
#76246 = ORIENTED_EDGE('',*,*,#52521,.F.) ;
#76247 = ORIENTED_EDGE('',*,*,#52518,.F.) ;
#76248 = ORIENTED_EDGE('',*,*,#52517,.F.) ;
#76249 = ORIENTED_EDGE('',*,*,#53293,.T.) ;
#76250 = ORIENTED_EDGE('',*,*,#52522,.F.) ;
#76251 = ORIENTED_EDGE('',*,*,#53294,.F.) ;
#76252 = ORIENTED_EDGE('',*,*,#49460,.F.) ;
#76253 = ORIENTED_EDGE('',*,*,#53295,.F.) ;
#76254 = ORIENTED_EDGE('',*,*,#52097,.F.) ;
#76255 = ORIENTED_EDGE('',*,*,#53295,.T.) ;
#76256 = ORIENTED_EDGE('',*,*,#49459,.F.) ;
#76257 = ORIENTED_EDGE('',*,*,#53296,.F.) ;
#76258 = ORIENTED_EDGE('',*,*,#52100,.F.) ;
#76259 = ORIENTED_EDGE('',*,*,#53294,.T.) ;
#76260 = ORIENTED_EDGE('',*,*,#52094,.F.) ;
#76261 = ORIENTED_EDGE('',*,*,#53297,.F.) ;
#76262 = ORIENTED_EDGE('',*,*,#49461,.F.) ;
#76263 = ORIENTED_EDGE('',*,*,#53296,.T.) ;
#76264 = ORIENTED_EDGE('',*,*,#49458,.F.) ;
#76265 = ORIENTED_EDGE('',*,*,#53298,.F.) ;
#76266 = ORIENTED_EDGE('',*,*,#52103,.F.) ;
#76267 = ORIENTED_EDGE('',*,*,#53297,.T.) ;
#76268 = ORIENTED_EDGE('',*,*,#52091,.F.) ;
#76269 = ORIENTED_EDGE('',*,*,#53299,.F.) ;
#76270 = ORIENTED_EDGE('',*,*,#49462,.F.) ;
#76271 = ORIENTED_EDGE('',*,*,#53298,.T.) ;
#76272 = ORIENTED_EDGE('',*,*,#49457,.F.) ;
#76273 = ORIENTED_EDGE('',*,*,#53300,.F.) ;
#76274 = ORIENTED_EDGE('',*,*,#52106,.F.) ;
#76275 = ORIENTED_EDGE('',*,*,#53299,.T.) ;
#76276 = ORIENTED_EDGE('',*,*,#52113,.F.) ;
#76277 = ORIENTED_EDGE('',*,*,#53301,.F.) ;
#76278 = ORIENTED_EDGE('',*,*,#49455,.F.) ;
#76279 = ORIENTED_EDGE('',*,*,#53300,.T.) ;
#76280 = ORIENTED_EDGE('',*,*,#49456,.F.) ;
#76281 = ORIENTED_EDGE('',*,*,#53301,.T.) ;
#76282 = ORIENTED_EDGE('',*,*,#52109,.F.) ;
#76283 = ORIENTED_EDGE('',*,*,#50954,.F.) ;
#76284 = ORIENTED_EDGE('',*,*,#50968,.F.) ;
#76285 = ORIENTED_EDGE('',*,*,#53302,.F.) ;
#76286 = ORIENTED_EDGE('',*,*,#50957,.F.) ;
#76287 = ORIENTED_EDGE('',*,*,#53303,.F.) ;
#76288 = ORIENTED_EDGE('',*,*,#50958,.F.) ;
#76289 = ORIENTED_EDGE('',*,*,#53304,.F.) ;
#76290 = ORIENTED_EDGE('',*,*,#51064,.F.) ;
#76291 = ORIENTED_EDGE('',*,*,#50956,.F.) ;
#76292 = ORIENTED_EDGE('',*,*,#50959,.F.) ;
#76293 = ORIENTED_EDGE('',*,*,#53305,.F.) ;
#76294 = ORIENTED_EDGE('',*,*,#50960,.F.) ;
#76295 = ORIENTED_EDGE('',*,*,#53304,.T.) ;
#76296 = ORIENTED_EDGE('',*,*,#53302,.T.) ;
#76297 = ORIENTED_EDGE('',*,*,#53306,.F.) ;
#76298 = ORIENTED_EDGE('',*,*,#53305,.T.) ;
#76299 = ORIENTED_EDGE('',*,*,#53303,.T.) ;
#76300 = ORIENTED_EDGE('',*,*,#53307,.F.) ;
#76301 = ORIENTED_EDGE('',*,*,#50952,.F.) ;
#76302 = ORIENTED_EDGE('',*,*,#50964,.F.) ;
#76303 = ORIENTED_EDGE('',*,*,#53308,.F.) ;
#76304 = ORIENTED_EDGE('',*,*,#50966,.F.) ;
#76305 = ORIENTED_EDGE('',*,*,#53306,.T.) ;
#76306 = ORIENTED_EDGE('',*,*,#50967,.F.) ;
#76307 = ORIENTED_EDGE('',*,*,#53309,.F.) ;
#76308 = ORIENTED_EDGE('',*,*,#51061,.F.) ;
#76309 = ORIENTED_EDGE('',*,*,#53307,.T.) ;
#76310 = ORIENTED_EDGE('',*,*,#51063,.F.) ;
#76311 = ORIENTED_EDGE('',*,*,#53310,.F.) ;
#76312 = ORIENTED_EDGE('',*,*,#50961,.F.) ;
#76313 = ORIENTED_EDGE('',*,*,#50950,.F.) ;
#76314 = ORIENTED_EDGE('',*,*,#50962,.F.) ;
#76315 = ORIENTED_EDGE('',*,*,#53311,.F.) ;
#76316 = ORIENTED_EDGE('',*,*,#50965,.F.) ;
#76317 = ORIENTED_EDGE('',*,*,#53309,.T.) ;
#76318 = ORIENTED_EDGE('',*,*,#53308,.T.) ;
#76319 = ORIENTED_EDGE('',*,*,#53312,.F.) ;
#76320 = ORIENTED_EDGE('',*,*,#53311,.T.) ;
#76321 = ORIENTED_EDGE('',*,*,#53310,.T.) ;
#76322 = ORIENTED_EDGE('',*,*,#53313,.F.) ;
#76323 = ORIENTED_EDGE('',*,*,#53312,.T.) ;
#76324 = ORIENTED_EDGE('',*,*,#50963,.F.) ;
#76325 = ORIENTED_EDGE('',*,*,#53313,.T.) ;
#76326 = ORIENTED_EDGE('',*,*,#51062,.F.) ;
#76327 = ORIENTED_EDGE('',*,*,#53314,.F.) ;
#76328 = ORIENTED_EDGE('',*,*,#49348,.F.) ;
#76329 = ORIENTED_EDGE('',*,*,#53315,.F.) ;
#76330 = ORIENTED_EDGE('',*,*,#51553,.F.) ;
#76331 = ORIENTED_EDGE('',*,*,#53315,.T.) ;
#76332 = ORIENTED_EDGE('',*,*,#49347,.T.) ;
#76333 = ORIENTED_EDGE('',*,*,#53316,.F.) ;
#76334 = ORIENTED_EDGE('',*,*,#53317,.F.) ;
#76335 = ORIENTED_EDGE('',*,*,#49349,.T.) ;
#76336 = ORIENTED_EDGE('',*,*,#53314,.T.) ;
#76337 = ORIENTED_EDGE('',*,*,#53318,.F.) ;
#76338 = ORIENTED_EDGE('',*,*,#53319,.F.) ;
#76339 = ORIENTED_EDGE('',*,*,#53316,.T.) ;
#76340 = ORIENTED_EDGE('',*,*,#49346,.F.) ;
#76341 = ORIENTED_EDGE('',*,*,#53320,.F.) ;
#76342 = ORIENTED_EDGE('',*,*,#51550,.F.) ;
#76343 = ORIENTED_EDGE('',*,*,#53317,.T.) ;
#76344 = ORIENTED_EDGE('',*,*,#51549,.F.) ;
#76345 = ORIENTED_EDGE('',*,*,#53321,.F.) ;
#76346 = ORIENTED_EDGE('',*,*,#51554,.F.) ;
#76347 = ORIENTED_EDGE('',*,*,#53322,.F.) ;
#76348 = ORIENTED_EDGE('',*,*,#51551,.F.) ;
#76349 = ORIENTED_EDGE('',*,*,#53323,.F.) ;
#76350 = ORIENTED_EDGE('',*,*,#51758,.F.) ;
#76351 = ORIENTED_EDGE('',*,*,#53318,.T.) ;
#76352 = ORIENTED_EDGE('',*,*,#51552,.F.) ;
#76353 = ORIENTED_EDGE('',*,*,#53324,.F.) ;
#76354 = ORIENTED_EDGE('',*,*,#51542,.F.) ;
#76355 = ORIENTED_EDGE('',*,*,#53319,.T.) ;
#76356 = ORIENTED_EDGE('',*,*,#51541,.F.) ;
#76357 = ORIENTED_EDGE('',*,*,#53325,.F.) ;
#76358 = ORIENTED_EDGE('',*,*,#49350,.F.) ;
#76359 = ORIENTED_EDGE('',*,*,#53326,.F.) ;
#76360 = ORIENTED_EDGE('',*,*,#49344,.F.) ;
#76361 = ORIENTED_EDGE('',*,*,#53327,.F.) ;
#76362 = ORIENTED_EDGE('',*,*,#51543,.F.) ;
#76363 = ORIENTED_EDGE('',*,*,#49345,.T.) ;
#76364 = ORIENTED_EDGE('',*,*,#53326,.T.) ;
#76365 = ORIENTED_EDGE('',*,*,#53328,.F.) ;
#76366 = ORIENTED_EDGE('',*,*,#53320,.T.) ;
#76367 = ORIENTED_EDGE('',*,*,#53323,.T.) ;
#76368 = ORIENTED_EDGE('',*,*,#53321,.T.) ;
#76369 = ORIENTED_EDGE('',*,*,#53329,.F.) ;
#76370 = ORIENTED_EDGE('',*,*,#53324,.T.) ;
#76371 = ORIENTED_EDGE('',*,*,#53322,.T.) ;
#76372 = ORIENTED_EDGE('',*,*,#53330,.F.) ;
#76373 = ORIENTED_EDGE('',*,*,#49343,.T.) ;
#76374 = ORIENTED_EDGE('',*,*,#53325,.T.) ;
#76375 = ORIENTED_EDGE('',*,*,#53331,.F.) ;
#76376 = ORIENTED_EDGE('',*,*,#53327,.T.) ;
#76377 = ORIENTED_EDGE('',*,*,#53328,.T.) ;
#76378 = ORIENTED_EDGE('',*,*,#51546,.F.) ;
#76379 = ORIENTED_EDGE('',*,*,#53332,.F.) ;
#76380 = ORIENTED_EDGE('',*,*,#51547,.F.) ;
#76381 = ORIENTED_EDGE('',*,*,#53329,.T.) ;
#76382 = ORIENTED_EDGE('',*,*,#51548,.F.) ;
#76383 = ORIENTED_EDGE('',*,*,#53333,.F.) ;
#76384 = ORIENTED_EDGE('',*,*,#51755,.F.) ;
#76385 = ORIENTED_EDGE('',*,*,#53330,.T.) ;
#76386 = ORIENTED_EDGE('',*,*,#51757,.F.) ;
#76387 = ORIENTED_EDGE('',*,*,#53334,.F.) ;
#76388 = ORIENTED_EDGE('',*,*,#51539,.F.) ;
#76389 = ORIENTED_EDGE('',*,*,#53331,.T.) ;
#76390 = ORIENTED_EDGE('',*,*,#51540,.F.) ;
#76391 = ORIENTED_EDGE('',*,*,#53335,.F.) ;
#76392 = ORIENTED_EDGE('',*,*,#51544,.F.) ;
#76393 = ORIENTED_EDGE('',*,*,#53333,.T.) ;
#76394 = ORIENTED_EDGE('',*,*,#53332,.T.) ;
#76395 = ORIENTED_EDGE('',*,*,#53336,.F.) ;
#76396 = ORIENTED_EDGE('',*,*,#53335,.T.) ;
#76397 = ORIENTED_EDGE('',*,*,#53334,.T.) ;
#76398 = ORIENTED_EDGE('',*,*,#53337,.F.) ;
#76399 = ORIENTED_EDGE('',*,*,#53336,.T.) ;
#76400 = ORIENTED_EDGE('',*,*,#51545,.F.) ;
#76401 = ORIENTED_EDGE('',*,*,#53337,.T.) ;
#76402 = ORIENTED_EDGE('',*,*,#51756,.F.) ;
#76403 = ORIENTED_EDGE('',*,*,#51764,.F.) ;
#76404 = ORIENTED_EDGE('',*,*,#51777,.F.) ;
#76405 = ORIENTED_EDGE('',*,*,#53338,.F.) ;
#76406 = ORIENTED_EDGE('',*,*,#51769,.F.) ;
#76407 = ORIENTED_EDGE('',*,*,#53339,.F.) ;
#76408 = ORIENTED_EDGE('',*,*,#51767,.F.) ;
#76409 = ORIENTED_EDGE('',*,*,#53340,.F.) ;
#76410 = ORIENTED_EDGE('',*,*,#51874,.F.) ;
#76411 = ORIENTED_EDGE('',*,*,#51766,.F.) ;
#76412 = ORIENTED_EDGE('',*,*,#51768,.F.) ;
#76413 = ORIENTED_EDGE('',*,*,#53341,.F.) ;
#76414 = ORIENTED_EDGE('',*,*,#51772,.F.) ;
#76415 = ORIENTED_EDGE('',*,*,#53340,.T.) ;
#76416 = ORIENTED_EDGE('',*,*,#53338,.T.) ;
#76417 = ORIENTED_EDGE('',*,*,#53342,.F.) ;
#76418 = ORIENTED_EDGE('',*,*,#53341,.T.) ;
#76419 = ORIENTED_EDGE('',*,*,#53339,.T.) ;
#76420 = ORIENTED_EDGE('',*,*,#53343,.F.) ;
#76421 = ORIENTED_EDGE('',*,*,#51762,.F.) ;
#76422 = ORIENTED_EDGE('',*,*,#51775,.F.) ;
#76423 = ORIENTED_EDGE('',*,*,#53344,.F.) ;
#76424 = ORIENTED_EDGE('',*,*,#51778,.F.) ;
#76425 = ORIENTED_EDGE('',*,*,#53342,.T.) ;
#76426 = ORIENTED_EDGE('',*,*,#51776,.F.) ;
#76427 = ORIENTED_EDGE('',*,*,#53345,.F.) ;
#76428 = ORIENTED_EDGE('',*,*,#51871,.F.) ;
#76429 = ORIENTED_EDGE('',*,*,#53343,.T.) ;
#76430 = ORIENTED_EDGE('',*,*,#51873,.F.) ;
#76431 = ORIENTED_EDGE('',*,*,#53346,.F.) ;
#76432 = ORIENTED_EDGE('',*,*,#51770,.F.) ;
#76433 = ORIENTED_EDGE('',*,*,#51760,.F.) ;
#76434 = ORIENTED_EDGE('',*,*,#51771,.F.) ;
#76435 = ORIENTED_EDGE('',*,*,#53347,.F.) ;
#76436 = ORIENTED_EDGE('',*,*,#51773,.F.) ;
#76437 = ORIENTED_EDGE('',*,*,#53345,.T.) ;
#76438 = ORIENTED_EDGE('',*,*,#53344,.T.) ;
#76439 = ORIENTED_EDGE('',*,*,#53348,.F.) ;
#76440 = ORIENTED_EDGE('',*,*,#53347,.T.) ;
#76441 = ORIENTED_EDGE('',*,*,#53346,.T.) ;
#76442 = ORIENTED_EDGE('',*,*,#53349,.F.) ;
#76443 = ORIENTED_EDGE('',*,*,#53348,.T.) ;
#76444 = ORIENTED_EDGE('',*,*,#51774,.F.) ;
#76445 = ORIENTED_EDGE('',*,*,#53349,.T.) ;
#76446 = ORIENTED_EDGE('',*,*,#51872,.F.) ;
#76447 = ORIENTED_EDGE('',*,*,#53350,.F.) ;
#76448 = ORIENTED_EDGE('',*,*,#52102,.F.) ;
#76449 = ORIENTED_EDGE('',*,*,#53351,.F.) ;
#76450 = ORIENTED_EDGE('',*,*,#52117,.F.) ;
#76451 = ORIENTED_EDGE('',*,*,#53351,.T.) ;
#76452 = ORIENTED_EDGE('',*,*,#52105,.F.) ;
#76453 = ORIENTED_EDGE('',*,*,#53352,.F.) ;
#76454 = ORIENTED_EDGE('',*,*,#52099,.F.) ;
#76455 = ORIENTED_EDGE('',*,*,#53350,.T.) ;
#76456 = ORIENTED_EDGE('',*,*,#53353,.F.) ;
#76457 = ORIENTED_EDGE('',*,*,#53352,.T.) ;
#76458 = ORIENTED_EDGE('',*,*,#52108,.F.) ;
#76459 = ORIENTED_EDGE('',*,*,#53354,.F.) ;
#76460 = ORIENTED_EDGE('',*,*,#52114,.F.) ;
#76461 = ORIENTED_EDGE('',*,*,#53353,.T.) ;
#76462 = ORIENTED_EDGE('',*,*,#52116,.F.) ;
#76463 = ORIENTED_EDGE('',*,*,#53355,.F.) ;
#76464 = ORIENTED_EDGE('',*,*,#52096,.F.) ;
#76465 = ORIENTED_EDGE('',*,*,#53354,.T.) ;
#76466 = ORIENTED_EDGE('',*,*,#52111,.F.) ;
#76467 = ORIENTED_EDGE('',*,*,#53356,.F.) ;
#76468 = ORIENTED_EDGE('',*,*,#52093,.F.) ;
#76469 = ORIENTED_EDGE('',*,*,#53355,.T.) ;
#76470 = ORIENTED_EDGE('',*,*,#53357,.F.) ;
#76471 = ORIENTED_EDGE('',*,*,#53356,.T.) ;
#76472 = ORIENTED_EDGE('',*,*,#52112,.F.) ;
#76473 = ORIENTED_EDGE('',*,*,#53357,.T.) ;
#76474 = ORIENTED_EDGE('',*,*,#52115,.F.) ;
#76475 = ORIENTED_EDGE('',*,*,#49178,.F.) ;
#76476 = ORIENTED_EDGE('',*,*,#51890,.F.) ;
#76477 = ORIENTED_EDGE('',*,*,#49192,.F.) ;
#76478 = ORIENTED_EDGE('',*,*,#51926,.F.) ;
#76479 = ORIENTED_EDGE('',*,*,#49180,.F.) ;
#76480 = ORIENTED_EDGE('',*,*,#51927,.F.) ;
#76481 = ORIENTED_EDGE('',*,*,#49190,.F.) ;
#76482 = ORIENTED_EDGE('',*,*,#51930,.F.) ;
#76483 = ORIENTED_EDGE('',*,*,#49188,.F.) ;
#76484 = ORIENTED_EDGE('',*,*,#51928,.F.) ;
#76485 = ORIENTED_EDGE('',*,*,#49182,.F.) ;
#76486 = ORIENTED_EDGE('',*,*,#51931,.F.) ;
#76487 = ORIENTED_EDGE('',*,*,#49186,.F.) ;
#76488 = ORIENTED_EDGE('',*,*,#49526,.F.) ;
#76489 = ORIENTED_EDGE('',*,*,#49184,.F.) ;
#76490 = ORIENTED_EDGE('',*,*,#51929,.F.) ;
#76491 = ORIENTED_EDGE('',*,*,#53358,.F.) ;
#76492 = ORIENTED_EDGE('',*,*,#53359,.F.) ;
#76493 = ORIENTED_EDGE('',*,*,#53360,.F.) ;
#76494 = ORIENTED_EDGE('',*,*,#53359,.T.) ;
#76495 = ORIENTED_EDGE('',*,*,#51449,.F.) ;
#76496 = ORIENTED_EDGE('',*,*,#53361,.F.) ;
#76497 = ORIENTED_EDGE('',*,*,#51444,.F.) ;
#76498 = ORIENTED_EDGE('',*,*,#53360,.T.) ;
#76499 = ORIENTED_EDGE('',*,*,#51443,.F.) ;
#76500 = ORIENTED_EDGE('',*,*,#53362,.F.) ;
#76501 = ORIENTED_EDGE('',*,*,#51445,.F.) ;
#76502 = ORIENTED_EDGE('',*,*,#53358,.T.) ;
#76503 = ORIENTED_EDGE('',*,*,#51448,.F.) ;
#76504 = ORIENTED_EDGE('',*,*,#53363,.F.) ;
#76505 = ORIENTED_EDGE('',*,*,#51450,.F.) ;
#76506 = ORIENTED_EDGE('',*,*,#51454,.F.) ;
#76507 = ORIENTED_EDGE('',*,*,#53364,.T.) ;
#76508 = ORIENTED_EDGE('',*,*,#51253,.F.) ;
#76509 = ORIENTED_EDGE('',*,*,#53365,.F.) ;
#76510 = ORIENTED_EDGE('',*,*,#53361,.T.) ;
#76511 = ORIENTED_EDGE('',*,*,#53365,.T.) ;
#76512 = ORIENTED_EDGE('',*,*,#53366,.F.) ;
#76513 = ORIENTED_EDGE('',*,*,#53367,.F.) ;
#76514 = ORIENTED_EDGE('',*,*,#53362,.T.) ;
#76515 = ORIENTED_EDGE('',*,*,#53368,.F.) ;
#76516 = ORIENTED_EDGE('',*,*,#49612,.T.) ;
#76517 = ORIENTED_EDGE('',*,*,#53369,.F.) ;
#76518 = ORIENTED_EDGE('',*,*,#53363,.T.) ;
#76519 = ORIENTED_EDGE('',*,*,#53370,.F.) ;
#76520 = ORIENTED_EDGE('',*,*,#51453,.F.) ;
#76521 = ORIENTED_EDGE('',*,*,#53371,.T.) ;
#76522 = ORIENTED_EDGE('',*,*,#49439,.F.) ;
#76523 = ORIENTED_EDGE('',*,*,#53372,.T.) ;
#76524 = ORIENTED_EDGE('',*,*,#53366,.T.) ;
#76525 = ORIENTED_EDGE('',*,*,#51252,.F.) ;
#76526 = ORIENTED_EDGE('',*,*,#53373,.F.) ;
#76527 = ORIENTED_EDGE('',*,*,#51441,.F.) ;
#76528 = ORIENTED_EDGE('',*,*,#53368,.T.) ;
#76529 = ORIENTED_EDGE('',*,*,#51442,.F.) ;
#76530 = ORIENTED_EDGE('',*,*,#53374,.F.) ;
#76531 = ORIENTED_EDGE('',*,*,#49613,.F.) ;
#76532 = ORIENTED_EDGE('',*,*,#53367,.T.) ;
#76533 = ORIENTED_EDGE('',*,*,#49619,.F.) ;
#76534 = ORIENTED_EDGE('',*,*,#53375,.F.) ;
#76535 = ORIENTED_EDGE('',*,*,#51446,.F.) ;
#76536 = ORIENTED_EDGE('',*,*,#53370,.T.) ;
#76537 = ORIENTED_EDGE('',*,*,#51447,.F.) ;
#76538 = ORIENTED_EDGE('',*,*,#53376,.F.) ;
#76539 = ORIENTED_EDGE('',*,*,#51437,.F.) ;
#76540 = ORIENTED_EDGE('',*,*,#53369,.T.) ;
#76541 = ORIENTED_EDGE('',*,*,#51440,.F.) ;
#76542 = ORIENTED_EDGE('',*,*,#53377,.F.) ;
#76543 = ORIENTED_EDGE('',*,*,#51451,.F.) ;
#76544 = ORIENTED_EDGE('',*,*,#51263,.F.) ;
#76545 = ORIENTED_EDGE('',*,*,#53378,.T.) ;
#76546 = ORIENTED_EDGE('',*,*,#51452,.F.) ;
#76547 = ORIENTED_EDGE('',*,*,#53379,.F.) ;
#76548 = ORIENTED_EDGE('',*,*,#53373,.T.) ;
#76549 = ORIENTED_EDGE('',*,*,#51251,.T.) ;
#76550 = ORIENTED_EDGE('',*,*,#53380,.F.) ;
#76551 = ORIENTED_EDGE('',*,*,#53374,.T.) ;
#76552 = ORIENTED_EDGE('',*,*,#53375,.T.) ;
#76553 = ORIENTED_EDGE('',*,*,#49618,.T.) ;
#76554 = ORIENTED_EDGE('',*,*,#53381,.F.) ;
#76555 = ORIENTED_EDGE('',*,*,#53376,.T.) ;
#76556 = ORIENTED_EDGE('',*,*,#53379,.T.) ;
#76557 = ORIENTED_EDGE('',*,*,#53377,.T.) ;
#76558 = ORIENTED_EDGE('',*,*,#53382,.F.) ;
#76559 = ORIENTED_EDGE('',*,*,#51247,.F.) ;
#76560 = ORIENTED_EDGE('',*,*,#53383,.T.) ;
#76561 = ORIENTED_EDGE('',*,*,#51241,.F.) ;
#76562 = ORIENTED_EDGE('',*,*,#53384,.F.) ;
#76563 = ORIENTED_EDGE('',*,*,#53380,.T.) ;
#76564 = ORIENTED_EDGE('',*,*,#51250,.F.) ;
#76565 = ORIENTED_EDGE('',*,*,#53385,.F.) ;
#76566 = ORIENTED_EDGE('',*,*,#49614,.F.) ;
#76567 = ORIENTED_EDGE('',*,*,#53381,.T.) ;
#76568 = ORIENTED_EDGE('',*,*,#49617,.F.) ;
#76569 = ORIENTED_EDGE('',*,*,#53386,.F.) ;
#76570 = ORIENTED_EDGE('',*,*,#51438,.F.) ;
#76571 = ORIENTED_EDGE('',*,*,#53382,.T.) ;
#76572 = ORIENTED_EDGE('',*,*,#51439,.F.) ;
#76573 = ORIENTED_EDGE('',*,*,#53387,.F.) ;
#76574 = ORIENTED_EDGE('',*,*,#51264,.F.) ;
#76575 = ORIENTED_EDGE('',*,*,#53384,.T.) ;
#76576 = ORIENTED_EDGE('',*,*,#53254,.F.) ;
#76577 = ORIENTED_EDGE('',*,*,#53388,.F.) ;
#76578 = ORIENTED_EDGE('',*,*,#53389,.F.) ;
#76579 = ORIENTED_EDGE('',*,*,#53385,.T.) ;
#76580 = ORIENTED_EDGE('',*,*,#53390,.F.) ;
#76581 = ORIENTED_EDGE('',*,*,#53387,.T.) ;
#76582 = ORIENTED_EDGE('',*,*,#53386,.T.) ;
#76583 = ORIENTED_EDGE('',*,*,#53391,.F.) ;
#76584 = ORIENTED_EDGE('',*,*,#51265,.T.) ;
#76585 = ORIENTED_EDGE('',*,*,#53388,.T.) ;
#76586 = ORIENTED_EDGE('',*,*,#49691,.F.) ;
#76587 = ORIENTED_EDGE('',*,*,#53392,.F.) ;
#76588 = ORIENTED_EDGE('',*,*,#51248,.F.) ;
#76589 = ORIENTED_EDGE('',*,*,#53390,.T.) ;
#76590 = ORIENTED_EDGE('',*,*,#51249,.F.) ;
#76591 = ORIENTED_EDGE('',*,*,#53393,.F.) ;
#76592 = ORIENTED_EDGE('',*,*,#51255,.F.) ;
#76593 = ORIENTED_EDGE('',*,*,#53389,.T.) ;
#76594 = ORIENTED_EDGE('',*,*,#51258,.F.) ;
#76595 = ORIENTED_EDGE('',*,*,#53394,.F.) ;
#76596 = ORIENTED_EDGE('',*,*,#49615,.F.) ;
#76597 = ORIENTED_EDGE('',*,*,#53391,.T.) ;
#76598 = ORIENTED_EDGE('',*,*,#49616,.F.) ;
#76599 = ORIENTED_EDGE('',*,*,#53395,.F.) ;
#76600 = ORIENTED_EDGE('',*,*,#51266,.F.) ;
#76601 = ORIENTED_EDGE('',*,*,#53392,.T.) ;
#76602 = ORIENTED_EDGE('',*,*,#49690,.T.) ;
#76603 = ORIENTED_EDGE('',*,*,#53396,.F.) ;
#76604 = ORIENTED_EDGE('',*,*,#53393,.T.) ;
#76605 = ORIENTED_EDGE('',*,*,#53395,.T.) ;
#76606 = ORIENTED_EDGE('',*,*,#53394,.T.) ;
#76607 = ORIENTED_EDGE('',*,*,#53397,.F.) ;
#76608 = ORIENTED_EDGE('',*,*,#53396,.T.) ;
#76609 = ORIENTED_EDGE('',*,*,#49689,.F.) ;
#76610 = ORIENTED_EDGE('',*,*,#53398,.F.) ;
#76611 = ORIENTED_EDGE('',*,*,#51256,.F.) ;
#76612 = ORIENTED_EDGE('',*,*,#53397,.T.) ;
#76613 = ORIENTED_EDGE('',*,*,#51257,.F.) ;
#76614 = ORIENTED_EDGE('',*,*,#53399,.F.) ;
#76615 = ORIENTED_EDGE('',*,*,#51267,.F.) ;
#76616 = ORIENTED_EDGE('',*,*,#51271,.F.) ;
#76617 = ORIENTED_EDGE('',*,*,#53400,.T.) ;
#76618 = ORIENTED_EDGE('',*,*,#51259,.F.) ;
#76619 = ORIENTED_EDGE('',*,*,#53401,.F.) ;
#76620 = ORIENTED_EDGE('',*,*,#49686,.F.) ;
#76621 = ORIENTED_EDGE('',*,*,#53402,.T.) ;
#76622 = ORIENTED_EDGE('',*,*,#51272,.F.) ;
#76623 = ORIENTED_EDGE('',*,*,#53403,.F.) ;
#76624 = ORIENTED_EDGE('',*,*,#53398,.T.) ;
#76625 = ORIENTED_EDGE('',*,*,#49688,.T.) ;
#76626 = ORIENTED_EDGE('',*,*,#53404,.F.) ;
#76627 = ORIENTED_EDGE('',*,*,#53399,.T.) ;
#76628 = ORIENTED_EDGE('',*,*,#53403,.T.) ;
#76629 = ORIENTED_EDGE('',*,*,#53401,.T.) ;
#76630 = ORIENTED_EDGE('',*,*,#53405,.F.) ;
#76631 = ORIENTED_EDGE('',*,*,#53404,.T.) ;
#76632 = ORIENTED_EDGE('',*,*,#49687,.F.) ;
#76633 = ORIENTED_EDGE('',*,*,#53405,.T.) ;
#76634 = ORIENTED_EDGE('',*,*,#51268,.F.) ;
#76635 = ORIENTED_EDGE('',*,*,#52294,.F.) ;
#76636 = ORIENTED_EDGE('',*,*,#52305,.F.) ;
#76637 = ORIENTED_EDGE('',*,*,#52304,.F.) ;
#76638 = ORIENTED_EDGE('',*,*,#53406,.F.) ;
#76639 = ORIENTED_EDGE('',*,*,#52295,.F.) ;
#76640 = ORIENTED_EDGE('',*,*,#53406,.T.) ;
#76641 = ORIENTED_EDGE('',*,*,#50728,.F.) ;
#76642 = ORIENTED_EDGE('',*,*,#53407,.F.) ;
#76643 = ORIENTED_EDGE('',*,*,#50714,.F.) ;
#76644 = ORIENTED_EDGE('',*,*,#52302,.F.) ;
#76645 = ORIENTED_EDGE('',*,*,#52301,.F.) ;
#76646 = ORIENTED_EDGE('',*,*,#52300,.F.) ;
#76647 = ORIENTED_EDGE('',*,*,#53408,.F.) ;
#76648 = ORIENTED_EDGE('',*,*,#52303,.F.) ;
#76649 = ORIENTED_EDGE('',*,*,#53409,.F.) ;
#76650 = ORIENTED_EDGE('',*,*,#53407,.T.) ;
#76651 = ORIENTED_EDGE('',*,*,#53410,.F.) ;
#76652 = ORIENTED_EDGE('',*,*,#52292,.F.) ;
#76653 = ORIENTED_EDGE('',*,*,#52297,.F.) ;
#76654 = ORIENTED_EDGE('',*,*,#52296,.F.) ;
#76655 = ORIENTED_EDGE('',*,*,#53411,.F.) ;
#76656 = ORIENTED_EDGE('',*,*,#52293,.F.) ;
#76657 = ORIENTED_EDGE('',*,*,#53408,.T.) ;
#76658 = ORIENTED_EDGE('',*,*,#50724,.F.) ;
#76659 = ORIENTED_EDGE('',*,*,#53412,.F.) ;
#76660 = ORIENTED_EDGE('',*,*,#50726,.F.) ;
#76661 = ORIENTED_EDGE('',*,*,#53410,.T.) ;
#76662 = ORIENTED_EDGE('',*,*,#50727,.F.) ;
#76663 = ORIENTED_EDGE('',*,*,#53413,.F.) ;
#76664 = ORIENTED_EDGE('',*,*,#50972,.F.) ;
#76665 = ORIENTED_EDGE('',*,*,#53409,.T.) ;
#76666 = ORIENTED_EDGE('',*,*,#50971,.F.) ;
#76667 = ORIENTED_EDGE('',*,*,#53414,.F.) ;
#76668 = ORIENTED_EDGE('',*,*,#50715,.F.) ;
#76669 = ORIENTED_EDGE('',*,*,#53411,.T.) ;
#76670 = ORIENTED_EDGE('',*,*,#50716,.F.) ;
#76671 = ORIENTED_EDGE('',*,*,#53415,.F.) ;
#76672 = ORIENTED_EDGE('',*,*,#50720,.F.) ;
#76673 = ORIENTED_EDGE('',*,*,#53413,.T.) ;
#76674 = ORIENTED_EDGE('',*,*,#53412,.T.) ;
#76675 = ORIENTED_EDGE('',*,*,#53416,.F.) ;
#76676 = ORIENTED_EDGE('',*,*,#53415,.T.) ;
#76677 = ORIENTED_EDGE('',*,*,#53414,.T.) ;
#76678 = ORIENTED_EDGE('',*,*,#53417,.F.) ;
#76679 = ORIENTED_EDGE('',*,*,#53416,.T.) ;
#76680 = ORIENTED_EDGE('',*,*,#50723,.F.) ;
#76681 = ORIENTED_EDGE('',*,*,#53418,.F.) ;
#76682 = ORIENTED_EDGE('',*,*,#50969,.F.) ;
#76683 = ORIENTED_EDGE('',*,*,#53417,.T.) ;
#76684 = ORIENTED_EDGE('',*,*,#50970,.F.) ;
#76685 = ORIENTED_EDGE('',*,*,#53419,.F.) ;
#76686 = ORIENTED_EDGE('',*,*,#50717,.F.) ;
#76687 = ORIENTED_EDGE('',*,*,#53419,.T.) ;
#76688 = ORIENTED_EDGE('',*,*,#53418,.T.) ;
#76689 = ORIENTED_EDGE('',*,*,#53420,.F.) ;
#76690 = ORIENTED_EDGE('',*,*,#53420,.T.) ;
#76691 = ORIENTED_EDGE('',*,*,#50722,.F.) ;
#76692 = ORIENTED_EDGE('',*,*,#53421,.F.) ;
#76693 = ORIENTED_EDGE('',*,*,#50718,.F.) ;
#76694 = ORIENTED_EDGE('',*,*,#52298,.F.) ;
#76695 = ORIENTED_EDGE('',*,*,#52291,.F.) ;
#76696 = ORIENTED_EDGE('',*,*,#52290,.F.) ;
#76697 = ORIENTED_EDGE('',*,*,#53421,.T.) ;
#76698 = ORIENTED_EDGE('',*,*,#52299,.F.) ;
#76699 = ORIENTED_EDGE('',*,*,#52531,.F.) ;
#76700 = ORIENTED_EDGE('',*,*,#52530,.F.) ;
#76701 = ORIENTED_EDGE('',*,*,#52529,.F.) ;
#76702 = ORIENTED_EDGE('',*,*,#53422,.F.) ;
#76703 = ORIENTED_EDGE('',*,*,#52532,.F.) ;
#76704 = ORIENTED_EDGE('',*,*,#53422,.T.) ;
#76705 = ORIENTED_EDGE('',*,*,#52528,.F.) ;
#76706 = ORIENTED_EDGE('',*,*,#53423,.F.) ;
#76707 = ORIENTED_EDGE('',*,*,#50600,.F.) ;
#76708 = ORIENTED_EDGE('',*,*,#53423,.T.) ;
#76709 = ORIENTED_EDGE('',*,*,#50426,.F.) ;
#76710 = ORIENTED_EDGE('',*,*,#53424,.F.) ;
#76711 = ORIENTED_EDGE('',*,*,#50601,.F.) ;
#76712 = ORIENTED_EDGE('',*,*,#50414,.F.) ;
#76713 = ORIENTED_EDGE('',*,*,#50602,.F.) ;
#76714 = ORIENTED_EDGE('',*,*,#53425,.F.) ;
#76715 = ORIENTED_EDGE('',*,*,#50420,.F.) ;
#76716 = ORIENTED_EDGE('',*,*,#53425,.T.) ;
#76717 = ORIENTED_EDGE('',*,*,#53424,.T.) ;
#76718 = ORIENTED_EDGE('',*,*,#53426,.F.) ;
#76719 = ORIENTED_EDGE('',*,*,#53426,.T.) ;
#76720 = ORIENTED_EDGE('',*,*,#50425,.F.) ;
#76721 = ORIENTED_EDGE('',*,*,#53427,.F.) ;
#76722 = ORIENTED_EDGE('',*,*,#50421,.F.) ;
#76723 = ORIENTED_EDGE('',*,*,#50416,.F.) ;
#76724 = ORIENTED_EDGE('',*,*,#50422,.F.) ;
#76725 = ORIENTED_EDGE('',*,*,#53428,.F.) ;
#76726 = ORIENTED_EDGE('',*,*,#50664,.F.) ;
#76727 = ORIENTED_EDGE('',*,*,#53428,.T.) ;
#76728 = ORIENTED_EDGE('',*,*,#53427,.T.) ;
#76729 = ORIENTED_EDGE('',*,*,#53429,.F.) ;
#76730 = ORIENTED_EDGE('',*,*,#53429,.T.) ;
#76731 = ORIENTED_EDGE('',*,*,#50424,.F.) ;
#76732 = ORIENTED_EDGE('',*,*,#53430,.F.) ;
#76733 = ORIENTED_EDGE('',*,*,#50665,.F.) ;
#76734 = ORIENTED_EDGE('',*,*,#53430,.T.) ;
#76735 = ORIENTED_EDGE('',*,*,#52527,.F.) ;
#76736 = ORIENTED_EDGE('',*,*,#53431,.F.) ;
#76737 = ORIENTED_EDGE('',*,*,#50666,.F.) ;
#76738 = ORIENTED_EDGE('',*,*,#53431,.T.) ;
#76739 = ORIENTED_EDGE('',*,*,#52526,.F.) ;
#76740 = ORIENTED_EDGE('',*,*,#52535,.F.) ;
#76741 = ORIENTED_EDGE('',*,*,#52536,.F.) ;
#76742 = ORIENTED_EDGE('',*,*,#52541,.F.) ;
#76743 = ORIENTED_EDGE('',*,*,#53432,.F.) ;
#76744 = ORIENTED_EDGE('',*,*,#53432,.T.) ;
#76745 = ORIENTED_EDGE('',*,*,#52540,.F.) ;
#76746 = ORIENTED_EDGE('',*,*,#53433,.F.) ;
#76747 = ORIENTED_EDGE('',*,*,#50661,.F.) ;
#76748 = ORIENTED_EDGE('',*,*,#53433,.T.) ;
#76749 = ORIENTED_EDGE('',*,*,#50408,.F.) ;
#76750 = ORIENTED_EDGE('',*,*,#53434,.F.) ;
#76751 = ORIENTED_EDGE('',*,*,#50662,.F.) ;
#76752 = ORIENTED_EDGE('',*,*,#50418,.F.) ;
#76753 = ORIENTED_EDGE('',*,*,#50663,.F.) ;
#76754 = ORIENTED_EDGE('',*,*,#53435,.F.) ;
#76755 = ORIENTED_EDGE('',*,*,#50412,.F.) ;
#76756 = ORIENTED_EDGE('',*,*,#53435,.T.) ;
#76757 = ORIENTED_EDGE('',*,*,#53434,.T.) ;
#76758 = ORIENTED_EDGE('',*,*,#53436,.F.) ;
#76759 = ORIENTED_EDGE('',*,*,#53436,.T.) ;
#76760 = ORIENTED_EDGE('',*,*,#50407,.F.) ;
#76761 = ORIENTED_EDGE('',*,*,#53437,.F.) ;
#76762 = ORIENTED_EDGE('',*,*,#50409,.F.) ;
#76763 = ORIENTED_EDGE('',*,*,#50419,.F.) ;
#76764 = ORIENTED_EDGE('',*,*,#50410,.F.) ;
#76765 = ORIENTED_EDGE('',*,*,#53438,.F.) ;
#76766 = ORIENTED_EDGE('',*,*,#50603,.F.) ;
#76767 = ORIENTED_EDGE('',*,*,#53438,.T.) ;
#76768 = ORIENTED_EDGE('',*,*,#53437,.T.) ;
#76769 = ORIENTED_EDGE('',*,*,#53439,.F.) ;
#76770 = ORIENTED_EDGE('',*,*,#53439,.T.) ;
#76771 = ORIENTED_EDGE('',*,*,#50406,.F.) ;
#76772 = ORIENTED_EDGE('',*,*,#53440,.F.) ;
#76773 = ORIENTED_EDGE('',*,*,#50604,.F.) ;
#76774 = ORIENTED_EDGE('',*,*,#53440,.T.) ;
#76775 = ORIENTED_EDGE('',*,*,#52539,.F.) ;
#76776 = ORIENTED_EDGE('',*,*,#53441,.F.) ;
#76777 = ORIENTED_EDGE('',*,*,#50605,.F.) ;
#76778 = ORIENTED_EDGE('',*,*,#52537,.F.) ;
#76779 = ORIENTED_EDGE('',*,*,#52534,.F.) ;
#76780 = ORIENTED_EDGE('',*,*,#52533,.F.) ;
#76781 = ORIENTED_EDGE('',*,*,#53441,.T.) ;
#76782 = ORIENTED_EDGE('',*,*,#52538,.F.) ;
#76783 = ORIENTED_EDGE('',*,*,#53442,.F.) ;
#76784 = ORIENTED_EDGE('',*,*,#49448,.F.) ;
#76785 = ORIENTED_EDGE('',*,*,#53443,.F.) ;
#76786 = ORIENTED_EDGE('',*,*,#52125,.F.) ;
#76787 = ORIENTED_EDGE('',*,*,#53443,.T.) ;
#76788 = ORIENTED_EDGE('',*,*,#49447,.F.) ;
#76789 = ORIENTED_EDGE('',*,*,#53444,.F.) ;
#76790 = ORIENTED_EDGE('',*,*,#52128,.F.) ;
#76791 = ORIENTED_EDGE('',*,*,#53442,.T.) ;
#76792 = ORIENTED_EDGE('',*,*,#52122,.F.) ;
#76793 = ORIENTED_EDGE('',*,*,#53445,.F.) ;
#76794 = ORIENTED_EDGE('',*,*,#49449,.F.) ;
#76795 = ORIENTED_EDGE('',*,*,#53444,.T.) ;
#76796 = ORIENTED_EDGE('',*,*,#49446,.F.) ;
#76797 = ORIENTED_EDGE('',*,*,#53446,.F.) ;
#76798 = ORIENTED_EDGE('',*,*,#52131,.F.) ;
#76799 = ORIENTED_EDGE('',*,*,#53445,.T.) ;
#76800 = ORIENTED_EDGE('',*,*,#52119,.F.) ;
#76801 = ORIENTED_EDGE('',*,*,#53447,.F.) ;
#76802 = ORIENTED_EDGE('',*,*,#49450,.F.) ;
#76803 = ORIENTED_EDGE('',*,*,#53446,.T.) ;
#76804 = ORIENTED_EDGE('',*,*,#49445,.F.) ;
#76805 = ORIENTED_EDGE('',*,*,#53448,.F.) ;
#76806 = ORIENTED_EDGE('',*,*,#52134,.F.) ;
#76807 = ORIENTED_EDGE('',*,*,#53447,.T.) ;
#76808 = ORIENTED_EDGE('',*,*,#52141,.F.) ;
#76809 = ORIENTED_EDGE('',*,*,#53449,.F.) ;
#76810 = ORIENTED_EDGE('',*,*,#49443,.F.) ;
#76811 = ORIENTED_EDGE('',*,*,#53448,.T.) ;
#76812 = ORIENTED_EDGE('',*,*,#49444,.F.) ;
#76813 = ORIENTED_EDGE('',*,*,#53449,.T.) ;
#76814 = ORIENTED_EDGE('',*,*,#52137,.F.) ;
#76815 = ORIENTED_EDGE('',*,*,#50978,.F.) ;
#76816 = ORIENTED_EDGE('',*,*,#50992,.F.) ;
#76817 = ORIENTED_EDGE('',*,*,#53450,.F.) ;
#76818 = ORIENTED_EDGE('',*,*,#50981,.F.) ;
#76819 = ORIENTED_EDGE('',*,*,#53451,.F.) ;
#76820 = ORIENTED_EDGE('',*,*,#50982,.F.) ;
#76821 = ORIENTED_EDGE('',*,*,#53452,.F.) ;
#76822 = ORIENTED_EDGE('',*,*,#51068,.F.) ;
#76823 = ORIENTED_EDGE('',*,*,#50980,.F.) ;
#76824 = ORIENTED_EDGE('',*,*,#50983,.F.) ;
#76825 = ORIENTED_EDGE('',*,*,#53453,.F.) ;
#76826 = ORIENTED_EDGE('',*,*,#50984,.F.) ;
#76827 = ORIENTED_EDGE('',*,*,#53452,.T.) ;
#76828 = ORIENTED_EDGE('',*,*,#53450,.T.) ;
#76829 = ORIENTED_EDGE('',*,*,#53454,.F.) ;
#76830 = ORIENTED_EDGE('',*,*,#53453,.T.) ;
#76831 = ORIENTED_EDGE('',*,*,#53451,.T.) ;
#76832 = ORIENTED_EDGE('',*,*,#53455,.F.) ;
#76833 = ORIENTED_EDGE('',*,*,#50976,.F.) ;
#76834 = ORIENTED_EDGE('',*,*,#50988,.F.) ;
#76835 = ORIENTED_EDGE('',*,*,#53456,.F.) ;
#76836 = ORIENTED_EDGE('',*,*,#50990,.F.) ;
#76837 = ORIENTED_EDGE('',*,*,#53454,.T.) ;
#76838 = ORIENTED_EDGE('',*,*,#50991,.F.) ;
#76839 = ORIENTED_EDGE('',*,*,#53457,.F.) ;
#76840 = ORIENTED_EDGE('',*,*,#51065,.F.) ;
#76841 = ORIENTED_EDGE('',*,*,#53455,.T.) ;
#76842 = ORIENTED_EDGE('',*,*,#51067,.F.) ;
#76843 = ORIENTED_EDGE('',*,*,#53458,.F.) ;
#76844 = ORIENTED_EDGE('',*,*,#50985,.F.) ;
#76845 = ORIENTED_EDGE('',*,*,#50974,.F.) ;
#76846 = ORIENTED_EDGE('',*,*,#50986,.F.) ;
#76847 = ORIENTED_EDGE('',*,*,#53459,.F.) ;
#76848 = ORIENTED_EDGE('',*,*,#50989,.F.) ;
#76849 = ORIENTED_EDGE('',*,*,#53457,.T.) ;
#76850 = ORIENTED_EDGE('',*,*,#53456,.T.) ;
#76851 = ORIENTED_EDGE('',*,*,#53460,.F.) ;
#76852 = ORIENTED_EDGE('',*,*,#53459,.T.) ;
#76853 = ORIENTED_EDGE('',*,*,#53458,.T.) ;
#76854 = ORIENTED_EDGE('',*,*,#53461,.F.) ;
#76855 = ORIENTED_EDGE('',*,*,#53460,.T.) ;
#76856 = ORIENTED_EDGE('',*,*,#50987,.F.) ;
#76857 = ORIENTED_EDGE('',*,*,#53461,.T.) ;
#76858 = ORIENTED_EDGE('',*,*,#51066,.F.) ;
#76859 = ORIENTED_EDGE('',*,*,#53462,.F.) ;
#76860 = ORIENTED_EDGE('',*,*,#49404,.F.) ;
#76861 = ORIENTED_EDGE('',*,*,#53463,.F.) ;
#76862 = ORIENTED_EDGE('',*,*,#51537,.F.) ;
#76863 = ORIENTED_EDGE('',*,*,#53463,.T.) ;
#76864 = ORIENTED_EDGE('',*,*,#49403,.T.) ;
#76865 = ORIENTED_EDGE('',*,*,#53464,.F.) ;
#76866 = ORIENTED_EDGE('',*,*,#53465,.F.) ;
#76867 = ORIENTED_EDGE('',*,*,#49405,.T.) ;
#76868 = ORIENTED_EDGE('',*,*,#53462,.T.) ;
#76869 = ORIENTED_EDGE('',*,*,#53466,.F.) ;
#76870 = ORIENTED_EDGE('',*,*,#53467,.F.) ;
#76871 = ORIENTED_EDGE('',*,*,#53464,.T.) ;
#76872 = ORIENTED_EDGE('',*,*,#49402,.F.) ;
#76873 = ORIENTED_EDGE('',*,*,#53468,.F.) ;
#76874 = ORIENTED_EDGE('',*,*,#51534,.F.) ;
#76875 = ORIENTED_EDGE('',*,*,#53465,.T.) ;
#76876 = ORIENTED_EDGE('',*,*,#51533,.F.) ;
#76877 = ORIENTED_EDGE('',*,*,#53469,.F.) ;
#76878 = ORIENTED_EDGE('',*,*,#51538,.F.) ;
#76879 = ORIENTED_EDGE('',*,*,#53470,.F.) ;
#76880 = ORIENTED_EDGE('',*,*,#51535,.F.) ;
#76881 = ORIENTED_EDGE('',*,*,#53471,.F.) ;
#76882 = ORIENTED_EDGE('',*,*,#51782,.F.) ;
#76883 = ORIENTED_EDGE('',*,*,#53466,.T.) ;
#76884 = ORIENTED_EDGE('',*,*,#51536,.F.) ;
#76885 = ORIENTED_EDGE('',*,*,#53472,.F.) ;
#76886 = ORIENTED_EDGE('',*,*,#51526,.F.) ;
#76887 = ORIENTED_EDGE('',*,*,#53467,.T.) ;
#76888 = ORIENTED_EDGE('',*,*,#51525,.F.) ;
#76889 = ORIENTED_EDGE('',*,*,#53473,.F.) ;
#76890 = ORIENTED_EDGE('',*,*,#49406,.F.) ;
#76891 = ORIENTED_EDGE('',*,*,#53474,.F.) ;
#76892 = ORIENTED_EDGE('',*,*,#49400,.F.) ;
#76893 = ORIENTED_EDGE('',*,*,#53475,.F.) ;
#76894 = ORIENTED_EDGE('',*,*,#51527,.F.) ;
#76895 = ORIENTED_EDGE('',*,*,#49401,.T.) ;
#76896 = ORIENTED_EDGE('',*,*,#53474,.T.) ;
#76897 = ORIENTED_EDGE('',*,*,#53476,.F.) ;
#76898 = ORIENTED_EDGE('',*,*,#53468,.T.) ;
#76899 = ORIENTED_EDGE('',*,*,#53471,.T.) ;
#76900 = ORIENTED_EDGE('',*,*,#53469,.T.) ;
#76901 = ORIENTED_EDGE('',*,*,#53477,.F.) ;
#76902 = ORIENTED_EDGE('',*,*,#53472,.T.) ;
#76903 = ORIENTED_EDGE('',*,*,#53470,.T.) ;
#76904 = ORIENTED_EDGE('',*,*,#53478,.F.) ;
#76905 = ORIENTED_EDGE('',*,*,#49399,.T.) ;
#76906 = ORIENTED_EDGE('',*,*,#53473,.T.) ;
#76907 = ORIENTED_EDGE('',*,*,#53479,.F.) ;
#76908 = ORIENTED_EDGE('',*,*,#53475,.T.) ;
#76909 = ORIENTED_EDGE('',*,*,#53476,.T.) ;
#76910 = ORIENTED_EDGE('',*,*,#51530,.F.) ;
#76911 = ORIENTED_EDGE('',*,*,#53480,.F.) ;
#76912 = ORIENTED_EDGE('',*,*,#51531,.F.) ;
#76913 = ORIENTED_EDGE('',*,*,#53477,.T.) ;
#76914 = ORIENTED_EDGE('',*,*,#51532,.F.) ;
#76915 = ORIENTED_EDGE('',*,*,#53481,.F.) ;
#76916 = ORIENTED_EDGE('',*,*,#51779,.F.) ;
#76917 = ORIENTED_EDGE('',*,*,#53478,.T.) ;
#76918 = ORIENTED_EDGE('',*,*,#51781,.F.) ;
#76919 = ORIENTED_EDGE('',*,*,#53482,.F.) ;
#76920 = ORIENTED_EDGE('',*,*,#51523,.F.) ;
#76921 = ORIENTED_EDGE('',*,*,#53479,.T.) ;
#76922 = ORIENTED_EDGE('',*,*,#51524,.F.) ;
#76923 = ORIENTED_EDGE('',*,*,#53483,.F.) ;
#76924 = ORIENTED_EDGE('',*,*,#51528,.F.) ;
#76925 = ORIENTED_EDGE('',*,*,#53481,.T.) ;
#76926 = ORIENTED_EDGE('',*,*,#53480,.T.) ;
#76927 = ORIENTED_EDGE('',*,*,#53484,.F.) ;
#76928 = ORIENTED_EDGE('',*,*,#53483,.T.) ;
#76929 = ORIENTED_EDGE('',*,*,#53482,.T.) ;
#76930 = ORIENTED_EDGE('',*,*,#53485,.F.) ;
#76931 = ORIENTED_EDGE('',*,*,#53484,.T.) ;
#76932 = ORIENTED_EDGE('',*,*,#51529,.F.) ;
#76933 = ORIENTED_EDGE('',*,*,#53485,.T.) ;
#76934 = ORIENTED_EDGE('',*,*,#51780,.F.) ;
#76935 = ORIENTED_EDGE('',*,*,#51788,.F.) ;
#76936 = ORIENTED_EDGE('',*,*,#51801,.F.) ;
#76937 = ORIENTED_EDGE('',*,*,#53486,.F.) ;
#76938 = ORIENTED_EDGE('',*,*,#51793,.F.) ;
#76939 = ORIENTED_EDGE('',*,*,#53487,.F.) ;
#76940 = ORIENTED_EDGE('',*,*,#51791,.F.) ;
#76941 = ORIENTED_EDGE('',*,*,#53488,.F.) ;
#76942 = ORIENTED_EDGE('',*,*,#51878,.F.) ;
#76943 = ORIENTED_EDGE('',*,*,#51790,.F.) ;
#76944 = ORIENTED_EDGE('',*,*,#51792,.F.) ;
#76945 = ORIENTED_EDGE('',*,*,#53489,.F.) ;
#76946 = ORIENTED_EDGE('',*,*,#51796,.F.) ;
#76947 = ORIENTED_EDGE('',*,*,#53488,.T.) ;
#76948 = ORIENTED_EDGE('',*,*,#53486,.T.) ;
#76949 = ORIENTED_EDGE('',*,*,#53490,.F.) ;
#76950 = ORIENTED_EDGE('',*,*,#53489,.T.) ;
#76951 = ORIENTED_EDGE('',*,*,#53487,.T.) ;
#76952 = ORIENTED_EDGE('',*,*,#53491,.F.) ;
#76953 = ORIENTED_EDGE('',*,*,#51786,.F.) ;
#76954 = ORIENTED_EDGE('',*,*,#51799,.F.) ;
#76955 = ORIENTED_EDGE('',*,*,#53492,.F.) ;
#76956 = ORIENTED_EDGE('',*,*,#51802,.F.) ;
#76957 = ORIENTED_EDGE('',*,*,#53490,.T.) ;
#76958 = ORIENTED_EDGE('',*,*,#51800,.F.) ;
#76959 = ORIENTED_EDGE('',*,*,#53493,.F.) ;
#76960 = ORIENTED_EDGE('',*,*,#51875,.F.) ;
#76961 = ORIENTED_EDGE('',*,*,#53491,.T.) ;
#76962 = ORIENTED_EDGE('',*,*,#51877,.F.) ;
#76963 = ORIENTED_EDGE('',*,*,#53494,.F.) ;
#76964 = ORIENTED_EDGE('',*,*,#51794,.F.) ;
#76965 = ORIENTED_EDGE('',*,*,#51784,.F.) ;
#76966 = ORIENTED_EDGE('',*,*,#51795,.F.) ;
#76967 = ORIENTED_EDGE('',*,*,#53495,.F.) ;
#76968 = ORIENTED_EDGE('',*,*,#51797,.F.) ;
#76969 = ORIENTED_EDGE('',*,*,#53493,.T.) ;
#76970 = ORIENTED_EDGE('',*,*,#53492,.T.) ;
#76971 = ORIENTED_EDGE('',*,*,#53496,.F.) ;
#76972 = ORIENTED_EDGE('',*,*,#53495,.T.) ;
#76973 = ORIENTED_EDGE('',*,*,#53494,.T.) ;
#76974 = ORIENTED_EDGE('',*,*,#53497,.F.) ;
#76975 = ORIENTED_EDGE('',*,*,#53496,.T.) ;
#76976 = ORIENTED_EDGE('',*,*,#51798,.F.) ;
#76977 = ORIENTED_EDGE('',*,*,#53497,.T.) ;
#76978 = ORIENTED_EDGE('',*,*,#51876,.F.) ;
#76979 = ORIENTED_EDGE('',*,*,#53498,.F.) ;
#76980 = ORIENTED_EDGE('',*,*,#52130,.F.) ;
#76981 = ORIENTED_EDGE('',*,*,#53499,.F.) ;
#76982 = ORIENTED_EDGE('',*,*,#52145,.F.) ;
#76983 = ORIENTED_EDGE('',*,*,#53499,.T.) ;
#76984 = ORIENTED_EDGE('',*,*,#52133,.F.) ;
#76985 = ORIENTED_EDGE('',*,*,#53500,.F.) ;
#76986 = ORIENTED_EDGE('',*,*,#52127,.F.) ;
#76987 = ORIENTED_EDGE('',*,*,#53498,.T.) ;
#76988 = ORIENTED_EDGE('',*,*,#53501,.F.) ;
#76989 = ORIENTED_EDGE('',*,*,#53500,.T.) ;
#76990 = ORIENTED_EDGE('',*,*,#52136,.F.) ;
#76991 = ORIENTED_EDGE('',*,*,#53502,.F.) ;
#76992 = ORIENTED_EDGE('',*,*,#52142,.F.) ;
#76993 = ORIENTED_EDGE('',*,*,#53501,.T.) ;
#76994 = ORIENTED_EDGE('',*,*,#52144,.F.) ;
#76995 = ORIENTED_EDGE('',*,*,#53503,.F.) ;
#76996 = ORIENTED_EDGE('',*,*,#52124,.F.) ;
#76997 = ORIENTED_EDGE('',*,*,#53502,.T.) ;
#76998 = ORIENTED_EDGE('',*,*,#52139,.F.) ;
#76999 = ORIENTED_EDGE('',*,*,#53504,.F.) ;
#77000 = ORIENTED_EDGE('',*,*,#52121,.F.) ;
#77001 = ORIENTED_EDGE('',*,*,#53503,.T.) ;
#77002 = ORIENTED_EDGE('',*,*,#53505,.F.) ;
#77003 = ORIENTED_EDGE('',*,*,#53504,.T.) ;
#77004 = ORIENTED_EDGE('',*,*,#52140,.F.) ;
#77005 = ORIENTED_EDGE('',*,*,#53505,.T.) ;
#77006 = ORIENTED_EDGE('',*,*,#52143,.F.) ;
#77007 = ORIENTED_EDGE('',*,*,#49196,.F.) ;
#77008 = ORIENTED_EDGE('',*,*,#51889,.F.) ;
#77009 = ORIENTED_EDGE('',*,*,#49210,.F.) ;
#77010 = ORIENTED_EDGE('',*,*,#51932,.F.) ;
#77011 = ORIENTED_EDGE('',*,*,#49198,.F.) ;
#77012 = ORIENTED_EDGE('',*,*,#51933,.F.) ;
#77013 = ORIENTED_EDGE('',*,*,#49208,.F.) ;
#77014 = ORIENTED_EDGE('',*,*,#51936,.F.) ;
#77015 = ORIENTED_EDGE('',*,*,#49206,.F.) ;
#77016 = ORIENTED_EDGE('',*,*,#51934,.F.) ;
#77017 = ORIENTED_EDGE('',*,*,#49200,.F.) ;
#77018 = ORIENTED_EDGE('',*,*,#51937,.F.) ;
#77019 = ORIENTED_EDGE('',*,*,#49204,.F.) ;
#77020 = ORIENTED_EDGE('',*,*,#49525,.F.) ;
#77021 = ORIENTED_EDGE('',*,*,#49202,.F.) ;
#77022 = ORIENTED_EDGE('',*,*,#51935,.F.) ;
#77023 = ORIENTED_EDGE('',*,*,#53506,.F.) ;
#77024 = ORIENTED_EDGE('',*,*,#53507,.F.) ;
#77025 = ORIENTED_EDGE('',*,*,#53508,.F.) ;
#77026 = ORIENTED_EDGE('',*,*,#53507,.T.) ;
#77027 = ORIENTED_EDGE('',*,*,#51467,.F.) ;
#77028 = ORIENTED_EDGE('',*,*,#53509,.F.) ;
#77029 = ORIENTED_EDGE('',*,*,#51462,.F.) ;
#77030 = ORIENTED_EDGE('',*,*,#53508,.T.) ;
#77031 = ORIENTED_EDGE('',*,*,#51461,.F.) ;
#77032 = ORIENTED_EDGE('',*,*,#53510,.F.) ;
#77033 = ORIENTED_EDGE('',*,*,#51463,.F.) ;
#77034 = ORIENTED_EDGE('',*,*,#53506,.T.) ;
#77035 = ORIENTED_EDGE('',*,*,#51466,.F.) ;
#77036 = ORIENTED_EDGE('',*,*,#53511,.F.) ;
#77037 = ORIENTED_EDGE('',*,*,#51468,.F.) ;
#77038 = ORIENTED_EDGE('',*,*,#51472,.F.) ;
#77039 = ORIENTED_EDGE('',*,*,#53512,.T.) ;
#77040 = ORIENTED_EDGE('',*,*,#51281,.F.) ;
#77041 = ORIENTED_EDGE('',*,*,#53513,.F.) ;
#77042 = ORIENTED_EDGE('',*,*,#53509,.T.) ;
#77043 = ORIENTED_EDGE('',*,*,#53513,.T.) ;
#77044 = ORIENTED_EDGE('',*,*,#53514,.F.) ;
#77045 = ORIENTED_EDGE('',*,*,#53515,.F.) ;
#77046 = ORIENTED_EDGE('',*,*,#53510,.T.) ;
#77047 = ORIENTED_EDGE('',*,*,#53516,.F.) ;
#77048 = ORIENTED_EDGE('',*,*,#49604,.T.) ;
#77049 = ORIENTED_EDGE('',*,*,#53517,.F.) ;
#77050 = ORIENTED_EDGE('',*,*,#53511,.T.) ;
#77051 = ORIENTED_EDGE('',*,*,#53518,.F.) ;
#77052 = ORIENTED_EDGE('',*,*,#51471,.F.) ;
#77053 = ORIENTED_EDGE('',*,*,#53519,.T.) ;
#77054 = ORIENTED_EDGE('',*,*,#49427,.F.) ;
#77055 = ORIENTED_EDGE('',*,*,#53520,.T.) ;
#77056 = ORIENTED_EDGE('',*,*,#53514,.T.) ;
#77057 = ORIENTED_EDGE('',*,*,#51280,.F.) ;
#77058 = ORIENTED_EDGE('',*,*,#53521,.F.) ;
#77059 = ORIENTED_EDGE('',*,*,#51459,.F.) ;
#77060 = ORIENTED_EDGE('',*,*,#53516,.T.) ;
#77061 = ORIENTED_EDGE('',*,*,#51460,.F.) ;
#77062 = ORIENTED_EDGE('',*,*,#53522,.F.) ;
#77063 = ORIENTED_EDGE('',*,*,#49605,.F.) ;
#77064 = ORIENTED_EDGE('',*,*,#53515,.T.) ;
#77065 = ORIENTED_EDGE('',*,*,#49611,.F.) ;
#77066 = ORIENTED_EDGE('',*,*,#53523,.F.) ;
#77067 = ORIENTED_EDGE('',*,*,#51464,.F.) ;
#77068 = ORIENTED_EDGE('',*,*,#53518,.T.) ;
#77069 = ORIENTED_EDGE('',*,*,#51465,.F.) ;
#77070 = ORIENTED_EDGE('',*,*,#53524,.F.) ;
#77071 = ORIENTED_EDGE('',*,*,#51455,.F.) ;
#77072 = ORIENTED_EDGE('',*,*,#53517,.T.) ;
#77073 = ORIENTED_EDGE('',*,*,#51458,.F.) ;
#77074 = ORIENTED_EDGE('',*,*,#53525,.F.) ;
#77075 = ORIENTED_EDGE('',*,*,#51469,.F.) ;
#77076 = ORIENTED_EDGE('',*,*,#51291,.F.) ;
#77077 = ORIENTED_EDGE('',*,*,#53526,.T.) ;
#77078 = ORIENTED_EDGE('',*,*,#51470,.F.) ;
#77079 = ORIENTED_EDGE('',*,*,#53527,.F.) ;
#77080 = ORIENTED_EDGE('',*,*,#53521,.T.) ;
#77081 = ORIENTED_EDGE('',*,*,#51279,.T.) ;
#77082 = ORIENTED_EDGE('',*,*,#53528,.F.) ;
#77083 = ORIENTED_EDGE('',*,*,#53522,.T.) ;
#77084 = ORIENTED_EDGE('',*,*,#53523,.T.) ;
#77085 = ORIENTED_EDGE('',*,*,#49610,.T.) ;
#77086 = ORIENTED_EDGE('',*,*,#53529,.F.) ;
#77087 = ORIENTED_EDGE('',*,*,#53524,.T.) ;
#77088 = ORIENTED_EDGE('',*,*,#53527,.T.) ;
#77089 = ORIENTED_EDGE('',*,*,#53525,.T.) ;
#77090 = ORIENTED_EDGE('',*,*,#53530,.F.) ;
#77091 = ORIENTED_EDGE('',*,*,#51275,.F.) ;
#77092 = ORIENTED_EDGE('',*,*,#53531,.T.) ;
#77093 = ORIENTED_EDGE('',*,*,#51269,.F.) ;
#77094 = ORIENTED_EDGE('',*,*,#53532,.F.) ;
#77095 = ORIENTED_EDGE('',*,*,#53528,.T.) ;
#77096 = ORIENTED_EDGE('',*,*,#51278,.F.) ;
#77097 = ORIENTED_EDGE('',*,*,#53533,.F.) ;
#77098 = ORIENTED_EDGE('',*,*,#49606,.F.) ;
#77099 = ORIENTED_EDGE('',*,*,#53529,.T.) ;
#77100 = ORIENTED_EDGE('',*,*,#49609,.F.) ;
#77101 = ORIENTED_EDGE('',*,*,#53534,.F.) ;
#77102 = ORIENTED_EDGE('',*,*,#51456,.F.) ;
#77103 = ORIENTED_EDGE('',*,*,#53530,.T.) ;
#77104 = ORIENTED_EDGE('',*,*,#51457,.F.) ;
#77105 = ORIENTED_EDGE('',*,*,#53535,.F.) ;
#77106 = ORIENTED_EDGE('',*,*,#51292,.F.) ;
#77107 = ORIENTED_EDGE('',*,*,#53532,.T.) ;
#77108 = ORIENTED_EDGE('',*,*,#53402,.F.) ;
#77109 = ORIENTED_EDGE('',*,*,#53536,.F.) ;
#77110 = ORIENTED_EDGE('',*,*,#53537,.F.) ;
#77111 = ORIENTED_EDGE('',*,*,#53533,.T.) ;
#77112 = ORIENTED_EDGE('',*,*,#53538,.F.) ;
#77113 = ORIENTED_EDGE('',*,*,#53535,.T.) ;
#77114 = ORIENTED_EDGE('',*,*,#53534,.T.) ;
#77115 = ORIENTED_EDGE('',*,*,#53539,.F.) ;
#77116 = ORIENTED_EDGE('',*,*,#51293,.T.) ;
#77117 = ORIENTED_EDGE('',*,*,#53536,.T.) ;
#77118 = ORIENTED_EDGE('',*,*,#49685,.F.) ;
#77119 = ORIENTED_EDGE('',*,*,#53540,.F.) ;
#77120 = ORIENTED_EDGE('',*,*,#51276,.F.) ;
#77121 = ORIENTED_EDGE('',*,*,#53538,.T.) ;
#77122 = ORIENTED_EDGE('',*,*,#51277,.F.) ;
#77123 = ORIENTED_EDGE('',*,*,#53541,.F.) ;
#77124 = ORIENTED_EDGE('',*,*,#51283,.F.) ;
#77125 = ORIENTED_EDGE('',*,*,#53537,.T.) ;
#77126 = ORIENTED_EDGE('',*,*,#51286,.F.) ;
#77127 = ORIENTED_EDGE('',*,*,#53542,.F.) ;
#77128 = ORIENTED_EDGE('',*,*,#49607,.F.) ;
#77129 = ORIENTED_EDGE('',*,*,#53539,.T.) ;
#77130 = ORIENTED_EDGE('',*,*,#49608,.F.) ;
#77131 = ORIENTED_EDGE('',*,*,#53543,.F.) ;
#77132 = ORIENTED_EDGE('',*,*,#51294,.F.) ;
#77133 = ORIENTED_EDGE('',*,*,#53540,.T.) ;
#77134 = ORIENTED_EDGE('',*,*,#49684,.T.) ;
#77135 = ORIENTED_EDGE('',*,*,#53544,.F.) ;
#77136 = ORIENTED_EDGE('',*,*,#53541,.T.) ;
#77137 = ORIENTED_EDGE('',*,*,#53543,.T.) ;
#77138 = ORIENTED_EDGE('',*,*,#53542,.T.) ;
#77139 = ORIENTED_EDGE('',*,*,#53545,.F.) ;
#77140 = ORIENTED_EDGE('',*,*,#53544,.T.) ;
#77141 = ORIENTED_EDGE('',*,*,#49683,.F.) ;
#77142 = ORIENTED_EDGE('',*,*,#53546,.F.) ;
#77143 = ORIENTED_EDGE('',*,*,#51284,.F.) ;
#77144 = ORIENTED_EDGE('',*,*,#53545,.T.) ;
#77145 = ORIENTED_EDGE('',*,*,#51285,.F.) ;
#77146 = ORIENTED_EDGE('',*,*,#53547,.F.) ;
#77147 = ORIENTED_EDGE('',*,*,#51295,.F.) ;
#77148 = ORIENTED_EDGE('',*,*,#51299,.F.) ;
#77149 = ORIENTED_EDGE('',*,*,#53548,.T.) ;
#77150 = ORIENTED_EDGE('',*,*,#51287,.F.) ;
#77151 = ORIENTED_EDGE('',*,*,#53549,.F.) ;
#77152 = ORIENTED_EDGE('',*,*,#49680,.F.) ;
#77153 = ORIENTED_EDGE('',*,*,#53550,.T.) ;
#77154 = ORIENTED_EDGE('',*,*,#51300,.F.) ;
#77155 = ORIENTED_EDGE('',*,*,#53551,.F.) ;
#77156 = ORIENTED_EDGE('',*,*,#53546,.T.) ;
#77157 = ORIENTED_EDGE('',*,*,#49682,.T.) ;
#77158 = ORIENTED_EDGE('',*,*,#53552,.F.) ;
#77159 = ORIENTED_EDGE('',*,*,#53547,.T.) ;
#77160 = ORIENTED_EDGE('',*,*,#53551,.T.) ;
#77161 = ORIENTED_EDGE('',*,*,#53549,.T.) ;
#77162 = ORIENTED_EDGE('',*,*,#53553,.F.) ;
#77163 = ORIENTED_EDGE('',*,*,#53552,.T.) ;
#77164 = ORIENTED_EDGE('',*,*,#49681,.F.) ;
#77165 = ORIENTED_EDGE('',*,*,#53553,.T.) ;
#77166 = ORIENTED_EDGE('',*,*,#51296,.F.) ;
#77167 = ORIENTED_EDGE('',*,*,#52278,.F.) ;
#77168 = ORIENTED_EDGE('',*,*,#52289,.F.) ;
#77169 = ORIENTED_EDGE('',*,*,#52288,.F.) ;
#77170 = ORIENTED_EDGE('',*,*,#53554,.F.) ;
#77171 = ORIENTED_EDGE('',*,*,#52279,.F.) ;
#77172 = ORIENTED_EDGE('',*,*,#53554,.T.) ;
#77173 = ORIENTED_EDGE('',*,*,#50712,.F.) ;
#77174 = ORIENTED_EDGE('',*,*,#53555,.F.) ;
#77175 = ORIENTED_EDGE('',*,*,#50698,.F.) ;
#77176 = ORIENTED_EDGE('',*,*,#52286,.F.) ;
#77177 = ORIENTED_EDGE('',*,*,#52285,.F.) ;
#77178 = ORIENTED_EDGE('',*,*,#52284,.F.) ;
#77179 = ORIENTED_EDGE('',*,*,#53556,.F.) ;
#77180 = ORIENTED_EDGE('',*,*,#52287,.F.) ;
#77181 = ORIENTED_EDGE('',*,*,#53557,.F.) ;
#77182 = ORIENTED_EDGE('',*,*,#53555,.T.) ;
#77183 = ORIENTED_EDGE('',*,*,#53558,.F.) ;
#77184 = ORIENTED_EDGE('',*,*,#52276,.F.) ;
#77185 = ORIENTED_EDGE('',*,*,#52281,.F.) ;
#77186 = ORIENTED_EDGE('',*,*,#52280,.F.) ;
#77187 = ORIENTED_EDGE('',*,*,#53559,.F.) ;
#77188 = ORIENTED_EDGE('',*,*,#52277,.F.) ;
#77189 = ORIENTED_EDGE('',*,*,#53556,.T.) ;
#77190 = ORIENTED_EDGE('',*,*,#50708,.F.) ;
#77191 = ORIENTED_EDGE('',*,*,#53560,.F.) ;
#77192 = ORIENTED_EDGE('',*,*,#50710,.F.) ;
#77193 = ORIENTED_EDGE('',*,*,#53558,.T.) ;
#77194 = ORIENTED_EDGE('',*,*,#50711,.F.) ;
#77195 = ORIENTED_EDGE('',*,*,#53561,.F.) ;
#77196 = ORIENTED_EDGE('',*,*,#50996,.F.) ;
#77197 = ORIENTED_EDGE('',*,*,#53557,.T.) ;
#77198 = ORIENTED_EDGE('',*,*,#50995,.F.) ;
#77199 = ORIENTED_EDGE('',*,*,#53562,.F.) ;
#77200 = ORIENTED_EDGE('',*,*,#50699,.F.) ;
#77201 = ORIENTED_EDGE('',*,*,#53559,.T.) ;
#77202 = ORIENTED_EDGE('',*,*,#50700,.F.) ;
#77203 = ORIENTED_EDGE('',*,*,#53563,.F.) ;
#77204 = ORIENTED_EDGE('',*,*,#50704,.F.) ;
#77205 = ORIENTED_EDGE('',*,*,#53561,.T.) ;
#77206 = ORIENTED_EDGE('',*,*,#53560,.T.) ;
#77207 = ORIENTED_EDGE('',*,*,#53564,.F.) ;
#77208 = ORIENTED_EDGE('',*,*,#53563,.T.) ;
#77209 = ORIENTED_EDGE('',*,*,#53562,.T.) ;
#77210 = ORIENTED_EDGE('',*,*,#53565,.F.) ;
#77211 = ORIENTED_EDGE('',*,*,#53564,.T.) ;
#77212 = ORIENTED_EDGE('',*,*,#50707,.F.) ;
#77213 = ORIENTED_EDGE('',*,*,#53566,.F.) ;
#77214 = ORIENTED_EDGE('',*,*,#50993,.F.) ;
#77215 = ORIENTED_EDGE('',*,*,#53565,.T.) ;
#77216 = ORIENTED_EDGE('',*,*,#50994,.F.) ;
#77217 = ORIENTED_EDGE('',*,*,#53567,.F.) ;
#77218 = ORIENTED_EDGE('',*,*,#50701,.F.) ;
#77219 = ORIENTED_EDGE('',*,*,#53567,.T.) ;
#77220 = ORIENTED_EDGE('',*,*,#53566,.T.) ;
#77221 = ORIENTED_EDGE('',*,*,#53568,.F.) ;
#77222 = ORIENTED_EDGE('',*,*,#53568,.T.) ;
#77223 = ORIENTED_EDGE('',*,*,#50706,.F.) ;
#77224 = ORIENTED_EDGE('',*,*,#53569,.F.) ;
#77225 = ORIENTED_EDGE('',*,*,#50702,.F.) ;
#77226 = ORIENTED_EDGE('',*,*,#52282,.F.) ;
#77227 = ORIENTED_EDGE('',*,*,#52275,.F.) ;
#77228 = ORIENTED_EDGE('',*,*,#52274,.F.) ;
#77229 = ORIENTED_EDGE('',*,*,#53569,.T.) ;
#77230 = ORIENTED_EDGE('',*,*,#52283,.F.) ;
#77231 = ORIENTED_EDGE('',*,*,#52547,.F.) ;
#77232 = ORIENTED_EDGE('',*,*,#52546,.F.) ;
#77233 = ORIENTED_EDGE('',*,*,#52545,.F.) ;
#77234 = ORIENTED_EDGE('',*,*,#53570,.F.) ;
#77235 = ORIENTED_EDGE('',*,*,#52548,.F.) ;
#77236 = ORIENTED_EDGE('',*,*,#53570,.T.) ;
#77237 = ORIENTED_EDGE('',*,*,#52544,.F.) ;
#77238 = ORIENTED_EDGE('',*,*,#53571,.F.) ;
#77239 = ORIENTED_EDGE('',*,*,#50607,.F.) ;
#77240 = ORIENTED_EDGE('',*,*,#53571,.T.) ;
#77241 = ORIENTED_EDGE('',*,*,#50404,.F.) ;
#77242 = ORIENTED_EDGE('',*,*,#53572,.F.) ;
#77243 = ORIENTED_EDGE('',*,*,#50608,.F.) ;
#77244 = ORIENTED_EDGE('',*,*,#50392,.F.) ;
#77245 = ORIENTED_EDGE('',*,*,#50609,.F.) ;
#77246 = ORIENTED_EDGE('',*,*,#53573,.F.) ;
#77247 = ORIENTED_EDGE('',*,*,#50398,.F.) ;
#77248 = ORIENTED_EDGE('',*,*,#53573,.T.) ;
#77249 = ORIENTED_EDGE('',*,*,#53572,.T.) ;
#77250 = ORIENTED_EDGE('',*,*,#53574,.F.) ;
#77251 = ORIENTED_EDGE('',*,*,#53574,.T.) ;
#77252 = ORIENTED_EDGE('',*,*,#50403,.F.) ;
#77253 = ORIENTED_EDGE('',*,*,#53575,.F.) ;
#77254 = ORIENTED_EDGE('',*,*,#50399,.F.) ;
#77255 = ORIENTED_EDGE('',*,*,#50394,.F.) ;
#77256 = ORIENTED_EDGE('',*,*,#50400,.F.) ;
#77257 = ORIENTED_EDGE('',*,*,#53576,.F.) ;
#77258 = ORIENTED_EDGE('',*,*,#50671,.F.) ;
#77259 = ORIENTED_EDGE('',*,*,#53576,.T.) ;
#77260 = ORIENTED_EDGE('',*,*,#53575,.T.) ;
#77261 = ORIENTED_EDGE('',*,*,#53577,.F.) ;
#77262 = ORIENTED_EDGE('',*,*,#53577,.T.) ;
#77263 = ORIENTED_EDGE('',*,*,#50402,.F.) ;
#77264 = ORIENTED_EDGE('',*,*,#53578,.F.) ;
#77265 = ORIENTED_EDGE('',*,*,#50672,.F.) ;
#77266 = ORIENTED_EDGE('',*,*,#53578,.T.) ;
#77267 = ORIENTED_EDGE('',*,*,#52543,.F.) ;
#77268 = ORIENTED_EDGE('',*,*,#53579,.F.) ;
#77269 = ORIENTED_EDGE('',*,*,#50673,.F.) ;
#77270 = ORIENTED_EDGE('',*,*,#53579,.T.) ;
#77271 = ORIENTED_EDGE('',*,*,#52542,.F.) ;
#77272 = ORIENTED_EDGE('',*,*,#52551,.F.) ;
#77273 = ORIENTED_EDGE('',*,*,#52552,.F.) ;
#77274 = ORIENTED_EDGE('',*,*,#52557,.F.) ;
#77275 = ORIENTED_EDGE('',*,*,#53580,.F.) ;
#77276 = ORIENTED_EDGE('',*,*,#53580,.T.) ;
#77277 = ORIENTED_EDGE('',*,*,#52556,.F.) ;
#77278 = ORIENTED_EDGE('',*,*,#53581,.F.) ;
#77279 = ORIENTED_EDGE('',*,*,#50668,.F.) ;
#77280 = ORIENTED_EDGE('',*,*,#53581,.T.) ;
#77281 = ORIENTED_EDGE('',*,*,#50386,.F.) ;
#77282 = ORIENTED_EDGE('',*,*,#53582,.F.) ;
#77283 = ORIENTED_EDGE('',*,*,#50669,.F.) ;
#77284 = ORIENTED_EDGE('',*,*,#50396,.F.) ;
#77285 = ORIENTED_EDGE('',*,*,#50670,.F.) ;
#77286 = ORIENTED_EDGE('',*,*,#53583,.F.) ;
#77287 = ORIENTED_EDGE('',*,*,#50390,.F.) ;
#77288 = ORIENTED_EDGE('',*,*,#53583,.T.) ;
#77289 = ORIENTED_EDGE('',*,*,#53582,.T.) ;
#77290 = ORIENTED_EDGE('',*,*,#53584,.F.) ;
#77291 = ORIENTED_EDGE('',*,*,#53584,.T.) ;
#77292 = ORIENTED_EDGE('',*,*,#50385,.F.) ;
#77293 = ORIENTED_EDGE('',*,*,#53585,.F.) ;
#77294 = ORIENTED_EDGE('',*,*,#50387,.F.) ;
#77295 = ORIENTED_EDGE('',*,*,#50397,.F.) ;
#77296 = ORIENTED_EDGE('',*,*,#50388,.F.) ;
#77297 = ORIENTED_EDGE('',*,*,#53586,.F.) ;
#77298 = ORIENTED_EDGE('',*,*,#50610,.F.) ;
#77299 = ORIENTED_EDGE('',*,*,#53586,.T.) ;
#77300 = ORIENTED_EDGE('',*,*,#53585,.T.) ;
#77301 = ORIENTED_EDGE('',*,*,#53587,.F.) ;
#77302 = ORIENTED_EDGE('',*,*,#53587,.T.) ;
#77303 = ORIENTED_EDGE('',*,*,#50384,.F.) ;
#77304 = ORIENTED_EDGE('',*,*,#53588,.F.) ;
#77305 = ORIENTED_EDGE('',*,*,#50611,.F.) ;
#77306 = ORIENTED_EDGE('',*,*,#53588,.T.) ;
#77307 = ORIENTED_EDGE('',*,*,#52555,.F.) ;
#77308 = ORIENTED_EDGE('',*,*,#53589,.F.) ;
#77309 = ORIENTED_EDGE('',*,*,#50612,.F.) ;
#77310 = ORIENTED_EDGE('',*,*,#52553,.F.) ;
#77311 = ORIENTED_EDGE('',*,*,#52550,.F.) ;
#77312 = ORIENTED_EDGE('',*,*,#52549,.F.) ;
#77313 = ORIENTED_EDGE('',*,*,#53589,.T.) ;
#77314 = ORIENTED_EDGE('',*,*,#52554,.F.) ;
#77315 = ORIENTED_EDGE('',*,*,#53590,.F.) ;
#77316 = ORIENTED_EDGE('',*,*,#49436,.F.) ;
#77317 = ORIENTED_EDGE('',*,*,#53591,.F.) ;
#77318 = ORIENTED_EDGE('',*,*,#52153,.F.) ;
#77319 = ORIENTED_EDGE('',*,*,#53591,.T.) ;
#77320 = ORIENTED_EDGE('',*,*,#49435,.F.) ;
#77321 = ORIENTED_EDGE('',*,*,#53592,.F.) ;
#77322 = ORIENTED_EDGE('',*,*,#52156,.F.) ;
#77323 = ORIENTED_EDGE('',*,*,#53590,.T.) ;
#77324 = ORIENTED_EDGE('',*,*,#52150,.F.) ;
#77325 = ORIENTED_EDGE('',*,*,#53593,.F.) ;
#77326 = ORIENTED_EDGE('',*,*,#49437,.F.) ;
#77327 = ORIENTED_EDGE('',*,*,#53592,.T.) ;
#77328 = ORIENTED_EDGE('',*,*,#49434,.F.) ;
#77329 = ORIENTED_EDGE('',*,*,#53594,.F.) ;
#77330 = ORIENTED_EDGE('',*,*,#52159,.F.) ;
#77331 = ORIENTED_EDGE('',*,*,#53593,.T.) ;
#77332 = ORIENTED_EDGE('',*,*,#52147,.F.) ;
#77333 = ORIENTED_EDGE('',*,*,#53595,.F.) ;
#77334 = ORIENTED_EDGE('',*,*,#49438,.F.) ;
#77335 = ORIENTED_EDGE('',*,*,#53594,.T.) ;
#77336 = ORIENTED_EDGE('',*,*,#49433,.F.) ;
#77337 = ORIENTED_EDGE('',*,*,#53596,.F.) ;
#77338 = ORIENTED_EDGE('',*,*,#52162,.F.) ;
#77339 = ORIENTED_EDGE('',*,*,#53595,.T.) ;
#77340 = ORIENTED_EDGE('',*,*,#52169,.F.) ;
#77341 = ORIENTED_EDGE('',*,*,#53597,.F.) ;
#77342 = ORIENTED_EDGE('',*,*,#49431,.F.) ;
#77343 = ORIENTED_EDGE('',*,*,#53596,.T.) ;
#77344 = ORIENTED_EDGE('',*,*,#49432,.F.) ;
#77345 = ORIENTED_EDGE('',*,*,#53597,.T.) ;
#77346 = ORIENTED_EDGE('',*,*,#52165,.F.) ;
#77347 = ORIENTED_EDGE('',*,*,#51002,.F.) ;
#77348 = ORIENTED_EDGE('',*,*,#51016,.F.) ;
#77349 = ORIENTED_EDGE('',*,*,#53598,.F.) ;
#77350 = ORIENTED_EDGE('',*,*,#51005,.F.) ;
#77351 = ORIENTED_EDGE('',*,*,#53599,.F.) ;
#77352 = ORIENTED_EDGE('',*,*,#51006,.F.) ;
#77353 = ORIENTED_EDGE('',*,*,#53600,.F.) ;
#77354 = ORIENTED_EDGE('',*,*,#51072,.F.) ;
#77355 = ORIENTED_EDGE('',*,*,#51004,.F.) ;
#77356 = ORIENTED_EDGE('',*,*,#51007,.F.) ;
#77357 = ORIENTED_EDGE('',*,*,#53601,.F.) ;
#77358 = ORIENTED_EDGE('',*,*,#51008,.F.) ;
#77359 = ORIENTED_EDGE('',*,*,#53600,.T.) ;
#77360 = ORIENTED_EDGE('',*,*,#53598,.T.) ;
#77361 = ORIENTED_EDGE('',*,*,#53602,.F.) ;
#77362 = ORIENTED_EDGE('',*,*,#53601,.T.) ;
#77363 = ORIENTED_EDGE('',*,*,#53599,.T.) ;
#77364 = ORIENTED_EDGE('',*,*,#53603,.F.) ;
#77365 = ORIENTED_EDGE('',*,*,#51000,.F.) ;
#77366 = ORIENTED_EDGE('',*,*,#51012,.F.) ;
#77367 = ORIENTED_EDGE('',*,*,#53604,.F.) ;
#77368 = ORIENTED_EDGE('',*,*,#51014,.F.) ;
#77369 = ORIENTED_EDGE('',*,*,#53602,.T.) ;
#77370 = ORIENTED_EDGE('',*,*,#51015,.F.) ;
#77371 = ORIENTED_EDGE('',*,*,#53605,.F.) ;
#77372 = ORIENTED_EDGE('',*,*,#51069,.F.) ;
#77373 = ORIENTED_EDGE('',*,*,#53603,.T.) ;
#77374 = ORIENTED_EDGE('',*,*,#51071,.F.) ;
#77375 = ORIENTED_EDGE('',*,*,#53606,.F.) ;
#77376 = ORIENTED_EDGE('',*,*,#51009,.F.) ;
#77377 = ORIENTED_EDGE('',*,*,#50998,.F.) ;
#77378 = ORIENTED_EDGE('',*,*,#51010,.F.) ;
#77379 = ORIENTED_EDGE('',*,*,#53607,.F.) ;
#77380 = ORIENTED_EDGE('',*,*,#51013,.F.) ;
#77381 = ORIENTED_EDGE('',*,*,#53605,.T.) ;
#77382 = ORIENTED_EDGE('',*,*,#53604,.T.) ;
#77383 = ORIENTED_EDGE('',*,*,#53608,.F.) ;
#77384 = ORIENTED_EDGE('',*,*,#53607,.T.) ;
#77385 = ORIENTED_EDGE('',*,*,#53606,.T.) ;
#77386 = ORIENTED_EDGE('',*,*,#53609,.F.) ;
#77387 = ORIENTED_EDGE('',*,*,#53608,.T.) ;
#77388 = ORIENTED_EDGE('',*,*,#51011,.F.) ;
#77389 = ORIENTED_EDGE('',*,*,#53609,.T.) ;
#77390 = ORIENTED_EDGE('',*,*,#51070,.F.) ;
#77391 = ORIENTED_EDGE('',*,*,#53610,.F.) ;
#77392 = ORIENTED_EDGE('',*,*,#49340,.F.) ;
#77393 = ORIENTED_EDGE('',*,*,#53611,.F.) ;
#77394 = ORIENTED_EDGE('',*,*,#51521,.F.) ;
#77395 = ORIENTED_EDGE('',*,*,#53611,.T.) ;
#77396 = ORIENTED_EDGE('',*,*,#49339,.T.) ;
#77397 = ORIENTED_EDGE('',*,*,#53612,.F.) ;
#77398 = ORIENTED_EDGE('',*,*,#53613,.F.) ;
#77399 = ORIENTED_EDGE('',*,*,#49341,.T.) ;
#77400 = ORIENTED_EDGE('',*,*,#53610,.T.) ;
#77401 = ORIENTED_EDGE('',*,*,#53614,.F.) ;
#77402 = ORIENTED_EDGE('',*,*,#53615,.F.) ;
#77403 = ORIENTED_EDGE('',*,*,#53612,.T.) ;
#77404 = ORIENTED_EDGE('',*,*,#49338,.F.) ;
#77405 = ORIENTED_EDGE('',*,*,#53616,.F.) ;
#77406 = ORIENTED_EDGE('',*,*,#51518,.F.) ;
#77407 = ORIENTED_EDGE('',*,*,#53613,.T.) ;
#77408 = ORIENTED_EDGE('',*,*,#51517,.F.) ;
#77409 = ORIENTED_EDGE('',*,*,#53617,.F.) ;
#77410 = ORIENTED_EDGE('',*,*,#51522,.F.) ;
#77411 = ORIENTED_EDGE('',*,*,#53618,.F.) ;
#77412 = ORIENTED_EDGE('',*,*,#51519,.F.) ;
#77413 = ORIENTED_EDGE('',*,*,#53619,.F.) ;
#77414 = ORIENTED_EDGE('',*,*,#51806,.F.) ;
#77415 = ORIENTED_EDGE('',*,*,#53614,.T.) ;
#77416 = ORIENTED_EDGE('',*,*,#51520,.F.) ;
#77417 = ORIENTED_EDGE('',*,*,#53620,.F.) ;
#77418 = ORIENTED_EDGE('',*,*,#51510,.F.) ;
#77419 = ORIENTED_EDGE('',*,*,#53615,.T.) ;
#77420 = ORIENTED_EDGE('',*,*,#51509,.F.) ;
#77421 = ORIENTED_EDGE('',*,*,#53621,.F.) ;
#77422 = ORIENTED_EDGE('',*,*,#49342,.F.) ;
#77423 = ORIENTED_EDGE('',*,*,#53622,.F.) ;
#77424 = ORIENTED_EDGE('',*,*,#49336,.F.) ;
#77425 = ORIENTED_EDGE('',*,*,#53623,.F.) ;
#77426 = ORIENTED_EDGE('',*,*,#51511,.F.) ;
#77427 = ORIENTED_EDGE('',*,*,#49337,.T.) ;
#77428 = ORIENTED_EDGE('',*,*,#53622,.T.) ;
#77429 = ORIENTED_EDGE('',*,*,#53624,.F.) ;
#77430 = ORIENTED_EDGE('',*,*,#53616,.T.) ;
#77431 = ORIENTED_EDGE('',*,*,#53619,.T.) ;
#77432 = ORIENTED_EDGE('',*,*,#53617,.T.) ;
#77433 = ORIENTED_EDGE('',*,*,#53625,.F.) ;
#77434 = ORIENTED_EDGE('',*,*,#53620,.T.) ;
#77435 = ORIENTED_EDGE('',*,*,#53618,.T.) ;
#77436 = ORIENTED_EDGE('',*,*,#53626,.F.) ;
#77437 = ORIENTED_EDGE('',*,*,#49335,.T.) ;
#77438 = ORIENTED_EDGE('',*,*,#53621,.T.) ;
#77439 = ORIENTED_EDGE('',*,*,#53627,.F.) ;
#77440 = ORIENTED_EDGE('',*,*,#53623,.T.) ;
#77441 = ORIENTED_EDGE('',*,*,#53624,.T.) ;
#77442 = ORIENTED_EDGE('',*,*,#51514,.F.) ;
#77443 = ORIENTED_EDGE('',*,*,#53628,.F.) ;
#77444 = ORIENTED_EDGE('',*,*,#51515,.F.) ;
#77445 = ORIENTED_EDGE('',*,*,#53625,.T.) ;
#77446 = ORIENTED_EDGE('',*,*,#51516,.F.) ;
#77447 = ORIENTED_EDGE('',*,*,#53629,.F.) ;
#77448 = ORIENTED_EDGE('',*,*,#51803,.F.) ;
#77449 = ORIENTED_EDGE('',*,*,#53626,.T.) ;
#77450 = ORIENTED_EDGE('',*,*,#51805,.F.) ;
#77451 = ORIENTED_EDGE('',*,*,#53630,.F.) ;
#77452 = ORIENTED_EDGE('',*,*,#51507,.F.) ;
#77453 = ORIENTED_EDGE('',*,*,#53627,.T.) ;
#77454 = ORIENTED_EDGE('',*,*,#51508,.F.) ;
#77455 = ORIENTED_EDGE('',*,*,#53631,.F.) ;
#77456 = ORIENTED_EDGE('',*,*,#51512,.F.) ;
#77457 = ORIENTED_EDGE('',*,*,#53629,.T.) ;
#77458 = ORIENTED_EDGE('',*,*,#53628,.T.) ;
#77459 = ORIENTED_EDGE('',*,*,#53632,.F.) ;
#77460 = ORIENTED_EDGE('',*,*,#53631,.T.) ;
#77461 = ORIENTED_EDGE('',*,*,#53630,.T.) ;
#77462 = ORIENTED_EDGE('',*,*,#53633,.F.) ;
#77463 = ORIENTED_EDGE('',*,*,#53632,.T.) ;
#77464 = ORIENTED_EDGE('',*,*,#51513,.F.) ;
#77465 = ORIENTED_EDGE('',*,*,#53633,.T.) ;
#77466 = ORIENTED_EDGE('',*,*,#51804,.F.) ;
#77467 = ORIENTED_EDGE('',*,*,#51812,.F.) ;
#77468 = ORIENTED_EDGE('',*,*,#51825,.F.) ;
#77469 = ORIENTED_EDGE('',*,*,#53634,.F.) ;
#77470 = ORIENTED_EDGE('',*,*,#51817,.F.) ;
#77471 = ORIENTED_EDGE('',*,*,#53635,.F.) ;
#77472 = ORIENTED_EDGE('',*,*,#51815,.F.) ;
#77473 = ORIENTED_EDGE('',*,*,#53636,.F.) ;
#77474 = ORIENTED_EDGE('',*,*,#51882,.F.) ;
#77475 = ORIENTED_EDGE('',*,*,#51814,.F.) ;
#77476 = ORIENTED_EDGE('',*,*,#51816,.F.) ;
#77477 = ORIENTED_EDGE('',*,*,#53637,.F.) ;
#77478 = ORIENTED_EDGE('',*,*,#51820,.F.) ;
#77479 = ORIENTED_EDGE('',*,*,#53636,.T.) ;
#77480 = ORIENTED_EDGE('',*,*,#53634,.T.) ;
#77481 = ORIENTED_EDGE('',*,*,#53638,.F.) ;
#77482 = ORIENTED_EDGE('',*,*,#53637,.T.) ;
#77483 = ORIENTED_EDGE('',*,*,#53635,.T.) ;
#77484 = ORIENTED_EDGE('',*,*,#53639,.F.) ;
#77485 = ORIENTED_EDGE('',*,*,#51810,.F.) ;
#77486 = ORIENTED_EDGE('',*,*,#51823,.F.) ;
#77487 = ORIENTED_EDGE('',*,*,#53640,.F.) ;
#77488 = ORIENTED_EDGE('',*,*,#51826,.F.) ;
#77489 = ORIENTED_EDGE('',*,*,#53638,.T.) ;
#77490 = ORIENTED_EDGE('',*,*,#51824,.F.) ;
#77491 = ORIENTED_EDGE('',*,*,#53641,.F.) ;
#77492 = ORIENTED_EDGE('',*,*,#51879,.F.) ;
#77493 = ORIENTED_EDGE('',*,*,#53639,.T.) ;
#77494 = ORIENTED_EDGE('',*,*,#51881,.F.) ;
#77495 = ORIENTED_EDGE('',*,*,#53642,.F.) ;
#77496 = ORIENTED_EDGE('',*,*,#51818,.F.) ;
#77497 = ORIENTED_EDGE('',*,*,#51808,.F.) ;
#77498 = ORIENTED_EDGE('',*,*,#51819,.F.) ;
#77499 = ORIENTED_EDGE('',*,*,#53643,.F.) ;
#77500 = ORIENTED_EDGE('',*,*,#51821,.F.) ;
#77501 = ORIENTED_EDGE('',*,*,#53641,.T.) ;
#77502 = ORIENTED_EDGE('',*,*,#53640,.T.) ;
#77503 = ORIENTED_EDGE('',*,*,#53644,.F.) ;
#77504 = ORIENTED_EDGE('',*,*,#53643,.T.) ;
#77505 = ORIENTED_EDGE('',*,*,#53642,.T.) ;
#77506 = ORIENTED_EDGE('',*,*,#53645,.F.) ;
#77507 = ORIENTED_EDGE('',*,*,#53644,.T.) ;
#77508 = ORIENTED_EDGE('',*,*,#51822,.F.) ;
#77509 = ORIENTED_EDGE('',*,*,#53645,.T.) ;
#77510 = ORIENTED_EDGE('',*,*,#51880,.F.) ;
#77511 = ORIENTED_EDGE('',*,*,#53646,.F.) ;
#77512 = ORIENTED_EDGE('',*,*,#52158,.F.) ;
#77513 = ORIENTED_EDGE('',*,*,#53647,.F.) ;
#77514 = ORIENTED_EDGE('',*,*,#52173,.F.) ;
#77515 = ORIENTED_EDGE('',*,*,#53647,.T.) ;
#77516 = ORIENTED_EDGE('',*,*,#52161,.F.) ;
#77517 = ORIENTED_EDGE('',*,*,#53648,.F.) ;
#77518 = ORIENTED_EDGE('',*,*,#52155,.F.) ;
#77519 = ORIENTED_EDGE('',*,*,#53646,.T.) ;
#77520 = ORIENTED_EDGE('',*,*,#53649,.F.) ;
#77521 = ORIENTED_EDGE('',*,*,#53648,.T.) ;
#77522 = ORIENTED_EDGE('',*,*,#52164,.F.) ;
#77523 = ORIENTED_EDGE('',*,*,#53650,.F.) ;
#77524 = ORIENTED_EDGE('',*,*,#52170,.F.) ;
#77525 = ORIENTED_EDGE('',*,*,#53649,.T.) ;
#77526 = ORIENTED_EDGE('',*,*,#52172,.F.) ;
#77527 = ORIENTED_EDGE('',*,*,#53651,.F.) ;
#77528 = ORIENTED_EDGE('',*,*,#52152,.F.) ;
#77529 = ORIENTED_EDGE('',*,*,#53650,.T.) ;
#77530 = ORIENTED_EDGE('',*,*,#52167,.F.) ;
#77531 = ORIENTED_EDGE('',*,*,#53652,.F.) ;
#77532 = ORIENTED_EDGE('',*,*,#52149,.F.) ;
#77533 = ORIENTED_EDGE('',*,*,#53651,.T.) ;
#77534 = ORIENTED_EDGE('',*,*,#53653,.F.) ;
#77535 = ORIENTED_EDGE('',*,*,#53652,.T.) ;
#77536 = ORIENTED_EDGE('',*,*,#52168,.F.) ;
#77537 = ORIENTED_EDGE('',*,*,#53653,.T.) ;
#77538 = ORIENTED_EDGE('',*,*,#52171,.F.) ;
#77539 = ORIENTED_EDGE('',*,*,#49214,.F.) ;
#77540 = ORIENTED_EDGE('',*,*,#51888,.F.) ;
#77541 = ORIENTED_EDGE('',*,*,#49228,.F.) ;
#77542 = ORIENTED_EDGE('',*,*,#51938,.F.) ;
#77543 = ORIENTED_EDGE('',*,*,#49216,.F.) ;
#77544 = ORIENTED_EDGE('',*,*,#51939,.F.) ;
#77545 = ORIENTED_EDGE('',*,*,#49226,.F.) ;
#77546 = ORIENTED_EDGE('',*,*,#51942,.F.) ;
#77547 = ORIENTED_EDGE('',*,*,#49224,.F.) ;
#77548 = ORIENTED_EDGE('',*,*,#51940,.F.) ;
#77549 = ORIENTED_EDGE('',*,*,#49218,.F.) ;
#77550 = ORIENTED_EDGE('',*,*,#51943,.F.) ;
#77551 = ORIENTED_EDGE('',*,*,#49222,.F.) ;
#77552 = ORIENTED_EDGE('',*,*,#49524,.F.) ;
#77553 = ORIENTED_EDGE('',*,*,#49220,.F.) ;
#77554 = ORIENTED_EDGE('',*,*,#51941,.F.) ;
#77555 = ORIENTED_EDGE('',*,*,#53654,.F.) ;
#77556 = ORIENTED_EDGE('',*,*,#53655,.F.) ;
#77557 = ORIENTED_EDGE('',*,*,#53656,.F.) ;
#77558 = ORIENTED_EDGE('',*,*,#53655,.T.) ;
#77559 = ORIENTED_EDGE('',*,*,#51485,.F.) ;
#77560 = ORIENTED_EDGE('',*,*,#53657,.F.) ;
#77561 = ORIENTED_EDGE('',*,*,#51480,.F.) ;
#77562 = ORIENTED_EDGE('',*,*,#53656,.T.) ;
#77563 = ORIENTED_EDGE('',*,*,#51479,.F.) ;
#77564 = ORIENTED_EDGE('',*,*,#53658,.F.) ;
#77565 = ORIENTED_EDGE('',*,*,#51481,.F.) ;
#77566 = ORIENTED_EDGE('',*,*,#53654,.T.) ;
#77567 = ORIENTED_EDGE('',*,*,#51484,.F.) ;
#77568 = ORIENTED_EDGE('',*,*,#53659,.F.) ;
#77569 = ORIENTED_EDGE('',*,*,#51486,.F.) ;
#77570 = ORIENTED_EDGE('',*,*,#51490,.F.) ;
#77571 = ORIENTED_EDGE('',*,*,#53660,.T.) ;
#77572 = ORIENTED_EDGE('',*,*,#51309,.F.) ;
#77573 = ORIENTED_EDGE('',*,*,#53661,.F.) ;
#77574 = ORIENTED_EDGE('',*,*,#53657,.T.) ;
#77575 = ORIENTED_EDGE('',*,*,#53661,.T.) ;
#77576 = ORIENTED_EDGE('',*,*,#53662,.F.) ;
#77577 = ORIENTED_EDGE('',*,*,#53663,.F.) ;
#77578 = ORIENTED_EDGE('',*,*,#53658,.T.) ;
#77579 = ORIENTED_EDGE('',*,*,#53664,.F.) ;
#77580 = ORIENTED_EDGE('',*,*,#49596,.T.) ;
#77581 = ORIENTED_EDGE('',*,*,#53665,.F.) ;
#77582 = ORIENTED_EDGE('',*,*,#53659,.T.) ;
#77583 = ORIENTED_EDGE('',*,*,#53666,.F.) ;
#77584 = ORIENTED_EDGE('',*,*,#51489,.F.) ;
#77585 = ORIENTED_EDGE('',*,*,#53667,.T.) ;
#77586 = ORIENTED_EDGE('',*,*,#49415,.F.) ;
#77587 = ORIENTED_EDGE('',*,*,#53668,.T.) ;
#77588 = ORIENTED_EDGE('',*,*,#53662,.T.) ;
#77589 = ORIENTED_EDGE('',*,*,#51308,.F.) ;
#77590 = ORIENTED_EDGE('',*,*,#53669,.F.) ;
#77591 = ORIENTED_EDGE('',*,*,#51477,.F.) ;
#77592 = ORIENTED_EDGE('',*,*,#53664,.T.) ;
#77593 = ORIENTED_EDGE('',*,*,#51478,.F.) ;
#77594 = ORIENTED_EDGE('',*,*,#53670,.F.) ;
#77595 = ORIENTED_EDGE('',*,*,#49597,.F.) ;
#77596 = ORIENTED_EDGE('',*,*,#53663,.T.) ;
#77597 = ORIENTED_EDGE('',*,*,#49603,.F.) ;
#77598 = ORIENTED_EDGE('',*,*,#53671,.F.) ;
#77599 = ORIENTED_EDGE('',*,*,#51482,.F.) ;
#77600 = ORIENTED_EDGE('',*,*,#53666,.T.) ;
#77601 = ORIENTED_EDGE('',*,*,#51483,.F.) ;
#77602 = ORIENTED_EDGE('',*,*,#53672,.F.) ;
#77603 = ORIENTED_EDGE('',*,*,#51473,.F.) ;
#77604 = ORIENTED_EDGE('',*,*,#53665,.T.) ;
#77605 = ORIENTED_EDGE('',*,*,#51476,.F.) ;
#77606 = ORIENTED_EDGE('',*,*,#53673,.F.) ;
#77607 = ORIENTED_EDGE('',*,*,#51487,.F.) ;
#77608 = ORIENTED_EDGE('',*,*,#51319,.F.) ;
#77609 = ORIENTED_EDGE('',*,*,#53674,.T.) ;
#77610 = ORIENTED_EDGE('',*,*,#51488,.F.) ;
#77611 = ORIENTED_EDGE('',*,*,#53675,.F.) ;
#77612 = ORIENTED_EDGE('',*,*,#53669,.T.) ;
#77613 = ORIENTED_EDGE('',*,*,#51307,.T.) ;
#77614 = ORIENTED_EDGE('',*,*,#53676,.F.) ;
#77615 = ORIENTED_EDGE('',*,*,#53670,.T.) ;
#77616 = ORIENTED_EDGE('',*,*,#53671,.T.) ;
#77617 = ORIENTED_EDGE('',*,*,#49602,.T.) ;
#77618 = ORIENTED_EDGE('',*,*,#53677,.F.) ;
#77619 = ORIENTED_EDGE('',*,*,#53672,.T.) ;
#77620 = ORIENTED_EDGE('',*,*,#53675,.T.) ;
#77621 = ORIENTED_EDGE('',*,*,#53673,.T.) ;
#77622 = ORIENTED_EDGE('',*,*,#53678,.F.) ;
#77623 = ORIENTED_EDGE('',*,*,#51303,.F.) ;
#77624 = ORIENTED_EDGE('',*,*,#53679,.T.) ;
#77625 = ORIENTED_EDGE('',*,*,#51297,.F.) ;
#77626 = ORIENTED_EDGE('',*,*,#53680,.F.) ;
#77627 = ORIENTED_EDGE('',*,*,#53676,.T.) ;
#77628 = ORIENTED_EDGE('',*,*,#51306,.F.) ;
#77629 = ORIENTED_EDGE('',*,*,#53681,.F.) ;
#77630 = ORIENTED_EDGE('',*,*,#49598,.F.) ;
#77631 = ORIENTED_EDGE('',*,*,#53677,.T.) ;
#77632 = ORIENTED_EDGE('',*,*,#49601,.F.) ;
#77633 = ORIENTED_EDGE('',*,*,#53682,.F.) ;
#77634 = ORIENTED_EDGE('',*,*,#51474,.F.) ;
#77635 = ORIENTED_EDGE('',*,*,#53678,.T.) ;
#77636 = ORIENTED_EDGE('',*,*,#51475,.F.) ;
#77637 = ORIENTED_EDGE('',*,*,#53683,.F.) ;
#77638 = ORIENTED_EDGE('',*,*,#51320,.F.) ;
#77639 = ORIENTED_EDGE('',*,*,#53680,.T.) ;
#77640 = ORIENTED_EDGE('',*,*,#53550,.F.) ;
#77641 = ORIENTED_EDGE('',*,*,#53684,.F.) ;
#77642 = ORIENTED_EDGE('',*,*,#53685,.F.) ;
#77643 = ORIENTED_EDGE('',*,*,#53681,.T.) ;
#77644 = ORIENTED_EDGE('',*,*,#53686,.F.) ;
#77645 = ORIENTED_EDGE('',*,*,#53683,.T.) ;
#77646 = ORIENTED_EDGE('',*,*,#53682,.T.) ;
#77647 = ORIENTED_EDGE('',*,*,#53687,.F.) ;
#77648 = ORIENTED_EDGE('',*,*,#51321,.T.) ;
#77649 = ORIENTED_EDGE('',*,*,#53684,.T.) ;
#77650 = ORIENTED_EDGE('',*,*,#49679,.F.) ;
#77651 = ORIENTED_EDGE('',*,*,#53688,.F.) ;
#77652 = ORIENTED_EDGE('',*,*,#51304,.F.) ;
#77653 = ORIENTED_EDGE('',*,*,#53686,.T.) ;
#77654 = ORIENTED_EDGE('',*,*,#51305,.F.) ;
#77655 = ORIENTED_EDGE('',*,*,#53689,.F.) ;
#77656 = ORIENTED_EDGE('',*,*,#51311,.F.) ;
#77657 = ORIENTED_EDGE('',*,*,#53685,.T.) ;
#77658 = ORIENTED_EDGE('',*,*,#51314,.F.) ;
#77659 = ORIENTED_EDGE('',*,*,#53690,.F.) ;
#77660 = ORIENTED_EDGE('',*,*,#49599,.F.) ;
#77661 = ORIENTED_EDGE('',*,*,#53687,.T.) ;
#77662 = ORIENTED_EDGE('',*,*,#49600,.F.) ;
#77663 = ORIENTED_EDGE('',*,*,#53691,.F.) ;
#77664 = ORIENTED_EDGE('',*,*,#51322,.F.) ;
#77665 = ORIENTED_EDGE('',*,*,#53688,.T.) ;
#77666 = ORIENTED_EDGE('',*,*,#49678,.T.) ;
#77667 = ORIENTED_EDGE('',*,*,#53692,.F.) ;
#77668 = ORIENTED_EDGE('',*,*,#53689,.T.) ;
#77669 = ORIENTED_EDGE('',*,*,#53691,.T.) ;
#77670 = ORIENTED_EDGE('',*,*,#53690,.T.) ;
#77671 = ORIENTED_EDGE('',*,*,#53693,.F.) ;
#77672 = ORIENTED_EDGE('',*,*,#53692,.T.) ;
#77673 = ORIENTED_EDGE('',*,*,#49677,.F.) ;
#77674 = ORIENTED_EDGE('',*,*,#53694,.F.) ;
#77675 = ORIENTED_EDGE('',*,*,#51312,.F.) ;
#77676 = ORIENTED_EDGE('',*,*,#53693,.T.) ;
#77677 = ORIENTED_EDGE('',*,*,#51313,.F.) ;
#77678 = ORIENTED_EDGE('',*,*,#53695,.F.) ;
#77679 = ORIENTED_EDGE('',*,*,#51323,.F.) ;
#77680 = ORIENTED_EDGE('',*,*,#51328,.F.) ;
#77681 = ORIENTED_EDGE('',*,*,#53696,.T.) ;
#77682 = ORIENTED_EDGE('',*,*,#51315,.F.) ;
#77683 = ORIENTED_EDGE('',*,*,#53697,.F.) ;
#77684 = ORIENTED_EDGE('',*,*,#49674,.F.) ;
#77685 = ORIENTED_EDGE('',*,*,#53698,.T.) ;
#77686 = ORIENTED_EDGE('',*,*,#51325,.F.) ;
#77687 = ORIENTED_EDGE('',*,*,#53699,.F.) ;
#77688 = ORIENTED_EDGE('',*,*,#53694,.T.) ;
#77689 = ORIENTED_EDGE('',*,*,#49676,.T.) ;
#77690 = ORIENTED_EDGE('',*,*,#53700,.F.) ;
#77691 = ORIENTED_EDGE('',*,*,#53695,.T.) ;
#77692 = ORIENTED_EDGE('',*,*,#53699,.T.) ;
#77693 = ORIENTED_EDGE('',*,*,#53697,.T.) ;
#77694 = ORIENTED_EDGE('',*,*,#53701,.F.) ;
#77695 = ORIENTED_EDGE('',*,*,#53700,.T.) ;
#77696 = ORIENTED_EDGE('',*,*,#49675,.F.) ;
#77697 = ORIENTED_EDGE('',*,*,#53701,.T.) ;
#77698 = ORIENTED_EDGE('',*,*,#51324,.F.) ;
#77699 = ORIENTED_EDGE('',*,*,#52262,.F.) ;
#77700 = ORIENTED_EDGE('',*,*,#52273,.F.) ;
#77701 = ORIENTED_EDGE('',*,*,#52272,.F.) ;
#77702 = ORIENTED_EDGE('',*,*,#53702,.F.) ;
#77703 = ORIENTED_EDGE('',*,*,#52263,.F.) ;
#77704 = ORIENTED_EDGE('',*,*,#53702,.T.) ;
#77705 = ORIENTED_EDGE('',*,*,#50696,.F.) ;
#77706 = ORIENTED_EDGE('',*,*,#53703,.F.) ;
#77707 = ORIENTED_EDGE('',*,*,#50682,.F.) ;
#77708 = ORIENTED_EDGE('',*,*,#52270,.F.) ;
#77709 = ORIENTED_EDGE('',*,*,#52269,.F.) ;
#77710 = ORIENTED_EDGE('',*,*,#52268,.F.) ;
#77711 = ORIENTED_EDGE('',*,*,#53704,.F.) ;
#77712 = ORIENTED_EDGE('',*,*,#52271,.F.) ;
#77713 = ORIENTED_EDGE('',*,*,#53705,.F.) ;
#77714 = ORIENTED_EDGE('',*,*,#53703,.T.) ;
#77715 = ORIENTED_EDGE('',*,*,#53706,.F.) ;
#77716 = ORIENTED_EDGE('',*,*,#52260,.F.) ;
#77717 = ORIENTED_EDGE('',*,*,#52265,.F.) ;
#77718 = ORIENTED_EDGE('',*,*,#52264,.F.) ;
#77719 = ORIENTED_EDGE('',*,*,#53707,.F.) ;
#77720 = ORIENTED_EDGE('',*,*,#52261,.F.) ;
#77721 = ORIENTED_EDGE('',*,*,#53704,.T.) ;
#77722 = ORIENTED_EDGE('',*,*,#50692,.F.) ;
#77723 = ORIENTED_EDGE('',*,*,#53708,.F.) ;
#77724 = ORIENTED_EDGE('',*,*,#50694,.F.) ;
#77725 = ORIENTED_EDGE('',*,*,#53706,.T.) ;
#77726 = ORIENTED_EDGE('',*,*,#50695,.F.) ;
#77727 = ORIENTED_EDGE('',*,*,#53709,.F.) ;
#77728 = ORIENTED_EDGE('',*,*,#51020,.F.) ;
#77729 = ORIENTED_EDGE('',*,*,#53705,.T.) ;
#77730 = ORIENTED_EDGE('',*,*,#51019,.F.) ;
#77731 = ORIENTED_EDGE('',*,*,#53710,.F.) ;
#77732 = ORIENTED_EDGE('',*,*,#50683,.F.) ;
#77733 = ORIENTED_EDGE('',*,*,#53707,.T.) ;
#77734 = ORIENTED_EDGE('',*,*,#50684,.F.) ;
#77735 = ORIENTED_EDGE('',*,*,#53711,.F.) ;
#77736 = ORIENTED_EDGE('',*,*,#50688,.F.) ;
#77737 = ORIENTED_EDGE('',*,*,#53709,.T.) ;
#77738 = ORIENTED_EDGE('',*,*,#53708,.T.) ;
#77739 = ORIENTED_EDGE('',*,*,#53712,.F.) ;
#77740 = ORIENTED_EDGE('',*,*,#53711,.T.) ;
#77741 = ORIENTED_EDGE('',*,*,#53710,.T.) ;
#77742 = ORIENTED_EDGE('',*,*,#53713,.F.) ;
#77743 = ORIENTED_EDGE('',*,*,#53712,.T.) ;
#77744 = ORIENTED_EDGE('',*,*,#50691,.F.) ;
#77745 = ORIENTED_EDGE('',*,*,#53714,.F.) ;
#77746 = ORIENTED_EDGE('',*,*,#51017,.F.) ;
#77747 = ORIENTED_EDGE('',*,*,#53713,.T.) ;
#77748 = ORIENTED_EDGE('',*,*,#51018,.F.) ;
#77749 = ORIENTED_EDGE('',*,*,#53715,.F.) ;
#77750 = ORIENTED_EDGE('',*,*,#50685,.F.) ;
#77751 = ORIENTED_EDGE('',*,*,#53715,.T.) ;
#77752 = ORIENTED_EDGE('',*,*,#53714,.T.) ;
#77753 = ORIENTED_EDGE('',*,*,#53716,.F.) ;
#77754 = ORIENTED_EDGE('',*,*,#53716,.T.) ;
#77755 = ORIENTED_EDGE('',*,*,#50690,.F.) ;
#77756 = ORIENTED_EDGE('',*,*,#53717,.F.) ;
#77757 = ORIENTED_EDGE('',*,*,#50686,.F.) ;
#77758 = ORIENTED_EDGE('',*,*,#52266,.F.) ;
#77759 = ORIENTED_EDGE('',*,*,#52259,.F.) ;
#77760 = ORIENTED_EDGE('',*,*,#52258,.F.) ;
#77761 = ORIENTED_EDGE('',*,*,#53717,.T.) ;
#77762 = ORIENTED_EDGE('',*,*,#52267,.F.) ;
#77763 = ORIENTED_EDGE('',*,*,#52563,.F.) ;
#77764 = ORIENTED_EDGE('',*,*,#52562,.F.) ;
#77765 = ORIENTED_EDGE('',*,*,#52561,.F.) ;
#77766 = ORIENTED_EDGE('',*,*,#53718,.F.) ;
#77767 = ORIENTED_EDGE('',*,*,#52564,.F.) ;
#77768 = ORIENTED_EDGE('',*,*,#53718,.T.) ;
#77769 = ORIENTED_EDGE('',*,*,#52560,.F.) ;
#77770 = ORIENTED_EDGE('',*,*,#53719,.F.) ;
#77771 = ORIENTED_EDGE('',*,*,#50614,.F.) ;
#77772 = ORIENTED_EDGE('',*,*,#53719,.T.) ;
#77773 = ORIENTED_EDGE('',*,*,#50382,.F.) ;
#77774 = ORIENTED_EDGE('',*,*,#53720,.F.) ;
#77775 = ORIENTED_EDGE('',*,*,#50615,.F.) ;
#77776 = ORIENTED_EDGE('',*,*,#50370,.F.) ;
#77777 = ORIENTED_EDGE('',*,*,#50616,.F.) ;
#77778 = ORIENTED_EDGE('',*,*,#53721,.F.) ;
#77779 = ORIENTED_EDGE('',*,*,#50376,.F.) ;
#77780 = ORIENTED_EDGE('',*,*,#53721,.T.) ;
#77781 = ORIENTED_EDGE('',*,*,#53720,.T.) ;
#77782 = ORIENTED_EDGE('',*,*,#53722,.F.) ;
#77783 = ORIENTED_EDGE('',*,*,#53722,.T.) ;
#77784 = ORIENTED_EDGE('',*,*,#50381,.F.) ;
#77785 = ORIENTED_EDGE('',*,*,#53723,.F.) ;
#77786 = ORIENTED_EDGE('',*,*,#50377,.F.) ;
#77787 = ORIENTED_EDGE('',*,*,#50372,.F.) ;
#77788 = ORIENTED_EDGE('',*,*,#50378,.F.) ;
#77789 = ORIENTED_EDGE('',*,*,#53724,.F.) ;
#77790 = ORIENTED_EDGE('',*,*,#50678,.F.) ;
#77791 = ORIENTED_EDGE('',*,*,#53724,.T.) ;
#77792 = ORIENTED_EDGE('',*,*,#53723,.T.) ;
#77793 = ORIENTED_EDGE('',*,*,#53725,.F.) ;
#77794 = ORIENTED_EDGE('',*,*,#53725,.T.) ;
#77795 = ORIENTED_EDGE('',*,*,#50380,.F.) ;
#77796 = ORIENTED_EDGE('',*,*,#53726,.F.) ;
#77797 = ORIENTED_EDGE('',*,*,#50679,.F.) ;
#77798 = ORIENTED_EDGE('',*,*,#53726,.T.) ;
#77799 = ORIENTED_EDGE('',*,*,#52559,.F.) ;
#77800 = ORIENTED_EDGE('',*,*,#53727,.F.) ;
#77801 = ORIENTED_EDGE('',*,*,#50680,.F.) ;
#77802 = ORIENTED_EDGE('',*,*,#53727,.T.) ;
#77803 = ORIENTED_EDGE('',*,*,#52558,.F.) ;
#77804 = ORIENTED_EDGE('',*,*,#52567,.F.) ;
#77805 = ORIENTED_EDGE('',*,*,#52568,.F.) ;
#77806 = ORIENTED_EDGE('',*,*,#52573,.F.) ;
#77807 = ORIENTED_EDGE('',*,*,#53728,.F.) ;
#77808 = ORIENTED_EDGE('',*,*,#53728,.T.) ;
#77809 = ORIENTED_EDGE('',*,*,#52572,.F.) ;
#77810 = ORIENTED_EDGE('',*,*,#53729,.F.) ;
#77811 = ORIENTED_EDGE('',*,*,#50675,.F.) ;
#77812 = ORIENTED_EDGE('',*,*,#53729,.T.) ;
#77813 = ORIENTED_EDGE('',*,*,#50364,.F.) ;
#77814 = ORIENTED_EDGE('',*,*,#53730,.F.) ;
#77815 = ORIENTED_EDGE('',*,*,#50676,.F.) ;
#77816 = ORIENTED_EDGE('',*,*,#50374,.F.) ;
#77817 = ORIENTED_EDGE('',*,*,#50677,.F.) ;
#77818 = ORIENTED_EDGE('',*,*,#53731,.F.) ;
#77819 = ORIENTED_EDGE('',*,*,#50368,.F.) ;
#77820 = ORIENTED_EDGE('',*,*,#53731,.T.) ;
#77821 = ORIENTED_EDGE('',*,*,#53730,.T.) ;
#77822 = ORIENTED_EDGE('',*,*,#53732,.F.) ;
#77823 = ORIENTED_EDGE('',*,*,#53732,.T.) ;
#77824 = ORIENTED_EDGE('',*,*,#50363,.F.) ;
#77825 = ORIENTED_EDGE('',*,*,#53733,.F.) ;
#77826 = ORIENTED_EDGE('',*,*,#50365,.F.) ;
#77827 = ORIENTED_EDGE('',*,*,#50375,.F.) ;
#77828 = ORIENTED_EDGE('',*,*,#50366,.F.) ;
#77829 = ORIENTED_EDGE('',*,*,#53734,.F.) ;
#77830 = ORIENTED_EDGE('',*,*,#50617,.F.) ;
#77831 = ORIENTED_EDGE('',*,*,#53734,.T.) ;
#77832 = ORIENTED_EDGE('',*,*,#53733,.T.) ;
#77833 = ORIENTED_EDGE('',*,*,#53735,.F.) ;
#77834 = ORIENTED_EDGE('',*,*,#53735,.T.) ;
#77835 = ORIENTED_EDGE('',*,*,#50362,.F.) ;
#77836 = ORIENTED_EDGE('',*,*,#53736,.F.) ;
#77837 = ORIENTED_EDGE('',*,*,#50618,.F.) ;
#77838 = ORIENTED_EDGE('',*,*,#53736,.T.) ;
#77839 = ORIENTED_EDGE('',*,*,#52571,.F.) ;
#77840 = ORIENTED_EDGE('',*,*,#53737,.F.) ;
#77841 = ORIENTED_EDGE('',*,*,#50619,.F.) ;
#77842 = ORIENTED_EDGE('',*,*,#52569,.F.) ;
#77843 = ORIENTED_EDGE('',*,*,#52566,.F.) ;
#77844 = ORIENTED_EDGE('',*,*,#52565,.F.) ;
#77845 = ORIENTED_EDGE('',*,*,#53737,.T.) ;
#77846 = ORIENTED_EDGE('',*,*,#52570,.F.) ;
#77847 = ORIENTED_EDGE('',*,*,#53738,.F.) ;
#77848 = ORIENTED_EDGE('',*,*,#49424,.F.) ;
#77849 = ORIENTED_EDGE('',*,*,#53739,.F.) ;
#77850 = ORIENTED_EDGE('',*,*,#52181,.F.) ;
#77851 = ORIENTED_EDGE('',*,*,#53739,.T.) ;
#77852 = ORIENTED_EDGE('',*,*,#49423,.F.) ;
#77853 = ORIENTED_EDGE('',*,*,#53740,.F.) ;
#77854 = ORIENTED_EDGE('',*,*,#52184,.F.) ;
#77855 = ORIENTED_EDGE('',*,*,#53738,.T.) ;
#77856 = ORIENTED_EDGE('',*,*,#52178,.F.) ;
#77857 = ORIENTED_EDGE('',*,*,#53741,.F.) ;
#77858 = ORIENTED_EDGE('',*,*,#49425,.F.) ;
#77859 = ORIENTED_EDGE('',*,*,#53740,.T.) ;
#77860 = ORIENTED_EDGE('',*,*,#49422,.F.) ;
#77861 = ORIENTED_EDGE('',*,*,#53742,.F.) ;
#77862 = ORIENTED_EDGE('',*,*,#52187,.F.) ;
#77863 = ORIENTED_EDGE('',*,*,#53741,.T.) ;
#77864 = ORIENTED_EDGE('',*,*,#52175,.F.) ;
#77865 = ORIENTED_EDGE('',*,*,#53743,.F.) ;
#77866 = ORIENTED_EDGE('',*,*,#49426,.F.) ;
#77867 = ORIENTED_EDGE('',*,*,#53742,.T.) ;
#77868 = ORIENTED_EDGE('',*,*,#49421,.F.) ;
#77869 = ORIENTED_EDGE('',*,*,#53744,.F.) ;
#77870 = ORIENTED_EDGE('',*,*,#52190,.F.) ;
#77871 = ORIENTED_EDGE('',*,*,#53743,.T.) ;
#77872 = ORIENTED_EDGE('',*,*,#52197,.F.) ;
#77873 = ORIENTED_EDGE('',*,*,#53745,.F.) ;
#77874 = ORIENTED_EDGE('',*,*,#49419,.F.) ;
#77875 = ORIENTED_EDGE('',*,*,#53744,.T.) ;
#77876 = ORIENTED_EDGE('',*,*,#49420,.F.) ;
#77877 = ORIENTED_EDGE('',*,*,#53745,.T.) ;
#77878 = ORIENTED_EDGE('',*,*,#52193,.F.) ;
#77879 = ORIENTED_EDGE('',*,*,#51026,.F.) ;
#77880 = ORIENTED_EDGE('',*,*,#51040,.F.) ;
#77881 = ORIENTED_EDGE('',*,*,#53746,.F.) ;
#77882 = ORIENTED_EDGE('',*,*,#51029,.F.) ;
#77883 = ORIENTED_EDGE('',*,*,#53747,.F.) ;
#77884 = ORIENTED_EDGE('',*,*,#51030,.F.) ;
#77885 = ORIENTED_EDGE('',*,*,#53748,.F.) ;
#77886 = ORIENTED_EDGE('',*,*,#51076,.F.) ;
#77887 = ORIENTED_EDGE('',*,*,#51028,.F.) ;
#77888 = ORIENTED_EDGE('',*,*,#51031,.F.) ;
#77889 = ORIENTED_EDGE('',*,*,#53749,.F.) ;
#77890 = ORIENTED_EDGE('',*,*,#51032,.F.) ;
#77891 = ORIENTED_EDGE('',*,*,#53748,.T.) ;
#77892 = ORIENTED_EDGE('',*,*,#53746,.T.) ;
#77893 = ORIENTED_EDGE('',*,*,#53750,.F.) ;
#77894 = ORIENTED_EDGE('',*,*,#53749,.T.) ;
#77895 = ORIENTED_EDGE('',*,*,#53747,.T.) ;
#77896 = ORIENTED_EDGE('',*,*,#53751,.F.) ;
#77897 = ORIENTED_EDGE('',*,*,#51024,.F.) ;
#77898 = ORIENTED_EDGE('',*,*,#51036,.F.) ;
#77899 = ORIENTED_EDGE('',*,*,#53752,.F.) ;
#77900 = ORIENTED_EDGE('',*,*,#51038,.F.) ;
#77901 = ORIENTED_EDGE('',*,*,#53750,.T.) ;
#77902 = ORIENTED_EDGE('',*,*,#51039,.F.) ;
#77903 = ORIENTED_EDGE('',*,*,#53753,.F.) ;
#77904 = ORIENTED_EDGE('',*,*,#51073,.F.) ;
#77905 = ORIENTED_EDGE('',*,*,#53751,.T.) ;
#77906 = ORIENTED_EDGE('',*,*,#51075,.F.) ;
#77907 = ORIENTED_EDGE('',*,*,#53754,.F.) ;
#77908 = ORIENTED_EDGE('',*,*,#51033,.F.) ;
#77909 = ORIENTED_EDGE('',*,*,#51022,.F.) ;
#77910 = ORIENTED_EDGE('',*,*,#51034,.F.) ;
#77911 = ORIENTED_EDGE('',*,*,#53755,.F.) ;
#77912 = ORIENTED_EDGE('',*,*,#51037,.F.) ;
#77913 = ORIENTED_EDGE('',*,*,#53753,.T.) ;
#77914 = ORIENTED_EDGE('',*,*,#53752,.T.) ;
#77915 = ORIENTED_EDGE('',*,*,#53756,.F.) ;
#77916 = ORIENTED_EDGE('',*,*,#53755,.T.) ;
#77917 = ORIENTED_EDGE('',*,*,#53754,.T.) ;
#77918 = ORIENTED_EDGE('',*,*,#53757,.F.) ;
#77919 = ORIENTED_EDGE('',*,*,#53756,.T.) ;
#77920 = ORIENTED_EDGE('',*,*,#51035,.F.) ;
#77921 = ORIENTED_EDGE('',*,*,#53757,.T.) ;
#77922 = ORIENTED_EDGE('',*,*,#51074,.F.) ;
#77923 = ORIENTED_EDGE('',*,*,#53758,.F.) ;
#77924 = ORIENTED_EDGE('',*,*,#49412,.F.) ;
#77925 = ORIENTED_EDGE('',*,*,#53759,.F.) ;
#77926 = ORIENTED_EDGE('',*,*,#51505,.F.) ;
#77927 = ORIENTED_EDGE('',*,*,#53759,.T.) ;
#77928 = ORIENTED_EDGE('',*,*,#49411,.T.) ;
#77929 = ORIENTED_EDGE('',*,*,#53760,.F.) ;
#77930 = ORIENTED_EDGE('',*,*,#53761,.F.) ;
#77931 = ORIENTED_EDGE('',*,*,#49413,.T.) ;
#77932 = ORIENTED_EDGE('',*,*,#53758,.T.) ;
#77933 = ORIENTED_EDGE('',*,*,#53762,.F.) ;
#77934 = ORIENTED_EDGE('',*,*,#53763,.F.) ;
#77935 = ORIENTED_EDGE('',*,*,#53760,.T.) ;
#77936 = ORIENTED_EDGE('',*,*,#49410,.F.) ;
#77937 = ORIENTED_EDGE('',*,*,#53764,.F.) ;
#77938 = ORIENTED_EDGE('',*,*,#51502,.F.) ;
#77939 = ORIENTED_EDGE('',*,*,#53761,.T.) ;
#77940 = ORIENTED_EDGE('',*,*,#51501,.F.) ;
#77941 = ORIENTED_EDGE('',*,*,#53765,.F.) ;
#77942 = ORIENTED_EDGE('',*,*,#51506,.F.) ;
#77943 = ORIENTED_EDGE('',*,*,#53766,.F.) ;
#77944 = ORIENTED_EDGE('',*,*,#51503,.F.) ;
#77945 = ORIENTED_EDGE('',*,*,#53767,.F.) ;
#77946 = ORIENTED_EDGE('',*,*,#51830,.F.) ;
#77947 = ORIENTED_EDGE('',*,*,#53762,.T.) ;
#77948 = ORIENTED_EDGE('',*,*,#51504,.F.) ;
#77949 = ORIENTED_EDGE('',*,*,#53768,.F.) ;
#77950 = ORIENTED_EDGE('',*,*,#51494,.F.) ;
#77951 = ORIENTED_EDGE('',*,*,#53763,.T.) ;
#77952 = ORIENTED_EDGE('',*,*,#51493,.F.) ;
#77953 = ORIENTED_EDGE('',*,*,#53769,.F.) ;
#77954 = ORIENTED_EDGE('',*,*,#49414,.F.) ;
#77955 = ORIENTED_EDGE('',*,*,#53770,.F.) ;
#77956 = ORIENTED_EDGE('',*,*,#49408,.F.) ;
#77957 = ORIENTED_EDGE('',*,*,#53771,.F.) ;
#77958 = ORIENTED_EDGE('',*,*,#51495,.F.) ;
#77959 = ORIENTED_EDGE('',*,*,#49409,.T.) ;
#77960 = ORIENTED_EDGE('',*,*,#53770,.T.) ;
#77961 = ORIENTED_EDGE('',*,*,#53772,.F.) ;
#77962 = ORIENTED_EDGE('',*,*,#53764,.T.) ;
#77963 = ORIENTED_EDGE('',*,*,#53767,.T.) ;
#77964 = ORIENTED_EDGE('',*,*,#53765,.T.) ;
#77965 = ORIENTED_EDGE('',*,*,#53773,.F.) ;
#77966 = ORIENTED_EDGE('',*,*,#53768,.T.) ;
#77967 = ORIENTED_EDGE('',*,*,#53766,.T.) ;
#77968 = ORIENTED_EDGE('',*,*,#53774,.F.) ;
#77969 = ORIENTED_EDGE('',*,*,#49407,.T.) ;
#77970 = ORIENTED_EDGE('',*,*,#53769,.T.) ;
#77971 = ORIENTED_EDGE('',*,*,#53775,.F.) ;
#77972 = ORIENTED_EDGE('',*,*,#53771,.T.) ;
#77973 = ORIENTED_EDGE('',*,*,#53772,.T.) ;
#77974 = ORIENTED_EDGE('',*,*,#51498,.F.) ;
#77975 = ORIENTED_EDGE('',*,*,#53776,.F.) ;
#77976 = ORIENTED_EDGE('',*,*,#51499,.F.) ;
#77977 = ORIENTED_EDGE('',*,*,#53773,.T.) ;
#77978 = ORIENTED_EDGE('',*,*,#51500,.F.) ;
#77979 = ORIENTED_EDGE('',*,*,#53777,.F.) ;
#77980 = ORIENTED_EDGE('',*,*,#51827,.F.) ;
#77981 = ORIENTED_EDGE('',*,*,#53774,.T.) ;
#77982 = ORIENTED_EDGE('',*,*,#51829,.F.) ;
#77983 = ORIENTED_EDGE('',*,*,#53778,.F.) ;
#77984 = ORIENTED_EDGE('',*,*,#51491,.F.) ;
#77985 = ORIENTED_EDGE('',*,*,#53775,.T.) ;
#77986 = ORIENTED_EDGE('',*,*,#51492,.F.) ;
#77987 = ORIENTED_EDGE('',*,*,#53779,.F.) ;
#77988 = ORIENTED_EDGE('',*,*,#51496,.F.) ;
#77989 = ORIENTED_EDGE('',*,*,#53777,.T.) ;
#77990 = ORIENTED_EDGE('',*,*,#53776,.T.) ;
#77991 = ORIENTED_EDGE('',*,*,#53780,.F.) ;
#77992 = ORIENTED_EDGE('',*,*,#53779,.T.) ;
#77993 = ORIENTED_EDGE('',*,*,#53778,.T.) ;
#77994 = ORIENTED_EDGE('',*,*,#53781,.F.) ;
#77995 = ORIENTED_EDGE('',*,*,#53780,.T.) ;
#77996 = ORIENTED_EDGE('',*,*,#51497,.F.) ;
#77997 = ORIENTED_EDGE('',*,*,#53781,.T.) ;
#77998 = ORIENTED_EDGE('',*,*,#51828,.F.) ;
#77999 = ORIENTED_EDGE('',*,*,#51836,.F.) ;
#78000 = ORIENTED_EDGE('',*,*,#51849,.F.) ;
#78001 = ORIENTED_EDGE('',*,*,#53782,.F.) ;
#78002 = ORIENTED_EDGE('',*,*,#51841,.F.) ;
#78003 = ORIENTED_EDGE('',*,*,#53783,.F.) ;
#78004 = ORIENTED_EDGE('',*,*,#51839,.F.) ;
#78005 = ORIENTED_EDGE('',*,*,#53784,.F.) ;
#78006 = ORIENTED_EDGE('',*,*,#51886,.F.) ;
#78007 = ORIENTED_EDGE('',*,*,#51838,.F.) ;
#78008 = ORIENTED_EDGE('',*,*,#51840,.F.) ;
#78009 = ORIENTED_EDGE('',*,*,#53785,.F.) ;
#78010 = ORIENTED_EDGE('',*,*,#51844,.F.) ;
#78011 = ORIENTED_EDGE('',*,*,#53784,.T.) ;
#78012 = ORIENTED_EDGE('',*,*,#53782,.T.) ;
#78013 = ORIENTED_EDGE('',*,*,#53786,.F.) ;
#78014 = ORIENTED_EDGE('',*,*,#53785,.T.) ;
#78015 = ORIENTED_EDGE('',*,*,#53783,.T.) ;
#78016 = ORIENTED_EDGE('',*,*,#53787,.F.) ;
#78017 = ORIENTED_EDGE('',*,*,#51834,.F.) ;
#78018 = ORIENTED_EDGE('',*,*,#51847,.F.) ;
#78019 = ORIENTED_EDGE('',*,*,#53788,.F.) ;
#78020 = ORIENTED_EDGE('',*,*,#51850,.F.) ;
#78021 = ORIENTED_EDGE('',*,*,#53786,.T.) ;
#78022 = ORIENTED_EDGE('',*,*,#51848,.F.) ;
#78023 = ORIENTED_EDGE('',*,*,#53789,.F.) ;
#78024 = ORIENTED_EDGE('',*,*,#51883,.F.) ;
#78025 = ORIENTED_EDGE('',*,*,#53787,.T.) ;
#78026 = ORIENTED_EDGE('',*,*,#51885,.F.) ;
#78027 = ORIENTED_EDGE('',*,*,#53790,.F.) ;
#78028 = ORIENTED_EDGE('',*,*,#51842,.F.) ;
#78029 = ORIENTED_EDGE('',*,*,#51832,.F.) ;
#78030 = ORIENTED_EDGE('',*,*,#51843,.F.) ;
#78031 = ORIENTED_EDGE('',*,*,#53791,.F.) ;
#78032 = ORIENTED_EDGE('',*,*,#51845,.F.) ;
#78033 = ORIENTED_EDGE('',*,*,#53789,.T.) ;
#78034 = ORIENTED_EDGE('',*,*,#53788,.T.) ;
#78035 = ORIENTED_EDGE('',*,*,#53792,.F.) ;
#78036 = ORIENTED_EDGE('',*,*,#53791,.T.) ;
#78037 = ORIENTED_EDGE('',*,*,#53790,.T.) ;
#78038 = ORIENTED_EDGE('',*,*,#53793,.F.) ;
#78039 = ORIENTED_EDGE('',*,*,#53792,.T.) ;
#78040 = ORIENTED_EDGE('',*,*,#51846,.F.) ;
#78041 = ORIENTED_EDGE('',*,*,#53793,.T.) ;
#78042 = ORIENTED_EDGE('',*,*,#51884,.F.) ;
#78043 = ORIENTED_EDGE('',*,*,#53794,.F.) ;
#78044 = ORIENTED_EDGE('',*,*,#52186,.F.) ;
#78045 = ORIENTED_EDGE('',*,*,#53795,.F.) ;
#78046 = ORIENTED_EDGE('',*,*,#52201,.F.) ;
#78047 = ORIENTED_EDGE('',*,*,#53795,.T.) ;
#78048 = ORIENTED_EDGE('',*,*,#52189,.F.) ;
#78049 = ORIENTED_EDGE('',*,*,#53796,.F.) ;
#78050 = ORIENTED_EDGE('',*,*,#52183,.F.) ;
#78051 = ORIENTED_EDGE('',*,*,#53794,.T.) ;
#78052 = ORIENTED_EDGE('',*,*,#53797,.F.) ;
#78053 = ORIENTED_EDGE('',*,*,#53796,.T.) ;
#78054 = ORIENTED_EDGE('',*,*,#52192,.F.) ;
#78055 = ORIENTED_EDGE('',*,*,#53798,.F.) ;
#78056 = ORIENTED_EDGE('',*,*,#52198,.F.) ;
#78057 = ORIENTED_EDGE('',*,*,#53797,.T.) ;
#78058 = ORIENTED_EDGE('',*,*,#52200,.F.) ;
#78059 = ORIENTED_EDGE('',*,*,#53799,.F.) ;
#78060 = ORIENTED_EDGE('',*,*,#52180,.F.) ;
#78061 = ORIENTED_EDGE('',*,*,#53798,.T.) ;
#78062 = ORIENTED_EDGE('',*,*,#52195,.F.) ;
#78063 = ORIENTED_EDGE('',*,*,#53800,.F.) ;
#78064 = ORIENTED_EDGE('',*,*,#52177,.F.) ;
#78065 = ORIENTED_EDGE('',*,*,#53799,.T.) ;
#78066 = ORIENTED_EDGE('',*,*,#53801,.F.) ;
#78067 = ORIENTED_EDGE('',*,*,#53800,.T.) ;
#78068 = ORIENTED_EDGE('',*,*,#52196,.F.) ;
#78069 = ORIENTED_EDGE('',*,*,#53801,.T.) ;
#78070 = ORIENTED_EDGE('',*,*,#52199,.F.) ;
#78071 = ORIENTED_EDGE('',*,*,#49232,.F.) ;
#78072 = ORIENTED_EDGE('',*,*,#51887,.F.) ;
#78073 = ORIENTED_EDGE('',*,*,#49246,.F.) ;
#78074 = ORIENTED_EDGE('',*,*,#51944,.F.) ;
#78075 = ORIENTED_EDGE('',*,*,#49234,.F.) ;
#78076 = ORIENTED_EDGE('',*,*,#51945,.F.) ;
#78077 = ORIENTED_EDGE('',*,*,#49244,.F.) ;
#78078 = ORIENTED_EDGE('',*,*,#51948,.F.) ;
#78079 = ORIENTED_EDGE('',*,*,#49242,.F.) ;
#78080 = ORIENTED_EDGE('',*,*,#51946,.F.) ;
#78081 = ORIENTED_EDGE('',*,*,#49236,.F.) ;
#78082 = ORIENTED_EDGE('',*,*,#51949,.F.) ;
#78083 = ORIENTED_EDGE('',*,*,#49240,.F.) ;
#78084 = ORIENTED_EDGE('',*,*,#49523,.F.) ;
#78085 = ORIENTED_EDGE('',*,*,#49238,.F.) ;
#78086 = ORIENTED_EDGE('',*,*,#51947,.F.) ;
#78087 = ORIENTED_EDGE('',*,*,#49513,.F.) ;
#78088 = ORIENTED_EDGE('',*,*,#53802,.T.) ;
#78089 = ORIENTED_EDGE('',*,*,#49545,.F.) ;
#78090 = ORIENTED_EDGE('',*,*,#53803,.T.) ;
#78091 = ORIENTED_EDGE('',*,*,#49501,.F.) ;
#78092 = ORIENTED_EDGE('',*,*,#53804,.T.) ;
#78093 = ORIENTED_EDGE('',*,*,#49551,.F.) ;
#78094 = ORIENTED_EDGE('',*,*,#53805,.T.) ;
#78095 = ORIENTED_EDGE('',*,*,#49489,.F.) ;
#78096 = ORIENTED_EDGE('',*,*,#53806,.T.) ;
#78097 = ORIENTED_EDGE('',*,*,#49557,.F.) ;
#78098 = ORIENTED_EDGE('',*,*,#53807,.T.) ;
#78099 = ORIENTED_EDGE('',*,*,#49477,.F.) ;
#78100 = ORIENTED_EDGE('',*,*,#53808,.T.) ;
#78101 = ORIENTED_EDGE('',*,*,#49563,.F.) ;
#78102 = ORIENTED_EDGE('',*,*,#53809,.T.) ;
#78103 = ORIENTED_EDGE('',*,*,#49465,.F.) ;
#78104 = ORIENTED_EDGE('',*,*,#53810,.T.) ;
#78105 = ORIENTED_EDGE('',*,*,#49569,.F.) ;
#78106 = ORIENTED_EDGE('',*,*,#53811,.T.) ;
#78107 = ORIENTED_EDGE('',*,*,#49453,.F.) ;
#78108 = ORIENTED_EDGE('',*,*,#53812,.T.) ;
#78109 = ORIENTED_EDGE('',*,*,#49575,.F.) ;
#78110 = ORIENTED_EDGE('',*,*,#53813,.T.) ;
#78111 = ORIENTED_EDGE('',*,*,#49441,.F.) ;
#78112 = ORIENTED_EDGE('',*,*,#53814,.T.) ;
#78113 = ORIENTED_EDGE('',*,*,#49581,.F.) ;
#78114 = ORIENTED_EDGE('',*,*,#53815,.T.) ;
#78115 = ORIENTED_EDGE('',*,*,#49429,.F.) ;
#78116 = ORIENTED_EDGE('',*,*,#53816,.T.) ;
#78117 = ORIENTED_EDGE('',*,*,#49587,.F.) ;
#78118 = ORIENTED_EDGE('',*,*,#53817,.T.) ;
#78119 = ORIENTED_EDGE('',*,*,#49417,.F.) ;
#78120 = ORIENTED_EDGE('',*,*,#53818,.T.) ;
#78121 = ORIENTED_EDGE('',*,*,#49593,.F.) ;
#78122 = ORIENTED_EDGE('',*,*,#53819,.T.) ;
#78123 = ORIENTED_EDGE('',*,*,#53820,.F.) ;
#78124 = ORIENTED_EDGE('',*,*,#53821,.T.) ;
#78125 = ORIENTED_EDGE('',*,*,#49549,.F.) ;
#78126 = ORIENTED_EDGE('',*,*,#53822,.T.) ;
#78127 = ORIENTED_EDGE('',*,*,#53820,.T.) ;
#78128 = ORIENTED_EDGE('',*,*,#49548,.F.) ;
#78129 = ORIENTED_EDGE('',*,*,#53823,.F.) ;
#78130 = ORIENTED_EDGE('',*,*,#53824,.F.) ;
#78131 = ORIENTED_EDGE('',*,*,#51102,.F.) ;
#78132 = ORIENTED_EDGE('',*,*,#49547,.F.) ;
#78133 = ORIENTED_EDGE('',*,*,#53825,.T.) ;
#78134 = ORIENTED_EDGE('',*,*,#53823,.T.) ;
#78135 = ORIENTED_EDGE('',*,*,#49741,.T.) ;
#78136 = ORIENTED_EDGE('',*,*,#53826,.T.) ;
#78137 = ORIENTED_EDGE('',*,*,#49543,.F.) ;
#78138 = ORIENTED_EDGE('',*,*,#53827,.F.) ;
#78139 = ORIENTED_EDGE('',*,*,#53828,.T.) ;
#78140 = ORIENTED_EDGE('',*,*,#49555,.F.) ;
#78141 = ORIENTED_EDGE('',*,*,#53829,.T.) ;
#78142 = ORIENTED_EDGE('',*,*,#53827,.T.) ;
#78143 = ORIENTED_EDGE('',*,*,#49554,.F.) ;
#78144 = ORIENTED_EDGE('',*,*,#53830,.F.) ;
#78145 = ORIENTED_EDGE('',*,*,#53831,.F.) ;
#78146 = ORIENTED_EDGE('',*,*,#51130,.F.) ;
#78147 = ORIENTED_EDGE('',*,*,#49553,.F.) ;
#78148 = ORIENTED_EDGE('',*,*,#53832,.T.) ;
#78149 = ORIENTED_EDGE('',*,*,#53830,.T.) ;
#78150 = ORIENTED_EDGE('',*,*,#53833,.F.) ;
#78151 = ORIENTED_EDGE('',*,*,#53834,.T.) ;
#78152 = ORIENTED_EDGE('',*,*,#49561,.F.) ;
#78153 = ORIENTED_EDGE('',*,*,#53835,.T.) ;
#78154 = ORIENTED_EDGE('',*,*,#53833,.T.) ;
#78155 = ORIENTED_EDGE('',*,*,#49560,.F.) ;
#78156 = ORIENTED_EDGE('',*,*,#53836,.F.) ;
#78157 = ORIENTED_EDGE('',*,*,#53837,.F.) ;
#78158 = ORIENTED_EDGE('',*,*,#51158,.F.) ;
#78159 = ORIENTED_EDGE('',*,*,#49559,.F.) ;
#78160 = ORIENTED_EDGE('',*,*,#53838,.T.) ;
#78161 = ORIENTED_EDGE('',*,*,#53836,.T.) ;
#78162 = ORIENTED_EDGE('',*,*,#53839,.F.) ;
#78163 = ORIENTED_EDGE('',*,*,#53840,.T.) ;
#78164 = ORIENTED_EDGE('',*,*,#49567,.F.) ;
#78165 = ORIENTED_EDGE('',*,*,#53841,.T.) ;
#78166 = ORIENTED_EDGE('',*,*,#53839,.T.) ;
#78167 = ORIENTED_EDGE('',*,*,#49566,.F.) ;
#78168 = ORIENTED_EDGE('',*,*,#53842,.F.) ;
#78169 = ORIENTED_EDGE('',*,*,#53843,.F.) ;
#78170 = ORIENTED_EDGE('',*,*,#51186,.F.) ;
#78171 = ORIENTED_EDGE('',*,*,#49565,.F.) ;
#78172 = ORIENTED_EDGE('',*,*,#53844,.T.) ;
#78173 = ORIENTED_EDGE('',*,*,#53842,.T.) ;
#78174 = ORIENTED_EDGE('',*,*,#53845,.F.) ;
#78175 = ORIENTED_EDGE('',*,*,#53846,.T.) ;
#78176 = ORIENTED_EDGE('',*,*,#49573,.F.) ;
#78177 = ORIENTED_EDGE('',*,*,#53847,.T.) ;
#78178 = ORIENTED_EDGE('',*,*,#53845,.T.) ;
#78179 = ORIENTED_EDGE('',*,*,#49572,.F.) ;
#78180 = ORIENTED_EDGE('',*,*,#53848,.F.) ;
#78181 = ORIENTED_EDGE('',*,*,#53849,.F.) ;
#78182 = ORIENTED_EDGE('',*,*,#51214,.F.) ;
#78183 = ORIENTED_EDGE('',*,*,#49571,.F.) ;
#78184 = ORIENTED_EDGE('',*,*,#53850,.T.) ;
#78185 = ORIENTED_EDGE('',*,*,#53848,.T.) ;
#78186 = ORIENTED_EDGE('',*,*,#53851,.F.) ;
#78187 = ORIENTED_EDGE('',*,*,#53852,.T.) ;
#78188 = ORIENTED_EDGE('',*,*,#49579,.F.) ;
#78189 = ORIENTED_EDGE('',*,*,#53853,.T.) ;
#78190 = ORIENTED_EDGE('',*,*,#53851,.T.) ;
#78191 = ORIENTED_EDGE('',*,*,#49578,.F.) ;
#78192 = ORIENTED_EDGE('',*,*,#53854,.F.) ;
#78193 = ORIENTED_EDGE('',*,*,#53855,.F.) ;
#78194 = ORIENTED_EDGE('',*,*,#51242,.F.) ;
#78195 = ORIENTED_EDGE('',*,*,#49577,.F.) ;
#78196 = ORIENTED_EDGE('',*,*,#53856,.T.) ;
#78197 = ORIENTED_EDGE('',*,*,#53854,.T.) ;
#78198 = ORIENTED_EDGE('',*,*,#53857,.F.) ;
#78199 = ORIENTED_EDGE('',*,*,#53858,.T.) ;
#78200 = ORIENTED_EDGE('',*,*,#49585,.F.) ;
#78201 = ORIENTED_EDGE('',*,*,#53859,.T.) ;
#78202 = ORIENTED_EDGE('',*,*,#53857,.T.) ;
#78203 = ORIENTED_EDGE('',*,*,#49584,.F.) ;
#78204 = ORIENTED_EDGE('',*,*,#53860,.F.) ;
#78205 = ORIENTED_EDGE('',*,*,#53861,.F.) ;
#78206 = ORIENTED_EDGE('',*,*,#51270,.F.) ;
#78207 = ORIENTED_EDGE('',*,*,#49583,.F.) ;
#78208 = ORIENTED_EDGE('',*,*,#53862,.T.) ;
#78209 = ORIENTED_EDGE('',*,*,#53860,.T.) ;
#78210 = ORIENTED_EDGE('',*,*,#53863,.F.) ;
#78211 = ORIENTED_EDGE('',*,*,#53864,.T.) ;
#78212 = ORIENTED_EDGE('',*,*,#49591,.F.) ;
#78213 = ORIENTED_EDGE('',*,*,#53865,.T.) ;
#78214 = ORIENTED_EDGE('',*,*,#53863,.T.) ;
#78215 = ORIENTED_EDGE('',*,*,#49590,.F.) ;
#78216 = ORIENTED_EDGE('',*,*,#53866,.F.) ;
#78217 = ORIENTED_EDGE('',*,*,#53867,.F.) ;
#78218 = ORIENTED_EDGE('',*,*,#51298,.F.) ;
#78219 = ORIENTED_EDGE('',*,*,#49589,.F.) ;
#78220 = ORIENTED_EDGE('',*,*,#53868,.T.) ;
#78221 = ORIENTED_EDGE('',*,*,#53866,.T.) ;
#78222 = ORIENTED_EDGE('',*,*,#51327,.F.) ;
#78223 = ORIENTED_EDGE('',*,*,#53869,.T.) ;
#78224 = ORIENTED_EDGE('',*,*,#49532,.F.) ;
#78225 = ORIENTED_EDGE('',*,*,#53870,.F.) ;
#78226 = ORIENTED_EDGE('',*,*,#53871,.F.) ;
#78227 = ORIENTED_EDGE('',*,*,#49595,.F.) ;
#78228 = ORIENTED_EDGE('',*,*,#53872,.T.) ;
#78229 = ORIENTED_EDGE('',*,*,#53870,.T.) ;
#78230 = ORIENTED_EDGE('',*,*,#51093,.F.) ;
#78231 = ORIENTED_EDGE('',*,*,#53873,.T.) ;
#78232 = ORIENTED_EDGE('',*,*,#53874,.F.) ;
#78233 = ORIENTED_EDGE('',*,*,#53874,.T.) ;
#78234 = ORIENTED_EDGE('',*,*,#53875,.T.) ;
#78235 = ORIENTED_EDGE('',*,*,#49512,.F.) ;
#78236 = ORIENTED_EDGE('',*,*,#53876,.F.) ;
#78237 = ORIENTED_EDGE('',*,*,#51094,.F.) ;
#78238 = ORIENTED_EDGE('',*,*,#52210,.F.) ;
#78239 = ORIENTED_EDGE('',*,*,#52208,.F.) ;
#78240 = ORIENTED_EDGE('',*,*,#53876,.T.) ;
#78241 = ORIENTED_EDGE('',*,*,#53877,.F.) ;
#78242 = ORIENTED_EDGE('',*,*,#53878,.T.) ;
#78243 = ORIENTED_EDGE('',*,*,#51077,.F.) ;
#78244 = ORIENTED_EDGE('',*,*,#53879,.T.) ;
#78245 = ORIENTED_EDGE('',*,*,#53877,.T.) ;
#78246 = ORIENTED_EDGE('',*,*,#51086,.F.) ;
#78247 = ORIENTED_EDGE('',*,*,#53880,.F.) ;
#78248 = ORIENTED_EDGE('',*,*,#49514,.F.) ;
#78249 = ORIENTED_EDGE('',*,*,#52217,.F.) ;
#78250 = ORIENTED_EDGE('',*,*,#52211,.F.) ;
#78251 = ORIENTED_EDGE('',*,*,#53880,.T.) ;
#78252 = ORIENTED_EDGE('',*,*,#51121,.F.) ;
#78253 = ORIENTED_EDGE('',*,*,#53881,.T.) ;
#78254 = ORIENTED_EDGE('',*,*,#53882,.F.) ;
#78255 = ORIENTED_EDGE('',*,*,#53882,.T.) ;
#78256 = ORIENTED_EDGE('',*,*,#53883,.T.) ;
#78257 = ORIENTED_EDGE('',*,*,#49500,.F.) ;
#78258 = ORIENTED_EDGE('',*,*,#53884,.F.) ;
#78259 = ORIENTED_EDGE('',*,*,#51122,.F.) ;
#78260 = ORIENTED_EDGE('',*,*,#53884,.T.) ;
#78261 = ORIENTED_EDGE('',*,*,#52631,.F.) ;
#78262 = ORIENTED_EDGE('',*,*,#52638,.F.) ;
#78263 = ORIENTED_EDGE('',*,*,#53885,.F.) ;
#78264 = ORIENTED_EDGE('',*,*,#53886,.T.) ;
#78265 = ORIENTED_EDGE('',*,*,#51105,.F.) ;
#78266 = ORIENTED_EDGE('',*,*,#53887,.T.) ;
#78267 = ORIENTED_EDGE('',*,*,#53885,.T.) ;
#78268 = ORIENTED_EDGE('',*,*,#51114,.F.) ;
#78269 = ORIENTED_EDGE('',*,*,#53888,.F.) ;
#78270 = ORIENTED_EDGE('',*,*,#49502,.F.) ;
#78271 = ORIENTED_EDGE('',*,*,#53888,.T.) ;
#78272 = ORIENTED_EDGE('',*,*,#52624,.F.) ;
#78273 = ORIENTED_EDGE('',*,*,#52632,.F.) ;
#78274 = ORIENTED_EDGE('',*,*,#51149,.F.) ;
#78275 = ORIENTED_EDGE('',*,*,#53889,.T.) ;
#78276 = ORIENTED_EDGE('',*,*,#53890,.F.) ;
#78277 = ORIENTED_EDGE('',*,*,#53890,.T.) ;
#78278 = ORIENTED_EDGE('',*,*,#53891,.T.) ;
#78279 = ORIENTED_EDGE('',*,*,#49488,.F.) ;
#78280 = ORIENTED_EDGE('',*,*,#53892,.F.) ;
#78281 = ORIENTED_EDGE('',*,*,#51150,.F.) ;
#78282 = ORIENTED_EDGE('',*,*,#53892,.T.) ;
#78283 = ORIENTED_EDGE('',*,*,#52779,.F.) ;
#78284 = ORIENTED_EDGE('',*,*,#52786,.F.) ;
#78285 = ORIENTED_EDGE('',*,*,#53893,.F.) ;
#78286 = ORIENTED_EDGE('',*,*,#53894,.T.) ;
#78287 = ORIENTED_EDGE('',*,*,#51133,.F.) ;
#78288 = ORIENTED_EDGE('',*,*,#53895,.T.) ;
#78289 = ORIENTED_EDGE('',*,*,#53893,.T.) ;
#78290 = ORIENTED_EDGE('',*,*,#51142,.F.) ;
#78291 = ORIENTED_EDGE('',*,*,#53896,.F.) ;
#78292 = ORIENTED_EDGE('',*,*,#49490,.F.) ;
#78293 = ORIENTED_EDGE('',*,*,#53896,.T.) ;
#78294 = ORIENTED_EDGE('',*,*,#52772,.F.) ;
#78295 = ORIENTED_EDGE('',*,*,#52780,.F.) ;
#78296 = ORIENTED_EDGE('',*,*,#51177,.F.) ;
#78297 = ORIENTED_EDGE('',*,*,#53897,.T.) ;
#78298 = ORIENTED_EDGE('',*,*,#53898,.F.) ;
#78299 = ORIENTED_EDGE('',*,*,#53898,.T.) ;
#78300 = ORIENTED_EDGE('',*,*,#53899,.T.) ;
#78301 = ORIENTED_EDGE('',*,*,#49476,.F.) ;
#78302 = ORIENTED_EDGE('',*,*,#53900,.F.) ;
#78303 = ORIENTED_EDGE('',*,*,#51178,.F.) ;
#78304 = ORIENTED_EDGE('',*,*,#53900,.T.) ;
#78305 = ORIENTED_EDGE('',*,*,#52927,.F.) ;
#78306 = ORIENTED_EDGE('',*,*,#52934,.F.) ;
#78307 = ORIENTED_EDGE('',*,*,#53901,.F.) ;
#78308 = ORIENTED_EDGE('',*,*,#53902,.T.) ;
#78309 = ORIENTED_EDGE('',*,*,#51161,.F.) ;
#78310 = ORIENTED_EDGE('',*,*,#53903,.T.) ;
#78311 = ORIENTED_EDGE('',*,*,#53901,.T.) ;
#78312 = ORIENTED_EDGE('',*,*,#51170,.F.) ;
#78313 = ORIENTED_EDGE('',*,*,#53904,.F.) ;
#78314 = ORIENTED_EDGE('',*,*,#49478,.F.) ;
#78315 = ORIENTED_EDGE('',*,*,#53904,.T.) ;
#78316 = ORIENTED_EDGE('',*,*,#52920,.F.) ;
#78317 = ORIENTED_EDGE('',*,*,#52928,.F.) ;
#78318 = ORIENTED_EDGE('',*,*,#51205,.F.) ;
#78319 = ORIENTED_EDGE('',*,*,#53905,.T.) ;
#78320 = ORIENTED_EDGE('',*,*,#53906,.F.) ;
#78321 = ORIENTED_EDGE('',*,*,#53906,.T.) ;
#78322 = ORIENTED_EDGE('',*,*,#53907,.T.) ;
#78323 = ORIENTED_EDGE('',*,*,#49464,.F.) ;
#78324 = ORIENTED_EDGE('',*,*,#53908,.F.) ;
#78325 = ORIENTED_EDGE('',*,*,#51206,.F.) ;
#78326 = ORIENTED_EDGE('',*,*,#53908,.T.) ;
#78327 = ORIENTED_EDGE('',*,*,#53075,.F.) ;
#78328 = ORIENTED_EDGE('',*,*,#53082,.F.) ;
#78329 = ORIENTED_EDGE('',*,*,#53909,.F.) ;
#78330 = ORIENTED_EDGE('',*,*,#53910,.T.) ;
#78331 = ORIENTED_EDGE('',*,*,#51189,.F.) ;
#78332 = ORIENTED_EDGE('',*,*,#53911,.T.) ;
#78333 = ORIENTED_EDGE('',*,*,#53909,.T.) ;
#78334 = ORIENTED_EDGE('',*,*,#51198,.F.) ;
#78335 = ORIENTED_EDGE('',*,*,#53912,.F.) ;
#78336 = ORIENTED_EDGE('',*,*,#49466,.F.) ;
#78337 = ORIENTED_EDGE('',*,*,#53912,.T.) ;
#78338 = ORIENTED_EDGE('',*,*,#53068,.F.) ;
#78339 = ORIENTED_EDGE('',*,*,#53076,.F.) ;
#78340 = ORIENTED_EDGE('',*,*,#51233,.F.) ;
#78341 = ORIENTED_EDGE('',*,*,#53913,.T.) ;
#78342 = ORIENTED_EDGE('',*,*,#53914,.F.) ;
#78343 = ORIENTED_EDGE('',*,*,#53914,.T.) ;
#78344 = ORIENTED_EDGE('',*,*,#53915,.T.) ;
#78345 = ORIENTED_EDGE('',*,*,#49452,.F.) ;
#78346 = ORIENTED_EDGE('',*,*,#53916,.F.) ;
#78347 = ORIENTED_EDGE('',*,*,#51234,.F.) ;
#78348 = ORIENTED_EDGE('',*,*,#53916,.T.) ;
#78349 = ORIENTED_EDGE('',*,*,#53223,.F.) ;
#78350 = ORIENTED_EDGE('',*,*,#53230,.F.) ;
#78351 = ORIENTED_EDGE('',*,*,#53917,.F.) ;
#78352 = ORIENTED_EDGE('',*,*,#53918,.T.) ;
#78353 = ORIENTED_EDGE('',*,*,#51217,.F.) ;
#78354 = ORIENTED_EDGE('',*,*,#53919,.T.) ;
#78355 = ORIENTED_EDGE('',*,*,#53917,.T.) ;
#78356 = ORIENTED_EDGE('',*,*,#51226,.F.) ;
#78357 = ORIENTED_EDGE('',*,*,#53920,.F.) ;
#78358 = ORIENTED_EDGE('',*,*,#49454,.F.) ;
#78359 = ORIENTED_EDGE('',*,*,#53920,.T.) ;
#78360 = ORIENTED_EDGE('',*,*,#53216,.F.) ;
#78361 = ORIENTED_EDGE('',*,*,#53224,.F.) ;
#78362 = ORIENTED_EDGE('',*,*,#51261,.F.) ;
#78363 = ORIENTED_EDGE('',*,*,#53921,.T.) ;
#78364 = ORIENTED_EDGE('',*,*,#53922,.F.) ;
#78365 = ORIENTED_EDGE('',*,*,#53922,.T.) ;
#78366 = ORIENTED_EDGE('',*,*,#53923,.T.) ;
#78367 = ORIENTED_EDGE('',*,*,#49440,.F.) ;
#78368 = ORIENTED_EDGE('',*,*,#53924,.F.) ;
#78369 = ORIENTED_EDGE('',*,*,#51262,.F.) ;
#78370 = ORIENTED_EDGE('',*,*,#53924,.T.) ;
#78371 = ORIENTED_EDGE('',*,*,#53371,.F.) ;
#78372 = ORIENTED_EDGE('',*,*,#53378,.F.) ;
#78373 = ORIENTED_EDGE('',*,*,#53925,.F.) ;
#78374 = ORIENTED_EDGE('',*,*,#53926,.T.) ;
#78375 = ORIENTED_EDGE('',*,*,#51245,.F.) ;
#78376 = ORIENTED_EDGE('',*,*,#53927,.T.) ;
#78377 = ORIENTED_EDGE('',*,*,#53925,.T.) ;
#78378 = ORIENTED_EDGE('',*,*,#51254,.F.) ;
#78379 = ORIENTED_EDGE('',*,*,#53928,.F.) ;
#78380 = ORIENTED_EDGE('',*,*,#49442,.F.) ;
#78381 = ORIENTED_EDGE('',*,*,#53928,.T.) ;
#78382 = ORIENTED_EDGE('',*,*,#53364,.F.) ;
#78383 = ORIENTED_EDGE('',*,*,#53372,.F.) ;
#78384 = ORIENTED_EDGE('',*,*,#51289,.F.) ;
#78385 = ORIENTED_EDGE('',*,*,#53929,.T.) ;
#78386 = ORIENTED_EDGE('',*,*,#53930,.F.) ;
#78387 = ORIENTED_EDGE('',*,*,#53930,.T.) ;
#78388 = ORIENTED_EDGE('',*,*,#53931,.T.) ;
#78389 = ORIENTED_EDGE('',*,*,#49428,.F.) ;
#78390 = ORIENTED_EDGE('',*,*,#53932,.F.) ;
#78391 = ORIENTED_EDGE('',*,*,#51290,.F.) ;
#78392 = ORIENTED_EDGE('',*,*,#53932,.T.) ;
#78393 = ORIENTED_EDGE('',*,*,#53519,.F.) ;
#78394 = ORIENTED_EDGE('',*,*,#53526,.F.) ;
#78395 = ORIENTED_EDGE('',*,*,#53933,.F.) ;
#78396 = ORIENTED_EDGE('',*,*,#53934,.T.) ;
#78397 = ORIENTED_EDGE('',*,*,#51273,.F.) ;
#78398 = ORIENTED_EDGE('',*,*,#53935,.T.) ;
#78399 = ORIENTED_EDGE('',*,*,#53933,.T.) ;
#78400 = ORIENTED_EDGE('',*,*,#51282,.F.) ;
#78401 = ORIENTED_EDGE('',*,*,#53936,.F.) ;
#78402 = ORIENTED_EDGE('',*,*,#49430,.F.) ;
#78403 = ORIENTED_EDGE('',*,*,#53936,.T.) ;
#78404 = ORIENTED_EDGE('',*,*,#53512,.F.) ;
#78405 = ORIENTED_EDGE('',*,*,#53520,.F.) ;
#78406 = ORIENTED_EDGE('',*,*,#51317,.F.) ;
#78407 = ORIENTED_EDGE('',*,*,#53937,.T.) ;
#78408 = ORIENTED_EDGE('',*,*,#53938,.F.) ;
#78409 = ORIENTED_EDGE('',*,*,#53938,.T.) ;
#78410 = ORIENTED_EDGE('',*,*,#53939,.T.) ;
#78411 = ORIENTED_EDGE('',*,*,#49416,.F.) ;
#78412 = ORIENTED_EDGE('',*,*,#53940,.F.) ;
#78413 = ORIENTED_EDGE('',*,*,#51318,.F.) ;
#78414 = ORIENTED_EDGE('',*,*,#53940,.T.) ;
#78415 = ORIENTED_EDGE('',*,*,#53667,.F.) ;
#78416 = ORIENTED_EDGE('',*,*,#53674,.F.) ;
#78417 = ORIENTED_EDGE('',*,*,#53941,.F.) ;
#78418 = ORIENTED_EDGE('',*,*,#53942,.T.) ;
#78419 = ORIENTED_EDGE('',*,*,#51301,.F.) ;
#78420 = ORIENTED_EDGE('',*,*,#53943,.T.) ;
#78421 = ORIENTED_EDGE('',*,*,#53941,.T.) ;
#78422 = ORIENTED_EDGE('',*,*,#51310,.F.) ;
#78423 = ORIENTED_EDGE('',*,*,#53944,.F.) ;
#78424 = ORIENTED_EDGE('',*,*,#49418,.F.) ;
#78425 = ORIENTED_EDGE('',*,*,#53944,.T.) ;
#78426 = ORIENTED_EDGE('',*,*,#53660,.F.) ;
#78427 = ORIENTED_EDGE('',*,*,#53668,.F.) ;
#78428 = ORIENTED_EDGE('',*,*,#53802,.F.) ;
#78429 = ORIENTED_EDGE('',*,*,#53875,.F.) ;
#78430 = ORIENTED_EDGE('',*,*,#53945,.F.) ;
#78431 = ORIENTED_EDGE('',*,*,#49546,.F.) ;
#78432 = ORIENTED_EDGE('',*,*,#53945,.T.) ;
#78433 = ORIENTED_EDGE('',*,*,#53873,.F.) ;
#78434 = ORIENTED_EDGE('',*,*,#53946,.F.) ;
#78435 = ORIENTED_EDGE('',*,*,#53825,.F.) ;
#78436 = ORIENTED_EDGE('',*,*,#52230,.F.) ;
#78437 = ORIENTED_EDGE('',*,*,#53824,.T.) ;
#78438 = ORIENTED_EDGE('',*,*,#53946,.T.) ;
#78439 = ORIENTED_EDGE('',*,*,#51092,.F.) ;
#78440 = ORIENTED_EDGE('',*,*,#53803,.F.) ;
#78441 = ORIENTED_EDGE('',*,*,#49544,.F.) ;
#78442 = ORIENTED_EDGE('',*,*,#53947,.F.) ;
#78443 = ORIENTED_EDGE('',*,*,#53879,.F.) ;
#78444 = ORIENTED_EDGE('',*,*,#53947,.T.) ;
#78445 = ORIENTED_EDGE('',*,*,#53826,.F.) ;
#78446 = ORIENTED_EDGE('',*,*,#53948,.F.) ;
#78447 = ORIENTED_EDGE('',*,*,#53878,.F.) ;
#78448 = ORIENTED_EDGE('',*,*,#53948,.T.) ;
#78449 = ORIENTED_EDGE('',*,*,#49740,.T.) ;
#78450 = ORIENTED_EDGE('',*,*,#52244,.F.) ;
#78451 = ORIENTED_EDGE('',*,*,#51078,.F.) ;
#78452 = ORIENTED_EDGE('',*,*,#53804,.F.) ;
#78453 = ORIENTED_EDGE('',*,*,#53883,.F.) ;
#78454 = ORIENTED_EDGE('',*,*,#53949,.F.) ;
#78455 = ORIENTED_EDGE('',*,*,#49552,.F.) ;
#78456 = ORIENTED_EDGE('',*,*,#53949,.T.) ;
#78457 = ORIENTED_EDGE('',*,*,#53881,.F.) ;
#78458 = ORIENTED_EDGE('',*,*,#53950,.F.) ;
#78459 = ORIENTED_EDGE('',*,*,#53832,.F.) ;
#78460 = ORIENTED_EDGE('',*,*,#52660,.F.) ;
#78461 = ORIENTED_EDGE('',*,*,#53831,.T.) ;
#78462 = ORIENTED_EDGE('',*,*,#53950,.T.) ;
#78463 = ORIENTED_EDGE('',*,*,#51120,.F.) ;
#78464 = ORIENTED_EDGE('',*,*,#53805,.F.) ;
#78465 = ORIENTED_EDGE('',*,*,#49550,.F.) ;
#78466 = ORIENTED_EDGE('',*,*,#53951,.F.) ;
#78467 = ORIENTED_EDGE('',*,*,#53887,.F.) ;
#78468 = ORIENTED_EDGE('',*,*,#53951,.T.) ;
#78469 = ORIENTED_EDGE('',*,*,#53821,.F.) ;
#78470 = ORIENTED_EDGE('',*,*,#53952,.F.) ;
#78471 = ORIENTED_EDGE('',*,*,#53886,.F.) ;
#78472 = ORIENTED_EDGE('',*,*,#53952,.T.) ;
#78473 = ORIENTED_EDGE('',*,*,#53822,.F.) ;
#78474 = ORIENTED_EDGE('',*,*,#52643,.F.) ;
#78475 = ORIENTED_EDGE('',*,*,#51106,.F.) ;
#78476 = ORIENTED_EDGE('',*,*,#53806,.F.) ;
#78477 = ORIENTED_EDGE('',*,*,#53891,.F.) ;
#78478 = ORIENTED_EDGE('',*,*,#53953,.F.) ;
#78479 = ORIENTED_EDGE('',*,*,#49558,.F.) ;
#78480 = ORIENTED_EDGE('',*,*,#53953,.T.) ;
#78481 = ORIENTED_EDGE('',*,*,#53889,.F.) ;
#78482 = ORIENTED_EDGE('',*,*,#53954,.F.) ;
#78483 = ORIENTED_EDGE('',*,*,#53838,.F.) ;
#78484 = ORIENTED_EDGE('',*,*,#52808,.F.) ;
#78485 = ORIENTED_EDGE('',*,*,#53837,.T.) ;
#78486 = ORIENTED_EDGE('',*,*,#53954,.T.) ;
#78487 = ORIENTED_EDGE('',*,*,#51148,.F.) ;
#78488 = ORIENTED_EDGE('',*,*,#53807,.F.) ;
#78489 = ORIENTED_EDGE('',*,*,#49556,.F.) ;
#78490 = ORIENTED_EDGE('',*,*,#53955,.F.) ;
#78491 = ORIENTED_EDGE('',*,*,#53895,.F.) ;
#78492 = ORIENTED_EDGE('',*,*,#53955,.T.) ;
#78493 = ORIENTED_EDGE('',*,*,#53828,.F.) ;
#78494 = ORIENTED_EDGE('',*,*,#53956,.F.) ;
#78495 = ORIENTED_EDGE('',*,*,#53894,.F.) ;
#78496 = ORIENTED_EDGE('',*,*,#53956,.T.) ;
#78497 = ORIENTED_EDGE('',*,*,#53829,.F.) ;
#78498 = ORIENTED_EDGE('',*,*,#52791,.F.) ;
#78499 = ORIENTED_EDGE('',*,*,#51134,.F.) ;
#78500 = ORIENTED_EDGE('',*,*,#53808,.F.) ;
#78501 = ORIENTED_EDGE('',*,*,#53899,.F.) ;
#78502 = ORIENTED_EDGE('',*,*,#53957,.F.) ;
#78503 = ORIENTED_EDGE('',*,*,#49564,.F.) ;
#78504 = ORIENTED_EDGE('',*,*,#53957,.T.) ;
#78505 = ORIENTED_EDGE('',*,*,#53897,.F.) ;
#78506 = ORIENTED_EDGE('',*,*,#53958,.F.) ;
#78507 = ORIENTED_EDGE('',*,*,#53844,.F.) ;
#78508 = ORIENTED_EDGE('',*,*,#52956,.F.) ;
#78509 = ORIENTED_EDGE('',*,*,#53843,.T.) ;
#78510 = ORIENTED_EDGE('',*,*,#53958,.T.) ;
#78511 = ORIENTED_EDGE('',*,*,#51176,.F.) ;
#78512 = ORIENTED_EDGE('',*,*,#53809,.F.) ;
#78513 = ORIENTED_EDGE('',*,*,#49562,.F.) ;
#78514 = ORIENTED_EDGE('',*,*,#53959,.F.) ;
#78515 = ORIENTED_EDGE('',*,*,#53903,.F.) ;
#78516 = ORIENTED_EDGE('',*,*,#53959,.T.) ;
#78517 = ORIENTED_EDGE('',*,*,#53834,.F.) ;
#78518 = ORIENTED_EDGE('',*,*,#53960,.F.) ;
#78519 = ORIENTED_EDGE('',*,*,#53902,.F.) ;
#78520 = ORIENTED_EDGE('',*,*,#53960,.T.) ;
#78521 = ORIENTED_EDGE('',*,*,#53835,.F.) ;
#78522 = ORIENTED_EDGE('',*,*,#52939,.F.) ;
#78523 = ORIENTED_EDGE('',*,*,#51162,.F.) ;
#78524 = ORIENTED_EDGE('',*,*,#53810,.F.) ;
#78525 = ORIENTED_EDGE('',*,*,#53907,.F.) ;
#78526 = ORIENTED_EDGE('',*,*,#53961,.F.) ;
#78527 = ORIENTED_EDGE('',*,*,#49570,.F.) ;
#78528 = ORIENTED_EDGE('',*,*,#53961,.T.) ;
#78529 = ORIENTED_EDGE('',*,*,#53905,.F.) ;
#78530 = ORIENTED_EDGE('',*,*,#53962,.F.) ;
#78531 = ORIENTED_EDGE('',*,*,#53850,.F.) ;
#78532 = ORIENTED_EDGE('',*,*,#53104,.F.) ;
#78533 = ORIENTED_EDGE('',*,*,#53849,.T.) ;
#78534 = ORIENTED_EDGE('',*,*,#53962,.T.) ;
#78535 = ORIENTED_EDGE('',*,*,#51204,.F.) ;
#78536 = ORIENTED_EDGE('',*,*,#53811,.F.) ;
#78537 = ORIENTED_EDGE('',*,*,#49568,.F.) ;
#78538 = ORIENTED_EDGE('',*,*,#53963,.F.) ;
#78539 = ORIENTED_EDGE('',*,*,#53911,.F.) ;
#78540 = ORIENTED_EDGE('',*,*,#53963,.T.) ;
#78541 = ORIENTED_EDGE('',*,*,#53840,.F.) ;
#78542 = ORIENTED_EDGE('',*,*,#53964,.F.) ;
#78543 = ORIENTED_EDGE('',*,*,#53910,.F.) ;
#78544 = ORIENTED_EDGE('',*,*,#53964,.T.) ;
#78545 = ORIENTED_EDGE('',*,*,#53841,.F.) ;
#78546 = ORIENTED_EDGE('',*,*,#53087,.F.) ;
#78547 = ORIENTED_EDGE('',*,*,#51190,.F.) ;
#78548 = ORIENTED_EDGE('',*,*,#53812,.F.) ;
#78549 = ORIENTED_EDGE('',*,*,#53915,.F.) ;
#78550 = ORIENTED_EDGE('',*,*,#53965,.F.) ;
#78551 = ORIENTED_EDGE('',*,*,#49576,.F.) ;
#78552 = ORIENTED_EDGE('',*,*,#53965,.T.) ;
#78553 = ORIENTED_EDGE('',*,*,#53913,.F.) ;
#78554 = ORIENTED_EDGE('',*,*,#53966,.F.) ;
#78555 = ORIENTED_EDGE('',*,*,#53856,.F.) ;
#78556 = ORIENTED_EDGE('',*,*,#53252,.F.) ;
#78557 = ORIENTED_EDGE('',*,*,#53855,.T.) ;
#78558 = ORIENTED_EDGE('',*,*,#53966,.T.) ;
#78559 = ORIENTED_EDGE('',*,*,#51232,.F.) ;
#78560 = ORIENTED_EDGE('',*,*,#53813,.F.) ;
#78561 = ORIENTED_EDGE('',*,*,#49574,.F.) ;
#78562 = ORIENTED_EDGE('',*,*,#53967,.F.) ;
#78563 = ORIENTED_EDGE('',*,*,#53919,.F.) ;
#78564 = ORIENTED_EDGE('',*,*,#53967,.T.) ;
#78565 = ORIENTED_EDGE('',*,*,#53846,.F.) ;
#78566 = ORIENTED_EDGE('',*,*,#53968,.F.) ;
#78567 = ORIENTED_EDGE('',*,*,#53918,.F.) ;
#78568 = ORIENTED_EDGE('',*,*,#53968,.T.) ;
#78569 = ORIENTED_EDGE('',*,*,#53847,.F.) ;
#78570 = ORIENTED_EDGE('',*,*,#53235,.F.) ;
#78571 = ORIENTED_EDGE('',*,*,#51218,.F.) ;
#78572 = ORIENTED_EDGE('',*,*,#53814,.F.) ;
#78573 = ORIENTED_EDGE('',*,*,#53923,.F.) ;
#78574 = ORIENTED_EDGE('',*,*,#53969,.F.) ;
#78575 = ORIENTED_EDGE('',*,*,#49582,.F.) ;
#78576 = ORIENTED_EDGE('',*,*,#53969,.T.) ;
#78577 = ORIENTED_EDGE('',*,*,#53921,.F.) ;
#78578 = ORIENTED_EDGE('',*,*,#53970,.F.) ;
#78579 = ORIENTED_EDGE('',*,*,#53862,.F.) ;
#78580 = ORIENTED_EDGE('',*,*,#53400,.F.) ;
#78581 = ORIENTED_EDGE('',*,*,#53861,.T.) ;
#78582 = ORIENTED_EDGE('',*,*,#53970,.T.) ;
#78583 = ORIENTED_EDGE('',*,*,#51260,.F.) ;
#78584 = ORIENTED_EDGE('',*,*,#53815,.F.) ;
#78585 = ORIENTED_EDGE('',*,*,#49580,.F.) ;
#78586 = ORIENTED_EDGE('',*,*,#53971,.F.) ;
#78587 = ORIENTED_EDGE('',*,*,#53927,.F.) ;
#78588 = ORIENTED_EDGE('',*,*,#53971,.T.) ;
#78589 = ORIENTED_EDGE('',*,*,#53852,.F.) ;
#78590 = ORIENTED_EDGE('',*,*,#53972,.F.) ;
#78591 = ORIENTED_EDGE('',*,*,#53926,.F.) ;
#78592 = ORIENTED_EDGE('',*,*,#53972,.T.) ;
#78593 = ORIENTED_EDGE('',*,*,#53853,.F.) ;
#78594 = ORIENTED_EDGE('',*,*,#53383,.F.) ;
#78595 = ORIENTED_EDGE('',*,*,#51246,.F.) ;
#78596 = ORIENTED_EDGE('',*,*,#53816,.F.) ;
#78597 = ORIENTED_EDGE('',*,*,#53931,.F.) ;
#78598 = ORIENTED_EDGE('',*,*,#53973,.F.) ;
#78599 = ORIENTED_EDGE('',*,*,#49588,.F.) ;
#78600 = ORIENTED_EDGE('',*,*,#53973,.T.) ;
#78601 = ORIENTED_EDGE('',*,*,#53929,.F.) ;
#78602 = ORIENTED_EDGE('',*,*,#53974,.F.) ;
#78603 = ORIENTED_EDGE('',*,*,#53868,.F.) ;
#78604 = ORIENTED_EDGE('',*,*,#53548,.F.) ;
#78605 = ORIENTED_EDGE('',*,*,#53867,.T.) ;
#78606 = ORIENTED_EDGE('',*,*,#53974,.T.) ;
#78607 = ORIENTED_EDGE('',*,*,#51288,.F.) ;
#78608 = ORIENTED_EDGE('',*,*,#53817,.F.) ;
#78609 = ORIENTED_EDGE('',*,*,#49586,.F.) ;
#78610 = ORIENTED_EDGE('',*,*,#53975,.F.) ;
#78611 = ORIENTED_EDGE('',*,*,#53935,.F.) ;
#78612 = ORIENTED_EDGE('',*,*,#53975,.T.) ;
#78613 = ORIENTED_EDGE('',*,*,#53858,.F.) ;
#78614 = ORIENTED_EDGE('',*,*,#53976,.F.) ;
#78615 = ORIENTED_EDGE('',*,*,#53934,.F.) ;
#78616 = ORIENTED_EDGE('',*,*,#53976,.T.) ;
#78617 = ORIENTED_EDGE('',*,*,#53859,.F.) ;
#78618 = ORIENTED_EDGE('',*,*,#53531,.F.) ;
#78619 = ORIENTED_EDGE('',*,*,#51274,.F.) ;
#78620 = ORIENTED_EDGE('',*,*,#53818,.F.) ;
#78621 = ORIENTED_EDGE('',*,*,#53939,.F.) ;
#78622 = ORIENTED_EDGE('',*,*,#53977,.F.) ;
#78623 = ORIENTED_EDGE('',*,*,#49594,.F.) ;
#78624 = ORIENTED_EDGE('',*,*,#53977,.T.) ;
#78625 = ORIENTED_EDGE('',*,*,#53937,.F.) ;
#78626 = ORIENTED_EDGE('',*,*,#53978,.F.) ;
#78627 = ORIENTED_EDGE('',*,*,#53872,.F.) ;
#78628 = ORIENTED_EDGE('',*,*,#53696,.F.) ;
#78629 = ORIENTED_EDGE('',*,*,#53871,.T.) ;
#78630 = ORIENTED_EDGE('',*,*,#53978,.T.) ;
#78631 = ORIENTED_EDGE('',*,*,#51316,.F.) ;
#78632 = ORIENTED_EDGE('',*,*,#53819,.F.) ;
#78633 = ORIENTED_EDGE('',*,*,#49592,.F.) ;
#78634 = ORIENTED_EDGE('',*,*,#53979,.F.) ;
#78635 = ORIENTED_EDGE('',*,*,#53943,.F.) ;
#78636 = ORIENTED_EDGE('',*,*,#53979,.T.) ;
#78637 = ORIENTED_EDGE('',*,*,#53864,.F.) ;
#78638 = ORIENTED_EDGE('',*,*,#53980,.F.) ;
#78639 = ORIENTED_EDGE('',*,*,#53942,.F.) ;
#78640 = ORIENTED_EDGE('',*,*,#53980,.T.) ;
#78641 = ORIENTED_EDGE('',*,*,#53865,.F.) ;
#78642 = ORIENTED_EDGE('',*,*,#53679,.F.) ;
#78643 = ORIENTED_EDGE('',*,*,#51302,.F.) ;
#78644 = ORIENTED_EDGE('',*,*,#49002,.T.) ;
#78645 = ORIENTED_EDGE('',*,*,#53981,.T.) ;
#78646 = ORIENTED_EDGE('',*,*,#49004,.F.) ;
#78647 = ORIENTED_EDGE('',*,*,#48927,.T.) ;
#78648 = ORIENTED_EDGE('',*,*,#48999,.T.) ;
#78649 = ORIENTED_EDGE('',*,*,#53982,.T.) ;
#78650 = ORIENTED_EDGE('',*,*,#49001,.F.) ;
#78651 = ORIENTED_EDGE('',*,*,#48935,.T.) ;
#78652 = ORIENTED_EDGE('',*,*,#48996,.T.) ;
#78653 = ORIENTED_EDGE('',*,*,#53983,.T.) ;
#78654 = ORIENTED_EDGE('',*,*,#48998,.F.) ;
#78655 = ORIENTED_EDGE('',*,*,#48943,.T.) ;
#78656 = ORIENTED_EDGE('',*,*,#48993,.T.) ;
#78657 = ORIENTED_EDGE('',*,*,#53984,.T.) ;
#78658 = ORIENTED_EDGE('',*,*,#48995,.F.) ;
#78659 = ORIENTED_EDGE('',*,*,#48951,.T.) ;
#78660 = ORIENTED_EDGE('',*,*,#48990,.T.) ;
#78661 = ORIENTED_EDGE('',*,*,#53985,.T.) ;
#78662 = ORIENTED_EDGE('',*,*,#48992,.F.) ;
#78663 = ORIENTED_EDGE('',*,*,#48959,.T.) ;
#78664 = ORIENTED_EDGE('',*,*,#48987,.T.) ;
#78665 = ORIENTED_EDGE('',*,*,#53986,.T.) ;
#78666 = ORIENTED_EDGE('',*,*,#48989,.F.) ;
#78667 = ORIENTED_EDGE('',*,*,#48967,.T.) ;
#78668 = ORIENTED_EDGE('',*,*,#50140,.F.) ;
#78669 = ORIENTED_EDGE('',*,*,#50144,.F.) ;
#78670 = ORIENTED_EDGE('',*,*,#53987,.F.) ;
#78671 = ORIENTED_EDGE('',*,*,#53987,.T.) ;
#78672 = ORIENTED_EDGE('',*,*,#49892,.F.) ;
#78673 = ORIENTED_EDGE('',*,*,#53988,.F.) ;
#78674 = ORIENTED_EDGE('',*,*,#49673,.F.) ;
#78675 = ORIENTED_EDGE('',*,*,#53988,.T.) ;
#78676 = ORIENTED_EDGE('',*,*,#49891,.F.) ;
#78677 = ORIENTED_EDGE('',*,*,#53989,.F.) ;
#78678 = ORIENTED_EDGE('',*,*,#53698,.F.) ;
#78679 = ORIENTED_EDGE('',*,*,#53990,.F.) ;
#78680 = ORIENTED_EDGE('',*,*,#51326,.F.) ;
#78681 = ORIENTED_EDGE('',*,*,#53989,.T.) ;
#78682 = ORIENTED_EDGE('',*,*,#49890,.F.) ;
#78683 = ORIENTED_EDGE('',*,*,#53869,.F.) ;
#78684 = ORIENTED_EDGE('',*,*,#53990,.T.) ;
#78685 = ORIENTED_EDGE('',*,*,#53991,.F.) ;
#78686 = ORIENTED_EDGE('',*,*,#53992,.F.) ;
#78687 = ORIENTED_EDGE('',*,*,#49533,.F.) ;
#78688 = ORIENTED_EDGE('',*,*,#53991,.T.) ;
#78689 = ORIENTED_EDGE('',*,*,#49889,.F.) ;
#78690 = ORIENTED_EDGE('',*,*,#49738,.F.) ;
#78691 = ORIENTED_EDGE('',*,*,#53992,.T.) ;
#78692 = ORIENTED_EDGE('',*,*,#53993,.F.) ;
#78693 = ORIENTED_EDGE('',*,*,#53993,.T.) ;
#78694 = ORIENTED_EDGE('',*,*,#49888,.F.) ;
#78695 = ORIENTED_EDGE('',*,*,#53994,.F.) ;
#78696 = ORIENTED_EDGE('',*,*,#49990,.F.) ;
#78697 = ORIENTED_EDGE('',*,*,#50165,.F.) ;
#78698 = ORIENTED_EDGE('',*,*,#50155,.F.) ;
#78699 = ORIENTED_EDGE('',*,*,#53995,.F.) ;
#78700 = ORIENTED_EDGE('',*,*,#53994,.T.) ;
#78701 = ORIENTED_EDGE('',*,*,#49887,.T.) ;
#78702 = ORIENTED_EDGE('',*,*,#53996,.F.) ;
#78703 = ORIENTED_EDGE('',*,*,#53997,.F.) ;
#78704 = ORIENTED_EDGE('',*,*,#53995,.T.) ;
#78705 = ORIENTED_EDGE('',*,*,#49334,.F.) ;
#78706 = ORIENTED_EDGE('',*,*,#53998,.F.) ;
#78707 = ORIENTED_EDGE('',*,*,#49885,.F.) ;
#78708 = ORIENTED_EDGE('',*,*,#53996,.T.) ;
#78709 = ORIENTED_EDGE('',*,*,#49886,.F.) ;
#78710 = ORIENTED_EDGE('',*,*,#53999,.F.) ;
#78711 = ORIENTED_EDGE('',*,*,#49668,.F.) ;
#78712 = ORIENTED_EDGE('',*,*,#53997,.T.) ;
#78713 = ORIENTED_EDGE('',*,*,#49671,.F.) ;
#78714 = ORIENTED_EDGE('',*,*,#54000,.F.) ;
#78715 = ORIENTED_EDGE('',*,*,#49991,.F.) ;
#78716 = ORIENTED_EDGE('',*,*,#53999,.T.) ;
#78717 = ORIENTED_EDGE('',*,*,#53998,.T.) ;
#78718 = ORIENTED_EDGE('',*,*,#54001,.F.) ;
#78719 = ORIENTED_EDGE('',*,*,#49992,.T.) ;
#78720 = ORIENTED_EDGE('',*,*,#54000,.T.) ;
#78721 = ORIENTED_EDGE('',*,*,#54002,.F.) ;
#78722 = ORIENTED_EDGE('',*,*,#54003,.F.) ;
#78723 = ORIENTED_EDGE('',*,*,#54001,.T.) ;
#78724 = ORIENTED_EDGE('',*,*,#49333,.F.) ;
#78725 = ORIENTED_EDGE('',*,*,#54004,.F.) ;
#78726 = ORIENTED_EDGE('',*,*,#49669,.F.) ;
#78727 = ORIENTED_EDGE('',*,*,#54002,.T.) ;
#78728 = ORIENTED_EDGE('',*,*,#49670,.F.) ;
#78729 = ORIENTED_EDGE('',*,*,#54005,.F.) ;
#78730 = ORIENTED_EDGE('',*,*,#50103,.F.) ;
#78731 = ORIENTED_EDGE('',*,*,#54003,.T.) ;
#78732 = ORIENTED_EDGE('',*,*,#50105,.F.) ;
#78733 = ORIENTED_EDGE('',*,*,#54006,.F.) ;
#78734 = ORIENTED_EDGE('',*,*,#49993,.F.) ;
#78735 = ORIENTED_EDGE('',*,*,#54005,.T.) ;
#78736 = ORIENTED_EDGE('',*,*,#54004,.T.) ;
#78737 = ORIENTED_EDGE('',*,*,#54007,.F.) ;
#78738 = ORIENTED_EDGE('',*,*,#54006,.T.) ;
#78739 = ORIENTED_EDGE('',*,*,#49288,.F.) ;
#78740 = ORIENTED_EDGE('',*,*,#48982,.F.) ;
#78741 = ORIENTED_EDGE('',*,*,#54007,.T.) ;
#78742 = ORIENTED_EDGE('',*,*,#49332,.F.) ;
#78743 = ORIENTED_EDGE('',*,*,#48980,.F.) ;
#78744 = ORIENTED_EDGE('',*,*,#50104,.F.) ;
#78745 = ORIENTED_EDGE('',*,*,#48984,.T.) ;
#78746 = ORIENTED_EDGE('',*,*,#49285,.F.) ;
#78747 = ORIENTED_EDGE('',*,*,#48974,.F.) ;
#78748 = ORIENTED_EDGE('',*,*,#48978,.T.) ;
#78749 = ORIENTED_EDGE('',*,*,#49331,.F.) ;
#78750 = ORIENTED_EDGE('',*,*,#48972,.F.) ;
#78751 = ORIENTED_EDGE('',*,*,#50106,.F.) ;
#78752 = ORIENTED_EDGE('',*,*,#48976,.T.) ;
#78753 = ORIENTED_EDGE('',*,*,#48985,.F.) ;
#78754 = ORIENTED_EDGE('',*,*,#48966,.F.) ;
#78755 = ORIENTED_EDGE('',*,*,#48970,.T.) ;
#78756 = ORIENTED_EDGE('',*,*,#49330,.F.) ;
#78757 = ORIENTED_EDGE('',*,*,#48964,.F.) ;
#78758 = ORIENTED_EDGE('',*,*,#50107,.F.) ;
#78759 = ORIENTED_EDGE('',*,*,#48968,.T.) ;
#78760 = ORIENTED_EDGE('',*,*,#48988,.F.) ;
#78761 = ORIENTED_EDGE('',*,*,#48958,.F.) ;
#78762 = ORIENTED_EDGE('',*,*,#48962,.T.) ;
#78763 = ORIENTED_EDGE('',*,*,#49329,.F.) ;
#78764 = ORIENTED_EDGE('',*,*,#48956,.F.) ;
#78765 = ORIENTED_EDGE('',*,*,#53986,.F.) ;
#78766 = ORIENTED_EDGE('',*,*,#48960,.T.) ;
#78767 = ORIENTED_EDGE('',*,*,#48991,.F.) ;
#78768 = ORIENTED_EDGE('',*,*,#48950,.F.) ;
#78769 = ORIENTED_EDGE('',*,*,#48954,.T.) ;
#78770 = ORIENTED_EDGE('',*,*,#49328,.F.) ;
#78771 = ORIENTED_EDGE('',*,*,#48948,.F.) ;
#78772 = ORIENTED_EDGE('',*,*,#53985,.F.) ;
#78773 = ORIENTED_EDGE('',*,*,#48952,.T.) ;
#78774 = ORIENTED_EDGE('',*,*,#48994,.F.) ;
#78775 = ORIENTED_EDGE('',*,*,#48942,.F.) ;
#78776 = ORIENTED_EDGE('',*,*,#48946,.T.) ;
#78777 = ORIENTED_EDGE('',*,*,#49327,.F.) ;
#78778 = ORIENTED_EDGE('',*,*,#48940,.F.) ;
#78779 = ORIENTED_EDGE('',*,*,#53984,.F.) ;
#78780 = ORIENTED_EDGE('',*,*,#48944,.T.) ;
#78781 = ORIENTED_EDGE('',*,*,#48997,.F.) ;
#78782 = ORIENTED_EDGE('',*,*,#48934,.F.) ;
#78783 = ORIENTED_EDGE('',*,*,#48938,.T.) ;
#78784 = ORIENTED_EDGE('',*,*,#49326,.F.) ;
#78785 = ORIENTED_EDGE('',*,*,#48932,.F.) ;
#78786 = ORIENTED_EDGE('',*,*,#53983,.F.) ;
#78787 = ORIENTED_EDGE('',*,*,#48936,.T.) ;
#78788 = ORIENTED_EDGE('',*,*,#49000,.F.) ;
#78789 = ORIENTED_EDGE('',*,*,#48926,.F.) ;
#78790 = ORIENTED_EDGE('',*,*,#48930,.T.) ;
#78791 = ORIENTED_EDGE('',*,*,#49325,.F.) ;
#78792 = ORIENTED_EDGE('',*,*,#48924,.F.) ;
#78793 = ORIENTED_EDGE('',*,*,#53982,.F.) ;
#78794 = ORIENTED_EDGE('',*,*,#48928,.T.) ;
#78795 = ORIENTED_EDGE('',*,*,#49003,.F.) ;
#78796 = ORIENTED_EDGE('',*,*,#48918,.F.) ;
#78797 = ORIENTED_EDGE('',*,*,#50136,.F.) ;
#78798 = ORIENTED_EDGE('',*,*,#50141,.F.) ;
#78799 = ORIENTED_EDGE('',*,*,#54008,.F.) ;
#78800 = ORIENTED_EDGE('',*,*,#48922,.T.) ;
#78801 = ORIENTED_EDGE('',*,*,#49324,.F.) ;
#78802 = ORIENTED_EDGE('',*,*,#48916,.F.) ;
#78803 = ORIENTED_EDGE('',*,*,#53981,.F.) ;
#78804 = ORIENTED_EDGE('',*,*,#54008,.T.) ;
#78805 = ORIENTED_EDGE('',*,*,#49735,.F.) ;
#78806 = ORIENTED_EDGE('',*,*,#54009,.F.) ;
#78807 = ORIENTED_EDGE('',*,*,#49908,.F.) ;
#78808 = ORIENTED_EDGE('',*,*,#48920,.T.) ;
#78809 = ORIENTED_EDGE('',*,*,#49294,.F.) ;
#78810 = ORIENTED_EDGE('',*,*,#48910,.F.) ;
#78811 = ORIENTED_EDGE('',*,*,#54009,.T.) ;
#78812 = ORIENTED_EDGE('',*,*,#50222,.F.) ;
#78813 = ORIENTED_EDGE('',*,*,#54010,.F.) ;
#78814 = ORIENTED_EDGE('',*,*,#49909,.F.) ;
#78815 = ORIENTED_EDGE('',*,*,#48914,.T.) ;
#78816 = ORIENTED_EDGE('',*,*,#49323,.F.) ;
#78817 = ORIENTED_EDGE('',*,*,#48908,.F.) ;
#78818 = ORIENTED_EDGE('',*,*,#50098,.F.) ;
#78819 = ORIENTED_EDGE('',*,*,#54010,.T.) ;
#78820 = ORIENTED_EDGE('',*,*,#49999,.F.) ;
#78821 = ORIENTED_EDGE('',*,*,#54011,.F.) ;
#78822 = ORIENTED_EDGE('',*,*,#49910,.F.) ;
#78823 = ORIENTED_EDGE('',*,*,#48912,.T.) ;
#78824 = ORIENTED_EDGE('',*,*,#49291,.F.) ;
#78825 = ORIENTED_EDGE('',*,*,#54012,.F.) ;
#78826 = ORIENTED_EDGE('',*,*,#54011,.T.) ;
#78827 = ORIENTED_EDGE('',*,*,#50345,.F.) ;
#78828 = ORIENTED_EDGE('',*,*,#54013,.F.) ;
#78829 = ORIENTED_EDGE('',*,*,#48906,.T.) ;
#78830 = ORIENTED_EDGE('',*,*,#49322,.F.) ;
#78831 = ORIENTED_EDGE('',*,*,#48904,.F.) ;
#78832 = ORIENTED_EDGE('',*,*,#50099,.F.) ;
#78833 = ORIENTED_EDGE('',*,*,#54012,.T.) ;
#78834 = ORIENTED_EDGE('',*,*,#50102,.F.) ;
#78835 = ORIENTED_EDGE('',*,*,#54014,.F.) ;
#78836 = ORIENTED_EDGE('',*,*,#49994,.F.) ;
#78837 = ORIENTED_EDGE('',*,*,#54013,.T.) ;
#78838 = ORIENTED_EDGE('',*,*,#49535,.F.) ;
#78839 = ORIENTED_EDGE('',*,*,#54015,.F.) ;
#78840 = ORIENTED_EDGE('',*,*,#49911,.F.) ;
#78841 = ORIENTED_EDGE('',*,*,#49995,.T.) ;
#78842 = ORIENTED_EDGE('',*,*,#54014,.T.) ;
#78843 = ORIENTED_EDGE('',*,*,#54016,.F.) ;
#78844 = ORIENTED_EDGE('',*,*,#54017,.F.) ;
#78845 = ORIENTED_EDGE('',*,*,#54015,.T.) ;
#78846 = ORIENTED_EDGE('',*,*,#49737,.F.) ;
#78847 = ORIENTED_EDGE('',*,*,#54018,.F.) ;
#78848 = ORIENTED_EDGE('',*,*,#48902,.T.) ;
#78849 = ORIENTED_EDGE('',*,*,#49321,.F.) ;
#78850 = ORIENTED_EDGE('',*,*,#54019,.F.) ;
#78851 = ORIENTED_EDGE('',*,*,#50100,.F.) ;
#78852 = ORIENTED_EDGE('',*,*,#54016,.T.) ;
#78853 = ORIENTED_EDGE('',*,*,#50101,.F.) ;
#78854 = ORIENTED_EDGE('',*,*,#54020,.F.) ;
#78855 = ORIENTED_EDGE('',*,*,#49808,.F.) ;
#78856 = ORIENTED_EDGE('',*,*,#54017,.T.) ;
#78857 = ORIENTED_EDGE('',*,*,#49811,.F.) ;
#78858 = ORIENTED_EDGE('',*,*,#54021,.F.) ;
#78859 = ORIENTED_EDGE('',*,*,#49996,.F.) ;
#78860 = ORIENTED_EDGE('',*,*,#54018,.T.) ;
#78861 = ORIENTED_EDGE('',*,*,#49997,.F.) ;
#78862 = ORIENTED_EDGE('',*,*,#54022,.F.) ;
#78863 = ORIENTED_EDGE('',*,*,#49912,.F.) ;
#78864 = ORIENTED_EDGE('',*,*,#54020,.T.) ;
#78865 = ORIENTED_EDGE('',*,*,#54019,.T.) ;
#78866 = ORIENTED_EDGE('',*,*,#54023,.F.) ;
#78867 = ORIENTED_EDGE('',*,*,#54022,.T.) ;
#78868 = ORIENTED_EDGE('',*,*,#54021,.T.) ;
#78869 = ORIENTED_EDGE('',*,*,#54024,.F.) ;
#78870 = ORIENTED_EDGE('',*,*,#49913,.T.) ;
#78871 = ORIENTED_EDGE('',*,*,#54023,.T.) ;
#78872 = ORIENTED_EDGE('',*,*,#49320,.F.) ;
#78873 = ORIENTED_EDGE('',*,*,#54025,.F.) ;
#78874 = ORIENTED_EDGE('',*,*,#49809,.F.) ;
#78875 = ORIENTED_EDGE('',*,*,#54024,.T.) ;
#78876 = ORIENTED_EDGE('',*,*,#49810,.F.) ;
#78877 = ORIENTED_EDGE('',*,*,#54026,.F.) ;
#78878 = ORIENTED_EDGE('',*,*,#49899,.F.) ;
#78879 = ORIENTED_EDGE('',*,*,#54026,.T.) ;
#78880 = ORIENTED_EDGE('',*,*,#54025,.T.) ;
#78881 = ORIENTED_EDGE('',*,*,#54027,.F.) ;
#78882 = ORIENTED_EDGE('',*,*,#54027,.T.) ;
#78883 = ORIENTED_EDGE('',*,*,#49319,.F.) ;
#78884 = ORIENTED_EDGE('',*,*,#54028,.F.) ;
#78885 = ORIENTED_EDGE('',*,*,#49900,.F.) ;
#78886 = ORIENTED_EDGE('',*,*,#50154,.F.) ;
#78887 = ORIENTED_EDGE('',*,*,#50146,.F.) ;
#78888 = ORIENTED_EDGE('',*,*,#54028,.T.) ;
#78889 = ORIENTED_EDGE('',*,*,#50158,.F.) ;
#78890 = ORIENTED_EDGE('',*,*,#50150,.F.) ;
#78891 = ORIENTED_EDGE('',*,*,#50149,.F.) ;
#78892 = ORIENTED_EDGE('',*,*,#54029,.F.) ;
#78893 = ORIENTED_EDGE('',*,*,#50159,.F.) ;
#78894 = ORIENTED_EDGE('',*,*,#54029,.T.) ;
#78895 = ORIENTED_EDGE('',*,*,#50157,.F.) ;
#78896 = ORIENTED_EDGE('',*,*,#48899,.F.) ;
#78897 = ORIENTED_EDGE('',*,*,#50160,.F.) ;
#78898 = ORIENTED_EDGE('',*,*,#50174,.F.) ;
#78899 = ORIENTED_EDGE('',*,*,#50179,.F.) ;
#78900 = ORIENTED_EDGE('',*,*,#50178,.F.) ;
#78901 = ORIENTED_EDGE('',*,*,#54030,.F.) ;
#78902 = ORIENTED_EDGE('',*,*,#50175,.F.) ;
#78903 = ORIENTED_EDGE('',*,*,#48897,.T.) ;
#78904 = ORIENTED_EDGE('',*,*,#50171,.F.) ;
#78905 = ORIENTED_EDGE('',*,*,#54030,.T.) ;
#78906 = ORIENTED_EDGE('',*,*,#50177,.F.) ;
#78907 = TOROIDAL_SURFACE('',#91124,0.2,0.1) ;
#78908 = TOROIDAL_SURFACE('',#91129,2.,0.1) ;
#78909 = TOROIDAL_SURFACE('',#91134,1.4,0.1) ;
#78910 = TOROIDAL_SURFACE('',#91138,1.6,0.1) ;
#78911 = TOROIDAL_SURFACE('',#91143,0.2,0.1) ;
#78912 = TOROIDAL_SURFACE('',#91167,0.2,0.1) ;
#78913 = TOROIDAL_SURFACE('',#91175,2.,0.1) ;
#78914 = TOROIDAL_SURFACE('',#91180,1.4,0.1) ;
#78915 = TOROIDAL_SURFACE('',#91184,1.6,0.1) ;
#78916 = TOROIDAL_SURFACE('',#91189,0.2,0.1) ;
#78917 = TOROIDAL_SURFACE('',#91443,0.2,0.1) ;
#78918 = TOROIDAL_SURFACE('',#91470,0.2,0.1) ;
#78919 = TOROIDAL_SURFACE('',#91473,0.2,0.1) ;
#78920 = TOROIDAL_SURFACE('',#91490,0.2,0.1) ;
#78921 = TOROIDAL_SURFACE('',#91496,0.2,0.1) ;
#78922 = TOROIDAL_SURFACE('',#91514,0.2,0.1) ;
#78923 = TOROIDAL_SURFACE('',#91517,0.2,0.1) ;
#78924 = TOROIDAL_SURFACE('',#91534,0.2,0.1) ;
#78925 = TOROIDAL_SURFACE('',#91540,0.2,0.1) ;
#78926 = TOROIDAL_SURFACE('',#91555,3.1,0.1) ;
#78927 = TOROIDAL_SURFACE('',#91565,0.2,0.1) ;
#78928 = TOROIDAL_SURFACE('',#91567,2.9,0.1) ;
#78929 = TOROIDAL_SURFACE('',#91572,0.2,0.1) ;
#78930 = TOROIDAL_SURFACE('',#91581,3.1,0.1) ;
#78931 = TOROIDAL_SURFACE('',#91608,0.2,0.1) ;
#78932 = TOROIDAL_SURFACE('',#91620,2.9,0.1) ;
#78933 = TOROIDAL_SURFACE('',#91808,0.2,0.1) ;
#78934 = TOROIDAL_SURFACE('',#91834,0.2,0.1) ;
#78935 = TOROIDAL_SURFACE('',#91837,0.2,0.1) ;
#78936 = TOROIDAL_SURFACE('',#91854,0.2,0.1) ;
#78937 = TOROIDAL_SURFACE('',#91860,0.2,0.1) ;
#78938 = TOROIDAL_SURFACE('',#91878,0.2,0.1) ;
#78939 = TOROIDAL_SURFACE('',#91881,0.2,0.1) ;
#78940 = TOROIDAL_SURFACE('',#91898,0.2,0.1) ;
#78941 = TOROIDAL_SURFACE('',#91904,0.2,0.1) ;
#78942 = TOROIDAL_SURFACE('',#91919,3.1,0.1) ;
#78943 = TOROIDAL_SURFACE('',#91925,0.2,0.1) ;
#78944 = TOROIDAL_SURFACE('',#91927,2.9,0.1) ;
#78945 = TOROIDAL_SURFACE('',#91931,0.2,0.1) ;
#78946 = TOROIDAL_SURFACE('',#91939,3.1,0.1) ;
#78947 = TOROIDAL_SURFACE('',#91948,0.2,0.1) ;
#78948 = TOROIDAL_SURFACE('',#91957,2.9,0.1) ;
#78949 = TOROIDAL_SURFACE('',#91994,0.199999999999999,0.1) ;
#78950 = TOROIDAL_SURFACE('',#91998,0.199999999999999,0.1) ;
#78951 = TOROIDAL_SURFACE('',#92008,0.2,0.1) ;
#78952 = TOROIDAL_SURFACE('',#92010,0.2,0.1) ;
#78953 = TOROIDAL_SURFACE('',#92013,0.2,0.1) ;
#78954 = TOROIDAL_SURFACE('',#92018,2.,0.1) ;
#78955 = TOROIDAL_SURFACE('',#92023,1.4,0.1) ;
#78956 = TOROIDAL_SURFACE('',#92027,1.6,0.1) ;
#78957 = TOROIDAL_SURFACE('',#92032,0.2,0.1) ;
#78958 = TOROIDAL_SURFACE('',#92056,0.2,0.1) ;
#78959 = TOROIDAL_SURFACE('',#92064,2.,0.1) ;
#78960 = TOROIDAL_SURFACE('',#92069,1.4,0.1) ;
#78961 = TOROIDAL_SURFACE('',#92073,1.6,0.1) ;
#78962 = TOROIDAL_SURFACE('',#92078,0.2,0.1) ;
#78963 = TOROIDAL_SURFACE('',#92332,0.2,0.1) ;
#78964 = TOROIDAL_SURFACE('',#92359,0.2,0.1) ;
#78965 = TOROIDAL_SURFACE('',#92362,0.2,0.1) ;
#78966 = TOROIDAL_SURFACE('',#92379,0.2,0.1) ;
#78967 = TOROIDAL_SURFACE('',#92385,0.2,0.1) ;
#78968 = TOROIDAL_SURFACE('',#92403,0.2,0.1) ;
#78969 = TOROIDAL_SURFACE('',#92406,0.2,0.1) ;
#78970 = TOROIDAL_SURFACE('',#92423,0.2,0.1) ;
#78971 = TOROIDAL_SURFACE('',#92429,0.2,0.1) ;
#78972 = TOROIDAL_SURFACE('',#92444,3.1,0.1) ;
#78973 = TOROIDAL_SURFACE('',#92456,0.2,0.1) ;
#78974 = TOROIDAL_SURFACE('',#92458,2.9,0.1) ;
#78975 = TOROIDAL_SURFACE('',#92462,0.2,0.1) ;
#78976 = TOROIDAL_SURFACE('',#92470,3.1,0.1) ;
#78977 = TOROIDAL_SURFACE('',#92497,0.2,0.1) ;
#78978 = TOROIDAL_SURFACE('',#92509,2.9,0.1) ;
#78979 = TOROIDAL_SURFACE('',#92696,0.2,0.1) ;
#78980 = TOROIDAL_SURFACE('',#92723,0.2,0.1) ;
#78981 = TOROIDAL_SURFACE('',#92726,0.2,0.1) ;
#78982 = TOROIDAL_SURFACE('',#92743,0.2,0.1) ;
#78983 = TOROIDAL_SURFACE('',#92749,0.2,0.1) ;
#78984 = TOROIDAL_SURFACE('',#92767,0.2,0.1) ;
#78985 = TOROIDAL_SURFACE('',#92770,0.2,0.1) ;
#78986 = TOROIDAL_SURFACE('',#92787,0.2,0.1) ;
#78987 = TOROIDAL_SURFACE('',#92793,0.2,0.1) ;
#78988 = TOROIDAL_SURFACE('',#92808,3.1,0.1) ;
#78989 = TOROIDAL_SURFACE('',#92818,0.2,0.1) ;
#78990 = TOROIDAL_SURFACE('',#92820,2.9,0.1) ;
#78991 = TOROIDAL_SURFACE('',#92822,0.2,0.1) ;
#78992 = TOROIDAL_SURFACE('',#92828,3.1,0.1) ;
#78993 = TOROIDAL_SURFACE('',#92837,0.2,0.1) ;
#78994 = TOROIDAL_SURFACE('',#92846,2.9,0.1) ;
#78995 = TOROIDAL_SURFACE('',#92883,0.199999999999999,0.1) ;
#78996 = TOROIDAL_SURFACE('',#92887,0.199999999999999,0.1) ;
#78997 = TOROIDAL_SURFACE('',#92897,0.2,0.1) ;
#78998 = TOROIDAL_SURFACE('',#92899,0.2,0.1) ;
#78999 = TOROIDAL_SURFACE('',#92902,0.2,0.1) ;
#79000 = TOROIDAL_SURFACE('',#92910,2.,0.1) ;
#79001 = TOROIDAL_SURFACE('',#92915,1.4,0.1) ;
#79002 = TOROIDAL_SURFACE('',#92919,1.6,0.1) ;
#79003 = TOROIDAL_SURFACE('',#92924,0.2,0.1) ;
#79004 = TOROIDAL_SURFACE('',#93171,0.2,0.1) ;
#79005 = TOROIDAL_SURFACE('',#93198,0.2,0.1) ;
#79006 = TOROIDAL_SURFACE('',#93201,0.2,0.1) ;
#79007 = TOROIDAL_SURFACE('',#93218,0.2,0.1) ;
#79008 = TOROIDAL_SURFACE('',#93224,0.2,0.1) ;
#79009 = TOROIDAL_SURFACE('',#93242,0.2,0.1) ;
#79010 = TOROIDAL_SURFACE('',#93245,0.2,0.1) ;
#79011 = TOROIDAL_SURFACE('',#93262,0.2,0.1) ;
#79012 = TOROIDAL_SURFACE('',#93268,0.2,0.1) ;
#79013 = TOROIDAL_SURFACE('',#93283,3.1,0.1) ;
#79014 = TOROIDAL_SURFACE('',#93293,0.2,0.1) ;
#79015 = TOROIDAL_SURFACE('',#93295,2.9,0.1) ;
#79016 = TOROIDAL_SURFACE('',#93299,0.2,0.1) ;
#79017 = TOROIDAL_SURFACE('',#93307,3.1,0.1) ;
#79018 = TOROIDAL_SURFACE('',#93329,0.2,0.1) ;
#79019 = TOROIDAL_SURFACE('',#93340,2.9,0.1) ;
#79020 = TOROIDAL_SURFACE('',#93349,0.9,0.1) ;
#79021 = TOROIDAL_SURFACE('',#93354,1.1,0.1) ;
#79022 = TOROIDAL_SURFACE('',#93366,0.9,0.1) ;
#79023 = TOROIDAL_SURFACE('',#93371,1.1,0.1) ;
#79024 = TOROIDAL_SURFACE('',#93383,0.9,0.1) ;
#79025 = TOROIDAL_SURFACE('',#93388,1.1,0.1) ;
#79026 = TOROIDAL_SURFACE('',#93400,0.9,0.1) ;
#79027 = TOROIDAL_SURFACE('',#93405,1.1,0.1) ;
#79028 = TOROIDAL_SURFACE('',#93417,0.9,0.1) ;
#79029 = TOROIDAL_SURFACE('',#93422,1.1,0.1) ;
#79030 = TOROIDAL_SURFACE('',#93434,0.9,0.1) ;
#79031 = TOROIDAL_SURFACE('',#93439,1.1,0.1) ;
#79032 = TOROIDAL_SURFACE('',#93451,0.9,0.1) ;
#79033 = TOROIDAL_SURFACE('',#93456,1.1,0.1) ;
#79034 = TOROIDAL_SURFACE('',#93468,0.9,0.1) ;
#79035 = TOROIDAL_SURFACE('',#93473,1.1,0.1) ;
#79036 = TOROIDAL_SURFACE('',#93485,0.9,0.1) ;
#79037 = TOROIDAL_SURFACE('',#93490,0.2,0.1) ;
#79038 = TOROIDAL_SURFACE('',#93495,0.2,0.1) ;
#79039 = TOROIDAL_SURFACE('',#93500,0.2,0.1) ;
#79040 = TOROIDAL_SURFACE('',#93505,0.2,0.1) ;
#79041 = TOROIDAL_SURFACE('',#93510,0.2,0.1) ;
#79042 = TOROIDAL_SURFACE('',#93515,0.2,0.1) ;
#79043 = TOROIDAL_SURFACE('',#93520,0.2,0.1) ;
#79044 = TOROIDAL_SURFACE('',#93525,0.2,0.1) ;
#79045 = TOROIDAL_SURFACE('',#93530,0.2,0.1) ;
#79046 = TOROIDAL_SURFACE('',#93535,1.1,0.1) ;
#79047 = TOROIDAL_SURFACE('',#93574,0.9,0.1) ;
#79048 = TOROIDAL_SURFACE('',#93579,0.2,0.1) ;
#79049 = TOROIDAL_SURFACE('',#93584,1.1,0.1) ;
#79050 = TOROIDAL_SURFACE('',#93982,0.2,0.1) ;
#79051 = TOROIDAL_SURFACE('',#93998,0.2,0.1) ;
#79052 = TOROIDAL_SURFACE('',#94000,0.2,0.1) ;
#79053 = TOROIDAL_SURFACE('',#94003,0.2,0.1) ;
#79054 = TOROIDAL_SURFACE('',#94016,0.2,0.1) ;
#79055 = TOROIDAL_SURFACE('',#94036,0.2,0.1) ;
#79056 = TOROIDAL_SURFACE('',#94047,0.2,0.1) ;
#79057 = TOROIDAL_SURFACE('',#94054,0.2,0.1) ;
#79058 = TOROIDAL_SURFACE('',#94060,0.2,0.1) ;
#79059 = TOROIDAL_SURFACE('',#94063,0.2,0.1) ;
#79060 = TOROIDAL_SURFACE('',#94077,0.2,0.1) ;
#79061 = TOROIDAL_SURFACE('',#94087,0.2,0.1) ;
#79062 = TOROIDAL_SURFACE('',#94109,0.2,0.1) ;
#79063 = TOROIDAL_SURFACE('',#94119,0.2,0.1) ;
#79064 = TOROIDAL_SURFACE('',#94137,0.2,0.1) ;
#79065 = TOROIDAL_SURFACE('',#94145,0.2,0.1) ;
#79066 = TOROIDAL_SURFACE('',#94159,1.75625,0.1) ;
#79067 = TOROIDAL_SURFACE('',#94182,0.2,0.1) ;
#79068 = TOROIDAL_SURFACE('',#94184,0.2,0.1) ;
#79069 = TOROIDAL_SURFACE('',#94198,0.2,0.1) ;
#79070 = TOROIDAL_SURFACE('',#94200,0.2,0.1) ;
#79071 = TOROIDAL_SURFACE('',#94205,0.2,0.1) ;
#79072 = TOROIDAL_SURFACE('',#94211,0.2,0.1) ;
#79073 = TOROIDAL_SURFACE('',#94213,0.2,0.1) ;
#79074 = TOROIDAL_SURFACE('',#94217,1.55625,0.1) ;
#79075 = TOROIDAL_SURFACE('',#94219,0.199999999999999,0.1) ;
#79076 = TOROIDAL_SURFACE('',#94221,0.2,0.1) ;
#79077 = TOROIDAL_SURFACE('',#94229,0.2,0.1) ;
#79078 = TOROIDAL_SURFACE('',#94237,0.2,0.1) ;
#79079 = TOROIDAL_SURFACE('',#94336,0.3,0.1) ;
#79080 = TOROIDAL_SURFACE('',#94348,0.9,0.1) ;
#79081 = TOROIDAL_SURFACE('',#94349,0.9,0.1) ;
#79082 = TOROIDAL_SURFACE('',#94361,0.3,0.1) ;
#79083 = TOROIDAL_SURFACE('',#95049,0.2,0.1) ;
#79084 = TOROIDAL_SURFACE('',#95065,0.2,0.1) ;
#79085 = TOROIDAL_SURFACE('',#95067,0.2,0.1) ;
#79086 = TOROIDAL_SURFACE('',#95070,0.2,0.1) ;
#79087 = TOROIDAL_SURFACE('',#95083,0.2,0.1) ;
#79088 = TOROIDAL_SURFACE('',#95103,0.2,0.1) ;
#79089 = TOROIDAL_SURFACE('',#95114,0.2,0.1) ;
#79090 = TOROIDAL_SURFACE('',#95121,0.2,0.1) ;
#79091 = TOROIDAL_SURFACE('',#95127,0.2,0.1) ;
#79092 = TOROIDAL_SURFACE('',#95130,0.2,0.1) ;
#79093 = TOROIDAL_SURFACE('',#95140,0.2,0.1) ;
#79094 = TOROIDAL_SURFACE('',#95148,0.2,0.1) ;
#79095 = TOROIDAL_SURFACE('',#95162,1.75625,0.1) ;
#79096 = TOROIDAL_SURFACE('',#95185,0.2,0.1) ;
#79097 = TOROIDAL_SURFACE('',#95187,0.2,0.1) ;
#79098 = TOROIDAL_SURFACE('',#95201,0.2,0.1) ;
#79099 = TOROIDAL_SURFACE('',#95203,0.2,0.1) ;
#79100 = TOROIDAL_SURFACE('',#95208,0.2,0.1) ;
#79101 = TOROIDAL_SURFACE('',#95214,0.2,0.1) ;
#79102 = TOROIDAL_SURFACE('',#95216,0.2,0.1) ;
#79103 = TOROIDAL_SURFACE('',#95220,1.55625,0.1) ;
#79104 = TOROIDAL_SURFACE('',#95222,0.199999999999999,0.1) ;
#79105 = TOROIDAL_SURFACE('',#95224,0.2,0.1) ;
#79106 = TOROIDAL_SURFACE('',#95232,0.2,0.1) ;
#79107 = TOROIDAL_SURFACE('',#95240,0.2,0.1) ;
#79108 = TOROIDAL_SURFACE('',#95254,0.2,0.1) ;
#79109 = TOROIDAL_SURFACE('',#95256,0.2,0.1) ;
#79110 = TOROIDAL_SURFACE('',#95261,0.2,0.1) ;
#79111 = TOROIDAL_SURFACE('',#95267,0.2,0.1) ;
#79112 = TOROIDAL_SURFACE('',#95269,0.2,0.1) ;
#79113 = TOROIDAL_SURFACE('',#95273,1.55625,0.1) ;
#79114 = TOROIDAL_SURFACE('',#95275,0.199999999999999,0.1) ;
#79115 = TOROIDAL_SURFACE('',#95277,0.2,0.1) ;
#79116 = TOROIDAL_SURFACE('',#95285,0.2,0.1) ;
#79117 = TOROIDAL_SURFACE('',#95293,0.2,0.1) ;
#79118 = TOROIDAL_SURFACE('',#95307,0.2,0.1) ;
#79119 = TOROIDAL_SURFACE('',#95309,0.2,0.1) ;
#79120 = TOROIDAL_SURFACE('',#95314,0.2,0.1) ;
#79121 = TOROIDAL_SURFACE('',#95320,0.2,0.1) ;
#79122 = TOROIDAL_SURFACE('',#95322,0.2,0.1) ;
#79123 = TOROIDAL_SURFACE('',#95326,1.55625,0.1) ;
#79124 = TOROIDAL_SURFACE('',#95328,0.199999999999999,0.1) ;
#79125 = TOROIDAL_SURFACE('',#95330,0.2,0.1) ;
#79126 = TOROIDAL_SURFACE('',#95338,0.2,0.1) ;
#79127 = TOROIDAL_SURFACE('',#95346,0.2,0.1) ;
#79128 = TOROIDAL_SURFACE('',#95360,0.2,0.1) ;
#79129 = TOROIDAL_SURFACE('',#95362,0.2,0.1) ;
#79130 = TOROIDAL_SURFACE('',#95367,0.2,0.1) ;
#79131 = TOROIDAL_SURFACE('',#95373,0.2,0.1) ;
#79132 = TOROIDAL_SURFACE('',#95375,0.2,0.1) ;
#79133 = TOROIDAL_SURFACE('',#95379,1.55625,0.1) ;
#79134 = TOROIDAL_SURFACE('',#95381,0.199999999999999,0.1) ;
#79135 = TOROIDAL_SURFACE('',#95383,0.2,0.1) ;
#79136 = TOROIDAL_SURFACE('',#95391,0.2,0.1) ;
#79137 = TOROIDAL_SURFACE('',#95399,0.2,0.1) ;
#79138 = TOROIDAL_SURFACE('',#95413,0.2,0.1) ;
#79139 = TOROIDAL_SURFACE('',#95415,0.2,0.1) ;
#79140 = TOROIDAL_SURFACE('',#95420,0.2,0.1) ;
#79141 = TOROIDAL_SURFACE('',#95426,0.2,0.1) ;
#79142 = TOROIDAL_SURFACE('',#95428,0.2,0.1) ;
#79143 = TOROIDAL_SURFACE('',#95432,1.55625,0.1) ;
#79144 = TOROIDAL_SURFACE('',#95434,0.199999999999999,0.1) ;
#79145 = TOROIDAL_SURFACE('',#95436,0.2,0.1) ;
#79146 = TOROIDAL_SURFACE('',#95444,0.2,0.1) ;
#79147 = TOROIDAL_SURFACE('',#95452,0.2,0.1) ;
#79148 = TOROIDAL_SURFACE('',#95466,0.2,0.1) ;
#79149 = TOROIDAL_SURFACE('',#95468,0.2,0.1) ;
#79150 = TOROIDAL_SURFACE('',#95473,0.2,0.1) ;
#79151 = TOROIDAL_SURFACE('',#95479,0.2,0.1) ;
#79152 = TOROIDAL_SURFACE('',#95481,0.2,0.1) ;
#79153 = TOROIDAL_SURFACE('',#95485,1.55625,0.1) ;
#79154 = TOROIDAL_SURFACE('',#95487,0.199999999999999,0.1) ;
#79155 = TOROIDAL_SURFACE('',#95489,0.2,0.1) ;
#79156 = TOROIDAL_SURFACE('',#95497,0.2,0.1) ;
#79157 = TOROIDAL_SURFACE('',#95505,0.2,0.1) ;
#79158 = TOROIDAL_SURFACE('',#95519,0.2,0.1) ;
#79159 = TOROIDAL_SURFACE('',#95521,0.2,0.1) ;
#79160 = TOROIDAL_SURFACE('',#95526,0.2,0.1) ;
#79161 = TOROIDAL_SURFACE('',#95532,0.2,0.1) ;
#79162 = TOROIDAL_SURFACE('',#95534,0.2,0.1) ;
#79163 = TOROIDAL_SURFACE('',#95538,1.55625,0.1) ;
#79164 = TOROIDAL_SURFACE('',#95540,0.199999999999999,0.1) ;
#79165 = TOROIDAL_SURFACE('',#95542,0.2,0.1) ;
#79166 = TOROIDAL_SURFACE('',#95550,0.2,0.1) ;
#79167 = TOROIDAL_SURFACE('',#95558,0.2,0.1) ;
#79168 = TOROIDAL_SURFACE('',#95572,0.2,0.1) ;
#79169 = TOROIDAL_SURFACE('',#95574,0.2,0.1) ;
#79170 = TOROIDAL_SURFACE('',#95579,0.2,0.1) ;
#79171 = TOROIDAL_SURFACE('',#95585,0.2,0.1) ;
#79172 = TOROIDAL_SURFACE('',#95587,0.2,0.1) ;
#79173 = TOROIDAL_SURFACE('',#95591,1.55625,0.1) ;
#79174 = TOROIDAL_SURFACE('',#95593,0.199999999999999,0.1) ;
#79175 = TOROIDAL_SURFACE('',#95595,0.2,0.1) ;
#79176 = TOROIDAL_SURFACE('',#95603,0.2,0.1) ;
#79177 = TOROIDAL_SURFACE('',#95611,0.2,0.1) ;
#79178 = TOROIDAL_SURFACE('',#95625,0.2,0.1) ;
#79179 = TOROIDAL_SURFACE('',#95627,0.2,0.1) ;
#79180 = TOROIDAL_SURFACE('',#95632,0.2,0.1) ;
#79181 = TOROIDAL_SURFACE('',#95638,0.2,0.1) ;
#79182 = TOROIDAL_SURFACE('',#95640,0.2,0.1) ;
#79183 = TOROIDAL_SURFACE('',#95644,1.55625,0.1) ;
#79184 = TOROIDAL_SURFACE('',#95646,0.199999999999999,0.1) ;
#79185 = TOROIDAL_SURFACE('',#95648,0.2,0.1) ;
#79186 = TOROIDAL_SURFACE('',#95656,0.2,0.1) ;
#79187 = TOROIDAL_SURFACE('',#95664,0.2,0.1) ;
#79188 = TOROIDAL_SURFACE('',#95679,0.2,0.1) ;
#79189 = TOROIDAL_SURFACE('',#95695,0.2,0.1) ;
#79190 = TOROIDAL_SURFACE('',#95697,0.2,0.1) ;
#79191 = TOROIDAL_SURFACE('',#95700,0.2,0.1) ;
#79192 = TOROIDAL_SURFACE('',#95713,0.2,0.1) ;
#79193 = TOROIDAL_SURFACE('',#95733,0.2,0.1) ;
#79194 = TOROIDAL_SURFACE('',#95744,0.2,0.1) ;
#79195 = TOROIDAL_SURFACE('',#95751,0.2,0.1) ;
#79196 = TOROIDAL_SURFACE('',#95757,0.2,0.1) ;
#79197 = TOROIDAL_SURFACE('',#95760,0.2,0.1) ;
#79198 = TOROIDAL_SURFACE('',#95770,0.2,0.1) ;
#79199 = TOROIDAL_SURFACE('',#95778,0.2,0.1) ;
#79200 = TOROIDAL_SURFACE('',#95792,1.75625,0.1) ;
#79201 = TOROIDAL_SURFACE('',#95815,0.2,0.1) ;
#79202 = TOROIDAL_SURFACE('',#95817,0.2,0.1) ;
#79203 = TOROIDAL_SURFACE('',#95832,0.2,0.1) ;
#79204 = TOROIDAL_SURFACE('',#95848,0.2,0.1) ;
#79205 = TOROIDAL_SURFACE('',#95850,0.2,0.1) ;
#79206 = TOROIDAL_SURFACE('',#95853,0.2,0.1) ;
#79207 = TOROIDAL_SURFACE('',#95866,0.2,0.1) ;
#79208 = TOROIDAL_SURFACE('',#95886,0.2,0.1) ;
#79209 = TOROIDAL_SURFACE('',#95897,0.2,0.1) ;
#79210 = TOROIDAL_SURFACE('',#95904,0.2,0.1) ;
#79211 = TOROIDAL_SURFACE('',#95910,0.2,0.1) ;
#79212 = TOROIDAL_SURFACE('',#95913,0.2,0.1) ;
#79213 = TOROIDAL_SURFACE('',#95923,0.2,0.1) ;
#79214 = TOROIDAL_SURFACE('',#95931,0.2,0.1) ;
#79215 = TOROIDAL_SURFACE('',#95945,1.75625,0.1) ;
#79216 = TOROIDAL_SURFACE('',#95968,0.2,0.1) ;
#79217 = TOROIDAL_SURFACE('',#95970,0.2,0.1) ;
#79218 = TOROIDAL_SURFACE('',#95985,0.2,0.1) ;
#79219 = TOROIDAL_SURFACE('',#96001,0.2,0.1) ;
#79220 = TOROIDAL_SURFACE('',#96003,0.2,0.1) ;
#79221 = TOROIDAL_SURFACE('',#96006,0.2,0.1) ;
#79222 = TOROIDAL_SURFACE('',#96019,0.2,0.1) ;
#79223 = TOROIDAL_SURFACE('',#96039,0.2,0.1) ;
#79224 = TOROIDAL_SURFACE('',#96050,0.2,0.1) ;
#79225 = TOROIDAL_SURFACE('',#96057,0.2,0.1) ;
#79226 = TOROIDAL_SURFACE('',#96063,0.2,0.1) ;
#79227 = TOROIDAL_SURFACE('',#96066,0.2,0.1) ;
#79228 = TOROIDAL_SURFACE('',#96076,0.2,0.1) ;
#79229 = TOROIDAL_SURFACE('',#96084,0.2,0.1) ;
#79230 = TOROIDAL_SURFACE('',#96098,1.75625,0.1) ;
#79231 = TOROIDAL_SURFACE('',#96121,0.2,0.1) ;
#79232 = TOROIDAL_SURFACE('',#96123,0.2,0.1) ;
#79233 = TOROIDAL_SURFACE('',#96138,0.2,0.1) ;
#79234 = TOROIDAL_SURFACE('',#96154,0.2,0.1) ;
#79235 = TOROIDAL_SURFACE('',#96156,0.2,0.1) ;
#79236 = TOROIDAL_SURFACE('',#96159,0.2,0.1) ;
#79237 = TOROIDAL_SURFACE('',#96172,0.2,0.1) ;
#79238 = TOROIDAL_SURFACE('',#96192,0.2,0.1) ;
#79239 = TOROIDAL_SURFACE('',#96203,0.2,0.1) ;
#79240 = TOROIDAL_SURFACE('',#96210,0.2,0.1) ;
#79241 = TOROIDAL_SURFACE('',#96216,0.2,0.1) ;
#79242 = TOROIDAL_SURFACE('',#96219,0.2,0.1) ;
#79243 = TOROIDAL_SURFACE('',#96229,0.2,0.1) ;
#79244 = TOROIDAL_SURFACE('',#96237,0.2,0.1) ;
#79245 = TOROIDAL_SURFACE('',#96251,1.75625,0.1) ;
#79246 = TOROIDAL_SURFACE('',#96274,0.2,0.1) ;
#79247 = TOROIDAL_SURFACE('',#96276,0.2,0.1) ;
#79248 = TOROIDAL_SURFACE('',#96291,0.2,0.1) ;
#79249 = TOROIDAL_SURFACE('',#96307,0.2,0.1) ;
#79250 = TOROIDAL_SURFACE('',#96309,0.2,0.1) ;
#79251 = TOROIDAL_SURFACE('',#96312,0.2,0.1) ;
#79252 = TOROIDAL_SURFACE('',#96325,0.2,0.1) ;
#79253 = TOROIDAL_SURFACE('',#96345,0.2,0.1) ;
#79254 = TOROIDAL_SURFACE('',#96356,0.2,0.1) ;
#79255 = TOROIDAL_SURFACE('',#96363,0.2,0.1) ;
#79256 = TOROIDAL_SURFACE('',#96369,0.2,0.1) ;
#79257 = TOROIDAL_SURFACE('',#96372,0.2,0.1) ;
#79258 = TOROIDAL_SURFACE('',#96382,0.2,0.1) ;
#79259 = TOROIDAL_SURFACE('',#96390,0.2,0.1) ;
#79260 = TOROIDAL_SURFACE('',#96404,1.75625,0.1) ;
#79261 = TOROIDAL_SURFACE('',#96427,0.2,0.1) ;
#79262 = TOROIDAL_SURFACE('',#96429,0.2,0.1) ;
#79263 = TOROIDAL_SURFACE('',#96444,0.2,0.1) ;
#79264 = TOROIDAL_SURFACE('',#96460,0.2,0.1) ;
#79265 = TOROIDAL_SURFACE('',#96462,0.2,0.1) ;
#79266 = TOROIDAL_SURFACE('',#96465,0.2,0.1) ;
#79267 = TOROIDAL_SURFACE('',#96478,0.2,0.1) ;
#79268 = TOROIDAL_SURFACE('',#96498,0.2,0.1) ;
#79269 = TOROIDAL_SURFACE('',#96509,0.2,0.1) ;
#79270 = TOROIDAL_SURFACE('',#96516,0.2,0.1) ;
#79271 = TOROIDAL_SURFACE('',#96522,0.2,0.1) ;
#79272 = TOROIDAL_SURFACE('',#96525,0.2,0.1) ;
#79273 = TOROIDAL_SURFACE('',#96535,0.2,0.1) ;
#79274 = TOROIDAL_SURFACE('',#96543,0.2,0.1) ;
#79275 = TOROIDAL_SURFACE('',#96557,1.75625,0.1) ;
#79276 = TOROIDAL_SURFACE('',#96580,0.2,0.1) ;
#79277 = TOROIDAL_SURFACE('',#96582,0.2,0.1) ;
#79278 = TOROIDAL_SURFACE('',#96597,0.2,0.1) ;
#79279 = TOROIDAL_SURFACE('',#96613,0.2,0.1) ;
#79280 = TOROIDAL_SURFACE('',#96615,0.2,0.1) ;
#79281 = TOROIDAL_SURFACE('',#96618,0.2,0.1) ;
#79282 = TOROIDAL_SURFACE('',#96631,0.2,0.1) ;
#79283 = TOROIDAL_SURFACE('',#96651,0.2,0.1) ;
#79284 = TOROIDAL_SURFACE('',#96662,0.2,0.1) ;
#79285 = TOROIDAL_SURFACE('',#96669,0.2,0.1) ;
#79286 = TOROIDAL_SURFACE('',#96675,0.2,0.1) ;
#79287 = TOROIDAL_SURFACE('',#96678,0.2,0.1) ;
#79288 = TOROIDAL_SURFACE('',#96688,0.2,0.1) ;
#79289 = TOROIDAL_SURFACE('',#96696,0.2,0.1) ;
#79290 = TOROIDAL_SURFACE('',#96710,1.75625,0.1) ;
#79291 = TOROIDAL_SURFACE('',#96733,0.2,0.1) ;
#79292 = TOROIDAL_SURFACE('',#96735,0.2,0.1) ;
#79293 = TOROIDAL_SURFACE('',#96750,0.2,0.1) ;
#79294 = TOROIDAL_SURFACE('',#96766,0.2,0.1) ;
#79295 = TOROIDAL_SURFACE('',#96768,0.2,0.1) ;
#79296 = TOROIDAL_SURFACE('',#96771,0.2,0.1) ;
#79297 = TOROIDAL_SURFACE('',#96784,0.2,0.1) ;
#79298 = TOROIDAL_SURFACE('',#96804,0.2,0.1) ;
#79299 = TOROIDAL_SURFACE('',#96815,0.2,0.1) ;
#79300 = TOROIDAL_SURFACE('',#96822,0.2,0.1) ;
#79301 = TOROIDAL_SURFACE('',#96828,0.2,0.1) ;
#79302 = TOROIDAL_SURFACE('',#96831,0.2,0.1) ;
#79303 = TOROIDAL_SURFACE('',#96841,0.2,0.1) ;
#79304 = TOROIDAL_SURFACE('',#96849,0.2,0.1) ;
#79305 = TOROIDAL_SURFACE('',#96863,1.75625,0.1) ;
#79306 = TOROIDAL_SURFACE('',#96886,0.2,0.1) ;
#79307 = TOROIDAL_SURFACE('',#96888,0.2,0.1) ;
#79308 = TOROIDAL_SURFACE('',#97755,0.3,0.1) ;
#79309 = TOROIDAL_SURFACE('',#97767,0.9,0.1) ;
#79310 = TOROIDAL_SURFACE('',#97768,0.9,0.1) ;
#79311 = TOROIDAL_SURFACE('',#97780,0.3,0.1) ;
#79312 = TOROIDAL_SURFACE('',#97799,0.3,0.1) ;
#79313 = TOROIDAL_SURFACE('',#97811,0.9,0.1) ;
#79314 = TOROIDAL_SURFACE('',#97812,0.9,0.1) ;
#79315 = TOROIDAL_SURFACE('',#97824,0.3,0.1) ;
#79316 = TOROIDAL_SURFACE('',#97843,0.3,0.1) ;
#79317 = TOROIDAL_SURFACE('',#97855,0.9,0.1) ;
#79318 = TOROIDAL_SURFACE('',#97856,0.9,0.1) ;
#79319 = TOROIDAL_SURFACE('',#97868,0.3,0.1) ;
#79320 = TOROIDAL_SURFACE('',#97887,0.3,0.1) ;
#79321 = TOROIDAL_SURFACE('',#97899,0.9,0.1) ;
#79322 = TOROIDAL_SURFACE('',#97900,0.9,0.1) ;
#79323 = TOROIDAL_SURFACE('',#97912,0.3,0.1) ;
#79324 = TOROIDAL_SURFACE('',#97931,0.3,0.1) ;
#79325 = TOROIDAL_SURFACE('',#97943,0.9,0.1) ;
#79326 = TOROIDAL_SURFACE('',#97944,0.9,0.1) ;
#79327 = TOROIDAL_SURFACE('',#97956,0.3,0.1) ;
#79328 = TOROIDAL_SURFACE('',#97975,0.3,0.1) ;
#79329 = TOROIDAL_SURFACE('',#97987,0.9,0.1) ;
#79330 = TOROIDAL_SURFACE('',#97988,0.9,0.1) ;
#79331 = TOROIDAL_SURFACE('',#98000,0.3,0.1) ;
#79332 = TOROIDAL_SURFACE('',#98019,0.3,0.1) ;
#79333 = TOROIDAL_SURFACE('',#98031,0.9,0.1) ;
#79334 = TOROIDAL_SURFACE('',#98032,0.9,0.1) ;
#79335 = TOROIDAL_SURFACE('',#98044,0.3,0.1) ;
#79336 = TOROIDAL_SURFACE('',#98063,0.3,0.1) ;
#79337 = TOROIDAL_SURFACE('',#98075,0.9,0.1) ;
#79338 = TOROIDAL_SURFACE('',#98076,0.9,0.1) ;
#79339 = TOROIDAL_SURFACE('',#98088,0.3,0.1) ;
#79340 = TOROIDAL_SURFACE('',#98107,0.3,0.1) ;
#79341 = TOROIDAL_SURFACE('',#98119,0.9,0.1) ;
#79342 = TOROIDAL_SURFACE('',#98120,0.9,0.1) ;
#79343 = TOROIDAL_SURFACE('',#98132,0.3,0.1) ;
#79344 = TOROIDAL_SURFACE('',#98155,0.1645125,0.1) ;
#79345 = TOROIDAL_SURFACE('',#98160,0.1645125,0.1) ;
#79346 = TOROIDAL_SURFACE('',#98165,2.35,0.1) ;
#79347 = TOROIDAL_SURFACE('',#98168,0.1645125,0.1) ;
#79348 = TOROIDAL_SURFACE('',#98173,2.35,0.1) ;
#79349 = TOROIDAL_SURFACE('',#98176,0.1645125,0.1) ;
#79350 = TOROIDAL_SURFACE('',#98181,2.35,0.1) ;
#79351 = TOROIDAL_SURFACE('',#98184,0.1645125,0.1) ;
#79352 = TOROIDAL_SURFACE('',#98189,2.35,0.1) ;
#79353 = TOROIDAL_SURFACE('',#98192,0.1645125,0.1) ;
#79354 = TOROIDAL_SURFACE('',#98197,2.35,0.1) ;
#79355 = TOROIDAL_SURFACE('',#98200,0.1645125,0.1) ;
#79356 = TOROIDAL_SURFACE('',#98205,2.35,0.1) ;
#79357 = TOROIDAL_SURFACE('',#98208,0.1645125,0.1) ;
#79358 = TOROIDAL_SURFACE('',#98213,2.35,0.1) ;
#79359 = TOROIDAL_SURFACE('',#98216,0.1645125,0.1) ;
#79360 = TOROIDAL_SURFACE('',#98221,2.35,0.1) ;
#79361 = TOROIDAL_SURFACE('',#98224,0.164512500000005,0.1) ;
#79362 = TOROIDAL_SURFACE('',#98229,2.35,0.1) ;
#79363 = TOROIDAL_SURFACE('',#98232,0.164512500000006,0.1) ;
#79364 = TOROIDAL_SURFACE('',#98237,2.35,0.1) ;
#79365 = TOROIDAL_SURFACE('',#98254,0.899999999999998,0.1) ;
#79366 = TOROIDAL_SURFACE('',#98258,1.6,0.1) ;
#79367 = TOROIDAL_SURFACE('',#98262,1.1,0.1) ;
#79368 = TOROIDAL_SURFACE('',#98266,0.900000000000001,0.1) ;
#79369 = TOROIDAL_SURFACE('',#98270,1.6,0.1) ;
#79370 = TOROIDAL_SURFACE('',#98274,1.1,0.1) ;
#79371 = TOROIDAL_SURFACE('',#98278,0.900000000000001,0.1) ;
#79372 = TOROIDAL_SURFACE('',#98282,1.6,0.1) ;
#79373 = TOROIDAL_SURFACE('',#98286,1.1,0.1) ;
#79374 = TOROIDAL_SURFACE('',#98290,0.900000000000001,0.1) ;
#79375 = TOROIDAL_SURFACE('',#98294,1.6,0.1) ;
#79376 = TOROIDAL_SURFACE('',#98298,1.1,0.1) ;
#79377 = TOROIDAL_SURFACE('',#98302,0.900000000000001,0.1) ;
#79378 = TOROIDAL_SURFACE('',#98306,1.6,0.1) ;
#79379 = TOROIDAL_SURFACE('',#98310,1.1,0.1) ;
#79380 = TOROIDAL_SURFACE('',#98314,0.900000000000001,0.1) ;
#79381 = TOROIDAL_SURFACE('',#98318,1.6,0.1) ;
#79382 = TOROIDAL_SURFACE('',#98322,1.1,0.1) ;
#79383 = TOROIDAL_SURFACE('',#98326,0.900000000000001,0.1) ;
#79384 = TOROIDAL_SURFACE('',#98330,1.6,0.1) ;
#79385 = TOROIDAL_SURFACE('',#98334,1.1,0.1) ;
#79386 = TOROIDAL_SURFACE('',#98338,0.9,0.1) ;
#79387 = TOROIDAL_SURFACE('',#98342,1.6,0.1) ;
#79388 = TOROIDAL_SURFACE('',#98346,1.1,0.1) ;
#79389 = TOROIDAL_SURFACE('',#98350,0.900000000000001,0.1) ;
#79390 = TOROIDAL_SURFACE('',#98354,1.6,0.1) ;
#79391 = TOROIDAL_SURFACE('',#98358,1.1,0.1) ;
#79392 = TOROIDAL_SURFACE('',#98443,0.9,0.1) ;
#79393 = TOROIDAL_SURFACE('',#98447,1.6,0.1) ;
#79394 = TOROIDAL_SURFACE('',#98451,1.1,0.1) ;
#79395 = TOROIDAL_SURFACE('',#98858,0.2,0.1) ;
#79396 = TOROIDAL_SURFACE('',#98872,0.2,0.1) ;
#79397 = TOROIDAL_SURFACE('',#98882,1.75625,0.1) ;
#79398 = TOROIDAL_SURFACE('',#98897,0.2,0.1) ;
#79399 = TOROIDAL_SURFACE('',#98909,1.55625,0.1) ;
#79400 = TOROIDAL_SURFACE('',#98917,0.2,0.1) ;
#79401 = TOROIDAL_SURFACE('',#98919,0.2,0.1) ;
#79402 = TOROIDAL_SURFACE('',#98933,0.2,0.1) ;
#79403 = TOROIDAL_SURFACE('',#98950,0.2,0.1) ;
#79404 = TOROIDAL_SURFACE('',#98964,0.2,0.1) ;
#79405 = TOROIDAL_SURFACE('',#98967,0.2,0.1) ;
#79406 = TOROIDAL_SURFACE('',#98974,0.2,0.1) ;
#79407 = TOROIDAL_SURFACE('',#98976,0.2,0.1) ;
#79408 = TOROIDAL_SURFACE('',#98982,0.2,0.1) ;
#79409 = TOROIDAL_SURFACE('',#98986,0.2,0.1) ;
#79410 = TOROIDAL_SURFACE('',#98989,0.2,0.1) ;
#79411 = TOROIDAL_SURFACE('',#99006,0.2,0.1) ;
#79412 = TOROIDAL_SURFACE('',#99012,0.2,0.1) ;
#79413 = TOROIDAL_SURFACE('',#99094,0.2,0.1) ;
#79414 = TOROIDAL_SURFACE('',#99097,0.2,0.1) ;
#79415 = TOROIDAL_SURFACE('',#99114,0.2,0.1) ;
#79416 = TOROIDAL_SURFACE('',#99120,0.2,0.1) ;
#79417 = TOROIDAL_SURFACE('',#99182,0.2,0.1) ;
#79418 = TOROIDAL_SURFACE('',#99187,0.2,0.1) ;
#79419 = TOROIDAL_SURFACE('',#99188,0.2,0.1) ;
#79420 = TOROIDAL_SURFACE('',#99194,0.2,0.1) ;
#79421 = TOROIDAL_SURFACE('',#99200,0.2,0.1) ;
#79422 = TOROIDAL_SURFACE('',#99203,0.2,0.1) ;
#79423 = TOROIDAL_SURFACE('',#99204,0.2,0.1) ;
#79424 = TOROIDAL_SURFACE('',#99207,0.2,0.1) ;
#79425 = TOROIDAL_SURFACE('',#99946,1.75625,0.1) ;
#79426 = TOROIDAL_SURFACE('',#99961,0.2,0.1) ;
#79427 = TOROIDAL_SURFACE('',#99973,1.55625,0.1) ;
#79428 = TOROIDAL_SURFACE('',#99981,0.2,0.1) ;
#79429 = TOROIDAL_SURFACE('',#99983,0.2,0.1) ;
#79430 = TOROIDAL_SURFACE('',#99997,0.2,0.1) ;
#79431 = TOROIDAL_SURFACE('',#100014,0.2,0.1) ;
#79432 = TOROIDAL_SURFACE('',#100025,0.2,0.1) ;
#79433 = TOROIDAL_SURFACE('',#100028,0.2,0.1) ;
#79434 = TOROIDAL_SURFACE('',#100035,0.2,0.1) ;
#79435 = TOROIDAL_SURFACE('',#100037,0.2,0.1) ;
#79436 = TOROIDAL_SURFACE('',#100043,0.2,0.1) ;
#79437 = TOROIDAL_SURFACE('',#100143,0.2,0.1) ;
#79438 = TOROIDAL_SURFACE('',#100146,0.2,0.1) ;
#79439 = TOROIDAL_SURFACE('',#100163,0.2,0.1) ;
#79440 = TOROIDAL_SURFACE('',#100169,0.2,0.1) ;
#79441 = TOROIDAL_SURFACE('',#100411,0.2,0.1) ;
#79442 = TOROIDAL_SURFACE('',#100414,0.2,0.1) ;
#79443 = TOROIDAL_SURFACE('',#100431,0.2,0.1) ;
#79444 = TOROIDAL_SURFACE('',#100437,0.2,0.1) ;
#79445 = TOROIDAL_SURFACE('',#100504,1.75625,0.1) ;
#79446 = TOROIDAL_SURFACE('',#100511,0.2,0.1) ;
#79447 = TOROIDAL_SURFACE('',#100524,1.55625,0.1) ;
#79448 = TOROIDAL_SURFACE('',#100533,0.2,0.1) ;
#79449 = TOROIDAL_SURFACE('',#100535,0.2,0.1) ;
#79450 = TOROIDAL_SURFACE('',#100553,0.2,0.1) ;
#79451 = TOROIDAL_SURFACE('',#100563,0.2,0.1) ;
#79452 = TOROIDAL_SURFACE('',#100577,0.2,0.1) ;
#79453 = TOROIDAL_SURFACE('',#100644,0.2,0.1) ;
#79454 = TOROIDAL_SURFACE('',#100651,0.2,0.1) ;
#79455 = TOROIDAL_SURFACE('',#100653,0.2,0.1) ;
#79456 = TOROIDAL_SURFACE('',#100659,0.2,0.1) ;
#79457 = TOROIDAL_SURFACE('',#100687,0.2,0.1) ;
#79458 = TOROIDAL_SURFACE('',#100690,0.2,0.1) ;
#79459 = TOROIDAL_SURFACE('',#100707,0.2,0.1) ;
#79460 = TOROIDAL_SURFACE('',#100713,0.2,0.1) ;
#79461 = TOROIDAL_SURFACE('',#100780,1.75625,0.1) ;
#79462 = TOROIDAL_SURFACE('',#100787,0.2,0.1) ;
#79463 = TOROIDAL_SURFACE('',#100800,1.55625,0.1) ;
#79464 = TOROIDAL_SURFACE('',#100809,0.2,0.1) ;
#79465 = TOROIDAL_SURFACE('',#100811,0.2,0.1) ;
#79466 = TOROIDAL_SURFACE('',#100829,0.2,0.1) ;
#79467 = TOROIDAL_SURFACE('',#100839,0.2,0.1) ;
#79468 = TOROIDAL_SURFACE('',#100853,0.2,0.1) ;
#79469 = TOROIDAL_SURFACE('',#100920,0.2,0.1) ;
#79470 = TOROIDAL_SURFACE('',#100927,0.2,0.1) ;
#79471 = TOROIDAL_SURFACE('',#100929,0.2,0.1) ;
#79472 = TOROIDAL_SURFACE('',#100935,0.2,0.1) ;
#79473 = TOROIDAL_SURFACE('',#100963,0.2,0.1) ;
#79474 = TOROIDAL_SURFACE('',#100966,0.2,0.1) ;
#79475 = TOROIDAL_SURFACE('',#100983,0.2,0.1) ;
#79476 = TOROIDAL_SURFACE('',#100989,0.2,0.1) ;
#79477 = TOROIDAL_SURFACE('',#101056,1.75625,0.1) ;
#79478 = TOROIDAL_SURFACE('',#101063,0.2,0.1) ;
#79479 = TOROIDAL_SURFACE('',#101076,1.55625,0.1) ;
#79480 = TOROIDAL_SURFACE('',#101085,0.2,0.1) ;
#79481 = TOROIDAL_SURFACE('',#101087,0.2,0.1) ;
#79482 = TOROIDAL_SURFACE('',#101105,0.2,0.1) ;
#79483 = TOROIDAL_SURFACE('',#101115,0.2,0.1) ;
#79484 = TOROIDAL_SURFACE('',#101129,0.2,0.1) ;
#79485 = TOROIDAL_SURFACE('',#101196,0.2,0.1) ;
#79486 = TOROIDAL_SURFACE('',#101203,0.2,0.1) ;
#79487 = TOROIDAL_SURFACE('',#101205,0.2,0.1) ;
#79488 = TOROIDAL_SURFACE('',#101211,0.2,0.1) ;
#79489 = TOROIDAL_SURFACE('',#101239,0.2,0.1) ;
#79490 = TOROIDAL_SURFACE('',#101242,0.2,0.1) ;
#79491 = TOROIDAL_SURFACE('',#101259,0.2,0.1) ;
#79492 = TOROIDAL_SURFACE('',#101265,0.2,0.1) ;
#79493 = TOROIDAL_SURFACE('',#101332,1.75625,0.1) ;
#79494 = TOROIDAL_SURFACE('',#101339,0.2,0.1) ;
#79495 = TOROIDAL_SURFACE('',#101352,1.55625,0.1) ;
#79496 = TOROIDAL_SURFACE('',#101361,0.2,0.1) ;
#79497 = TOROIDAL_SURFACE('',#101363,0.2,0.1) ;
#79498 = TOROIDAL_SURFACE('',#101381,0.2,0.1) ;
#79499 = TOROIDAL_SURFACE('',#101391,0.2,0.1) ;
#79500 = TOROIDAL_SURFACE('',#101405,0.2,0.1) ;
#79501 = TOROIDAL_SURFACE('',#101472,0.2,0.1) ;
#79502 = TOROIDAL_SURFACE('',#101479,0.2,0.1) ;
#79503 = TOROIDAL_SURFACE('',#101481,0.2,0.1) ;
#79504 = TOROIDAL_SURFACE('',#101487,0.2,0.1) ;
#79505 = TOROIDAL_SURFACE('',#101515,0.2,0.1) ;
#79506 = TOROIDAL_SURFACE('',#101518,0.2,0.1) ;
#79507 = TOROIDAL_SURFACE('',#101535,0.2,0.1) ;
#79508 = TOROIDAL_SURFACE('',#101541,0.2,0.1) ;
#79509 = TOROIDAL_SURFACE('',#101608,1.75625,0.1) ;
#79510 = TOROIDAL_SURFACE('',#101615,0.2,0.1) ;
#79511 = TOROIDAL_SURFACE('',#101628,1.55625,0.1) ;
#79512 = TOROIDAL_SURFACE('',#101637,0.2,0.1) ;
#79513 = TOROIDAL_SURFACE('',#101639,0.2,0.1) ;
#79514 = TOROIDAL_SURFACE('',#101657,0.2,0.1) ;
#79515 = TOROIDAL_SURFACE('',#101667,0.2,0.1) ;
#79516 = TOROIDAL_SURFACE('',#101681,0.2,0.1) ;
#79517 = TOROIDAL_SURFACE('',#101748,0.2,0.1) ;
#79518 = TOROIDAL_SURFACE('',#101755,0.2,0.1) ;
#79519 = TOROIDAL_SURFACE('',#101757,0.2,0.1) ;
#79520 = TOROIDAL_SURFACE('',#101763,0.2,0.1) ;
#79521 = TOROIDAL_SURFACE('',#101791,0.2,0.1) ;
#79522 = TOROIDAL_SURFACE('',#101794,0.2,0.1) ;
#79523 = TOROIDAL_SURFACE('',#101811,0.2,0.1) ;
#79524 = TOROIDAL_SURFACE('',#101817,0.2,0.1) ;
#79525 = TOROIDAL_SURFACE('',#101884,1.75625,0.1) ;
#79526 = TOROIDAL_SURFACE('',#101891,0.2,0.1) ;
#79527 = TOROIDAL_SURFACE('',#101904,1.55625,0.1) ;
#79528 = TOROIDAL_SURFACE('',#101913,0.2,0.1) ;
#79529 = TOROIDAL_SURFACE('',#101915,0.2,0.1) ;
#79530 = TOROIDAL_SURFACE('',#101933,0.2,0.1) ;
#79531 = TOROIDAL_SURFACE('',#101943,0.2,0.1) ;
#79532 = TOROIDAL_SURFACE('',#101957,0.2,0.1) ;
#79533 = TOROIDAL_SURFACE('',#102024,0.2,0.1) ;
#79534 = TOROIDAL_SURFACE('',#102031,0.2,0.1) ;
#79535 = TOROIDAL_SURFACE('',#102033,0.2,0.1) ;
#79536 = TOROIDAL_SURFACE('',#102039,0.2,0.1) ;
#79537 = TOROIDAL_SURFACE('',#102067,0.2,0.1) ;
#79538 = TOROIDAL_SURFACE('',#102070,0.2,0.1) ;
#79539 = TOROIDAL_SURFACE('',#102087,0.2,0.1) ;
#79540 = TOROIDAL_SURFACE('',#102093,0.2,0.1) ;
#79541 = TOROIDAL_SURFACE('',#102160,1.75625,0.1) ;
#79542 = TOROIDAL_SURFACE('',#102167,0.2,0.1) ;
#79543 = TOROIDAL_SURFACE('',#102180,1.55625,0.1) ;
#79544 = TOROIDAL_SURFACE('',#102189,0.2,0.1) ;
#79545 = TOROIDAL_SURFACE('',#102191,0.2,0.1) ;
#79546 = TOROIDAL_SURFACE('',#102209,0.2,0.1) ;
#79547 = TOROIDAL_SURFACE('',#102219,0.2,0.1) ;
#79548 = TOROIDAL_SURFACE('',#102233,0.2,0.1) ;
#79549 = TOROIDAL_SURFACE('',#102300,0.2,0.1) ;
#79550 = TOROIDAL_SURFACE('',#102307,0.2,0.1) ;
#79551 = TOROIDAL_SURFACE('',#102309,0.2,0.1) ;
#79552 = TOROIDAL_SURFACE('',#102315,0.2,0.1) ;
#79553 = TOROIDAL_SURFACE('',#102343,0.2,0.1) ;
#79554 = TOROIDAL_SURFACE('',#102346,0.2,0.1) ;
#79555 = TOROIDAL_SURFACE('',#102363,0.2,0.1) ;
#79556 = TOROIDAL_SURFACE('',#102369,0.2,0.1) ;
#79557 = TOROIDAL_SURFACE('',#102436,1.75625,0.1) ;
#79558 = TOROIDAL_SURFACE('',#102443,0.2,0.1) ;
#79559 = TOROIDAL_SURFACE('',#102456,1.55625,0.1) ;
#79560 = TOROIDAL_SURFACE('',#102465,0.2,0.1) ;
#79561 = TOROIDAL_SURFACE('',#102467,0.2,0.1) ;
#79562 = TOROIDAL_SURFACE('',#102485,0.2,0.1) ;
#79563 = TOROIDAL_SURFACE('',#102495,0.2,0.1) ;
#79564 = TOROIDAL_SURFACE('',#102509,0.2,0.1) ;
#79565 = TOROIDAL_SURFACE('',#102576,0.2,0.1) ;
#79566 = TOROIDAL_SURFACE('',#102583,0.2,0.1) ;
#79567 = TOROIDAL_SURFACE('',#102585,0.2,0.1) ;
#79568 = TOROIDAL_SURFACE('',#102591,0.2,0.1) ;
#79569 = TOROIDAL_SURFACE('',#102619,0.2,0.1) ;
#79570 = TOROIDAL_SURFACE('',#102622,0.2,0.1) ;
#79571 = TOROIDAL_SURFACE('',#102639,0.2,0.1) ;
#79572 = TOROIDAL_SURFACE('',#102645,0.2,0.1) ;
#79573 = TOROIDAL_SURFACE('',#102731,0.2,0.1) ;
#79574 = TOROIDAL_SURFACE('',#102737,0.2,0.1) ;
#79575 = TOROIDAL_SURFACE('',#102738,0.2,0.1) ;
#79576 = TOROIDAL_SURFACE('',#102739,0.2,0.1) ;
#79577 = TOROIDAL_SURFACE('',#102745,0.2,0.1) ;
#79578 = TOROIDAL_SURFACE('',#102746,0.2,0.1) ;
#79579 = TOROIDAL_SURFACE('',#102752,0.2,0.1) ;
#79580 = TOROIDAL_SURFACE('',#102753,0.2,0.1) ;
#79581 = TOROIDAL_SURFACE('',#102759,0.2,0.1) ;
#79582 = TOROIDAL_SURFACE('',#102760,0.2,0.1) ;
#79583 = TOROIDAL_SURFACE('',#102766,0.2,0.1) ;
#79584 = TOROIDAL_SURFACE('',#102767,0.2,0.1) ;
#79585 = TOROIDAL_SURFACE('',#102773,0.2,0.1) ;
#79586 = TOROIDAL_SURFACE('',#102774,0.2,0.1) ;
#79587 = TOROIDAL_SURFACE('',#102780,0.2,0.1) ;
#79588 = TOROIDAL_SURFACE('',#102781,0.2,0.1) ;
#79589 = TOROIDAL_SURFACE('',#102787,0.2,0.1) ;
#79590 = TOROIDAL_SURFACE('',#102792,0.2,0.1) ;
#79591 = TOROIDAL_SURFACE('',#102793,0.2,0.1) ;
#79592 = TOROIDAL_SURFACE('',#102799,0.2,0.1) ;
#79593 = TOROIDAL_SURFACE('',#102805,0.2,0.1) ;
#79594 = TOROIDAL_SURFACE('',#102811,0.2,0.1) ;
#79595 = TOROIDAL_SURFACE('',#102817,0.2,0.1) ;
#79596 = TOROIDAL_SURFACE('',#102823,0.2,0.1) ;
#79597 = TOROIDAL_SURFACE('',#102829,0.2,0.1) ;
#79598 = TOROIDAL_SURFACE('',#102835,0.2,0.1) ;
#79599 = TOROIDAL_SURFACE('',#102841,0.2,0.1) ;
#79600 = TOROIDAL_SURFACE('',#102847,0.2,0.1) ;
#79601 = TOROIDAL_SURFACE('',#102853,0.2,0.1) ;
#79602 = TOROIDAL_SURFACE('',#102859,0.2,0.1) ;
#79603 = TOROIDAL_SURFACE('',#102865,0.2,0.1) ;
#79604 = TOROIDAL_SURFACE('',#102871,0.2,0.1) ;
#79605 = TOROIDAL_SURFACE('',#102877,0.2,0.1) ;
#79606 = TOROIDAL_SURFACE('',#102883,0.2,0.1) ;
#79607 = TOROIDAL_SURFACE('',#102889,0.2,0.1) ;
#79608 = TOROIDAL_SURFACE('',#102895,0.2,0.1) ;
#79609 = TOROIDAL_SURFACE('',#102901,0.2,0.1) ;
#79610 = TOROIDAL_SURFACE('',#102904,0.2,0.1) ;
#79611 = TOROIDAL_SURFACE('',#102905,0.2,0.1) ;
#79612 = TOROIDAL_SURFACE('',#102908,0.2,0.1) ;
#79613 = TOROIDAL_SURFACE('',#102909,0.2,0.1) ;
#79614 = TOROIDAL_SURFACE('',#102912,0.2,0.1) ;
#79615 = TOROIDAL_SURFACE('',#102913,0.2,0.1) ;
#79616 = TOROIDAL_SURFACE('',#102916,0.2,0.1) ;
#79617 = TOROIDAL_SURFACE('',#102917,0.2,0.1) ;
#79618 = TOROIDAL_SURFACE('',#102920,0.2,0.1) ;
#79619 = TOROIDAL_SURFACE('',#102921,0.2,0.1) ;
#79620 = TOROIDAL_SURFACE('',#102924,0.2,0.1) ;
#79621 = TOROIDAL_SURFACE('',#102925,0.2,0.1) ;
#79622 = TOROIDAL_SURFACE('',#102928,0.2,0.1) ;
#79623 = TOROIDAL_SURFACE('',#102929,0.2,0.1) ;
#79624 = TOROIDAL_SURFACE('',#102932,0.2,0.1) ;
#79625 = TOROIDAL_SURFACE('',#102933,0.2,0.1) ;
#79626 = TOROIDAL_SURFACE('',#102936,0.2,0.1) ;
#79627 = TOROIDAL_SURFACE('',#102937,0.2,0.1) ;
#79628 = TOROIDAL_SURFACE('',#102940,0.2,0.1) ;
#79629 = TOROIDAL_SURFACE('',#102941,0.2,0.1) ;
#79630 = TOROIDAL_SURFACE('',#102944,0.2,0.1) ;
#79631 = TOROIDAL_SURFACE('',#102945,0.2,0.1) ;
#79632 = TOROIDAL_SURFACE('',#102948,0.2,0.1) ;
#79633 = TOROIDAL_SURFACE('',#102949,0.2,0.1) ;
#79634 = TOROIDAL_SURFACE('',#102952,0.2,0.1) ;
#79635 = TOROIDAL_SURFACE('',#102953,0.2,0.1) ;
#79636 = TOROIDAL_SURFACE('',#102956,0.2,0.1) ;
#79637 = TOROIDAL_SURFACE('',#102957,0.2,0.1) ;
#79638 = TOROIDAL_SURFACE('',#102960,0.2,0.1) ;
#79639 = TOROIDAL_SURFACE('',#102961,0.2,0.1) ;
#79640 = TOROIDAL_SURFACE('',#102964,0.2,0.1) ;
#79641 = TOROIDAL_SURFACE('',#102965,0.2,0.1) ;
#79642 = TOROIDAL_SURFACE('',#102968,0.2,0.1) ;
#79643 = TOROIDAL_SURFACE('',#102969,0.2,0.1) ;
#79644 = TOROIDAL_SURFACE('',#102972,0.2,0.1) ;
#79645 = TOROIDAL_SURFACE('',#102989,0.2,0.1) ;
#79646 = TOROIDAL_SURFACE('',#103003,0.2,0.1) ;
#79647 = TOROIDAL_SURFACE('',#103014,0.2,0.1) ;
#79648 = TOROIDAL_SURFACE('',#103025,2.15,0.1) ;
#79649 = TOROIDAL_SURFACE('',#103026,2.15,0.1) ;
#79650 = TOROIDAL_SURFACE('',#103027,2.15,0.1) ;
#79651 = TOROIDAL_SURFACE('',#103028,2.15,0.1) ;
#79652 = TOROIDAL_SURFACE('',#103029,2.15,0.1) ;
#79653 = TOROIDAL_SURFACE('',#103030,2.15,0.1) ;
#79654 = TOROIDAL_SURFACE('',#103031,2.15,0.1) ;
#79655 = TOROIDAL_SURFACE('',#103034,2.15,0.1) ;
#79656 = TOROIDAL_SURFACE('',#103037,0.2,0.1) ;
#79657 = TOROIDAL_SURFACE('',#103039,2.15,0.1) ;
#79658 = TOROIDAL_SURFACE('',#103044,2.15,0.1) ;
#79659 = TOROIDAL_SURFACE('',#103049,0.2,0.1) ;
#79660 = TOROIDAL_SURFACE('',#103064,0.2,0.1) ;
#79661 = STYLED_ITEM('',(#170169),#85367) ;
#79662 = STYLED_ITEM('',(#170169),#85368) ;
#79663 = STYLED_ITEM('',(#170169),#85369) ;
#79664 = STYLED_ITEM('',(#170169),#85370) ;
#79665 = STYLED_ITEM('',(#170169),#85371) ;
#79666 = STYLED_ITEM('',(#170169),#85372) ;
#79667 = STYLED_ITEM('',(#170169),#85373) ;
#79668 = STYLED_ITEM('',(#170169),#85374) ;
#79669 = STYLED_ITEM('',(#170169),#85375) ;
#79670 = STYLED_ITEM('',(#170169),#85376) ;
#79671 = STYLED_ITEM('',(#170169),#85377) ;
#79672 = STYLED_ITEM('',(#170169),#85378) ;
#79673 = STYLED_ITEM('',(#170169),#85379) ;
#79674 = STYLED_ITEM('',(#170169),#85380) ;
#79675 = STYLED_ITEM('',(#170169),#85381) ;
#79676 = STYLED_ITEM('',(#170169),#85382) ;
#79677 = STYLED_ITEM('',(#170169),#85383) ;
#79678 = STYLED_ITEM('',(#170169),#85384) ;
#79679 = STYLED_ITEM('',(#170169),#85385) ;
#79680 = STYLED_ITEM('',(#170169),#85386) ;
#79681 = STYLED_ITEM('',(#170169),#85387) ;
#79682 = STYLED_ITEM('',(#170169),#85388) ;
#79683 = STYLED_ITEM('',(#170169),#85389) ;
#79684 = STYLED_ITEM('',(#170169),#85390) ;
#79685 = STYLED_ITEM('',(#170169),#85391) ;
#79686 = STYLED_ITEM('',(#170169),#85392) ;
#79687 = STYLED_ITEM('',(#170169),#85393) ;
#79688 = STYLED_ITEM('',(#170169),#85394) ;
#79689 = STYLED_ITEM('',(#170169),#85395) ;
#79690 = STYLED_ITEM('',(#170169),#85396) ;
#79691 = STYLED_ITEM('',(#170169),#85397) ;
#79692 = STYLED_ITEM('',(#170169),#85398) ;
#79693 = STYLED_ITEM('',(#170169),#85399) ;
#79694 = STYLED_ITEM('',(#170169),#85400) ;
#79695 = STYLED_ITEM('',(#170170),#85401) ;
#79696 = STYLED_ITEM('',(#170169),#85402) ;
#79697 = STYLED_ITEM('',(#170169),#85403) ;
#79698 = STYLED_ITEM('',(#170169),#85404) ;
#79699 = STYLED_ITEM('',(#170169),#85405) ;
#79700 = STYLED_ITEM('',(#170169),#85406) ;
#79701 = STYLED_ITEM('',(#170169),#85407) ;
#79702 = STYLED_ITEM('',(#170169),#85408) ;
#79703 = STYLED_ITEM('',(#170169),#85409) ;
#79704 = STYLED_ITEM('',(#170169),#85410) ;
#79705 = STYLED_ITEM('',(#170169),#85411) ;
#79706 = STYLED_ITEM('',(#170169),#85412) ;
#79707 = STYLED_ITEM('',(#170169),#85413) ;
#79708 = STYLED_ITEM('',(#170169),#85414) ;
#79709 = STYLED_ITEM('',(#170169),#85415) ;
#79710 = STYLED_ITEM('',(#170169),#85416) ;
#79711 = STYLED_ITEM('',(#170169),#85417) ;
#79712 = STYLED_ITEM('',(#170169),#85418) ;
#79713 = STYLED_ITEM('',(#170169),#85419) ;
#79714 = STYLED_ITEM('',(#170169),#85420) ;
#79715 = STYLED_ITEM('',(#170171),#85421) ;
#79716 = STYLED_ITEM('',(#170169),#85422) ;
#79717 = STYLED_ITEM('',(#170169),#85423) ;
#79718 = STYLED_ITEM('',(#170169),#85424) ;
#79719 = STYLED_ITEM('',(#170169),#85425) ;
#79720 = STYLED_ITEM('',(#170169),#85426) ;
#79721 = STYLED_ITEM('',(#170169),#85427) ;
#79722 = STYLED_ITEM('',(#170169),#85428) ;
#79723 = STYLED_ITEM('',(#170169),#85429) ;
#79724 = STYLED_ITEM('',(#170169),#85430) ;
#79725 = STYLED_ITEM('',(#170169),#85431) ;
#79726 = STYLED_ITEM('',(#170169),#85432) ;
#79727 = STYLED_ITEM('',(#170169),#85433) ;
#79728 = STYLED_ITEM('',(#170169),#85434) ;
#79729 = STYLED_ITEM('',(#170169),#85435) ;
#79730 = STYLED_ITEM('',(#170169),#85436) ;
#79731 = STYLED_ITEM('',(#170169),#85437) ;
#79732 = STYLED_ITEM('',(#170169),#85438) ;
#79733 = STYLED_ITEM('',(#170169),#85439) ;
#79734 = STYLED_ITEM('',(#170169),#85440) ;
#79735 = STYLED_ITEM('',(#170170),#85441) ;
#79736 = STYLED_ITEM('',(#170170),#85442) ;
#79737 = STYLED_ITEM('',(#170170),#85443) ;
#79738 = STYLED_ITEM('',(#170170),#85444) ;
#79739 = STYLED_ITEM('',(#170169),#85445) ;
#79740 = STYLED_ITEM('',(#170169),#85446) ;
#79741 = STYLED_ITEM('',(#170169),#85447) ;
#79742 = STYLED_ITEM('',(#170169),#85448) ;
#79743 = STYLED_ITEM('',(#170169),#85449) ;
#79744 = STYLED_ITEM('',(#170169),#85450) ;
#79745 = STYLED_ITEM('',(#170169),#85451) ;
#79746 = STYLED_ITEM('',(#170169),#85452) ;
#79747 = STYLED_ITEM('',(#170169),#85453) ;
#79748 = STYLED_ITEM('',(#170169),#85454) ;
#79749 = STYLED_ITEM('',(#170169),#85455) ;
#79750 = STYLED_ITEM('',(#170169),#85456) ;
#79751 = STYLED_ITEM('',(#170169),#85457) ;
#79752 = STYLED_ITEM('',(#170169),#85458) ;
#79753 = STYLED_ITEM('',(#170169),#85459) ;
#79754 = STYLED_ITEM('',(#170169),#85460) ;
#79755 = STYLED_ITEM('',(#170169),#85461) ;
#79756 = STYLED_ITEM('',(#170169),#85462) ;
#79757 = STYLED_ITEM('',(#170171),#85463) ;
#79758 = STYLED_ITEM('',(#170169),#85464) ;
#79759 = STYLED_ITEM('',(#170169),#85465) ;
#79760 = STYLED_ITEM('',(#170169),#85466) ;
#79761 = STYLED_ITEM('',(#170169),#85467) ;
#79762 = STYLED_ITEM('',(#170169),#85468) ;
#79763 = STYLED_ITEM('',(#170169),#85469) ;
#79764 = STYLED_ITEM('',(#170169),#85470) ;
#79765 = STYLED_ITEM('',(#170169),#85471) ;
#79766 = STYLED_ITEM('',(#170169),#85472) ;
#79767 = STYLED_ITEM('',(#170169),#85473) ;
#79768 = STYLED_ITEM('',(#170169),#85474) ;
#79769 = STYLED_ITEM('',(#170169),#85475) ;
#79770 = STYLED_ITEM('',(#170169),#85476) ;
#79771 = STYLED_ITEM('',(#170169),#85477) ;
#79772 = STYLED_ITEM('',(#170169),#85478) ;
#79773 = STYLED_ITEM('',(#170169),#85479) ;
#79774 = STYLED_ITEM('',(#170169),#85480) ;
#79775 = STYLED_ITEM('',(#170169),#85481) ;
#79776 = STYLED_ITEM('',(#170169),#85482) ;
#79777 = STYLED_ITEM('',(#170169),#85483) ;
#79778 = STYLED_ITEM('',(#170169),#85485) ;
#79779 = STYLED_ITEM('',(#170169),#85486) ;
#79780 = STYLED_ITEM('',(#170169),#85487) ;
#79781 = STYLED_ITEM('',(#170169),#85488) ;
#79782 = STYLED_ITEM('',(#170169),#85489) ;
#79783 = STYLED_ITEM('',(#170169),#85490) ;
#79784 = STYLED_ITEM('',(#170169),#85491) ;
#79785 = STYLED_ITEM('',(#170169),#85492) ;
#79786 = STYLED_ITEM('',(#170169),#85493) ;
#79787 = STYLED_ITEM('',(#170169),#85494) ;
#79788 = STYLED_ITEM('',(#170169),#85495) ;
#79789 = STYLED_ITEM('',(#170169),#85496) ;
#79790 = STYLED_ITEM('',(#170169),#85497) ;
#79791 = STYLED_ITEM('',(#170169),#85498) ;
#79792 = STYLED_ITEM('',(#170169),#85499) ;
#79793 = STYLED_ITEM('',(#170169),#85500) ;
#79794 = STYLED_ITEM('',(#170169),#85501) ;
#79795 = STYLED_ITEM('',(#170169),#85502) ;
#79796 = STYLED_ITEM('',(#170169),#85503) ;
#79797 = STYLED_ITEM('',(#170169),#85504) ;
#79798 = STYLED_ITEM('',(#170169),#85505) ;
#79799 = STYLED_ITEM('',(#170169),#85506) ;
#79800 = STYLED_ITEM('',(#170169),#85507) ;
#79801 = STYLED_ITEM('',(#170169),#85508) ;
#79802 = STYLED_ITEM('',(#170169),#85509) ;
#79803 = STYLED_ITEM('',(#170169),#85510) ;
#79804 = STYLED_ITEM('',(#170169),#85511) ;
#79805 = STYLED_ITEM('',(#170169),#85512) ;
#79806 = STYLED_ITEM('',(#170169),#85513) ;
#79807 = STYLED_ITEM('',(#170169),#85514) ;
#79808 = STYLED_ITEM('',(#170169),#85515) ;
#79809 = STYLED_ITEM('',(#170169),#85516) ;
#79810 = STYLED_ITEM('',(#170169),#85517) ;
#79811 = STYLED_ITEM('',(#170169),#85518) ;
#79812 = STYLED_ITEM('',(#170169),#85519) ;
#79813 = STYLED_ITEM('',(#170169),#85520) ;
#79814 = STYLED_ITEM('',(#170169),#85521) ;
#79815 = STYLED_ITEM('',(#170169),#85522) ;
#79816 = STYLED_ITEM('',(#170169),#85523) ;
#79817 = STYLED_ITEM('',(#170169),#85524) ;
#79818 = STYLED_ITEM('',(#170169),#85525) ;
#79819 = STYLED_ITEM('',(#170169),#85526) ;
#79820 = STYLED_ITEM('',(#170169),#85527) ;
#79821 = STYLED_ITEM('',(#170169),#85528) ;
#79822 = STYLED_ITEM('',(#170169),#85529) ;
#79823 = STYLED_ITEM('',(#170169),#85530) ;
#79824 = STYLED_ITEM('',(#170169),#85531) ;
#79825 = STYLED_ITEM('',(#170169),#85532) ;
#79826 = STYLED_ITEM('',(#170169),#85533) ;
#79827 = STYLED_ITEM('',(#170169),#85534) ;
#79828 = STYLED_ITEM('',(#170169),#85535) ;
#79829 = STYLED_ITEM('',(#170169),#85536) ;
#79830 = STYLED_ITEM('',(#170169),#85537) ;
#79831 = STYLED_ITEM('',(#170169),#85538) ;
#79832 = STYLED_ITEM('',(#170169),#85539) ;
#79833 = STYLED_ITEM('',(#170169),#85540) ;
#79834 = STYLED_ITEM('',(#170169),#85541) ;
#79835 = STYLED_ITEM('',(#170169),#85542) ;
#79836 = STYLED_ITEM('',(#170169),#85543) ;
#79837 = STYLED_ITEM('',(#170169),#85544) ;
#79838 = STYLED_ITEM('',(#170169),#85545) ;
#79839 = STYLED_ITEM('',(#170169),#85546) ;
#79840 = STYLED_ITEM('',(#170169),#85547) ;
#79841 = STYLED_ITEM('',(#170169),#85548) ;
#79842 = STYLED_ITEM('',(#170169),#85549) ;
#79843 = STYLED_ITEM('',(#170169),#85550) ;
#79844 = STYLED_ITEM('',(#170169),#85551) ;
#79845 = STYLED_ITEM('',(#170169),#85552) ;
#79846 = STYLED_ITEM('',(#170169),#85553) ;
#79847 = STYLED_ITEM('',(#170169),#85554) ;
#79848 = STYLED_ITEM('',(#170169),#85555) ;
#79849 = STYLED_ITEM('',(#170169),#85556) ;
#79850 = STYLED_ITEM('',(#170169),#85557) ;
#79851 = STYLED_ITEM('',(#170169),#85558) ;
#79852 = STYLED_ITEM('',(#170169),#85559) ;
#79853 = STYLED_ITEM('',(#170169),#85560) ;
#79854 = STYLED_ITEM('',(#170169),#85561) ;
#79855 = STYLED_ITEM('',(#170169),#85562) ;
#79856 = STYLED_ITEM('',(#170169),#85563) ;
#79857 = STYLED_ITEM('',(#170169),#85564) ;
#79858 = STYLED_ITEM('',(#170169),#85565) ;
#79859 = STYLED_ITEM('',(#170169),#85566) ;
#79860 = STYLED_ITEM('',(#170169),#85567) ;
#79861 = STYLED_ITEM('',(#170169),#85568) ;
#79862 = STYLED_ITEM('',(#170169),#85569) ;
#79863 = STYLED_ITEM('',(#170169),#85570) ;
#79864 = STYLED_ITEM('',(#170169),#85571) ;
#79865 = STYLED_ITEM('',(#170169),#85572) ;
#79866 = STYLED_ITEM('',(#170169),#85573) ;
#79867 = STYLED_ITEM('',(#170169),#85574) ;
#79868 = STYLED_ITEM('',(#170170),#85575) ;
#79869 = STYLED_ITEM('',(#170170),#85576) ;
#79870 = STYLED_ITEM('',(#170170),#85577) ;
#79871 = STYLED_ITEM('',(#170170),#85578) ;
#79872 = STYLED_ITEM('',(#170169),#85579) ;
#79873 = STYLED_ITEM('',(#170169),#85580) ;
#79874 = STYLED_ITEM('',(#170169),#85581) ;
#79875 = STYLED_ITEM('',(#170169),#85582) ;
#79876 = STYLED_ITEM('',(#170169),#85583) ;
#79877 = STYLED_ITEM('',(#170169),#85584) ;
#79878 = STYLED_ITEM('',(#170169),#85585) ;
#79879 = STYLED_ITEM('',(#170169),#85586) ;
#79880 = STYLED_ITEM('',(#170169),#85587) ;
#79881 = STYLED_ITEM('',(#170169),#85588) ;
#79882 = STYLED_ITEM('',(#170169),#85589) ;
#79883 = STYLED_ITEM('',(#170169),#85590) ;
#79884 = STYLED_ITEM('',(#170169),#85591) ;
#79885 = STYLED_ITEM('',(#170169),#85592) ;
#79886 = STYLED_ITEM('',(#170169),#85593) ;
#79887 = STYLED_ITEM('',(#170169),#85594) ;
#79888 = STYLED_ITEM('',(#170169),#85595) ;
#79889 = STYLED_ITEM('',(#170169),#85596) ;
#79890 = STYLED_ITEM('',(#170169),#85597) ;
#79891 = STYLED_ITEM('',(#170169),#85598) ;
#79892 = STYLED_ITEM('',(#170169),#85599) ;
#79893 = STYLED_ITEM('',(#170169),#85600) ;
#79894 = STYLED_ITEM('',(#170169),#85601) ;
#79895 = STYLED_ITEM('',(#170169),#85602) ;
#79896 = STYLED_ITEM('',(#170169),#85603) ;
#79897 = STYLED_ITEM('',(#170169),#85604) ;
#79898 = STYLED_ITEM('',(#170169),#85605) ;
#79899 = STYLED_ITEM('',(#170169),#85606) ;
#79900 = STYLED_ITEM('',(#170169),#85607) ;
#79901 = STYLED_ITEM('',(#170169),#85608) ;
#79902 = STYLED_ITEM('',(#170169),#85609) ;
#79903 = STYLED_ITEM('',(#170169),#85610) ;
#79904 = STYLED_ITEM('',(#170169),#85611) ;
#79905 = STYLED_ITEM('',(#170169),#85612) ;
#79906 = STYLED_ITEM('',(#170169),#85613) ;
#79907 = STYLED_ITEM('',(#170169),#85614) ;
#79908 = STYLED_ITEM('',(#170169),#85615) ;
#79909 = STYLED_ITEM('',(#170170),#85616) ;
#79910 = STYLED_ITEM('',(#170169),#85617) ;
#79911 = STYLED_ITEM('',(#170169),#85618) ;
#79912 = STYLED_ITEM('',(#170169),#85619) ;
#79913 = STYLED_ITEM('',(#170169),#85620) ;
#79914 = STYLED_ITEM('',(#170169),#85621) ;
#79915 = STYLED_ITEM('',(#170171),#85622) ;
#79916 = STYLED_ITEM('',(#170169),#85623) ;
#79917 = STYLED_ITEM('',(#170169),#85624) ;
#79918 = STYLED_ITEM('',(#170169),#85625) ;
#79919 = STYLED_ITEM('',(#170169),#85626) ;
#79920 = STYLED_ITEM('',(#170169),#85627) ;
#79921 = STYLED_ITEM('',(#170169),#85628) ;
#79922 = STYLED_ITEM('',(#170169),#85629) ;
#79923 = STYLED_ITEM('',(#170169),#85630) ;
#79924 = STYLED_ITEM('',(#170169),#85631) ;
#79925 = STYLED_ITEM('',(#170169),#85632) ;
#79926 = STYLED_ITEM('',(#170169),#85633) ;
#79927 = STYLED_ITEM('',(#170169),#85634) ;
#79928 = STYLED_ITEM('',(#170169),#85635) ;
#79929 = STYLED_ITEM('',(#170169),#85636) ;
#79930 = STYLED_ITEM('',(#170169),#85637) ;
#79931 = STYLED_ITEM('',(#170169),#85638) ;
#79932 = STYLED_ITEM('',(#170169),#85639) ;
#79933 = STYLED_ITEM('',(#170169),#85640) ;
#79934 = STYLED_ITEM('',(#170169),#85641) ;
#79935 = STYLED_ITEM('',(#170170),#85642) ;
#79936 = STYLED_ITEM('',(#170170),#85643) ;
#79937 = STYLED_ITEM('',(#170170),#85644) ;
#79938 = STYLED_ITEM('',(#170170),#85645) ;
#79939 = STYLED_ITEM('',(#170169),#85646) ;
#79940 = STYLED_ITEM('',(#170169),#85647) ;
#79941 = STYLED_ITEM('',(#170169),#85648) ;
#79942 = STYLED_ITEM('',(#170169),#85649) ;
#79943 = STYLED_ITEM('',(#170169),#85650) ;
#79944 = STYLED_ITEM('',(#170169),#85651) ;
#79945 = STYLED_ITEM('',(#170169),#85652) ;
#79946 = STYLED_ITEM('',(#170169),#85653) ;
#79947 = STYLED_ITEM('',(#170169),#85654) ;
#79948 = STYLED_ITEM('',(#170169),#85655) ;
#79949 = STYLED_ITEM('',(#170169),#85656) ;
#79950 = STYLED_ITEM('',(#170169),#85657) ;
#79951 = STYLED_ITEM('',(#170169),#85658) ;
#79952 = STYLED_ITEM('',(#170169),#85659) ;
#79953 = STYLED_ITEM('',(#170169),#85660) ;
#79954 = STYLED_ITEM('',(#170169),#85661) ;
#79955 = STYLED_ITEM('',(#170169),#85662) ;
#79956 = STYLED_ITEM('',(#170169),#85663) ;
#79957 = STYLED_ITEM('',(#170171),#85664) ;
#79958 = STYLED_ITEM('',(#170169),#85665) ;
#79959 = STYLED_ITEM('',(#170169),#85666) ;
#79960 = STYLED_ITEM('',(#170169),#85667) ;
#79961 = STYLED_ITEM('',(#170169),#85668) ;
#79962 = STYLED_ITEM('',(#170169),#85669) ;
#79963 = STYLED_ITEM('',(#170169),#85670) ;
#79964 = STYLED_ITEM('',(#170169),#85671) ;
#79965 = STYLED_ITEM('',(#170169),#85672) ;
#79966 = STYLED_ITEM('',(#170169),#85673) ;
#79967 = STYLED_ITEM('',(#170169),#85674) ;
#79968 = STYLED_ITEM('',(#170169),#85675) ;
#79969 = STYLED_ITEM('',(#170169),#85676) ;
#79970 = STYLED_ITEM('',(#170169),#85677) ;
#79971 = STYLED_ITEM('',(#170169),#85678) ;
#79972 = STYLED_ITEM('',(#170169),#85679) ;
#79973 = STYLED_ITEM('',(#170169),#85680) ;
#79974 = STYLED_ITEM('',(#170169),#85681) ;
#79975 = STYLED_ITEM('',(#170169),#85682) ;
#79976 = STYLED_ITEM('',(#170169),#85683) ;
#79977 = STYLED_ITEM('',(#170169),#85684) ;
#79978 = STYLED_ITEM('',(#170169),#85685) ;
#79979 = STYLED_ITEM('',(#170169),#85686) ;
#79980 = STYLED_ITEM('',(#170169),#85687) ;
#79981 = STYLED_ITEM('',(#170169),#85688) ;
#79982 = STYLED_ITEM('',(#170169),#85689) ;
#79983 = STYLED_ITEM('',(#170169),#85690) ;
#79984 = STYLED_ITEM('',(#170169),#85691) ;
#79985 = STYLED_ITEM('',(#170169),#85692) ;
#79986 = STYLED_ITEM('',(#170169),#85693) ;
#79987 = STYLED_ITEM('',(#170169),#85694) ;
#79988 = STYLED_ITEM('',(#170169),#85695) ;
#79989 = STYLED_ITEM('',(#170169),#85696) ;
#79990 = STYLED_ITEM('',(#170169),#85697) ;
#79991 = STYLED_ITEM('',(#170169),#85698) ;
#79992 = STYLED_ITEM('',(#170169),#85699) ;
#79993 = STYLED_ITEM('',(#170169),#85700) ;
#79994 = STYLED_ITEM('',(#170169),#85701) ;
#79995 = STYLED_ITEM('',(#170169),#85702) ;
#79996 = STYLED_ITEM('',(#170169),#85703) ;
#79997 = STYLED_ITEM('',(#170169),#85704) ;
#79998 = STYLED_ITEM('',(#170169),#85705) ;
#79999 = STYLED_ITEM('',(#170169),#85706) ;
#80000 = STYLED_ITEM('',(#170169),#85707) ;
#80001 = STYLED_ITEM('',(#170169),#85708) ;
#80002 = STYLED_ITEM('',(#170169),#85709) ;
#80003 = STYLED_ITEM('',(#170169),#85710) ;
#80004 = STYLED_ITEM('',(#170169),#85711) ;
#80005 = STYLED_ITEM('',(#170169),#85712) ;
#80006 = STYLED_ITEM('',(#170169),#85713) ;
#80007 = STYLED_ITEM('',(#170169),#85714) ;
#80008 = STYLED_ITEM('',(#170169),#85715) ;
#80009 = STYLED_ITEM('',(#170169),#85716) ;
#80010 = STYLED_ITEM('',(#170169),#85717) ;
#80011 = STYLED_ITEM('',(#170169),#85718) ;
#80012 = STYLED_ITEM('',(#170169),#85719) ;
#80013 = STYLED_ITEM('',(#170169),#85720) ;
#80014 = STYLED_ITEM('',(#170169),#85721) ;
#80015 = STYLED_ITEM('',(#170169),#85722) ;
#80016 = STYLED_ITEM('',(#170169),#85723) ;
#80017 = STYLED_ITEM('',(#170169),#85724) ;
#80018 = STYLED_ITEM('',(#170169),#85725) ;
#80019 = STYLED_ITEM('',(#170169),#85726) ;
#80020 = STYLED_ITEM('',(#170169),#85727) ;
#80021 = STYLED_ITEM('',(#170169),#85728) ;
#80022 = STYLED_ITEM('',(#170169),#85729) ;
#80023 = STYLED_ITEM('',(#170169),#85730) ;
#80024 = STYLED_ITEM('',(#170169),#85731) ;
#80025 = STYLED_ITEM('',(#170169),#85732) ;
#80026 = STYLED_ITEM('',(#170169),#85733) ;
#80027 = STYLED_ITEM('',(#170169),#85734) ;
#80028 = STYLED_ITEM('',(#170169),#85735) ;
#80029 = STYLED_ITEM('',(#170169),#85736) ;
#80030 = STYLED_ITEM('',(#170169),#85737) ;
#80031 = STYLED_ITEM('',(#170169),#85738) ;
#80032 = STYLED_ITEM('',(#170169),#85739) ;
#80033 = STYLED_ITEM('',(#170169),#85740) ;
#80034 = STYLED_ITEM('',(#170169),#85741) ;
#80035 = STYLED_ITEM('',(#170169),#85742) ;
#80036 = STYLED_ITEM('',(#170169),#85743) ;
#80037 = STYLED_ITEM('',(#170169),#85744) ;
#80038 = STYLED_ITEM('',(#170169),#85745) ;
#80039 = STYLED_ITEM('',(#170169),#85746) ;
#80040 = STYLED_ITEM('',(#170169),#85747) ;
#80041 = STYLED_ITEM('',(#170169),#85748) ;
#80042 = STYLED_ITEM('',(#170169),#85749) ;
#80043 = STYLED_ITEM('',(#170169),#85750) ;
#80044 = STYLED_ITEM('',(#170169),#85751) ;
#80045 = STYLED_ITEM('',(#170169),#85752) ;
#80046 = STYLED_ITEM('',(#170169),#85753) ;
#80047 = STYLED_ITEM('',(#170169),#85754) ;
#80048 = STYLED_ITEM('',(#170169),#85755) ;
#80049 = STYLED_ITEM('',(#170169),#85756) ;
#80050 = STYLED_ITEM('',(#170169),#85757) ;
#80051 = STYLED_ITEM('',(#170169),#85758) ;
#80052 = STYLED_ITEM('',(#170169),#85759) ;
#80053 = STYLED_ITEM('',(#170169),#85760) ;
#80054 = STYLED_ITEM('',(#170169),#85761) ;
#80055 = STYLED_ITEM('',(#170169),#85762) ;
#80056 = STYLED_ITEM('',(#170169),#85763) ;
#80057 = STYLED_ITEM('',(#170169),#85764) ;
#80058 = STYLED_ITEM('',(#170169),#85765) ;
#80059 = STYLED_ITEM('',(#170169),#85766) ;
#80060 = STYLED_ITEM('',(#170170),#85767) ;
#80061 = STYLED_ITEM('',(#170170),#85768) ;
#80062 = STYLED_ITEM('',(#170170),#85769) ;
#80063 = STYLED_ITEM('',(#170170),#85770) ;
#80064 = STYLED_ITEM('',(#170169),#85771) ;
#80065 = STYLED_ITEM('',(#170169),#85772) ;
#80066 = STYLED_ITEM('',(#170169),#85773) ;
#80067 = STYLED_ITEM('',(#170169),#85774) ;
#80068 = STYLED_ITEM('',(#170169),#85775) ;
#80069 = STYLED_ITEM('',(#170169),#85776) ;
#80070 = STYLED_ITEM('',(#170169),#85777) ;
#80071 = STYLED_ITEM('',(#170169),#85778) ;
#80072 = STYLED_ITEM('',(#170169),#85779) ;
#80073 = STYLED_ITEM('',(#170169),#85780) ;
#80074 = STYLED_ITEM('',(#170169),#85781) ;
#80075 = STYLED_ITEM('',(#170169),#85782) ;
#80076 = STYLED_ITEM('',(#170169),#85783) ;
#80077 = STYLED_ITEM('',(#170169),#85784) ;
#80078 = STYLED_ITEM('',(#170169),#85785) ;
#80079 = STYLED_ITEM('',(#170169),#85786) ;
#80080 = STYLED_ITEM('',(#170169),#85787) ;
#80081 = STYLED_ITEM('',(#170169),#85788) ;
#80082 = STYLED_ITEM('',(#170169),#85789) ;
#80083 = STYLED_ITEM('',(#170169),#85790) ;
#80084 = STYLED_ITEM('',(#170169),#85791) ;
#80085 = STYLED_ITEM('',(#170169),#85792) ;
#80086 = STYLED_ITEM('',(#170169),#85793) ;
#80087 = STYLED_ITEM('',(#170169),#85794) ;
#80088 = STYLED_ITEM('',(#170169),#85795) ;
#80089 = STYLED_ITEM('',(#170169),#85796) ;
#80090 = STYLED_ITEM('',(#170169),#85797) ;
#80091 = STYLED_ITEM('',(#170169),#85798) ;
#80092 = STYLED_ITEM('',(#170169),#85799) ;
#80093 = STYLED_ITEM('',(#170169),#85800) ;
#80094 = STYLED_ITEM('',(#170169),#85801) ;
#80095 = STYLED_ITEM('',(#170169),#85802) ;
#80096 = STYLED_ITEM('',(#170169),#85803) ;
#80097 = STYLED_ITEM('',(#170169),#85804) ;
#80098 = STYLED_ITEM('',(#170169),#85805) ;
#80099 = STYLED_ITEM('',(#170169),#85806) ;
#80100 = STYLED_ITEM('',(#170169),#85807) ;
#80101 = STYLED_ITEM('',(#170169),#85808) ;
#80102 = STYLED_ITEM('',(#170169),#85809) ;
#80103 = STYLED_ITEM('',(#170169),#85810) ;
#80104 = STYLED_ITEM('',(#170169),#85811) ;
#80105 = STYLED_ITEM('',(#170169),#85812) ;
#80106 = STYLED_ITEM('',(#170169),#85813) ;
#80107 = STYLED_ITEM('',(#170169),#85814) ;
#80108 = STYLED_ITEM('',(#170168),#29) ;
#80109 = STYLED_ITEM('',(#170169),#85815) ;
#80110 = STYLED_ITEM('',(#170169),#85816) ;
#80111 = STYLED_ITEM('',(#170169),#85817) ;
#80112 = STYLED_ITEM('',(#170169),#85818) ;
#80113 = STYLED_ITEM('',(#170169),#85819) ;
#80114 = STYLED_ITEM('',(#170169),#85820) ;
#80115 = STYLED_ITEM('',(#170169),#85821) ;
#80116 = STYLED_ITEM('',(#170169),#85822) ;
#80117 = STYLED_ITEM('',(#170169),#85823) ;
#80118 = STYLED_ITEM('',(#170169),#85824) ;
#80119 = STYLED_ITEM('',(#170169),#85825) ;
#80120 = STYLED_ITEM('',(#170169),#85826) ;
#80121 = STYLED_ITEM('',(#170169),#85827) ;
#80122 = STYLED_ITEM('',(#170169),#85828) ;
#80123 = STYLED_ITEM('',(#170169),#85829) ;
#80124 = STYLED_ITEM('',(#170169),#85830) ;
#80125 = STYLED_ITEM('',(#170169),#85831) ;
#80126 = STYLED_ITEM('',(#170169),#85832) ;
#80127 = STYLED_ITEM('',(#170169),#85833) ;
#80128 = STYLED_ITEM('',(#170169),#85834) ;
#80129 = STYLED_ITEM('',(#170169),#85835) ;
#80130 = STYLED_ITEM('',(#170169),#85836) ;
#80131 = STYLED_ITEM('',(#170169),#85837) ;
#80132 = STYLED_ITEM('',(#170169),#85838) ;
#80133 = STYLED_ITEM('',(#170169),#85839) ;
#80134 = STYLED_ITEM('',(#170169),#85840) ;
#80135 = STYLED_ITEM('',(#170169),#85841) ;
#80136 = STYLED_ITEM('',(#170169),#85842) ;
#80137 = STYLED_ITEM('',(#170169),#85843) ;
#80138 = STYLED_ITEM('',(#170169),#85844) ;
#80139 = STYLED_ITEM('',(#170169),#85845) ;
#80140 = STYLED_ITEM('',(#170169),#85847) ;
#80141 = STYLED_ITEM('',(#170170),#85849) ;
#80142 = STYLED_ITEM('',(#170169),#85850) ;
#80143 = STYLED_ITEM('',(#170169),#85851) ;
#80144 = STYLED_ITEM('',(#170169),#85852) ;
#80145 = STYLED_ITEM('',(#170169),#85853) ;
#80146 = STYLED_ITEM('',(#170169),#85854) ;
#80147 = STYLED_ITEM('',(#170169),#85855) ;
#80148 = STYLED_ITEM('',(#170169),#85856) ;
#80149 = STYLED_ITEM('',(#170169),#85857) ;
#80150 = STYLED_ITEM('',(#170169),#85858) ;
#80151 = STYLED_ITEM('',(#170169),#85859) ;
#80152 = STYLED_ITEM('',(#170169),#85860) ;
#80153 = STYLED_ITEM('',(#170169),#85861) ;
#80154 = STYLED_ITEM('',(#170169),#85862) ;
#80155 = STYLED_ITEM('',(#170169),#85863) ;
#80156 = STYLED_ITEM('',(#170169),#85866) ;
#80157 = STYLED_ITEM('',(#170169),#85867) ;
#80158 = STYLED_ITEM('',(#170169),#85868) ;
#80159 = STYLED_ITEM('',(#170171),#85869) ;
#80160 = STYLED_ITEM('',(#170169),#85870) ;
#80161 = STYLED_ITEM('',(#170169),#85871) ;
#80162 = STYLED_ITEM('',(#170169),#85872) ;
#80163 = STYLED_ITEM('',(#170169),#85873) ;
#80164 = STYLED_ITEM('',(#170169),#85874) ;
#80165 = STYLED_ITEM('',(#170169),#85875) ;
#80166 = STYLED_ITEM('',(#170169),#85876) ;
#80167 = STYLED_ITEM('',(#170169),#85877) ;
#80168 = STYLED_ITEM('',(#170169),#85878) ;
#80169 = STYLED_ITEM('',(#170169),#85879) ;
#80170 = STYLED_ITEM('',(#170169),#85880) ;
#80171 = STYLED_ITEM('',(#170169),#85881) ;
#80172 = STYLED_ITEM('',(#170169),#85882) ;
#80173 = STYLED_ITEM('',(#170169),#85883) ;
#80174 = STYLED_ITEM('',(#170169),#85884) ;
#80175 = STYLED_ITEM('',(#170169),#85885) ;
#80176 = STYLED_ITEM('',(#170169),#85886) ;
#80177 = STYLED_ITEM('',(#170169),#85887) ;
#80178 = STYLED_ITEM('',(#170169),#85888) ;
#80179 = STYLED_ITEM('',(#170170),#85889) ;
#80180 = STYLED_ITEM('',(#170170),#85890) ;
#80181 = STYLED_ITEM('',(#170170),#85891) ;
#80182 = STYLED_ITEM('',(#170170),#85892) ;
#80183 = STYLED_ITEM('',(#170169),#85893) ;
#80184 = STYLED_ITEM('',(#170169),#85894) ;
#80185 = STYLED_ITEM('',(#170169),#85895) ;
#80186 = STYLED_ITEM('',(#170169),#85896) ;
#80187 = STYLED_ITEM('',(#170169),#85897) ;
#80188 = STYLED_ITEM('',(#170169),#85898) ;
#80189 = STYLED_ITEM('',(#170169),#85899) ;
#80190 = STYLED_ITEM('',(#170169),#85900) ;
#80191 = STYLED_ITEM('',(#170169),#85901) ;
#80192 = STYLED_ITEM('',(#170169),#85902) ;
#80193 = STYLED_ITEM('',(#170169),#85903) ;
#80194 = STYLED_ITEM('',(#170169),#85904) ;
#80195 = STYLED_ITEM('',(#170169),#85905) ;
#80196 = STYLED_ITEM('',(#170169),#85906) ;
#80197 = STYLED_ITEM('',(#170169),#85907) ;
#80198 = STYLED_ITEM('',(#170169),#85908) ;
#80199 = STYLED_ITEM('',(#170169),#85909) ;
#80200 = STYLED_ITEM('',(#170169),#85910) ;
#80201 = STYLED_ITEM('',(#170171),#85911) ;
#80202 = STYLED_ITEM('',(#170169),#85912) ;
#80203 = STYLED_ITEM('',(#170169),#85913) ;
#80204 = STYLED_ITEM('',(#170169),#85914) ;
#80205 = STYLED_ITEM('',(#170169),#85915) ;
#80206 = STYLED_ITEM('',(#170169),#85916) ;
#80207 = STYLED_ITEM('',(#170169),#85917) ;
#80208 = STYLED_ITEM('',(#170169),#85918) ;
#80209 = STYLED_ITEM('',(#170169),#85919) ;
#80210 = STYLED_ITEM('',(#170169),#85920) ;
#80211 = STYLED_ITEM('',(#170169),#85921) ;
#80212 = STYLED_ITEM('',(#170169),#85922) ;
#80213 = STYLED_ITEM('',(#170169),#85923) ;
#80214 = STYLED_ITEM('',(#170169),#85924) ;
#80215 = STYLED_ITEM('',(#170169),#85925) ;
#80216 = STYLED_ITEM('',(#170169),#85926) ;
#80217 = STYLED_ITEM('',(#170169),#85927) ;
#80218 = STYLED_ITEM('',(#170169),#85928) ;
#80219 = STYLED_ITEM('',(#170169),#85929) ;
#80220 = STYLED_ITEM('',(#170169),#85930) ;
#80221 = STYLED_ITEM('',(#170169),#85931) ;
#80222 = STYLED_ITEM('',(#170169),#85932) ;
#80223 = STYLED_ITEM('',(#170169),#85933) ;
#80224 = STYLED_ITEM('',(#170169),#85934) ;
#80225 = STYLED_ITEM('',(#170169),#85935) ;
#80226 = STYLED_ITEM('',(#170169),#85936) ;
#80227 = STYLED_ITEM('',(#170169),#85937) ;
#80228 = STYLED_ITEM('',(#170169),#85938) ;
#80229 = STYLED_ITEM('',(#170169),#85939) ;
#80230 = STYLED_ITEM('',(#170169),#85940) ;
#80231 = STYLED_ITEM('',(#170169),#85941) ;
#80232 = STYLED_ITEM('',(#170169),#85942) ;
#80233 = STYLED_ITEM('',(#170169),#85943) ;
#80234 = STYLED_ITEM('',(#170169),#85944) ;
#80235 = STYLED_ITEM('',(#170169),#85945) ;
#80236 = STYLED_ITEM('',(#170169),#85946) ;
#80237 = STYLED_ITEM('',(#170169),#85947) ;
#80238 = STYLED_ITEM('',(#170169),#85948) ;
#80239 = STYLED_ITEM('',(#170169),#85949) ;
#80240 = STYLED_ITEM('',(#170169),#85950) ;
#80241 = STYLED_ITEM('',(#170169),#85951) ;
#80242 = STYLED_ITEM('',(#170169),#85952) ;
#80243 = STYLED_ITEM('',(#170169),#85953) ;
#80244 = STYLED_ITEM('',(#170169),#85954) ;
#80245 = STYLED_ITEM('',(#170169),#85955) ;
#80246 = STYLED_ITEM('',(#170169),#85956) ;
#80247 = STYLED_ITEM('',(#170169),#85957) ;
#80248 = STYLED_ITEM('',(#170169),#85958) ;
#80249 = STYLED_ITEM('',(#170169),#85959) ;
#80250 = STYLED_ITEM('',(#170169),#85960) ;
#80251 = STYLED_ITEM('',(#170169),#85961) ;
#80252 = STYLED_ITEM('',(#170169),#85962) ;
#80253 = STYLED_ITEM('',(#170169),#85963) ;
#80254 = STYLED_ITEM('',(#170169),#85964) ;
#80255 = STYLED_ITEM('',(#170169),#85965) ;
#80256 = STYLED_ITEM('',(#170169),#85966) ;
#80257 = STYLED_ITEM('',(#170169),#85967) ;
#80258 = STYLED_ITEM('',(#170169),#85968) ;
#80259 = STYLED_ITEM('',(#170169),#85969) ;
#80260 = STYLED_ITEM('',(#170169),#85970) ;
#80261 = STYLED_ITEM('',(#170169),#85971) ;
#80262 = STYLED_ITEM('',(#170169),#85972) ;
#80263 = STYLED_ITEM('',(#170169),#85973) ;
#80264 = STYLED_ITEM('',(#170169),#85974) ;
#80265 = STYLED_ITEM('',(#170169),#85975) ;
#80266 = STYLED_ITEM('',(#170169),#85976) ;
#80267 = STYLED_ITEM('',(#170169),#85977) ;
#80268 = STYLED_ITEM('',(#170169),#85978) ;
#80269 = STYLED_ITEM('',(#170169),#85979) ;
#80270 = STYLED_ITEM('',(#170169),#85980) ;
#80271 = STYLED_ITEM('',(#170169),#85981) ;
#80272 = STYLED_ITEM('',(#170169),#85982) ;
#80273 = STYLED_ITEM('',(#170169),#85983) ;
#80274 = STYLED_ITEM('',(#170169),#85984) ;
#80275 = STYLED_ITEM('',(#170169),#85985) ;
#80276 = STYLED_ITEM('',(#170169),#85986) ;
#80277 = STYLED_ITEM('',(#170169),#85987) ;
#80278 = STYLED_ITEM('',(#170169),#85988) ;
#80279 = STYLED_ITEM('',(#170169),#85989) ;
#80280 = STYLED_ITEM('',(#170169),#85990) ;
#80281 = STYLED_ITEM('',(#170169),#85991) ;
#80282 = STYLED_ITEM('',(#170169),#85992) ;
#80283 = STYLED_ITEM('',(#170169),#85993) ;
#80284 = STYLED_ITEM('',(#170169),#85994) ;
#80285 = STYLED_ITEM('',(#170169),#85995) ;
#80286 = STYLED_ITEM('',(#170169),#85996) ;
#80287 = STYLED_ITEM('',(#170169),#85997) ;
#80288 = STYLED_ITEM('',(#170169),#85998) ;
#80289 = STYLED_ITEM('',(#170169),#85999) ;
#80290 = STYLED_ITEM('',(#170169),#86000) ;
#80291 = STYLED_ITEM('',(#170169),#86001) ;
#80292 = STYLED_ITEM('',(#170169),#86002) ;
#80293 = STYLED_ITEM('',(#170169),#86003) ;
#80294 = STYLED_ITEM('',(#170169),#86004) ;
#80295 = STYLED_ITEM('',(#170169),#86005) ;
#80296 = STYLED_ITEM('',(#170169),#86006) ;
#80297 = STYLED_ITEM('',(#170169),#86007) ;
#80298 = STYLED_ITEM('',(#170169),#86008) ;
#80299 = STYLED_ITEM('',(#170169),#86009) ;
#80300 = STYLED_ITEM('',(#170169),#86010) ;
#80301 = STYLED_ITEM('',(#170169),#86011) ;
#80302 = STYLED_ITEM('',(#170169),#86012) ;
#80303 = STYLED_ITEM('',(#170169),#86013) ;
#80304 = STYLED_ITEM('',(#170169),#86014) ;
#80305 = STYLED_ITEM('',(#170169),#86015) ;
#80306 = STYLED_ITEM('',(#170169),#86016) ;
#80307 = STYLED_ITEM('',(#170169),#86017) ;
#80308 = STYLED_ITEM('',(#170169),#86018) ;
#80309 = STYLED_ITEM('',(#170169),#86019) ;
#80310 = STYLED_ITEM('',(#170169),#86020) ;
#80311 = STYLED_ITEM('',(#170169),#86021) ;
#80312 = STYLED_ITEM('',(#170169),#86022) ;
#80313 = STYLED_ITEM('',(#170170),#86023) ;
#80314 = STYLED_ITEM('',(#170170),#86024) ;
#80315 = STYLED_ITEM('',(#170170),#86025) ;
#80316 = STYLED_ITEM('',(#170170),#86026) ;
#80317 = STYLED_ITEM('',(#170169),#86027) ;
#80318 = STYLED_ITEM('',(#170169),#86028) ;
#80319 = STYLED_ITEM('',(#170169),#86029) ;
#80320 = STYLED_ITEM('',(#170169),#86030) ;
#80321 = STYLED_ITEM('',(#170169),#86031) ;
#80322 = STYLED_ITEM('',(#170169),#86032) ;
#80323 = STYLED_ITEM('',(#170169),#86033) ;
#80324 = STYLED_ITEM('',(#170169),#86034) ;
#80325 = STYLED_ITEM('',(#170169),#86035) ;
#80326 = STYLED_ITEM('',(#170169),#86036) ;
#80327 = STYLED_ITEM('',(#170169),#86037) ;
#80328 = STYLED_ITEM('',(#170169),#86038) ;
#80329 = STYLED_ITEM('',(#170169),#86039) ;
#80330 = STYLED_ITEM('',(#170169),#86040) ;
#80331 = STYLED_ITEM('',(#170169),#86041) ;
#80332 = STYLED_ITEM('',(#170169),#86042) ;
#80333 = STYLED_ITEM('',(#170169),#86043) ;
#80334 = STYLED_ITEM('',(#170169),#86044) ;
#80335 = STYLED_ITEM('',(#170169),#86045) ;
#80336 = STYLED_ITEM('',(#170169),#86046) ;
#80337 = STYLED_ITEM('',(#170169),#86047) ;
#80338 = STYLED_ITEM('',(#170169),#86048) ;
#80339 = STYLED_ITEM('',(#170169),#86049) ;
#80340 = STYLED_ITEM('',(#170169),#86050) ;
#80341 = STYLED_ITEM('',(#170169),#86051) ;
#80342 = STYLED_ITEM('',(#170169),#86052) ;
#80343 = STYLED_ITEM('',(#170169),#86053) ;
#80344 = STYLED_ITEM('',(#170169),#86054) ;
#80345 = STYLED_ITEM('',(#170169),#86055) ;
#80346 = STYLED_ITEM('',(#170169),#86056) ;
#80347 = STYLED_ITEM('',(#170169),#86057) ;
#80348 = STYLED_ITEM('',(#170169),#86058) ;
#80349 = STYLED_ITEM('',(#170169),#86059) ;
#80350 = STYLED_ITEM('',(#170169),#86060) ;
#80351 = STYLED_ITEM('',(#170169),#86061) ;
#80352 = STYLED_ITEM('',(#170169),#86062) ;
#80353 = STYLED_ITEM('',(#170170),#86063) ;
#80354 = STYLED_ITEM('',(#170169),#86064) ;
#80355 = STYLED_ITEM('',(#170169),#86065) ;
#80356 = STYLED_ITEM('',(#170169),#86066) ;
#80357 = STYLED_ITEM('',(#170169),#86067) ;
#80358 = STYLED_ITEM('',(#170169),#86068) ;
#80359 = STYLED_ITEM('',(#170169),#86069) ;
#80360 = STYLED_ITEM('',(#170171),#86070) ;
#80361 = STYLED_ITEM('',(#170169),#86071) ;
#80362 = STYLED_ITEM('',(#170169),#86072) ;
#80363 = STYLED_ITEM('',(#170169),#86073) ;
#80364 = STYLED_ITEM('',(#170169),#86074) ;
#80365 = STYLED_ITEM('',(#170169),#86075) ;
#80366 = STYLED_ITEM('',(#170169),#86076) ;
#80367 = STYLED_ITEM('',(#170169),#86077) ;
#80368 = STYLED_ITEM('',(#170169),#86078) ;
#80369 = STYLED_ITEM('',(#170169),#86079) ;
#80370 = STYLED_ITEM('',(#170169),#86080) ;
#80371 = STYLED_ITEM('',(#170169),#86081) ;
#80372 = STYLED_ITEM('',(#170169),#86082) ;
#80373 = STYLED_ITEM('',(#170169),#86083) ;
#80374 = STYLED_ITEM('',(#170169),#86084) ;
#80375 = STYLED_ITEM('',(#170169),#86085) ;
#80376 = STYLED_ITEM('',(#170169),#86086) ;
#80377 = STYLED_ITEM('',(#170169),#86087) ;
#80378 = STYLED_ITEM('',(#170169),#86088) ;
#80379 = STYLED_ITEM('',(#170169),#86089) ;
#80380 = STYLED_ITEM('',(#170170),#86090) ;
#80381 = STYLED_ITEM('',(#170170),#86091) ;
#80382 = STYLED_ITEM('',(#170170),#86092) ;
#80383 = STYLED_ITEM('',(#170170),#86093) ;
#80384 = STYLED_ITEM('',(#170169),#86094) ;
#80385 = STYLED_ITEM('',(#170169),#86095) ;
#80386 = STYLED_ITEM('',(#170169),#86096) ;
#80387 = STYLED_ITEM('',(#170169),#86097) ;
#80388 = STYLED_ITEM('',(#170169),#86098) ;
#80389 = STYLED_ITEM('',(#170169),#86099) ;
#80390 = STYLED_ITEM('',(#170169),#86100) ;
#80391 = STYLED_ITEM('',(#170169),#86101) ;
#80392 = STYLED_ITEM('',(#170169),#86102) ;
#80393 = STYLED_ITEM('',(#170169),#86103) ;
#80394 = STYLED_ITEM('',(#170169),#86104) ;
#80395 = STYLED_ITEM('',(#170169),#86105) ;
#80396 = STYLED_ITEM('',(#170169),#86106) ;
#80397 = STYLED_ITEM('',(#170169),#86107) ;
#80398 = STYLED_ITEM('',(#170169),#86108) ;
#80399 = STYLED_ITEM('',(#170169),#86109) ;
#80400 = STYLED_ITEM('',(#170169),#86110) ;
#80401 = STYLED_ITEM('',(#170169),#86111) ;
#80402 = STYLED_ITEM('',(#170171),#86112) ;
#80403 = STYLED_ITEM('',(#170169),#86113) ;
#80404 = STYLED_ITEM('',(#170169),#86114) ;
#80405 = STYLED_ITEM('',(#170169),#86115) ;
#80406 = STYLED_ITEM('',(#170169),#86116) ;
#80407 = STYLED_ITEM('',(#170169),#86117) ;
#80408 = STYLED_ITEM('',(#170169),#86118) ;
#80409 = STYLED_ITEM('',(#170169),#86119) ;
#80410 = STYLED_ITEM('',(#170169),#86120) ;
#80411 = STYLED_ITEM('',(#170169),#86121) ;
#80412 = STYLED_ITEM('',(#170169),#86122) ;
#80413 = STYLED_ITEM('',(#170169),#86123) ;
#80414 = STYLED_ITEM('',(#170169),#86124) ;
#80415 = STYLED_ITEM('',(#170169),#86125) ;
#80416 = STYLED_ITEM('',(#170169),#86126) ;
#80417 = STYLED_ITEM('',(#170169),#86127) ;
#80418 = STYLED_ITEM('',(#170169),#86128) ;
#80419 = STYLED_ITEM('',(#170169),#86129) ;
#80420 = STYLED_ITEM('',(#170169),#86130) ;
#80421 = STYLED_ITEM('',(#170169),#86131) ;
#80422 = STYLED_ITEM('',(#170169),#86132) ;
#80423 = STYLED_ITEM('',(#170169),#86133) ;
#80424 = STYLED_ITEM('',(#170169),#86134) ;
#80425 = STYLED_ITEM('',(#170169),#86135) ;
#80426 = STYLED_ITEM('',(#170169),#86136) ;
#80427 = STYLED_ITEM('',(#170169),#86137) ;
#80428 = STYLED_ITEM('',(#170169),#86138) ;
#80429 = STYLED_ITEM('',(#170169),#86139) ;
#80430 = STYLED_ITEM('',(#170169),#86140) ;
#80431 = STYLED_ITEM('',(#170169),#86141) ;
#80432 = STYLED_ITEM('',(#170169),#86142) ;
#80433 = STYLED_ITEM('',(#170169),#86143) ;
#80434 = STYLED_ITEM('',(#170169),#86144) ;
#80435 = STYLED_ITEM('',(#170169),#86145) ;
#80436 = STYLED_ITEM('',(#170169),#86146) ;
#80437 = STYLED_ITEM('',(#170169),#86147) ;
#80438 = STYLED_ITEM('',(#170169),#86148) ;
#80439 = STYLED_ITEM('',(#170169),#86149) ;
#80440 = STYLED_ITEM('',(#170169),#86150) ;
#80441 = STYLED_ITEM('',(#170169),#86151) ;
#80442 = STYLED_ITEM('',(#170169),#86152) ;
#80443 = STYLED_ITEM('',(#170169),#86153) ;
#80444 = STYLED_ITEM('',(#170169),#86154) ;
#80445 = STYLED_ITEM('',(#170169),#86155) ;
#80446 = STYLED_ITEM('',(#170169),#86156) ;
#80447 = STYLED_ITEM('',(#170169),#86157) ;
#80448 = STYLED_ITEM('',(#170169),#86158) ;
#80449 = STYLED_ITEM('',(#170169),#86159) ;
#80450 = STYLED_ITEM('',(#170169),#86160) ;
#80451 = STYLED_ITEM('',(#170169),#86161) ;
#80452 = STYLED_ITEM('',(#170169),#86162) ;
#80453 = STYLED_ITEM('',(#170169),#86163) ;
#80454 = STYLED_ITEM('',(#170169),#86164) ;
#80455 = STYLED_ITEM('',(#170169),#86165) ;
#80456 = STYLED_ITEM('',(#170169),#86166) ;
#80457 = STYLED_ITEM('',(#170169),#86167) ;
#80458 = STYLED_ITEM('',(#170169),#86168) ;
#80459 = STYLED_ITEM('',(#170169),#86169) ;
#80460 = STYLED_ITEM('',(#170169),#86170) ;
#80461 = STYLED_ITEM('',(#170169),#86171) ;
#80462 = STYLED_ITEM('',(#170169),#86172) ;
#80463 = STYLED_ITEM('',(#170169),#86173) ;
#80464 = STYLED_ITEM('',(#170169),#86174) ;
#80465 = STYLED_ITEM('',(#170169),#86175) ;
#80466 = STYLED_ITEM('',(#170169),#86176) ;
#80467 = STYLED_ITEM('',(#170169),#86177) ;
#80468 = STYLED_ITEM('',(#170169),#86178) ;
#80469 = STYLED_ITEM('',(#170169),#86179) ;
#80470 = STYLED_ITEM('',(#170169),#86180) ;
#80471 = STYLED_ITEM('',(#170169),#86181) ;
#80472 = STYLED_ITEM('',(#170169),#86182) ;
#80473 = STYLED_ITEM('',(#170169),#86183) ;
#80474 = STYLED_ITEM('',(#170169),#86184) ;
#80475 = STYLED_ITEM('',(#170169),#86185) ;
#80476 = STYLED_ITEM('',(#170169),#86186) ;
#80477 = STYLED_ITEM('',(#170169),#86187) ;
#80478 = STYLED_ITEM('',(#170169),#86188) ;
#80479 = STYLED_ITEM('',(#170169),#86189) ;
#80480 = STYLED_ITEM('',(#170169),#86190) ;
#80481 = STYLED_ITEM('',(#170169),#86191) ;
#80482 = STYLED_ITEM('',(#170169),#86192) ;
#80483 = STYLED_ITEM('',(#170169),#86193) ;
#80484 = STYLED_ITEM('',(#170169),#86194) ;
#80485 = STYLED_ITEM('',(#170169),#86195) ;
#80486 = STYLED_ITEM('',(#170169),#86196) ;
#80487 = STYLED_ITEM('',(#170169),#86197) ;
#80488 = STYLED_ITEM('',(#170169),#86198) ;
#80489 = STYLED_ITEM('',(#170169),#86199) ;
#80490 = STYLED_ITEM('',(#170169),#86200) ;
#80491 = STYLED_ITEM('',(#170169),#86201) ;
#80492 = STYLED_ITEM('',(#170169),#86202) ;
#80493 = STYLED_ITEM('',(#170169),#86203) ;
#80494 = STYLED_ITEM('',(#170169),#86204) ;
#80495 = STYLED_ITEM('',(#170169),#86205) ;
#80496 = STYLED_ITEM('',(#170169),#86206) ;
#80497 = STYLED_ITEM('',(#170169),#86207) ;
#80498 = STYLED_ITEM('',(#170169),#86208) ;
#80499 = STYLED_ITEM('',(#170169),#86209) ;
#80500 = STYLED_ITEM('',(#170169),#86210) ;
#80501 = STYLED_ITEM('',(#170169),#86211) ;
#80502 = STYLED_ITEM('',(#170169),#86212) ;
#80503 = STYLED_ITEM('',(#170169),#86213) ;
#80504 = STYLED_ITEM('',(#170169),#86214) ;
#80505 = STYLED_ITEM('',(#170170),#86215) ;
#80506 = STYLED_ITEM('',(#170170),#86216) ;
#80507 = STYLED_ITEM('',(#170170),#86217) ;
#80508 = STYLED_ITEM('',(#170170),#86218) ;
#80509 = STYLED_ITEM('',(#170169),#86219) ;
#80510 = STYLED_ITEM('',(#170169),#86220) ;
#80511 = STYLED_ITEM('',(#170169),#86221) ;
#80512 = STYLED_ITEM('',(#170169),#86222) ;
#80513 = STYLED_ITEM('',(#170169),#86223) ;
#80514 = STYLED_ITEM('',(#170169),#86224) ;
#80515 = STYLED_ITEM('',(#170169),#86225) ;
#80516 = STYLED_ITEM('',(#170169),#86226) ;
#80517 = STYLED_ITEM('',(#170169),#86227) ;
#80518 = STYLED_ITEM('',(#170169),#86228) ;
#80519 = STYLED_ITEM('',(#170169),#86229) ;
#80520 = STYLED_ITEM('',(#170169),#86230) ;
#80521 = STYLED_ITEM('',(#170169),#86231) ;
#80522 = STYLED_ITEM('',(#170169),#86232) ;
#80523 = STYLED_ITEM('',(#170169),#86233) ;
#80524 = STYLED_ITEM('',(#170169),#86234) ;
#80525 = STYLED_ITEM('',(#170169),#86235) ;
#80526 = STYLED_ITEM('',(#170169),#86236) ;
#80527 = STYLED_ITEM('',(#170169),#86237) ;
#80528 = STYLED_ITEM('',(#170169),#86238) ;
#80529 = STYLED_ITEM('',(#170169),#86239) ;
#80530 = STYLED_ITEM('',(#170169),#86240) ;
#80531 = STYLED_ITEM('',(#170169),#86241) ;
#80532 = STYLED_ITEM('',(#170169),#86242) ;
#80533 = STYLED_ITEM('',(#170169),#86243) ;
#80534 = STYLED_ITEM('',(#170169),#86244) ;
#80535 = STYLED_ITEM('',(#170169),#86245) ;
#80536 = STYLED_ITEM('',(#170169),#86246) ;
#80537 = STYLED_ITEM('',(#170169),#86247) ;
#80538 = STYLED_ITEM('',(#170169),#86248) ;
#80539 = STYLED_ITEM('',(#170169),#86249) ;
#80540 = STYLED_ITEM('',(#170169),#86250) ;
#80541 = STYLED_ITEM('',(#170169),#86251) ;
#80542 = STYLED_ITEM('',(#170169),#86252) ;
#80543 = STYLED_ITEM('',(#170169),#86253) ;
#80544 = STYLED_ITEM('',(#170169),#86254) ;
#80545 = STYLED_ITEM('',(#170169),#86255) ;
#80546 = STYLED_ITEM('',(#170169),#86256) ;
#80547 = STYLED_ITEM('',(#170169),#86257) ;
#80548 = STYLED_ITEM('',(#170169),#86258) ;
#80549 = STYLED_ITEM('',(#170169),#86259) ;
#80550 = STYLED_ITEM('',(#170169),#86260) ;
#80551 = STYLED_ITEM('',(#170169),#86261) ;
#80552 = STYLED_ITEM('',(#170169),#86262) ;
#80553 = STYLED_ITEM('',(#170168),#30) ;
#80554 = STYLED_ITEM('',(#170169),#86263) ;
#80555 = STYLED_ITEM('',(#170169),#86264) ;
#80556 = STYLED_ITEM('',(#170169),#86265) ;
#80557 = STYLED_ITEM('',(#170169),#86266) ;
#80558 = STYLED_ITEM('',(#170169),#86267) ;
#80559 = STYLED_ITEM('',(#170169),#86268) ;
#80560 = STYLED_ITEM('',(#170169),#86269) ;
#80561 = STYLED_ITEM('',(#170169),#86270) ;
#80562 = STYLED_ITEM('',(#170169),#86271) ;
#80563 = STYLED_ITEM('',(#170169),#86272) ;
#80564 = STYLED_ITEM('',(#170169),#86273) ;
#80565 = STYLED_ITEM('',(#170169),#86274) ;
#80566 = STYLED_ITEM('',(#170169),#86275) ;
#80567 = STYLED_ITEM('',(#170169),#86276) ;
#80568 = STYLED_ITEM('',(#170169),#86277) ;
#80569 = STYLED_ITEM('',(#170170),#86278) ;
#80570 = STYLED_ITEM('',(#170169),#86279) ;
#80571 = STYLED_ITEM('',(#170169),#86280) ;
#80572 = STYLED_ITEM('',(#170169),#86281) ;
#80573 = STYLED_ITEM('',(#170169),#86282) ;
#80574 = STYLED_ITEM('',(#170169),#86283) ;
#80575 = STYLED_ITEM('',(#170169),#86284) ;
#80576 = STYLED_ITEM('',(#170169),#86285) ;
#80577 = STYLED_ITEM('',(#170169),#86286) ;
#80578 = STYLED_ITEM('',(#170169),#86287) ;
#80579 = STYLED_ITEM('',(#170169),#86288) ;
#80580 = STYLED_ITEM('',(#170169),#86289) ;
#80581 = STYLED_ITEM('',(#170169),#86290) ;
#80582 = STYLED_ITEM('',(#170169),#86291) ;
#80583 = STYLED_ITEM('',(#170169),#86292) ;
#80584 = STYLED_ITEM('',(#170169),#86293) ;
#80585 = STYLED_ITEM('',(#170169),#86294) ;
#80586 = STYLED_ITEM('',(#170169),#86295) ;
#80587 = STYLED_ITEM('',(#170169),#86296) ;
#80588 = STYLED_ITEM('',(#170169),#86297) ;
#80589 = STYLED_ITEM('',(#170169),#86298) ;
#80590 = STYLED_ITEM('',(#170169),#86299) ;
#80591 = STYLED_ITEM('',(#170169),#86300) ;
#80592 = STYLED_ITEM('',(#170169),#86301) ;
#80593 = STYLED_ITEM('',(#170169),#86302) ;
#80594 = STYLED_ITEM('',(#170171),#86303) ;
#80595 = STYLED_ITEM('',(#170169),#86304) ;
#80596 = STYLED_ITEM('',(#170169),#86305) ;
#80597 = STYLED_ITEM('',(#170169),#86306) ;
#80598 = STYLED_ITEM('',(#170169),#86307) ;
#80599 = STYLED_ITEM('',(#170169),#86308) ;
#80600 = STYLED_ITEM('',(#170169),#86309) ;
#80601 = STYLED_ITEM('',(#170169),#86310) ;
#80602 = STYLED_ITEM('',(#170169),#86311) ;
#80603 = STYLED_ITEM('',(#170169),#86312) ;
#80604 = STYLED_ITEM('',(#170169),#86313) ;
#80605 = STYLED_ITEM('',(#170169),#86314) ;
#80606 = STYLED_ITEM('',(#170169),#86315) ;
#80607 = STYLED_ITEM('',(#170169),#86316) ;
#80608 = STYLED_ITEM('',(#170169),#86317) ;
#80609 = STYLED_ITEM('',(#170169),#86318) ;
#80610 = STYLED_ITEM('',(#170169),#86319) ;
#80611 = STYLED_ITEM('',(#170169),#86320) ;
#80612 = STYLED_ITEM('',(#170169),#86321) ;
#80613 = STYLED_ITEM('',(#170169),#86322) ;
#80614 = STYLED_ITEM('',(#170170),#86323) ;
#80615 = STYLED_ITEM('',(#170170),#86324) ;
#80616 = STYLED_ITEM('',(#170170),#86325) ;
#80617 = STYLED_ITEM('',(#170170),#86326) ;
#80618 = STYLED_ITEM('',(#170169),#86327) ;
#80619 = STYLED_ITEM('',(#170169),#86328) ;
#80620 = STYLED_ITEM('',(#170169),#86329) ;
#80621 = STYLED_ITEM('',(#170169),#86330) ;
#80622 = STYLED_ITEM('',(#170169),#86331) ;
#80623 = STYLED_ITEM('',(#170169),#86332) ;
#80624 = STYLED_ITEM('',(#170169),#86333) ;
#80625 = STYLED_ITEM('',(#170169),#86334) ;
#80626 = STYLED_ITEM('',(#170169),#86335) ;
#80627 = STYLED_ITEM('',(#170169),#86336) ;
#80628 = STYLED_ITEM('',(#170169),#86337) ;
#80629 = STYLED_ITEM('',(#170169),#86338) ;
#80630 = STYLED_ITEM('',(#170169),#86339) ;
#80631 = STYLED_ITEM('',(#170169),#86340) ;
#80632 = STYLED_ITEM('',(#170169),#86341) ;
#80633 = STYLED_ITEM('',(#170169),#86342) ;
#80634 = STYLED_ITEM('',(#170169),#86343) ;
#80635 = STYLED_ITEM('',(#170169),#86344) ;
#80636 = STYLED_ITEM('',(#170171),#86345) ;
#80637 = STYLED_ITEM('',(#170169),#86346) ;
#80638 = STYLED_ITEM('',(#170169),#86347) ;
#80639 = STYLED_ITEM('',(#170169),#86348) ;
#80640 = STYLED_ITEM('',(#170169),#86349) ;
#80641 = STYLED_ITEM('',(#170169),#86350) ;
#80642 = STYLED_ITEM('',(#170169),#86351) ;
#80643 = STYLED_ITEM('',(#170169),#86352) ;
#80644 = STYLED_ITEM('',(#170169),#86353) ;
#80645 = STYLED_ITEM('',(#170169),#86354) ;
#80646 = STYLED_ITEM('',(#170169),#86355) ;
#80647 = STYLED_ITEM('',(#170169),#86356) ;
#80648 = STYLED_ITEM('',(#170169),#86357) ;
#80649 = STYLED_ITEM('',(#170169),#86358) ;
#80650 = STYLED_ITEM('',(#170169),#86359) ;
#80651 = STYLED_ITEM('',(#170169),#86360) ;
#80652 = STYLED_ITEM('',(#170169),#86361) ;
#80653 = STYLED_ITEM('',(#170169),#86362) ;
#80654 = STYLED_ITEM('',(#170169),#86363) ;
#80655 = STYLED_ITEM('',(#170169),#86364) ;
#80656 = STYLED_ITEM('',(#170169),#86365) ;
#80657 = STYLED_ITEM('',(#170169),#86366) ;
#80658 = STYLED_ITEM('',(#170169),#86367) ;
#80659 = STYLED_ITEM('',(#170169),#86368) ;
#80660 = STYLED_ITEM('',(#170169),#86369) ;
#80661 = STYLED_ITEM('',(#170169),#86370) ;
#80662 = STYLED_ITEM('',(#170169),#86371) ;
#80663 = STYLED_ITEM('',(#170169),#86372) ;
#80664 = STYLED_ITEM('',(#170169),#86373) ;
#80665 = STYLED_ITEM('',(#170169),#86374) ;
#80666 = STYLED_ITEM('',(#170169),#86375) ;
#80667 = STYLED_ITEM('',(#170169),#86376) ;
#80668 = STYLED_ITEM('',(#170169),#86377) ;
#80669 = STYLED_ITEM('',(#170169),#86378) ;
#80670 = STYLED_ITEM('',(#170169),#86379) ;
#80671 = STYLED_ITEM('',(#170169),#86380) ;
#80672 = STYLED_ITEM('',(#170169),#86381) ;
#80673 = STYLED_ITEM('',(#170169),#86382) ;
#80674 = STYLED_ITEM('',(#170169),#86383) ;
#80675 = STYLED_ITEM('',(#170169),#86384) ;
#80676 = STYLED_ITEM('',(#170169),#86385) ;
#80677 = STYLED_ITEM('',(#170169),#86386) ;
#80678 = STYLED_ITEM('',(#170169),#86387) ;
#80679 = STYLED_ITEM('',(#170169),#86388) ;
#80680 = STYLED_ITEM('',(#170169),#86389) ;
#80681 = STYLED_ITEM('',(#170169),#86390) ;
#80682 = STYLED_ITEM('',(#170169),#86391) ;
#80683 = STYLED_ITEM('',(#170169),#86392) ;
#80684 = STYLED_ITEM('',(#170169),#86393) ;
#80685 = STYLED_ITEM('',(#170169),#86394) ;
#80686 = STYLED_ITEM('',(#170169),#86395) ;
#80687 = STYLED_ITEM('',(#170169),#86396) ;
#80688 = STYLED_ITEM('',(#170169),#86397) ;
#80689 = STYLED_ITEM('',(#170169),#86398) ;
#80690 = STYLED_ITEM('',(#170169),#86399) ;
#80691 = STYLED_ITEM('',(#170169),#86400) ;
#80692 = STYLED_ITEM('',(#170169),#86401) ;
#80693 = STYLED_ITEM('',(#170169),#86402) ;
#80694 = STYLED_ITEM('',(#170169),#86403) ;
#80695 = STYLED_ITEM('',(#170169),#86404) ;
#80696 = STYLED_ITEM('',(#170169),#86405) ;
#80697 = STYLED_ITEM('',(#170169),#86406) ;
#80698 = STYLED_ITEM('',(#170169),#86407) ;
#80699 = STYLED_ITEM('',(#170169),#86408) ;
#80700 = STYLED_ITEM('',(#170169),#86409) ;
#80701 = STYLED_ITEM('',(#170169),#86410) ;
#80702 = STYLED_ITEM('',(#170169),#86411) ;
#80703 = STYLED_ITEM('',(#170169),#86412) ;
#80704 = STYLED_ITEM('',(#170169),#86413) ;
#80705 = STYLED_ITEM('',(#170169),#86414) ;
#80706 = STYLED_ITEM('',(#170169),#86415) ;
#80707 = STYLED_ITEM('',(#170169),#86416) ;
#80708 = STYLED_ITEM('',(#170169),#86417) ;
#80709 = STYLED_ITEM('',(#170169),#86418) ;
#80710 = STYLED_ITEM('',(#170169),#86419) ;
#80711 = STYLED_ITEM('',(#170169),#86420) ;
#80712 = STYLED_ITEM('',(#170169),#86421) ;
#80713 = STYLED_ITEM('',(#170169),#86422) ;
#80714 = STYLED_ITEM('',(#170169),#86423) ;
#80715 = STYLED_ITEM('',(#170169),#86424) ;
#80716 = STYLED_ITEM('',(#170169),#86425) ;
#80717 = STYLED_ITEM('',(#170169),#86426) ;
#80718 = STYLED_ITEM('',(#170169),#86427) ;
#80719 = STYLED_ITEM('',(#170169),#86428) ;
#80720 = STYLED_ITEM('',(#170169),#86429) ;
#80721 = STYLED_ITEM('',(#170169),#86430) ;
#80722 = STYLED_ITEM('',(#170169),#86431) ;
#80723 = STYLED_ITEM('',(#170169),#86432) ;
#80724 = STYLED_ITEM('',(#170169),#86433) ;
#80725 = STYLED_ITEM('',(#170169),#86434) ;
#80726 = STYLED_ITEM('',(#170169),#86435) ;
#80727 = STYLED_ITEM('',(#170169),#86436) ;
#80728 = STYLED_ITEM('',(#170169),#86437) ;
#80729 = STYLED_ITEM('',(#170169),#86438) ;
#80730 = STYLED_ITEM('',(#170169),#86439) ;
#80731 = STYLED_ITEM('',(#170169),#86440) ;
#80732 = STYLED_ITEM('',(#170169),#86441) ;
#80733 = STYLED_ITEM('',(#170169),#86442) ;
#80734 = STYLED_ITEM('',(#170169),#86443) ;
#80735 = STYLED_ITEM('',(#170169),#86444) ;
#80736 = STYLED_ITEM('',(#170169),#86445) ;
#80737 = STYLED_ITEM('',(#170169),#86446) ;
#80738 = STYLED_ITEM('',(#170169),#86447) ;
#80739 = STYLED_ITEM('',(#170169),#86448) ;
#80740 = STYLED_ITEM('',(#170169),#86449) ;
#80741 = STYLED_ITEM('',(#170169),#86450) ;
#80742 = STYLED_ITEM('',(#170169),#86451) ;
#80743 = STYLED_ITEM('',(#170169),#86452) ;
#80744 = STYLED_ITEM('',(#170169),#86453) ;
#80745 = STYLED_ITEM('',(#170169),#86454) ;
#80746 = STYLED_ITEM('',(#170169),#86455) ;
#80747 = STYLED_ITEM('',(#170169),#86456) ;
#80748 = STYLED_ITEM('',(#170170),#86457) ;
#80749 = STYLED_ITEM('',(#170170),#86458) ;
#80750 = STYLED_ITEM('',(#170170),#86459) ;
#80751 = STYLED_ITEM('',(#170170),#86460) ;
#80752 = STYLED_ITEM('',(#170169),#86461) ;
#80753 = STYLED_ITEM('',(#170169),#86462) ;
#80754 = STYLED_ITEM('',(#170169),#86463) ;
#80755 = STYLED_ITEM('',(#170169),#86464) ;
#80756 = STYLED_ITEM('',(#170169),#86465) ;
#80757 = STYLED_ITEM('',(#170169),#86466) ;
#80758 = STYLED_ITEM('',(#170169),#86467) ;
#80759 = STYLED_ITEM('',(#170169),#86468) ;
#80760 = STYLED_ITEM('',(#170169),#86469) ;
#80761 = STYLED_ITEM('',(#170169),#86470) ;
#80762 = STYLED_ITEM('',(#170169),#86471) ;
#80763 = STYLED_ITEM('',(#170169),#86472) ;
#80764 = STYLED_ITEM('',(#170169),#86473) ;
#80765 = STYLED_ITEM('',(#170169),#86474) ;
#80766 = STYLED_ITEM('',(#170169),#86475) ;
#80767 = STYLED_ITEM('',(#170169),#86476) ;
#80768 = STYLED_ITEM('',(#170169),#86477) ;
#80769 = STYLED_ITEM('',(#170169),#86478) ;
#80770 = STYLED_ITEM('',(#170169),#86479) ;
#80771 = STYLED_ITEM('',(#170169),#86480) ;
#80772 = STYLED_ITEM('',(#170169),#86481) ;
#80773 = STYLED_ITEM('',(#170169),#86482) ;
#80774 = STYLED_ITEM('',(#170169),#86483) ;
#80775 = STYLED_ITEM('',(#170169),#86484) ;
#80776 = STYLED_ITEM('',(#170169),#86485) ;
#80777 = STYLED_ITEM('',(#170169),#86486) ;
#80778 = STYLED_ITEM('',(#170169),#86487) ;
#80779 = STYLED_ITEM('',(#170168),#31) ;
#80780 = STYLED_ITEM('',(#170169),#86488) ;
#80781 = STYLED_ITEM('',(#170169),#86489) ;
#80782 = STYLED_ITEM('',(#170169),#86490) ;
#80783 = STYLED_ITEM('',(#170169),#86491) ;
#80784 = STYLED_ITEM('',(#170169),#86492) ;
#80785 = STYLED_ITEM('',(#170169),#86493) ;
#80786 = STYLED_ITEM('',(#170169),#86494) ;
#80787 = STYLED_ITEM('',(#170169),#86495) ;
#80788 = STYLED_ITEM('',(#170169),#86496) ;
#80789 = STYLED_ITEM('',(#170169),#86497) ;
#80790 = STYLED_ITEM('',(#170169),#86498) ;
#80791 = STYLED_ITEM('',(#170169),#86499) ;
#80792 = STYLED_ITEM('',(#170169),#86500) ;
#80793 = STYLED_ITEM('',(#170169),#86501) ;
#80794 = STYLED_ITEM('',(#170169),#86502) ;
#80795 = STYLED_ITEM('',(#170169),#86503) ;
#80796 = STYLED_ITEM('',(#170169),#86504) ;
#80797 = STYLED_ITEM('',(#170169),#86505) ;
#80798 = STYLED_ITEM('',(#170169),#86506) ;
#80799 = STYLED_ITEM('',(#170169),#86507) ;
#80800 = STYLED_ITEM('',(#170169),#86508) ;
#80801 = STYLED_ITEM('',(#170169),#86509) ;
#80802 = STYLED_ITEM('',(#170169),#86510) ;
#80803 = STYLED_ITEM('',(#170169),#86511) ;
#80804 = STYLED_ITEM('',(#170169),#86512) ;
#80805 = STYLED_ITEM('',(#170169),#86513) ;
#80806 = STYLED_ITEM('',(#170169),#86514) ;
#80807 = STYLED_ITEM('',(#170169),#86515) ;
#80808 = STYLED_ITEM('',(#170169),#86516) ;
#80809 = STYLED_ITEM('',(#170169),#86517) ;
#80810 = STYLED_ITEM('',(#170169),#86518) ;
#80811 = STYLED_ITEM('',(#170169),#86519) ;
#80812 = STYLED_ITEM('',(#170169),#86520) ;
#80813 = STYLED_ITEM('',(#170169),#86521) ;
#80814 = STYLED_ITEM('',(#170169),#86522) ;
#80815 = STYLED_ITEM('',(#170169),#86523) ;
#80816 = STYLED_ITEM('',(#170169),#86524) ;
#80817 = STYLED_ITEM('',(#170169),#86525) ;
#80818 = STYLED_ITEM('',(#170169),#86526) ;
#80819 = STYLED_ITEM('',(#170169),#86527) ;
#80820 = STYLED_ITEM('',(#170169),#86528) ;
#80821 = STYLED_ITEM('',(#170169),#86529) ;
#80822 = STYLED_ITEM('',(#170169),#86530) ;
#80823 = STYLED_ITEM('',(#170169),#86531) ;
#80824 = STYLED_ITEM('',(#170169),#86532) ;
#80825 = STYLED_ITEM('',(#170169),#86533) ;
#80826 = STYLED_ITEM('',(#170169),#86534) ;
#80827 = STYLED_ITEM('',(#170169),#86535) ;
#80828 = STYLED_ITEM('',(#170169),#86536) ;
#80829 = STYLED_ITEM('',(#170169),#86537) ;
#80830 = STYLED_ITEM('',(#170169),#86538) ;
#80831 = STYLED_ITEM('',(#170169),#86539) ;
#80832 = STYLED_ITEM('',(#170169),#86540) ;
#80833 = STYLED_ITEM('',(#170169),#86541) ;
#80834 = STYLED_ITEM('',(#170169),#86542) ;
#80835 = STYLED_ITEM('',(#170169),#86543) ;
#80836 = STYLED_ITEM('',(#170169),#86544) ;
#80837 = STYLED_ITEM('',(#170169),#86545) ;
#80838 = STYLED_ITEM('',(#170169),#86546) ;
#80839 = STYLED_ITEM('',(#170169),#86547) ;
#80840 = STYLED_ITEM('',(#170169),#86548) ;
#80841 = STYLED_ITEM('',(#170169),#86549) ;
#80842 = STYLED_ITEM('',(#170169),#86550) ;
#80843 = STYLED_ITEM('',(#170169),#86551) ;
#80844 = STYLED_ITEM('',(#170169),#86552) ;
#80845 = STYLED_ITEM('',(#170169),#86553) ;
#80846 = STYLED_ITEM('',(#170169),#86554) ;
#80847 = STYLED_ITEM('',(#170169),#86555) ;
#80848 = STYLED_ITEM('',(#170169),#86556) ;
#80849 = STYLED_ITEM('',(#170169),#86557) ;
#80850 = STYLED_ITEM('',(#170169),#86558) ;
#80851 = STYLED_ITEM('',(#170169),#86559) ;
#80852 = STYLED_ITEM('',(#170169),#86560) ;
#80853 = STYLED_ITEM('',(#170169),#86561) ;
#80854 = STYLED_ITEM('',(#170169),#86562) ;
#80855 = STYLED_ITEM('',(#170169),#86563) ;
#80856 = STYLED_ITEM('',(#170169),#86564) ;
#80857 = STYLED_ITEM('',(#170169),#86565) ;
#80858 = STYLED_ITEM('',(#170169),#86566) ;
#80859 = STYLED_ITEM('',(#170169),#86567) ;
#80860 = STYLED_ITEM('',(#170169),#86568) ;
#80861 = STYLED_ITEM('',(#170169),#86569) ;
#80862 = STYLED_ITEM('',(#170169),#86570) ;
#80863 = STYLED_ITEM('',(#170169),#86571) ;
#80864 = STYLED_ITEM('',(#170169),#86572) ;
#80865 = STYLED_ITEM('',(#170169),#86573) ;
#80866 = STYLED_ITEM('',(#170169),#86574) ;
#80867 = STYLED_ITEM('',(#170169),#86575) ;
#80868 = STYLED_ITEM('',(#170169),#86576) ;
#80869 = STYLED_ITEM('',(#170169),#86577) ;
#80870 = STYLED_ITEM('',(#170169),#86578) ;
#80871 = STYLED_ITEM('',(#170169),#86579) ;
#80872 = STYLED_ITEM('',(#170169),#86580) ;
#80873 = STYLED_ITEM('',(#170169),#86581) ;
#80874 = STYLED_ITEM('',(#170169),#86582) ;
#80875 = STYLED_ITEM('',(#170169),#86583) ;
#80876 = STYLED_ITEM('',(#170169),#86584) ;
#80877 = STYLED_ITEM('',(#170169),#86585) ;
#80878 = STYLED_ITEM('',(#170169),#86586) ;
#80879 = STYLED_ITEM('',(#170169),#86587) ;
#80880 = STYLED_ITEM('',(#170169),#86588) ;
#80881 = STYLED_ITEM('',(#170169),#86589) ;
#80882 = STYLED_ITEM('',(#170169),#86590) ;
#80883 = STYLED_ITEM('',(#170169),#86591) ;
#80884 = STYLED_ITEM('',(#170169),#86592) ;
#80885 = STYLED_ITEM('',(#170169),#86593) ;
#80886 = STYLED_ITEM('',(#170169),#86594) ;
#80887 = STYLED_ITEM('',(#170169),#86595) ;
#80888 = STYLED_ITEM('',(#170169),#86596) ;
#80889 = STYLED_ITEM('',(#170169),#86597) ;
#80890 = STYLED_ITEM('',(#170169),#86598) ;
#80891 = STYLED_ITEM('',(#170169),#86599) ;
#80892 = STYLED_ITEM('',(#170169),#86600) ;
#80893 = STYLED_ITEM('',(#170169),#86601) ;
#80894 = STYLED_ITEM('',(#170169),#86602) ;
#80895 = STYLED_ITEM('',(#170169),#86603) ;
#80896 = STYLED_ITEM('',(#170169),#86604) ;
#80897 = STYLED_ITEM('',(#170169),#86605) ;
#80898 = STYLED_ITEM('',(#170169),#86606) ;
#80899 = STYLED_ITEM('',(#170169),#86607) ;
#80900 = STYLED_ITEM('',(#170169),#86608) ;
#80901 = STYLED_ITEM('',(#170169),#86609) ;
#80902 = STYLED_ITEM('',(#170169),#86610) ;
#80903 = STYLED_ITEM('',(#170169),#86611) ;
#80904 = STYLED_ITEM('',(#170169),#86612) ;
#80905 = STYLED_ITEM('',(#170169),#86613) ;
#80906 = STYLED_ITEM('',(#170169),#86614) ;
#80907 = STYLED_ITEM('',(#170169),#86615) ;
#80908 = STYLED_ITEM('',(#170169),#86616) ;
#80909 = STYLED_ITEM('',(#170169),#86617) ;
#80910 = STYLED_ITEM('',(#170169),#86618) ;
#80911 = STYLED_ITEM('',(#170169),#86619) ;
#80912 = STYLED_ITEM('',(#170169),#86620) ;
#80913 = STYLED_ITEM('',(#170169),#86621) ;
#80914 = STYLED_ITEM('',(#170169),#86622) ;
#80915 = STYLED_ITEM('',(#170169),#86623) ;
#80916 = STYLED_ITEM('',(#170169),#86624) ;
#80917 = STYLED_ITEM('',(#170169),#86625) ;
#80918 = STYLED_ITEM('',(#170169),#86626) ;
#80919 = STYLED_ITEM('',(#170169),#86627) ;
#80920 = STYLED_ITEM('',(#170169),#86628) ;
#80921 = STYLED_ITEM('',(#170169),#86629) ;
#80922 = STYLED_ITEM('',(#170169),#86630) ;
#80923 = STYLED_ITEM('',(#170169),#86631) ;
#80924 = STYLED_ITEM('',(#170169),#86632) ;
#80925 = STYLED_ITEM('',(#170169),#86633) ;
#80926 = STYLED_ITEM('',(#170169),#86634) ;
#80927 = STYLED_ITEM('',(#170169),#86635) ;
#80928 = STYLED_ITEM('',(#170169),#86636) ;
#80929 = STYLED_ITEM('',(#170169),#86637) ;
#80930 = STYLED_ITEM('',(#170169),#86638) ;
#80931 = STYLED_ITEM('',(#170169),#86639) ;
#80932 = STYLED_ITEM('',(#170169),#86640) ;
#80933 = STYLED_ITEM('',(#170169),#86641) ;
#80934 = STYLED_ITEM('',(#170169),#86642) ;
#80935 = STYLED_ITEM('',(#170169),#86643) ;
#80936 = STYLED_ITEM('',(#170169),#86644) ;
#80937 = STYLED_ITEM('',(#170169),#86645) ;
#80938 = STYLED_ITEM('',(#170169),#86646) ;
#80939 = STYLED_ITEM('',(#170169),#86647) ;
#80940 = STYLED_ITEM('',(#170169),#86648) ;
#80941 = STYLED_ITEM('',(#170169),#86649) ;
#80942 = STYLED_ITEM('',(#170169),#86650) ;
#80943 = STYLED_ITEM('',(#170169),#86651) ;
#80944 = STYLED_ITEM('',(#170169),#86652) ;
#80945 = STYLED_ITEM('',(#170169),#86653) ;
#80946 = STYLED_ITEM('',(#170169),#86654) ;
#80947 = STYLED_ITEM('',(#170169),#86655) ;
#80948 = STYLED_ITEM('',(#170169),#86656) ;
#80949 = STYLED_ITEM('',(#170169),#86657) ;
#80950 = STYLED_ITEM('',(#170169),#86658) ;
#80951 = STYLED_ITEM('',(#170169),#86659) ;
#80952 = STYLED_ITEM('',(#170169),#86660) ;
#80953 = STYLED_ITEM('',(#170169),#86661) ;
#80954 = STYLED_ITEM('',(#170169),#86662) ;
#80955 = STYLED_ITEM('',(#170169),#86663) ;
#80956 = STYLED_ITEM('',(#170169),#86664) ;
#80957 = STYLED_ITEM('',(#170169),#86665) ;
#80958 = STYLED_ITEM('',(#170169),#86666) ;
#80959 = STYLED_ITEM('',(#170169),#86667) ;
#80960 = STYLED_ITEM('',(#170169),#86668) ;
#80961 = STYLED_ITEM('',(#170169),#86669) ;
#80962 = STYLED_ITEM('',(#170169),#86670) ;
#80963 = STYLED_ITEM('',(#170169),#86671) ;
#80964 = STYLED_ITEM('',(#170169),#86672) ;
#80965 = STYLED_ITEM('',(#170169),#86673) ;
#80966 = STYLED_ITEM('',(#170169),#86674) ;
#80967 = STYLED_ITEM('',(#170169),#86675) ;
#80968 = STYLED_ITEM('',(#170169),#86676) ;
#80969 = STYLED_ITEM('',(#170169),#86677) ;
#80970 = STYLED_ITEM('',(#170169),#86678) ;
#80971 = STYLED_ITEM('',(#170169),#86679) ;
#80972 = STYLED_ITEM('',(#170169),#86680) ;
#80973 = STYLED_ITEM('',(#170169),#86681) ;
#80974 = STYLED_ITEM('',(#170169),#86682) ;
#80975 = STYLED_ITEM('',(#170169),#86683) ;
#80976 = STYLED_ITEM('',(#170169),#86684) ;
#80977 = STYLED_ITEM('',(#170169),#86685) ;
#80978 = STYLED_ITEM('',(#170169),#86686) ;
#80979 = STYLED_ITEM('',(#170169),#86687) ;
#80980 = STYLED_ITEM('',(#170169),#86688) ;
#80981 = STYLED_ITEM('',(#170169),#86689) ;
#80982 = STYLED_ITEM('',(#170169),#86690) ;
#80983 = STYLED_ITEM('',(#170169),#86691) ;
#80984 = STYLED_ITEM('',(#170169),#86692) ;
#80985 = STYLED_ITEM('',(#170169),#86693) ;
#80986 = STYLED_ITEM('',(#170169),#86694) ;
#80987 = STYLED_ITEM('',(#170169),#86695) ;
#80988 = STYLED_ITEM('',(#170169),#86696) ;
#80989 = STYLED_ITEM('',(#170169),#86697) ;
#80990 = STYLED_ITEM('',(#170169),#86698) ;
#80991 = STYLED_ITEM('',(#170169),#86699) ;
#80992 = STYLED_ITEM('',(#170169),#86700) ;
#80993 = STYLED_ITEM('',(#170169),#86701) ;
#80994 = STYLED_ITEM('',(#170169),#86702) ;
#80995 = STYLED_ITEM('',(#170169),#86703) ;
#80996 = STYLED_ITEM('',(#170169),#86704) ;
#80997 = STYLED_ITEM('',(#170169),#86705) ;
#80998 = STYLED_ITEM('',(#170169),#86706) ;
#80999 = STYLED_ITEM('',(#170169),#86707) ;
#81000 = STYLED_ITEM('',(#170169),#86708) ;
#81001 = STYLED_ITEM('',(#170169),#86709) ;
#81002 = STYLED_ITEM('',(#170169),#86710) ;
#81003 = STYLED_ITEM('',(#170169),#86711) ;
#81004 = STYLED_ITEM('',(#170169),#86712) ;
#81005 = STYLED_ITEM('',(#170169),#86713) ;
#81006 = STYLED_ITEM('',(#170169),#86714) ;
#81007 = STYLED_ITEM('',(#170169),#86715) ;
#81008 = STYLED_ITEM('',(#170169),#86716) ;
#81009 = STYLED_ITEM('',(#170169),#86717) ;
#81010 = STYLED_ITEM('',(#170169),#86718) ;
#81011 = STYLED_ITEM('',(#170169),#86719) ;
#81012 = STYLED_ITEM('',(#170169),#86720) ;
#81013 = STYLED_ITEM('',(#170169),#86721) ;
#81014 = STYLED_ITEM('',(#170169),#86722) ;
#81015 = STYLED_ITEM('',(#170169),#86723) ;
#81016 = STYLED_ITEM('',(#170169),#86724) ;
#81017 = STYLED_ITEM('',(#170169),#86725) ;
#81018 = STYLED_ITEM('',(#170169),#86726) ;
#81019 = STYLED_ITEM('',(#170169),#86727) ;
#81020 = STYLED_ITEM('',(#170169),#86728) ;
#81021 = STYLED_ITEM('',(#170169),#86729) ;
#81022 = STYLED_ITEM('',(#170169),#86730) ;
#81023 = STYLED_ITEM('',(#170169),#86731) ;
#81024 = STYLED_ITEM('',(#170169),#86732) ;
#81025 = STYLED_ITEM('',(#170169),#86733) ;
#81026 = STYLED_ITEM('',(#170169),#86734) ;
#81027 = STYLED_ITEM('',(#170169),#86735) ;
#81028 = STYLED_ITEM('',(#170169),#86736) ;
#81029 = STYLED_ITEM('',(#170169),#86737) ;
#81030 = STYLED_ITEM('',(#170169),#86738) ;
#81031 = STYLED_ITEM('',(#170169),#86739) ;
#81032 = STYLED_ITEM('',(#170169),#86740) ;
#81033 = STYLED_ITEM('',(#170169),#86741) ;
#81034 = STYLED_ITEM('',(#170169),#86742) ;
#81035 = STYLED_ITEM('',(#170169),#86743) ;
#81036 = STYLED_ITEM('',(#170169),#86744) ;
#81037 = STYLED_ITEM('',(#170169),#86745) ;
#81038 = STYLED_ITEM('',(#170169),#86746) ;
#81039 = STYLED_ITEM('',(#170169),#86747) ;
#81040 = STYLED_ITEM('',(#170169),#86748) ;
#81041 = STYLED_ITEM('',(#170169),#86749) ;
#81042 = STYLED_ITEM('',(#170169),#86750) ;
#81043 = STYLED_ITEM('',(#170169),#86751) ;
#81044 = STYLED_ITEM('',(#170169),#86752) ;
#81045 = STYLED_ITEM('',(#170169),#86753) ;
#81046 = STYLED_ITEM('',(#170169),#86754) ;
#81047 = STYLED_ITEM('',(#170169),#86755) ;
#81048 = STYLED_ITEM('',(#170169),#86756) ;
#81049 = STYLED_ITEM('',(#170169),#86757) ;
#81050 = STYLED_ITEM('',(#170169),#86758) ;
#81051 = STYLED_ITEM('',(#170169),#86759) ;
#81052 = STYLED_ITEM('',(#170169),#86760) ;
#81053 = STYLED_ITEM('',(#170169),#86761) ;
#81054 = STYLED_ITEM('',(#170169),#86762) ;
#81055 = STYLED_ITEM('',(#170169),#86763) ;
#81056 = STYLED_ITEM('',(#170169),#86764) ;
#81057 = STYLED_ITEM('',(#170169),#86765) ;
#81058 = STYLED_ITEM('',(#170169),#86766) ;
#81059 = STYLED_ITEM('',(#170169),#86767) ;
#81060 = STYLED_ITEM('',(#170169),#86768) ;
#81061 = STYLED_ITEM('',(#170169),#86769) ;
#81062 = STYLED_ITEM('',(#170169),#86770) ;
#81063 = STYLED_ITEM('',(#170169),#86771) ;
#81064 = STYLED_ITEM('',(#170169),#86772) ;
#81065 = STYLED_ITEM('',(#170169),#86773) ;
#81066 = STYLED_ITEM('',(#170169),#86774) ;
#81067 = STYLED_ITEM('',(#170169),#86775) ;
#81068 = STYLED_ITEM('',(#170169),#86776) ;
#81069 = STYLED_ITEM('',(#170169),#86777) ;
#81070 = STYLED_ITEM('',(#170169),#86778) ;
#81071 = STYLED_ITEM('',(#170169),#86779) ;
#81072 = STYLED_ITEM('',(#170169),#86780) ;
#81073 = STYLED_ITEM('',(#170169),#86781) ;
#81074 = STYLED_ITEM('',(#170169),#86782) ;
#81075 = STYLED_ITEM('',(#170171),#86783) ;
#81076 = STYLED_ITEM('',(#170171),#86784) ;
#81077 = STYLED_ITEM('',(#170171),#86785) ;
#81078 = STYLED_ITEM('',(#170171),#86786) ;
#81079 = STYLED_ITEM('',(#170171),#86787) ;
#81080 = STYLED_ITEM('',(#170171),#86788) ;
#81081 = STYLED_ITEM('',(#170171),#86789) ;
#81082 = STYLED_ITEM('',(#170171),#86790) ;
#81083 = STYLED_ITEM('',(#170171),#86791) ;
#81084 = STYLED_ITEM('',(#170171),#86792) ;
#81085 = STYLED_ITEM('',(#170171),#86793) ;
#81086 = STYLED_ITEM('',(#170171),#86794) ;
#81087 = STYLED_ITEM('',(#170171),#86795) ;
#81088 = STYLED_ITEM('',(#170171),#86796) ;
#81089 = STYLED_ITEM('',(#170171),#86797) ;
#81090 = STYLED_ITEM('',(#170171),#86798) ;
#81091 = STYLED_ITEM('',(#170171),#86799) ;
#81092 = STYLED_ITEM('',(#170171),#86800) ;
#81093 = STYLED_ITEM('',(#170171),#86801) ;
#81094 = STYLED_ITEM('',(#170171),#86802) ;
#81095 = STYLED_ITEM('',(#170171),#86803) ;
#81096 = STYLED_ITEM('',(#170171),#86804) ;
#81097 = STYLED_ITEM('',(#170171),#86805) ;
#81098 = STYLED_ITEM('',(#170171),#86806) ;
#81099 = STYLED_ITEM('',(#170171),#86807) ;
#81100 = STYLED_ITEM('',(#170171),#86808) ;
#81101 = STYLED_ITEM('',(#170171),#86809) ;
#81102 = STYLED_ITEM('',(#170171),#86810) ;
#81103 = STYLED_ITEM('',(#170171),#86811) ;
#81104 = STYLED_ITEM('',(#170171),#86812) ;
#81105 = STYLED_ITEM('',(#170171),#86813) ;
#81106 = STYLED_ITEM('',(#170171),#86814) ;
#81107 = STYLED_ITEM('',(#170171),#86815) ;
#81108 = STYLED_ITEM('',(#170171),#86816) ;
#81109 = STYLED_ITEM('',(#170171),#86817) ;
#81110 = STYLED_ITEM('',(#170171),#86818) ;
#81111 = STYLED_ITEM('',(#170171),#86819) ;
#81112 = STYLED_ITEM('',(#170171),#86820) ;
#81113 = STYLED_ITEM('',(#170171),#86821) ;
#81114 = STYLED_ITEM('',(#170171),#86822) ;
#81115 = STYLED_ITEM('',(#170171),#86823) ;
#81116 = STYLED_ITEM('',(#170171),#86824) ;
#81117 = STYLED_ITEM('',(#170171),#86825) ;
#81118 = STYLED_ITEM('',(#170171),#86826) ;
#81119 = STYLED_ITEM('',(#170171),#86827) ;
#81120 = STYLED_ITEM('',(#170171),#86828) ;
#81121 = STYLED_ITEM('',(#170171),#86829) ;
#81122 = STYLED_ITEM('',(#170171),#86830) ;
#81123 = STYLED_ITEM('',(#170171),#86831) ;
#81124 = STYLED_ITEM('',(#170171),#86832) ;
#81125 = STYLED_ITEM('',(#170171),#86833) ;
#81126 = STYLED_ITEM('',(#170171),#86834) ;
#81127 = STYLED_ITEM('',(#170171),#86835) ;
#81128 = STYLED_ITEM('',(#170171),#86836) ;
#81129 = STYLED_ITEM('',(#170171),#86837) ;
#81130 = STYLED_ITEM('',(#170171),#86838) ;
#81131 = STYLED_ITEM('',(#170171),#86839) ;
#81132 = STYLED_ITEM('',(#170171),#86840) ;
#81133 = STYLED_ITEM('',(#170171),#86841) ;
#81134 = STYLED_ITEM('',(#170171),#86842) ;
#81135 = STYLED_ITEM('',(#170171),#86843) ;
#81136 = STYLED_ITEM('',(#170171),#86844) ;
#81137 = STYLED_ITEM('',(#170171),#86845) ;
#81138 = STYLED_ITEM('',(#170171),#86846) ;
#81139 = STYLED_ITEM('',(#170171),#86847) ;
#81140 = STYLED_ITEM('',(#170171),#86848) ;
#81141 = STYLED_ITEM('',(#170171),#86849) ;
#81142 = STYLED_ITEM('',(#170171),#86850) ;
#81143 = STYLED_ITEM('',(#170171),#86851) ;
#81144 = STYLED_ITEM('',(#170171),#86852) ;
#81145 = STYLED_ITEM('',(#170171),#86853) ;
#81146 = STYLED_ITEM('',(#170171),#86854) ;
#81147 = STYLED_ITEM('',(#170169),#86855) ;
#81148 = STYLED_ITEM('',(#170169),#86856) ;
#81149 = STYLED_ITEM('',(#170169),#86857) ;
#81150 = STYLED_ITEM('',(#170169),#86858) ;
#81151 = STYLED_ITEM('',(#170169),#86859) ;
#81152 = STYLED_ITEM('',(#170169),#86860) ;
#81153 = STYLED_ITEM('',(#170169),#86861) ;
#81154 = STYLED_ITEM('',(#170169),#86862) ;
#81155 = STYLED_ITEM('',(#170169),#86863) ;
#81156 = STYLED_ITEM('',(#170169),#86864) ;
#81157 = STYLED_ITEM('',(#170169),#86865) ;
#81158 = STYLED_ITEM('',(#170169),#86866) ;
#81159 = STYLED_ITEM('',(#170169),#86867) ;
#81160 = STYLED_ITEM('',(#170169),#86868) ;
#81161 = STYLED_ITEM('',(#170169),#86869) ;
#81162 = STYLED_ITEM('',(#170169),#86870) ;
#81163 = STYLED_ITEM('',(#170169),#86871) ;
#81164 = STYLED_ITEM('',(#170169),#86872) ;
#81165 = STYLED_ITEM('',(#170169),#86873) ;
#81166 = STYLED_ITEM('',(#170169),#86874) ;
#81167 = STYLED_ITEM('',(#170169),#86875) ;
#81168 = STYLED_ITEM('',(#170169),#86876) ;
#81169 = STYLED_ITEM('',(#170169),#86877) ;
#81170 = STYLED_ITEM('',(#170169),#86878) ;
#81171 = STYLED_ITEM('',(#170169),#86879) ;
#81172 = STYLED_ITEM('',(#170169),#86880) ;
#81173 = STYLED_ITEM('',(#170169),#86881) ;
#81174 = STYLED_ITEM('',(#170169),#86882) ;
#81175 = STYLED_ITEM('',(#170169),#86883) ;
#81176 = STYLED_ITEM('',(#170169),#86884) ;
#81177 = STYLED_ITEM('',(#170169),#86885) ;
#81178 = STYLED_ITEM('',(#170169),#86886) ;
#81179 = STYLED_ITEM('',(#170169),#86887) ;
#81180 = STYLED_ITEM('',(#170169),#86888) ;
#81181 = STYLED_ITEM('',(#170169),#86889) ;
#81182 = STYLED_ITEM('',(#170169),#86890) ;
#81183 = STYLED_ITEM('',(#170169),#86891) ;
#81184 = STYLED_ITEM('',(#170169),#86892) ;
#81185 = STYLED_ITEM('',(#170169),#86893) ;
#81186 = STYLED_ITEM('',(#170169),#86894) ;
#81187 = STYLED_ITEM('',(#170169),#86895) ;
#81188 = STYLED_ITEM('',(#170169),#86896) ;
#81189 = STYLED_ITEM('',(#170169),#86897) ;
#81190 = STYLED_ITEM('',(#170169),#86898) ;
#81191 = STYLED_ITEM('',(#170169),#86899) ;
#81192 = STYLED_ITEM('',(#170169),#86900) ;
#81193 = STYLED_ITEM('',(#170169),#86901) ;
#81194 = STYLED_ITEM('',(#170169),#86902) ;
#81195 = STYLED_ITEM('',(#170169),#86903) ;
#81196 = STYLED_ITEM('',(#170169),#86904) ;
#81197 = STYLED_ITEM('',(#170169),#86905) ;
#81198 = STYLED_ITEM('',(#170169),#86906) ;
#81199 = STYLED_ITEM('',(#170169),#86907) ;
#81200 = STYLED_ITEM('',(#170169),#86908) ;
#81201 = STYLED_ITEM('',(#170169),#86909) ;
#81202 = STYLED_ITEM('',(#170169),#86910) ;
#81203 = STYLED_ITEM('',(#170169),#86911) ;
#81204 = STYLED_ITEM('',(#170169),#86912) ;
#81205 = STYLED_ITEM('',(#170169),#86913) ;
#81206 = STYLED_ITEM('',(#170169),#86914) ;
#81207 = STYLED_ITEM('',(#170169),#86915) ;
#81208 = STYLED_ITEM('',(#170169),#86916) ;
#81209 = STYLED_ITEM('',(#170169),#86917) ;
#81210 = STYLED_ITEM('',(#170169),#86918) ;
#81211 = STYLED_ITEM('',(#170169),#86919) ;
#81212 = STYLED_ITEM('',(#170169),#86920) ;
#81213 = STYLED_ITEM('',(#170169),#86921) ;
#81214 = STYLED_ITEM('',(#170169),#86922) ;
#81215 = STYLED_ITEM('',(#170169),#86923) ;
#81216 = STYLED_ITEM('',(#170169),#86924) ;
#81217 = STYLED_ITEM('',(#170169),#86925) ;
#81218 = STYLED_ITEM('',(#170169),#86926) ;
#81219 = STYLED_ITEM('',(#170169),#86927) ;
#81220 = STYLED_ITEM('',(#170169),#86928) ;
#81221 = STYLED_ITEM('',(#170169),#86929) ;
#81222 = STYLED_ITEM('',(#170169),#86930) ;
#81223 = STYLED_ITEM('',(#170169),#86931) ;
#81224 = STYLED_ITEM('',(#170169),#86932) ;
#81225 = STYLED_ITEM('',(#170169),#86933) ;
#81226 = STYLED_ITEM('',(#170169),#86934) ;
#81227 = STYLED_ITEM('',(#170169),#86935) ;
#81228 = STYLED_ITEM('',(#170169),#86936) ;
#81229 = STYLED_ITEM('',(#170169),#86937) ;
#81230 = STYLED_ITEM('',(#170169),#86938) ;
#81231 = STYLED_ITEM('',(#170169),#86939) ;
#81232 = STYLED_ITEM('',(#170169),#86940) ;
#81233 = STYLED_ITEM('',(#170169),#86941) ;
#81234 = STYLED_ITEM('',(#170169),#86942) ;
#81235 = STYLED_ITEM('',(#170169),#86943) ;
#81236 = STYLED_ITEM('',(#170169),#86944) ;
#81237 = STYLED_ITEM('',(#170169),#86945) ;
#81238 = STYLED_ITEM('',(#170169),#86946) ;
#81239 = STYLED_ITEM('',(#170169),#86947) ;
#81240 = STYLED_ITEM('',(#170169),#86948) ;
#81241 = STYLED_ITEM('',(#170169),#86949) ;
#81242 = STYLED_ITEM('',(#170169),#86950) ;
#81243 = STYLED_ITEM('',(#170169),#86951) ;
#81244 = STYLED_ITEM('',(#170169),#86952) ;
#81245 = STYLED_ITEM('',(#170169),#86953) ;
#81246 = STYLED_ITEM('',(#170169),#86954) ;
#81247 = STYLED_ITEM('',(#170169),#86955) ;
#81248 = STYLED_ITEM('',(#170169),#86956) ;
#81249 = STYLED_ITEM('',(#170169),#86957) ;
#81250 = STYLED_ITEM('',(#170169),#86958) ;
#81251 = STYLED_ITEM('',(#170169),#86959) ;
#81252 = STYLED_ITEM('',(#170169),#86960) ;
#81253 = STYLED_ITEM('',(#170169),#86961) ;
#81254 = STYLED_ITEM('',(#170169),#86962) ;
#81255 = STYLED_ITEM('',(#170169),#86963) ;
#81256 = STYLED_ITEM('',(#170169),#86964) ;
#81257 = STYLED_ITEM('',(#170169),#86965) ;
#81258 = STYLED_ITEM('',(#170169),#86966) ;
#81259 = STYLED_ITEM('',(#170169),#86967) ;
#81260 = STYLED_ITEM('',(#170169),#86968) ;
#81261 = STYLED_ITEM('',(#170169),#86969) ;
#81262 = STYLED_ITEM('',(#170169),#86970) ;
#81263 = STYLED_ITEM('',(#170169),#86971) ;
#81264 = STYLED_ITEM('',(#170169),#86972) ;
#81265 = STYLED_ITEM('',(#170169),#86973) ;
#81266 = STYLED_ITEM('',(#170169),#86974) ;
#81267 = STYLED_ITEM('',(#170169),#86975) ;
#81268 = STYLED_ITEM('',(#170169),#86976) ;
#81269 = STYLED_ITEM('',(#170169),#86977) ;
#81270 = STYLED_ITEM('',(#170169),#86978) ;
#81271 = STYLED_ITEM('',(#170169),#86979) ;
#81272 = STYLED_ITEM('',(#170169),#86980) ;
#81273 = STYLED_ITEM('',(#170169),#86981) ;
#81274 = STYLED_ITEM('',(#170169),#86982) ;
#81275 = STYLED_ITEM('',(#170169),#86983) ;
#81276 = STYLED_ITEM('',(#170169),#86984) ;
#81277 = STYLED_ITEM('',(#170169),#86985) ;
#81278 = STYLED_ITEM('',(#170169),#86986) ;
#81279 = STYLED_ITEM('',(#170169),#86987) ;
#81280 = STYLED_ITEM('',(#170169),#86988) ;
#81281 = STYLED_ITEM('',(#170169),#86989) ;
#81282 = STYLED_ITEM('',(#170169),#86990) ;
#81283 = STYLED_ITEM('',(#170169),#86991) ;
#81284 = STYLED_ITEM('',(#170169),#86992) ;
#81285 = STYLED_ITEM('',(#170169),#86993) ;
#81286 = STYLED_ITEM('',(#170169),#86994) ;
#81287 = STYLED_ITEM('',(#170169),#86995) ;
#81288 = STYLED_ITEM('',(#170169),#86996) ;
#81289 = STYLED_ITEM('',(#170169),#86997) ;
#81290 = STYLED_ITEM('',(#170169),#86998) ;
#81291 = STYLED_ITEM('',(#170169),#86999) ;
#81292 = STYLED_ITEM('',(#170169),#87000) ;
#81293 = STYLED_ITEM('',(#170169),#87001) ;
#81294 = STYLED_ITEM('',(#170169),#87002) ;
#81295 = STYLED_ITEM('',(#170169),#87003) ;
#81296 = STYLED_ITEM('',(#170169),#87004) ;
#81297 = STYLED_ITEM('',(#170169),#87005) ;
#81298 = STYLED_ITEM('',(#170169),#87006) ;
#81299 = STYLED_ITEM('',(#170169),#87007) ;
#81300 = STYLED_ITEM('',(#170169),#87008) ;
#81301 = STYLED_ITEM('',(#170169),#87009) ;
#81302 = STYLED_ITEM('',(#170169),#87010) ;
#81303 = STYLED_ITEM('',(#170169),#87011) ;
#81304 = STYLED_ITEM('',(#170169),#87012) ;
#81305 = STYLED_ITEM('',(#170169),#87013) ;
#81306 = STYLED_ITEM('',(#170169),#87014) ;
#81307 = STYLED_ITEM('',(#170169),#87015) ;
#81308 = STYLED_ITEM('',(#170169),#87016) ;
#81309 = STYLED_ITEM('',(#170169),#87017) ;
#81310 = STYLED_ITEM('',(#170169),#87018) ;
#81311 = STYLED_ITEM('',(#170169),#87019) ;
#81312 = STYLED_ITEM('',(#170169),#87020) ;
#81313 = STYLED_ITEM('',(#170169),#87021) ;
#81314 = STYLED_ITEM('',(#170169),#87022) ;
#81315 = STYLED_ITEM('',(#170169),#87023) ;
#81316 = STYLED_ITEM('',(#170169),#87024) ;
#81317 = STYLED_ITEM('',(#170169),#87025) ;
#81318 = STYLED_ITEM('',(#170169),#87026) ;
#81319 = STYLED_ITEM('',(#170169),#87027) ;
#81320 = STYLED_ITEM('',(#170169),#87028) ;
#81321 = STYLED_ITEM('',(#170169),#87029) ;
#81322 = STYLED_ITEM('',(#170169),#87030) ;
#81323 = STYLED_ITEM('',(#170169),#87031) ;
#81324 = STYLED_ITEM('',(#170169),#87032) ;
#81325 = STYLED_ITEM('',(#170169),#87033) ;
#81326 = STYLED_ITEM('',(#170169),#87034) ;
#81327 = STYLED_ITEM('',(#170169),#87035) ;
#81328 = STYLED_ITEM('',(#170169),#87036) ;
#81329 = STYLED_ITEM('',(#170169),#87037) ;
#81330 = STYLED_ITEM('',(#170169),#87038) ;
#81331 = STYLED_ITEM('',(#170169),#87039) ;
#81332 = STYLED_ITEM('',(#170169),#87040) ;
#81333 = STYLED_ITEM('',(#170169),#87041) ;
#81334 = STYLED_ITEM('',(#170169),#87042) ;
#81335 = STYLED_ITEM('',(#170169),#87043) ;
#81336 = STYLED_ITEM('',(#170169),#87044) ;
#81337 = STYLED_ITEM('',(#170169),#87045) ;
#81338 = STYLED_ITEM('',(#170169),#87046) ;
#81339 = STYLED_ITEM('',(#170169),#87047) ;
#81340 = STYLED_ITEM('',(#170169),#87048) ;
#81341 = STYLED_ITEM('',(#170169),#87049) ;
#81342 = STYLED_ITEM('',(#170169),#87050) ;
#81343 = STYLED_ITEM('',(#170169),#87051) ;
#81344 = STYLED_ITEM('',(#170169),#87052) ;
#81345 = STYLED_ITEM('',(#170169),#87053) ;
#81346 = STYLED_ITEM('',(#170169),#87054) ;
#81347 = STYLED_ITEM('',(#170169),#87055) ;
#81348 = STYLED_ITEM('',(#170169),#87056) ;
#81349 = STYLED_ITEM('',(#170169),#87057) ;
#81350 = STYLED_ITEM('',(#170169),#87058) ;
#81351 = STYLED_ITEM('',(#170169),#87059) ;
#81352 = STYLED_ITEM('',(#170169),#87060) ;
#81353 = STYLED_ITEM('',(#170169),#87061) ;
#81354 = STYLED_ITEM('',(#170169),#87062) ;
#81355 = STYLED_ITEM('',(#170169),#87063) ;
#81356 = STYLED_ITEM('',(#170169),#87064) ;
#81357 = STYLED_ITEM('',(#170169),#87065) ;
#81358 = STYLED_ITEM('',(#170169),#87066) ;
#81359 = STYLED_ITEM('',(#170169),#87067) ;
#81360 = STYLED_ITEM('',(#170169),#87068) ;
#81361 = STYLED_ITEM('',(#170169),#87069) ;
#81362 = STYLED_ITEM('',(#170169),#87070) ;
#81363 = STYLED_ITEM('',(#170169),#87071) ;
#81364 = STYLED_ITEM('',(#170169),#87072) ;
#81365 = STYLED_ITEM('',(#170169),#87073) ;
#81366 = STYLED_ITEM('',(#170169),#87074) ;
#81367 = STYLED_ITEM('',(#170169),#87075) ;
#81368 = STYLED_ITEM('',(#170169),#87076) ;
#81369 = STYLED_ITEM('',(#170169),#87077) ;
#81370 = STYLED_ITEM('',(#170169),#87078) ;
#81371 = STYLED_ITEM('',(#170169),#87079) ;
#81372 = STYLED_ITEM('',(#170169),#87080) ;
#81373 = STYLED_ITEM('',(#170169),#87081) ;
#81374 = STYLED_ITEM('',(#170169),#87082) ;
#81375 = STYLED_ITEM('',(#170169),#87083) ;
#81376 = STYLED_ITEM('',(#170169),#87084) ;
#81377 = STYLED_ITEM('',(#170169),#87085) ;
#81378 = STYLED_ITEM('',(#170169),#87086) ;
#81379 = STYLED_ITEM('',(#170169),#87087) ;
#81380 = STYLED_ITEM('',(#170169),#87088) ;
#81381 = STYLED_ITEM('',(#170169),#87089) ;
#81382 = STYLED_ITEM('',(#170169),#87090) ;
#81383 = STYLED_ITEM('',(#170169),#87091) ;
#81384 = STYLED_ITEM('',(#170169),#87092) ;
#81385 = STYLED_ITEM('',(#170169),#87093) ;
#81386 = STYLED_ITEM('',(#170169),#87094) ;
#81387 = STYLED_ITEM('',(#170169),#87095) ;
#81388 = STYLED_ITEM('',(#170169),#87096) ;
#81389 = STYLED_ITEM('',(#170169),#87097) ;
#81390 = STYLED_ITEM('',(#170169),#87098) ;
#81391 = STYLED_ITEM('',(#170169),#87099) ;
#81392 = STYLED_ITEM('',(#170169),#87100) ;
#81393 = STYLED_ITEM('',(#170169),#87101) ;
#81394 = STYLED_ITEM('',(#170169),#87102) ;
#81395 = STYLED_ITEM('',(#170169),#87103) ;
#81396 = STYLED_ITEM('',(#170169),#87104) ;
#81397 = STYLED_ITEM('',(#170169),#87105) ;
#81398 = STYLED_ITEM('',(#170169),#87106) ;
#81399 = STYLED_ITEM('',(#170169),#87107) ;
#81400 = STYLED_ITEM('',(#170169),#87108) ;
#81401 = STYLED_ITEM('',(#170169),#87109) ;
#81402 = STYLED_ITEM('',(#170169),#87110) ;
#81403 = STYLED_ITEM('',(#170169),#87111) ;
#81404 = STYLED_ITEM('',(#170169),#87112) ;
#81405 = STYLED_ITEM('',(#170169),#87113) ;
#81406 = STYLED_ITEM('',(#170169),#87114) ;
#81407 = STYLED_ITEM('',(#170169),#87115) ;
#81408 = STYLED_ITEM('',(#170169),#87116) ;
#81409 = STYLED_ITEM('',(#170169),#87117) ;
#81410 = STYLED_ITEM('',(#170169),#87118) ;
#81411 = STYLED_ITEM('',(#170169),#87119) ;
#81412 = STYLED_ITEM('',(#170169),#87120) ;
#81413 = STYLED_ITEM('',(#170169),#87121) ;
#81414 = STYLED_ITEM('',(#170169),#87122) ;
#81415 = STYLED_ITEM('',(#170169),#87123) ;
#81416 = STYLED_ITEM('',(#170169),#87124) ;
#81417 = STYLED_ITEM('',(#170169),#87125) ;
#81418 = STYLED_ITEM('',(#170169),#87126) ;
#81419 = STYLED_ITEM('',(#170169),#87127) ;
#81420 = STYLED_ITEM('',(#170169),#87128) ;
#81421 = STYLED_ITEM('',(#170169),#87129) ;
#81422 = STYLED_ITEM('',(#170169),#87130) ;
#81423 = STYLED_ITEM('',(#170169),#87131) ;
#81424 = STYLED_ITEM('',(#170169),#87132) ;
#81425 = STYLED_ITEM('',(#170169),#87133) ;
#81426 = STYLED_ITEM('',(#170169),#87134) ;
#81427 = STYLED_ITEM('',(#170169),#87135) ;
#81428 = STYLED_ITEM('',(#170169),#87136) ;
#81429 = STYLED_ITEM('',(#170169),#87137) ;
#81430 = STYLED_ITEM('',(#170169),#87138) ;
#81431 = STYLED_ITEM('',(#170169),#87139) ;
#81432 = STYLED_ITEM('',(#170169),#87140) ;
#81433 = STYLED_ITEM('',(#170169),#87141) ;
#81434 = STYLED_ITEM('',(#170169),#87142) ;
#81435 = STYLED_ITEM('',(#170169),#87143) ;
#81436 = STYLED_ITEM('',(#170169),#87144) ;
#81437 = STYLED_ITEM('',(#170169),#87145) ;
#81438 = STYLED_ITEM('',(#170169),#87146) ;
#81439 = STYLED_ITEM('',(#170169),#87147) ;
#81440 = STYLED_ITEM('',(#170169),#87148) ;
#81441 = STYLED_ITEM('',(#170169),#87149) ;
#81442 = STYLED_ITEM('',(#170169),#87150) ;
#81443 = STYLED_ITEM('',(#170169),#87151) ;
#81444 = STYLED_ITEM('',(#170169),#87152) ;
#81445 = STYLED_ITEM('',(#170169),#87153) ;
#81446 = STYLED_ITEM('',(#170169),#87154) ;
#81447 = STYLED_ITEM('',(#170169),#87155) ;
#81448 = STYLED_ITEM('',(#170169),#87156) ;
#81449 = STYLED_ITEM('',(#170169),#87157) ;
#81450 = STYLED_ITEM('',(#170169),#87158) ;
#81451 = STYLED_ITEM('',(#170169),#87159) ;
#81452 = STYLED_ITEM('',(#170169),#87160) ;
#81453 = STYLED_ITEM('',(#170169),#87161) ;
#81454 = STYLED_ITEM('',(#170169),#87162) ;
#81455 = STYLED_ITEM('',(#170169),#87163) ;
#81456 = STYLED_ITEM('',(#170169),#87164) ;
#81457 = STYLED_ITEM('',(#170169),#87165) ;
#81458 = STYLED_ITEM('',(#170169),#87166) ;
#81459 = STYLED_ITEM('',(#170169),#87167) ;
#81460 = STYLED_ITEM('',(#170169),#87168) ;
#81461 = STYLED_ITEM('',(#170169),#87169) ;
#81462 = STYLED_ITEM('',(#170169),#87170) ;
#81463 = STYLED_ITEM('',(#170169),#87171) ;
#81464 = STYLED_ITEM('',(#170169),#87172) ;
#81465 = STYLED_ITEM('',(#170169),#87173) ;
#81466 = STYLED_ITEM('',(#170169),#87174) ;
#81467 = STYLED_ITEM('',(#170169),#87175) ;
#81468 = STYLED_ITEM('',(#170169),#87176) ;
#81469 = STYLED_ITEM('',(#170169),#87177) ;
#81470 = STYLED_ITEM('',(#170169),#87178) ;
#81471 = STYLED_ITEM('',(#170169),#87179) ;
#81472 = STYLED_ITEM('',(#170169),#87180) ;
#81473 = STYLED_ITEM('',(#170169),#87181) ;
#81474 = STYLED_ITEM('',(#170169),#87182) ;
#81475 = STYLED_ITEM('',(#170169),#87183) ;
#81476 = STYLED_ITEM('',(#170169),#87184) ;
#81477 = STYLED_ITEM('',(#170169),#87185) ;
#81478 = STYLED_ITEM('',(#170169),#87186) ;
#81479 = STYLED_ITEM('',(#170169),#87187) ;
#81480 = STYLED_ITEM('',(#170169),#87188) ;
#81481 = STYLED_ITEM('',(#170169),#87189) ;
#81482 = STYLED_ITEM('',(#170169),#87190) ;
#81483 = STYLED_ITEM('',(#170169),#87191) ;
#81484 = STYLED_ITEM('',(#170169),#87192) ;
#81485 = STYLED_ITEM('',(#170169),#87193) ;
#81486 = STYLED_ITEM('',(#170169),#87194) ;
#81487 = STYLED_ITEM('',(#170169),#87195) ;
#81488 = STYLED_ITEM('',(#170169),#87196) ;
#81489 = STYLED_ITEM('',(#170169),#87197) ;
#81490 = STYLED_ITEM('',(#170169),#87198) ;
#81491 = STYLED_ITEM('',(#170169),#87199) ;
#81492 = STYLED_ITEM('',(#170169),#87200) ;
#81493 = STYLED_ITEM('',(#170169),#87201) ;
#81494 = STYLED_ITEM('',(#170169),#87202) ;
#81495 = STYLED_ITEM('',(#170169),#87203) ;
#81496 = STYLED_ITEM('',(#170169),#87204) ;
#81497 = STYLED_ITEM('',(#170169),#87205) ;
#81498 = STYLED_ITEM('',(#170169),#87206) ;
#81499 = STYLED_ITEM('',(#170169),#87207) ;
#81500 = STYLED_ITEM('',(#170169),#87208) ;
#81501 = STYLED_ITEM('',(#170169),#87209) ;
#81502 = STYLED_ITEM('',(#170169),#87210) ;
#81503 = STYLED_ITEM('',(#170169),#87211) ;
#81504 = STYLED_ITEM('',(#170169),#87212) ;
#81505 = STYLED_ITEM('',(#170169),#87213) ;
#81506 = STYLED_ITEM('',(#170169),#87214) ;
#81507 = STYLED_ITEM('',(#170169),#87215) ;
#81508 = STYLED_ITEM('',(#170169),#87216) ;
#81509 = STYLED_ITEM('',(#170169),#87217) ;
#81510 = STYLED_ITEM('',(#170169),#87218) ;
#81511 = STYLED_ITEM('',(#170169),#87219) ;
#81512 = STYLED_ITEM('',(#170169),#87220) ;
#81513 = STYLED_ITEM('',(#170169),#87221) ;
#81514 = STYLED_ITEM('',(#170169),#87222) ;
#81515 = STYLED_ITEM('',(#170169),#87223) ;
#81516 = STYLED_ITEM('',(#170169),#87224) ;
#81517 = STYLED_ITEM('',(#170169),#87225) ;
#81518 = STYLED_ITEM('',(#170169),#87226) ;
#81519 = STYLED_ITEM('',(#170169),#87227) ;
#81520 = STYLED_ITEM('',(#170169),#87228) ;
#81521 = STYLED_ITEM('',(#170169),#87229) ;
#81522 = STYLED_ITEM('',(#170169),#87230) ;
#81523 = STYLED_ITEM('',(#170169),#87231) ;
#81524 = STYLED_ITEM('',(#170169),#87232) ;
#81525 = STYLED_ITEM('',(#170169),#87233) ;
#81526 = STYLED_ITEM('',(#170169),#87234) ;
#81527 = STYLED_ITEM('',(#170169),#87235) ;
#81528 = STYLED_ITEM('',(#170169),#87236) ;
#81529 = STYLED_ITEM('',(#170169),#87237) ;
#81530 = STYLED_ITEM('',(#170169),#87238) ;
#81531 = STYLED_ITEM('',(#170169),#87239) ;
#81532 = STYLED_ITEM('',(#170169),#87240) ;
#81533 = STYLED_ITEM('',(#170169),#87241) ;
#81534 = STYLED_ITEM('',(#170169),#87242) ;
#81535 = STYLED_ITEM('',(#170169),#87243) ;
#81536 = STYLED_ITEM('',(#170169),#87244) ;
#81537 = STYLED_ITEM('',(#170169),#87245) ;
#81538 = STYLED_ITEM('',(#170169),#87246) ;
#81539 = STYLED_ITEM('',(#170169),#87247) ;
#81540 = STYLED_ITEM('',(#170169),#87248) ;
#81541 = STYLED_ITEM('',(#170169),#87249) ;
#81542 = STYLED_ITEM('',(#170169),#87250) ;
#81543 = STYLED_ITEM('',(#170169),#87251) ;
#81544 = STYLED_ITEM('',(#170169),#87252) ;
#81545 = STYLED_ITEM('',(#170169),#87253) ;
#81546 = STYLED_ITEM('',(#170169),#87254) ;
#81547 = STYLED_ITEM('',(#170169),#87255) ;
#81548 = STYLED_ITEM('',(#170169),#87256) ;
#81549 = STYLED_ITEM('',(#170169),#87257) ;
#81550 = STYLED_ITEM('',(#170169),#87258) ;
#81551 = STYLED_ITEM('',(#170169),#87259) ;
#81552 = STYLED_ITEM('',(#170169),#87260) ;
#81553 = STYLED_ITEM('',(#170169),#87261) ;
#81554 = STYLED_ITEM('',(#170169),#87262) ;
#81555 = STYLED_ITEM('',(#170169),#87263) ;
#81556 = STYLED_ITEM('',(#170169),#87264) ;
#81557 = STYLED_ITEM('',(#170169),#87265) ;
#81558 = STYLED_ITEM('',(#170169),#87266) ;
#81559 = STYLED_ITEM('',(#170169),#87267) ;
#81560 = STYLED_ITEM('',(#170169),#87268) ;
#81561 = STYLED_ITEM('',(#170169),#87269) ;
#81562 = STYLED_ITEM('',(#170169),#87270) ;
#81563 = STYLED_ITEM('',(#170169),#87271) ;
#81564 = STYLED_ITEM('',(#170169),#87272) ;
#81565 = STYLED_ITEM('',(#170169),#87273) ;
#81566 = STYLED_ITEM('',(#170169),#87274) ;
#81567 = STYLED_ITEM('',(#170169),#87275) ;
#81568 = STYLED_ITEM('',(#170169),#87276) ;
#81569 = STYLED_ITEM('',(#170169),#87277) ;
#81570 = STYLED_ITEM('',(#170169),#87278) ;
#81571 = STYLED_ITEM('',(#170169),#87279) ;
#81572 = STYLED_ITEM('',(#170169),#87280) ;
#81573 = STYLED_ITEM('',(#170169),#87281) ;
#81574 = STYLED_ITEM('',(#170169),#87282) ;
#81575 = STYLED_ITEM('',(#170169),#87283) ;
#81576 = STYLED_ITEM('',(#170169),#87284) ;
#81577 = STYLED_ITEM('',(#170169),#87285) ;
#81578 = STYLED_ITEM('',(#170169),#87286) ;
#81579 = STYLED_ITEM('',(#170169),#87287) ;
#81580 = STYLED_ITEM('',(#170169),#87288) ;
#81581 = STYLED_ITEM('',(#170169),#87289) ;
#81582 = STYLED_ITEM('',(#170169),#87290) ;
#81583 = STYLED_ITEM('',(#170169),#87291) ;
#81584 = STYLED_ITEM('',(#170169),#87292) ;
#81585 = STYLED_ITEM('',(#170169),#87293) ;
#81586 = STYLED_ITEM('',(#170169),#87294) ;
#81587 = STYLED_ITEM('',(#170169),#87295) ;
#81588 = STYLED_ITEM('',(#170169),#87296) ;
#81589 = STYLED_ITEM('',(#170169),#87297) ;
#81590 = STYLED_ITEM('',(#170169),#87298) ;
#81591 = STYLED_ITEM('',(#170169),#87299) ;
#81592 = STYLED_ITEM('',(#170169),#87300) ;
#81593 = STYLED_ITEM('',(#170169),#87301) ;
#81594 = STYLED_ITEM('',(#170169),#87302) ;
#81595 = STYLED_ITEM('',(#170169),#87303) ;
#81596 = STYLED_ITEM('',(#170169),#87304) ;
#81597 = STYLED_ITEM('',(#170169),#87305) ;
#81598 = STYLED_ITEM('',(#170169),#87306) ;
#81599 = STYLED_ITEM('',(#170169),#87307) ;
#81600 = STYLED_ITEM('',(#170169),#87308) ;
#81601 = STYLED_ITEM('',(#170169),#87309) ;
#81602 = STYLED_ITEM('',(#170169),#87310) ;
#81603 = STYLED_ITEM('',(#170169),#87311) ;
#81604 = STYLED_ITEM('',(#170169),#87312) ;
#81605 = STYLED_ITEM('',(#170169),#87313) ;
#81606 = STYLED_ITEM('',(#170169),#87314) ;
#81607 = STYLED_ITEM('',(#170169),#87315) ;
#81608 = STYLED_ITEM('',(#170169),#87316) ;
#81609 = STYLED_ITEM('',(#170169),#87317) ;
#81610 = STYLED_ITEM('',(#170169),#87318) ;
#81611 = STYLED_ITEM('',(#170169),#87319) ;
#81612 = STYLED_ITEM('',(#170169),#87320) ;
#81613 = STYLED_ITEM('',(#170169),#87321) ;
#81614 = STYLED_ITEM('',(#170169),#87322) ;
#81615 = STYLED_ITEM('',(#170169),#87323) ;
#81616 = STYLED_ITEM('',(#170169),#87324) ;
#81617 = STYLED_ITEM('',(#170169),#87325) ;
#81618 = STYLED_ITEM('',(#170169),#87326) ;
#81619 = STYLED_ITEM('',(#170169),#87327) ;
#81620 = STYLED_ITEM('',(#170169),#87328) ;
#81621 = STYLED_ITEM('',(#170169),#87329) ;
#81622 = STYLED_ITEM('',(#170169),#87330) ;
#81623 = STYLED_ITEM('',(#170169),#87331) ;
#81624 = STYLED_ITEM('',(#170169),#87332) ;
#81625 = STYLED_ITEM('',(#170169),#87333) ;
#81626 = STYLED_ITEM('',(#170169),#87334) ;
#81627 = STYLED_ITEM('',(#170169),#87335) ;
#81628 = STYLED_ITEM('',(#170169),#87336) ;
#81629 = STYLED_ITEM('',(#170169),#87337) ;
#81630 = STYLED_ITEM('',(#170169),#87338) ;
#81631 = STYLED_ITEM('',(#170169),#87339) ;
#81632 = STYLED_ITEM('',(#170169),#87340) ;
#81633 = STYLED_ITEM('',(#170169),#87341) ;
#81634 = STYLED_ITEM('',(#170169),#87342) ;
#81635 = STYLED_ITEM('',(#170169),#87343) ;
#81636 = STYLED_ITEM('',(#170169),#87344) ;
#81637 = STYLED_ITEM('',(#170169),#87345) ;
#81638 = STYLED_ITEM('',(#170169),#87346) ;
#81639 = STYLED_ITEM('',(#170169),#87347) ;
#81640 = STYLED_ITEM('',(#170169),#87348) ;
#81641 = STYLED_ITEM('',(#170169),#87349) ;
#81642 = STYLED_ITEM('',(#170169),#87350) ;
#81643 = STYLED_ITEM('',(#170169),#87351) ;
#81644 = STYLED_ITEM('',(#170169),#87352) ;
#81645 = STYLED_ITEM('',(#170169),#87353) ;
#81646 = STYLED_ITEM('',(#170169),#87354) ;
#81647 = STYLED_ITEM('',(#170169),#87355) ;
#81648 = STYLED_ITEM('',(#170169),#87356) ;
#81649 = STYLED_ITEM('',(#170169),#87357) ;
#81650 = STYLED_ITEM('',(#170169),#87358) ;
#81651 = STYLED_ITEM('',(#170169),#87359) ;
#81652 = STYLED_ITEM('',(#170169),#87360) ;
#81653 = STYLED_ITEM('',(#170169),#87361) ;
#81654 = STYLED_ITEM('',(#170169),#87362) ;
#81655 = STYLED_ITEM('',(#170169),#87363) ;
#81656 = STYLED_ITEM('',(#170169),#87364) ;
#81657 = STYLED_ITEM('',(#170169),#87365) ;
#81658 = STYLED_ITEM('',(#170169),#87366) ;
#81659 = STYLED_ITEM('',(#170169),#87367) ;
#81660 = STYLED_ITEM('',(#170169),#87368) ;
#81661 = STYLED_ITEM('',(#170169),#87369) ;
#81662 = STYLED_ITEM('',(#170169),#87370) ;
#81663 = STYLED_ITEM('',(#170169),#87371) ;
#81664 = STYLED_ITEM('',(#170169),#87372) ;
#81665 = STYLED_ITEM('',(#170169),#87373) ;
#81666 = STYLED_ITEM('',(#170169),#87374) ;
#81667 = STYLED_ITEM('',(#170169),#87375) ;
#81668 = STYLED_ITEM('',(#170169),#87376) ;
#81669 = STYLED_ITEM('',(#170169),#87377) ;
#81670 = STYLED_ITEM('',(#170169),#87378) ;
#81671 = STYLED_ITEM('',(#170169),#87379) ;
#81672 = STYLED_ITEM('',(#170169),#87380) ;
#81673 = STYLED_ITEM('',(#170169),#87381) ;
#81674 = STYLED_ITEM('',(#170169),#87382) ;
#81675 = STYLED_ITEM('',(#170169),#87383) ;
#81676 = STYLED_ITEM('',(#170169),#87384) ;
#81677 = STYLED_ITEM('',(#170169),#87385) ;
#81678 = STYLED_ITEM('',(#170169),#87386) ;
#81679 = STYLED_ITEM('',(#170169),#87387) ;
#81680 = STYLED_ITEM('',(#170169),#87388) ;
#81681 = STYLED_ITEM('',(#170169),#87389) ;
#81682 = STYLED_ITEM('',(#170169),#87390) ;
#81683 = STYLED_ITEM('',(#170169),#87391) ;
#81684 = STYLED_ITEM('',(#170169),#87392) ;
#81685 = STYLED_ITEM('',(#170169),#87393) ;
#81686 = STYLED_ITEM('',(#170169),#87394) ;
#81687 = STYLED_ITEM('',(#170169),#87395) ;
#81688 = STYLED_ITEM('',(#170169),#87396) ;
#81689 = STYLED_ITEM('',(#170169),#87397) ;
#81690 = STYLED_ITEM('',(#170169),#87398) ;
#81691 = STYLED_ITEM('',(#170169),#87399) ;
#81692 = STYLED_ITEM('',(#170169),#87400) ;
#81693 = STYLED_ITEM('',(#170169),#87401) ;
#81694 = STYLED_ITEM('',(#170169),#87402) ;
#81695 = STYLED_ITEM('',(#170169),#87403) ;
#81696 = STYLED_ITEM('',(#170169),#87404) ;
#81697 = STYLED_ITEM('',(#170169),#87405) ;
#81698 = STYLED_ITEM('',(#170169),#87406) ;
#81699 = STYLED_ITEM('',(#170169),#87407) ;
#81700 = STYLED_ITEM('',(#170169),#87408) ;
#81701 = STYLED_ITEM('',(#170169),#87409) ;
#81702 = STYLED_ITEM('',(#170169),#87410) ;
#81703 = STYLED_ITEM('',(#170169),#87411) ;
#81704 = STYLED_ITEM('',(#170169),#87412) ;
#81705 = STYLED_ITEM('',(#170169),#87413) ;
#81706 = STYLED_ITEM('',(#170169),#87414) ;
#81707 = STYLED_ITEM('',(#170169),#87415) ;
#81708 = STYLED_ITEM('',(#170169),#87416) ;
#81709 = STYLED_ITEM('',(#170169),#87417) ;
#81710 = STYLED_ITEM('',(#170169),#87418) ;
#81711 = STYLED_ITEM('',(#170169),#87419) ;
#81712 = STYLED_ITEM('',(#170169),#87420) ;
#81713 = STYLED_ITEM('',(#170169),#87421) ;
#81714 = STYLED_ITEM('',(#170169),#87422) ;
#81715 = STYLED_ITEM('',(#170169),#87423) ;
#81716 = STYLED_ITEM('',(#170169),#87424) ;
#81717 = STYLED_ITEM('',(#170169),#87425) ;
#81718 = STYLED_ITEM('',(#170169),#87426) ;
#81719 = STYLED_ITEM('',(#170169),#87427) ;
#81720 = STYLED_ITEM('',(#170169),#87428) ;
#81721 = STYLED_ITEM('',(#170169),#87429) ;
#81722 = STYLED_ITEM('',(#170169),#87430) ;
#81723 = STYLED_ITEM('',(#170169),#87431) ;
#81724 = STYLED_ITEM('',(#170169),#87432) ;
#81725 = STYLED_ITEM('',(#170169),#87433) ;
#81726 = STYLED_ITEM('',(#170169),#87434) ;
#81727 = STYLED_ITEM('',(#170169),#87435) ;
#81728 = STYLED_ITEM('',(#170169),#87436) ;
#81729 = STYLED_ITEM('',(#170169),#87437) ;
#81730 = STYLED_ITEM('',(#170169),#87438) ;
#81731 = STYLED_ITEM('',(#170169),#87439) ;
#81732 = STYLED_ITEM('',(#170169),#87440) ;
#81733 = STYLED_ITEM('',(#170169),#87441) ;
#81734 = STYLED_ITEM('',(#170169),#87442) ;
#81735 = STYLED_ITEM('',(#170169),#87443) ;
#81736 = STYLED_ITEM('',(#170169),#87444) ;
#81737 = STYLED_ITEM('',(#170169),#87445) ;
#81738 = STYLED_ITEM('',(#170169),#87446) ;
#81739 = STYLED_ITEM('',(#170169),#87447) ;
#81740 = STYLED_ITEM('',(#170169),#87448) ;
#81741 = STYLED_ITEM('',(#170169),#87449) ;
#81742 = STYLED_ITEM('',(#170169),#87450) ;
#81743 = STYLED_ITEM('',(#170169),#87451) ;
#81744 = STYLED_ITEM('',(#170169),#87452) ;
#81745 = STYLED_ITEM('',(#170169),#87453) ;
#81746 = STYLED_ITEM('',(#170169),#87454) ;
#81747 = STYLED_ITEM('',(#170169),#87455) ;
#81748 = STYLED_ITEM('',(#170169),#87456) ;
#81749 = STYLED_ITEM('',(#170169),#87457) ;
#81750 = STYLED_ITEM('',(#170169),#87458) ;
#81751 = STYLED_ITEM('',(#170169),#87459) ;
#81752 = STYLED_ITEM('',(#170169),#87460) ;
#81753 = STYLED_ITEM('',(#170169),#87461) ;
#81754 = STYLED_ITEM('',(#170169),#87462) ;
#81755 = STYLED_ITEM('',(#170169),#87463) ;
#81756 = STYLED_ITEM('',(#170169),#87464) ;
#81757 = STYLED_ITEM('',(#170169),#87465) ;
#81758 = STYLED_ITEM('',(#170169),#87466) ;
#81759 = STYLED_ITEM('',(#170169),#87467) ;
#81760 = STYLED_ITEM('',(#170169),#87468) ;
#81761 = STYLED_ITEM('',(#170169),#87469) ;
#81762 = STYLED_ITEM('',(#170169),#87470) ;
#81763 = STYLED_ITEM('',(#170169),#87471) ;
#81764 = STYLED_ITEM('',(#170169),#87472) ;
#81765 = STYLED_ITEM('',(#170169),#87473) ;
#81766 = STYLED_ITEM('',(#170169),#87474) ;
#81767 = STYLED_ITEM('',(#170169),#87475) ;
#81768 = STYLED_ITEM('',(#170169),#87476) ;
#81769 = STYLED_ITEM('',(#170169),#87477) ;
#81770 = STYLED_ITEM('',(#170169),#87478) ;
#81771 = STYLED_ITEM('',(#170169),#87479) ;
#81772 = STYLED_ITEM('',(#170169),#87480) ;
#81773 = STYLED_ITEM('',(#170169),#87481) ;
#81774 = STYLED_ITEM('',(#170169),#87482) ;
#81775 = STYLED_ITEM('',(#170169),#87483) ;
#81776 = STYLED_ITEM('',(#170169),#87484) ;
#81777 = STYLED_ITEM('',(#170169),#87485) ;
#81778 = STYLED_ITEM('',(#170169),#87486) ;
#81779 = STYLED_ITEM('',(#170169),#87487) ;
#81780 = STYLED_ITEM('',(#170169),#87488) ;
#81781 = STYLED_ITEM('',(#170169),#87489) ;
#81782 = STYLED_ITEM('',(#170169),#87490) ;
#81783 = STYLED_ITEM('',(#170169),#87491) ;
#81784 = STYLED_ITEM('',(#170169),#87492) ;
#81785 = STYLED_ITEM('',(#170169),#87493) ;
#81786 = STYLED_ITEM('',(#170169),#87494) ;
#81787 = STYLED_ITEM('',(#170169),#87495) ;
#81788 = STYLED_ITEM('',(#170169),#87496) ;
#81789 = STYLED_ITEM('',(#170169),#87497) ;
#81790 = STYLED_ITEM('',(#170169),#87498) ;
#81791 = STYLED_ITEM('',(#170169),#87499) ;
#81792 = STYLED_ITEM('',(#170169),#87500) ;
#81793 = STYLED_ITEM('',(#170169),#87501) ;
#81794 = STYLED_ITEM('',(#170169),#87502) ;
#81795 = STYLED_ITEM('',(#170169),#87503) ;
#81796 = STYLED_ITEM('',(#170169),#87504) ;
#81797 = STYLED_ITEM('',(#170169),#87505) ;
#81798 = STYLED_ITEM('',(#170169),#87506) ;
#81799 = STYLED_ITEM('',(#170169),#87507) ;
#81800 = STYLED_ITEM('',(#170169),#87508) ;
#81801 = STYLED_ITEM('',(#170169),#87509) ;
#81802 = STYLED_ITEM('',(#170169),#87510) ;
#81803 = STYLED_ITEM('',(#170169),#87511) ;
#81804 = STYLED_ITEM('',(#170169),#87512) ;
#81805 = STYLED_ITEM('',(#170169),#87513) ;
#81806 = STYLED_ITEM('',(#170169),#87514) ;
#81807 = STYLED_ITEM('',(#170169),#87515) ;
#81808 = STYLED_ITEM('',(#170169),#87516) ;
#81809 = STYLED_ITEM('',(#170169),#87517) ;
#81810 = STYLED_ITEM('',(#170169),#87518) ;
#81811 = STYLED_ITEM('',(#170169),#87519) ;
#81812 = STYLED_ITEM('',(#170169),#87520) ;
#81813 = STYLED_ITEM('',(#170169),#87521) ;
#81814 = STYLED_ITEM('',(#170169),#87522) ;
#81815 = STYLED_ITEM('',(#170169),#87523) ;
#81816 = STYLED_ITEM('',(#170169),#87524) ;
#81817 = STYLED_ITEM('',(#170169),#87525) ;
#81818 = STYLED_ITEM('',(#170169),#87526) ;
#81819 = STYLED_ITEM('',(#170169),#87527) ;
#81820 = STYLED_ITEM('',(#170169),#87528) ;
#81821 = STYLED_ITEM('',(#170169),#87529) ;
#81822 = STYLED_ITEM('',(#170169),#87530) ;
#81823 = STYLED_ITEM('',(#170169),#87531) ;
#81824 = STYLED_ITEM('',(#170169),#87532) ;
#81825 = STYLED_ITEM('',(#170169),#87533) ;
#81826 = STYLED_ITEM('',(#170169),#87534) ;
#81827 = STYLED_ITEM('',(#170169),#87535) ;
#81828 = STYLED_ITEM('',(#170169),#87536) ;
#81829 = STYLED_ITEM('',(#170169),#87537) ;
#81830 = STYLED_ITEM('',(#170169),#87538) ;
#81831 = STYLED_ITEM('',(#170169),#87539) ;
#81832 = STYLED_ITEM('',(#170169),#87540) ;
#81833 = STYLED_ITEM('',(#170169),#87541) ;
#81834 = STYLED_ITEM('',(#170169),#87542) ;
#81835 = STYLED_ITEM('',(#170169),#87543) ;
#81836 = STYLED_ITEM('',(#170169),#87544) ;
#81837 = STYLED_ITEM('',(#170169),#87545) ;
#81838 = STYLED_ITEM('',(#170169),#87546) ;
#81839 = STYLED_ITEM('',(#170169),#87547) ;
#81840 = STYLED_ITEM('',(#170169),#87548) ;
#81841 = STYLED_ITEM('',(#170169),#87549) ;
#81842 = STYLED_ITEM('',(#170169),#87550) ;
#81843 = STYLED_ITEM('',(#170169),#87551) ;
#81844 = STYLED_ITEM('',(#170169),#87552) ;
#81845 = STYLED_ITEM('',(#170169),#87553) ;
#81846 = STYLED_ITEM('',(#170169),#87554) ;
#81847 = STYLED_ITEM('',(#170169),#87555) ;
#81848 = STYLED_ITEM('',(#170169),#87556) ;
#81849 = STYLED_ITEM('',(#170169),#87557) ;
#81850 = STYLED_ITEM('',(#170169),#87558) ;
#81851 = STYLED_ITEM('',(#170169),#87559) ;
#81852 = STYLED_ITEM('',(#170169),#87560) ;
#81853 = STYLED_ITEM('',(#170169),#87561) ;
#81854 = STYLED_ITEM('',(#170169),#87562) ;
#81855 = STYLED_ITEM('',(#170169),#87563) ;
#81856 = STYLED_ITEM('',(#170169),#87564) ;
#81857 = STYLED_ITEM('',(#170169),#87565) ;
#81858 = STYLED_ITEM('',(#170169),#87566) ;
#81859 = STYLED_ITEM('',(#170169),#87567) ;
#81860 = STYLED_ITEM('',(#170169),#87568) ;
#81861 = STYLED_ITEM('',(#170169),#87569) ;
#81862 = STYLED_ITEM('',(#170169),#87570) ;
#81863 = STYLED_ITEM('',(#170169),#87571) ;
#81864 = STYLED_ITEM('',(#170169),#87572) ;
#81865 = STYLED_ITEM('',(#170169),#87573) ;
#81866 = STYLED_ITEM('',(#170169),#87574) ;
#81867 = STYLED_ITEM('',(#170169),#87575) ;
#81868 = STYLED_ITEM('',(#170169),#87576) ;
#81869 = STYLED_ITEM('',(#170169),#87577) ;
#81870 = STYLED_ITEM('',(#170169),#87578) ;
#81871 = STYLED_ITEM('',(#170169),#87579) ;
#81872 = STYLED_ITEM('',(#170169),#87580) ;
#81873 = STYLED_ITEM('',(#170169),#87581) ;
#81874 = STYLED_ITEM('',(#170169),#87582) ;
#81875 = STYLED_ITEM('',(#170169),#87583) ;
#81876 = STYLED_ITEM('',(#170169),#87584) ;
#81877 = STYLED_ITEM('',(#170169),#87585) ;
#81878 = STYLED_ITEM('',(#170169),#87586) ;
#81879 = STYLED_ITEM('',(#170169),#87587) ;
#81880 = STYLED_ITEM('',(#170169),#87588) ;
#81881 = STYLED_ITEM('',(#170169),#87589) ;
#81882 = STYLED_ITEM('',(#170169),#87590) ;
#81883 = STYLED_ITEM('',(#170169),#87591) ;
#81884 = STYLED_ITEM('',(#170169),#87592) ;
#81885 = STYLED_ITEM('',(#170169),#87593) ;
#81886 = STYLED_ITEM('',(#170169),#87594) ;
#81887 = STYLED_ITEM('',(#170169),#87595) ;
#81888 = STYLED_ITEM('',(#170169),#87596) ;
#81889 = STYLED_ITEM('',(#170169),#87597) ;
#81890 = STYLED_ITEM('',(#170169),#87598) ;
#81891 = STYLED_ITEM('',(#170169),#87599) ;
#81892 = STYLED_ITEM('',(#170169),#87600) ;
#81893 = STYLED_ITEM('',(#170169),#87601) ;
#81894 = STYLED_ITEM('',(#170169),#87602) ;
#81895 = STYLED_ITEM('',(#170169),#87603) ;
#81896 = STYLED_ITEM('',(#170169),#87604) ;
#81897 = STYLED_ITEM('',(#170169),#87605) ;
#81898 = STYLED_ITEM('',(#170169),#87606) ;
#81899 = STYLED_ITEM('',(#170169),#87607) ;
#81900 = STYLED_ITEM('',(#170169),#87608) ;
#81901 = STYLED_ITEM('',(#170169),#87609) ;
#81902 = STYLED_ITEM('',(#170169),#87610) ;
#81903 = STYLED_ITEM('',(#170169),#87611) ;
#81904 = STYLED_ITEM('',(#170169),#87612) ;
#81905 = STYLED_ITEM('',(#170169),#87613) ;
#81906 = STYLED_ITEM('',(#170169),#87614) ;
#81907 = STYLED_ITEM('',(#170169),#87615) ;
#81908 = STYLED_ITEM('',(#170169),#87616) ;
#81909 = STYLED_ITEM('',(#170169),#87617) ;
#81910 = STYLED_ITEM('',(#170169),#87618) ;
#81911 = STYLED_ITEM('',(#170169),#87619) ;
#81912 = STYLED_ITEM('',(#170169),#87620) ;
#81913 = STYLED_ITEM('',(#170169),#87621) ;
#81914 = STYLED_ITEM('',(#170169),#87622) ;
#81915 = STYLED_ITEM('',(#170169),#87623) ;
#81916 = STYLED_ITEM('',(#170169),#87624) ;
#81917 = STYLED_ITEM('',(#170169),#87625) ;
#81918 = STYLED_ITEM('',(#170169),#87626) ;
#81919 = STYLED_ITEM('',(#170169),#87627) ;
#81920 = STYLED_ITEM('',(#170169),#87628) ;
#81921 = STYLED_ITEM('',(#170169),#87629) ;
#81922 = STYLED_ITEM('',(#170169),#87630) ;
#81923 = STYLED_ITEM('',(#170169),#87631) ;
#81924 = STYLED_ITEM('',(#170169),#87632) ;
#81925 = STYLED_ITEM('',(#170169),#87633) ;
#81926 = STYLED_ITEM('',(#170169),#87634) ;
#81927 = STYLED_ITEM('',(#170169),#87635) ;
#81928 = STYLED_ITEM('',(#170169),#87636) ;
#81929 = STYLED_ITEM('',(#170169),#87637) ;
#81930 = STYLED_ITEM('',(#170169),#87638) ;
#81931 = STYLED_ITEM('',(#170169),#87639) ;
#81932 = STYLED_ITEM('',(#170169),#87640) ;
#81933 = STYLED_ITEM('',(#170169),#87641) ;
#81934 = STYLED_ITEM('',(#170169),#87642) ;
#81935 = STYLED_ITEM('',(#170169),#87643) ;
#81936 = STYLED_ITEM('',(#170169),#87644) ;
#81937 = STYLED_ITEM('',(#170169),#87645) ;
#81938 = STYLED_ITEM('',(#170169),#87646) ;
#81939 = STYLED_ITEM('',(#170169),#87647) ;
#81940 = STYLED_ITEM('',(#170169),#87648) ;
#81941 = STYLED_ITEM('',(#170169),#87649) ;
#81942 = STYLED_ITEM('',(#170169),#87650) ;
#81943 = STYLED_ITEM('',(#170169),#87651) ;
#81944 = STYLED_ITEM('',(#170169),#87652) ;
#81945 = STYLED_ITEM('',(#170169),#87653) ;
#81946 = STYLED_ITEM('',(#170169),#87654) ;
#81947 = STYLED_ITEM('',(#170169),#87655) ;
#81948 = STYLED_ITEM('',(#170169),#87656) ;
#81949 = STYLED_ITEM('',(#170169),#87657) ;
#81950 = STYLED_ITEM('',(#170169),#87658) ;
#81951 = STYLED_ITEM('',(#170169),#87659) ;
#81952 = STYLED_ITEM('',(#170169),#87660) ;
#81953 = STYLED_ITEM('',(#170169),#87661) ;
#81954 = STYLED_ITEM('',(#170169),#87662) ;
#81955 = STYLED_ITEM('',(#170169),#87663) ;
#81956 = STYLED_ITEM('',(#170169),#87664) ;
#81957 = STYLED_ITEM('',(#170169),#87665) ;
#81958 = STYLED_ITEM('',(#170169),#87666) ;
#81959 = STYLED_ITEM('',(#170169),#87667) ;
#81960 = STYLED_ITEM('',(#170169),#87668) ;
#81961 = STYLED_ITEM('',(#170169),#87669) ;
#81962 = STYLED_ITEM('',(#170169),#87670) ;
#81963 = STYLED_ITEM('',(#170169),#87671) ;
#81964 = STYLED_ITEM('',(#170169),#87672) ;
#81965 = STYLED_ITEM('',(#170169),#87673) ;
#81966 = STYLED_ITEM('',(#170169),#87674) ;
#81967 = STYLED_ITEM('',(#170169),#87675) ;
#81968 = STYLED_ITEM('',(#170169),#87676) ;
#81969 = STYLED_ITEM('',(#170169),#87677) ;
#81970 = STYLED_ITEM('',(#170169),#87678) ;
#81971 = STYLED_ITEM('',(#170169),#87679) ;
#81972 = STYLED_ITEM('',(#170169),#87680) ;
#81973 = STYLED_ITEM('',(#170169),#87681) ;
#81974 = STYLED_ITEM('',(#170169),#87682) ;
#81975 = STYLED_ITEM('',(#170169),#87683) ;
#81976 = STYLED_ITEM('',(#170169),#87684) ;
#81977 = STYLED_ITEM('',(#170169),#87685) ;
#81978 = STYLED_ITEM('',(#170169),#87686) ;
#81979 = STYLED_ITEM('',(#170169),#87687) ;
#81980 = STYLED_ITEM('',(#170169),#87688) ;
#81981 = STYLED_ITEM('',(#170169),#87689) ;
#81982 = STYLED_ITEM('',(#170169),#87690) ;
#81983 = STYLED_ITEM('',(#170169),#87691) ;
#81984 = STYLED_ITEM('',(#170169),#87692) ;
#81985 = STYLED_ITEM('',(#170169),#87693) ;
#81986 = STYLED_ITEM('',(#170169),#87694) ;
#81987 = STYLED_ITEM('',(#170169),#87695) ;
#81988 = STYLED_ITEM('',(#170169),#87696) ;
#81989 = STYLED_ITEM('',(#170169),#87697) ;
#81990 = STYLED_ITEM('',(#170169),#87698) ;
#81991 = STYLED_ITEM('',(#170169),#87699) ;
#81992 = STYLED_ITEM('',(#170169),#87700) ;
#81993 = STYLED_ITEM('',(#170169),#87701) ;
#81994 = STYLED_ITEM('',(#170169),#87702) ;
#81995 = STYLED_ITEM('',(#170169),#87703) ;
#81996 = STYLED_ITEM('',(#170169),#87704) ;
#81997 = STYLED_ITEM('',(#170169),#87705) ;
#81998 = STYLED_ITEM('',(#170169),#87706) ;
#81999 = STYLED_ITEM('',(#170169),#87707) ;
#82000 = STYLED_ITEM('',(#170169),#87708) ;
#82001 = STYLED_ITEM('',(#170169),#87709) ;
#82002 = STYLED_ITEM('',(#170169),#87710) ;
#82003 = STYLED_ITEM('',(#170169),#87711) ;
#82004 = STYLED_ITEM('',(#170169),#87712) ;
#82005 = STYLED_ITEM('',(#170169),#87713) ;
#82006 = STYLED_ITEM('',(#170169),#87714) ;
#82007 = STYLED_ITEM('',(#170169),#87715) ;
#82008 = STYLED_ITEM('',(#170169),#87716) ;
#82009 = STYLED_ITEM('',(#170169),#87717) ;
#82010 = STYLED_ITEM('',(#170169),#87718) ;
#82011 = STYLED_ITEM('',(#170169),#87719) ;
#82012 = STYLED_ITEM('',(#170169),#87720) ;
#82013 = STYLED_ITEM('',(#170169),#87721) ;
#82014 = STYLED_ITEM('',(#170169),#87722) ;
#82015 = STYLED_ITEM('',(#170169),#87723) ;
#82016 = STYLED_ITEM('',(#170169),#87724) ;
#82017 = STYLED_ITEM('',(#170169),#87725) ;
#82018 = STYLED_ITEM('',(#170169),#87726) ;
#82019 = STYLED_ITEM('',(#170169),#87727) ;
#82020 = STYLED_ITEM('',(#170169),#87728) ;
#82021 = STYLED_ITEM('',(#170169),#87729) ;
#82022 = STYLED_ITEM('',(#170169),#87730) ;
#82023 = STYLED_ITEM('',(#170169),#87731) ;
#82024 = STYLED_ITEM('',(#170169),#87732) ;
#82025 = STYLED_ITEM('',(#170169),#87733) ;
#82026 = STYLED_ITEM('',(#170169),#87734) ;
#82027 = STYLED_ITEM('',(#170169),#87735) ;
#82028 = STYLED_ITEM('',(#170169),#87736) ;
#82029 = STYLED_ITEM('',(#170169),#87737) ;
#82030 = STYLED_ITEM('',(#170169),#87738) ;
#82031 = STYLED_ITEM('',(#170169),#87739) ;
#82032 = STYLED_ITEM('',(#170169),#87740) ;
#82033 = STYLED_ITEM('',(#170169),#87741) ;
#82034 = STYLED_ITEM('',(#170169),#87742) ;
#82035 = STYLED_ITEM('',(#170169),#87743) ;
#82036 = STYLED_ITEM('',(#170169),#87744) ;
#82037 = STYLED_ITEM('',(#170169),#87745) ;
#82038 = STYLED_ITEM('',(#170169),#87746) ;
#82039 = STYLED_ITEM('',(#170169),#87747) ;
#82040 = STYLED_ITEM('',(#170169),#87748) ;
#82041 = STYLED_ITEM('',(#170169),#87749) ;
#82042 = STYLED_ITEM('',(#170169),#87750) ;
#82043 = STYLED_ITEM('',(#170169),#87751) ;
#82044 = STYLED_ITEM('',(#170169),#87752) ;
#82045 = STYLED_ITEM('',(#170169),#87753) ;
#82046 = STYLED_ITEM('',(#170169),#87754) ;
#82047 = STYLED_ITEM('',(#170169),#87755) ;
#82048 = STYLED_ITEM('',(#170169),#87756) ;
#82049 = STYLED_ITEM('',(#170169),#87757) ;
#82050 = STYLED_ITEM('',(#170169),#87758) ;
#82051 = STYLED_ITEM('',(#170169),#87759) ;
#82052 = STYLED_ITEM('',(#170169),#87760) ;
#82053 = STYLED_ITEM('',(#170169),#87761) ;
#82054 = STYLED_ITEM('',(#170169),#87762) ;
#82055 = STYLED_ITEM('',(#170169),#87763) ;
#82056 = STYLED_ITEM('',(#170169),#87764) ;
#82057 = STYLED_ITEM('',(#170169),#87765) ;
#82058 = STYLED_ITEM('',(#170169),#87766) ;
#82059 = STYLED_ITEM('',(#170169),#87767) ;
#82060 = STYLED_ITEM('',(#170169),#87768) ;
#82061 = STYLED_ITEM('',(#170169),#87769) ;
#82062 = STYLED_ITEM('',(#170169),#87770) ;
#82063 = STYLED_ITEM('',(#170169),#87771) ;
#82064 = STYLED_ITEM('',(#170169),#87772) ;
#82065 = STYLED_ITEM('',(#170169),#87773) ;
#82066 = STYLED_ITEM('',(#170169),#87774) ;
#82067 = STYLED_ITEM('',(#170169),#87775) ;
#82068 = STYLED_ITEM('',(#170169),#87776) ;
#82069 = STYLED_ITEM('',(#170169),#87777) ;
#82070 = STYLED_ITEM('',(#170169),#87778) ;
#82071 = STYLED_ITEM('',(#170169),#87779) ;
#82072 = STYLED_ITEM('',(#170169),#87780) ;
#82073 = STYLED_ITEM('',(#170169),#87781) ;
#82074 = STYLED_ITEM('',(#170169),#87782) ;
#82075 = STYLED_ITEM('',(#170169),#87783) ;
#82076 = STYLED_ITEM('',(#170169),#87784) ;
#82077 = STYLED_ITEM('',(#170169),#87785) ;
#82078 = STYLED_ITEM('',(#170169),#87786) ;
#82079 = STYLED_ITEM('',(#170169),#87787) ;
#82080 = STYLED_ITEM('',(#170169),#87788) ;
#82081 = STYLED_ITEM('',(#170169),#87789) ;
#82082 = STYLED_ITEM('',(#170169),#87790) ;
#82083 = STYLED_ITEM('',(#170169),#87791) ;
#82084 = STYLED_ITEM('',(#170169),#87792) ;
#82085 = STYLED_ITEM('',(#170169),#87793) ;
#82086 = STYLED_ITEM('',(#170169),#87794) ;
#82087 = STYLED_ITEM('',(#170169),#87795) ;
#82088 = STYLED_ITEM('',(#170169),#87796) ;
#82089 = STYLED_ITEM('',(#170169),#87797) ;
#82090 = STYLED_ITEM('',(#170169),#87798) ;
#82091 = STYLED_ITEM('',(#170169),#87799) ;
#82092 = STYLED_ITEM('',(#170169),#87800) ;
#82093 = STYLED_ITEM('',(#170169),#87801) ;
#82094 = STYLED_ITEM('',(#170169),#87802) ;
#82095 = STYLED_ITEM('',(#170169),#87803) ;
#82096 = STYLED_ITEM('',(#170169),#87804) ;
#82097 = STYLED_ITEM('',(#170169),#87805) ;
#82098 = STYLED_ITEM('',(#170169),#87806) ;
#82099 = STYLED_ITEM('',(#170169),#87807) ;
#82100 = STYLED_ITEM('',(#170169),#87808) ;
#82101 = STYLED_ITEM('',(#170169),#87809) ;
#82102 = STYLED_ITEM('',(#170169),#87810) ;
#82103 = STYLED_ITEM('',(#170169),#87811) ;
#82104 = STYLED_ITEM('',(#170169),#87812) ;
#82105 = STYLED_ITEM('',(#170169),#87813) ;
#82106 = STYLED_ITEM('',(#170169),#87814) ;
#82107 = STYLED_ITEM('',(#170169),#87815) ;
#82108 = STYLED_ITEM('',(#170169),#87816) ;
#82109 = STYLED_ITEM('',(#170169),#87817) ;
#82110 = STYLED_ITEM('',(#170169),#87818) ;
#82111 = STYLED_ITEM('',(#170169),#87819) ;
#82112 = STYLED_ITEM('',(#170169),#87820) ;
#82113 = STYLED_ITEM('',(#170169),#87821) ;
#82114 = STYLED_ITEM('',(#170169),#87822) ;
#82115 = STYLED_ITEM('',(#170169),#87823) ;
#82116 = STYLED_ITEM('',(#170169),#87824) ;
#82117 = STYLED_ITEM('',(#170169),#87825) ;
#82118 = STYLED_ITEM('',(#170169),#87826) ;
#82119 = STYLED_ITEM('',(#170169),#87827) ;
#82120 = STYLED_ITEM('',(#170169),#87828) ;
#82121 = STYLED_ITEM('',(#170169),#87829) ;
#82122 = STYLED_ITEM('',(#170169),#87830) ;
#82123 = STYLED_ITEM('',(#170169),#87831) ;
#82124 = STYLED_ITEM('',(#170169),#87832) ;
#82125 = STYLED_ITEM('',(#170169),#87833) ;
#82126 = STYLED_ITEM('',(#170169),#87834) ;
#82127 = STYLED_ITEM('',(#170169),#87835) ;
#82128 = STYLED_ITEM('',(#170169),#87836) ;
#82129 = STYLED_ITEM('',(#170169),#87837) ;
#82130 = STYLED_ITEM('',(#170169),#87838) ;
#82131 = STYLED_ITEM('',(#170169),#87839) ;
#82132 = STYLED_ITEM('',(#170169),#87840) ;
#82133 = STYLED_ITEM('',(#170169),#87841) ;
#82134 = STYLED_ITEM('',(#170169),#87842) ;
#82135 = STYLED_ITEM('',(#170169),#87843) ;
#82136 = STYLED_ITEM('',(#170169),#87844) ;
#82137 = STYLED_ITEM('',(#170169),#87845) ;
#82138 = STYLED_ITEM('',(#170169),#87846) ;
#82139 = STYLED_ITEM('',(#170169),#87847) ;
#82140 = STYLED_ITEM('',(#170169),#87848) ;
#82141 = STYLED_ITEM('',(#170169),#87849) ;
#82142 = STYLED_ITEM('',(#170169),#87850) ;
#82143 = STYLED_ITEM('',(#170169),#87851) ;
#82144 = STYLED_ITEM('',(#170169),#87852) ;
#82145 = STYLED_ITEM('',(#170169),#87853) ;
#82146 = STYLED_ITEM('',(#170169),#87854) ;
#82147 = STYLED_ITEM('',(#170169),#87855) ;
#82148 = STYLED_ITEM('',(#170169),#87856) ;
#82149 = STYLED_ITEM('',(#170169),#87857) ;
#82150 = STYLED_ITEM('',(#170169),#87858) ;
#82151 = STYLED_ITEM('',(#170169),#87859) ;
#82152 = STYLED_ITEM('',(#170169),#87860) ;
#82153 = STYLED_ITEM('',(#170169),#87861) ;
#82154 = STYLED_ITEM('',(#170169),#87862) ;
#82155 = STYLED_ITEM('',(#170169),#87863) ;
#82156 = STYLED_ITEM('',(#170169),#87864) ;
#82157 = STYLED_ITEM('',(#170169),#87865) ;
#82158 = STYLED_ITEM('',(#170169),#87866) ;
#82159 = STYLED_ITEM('',(#170169),#87867) ;
#82160 = STYLED_ITEM('',(#170169),#87868) ;
#82161 = STYLED_ITEM('',(#170169),#87869) ;
#82162 = STYLED_ITEM('',(#170169),#87870) ;
#82163 = STYLED_ITEM('',(#170169),#87871) ;
#82164 = STYLED_ITEM('',(#170169),#87872) ;
#82165 = STYLED_ITEM('',(#170169),#87873) ;
#82166 = STYLED_ITEM('',(#170169),#87874) ;
#82167 = STYLED_ITEM('',(#170169),#87875) ;
#82168 = STYLED_ITEM('',(#170169),#87876) ;
#82169 = STYLED_ITEM('',(#170169),#87877) ;
#82170 = STYLED_ITEM('',(#170169),#87878) ;
#82171 = STYLED_ITEM('',(#170169),#87879) ;
#82172 = STYLED_ITEM('',(#170169),#87880) ;
#82173 = STYLED_ITEM('',(#170169),#87881) ;
#82174 = STYLED_ITEM('',(#170169),#87882) ;
#82175 = STYLED_ITEM('',(#170169),#87883) ;
#82176 = STYLED_ITEM('',(#170169),#87884) ;
#82177 = STYLED_ITEM('',(#170169),#87885) ;
#82178 = STYLED_ITEM('',(#170169),#87886) ;
#82179 = STYLED_ITEM('',(#170169),#87887) ;
#82180 = STYLED_ITEM('',(#170169),#87888) ;
#82181 = STYLED_ITEM('',(#170169),#87889) ;
#82182 = STYLED_ITEM('',(#170169),#87890) ;
#82183 = STYLED_ITEM('',(#170169),#87891) ;
#82184 = STYLED_ITEM('',(#170169),#87892) ;
#82185 = STYLED_ITEM('',(#170169),#87893) ;
#82186 = STYLED_ITEM('',(#170169),#87894) ;
#82187 = STYLED_ITEM('',(#170169),#87895) ;
#82188 = STYLED_ITEM('',(#170169),#87896) ;
#82189 = STYLED_ITEM('',(#170169),#87897) ;
#82190 = STYLED_ITEM('',(#170169),#87898) ;
#82191 = STYLED_ITEM('',(#170169),#87899) ;
#82192 = STYLED_ITEM('',(#170169),#87900) ;
#82193 = STYLED_ITEM('',(#170169),#87901) ;
#82194 = STYLED_ITEM('',(#170169),#87902) ;
#82195 = STYLED_ITEM('',(#170169),#87903) ;
#82196 = STYLED_ITEM('',(#170169),#87904) ;
#82197 = STYLED_ITEM('',(#170169),#87905) ;
#82198 = STYLED_ITEM('',(#170169),#87906) ;
#82199 = STYLED_ITEM('',(#170169),#87907) ;
#82200 = STYLED_ITEM('',(#170169),#87908) ;
#82201 = STYLED_ITEM('',(#170169),#87909) ;
#82202 = STYLED_ITEM('',(#170169),#87910) ;
#82203 = STYLED_ITEM('',(#170169),#87911) ;
#82204 = STYLED_ITEM('',(#170169),#87912) ;
#82205 = STYLED_ITEM('',(#170169),#87913) ;
#82206 = STYLED_ITEM('',(#170169),#87914) ;
#82207 = STYLED_ITEM('',(#170169),#87915) ;
#82208 = STYLED_ITEM('',(#170169),#87916) ;
#82209 = STYLED_ITEM('',(#170169),#87917) ;
#82210 = STYLED_ITEM('',(#170169),#87918) ;
#82211 = STYLED_ITEM('',(#170169),#87919) ;
#82212 = STYLED_ITEM('',(#170169),#87920) ;
#82213 = STYLED_ITEM('',(#170169),#87921) ;
#82214 = STYLED_ITEM('',(#170169),#87922) ;
#82215 = STYLED_ITEM('',(#170169),#87923) ;
#82216 = STYLED_ITEM('',(#170169),#87924) ;
#82217 = STYLED_ITEM('',(#170169),#87925) ;
#82218 = STYLED_ITEM('',(#170169),#87926) ;
#82219 = STYLED_ITEM('',(#170169),#87927) ;
#82220 = STYLED_ITEM('',(#170169),#87928) ;
#82221 = STYLED_ITEM('',(#170169),#87929) ;
#82222 = STYLED_ITEM('',(#170169),#87930) ;
#82223 = STYLED_ITEM('',(#170169),#87931) ;
#82224 = STYLED_ITEM('',(#170169),#87932) ;
#82225 = STYLED_ITEM('',(#170169),#87933) ;
#82226 = STYLED_ITEM('',(#170169),#87934) ;
#82227 = STYLED_ITEM('',(#170169),#87935) ;
#82228 = STYLED_ITEM('',(#170169),#87936) ;
#82229 = STYLED_ITEM('',(#170169),#87937) ;
#82230 = STYLED_ITEM('',(#170169),#87938) ;
#82231 = STYLED_ITEM('',(#170169),#87939) ;
#82232 = STYLED_ITEM('',(#170169),#87940) ;
#82233 = STYLED_ITEM('',(#170169),#87941) ;
#82234 = STYLED_ITEM('',(#170169),#87942) ;
#82235 = STYLED_ITEM('',(#170169),#87943) ;
#82236 = STYLED_ITEM('',(#170169),#87944) ;
#82237 = STYLED_ITEM('',(#170169),#87945) ;
#82238 = STYLED_ITEM('',(#170169),#87946) ;
#82239 = STYLED_ITEM('',(#170169),#87947) ;
#82240 = STYLED_ITEM('',(#170169),#87948) ;
#82241 = STYLED_ITEM('',(#170169),#87949) ;
#82242 = STYLED_ITEM('',(#170169),#87950) ;
#82243 = STYLED_ITEM('',(#170169),#87951) ;
#82244 = STYLED_ITEM('',(#170169),#87952) ;
#82245 = STYLED_ITEM('',(#170169),#87953) ;
#82246 = STYLED_ITEM('',(#170169),#87954) ;
#82247 = STYLED_ITEM('',(#170169),#87955) ;
#82248 = STYLED_ITEM('',(#170169),#87956) ;
#82249 = STYLED_ITEM('',(#170169),#87957) ;
#82250 = STYLED_ITEM('',(#170169),#87958) ;
#82251 = STYLED_ITEM('',(#170169),#87959) ;
#82252 = STYLED_ITEM('',(#170169),#87960) ;
#82253 = STYLED_ITEM('',(#170169),#87961) ;
#82254 = STYLED_ITEM('',(#170169),#87962) ;
#82255 = STYLED_ITEM('',(#170169),#87963) ;
#82256 = STYLED_ITEM('',(#170169),#87964) ;
#82257 = STYLED_ITEM('',(#170169),#87965) ;
#82258 = STYLED_ITEM('',(#170169),#87966) ;
#82259 = STYLED_ITEM('',(#170169),#87967) ;
#82260 = STYLED_ITEM('',(#170169),#87968) ;
#82261 = STYLED_ITEM('',(#170169),#87969) ;
#82262 = STYLED_ITEM('',(#170169),#87970) ;
#82263 = STYLED_ITEM('',(#170169),#87971) ;
#82264 = STYLED_ITEM('',(#170169),#87972) ;
#82265 = STYLED_ITEM('',(#170169),#87973) ;
#82266 = STYLED_ITEM('',(#170169),#87974) ;
#82267 = STYLED_ITEM('',(#170169),#87975) ;
#82268 = STYLED_ITEM('',(#170169),#87976) ;
#82269 = STYLED_ITEM('',(#170169),#87977) ;
#82270 = STYLED_ITEM('',(#170169),#87978) ;
#82271 = STYLED_ITEM('',(#170169),#87979) ;
#82272 = STYLED_ITEM('',(#170169),#87980) ;
#82273 = STYLED_ITEM('',(#170169),#87981) ;
#82274 = STYLED_ITEM('',(#170169),#87982) ;
#82275 = STYLED_ITEM('',(#170169),#87983) ;
#82276 = STYLED_ITEM('',(#170169),#87984) ;
#82277 = STYLED_ITEM('',(#170169),#87985) ;
#82278 = STYLED_ITEM('',(#170169),#87986) ;
#82279 = STYLED_ITEM('',(#170169),#87987) ;
#82280 = STYLED_ITEM('',(#170169),#87988) ;
#82281 = STYLED_ITEM('',(#170169),#87989) ;
#82282 = STYLED_ITEM('',(#170169),#87990) ;
#82283 = STYLED_ITEM('',(#170169),#87991) ;
#82284 = STYLED_ITEM('',(#170169),#87992) ;
#82285 = STYLED_ITEM('',(#170169),#87993) ;
#82286 = STYLED_ITEM('',(#170169),#87994) ;
#82287 = STYLED_ITEM('',(#170169),#87995) ;
#82288 = STYLED_ITEM('',(#170169),#87996) ;
#82289 = STYLED_ITEM('',(#170169),#87997) ;
#82290 = STYLED_ITEM('',(#170169),#87998) ;
#82291 = STYLED_ITEM('',(#170169),#87999) ;
#82292 = STYLED_ITEM('',(#170169),#88000) ;
#82293 = STYLED_ITEM('',(#170169),#88001) ;
#82294 = STYLED_ITEM('',(#170169),#88002) ;
#82295 = STYLED_ITEM('',(#170169),#88003) ;
#82296 = STYLED_ITEM('',(#170169),#88004) ;
#82297 = STYLED_ITEM('',(#170169),#88005) ;
#82298 = STYLED_ITEM('',(#170169),#88006) ;
#82299 = STYLED_ITEM('',(#170169),#88007) ;
#82300 = STYLED_ITEM('',(#170169),#88008) ;
#82301 = STYLED_ITEM('',(#170169),#88009) ;
#82302 = STYLED_ITEM('',(#170169),#88010) ;
#82303 = STYLED_ITEM('',(#170169),#88011) ;
#82304 = STYLED_ITEM('',(#170169),#88012) ;
#82305 = STYLED_ITEM('',(#170169),#88013) ;
#82306 = STYLED_ITEM('',(#170169),#88014) ;
#82307 = STYLED_ITEM('',(#170169),#88015) ;
#82308 = STYLED_ITEM('',(#170169),#88016) ;
#82309 = STYLED_ITEM('',(#170169),#88017) ;
#82310 = STYLED_ITEM('',(#170169),#88018) ;
#82311 = STYLED_ITEM('',(#170169),#88019) ;
#82312 = STYLED_ITEM('',(#170169),#88020) ;
#82313 = STYLED_ITEM('',(#170169),#88021) ;
#82314 = STYLED_ITEM('',(#170169),#88022) ;
#82315 = STYLED_ITEM('',(#170169),#88023) ;
#82316 = STYLED_ITEM('',(#170169),#88024) ;
#82317 = STYLED_ITEM('',(#170169),#88025) ;
#82318 = STYLED_ITEM('',(#170169),#88026) ;
#82319 = STYLED_ITEM('',(#170169),#88027) ;
#82320 = STYLED_ITEM('',(#170169),#88028) ;
#82321 = STYLED_ITEM('',(#170169),#88029) ;
#82322 = STYLED_ITEM('',(#170169),#88030) ;
#82323 = STYLED_ITEM('',(#170169),#88031) ;
#82324 = STYLED_ITEM('',(#170169),#88032) ;
#82325 = STYLED_ITEM('',(#170169),#88033) ;
#82326 = STYLED_ITEM('',(#170169),#88034) ;
#82327 = STYLED_ITEM('',(#170169),#88035) ;
#82328 = STYLED_ITEM('',(#170169),#88036) ;
#82329 = STYLED_ITEM('',(#170169),#88037) ;
#82330 = STYLED_ITEM('',(#170169),#88038) ;
#82331 = STYLED_ITEM('',(#170169),#88039) ;
#82332 = STYLED_ITEM('',(#170169),#88040) ;
#82333 = STYLED_ITEM('',(#170169),#88041) ;
#82334 = STYLED_ITEM('',(#170169),#88042) ;
#82335 = STYLED_ITEM('',(#170169),#88043) ;
#82336 = STYLED_ITEM('',(#170169),#88044) ;
#82337 = STYLED_ITEM('',(#170169),#88045) ;
#82338 = STYLED_ITEM('',(#170169),#88046) ;
#82339 = STYLED_ITEM('',(#170169),#88047) ;
#82340 = STYLED_ITEM('',(#170169),#88048) ;
#82341 = STYLED_ITEM('',(#170169),#88049) ;
#82342 = STYLED_ITEM('',(#170169),#88050) ;
#82343 = STYLED_ITEM('',(#170169),#88051) ;
#82344 = STYLED_ITEM('',(#170169),#88052) ;
#82345 = STYLED_ITEM('',(#170169),#88053) ;
#82346 = STYLED_ITEM('',(#170169),#88054) ;
#82347 = STYLED_ITEM('',(#170169),#88055) ;
#82348 = STYLED_ITEM('',(#170169),#88056) ;
#82349 = STYLED_ITEM('',(#170169),#88057) ;
#82350 = STYLED_ITEM('',(#170169),#88058) ;
#82351 = STYLED_ITEM('',(#170169),#88059) ;
#82352 = STYLED_ITEM('',(#170169),#88060) ;
#82353 = STYLED_ITEM('',(#170169),#88061) ;
#82354 = STYLED_ITEM('',(#170169),#88062) ;
#82355 = STYLED_ITEM('',(#170169),#88063) ;
#82356 = STYLED_ITEM('',(#170169),#88064) ;
#82357 = STYLED_ITEM('',(#170169),#88065) ;
#82358 = STYLED_ITEM('',(#170169),#88066) ;
#82359 = STYLED_ITEM('',(#170169),#88067) ;
#82360 = STYLED_ITEM('',(#170169),#88068) ;
#82361 = STYLED_ITEM('',(#170169),#88069) ;
#82362 = STYLED_ITEM('',(#170171),#88070) ;
#82363 = STYLED_ITEM('',(#170171),#88071) ;
#82364 = STYLED_ITEM('',(#170171),#88072) ;
#82365 = STYLED_ITEM('',(#170171),#88073) ;
#82366 = STYLED_ITEM('',(#170171),#88074) ;
#82367 = STYLED_ITEM('',(#170171),#88075) ;
#82368 = STYLED_ITEM('',(#170171),#88076) ;
#82369 = STYLED_ITEM('',(#170171),#88077) ;
#82370 = STYLED_ITEM('',(#170171),#88078) ;
#82371 = STYLED_ITEM('',(#170171),#88079) ;
#82372 = STYLED_ITEM('',(#170171),#88080) ;
#82373 = STYLED_ITEM('',(#170171),#88081) ;
#82374 = STYLED_ITEM('',(#170171),#88082) ;
#82375 = STYLED_ITEM('',(#170171),#88083) ;
#82376 = STYLED_ITEM('',(#170171),#88084) ;
#82377 = STYLED_ITEM('',(#170171),#88085) ;
#82378 = STYLED_ITEM('',(#170171),#88086) ;
#82379 = STYLED_ITEM('',(#170171),#88087) ;
#82380 = STYLED_ITEM('',(#170171),#88088) ;
#82381 = STYLED_ITEM('',(#170171),#88089) ;
#82382 = STYLED_ITEM('',(#170171),#88090) ;
#82383 = STYLED_ITEM('',(#170171),#88091) ;
#82384 = STYLED_ITEM('',(#170171),#88092) ;
#82385 = STYLED_ITEM('',(#170171),#88093) ;
#82386 = STYLED_ITEM('',(#170171),#88094) ;
#82387 = STYLED_ITEM('',(#170171),#88095) ;
#82388 = STYLED_ITEM('',(#170171),#88096) ;
#82389 = STYLED_ITEM('',(#170171),#88097) ;
#82390 = STYLED_ITEM('',(#170171),#88098) ;
#82391 = STYLED_ITEM('',(#170171),#88099) ;
#82392 = STYLED_ITEM('',(#170171),#88100) ;
#82393 = STYLED_ITEM('',(#170171),#88101) ;
#82394 = STYLED_ITEM('',(#170171),#88102) ;
#82395 = STYLED_ITEM('',(#170171),#88103) ;
#82396 = STYLED_ITEM('',(#170171),#88104) ;
#82397 = STYLED_ITEM('',(#170171),#88105) ;
#82398 = STYLED_ITEM('',(#170171),#88106) ;
#82399 = STYLED_ITEM('',(#170171),#88107) ;
#82400 = STYLED_ITEM('',(#170171),#88108) ;
#82401 = STYLED_ITEM('',(#170171),#88109) ;
#82402 = STYLED_ITEM('',(#170171),#88110) ;
#82403 = STYLED_ITEM('',(#170171),#88111) ;
#82404 = STYLED_ITEM('',(#170171),#88112) ;
#82405 = STYLED_ITEM('',(#170171),#88113) ;
#82406 = STYLED_ITEM('',(#170171),#88114) ;
#82407 = STYLED_ITEM('',(#170171),#88115) ;
#82408 = STYLED_ITEM('',(#170171),#88116) ;
#82409 = STYLED_ITEM('',(#170171),#88117) ;
#82410 = STYLED_ITEM('',(#170171),#88118) ;
#82411 = STYLED_ITEM('',(#170171),#88119) ;
#82412 = STYLED_ITEM('',(#170171),#88120) ;
#82413 = STYLED_ITEM('',(#170171),#88121) ;
#82414 = STYLED_ITEM('',(#170171),#88122) ;
#82415 = STYLED_ITEM('',(#170171),#88123) ;
#82416 = STYLED_ITEM('',(#170171),#88124) ;
#82417 = STYLED_ITEM('',(#170171),#88125) ;
#82418 = STYLED_ITEM('',(#170171),#88126) ;
#82419 = STYLED_ITEM('',(#170171),#88127) ;
#82420 = STYLED_ITEM('',(#170171),#88128) ;
#82421 = STYLED_ITEM('',(#170171),#88129) ;
#82422 = STYLED_ITEM('',(#170171),#88130) ;
#82423 = STYLED_ITEM('',(#170171),#88131) ;
#82424 = STYLED_ITEM('',(#170171),#88132) ;
#82425 = STYLED_ITEM('',(#170171),#88133) ;
#82426 = STYLED_ITEM('',(#170171),#88134) ;
#82427 = STYLED_ITEM('',(#170171),#88135) ;
#82428 = STYLED_ITEM('',(#170171),#88136) ;
#82429 = STYLED_ITEM('',(#170171),#88137) ;
#82430 = STYLED_ITEM('',(#170171),#88138) ;
#82431 = STYLED_ITEM('',(#170171),#88139) ;
#82432 = STYLED_ITEM('',(#170171),#88140) ;
#82433 = STYLED_ITEM('',(#170171),#88141) ;
#82434 = STYLED_ITEM('',(#170171),#88142) ;
#82435 = STYLED_ITEM('',(#170171),#88143) ;
#82436 = STYLED_ITEM('',(#170171),#88144) ;
#82437 = STYLED_ITEM('',(#170171),#88145) ;
#82438 = STYLED_ITEM('',(#170171),#88146) ;
#82439 = STYLED_ITEM('',(#170171),#88147) ;
#82440 = STYLED_ITEM('',(#170171),#88148) ;
#82441 = STYLED_ITEM('',(#170171),#88149) ;
#82442 = STYLED_ITEM('',(#170171),#88150) ;
#82443 = STYLED_ITEM('',(#170171),#88151) ;
#82444 = STYLED_ITEM('',(#170171),#88152) ;
#82445 = STYLED_ITEM('',(#170171),#88153) ;
#82446 = STYLED_ITEM('',(#170171),#88154) ;
#82447 = STYLED_ITEM('',(#170171),#88155) ;
#82448 = STYLED_ITEM('',(#170171),#88156) ;
#82449 = STYLED_ITEM('',(#170171),#88157) ;
#82450 = STYLED_ITEM('',(#170171),#88158) ;
#82451 = STYLED_ITEM('',(#170171),#88159) ;
#82452 = STYLED_ITEM('',(#170171),#88160) ;
#82453 = STYLED_ITEM('',(#170171),#88161) ;
#82454 = STYLED_ITEM('',(#170171),#88162) ;
#82455 = STYLED_ITEM('',(#170171),#88163) ;
#82456 = STYLED_ITEM('',(#170171),#88164) ;
#82457 = STYLED_ITEM('',(#170171),#88165) ;
#82458 = STYLED_ITEM('',(#170171),#88166) ;
#82459 = STYLED_ITEM('',(#170171),#88167) ;
#82460 = STYLED_ITEM('',(#170171),#88168) ;
#82461 = STYLED_ITEM('',(#170171),#88169) ;
#82462 = STYLED_ITEM('',(#170171),#88170) ;
#82463 = STYLED_ITEM('',(#170171),#88171) ;
#82464 = STYLED_ITEM('',(#170171),#88172) ;
#82465 = STYLED_ITEM('',(#170171),#88173) ;
#82466 = STYLED_ITEM('',(#170171),#88174) ;
#82467 = STYLED_ITEM('',(#170171),#88175) ;
#82468 = STYLED_ITEM('',(#170171),#88176) ;
#82469 = STYLED_ITEM('',(#170171),#88177) ;
#82470 = STYLED_ITEM('',(#170171),#88178) ;
#82471 = STYLED_ITEM('',(#170171),#88179) ;
#82472 = STYLED_ITEM('',(#170171),#88180) ;
#82473 = STYLED_ITEM('',(#170171),#88181) ;
#82474 = STYLED_ITEM('',(#170171),#88182) ;
#82475 = STYLED_ITEM('',(#170171),#88183) ;
#82476 = STYLED_ITEM('',(#170171),#88184) ;
#82477 = STYLED_ITEM('',(#170171),#88185) ;
#82478 = STYLED_ITEM('',(#170171),#88186) ;
#82479 = STYLED_ITEM('',(#170171),#88187) ;
#82480 = STYLED_ITEM('',(#170171),#88188) ;
#82481 = STYLED_ITEM('',(#170171),#88189) ;
#82482 = STYLED_ITEM('',(#170171),#88190) ;
#82483 = STYLED_ITEM('',(#170171),#88191) ;
#82484 = STYLED_ITEM('',(#170171),#88192) ;
#82485 = STYLED_ITEM('',(#170171),#88193) ;
#82486 = STYLED_ITEM('',(#170171),#88194) ;
#82487 = STYLED_ITEM('',(#170171),#88195) ;
#82488 = STYLED_ITEM('',(#170171),#88196) ;
#82489 = STYLED_ITEM('',(#170171),#88197) ;
#82490 = STYLED_ITEM('',(#170171),#88198) ;
#82491 = STYLED_ITEM('',(#170171),#88199) ;
#82492 = STYLED_ITEM('',(#170171),#88200) ;
#82493 = STYLED_ITEM('',(#170171),#88201) ;
#82494 = STYLED_ITEM('',(#170171),#88202) ;
#82495 = STYLED_ITEM('',(#170171),#88203) ;
#82496 = STYLED_ITEM('',(#170171),#88204) ;
#82497 = STYLED_ITEM('',(#170171),#88205) ;
#82498 = STYLED_ITEM('',(#170171),#88206) ;
#82499 = STYLED_ITEM('',(#170171),#88207) ;
#82500 = STYLED_ITEM('',(#170171),#88208) ;
#82501 = STYLED_ITEM('',(#170171),#88209) ;
#82502 = STYLED_ITEM('',(#170171),#88210) ;
#82503 = STYLED_ITEM('',(#170171),#88211) ;
#82504 = STYLED_ITEM('',(#170171),#88212) ;
#82505 = STYLED_ITEM('',(#170171),#88213) ;
#82506 = STYLED_ITEM('',(#170171),#88214) ;
#82507 = STYLED_ITEM('',(#170171),#88215) ;
#82508 = STYLED_ITEM('',(#170171),#88216) ;
#82509 = STYLED_ITEM('',(#170171),#88217) ;
#82510 = STYLED_ITEM('',(#170171),#88218) ;
#82511 = STYLED_ITEM('',(#170171),#88219) ;
#82512 = STYLED_ITEM('',(#170171),#88220) ;
#82513 = STYLED_ITEM('',(#170171),#88221) ;
#82514 = STYLED_ITEM('',(#170171),#88222) ;
#82515 = STYLED_ITEM('',(#170171),#88223) ;
#82516 = STYLED_ITEM('',(#170171),#88224) ;
#82517 = STYLED_ITEM('',(#170171),#88225) ;
#82518 = STYLED_ITEM('',(#170171),#88226) ;
#82519 = STYLED_ITEM('',(#170171),#88227) ;
#82520 = STYLED_ITEM('',(#170171),#88228) ;
#82521 = STYLED_ITEM('',(#170171),#88229) ;
#82522 = STYLED_ITEM('',(#170171),#88230) ;
#82523 = STYLED_ITEM('',(#170171),#88231) ;
#82524 = STYLED_ITEM('',(#170171),#88232) ;
#82525 = STYLED_ITEM('',(#170171),#88233) ;
#82526 = STYLED_ITEM('',(#170171),#88234) ;
#82527 = STYLED_ITEM('',(#170171),#88235) ;
#82528 = STYLED_ITEM('',(#170171),#88236) ;
#82529 = STYLED_ITEM('',(#170171),#88237) ;
#82530 = STYLED_ITEM('',(#170171),#88238) ;
#82531 = STYLED_ITEM('',(#170171),#88239) ;
#82532 = STYLED_ITEM('',(#170171),#88240) ;
#82533 = STYLED_ITEM('',(#170171),#88241) ;
#82534 = STYLED_ITEM('',(#170171),#88242) ;
#82535 = STYLED_ITEM('',(#170171),#88243) ;
#82536 = STYLED_ITEM('',(#170171),#88244) ;
#82537 = STYLED_ITEM('',(#170171),#88245) ;
#82538 = STYLED_ITEM('',(#170171),#88246) ;
#82539 = STYLED_ITEM('',(#170171),#88247) ;
#82540 = STYLED_ITEM('',(#170171),#88248) ;
#82541 = STYLED_ITEM('',(#170171),#88249) ;
#82542 = STYLED_ITEM('',(#170171),#88250) ;
#82543 = STYLED_ITEM('',(#170171),#88251) ;
#82544 = STYLED_ITEM('',(#170171),#88252) ;
#82545 = STYLED_ITEM('',(#170171),#88253) ;
#82546 = STYLED_ITEM('',(#170171),#88254) ;
#82547 = STYLED_ITEM('',(#170171),#88255) ;
#82548 = STYLED_ITEM('',(#170171),#88256) ;
#82549 = STYLED_ITEM('',(#170171),#88257) ;
#82550 = STYLED_ITEM('',(#170171),#88258) ;
#82551 = STYLED_ITEM('',(#170171),#88259) ;
#82552 = STYLED_ITEM('',(#170171),#88260) ;
#82553 = STYLED_ITEM('',(#170171),#88261) ;
#82554 = STYLED_ITEM('',(#170171),#88262) ;
#82555 = STYLED_ITEM('',(#170171),#88263) ;
#82556 = STYLED_ITEM('',(#170171),#88264) ;
#82557 = STYLED_ITEM('',(#170171),#88265) ;
#82558 = STYLED_ITEM('',(#170171),#88266) ;
#82559 = STYLED_ITEM('',(#170171),#88267) ;
#82560 = STYLED_ITEM('',(#170171),#88268) ;
#82561 = STYLED_ITEM('',(#170171),#88269) ;
#82562 = STYLED_ITEM('',(#170171),#88270) ;
#82563 = STYLED_ITEM('',(#170171),#88271) ;
#82564 = STYLED_ITEM('',(#170171),#88272) ;
#82565 = STYLED_ITEM('',(#170171),#88273) ;
#82566 = STYLED_ITEM('',(#170171),#88274) ;
#82567 = STYLED_ITEM('',(#170171),#88275) ;
#82568 = STYLED_ITEM('',(#170171),#88276) ;
#82569 = STYLED_ITEM('',(#170171),#88277) ;
#82570 = STYLED_ITEM('',(#170171),#88278) ;
#82571 = STYLED_ITEM('',(#170171),#88279) ;
#82572 = STYLED_ITEM('',(#170171),#88280) ;
#82573 = STYLED_ITEM('',(#170171),#88281) ;
#82574 = STYLED_ITEM('',(#170171),#88282) ;
#82575 = STYLED_ITEM('',(#170171),#88283) ;
#82576 = STYLED_ITEM('',(#170171),#88284) ;
#82577 = STYLED_ITEM('',(#170171),#88285) ;
#82578 = STYLED_ITEM('',(#170171),#88286) ;
#82579 = STYLED_ITEM('',(#170171),#88287) ;
#82580 = STYLED_ITEM('',(#170171),#88288) ;
#82581 = STYLED_ITEM('',(#170171),#88289) ;
#82582 = STYLED_ITEM('',(#170171),#88290) ;
#82583 = STYLED_ITEM('',(#170171),#88291) ;
#82584 = STYLED_ITEM('',(#170171),#88292) ;
#82585 = STYLED_ITEM('',(#170171),#88293) ;
#82586 = STYLED_ITEM('',(#170171),#88294) ;
#82587 = STYLED_ITEM('',(#170171),#88295) ;
#82588 = STYLED_ITEM('',(#170171),#88296) ;
#82589 = STYLED_ITEM('',(#170171),#88297) ;
#82590 = STYLED_ITEM('',(#170171),#88298) ;
#82591 = STYLED_ITEM('',(#170171),#88299) ;
#82592 = STYLED_ITEM('',(#170171),#88300) ;
#82593 = STYLED_ITEM('',(#170171),#88301) ;
#82594 = STYLED_ITEM('',(#170171),#88302) ;
#82595 = STYLED_ITEM('',(#170171),#88303) ;
#82596 = STYLED_ITEM('',(#170171),#88304) ;
#82597 = STYLED_ITEM('',(#170171),#88305) ;
#82598 = STYLED_ITEM('',(#170171),#88306) ;
#82599 = STYLED_ITEM('',(#170171),#88307) ;
#82600 = STYLED_ITEM('',(#170171),#88308) ;
#82601 = STYLED_ITEM('',(#170171),#88309) ;
#82602 = STYLED_ITEM('',(#170171),#88310) ;
#82603 = STYLED_ITEM('',(#170171),#88311) ;
#82604 = STYLED_ITEM('',(#170171),#88312) ;
#82605 = STYLED_ITEM('',(#170171),#88313) ;
#82606 = STYLED_ITEM('',(#170171),#88314) ;
#82607 = STYLED_ITEM('',(#170171),#88315) ;
#82608 = STYLED_ITEM('',(#170171),#88316) ;
#82609 = STYLED_ITEM('',(#170171),#88317) ;
#82610 = STYLED_ITEM('',(#170171),#88318) ;
#82611 = STYLED_ITEM('',(#170171),#88319) ;
#82612 = STYLED_ITEM('',(#170171),#88320) ;
#82613 = STYLED_ITEM('',(#170171),#88321) ;
#82614 = STYLED_ITEM('',(#170171),#88322) ;
#82615 = STYLED_ITEM('',(#170171),#88323) ;
#82616 = STYLED_ITEM('',(#170171),#88324) ;
#82617 = STYLED_ITEM('',(#170171),#88325) ;
#82618 = STYLED_ITEM('',(#170171),#88326) ;
#82619 = STYLED_ITEM('',(#170171),#88327) ;
#82620 = STYLED_ITEM('',(#170171),#88328) ;
#82621 = STYLED_ITEM('',(#170171),#88329) ;
#82622 = STYLED_ITEM('',(#170171),#88330) ;
#82623 = STYLED_ITEM('',(#170171),#88331) ;
#82624 = STYLED_ITEM('',(#170171),#88332) ;
#82625 = STYLED_ITEM('',(#170171),#88333) ;
#82626 = STYLED_ITEM('',(#170171),#88334) ;
#82627 = STYLED_ITEM('',(#170171),#88335) ;
#82628 = STYLED_ITEM('',(#170171),#88336) ;
#82629 = STYLED_ITEM('',(#170171),#88337) ;
#82630 = STYLED_ITEM('',(#170171),#88338) ;
#82631 = STYLED_ITEM('',(#170171),#88339) ;
#82632 = STYLED_ITEM('',(#170171),#88340) ;
#82633 = STYLED_ITEM('',(#170171),#88341) ;
#82634 = STYLED_ITEM('',(#170171),#88342) ;
#82635 = STYLED_ITEM('',(#170171),#88343) ;
#82636 = STYLED_ITEM('',(#170171),#88344) ;
#82637 = STYLED_ITEM('',(#170171),#88345) ;
#82638 = STYLED_ITEM('',(#170171),#88346) ;
#82639 = STYLED_ITEM('',(#170171),#88347) ;
#82640 = STYLED_ITEM('',(#170171),#88348) ;
#82641 = STYLED_ITEM('',(#170171),#88349) ;
#82642 = STYLED_ITEM('',(#170171),#88350) ;
#82643 = STYLED_ITEM('',(#170171),#88351) ;
#82644 = STYLED_ITEM('',(#170171),#88352) ;
#82645 = STYLED_ITEM('',(#170171),#88353) ;
#82646 = STYLED_ITEM('',(#170171),#88354) ;
#82647 = STYLED_ITEM('',(#170171),#88355) ;
#82648 = STYLED_ITEM('',(#170171),#88356) ;
#82649 = STYLED_ITEM('',(#170171),#88357) ;
#82650 = STYLED_ITEM('',(#170171),#88358) ;
#82651 = STYLED_ITEM('',(#170171),#88359) ;
#82652 = STYLED_ITEM('',(#170171),#88360) ;
#82653 = STYLED_ITEM('',(#170171),#88361) ;
#82654 = STYLED_ITEM('',(#170171),#88362) ;
#82655 = STYLED_ITEM('',(#170171),#88363) ;
#82656 = STYLED_ITEM('',(#170171),#88364) ;
#82657 = STYLED_ITEM('',(#170171),#88365) ;
#82658 = STYLED_ITEM('',(#170171),#88366) ;
#82659 = STYLED_ITEM('',(#170171),#88367) ;
#82660 = STYLED_ITEM('',(#170171),#88368) ;
#82661 = STYLED_ITEM('',(#170171),#88369) ;
#82662 = STYLED_ITEM('',(#170171),#88370) ;
#82663 = STYLED_ITEM('',(#170171),#88371) ;
#82664 = STYLED_ITEM('',(#170171),#88372) ;
#82665 = STYLED_ITEM('',(#170171),#88373) ;
#82666 = STYLED_ITEM('',(#170171),#88374) ;
#82667 = STYLED_ITEM('',(#170171),#88375) ;
#82668 = STYLED_ITEM('',(#170171),#88376) ;
#82669 = STYLED_ITEM('',(#170171),#88377) ;
#82670 = STYLED_ITEM('',(#170171),#88378) ;
#82671 = STYLED_ITEM('',(#170171),#88379) ;
#82672 = STYLED_ITEM('',(#170171),#88380) ;
#82673 = STYLED_ITEM('',(#170171),#88381) ;
#82674 = STYLED_ITEM('',(#170171),#88382) ;
#82675 = STYLED_ITEM('',(#170171),#88383) ;
#82676 = STYLED_ITEM('',(#170171),#88384) ;
#82677 = STYLED_ITEM('',(#170171),#88385) ;
#82678 = STYLED_ITEM('',(#170171),#88386) ;
#82679 = STYLED_ITEM('',(#170171),#88387) ;
#82680 = STYLED_ITEM('',(#170171),#88388) ;
#82681 = STYLED_ITEM('',(#170171),#88389) ;
#82682 = STYLED_ITEM('',(#170171),#88390) ;
#82683 = STYLED_ITEM('',(#170171),#88391) ;
#82684 = STYLED_ITEM('',(#170171),#88392) ;
#82685 = STYLED_ITEM('',(#170171),#88393) ;
#82686 = STYLED_ITEM('',(#170171),#88394) ;
#82687 = STYLED_ITEM('',(#170171),#88395) ;
#82688 = STYLED_ITEM('',(#170171),#88396) ;
#82689 = STYLED_ITEM('',(#170171),#88397) ;
#82690 = STYLED_ITEM('',(#170171),#88398) ;
#82691 = STYLED_ITEM('',(#170171),#88399) ;
#82692 = STYLED_ITEM('',(#170171),#88400) ;
#82693 = STYLED_ITEM('',(#170171),#88401) ;
#82694 = STYLED_ITEM('',(#170171),#88402) ;
#82695 = STYLED_ITEM('',(#170171),#88403) ;
#82696 = STYLED_ITEM('',(#170171),#88404) ;
#82697 = STYLED_ITEM('',(#170171),#88405) ;
#82698 = STYLED_ITEM('',(#170171),#88406) ;
#82699 = STYLED_ITEM('',(#170171),#88407) ;
#82700 = STYLED_ITEM('',(#170171),#88408) ;
#82701 = STYLED_ITEM('',(#170171),#88409) ;
#82702 = STYLED_ITEM('',(#170171),#88410) ;
#82703 = STYLED_ITEM('',(#170171),#88411) ;
#82704 = STYLED_ITEM('',(#170171),#88412) ;
#82705 = STYLED_ITEM('',(#170171),#88413) ;
#82706 = STYLED_ITEM('',(#170171),#88414) ;
#82707 = STYLED_ITEM('',(#170171),#88415) ;
#82708 = STYLED_ITEM('',(#170171),#88416) ;
#82709 = STYLED_ITEM('',(#170171),#88417) ;
#82710 = STYLED_ITEM('',(#170171),#88418) ;
#82711 = STYLED_ITEM('',(#170171),#88419) ;
#82712 = STYLED_ITEM('',(#170171),#88420) ;
#82713 = STYLED_ITEM('',(#170171),#88421) ;
#82714 = STYLED_ITEM('',(#170171),#88422) ;
#82715 = STYLED_ITEM('',(#170171),#88423) ;
#82716 = STYLED_ITEM('',(#170171),#88424) ;
#82717 = STYLED_ITEM('',(#170171),#88425) ;
#82718 = STYLED_ITEM('',(#170171),#88426) ;
#82719 = STYLED_ITEM('',(#170171),#88427) ;
#82720 = STYLED_ITEM('',(#170171),#88428) ;
#82721 = STYLED_ITEM('',(#170171),#88429) ;
#82722 = STYLED_ITEM('',(#170171),#88430) ;
#82723 = STYLED_ITEM('',(#170171),#88431) ;
#82724 = STYLED_ITEM('',(#170171),#88432) ;
#82725 = STYLED_ITEM('',(#170171),#88433) ;
#82726 = STYLED_ITEM('',(#170171),#88434) ;
#82727 = STYLED_ITEM('',(#170171),#88435) ;
#82728 = STYLED_ITEM('',(#170171),#88436) ;
#82729 = STYLED_ITEM('',(#170171),#88437) ;
#82730 = STYLED_ITEM('',(#170171),#88438) ;
#82731 = STYLED_ITEM('',(#170171),#88439) ;
#82732 = STYLED_ITEM('',(#170171),#88440) ;
#82733 = STYLED_ITEM('',(#170171),#88441) ;
#82734 = STYLED_ITEM('',(#170171),#88442) ;
#82735 = STYLED_ITEM('',(#170171),#88443) ;
#82736 = STYLED_ITEM('',(#170171),#88444) ;
#82737 = STYLED_ITEM('',(#170171),#88445) ;
#82738 = STYLED_ITEM('',(#170171),#88446) ;
#82739 = STYLED_ITEM('',(#170171),#88447) ;
#82740 = STYLED_ITEM('',(#170171),#88448) ;
#82741 = STYLED_ITEM('',(#170171),#88449) ;
#82742 = STYLED_ITEM('',(#170171),#88450) ;
#82743 = STYLED_ITEM('',(#170171),#88451) ;
#82744 = STYLED_ITEM('',(#170171),#88452) ;
#82745 = STYLED_ITEM('',(#170171),#88453) ;
#82746 = STYLED_ITEM('',(#170171),#88454) ;
#82747 = STYLED_ITEM('',(#170171),#88455) ;
#82748 = STYLED_ITEM('',(#170171),#88456) ;
#82749 = STYLED_ITEM('',(#170171),#88457) ;
#82750 = STYLED_ITEM('',(#170171),#88458) ;
#82751 = STYLED_ITEM('',(#170171),#88459) ;
#82752 = STYLED_ITEM('',(#170171),#88460) ;
#82753 = STYLED_ITEM('',(#170171),#88461) ;
#82754 = STYLED_ITEM('',(#170171),#88462) ;
#82755 = STYLED_ITEM('',(#170171),#88463) ;
#82756 = STYLED_ITEM('',(#170171),#88464) ;
#82757 = STYLED_ITEM('',(#170171),#88465) ;
#82758 = STYLED_ITEM('',(#170171),#88466) ;
#82759 = STYLED_ITEM('',(#170171),#88467) ;
#82760 = STYLED_ITEM('',(#170171),#88468) ;
#82761 = STYLED_ITEM('',(#170171),#88469) ;
#82762 = STYLED_ITEM('',(#170171),#88470) ;
#82763 = STYLED_ITEM('',(#170171),#88471) ;
#82764 = STYLED_ITEM('',(#170171),#88472) ;
#82765 = STYLED_ITEM('',(#170171),#88473) ;
#82766 = STYLED_ITEM('',(#170171),#88474) ;
#82767 = STYLED_ITEM('',(#170171),#88475) ;
#82768 = STYLED_ITEM('',(#170171),#88476) ;
#82769 = STYLED_ITEM('',(#170171),#88477) ;
#82770 = STYLED_ITEM('',(#170171),#88478) ;
#82771 = STYLED_ITEM('',(#170171),#88479) ;
#82772 = STYLED_ITEM('',(#170171),#88480) ;
#82773 = STYLED_ITEM('',(#170171),#88481) ;
#82774 = STYLED_ITEM('',(#170171),#88482) ;
#82775 = STYLED_ITEM('',(#170171),#88483) ;
#82776 = STYLED_ITEM('',(#170171),#88484) ;
#82777 = STYLED_ITEM('',(#170171),#88485) ;
#82778 = STYLED_ITEM('',(#170171),#88486) ;
#82779 = STYLED_ITEM('',(#170171),#88487) ;
#82780 = STYLED_ITEM('',(#170171),#88488) ;
#82781 = STYLED_ITEM('',(#170171),#88489) ;
#82782 = STYLED_ITEM('',(#170171),#88490) ;
#82783 = STYLED_ITEM('',(#170171),#88491) ;
#82784 = STYLED_ITEM('',(#170171),#88492) ;
#82785 = STYLED_ITEM('',(#170171),#88493) ;
#82786 = STYLED_ITEM('',(#170171),#88494) ;
#82787 = STYLED_ITEM('',(#170171),#88495) ;
#82788 = STYLED_ITEM('',(#170171),#88496) ;
#82789 = STYLED_ITEM('',(#170171),#88497) ;
#82790 = STYLED_ITEM('',(#170171),#88498) ;
#82791 = STYLED_ITEM('',(#170171),#88499) ;
#82792 = STYLED_ITEM('',(#170171),#88500) ;
#82793 = STYLED_ITEM('',(#170171),#88501) ;
#82794 = STYLED_ITEM('',(#170171),#88502) ;
#82795 = STYLED_ITEM('',(#170171),#88503) ;
#82796 = STYLED_ITEM('',(#170171),#88504) ;
#82797 = STYLED_ITEM('',(#170171),#88505) ;
#82798 = STYLED_ITEM('',(#170171),#88506) ;
#82799 = STYLED_ITEM('',(#170171),#88507) ;
#82800 = STYLED_ITEM('',(#170171),#88508) ;
#82801 = STYLED_ITEM('',(#170171),#88509) ;
#82802 = STYLED_ITEM('',(#170171),#88510) ;
#82803 = STYLED_ITEM('',(#170171),#88511) ;
#82804 = STYLED_ITEM('',(#170171),#88512) ;
#82805 = STYLED_ITEM('',(#170171),#88513) ;
#82806 = STYLED_ITEM('',(#170171),#88514) ;
#82807 = STYLED_ITEM('',(#170171),#88515) ;
#82808 = STYLED_ITEM('',(#170171),#88516) ;
#82809 = STYLED_ITEM('',(#170171),#88517) ;
#82810 = STYLED_ITEM('',(#170171),#88518) ;
#82811 = STYLED_ITEM('',(#170171),#88519) ;
#82812 = STYLED_ITEM('',(#170171),#88520) ;
#82813 = STYLED_ITEM('',(#170171),#88521) ;
#82814 = STYLED_ITEM('',(#170171),#88522) ;
#82815 = STYLED_ITEM('',(#170171),#88523) ;
#82816 = STYLED_ITEM('',(#170171),#88524) ;
#82817 = STYLED_ITEM('',(#170171),#88525) ;
#82818 = STYLED_ITEM('',(#170171),#88526) ;
#82819 = STYLED_ITEM('',(#170171),#88527) ;
#82820 = STYLED_ITEM('',(#170171),#88528) ;
#82821 = STYLED_ITEM('',(#170171),#88529) ;
#82822 = STYLED_ITEM('',(#170171),#88530) ;
#82823 = STYLED_ITEM('',(#170171),#88531) ;
#82824 = STYLED_ITEM('',(#170171),#88532) ;
#82825 = STYLED_ITEM('',(#170171),#88533) ;
#82826 = STYLED_ITEM('',(#170171),#88534) ;
#82827 = STYLED_ITEM('',(#170171),#88535) ;
#82828 = STYLED_ITEM('',(#170171),#88536) ;
#82829 = STYLED_ITEM('',(#170171),#88537) ;
#82830 = STYLED_ITEM('',(#170171),#88538) ;
#82831 = STYLED_ITEM('',(#170171),#88539) ;
#82832 = STYLED_ITEM('',(#170171),#88540) ;
#82833 = STYLED_ITEM('',(#170171),#88541) ;
#82834 = STYLED_ITEM('',(#170171),#88542) ;
#82835 = STYLED_ITEM('',(#170171),#88543) ;
#82836 = STYLED_ITEM('',(#170171),#88544) ;
#82837 = STYLED_ITEM('',(#170171),#88545) ;
#82838 = STYLED_ITEM('',(#170171),#88546) ;
#82839 = STYLED_ITEM('',(#170171),#88547) ;
#82840 = STYLED_ITEM('',(#170171),#88548) ;
#82841 = STYLED_ITEM('',(#170171),#88549) ;
#82842 = STYLED_ITEM('',(#170171),#88550) ;
#82843 = STYLED_ITEM('',(#170171),#88551) ;
#82844 = STYLED_ITEM('',(#170171),#88552) ;
#82845 = STYLED_ITEM('',(#170171),#88553) ;
#82846 = STYLED_ITEM('',(#170171),#88554) ;
#82847 = STYLED_ITEM('',(#170171),#88555) ;
#82848 = STYLED_ITEM('',(#170171),#88556) ;
#82849 = STYLED_ITEM('',(#170171),#88557) ;
#82850 = STYLED_ITEM('',(#170171),#88558) ;
#82851 = STYLED_ITEM('',(#170171),#88559) ;
#82852 = STYLED_ITEM('',(#170171),#88560) ;
#82853 = STYLED_ITEM('',(#170171),#88561) ;
#82854 = STYLED_ITEM('',(#170171),#88562) ;
#82855 = STYLED_ITEM('',(#170171),#88563) ;
#82856 = STYLED_ITEM('',(#170171),#88564) ;
#82857 = STYLED_ITEM('',(#170171),#88565) ;
#82858 = STYLED_ITEM('',(#170171),#88566) ;
#82859 = STYLED_ITEM('',(#170171),#88567) ;
#82860 = STYLED_ITEM('',(#170171),#88568) ;
#82861 = STYLED_ITEM('',(#170171),#88569) ;
#82862 = STYLED_ITEM('',(#170171),#88570) ;
#82863 = STYLED_ITEM('',(#170171),#88571) ;
#82864 = STYLED_ITEM('',(#170171),#88572) ;
#82865 = STYLED_ITEM('',(#170171),#88573) ;
#82866 = STYLED_ITEM('',(#170171),#88574) ;
#82867 = STYLED_ITEM('',(#170171),#88575) ;
#82868 = STYLED_ITEM('',(#170171),#88576) ;
#82869 = STYLED_ITEM('',(#170171),#88577) ;
#82870 = STYLED_ITEM('',(#170171),#88578) ;
#82871 = STYLED_ITEM('',(#170171),#88579) ;
#82872 = STYLED_ITEM('',(#170171),#88580) ;
#82873 = STYLED_ITEM('',(#170171),#88581) ;
#82874 = STYLED_ITEM('',(#170171),#88582) ;
#82875 = STYLED_ITEM('',(#170171),#88583) ;
#82876 = STYLED_ITEM('',(#170171),#88584) ;
#82877 = STYLED_ITEM('',(#170171),#88585) ;
#82878 = STYLED_ITEM('',(#170171),#88586) ;
#82879 = STYLED_ITEM('',(#170171),#88587) ;
#82880 = STYLED_ITEM('',(#170171),#88588) ;
#82881 = STYLED_ITEM('',(#170171),#88589) ;
#82882 = STYLED_ITEM('',(#170171),#88590) ;
#82883 = STYLED_ITEM('',(#170171),#88591) ;
#82884 = STYLED_ITEM('',(#170171),#88592) ;
#82885 = STYLED_ITEM('',(#170171),#88593) ;
#82886 = STYLED_ITEM('',(#170171),#88594) ;
#82887 = STYLED_ITEM('',(#170171),#88595) ;
#82888 = STYLED_ITEM('',(#170171),#88596) ;
#82889 = STYLED_ITEM('',(#170171),#88597) ;
#82890 = STYLED_ITEM('',(#170171),#88598) ;
#82891 = STYLED_ITEM('',(#170171),#88599) ;
#82892 = STYLED_ITEM('',(#170171),#88600) ;
#82893 = STYLED_ITEM('',(#170171),#88601) ;
#82894 = STYLED_ITEM('',(#170171),#88602) ;
#82895 = STYLED_ITEM('',(#170171),#88603) ;
#82896 = STYLED_ITEM('',(#170171),#88604) ;
#82897 = STYLED_ITEM('',(#170171),#88605) ;
#82898 = STYLED_ITEM('',(#170171),#88606) ;
#82899 = STYLED_ITEM('',(#170171),#88607) ;
#82900 = STYLED_ITEM('',(#170171),#88608) ;
#82901 = STYLED_ITEM('',(#170171),#88609) ;
#82902 = STYLED_ITEM('',(#170171),#88610) ;
#82903 = STYLED_ITEM('',(#170171),#88611) ;
#82904 = STYLED_ITEM('',(#170171),#88612) ;
#82905 = STYLED_ITEM('',(#170171),#88613) ;
#82906 = STYLED_ITEM('',(#170171),#88614) ;
#82907 = STYLED_ITEM('',(#170171),#88615) ;
#82908 = STYLED_ITEM('',(#170171),#88616) ;
#82909 = STYLED_ITEM('',(#170171),#88617) ;
#82910 = STYLED_ITEM('',(#170171),#88618) ;
#82911 = STYLED_ITEM('',(#170171),#88619) ;
#82912 = STYLED_ITEM('',(#170171),#88620) ;
#82913 = STYLED_ITEM('',(#170171),#88621) ;
#82914 = STYLED_ITEM('',(#170171),#88622) ;
#82915 = STYLED_ITEM('',(#170171),#88623) ;
#82916 = STYLED_ITEM('',(#170171),#88624) ;
#82917 = STYLED_ITEM('',(#170171),#88625) ;
#82918 = STYLED_ITEM('',(#170171),#88626) ;
#82919 = STYLED_ITEM('',(#170171),#88627) ;
#82920 = STYLED_ITEM('',(#170171),#88628) ;
#82921 = STYLED_ITEM('',(#170171),#88629) ;
#82922 = STYLED_ITEM('',(#170171),#88630) ;
#82923 = STYLED_ITEM('',(#170171),#88631) ;
#82924 = STYLED_ITEM('',(#170171),#88632) ;
#82925 = STYLED_ITEM('',(#170171),#88633) ;
#82926 = STYLED_ITEM('',(#170171),#88634) ;
#82927 = STYLED_ITEM('',(#170171),#88635) ;
#82928 = STYLED_ITEM('',(#170171),#88636) ;
#82929 = STYLED_ITEM('',(#170171),#88637) ;
#82930 = STYLED_ITEM('',(#170171),#88638) ;
#82931 = STYLED_ITEM('',(#170171),#88639) ;
#82932 = STYLED_ITEM('',(#170171),#88640) ;
#82933 = STYLED_ITEM('',(#170171),#88641) ;
#82934 = STYLED_ITEM('',(#170171),#88642) ;
#82935 = STYLED_ITEM('',(#170171),#88643) ;
#82936 = STYLED_ITEM('',(#170171),#88644) ;
#82937 = STYLED_ITEM('',(#170171),#88645) ;
#82938 = STYLED_ITEM('',(#170171),#88646) ;
#82939 = STYLED_ITEM('',(#170171),#88647) ;
#82940 = STYLED_ITEM('',(#170171),#88648) ;
#82941 = STYLED_ITEM('',(#170171),#88649) ;
#82942 = STYLED_ITEM('',(#170171),#88650) ;
#82943 = STYLED_ITEM('',(#170171),#88651) ;
#82944 = STYLED_ITEM('',(#170171),#88652) ;
#82945 = STYLED_ITEM('',(#170171),#88653) ;
#82946 = STYLED_ITEM('',(#170171),#88654) ;
#82947 = STYLED_ITEM('',(#170171),#88655) ;
#82948 = STYLED_ITEM('',(#170171),#88656) ;
#82949 = STYLED_ITEM('',(#170171),#88657) ;
#82950 = STYLED_ITEM('',(#170171),#88658) ;
#82951 = STYLED_ITEM('',(#170171),#88659) ;
#82952 = STYLED_ITEM('',(#170171),#88660) ;
#82953 = STYLED_ITEM('',(#170171),#88661) ;
#82954 = STYLED_ITEM('',(#170171),#88662) ;
#82955 = STYLED_ITEM('',(#170171),#88663) ;
#82956 = STYLED_ITEM('',(#170171),#88664) ;
#82957 = STYLED_ITEM('',(#170171),#88665) ;
#82958 = STYLED_ITEM('',(#170171),#88666) ;
#82959 = STYLED_ITEM('',(#170171),#88667) ;
#82960 = STYLED_ITEM('',(#170171),#88668) ;
#82961 = STYLED_ITEM('',(#170171),#88669) ;
#82962 = STYLED_ITEM('',(#170171),#88670) ;
#82963 = STYLED_ITEM('',(#170171),#88671) ;
#82964 = STYLED_ITEM('',(#170171),#88672) ;
#82965 = STYLED_ITEM('',(#170171),#88673) ;
#82966 = STYLED_ITEM('',(#170171),#88674) ;
#82967 = STYLED_ITEM('',(#170171),#88675) ;
#82968 = STYLED_ITEM('',(#170171),#88676) ;
#82969 = STYLED_ITEM('',(#170171),#88677) ;
#82970 = STYLED_ITEM('',(#170171),#88678) ;
#82971 = STYLED_ITEM('',(#170171),#88679) ;
#82972 = STYLED_ITEM('',(#170171),#88680) ;
#82973 = STYLED_ITEM('',(#170171),#88681) ;
#82974 = STYLED_ITEM('',(#170171),#88682) ;
#82975 = STYLED_ITEM('',(#170171),#88683) ;
#82976 = STYLED_ITEM('',(#170171),#88684) ;
#82977 = STYLED_ITEM('',(#170171),#88685) ;
#82978 = STYLED_ITEM('',(#170171),#88686) ;
#82979 = STYLED_ITEM('',(#170171),#88687) ;
#82980 = STYLED_ITEM('',(#170171),#88688) ;
#82981 = STYLED_ITEM('',(#170171),#88689) ;
#82982 = STYLED_ITEM('',(#170171),#88690) ;
#82983 = STYLED_ITEM('',(#170171),#88691) ;
#82984 = STYLED_ITEM('',(#170171),#88692) ;
#82985 = STYLED_ITEM('',(#170171),#88693) ;
#82986 = STYLED_ITEM('',(#170171),#88694) ;
#82987 = STYLED_ITEM('',(#170171),#88695) ;
#82988 = STYLED_ITEM('',(#170171),#88696) ;
#82989 = STYLED_ITEM('',(#170171),#88697) ;
#82990 = STYLED_ITEM('',(#170171),#88698) ;
#82991 = STYLED_ITEM('',(#170171),#88699) ;
#82992 = STYLED_ITEM('',(#170171),#88700) ;
#82993 = STYLED_ITEM('',(#170171),#88701) ;
#82994 = STYLED_ITEM('',(#170171),#88702) ;
#82995 = STYLED_ITEM('',(#170171),#88703) ;
#82996 = STYLED_ITEM('',(#170171),#88704) ;
#82997 = STYLED_ITEM('',(#170171),#88705) ;
#82998 = STYLED_ITEM('',(#170171),#88706) ;
#82999 = STYLED_ITEM('',(#170171),#88707) ;
#83000 = STYLED_ITEM('',(#170171),#88708) ;
#83001 = STYLED_ITEM('',(#170171),#88709) ;
#83002 = STYLED_ITEM('',(#170171),#88710) ;
#83003 = STYLED_ITEM('',(#170171),#88711) ;
#83004 = STYLED_ITEM('',(#170171),#88712) ;
#83005 = STYLED_ITEM('',(#170171),#88713) ;
#83006 = STYLED_ITEM('',(#170171),#88714) ;
#83007 = STYLED_ITEM('',(#170171),#88715) ;
#83008 = STYLED_ITEM('',(#170171),#88716) ;
#83009 = STYLED_ITEM('',(#170171),#88717) ;
#83010 = STYLED_ITEM('',(#170168),#32) ;
#83011 = STYLED_ITEM('',(#170169),#88718) ;
#83012 = STYLED_ITEM('',(#170169),#88719) ;
#83013 = STYLED_ITEM('',(#170169),#88720) ;
#83014 = STYLED_ITEM('',(#170169),#88721) ;
#83015 = STYLED_ITEM('',(#170169),#88722) ;
#83016 = STYLED_ITEM('',(#170169),#88723) ;
#83017 = STYLED_ITEM('',(#170169),#88724) ;
#83018 = STYLED_ITEM('',(#170169),#88725) ;
#83019 = STYLED_ITEM('',(#170169),#88726) ;
#83020 = STYLED_ITEM('',(#170169),#88727) ;
#83021 = STYLED_ITEM('',(#170169),#88728) ;
#83022 = STYLED_ITEM('',(#170169),#88729) ;
#83023 = STYLED_ITEM('',(#170169),#88730) ;
#83024 = STYLED_ITEM('',(#170169),#88731) ;
#83025 = STYLED_ITEM('',(#170169),#88732) ;
#83026 = STYLED_ITEM('',(#170169),#88733) ;
#83027 = STYLED_ITEM('',(#170169),#88734) ;
#83028 = STYLED_ITEM('',(#170169),#88735) ;
#83029 = STYLED_ITEM('',(#170169),#88736) ;
#83030 = STYLED_ITEM('',(#170169),#88737) ;
#83031 = STYLED_ITEM('',(#170169),#88738) ;
#83032 = STYLED_ITEM('',(#170169),#88739) ;
#83033 = STYLED_ITEM('',(#170169),#88740) ;
#83034 = STYLED_ITEM('',(#170169),#88741) ;
#83035 = STYLED_ITEM('',(#170169),#88742) ;
#83036 = STYLED_ITEM('',(#170169),#88743) ;
#83037 = STYLED_ITEM('',(#170169),#88744) ;
#83038 = STYLED_ITEM('',(#170169),#88745) ;
#83039 = STYLED_ITEM('',(#170169),#88746) ;
#83040 = STYLED_ITEM('',(#170169),#88747) ;
#83041 = STYLED_ITEM('',(#170169),#88748) ;
#83042 = STYLED_ITEM('',(#170169),#88749) ;
#83043 = STYLED_ITEM('',(#170169),#88750) ;
#83044 = STYLED_ITEM('',(#170169),#88751) ;
#83045 = STYLED_ITEM('',(#170169),#88752) ;
#83046 = STYLED_ITEM('',(#170169),#88753) ;
#83047 = STYLED_ITEM('',(#170169),#88754) ;
#83048 = STYLED_ITEM('',(#170169),#88755) ;
#83049 = STYLED_ITEM('',(#170169),#88756) ;
#83050 = STYLED_ITEM('',(#170169),#88757) ;
#83051 = STYLED_ITEM('',(#170169),#88758) ;
#83052 = STYLED_ITEM('',(#170169),#88759) ;
#83053 = STYLED_ITEM('',(#170169),#88760) ;
#83054 = STYLED_ITEM('',(#170169),#88761) ;
#83055 = STYLED_ITEM('',(#170169),#88762) ;
#83056 = STYLED_ITEM('',(#170169),#88763) ;
#83057 = STYLED_ITEM('',(#170169),#88764) ;
#83058 = STYLED_ITEM('',(#170169),#88765) ;
#83059 = STYLED_ITEM('',(#170169),#88766) ;
#83060 = STYLED_ITEM('',(#170169),#88767) ;
#83061 = STYLED_ITEM('',(#170169),#88768) ;
#83062 = STYLED_ITEM('',(#170169),#88769) ;
#83063 = STYLED_ITEM('',(#170169),#88770) ;
#83064 = STYLED_ITEM('',(#170169),#88771) ;
#83065 = STYLED_ITEM('',(#170169),#88772) ;
#83066 = STYLED_ITEM('',(#170169),#88773) ;
#83067 = STYLED_ITEM('',(#170169),#88774) ;
#83068 = STYLED_ITEM('',(#170169),#88775) ;
#83069 = STYLED_ITEM('',(#170169),#88776) ;
#83070 = STYLED_ITEM('',(#170169),#88777) ;
#83071 = STYLED_ITEM('',(#170169),#88778) ;
#83072 = STYLED_ITEM('',(#170169),#88779) ;
#83073 = STYLED_ITEM('',(#170169),#88780) ;
#83074 = STYLED_ITEM('',(#170169),#88781) ;
#83075 = STYLED_ITEM('',(#170169),#88782) ;
#83076 = STYLED_ITEM('',(#170169),#88783) ;
#83077 = STYLED_ITEM('',(#170169),#88784) ;
#83078 = STYLED_ITEM('',(#170169),#88785) ;
#83079 = STYLED_ITEM('',(#170169),#88786) ;
#83080 = STYLED_ITEM('',(#170169),#88787) ;
#83081 = STYLED_ITEM('',(#170169),#88788) ;
#83082 = STYLED_ITEM('',(#170169),#88789) ;
#83083 = STYLED_ITEM('',(#170169),#88790) ;
#83084 = STYLED_ITEM('',(#170169),#88791) ;
#83085 = STYLED_ITEM('',(#170169),#88792) ;
#83086 = STYLED_ITEM('',(#170169),#88793) ;
#83087 = STYLED_ITEM('',(#170169),#88794) ;
#83088 = STYLED_ITEM('',(#170169),#88795) ;
#83089 = STYLED_ITEM('',(#170169),#88796) ;
#83090 = STYLED_ITEM('',(#170169),#88797) ;
#83091 = STYLED_ITEM('',(#170169),#88798) ;
#83092 = STYLED_ITEM('',(#170169),#88799) ;
#83093 = STYLED_ITEM('',(#170169),#88800) ;
#83094 = STYLED_ITEM('',(#170169),#88801) ;
#83095 = STYLED_ITEM('',(#170169),#88802) ;
#83096 = STYLED_ITEM('',(#170169),#88803) ;
#83097 = STYLED_ITEM('',(#170169),#88804) ;
#83098 = STYLED_ITEM('',(#170169),#88805) ;
#83099 = STYLED_ITEM('',(#170169),#88806) ;
#83100 = STYLED_ITEM('',(#170169),#88807) ;
#83101 = STYLED_ITEM('',(#170169),#88808) ;
#83102 = STYLED_ITEM('',(#170169),#88809) ;
#83103 = STYLED_ITEM('',(#170169),#88810) ;
#83104 = STYLED_ITEM('',(#170169),#88811) ;
#83105 = STYLED_ITEM('',(#170169),#88812) ;
#83106 = STYLED_ITEM('',(#170169),#88813) ;
#83107 = STYLED_ITEM('',(#170169),#88814) ;
#83108 = STYLED_ITEM('',(#170169),#88815) ;
#83109 = STYLED_ITEM('',(#170169),#88816) ;
#83110 = STYLED_ITEM('',(#170169),#88817) ;
#83111 = STYLED_ITEM('',(#170169),#88818) ;
#83112 = STYLED_ITEM('',(#170169),#88819) ;
#83113 = STYLED_ITEM('',(#170169),#88820) ;
#83114 = STYLED_ITEM('',(#170172),#88821) ;
#83115 = STYLED_ITEM('',(#170172),#88822) ;
#83116 = STYLED_ITEM('',(#170172),#88823) ;
#83117 = STYLED_ITEM('',(#170172),#88824) ;
#83118 = STYLED_ITEM('',(#170172),#88825) ;
#83119 = STYLED_ITEM('',(#170172),#88826) ;
#83120 = STYLED_ITEM('',(#170172),#88827) ;
#83121 = STYLED_ITEM('',(#170172),#88828) ;
#83122 = STYLED_ITEM('',(#170172),#88829) ;
#83123 = STYLED_ITEM('',(#170169),#88830) ;
#83124 = STYLED_ITEM('',(#170169),#88831) ;
#83125 = STYLED_ITEM('',(#170169),#88832) ;
#83126 = STYLED_ITEM('',(#170169),#88833) ;
#83127 = STYLED_ITEM('',(#170169),#88834) ;
#83128 = STYLED_ITEM('',(#170169),#88835) ;
#83129 = STYLED_ITEM('',(#170169),#88836) ;
#83130 = STYLED_ITEM('',(#170169),#88837) ;
#83131 = STYLED_ITEM('',(#170169),#88838) ;
#83132 = STYLED_ITEM('',(#170169),#88839) ;
#83133 = STYLED_ITEM('',(#170169),#88840) ;
#83134 = STYLED_ITEM('',(#170169),#88841) ;
#83135 = STYLED_ITEM('',(#170169),#88842) ;
#83136 = STYLED_ITEM('',(#170169),#88843) ;
#83137 = STYLED_ITEM('',(#170169),#88844) ;
#83138 = STYLED_ITEM('',(#170169),#88845) ;
#83139 = STYLED_ITEM('',(#170169),#88846) ;
#83140 = STYLED_ITEM('',(#170172),#88847) ;
#83141 = STYLED_ITEM('',(#170169),#88848) ;
#83142 = STYLED_ITEM('',(#170169),#88849) ;
#83143 = STYLED_ITEM('',(#170169),#88850) ;
#83144 = STYLED_ITEM('',(#170169),#88851) ;
#83145 = STYLED_ITEM('',(#170169),#88852) ;
#83146 = STYLED_ITEM('',(#170169),#88853) ;
#83147 = STYLED_ITEM('',(#170169),#88854) ;
#83148 = STYLED_ITEM('',(#170169),#88855) ;
#83149 = STYLED_ITEM('',(#170169),#88856) ;
#83150 = STYLED_ITEM('',(#170171),#88857) ;
#83151 = STYLED_ITEM('',(#170169),#88858) ;
#83152 = STYLED_ITEM('',(#170169),#88859) ;
#83153 = STYLED_ITEM('',(#170169),#88860) ;
#83154 = STYLED_ITEM('',(#170169),#88861) ;
#83155 = STYLED_ITEM('',(#170169),#88862) ;
#83156 = STYLED_ITEM('',(#170169),#88863) ;
#83157 = STYLED_ITEM('',(#170169),#88864) ;
#83158 = STYLED_ITEM('',(#170169),#88865) ;
#83159 = STYLED_ITEM('',(#170169),#88866) ;
#83160 = STYLED_ITEM('',(#170169),#88867) ;
#83161 = STYLED_ITEM('',(#170169),#88868) ;
#83162 = STYLED_ITEM('',(#170169),#88869) ;
#83163 = STYLED_ITEM('',(#170169),#88870) ;
#83164 = STYLED_ITEM('',(#170169),#88871) ;
#83165 = STYLED_ITEM('',(#170169),#88872) ;
#83166 = STYLED_ITEM('',(#170169),#88873) ;
#83167 = STYLED_ITEM('',(#170169),#88874) ;
#83168 = STYLED_ITEM('',(#170169),#88875) ;
#83169 = STYLED_ITEM('',(#170169),#88876) ;
#83170 = STYLED_ITEM('',(#170169),#88877) ;
#83171 = STYLED_ITEM('',(#170169),#88878) ;
#83172 = STYLED_ITEM('',(#170169),#88879) ;
#83173 = STYLED_ITEM('',(#170169),#88880) ;
#83174 = STYLED_ITEM('',(#170169),#88881) ;
#83175 = STYLED_ITEM('',(#170171),#88882) ;
#83176 = STYLED_ITEM('',(#170169),#88883) ;
#83177 = STYLED_ITEM('',(#170169),#88884) ;
#83178 = STYLED_ITEM('',(#170169),#88885) ;
#83179 = STYLED_ITEM('',(#170169),#88886) ;
#83180 = STYLED_ITEM('',(#170169),#88887) ;
#83181 = STYLED_ITEM('',(#170169),#88888) ;
#83182 = STYLED_ITEM('',(#170169),#88889) ;
#83183 = STYLED_ITEM('',(#170169),#88890) ;
#83184 = STYLED_ITEM('',(#170169),#88891) ;
#83185 = STYLED_ITEM('',(#170169),#88892) ;
#83186 = STYLED_ITEM('',(#170172),#88893) ;
#83187 = STYLED_ITEM('',(#170172),#88894) ;
#83188 = STYLED_ITEM('',(#170172),#88895) ;
#83189 = STYLED_ITEM('',(#170172),#88896) ;
#83190 = STYLED_ITEM('',(#170169),#88897) ;
#83191 = STYLED_ITEM('',(#170169),#88898) ;
#83192 = STYLED_ITEM('',(#170169),#88899) ;
#83193 = STYLED_ITEM('',(#170169),#88900) ;
#83194 = STYLED_ITEM('',(#170169),#88901) ;
#83195 = STYLED_ITEM('',(#170169),#88902) ;
#83196 = STYLED_ITEM('',(#170169),#88903) ;
#83197 = STYLED_ITEM('',(#170169),#88904) ;
#83198 = STYLED_ITEM('',(#170169),#88905) ;
#83199 = STYLED_ITEM('',(#170169),#88906) ;
#83200 = STYLED_ITEM('',(#170169),#88907) ;
#83201 = STYLED_ITEM('',(#170169),#88908) ;
#83202 = STYLED_ITEM('',(#170169),#88909) ;
#83203 = STYLED_ITEM('',(#170169),#88910) ;
#83204 = STYLED_ITEM('',(#170169),#88911) ;
#83205 = STYLED_ITEM('',(#170169),#88912) ;
#83206 = STYLED_ITEM('',(#170169),#88913) ;
#83207 = STYLED_ITEM('',(#170169),#88914) ;
#83208 = STYLED_ITEM('',(#170169),#88915) ;
#83209 = STYLED_ITEM('',(#170169),#88916) ;
#83210 = STYLED_ITEM('',(#170169),#88918) ;
#83211 = STYLED_ITEM('',(#170169),#88919) ;
#83212 = STYLED_ITEM('',(#170169),#88920) ;
#83213 = STYLED_ITEM('',(#170169),#88922) ;
#83214 = STYLED_ITEM('',(#170169),#88923) ;
#83215 = STYLED_ITEM('',(#170169),#88924) ;
#83216 = STYLED_ITEM('',(#170169),#88925) ;
#83217 = STYLED_ITEM('',(#170169),#88926) ;
#83218 = STYLED_ITEM('',(#170169),#88929) ;
#83219 = STYLED_ITEM('',(#170169),#88930) ;
#83220 = STYLED_ITEM('',(#170169),#88933) ;
#83221 = STYLED_ITEM('',(#170169),#88938) ;
#83222 = STYLED_ITEM('',(#170169),#88939) ;
#83223 = STYLED_ITEM('',(#170169),#88940) ;
#83224 = STYLED_ITEM('',(#170169),#88941) ;
#83225 = STYLED_ITEM('',(#170169),#88942) ;
#83226 = STYLED_ITEM('',(#170169),#88943) ;
#83227 = STYLED_ITEM('',(#170169),#88944) ;
#83228 = STYLED_ITEM('',(#170169),#88945) ;
#83229 = STYLED_ITEM('',(#170169),#88946) ;
#83230 = STYLED_ITEM('',(#170169),#88947) ;
#83231 = STYLED_ITEM('',(#170169),#88948) ;
#83232 = STYLED_ITEM('',(#170169),#88949) ;
#83233 = STYLED_ITEM('',(#170169),#88950) ;
#83234 = STYLED_ITEM('',(#170169),#88951) ;
#83235 = STYLED_ITEM('',(#170169),#88952) ;
#83236 = STYLED_ITEM('',(#170169),#88953) ;
#83237 = STYLED_ITEM('',(#170169),#88954) ;
#83238 = STYLED_ITEM('',(#170169),#88955) ;
#83239 = STYLED_ITEM('',(#170169),#88956) ;
#83240 = STYLED_ITEM('',(#170169),#88957) ;
#83241 = STYLED_ITEM('',(#170169),#88958) ;
#83242 = STYLED_ITEM('',(#170169),#88959) ;
#83243 = STYLED_ITEM('',(#170169),#88960) ;
#83244 = STYLED_ITEM('',(#170169),#88961) ;
#83245 = STYLED_ITEM('',(#170169),#88962) ;
#83246 = STYLED_ITEM('',(#170169),#88963) ;
#83247 = STYLED_ITEM('',(#170169),#88964) ;
#83248 = STYLED_ITEM('',(#170169),#88965) ;
#83249 = STYLED_ITEM('',(#170169),#88966) ;
#83250 = STYLED_ITEM('',(#170169),#88967) ;
#83251 = STYLED_ITEM('',(#170169),#88968) ;
#83252 = STYLED_ITEM('',(#170169),#88969) ;
#83253 = STYLED_ITEM('',(#170169),#88970) ;
#83254 = STYLED_ITEM('',(#170169),#88971) ;
#83255 = STYLED_ITEM('',(#170169),#88972) ;
#83256 = STYLED_ITEM('',(#170169),#88973) ;
#83257 = STYLED_ITEM('',(#170169),#88974) ;
#83258 = STYLED_ITEM('',(#170169),#88975) ;
#83259 = STYLED_ITEM('',(#170169),#88976) ;
#83260 = STYLED_ITEM('',(#170169),#88977) ;
#83261 = STYLED_ITEM('',(#170169),#88978) ;
#83262 = STYLED_ITEM('',(#170169),#88979) ;
#83263 = STYLED_ITEM('',(#170169),#88980) ;
#83264 = STYLED_ITEM('',(#170169),#88981) ;
#83265 = STYLED_ITEM('',(#170169),#88982) ;
#83266 = STYLED_ITEM('',(#170169),#88983) ;
#83267 = STYLED_ITEM('',(#170169),#88984) ;
#83268 = STYLED_ITEM('',(#170169),#88985) ;
#83269 = STYLED_ITEM('',(#170169),#88986) ;
#83270 = STYLED_ITEM('',(#170169),#88987) ;
#83271 = STYLED_ITEM('',(#170169),#88988) ;
#83272 = STYLED_ITEM('',(#170169),#88989) ;
#83273 = STYLED_ITEM('',(#170169),#88990) ;
#83274 = STYLED_ITEM('',(#170169),#88991) ;
#83275 = STYLED_ITEM('',(#170169),#88992) ;
#83276 = STYLED_ITEM('',(#170169),#88993) ;
#83277 = STYLED_ITEM('',(#170169),#88994) ;
#83278 = STYLED_ITEM('',(#170169),#88995) ;
#83279 = STYLED_ITEM('',(#170169),#88996) ;
#83280 = STYLED_ITEM('',(#170169),#88997) ;
#83281 = STYLED_ITEM('',(#170169),#88998) ;
#83282 = STYLED_ITEM('',(#170169),#88999) ;
#83283 = STYLED_ITEM('',(#170169),#89000) ;
#83284 = STYLED_ITEM('',(#170169),#89001) ;
#83285 = STYLED_ITEM('',(#170169),#89002) ;
#83286 = STYLED_ITEM('',(#170169),#89003) ;
#83287 = STYLED_ITEM('',(#170169),#89004) ;
#83288 = STYLED_ITEM('',(#170169),#89005) ;
#83289 = STYLED_ITEM('',(#170169),#89006) ;
#83290 = STYLED_ITEM('',(#170169),#89007) ;
#83291 = STYLED_ITEM('',(#170169),#89008) ;
#83292 = STYLED_ITEM('',(#170169),#89009) ;
#83293 = STYLED_ITEM('',(#170169),#89010) ;
#83294 = STYLED_ITEM('',(#170169),#89011) ;
#83295 = STYLED_ITEM('',(#170169),#89012) ;
#83296 = STYLED_ITEM('',(#170169),#89013) ;
#83297 = STYLED_ITEM('',(#170169),#89014) ;
#83298 = STYLED_ITEM('',(#170169),#89015) ;
#83299 = STYLED_ITEM('',(#170169),#89016) ;
#83300 = STYLED_ITEM('',(#170169),#89017) ;
#83301 = STYLED_ITEM('',(#170169),#89018) ;
#83302 = STYLED_ITEM('',(#170169),#89019) ;
#83303 = STYLED_ITEM('',(#170169),#89020) ;
#83304 = STYLED_ITEM('',(#170169),#89021) ;
#83305 = STYLED_ITEM('',(#170169),#89022) ;
#83306 = STYLED_ITEM('',(#170169),#89023) ;
#83307 = STYLED_ITEM('',(#170169),#89024) ;
#83308 = STYLED_ITEM('',(#170169),#89025) ;
#83309 = STYLED_ITEM('',(#170169),#89026) ;
#83310 = STYLED_ITEM('',(#170169),#89027) ;
#83311 = STYLED_ITEM('',(#170169),#89028) ;
#83312 = STYLED_ITEM('',(#170169),#89029) ;
#83313 = STYLED_ITEM('',(#170169),#89030) ;
#83314 = STYLED_ITEM('',(#170169),#89031) ;
#83315 = STYLED_ITEM('',(#170169),#89032) ;
#83316 = STYLED_ITEM('',(#170169),#89033) ;
#83317 = STYLED_ITEM('',(#170169),#89034) ;
#83318 = STYLED_ITEM('',(#170169),#89035) ;
#83319 = STYLED_ITEM('',(#170169),#89036) ;
#83320 = STYLED_ITEM('',(#170169),#89037) ;
#83321 = STYLED_ITEM('',(#170169),#89038) ;
#83322 = STYLED_ITEM('',(#170169),#89039) ;
#83323 = STYLED_ITEM('',(#170169),#89040) ;
#83324 = STYLED_ITEM('',(#170169),#89041) ;
#83325 = STYLED_ITEM('',(#170169),#89042) ;
#83326 = STYLED_ITEM('',(#170169),#89043) ;
#83327 = STYLED_ITEM('',(#170169),#89044) ;
#83328 = STYLED_ITEM('',(#170169),#89045) ;
#83329 = STYLED_ITEM('',(#170169),#89046) ;
#83330 = STYLED_ITEM('',(#170169),#89047) ;
#83331 = STYLED_ITEM('',(#170169),#89048) ;
#83332 = STYLED_ITEM('',(#170169),#89049) ;
#83333 = STYLED_ITEM('',(#170169),#89050) ;
#83334 = STYLED_ITEM('',(#170169),#89051) ;
#83335 = STYLED_ITEM('',(#170169),#89052) ;
#83336 = STYLED_ITEM('',(#170169),#89053) ;
#83337 = STYLED_ITEM('',(#170169),#89054) ;
#83338 = STYLED_ITEM('',(#170169),#89055) ;
#83339 = STYLED_ITEM('',(#170169),#89056) ;
#83340 = STYLED_ITEM('',(#170169),#89057) ;
#83341 = STYLED_ITEM('',(#170169),#89058) ;
#83342 = STYLED_ITEM('',(#170169),#89059) ;
#83343 = STYLED_ITEM('',(#170169),#89060) ;
#83344 = STYLED_ITEM('',(#170169),#89061) ;
#83345 = STYLED_ITEM('',(#170169),#89062) ;
#83346 = STYLED_ITEM('',(#170169),#89063) ;
#83347 = STYLED_ITEM('',(#170169),#89064) ;
#83348 = STYLED_ITEM('',(#170169),#89065) ;
#83349 = STYLED_ITEM('',(#170169),#89066) ;
#83350 = STYLED_ITEM('',(#170169),#89067) ;
#83351 = STYLED_ITEM('',(#170169),#89068) ;
#83352 = STYLED_ITEM('',(#170169),#89069) ;
#83353 = STYLED_ITEM('',(#170169),#89070) ;
#83354 = STYLED_ITEM('',(#170169),#89071) ;
#83355 = STYLED_ITEM('',(#170169),#89072) ;
#83356 = STYLED_ITEM('',(#170169),#89073) ;
#83357 = STYLED_ITEM('',(#170169),#89074) ;
#83358 = STYLED_ITEM('',(#170169),#89075) ;
#83359 = STYLED_ITEM('',(#170169),#89076) ;
#83360 = STYLED_ITEM('',(#170169),#89077) ;
#83361 = STYLED_ITEM('',(#170169),#89078) ;
#83362 = STYLED_ITEM('',(#170172),#89079) ;
#83363 = STYLED_ITEM('',(#170172),#89080) ;
#83364 = STYLED_ITEM('',(#170172),#89081) ;
#83365 = STYLED_ITEM('',(#170172),#89082) ;
#83366 = STYLED_ITEM('',(#170169),#89083) ;
#83367 = STYLED_ITEM('',(#170169),#89084) ;
#83368 = STYLED_ITEM('',(#170169),#89085) ;
#83369 = STYLED_ITEM('',(#170169),#89086) ;
#83370 = STYLED_ITEM('',(#170169),#89087) ;
#83371 = STYLED_ITEM('',(#170169),#89088) ;
#83372 = STYLED_ITEM('',(#170169),#89089) ;
#83373 = STYLED_ITEM('',(#170169),#89090) ;
#83374 = STYLED_ITEM('',(#170169),#89091) ;
#83375 = STYLED_ITEM('',(#170169),#89092) ;
#83376 = STYLED_ITEM('',(#170169),#89093) ;
#83377 = STYLED_ITEM('',(#170169),#89094) ;
#83378 = STYLED_ITEM('',(#170169),#89095) ;
#83379 = STYLED_ITEM('',(#170169),#89096) ;
#83380 = STYLED_ITEM('',(#170169),#89097) ;
#83381 = STYLED_ITEM('',(#170169),#89098) ;
#83382 = STYLED_ITEM('',(#170169),#89099) ;
#83383 = STYLED_ITEM('',(#170169),#89100) ;
#83384 = STYLED_ITEM('',(#170171),#89101) ;
#83385 = STYLED_ITEM('',(#170169),#89102) ;
#83386 = STYLED_ITEM('',(#170169),#89103) ;
#83387 = STYLED_ITEM('',(#170169),#89104) ;
#83388 = STYLED_ITEM('',(#170169),#89105) ;
#83389 = STYLED_ITEM('',(#170171),#89106) ;
#83390 = STYLED_ITEM('',(#170169),#89107) ;
#83391 = STYLED_ITEM('',(#170169),#89108) ;
#83392 = STYLED_ITEM('',(#170169),#89109) ;
#83393 = STYLED_ITEM('',(#170169),#89110) ;
#83394 = STYLED_ITEM('',(#170171),#89111) ;
#83395 = STYLED_ITEM('',(#170169),#89112) ;
#83396 = STYLED_ITEM('',(#170169),#89113) ;
#83397 = STYLED_ITEM('',(#170169),#89114) ;
#83398 = STYLED_ITEM('',(#170169),#89115) ;
#83399 = STYLED_ITEM('',(#170171),#89116) ;
#83400 = STYLED_ITEM('',(#170169),#89117) ;
#83401 = STYLED_ITEM('',(#170169),#89118) ;
#83402 = STYLED_ITEM('',(#170169),#89119) ;
#83403 = STYLED_ITEM('',(#170169),#89120) ;
#83404 = STYLED_ITEM('',(#170171),#89121) ;
#83405 = STYLED_ITEM('',(#170169),#89122) ;
#83406 = STYLED_ITEM('',(#170169),#89123) ;
#83407 = STYLED_ITEM('',(#170169),#89124) ;
#83408 = STYLED_ITEM('',(#170169),#89125) ;
#83409 = STYLED_ITEM('',(#170171),#89126) ;
#83410 = STYLED_ITEM('',(#170169),#89127) ;
#83411 = STYLED_ITEM('',(#170169),#89128) ;
#83412 = STYLED_ITEM('',(#170169),#89129) ;
#83413 = STYLED_ITEM('',(#170169),#89130) ;
#83414 = STYLED_ITEM('',(#170171),#89131) ;
#83415 = STYLED_ITEM('',(#170169),#89132) ;
#83416 = STYLED_ITEM('',(#170169),#89133) ;
#83417 = STYLED_ITEM('',(#170169),#89134) ;
#83418 = STYLED_ITEM('',(#170169),#89135) ;
#83419 = STYLED_ITEM('',(#170171),#89136) ;
#83420 = STYLED_ITEM('',(#170169),#89137) ;
#83421 = STYLED_ITEM('',(#170169),#89138) ;
#83422 = STYLED_ITEM('',(#170169),#89139) ;
#83423 = STYLED_ITEM('',(#170169),#89140) ;
#83424 = STYLED_ITEM('',(#170171),#89141) ;
#83425 = STYLED_ITEM('',(#170169),#89142) ;
#83426 = STYLED_ITEM('',(#170169),#89143) ;
#83427 = STYLED_ITEM('',(#170169),#89144) ;
#83428 = STYLED_ITEM('',(#170169),#89145) ;
#83429 = STYLED_ITEM('',(#170169),#89146) ;
#83430 = STYLED_ITEM('',(#170169),#89147) ;
#83431 = STYLED_ITEM('',(#170169),#89148) ;
#83432 = STYLED_ITEM('',(#170169),#89149) ;
#83433 = STYLED_ITEM('',(#170169),#89150) ;
#83434 = STYLED_ITEM('',(#170169),#89151) ;
#83435 = STYLED_ITEM('',(#170169),#89152) ;
#83436 = STYLED_ITEM('',(#170169),#89153) ;
#83437 = STYLED_ITEM('',(#170169),#89154) ;
#83438 = STYLED_ITEM('',(#170169),#89155) ;
#83439 = STYLED_ITEM('',(#170169),#89156) ;
#83440 = STYLED_ITEM('',(#170169),#89157) ;
#83441 = STYLED_ITEM('',(#170169),#89158) ;
#83442 = STYLED_ITEM('',(#170169),#89159) ;
#83443 = STYLED_ITEM('',(#170169),#89160) ;
#83444 = STYLED_ITEM('',(#170169),#89161) ;
#83445 = STYLED_ITEM('',(#170169),#89162) ;
#83446 = STYLED_ITEM('',(#170169),#89163) ;
#83447 = STYLED_ITEM('',(#170169),#89164) ;
#83448 = STYLED_ITEM('',(#170169),#89165) ;
#83449 = STYLED_ITEM('',(#170169),#89166) ;
#83450 = STYLED_ITEM('',(#170169),#89167) ;
#83451 = STYLED_ITEM('',(#170169),#89168) ;
#83452 = STYLED_ITEM('',(#170169),#89169) ;
#83453 = STYLED_ITEM('',(#170169),#89170) ;
#83454 = STYLED_ITEM('',(#170169),#89171) ;
#83455 = STYLED_ITEM('',(#170169),#89172) ;
#83456 = STYLED_ITEM('',(#170169),#89173) ;
#83457 = STYLED_ITEM('',(#170169),#89174) ;
#83458 = STYLED_ITEM('',(#170169),#89175) ;
#83459 = STYLED_ITEM('',(#170169),#89176) ;
#83460 = STYLED_ITEM('',(#170169),#89177) ;
#83461 = STYLED_ITEM('',(#170169),#89178) ;
#83462 = STYLED_ITEM('',(#170169),#89179) ;
#83463 = STYLED_ITEM('',(#170169),#89180) ;
#83464 = STYLED_ITEM('',(#170169),#89181) ;
#83465 = STYLED_ITEM('',(#170169),#89182) ;
#83466 = STYLED_ITEM('',(#170169),#89183) ;
#83467 = STYLED_ITEM('',(#170169),#89184) ;
#83468 = STYLED_ITEM('',(#170169),#89185) ;
#83469 = STYLED_ITEM('',(#170169),#89186) ;
#83470 = STYLED_ITEM('',(#170169),#89187) ;
#83471 = STYLED_ITEM('',(#170169),#89188) ;
#83472 = STYLED_ITEM('',(#170169),#89189) ;
#83473 = STYLED_ITEM('',(#170169),#89190) ;
#83474 = STYLED_ITEM('',(#170169),#89191) ;
#83475 = STYLED_ITEM('',(#170169),#89192) ;
#83476 = STYLED_ITEM('',(#170169),#89193) ;
#83477 = STYLED_ITEM('',(#170169),#89194) ;
#83478 = STYLED_ITEM('',(#170169),#89195) ;
#83479 = STYLED_ITEM('',(#170169),#89196) ;
#83480 = STYLED_ITEM('',(#170169),#89197) ;
#83481 = STYLED_ITEM('',(#170169),#89198) ;
#83482 = STYLED_ITEM('',(#170169),#89199) ;
#83483 = STYLED_ITEM('',(#170169),#89200) ;
#83484 = STYLED_ITEM('',(#170169),#89201) ;
#83485 = STYLED_ITEM('',(#170169),#89202) ;
#83486 = STYLED_ITEM('',(#170169),#89203) ;
#83487 = STYLED_ITEM('',(#170169),#89204) ;
#83488 = STYLED_ITEM('',(#170169),#89205) ;
#83489 = STYLED_ITEM('',(#170169),#89206) ;
#83490 = STYLED_ITEM('',(#170169),#89207) ;
#83491 = STYLED_ITEM('',(#170169),#89208) ;
#83492 = STYLED_ITEM('',(#170169),#89209) ;
#83493 = STYLED_ITEM('',(#170169),#89210) ;
#83494 = STYLED_ITEM('',(#170169),#89211) ;
#83495 = STYLED_ITEM('',(#170169),#89212) ;
#83496 = STYLED_ITEM('',(#170169),#89213) ;
#83497 = STYLED_ITEM('',(#170169),#89214) ;
#83498 = STYLED_ITEM('',(#170169),#89215) ;
#83499 = STYLED_ITEM('',(#170169),#89216) ;
#83500 = STYLED_ITEM('',(#170169),#89217) ;
#83501 = STYLED_ITEM('',(#170169),#89218) ;
#83502 = STYLED_ITEM('',(#170169),#89219) ;
#83503 = STYLED_ITEM('',(#170169),#89220) ;
#83504 = STYLED_ITEM('',(#170169),#89221) ;
#83505 = STYLED_ITEM('',(#170169),#89222) ;
#83506 = STYLED_ITEM('',(#170169),#89223) ;
#83507 = STYLED_ITEM('',(#170169),#89224) ;
#83508 = STYLED_ITEM('',(#170169),#89225) ;
#83509 = STYLED_ITEM('',(#170169),#89226) ;
#83510 = STYLED_ITEM('',(#170169),#89227) ;
#83511 = STYLED_ITEM('',(#170169),#89228) ;
#83512 = STYLED_ITEM('',(#170169),#89229) ;
#83513 = STYLED_ITEM('',(#170169),#89230) ;
#83514 = STYLED_ITEM('',(#170169),#89231) ;
#83515 = STYLED_ITEM('',(#170169),#89232) ;
#83516 = STYLED_ITEM('',(#170169),#89233) ;
#83517 = STYLED_ITEM('',(#170169),#89234) ;
#83518 = STYLED_ITEM('',(#170169),#89235) ;
#83519 = STYLED_ITEM('',(#170169),#89236) ;
#83520 = STYLED_ITEM('',(#170169),#89237) ;
#83521 = STYLED_ITEM('',(#170169),#89238) ;
#83522 = STYLED_ITEM('',(#170169),#89239) ;
#83523 = STYLED_ITEM('',(#170169),#89240) ;
#83524 = STYLED_ITEM('',(#170169),#89241) ;
#83525 = STYLED_ITEM('',(#170169),#89242) ;
#83526 = STYLED_ITEM('',(#170169),#89243) ;
#83527 = STYLED_ITEM('',(#170169),#89244) ;
#83528 = STYLED_ITEM('',(#170169),#89245) ;
#83529 = STYLED_ITEM('',(#170169),#89246) ;
#83530 = STYLED_ITEM('',(#170169),#89247) ;
#83531 = STYLED_ITEM('',(#170169),#89248) ;
#83532 = STYLED_ITEM('',(#170169),#89249) ;
#83533 = STYLED_ITEM('',(#170169),#89250) ;
#83534 = STYLED_ITEM('',(#170169),#89251) ;
#83535 = STYLED_ITEM('',(#170169),#89252) ;
#83536 = STYLED_ITEM('',(#170169),#89253) ;
#83537 = STYLED_ITEM('',(#170169),#89254) ;
#83538 = STYLED_ITEM('',(#170169),#89255) ;
#83539 = STYLED_ITEM('',(#170169),#89256) ;
#83540 = STYLED_ITEM('',(#170169),#89257) ;
#83541 = STYLED_ITEM('',(#170169),#89258) ;
#83542 = STYLED_ITEM('',(#170169),#89259) ;
#83543 = STYLED_ITEM('',(#170169),#89260) ;
#83544 = STYLED_ITEM('',(#170169),#89261) ;
#83545 = STYLED_ITEM('',(#170169),#89262) ;
#83546 = STYLED_ITEM('',(#170169),#89263) ;
#83547 = STYLED_ITEM('',(#170169),#89264) ;
#83548 = STYLED_ITEM('',(#170169),#89265) ;
#83549 = STYLED_ITEM('',(#170169),#89266) ;
#83550 = STYLED_ITEM('',(#170169),#89267) ;
#83551 = STYLED_ITEM('',(#170169),#89268) ;
#83552 = STYLED_ITEM('',(#170169),#89269) ;
#83553 = STYLED_ITEM('',(#170169),#89270) ;
#83554 = STYLED_ITEM('',(#170169),#89271) ;
#83555 = STYLED_ITEM('',(#170169),#89272) ;
#83556 = STYLED_ITEM('',(#170169),#89273) ;
#83557 = STYLED_ITEM('',(#170169),#89274) ;
#83558 = STYLED_ITEM('',(#170169),#89275) ;
#83559 = STYLED_ITEM('',(#170169),#89276) ;
#83560 = STYLED_ITEM('',(#170169),#89277) ;
#83561 = STYLED_ITEM('',(#170169),#89278) ;
#83562 = STYLED_ITEM('',(#170169),#89279) ;
#83563 = STYLED_ITEM('',(#170169),#89280) ;
#83564 = STYLED_ITEM('',(#170169),#89281) ;
#83565 = STYLED_ITEM('',(#170169),#89282) ;
#83566 = STYLED_ITEM('',(#170169),#89283) ;
#83567 = STYLED_ITEM('',(#170169),#89284) ;
#83568 = STYLED_ITEM('',(#170169),#89285) ;
#83569 = STYLED_ITEM('',(#170169),#89286) ;
#83570 = STYLED_ITEM('',(#170169),#89287) ;
#83571 = STYLED_ITEM('',(#170169),#89288) ;
#83572 = STYLED_ITEM('',(#170169),#89289) ;
#83573 = STYLED_ITEM('',(#170169),#89290) ;
#83574 = STYLED_ITEM('',(#170169),#89291) ;
#83575 = STYLED_ITEM('',(#170169),#89292) ;
#83576 = STYLED_ITEM('',(#170169),#89293) ;
#83577 = STYLED_ITEM('',(#170169),#89294) ;
#83578 = STYLED_ITEM('',(#170169),#89295) ;
#83579 = STYLED_ITEM('',(#170169),#89296) ;
#83580 = STYLED_ITEM('',(#170169),#89297) ;
#83581 = STYLED_ITEM('',(#170169),#89298) ;
#83582 = STYLED_ITEM('',(#170169),#89299) ;
#83583 = STYLED_ITEM('',(#170169),#89300) ;
#83584 = STYLED_ITEM('',(#170169),#89301) ;
#83585 = STYLED_ITEM('',(#170169),#89302) ;
#83586 = STYLED_ITEM('',(#170169),#89303) ;
#83587 = STYLED_ITEM('',(#170169),#89304) ;
#83588 = STYLED_ITEM('',(#170169),#89305) ;
#83589 = STYLED_ITEM('',(#170169),#89306) ;
#83590 = STYLED_ITEM('',(#170169),#89307) ;
#83591 = STYLED_ITEM('',(#170169),#89308) ;
#83592 = STYLED_ITEM('',(#170169),#89309) ;
#83593 = STYLED_ITEM('',(#170169),#89310) ;
#83594 = STYLED_ITEM('',(#170169),#89311) ;
#83595 = STYLED_ITEM('',(#170169),#89312) ;
#83596 = STYLED_ITEM('',(#170169),#89313) ;
#83597 = STYLED_ITEM('',(#170169),#89314) ;
#83598 = STYLED_ITEM('',(#170169),#89315) ;
#83599 = STYLED_ITEM('',(#170169),#89316) ;
#83600 = STYLED_ITEM('',(#170169),#89317) ;
#83601 = STYLED_ITEM('',(#170169),#89318) ;
#83602 = STYLED_ITEM('',(#170169),#89319) ;
#83603 = STYLED_ITEM('',(#170169),#89320) ;
#83604 = STYLED_ITEM('',(#170169),#89321) ;
#83605 = STYLED_ITEM('',(#170169),#89322) ;
#83606 = STYLED_ITEM('',(#170169),#89323) ;
#83607 = STYLED_ITEM('',(#170171),#89324) ;
#83608 = STYLED_ITEM('',(#170171),#89325) ;
#83609 = STYLED_ITEM('',(#170171),#89326) ;
#83610 = STYLED_ITEM('',(#170171),#89327) ;
#83611 = STYLED_ITEM('',(#170171),#89328) ;
#83612 = STYLED_ITEM('',(#170171),#89329) ;
#83613 = STYLED_ITEM('',(#170171),#89330) ;
#83614 = STYLED_ITEM('',(#170171),#89331) ;
#83615 = STYLED_ITEM('',(#170171),#89332) ;
#83616 = STYLED_ITEM('',(#170169),#89333) ;
#83617 = STYLED_ITEM('',(#170169),#89334) ;
#83618 = STYLED_ITEM('',(#170169),#89335) ;
#83619 = STYLED_ITEM('',(#170169),#89336) ;
#83620 = STYLED_ITEM('',(#170169),#89337) ;
#83621 = STYLED_ITEM('',(#170169),#89338) ;
#83622 = STYLED_ITEM('',(#170169),#89339) ;
#83623 = STYLED_ITEM('',(#170169),#89340) ;
#83624 = STYLED_ITEM('',(#170169),#89341) ;
#83625 = STYLED_ITEM('',(#170169),#89342) ;
#83626 = STYLED_ITEM('',(#170169),#89343) ;
#83627 = STYLED_ITEM('',(#170169),#89344) ;
#83628 = STYLED_ITEM('',(#170169),#89345) ;
#83629 = STYLED_ITEM('',(#170169),#89346) ;
#83630 = STYLED_ITEM('',(#170169),#89347) ;
#83631 = STYLED_ITEM('',(#170169),#89348) ;
#83632 = STYLED_ITEM('',(#170169),#89349) ;
#83633 = STYLED_ITEM('',(#170169),#89350) ;
#83634 = STYLED_ITEM('',(#170169),#89351) ;
#83635 = STYLED_ITEM('',(#170169),#89352) ;
#83636 = STYLED_ITEM('',(#170169),#89353) ;
#83637 = STYLED_ITEM('',(#170169),#89354) ;
#83638 = STYLED_ITEM('',(#170169),#89355) ;
#83639 = STYLED_ITEM('',(#170169),#89356) ;
#83640 = STYLED_ITEM('',(#170169),#89357) ;
#83641 = STYLED_ITEM('',(#170169),#89358) ;
#83642 = STYLED_ITEM('',(#170169),#89359) ;
#83643 = STYLED_ITEM('',(#170169),#89360) ;
#83644 = STYLED_ITEM('',(#170169),#89361) ;
#83645 = STYLED_ITEM('',(#170169),#89362) ;
#83646 = STYLED_ITEM('',(#170169),#89363) ;
#83647 = STYLED_ITEM('',(#170169),#89364) ;
#83648 = STYLED_ITEM('',(#170169),#89365) ;
#83649 = STYLED_ITEM('',(#170169),#89366) ;
#83650 = STYLED_ITEM('',(#170169),#89367) ;
#83651 = STYLED_ITEM('',(#170169),#89368) ;
#83652 = STYLED_ITEM('',(#170169),#89369) ;
#83653 = STYLED_ITEM('',(#170169),#89370) ;
#83654 = STYLED_ITEM('',(#170169),#89371) ;
#83655 = STYLED_ITEM('',(#170169),#89372) ;
#83656 = STYLED_ITEM('',(#170169),#89373) ;
#83657 = STYLED_ITEM('',(#170169),#89374) ;
#83658 = STYLED_ITEM('',(#170169),#89375) ;
#83659 = STYLED_ITEM('',(#170169),#89376) ;
#83660 = STYLED_ITEM('',(#170169),#89377) ;
#83661 = STYLED_ITEM('',(#170169),#89378) ;
#83662 = STYLED_ITEM('',(#170169),#89379) ;
#83663 = STYLED_ITEM('',(#170169),#89380) ;
#83664 = STYLED_ITEM('',(#170169),#89381) ;
#83665 = STYLED_ITEM('',(#170169),#89382) ;
#83666 = STYLED_ITEM('',(#170169),#89383) ;
#83667 = STYLED_ITEM('',(#170169),#89384) ;
#83668 = STYLED_ITEM('',(#170169),#89385) ;
#83669 = STYLED_ITEM('',(#170169),#89386) ;
#83670 = STYLED_ITEM('',(#170169),#89387) ;
#83671 = STYLED_ITEM('',(#170169),#89388) ;
#83672 = STYLED_ITEM('',(#170169),#89389) ;
#83673 = STYLED_ITEM('',(#170169),#89390) ;
#83674 = STYLED_ITEM('',(#170169),#89391) ;
#83675 = STYLED_ITEM('',(#170169),#89392) ;
#83676 = STYLED_ITEM('',(#170169),#89393) ;
#83677 = STYLED_ITEM('',(#170169),#89394) ;
#83678 = STYLED_ITEM('',(#170169),#89395) ;
#83679 = STYLED_ITEM('',(#170169),#89396) ;
#83680 = STYLED_ITEM('',(#170169),#89397) ;
#83681 = STYLED_ITEM('',(#170169),#89398) ;
#83682 = STYLED_ITEM('',(#170169),#89399) ;
#83683 = STYLED_ITEM('',(#170169),#89400) ;
#83684 = STYLED_ITEM('',(#170169),#89401) ;
#83685 = STYLED_ITEM('',(#170169),#89402) ;
#83686 = STYLED_ITEM('',(#170169),#89403) ;
#83687 = STYLED_ITEM('',(#170169),#89404) ;
#83688 = STYLED_ITEM('',(#170169),#89405) ;
#83689 = STYLED_ITEM('',(#170169),#89406) ;
#83690 = STYLED_ITEM('',(#170169),#89407) ;
#83691 = STYLED_ITEM('',(#170169),#89408) ;
#83692 = STYLED_ITEM('',(#170169),#89409) ;
#83693 = STYLED_ITEM('',(#170169),#89410) ;
#83694 = STYLED_ITEM('',(#170169),#89411) ;
#83695 = STYLED_ITEM('',(#170169),#89412) ;
#83696 = STYLED_ITEM('',(#170169),#89413) ;
#83697 = STYLED_ITEM('',(#170169),#89414) ;
#83698 = STYLED_ITEM('',(#170169),#89415) ;
#83699 = STYLED_ITEM('',(#170169),#89416) ;
#83700 = STYLED_ITEM('',(#170169),#89417) ;
#83701 = STYLED_ITEM('',(#170169),#89418) ;
#83702 = STYLED_ITEM('',(#170169),#89419) ;
#83703 = STYLED_ITEM('',(#170169),#89420) ;
#83704 = STYLED_ITEM('',(#170169),#89421) ;
#83705 = STYLED_ITEM('',(#170169),#89422) ;
#83706 = STYLED_ITEM('',(#170172),#89423) ;
#83707 = STYLED_ITEM('',(#170172),#89424) ;
#83708 = STYLED_ITEM('',(#170172),#89425) ;
#83709 = STYLED_ITEM('',(#170172),#89426) ;
#83710 = STYLED_ITEM('',(#170172),#89427) ;
#83711 = STYLED_ITEM('',(#170172),#89428) ;
#83712 = STYLED_ITEM('',(#170172),#89429) ;
#83713 = STYLED_ITEM('',(#170172),#89430) ;
#83714 = STYLED_ITEM('',(#170172),#89431) ;
#83715 = STYLED_ITEM('',(#170172),#89432) ;
#83716 = STYLED_ITEM('',(#170172),#89433) ;
#83717 = STYLED_ITEM('',(#170172),#89434) ;
#83718 = STYLED_ITEM('',(#170172),#89435) ;
#83719 = STYLED_ITEM('',(#170172),#89436) ;
#83720 = STYLED_ITEM('',(#170172),#89437) ;
#83721 = STYLED_ITEM('',(#170172),#89438) ;
#83722 = STYLED_ITEM('',(#170172),#89439) ;
#83723 = STYLED_ITEM('',(#170172),#89440) ;
#83724 = STYLED_ITEM('',(#170172),#89441) ;
#83725 = STYLED_ITEM('',(#170172),#89442) ;
#83726 = STYLED_ITEM('',(#170172),#89443) ;
#83727 = STYLED_ITEM('',(#170172),#89444) ;
#83728 = STYLED_ITEM('',(#170172),#89445) ;
#83729 = STYLED_ITEM('',(#170172),#89446) ;
#83730 = STYLED_ITEM('',(#170172),#89447) ;
#83731 = STYLED_ITEM('',(#170172),#89448) ;
#83732 = STYLED_ITEM('',(#170172),#89449) ;
#83733 = STYLED_ITEM('',(#170172),#89450) ;
#83734 = STYLED_ITEM('',(#170172),#89451) ;
#83735 = STYLED_ITEM('',(#170172),#89452) ;
#83736 = STYLED_ITEM('',(#170172),#89453) ;
#83737 = STYLED_ITEM('',(#170172),#89454) ;
#83738 = STYLED_ITEM('',(#170172),#89455) ;
#83739 = STYLED_ITEM('',(#170172),#89456) ;
#83740 = STYLED_ITEM('',(#170172),#89457) ;
#83741 = STYLED_ITEM('',(#170172),#89458) ;
#83742 = STYLED_ITEM('',(#170169),#89459) ;
#83743 = STYLED_ITEM('',(#170169),#89460) ;
#83744 = STYLED_ITEM('',(#170169),#89461) ;
#83745 = STYLED_ITEM('',(#170169),#89462) ;
#83746 = STYLED_ITEM('',(#170169),#89463) ;
#83747 = STYLED_ITEM('',(#170169),#89464) ;
#83748 = STYLED_ITEM('',(#170169),#89465) ;
#83749 = STYLED_ITEM('',(#170169),#89466) ;
#83750 = STYLED_ITEM('',(#170169),#89467) ;
#83751 = STYLED_ITEM('',(#170169),#89468) ;
#83752 = STYLED_ITEM('',(#170169),#89469) ;
#83753 = STYLED_ITEM('',(#170169),#89470) ;
#83754 = STYLED_ITEM('',(#170169),#89471) ;
#83755 = STYLED_ITEM('',(#170169),#89472) ;
#83756 = STYLED_ITEM('',(#170169),#89473) ;
#83757 = STYLED_ITEM('',(#170169),#89474) ;
#83758 = STYLED_ITEM('',(#170169),#89475) ;
#83759 = STYLED_ITEM('',(#170169),#89476) ;
#83760 = STYLED_ITEM('',(#170169),#89477) ;
#83761 = STYLED_ITEM('',(#170169),#89478) ;
#83762 = STYLED_ITEM('',(#170169),#89479) ;
#83763 = STYLED_ITEM('',(#170169),#89480) ;
#83764 = STYLED_ITEM('',(#170169),#89481) ;
#83765 = STYLED_ITEM('',(#170169),#89482) ;
#83766 = STYLED_ITEM('',(#170169),#89483) ;
#83767 = STYLED_ITEM('',(#170169),#89484) ;
#83768 = STYLED_ITEM('',(#170169),#89485) ;
#83769 = STYLED_ITEM('',(#170169),#89486) ;
#83770 = STYLED_ITEM('',(#170169),#89487) ;
#83771 = STYLED_ITEM('',(#170169),#89488) ;
#83772 = STYLED_ITEM('',(#170169),#89489) ;
#83773 = STYLED_ITEM('',(#170169),#89490) ;
#83774 = STYLED_ITEM('',(#170169),#89491) ;
#83775 = STYLED_ITEM('',(#170169),#89492) ;
#83776 = STYLED_ITEM('',(#170169),#89493) ;
#83777 = STYLED_ITEM('',(#170169),#89494) ;
#83778 = STYLED_ITEM('',(#170169),#89495) ;
#83779 = STYLED_ITEM('',(#170169),#89496) ;
#83780 = STYLED_ITEM('',(#170169),#89497) ;
#83781 = STYLED_ITEM('',(#170169),#89498) ;
#83782 = STYLED_ITEM('',(#170169),#89499) ;
#83783 = STYLED_ITEM('',(#170169),#89500) ;
#83784 = STYLED_ITEM('',(#170169),#89501) ;
#83785 = STYLED_ITEM('',(#170169),#89502) ;
#83786 = STYLED_ITEM('',(#170169),#89503) ;
#83787 = STYLED_ITEM('',(#170169),#89504) ;
#83788 = STYLED_ITEM('',(#170169),#89505) ;
#83789 = STYLED_ITEM('',(#170169),#89506) ;
#83790 = STYLED_ITEM('',(#170169),#89507) ;
#83791 = STYLED_ITEM('',(#170169),#89508) ;
#83792 = STYLED_ITEM('',(#170169),#89509) ;
#83793 = STYLED_ITEM('',(#170169),#89510) ;
#83794 = STYLED_ITEM('',(#170169),#89511) ;
#83795 = STYLED_ITEM('',(#170169),#89512) ;
#83796 = STYLED_ITEM('',(#170169),#89513) ;
#83797 = STYLED_ITEM('',(#170169),#89514) ;
#83798 = STYLED_ITEM('',(#170169),#89515) ;
#83799 = STYLED_ITEM('',(#170169),#89516) ;
#83800 = STYLED_ITEM('',(#170169),#89517) ;
#83801 = STYLED_ITEM('',(#170169),#89518) ;
#83802 = STYLED_ITEM('',(#170169),#89519) ;
#83803 = STYLED_ITEM('',(#170169),#89520) ;
#83804 = STYLED_ITEM('',(#170169),#89521) ;
#83805 = STYLED_ITEM('',(#170169),#89522) ;
#83806 = STYLED_ITEM('',(#170169),#89523) ;
#83807 = STYLED_ITEM('',(#170169),#89524) ;
#83808 = STYLED_ITEM('',(#170169),#89525) ;
#83809 = STYLED_ITEM('',(#170169),#89526) ;
#83810 = STYLED_ITEM('',(#170169),#89527) ;
#83811 = STYLED_ITEM('',(#170169),#89528) ;
#83812 = STYLED_ITEM('',(#170169),#89529) ;
#83813 = STYLED_ITEM('',(#170169),#89530) ;
#83814 = STYLED_ITEM('',(#170169),#89531) ;
#83815 = STYLED_ITEM('',(#170169),#89532) ;
#83816 = STYLED_ITEM('',(#170169),#89533) ;
#83817 = STYLED_ITEM('',(#170169),#89534) ;
#83818 = STYLED_ITEM('',(#170169),#89535) ;
#83819 = STYLED_ITEM('',(#170169),#89536) ;
#83820 = STYLED_ITEM('',(#170169),#89537) ;
#83821 = STYLED_ITEM('',(#170169),#89538) ;
#83822 = STYLED_ITEM('',(#170169),#89539) ;
#83823 = STYLED_ITEM('',(#170169),#89540) ;
#83824 = STYLED_ITEM('',(#170169),#89541) ;
#83825 = STYLED_ITEM('',(#170169),#89542) ;
#83826 = STYLED_ITEM('',(#170169),#89543) ;
#83827 = STYLED_ITEM('',(#170169),#89544) ;
#83828 = STYLED_ITEM('',(#170169),#89545) ;
#83829 = STYLED_ITEM('',(#170169),#89546) ;
#83830 = STYLED_ITEM('',(#170169),#89547) ;
#83831 = STYLED_ITEM('',(#170169),#89548) ;
#83832 = STYLED_ITEM('',(#170169),#89549) ;
#83833 = STYLED_ITEM('',(#170169),#89550) ;
#83834 = STYLED_ITEM('',(#170169),#89551) ;
#83835 = STYLED_ITEM('',(#170169),#89552) ;
#83836 = STYLED_ITEM('',(#170169),#89553) ;
#83837 = STYLED_ITEM('',(#170169),#89554) ;
#83838 = STYLED_ITEM('',(#170169),#89555) ;
#83839 = STYLED_ITEM('',(#170169),#89556) ;
#83840 = STYLED_ITEM('',(#170169),#89557) ;
#83841 = STYLED_ITEM('',(#170169),#89558) ;
#83842 = STYLED_ITEM('',(#170169),#89559) ;
#83843 = STYLED_ITEM('',(#170169),#89560) ;
#83844 = STYLED_ITEM('',(#170169),#89561) ;
#83845 = STYLED_ITEM('',(#170169),#89562) ;
#83846 = STYLED_ITEM('',(#170169),#89563) ;
#83847 = STYLED_ITEM('',(#170169),#89564) ;
#83848 = STYLED_ITEM('',(#170169),#89565) ;
#83849 = STYLED_ITEM('',(#170169),#89566) ;
#83850 = STYLED_ITEM('',(#170169),#89567) ;
#83851 = STYLED_ITEM('',(#170169),#89568) ;
#83852 = STYLED_ITEM('',(#170169),#89569) ;
#83853 = STYLED_ITEM('',(#170169),#89570) ;
#83854 = STYLED_ITEM('',(#170169),#89571) ;
#83855 = STYLED_ITEM('',(#170169),#89572) ;
#83856 = STYLED_ITEM('',(#170169),#89573) ;
#83857 = STYLED_ITEM('',(#170169),#89574) ;
#83858 = STYLED_ITEM('',(#170169),#89575) ;
#83859 = STYLED_ITEM('',(#170169),#89576) ;
#83860 = STYLED_ITEM('',(#170169),#89577) ;
#83861 = STYLED_ITEM('',(#170169),#89578) ;
#83862 = STYLED_ITEM('',(#170169),#89579) ;
#83863 = STYLED_ITEM('',(#170169),#89580) ;
#83864 = STYLED_ITEM('',(#170169),#89581) ;
#83865 = STYLED_ITEM('',(#170169),#89582) ;
#83866 = STYLED_ITEM('',(#170169),#89583) ;
#83867 = STYLED_ITEM('',(#170169),#89584) ;
#83868 = STYLED_ITEM('',(#170169),#89585) ;
#83869 = STYLED_ITEM('',(#170169),#89586) ;
#83870 = STYLED_ITEM('',(#170169),#89587) ;
#83871 = STYLED_ITEM('',(#170169),#89588) ;
#83872 = STYLED_ITEM('',(#170169),#89589) ;
#83873 = STYLED_ITEM('',(#170169),#89590) ;
#83874 = STYLED_ITEM('',(#170169),#89591) ;
#83875 = STYLED_ITEM('',(#170169),#89592) ;
#83876 = STYLED_ITEM('',(#170169),#89593) ;
#83877 = STYLED_ITEM('',(#170169),#89594) ;
#83878 = STYLED_ITEM('',(#170169),#89595) ;
#83879 = STYLED_ITEM('',(#170169),#89596) ;
#83880 = STYLED_ITEM('',(#170169),#89597) ;
#83881 = STYLED_ITEM('',(#170169),#89598) ;
#83882 = STYLED_ITEM('',(#170169),#89599) ;
#83883 = STYLED_ITEM('',(#170169),#89600) ;
#83884 = STYLED_ITEM('',(#170169),#89601) ;
#83885 = STYLED_ITEM('',(#170169),#89602) ;
#83886 = STYLED_ITEM('',(#170169),#89603) ;
#83887 = STYLED_ITEM('',(#170169),#89604) ;
#83888 = STYLED_ITEM('',(#170169),#89605) ;
#83889 = STYLED_ITEM('',(#170169),#89606) ;
#83890 = STYLED_ITEM('',(#170169),#89607) ;
#83891 = STYLED_ITEM('',(#170169),#89608) ;
#83892 = STYLED_ITEM('',(#170169),#89609) ;
#83893 = STYLED_ITEM('',(#170169),#89610) ;
#83894 = STYLED_ITEM('',(#170169),#89611) ;
#83895 = STYLED_ITEM('',(#170169),#89612) ;
#83896 = STYLED_ITEM('',(#170169),#89613) ;
#83897 = STYLED_ITEM('',(#170169),#89614) ;
#83898 = STYLED_ITEM('',(#170169),#89615) ;
#83899 = STYLED_ITEM('',(#170169),#89616) ;
#83900 = STYLED_ITEM('',(#170169),#89617) ;
#83901 = STYLED_ITEM('',(#170169),#89618) ;
#83902 = STYLED_ITEM('',(#170169),#89619) ;
#83903 = STYLED_ITEM('',(#170169),#89620) ;
#83904 = STYLED_ITEM('',(#170169),#89621) ;
#83905 = STYLED_ITEM('',(#170169),#89622) ;
#83906 = STYLED_ITEM('',(#170169),#89623) ;
#83907 = STYLED_ITEM('',(#170169),#89624) ;
#83908 = STYLED_ITEM('',(#170169),#89625) ;
#83909 = STYLED_ITEM('',(#170169),#89626) ;
#83910 = STYLED_ITEM('',(#170169),#89627) ;
#83911 = STYLED_ITEM('',(#170169),#89628) ;
#83912 = STYLED_ITEM('',(#170169),#89629) ;
#83913 = STYLED_ITEM('',(#170169),#89630) ;
#83914 = STYLED_ITEM('',(#170169),#89631) ;
#83915 = STYLED_ITEM('',(#170169),#89632) ;
#83916 = STYLED_ITEM('',(#170169),#89633) ;
#83917 = STYLED_ITEM('',(#170169),#89634) ;
#83918 = STYLED_ITEM('',(#170169),#89635) ;
#83919 = STYLED_ITEM('',(#170169),#89636) ;
#83920 = STYLED_ITEM('',(#170169),#89637) ;
#83921 = STYLED_ITEM('',(#170169),#89638) ;
#83922 = STYLED_ITEM('',(#170169),#89639) ;
#83923 = STYLED_ITEM('',(#170169),#89640) ;
#83924 = STYLED_ITEM('',(#170169),#89641) ;
#83925 = STYLED_ITEM('',(#170169),#89642) ;
#83926 = STYLED_ITEM('',(#170169),#89643) ;
#83927 = STYLED_ITEM('',(#170169),#89644) ;
#83928 = STYLED_ITEM('',(#170169),#89645) ;
#83929 = STYLED_ITEM('',(#170169),#89646) ;
#83930 = STYLED_ITEM('',(#170169),#89647) ;
#83931 = STYLED_ITEM('',(#170169),#89648) ;
#83932 = STYLED_ITEM('',(#170169),#89649) ;
#83933 = STYLED_ITEM('',(#170169),#89650) ;
#83934 = STYLED_ITEM('',(#170169),#89651) ;
#83935 = STYLED_ITEM('',(#170169),#89652) ;
#83936 = STYLED_ITEM('',(#170169),#89653) ;
#83937 = STYLED_ITEM('',(#170169),#89654) ;
#83938 = STYLED_ITEM('',(#170169),#89655) ;
#83939 = STYLED_ITEM('',(#170169),#89656) ;
#83940 = STYLED_ITEM('',(#170169),#89657) ;
#83941 = STYLED_ITEM('',(#170169),#89658) ;
#83942 = STYLED_ITEM('',(#170169),#89659) ;
#83943 = STYLED_ITEM('',(#170169),#89660) ;
#83944 = STYLED_ITEM('',(#170169),#89661) ;
#83945 = STYLED_ITEM('',(#170169),#89662) ;
#83946 = STYLED_ITEM('',(#170169),#89663) ;
#83947 = STYLED_ITEM('',(#170169),#89664) ;
#83948 = STYLED_ITEM('',(#170169),#89665) ;
#83949 = STYLED_ITEM('',(#170169),#89666) ;
#83950 = STYLED_ITEM('',(#170169),#89667) ;
#83951 = STYLED_ITEM('',(#170169),#89668) ;
#83952 = STYLED_ITEM('',(#170169),#89669) ;
#83953 = STYLED_ITEM('',(#170169),#89670) ;
#83954 = STYLED_ITEM('',(#170169),#89671) ;
#83955 = STYLED_ITEM('',(#170169),#89672) ;
#83956 = STYLED_ITEM('',(#170169),#89673) ;
#83957 = STYLED_ITEM('',(#170169),#89674) ;
#83958 = STYLED_ITEM('',(#170169),#89675) ;
#83959 = STYLED_ITEM('',(#170169),#89676) ;
#83960 = STYLED_ITEM('',(#170169),#89677) ;
#83961 = STYLED_ITEM('',(#170169),#89678) ;
#83962 = STYLED_ITEM('',(#170169),#89679) ;
#83963 = STYLED_ITEM('',(#170169),#89680) ;
#83964 = STYLED_ITEM('',(#170169),#89681) ;
#83965 = STYLED_ITEM('',(#170169),#89682) ;
#83966 = STYLED_ITEM('',(#170169),#89683) ;
#83967 = STYLED_ITEM('',(#170169),#89684) ;
#83968 = STYLED_ITEM('',(#170169),#89685) ;
#83969 = STYLED_ITEM('',(#170169),#89686) ;
#83970 = STYLED_ITEM('',(#170169),#89687) ;
#83971 = STYLED_ITEM('',(#170169),#89688) ;
#83972 = STYLED_ITEM('',(#170169),#89689) ;
#83973 = STYLED_ITEM('',(#170169),#89690) ;
#83974 = STYLED_ITEM('',(#170169),#89691) ;
#83975 = STYLED_ITEM('',(#170169),#89692) ;
#83976 = STYLED_ITEM('',(#170169),#89693) ;
#83977 = STYLED_ITEM('',(#170169),#89694) ;
#83978 = STYLED_ITEM('',(#170169),#89695) ;
#83979 = STYLED_ITEM('',(#170169),#89696) ;
#83980 = STYLED_ITEM('',(#170169),#89697) ;
#83981 = STYLED_ITEM('',(#170169),#89698) ;
#83982 = STYLED_ITEM('',(#170169),#89699) ;
#83983 = STYLED_ITEM('',(#170169),#89700) ;
#83984 = STYLED_ITEM('',(#170169),#89701) ;
#83985 = STYLED_ITEM('',(#170169),#89702) ;
#83986 = STYLED_ITEM('',(#170169),#89703) ;
#83987 = STYLED_ITEM('',(#170169),#89704) ;
#83988 = STYLED_ITEM('',(#170169),#89705) ;
#83989 = STYLED_ITEM('',(#170169),#89706) ;
#83990 = STYLED_ITEM('',(#170169),#89707) ;
#83991 = STYLED_ITEM('',(#170169),#89708) ;
#83992 = STYLED_ITEM('',(#170169),#89709) ;
#83993 = STYLED_ITEM('',(#170169),#89710) ;
#83994 = STYLED_ITEM('',(#170169),#89711) ;
#83995 = STYLED_ITEM('',(#170169),#89712) ;
#83996 = STYLED_ITEM('',(#170169),#89713) ;
#83997 = STYLED_ITEM('',(#170169),#89714) ;
#83998 = STYLED_ITEM('',(#170169),#89715) ;
#83999 = STYLED_ITEM('',(#170169),#89716) ;
#84000 = STYLED_ITEM('',(#170169),#89717) ;
#84001 = STYLED_ITEM('',(#170169),#89718) ;
#84002 = STYLED_ITEM('',(#170169),#89719) ;
#84003 = STYLED_ITEM('',(#170169),#89720) ;
#84004 = STYLED_ITEM('',(#170169),#89721) ;
#84005 = STYLED_ITEM('',(#170169),#89722) ;
#84006 = STYLED_ITEM('',(#170169),#89723) ;
#84007 = STYLED_ITEM('',(#170169),#89724) ;
#84008 = STYLED_ITEM('',(#170169),#89725) ;
#84009 = STYLED_ITEM('',(#170169),#89726) ;
#84010 = STYLED_ITEM('',(#170169),#89727) ;
#84011 = STYLED_ITEM('',(#170169),#89728) ;
#84012 = STYLED_ITEM('',(#170169),#89729) ;
#84013 = STYLED_ITEM('',(#170169),#89730) ;
#84014 = STYLED_ITEM('',(#170169),#89731) ;
#84015 = STYLED_ITEM('',(#170169),#89732) ;
#84016 = STYLED_ITEM('',(#170169),#89733) ;
#84017 = STYLED_ITEM('',(#170169),#89734) ;
#84018 = STYLED_ITEM('',(#170169),#89735) ;
#84019 = STYLED_ITEM('',(#170169),#89736) ;
#84020 = STYLED_ITEM('',(#170169),#89737) ;
#84021 = STYLED_ITEM('',(#170169),#89738) ;
#84022 = STYLED_ITEM('',(#170169),#89739) ;
#84023 = STYLED_ITEM('',(#170169),#89740) ;
#84024 = STYLED_ITEM('',(#170169),#89741) ;
#84025 = STYLED_ITEM('',(#170169),#89742) ;
#84026 = STYLED_ITEM('',(#170169),#89743) ;
#84027 = STYLED_ITEM('',(#170172),#89744) ;
#84028 = STYLED_ITEM('',(#170172),#89745) ;
#84029 = STYLED_ITEM('',(#170172),#89746) ;
#84030 = STYLED_ITEM('',(#170172),#89747) ;
#84031 = STYLED_ITEM('',(#170169),#89748) ;
#84032 = STYLED_ITEM('',(#170169),#89749) ;
#84033 = STYLED_ITEM('',(#170169),#89750) ;
#84034 = STYLED_ITEM('',(#170169),#89751) ;
#84035 = STYLED_ITEM('',(#170169),#89752) ;
#84036 = STYLED_ITEM('',(#170169),#89753) ;
#84037 = STYLED_ITEM('',(#170169),#89754) ;
#84038 = STYLED_ITEM('',(#170169),#89755) ;
#84039 = STYLED_ITEM('',(#170169),#89756) ;
#84040 = STYLED_ITEM('',(#170169),#89757) ;
#84041 = STYLED_ITEM('',(#170169),#89758) ;
#84042 = STYLED_ITEM('',(#170169),#89759) ;
#84043 = STYLED_ITEM('',(#170169),#89760) ;
#84044 = STYLED_ITEM('',(#170169),#89761) ;
#84045 = STYLED_ITEM('',(#170169),#89762) ;
#84046 = STYLED_ITEM('',(#170169),#89763) ;
#84047 = STYLED_ITEM('',(#170169),#89764) ;
#84048 = STYLED_ITEM('',(#170169),#89765) ;
#84049 = STYLED_ITEM('',(#170169),#89766) ;
#84050 = STYLED_ITEM('',(#170169),#89767) ;
#84051 = STYLED_ITEM('',(#170169),#89768) ;
#84052 = STYLED_ITEM('',(#170169),#89769) ;
#84053 = STYLED_ITEM('',(#170169),#89770) ;
#84054 = STYLED_ITEM('',(#170169),#89771) ;
#84055 = STYLED_ITEM('',(#170169),#89772) ;
#84056 = STYLED_ITEM('',(#170169),#89773) ;
#84057 = STYLED_ITEM('',(#170169),#89774) ;
#84058 = STYLED_ITEM('',(#170169),#89775) ;
#84059 = STYLED_ITEM('',(#170169),#89776) ;
#84060 = STYLED_ITEM('',(#170169),#89777) ;
#84061 = STYLED_ITEM('',(#170169),#89778) ;
#84062 = STYLED_ITEM('',(#170169),#89779) ;
#84063 = STYLED_ITEM('',(#170169),#89780) ;
#84064 = STYLED_ITEM('',(#170169),#89781) ;
#84065 = STYLED_ITEM('',(#170169),#89782) ;
#84066 = STYLED_ITEM('',(#170169),#89783) ;
#84067 = STYLED_ITEM('',(#170169),#89784) ;
#84068 = STYLED_ITEM('',(#170169),#89785) ;
#84069 = STYLED_ITEM('',(#170169),#89786) ;
#84070 = STYLED_ITEM('',(#170169),#89787) ;
#84071 = STYLED_ITEM('',(#170169),#89788) ;
#84072 = STYLED_ITEM('',(#170169),#89789) ;
#84073 = STYLED_ITEM('',(#170169),#89790) ;
#84074 = STYLED_ITEM('',(#170169),#89791) ;
#84075 = STYLED_ITEM('',(#170169),#89792) ;
#84076 = STYLED_ITEM('',(#170169),#89793) ;
#84077 = STYLED_ITEM('',(#170169),#89794) ;
#84078 = STYLED_ITEM('',(#170169),#89795) ;
#84079 = STYLED_ITEM('',(#170169),#89796) ;
#84080 = STYLED_ITEM('',(#170169),#89797) ;
#84081 = STYLED_ITEM('',(#170169),#89798) ;
#84082 = STYLED_ITEM('',(#170169),#89799) ;
#84083 = STYLED_ITEM('',(#170169),#89800) ;
#84084 = STYLED_ITEM('',(#170169),#89801) ;
#84085 = STYLED_ITEM('',(#170169),#89802) ;
#84086 = STYLED_ITEM('',(#170169),#89803) ;
#84087 = STYLED_ITEM('',(#170169),#89804) ;
#84088 = STYLED_ITEM('',(#170169),#89805) ;
#84089 = STYLED_ITEM('',(#170169),#89806) ;
#84090 = STYLED_ITEM('',(#170169),#89807) ;
#84091 = STYLED_ITEM('',(#170169),#89808) ;
#84092 = STYLED_ITEM('',(#170169),#89809) ;
#84093 = STYLED_ITEM('',(#170169),#89810) ;
#84094 = STYLED_ITEM('',(#170169),#89811) ;
#84095 = STYLED_ITEM('',(#170169),#89812) ;
#84096 = STYLED_ITEM('',(#170169),#89813) ;
#84097 = STYLED_ITEM('',(#170169),#89814) ;
#84098 = STYLED_ITEM('',(#170169),#89815) ;
#84099 = STYLED_ITEM('',(#170169),#89816) ;
#84100 = STYLED_ITEM('',(#170169),#89817) ;
#84101 = STYLED_ITEM('',(#170169),#89818) ;
#84102 = STYLED_ITEM('',(#170169),#89819) ;
#84103 = STYLED_ITEM('',(#170169),#89820) ;
#84104 = STYLED_ITEM('',(#170169),#89821) ;
#84105 = STYLED_ITEM('',(#170169),#89822) ;
#84106 = STYLED_ITEM('',(#170169),#89823) ;
#84107 = STYLED_ITEM('',(#170169),#89824) ;
#84108 = STYLED_ITEM('',(#170169),#89825) ;
#84109 = STYLED_ITEM('',(#170169),#89826) ;
#84110 = STYLED_ITEM('',(#170169),#89827) ;
#84111 = STYLED_ITEM('',(#170169),#89828) ;
#84112 = STYLED_ITEM('',(#170169),#89829) ;
#84113 = STYLED_ITEM('',(#170169),#89830) ;
#84114 = STYLED_ITEM('',(#170169),#89831) ;
#84115 = STYLED_ITEM('',(#170169),#89832) ;
#84116 = STYLED_ITEM('',(#170169),#89833) ;
#84117 = STYLED_ITEM('',(#170169),#89834) ;
#84118 = STYLED_ITEM('',(#170169),#89835) ;
#84119 = STYLED_ITEM('',(#170169),#89836) ;
#84120 = STYLED_ITEM('',(#170169),#89837) ;
#84121 = STYLED_ITEM('',(#170169),#89838) ;
#84122 = STYLED_ITEM('',(#170169),#89839) ;
#84123 = STYLED_ITEM('',(#170169),#89840) ;
#84124 = STYLED_ITEM('',(#170169),#89841) ;
#84125 = STYLED_ITEM('',(#170169),#89842) ;
#84126 = STYLED_ITEM('',(#170169),#89843) ;
#84127 = STYLED_ITEM('',(#170169),#89844) ;
#84128 = STYLED_ITEM('',(#170169),#89845) ;
#84129 = STYLED_ITEM('',(#170169),#89846) ;
#84130 = STYLED_ITEM('',(#170169),#89847) ;
#84131 = STYLED_ITEM('',(#170169),#89848) ;
#84132 = STYLED_ITEM('',(#170169),#89849) ;
#84133 = STYLED_ITEM('',(#170169),#89850) ;
#84134 = STYLED_ITEM('',(#170169),#89851) ;
#84135 = STYLED_ITEM('',(#170169),#89852) ;
#84136 = STYLED_ITEM('',(#170169),#89853) ;
#84137 = STYLED_ITEM('',(#170169),#89854) ;
#84138 = STYLED_ITEM('',(#170169),#89855) ;
#84139 = STYLED_ITEM('',(#170169),#89856) ;
#84140 = STYLED_ITEM('',(#170169),#89857) ;
#84141 = STYLED_ITEM('',(#170169),#89858) ;
#84142 = STYLED_ITEM('',(#170169),#89859) ;
#84143 = STYLED_ITEM('',(#170169),#89860) ;
#84144 = STYLED_ITEM('',(#170169),#89861) ;
#84145 = STYLED_ITEM('',(#170169),#89862) ;
#84146 = STYLED_ITEM('',(#170169),#89863) ;
#84147 = STYLED_ITEM('',(#170169),#89864) ;
#84148 = STYLED_ITEM('',(#170169),#89865) ;
#84149 = STYLED_ITEM('',(#170169),#89866) ;
#84150 = STYLED_ITEM('',(#170169),#89867) ;
#84151 = STYLED_ITEM('',(#170169),#89868) ;
#84152 = STYLED_ITEM('',(#170169),#89869) ;
#84153 = STYLED_ITEM('',(#170169),#89870) ;
#84154 = STYLED_ITEM('',(#170169),#89871) ;
#84155 = STYLED_ITEM('',(#170169),#89872) ;
#84156 = STYLED_ITEM('',(#170169),#89873) ;
#84157 = STYLED_ITEM('',(#170169),#89874) ;
#84158 = STYLED_ITEM('',(#170169),#89875) ;
#84159 = STYLED_ITEM('',(#170169),#89876) ;
#84160 = STYLED_ITEM('',(#170169),#89877) ;
#84161 = STYLED_ITEM('',(#170169),#89878) ;
#84162 = STYLED_ITEM('',(#170169),#89879) ;
#84163 = STYLED_ITEM('',(#170169),#89880) ;
#84164 = STYLED_ITEM('',(#170169),#89881) ;
#84165 = STYLED_ITEM('',(#170169),#89882) ;
#84166 = STYLED_ITEM('',(#170169),#89883) ;
#84167 = STYLED_ITEM('',(#170172),#89884) ;
#84168 = STYLED_ITEM('',(#170172),#89885) ;
#84169 = STYLED_ITEM('',(#170172),#89886) ;
#84170 = STYLED_ITEM('',(#170172),#89887) ;
#84171 = STYLED_ITEM('',(#170169),#89888) ;
#84172 = STYLED_ITEM('',(#170169),#89889) ;
#84173 = STYLED_ITEM('',(#170169),#89890) ;
#84174 = STYLED_ITEM('',(#170169),#89891) ;
#84175 = STYLED_ITEM('',(#170169),#89892) ;
#84176 = STYLED_ITEM('',(#170169),#89893) ;
#84177 = STYLED_ITEM('',(#170169),#89894) ;
#84178 = STYLED_ITEM('',(#170169),#89895) ;
#84179 = STYLED_ITEM('',(#170169),#89896) ;
#84180 = STYLED_ITEM('',(#170169),#89897) ;
#84181 = STYLED_ITEM('',(#170169),#89898) ;
#84182 = STYLED_ITEM('',(#170169),#89899) ;
#84183 = STYLED_ITEM('',(#170169),#89900) ;
#84184 = STYLED_ITEM('',(#170169),#89901) ;
#84185 = STYLED_ITEM('',(#170169),#89902) ;
#84186 = STYLED_ITEM('',(#170169),#89903) ;
#84187 = STYLED_ITEM('',(#170169),#89904) ;
#84188 = STYLED_ITEM('',(#170169),#89905) ;
#84189 = STYLED_ITEM('',(#170169),#89906) ;
#84190 = STYLED_ITEM('',(#170169),#89907) ;
#84191 = STYLED_ITEM('',(#170169),#89908) ;
#84192 = STYLED_ITEM('',(#170169),#89909) ;
#84193 = STYLED_ITEM('',(#170169),#89910) ;
#84194 = STYLED_ITEM('',(#170169),#89911) ;
#84195 = STYLED_ITEM('',(#170169),#89912) ;
#84196 = STYLED_ITEM('',(#170169),#89913) ;
#84197 = STYLED_ITEM('',(#170169),#89914) ;
#84198 = STYLED_ITEM('',(#170169),#89915) ;
#84199 = STYLED_ITEM('',(#170169),#89916) ;
#84200 = STYLED_ITEM('',(#170169),#89917) ;
#84201 = STYLED_ITEM('',(#170169),#89918) ;
#84202 = STYLED_ITEM('',(#170169),#89919) ;
#84203 = STYLED_ITEM('',(#170169),#89920) ;
#84204 = STYLED_ITEM('',(#170169),#89921) ;
#84205 = STYLED_ITEM('',(#170169),#89922) ;
#84206 = STYLED_ITEM('',(#170169),#89923) ;
#84207 = STYLED_ITEM('',(#170169),#89924) ;
#84208 = STYLED_ITEM('',(#170169),#89925) ;
#84209 = STYLED_ITEM('',(#170169),#89926) ;
#84210 = STYLED_ITEM('',(#170169),#89927) ;
#84211 = STYLED_ITEM('',(#170169),#89928) ;
#84212 = STYLED_ITEM('',(#170169),#89929) ;
#84213 = STYLED_ITEM('',(#170169),#89930) ;
#84214 = STYLED_ITEM('',(#170169),#89931) ;
#84215 = STYLED_ITEM('',(#170169),#89932) ;
#84216 = STYLED_ITEM('',(#170169),#89933) ;
#84217 = STYLED_ITEM('',(#170169),#89934) ;
#84218 = STYLED_ITEM('',(#170169),#89935) ;
#84219 = STYLED_ITEM('',(#170169),#89936) ;
#84220 = STYLED_ITEM('',(#170169),#89937) ;
#84221 = STYLED_ITEM('',(#170169),#89938) ;
#84222 = STYLED_ITEM('',(#170169),#89939) ;
#84223 = STYLED_ITEM('',(#170169),#89940) ;
#84224 = STYLED_ITEM('',(#170169),#89941) ;
#84225 = STYLED_ITEM('',(#170169),#89942) ;
#84226 = STYLED_ITEM('',(#170169),#89943) ;
#84227 = STYLED_ITEM('',(#170169),#89944) ;
#84228 = STYLED_ITEM('',(#170169),#89945) ;
#84229 = STYLED_ITEM('',(#170169),#89946) ;
#84230 = STYLED_ITEM('',(#170169),#89947) ;
#84231 = STYLED_ITEM('',(#170169),#89948) ;
#84232 = STYLED_ITEM('',(#170169),#89949) ;
#84233 = STYLED_ITEM('',(#170169),#89950) ;
#84234 = STYLED_ITEM('',(#170169),#89951) ;
#84235 = STYLED_ITEM('',(#170169),#89952) ;
#84236 = STYLED_ITEM('',(#170169),#89953) ;
#84237 = STYLED_ITEM('',(#170169),#89954) ;
#84238 = STYLED_ITEM('',(#170169),#89955) ;
#84239 = STYLED_ITEM('',(#170169),#89956) ;
#84240 = STYLED_ITEM('',(#170169),#89957) ;
#84241 = STYLED_ITEM('',(#170169),#89958) ;
#84242 = STYLED_ITEM('',(#170169),#89959) ;
#84243 = STYLED_ITEM('',(#170169),#89960) ;
#84244 = STYLED_ITEM('',(#170169),#89961) ;
#84245 = STYLED_ITEM('',(#170169),#89962) ;
#84246 = STYLED_ITEM('',(#170169),#89963) ;
#84247 = STYLED_ITEM('',(#170169),#89964) ;
#84248 = STYLED_ITEM('',(#170169),#89965) ;
#84249 = STYLED_ITEM('',(#170169),#89966) ;
#84250 = STYLED_ITEM('',(#170169),#89967) ;
#84251 = STYLED_ITEM('',(#170169),#89968) ;
#84252 = STYLED_ITEM('',(#170169),#89969) ;
#84253 = STYLED_ITEM('',(#170169),#89970) ;
#84254 = STYLED_ITEM('',(#170169),#89971) ;
#84255 = STYLED_ITEM('',(#170169),#89972) ;
#84256 = STYLED_ITEM('',(#170169),#89973) ;
#84257 = STYLED_ITEM('',(#170169),#89974) ;
#84258 = STYLED_ITEM('',(#170169),#89975) ;
#84259 = STYLED_ITEM('',(#170169),#89976) ;
#84260 = STYLED_ITEM('',(#170169),#89977) ;
#84261 = STYLED_ITEM('',(#170169),#89978) ;
#84262 = STYLED_ITEM('',(#170169),#89979) ;
#84263 = STYLED_ITEM('',(#170169),#89980) ;
#84264 = STYLED_ITEM('',(#170169),#89981) ;
#84265 = STYLED_ITEM('',(#170169),#89982) ;
#84266 = STYLED_ITEM('',(#170169),#89983) ;
#84267 = STYLED_ITEM('',(#170169),#89984) ;
#84268 = STYLED_ITEM('',(#170169),#89985) ;
#84269 = STYLED_ITEM('',(#170169),#89986) ;
#84270 = STYLED_ITEM('',(#170169),#89987) ;
#84271 = STYLED_ITEM('',(#170169),#89988) ;
#84272 = STYLED_ITEM('',(#170169),#89989) ;
#84273 = STYLED_ITEM('',(#170169),#89990) ;
#84274 = STYLED_ITEM('',(#170169),#89991) ;
#84275 = STYLED_ITEM('',(#170169),#89992) ;
#84276 = STYLED_ITEM('',(#170169),#89993) ;
#84277 = STYLED_ITEM('',(#170169),#89994) ;
#84278 = STYLED_ITEM('',(#170169),#89995) ;
#84279 = STYLED_ITEM('',(#170169),#89996) ;
#84280 = STYLED_ITEM('',(#170169),#89997) ;
#84281 = STYLED_ITEM('',(#170169),#89998) ;
#84282 = STYLED_ITEM('',(#170169),#89999) ;
#84283 = STYLED_ITEM('',(#170169),#90000) ;
#84284 = STYLED_ITEM('',(#170169),#90001) ;
#84285 = STYLED_ITEM('',(#170169),#90002) ;
#84286 = STYLED_ITEM('',(#170169),#90003) ;
#84287 = STYLED_ITEM('',(#170169),#90004) ;
#84288 = STYLED_ITEM('',(#170169),#90005) ;
#84289 = STYLED_ITEM('',(#170169),#90006) ;
#84290 = STYLED_ITEM('',(#170169),#90007) ;
#84291 = STYLED_ITEM('',(#170169),#90008) ;
#84292 = STYLED_ITEM('',(#170169),#90009) ;
#84293 = STYLED_ITEM('',(#170169),#90010) ;
#84294 = STYLED_ITEM('',(#170169),#90011) ;
#84295 = STYLED_ITEM('',(#170169),#90012) ;
#84296 = STYLED_ITEM('',(#170169),#90013) ;
#84297 = STYLED_ITEM('',(#170169),#90014) ;
#84298 = STYLED_ITEM('',(#170169),#90015) ;
#84299 = STYLED_ITEM('',(#170169),#90016) ;
#84300 = STYLED_ITEM('',(#170169),#90017) ;
#84301 = STYLED_ITEM('',(#170169),#90018) ;
#84302 = STYLED_ITEM('',(#170169),#90019) ;
#84303 = STYLED_ITEM('',(#170169),#90020) ;
#84304 = STYLED_ITEM('',(#170169),#90021) ;
#84305 = STYLED_ITEM('',(#170169),#90022) ;
#84306 = STYLED_ITEM('',(#170169),#90023) ;
#84307 = STYLED_ITEM('',(#170172),#90024) ;
#84308 = STYLED_ITEM('',(#170172),#90025) ;
#84309 = STYLED_ITEM('',(#170172),#90026) ;
#84310 = STYLED_ITEM('',(#170172),#90027) ;
#84311 = STYLED_ITEM('',(#170169),#90028) ;
#84312 = STYLED_ITEM('',(#170169),#90029) ;
#84313 = STYLED_ITEM('',(#170169),#90030) ;
#84314 = STYLED_ITEM('',(#170169),#90031) ;
#84315 = STYLED_ITEM('',(#170169),#90032) ;
#84316 = STYLED_ITEM('',(#170169),#90033) ;
#84317 = STYLED_ITEM('',(#170169),#90034) ;
#84318 = STYLED_ITEM('',(#170169),#90035) ;
#84319 = STYLED_ITEM('',(#170169),#90036) ;
#84320 = STYLED_ITEM('',(#170169),#90037) ;
#84321 = STYLED_ITEM('',(#170169),#90038) ;
#84322 = STYLED_ITEM('',(#170169),#90039) ;
#84323 = STYLED_ITEM('',(#170169),#90040) ;
#84324 = STYLED_ITEM('',(#170169),#90041) ;
#84325 = STYLED_ITEM('',(#170169),#90042) ;
#84326 = STYLED_ITEM('',(#170169),#90043) ;
#84327 = STYLED_ITEM('',(#170169),#90044) ;
#84328 = STYLED_ITEM('',(#170169),#90045) ;
#84329 = STYLED_ITEM('',(#170169),#90046) ;
#84330 = STYLED_ITEM('',(#170169),#90047) ;
#84331 = STYLED_ITEM('',(#170169),#90048) ;
#84332 = STYLED_ITEM('',(#170169),#90049) ;
#84333 = STYLED_ITEM('',(#170169),#90050) ;
#84334 = STYLED_ITEM('',(#170169),#90051) ;
#84335 = STYLED_ITEM('',(#170169),#90052) ;
#84336 = STYLED_ITEM('',(#170169),#90053) ;
#84337 = STYLED_ITEM('',(#170169),#90054) ;
#84338 = STYLED_ITEM('',(#170169),#90055) ;
#84339 = STYLED_ITEM('',(#170169),#90056) ;
#84340 = STYLED_ITEM('',(#170169),#90057) ;
#84341 = STYLED_ITEM('',(#170169),#90058) ;
#84342 = STYLED_ITEM('',(#170169),#90059) ;
#84343 = STYLED_ITEM('',(#170169),#90060) ;
#84344 = STYLED_ITEM('',(#170169),#90061) ;
#84345 = STYLED_ITEM('',(#170169),#90062) ;
#84346 = STYLED_ITEM('',(#170169),#90063) ;
#84347 = STYLED_ITEM('',(#170169),#90064) ;
#84348 = STYLED_ITEM('',(#170169),#90065) ;
#84349 = STYLED_ITEM('',(#170169),#90066) ;
#84350 = STYLED_ITEM('',(#170169),#90067) ;
#84351 = STYLED_ITEM('',(#170169),#90068) ;
#84352 = STYLED_ITEM('',(#170169),#90069) ;
#84353 = STYLED_ITEM('',(#170169),#90070) ;
#84354 = STYLED_ITEM('',(#170169),#90071) ;
#84355 = STYLED_ITEM('',(#170169),#90072) ;
#84356 = STYLED_ITEM('',(#170169),#90073) ;
#84357 = STYLED_ITEM('',(#170169),#90074) ;
#84358 = STYLED_ITEM('',(#170169),#90075) ;
#84359 = STYLED_ITEM('',(#170169),#90076) ;
#84360 = STYLED_ITEM('',(#170169),#90077) ;
#84361 = STYLED_ITEM('',(#170169),#90078) ;
#84362 = STYLED_ITEM('',(#170169),#90079) ;
#84363 = STYLED_ITEM('',(#170169),#90080) ;
#84364 = STYLED_ITEM('',(#170169),#90081) ;
#84365 = STYLED_ITEM('',(#170169),#90082) ;
#84366 = STYLED_ITEM('',(#170169),#90083) ;
#84367 = STYLED_ITEM('',(#170169),#90084) ;
#84368 = STYLED_ITEM('',(#170169),#90085) ;
#84369 = STYLED_ITEM('',(#170169),#90086) ;
#84370 = STYLED_ITEM('',(#170169),#90087) ;
#84371 = STYLED_ITEM('',(#170169),#90088) ;
#84372 = STYLED_ITEM('',(#170169),#90089) ;
#84373 = STYLED_ITEM('',(#170169),#90090) ;
#84374 = STYLED_ITEM('',(#170169),#90091) ;
#84375 = STYLED_ITEM('',(#170169),#90092) ;
#84376 = STYLED_ITEM('',(#170169),#90093) ;
#84377 = STYLED_ITEM('',(#170169),#90094) ;
#84378 = STYLED_ITEM('',(#170169),#90095) ;
#84379 = STYLED_ITEM('',(#170169),#90096) ;
#84380 = STYLED_ITEM('',(#170169),#90097) ;
#84381 = STYLED_ITEM('',(#170169),#90098) ;
#84382 = STYLED_ITEM('',(#170169),#90099) ;
#84383 = STYLED_ITEM('',(#170169),#90100) ;
#84384 = STYLED_ITEM('',(#170169),#90101) ;
#84385 = STYLED_ITEM('',(#170169),#90102) ;
#84386 = STYLED_ITEM('',(#170169),#90103) ;
#84387 = STYLED_ITEM('',(#170169),#90104) ;
#84388 = STYLED_ITEM('',(#170169),#90105) ;
#84389 = STYLED_ITEM('',(#170169),#90106) ;
#84390 = STYLED_ITEM('',(#170169),#90107) ;
#84391 = STYLED_ITEM('',(#170169),#90108) ;
#84392 = STYLED_ITEM('',(#170169),#90109) ;
#84393 = STYLED_ITEM('',(#170169),#90110) ;
#84394 = STYLED_ITEM('',(#170169),#90111) ;
#84395 = STYLED_ITEM('',(#170169),#90112) ;
#84396 = STYLED_ITEM('',(#170169),#90113) ;
#84397 = STYLED_ITEM('',(#170169),#90114) ;
#84398 = STYLED_ITEM('',(#170169),#90115) ;
#84399 = STYLED_ITEM('',(#170169),#90116) ;
#84400 = STYLED_ITEM('',(#170169),#90117) ;
#84401 = STYLED_ITEM('',(#170169),#90118) ;
#84402 = STYLED_ITEM('',(#170169),#90119) ;
#84403 = STYLED_ITEM('',(#170169),#90120) ;
#84404 = STYLED_ITEM('',(#170169),#90121) ;
#84405 = STYLED_ITEM('',(#170169),#90122) ;
#84406 = STYLED_ITEM('',(#170169),#90123) ;
#84407 = STYLED_ITEM('',(#170169),#90124) ;
#84408 = STYLED_ITEM('',(#170169),#90125) ;
#84409 = STYLED_ITEM('',(#170169),#90126) ;
#84410 = STYLED_ITEM('',(#170169),#90127) ;
#84411 = STYLED_ITEM('',(#170169),#90128) ;
#84412 = STYLED_ITEM('',(#170169),#90129) ;
#84413 = STYLED_ITEM('',(#170169),#90130) ;
#84414 = STYLED_ITEM('',(#170169),#90131) ;
#84415 = STYLED_ITEM('',(#170169),#90132) ;
#84416 = STYLED_ITEM('',(#170169),#90133) ;
#84417 = STYLED_ITEM('',(#170169),#90134) ;
#84418 = STYLED_ITEM('',(#170169),#90135) ;
#84419 = STYLED_ITEM('',(#170169),#90136) ;
#84420 = STYLED_ITEM('',(#170169),#90137) ;
#84421 = STYLED_ITEM('',(#170169),#90138) ;
#84422 = STYLED_ITEM('',(#170169),#90139) ;
#84423 = STYLED_ITEM('',(#170169),#90140) ;
#84424 = STYLED_ITEM('',(#170169),#90141) ;
#84425 = STYLED_ITEM('',(#170169),#90142) ;
#84426 = STYLED_ITEM('',(#170169),#90143) ;
#84427 = STYLED_ITEM('',(#170169),#90144) ;
#84428 = STYLED_ITEM('',(#170169),#90145) ;
#84429 = STYLED_ITEM('',(#170169),#90146) ;
#84430 = STYLED_ITEM('',(#170169),#90147) ;
#84431 = STYLED_ITEM('',(#170169),#90148) ;
#84432 = STYLED_ITEM('',(#170169),#90149) ;
#84433 = STYLED_ITEM('',(#170169),#90150) ;
#84434 = STYLED_ITEM('',(#170169),#90151) ;
#84435 = STYLED_ITEM('',(#170169),#90152) ;
#84436 = STYLED_ITEM('',(#170169),#90153) ;
#84437 = STYLED_ITEM('',(#170169),#90154) ;
#84438 = STYLED_ITEM('',(#170169),#90155) ;
#84439 = STYLED_ITEM('',(#170169),#90156) ;
#84440 = STYLED_ITEM('',(#170169),#90157) ;
#84441 = STYLED_ITEM('',(#170169),#90158) ;
#84442 = STYLED_ITEM('',(#170169),#90159) ;
#84443 = STYLED_ITEM('',(#170169),#90160) ;
#84444 = STYLED_ITEM('',(#170169),#90161) ;
#84445 = STYLED_ITEM('',(#170169),#90162) ;
#84446 = STYLED_ITEM('',(#170169),#90163) ;
#84447 = STYLED_ITEM('',(#170172),#90164) ;
#84448 = STYLED_ITEM('',(#170172),#90165) ;
#84449 = STYLED_ITEM('',(#170172),#90166) ;
#84450 = STYLED_ITEM('',(#170172),#90167) ;
#84451 = STYLED_ITEM('',(#170169),#90168) ;
#84452 = STYLED_ITEM('',(#170169),#90169) ;
#84453 = STYLED_ITEM('',(#170169),#90170) ;
#84454 = STYLED_ITEM('',(#170169),#90171) ;
#84455 = STYLED_ITEM('',(#170169),#90172) ;
#84456 = STYLED_ITEM('',(#170169),#90173) ;
#84457 = STYLED_ITEM('',(#170169),#90174) ;
#84458 = STYLED_ITEM('',(#170169),#90175) ;
#84459 = STYLED_ITEM('',(#170169),#90176) ;
#84460 = STYLED_ITEM('',(#170169),#90177) ;
#84461 = STYLED_ITEM('',(#170169),#90178) ;
#84462 = STYLED_ITEM('',(#170169),#90179) ;
#84463 = STYLED_ITEM('',(#170169),#90180) ;
#84464 = STYLED_ITEM('',(#170169),#90181) ;
#84465 = STYLED_ITEM('',(#170169),#90182) ;
#84466 = STYLED_ITEM('',(#170169),#90183) ;
#84467 = STYLED_ITEM('',(#170169),#90184) ;
#84468 = STYLED_ITEM('',(#170169),#90185) ;
#84469 = STYLED_ITEM('',(#170169),#90186) ;
#84470 = STYLED_ITEM('',(#170169),#90187) ;
#84471 = STYLED_ITEM('',(#170169),#90188) ;
#84472 = STYLED_ITEM('',(#170169),#90189) ;
#84473 = STYLED_ITEM('',(#170169),#90190) ;
#84474 = STYLED_ITEM('',(#170169),#90191) ;
#84475 = STYLED_ITEM('',(#170169),#90192) ;
#84476 = STYLED_ITEM('',(#170169),#90193) ;
#84477 = STYLED_ITEM('',(#170169),#90194) ;
#84478 = STYLED_ITEM('',(#170169),#90195) ;
#84479 = STYLED_ITEM('',(#170169),#90196) ;
#84480 = STYLED_ITEM('',(#170169),#90197) ;
#84481 = STYLED_ITEM('',(#170169),#90198) ;
#84482 = STYLED_ITEM('',(#170169),#90199) ;
#84483 = STYLED_ITEM('',(#170169),#90200) ;
#84484 = STYLED_ITEM('',(#170169),#90201) ;
#84485 = STYLED_ITEM('',(#170169),#90202) ;
#84486 = STYLED_ITEM('',(#170169),#90203) ;
#84487 = STYLED_ITEM('',(#170169),#90204) ;
#84488 = STYLED_ITEM('',(#170169),#90205) ;
#84489 = STYLED_ITEM('',(#170169),#90206) ;
#84490 = STYLED_ITEM('',(#170169),#90207) ;
#84491 = STYLED_ITEM('',(#170169),#90208) ;
#84492 = STYLED_ITEM('',(#170169),#90209) ;
#84493 = STYLED_ITEM('',(#170169),#90210) ;
#84494 = STYLED_ITEM('',(#170169),#90211) ;
#84495 = STYLED_ITEM('',(#170169),#90212) ;
#84496 = STYLED_ITEM('',(#170169),#90213) ;
#84497 = STYLED_ITEM('',(#170169),#90214) ;
#84498 = STYLED_ITEM('',(#170169),#90215) ;
#84499 = STYLED_ITEM('',(#170169),#90216) ;
#84500 = STYLED_ITEM('',(#170169),#90217) ;
#84501 = STYLED_ITEM('',(#170169),#90218) ;
#84502 = STYLED_ITEM('',(#170169),#90219) ;
#84503 = STYLED_ITEM('',(#170169),#90220) ;
#84504 = STYLED_ITEM('',(#170169),#90221) ;
#84505 = STYLED_ITEM('',(#170169),#90222) ;
#84506 = STYLED_ITEM('',(#170169),#90223) ;
#84507 = STYLED_ITEM('',(#170169),#90224) ;
#84508 = STYLED_ITEM('',(#170169),#90225) ;
#84509 = STYLED_ITEM('',(#170169),#90226) ;
#84510 = STYLED_ITEM('',(#170169),#90227) ;
#84511 = STYLED_ITEM('',(#170169),#90228) ;
#84512 = STYLED_ITEM('',(#170169),#90229) ;
#84513 = STYLED_ITEM('',(#170169),#90230) ;
#84514 = STYLED_ITEM('',(#170169),#90231) ;
#84515 = STYLED_ITEM('',(#170169),#90232) ;
#84516 = STYLED_ITEM('',(#170169),#90233) ;
#84517 = STYLED_ITEM('',(#170169),#90234) ;
#84518 = STYLED_ITEM('',(#170169),#90235) ;
#84519 = STYLED_ITEM('',(#170169),#90236) ;
#84520 = STYLED_ITEM('',(#170169),#90237) ;
#84521 = STYLED_ITEM('',(#170169),#90238) ;
#84522 = STYLED_ITEM('',(#170169),#90239) ;
#84523 = STYLED_ITEM('',(#170169),#90240) ;
#84524 = STYLED_ITEM('',(#170169),#90241) ;
#84525 = STYLED_ITEM('',(#170169),#90242) ;
#84526 = STYLED_ITEM('',(#170169),#90243) ;
#84527 = STYLED_ITEM('',(#170169),#90244) ;
#84528 = STYLED_ITEM('',(#170169),#90245) ;
#84529 = STYLED_ITEM('',(#170169),#90246) ;
#84530 = STYLED_ITEM('',(#170169),#90247) ;
#84531 = STYLED_ITEM('',(#170169),#90248) ;
#84532 = STYLED_ITEM('',(#170169),#90249) ;
#84533 = STYLED_ITEM('',(#170169),#90250) ;
#84534 = STYLED_ITEM('',(#170169),#90251) ;
#84535 = STYLED_ITEM('',(#170169),#90252) ;
#84536 = STYLED_ITEM('',(#170169),#90253) ;
#84537 = STYLED_ITEM('',(#170169),#90254) ;
#84538 = STYLED_ITEM('',(#170169),#90255) ;
#84539 = STYLED_ITEM('',(#170169),#90256) ;
#84540 = STYLED_ITEM('',(#170169),#90257) ;
#84541 = STYLED_ITEM('',(#170169),#90258) ;
#84542 = STYLED_ITEM('',(#170169),#90259) ;
#84543 = STYLED_ITEM('',(#170169),#90260) ;
#84544 = STYLED_ITEM('',(#170169),#90261) ;
#84545 = STYLED_ITEM('',(#170169),#90262) ;
#84546 = STYLED_ITEM('',(#170169),#90263) ;
#84547 = STYLED_ITEM('',(#170169),#90264) ;
#84548 = STYLED_ITEM('',(#170169),#90265) ;
#84549 = STYLED_ITEM('',(#170169),#90266) ;
#84550 = STYLED_ITEM('',(#170169),#90267) ;
#84551 = STYLED_ITEM('',(#170169),#90268) ;
#84552 = STYLED_ITEM('',(#170169),#90269) ;
#84553 = STYLED_ITEM('',(#170169),#90270) ;
#84554 = STYLED_ITEM('',(#170169),#90271) ;
#84555 = STYLED_ITEM('',(#170169),#90272) ;
#84556 = STYLED_ITEM('',(#170169),#90273) ;
#84557 = STYLED_ITEM('',(#170169),#90274) ;
#84558 = STYLED_ITEM('',(#170169),#90275) ;
#84559 = STYLED_ITEM('',(#170169),#90276) ;
#84560 = STYLED_ITEM('',(#170169),#90277) ;
#84561 = STYLED_ITEM('',(#170169),#90278) ;
#84562 = STYLED_ITEM('',(#170169),#90279) ;
#84563 = STYLED_ITEM('',(#170169),#90280) ;
#84564 = STYLED_ITEM('',(#170169),#90281) ;
#84565 = STYLED_ITEM('',(#170169),#90282) ;
#84566 = STYLED_ITEM('',(#170169),#90283) ;
#84567 = STYLED_ITEM('',(#170169),#90284) ;
#84568 = STYLED_ITEM('',(#170169),#90285) ;
#84569 = STYLED_ITEM('',(#170169),#90286) ;
#84570 = STYLED_ITEM('',(#170169),#90287) ;
#84571 = STYLED_ITEM('',(#170169),#90288) ;
#84572 = STYLED_ITEM('',(#170169),#90289) ;
#84573 = STYLED_ITEM('',(#170169),#90290) ;
#84574 = STYLED_ITEM('',(#170169),#90291) ;
#84575 = STYLED_ITEM('',(#170169),#90292) ;
#84576 = STYLED_ITEM('',(#170169),#90293) ;
#84577 = STYLED_ITEM('',(#170169),#90294) ;
#84578 = STYLED_ITEM('',(#170169),#90295) ;
#84579 = STYLED_ITEM('',(#170169),#90296) ;
#84580 = STYLED_ITEM('',(#170169),#90297) ;
#84581 = STYLED_ITEM('',(#170169),#90298) ;
#84582 = STYLED_ITEM('',(#170169),#90299) ;
#84583 = STYLED_ITEM('',(#170169),#90300) ;
#84584 = STYLED_ITEM('',(#170169),#90301) ;
#84585 = STYLED_ITEM('',(#170169),#90302) ;
#84586 = STYLED_ITEM('',(#170169),#90303) ;
#84587 = STYLED_ITEM('',(#170172),#90304) ;
#84588 = STYLED_ITEM('',(#170172),#90305) ;
#84589 = STYLED_ITEM('',(#170172),#90306) ;
#84590 = STYLED_ITEM('',(#170172),#90307) ;
#84591 = STYLED_ITEM('',(#170169),#90308) ;
#84592 = STYLED_ITEM('',(#170169),#90309) ;
#84593 = STYLED_ITEM('',(#170169),#90310) ;
#84594 = STYLED_ITEM('',(#170169),#90311) ;
#84595 = STYLED_ITEM('',(#170169),#90312) ;
#84596 = STYLED_ITEM('',(#170169),#90313) ;
#84597 = STYLED_ITEM('',(#170169),#90314) ;
#84598 = STYLED_ITEM('',(#170169),#90315) ;
#84599 = STYLED_ITEM('',(#170169),#90316) ;
#84600 = STYLED_ITEM('',(#170169),#90317) ;
#84601 = STYLED_ITEM('',(#170169),#90318) ;
#84602 = STYLED_ITEM('',(#170169),#90319) ;
#84603 = STYLED_ITEM('',(#170169),#90320) ;
#84604 = STYLED_ITEM('',(#170169),#90321) ;
#84605 = STYLED_ITEM('',(#170169),#90322) ;
#84606 = STYLED_ITEM('',(#170169),#90323) ;
#84607 = STYLED_ITEM('',(#170169),#90324) ;
#84608 = STYLED_ITEM('',(#170169),#90325) ;
#84609 = STYLED_ITEM('',(#170169),#90326) ;
#84610 = STYLED_ITEM('',(#170169),#90327) ;
#84611 = STYLED_ITEM('',(#170169),#90328) ;
#84612 = STYLED_ITEM('',(#170169),#90329) ;
#84613 = STYLED_ITEM('',(#170169),#90330) ;
#84614 = STYLED_ITEM('',(#170169),#90331) ;
#84615 = STYLED_ITEM('',(#170169),#90332) ;
#84616 = STYLED_ITEM('',(#170169),#90333) ;
#84617 = STYLED_ITEM('',(#170169),#90334) ;
#84618 = STYLED_ITEM('',(#170169),#90335) ;
#84619 = STYLED_ITEM('',(#170169),#90336) ;
#84620 = STYLED_ITEM('',(#170169),#90337) ;
#84621 = STYLED_ITEM('',(#170169),#90338) ;
#84622 = STYLED_ITEM('',(#170169),#90339) ;
#84623 = STYLED_ITEM('',(#170169),#90340) ;
#84624 = STYLED_ITEM('',(#170169),#90341) ;
#84625 = STYLED_ITEM('',(#170169),#90342) ;
#84626 = STYLED_ITEM('',(#170169),#90343) ;
#84627 = STYLED_ITEM('',(#170169),#90344) ;
#84628 = STYLED_ITEM('',(#170169),#90345) ;
#84629 = STYLED_ITEM('',(#170169),#90346) ;
#84630 = STYLED_ITEM('',(#170169),#90347) ;
#84631 = STYLED_ITEM('',(#170169),#90348) ;
#84632 = STYLED_ITEM('',(#170169),#90349) ;
#84633 = STYLED_ITEM('',(#170169),#90350) ;
#84634 = STYLED_ITEM('',(#170169),#90351) ;
#84635 = STYLED_ITEM('',(#170169),#90352) ;
#84636 = STYLED_ITEM('',(#170169),#90353) ;
#84637 = STYLED_ITEM('',(#170169),#90354) ;
#84638 = STYLED_ITEM('',(#170169),#90355) ;
#84639 = STYLED_ITEM('',(#170169),#90356) ;
#84640 = STYLED_ITEM('',(#170169),#90357) ;
#84641 = STYLED_ITEM('',(#170169),#90358) ;
#84642 = STYLED_ITEM('',(#170169),#90359) ;
#84643 = STYLED_ITEM('',(#170169),#90360) ;
#84644 = STYLED_ITEM('',(#170169),#90361) ;
#84645 = STYLED_ITEM('',(#170169),#90362) ;
#84646 = STYLED_ITEM('',(#170169),#90363) ;
#84647 = STYLED_ITEM('',(#170169),#90364) ;
#84648 = STYLED_ITEM('',(#170169),#90365) ;
#84649 = STYLED_ITEM('',(#170169),#90366) ;
#84650 = STYLED_ITEM('',(#170169),#90367) ;
#84651 = STYLED_ITEM('',(#170169),#90368) ;
#84652 = STYLED_ITEM('',(#170169),#90369) ;
#84653 = STYLED_ITEM('',(#170169),#90370) ;
#84654 = STYLED_ITEM('',(#170169),#90371) ;
#84655 = STYLED_ITEM('',(#170169),#90372) ;
#84656 = STYLED_ITEM('',(#170169),#90373) ;
#84657 = STYLED_ITEM('',(#170169),#90374) ;
#84658 = STYLED_ITEM('',(#170169),#90375) ;
#84659 = STYLED_ITEM('',(#170169),#90376) ;
#84660 = STYLED_ITEM('',(#170169),#90377) ;
#84661 = STYLED_ITEM('',(#170169),#90378) ;
#84662 = STYLED_ITEM('',(#170169),#90379) ;
#84663 = STYLED_ITEM('',(#170169),#90380) ;
#84664 = STYLED_ITEM('',(#170169),#90381) ;
#84665 = STYLED_ITEM('',(#170169),#90382) ;
#84666 = STYLED_ITEM('',(#170169),#90383) ;
#84667 = STYLED_ITEM('',(#170169),#90384) ;
#84668 = STYLED_ITEM('',(#170169),#90385) ;
#84669 = STYLED_ITEM('',(#170169),#90386) ;
#84670 = STYLED_ITEM('',(#170169),#90387) ;
#84671 = STYLED_ITEM('',(#170169),#90388) ;
#84672 = STYLED_ITEM('',(#170169),#90389) ;
#84673 = STYLED_ITEM('',(#170169),#90390) ;
#84674 = STYLED_ITEM('',(#170169),#90391) ;
#84675 = STYLED_ITEM('',(#170169),#90392) ;
#84676 = STYLED_ITEM('',(#170169),#90393) ;
#84677 = STYLED_ITEM('',(#170169),#90394) ;
#84678 = STYLED_ITEM('',(#170169),#90395) ;
#84679 = STYLED_ITEM('',(#170169),#90396) ;
#84680 = STYLED_ITEM('',(#170169),#90397) ;
#84681 = STYLED_ITEM('',(#170169),#90398) ;
#84682 = STYLED_ITEM('',(#170169),#90399) ;
#84683 = STYLED_ITEM('',(#170169),#90400) ;
#84684 = STYLED_ITEM('',(#170169),#90401) ;
#84685 = STYLED_ITEM('',(#170169),#90402) ;
#84686 = STYLED_ITEM('',(#170169),#90403) ;
#84687 = STYLED_ITEM('',(#170169),#90404) ;
#84688 = STYLED_ITEM('',(#170169),#90405) ;
#84689 = STYLED_ITEM('',(#170169),#90406) ;
#84690 = STYLED_ITEM('',(#170169),#90407) ;
#84691 = STYLED_ITEM('',(#170169),#90408) ;
#84692 = STYLED_ITEM('',(#170169),#90409) ;
#84693 = STYLED_ITEM('',(#170169),#90410) ;
#84694 = STYLED_ITEM('',(#170169),#90411) ;
#84695 = STYLED_ITEM('',(#170169),#90412) ;
#84696 = STYLED_ITEM('',(#170169),#90413) ;
#84697 = STYLED_ITEM('',(#170169),#90414) ;
#84698 = STYLED_ITEM('',(#170169),#90415) ;
#84699 = STYLED_ITEM('',(#170169),#90416) ;
#84700 = STYLED_ITEM('',(#170169),#90417) ;
#84701 = STYLED_ITEM('',(#170169),#90418) ;
#84702 = STYLED_ITEM('',(#170169),#90419) ;
#84703 = STYLED_ITEM('',(#170169),#90420) ;
#84704 = STYLED_ITEM('',(#170169),#90421) ;
#84705 = STYLED_ITEM('',(#170169),#90422) ;
#84706 = STYLED_ITEM('',(#170169),#90423) ;
#84707 = STYLED_ITEM('',(#170169),#90424) ;
#84708 = STYLED_ITEM('',(#170169),#90425) ;
#84709 = STYLED_ITEM('',(#170169),#90426) ;
#84710 = STYLED_ITEM('',(#170169),#90427) ;
#84711 = STYLED_ITEM('',(#170169),#90428) ;
#84712 = STYLED_ITEM('',(#170169),#90429) ;
#84713 = STYLED_ITEM('',(#170169),#90430) ;
#84714 = STYLED_ITEM('',(#170169),#90431) ;
#84715 = STYLED_ITEM('',(#170169),#90432) ;
#84716 = STYLED_ITEM('',(#170169),#90433) ;
#84717 = STYLED_ITEM('',(#170169),#90434) ;
#84718 = STYLED_ITEM('',(#170169),#90435) ;
#84719 = STYLED_ITEM('',(#170169),#90436) ;
#84720 = STYLED_ITEM('',(#170169),#90437) ;
#84721 = STYLED_ITEM('',(#170169),#90438) ;
#84722 = STYLED_ITEM('',(#170169),#90439) ;
#84723 = STYLED_ITEM('',(#170169),#90440) ;
#84724 = STYLED_ITEM('',(#170169),#90441) ;
#84725 = STYLED_ITEM('',(#170169),#90442) ;
#84726 = STYLED_ITEM('',(#170169),#90443) ;
#84727 = STYLED_ITEM('',(#170172),#90444) ;
#84728 = STYLED_ITEM('',(#170172),#90445) ;
#84729 = STYLED_ITEM('',(#170172),#90446) ;
#84730 = STYLED_ITEM('',(#170172),#90447) ;
#84731 = STYLED_ITEM('',(#170169),#90448) ;
#84732 = STYLED_ITEM('',(#170169),#90449) ;
#84733 = STYLED_ITEM('',(#170169),#90450) ;
#84734 = STYLED_ITEM('',(#170169),#90451) ;
#84735 = STYLED_ITEM('',(#170169),#90452) ;
#84736 = STYLED_ITEM('',(#170169),#90453) ;
#84737 = STYLED_ITEM('',(#170169),#90454) ;
#84738 = STYLED_ITEM('',(#170169),#90455) ;
#84739 = STYLED_ITEM('',(#170169),#90456) ;
#84740 = STYLED_ITEM('',(#170169),#90457) ;
#84741 = STYLED_ITEM('',(#170169),#90458) ;
#84742 = STYLED_ITEM('',(#170169),#90459) ;
#84743 = STYLED_ITEM('',(#170169),#90460) ;
#84744 = STYLED_ITEM('',(#170169),#90461) ;
#84745 = STYLED_ITEM('',(#170169),#90462) ;
#84746 = STYLED_ITEM('',(#170169),#90463) ;
#84747 = STYLED_ITEM('',(#170169),#90464) ;
#84748 = STYLED_ITEM('',(#170169),#90465) ;
#84749 = STYLED_ITEM('',(#170169),#90466) ;
#84750 = STYLED_ITEM('',(#170169),#90467) ;
#84751 = STYLED_ITEM('',(#170169),#90468) ;
#84752 = STYLED_ITEM('',(#170169),#90469) ;
#84753 = STYLED_ITEM('',(#170169),#90470) ;
#84754 = STYLED_ITEM('',(#170169),#90471) ;
#84755 = STYLED_ITEM('',(#170169),#90472) ;
#84756 = STYLED_ITEM('',(#170169),#90473) ;
#84757 = STYLED_ITEM('',(#170169),#90474) ;
#84758 = STYLED_ITEM('',(#170169),#90475) ;
#84759 = STYLED_ITEM('',(#170169),#90476) ;
#84760 = STYLED_ITEM('',(#170169),#90477) ;
#84761 = STYLED_ITEM('',(#170169),#90478) ;
#84762 = STYLED_ITEM('',(#170169),#90479) ;
#84763 = STYLED_ITEM('',(#170169),#90480) ;
#84764 = STYLED_ITEM('',(#170169),#90481) ;
#84765 = STYLED_ITEM('',(#170169),#90482) ;
#84766 = STYLED_ITEM('',(#170169),#90483) ;
#84767 = STYLED_ITEM('',(#170169),#90484) ;
#84768 = STYLED_ITEM('',(#170169),#90485) ;
#84769 = STYLED_ITEM('',(#170169),#90486) ;
#84770 = STYLED_ITEM('',(#170169),#90487) ;
#84771 = STYLED_ITEM('',(#170169),#90488) ;
#84772 = STYLED_ITEM('',(#170169),#90489) ;
#84773 = STYLED_ITEM('',(#170169),#90490) ;
#84774 = STYLED_ITEM('',(#170169),#90491) ;
#84775 = STYLED_ITEM('',(#170169),#90492) ;
#84776 = STYLED_ITEM('',(#170169),#90493) ;
#84777 = STYLED_ITEM('',(#170169),#90494) ;
#84778 = STYLED_ITEM('',(#170169),#90495) ;
#84779 = STYLED_ITEM('',(#170169),#90496) ;
#84780 = STYLED_ITEM('',(#170169),#90497) ;
#84781 = STYLED_ITEM('',(#170169),#90498) ;
#84782 = STYLED_ITEM('',(#170169),#90499) ;
#84783 = STYLED_ITEM('',(#170169),#90500) ;
#84784 = STYLED_ITEM('',(#170169),#90501) ;
#84785 = STYLED_ITEM('',(#170169),#90502) ;
#84786 = STYLED_ITEM('',(#170169),#90503) ;
#84787 = STYLED_ITEM('',(#170169),#90504) ;
#84788 = STYLED_ITEM('',(#170169),#90505) ;
#84789 = STYLED_ITEM('',(#170169),#90506) ;
#84790 = STYLED_ITEM('',(#170169),#90507) ;
#84791 = STYLED_ITEM('',(#170169),#90508) ;
#84792 = STYLED_ITEM('',(#170169),#90509) ;
#84793 = STYLED_ITEM('',(#170169),#90510) ;
#84794 = STYLED_ITEM('',(#170169),#90511) ;
#84795 = STYLED_ITEM('',(#170169),#90512) ;
#84796 = STYLED_ITEM('',(#170169),#90513) ;
#84797 = STYLED_ITEM('',(#170169),#90514) ;
#84798 = STYLED_ITEM('',(#170169),#90515) ;
#84799 = STYLED_ITEM('',(#170169),#90516) ;
#84800 = STYLED_ITEM('',(#170169),#90517) ;
#84801 = STYLED_ITEM('',(#170169),#90518) ;
#84802 = STYLED_ITEM('',(#170169),#90519) ;
#84803 = STYLED_ITEM('',(#170169),#90520) ;
#84804 = STYLED_ITEM('',(#170169),#90521) ;
#84805 = STYLED_ITEM('',(#170169),#90522) ;
#84806 = STYLED_ITEM('',(#170169),#90523) ;
#84807 = STYLED_ITEM('',(#170169),#90524) ;
#84808 = STYLED_ITEM('',(#170169),#90525) ;
#84809 = STYLED_ITEM('',(#170169),#90526) ;
#84810 = STYLED_ITEM('',(#170169),#90527) ;
#84811 = STYLED_ITEM('',(#170169),#90528) ;
#84812 = STYLED_ITEM('',(#170169),#90529) ;
#84813 = STYLED_ITEM('',(#170169),#90530) ;
#84814 = STYLED_ITEM('',(#170169),#90531) ;
#84815 = STYLED_ITEM('',(#170169),#90532) ;
#84816 = STYLED_ITEM('',(#170169),#90533) ;
#84817 = STYLED_ITEM('',(#170169),#90534) ;
#84818 = STYLED_ITEM('',(#170169),#90535) ;
#84819 = STYLED_ITEM('',(#170169),#90536) ;
#84820 = STYLED_ITEM('',(#170169),#90537) ;
#84821 = STYLED_ITEM('',(#170169),#90538) ;
#84822 = STYLED_ITEM('',(#170169),#90539) ;
#84823 = STYLED_ITEM('',(#170169),#90540) ;
#84824 = STYLED_ITEM('',(#170169),#90541) ;
#84825 = STYLED_ITEM('',(#170169),#90542) ;
#84826 = STYLED_ITEM('',(#170169),#90543) ;
#84827 = STYLED_ITEM('',(#170169),#90544) ;
#84828 = STYLED_ITEM('',(#170169),#90545) ;
#84829 = STYLED_ITEM('',(#170169),#90546) ;
#84830 = STYLED_ITEM('',(#170169),#90547) ;
#84831 = STYLED_ITEM('',(#170169),#90548) ;
#84832 = STYLED_ITEM('',(#170169),#90549) ;
#84833 = STYLED_ITEM('',(#170169),#90550) ;
#84834 = STYLED_ITEM('',(#170169),#90551) ;
#84835 = STYLED_ITEM('',(#170169),#90552) ;
#84836 = STYLED_ITEM('',(#170169),#90553) ;
#84837 = STYLED_ITEM('',(#170169),#90554) ;
#84838 = STYLED_ITEM('',(#170169),#90555) ;
#84839 = STYLED_ITEM('',(#170169),#90556) ;
#84840 = STYLED_ITEM('',(#170169),#90557) ;
#84841 = STYLED_ITEM('',(#170169),#90558) ;
#84842 = STYLED_ITEM('',(#170169),#90559) ;
#84843 = STYLED_ITEM('',(#170169),#90560) ;
#84844 = STYLED_ITEM('',(#170169),#90561) ;
#84845 = STYLED_ITEM('',(#170169),#90562) ;
#84846 = STYLED_ITEM('',(#170169),#90563) ;
#84847 = STYLED_ITEM('',(#170169),#90564) ;
#84848 = STYLED_ITEM('',(#170169),#90565) ;
#84849 = STYLED_ITEM('',(#170169),#90566) ;
#84850 = STYLED_ITEM('',(#170169),#90567) ;
#84851 = STYLED_ITEM('',(#170169),#90568) ;
#84852 = STYLED_ITEM('',(#170169),#90569) ;
#84853 = STYLED_ITEM('',(#170169),#90570) ;
#84854 = STYLED_ITEM('',(#170169),#90571) ;
#84855 = STYLED_ITEM('',(#170169),#90572) ;
#84856 = STYLED_ITEM('',(#170169),#90573) ;
#84857 = STYLED_ITEM('',(#170169),#90574) ;
#84858 = STYLED_ITEM('',(#170169),#90575) ;
#84859 = STYLED_ITEM('',(#170169),#90576) ;
#84860 = STYLED_ITEM('',(#170169),#90577) ;
#84861 = STYLED_ITEM('',(#170169),#90578) ;
#84862 = STYLED_ITEM('',(#170169),#90579) ;
#84863 = STYLED_ITEM('',(#170169),#90580) ;
#84864 = STYLED_ITEM('',(#170169),#90581) ;
#84865 = STYLED_ITEM('',(#170169),#90582) ;
#84866 = STYLED_ITEM('',(#170169),#90583) ;
#84867 = STYLED_ITEM('',(#170172),#90584) ;
#84868 = STYLED_ITEM('',(#170172),#90585) ;
#84869 = STYLED_ITEM('',(#170172),#90586) ;
#84870 = STYLED_ITEM('',(#170172),#90587) ;
#84871 = STYLED_ITEM('',(#170169),#90588) ;
#84872 = STYLED_ITEM('',(#170169),#90589) ;
#84873 = STYLED_ITEM('',(#170169),#90590) ;
#84874 = STYLED_ITEM('',(#170169),#90591) ;
#84875 = STYLED_ITEM('',(#170169),#90592) ;
#84876 = STYLED_ITEM('',(#170169),#90593) ;
#84877 = STYLED_ITEM('',(#170169),#90594) ;
#84878 = STYLED_ITEM('',(#170169),#90595) ;
#84879 = STYLED_ITEM('',(#170169),#90596) ;
#84880 = STYLED_ITEM('',(#170169),#90597) ;
#84881 = STYLED_ITEM('',(#170169),#90598) ;
#84882 = STYLED_ITEM('',(#170169),#90599) ;
#84883 = STYLED_ITEM('',(#170169),#90600) ;
#84884 = STYLED_ITEM('',(#170169),#90601) ;
#84885 = STYLED_ITEM('',(#170169),#90602) ;
#84886 = STYLED_ITEM('',(#170169),#90603) ;
#84887 = STYLED_ITEM('',(#170169),#90604) ;
#84888 = STYLED_ITEM('',(#170169),#90605) ;
#84889 = STYLED_ITEM('',(#170169),#90606) ;
#84890 = STYLED_ITEM('',(#170169),#90607) ;
#84891 = STYLED_ITEM('',(#170169),#90608) ;
#84892 = STYLED_ITEM('',(#170169),#90609) ;
#84893 = STYLED_ITEM('',(#170169),#90610) ;
#84894 = STYLED_ITEM('',(#170169),#90611) ;
#84895 = STYLED_ITEM('',(#170169),#90612) ;
#84896 = STYLED_ITEM('',(#170169),#90613) ;
#84897 = STYLED_ITEM('',(#170169),#90614) ;
#84898 = STYLED_ITEM('',(#170169),#90615) ;
#84899 = STYLED_ITEM('',(#170169),#90616) ;
#84900 = STYLED_ITEM('',(#170169),#90617) ;
#84901 = STYLED_ITEM('',(#170169),#90618) ;
#84902 = STYLED_ITEM('',(#170169),#90619) ;
#84903 = STYLED_ITEM('',(#170169),#90620) ;
#84904 = STYLED_ITEM('',(#170169),#90621) ;
#84905 = STYLED_ITEM('',(#170169),#90622) ;
#84906 = STYLED_ITEM('',(#170169),#90623) ;
#84907 = STYLED_ITEM('',(#170169),#90624) ;
#84908 = STYLED_ITEM('',(#170169),#90625) ;
#84909 = STYLED_ITEM('',(#170169),#90626) ;
#84910 = STYLED_ITEM('',(#170169),#90627) ;
#84911 = STYLED_ITEM('',(#170169),#90628) ;
#84912 = STYLED_ITEM('',(#170169),#90629) ;
#84913 = STYLED_ITEM('',(#170169),#90630) ;
#84914 = STYLED_ITEM('',(#170169),#90631) ;
#84915 = STYLED_ITEM('',(#170169),#90632) ;
#84916 = STYLED_ITEM('',(#170169),#90633) ;
#84917 = STYLED_ITEM('',(#170169),#90634) ;
#84918 = STYLED_ITEM('',(#170169),#90635) ;
#84919 = STYLED_ITEM('',(#170169),#90636) ;
#84920 = STYLED_ITEM('',(#170169),#90637) ;
#84921 = STYLED_ITEM('',(#170169),#90638) ;
#84922 = STYLED_ITEM('',(#170169),#90639) ;
#84923 = STYLED_ITEM('',(#170169),#90640) ;
#84924 = STYLED_ITEM('',(#170169),#90641) ;
#84925 = STYLED_ITEM('',(#170169),#90642) ;
#84926 = STYLED_ITEM('',(#170169),#90643) ;
#84927 = STYLED_ITEM('',(#170169),#90644) ;
#84928 = STYLED_ITEM('',(#170169),#90645) ;
#84929 = STYLED_ITEM('',(#170169),#90646) ;
#84930 = STYLED_ITEM('',(#170169),#90647) ;
#84931 = STYLED_ITEM('',(#170169),#90648) ;
#84932 = STYLED_ITEM('',(#170169),#90649) ;
#84933 = STYLED_ITEM('',(#170169),#90650) ;
#84934 = STYLED_ITEM('',(#170169),#90651) ;
#84935 = STYLED_ITEM('',(#170169),#90652) ;
#84936 = STYLED_ITEM('',(#170169),#90653) ;
#84937 = STYLED_ITEM('',(#170169),#90654) ;
#84938 = STYLED_ITEM('',(#170169),#90655) ;
#84939 = STYLED_ITEM('',(#170169),#90656) ;
#84940 = STYLED_ITEM('',(#170169),#90657) ;
#84941 = STYLED_ITEM('',(#170169),#90658) ;
#84942 = STYLED_ITEM('',(#170169),#90659) ;
#84943 = STYLED_ITEM('',(#170169),#90660) ;
#84944 = STYLED_ITEM('',(#170169),#90661) ;
#84945 = STYLED_ITEM('',(#170169),#90662) ;
#84946 = STYLED_ITEM('',(#170169),#90663) ;
#84947 = STYLED_ITEM('',(#170169),#90664) ;
#84948 = STYLED_ITEM('',(#170169),#90665) ;
#84949 = STYLED_ITEM('',(#170169),#90666) ;
#84950 = STYLED_ITEM('',(#170169),#90667) ;
#84951 = STYLED_ITEM('',(#170169),#90668) ;
#84952 = STYLED_ITEM('',(#170169),#90669) ;
#84953 = STYLED_ITEM('',(#170169),#90670) ;
#84954 = STYLED_ITEM('',(#170169),#90671) ;
#84955 = STYLED_ITEM('',(#170169),#90672) ;
#84956 = STYLED_ITEM('',(#170169),#90673) ;
#84957 = STYLED_ITEM('',(#170169),#90674) ;
#84958 = STYLED_ITEM('',(#170169),#90675) ;
#84959 = STYLED_ITEM('',(#170169),#90676) ;
#84960 = STYLED_ITEM('',(#170169),#90677) ;
#84961 = STYLED_ITEM('',(#170169),#90678) ;
#84962 = STYLED_ITEM('',(#170169),#90679) ;
#84963 = STYLED_ITEM('',(#170169),#90680) ;
#84964 = STYLED_ITEM('',(#170169),#90681) ;
#84965 = STYLED_ITEM('',(#170169),#90682) ;
#84966 = STYLED_ITEM('',(#170169),#90683) ;
#84967 = STYLED_ITEM('',(#170169),#90684) ;
#84968 = STYLED_ITEM('',(#170169),#90685) ;
#84969 = STYLED_ITEM('',(#170169),#90686) ;
#84970 = STYLED_ITEM('',(#170169),#90687) ;
#84971 = STYLED_ITEM('',(#170169),#90688) ;
#84972 = STYLED_ITEM('',(#170169),#90689) ;
#84973 = STYLED_ITEM('',(#170169),#90690) ;
#84974 = STYLED_ITEM('',(#170169),#90691) ;
#84975 = STYLED_ITEM('',(#170169),#90692) ;
#84976 = STYLED_ITEM('',(#170169),#90693) ;
#84977 = STYLED_ITEM('',(#170169),#90694) ;
#84978 = STYLED_ITEM('',(#170169),#90695) ;
#84979 = STYLED_ITEM('',(#170169),#90696) ;
#84980 = STYLED_ITEM('',(#170169),#90697) ;
#84981 = STYLED_ITEM('',(#170169),#90698) ;
#84982 = STYLED_ITEM('',(#170169),#90699) ;
#84983 = STYLED_ITEM('',(#170169),#90700) ;
#84984 = STYLED_ITEM('',(#170169),#90701) ;
#84985 = STYLED_ITEM('',(#170169),#90702) ;
#84986 = STYLED_ITEM('',(#170169),#90703) ;
#84987 = STYLED_ITEM('',(#170169),#90704) ;
#84988 = STYLED_ITEM('',(#170169),#90705) ;
#84989 = STYLED_ITEM('',(#170169),#90706) ;
#84990 = STYLED_ITEM('',(#170169),#90707) ;
#84991 = STYLED_ITEM('',(#170169),#90708) ;
#84992 = STYLED_ITEM('',(#170169),#90709) ;
#84993 = STYLED_ITEM('',(#170169),#90710) ;
#84994 = STYLED_ITEM('',(#170169),#90711) ;
#84995 = STYLED_ITEM('',(#170169),#90712) ;
#84996 = STYLED_ITEM('',(#170169),#90713) ;
#84997 = STYLED_ITEM('',(#170169),#90714) ;
#84998 = STYLED_ITEM('',(#170169),#90715) ;
#84999 = STYLED_ITEM('',(#170169),#90716) ;
#85000 = STYLED_ITEM('',(#170169),#90717) ;
#85001 = STYLED_ITEM('',(#170169),#90718) ;
#85002 = STYLED_ITEM('',(#170169),#90719) ;
#85003 = STYLED_ITEM('',(#170169),#90720) ;
#85004 = STYLED_ITEM('',(#170169),#90721) ;
#85005 = STYLED_ITEM('',(#170169),#90722) ;
#85006 = STYLED_ITEM('',(#170169),#90723) ;
#85007 = STYLED_ITEM('',(#170172),#90724) ;
#85008 = STYLED_ITEM('',(#170172),#90725) ;
#85009 = STYLED_ITEM('',(#170172),#90726) ;
#85010 = STYLED_ITEM('',(#170172),#90727) ;
#85011 = STYLED_ITEM('',(#170169),#90728) ;
#85012 = STYLED_ITEM('',(#170169),#90729) ;
#85013 = STYLED_ITEM('',(#170169),#90730) ;
#85014 = STYLED_ITEM('',(#170169),#90731) ;
#85015 = STYLED_ITEM('',(#170169),#90732) ;
#85016 = STYLED_ITEM('',(#170169),#90733) ;
#85017 = STYLED_ITEM('',(#170169),#90734) ;
#85018 = STYLED_ITEM('',(#170169),#90735) ;
#85019 = STYLED_ITEM('',(#170169),#90736) ;
#85020 = STYLED_ITEM('',(#170169),#90737) ;
#85021 = STYLED_ITEM('',(#170169),#90738) ;
#85022 = STYLED_ITEM('',(#170169),#90739) ;
#85023 = STYLED_ITEM('',(#170169),#90740) ;
#85024 = STYLED_ITEM('',(#170169),#90741) ;
#85025 = STYLED_ITEM('',(#170169),#90742) ;
#85026 = STYLED_ITEM('',(#170169),#90743) ;
#85027 = STYLED_ITEM('',(#170169),#90744) ;
#85028 = STYLED_ITEM('',(#170169),#90745) ;
#85029 = STYLED_ITEM('',(#170169),#90746) ;
#85030 = STYLED_ITEM('',(#170169),#90747) ;
#85031 = STYLED_ITEM('',(#170169),#90748) ;
#85032 = STYLED_ITEM('',(#170169),#90749) ;
#85033 = STYLED_ITEM('',(#170169),#90750) ;
#85034 = STYLED_ITEM('',(#170169),#90751) ;
#85035 = STYLED_ITEM('',(#170169),#90752) ;
#85036 = STYLED_ITEM('',(#170169),#90753) ;
#85037 = STYLED_ITEM('',(#170169),#90754) ;
#85038 = STYLED_ITEM('',(#170169),#90755) ;
#85039 = STYLED_ITEM('',(#170169),#90756) ;
#85040 = STYLED_ITEM('',(#170169),#90757) ;
#85041 = STYLED_ITEM('',(#170169),#90758) ;
#85042 = STYLED_ITEM('',(#170169),#90759) ;
#85043 = STYLED_ITEM('',(#170169),#90760) ;
#85044 = STYLED_ITEM('',(#170169),#90761) ;
#85045 = STYLED_ITEM('',(#170169),#90762) ;
#85046 = STYLED_ITEM('',(#170169),#90763) ;
#85047 = STYLED_ITEM('',(#170169),#90764) ;
#85048 = STYLED_ITEM('',(#170169),#90765) ;
#85049 = STYLED_ITEM('',(#170169),#90766) ;
#85050 = STYLED_ITEM('',(#170169),#90767) ;
#85051 = STYLED_ITEM('',(#170169),#90768) ;
#85052 = STYLED_ITEM('',(#170169),#90769) ;
#85053 = STYLED_ITEM('',(#170169),#90770) ;
#85054 = STYLED_ITEM('',(#170169),#90771) ;
#85055 = STYLED_ITEM('',(#170169),#90772) ;
#85056 = STYLED_ITEM('',(#170169),#90773) ;
#85057 = STYLED_ITEM('',(#170169),#90774) ;
#85058 = STYLED_ITEM('',(#170169),#90775) ;
#85059 = STYLED_ITEM('',(#170169),#90776) ;
#85060 = STYLED_ITEM('',(#170169),#90777) ;
#85061 = STYLED_ITEM('',(#170169),#90778) ;
#85062 = STYLED_ITEM('',(#170169),#90779) ;
#85063 = STYLED_ITEM('',(#170169),#90780) ;
#85064 = STYLED_ITEM('',(#170169),#90781) ;
#85065 = STYLED_ITEM('',(#170169),#90782) ;
#85066 = STYLED_ITEM('',(#170169),#90783) ;
#85067 = STYLED_ITEM('',(#170169),#90784) ;
#85068 = STYLED_ITEM('',(#170169),#90785) ;
#85069 = STYLED_ITEM('',(#170169),#90786) ;
#85070 = STYLED_ITEM('',(#170169),#90787) ;
#85071 = STYLED_ITEM('',(#170169),#90788) ;
#85072 = STYLED_ITEM('',(#170169),#90789) ;
#85073 = STYLED_ITEM('',(#170169),#90790) ;
#85074 = STYLED_ITEM('',(#170169),#90791) ;
#85075 = STYLED_ITEM('',(#170169),#90792) ;
#85076 = STYLED_ITEM('',(#170169),#90793) ;
#85077 = STYLED_ITEM('',(#170169),#90794) ;
#85078 = STYLED_ITEM('',(#170169),#90795) ;
#85079 = STYLED_ITEM('',(#170169),#90796) ;
#85080 = STYLED_ITEM('',(#170169),#90797) ;
#85081 = STYLED_ITEM('',(#170169),#90798) ;
#85082 = STYLED_ITEM('',(#170169),#90799) ;
#85083 = STYLED_ITEM('',(#170169),#90800) ;
#85084 = STYLED_ITEM('',(#170169),#90801) ;
#85085 = STYLED_ITEM('',(#170169),#90802) ;
#85086 = STYLED_ITEM('',(#170169),#90803) ;
#85087 = STYLED_ITEM('',(#170169),#90804) ;
#85088 = STYLED_ITEM('',(#170169),#90805) ;
#85089 = STYLED_ITEM('',(#170169),#90806) ;
#85090 = STYLED_ITEM('',(#170169),#90807) ;
#85091 = STYLED_ITEM('',(#170169),#90808) ;
#85092 = STYLED_ITEM('',(#170169),#90809) ;
#85093 = STYLED_ITEM('',(#170169),#90810) ;
#85094 = STYLED_ITEM('',(#170169),#90811) ;
#85095 = STYLED_ITEM('',(#170169),#90812) ;
#85096 = STYLED_ITEM('',(#170169),#90813) ;
#85097 = STYLED_ITEM('',(#170169),#90814) ;
#85098 = STYLED_ITEM('',(#170169),#90815) ;
#85099 = STYLED_ITEM('',(#170169),#90816) ;
#85100 = STYLED_ITEM('',(#170169),#90817) ;
#85101 = STYLED_ITEM('',(#170169),#90818) ;
#85102 = STYLED_ITEM('',(#170169),#90819) ;
#85103 = STYLED_ITEM('',(#170169),#90820) ;
#85104 = STYLED_ITEM('',(#170169),#90821) ;
#85105 = STYLED_ITEM('',(#170169),#90822) ;
#85106 = STYLED_ITEM('',(#170169),#90823) ;
#85107 = STYLED_ITEM('',(#170169),#90824) ;
#85108 = STYLED_ITEM('',(#170169),#90825) ;
#85109 = STYLED_ITEM('',(#170169),#90826) ;
#85110 = STYLED_ITEM('',(#170169),#90827) ;
#85111 = STYLED_ITEM('',(#170169),#90828) ;
#85112 = STYLED_ITEM('',(#170169),#90829) ;
#85113 = STYLED_ITEM('',(#170169),#90830) ;
#85114 = STYLED_ITEM('',(#170169),#90831) ;
#85115 = STYLED_ITEM('',(#170169),#90832) ;
#85116 = STYLED_ITEM('',(#170169),#90833) ;
#85117 = STYLED_ITEM('',(#170169),#90834) ;
#85118 = STYLED_ITEM('',(#170169),#90835) ;
#85119 = STYLED_ITEM('',(#170169),#90836) ;
#85120 = STYLED_ITEM('',(#170169),#90837) ;
#85121 = STYLED_ITEM('',(#170169),#90838) ;
#85122 = STYLED_ITEM('',(#170169),#90839) ;
#85123 = STYLED_ITEM('',(#170169),#90840) ;
#85124 = STYLED_ITEM('',(#170169),#90841) ;
#85125 = STYLED_ITEM('',(#170169),#90842) ;
#85126 = STYLED_ITEM('',(#170169),#90843) ;
#85127 = STYLED_ITEM('',(#170169),#90844) ;
#85128 = STYLED_ITEM('',(#170169),#90845) ;
#85129 = STYLED_ITEM('',(#170169),#90846) ;
#85130 = STYLED_ITEM('',(#170169),#90847) ;
#85131 = STYLED_ITEM('',(#170169),#90848) ;
#85132 = STYLED_ITEM('',(#170169),#90849) ;
#85133 = STYLED_ITEM('',(#170169),#90850) ;
#85134 = STYLED_ITEM('',(#170169),#90851) ;
#85135 = STYLED_ITEM('',(#170169),#90852) ;
#85136 = STYLED_ITEM('',(#170169),#90853) ;
#85137 = STYLED_ITEM('',(#170169),#90854) ;
#85138 = STYLED_ITEM('',(#170169),#90855) ;
#85139 = STYLED_ITEM('',(#170169),#90856) ;
#85140 = STYLED_ITEM('',(#170169),#90857) ;
#85141 = STYLED_ITEM('',(#170169),#90858) ;
#85142 = STYLED_ITEM('',(#170169),#90859) ;
#85143 = STYLED_ITEM('',(#170169),#90860) ;
#85144 = STYLED_ITEM('',(#170169),#90861) ;
#85145 = STYLED_ITEM('',(#170169),#90862) ;
#85146 = STYLED_ITEM('',(#170169),#90863) ;
#85147 = STYLED_ITEM('',(#170172),#90864) ;
#85148 = STYLED_ITEM('',(#170172),#90865) ;
#85149 = STYLED_ITEM('',(#170172),#90866) ;
#85150 = STYLED_ITEM('',(#170172),#90867) ;
#85151 = STYLED_ITEM('',(#170169),#90868) ;
#85152 = STYLED_ITEM('',(#170169),#90869) ;
#85153 = STYLED_ITEM('',(#170169),#90870) ;
#85154 = STYLED_ITEM('',(#170169),#90871) ;
#85155 = STYLED_ITEM('',(#170169),#90872) ;
#85156 = STYLED_ITEM('',(#170169),#90873) ;
#85157 = STYLED_ITEM('',(#170169),#90874) ;
#85158 = STYLED_ITEM('',(#170169),#90875) ;
#85159 = STYLED_ITEM('',(#170169),#90876) ;
#85160 = STYLED_ITEM('',(#170169),#90877) ;
#85161 = STYLED_ITEM('',(#170169),#90878) ;
#85162 = STYLED_ITEM('',(#170169),#90879) ;
#85163 = STYLED_ITEM('',(#170169),#90880) ;
#85164 = STYLED_ITEM('',(#170169),#90881) ;
#85165 = STYLED_ITEM('',(#170169),#90882) ;
#85166 = STYLED_ITEM('',(#170169),#90883) ;
#85167 = STYLED_ITEM('',(#170169),#90884) ;
#85168 = STYLED_ITEM('',(#170169),#90885) ;
#85169 = STYLED_ITEM('',(#170169),#90886) ;
#85170 = STYLED_ITEM('',(#170169),#90887) ;
#85171 = STYLED_ITEM('',(#170169),#90888) ;
#85172 = STYLED_ITEM('',(#170169),#90889) ;
#85173 = STYLED_ITEM('',(#170169),#90890) ;
#85174 = STYLED_ITEM('',(#170169),#90891) ;
#85175 = STYLED_ITEM('',(#170169),#90892) ;
#85176 = STYLED_ITEM('',(#170169),#90893) ;
#85177 = STYLED_ITEM('',(#170169),#90894) ;
#85178 = STYLED_ITEM('',(#170169),#90895) ;
#85179 = STYLED_ITEM('',(#170169),#90896) ;
#85180 = STYLED_ITEM('',(#170169),#90897) ;
#85181 = STYLED_ITEM('',(#170169),#90898) ;
#85182 = STYLED_ITEM('',(#170169),#90899) ;
#85183 = STYLED_ITEM('',(#170169),#90900) ;
#85184 = STYLED_ITEM('',(#170169),#90901) ;
#85185 = STYLED_ITEM('',(#170169),#90902) ;
#85186 = STYLED_ITEM('',(#170169),#90903) ;
#85187 = STYLED_ITEM('',(#170169),#90904) ;
#85188 = STYLED_ITEM('',(#170169),#90905) ;
#85189 = STYLED_ITEM('',(#170169),#90906) ;
#85190 = STYLED_ITEM('',(#170169),#90907) ;
#85191 = STYLED_ITEM('',(#170169),#90908) ;
#85192 = STYLED_ITEM('',(#170169),#90909) ;
#85193 = STYLED_ITEM('',(#170169),#90910) ;
#85194 = STYLED_ITEM('',(#170169),#90911) ;
#85195 = STYLED_ITEM('',(#170169),#90912) ;
#85196 = STYLED_ITEM('',(#170169),#90913) ;
#85197 = STYLED_ITEM('',(#170169),#90914) ;
#85198 = STYLED_ITEM('',(#170169),#90915) ;
#85199 = STYLED_ITEM('',(#170169),#90916) ;
#85200 = STYLED_ITEM('',(#170169),#90917) ;
#85201 = STYLED_ITEM('',(#170169),#90918) ;
#85202 = STYLED_ITEM('',(#170169),#90919) ;
#85203 = STYLED_ITEM('',(#170169),#90920) ;
#85204 = STYLED_ITEM('',(#170169),#90921) ;
#85205 = STYLED_ITEM('',(#170169),#90922) ;
#85206 = STYLED_ITEM('',(#170169),#90923) ;
#85207 = STYLED_ITEM('',(#170169),#90924) ;
#85208 = STYLED_ITEM('',(#170169),#90925) ;
#85209 = STYLED_ITEM('',(#170169),#90926) ;
#85210 = STYLED_ITEM('',(#170169),#90927) ;
#85211 = STYLED_ITEM('',(#170169),#90928) ;
#85212 = STYLED_ITEM('',(#170169),#90929) ;
#85213 = STYLED_ITEM('',(#170169),#90930) ;
#85214 = STYLED_ITEM('',(#170169),#90931) ;
#85215 = STYLED_ITEM('',(#170169),#90932) ;
#85216 = STYLED_ITEM('',(#170169),#90933) ;
#85217 = STYLED_ITEM('',(#170169),#90934) ;
#85218 = STYLED_ITEM('',(#170169),#90935) ;
#85219 = STYLED_ITEM('',(#170169),#90936) ;
#85220 = STYLED_ITEM('',(#170169),#90937) ;
#85221 = STYLED_ITEM('',(#170169),#90938) ;
#85222 = STYLED_ITEM('',(#170169),#90939) ;
#85223 = STYLED_ITEM('',(#170169),#90940) ;
#85224 = STYLED_ITEM('',(#170169),#90941) ;
#85225 = STYLED_ITEM('',(#170169),#90942) ;
#85226 = STYLED_ITEM('',(#170169),#90943) ;
#85227 = STYLED_ITEM('',(#170169),#90944) ;
#85228 = STYLED_ITEM('',(#170169),#90945) ;
#85229 = STYLED_ITEM('',(#170169),#90946) ;
#85230 = STYLED_ITEM('',(#170169),#90947) ;
#85231 = STYLED_ITEM('',(#170169),#90948) ;
#85232 = STYLED_ITEM('',(#170169),#90949) ;
#85233 = STYLED_ITEM('',(#170169),#90950) ;
#85234 = STYLED_ITEM('',(#170169),#90951) ;
#85235 = STYLED_ITEM('',(#170169),#90952) ;
#85236 = STYLED_ITEM('',(#170169),#90953) ;
#85237 = STYLED_ITEM('',(#170169),#90954) ;
#85238 = STYLED_ITEM('',(#170169),#90955) ;
#85239 = STYLED_ITEM('',(#170169),#90956) ;
#85240 = STYLED_ITEM('',(#170169),#90957) ;
#85241 = STYLED_ITEM('',(#170169),#90958) ;
#85242 = STYLED_ITEM('',(#170169),#90959) ;
#85243 = STYLED_ITEM('',(#170169),#90960) ;
#85244 = STYLED_ITEM('',(#170169),#90961) ;
#85245 = STYLED_ITEM('',(#170169),#90962) ;
#85246 = STYLED_ITEM('',(#170169),#90963) ;
#85247 = STYLED_ITEM('',(#170169),#90964) ;
#85248 = STYLED_ITEM('',(#170169),#90965) ;
#85249 = STYLED_ITEM('',(#170169),#90966) ;
#85250 = STYLED_ITEM('',(#170169),#90967) ;
#85251 = STYLED_ITEM('',(#170169),#90968) ;
#85252 = STYLED_ITEM('',(#170169),#90969) ;
#85253 = STYLED_ITEM('',(#170169),#90970) ;
#85254 = STYLED_ITEM('',(#170169),#90971) ;
#85255 = STYLED_ITEM('',(#170169),#90972) ;
#85256 = STYLED_ITEM('',(#170169),#90973) ;
#85257 = STYLED_ITEM('',(#170169),#90974) ;
#85258 = STYLED_ITEM('',(#170169),#90975) ;
#85259 = STYLED_ITEM('',(#170169),#90976) ;
#85260 = STYLED_ITEM('',(#170169),#90977) ;
#85261 = STYLED_ITEM('',(#170169),#90978) ;
#85262 = STYLED_ITEM('',(#170169),#90979) ;
#85263 = STYLED_ITEM('',(#170169),#90980) ;
#85264 = STYLED_ITEM('',(#170169),#90981) ;
#85265 = STYLED_ITEM('',(#170169),#90982) ;
#85266 = STYLED_ITEM('',(#170169),#90983) ;
#85267 = STYLED_ITEM('',(#170169),#90984) ;
#85268 = STYLED_ITEM('',(#170169),#90985) ;
#85269 = STYLED_ITEM('',(#170169),#90986) ;
#85270 = STYLED_ITEM('',(#170169),#90987) ;
#85271 = STYLED_ITEM('',(#170169),#90988) ;
#85272 = STYLED_ITEM('',(#170169),#90989) ;
#85273 = STYLED_ITEM('',(#170169),#90990) ;
#85274 = STYLED_ITEM('',(#170169),#90991) ;
#85275 = STYLED_ITEM('',(#170169),#90992) ;
#85276 = STYLED_ITEM('',(#170169),#90993) ;
#85277 = STYLED_ITEM('',(#170169),#90994) ;
#85278 = STYLED_ITEM('',(#170169),#90995) ;
#85279 = STYLED_ITEM('',(#170169),#90996) ;
#85280 = STYLED_ITEM('',(#170169),#90997) ;
#85281 = STYLED_ITEM('',(#170169),#90998) ;
#85282 = STYLED_ITEM('',(#170169),#90999) ;
#85283 = STYLED_ITEM('',(#170169),#91000) ;
#85284 = STYLED_ITEM('',(#170169),#91001) ;
#85285 = STYLED_ITEM('',(#170169),#91002) ;
#85286 = STYLED_ITEM('',(#170169),#91003) ;
#85287 = STYLED_ITEM('',(#170169),#91004) ;
#85288 = STYLED_ITEM('',(#170169),#91005) ;
#85289 = STYLED_ITEM('',(#170169),#91006) ;
#85290 = STYLED_ITEM('',(#170169),#91007) ;
#85291 = STYLED_ITEM('',(#170169),#91008) ;
#85292 = STYLED_ITEM('',(#170169),#91009) ;
#85293 = STYLED_ITEM('',(#170169),#91010) ;
#85294 = STYLED_ITEM('',(#170169),#91011) ;
#85295 = STYLED_ITEM('',(#170169),#91012) ;
#85296 = STYLED_ITEM('',(#170169),#91013) ;
#85297 = STYLED_ITEM('',(#170169),#91014) ;
#85298 = STYLED_ITEM('',(#170169),#91015) ;
#85299 = STYLED_ITEM('',(#170169),#91016) ;
#85300 = STYLED_ITEM('',(#170169),#91017) ;
#85301 = STYLED_ITEM('',(#170169),#91018) ;
#85302 = STYLED_ITEM('',(#170169),#91019) ;
#85303 = STYLED_ITEM('',(#170169),#91020) ;
#85304 = STYLED_ITEM('',(#170169),#91021) ;
#85305 = STYLED_ITEM('',(#170169),#91022) ;
#85306 = STYLED_ITEM('',(#170169),#91023) ;
#85307 = STYLED_ITEM('',(#170169),#91024) ;
#85308 = STYLED_ITEM('',(#170169),#91025) ;
#85309 = STYLED_ITEM('',(#170169),#91026) ;
#85310 = STYLED_ITEM('',(#170169),#91027) ;
#85311 = STYLED_ITEM('',(#170169),#91028) ;
#85312 = STYLED_ITEM('',(#170169),#91029) ;
#85313 = STYLED_ITEM('',(#170169),#91030) ;
#85314 = STYLED_ITEM('',(#170169),#91031) ;
#85315 = STYLED_ITEM('',(#170169),#91032) ;
#85316 = STYLED_ITEM('',(#170169),#91033) ;
#85317 = STYLED_ITEM('',(#170169),#91034) ;
#85318 = STYLED_ITEM('',(#170169),#91035) ;
#85319 = STYLED_ITEM('',(#170169),#91036) ;
#85320 = STYLED_ITEM('',(#170169),#91037) ;
#85321 = STYLED_ITEM('',(#170169),#91038) ;
#85322 = STYLED_ITEM('',(#170169),#91039) ;
#85323 = STYLED_ITEM('',(#170169),#91040) ;
#85324 = STYLED_ITEM('',(#170169),#91041) ;
#85325 = STYLED_ITEM('',(#170169),#91042) ;
#85326 = STYLED_ITEM('',(#170169),#91043) ;
#85327 = STYLED_ITEM('',(#170169),#91044) ;
#85328 = STYLED_ITEM('',(#170169),#91045) ;
#85329 = STYLED_ITEM('',(#170169),#91046) ;
#85330 = STYLED_ITEM('',(#170169),#91047) ;
#85331 = STYLED_ITEM('',(#170169),#91048) ;
#85332 = STYLED_ITEM('',(#170169),#91049) ;
#85333 = STYLED_ITEM('',(#170169),#91050) ;
#85334 = STYLED_ITEM('',(#170169),#91051) ;
#85335 = STYLED_ITEM('',(#170169),#91052) ;
#85336 = STYLED_ITEM('',(#170169),#91053) ;
#85337 = STYLED_ITEM('',(#170169),#91054) ;
#85338 = STYLED_ITEM('',(#170169),#91055) ;
#85339 = STYLED_ITEM('',(#170169),#91056) ;
#85340 = STYLED_ITEM('',(#170169),#91057) ;
#85341 = STYLED_ITEM('',(#170169),#91058) ;
#85342 = STYLED_ITEM('',(#170169),#91059) ;
#85343 = STYLED_ITEM('',(#170169),#91060) ;
#85344 = STYLED_ITEM('',(#170169),#91061) ;
#85345 = STYLED_ITEM('',(#170169),#91062) ;
#85346 = STYLED_ITEM('',(#170169),#91063) ;
#85347 = STYLED_ITEM('',(#170169),#91064) ;
#85348 = STYLED_ITEM('',(#170169),#91065) ;
#85349 = STYLED_ITEM('',(#170169),#91066) ;
#85350 = STYLED_ITEM('',(#170169),#91067) ;
#85351 = STYLED_ITEM('',(#170169),#91068) ;
#85352 = STYLED_ITEM('',(#170169),#91069) ;
#85353 = STYLED_ITEM('',(#170169),#91070) ;
#85354 = STYLED_ITEM('',(#170169),#91071) ;
#85355 = STYLED_ITEM('',(#170169),#91072) ;
#85356 = STYLED_ITEM('',(#170169),#91073) ;
#85357 = STYLED_ITEM('',(#170169),#91074) ;
#85358 = STYLED_ITEM('',(#170169),#91075) ;
#85359 = STYLED_ITEM('',(#170169),#91076) ;
#85360 = STYLED_ITEM('',(#170169),#91077) ;
#85361 = STYLED_ITEM('',(#170169),#91078) ;
#85362 = STYLED_ITEM('',(#170169),#91079) ;
#85363 = STYLED_ITEM('',(#170169),#91080) ;
#85364 = STYLED_ITEM('',(#170169),#91081) ;
#85365 = STYLED_ITEM('',(#170169),#91082) ;
#85366 = STYLED_ITEM('',(#170168),#33) ;
#85367 = ADVANCED_FACE('',(#17047),#78907,.F.) ;
#85368 = ADVANCED_FACE('',(#17048),#78908,.T.) ;
#85369 = ADVANCED_FACE('',(#17049),#78909,.F.) ;
#85370 = ADVANCED_FACE('',(#17050),#78910,.T.) ;
#85371 = ADVANCED_FACE('',(#17051),#78911,.T.) ;
#85372 = ADVANCED_FACE('',(#17052),#16155,.T.) ;
#85373 = ADVANCED_FACE('',(#17053),#13538,.F.) ;
#85374 = ADVANCED_FACE('',(#17054),#16156,.T.) ;
#85375 = ADVANCED_FACE('',(#17055),#2415,.F.) ;
#85376 = ADVANCED_FACE('',(#17056),#13539,.F.) ;
#85377 = ADVANCED_FACE('',(#17057),#13540,.F.) ;
#85378 = ADVANCED_FACE('',(#17058),#78912,.F.) ;
#85379 = ADVANCED_FACE('',(#17059),#13541,.F.) ;
#85380 = ADVANCED_FACE('',(#17060),#78913,.T.) ;
#85381 = ADVANCED_FACE('',(#17061),#78914,.F.) ;
#85382 = ADVANCED_FACE('',(#17062),#78915,.T.) ;
#85383 = ADVANCED_FACE('',(#17063),#78916,.T.) ;
#85384 = ADVANCED_FACE('',(#17064),#16157,.T.) ;
#85385 = ADVANCED_FACE('',(#17065),#13542,.F.) ;
#85386 = ADVANCED_FACE('',(#17066),#16158,.T.) ;
#85387 = ADVANCED_FACE('',(#17067),#2416,.F.) ;
#85388 = ADVANCED_FACE('',(#17068),#13543,.F.) ;
#85389 = ADVANCED_FACE('',(#17069),#13544,.F.) ;
#85390 = ADVANCED_FACE('',(#17070,#647),#794,.F.) ;
#85391 = ADVANCED_FACE('',(#17071),#795,.F.) ;
#85392 = ADVANCED_FACE('',(#17072),#796,.F.) ;
#85393 = ADVANCED_FACE('',(#17073),#797,.F.) ;
#85394 = ADVANCED_FACE('',(#17074),#13545,.T.) ;
#85395 = ADVANCED_FACE('',(#17075),#13546,.F.) ;
#85396 = ADVANCED_FACE('',(#17076),#13547,.F.) ;
#85397 = ADVANCED_FACE('',(#17077),#13548,.T.) ;
#85398 = ADVANCED_FACE('',(#17078),#798,.F.) ;
#85399 = ADVANCED_FACE('',(#17079),#799,.F.) ;
#85400 = ADVANCED_FACE('',(#17080),#800,.F.) ;
#85401 = ADVANCED_FACE('',(#17081),#801,.T.) ;
#85402 = ADVANCED_FACE('',(#17082,#648,#649),#802,.F.) ;
#85403 = ADVANCED_FACE('',(#17083),#803,.F.) ;
#85404 = ADVANCED_FACE('',(#17084),#804,.F.) ;
#85405 = ADVANCED_FACE('',(#17085),#805,.F.) ;
#85406 = ADVANCED_FACE('',(#17086),#806,.F.) ;
#85407 = ADVANCED_FACE('',(#17087,#650,#651,#652,#653),#807,.F.) ;
#85408 = ADVANCED_FACE('',(#17088),#808,.F.) ;
#85409 = ADVANCED_FACE('',(#17089),#809,.F.) ;
#85410 = ADVANCED_FACE('',(#17090),#810,.F.) ;
#85411 = ADVANCED_FACE('',(#17091,#654,#655),#811,.F.) ;
#85412 = ADVANCED_FACE('',(#17092,#656,#657),#812,.F.) ;
#85413 = ADVANCED_FACE('',(#17093),#813,.F.) ;
#85414 = ADVANCED_FACE('',(#17094),#814,.F.) ;
#85415 = ADVANCED_FACE('',(#17095),#815,.F.) ;
#85416 = ADVANCED_FACE('',(#17096),#816,.F.) ;
#85417 = ADVANCED_FACE('',(#17097),#817,.T.) ;
#85418 = ADVANCED_FACE('',(#17098),#818,.T.) ;
#85419 = ADVANCED_FACE('',(#17099),#819,.T.) ;
#85420 = ADVANCED_FACE('',(#17100),#820,.T.) ;
#85421 = ADVANCED_FACE('',(#17101),#821,.T.) ;
#85422 = ADVANCED_FACE('',(#17102),#822,.T.) ;
#85423 = ADVANCED_FACE('',(#17103),#823,.F.) ;
#85424 = ADVANCED_FACE('',(#17104),#824,.T.) ;
#85425 = ADVANCED_FACE('',(#17105),#825,.T.) ;
#85426 = ADVANCED_FACE('',(#17106),#826,.F.) ;
#85427 = ADVANCED_FACE('',(#17107),#827,.F.) ;
#85428 = ADVANCED_FACE('',(#17108),#828,.F.) ;
#85429 = ADVANCED_FACE('',(#17109),#829,.F.) ;
#85430 = ADVANCED_FACE('',(#17110),#830,.F.) ;
#85431 = ADVANCED_FACE('',(#17111,#658),#831,.T.) ;
#85432 = ADVANCED_FACE('',(#17112),#13549,.T.) ;
#85433 = ADVANCED_FACE('',(#17113),#832,.T.) ;
#85434 = ADVANCED_FACE('',(#17114),#13550,.T.) ;
#85435 = ADVANCED_FACE('',(#17115),#833,.T.) ;
#85436 = ADVANCED_FACE('',(#17116),#13551,.T.) ;
#85437 = ADVANCED_FACE('',(#17117),#834,.T.) ;
#85438 = ADVANCED_FACE('',(#17118),#13552,.T.) ;
#85439 = ADVANCED_FACE('',(#17119),#835,.T.) ;
#85440 = ADVANCED_FACE('',(#17120),#836,.T.) ;
#85441 = ADVANCED_FACE('',(#17121),#837,.T.) ;
#85442 = ADVANCED_FACE('',(#17122),#838,.F.) ;
#85443 = ADVANCED_FACE('',(#17123),#839,.F.) ;
#85444 = ADVANCED_FACE('',(#17124),#840,.T.) ;
#85445 = ADVANCED_FACE('',(#17125),#841,.F.) ;
#85446 = ADVANCED_FACE('',(#17126),#842,.F.) ;
#85447 = ADVANCED_FACE('',(#17127),#843,.F.) ;
#85448 = ADVANCED_FACE('',(#17128),#844,.F.) ;
#85449 = ADVANCED_FACE('',(#17129,#659),#845,.T.) ;
#85450 = ADVANCED_FACE('',(#17130),#13553,.T.) ;
#85451 = ADVANCED_FACE('',(#17131),#846,.T.) ;
#85452 = ADVANCED_FACE('',(#17132),#13554,.T.) ;
#85453 = ADVANCED_FACE('',(#17133),#847,.T.) ;
#85454 = ADVANCED_FACE('',(#17134),#13555,.T.) ;
#85455 = ADVANCED_FACE('',(#17135),#848,.T.) ;
#85456 = ADVANCED_FACE('',(#17136),#13556,.T.) ;
#85457 = ADVANCED_FACE('',(#17137),#849,.T.) ;
#85458 = ADVANCED_FACE('',(#17138),#850,.T.) ;
#85459 = ADVANCED_FACE('',(#17139),#851,.F.) ;
#85460 = ADVANCED_FACE('',(#17140),#852,.F.) ;
#85461 = ADVANCED_FACE('',(#17141),#853,.F.) ;
#85462 = ADVANCED_FACE('',(#17142),#854,.F.) ;
#85463 = ADVANCED_FACE('',(#17143),#855,.T.) ;
#85464 = ADVANCED_FACE('',(#17144),#13557,.T.) ;
#85465 = ADVANCED_FACE('',(#17145),#34,.T.) ;
#85466 = ADVANCED_FACE('',(#17146),#13558,.F.) ;
#85467 = ADVANCED_FACE('',(#17147),#35,.F.) ;
#85468 = ADVANCED_FACE('',(#17148),#13559,.F.) ;
#85469 = ADVANCED_FACE('',(#17149),#13560,.F.) ;
#85470 = ADVANCED_FACE('',(#17150),#13561,.T.) ;
#85471 = ADVANCED_FACE('',(#17151),#13562,.T.) ;
#85472 = ADVANCED_FACE('',(#17152),#13563,.T.) ;
#85473 = ADVANCED_FACE('',(#17153),#13564,.F.) ;
#85474 = ADVANCED_FACE('',(#17154),#16159,.F.) ;
#85475 = ADVANCED_FACE('',(#17155),#36,.T.) ;
#85476 = ADVANCED_FACE('',(#17156),#37,.T.) ;
#85477 = ADVANCED_FACE('',(#17157),#38,.F.) ;
#85478 = ADVANCED_FACE('',(#17158),#13565,.F.) ;
#85479 = ADVANCED_FACE('',(#17159),#13566,.F.) ;
#85480 = ADVANCED_FACE('',(#17160),#13567,.T.) ;
#85481 = ADVANCED_FACE('',(#17161),#13568,.T.) ;
#85482 = ADVANCED_FACE('',(#17162),#13569,.F.) ;
#85483 = ADVANCED_FACE('',(#17163),#13570,.F.) ;
#85484 = ADVANCED_FACE('',(#17164),#16160,.F.) ;
#85485 = ADVANCED_FACE('',(#17165),#39,.T.) ;
#85486 = ADVANCED_FACE('',(#17166),#16161,.F.) ;
#85487 = ADVANCED_FACE('',(#17167),#13571,.F.) ;
#85488 = ADVANCED_FACE('',(#17168),#13572,.F.) ;
#85489 = ADVANCED_FACE('',(#17169),#13573,.F.) ;
#85490 = ADVANCED_FACE('',(#17170),#13574,.F.) ;
#85491 = ADVANCED_FACE('',(#17171),#40,.F.) ;
#85492 = ADVANCED_FACE('',(#17172),#16162,.F.) ;
#85493 = ADVANCED_FACE('',(#17173),#13575,.T.) ;
#85494 = ADVANCED_FACE('',(#17174),#13576,.F.) ;
#85495 = ADVANCED_FACE('',(#17175),#41,.F.) ;
#85496 = ADVANCED_FACE('',(#17176),#13577,.F.) ;
#85497 = ADVANCED_FACE('',(#17177),#13578,.T.) ;
#85498 = ADVANCED_FACE('',(#17178),#13579,.T.) ;
#85499 = ADVANCED_FACE('',(#17179),#13580,.F.) ;
#85500 = ADVANCED_FACE('',(#17180),#13581,.T.) ;
#85501 = ADVANCED_FACE('',(#17181),#13582,.T.) ;
#85502 = ADVANCED_FACE('',(#17182),#13583,.F.) ;
#85503 = ADVANCED_FACE('',(#17183),#78917,.T.) ;
#85504 = ADVANCED_FACE('',(#17184),#13584,.T.) ;
#85505 = ADVANCED_FACE('',(#17185),#13585,.T.) ;
#85506 = ADVANCED_FACE('',(#17186),#13586,.T.) ;
#85507 = ADVANCED_FACE('',(#17187),#13587,.T.) ;
#85508 = ADVANCED_FACE('',(#17188),#16163,.T.) ;
#85509 = ADVANCED_FACE('',(#17189),#13588,.T.) ;
#85510 = ADVANCED_FACE('',(#17190),#13589,.T.) ;
#85511 = ADVANCED_FACE('',(#17191),#16164,.T.) ;
#85512 = ADVANCED_FACE('',(#17192),#16165,.T.) ;
#85513 = ADVANCED_FACE('',(#17193),#13590,.T.) ;
#85514 = ADVANCED_FACE('',(#17194),#13591,.T.) ;
#85515 = ADVANCED_FACE('',(#17195),#16166,.T.) ;
#85516 = ADVANCED_FACE('',(#17196),#13592,.T.) ;
#85517 = ADVANCED_FACE('',(#17197),#78918,.T.) ;
#85518 = ADVANCED_FACE('',(#17198),#78919,.T.) ;
#85519 = ADVANCED_FACE('',(#17199),#13593,.T.) ;
#85520 = ADVANCED_FACE('',(#17200),#13594,.F.) ;
#85521 = ADVANCED_FACE('',(#17201),#13595,.F.) ;
#85522 = ADVANCED_FACE('',(#17202),#13596,.F.) ;
#85523 = ADVANCED_FACE('',(#17203),#13597,.T.) ;
#85524 = ADVANCED_FACE('',(#17204),#13598,.T.) ;
#85525 = ADVANCED_FACE('',(#17205),#78920,.T.) ;
#85526 = ADVANCED_FACE('',(#17206),#16167,.F.) ;
#85527 = ADVANCED_FACE('',(#17207),#16168,.F.) ;
#85528 = ADVANCED_FACE('',(#17208),#78921,.T.) ;
#85529 = ADVANCED_FACE('',(#17209),#13599,.F.) ;
#85530 = ADVANCED_FACE('',(#17210),#13600,.F.) ;
#85531 = ADVANCED_FACE('',(#17211),#13601,.F.) ;
#85532 = ADVANCED_FACE('',(#17212),#13602,.F.) ;
#85533 = ADVANCED_FACE('',(#17213),#16169,.F.) ;
#85534 = ADVANCED_FACE('',(#17214),#16170,.F.) ;
#85535 = ADVANCED_FACE('',(#17215),#13603,.F.) ;
#85536 = ADVANCED_FACE('',(#17216),#13604,.T.) ;
#85537 = ADVANCED_FACE('',(#17217),#78922,.T.) ;
#85538 = ADVANCED_FACE('',(#17218),#78923,.T.) ;
#85539 = ADVANCED_FACE('',(#17219),#13605,.T.) ;
#85540 = ADVANCED_FACE('',(#17220),#13606,.F.) ;
#85541 = ADVANCED_FACE('',(#17221),#13607,.F.) ;
#85542 = ADVANCED_FACE('',(#17222),#13608,.F.) ;
#85543 = ADVANCED_FACE('',(#17223),#13609,.T.) ;
#85544 = ADVANCED_FACE('',(#17224),#13610,.T.) ;
#85545 = ADVANCED_FACE('',(#17225),#78924,.T.) ;
#85546 = ADVANCED_FACE('',(#17226),#16171,.F.) ;
#85547 = ADVANCED_FACE('',(#17227),#16172,.F.) ;
#85548 = ADVANCED_FACE('',(#17228),#78925,.T.) ;
#85549 = ADVANCED_FACE('',(#17229),#13611,.F.) ;
#85550 = ADVANCED_FACE('',(#17230),#13612,.F.) ;
#85551 = ADVANCED_FACE('',(#17231),#13613,.F.) ;
#85552 = ADVANCED_FACE('',(#17232),#13614,.F.) ;
#85553 = ADVANCED_FACE('',(#17233),#16173,.F.) ;
#85554 = ADVANCED_FACE('',(#17234),#16174,.F.) ;
#85555 = ADVANCED_FACE('',(#17235),#13615,.F.) ;
#85556 = ADVANCED_FACE('',(#17236),#78926,.F.) ;
#85557 = ADVANCED_FACE('',(#17237),#13616,.F.) ;
#85558 = ADVANCED_FACE('',(#17238),#16175,.F.) ;
#85559 = ADVANCED_FACE('',(#17239),#13617,.F.) ;
#85560 = ADVANCED_FACE('',(#17240),#13618,.T.) ;
#85561 = ADVANCED_FACE('',(#17241),#78927,.T.) ;
#85562 = ADVANCED_FACE('',(#17242),#78928,.T.) ;
#85563 = ADVANCED_FACE('',(#17243),#13619,.T.) ;
#85564 = ADVANCED_FACE('',(#17244),#78929,.T.) ;
#85565 = ADVANCED_FACE('',(#17245),#13620,.F.) ;
#85566 = ADVANCED_FACE('',(#17246),#13621,.F.) ;
#85567 = ADVANCED_FACE('',(#17247),#16176,.F.) ;
#85568 = ADVANCED_FACE('',(#17248),#78930,.F.) ;
#85569 = ADVANCED_FACE('',(#17249),#13622,.F.) ;
#85570 = ADVANCED_FACE('',(#17250),#13623,.T.) ;
#85571 = ADVANCED_FACE('',(#17251),#13624,.T.) ;
#85572 = ADVANCED_FACE('',(#17252),#13625,.T.) ;
#85573 = ADVANCED_FACE('',(#17253),#13626,.T.) ;
#85574 = ADVANCED_FACE('',(#17254),#13627,.T.) ;
#85575 = ADVANCED_FACE('',(#17255),#13628,.F.) ;
#85576 = ADVANCED_FACE('',(#17256),#13629,.F.) ;
#85577 = ADVANCED_FACE('',(#17257),#13630,.T.) ;
#85578 = ADVANCED_FACE('',(#17258),#13631,.T.) ;
#85579 = ADVANCED_FACE('',(#17259),#13632,.T.) ;
#85580 = ADVANCED_FACE('',(#17260),#13633,.T.) ;
#85581 = ADVANCED_FACE('',(#17261),#13634,.F.) ;
#85582 = ADVANCED_FACE('',(#17262),#16177,.F.) ;
#85583 = ADVANCED_FACE('',(#17263),#13635,.F.) ;
#85584 = ADVANCED_FACE('',(#17264),#78931,.F.) ;
#85585 = ADVANCED_FACE('',(#17265),#42,.F.) ;
#85586 = ADVANCED_FACE('',(#17266),#43,.F.) ;
#85587 = ADVANCED_FACE('',(#17267),#13636,.F.) ;
#85588 = ADVANCED_FACE('',(#17268),#13637,.F.) ;
#85589 = ADVANCED_FACE('',(#17269),#44,.F.) ;
#85590 = ADVANCED_FACE('',(#17270),#45,.F.) ;
#85591 = ADVANCED_FACE('',(#17271),#13638,.F.) ;
#85592 = ADVANCED_FACE('',(#17272),#16178,.F.) ;
#85593 = ADVANCED_FACE('',(#17273),#78932,.T.) ;
#85594 = ADVANCED_FACE('',(#17274),#13639,.T.) ;
#85595 = ADVANCED_FACE('',(#17275),#46,.T.) ;
#85596 = ADVANCED_FACE('',(#17276),#13640,.T.) ;
#85597 = ADVANCED_FACE('',(#17277),#47,.T.) ;
#85598 = ADVANCED_FACE('',(#17278),#48,.F.) ;
#85599 = ADVANCED_FACE('',(#17279),#49,.F.) ;
#85600 = ADVANCED_FACE('',(#17280),#50,.F.) ;
#85601 = ADVANCED_FACE('',(#17281),#51,.F.) ;
#85602 = ADVANCED_FACE('',(#17282),#856,.F.) ;
#85603 = ADVANCED_FACE('',(#17283),#857,.T.) ;
#85604 = ADVANCED_FACE('',(#17284),#13641,.T.) ;
#85605 = ADVANCED_FACE('',(#17285),#858,.T.) ;
#85606 = ADVANCED_FACE('',(#17286),#13642,.T.) ;
#85607 = ADVANCED_FACE('',(#17287),#859,.T.) ;
#85608 = ADVANCED_FACE('',(#17288),#13643,.T.) ;
#85609 = ADVANCED_FACE('',(#17289),#860,.T.) ;
#85610 = ADVANCED_FACE('',(#17290),#13644,.F.) ;
#85611 = ADVANCED_FACE('',(#17291),#861,.T.) ;
#85612 = ADVANCED_FACE('',(#17292),#862,.F.) ;
#85613 = ADVANCED_FACE('',(#17293),#863,.T.) ;
#85614 = ADVANCED_FACE('',(#17294),#864,.F.) ;
#85615 = ADVANCED_FACE('',(#17295),#865,.F.) ;
#85616 = ADVANCED_FACE('',(#17296),#866,.T.) ;
#85617 = ADVANCED_FACE('',(#17297),#867,.F.) ;
#85618 = ADVANCED_FACE('',(#17298),#868,.F.) ;
#85619 = ADVANCED_FACE('',(#17299),#869,.T.) ;
#85620 = ADVANCED_FACE('',(#17300),#870,.T.) ;
#85621 = ADVANCED_FACE('',(#17301),#871,.T.) ;
#85622 = ADVANCED_FACE('',(#17302),#872,.T.) ;
#85623 = ADVANCED_FACE('',(#17303),#873,.T.) ;
#85624 = ADVANCED_FACE('',(#17304),#874,.F.) ;
#85625 = ADVANCED_FACE('',(#17305),#875,.T.) ;
#85626 = ADVANCED_FACE('',(#17306),#876,.T.) ;
#85627 = ADVANCED_FACE('',(#17307),#877,.F.) ;
#85628 = ADVANCED_FACE('',(#17308),#878,.F.) ;
#85629 = ADVANCED_FACE('',(#17309),#879,.F.) ;
#85630 = ADVANCED_FACE('',(#17310),#880,.F.) ;
#85631 = ADVANCED_FACE('',(#17311),#881,.F.) ;
#85632 = ADVANCED_FACE('',(#17312,#660),#882,.T.) ;
#85633 = ADVANCED_FACE('',(#17313),#13645,.T.) ;
#85634 = ADVANCED_FACE('',(#17314),#883,.T.) ;
#85635 = ADVANCED_FACE('',(#17315),#13646,.T.) ;
#85636 = ADVANCED_FACE('',(#17316),#884,.T.) ;
#85637 = ADVANCED_FACE('',(#17317),#13647,.T.) ;
#85638 = ADVANCED_FACE('',(#17318),#885,.T.) ;
#85639 = ADVANCED_FACE('',(#17319),#13648,.T.) ;
#85640 = ADVANCED_FACE('',(#17320),#886,.T.) ;
#85641 = ADVANCED_FACE('',(#17321),#887,.T.) ;
#85642 = ADVANCED_FACE('',(#17322),#888,.T.) ;
#85643 = ADVANCED_FACE('',(#17323),#889,.F.) ;
#85644 = ADVANCED_FACE('',(#17324),#890,.F.) ;
#85645 = ADVANCED_FACE('',(#17325),#891,.T.) ;
#85646 = ADVANCED_FACE('',(#17326),#892,.F.) ;
#85647 = ADVANCED_FACE('',(#17327),#893,.F.) ;
#85648 = ADVANCED_FACE('',(#17328),#894,.F.) ;
#85649 = ADVANCED_FACE('',(#17329),#895,.F.) ;
#85650 = ADVANCED_FACE('',(#17330,#661),#896,.T.) ;
#85651 = ADVANCED_FACE('',(#17331),#13649,.T.) ;
#85652 = ADVANCED_FACE('',(#17332),#897,.T.) ;
#85653 = ADVANCED_FACE('',(#17333),#13650,.T.) ;
#85654 = ADVANCED_FACE('',(#17334),#898,.T.) ;
#85655 = ADVANCED_FACE('',(#17335),#13651,.T.) ;
#85656 = ADVANCED_FACE('',(#17336),#899,.T.) ;
#85657 = ADVANCED_FACE('',(#17337),#13652,.T.) ;
#85658 = ADVANCED_FACE('',(#17338),#900,.T.) ;
#85659 = ADVANCED_FACE('',(#17339),#901,.T.) ;
#85660 = ADVANCED_FACE('',(#17340),#902,.F.) ;
#85661 = ADVANCED_FACE('',(#17341),#903,.F.) ;
#85662 = ADVANCED_FACE('',(#17342),#904,.F.) ;
#85663 = ADVANCED_FACE('',(#17343),#905,.F.) ;
#85664 = ADVANCED_FACE('',(#17344),#906,.T.) ;
#85665 = ADVANCED_FACE('',(#17345),#13653,.T.) ;
#85666 = ADVANCED_FACE('',(#17346),#52,.T.) ;
#85667 = ADVANCED_FACE('',(#17347),#13654,.F.) ;
#85668 = ADVANCED_FACE('',(#17348),#53,.F.) ;
#85669 = ADVANCED_FACE('',(#17349),#13655,.F.) ;
#85670 = ADVANCED_FACE('',(#17350),#13656,.F.) ;
#85671 = ADVANCED_FACE('',(#17351),#13657,.T.) ;
#85672 = ADVANCED_FACE('',(#17352),#13658,.T.) ;
#85673 = ADVANCED_FACE('',(#17353),#13659,.T.) ;
#85674 = ADVANCED_FACE('',(#17354),#13660,.F.) ;
#85675 = ADVANCED_FACE('',(#17355),#16179,.F.) ;
#85676 = ADVANCED_FACE('',(#17356),#54,.T.) ;
#85677 = ADVANCED_FACE('',(#17357),#55,.T.) ;
#85678 = ADVANCED_FACE('',(#17358),#56,.F.) ;
#85679 = ADVANCED_FACE('',(#17359),#13661,.F.) ;
#85680 = ADVANCED_FACE('',(#17360),#13662,.F.) ;
#85681 = ADVANCED_FACE('',(#17361),#13663,.T.) ;
#85682 = ADVANCED_FACE('',(#17362),#13664,.T.) ;
#85683 = ADVANCED_FACE('',(#17363),#13665,.F.) ;
#85684 = ADVANCED_FACE('',(#17364),#13666,.F.) ;
#85685 = ADVANCED_FACE('',(#17365),#16180,.F.) ;
#85686 = ADVANCED_FACE('',(#17366),#57,.T.) ;
#85687 = ADVANCED_FACE('',(#17367),#16181,.F.) ;
#85688 = ADVANCED_FACE('',(#17368),#13667,.F.) ;
#85689 = ADVANCED_FACE('',(#17369),#13668,.F.) ;
#85690 = ADVANCED_FACE('',(#17370),#13669,.F.) ;
#85691 = ADVANCED_FACE('',(#17371),#13670,.F.) ;
#85692 = ADVANCED_FACE('',(#17372),#58,.F.) ;
#85693 = ADVANCED_FACE('',(#17373),#16182,.F.) ;
#85694 = ADVANCED_FACE('',(#17374),#13671,.T.) ;
#85695 = ADVANCED_FACE('',(#17375),#13672,.F.) ;
#85696 = ADVANCED_FACE('',(#17376),#59,.F.) ;
#85697 = ADVANCED_FACE('',(#17377),#13673,.F.) ;
#85698 = ADVANCED_FACE('',(#17378),#13674,.T.) ;
#85699 = ADVANCED_FACE('',(#17379),#13675,.T.) ;
#85700 = ADVANCED_FACE('',(#17380),#13676,.F.) ;
#85701 = ADVANCED_FACE('',(#17381),#13677,.T.) ;
#85702 = ADVANCED_FACE('',(#17382),#13678,.T.) ;
#85703 = ADVANCED_FACE('',(#17383),#13679,.F.) ;
#85704 = ADVANCED_FACE('',(#17384),#78933,.T.) ;
#85705 = ADVANCED_FACE('',(#17385),#13680,.T.) ;
#85706 = ADVANCED_FACE('',(#17386),#13681,.T.) ;
#85707 = ADVANCED_FACE('',(#17387),#13682,.T.) ;
#85708 = ADVANCED_FACE('',(#17388),#16183,.T.) ;
#85709 = ADVANCED_FACE('',(#17389),#13683,.T.) ;
#85710 = ADVANCED_FACE('',(#17390),#13684,.T.) ;
#85711 = ADVANCED_FACE('',(#17391),#16184,.T.) ;
#85712 = ADVANCED_FACE('',(#17392),#16185,.T.) ;
#85713 = ADVANCED_FACE('',(#17393),#13685,.T.) ;
#85714 = ADVANCED_FACE('',(#17394),#13686,.T.) ;
#85715 = ADVANCED_FACE('',(#17395),#16186,.T.) ;
#85716 = ADVANCED_FACE('',(#17396),#13687,.T.) ;
#85717 = ADVANCED_FACE('',(#17397),#78934,.T.) ;
#85718 = ADVANCED_FACE('',(#17398),#78935,.T.) ;
#85719 = ADVANCED_FACE('',(#17399),#13688,.T.) ;
#85720 = ADVANCED_FACE('',(#17400),#13689,.F.) ;
#85721 = ADVANCED_FACE('',(#17401),#13690,.F.) ;
#85722 = ADVANCED_FACE('',(#17402),#13691,.F.) ;
#85723 = ADVANCED_FACE('',(#17403),#13692,.T.) ;
#85724 = ADVANCED_FACE('',(#17404),#13693,.T.) ;
#85725 = ADVANCED_FACE('',(#17405),#78936,.T.) ;
#85726 = ADVANCED_FACE('',(#17406),#16187,.F.) ;
#85727 = ADVANCED_FACE('',(#17407),#16188,.F.) ;
#85728 = ADVANCED_FACE('',(#17408),#78937,.T.) ;
#85729 = ADVANCED_FACE('',(#17409),#13694,.F.) ;
#85730 = ADVANCED_FACE('',(#17410),#13695,.F.) ;
#85731 = ADVANCED_FACE('',(#17411),#13696,.F.) ;
#85732 = ADVANCED_FACE('',(#17412),#13697,.F.) ;
#85733 = ADVANCED_FACE('',(#17413),#16189,.F.) ;
#85734 = ADVANCED_FACE('',(#17414),#16190,.F.) ;
#85735 = ADVANCED_FACE('',(#17415),#13698,.F.) ;
#85736 = ADVANCED_FACE('',(#17416),#13699,.T.) ;
#85737 = ADVANCED_FACE('',(#17417),#78938,.T.) ;
#85738 = ADVANCED_FACE('',(#17418),#78939,.T.) ;
#85739 = ADVANCED_FACE('',(#17419),#13700,.T.) ;
#85740 = ADVANCED_FACE('',(#17420),#13701,.F.) ;
#85741 = ADVANCED_FACE('',(#17421),#13702,.F.) ;
#85742 = ADVANCED_FACE('',(#17422),#13703,.F.) ;
#85743 = ADVANCED_FACE('',(#17423),#13704,.T.) ;
#85744 = ADVANCED_FACE('',(#17424),#13705,.T.) ;
#85745 = ADVANCED_FACE('',(#17425),#78940,.T.) ;
#85746 = ADVANCED_FACE('',(#17426),#16191,.F.) ;
#85747 = ADVANCED_FACE('',(#17427),#16192,.F.) ;
#85748 = ADVANCED_FACE('',(#17428),#78941,.T.) ;
#85749 = ADVANCED_FACE('',(#17429),#13706,.F.) ;
#85750 = ADVANCED_FACE('',(#17430),#13707,.F.) ;
#85751 = ADVANCED_FACE('',(#17431),#13708,.F.) ;
#85752 = ADVANCED_FACE('',(#17432),#13709,.F.) ;
#85753 = ADVANCED_FACE('',(#17433),#16193,.F.) ;
#85754 = ADVANCED_FACE('',(#17434),#16194,.F.) ;
#85755 = ADVANCED_FACE('',(#17435),#13710,.F.) ;
#85756 = ADVANCED_FACE('',(#17436),#78942,.F.) ;
#85757 = ADVANCED_FACE('',(#17437),#16195,.F.) ;
#85758 = ADVANCED_FACE('',(#17438),#13711,.F.) ;
#85759 = ADVANCED_FACE('',(#17439),#78943,.T.) ;
#85760 = ADVANCED_FACE('',(#17440),#78944,.T.) ;
#85761 = ADVANCED_FACE('',(#17441),#13712,.T.) ;
#85762 = ADVANCED_FACE('',(#17442),#78945,.T.) ;
#85763 = ADVANCED_FACE('',(#17443),#13713,.F.) ;
#85764 = ADVANCED_FACE('',(#17444),#13714,.F.) ;
#85765 = ADVANCED_FACE('',(#17445),#16196,.F.) ;
#85766 = ADVANCED_FACE('',(#17446),#78946,.F.) ;
#85767 = ADVANCED_FACE('',(#17447),#13715,.F.) ;
#85768 = ADVANCED_FACE('',(#17448),#13716,.F.) ;
#85769 = ADVANCED_FACE('',(#17449),#13717,.T.) ;
#85770 = ADVANCED_FACE('',(#17450),#13718,.T.) ;
#85771 = ADVANCED_FACE('',(#17451),#16197,.F.) ;
#85772 = ADVANCED_FACE('',(#17452),#13719,.F.) ;
#85773 = ADVANCED_FACE('',(#17453),#78947,.F.) ;
#85774 = ADVANCED_FACE('',(#17454),#60,.F.) ;
#85775 = ADVANCED_FACE('',(#17455),#61,.F.) ;
#85776 = ADVANCED_FACE('',(#17456),#13720,.F.) ;
#85777 = ADVANCED_FACE('',(#17457),#62,.F.) ;
#85778 = ADVANCED_FACE('',(#17458),#63,.F.) ;
#85779 = ADVANCED_FACE('',(#17459),#13721,.F.) ;
#85780 = ADVANCED_FACE('',(#17460),#16198,.F.) ;
#85781 = ADVANCED_FACE('',(#17461),#78948,.T.) ;
#85782 = ADVANCED_FACE('',(#17462),#64,.T.) ;
#85783 = ADVANCED_FACE('',(#17463),#13722,.T.) ;
#85784 = ADVANCED_FACE('',(#17464),#65,.T.) ;
#85785 = ADVANCED_FACE('',(#17465),#66,.F.) ;
#85786 = ADVANCED_FACE('',(#17466),#67,.F.) ;
#85787 = ADVANCED_FACE('',(#17467),#68,.F.) ;
#85788 = ADVANCED_FACE('',(#17468),#69,.F.) ;
#85789 = ADVANCED_FACE('',(#17469),#16199,.T.) ;
#85790 = ADVANCED_FACE('',(#17470),#16200,.T.) ;
#85791 = ADVANCED_FACE('',(#17471),#13723,.T.) ;
#85792 = ADVANCED_FACE('',(#17472),#13724,.T.) ;
#85793 = ADVANCED_FACE('',(#17473),#13725,.T.) ;
#85794 = ADVANCED_FACE('',(#17474),#13726,.T.) ;
#85795 = ADVANCED_FACE('',(#17475),#16201,.T.) ;
#85796 = ADVANCED_FACE('',(#17476),#16202,.T.) ;
#85797 = ADVANCED_FACE('',(#17477),#16203,.T.) ;
#85798 = ADVANCED_FACE('',(#17478),#16204,.T.) ;
#85799 = ADVANCED_FACE('',(#17479),#13727,.T.) ;
#85800 = ADVANCED_FACE('',(#17480),#13728,.T.) ;
#85801 = ADVANCED_FACE('',(#17481),#13729,.F.) ;
#85802 = ADVANCED_FACE('',(#17482),#13730,.T.) ;
#85803 = ADVANCED_FACE('',(#17483),#13731,.T.) ;
#85804 = ADVANCED_FACE('',(#17484),#78949,.T.) ;
#85805 = ADVANCED_FACE('',(#17485),#70,.F.) ;
#85806 = ADVANCED_FACE('',(#17486),#71,.F.) ;
#85807 = ADVANCED_FACE('',(#17487),#78950,.T.) ;
#85808 = ADVANCED_FACE('',(#17488),#13732,.T.) ;
#85809 = ADVANCED_FACE('',(#17489),#13733,.F.) ;
#85810 = ADVANCED_FACE('',(#17490),#13734,.F.) ;
#85811 = ADVANCED_FACE('',(#17491),#13735,.T.) ;
#85812 = ADVANCED_FACE('',(#17492),#78951,.F.) ;
#85813 = ADVANCED_FACE('',(#17493),#78952,.F.) ;
#85814 = ADVANCED_FACE('',(#17494),#13736,.F.) ;
#85815 = ADVANCED_FACE('',(#17495),#78953,.F.) ;
#85816 = ADVANCED_FACE('',(#17496),#78954,.T.) ;
#85817 = ADVANCED_FACE('',(#17497),#78955,.F.) ;
#85818 = ADVANCED_FACE('',(#17498),#78956,.T.) ;
#85819 = ADVANCED_FACE('',(#17499),#78957,.T.) ;
#85820 = ADVANCED_FACE('',(#17500),#16205,.T.) ;
#85821 = ADVANCED_FACE('',(#17501),#13737,.F.) ;
#85822 = ADVANCED_FACE('',(#17502),#16206,.T.) ;
#85823 = ADVANCED_FACE('',(#17503),#2417,.F.) ;
#85824 = ADVANCED_FACE('',(#17504),#13738,.F.) ;
#85825 = ADVANCED_FACE('',(#17505),#13739,.F.) ;
#85826 = ADVANCED_FACE('',(#17506),#78958,.F.) ;
#85827 = ADVANCED_FACE('',(#17507),#13740,.F.) ;
#85828 = ADVANCED_FACE('',(#17508),#78959,.T.) ;
#85829 = ADVANCED_FACE('',(#17509),#78960,.F.) ;
#85830 = ADVANCED_FACE('',(#17510),#78961,.T.) ;
#85831 = ADVANCED_FACE('',(#17511),#78962,.T.) ;
#85832 = ADVANCED_FACE('',(#17512),#16207,.T.) ;
#85833 = ADVANCED_FACE('',(#17513),#13741,.F.) ;
#85834 = ADVANCED_FACE('',(#17514),#16208,.T.) ;
#85835 = ADVANCED_FACE('',(#17515),#2418,.F.) ;
#85836 = ADVANCED_FACE('',(#17516),#13742,.F.) ;
#85837 = ADVANCED_FACE('',(#17517),#13743,.F.) ;
#85838 = ADVANCED_FACE('',(#17518,#662),#907,.F.) ;
#85839 = ADVANCED_FACE('',(#17519),#908,.F.) ;
#85840 = ADVANCED_FACE('',(#17520),#909,.F.) ;
#85841 = ADVANCED_FACE('',(#17521),#910,.F.) ;
#85842 = ADVANCED_FACE('',(#17522),#13744,.T.) ;
#85843 = ADVANCED_FACE('',(#17523),#13745,.F.) ;
#85844 = ADVANCED_FACE('',(#17524),#13746,.F.) ;
#85845 = ADVANCED_FACE('',(#17525),#13747,.T.) ;
#85846 = ADVANCED_FACE('',(#17526),#911,.F.) ;
#85847 = ADVANCED_FACE('',(#17527),#912,.F.) ;
#85848 = ADVANCED_FACE('',(#17528),#913,.F.) ;
#85849 = ADVANCED_FACE('',(#17529),#914,.T.) ;
#85850 = ADVANCED_FACE('',(#17530,#663,#664),#915,.F.) ;
#85851 = ADVANCED_FACE('',(#17531),#916,.F.) ;
#85852 = ADVANCED_FACE('',(#17532),#917,.F.) ;
#85853 = ADVANCED_FACE('',(#17533),#918,.F.) ;
#85854 = ADVANCED_FACE('',(#17534),#919,.F.) ;
#85855 = ADVANCED_FACE('',(#17535,#665,#666,#667,#668),#920,.F.) ;
#85856 = ADVANCED_FACE('',(#17536),#921,.F.) ;
#85857 = ADVANCED_FACE('',(#17537),#922,.F.) ;
#85858 = ADVANCED_FACE('',(#17538),#923,.F.) ;
#85859 = ADVANCED_FACE('',(#17539,#669,#670),#924,.F.) ;
#85860 = ADVANCED_FACE('',(#17540,#671,#672),#925,.F.) ;
#85861 = ADVANCED_FACE('',(#17541),#926,.F.) ;
#85862 = ADVANCED_FACE('',(#17542),#927,.F.) ;
#85863 = ADVANCED_FACE('',(#17543),#928,.F.) ;
#85864 = ADVANCED_FACE('',(#17544),#929,.F.) ;
#85865 = ADVANCED_FACE('',(#17545),#930,.F.) ;
#85866 = ADVANCED_FACE('',(#17546),#931,.T.) ;
#85867 = ADVANCED_FACE('',(#17547),#932,.T.) ;
#85868 = ADVANCED_FACE('',(#17548),#933,.T.) ;
#85869 = ADVANCED_FACE('',(#17549),#934,.T.) ;
#85870 = ADVANCED_FACE('',(#17550),#935,.T.) ;
#85871 = ADVANCED_FACE('',(#17551),#936,.F.) ;
#85872 = ADVANCED_FACE('',(#17552),#937,.T.) ;
#85873 = ADVANCED_FACE('',(#17553),#938,.T.) ;
#85874 = ADVANCED_FACE('',(#17554),#939,.F.) ;
#85875 = ADVANCED_FACE('',(#17555),#940,.F.) ;
#85876 = ADVANCED_FACE('',(#17556),#941,.F.) ;
#85877 = ADVANCED_FACE('',(#17557),#942,.F.) ;
#85878 = ADVANCED_FACE('',(#17558),#943,.F.) ;
#85879 = ADVANCED_FACE('',(#17559,#673),#944,.T.) ;
#85880 = ADVANCED_FACE('',(#17560),#13748,.T.) ;
#85881 = ADVANCED_FACE('',(#17561),#945,.T.) ;
#85882 = ADVANCED_FACE('',(#17562),#13749,.T.) ;
#85883 = ADVANCED_FACE('',(#17563),#946,.T.) ;
#85884 = ADVANCED_FACE('',(#17564),#13750,.T.) ;
#85885 = ADVANCED_FACE('',(#17565),#947,.T.) ;
#85886 = ADVANCED_FACE('',(#17566),#13751,.T.) ;
#85887 = ADVANCED_FACE('',(#17567),#948,.T.) ;
#85888 = ADVANCED_FACE('',(#17568),#949,.T.) ;
#85889 = ADVANCED_FACE('',(#17569),#950,.T.) ;
#85890 = ADVANCED_FACE('',(#17570),#951,.F.) ;
#85891 = ADVANCED_FACE('',(#17571),#952,.F.) ;
#85892 = ADVANCED_FACE('',(#17572),#953,.T.) ;
#85893 = ADVANCED_FACE('',(#17573),#954,.F.) ;
#85894 = ADVANCED_FACE('',(#17574),#955,.F.) ;
#85895 = ADVANCED_FACE('',(#17575),#956,.F.) ;
#85896 = ADVANCED_FACE('',(#17576),#957,.F.) ;
#85897 = ADVANCED_FACE('',(#17577,#674),#958,.T.) ;
#85898 = ADVANCED_FACE('',(#17578),#13752,.T.) ;
#85899 = ADVANCED_FACE('',(#17579),#959,.T.) ;
#85900 = ADVANCED_FACE('',(#17580),#13753,.T.) ;
#85901 = ADVANCED_FACE('',(#17581),#960,.T.) ;
#85902 = ADVANCED_FACE('',(#17582),#13754,.T.) ;
#85903 = ADVANCED_FACE('',(#17583),#961,.T.) ;
#85904 = ADVANCED_FACE('',(#17584),#13755,.T.) ;
#85905 = ADVANCED_FACE('',(#17585),#962,.T.) ;
#85906 = ADVANCED_FACE('',(#17586),#963,.T.) ;
#85907 = ADVANCED_FACE('',(#17587),#964,.F.) ;
#85908 = ADVANCED_FACE('',(#17588),#965,.F.) ;
#85909 = ADVANCED_FACE('',(#17589),#966,.F.) ;
#85910 = ADVANCED_FACE('',(#17590),#967,.F.) ;
#85911 = ADVANCED_FACE('',(#17591),#968,.T.) ;
#85912 = ADVANCED_FACE('',(#17592),#13756,.T.) ;
#85913 = ADVANCED_FACE('',(#17593),#72,.T.) ;
#85914 = ADVANCED_FACE('',(#17594),#13757,.F.) ;
#85915 = ADVANCED_FACE('',(#17595),#73,.F.) ;
#85916 = ADVANCED_FACE('',(#17596),#13758,.F.) ;
#85917 = ADVANCED_FACE('',(#17597),#13759,.F.) ;
#85918 = ADVANCED_FACE('',(#17598),#13760,.T.) ;
#85919 = ADVANCED_FACE('',(#17599),#13761,.T.) ;
#85920 = ADVANCED_FACE('',(#17600),#13762,.T.) ;
#85921 = ADVANCED_FACE('',(#17601),#13763,.F.) ;
#85922 = ADVANCED_FACE('',(#17602),#16209,.F.) ;
#85923 = ADVANCED_FACE('',(#17603),#74,.T.) ;
#85924 = ADVANCED_FACE('',(#17604),#75,.T.) ;
#85925 = ADVANCED_FACE('',(#17605),#76,.F.) ;
#85926 = ADVANCED_FACE('',(#17606),#13764,.F.) ;
#85927 = ADVANCED_FACE('',(#17607),#13765,.F.) ;
#85928 = ADVANCED_FACE('',(#17608),#13766,.T.) ;
#85929 = ADVANCED_FACE('',(#17609),#13767,.T.) ;
#85930 = ADVANCED_FACE('',(#17610),#13768,.F.) ;
#85931 = ADVANCED_FACE('',(#17611),#13769,.F.) ;
#85932 = ADVANCED_FACE('',(#17612),#16210,.F.) ;
#85933 = ADVANCED_FACE('',(#17613),#77,.T.) ;
#85934 = ADVANCED_FACE('',(#17614),#16211,.F.) ;
#85935 = ADVANCED_FACE('',(#17615),#13770,.F.) ;
#85936 = ADVANCED_FACE('',(#17616),#13771,.F.) ;
#85937 = ADVANCED_FACE('',(#17617),#13772,.F.) ;
#85938 = ADVANCED_FACE('',(#17618),#13773,.F.) ;
#85939 = ADVANCED_FACE('',(#17619),#78,.F.) ;
#85940 = ADVANCED_FACE('',(#17620),#16212,.F.) ;
#85941 = ADVANCED_FACE('',(#17621),#13774,.T.) ;
#85942 = ADVANCED_FACE('',(#17622),#13775,.F.) ;
#85943 = ADVANCED_FACE('',(#17623),#79,.F.) ;
#85944 = ADVANCED_FACE('',(#17624),#13776,.F.) ;
#85945 = ADVANCED_FACE('',(#17625),#13777,.T.) ;
#85946 = ADVANCED_FACE('',(#17626),#13778,.T.) ;
#85947 = ADVANCED_FACE('',(#17627),#13779,.F.) ;
#85948 = ADVANCED_FACE('',(#17628),#13780,.T.) ;
#85949 = ADVANCED_FACE('',(#17629),#13781,.T.) ;
#85950 = ADVANCED_FACE('',(#17630),#13782,.F.) ;
#85951 = ADVANCED_FACE('',(#17631),#78963,.T.) ;
#85952 = ADVANCED_FACE('',(#17632),#13783,.T.) ;
#85953 = ADVANCED_FACE('',(#17633),#13784,.T.) ;
#85954 = ADVANCED_FACE('',(#17634),#13785,.T.) ;
#85955 = ADVANCED_FACE('',(#17635),#13786,.T.) ;
#85956 = ADVANCED_FACE('',(#17636),#16213,.T.) ;
#85957 = ADVANCED_FACE('',(#17637),#13787,.T.) ;
#85958 = ADVANCED_FACE('',(#17638),#13788,.T.) ;
#85959 = ADVANCED_FACE('',(#17639),#16214,.T.) ;
#85960 = ADVANCED_FACE('',(#17640),#16215,.T.) ;
#85961 = ADVANCED_FACE('',(#17641),#13789,.T.) ;
#85962 = ADVANCED_FACE('',(#17642),#13790,.T.) ;
#85963 = ADVANCED_FACE('',(#17643),#16216,.T.) ;
#85964 = ADVANCED_FACE('',(#17644),#13791,.T.) ;
#85965 = ADVANCED_FACE('',(#17645),#78964,.T.) ;
#85966 = ADVANCED_FACE('',(#17646),#78965,.T.) ;
#85967 = ADVANCED_FACE('',(#17647),#13792,.T.) ;
#85968 = ADVANCED_FACE('',(#17648),#13793,.F.) ;
#85969 = ADVANCED_FACE('',(#17649),#13794,.F.) ;
#85970 = ADVANCED_FACE('',(#17650),#13795,.F.) ;
#85971 = ADVANCED_FACE('',(#17651),#13796,.T.) ;
#85972 = ADVANCED_FACE('',(#17652),#13797,.T.) ;
#85973 = ADVANCED_FACE('',(#17653),#78966,.T.) ;
#85974 = ADVANCED_FACE('',(#17654),#16217,.F.) ;
#85975 = ADVANCED_FACE('',(#17655),#16218,.F.) ;
#85976 = ADVANCED_FACE('',(#17656),#78967,.T.) ;
#85977 = ADVANCED_FACE('',(#17657),#13798,.F.) ;
#85978 = ADVANCED_FACE('',(#17658),#13799,.F.) ;
#85979 = ADVANCED_FACE('',(#17659),#13800,.F.) ;
#85980 = ADVANCED_FACE('',(#17660),#13801,.F.) ;
#85981 = ADVANCED_FACE('',(#17661),#16219,.F.) ;
#85982 = ADVANCED_FACE('',(#17662),#16220,.F.) ;
#85983 = ADVANCED_FACE('',(#17663),#13802,.F.) ;
#85984 = ADVANCED_FACE('',(#17664),#13803,.T.) ;
#85985 = ADVANCED_FACE('',(#17665),#78968,.T.) ;
#85986 = ADVANCED_FACE('',(#17666),#78969,.T.) ;
#85987 = ADVANCED_FACE('',(#17667),#13804,.T.) ;
#85988 = ADVANCED_FACE('',(#17668),#13805,.F.) ;
#85989 = ADVANCED_FACE('',(#17669),#13806,.F.) ;
#85990 = ADVANCED_FACE('',(#17670),#13807,.F.) ;
#85991 = ADVANCED_FACE('',(#17671),#13808,.T.) ;
#85992 = ADVANCED_FACE('',(#17672),#13809,.T.) ;
#85993 = ADVANCED_FACE('',(#17673),#78970,.T.) ;
#85994 = ADVANCED_FACE('',(#17674),#16221,.F.) ;
#85995 = ADVANCED_FACE('',(#17675),#16222,.F.) ;
#85996 = ADVANCED_FACE('',(#17676),#78971,.T.) ;
#85997 = ADVANCED_FACE('',(#17677),#13810,.F.) ;
#85998 = ADVANCED_FACE('',(#17678),#13811,.F.) ;
#85999 = ADVANCED_FACE('',(#17679),#13812,.F.) ;
#86000 = ADVANCED_FACE('',(#17680),#13813,.F.) ;
#86001 = ADVANCED_FACE('',(#17681),#16223,.F.) ;
#86002 = ADVANCED_FACE('',(#17682),#16224,.F.) ;
#86003 = ADVANCED_FACE('',(#17683),#13814,.F.) ;
#86004 = ADVANCED_FACE('',(#17684),#78972,.F.) ;
#86005 = ADVANCED_FACE('',(#17685),#13815,.F.) ;
#86006 = ADVANCED_FACE('',(#17686),#16225,.F.) ;
#86007 = ADVANCED_FACE('',(#17687),#13816,.F.) ;
#86008 = ADVANCED_FACE('',(#17688),#13817,.T.) ;
#86009 = ADVANCED_FACE('',(#17689),#78973,.T.) ;
#86010 = ADVANCED_FACE('',(#17690),#78974,.T.) ;
#86011 = ADVANCED_FACE('',(#17691),#13818,.T.) ;
#86012 = ADVANCED_FACE('',(#17692),#78975,.T.) ;
#86013 = ADVANCED_FACE('',(#17693),#13819,.F.) ;
#86014 = ADVANCED_FACE('',(#17694),#13820,.F.) ;
#86015 = ADVANCED_FACE('',(#17695),#16226,.F.) ;
#86016 = ADVANCED_FACE('',(#17696),#78976,.F.) ;
#86017 = ADVANCED_FACE('',(#17697),#13821,.F.) ;
#86018 = ADVANCED_FACE('',(#17698),#13822,.T.) ;
#86019 = ADVANCED_FACE('',(#17699),#13823,.T.) ;
#86020 = ADVANCED_FACE('',(#17700),#13824,.T.) ;
#86021 = ADVANCED_FACE('',(#17701),#13825,.T.) ;
#86022 = ADVANCED_FACE('',(#17702),#13826,.T.) ;
#86023 = ADVANCED_FACE('',(#17703),#13827,.F.) ;
#86024 = ADVANCED_FACE('',(#17704),#13828,.F.) ;
#86025 = ADVANCED_FACE('',(#17705),#13829,.T.) ;
#86026 = ADVANCED_FACE('',(#17706),#13830,.T.) ;
#86027 = ADVANCED_FACE('',(#17707),#13831,.T.) ;
#86028 = ADVANCED_FACE('',(#17708),#13832,.T.) ;
#86029 = ADVANCED_FACE('',(#17709),#13833,.F.) ;
#86030 = ADVANCED_FACE('',(#17710),#16227,.F.) ;
#86031 = ADVANCED_FACE('',(#17711),#13834,.F.) ;
#86032 = ADVANCED_FACE('',(#17712),#78977,.F.) ;
#86033 = ADVANCED_FACE('',(#17713),#80,.F.) ;
#86034 = ADVANCED_FACE('',(#17714),#81,.F.) ;
#86035 = ADVANCED_FACE('',(#17715),#13835,.F.) ;
#86036 = ADVANCED_FACE('',(#17716),#13836,.F.) ;
#86037 = ADVANCED_FACE('',(#17717),#82,.F.) ;
#86038 = ADVANCED_FACE('',(#17718),#83,.F.) ;
#86039 = ADVANCED_FACE('',(#17719),#13837,.F.) ;
#86040 = ADVANCED_FACE('',(#17720),#16228,.F.) ;
#86041 = ADVANCED_FACE('',(#17721),#78978,.T.) ;
#86042 = ADVANCED_FACE('',(#17722),#13838,.T.) ;
#86043 = ADVANCED_FACE('',(#17723),#84,.T.) ;
#86044 = ADVANCED_FACE('',(#17724),#13839,.T.) ;
#86045 = ADVANCED_FACE('',(#17725),#85,.T.) ;
#86046 = ADVANCED_FACE('',(#17726),#86,.F.) ;
#86047 = ADVANCED_FACE('',(#17727),#87,.F.) ;
#86048 = ADVANCED_FACE('',(#17728),#88,.F.) ;
#86049 = ADVANCED_FACE('',(#17729),#89,.F.) ;
#86050 = ADVANCED_FACE('',(#17730),#969,.F.) ;
#86051 = ADVANCED_FACE('',(#17731),#970,.T.) ;
#86052 = ADVANCED_FACE('',(#17732),#13840,.T.) ;
#86053 = ADVANCED_FACE('',(#17733),#971,.T.) ;
#86054 = ADVANCED_FACE('',(#17734),#13841,.T.) ;
#86055 = ADVANCED_FACE('',(#17735),#972,.T.) ;
#86056 = ADVANCED_FACE('',(#17736),#13842,.T.) ;
#86057 = ADVANCED_FACE('',(#17737),#973,.T.) ;
#86058 = ADVANCED_FACE('',(#17738),#13843,.F.) ;
#86059 = ADVANCED_FACE('',(#17739),#974,.T.) ;
#86060 = ADVANCED_FACE('',(#17740),#975,.F.) ;
#86061 = ADVANCED_FACE('',(#17741),#976,.T.) ;
#86062 = ADVANCED_FACE('',(#17742),#977,.F.) ;
#86063 = ADVANCED_FACE('',(#17743),#978,.T.) ;
#86064 = ADVANCED_FACE('',(#17744),#979,.F.) ;
#86065 = ADVANCED_FACE('',(#17745),#980,.F.) ;
#86066 = ADVANCED_FACE('',(#17746),#981,.T.) ;
#86067 = ADVANCED_FACE('',(#17747),#982,.T.) ;
#86068 = ADVANCED_FACE('',(#17748),#983,.T.) ;
#86069 = ADVANCED_FACE('',(#17749),#984,.T.) ;
#86070 = ADVANCED_FACE('',(#17750),#985,.T.) ;
#86071 = ADVANCED_FACE('',(#17751),#986,.T.) ;
#86072 = ADVANCED_FACE('',(#17752),#987,.F.) ;
#86073 = ADVANCED_FACE('',(#17753),#988,.T.) ;
#86074 = ADVANCED_FACE('',(#17754),#989,.T.) ;
#86075 = ADVANCED_FACE('',(#17755),#990,.F.) ;
#86076 = ADVANCED_FACE('',(#17756),#991,.F.) ;
#86077 = ADVANCED_FACE('',(#17757),#992,.F.) ;
#86078 = ADVANCED_FACE('',(#17758),#993,.F.) ;
#86079 = ADVANCED_FACE('',(#17759),#994,.F.) ;
#86080 = ADVANCED_FACE('',(#17760,#675),#995,.T.) ;
#86081 = ADVANCED_FACE('',(#17761),#13844,.T.) ;
#86082 = ADVANCED_FACE('',(#17762),#996,.T.) ;
#86083 = ADVANCED_FACE('',(#17763),#13845,.T.) ;
#86084 = ADVANCED_FACE('',(#17764),#997,.T.) ;
#86085 = ADVANCED_FACE('',(#17765),#13846,.T.) ;
#86086 = ADVANCED_FACE('',(#17766),#998,.T.) ;
#86087 = ADVANCED_FACE('',(#17767),#13847,.T.) ;
#86088 = ADVANCED_FACE('',(#17768),#999,.T.) ;
#86089 = ADVANCED_FACE('',(#17769),#1000,.T.) ;
#86090 = ADVANCED_FACE('',(#17770),#1001,.T.) ;
#86091 = ADVANCED_FACE('',(#17771),#1002,.F.) ;
#86092 = ADVANCED_FACE('',(#17772),#1003,.F.) ;
#86093 = ADVANCED_FACE('',(#17773),#1004,.T.) ;
#86094 = ADVANCED_FACE('',(#17774),#1005,.F.) ;
#86095 = ADVANCED_FACE('',(#17775),#1006,.F.) ;
#86096 = ADVANCED_FACE('',(#17776),#1007,.F.) ;
#86097 = ADVANCED_FACE('',(#17777),#1008,.F.) ;
#86098 = ADVANCED_FACE('',(#17778,#676),#1009,.T.) ;
#86099 = ADVANCED_FACE('',(#17779),#13848,.T.) ;
#86100 = ADVANCED_FACE('',(#17780),#1010,.T.) ;
#86101 = ADVANCED_FACE('',(#17781),#13849,.T.) ;
#86102 = ADVANCED_FACE('',(#17782),#1011,.T.) ;
#86103 = ADVANCED_FACE('',(#17783),#13850,.T.) ;
#86104 = ADVANCED_FACE('',(#17784),#1012,.T.) ;
#86105 = ADVANCED_FACE('',(#17785),#13851,.T.) ;
#86106 = ADVANCED_FACE('',(#17786),#1013,.T.) ;
#86107 = ADVANCED_FACE('',(#17787),#1014,.T.) ;
#86108 = ADVANCED_FACE('',(#17788),#1015,.F.) ;
#86109 = ADVANCED_FACE('',(#17789),#1016,.F.) ;
#86110 = ADVANCED_FACE('',(#17790),#1017,.F.) ;
#86111 = ADVANCED_FACE('',(#17791),#1018,.F.) ;
#86112 = ADVANCED_FACE('',(#17792),#1019,.T.) ;
#86113 = ADVANCED_FACE('',(#17793),#13852,.T.) ;
#86114 = ADVANCED_FACE('',(#17794),#90,.T.) ;
#86115 = ADVANCED_FACE('',(#17795),#13853,.F.) ;
#86116 = ADVANCED_FACE('',(#17796),#91,.F.) ;
#86117 = ADVANCED_FACE('',(#17797),#13854,.F.) ;
#86118 = ADVANCED_FACE('',(#17798),#13855,.F.) ;
#86119 = ADVANCED_FACE('',(#17799),#13856,.T.) ;
#86120 = ADVANCED_FACE('',(#17800),#13857,.T.) ;
#86121 = ADVANCED_FACE('',(#17801),#13858,.T.) ;
#86122 = ADVANCED_FACE('',(#17802),#13859,.F.) ;
#86123 = ADVANCED_FACE('',(#17803),#16229,.F.) ;
#86124 = ADVANCED_FACE('',(#17804),#92,.T.) ;
#86125 = ADVANCED_FACE('',(#17805),#93,.T.) ;
#86126 = ADVANCED_FACE('',(#17806),#94,.F.) ;
#86127 = ADVANCED_FACE('',(#17807),#13860,.F.) ;
#86128 = ADVANCED_FACE('',(#17808),#13861,.F.) ;
#86129 = ADVANCED_FACE('',(#17809),#13862,.T.) ;
#86130 = ADVANCED_FACE('',(#17810),#13863,.T.) ;
#86131 = ADVANCED_FACE('',(#17811),#13864,.F.) ;
#86132 = ADVANCED_FACE('',(#17812),#13865,.F.) ;
#86133 = ADVANCED_FACE('',(#17813),#16230,.F.) ;
#86134 = ADVANCED_FACE('',(#17814),#95,.T.) ;
#86135 = ADVANCED_FACE('',(#17815),#16231,.F.) ;
#86136 = ADVANCED_FACE('',(#17816),#13866,.F.) ;
#86137 = ADVANCED_FACE('',(#17817),#13867,.F.) ;
#86138 = ADVANCED_FACE('',(#17818),#13868,.F.) ;
#86139 = ADVANCED_FACE('',(#17819),#13869,.F.) ;
#86140 = ADVANCED_FACE('',(#17820),#96,.F.) ;
#86141 = ADVANCED_FACE('',(#17821),#16232,.F.) ;
#86142 = ADVANCED_FACE('',(#17822),#13870,.T.) ;
#86143 = ADVANCED_FACE('',(#17823),#13871,.F.) ;
#86144 = ADVANCED_FACE('',(#17824),#97,.F.) ;
#86145 = ADVANCED_FACE('',(#17825),#13872,.F.) ;
#86146 = ADVANCED_FACE('',(#17826),#13873,.T.) ;
#86147 = ADVANCED_FACE('',(#17827),#13874,.F.) ;
#86148 = ADVANCED_FACE('',(#17828),#13875,.T.) ;
#86149 = ADVANCED_FACE('',(#17829),#13876,.T.) ;
#86150 = ADVANCED_FACE('',(#17830),#13877,.F.) ;
#86151 = ADVANCED_FACE('',(#17831),#78979,.T.) ;
#86152 = ADVANCED_FACE('',(#17832),#13878,.T.) ;
#86153 = ADVANCED_FACE('',(#17833),#13879,.T.) ;
#86154 = ADVANCED_FACE('',(#17834),#13880,.T.) ;
#86155 = ADVANCED_FACE('',(#17835),#13881,.T.) ;
#86156 = ADVANCED_FACE('',(#17836),#16233,.T.) ;
#86157 = ADVANCED_FACE('',(#17837),#13882,.T.) ;
#86158 = ADVANCED_FACE('',(#17838),#13883,.T.) ;
#86159 = ADVANCED_FACE('',(#17839),#16234,.T.) ;
#86160 = ADVANCED_FACE('',(#17840),#16235,.T.) ;
#86161 = ADVANCED_FACE('',(#17841),#13884,.T.) ;
#86162 = ADVANCED_FACE('',(#17842),#13885,.T.) ;
#86163 = ADVANCED_FACE('',(#17843),#16236,.T.) ;
#86164 = ADVANCED_FACE('',(#17844),#13886,.T.) ;
#86165 = ADVANCED_FACE('',(#17845),#78980,.T.) ;
#86166 = ADVANCED_FACE('',(#17846),#78981,.T.) ;
#86167 = ADVANCED_FACE('',(#17847),#13887,.T.) ;
#86168 = ADVANCED_FACE('',(#17848),#13888,.F.) ;
#86169 = ADVANCED_FACE('',(#17849),#13889,.F.) ;
#86170 = ADVANCED_FACE('',(#17850),#13890,.F.) ;
#86171 = ADVANCED_FACE('',(#17851),#13891,.T.) ;
#86172 = ADVANCED_FACE('',(#17852),#13892,.T.) ;
#86173 = ADVANCED_FACE('',(#17853),#78982,.T.) ;
#86174 = ADVANCED_FACE('',(#17854),#16237,.F.) ;
#86175 = ADVANCED_FACE('',(#17855),#16238,.F.) ;
#86176 = ADVANCED_FACE('',(#17856),#78983,.T.) ;
#86177 = ADVANCED_FACE('',(#17857),#13893,.F.) ;
#86178 = ADVANCED_FACE('',(#17858),#13894,.F.) ;
#86179 = ADVANCED_FACE('',(#17859),#13895,.F.) ;
#86180 = ADVANCED_FACE('',(#17860),#13896,.F.) ;
#86181 = ADVANCED_FACE('',(#17861),#16239,.F.) ;
#86182 = ADVANCED_FACE('',(#17862),#16240,.F.) ;
#86183 = ADVANCED_FACE('',(#17863),#13897,.F.) ;
#86184 = ADVANCED_FACE('',(#17864),#13898,.T.) ;
#86185 = ADVANCED_FACE('',(#17865),#78984,.T.) ;
#86186 = ADVANCED_FACE('',(#17866),#78985,.T.) ;
#86187 = ADVANCED_FACE('',(#17867),#13899,.T.) ;
#86188 = ADVANCED_FACE('',(#17868),#13900,.F.) ;
#86189 = ADVANCED_FACE('',(#17869),#13901,.F.) ;
#86190 = ADVANCED_FACE('',(#17870),#13902,.F.) ;
#86191 = ADVANCED_FACE('',(#17871),#13903,.T.) ;
#86192 = ADVANCED_FACE('',(#17872),#13904,.T.) ;
#86193 = ADVANCED_FACE('',(#17873),#78986,.T.) ;
#86194 = ADVANCED_FACE('',(#17874),#16241,.F.) ;
#86195 = ADVANCED_FACE('',(#17875),#16242,.F.) ;
#86196 = ADVANCED_FACE('',(#17876),#78987,.T.) ;
#86197 = ADVANCED_FACE('',(#17877),#13905,.F.) ;
#86198 = ADVANCED_FACE('',(#17878),#13906,.F.) ;
#86199 = ADVANCED_FACE('',(#17879),#13907,.F.) ;
#86200 = ADVANCED_FACE('',(#17880),#13908,.F.) ;
#86201 = ADVANCED_FACE('',(#17881),#16243,.F.) ;
#86202 = ADVANCED_FACE('',(#17882),#16244,.F.) ;
#86203 = ADVANCED_FACE('',(#17883),#13909,.F.) ;
#86204 = ADVANCED_FACE('',(#17884),#78988,.F.) ;
#86205 = ADVANCED_FACE('',(#17885),#13910,.F.) ;
#86206 = ADVANCED_FACE('',(#17886),#16245,.F.) ;
#86207 = ADVANCED_FACE('',(#17887),#13911,.F.) ;
#86208 = ADVANCED_FACE('',(#17888),#13912,.T.) ;
#86209 = ADVANCED_FACE('',(#17889),#78989,.T.) ;
#86210 = ADVANCED_FACE('',(#17890),#78990,.T.) ;
#86211 = ADVANCED_FACE('',(#17891),#78991,.T.) ;
#86212 = ADVANCED_FACE('',(#17892),#13913,.F.) ;
#86213 = ADVANCED_FACE('',(#17893),#16246,.F.) ;
#86214 = ADVANCED_FACE('',(#17894),#78992,.F.) ;
#86215 = ADVANCED_FACE('',(#17895),#13914,.F.) ;
#86216 = ADVANCED_FACE('',(#17896),#13915,.F.) ;
#86217 = ADVANCED_FACE('',(#17897),#13916,.T.) ;
#86218 = ADVANCED_FACE('',(#17898),#13917,.T.) ;
#86219 = ADVANCED_FACE('',(#17899),#16247,.F.) ;
#86220 = ADVANCED_FACE('',(#17900),#13918,.F.) ;
#86221 = ADVANCED_FACE('',(#17901),#78993,.F.) ;
#86222 = ADVANCED_FACE('',(#17902),#98,.F.) ;
#86223 = ADVANCED_FACE('',(#17903),#99,.F.) ;
#86224 = ADVANCED_FACE('',(#17904),#13919,.F.) ;
#86225 = ADVANCED_FACE('',(#17905),#100,.F.) ;
#86226 = ADVANCED_FACE('',(#17906),#101,.F.) ;
#86227 = ADVANCED_FACE('',(#17907),#13920,.F.) ;
#86228 = ADVANCED_FACE('',(#17908),#16248,.F.) ;
#86229 = ADVANCED_FACE('',(#17909),#78994,.T.) ;
#86230 = ADVANCED_FACE('',(#17910),#13921,.T.) ;
#86231 = ADVANCED_FACE('',(#17911),#102,.T.) ;
#86232 = ADVANCED_FACE('',(#17912),#103,.T.) ;
#86233 = ADVANCED_FACE('',(#17913),#104,.F.) ;
#86234 = ADVANCED_FACE('',(#17914),#105,.F.) ;
#86235 = ADVANCED_FACE('',(#17915),#106,.F.) ;
#86236 = ADVANCED_FACE('',(#17916),#107,.F.) ;
#86237 = ADVANCED_FACE('',(#17917),#16249,.T.) ;
#86238 = ADVANCED_FACE('',(#17918),#16250,.T.) ;
#86239 = ADVANCED_FACE('',(#17919),#13922,.T.) ;
#86240 = ADVANCED_FACE('',(#17920),#13923,.T.) ;
#86241 = ADVANCED_FACE('',(#17921),#13924,.T.) ;
#86242 = ADVANCED_FACE('',(#17922),#13925,.T.) ;
#86243 = ADVANCED_FACE('',(#17923),#16251,.T.) ;
#86244 = ADVANCED_FACE('',(#17924),#16252,.T.) ;
#86245 = ADVANCED_FACE('',(#17925),#16253,.T.) ;
#86246 = ADVANCED_FACE('',(#17926),#16254,.T.) ;
#86247 = ADVANCED_FACE('',(#17927),#13926,.T.) ;
#86248 = ADVANCED_FACE('',(#17928),#13927,.T.) ;
#86249 = ADVANCED_FACE('',(#17929),#13928,.F.) ;
#86250 = ADVANCED_FACE('',(#17930),#13929,.T.) ;
#86251 = ADVANCED_FACE('',(#17931),#13930,.T.) ;
#86252 = ADVANCED_FACE('',(#17932),#78995,.T.) ;
#86253 = ADVANCED_FACE('',(#17933),#108,.F.) ;
#86254 = ADVANCED_FACE('',(#17934),#109,.F.) ;
#86255 = ADVANCED_FACE('',(#17935),#78996,.T.) ;
#86256 = ADVANCED_FACE('',(#17936),#13931,.T.) ;
#86257 = ADVANCED_FACE('',(#17937),#13932,.F.) ;
#86258 = ADVANCED_FACE('',(#17938),#13933,.F.) ;
#86259 = ADVANCED_FACE('',(#17939),#13934,.T.) ;
#86260 = ADVANCED_FACE('',(#17940),#78997,.F.) ;
#86261 = ADVANCED_FACE('',(#17941),#78998,.F.) ;
#86262 = ADVANCED_FACE('',(#17942),#13935,.F.) ;
#86263 = ADVANCED_FACE('',(#17943),#78999,.F.) ;
#86264 = ADVANCED_FACE('',(#17944),#13936,.F.) ;
#86265 = ADVANCED_FACE('',(#17945),#79000,.T.) ;
#86266 = ADVANCED_FACE('',(#17946),#79001,.F.) ;
#86267 = ADVANCED_FACE('',(#17947),#79002,.T.) ;
#86268 = ADVANCED_FACE('',(#17948),#79003,.T.) ;
#86269 = ADVANCED_FACE('',(#17949),#16255,.T.) ;
#86270 = ADVANCED_FACE('',(#17950),#13937,.F.) ;
#86271 = ADVANCED_FACE('',(#17951),#16256,.T.) ;
#86272 = ADVANCED_FACE('',(#17952),#2419,.F.) ;
#86273 = ADVANCED_FACE('',(#17953),#13938,.F.) ;
#86274 = ADVANCED_FACE('',(#17954),#13939,.F.) ;
#86275 = ADVANCED_FACE('',(#17955),#1020,.F.) ;
#86276 = ADVANCED_FACE('',(#17956),#1021,.F.) ;
#86277 = ADVANCED_FACE('',(#17957),#1022,.F.) ;
#86278 = ADVANCED_FACE('',(#17958),#1023,.T.) ;
#86279 = ADVANCED_FACE('',(#17959,#677),#1024,.F.) ;
#86280 = ADVANCED_FACE('',(#17960),#1025,.F.) ;
#86281 = ADVANCED_FACE('',(#17961),#1026,.F.) ;
#86282 = ADVANCED_FACE('',(#17962),#1027,.F.) ;
#86283 = ADVANCED_FACE('',(#17963),#1028,.F.) ;
#86284 = ADVANCED_FACE('',(#17964),#1029,.F.) ;
#86285 = ADVANCED_FACE('',(#17965),#1030,.F.) ;
#86286 = ADVANCED_FACE('',(#17966),#1031,.F.) ;
#86287 = ADVANCED_FACE('',(#17967),#1032,.F.) ;
#86288 = ADVANCED_FACE('',(#17968,#678,#679),#1033,.F.) ;
#86289 = ADVANCED_FACE('',(#17969),#1034,.F.) ;
#86290 = ADVANCED_FACE('',(#17970),#1035,.F.) ;
#86291 = ADVANCED_FACE('',(#17971),#1036,.F.) ;
#86292 = ADVANCED_FACE('',(#17972,#680),#1037,.F.) ;
#86293 = ADVANCED_FACE('',(#17973,#681),#1038,.F.) ;
#86294 = ADVANCED_FACE('',(#17974),#1039,.F.) ;
#86295 = ADVANCED_FACE('',(#17975),#1040,.F.) ;
#86296 = ADVANCED_FACE('',(#17976),#1041,.F.) ;
#86297 = ADVANCED_FACE('',(#17977),#1042,.F.) ;
#86298 = ADVANCED_FACE('',(#17978),#1043,.T.) ;
#86299 = ADVANCED_FACE('',(#17979),#1044,.F.) ;
#86300 = ADVANCED_FACE('',(#17980),#1045,.T.) ;
#86301 = ADVANCED_FACE('',(#17981),#1046,.T.) ;
#86302 = ADVANCED_FACE('',(#17982),#1047,.T.) ;
#86303 = ADVANCED_FACE('',(#17983),#1048,.T.) ;
#86304 = ADVANCED_FACE('',(#17984),#1049,.T.) ;
#86305 = ADVANCED_FACE('',(#17985),#1050,.F.) ;
#86306 = ADVANCED_FACE('',(#17986),#1051,.T.) ;
#86307 = ADVANCED_FACE('',(#17987),#1052,.T.) ;
#86308 = ADVANCED_FACE('',(#17988),#1053,.F.) ;
#86309 = ADVANCED_FACE('',(#17989),#1054,.F.) ;
#86310 = ADVANCED_FACE('',(#17990),#1055,.F.) ;
#86311 = ADVANCED_FACE('',(#17991),#1056,.F.) ;
#86312 = ADVANCED_FACE('',(#17992),#1057,.F.) ;
#86313 = ADVANCED_FACE('',(#17993,#682),#1058,.T.) ;
#86314 = ADVANCED_FACE('',(#17994),#13940,.T.) ;
#86315 = ADVANCED_FACE('',(#17995),#1059,.T.) ;
#86316 = ADVANCED_FACE('',(#17996),#13941,.T.) ;
#86317 = ADVANCED_FACE('',(#17997),#1060,.T.) ;
#86318 = ADVANCED_FACE('',(#17998),#13942,.T.) ;
#86319 = ADVANCED_FACE('',(#17999),#1061,.T.) ;
#86320 = ADVANCED_FACE('',(#18000),#13943,.T.) ;
#86321 = ADVANCED_FACE('',(#18001),#1062,.T.) ;
#86322 = ADVANCED_FACE('',(#18002),#1063,.T.) ;
#86323 = ADVANCED_FACE('',(#18003),#1064,.T.) ;
#86324 = ADVANCED_FACE('',(#18004),#1065,.F.) ;
#86325 = ADVANCED_FACE('',(#18005),#1066,.F.) ;
#86326 = ADVANCED_FACE('',(#18006),#1067,.T.) ;
#86327 = ADVANCED_FACE('',(#18007),#1068,.F.) ;
#86328 = ADVANCED_FACE('',(#18008),#1069,.F.) ;
#86329 = ADVANCED_FACE('',(#18009),#1070,.F.) ;
#86330 = ADVANCED_FACE('',(#18010),#1071,.F.) ;
#86331 = ADVANCED_FACE('',(#18011,#683),#1072,.T.) ;
#86332 = ADVANCED_FACE('',(#18012),#13944,.T.) ;
#86333 = ADVANCED_FACE('',(#18013),#1073,.T.) ;
#86334 = ADVANCED_FACE('',(#18014),#13945,.T.) ;
#86335 = ADVANCED_FACE('',(#18015),#1074,.T.) ;
#86336 = ADVANCED_FACE('',(#18016),#13946,.T.) ;
#86337 = ADVANCED_FACE('',(#18017),#1075,.T.) ;
#86338 = ADVANCED_FACE('',(#18018),#13947,.T.) ;
#86339 = ADVANCED_FACE('',(#18019),#1076,.T.) ;
#86340 = ADVANCED_FACE('',(#18020),#1077,.T.) ;
#86341 = ADVANCED_FACE('',(#18021),#1078,.F.) ;
#86342 = ADVANCED_FACE('',(#18022),#1079,.F.) ;
#86343 = ADVANCED_FACE('',(#18023),#1080,.F.) ;
#86344 = ADVANCED_FACE('',(#18024),#1081,.F.) ;
#86345 = ADVANCED_FACE('',(#18025),#1082,.T.) ;
#86346 = ADVANCED_FACE('',(#18026),#13948,.T.) ;
#86347 = ADVANCED_FACE('',(#18027),#110,.T.) ;
#86348 = ADVANCED_FACE('',(#18028),#13949,.F.) ;
#86349 = ADVANCED_FACE('',(#18029),#111,.F.) ;
#86350 = ADVANCED_FACE('',(#18030),#13950,.F.) ;
#86351 = ADVANCED_FACE('',(#18031),#13951,.F.) ;
#86352 = ADVANCED_FACE('',(#18032),#13952,.T.) ;
#86353 = ADVANCED_FACE('',(#18033),#13953,.T.) ;
#86354 = ADVANCED_FACE('',(#18034),#13954,.T.) ;
#86355 = ADVANCED_FACE('',(#18035),#13955,.F.) ;
#86356 = ADVANCED_FACE('',(#18036),#16257,.F.) ;
#86357 = ADVANCED_FACE('',(#18037),#112,.T.) ;
#86358 = ADVANCED_FACE('',(#18038),#113,.T.) ;
#86359 = ADVANCED_FACE('',(#18039),#114,.F.) ;
#86360 = ADVANCED_FACE('',(#18040),#13956,.F.) ;
#86361 = ADVANCED_FACE('',(#18041),#13957,.F.) ;
#86362 = ADVANCED_FACE('',(#18042),#13958,.T.) ;
#86363 = ADVANCED_FACE('',(#18043),#13959,.T.) ;
#86364 = ADVANCED_FACE('',(#18044),#13960,.F.) ;
#86365 = ADVANCED_FACE('',(#18045),#13961,.F.) ;
#86366 = ADVANCED_FACE('',(#18046),#16258,.F.) ;
#86367 = ADVANCED_FACE('',(#18047),#115,.T.) ;
#86368 = ADVANCED_FACE('',(#18048),#16259,.F.) ;
#86369 = ADVANCED_FACE('',(#18049),#13962,.F.) ;
#86370 = ADVANCED_FACE('',(#18050),#13963,.F.) ;
#86371 = ADVANCED_FACE('',(#18051),#13964,.F.) ;
#86372 = ADVANCED_FACE('',(#18052),#13965,.F.) ;
#86373 = ADVANCED_FACE('',(#18053),#116,.F.) ;
#86374 = ADVANCED_FACE('',(#18054),#16260,.F.) ;
#86375 = ADVANCED_FACE('',(#18055),#13966,.T.) ;
#86376 = ADVANCED_FACE('',(#18056),#13967,.F.) ;
#86377 = ADVANCED_FACE('',(#18057),#117,.F.) ;
#86378 = ADVANCED_FACE('',(#18058),#13968,.F.) ;
#86379 = ADVANCED_FACE('',(#18059),#13969,.T.) ;
#86380 = ADVANCED_FACE('',(#18060),#13970,.T.) ;
#86381 = ADVANCED_FACE('',(#18061),#13971,.F.) ;
#86382 = ADVANCED_FACE('',(#18062),#13972,.T.) ;
#86383 = ADVANCED_FACE('',(#18063),#13973,.T.) ;
#86384 = ADVANCED_FACE('',(#18064),#13974,.F.) ;
#86385 = ADVANCED_FACE('',(#18065),#79004,.T.) ;
#86386 = ADVANCED_FACE('',(#18066),#13975,.T.) ;
#86387 = ADVANCED_FACE('',(#18067),#13976,.T.) ;
#86388 = ADVANCED_FACE('',(#18068),#13977,.T.) ;
#86389 = ADVANCED_FACE('',(#18069),#13978,.T.) ;
#86390 = ADVANCED_FACE('',(#18070),#16261,.T.) ;
#86391 = ADVANCED_FACE('',(#18071),#13979,.T.) ;
#86392 = ADVANCED_FACE('',(#18072),#13980,.T.) ;
#86393 = ADVANCED_FACE('',(#18073),#16262,.T.) ;
#86394 = ADVANCED_FACE('',(#18074),#16263,.T.) ;
#86395 = ADVANCED_FACE('',(#18075),#13981,.T.) ;
#86396 = ADVANCED_FACE('',(#18076),#13982,.T.) ;
#86397 = ADVANCED_FACE('',(#18077),#16264,.T.) ;
#86398 = ADVANCED_FACE('',(#18078),#13983,.T.) ;
#86399 = ADVANCED_FACE('',(#18079),#79005,.T.) ;
#86400 = ADVANCED_FACE('',(#18080),#79006,.T.) ;
#86401 = ADVANCED_FACE('',(#18081),#13984,.T.) ;
#86402 = ADVANCED_FACE('',(#18082),#13985,.F.) ;
#86403 = ADVANCED_FACE('',(#18083),#13986,.F.) ;
#86404 = ADVANCED_FACE('',(#18084),#13987,.F.) ;
#86405 = ADVANCED_FACE('',(#18085),#13988,.T.) ;
#86406 = ADVANCED_FACE('',(#18086),#13989,.T.) ;
#86407 = ADVANCED_FACE('',(#18087),#79007,.T.) ;
#86408 = ADVANCED_FACE('',(#18088),#16265,.F.) ;
#86409 = ADVANCED_FACE('',(#18089),#16266,.F.) ;
#86410 = ADVANCED_FACE('',(#18090),#79008,.T.) ;
#86411 = ADVANCED_FACE('',(#18091),#13990,.F.) ;
#86412 = ADVANCED_FACE('',(#18092),#13991,.F.) ;
#86413 = ADVANCED_FACE('',(#18093),#13992,.F.) ;
#86414 = ADVANCED_FACE('',(#18094),#13993,.F.) ;
#86415 = ADVANCED_FACE('',(#18095),#16267,.F.) ;
#86416 = ADVANCED_FACE('',(#18096),#16268,.F.) ;
#86417 = ADVANCED_FACE('',(#18097),#13994,.F.) ;
#86418 = ADVANCED_FACE('',(#18098),#13995,.T.) ;
#86419 = ADVANCED_FACE('',(#18099),#79009,.T.) ;
#86420 = ADVANCED_FACE('',(#18100),#79010,.T.) ;
#86421 = ADVANCED_FACE('',(#18101),#13996,.T.) ;
#86422 = ADVANCED_FACE('',(#18102),#13997,.F.) ;
#86423 = ADVANCED_FACE('',(#18103),#13998,.F.) ;
#86424 = ADVANCED_FACE('',(#18104),#13999,.F.) ;
#86425 = ADVANCED_FACE('',(#18105),#14000,.T.) ;
#86426 = ADVANCED_FACE('',(#18106),#14001,.T.) ;
#86427 = ADVANCED_FACE('',(#18107),#79011,.T.) ;
#86428 = ADVANCED_FACE('',(#18108),#16269,.F.) ;
#86429 = ADVANCED_FACE('',(#18109),#16270,.F.) ;
#86430 = ADVANCED_FACE('',(#18110),#79012,.T.) ;
#86431 = ADVANCED_FACE('',(#18111),#14002,.F.) ;
#86432 = ADVANCED_FACE('',(#18112),#14003,.F.) ;
#86433 = ADVANCED_FACE('',(#18113),#14004,.F.) ;
#86434 = ADVANCED_FACE('',(#18114),#14005,.F.) ;
#86435 = ADVANCED_FACE('',(#18115),#16271,.F.) ;
#86436 = ADVANCED_FACE('',(#18116),#16272,.F.) ;
#86437 = ADVANCED_FACE('',(#18117),#14006,.F.) ;
#86438 = ADVANCED_FACE('',(#18118),#79013,.F.) ;
#86439 = ADVANCED_FACE('',(#18119),#14007,.F.) ;
#86440 = ADVANCED_FACE('',(#18120),#16273,.F.) ;
#86441 = ADVANCED_FACE('',(#18121),#14008,.F.) ;
#86442 = ADVANCED_FACE('',(#18122),#14009,.T.) ;
#86443 = ADVANCED_FACE('',(#18123),#79014,.T.) ;
#86444 = ADVANCED_FACE('',(#18124),#79015,.T.) ;
#86445 = ADVANCED_FACE('',(#18125),#14010,.T.) ;
#86446 = ADVANCED_FACE('',(#18126),#79016,.T.) ;
#86447 = ADVANCED_FACE('',(#18127),#14011,.F.) ;
#86448 = ADVANCED_FACE('',(#18128),#14012,.F.) ;
#86449 = ADVANCED_FACE('',(#18129),#16274,.F.) ;
#86450 = ADVANCED_FACE('',(#18130),#79017,.F.) ;
#86451 = ADVANCED_FACE('',(#18131),#14013,.F.) ;
#86452 = ADVANCED_FACE('',(#18132),#14014,.T.) ;
#86453 = ADVANCED_FACE('',(#18133),#14015,.T.) ;
#86454 = ADVANCED_FACE('',(#18134),#14016,.T.) ;
#86455 = ADVANCED_FACE('',(#18135),#14017,.T.) ;
#86456 = ADVANCED_FACE('',(#18136),#14018,.T.) ;
#86457 = ADVANCED_FACE('',(#18137),#14019,.F.) ;
#86458 = ADVANCED_FACE('',(#18138),#14020,.F.) ;
#86459 = ADVANCED_FACE('',(#18139),#14021,.T.) ;
#86460 = ADVANCED_FACE('',(#18140),#14022,.T.) ;
#86461 = ADVANCED_FACE('',(#18141),#14023,.T.) ;
#86462 = ADVANCED_FACE('',(#18142),#14024,.T.) ;
#86463 = ADVANCED_FACE('',(#18143),#14025,.F.) ;
#86464 = ADVANCED_FACE('',(#18144),#14026,.F.) ;
#86465 = ADVANCED_FACE('',(#18145),#14027,.T.) ;
#86466 = ADVANCED_FACE('',(#18146),#14028,.T.) ;
#86467 = ADVANCED_FACE('',(#18147),#14029,.F.) ;
#86468 = ADVANCED_FACE('',(#18148),#16275,.F.) ;
#86469 = ADVANCED_FACE('',(#18149),#14030,.F.) ;
#86470 = ADVANCED_FACE('',(#18150),#79018,.F.) ;
#86471 = ADVANCED_FACE('',(#18151),#118,.F.) ;
#86472 = ADVANCED_FACE('',(#18152),#119,.F.) ;
#86473 = ADVANCED_FACE('',(#18153),#14031,.F.) ;
#86474 = ADVANCED_FACE('',(#18154),#14032,.F.) ;
#86475 = ADVANCED_FACE('',(#18155),#120,.F.) ;
#86476 = ADVANCED_FACE('',(#18156),#121,.F.) ;
#86477 = ADVANCED_FACE('',(#18157),#14033,.F.) ;
#86478 = ADVANCED_FACE('',(#18158),#16276,.F.) ;
#86479 = ADVANCED_FACE('',(#18159),#79019,.T.) ;
#86480 = ADVANCED_FACE('',(#18160),#14034,.T.) ;
#86481 = ADVANCED_FACE('',(#18161),#122,.T.) ;
#86482 = ADVANCED_FACE('',(#18162),#14035,.T.) ;
#86483 = ADVANCED_FACE('',(#18163),#123,.T.) ;
#86484 = ADVANCED_FACE('',(#18164),#124,.F.) ;
#86485 = ADVANCED_FACE('',(#18165),#125,.F.) ;
#86486 = ADVANCED_FACE('',(#18166),#126,.F.) ;
#86487 = ADVANCED_FACE('',(#18167),#127,.F.) ;
#86488 = ADVANCED_FACE('',(#18168),#79020,.T.) ;
#86489 = ADVANCED_FACE('',(#18169),#79021,.F.) ;
#86490 = ADVANCED_FACE('',(#18170),#16277,.F.) ;
#86491 = ADVANCED_FACE('',(#18171),#14036,.F.) ;
#86492 = ADVANCED_FACE('',(#18172),#79022,.T.) ;
#86493 = ADVANCED_FACE('',(#18173),#79023,.F.) ;
#86494 = ADVANCED_FACE('',(#18174),#16278,.F.) ;
#86495 = ADVANCED_FACE('',(#18175),#14037,.F.) ;
#86496 = ADVANCED_FACE('',(#18176),#79024,.T.) ;
#86497 = ADVANCED_FACE('',(#18177),#79025,.F.) ;
#86498 = ADVANCED_FACE('',(#18178),#16279,.F.) ;
#86499 = ADVANCED_FACE('',(#18179),#14038,.F.) ;
#86500 = ADVANCED_FACE('',(#18180),#79026,.T.) ;
#86501 = ADVANCED_FACE('',(#18181),#79027,.F.) ;
#86502 = ADVANCED_FACE('',(#18182),#16280,.F.) ;
#86503 = ADVANCED_FACE('',(#18183),#14039,.F.) ;
#86504 = ADVANCED_FACE('',(#18184),#79028,.T.) ;
#86505 = ADVANCED_FACE('',(#18185),#79029,.F.) ;
#86506 = ADVANCED_FACE('',(#18186),#16281,.F.) ;
#86507 = ADVANCED_FACE('',(#18187),#14040,.F.) ;
#86508 = ADVANCED_FACE('',(#18188),#79030,.T.) ;
#86509 = ADVANCED_FACE('',(#18189),#79031,.F.) ;
#86510 = ADVANCED_FACE('',(#18190),#16282,.F.) ;
#86511 = ADVANCED_FACE('',(#18191),#14041,.F.) ;
#86512 = ADVANCED_FACE('',(#18192),#79032,.T.) ;
#86513 = ADVANCED_FACE('',(#18193),#79033,.F.) ;
#86514 = ADVANCED_FACE('',(#18194),#16283,.F.) ;
#86515 = ADVANCED_FACE('',(#18195),#14042,.F.) ;
#86516 = ADVANCED_FACE('',(#18196),#79034,.T.) ;
#86517 = ADVANCED_FACE('',(#18197),#79035,.F.) ;
#86518 = ADVANCED_FACE('',(#18198),#16284,.F.) ;
#86519 = ADVANCED_FACE('',(#18199),#14043,.F.) ;
#86520 = ADVANCED_FACE('',(#18200),#79036,.T.) ;
#86521 = ADVANCED_FACE('',(#18201),#79037,.T.) ;
#86522 = ADVANCED_FACE('',(#18202),#79038,.T.) ;
#86523 = ADVANCED_FACE('',(#18203),#79039,.T.) ;
#86524 = ADVANCED_FACE('',(#18204),#79040,.T.) ;
#86525 = ADVANCED_FACE('',(#18205),#79041,.T.) ;
#86526 = ADVANCED_FACE('',(#18206),#79042,.T.) ;
#86527 = ADVANCED_FACE('',(#18207),#79043,.T.) ;
#86528 = ADVANCED_FACE('',(#18208),#79044,.T.) ;
#86529 = ADVANCED_FACE('',(#18209),#79045,.T.) ;
#86530 = ADVANCED_FACE('',(#18210),#79046,.F.) ;
#86531 = ADVANCED_FACE('',(#18211),#16285,.F.) ;
#86532 = ADVANCED_FACE('',(#18212),#14044,.F.) ;
#86533 = ADVANCED_FACE('',(#18213),#14045,.T.) ;
#86534 = ADVANCED_FACE('',(#18214),#14046,.T.) ;
#86535 = ADVANCED_FACE('',(#18215),#14047,.T.) ;
#86536 = ADVANCED_FACE('',(#18216),#14048,.T.) ;
#86537 = ADVANCED_FACE('',(#18217),#14049,.T.) ;
#86538 = ADVANCED_FACE('',(#18218),#14050,.T.) ;
#86539 = ADVANCED_FACE('',(#18219),#14051,.T.) ;
#86540 = ADVANCED_FACE('',(#18220),#14052,.T.) ;
#86541 = ADVANCED_FACE('',(#18221),#14053,.T.) ;
#86542 = ADVANCED_FACE('',(#18222),#14054,.F.) ;
#86543 = ADVANCED_FACE('',(#18223),#14055,.F.) ;
#86544 = ADVANCED_FACE('',(#18224),#14056,.F.) ;
#86545 = ADVANCED_FACE('',(#18225),#14057,.F.) ;
#86546 = ADVANCED_FACE('',(#18226),#14058,.F.) ;
#86547 = ADVANCED_FACE('',(#18227),#14059,.F.) ;
#86548 = ADVANCED_FACE('',(#18228),#14060,.F.) ;
#86549 = ADVANCED_FACE('',(#18229),#14061,.F.) ;
#86550 = ADVANCED_FACE('',(#18230),#14062,.F.) ;
#86551 = ADVANCED_FACE('',(#18231),#79047,.T.) ;
#86552 = ADVANCED_FACE('',(#18232),#79048,.T.) ;
#86553 = ADVANCED_FACE('',(#18233),#79049,.F.) ;
#86554 = ADVANCED_FACE('',(#18234),#16286,.F.) ;
#86555 = ADVANCED_FACE('',(#18235),#14063,.F.) ;
#86556 = ADVANCED_FACE('',(#18236),#14064,.T.) ;
#86557 = ADVANCED_FACE('',(#18237),#14065,.F.) ;
#86558 = ADVANCED_FACE('',(#18238),#1083,.T.) ;
#86559 = ADVANCED_FACE('',(#18239),#1084,.T.) ;
#86560 = ADVANCED_FACE('',(#18240),#1085,.T.) ;
#86561 = ADVANCED_FACE('',(#18241),#1086,.T.) ;
#86562 = ADVANCED_FACE('',(#18242),#1087,.T.) ;
#86563 = ADVANCED_FACE('',(#18243),#1088,.T.) ;
#86564 = ADVANCED_FACE('',(#18244),#1089,.T.) ;
#86565 = ADVANCED_FACE('',(#18245),#1090,.T.) ;
#86566 = ADVANCED_FACE('',(#18246),#1091,.T.) ;
#86567 = ADVANCED_FACE('',(#18247),#1092,.F.) ;
#86568 = ADVANCED_FACE('',(#18248),#1093,.F.) ;
#86569 = ADVANCED_FACE('',(#18249),#1094,.F.) ;
#86570 = ADVANCED_FACE('',(#18250),#1095,.F.) ;
#86571 = ADVANCED_FACE('',(#18251),#1096,.F.) ;
#86572 = ADVANCED_FACE('',(#18252),#1097,.F.) ;
#86573 = ADVANCED_FACE('',(#18253),#1098,.F.) ;
#86574 = ADVANCED_FACE('',(#18254),#1099,.F.) ;
#86575 = ADVANCED_FACE('',(#18255),#1100,.F.) ;
#86576 = ADVANCED_FACE('',(#18256),#1101,.F.) ;
#86577 = ADVANCED_FACE('',(#18257),#1102,.F.) ;
#86578 = ADVANCED_FACE('',(#18258),#1103,.F.) ;
#86579 = ADVANCED_FACE('',(#18259),#1104,.F.) ;
#86580 = ADVANCED_FACE('',(#18260),#1105,.F.) ;
#86581 = ADVANCED_FACE('',(#18261),#1106,.F.) ;
#86582 = ADVANCED_FACE('',(#18262),#1107,.F.) ;
#86583 = ADVANCED_FACE('',(#18263),#1108,.F.) ;
#86584 = ADVANCED_FACE('',(#18264),#1109,.F.) ;
#86585 = ADVANCED_FACE('',(#18265),#14066,.T.) ;
#86586 = ADVANCED_FACE('',(#18266),#14067,.T.) ;
#86587 = ADVANCED_FACE('',(#18267),#14068,.T.) ;
#86588 = ADVANCED_FACE('',(#18268),#14069,.T.) ;
#86589 = ADVANCED_FACE('',(#18269),#14070,.T.) ;
#86590 = ADVANCED_FACE('',(#18270),#14071,.T.) ;
#86591 = ADVANCED_FACE('',(#18271),#14072,.T.) ;
#86592 = ADVANCED_FACE('',(#18272),#14073,.T.) ;
#86593 = ADVANCED_FACE('',(#18273),#14074,.T.) ;
#86594 = ADVANCED_FACE('',(#18274),#1110,.T.) ;
#86595 = ADVANCED_FACE('',(#18275),#1111,.F.) ;
#86596 = ADVANCED_FACE('',(#18276),#1112,.F.) ;
#86597 = ADVANCED_FACE('',(#18277),#14075,.T.) ;
#86598 = ADVANCED_FACE('',(#18278),#14076,.T.) ;
#86599 = ADVANCED_FACE('',(#18279),#1113,.T.) ;
#86600 = ADVANCED_FACE('',(#18280),#14077,.T.) ;
#86601 = ADVANCED_FACE('',(#18281),#1114,.T.) ;
#86602 = ADVANCED_FACE('',(#18282),#14078,.T.) ;
#86603 = ADVANCED_FACE('',(#18283),#1115,.T.) ;
#86604 = ADVANCED_FACE('',(#18284),#14079,.F.) ;
#86605 = ADVANCED_FACE('',(#18285),#1116,.T.) ;
#86606 = ADVANCED_FACE('',(#18286),#14080,.T.) ;
#86607 = ADVANCED_FACE('',(#18287),#1117,.T.) ;
#86608 = ADVANCED_FACE('',(#18288),#14081,.T.) ;
#86609 = ADVANCED_FACE('',(#18289),#1118,.T.) ;
#86610 = ADVANCED_FACE('',(#18290),#14082,.F.) ;
#86611 = ADVANCED_FACE('',(#18291),#1119,.T.) ;
#86612 = ADVANCED_FACE('',(#18292),#14083,.T.) ;
#86613 = ADVANCED_FACE('',(#18293,#684,#685,#686,#687,#688,#689,#690,#691,
#692,#693),#1120,.T.) ;
#86614 = ADVANCED_FACE('',(#18294),#1121,.F.) ;
#86615 = ADVANCED_FACE('',(#18295),#1122,.T.) ;
#86616 = ADVANCED_FACE('',(#18296),#1123,.T.) ;
#86617 = ADVANCED_FACE('',(#18297),#1124,.F.) ;
#86618 = ADVANCED_FACE('',(#18298),#1125,.F.) ;
#86619 = ADVANCED_FACE('',(#18299),#1126,.F.) ;
#86620 = ADVANCED_FACE('',(#18300),#1127,.F.) ;
#86621 = ADVANCED_FACE('',(#18301),#1128,.F.) ;
#86622 = ADVANCED_FACE('',(#18302),#14084,.T.) ;
#86623 = ADVANCED_FACE('',(#18303),#1129,.F.) ;
#86624 = ADVANCED_FACE('',(#18304),#14085,.T.) ;
#86625 = ADVANCED_FACE('',(#18305),#1130,.F.) ;
#86626 = ADVANCED_FACE('',(#18306),#14086,.F.) ;
#86627 = ADVANCED_FACE('',(#18307),#1131,.F.) ;
#86628 = ADVANCED_FACE('',(#18308),#14087,.F.) ;
#86629 = ADVANCED_FACE('',(#18309),#1132,.F.) ;
#86630 = ADVANCED_FACE('',(#18310),#1133,.F.) ;
#86631 = ADVANCED_FACE('',(#18311),#14088,.F.) ;
#86632 = ADVANCED_FACE('',(#18312),#1134,.F.) ;
#86633 = ADVANCED_FACE('',(#18313),#14089,.T.) ;
#86634 = ADVANCED_FACE('',(#18314),#1135,.F.) ;
#86635 = ADVANCED_FACE('',(#18315),#14090,.T.) ;
#86636 = ADVANCED_FACE('',(#18316),#1136,.F.) ;
#86637 = ADVANCED_FACE('',(#18317),#14091,.F.) ;
#86638 = ADVANCED_FACE('',(#18318),#1137,.F.) ;
#86639 = ADVANCED_FACE('',(#18319),#14092,.F.) ;
#86640 = ADVANCED_FACE('',(#18320),#1138,.F.) ;
#86641 = ADVANCED_FACE('',(#18321),#14093,.F.) ;
#86642 = ADVANCED_FACE('',(#18322),#14094,.T.) ;
#86643 = ADVANCED_FACE('',(#18323),#14095,.F.) ;
#86644 = ADVANCED_FACE('',(#18324),#1139,.F.) ;
#86645 = ADVANCED_FACE('',(#18325),#14096,.F.) ;
#86646 = ADVANCED_FACE('',(#18326),#1140,.F.) ;
#86647 = ADVANCED_FACE('',(#18327),#14097,.F.) ;
#86648 = ADVANCED_FACE('',(#18328),#1141,.F.) ;
#86649 = ADVANCED_FACE('',(#18329,#694),#1142,.F.) ;
#86650 = ADVANCED_FACE('',(#18330,#695),#1143,.T.) ;
#86651 = ADVANCED_FACE('',(#18331),#14098,.T.) ;
#86652 = ADVANCED_FACE('',(#18332),#14099,.F.) ;
#86653 = ADVANCED_FACE('',(#18333),#16287,.F.) ;
#86654 = ADVANCED_FACE('',(#18334),#16288,.T.) ;
#86655 = ADVANCED_FACE('',(#18335),#79050,.T.) ;
#86656 = ADVANCED_FACE('',(#18336),#14100,.F.) ;
#86657 = ADVANCED_FACE('',(#18337),#14101,.F.) ;
#86658 = ADVANCED_FACE('',(#18338),#14102,.T.) ;
#86659 = ADVANCED_FACE('',(#18339),#14103,.T.) ;
#86660 = ADVANCED_FACE('',(#18340),#14104,.T.) ;
#86661 = ADVANCED_FACE('',(#18341),#14105,.F.) ;
#86662 = ADVANCED_FACE('',(#18342),#16289,.F.) ;
#86663 = ADVANCED_FACE('',(#18343),#79051,.F.) ;
#86664 = ADVANCED_FACE('',(#18344),#79052,.F.) ;
#86665 = ADVANCED_FACE('',(#18345),#79053,.T.) ;
#86666 = ADVANCED_FACE('',(#18346),#14106,.F.) ;
#86667 = ADVANCED_FACE('',(#18347),#14107,.F.) ;
#86668 = ADVANCED_FACE('',(#18348),#14108,.F.) ;
#86669 = ADVANCED_FACE('',(#18349),#14109,.T.) ;
#86670 = ADVANCED_FACE('',(#18350),#14110,.T.) ;
#86671 = ADVANCED_FACE('',(#18351),#79054,.F.) ;
#86672 = ADVANCED_FACE('',(#18352),#16290,.F.) ;
#86673 = ADVANCED_FACE('',(#18353),#16291,.T.) ;
#86674 = ADVANCED_FACE('',(#18354),#14111,.T.) ;
#86675 = ADVANCED_FACE('',(#18355),#16292,.F.) ;
#86676 = ADVANCED_FACE('',(#18356),#16293,.T.) ;
#86677 = ADVANCED_FACE('',(#18357),#14112,.F.) ;
#86678 = ADVANCED_FACE('',(#18358),#14113,.F.) ;
#86679 = ADVANCED_FACE('',(#18359),#14114,.T.) ;
#86680 = ADVANCED_FACE('',(#18360),#79055,.T.) ;
#86681 = ADVANCED_FACE('',(#18361),#14115,.F.) ;
#86682 = ADVANCED_FACE('',(#18362),#14116,.T.) ;
#86683 = ADVANCED_FACE('',(#18363),#14117,.F.) ;
#86684 = ADVANCED_FACE('',(#18364),#16294,.F.) ;
#86685 = ADVANCED_FACE('',(#18365),#79056,.T.) ;
#86686 = ADVANCED_FACE('',(#18366),#14118,.T.) ;
#86687 = ADVANCED_FACE('',(#18367),#16295,.F.) ;
#86688 = ADVANCED_FACE('',(#18368),#79057,.F.) ;
#86689 = ADVANCED_FACE('',(#18369),#14119,.F.) ;
#86690 = ADVANCED_FACE('',(#18370),#14120,.T.) ;
#86691 = ADVANCED_FACE('',(#18371),#79058,.T.) ;
#86692 = ADVANCED_FACE('',(#18372),#14121,.F.) ;
#86693 = ADVANCED_FACE('',(#18373),#79059,.T.) ;
#86694 = ADVANCED_FACE('',(#18374),#14122,.T.) ;
#86695 = ADVANCED_FACE('',(#18375),#14123,.T.) ;
#86696 = ADVANCED_FACE('',(#18376),#16296,.T.) ;
#86697 = ADVANCED_FACE('',(#18377),#16297,.T.) ;
#86698 = ADVANCED_FACE('',(#18378),#14124,.T.) ;
#86699 = ADVANCED_FACE('',(#18379),#14125,.T.) ;
#86700 = ADVANCED_FACE('',(#18380),#79060,.T.) ;
#86701 = ADVANCED_FACE('',(#18381),#16298,.T.) ;
#86702 = ADVANCED_FACE('',(#18382),#14126,.T.) ;
#86703 = ADVANCED_FACE('',(#18383),#14127,.T.) ;
#86704 = ADVANCED_FACE('',(#18384),#16299,.T.) ;
#86705 = ADVANCED_FACE('',(#18385),#79061,.T.) ;
#86706 = ADVANCED_FACE('',(#18386),#14128,.T.) ;
#86707 = ADVANCED_FACE('',(#18387),#14129,.T.) ;
#86708 = ADVANCED_FACE('',(#18388),#16300,.T.) ;
#86709 = ADVANCED_FACE('',(#18389),#16301,.T.) ;
#86710 = ADVANCED_FACE('',(#18390),#14130,.T.) ;
#86711 = ADVANCED_FACE('',(#18391),#14131,.T.) ;
#86712 = ADVANCED_FACE('',(#18392),#16302,.T.) ;
#86713 = ADVANCED_FACE('',(#18393),#16303,.T.) ;
#86714 = ADVANCED_FACE('',(#18394),#14132,.T.) ;
#86715 = ADVANCED_FACE('',(#18395),#14133,.T.) ;
#86716 = ADVANCED_FACE('',(#18396),#79062,.T.) ;
#86717 = ADVANCED_FACE('',(#18397),#16304,.T.) ;
#86718 = ADVANCED_FACE('',(#18398),#14134,.T.) ;
#86719 = ADVANCED_FACE('',(#18399),#14135,.T.) ;
#86720 = ADVANCED_FACE('',(#18400),#16305,.T.) ;
#86721 = ADVANCED_FACE('',(#18401),#79063,.T.) ;
#86722 = ADVANCED_FACE('',(#18402),#14136,.T.) ;
#86723 = ADVANCED_FACE('',(#18403),#14137,.T.) ;
#86724 = ADVANCED_FACE('',(#18404),#16306,.T.) ;
#86725 = ADVANCED_FACE('',(#18405),#16307,.T.) ;
#86726 = ADVANCED_FACE('',(#18406),#14138,.T.) ;
#86727 = ADVANCED_FACE('',(#18407),#14139,.T.) ;
#86728 = ADVANCED_FACE('',(#18408),#16308,.T.) ;
#86729 = ADVANCED_FACE('',(#18409),#14140,.F.) ;
#86730 = ADVANCED_FACE('',(#18410),#79064,.F.) ;
#86731 = ADVANCED_FACE('',(#18411),#16309,.F.) ;
#86732 = ADVANCED_FACE('',(#18412),#14141,.F.) ;
#86733 = ADVANCED_FACE('',(#18413),#14142,.F.) ;
#86734 = ADVANCED_FACE('',(#18414),#79065,.F.) ;
#86735 = ADVANCED_FACE('',(#18415),#16310,.F.) ;
#86736 = ADVANCED_FACE('',(#18416),#14143,.F.) ;
#86737 = ADVANCED_FACE('',(#18417),#14144,.F.) ;
#86738 = ADVANCED_FACE('',(#18418),#16311,.F.) ;
#86739 = ADVANCED_FACE('',(#18419),#16312,.F.) ;
#86740 = ADVANCED_FACE('',(#18420),#14145,.F.) ;
#86741 = ADVANCED_FACE('',(#18421),#79066,.F.) ;
#86742 = ADVANCED_FACE('',(#18422),#16313,.F.) ;
#86743 = ADVANCED_FACE('',(#18423),#16314,.F.) ;
#86744 = ADVANCED_FACE('',(#18424),#14146,.F.) ;
#86745 = ADVANCED_FACE('',(#18425),#14147,.F.) ;
#86746 = ADVANCED_FACE('',(#18426),#16315,.F.) ;
#86747 = ADVANCED_FACE('',(#18427),#14148,.F.) ;
#86748 = ADVANCED_FACE('',(#18428),#14149,.F.) ;
#86749 = ADVANCED_FACE('',(#18429),#16316,.F.) ;
#86750 = ADVANCED_FACE('',(#18430),#16317,.F.) ;
#86751 = ADVANCED_FACE('',(#18431),#14150,.F.) ;
#86752 = ADVANCED_FACE('',(#18432),#14151,.F.) ;
#86753 = ADVANCED_FACE('',(#18433),#79067,.F.) ;
#86754 = ADVANCED_FACE('',(#18434),#79068,.F.) ;
#86755 = ADVANCED_FACE('',(#18435),#14152,.F.) ;
#86756 = ADVANCED_FACE('',(#18436),#14153,.T.) ;
#86757 = ADVANCED_FACE('',(#18437),#16318,.T.) ;
#86758 = ADVANCED_FACE('',(#18438),#16319,.T.) ;
#86759 = ADVANCED_FACE('',(#18439),#14154,.T.) ;
#86760 = ADVANCED_FACE('',(#18440),#14155,.T.) ;
#86761 = ADVANCED_FACE('',(#18441),#79069,.T.) ;
#86762 = ADVANCED_FACE('',(#18442),#79070,.T.) ;
#86763 = ADVANCED_FACE('',(#18443),#14156,.T.) ;
#86764 = ADVANCED_FACE('',(#18444),#14157,.T.) ;
#86765 = ADVANCED_FACE('',(#18445),#79071,.T.) ;
#86766 = ADVANCED_FACE('',(#18446),#14158,.T.) ;
#86767 = ADVANCED_FACE('',(#18447),#14159,.T.) ;
#86768 = ADVANCED_FACE('',(#18448),#79072,.T.) ;
#86769 = ADVANCED_FACE('',(#18449),#79073,.T.) ;
#86770 = ADVANCED_FACE('',(#18450),#14160,.T.) ;
#86771 = ADVANCED_FACE('',(#18451),#79074,.T.) ;
#86772 = ADVANCED_FACE('',(#18452),#79075,.T.) ;
#86773 = ADVANCED_FACE('',(#18453),#79076,.T.) ;
#86774 = ADVANCED_FACE('',(#18454),#14161,.T.) ;
#86775 = ADVANCED_FACE('',(#18455),#14162,.T.) ;
#86776 = ADVANCED_FACE('',(#18456),#16320,.T.) ;
#86777 = ADVANCED_FACE('',(#18457),#79077,.T.) ;
#86778 = ADVANCED_FACE('',(#18458),#14163,.T.) ;
#86779 = ADVANCED_FACE('',(#18459),#14164,.T.) ;
#86780 = ADVANCED_FACE('',(#18460),#16321,.T.) ;
#86781 = ADVANCED_FACE('',(#18461),#79078,.T.) ;
#86782 = ADVANCED_FACE('',(#18462),#14165,.T.) ;
#86783 = ADVANCED_FACE('',(#18463),#1144,.F.) ;
#86784 = ADVANCED_FACE('',(#18464),#1145,.F.) ;
#86785 = ADVANCED_FACE('',(#18465),#1146,.F.) ;
#86786 = ADVANCED_FACE('',(#18466),#1147,.F.) ;
#86787 = ADVANCED_FACE('',(#18467),#1148,.F.) ;
#86788 = ADVANCED_FACE('',(#18468),#1149,.T.) ;
#86789 = ADVANCED_FACE('',(#18469),#1150,.F.) ;
#86790 = ADVANCED_FACE('',(#18470),#14166,.T.) ;
#86791 = ADVANCED_FACE('',(#18471),#14167,.F.) ;
#86792 = ADVANCED_FACE('',(#18472),#1151,.F.) ;
#86793 = ADVANCED_FACE('',(#18473),#1152,.F.) ;
#86794 = ADVANCED_FACE('',(#18474),#1153,.F.) ;
#86795 = ADVANCED_FACE('',(#18475),#1154,.F.) ;
#86796 = ADVANCED_FACE('',(#18476),#1155,.F.) ;
#86797 = ADVANCED_FACE('',(#18477),#1156,.T.) ;
#86798 = ADVANCED_FACE('',(#18478),#1157,.F.) ;
#86799 = ADVANCED_FACE('',(#18479),#1158,.F.) ;
#86800 = ADVANCED_FACE('',(#18480),#1159,.F.) ;
#86801 = ADVANCED_FACE('',(#18481),#1160,.F.) ;
#86802 = ADVANCED_FACE('',(#18482),#1161,.F.) ;
#86803 = ADVANCED_FACE('',(#18483),#14168,.T.) ;
#86804 = ADVANCED_FACE('',(#18484),#14169,.T.) ;
#86805 = ADVANCED_FACE('',(#18485),#16322,.T.) ;
#86806 = ADVANCED_FACE('',(#18486),#14170,.T.) ;
#86807 = ADVANCED_FACE('',(#18487),#14171,.T.) ;
#86808 = ADVANCED_FACE('',(#18488),#14172,.T.) ;
#86809 = ADVANCED_FACE('',(#18489),#16323,.T.) ;
#86810 = ADVANCED_FACE('',(#18490),#16324,.T.) ;
#86811 = ADVANCED_FACE('',(#18491),#14173,.T.) ;
#86812 = ADVANCED_FACE('',(#18492),#14174,.T.) ;
#86813 = ADVANCED_FACE('',(#18493),#14175,.T.) ;
#86814 = ADVANCED_FACE('',(#18494),#16325,.T.) ;
#86815 = ADVANCED_FACE('',(#18495),#14176,.T.) ;
#86816 = ADVANCED_FACE('',(#18496),#14177,.T.) ;
#86817 = ADVANCED_FACE('',(#18497),#14178,.T.) ;
#86818 = ADVANCED_FACE('',(#18498),#14179,.T.) ;
#86819 = ADVANCED_FACE('',(#18499),#16326,.T.) ;
#86820 = ADVANCED_FACE('',(#18500),#14180,.T.) ;
#86821 = ADVANCED_FACE('',(#18501),#14181,.T.) ;
#86822 = ADVANCED_FACE('',(#18502),#14182,.T.) ;
#86823 = ADVANCED_FACE('',(#18503),#16327,.T.) ;
#86824 = ADVANCED_FACE('',(#18504),#16328,.T.) ;
#86825 = ADVANCED_FACE('',(#18505),#14183,.T.) ;
#86826 = ADVANCED_FACE('',(#18506),#14184,.T.) ;
#86827 = ADVANCED_FACE('',(#18507),#14185,.T.) ;
#86828 = ADVANCED_FACE('',(#18508),#16329,.T.) ;
#86829 = ADVANCED_FACE('',(#18509),#14186,.T.) ;
#86830 = ADVANCED_FACE('',(#18510),#14187,.T.) ;
#86831 = ADVANCED_FACE('',(#18511),#79079,.T.) ;
#86832 = ADVANCED_FACE('',(#18512),#14188,.T.) ;
#86833 = ADVANCED_FACE('',(#18513),#16330,.T.) ;
#86834 = ADVANCED_FACE('',(#18514),#14189,.T.) ;
#86835 = ADVANCED_FACE('',(#18515),#16331,.T.) ;
#86836 = ADVANCED_FACE('',(#18516),#14190,.T.) ;
#86837 = ADVANCED_FACE('',(#18517),#79080,.T.) ;
#86838 = ADVANCED_FACE('',(#18518),#79081,.T.) ;
#86839 = ADVANCED_FACE('',(#18519),#14191,.T.) ;
#86840 = ADVANCED_FACE('',(#18520),#16332,.T.) ;
#86841 = ADVANCED_FACE('',(#18521),#14192,.T.) ;
#86842 = ADVANCED_FACE('',(#18522),#16333,.T.) ;
#86843 = ADVANCED_FACE('',(#18523),#14193,.T.) ;
#86844 = ADVANCED_FACE('',(#18524),#79082,.T.) ;
#86845 = ADVANCED_FACE('',(#18525),#14194,.T.) ;
#86846 = ADVANCED_FACE('',(#18526),#16334,.T.) ;
#86847 = ADVANCED_FACE('',(#18527),#14195,.T.) ;
#86848 = ADVANCED_FACE('',(#18528),#16335,.T.) ;
#86849 = ADVANCED_FACE('',(#18529),#14196,.T.) ;
#86850 = ADVANCED_FACE('',(#18530),#14197,.T.) ;
#86851 = ADVANCED_FACE('',(#18531),#16336,.T.) ;
#86852 = ADVANCED_FACE('',(#18532),#14198,.T.) ;
#86853 = ADVANCED_FACE('',(#18533),#14199,.T.) ;
#86854 = ADVANCED_FACE('',(#18534),#16337,.T.) ;
#86855 = ADVANCED_FACE('',(#18535),#1162,.T.) ;
#86856 = ADVANCED_FACE('',(#18536),#1163,.T.) ;
#86857 = ADVANCED_FACE('',(#18537),#1164,.T.) ;
#86858 = ADVANCED_FACE('',(#18538),#1165,.T.) ;
#86859 = ADVANCED_FACE('',(#18539),#1166,.T.) ;
#86860 = ADVANCED_FACE('',(#18540),#1167,.T.) ;
#86861 = ADVANCED_FACE('',(#18541),#1168,.T.) ;
#86862 = ADVANCED_FACE('',(#18542),#1169,.T.) ;
#86863 = ADVANCED_FACE('',(#18543),#1170,.T.) ;
#86864 = ADVANCED_FACE('',(#18544),#1171,.F.) ;
#86865 = ADVANCED_FACE('',(#18545),#1172,.F.) ;
#86866 = ADVANCED_FACE('',(#18546),#1173,.F.) ;
#86867 = ADVANCED_FACE('',(#18547),#1174,.F.) ;
#86868 = ADVANCED_FACE('',(#18548),#1175,.F.) ;
#86869 = ADVANCED_FACE('',(#18549),#1176,.F.) ;
#86870 = ADVANCED_FACE('',(#18550),#1177,.F.) ;
#86871 = ADVANCED_FACE('',(#18551),#1178,.F.) ;
#86872 = ADVANCED_FACE('',(#18552),#1179,.F.) ;
#86873 = ADVANCED_FACE('',(#18553),#1180,.F.) ;
#86874 = ADVANCED_FACE('',(#18554),#1181,.F.) ;
#86875 = ADVANCED_FACE('',(#18555),#1182,.F.) ;
#86876 = ADVANCED_FACE('',(#18556),#1183,.F.) ;
#86877 = ADVANCED_FACE('',(#18557),#1184,.F.) ;
#86878 = ADVANCED_FACE('',(#18558),#1185,.F.) ;
#86879 = ADVANCED_FACE('',(#18559),#1186,.F.) ;
#86880 = ADVANCED_FACE('',(#18560),#1187,.F.) ;
#86881 = ADVANCED_FACE('',(#18561),#1188,.F.) ;
#86882 = ADVANCED_FACE('',(#18562),#1189,.F.) ;
#86883 = ADVANCED_FACE('',(#18563),#1190,.F.) ;
#86884 = ADVANCED_FACE('',(#18564),#1191,.F.) ;
#86885 = ADVANCED_FACE('',(#18565),#1192,.F.) ;
#86886 = ADVANCED_FACE('',(#18566),#1193,.F.) ;
#86887 = ADVANCED_FACE('',(#18567),#1194,.F.) ;
#86888 = ADVANCED_FACE('',(#18568),#1195,.F.) ;
#86889 = ADVANCED_FACE('',(#18569),#1196,.F.) ;
#86890 = ADVANCED_FACE('',(#18570),#1197,.F.) ;
#86891 = ADVANCED_FACE('',(#18571),#1198,.F.) ;
#86892 = ADVANCED_FACE('',(#18572),#1199,.F.) ;
#86893 = ADVANCED_FACE('',(#18573),#1200,.F.) ;
#86894 = ADVANCED_FACE('',(#18574),#1201,.F.) ;
#86895 = ADVANCED_FACE('',(#18575),#1202,.F.) ;
#86896 = ADVANCED_FACE('',(#18576),#1203,.F.) ;
#86897 = ADVANCED_FACE('',(#18577),#1204,.F.) ;
#86898 = ADVANCED_FACE('',(#18578),#1205,.F.) ;
#86899 = ADVANCED_FACE('',(#18579),#1206,.F.) ;
#86900 = ADVANCED_FACE('',(#18580),#1207,.F.) ;
#86901 = ADVANCED_FACE('',(#18581),#1208,.F.) ;
#86902 = ADVANCED_FACE('',(#18582),#1209,.F.) ;
#86903 = ADVANCED_FACE('',(#18583),#1210,.F.) ;
#86904 = ADVANCED_FACE('',(#18584),#1211,.F.) ;
#86905 = ADVANCED_FACE('',(#18585),#1212,.F.) ;
#86906 = ADVANCED_FACE('',(#18586),#1213,.F.) ;
#86907 = ADVANCED_FACE('',(#18587),#1214,.F.) ;
#86908 = ADVANCED_FACE('',(#18588),#1215,.F.) ;
#86909 = ADVANCED_FACE('',(#18589),#14200,.T.) ;
#86910 = ADVANCED_FACE('',(#18590),#1216,.F.) ;
#86911 = ADVANCED_FACE('',(#18591),#14201,.T.) ;
#86912 = ADVANCED_FACE('',(#18592),#1217,.F.) ;
#86913 = ADVANCED_FACE('',(#18593),#14202,.F.) ;
#86914 = ADVANCED_FACE('',(#18594),#1218,.F.) ;
#86915 = ADVANCED_FACE('',(#18595),#14203,.F.) ;
#86916 = ADVANCED_FACE('',(#18596),#1219,.F.) ;
#86917 = ADVANCED_FACE('',(#18597),#1220,.F.) ;
#86918 = ADVANCED_FACE('',(#18598),#14204,.F.) ;
#86919 = ADVANCED_FACE('',(#18599),#1221,.F.) ;
#86920 = ADVANCED_FACE('',(#18600),#14205,.T.) ;
#86921 = ADVANCED_FACE('',(#18601),#1222,.F.) ;
#86922 = ADVANCED_FACE('',(#18602),#14206,.T.) ;
#86923 = ADVANCED_FACE('',(#18603),#1223,.F.) ;
#86924 = ADVANCED_FACE('',(#18604),#14207,.F.) ;
#86925 = ADVANCED_FACE('',(#18605),#1224,.F.) ;
#86926 = ADVANCED_FACE('',(#18606),#14208,.F.) ;
#86927 = ADVANCED_FACE('',(#18607),#1225,.F.) ;
#86928 = ADVANCED_FACE('',(#18608),#14209,.F.) ;
#86929 = ADVANCED_FACE('',(#18609),#14210,.T.) ;
#86930 = ADVANCED_FACE('',(#18610),#14211,.F.) ;
#86931 = ADVANCED_FACE('',(#18611),#1226,.F.) ;
#86932 = ADVANCED_FACE('',(#18612),#14212,.F.) ;
#86933 = ADVANCED_FACE('',(#18613),#1227,.F.) ;
#86934 = ADVANCED_FACE('',(#18614),#14213,.F.) ;
#86935 = ADVANCED_FACE('',(#18615),#1228,.F.) ;
#86936 = ADVANCED_FACE('',(#18616,#696),#1229,.F.) ;
#86937 = ADVANCED_FACE('',(#18617),#14214,.T.) ;
#86938 = ADVANCED_FACE('',(#18618),#1230,.F.) ;
#86939 = ADVANCED_FACE('',(#18619),#14215,.T.) ;
#86940 = ADVANCED_FACE('',(#18620),#1231,.F.) ;
#86941 = ADVANCED_FACE('',(#18621),#14216,.F.) ;
#86942 = ADVANCED_FACE('',(#18622),#1232,.F.) ;
#86943 = ADVANCED_FACE('',(#18623),#14217,.F.) ;
#86944 = ADVANCED_FACE('',(#18624),#1233,.F.) ;
#86945 = ADVANCED_FACE('',(#18625),#1234,.F.) ;
#86946 = ADVANCED_FACE('',(#18626),#14218,.F.) ;
#86947 = ADVANCED_FACE('',(#18627),#1235,.F.) ;
#86948 = ADVANCED_FACE('',(#18628),#14219,.T.) ;
#86949 = ADVANCED_FACE('',(#18629),#1236,.F.) ;
#86950 = ADVANCED_FACE('',(#18630),#14220,.T.) ;
#86951 = ADVANCED_FACE('',(#18631),#1237,.F.) ;
#86952 = ADVANCED_FACE('',(#18632),#14221,.F.) ;
#86953 = ADVANCED_FACE('',(#18633),#1238,.F.) ;
#86954 = ADVANCED_FACE('',(#18634),#14222,.F.) ;
#86955 = ADVANCED_FACE('',(#18635),#1239,.F.) ;
#86956 = ADVANCED_FACE('',(#18636),#14223,.F.) ;
#86957 = ADVANCED_FACE('',(#18637),#14224,.T.) ;
#86958 = ADVANCED_FACE('',(#18638),#14225,.F.) ;
#86959 = ADVANCED_FACE('',(#18639),#1240,.F.) ;
#86960 = ADVANCED_FACE('',(#18640),#14226,.F.) ;
#86961 = ADVANCED_FACE('',(#18641),#1241,.F.) ;
#86962 = ADVANCED_FACE('',(#18642),#14227,.F.) ;
#86963 = ADVANCED_FACE('',(#18643),#1242,.F.) ;
#86964 = ADVANCED_FACE('',(#18644,#697),#1243,.F.) ;
#86965 = ADVANCED_FACE('',(#18645),#14228,.T.) ;
#86966 = ADVANCED_FACE('',(#18646),#1244,.F.) ;
#86967 = ADVANCED_FACE('',(#18647),#14229,.T.) ;
#86968 = ADVANCED_FACE('',(#18648),#1245,.F.) ;
#86969 = ADVANCED_FACE('',(#18649),#14230,.F.) ;
#86970 = ADVANCED_FACE('',(#18650),#1246,.F.) ;
#86971 = ADVANCED_FACE('',(#18651),#14231,.F.) ;
#86972 = ADVANCED_FACE('',(#18652),#1247,.F.) ;
#86973 = ADVANCED_FACE('',(#18653),#1248,.F.) ;
#86974 = ADVANCED_FACE('',(#18654),#14232,.F.) ;
#86975 = ADVANCED_FACE('',(#18655),#1249,.F.) ;
#86976 = ADVANCED_FACE('',(#18656),#14233,.T.) ;
#86977 = ADVANCED_FACE('',(#18657),#1250,.F.) ;
#86978 = ADVANCED_FACE('',(#18658),#14234,.T.) ;
#86979 = ADVANCED_FACE('',(#18659),#1251,.F.) ;
#86980 = ADVANCED_FACE('',(#18660),#14235,.F.) ;
#86981 = ADVANCED_FACE('',(#18661),#1252,.F.) ;
#86982 = ADVANCED_FACE('',(#18662),#14236,.F.) ;
#86983 = ADVANCED_FACE('',(#18663),#1253,.F.) ;
#86984 = ADVANCED_FACE('',(#18664),#14237,.F.) ;
#86985 = ADVANCED_FACE('',(#18665),#14238,.T.) ;
#86986 = ADVANCED_FACE('',(#18666),#14239,.F.) ;
#86987 = ADVANCED_FACE('',(#18667),#1254,.F.) ;
#86988 = ADVANCED_FACE('',(#18668),#14240,.F.) ;
#86989 = ADVANCED_FACE('',(#18669),#1255,.F.) ;
#86990 = ADVANCED_FACE('',(#18670),#14241,.F.) ;
#86991 = ADVANCED_FACE('',(#18671),#1256,.F.) ;
#86992 = ADVANCED_FACE('',(#18672,#698),#1257,.F.) ;
#86993 = ADVANCED_FACE('',(#18673),#14242,.T.) ;
#86994 = ADVANCED_FACE('',(#18674),#1258,.F.) ;
#86995 = ADVANCED_FACE('',(#18675),#14243,.T.) ;
#86996 = ADVANCED_FACE('',(#18676),#1259,.F.) ;
#86997 = ADVANCED_FACE('',(#18677),#14244,.F.) ;
#86998 = ADVANCED_FACE('',(#18678),#1260,.F.) ;
#86999 = ADVANCED_FACE('',(#18679),#14245,.F.) ;
#87000 = ADVANCED_FACE('',(#18680),#1261,.F.) ;
#87001 = ADVANCED_FACE('',(#18681),#1262,.F.) ;
#87002 = ADVANCED_FACE('',(#18682),#14246,.F.) ;
#87003 = ADVANCED_FACE('',(#18683),#1263,.F.) ;
#87004 = ADVANCED_FACE('',(#18684),#14247,.T.) ;
#87005 = ADVANCED_FACE('',(#18685),#1264,.F.) ;
#87006 = ADVANCED_FACE('',(#18686),#14248,.T.) ;
#87007 = ADVANCED_FACE('',(#18687),#1265,.F.) ;
#87008 = ADVANCED_FACE('',(#18688),#14249,.F.) ;
#87009 = ADVANCED_FACE('',(#18689),#1266,.F.) ;
#87010 = ADVANCED_FACE('',(#18690),#14250,.F.) ;
#87011 = ADVANCED_FACE('',(#18691),#1267,.F.) ;
#87012 = ADVANCED_FACE('',(#18692),#14251,.F.) ;
#87013 = ADVANCED_FACE('',(#18693),#14252,.T.) ;
#87014 = ADVANCED_FACE('',(#18694),#14253,.F.) ;
#87015 = ADVANCED_FACE('',(#18695),#1268,.F.) ;
#87016 = ADVANCED_FACE('',(#18696),#14254,.F.) ;
#87017 = ADVANCED_FACE('',(#18697),#1269,.F.) ;
#87018 = ADVANCED_FACE('',(#18698),#14255,.F.) ;
#87019 = ADVANCED_FACE('',(#18699),#1270,.F.) ;
#87020 = ADVANCED_FACE('',(#18700,#699),#1271,.F.) ;
#87021 = ADVANCED_FACE('',(#18701),#14256,.T.) ;
#87022 = ADVANCED_FACE('',(#18702),#1272,.F.) ;
#87023 = ADVANCED_FACE('',(#18703),#14257,.T.) ;
#87024 = ADVANCED_FACE('',(#18704),#1273,.F.) ;
#87025 = ADVANCED_FACE('',(#18705),#14258,.F.) ;
#87026 = ADVANCED_FACE('',(#18706),#1274,.F.) ;
#87027 = ADVANCED_FACE('',(#18707),#14259,.F.) ;
#87028 = ADVANCED_FACE('',(#18708),#1275,.F.) ;
#87029 = ADVANCED_FACE('',(#18709),#1276,.F.) ;
#87030 = ADVANCED_FACE('',(#18710),#14260,.F.) ;
#87031 = ADVANCED_FACE('',(#18711),#1277,.F.) ;
#87032 = ADVANCED_FACE('',(#18712),#14261,.T.) ;
#87033 = ADVANCED_FACE('',(#18713),#1278,.F.) ;
#87034 = ADVANCED_FACE('',(#18714),#14262,.T.) ;
#87035 = ADVANCED_FACE('',(#18715),#1279,.F.) ;
#87036 = ADVANCED_FACE('',(#18716),#14263,.F.) ;
#87037 = ADVANCED_FACE('',(#18717),#1280,.F.) ;
#87038 = ADVANCED_FACE('',(#18718),#14264,.F.) ;
#87039 = ADVANCED_FACE('',(#18719),#1281,.F.) ;
#87040 = ADVANCED_FACE('',(#18720),#14265,.F.) ;
#87041 = ADVANCED_FACE('',(#18721),#14266,.T.) ;
#87042 = ADVANCED_FACE('',(#18722),#14267,.F.) ;
#87043 = ADVANCED_FACE('',(#18723),#1282,.F.) ;
#87044 = ADVANCED_FACE('',(#18724),#14268,.F.) ;
#87045 = ADVANCED_FACE('',(#18725),#1283,.F.) ;
#87046 = ADVANCED_FACE('',(#18726),#14269,.F.) ;
#87047 = ADVANCED_FACE('',(#18727),#1284,.F.) ;
#87048 = ADVANCED_FACE('',(#18728,#700),#1285,.F.) ;
#87049 = ADVANCED_FACE('',(#18729),#14270,.T.) ;
#87050 = ADVANCED_FACE('',(#18730),#1286,.F.) ;
#87051 = ADVANCED_FACE('',(#18731),#14271,.T.) ;
#87052 = ADVANCED_FACE('',(#18732),#1287,.F.) ;
#87053 = ADVANCED_FACE('',(#18733),#14272,.F.) ;
#87054 = ADVANCED_FACE('',(#18734),#1288,.F.) ;
#87055 = ADVANCED_FACE('',(#18735),#14273,.F.) ;
#87056 = ADVANCED_FACE('',(#18736),#1289,.F.) ;
#87057 = ADVANCED_FACE('',(#18737),#1290,.F.) ;
#87058 = ADVANCED_FACE('',(#18738),#14274,.F.) ;
#87059 = ADVANCED_FACE('',(#18739),#1291,.F.) ;
#87060 = ADVANCED_FACE('',(#18740),#14275,.T.) ;
#87061 = ADVANCED_FACE('',(#18741),#1292,.F.) ;
#87062 = ADVANCED_FACE('',(#18742),#14276,.T.) ;
#87063 = ADVANCED_FACE('',(#18743),#1293,.F.) ;
#87064 = ADVANCED_FACE('',(#18744),#14277,.F.) ;
#87065 = ADVANCED_FACE('',(#18745),#1294,.F.) ;
#87066 = ADVANCED_FACE('',(#18746),#14278,.F.) ;
#87067 = ADVANCED_FACE('',(#18747),#1295,.F.) ;
#87068 = ADVANCED_FACE('',(#18748),#14279,.F.) ;
#87069 = ADVANCED_FACE('',(#18749),#14280,.T.) ;
#87070 = ADVANCED_FACE('',(#18750),#14281,.F.) ;
#87071 = ADVANCED_FACE('',(#18751),#1296,.F.) ;
#87072 = ADVANCED_FACE('',(#18752),#14282,.F.) ;
#87073 = ADVANCED_FACE('',(#18753),#1297,.F.) ;
#87074 = ADVANCED_FACE('',(#18754),#14283,.F.) ;
#87075 = ADVANCED_FACE('',(#18755),#1298,.F.) ;
#87076 = ADVANCED_FACE('',(#18756,#701),#1299,.F.) ;
#87077 = ADVANCED_FACE('',(#18757),#14284,.T.) ;
#87078 = ADVANCED_FACE('',(#18758),#1300,.F.) ;
#87079 = ADVANCED_FACE('',(#18759),#14285,.T.) ;
#87080 = ADVANCED_FACE('',(#18760),#1301,.F.) ;
#87081 = ADVANCED_FACE('',(#18761),#14286,.F.) ;
#87082 = ADVANCED_FACE('',(#18762),#1302,.F.) ;
#87083 = ADVANCED_FACE('',(#18763),#14287,.F.) ;
#87084 = ADVANCED_FACE('',(#18764),#1303,.F.) ;
#87085 = ADVANCED_FACE('',(#18765),#1304,.F.) ;
#87086 = ADVANCED_FACE('',(#18766),#14288,.F.) ;
#87087 = ADVANCED_FACE('',(#18767),#1305,.F.) ;
#87088 = ADVANCED_FACE('',(#18768),#14289,.T.) ;
#87089 = ADVANCED_FACE('',(#18769),#1306,.F.) ;
#87090 = ADVANCED_FACE('',(#18770),#14290,.T.) ;
#87091 = ADVANCED_FACE('',(#18771),#1307,.F.) ;
#87092 = ADVANCED_FACE('',(#18772),#14291,.F.) ;
#87093 = ADVANCED_FACE('',(#18773),#1308,.F.) ;
#87094 = ADVANCED_FACE('',(#18774),#14292,.F.) ;
#87095 = ADVANCED_FACE('',(#18775),#1309,.F.) ;
#87096 = ADVANCED_FACE('',(#18776),#14293,.F.) ;
#87097 = ADVANCED_FACE('',(#18777),#14294,.T.) ;
#87098 = ADVANCED_FACE('',(#18778),#14295,.F.) ;
#87099 = ADVANCED_FACE('',(#18779),#1310,.F.) ;
#87100 = ADVANCED_FACE('',(#18780),#14296,.F.) ;
#87101 = ADVANCED_FACE('',(#18781),#1311,.F.) ;
#87102 = ADVANCED_FACE('',(#18782),#14297,.F.) ;
#87103 = ADVANCED_FACE('',(#18783),#1312,.F.) ;
#87104 = ADVANCED_FACE('',(#18784,#702),#1313,.F.) ;
#87105 = ADVANCED_FACE('',(#18785),#14298,.T.) ;
#87106 = ADVANCED_FACE('',(#18786),#1314,.F.) ;
#87107 = ADVANCED_FACE('',(#18787),#14299,.T.) ;
#87108 = ADVANCED_FACE('',(#18788),#1315,.F.) ;
#87109 = ADVANCED_FACE('',(#18789),#14300,.F.) ;
#87110 = ADVANCED_FACE('',(#18790),#1316,.F.) ;
#87111 = ADVANCED_FACE('',(#18791),#14301,.F.) ;
#87112 = ADVANCED_FACE('',(#18792),#1317,.F.) ;
#87113 = ADVANCED_FACE('',(#18793),#1318,.F.) ;
#87114 = ADVANCED_FACE('',(#18794),#14302,.F.) ;
#87115 = ADVANCED_FACE('',(#18795),#1319,.F.) ;
#87116 = ADVANCED_FACE('',(#18796),#14303,.T.) ;
#87117 = ADVANCED_FACE('',(#18797),#1320,.F.) ;
#87118 = ADVANCED_FACE('',(#18798),#14304,.T.) ;
#87119 = ADVANCED_FACE('',(#18799),#1321,.F.) ;
#87120 = ADVANCED_FACE('',(#18800),#14305,.F.) ;
#87121 = ADVANCED_FACE('',(#18801),#1322,.F.) ;
#87122 = ADVANCED_FACE('',(#18802),#14306,.F.) ;
#87123 = ADVANCED_FACE('',(#18803),#1323,.F.) ;
#87124 = ADVANCED_FACE('',(#18804),#14307,.F.) ;
#87125 = ADVANCED_FACE('',(#18805),#14308,.T.) ;
#87126 = ADVANCED_FACE('',(#18806),#14309,.F.) ;
#87127 = ADVANCED_FACE('',(#18807),#1324,.F.) ;
#87128 = ADVANCED_FACE('',(#18808),#14310,.F.) ;
#87129 = ADVANCED_FACE('',(#18809),#1325,.F.) ;
#87130 = ADVANCED_FACE('',(#18810),#14311,.F.) ;
#87131 = ADVANCED_FACE('',(#18811),#1326,.F.) ;
#87132 = ADVANCED_FACE('',(#18812,#703),#1327,.F.) ;
#87133 = ADVANCED_FACE('',(#18813),#14312,.T.) ;
#87134 = ADVANCED_FACE('',(#18814),#1328,.F.) ;
#87135 = ADVANCED_FACE('',(#18815),#14313,.T.) ;
#87136 = ADVANCED_FACE('',(#18816),#1329,.F.) ;
#87137 = ADVANCED_FACE('',(#18817),#14314,.F.) ;
#87138 = ADVANCED_FACE('',(#18818),#1330,.F.) ;
#87139 = ADVANCED_FACE('',(#18819),#14315,.F.) ;
#87140 = ADVANCED_FACE('',(#18820),#1331,.F.) ;
#87141 = ADVANCED_FACE('',(#18821),#1332,.F.) ;
#87142 = ADVANCED_FACE('',(#18822),#14316,.F.) ;
#87143 = ADVANCED_FACE('',(#18823),#1333,.F.) ;
#87144 = ADVANCED_FACE('',(#18824),#14317,.T.) ;
#87145 = ADVANCED_FACE('',(#18825),#1334,.F.) ;
#87146 = ADVANCED_FACE('',(#18826),#14318,.T.) ;
#87147 = ADVANCED_FACE('',(#18827),#1335,.F.) ;
#87148 = ADVANCED_FACE('',(#18828),#14319,.F.) ;
#87149 = ADVANCED_FACE('',(#18829),#1336,.F.) ;
#87150 = ADVANCED_FACE('',(#18830),#14320,.F.) ;
#87151 = ADVANCED_FACE('',(#18831),#1337,.F.) ;
#87152 = ADVANCED_FACE('',(#18832),#14321,.F.) ;
#87153 = ADVANCED_FACE('',(#18833),#14322,.T.) ;
#87154 = ADVANCED_FACE('',(#18834),#14323,.F.) ;
#87155 = ADVANCED_FACE('',(#18835),#1338,.F.) ;
#87156 = ADVANCED_FACE('',(#18836),#14324,.F.) ;
#87157 = ADVANCED_FACE('',(#18837),#1339,.F.) ;
#87158 = ADVANCED_FACE('',(#18838),#14325,.F.) ;
#87159 = ADVANCED_FACE('',(#18839),#1340,.F.) ;
#87160 = ADVANCED_FACE('',(#18840,#704),#1341,.F.) ;
#87161 = ADVANCED_FACE('',(#18841,#705),#1342,.T.) ;
#87162 = ADVANCED_FACE('',(#18842,#706),#1343,.T.) ;
#87163 = ADVANCED_FACE('',(#18843,#707),#1344,.T.) ;
#87164 = ADVANCED_FACE('',(#18844,#708),#1345,.T.) ;
#87165 = ADVANCED_FACE('',(#18845,#709),#1346,.T.) ;
#87166 = ADVANCED_FACE('',(#18846,#710),#1347,.T.) ;
#87167 = ADVANCED_FACE('',(#18847,#711),#1348,.T.) ;
#87168 = ADVANCED_FACE('',(#18848,#712),#1349,.T.) ;
#87169 = ADVANCED_FACE('',(#18849,#713),#1350,.T.) ;
#87170 = ADVANCED_FACE('',(#18850),#14326,.T.) ;
#87171 = ADVANCED_FACE('',(#18851),#14327,.F.) ;
#87172 = ADVANCED_FACE('',(#18852),#16338,.F.) ;
#87173 = ADVANCED_FACE('',(#18853),#16339,.T.) ;
#87174 = ADVANCED_FACE('',(#18854),#79083,.T.) ;
#87175 = ADVANCED_FACE('',(#18855),#14328,.F.) ;
#87176 = ADVANCED_FACE('',(#18856),#14329,.F.) ;
#87177 = ADVANCED_FACE('',(#18857),#14330,.T.) ;
#87178 = ADVANCED_FACE('',(#18858),#14331,.T.) ;
#87179 = ADVANCED_FACE('',(#18859),#14332,.T.) ;
#87180 = ADVANCED_FACE('',(#18860),#14333,.F.) ;
#87181 = ADVANCED_FACE('',(#18861),#16340,.F.) ;
#87182 = ADVANCED_FACE('',(#18862),#79084,.F.) ;
#87183 = ADVANCED_FACE('',(#18863),#79085,.F.) ;
#87184 = ADVANCED_FACE('',(#18864),#79086,.T.) ;
#87185 = ADVANCED_FACE('',(#18865),#14334,.F.) ;
#87186 = ADVANCED_FACE('',(#18866),#14335,.F.) ;
#87187 = ADVANCED_FACE('',(#18867),#14336,.F.) ;
#87188 = ADVANCED_FACE('',(#18868),#14337,.T.) ;
#87189 = ADVANCED_FACE('',(#18869),#14338,.T.) ;
#87190 = ADVANCED_FACE('',(#18870),#79087,.F.) ;
#87191 = ADVANCED_FACE('',(#18871),#16341,.F.) ;
#87192 = ADVANCED_FACE('',(#18872),#16342,.T.) ;
#87193 = ADVANCED_FACE('',(#18873),#14339,.T.) ;
#87194 = ADVANCED_FACE('',(#18874),#16343,.F.) ;
#87195 = ADVANCED_FACE('',(#18875),#16344,.T.) ;
#87196 = ADVANCED_FACE('',(#18876),#14340,.F.) ;
#87197 = ADVANCED_FACE('',(#18877),#14341,.F.) ;
#87198 = ADVANCED_FACE('',(#18878),#14342,.T.) ;
#87199 = ADVANCED_FACE('',(#18879),#79088,.T.) ;
#87200 = ADVANCED_FACE('',(#18880),#14343,.F.) ;
#87201 = ADVANCED_FACE('',(#18881),#14344,.T.) ;
#87202 = ADVANCED_FACE('',(#18882),#14345,.F.) ;
#87203 = ADVANCED_FACE('',(#18883),#16345,.F.) ;
#87204 = ADVANCED_FACE('',(#18884),#79089,.T.) ;
#87205 = ADVANCED_FACE('',(#18885),#14346,.T.) ;
#87206 = ADVANCED_FACE('',(#18886),#16346,.F.) ;
#87207 = ADVANCED_FACE('',(#18887),#79090,.F.) ;
#87208 = ADVANCED_FACE('',(#18888),#14347,.F.) ;
#87209 = ADVANCED_FACE('',(#18889),#14348,.T.) ;
#87210 = ADVANCED_FACE('',(#18890),#79091,.T.) ;
#87211 = ADVANCED_FACE('',(#18891),#14349,.F.) ;
#87212 = ADVANCED_FACE('',(#18892),#79092,.T.) ;
#87213 = ADVANCED_FACE('',(#18893),#14350,.T.) ;
#87214 = ADVANCED_FACE('',(#18894),#14351,.T.) ;
#87215 = ADVANCED_FACE('',(#18895),#16347,.T.) ;
#87216 = ADVANCED_FACE('',(#18896),#14352,.F.) ;
#87217 = ADVANCED_FACE('',(#18897),#79093,.F.) ;
#87218 = ADVANCED_FACE('',(#18898),#16348,.F.) ;
#87219 = ADVANCED_FACE('',(#18899),#14353,.F.) ;
#87220 = ADVANCED_FACE('',(#18900),#14354,.F.) ;
#87221 = ADVANCED_FACE('',(#18901),#79094,.F.) ;
#87222 = ADVANCED_FACE('',(#18902),#16349,.F.) ;
#87223 = ADVANCED_FACE('',(#18903),#14355,.F.) ;
#87224 = ADVANCED_FACE('',(#18904),#14356,.F.) ;
#87225 = ADVANCED_FACE('',(#18905),#16350,.F.) ;
#87226 = ADVANCED_FACE('',(#18906),#16351,.F.) ;
#87227 = ADVANCED_FACE('',(#18907),#14357,.F.) ;
#87228 = ADVANCED_FACE('',(#18908),#79095,.F.) ;
#87229 = ADVANCED_FACE('',(#18909),#16352,.F.) ;
#87230 = ADVANCED_FACE('',(#18910),#16353,.F.) ;
#87231 = ADVANCED_FACE('',(#18911),#14358,.F.) ;
#87232 = ADVANCED_FACE('',(#18912),#14359,.F.) ;
#87233 = ADVANCED_FACE('',(#18913),#16354,.F.) ;
#87234 = ADVANCED_FACE('',(#18914),#14360,.F.) ;
#87235 = ADVANCED_FACE('',(#18915),#14361,.F.) ;
#87236 = ADVANCED_FACE('',(#18916),#16355,.F.) ;
#87237 = ADVANCED_FACE('',(#18917),#16356,.F.) ;
#87238 = ADVANCED_FACE('',(#18918),#14362,.F.) ;
#87239 = ADVANCED_FACE('',(#18919),#14363,.F.) ;
#87240 = ADVANCED_FACE('',(#18920),#79096,.F.) ;
#87241 = ADVANCED_FACE('',(#18921),#79097,.F.) ;
#87242 = ADVANCED_FACE('',(#18922),#14364,.F.) ;
#87243 = ADVANCED_FACE('',(#18923),#14365,.T.) ;
#87244 = ADVANCED_FACE('',(#18924),#16357,.T.) ;
#87245 = ADVANCED_FACE('',(#18925),#16358,.T.) ;
#87246 = ADVANCED_FACE('',(#18926),#14366,.T.) ;
#87247 = ADVANCED_FACE('',(#18927),#14367,.T.) ;
#87248 = ADVANCED_FACE('',(#18928),#79098,.T.) ;
#87249 = ADVANCED_FACE('',(#18929),#79099,.T.) ;
#87250 = ADVANCED_FACE('',(#18930),#14368,.T.) ;
#87251 = ADVANCED_FACE('',(#18931),#14369,.T.) ;
#87252 = ADVANCED_FACE('',(#18932),#79100,.T.) ;
#87253 = ADVANCED_FACE('',(#18933),#14370,.T.) ;
#87254 = ADVANCED_FACE('',(#18934),#14371,.T.) ;
#87255 = ADVANCED_FACE('',(#18935),#79101,.T.) ;
#87256 = ADVANCED_FACE('',(#18936),#79102,.T.) ;
#87257 = ADVANCED_FACE('',(#18937),#14372,.T.) ;
#87258 = ADVANCED_FACE('',(#18938),#79103,.T.) ;
#87259 = ADVANCED_FACE('',(#18939),#79104,.T.) ;
#87260 = ADVANCED_FACE('',(#18940),#79105,.T.) ;
#87261 = ADVANCED_FACE('',(#18941),#14373,.T.) ;
#87262 = ADVANCED_FACE('',(#18942),#14374,.T.) ;
#87263 = ADVANCED_FACE('',(#18943),#16359,.T.) ;
#87264 = ADVANCED_FACE('',(#18944),#79106,.T.) ;
#87265 = ADVANCED_FACE('',(#18945),#14375,.T.) ;
#87266 = ADVANCED_FACE('',(#18946),#14376,.T.) ;
#87267 = ADVANCED_FACE('',(#18947),#16360,.T.) ;
#87268 = ADVANCED_FACE('',(#18948),#79107,.T.) ;
#87269 = ADVANCED_FACE('',(#18949),#14377,.T.) ;
#87270 = ADVANCED_FACE('',(#18950),#14378,.T.) ;
#87271 = ADVANCED_FACE('',(#18951),#16361,.T.) ;
#87272 = ADVANCED_FACE('',(#18952),#16362,.T.) ;
#87273 = ADVANCED_FACE('',(#18953),#14379,.T.) ;
#87274 = ADVANCED_FACE('',(#18954),#14380,.T.) ;
#87275 = ADVANCED_FACE('',(#18955),#79108,.T.) ;
#87276 = ADVANCED_FACE('',(#18956),#79109,.T.) ;
#87277 = ADVANCED_FACE('',(#18957),#14381,.T.) ;
#87278 = ADVANCED_FACE('',(#18958),#14382,.T.) ;
#87279 = ADVANCED_FACE('',(#18959),#79110,.T.) ;
#87280 = ADVANCED_FACE('',(#18960),#14383,.T.) ;
#87281 = ADVANCED_FACE('',(#18961),#14384,.T.) ;
#87282 = ADVANCED_FACE('',(#18962),#79111,.T.) ;
#87283 = ADVANCED_FACE('',(#18963),#79112,.T.) ;
#87284 = ADVANCED_FACE('',(#18964),#14385,.T.) ;
#87285 = ADVANCED_FACE('',(#18965),#79113,.T.) ;
#87286 = ADVANCED_FACE('',(#18966),#79114,.T.) ;
#87287 = ADVANCED_FACE('',(#18967),#79115,.T.) ;
#87288 = ADVANCED_FACE('',(#18968),#14386,.T.) ;
#87289 = ADVANCED_FACE('',(#18969),#14387,.T.) ;
#87290 = ADVANCED_FACE('',(#18970),#16363,.T.) ;
#87291 = ADVANCED_FACE('',(#18971),#79116,.T.) ;
#87292 = ADVANCED_FACE('',(#18972),#14388,.T.) ;
#87293 = ADVANCED_FACE('',(#18973),#14389,.T.) ;
#87294 = ADVANCED_FACE('',(#18974),#16364,.T.) ;
#87295 = ADVANCED_FACE('',(#18975),#79117,.T.) ;
#87296 = ADVANCED_FACE('',(#18976),#14390,.T.) ;
#87297 = ADVANCED_FACE('',(#18977),#14391,.T.) ;
#87298 = ADVANCED_FACE('',(#18978),#16365,.T.) ;
#87299 = ADVANCED_FACE('',(#18979),#16366,.T.) ;
#87300 = ADVANCED_FACE('',(#18980),#14392,.T.) ;
#87301 = ADVANCED_FACE('',(#18981),#14393,.T.) ;
#87302 = ADVANCED_FACE('',(#18982),#79118,.T.) ;
#87303 = ADVANCED_FACE('',(#18983),#79119,.T.) ;
#87304 = ADVANCED_FACE('',(#18984),#14394,.T.) ;
#87305 = ADVANCED_FACE('',(#18985),#14395,.T.) ;
#87306 = ADVANCED_FACE('',(#18986),#79120,.T.) ;
#87307 = ADVANCED_FACE('',(#18987),#14396,.T.) ;
#87308 = ADVANCED_FACE('',(#18988),#14397,.T.) ;
#87309 = ADVANCED_FACE('',(#18989),#79121,.T.) ;
#87310 = ADVANCED_FACE('',(#18990),#79122,.T.) ;
#87311 = ADVANCED_FACE('',(#18991),#14398,.T.) ;
#87312 = ADVANCED_FACE('',(#18992),#79123,.T.) ;
#87313 = ADVANCED_FACE('',(#18993),#79124,.T.) ;
#87314 = ADVANCED_FACE('',(#18994),#79125,.T.) ;
#87315 = ADVANCED_FACE('',(#18995),#14399,.T.) ;
#87316 = ADVANCED_FACE('',(#18996),#14400,.T.) ;
#87317 = ADVANCED_FACE('',(#18997),#16367,.T.) ;
#87318 = ADVANCED_FACE('',(#18998),#79126,.T.) ;
#87319 = ADVANCED_FACE('',(#18999),#14401,.T.) ;
#87320 = ADVANCED_FACE('',(#19000),#14402,.T.) ;
#87321 = ADVANCED_FACE('',(#19001),#16368,.T.) ;
#87322 = ADVANCED_FACE('',(#19002),#79127,.T.) ;
#87323 = ADVANCED_FACE('',(#19003),#14403,.T.) ;
#87324 = ADVANCED_FACE('',(#19004),#14404,.T.) ;
#87325 = ADVANCED_FACE('',(#19005),#16369,.T.) ;
#87326 = ADVANCED_FACE('',(#19006),#16370,.T.) ;
#87327 = ADVANCED_FACE('',(#19007),#14405,.T.) ;
#87328 = ADVANCED_FACE('',(#19008),#14406,.T.) ;
#87329 = ADVANCED_FACE('',(#19009),#79128,.T.) ;
#87330 = ADVANCED_FACE('',(#19010),#79129,.T.) ;
#87331 = ADVANCED_FACE('',(#19011),#14407,.T.) ;
#87332 = ADVANCED_FACE('',(#19012),#14408,.T.) ;
#87333 = ADVANCED_FACE('',(#19013),#79130,.T.) ;
#87334 = ADVANCED_FACE('',(#19014),#14409,.T.) ;
#87335 = ADVANCED_FACE('',(#19015),#14410,.T.) ;
#87336 = ADVANCED_FACE('',(#19016),#79131,.T.) ;
#87337 = ADVANCED_FACE('',(#19017),#79132,.T.) ;
#87338 = ADVANCED_FACE('',(#19018),#14411,.T.) ;
#87339 = ADVANCED_FACE('',(#19019),#79133,.T.) ;
#87340 = ADVANCED_FACE('',(#19020),#79134,.T.) ;
#87341 = ADVANCED_FACE('',(#19021),#79135,.T.) ;
#87342 = ADVANCED_FACE('',(#19022),#14412,.T.) ;
#87343 = ADVANCED_FACE('',(#19023),#14413,.T.) ;
#87344 = ADVANCED_FACE('',(#19024),#16371,.T.) ;
#87345 = ADVANCED_FACE('',(#19025),#79136,.T.) ;
#87346 = ADVANCED_FACE('',(#19026),#14414,.T.) ;
#87347 = ADVANCED_FACE('',(#19027),#14415,.T.) ;
#87348 = ADVANCED_FACE('',(#19028),#16372,.T.) ;
#87349 = ADVANCED_FACE('',(#19029),#79137,.T.) ;
#87350 = ADVANCED_FACE('',(#19030),#14416,.T.) ;
#87351 = ADVANCED_FACE('',(#19031),#14417,.T.) ;
#87352 = ADVANCED_FACE('',(#19032),#16373,.T.) ;
#87353 = ADVANCED_FACE('',(#19033),#16374,.T.) ;
#87354 = ADVANCED_FACE('',(#19034),#14418,.T.) ;
#87355 = ADVANCED_FACE('',(#19035),#14419,.T.) ;
#87356 = ADVANCED_FACE('',(#19036),#79138,.T.) ;
#87357 = ADVANCED_FACE('',(#19037),#79139,.T.) ;
#87358 = ADVANCED_FACE('',(#19038),#14420,.T.) ;
#87359 = ADVANCED_FACE('',(#19039),#14421,.T.) ;
#87360 = ADVANCED_FACE('',(#19040),#79140,.T.) ;
#87361 = ADVANCED_FACE('',(#19041),#14422,.T.) ;
#87362 = ADVANCED_FACE('',(#19042),#14423,.T.) ;
#87363 = ADVANCED_FACE('',(#19043),#79141,.T.) ;
#87364 = ADVANCED_FACE('',(#19044),#79142,.T.) ;
#87365 = ADVANCED_FACE('',(#19045),#14424,.T.) ;
#87366 = ADVANCED_FACE('',(#19046),#79143,.T.) ;
#87367 = ADVANCED_FACE('',(#19047),#79144,.T.) ;
#87368 = ADVANCED_FACE('',(#19048),#79145,.T.) ;
#87369 = ADVANCED_FACE('',(#19049),#14425,.T.) ;
#87370 = ADVANCED_FACE('',(#19050),#14426,.T.) ;
#87371 = ADVANCED_FACE('',(#19051),#16375,.T.) ;
#87372 = ADVANCED_FACE('',(#19052),#79146,.T.) ;
#87373 = ADVANCED_FACE('',(#19053),#14427,.T.) ;
#87374 = ADVANCED_FACE('',(#19054),#14428,.T.) ;
#87375 = ADVANCED_FACE('',(#19055),#16376,.T.) ;
#87376 = ADVANCED_FACE('',(#19056),#79147,.T.) ;
#87377 = ADVANCED_FACE('',(#19057),#14429,.T.) ;
#87378 = ADVANCED_FACE('',(#19058),#14430,.T.) ;
#87379 = ADVANCED_FACE('',(#19059),#16377,.T.) ;
#87380 = ADVANCED_FACE('',(#19060),#16378,.T.) ;
#87381 = ADVANCED_FACE('',(#19061),#14431,.T.) ;
#87382 = ADVANCED_FACE('',(#19062),#14432,.T.) ;
#87383 = ADVANCED_FACE('',(#19063),#79148,.T.) ;
#87384 = ADVANCED_FACE('',(#19064),#79149,.T.) ;
#87385 = ADVANCED_FACE('',(#19065),#14433,.T.) ;
#87386 = ADVANCED_FACE('',(#19066),#14434,.T.) ;
#87387 = ADVANCED_FACE('',(#19067),#79150,.T.) ;
#87388 = ADVANCED_FACE('',(#19068),#14435,.T.) ;
#87389 = ADVANCED_FACE('',(#19069),#14436,.T.) ;
#87390 = ADVANCED_FACE('',(#19070),#79151,.T.) ;
#87391 = ADVANCED_FACE('',(#19071),#79152,.T.) ;
#87392 = ADVANCED_FACE('',(#19072),#14437,.T.) ;
#87393 = ADVANCED_FACE('',(#19073),#79153,.T.) ;
#87394 = ADVANCED_FACE('',(#19074),#79154,.T.) ;
#87395 = ADVANCED_FACE('',(#19075),#79155,.T.) ;
#87396 = ADVANCED_FACE('',(#19076),#14438,.T.) ;
#87397 = ADVANCED_FACE('',(#19077),#14439,.T.) ;
#87398 = ADVANCED_FACE('',(#19078),#16379,.T.) ;
#87399 = ADVANCED_FACE('',(#19079),#79156,.T.) ;
#87400 = ADVANCED_FACE('',(#19080),#14440,.T.) ;
#87401 = ADVANCED_FACE('',(#19081),#14441,.T.) ;
#87402 = ADVANCED_FACE('',(#19082),#16380,.T.) ;
#87403 = ADVANCED_FACE('',(#19083),#79157,.T.) ;
#87404 = ADVANCED_FACE('',(#19084),#14442,.T.) ;
#87405 = ADVANCED_FACE('',(#19085),#14443,.T.) ;
#87406 = ADVANCED_FACE('',(#19086),#16381,.T.) ;
#87407 = ADVANCED_FACE('',(#19087),#16382,.T.) ;
#87408 = ADVANCED_FACE('',(#19088),#14444,.T.) ;
#87409 = ADVANCED_FACE('',(#19089),#14445,.T.) ;
#87410 = ADVANCED_FACE('',(#19090),#79158,.T.) ;
#87411 = ADVANCED_FACE('',(#19091),#79159,.T.) ;
#87412 = ADVANCED_FACE('',(#19092),#14446,.T.) ;
#87413 = ADVANCED_FACE('',(#19093),#14447,.T.) ;
#87414 = ADVANCED_FACE('',(#19094),#79160,.T.) ;
#87415 = ADVANCED_FACE('',(#19095),#14448,.T.) ;
#87416 = ADVANCED_FACE('',(#19096),#14449,.T.) ;
#87417 = ADVANCED_FACE('',(#19097),#79161,.T.) ;
#87418 = ADVANCED_FACE('',(#19098),#79162,.T.) ;
#87419 = ADVANCED_FACE('',(#19099),#14450,.T.) ;
#87420 = ADVANCED_FACE('',(#19100),#79163,.T.) ;
#87421 = ADVANCED_FACE('',(#19101),#79164,.T.) ;
#87422 = ADVANCED_FACE('',(#19102),#79165,.T.) ;
#87423 = ADVANCED_FACE('',(#19103),#14451,.T.) ;
#87424 = ADVANCED_FACE('',(#19104),#14452,.T.) ;
#87425 = ADVANCED_FACE('',(#19105),#16383,.T.) ;
#87426 = ADVANCED_FACE('',(#19106),#79166,.T.) ;
#87427 = ADVANCED_FACE('',(#19107),#14453,.T.) ;
#87428 = ADVANCED_FACE('',(#19108),#14454,.T.) ;
#87429 = ADVANCED_FACE('',(#19109),#16384,.T.) ;
#87430 = ADVANCED_FACE('',(#19110),#79167,.T.) ;
#87431 = ADVANCED_FACE('',(#19111),#14455,.T.) ;
#87432 = ADVANCED_FACE('',(#19112),#14456,.T.) ;
#87433 = ADVANCED_FACE('',(#19113),#16385,.T.) ;
#87434 = ADVANCED_FACE('',(#19114),#16386,.T.) ;
#87435 = ADVANCED_FACE('',(#19115),#14457,.T.) ;
#87436 = ADVANCED_FACE('',(#19116),#14458,.T.) ;
#87437 = ADVANCED_FACE('',(#19117),#79168,.T.) ;
#87438 = ADVANCED_FACE('',(#19118),#79169,.T.) ;
#87439 = ADVANCED_FACE('',(#19119),#14459,.T.) ;
#87440 = ADVANCED_FACE('',(#19120),#14460,.T.) ;
#87441 = ADVANCED_FACE('',(#19121),#79170,.T.) ;
#87442 = ADVANCED_FACE('',(#19122),#14461,.T.) ;
#87443 = ADVANCED_FACE('',(#19123),#14462,.T.) ;
#87444 = ADVANCED_FACE('',(#19124),#79171,.T.) ;
#87445 = ADVANCED_FACE('',(#19125),#79172,.T.) ;
#87446 = ADVANCED_FACE('',(#19126),#14463,.T.) ;
#87447 = ADVANCED_FACE('',(#19127),#79173,.T.) ;
#87448 = ADVANCED_FACE('',(#19128),#79174,.T.) ;
#87449 = ADVANCED_FACE('',(#19129),#79175,.T.) ;
#87450 = ADVANCED_FACE('',(#19130),#14464,.T.) ;
#87451 = ADVANCED_FACE('',(#19131),#14465,.T.) ;
#87452 = ADVANCED_FACE('',(#19132),#16387,.T.) ;
#87453 = ADVANCED_FACE('',(#19133),#79176,.T.) ;
#87454 = ADVANCED_FACE('',(#19134),#14466,.T.) ;
#87455 = ADVANCED_FACE('',(#19135),#14467,.T.) ;
#87456 = ADVANCED_FACE('',(#19136),#16388,.T.) ;
#87457 = ADVANCED_FACE('',(#19137),#79177,.T.) ;
#87458 = ADVANCED_FACE('',(#19138),#14468,.T.) ;
#87459 = ADVANCED_FACE('',(#19139),#14469,.T.) ;
#87460 = ADVANCED_FACE('',(#19140),#16389,.T.) ;
#87461 = ADVANCED_FACE('',(#19141),#16390,.T.) ;
#87462 = ADVANCED_FACE('',(#19142),#14470,.T.) ;
#87463 = ADVANCED_FACE('',(#19143),#14471,.T.) ;
#87464 = ADVANCED_FACE('',(#19144),#79178,.T.) ;
#87465 = ADVANCED_FACE('',(#19145),#79179,.T.) ;
#87466 = ADVANCED_FACE('',(#19146),#14472,.T.) ;
#87467 = ADVANCED_FACE('',(#19147),#14473,.T.) ;
#87468 = ADVANCED_FACE('',(#19148),#79180,.T.) ;
#87469 = ADVANCED_FACE('',(#19149),#14474,.T.) ;
#87470 = ADVANCED_FACE('',(#19150),#14475,.T.) ;
#87471 = ADVANCED_FACE('',(#19151),#79181,.T.) ;
#87472 = ADVANCED_FACE('',(#19152),#79182,.T.) ;
#87473 = ADVANCED_FACE('',(#19153),#14476,.T.) ;
#87474 = ADVANCED_FACE('',(#19154),#79183,.T.) ;
#87475 = ADVANCED_FACE('',(#19155),#79184,.T.) ;
#87476 = ADVANCED_FACE('',(#19156),#79185,.T.) ;
#87477 = ADVANCED_FACE('',(#19157),#14477,.T.) ;
#87478 = ADVANCED_FACE('',(#19158),#14478,.T.) ;
#87479 = ADVANCED_FACE('',(#19159),#16391,.T.) ;
#87480 = ADVANCED_FACE('',(#19160),#79186,.T.) ;
#87481 = ADVANCED_FACE('',(#19161),#14479,.T.) ;
#87482 = ADVANCED_FACE('',(#19162),#14480,.T.) ;
#87483 = ADVANCED_FACE('',(#19163),#16392,.T.) ;
#87484 = ADVANCED_FACE('',(#19164),#79187,.T.) ;
#87485 = ADVANCED_FACE('',(#19165),#14481,.T.) ;
#87486 = ADVANCED_FACE('',(#19166),#14482,.T.) ;
#87487 = ADVANCED_FACE('',(#19167),#14483,.F.) ;
#87488 = ADVANCED_FACE('',(#19168),#16393,.F.) ;
#87489 = ADVANCED_FACE('',(#19169),#16394,.T.) ;
#87490 = ADVANCED_FACE('',(#19170),#79188,.T.) ;
#87491 = ADVANCED_FACE('',(#19171),#14484,.F.) ;
#87492 = ADVANCED_FACE('',(#19172),#14485,.F.) ;
#87493 = ADVANCED_FACE('',(#19173),#14486,.T.) ;
#87494 = ADVANCED_FACE('',(#19174),#14487,.T.) ;
#87495 = ADVANCED_FACE('',(#19175),#14488,.T.) ;
#87496 = ADVANCED_FACE('',(#19176),#14489,.F.) ;
#87497 = ADVANCED_FACE('',(#19177),#16395,.F.) ;
#87498 = ADVANCED_FACE('',(#19178),#79189,.F.) ;
#87499 = ADVANCED_FACE('',(#19179),#79190,.F.) ;
#87500 = ADVANCED_FACE('',(#19180),#79191,.T.) ;
#87501 = ADVANCED_FACE('',(#19181),#14490,.F.) ;
#87502 = ADVANCED_FACE('',(#19182),#14491,.F.) ;
#87503 = ADVANCED_FACE('',(#19183),#14492,.F.) ;
#87504 = ADVANCED_FACE('',(#19184),#14493,.T.) ;
#87505 = ADVANCED_FACE('',(#19185),#14494,.T.) ;
#87506 = ADVANCED_FACE('',(#19186),#79192,.F.) ;
#87507 = ADVANCED_FACE('',(#19187),#16396,.F.) ;
#87508 = ADVANCED_FACE('',(#19188),#16397,.T.) ;
#87509 = ADVANCED_FACE('',(#19189),#14495,.T.) ;
#87510 = ADVANCED_FACE('',(#19190),#16398,.F.) ;
#87511 = ADVANCED_FACE('',(#19191),#16399,.T.) ;
#87512 = ADVANCED_FACE('',(#19192),#14496,.F.) ;
#87513 = ADVANCED_FACE('',(#19193),#14497,.F.) ;
#87514 = ADVANCED_FACE('',(#19194),#14498,.T.) ;
#87515 = ADVANCED_FACE('',(#19195),#79193,.T.) ;
#87516 = ADVANCED_FACE('',(#19196),#14499,.F.) ;
#87517 = ADVANCED_FACE('',(#19197),#14500,.T.) ;
#87518 = ADVANCED_FACE('',(#19198),#14501,.F.) ;
#87519 = ADVANCED_FACE('',(#19199),#16400,.F.) ;
#87520 = ADVANCED_FACE('',(#19200),#79194,.T.) ;
#87521 = ADVANCED_FACE('',(#19201),#14502,.T.) ;
#87522 = ADVANCED_FACE('',(#19202),#16401,.F.) ;
#87523 = ADVANCED_FACE('',(#19203),#79195,.F.) ;
#87524 = ADVANCED_FACE('',(#19204),#14503,.F.) ;
#87525 = ADVANCED_FACE('',(#19205),#14504,.T.) ;
#87526 = ADVANCED_FACE('',(#19206),#79196,.T.) ;
#87527 = ADVANCED_FACE('',(#19207),#14505,.F.) ;
#87528 = ADVANCED_FACE('',(#19208),#79197,.T.) ;
#87529 = ADVANCED_FACE('',(#19209),#14506,.T.) ;
#87530 = ADVANCED_FACE('',(#19210),#14507,.T.) ;
#87531 = ADVANCED_FACE('',(#19211),#16402,.T.) ;
#87532 = ADVANCED_FACE('',(#19212),#14508,.F.) ;
#87533 = ADVANCED_FACE('',(#19213),#79198,.F.) ;
#87534 = ADVANCED_FACE('',(#19214),#16403,.F.) ;
#87535 = ADVANCED_FACE('',(#19215),#14509,.F.) ;
#87536 = ADVANCED_FACE('',(#19216),#14510,.F.) ;
#87537 = ADVANCED_FACE('',(#19217),#79199,.F.) ;
#87538 = ADVANCED_FACE('',(#19218),#16404,.F.) ;
#87539 = ADVANCED_FACE('',(#19219),#14511,.F.) ;
#87540 = ADVANCED_FACE('',(#19220),#14512,.F.) ;
#87541 = ADVANCED_FACE('',(#19221),#16405,.F.) ;
#87542 = ADVANCED_FACE('',(#19222),#16406,.F.) ;
#87543 = ADVANCED_FACE('',(#19223),#14513,.F.) ;
#87544 = ADVANCED_FACE('',(#19224),#79200,.F.) ;
#87545 = ADVANCED_FACE('',(#19225),#16407,.F.) ;
#87546 = ADVANCED_FACE('',(#19226),#16408,.F.) ;
#87547 = ADVANCED_FACE('',(#19227),#14514,.F.) ;
#87548 = ADVANCED_FACE('',(#19228),#14515,.F.) ;
#87549 = ADVANCED_FACE('',(#19229),#16409,.F.) ;
#87550 = ADVANCED_FACE('',(#19230),#14516,.F.) ;
#87551 = ADVANCED_FACE('',(#19231),#14517,.F.) ;
#87552 = ADVANCED_FACE('',(#19232),#16410,.F.) ;
#87553 = ADVANCED_FACE('',(#19233),#16411,.F.) ;
#87554 = ADVANCED_FACE('',(#19234),#14518,.F.) ;
#87555 = ADVANCED_FACE('',(#19235),#14519,.F.) ;
#87556 = ADVANCED_FACE('',(#19236),#79201,.F.) ;
#87557 = ADVANCED_FACE('',(#19237),#79202,.F.) ;
#87558 = ADVANCED_FACE('',(#19238),#14520,.F.) ;
#87559 = ADVANCED_FACE('',(#19239),#14521,.T.) ;
#87560 = ADVANCED_FACE('',(#19240),#14522,.F.) ;
#87561 = ADVANCED_FACE('',(#19241),#16412,.F.) ;
#87562 = ADVANCED_FACE('',(#19242),#16413,.T.) ;
#87563 = ADVANCED_FACE('',(#19243),#79203,.T.) ;
#87564 = ADVANCED_FACE('',(#19244),#14523,.F.) ;
#87565 = ADVANCED_FACE('',(#19245),#14524,.F.) ;
#87566 = ADVANCED_FACE('',(#19246),#14525,.T.) ;
#87567 = ADVANCED_FACE('',(#19247),#14526,.T.) ;
#87568 = ADVANCED_FACE('',(#19248),#14527,.T.) ;
#87569 = ADVANCED_FACE('',(#19249),#14528,.F.) ;
#87570 = ADVANCED_FACE('',(#19250),#16414,.F.) ;
#87571 = ADVANCED_FACE('',(#19251),#79204,.F.) ;
#87572 = ADVANCED_FACE('',(#19252),#79205,.F.) ;
#87573 = ADVANCED_FACE('',(#19253),#79206,.T.) ;
#87574 = ADVANCED_FACE('',(#19254),#14529,.F.) ;
#87575 = ADVANCED_FACE('',(#19255),#14530,.F.) ;
#87576 = ADVANCED_FACE('',(#19256),#14531,.F.) ;
#87577 = ADVANCED_FACE('',(#19257),#14532,.T.) ;
#87578 = ADVANCED_FACE('',(#19258),#14533,.T.) ;
#87579 = ADVANCED_FACE('',(#19259),#79207,.F.) ;
#87580 = ADVANCED_FACE('',(#19260),#16415,.F.) ;
#87581 = ADVANCED_FACE('',(#19261),#16416,.T.) ;
#87582 = ADVANCED_FACE('',(#19262),#14534,.T.) ;
#87583 = ADVANCED_FACE('',(#19263),#16417,.F.) ;
#87584 = ADVANCED_FACE('',(#19264),#16418,.T.) ;
#87585 = ADVANCED_FACE('',(#19265),#14535,.F.) ;
#87586 = ADVANCED_FACE('',(#19266),#14536,.F.) ;
#87587 = ADVANCED_FACE('',(#19267),#14537,.T.) ;
#87588 = ADVANCED_FACE('',(#19268),#79208,.T.) ;
#87589 = ADVANCED_FACE('',(#19269),#14538,.F.) ;
#87590 = ADVANCED_FACE('',(#19270),#14539,.T.) ;
#87591 = ADVANCED_FACE('',(#19271),#14540,.F.) ;
#87592 = ADVANCED_FACE('',(#19272),#16419,.F.) ;
#87593 = ADVANCED_FACE('',(#19273),#79209,.T.) ;
#87594 = ADVANCED_FACE('',(#19274),#14541,.T.) ;
#87595 = ADVANCED_FACE('',(#19275),#16420,.F.) ;
#87596 = ADVANCED_FACE('',(#19276),#79210,.F.) ;
#87597 = ADVANCED_FACE('',(#19277),#14542,.F.) ;
#87598 = ADVANCED_FACE('',(#19278),#14543,.T.) ;
#87599 = ADVANCED_FACE('',(#19279),#79211,.T.) ;
#87600 = ADVANCED_FACE('',(#19280),#14544,.F.) ;
#87601 = ADVANCED_FACE('',(#19281),#79212,.T.) ;
#87602 = ADVANCED_FACE('',(#19282),#14545,.T.) ;
#87603 = ADVANCED_FACE('',(#19283),#14546,.T.) ;
#87604 = ADVANCED_FACE('',(#19284),#16421,.T.) ;
#87605 = ADVANCED_FACE('',(#19285),#14547,.F.) ;
#87606 = ADVANCED_FACE('',(#19286),#79213,.F.) ;
#87607 = ADVANCED_FACE('',(#19287),#16422,.F.) ;
#87608 = ADVANCED_FACE('',(#19288),#14548,.F.) ;
#87609 = ADVANCED_FACE('',(#19289),#14549,.F.) ;
#87610 = ADVANCED_FACE('',(#19290),#79214,.F.) ;
#87611 = ADVANCED_FACE('',(#19291),#16423,.F.) ;
#87612 = ADVANCED_FACE('',(#19292),#14550,.F.) ;
#87613 = ADVANCED_FACE('',(#19293),#14551,.F.) ;
#87614 = ADVANCED_FACE('',(#19294),#16424,.F.) ;
#87615 = ADVANCED_FACE('',(#19295),#16425,.F.) ;
#87616 = ADVANCED_FACE('',(#19296),#14552,.F.) ;
#87617 = ADVANCED_FACE('',(#19297),#79215,.F.) ;
#87618 = ADVANCED_FACE('',(#19298),#16426,.F.) ;
#87619 = ADVANCED_FACE('',(#19299),#16427,.F.) ;
#87620 = ADVANCED_FACE('',(#19300),#14553,.F.) ;
#87621 = ADVANCED_FACE('',(#19301),#14554,.F.) ;
#87622 = ADVANCED_FACE('',(#19302),#16428,.F.) ;
#87623 = ADVANCED_FACE('',(#19303),#14555,.F.) ;
#87624 = ADVANCED_FACE('',(#19304),#14556,.F.) ;
#87625 = ADVANCED_FACE('',(#19305),#16429,.F.) ;
#87626 = ADVANCED_FACE('',(#19306),#16430,.F.) ;
#87627 = ADVANCED_FACE('',(#19307),#14557,.F.) ;
#87628 = ADVANCED_FACE('',(#19308),#14558,.F.) ;
#87629 = ADVANCED_FACE('',(#19309),#79216,.F.) ;
#87630 = ADVANCED_FACE('',(#19310),#79217,.F.) ;
#87631 = ADVANCED_FACE('',(#19311),#14559,.F.) ;
#87632 = ADVANCED_FACE('',(#19312),#14560,.T.) ;
#87633 = ADVANCED_FACE('',(#19313),#14561,.F.) ;
#87634 = ADVANCED_FACE('',(#19314),#16431,.F.) ;
#87635 = ADVANCED_FACE('',(#19315),#16432,.T.) ;
#87636 = ADVANCED_FACE('',(#19316),#79218,.T.) ;
#87637 = ADVANCED_FACE('',(#19317),#14562,.F.) ;
#87638 = ADVANCED_FACE('',(#19318),#14563,.F.) ;
#87639 = ADVANCED_FACE('',(#19319),#14564,.T.) ;
#87640 = ADVANCED_FACE('',(#19320),#14565,.T.) ;
#87641 = ADVANCED_FACE('',(#19321),#14566,.T.) ;
#87642 = ADVANCED_FACE('',(#19322),#14567,.F.) ;
#87643 = ADVANCED_FACE('',(#19323),#16433,.F.) ;
#87644 = ADVANCED_FACE('',(#19324),#79219,.F.) ;
#87645 = ADVANCED_FACE('',(#19325),#79220,.F.) ;
#87646 = ADVANCED_FACE('',(#19326),#79221,.T.) ;
#87647 = ADVANCED_FACE('',(#19327),#14568,.F.) ;
#87648 = ADVANCED_FACE('',(#19328),#14569,.F.) ;
#87649 = ADVANCED_FACE('',(#19329),#14570,.F.) ;
#87650 = ADVANCED_FACE('',(#19330),#14571,.T.) ;
#87651 = ADVANCED_FACE('',(#19331),#14572,.T.) ;
#87652 = ADVANCED_FACE('',(#19332),#79222,.F.) ;
#87653 = ADVANCED_FACE('',(#19333),#16434,.F.) ;
#87654 = ADVANCED_FACE('',(#19334),#16435,.T.) ;
#87655 = ADVANCED_FACE('',(#19335),#14573,.T.) ;
#87656 = ADVANCED_FACE('',(#19336),#16436,.F.) ;
#87657 = ADVANCED_FACE('',(#19337),#16437,.T.) ;
#87658 = ADVANCED_FACE('',(#19338),#14574,.F.) ;
#87659 = ADVANCED_FACE('',(#19339),#14575,.F.) ;
#87660 = ADVANCED_FACE('',(#19340),#14576,.T.) ;
#87661 = ADVANCED_FACE('',(#19341),#79223,.T.) ;
#87662 = ADVANCED_FACE('',(#19342),#14577,.F.) ;
#87663 = ADVANCED_FACE('',(#19343),#14578,.T.) ;
#87664 = ADVANCED_FACE('',(#19344),#14579,.F.) ;
#87665 = ADVANCED_FACE('',(#19345),#16438,.F.) ;
#87666 = ADVANCED_FACE('',(#19346),#79224,.T.) ;
#87667 = ADVANCED_FACE('',(#19347),#14580,.T.) ;
#87668 = ADVANCED_FACE('',(#19348),#16439,.F.) ;
#87669 = ADVANCED_FACE('',(#19349),#79225,.F.) ;
#87670 = ADVANCED_FACE('',(#19350),#14581,.F.) ;
#87671 = ADVANCED_FACE('',(#19351),#14582,.T.) ;
#87672 = ADVANCED_FACE('',(#19352),#79226,.T.) ;
#87673 = ADVANCED_FACE('',(#19353),#14583,.F.) ;
#87674 = ADVANCED_FACE('',(#19354),#79227,.T.) ;
#87675 = ADVANCED_FACE('',(#19355),#14584,.T.) ;
#87676 = ADVANCED_FACE('',(#19356),#14585,.T.) ;
#87677 = ADVANCED_FACE('',(#19357),#16440,.T.) ;
#87678 = ADVANCED_FACE('',(#19358),#14586,.F.) ;
#87679 = ADVANCED_FACE('',(#19359),#79228,.F.) ;
#87680 = ADVANCED_FACE('',(#19360),#16441,.F.) ;
#87681 = ADVANCED_FACE('',(#19361),#14587,.F.) ;
#87682 = ADVANCED_FACE('',(#19362),#14588,.F.) ;
#87683 = ADVANCED_FACE('',(#19363),#79229,.F.) ;
#87684 = ADVANCED_FACE('',(#19364),#16442,.F.) ;
#87685 = ADVANCED_FACE('',(#19365),#14589,.F.) ;
#87686 = ADVANCED_FACE('',(#19366),#14590,.F.) ;
#87687 = ADVANCED_FACE('',(#19367),#16443,.F.) ;
#87688 = ADVANCED_FACE('',(#19368),#16444,.F.) ;
#87689 = ADVANCED_FACE('',(#19369),#14591,.F.) ;
#87690 = ADVANCED_FACE('',(#19370),#79230,.F.) ;
#87691 = ADVANCED_FACE('',(#19371),#16445,.F.) ;
#87692 = ADVANCED_FACE('',(#19372),#16446,.F.) ;
#87693 = ADVANCED_FACE('',(#19373),#14592,.F.) ;
#87694 = ADVANCED_FACE('',(#19374),#14593,.F.) ;
#87695 = ADVANCED_FACE('',(#19375),#16447,.F.) ;
#87696 = ADVANCED_FACE('',(#19376),#14594,.F.) ;
#87697 = ADVANCED_FACE('',(#19377),#14595,.F.) ;
#87698 = ADVANCED_FACE('',(#19378),#16448,.F.) ;
#87699 = ADVANCED_FACE('',(#19379),#16449,.F.) ;
#87700 = ADVANCED_FACE('',(#19380),#14596,.F.) ;
#87701 = ADVANCED_FACE('',(#19381),#14597,.F.) ;
#87702 = ADVANCED_FACE('',(#19382),#79231,.F.) ;
#87703 = ADVANCED_FACE('',(#19383),#79232,.F.) ;
#87704 = ADVANCED_FACE('',(#19384),#14598,.F.) ;
#87705 = ADVANCED_FACE('',(#19385),#14599,.T.) ;
#87706 = ADVANCED_FACE('',(#19386),#14600,.F.) ;
#87707 = ADVANCED_FACE('',(#19387),#16450,.F.) ;
#87708 = ADVANCED_FACE('',(#19388),#16451,.T.) ;
#87709 = ADVANCED_FACE('',(#19389),#79233,.T.) ;
#87710 = ADVANCED_FACE('',(#19390),#14601,.F.) ;
#87711 = ADVANCED_FACE('',(#19391),#14602,.F.) ;
#87712 = ADVANCED_FACE('',(#19392),#14603,.T.) ;
#87713 = ADVANCED_FACE('',(#19393),#14604,.T.) ;
#87714 = ADVANCED_FACE('',(#19394),#14605,.T.) ;
#87715 = ADVANCED_FACE('',(#19395),#14606,.F.) ;
#87716 = ADVANCED_FACE('',(#19396),#16452,.F.) ;
#87717 = ADVANCED_FACE('',(#19397),#79234,.F.) ;
#87718 = ADVANCED_FACE('',(#19398),#79235,.F.) ;
#87719 = ADVANCED_FACE('',(#19399),#79236,.T.) ;
#87720 = ADVANCED_FACE('',(#19400),#14607,.F.) ;
#87721 = ADVANCED_FACE('',(#19401),#14608,.F.) ;
#87722 = ADVANCED_FACE('',(#19402),#14609,.F.) ;
#87723 = ADVANCED_FACE('',(#19403),#14610,.T.) ;
#87724 = ADVANCED_FACE('',(#19404),#14611,.T.) ;
#87725 = ADVANCED_FACE('',(#19405),#79237,.F.) ;
#87726 = ADVANCED_FACE('',(#19406),#16453,.F.) ;
#87727 = ADVANCED_FACE('',(#19407),#16454,.T.) ;
#87728 = ADVANCED_FACE('',(#19408),#14612,.T.) ;
#87729 = ADVANCED_FACE('',(#19409),#16455,.F.) ;
#87730 = ADVANCED_FACE('',(#19410),#16456,.T.) ;
#87731 = ADVANCED_FACE('',(#19411),#14613,.F.) ;
#87732 = ADVANCED_FACE('',(#19412),#14614,.F.) ;
#87733 = ADVANCED_FACE('',(#19413),#14615,.T.) ;
#87734 = ADVANCED_FACE('',(#19414),#79238,.T.) ;
#87735 = ADVANCED_FACE('',(#19415),#14616,.F.) ;
#87736 = ADVANCED_FACE('',(#19416),#14617,.T.) ;
#87737 = ADVANCED_FACE('',(#19417),#14618,.F.) ;
#87738 = ADVANCED_FACE('',(#19418),#16457,.F.) ;
#87739 = ADVANCED_FACE('',(#19419),#79239,.T.) ;
#87740 = ADVANCED_FACE('',(#19420),#14619,.T.) ;
#87741 = ADVANCED_FACE('',(#19421),#16458,.F.) ;
#87742 = ADVANCED_FACE('',(#19422),#79240,.F.) ;
#87743 = ADVANCED_FACE('',(#19423),#14620,.F.) ;
#87744 = ADVANCED_FACE('',(#19424),#14621,.T.) ;
#87745 = ADVANCED_FACE('',(#19425),#79241,.T.) ;
#87746 = ADVANCED_FACE('',(#19426),#14622,.F.) ;
#87747 = ADVANCED_FACE('',(#19427),#79242,.T.) ;
#87748 = ADVANCED_FACE('',(#19428),#14623,.T.) ;
#87749 = ADVANCED_FACE('',(#19429),#14624,.T.) ;
#87750 = ADVANCED_FACE('',(#19430),#16459,.T.) ;
#87751 = ADVANCED_FACE('',(#19431),#14625,.F.) ;
#87752 = ADVANCED_FACE('',(#19432),#79243,.F.) ;
#87753 = ADVANCED_FACE('',(#19433),#16460,.F.) ;
#87754 = ADVANCED_FACE('',(#19434),#14626,.F.) ;
#87755 = ADVANCED_FACE('',(#19435),#14627,.F.) ;
#87756 = ADVANCED_FACE('',(#19436),#79244,.F.) ;
#87757 = ADVANCED_FACE('',(#19437),#16461,.F.) ;
#87758 = ADVANCED_FACE('',(#19438),#14628,.F.) ;
#87759 = ADVANCED_FACE('',(#19439),#14629,.F.) ;
#87760 = ADVANCED_FACE('',(#19440),#16462,.F.) ;
#87761 = ADVANCED_FACE('',(#19441),#16463,.F.) ;
#87762 = ADVANCED_FACE('',(#19442),#14630,.F.) ;
#87763 = ADVANCED_FACE('',(#19443),#79245,.F.) ;
#87764 = ADVANCED_FACE('',(#19444),#16464,.F.) ;
#87765 = ADVANCED_FACE('',(#19445),#16465,.F.) ;
#87766 = ADVANCED_FACE('',(#19446),#14631,.F.) ;
#87767 = ADVANCED_FACE('',(#19447),#14632,.F.) ;
#87768 = ADVANCED_FACE('',(#19448),#16466,.F.) ;
#87769 = ADVANCED_FACE('',(#19449),#14633,.F.) ;
#87770 = ADVANCED_FACE('',(#19450),#14634,.F.) ;
#87771 = ADVANCED_FACE('',(#19451),#16467,.F.) ;
#87772 = ADVANCED_FACE('',(#19452),#16468,.F.) ;
#87773 = ADVANCED_FACE('',(#19453),#14635,.F.) ;
#87774 = ADVANCED_FACE('',(#19454),#14636,.F.) ;
#87775 = ADVANCED_FACE('',(#19455),#79246,.F.) ;
#87776 = ADVANCED_FACE('',(#19456),#79247,.F.) ;
#87777 = ADVANCED_FACE('',(#19457),#14637,.F.) ;
#87778 = ADVANCED_FACE('',(#19458),#14638,.T.) ;
#87779 = ADVANCED_FACE('',(#19459),#14639,.F.) ;
#87780 = ADVANCED_FACE('',(#19460),#16469,.F.) ;
#87781 = ADVANCED_FACE('',(#19461),#16470,.T.) ;
#87782 = ADVANCED_FACE('',(#19462),#79248,.T.) ;
#87783 = ADVANCED_FACE('',(#19463),#14640,.F.) ;
#87784 = ADVANCED_FACE('',(#19464),#14641,.F.) ;
#87785 = ADVANCED_FACE('',(#19465),#14642,.T.) ;
#87786 = ADVANCED_FACE('',(#19466),#14643,.T.) ;
#87787 = ADVANCED_FACE('',(#19467),#14644,.T.) ;
#87788 = ADVANCED_FACE('',(#19468),#14645,.F.) ;
#87789 = ADVANCED_FACE('',(#19469),#16471,.F.) ;
#87790 = ADVANCED_FACE('',(#19470),#79249,.F.) ;
#87791 = ADVANCED_FACE('',(#19471),#79250,.F.) ;
#87792 = ADVANCED_FACE('',(#19472),#79251,.T.) ;
#87793 = ADVANCED_FACE('',(#19473),#14646,.F.) ;
#87794 = ADVANCED_FACE('',(#19474),#14647,.F.) ;
#87795 = ADVANCED_FACE('',(#19475),#14648,.F.) ;
#87796 = ADVANCED_FACE('',(#19476),#14649,.T.) ;
#87797 = ADVANCED_FACE('',(#19477),#14650,.T.) ;
#87798 = ADVANCED_FACE('',(#19478),#79252,.F.) ;
#87799 = ADVANCED_FACE('',(#19479),#16472,.F.) ;
#87800 = ADVANCED_FACE('',(#19480),#16473,.T.) ;
#87801 = ADVANCED_FACE('',(#19481),#14651,.T.) ;
#87802 = ADVANCED_FACE('',(#19482),#16474,.F.) ;
#87803 = ADVANCED_FACE('',(#19483),#16475,.T.) ;
#87804 = ADVANCED_FACE('',(#19484),#14652,.F.) ;
#87805 = ADVANCED_FACE('',(#19485),#14653,.F.) ;
#87806 = ADVANCED_FACE('',(#19486),#14654,.T.) ;
#87807 = ADVANCED_FACE('',(#19487),#79253,.T.) ;
#87808 = ADVANCED_FACE('',(#19488),#14655,.F.) ;
#87809 = ADVANCED_FACE('',(#19489),#14656,.T.) ;
#87810 = ADVANCED_FACE('',(#19490),#14657,.F.) ;
#87811 = ADVANCED_FACE('',(#19491),#16476,.F.) ;
#87812 = ADVANCED_FACE('',(#19492),#79254,.T.) ;
#87813 = ADVANCED_FACE('',(#19493),#14658,.T.) ;
#87814 = ADVANCED_FACE('',(#19494),#16477,.F.) ;
#87815 = ADVANCED_FACE('',(#19495),#79255,.F.) ;
#87816 = ADVANCED_FACE('',(#19496),#14659,.F.) ;
#87817 = ADVANCED_FACE('',(#19497),#14660,.T.) ;
#87818 = ADVANCED_FACE('',(#19498),#79256,.T.) ;
#87819 = ADVANCED_FACE('',(#19499),#14661,.F.) ;
#87820 = ADVANCED_FACE('',(#19500),#79257,.T.) ;
#87821 = ADVANCED_FACE('',(#19501),#14662,.T.) ;
#87822 = ADVANCED_FACE('',(#19502),#14663,.T.) ;
#87823 = ADVANCED_FACE('',(#19503),#16478,.T.) ;
#87824 = ADVANCED_FACE('',(#19504),#14664,.F.) ;
#87825 = ADVANCED_FACE('',(#19505),#79258,.F.) ;
#87826 = ADVANCED_FACE('',(#19506),#16479,.F.) ;
#87827 = ADVANCED_FACE('',(#19507),#14665,.F.) ;
#87828 = ADVANCED_FACE('',(#19508),#14666,.F.) ;
#87829 = ADVANCED_FACE('',(#19509),#79259,.F.) ;
#87830 = ADVANCED_FACE('',(#19510),#16480,.F.) ;
#87831 = ADVANCED_FACE('',(#19511),#14667,.F.) ;
#87832 = ADVANCED_FACE('',(#19512),#14668,.F.) ;
#87833 = ADVANCED_FACE('',(#19513),#16481,.F.) ;
#87834 = ADVANCED_FACE('',(#19514),#16482,.F.) ;
#87835 = ADVANCED_FACE('',(#19515),#14669,.F.) ;
#87836 = ADVANCED_FACE('',(#19516),#79260,.F.) ;
#87837 = ADVANCED_FACE('',(#19517),#16483,.F.) ;
#87838 = ADVANCED_FACE('',(#19518),#16484,.F.) ;
#87839 = ADVANCED_FACE('',(#19519),#14670,.F.) ;
#87840 = ADVANCED_FACE('',(#19520),#14671,.F.) ;
#87841 = ADVANCED_FACE('',(#19521),#16485,.F.) ;
#87842 = ADVANCED_FACE('',(#19522),#14672,.F.) ;
#87843 = ADVANCED_FACE('',(#19523),#14673,.F.) ;
#87844 = ADVANCED_FACE('',(#19524),#16486,.F.) ;
#87845 = ADVANCED_FACE('',(#19525),#16487,.F.) ;
#87846 = ADVANCED_FACE('',(#19526),#14674,.F.) ;
#87847 = ADVANCED_FACE('',(#19527),#14675,.F.) ;
#87848 = ADVANCED_FACE('',(#19528),#79261,.F.) ;
#87849 = ADVANCED_FACE('',(#19529),#79262,.F.) ;
#87850 = ADVANCED_FACE('',(#19530),#14676,.F.) ;
#87851 = ADVANCED_FACE('',(#19531),#14677,.T.) ;
#87852 = ADVANCED_FACE('',(#19532),#14678,.F.) ;
#87853 = ADVANCED_FACE('',(#19533),#16488,.F.) ;
#87854 = ADVANCED_FACE('',(#19534),#16489,.T.) ;
#87855 = ADVANCED_FACE('',(#19535),#79263,.T.) ;
#87856 = ADVANCED_FACE('',(#19536),#14679,.F.) ;
#87857 = ADVANCED_FACE('',(#19537),#14680,.F.) ;
#87858 = ADVANCED_FACE('',(#19538),#14681,.T.) ;
#87859 = ADVANCED_FACE('',(#19539),#14682,.T.) ;
#87860 = ADVANCED_FACE('',(#19540),#14683,.T.) ;
#87861 = ADVANCED_FACE('',(#19541),#14684,.F.) ;
#87862 = ADVANCED_FACE('',(#19542),#16490,.F.) ;
#87863 = ADVANCED_FACE('',(#19543),#79264,.F.) ;
#87864 = ADVANCED_FACE('',(#19544),#79265,.F.) ;
#87865 = ADVANCED_FACE('',(#19545),#79266,.T.) ;
#87866 = ADVANCED_FACE('',(#19546),#14685,.F.) ;
#87867 = ADVANCED_FACE('',(#19547),#14686,.F.) ;
#87868 = ADVANCED_FACE('',(#19548),#14687,.F.) ;
#87869 = ADVANCED_FACE('',(#19549),#14688,.T.) ;
#87870 = ADVANCED_FACE('',(#19550),#14689,.T.) ;
#87871 = ADVANCED_FACE('',(#19551),#79267,.F.) ;
#87872 = ADVANCED_FACE('',(#19552),#16491,.F.) ;
#87873 = ADVANCED_FACE('',(#19553),#16492,.T.) ;
#87874 = ADVANCED_FACE('',(#19554),#14690,.T.) ;
#87875 = ADVANCED_FACE('',(#19555),#16493,.F.) ;
#87876 = ADVANCED_FACE('',(#19556),#16494,.T.) ;
#87877 = ADVANCED_FACE('',(#19557),#14691,.F.) ;
#87878 = ADVANCED_FACE('',(#19558),#14692,.F.) ;
#87879 = ADVANCED_FACE('',(#19559),#14693,.T.) ;
#87880 = ADVANCED_FACE('',(#19560),#79268,.T.) ;
#87881 = ADVANCED_FACE('',(#19561),#14694,.F.) ;
#87882 = ADVANCED_FACE('',(#19562),#14695,.T.) ;
#87883 = ADVANCED_FACE('',(#19563),#14696,.F.) ;
#87884 = ADVANCED_FACE('',(#19564),#16495,.F.) ;
#87885 = ADVANCED_FACE('',(#19565),#79269,.T.) ;
#87886 = ADVANCED_FACE('',(#19566),#14697,.T.) ;
#87887 = ADVANCED_FACE('',(#19567),#16496,.F.) ;
#87888 = ADVANCED_FACE('',(#19568),#79270,.F.) ;
#87889 = ADVANCED_FACE('',(#19569),#14698,.F.) ;
#87890 = ADVANCED_FACE('',(#19570),#14699,.T.) ;
#87891 = ADVANCED_FACE('',(#19571),#79271,.T.) ;
#87892 = ADVANCED_FACE('',(#19572),#14700,.F.) ;
#87893 = ADVANCED_FACE('',(#19573),#79272,.T.) ;
#87894 = ADVANCED_FACE('',(#19574),#14701,.T.) ;
#87895 = ADVANCED_FACE('',(#19575),#14702,.T.) ;
#87896 = ADVANCED_FACE('',(#19576),#16497,.T.) ;
#87897 = ADVANCED_FACE('',(#19577),#14703,.F.) ;
#87898 = ADVANCED_FACE('',(#19578),#79273,.F.) ;
#87899 = ADVANCED_FACE('',(#19579),#16498,.F.) ;
#87900 = ADVANCED_FACE('',(#19580),#14704,.F.) ;
#87901 = ADVANCED_FACE('',(#19581),#14705,.F.) ;
#87902 = ADVANCED_FACE('',(#19582),#79274,.F.) ;
#87903 = ADVANCED_FACE('',(#19583),#16499,.F.) ;
#87904 = ADVANCED_FACE('',(#19584),#14706,.F.) ;
#87905 = ADVANCED_FACE('',(#19585),#14707,.F.) ;
#87906 = ADVANCED_FACE('',(#19586),#16500,.F.) ;
#87907 = ADVANCED_FACE('',(#19587),#16501,.F.) ;
#87908 = ADVANCED_FACE('',(#19588),#14708,.F.) ;
#87909 = ADVANCED_FACE('',(#19589),#79275,.F.) ;
#87910 = ADVANCED_FACE('',(#19590),#16502,.F.) ;
#87911 = ADVANCED_FACE('',(#19591),#16503,.F.) ;
#87912 = ADVANCED_FACE('',(#19592),#14709,.F.) ;
#87913 = ADVANCED_FACE('',(#19593),#14710,.F.) ;
#87914 = ADVANCED_FACE('',(#19594),#16504,.F.) ;
#87915 = ADVANCED_FACE('',(#19595),#14711,.F.) ;
#87916 = ADVANCED_FACE('',(#19596),#14712,.F.) ;
#87917 = ADVANCED_FACE('',(#19597),#16505,.F.) ;
#87918 = ADVANCED_FACE('',(#19598),#16506,.F.) ;
#87919 = ADVANCED_FACE('',(#19599),#14713,.F.) ;
#87920 = ADVANCED_FACE('',(#19600),#14714,.F.) ;
#87921 = ADVANCED_FACE('',(#19601),#79276,.F.) ;
#87922 = ADVANCED_FACE('',(#19602),#79277,.F.) ;
#87923 = ADVANCED_FACE('',(#19603),#14715,.F.) ;
#87924 = ADVANCED_FACE('',(#19604),#14716,.T.) ;
#87925 = ADVANCED_FACE('',(#19605),#14717,.F.) ;
#87926 = ADVANCED_FACE('',(#19606),#16507,.F.) ;
#87927 = ADVANCED_FACE('',(#19607),#16508,.T.) ;
#87928 = ADVANCED_FACE('',(#19608),#79278,.T.) ;
#87929 = ADVANCED_FACE('',(#19609),#14718,.F.) ;
#87930 = ADVANCED_FACE('',(#19610),#14719,.F.) ;
#87931 = ADVANCED_FACE('',(#19611),#14720,.T.) ;
#87932 = ADVANCED_FACE('',(#19612),#14721,.T.) ;
#87933 = ADVANCED_FACE('',(#19613),#14722,.T.) ;
#87934 = ADVANCED_FACE('',(#19614),#14723,.F.) ;
#87935 = ADVANCED_FACE('',(#19615),#16509,.F.) ;
#87936 = ADVANCED_FACE('',(#19616),#79279,.F.) ;
#87937 = ADVANCED_FACE('',(#19617),#79280,.F.) ;
#87938 = ADVANCED_FACE('',(#19618),#79281,.T.) ;
#87939 = ADVANCED_FACE('',(#19619),#14724,.F.) ;
#87940 = ADVANCED_FACE('',(#19620),#14725,.F.) ;
#87941 = ADVANCED_FACE('',(#19621),#14726,.F.) ;
#87942 = ADVANCED_FACE('',(#19622),#14727,.T.) ;
#87943 = ADVANCED_FACE('',(#19623),#14728,.T.) ;
#87944 = ADVANCED_FACE('',(#19624),#79282,.F.) ;
#87945 = ADVANCED_FACE('',(#19625),#16510,.F.) ;
#87946 = ADVANCED_FACE('',(#19626),#16511,.T.) ;
#87947 = ADVANCED_FACE('',(#19627),#14729,.T.) ;
#87948 = ADVANCED_FACE('',(#19628),#16512,.F.) ;
#87949 = ADVANCED_FACE('',(#19629),#16513,.T.) ;
#87950 = ADVANCED_FACE('',(#19630),#14730,.F.) ;
#87951 = ADVANCED_FACE('',(#19631),#14731,.F.) ;
#87952 = ADVANCED_FACE('',(#19632),#14732,.T.) ;
#87953 = ADVANCED_FACE('',(#19633),#79283,.T.) ;
#87954 = ADVANCED_FACE('',(#19634),#14733,.F.) ;
#87955 = ADVANCED_FACE('',(#19635),#14734,.T.) ;
#87956 = ADVANCED_FACE('',(#19636),#14735,.F.) ;
#87957 = ADVANCED_FACE('',(#19637),#16514,.F.) ;
#87958 = ADVANCED_FACE('',(#19638),#79284,.T.) ;
#87959 = ADVANCED_FACE('',(#19639),#14736,.T.) ;
#87960 = ADVANCED_FACE('',(#19640),#16515,.F.) ;
#87961 = ADVANCED_FACE('',(#19641),#79285,.F.) ;
#87962 = ADVANCED_FACE('',(#19642),#14737,.F.) ;
#87963 = ADVANCED_FACE('',(#19643),#14738,.T.) ;
#87964 = ADVANCED_FACE('',(#19644),#79286,.T.) ;
#87965 = ADVANCED_FACE('',(#19645),#14739,.F.) ;
#87966 = ADVANCED_FACE('',(#19646),#79287,.T.) ;
#87967 = ADVANCED_FACE('',(#19647),#14740,.T.) ;
#87968 = ADVANCED_FACE('',(#19648),#14741,.T.) ;
#87969 = ADVANCED_FACE('',(#19649),#16516,.T.) ;
#87970 = ADVANCED_FACE('',(#19650),#14742,.F.) ;
#87971 = ADVANCED_FACE('',(#19651),#79288,.F.) ;
#87972 = ADVANCED_FACE('',(#19652),#16517,.F.) ;
#87973 = ADVANCED_FACE('',(#19653),#14743,.F.) ;
#87974 = ADVANCED_FACE('',(#19654),#14744,.F.) ;
#87975 = ADVANCED_FACE('',(#19655),#79289,.F.) ;
#87976 = ADVANCED_FACE('',(#19656),#16518,.F.) ;
#87977 = ADVANCED_FACE('',(#19657),#14745,.F.) ;
#87978 = ADVANCED_FACE('',(#19658),#14746,.F.) ;
#87979 = ADVANCED_FACE('',(#19659),#16519,.F.) ;
#87980 = ADVANCED_FACE('',(#19660),#16520,.F.) ;
#87981 = ADVANCED_FACE('',(#19661),#14747,.F.) ;
#87982 = ADVANCED_FACE('',(#19662),#79290,.F.) ;
#87983 = ADVANCED_FACE('',(#19663),#16521,.F.) ;
#87984 = ADVANCED_FACE('',(#19664),#16522,.F.) ;
#87985 = ADVANCED_FACE('',(#19665),#14748,.F.) ;
#87986 = ADVANCED_FACE('',(#19666),#14749,.F.) ;
#87987 = ADVANCED_FACE('',(#19667),#16523,.F.) ;
#87988 = ADVANCED_FACE('',(#19668),#14750,.F.) ;
#87989 = ADVANCED_FACE('',(#19669),#14751,.F.) ;
#87990 = ADVANCED_FACE('',(#19670),#16524,.F.) ;
#87991 = ADVANCED_FACE('',(#19671),#16525,.F.) ;
#87992 = ADVANCED_FACE('',(#19672),#14752,.F.) ;
#87993 = ADVANCED_FACE('',(#19673),#14753,.F.) ;
#87994 = ADVANCED_FACE('',(#19674),#79291,.F.) ;
#87995 = ADVANCED_FACE('',(#19675),#79292,.F.) ;
#87996 = ADVANCED_FACE('',(#19676),#14754,.F.) ;
#87997 = ADVANCED_FACE('',(#19677),#14755,.T.) ;
#87998 = ADVANCED_FACE('',(#19678),#14756,.F.) ;
#87999 = ADVANCED_FACE('',(#19679),#16526,.F.) ;
#88000 = ADVANCED_FACE('',(#19680),#16527,.T.) ;
#88001 = ADVANCED_FACE('',(#19681),#79293,.T.) ;
#88002 = ADVANCED_FACE('',(#19682),#14757,.F.) ;
#88003 = ADVANCED_FACE('',(#19683),#14758,.F.) ;
#88004 = ADVANCED_FACE('',(#19684),#14759,.T.) ;
#88005 = ADVANCED_FACE('',(#19685),#14760,.T.) ;
#88006 = ADVANCED_FACE('',(#19686),#14761,.T.) ;
#88007 = ADVANCED_FACE('',(#19687),#14762,.F.) ;
#88008 = ADVANCED_FACE('',(#19688),#16528,.F.) ;
#88009 = ADVANCED_FACE('',(#19689),#79294,.F.) ;
#88010 = ADVANCED_FACE('',(#19690),#79295,.F.) ;
#88011 = ADVANCED_FACE('',(#19691),#79296,.T.) ;
#88012 = ADVANCED_FACE('',(#19692),#14763,.F.) ;
#88013 = ADVANCED_FACE('',(#19693),#14764,.F.) ;
#88014 = ADVANCED_FACE('',(#19694),#14765,.F.) ;
#88015 = ADVANCED_FACE('',(#19695),#14766,.T.) ;
#88016 = ADVANCED_FACE('',(#19696),#14767,.T.) ;
#88017 = ADVANCED_FACE('',(#19697),#79297,.F.) ;
#88018 = ADVANCED_FACE('',(#19698),#16529,.F.) ;
#88019 = ADVANCED_FACE('',(#19699),#16530,.T.) ;
#88020 = ADVANCED_FACE('',(#19700),#14768,.T.) ;
#88021 = ADVANCED_FACE('',(#19701),#16531,.F.) ;
#88022 = ADVANCED_FACE('',(#19702),#16532,.T.) ;
#88023 = ADVANCED_FACE('',(#19703),#14769,.F.) ;
#88024 = ADVANCED_FACE('',(#19704),#14770,.F.) ;
#88025 = ADVANCED_FACE('',(#19705),#14771,.T.) ;
#88026 = ADVANCED_FACE('',(#19706),#79298,.T.) ;
#88027 = ADVANCED_FACE('',(#19707),#14772,.F.) ;
#88028 = ADVANCED_FACE('',(#19708),#14773,.T.) ;
#88029 = ADVANCED_FACE('',(#19709),#14774,.F.) ;
#88030 = ADVANCED_FACE('',(#19710),#16533,.F.) ;
#88031 = ADVANCED_FACE('',(#19711),#79299,.T.) ;
#88032 = ADVANCED_FACE('',(#19712),#14775,.T.) ;
#88033 = ADVANCED_FACE('',(#19713),#16534,.F.) ;
#88034 = ADVANCED_FACE('',(#19714),#79300,.F.) ;
#88035 = ADVANCED_FACE('',(#19715),#14776,.F.) ;
#88036 = ADVANCED_FACE('',(#19716),#14777,.T.) ;
#88037 = ADVANCED_FACE('',(#19717),#79301,.T.) ;
#88038 = ADVANCED_FACE('',(#19718),#14778,.F.) ;
#88039 = ADVANCED_FACE('',(#19719),#79302,.T.) ;
#88040 = ADVANCED_FACE('',(#19720),#14779,.T.) ;
#88041 = ADVANCED_FACE('',(#19721),#14780,.T.) ;
#88042 = ADVANCED_FACE('',(#19722),#16535,.T.) ;
#88043 = ADVANCED_FACE('',(#19723),#14781,.F.) ;
#88044 = ADVANCED_FACE('',(#19724),#79303,.F.) ;
#88045 = ADVANCED_FACE('',(#19725),#16536,.F.) ;
#88046 = ADVANCED_FACE('',(#19726),#14782,.F.) ;
#88047 = ADVANCED_FACE('',(#19727),#14783,.F.) ;
#88048 = ADVANCED_FACE('',(#19728),#79304,.F.) ;
#88049 = ADVANCED_FACE('',(#19729),#16537,.F.) ;
#88050 = ADVANCED_FACE('',(#19730),#14784,.F.) ;
#88051 = ADVANCED_FACE('',(#19731),#14785,.F.) ;
#88052 = ADVANCED_FACE('',(#19732),#16538,.F.) ;
#88053 = ADVANCED_FACE('',(#19733),#16539,.F.) ;
#88054 = ADVANCED_FACE('',(#19734),#14786,.F.) ;
#88055 = ADVANCED_FACE('',(#19735),#79305,.F.) ;
#88056 = ADVANCED_FACE('',(#19736),#16540,.F.) ;
#88057 = ADVANCED_FACE('',(#19737),#16541,.F.) ;
#88058 = ADVANCED_FACE('',(#19738),#14787,.F.) ;
#88059 = ADVANCED_FACE('',(#19739),#14788,.F.) ;
#88060 = ADVANCED_FACE('',(#19740),#16542,.F.) ;
#88061 = ADVANCED_FACE('',(#19741),#14789,.F.) ;
#88062 = ADVANCED_FACE('',(#19742),#14790,.F.) ;
#88063 = ADVANCED_FACE('',(#19743),#16543,.F.) ;
#88064 = ADVANCED_FACE('',(#19744),#16544,.F.) ;
#88065 = ADVANCED_FACE('',(#19745),#14791,.F.) ;
#88066 = ADVANCED_FACE('',(#19746),#14792,.F.) ;
#88067 = ADVANCED_FACE('',(#19747),#79306,.F.) ;
#88068 = ADVANCED_FACE('',(#19748),#79307,.F.) ;
#88069 = ADVANCED_FACE('',(#19749),#14793,.F.) ;
#88070 = ADVANCED_FACE('',(#19750),#1351,.F.) ;
#88071 = ADVANCED_FACE('',(#19751),#1352,.F.) ;
#88072 = ADVANCED_FACE('',(#19752),#1353,.F.) ;
#88073 = ADVANCED_FACE('',(#19753),#1354,.F.) ;
#88074 = ADVANCED_FACE('',(#19754),#1355,.F.) ;
#88075 = ADVANCED_FACE('',(#19755),#1356,.T.) ;
#88076 = ADVANCED_FACE('',(#19756),#1357,.F.) ;
#88077 = ADVANCED_FACE('',(#19757),#14794,.T.) ;
#88078 = ADVANCED_FACE('',(#19758),#14795,.F.) ;
#88079 = ADVANCED_FACE('',(#19759),#1358,.F.) ;
#88080 = ADVANCED_FACE('',(#19760),#1359,.F.) ;
#88081 = ADVANCED_FACE('',(#19761),#1360,.F.) ;
#88082 = ADVANCED_FACE('',(#19762),#1361,.F.) ;
#88083 = ADVANCED_FACE('',(#19763),#1362,.F.) ;
#88084 = ADVANCED_FACE('',(#19764),#1363,.T.) ;
#88085 = ADVANCED_FACE('',(#19765),#1364,.F.) ;
#88086 = ADVANCED_FACE('',(#19766),#1365,.F.) ;
#88087 = ADVANCED_FACE('',(#19767),#1366,.F.) ;
#88088 = ADVANCED_FACE('',(#19768),#1367,.F.) ;
#88089 = ADVANCED_FACE('',(#19769),#1368,.F.) ;
#88090 = ADVANCED_FACE('',(#19770),#1369,.F.) ;
#88091 = ADVANCED_FACE('',(#19771),#1370,.T.) ;
#88092 = ADVANCED_FACE('',(#19772),#1371,.F.) ;
#88093 = ADVANCED_FACE('',(#19773),#14796,.T.) ;
#88094 = ADVANCED_FACE('',(#19774),#14797,.F.) ;
#88095 = ADVANCED_FACE('',(#19775),#1372,.F.) ;
#88096 = ADVANCED_FACE('',(#19776),#1373,.F.) ;
#88097 = ADVANCED_FACE('',(#19777),#1374,.F.) ;
#88098 = ADVANCED_FACE('',(#19778),#1375,.F.) ;
#88099 = ADVANCED_FACE('',(#19779),#1376,.F.) ;
#88100 = ADVANCED_FACE('',(#19780),#1377,.T.) ;
#88101 = ADVANCED_FACE('',(#19781),#1378,.F.) ;
#88102 = ADVANCED_FACE('',(#19782),#1379,.F.) ;
#88103 = ADVANCED_FACE('',(#19783),#1380,.F.) ;
#88104 = ADVANCED_FACE('',(#19784),#1381,.F.) ;
#88105 = ADVANCED_FACE('',(#19785),#1382,.F.) ;
#88106 = ADVANCED_FACE('',(#19786),#1383,.F.) ;
#88107 = ADVANCED_FACE('',(#19787),#1384,.T.) ;
#88108 = ADVANCED_FACE('',(#19788),#1385,.F.) ;
#88109 = ADVANCED_FACE('',(#19789),#14798,.T.) ;
#88110 = ADVANCED_FACE('',(#19790),#14799,.F.) ;
#88111 = ADVANCED_FACE('',(#19791),#1386,.F.) ;
#88112 = ADVANCED_FACE('',(#19792),#1387,.F.) ;
#88113 = ADVANCED_FACE('',(#19793),#1388,.F.) ;
#88114 = ADVANCED_FACE('',(#19794),#1389,.F.) ;
#88115 = ADVANCED_FACE('',(#19795),#1390,.F.) ;
#88116 = ADVANCED_FACE('',(#19796),#1391,.T.) ;
#88117 = ADVANCED_FACE('',(#19797),#1392,.F.) ;
#88118 = ADVANCED_FACE('',(#19798),#1393,.F.) ;
#88119 = ADVANCED_FACE('',(#19799),#1394,.F.) ;
#88120 = ADVANCED_FACE('',(#19800),#1395,.F.) ;
#88121 = ADVANCED_FACE('',(#19801),#1396,.F.) ;
#88122 = ADVANCED_FACE('',(#19802),#1397,.F.) ;
#88123 = ADVANCED_FACE('',(#19803),#1398,.T.) ;
#88124 = ADVANCED_FACE('',(#19804),#1399,.F.) ;
#88125 = ADVANCED_FACE('',(#19805),#14800,.T.) ;
#88126 = ADVANCED_FACE('',(#19806),#14801,.F.) ;
#88127 = ADVANCED_FACE('',(#19807),#1400,.F.) ;
#88128 = ADVANCED_FACE('',(#19808),#1401,.F.) ;
#88129 = ADVANCED_FACE('',(#19809),#1402,.F.) ;
#88130 = ADVANCED_FACE('',(#19810),#1403,.F.) ;
#88131 = ADVANCED_FACE('',(#19811),#1404,.F.) ;
#88132 = ADVANCED_FACE('',(#19812),#1405,.T.) ;
#88133 = ADVANCED_FACE('',(#19813),#1406,.F.) ;
#88134 = ADVANCED_FACE('',(#19814),#1407,.F.) ;
#88135 = ADVANCED_FACE('',(#19815),#1408,.F.) ;
#88136 = ADVANCED_FACE('',(#19816),#1409,.F.) ;
#88137 = ADVANCED_FACE('',(#19817),#1410,.F.) ;
#88138 = ADVANCED_FACE('',(#19818),#1411,.F.) ;
#88139 = ADVANCED_FACE('',(#19819),#1412,.T.) ;
#88140 = ADVANCED_FACE('',(#19820),#1413,.F.) ;
#88141 = ADVANCED_FACE('',(#19821),#14802,.T.) ;
#88142 = ADVANCED_FACE('',(#19822),#14803,.F.) ;
#88143 = ADVANCED_FACE('',(#19823),#1414,.F.) ;
#88144 = ADVANCED_FACE('',(#19824),#1415,.F.) ;
#88145 = ADVANCED_FACE('',(#19825),#1416,.F.) ;
#88146 = ADVANCED_FACE('',(#19826),#1417,.F.) ;
#88147 = ADVANCED_FACE('',(#19827),#1418,.F.) ;
#88148 = ADVANCED_FACE('',(#19828),#1419,.T.) ;
#88149 = ADVANCED_FACE('',(#19829),#1420,.F.) ;
#88150 = ADVANCED_FACE('',(#19830),#1421,.F.) ;
#88151 = ADVANCED_FACE('',(#19831),#1422,.F.) ;
#88152 = ADVANCED_FACE('',(#19832),#1423,.F.) ;
#88153 = ADVANCED_FACE('',(#19833),#1424,.F.) ;
#88154 = ADVANCED_FACE('',(#19834),#1425,.F.) ;
#88155 = ADVANCED_FACE('',(#19835),#1426,.T.) ;
#88156 = ADVANCED_FACE('',(#19836),#1427,.F.) ;
#88157 = ADVANCED_FACE('',(#19837),#14804,.T.) ;
#88158 = ADVANCED_FACE('',(#19838),#14805,.F.) ;
#88159 = ADVANCED_FACE('',(#19839),#1428,.F.) ;
#88160 = ADVANCED_FACE('',(#19840),#1429,.F.) ;
#88161 = ADVANCED_FACE('',(#19841),#1430,.F.) ;
#88162 = ADVANCED_FACE('',(#19842),#1431,.F.) ;
#88163 = ADVANCED_FACE('',(#19843),#1432,.F.) ;
#88164 = ADVANCED_FACE('',(#19844),#1433,.T.) ;
#88165 = ADVANCED_FACE('',(#19845),#1434,.F.) ;
#88166 = ADVANCED_FACE('',(#19846),#1435,.F.) ;
#88167 = ADVANCED_FACE('',(#19847),#1436,.F.) ;
#88168 = ADVANCED_FACE('',(#19848),#1437,.F.) ;
#88169 = ADVANCED_FACE('',(#19849),#1438,.F.) ;
#88170 = ADVANCED_FACE('',(#19850),#1439,.F.) ;
#88171 = ADVANCED_FACE('',(#19851),#1440,.T.) ;
#88172 = ADVANCED_FACE('',(#19852),#1441,.F.) ;
#88173 = ADVANCED_FACE('',(#19853),#14806,.T.) ;
#88174 = ADVANCED_FACE('',(#19854),#14807,.F.) ;
#88175 = ADVANCED_FACE('',(#19855),#1442,.F.) ;
#88176 = ADVANCED_FACE('',(#19856),#1443,.F.) ;
#88177 = ADVANCED_FACE('',(#19857),#1444,.F.) ;
#88178 = ADVANCED_FACE('',(#19858),#1445,.F.) ;
#88179 = ADVANCED_FACE('',(#19859),#1446,.F.) ;
#88180 = ADVANCED_FACE('',(#19860),#1447,.T.) ;
#88181 = ADVANCED_FACE('',(#19861),#1448,.F.) ;
#88182 = ADVANCED_FACE('',(#19862),#1449,.F.) ;
#88183 = ADVANCED_FACE('',(#19863),#1450,.F.) ;
#88184 = ADVANCED_FACE('',(#19864),#1451,.F.) ;
#88185 = ADVANCED_FACE('',(#19865),#1452,.F.) ;
#88186 = ADVANCED_FACE('',(#19866),#1453,.F.) ;
#88187 = ADVANCED_FACE('',(#19867),#1454,.T.) ;
#88188 = ADVANCED_FACE('',(#19868),#1455,.F.) ;
#88189 = ADVANCED_FACE('',(#19869),#14808,.T.) ;
#88190 = ADVANCED_FACE('',(#19870),#14809,.F.) ;
#88191 = ADVANCED_FACE('',(#19871),#1456,.F.) ;
#88192 = ADVANCED_FACE('',(#19872),#1457,.F.) ;
#88193 = ADVANCED_FACE('',(#19873),#1458,.F.) ;
#88194 = ADVANCED_FACE('',(#19874),#1459,.F.) ;
#88195 = ADVANCED_FACE('',(#19875),#1460,.F.) ;
#88196 = ADVANCED_FACE('',(#19876),#1461,.T.) ;
#88197 = ADVANCED_FACE('',(#19877),#1462,.F.) ;
#88198 = ADVANCED_FACE('',(#19878),#1463,.F.) ;
#88199 = ADVANCED_FACE('',(#19879),#1464,.F.) ;
#88200 = ADVANCED_FACE('',(#19880),#1465,.F.) ;
#88201 = ADVANCED_FACE('',(#19881),#1466,.F.) ;
#88202 = ADVANCED_FACE('',(#19882),#1467,.F.) ;
#88203 = ADVANCED_FACE('',(#19883),#1468,.T.) ;
#88204 = ADVANCED_FACE('',(#19884),#1469,.F.) ;
#88205 = ADVANCED_FACE('',(#19885),#14810,.T.) ;
#88206 = ADVANCED_FACE('',(#19886),#14811,.F.) ;
#88207 = ADVANCED_FACE('',(#19887),#1470,.F.) ;
#88208 = ADVANCED_FACE('',(#19888),#1471,.F.) ;
#88209 = ADVANCED_FACE('',(#19889),#1472,.F.) ;
#88210 = ADVANCED_FACE('',(#19890),#1473,.F.) ;
#88211 = ADVANCED_FACE('',(#19891),#1474,.F.) ;
#88212 = ADVANCED_FACE('',(#19892),#1475,.T.) ;
#88213 = ADVANCED_FACE('',(#19893),#1476,.F.) ;
#88214 = ADVANCED_FACE('',(#19894),#1477,.F.) ;
#88215 = ADVANCED_FACE('',(#19895),#1478,.F.) ;
#88216 = ADVANCED_FACE('',(#19896),#1479,.F.) ;
#88217 = ADVANCED_FACE('',(#19897),#1480,.F.) ;
#88218 = ADVANCED_FACE('',(#19898),#1481,.F.) ;
#88219 = ADVANCED_FACE('',(#19899),#1482,.F.) ;
#88220 = ADVANCED_FACE('',(#19900),#1483,.F.) ;
#88221 = ADVANCED_FACE('',(#19901),#1484,.F.) ;
#88222 = ADVANCED_FACE('',(#19902),#1485,.F.) ;
#88223 = ADVANCED_FACE('',(#19903),#1486,.F.) ;
#88224 = ADVANCED_FACE('',(#19904),#1487,.F.) ;
#88225 = ADVANCED_FACE('',(#19905),#1488,.F.) ;
#88226 = ADVANCED_FACE('',(#19906),#1489,.F.) ;
#88227 = ADVANCED_FACE('',(#19907),#1490,.F.) ;
#88228 = ADVANCED_FACE('',(#19908),#1491,.F.) ;
#88229 = ADVANCED_FACE('',(#19909),#1492,.F.) ;
#88230 = ADVANCED_FACE('',(#19910),#1493,.F.) ;
#88231 = ADVANCED_FACE('',(#19911),#1494,.F.) ;
#88232 = ADVANCED_FACE('',(#19912),#1495,.F.) ;
#88233 = ADVANCED_FACE('',(#19913),#1496,.F.) ;
#88234 = ADVANCED_FACE('',(#19914),#1497,.F.) ;
#88235 = ADVANCED_FACE('',(#19915),#1498,.F.) ;
#88236 = ADVANCED_FACE('',(#19916),#1499,.F.) ;
#88237 = ADVANCED_FACE('',(#19917),#1500,.F.) ;
#88238 = ADVANCED_FACE('',(#19918),#1501,.F.) ;
#88239 = ADVANCED_FACE('',(#19919),#1502,.F.) ;
#88240 = ADVANCED_FACE('',(#19920),#1503,.F.) ;
#88241 = ADVANCED_FACE('',(#19921),#1504,.F.) ;
#88242 = ADVANCED_FACE('',(#19922),#1505,.F.) ;
#88243 = ADVANCED_FACE('',(#19923),#1506,.F.) ;
#88244 = ADVANCED_FACE('',(#19924),#1507,.F.) ;
#88245 = ADVANCED_FACE('',(#19925),#1508,.F.) ;
#88246 = ADVANCED_FACE('',(#19926),#1509,.F.) ;
#88247 = ADVANCED_FACE('',(#19927),#1510,.F.) ;
#88248 = ADVANCED_FACE('',(#19928),#1511,.F.) ;
#88249 = ADVANCED_FACE('',(#19929),#1512,.F.) ;
#88250 = ADVANCED_FACE('',(#19930),#14812,.T.) ;
#88251 = ADVANCED_FACE('',(#19931),#14813,.T.) ;
#88252 = ADVANCED_FACE('',(#19932),#16545,.T.) ;
#88253 = ADVANCED_FACE('',(#19933),#14814,.T.) ;
#88254 = ADVANCED_FACE('',(#19934),#14815,.T.) ;
#88255 = ADVANCED_FACE('',(#19935),#14816,.T.) ;
#88256 = ADVANCED_FACE('',(#19936),#16546,.T.) ;
#88257 = ADVANCED_FACE('',(#19937),#16547,.T.) ;
#88258 = ADVANCED_FACE('',(#19938),#14817,.T.) ;
#88259 = ADVANCED_FACE('',(#19939),#14818,.T.) ;
#88260 = ADVANCED_FACE('',(#19940),#14819,.T.) ;
#88261 = ADVANCED_FACE('',(#19941),#16548,.T.) ;
#88262 = ADVANCED_FACE('',(#19942),#14820,.T.) ;
#88263 = ADVANCED_FACE('',(#19943),#14821,.T.) ;
#88264 = ADVANCED_FACE('',(#19944),#14822,.T.) ;
#88265 = ADVANCED_FACE('',(#19945),#14823,.T.) ;
#88266 = ADVANCED_FACE('',(#19946),#16549,.T.) ;
#88267 = ADVANCED_FACE('',(#19947),#14824,.T.) ;
#88268 = ADVANCED_FACE('',(#19948),#14825,.T.) ;
#88269 = ADVANCED_FACE('',(#19949),#14826,.T.) ;
#88270 = ADVANCED_FACE('',(#19950),#16550,.T.) ;
#88271 = ADVANCED_FACE('',(#19951),#16551,.T.) ;
#88272 = ADVANCED_FACE('',(#19952),#14827,.T.) ;
#88273 = ADVANCED_FACE('',(#19953),#14828,.T.) ;
#88274 = ADVANCED_FACE('',(#19954),#14829,.T.) ;
#88275 = ADVANCED_FACE('',(#19955),#16552,.T.) ;
#88276 = ADVANCED_FACE('',(#19956),#14830,.T.) ;
#88277 = ADVANCED_FACE('',(#19957),#14831,.T.) ;
#88278 = ADVANCED_FACE('',(#19958),#14832,.T.) ;
#88279 = ADVANCED_FACE('',(#19959),#14833,.T.) ;
#88280 = ADVANCED_FACE('',(#19960),#16553,.T.) ;
#88281 = ADVANCED_FACE('',(#19961),#14834,.T.) ;
#88282 = ADVANCED_FACE('',(#19962),#14835,.T.) ;
#88283 = ADVANCED_FACE('',(#19963),#14836,.T.) ;
#88284 = ADVANCED_FACE('',(#19964),#16554,.T.) ;
#88285 = ADVANCED_FACE('',(#19965),#16555,.T.) ;
#88286 = ADVANCED_FACE('',(#19966),#14837,.T.) ;
#88287 = ADVANCED_FACE('',(#19967),#14838,.T.) ;
#88288 = ADVANCED_FACE('',(#19968),#14839,.T.) ;
#88289 = ADVANCED_FACE('',(#19969),#16556,.T.) ;
#88290 = ADVANCED_FACE('',(#19970),#14840,.T.) ;
#88291 = ADVANCED_FACE('',(#19971),#14841,.T.) ;
#88292 = ADVANCED_FACE('',(#19972),#14842,.T.) ;
#88293 = ADVANCED_FACE('',(#19973),#14843,.T.) ;
#88294 = ADVANCED_FACE('',(#19974),#16557,.T.) ;
#88295 = ADVANCED_FACE('',(#19975),#14844,.T.) ;
#88296 = ADVANCED_FACE('',(#19976),#14845,.T.) ;
#88297 = ADVANCED_FACE('',(#19977),#14846,.T.) ;
#88298 = ADVANCED_FACE('',(#19978),#16558,.T.) ;
#88299 = ADVANCED_FACE('',(#19979),#16559,.T.) ;
#88300 = ADVANCED_FACE('',(#19980),#14847,.T.) ;
#88301 = ADVANCED_FACE('',(#19981),#14848,.T.) ;
#88302 = ADVANCED_FACE('',(#19982),#14849,.T.) ;
#88303 = ADVANCED_FACE('',(#19983),#16560,.T.) ;
#88304 = ADVANCED_FACE('',(#19984),#14850,.T.) ;
#88305 = ADVANCED_FACE('',(#19985),#14851,.T.) ;
#88306 = ADVANCED_FACE('',(#19986),#14852,.T.) ;
#88307 = ADVANCED_FACE('',(#19987),#14853,.T.) ;
#88308 = ADVANCED_FACE('',(#19988),#16561,.T.) ;
#88309 = ADVANCED_FACE('',(#19989),#14854,.T.) ;
#88310 = ADVANCED_FACE('',(#19990),#14855,.T.) ;
#88311 = ADVANCED_FACE('',(#19991),#14856,.T.) ;
#88312 = ADVANCED_FACE('',(#19992),#16562,.T.) ;
#88313 = ADVANCED_FACE('',(#19993),#16563,.T.) ;
#88314 = ADVANCED_FACE('',(#19994),#14857,.T.) ;
#88315 = ADVANCED_FACE('',(#19995),#14858,.T.) ;
#88316 = ADVANCED_FACE('',(#19996),#14859,.T.) ;
#88317 = ADVANCED_FACE('',(#19997),#16564,.T.) ;
#88318 = ADVANCED_FACE('',(#19998),#14860,.T.) ;
#88319 = ADVANCED_FACE('',(#19999),#14861,.T.) ;
#88320 = ADVANCED_FACE('',(#20000),#14862,.T.) ;
#88321 = ADVANCED_FACE('',(#20001),#14863,.T.) ;
#88322 = ADVANCED_FACE('',(#20002),#16565,.T.) ;
#88323 = ADVANCED_FACE('',(#20003),#14864,.T.) ;
#88324 = ADVANCED_FACE('',(#20004),#14865,.T.) ;
#88325 = ADVANCED_FACE('',(#20005),#14866,.T.) ;
#88326 = ADVANCED_FACE('',(#20006),#16566,.T.) ;
#88327 = ADVANCED_FACE('',(#20007),#16567,.T.) ;
#88328 = ADVANCED_FACE('',(#20008),#14867,.T.) ;
#88329 = ADVANCED_FACE('',(#20009),#14868,.T.) ;
#88330 = ADVANCED_FACE('',(#20010),#14869,.T.) ;
#88331 = ADVANCED_FACE('',(#20011),#16568,.T.) ;
#88332 = ADVANCED_FACE('',(#20012),#14870,.T.) ;
#88333 = ADVANCED_FACE('',(#20013),#14871,.T.) ;
#88334 = ADVANCED_FACE('',(#20014),#14872,.T.) ;
#88335 = ADVANCED_FACE('',(#20015),#14873,.T.) ;
#88336 = ADVANCED_FACE('',(#20016),#16569,.T.) ;
#88337 = ADVANCED_FACE('',(#20017),#14874,.T.) ;
#88338 = ADVANCED_FACE('',(#20018),#14875,.T.) ;
#88339 = ADVANCED_FACE('',(#20019),#14876,.T.) ;
#88340 = ADVANCED_FACE('',(#20020),#16570,.T.) ;
#88341 = ADVANCED_FACE('',(#20021),#16571,.T.) ;
#88342 = ADVANCED_FACE('',(#20022),#14877,.T.) ;
#88343 = ADVANCED_FACE('',(#20023),#14878,.T.) ;
#88344 = ADVANCED_FACE('',(#20024),#14879,.T.) ;
#88345 = ADVANCED_FACE('',(#20025),#16572,.T.) ;
#88346 = ADVANCED_FACE('',(#20026),#14880,.T.) ;
#88347 = ADVANCED_FACE('',(#20027),#14881,.T.) ;
#88348 = ADVANCED_FACE('',(#20028),#14882,.T.) ;
#88349 = ADVANCED_FACE('',(#20029),#14883,.T.) ;
#88350 = ADVANCED_FACE('',(#20030),#16573,.T.) ;
#88351 = ADVANCED_FACE('',(#20031),#14884,.T.) ;
#88352 = ADVANCED_FACE('',(#20032),#14885,.T.) ;
#88353 = ADVANCED_FACE('',(#20033),#14886,.T.) ;
#88354 = ADVANCED_FACE('',(#20034),#16574,.T.) ;
#88355 = ADVANCED_FACE('',(#20035),#16575,.T.) ;
#88356 = ADVANCED_FACE('',(#20036),#14887,.T.) ;
#88357 = ADVANCED_FACE('',(#20037),#14888,.T.) ;
#88358 = ADVANCED_FACE('',(#20038),#14889,.T.) ;
#88359 = ADVANCED_FACE('',(#20039),#16576,.T.) ;
#88360 = ADVANCED_FACE('',(#20040),#14890,.T.) ;
#88361 = ADVANCED_FACE('',(#20041),#14891,.T.) ;
#88362 = ADVANCED_FACE('',(#20042),#14892,.T.) ;
#88363 = ADVANCED_FACE('',(#20043),#14893,.T.) ;
#88364 = ADVANCED_FACE('',(#20044),#16577,.T.) ;
#88365 = ADVANCED_FACE('',(#20045),#14894,.T.) ;
#88366 = ADVANCED_FACE('',(#20046),#14895,.T.) ;
#88367 = ADVANCED_FACE('',(#20047),#14896,.T.) ;
#88368 = ADVANCED_FACE('',(#20048),#16578,.T.) ;
#88369 = ADVANCED_FACE('',(#20049),#16579,.T.) ;
#88370 = ADVANCED_FACE('',(#20050),#14897,.T.) ;
#88371 = ADVANCED_FACE('',(#20051),#14898,.T.) ;
#88372 = ADVANCED_FACE('',(#20052),#14899,.T.) ;
#88373 = ADVANCED_FACE('',(#20053),#16580,.T.) ;
#88374 = ADVANCED_FACE('',(#20054),#14900,.T.) ;
#88375 = ADVANCED_FACE('',(#20055),#14901,.T.) ;
#88376 = ADVANCED_FACE('',(#20056),#14902,.T.) ;
#88377 = ADVANCED_FACE('',(#20057),#14903,.T.) ;
#88378 = ADVANCED_FACE('',(#20058),#16581,.T.) ;
#88379 = ADVANCED_FACE('',(#20059),#14904,.T.) ;
#88380 = ADVANCED_FACE('',(#20060),#14905,.T.) ;
#88381 = ADVANCED_FACE('',(#20061),#14906,.T.) ;
#88382 = ADVANCED_FACE('',(#20062),#16582,.T.) ;
#88383 = ADVANCED_FACE('',(#20063),#16583,.T.) ;
#88384 = ADVANCED_FACE('',(#20064),#14907,.T.) ;
#88385 = ADVANCED_FACE('',(#20065),#14908,.T.) ;
#88386 = ADVANCED_FACE('',(#20066),#14909,.T.) ;
#88387 = ADVANCED_FACE('',(#20067),#16584,.T.) ;
#88388 = ADVANCED_FACE('',(#20068),#14910,.T.) ;
#88389 = ADVANCED_FACE('',(#20069),#14911,.T.) ;
#88390 = ADVANCED_FACE('',(#20070),#14912,.T.) ;
#88391 = ADVANCED_FACE('',(#20071),#14913,.T.) ;
#88392 = ADVANCED_FACE('',(#20072),#16585,.T.) ;
#88393 = ADVANCED_FACE('',(#20073),#14914,.T.) ;
#88394 = ADVANCED_FACE('',(#20074),#14915,.T.) ;
#88395 = ADVANCED_FACE('',(#20075),#14916,.T.) ;
#88396 = ADVANCED_FACE('',(#20076),#16586,.T.) ;
#88397 = ADVANCED_FACE('',(#20077),#16587,.T.) ;
#88398 = ADVANCED_FACE('',(#20078),#14917,.T.) ;
#88399 = ADVANCED_FACE('',(#20079),#14918,.T.) ;
#88400 = ADVANCED_FACE('',(#20080),#14919,.T.) ;
#88401 = ADVANCED_FACE('',(#20081),#16588,.T.) ;
#88402 = ADVANCED_FACE('',(#20082),#14920,.T.) ;
#88403 = ADVANCED_FACE('',(#20083),#14921,.T.) ;
#88404 = ADVANCED_FACE('',(#20084),#14922,.T.) ;
#88405 = ADVANCED_FACE('',(#20085),#14923,.T.) ;
#88406 = ADVANCED_FACE('',(#20086),#16589,.T.) ;
#88407 = ADVANCED_FACE('',(#20087),#14924,.T.) ;
#88408 = ADVANCED_FACE('',(#20088),#14925,.T.) ;
#88409 = ADVANCED_FACE('',(#20089),#14926,.T.) ;
#88410 = ADVANCED_FACE('',(#20090),#16590,.T.) ;
#88411 = ADVANCED_FACE('',(#20091),#16591,.T.) ;
#88412 = ADVANCED_FACE('',(#20092),#14927,.T.) ;
#88413 = ADVANCED_FACE('',(#20093),#14928,.T.) ;
#88414 = ADVANCED_FACE('',(#20094),#14929,.T.) ;
#88415 = ADVANCED_FACE('',(#20095),#16592,.T.) ;
#88416 = ADVANCED_FACE('',(#20096),#14930,.T.) ;
#88417 = ADVANCED_FACE('',(#20097),#14931,.T.) ;
#88418 = ADVANCED_FACE('',(#20098),#14932,.T.) ;
#88419 = ADVANCED_FACE('',(#20099),#14933,.T.) ;
#88420 = ADVANCED_FACE('',(#20100),#16593,.T.) ;
#88421 = ADVANCED_FACE('',(#20101),#14934,.T.) ;
#88422 = ADVANCED_FACE('',(#20102),#14935,.T.) ;
#88423 = ADVANCED_FACE('',(#20103),#14936,.T.) ;
#88424 = ADVANCED_FACE('',(#20104),#16594,.T.) ;
#88425 = ADVANCED_FACE('',(#20105),#16595,.T.) ;
#88426 = ADVANCED_FACE('',(#20106),#14937,.T.) ;
#88427 = ADVANCED_FACE('',(#20107),#14938,.T.) ;
#88428 = ADVANCED_FACE('',(#20108),#14939,.T.) ;
#88429 = ADVANCED_FACE('',(#20109),#16596,.T.) ;
#88430 = ADVANCED_FACE('',(#20110),#14940,.T.) ;
#88431 = ADVANCED_FACE('',(#20111),#14941,.T.) ;
#88432 = ADVANCED_FACE('',(#20112),#14942,.T.) ;
#88433 = ADVANCED_FACE('',(#20113),#14943,.T.) ;
#88434 = ADVANCED_FACE('',(#20114),#16597,.T.) ;
#88435 = ADVANCED_FACE('',(#20115),#14944,.T.) ;
#88436 = ADVANCED_FACE('',(#20116),#14945,.T.) ;
#88437 = ADVANCED_FACE('',(#20117),#14946,.T.) ;
#88438 = ADVANCED_FACE('',(#20118),#16598,.T.) ;
#88439 = ADVANCED_FACE('',(#20119),#16599,.T.) ;
#88440 = ADVANCED_FACE('',(#20120),#14947,.T.) ;
#88441 = ADVANCED_FACE('',(#20121),#14948,.T.) ;
#88442 = ADVANCED_FACE('',(#20122),#14949,.T.) ;
#88443 = ADVANCED_FACE('',(#20123),#16600,.T.) ;
#88444 = ADVANCED_FACE('',(#20124),#14950,.T.) ;
#88445 = ADVANCED_FACE('',(#20125),#14951,.T.) ;
#88446 = ADVANCED_FACE('',(#20126),#14952,.T.) ;
#88447 = ADVANCED_FACE('',(#20127),#14953,.T.) ;
#88448 = ADVANCED_FACE('',(#20128),#16601,.T.) ;
#88449 = ADVANCED_FACE('',(#20129),#14954,.T.) ;
#88450 = ADVANCED_FACE('',(#20130),#14955,.T.) ;
#88451 = ADVANCED_FACE('',(#20131),#14956,.T.) ;
#88452 = ADVANCED_FACE('',(#20132),#16602,.T.) ;
#88453 = ADVANCED_FACE('',(#20133),#16603,.T.) ;
#88454 = ADVANCED_FACE('',(#20134),#14957,.T.) ;
#88455 = ADVANCED_FACE('',(#20135),#14958,.T.) ;
#88456 = ADVANCED_FACE('',(#20136),#14959,.T.) ;
#88457 = ADVANCED_FACE('',(#20137),#16604,.T.) ;
#88458 = ADVANCED_FACE('',(#20138),#14960,.T.) ;
#88459 = ADVANCED_FACE('',(#20139),#14961,.T.) ;
#88460 = ADVANCED_FACE('',(#20140),#14962,.T.) ;
#88461 = ADVANCED_FACE('',(#20141),#14963,.T.) ;
#88462 = ADVANCED_FACE('',(#20142),#16605,.T.) ;
#88463 = ADVANCED_FACE('',(#20143),#14964,.T.) ;
#88464 = ADVANCED_FACE('',(#20144),#14965,.T.) ;
#88465 = ADVANCED_FACE('',(#20145),#14966,.T.) ;
#88466 = ADVANCED_FACE('',(#20146),#16606,.T.) ;
#88467 = ADVANCED_FACE('',(#20147),#16607,.T.) ;
#88468 = ADVANCED_FACE('',(#20148),#14967,.T.) ;
#88469 = ADVANCED_FACE('',(#20149),#14968,.T.) ;
#88470 = ADVANCED_FACE('',(#20150),#14969,.T.) ;
#88471 = ADVANCED_FACE('',(#20151),#16608,.T.) ;
#88472 = ADVANCED_FACE('',(#20152),#14970,.T.) ;
#88473 = ADVANCED_FACE('',(#20153),#14971,.T.) ;
#88474 = ADVANCED_FACE('',(#20154),#14972,.T.) ;
#88475 = ADVANCED_FACE('',(#20155),#14973,.T.) ;
#88476 = ADVANCED_FACE('',(#20156),#16609,.T.) ;
#88477 = ADVANCED_FACE('',(#20157),#14974,.T.) ;
#88478 = ADVANCED_FACE('',(#20158),#14975,.T.) ;
#88479 = ADVANCED_FACE('',(#20159),#14976,.T.) ;
#88480 = ADVANCED_FACE('',(#20160),#16610,.T.) ;
#88481 = ADVANCED_FACE('',(#20161),#16611,.T.) ;
#88482 = ADVANCED_FACE('',(#20162),#14977,.T.) ;
#88483 = ADVANCED_FACE('',(#20163),#14978,.T.) ;
#88484 = ADVANCED_FACE('',(#20164),#14979,.T.) ;
#88485 = ADVANCED_FACE('',(#20165),#16612,.T.) ;
#88486 = ADVANCED_FACE('',(#20166),#14980,.T.) ;
#88487 = ADVANCED_FACE('',(#20167),#14981,.T.) ;
#88488 = ADVANCED_FACE('',(#20168),#14982,.T.) ;
#88489 = ADVANCED_FACE('',(#20169),#14983,.T.) ;
#88490 = ADVANCED_FACE('',(#20170),#16613,.T.) ;
#88491 = ADVANCED_FACE('',(#20171),#14984,.T.) ;
#88492 = ADVANCED_FACE('',(#20172),#14985,.T.) ;
#88493 = ADVANCED_FACE('',(#20173),#14986,.T.) ;
#88494 = ADVANCED_FACE('',(#20174),#16614,.T.) ;
#88495 = ADVANCED_FACE('',(#20175),#16615,.T.) ;
#88496 = ADVANCED_FACE('',(#20176),#14987,.T.) ;
#88497 = ADVANCED_FACE('',(#20177),#14988,.T.) ;
#88498 = ADVANCED_FACE('',(#20178),#14989,.T.) ;
#88499 = ADVANCED_FACE('',(#20179),#16616,.T.) ;
#88500 = ADVANCED_FACE('',(#20180),#14990,.T.) ;
#88501 = ADVANCED_FACE('',(#20181),#14991,.T.) ;
#88502 = ADVANCED_FACE('',(#20182),#79308,.T.) ;
#88503 = ADVANCED_FACE('',(#20183),#14992,.T.) ;
#88504 = ADVANCED_FACE('',(#20184),#16617,.T.) ;
#88505 = ADVANCED_FACE('',(#20185),#14993,.T.) ;
#88506 = ADVANCED_FACE('',(#20186),#16618,.T.) ;
#88507 = ADVANCED_FACE('',(#20187),#14994,.T.) ;
#88508 = ADVANCED_FACE('',(#20188),#79309,.T.) ;
#88509 = ADVANCED_FACE('',(#20189),#79310,.T.) ;
#88510 = ADVANCED_FACE('',(#20190),#14995,.T.) ;
#88511 = ADVANCED_FACE('',(#20191),#16619,.T.) ;
#88512 = ADVANCED_FACE('',(#20192),#14996,.T.) ;
#88513 = ADVANCED_FACE('',(#20193),#16620,.T.) ;
#88514 = ADVANCED_FACE('',(#20194),#14997,.T.) ;
#88515 = ADVANCED_FACE('',(#20195),#79311,.T.) ;
#88516 = ADVANCED_FACE('',(#20196),#14998,.T.) ;
#88517 = ADVANCED_FACE('',(#20197),#16621,.T.) ;
#88518 = ADVANCED_FACE('',(#20198),#14999,.T.) ;
#88519 = ADVANCED_FACE('',(#20199),#16622,.T.) ;
#88520 = ADVANCED_FACE('',(#20200),#15000,.T.) ;
#88521 = ADVANCED_FACE('',(#20201),#15001,.T.) ;
#88522 = ADVANCED_FACE('',(#20202),#16623,.T.) ;
#88523 = ADVANCED_FACE('',(#20203),#15002,.T.) ;
#88524 = ADVANCED_FACE('',(#20204),#15003,.T.) ;
#88525 = ADVANCED_FACE('',(#20205),#16624,.T.) ;
#88526 = ADVANCED_FACE('',(#20206),#79312,.T.) ;
#88527 = ADVANCED_FACE('',(#20207),#15004,.T.) ;
#88528 = ADVANCED_FACE('',(#20208),#16625,.T.) ;
#88529 = ADVANCED_FACE('',(#20209),#15005,.T.) ;
#88530 = ADVANCED_FACE('',(#20210),#16626,.T.) ;
#88531 = ADVANCED_FACE('',(#20211),#15006,.T.) ;
#88532 = ADVANCED_FACE('',(#20212),#79313,.T.) ;
#88533 = ADVANCED_FACE('',(#20213),#79314,.T.) ;
#88534 = ADVANCED_FACE('',(#20214),#15007,.T.) ;
#88535 = ADVANCED_FACE('',(#20215),#16627,.T.) ;
#88536 = ADVANCED_FACE('',(#20216),#15008,.T.) ;
#88537 = ADVANCED_FACE('',(#20217),#16628,.T.) ;
#88538 = ADVANCED_FACE('',(#20218),#15009,.T.) ;
#88539 = ADVANCED_FACE('',(#20219),#79315,.T.) ;
#88540 = ADVANCED_FACE('',(#20220),#15010,.T.) ;
#88541 = ADVANCED_FACE('',(#20221),#16629,.T.) ;
#88542 = ADVANCED_FACE('',(#20222),#15011,.T.) ;
#88543 = ADVANCED_FACE('',(#20223),#16630,.T.) ;
#88544 = ADVANCED_FACE('',(#20224),#15012,.T.) ;
#88545 = ADVANCED_FACE('',(#20225),#15013,.T.) ;
#88546 = ADVANCED_FACE('',(#20226),#16631,.T.) ;
#88547 = ADVANCED_FACE('',(#20227),#15014,.T.) ;
#88548 = ADVANCED_FACE('',(#20228),#15015,.T.) ;
#88549 = ADVANCED_FACE('',(#20229),#16632,.T.) ;
#88550 = ADVANCED_FACE('',(#20230),#79316,.T.) ;
#88551 = ADVANCED_FACE('',(#20231),#15016,.T.) ;
#88552 = ADVANCED_FACE('',(#20232),#16633,.T.) ;
#88553 = ADVANCED_FACE('',(#20233),#15017,.T.) ;
#88554 = ADVANCED_FACE('',(#20234),#16634,.T.) ;
#88555 = ADVANCED_FACE('',(#20235),#15018,.T.) ;
#88556 = ADVANCED_FACE('',(#20236),#79317,.T.) ;
#88557 = ADVANCED_FACE('',(#20237),#79318,.T.) ;
#88558 = ADVANCED_FACE('',(#20238),#15019,.T.) ;
#88559 = ADVANCED_FACE('',(#20239),#16635,.T.) ;
#88560 = ADVANCED_FACE('',(#20240),#15020,.T.) ;
#88561 = ADVANCED_FACE('',(#20241),#16636,.T.) ;
#88562 = ADVANCED_FACE('',(#20242),#15021,.T.) ;
#88563 = ADVANCED_FACE('',(#20243),#79319,.T.) ;
#88564 = ADVANCED_FACE('',(#20244),#15022,.T.) ;
#88565 = ADVANCED_FACE('',(#20245),#16637,.T.) ;
#88566 = ADVANCED_FACE('',(#20246),#15023,.T.) ;
#88567 = ADVANCED_FACE('',(#20247),#16638,.T.) ;
#88568 = ADVANCED_FACE('',(#20248),#15024,.T.) ;
#88569 = ADVANCED_FACE('',(#20249),#15025,.T.) ;
#88570 = ADVANCED_FACE('',(#20250),#16639,.T.) ;
#88571 = ADVANCED_FACE('',(#20251),#15026,.T.) ;
#88572 = ADVANCED_FACE('',(#20252),#15027,.T.) ;
#88573 = ADVANCED_FACE('',(#20253),#16640,.T.) ;
#88574 = ADVANCED_FACE('',(#20254),#79320,.T.) ;
#88575 = ADVANCED_FACE('',(#20255),#15028,.T.) ;
#88576 = ADVANCED_FACE('',(#20256),#16641,.T.) ;
#88577 = ADVANCED_FACE('',(#20257),#15029,.T.) ;
#88578 = ADVANCED_FACE('',(#20258),#16642,.T.) ;
#88579 = ADVANCED_FACE('',(#20259),#15030,.T.) ;
#88580 = ADVANCED_FACE('',(#20260),#79321,.T.) ;
#88581 = ADVANCED_FACE('',(#20261),#79322,.T.) ;
#88582 = ADVANCED_FACE('',(#20262),#15031,.T.) ;
#88583 = ADVANCED_FACE('',(#20263),#16643,.T.) ;
#88584 = ADVANCED_FACE('',(#20264),#15032,.T.) ;
#88585 = ADVANCED_FACE('',(#20265),#16644,.T.) ;
#88586 = ADVANCED_FACE('',(#20266),#15033,.T.) ;
#88587 = ADVANCED_FACE('',(#20267),#79323,.T.) ;
#88588 = ADVANCED_FACE('',(#20268),#15034,.T.) ;
#88589 = ADVANCED_FACE('',(#20269),#16645,.T.) ;
#88590 = ADVANCED_FACE('',(#20270),#15035,.T.) ;
#88591 = ADVANCED_FACE('',(#20271),#16646,.T.) ;
#88592 = ADVANCED_FACE('',(#20272),#15036,.T.) ;
#88593 = ADVANCED_FACE('',(#20273),#15037,.T.) ;
#88594 = ADVANCED_FACE('',(#20274),#16647,.T.) ;
#88595 = ADVANCED_FACE('',(#20275),#15038,.T.) ;
#88596 = ADVANCED_FACE('',(#20276),#15039,.T.) ;
#88597 = ADVANCED_FACE('',(#20277),#16648,.T.) ;
#88598 = ADVANCED_FACE('',(#20278),#79324,.T.) ;
#88599 = ADVANCED_FACE('',(#20279),#15040,.T.) ;
#88600 = ADVANCED_FACE('',(#20280),#16649,.T.) ;
#88601 = ADVANCED_FACE('',(#20281),#15041,.T.) ;
#88602 = ADVANCED_FACE('',(#20282),#16650,.T.) ;
#88603 = ADVANCED_FACE('',(#20283),#15042,.T.) ;
#88604 = ADVANCED_FACE('',(#20284),#79325,.T.) ;
#88605 = ADVANCED_FACE('',(#20285),#79326,.T.) ;
#88606 = ADVANCED_FACE('',(#20286),#15043,.T.) ;
#88607 = ADVANCED_FACE('',(#20287),#16651,.T.) ;
#88608 = ADVANCED_FACE('',(#20288),#15044,.T.) ;
#88609 = ADVANCED_FACE('',(#20289),#16652,.T.) ;
#88610 = ADVANCED_FACE('',(#20290),#15045,.T.) ;
#88611 = ADVANCED_FACE('',(#20291),#79327,.T.) ;
#88612 = ADVANCED_FACE('',(#20292),#15046,.T.) ;
#88613 = ADVANCED_FACE('',(#20293),#16653,.T.) ;
#88614 = ADVANCED_FACE('',(#20294),#15047,.T.) ;
#88615 = ADVANCED_FACE('',(#20295),#16654,.T.) ;
#88616 = ADVANCED_FACE('',(#20296),#15048,.T.) ;
#88617 = ADVANCED_FACE('',(#20297),#15049,.T.) ;
#88618 = ADVANCED_FACE('',(#20298),#16655,.T.) ;
#88619 = ADVANCED_FACE('',(#20299),#15050,.T.) ;
#88620 = ADVANCED_FACE('',(#20300),#15051,.T.) ;
#88621 = ADVANCED_FACE('',(#20301),#16656,.T.) ;
#88622 = ADVANCED_FACE('',(#20302),#79328,.T.) ;
#88623 = ADVANCED_FACE('',(#20303),#15052,.T.) ;
#88624 = ADVANCED_FACE('',(#20304),#16657,.T.) ;
#88625 = ADVANCED_FACE('',(#20305),#15053,.T.) ;
#88626 = ADVANCED_FACE('',(#20306),#16658,.T.) ;
#88627 = ADVANCED_FACE('',(#20307),#15054,.T.) ;
#88628 = ADVANCED_FACE('',(#20308),#79329,.T.) ;
#88629 = ADVANCED_FACE('',(#20309),#79330,.T.) ;
#88630 = ADVANCED_FACE('',(#20310),#15055,.T.) ;
#88631 = ADVANCED_FACE('',(#20311),#16659,.T.) ;
#88632 = ADVANCED_FACE('',(#20312),#15056,.T.) ;
#88633 = ADVANCED_FACE('',(#20313),#16660,.T.) ;
#88634 = ADVANCED_FACE('',(#20314),#15057,.T.) ;
#88635 = ADVANCED_FACE('',(#20315),#79331,.T.) ;
#88636 = ADVANCED_FACE('',(#20316),#15058,.T.) ;
#88637 = ADVANCED_FACE('',(#20317),#16661,.T.) ;
#88638 = ADVANCED_FACE('',(#20318),#15059,.T.) ;
#88639 = ADVANCED_FACE('',(#20319),#16662,.T.) ;
#88640 = ADVANCED_FACE('',(#20320),#15060,.T.) ;
#88641 = ADVANCED_FACE('',(#20321),#15061,.T.) ;
#88642 = ADVANCED_FACE('',(#20322),#16663,.T.) ;
#88643 = ADVANCED_FACE('',(#20323),#15062,.T.) ;
#88644 = ADVANCED_FACE('',(#20324),#15063,.T.) ;
#88645 = ADVANCED_FACE('',(#20325),#16664,.T.) ;
#88646 = ADVANCED_FACE('',(#20326),#79332,.T.) ;
#88647 = ADVANCED_FACE('',(#20327),#15064,.T.) ;
#88648 = ADVANCED_FACE('',(#20328),#16665,.T.) ;
#88649 = ADVANCED_FACE('',(#20329),#15065,.T.) ;
#88650 = ADVANCED_FACE('',(#20330),#16666,.T.) ;
#88651 = ADVANCED_FACE('',(#20331),#15066,.T.) ;
#88652 = ADVANCED_FACE('',(#20332),#79333,.T.) ;
#88653 = ADVANCED_FACE('',(#20333),#79334,.T.) ;
#88654 = ADVANCED_FACE('',(#20334),#15067,.T.) ;
#88655 = ADVANCED_FACE('',(#20335),#16667,.T.) ;
#88656 = ADVANCED_FACE('',(#20336),#15068,.T.) ;
#88657 = ADVANCED_FACE('',(#20337),#16668,.T.) ;
#88658 = ADVANCED_FACE('',(#20338),#15069,.T.) ;
#88659 = ADVANCED_FACE('',(#20339),#79335,.T.) ;
#88660 = ADVANCED_FACE('',(#20340),#15070,.T.) ;
#88661 = ADVANCED_FACE('',(#20341),#16669,.T.) ;
#88662 = ADVANCED_FACE('',(#20342),#15071,.T.) ;
#88663 = ADVANCED_FACE('',(#20343),#16670,.T.) ;
#88664 = ADVANCED_FACE('',(#20344),#15072,.T.) ;
#88665 = ADVANCED_FACE('',(#20345),#15073,.T.) ;
#88666 = ADVANCED_FACE('',(#20346),#16671,.T.) ;
#88667 = ADVANCED_FACE('',(#20347),#15074,.T.) ;
#88668 = ADVANCED_FACE('',(#20348),#15075,.T.) ;
#88669 = ADVANCED_FACE('',(#20349),#16672,.T.) ;
#88670 = ADVANCED_FACE('',(#20350),#79336,.T.) ;
#88671 = ADVANCED_FACE('',(#20351),#15076,.T.) ;
#88672 = ADVANCED_FACE('',(#20352),#16673,.T.) ;
#88673 = ADVANCED_FACE('',(#20353),#15077,.T.) ;
#88674 = ADVANCED_FACE('',(#20354),#16674,.T.) ;
#88675 = ADVANCED_FACE('',(#20355),#15078,.T.) ;
#88676 = ADVANCED_FACE('',(#20356),#79337,.T.) ;
#88677 = ADVANCED_FACE('',(#20357),#79338,.T.) ;
#88678 = ADVANCED_FACE('',(#20358),#15079,.T.) ;
#88679 = ADVANCED_FACE('',(#20359),#16675,.T.) ;
#88680 = ADVANCED_FACE('',(#20360),#15080,.T.) ;
#88681 = ADVANCED_FACE('',(#20361),#16676,.T.) ;
#88682 = ADVANCED_FACE('',(#20362),#15081,.T.) ;
#88683 = ADVANCED_FACE('',(#20363),#79339,.T.) ;
#88684 = ADVANCED_FACE('',(#20364),#15082,.T.) ;
#88685 = ADVANCED_FACE('',(#20365),#16677,.T.) ;
#88686 = ADVANCED_FACE('',(#20366),#15083,.T.) ;
#88687 = ADVANCED_FACE('',(#20367),#16678,.T.) ;
#88688 = ADVANCED_FACE('',(#20368),#15084,.T.) ;
#88689 = ADVANCED_FACE('',(#20369),#15085,.T.) ;
#88690 = ADVANCED_FACE('',(#20370),#16679,.T.) ;
#88691 = ADVANCED_FACE('',(#20371),#15086,.T.) ;
#88692 = ADVANCED_FACE('',(#20372),#15087,.T.) ;
#88693 = ADVANCED_FACE('',(#20373),#16680,.T.) ;
#88694 = ADVANCED_FACE('',(#20374),#79340,.T.) ;
#88695 = ADVANCED_FACE('',(#20375),#15088,.T.) ;
#88696 = ADVANCED_FACE('',(#20376),#16681,.T.) ;
#88697 = ADVANCED_FACE('',(#20377),#15089,.T.) ;
#88698 = ADVANCED_FACE('',(#20378),#16682,.T.) ;
#88699 = ADVANCED_FACE('',(#20379),#15090,.T.) ;
#88700 = ADVANCED_FACE('',(#20380),#79341,.T.) ;
#88701 = ADVANCED_FACE('',(#20381),#79342,.T.) ;
#88702 = ADVANCED_FACE('',(#20382),#15091,.T.) ;
#88703 = ADVANCED_FACE('',(#20383),#16683,.T.) ;
#88704 = ADVANCED_FACE('',(#20384),#15092,.T.) ;
#88705 = ADVANCED_FACE('',(#20385),#16684,.T.) ;
#88706 = ADVANCED_FACE('',(#20386),#15093,.T.) ;
#88707 = ADVANCED_FACE('',(#20387),#79343,.T.) ;
#88708 = ADVANCED_FACE('',(#20388),#15094,.T.) ;
#88709 = ADVANCED_FACE('',(#20389),#16685,.T.) ;
#88710 = ADVANCED_FACE('',(#20390),#15095,.T.) ;
#88711 = ADVANCED_FACE('',(#20391),#16686,.T.) ;
#88712 = ADVANCED_FACE('',(#20392),#15096,.T.) ;
#88713 = ADVANCED_FACE('',(#20393),#15097,.T.) ;
#88714 = ADVANCED_FACE('',(#20394),#16687,.T.) ;
#88715 = ADVANCED_FACE('',(#20395),#15098,.T.) ;
#88716 = ADVANCED_FACE('',(#20396),#15099,.T.) ;
#88717 = ADVANCED_FACE('',(#20397),#16688,.T.) ;
#88718 = ADVANCED_FACE('',(#20398),#15100,.F.) ;
#88719 = ADVANCED_FACE('',(#20399),#79344,.T.) ;
#88720 = ADVANCED_FACE('',(#20400),#79345,.T.) ;
#88721 = ADVANCED_FACE('',(#20401),#79346,.F.) ;
#88722 = ADVANCED_FACE('',(#20402),#79347,.T.) ;
#88723 = ADVANCED_FACE('',(#20403),#79348,.F.) ;
#88724 = ADVANCED_FACE('',(#20404),#79349,.T.) ;
#88725 = ADVANCED_FACE('',(#20405),#79350,.F.) ;
#88726 = ADVANCED_FACE('',(#20406),#79351,.T.) ;
#88727 = ADVANCED_FACE('',(#20407),#79352,.F.) ;
#88728 = ADVANCED_FACE('',(#20408),#79353,.T.) ;
#88729 = ADVANCED_FACE('',(#20409),#79354,.F.) ;
#88730 = ADVANCED_FACE('',(#20410),#79355,.T.) ;
#88731 = ADVANCED_FACE('',(#20411),#79356,.F.) ;
#88732 = ADVANCED_FACE('',(#20412),#79357,.T.) ;
#88733 = ADVANCED_FACE('',(#20413),#79358,.F.) ;
#88734 = ADVANCED_FACE('',(#20414),#79359,.T.) ;
#88735 = ADVANCED_FACE('',(#20415),#79360,.F.) ;
#88736 = ADVANCED_FACE('',(#20416),#79361,.T.) ;
#88737 = ADVANCED_FACE('',(#20417),#79362,.F.) ;
#88738 = ADVANCED_FACE('',(#20418),#79363,.T.) ;
#88739 = ADVANCED_FACE('',(#20419),#79364,.F.) ;
#88740 = ADVANCED_FACE('',(#20420),#15101,.F.) ;
#88741 = ADVANCED_FACE('',(#20421),#15102,.F.) ;
#88742 = ADVANCED_FACE('',(#20422),#15103,.F.) ;
#88743 = ADVANCED_FACE('',(#20423),#15104,.F.) ;
#88744 = ADVANCED_FACE('',(#20424),#15105,.F.) ;
#88745 = ADVANCED_FACE('',(#20425),#15106,.F.) ;
#88746 = ADVANCED_FACE('',(#20426),#15107,.F.) ;
#88747 = ADVANCED_FACE('',(#20427),#79365,.F.) ;
#88748 = ADVANCED_FACE('',(#20428),#79366,.T.) ;
#88749 = ADVANCED_FACE('',(#20429),#79367,.T.) ;
#88750 = ADVANCED_FACE('',(#20430),#79368,.F.) ;
#88751 = ADVANCED_FACE('',(#20431),#79369,.T.) ;
#88752 = ADVANCED_FACE('',(#20432),#79370,.T.) ;
#88753 = ADVANCED_FACE('',(#20433),#79371,.F.) ;
#88754 = ADVANCED_FACE('',(#20434),#79372,.T.) ;
#88755 = ADVANCED_FACE('',(#20435),#79373,.T.) ;
#88756 = ADVANCED_FACE('',(#20436),#79374,.F.) ;
#88757 = ADVANCED_FACE('',(#20437),#79375,.T.) ;
#88758 = ADVANCED_FACE('',(#20438),#79376,.T.) ;
#88759 = ADVANCED_FACE('',(#20439),#79377,.F.) ;
#88760 = ADVANCED_FACE('',(#20440),#79378,.T.) ;
#88761 = ADVANCED_FACE('',(#20441),#79379,.T.) ;
#88762 = ADVANCED_FACE('',(#20442),#79380,.F.) ;
#88763 = ADVANCED_FACE('',(#20443),#79381,.T.) ;
#88764 = ADVANCED_FACE('',(#20444),#79382,.T.) ;
#88765 = ADVANCED_FACE('',(#20445),#79383,.F.) ;
#88766 = ADVANCED_FACE('',(#20446),#79384,.T.) ;
#88767 = ADVANCED_FACE('',(#20447),#79385,.T.) ;
#88768 = ADVANCED_FACE('',(#20448),#79386,.F.) ;
#88769 = ADVANCED_FACE('',(#20449),#79387,.T.) ;
#88770 = ADVANCED_FACE('',(#20450),#79388,.T.) ;
#88771 = ADVANCED_FACE('',(#20451),#79389,.F.) ;
#88772 = ADVANCED_FACE('',(#20452),#79390,.T.) ;
#88773 = ADVANCED_FACE('',(#20453),#79391,.T.) ;
#88774 = ADVANCED_FACE('',(#20454),#15108,.F.) ;
#88775 = ADVANCED_FACE('',(#20455),#15109,.F.) ;
#88776 = ADVANCED_FACE('',(#20456),#15110,.F.) ;
#88777 = ADVANCED_FACE('',(#20457),#15111,.F.) ;
#88778 = ADVANCED_FACE('',(#20458),#15112,.F.) ;
#88779 = ADVANCED_FACE('',(#20459),#15113,.F.) ;
#88780 = ADVANCED_FACE('',(#20460),#15114,.F.) ;
#88781 = ADVANCED_FACE('',(#20461),#15115,.F.) ;
#88782 = ADVANCED_FACE('',(#20462),#15116,.F.) ;
#88783 = ADVANCED_FACE('',(#20463),#2420,.F.) ;
#88784 = ADVANCED_FACE('',(#20464),#2421,.F.) ;
#88785 = ADVANCED_FACE('',(#20465),#2422,.F.) ;
#88786 = ADVANCED_FACE('',(#20466),#2423,.F.) ;
#88787 = ADVANCED_FACE('',(#20467),#2424,.F.) ;
#88788 = ADVANCED_FACE('',(#20468),#2425,.F.) ;
#88789 = ADVANCED_FACE('',(#20469),#2426,.F.) ;
#88790 = ADVANCED_FACE('',(#20470),#2427,.F.) ;
#88791 = ADVANCED_FACE('',(#20471),#2428,.F.) ;
#88792 = ADVANCED_FACE('',(#20472),#15117,.F.) ;
#88793 = ADVANCED_FACE('',(#20473),#15118,.F.) ;
#88794 = ADVANCED_FACE('',(#20474),#15119,.F.) ;
#88795 = ADVANCED_FACE('',(#20475),#15120,.F.) ;
#88796 = ADVANCED_FACE('',(#20476),#15121,.F.) ;
#88797 = ADVANCED_FACE('',(#20477),#15122,.F.) ;
#88798 = ADVANCED_FACE('',(#20478),#15123,.F.) ;
#88799 = ADVANCED_FACE('',(#20479),#15124,.F.) ;
#88800 = ADVANCED_FACE('',(#20480),#15125,.F.) ;
#88801 = ADVANCED_FACE('',(#20481),#79392,.F.) ;
#88802 = ADVANCED_FACE('',(#20482),#79393,.T.) ;
#88803 = ADVANCED_FACE('',(#20483),#79394,.T.) ;
#88804 = ADVANCED_FACE('',(#20484),#15126,.F.) ;
#88805 = ADVANCED_FACE('',(#20485),#15127,.F.) ;
#88806 = ADVANCED_FACE('',(#20486),#15128,.F.) ;
#88807 = ADVANCED_FACE('',(#20487),#15129,.F.) ;
#88808 = ADVANCED_FACE('',(#20488),#15130,.F.) ;
#88809 = ADVANCED_FACE('',(#20489),#2429,.F.) ;
#88810 = ADVANCED_FACE('',(#20490),#15131,.F.) ;
#88811 = ADVANCED_FACE('',(#20491,#714,#715,#716,#717,#718,#719,#720,#721,
#722,#723,#724,#725,#726,#727,#728,#729,#730,#731,#732,#733),#1513,.T.) ;
#88812 = ADVANCED_FACE('',(#20492,#734),#1514,.F.) ;
#88813 = ADVANCED_FACE('',(#20493,#735),#1515,.F.) ;
#88814 = ADVANCED_FACE('',(#20494,#736),#1516,.F.) ;
#88815 = ADVANCED_FACE('',(#20495,#737),#1517,.F.) ;
#88816 = ADVANCED_FACE('',(#20496,#738),#1518,.F.) ;
#88817 = ADVANCED_FACE('',(#20497,#739),#1519,.F.) ;
#88818 = ADVANCED_FACE('',(#20498,#740),#1520,.F.) ;
#88819 = ADVANCED_FACE('',(#20499,#741),#1521,.F.) ;
#88820 = ADVANCED_FACE('',(#20500,#742),#1522,.F.) ;
#88821 = ADVANCED_FACE('',(#20501),#1523,.T.) ;
#88822 = ADVANCED_FACE('',(#20502),#1524,.T.) ;
#88823 = ADVANCED_FACE('',(#20503),#1525,.T.) ;
#88824 = ADVANCED_FACE('',(#20504),#1526,.T.) ;
#88825 = ADVANCED_FACE('',(#20505),#1527,.T.) ;
#88826 = ADVANCED_FACE('',(#20506),#1528,.T.) ;
#88827 = ADVANCED_FACE('',(#20507),#1529,.T.) ;
#88828 = ADVANCED_FACE('',(#20508),#1530,.T.) ;
#88829 = ADVANCED_FACE('',(#20509),#1531,.T.) ;
#88830 = ADVANCED_FACE('',(#20510),#1532,.T.) ;
#88831 = ADVANCED_FACE('',(#20511),#1533,.T.) ;
#88832 = ADVANCED_FACE('',(#20512),#1534,.T.) ;
#88833 = ADVANCED_FACE('',(#20513),#1535,.T.) ;
#88834 = ADVANCED_FACE('',(#20514),#1536,.T.) ;
#88835 = ADVANCED_FACE('',(#20515),#1537,.T.) ;
#88836 = ADVANCED_FACE('',(#20516),#1538,.T.) ;
#88837 = ADVANCED_FACE('',(#20517),#1539,.T.) ;
#88838 = ADVANCED_FACE('',(#20518),#1540,.T.) ;
#88839 = ADVANCED_FACE('',(#20519),#1541,.T.) ;
#88840 = ADVANCED_FACE('',(#20520),#1542,.T.) ;
#88841 = ADVANCED_FACE('',(#20521),#1543,.T.) ;
#88842 = ADVANCED_FACE('',(#20522),#15132,.T.) ;
#88843 = ADVANCED_FACE('',(#20523),#15133,.T.) ;
#88844 = ADVANCED_FACE('',(#20524,#743,#744,#745,#746,#747,#748,#749,#750,
#751,#752),#1544,.T.) ;
#88845 = ADVANCED_FACE('',(#20525,#753),#1545,.F.) ;
#88846 = ADVANCED_FACE('',(#20526),#1546,.T.) ;
#88847 = ADVANCED_FACE('',(#20527),#1547,.T.) ;
#88848 = ADVANCED_FACE('',(#20528),#1548,.T.) ;
#88849 = ADVANCED_FACE('',(#20529),#1549,.T.) ;
#88850 = ADVANCED_FACE('',(#20530),#1550,.T.) ;
#88851 = ADVANCED_FACE('',(#20531),#1551,.T.) ;
#88852 = ADVANCED_FACE('',(#20532,#754,#755,#756,#757,#758,#759,#760,#761,
#762,#763),#1552,.T.) ;
#88853 = ADVANCED_FACE('',(#20533),#1553,.T.) ;
#88854 = ADVANCED_FACE('',(#20534),#1554,.F.) ;
#88855 = ADVANCED_FACE('',(#20535),#1555,.F.) ;
#88856 = ADVANCED_FACE('',(#20536),#1556,.F.) ;
#88857 = ADVANCED_FACE('',(#20537),#1557,.F.) ;
#88858 = ADVANCED_FACE('',(#20538),#1558,.F.) ;
#88859 = ADVANCED_FACE('',(#20539),#1559,.F.) ;
#88860 = ADVANCED_FACE('',(#20540),#1560,.F.) ;
#88861 = ADVANCED_FACE('',(#20541),#1561,.T.) ;
#88862 = ADVANCED_FACE('',(#20542),#1562,.F.) ;
#88863 = ADVANCED_FACE('',(#20543),#1563,.F.) ;
#88864 = ADVANCED_FACE('',(#20544),#1564,.F.) ;
#88865 = ADVANCED_FACE('',(#20545),#1565,.F.) ;
#88866 = ADVANCED_FACE('',(#20546,#764),#1566,.T.) ;
#88867 = ADVANCED_FACE('',(#20547),#1567,.T.) ;
#88868 = ADVANCED_FACE('',(#20548),#1568,.T.) ;
#88869 = ADVANCED_FACE('',(#20549),#1569,.T.) ;
#88870 = ADVANCED_FACE('',(#20550),#1570,.T.) ;
#88871 = ADVANCED_FACE('',(#20551),#1571,.T.) ;
#88872 = ADVANCED_FACE('',(#20552),#1572,.F.) ;
#88873 = ADVANCED_FACE('',(#20553),#1573,.F.) ;
#88874 = ADVANCED_FACE('',(#20554),#1574,.F.) ;
#88875 = ADVANCED_FACE('',(#20555),#1575,.F.) ;
#88876 = ADVANCED_FACE('',(#20556),#1576,.F.) ;
#88877 = ADVANCED_FACE('',(#20557),#1577,.F.) ;
#88878 = ADVANCED_FACE('',(#20558),#1578,.F.) ;
#88879 = ADVANCED_FACE('',(#20559),#1579,.F.) ;
#88880 = ADVANCED_FACE('',(#20560),#15134,.F.) ;
#88881 = ADVANCED_FACE('',(#20561,#765),#1580,.T.) ;
#88882 = ADVANCED_FACE('',(#20562),#1581,.T.) ;
#88883 = ADVANCED_FACE('',(#20563),#1582,.F.) ;
#88884 = ADVANCED_FACE('',(#20564),#1583,.F.) ;
#88885 = ADVANCED_FACE('',(#20565),#1584,.F.) ;
#88886 = ADVANCED_FACE('',(#20566),#1585,.F.) ;
#88887 = ADVANCED_FACE('',(#20567,#766),#1586,.T.) ;
#88888 = ADVANCED_FACE('',(#20568),#1587,.T.) ;
#88889 = ADVANCED_FACE('',(#20569),#1588,.T.) ;
#88890 = ADVANCED_FACE('',(#20570),#1589,.T.) ;
#88891 = ADVANCED_FACE('',(#20571),#1590,.T.) ;
#88892 = ADVANCED_FACE('',(#20572),#1591,.T.) ;
#88893 = ADVANCED_FACE('',(#20573),#1592,.T.) ;
#88894 = ADVANCED_FACE('',(#20574),#1593,.F.) ;
#88895 = ADVANCED_FACE('',(#20575),#1594,.F.) ;
#88896 = ADVANCED_FACE('',(#20576),#1595,.T.) ;
#88897 = ADVANCED_FACE('',(#20577),#15135,.T.) ;
#88898 = ADVANCED_FACE('',(#20578),#15136,.T.) ;
#88899 = ADVANCED_FACE('',(#20579),#1596,.F.) ;
#88900 = ADVANCED_FACE('',(#20580),#1597,.F.) ;
#88901 = ADVANCED_FACE('',(#20581),#15137,.T.) ;
#88902 = ADVANCED_FACE('',(#20582),#15138,.T.) ;
#88903 = ADVANCED_FACE('',(#20583),#15139,.T.) ;
#88904 = ADVANCED_FACE('',(#20584),#1598,.F.) ;
#88905 = ADVANCED_FACE('',(#20585),#15140,.T.) ;
#88906 = ADVANCED_FACE('',(#20586),#1599,.F.) ;
#88907 = ADVANCED_FACE('',(#20587),#15141,.T.) ;
#88908 = ADVANCED_FACE('',(#20588),#1600,.F.) ;
#88909 = ADVANCED_FACE('',(#20589),#15142,.T.) ;
#88910 = ADVANCED_FACE('',(#20590),#1601,.F.) ;
#88911 = ADVANCED_FACE('',(#20591),#1602,.F.) ;
#88912 = ADVANCED_FACE('',(#20592),#15143,.T.) ;
#88913 = ADVANCED_FACE('',(#20593),#16689,.T.) ;
#88914 = ADVANCED_FACE('',(#20594),#15144,.T.) ;
#88915 = ADVANCED_FACE('',(#20595),#15145,.T.) ;
#88916 = ADVANCED_FACE('',(#20596),#15146,.T.) ;
#88917 = ADVANCED_FACE('',(#20597),#15147,.T.) ;
#88918 = ADVANCED_FACE('',(#20598),#15148,.T.) ;
#88919 = ADVANCED_FACE('',(#20599),#15149,.T.) ;
#88920 = ADVANCED_FACE('',(#20600),#16690,.T.) ;
#88921 = ADVANCED_FACE('',(#20601),#16691,.T.) ;
#88922 = ADVANCED_FACE('',(#20602),#15150,.T.) ;
#88923 = ADVANCED_FACE('',(#20603),#16692,.T.) ;
#88924 = ADVANCED_FACE('',(#20604),#15151,.T.) ;
#88925 = ADVANCED_FACE('',(#20605),#15152,.T.) ;
#88926 = ADVANCED_FACE('',(#20606),#15153,.T.) ;
#88927 = ADVANCED_FACE('',(#20607),#15154,.T.) ;
#88928 = ADVANCED_FACE('',(#20608),#15155,.T.) ;
#88929 = ADVANCED_FACE('',(#20609),#15156,.T.) ;
#88930 = ADVANCED_FACE('',(#20610),#79395,.T.) ;
#88931 = ADVANCED_FACE('',(#20611),#16693,.T.) ;
#88932 = ADVANCED_FACE('',(#20612),#16694,.T.) ;
#88933 = ADVANCED_FACE('',(#20613),#15157,.F.) ;
#88934 = ADVANCED_FACE('',(#20614),#15158,.T.) ;
#88935 = ADVANCED_FACE('',(#20615),#15159,.T.) ;
#88936 = ADVANCED_FACE('',(#20616),#79396,.T.) ;
#88937 = ADVANCED_FACE('',(#20617),#15160,.T.) ;
#88938 = ADVANCED_FACE('',(#20618),#16695,.T.) ;
#88939 = ADVANCED_FACE('',(#20619),#79397,.T.) ;
#88940 = ADVANCED_FACE('',(#20620),#15161,.T.) ;
#88941 = ADVANCED_FACE('',(#20621),#15162,.T.) ;
#88942 = ADVANCED_FACE('',(#20622),#15163,.T.) ;
#88943 = ADVANCED_FACE('',(#20623),#15164,.T.) ;
#88944 = ADVANCED_FACE('',(#20624),#16696,.T.) ;
#88945 = ADVANCED_FACE('',(#20625),#79398,.F.) ;
#88946 = ADVANCED_FACE('',(#20626),#16697,.T.) ;
#88947 = ADVANCED_FACE('',(#20627),#15165,.T.) ;
#88948 = ADVANCED_FACE('',(#20628),#15166,.T.) ;
#88949 = ADVANCED_FACE('',(#20629),#15167,.T.) ;
#88950 = ADVANCED_FACE('',(#20630),#79399,.F.) ;
#88951 = ADVANCED_FACE('',(#20631),#15168,.F.) ;
#88952 = ADVANCED_FACE('',(#20632),#15169,.T.) ;
#88953 = ADVANCED_FACE('',(#20633),#16698,.T.) ;
#88954 = ADVANCED_FACE('',(#20634),#79400,.F.) ;
#88955 = ADVANCED_FACE('',(#20635),#79401,.T.) ;
#88956 = ADVANCED_FACE('',(#20636),#15170,.T.) ;
#88957 = ADVANCED_FACE('',(#20637),#15171,.F.) ;
#88958 = ADVANCED_FACE('',(#20638),#15172,.T.) ;
#88959 = ADVANCED_FACE('',(#20639),#15173,.F.) ;
#88960 = ADVANCED_FACE('',(#20640),#15174,.F.) ;
#88961 = ADVANCED_FACE('',(#20641),#79402,.T.) ;
#88962 = ADVANCED_FACE('',(#20642),#16699,.T.) ;
#88963 = ADVANCED_FACE('',(#20643),#16700,.F.) ;
#88964 = ADVANCED_FACE('',(#20644),#15175,.T.) ;
#88965 = ADVANCED_FACE('',(#20645),#15176,.T.) ;
#88966 = ADVANCED_FACE('',(#20646),#15177,.T.) ;
#88967 = ADVANCED_FACE('',(#20647),#15178,.F.) ;
#88968 = ADVANCED_FACE('',(#20648),#16701,.T.) ;
#88969 = ADVANCED_FACE('',(#20649),#79403,.F.) ;
#88970 = ADVANCED_FACE('',(#20650),#15179,.F.) ;
#88971 = ADVANCED_FACE('',(#20651),#15180,.F.) ;
#88972 = ADVANCED_FACE('',(#20652),#15181,.T.) ;
#88973 = ADVANCED_FACE('',(#20653),#15182,.F.) ;
#88974 = ADVANCED_FACE('',(#20654),#16702,.F.) ;
#88975 = ADVANCED_FACE('',(#20655),#79404,.F.) ;
#88976 = ADVANCED_FACE('',(#20656),#15183,.F.) ;
#88977 = ADVANCED_FACE('',(#20657),#79405,.F.) ;
#88978 = ADVANCED_FACE('',(#20658),#15184,.F.) ;
#88979 = ADVANCED_FACE('',(#20659),#15185,.F.) ;
#88980 = ADVANCED_FACE('',(#20660),#79406,.F.) ;
#88981 = ADVANCED_FACE('',(#20661),#79407,.F.) ;
#88982 = ADVANCED_FACE('',(#20662),#15186,.F.) ;
#88983 = ADVANCED_FACE('',(#20663),#15187,.F.) ;
#88984 = ADVANCED_FACE('',(#20664),#79408,.F.) ;
#88985 = ADVANCED_FACE('',(#20665),#15188,.T.) ;
#88986 = ADVANCED_FACE('',(#20666),#79409,.T.) ;
#88987 = ADVANCED_FACE('',(#20667),#79410,.T.) ;
#88988 = ADVANCED_FACE('',(#20668),#15189,.T.) ;
#88989 = ADVANCED_FACE('',(#20669),#15190,.F.) ;
#88990 = ADVANCED_FACE('',(#20670),#15191,.F.) ;
#88991 = ADVANCED_FACE('',(#20671),#15192,.F.) ;
#88992 = ADVANCED_FACE('',(#20672),#15193,.T.) ;
#88993 = ADVANCED_FACE('',(#20673),#15194,.T.) ;
#88994 = ADVANCED_FACE('',(#20674),#79411,.T.) ;
#88995 = ADVANCED_FACE('',(#20675),#16703,.F.) ;
#88996 = ADVANCED_FACE('',(#20676),#16704,.F.) ;
#88997 = ADVANCED_FACE('',(#20677),#79412,.T.) ;
#88998 = ADVANCED_FACE('',(#20678),#15195,.F.) ;
#88999 = ADVANCED_FACE('',(#20679),#15196,.F.) ;
#89000 = ADVANCED_FACE('',(#20680),#15197,.F.) ;
#89001 = ADVANCED_FACE('',(#20681),#15198,.F.) ;
#89002 = ADVANCED_FACE('',(#20682),#16705,.F.) ;
#89003 = ADVANCED_FACE('',(#20683),#16706,.F.) ;
#89004 = ADVANCED_FACE('',(#20684),#15199,.F.) ;
#89005 = ADVANCED_FACE('',(#20685),#15200,.T.) ;
#89006 = ADVANCED_FACE('',(#20686),#15201,.T.) ;
#89007 = ADVANCED_FACE('',(#20687),#15202,.T.) ;
#89008 = ADVANCED_FACE('',(#20688),#16707,.T.) ;
#89009 = ADVANCED_FACE('',(#20689),#16708,.T.) ;
#89010 = ADVANCED_FACE('',(#20690),#15203,.T.) ;
#89011 = ADVANCED_FACE('',(#20691),#15204,.T.) ;
#89012 = ADVANCED_FACE('',(#20692),#15205,.T.) ;
#89013 = ADVANCED_FACE('',(#20693),#15206,.T.) ;
#89014 = ADVANCED_FACE('',(#20694),#16709,.T.) ;
#89015 = ADVANCED_FACE('',(#20695),#16710,.T.) ;
#89016 = ADVANCED_FACE('',(#20696),#15207,.T.) ;
#89017 = ADVANCED_FACE('',(#20697),#15208,.F.) ;
#89018 = ADVANCED_FACE('',(#20698),#16711,.F.) ;
#89019 = ADVANCED_FACE('',(#20699),#15209,.F.) ;
#89020 = ADVANCED_FACE('',(#20700),#15210,.F.) ;
#89021 = ADVANCED_FACE('',(#20701),#15211,.F.) ;
#89022 = ADVANCED_FACE('',(#20702),#128,.T.) ;
#89023 = ADVANCED_FACE('',(#20703),#16712,.F.) ;
#89024 = ADVANCED_FACE('',(#20704),#15212,.F.) ;
#89025 = ADVANCED_FACE('',(#20705),#15213,.F.) ;
#89026 = ADVANCED_FACE('',(#20706),#15214,.T.) ;
#89027 = ADVANCED_FACE('',(#20707),#15215,.T.) ;
#89028 = ADVANCED_FACE('',(#20708),#15216,.F.) ;
#89029 = ADVANCED_FACE('',(#20709),#16713,.F.) ;
#89030 = ADVANCED_FACE('',(#20710),#129,.T.) ;
#89031 = ADVANCED_FACE('',(#20711),#130,.T.) ;
#89032 = ADVANCED_FACE('',(#20712),#15217,.F.) ;
#89033 = ADVANCED_FACE('',(#20713),#15218,.F.) ;
#89034 = ADVANCED_FACE('',(#20714),#15219,.T.) ;
#89035 = ADVANCED_FACE('',(#20715),#15220,.T.) ;
#89036 = ADVANCED_FACE('',(#20716),#16714,.F.) ;
#89037 = ADVANCED_FACE('',(#20717),#131,.T.) ;
#89038 = ADVANCED_FACE('',(#20718),#15221,.F.) ;
#89039 = ADVANCED_FACE('',(#20719),#15222,.T.) ;
#89040 = ADVANCED_FACE('',(#20720),#79413,.T.) ;
#89041 = ADVANCED_FACE('',(#20721),#79414,.T.) ;
#89042 = ADVANCED_FACE('',(#20722),#15223,.T.) ;
#89043 = ADVANCED_FACE('',(#20723),#15224,.F.) ;
#89044 = ADVANCED_FACE('',(#20724),#15225,.F.) ;
#89045 = ADVANCED_FACE('',(#20725),#15226,.F.) ;
#89046 = ADVANCED_FACE('',(#20726),#15227,.T.) ;
#89047 = ADVANCED_FACE('',(#20727),#15228,.T.) ;
#89048 = ADVANCED_FACE('',(#20728),#79415,.T.) ;
#89049 = ADVANCED_FACE('',(#20729),#16715,.F.) ;
#89050 = ADVANCED_FACE('',(#20730),#16716,.F.) ;
#89051 = ADVANCED_FACE('',(#20731),#79416,.T.) ;
#89052 = ADVANCED_FACE('',(#20732),#15229,.F.) ;
#89053 = ADVANCED_FACE('',(#20733),#15230,.F.) ;
#89054 = ADVANCED_FACE('',(#20734),#15231,.F.) ;
#89055 = ADVANCED_FACE('',(#20735),#15232,.F.) ;
#89056 = ADVANCED_FACE('',(#20736),#16717,.F.) ;
#89057 = ADVANCED_FACE('',(#20737),#16718,.F.) ;
#89058 = ADVANCED_FACE('',(#20738),#15233,.F.) ;
#89059 = ADVANCED_FACE('',(#20739),#15234,.T.) ;
#89060 = ADVANCED_FACE('',(#20740),#15235,.T.) ;
#89061 = ADVANCED_FACE('',(#20741),#15236,.T.) ;
#89062 = ADVANCED_FACE('',(#20742),#16719,.T.) ;
#89063 = ADVANCED_FACE('',(#20743),#16720,.T.) ;
#89064 = ADVANCED_FACE('',(#20744),#15237,.T.) ;
#89065 = ADVANCED_FACE('',(#20745),#15238,.T.) ;
#89066 = ADVANCED_FACE('',(#20746),#15239,.T.) ;
#89067 = ADVANCED_FACE('',(#20747),#15240,.T.) ;
#89068 = ADVANCED_FACE('',(#20748),#16721,.T.) ;
#89069 = ADVANCED_FACE('',(#20749),#16722,.T.) ;
#89070 = ADVANCED_FACE('',(#20750),#15241,.T.) ;
#89071 = ADVANCED_FACE('',(#20751),#15242,.T.) ;
#89072 = ADVANCED_FACE('',(#20752),#16723,.T.) ;
#89073 = ADVANCED_FACE('',(#20753),#16724,.T.) ;
#89074 = ADVANCED_FACE('',(#20754),#15243,.T.) ;
#89075 = ADVANCED_FACE('',(#20755),#15244,.T.) ;
#89076 = ADVANCED_FACE('',(#20756),#16725,.T.) ;
#89077 = ADVANCED_FACE('',(#20757),#16726,.T.) ;
#89078 = ADVANCED_FACE('',(#20758),#15245,.T.) ;
#89079 = ADVANCED_FACE('',(#20759),#15246,.T.) ;
#89080 = ADVANCED_FACE('',(#20760),#15247,.F.) ;
#89081 = ADVANCED_FACE('',(#20761),#15248,.F.) ;
#89082 = ADVANCED_FACE('',(#20762),#15249,.T.) ;
#89083 = ADVANCED_FACE('',(#20763),#15250,.F.) ;
#89084 = ADVANCED_FACE('',(#20764),#79417,.T.) ;
#89085 = ADVANCED_FACE('',(#20765),#15251,.T.) ;
#89086 = ADVANCED_FACE('',(#20766),#79418,.T.) ;
#89087 = ADVANCED_FACE('',(#20767),#79419,.T.) ;
#89088 = ADVANCED_FACE('',(#20768),#15252,.T.) ;
#89089 = ADVANCED_FACE('',(#20769),#16727,.T.) ;
#89090 = ADVANCED_FACE('',(#20770),#79420,.T.) ;
#89091 = ADVANCED_FACE('',(#20771),#15253,.T.) ;
#89092 = ADVANCED_FACE('',(#20772),#16728,.T.) ;
#89093 = ADVANCED_FACE('',(#20773),#79421,.F.) ;
#89094 = ADVANCED_FACE('',(#20774),#132,.F.) ;
#89095 = ADVANCED_FACE('',(#20775),#79422,.F.) ;
#89096 = ADVANCED_FACE('',(#20776),#79423,.F.) ;
#89097 = ADVANCED_FACE('',(#20777),#133,.F.) ;
#89098 = ADVANCED_FACE('',(#20778),#79424,.F.) ;
#89099 = ADVANCED_FACE('',(#20779),#1603,.F.) ;
#89100 = ADVANCED_FACE('',(#20780),#1604,.F.) ;
#89101 = ADVANCED_FACE('',(#20781),#1605,.F.) ;
#89102 = ADVANCED_FACE('',(#20782),#1606,.F.) ;
#89103 = ADVANCED_FACE('',(#20783),#1607,.F.) ;
#89104 = ADVANCED_FACE('',(#20784),#1608,.F.) ;
#89105 = ADVANCED_FACE('',(#20785),#1609,.F.) ;
#89106 = ADVANCED_FACE('',(#20786),#1610,.F.) ;
#89107 = ADVANCED_FACE('',(#20787),#1611,.F.) ;
#89108 = ADVANCED_FACE('',(#20788),#1612,.F.) ;
#89109 = ADVANCED_FACE('',(#20789),#1613,.F.) ;
#89110 = ADVANCED_FACE('',(#20790),#1614,.F.) ;
#89111 = ADVANCED_FACE('',(#20791),#1615,.F.) ;
#89112 = ADVANCED_FACE('',(#20792),#1616,.F.) ;
#89113 = ADVANCED_FACE('',(#20793),#1617,.F.) ;
#89114 = ADVANCED_FACE('',(#20794),#1618,.F.) ;
#89115 = ADVANCED_FACE('',(#20795),#1619,.F.) ;
#89116 = ADVANCED_FACE('',(#20796),#1620,.F.) ;
#89117 = ADVANCED_FACE('',(#20797),#1621,.F.) ;
#89118 = ADVANCED_FACE('',(#20798),#1622,.F.) ;
#89119 = ADVANCED_FACE('',(#20799),#1623,.F.) ;
#89120 = ADVANCED_FACE('',(#20800),#1624,.F.) ;
#89121 = ADVANCED_FACE('',(#20801),#1625,.F.) ;
#89122 = ADVANCED_FACE('',(#20802),#1626,.F.) ;
#89123 = ADVANCED_FACE('',(#20803),#1627,.F.) ;
#89124 = ADVANCED_FACE('',(#20804),#1628,.F.) ;
#89125 = ADVANCED_FACE('',(#20805),#1629,.F.) ;
#89126 = ADVANCED_FACE('',(#20806),#1630,.F.) ;
#89127 = ADVANCED_FACE('',(#20807),#1631,.F.) ;
#89128 = ADVANCED_FACE('',(#20808),#1632,.F.) ;
#89129 = ADVANCED_FACE('',(#20809),#1633,.F.) ;
#89130 = ADVANCED_FACE('',(#20810),#1634,.F.) ;
#89131 = ADVANCED_FACE('',(#20811),#1635,.F.) ;
#89132 = ADVANCED_FACE('',(#20812),#1636,.F.) ;
#89133 = ADVANCED_FACE('',(#20813),#1637,.F.) ;
#89134 = ADVANCED_FACE('',(#20814),#1638,.F.) ;
#89135 = ADVANCED_FACE('',(#20815),#1639,.F.) ;
#89136 = ADVANCED_FACE('',(#20816),#1640,.F.) ;
#89137 = ADVANCED_FACE('',(#20817),#1641,.F.) ;
#89138 = ADVANCED_FACE('',(#20818),#1642,.F.) ;
#89139 = ADVANCED_FACE('',(#20819),#1643,.F.) ;
#89140 = ADVANCED_FACE('',(#20820),#1644,.F.) ;
#89141 = ADVANCED_FACE('',(#20821),#1645,.F.) ;
#89142 = ADVANCED_FACE('',(#20822),#1646,.F.) ;
#89143 = ADVANCED_FACE('',(#20823),#1647,.F.) ;
#89144 = ADVANCED_FACE('',(#20824),#1648,.F.) ;
#89145 = ADVANCED_FACE('',(#20825),#1649,.F.) ;
#89146 = ADVANCED_FACE('',(#20826),#1650,.F.) ;
#89147 = ADVANCED_FACE('',(#20827),#1651,.F.) ;
#89148 = ADVANCED_FACE('',(#20828),#1652,.F.) ;
#89149 = ADVANCED_FACE('',(#20829),#1653,.F.) ;
#89150 = ADVANCED_FACE('',(#20830),#1654,.F.) ;
#89151 = ADVANCED_FACE('',(#20831),#1655,.F.) ;
#89152 = ADVANCED_FACE('',(#20832),#1656,.F.) ;
#89153 = ADVANCED_FACE('',(#20833),#1657,.T.) ;
#89154 = ADVANCED_FACE('',(#20834),#1658,.T.) ;
#89155 = ADVANCED_FACE('',(#20835),#1659,.T.) ;
#89156 = ADVANCED_FACE('',(#20836),#1660,.T.) ;
#89157 = ADVANCED_FACE('',(#20837),#1661,.T.) ;
#89158 = ADVANCED_FACE('',(#20838),#1662,.T.) ;
#89159 = ADVANCED_FACE('',(#20839),#1663,.T.) ;
#89160 = ADVANCED_FACE('',(#20840),#1664,.T.) ;
#89161 = ADVANCED_FACE('',(#20841),#1665,.T.) ;
#89162 = ADVANCED_FACE('',(#20842),#1666,.F.) ;
#89163 = ADVANCED_FACE('',(#20843),#1667,.F.) ;
#89164 = ADVANCED_FACE('',(#20844),#1668,.F.) ;
#89165 = ADVANCED_FACE('',(#20845),#1669,.F.) ;
#89166 = ADVANCED_FACE('',(#20846),#1670,.F.) ;
#89167 = ADVANCED_FACE('',(#20847),#1671,.F.) ;
#89168 = ADVANCED_FACE('',(#20848),#1672,.F.) ;
#89169 = ADVANCED_FACE('',(#20849),#1673,.F.) ;
#89170 = ADVANCED_FACE('',(#20850),#1674,.F.) ;
#89171 = ADVANCED_FACE('',(#20851),#1675,.F.) ;
#89172 = ADVANCED_FACE('',(#20852),#1676,.F.) ;
#89173 = ADVANCED_FACE('',(#20853),#1677,.F.) ;
#89174 = ADVANCED_FACE('',(#20854),#1678,.F.) ;
#89175 = ADVANCED_FACE('',(#20855),#1679,.F.) ;
#89176 = ADVANCED_FACE('',(#20856),#1680,.F.) ;
#89177 = ADVANCED_FACE('',(#20857),#1681,.F.) ;
#89178 = ADVANCED_FACE('',(#20858),#1682,.F.) ;
#89179 = ADVANCED_FACE('',(#20859),#1683,.F.) ;
#89180 = ADVANCED_FACE('',(#20860),#1684,.F.) ;
#89181 = ADVANCED_FACE('',(#20861),#1685,.F.) ;
#89182 = ADVANCED_FACE('',(#20862),#1686,.F.) ;
#89183 = ADVANCED_FACE('',(#20863),#1687,.F.) ;
#89184 = ADVANCED_FACE('',(#20864),#1688,.F.) ;
#89185 = ADVANCED_FACE('',(#20865),#1689,.F.) ;
#89186 = ADVANCED_FACE('',(#20866),#1690,.F.) ;
#89187 = ADVANCED_FACE('',(#20867),#1691,.F.) ;
#89188 = ADVANCED_FACE('',(#20868),#1692,.F.) ;
#89189 = ADVANCED_FACE('',(#20869),#1693,.F.) ;
#89190 = ADVANCED_FACE('',(#20870),#1694,.F.) ;
#89191 = ADVANCED_FACE('',(#20871),#1695,.F.) ;
#89192 = ADVANCED_FACE('',(#20872),#1696,.F.) ;
#89193 = ADVANCED_FACE('',(#20873),#1697,.F.) ;
#89194 = ADVANCED_FACE('',(#20874),#1698,.F.) ;
#89195 = ADVANCED_FACE('',(#20875),#1699,.F.) ;
#89196 = ADVANCED_FACE('',(#20876),#1700,.F.) ;
#89197 = ADVANCED_FACE('',(#20877),#1701,.F.) ;
#89198 = ADVANCED_FACE('',(#20878,#767),#1702,.T.) ;
#89199 = ADVANCED_FACE('',(#20879),#1703,.T.) ;
#89200 = ADVANCED_FACE('',(#20880),#1704,.T.) ;
#89201 = ADVANCED_FACE('',(#20881),#1705,.T.) ;
#89202 = ADVANCED_FACE('',(#20882),#1706,.T.) ;
#89203 = ADVANCED_FACE('',(#20883,#768),#1707,.T.) ;
#89204 = ADVANCED_FACE('',(#20884),#1708,.T.) ;
#89205 = ADVANCED_FACE('',(#20885),#1709,.T.) ;
#89206 = ADVANCED_FACE('',(#20886),#1710,.T.) ;
#89207 = ADVANCED_FACE('',(#20887),#1711,.T.) ;
#89208 = ADVANCED_FACE('',(#20888,#769),#1712,.T.) ;
#89209 = ADVANCED_FACE('',(#20889),#1713,.T.) ;
#89210 = ADVANCED_FACE('',(#20890),#1714,.T.) ;
#89211 = ADVANCED_FACE('',(#20891),#1715,.T.) ;
#89212 = ADVANCED_FACE('',(#20892),#1716,.T.) ;
#89213 = ADVANCED_FACE('',(#20893,#770),#1717,.T.) ;
#89214 = ADVANCED_FACE('',(#20894),#1718,.T.) ;
#89215 = ADVANCED_FACE('',(#20895),#1719,.T.) ;
#89216 = ADVANCED_FACE('',(#20896),#1720,.T.) ;
#89217 = ADVANCED_FACE('',(#20897),#1721,.T.) ;
#89218 = ADVANCED_FACE('',(#20898,#771),#1722,.T.) ;
#89219 = ADVANCED_FACE('',(#20899),#1723,.T.) ;
#89220 = ADVANCED_FACE('',(#20900),#1724,.T.) ;
#89221 = ADVANCED_FACE('',(#20901),#1725,.T.) ;
#89222 = ADVANCED_FACE('',(#20902),#1726,.T.) ;
#89223 = ADVANCED_FACE('',(#20903,#772),#1727,.T.) ;
#89224 = ADVANCED_FACE('',(#20904),#1728,.T.) ;
#89225 = ADVANCED_FACE('',(#20905),#1729,.T.) ;
#89226 = ADVANCED_FACE('',(#20906),#1730,.T.) ;
#89227 = ADVANCED_FACE('',(#20907),#1731,.T.) ;
#89228 = ADVANCED_FACE('',(#20908,#773),#1732,.T.) ;
#89229 = ADVANCED_FACE('',(#20909),#1733,.T.) ;
#89230 = ADVANCED_FACE('',(#20910),#1734,.T.) ;
#89231 = ADVANCED_FACE('',(#20911),#1735,.T.) ;
#89232 = ADVANCED_FACE('',(#20912),#1736,.T.) ;
#89233 = ADVANCED_FACE('',(#20913,#774),#1737,.T.) ;
#89234 = ADVANCED_FACE('',(#20914),#1738,.T.) ;
#89235 = ADVANCED_FACE('',(#20915),#1739,.T.) ;
#89236 = ADVANCED_FACE('',(#20916),#1740,.T.) ;
#89237 = ADVANCED_FACE('',(#20917),#1741,.T.) ;
#89238 = ADVANCED_FACE('',(#20918,#775),#1742,.T.) ;
#89239 = ADVANCED_FACE('',(#20919),#1743,.T.) ;
#89240 = ADVANCED_FACE('',(#20920),#1744,.T.) ;
#89241 = ADVANCED_FACE('',(#20921),#1745,.T.) ;
#89242 = ADVANCED_FACE('',(#20922),#1746,.T.) ;
#89243 = ADVANCED_FACE('',(#20923),#1747,.T.) ;
#89244 = ADVANCED_FACE('',(#20924),#1748,.T.) ;
#89245 = ADVANCED_FACE('',(#20925),#1749,.T.) ;
#89246 = ADVANCED_FACE('',(#20926),#1750,.T.) ;
#89247 = ADVANCED_FACE('',(#20927),#1751,.T.) ;
#89248 = ADVANCED_FACE('',(#20928),#1752,.T.) ;
#89249 = ADVANCED_FACE('',(#20929),#1753,.T.) ;
#89250 = ADVANCED_FACE('',(#20930),#1754,.T.) ;
#89251 = ADVANCED_FACE('',(#20931),#1755,.T.) ;
#89252 = ADVANCED_FACE('',(#20932),#1756,.F.) ;
#89253 = ADVANCED_FACE('',(#20933),#1757,.F.) ;
#89254 = ADVANCED_FACE('',(#20934),#1758,.F.) ;
#89255 = ADVANCED_FACE('',(#20935),#1759,.F.) ;
#89256 = ADVANCED_FACE('',(#20936),#1760,.F.) ;
#89257 = ADVANCED_FACE('',(#20937),#1761,.F.) ;
#89258 = ADVANCED_FACE('',(#20938),#1762,.F.) ;
#89259 = ADVANCED_FACE('',(#20939),#1763,.F.) ;
#89260 = ADVANCED_FACE('',(#20940),#1764,.F.) ;
#89261 = ADVANCED_FACE('',(#20941),#1765,.F.) ;
#89262 = ADVANCED_FACE('',(#20942),#1766,.F.) ;
#89263 = ADVANCED_FACE('',(#20943),#1767,.F.) ;
#89264 = ADVANCED_FACE('',(#20944),#1768,.F.) ;
#89265 = ADVANCED_FACE('',(#20945),#1769,.F.) ;
#89266 = ADVANCED_FACE('',(#20946),#1770,.F.) ;
#89267 = ADVANCED_FACE('',(#20947),#1771,.F.) ;
#89268 = ADVANCED_FACE('',(#20948),#1772,.F.) ;
#89269 = ADVANCED_FACE('',(#20949),#1773,.F.) ;
#89270 = ADVANCED_FACE('',(#20950),#1774,.F.) ;
#89271 = ADVANCED_FACE('',(#20951),#1775,.F.) ;
#89272 = ADVANCED_FACE('',(#20952),#1776,.F.) ;
#89273 = ADVANCED_FACE('',(#20953),#1777,.F.) ;
#89274 = ADVANCED_FACE('',(#20954),#1778,.F.) ;
#89275 = ADVANCED_FACE('',(#20955),#1779,.F.) ;
#89276 = ADVANCED_FACE('',(#20956),#1780,.F.) ;
#89277 = ADVANCED_FACE('',(#20957),#1781,.F.) ;
#89278 = ADVANCED_FACE('',(#20958),#1782,.F.) ;
#89279 = ADVANCED_FACE('',(#20959),#1783,.F.) ;
#89280 = ADVANCED_FACE('',(#20960),#1784,.F.) ;
#89281 = ADVANCED_FACE('',(#20961),#1785,.F.) ;
#89282 = ADVANCED_FACE('',(#20962),#1786,.F.) ;
#89283 = ADVANCED_FACE('',(#20963),#1787,.F.) ;
#89284 = ADVANCED_FACE('',(#20964),#1788,.F.) ;
#89285 = ADVANCED_FACE('',(#20965),#1789,.F.) ;
#89286 = ADVANCED_FACE('',(#20966),#1790,.F.) ;
#89287 = ADVANCED_FACE('',(#20967),#1791,.F.) ;
#89288 = ADVANCED_FACE('',(#20968),#1792,.F.) ;
#89289 = ADVANCED_FACE('',(#20969),#1793,.F.) ;
#89290 = ADVANCED_FACE('',(#20970),#15254,.F.) ;
#89291 = ADVANCED_FACE('',(#20971,#776),#1794,.T.) ;
#89292 = ADVANCED_FACE('',(#20972),#1795,.F.) ;
#89293 = ADVANCED_FACE('',(#20973),#1796,.F.) ;
#89294 = ADVANCED_FACE('',(#20974),#15255,.F.) ;
#89295 = ADVANCED_FACE('',(#20975,#777),#1797,.T.) ;
#89296 = ADVANCED_FACE('',(#20976),#1798,.F.) ;
#89297 = ADVANCED_FACE('',(#20977),#1799,.F.) ;
#89298 = ADVANCED_FACE('',(#20978),#15256,.F.) ;
#89299 = ADVANCED_FACE('',(#20979,#778),#1800,.T.) ;
#89300 = ADVANCED_FACE('',(#20980),#1801,.F.) ;
#89301 = ADVANCED_FACE('',(#20981),#1802,.F.) ;
#89302 = ADVANCED_FACE('',(#20982),#15257,.F.) ;
#89303 = ADVANCED_FACE('',(#20983,#779),#1803,.T.) ;
#89304 = ADVANCED_FACE('',(#20984),#1804,.F.) ;
#89305 = ADVANCED_FACE('',(#20985),#1805,.F.) ;
#89306 = ADVANCED_FACE('',(#20986),#15258,.F.) ;
#89307 = ADVANCED_FACE('',(#20987,#780),#1806,.T.) ;
#89308 = ADVANCED_FACE('',(#20988),#1807,.F.) ;
#89309 = ADVANCED_FACE('',(#20989),#1808,.F.) ;
#89310 = ADVANCED_FACE('',(#20990),#15259,.F.) ;
#89311 = ADVANCED_FACE('',(#20991,#781),#1809,.T.) ;
#89312 = ADVANCED_FACE('',(#20992),#1810,.F.) ;
#89313 = ADVANCED_FACE('',(#20993),#1811,.F.) ;
#89314 = ADVANCED_FACE('',(#20994),#15260,.F.) ;
#89315 = ADVANCED_FACE('',(#20995,#782),#1812,.T.) ;
#89316 = ADVANCED_FACE('',(#20996),#1813,.F.) ;
#89317 = ADVANCED_FACE('',(#20997),#1814,.F.) ;
#89318 = ADVANCED_FACE('',(#20998),#15261,.F.) ;
#89319 = ADVANCED_FACE('',(#20999,#783),#1815,.T.) ;
#89320 = ADVANCED_FACE('',(#21000),#1816,.F.) ;
#89321 = ADVANCED_FACE('',(#21001),#1817,.F.) ;
#89322 = ADVANCED_FACE('',(#21002),#15262,.F.) ;
#89323 = ADVANCED_FACE('',(#21003,#784),#1818,.T.) ;
#89324 = ADVANCED_FACE('',(#21004),#1819,.T.) ;
#89325 = ADVANCED_FACE('',(#21005),#1820,.T.) ;
#89326 = ADVANCED_FACE('',(#21006),#1821,.T.) ;
#89327 = ADVANCED_FACE('',(#21007),#1822,.T.) ;
#89328 = ADVANCED_FACE('',(#21008),#1823,.T.) ;
#89329 = ADVANCED_FACE('',(#21009),#1824,.T.) ;
#89330 = ADVANCED_FACE('',(#21010),#1825,.T.) ;
#89331 = ADVANCED_FACE('',(#21011),#1826,.T.) ;
#89332 = ADVANCED_FACE('',(#21012),#1827,.T.) ;
#89333 = ADVANCED_FACE('',(#21013),#1828,.F.) ;
#89334 = ADVANCED_FACE('',(#21014),#1829,.F.) ;
#89335 = ADVANCED_FACE('',(#21015),#1830,.F.) ;
#89336 = ADVANCED_FACE('',(#21016),#1831,.F.) ;
#89337 = ADVANCED_FACE('',(#21017),#1832,.F.) ;
#89338 = ADVANCED_FACE('',(#21018),#1833,.F.) ;
#89339 = ADVANCED_FACE('',(#21019),#1834,.F.) ;
#89340 = ADVANCED_FACE('',(#21020),#1835,.F.) ;
#89341 = ADVANCED_FACE('',(#21021),#1836,.F.) ;
#89342 = ADVANCED_FACE('',(#21022),#1837,.F.) ;
#89343 = ADVANCED_FACE('',(#21023),#1838,.F.) ;
#89344 = ADVANCED_FACE('',(#21024),#1839,.F.) ;
#89345 = ADVANCED_FACE('',(#21025),#1840,.F.) ;
#89346 = ADVANCED_FACE('',(#21026),#1841,.F.) ;
#89347 = ADVANCED_FACE('',(#21027),#1842,.F.) ;
#89348 = ADVANCED_FACE('',(#21028),#1843,.F.) ;
#89349 = ADVANCED_FACE('',(#21029),#1844,.F.) ;
#89350 = ADVANCED_FACE('',(#21030),#1845,.F.) ;
#89351 = ADVANCED_FACE('',(#21031),#1846,.F.) ;
#89352 = ADVANCED_FACE('',(#21032),#1847,.F.) ;
#89353 = ADVANCED_FACE('',(#21033),#1848,.F.) ;
#89354 = ADVANCED_FACE('',(#21034),#1849,.F.) ;
#89355 = ADVANCED_FACE('',(#21035),#1850,.F.) ;
#89356 = ADVANCED_FACE('',(#21036),#1851,.F.) ;
#89357 = ADVANCED_FACE('',(#21037),#1852,.F.) ;
#89358 = ADVANCED_FACE('',(#21038),#1853,.F.) ;
#89359 = ADVANCED_FACE('',(#21039),#1854,.F.) ;
#89360 = ADVANCED_FACE('',(#21040),#1855,.F.) ;
#89361 = ADVANCED_FACE('',(#21041),#1856,.F.) ;
#89362 = ADVANCED_FACE('',(#21042),#1857,.F.) ;
#89363 = ADVANCED_FACE('',(#21043),#1858,.F.) ;
#89364 = ADVANCED_FACE('',(#21044),#1859,.F.) ;
#89365 = ADVANCED_FACE('',(#21045),#1860,.F.) ;
#89366 = ADVANCED_FACE('',(#21046),#1861,.F.) ;
#89367 = ADVANCED_FACE('',(#21047),#1862,.F.) ;
#89368 = ADVANCED_FACE('',(#21048),#1863,.F.) ;
#89369 = ADVANCED_FACE('',(#21049,#785),#1864,.T.) ;
#89370 = ADVANCED_FACE('',(#21050),#1865,.T.) ;
#89371 = ADVANCED_FACE('',(#21051),#1866,.T.) ;
#89372 = ADVANCED_FACE('',(#21052),#1867,.T.) ;
#89373 = ADVANCED_FACE('',(#21053),#1868,.T.) ;
#89374 = ADVANCED_FACE('',(#21054,#786),#1869,.T.) ;
#89375 = ADVANCED_FACE('',(#21055),#1870,.T.) ;
#89376 = ADVANCED_FACE('',(#21056),#1871,.T.) ;
#89377 = ADVANCED_FACE('',(#21057),#1872,.T.) ;
#89378 = ADVANCED_FACE('',(#21058),#1873,.T.) ;
#89379 = ADVANCED_FACE('',(#21059,#787),#1874,.T.) ;
#89380 = ADVANCED_FACE('',(#21060),#1875,.T.) ;
#89381 = ADVANCED_FACE('',(#21061),#1876,.T.) ;
#89382 = ADVANCED_FACE('',(#21062),#1877,.T.) ;
#89383 = ADVANCED_FACE('',(#21063),#1878,.T.) ;
#89384 = ADVANCED_FACE('',(#21064,#788),#1879,.T.) ;
#89385 = ADVANCED_FACE('',(#21065),#1880,.T.) ;
#89386 = ADVANCED_FACE('',(#21066),#1881,.T.) ;
#89387 = ADVANCED_FACE('',(#21067),#1882,.T.) ;
#89388 = ADVANCED_FACE('',(#21068),#1883,.T.) ;
#89389 = ADVANCED_FACE('',(#21069,#789),#1884,.T.) ;
#89390 = ADVANCED_FACE('',(#21070),#1885,.T.) ;
#89391 = ADVANCED_FACE('',(#21071),#1886,.T.) ;
#89392 = ADVANCED_FACE('',(#21072),#1887,.T.) ;
#89393 = ADVANCED_FACE('',(#21073),#1888,.T.) ;
#89394 = ADVANCED_FACE('',(#21074,#790),#1889,.T.) ;
#89395 = ADVANCED_FACE('',(#21075),#1890,.T.) ;
#89396 = ADVANCED_FACE('',(#21076),#1891,.T.) ;
#89397 = ADVANCED_FACE('',(#21077),#1892,.T.) ;
#89398 = ADVANCED_FACE('',(#21078),#1893,.T.) ;
#89399 = ADVANCED_FACE('',(#21079,#791),#1894,.T.) ;
#89400 = ADVANCED_FACE('',(#21080),#1895,.T.) ;
#89401 = ADVANCED_FACE('',(#21081),#1896,.T.) ;
#89402 = ADVANCED_FACE('',(#21082),#1897,.T.) ;
#89403 = ADVANCED_FACE('',(#21083),#1898,.T.) ;
#89404 = ADVANCED_FACE('',(#21084,#792),#1899,.T.) ;
#89405 = ADVANCED_FACE('',(#21085),#1900,.T.) ;
#89406 = ADVANCED_FACE('',(#21086),#1901,.T.) ;
#89407 = ADVANCED_FACE('',(#21087),#1902,.T.) ;
#89408 = ADVANCED_FACE('',(#21088),#1903,.T.) ;
#89409 = ADVANCED_FACE('',(#21089,#793),#1904,.T.) ;
#89410 = ADVANCED_FACE('',(#21090),#1905,.T.) ;
#89411 = ADVANCED_FACE('',(#21091),#1906,.T.) ;
#89412 = ADVANCED_FACE('',(#21092),#1907,.T.) ;
#89413 = ADVANCED_FACE('',(#21093),#1908,.T.) ;
#89414 = ADVANCED_FACE('',(#21094),#1909,.T.) ;
#89415 = ADVANCED_FACE('',(#21095),#1910,.T.) ;
#89416 = ADVANCED_FACE('',(#21096),#1911,.T.) ;
#89417 = ADVANCED_FACE('',(#21097),#1912,.T.) ;
#89418 = ADVANCED_FACE('',(#21098),#1913,.T.) ;
#89419 = ADVANCED_FACE('',(#21099),#1914,.T.) ;
#89420 = ADVANCED_FACE('',(#21100),#1915,.T.) ;
#89421 = ADVANCED_FACE('',(#21101),#1916,.T.) ;
#89422 = ADVANCED_FACE('',(#21102),#1917,.T.) ;
#89423 = ADVANCED_FACE('',(#21103),#1918,.T.) ;
#89424 = ADVANCED_FACE('',(#21104),#1919,.T.) ;
#89425 = ADVANCED_FACE('',(#21105),#1920,.T.) ;
#89426 = ADVANCED_FACE('',(#21106),#1921,.T.) ;
#89427 = ADVANCED_FACE('',(#21107),#1922,.T.) ;
#89428 = ADVANCED_FACE('',(#21108),#1923,.T.) ;
#89429 = ADVANCED_FACE('',(#21109),#1924,.T.) ;
#89430 = ADVANCED_FACE('',(#21110),#1925,.T.) ;
#89431 = ADVANCED_FACE('',(#21111),#1926,.T.) ;
#89432 = ADVANCED_FACE('',(#21112),#1927,.F.) ;
#89433 = ADVANCED_FACE('',(#21113),#1928,.F.) ;
#89434 = ADVANCED_FACE('',(#21114),#1929,.T.) ;
#89435 = ADVANCED_FACE('',(#21115),#1930,.F.) ;
#89436 = ADVANCED_FACE('',(#21116),#1931,.F.) ;
#89437 = ADVANCED_FACE('',(#21117),#1932,.T.) ;
#89438 = ADVANCED_FACE('',(#21118),#1933,.F.) ;
#89439 = ADVANCED_FACE('',(#21119),#1934,.F.) ;
#89440 = ADVANCED_FACE('',(#21120),#1935,.T.) ;
#89441 = ADVANCED_FACE('',(#21121),#1936,.F.) ;
#89442 = ADVANCED_FACE('',(#21122),#1937,.F.) ;
#89443 = ADVANCED_FACE('',(#21123),#1938,.T.) ;
#89444 = ADVANCED_FACE('',(#21124),#1939,.F.) ;
#89445 = ADVANCED_FACE('',(#21125),#1940,.F.) ;
#89446 = ADVANCED_FACE('',(#21126),#1941,.T.) ;
#89447 = ADVANCED_FACE('',(#21127),#1942,.F.) ;
#89448 = ADVANCED_FACE('',(#21128),#1943,.F.) ;
#89449 = ADVANCED_FACE('',(#21129),#1944,.T.) ;
#89450 = ADVANCED_FACE('',(#21130),#1945,.F.) ;
#89451 = ADVANCED_FACE('',(#21131),#1946,.F.) ;
#89452 = ADVANCED_FACE('',(#21132),#1947,.T.) ;
#89453 = ADVANCED_FACE('',(#21133),#1948,.F.) ;
#89454 = ADVANCED_FACE('',(#21134),#1949,.F.) ;
#89455 = ADVANCED_FACE('',(#21135),#1950,.T.) ;
#89456 = ADVANCED_FACE('',(#21136),#1951,.F.) ;
#89457 = ADVANCED_FACE('',(#21137),#1952,.F.) ;
#89458 = ADVANCED_FACE('',(#21138),#1953,.T.) ;
#89459 = ADVANCED_FACE('',(#21139),#15263,.T.) ;
#89460 = ADVANCED_FACE('',(#21140),#1954,.F.) ;
#89461 = ADVANCED_FACE('',(#21141),#15264,.T.) ;
#89462 = ADVANCED_FACE('',(#21142),#1955,.F.) ;
#89463 = ADVANCED_FACE('',(#21143),#15265,.T.) ;
#89464 = ADVANCED_FACE('',(#21144),#1956,.F.) ;
#89465 = ADVANCED_FACE('',(#21145),#15266,.T.) ;
#89466 = ADVANCED_FACE('',(#21146),#1957,.F.) ;
#89467 = ADVANCED_FACE('',(#21147),#1958,.F.) ;
#89468 = ADVANCED_FACE('',(#21148),#15267,.T.) ;
#89469 = ADVANCED_FACE('',(#21149),#1959,.F.) ;
#89470 = ADVANCED_FACE('',(#21150),#15268,.T.) ;
#89471 = ADVANCED_FACE('',(#21151),#1960,.F.) ;
#89472 = ADVANCED_FACE('',(#21152),#15269,.T.) ;
#89473 = ADVANCED_FACE('',(#21153),#1961,.F.) ;
#89474 = ADVANCED_FACE('',(#21154),#15270,.T.) ;
#89475 = ADVANCED_FACE('',(#21155),#1962,.F.) ;
#89476 = ADVANCED_FACE('',(#21156),#1963,.F.) ;
#89477 = ADVANCED_FACE('',(#21157),#15271,.T.) ;
#89478 = ADVANCED_FACE('',(#21158),#1964,.F.) ;
#89479 = ADVANCED_FACE('',(#21159),#15272,.T.) ;
#89480 = ADVANCED_FACE('',(#21160),#1965,.F.) ;
#89481 = ADVANCED_FACE('',(#21161),#15273,.T.) ;
#89482 = ADVANCED_FACE('',(#21162),#1966,.F.) ;
#89483 = ADVANCED_FACE('',(#21163),#15274,.T.) ;
#89484 = ADVANCED_FACE('',(#21164),#1967,.F.) ;
#89485 = ADVANCED_FACE('',(#21165),#1968,.F.) ;
#89486 = ADVANCED_FACE('',(#21166),#15275,.T.) ;
#89487 = ADVANCED_FACE('',(#21167),#1969,.F.) ;
#89488 = ADVANCED_FACE('',(#21168),#15276,.T.) ;
#89489 = ADVANCED_FACE('',(#21169),#1970,.F.) ;
#89490 = ADVANCED_FACE('',(#21170),#15277,.T.) ;
#89491 = ADVANCED_FACE('',(#21171),#1971,.F.) ;
#89492 = ADVANCED_FACE('',(#21172),#15278,.T.) ;
#89493 = ADVANCED_FACE('',(#21173),#1972,.F.) ;
#89494 = ADVANCED_FACE('',(#21174),#1973,.F.) ;
#89495 = ADVANCED_FACE('',(#21175),#15279,.T.) ;
#89496 = ADVANCED_FACE('',(#21176),#1974,.F.) ;
#89497 = ADVANCED_FACE('',(#21177),#15280,.T.) ;
#89498 = ADVANCED_FACE('',(#21178),#1975,.F.) ;
#89499 = ADVANCED_FACE('',(#21179),#15281,.T.) ;
#89500 = ADVANCED_FACE('',(#21180),#1976,.F.) ;
#89501 = ADVANCED_FACE('',(#21181),#15282,.T.) ;
#89502 = ADVANCED_FACE('',(#21182),#1977,.F.) ;
#89503 = ADVANCED_FACE('',(#21183),#1978,.F.) ;
#89504 = ADVANCED_FACE('',(#21184),#15283,.T.) ;
#89505 = ADVANCED_FACE('',(#21185),#1979,.F.) ;
#89506 = ADVANCED_FACE('',(#21186),#15284,.T.) ;
#89507 = ADVANCED_FACE('',(#21187),#1980,.F.) ;
#89508 = ADVANCED_FACE('',(#21188),#15285,.T.) ;
#89509 = ADVANCED_FACE('',(#21189),#1981,.F.) ;
#89510 = ADVANCED_FACE('',(#21190),#15286,.T.) ;
#89511 = ADVANCED_FACE('',(#21191),#1982,.F.) ;
#89512 = ADVANCED_FACE('',(#21192),#1983,.F.) ;
#89513 = ADVANCED_FACE('',(#21193),#15287,.T.) ;
#89514 = ADVANCED_FACE('',(#21194),#1984,.F.) ;
#89515 = ADVANCED_FACE('',(#21195),#15288,.T.) ;
#89516 = ADVANCED_FACE('',(#21196),#1985,.F.) ;
#89517 = ADVANCED_FACE('',(#21197),#15289,.T.) ;
#89518 = ADVANCED_FACE('',(#21198),#1986,.F.) ;
#89519 = ADVANCED_FACE('',(#21199),#15290,.T.) ;
#89520 = ADVANCED_FACE('',(#21200),#1987,.F.) ;
#89521 = ADVANCED_FACE('',(#21201),#1988,.F.) ;
#89522 = ADVANCED_FACE('',(#21202),#15291,.T.) ;
#89523 = ADVANCED_FACE('',(#21203),#1989,.F.) ;
#89524 = ADVANCED_FACE('',(#21204),#15292,.T.) ;
#89525 = ADVANCED_FACE('',(#21205),#1990,.F.) ;
#89526 = ADVANCED_FACE('',(#21206),#15293,.T.) ;
#89527 = ADVANCED_FACE('',(#21207),#1991,.F.) ;
#89528 = ADVANCED_FACE('',(#21208),#15294,.T.) ;
#89529 = ADVANCED_FACE('',(#21209),#1992,.F.) ;
#89530 = ADVANCED_FACE('',(#21210),#1993,.F.) ;
#89531 = ADVANCED_FACE('',(#21211),#15295,.T.) ;
#89532 = ADVANCED_FACE('',(#21212),#1994,.F.) ;
#89533 = ADVANCED_FACE('',(#21213),#15296,.T.) ;
#89534 = ADVANCED_FACE('',(#21214),#1995,.F.) ;
#89535 = ADVANCED_FACE('',(#21215),#15297,.T.) ;
#89536 = ADVANCED_FACE('',(#21216),#1996,.F.) ;
#89537 = ADVANCED_FACE('',(#21217),#15298,.T.) ;
#89538 = ADVANCED_FACE('',(#21218),#1997,.F.) ;
#89539 = ADVANCED_FACE('',(#21219),#1998,.F.) ;
#89540 = ADVANCED_FACE('',(#21220),#16729,.T.) ;
#89541 = ADVANCED_FACE('',(#21221),#79425,.T.) ;
#89542 = ADVANCED_FACE('',(#21222),#15299,.T.) ;
#89543 = ADVANCED_FACE('',(#21223),#15300,.T.) ;
#89544 = ADVANCED_FACE('',(#21224),#15301,.T.) ;
#89545 = ADVANCED_FACE('',(#21225),#15302,.T.) ;
#89546 = ADVANCED_FACE('',(#21226),#16730,.T.) ;
#89547 = ADVANCED_FACE('',(#21227),#79426,.F.) ;
#89548 = ADVANCED_FACE('',(#21228),#16731,.T.) ;
#89549 = ADVANCED_FACE('',(#21229),#15303,.T.) ;
#89550 = ADVANCED_FACE('',(#21230),#15304,.T.) ;
#89551 = ADVANCED_FACE('',(#21231),#15305,.T.) ;
#89552 = ADVANCED_FACE('',(#21232),#79427,.F.) ;
#89553 = ADVANCED_FACE('',(#21233),#15306,.F.) ;
#89554 = ADVANCED_FACE('',(#21234),#15307,.T.) ;
#89555 = ADVANCED_FACE('',(#21235),#16732,.T.) ;
#89556 = ADVANCED_FACE('',(#21236),#79428,.F.) ;
#89557 = ADVANCED_FACE('',(#21237),#79429,.T.) ;
#89558 = ADVANCED_FACE('',(#21238),#15308,.T.) ;
#89559 = ADVANCED_FACE('',(#21239),#15309,.F.) ;
#89560 = ADVANCED_FACE('',(#21240),#15310,.T.) ;
#89561 = ADVANCED_FACE('',(#21241),#15311,.F.) ;
#89562 = ADVANCED_FACE('',(#21242),#15312,.F.) ;
#89563 = ADVANCED_FACE('',(#21243),#79430,.T.) ;
#89564 = ADVANCED_FACE('',(#21244),#16733,.T.) ;
#89565 = ADVANCED_FACE('',(#21245),#16734,.F.) ;
#89566 = ADVANCED_FACE('',(#21246),#15313,.T.) ;
#89567 = ADVANCED_FACE('',(#21247),#15314,.T.) ;
#89568 = ADVANCED_FACE('',(#21248),#15315,.T.) ;
#89569 = ADVANCED_FACE('',(#21249),#15316,.F.) ;
#89570 = ADVANCED_FACE('',(#21250),#16735,.T.) ;
#89571 = ADVANCED_FACE('',(#21251),#79431,.F.) ;
#89572 = ADVANCED_FACE('',(#21252),#15317,.F.) ;
#89573 = ADVANCED_FACE('',(#21253),#15318,.T.) ;
#89574 = ADVANCED_FACE('',(#21254),#15319,.F.) ;
#89575 = ADVANCED_FACE('',(#21255),#16736,.F.) ;
#89576 = ADVANCED_FACE('',(#21256),#79432,.F.) ;
#89577 = ADVANCED_FACE('',(#21257),#15320,.F.) ;
#89578 = ADVANCED_FACE('',(#21258),#79433,.F.) ;
#89579 = ADVANCED_FACE('',(#21259),#15321,.F.) ;
#89580 = ADVANCED_FACE('',(#21260),#15322,.F.) ;
#89581 = ADVANCED_FACE('',(#21261),#79434,.F.) ;
#89582 = ADVANCED_FACE('',(#21262),#79435,.F.) ;
#89583 = ADVANCED_FACE('',(#21263),#15323,.F.) ;
#89584 = ADVANCED_FACE('',(#21264),#15324,.F.) ;
#89585 = ADVANCED_FACE('',(#21265),#79436,.F.) ;
#89586 = ADVANCED_FACE('',(#21266),#15325,.T.) ;
#89587 = ADVANCED_FACE('',(#21267),#15326,.T.) ;
#89588 = ADVANCED_FACE('',(#21268),#15327,.T.) ;
#89589 = ADVANCED_FACE('',(#21269),#15328,.T.) ;
#89590 = ADVANCED_FACE('',(#21270),#15329,.T.) ;
#89591 = ADVANCED_FACE('',(#21271),#15330,.T.) ;
#89592 = ADVANCED_FACE('',(#21272),#15331,.T.) ;
#89593 = ADVANCED_FACE('',(#21273),#15332,.T.) ;
#89594 = ADVANCED_FACE('',(#21274),#15333,.T.) ;
#89595 = ADVANCED_FACE('',(#21275),#15334,.T.) ;
#89596 = ADVANCED_FACE('',(#21276),#15335,.T.) ;
#89597 = ADVANCED_FACE('',(#21277),#15336,.T.) ;
#89598 = ADVANCED_FACE('',(#21278),#15337,.T.) ;
#89599 = ADVANCED_FACE('',(#21279),#15338,.T.) ;
#89600 = ADVANCED_FACE('',(#21280),#15339,.T.) ;
#89601 = ADVANCED_FACE('',(#21281),#15340,.T.) ;
#89602 = ADVANCED_FACE('',(#21282),#15341,.T.) ;
#89603 = ADVANCED_FACE('',(#21283),#15342,.T.) ;
#89604 = ADVANCED_FACE('',(#21284),#15343,.T.) ;
#89605 = ADVANCED_FACE('',(#21285),#15344,.T.) ;
#89606 = ADVANCED_FACE('',(#21286),#15345,.T.) ;
#89607 = ADVANCED_FACE('',(#21287),#15346,.T.) ;
#89608 = ADVANCED_FACE('',(#21288),#15347,.T.) ;
#89609 = ADVANCED_FACE('',(#21289),#15348,.T.) ;
#89610 = ADVANCED_FACE('',(#21290),#15349,.T.) ;
#89611 = ADVANCED_FACE('',(#21291),#15350,.T.) ;
#89612 = ADVANCED_FACE('',(#21292),#15351,.T.) ;
#89613 = ADVANCED_FACE('',(#21293),#15352,.T.) ;
#89614 = ADVANCED_FACE('',(#21294),#15353,.T.) ;
#89615 = ADVANCED_FACE('',(#21295),#15354,.T.) ;
#89616 = ADVANCED_FACE('',(#21296),#15355,.T.) ;
#89617 = ADVANCED_FACE('',(#21297),#15356,.T.) ;
#89618 = ADVANCED_FACE('',(#21298),#15357,.T.) ;
#89619 = ADVANCED_FACE('',(#21299),#79437,.T.) ;
#89620 = ADVANCED_FACE('',(#21300),#79438,.T.) ;
#89621 = ADVANCED_FACE('',(#21301),#15358,.T.) ;
#89622 = ADVANCED_FACE('',(#21302),#15359,.F.) ;
#89623 = ADVANCED_FACE('',(#21303),#15360,.F.) ;
#89624 = ADVANCED_FACE('',(#21304),#15361,.F.) ;
#89625 = ADVANCED_FACE('',(#21305),#15362,.T.) ;
#89626 = ADVANCED_FACE('',(#21306),#15363,.T.) ;
#89627 = ADVANCED_FACE('',(#21307),#79439,.T.) ;
#89628 = ADVANCED_FACE('',(#21308),#16737,.F.) ;
#89629 = ADVANCED_FACE('',(#21309),#16738,.F.) ;
#89630 = ADVANCED_FACE('',(#21310),#79440,.T.) ;
#89631 = ADVANCED_FACE('',(#21311),#15364,.F.) ;
#89632 = ADVANCED_FACE('',(#21312),#15365,.F.) ;
#89633 = ADVANCED_FACE('',(#21313),#15366,.F.) ;
#89634 = ADVANCED_FACE('',(#21314),#15367,.F.) ;
#89635 = ADVANCED_FACE('',(#21315),#16739,.F.) ;
#89636 = ADVANCED_FACE('',(#21316),#16740,.F.) ;
#89637 = ADVANCED_FACE('',(#21317),#15368,.F.) ;
#89638 = ADVANCED_FACE('',(#21318),#15369,.T.) ;
#89639 = ADVANCED_FACE('',(#21319),#15370,.T.) ;
#89640 = ADVANCED_FACE('',(#21320),#15371,.T.) ;
#89641 = ADVANCED_FACE('',(#21321),#16741,.T.) ;
#89642 = ADVANCED_FACE('',(#21322),#16742,.T.) ;
#89643 = ADVANCED_FACE('',(#21323),#15372,.T.) ;
#89644 = ADVANCED_FACE('',(#21324),#15373,.T.) ;
#89645 = ADVANCED_FACE('',(#21325),#15374,.T.) ;
#89646 = ADVANCED_FACE('',(#21326),#15375,.T.) ;
#89647 = ADVANCED_FACE('',(#21327),#16743,.T.) ;
#89648 = ADVANCED_FACE('',(#21328),#16744,.T.) ;
#89649 = ADVANCED_FACE('',(#21329),#15376,.T.) ;
#89650 = ADVANCED_FACE('',(#21330),#15377,.F.) ;
#89651 = ADVANCED_FACE('',(#21331),#16745,.F.) ;
#89652 = ADVANCED_FACE('',(#21332),#15378,.F.) ;
#89653 = ADVANCED_FACE('',(#21333),#15379,.F.) ;
#89654 = ADVANCED_FACE('',(#21334),#15380,.F.) ;
#89655 = ADVANCED_FACE('',(#21335),#134,.T.) ;
#89656 = ADVANCED_FACE('',(#21336),#16746,.F.) ;
#89657 = ADVANCED_FACE('',(#21337),#15381,.F.) ;
#89658 = ADVANCED_FACE('',(#21338),#15382,.F.) ;
#89659 = ADVANCED_FACE('',(#21339),#15383,.T.) ;
#89660 = ADVANCED_FACE('',(#21340),#15384,.T.) ;
#89661 = ADVANCED_FACE('',(#21341),#15385,.F.) ;
#89662 = ADVANCED_FACE('',(#21342),#16747,.F.) ;
#89663 = ADVANCED_FACE('',(#21343),#135,.T.) ;
#89664 = ADVANCED_FACE('',(#21344),#136,.T.) ;
#89665 = ADVANCED_FACE('',(#21345),#15386,.F.) ;
#89666 = ADVANCED_FACE('',(#21346),#15387,.F.) ;
#89667 = ADVANCED_FACE('',(#21347),#15388,.T.) ;
#89668 = ADVANCED_FACE('',(#21348),#15389,.T.) ;
#89669 = ADVANCED_FACE('',(#21349),#16748,.F.) ;
#89670 = ADVANCED_FACE('',(#21350),#137,.T.) ;
#89671 = ADVANCED_FACE('',(#21351),#15390,.F.) ;
#89672 = ADVANCED_FACE('',(#21352),#15391,.T.) ;
#89673 = ADVANCED_FACE('',(#21353),#15392,.T.) ;
#89674 = ADVANCED_FACE('',(#21354),#15393,.T.) ;
#89675 = ADVANCED_FACE('',(#21355),#15394,.T.) ;
#89676 = ADVANCED_FACE('',(#21356),#15395,.T.) ;
#89677 = ADVANCED_FACE('',(#21357),#15396,.T.) ;
#89678 = ADVANCED_FACE('',(#21358),#15397,.T.) ;
#89679 = ADVANCED_FACE('',(#21359),#15398,.T.) ;
#89680 = ADVANCED_FACE('',(#21360),#15399,.T.) ;
#89681 = ADVANCED_FACE('',(#21361),#15400,.T.) ;
#89682 = ADVANCED_FACE('',(#21362),#15401,.T.) ;
#89683 = ADVANCED_FACE('',(#21363),#15402,.T.) ;
#89684 = ADVANCED_FACE('',(#21364),#15403,.T.) ;
#89685 = ADVANCED_FACE('',(#21365),#15404,.T.) ;
#89686 = ADVANCED_FACE('',(#21366),#15405,.T.) ;
#89687 = ADVANCED_FACE('',(#21367),#15406,.T.) ;
#89688 = ADVANCED_FACE('',(#21368),#15407,.T.) ;
#89689 = ADVANCED_FACE('',(#21369),#15408,.T.) ;
#89690 = ADVANCED_FACE('',(#21370),#15409,.T.) ;
#89691 = ADVANCED_FACE('',(#21371),#15410,.T.) ;
#89692 = ADVANCED_FACE('',(#21372),#15411,.T.) ;
#89693 = ADVANCED_FACE('',(#21373),#15412,.T.) ;
#89694 = ADVANCED_FACE('',(#21374),#15413,.T.) ;
#89695 = ADVANCED_FACE('',(#21375),#15414,.T.) ;
#89696 = ADVANCED_FACE('',(#21376),#15415,.T.) ;
#89697 = ADVANCED_FACE('',(#21377),#15416,.T.) ;
#89698 = ADVANCED_FACE('',(#21378),#15417,.T.) ;
#89699 = ADVANCED_FACE('',(#21379),#15418,.T.) ;
#89700 = ADVANCED_FACE('',(#21380),#15419,.T.) ;
#89701 = ADVANCED_FACE('',(#21381),#15420,.T.) ;
#89702 = ADVANCED_FACE('',(#21382),#15421,.T.) ;
#89703 = ADVANCED_FACE('',(#21383),#15422,.T.) ;
#89704 = ADVANCED_FACE('',(#21384),#15423,.T.) ;
#89705 = ADVANCED_FACE('',(#21385),#79441,.T.) ;
#89706 = ADVANCED_FACE('',(#21386),#79442,.T.) ;
#89707 = ADVANCED_FACE('',(#21387),#15424,.T.) ;
#89708 = ADVANCED_FACE('',(#21388),#15425,.F.) ;
#89709 = ADVANCED_FACE('',(#21389),#15426,.F.) ;
#89710 = ADVANCED_FACE('',(#21390),#15427,.F.) ;
#89711 = ADVANCED_FACE('',(#21391),#15428,.T.) ;
#89712 = ADVANCED_FACE('',(#21392),#15429,.T.) ;
#89713 = ADVANCED_FACE('',(#21393),#79443,.T.) ;
#89714 = ADVANCED_FACE('',(#21394),#16749,.F.) ;
#89715 = ADVANCED_FACE('',(#21395),#16750,.F.) ;
#89716 = ADVANCED_FACE('',(#21396),#79444,.T.) ;
#89717 = ADVANCED_FACE('',(#21397),#15430,.F.) ;
#89718 = ADVANCED_FACE('',(#21398),#15431,.F.) ;
#89719 = ADVANCED_FACE('',(#21399),#15432,.F.) ;
#89720 = ADVANCED_FACE('',(#21400),#15433,.F.) ;
#89721 = ADVANCED_FACE('',(#21401),#16751,.F.) ;
#89722 = ADVANCED_FACE('',(#21402),#16752,.F.) ;
#89723 = ADVANCED_FACE('',(#21403),#15434,.F.) ;
#89724 = ADVANCED_FACE('',(#21404),#15435,.T.) ;
#89725 = ADVANCED_FACE('',(#21405),#15436,.T.) ;
#89726 = ADVANCED_FACE('',(#21406),#15437,.T.) ;
#89727 = ADVANCED_FACE('',(#21407),#16753,.T.) ;
#89728 = ADVANCED_FACE('',(#21408),#16754,.T.) ;
#89729 = ADVANCED_FACE('',(#21409),#15438,.T.) ;
#89730 = ADVANCED_FACE('',(#21410),#15439,.T.) ;
#89731 = ADVANCED_FACE('',(#21411),#15440,.T.) ;
#89732 = ADVANCED_FACE('',(#21412),#15441,.T.) ;
#89733 = ADVANCED_FACE('',(#21413),#16755,.T.) ;
#89734 = ADVANCED_FACE('',(#21414),#16756,.T.) ;
#89735 = ADVANCED_FACE('',(#21415),#15442,.T.) ;
#89736 = ADVANCED_FACE('',(#21416),#15443,.T.) ;
#89737 = ADVANCED_FACE('',(#21417),#16757,.T.) ;
#89738 = ADVANCED_FACE('',(#21418),#16758,.T.) ;
#89739 = ADVANCED_FACE('',(#21419),#15444,.T.) ;
#89740 = ADVANCED_FACE('',(#21420),#15445,.T.) ;
#89741 = ADVANCED_FACE('',(#21421),#16759,.T.) ;
#89742 = ADVANCED_FACE('',(#21422),#16760,.T.) ;
#89743 = ADVANCED_FACE('',(#21423),#15446,.T.) ;
#89744 = ADVANCED_FACE('',(#21424),#15447,.T.) ;
#89745 = ADVANCED_FACE('',(#21425),#15448,.F.) ;
#89746 = ADVANCED_FACE('',(#21426),#15449,.F.) ;
#89747 = ADVANCED_FACE('',(#21427),#15450,.T.) ;
#89748 = ADVANCED_FACE('',(#21428),#16761,.T.) ;
#89749 = ADVANCED_FACE('',(#21429),#15451,.T.) ;
#89750 = ADVANCED_FACE('',(#21430),#15452,.T.) ;
#89751 = ADVANCED_FACE('',(#21431),#79445,.T.) ;
#89752 = ADVANCED_FACE('',(#21432),#15453,.T.) ;
#89753 = ADVANCED_FACE('',(#21433),#16762,.T.) ;
#89754 = ADVANCED_FACE('',(#21434),#79446,.F.) ;
#89755 = ADVANCED_FACE('',(#21435),#16763,.T.) ;
#89756 = ADVANCED_FACE('',(#21436),#15454,.T.) ;
#89757 = ADVANCED_FACE('',(#21437),#15455,.T.) ;
#89758 = ADVANCED_FACE('',(#21438),#15456,.F.) ;
#89759 = ADVANCED_FACE('',(#21439),#79447,.F.) ;
#89760 = ADVANCED_FACE('',(#21440),#15457,.T.) ;
#89761 = ADVANCED_FACE('',(#21441),#15458,.T.) ;
#89762 = ADVANCED_FACE('',(#21442),#15459,.T.) ;
#89763 = ADVANCED_FACE('',(#21443),#79448,.T.) ;
#89764 = ADVANCED_FACE('',(#21444),#79449,.F.) ;
#89765 = ADVANCED_FACE('',(#21445),#16764,.T.) ;
#89766 = ADVANCED_FACE('',(#21446),#15460,.F.) ;
#89767 = ADVANCED_FACE('',(#21447),#15461,.T.) ;
#89768 = ADVANCED_FACE('',(#21448),#15462,.F.) ;
#89769 = ADVANCED_FACE('',(#21449),#15463,.T.) ;
#89770 = ADVANCED_FACE('',(#21450),#16765,.F.) ;
#89771 = ADVANCED_FACE('',(#21451),#16766,.T.) ;
#89772 = ADVANCED_FACE('',(#21452),#79450,.T.) ;
#89773 = ADVANCED_FACE('',(#21453),#15464,.F.) ;
#89774 = ADVANCED_FACE('',(#21454),#15465,.T.) ;
#89775 = ADVANCED_FACE('',(#21455),#15466,.T.) ;
#89776 = ADVANCED_FACE('',(#21456),#15467,.T.) ;
#89777 = ADVANCED_FACE('',(#21457),#79451,.F.) ;
#89778 = ADVANCED_FACE('',(#21458),#16767,.T.) ;
#89779 = ADVANCED_FACE('',(#21459),#15468,.F.) ;
#89780 = ADVANCED_FACE('',(#21460),#15469,.T.) ;
#89781 = ADVANCED_FACE('',(#21461),#15470,.F.) ;
#89782 = ADVANCED_FACE('',(#21462),#15471,.F.) ;
#89783 = ADVANCED_FACE('',(#21463),#79452,.F.) ;
#89784 = ADVANCED_FACE('',(#21464),#16768,.F.) ;
#89785 = ADVANCED_FACE('',(#21465),#15472,.F.) ;
#89786 = ADVANCED_FACE('',(#21466),#138,.F.) ;
#89787 = ADVANCED_FACE('',(#21467),#15473,.F.) ;
#89788 = ADVANCED_FACE('',(#21468),#139,.F.) ;
#89789 = ADVANCED_FACE('',(#21469),#16769,.F.) ;
#89790 = ADVANCED_FACE('',(#21470),#140,.F.) ;
#89791 = ADVANCED_FACE('',(#21471),#15474,.F.) ;
#89792 = ADVANCED_FACE('',(#21472),#15475,.F.) ;
#89793 = ADVANCED_FACE('',(#21473),#15476,.F.) ;
#89794 = ADVANCED_FACE('',(#21474),#15477,.F.) ;
#89795 = ADVANCED_FACE('',(#21475),#16770,.F.) ;
#89796 = ADVANCED_FACE('',(#21476),#16771,.F.) ;
#89797 = ADVANCED_FACE('',(#21477),#15478,.F.) ;
#89798 = ADVANCED_FACE('',(#21478),#15479,.F.) ;
#89799 = ADVANCED_FACE('',(#21479),#16772,.F.) ;
#89800 = ADVANCED_FACE('',(#21480),#15480,.F.) ;
#89801 = ADVANCED_FACE('',(#21481),#141,.F.) ;
#89802 = ADVANCED_FACE('',(#21482),#142,.F.) ;
#89803 = ADVANCED_FACE('',(#21483),#143,.F.) ;
#89804 = ADVANCED_FACE('',(#21484),#15481,.F.) ;
#89805 = ADVANCED_FACE('',(#21485),#15482,.F.) ;
#89806 = ADVANCED_FACE('',(#21486),#16773,.F.) ;
#89807 = ADVANCED_FACE('',(#21487),#15483,.F.) ;
#89808 = ADVANCED_FACE('',(#21488),#15484,.F.) ;
#89809 = ADVANCED_FACE('',(#21489),#16774,.F.) ;
#89810 = ADVANCED_FACE('',(#21490),#15485,.F.) ;
#89811 = ADVANCED_FACE('',(#21491),#144,.F.) ;
#89812 = ADVANCED_FACE('',(#21492),#145,.F.) ;
#89813 = ADVANCED_FACE('',(#21493),#146,.F.) ;
#89814 = ADVANCED_FACE('',(#21494),#147,.F.) ;
#89815 = ADVANCED_FACE('',(#21495),#15486,.F.) ;
#89816 = ADVANCED_FACE('',(#21496),#15487,.F.) ;
#89817 = ADVANCED_FACE('',(#21497),#16775,.F.) ;
#89818 = ADVANCED_FACE('',(#21498),#15488,.F.) ;
#89819 = ADVANCED_FACE('',(#21499),#15489,.F.) ;
#89820 = ADVANCED_FACE('',(#21500),#16776,.F.) ;
#89821 = ADVANCED_FACE('',(#21501),#15490,.F.) ;
#89822 = ADVANCED_FACE('',(#21502),#148,.F.) ;
#89823 = ADVANCED_FACE('',(#21503),#149,.F.) ;
#89824 = ADVANCED_FACE('',(#21504),#79453,.F.) ;
#89825 = ADVANCED_FACE('',(#21505),#15491,.F.) ;
#89826 = ADVANCED_FACE('',(#21506),#15492,.F.) ;
#89827 = ADVANCED_FACE('',(#21507),#79454,.F.) ;
#89828 = ADVANCED_FACE('',(#21508),#79455,.F.) ;
#89829 = ADVANCED_FACE('',(#21509),#15493,.F.) ;
#89830 = ADVANCED_FACE('',(#21510),#15494,.F.) ;
#89831 = ADVANCED_FACE('',(#21511),#79456,.F.) ;
#89832 = ADVANCED_FACE('',(#21512),#15495,.T.) ;
#89833 = ADVANCED_FACE('',(#21513),#15496,.T.) ;
#89834 = ADVANCED_FACE('',(#21514),#15497,.T.) ;
#89835 = ADVANCED_FACE('',(#21515),#16777,.T.) ;
#89836 = ADVANCED_FACE('',(#21516),#16778,.T.) ;
#89837 = ADVANCED_FACE('',(#21517),#15498,.T.) ;
#89838 = ADVANCED_FACE('',(#21518),#15499,.T.) ;
#89839 = ADVANCED_FACE('',(#21519),#15500,.T.) ;
#89840 = ADVANCED_FACE('',(#21520),#15501,.T.) ;
#89841 = ADVANCED_FACE('',(#21521),#16779,.T.) ;
#89842 = ADVANCED_FACE('',(#21522),#16780,.T.) ;
#89843 = ADVANCED_FACE('',(#21523),#15502,.T.) ;
#89844 = ADVANCED_FACE('',(#21524),#15503,.T.) ;
#89845 = ADVANCED_FACE('',(#21525),#79457,.T.) ;
#89846 = ADVANCED_FACE('',(#21526),#79458,.T.) ;
#89847 = ADVANCED_FACE('',(#21527),#15504,.T.) ;
#89848 = ADVANCED_FACE('',(#21528),#15505,.F.) ;
#89849 = ADVANCED_FACE('',(#21529),#15506,.F.) ;
#89850 = ADVANCED_FACE('',(#21530),#15507,.F.) ;
#89851 = ADVANCED_FACE('',(#21531),#15508,.T.) ;
#89852 = ADVANCED_FACE('',(#21532),#15509,.T.) ;
#89853 = ADVANCED_FACE('',(#21533),#79459,.T.) ;
#89854 = ADVANCED_FACE('',(#21534),#16781,.F.) ;
#89855 = ADVANCED_FACE('',(#21535),#16782,.F.) ;
#89856 = ADVANCED_FACE('',(#21536),#79460,.T.) ;
#89857 = ADVANCED_FACE('',(#21537),#15510,.F.) ;
#89858 = ADVANCED_FACE('',(#21538),#15511,.F.) ;
#89859 = ADVANCED_FACE('',(#21539),#15512,.F.) ;
#89860 = ADVANCED_FACE('',(#21540),#15513,.F.) ;
#89861 = ADVANCED_FACE('',(#21541),#16783,.F.) ;
#89862 = ADVANCED_FACE('',(#21542),#16784,.F.) ;
#89863 = ADVANCED_FACE('',(#21543),#15514,.F.) ;
#89864 = ADVANCED_FACE('',(#21544),#15515,.T.) ;
#89865 = ADVANCED_FACE('',(#21545),#15516,.T.) ;
#89866 = ADVANCED_FACE('',(#21546),#15517,.T.) ;
#89867 = ADVANCED_FACE('',(#21547),#16785,.T.) ;
#89868 = ADVANCED_FACE('',(#21548),#16786,.T.) ;
#89869 = ADVANCED_FACE('',(#21549),#15518,.T.) ;
#89870 = ADVANCED_FACE('',(#21550),#15519,.T.) ;
#89871 = ADVANCED_FACE('',(#21551),#15520,.T.) ;
#89872 = ADVANCED_FACE('',(#21552),#15521,.T.) ;
#89873 = ADVANCED_FACE('',(#21553),#16787,.T.) ;
#89874 = ADVANCED_FACE('',(#21554),#16788,.T.) ;
#89875 = ADVANCED_FACE('',(#21555),#15522,.T.) ;
#89876 = ADVANCED_FACE('',(#21556),#15523,.T.) ;
#89877 = ADVANCED_FACE('',(#21557),#16789,.T.) ;
#89878 = ADVANCED_FACE('',(#21558),#16790,.T.) ;
#89879 = ADVANCED_FACE('',(#21559),#15524,.T.) ;
#89880 = ADVANCED_FACE('',(#21560),#15525,.T.) ;
#89881 = ADVANCED_FACE('',(#21561),#16791,.T.) ;
#89882 = ADVANCED_FACE('',(#21562),#16792,.T.) ;
#89883 = ADVANCED_FACE('',(#21563),#15526,.T.) ;
#89884 = ADVANCED_FACE('',(#21564),#15527,.T.) ;
#89885 = ADVANCED_FACE('',(#21565),#15528,.F.) ;
#89886 = ADVANCED_FACE('',(#21566),#15529,.F.) ;
#89887 = ADVANCED_FACE('',(#21567),#15530,.T.) ;
#89888 = ADVANCED_FACE('',(#21568),#16793,.T.) ;
#89889 = ADVANCED_FACE('',(#21569),#15531,.T.) ;
#89890 = ADVANCED_FACE('',(#21570),#15532,.T.) ;
#89891 = ADVANCED_FACE('',(#21571),#79461,.T.) ;
#89892 = ADVANCED_FACE('',(#21572),#15533,.T.) ;
#89893 = ADVANCED_FACE('',(#21573),#16794,.T.) ;
#89894 = ADVANCED_FACE('',(#21574),#79462,.F.) ;
#89895 = ADVANCED_FACE('',(#21575),#16795,.T.) ;
#89896 = ADVANCED_FACE('',(#21576),#15534,.T.) ;
#89897 = ADVANCED_FACE('',(#21577),#15535,.T.) ;
#89898 = ADVANCED_FACE('',(#21578),#15536,.F.) ;
#89899 = ADVANCED_FACE('',(#21579),#79463,.F.) ;
#89900 = ADVANCED_FACE('',(#21580),#15537,.T.) ;
#89901 = ADVANCED_FACE('',(#21581),#15538,.T.) ;
#89902 = ADVANCED_FACE('',(#21582),#15539,.T.) ;
#89903 = ADVANCED_FACE('',(#21583),#79464,.T.) ;
#89904 = ADVANCED_FACE('',(#21584),#79465,.F.) ;
#89905 = ADVANCED_FACE('',(#21585),#16796,.T.) ;
#89906 = ADVANCED_FACE('',(#21586),#15540,.F.) ;
#89907 = ADVANCED_FACE('',(#21587),#15541,.T.) ;
#89908 = ADVANCED_FACE('',(#21588),#15542,.F.) ;
#89909 = ADVANCED_FACE('',(#21589),#15543,.T.) ;
#89910 = ADVANCED_FACE('',(#21590),#16797,.F.) ;
#89911 = ADVANCED_FACE('',(#21591),#16798,.T.) ;
#89912 = ADVANCED_FACE('',(#21592),#79466,.T.) ;
#89913 = ADVANCED_FACE('',(#21593),#15544,.F.) ;
#89914 = ADVANCED_FACE('',(#21594),#15545,.T.) ;
#89915 = ADVANCED_FACE('',(#21595),#15546,.T.) ;
#89916 = ADVANCED_FACE('',(#21596),#15547,.T.) ;
#89917 = ADVANCED_FACE('',(#21597),#79467,.F.) ;
#89918 = ADVANCED_FACE('',(#21598),#16799,.T.) ;
#89919 = ADVANCED_FACE('',(#21599),#15548,.F.) ;
#89920 = ADVANCED_FACE('',(#21600),#15549,.T.) ;
#89921 = ADVANCED_FACE('',(#21601),#15550,.F.) ;
#89922 = ADVANCED_FACE('',(#21602),#15551,.F.) ;
#89923 = ADVANCED_FACE('',(#21603),#79468,.F.) ;
#89924 = ADVANCED_FACE('',(#21604),#16800,.F.) ;
#89925 = ADVANCED_FACE('',(#21605),#15552,.F.) ;
#89926 = ADVANCED_FACE('',(#21606),#150,.F.) ;
#89927 = ADVANCED_FACE('',(#21607),#15553,.F.) ;
#89928 = ADVANCED_FACE('',(#21608),#151,.F.) ;
#89929 = ADVANCED_FACE('',(#21609),#16801,.F.) ;
#89930 = ADVANCED_FACE('',(#21610),#152,.F.) ;
#89931 = ADVANCED_FACE('',(#21611),#15554,.F.) ;
#89932 = ADVANCED_FACE('',(#21612),#15555,.F.) ;
#89933 = ADVANCED_FACE('',(#21613),#15556,.F.) ;
#89934 = ADVANCED_FACE('',(#21614),#15557,.F.) ;
#89935 = ADVANCED_FACE('',(#21615),#16802,.F.) ;
#89936 = ADVANCED_FACE('',(#21616),#16803,.F.) ;
#89937 = ADVANCED_FACE('',(#21617),#15558,.F.) ;
#89938 = ADVANCED_FACE('',(#21618),#15559,.F.) ;
#89939 = ADVANCED_FACE('',(#21619),#16804,.F.) ;
#89940 = ADVANCED_FACE('',(#21620),#15560,.F.) ;
#89941 = ADVANCED_FACE('',(#21621),#153,.F.) ;
#89942 = ADVANCED_FACE('',(#21622),#154,.F.) ;
#89943 = ADVANCED_FACE('',(#21623),#155,.F.) ;
#89944 = ADVANCED_FACE('',(#21624),#15561,.F.) ;
#89945 = ADVANCED_FACE('',(#21625),#15562,.F.) ;
#89946 = ADVANCED_FACE('',(#21626),#16805,.F.) ;
#89947 = ADVANCED_FACE('',(#21627),#15563,.F.) ;
#89948 = ADVANCED_FACE('',(#21628),#15564,.F.) ;
#89949 = ADVANCED_FACE('',(#21629),#16806,.F.) ;
#89950 = ADVANCED_FACE('',(#21630),#15565,.F.) ;
#89951 = ADVANCED_FACE('',(#21631),#156,.F.) ;
#89952 = ADVANCED_FACE('',(#21632),#157,.F.) ;
#89953 = ADVANCED_FACE('',(#21633),#158,.F.) ;
#89954 = ADVANCED_FACE('',(#21634),#159,.F.) ;
#89955 = ADVANCED_FACE('',(#21635),#15566,.F.) ;
#89956 = ADVANCED_FACE('',(#21636),#15567,.F.) ;
#89957 = ADVANCED_FACE('',(#21637),#16807,.F.) ;
#89958 = ADVANCED_FACE('',(#21638),#15568,.F.) ;
#89959 = ADVANCED_FACE('',(#21639),#15569,.F.) ;
#89960 = ADVANCED_FACE('',(#21640),#16808,.F.) ;
#89961 = ADVANCED_FACE('',(#21641),#15570,.F.) ;
#89962 = ADVANCED_FACE('',(#21642),#160,.F.) ;
#89963 = ADVANCED_FACE('',(#21643),#161,.F.) ;
#89964 = ADVANCED_FACE('',(#21644),#79469,.F.) ;
#89965 = ADVANCED_FACE('',(#21645),#15571,.F.) ;
#89966 = ADVANCED_FACE('',(#21646),#15572,.F.) ;
#89967 = ADVANCED_FACE('',(#21647),#79470,.F.) ;
#89968 = ADVANCED_FACE('',(#21648),#79471,.F.) ;
#89969 = ADVANCED_FACE('',(#21649),#15573,.F.) ;
#89970 = ADVANCED_FACE('',(#21650),#15574,.F.) ;
#89971 = ADVANCED_FACE('',(#21651),#79472,.F.) ;
#89972 = ADVANCED_FACE('',(#21652),#15575,.T.) ;
#89973 = ADVANCED_FACE('',(#21653),#15576,.T.) ;
#89974 = ADVANCED_FACE('',(#21654),#15577,.T.) ;
#89975 = ADVANCED_FACE('',(#21655),#16809,.T.) ;
#89976 = ADVANCED_FACE('',(#21656),#16810,.T.) ;
#89977 = ADVANCED_FACE('',(#21657),#15578,.T.) ;
#89978 = ADVANCED_FACE('',(#21658),#15579,.T.) ;
#89979 = ADVANCED_FACE('',(#21659),#15580,.T.) ;
#89980 = ADVANCED_FACE('',(#21660),#15581,.T.) ;
#89981 = ADVANCED_FACE('',(#21661),#16811,.T.) ;
#89982 = ADVANCED_FACE('',(#21662),#16812,.T.) ;
#89983 = ADVANCED_FACE('',(#21663),#15582,.T.) ;
#89984 = ADVANCED_FACE('',(#21664),#15583,.T.) ;
#89985 = ADVANCED_FACE('',(#21665),#79473,.T.) ;
#89986 = ADVANCED_FACE('',(#21666),#79474,.T.) ;
#89987 = ADVANCED_FACE('',(#21667),#15584,.T.) ;
#89988 = ADVANCED_FACE('',(#21668),#15585,.F.) ;
#89989 = ADVANCED_FACE('',(#21669),#15586,.F.) ;
#89990 = ADVANCED_FACE('',(#21670),#15587,.F.) ;
#89991 = ADVANCED_FACE('',(#21671),#15588,.T.) ;
#89992 = ADVANCED_FACE('',(#21672),#15589,.T.) ;
#89993 = ADVANCED_FACE('',(#21673),#79475,.T.) ;
#89994 = ADVANCED_FACE('',(#21674),#16813,.F.) ;
#89995 = ADVANCED_FACE('',(#21675),#16814,.F.) ;
#89996 = ADVANCED_FACE('',(#21676),#79476,.T.) ;
#89997 = ADVANCED_FACE('',(#21677),#15590,.F.) ;
#89998 = ADVANCED_FACE('',(#21678),#15591,.F.) ;
#89999 = ADVANCED_FACE('',(#21679),#15592,.F.) ;
#90000 = ADVANCED_FACE('',(#21680),#15593,.F.) ;
#90001 = ADVANCED_FACE('',(#21681),#16815,.F.) ;
#90002 = ADVANCED_FACE('',(#21682),#16816,.F.) ;
#90003 = ADVANCED_FACE('',(#21683),#15594,.F.) ;
#90004 = ADVANCED_FACE('',(#21684),#15595,.T.) ;
#90005 = ADVANCED_FACE('',(#21685),#15596,.T.) ;
#90006 = ADVANCED_FACE('',(#21686),#15597,.T.) ;
#90007 = ADVANCED_FACE('',(#21687),#16817,.T.) ;
#90008 = ADVANCED_FACE('',(#21688),#16818,.T.) ;
#90009 = ADVANCED_FACE('',(#21689),#15598,.T.) ;
#90010 = ADVANCED_FACE('',(#21690),#15599,.T.) ;
#90011 = ADVANCED_FACE('',(#21691),#15600,.T.) ;
#90012 = ADVANCED_FACE('',(#21692),#15601,.T.) ;
#90013 = ADVANCED_FACE('',(#21693),#16819,.T.) ;
#90014 = ADVANCED_FACE('',(#21694),#16820,.T.) ;
#90015 = ADVANCED_FACE('',(#21695),#15602,.T.) ;
#90016 = ADVANCED_FACE('',(#21696),#15603,.T.) ;
#90017 = ADVANCED_FACE('',(#21697),#16821,.T.) ;
#90018 = ADVANCED_FACE('',(#21698),#16822,.T.) ;
#90019 = ADVANCED_FACE('',(#21699),#15604,.T.) ;
#90020 = ADVANCED_FACE('',(#21700),#15605,.T.) ;
#90021 = ADVANCED_FACE('',(#21701),#16823,.T.) ;
#90022 = ADVANCED_FACE('',(#21702),#16824,.T.) ;
#90023 = ADVANCED_FACE('',(#21703),#15606,.T.) ;
#90024 = ADVANCED_FACE('',(#21704),#15607,.T.) ;
#90025 = ADVANCED_FACE('',(#21705),#15608,.F.) ;
#90026 = ADVANCED_FACE('',(#21706),#15609,.F.) ;
#90027 = ADVANCED_FACE('',(#21707),#15610,.T.) ;
#90028 = ADVANCED_FACE('',(#21708),#16825,.T.) ;
#90029 = ADVANCED_FACE('',(#21709),#15611,.T.) ;
#90030 = ADVANCED_FACE('',(#21710),#15612,.T.) ;
#90031 = ADVANCED_FACE('',(#21711),#79477,.T.) ;
#90032 = ADVANCED_FACE('',(#21712),#15613,.T.) ;
#90033 = ADVANCED_FACE('',(#21713),#16826,.T.) ;
#90034 = ADVANCED_FACE('',(#21714),#79478,.F.) ;
#90035 = ADVANCED_FACE('',(#21715),#16827,.T.) ;
#90036 = ADVANCED_FACE('',(#21716),#15614,.T.) ;
#90037 = ADVANCED_FACE('',(#21717),#15615,.T.) ;
#90038 = ADVANCED_FACE('',(#21718),#15616,.F.) ;
#90039 = ADVANCED_FACE('',(#21719),#79479,.F.) ;
#90040 = ADVANCED_FACE('',(#21720),#15617,.T.) ;
#90041 = ADVANCED_FACE('',(#21721),#15618,.T.) ;
#90042 = ADVANCED_FACE('',(#21722),#15619,.T.) ;
#90043 = ADVANCED_FACE('',(#21723),#79480,.T.) ;
#90044 = ADVANCED_FACE('',(#21724),#79481,.F.) ;
#90045 = ADVANCED_FACE('',(#21725),#16828,.T.) ;
#90046 = ADVANCED_FACE('',(#21726),#15620,.F.) ;
#90047 = ADVANCED_FACE('',(#21727),#15621,.T.) ;
#90048 = ADVANCED_FACE('',(#21728),#15622,.F.) ;
#90049 = ADVANCED_FACE('',(#21729),#15623,.T.) ;
#90050 = ADVANCED_FACE('',(#21730),#16829,.F.) ;
#90051 = ADVANCED_FACE('',(#21731),#16830,.T.) ;
#90052 = ADVANCED_FACE('',(#21732),#79482,.T.) ;
#90053 = ADVANCED_FACE('',(#21733),#15624,.F.) ;
#90054 = ADVANCED_FACE('',(#21734),#15625,.T.) ;
#90055 = ADVANCED_FACE('',(#21735),#15626,.T.) ;
#90056 = ADVANCED_FACE('',(#21736),#15627,.T.) ;
#90057 = ADVANCED_FACE('',(#21737),#79483,.F.) ;
#90058 = ADVANCED_FACE('',(#21738),#16831,.T.) ;
#90059 = ADVANCED_FACE('',(#21739),#15628,.F.) ;
#90060 = ADVANCED_FACE('',(#21740),#15629,.T.) ;
#90061 = ADVANCED_FACE('',(#21741),#15630,.F.) ;
#90062 = ADVANCED_FACE('',(#21742),#15631,.F.) ;
#90063 = ADVANCED_FACE('',(#21743),#79484,.F.) ;
#90064 = ADVANCED_FACE('',(#21744),#16832,.F.) ;
#90065 = ADVANCED_FACE('',(#21745),#15632,.F.) ;
#90066 = ADVANCED_FACE('',(#21746),#162,.F.) ;
#90067 = ADVANCED_FACE('',(#21747),#15633,.F.) ;
#90068 = ADVANCED_FACE('',(#21748),#163,.F.) ;
#90069 = ADVANCED_FACE('',(#21749),#16833,.F.) ;
#90070 = ADVANCED_FACE('',(#21750),#164,.F.) ;
#90071 = ADVANCED_FACE('',(#21751),#15634,.F.) ;
#90072 = ADVANCED_FACE('',(#21752),#15635,.F.) ;
#90073 = ADVANCED_FACE('',(#21753),#15636,.F.) ;
#90074 = ADVANCED_FACE('',(#21754),#15637,.F.) ;
#90075 = ADVANCED_FACE('',(#21755),#16834,.F.) ;
#90076 = ADVANCED_FACE('',(#21756),#16835,.F.) ;
#90077 = ADVANCED_FACE('',(#21757),#15638,.F.) ;
#90078 = ADVANCED_FACE('',(#21758),#15639,.F.) ;
#90079 = ADVANCED_FACE('',(#21759),#16836,.F.) ;
#90080 = ADVANCED_FACE('',(#21760),#15640,.F.) ;
#90081 = ADVANCED_FACE('',(#21761),#165,.F.) ;
#90082 = ADVANCED_FACE('',(#21762),#166,.F.) ;
#90083 = ADVANCED_FACE('',(#21763),#167,.F.) ;
#90084 = ADVANCED_FACE('',(#21764),#15641,.F.) ;
#90085 = ADVANCED_FACE('',(#21765),#15642,.F.) ;
#90086 = ADVANCED_FACE('',(#21766),#16837,.F.) ;
#90087 = ADVANCED_FACE('',(#21767),#15643,.F.) ;
#90088 = ADVANCED_FACE('',(#21768),#15644,.F.) ;
#90089 = ADVANCED_FACE('',(#21769),#16838,.F.) ;
#90090 = ADVANCED_FACE('',(#21770),#15645,.F.) ;
#90091 = ADVANCED_FACE('',(#21771),#168,.F.) ;
#90092 = ADVANCED_FACE('',(#21772),#169,.F.) ;
#90093 = ADVANCED_FACE('',(#21773),#170,.F.) ;
#90094 = ADVANCED_FACE('',(#21774),#171,.F.) ;
#90095 = ADVANCED_FACE('',(#21775),#15646,.F.) ;
#90096 = ADVANCED_FACE('',(#21776),#15647,.F.) ;
#90097 = ADVANCED_FACE('',(#21777),#16839,.F.) ;
#90098 = ADVANCED_FACE('',(#21778),#15648,.F.) ;
#90099 = ADVANCED_FACE('',(#21779),#15649,.F.) ;
#90100 = ADVANCED_FACE('',(#21780),#16840,.F.) ;
#90101 = ADVANCED_FACE('',(#21781),#15650,.F.) ;
#90102 = ADVANCED_FACE('',(#21782),#172,.F.) ;
#90103 = ADVANCED_FACE('',(#21783),#173,.F.) ;
#90104 = ADVANCED_FACE('',(#21784),#79485,.F.) ;
#90105 = ADVANCED_FACE('',(#21785),#15651,.F.) ;
#90106 = ADVANCED_FACE('',(#21786),#15652,.F.) ;
#90107 = ADVANCED_FACE('',(#21787),#79486,.F.) ;
#90108 = ADVANCED_FACE('',(#21788),#79487,.F.) ;
#90109 = ADVANCED_FACE('',(#21789),#15653,.F.) ;
#90110 = ADVANCED_FACE('',(#21790),#15654,.F.) ;
#90111 = ADVANCED_FACE('',(#21791),#79488,.F.) ;
#90112 = ADVANCED_FACE('',(#21792),#15655,.T.) ;
#90113 = ADVANCED_FACE('',(#21793),#15656,.T.) ;
#90114 = ADVANCED_FACE('',(#21794),#15657,.T.) ;
#90115 = ADVANCED_FACE('',(#21795),#16841,.T.) ;
#90116 = ADVANCED_FACE('',(#21796),#16842,.T.) ;
#90117 = ADVANCED_FACE('',(#21797),#15658,.T.) ;
#90118 = ADVANCED_FACE('',(#21798),#15659,.T.) ;
#90119 = ADVANCED_FACE('',(#21799),#15660,.T.) ;
#90120 = ADVANCED_FACE('',(#21800),#15661,.T.) ;
#90121 = ADVANCED_FACE('',(#21801),#16843,.T.) ;
#90122 = ADVANCED_FACE('',(#21802),#16844,.T.) ;
#90123 = ADVANCED_FACE('',(#21803),#15662,.T.) ;
#90124 = ADVANCED_FACE('',(#21804),#15663,.T.) ;
#90125 = ADVANCED_FACE('',(#21805),#79489,.T.) ;
#90126 = ADVANCED_FACE('',(#21806),#79490,.T.) ;
#90127 = ADVANCED_FACE('',(#21807),#15664,.T.) ;
#90128 = ADVANCED_FACE('',(#21808),#15665,.F.) ;
#90129 = ADVANCED_FACE('',(#21809),#15666,.F.) ;
#90130 = ADVANCED_FACE('',(#21810),#15667,.F.) ;
#90131 = ADVANCED_FACE('',(#21811),#15668,.T.) ;
#90132 = ADVANCED_FACE('',(#21812),#15669,.T.) ;
#90133 = ADVANCED_FACE('',(#21813),#79491,.T.) ;
#90134 = ADVANCED_FACE('',(#21814),#16845,.F.) ;
#90135 = ADVANCED_FACE('',(#21815),#16846,.F.) ;
#90136 = ADVANCED_FACE('',(#21816),#79492,.T.) ;
#90137 = ADVANCED_FACE('',(#21817),#15670,.F.) ;
#90138 = ADVANCED_FACE('',(#21818),#15671,.F.) ;
#90139 = ADVANCED_FACE('',(#21819),#15672,.F.) ;
#90140 = ADVANCED_FACE('',(#21820),#15673,.F.) ;
#90141 = ADVANCED_FACE('',(#21821),#16847,.F.) ;
#90142 = ADVANCED_FACE('',(#21822),#16848,.F.) ;
#90143 = ADVANCED_FACE('',(#21823),#15674,.F.) ;
#90144 = ADVANCED_FACE('',(#21824),#15675,.T.) ;
#90145 = ADVANCED_FACE('',(#21825),#15676,.T.) ;
#90146 = ADVANCED_FACE('',(#21826),#15677,.T.) ;
#90147 = ADVANCED_FACE('',(#21827),#16849,.T.) ;
#90148 = ADVANCED_FACE('',(#21828),#16850,.T.) ;
#90149 = ADVANCED_FACE('',(#21829),#15678,.T.) ;
#90150 = ADVANCED_FACE('',(#21830),#15679,.T.) ;
#90151 = ADVANCED_FACE('',(#21831),#15680,.T.) ;
#90152 = ADVANCED_FACE('',(#21832),#15681,.T.) ;
#90153 = ADVANCED_FACE('',(#21833),#16851,.T.) ;
#90154 = ADVANCED_FACE('',(#21834),#16852,.T.) ;
#90155 = ADVANCED_FACE('',(#21835),#15682,.T.) ;
#90156 = ADVANCED_FACE('',(#21836),#15683,.T.) ;
#90157 = ADVANCED_FACE('',(#21837),#16853,.T.) ;
#90158 = ADVANCED_FACE('',(#21838),#16854,.T.) ;
#90159 = ADVANCED_FACE('',(#21839),#15684,.T.) ;
#90160 = ADVANCED_FACE('',(#21840),#15685,.T.) ;
#90161 = ADVANCED_FACE('',(#21841),#16855,.T.) ;
#90162 = ADVANCED_FACE('',(#21842),#16856,.T.) ;
#90163 = ADVANCED_FACE('',(#21843),#15686,.T.) ;
#90164 = ADVANCED_FACE('',(#21844),#15687,.T.) ;
#90165 = ADVANCED_FACE('',(#21845),#15688,.F.) ;
#90166 = ADVANCED_FACE('',(#21846),#15689,.F.) ;
#90167 = ADVANCED_FACE('',(#21847),#15690,.T.) ;
#90168 = ADVANCED_FACE('',(#21848),#16857,.T.) ;
#90169 = ADVANCED_FACE('',(#21849),#15691,.T.) ;
#90170 = ADVANCED_FACE('',(#21850),#15692,.T.) ;
#90171 = ADVANCED_FACE('',(#21851),#79493,.T.) ;
#90172 = ADVANCED_FACE('',(#21852),#15693,.T.) ;
#90173 = ADVANCED_FACE('',(#21853),#16858,.T.) ;
#90174 = ADVANCED_FACE('',(#21854),#79494,.F.) ;
#90175 = ADVANCED_FACE('',(#21855),#16859,.T.) ;
#90176 = ADVANCED_FACE('',(#21856),#15694,.T.) ;
#90177 = ADVANCED_FACE('',(#21857),#15695,.T.) ;
#90178 = ADVANCED_FACE('',(#21858),#15696,.F.) ;
#90179 = ADVANCED_FACE('',(#21859),#79495,.F.) ;
#90180 = ADVANCED_FACE('',(#21860),#15697,.T.) ;
#90181 = ADVANCED_FACE('',(#21861),#15698,.T.) ;
#90182 = ADVANCED_FACE('',(#21862),#15699,.T.) ;
#90183 = ADVANCED_FACE('',(#21863),#79496,.T.) ;
#90184 = ADVANCED_FACE('',(#21864),#79497,.F.) ;
#90185 = ADVANCED_FACE('',(#21865),#16860,.T.) ;
#90186 = ADVANCED_FACE('',(#21866),#15700,.F.) ;
#90187 = ADVANCED_FACE('',(#21867),#15701,.T.) ;
#90188 = ADVANCED_FACE('',(#21868),#15702,.F.) ;
#90189 = ADVANCED_FACE('',(#21869),#15703,.T.) ;
#90190 = ADVANCED_FACE('',(#21870),#16861,.F.) ;
#90191 = ADVANCED_FACE('',(#21871),#16862,.T.) ;
#90192 = ADVANCED_FACE('',(#21872),#79498,.T.) ;
#90193 = ADVANCED_FACE('',(#21873),#15704,.F.) ;
#90194 = ADVANCED_FACE('',(#21874),#15705,.T.) ;
#90195 = ADVANCED_FACE('',(#21875),#15706,.T.) ;
#90196 = ADVANCED_FACE('',(#21876),#15707,.T.) ;
#90197 = ADVANCED_FACE('',(#21877),#79499,.F.) ;
#90198 = ADVANCED_FACE('',(#21878),#16863,.T.) ;
#90199 = ADVANCED_FACE('',(#21879),#15708,.F.) ;
#90200 = ADVANCED_FACE('',(#21880),#15709,.T.) ;
#90201 = ADVANCED_FACE('',(#21881),#15710,.F.) ;
#90202 = ADVANCED_FACE('',(#21882),#15711,.F.) ;
#90203 = ADVANCED_FACE('',(#21883),#79500,.F.) ;
#90204 = ADVANCED_FACE('',(#21884),#16864,.F.) ;
#90205 = ADVANCED_FACE('',(#21885),#15712,.F.) ;
#90206 = ADVANCED_FACE('',(#21886),#174,.F.) ;
#90207 = ADVANCED_FACE('',(#21887),#15713,.F.) ;
#90208 = ADVANCED_FACE('',(#21888),#175,.F.) ;
#90209 = ADVANCED_FACE('',(#21889),#16865,.F.) ;
#90210 = ADVANCED_FACE('',(#21890),#176,.F.) ;
#90211 = ADVANCED_FACE('',(#21891),#15714,.F.) ;
#90212 = ADVANCED_FACE('',(#21892),#15715,.F.) ;
#90213 = ADVANCED_FACE('',(#21893),#15716,.F.) ;
#90214 = ADVANCED_FACE('',(#21894),#15717,.F.) ;
#90215 = ADVANCED_FACE('',(#21895),#16866,.F.) ;
#90216 = ADVANCED_FACE('',(#21896),#16867,.F.) ;
#90217 = ADVANCED_FACE('',(#21897),#15718,.F.) ;
#90218 = ADVANCED_FACE('',(#21898),#15719,.F.) ;
#90219 = ADVANCED_FACE('',(#21899),#16868,.F.) ;
#90220 = ADVANCED_FACE('',(#21900),#15720,.F.) ;
#90221 = ADVANCED_FACE('',(#21901),#177,.F.) ;
#90222 = ADVANCED_FACE('',(#21902),#178,.F.) ;
#90223 = ADVANCED_FACE('',(#21903),#179,.F.) ;
#90224 = ADVANCED_FACE('',(#21904),#15721,.F.) ;
#90225 = ADVANCED_FACE('',(#21905),#15722,.F.) ;
#90226 = ADVANCED_FACE('',(#21906),#16869,.F.) ;
#90227 = ADVANCED_FACE('',(#21907),#15723,.F.) ;
#90228 = ADVANCED_FACE('',(#21908),#15724,.F.) ;
#90229 = ADVANCED_FACE('',(#21909),#16870,.F.) ;
#90230 = ADVANCED_FACE('',(#21910),#15725,.F.) ;
#90231 = ADVANCED_FACE('',(#21911),#180,.F.) ;
#90232 = ADVANCED_FACE('',(#21912),#181,.F.) ;
#90233 = ADVANCED_FACE('',(#21913),#182,.F.) ;
#90234 = ADVANCED_FACE('',(#21914),#183,.F.) ;
#90235 = ADVANCED_FACE('',(#21915),#15726,.F.) ;
#90236 = ADVANCED_FACE('',(#21916),#15727,.F.) ;
#90237 = ADVANCED_FACE('',(#21917),#16871,.F.) ;
#90238 = ADVANCED_FACE('',(#21918),#15728,.F.) ;
#90239 = ADVANCED_FACE('',(#21919),#15729,.F.) ;
#90240 = ADVANCED_FACE('',(#21920),#16872,.F.) ;
#90241 = ADVANCED_FACE('',(#21921),#15730,.F.) ;
#90242 = ADVANCED_FACE('',(#21922),#184,.F.) ;
#90243 = ADVANCED_FACE('',(#21923),#185,.F.) ;
#90244 = ADVANCED_FACE('',(#21924),#79501,.F.) ;
#90245 = ADVANCED_FACE('',(#21925),#15731,.F.) ;
#90246 = ADVANCED_FACE('',(#21926),#15732,.F.) ;
#90247 = ADVANCED_FACE('',(#21927),#79502,.F.) ;
#90248 = ADVANCED_FACE('',(#21928),#79503,.F.) ;
#90249 = ADVANCED_FACE('',(#21929),#15733,.F.) ;
#90250 = ADVANCED_FACE('',(#21930),#15734,.F.) ;
#90251 = ADVANCED_FACE('',(#21931),#79504,.F.) ;
#90252 = ADVANCED_FACE('',(#21932),#15735,.T.) ;
#90253 = ADVANCED_FACE('',(#21933),#15736,.T.) ;
#90254 = ADVANCED_FACE('',(#21934),#15737,.T.) ;
#90255 = ADVANCED_FACE('',(#21935),#16873,.T.) ;
#90256 = ADVANCED_FACE('',(#21936),#16874,.T.) ;
#90257 = ADVANCED_FACE('',(#21937),#15738,.T.) ;
#90258 = ADVANCED_FACE('',(#21938),#15739,.T.) ;
#90259 = ADVANCED_FACE('',(#21939),#15740,.T.) ;
#90260 = ADVANCED_FACE('',(#21940),#15741,.T.) ;
#90261 = ADVANCED_FACE('',(#21941),#16875,.T.) ;
#90262 = ADVANCED_FACE('',(#21942),#16876,.T.) ;
#90263 = ADVANCED_FACE('',(#21943),#15742,.T.) ;
#90264 = ADVANCED_FACE('',(#21944),#15743,.T.) ;
#90265 = ADVANCED_FACE('',(#21945),#79505,.T.) ;
#90266 = ADVANCED_FACE('',(#21946),#79506,.T.) ;
#90267 = ADVANCED_FACE('',(#21947),#15744,.T.) ;
#90268 = ADVANCED_FACE('',(#21948),#15745,.F.) ;
#90269 = ADVANCED_FACE('',(#21949),#15746,.F.) ;
#90270 = ADVANCED_FACE('',(#21950),#15747,.F.) ;
#90271 = ADVANCED_FACE('',(#21951),#15748,.T.) ;
#90272 = ADVANCED_FACE('',(#21952),#15749,.T.) ;
#90273 = ADVANCED_FACE('',(#21953),#79507,.T.) ;
#90274 = ADVANCED_FACE('',(#21954),#16877,.F.) ;
#90275 = ADVANCED_FACE('',(#21955),#16878,.F.) ;
#90276 = ADVANCED_FACE('',(#21956),#79508,.T.) ;
#90277 = ADVANCED_FACE('',(#21957),#15750,.F.) ;
#90278 = ADVANCED_FACE('',(#21958),#15751,.F.) ;
#90279 = ADVANCED_FACE('',(#21959),#15752,.F.) ;
#90280 = ADVANCED_FACE('',(#21960),#15753,.F.) ;
#90281 = ADVANCED_FACE('',(#21961),#16879,.F.) ;
#90282 = ADVANCED_FACE('',(#21962),#16880,.F.) ;
#90283 = ADVANCED_FACE('',(#21963),#15754,.F.) ;
#90284 = ADVANCED_FACE('',(#21964),#15755,.T.) ;
#90285 = ADVANCED_FACE('',(#21965),#15756,.T.) ;
#90286 = ADVANCED_FACE('',(#21966),#15757,.T.) ;
#90287 = ADVANCED_FACE('',(#21967),#16881,.T.) ;
#90288 = ADVANCED_FACE('',(#21968),#16882,.T.) ;
#90289 = ADVANCED_FACE('',(#21969),#15758,.T.) ;
#90290 = ADVANCED_FACE('',(#21970),#15759,.T.) ;
#90291 = ADVANCED_FACE('',(#21971),#15760,.T.) ;
#90292 = ADVANCED_FACE('',(#21972),#15761,.T.) ;
#90293 = ADVANCED_FACE('',(#21973),#16883,.T.) ;
#90294 = ADVANCED_FACE('',(#21974),#16884,.T.) ;
#90295 = ADVANCED_FACE('',(#21975),#15762,.T.) ;
#90296 = ADVANCED_FACE('',(#21976),#15763,.T.) ;
#90297 = ADVANCED_FACE('',(#21977),#16885,.T.) ;
#90298 = ADVANCED_FACE('',(#21978),#16886,.T.) ;
#90299 = ADVANCED_FACE('',(#21979),#15764,.T.) ;
#90300 = ADVANCED_FACE('',(#21980),#15765,.T.) ;
#90301 = ADVANCED_FACE('',(#21981),#16887,.T.) ;
#90302 = ADVANCED_FACE('',(#21982),#16888,.T.) ;
#90303 = ADVANCED_FACE('',(#21983),#15766,.T.) ;
#90304 = ADVANCED_FACE('',(#21984),#15767,.T.) ;
#90305 = ADVANCED_FACE('',(#21985),#15768,.F.) ;
#90306 = ADVANCED_FACE('',(#21986),#15769,.F.) ;
#90307 = ADVANCED_FACE('',(#21987),#15770,.T.) ;
#90308 = ADVANCED_FACE('',(#21988),#16889,.T.) ;
#90309 = ADVANCED_FACE('',(#21989),#15771,.T.) ;
#90310 = ADVANCED_FACE('',(#21990),#15772,.T.) ;
#90311 = ADVANCED_FACE('',(#21991),#79509,.T.) ;
#90312 = ADVANCED_FACE('',(#21992),#15773,.T.) ;
#90313 = ADVANCED_FACE('',(#21993),#16890,.T.) ;
#90314 = ADVANCED_FACE('',(#21994),#79510,.F.) ;
#90315 = ADVANCED_FACE('',(#21995),#16891,.T.) ;
#90316 = ADVANCED_FACE('',(#21996),#15774,.T.) ;
#90317 = ADVANCED_FACE('',(#21997),#15775,.T.) ;
#90318 = ADVANCED_FACE('',(#21998),#15776,.F.) ;
#90319 = ADVANCED_FACE('',(#21999),#79511,.F.) ;
#90320 = ADVANCED_FACE('',(#22000),#15777,.T.) ;
#90321 = ADVANCED_FACE('',(#22001),#15778,.T.) ;
#90322 = ADVANCED_FACE('',(#22002),#15779,.T.) ;
#90323 = ADVANCED_FACE('',(#22003),#79512,.T.) ;
#90324 = ADVANCED_FACE('',(#22004),#79513,.F.) ;
#90325 = ADVANCED_FACE('',(#22005),#16892,.T.) ;
#90326 = ADVANCED_FACE('',(#22006),#15780,.F.) ;
#90327 = ADVANCED_FACE('',(#22007),#15781,.T.) ;
#90328 = ADVANCED_FACE('',(#22008),#15782,.F.) ;
#90329 = ADVANCED_FACE('',(#22009),#15783,.T.) ;
#90330 = ADVANCED_FACE('',(#22010),#16893,.F.) ;
#90331 = ADVANCED_FACE('',(#22011),#16894,.T.) ;
#90332 = ADVANCED_FACE('',(#22012),#79514,.T.) ;
#90333 = ADVANCED_FACE('',(#22013),#15784,.F.) ;
#90334 = ADVANCED_FACE('',(#22014),#15785,.T.) ;
#90335 = ADVANCED_FACE('',(#22015),#15786,.T.) ;
#90336 = ADVANCED_FACE('',(#22016),#15787,.T.) ;
#90337 = ADVANCED_FACE('',(#22017),#79515,.F.) ;
#90338 = ADVANCED_FACE('',(#22018),#16895,.T.) ;
#90339 = ADVANCED_FACE('',(#22019),#15788,.F.) ;
#90340 = ADVANCED_FACE('',(#22020),#15789,.T.) ;
#90341 = ADVANCED_FACE('',(#22021),#15790,.F.) ;
#90342 = ADVANCED_FACE('',(#22022),#15791,.F.) ;
#90343 = ADVANCED_FACE('',(#22023),#79516,.F.) ;
#90344 = ADVANCED_FACE('',(#22024),#16896,.F.) ;
#90345 = ADVANCED_FACE('',(#22025),#15792,.F.) ;
#90346 = ADVANCED_FACE('',(#22026),#186,.F.) ;
#90347 = ADVANCED_FACE('',(#22027),#15793,.F.) ;
#90348 = ADVANCED_FACE('',(#22028),#187,.F.) ;
#90349 = ADVANCED_FACE('',(#22029),#16897,.F.) ;
#90350 = ADVANCED_FACE('',(#22030),#188,.F.) ;
#90351 = ADVANCED_FACE('',(#22031),#15794,.F.) ;
#90352 = ADVANCED_FACE('',(#22032),#15795,.F.) ;
#90353 = ADVANCED_FACE('',(#22033),#15796,.F.) ;
#90354 = ADVANCED_FACE('',(#22034),#15797,.F.) ;
#90355 = ADVANCED_FACE('',(#22035),#16898,.F.) ;
#90356 = ADVANCED_FACE('',(#22036),#16899,.F.) ;
#90357 = ADVANCED_FACE('',(#22037),#15798,.F.) ;
#90358 = ADVANCED_FACE('',(#22038),#15799,.F.) ;
#90359 = ADVANCED_FACE('',(#22039),#16900,.F.) ;
#90360 = ADVANCED_FACE('',(#22040),#15800,.F.) ;
#90361 = ADVANCED_FACE('',(#22041),#189,.F.) ;
#90362 = ADVANCED_FACE('',(#22042),#190,.F.) ;
#90363 = ADVANCED_FACE('',(#22043),#191,.F.) ;
#90364 = ADVANCED_FACE('',(#22044),#15801,.F.) ;
#90365 = ADVANCED_FACE('',(#22045),#15802,.F.) ;
#90366 = ADVANCED_FACE('',(#22046),#16901,.F.) ;
#90367 = ADVANCED_FACE('',(#22047),#15803,.F.) ;
#90368 = ADVANCED_FACE('',(#22048),#15804,.F.) ;
#90369 = ADVANCED_FACE('',(#22049),#16902,.F.) ;
#90370 = ADVANCED_FACE('',(#22050),#15805,.F.) ;
#90371 = ADVANCED_FACE('',(#22051),#192,.F.) ;
#90372 = ADVANCED_FACE('',(#22052),#193,.F.) ;
#90373 = ADVANCED_FACE('',(#22053),#194,.F.) ;
#90374 = ADVANCED_FACE('',(#22054),#195,.F.) ;
#90375 = ADVANCED_FACE('',(#22055),#15806,.F.) ;
#90376 = ADVANCED_FACE('',(#22056),#15807,.F.) ;
#90377 = ADVANCED_FACE('',(#22057),#16903,.F.) ;
#90378 = ADVANCED_FACE('',(#22058),#15808,.F.) ;
#90379 = ADVANCED_FACE('',(#22059),#15809,.F.) ;
#90380 = ADVANCED_FACE('',(#22060),#16904,.F.) ;
#90381 = ADVANCED_FACE('',(#22061),#15810,.F.) ;
#90382 = ADVANCED_FACE('',(#22062),#196,.F.) ;
#90383 = ADVANCED_FACE('',(#22063),#197,.F.) ;
#90384 = ADVANCED_FACE('',(#22064),#79517,.F.) ;
#90385 = ADVANCED_FACE('',(#22065),#15811,.F.) ;
#90386 = ADVANCED_FACE('',(#22066),#15812,.F.) ;
#90387 = ADVANCED_FACE('',(#22067),#79518,.F.) ;
#90388 = ADVANCED_FACE('',(#22068),#79519,.F.) ;
#90389 = ADVANCED_FACE('',(#22069),#15813,.F.) ;
#90390 = ADVANCED_FACE('',(#22070),#15814,.F.) ;
#90391 = ADVANCED_FACE('',(#22071),#79520,.F.) ;
#90392 = ADVANCED_FACE('',(#22072),#15815,.T.) ;
#90393 = ADVANCED_FACE('',(#22073),#15816,.T.) ;
#90394 = ADVANCED_FACE('',(#22074),#15817,.T.) ;
#90395 = ADVANCED_FACE('',(#22075),#16905,.T.) ;
#90396 = ADVANCED_FACE('',(#22076),#16906,.T.) ;
#90397 = ADVANCED_FACE('',(#22077),#15818,.T.) ;
#90398 = ADVANCED_FACE('',(#22078),#15819,.T.) ;
#90399 = ADVANCED_FACE('',(#22079),#15820,.T.) ;
#90400 = ADVANCED_FACE('',(#22080),#15821,.T.) ;
#90401 = ADVANCED_FACE('',(#22081),#16907,.T.) ;
#90402 = ADVANCED_FACE('',(#22082),#16908,.T.) ;
#90403 = ADVANCED_FACE('',(#22083),#15822,.T.) ;
#90404 = ADVANCED_FACE('',(#22084),#15823,.T.) ;
#90405 = ADVANCED_FACE('',(#22085),#79521,.T.) ;
#90406 = ADVANCED_FACE('',(#22086),#79522,.T.) ;
#90407 = ADVANCED_FACE('',(#22087),#15824,.T.) ;
#90408 = ADVANCED_FACE('',(#22088),#15825,.F.) ;
#90409 = ADVANCED_FACE('',(#22089),#15826,.F.) ;
#90410 = ADVANCED_FACE('',(#22090),#15827,.F.) ;
#90411 = ADVANCED_FACE('',(#22091),#15828,.T.) ;
#90412 = ADVANCED_FACE('',(#22092),#15829,.T.) ;
#90413 = ADVANCED_FACE('',(#22093),#79523,.T.) ;
#90414 = ADVANCED_FACE('',(#22094),#16909,.F.) ;
#90415 = ADVANCED_FACE('',(#22095),#16910,.F.) ;
#90416 = ADVANCED_FACE('',(#22096),#79524,.T.) ;
#90417 = ADVANCED_FACE('',(#22097),#15830,.F.) ;
#90418 = ADVANCED_FACE('',(#22098),#15831,.F.) ;
#90419 = ADVANCED_FACE('',(#22099),#15832,.F.) ;
#90420 = ADVANCED_FACE('',(#22100),#15833,.F.) ;
#90421 = ADVANCED_FACE('',(#22101),#16911,.F.) ;
#90422 = ADVANCED_FACE('',(#22102),#16912,.F.) ;
#90423 = ADVANCED_FACE('',(#22103),#15834,.F.) ;
#90424 = ADVANCED_FACE('',(#22104),#15835,.T.) ;
#90425 = ADVANCED_FACE('',(#22105),#15836,.T.) ;
#90426 = ADVANCED_FACE('',(#22106),#15837,.T.) ;
#90427 = ADVANCED_FACE('',(#22107),#16913,.T.) ;
#90428 = ADVANCED_FACE('',(#22108),#16914,.T.) ;
#90429 = ADVANCED_FACE('',(#22109),#15838,.T.) ;
#90430 = ADVANCED_FACE('',(#22110),#15839,.T.) ;
#90431 = ADVANCED_FACE('',(#22111),#15840,.T.) ;
#90432 = ADVANCED_FACE('',(#22112),#15841,.T.) ;
#90433 = ADVANCED_FACE('',(#22113),#16915,.T.) ;
#90434 = ADVANCED_FACE('',(#22114),#16916,.T.) ;
#90435 = ADVANCED_FACE('',(#22115),#15842,.T.) ;
#90436 = ADVANCED_FACE('',(#22116),#15843,.T.) ;
#90437 = ADVANCED_FACE('',(#22117),#16917,.T.) ;
#90438 = ADVANCED_FACE('',(#22118),#16918,.T.) ;
#90439 = ADVANCED_FACE('',(#22119),#15844,.T.) ;
#90440 = ADVANCED_FACE('',(#22120),#15845,.T.) ;
#90441 = ADVANCED_FACE('',(#22121),#16919,.T.) ;
#90442 = ADVANCED_FACE('',(#22122),#16920,.T.) ;
#90443 = ADVANCED_FACE('',(#22123),#15846,.T.) ;
#90444 = ADVANCED_FACE('',(#22124),#15847,.T.) ;
#90445 = ADVANCED_FACE('',(#22125),#15848,.F.) ;
#90446 = ADVANCED_FACE('',(#22126),#15849,.F.) ;
#90447 = ADVANCED_FACE('',(#22127),#15850,.T.) ;
#90448 = ADVANCED_FACE('',(#22128),#16921,.T.) ;
#90449 = ADVANCED_FACE('',(#22129),#15851,.T.) ;
#90450 = ADVANCED_FACE('',(#22130),#15852,.T.) ;
#90451 = ADVANCED_FACE('',(#22131),#79525,.T.) ;
#90452 = ADVANCED_FACE('',(#22132),#15853,.T.) ;
#90453 = ADVANCED_FACE('',(#22133),#16922,.T.) ;
#90454 = ADVANCED_FACE('',(#22134),#79526,.F.) ;
#90455 = ADVANCED_FACE('',(#22135),#16923,.T.) ;
#90456 = ADVANCED_FACE('',(#22136),#15854,.T.) ;
#90457 = ADVANCED_FACE('',(#22137),#15855,.T.) ;
#90458 = ADVANCED_FACE('',(#22138),#15856,.F.) ;
#90459 = ADVANCED_FACE('',(#22139),#79527,.F.) ;
#90460 = ADVANCED_FACE('',(#22140),#15857,.T.) ;
#90461 = ADVANCED_FACE('',(#22141),#15858,.T.) ;
#90462 = ADVANCED_FACE('',(#22142),#15859,.T.) ;
#90463 = ADVANCED_FACE('',(#22143),#79528,.T.) ;
#90464 = ADVANCED_FACE('',(#22144),#79529,.F.) ;
#90465 = ADVANCED_FACE('',(#22145),#16924,.T.) ;
#90466 = ADVANCED_FACE('',(#22146),#15860,.F.) ;
#90467 = ADVANCED_FACE('',(#22147),#15861,.T.) ;
#90468 = ADVANCED_FACE('',(#22148),#15862,.F.) ;
#90469 = ADVANCED_FACE('',(#22149),#15863,.T.) ;
#90470 = ADVANCED_FACE('',(#22150),#16925,.F.) ;
#90471 = ADVANCED_FACE('',(#22151),#16926,.T.) ;
#90472 = ADVANCED_FACE('',(#22152),#79530,.T.) ;
#90473 = ADVANCED_FACE('',(#22153),#15864,.F.) ;
#90474 = ADVANCED_FACE('',(#22154),#15865,.T.) ;
#90475 = ADVANCED_FACE('',(#22155),#15866,.T.) ;
#90476 = ADVANCED_FACE('',(#22156),#15867,.T.) ;
#90477 = ADVANCED_FACE('',(#22157),#79531,.F.) ;
#90478 = ADVANCED_FACE('',(#22158),#16927,.T.) ;
#90479 = ADVANCED_FACE('',(#22159),#15868,.F.) ;
#90480 = ADVANCED_FACE('',(#22160),#15869,.T.) ;
#90481 = ADVANCED_FACE('',(#22161),#15870,.F.) ;
#90482 = ADVANCED_FACE('',(#22162),#15871,.F.) ;
#90483 = ADVANCED_FACE('',(#22163),#79532,.F.) ;
#90484 = ADVANCED_FACE('',(#22164),#16928,.F.) ;
#90485 = ADVANCED_FACE('',(#22165),#15872,.F.) ;
#90486 = ADVANCED_FACE('',(#22166),#198,.F.) ;
#90487 = ADVANCED_FACE('',(#22167),#15873,.F.) ;
#90488 = ADVANCED_FACE('',(#22168),#199,.F.) ;
#90489 = ADVANCED_FACE('',(#22169),#16929,.F.) ;
#90490 = ADVANCED_FACE('',(#22170),#200,.F.) ;
#90491 = ADVANCED_FACE('',(#22171),#15874,.F.) ;
#90492 = ADVANCED_FACE('',(#22172),#15875,.F.) ;
#90493 = ADVANCED_FACE('',(#22173),#15876,.F.) ;
#90494 = ADVANCED_FACE('',(#22174),#15877,.F.) ;
#90495 = ADVANCED_FACE('',(#22175),#16930,.F.) ;
#90496 = ADVANCED_FACE('',(#22176),#16931,.F.) ;
#90497 = ADVANCED_FACE('',(#22177),#15878,.F.) ;
#90498 = ADVANCED_FACE('',(#22178),#15879,.F.) ;
#90499 = ADVANCED_FACE('',(#22179),#16932,.F.) ;
#90500 = ADVANCED_FACE('',(#22180),#15880,.F.) ;
#90501 = ADVANCED_FACE('',(#22181),#201,.F.) ;
#90502 = ADVANCED_FACE('',(#22182),#202,.F.) ;
#90503 = ADVANCED_FACE('',(#22183),#203,.F.) ;
#90504 = ADVANCED_FACE('',(#22184),#15881,.F.) ;
#90505 = ADVANCED_FACE('',(#22185),#15882,.F.) ;
#90506 = ADVANCED_FACE('',(#22186),#16933,.F.) ;
#90507 = ADVANCED_FACE('',(#22187),#15883,.F.) ;
#90508 = ADVANCED_FACE('',(#22188),#15884,.F.) ;
#90509 = ADVANCED_FACE('',(#22189),#16934,.F.) ;
#90510 = ADVANCED_FACE('',(#22190),#15885,.F.) ;
#90511 = ADVANCED_FACE('',(#22191),#204,.F.) ;
#90512 = ADVANCED_FACE('',(#22192),#205,.F.) ;
#90513 = ADVANCED_FACE('',(#22193),#206,.F.) ;
#90514 = ADVANCED_FACE('',(#22194),#207,.F.) ;
#90515 = ADVANCED_FACE('',(#22195),#15886,.F.) ;
#90516 = ADVANCED_FACE('',(#22196),#15887,.F.) ;
#90517 = ADVANCED_FACE('',(#22197),#16935,.F.) ;
#90518 = ADVANCED_FACE('',(#22198),#15888,.F.) ;
#90519 = ADVANCED_FACE('',(#22199),#15889,.F.) ;
#90520 = ADVANCED_FACE('',(#22200),#16936,.F.) ;
#90521 = ADVANCED_FACE('',(#22201),#15890,.F.) ;
#90522 = ADVANCED_FACE('',(#22202),#208,.F.) ;
#90523 = ADVANCED_FACE('',(#22203),#209,.F.) ;
#90524 = ADVANCED_FACE('',(#22204),#79533,.F.) ;
#90525 = ADVANCED_FACE('',(#22205),#15891,.F.) ;
#90526 = ADVANCED_FACE('',(#22206),#15892,.F.) ;
#90527 = ADVANCED_FACE('',(#22207),#79534,.F.) ;
#90528 = ADVANCED_FACE('',(#22208),#79535,.F.) ;
#90529 = ADVANCED_FACE('',(#22209),#15893,.F.) ;
#90530 = ADVANCED_FACE('',(#22210),#15894,.F.) ;
#90531 = ADVANCED_FACE('',(#22211),#79536,.F.) ;
#90532 = ADVANCED_FACE('',(#22212),#15895,.T.) ;
#90533 = ADVANCED_FACE('',(#22213),#15896,.T.) ;
#90534 = ADVANCED_FACE('',(#22214),#15897,.T.) ;
#90535 = ADVANCED_FACE('',(#22215),#16937,.T.) ;
#90536 = ADVANCED_FACE('',(#22216),#16938,.T.) ;
#90537 = ADVANCED_FACE('',(#22217),#15898,.T.) ;
#90538 = ADVANCED_FACE('',(#22218),#15899,.T.) ;
#90539 = ADVANCED_FACE('',(#22219),#15900,.T.) ;
#90540 = ADVANCED_FACE('',(#22220),#15901,.T.) ;
#90541 = ADVANCED_FACE('',(#22221),#16939,.T.) ;
#90542 = ADVANCED_FACE('',(#22222),#16940,.T.) ;
#90543 = ADVANCED_FACE('',(#22223),#15902,.T.) ;
#90544 = ADVANCED_FACE('',(#22224),#15903,.T.) ;
#90545 = ADVANCED_FACE('',(#22225),#79537,.T.) ;
#90546 = ADVANCED_FACE('',(#22226),#79538,.T.) ;
#90547 = ADVANCED_FACE('',(#22227),#15904,.T.) ;
#90548 = ADVANCED_FACE('',(#22228),#15905,.F.) ;
#90549 = ADVANCED_FACE('',(#22229),#15906,.F.) ;
#90550 = ADVANCED_FACE('',(#22230),#15907,.F.) ;
#90551 = ADVANCED_FACE('',(#22231),#15908,.T.) ;
#90552 = ADVANCED_FACE('',(#22232),#15909,.T.) ;
#90553 = ADVANCED_FACE('',(#22233),#79539,.T.) ;
#90554 = ADVANCED_FACE('',(#22234),#16941,.F.) ;
#90555 = ADVANCED_FACE('',(#22235),#16942,.F.) ;
#90556 = ADVANCED_FACE('',(#22236),#79540,.T.) ;
#90557 = ADVANCED_FACE('',(#22237),#15910,.F.) ;
#90558 = ADVANCED_FACE('',(#22238),#15911,.F.) ;
#90559 = ADVANCED_FACE('',(#22239),#15912,.F.) ;
#90560 = ADVANCED_FACE('',(#22240),#15913,.F.) ;
#90561 = ADVANCED_FACE('',(#22241),#16943,.F.) ;
#90562 = ADVANCED_FACE('',(#22242),#16944,.F.) ;
#90563 = ADVANCED_FACE('',(#22243),#15914,.F.) ;
#90564 = ADVANCED_FACE('',(#22244),#15915,.T.) ;
#90565 = ADVANCED_FACE('',(#22245),#15916,.T.) ;
#90566 = ADVANCED_FACE('',(#22246),#15917,.T.) ;
#90567 = ADVANCED_FACE('',(#22247),#16945,.T.) ;
#90568 = ADVANCED_FACE('',(#22248),#16946,.T.) ;
#90569 = ADVANCED_FACE('',(#22249),#15918,.T.) ;
#90570 = ADVANCED_FACE('',(#22250),#15919,.T.) ;
#90571 = ADVANCED_FACE('',(#22251),#15920,.T.) ;
#90572 = ADVANCED_FACE('',(#22252),#15921,.T.) ;
#90573 = ADVANCED_FACE('',(#22253),#16947,.T.) ;
#90574 = ADVANCED_FACE('',(#22254),#16948,.T.) ;
#90575 = ADVANCED_FACE('',(#22255),#15922,.T.) ;
#90576 = ADVANCED_FACE('',(#22256),#15923,.T.) ;
#90577 = ADVANCED_FACE('',(#22257),#16949,.T.) ;
#90578 = ADVANCED_FACE('',(#22258),#16950,.T.) ;
#90579 = ADVANCED_FACE('',(#22259),#15924,.T.) ;
#90580 = ADVANCED_FACE('',(#22260),#15925,.T.) ;
#90581 = ADVANCED_FACE('',(#22261),#16951,.T.) ;
#90582 = ADVANCED_FACE('',(#22262),#16952,.T.) ;
#90583 = ADVANCED_FACE('',(#22263),#15926,.T.) ;
#90584 = ADVANCED_FACE('',(#22264),#15927,.T.) ;
#90585 = ADVANCED_FACE('',(#22265),#15928,.F.) ;
#90586 = ADVANCED_FACE('',(#22266),#15929,.F.) ;
#90587 = ADVANCED_FACE('',(#22267),#15930,.T.) ;
#90588 = ADVANCED_FACE('',(#22268),#16953,.T.) ;
#90589 = ADVANCED_FACE('',(#22269),#15931,.T.) ;
#90590 = ADVANCED_FACE('',(#22270),#15932,.T.) ;
#90591 = ADVANCED_FACE('',(#22271),#79541,.T.) ;
#90592 = ADVANCED_FACE('',(#22272),#15933,.T.) ;
#90593 = ADVANCED_FACE('',(#22273),#16954,.T.) ;
#90594 = ADVANCED_FACE('',(#22274),#79542,.F.) ;
#90595 = ADVANCED_FACE('',(#22275),#16955,.T.) ;
#90596 = ADVANCED_FACE('',(#22276),#15934,.T.) ;
#90597 = ADVANCED_FACE('',(#22277),#15935,.T.) ;
#90598 = ADVANCED_FACE('',(#22278),#15936,.F.) ;
#90599 = ADVANCED_FACE('',(#22279),#79543,.F.) ;
#90600 = ADVANCED_FACE('',(#22280),#15937,.T.) ;
#90601 = ADVANCED_FACE('',(#22281),#15938,.T.) ;
#90602 = ADVANCED_FACE('',(#22282),#15939,.T.) ;
#90603 = ADVANCED_FACE('',(#22283),#79544,.T.) ;
#90604 = ADVANCED_FACE('',(#22284),#79545,.F.) ;
#90605 = ADVANCED_FACE('',(#22285),#16956,.T.) ;
#90606 = ADVANCED_FACE('',(#22286),#15940,.F.) ;
#90607 = ADVANCED_FACE('',(#22287),#15941,.T.) ;
#90608 = ADVANCED_FACE('',(#22288),#15942,.F.) ;
#90609 = ADVANCED_FACE('',(#22289),#15943,.T.) ;
#90610 = ADVANCED_FACE('',(#22290),#16957,.F.) ;
#90611 = ADVANCED_FACE('',(#22291),#16958,.T.) ;
#90612 = ADVANCED_FACE('',(#22292),#79546,.T.) ;
#90613 = ADVANCED_FACE('',(#22293),#15944,.F.) ;
#90614 = ADVANCED_FACE('',(#22294),#15945,.T.) ;
#90615 = ADVANCED_FACE('',(#22295),#15946,.T.) ;
#90616 = ADVANCED_FACE('',(#22296),#15947,.T.) ;
#90617 = ADVANCED_FACE('',(#22297),#79547,.F.) ;
#90618 = ADVANCED_FACE('',(#22298),#16959,.T.) ;
#90619 = ADVANCED_FACE('',(#22299),#15948,.F.) ;
#90620 = ADVANCED_FACE('',(#22300),#15949,.T.) ;
#90621 = ADVANCED_FACE('',(#22301),#15950,.F.) ;
#90622 = ADVANCED_FACE('',(#22302),#15951,.F.) ;
#90623 = ADVANCED_FACE('',(#22303),#79548,.F.) ;
#90624 = ADVANCED_FACE('',(#22304),#16960,.F.) ;
#90625 = ADVANCED_FACE('',(#22305),#15952,.F.) ;
#90626 = ADVANCED_FACE('',(#22306),#210,.F.) ;
#90627 = ADVANCED_FACE('',(#22307),#15953,.F.) ;
#90628 = ADVANCED_FACE('',(#22308),#211,.F.) ;
#90629 = ADVANCED_FACE('',(#22309),#16961,.F.) ;
#90630 = ADVANCED_FACE('',(#22310),#212,.F.) ;
#90631 = ADVANCED_FACE('',(#22311),#15954,.F.) ;
#90632 = ADVANCED_FACE('',(#22312),#15955,.F.) ;
#90633 = ADVANCED_FACE('',(#22313),#15956,.F.) ;
#90634 = ADVANCED_FACE('',(#22314),#15957,.F.) ;
#90635 = ADVANCED_FACE('',(#22315),#16962,.F.) ;
#90636 = ADVANCED_FACE('',(#22316),#16963,.F.) ;
#90637 = ADVANCED_FACE('',(#22317),#15958,.F.) ;
#90638 = ADVANCED_FACE('',(#22318),#15959,.F.) ;
#90639 = ADVANCED_FACE('',(#22319),#16964,.F.) ;
#90640 = ADVANCED_FACE('',(#22320),#15960,.F.) ;
#90641 = ADVANCED_FACE('',(#22321),#213,.F.) ;
#90642 = ADVANCED_FACE('',(#22322),#214,.F.) ;
#90643 = ADVANCED_FACE('',(#22323),#215,.F.) ;
#90644 = ADVANCED_FACE('',(#22324),#15961,.F.) ;
#90645 = ADVANCED_FACE('',(#22325),#15962,.F.) ;
#90646 = ADVANCED_FACE('',(#22326),#16965,.F.) ;
#90647 = ADVANCED_FACE('',(#22327),#15963,.F.) ;
#90648 = ADVANCED_FACE('',(#22328),#15964,.F.) ;
#90649 = ADVANCED_FACE('',(#22329),#16966,.F.) ;
#90650 = ADVANCED_FACE('',(#22330),#15965,.F.) ;
#90651 = ADVANCED_FACE('',(#22331),#216,.F.) ;
#90652 = ADVANCED_FACE('',(#22332),#217,.F.) ;
#90653 = ADVANCED_FACE('',(#22333),#218,.F.) ;
#90654 = ADVANCED_FACE('',(#22334),#219,.F.) ;
#90655 = ADVANCED_FACE('',(#22335),#15966,.F.) ;
#90656 = ADVANCED_FACE('',(#22336),#15967,.F.) ;
#90657 = ADVANCED_FACE('',(#22337),#16967,.F.) ;
#90658 = ADVANCED_FACE('',(#22338),#15968,.F.) ;
#90659 = ADVANCED_FACE('',(#22339),#15969,.F.) ;
#90660 = ADVANCED_FACE('',(#22340),#16968,.F.) ;
#90661 = ADVANCED_FACE('',(#22341),#15970,.F.) ;
#90662 = ADVANCED_FACE('',(#22342),#220,.F.) ;
#90663 = ADVANCED_FACE('',(#22343),#221,.F.) ;
#90664 = ADVANCED_FACE('',(#22344),#79549,.F.) ;
#90665 = ADVANCED_FACE('',(#22345),#15971,.F.) ;
#90666 = ADVANCED_FACE('',(#22346),#15972,.F.) ;
#90667 = ADVANCED_FACE('',(#22347),#79550,.F.) ;
#90668 = ADVANCED_FACE('',(#22348),#79551,.F.) ;
#90669 = ADVANCED_FACE('',(#22349),#15973,.F.) ;
#90670 = ADVANCED_FACE('',(#22350),#15974,.F.) ;
#90671 = ADVANCED_FACE('',(#22351),#79552,.F.) ;
#90672 = ADVANCED_FACE('',(#22352),#15975,.T.) ;
#90673 = ADVANCED_FACE('',(#22353),#15976,.T.) ;
#90674 = ADVANCED_FACE('',(#22354),#15977,.T.) ;
#90675 = ADVANCED_FACE('',(#22355),#16969,.T.) ;
#90676 = ADVANCED_FACE('',(#22356),#16970,.T.) ;
#90677 = ADVANCED_FACE('',(#22357),#15978,.T.) ;
#90678 = ADVANCED_FACE('',(#22358),#15979,.T.) ;
#90679 = ADVANCED_FACE('',(#22359),#15980,.T.) ;
#90680 = ADVANCED_FACE('',(#22360),#15981,.T.) ;
#90681 = ADVANCED_FACE('',(#22361),#16971,.T.) ;
#90682 = ADVANCED_FACE('',(#22362),#16972,.T.) ;
#90683 = ADVANCED_FACE('',(#22363),#15982,.T.) ;
#90684 = ADVANCED_FACE('',(#22364),#15983,.T.) ;
#90685 = ADVANCED_FACE('',(#22365),#79553,.T.) ;
#90686 = ADVANCED_FACE('',(#22366),#79554,.T.) ;
#90687 = ADVANCED_FACE('',(#22367),#15984,.T.) ;
#90688 = ADVANCED_FACE('',(#22368),#15985,.F.) ;
#90689 = ADVANCED_FACE('',(#22369),#15986,.F.) ;
#90690 = ADVANCED_FACE('',(#22370),#15987,.F.) ;
#90691 = ADVANCED_FACE('',(#22371),#15988,.T.) ;
#90692 = ADVANCED_FACE('',(#22372),#15989,.T.) ;
#90693 = ADVANCED_FACE('',(#22373),#79555,.T.) ;
#90694 = ADVANCED_FACE('',(#22374),#16973,.F.) ;
#90695 = ADVANCED_FACE('',(#22375),#16974,.F.) ;
#90696 = ADVANCED_FACE('',(#22376),#79556,.T.) ;
#90697 = ADVANCED_FACE('',(#22377),#15990,.F.) ;
#90698 = ADVANCED_FACE('',(#22378),#15991,.F.) ;
#90699 = ADVANCED_FACE('',(#22379),#15992,.F.) ;
#90700 = ADVANCED_FACE('',(#22380),#15993,.F.) ;
#90701 = ADVANCED_FACE('',(#22381),#16975,.F.) ;
#90702 = ADVANCED_FACE('',(#22382),#16976,.F.) ;
#90703 = ADVANCED_FACE('',(#22383),#15994,.F.) ;
#90704 = ADVANCED_FACE('',(#22384),#15995,.T.) ;
#90705 = ADVANCED_FACE('',(#22385),#15996,.T.) ;
#90706 = ADVANCED_FACE('',(#22386),#15997,.T.) ;
#90707 = ADVANCED_FACE('',(#22387),#16977,.T.) ;
#90708 = ADVANCED_FACE('',(#22388),#16978,.T.) ;
#90709 = ADVANCED_FACE('',(#22389),#15998,.T.) ;
#90710 = ADVANCED_FACE('',(#22390),#15999,.T.) ;
#90711 = ADVANCED_FACE('',(#22391),#16000,.T.) ;
#90712 = ADVANCED_FACE('',(#22392),#16001,.T.) ;
#90713 = ADVANCED_FACE('',(#22393),#16979,.T.) ;
#90714 = ADVANCED_FACE('',(#22394),#16980,.T.) ;
#90715 = ADVANCED_FACE('',(#22395),#16002,.T.) ;
#90716 = ADVANCED_FACE('',(#22396),#16003,.T.) ;
#90717 = ADVANCED_FACE('',(#22397),#16981,.T.) ;
#90718 = ADVANCED_FACE('',(#22398),#16982,.T.) ;
#90719 = ADVANCED_FACE('',(#22399),#16004,.T.) ;
#90720 = ADVANCED_FACE('',(#22400),#16005,.T.) ;
#90721 = ADVANCED_FACE('',(#22401),#16983,.T.) ;
#90722 = ADVANCED_FACE('',(#22402),#16984,.T.) ;
#90723 = ADVANCED_FACE('',(#22403),#16006,.T.) ;
#90724 = ADVANCED_FACE('',(#22404),#16007,.T.) ;
#90725 = ADVANCED_FACE('',(#22405),#16008,.F.) ;
#90726 = ADVANCED_FACE('',(#22406),#16009,.F.) ;
#90727 = ADVANCED_FACE('',(#22407),#16010,.T.) ;
#90728 = ADVANCED_FACE('',(#22408),#16985,.T.) ;
#90729 = ADVANCED_FACE('',(#22409),#16011,.T.) ;
#90730 = ADVANCED_FACE('',(#22410),#16012,.T.) ;
#90731 = ADVANCED_FACE('',(#22411),#79557,.T.) ;
#90732 = ADVANCED_FACE('',(#22412),#16013,.T.) ;
#90733 = ADVANCED_FACE('',(#22413),#16986,.T.) ;
#90734 = ADVANCED_FACE('',(#22414),#79558,.F.) ;
#90735 = ADVANCED_FACE('',(#22415),#16987,.T.) ;
#90736 = ADVANCED_FACE('',(#22416),#16014,.T.) ;
#90737 = ADVANCED_FACE('',(#22417),#16015,.T.) ;
#90738 = ADVANCED_FACE('',(#22418),#16016,.F.) ;
#90739 = ADVANCED_FACE('',(#22419),#79559,.F.) ;
#90740 = ADVANCED_FACE('',(#22420),#16017,.T.) ;
#90741 = ADVANCED_FACE('',(#22421),#16018,.T.) ;
#90742 = ADVANCED_FACE('',(#22422),#16019,.T.) ;
#90743 = ADVANCED_FACE('',(#22423),#79560,.T.) ;
#90744 = ADVANCED_FACE('',(#22424),#79561,.F.) ;
#90745 = ADVANCED_FACE('',(#22425),#16988,.T.) ;
#90746 = ADVANCED_FACE('',(#22426),#16020,.F.) ;
#90747 = ADVANCED_FACE('',(#22427),#16021,.T.) ;
#90748 = ADVANCED_FACE('',(#22428),#16022,.F.) ;
#90749 = ADVANCED_FACE('',(#22429),#16023,.T.) ;
#90750 = ADVANCED_FACE('',(#22430),#16989,.F.) ;
#90751 = ADVANCED_FACE('',(#22431),#16990,.T.) ;
#90752 = ADVANCED_FACE('',(#22432),#79562,.T.) ;
#90753 = ADVANCED_FACE('',(#22433),#16024,.F.) ;
#90754 = ADVANCED_FACE('',(#22434),#16025,.T.) ;
#90755 = ADVANCED_FACE('',(#22435),#16026,.T.) ;
#90756 = ADVANCED_FACE('',(#22436),#16027,.T.) ;
#90757 = ADVANCED_FACE('',(#22437),#79563,.F.) ;
#90758 = ADVANCED_FACE('',(#22438),#16991,.T.) ;
#90759 = ADVANCED_FACE('',(#22439),#16028,.F.) ;
#90760 = ADVANCED_FACE('',(#22440),#16029,.T.) ;
#90761 = ADVANCED_FACE('',(#22441),#16030,.F.) ;
#90762 = ADVANCED_FACE('',(#22442),#16031,.F.) ;
#90763 = ADVANCED_FACE('',(#22443),#79564,.F.) ;
#90764 = ADVANCED_FACE('',(#22444),#16992,.F.) ;
#90765 = ADVANCED_FACE('',(#22445),#16032,.F.) ;
#90766 = ADVANCED_FACE('',(#22446),#222,.F.) ;
#90767 = ADVANCED_FACE('',(#22447),#16033,.F.) ;
#90768 = ADVANCED_FACE('',(#22448),#223,.F.) ;
#90769 = ADVANCED_FACE('',(#22449),#16993,.F.) ;
#90770 = ADVANCED_FACE('',(#22450),#224,.F.) ;
#90771 = ADVANCED_FACE('',(#22451),#16034,.F.) ;
#90772 = ADVANCED_FACE('',(#22452),#16035,.F.) ;
#90773 = ADVANCED_FACE('',(#22453),#16036,.F.) ;
#90774 = ADVANCED_FACE('',(#22454),#16037,.F.) ;
#90775 = ADVANCED_FACE('',(#22455),#16994,.F.) ;
#90776 = ADVANCED_FACE('',(#22456),#16995,.F.) ;
#90777 = ADVANCED_FACE('',(#22457),#16038,.F.) ;
#90778 = ADVANCED_FACE('',(#22458),#16039,.F.) ;
#90779 = ADVANCED_FACE('',(#22459),#16996,.F.) ;
#90780 = ADVANCED_FACE('',(#22460),#16040,.F.) ;
#90781 = ADVANCED_FACE('',(#22461),#225,.F.) ;
#90782 = ADVANCED_FACE('',(#22462),#226,.F.) ;
#90783 = ADVANCED_FACE('',(#22463),#227,.F.) ;
#90784 = ADVANCED_FACE('',(#22464),#16041,.F.) ;
#90785 = ADVANCED_FACE('',(#22465),#16042,.F.) ;
#90786 = ADVANCED_FACE('',(#22466),#16997,.F.) ;
#90787 = ADVANCED_FACE('',(#22467),#16043,.F.) ;
#90788 = ADVANCED_FACE('',(#22468),#16044,.F.) ;
#90789 = ADVANCED_FACE('',(#22469),#16998,.F.) ;
#90790 = ADVANCED_FACE('',(#22470),#16045,.F.) ;
#90791 = ADVANCED_FACE('',(#22471),#228,.F.) ;
#90792 = ADVANCED_FACE('',(#22472),#229,.F.) ;
#90793 = ADVANCED_FACE('',(#22473),#230,.F.) ;
#90794 = ADVANCED_FACE('',(#22474),#231,.F.) ;
#90795 = ADVANCED_FACE('',(#22475),#16046,.F.) ;
#90796 = ADVANCED_FACE('',(#22476),#16047,.F.) ;
#90797 = ADVANCED_FACE('',(#22477),#16999,.F.) ;
#90798 = ADVANCED_FACE('',(#22478),#16048,.F.) ;
#90799 = ADVANCED_FACE('',(#22479),#16049,.F.) ;
#90800 = ADVANCED_FACE('',(#22480),#17000,.F.) ;
#90801 = ADVANCED_FACE('',(#22481),#16050,.F.) ;
#90802 = ADVANCED_FACE('',(#22482),#232,.F.) ;
#90803 = ADVANCED_FACE('',(#22483),#233,.F.) ;
#90804 = ADVANCED_FACE('',(#22484),#79565,.F.) ;
#90805 = ADVANCED_FACE('',(#22485),#16051,.F.) ;
#90806 = ADVANCED_FACE('',(#22486),#16052,.F.) ;
#90807 = ADVANCED_FACE('',(#22487),#79566,.F.) ;
#90808 = ADVANCED_FACE('',(#22488),#79567,.F.) ;
#90809 = ADVANCED_FACE('',(#22489),#16053,.F.) ;
#90810 = ADVANCED_FACE('',(#22490),#16054,.F.) ;
#90811 = ADVANCED_FACE('',(#22491),#79568,.F.) ;
#90812 = ADVANCED_FACE('',(#22492),#16055,.T.) ;
#90813 = ADVANCED_FACE('',(#22493),#16056,.T.) ;
#90814 = ADVANCED_FACE('',(#22494),#16057,.T.) ;
#90815 = ADVANCED_FACE('',(#22495),#17001,.T.) ;
#90816 = ADVANCED_FACE('',(#22496),#17002,.T.) ;
#90817 = ADVANCED_FACE('',(#22497),#16058,.T.) ;
#90818 = ADVANCED_FACE('',(#22498),#16059,.T.) ;
#90819 = ADVANCED_FACE('',(#22499),#16060,.T.) ;
#90820 = ADVANCED_FACE('',(#22500),#16061,.T.) ;
#90821 = ADVANCED_FACE('',(#22501),#17003,.T.) ;
#90822 = ADVANCED_FACE('',(#22502),#17004,.T.) ;
#90823 = ADVANCED_FACE('',(#22503),#16062,.T.) ;
#90824 = ADVANCED_FACE('',(#22504),#16063,.T.) ;
#90825 = ADVANCED_FACE('',(#22505),#79569,.T.) ;
#90826 = ADVANCED_FACE('',(#22506),#79570,.T.) ;
#90827 = ADVANCED_FACE('',(#22507),#16064,.T.) ;
#90828 = ADVANCED_FACE('',(#22508),#16065,.F.) ;
#90829 = ADVANCED_FACE('',(#22509),#16066,.F.) ;
#90830 = ADVANCED_FACE('',(#22510),#16067,.F.) ;
#90831 = ADVANCED_FACE('',(#22511),#16068,.T.) ;
#90832 = ADVANCED_FACE('',(#22512),#16069,.T.) ;
#90833 = ADVANCED_FACE('',(#22513),#79571,.T.) ;
#90834 = ADVANCED_FACE('',(#22514),#17005,.F.) ;
#90835 = ADVANCED_FACE('',(#22515),#17006,.F.) ;
#90836 = ADVANCED_FACE('',(#22516),#79572,.T.) ;
#90837 = ADVANCED_FACE('',(#22517),#16070,.F.) ;
#90838 = ADVANCED_FACE('',(#22518),#16071,.F.) ;
#90839 = ADVANCED_FACE('',(#22519),#16072,.F.) ;
#90840 = ADVANCED_FACE('',(#22520),#16073,.F.) ;
#90841 = ADVANCED_FACE('',(#22521),#17007,.F.) ;
#90842 = ADVANCED_FACE('',(#22522),#17008,.F.) ;
#90843 = ADVANCED_FACE('',(#22523),#16074,.F.) ;
#90844 = ADVANCED_FACE('',(#22524),#16075,.T.) ;
#90845 = ADVANCED_FACE('',(#22525),#16076,.T.) ;
#90846 = ADVANCED_FACE('',(#22526),#16077,.T.) ;
#90847 = ADVANCED_FACE('',(#22527),#17009,.T.) ;
#90848 = ADVANCED_FACE('',(#22528),#17010,.T.) ;
#90849 = ADVANCED_FACE('',(#22529),#16078,.T.) ;
#90850 = ADVANCED_FACE('',(#22530),#16079,.T.) ;
#90851 = ADVANCED_FACE('',(#22531),#16080,.T.) ;
#90852 = ADVANCED_FACE('',(#22532),#16081,.T.) ;
#90853 = ADVANCED_FACE('',(#22533),#17011,.T.) ;
#90854 = ADVANCED_FACE('',(#22534),#17012,.T.) ;
#90855 = ADVANCED_FACE('',(#22535),#16082,.T.) ;
#90856 = ADVANCED_FACE('',(#22536),#16083,.T.) ;
#90857 = ADVANCED_FACE('',(#22537),#17013,.T.) ;
#90858 = ADVANCED_FACE('',(#22538),#17014,.T.) ;
#90859 = ADVANCED_FACE('',(#22539),#16084,.T.) ;
#90860 = ADVANCED_FACE('',(#22540),#16085,.T.) ;
#90861 = ADVANCED_FACE('',(#22541),#17015,.T.) ;
#90862 = ADVANCED_FACE('',(#22542),#17016,.T.) ;
#90863 = ADVANCED_FACE('',(#22543),#16086,.T.) ;
#90864 = ADVANCED_FACE('',(#22544),#16087,.T.) ;
#90865 = ADVANCED_FACE('',(#22545),#16088,.F.) ;
#90866 = ADVANCED_FACE('',(#22546),#16089,.F.) ;
#90867 = ADVANCED_FACE('',(#22547),#16090,.T.) ;
#90868 = ADVANCED_FACE('',(#22548),#16091,.F.) ;
#90869 = ADVANCED_FACE('',(#22549),#16092,.F.) ;
#90870 = ADVANCED_FACE('',(#22550),#16093,.F.) ;
#90871 = ADVANCED_FACE('',(#22551),#16094,.F.) ;
#90872 = ADVANCED_FACE('',(#22552),#16095,.F.) ;
#90873 = ADVANCED_FACE('',(#22553),#16096,.F.) ;
#90874 = ADVANCED_FACE('',(#22554),#16097,.F.) ;
#90875 = ADVANCED_FACE('',(#22555),#16098,.F.) ;
#90876 = ADVANCED_FACE('',(#22556),#16099,.F.) ;
#90877 = ADVANCED_FACE('',(#22557),#79573,.T.) ;
#90878 = ADVANCED_FACE('',(#22558),#16100,.T.) ;
#90879 = ADVANCED_FACE('',(#22559),#79574,.T.) ;
#90880 = ADVANCED_FACE('',(#22560),#79575,.T.) ;
#90881 = ADVANCED_FACE('',(#22561),#79576,.T.) ;
#90882 = ADVANCED_FACE('',(#22562),#16101,.T.) ;
#90883 = ADVANCED_FACE('',(#22563),#79577,.T.) ;
#90884 = ADVANCED_FACE('',(#22564),#79578,.T.) ;
#90885 = ADVANCED_FACE('',(#22565),#16102,.T.) ;
#90886 = ADVANCED_FACE('',(#22566),#79579,.T.) ;
#90887 = ADVANCED_FACE('',(#22567),#79580,.T.) ;
#90888 = ADVANCED_FACE('',(#22568),#16103,.T.) ;
#90889 = ADVANCED_FACE('',(#22569),#79581,.T.) ;
#90890 = ADVANCED_FACE('',(#22570),#79582,.T.) ;
#90891 = ADVANCED_FACE('',(#22571),#16104,.T.) ;
#90892 = ADVANCED_FACE('',(#22572),#79583,.T.) ;
#90893 = ADVANCED_FACE('',(#22573),#79584,.T.) ;
#90894 = ADVANCED_FACE('',(#22574),#16105,.T.) ;
#90895 = ADVANCED_FACE('',(#22575),#79585,.T.) ;
#90896 = ADVANCED_FACE('',(#22576),#79586,.T.) ;
#90897 = ADVANCED_FACE('',(#22577),#16106,.T.) ;
#90898 = ADVANCED_FACE('',(#22578),#79587,.T.) ;
#90899 = ADVANCED_FACE('',(#22579),#79588,.T.) ;
#90900 = ADVANCED_FACE('',(#22580),#16107,.T.) ;
#90901 = ADVANCED_FACE('',(#22581),#79589,.T.) ;
#90902 = ADVANCED_FACE('',(#22582),#16108,.T.) ;
#90903 = ADVANCED_FACE('',(#22583),#79590,.T.) ;
#90904 = ADVANCED_FACE('',(#22584),#79591,.T.) ;
#90905 = ADVANCED_FACE('',(#22585),#16109,.T.) ;
#90906 = ADVANCED_FACE('',(#22586),#17017,.T.) ;
#90907 = ADVANCED_FACE('',(#22587),#79592,.T.) ;
#90908 = ADVANCED_FACE('',(#22588),#16110,.T.) ;
#90909 = ADVANCED_FACE('',(#22589),#17018,.T.) ;
#90910 = ADVANCED_FACE('',(#22590),#79593,.T.) ;
#90911 = ADVANCED_FACE('',(#22591),#16111,.T.) ;
#90912 = ADVANCED_FACE('',(#22592),#17019,.T.) ;
#90913 = ADVANCED_FACE('',(#22593),#79594,.T.) ;
#90914 = ADVANCED_FACE('',(#22594),#16112,.T.) ;
#90915 = ADVANCED_FACE('',(#22595),#17020,.T.) ;
#90916 = ADVANCED_FACE('',(#22596),#79595,.T.) ;
#90917 = ADVANCED_FACE('',(#22597),#16113,.T.) ;
#90918 = ADVANCED_FACE('',(#22598),#17021,.T.) ;
#90919 = ADVANCED_FACE('',(#22599),#79596,.T.) ;
#90920 = ADVANCED_FACE('',(#22600),#16114,.T.) ;
#90921 = ADVANCED_FACE('',(#22601),#17022,.T.) ;
#90922 = ADVANCED_FACE('',(#22602),#79597,.T.) ;
#90923 = ADVANCED_FACE('',(#22603),#16115,.T.) ;
#90924 = ADVANCED_FACE('',(#22604),#17023,.T.) ;
#90925 = ADVANCED_FACE('',(#22605),#79598,.T.) ;
#90926 = ADVANCED_FACE('',(#22606),#16116,.T.) ;
#90927 = ADVANCED_FACE('',(#22607),#17024,.T.) ;
#90928 = ADVANCED_FACE('',(#22608),#79599,.T.) ;
#90929 = ADVANCED_FACE('',(#22609),#16117,.T.) ;
#90930 = ADVANCED_FACE('',(#22610),#17025,.T.) ;
#90931 = ADVANCED_FACE('',(#22611),#79600,.T.) ;
#90932 = ADVANCED_FACE('',(#22612),#16118,.T.) ;
#90933 = ADVANCED_FACE('',(#22613),#17026,.T.) ;
#90934 = ADVANCED_FACE('',(#22614),#79601,.T.) ;
#90935 = ADVANCED_FACE('',(#22615),#16119,.T.) ;
#90936 = ADVANCED_FACE('',(#22616),#17027,.T.) ;
#90937 = ADVANCED_FACE('',(#22617),#79602,.T.) ;
#90938 = ADVANCED_FACE('',(#22618),#16120,.T.) ;
#90939 = ADVANCED_FACE('',(#22619),#17028,.T.) ;
#90940 = ADVANCED_FACE('',(#22620),#79603,.T.) ;
#90941 = ADVANCED_FACE('',(#22621),#16121,.T.) ;
#90942 = ADVANCED_FACE('',(#22622),#17029,.T.) ;
#90943 = ADVANCED_FACE('',(#22623),#79604,.T.) ;
#90944 = ADVANCED_FACE('',(#22624),#16122,.T.) ;
#90945 = ADVANCED_FACE('',(#22625),#17030,.T.) ;
#90946 = ADVANCED_FACE('',(#22626),#79605,.T.) ;
#90947 = ADVANCED_FACE('',(#22627),#16123,.T.) ;
#90948 = ADVANCED_FACE('',(#22628),#17031,.T.) ;
#90949 = ADVANCED_FACE('',(#22629),#79606,.T.) ;
#90950 = ADVANCED_FACE('',(#22630),#16124,.T.) ;
#90951 = ADVANCED_FACE('',(#22631),#17032,.T.) ;
#90952 = ADVANCED_FACE('',(#22632),#79607,.T.) ;
#90953 = ADVANCED_FACE('',(#22633),#16125,.T.) ;
#90954 = ADVANCED_FACE('',(#22634),#17033,.T.) ;
#90955 = ADVANCED_FACE('',(#22635),#79608,.T.) ;
#90956 = ADVANCED_FACE('',(#22636),#16126,.T.) ;
#90957 = ADVANCED_FACE('',(#22637),#17034,.T.) ;
#90958 = ADVANCED_FACE('',(#22638),#79609,.F.) ;
#90959 = ADVANCED_FACE('',(#22639),#234,.F.) ;
#90960 = ADVANCED_FACE('',(#22640),#79610,.F.) ;
#90961 = ADVANCED_FACE('',(#22641),#79611,.F.) ;
#90962 = ADVANCED_FACE('',(#22642),#235,.F.) ;
#90963 = ADVANCED_FACE('',(#22643),#79612,.F.) ;
#90964 = ADVANCED_FACE('',(#22644),#79613,.F.) ;
#90965 = ADVANCED_FACE('',(#22645),#236,.F.) ;
#90966 = ADVANCED_FACE('',(#22646),#79614,.F.) ;
#90967 = ADVANCED_FACE('',(#22647),#79615,.F.) ;
#90968 = ADVANCED_FACE('',(#22648),#237,.F.) ;
#90969 = ADVANCED_FACE('',(#22649),#79616,.F.) ;
#90970 = ADVANCED_FACE('',(#22650),#79617,.F.) ;
#90971 = ADVANCED_FACE('',(#22651),#238,.F.) ;
#90972 = ADVANCED_FACE('',(#22652),#79618,.F.) ;
#90973 = ADVANCED_FACE('',(#22653),#79619,.F.) ;
#90974 = ADVANCED_FACE('',(#22654),#239,.F.) ;
#90975 = ADVANCED_FACE('',(#22655),#79620,.F.) ;
#90976 = ADVANCED_FACE('',(#22656),#79621,.F.) ;
#90977 = ADVANCED_FACE('',(#22657),#240,.F.) ;
#90978 = ADVANCED_FACE('',(#22658),#79622,.F.) ;
#90979 = ADVANCED_FACE('',(#22659),#79623,.F.) ;
#90980 = ADVANCED_FACE('',(#22660),#241,.F.) ;
#90981 = ADVANCED_FACE('',(#22661),#79624,.F.) ;
#90982 = ADVANCED_FACE('',(#22662),#79625,.F.) ;
#90983 = ADVANCED_FACE('',(#22663),#242,.F.) ;
#90984 = ADVANCED_FACE('',(#22664),#79626,.F.) ;
#90985 = ADVANCED_FACE('',(#22665),#79627,.F.) ;
#90986 = ADVANCED_FACE('',(#22666),#243,.F.) ;
#90987 = ADVANCED_FACE('',(#22667),#79628,.F.) ;
#90988 = ADVANCED_FACE('',(#22668),#79629,.F.) ;
#90989 = ADVANCED_FACE('',(#22669),#244,.F.) ;
#90990 = ADVANCED_FACE('',(#22670),#79630,.F.) ;
#90991 = ADVANCED_FACE('',(#22671),#79631,.F.) ;
#90992 = ADVANCED_FACE('',(#22672),#245,.F.) ;
#90993 = ADVANCED_FACE('',(#22673),#79632,.F.) ;
#90994 = ADVANCED_FACE('',(#22674),#79633,.F.) ;
#90995 = ADVANCED_FACE('',(#22675),#246,.F.) ;
#90996 = ADVANCED_FACE('',(#22676),#79634,.F.) ;
#90997 = ADVANCED_FACE('',(#22677),#79635,.F.) ;
#90998 = ADVANCED_FACE('',(#22678),#247,.F.) ;
#90999 = ADVANCED_FACE('',(#22679),#79636,.F.) ;
#91000 = ADVANCED_FACE('',(#22680),#79637,.F.) ;
#91001 = ADVANCED_FACE('',(#22681),#248,.F.) ;
#91002 = ADVANCED_FACE('',(#22682),#79638,.F.) ;
#91003 = ADVANCED_FACE('',(#22683),#79639,.F.) ;
#91004 = ADVANCED_FACE('',(#22684),#249,.F.) ;
#91005 = ADVANCED_FACE('',(#22685),#79640,.F.) ;
#91006 = ADVANCED_FACE('',(#22686),#79641,.F.) ;
#91007 = ADVANCED_FACE('',(#22687),#250,.F.) ;
#91008 = ADVANCED_FACE('',(#22688),#79642,.F.) ;
#91009 = ADVANCED_FACE('',(#22689),#79643,.F.) ;
#91010 = ADVANCED_FACE('',(#22690),#251,.F.) ;
#91011 = ADVANCED_FACE('',(#22691),#79644,.F.) ;
#91012 = ADVANCED_FACE('',(#22692),#16127,.T.) ;
#91013 = ADVANCED_FACE('',(#22693),#16128,.T.) ;
#91014 = ADVANCED_FACE('',(#22694),#16129,.T.) ;
#91015 = ADVANCED_FACE('',(#22695),#16130,.T.) ;
#91016 = ADVANCED_FACE('',(#22696),#16131,.T.) ;
#91017 = ADVANCED_FACE('',(#22697),#16132,.T.) ;
#91018 = ADVANCED_FACE('',(#22698),#17035,.T.) ;
#91019 = ADVANCED_FACE('',(#22699),#16133,.T.) ;
#91020 = ADVANCED_FACE('',(#22700),#79645,.T.) ;
#91021 = ADVANCED_FACE('',(#22701),#16134,.T.) ;
#91022 = ADVANCED_FACE('',(#22702),#17036,.T.) ;
#91023 = ADVANCED_FACE('',(#22703),#16135,.T.) ;
#91024 = ADVANCED_FACE('',(#22704),#17037,.T.) ;
#91025 = ADVANCED_FACE('',(#22705),#16136,.T.) ;
#91026 = ADVANCED_FACE('',(#22706),#17038,.T.) ;
#91027 = ADVANCED_FACE('',(#22707),#79646,.T.) ;
#91028 = ADVANCED_FACE('',(#22708),#16137,.T.) ;
#91029 = ADVANCED_FACE('',(#22709),#16138,.T.) ;
#91030 = ADVANCED_FACE('',(#22710),#16139,.F.) ;
#91031 = ADVANCED_FACE('',(#22711),#17039,.T.) ;
#91032 = ADVANCED_FACE('',(#22712),#79647,.F.) ;
#91033 = ADVANCED_FACE('',(#22713),#16140,.T.) ;
#91034 = ADVANCED_FACE('',(#22714),#16141,.T.) ;
#91035 = ADVANCED_FACE('',(#22715),#16142,.F.) ;
#91036 = ADVANCED_FACE('',(#22716),#17040,.T.) ;
#91037 = ADVANCED_FACE('',(#22717),#252,.F.) ;
#91038 = ADVANCED_FACE('',(#22718),#16143,.T.) ;
#91039 = ADVANCED_FACE('',(#22719),#253,.F.) ;
#91040 = ADVANCED_FACE('',(#22720),#79648,.T.) ;
#91041 = ADVANCED_FACE('',(#22721),#254,.F.) ;
#91042 = ADVANCED_FACE('',(#22722),#79649,.T.) ;
#91043 = ADVANCED_FACE('',(#22723),#255,.F.) ;
#91044 = ADVANCED_FACE('',(#22724),#79650,.T.) ;
#91045 = ADVANCED_FACE('',(#22725),#256,.F.) ;
#91046 = ADVANCED_FACE('',(#22726),#79651,.T.) ;
#91047 = ADVANCED_FACE('',(#22727),#257,.F.) ;
#91048 = ADVANCED_FACE('',(#22728),#79652,.T.) ;
#91049 = ADVANCED_FACE('',(#22729),#258,.F.) ;
#91050 = ADVANCED_FACE('',(#22730),#79653,.T.) ;
#91051 = ADVANCED_FACE('',(#22731),#259,.F.) ;
#91052 = ADVANCED_FACE('',(#22732),#79654,.T.) ;
#91053 = ADVANCED_FACE('',(#22733),#260,.F.) ;
#91054 = ADVANCED_FACE('',(#22734),#17041,.T.) ;
#91055 = ADVANCED_FACE('',(#22735),#79655,.T.) ;
#91056 = ADVANCED_FACE('',(#22736),#16144,.T.) ;
#91057 = ADVANCED_FACE('',(#22737),#261,.F.) ;
#91058 = ADVANCED_FACE('',(#22738),#79656,.T.) ;
#91059 = ADVANCED_FACE('',(#22739),#79657,.T.) ;
#91060 = ADVANCED_FACE('',(#22740),#16145,.T.) ;
#91061 = ADVANCED_FACE('',(#22741),#262,.F.) ;
#91062 = ADVANCED_FACE('',(#22742),#17042,.T.) ;
#91063 = ADVANCED_FACE('',(#22743),#79658,.T.) ;
#91064 = ADVANCED_FACE('',(#22744),#16146,.F.) ;
#91065 = ADVANCED_FACE('',(#22745),#16147,.T.) ;
#91066 = ADVANCED_FACE('',(#22746),#79659,.F.) ;
#91067 = ADVANCED_FACE('',(#22747),#17043,.T.) ;
#91068 = ADVANCED_FACE('',(#22748),#16148,.T.) ;
#91069 = ADVANCED_FACE('',(#22749),#16149,.T.) ;
#91070 = ADVANCED_FACE('',(#22750),#16150,.F.) ;
#91071 = ADVANCED_FACE('',(#22751),#16151,.T.) ;
#91072 = ADVANCED_FACE('',(#22752),#17044,.T.) ;
#91073 = ADVANCED_FACE('',(#22753),#79660,.T.) ;
#91074 = ADVANCED_FACE('',(#22754),#16152,.T.) ;
#91075 = ADVANCED_FACE('',(#22755),#16153,.T.) ;
#91076 = ADVANCED_FACE('',(#22756),#17045,.T.) ;
#91077 = ADVANCED_FACE('',(#22757),#16154,.T.) ;
#91078 = ADVANCED_FACE('',(#22758),#17046,.T.) ;
#91079 = ADVANCED_FACE('',(#22759),#263,.F.) ;
#91080 = ADVANCED_FACE('',(#22760),#264,.F.) ;
#91081 = ADVANCED_FACE('',(#22761),#265,.F.) ;
#91082 = ADVANCED_FACE('',(#22762),#266,.F.) ;
#91083 = CLOSED_SHELL('',(#85367,#85368,#85369,#85370,#85371,#85372,#85373,
#85374,#85375,#85376,#85377,#85378,#85379,#85380,#85381,#85382,#85383,#85384,
#85385,#85386,#85387,#85388,#85389,#85390,#85391,#85392,#85393,#85394,#85395,
#85396,#85397,#85398,#85399,#85400,#85401,#85402,#85403,#85404,#85405,#85406,
#85407,#85408,#85409,#85410,#85411,#85412,#85413,#85414,#85415,#85416,#85417,
#85418,#85419,#85420,#85421,#85422,#85423,#85424,#85425,#85426,#85427,#85428,
#85429,#85430,#85431,#85432,#85433,#85434,#85435,#85436,#85437,#85438,#85439,
#85440,#85441,#85442,#85443,#85444,#85445,#85446,#85447,#85448,#85449,#85450,
#85451,#85452,#85453,#85454,#85455,#85456,#85457,#85458,#85459,#85460,#85461,
#85462,#85463,#85464,#85465,#85466,#85467,#85468,#85469,#85470,#85471,#85472,
#85473,#85474,#85475,#85476,#85477,#85478,#85479,#85480,#85481,#85482,#85483,
#85484,#85485,#85486,#85487,#85488,#85489,#85490,#85491,#85492,#85493,#85494,
#85495,#85496,#85497,#85498,#85499,#85500,#85501,#85502,#85503,#85504,#85505,
#85506,#85507,#85508,#85509,#85510,#85511,#85512,#85513,#85514,#85515,#85516,
#85517,#85518,#85519,#85520,#85521,#85522,#85523,#85524,#85525,#85526,#85527,
#85528,#85529,#85530,#85531,#85532,#85533,#85534,#85535,#85536,#85537,#85538,
#85539,#85540,#85541,#85542,#85543,#85544,#85545,#85546,#85547,#85548,#85549,
#85550,#85551,#85552,#85553,#85554,#85555,#85556,#85557,#85558,#85559,#85560,
#85561,#85562,#85563,#85564,#85565,#85566,#85567,#85568,#85569,#85570,#85571,
#85572,#85573,#85574,#85575,#85576,#85577,#85578,#85579,#85580,#85581,#85582,
#85583,#85584,#85585,#85586,#85587,#85588,#85589,#85590,#85591,#85592,#85593,
#85594,#85595,#85596,#85597,#85598,#85599,#85600,#85601,#85602,#85603,#85604,
#85605,#85606,#85607,#85608,#85609,#85610,#85611,#85612,#85613,#85614,#85615,
#85616,#85617,#85618,#85619,#85620,#85621,#85622,#85623,#85624,#85625,#85626,
#85627,#85628,#85629,#85630,#85631,#85632,#85633,#85634,#85635,#85636,#85637,
#85638,#85639,#85640,#85641,#85642,#85643,#85644,#85645,#85646,#85647,#85648,
#85649,#85650,#85651,#85652,#85653,#85654,#85655,#85656,#85657,#85658,#85659,
#85660,#85661,#85662,#85663,#85664,#85665,#85666,#85667,#85668,#85669,#85670,
#85671,#85672,#85673,#85674,#85675,#85676,#85677,#85678,#85679,#85680,#85681,
#85682,#85683,#85684,#85685,#85686,#85687,#85688,#85689,#85690,#85691,#85692,
#85693,#85694,#85695,#85696,#85697,#85698,#85699,#85700,#85701,#85702,#85703,
#85704,#85705,#85706,#85707,#85708,#85709,#85710,#85711,#85712,#85713,#85714,
#85715,#85716,#85717,#85718,#85719,#85720,#85721,#85722,#85723,#85724,#85725,
#85726,#85727,#85728,#85729,#85730,#85731,#85732,#85733,#85734,#85735,#85736,
#85737,#85738,#85739,#85740,#85741,#85742,#85743,#85744,#85745,#85746,#85747,
#85748,#85749,#85750,#85751,#85752,#85753,#85754,#85755,#85756,#85757,#85758,
#85759,#85760,#85761,#85762,#85763,#85764,#85765,#85766,#85767,#85768,#85769,
#85770,#85771,#85772,#85773,#85774,#85775,#85776,#85777,#85778,#85779,#85780,
#85781,#85782,#85783,#85784,#85785,#85786,#85787,#85788,#85789,#85790,#85791,
#85792,#85793,#85794,#85795,#85796,#85797,#85798,#85799,#85800,#85801,#85802,
#85803,#85804,#85805,#85806,#85807,#85808,#85809,#85810,#85811,#85812,#85813,
#85814)) ;
#91084 = CLOSED_SHELL('',(#85815,#85816,#85817,#85818,#85819,#85820,#85821,
#85822,#85823,#85824,#85825,#85826,#85827,#85828,#85829,#85830,#85831,#85832,
#85833,#85834,#85835,#85836,#85837,#85838,#85839,#85840,#85841,#85842,#85843,
#85844,#85845,#85846,#85847,#85848,#85849,#85850,#85851,#85852,#85853,#85854,
#85855,#85856,#85857,#85858,#85859,#85860,#85861,#85862,#85863,#85864,#85865,
#85866,#85867,#85868,#85869,#85870,#85871,#85872,#85873,#85874,#85875,#85876,
#85877,#85878,#85879,#85880,#85881,#85882,#85883,#85884,#85885,#85886,#85887,
#85888,#85889,#85890,#85891,#85892,#85893,#85894,#85895,#85896,#85897,#85898,
#85899,#85900,#85901,#85902,#85903,#85904,#85905,#85906,#85907,#85908,#85909,
#85910,#85911,#85912,#85913,#85914,#85915,#85916,#85917,#85918,#85919,#85920,
#85921,#85922,#85923,#85924,#85925,#85926,#85927,#85928,#85929,#85930,#85931,
#85932,#85933,#85934,#85935,#85936,#85937,#85938,#85939,#85940,#85941,#85942,
#85943,#85944,#85945,#85946,#85947,#85948,#85949,#85950,#85951,#85952,#85953,
#85954,#85955,#85956,#85957,#85958,#85959,#85960,#85961,#85962,#85963,#85964,
#85965,#85966,#85967,#85968,#85969,#85970,#85971,#85972,#85973,#85974,#85975,
#85976,#85977,#85978,#85979,#85980,#85981,#85982,#85983,#85984,#85985,#85986,
#85987,#85988,#85989,#85990,#85991,#85992,#85993,#85994,#85995,#85996,#85997,
#85998,#85999,#86000,#86001,#86002,#86003,#86004,#86005,#86006,#86007,#86008,
#86009,#86010,#86011,#86012,#86013,#86014,#86015,#86016,#86017,#86018,#86019,
#86020,#86021,#86022,#86023,#86024,#86025,#86026,#86027,#86028,#86029,#86030,
#86031,#86032,#86033,#86034,#86035,#86036,#86037,#86038,#86039,#86040,#86041,
#86042,#86043,#86044,#86045,#86046,#86047,#86048,#86049,#86050,#86051,#86052,
#86053,#86054,#86055,#86056,#86057,#86058,#86059,#86060,#86061,#86062,#86063,
#86064,#86065,#86066,#86067,#86068,#86069,#86070,#86071,#86072,#86073,#86074,
#86075,#86076,#86077,#86078,#86079,#86080,#86081,#86082,#86083,#86084,#86085,
#86086,#86087,#86088,#86089,#86090,#86091,#86092,#86093,#86094,#86095,#86096,
#86097,#86098,#86099,#86100,#86101,#86102,#86103,#86104,#86105,#86106,#86107,
#86108,#86109,#86110,#86111,#86112,#86113,#86114,#86115,#86116,#86117,#86118,
#86119,#86120,#86121,#86122,#86123,#86124,#86125,#86126,#86127,#86128,#86129,
#86130,#86131,#86132,#86133,#86134,#86135,#86136,#86137,#86138,#86139,#86140,
#86141,#86142,#86143,#86144,#86145,#86146,#86147,#86148,#86149,#86150,#86151,
#86152,#86153,#86154,#86155,#86156,#86157,#86158,#86159,#86160,#86161,#86162,
#86163,#86164,#86165,#86166,#86167,#86168,#86169,#86170,#86171,#86172,#86173,
#86174,#86175,#86176,#86177,#86178,#86179,#86180,#86181,#86182,#86183,#86184,
#86185,#86186,#86187,#86188,#86189,#86190,#86191,#86192,#86193,#86194,#86195,
#86196,#86197,#86198,#86199,#86200,#86201,#86202,#86203,#86204,#86205,#86206,
#86207,#86208,#86209,#86210,#86211,#86212,#86213,#86214,#86215,#86216,#86217,
#86218,#86219,#86220,#86221,#86222,#86223,#86224,#86225,#86226,#86227,#86228,
#86229,#86230,#86231,#86232,#86233,#86234,#86235,#86236,#86237,#86238,#86239,
#86240,#86241,#86242,#86243,#86244,#86245,#86246,#86247,#86248,#86249,#86250,
#86251,#86252,#86253,#86254,#86255,#86256,#86257,#86258,#86259,#86260,#86261,
#86262)) ;
#91085 = CLOSED_SHELL('',(#86263,#86264,#86265,#86266,#86267,#86268,#86269,
#86270,#86271,#86272,#86273,#86274,#86275,#86276,#86277,#86278,#86279,#86280,
#86281,#86282,#86283,#86284,#86285,#86286,#86287,#86288,#86289,#86290,#86291,
#86292,#86293,#86294,#86295,#86296,#86297,#86298,#86299,#86300,#86301,#86302,
#86303,#86304,#86305,#86306,#86307,#86308,#86309,#86310,#86311,#86312,#86313,
#86314,#86315,#86316,#86317,#86318,#86319,#86320,#86321,#86322,#86323,#86324,
#86325,#86326,#86327,#86328,#86329,#86330,#86331,#86332,#86333,#86334,#86335,
#86336,#86337,#86338,#86339,#86340,#86341,#86342,#86343,#86344,#86345,#86346,
#86347,#86348,#86349,#86350,#86351,#86352,#86353,#86354,#86355,#86356,#86357,
#86358,#86359,#86360,#86361,#86362,#86363,#86364,#86365,#86366,#86367,#86368,
#86369,#86370,#86371,#86372,#86373,#86374,#86375,#86376,#86377,#86378,#86379,
#86380,#86381,#86382,#86383,#86384,#86385,#86386,#86387,#86388,#86389,#86390,
#86391,#86392,#86393,#86394,#86395,#86396,#86397,#86398,#86399,#86400,#86401,
#86402,#86403,#86404,#86405,#86406,#86407,#86408,#86409,#86410,#86411,#86412,
#86413,#86414,#86415,#86416,#86417,#86418,#86419,#86420,#86421,#86422,#86423,
#86424,#86425,#86426,#86427,#86428,#86429,#86430,#86431,#86432,#86433,#86434,
#86435,#86436,#86437,#86438,#86439,#86440,#86441,#86442,#86443,#86444,#86445,
#86446,#86447,#86448,#86449,#86450,#86451,#86452,#86453,#86454,#86455,#86456,
#86457,#86458,#86459,#86460,#86461,#86462,#86463,#86464,#86465,#86466,#86467,
#86468,#86469,#86470,#86471,#86472,#86473,#86474,#86475,#86476,#86477,#86478,
#86479,#86480,#86481,#86482,#86483,#86484,#86485,#86486,#86487)) ;
#91086 = CLOSED_SHELL('',(#86488,#86489,#86490,#86491,#86492,#86493,#86494,
#86495,#86496,#86497,#86498,#86499,#86500,#86501,#86502,#86503,#86504,#86505,
#86506,#86507,#86508,#86509,#86510,#86511,#86512,#86513,#86514,#86515,#86516,
#86517,#86518,#86519,#86520,#86521,#86522,#86523,#86524,#86525,#86526,#86527,
#86528,#86529,#86530,#86531,#86532,#86533,#86534,#86535,#86536,#86537,#86538,
#86539,#86540,#86541,#86542,#86543,#86544,#86545,#86546,#86547,#86548,#86549,
#86550,#86551,#86552,#86553,#86554,#86555,#86556,#86557,#86558,#86559,#86560,
#86561,#86562,#86563,#86564,#86565,#86566,#86567,#86568,#86569,#86570,#86571,
#86572,#86573,#86574,#86575,#86576,#86577,#86578,#86579,#86580,#86581,#86582,
#86583,#86584,#86585,#86586,#86587,#86588,#86589,#86590,#86591,#86592,#86593,
#86594,#86595,#86596,#86597,#86598,#86599,#86600,#86601,#86602,#86603,#86604,
#86605,#86606,#86607,#86608,#86609,#86610,#86611,#86612,#86613,#86614,#86615,
#86616,#86617,#86618,#86619,#86620,#86621,#86622,#86623,#86624,#86625,#86626,
#86627,#86628,#86629,#86630,#86631,#86632,#86633,#86634,#86635,#86636,#86637,
#86638,#86639,#86640,#86641,#86642,#86643,#86644,#86645,#86646,#86647,#86648,
#86649,#86650,#86651,#86652,#86653,#86654,#86655,#86656,#86657,#86658,#86659,
#86660,#86661,#86662,#86663,#86664,#86665,#86666,#86667,#86668,#86669,#86670,
#86671,#86672,#86673,#86674,#86675,#86676,#86677,#86678,#86679,#86680,#86681,
#86682,#86683,#86684,#86685,#86686,#86687,#86688,#86689,#86690,#86691,#86692,
#86693,#86694,#86695,#86696,#86697,#86698,#86699,#86700,#86701,#86702,#86703,
#86704,#86705,#86706,#86707,#86708,#86709,#86710,#86711,#86712,#86713,#86714,
#86715,#86716,#86717,#86718,#86719,#86720,#86721,#86722,#86723,#86724,#86725,
#86726,#86727,#86728,#86729,#86730,#86731,#86732,#86733,#86734,#86735,#86736,
#86737,#86738,#86739,#86740,#86741,#86742,#86743,#86744,#86745,#86746,#86747,
#86748,#86749,#86750,#86751,#86752,#86753,#86754,#86755,#86756,#86757,#86758,
#86759,#86760,#86761,#86762,#86763,#86764,#86765,#86766,#86767,#86768,#86769,
#86770,#86771,#86772,#86773,#86774,#86775,#86776,#86777,#86778,#86779,#86780,
#86781,#86782,#86783,#86784,#86785,#86786,#86787,#86788,#86789,#86790,#86791,
#86792,#86793,#86794,#86795,#86796,#86797,#86798,#86799,#86800,#86801,#86802,
#86803,#86804,#86805,#86806,#86807,#86808,#86809,#86810,#86811,#86812,#86813,
#86814,#86815,#86816,#86817,#86818,#86819,#86820,#86821,#86822,#86823,#86824,
#86825,#86826,#86827,#86828,#86829,#86830,#86831,#86832,#86833,#86834,#86835,
#86836,#86837,#86838,#86839,#86840,#86841,#86842,#86843,#86844,#86845,#86846,
#86847,#86848,#86849,#86850,#86851,#86852,#86853,#86854,#86855,#86856,#86857,
#86858,#86859,#86860,#86861,#86862,#86863,#86864,#86865,#86866,#86867,#86868,
#86869,#86870,#86871,#86872,#86873,#86874,#86875,#86876,#86877,#86878,#86879,
#86880,#86881,#86882,#86883,#86884,#86885,#86886,#86887,#86888,#86889,#86890,
#86891,#86892,#86893,#86894,#86895,#86896,#86897,#86898,#86899,#86900,#86901,
#86902,#86903,#86904,#86905,#86906,#86907,#86908,#86909,#86910,#86911,#86912,
#86913,#86914,#86915,#86916,#86917,#86918,#86919,#86920,#86921,#86922,#86923,
#86924,#86925,#86926,#86927,#86928,#86929,#86930,#86931,#86932,#86933,#86934,
#86935,#86936,#86937,#86938,#86939,#86940,#86941,#86942,#86943,#86944,#86945,
#86946,#86947,#86948,#86949,#86950,#86951,#86952,#86953,#86954,#86955,#86956,
#86957,#86958,#86959,#86960,#86961,#86962,#86963,#86964,#86965,#86966,#86967,
#86968,#86969,#86970,#86971,#86972,#86973,#86974,#86975,#86976,#86977,#86978,
#86979,#86980,#86981,#86982,#86983,#86984,#86985,#86986,#86987,#86988,#86989,
#86990,#86991,#86992,#86993,#86994,#86995,#86996,#86997,#86998,#86999,#87000,
#87001,#87002,#87003,#87004,#87005,#87006,#87007,#87008,#87009,#87010,#87011,
#87012,#87013,#87014,#87015,#87016,#87017,#87018,#87019,#87020,#87021,#87022,
#87023,#87024,#87025,#87026,#87027,#87028,#87029,#87030,#87031,#87032,#87033,
#87034,#87035,#87036,#87037,#87038,#87039,#87040,#87041,#87042,#87043,#87044,
#87045,#87046,#87047,#87048,#87049,#87050,#87051,#87052,#87053,#87054,#87055,
#87056,#87057,#87058,#87059,#87060,#87061,#87062,#87063,#87064,#87065,#87066,
#87067,#87068,#87069,#87070,#87071,#87072,#87073,#87074,#87075,#87076,#87077,
#87078,#87079,#87080,#87081,#87082,#87083,#87084,#87085,#87086,#87087,#87088,
#87089,#87090,#87091,#87092,#87093,#87094,#87095,#87096,#87097,#87098,#87099,
#87100,#87101,#87102,#87103,#87104,#87105,#87106,#87107,#87108,#87109,#87110,
#87111,#87112,#87113,#87114,#87115,#87116,#87117,#87118,#87119,#87120,#87121,
#87122,#87123,#87124,#87125,#87126,#87127,#87128,#87129,#87130,#87131,#87132,
#87133,#87134,#87135,#87136,#87137,#87138,#87139,#87140,#87141,#87142,#87143,
#87144,#87145,#87146,#87147,#87148,#87149,#87150,#87151,#87152,#87153,#87154,
#87155,#87156,#87157,#87158,#87159,#87160,#87161,#87162,#87163,#87164,#87165,
#87166,#87167,#87168,#87169,#87170,#87171,#87172,#87173,#87174,#87175,#87176,
#87177,#87178,#87179,#87180,#87181,#87182,#87183,#87184,#87185,#87186,#87187,
#87188,#87189,#87190,#87191,#87192,#87193,#87194,#87195,#87196,#87197,#87198,
#87199,#87200,#87201,#87202,#87203,#87204,#87205,#87206,#87207,#87208,#87209,
#87210,#87211,#87212,#87213,#87214,#87215,#87216,#87217,#87218,#87219,#87220,
#87221,#87222,#87223,#87224,#87225,#87226,#87227,#87228,#87229,#87230,#87231,
#87232,#87233,#87234,#87235,#87236,#87237,#87238,#87239,#87240,#87241,#87242,
#87243,#87244,#87245,#87246,#87247,#87248,#87249,#87250,#87251,#87252,#87253,
#87254,#87255,#87256,#87257,#87258,#87259,#87260,#87261,#87262,#87263,#87264,
#87265,#87266,#87267,#87268,#87269,#87270,#87271,#87272,#87273,#87274,#87275,
#87276,#87277,#87278,#87279,#87280,#87281,#87282,#87283,#87284,#87285,#87286,
#87287,#87288,#87289,#87290,#87291,#87292,#87293,#87294,#87295,#87296,#87297,
#87298,#87299,#87300,#87301,#87302,#87303,#87304,#87305,#87306,#87307,#87308,
#87309,#87310,#87311,#87312,#87313,#87314,#87315,#87316,#87317,#87318,#87319,
#87320,#87321,#87322,#87323,#87324,#87325,#87326,#87327,#87328,#87329,#87330,
#87331,#87332,#87333,#87334,#87335,#87336,#87337,#87338,#87339,#87340,#87341,
#87342,#87343,#87344,#87345,#87346,#87347,#87348,#87349,#87350,#87351,#87352,
#87353,#87354,#87355,#87356,#87357,#87358,#87359,#87360,#87361,#87362,#87363,
#87364,#87365,#87366,#87367,#87368,#87369,#87370,#87371,#87372,#87373,#87374,
#87375,#87376,#87377,#87378,#87379,#87380,#87381,#87382,#87383,#87384,#87385,
#87386,#87387,#87388,#87389,#87390,#87391,#87392,#87393,#87394,#87395,#87396,
#87397,#87398,#87399,#87400,#87401,#87402,#87403,#87404,#87405,#87406,#87407,
#87408,#87409,#87410,#87411,#87412,#87413,#87414,#87415,#87416,#87417,#87418,
#87419,#87420,#87421,#87422,#87423,#87424,#87425,#87426,#87427,#87428,#87429,
#87430,#87431,#87432,#87433,#87434,#87435,#87436,#87437,#87438,#87439,#87440,
#87441,#87442,#87443,#87444,#87445,#87446,#87447,#87448,#87449,#87450,#87451,
#87452,#87453,#87454,#87455,#87456,#87457,#87458,#87459,#87460,#87461,#87462,
#87463,#87464,#87465,#87466,#87467,#87468,#87469,#87470,#87471,#87472,#87473,
#87474,#87475,#87476,#87477,#87478,#87479,#87480,#87481,#87482,#87483,#87484,
#87485,#87486,#87487,#87488,#87489,#87490,#87491,#87492,#87493,#87494,#87495,
#87496,#87497,#87498,#87499,#87500,#87501,#87502,#87503,#87504,#87505,#87506,
#87507,#87508,#87509,#87510,#87511,#87512,#87513,#87514,#87515,#87516,#87517,
#87518,#87519,#87520,#87521,#87522,#87523,#87524,#87525,#87526,#87527,#87528,
#87529,#87530,#87531,#87532,#87533,#87534,#87535,#87536,#87537,#87538,#87539,
#87540,#87541,#87542,#87543,#87544,#87545,#87546,#87547,#87548,#87549,#87550,
#87551,#87552,#87553,#87554,#87555,#87556,#87557,#87558,#87559,#87560,#87561,
#87562,#87563,#87564,#87565,#87566,#87567,#87568,#87569,#87570,#87571,#87572,
#87573,#87574,#87575,#87576,#87577,#87578,#87579,#87580,#87581,#87582,#87583,
#87584,#87585,#87586,#87587,#87588,#87589,#87590,#87591,#87592,#87593,#87594,
#87595,#87596,#87597,#87598,#87599,#87600,#87601,#87602,#87603,#87604,#87605,
#87606,#87607,#87608,#87609,#87610,#87611,#87612,#87613,#87614,#87615,#87616,
#87617,#87618,#87619,#87620,#87621,#87622,#87623,#87624,#87625,#87626,#87627,
#87628,#87629,#87630,#87631,#87632,#87633,#87634,#87635,#87636,#87637,#87638,
#87639,#87640,#87641,#87642,#87643,#87644,#87645,#87646,#87647,#87648,#87649,
#87650,#87651,#87652,#87653,#87654,#87655,#87656,#87657,#87658,#87659,#87660,
#87661,#87662,#87663,#87664,#87665,#87666,#87667,#87668,#87669,#87670,#87671,
#87672,#87673,#87674,#87675,#87676,#87677,#87678,#87679,#87680,#87681,#87682,
#87683,#87684,#87685,#87686,#87687,#87688,#87689,#87690,#87691,#87692,#87693,
#87694,#87695,#87696,#87697,#87698,#87699,#87700,#87701,#87702,#87703,#87704,
#87705,#87706,#87707,#87708,#87709,#87710,#87711,#87712,#87713,#87714,#87715,
#87716,#87717,#87718,#87719,#87720,#87721,#87722,#87723,#87724,#87725,#87726,
#87727,#87728,#87729,#87730,#87731,#87732,#87733,#87734,#87735,#87736,#87737,
#87738,#87739,#87740,#87741,#87742,#87743,#87744,#87745,#87746,#87747,#87748,
#87749,#87750,#87751,#87752,#87753,#87754,#87755,#87756,#87757,#87758,#87759,
#87760,#87761,#87762,#87763,#87764,#87765,#87766,#87767,#87768,#87769,#87770,
#87771,#87772,#87773,#87774,#87775,#87776,#87777,#87778,#87779,#87780,#87781,
#87782,#87783,#87784,#87785,#87786,#87787,#87788,#87789,#87790,#87791,#87792,
#87793,#87794,#87795,#87796,#87797,#87798,#87799,#87800,#87801,#87802,#87803,
#87804,#87805,#87806,#87807,#87808,#87809,#87810,#87811,#87812,#87813,#87814,
#87815,#87816,#87817,#87818,#87819,#87820,#87821,#87822,#87823,#87824,#87825,
#87826,#87827,#87828,#87829,#87830,#87831,#87832,#87833,#87834,#87835,#87836,
#87837,#87838,#87839,#87840,#87841,#87842,#87843,#87844,#87845,#87846,#87847,
#87848,#87849,#87850,#87851,#87852,#87853,#87854,#87855,#87856,#87857,#87858,
#87859,#87860,#87861,#87862,#87863,#87864,#87865,#87866,#87867,#87868,#87869,
#87870,#87871,#87872,#87873,#87874,#87875,#87876,#87877,#87878,#87879,#87880,
#87881,#87882,#87883,#87884,#87885,#87886,#87887,#87888,#87889,#87890,#87891,
#87892,#87893,#87894,#87895,#87896,#87897,#87898,#87899,#87900,#87901,#87902,
#87903,#87904,#87905,#87906,#87907,#87908,#87909,#87910,#87911,#87912,#87913,
#87914,#87915,#87916,#87917,#87918,#87919,#87920,#87921,#87922,#87923,#87924,
#87925,#87926,#87927,#87928,#87929,#87930,#87931,#87932,#87933,#87934,#87935,
#87936,#87937,#87938,#87939,#87940,#87941,#87942,#87943,#87944,#87945,#87946,
#87947,#87948,#87949,#87950,#87951,#87952,#87953,#87954,#87955,#87956,#87957,
#87958,#87959,#87960,#87961,#87962,#87963,#87964,#87965,#87966,#87967,#87968,
#87969,#87970,#87971,#87972,#87973,#87974,#87975,#87976,#87977,#87978,#87979,
#87980,#87981,#87982,#87983,#87984,#87985,#87986,#87987,#87988,#87989,#87990,
#87991,#87992,#87993,#87994,#87995,#87996,#87997,#87998,#87999,#88000,#88001,
#88002,#88003,#88004,#88005,#88006,#88007,#88008,#88009,#88010,#88011,#88012,
#88013,#88014,#88015,#88016,#88017,#88018,#88019,#88020,#88021,#88022,#88023,
#88024,#88025,#88026,#88027,#88028,#88029,#88030,#88031,#88032,#88033,#88034,
#88035,#88036,#88037,#88038,#88039,#88040,#88041,#88042,#88043,#88044,#88045,
#88046,#88047,#88048,#88049,#88050,#88051,#88052,#88053,#88054,#88055,#88056,
#88057,#88058,#88059,#88060,#88061,#88062,#88063,#88064,#88065,#88066,#88067,
#88068,#88069,#88070,#88071,#88072,#88073,#88074,#88075,#88076,#88077,#88078,
#88079,#88080,#88081,#88082,#88083,#88084,#88085,#88086,#88087,#88088,#88089,
#88090,#88091,#88092,#88093,#88094,#88095,#88096,#88097,#88098,#88099,#88100,
#88101,#88102,#88103,#88104,#88105,#88106,#88107,#88108,#88109,#88110,#88111,
#88112,#88113,#88114,#88115,#88116,#88117,#88118,#88119,#88120,#88121,#88122,
#88123,#88124,#88125,#88126,#88127,#88128,#88129,#88130,#88131,#88132,#88133,
#88134,#88135,#88136,#88137,#88138,#88139,#88140,#88141,#88142,#88143,#88144,
#88145,#88146,#88147,#88148,#88149,#88150,#88151,#88152,#88153,#88154,#88155,
#88156,#88157,#88158,#88159,#88160,#88161,#88162,#88163,#88164,#88165,#88166,
#88167,#88168,#88169,#88170,#88171,#88172,#88173,#88174,#88175,#88176,#88177,
#88178,#88179,#88180,#88181,#88182,#88183,#88184,#88185,#88186,#88187,#88188,
#88189,#88190,#88191,#88192,#88193,#88194,#88195,#88196,#88197,#88198,#88199,
#88200,#88201,#88202,#88203,#88204,#88205,#88206,#88207,#88208,#88209,#88210,
#88211,#88212,#88213,#88214,#88215,#88216,#88217,#88218,#88219,#88220,#88221,
#88222,#88223,#88224,#88225,#88226,#88227,#88228,#88229,#88230,#88231,#88232,
#88233,#88234,#88235,#88236,#88237,#88238,#88239,#88240,#88241,#88242,#88243,
#88244,#88245,#88246,#88247,#88248,#88249,#88250,#88251,#88252,#88253,#88254,
#88255,#88256,#88257,#88258,#88259,#88260,#88261,#88262,#88263,#88264,#88265,
#88266,#88267,#88268,#88269,#88270,#88271,#88272,#88273,#88274,#88275,#88276,
#88277,#88278,#88279,#88280,#88281,#88282,#88283,#88284,#88285,#88286,#88287,
#88288,#88289,#88290,#88291,#88292,#88293,#88294,#88295,#88296,#88297,#88298,
#88299,#88300,#88301,#88302,#88303,#88304,#88305,#88306,#88307,#88308,#88309,
#88310,#88311,#88312,#88313,#88314,#88315,#88316,#88317,#88318,#88319,#88320,
#88321,#88322,#88323,#88324,#88325,#88326,#88327,#88328,#88329,#88330,#88331,
#88332,#88333,#88334,#88335,#88336,#88337,#88338,#88339,#88340,#88341,#88342,
#88343,#88344,#88345,#88346,#88347,#88348,#88349,#88350,#88351,#88352,#88353,
#88354,#88355,#88356,#88357,#88358,#88359,#88360,#88361,#88362,#88363,#88364,
#88365,#88366,#88367,#88368,#88369,#88370,#88371,#88372,#88373,#88374,#88375,
#88376,#88377,#88378,#88379,#88380,#88381,#88382,#88383,#88384,#88385,#88386,
#88387,#88388,#88389,#88390,#88391,#88392,#88393,#88394,#88395,#88396,#88397,
#88398,#88399,#88400,#88401,#88402,#88403,#88404,#88405,#88406,#88407,#88408,
#88409,#88410,#88411,#88412,#88413,#88414,#88415,#88416,#88417,#88418,#88419,
#88420,#88421,#88422,#88423,#88424,#88425,#88426,#88427,#88428,#88429,#88430,
#88431,#88432,#88433,#88434,#88435,#88436,#88437,#88438,#88439,#88440,#88441,
#88442,#88443,#88444,#88445,#88446,#88447,#88448,#88449,#88450,#88451,#88452,
#88453,#88454,#88455,#88456,#88457,#88458,#88459,#88460,#88461,#88462,#88463,
#88464,#88465,#88466,#88467,#88468,#88469,#88470,#88471,#88472,#88473,#88474,
#88475,#88476,#88477,#88478,#88479,#88480,#88481,#88482,#88483,#88484,#88485,
#88486,#88487,#88488,#88489,#88490,#88491,#88492,#88493,#88494,#88495,#88496,
#88497,#88498,#88499,#88500,#88501,#88502,#88503,#88504,#88505,#88506,#88507,
#88508,#88509,#88510,#88511,#88512,#88513,#88514,#88515,#88516,#88517,#88518,
#88519,#88520,#88521,#88522,#88523,#88524,#88525,#88526,#88527,#88528,#88529,
#88530,#88531,#88532,#88533,#88534,#88535,#88536,#88537,#88538,#88539,#88540,
#88541,#88542,#88543,#88544,#88545,#88546,#88547,#88548,#88549,#88550,#88551,
#88552,#88553,#88554,#88555,#88556,#88557,#88558,#88559,#88560,#88561,#88562,
#88563,#88564,#88565,#88566,#88567,#88568,#88569,#88570,#88571,#88572,#88573,
#88574,#88575,#88576,#88577,#88578,#88579,#88580,#88581,#88582,#88583,#88584,
#88585,#88586,#88587,#88588,#88589,#88590,#88591,#88592,#88593,#88594,#88595,
#88596,#88597,#88598,#88599,#88600,#88601,#88602,#88603,#88604,#88605,#88606,
#88607,#88608,#88609,#88610,#88611,#88612,#88613,#88614,#88615,#88616,#88617,
#88618,#88619,#88620,#88621,#88622,#88623,#88624,#88625,#88626,#88627,#88628,
#88629,#88630,#88631,#88632,#88633,#88634,#88635,#88636,#88637,#88638,#88639,
#88640,#88641,#88642,#88643,#88644,#88645,#88646,#88647,#88648,#88649,#88650,
#88651,#88652,#88653,#88654,#88655,#88656,#88657,#88658,#88659,#88660,#88661,
#88662,#88663,#88664,#88665,#88666,#88667,#88668,#88669,#88670,#88671,#88672,
#88673,#88674,#88675,#88676,#88677,#88678,#88679,#88680,#88681,#88682,#88683,
#88684,#88685,#88686,#88687,#88688,#88689,#88690,#88691,#88692,#88693,#88694,
#88695,#88696,#88697,#88698,#88699,#88700,#88701,#88702,#88703,#88704,#88705,
#88706,#88707,#88708,#88709,#88710,#88711,#88712,#88713,#88714,#88715,#88716,
#88717)) ;
#91087 = CLOSED_SHELL('',(#88718,#88719,#88720,#88721,#88722,#88723,#88724,
#88725,#88726,#88727,#88728,#88729,#88730,#88731,#88732,#88733,#88734,#88735,
#88736,#88737,#88738,#88739,#88740,#88741,#88742,#88743,#88744,#88745,#88746,
#88747,#88748,#88749,#88750,#88751,#88752,#88753,#88754,#88755,#88756,#88757,
#88758,#88759,#88760,#88761,#88762,#88763,#88764,#88765,#88766,#88767,#88768,
#88769,#88770,#88771,#88772,#88773,#88774,#88775,#88776,#88777,#88778,#88779,
#88780,#88781,#88782,#88783,#88784,#88785,#88786,#88787,#88788,#88789,#88790,
#88791,#88792,#88793,#88794,#88795,#88796,#88797,#88798,#88799,#88800,#88801,
#88802,#88803,#88804,#88805,#88806,#88807,#88808,#88809,#88810,#88811,#88812,
#88813,#88814,#88815,#88816,#88817,#88818,#88819,#88820,#88821,#88822,#88823,
#88824,#88825,#88826,#88827,#88828,#88829,#88830,#88831,#88832,#88833,#88834,
#88835,#88836,#88837,#88838,#88839,#88840,#88841,#88842,#88843,#88844,#88845,
#88846,#88847,#88848,#88849,#88850,#88851,#88852,#88853,#88854,#88855,#88856,
#88857,#88858,#88859,#88860,#88861,#88862,#88863,#88864,#88865,#88866,#88867,
#88868,#88869,#88870,#88871,#88872,#88873,#88874,#88875,#88876,#88877,#88878,
#88879,#88880,#88881,#88882,#88883,#88884,#88885,#88886,#88887,#88888,#88889,
#88890,#88891,#88892,#88893,#88894,#88895,#88896,#88897,#88898,#88899,#88900,
#88901,#88902,#88903,#88904,#88905,#88906,#88907,#88908,#88909,#88910,#88911,
#88912,#88913,#88914,#88915,#88916,#88917,#88918,#88919,#88920,#88921,#88922,
#88923,#88924,#88925,#88926,#88927,#88928,#88929,#88930,#88931,#88932,#88933,
#88934,#88935,#88936,#88937,#88938,#88939,#88940,#88941,#88942,#88943,#88944,
#88945,#88946,#88947,#88948,#88949,#88950,#88951,#88952,#88953,#88954,#88955,
#88956,#88957,#88958,#88959,#88960,#88961,#88962,#88963,#88964,#88965,#88966,
#88967,#88968,#88969,#88970,#88971,#88972,#88973,#88974,#88975,#88976,#88977,
#88978,#88979,#88980,#88981,#88982,#88983,#88984,#88985,#88986,#88987,#88988,
#88989,#88990,#88991,#88992,#88993,#88994,#88995,#88996,#88997,#88998,#88999,
#89000,#89001,#89002,#89003,#89004,#89005,#89006,#89007,#89008,#89009,#89010,
#89011,#89012,#89013,#89014,#89015,#89016,#89017,#89018,#89019,#89020,#89021,
#89022,#89023,#89024,#89025,#89026,#89027,#89028,#89029,#89030,#89031,#89032,
#89033,#89034,#89035,#89036,#89037,#89038,#89039,#89040,#89041,#89042,#89043,
#89044,#89045,#89046,#89047,#89048,#89049,#89050,#89051,#89052,#89053,#89054,
#89055,#89056,#89057,#89058,#89059,#89060,#89061,#89062,#89063,#89064,#89065,
#89066,#89067,#89068,#89069,#89070,#89071,#89072,#89073,#89074,#89075,#89076,
#89077,#89078,#89079,#89080,#89081,#89082,#89083,#89084,#89085,#89086,#89087,
#89088,#89089,#89090,#89091,#89092,#89093,#89094,#89095,#89096,#89097,#89098,
#89099,#89100,#89101,#89102,#89103,#89104,#89105,#89106,#89107,#89108,#89109,
#89110,#89111,#89112,#89113,#89114,#89115,#89116,#89117,#89118,#89119,#89120,
#89121,#89122,#89123,#89124,#89125,#89126,#89127,#89128,#89129,#89130,#89131,
#89132,#89133,#89134,#89135,#89136,#89137,#89138,#89139,#89140,#89141,#89142,
#89143,#89144,#89145,#89146,#89147,#89148,#89149,#89150,#89151,#89152,#89153,
#89154,#89155,#89156,#89157,#89158,#89159,#89160,#89161,#89162,#89163,#89164,
#89165,#89166,#89167,#89168,#89169,#89170,#89171,#89172,#89173,#89174,#89175,
#89176,#89177,#89178,#89179,#89180,#89181,#89182,#89183,#89184,#89185,#89186,
#89187,#89188,#89189,#89190,#89191,#89192,#89193,#89194,#89195,#89196,#89197,
#89198,#89199,#89200,#89201,#89202,#89203,#89204,#89205,#89206,#89207,#89208,
#89209,#89210,#89211,#89212,#89213,#89214,#89215,#89216,#89217,#89218,#89219,
#89220,#89221,#89222,#89223,#89224,#89225,#89226,#89227,#89228,#89229,#89230,
#89231,#89232,#89233,#89234,#89235,#89236,#89237,#89238,#89239,#89240,#89241,
#89242,#89243,#89244,#89245,#89246,#89247,#89248,#89249,#89250,#89251,#89252,
#89253,#89254,#89255,#89256,#89257,#89258,#89259,#89260,#89261,#89262,#89263,
#89264,#89265,#89266,#89267,#89268,#89269,#89270,#89271,#89272,#89273,#89274,
#89275,#89276,#89277,#89278,#89279,#89280,#89281,#89282,#89283,#89284,#89285,
#89286,#89287,#89288,#89289,#89290,#89291,#89292,#89293,#89294,#89295,#89296,
#89297,#89298,#89299,#89300,#89301,#89302,#89303,#89304,#89305,#89306,#89307,
#89308,#89309,#89310,#89311,#89312,#89313,#89314,#89315,#89316,#89317,#89318,
#89319,#89320,#89321,#89322,#89323,#89324,#89325,#89326,#89327,#89328,#89329,
#89330,#89331,#89332,#89333,#89334,#89335,#89336,#89337,#89338,#89339,#89340,
#89341,#89342,#89343,#89344,#89345,#89346,#89347,#89348,#89349,#89350,#89351,
#89352,#89353,#89354,#89355,#89356,#89357,#89358,#89359,#89360,#89361,#89362,
#89363,#89364,#89365,#89366,#89367,#89368,#89369,#89370,#89371,#89372,#89373,
#89374,#89375,#89376,#89377,#89378,#89379,#89380,#89381,#89382,#89383,#89384,
#89385,#89386,#89387,#89388,#89389,#89390,#89391,#89392,#89393,#89394,#89395,
#89396,#89397,#89398,#89399,#89400,#89401,#89402,#89403,#89404,#89405,#89406,
#89407,#89408,#89409,#89410,#89411,#89412,#89413,#89414,#89415,#89416,#89417,
#89418,#89419,#89420,#89421,#89422,#89423,#89424,#89425,#89426,#89427,#89428,
#89429,#89430,#89431,#89432,#89433,#89434,#89435,#89436,#89437,#89438,#89439,
#89440,#89441,#89442,#89443,#89444,#89445,#89446,#89447,#89448,#89449,#89450,
#89451,#89452,#89453,#89454,#89455,#89456,#89457,#89458,#89459,#89460,#89461,
#89462,#89463,#89464,#89465,#89466,#89467,#89468,#89469,#89470,#89471,#89472,
#89473,#89474,#89475,#89476,#89477,#89478,#89479,#89480,#89481,#89482,#89483,
#89484,#89485,#89486,#89487,#89488,#89489,#89490,#89491,#89492,#89493,#89494,
#89495,#89496,#89497,#89498,#89499,#89500,#89501,#89502,#89503,#89504,#89505,
#89506,#89507,#89508,#89509,#89510,#89511,#89512,#89513,#89514,#89515,#89516,
#89517,#89518,#89519,#89520,#89521,#89522,#89523,#89524,#89525,#89526,#89527,
#89528,#89529,#89530,#89531,#89532,#89533,#89534,#89535,#89536,#89537,#89538,
#89539,#89540,#89541,#89542,#89543,#89544,#89545,#89546,#89547,#89548,#89549,
#89550,#89551,#89552,#89553,#89554,#89555,#89556,#89557,#89558,#89559,#89560,
#89561,#89562,#89563,#89564,#89565,#89566,#89567,#89568,#89569,#89570,#89571,
#89572,#89573,#89574,#89575,#89576,#89577,#89578,#89579,#89580,#89581,#89582,
#89583,#89584,#89585,#89586,#89587,#89588,#89589,#89590,#89591,#89592,#89593,
#89594,#89595,#89596,#89597,#89598,#89599,#89600,#89601,#89602,#89603,#89604,
#89605,#89606,#89607,#89608,#89609,#89610,#89611,#89612,#89613,#89614,#89615,
#89616,#89617,#89618,#89619,#89620,#89621,#89622,#89623,#89624,#89625,#89626,
#89627,#89628,#89629,#89630,#89631,#89632,#89633,#89634,#89635,#89636,#89637,
#89638,#89639,#89640,#89641,#89642,#89643,#89644,#89645,#89646,#89647,#89648,
#89649,#89650,#89651,#89652,#89653,#89654,#89655,#89656,#89657,#89658,#89659,
#89660,#89661,#89662,#89663,#89664,#89665,#89666,#89667,#89668,#89669,#89670,
#89671,#89672,#89673,#89674,#89675,#89676,#89677,#89678,#89679,#89680,#89681,
#89682,#89683,#89684,#89685,#89686,#89687,#89688,#89689,#89690,#89691,#89692,
#89693,#89694,#89695,#89696,#89697,#89698,#89699,#89700,#89701,#89702,#89703,
#89704,#89705,#89706,#89707,#89708,#89709,#89710,#89711,#89712,#89713,#89714,
#89715,#89716,#89717,#89718,#89719,#89720,#89721,#89722,#89723,#89724,#89725,
#89726,#89727,#89728,#89729,#89730,#89731,#89732,#89733,#89734,#89735,#89736,
#89737,#89738,#89739,#89740,#89741,#89742,#89743,#89744,#89745,#89746,#89747,
#89748,#89749,#89750,#89751,#89752,#89753,#89754,#89755,#89756,#89757,#89758,
#89759,#89760,#89761,#89762,#89763,#89764,#89765,#89766,#89767,#89768,#89769,
#89770,#89771,#89772,#89773,#89774,#89775,#89776,#89777,#89778,#89779,#89780,
#89781,#89782,#89783,#89784,#89785,#89786,#89787,#89788,#89789,#89790,#89791,
#89792,#89793,#89794,#89795,#89796,#89797,#89798,#89799,#89800,#89801,#89802,
#89803,#89804,#89805,#89806,#89807,#89808,#89809,#89810,#89811,#89812,#89813,
#89814,#89815,#89816,#89817,#89818,#89819,#89820,#89821,#89822,#89823,#89824,
#89825,#89826,#89827,#89828,#89829,#89830,#89831,#89832,#89833,#89834,#89835,
#89836,#89837,#89838,#89839,#89840,#89841,#89842,#89843,#89844,#89845,#89846,
#89847,#89848,#89849,#89850,#89851,#89852,#89853,#89854,#89855,#89856,#89857,
#89858,#89859,#89860,#89861,#89862,#89863,#89864,#89865,#89866,#89867,#89868,
#89869,#89870,#89871,#89872,#89873,#89874,#89875,#89876,#89877,#89878,#89879,
#89880,#89881,#89882,#89883,#89884,#89885,#89886,#89887,#89888,#89889,#89890,
#89891,#89892,#89893,#89894,#89895,#89896,#89897,#89898,#89899,#89900,#89901,
#89902,#89903,#89904,#89905,#89906,#89907,#89908,#89909,#89910,#89911,#89912,
#89913,#89914,#89915,#89916,#89917,#89918,#89919,#89920,#89921,#89922,#89923,
#89924,#89925,#89926,#89927,#89928,#89929,#89930,#89931,#89932,#89933,#89934,
#89935,#89936,#89937,#89938,#89939,#89940,#89941,#89942,#89943,#89944,#89945,
#89946,#89947,#89948,#89949,#89950,#89951,#89952,#89953,#89954,#89955,#89956,
#89957,#89958,#89959,#89960,#89961,#89962,#89963,#89964,#89965,#89966,#89967,
#89968,#89969,#89970,#89971,#89972,#89973,#89974,#89975,#89976,#89977,#89978,
#89979,#89980,#89981,#89982,#89983,#89984,#89985,#89986,#89987,#89988,#89989,
#89990,#89991,#89992,#89993,#89994,#89995,#89996,#89997,#89998,#89999,#90000,
#90001,#90002,#90003,#90004,#90005,#90006,#90007,#90008,#90009,#90010,#90011,
#90012,#90013,#90014,#90015,#90016,#90017,#90018,#90019,#90020,#90021,#90022,
#90023,#90024,#90025,#90026,#90027,#90028,#90029,#90030,#90031,#90032,#90033,
#90034,#90035,#90036,#90037,#90038,#90039,#90040,#90041,#90042,#90043,#90044,
#90045,#90046,#90047,#90048,#90049,#90050,#90051,#90052,#90053,#90054,#90055,
#90056,#90057,#90058,#90059,#90060,#90061,#90062,#90063,#90064,#90065,#90066,
#90067,#90068,#90069,#90070,#90071,#90072,#90073,#90074,#90075,#90076,#90077,
#90078,#90079,#90080,#90081,#90082,#90083,#90084,#90085,#90086,#90087,#90088,
#90089,#90090,#90091,#90092,#90093,#90094,#90095,#90096,#90097,#90098,#90099,
#90100,#90101,#90102,#90103,#90104,#90105,#90106,#90107,#90108,#90109,#90110,
#90111,#90112,#90113,#90114,#90115,#90116,#90117,#90118,#90119,#90120,#90121,
#90122,#90123,#90124,#90125,#90126,#90127,#90128,#90129,#90130,#90131,#90132,
#90133,#90134,#90135,#90136,#90137,#90138,#90139,#90140,#90141,#90142,#90143,
#90144,#90145,#90146,#90147,#90148,#90149,#90150,#90151,#90152,#90153,#90154,
#90155,#90156,#90157,#90158,#90159,#90160,#90161,#90162,#90163,#90164,#90165,
#90166,#90167,#90168,#90169,#90170,#90171,#90172,#90173,#90174,#90175,#90176,
#90177,#90178,#90179,#90180,#90181,#90182,#90183,#90184,#90185,#90186,#90187,
#90188,#90189,#90190,#90191,#90192,#90193,#90194,#90195,#90196,#90197,#90198,
#90199,#90200,#90201,#90202,#90203,#90204,#90205,#90206,#90207,#90208,#90209,
#90210,#90211,#90212,#90213,#90214,#90215,#90216,#90217,#90218,#90219,#90220,
#90221,#90222,#90223,#90224,#90225,#90226,#90227,#90228,#90229,#90230,#90231,
#90232,#90233,#90234,#90235,#90236,#90237,#90238,#90239,#90240,#90241,#90242,
#90243,#90244,#90245,#90246,#90247,#90248,#90249,#90250,#90251,#90252,#90253,
#90254,#90255,#90256,#90257,#90258,#90259,#90260,#90261,#90262,#90263,#90264,
#90265,#90266,#90267,#90268,#90269,#90270,#90271,#90272,#90273,#90274,#90275,
#90276,#90277,#90278,#90279,#90280,#90281,#90282,#90283,#90284,#90285,#90286,
#90287,#90288,#90289,#90290,#90291,#90292,#90293,#90294,#90295,#90296,#90297,
#90298,#90299,#90300,#90301,#90302,#90303,#90304,#90305,#90306,#90307,#90308,
#90309,#90310,#90311,#90312,#90313,#90314,#90315,#90316,#90317,#90318,#90319,
#90320,#90321,#90322,#90323,#90324,#90325,#90326,#90327,#90328,#90329,#90330,
#90331,#90332,#90333,#90334,#90335,#90336,#90337,#90338,#90339,#90340,#90341,
#90342,#90343,#90344,#90345,#90346,#90347,#90348,#90349,#90350,#90351,#90352,
#90353,#90354,#90355,#90356,#90357,#90358,#90359,#90360,#90361,#90362,#90363,
#90364,#90365,#90366,#90367,#90368,#90369,#90370,#90371,#90372,#90373,#90374,
#90375,#90376,#90377,#90378,#90379,#90380,#90381,#90382,#90383,#90384,#90385,
#90386,#90387,#90388,#90389,#90390,#90391,#90392,#90393,#90394,#90395,#90396,
#90397,#90398,#90399,#90400,#90401,#90402,#90403,#90404,#90405,#90406,#90407,
#90408,#90409,#90410,#90411,#90412,#90413,#90414,#90415,#90416,#90417,#90418,
#90419,#90420,#90421,#90422,#90423,#90424,#90425,#90426,#90427,#90428,#90429,
#90430,#90431,#90432,#90433,#90434,#90435,#90436,#90437,#90438,#90439,#90440,
#90441,#90442,#90443,#90444,#90445,#90446,#90447,#90448,#90449,#90450,#90451,
#90452,#90453,#90454,#90455,#90456,#90457,#90458,#90459,#90460,#90461,#90462,
#90463,#90464,#90465,#90466,#90467,#90468,#90469,#90470,#90471,#90472,#90473,
#90474,#90475,#90476,#90477,#90478,#90479,#90480,#90481,#90482,#90483,#90484,
#90485,#90486,#90487,#90488,#90489,#90490,#90491,#90492,#90493,#90494,#90495,
#90496,#90497,#90498,#90499,#90500,#90501,#90502,#90503,#90504,#90505,#90506,
#90507,#90508,#90509,#90510,#90511,#90512,#90513,#90514,#90515,#90516,#90517,
#90518,#90519,#90520,#90521,#90522,#90523,#90524,#90525,#90526,#90527,#90528,
#90529,#90530,#90531,#90532,#90533,#90534,#90535,#90536,#90537,#90538,#90539,
#90540,#90541,#90542,#90543,#90544,#90545,#90546,#90547,#90548,#90549,#90550,
#90551,#90552,#90553,#90554,#90555,#90556,#90557,#90558,#90559,#90560,#90561,
#90562,#90563,#90564,#90565,#90566,#90567,#90568,#90569,#90570,#90571,#90572,
#90573,#90574,#90575,#90576,#90577,#90578,#90579,#90580,#90581,#90582,#90583,
#90584,#90585,#90586,#90587,#90588,#90589,#90590,#90591,#90592,#90593,#90594,
#90595,#90596,#90597,#90598,#90599,#90600,#90601,#90602,#90603,#90604,#90605,
#90606,#90607,#90608,#90609,#90610,#90611,#90612,#90613,#90614,#90615,#90616,
#90617,#90618,#90619,#90620,#90621,#90622,#90623,#90624,#90625,#90626,#90627,
#90628,#90629,#90630,#90631,#90632,#90633,#90634,#90635,#90636,#90637,#90638,
#90639,#90640,#90641,#90642,#90643,#90644,#90645,#90646,#90647,#90648,#90649,
#90650,#90651,#90652,#90653,#90654,#90655,#90656,#90657,#90658,#90659,#90660,
#90661,#90662,#90663,#90664,#90665,#90666,#90667,#90668,#90669,#90670,#90671,
#90672,#90673,#90674,#90675,#90676,#90677,#90678,#90679,#90680,#90681,#90682,
#90683,#90684,#90685,#90686,#90687,#90688,#90689,#90690,#90691,#90692,#90693,
#90694,#90695,#90696,#90697,#90698,#90699,#90700,#90701,#90702,#90703,#90704,
#90705,#90706,#90707,#90708,#90709,#90710,#90711,#90712,#90713,#90714,#90715,
#90716,#90717,#90718,#90719,#90720,#90721,#90722,#90723,#90724,#90725,#90726,
#90727,#90728,#90729,#90730,#90731,#90732,#90733,#90734,#90735,#90736,#90737,
#90738,#90739,#90740,#90741,#90742,#90743,#90744,#90745,#90746,#90747,#90748,
#90749,#90750,#90751,#90752,#90753,#90754,#90755,#90756,#90757,#90758,#90759,
#90760,#90761,#90762,#90763,#90764,#90765,#90766,#90767,#90768,#90769,#90770,
#90771,#90772,#90773,#90774,#90775,#90776,#90777,#90778,#90779,#90780,#90781,
#90782,#90783,#90784,#90785,#90786,#90787,#90788,#90789,#90790,#90791,#90792,
#90793,#90794,#90795,#90796,#90797,#90798,#90799,#90800,#90801,#90802,#90803,
#90804,#90805,#90806,#90807,#90808,#90809,#90810,#90811,#90812,#90813,#90814,
#90815,#90816,#90817,#90818,#90819,#90820,#90821,#90822,#90823,#90824,#90825,
#90826,#90827,#90828,#90829,#90830,#90831,#90832,#90833,#90834,#90835,#90836,
#90837,#90838,#90839,#90840,#90841,#90842,#90843,#90844,#90845,#90846,#90847,
#90848,#90849,#90850,#90851,#90852,#90853,#90854,#90855,#90856,#90857,#90858,
#90859,#90860,#90861,#90862,#90863,#90864,#90865,#90866,#90867,#90868,#90869,
#90870,#90871,#90872,#90873,#90874,#90875,#90876,#90877,#90878,#90879,#90880,
#90881,#90882,#90883,#90884,#90885,#90886,#90887,#90888,#90889,#90890,#90891,
#90892,#90893,#90894,#90895,#90896,#90897,#90898,#90899,#90900,#90901,#90902,
#90903,#90904,#90905,#90906,#90907,#90908,#90909,#90910,#90911,#90912,#90913,
#90914,#90915,#90916,#90917,#90918,#90919,#90920,#90921,#90922,#90923,#90924,
#90925,#90926,#90927,#90928,#90929,#90930,#90931,#90932,#90933,#90934,#90935,
#90936,#90937,#90938,#90939,#90940,#90941,#90942,#90943,#90944,#90945,#90946,
#90947,#90948,#90949,#90950,#90951,#90952,#90953,#90954,#90955,#90956,#90957,
#90958,#90959,#90960,#90961,#90962,#90963,#90964,#90965,#90966,#90967,#90968,
#90969,#90970,#90971,#90972,#90973,#90974,#90975,#90976,#90977,#90978,#90979,
#90980,#90981,#90982,#90983,#90984,#90985,#90986,#90987,#90988,#90989,#90990,
#90991,#90992,#90993,#90994,#90995,#90996,#90997,#90998,#90999,#91000,#91001,
#91002,#91003,#91004,#91005,#91006,#91007,#91008,#91009,#91010,#91011,#91012,
#91013,#91014,#91015,#91016,#91017,#91018,#91019,#91020,#91021,#91022,#91023,
#91024,#91025,#91026,#91027,#91028,#91029,#91030,#91031,#91032,#91033,#91034,
#91035,#91036,#91037,#91038,#91039,#91040,#91041,#91042,#91043,#91044,#91045,
#91046,#91047,#91048,#91049,#91050,#91051,#91052,#91053,#91054,#91055,#91056,
#91057,#91058,#91059,#91060,#91061,#91062,#91063,#91064,#91065,#91066,#91067,
#91068,#91069,#91070,#91071,#91072,#91073,#91074,#91075,#91076,#91077,#91078,
#91079,#91080,#91081,#91082)) ;
#91088 = DERIVED_UNIT_ELEMENT(#91094,1.) ;
#91089 = DERIVED_UNIT_ELEMENT(#170129,-3.) ;
#91090 = DERIVED_UNIT_ELEMENT(#91094,1.) ;
#91091 = DERIVED_UNIT_ELEMENT(#170129,-3.) ;
#91092 = DERIVED_UNIT_ELEMENT(#91094,1.) ;
#91093 = DERIVED_UNIT_ELEMENT(#170129,-3.) ;
#91094 = (
MASS_UNIT()
NAMED_UNIT(*)
SI_UNIT(.KILO.,.GRAM.)
) ;
#91095 = DERIVED_UNIT((#91088,#91089)) ;
#91096 = DERIVED_UNIT((#91090,#91091)) ;
#91097 = DERIVED_UNIT((#91092,#91093)) ;
#91098 = MEASURE_REPRESENTATION_ITEM('density measure',
POSITIVE_RATIO_MEASURE(7850.),#91095) ;
#91099 = MEASURE_REPRESENTATION_ITEM('density measure',
POSITIVE_RATIO_MEASURE(7850.),#91096) ;
#91100 = MEASURE_REPRESENTATION_ITEM('density measure',
POSITIVE_RATIO_MEASURE(7850.),#91097) ;
#91101 = PROPERTY_DEFINITION_REPRESENTATION(#91116,#91107) ;
#91102 = PROPERTY_DEFINITION_REPRESENTATION(#91117,#91108) ;
#91103 = PROPERTY_DEFINITION_REPRESENTATION(#91118,#91109) ;
#91104 = PROPERTY_DEFINITION_REPRESENTATION(#91119,#91110) ;
#91105 = PROPERTY_DEFINITION_REPRESENTATION(#91120,#91111) ;
#91106 = PROPERTY_DEFINITION_REPRESENTATION(#91121,#91112) ;
#91107 = REPRESENTATION('material name',(#91113),#170124) ;
#91108 = REPRESENTATION('density',(#91098),#170124) ;
#91109 = REPRESENTATION('material name',(#91114),#170125) ;
#91110 = REPRESENTATION('density',(#91099),#170125) ;
#91111 = REPRESENTATION('material name',(#91115),#170126) ;
#91112 = REPRESENTATION('density',(#91100),#170126) ;
#91113 = DESCRIPTIVE_REPRESENTATION_ITEM('Steel','Steel') ;
#91114 = DESCRIPTIVE_REPRESENTATION_ITEM('Steel','Steel') ;
#91115 = DESCRIPTIVE_REPRESENTATION_ITEM('Steel','Steel') ;
#91116 = PROPERTY_DEFINITION('material property','material name',#170149) ;
#91117 = PROPERTY_DEFINITION('material property','density of part',#170149) ;
#91118 = PROPERTY_DEFINITION('material property','material name',#170150) ;
#91119 = PROPERTY_DEFINITION('material property','density of part',#170150) ;
#91120 = PROPERTY_DEFINITION('material property','material name',#170151) ;
#91121 = PROPERTY_DEFINITION('material property','density of part',#170151) ;
#91122 = AXIS2_PLACEMENT_3D('',#132550,#103080,#103081) ;
#91123 = AXIS2_PLACEMENT_3D('',#132551,#103082,#103083) ;
#91124 = AXIS2_PLACEMENT_3D('',#132552,#103084,#103085) ;
#91125 = AXIS2_PLACEMENT_3D('',#132555,#103086,#103087) ;
#91126 = AXIS2_PLACEMENT_3D('',#132557,#103088,#103089) ;
#91127 = AXIS2_PLACEMENT_3D('',#132559,#103090,#103091) ;
#91128 = AXIS2_PLACEMENT_3D('',#132560,#103092,#103093) ;
#91129 = AXIS2_PLACEMENT_3D('',#132561,#103094,#103095) ;
#91130 = AXIS2_PLACEMENT_3D('',#132563,#103096,#103097) ;
#91131 = AXIS2_PLACEMENT_3D('',#132565,#103098,#103099) ;
#91132 = AXIS2_PLACEMENT_3D('',#132567,#103100,#103101) ;
#91133 = AXIS2_PLACEMENT_3D('',#132568,#103102,#103103) ;
#91134 = AXIS2_PLACEMENT_3D('',#132569,#103104,#103105) ;
#91135 = AXIS2_PLACEMENT_3D('',#132571,#103106,#103107) ;
#91136 = AXIS2_PLACEMENT_3D('',#132573,#103108,#103109) ;
#91137 = AXIS2_PLACEMENT_3D('',#132574,#103110,#103111) ;
#91138 = AXIS2_PLACEMENT_3D('',#132575,#103112,#103113) ;
#91139 = AXIS2_PLACEMENT_3D('',#132577,#103114,#103115) ;
#91140 = AXIS2_PLACEMENT_3D('',#132579,#103116,#103117) ;
#91141 = AXIS2_PLACEMENT_3D('',#132581,#103118,#103119) ;
#91142 = AXIS2_PLACEMENT_3D('',#132582,#103120,#103121) ;
#91143 = AXIS2_PLACEMENT_3D('',#132583,#103122,#103123) ;
#91144 = AXIS2_PLACEMENT_3D('',#132586,#103124,#103125) ;
#91145 = AXIS2_PLACEMENT_3D('',#132588,#103126,#103127) ;
#91146 = AXIS2_PLACEMENT_3D('',#132590,#103128,#103129) ;
#91147 = AXIS2_PLACEMENT_3D('',#132591,#103130,#103131) ;
#91148 = AXIS2_PLACEMENT_3D('',#132592,#103132,#103133) ;
#91149 = AXIS2_PLACEMENT_3D('',#132595,#103134,#103135) ;
#91150 = AXIS2_PLACEMENT_3D('',#132597,#103136,#103137) ;
#91151 = AXIS2_PLACEMENT_3D('',#132598,#103138,#103139) ;
#91152 = AXIS2_PLACEMENT_3D('',#132599,#103140,#103141) ;
#91153 = AXIS2_PLACEMENT_3D('',#132603,#103143,#103144) ;
#91154 = AXIS2_PLACEMENT_3D('',#132605,#103146,#103147) ;
#91155 = AXIS2_PLACEMENT_3D('',#132608,#103148,#103149) ;
#91156 = AXIS2_PLACEMENT_3D('',#132610,#103150,#103151) ;
#91157 = AXIS2_PLACEMENT_3D('',#132611,#103152,#103153) ;
#91158 = AXIS2_PLACEMENT_3D('',#132612,#103154,#103155) ;
#91159 = AXIS2_PLACEMENT_3D('',#132614,#103156,#103157) ;
#91160 = AXIS2_PLACEMENT_3D('',#132616,#103159,#103160) ;
#91161 = AXIS2_PLACEMENT_3D('',#132618,#103162,#103163) ;
#91162 = AXIS2_PLACEMENT_3D('',#132621,#103164,#103165) ;
#91163 = AXIS2_PLACEMENT_3D('',#132647,#103167,#103168) ;
#91164 = AXIS2_PLACEMENT_3D('',#132694,#103170,#103171) ;
#91165 = AXIS2_PLACEMENT_3D('',#132720,#103173,#103174) ;
#91166 = AXIS2_PLACEMENT_3D('',#132766,#103176,#103177) ;
#91167 = AXIS2_PLACEMENT_3D('',#132768,#103179,#103180) ;
#91168 = AXIS2_PLACEMENT_3D('',#132771,#103181,#103182) ;
#91169 = AXIS2_PLACEMENT_3D('',#132773,#103183,#103184) ;
#91170 = AXIS2_PLACEMENT_3D('',#132775,#103185,#103186) ;
#91171 = AXIS2_PLACEMENT_3D('',#132776,#103187,#103188) ;
#91172 = AXIS2_PLACEMENT_3D('',#132777,#103189,#103190) ;
#91173 = AXIS2_PLACEMENT_3D('',#132780,#103191,#103192) ;
#91174 = AXIS2_PLACEMENT_3D('',#132784,#103194,#103195) ;
#91175 = AXIS2_PLACEMENT_3D('',#132786,#103197,#103198) ;
#91176 = AXIS2_PLACEMENT_3D('',#132788,#103199,#103200) ;
#91177 = AXIS2_PLACEMENT_3D('',#132790,#103201,#103202) ;
#91178 = AXIS2_PLACEMENT_3D('',#132792,#103203,#103204) ;
#91179 = AXIS2_PLACEMENT_3D('',#132793,#103205,#103206) ;
#91180 = AXIS2_PLACEMENT_3D('',#132794,#103207,#103208) ;
#91181 = AXIS2_PLACEMENT_3D('',#132796,#103209,#103210) ;
#91182 = AXIS2_PLACEMENT_3D('',#132798,#103211,#103212) ;
#91183 = AXIS2_PLACEMENT_3D('',#132799,#103213,#103214) ;
#91184 = AXIS2_PLACEMENT_3D('',#132800,#103215,#103216) ;
#91185 = AXIS2_PLACEMENT_3D('',#132802,#103217,#103218) ;
#91186 = AXIS2_PLACEMENT_3D('',#132804,#103219,#103220) ;
#91187 = AXIS2_PLACEMENT_3D('',#132806,#103221,#103222) ;
#91188 = AXIS2_PLACEMENT_3D('',#132807,#103223,#103224) ;
#91189 = AXIS2_PLACEMENT_3D('',#132808,#103225,#103226) ;
#91190 = AXIS2_PLACEMENT_3D('',#132811,#103227,#103228) ;
#91191 = AXIS2_PLACEMENT_3D('',#132813,#103229,#103230) ;
#91192 = AXIS2_PLACEMENT_3D('',#132815,#103231,#103232) ;
#91193 = AXIS2_PLACEMENT_3D('',#132816,#103233,#103234) ;
#91194 = AXIS2_PLACEMENT_3D('',#132817,#103235,#103236) ;
#91195 = AXIS2_PLACEMENT_3D('',#132820,#103237,#103238) ;
#91196 = AXIS2_PLACEMENT_3D('',#132822,#103239,#103240) ;
#91197 = AXIS2_PLACEMENT_3D('',#132823,#103241,#103242) ;
#91198 = AXIS2_PLACEMENT_3D('',#132824,#103243,#103244) ;
#91199 = AXIS2_PLACEMENT_3D('',#132828,#103246,#103247) ;
#91200 = AXIS2_PLACEMENT_3D('',#132830,#103249,#103250) ;
#91201 = AXIS2_PLACEMENT_3D('',#132833,#103251,#103252) ;
#91202 = AXIS2_PLACEMENT_3D('',#132835,#103253,#103254) ;
#91203 = AXIS2_PLACEMENT_3D('',#132836,#103255,#103256) ;
#91204 = AXIS2_PLACEMENT_3D('',#132837,#103257,#103258) ;
#91205 = AXIS2_PLACEMENT_3D('',#132839,#103259,#103260) ;
#91206 = AXIS2_PLACEMENT_3D('',#132841,#103262,#103263) ;
#91207 = AXIS2_PLACEMENT_3D('',#132843,#103265,#103266) ;
#91208 = AXIS2_PLACEMENT_3D('',#132846,#103267,#103268) ;
#91209 = AXIS2_PLACEMENT_3D('',#132872,#103270,#103271) ;
#91210 = AXIS2_PLACEMENT_3D('',#132919,#103273,#103274) ;
#91211 = AXIS2_PLACEMENT_3D('',#132945,#103276,#103277) ;
#91212 = AXIS2_PLACEMENT_3D('',#132991,#103279,#103280) ;
#91213 = AXIS2_PLACEMENT_3D('',#132993,#103282,#103283) ;
#91214 = AXIS2_PLACEMENT_3D('',#133004,#103288,#103289) ;
#91215 = AXIS2_PLACEMENT_3D('',#133022,#103293,#103294) ;
#91216 = AXIS2_PLACEMENT_3D('',#133024,#103296,#103297) ;
#91217 = AXIS2_PLACEMENT_3D('',#133033,#103302,#103303) ;
#91218 = AXIS2_PLACEMENT_3D('',#133042,#103308,#103309) ;
#91219 = AXIS2_PLACEMENT_3D('',#133051,#103314,#103315) ;
#91220 = AXIS2_PLACEMENT_3D('',#133055,#103317,#103318) ;
#91221 = AXIS2_PLACEMENT_3D('',#133056,#103319,#103320) ;
#91222 = AXIS2_PLACEMENT_3D('',#133057,#103321,#103322) ;
#91223 = AXIS2_PLACEMENT_3D('',#133058,#103323,#103324) ;
#91224 = AXIS2_PLACEMENT_3D('',#133059,#103325,#103326) ;
#91225 = AXIS2_PLACEMENT_3D('',#133060,#103327,#103328) ;
#91226 = AXIS2_PLACEMENT_3D('',#133061,#103329,#103330) ;
#91227 = AXIS2_PLACEMENT_3D('',#133062,#103331,#103332) ;
#91228 = AXIS2_PLACEMENT_3D('',#133063,#103333,#103334) ;
#91229 = AXIS2_PLACEMENT_3D('',#133065,#103335,#103336) ;
#91230 = AXIS2_PLACEMENT_3D('',#133069,#103338,#103339) ;
#91231 = AXIS2_PLACEMENT_3D('',#133072,#103341,#103342) ;
#91232 = AXIS2_PLACEMENT_3D('',#133073,#103343,#103344) ;
#91233 = AXIS2_PLACEMENT_3D('',#133076,#103345,#103346) ;
#91234 = AXIS2_PLACEMENT_3D('',#133080,#103348,#103349) ;
#91235 = AXIS2_PLACEMENT_3D('',#133082,#103351,#103352) ;
#91236 = AXIS2_PLACEMENT_3D('',#133091,#103357,#103358) ;
#91237 = AXIS2_PLACEMENT_3D('',#133098,#103363,#103364) ;
#91238 = AXIS2_PLACEMENT_3D('',#133100,#103366,#103367) ;
#91239 = AXIS2_PLACEMENT_3D('',#133109,#103372,#103373) ;
#91240 = AXIS2_PLACEMENT_3D('',#133111,#103374,#103375) ;
#91241 = AXIS2_PLACEMENT_3D('',#133113,#103376,#103377) ;
#91242 = AXIS2_PLACEMENT_3D('',#133117,#103379,#103380) ;
#91243 = AXIS2_PLACEMENT_3D('',#133119,#103381,#103382) ;
#91244 = AXIS2_PLACEMENT_3D('',#133121,#103383,#103384) ;
#91245 = AXIS2_PLACEMENT_3D('',#133130,#103389,#103390) ;
#91246 = AXIS2_PLACEMENT_3D('',#133137,#103395,#103396) ;
#91247 = AXIS2_PLACEMENT_3D('',#133139,#103398,#103399) ;
#91248 = AXIS2_PLACEMENT_3D('',#133147,#103404,#103405) ;
#91249 = AXIS2_PLACEMENT_3D('',#133154,#103408,#103409) ;
#91250 = AXIS2_PLACEMENT_3D('',#133158,#103411,#103412) ;
#91251 = AXIS2_PLACEMENT_3D('',#133162,#103414,#103415) ;
#91252 = AXIS2_PLACEMENT_3D('',#133166,#103417,#103418) ;
#91253 = AXIS2_PLACEMENT_3D('',#133172,#103422,#103423) ;
#91254 = AXIS2_PLACEMENT_3D('',#133178,#103427,#103428) ;
#91255 = AXIS2_PLACEMENT_3D('',#133185,#103433,#103434) ;
#91256 = AXIS2_PLACEMENT_3D('',#133196,#103439,#103440) ;
#91257 = AXIS2_PLACEMENT_3D('',#133200,#103442,#103443) ;
#91258 = AXIS2_PLACEMENT_3D('',#133204,#103445,#103446) ;
#91259 = AXIS2_PLACEMENT_3D('',#133208,#103448,#103449) ;
#91260 = AXIS2_PLACEMENT_3D('',#133212,#103451,#103452) ;
#91261 = AXIS2_PLACEMENT_3D('',#133216,#103454,#103455) ;
#91262 = AXIS2_PLACEMENT_3D('',#133220,#103457,#103458) ;
#91263 = AXIS2_PLACEMENT_3D('',#133224,#103460,#103461) ;
#91264 = AXIS2_PLACEMENT_3D('',#133226,#103463,#103464) ;
#91265 = AXIS2_PLACEMENT_3D('',#133235,#103469,#103470) ;
#91266 = AXIS2_PLACEMENT_3D('',#133241,#103474,#103475) ;
#91267 = AXIS2_PLACEMENT_3D('',#133247,#103479,#103480) ;
#91268 = AXIS2_PLACEMENT_3D('',#133328,#103493,#103494) ;
#91269 = AXIS2_PLACEMENT_3D('',#133339,#103499,#103500) ;
#91270 = AXIS2_PLACEMENT_3D('',#133343,#103502,#103503) ;
#91271 = AXIS2_PLACEMENT_3D('',#133347,#103505,#103506) ;
#91272 = AXIS2_PLACEMENT_3D('',#133351,#103508,#103509) ;
#91273 = AXIS2_PLACEMENT_3D('',#133355,#103511,#103512) ;
#91274 = AXIS2_PLACEMENT_3D('',#133359,#103514,#103515) ;
#91275 = AXIS2_PLACEMENT_3D('',#133363,#103517,#103518) ;
#91276 = AXIS2_PLACEMENT_3D('',#133367,#103520,#103521) ;
#91277 = AXIS2_PLACEMENT_3D('',#133369,#103523,#103524) ;
#91278 = AXIS2_PLACEMENT_3D('',#133378,#103529,#103530) ;
#91279 = AXIS2_PLACEMENT_3D('',#133557,#103537,#103538) ;
#91280 = AXIS2_PLACEMENT_3D('',#133564,#103541,#103542) ;
#91281 = AXIS2_PLACEMENT_3D('',#133566,#103544,#103545) ;
#91282 = AXIS2_PLACEMENT_3D('',#133575,#103550,#103551) ;
#91283 = AXIS2_PLACEMENT_3D('',#133576,#103552,#103553) ;
#91284 = AXIS2_PLACEMENT_3D('',#133577,#103554,#103555) ;
#91285 = AXIS2_PLACEMENT_3D('',#133578,#103556,#103557) ;
#91286 = AXIS2_PLACEMENT_3D('',#133579,#103558,#103559) ;
#91287 = AXIS2_PLACEMENT_3D('',#133580,#103560,#103561) ;
#91288 = AXIS2_PLACEMENT_3D('',#133581,#103562,#103563) ;
#91289 = AXIS2_PLACEMENT_3D('',#133582,#103564,#103565) ;
#91290 = AXIS2_PLACEMENT_3D('',#133583,#103566,#103567) ;
#91291 = AXIS2_PLACEMENT_3D('',#133584,#103568,#103569) ;
#91292 = AXIS2_PLACEMENT_3D('',#133585,#103570,#103571) ;
#91293 = AXIS2_PLACEMENT_3D('',#133586,#103572,#103573) ;
#91294 = AXIS2_PLACEMENT_3D('',#133587,#103574,#103575) ;
#91295 = AXIS2_PLACEMENT_3D('',#133588,#103576,#103577) ;
#91296 = AXIS2_PLACEMENT_3D('',#133589,#103578,#103579) ;
#91297 = AXIS2_PLACEMENT_3D('',#133590,#103580,#103581) ;
#91298 = AXIS2_PLACEMENT_3D('',#133599,#103586,#103587) ;
#91299 = AXIS2_PLACEMENT_3D('',#133608,#103592,#103593) ;
#91300 = AXIS2_PLACEMENT_3D('',#133611,#103594,#103595) ;
#91301 = AXIS2_PLACEMENT_3D('',#133619,#103599,#103600) ;
#91302 = AXIS2_PLACEMENT_3D('',#133625,#103604,#103605) ;
#91303 = AXIS2_PLACEMENT_3D('',#133630,#103607,#103608) ;
#91304 = AXIS2_PLACEMENT_3D('',#133633,#103610,#103611) ;
#91305 = AXIS2_PLACEMENT_3D('',#133635,#103612,#103613) ;
#91306 = AXIS2_PLACEMENT_3D('',#133638,#103615,#103616) ;
#91307 = AXIS2_PLACEMENT_3D('',#133639,#103617,#103618) ;
#91308 = AXIS2_PLACEMENT_3D('',#133642,#103619,#103620) ;
#91309 = AXIS2_PLACEMENT_3D('',#133647,#103623,#103624) ;
#91310 = AXIS2_PLACEMENT_3D('',#133653,#103628,#103629) ;
#91311 = AXIS2_PLACEMENT_3D('',#133659,#103633,#103634) ;
#91312 = AXIS2_PLACEMENT_3D('',#133665,#103638,#103639) ;
#91313 = AXIS2_PLACEMENT_3D('',#133678,#103646,#103647) ;
#91314 = AXIS2_PLACEMENT_3D('',#133691,#103654,#103655) ;
#91315 = AXIS2_PLACEMENT_3D('',#133700,#103660,#103661) ;
#91316 = AXIS2_PLACEMENT_3D('',#133709,#103666,#103667) ;
#91317 = AXIS2_PLACEMENT_3D('',#133718,#103672,#103673) ;
#91318 = AXIS2_PLACEMENT_3D('',#133727,#103678,#103679) ;
#91319 = AXIS2_PLACEMENT_3D('',#133740,#103685,#103686) ;
#91320 = AXIS2_PLACEMENT_3D('',#133744,#103688,#103689) ;
#91321 = AXIS2_PLACEMENT_3D('',#133748,#103691,#103692) ;
#91322 = AXIS2_PLACEMENT_3D('',#133751,#103694,#103695) ;
#91323 = AXIS2_PLACEMENT_3D('',#133752,#103696,#103697) ;
#91324 = AXIS2_PLACEMENT_3D('',#133755,#103698,#103699) ;
#91325 = AXIS2_PLACEMENT_3D('',#133758,#103702,#103703) ;
#91326 = AXIS2_PLACEMENT_3D('',#133762,#103706,#103707) ;
#91327 = AXIS2_PLACEMENT_3D('',#133764,#103708,#103709) ;
#91328 = AXIS2_PLACEMENT_3D('',#133766,#103711,#103712) ;
#91329 = AXIS2_PLACEMENT_3D('',#133770,#103715,#103716) ;
#91330 = AXIS2_PLACEMENT_3D('',#133772,#103717,#103718) ;
#91331 = AXIS2_PLACEMENT_3D('',#133774,#103720,#103721) ;
#91332 = AXIS2_PLACEMENT_3D('',#133778,#103724,#103725) ;
#91333 = AXIS2_PLACEMENT_3D('',#133780,#103726,#103727) ;
#91334 = AXIS2_PLACEMENT_3D('',#133782,#103729,#103730) ;
#91335 = AXIS2_PLACEMENT_3D('',#133784,#103732,#103733) ;
#91336 = AXIS2_PLACEMENT_3D('',#133785,#103734,#103735) ;
#91337 = AXIS2_PLACEMENT_3D('',#133787,#103737,#103738) ;
#91338 = AXIS2_PLACEMENT_3D('',#133790,#103741,#103742) ;
#91339 = AXIS2_PLACEMENT_3D('',#133793,#103745,#103746) ;
#91340 = AXIS2_PLACEMENT_3D('',#133796,#103749,#103750) ;
#91341 = AXIS2_PLACEMENT_3D('',#133805,#103755,#103756) ;
#91342 = AXIS2_PLACEMENT_3D('',#133814,#103761,#103762) ;
#91343 = AXIS2_PLACEMENT_3D('',#133823,#103767,#103768) ;
#91344 = AXIS2_PLACEMENT_3D('',#133832,#103773,#103774) ;
#91345 = AXIS2_PLACEMENT_3D('',#133845,#103780,#103781) ;
#91346 = AXIS2_PLACEMENT_3D('',#133849,#103783,#103784) ;
#91347 = AXIS2_PLACEMENT_3D('',#133853,#103786,#103787) ;
#91348 = AXIS2_PLACEMENT_3D('',#133856,#103789,#103790) ;
#91349 = AXIS2_PLACEMENT_3D('',#133857,#103791,#103792) ;
#91350 = AXIS2_PLACEMENT_3D('',#133861,#103794,#103795) ;
#91351 = AXIS2_PLACEMENT_3D('',#133863,#103797,#103798) ;
#91352 = AXIS2_PLACEMENT_3D('',#133867,#103801,#103802) ;
#91353 = AXIS2_PLACEMENT_3D('',#133869,#103803,#103804) ;
#91354 = AXIS2_PLACEMENT_3D('',#133871,#103806,#103807) ;
#91355 = AXIS2_PLACEMENT_3D('',#133875,#103810,#103811) ;
#91356 = AXIS2_PLACEMENT_3D('',#133877,#103812,#103813) ;
#91357 = AXIS2_PLACEMENT_3D('',#133879,#103815,#103816) ;
#91358 = AXIS2_PLACEMENT_3D('',#133883,#103819,#103820) ;
#91359 = AXIS2_PLACEMENT_3D('',#133885,#103821,#103822) ;
#91360 = AXIS2_PLACEMENT_3D('',#133887,#103824,#103825) ;
#91361 = AXIS2_PLACEMENT_3D('',#133889,#103827,#103828) ;
#91362 = AXIS2_PLACEMENT_3D('',#133898,#103833,#103834) ;
#91363 = AXIS2_PLACEMENT_3D('',#133905,#103839,#103840) ;
#91364 = AXIS2_PLACEMENT_3D('',#133911,#103844,#103845) ;
#91365 = AXIS2_PLACEMENT_3D('',#133916,#103849,#103850) ;
#91366 = AXIS2_PLACEMENT_3D('',#133920,#103852,#103853) ;
#91367 = AXIS2_PLACEMENT_3D('',#133926,#103857,#103858) ;
#91368 = AXIS2_PLACEMENT_3D('',#133927,#103859,#103860) ;
#91369 = AXIS2_PLACEMENT_3D('',#133930,#103861,#103862) ;
#91370 = AXIS2_PLACEMENT_3D('',#133932,#103863,#103864) ;
#91371 = AXIS2_PLACEMENT_3D('',#133934,#103865,#103866) ;
#91372 = AXIS2_PLACEMENT_3D('',#133938,#103868,#103869) ;
#91373 = AXIS2_PLACEMENT_3D('',#133958,#103871,#103872) ;
#91374 = AXIS2_PLACEMENT_3D('',#133965,#103873,#103874) ;
#91375 = AXIS2_PLACEMENT_3D('',#133966,#103875,#103876) ;
#91376 = AXIS2_PLACEMENT_3D('',#133967,#103877,#103878) ;
#91377 = AXIS2_PLACEMENT_3D('',#133980,#103879,#103880) ;
#91378 = AXIS2_PLACEMENT_3D('',#133981,#103881,#103882) ;
#91379 = AXIS2_PLACEMENT_3D('',#133982,#103883,#103884) ;
#91380 = AXIS2_PLACEMENT_3D('',#133983,#103885,#103886) ;
#91381 = AXIS2_PLACEMENT_3D('',#133984,#103887,#103888) ;
#91382 = AXIS2_PLACEMENT_3D('',#133985,#103889,#103890) ;
#91383 = AXIS2_PLACEMENT_3D('',#133986,#103891,#103892) ;
#91384 = AXIS2_PLACEMENT_3D('',#133987,#103893,#103894) ;
#91385 = AXIS2_PLACEMENT_3D('',#133988,#103895,#103896) ;
#91386 = AXIS2_PLACEMENT_3D('',#133989,#103897,#103898) ;
#91387 = AXIS2_PLACEMENT_3D('',#133990,#103899,#103900) ;
#91388 = AXIS2_PLACEMENT_3D('',#133991,#103901,#103902) ;
#91389 = AXIS2_PLACEMENT_3D('',#133992,#103903,#103904) ;
#91390 = AXIS2_PLACEMENT_3D('',#133993,#103905,#103906) ;
#91391 = AXIS2_PLACEMENT_3D('',#133994,#103907,#103908) ;
#91392 = AXIS2_PLACEMENT_3D('',#133995,#103909,#103910) ;
#91393 = AXIS2_PLACEMENT_3D('',#134014,#103911,#103912) ;
#91394 = AXIS2_PLACEMENT_3D('',#134015,#103913,#103914) ;
#91395 = AXIS2_PLACEMENT_3D('',#134034,#103915,#103916) ;
#91396 = AXIS2_PLACEMENT_3D('',#134053,#103917,#103918) ;
#91397 = AXIS2_PLACEMENT_3D('',#134054,#103919,#103920) ;
#91398 = AXIS2_PLACEMENT_3D('',#134055,#103921,#103922) ;
#91399 = AXIS2_PLACEMENT_3D('',#134056,#103923,#103924) ;
#91400 = AXIS2_PLACEMENT_3D('',#134057,#103925,#103926) ;
#91401 = AXIS2_PLACEMENT_3D('',#134058,#103927,#103928) ;
#91402 = AXIS2_PLACEMENT_3D('',#134059,#103929,#103930) ;
#91403 = AXIS2_PLACEMENT_3D('',#134060,#103931,#103932) ;
#91404 = AXIS2_PLACEMENT_3D('',#134061,#103933,#103934) ;
#91405 = AXIS2_PLACEMENT_3D('',#134062,#103935,#103936) ;
#91406 = AXIS2_PLACEMENT_3D('',#134063,#103937,#103938) ;
#91407 = AXIS2_PLACEMENT_3D('',#134064,#103939,#103940) ;
#91408 = AXIS2_PLACEMENT_3D('',#134065,#103941,#103942) ;
#91409 = AXIS2_PLACEMENT_3D('',#134066,#103943,#103944) ;
#91410 = AXIS2_PLACEMENT_3D('',#134067,#103945,#103946) ;
#91411 = AXIS2_PLACEMENT_3D('',#134086,#103947,#103948) ;
#91412 = AXIS2_PLACEMENT_3D('',#134087,#103949,#103950) ;
#91413 = AXIS2_PLACEMENT_3D('',#134088,#103951,#103952) ;
#91414 = AXIS2_PLACEMENT_3D('',#134089,#103953,#103954) ;
#91415 = AXIS2_PLACEMENT_3D('',#134090,#103955,#103956) ;
#91416 = AXIS2_PLACEMENT_3D('',#134091,#103957,#103958) ;
#91417 = AXIS2_PLACEMENT_3D('',#134092,#103959,#103960) ;
#91418 = AXIS2_PLACEMENT_3D('',#134093,#103961,#103962) ;
#91419 = AXIS2_PLACEMENT_3D('',#134094,#103963,#103964) ;
#91420 = AXIS2_PLACEMENT_3D('',#134095,#103965,#103966) ;
#91421 = AXIS2_PLACEMENT_3D('',#134096,#103967,#103968) ;
#91422 = AXIS2_PLACEMENT_3D('',#134109,#103969,#103970) ;
#91423 = AXIS2_PLACEMENT_3D('',#134110,#103971,#103972) ;
#91424 = AXIS2_PLACEMENT_3D('',#134111,#103973,#103974) ;
#91425 = AXIS2_PLACEMENT_3D('',#134112,#103975,#103976) ;
#91426 = AXIS2_PLACEMENT_3D('',#134113,#103977,#103978) ;
#91427 = AXIS2_PLACEMENT_3D('',#134114,#103979,#103980) ;
#91428 = AXIS2_PLACEMENT_3D('',#134115,#103981,#103982) ;
#91429 = AXIS2_PLACEMENT_3D('',#134128,#103983,#103984) ;
#91430 = AXIS2_PLACEMENT_3D('',#134129,#103985,#103986) ;
#91431 = AXIS2_PLACEMENT_3D('',#134130,#103987,#103988) ;
#91432 = AXIS2_PLACEMENT_3D('',#134131,#103989,#103990) ;
#91433 = AXIS2_PLACEMENT_3D('',#134133,#103991,#103992) ;
#91434 = AXIS2_PLACEMENT_3D('',#134153,#103993,#103994) ;
#91435 = AXIS2_PLACEMENT_3D('',#134154,#103995,#103996) ;
#91436 = AXIS2_PLACEMENT_3D('',#134155,#103997,#103998) ;
#91437 = AXIS2_PLACEMENT_3D('',#134156,#103999,#104000) ;
#91438 = AXIS2_PLACEMENT_3D('',#134157,#104001,#104002) ;
#91439 = AXIS2_PLACEMENT_3D('',#134158,#104003,#104004) ;
#91440 = AXIS2_PLACEMENT_3D('',#134187,#104005,#104006) ;
#91441 = AXIS2_PLACEMENT_3D('',#134188,#104007,#104008) ;
#91442 = AXIS2_PLACEMENT_3D('',#134189,#104009,#104010) ;
#91443 = AXIS2_PLACEMENT_3D('',#134190,#104011,#104012) ;
#91444 = AXIS2_PLACEMENT_3D('',#134191,#104013,#104014) ;
#91445 = AXIS2_PLACEMENT_3D('',#134192,#104015,#104016) ;
#91446 = AXIS2_PLACEMENT_3D('',#134193,#104017,#104018) ;
#91447 = AXIS2_PLACEMENT_3D('',#134215,#104019,#104020) ;
#91448 = AXIS2_PLACEMENT_3D('',#134216,#104021,#104022) ;
#91449 = AXIS2_PLACEMENT_3D('',#134217,#104023,#104024) ;
#91450 = AXIS2_PLACEMENT_3D('',#134218,#104025,#104026) ;
#91451 = AXIS2_PLACEMENT_3D('',#134219,#104027,#104028) ;
#91452 = AXIS2_PLACEMENT_3D('',#134220,#104029,#104030) ;
#91453 = AXIS2_PLACEMENT_3D('',#134221,#104031,#104032) ;
#91454 = AXIS2_PLACEMENT_3D('',#134222,#104033,#104034) ;
#91455 = AXIS2_PLACEMENT_3D('',#134223,#104035,#104036) ;
#91456 = AXIS2_PLACEMENT_3D('',#134224,#104037,#104038) ;
#91457 = AXIS2_PLACEMENT_3D('',#134225,#104039,#104040) ;
#91458 = AXIS2_PLACEMENT_3D('',#134226,#104041,#104042) ;
#91459 = AXIS2_PLACEMENT_3D('',#134227,#104043,#104044) ;
#91460 = AXIS2_PLACEMENT_3D('',#134228,#104045,#104046) ;
#91461 = AXIS2_PLACEMENT_3D('',#134229,#104047,#104048) ;
#91462 = AXIS2_PLACEMENT_3D('',#134230,#104049,#104050) ;
#91463 = AXIS2_PLACEMENT_3D('',#134231,#104051,#104052) ;
#91464 = AXIS2_PLACEMENT_3D('',#134232,#104053,#104054) ;
#91465 = AXIS2_PLACEMENT_3D('',#134233,#104055,#104056) ;
#91466 = AXIS2_PLACEMENT_3D('',#134234,#104057,#104058) ;
#91467 = AXIS2_PLACEMENT_3D('',#134235,#104059,#104060) ;
#91468 = AXIS2_PLACEMENT_3D('',#134236,#104061,#104062) ;
#91469 = AXIS2_PLACEMENT_3D('',#134237,#104063,#104064) ;
#91470 = AXIS2_PLACEMENT_3D('',#134238,#104065,#104066) ;
#91471 = AXIS2_PLACEMENT_3D('',#134239,#104067,#104068) ;
#91472 = AXIS2_PLACEMENT_3D('',#134240,#104069,#104070) ;
#91473 = AXIS2_PLACEMENT_3D('',#134241,#104071,#104072) ;
#91474 = AXIS2_PLACEMENT_3D('',#134242,#104073,#104074) ;
#91475 = AXIS2_PLACEMENT_3D('',#134243,#104075,#104076) ;
#91476 = AXIS2_PLACEMENT_3D('',#134244,#104077,#104078) ;
#91477 = AXIS2_PLACEMENT_3D('',#134245,#104079,#104080) ;
#91478 = AXIS2_PLACEMENT_3D('',#134246,#104081,#104082) ;
#91479 = AXIS2_PLACEMENT_3D('',#134247,#104083,#104084) ;
#91480 = AXIS2_PLACEMENT_3D('',#134248,#104085,#104086) ;
#91481 = AXIS2_PLACEMENT_3D('',#134249,#104087,#104088) ;
#91482 = AXIS2_PLACEMENT_3D('',#134250,#104089,#104090) ;
#91483 = AXIS2_PLACEMENT_3D('',#134251,#104091,#104092) ;
#91484 = AXIS2_PLACEMENT_3D('',#134252,#104093,#104094) ;
#91485 = AXIS2_PLACEMENT_3D('',#134253,#104095,#104096) ;
#91486 = AXIS2_PLACEMENT_3D('',#134254,#104097,#104098) ;
#91487 = AXIS2_PLACEMENT_3D('',#134255,#104099,#104100) ;
#91488 = AXIS2_PLACEMENT_3D('',#134256,#104101,#104102) ;
#91489 = AXIS2_PLACEMENT_3D('',#134257,#104103,#104104) ;
#91490 = AXIS2_PLACEMENT_3D('',#134258,#104105,#104106) ;
#91491 = AXIS2_PLACEMENT_3D('',#134259,#104107,#104108) ;
#91492 = AXIS2_PLACEMENT_3D('',#134260,#104109,#104110) ;
#91493 = AXIS2_PLACEMENT_3D('',#134261,#104111,#104112) ;
#91494 = AXIS2_PLACEMENT_3D('',#134262,#104113,#104114) ;
#91495 = AXIS2_PLACEMENT_3D('',#134263,#104115,#104116) ;
#91496 = AXIS2_PLACEMENT_3D('',#134264,#104117,#104118) ;
#91497 = AXIS2_PLACEMENT_3D('',#134265,#104119,#104120) ;
#91498 = AXIS2_PLACEMENT_3D('',#134266,#104121,#104122) ;
#91499 = AXIS2_PLACEMENT_3D('',#134267,#104123,#104124) ;
#91500 = AXIS2_PLACEMENT_3D('',#134268,#104125,#104126) ;
#91501 = AXIS2_PLACEMENT_3D('',#134269,#104127,#104128) ;
#91502 = AXIS2_PLACEMENT_3D('',#134270,#104129,#104130) ;
#91503 = AXIS2_PLACEMENT_3D('',#134271,#104131,#104132) ;
#91504 = AXIS2_PLACEMENT_3D('',#134272,#104133,#104134) ;
#91505 = AXIS2_PLACEMENT_3D('',#134273,#104135,#104136) ;
#91506 = AXIS2_PLACEMENT_3D('',#134274,#104137,#104138) ;
#91507 = AXIS2_PLACEMENT_3D('',#134275,#104139,#104140) ;
#91508 = AXIS2_PLACEMENT_3D('',#134276,#104141,#104142) ;
#91509 = AXIS2_PLACEMENT_3D('',#134277,#104143,#104144) ;
#91510 = AXIS2_PLACEMENT_3D('',#134278,#104145,#104146) ;
#91511 = AXIS2_PLACEMENT_3D('',#134279,#104147,#104148) ;
#91512 = AXIS2_PLACEMENT_3D('',#134280,#104149,#104150) ;
#91513 = AXIS2_PLACEMENT_3D('',#134281,#104151,#104152) ;
#91514 = AXIS2_PLACEMENT_3D('',#134282,#104153,#104154) ;
#91515 = AXIS2_PLACEMENT_3D('',#134283,#104155,#104156) ;
#91516 = AXIS2_PLACEMENT_3D('',#134284,#104157,#104158) ;
#91517 = AXIS2_PLACEMENT_3D('',#134285,#104159,#104160) ;
#91518 = AXIS2_PLACEMENT_3D('',#134286,#104161,#104162) ;
#91519 = AXIS2_PLACEMENT_3D('',#134287,#104163,#104164) ;
#91520 = AXIS2_PLACEMENT_3D('',#134288,#104165,#104166) ;
#91521 = AXIS2_PLACEMENT_3D('',#134289,#104167,#104168) ;
#91522 = AXIS2_PLACEMENT_3D('',#134290,#104169,#104170) ;
#91523 = AXIS2_PLACEMENT_3D('',#134291,#104171,#104172) ;
#91524 = AXIS2_PLACEMENT_3D('',#134292,#104173,#104174) ;
#91525 = AXIS2_PLACEMENT_3D('',#134293,#104175,#104176) ;
#91526 = AXIS2_PLACEMENT_3D('',#134294,#104177,#104178) ;
#91527 = AXIS2_PLACEMENT_3D('',#134295,#104179,#104180) ;
#91528 = AXIS2_PLACEMENT_3D('',#134296,#104181,#104182) ;
#91529 = AXIS2_PLACEMENT_3D('',#134297,#104183,#104184) ;
#91530 = AXIS2_PLACEMENT_3D('',#134298,#104185,#104186) ;
#91531 = AXIS2_PLACEMENT_3D('',#134299,#104187,#104188) ;
#91532 = AXIS2_PLACEMENT_3D('',#134300,#104189,#104190) ;
#91533 = AXIS2_PLACEMENT_3D('',#134301,#104191,#104192) ;
#91534 = AXIS2_PLACEMENT_3D('',#134302,#104193,#104194) ;
#91535 = AXIS2_PLACEMENT_3D('',#134303,#104195,#104196) ;
#91536 = AXIS2_PLACEMENT_3D('',#134304,#104197,#104198) ;
#91537 = AXIS2_PLACEMENT_3D('',#134305,#104199,#104200) ;
#91538 = AXIS2_PLACEMENT_3D('',#134306,#104201,#104202) ;
#91539 = AXIS2_PLACEMENT_3D('',#134307,#104203,#104204) ;
#91540 = AXIS2_PLACEMENT_3D('',#134308,#104205,#104206) ;
#91541 = AXIS2_PLACEMENT_3D('',#134309,#104207,#104208) ;
#91542 = AXIS2_PLACEMENT_3D('',#134310,#104209,#104210) ;
#91543 = AXIS2_PLACEMENT_3D('',#134311,#104211,#104212) ;
#91544 = AXIS2_PLACEMENT_3D('',#134312,#104213,#104214) ;
#91545 = AXIS2_PLACEMENT_3D('',#134313,#104215,#104216) ;
#91546 = AXIS2_PLACEMENT_3D('',#134314,#104217,#104218) ;
#91547 = AXIS2_PLACEMENT_3D('',#134315,#104219,#104220) ;
#91548 = AXIS2_PLACEMENT_3D('',#134316,#104221,#104222) ;
#91549 = AXIS2_PLACEMENT_3D('',#134317,#104223,#104224) ;
#91550 = AXIS2_PLACEMENT_3D('',#134318,#104225,#104226) ;
#91551 = AXIS2_PLACEMENT_3D('',#134319,#104227,#104228) ;
#91552 = AXIS2_PLACEMENT_3D('',#134320,#104229,#104230) ;
#91553 = AXIS2_PLACEMENT_3D('',#134321,#104231,#104232) ;
#91554 = AXIS2_PLACEMENT_3D('',#134322,#104233,#104234) ;
#91555 = AXIS2_PLACEMENT_3D('',#134323,#104235,#104236) ;
#91556 = AXIS2_PLACEMENT_3D('',#134336,#104237,#104238) ;
#91557 = AXIS2_PLACEMENT_3D('',#134337,#104239,#104240) ;
#91558 = AXIS2_PLACEMENT_3D('',#134338,#104241,#104242) ;
#91559 = AXIS2_PLACEMENT_3D('',#134339,#104243,#104244) ;
#91560 = AXIS2_PLACEMENT_3D('',#134340,#104245,#104246) ;
#91561 = AXIS2_PLACEMENT_3D('',#134341,#104247,#104248) ;
#91562 = AXIS2_PLACEMENT_3D('',#134342,#104249,#104250) ;
#91563 = AXIS2_PLACEMENT_3D('',#134343,#104251,#104252) ;
#91564 = AXIS2_PLACEMENT_3D('',#134344,#104253,#104254) ;
#91565 = AXIS2_PLACEMENT_3D('',#134345,#104255,#104256) ;
#91566 = AXIS2_PLACEMENT_3D('',#134346,#104257,#104258) ;
#91567 = AXIS2_PLACEMENT_3D('',#134347,#104259,#104260) ;
#91568 = AXIS2_PLACEMENT_3D('',#134348,#104261,#104262) ;
#91569 = AXIS2_PLACEMENT_3D('',#134349,#104263,#104264) ;
#91570 = AXIS2_PLACEMENT_3D('',#134350,#104265,#104266) ;
#91571 = AXIS2_PLACEMENT_3D('',#134351,#104267,#104268) ;
#91572 = AXIS2_PLACEMENT_3D('',#134352,#104269,#104270) ;
#91573 = AXIS2_PLACEMENT_3D('',#134353,#104271,#104272) ;
#91574 = AXIS2_PLACEMENT_3D('',#134354,#104273,#104274) ;
#91575 = AXIS2_PLACEMENT_3D('',#134355,#104275,#104276) ;
#91576 = AXIS2_PLACEMENT_3D('',#134356,#104277,#104278) ;
#91577 = AXIS2_PLACEMENT_3D('',#134357,#104279,#104280) ;
#91578 = AXIS2_PLACEMENT_3D('',#134358,#104281,#104282) ;
#91579 = AXIS2_PLACEMENT_3D('',#134359,#104283,#104284) ;
#91580 = AXIS2_PLACEMENT_3D('',#134360,#104285,#104286) ;
#91581 = AXIS2_PLACEMENT_3D('',#134361,#104287,#104288) ;
#91582 = AXIS2_PLACEMENT_3D('',#134374,#104289,#104290) ;
#91583 = AXIS2_PLACEMENT_3D('',#134375,#104291,#104292) ;
#91584 = AXIS2_PLACEMENT_3D('',#134376,#104293,#104294) ;
#91585 = AXIS2_PLACEMENT_3D('',#134377,#104295,#104296) ;
#91586 = AXIS2_PLACEMENT_3D('',#134378,#104297,#104298) ;
#91587 = AXIS2_PLACEMENT_3D('',#134379,#104299,#104300) ;
#91588 = AXIS2_PLACEMENT_3D('',#134380,#104301,#104302) ;
#91589 = AXIS2_PLACEMENT_3D('',#134381,#104303,#104304) ;
#91590 = AXIS2_PLACEMENT_3D('',#134382,#104305,#104306) ;
#91591 = AXIS2_PLACEMENT_3D('',#134383,#104307,#104308) ;
#91592 = AXIS2_PLACEMENT_3D('',#134384,#104309,#104310) ;
#91593 = AXIS2_PLACEMENT_3D('',#134385,#104311,#104312) ;
#91594 = AXIS2_PLACEMENT_3D('',#134386,#104313,#104314) ;
#91595 = AXIS2_PLACEMENT_3D('',#134387,#104315,#104316) ;
#91596 = AXIS2_PLACEMENT_3D('',#134388,#104317,#104318) ;
#91597 = AXIS2_PLACEMENT_3D('',#134389,#104319,#104320) ;
#91598 = AXIS2_PLACEMENT_3D('',#134390,#104321,#104322) ;
#91599 = AXIS2_PLACEMENT_3D('',#134391,#104323,#104324) ;
#91600 = AXIS2_PLACEMENT_3D('',#134392,#104325,#104326) ;
#91601 = AXIS2_PLACEMENT_3D('',#134393,#104327,#104328) ;
#91602 = AXIS2_PLACEMENT_3D('',#134394,#104329,#104330) ;
#91603 = AXIS2_PLACEMENT_3D('',#134395,#104331,#104332) ;
#91604 = AXIS2_PLACEMENT_3D('',#134396,#104333,#104334) ;
#91605 = AXIS2_PLACEMENT_3D('',#134397,#104335,#104336) ;
#91606 = AXIS2_PLACEMENT_3D('',#134398,#104337,#104338) ;
#91607 = AXIS2_PLACEMENT_3D('',#134399,#104339,#104340) ;
#91608 = AXIS2_PLACEMENT_3D('',#134400,#104341,#104342) ;
#91609 = AXIS2_PLACEMENT_3D('',#134401,#104343,#104344) ;
#91610 = AXIS2_PLACEMENT_3D('',#134414,#104345,#104346) ;
#91611 = AXIS2_PLACEMENT_3D('',#134427,#104347,#104348) ;
#91612 = AXIS2_PLACEMENT_3D('',#134428,#104349,#104350) ;
#91613 = AXIS2_PLACEMENT_3D('',#134429,#104351,#104352) ;
#91614 = AXIS2_PLACEMENT_3D('',#134430,#104353,#104354) ;
#91615 = AXIS2_PLACEMENT_3D('',#134431,#104355,#104356) ;
#91616 = AXIS2_PLACEMENT_3D('',#134444,#104357,#104358) ;
#91617 = AXIS2_PLACEMENT_3D('',#134457,#104359,#104360) ;
#91618 = AXIS2_PLACEMENT_3D('',#134458,#104361,#104362) ;
#91619 = AXIS2_PLACEMENT_3D('',#134459,#104363,#104364) ;
#91620 = AXIS2_PLACEMENT_3D('',#134460,#104365,#104366) ;
#91621 = AXIS2_PLACEMENT_3D('',#134538,#104367,#104368) ;
#91622 = AXIS2_PLACEMENT_3D('',#134539,#104369,#104370) ;
#91623 = AXIS2_PLACEMENT_3D('',#134608,#104371,#104372) ;
#91624 = AXIS2_PLACEMENT_3D('',#134609,#104373,#104374) ;
#91625 = AXIS2_PLACEMENT_3D('',#134610,#104375,#104376) ;
#91626 = AXIS2_PLACEMENT_3D('',#134725,#104377,#104378) ;
#91627 = AXIS2_PLACEMENT_3D('',#134756,#104379,#104380) ;
#91628 = AXIS2_PLACEMENT_3D('',#134787,#104381,#104382) ;
#91629 = AXIS2_PLACEMENT_3D('',#134836,#104383,#104384) ;
#91630 = AXIS2_PLACEMENT_3D('',#134837,#104385,#104386) ;
#91631 = AXIS2_PLACEMENT_3D('',#134846,#104391,#104392) ;
#91632 = AXIS2_PLACEMENT_3D('',#134848,#104393,#104394) ;
#91633 = AXIS2_PLACEMENT_3D('',#134851,#104396,#104397) ;
#91634 = AXIS2_PLACEMENT_3D('',#134852,#104398,#104399) ;
#91635 = AXIS2_PLACEMENT_3D('',#134858,#104403,#104404) ;
#91636 = AXIS2_PLACEMENT_3D('',#134860,#104405,#104406) ;
#91637 = AXIS2_PLACEMENT_3D('',#134863,#104408,#104409) ;
#91638 = AXIS2_PLACEMENT_3D('',#134864,#104410,#104411) ;
#91639 = AXIS2_PLACEMENT_3D('',#134870,#104415,#104416) ;
#91640 = AXIS2_PLACEMENT_3D('',#134872,#104417,#104418) ;
#91641 = AXIS2_PLACEMENT_3D('',#134875,#104420,#104421) ;
#91642 = AXIS2_PLACEMENT_3D('',#134876,#104422,#104423) ;
#91643 = AXIS2_PLACEMENT_3D('',#134882,#104427,#104428) ;
#91644 = AXIS2_PLACEMENT_3D('',#134884,#104429,#104430) ;
#91645 = AXIS2_PLACEMENT_3D('',#134887,#104432,#104433) ;
#91646 = AXIS2_PLACEMENT_3D('',#134888,#104434,#104435) ;
#91647 = AXIS2_PLACEMENT_3D('',#134894,#104439,#104440) ;
#91648 = AXIS2_PLACEMENT_3D('',#134897,#104441,#104442) ;
#91649 = AXIS2_PLACEMENT_3D('',#134909,#104449,#104450) ;
#91650 = AXIS2_PLACEMENT_3D('',#134920,#104455,#104456) ;
#91651 = AXIS2_PLACEMENT_3D('',#134924,#104459,#104460) ;
#91652 = AXIS2_PLACEMENT_3D('',#134927,#104461,#104462) ;
#91653 = AXIS2_PLACEMENT_3D('',#134933,#104466,#104467) ;
#91654 = AXIS2_PLACEMENT_3D('',#134941,#104472,#104473) ;
#91655 = AXIS2_PLACEMENT_3D('',#134943,#104475,#104476) ;
#91656 = AXIS2_PLACEMENT_3D('',#134952,#104481,#104482) ;
#91657 = AXIS2_PLACEMENT_3D('',#134953,#104483,#104484) ;
#91658 = AXIS2_PLACEMENT_3D('',#134954,#104485,#104486) ;
#91659 = AXIS2_PLACEMENT_3D('',#134955,#104487,#104488) ;
#91660 = AXIS2_PLACEMENT_3D('',#134956,#104489,#104490) ;
#91661 = AXIS2_PLACEMENT_3D('',#134957,#104491,#104492) ;
#91662 = AXIS2_PLACEMENT_3D('',#134958,#104493,#104494) ;
#91663 = AXIS2_PLACEMENT_3D('',#134967,#104499,#104500) ;
#91664 = AXIS2_PLACEMENT_3D('',#134976,#104505,#104506) ;
#91665 = AXIS2_PLACEMENT_3D('',#134979,#104507,#104508) ;
#91666 = AXIS2_PLACEMENT_3D('',#134987,#104512,#104513) ;
#91667 = AXIS2_PLACEMENT_3D('',#134993,#104517,#104518) ;
#91668 = AXIS2_PLACEMENT_3D('',#134998,#104520,#104521) ;
#91669 = AXIS2_PLACEMENT_3D('',#135001,#104523,#104524) ;
#91670 = AXIS2_PLACEMENT_3D('',#135003,#104525,#104526) ;
#91671 = AXIS2_PLACEMENT_3D('',#135006,#104528,#104529) ;
#91672 = AXIS2_PLACEMENT_3D('',#135007,#104530,#104531) ;
#91673 = AXIS2_PLACEMENT_3D('',#135010,#104532,#104533) ;
#91674 = AXIS2_PLACEMENT_3D('',#135015,#104536,#104537) ;
#91675 = AXIS2_PLACEMENT_3D('',#135021,#104541,#104542) ;
#91676 = AXIS2_PLACEMENT_3D('',#135027,#104546,#104547) ;
#91677 = AXIS2_PLACEMENT_3D('',#135033,#104551,#104552) ;
#91678 = AXIS2_PLACEMENT_3D('',#135046,#104559,#104560) ;
#91679 = AXIS2_PLACEMENT_3D('',#135059,#104567,#104568) ;
#91680 = AXIS2_PLACEMENT_3D('',#135068,#104573,#104574) ;
#91681 = AXIS2_PLACEMENT_3D('',#135077,#104579,#104580) ;
#91682 = AXIS2_PLACEMENT_3D('',#135086,#104585,#104586) ;
#91683 = AXIS2_PLACEMENT_3D('',#135095,#104591,#104592) ;
#91684 = AXIS2_PLACEMENT_3D('',#135108,#104598,#104599) ;
#91685 = AXIS2_PLACEMENT_3D('',#135112,#104601,#104602) ;
#91686 = AXIS2_PLACEMENT_3D('',#135116,#104604,#104605) ;
#91687 = AXIS2_PLACEMENT_3D('',#135119,#104607,#104608) ;
#91688 = AXIS2_PLACEMENT_3D('',#135120,#104609,#104610) ;
#91689 = AXIS2_PLACEMENT_3D('',#135123,#104611,#104612) ;
#91690 = AXIS2_PLACEMENT_3D('',#135126,#104615,#104616) ;
#91691 = AXIS2_PLACEMENT_3D('',#135130,#104619,#104620) ;
#91692 = AXIS2_PLACEMENT_3D('',#135132,#104621,#104622) ;
#91693 = AXIS2_PLACEMENT_3D('',#135134,#104624,#104625) ;
#91694 = AXIS2_PLACEMENT_3D('',#135138,#104628,#104629) ;
#91695 = AXIS2_PLACEMENT_3D('',#135140,#104630,#104631) ;
#91696 = AXIS2_PLACEMENT_3D('',#135142,#104633,#104634) ;
#91697 = AXIS2_PLACEMENT_3D('',#135146,#104637,#104638) ;
#91698 = AXIS2_PLACEMENT_3D('',#135148,#104639,#104640) ;
#91699 = AXIS2_PLACEMENT_3D('',#135150,#104642,#104643) ;
#91700 = AXIS2_PLACEMENT_3D('',#135152,#104645,#104646) ;
#91701 = AXIS2_PLACEMENT_3D('',#135153,#104647,#104648) ;
#91702 = AXIS2_PLACEMENT_3D('',#135155,#104650,#104651) ;
#91703 = AXIS2_PLACEMENT_3D('',#135158,#104654,#104655) ;
#91704 = AXIS2_PLACEMENT_3D('',#135161,#104658,#104659) ;
#91705 = AXIS2_PLACEMENT_3D('',#135164,#104662,#104663) ;
#91706 = AXIS2_PLACEMENT_3D('',#135173,#104668,#104669) ;
#91707 = AXIS2_PLACEMENT_3D('',#135182,#104674,#104675) ;
#91708 = AXIS2_PLACEMENT_3D('',#135191,#104680,#104681) ;
#91709 = AXIS2_PLACEMENT_3D('',#135200,#104686,#104687) ;
#91710 = AXIS2_PLACEMENT_3D('',#135213,#104693,#104694) ;
#91711 = AXIS2_PLACEMENT_3D('',#135217,#104696,#104697) ;
#91712 = AXIS2_PLACEMENT_3D('',#135221,#104699,#104700) ;
#91713 = AXIS2_PLACEMENT_3D('',#135224,#104702,#104703) ;
#91714 = AXIS2_PLACEMENT_3D('',#135225,#104704,#104705) ;
#91715 = AXIS2_PLACEMENT_3D('',#135229,#104707,#104708) ;
#91716 = AXIS2_PLACEMENT_3D('',#135231,#104710,#104711) ;
#91717 = AXIS2_PLACEMENT_3D('',#135235,#104714,#104715) ;
#91718 = AXIS2_PLACEMENT_3D('',#135237,#104716,#104717) ;
#91719 = AXIS2_PLACEMENT_3D('',#135239,#104719,#104720) ;
#91720 = AXIS2_PLACEMENT_3D('',#135243,#104723,#104724) ;
#91721 = AXIS2_PLACEMENT_3D('',#135245,#104725,#104726) ;
#91722 = AXIS2_PLACEMENT_3D('',#135247,#104728,#104729) ;
#91723 = AXIS2_PLACEMENT_3D('',#135251,#104732,#104733) ;
#91724 = AXIS2_PLACEMENT_3D('',#135253,#104734,#104735) ;
#91725 = AXIS2_PLACEMENT_3D('',#135255,#104737,#104738) ;
#91726 = AXIS2_PLACEMENT_3D('',#135257,#104740,#104741) ;
#91727 = AXIS2_PLACEMENT_3D('',#135266,#104746,#104747) ;
#91728 = AXIS2_PLACEMENT_3D('',#135273,#104752,#104753) ;
#91729 = AXIS2_PLACEMENT_3D('',#135279,#104757,#104758) ;
#91730 = AXIS2_PLACEMENT_3D('',#135284,#104762,#104763) ;
#91731 = AXIS2_PLACEMENT_3D('',#135288,#104765,#104766) ;
#91732 = AXIS2_PLACEMENT_3D('',#135294,#104770,#104771) ;
#91733 = AXIS2_PLACEMENT_3D('',#135295,#104772,#104773) ;
#91734 = AXIS2_PLACEMENT_3D('',#135298,#104774,#104775) ;
#91735 = AXIS2_PLACEMENT_3D('',#135300,#104776,#104777) ;
#91736 = AXIS2_PLACEMENT_3D('',#135302,#104778,#104779) ;
#91737 = AXIS2_PLACEMENT_3D('',#135306,#104781,#104782) ;
#91738 = AXIS2_PLACEMENT_3D('',#135326,#104784,#104785) ;
#91739 = AXIS2_PLACEMENT_3D('',#135333,#104786,#104787) ;
#91740 = AXIS2_PLACEMENT_3D('',#135334,#104788,#104789) ;
#91741 = AXIS2_PLACEMENT_3D('',#135335,#104790,#104791) ;
#91742 = AXIS2_PLACEMENT_3D('',#135348,#104792,#104793) ;
#91743 = AXIS2_PLACEMENT_3D('',#135349,#104794,#104795) ;
#91744 = AXIS2_PLACEMENT_3D('',#135350,#104796,#104797) ;
#91745 = AXIS2_PLACEMENT_3D('',#135351,#104798,#104799) ;
#91746 = AXIS2_PLACEMENT_3D('',#135352,#104800,#104801) ;
#91747 = AXIS2_PLACEMENT_3D('',#135353,#104802,#104803) ;
#91748 = AXIS2_PLACEMENT_3D('',#135354,#104804,#104805) ;
#91749 = AXIS2_PLACEMENT_3D('',#135355,#104806,#104807) ;
#91750 = AXIS2_PLACEMENT_3D('',#135356,#104808,#104809) ;
#91751 = AXIS2_PLACEMENT_3D('',#135357,#104810,#104811) ;
#91752 = AXIS2_PLACEMENT_3D('',#135358,#104812,#104813) ;
#91753 = AXIS2_PLACEMENT_3D('',#135359,#104814,#104815) ;
#91754 = AXIS2_PLACEMENT_3D('',#135360,#104816,#104817) ;
#91755 = AXIS2_PLACEMENT_3D('',#135361,#104818,#104819) ;
#91756 = AXIS2_PLACEMENT_3D('',#135362,#104820,#104821) ;
#91757 = AXIS2_PLACEMENT_3D('',#135363,#104822,#104823) ;
#91758 = AXIS2_PLACEMENT_3D('',#135382,#104824,#104825) ;
#91759 = AXIS2_PLACEMENT_3D('',#135383,#104826,#104827) ;
#91760 = AXIS2_PLACEMENT_3D('',#135402,#104828,#104829) ;
#91761 = AXIS2_PLACEMENT_3D('',#135421,#104830,#104831) ;
#91762 = AXIS2_PLACEMENT_3D('',#135422,#104832,#104833) ;
#91763 = AXIS2_PLACEMENT_3D('',#135423,#104834,#104835) ;
#91764 = AXIS2_PLACEMENT_3D('',#135424,#104836,#104837) ;
#91765 = AXIS2_PLACEMENT_3D('',#135425,#104838,#104839) ;
#91766 = AXIS2_PLACEMENT_3D('',#135426,#104840,#104841) ;
#91767 = AXIS2_PLACEMENT_3D('',#135427,#104842,#104843) ;
#91768 = AXIS2_PLACEMENT_3D('',#135428,#104844,#104845) ;
#91769 = AXIS2_PLACEMENT_3D('',#135429,#104846,#104847) ;
#91770 = AXIS2_PLACEMENT_3D('',#135430,#104848,#104849) ;
#91771 = AXIS2_PLACEMENT_3D('',#135431,#104850,#104851) ;
#91772 = AXIS2_PLACEMENT_3D('',#135432,#104852,#104853) ;
#91773 = AXIS2_PLACEMENT_3D('',#135433,#104854,#104855) ;
#91774 = AXIS2_PLACEMENT_3D('',#135434,#104856,#104857) ;
#91775 = AXIS2_PLACEMENT_3D('',#135435,#104858,#104859) ;
#91776 = AXIS2_PLACEMENT_3D('',#135454,#104860,#104861) ;
#91777 = AXIS2_PLACEMENT_3D('',#135455,#104862,#104863) ;
#91778 = AXIS2_PLACEMENT_3D('',#135456,#104864,#104865) ;
#91779 = AXIS2_PLACEMENT_3D('',#135457,#104866,#104867) ;
#91780 = AXIS2_PLACEMENT_3D('',#135458,#104868,#104869) ;
#91781 = AXIS2_PLACEMENT_3D('',#135459,#104870,#104871) ;
#91782 = AXIS2_PLACEMENT_3D('',#135460,#104872,#104873) ;
#91783 = AXIS2_PLACEMENT_3D('',#135461,#104874,#104875) ;
#91784 = AXIS2_PLACEMENT_3D('',#135462,#104876,#104877) ;
#91785 = AXIS2_PLACEMENT_3D('',#135463,#104878,#104879) ;
#91786 = AXIS2_PLACEMENT_3D('',#135464,#104880,#104881) ;
#91787 = AXIS2_PLACEMENT_3D('',#135477,#104882,#104883) ;
#91788 = AXIS2_PLACEMENT_3D('',#135478,#104884,#104885) ;
#91789 = AXIS2_PLACEMENT_3D('',#135479,#104886,#104887) ;
#91790 = AXIS2_PLACEMENT_3D('',#135480,#104888,#104889) ;
#91791 = AXIS2_PLACEMENT_3D('',#135481,#104890,#104891) ;
#91792 = AXIS2_PLACEMENT_3D('',#135482,#104892,#104893) ;
#91793 = AXIS2_PLACEMENT_3D('',#135483,#104894,#104895) ;
#91794 = AXIS2_PLACEMENT_3D('',#135496,#104896,#104897) ;
#91795 = AXIS2_PLACEMENT_3D('',#135497,#104898,#104899) ;
#91796 = AXIS2_PLACEMENT_3D('',#135498,#104900,#104901) ;
#91797 = AXIS2_PLACEMENT_3D('',#135499,#104902,#104903) ;
#91798 = AXIS2_PLACEMENT_3D('',#135501,#104904,#104905) ;
#91799 = AXIS2_PLACEMENT_3D('',#135521,#104906,#104907) ;
#91800 = AXIS2_PLACEMENT_3D('',#135522,#104908,#104909) ;
#91801 = AXIS2_PLACEMENT_3D('',#135523,#104910,#104911) ;
#91802 = AXIS2_PLACEMENT_3D('',#135524,#104912,#104913) ;
#91803 = AXIS2_PLACEMENT_3D('',#135525,#104914,#104915) ;
#91804 = AXIS2_PLACEMENT_3D('',#135526,#104916,#104917) ;
#91805 = AXIS2_PLACEMENT_3D('',#135555,#104918,#104919) ;
#91806 = AXIS2_PLACEMENT_3D('',#135556,#104920,#104921) ;
#91807 = AXIS2_PLACEMENT_3D('',#135557,#104922,#104923) ;
#91808 = AXIS2_PLACEMENT_3D('',#135558,#104924,#104925) ;
#91809 = AXIS2_PLACEMENT_3D('',#135559,#104926,#104927) ;
#91810 = AXIS2_PLACEMENT_3D('',#135560,#104928,#104929) ;
#91811 = AXIS2_PLACEMENT_3D('',#135582,#104930,#104931) ;
#91812 = AXIS2_PLACEMENT_3D('',#135583,#104932,#104933) ;
#91813 = AXIS2_PLACEMENT_3D('',#135584,#104934,#104935) ;
#91814 = AXIS2_PLACEMENT_3D('',#135585,#104936,#104937) ;
#91815 = AXIS2_PLACEMENT_3D('',#135586,#104938,#104939) ;
#91816 = AXIS2_PLACEMENT_3D('',#135587,#104940,#104941) ;
#91817 = AXIS2_PLACEMENT_3D('',#135588,#104942,#104943) ;
#91818 = AXIS2_PLACEMENT_3D('',#135589,#104944,#104945) ;
#91819 = AXIS2_PLACEMENT_3D('',#135590,#104946,#104947) ;
#91820 = AXIS2_PLACEMENT_3D('',#135591,#104948,#104949) ;
#91821 = AXIS2_PLACEMENT_3D('',#135592,#104950,#104951) ;
#91822 = AXIS2_PLACEMENT_3D('',#135593,#104952,#104953) ;
#91823 = AXIS2_PLACEMENT_3D('',#135594,#104954,#104955) ;
#91824 = AXIS2_PLACEMENT_3D('',#135595,#104956,#104957) ;
#91825 = AXIS2_PLACEMENT_3D('',#135596,#104958,#104959) ;
#91826 = AXIS2_PLACEMENT_3D('',#135597,#104960,#104961) ;
#91827 = AXIS2_PLACEMENT_3D('',#135598,#104962,#104963) ;
#91828 = AXIS2_PLACEMENT_3D('',#135599,#104964,#104965) ;
#91829 = AXIS2_PLACEMENT_3D('',#135600,#104966,#104967) ;
#91830 = AXIS2_PLACEMENT_3D('',#135601,#104968,#104969) ;
#91831 = AXIS2_PLACEMENT_3D('',#135602,#104970,#104971) ;
#91832 = AXIS2_PLACEMENT_3D('',#135603,#104972,#104973) ;
#91833 = AXIS2_PLACEMENT_3D('',#135604,#104974,#104975) ;
#91834 = AXIS2_PLACEMENT_3D('',#135605,#104976,#104977) ;
#91835 = AXIS2_PLACEMENT_3D('',#135606,#104978,#104979) ;
#91836 = AXIS2_PLACEMENT_3D('',#135607,#104980,#104981) ;
#91837 = AXIS2_PLACEMENT_3D('',#135608,#104982,#104983) ;
#91838 = AXIS2_PLACEMENT_3D('',#135609,#104984,#104985) ;
#91839 = AXIS2_PLACEMENT_3D('',#135610,#104986,#104987) ;
#91840 = AXIS2_PLACEMENT_3D('',#135611,#104988,#104989) ;
#91841 = AXIS2_PLACEMENT_3D('',#135612,#104990,#104991) ;
#91842 = AXIS2_PLACEMENT_3D('',#135613,#104992,#104993) ;
#91843 = AXIS2_PLACEMENT_3D('',#135614,#104994,#104995) ;
#91844 = AXIS2_PLACEMENT_3D('',#135615,#104996,#104997) ;
#91845 = AXIS2_PLACEMENT_3D('',#135616,#104998,#104999) ;
#91846 = AXIS2_PLACEMENT_3D('',#135617,#105000,#105001) ;
#91847 = AXIS2_PLACEMENT_3D('',#135618,#105002,#105003) ;
#91848 = AXIS2_PLACEMENT_3D('',#135619,#105004,#105005) ;
#91849 = AXIS2_PLACEMENT_3D('',#135620,#105006,#105007) ;
#91850 = AXIS2_PLACEMENT_3D('',#135621,#105008,#105009) ;
#91851 = AXIS2_PLACEMENT_3D('',#135622,#105010,#105011) ;
#91852 = AXIS2_PLACEMENT_3D('',#135623,#105012,#105013) ;
#91853 = AXIS2_PLACEMENT_3D('',#135624,#105014,#105015) ;
#91854 = AXIS2_PLACEMENT_3D('',#135625,#105016,#105017) ;
#91855 = AXIS2_PLACEMENT_3D('',#135626,#105018,#105019) ;
#91856 = AXIS2_PLACEMENT_3D('',#135627,#105020,#105021) ;
#91857 = AXIS2_PLACEMENT_3D('',#135628,#105022,#105023) ;
#91858 = AXIS2_PLACEMENT_3D('',#135629,#105024,#105025) ;
#91859 = AXIS2_PLACEMENT_3D('',#135630,#105026,#105027) ;
#91860 = AXIS2_PLACEMENT_3D('',#135631,#105028,#105029) ;
#91861 = AXIS2_PLACEMENT_3D('',#135632,#105030,#105031) ;
#91862 = AXIS2_PLACEMENT_3D('',#135633,#105032,#105033) ;
#91863 = AXIS2_PLACEMENT_3D('',#135634,#105034,#105035) ;
#91864 = AXIS2_PLACEMENT_3D('',#135635,#105036,#105037) ;
#91865 = AXIS2_PLACEMENT_3D('',#135636,#105038,#105039) ;
#91866 = AXIS2_PLACEMENT_3D('',#135637,#105040,#105041) ;
#91867 = AXIS2_PLACEMENT_3D('',#135638,#105042,#105043) ;
#91868 = AXIS2_PLACEMENT_3D('',#135639,#105044,#105045) ;
#91869 = AXIS2_PLACEMENT_3D('',#135640,#105046,#105047) ;
#91870 = AXIS2_PLACEMENT_3D('',#135641,#105048,#105049) ;
#91871 = AXIS2_PLACEMENT_3D('',#135642,#105050,#105051) ;
#91872 = AXIS2_PLACEMENT_3D('',#135643,#105052,#105053) ;
#91873 = AXIS2_PLACEMENT_3D('',#135644,#105054,#105055) ;
#91874 = AXIS2_PLACEMENT_3D('',#135645,#105056,#105057) ;
#91875 = AXIS2_PLACEMENT_3D('',#135646,#105058,#105059) ;
#91876 = AXIS2_PLACEMENT_3D('',#135647,#105060,#105061) ;
#91877 = AXIS2_PLACEMENT_3D('',#135648,#105062,#105063) ;
#91878 = AXIS2_PLACEMENT_3D('',#135649,#105064,#105065) ;
#91879 = AXIS2_PLACEMENT_3D('',#135650,#105066,#105067) ;
#91880 = AXIS2_PLACEMENT_3D('',#135651,#105068,#105069) ;
#91881 = AXIS2_PLACEMENT_3D('',#135652,#105070,#105071) ;
#91882 = AXIS2_PLACEMENT_3D('',#135653,#105072,#105073) ;
#91883 = AXIS2_PLACEMENT_3D('',#135654,#105074,#105075) ;
#91884 = AXIS2_PLACEMENT_3D('',#135655,#105076,#105077) ;
#91885 = AXIS2_PLACEMENT_3D('',#135656,#105078,#105079) ;
#91886 = AXIS2_PLACEMENT_3D('',#135657,#105080,#105081) ;
#91887 = AXIS2_PLACEMENT_3D('',#135658,#105082,#105083) ;
#91888 = AXIS2_PLACEMENT_3D('',#135659,#105084,#105085) ;
#91889 = AXIS2_PLACEMENT_3D('',#135660,#105086,#105087) ;
#91890 = AXIS2_PLACEMENT_3D('',#135661,#105088,#105089) ;
#91891 = AXIS2_PLACEMENT_3D('',#135662,#105090,#105091) ;
#91892 = AXIS2_PLACEMENT_3D('',#135663,#105092,#105093) ;
#91893 = AXIS2_PLACEMENT_3D('',#135664,#105094,#105095) ;
#91894 = AXIS2_PLACEMENT_3D('',#135665,#105096,#105097) ;
#91895 = AXIS2_PLACEMENT_3D('',#135666,#105098,#105099) ;
#91896 = AXIS2_PLACEMENT_3D('',#135667,#105100,#105101) ;
#91897 = AXIS2_PLACEMENT_3D('',#135668,#105102,#105103) ;
#91898 = AXIS2_PLACEMENT_3D('',#135669,#105104,#105105) ;
#91899 = AXIS2_PLACEMENT_3D('',#135670,#105106,#105107) ;
#91900 = AXIS2_PLACEMENT_3D('',#135671,#105108,#105109) ;
#91901 = AXIS2_PLACEMENT_3D('',#135672,#105110,#105111) ;
#91902 = AXIS2_PLACEMENT_3D('',#135673,#105112,#105113) ;
#91903 = AXIS2_PLACEMENT_3D('',#135674,#105114,#105115) ;
#91904 = AXIS2_PLACEMENT_3D('',#135675,#105116,#105117) ;
#91905 = AXIS2_PLACEMENT_3D('',#135676,#105118,#105119) ;
#91906 = AXIS2_PLACEMENT_3D('',#135677,#105120,#105121) ;
#91907 = AXIS2_PLACEMENT_3D('',#135678,#105122,#105123) ;
#91908 = AXIS2_PLACEMENT_3D('',#135679,#105124,#105125) ;
#91909 = AXIS2_PLACEMENT_3D('',#135680,#105126,#105127) ;
#91910 = AXIS2_PLACEMENT_3D('',#135681,#105128,#105129) ;
#91911 = AXIS2_PLACEMENT_3D('',#135682,#105130,#105131) ;
#91912 = AXIS2_PLACEMENT_3D('',#135683,#105132,#105133) ;
#91913 = AXIS2_PLACEMENT_3D('',#135684,#105134,#105135) ;
#91914 = AXIS2_PLACEMENT_3D('',#135685,#105136,#105137) ;
#91915 = AXIS2_PLACEMENT_3D('',#135686,#105138,#105139) ;
#91916 = AXIS2_PLACEMENT_3D('',#135687,#105140,#105141) ;
#91917 = AXIS2_PLACEMENT_3D('',#135688,#105142,#105143) ;
#91918 = AXIS2_PLACEMENT_3D('',#135689,#105144,#105145) ;
#91919 = AXIS2_PLACEMENT_3D('',#135690,#105146,#105147) ;
#91920 = AXIS2_PLACEMENT_3D('',#135703,#105148,#105149) ;
#91921 = AXIS2_PLACEMENT_3D('',#135704,#105150,#105151) ;
#91922 = AXIS2_PLACEMENT_3D('',#135705,#105152,#105153) ;
#91923 = AXIS2_PLACEMENT_3D('',#135706,#105154,#105155) ;
#91924 = AXIS2_PLACEMENT_3D('',#135707,#105156,#105157) ;
#91925 = AXIS2_PLACEMENT_3D('',#135708,#105158,#105159) ;
#91926 = AXIS2_PLACEMENT_3D('',#135709,#105160,#105161) ;
#91927 = AXIS2_PLACEMENT_3D('',#135710,#105162,#105163) ;
#91928 = AXIS2_PLACEMENT_3D('',#135711,#105164,#105165) ;
#91929 = AXIS2_PLACEMENT_3D('',#135712,#105166,#105167) ;
#91930 = AXIS2_PLACEMENT_3D('',#135713,#105168,#105169) ;
#91931 = AXIS2_PLACEMENT_3D('',#135714,#105170,#105171) ;
#91932 = AXIS2_PLACEMENT_3D('',#135715,#105172,#105173) ;
#91933 = AXIS2_PLACEMENT_3D('',#135716,#105174,#105175) ;
#91934 = AXIS2_PLACEMENT_3D('',#135717,#105176,#105177) ;
#91935 = AXIS2_PLACEMENT_3D('',#135718,#105178,#105179) ;
#91936 = AXIS2_PLACEMENT_3D('',#135719,#105180,#105181) ;
#91937 = AXIS2_PLACEMENT_3D('',#135720,#105182,#105183) ;
#91938 = AXIS2_PLACEMENT_3D('',#135721,#105184,#105185) ;
#91939 = AXIS2_PLACEMENT_3D('',#135722,#105186,#105187) ;
#91940 = AXIS2_PLACEMENT_3D('',#135735,#105188,#105189) ;
#91941 = AXIS2_PLACEMENT_3D('',#135736,#105190,#105191) ;
#91942 = AXIS2_PLACEMENT_3D('',#135737,#105192,#105193) ;
#91943 = AXIS2_PLACEMENT_3D('',#135738,#105194,#105195) ;
#91944 = AXIS2_PLACEMENT_3D('',#135739,#105196,#105197) ;
#91945 = AXIS2_PLACEMENT_3D('',#135740,#105198,#105199) ;
#91946 = AXIS2_PLACEMENT_3D('',#135741,#105200,#105201) ;
#91947 = AXIS2_PLACEMENT_3D('',#135742,#105202,#105203) ;
#91948 = AXIS2_PLACEMENT_3D('',#135743,#105204,#105205) ;
#91949 = AXIS2_PLACEMENT_3D('',#135744,#105206,#105207) ;
#91950 = AXIS2_PLACEMENT_3D('',#135757,#105208,#105209) ;
#91951 = AXIS2_PLACEMENT_3D('',#135770,#105210,#105211) ;
#91952 = AXIS2_PLACEMENT_3D('',#135771,#105212,#105213) ;
#91953 = AXIS2_PLACEMENT_3D('',#135784,#105214,#105215) ;
#91954 = AXIS2_PLACEMENT_3D('',#135797,#105216,#105217) ;
#91955 = AXIS2_PLACEMENT_3D('',#135798,#105218,#105219) ;
#91956 = AXIS2_PLACEMENT_3D('',#135799,#105220,#105221) ;
#91957 = AXIS2_PLACEMENT_3D('',#135800,#105222,#105223) ;
#91958 = AXIS2_PLACEMENT_3D('',#135946,#105224,#105225) ;
#91959 = AXIS2_PLACEMENT_3D('',#135947,#105226,#105227) ;
#91960 = AXIS2_PLACEMENT_3D('',#136062,#105228,#105229) ;
#91961 = AXIS2_PLACEMENT_3D('',#136093,#105230,#105231) ;
#91962 = AXIS2_PLACEMENT_3D('',#136124,#105232,#105233) ;
#91963 = AXIS2_PLACEMENT_3D('',#136173,#105234,#105235) ;
#91964 = AXIS2_PLACEMENT_3D('',#136174,#105236,#105237) ;
#91965 = AXIS2_PLACEMENT_3D('',#136175,#105238,#105239) ;
#91966 = AXIS2_PLACEMENT_3D('',#136176,#105240,#105241) ;
#91967 = AXIS2_PLACEMENT_3D('',#136177,#105242,#105243) ;
#91968 = AXIS2_PLACEMENT_3D('',#136178,#105244,#105245) ;
#91969 = AXIS2_PLACEMENT_3D('',#136179,#105246,#105247) ;
#91970 = AXIS2_PLACEMENT_3D('',#136180,#105248,#105249) ;
#91971 = AXIS2_PLACEMENT_3D('',#136181,#105250,#105251) ;
#91972 = AXIS2_PLACEMENT_3D('',#136182,#105252,#105253) ;
#91973 = AXIS2_PLACEMENT_3D('',#136183,#105254,#105255) ;
#91974 = AXIS2_PLACEMENT_3D('',#136184,#105256,#105257) ;
#91975 = AXIS2_PLACEMENT_3D('',#136185,#105258,#105259) ;
#91976 = AXIS2_PLACEMENT_3D('',#136186,#105260,#105261) ;
#91977 = AXIS2_PLACEMENT_3D('',#136187,#105262,#105263) ;
#91978 = AXIS2_PLACEMENT_3D('',#136188,#105264,#105265) ;
#91979 = AXIS2_PLACEMENT_3D('',#136189,#105266,#105267) ;
#91980 = AXIS2_PLACEMENT_3D('',#136190,#105268,#105269) ;
#91981 = AXIS2_PLACEMENT_3D('',#136191,#105270,#105271) ;
#91982 = AXIS2_PLACEMENT_3D('',#136192,#105272,#105273) ;
#91983 = AXIS2_PLACEMENT_3D('',#136193,#105274,#105275) ;
#91984 = AXIS2_PLACEMENT_3D('',#136194,#105276,#105277) ;
#91985 = AXIS2_PLACEMENT_3D('',#136195,#105278,#105279) ;
#91986 = AXIS2_PLACEMENT_3D('',#136196,#105280,#105281) ;
#91987 = AXIS2_PLACEMENT_3D('',#136197,#105282,#105283) ;
#91988 = AXIS2_PLACEMENT_3D('',#136202,#105284,#105285) ;
#91989 = AXIS2_PLACEMENT_3D('',#136203,#105286,#105287) ;
#91990 = AXIS2_PLACEMENT_3D('',#136204,#105288,#105289) ;
#91991 = AXIS2_PLACEMENT_3D('',#136205,#105290,#105291) ;
#91992 = AXIS2_PLACEMENT_3D('',#136210,#105292,#105293) ;
#91993 = AXIS2_PLACEMENT_3D('',#136211,#105294,#105295) ;
#91994 = AXIS2_PLACEMENT_3D('',#136212,#105296,#105297) ;
#91995 = AXIS2_PLACEMENT_3D('',#136213,#105298,#105299) ;
#91996 = AXIS2_PLACEMENT_3D('',#136226,#105300,#105301) ;
#91997 = AXIS2_PLACEMENT_3D('',#136239,#105302,#105303) ;
#91998 = AXIS2_PLACEMENT_3D('',#136240,#105304,#105305) ;
#91999 = AXIS2_PLACEMENT_3D('',#136241,#105306,#105307) ;
#92000 = AXIS2_PLACEMENT_3D('',#136242,#105308,#105309) ;
#92001 = AXIS2_PLACEMENT_3D('',#136243,#105310,#105311) ;
#92002 = AXIS2_PLACEMENT_3D('',#136244,#105312,#105313) ;
#92003 = AXIS2_PLACEMENT_3D('',#136245,#105314,#105315) ;
#92004 = AXIS2_PLACEMENT_3D('',#136246,#105316,#105317) ;
#92005 = AXIS2_PLACEMENT_3D('',#136247,#105318,#105319) ;
#92006 = AXIS2_PLACEMENT_3D('',#136248,#105320,#105321) ;
#92007 = AXIS2_PLACEMENT_3D('',#136249,#105322,#105323) ;
#92008 = AXIS2_PLACEMENT_3D('',#136250,#105324,#105325) ;
#92009 = AXIS2_PLACEMENT_3D('',#136251,#105326,#105327) ;
#92010 = AXIS2_PLACEMENT_3D('',#136252,#105328,#105329) ;
#92011 = AXIS2_PLACEMENT_3D('',#136253,#105330,#105331) ;
#92012 = AXIS2_PLACEMENT_3D('',#136254,#105332,#105333) ;
#92013 = AXIS2_PLACEMENT_3D('',#136255,#105334,#105335) ;
#92014 = AXIS2_PLACEMENT_3D('',#136258,#105336,#105337) ;
#92015 = AXIS2_PLACEMENT_3D('',#136260,#105338,#105339) ;
#92016 = AXIS2_PLACEMENT_3D('',#136262,#105340,#105341) ;
#92017 = AXIS2_PLACEMENT_3D('',#136263,#105342,#105343) ;
#92018 = AXIS2_PLACEMENT_3D('',#136264,#105344,#105345) ;
#92019 = AXIS2_PLACEMENT_3D('',#136266,#105346,#105347) ;
#92020 = AXIS2_PLACEMENT_3D('',#136268,#105348,#105349) ;
#92021 = AXIS2_PLACEMENT_3D('',#136270,#105350,#105351) ;
#92022 = AXIS2_PLACEMENT_3D('',#136271,#105352,#105353) ;
#92023 = AXIS2_PLACEMENT_3D('',#136272,#105354,#105355) ;
#92024 = AXIS2_PLACEMENT_3D('',#136274,#105356,#105357) ;
#92025 = AXIS2_PLACEMENT_3D('',#136276,#105358,#105359) ;
#92026 = AXIS2_PLACEMENT_3D('',#136277,#105360,#105361) ;
#92027 = AXIS2_PLACEMENT_3D('',#136278,#105362,#105363) ;
#92028 = AXIS2_PLACEMENT_3D('',#136280,#105364,#105365) ;
#92029 = AXIS2_PLACEMENT_3D('',#136282,#105366,#105367) ;
#92030 = AXIS2_PLACEMENT_3D('',#136284,#105368,#105369) ;
#92031 = AXIS2_PLACEMENT_3D('',#136285,#105370,#105371) ;
#92032 = AXIS2_PLACEMENT_3D('',#136286,#105372,#105373) ;
#92033 = AXIS2_PLACEMENT_3D('',#136289,#105374,#105375) ;
#92034 = AXIS2_PLACEMENT_3D('',#136291,#105376,#105377) ;
#92035 = AXIS2_PLACEMENT_3D('',#136293,#105378,#105379) ;
#92036 = AXIS2_PLACEMENT_3D('',#136294,#105380,#105381) ;
#92037 = AXIS2_PLACEMENT_3D('',#136295,#105382,#105383) ;
#92038 = AXIS2_PLACEMENT_3D('',#136298,#105384,#105385) ;
#92039 = AXIS2_PLACEMENT_3D('',#136300,#105386,#105387) ;
#92040 = AXIS2_PLACEMENT_3D('',#136301,#105388,#105389) ;
#92041 = AXIS2_PLACEMENT_3D('',#136302,#105390,#105391) ;
#92042 = AXIS2_PLACEMENT_3D('',#136306,#105393,#105394) ;
#92043 = AXIS2_PLACEMENT_3D('',#136308,#105396,#105397) ;
#92044 = AXIS2_PLACEMENT_3D('',#136311,#105398,#105399) ;
#92045 = AXIS2_PLACEMENT_3D('',#136313,#105400,#105401) ;
#92046 = AXIS2_PLACEMENT_3D('',#136314,#105402,#105403) ;
#92047 = AXIS2_PLACEMENT_3D('',#136315,#105404,#105405) ;
#92048 = AXIS2_PLACEMENT_3D('',#136317,#105406,#105407) ;
#92049 = AXIS2_PLACEMENT_3D('',#136319,#105409,#105410) ;
#92050 = AXIS2_PLACEMENT_3D('',#136321,#105412,#105413) ;
#92051 = AXIS2_PLACEMENT_3D('',#136324,#105414,#105415) ;
#92052 = AXIS2_PLACEMENT_3D('',#136350,#105417,#105418) ;
#92053 = AXIS2_PLACEMENT_3D('',#136397,#105420,#105421) ;
#92054 = AXIS2_PLACEMENT_3D('',#136423,#105423,#105424) ;
#92055 = AXIS2_PLACEMENT_3D('',#136469,#105426,#105427) ;
#92056 = AXIS2_PLACEMENT_3D('',#136471,#105429,#105430) ;
#92057 = AXIS2_PLACEMENT_3D('',#136474,#105431,#105432) ;
#92058 = AXIS2_PLACEMENT_3D('',#136476,#105433,#105434) ;
#92059 = AXIS2_PLACEMENT_3D('',#136478,#105435,#105436) ;
#92060 = AXIS2_PLACEMENT_3D('',#136479,#105437,#105438) ;
#92061 = AXIS2_PLACEMENT_3D('',#136480,#105439,#105440) ;
#92062 = AXIS2_PLACEMENT_3D('',#136483,#105441,#105442) ;
#92063 = AXIS2_PLACEMENT_3D('',#136487,#105444,#105445) ;
#92064 = AXIS2_PLACEMENT_3D('',#136489,#105447,#105448) ;
#92065 = AXIS2_PLACEMENT_3D('',#136491,#105449,#105450) ;
#92066 = AXIS2_PLACEMENT_3D('',#136493,#105451,#105452) ;
#92067 = AXIS2_PLACEMENT_3D('',#136495,#105453,#105454) ;
#92068 = AXIS2_PLACEMENT_3D('',#136496,#105455,#105456) ;
#92069 = AXIS2_PLACEMENT_3D('',#136497,#105457,#105458) ;
#92070 = AXIS2_PLACEMENT_3D('',#136499,#105459,#105460) ;
#92071 = AXIS2_PLACEMENT_3D('',#136501,#105461,#105462) ;
#92072 = AXIS2_PLACEMENT_3D('',#136502,#105463,#105464) ;
#92073 = AXIS2_PLACEMENT_3D('',#136503,#105465,#105466) ;
#92074 = AXIS2_PLACEMENT_3D('',#136505,#105467,#105468) ;
#92075 = AXIS2_PLACEMENT_3D('',#136507,#105469,#105470) ;
#92076 = AXIS2_PLACEMENT_3D('',#136509,#105471,#105472) ;
#92077 = AXIS2_PLACEMENT_3D('',#136510,#105473,#105474) ;
#92078 = AXIS2_PLACEMENT_3D('',#136511,#105475,#105476) ;
#92079 = AXIS2_PLACEMENT_3D('',#136514,#105477,#105478) ;
#92080 = AXIS2_PLACEMENT_3D('',#136516,#105479,#105480) ;
#92081 = AXIS2_PLACEMENT_3D('',#136518,#105481,#105482) ;
#92082 = AXIS2_PLACEMENT_3D('',#136519,#105483,#105484) ;
#92083 = AXIS2_PLACEMENT_3D('',#136520,#105485,#105486) ;
#92084 = AXIS2_PLACEMENT_3D('',#136523,#105487,#105488) ;
#92085 = AXIS2_PLACEMENT_3D('',#136525,#105489,#105490) ;
#92086 = AXIS2_PLACEMENT_3D('',#136526,#105491,#105492) ;
#92087 = AXIS2_PLACEMENT_3D('',#136527,#105493,#105494) ;
#92088 = AXIS2_PLACEMENT_3D('',#136531,#105496,#105497) ;
#92089 = AXIS2_PLACEMENT_3D('',#136533,#105499,#105500) ;
#92090 = AXIS2_PLACEMENT_3D('',#136536,#105501,#105502) ;
#92091 = AXIS2_PLACEMENT_3D('',#136538,#105503,#105504) ;
#92092 = AXIS2_PLACEMENT_3D('',#136539,#105505,#105506) ;
#92093 = AXIS2_PLACEMENT_3D('',#136540,#105507,#105508) ;
#92094 = AXIS2_PLACEMENT_3D('',#136542,#105509,#105510) ;
#92095 = AXIS2_PLACEMENT_3D('',#136544,#105512,#105513) ;
#92096 = AXIS2_PLACEMENT_3D('',#136546,#105515,#105516) ;
#92097 = AXIS2_PLACEMENT_3D('',#136549,#105517,#105518) ;
#92098 = AXIS2_PLACEMENT_3D('',#136575,#105520,#105521) ;
#92099 = AXIS2_PLACEMENT_3D('',#136622,#105523,#105524) ;
#92100 = AXIS2_PLACEMENT_3D('',#136648,#105526,#105527) ;
#92101 = AXIS2_PLACEMENT_3D('',#136694,#105529,#105530) ;
#92102 = AXIS2_PLACEMENT_3D('',#136696,#105532,#105533) ;
#92103 = AXIS2_PLACEMENT_3D('',#136707,#105538,#105539) ;
#92104 = AXIS2_PLACEMENT_3D('',#136725,#105543,#105544) ;
#92105 = AXIS2_PLACEMENT_3D('',#136727,#105546,#105547) ;
#92106 = AXIS2_PLACEMENT_3D('',#136736,#105552,#105553) ;
#92107 = AXIS2_PLACEMENT_3D('',#136745,#105558,#105559) ;
#92108 = AXIS2_PLACEMENT_3D('',#136754,#105564,#105565) ;
#92109 = AXIS2_PLACEMENT_3D('',#136756,#105566,#105567) ;
#92110 = AXIS2_PLACEMENT_3D('',#136759,#105569,#105570) ;
#92111 = AXIS2_PLACEMENT_3D('',#136760,#105571,#105572) ;
#92112 = AXIS2_PLACEMENT_3D('',#136761,#105573,#105574) ;
#92113 = AXIS2_PLACEMENT_3D('',#136762,#105575,#105576) ;
#92114 = AXIS2_PLACEMENT_3D('',#136763,#105577,#105578) ;
#92115 = AXIS2_PLACEMENT_3D('',#136764,#105579,#105580) ;
#92116 = AXIS2_PLACEMENT_3D('',#136765,#105581,#105582) ;
#92117 = AXIS2_PLACEMENT_3D('',#136766,#105583,#105584) ;
#92118 = AXIS2_PLACEMENT_3D('',#136769,#105585,#105586) ;
#92119 = AXIS2_PLACEMENT_3D('',#136772,#105588,#105589) ;
#92120 = AXIS2_PLACEMENT_3D('',#136774,#105590,#105591) ;
#92121 = AXIS2_PLACEMENT_3D('',#136776,#105593,#105594) ;
#92122 = AXIS2_PLACEMENT_3D('',#136779,#105595,#105596) ;
#92123 = AXIS2_PLACEMENT_3D('',#136785,#105600,#105601) ;
#92124 = AXIS2_PLACEMENT_3D('',#136794,#105606,#105607) ;
#92125 = AXIS2_PLACEMENT_3D('',#136802,#105612,#105613) ;
#92126 = AXIS2_PLACEMENT_3D('',#136804,#105615,#105616) ;
#92127 = AXIS2_PLACEMENT_3D('',#136810,#105620,#105621) ;
#92128 = AXIS2_PLACEMENT_3D('',#136820,#105627,#105628) ;
#92129 = AXIS2_PLACEMENT_3D('',#136822,#105629,#105630) ;
#92130 = AXIS2_PLACEMENT_3D('',#136824,#105631,#105632) ;
#92131 = AXIS2_PLACEMENT_3D('',#136828,#105634,#105635) ;
#92132 = AXIS2_PLACEMENT_3D('',#136830,#105636,#105637) ;
#92133 = AXIS2_PLACEMENT_3D('',#136832,#105638,#105639) ;
#92134 = AXIS2_PLACEMENT_3D('',#136841,#105644,#105645) ;
#92135 = AXIS2_PLACEMENT_3D('',#136843,#105647,#105648) ;
#92136 = AXIS2_PLACEMENT_3D('',#136850,#105653,#105654) ;
#92137 = AXIS2_PLACEMENT_3D('',#136859,#105658,#105659) ;
#92138 = AXIS2_PLACEMENT_3D('',#136863,#105661,#105662) ;
#92139 = AXIS2_PLACEMENT_3D('',#136867,#105664,#105665) ;
#92140 = AXIS2_PLACEMENT_3D('',#136871,#105667,#105668) ;
#92141 = AXIS2_PLACEMENT_3D('',#136875,#105671,#105672) ;
#92142 = AXIS2_PLACEMENT_3D('',#136881,#105676,#105677) ;
#92143 = AXIS2_PLACEMENT_3D('',#136888,#105682,#105683) ;
#92144 = AXIS2_PLACEMENT_3D('',#136899,#105688,#105689) ;
#92145 = AXIS2_PLACEMENT_3D('',#136903,#105691,#105692) ;
#92146 = AXIS2_PLACEMENT_3D('',#136907,#105694,#105695) ;
#92147 = AXIS2_PLACEMENT_3D('',#136911,#105697,#105698) ;
#92148 = AXIS2_PLACEMENT_3D('',#136915,#105700,#105701) ;
#92149 = AXIS2_PLACEMENT_3D('',#136919,#105703,#105704) ;
#92150 = AXIS2_PLACEMENT_3D('',#136923,#105706,#105707) ;
#92151 = AXIS2_PLACEMENT_3D('',#136927,#105709,#105710) ;
#92152 = AXIS2_PLACEMENT_3D('',#136929,#105712,#105713) ;
#92153 = AXIS2_PLACEMENT_3D('',#136938,#105718,#105719) ;
#92154 = AXIS2_PLACEMENT_3D('',#136944,#105723,#105724) ;
#92155 = AXIS2_PLACEMENT_3D('',#136950,#105728,#105729) ;
#92156 = AXIS2_PLACEMENT_3D('',#137031,#105742,#105743) ;
#92157 = AXIS2_PLACEMENT_3D('',#137042,#105748,#105749) ;
#92158 = AXIS2_PLACEMENT_3D('',#137046,#105751,#105752) ;
#92159 = AXIS2_PLACEMENT_3D('',#137050,#105754,#105755) ;
#92160 = AXIS2_PLACEMENT_3D('',#137054,#105757,#105758) ;
#92161 = AXIS2_PLACEMENT_3D('',#137058,#105760,#105761) ;
#92162 = AXIS2_PLACEMENT_3D('',#137062,#105763,#105764) ;
#92163 = AXIS2_PLACEMENT_3D('',#137066,#105766,#105767) ;
#92164 = AXIS2_PLACEMENT_3D('',#137070,#105769,#105770) ;
#92165 = AXIS2_PLACEMENT_3D('',#137072,#105772,#105773) ;
#92166 = AXIS2_PLACEMENT_3D('',#137081,#105778,#105779) ;
#92167 = AXIS2_PLACEMENT_3D('',#137260,#105786,#105787) ;
#92168 = AXIS2_PLACEMENT_3D('',#137265,#105789,#105790) ;
#92169 = AXIS2_PLACEMENT_3D('',#137268,#105792,#105793) ;
#92170 = AXIS2_PLACEMENT_3D('',#137269,#105794,#105795) ;
#92171 = AXIS2_PLACEMENT_3D('',#137278,#105800,#105801) ;
#92172 = AXIS2_PLACEMENT_3D('',#137279,#105802,#105803) ;
#92173 = AXIS2_PLACEMENT_3D('',#137280,#105804,#105805) ;
#92174 = AXIS2_PLACEMENT_3D('',#137281,#105806,#105807) ;
#92175 = AXIS2_PLACEMENT_3D('',#137282,#105808,#105809) ;
#92176 = AXIS2_PLACEMENT_3D('',#137283,#105810,#105811) ;
#92177 = AXIS2_PLACEMENT_3D('',#137284,#105812,#105813) ;
#92178 = AXIS2_PLACEMENT_3D('',#137285,#105814,#105815) ;
#92179 = AXIS2_PLACEMENT_3D('',#137286,#105816,#105817) ;
#92180 = AXIS2_PLACEMENT_3D('',#137287,#105818,#105819) ;
#92181 = AXIS2_PLACEMENT_3D('',#137288,#105820,#105821) ;
#92182 = AXIS2_PLACEMENT_3D('',#137289,#105822,#105823) ;
#92183 = AXIS2_PLACEMENT_3D('',#137290,#105824,#105825) ;
#92184 = AXIS2_PLACEMENT_3D('',#137291,#105826,#105827) ;
#92185 = AXIS2_PLACEMENT_3D('',#137292,#105828,#105829) ;
#92186 = AXIS2_PLACEMENT_3D('',#137293,#105830,#105831) ;
#92187 = AXIS2_PLACEMENT_3D('',#137302,#105836,#105837) ;
#92188 = AXIS2_PLACEMENT_3D('',#137311,#105842,#105843) ;
#92189 = AXIS2_PLACEMENT_3D('',#137314,#105844,#105845) ;
#92190 = AXIS2_PLACEMENT_3D('',#137322,#105849,#105850) ;
#92191 = AXIS2_PLACEMENT_3D('',#137328,#105854,#105855) ;
#92192 = AXIS2_PLACEMENT_3D('',#137333,#105857,#105858) ;
#92193 = AXIS2_PLACEMENT_3D('',#137336,#105860,#105861) ;
#92194 = AXIS2_PLACEMENT_3D('',#137338,#105862,#105863) ;
#92195 = AXIS2_PLACEMENT_3D('',#137341,#105865,#105866) ;
#92196 = AXIS2_PLACEMENT_3D('',#137342,#105867,#105868) ;
#92197 = AXIS2_PLACEMENT_3D('',#137345,#105869,#105870) ;
#92198 = AXIS2_PLACEMENT_3D('',#137350,#105873,#105874) ;
#92199 = AXIS2_PLACEMENT_3D('',#137356,#105878,#105879) ;
#92200 = AXIS2_PLACEMENT_3D('',#137362,#105883,#105884) ;
#92201 = AXIS2_PLACEMENT_3D('',#137368,#105888,#105889) ;
#92202 = AXIS2_PLACEMENT_3D('',#137381,#105896,#105897) ;
#92203 = AXIS2_PLACEMENT_3D('',#137394,#105904,#105905) ;
#92204 = AXIS2_PLACEMENT_3D('',#137403,#105910,#105911) ;
#92205 = AXIS2_PLACEMENT_3D('',#137412,#105916,#105917) ;
#92206 = AXIS2_PLACEMENT_3D('',#137421,#105922,#105923) ;
#92207 = AXIS2_PLACEMENT_3D('',#137430,#105928,#105929) ;
#92208 = AXIS2_PLACEMENT_3D('',#137443,#105935,#105936) ;
#92209 = AXIS2_PLACEMENT_3D('',#137447,#105938,#105939) ;
#92210 = AXIS2_PLACEMENT_3D('',#137451,#105941,#105942) ;
#92211 = AXIS2_PLACEMENT_3D('',#137454,#105944,#105945) ;
#92212 = AXIS2_PLACEMENT_3D('',#137455,#105946,#105947) ;
#92213 = AXIS2_PLACEMENT_3D('',#137458,#105948,#105949) ;
#92214 = AXIS2_PLACEMENT_3D('',#137461,#105952,#105953) ;
#92215 = AXIS2_PLACEMENT_3D('',#137465,#105956,#105957) ;
#92216 = AXIS2_PLACEMENT_3D('',#137467,#105958,#105959) ;
#92217 = AXIS2_PLACEMENT_3D('',#137469,#105961,#105962) ;
#92218 = AXIS2_PLACEMENT_3D('',#137473,#105965,#105966) ;
#92219 = AXIS2_PLACEMENT_3D('',#137475,#105967,#105968) ;
#92220 = AXIS2_PLACEMENT_3D('',#137477,#105970,#105971) ;
#92221 = AXIS2_PLACEMENT_3D('',#137481,#105974,#105975) ;
#92222 = AXIS2_PLACEMENT_3D('',#137483,#105976,#105977) ;
#92223 = AXIS2_PLACEMENT_3D('',#137485,#105979,#105980) ;
#92224 = AXIS2_PLACEMENT_3D('',#137487,#105982,#105983) ;
#92225 = AXIS2_PLACEMENT_3D('',#137488,#105984,#105985) ;
#92226 = AXIS2_PLACEMENT_3D('',#137490,#105987,#105988) ;
#92227 = AXIS2_PLACEMENT_3D('',#137493,#105991,#105992) ;
#92228 = AXIS2_PLACEMENT_3D('',#137496,#105995,#105996) ;
#92229 = AXIS2_PLACEMENT_3D('',#137499,#105999,#106000) ;
#92230 = AXIS2_PLACEMENT_3D('',#137508,#106005,#106006) ;
#92231 = AXIS2_PLACEMENT_3D('',#137517,#106011,#106012) ;
#92232 = AXIS2_PLACEMENT_3D('',#137526,#106017,#106018) ;
#92233 = AXIS2_PLACEMENT_3D('',#137535,#106023,#106024) ;
#92234 = AXIS2_PLACEMENT_3D('',#137548,#106030,#106031) ;
#92235 = AXIS2_PLACEMENT_3D('',#137552,#106033,#106034) ;
#92236 = AXIS2_PLACEMENT_3D('',#137556,#106036,#106037) ;
#92237 = AXIS2_PLACEMENT_3D('',#137559,#106039,#106040) ;
#92238 = AXIS2_PLACEMENT_3D('',#137560,#106041,#106042) ;
#92239 = AXIS2_PLACEMENT_3D('',#137564,#106044,#106045) ;
#92240 = AXIS2_PLACEMENT_3D('',#137566,#106047,#106048) ;
#92241 = AXIS2_PLACEMENT_3D('',#137570,#106051,#106052) ;
#92242 = AXIS2_PLACEMENT_3D('',#137572,#106053,#106054) ;
#92243 = AXIS2_PLACEMENT_3D('',#137574,#106056,#106057) ;
#92244 = AXIS2_PLACEMENT_3D('',#137578,#106060,#106061) ;
#92245 = AXIS2_PLACEMENT_3D('',#137580,#106062,#106063) ;
#92246 = AXIS2_PLACEMENT_3D('',#137582,#106065,#106066) ;
#92247 = AXIS2_PLACEMENT_3D('',#137586,#106069,#106070) ;
#92248 = AXIS2_PLACEMENT_3D('',#137588,#106071,#106072) ;
#92249 = AXIS2_PLACEMENT_3D('',#137590,#106074,#106075) ;
#92250 = AXIS2_PLACEMENT_3D('',#137592,#106077,#106078) ;
#92251 = AXIS2_PLACEMENT_3D('',#137601,#106083,#106084) ;
#92252 = AXIS2_PLACEMENT_3D('',#137608,#106089,#106090) ;
#92253 = AXIS2_PLACEMENT_3D('',#137614,#106094,#106095) ;
#92254 = AXIS2_PLACEMENT_3D('',#137619,#106099,#106100) ;
#92255 = AXIS2_PLACEMENT_3D('',#137623,#106102,#106103) ;
#92256 = AXIS2_PLACEMENT_3D('',#137629,#106107,#106108) ;
#92257 = AXIS2_PLACEMENT_3D('',#137630,#106109,#106110) ;
#92258 = AXIS2_PLACEMENT_3D('',#137633,#106111,#106112) ;
#92259 = AXIS2_PLACEMENT_3D('',#137635,#106113,#106114) ;
#92260 = AXIS2_PLACEMENT_3D('',#137637,#106115,#106116) ;
#92261 = AXIS2_PLACEMENT_3D('',#137641,#106118,#106119) ;
#92262 = AXIS2_PLACEMENT_3D('',#137661,#106121,#106122) ;
#92263 = AXIS2_PLACEMENT_3D('',#137668,#106123,#106124) ;
#92264 = AXIS2_PLACEMENT_3D('',#137669,#106125,#106126) ;
#92265 = AXIS2_PLACEMENT_3D('',#137670,#106127,#106128) ;
#92266 = AXIS2_PLACEMENT_3D('',#137683,#106129,#106130) ;
#92267 = AXIS2_PLACEMENT_3D('',#137684,#106131,#106132) ;
#92268 = AXIS2_PLACEMENT_3D('',#137685,#106133,#106134) ;
#92269 = AXIS2_PLACEMENT_3D('',#137686,#106135,#106136) ;
#92270 = AXIS2_PLACEMENT_3D('',#137687,#106137,#106138) ;
#92271 = AXIS2_PLACEMENT_3D('',#137688,#106139,#106140) ;
#92272 = AXIS2_PLACEMENT_3D('',#137689,#106141,#106142) ;
#92273 = AXIS2_PLACEMENT_3D('',#137690,#106143,#106144) ;
#92274 = AXIS2_PLACEMENT_3D('',#137691,#106145,#106146) ;
#92275 = AXIS2_PLACEMENT_3D('',#137692,#106147,#106148) ;
#92276 = AXIS2_PLACEMENT_3D('',#137693,#106149,#106150) ;
#92277 = AXIS2_PLACEMENT_3D('',#137694,#106151,#106152) ;
#92278 = AXIS2_PLACEMENT_3D('',#137695,#106153,#106154) ;
#92279 = AXIS2_PLACEMENT_3D('',#137696,#106155,#106156) ;
#92280 = AXIS2_PLACEMENT_3D('',#137697,#106157,#106158) ;
#92281 = AXIS2_PLACEMENT_3D('',#137698,#106159,#106160) ;
#92282 = AXIS2_PLACEMENT_3D('',#137717,#106161,#106162) ;
#92283 = AXIS2_PLACEMENT_3D('',#137718,#106163,#106164) ;
#92284 = AXIS2_PLACEMENT_3D('',#137737,#106165,#106166) ;
#92285 = AXIS2_PLACEMENT_3D('',#137756,#106167,#106168) ;
#92286 = AXIS2_PLACEMENT_3D('',#137757,#106169,#106170) ;
#92287 = AXIS2_PLACEMENT_3D('',#137758,#106171,#106172) ;
#92288 = AXIS2_PLACEMENT_3D('',#137759,#106173,#106174) ;
#92289 = AXIS2_PLACEMENT_3D('',#137760,#106175,#106176) ;
#92290 = AXIS2_PLACEMENT_3D('',#137761,#106177,#106178) ;
#92291 = AXIS2_PLACEMENT_3D('',#137762,#106179,#106180) ;
#92292 = AXIS2_PLACEMENT_3D('',#137763,#106181,#106182) ;
#92293 = AXIS2_PLACEMENT_3D('',#137764,#106183,#106184) ;
#92294 = AXIS2_PLACEMENT_3D('',#137765,#106185,#106186) ;
#92295 = AXIS2_PLACEMENT_3D('',#137766,#106187,#106188) ;
#92296 = AXIS2_PLACEMENT_3D('',#137767,#106189,#106190) ;
#92297 = AXIS2_PLACEMENT_3D('',#137768,#106191,#106192) ;
#92298 = AXIS2_PLACEMENT_3D('',#137769,#106193,#106194) ;
#92299 = AXIS2_PLACEMENT_3D('',#137770,#106195,#106196) ;
#92300 = AXIS2_PLACEMENT_3D('',#137789,#106197,#106198) ;
#92301 = AXIS2_PLACEMENT_3D('',#137790,#106199,#106200) ;
#92302 = AXIS2_PLACEMENT_3D('',#137791,#106201,#106202) ;
#92303 = AXIS2_PLACEMENT_3D('',#137792,#106203,#106204) ;
#92304 = AXIS2_PLACEMENT_3D('',#137793,#106205,#106206) ;
#92305 = AXIS2_PLACEMENT_3D('',#137794,#106207,#106208) ;
#92306 = AXIS2_PLACEMENT_3D('',#137795,#106209,#106210) ;
#92307 = AXIS2_PLACEMENT_3D('',#137796,#106211,#106212) ;
#92308 = AXIS2_PLACEMENT_3D('',#137797,#106213,#106214) ;
#92309 = AXIS2_PLACEMENT_3D('',#137798,#106215,#106216) ;
#92310 = AXIS2_PLACEMENT_3D('',#137799,#106217,#106218) ;
#92311 = AXIS2_PLACEMENT_3D('',#137812,#106219,#106220) ;
#92312 = AXIS2_PLACEMENT_3D('',#137813,#106221,#106222) ;
#92313 = AXIS2_PLACEMENT_3D('',#137814,#106223,#106224) ;
#92314 = AXIS2_PLACEMENT_3D('',#137815,#106225,#106226) ;
#92315 = AXIS2_PLACEMENT_3D('',#137816,#106227,#106228) ;
#92316 = AXIS2_PLACEMENT_3D('',#137817,#106229,#106230) ;
#92317 = AXIS2_PLACEMENT_3D('',#137818,#106231,#106232) ;
#92318 = AXIS2_PLACEMENT_3D('',#137831,#106233,#106234) ;
#92319 = AXIS2_PLACEMENT_3D('',#137832,#106235,#106236) ;
#92320 = AXIS2_PLACEMENT_3D('',#137833,#106237,#106238) ;
#92321 = AXIS2_PLACEMENT_3D('',#137834,#106239,#106240) ;
#92322 = AXIS2_PLACEMENT_3D('',#137836,#106241,#106242) ;
#92323 = AXIS2_PLACEMENT_3D('',#137856,#106243,#106244) ;
#92324 = AXIS2_PLACEMENT_3D('',#137857,#106245,#106246) ;
#92325 = AXIS2_PLACEMENT_3D('',#137858,#106247,#106248) ;
#92326 = AXIS2_PLACEMENT_3D('',#137859,#106249,#106250) ;
#92327 = AXIS2_PLACEMENT_3D('',#137860,#106251,#106252) ;
#92328 = AXIS2_PLACEMENT_3D('',#137861,#106253,#106254) ;
#92329 = AXIS2_PLACEMENT_3D('',#137890,#106255,#106256) ;
#92330 = AXIS2_PLACEMENT_3D('',#137891,#106257,#106258) ;
#92331 = AXIS2_PLACEMENT_3D('',#137892,#106259,#106260) ;
#92332 = AXIS2_PLACEMENT_3D('',#137893,#106261,#106262) ;
#92333 = AXIS2_PLACEMENT_3D('',#137894,#106263,#106264) ;
#92334 = AXIS2_PLACEMENT_3D('',#137895,#106265,#106266) ;
#92335 = AXIS2_PLACEMENT_3D('',#137896,#106267,#106268) ;
#92336 = AXIS2_PLACEMENT_3D('',#137918,#106269,#106270) ;
#92337 = AXIS2_PLACEMENT_3D('',#137919,#106271,#106272) ;
#92338 = AXIS2_PLACEMENT_3D('',#137920,#106273,#106274) ;
#92339 = AXIS2_PLACEMENT_3D('',#137921,#106275,#106276) ;
#92340 = AXIS2_PLACEMENT_3D('',#137922,#106277,#106278) ;
#92341 = AXIS2_PLACEMENT_3D('',#137923,#106279,#106280) ;
#92342 = AXIS2_PLACEMENT_3D('',#137924,#106281,#106282) ;
#92343 = AXIS2_PLACEMENT_3D('',#137925,#106283,#106284) ;
#92344 = AXIS2_PLACEMENT_3D('',#137926,#106285,#106286) ;
#92345 = AXIS2_PLACEMENT_3D('',#137927,#106287,#106288) ;
#92346 = AXIS2_PLACEMENT_3D('',#137928,#106289,#106290) ;
#92347 = AXIS2_PLACEMENT_3D('',#137929,#106291,#106292) ;
#92348 = AXIS2_PLACEMENT_3D('',#137930,#106293,#106294) ;
#92349 = AXIS2_PLACEMENT_3D('',#137931,#106295,#106296) ;
#92350 = AXIS2_PLACEMENT_3D('',#137932,#106297,#106298) ;
#92351 = AXIS2_PLACEMENT_3D('',#137933,#106299,#106300) ;
#92352 = AXIS2_PLACEMENT_3D('',#137934,#106301,#106302) ;
#92353 = AXIS2_PLACEMENT_3D('',#137935,#106303,#106304) ;
#92354 = AXIS2_PLACEMENT_3D('',#137936,#106305,#106306) ;
#92355 = AXIS2_PLACEMENT_3D('',#137937,#106307,#106308) ;
#92356 = AXIS2_PLACEMENT_3D('',#137938,#106309,#106310) ;
#92357 = AXIS2_PLACEMENT_3D('',#137939,#106311,#106312) ;
#92358 = AXIS2_PLACEMENT_3D('',#137940,#106313,#106314) ;
#92359 = AXIS2_PLACEMENT_3D('',#137941,#106315,#106316) ;
#92360 = AXIS2_PLACEMENT_3D('',#137942,#106317,#106318) ;
#92361 = AXIS2_PLACEMENT_3D('',#137943,#106319,#106320) ;
#92362 = AXIS2_PLACEMENT_3D('',#137944,#106321,#106322) ;
#92363 = AXIS2_PLACEMENT_3D('',#137945,#106323,#106324) ;
#92364 = AXIS2_PLACEMENT_3D('',#137946,#106325,#106326) ;
#92365 = AXIS2_PLACEMENT_3D('',#137947,#106327,#106328) ;
#92366 = AXIS2_PLACEMENT_3D('',#137948,#106329,#106330) ;
#92367 = AXIS2_PLACEMENT_3D('',#137949,#106331,#106332) ;
#92368 = AXIS2_PLACEMENT_3D('',#137950,#106333,#106334) ;
#92369 = AXIS2_PLACEMENT_3D('',#137951,#106335,#106336) ;
#92370 = AXIS2_PLACEMENT_3D('',#137952,#106337,#106338) ;
#92371 = AXIS2_PLACEMENT_3D('',#137953,#106339,#106340) ;
#92372 = AXIS2_PLACEMENT_3D('',#137954,#106341,#106342) ;
#92373 = AXIS2_PLACEMENT_3D('',#137955,#106343,#106344) ;
#92374 = AXIS2_PLACEMENT_3D('',#137956,#106345,#106346) ;
#92375 = AXIS2_PLACEMENT_3D('',#137957,#106347,#106348) ;
#92376 = AXIS2_PLACEMENT_3D('',#137958,#106349,#106350) ;
#92377 = AXIS2_PLACEMENT_3D('',#137959,#106351,#106352) ;
#92378 = AXIS2_PLACEMENT_3D('',#137960,#106353,#106354) ;
#92379 = AXIS2_PLACEMENT_3D('',#137961,#106355,#106356) ;
#92380 = AXIS2_PLACEMENT_3D('',#137962,#106357,#106358) ;
#92381 = AXIS2_PLACEMENT_3D('',#137963,#106359,#106360) ;
#92382 = AXIS2_PLACEMENT_3D('',#137964,#106361,#106362) ;
#92383 = AXIS2_PLACEMENT_3D('',#137965,#106363,#106364) ;
#92384 = AXIS2_PLACEMENT_3D('',#137966,#106365,#106366) ;
#92385 = AXIS2_PLACEMENT_3D('',#137967,#106367,#106368) ;
#92386 = AXIS2_PLACEMENT_3D('',#137968,#106369,#106370) ;
#92387 = AXIS2_PLACEMENT_3D('',#137969,#106371,#106372) ;
#92388 = AXIS2_PLACEMENT_3D('',#137970,#106373,#106374) ;
#92389 = AXIS2_PLACEMENT_3D('',#137971,#106375,#106376) ;
#92390 = AXIS2_PLACEMENT_3D('',#137972,#106377,#106378) ;
#92391 = AXIS2_PLACEMENT_3D('',#137973,#106379,#106380) ;
#92392 = AXIS2_PLACEMENT_3D('',#137974,#106381,#106382) ;
#92393 = AXIS2_PLACEMENT_3D('',#137975,#106383,#106384) ;
#92394 = AXIS2_PLACEMENT_3D('',#137976,#106385,#106386) ;
#92395 = AXIS2_PLACEMENT_3D('',#137977,#106387,#106388) ;
#92396 = AXIS2_PLACEMENT_3D('',#137978,#106389,#106390) ;
#92397 = AXIS2_PLACEMENT_3D('',#137979,#106391,#106392) ;
#92398 = AXIS2_PLACEMENT_3D('',#137980,#106393,#106394) ;
#92399 = AXIS2_PLACEMENT_3D('',#137981,#106395,#106396) ;
#92400 = AXIS2_PLACEMENT_3D('',#137982,#106397,#106398) ;
#92401 = AXIS2_PLACEMENT_3D('',#137983,#106399,#106400) ;
#92402 = AXIS2_PLACEMENT_3D('',#137984,#106401,#106402) ;
#92403 = AXIS2_PLACEMENT_3D('',#137985,#106403,#106404) ;
#92404 = AXIS2_PLACEMENT_3D('',#137986,#106405,#106406) ;
#92405 = AXIS2_PLACEMENT_3D('',#137987,#106407,#106408) ;
#92406 = AXIS2_PLACEMENT_3D('',#137988,#106409,#106410) ;
#92407 = AXIS2_PLACEMENT_3D('',#137989,#106411,#106412) ;
#92408 = AXIS2_PLACEMENT_3D('',#137990,#106413,#106414) ;
#92409 = AXIS2_PLACEMENT_3D('',#137991,#106415,#106416) ;
#92410 = AXIS2_PLACEMENT_3D('',#137992,#106417,#106418) ;
#92411 = AXIS2_PLACEMENT_3D('',#137993,#106419,#106420) ;
#92412 = AXIS2_PLACEMENT_3D('',#137994,#106421,#106422) ;
#92413 = AXIS2_PLACEMENT_3D('',#137995,#106423,#106424) ;
#92414 = AXIS2_PLACEMENT_3D('',#137996,#106425,#106426) ;
#92415 = AXIS2_PLACEMENT_3D('',#137997,#106427,#106428) ;
#92416 = AXIS2_PLACEMENT_3D('',#137998,#106429,#106430) ;
#92417 = AXIS2_PLACEMENT_3D('',#137999,#106431,#106432) ;
#92418 = AXIS2_PLACEMENT_3D('',#138000,#106433,#106434) ;
#92419 = AXIS2_PLACEMENT_3D('',#138001,#106435,#106436) ;
#92420 = AXIS2_PLACEMENT_3D('',#138002,#106437,#106438) ;
#92421 = AXIS2_PLACEMENT_3D('',#138003,#106439,#106440) ;
#92422 = AXIS2_PLACEMENT_3D('',#138004,#106441,#106442) ;
#92423 = AXIS2_PLACEMENT_3D('',#138005,#106443,#106444) ;
#92424 = AXIS2_PLACEMENT_3D('',#138006,#106445,#106446) ;
#92425 = AXIS2_PLACEMENT_3D('',#138007,#106447,#106448) ;
#92426 = AXIS2_PLACEMENT_3D('',#138008,#106449,#106450) ;
#92427 = AXIS2_PLACEMENT_3D('',#138009,#106451,#106452) ;
#92428 = AXIS2_PLACEMENT_3D('',#138010,#106453,#106454) ;
#92429 = AXIS2_PLACEMENT_3D('',#138011,#106455,#106456) ;
#92430 = AXIS2_PLACEMENT_3D('',#138012,#106457,#106458) ;
#92431 = AXIS2_PLACEMENT_3D('',#138013,#106459,#106460) ;
#92432 = AXIS2_PLACEMENT_3D('',#138014,#106461,#106462) ;
#92433 = AXIS2_PLACEMENT_3D('',#138015,#106463,#106464) ;
#92434 = AXIS2_PLACEMENT_3D('',#138016,#106465,#106466) ;
#92435 = AXIS2_PLACEMENT_3D('',#138017,#106467,#106468) ;
#92436 = AXIS2_PLACEMENT_3D('',#138018,#106469,#106470) ;
#92437 = AXIS2_PLACEMENT_3D('',#138019,#106471,#106472) ;
#92438 = AXIS2_PLACEMENT_3D('',#138020,#106473,#106474) ;
#92439 = AXIS2_PLACEMENT_3D('',#138021,#106475,#106476) ;
#92440 = AXIS2_PLACEMENT_3D('',#138022,#106477,#106478) ;
#92441 = AXIS2_PLACEMENT_3D('',#138023,#106479,#106480) ;
#92442 = AXIS2_PLACEMENT_3D('',#138024,#106481,#106482) ;
#92443 = AXIS2_PLACEMENT_3D('',#138025,#106483,#106484) ;
#92444 = AXIS2_PLACEMENT_3D('',#138026,#106485,#106486) ;
#92445 = AXIS2_PLACEMENT_3D('',#138039,#106487,#106488) ;
#92446 = AXIS2_PLACEMENT_3D('',#138040,#106489,#106490) ;
#92447 = AXIS2_PLACEMENT_3D('',#138041,#106491,#106492) ;
#92448 = AXIS2_PLACEMENT_3D('',#138042,#106493,#106494) ;
#92449 = AXIS2_PLACEMENT_3D('',#138043,#106495,#106496) ;
#92450 = AXIS2_PLACEMENT_3D('',#138044,#106497,#106498) ;
#92451 = AXIS2_PLACEMENT_3D('',#138045,#106499,#106500) ;
#92452 = AXIS2_PLACEMENT_3D('',#138046,#106501,#106502) ;
#92453 = AXIS2_PLACEMENT_3D('',#138047,#106503,#106504) ;
#92454 = AXIS2_PLACEMENT_3D('',#138048,#106505,#106506) ;
#92455 = AXIS2_PLACEMENT_3D('',#138049,#106507,#106508) ;
#92456 = AXIS2_PLACEMENT_3D('',#138050,#106509,#106510) ;
#92457 = AXIS2_PLACEMENT_3D('',#138051,#106511,#106512) ;
#92458 = AXIS2_PLACEMENT_3D('',#138052,#106513,#106514) ;
#92459 = AXIS2_PLACEMENT_3D('',#138053,#106515,#106516) ;
#92460 = AXIS2_PLACEMENT_3D('',#138054,#106517,#106518) ;
#92461 = AXIS2_PLACEMENT_3D('',#138055,#106519,#106520) ;
#92462 = AXIS2_PLACEMENT_3D('',#138056,#106521,#106522) ;
#92463 = AXIS2_PLACEMENT_3D('',#138057,#106523,#106524) ;
#92464 = AXIS2_PLACEMENT_3D('',#138058,#106525,#106526) ;
#92465 = AXIS2_PLACEMENT_3D('',#138059,#106527,#106528) ;
#92466 = AXIS2_PLACEMENT_3D('',#138060,#106529,#106530) ;
#92467 = AXIS2_PLACEMENT_3D('',#138061,#106531,#106532) ;
#92468 = AXIS2_PLACEMENT_3D('',#138062,#106533,#106534) ;
#92469 = AXIS2_PLACEMENT_3D('',#138063,#106535,#106536) ;
#92470 = AXIS2_PLACEMENT_3D('',#138064,#106537,#106538) ;
#92471 = AXIS2_PLACEMENT_3D('',#138077,#106539,#106540) ;
#92472 = AXIS2_PLACEMENT_3D('',#138078,#106541,#106542) ;
#92473 = AXIS2_PLACEMENT_3D('',#138079,#106543,#106544) ;
#92474 = AXIS2_PLACEMENT_3D('',#138080,#106545,#106546) ;
#92475 = AXIS2_PLACEMENT_3D('',#138081,#106547,#106548) ;
#92476 = AXIS2_PLACEMENT_3D('',#138082,#106549,#106550) ;
#92477 = AXIS2_PLACEMENT_3D('',#138083,#106551,#106552) ;
#92478 = AXIS2_PLACEMENT_3D('',#138084,#106553,#106554) ;
#92479 = AXIS2_PLACEMENT_3D('',#138085,#106555,#106556) ;
#92480 = AXIS2_PLACEMENT_3D('',#138086,#106557,#106558) ;
#92481 = AXIS2_PLACEMENT_3D('',#138087,#106559,#106560) ;
#92482 = AXIS2_PLACEMENT_3D('',#138088,#106561,#106562) ;
#92483 = AXIS2_PLACEMENT_3D('',#138089,#106563,#106564) ;
#92484 = AXIS2_PLACEMENT_3D('',#138090,#106565,#106566) ;
#92485 = AXIS2_PLACEMENT_3D('',#138091,#106567,#106568) ;
#92486 = AXIS2_PLACEMENT_3D('',#138092,#106569,#106570) ;
#92487 = AXIS2_PLACEMENT_3D('',#138093,#106571,#106572) ;
#92488 = AXIS2_PLACEMENT_3D('',#138094,#106573,#106574) ;
#92489 = AXIS2_PLACEMENT_3D('',#138095,#106575,#106576) ;
#92490 = AXIS2_PLACEMENT_3D('',#138096,#106577,#106578) ;
#92491 = AXIS2_PLACEMENT_3D('',#138097,#106579,#106580) ;
#92492 = AXIS2_PLACEMENT_3D('',#138098,#106581,#106582) ;
#92493 = AXIS2_PLACEMENT_3D('',#138099,#106583,#106584) ;
#92494 = AXIS2_PLACEMENT_3D('',#138100,#106585,#106586) ;
#92495 = AXIS2_PLACEMENT_3D('',#138101,#106587,#106588) ;
#92496 = AXIS2_PLACEMENT_3D('',#138102,#106589,#106590) ;
#92497 = AXIS2_PLACEMENT_3D('',#138103,#106591,#106592) ;
#92498 = AXIS2_PLACEMENT_3D('',#138104,#106593,#106594) ;
#92499 = AXIS2_PLACEMENT_3D('',#138117,#106595,#106596) ;
#92500 = AXIS2_PLACEMENT_3D('',#138130,#106597,#106598) ;
#92501 = AXIS2_PLACEMENT_3D('',#138131,#106599,#106600) ;
#92502 = AXIS2_PLACEMENT_3D('',#138132,#106601,#106602) ;
#92503 = AXIS2_PLACEMENT_3D('',#138133,#106603,#106604) ;
#92504 = AXIS2_PLACEMENT_3D('',#138134,#106605,#106606) ;
#92505 = AXIS2_PLACEMENT_3D('',#138147,#106607,#106608) ;
#92506 = AXIS2_PLACEMENT_3D('',#138160,#106609,#106610) ;
#92507 = AXIS2_PLACEMENT_3D('',#138161,#106611,#106612) ;
#92508 = AXIS2_PLACEMENT_3D('',#138162,#106613,#106614) ;
#92509 = AXIS2_PLACEMENT_3D('',#138163,#106615,#106616) ;
#92510 = AXIS2_PLACEMENT_3D('',#138241,#106617,#106618) ;
#92511 = AXIS2_PLACEMENT_3D('',#138242,#106619,#106620) ;
#92512 = AXIS2_PLACEMENT_3D('',#138243,#106621,#106622) ;
#92513 = AXIS2_PLACEMENT_3D('',#138312,#106623,#106624) ;
#92514 = AXIS2_PLACEMENT_3D('',#138313,#106625,#106626) ;
#92515 = AXIS2_PLACEMENT_3D('',#138428,#106627,#106628) ;
#92516 = AXIS2_PLACEMENT_3D('',#138459,#106629,#106630) ;
#92517 = AXIS2_PLACEMENT_3D('',#138490,#106631,#106632) ;
#92518 = AXIS2_PLACEMENT_3D('',#138539,#106633,#106634) ;
#92519 = AXIS2_PLACEMENT_3D('',#138540,#106635,#106636) ;
#92520 = AXIS2_PLACEMENT_3D('',#138549,#106641,#106642) ;
#92521 = AXIS2_PLACEMENT_3D('',#138551,#106643,#106644) ;
#92522 = AXIS2_PLACEMENT_3D('',#138554,#106646,#106647) ;
#92523 = AXIS2_PLACEMENT_3D('',#138555,#106648,#106649) ;
#92524 = AXIS2_PLACEMENT_3D('',#138561,#106653,#106654) ;
#92525 = AXIS2_PLACEMENT_3D('',#138563,#106655,#106656) ;
#92526 = AXIS2_PLACEMENT_3D('',#138566,#106658,#106659) ;
#92527 = AXIS2_PLACEMENT_3D('',#138567,#106660,#106661) ;
#92528 = AXIS2_PLACEMENT_3D('',#138573,#106665,#106666) ;
#92529 = AXIS2_PLACEMENT_3D('',#138575,#106667,#106668) ;
#92530 = AXIS2_PLACEMENT_3D('',#138578,#106670,#106671) ;
#92531 = AXIS2_PLACEMENT_3D('',#138579,#106672,#106673) ;
#92532 = AXIS2_PLACEMENT_3D('',#138585,#106677,#106678) ;
#92533 = AXIS2_PLACEMENT_3D('',#138587,#106679,#106680) ;
#92534 = AXIS2_PLACEMENT_3D('',#138590,#106682,#106683) ;
#92535 = AXIS2_PLACEMENT_3D('',#138591,#106684,#106685) ;
#92536 = AXIS2_PLACEMENT_3D('',#138597,#106689,#106690) ;
#92537 = AXIS2_PLACEMENT_3D('',#138600,#106691,#106692) ;
#92538 = AXIS2_PLACEMENT_3D('',#138612,#106699,#106700) ;
#92539 = AXIS2_PLACEMENT_3D('',#138623,#106705,#106706) ;
#92540 = AXIS2_PLACEMENT_3D('',#138627,#106709,#106710) ;
#92541 = AXIS2_PLACEMENT_3D('',#138636,#106715,#106716) ;
#92542 = AXIS2_PLACEMENT_3D('',#138638,#106718,#106719) ;
#92543 = AXIS2_PLACEMENT_3D('',#138646,#106724,#106725) ;
#92544 = AXIS2_PLACEMENT_3D('',#138653,#106728,#106729) ;
#92545 = AXIS2_PLACEMENT_3D('',#138655,#106731,#106732) ;
#92546 = AXIS2_PLACEMENT_3D('',#138656,#106733,#106734) ;
#92547 = AXIS2_PLACEMENT_3D('',#138657,#106735,#106736) ;
#92548 = AXIS2_PLACEMENT_3D('',#138658,#106737,#106738) ;
#92549 = AXIS2_PLACEMENT_3D('',#138659,#106739,#106740) ;
#92550 = AXIS2_PLACEMENT_3D('',#138660,#106741,#106742) ;
#92551 = AXIS2_PLACEMENT_3D('',#138661,#106743,#106744) ;
#92552 = AXIS2_PLACEMENT_3D('',#138670,#106749,#106750) ;
#92553 = AXIS2_PLACEMENT_3D('',#138679,#106755,#106756) ;
#92554 = AXIS2_PLACEMENT_3D('',#138682,#106757,#106758) ;
#92555 = AXIS2_PLACEMENT_3D('',#138690,#106762,#106763) ;
#92556 = AXIS2_PLACEMENT_3D('',#138696,#106767,#106768) ;
#92557 = AXIS2_PLACEMENT_3D('',#138701,#106770,#106771) ;
#92558 = AXIS2_PLACEMENT_3D('',#138704,#106773,#106774) ;
#92559 = AXIS2_PLACEMENT_3D('',#138706,#106775,#106776) ;
#92560 = AXIS2_PLACEMENT_3D('',#138709,#106778,#106779) ;
#92561 = AXIS2_PLACEMENT_3D('',#138710,#106780,#106781) ;
#92562 = AXIS2_PLACEMENT_3D('',#138713,#106782,#106783) ;
#92563 = AXIS2_PLACEMENT_3D('',#138718,#106786,#106787) ;
#92564 = AXIS2_PLACEMENT_3D('',#138724,#106791,#106792) ;
#92565 = AXIS2_PLACEMENT_3D('',#138730,#106796,#106797) ;
#92566 = AXIS2_PLACEMENT_3D('',#138736,#106801,#106802) ;
#92567 = AXIS2_PLACEMENT_3D('',#138749,#106809,#106810) ;
#92568 = AXIS2_PLACEMENT_3D('',#138762,#106817,#106818) ;
#92569 = AXIS2_PLACEMENT_3D('',#138771,#106823,#106824) ;
#92570 = AXIS2_PLACEMENT_3D('',#138780,#106829,#106830) ;
#92571 = AXIS2_PLACEMENT_3D('',#138789,#106835,#106836) ;
#92572 = AXIS2_PLACEMENT_3D('',#138798,#106841,#106842) ;
#92573 = AXIS2_PLACEMENT_3D('',#138811,#106848,#106849) ;
#92574 = AXIS2_PLACEMENT_3D('',#138815,#106851,#106852) ;
#92575 = AXIS2_PLACEMENT_3D('',#138819,#106854,#106855) ;
#92576 = AXIS2_PLACEMENT_3D('',#138822,#106857,#106858) ;
#92577 = AXIS2_PLACEMENT_3D('',#138823,#106859,#106860) ;
#92578 = AXIS2_PLACEMENT_3D('',#138826,#106861,#106862) ;
#92579 = AXIS2_PLACEMENT_3D('',#138829,#106865,#106866) ;
#92580 = AXIS2_PLACEMENT_3D('',#138833,#106869,#106870) ;
#92581 = AXIS2_PLACEMENT_3D('',#138835,#106871,#106872) ;
#92582 = AXIS2_PLACEMENT_3D('',#138837,#106874,#106875) ;
#92583 = AXIS2_PLACEMENT_3D('',#138841,#106878,#106879) ;
#92584 = AXIS2_PLACEMENT_3D('',#138843,#106880,#106881) ;
#92585 = AXIS2_PLACEMENT_3D('',#138845,#106883,#106884) ;
#92586 = AXIS2_PLACEMENT_3D('',#138849,#106887,#106888) ;
#92587 = AXIS2_PLACEMENT_3D('',#138851,#106889,#106890) ;
#92588 = AXIS2_PLACEMENT_3D('',#138853,#106892,#106893) ;
#92589 = AXIS2_PLACEMENT_3D('',#138855,#106895,#106896) ;
#92590 = AXIS2_PLACEMENT_3D('',#138856,#106897,#106898) ;
#92591 = AXIS2_PLACEMENT_3D('',#138858,#106900,#106901) ;
#92592 = AXIS2_PLACEMENT_3D('',#138861,#106904,#106905) ;
#92593 = AXIS2_PLACEMENT_3D('',#138864,#106908,#106909) ;
#92594 = AXIS2_PLACEMENT_3D('',#138867,#106912,#106913) ;
#92595 = AXIS2_PLACEMENT_3D('',#138876,#106918,#106919) ;
#92596 = AXIS2_PLACEMENT_3D('',#138885,#106924,#106925) ;
#92597 = AXIS2_PLACEMENT_3D('',#138894,#106930,#106931) ;
#92598 = AXIS2_PLACEMENT_3D('',#138903,#106936,#106937) ;
#92599 = AXIS2_PLACEMENT_3D('',#138916,#106943,#106944) ;
#92600 = AXIS2_PLACEMENT_3D('',#138920,#106946,#106947) ;
#92601 = AXIS2_PLACEMENT_3D('',#138924,#106949,#106950) ;
#92602 = AXIS2_PLACEMENT_3D('',#138927,#106952,#106953) ;
#92603 = AXIS2_PLACEMENT_3D('',#138928,#106954,#106955) ;
#92604 = AXIS2_PLACEMENT_3D('',#138932,#106957,#106958) ;
#92605 = AXIS2_PLACEMENT_3D('',#138934,#106960,#106961) ;
#92606 = AXIS2_PLACEMENT_3D('',#138938,#106964,#106965) ;
#92607 = AXIS2_PLACEMENT_3D('',#138940,#106966,#106967) ;
#92608 = AXIS2_PLACEMENT_3D('',#138942,#106969,#106970) ;
#92609 = AXIS2_PLACEMENT_3D('',#138946,#106973,#106974) ;
#92610 = AXIS2_PLACEMENT_3D('',#138948,#106975,#106976) ;
#92611 = AXIS2_PLACEMENT_3D('',#138950,#106978,#106979) ;
#92612 = AXIS2_PLACEMENT_3D('',#138954,#106982,#106983) ;
#92613 = AXIS2_PLACEMENT_3D('',#138956,#106984,#106985) ;
#92614 = AXIS2_PLACEMENT_3D('',#138958,#106987,#106988) ;
#92615 = AXIS2_PLACEMENT_3D('',#138960,#106990,#106991) ;
#92616 = AXIS2_PLACEMENT_3D('',#138969,#106996,#106997) ;
#92617 = AXIS2_PLACEMENT_3D('',#138976,#107002,#107003) ;
#92618 = AXIS2_PLACEMENT_3D('',#138982,#107007,#107008) ;
#92619 = AXIS2_PLACEMENT_3D('',#138987,#107012,#107013) ;
#92620 = AXIS2_PLACEMENT_3D('',#138991,#107015,#107016) ;
#92621 = AXIS2_PLACEMENT_3D('',#138997,#107020,#107021) ;
#92622 = AXIS2_PLACEMENT_3D('',#138998,#107022,#107023) ;
#92623 = AXIS2_PLACEMENT_3D('',#139001,#107024,#107025) ;
#92624 = AXIS2_PLACEMENT_3D('',#139003,#107026,#107027) ;
#92625 = AXIS2_PLACEMENT_3D('',#139005,#107028,#107029) ;
#92626 = AXIS2_PLACEMENT_3D('',#139009,#107031,#107032) ;
#92627 = AXIS2_PLACEMENT_3D('',#139029,#107034,#107035) ;
#92628 = AXIS2_PLACEMENT_3D('',#139036,#107036,#107037) ;
#92629 = AXIS2_PLACEMENT_3D('',#139037,#107038,#107039) ;
#92630 = AXIS2_PLACEMENT_3D('',#139038,#107040,#107041) ;
#92631 = AXIS2_PLACEMENT_3D('',#139051,#107042,#107043) ;
#92632 = AXIS2_PLACEMENT_3D('',#139052,#107044,#107045) ;
#92633 = AXIS2_PLACEMENT_3D('',#139053,#107046,#107047) ;
#92634 = AXIS2_PLACEMENT_3D('',#139054,#107048,#107049) ;
#92635 = AXIS2_PLACEMENT_3D('',#139055,#107050,#107051) ;
#92636 = AXIS2_PLACEMENT_3D('',#139056,#107052,#107053) ;
#92637 = AXIS2_PLACEMENT_3D('',#139057,#107054,#107055) ;
#92638 = AXIS2_PLACEMENT_3D('',#139058,#107056,#107057) ;
#92639 = AXIS2_PLACEMENT_3D('',#139059,#107058,#107059) ;
#92640 = AXIS2_PLACEMENT_3D('',#139060,#107060,#107061) ;
#92641 = AXIS2_PLACEMENT_3D('',#139061,#107062,#107063) ;
#92642 = AXIS2_PLACEMENT_3D('',#139062,#107064,#107065) ;
#92643 = AXIS2_PLACEMENT_3D('',#139063,#107066,#107067) ;
#92644 = AXIS2_PLACEMENT_3D('',#139064,#107068,#107069) ;
#92645 = AXIS2_PLACEMENT_3D('',#139065,#107070,#107071) ;
#92646 = AXIS2_PLACEMENT_3D('',#139066,#107072,#107073) ;
#92647 = AXIS2_PLACEMENT_3D('',#139085,#107074,#107075) ;
#92648 = AXIS2_PLACEMENT_3D('',#139086,#107076,#107077) ;
#92649 = AXIS2_PLACEMENT_3D('',#139105,#107078,#107079) ;
#92650 = AXIS2_PLACEMENT_3D('',#139124,#107080,#107081) ;
#92651 = AXIS2_PLACEMENT_3D('',#139125,#107082,#107083) ;
#92652 = AXIS2_PLACEMENT_3D('',#139126,#107084,#107085) ;
#92653 = AXIS2_PLACEMENT_3D('',#139127,#107086,#107087) ;
#92654 = AXIS2_PLACEMENT_3D('',#139128,#107088,#107089) ;
#92655 = AXIS2_PLACEMENT_3D('',#139129,#107090,#107091) ;
#92656 = AXIS2_PLACEMENT_3D('',#139130,#107092,#107093) ;
#92657 = AXIS2_PLACEMENT_3D('',#139131,#107094,#107095) ;
#92658 = AXIS2_PLACEMENT_3D('',#139132,#107096,#107097) ;
#92659 = AXIS2_PLACEMENT_3D('',#139133,#107098,#107099) ;
#92660 = AXIS2_PLACEMENT_3D('',#139134,#107100,#107101) ;
#92661 = AXIS2_PLACEMENT_3D('',#139135,#107102,#107103) ;
#92662 = AXIS2_PLACEMENT_3D('',#139136,#107104,#107105) ;
#92663 = AXIS2_PLACEMENT_3D('',#139137,#107106,#107107) ;
#92664 = AXIS2_PLACEMENT_3D('',#139138,#107108,#107109) ;
#92665 = AXIS2_PLACEMENT_3D('',#139157,#107110,#107111) ;
#92666 = AXIS2_PLACEMENT_3D('',#139158,#107112,#107113) ;
#92667 = AXIS2_PLACEMENT_3D('',#139159,#107114,#107115) ;
#92668 = AXIS2_PLACEMENT_3D('',#139160,#107116,#107117) ;
#92669 = AXIS2_PLACEMENT_3D('',#139161,#107118,#107119) ;
#92670 = AXIS2_PLACEMENT_3D('',#139162,#107120,#107121) ;
#92671 = AXIS2_PLACEMENT_3D('',#139163,#107122,#107123) ;
#92672 = AXIS2_PLACEMENT_3D('',#139164,#107124,#107125) ;
#92673 = AXIS2_PLACEMENT_3D('',#139165,#107126,#107127) ;
#92674 = AXIS2_PLACEMENT_3D('',#139166,#107128,#107129) ;
#92675 = AXIS2_PLACEMENT_3D('',#139167,#107130,#107131) ;
#92676 = AXIS2_PLACEMENT_3D('',#139180,#107132,#107133) ;
#92677 = AXIS2_PLACEMENT_3D('',#139181,#107134,#107135) ;
#92678 = AXIS2_PLACEMENT_3D('',#139182,#107136,#107137) ;
#92679 = AXIS2_PLACEMENT_3D('',#139183,#107138,#107139) ;
#92680 = AXIS2_PLACEMENT_3D('',#139184,#107140,#107141) ;
#92681 = AXIS2_PLACEMENT_3D('',#139185,#107142,#107143) ;
#92682 = AXIS2_PLACEMENT_3D('',#139186,#107144,#107145) ;
#92683 = AXIS2_PLACEMENT_3D('',#139199,#107146,#107147) ;
#92684 = AXIS2_PLACEMENT_3D('',#139200,#107148,#107149) ;
#92685 = AXIS2_PLACEMENT_3D('',#139201,#107150,#107151) ;
#92686 = AXIS2_PLACEMENT_3D('',#139203,#107152,#107153) ;
#92687 = AXIS2_PLACEMENT_3D('',#139223,#107154,#107155) ;
#92688 = AXIS2_PLACEMENT_3D('',#139224,#107156,#107157) ;
#92689 = AXIS2_PLACEMENT_3D('',#139225,#107158,#107159) ;
#92690 = AXIS2_PLACEMENT_3D('',#139226,#107160,#107161) ;
#92691 = AXIS2_PLACEMENT_3D('',#139227,#107162,#107163) ;
#92692 = AXIS2_PLACEMENT_3D('',#139228,#107164,#107165) ;
#92693 = AXIS2_PLACEMENT_3D('',#139257,#107166,#107167) ;
#92694 = AXIS2_PLACEMENT_3D('',#139258,#107168,#107169) ;
#92695 = AXIS2_PLACEMENT_3D('',#139259,#107170,#107171) ;
#92696 = AXIS2_PLACEMENT_3D('',#139260,#107172,#107173) ;
#92697 = AXIS2_PLACEMENT_3D('',#139261,#107174,#107175) ;
#92698 = AXIS2_PLACEMENT_3D('',#139262,#107176,#107177) ;
#92699 = AXIS2_PLACEMENT_3D('',#139263,#107178,#107179) ;
#92700 = AXIS2_PLACEMENT_3D('',#139285,#107180,#107181) ;
#92701 = AXIS2_PLACEMENT_3D('',#139286,#107182,#107183) ;
#92702 = AXIS2_PLACEMENT_3D('',#139287,#107184,#107185) ;
#92703 = AXIS2_PLACEMENT_3D('',#139288,#107186,#107187) ;
#92704 = AXIS2_PLACEMENT_3D('',#139289,#107188,#107189) ;
#92705 = AXIS2_PLACEMENT_3D('',#139290,#107190,#107191) ;
#92706 = AXIS2_PLACEMENT_3D('',#139291,#107192,#107193) ;
#92707 = AXIS2_PLACEMENT_3D('',#139292,#107194,#107195) ;
#92708 = AXIS2_PLACEMENT_3D('',#139293,#107196,#107197) ;
#92709 = AXIS2_PLACEMENT_3D('',#139294,#107198,#107199) ;
#92710 = AXIS2_PLACEMENT_3D('',#139295,#107200,#107201) ;
#92711 = AXIS2_PLACEMENT_3D('',#139296,#107202,#107203) ;
#92712 = AXIS2_PLACEMENT_3D('',#139297,#107204,#107205) ;
#92713 = AXIS2_PLACEMENT_3D('',#139298,#107206,#107207) ;
#92714 = AXIS2_PLACEMENT_3D('',#139299,#107208,#107209) ;
#92715 = AXIS2_PLACEMENT_3D('',#139300,#107210,#107211) ;
#92716 = AXIS2_PLACEMENT_3D('',#139301,#107212,#107213) ;
#92717 = AXIS2_PLACEMENT_3D('',#139302,#107214,#107215) ;
#92718 = AXIS2_PLACEMENT_3D('',#139303,#107216,#107217) ;
#92719 = AXIS2_PLACEMENT_3D('',#139304,#107218,#107219) ;
#92720 = AXIS2_PLACEMENT_3D('',#139305,#107220,#107221) ;
#92721 = AXIS2_PLACEMENT_3D('',#139306,#107222,#107223) ;
#92722 = AXIS2_PLACEMENT_3D('',#139307,#107224,#107225) ;
#92723 = AXIS2_PLACEMENT_3D('',#139308,#107226,#107227) ;
#92724 = AXIS2_PLACEMENT_3D('',#139309,#107228,#107229) ;
#92725 = AXIS2_PLACEMENT_3D('',#139310,#107230,#107231) ;
#92726 = AXIS2_PLACEMENT_3D('',#139311,#107232,#107233) ;
#92727 = AXIS2_PLACEMENT_3D('',#139312,#107234,#107235) ;
#92728 = AXIS2_PLACEMENT_3D('',#139313,#107236,#107237) ;
#92729 = AXIS2_PLACEMENT_3D('',#139314,#107238,#107239) ;
#92730 = AXIS2_PLACEMENT_3D('',#139315,#107240,#107241) ;
#92731 = AXIS2_PLACEMENT_3D('',#139316,#107242,#107243) ;
#92732 = AXIS2_PLACEMENT_3D('',#139317,#107244,#107245) ;
#92733 = AXIS2_PLACEMENT_3D('',#139318,#107246,#107247) ;
#92734 = AXIS2_PLACEMENT_3D('',#139319,#107248,#107249) ;
#92735 = AXIS2_PLACEMENT_3D('',#139320,#107250,#107251) ;
#92736 = AXIS2_PLACEMENT_3D('',#139321,#107252,#107253) ;
#92737 = AXIS2_PLACEMENT_3D('',#139322,#107254,#107255) ;
#92738 = AXIS2_PLACEMENT_3D('',#139323,#107256,#107257) ;
#92739 = AXIS2_PLACEMENT_3D('',#139324,#107258,#107259) ;
#92740 = AXIS2_PLACEMENT_3D('',#139325,#107260,#107261) ;
#92741 = AXIS2_PLACEMENT_3D('',#139326,#107262,#107263) ;
#92742 = AXIS2_PLACEMENT_3D('',#139327,#107264,#107265) ;
#92743 = AXIS2_PLACEMENT_3D('',#139328,#107266,#107267) ;
#92744 = AXIS2_PLACEMENT_3D('',#139329,#107268,#107269) ;
#92745 = AXIS2_PLACEMENT_3D('',#139330,#107270,#107271) ;
#92746 = AXIS2_PLACEMENT_3D('',#139331,#107272,#107273) ;
#92747 = AXIS2_PLACEMENT_3D('',#139332,#107274,#107275) ;
#92748 = AXIS2_PLACEMENT_3D('',#139333,#107276,#107277) ;
#92749 = AXIS2_PLACEMENT_3D('',#139334,#107278,#107279) ;
#92750 = AXIS2_PLACEMENT_3D('',#139335,#107280,#107281) ;
#92751 = AXIS2_PLACEMENT_3D('',#139336,#107282,#107283) ;
#92752 = AXIS2_PLACEMENT_3D('',#139337,#107284,#107285) ;
#92753 = AXIS2_PLACEMENT_3D('',#139338,#107286,#107287) ;
#92754 = AXIS2_PLACEMENT_3D('',#139339,#107288,#107289) ;
#92755 = AXIS2_PLACEMENT_3D('',#139340,#107290,#107291) ;
#92756 = AXIS2_PLACEMENT_3D('',#139341,#107292,#107293) ;
#92757 = AXIS2_PLACEMENT_3D('',#139342,#107294,#107295) ;
#92758 = AXIS2_PLACEMENT_3D('',#139343,#107296,#107297) ;
#92759 = AXIS2_PLACEMENT_3D('',#139344,#107298,#107299) ;
#92760 = AXIS2_PLACEMENT_3D('',#139345,#107300,#107301) ;
#92761 = AXIS2_PLACEMENT_3D('',#139346,#107302,#107303) ;
#92762 = AXIS2_PLACEMENT_3D('',#139347,#107304,#107305) ;
#92763 = AXIS2_PLACEMENT_3D('',#139348,#107306,#107307) ;
#92764 = AXIS2_PLACEMENT_3D('',#139349,#107308,#107309) ;
#92765 = AXIS2_PLACEMENT_3D('',#139350,#107310,#107311) ;
#92766 = AXIS2_PLACEMENT_3D('',#139351,#107312,#107313) ;
#92767 = AXIS2_PLACEMENT_3D('',#139352,#107314,#107315) ;
#92768 = AXIS2_PLACEMENT_3D('',#139353,#107316,#107317) ;
#92769 = AXIS2_PLACEMENT_3D('',#139354,#107318,#107319) ;
#92770 = AXIS2_PLACEMENT_3D('',#139355,#107320,#107321) ;
#92771 = AXIS2_PLACEMENT_3D('',#139356,#107322,#107323) ;
#92772 = AXIS2_PLACEMENT_3D('',#139357,#107324,#107325) ;
#92773 = AXIS2_PLACEMENT_3D('',#139358,#107326,#107327) ;
#92774 = AXIS2_PLACEMENT_3D('',#139359,#107328,#107329) ;
#92775 = AXIS2_PLACEMENT_3D('',#139360,#107330,#107331) ;
#92776 = AXIS2_PLACEMENT_3D('',#139361,#107332,#107333) ;
#92777 = AXIS2_PLACEMENT_3D('',#139362,#107334,#107335) ;
#92778 = AXIS2_PLACEMENT_3D('',#139363,#107336,#107337) ;
#92779 = AXIS2_PLACEMENT_3D('',#139364,#107338,#107339) ;
#92780 = AXIS2_PLACEMENT_3D('',#139365,#107340,#107341) ;
#92781 = AXIS2_PLACEMENT_3D('',#139366,#107342,#107343) ;
#92782 = AXIS2_PLACEMENT_3D('',#139367,#107344,#107345) ;
#92783 = AXIS2_PLACEMENT_3D('',#139368,#107346,#107347) ;
#92784 = AXIS2_PLACEMENT_3D('',#139369,#107348,#107349) ;
#92785 = AXIS2_PLACEMENT_3D('',#139370,#107350,#107351) ;
#92786 = AXIS2_PLACEMENT_3D('',#139371,#107352,#107353) ;
#92787 = AXIS2_PLACEMENT_3D('',#139372,#107354,#107355) ;
#92788 = AXIS2_PLACEMENT_3D('',#139373,#107356,#107357) ;
#92789 = AXIS2_PLACEMENT_3D('',#139374,#107358,#107359) ;
#92790 = AXIS2_PLACEMENT_3D('',#139375,#107360,#107361) ;
#92791 = AXIS2_PLACEMENT_3D('',#139376,#107362,#107363) ;
#92792 = AXIS2_PLACEMENT_3D('',#139377,#107364,#107365) ;
#92793 = AXIS2_PLACEMENT_3D('',#139378,#107366,#107367) ;
#92794 = AXIS2_PLACEMENT_3D('',#139379,#107368,#107369) ;
#92795 = AXIS2_PLACEMENT_3D('',#139380,#107370,#107371) ;
#92796 = AXIS2_PLACEMENT_3D('',#139381,#107372,#107373) ;
#92797 = AXIS2_PLACEMENT_3D('',#139382,#107374,#107375) ;
#92798 = AXIS2_PLACEMENT_3D('',#139383,#107376,#107377) ;
#92799 = AXIS2_PLACEMENT_3D('',#139384,#107378,#107379) ;
#92800 = AXIS2_PLACEMENT_3D('',#139385,#107380,#107381) ;
#92801 = AXIS2_PLACEMENT_3D('',#139386,#107382,#107383) ;
#92802 = AXIS2_PLACEMENT_3D('',#139387,#107384,#107385) ;
#92803 = AXIS2_PLACEMENT_3D('',#139388,#107386,#107387) ;
#92804 = AXIS2_PLACEMENT_3D('',#139389,#107388,#107389) ;
#92805 = AXIS2_PLACEMENT_3D('',#139390,#107390,#107391) ;
#92806 = AXIS2_PLACEMENT_3D('',#139391,#107392,#107393) ;
#92807 = AXIS2_PLACEMENT_3D('',#139392,#107394,#107395) ;
#92808 = AXIS2_PLACEMENT_3D('',#139393,#107396,#107397) ;
#92809 = AXIS2_PLACEMENT_3D('',#139406,#107398,#107399) ;
#92810 = AXIS2_PLACEMENT_3D('',#139407,#107400,#107401) ;
#92811 = AXIS2_PLACEMENT_3D('',#139408,#107402,#107403) ;
#92812 = AXIS2_PLACEMENT_3D('',#139409,#107404,#107405) ;
#92813 = AXIS2_PLACEMENT_3D('',#139410,#107406,#107407) ;
#92814 = AXIS2_PLACEMENT_3D('',#139411,#107408,#107409) ;
#92815 = AXIS2_PLACEMENT_3D('',#139412,#107410,#107411) ;
#92816 = AXIS2_PLACEMENT_3D('',#139413,#107412,#107413) ;
#92817 = AXIS2_PLACEMENT_3D('',#139414,#107414,#107415) ;
#92818 = AXIS2_PLACEMENT_3D('',#139415,#107416,#107417) ;
#92819 = AXIS2_PLACEMENT_3D('',#139416,#107418,#107419) ;
#92820 = AXIS2_PLACEMENT_3D('',#139417,#107420,#107421) ;
#92821 = AXIS2_PLACEMENT_3D('',#139418,#107422,#107423) ;
#92822 = AXIS2_PLACEMENT_3D('',#139419,#107424,#107425) ;
#92823 = AXIS2_PLACEMENT_3D('',#139420,#107426,#107427) ;
#92824 = AXIS2_PLACEMENT_3D('',#139421,#107428,#107429) ;
#92825 = AXIS2_PLACEMENT_3D('',#139422,#107430,#107431) ;
#92826 = AXIS2_PLACEMENT_3D('',#139423,#107432,#107433) ;
#92827 = AXIS2_PLACEMENT_3D('',#139424,#107434,#107435) ;
#92828 = AXIS2_PLACEMENT_3D('',#139425,#107436,#107437) ;
#92829 = AXIS2_PLACEMENT_3D('',#139438,#107438,#107439) ;
#92830 = AXIS2_PLACEMENT_3D('',#139439,#107440,#107441) ;
#92831 = AXIS2_PLACEMENT_3D('',#139440,#107442,#107443) ;
#92832 = AXIS2_PLACEMENT_3D('',#139441,#107444,#107445) ;
#92833 = AXIS2_PLACEMENT_3D('',#139442,#107446,#107447) ;
#92834 = AXIS2_PLACEMENT_3D('',#139443,#107448,#107449) ;
#92835 = AXIS2_PLACEMENT_3D('',#139444,#107450,#107451) ;
#92836 = AXIS2_PLACEMENT_3D('',#139445,#107452,#107453) ;
#92837 = AXIS2_PLACEMENT_3D('',#139446,#107454,#107455) ;
#92838 = AXIS2_PLACEMENT_3D('',#139447,#107456,#107457) ;
#92839 = AXIS2_PLACEMENT_3D('',#139460,#107458,#107459) ;
#92840 = AXIS2_PLACEMENT_3D('',#139473,#107460,#107461) ;
#92841 = AXIS2_PLACEMENT_3D('',#139474,#107462,#107463) ;
#92842 = AXIS2_PLACEMENT_3D('',#139487,#107464,#107465) ;
#92843 = AXIS2_PLACEMENT_3D('',#139500,#107466,#107467) ;
#92844 = AXIS2_PLACEMENT_3D('',#139501,#107468,#107469) ;
#92845 = AXIS2_PLACEMENT_3D('',#139502,#107470,#107471) ;
#92846 = AXIS2_PLACEMENT_3D('',#139503,#107472,#107473) ;
#92847 = AXIS2_PLACEMENT_3D('',#139581,#107474,#107475) ;
#92848 = AXIS2_PLACEMENT_3D('',#139582,#107476,#107477) ;
#92849 = AXIS2_PLACEMENT_3D('',#139765,#107478,#107479) ;
#92850 = AXIS2_PLACEMENT_3D('',#139796,#107480,#107481) ;
#92851 = AXIS2_PLACEMENT_3D('',#139827,#107482,#107483) ;
#92852 = AXIS2_PLACEMENT_3D('',#139876,#107484,#107485) ;
#92853 = AXIS2_PLACEMENT_3D('',#139877,#107486,#107487) ;
#92854 = AXIS2_PLACEMENT_3D('',#139878,#107488,#107489) ;
#92855 = AXIS2_PLACEMENT_3D('',#139879,#107490,#107491) ;
#92856 = AXIS2_PLACEMENT_3D('',#139880,#107492,#107493) ;
#92857 = AXIS2_PLACEMENT_3D('',#139881,#107494,#107495) ;
#92858 = AXIS2_PLACEMENT_3D('',#139882,#107496,#107497) ;
#92859 = AXIS2_PLACEMENT_3D('',#139883,#107498,#107499) ;
#92860 = AXIS2_PLACEMENT_3D('',#139884,#107500,#107501) ;
#92861 = AXIS2_PLACEMENT_3D('',#139885,#107502,#107503) ;
#92862 = AXIS2_PLACEMENT_3D('',#139886,#107504,#107505) ;
#92863 = AXIS2_PLACEMENT_3D('',#139887,#107506,#107507) ;
#92864 = AXIS2_PLACEMENT_3D('',#139888,#107508,#107509) ;
#92865 = AXIS2_PLACEMENT_3D('',#139889,#107510,#107511) ;
#92866 = AXIS2_PLACEMENT_3D('',#139890,#107512,#107513) ;
#92867 = AXIS2_PLACEMENT_3D('',#139891,#107514,#107515) ;
#92868 = AXIS2_PLACEMENT_3D('',#139892,#107516,#107517) ;
#92869 = AXIS2_PLACEMENT_3D('',#139893,#107518,#107519) ;
#92870 = AXIS2_PLACEMENT_3D('',#139894,#107520,#107521) ;
#92871 = AXIS2_PLACEMENT_3D('',#139895,#107522,#107523) ;
#92872 = AXIS2_PLACEMENT_3D('',#139896,#107524,#107525) ;
#92873 = AXIS2_PLACEMENT_3D('',#139897,#107526,#107527) ;
#92874 = AXIS2_PLACEMENT_3D('',#139898,#107528,#107529) ;
#92875 = AXIS2_PLACEMENT_3D('',#139899,#107530,#107531) ;
#92876 = AXIS2_PLACEMENT_3D('',#139900,#107532,#107533) ;
#92877 = AXIS2_PLACEMENT_3D('',#139905,#107534,#107535) ;
#92878 = AXIS2_PLACEMENT_3D('',#139906,#107536,#107537) ;
#92879 = AXIS2_PLACEMENT_3D('',#139907,#107538,#107539) ;
#92880 = AXIS2_PLACEMENT_3D('',#139908,#107540,#107541) ;
#92881 = AXIS2_PLACEMENT_3D('',#139913,#107542,#107543) ;
#92882 = AXIS2_PLACEMENT_3D('',#139914,#107544,#107545) ;
#92883 = AXIS2_PLACEMENT_3D('',#139915,#107546,#107547) ;
#92884 = AXIS2_PLACEMENT_3D('',#139916,#107548,#107549) ;
#92885 = AXIS2_PLACEMENT_3D('',#139929,#107550,#107551) ;
#92886 = AXIS2_PLACEMENT_3D('',#139942,#107552,#107553) ;
#92887 = AXIS2_PLACEMENT_3D('',#139943,#107554,#107555) ;
#92888 = AXIS2_PLACEMENT_3D('',#139944,#107556,#107557) ;
#92889 = AXIS2_PLACEMENT_3D('',#139945,#107558,#107559) ;
#92890 = AXIS2_PLACEMENT_3D('',#139946,#107560,#107561) ;
#92891 = AXIS2_PLACEMENT_3D('',#139947,#107562,#107563) ;
#92892 = AXIS2_PLACEMENT_3D('',#139948,#107564,#107565) ;
#92893 = AXIS2_PLACEMENT_3D('',#139949,#107566,#107567) ;
#92894 = AXIS2_PLACEMENT_3D('',#139950,#107568,#107569) ;
#92895 = AXIS2_PLACEMENT_3D('',#139951,#107570,#107571) ;
#92896 = AXIS2_PLACEMENT_3D('',#139952,#107572,#107573) ;
#92897 = AXIS2_PLACEMENT_3D('',#139953,#107574,#107575) ;
#92898 = AXIS2_PLACEMENT_3D('',#139954,#107576,#107577) ;
#92899 = AXIS2_PLACEMENT_3D('',#139955,#107578,#107579) ;
#92900 = AXIS2_PLACEMENT_3D('',#139956,#107580,#107581) ;
#92901 = AXIS2_PLACEMENT_3D('',#139957,#107582,#107583) ;
#92902 = AXIS2_PLACEMENT_3D('',#139958,#107584,#107585) ;
#92903 = AXIS2_PLACEMENT_3D('',#139961,#107586,#107587) ;
#92904 = AXIS2_PLACEMENT_3D('',#139963,#107588,#107589) ;
#92905 = AXIS2_PLACEMENT_3D('',#139965,#107590,#107591) ;
#92906 = AXIS2_PLACEMENT_3D('',#139966,#107592,#107593) ;
#92907 = AXIS2_PLACEMENT_3D('',#139967,#107594,#107595) ;
#92908 = AXIS2_PLACEMENT_3D('',#139970,#107596,#107597) ;
#92909 = AXIS2_PLACEMENT_3D('',#139974,#107599,#107600) ;
#92910 = AXIS2_PLACEMENT_3D('',#139976,#107602,#107603) ;
#92911 = AXIS2_PLACEMENT_3D('',#139978,#107604,#107605) ;
#92912 = AXIS2_PLACEMENT_3D('',#139980,#107606,#107607) ;
#92913 = AXIS2_PLACEMENT_3D('',#139982,#107608,#107609) ;
#92914 = AXIS2_PLACEMENT_3D('',#139983,#107610,#107611) ;
#92915 = AXIS2_PLACEMENT_3D('',#139984,#107612,#107613) ;
#92916 = AXIS2_PLACEMENT_3D('',#139986,#107614,#107615) ;
#92917 = AXIS2_PLACEMENT_3D('',#139988,#107616,#107617) ;
#92918 = AXIS2_PLACEMENT_3D('',#139989,#107618,#107619) ;
#92919 = AXIS2_PLACEMENT_3D('',#139990,#107620,#107621) ;
#92920 = AXIS2_PLACEMENT_3D('',#139992,#107622,#107623) ;
#92921 = AXIS2_PLACEMENT_3D('',#139994,#107624,#107625) ;
#92922 = AXIS2_PLACEMENT_3D('',#139996,#107626,#107627) ;
#92923 = AXIS2_PLACEMENT_3D('',#139997,#107628,#107629) ;
#92924 = AXIS2_PLACEMENT_3D('',#139998,#107630,#107631) ;
#92925 = AXIS2_PLACEMENT_3D('',#140001,#107632,#107633) ;
#92926 = AXIS2_PLACEMENT_3D('',#140003,#107634,#107635) ;
#92927 = AXIS2_PLACEMENT_3D('',#140005,#107636,#107637) ;
#92928 = AXIS2_PLACEMENT_3D('',#140006,#107638,#107639) ;
#92929 = AXIS2_PLACEMENT_3D('',#140007,#107640,#107641) ;
#92930 = AXIS2_PLACEMENT_3D('',#140010,#107642,#107643) ;
#92931 = AXIS2_PLACEMENT_3D('',#140012,#107644,#107645) ;
#92932 = AXIS2_PLACEMENT_3D('',#140013,#107646,#107647) ;
#92933 = AXIS2_PLACEMENT_3D('',#140014,#107648,#107649) ;
#92934 = AXIS2_PLACEMENT_3D('',#140018,#107651,#107652) ;
#92935 = AXIS2_PLACEMENT_3D('',#140020,#107654,#107655) ;
#92936 = AXIS2_PLACEMENT_3D('',#140023,#107656,#107657) ;
#92937 = AXIS2_PLACEMENT_3D('',#140025,#107658,#107659) ;
#92938 = AXIS2_PLACEMENT_3D('',#140026,#107660,#107661) ;
#92939 = AXIS2_PLACEMENT_3D('',#140027,#107662,#107663) ;
#92940 = AXIS2_PLACEMENT_3D('',#140029,#107664,#107665) ;
#92941 = AXIS2_PLACEMENT_3D('',#140031,#107667,#107668) ;
#92942 = AXIS2_PLACEMENT_3D('',#140033,#107670,#107671) ;
#92943 = AXIS2_PLACEMENT_3D('',#140036,#107672,#107673) ;
#92944 = AXIS2_PLACEMENT_3D('',#140062,#107675,#107676) ;
#92945 = AXIS2_PLACEMENT_3D('',#140109,#107678,#107679) ;
#92946 = AXIS2_PLACEMENT_3D('',#140135,#107681,#107682) ;
#92947 = AXIS2_PLACEMENT_3D('',#140181,#107684,#107685) ;
#92948 = AXIS2_PLACEMENT_3D('',#140183,#107687,#107688) ;
#92949 = AXIS2_PLACEMENT_3D('',#140186,#107689,#107690) ;
#92950 = AXIS2_PLACEMENT_3D('',#140192,#107694,#107695) ;
#92951 = AXIS2_PLACEMENT_3D('',#140201,#107700,#107701) ;
#92952 = AXIS2_PLACEMENT_3D('',#140209,#107706,#107707) ;
#92953 = AXIS2_PLACEMENT_3D('',#140211,#107709,#107710) ;
#92954 = AXIS2_PLACEMENT_3D('',#140220,#107715,#107716) ;
#92955 = AXIS2_PLACEMENT_3D('',#140222,#107717,#107718) ;
#92956 = AXIS2_PLACEMENT_3D('',#140224,#107719,#107720) ;
#92957 = AXIS2_PLACEMENT_3D('',#140233,#107725,#107726) ;
#92958 = AXIS2_PLACEMENT_3D('',#140235,#107728,#107729) ;
#92959 = AXIS2_PLACEMENT_3D('',#140243,#107734,#107735) ;
#92960 = AXIS2_PLACEMENT_3D('',#140250,#107738,#107739) ;
#92961 = AXIS2_PLACEMENT_3D('',#140254,#107741,#107742) ;
#92962 = AXIS2_PLACEMENT_3D('',#140260,#107746,#107747) ;
#92963 = AXIS2_PLACEMENT_3D('',#140269,#107752,#107753) ;
#92964 = AXIS2_PLACEMENT_3D('',#140278,#107758,#107759) ;
#92965 = AXIS2_PLACEMENT_3D('',#140287,#107764,#107765) ;
#92966 = AXIS2_PLACEMENT_3D('',#140296,#107770,#107771) ;
#92967 = AXIS2_PLACEMENT_3D('',#140305,#107776,#107777) ;
#92968 = AXIS2_PLACEMENT_3D('',#140314,#107782,#107783) ;
#92969 = AXIS2_PLACEMENT_3D('',#140325,#107788,#107789) ;
#92970 = AXIS2_PLACEMENT_3D('',#140329,#107791,#107792) ;
#92971 = AXIS2_PLACEMENT_3D('',#140333,#107794,#107795) ;
#92972 = AXIS2_PLACEMENT_3D('',#140337,#107797,#107798) ;
#92973 = AXIS2_PLACEMENT_3D('',#140339,#107800,#107801) ;
#92974 = AXIS2_PLACEMENT_3D('',#140348,#107806,#107807) ;
#92975 = AXIS2_PLACEMENT_3D('',#140354,#107811,#107812) ;
#92976 = AXIS2_PLACEMENT_3D('',#140360,#107816,#107817) ;
#92977 = AXIS2_PLACEMENT_3D('',#140405,#107826,#107827) ;
#92978 = AXIS2_PLACEMENT_3D('',#140416,#107832,#107833) ;
#92979 = AXIS2_PLACEMENT_3D('',#140420,#107835,#107836) ;
#92980 = AXIS2_PLACEMENT_3D('',#140424,#107838,#107839) ;
#92981 = AXIS2_PLACEMENT_3D('',#140428,#107841,#107842) ;
#92982 = AXIS2_PLACEMENT_3D('',#140430,#107844,#107845) ;
#92983 = AXIS2_PLACEMENT_3D('',#140439,#107850,#107851) ;
#92984 = AXIS2_PLACEMENT_3D('',#140533,#107857,#107858) ;
#92985 = AXIS2_PLACEMENT_3D('',#140540,#107861,#107862) ;
#92986 = AXIS2_PLACEMENT_3D('',#140542,#107864,#107865) ;
#92987 = AXIS2_PLACEMENT_3D('',#140551,#107870,#107871) ;
#92988 = AXIS2_PLACEMENT_3D('',#140552,#107872,#107873) ;
#92989 = AXIS2_PLACEMENT_3D('',#140553,#107874,#107875) ;
#92990 = AXIS2_PLACEMENT_3D('',#140554,#107876,#107877) ;
#92991 = AXIS2_PLACEMENT_3D('',#140555,#107878,#107879) ;
#92992 = AXIS2_PLACEMENT_3D('',#140556,#107880,#107881) ;
#92993 = AXIS2_PLACEMENT_3D('',#140557,#107882,#107883) ;
#92994 = AXIS2_PLACEMENT_3D('',#140558,#107884,#107885) ;
#92995 = AXIS2_PLACEMENT_3D('',#140559,#107886,#107887) ;
#92996 = AXIS2_PLACEMENT_3D('',#140560,#107888,#107889) ;
#92997 = AXIS2_PLACEMENT_3D('',#140561,#107890,#107891) ;
#92998 = AXIS2_PLACEMENT_3D('',#140562,#107892,#107893) ;
#92999 = AXIS2_PLACEMENT_3D('',#140563,#107894,#107895) ;
#93000 = AXIS2_PLACEMENT_3D('',#140564,#107896,#107897) ;
#93001 = AXIS2_PLACEMENT_3D('',#140565,#107898,#107899) ;
#93002 = AXIS2_PLACEMENT_3D('',#140566,#107900,#107901) ;
#93003 = AXIS2_PLACEMENT_3D('',#140567,#107902,#107903) ;
#93004 = AXIS2_PLACEMENT_3D('',#140568,#107904,#107905) ;
#93005 = AXIS2_PLACEMENT_3D('',#140569,#107906,#107907) ;
#93006 = AXIS2_PLACEMENT_3D('',#140570,#107908,#107909) ;
#93007 = AXIS2_PLACEMENT_3D('',#140571,#107910,#107911) ;
#93008 = AXIS2_PLACEMENT_3D('',#140572,#107912,#107913) ;
#93009 = AXIS2_PLACEMENT_3D('',#140573,#107914,#107915) ;
#93010 = AXIS2_PLACEMENT_3D('',#140574,#107916,#107917) ;
#93011 = AXIS2_PLACEMENT_3D('',#140575,#107918,#107919) ;
#93012 = AXIS2_PLACEMENT_3D('',#140576,#107920,#107921) ;
#93013 = AXIS2_PLACEMENT_3D('',#140577,#107922,#107923) ;
#93014 = AXIS2_PLACEMENT_3D('',#140578,#107924,#107925) ;
#93015 = AXIS2_PLACEMENT_3D('',#140579,#107926,#107927) ;
#93016 = AXIS2_PLACEMENT_3D('',#140580,#107928,#107929) ;
#93017 = AXIS2_PLACEMENT_3D('',#140581,#107930,#107931) ;
#93018 = AXIS2_PLACEMENT_3D('',#140582,#107932,#107933) ;
#93019 = AXIS2_PLACEMENT_3D('',#140583,#107934,#107935) ;
#93020 = AXIS2_PLACEMENT_3D('',#140584,#107936,#107937) ;
#93021 = AXIS2_PLACEMENT_3D('',#140585,#107938,#107939) ;
#93022 = AXIS2_PLACEMENT_3D('',#140586,#107940,#107941) ;
#93023 = AXIS2_PLACEMENT_3D('',#140587,#107942,#107943) ;
#93024 = AXIS2_PLACEMENT_3D('',#140588,#107944,#107945) ;
#93025 = AXIS2_PLACEMENT_3D('',#140589,#107946,#107947) ;
#93026 = AXIS2_PLACEMENT_3D('',#140598,#107952,#107953) ;
#93027 = AXIS2_PLACEMENT_3D('',#140607,#107958,#107959) ;
#93028 = AXIS2_PLACEMENT_3D('',#140610,#107960,#107961) ;
#93029 = AXIS2_PLACEMENT_3D('',#140618,#107965,#107966) ;
#93030 = AXIS2_PLACEMENT_3D('',#140624,#107970,#107971) ;
#93031 = AXIS2_PLACEMENT_3D('',#140629,#107973,#107974) ;
#93032 = AXIS2_PLACEMENT_3D('',#140632,#107976,#107977) ;
#93033 = AXIS2_PLACEMENT_3D('',#140634,#107978,#107979) ;
#93034 = AXIS2_PLACEMENT_3D('',#140637,#107981,#107982) ;
#93035 = AXIS2_PLACEMENT_3D('',#140638,#107983,#107984) ;
#93036 = AXIS2_PLACEMENT_3D('',#140641,#107985,#107986) ;
#93037 = AXIS2_PLACEMENT_3D('',#140646,#107989,#107990) ;
#93038 = AXIS2_PLACEMENT_3D('',#140652,#107994,#107995) ;
#93039 = AXIS2_PLACEMENT_3D('',#140658,#107999,#108000) ;
#93040 = AXIS2_PLACEMENT_3D('',#140664,#108004,#108005) ;
#93041 = AXIS2_PLACEMENT_3D('',#140677,#108012,#108013) ;
#93042 = AXIS2_PLACEMENT_3D('',#140690,#108020,#108021) ;
#93043 = AXIS2_PLACEMENT_3D('',#140699,#108026,#108027) ;
#93044 = AXIS2_PLACEMENT_3D('',#140708,#108032,#108033) ;
#93045 = AXIS2_PLACEMENT_3D('',#140717,#108038,#108039) ;
#93046 = AXIS2_PLACEMENT_3D('',#140726,#108044,#108045) ;
#93047 = AXIS2_PLACEMENT_3D('',#140739,#108051,#108052) ;
#93048 = AXIS2_PLACEMENT_3D('',#140743,#108054,#108055) ;
#93049 = AXIS2_PLACEMENT_3D('',#140747,#108057,#108058) ;
#93050 = AXIS2_PLACEMENT_3D('',#140750,#108060,#108061) ;
#93051 = AXIS2_PLACEMENT_3D('',#140751,#108062,#108063) ;
#93052 = AXIS2_PLACEMENT_3D('',#140754,#108064,#108065) ;
#93053 = AXIS2_PLACEMENT_3D('',#140757,#108068,#108069) ;
#93054 = AXIS2_PLACEMENT_3D('',#140761,#108072,#108073) ;
#93055 = AXIS2_PLACEMENT_3D('',#140763,#108074,#108075) ;
#93056 = AXIS2_PLACEMENT_3D('',#140765,#108077,#108078) ;
#93057 = AXIS2_PLACEMENT_3D('',#140769,#108081,#108082) ;
#93058 = AXIS2_PLACEMENT_3D('',#140771,#108083,#108084) ;
#93059 = AXIS2_PLACEMENT_3D('',#140773,#108086,#108087) ;
#93060 = AXIS2_PLACEMENT_3D('',#140777,#108090,#108091) ;
#93061 = AXIS2_PLACEMENT_3D('',#140779,#108092,#108093) ;
#93062 = AXIS2_PLACEMENT_3D('',#140781,#108095,#108096) ;
#93063 = AXIS2_PLACEMENT_3D('',#140783,#108098,#108099) ;
#93064 = AXIS2_PLACEMENT_3D('',#140784,#108100,#108101) ;
#93065 = AXIS2_PLACEMENT_3D('',#140786,#108103,#108104) ;
#93066 = AXIS2_PLACEMENT_3D('',#140789,#108107,#108108) ;
#93067 = AXIS2_PLACEMENT_3D('',#140792,#108111,#108112) ;
#93068 = AXIS2_PLACEMENT_3D('',#140795,#108115,#108116) ;
#93069 = AXIS2_PLACEMENT_3D('',#140804,#108121,#108122) ;
#93070 = AXIS2_PLACEMENT_3D('',#140813,#108127,#108128) ;
#93071 = AXIS2_PLACEMENT_3D('',#140822,#108133,#108134) ;
#93072 = AXIS2_PLACEMENT_3D('',#140831,#108139,#108140) ;
#93073 = AXIS2_PLACEMENT_3D('',#140844,#108146,#108147) ;
#93074 = AXIS2_PLACEMENT_3D('',#140848,#108149,#108150) ;
#93075 = AXIS2_PLACEMENT_3D('',#140852,#108152,#108153) ;
#93076 = AXIS2_PLACEMENT_3D('',#140855,#108155,#108156) ;
#93077 = AXIS2_PLACEMENT_3D('',#140856,#108157,#108158) ;
#93078 = AXIS2_PLACEMENT_3D('',#140860,#108160,#108161) ;
#93079 = AXIS2_PLACEMENT_3D('',#140862,#108163,#108164) ;
#93080 = AXIS2_PLACEMENT_3D('',#140866,#108167,#108168) ;
#93081 = AXIS2_PLACEMENT_3D('',#140868,#108169,#108170) ;
#93082 = AXIS2_PLACEMENT_3D('',#140870,#108172,#108173) ;
#93083 = AXIS2_PLACEMENT_3D('',#140874,#108176,#108177) ;
#93084 = AXIS2_PLACEMENT_3D('',#140876,#108178,#108179) ;
#93085 = AXIS2_PLACEMENT_3D('',#140878,#108181,#108182) ;
#93086 = AXIS2_PLACEMENT_3D('',#140882,#108185,#108186) ;
#93087 = AXIS2_PLACEMENT_3D('',#140884,#108187,#108188) ;
#93088 = AXIS2_PLACEMENT_3D('',#140886,#108190,#108191) ;
#93089 = AXIS2_PLACEMENT_3D('',#140888,#108193,#108194) ;
#93090 = AXIS2_PLACEMENT_3D('',#140897,#108199,#108200) ;
#93091 = AXIS2_PLACEMENT_3D('',#140904,#108205,#108206) ;
#93092 = AXIS2_PLACEMENT_3D('',#140910,#108210,#108211) ;
#93093 = AXIS2_PLACEMENT_3D('',#140915,#108215,#108216) ;
#93094 = AXIS2_PLACEMENT_3D('',#140919,#108218,#108219) ;
#93095 = AXIS2_PLACEMENT_3D('',#140925,#108223,#108224) ;
#93096 = AXIS2_PLACEMENT_3D('',#140926,#108225,#108226) ;
#93097 = AXIS2_PLACEMENT_3D('',#140929,#108227,#108228) ;
#93098 = AXIS2_PLACEMENT_3D('',#140931,#108229,#108230) ;
#93099 = AXIS2_PLACEMENT_3D('',#140933,#108231,#108232) ;
#93100 = AXIS2_PLACEMENT_3D('',#140937,#108234,#108235) ;
#93101 = AXIS2_PLACEMENT_3D('',#140957,#108237,#108238) ;
#93102 = AXIS2_PLACEMENT_3D('',#140964,#108239,#108240) ;
#93103 = AXIS2_PLACEMENT_3D('',#140965,#108241,#108242) ;
#93104 = AXIS2_PLACEMENT_3D('',#140966,#108243,#108244) ;
#93105 = AXIS2_PLACEMENT_3D('',#140979,#108245,#108246) ;
#93106 = AXIS2_PLACEMENT_3D('',#140980,#108247,#108248) ;
#93107 = AXIS2_PLACEMENT_3D('',#140981,#108249,#108250) ;
#93108 = AXIS2_PLACEMENT_3D('',#140982,#108251,#108252) ;
#93109 = AXIS2_PLACEMENT_3D('',#140983,#108253,#108254) ;
#93110 = AXIS2_PLACEMENT_3D('',#140984,#108255,#108256) ;
#93111 = AXIS2_PLACEMENT_3D('',#140985,#108257,#108258) ;
#93112 = AXIS2_PLACEMENT_3D('',#140986,#108259,#108260) ;
#93113 = AXIS2_PLACEMENT_3D('',#140987,#108261,#108262) ;
#93114 = AXIS2_PLACEMENT_3D('',#140988,#108263,#108264) ;
#93115 = AXIS2_PLACEMENT_3D('',#140989,#108265,#108266) ;
#93116 = AXIS2_PLACEMENT_3D('',#140990,#108267,#108268) ;
#93117 = AXIS2_PLACEMENT_3D('',#140991,#108269,#108270) ;
#93118 = AXIS2_PLACEMENT_3D('',#140992,#108271,#108272) ;
#93119 = AXIS2_PLACEMENT_3D('',#140993,#108273,#108274) ;
#93120 = AXIS2_PLACEMENT_3D('',#140994,#108275,#108276) ;
#93121 = AXIS2_PLACEMENT_3D('',#141013,#108277,#108278) ;
#93122 = AXIS2_PLACEMENT_3D('',#141014,#108279,#108280) ;
#93123 = AXIS2_PLACEMENT_3D('',#141033,#108281,#108282) ;
#93124 = AXIS2_PLACEMENT_3D('',#141052,#108283,#108284) ;
#93125 = AXIS2_PLACEMENT_3D('',#141053,#108285,#108286) ;
#93126 = AXIS2_PLACEMENT_3D('',#141054,#108287,#108288) ;
#93127 = AXIS2_PLACEMENT_3D('',#141055,#108289,#108290) ;
#93128 = AXIS2_PLACEMENT_3D('',#141056,#108291,#108292) ;
#93129 = AXIS2_PLACEMENT_3D('',#141057,#108293,#108294) ;
#93130 = AXIS2_PLACEMENT_3D('',#141058,#108295,#108296) ;
#93131 = AXIS2_PLACEMENT_3D('',#141059,#108297,#108298) ;
#93132 = AXIS2_PLACEMENT_3D('',#141060,#108299,#108300) ;
#93133 = AXIS2_PLACEMENT_3D('',#141061,#108301,#108302) ;
#93134 = AXIS2_PLACEMENT_3D('',#141062,#108303,#108304) ;
#93135 = AXIS2_PLACEMENT_3D('',#141063,#108305,#108306) ;
#93136 = AXIS2_PLACEMENT_3D('',#141064,#108307,#108308) ;
#93137 = AXIS2_PLACEMENT_3D('',#141065,#108309,#108310) ;
#93138 = AXIS2_PLACEMENT_3D('',#141066,#108311,#108312) ;
#93139 = AXIS2_PLACEMENT_3D('',#141085,#108313,#108314) ;
#93140 = AXIS2_PLACEMENT_3D('',#141086,#108315,#108316) ;
#93141 = AXIS2_PLACEMENT_3D('',#141087,#108317,#108318) ;
#93142 = AXIS2_PLACEMENT_3D('',#141088,#108319,#108320) ;
#93143 = AXIS2_PLACEMENT_3D('',#141089,#108321,#108322) ;
#93144 = AXIS2_PLACEMENT_3D('',#141090,#108323,#108324) ;
#93145 = AXIS2_PLACEMENT_3D('',#141091,#108325,#108326) ;
#93146 = AXIS2_PLACEMENT_3D('',#141092,#108327,#108328) ;
#93147 = AXIS2_PLACEMENT_3D('',#141093,#108329,#108330) ;
#93148 = AXIS2_PLACEMENT_3D('',#141094,#108331,#108332) ;
#93149 = AXIS2_PLACEMENT_3D('',#141095,#108333,#108334) ;
#93150 = AXIS2_PLACEMENT_3D('',#141108,#108335,#108336) ;
#93151 = AXIS2_PLACEMENT_3D('',#141109,#108337,#108338) ;
#93152 = AXIS2_PLACEMENT_3D('',#141110,#108339,#108340) ;
#93153 = AXIS2_PLACEMENT_3D('',#141111,#108341,#108342) ;
#93154 = AXIS2_PLACEMENT_3D('',#141112,#108343,#108344) ;
#93155 = AXIS2_PLACEMENT_3D('',#141113,#108345,#108346) ;
#93156 = AXIS2_PLACEMENT_3D('',#141114,#108347,#108348) ;
#93157 = AXIS2_PLACEMENT_3D('',#141127,#108349,#108350) ;
#93158 = AXIS2_PLACEMENT_3D('',#141128,#108351,#108352) ;
#93159 = AXIS2_PLACEMENT_3D('',#141129,#108353,#108354) ;
#93160 = AXIS2_PLACEMENT_3D('',#141130,#108355,#108356) ;
#93161 = AXIS2_PLACEMENT_3D('',#141132,#108357,#108358) ;
#93162 = AXIS2_PLACEMENT_3D('',#141152,#108359,#108360) ;
#93163 = AXIS2_PLACEMENT_3D('',#141153,#108361,#108362) ;
#93164 = AXIS2_PLACEMENT_3D('',#141154,#108363,#108364) ;
#93165 = AXIS2_PLACEMENT_3D('',#141155,#108365,#108366) ;
#93166 = AXIS2_PLACEMENT_3D('',#141156,#108367,#108368) ;
#93167 = AXIS2_PLACEMENT_3D('',#141157,#108369,#108370) ;
#93168 = AXIS2_PLACEMENT_3D('',#141186,#108371,#108372) ;
#93169 = AXIS2_PLACEMENT_3D('',#141187,#108373,#108374) ;
#93170 = AXIS2_PLACEMENT_3D('',#141188,#108375,#108376) ;
#93171 = AXIS2_PLACEMENT_3D('',#141189,#108377,#108378) ;
#93172 = AXIS2_PLACEMENT_3D('',#141190,#108379,#108380) ;
#93173 = AXIS2_PLACEMENT_3D('',#141191,#108381,#108382) ;
#93174 = AXIS2_PLACEMENT_3D('',#141192,#108383,#108384) ;
#93175 = AXIS2_PLACEMENT_3D('',#141214,#108385,#108386) ;
#93176 = AXIS2_PLACEMENT_3D('',#141215,#108387,#108388) ;
#93177 = AXIS2_PLACEMENT_3D('',#141216,#108389,#108390) ;
#93178 = AXIS2_PLACEMENT_3D('',#141217,#108391,#108392) ;
#93179 = AXIS2_PLACEMENT_3D('',#141218,#108393,#108394) ;
#93180 = AXIS2_PLACEMENT_3D('',#141219,#108395,#108396) ;
#93181 = AXIS2_PLACEMENT_3D('',#141220,#108397,#108398) ;
#93182 = AXIS2_PLACEMENT_3D('',#141221,#108399,#108400) ;
#93183 = AXIS2_PLACEMENT_3D('',#141222,#108401,#108402) ;
#93184 = AXIS2_PLACEMENT_3D('',#141223,#108403,#108404) ;
#93185 = AXIS2_PLACEMENT_3D('',#141224,#108405,#108406) ;
#93186 = AXIS2_PLACEMENT_3D('',#141225,#108407,#108408) ;
#93187 = AXIS2_PLACEMENT_3D('',#141226,#108409,#108410) ;
#93188 = AXIS2_PLACEMENT_3D('',#141227,#108411,#108412) ;
#93189 = AXIS2_PLACEMENT_3D('',#141228,#108413,#108414) ;
#93190 = AXIS2_PLACEMENT_3D('',#141229,#108415,#108416) ;
#93191 = AXIS2_PLACEMENT_3D('',#141230,#108417,#108418) ;
#93192 = AXIS2_PLACEMENT_3D('',#141231,#108419,#108420) ;
#93193 = AXIS2_PLACEMENT_3D('',#141232,#108421,#108422) ;
#93194 = AXIS2_PLACEMENT_3D('',#141233,#108423,#108424) ;
#93195 = AXIS2_PLACEMENT_3D('',#141234,#108425,#108426) ;
#93196 = AXIS2_PLACEMENT_3D('',#141235,#108427,#108428) ;
#93197 = AXIS2_PLACEMENT_3D('',#141236,#108429,#108430) ;
#93198 = AXIS2_PLACEMENT_3D('',#141237,#108431,#108432) ;
#93199 = AXIS2_PLACEMENT_3D('',#141238,#108433,#108434) ;
#93200 = AXIS2_PLACEMENT_3D('',#141239,#108435,#108436) ;
#93201 = AXIS2_PLACEMENT_3D('',#141240,#108437,#108438) ;
#93202 = AXIS2_PLACEMENT_3D('',#141241,#108439,#108440) ;
#93203 = AXIS2_PLACEMENT_3D('',#141242,#108441,#108442) ;
#93204 = AXIS2_PLACEMENT_3D('',#141243,#108443,#108444) ;
#93205 = AXIS2_PLACEMENT_3D('',#141244,#108445,#108446) ;
#93206 = AXIS2_PLACEMENT_3D('',#141245,#108447,#108448) ;
#93207 = AXIS2_PLACEMENT_3D('',#141246,#108449,#108450) ;
#93208 = AXIS2_PLACEMENT_3D('',#141247,#108451,#108452) ;
#93209 = AXIS2_PLACEMENT_3D('',#141248,#108453,#108454) ;
#93210 = AXIS2_PLACEMENT_3D('',#141249,#108455,#108456) ;
#93211 = AXIS2_PLACEMENT_3D('',#141250,#108457,#108458) ;
#93212 = AXIS2_PLACEMENT_3D('',#141251,#108459,#108460) ;
#93213 = AXIS2_PLACEMENT_3D('',#141252,#108461,#108462) ;
#93214 = AXIS2_PLACEMENT_3D('',#141253,#108463,#108464) ;
#93215 = AXIS2_PLACEMENT_3D('',#141254,#108465,#108466) ;
#93216 = AXIS2_PLACEMENT_3D('',#141255,#108467,#108468) ;
#93217 = AXIS2_PLACEMENT_3D('',#141256,#108469,#108470) ;
#93218 = AXIS2_PLACEMENT_3D('',#141257,#108471,#108472) ;
#93219 = AXIS2_PLACEMENT_3D('',#141258,#108473,#108474) ;
#93220 = AXIS2_PLACEMENT_3D('',#141259,#108475,#108476) ;
#93221 = AXIS2_PLACEMENT_3D('',#141260,#108477,#108478) ;
#93222 = AXIS2_PLACEMENT_3D('',#141261,#108479,#108480) ;
#93223 = AXIS2_PLACEMENT_3D('',#141262,#108481,#108482) ;
#93224 = AXIS2_PLACEMENT_3D('',#141263,#108483,#108484) ;
#93225 = AXIS2_PLACEMENT_3D('',#141264,#108485,#108486) ;
#93226 = AXIS2_PLACEMENT_3D('',#141265,#108487,#108488) ;
#93227 = AXIS2_PLACEMENT_3D('',#141266,#108489,#108490) ;
#93228 = AXIS2_PLACEMENT_3D('',#141267,#108491,#108492) ;
#93229 = AXIS2_PLACEMENT_3D('',#141268,#108493,#108494) ;
#93230 = AXIS2_PLACEMENT_3D('',#141269,#108495,#108496) ;
#93231 = AXIS2_PLACEMENT_3D('',#141270,#108497,#108498) ;
#93232 = AXIS2_PLACEMENT_3D('',#141271,#108499,#108500) ;
#93233 = AXIS2_PLACEMENT_3D('',#141272,#108501,#108502) ;
#93234 = AXIS2_PLACEMENT_3D('',#141273,#108503,#108504) ;
#93235 = AXIS2_PLACEMENT_3D('',#141274,#108505,#108506) ;
#93236 = AXIS2_PLACEMENT_3D('',#141275,#108507,#108508) ;
#93237 = AXIS2_PLACEMENT_3D('',#141276,#108509,#108510) ;
#93238 = AXIS2_PLACEMENT_3D('',#141277,#108511,#108512) ;
#93239 = AXIS2_PLACEMENT_3D('',#141278,#108513,#108514) ;
#93240 = AXIS2_PLACEMENT_3D('',#141279,#108515,#108516) ;
#93241 = AXIS2_PLACEMENT_3D('',#141280,#108517,#108518) ;
#93242 = AXIS2_PLACEMENT_3D('',#141281,#108519,#108520) ;
#93243 = AXIS2_PLACEMENT_3D('',#141282,#108521,#108522) ;
#93244 = AXIS2_PLACEMENT_3D('',#141283,#108523,#108524) ;
#93245 = AXIS2_PLACEMENT_3D('',#141284,#108525,#108526) ;
#93246 = AXIS2_PLACEMENT_3D('',#141285,#108527,#108528) ;
#93247 = AXIS2_PLACEMENT_3D('',#141286,#108529,#108530) ;
#93248 = AXIS2_PLACEMENT_3D('',#141287,#108531,#108532) ;
#93249 = AXIS2_PLACEMENT_3D('',#141288,#108533,#108534) ;
#93250 = AXIS2_PLACEMENT_3D('',#141289,#108535,#108536) ;
#93251 = AXIS2_PLACEMENT_3D('',#141290,#108537,#108538) ;
#93252 = AXIS2_PLACEMENT_3D('',#141291,#108539,#108540) ;
#93253 = AXIS2_PLACEMENT_3D('',#141292,#108541,#108542) ;
#93254 = AXIS2_PLACEMENT_3D('',#141293,#108543,#108544) ;
#93255 = AXIS2_PLACEMENT_3D('',#141294,#108545,#108546) ;
#93256 = AXIS2_PLACEMENT_3D('',#141295,#108547,#108548) ;
#93257 = AXIS2_PLACEMENT_3D('',#141296,#108549,#108550) ;
#93258 = AXIS2_PLACEMENT_3D('',#141297,#108551,#108552) ;
#93259 = AXIS2_PLACEMENT_3D('',#141298,#108553,#108554) ;
#93260 = AXIS2_PLACEMENT_3D('',#141299,#108555,#108556) ;
#93261 = AXIS2_PLACEMENT_3D('',#141300,#108557,#108558) ;
#93262 = AXIS2_PLACEMENT_3D('',#141301,#108559,#108560) ;
#93263 = AXIS2_PLACEMENT_3D('',#141302,#108561,#108562) ;
#93264 = AXIS2_PLACEMENT_3D('',#141303,#108563,#108564) ;
#93265 = AXIS2_PLACEMENT_3D('',#141304,#108565,#108566) ;
#93266 = AXIS2_PLACEMENT_3D('',#141305,#108567,#108568) ;
#93267 = AXIS2_PLACEMENT_3D('',#141306,#108569,#108570) ;
#93268 = AXIS2_PLACEMENT_3D('',#141307,#108571,#108572) ;
#93269 = AXIS2_PLACEMENT_3D('',#141308,#108573,#108574) ;
#93270 = AXIS2_PLACEMENT_3D('',#141309,#108575,#108576) ;
#93271 = AXIS2_PLACEMENT_3D('',#141310,#108577,#108578) ;
#93272 = AXIS2_PLACEMENT_3D('',#141311,#108579,#108580) ;
#93273 = AXIS2_PLACEMENT_3D('',#141312,#108581,#108582) ;
#93274 = AXIS2_PLACEMENT_3D('',#141313,#108583,#108584) ;
#93275 = AXIS2_PLACEMENT_3D('',#141314,#108585,#108586) ;
#93276 = AXIS2_PLACEMENT_3D('',#141315,#108587,#108588) ;
#93277 = AXIS2_PLACEMENT_3D('',#141316,#108589,#108590) ;
#93278 = AXIS2_PLACEMENT_3D('',#141317,#108591,#108592) ;
#93279 = AXIS2_PLACEMENT_3D('',#141318,#108593,#108594) ;
#93280 = AXIS2_PLACEMENT_3D('',#141319,#108595,#108596) ;
#93281 = AXIS2_PLACEMENT_3D('',#141320,#108597,#108598) ;
#93282 = AXIS2_PLACEMENT_3D('',#141321,#108599,#108600) ;
#93283 = AXIS2_PLACEMENT_3D('',#141322,#108601,#108602) ;
#93284 = AXIS2_PLACEMENT_3D('',#141335,#108603,#108604) ;
#93285 = AXIS2_PLACEMENT_3D('',#141336,#108605,#108606) ;
#93286 = AXIS2_PLACEMENT_3D('',#141337,#108607,#108608) ;
#93287 = AXIS2_PLACEMENT_3D('',#141338,#108609,#108610) ;
#93288 = AXIS2_PLACEMENT_3D('',#141339,#108611,#108612) ;
#93289 = AXIS2_PLACEMENT_3D('',#141340,#108613,#108614) ;
#93290 = AXIS2_PLACEMENT_3D('',#141341,#108615,#108616) ;
#93291 = AXIS2_PLACEMENT_3D('',#141342,#108617,#108618) ;
#93292 = AXIS2_PLACEMENT_3D('',#141343,#108619,#108620) ;
#93293 = AXIS2_PLACEMENT_3D('',#141344,#108621,#108622) ;
#93294 = AXIS2_PLACEMENT_3D('',#141345,#108623,#108624) ;
#93295 = AXIS2_PLACEMENT_3D('',#141346,#108625,#108626) ;
#93296 = AXIS2_PLACEMENT_3D('',#141347,#108627,#108628) ;
#93297 = AXIS2_PLACEMENT_3D('',#141348,#108629,#108630) ;
#93298 = AXIS2_PLACEMENT_3D('',#141349,#108631,#108632) ;
#93299 = AXIS2_PLACEMENT_3D('',#141350,#108633,#108634) ;
#93300 = AXIS2_PLACEMENT_3D('',#141351,#108635,#108636) ;
#93301 = AXIS2_PLACEMENT_3D('',#141352,#108637,#108638) ;
#93302 = AXIS2_PLACEMENT_3D('',#141353,#108639,#108640) ;
#93303 = AXIS2_PLACEMENT_3D('',#141354,#108641,#108642) ;
#93304 = AXIS2_PLACEMENT_3D('',#141355,#108643,#108644) ;
#93305 = AXIS2_PLACEMENT_3D('',#141356,#108645,#108646) ;
#93306 = AXIS2_PLACEMENT_3D('',#141357,#108647,#108648) ;
#93307 = AXIS2_PLACEMENT_3D('',#141358,#108649,#108650) ;
#93308 = AXIS2_PLACEMENT_3D('',#141371,#108651,#108652) ;
#93309 = AXIS2_PLACEMENT_3D('',#141372,#108653,#108654) ;
#93310 = AXIS2_PLACEMENT_3D('',#141373,#108655,#108656) ;
#93311 = AXIS2_PLACEMENT_3D('',#141374,#108657,#108658) ;
#93312 = AXIS2_PLACEMENT_3D('',#141375,#108659,#108660) ;
#93313 = AXIS2_PLACEMENT_3D('',#141376,#108661,#108662) ;
#93314 = AXIS2_PLACEMENT_3D('',#141377,#108663,#108664) ;
#93315 = AXIS2_PLACEMENT_3D('',#141378,#108665,#108666) ;
#93316 = AXIS2_PLACEMENT_3D('',#141379,#108667,#108668) ;
#93317 = AXIS2_PLACEMENT_3D('',#141380,#108669,#108670) ;
#93318 = AXIS2_PLACEMENT_3D('',#141381,#108671,#108672) ;
#93319 = AXIS2_PLACEMENT_3D('',#141382,#108673,#108674) ;
#93320 = AXIS2_PLACEMENT_3D('',#141383,#108675,#108676) ;
#93321 = AXIS2_PLACEMENT_3D('',#141384,#108677,#108678) ;
#93322 = AXIS2_PLACEMENT_3D('',#141385,#108679,#108680) ;
#93323 = AXIS2_PLACEMENT_3D('',#141386,#108681,#108682) ;
#93324 = AXIS2_PLACEMENT_3D('',#141387,#108683,#108684) ;
#93325 = AXIS2_PLACEMENT_3D('',#141388,#108685,#108686) ;
#93326 = AXIS2_PLACEMENT_3D('',#141389,#108687,#108688) ;
#93327 = AXIS2_PLACEMENT_3D('',#141390,#108689,#108690) ;
#93328 = AXIS2_PLACEMENT_3D('',#141391,#108691,#108692) ;
#93329 = AXIS2_PLACEMENT_3D('',#141392,#108693,#108694) ;
#93330 = AXIS2_PLACEMENT_3D('',#141393,#108695,#108696) ;
#93331 = AXIS2_PLACEMENT_3D('',#141406,#108697,#108698) ;
#93332 = AXIS2_PLACEMENT_3D('',#141419,#108699,#108700) ;
#93333 = AXIS2_PLACEMENT_3D('',#141420,#108701,#108702) ;
#93334 = AXIS2_PLACEMENT_3D('',#141421,#108703,#108704) ;
#93335 = AXIS2_PLACEMENT_3D('',#141422,#108705,#108706) ;
#93336 = AXIS2_PLACEMENT_3D('',#141435,#108707,#108708) ;
#93337 = AXIS2_PLACEMENT_3D('',#141448,#108709,#108710) ;
#93338 = AXIS2_PLACEMENT_3D('',#141449,#108711,#108712) ;
#93339 = AXIS2_PLACEMENT_3D('',#141450,#108713,#108714) ;
#93340 = AXIS2_PLACEMENT_3D('',#141451,#108715,#108716) ;
#93341 = AXIS2_PLACEMENT_3D('',#141529,#108717,#108718) ;
#93342 = AXIS2_PLACEMENT_3D('',#141530,#108719,#108720) ;
#93343 = AXIS2_PLACEMENT_3D('',#141599,#108721,#108722) ;
#93344 = AXIS2_PLACEMENT_3D('',#141600,#108723,#108724) ;
#93345 = AXIS2_PLACEMENT_3D('',#141715,#108725,#108726) ;
#93346 = AXIS2_PLACEMENT_3D('',#141746,#108727,#108728) ;
#93347 = AXIS2_PLACEMENT_3D('',#141777,#108729,#108730) ;
#93348 = AXIS2_PLACEMENT_3D('',#141826,#108731,#108732) ;
#93349 = AXIS2_PLACEMENT_3D('',#141827,#108733,#108734) ;
#93350 = AXIS2_PLACEMENT_3D('',#141829,#108735,#108736) ;
#93351 = AXIS2_PLACEMENT_3D('',#141831,#108737,#108738) ;
#93352 = AXIS2_PLACEMENT_3D('',#141833,#108739,#108740) ;
#93353 = AXIS2_PLACEMENT_3D('',#141834,#108741,#108742) ;
#93354 = AXIS2_PLACEMENT_3D('',#141835,#108743,#108744) ;
#93355 = AXIS2_PLACEMENT_3D('',#141837,#108745,#108746) ;
#93356 = AXIS2_PLACEMENT_3D('',#141839,#108747,#108748) ;
#93357 = AXIS2_PLACEMENT_3D('',#141840,#108749,#108750) ;
#93358 = AXIS2_PLACEMENT_3D('',#141841,#108751,#108752) ;
#93359 = AXIS2_PLACEMENT_3D('',#141844,#108753,#108754) ;
#93360 = AXIS2_PLACEMENT_3D('',#141846,#108755,#108756) ;
#93361 = AXIS2_PLACEMENT_3D('',#141847,#108757,#108758) ;
#93362 = AXIS2_PLACEMENT_3D('',#141848,#108759,#108760) ;
#93363 = AXIS2_PLACEMENT_3D('',#141851,#108761,#108762) ;
#93364 = AXIS2_PLACEMENT_3D('',#141853,#108763,#108764) ;
#93365 = AXIS2_PLACEMENT_3D('',#141857,#108766,#108767) ;
#93366 = AXIS2_PLACEMENT_3D('',#141870,#108770,#108771) ;
#93367 = AXIS2_PLACEMENT_3D('',#141872,#108772,#108773) ;
#93368 = AXIS2_PLACEMENT_3D('',#141874,#108774,#108775) ;
#93369 = AXIS2_PLACEMENT_3D('',#141876,#108776,#108777) ;
#93370 = AXIS2_PLACEMENT_3D('',#141877,#108778,#108779) ;
#93371 = AXIS2_PLACEMENT_3D('',#141878,#108780,#108781) ;
#93372 = AXIS2_PLACEMENT_3D('',#141880,#108782,#108783) ;
#93373 = AXIS2_PLACEMENT_3D('',#141882,#108784,#108785) ;
#93374 = AXIS2_PLACEMENT_3D('',#141883,#108786,#108787) ;
#93375 = AXIS2_PLACEMENT_3D('',#141884,#108788,#108789) ;
#93376 = AXIS2_PLACEMENT_3D('',#141887,#108790,#108791) ;
#93377 = AXIS2_PLACEMENT_3D('',#141889,#108792,#108793) ;
#93378 = AXIS2_PLACEMENT_3D('',#141890,#108794,#108795) ;
#93379 = AXIS2_PLACEMENT_3D('',#141891,#108796,#108797) ;
#93380 = AXIS2_PLACEMENT_3D('',#141894,#108798,#108799) ;
#93381 = AXIS2_PLACEMENT_3D('',#141896,#108800,#108801) ;
#93382 = AXIS2_PLACEMENT_3D('',#141900,#108803,#108804) ;
#93383 = AXIS2_PLACEMENT_3D('',#141913,#108807,#108808) ;
#93384 = AXIS2_PLACEMENT_3D('',#141915,#108809,#108810) ;
#93385 = AXIS2_PLACEMENT_3D('',#141917,#108811,#108812) ;
#93386 = AXIS2_PLACEMENT_3D('',#141919,#108813,#108814) ;
#93387 = AXIS2_PLACEMENT_3D('',#141920,#108815,#108816) ;
#93388 = AXIS2_PLACEMENT_3D('',#141921,#108817,#108818) ;
#93389 = AXIS2_PLACEMENT_3D('',#141923,#108819,#108820) ;
#93390 = AXIS2_PLACEMENT_3D('',#141925,#108821,#108822) ;
#93391 = AXIS2_PLACEMENT_3D('',#141926,#108823,#108824) ;
#93392 = AXIS2_PLACEMENT_3D('',#141927,#108825,#108826) ;
#93393 = AXIS2_PLACEMENT_3D('',#141930,#108827,#108828) ;
#93394 = AXIS2_PLACEMENT_3D('',#141932,#108829,#108830) ;
#93395 = AXIS2_PLACEMENT_3D('',#141933,#108831,#108832) ;
#93396 = AXIS2_PLACEMENT_3D('',#141934,#108833,#108834) ;
#93397 = AXIS2_PLACEMENT_3D('',#141937,#108835,#108836) ;
#93398 = AXIS2_PLACEMENT_3D('',#141939,#108837,#108838) ;
#93399 = AXIS2_PLACEMENT_3D('',#141943,#108840,#108841) ;
#93400 = AXIS2_PLACEMENT_3D('',#141956,#108844,#108845) ;
#93401 = AXIS2_PLACEMENT_3D('',#141958,#108846,#108847) ;
#93402 = AXIS2_PLACEMENT_3D('',#141960,#108848,#108849) ;
#93403 = AXIS2_PLACEMENT_3D('',#141962,#108850,#108851) ;
#93404 = AXIS2_PLACEMENT_3D('',#141963,#108852,#108853) ;
#93405 = AXIS2_PLACEMENT_3D('',#141964,#108854,#108855) ;
#93406 = AXIS2_PLACEMENT_3D('',#141966,#108856,#108857) ;
#93407 = AXIS2_PLACEMENT_3D('',#141968,#108858,#108859) ;
#93408 = AXIS2_PLACEMENT_3D('',#141969,#108860,#108861) ;
#93409 = AXIS2_PLACEMENT_3D('',#141970,#108862,#108863) ;
#93410 = AXIS2_PLACEMENT_3D('',#141973,#108864,#108865) ;
#93411 = AXIS2_PLACEMENT_3D('',#141975,#108866,#108867) ;
#93412 = AXIS2_PLACEMENT_3D('',#141976,#108868,#108869) ;
#93413 = AXIS2_PLACEMENT_3D('',#141977,#108870,#108871) ;
#93414 = AXIS2_PLACEMENT_3D('',#141980,#108872,#108873) ;
#93415 = AXIS2_PLACEMENT_3D('',#141982,#108874,#108875) ;
#93416 = AXIS2_PLACEMENT_3D('',#141986,#108877,#108878) ;
#93417 = AXIS2_PLACEMENT_3D('',#141999,#108881,#108882) ;
#93418 = AXIS2_PLACEMENT_3D('',#142001,#108883,#108884) ;
#93419 = AXIS2_PLACEMENT_3D('',#142003,#108885,#108886) ;
#93420 = AXIS2_PLACEMENT_3D('',#142005,#108887,#108888) ;
#93421 = AXIS2_PLACEMENT_3D('',#142006,#108889,#108890) ;
#93422 = AXIS2_PLACEMENT_3D('',#142007,#108891,#108892) ;
#93423 = AXIS2_PLACEMENT_3D('',#142009,#108893,#108894) ;
#93424 = AXIS2_PLACEMENT_3D('',#142011,#108895,#108896) ;
#93425 = AXIS2_PLACEMENT_3D('',#142012,#108897,#108898) ;
#93426 = AXIS2_PLACEMENT_3D('',#142013,#108899,#108900) ;
#93427 = AXIS2_PLACEMENT_3D('',#142016,#108901,#108902) ;
#93428 = AXIS2_PLACEMENT_3D('',#142018,#108903,#108904) ;
#93429 = AXIS2_PLACEMENT_3D('',#142019,#108905,#108906) ;
#93430 = AXIS2_PLACEMENT_3D('',#142020,#108907,#108908) ;
#93431 = AXIS2_PLACEMENT_3D('',#142023,#108909,#108910) ;
#93432 = AXIS2_PLACEMENT_3D('',#142025,#108911,#108912) ;
#93433 = AXIS2_PLACEMENT_3D('',#142029,#108914,#108915) ;
#93434 = AXIS2_PLACEMENT_3D('',#142042,#108918,#108919) ;
#93435 = AXIS2_PLACEMENT_3D('',#142044,#108920,#108921) ;
#93436 = AXIS2_PLACEMENT_3D('',#142046,#108922,#108923) ;
#93437 = AXIS2_PLACEMENT_3D('',#142048,#108924,#108925) ;
#93438 = AXIS2_PLACEMENT_3D('',#142049,#108926,#108927) ;
#93439 = AXIS2_PLACEMENT_3D('',#142050,#108928,#108929) ;
#93440 = AXIS2_PLACEMENT_3D('',#142052,#108930,#108931) ;
#93441 = AXIS2_PLACEMENT_3D('',#142054,#108932,#108933) ;
#93442 = AXIS2_PLACEMENT_3D('',#142055,#108934,#108935) ;
#93443 = AXIS2_PLACEMENT_3D('',#142056,#108936,#108937) ;
#93444 = AXIS2_PLACEMENT_3D('',#142059,#108938,#108939) ;
#93445 = AXIS2_PLACEMENT_3D('',#142061,#108940,#108941) ;
#93446 = AXIS2_PLACEMENT_3D('',#142062,#108942,#108943) ;
#93447 = AXIS2_PLACEMENT_3D('',#142063,#108944,#108945) ;
#93448 = AXIS2_PLACEMENT_3D('',#142066,#108946,#108947) ;
#93449 = AXIS2_PLACEMENT_3D('',#142068,#108948,#108949) ;
#93450 = AXIS2_PLACEMENT_3D('',#142072,#108951,#108952) ;
#93451 = AXIS2_PLACEMENT_3D('',#142085,#108955,#108956) ;
#93452 = AXIS2_PLACEMENT_3D('',#142087,#108957,#108958) ;
#93453 = AXIS2_PLACEMENT_3D('',#142089,#108959,#108960) ;
#93454 = AXIS2_PLACEMENT_3D('',#142091,#108961,#108962) ;
#93455 = AXIS2_PLACEMENT_3D('',#142092,#108963,#108964) ;
#93456 = AXIS2_PLACEMENT_3D('',#142093,#108965,#108966) ;
#93457 = AXIS2_PLACEMENT_3D('',#142095,#108967,#108968) ;
#93458 = AXIS2_PLACEMENT_3D('',#142097,#108969,#108970) ;
#93459 = AXIS2_PLACEMENT_3D('',#142098,#108971,#108972) ;
#93460 = AXIS2_PLACEMENT_3D('',#142099,#108973,#108974) ;
#93461 = AXIS2_PLACEMENT_3D('',#142102,#108975,#108976) ;
#93462 = AXIS2_PLACEMENT_3D('',#142104,#108977,#108978) ;
#93463 = AXIS2_PLACEMENT_3D('',#142105,#108979,#108980) ;
#93464 = AXIS2_PLACEMENT_3D('',#142106,#108981,#108982) ;
#93465 = AXIS2_PLACEMENT_3D('',#142109,#108983,#108984) ;
#93466 = AXIS2_PLACEMENT_3D('',#142111,#108985,#108986) ;
#93467 = AXIS2_PLACEMENT_3D('',#142115,#108988,#108989) ;
#93468 = AXIS2_PLACEMENT_3D('',#142128,#108992,#108993) ;
#93469 = AXIS2_PLACEMENT_3D('',#142130,#108994,#108995) ;
#93470 = AXIS2_PLACEMENT_3D('',#142132,#108996,#108997) ;
#93471 = AXIS2_PLACEMENT_3D('',#142134,#108998,#108999) ;
#93472 = AXIS2_PLACEMENT_3D('',#142135,#109000,#109001) ;
#93473 = AXIS2_PLACEMENT_3D('',#142136,#109002,#109003) ;
#93474 = AXIS2_PLACEMENT_3D('',#142138,#109004,#109005) ;
#93475 = AXIS2_PLACEMENT_3D('',#142140,#109006,#109007) ;
#93476 = AXIS2_PLACEMENT_3D('',#142141,#109008,#109009) ;
#93477 = AXIS2_PLACEMENT_3D('',#142142,#109010,#109011) ;
#93478 = AXIS2_PLACEMENT_3D('',#142145,#109012,#109013) ;
#93479 = AXIS2_PLACEMENT_3D('',#142147,#109014,#109015) ;
#93480 = AXIS2_PLACEMENT_3D('',#142148,#109016,#109017) ;
#93481 = AXIS2_PLACEMENT_3D('',#142149,#109018,#109019) ;
#93482 = AXIS2_PLACEMENT_3D('',#142152,#109020,#109021) ;
#93483 = AXIS2_PLACEMENT_3D('',#142154,#109022,#109023) ;
#93484 = AXIS2_PLACEMENT_3D('',#142158,#109025,#109026) ;
#93485 = AXIS2_PLACEMENT_3D('',#142171,#109029,#109030) ;
#93486 = AXIS2_PLACEMENT_3D('',#142173,#109031,#109032) ;
#93487 = AXIS2_PLACEMENT_3D('',#142175,#109033,#109034) ;
#93488 = AXIS2_PLACEMENT_3D('',#142177,#109035,#109036) ;
#93489 = AXIS2_PLACEMENT_3D('',#142178,#109037,#109038) ;
#93490 = AXIS2_PLACEMENT_3D('',#142179,#109039,#109040) ;
#93491 = AXIS2_PLACEMENT_3D('',#142182,#109041,#109042) ;
#93492 = AXIS2_PLACEMENT_3D('',#142184,#109043,#109044) ;
#93493 = AXIS2_PLACEMENT_3D('',#142186,#109045,#109046) ;
#93494 = AXIS2_PLACEMENT_3D('',#142187,#109047,#109048) ;
#93495 = AXIS2_PLACEMENT_3D('',#142188,#109049,#109050) ;
#93496 = AXIS2_PLACEMENT_3D('',#142191,#109051,#109052) ;
#93497 = AXIS2_PLACEMENT_3D('',#142193,#109053,#109054) ;
#93498 = AXIS2_PLACEMENT_3D('',#142195,#109055,#109056) ;
#93499 = AXIS2_PLACEMENT_3D('',#142196,#109057,#109058) ;
#93500 = AXIS2_PLACEMENT_3D('',#142197,#109059,#109060) ;
#93501 = AXIS2_PLACEMENT_3D('',#142200,#109061,#109062) ;
#93502 = AXIS2_PLACEMENT_3D('',#142202,#109063,#109064) ;
#93503 = AXIS2_PLACEMENT_3D('',#142204,#109065,#109066) ;
#93504 = AXIS2_PLACEMENT_3D('',#142205,#109067,#109068) ;
#93505 = AXIS2_PLACEMENT_3D('',#142206,#109069,#109070) ;
#93506 = AXIS2_PLACEMENT_3D('',#142209,#109071,#109072) ;
#93507 = AXIS2_PLACEMENT_3D('',#142211,#109073,#109074) ;
#93508 = AXIS2_PLACEMENT_3D('',#142213,#109075,#109076) ;
#93509 = AXIS2_PLACEMENT_3D('',#142214,#109077,#109078) ;
#93510 = AXIS2_PLACEMENT_3D('',#142215,#109079,#109080) ;
#93511 = AXIS2_PLACEMENT_3D('',#142218,#109081,#109082) ;
#93512 = AXIS2_PLACEMENT_3D('',#142220,#109083,#109084) ;
#93513 = AXIS2_PLACEMENT_3D('',#142222,#109085,#109086) ;
#93514 = AXIS2_PLACEMENT_3D('',#142223,#109087,#109088) ;
#93515 = AXIS2_PLACEMENT_3D('',#142224,#109089,#109090) ;
#93516 = AXIS2_PLACEMENT_3D('',#142227,#109091,#109092) ;
#93517 = AXIS2_PLACEMENT_3D('',#142229,#109093,#109094) ;
#93518 = AXIS2_PLACEMENT_3D('',#142231,#109095,#109096) ;
#93519 = AXIS2_PLACEMENT_3D('',#142232,#109097,#109098) ;
#93520 = AXIS2_PLACEMENT_3D('',#142233,#109099,#109100) ;
#93521 = AXIS2_PLACEMENT_3D('',#142236,#109101,#109102) ;
#93522 = AXIS2_PLACEMENT_3D('',#142238,#109103,#109104) ;
#93523 = AXIS2_PLACEMENT_3D('',#142240,#109105,#109106) ;
#93524 = AXIS2_PLACEMENT_3D('',#142241,#109107,#109108) ;
#93525 = AXIS2_PLACEMENT_3D('',#142242,#109109,#109110) ;
#93526 = AXIS2_PLACEMENT_3D('',#142245,#109111,#109112) ;
#93527 = AXIS2_PLACEMENT_3D('',#142247,#109113,#109114) ;
#93528 = AXIS2_PLACEMENT_3D('',#142249,#109115,#109116) ;
#93529 = AXIS2_PLACEMENT_3D('',#142250,#109117,#109118) ;
#93530 = AXIS2_PLACEMENT_3D('',#142251,#109119,#109120) ;
#93531 = AXIS2_PLACEMENT_3D('',#142254,#109121,#109122) ;
#93532 = AXIS2_PLACEMENT_3D('',#142256,#109123,#109124) ;
#93533 = AXIS2_PLACEMENT_3D('',#142258,#109125,#109126) ;
#93534 = AXIS2_PLACEMENT_3D('',#142259,#109127,#109128) ;
#93535 = AXIS2_PLACEMENT_3D('',#142260,#109129,#109130) ;
#93536 = AXIS2_PLACEMENT_3D('',#142262,#109131,#109132) ;
#93537 = AXIS2_PLACEMENT_3D('',#142264,#109133,#109134) ;
#93538 = AXIS2_PLACEMENT_3D('',#142265,#109135,#109136) ;
#93539 = AXIS2_PLACEMENT_3D('',#142266,#109137,#109138) ;
#93540 = AXIS2_PLACEMENT_3D('',#142269,#109139,#109140) ;
#93541 = AXIS2_PLACEMENT_3D('',#142271,#109141,#109142) ;
#93542 = AXIS2_PLACEMENT_3D('',#142272,#109143,#109144) ;
#93543 = AXIS2_PLACEMENT_3D('',#142273,#109145,#109146) ;
#93544 = AXIS2_PLACEMENT_3D('',#142276,#109147,#109148) ;
#93545 = AXIS2_PLACEMENT_3D('',#142278,#109149,#109150) ;
#93546 = AXIS2_PLACEMENT_3D('',#142282,#109152,#109153) ;
#93547 = AXIS2_PLACEMENT_3D('',#142295,#109156,#109157) ;
#93548 = AXIS2_PLACEMENT_3D('',#142297,#109159,#109160) ;
#93549 = AXIS2_PLACEMENT_3D('',#142299,#109162,#109163) ;
#93550 = AXIS2_PLACEMENT_3D('',#142301,#109165,#109166) ;
#93551 = AXIS2_PLACEMENT_3D('',#142303,#109168,#109169) ;
#93552 = AXIS2_PLACEMENT_3D('',#142305,#109171,#109172) ;
#93553 = AXIS2_PLACEMENT_3D('',#142307,#109174,#109175) ;
#93554 = AXIS2_PLACEMENT_3D('',#142309,#109177,#109178) ;
#93555 = AXIS2_PLACEMENT_3D('',#142311,#109180,#109181) ;
#93556 = AXIS2_PLACEMENT_3D('',#142313,#109183,#109184) ;
#93557 = AXIS2_PLACEMENT_3D('',#142316,#109185,#109186) ;
#93558 = AXIS2_PLACEMENT_3D('',#142319,#109189,#109190) ;
#93559 = AXIS2_PLACEMENT_3D('',#142322,#109191,#109192) ;
#93560 = AXIS2_PLACEMENT_3D('',#142325,#109195,#109196) ;
#93561 = AXIS2_PLACEMENT_3D('',#142328,#109197,#109198) ;
#93562 = AXIS2_PLACEMENT_3D('',#142331,#109201,#109202) ;
#93563 = AXIS2_PLACEMENT_3D('',#142334,#109203,#109204) ;
#93564 = AXIS2_PLACEMENT_3D('',#142337,#109207,#109208) ;
#93565 = AXIS2_PLACEMENT_3D('',#142340,#109209,#109210) ;
#93566 = AXIS2_PLACEMENT_3D('',#142343,#109213,#109214) ;
#93567 = AXIS2_PLACEMENT_3D('',#142346,#109215,#109216) ;
#93568 = AXIS2_PLACEMENT_3D('',#142349,#109219,#109220) ;
#93569 = AXIS2_PLACEMENT_3D('',#142352,#109221,#109222) ;
#93570 = AXIS2_PLACEMENT_3D('',#142355,#109225,#109226) ;
#93571 = AXIS2_PLACEMENT_3D('',#142358,#109227,#109228) ;
#93572 = AXIS2_PLACEMENT_3D('',#142361,#109231,#109232) ;
#93573 = AXIS2_PLACEMENT_3D('',#142364,#109233,#109234) ;
#93574 = AXIS2_PLACEMENT_3D('',#142367,#109237,#109238) ;
#93575 = AXIS2_PLACEMENT_3D('',#142369,#109239,#109240) ;
#93576 = AXIS2_PLACEMENT_3D('',#142371,#109241,#109242) ;
#93577 = AXIS2_PLACEMENT_3D('',#142373,#109243,#109244) ;
#93578 = AXIS2_PLACEMENT_3D('',#142374,#109245,#109246) ;
#93579 = AXIS2_PLACEMENT_3D('',#142375,#109247,#109248) ;
#93580 = AXIS2_PLACEMENT_3D('',#142378,#109249,#109250) ;
#93581 = AXIS2_PLACEMENT_3D('',#142380,#109251,#109252) ;
#93582 = AXIS2_PLACEMENT_3D('',#142382,#109253,#109254) ;
#93583 = AXIS2_PLACEMENT_3D('',#142383,#109255,#109256) ;
#93584 = AXIS2_PLACEMENT_3D('',#142384,#109257,#109258) ;
#93585 = AXIS2_PLACEMENT_3D('',#142386,#109259,#109260) ;
#93586 = AXIS2_PLACEMENT_3D('',#142388,#109261,#109262) ;
#93587 = AXIS2_PLACEMENT_3D('',#142389,#109263,#109264) ;
#93588 = AXIS2_PLACEMENT_3D('',#142390,#109265,#109266) ;
#93589 = AXIS2_PLACEMENT_3D('',#142393,#109267,#109268) ;
#93590 = AXIS2_PLACEMENT_3D('',#142395,#109269,#109270) ;
#93591 = AXIS2_PLACEMENT_3D('',#142396,#109271,#109272) ;
#93592 = AXIS2_PLACEMENT_3D('',#142397,#109273,#109274) ;
#93593 = AXIS2_PLACEMENT_3D('',#142400,#109275,#109276) ;
#93594 = AXIS2_PLACEMENT_3D('',#142402,#109277,#109278) ;
#93595 = AXIS2_PLACEMENT_3D('',#142406,#109280,#109281) ;
#93596 = AXIS2_PLACEMENT_3D('',#142419,#109284,#109285) ;
#93597 = AXIS2_PLACEMENT_3D('',#142421,#109287,#109288) ;
#93598 = AXIS2_PLACEMENT_3D('',#142424,#109289,#109290) ;
#93599 = AXIS2_PLACEMENT_3D('',#142427,#109293,#109294) ;
#93600 = AXIS2_PLACEMENT_3D('',#142432,#109296,#109297) ;
#93601 = AXIS2_PLACEMENT_3D('',#142435,#109299,#109300) ;
#93602 = AXIS2_PLACEMENT_3D('',#142437,#109301,#109302) ;
#93603 = AXIS2_PLACEMENT_3D('',#142448,#109308,#109309) ;
#93604 = AXIS2_PLACEMENT_3D('',#142449,#109310,#109311) ;
#93605 = AXIS2_PLACEMENT_3D('',#142454,#109313,#109314) ;
#93606 = AXIS2_PLACEMENT_3D('',#142457,#109316,#109317) ;
#93607 = AXIS2_PLACEMENT_3D('',#142459,#109318,#109319) ;
#93608 = AXIS2_PLACEMENT_3D('',#142470,#109325,#109326) ;
#93609 = AXIS2_PLACEMENT_3D('',#142471,#109327,#109328) ;
#93610 = AXIS2_PLACEMENT_3D('',#142476,#109330,#109331) ;
#93611 = AXIS2_PLACEMENT_3D('',#142479,#109333,#109334) ;
#93612 = AXIS2_PLACEMENT_3D('',#142481,#109335,#109336) ;
#93613 = AXIS2_PLACEMENT_3D('',#142492,#109342,#109343) ;
#93614 = AXIS2_PLACEMENT_3D('',#142493,#109344,#109345) ;
#93615 = AXIS2_PLACEMENT_3D('',#142498,#109347,#109348) ;
#93616 = AXIS2_PLACEMENT_3D('',#142501,#109350,#109351) ;
#93617 = AXIS2_PLACEMENT_3D('',#142503,#109352,#109353) ;
#93618 = AXIS2_PLACEMENT_3D('',#142514,#109359,#109360) ;
#93619 = AXIS2_PLACEMENT_3D('',#142515,#109361,#109362) ;
#93620 = AXIS2_PLACEMENT_3D('',#142520,#109364,#109365) ;
#93621 = AXIS2_PLACEMENT_3D('',#142523,#109367,#109368) ;
#93622 = AXIS2_PLACEMENT_3D('',#142525,#109369,#109370) ;
#93623 = AXIS2_PLACEMENT_3D('',#142536,#109376,#109377) ;
#93624 = AXIS2_PLACEMENT_3D('',#142537,#109378,#109379) ;
#93625 = AXIS2_PLACEMENT_3D('',#142542,#109381,#109382) ;
#93626 = AXIS2_PLACEMENT_3D('',#142545,#109384,#109385) ;
#93627 = AXIS2_PLACEMENT_3D('',#142547,#109386,#109387) ;
#93628 = AXIS2_PLACEMENT_3D('',#142558,#109393,#109394) ;
#93629 = AXIS2_PLACEMENT_3D('',#142559,#109395,#109396) ;
#93630 = AXIS2_PLACEMENT_3D('',#142564,#109398,#109399) ;
#93631 = AXIS2_PLACEMENT_3D('',#142567,#109401,#109402) ;
#93632 = AXIS2_PLACEMENT_3D('',#142569,#109403,#109404) ;
#93633 = AXIS2_PLACEMENT_3D('',#142580,#109410,#109411) ;
#93634 = AXIS2_PLACEMENT_3D('',#142581,#109412,#109413) ;
#93635 = AXIS2_PLACEMENT_3D('',#142586,#109415,#109416) ;
#93636 = AXIS2_PLACEMENT_3D('',#142589,#109418,#109419) ;
#93637 = AXIS2_PLACEMENT_3D('',#142591,#109420,#109421) ;
#93638 = AXIS2_PLACEMENT_3D('',#142602,#109427,#109428) ;
#93639 = AXIS2_PLACEMENT_3D('',#142603,#109429,#109430) ;
#93640 = AXIS2_PLACEMENT_3D('',#142608,#109432,#109433) ;
#93641 = AXIS2_PLACEMENT_3D('',#142611,#109435,#109436) ;
#93642 = AXIS2_PLACEMENT_3D('',#142613,#109437,#109438) ;
#93643 = AXIS2_PLACEMENT_3D('',#142624,#109444,#109445) ;
#93644 = AXIS2_PLACEMENT_3D('',#142625,#109446,#109447) ;
#93645 = AXIS2_PLACEMENT_3D('',#142628,#109448,#109449) ;
#93646 = AXIS2_PLACEMENT_3D('',#142636,#109454,#109455) ;
#93647 = AXIS2_PLACEMENT_3D('',#142639,#109456,#109457) ;
#93648 = AXIS2_PLACEMENT_3D('',#142647,#109462,#109463) ;
#93649 = AXIS2_PLACEMENT_3D('',#142650,#109464,#109465) ;
#93650 = AXIS2_PLACEMENT_3D('',#142658,#109470,#109471) ;
#93651 = AXIS2_PLACEMENT_3D('',#142661,#109472,#109473) ;
#93652 = AXIS2_PLACEMENT_3D('',#142669,#109478,#109479) ;
#93653 = AXIS2_PLACEMENT_3D('',#142672,#109480,#109481) ;
#93654 = AXIS2_PLACEMENT_3D('',#142680,#109486,#109487) ;
#93655 = AXIS2_PLACEMENT_3D('',#142683,#109488,#109489) ;
#93656 = AXIS2_PLACEMENT_3D('',#142691,#109494,#109495) ;
#93657 = AXIS2_PLACEMENT_3D('',#142694,#109496,#109497) ;
#93658 = AXIS2_PLACEMENT_3D('',#142702,#109502,#109503) ;
#93659 = AXIS2_PLACEMENT_3D('',#142705,#109504,#109505) ;
#93660 = AXIS2_PLACEMENT_3D('',#142713,#109510,#109511) ;
#93661 = AXIS2_PLACEMENT_3D('',#142716,#109512,#109513) ;
#93662 = AXIS2_PLACEMENT_3D('',#142724,#109518,#109519) ;
#93663 = AXIS2_PLACEMENT_3D('',#142727,#109520,#109521) ;
#93664 = AXIS2_PLACEMENT_3D('',#142735,#109526,#109527) ;
#93665 = AXIS2_PLACEMENT_3D('',#142738,#109528,#109529) ;
#93666 = AXIS2_PLACEMENT_3D('',#142746,#109534,#109535) ;
#93667 = AXIS2_PLACEMENT_3D('',#142749,#109536,#109537) ;
#93668 = AXIS2_PLACEMENT_3D('',#142757,#109542,#109543) ;
#93669 = AXIS2_PLACEMENT_3D('',#142760,#109544,#109545) ;
#93670 = AXIS2_PLACEMENT_3D('',#142768,#109550,#109551) ;
#93671 = AXIS2_PLACEMENT_3D('',#142771,#109552,#109553) ;
#93672 = AXIS2_PLACEMENT_3D('',#142779,#109558,#109559) ;
#93673 = AXIS2_PLACEMENT_3D('',#142782,#109560,#109561) ;
#93674 = AXIS2_PLACEMENT_3D('',#142790,#109566,#109567) ;
#93675 = AXIS2_PLACEMENT_3D('',#142793,#109568,#109569) ;
#93676 = AXIS2_PLACEMENT_3D('',#142801,#109574,#109575) ;
#93677 = AXIS2_PLACEMENT_3D('',#142804,#109576,#109577) ;
#93678 = AXIS2_PLACEMENT_3D('',#142812,#109582,#109583) ;
#93679 = AXIS2_PLACEMENT_3D('',#142815,#109584,#109585) ;
#93680 = AXIS2_PLACEMENT_3D('',#142823,#109590,#109591) ;
#93681 = AXIS2_PLACEMENT_3D('',#142828,#109593,#109594) ;
#93682 = AXIS2_PLACEMENT_3D('',#142831,#109596,#109597) ;
#93683 = AXIS2_PLACEMENT_3D('',#142832,#109598,#109599) ;
#93684 = AXIS2_PLACEMENT_3D('',#142837,#109601,#109602) ;
#93685 = AXIS2_PLACEMENT_3D('',#142840,#109604,#109605) ;
#93686 = AXIS2_PLACEMENT_3D('',#142841,#109606,#109607) ;
#93687 = AXIS2_PLACEMENT_3D('',#142846,#109609,#109610) ;
#93688 = AXIS2_PLACEMENT_3D('',#142849,#109612,#109613) ;
#93689 = AXIS2_PLACEMENT_3D('',#142850,#109614,#109615) ;
#93690 = AXIS2_PLACEMENT_3D('',#142855,#109617,#109618) ;
#93691 = AXIS2_PLACEMENT_3D('',#142858,#109620,#109621) ;
#93692 = AXIS2_PLACEMENT_3D('',#142859,#109622,#109623) ;
#93693 = AXIS2_PLACEMENT_3D('',#142864,#109625,#109626) ;
#93694 = AXIS2_PLACEMENT_3D('',#142867,#109628,#109629) ;
#93695 = AXIS2_PLACEMENT_3D('',#142868,#109630,#109631) ;
#93696 = AXIS2_PLACEMENT_3D('',#142873,#109633,#109634) ;
#93697 = AXIS2_PLACEMENT_3D('',#142876,#109636,#109637) ;
#93698 = AXIS2_PLACEMENT_3D('',#142877,#109638,#109639) ;
#93699 = AXIS2_PLACEMENT_3D('',#142882,#109641,#109642) ;
#93700 = AXIS2_PLACEMENT_3D('',#142885,#109644,#109645) ;
#93701 = AXIS2_PLACEMENT_3D('',#142886,#109646,#109647) ;
#93702 = AXIS2_PLACEMENT_3D('',#142891,#109649,#109650) ;
#93703 = AXIS2_PLACEMENT_3D('',#142894,#109652,#109653) ;
#93704 = AXIS2_PLACEMENT_3D('',#142895,#109654,#109655) ;
#93705 = AXIS2_PLACEMENT_3D('',#142900,#109657,#109658) ;
#93706 = AXIS2_PLACEMENT_3D('',#142903,#109660,#109661) ;
#93707 = AXIS2_PLACEMENT_3D('',#142904,#109662,#109663) ;
#93708 = AXIS2_PLACEMENT_3D('',#142909,#109665,#109666) ;
#93709 = AXIS2_PLACEMENT_3D('',#142912,#109668,#109669) ;
#93710 = AXIS2_PLACEMENT_3D('',#142914,#109670,#109671) ;
#93711 = AXIS2_PLACEMENT_3D('',#142925,#109677,#109678) ;
#93712 = AXIS2_PLACEMENT_3D('',#142926,#109679,#109680) ;
#93713 = AXIS2_PLACEMENT_3D('',#142929,#109681,#109682) ;
#93714 = AXIS2_PLACEMENT_3D('',#142937,#109687,#109688) ;
#93715 = AXIS2_PLACEMENT_3D('',#142940,#109689,#109690) ;
#93716 = AXIS2_PLACEMENT_3D('',#142948,#109695,#109696) ;
#93717 = AXIS2_PLACEMENT_3D('',#142953,#109698,#109699) ;
#93718 = AXIS2_PLACEMENT_3D('',#142956,#109701,#109702) ;
#93719 = AXIS2_PLACEMENT_3D('',#142957,#109703,#109704) ;
#93720 = AXIS2_PLACEMENT_3D('',#142962,#109706,#109707) ;
#93721 = AXIS2_PLACEMENT_3D('',#142965,#109709,#109710) ;
#93722 = AXIS2_PLACEMENT_3D('',#142966,#109711,#109712) ;
#93723 = AXIS2_PLACEMENT_3D('',#142969,#109713,#109714) ;
#93724 = AXIS2_PLACEMENT_3D('',#142979,#109720,#109721) ;
#93725 = AXIS2_PLACEMENT_3D('',#142983,#109723,#109724) ;
#93726 = AXIS2_PLACEMENT_3D('',#142988,#109727,#109728) ;
#93727 = AXIS2_PLACEMENT_3D('',#142992,#109730,#109731) ;
#93728 = AXIS2_PLACEMENT_3D('',#142997,#109734,#109735) ;
#93729 = AXIS2_PLACEMENT_3D('',#143001,#109737,#109738) ;
#93730 = AXIS2_PLACEMENT_3D('',#143006,#109741,#109742) ;
#93731 = AXIS2_PLACEMENT_3D('',#143010,#109744,#109745) ;
#93732 = AXIS2_PLACEMENT_3D('',#143015,#109748,#109749) ;
#93733 = AXIS2_PLACEMENT_3D('',#143019,#109751,#109752) ;
#93734 = AXIS2_PLACEMENT_3D('',#143024,#109755,#109756) ;
#93735 = AXIS2_PLACEMENT_3D('',#143028,#109758,#109759) ;
#93736 = AXIS2_PLACEMENT_3D('',#143033,#109762,#109763) ;
#93737 = AXIS2_PLACEMENT_3D('',#143037,#109765,#109766) ;
#93738 = AXIS2_PLACEMENT_3D('',#143042,#109769,#109770) ;
#93739 = AXIS2_PLACEMENT_3D('',#143046,#109772,#109773) ;
#93740 = AXIS2_PLACEMENT_3D('',#143051,#109776,#109777) ;
#93741 = AXIS2_PLACEMENT_3D('',#143055,#109779,#109780) ;
#93742 = AXIS2_PLACEMENT_3D('',#143060,#109783,#109784) ;
#93743 = AXIS2_PLACEMENT_3D('',#143062,#109786,#109787) ;
#93744 = AXIS2_PLACEMENT_3D('',#143064,#109788,#109789) ;
#93745 = AXIS2_PLACEMENT_3D('',#143067,#109791,#109792) ;
#93746 = AXIS2_PLACEMENT_3D('',#143068,#109793,#109794) ;
#93747 = AXIS2_PLACEMENT_3D('',#143071,#109795,#109796) ;
#93748 = AXIS2_PLACEMENT_3D('',#143076,#109799,#109800) ;
#93749 = AXIS2_PLACEMENT_3D('',#143080,#109802,#109803) ;
#93750 = AXIS2_PLACEMENT_3D('',#143085,#109806,#109807) ;
#93751 = AXIS2_PLACEMENT_3D('',#143089,#109809,#109810) ;
#93752 = AXIS2_PLACEMENT_3D('',#143094,#109813,#109814) ;
#93753 = AXIS2_PLACEMENT_3D('',#143098,#109816,#109817) ;
#93754 = AXIS2_PLACEMENT_3D('',#143103,#109820,#109821) ;
#93755 = AXIS2_PLACEMENT_3D('',#143107,#109823,#109824) ;
#93756 = AXIS2_PLACEMENT_3D('',#143112,#109827,#109828) ;
#93757 = AXIS2_PLACEMENT_3D('',#143116,#109830,#109831) ;
#93758 = AXIS2_PLACEMENT_3D('',#143121,#109834,#109835) ;
#93759 = AXIS2_PLACEMENT_3D('',#143125,#109837,#109838) ;
#93760 = AXIS2_PLACEMENT_3D('',#143130,#109841,#109842) ;
#93761 = AXIS2_PLACEMENT_3D('',#143134,#109844,#109845) ;
#93762 = AXIS2_PLACEMENT_3D('',#143139,#109848,#109849) ;
#93763 = AXIS2_PLACEMENT_3D('',#143143,#109851,#109852) ;
#93764 = AXIS2_PLACEMENT_3D('',#143148,#109855,#109856) ;
#93765 = AXIS2_PLACEMENT_3D('',#143152,#109858,#109859) ;
#93766 = AXIS2_PLACEMENT_3D('',#143162,#109865,#109866) ;
#93767 = AXIS2_PLACEMENT_3D('',#143164,#109868,#109869) ;
#93768 = AXIS2_PLACEMENT_3D('',#143168,#109871,#109872) ;
#93769 = AXIS2_PLACEMENT_3D('',#143169,#109873,#109874) ;
#93770 = AXIS2_PLACEMENT_3D('',#143170,#109875,#109876) ;
#93771 = AXIS2_PLACEMENT_3D('',#143176,#109880,#109881) ;
#93772 = AXIS2_PLACEMENT_3D('',#143180,#109883,#109884) ;
#93773 = AXIS2_PLACEMENT_3D('',#143181,#109885,#109886) ;
#93774 = AXIS2_PLACEMENT_3D('',#143182,#109887,#109888) ;
#93775 = AXIS2_PLACEMENT_3D('',#143188,#109892,#109893) ;
#93776 = AXIS2_PLACEMENT_3D('',#143192,#109895,#109896) ;
#93777 = AXIS2_PLACEMENT_3D('',#143193,#109897,#109898) ;
#93778 = AXIS2_PLACEMENT_3D('',#143194,#109899,#109900) ;
#93779 = AXIS2_PLACEMENT_3D('',#143200,#109904,#109905) ;
#93780 = AXIS2_PLACEMENT_3D('',#143204,#109907,#109908) ;
#93781 = AXIS2_PLACEMENT_3D('',#143205,#109909,#109910) ;
#93782 = AXIS2_PLACEMENT_3D('',#143206,#109911,#109912) ;
#93783 = AXIS2_PLACEMENT_3D('',#143212,#109916,#109917) ;
#93784 = AXIS2_PLACEMENT_3D('',#143216,#109919,#109920) ;
#93785 = AXIS2_PLACEMENT_3D('',#143217,#109921,#109922) ;
#93786 = AXIS2_PLACEMENT_3D('',#143218,#109923,#109924) ;
#93787 = AXIS2_PLACEMENT_3D('',#143224,#109928,#109929) ;
#93788 = AXIS2_PLACEMENT_3D('',#143228,#109931,#109932) ;
#93789 = AXIS2_PLACEMENT_3D('',#143229,#109933,#109934) ;
#93790 = AXIS2_PLACEMENT_3D('',#143230,#109935,#109936) ;
#93791 = AXIS2_PLACEMENT_3D('',#143235,#109939,#109940) ;
#93792 = AXIS2_PLACEMENT_3D('',#143243,#109944,#109945) ;
#93793 = AXIS2_PLACEMENT_3D('',#143247,#109947,#109948) ;
#93794 = AXIS2_PLACEMENT_3D('',#143252,#109951,#109952) ;
#93795 = AXIS2_PLACEMENT_3D('',#143260,#109956,#109957) ;
#93796 = AXIS2_PLACEMENT_3D('',#143264,#109959,#109960) ;
#93797 = AXIS2_PLACEMENT_3D('',#143268,#109962,#109963) ;
#93798 = AXIS2_PLACEMENT_3D('',#143270,#109964,#109965) ;
#93799 = AXIS2_PLACEMENT_3D('',#143272,#109966,#109967) ;
#93800 = AXIS2_PLACEMENT_3D('',#143276,#109969,#109970) ;
#93801 = AXIS2_PLACEMENT_3D('',#143280,#109972,#109973) ;
#93802 = AXIS2_PLACEMENT_3D('',#143288,#109977,#109978) ;
#93803 = AXIS2_PLACEMENT_3D('',#143292,#109980,#109981) ;
#93804 = AXIS2_PLACEMENT_3D('',#143297,#109984,#109985) ;
#93805 = AXIS2_PLACEMENT_3D('',#143305,#109989,#109990) ;
#93806 = AXIS2_PLACEMENT_3D('',#143309,#109992,#109993) ;
#93807 = AXIS2_PLACEMENT_3D('',#143313,#109995,#109996) ;
#93808 = AXIS2_PLACEMENT_3D('',#143315,#109997,#109998) ;
#93809 = AXIS2_PLACEMENT_3D('',#143317,#109999,#110000) ;
#93810 = AXIS2_PLACEMENT_3D('',#143321,#110002,#110003) ;
#93811 = AXIS2_PLACEMENT_3D('',#143325,#110005,#110006) ;
#93812 = AXIS2_PLACEMENT_3D('',#143333,#110010,#110011) ;
#93813 = AXIS2_PLACEMENT_3D('',#143337,#110013,#110014) ;
#93814 = AXIS2_PLACEMENT_3D('',#143342,#110017,#110018) ;
#93815 = AXIS2_PLACEMENT_3D('',#143350,#110022,#110023) ;
#93816 = AXIS2_PLACEMENT_3D('',#143354,#110025,#110026) ;
#93817 = AXIS2_PLACEMENT_3D('',#143358,#110028,#110029) ;
#93818 = AXIS2_PLACEMENT_3D('',#143360,#110030,#110031) ;
#93819 = AXIS2_PLACEMENT_3D('',#143362,#110032,#110033) ;
#93820 = AXIS2_PLACEMENT_3D('',#143366,#110035,#110036) ;
#93821 = AXIS2_PLACEMENT_3D('',#143370,#110038,#110039) ;
#93822 = AXIS2_PLACEMENT_3D('',#143378,#110043,#110044) ;
#93823 = AXIS2_PLACEMENT_3D('',#143382,#110046,#110047) ;
#93824 = AXIS2_PLACEMENT_3D('',#143387,#110050,#110051) ;
#93825 = AXIS2_PLACEMENT_3D('',#143395,#110055,#110056) ;
#93826 = AXIS2_PLACEMENT_3D('',#143399,#110058,#110059) ;
#93827 = AXIS2_PLACEMENT_3D('',#143403,#110061,#110062) ;
#93828 = AXIS2_PLACEMENT_3D('',#143405,#110063,#110064) ;
#93829 = AXIS2_PLACEMENT_3D('',#143407,#110065,#110066) ;
#93830 = AXIS2_PLACEMENT_3D('',#143411,#110068,#110069) ;
#93831 = AXIS2_PLACEMENT_3D('',#143415,#110071,#110072) ;
#93832 = AXIS2_PLACEMENT_3D('',#143423,#110076,#110077) ;
#93833 = AXIS2_PLACEMENT_3D('',#143427,#110079,#110080) ;
#93834 = AXIS2_PLACEMENT_3D('',#143432,#110083,#110084) ;
#93835 = AXIS2_PLACEMENT_3D('',#143440,#110088,#110089) ;
#93836 = AXIS2_PLACEMENT_3D('',#143444,#110091,#110092) ;
#93837 = AXIS2_PLACEMENT_3D('',#143448,#110094,#110095) ;
#93838 = AXIS2_PLACEMENT_3D('',#143450,#110096,#110097) ;
#93839 = AXIS2_PLACEMENT_3D('',#143452,#110098,#110099) ;
#93840 = AXIS2_PLACEMENT_3D('',#143456,#110101,#110102) ;
#93841 = AXIS2_PLACEMENT_3D('',#143460,#110104,#110105) ;
#93842 = AXIS2_PLACEMENT_3D('',#143468,#110109,#110110) ;
#93843 = AXIS2_PLACEMENT_3D('',#143472,#110112,#110113) ;
#93844 = AXIS2_PLACEMENT_3D('',#143477,#110116,#110117) ;
#93845 = AXIS2_PLACEMENT_3D('',#143485,#110121,#110122) ;
#93846 = AXIS2_PLACEMENT_3D('',#143489,#110124,#110125) ;
#93847 = AXIS2_PLACEMENT_3D('',#143493,#110127,#110128) ;
#93848 = AXIS2_PLACEMENT_3D('',#143495,#110129,#110130) ;
#93849 = AXIS2_PLACEMENT_3D('',#143497,#110131,#110132) ;
#93850 = AXIS2_PLACEMENT_3D('',#143501,#110134,#110135) ;
#93851 = AXIS2_PLACEMENT_3D('',#143505,#110137,#110138) ;
#93852 = AXIS2_PLACEMENT_3D('',#143513,#110142,#110143) ;
#93853 = AXIS2_PLACEMENT_3D('',#143517,#110145,#110146) ;
#93854 = AXIS2_PLACEMENT_3D('',#143522,#110149,#110150) ;
#93855 = AXIS2_PLACEMENT_3D('',#143530,#110154,#110155) ;
#93856 = AXIS2_PLACEMENT_3D('',#143534,#110157,#110158) ;
#93857 = AXIS2_PLACEMENT_3D('',#143538,#110160,#110161) ;
#93858 = AXIS2_PLACEMENT_3D('',#143540,#110162,#110163) ;
#93859 = AXIS2_PLACEMENT_3D('',#143542,#110164,#110165) ;
#93860 = AXIS2_PLACEMENT_3D('',#143546,#110167,#110168) ;
#93861 = AXIS2_PLACEMENT_3D('',#143550,#110170,#110171) ;
#93862 = AXIS2_PLACEMENT_3D('',#143558,#110175,#110176) ;
#93863 = AXIS2_PLACEMENT_3D('',#143562,#110178,#110179) ;
#93864 = AXIS2_PLACEMENT_3D('',#143567,#110182,#110183) ;
#93865 = AXIS2_PLACEMENT_3D('',#143575,#110187,#110188) ;
#93866 = AXIS2_PLACEMENT_3D('',#143579,#110190,#110191) ;
#93867 = AXIS2_PLACEMENT_3D('',#143583,#110193,#110194) ;
#93868 = AXIS2_PLACEMENT_3D('',#143585,#110195,#110196) ;
#93869 = AXIS2_PLACEMENT_3D('',#143587,#110197,#110198) ;
#93870 = AXIS2_PLACEMENT_3D('',#143591,#110200,#110201) ;
#93871 = AXIS2_PLACEMENT_3D('',#143595,#110203,#110204) ;
#93872 = AXIS2_PLACEMENT_3D('',#143603,#110208,#110209) ;
#93873 = AXIS2_PLACEMENT_3D('',#143607,#110211,#110212) ;
#93874 = AXIS2_PLACEMENT_3D('',#143612,#110215,#110216) ;
#93875 = AXIS2_PLACEMENT_3D('',#143620,#110220,#110221) ;
#93876 = AXIS2_PLACEMENT_3D('',#143624,#110223,#110224) ;
#93877 = AXIS2_PLACEMENT_3D('',#143628,#110226,#110227) ;
#93878 = AXIS2_PLACEMENT_3D('',#143630,#110228,#110229) ;
#93879 = AXIS2_PLACEMENT_3D('',#143632,#110230,#110231) ;
#93880 = AXIS2_PLACEMENT_3D('',#143636,#110233,#110234) ;
#93881 = AXIS2_PLACEMENT_3D('',#143640,#110236,#110237) ;
#93882 = AXIS2_PLACEMENT_3D('',#143648,#110241,#110242) ;
#93883 = AXIS2_PLACEMENT_3D('',#143652,#110244,#110245) ;
#93884 = AXIS2_PLACEMENT_3D('',#143657,#110248,#110249) ;
#93885 = AXIS2_PLACEMENT_3D('',#143665,#110253,#110254) ;
#93886 = AXIS2_PLACEMENT_3D('',#143669,#110256,#110257) ;
#93887 = AXIS2_PLACEMENT_3D('',#143673,#110259,#110260) ;
#93888 = AXIS2_PLACEMENT_3D('',#143675,#110261,#110262) ;
#93889 = AXIS2_PLACEMENT_3D('',#143677,#110263,#110264) ;
#93890 = AXIS2_PLACEMENT_3D('',#143681,#110266,#110267) ;
#93891 = AXIS2_PLACEMENT_3D('',#143683,#110269,#110270) ;
#93892 = AXIS2_PLACEMENT_3D('',#143694,#110275,#110276) ;
#93893 = AXIS2_PLACEMENT_3D('',#143702,#110280,#110281) ;
#93894 = AXIS2_PLACEMENT_3D('',#143704,#110283,#110284) ;
#93895 = AXIS2_PLACEMENT_3D('',#143715,#110289,#110290) ;
#93896 = AXIS2_PLACEMENT_3D('',#143723,#110294,#110295) ;
#93897 = AXIS2_PLACEMENT_3D('',#143725,#110297,#110298) ;
#93898 = AXIS2_PLACEMENT_3D('',#143740,#110305,#110306) ;
#93899 = AXIS2_PLACEMENT_3D('',#143744,#110308,#110309) ;
#93900 = AXIS2_PLACEMENT_3D('',#143746,#110311,#110312) ;
#93901 = AXIS2_PLACEMENT_3D('',#143755,#110317,#110318) ;
#93902 = AXIS2_PLACEMENT_3D('',#143761,#110322,#110323) ;
#93903 = AXIS2_PLACEMENT_3D('',#143770,#110328,#110329) ;
#93904 = AXIS2_PLACEMENT_3D('',#143779,#110334,#110335) ;
#93905 = AXIS2_PLACEMENT_3D('',#143788,#110340,#110341) ;
#93906 = AXIS2_PLACEMENT_3D('',#143793,#110343,#110344) ;
#93907 = AXIS2_PLACEMENT_3D('',#143796,#110346,#110347) ;
#93908 = AXIS2_PLACEMENT_3D('',#143797,#110348,#110349) ;
#93909 = AXIS2_PLACEMENT_3D('',#143803,#110353,#110354) ;
#93910 = AXIS2_PLACEMENT_3D('',#143805,#110355,#110356) ;
#93911 = AXIS2_PLACEMENT_3D('',#143808,#110358,#110359) ;
#93912 = AXIS2_PLACEMENT_3D('',#143809,#110360,#110361) ;
#93913 = AXIS2_PLACEMENT_3D('',#143815,#110365,#110366) ;
#93914 = AXIS2_PLACEMENT_3D('',#143817,#110367,#110368) ;
#93915 = AXIS2_PLACEMENT_3D('',#143820,#110370,#110371) ;
#93916 = AXIS2_PLACEMENT_3D('',#143821,#110372,#110373) ;
#93917 = AXIS2_PLACEMENT_3D('',#143826,#110377,#110378) ;
#93918 = AXIS2_PLACEMENT_3D('',#143829,#110380,#110381) ;
#93919 = AXIS2_PLACEMENT_3D('',#143830,#110382,#110383) ;
#93920 = AXIS2_PLACEMENT_3D('',#143833,#110386,#110387) ;
#93921 = AXIS2_PLACEMENT_3D('',#143839,#110391,#110392) ;
#93922 = AXIS2_PLACEMENT_3D('',#143841,#110393,#110394) ;
#93923 = AXIS2_PLACEMENT_3D('',#143844,#110396,#110397) ;
#93924 = AXIS2_PLACEMENT_3D('',#143845,#110398,#110399) ;
#93925 = AXIS2_PLACEMENT_3D('',#143851,#110403,#110404) ;
#93926 = AXIS2_PLACEMENT_3D('',#143853,#110405,#110406) ;
#93927 = AXIS2_PLACEMENT_3D('',#143856,#110408,#110409) ;
#93928 = AXIS2_PLACEMENT_3D('',#143857,#110410,#110411) ;
#93929 = AXIS2_PLACEMENT_3D('',#143863,#110415,#110416) ;
#93930 = AXIS2_PLACEMENT_3D('',#143865,#110417,#110418) ;
#93931 = AXIS2_PLACEMENT_3D('',#143868,#110420,#110421) ;
#93932 = AXIS2_PLACEMENT_3D('',#143869,#110422,#110423) ;
#93933 = AXIS2_PLACEMENT_3D('',#143875,#110427,#110428) ;
#93934 = AXIS2_PLACEMENT_3D('',#143877,#110429,#110430) ;
#93935 = AXIS2_PLACEMENT_3D('',#143880,#110432,#110433) ;
#93936 = AXIS2_PLACEMENT_3D('',#143881,#110434,#110435) ;
#93937 = AXIS2_PLACEMENT_3D('',#143887,#110439,#110440) ;
#93938 = AXIS2_PLACEMENT_3D('',#143889,#110441,#110442) ;
#93939 = AXIS2_PLACEMENT_3D('',#143892,#110444,#110445) ;
#93940 = AXIS2_PLACEMENT_3D('',#143893,#110446,#110447) ;
#93941 = AXIS2_PLACEMENT_3D('',#143899,#110451,#110452) ;
#93942 = AXIS2_PLACEMENT_3D('',#143901,#110453,#110454) ;
#93943 = AXIS2_PLACEMENT_3D('',#143904,#110456,#110457) ;
#93944 = AXIS2_PLACEMENT_3D('',#143905,#110458,#110459) ;
#93945 = AXIS2_PLACEMENT_3D('',#143907,#110460,#110461) ;
#93946 = AXIS2_PLACEMENT_3D('',#143910,#110463,#110464) ;
#93947 = AXIS2_PLACEMENT_3D('',#143911,#110465,#110466) ;
#93948 = AXIS2_PLACEMENT_3D('',#143913,#110467,#110468) ;
#93949 = AXIS2_PLACEMENT_3D('',#143916,#110470,#110471) ;
#93950 = AXIS2_PLACEMENT_3D('',#143917,#110472,#110473) ;
#93951 = AXIS2_PLACEMENT_3D('',#143923,#110477,#110478) ;
#93952 = AXIS2_PLACEMENT_3D('',#143925,#110479,#110480) ;
#93953 = AXIS2_PLACEMENT_3D('',#143928,#110482,#110483) ;
#93954 = AXIS2_PLACEMENT_3D('',#143929,#110484,#110485) ;
#93955 = AXIS2_PLACEMENT_3D('',#143935,#110489,#110490) ;
#93956 = AXIS2_PLACEMENT_3D('',#143937,#110491,#110492) ;
#93957 = AXIS2_PLACEMENT_3D('',#143940,#110494,#110495) ;
#93958 = AXIS2_PLACEMENT_3D('',#143941,#110496,#110497) ;
#93959 = AXIS2_PLACEMENT_3D('',#143944,#110500,#110501) ;
#93960 = AXIS2_PLACEMENT_3D('',#143947,#110502,#110503) ;
#93961 = AXIS2_PLACEMENT_3D('',#143951,#110505,#110506) ;
#93962 = AXIS2_PLACEMENT_3D('',#143959,#110510,#110511) ;
#93963 = AXIS2_PLACEMENT_3D('',#143967,#110515,#110516) ;
#93964 = AXIS2_PLACEMENT_3D('',#143971,#110518,#110519) ;
#93965 = AXIS2_PLACEMENT_3D('',#143980,#110525,#110526) ;
#93966 = AXIS2_PLACEMENT_3D('',#143985,#110528,#110529) ;
#93967 = AXIS2_PLACEMENT_3D('',#143989,#110531,#110532) ;
#93968 = AXIS2_PLACEMENT_3D('',#143993,#110534,#110535) ;
#93969 = AXIS2_PLACEMENT_3D('',#143996,#110537,#110538) ;
#93970 = AXIS2_PLACEMENT_3D('',#143997,#110539,#110540) ;
#93971 = AXIS2_PLACEMENT_3D('',#143998,#110541,#110542) ;
#93972 = AXIS2_PLACEMENT_3D('',#143999,#110543,#110544) ;
#93973 = AXIS2_PLACEMENT_3D('',#144000,#110545,#110546) ;
#93974 = AXIS2_PLACEMENT_3D('',#144001,#110547,#110548) ;
#93975 = AXIS2_PLACEMENT_3D('',#144002,#110549,#110550) ;
#93976 = AXIS2_PLACEMENT_3D('',#144003,#110551,#110552) ;
#93977 = AXIS2_PLACEMENT_3D('',#144005,#110553,#110554) ;
#93978 = AXIS2_PLACEMENT_3D('',#144006,#110555,#110556) ;
#93979 = AXIS2_PLACEMENT_3D('',#144007,#110557,#110558) ;
#93980 = AXIS2_PLACEMENT_3D('',#144008,#110559,#110560) ;
#93981 = AXIS2_PLACEMENT_3D('',#144009,#110561,#110562) ;
#93982 = AXIS2_PLACEMENT_3D('',#144010,#110563,#110564) ;
#93983 = AXIS2_PLACEMENT_3D('',#144011,#110565,#110566) ;
#93984 = AXIS2_PLACEMENT_3D('',#144012,#110567,#110568) ;
#93985 = AXIS2_PLACEMENT_3D('',#144013,#110569,#110570) ;
#93986 = AXIS2_PLACEMENT_3D('',#144024,#110572,#110573) ;
#93987 = AXIS2_PLACEMENT_3D('',#144081,#110575,#110576) ;
#93988 = AXIS2_PLACEMENT_3D('',#144082,#110577,#110578) ;
#93989 = AXIS2_PLACEMENT_3D('',#144083,#110579,#110580) ;
#93990 = AXIS2_PLACEMENT_3D('',#144084,#110581,#110582) ;
#93991 = AXIS2_PLACEMENT_3D('',#144085,#110583,#110584) ;
#93992 = AXIS2_PLACEMENT_3D('',#144086,#110585,#110586) ;
#93993 = AXIS2_PLACEMENT_3D('',#144087,#110587,#110588) ;
#93994 = AXIS2_PLACEMENT_3D('',#144088,#110589,#110590) ;
#93995 = AXIS2_PLACEMENT_3D('',#144089,#110591,#110592) ;
#93996 = AXIS2_PLACEMENT_3D('',#144090,#110593,#110594) ;
#93997 = AXIS2_PLACEMENT_3D('',#144091,#110595,#110596) ;
#93998 = AXIS2_PLACEMENT_3D('',#144092,#110597,#110598) ;
#93999 = AXIS2_PLACEMENT_3D('',#144093,#110599,#110600) ;
#94000 = AXIS2_PLACEMENT_3D('',#144094,#110601,#110602) ;
#94001 = AXIS2_PLACEMENT_3D('',#144095,#110603,#110604) ;
#94002 = AXIS2_PLACEMENT_3D('',#144096,#110605,#110606) ;
#94003 = AXIS2_PLACEMENT_3D('',#144097,#110607,#110608) ;
#94004 = AXIS2_PLACEMENT_3D('',#144098,#110609,#110610) ;
#94005 = AXIS2_PLACEMENT_3D('',#144099,#110611,#110612) ;
#94006 = AXIS2_PLACEMENT_3D('',#144100,#110613,#110614) ;
#94007 = AXIS2_PLACEMENT_3D('',#144101,#110615,#110616) ;
#94008 = AXIS2_PLACEMENT_3D('',#144102,#110617,#110618) ;
#94009 = AXIS2_PLACEMENT_3D('',#144103,#110619,#110620) ;
#94010 = AXIS2_PLACEMENT_3D('',#144106,#110622,#110623) ;
#94011 = AXIS2_PLACEMENT_3D('',#144107,#110624,#110625) ;
#94012 = AXIS2_PLACEMENT_3D('',#144108,#110626,#110627) ;
#94013 = AXIS2_PLACEMENT_3D('',#144109,#110628,#110629) ;
#94014 = AXIS2_PLACEMENT_3D('',#144110,#110630,#110631) ;
#94015 = AXIS2_PLACEMENT_3D('',#144111,#110632,#110633) ;
#94016 = AXIS2_PLACEMENT_3D('',#144112,#110634,#110635) ;
#94017 = AXIS2_PLACEMENT_3D('',#144113,#110636,#110637) ;
#94018 = AXIS2_PLACEMENT_3D('',#144114,#110638,#110639) ;
#94019 = AXIS2_PLACEMENT_3D('',#144115,#110640,#110641) ;
#94020 = AXIS2_PLACEMENT_3D('',#144116,#110642,#110643) ;
#94021 = AXIS2_PLACEMENT_3D('',#144117,#110644,#110645) ;
#94022 = AXIS2_PLACEMENT_3D('',#144118,#110646,#110647) ;
#94023 = AXIS2_PLACEMENT_3D('',#144119,#110648,#110649) ;
#94024 = AXIS2_PLACEMENT_3D('',#144120,#110650,#110651) ;
#94025 = AXIS2_PLACEMENT_3D('',#144121,#110652,#110653) ;
#94026 = AXIS2_PLACEMENT_3D('',#144123,#110654,#110655) ;
#94027 = AXIS2_PLACEMENT_3D('',#144124,#110656,#110657) ;
#94028 = AXIS2_PLACEMENT_3D('',#144125,#110658,#110659) ;
#94029 = AXIS2_PLACEMENT_3D('',#144126,#110660,#110661) ;
#94030 = AXIS2_PLACEMENT_3D('',#144127,#110662,#110663) ;
#94031 = AXIS2_PLACEMENT_3D('',#144128,#110664,#110665) ;
#94032 = AXIS2_PLACEMENT_3D('',#144129,#110666,#110667) ;
#94033 = AXIS2_PLACEMENT_3D('',#144130,#110668,#110669) ;
#94034 = AXIS2_PLACEMENT_3D('',#144131,#110670,#110671) ;
#94035 = AXIS2_PLACEMENT_3D('',#144132,#110672,#110673) ;
#94036 = AXIS2_PLACEMENT_3D('',#144133,#110674,#110675) ;
#94037 = AXIS2_PLACEMENT_3D('',#144134,#110676,#110677) ;
#94038 = AXIS2_PLACEMENT_3D('',#144135,#110678,#110679) ;
#94039 = AXIS2_PLACEMENT_3D('',#144138,#110681,#110682) ;
#94040 = AXIS2_PLACEMENT_3D('',#144139,#110683,#110684) ;
#94041 = AXIS2_PLACEMENT_3D('',#144140,#110685,#110686) ;
#94042 = AXIS2_PLACEMENT_3D('',#144141,#110687,#110688) ;
#94043 = AXIS2_PLACEMENT_3D('',#144142,#110689,#110690) ;
#94044 = AXIS2_PLACEMENT_3D('',#144143,#110691,#110692) ;
#94045 = AXIS2_PLACEMENT_3D('',#144144,#110693,#110694) ;
#94046 = AXIS2_PLACEMENT_3D('',#144145,#110695,#110696) ;
#94047 = AXIS2_PLACEMENT_3D('',#144146,#110697,#110698) ;
#94048 = AXIS2_PLACEMENT_3D('',#144147,#110699,#110700) ;
#94049 = AXIS2_PLACEMENT_3D('',#144148,#110701,#110702) ;
#94050 = AXIS2_PLACEMENT_3D('',#144149,#110703,#110704) ;
#94051 = AXIS2_PLACEMENT_3D('',#144150,#110705,#110706) ;
#94052 = AXIS2_PLACEMENT_3D('',#144152,#110707,#110708) ;
#94053 = AXIS2_PLACEMENT_3D('',#144153,#110709,#110710) ;
#94054 = AXIS2_PLACEMENT_3D('',#144154,#110711,#110712) ;
#94055 = AXIS2_PLACEMENT_3D('',#144155,#110713,#110714) ;
#94056 = AXIS2_PLACEMENT_3D('',#144156,#110715,#110716) ;
#94057 = AXIS2_PLACEMENT_3D('',#144157,#110717,#110718) ;
#94058 = AXIS2_PLACEMENT_3D('',#144158,#110719,#110720) ;
#94059 = AXIS2_PLACEMENT_3D('',#144159,#110721,#110722) ;
#94060 = AXIS2_PLACEMENT_3D('',#144160,#110723,#110724) ;
#94061 = AXIS2_PLACEMENT_3D('',#144161,#110725,#110726) ;
#94062 = AXIS2_PLACEMENT_3D('',#144162,#110727,#110728) ;
#94063 = AXIS2_PLACEMENT_3D('',#144164,#110730,#110731) ;
#94064 = AXIS2_PLACEMENT_3D('',#144165,#110732,#110733) ;
#94065 = AXIS2_PLACEMENT_3D('',#144166,#110734,#110735) ;
#94066 = AXIS2_PLACEMENT_3D('',#144167,#110736,#110737) ;
#94067 = AXIS2_PLACEMENT_3D('',#144168,#110738,#110739) ;
#94068 = AXIS2_PLACEMENT_3D('',#144169,#110740,#110741) ;
#94069 = AXIS2_PLACEMENT_3D('',#144170,#110742,#110743) ;
#94070 = AXIS2_PLACEMENT_3D('',#144171,#110744,#110745) ;
#94071 = AXIS2_PLACEMENT_3D('',#144172,#110746,#110747) ;
#94072 = AXIS2_PLACEMENT_3D('',#144173,#110748,#110749) ;
#94073 = AXIS2_PLACEMENT_3D('',#144174,#110750,#110751) ;
#94074 = AXIS2_PLACEMENT_3D('',#144175,#110752,#110753) ;
#94075 = AXIS2_PLACEMENT_3D('',#144176,#110754,#110755) ;
#94076 = AXIS2_PLACEMENT_3D('',#144177,#110756,#110757) ;
#94077 = AXIS2_PLACEMENT_3D('',#144178,#110758,#110759) ;
#94078 = AXIS2_PLACEMENT_3D('',#144179,#110760,#110761) ;
#94079 = AXIS2_PLACEMENT_3D('',#144180,#110762,#110763) ;
#94080 = AXIS2_PLACEMENT_3D('',#144181,#110764,#110765) ;
#94081 = AXIS2_PLACEMENT_3D('',#144182,#110766,#110767) ;
#94082 = AXIS2_PLACEMENT_3D('',#144183,#110768,#110769) ;
#94083 = AXIS2_PLACEMENT_3D('',#144184,#110770,#110771) ;
#94084 = AXIS2_PLACEMENT_3D('',#144185,#110772,#110773) ;
#94085 = AXIS2_PLACEMENT_3D('',#144186,#110774,#110775) ;
#94086 = AXIS2_PLACEMENT_3D('',#144187,#110776,#110777) ;
#94087 = AXIS2_PLACEMENT_3D('',#144188,#110778,#110779) ;
#94088 = AXIS2_PLACEMENT_3D('',#144189,#110780,#110781) ;
#94089 = AXIS2_PLACEMENT_3D('',#144190,#110782,#110783) ;
#94090 = AXIS2_PLACEMENT_3D('',#144191,#110784,#110785) ;
#94091 = AXIS2_PLACEMENT_3D('',#144192,#110786,#110787) ;
#94092 = AXIS2_PLACEMENT_3D('',#144193,#110788,#110789) ;
#94093 = AXIS2_PLACEMENT_3D('',#144194,#110790,#110791) ;
#94094 = AXIS2_PLACEMENT_3D('',#144195,#110792,#110793) ;
#94095 = AXIS2_PLACEMENT_3D('',#144196,#110794,#110795) ;
#94096 = AXIS2_PLACEMENT_3D('',#144197,#110796,#110797) ;
#94097 = AXIS2_PLACEMENT_3D('',#144198,#110798,#110799) ;
#94098 = AXIS2_PLACEMENT_3D('',#144199,#110800,#110801) ;
#94099 = AXIS2_PLACEMENT_3D('',#144200,#110802,#110803) ;
#94100 = AXIS2_PLACEMENT_3D('',#144201,#110804,#110805) ;
#94101 = AXIS2_PLACEMENT_3D('',#144202,#110806,#110807) ;
#94102 = AXIS2_PLACEMENT_3D('',#144203,#110808,#110809) ;
#94103 = AXIS2_PLACEMENT_3D('',#144204,#110810,#110811) ;
#94104 = AXIS2_PLACEMENT_3D('',#144205,#110812,#110813) ;
#94105 = AXIS2_PLACEMENT_3D('',#144206,#110814,#110815) ;
#94106 = AXIS2_PLACEMENT_3D('',#144207,#110816,#110817) ;
#94107 = AXIS2_PLACEMENT_3D('',#144208,#110818,#110819) ;
#94108 = AXIS2_PLACEMENT_3D('',#144209,#110820,#110821) ;
#94109 = AXIS2_PLACEMENT_3D('',#144210,#110822,#110823) ;
#94110 = AXIS2_PLACEMENT_3D('',#144211,#110824,#110825) ;
#94111 = AXIS2_PLACEMENT_3D('',#144212,#110826,#110827) ;
#94112 = AXIS2_PLACEMENT_3D('',#144213,#110828,#110829) ;
#94113 = AXIS2_PLACEMENT_3D('',#144214,#110830,#110831) ;
#94114 = AXIS2_PLACEMENT_3D('',#144215,#110832,#110833) ;
#94115 = AXIS2_PLACEMENT_3D('',#144216,#110834,#110835) ;
#94116 = AXIS2_PLACEMENT_3D('',#144217,#110836,#110837) ;
#94117 = AXIS2_PLACEMENT_3D('',#144218,#110838,#110839) ;
#94118 = AXIS2_PLACEMENT_3D('',#144219,#110840,#110841) ;
#94119 = AXIS2_PLACEMENT_3D('',#144220,#110842,#110843) ;
#94120 = AXIS2_PLACEMENT_3D('',#144221,#110844,#110845) ;
#94121 = AXIS2_PLACEMENT_3D('',#144222,#110846,#110847) ;
#94122 = AXIS2_PLACEMENT_3D('',#144223,#110848,#110849) ;
#94123 = AXIS2_PLACEMENT_3D('',#144224,#110850,#110851) ;
#94124 = AXIS2_PLACEMENT_3D('',#144225,#110852,#110853) ;
#94125 = AXIS2_PLACEMENT_3D('',#144226,#110854,#110855) ;
#94126 = AXIS2_PLACEMENT_3D('',#144227,#110856,#110857) ;
#94127 = AXIS2_PLACEMENT_3D('',#144228,#110858,#110859) ;
#94128 = AXIS2_PLACEMENT_3D('',#144229,#110860,#110861) ;
#94129 = AXIS2_PLACEMENT_3D('',#144230,#110862,#110863) ;
#94130 = AXIS2_PLACEMENT_3D('',#144231,#110864,#110865) ;
#94131 = AXIS2_PLACEMENT_3D('',#144232,#110866,#110867) ;
#94132 = AXIS2_PLACEMENT_3D('',#144233,#110868,#110869) ;
#94133 = AXIS2_PLACEMENT_3D('',#144234,#110870,#110871) ;
#94134 = AXIS2_PLACEMENT_3D('',#144235,#110872,#110873) ;
#94135 = AXIS2_PLACEMENT_3D('',#144236,#110874,#110875) ;
#94136 = AXIS2_PLACEMENT_3D('',#144237,#110876,#110877) ;
#94137 = AXIS2_PLACEMENT_3D('',#144238,#110878,#110879) ;
#94138 = AXIS2_PLACEMENT_3D('',#144239,#110880,#110881) ;
#94139 = AXIS2_PLACEMENT_3D('',#144240,#110882,#110883) ;
#94140 = AXIS2_PLACEMENT_3D('',#144241,#110884,#110885) ;
#94141 = AXIS2_PLACEMENT_3D('',#144242,#110886,#110887) ;
#94142 = AXIS2_PLACEMENT_3D('',#144243,#110888,#110889) ;
#94143 = AXIS2_PLACEMENT_3D('',#144244,#110890,#110891) ;
#94144 = AXIS2_PLACEMENT_3D('',#144245,#110892,#110893) ;
#94145 = AXIS2_PLACEMENT_3D('',#144246,#110894,#110895) ;
#94146 = AXIS2_PLACEMENT_3D('',#144247,#110896,#110897) ;
#94147 = AXIS2_PLACEMENT_3D('',#144248,#110898,#110899) ;
#94148 = AXIS2_PLACEMENT_3D('',#144249,#110900,#110901) ;
#94149 = AXIS2_PLACEMENT_3D('',#144250,#110902,#110903) ;
#94150 = AXIS2_PLACEMENT_3D('',#144251,#110904,#110905) ;
#94151 = AXIS2_PLACEMENT_3D('',#144252,#110906,#110907) ;
#94152 = AXIS2_PLACEMENT_3D('',#144253,#110908,#110909) ;
#94153 = AXIS2_PLACEMENT_3D('',#144254,#110910,#110911) ;
#94154 = AXIS2_PLACEMENT_3D('',#144255,#110912,#110913) ;
#94155 = AXIS2_PLACEMENT_3D('',#144256,#110914,#110915) ;
#94156 = AXIS2_PLACEMENT_3D('',#144257,#110916,#110917) ;
#94157 = AXIS2_PLACEMENT_3D('',#144258,#110918,#110919) ;
#94158 = AXIS2_PLACEMENT_3D('',#144259,#110920,#110921) ;
#94159 = AXIS2_PLACEMENT_3D('',#144260,#110922,#110923) ;
#94160 = AXIS2_PLACEMENT_3D('',#144261,#110924,#110925) ;
#94161 = AXIS2_PLACEMENT_3D('',#144262,#110926,#110927) ;
#94162 = AXIS2_PLACEMENT_3D('',#144263,#110928,#110929) ;
#94163 = AXIS2_PLACEMENT_3D('',#144264,#110930,#110931) ;
#94164 = AXIS2_PLACEMENT_3D('',#144265,#110932,#110933) ;
#94165 = AXIS2_PLACEMENT_3D('',#144266,#110934,#110935) ;
#94166 = AXIS2_PLACEMENT_3D('',#144267,#110936,#110937) ;
#94167 = AXIS2_PLACEMENT_3D('',#144268,#110938,#110939) ;
#94168 = AXIS2_PLACEMENT_3D('',#144269,#110940,#110941) ;
#94169 = AXIS2_PLACEMENT_3D('',#144270,#110942,#110943) ;
#94170 = AXIS2_PLACEMENT_3D('',#144271,#110944,#110945) ;
#94171 = AXIS2_PLACEMENT_3D('',#144272,#110946,#110947) ;
#94172 = AXIS2_PLACEMENT_3D('',#144273,#110948,#110949) ;
#94173 = AXIS2_PLACEMENT_3D('',#144274,#110950,#110951) ;
#94174 = AXIS2_PLACEMENT_3D('',#144275,#110952,#110953) ;
#94175 = AXIS2_PLACEMENT_3D('',#144276,#110954,#110955) ;
#94176 = AXIS2_PLACEMENT_3D('',#144277,#110956,#110957) ;
#94177 = AXIS2_PLACEMENT_3D('',#144278,#110958,#110959) ;
#94178 = AXIS2_PLACEMENT_3D('',#144279,#110960,#110961) ;
#94179 = AXIS2_PLACEMENT_3D('',#144280,#110962,#110963) ;
#94180 = AXIS2_PLACEMENT_3D('',#144281,#110964,#110965) ;
#94181 = AXIS2_PLACEMENT_3D('',#144282,#110966,#110967) ;
#94182 = AXIS2_PLACEMENT_3D('',#144283,#110968,#110969) ;
#94183 = AXIS2_PLACEMENT_3D('',#144284,#110970,#110971) ;
#94184 = AXIS2_PLACEMENT_3D('',#144285,#110972,#110973) ;
#94185 = AXIS2_PLACEMENT_3D('',#144286,#110974,#110975) ;
#94186 = AXIS2_PLACEMENT_3D('',#144287,#110976,#110977) ;
#94187 = AXIS2_PLACEMENT_3D('',#144288,#110978,#110979) ;
#94188 = AXIS2_PLACEMENT_3D('',#144289,#110980,#110981) ;
#94189 = AXIS2_PLACEMENT_3D('',#144290,#110982,#110983) ;
#94190 = AXIS2_PLACEMENT_3D('',#144291,#110984,#110985) ;
#94191 = AXIS2_PLACEMENT_3D('',#144292,#110986,#110987) ;
#94192 = AXIS2_PLACEMENT_3D('',#144293,#110988,#110989) ;
#94193 = AXIS2_PLACEMENT_3D('',#144294,#110990,#110991) ;
#94194 = AXIS2_PLACEMENT_3D('',#144295,#110992,#110993) ;
#94195 = AXIS2_PLACEMENT_3D('',#144296,#110994,#110995) ;
#94196 = AXIS2_PLACEMENT_3D('',#144297,#110996,#110997) ;
#94197 = AXIS2_PLACEMENT_3D('',#144298,#110998,#110999) ;
#94198 = AXIS2_PLACEMENT_3D('',#144299,#111000,#111001) ;
#94199 = AXIS2_PLACEMENT_3D('',#144300,#111002,#111003) ;
#94200 = AXIS2_PLACEMENT_3D('',#144301,#111004,#111005) ;
#94201 = AXIS2_PLACEMENT_3D('',#144302,#111006,#111007) ;
#94202 = AXIS2_PLACEMENT_3D('',#144303,#111008,#111009) ;
#94203 = AXIS2_PLACEMENT_3D('',#144304,#111010,#111011) ;
#94204 = AXIS2_PLACEMENT_3D('',#144305,#111012,#111013) ;
#94205 = AXIS2_PLACEMENT_3D('',#144306,#111014,#111015) ;
#94206 = AXIS2_PLACEMENT_3D('',#144307,#111016,#111017) ;
#94207 = AXIS2_PLACEMENT_3D('',#144308,#111018,#111019) ;
#94208 = AXIS2_PLACEMENT_3D('',#144309,#111020,#111021) ;
#94209 = AXIS2_PLACEMENT_3D('',#144310,#111022,#111023) ;
#94210 = AXIS2_PLACEMENT_3D('',#144311,#111024,#111025) ;
#94211 = AXIS2_PLACEMENT_3D('',#144312,#111026,#111027) ;
#94212 = AXIS2_PLACEMENT_3D('',#144313,#111028,#111029) ;
#94213 = AXIS2_PLACEMENT_3D('',#144314,#111030,#111031) ;
#94214 = AXIS2_PLACEMENT_3D('',#144315,#111032,#111033) ;
#94215 = AXIS2_PLACEMENT_3D('',#144316,#111034,#111035) ;
#94216 = AXIS2_PLACEMENT_3D('',#144317,#111036,#111037) ;
#94217 = AXIS2_PLACEMENT_3D('',#144318,#111038,#111039) ;
#94218 = AXIS2_PLACEMENT_3D('',#144319,#111040,#111041) ;
#94219 = AXIS2_PLACEMENT_3D('',#144320,#111042,#111043) ;
#94220 = AXIS2_PLACEMENT_3D('',#144321,#111044,#111045) ;
#94221 = AXIS2_PLACEMENT_3D('',#144322,#111046,#111047) ;
#94222 = AXIS2_PLACEMENT_3D('',#144323,#111048,#111049) ;
#94223 = AXIS2_PLACEMENT_3D('',#144324,#111050,#111051) ;
#94224 = AXIS2_PLACEMENT_3D('',#144325,#111052,#111053) ;
#94225 = AXIS2_PLACEMENT_3D('',#144326,#111054,#111055) ;
#94226 = AXIS2_PLACEMENT_3D('',#144327,#111056,#111057) ;
#94227 = AXIS2_PLACEMENT_3D('',#144328,#111058,#111059) ;
#94228 = AXIS2_PLACEMENT_3D('',#144329,#111060,#111061) ;
#94229 = AXIS2_PLACEMENT_3D('',#144330,#111062,#111063) ;
#94230 = AXIS2_PLACEMENT_3D('',#144331,#111064,#111065) ;
#94231 = AXIS2_PLACEMENT_3D('',#144332,#111066,#111067) ;
#94232 = AXIS2_PLACEMENT_3D('',#144333,#111068,#111069) ;
#94233 = AXIS2_PLACEMENT_3D('',#144334,#111070,#111071) ;
#94234 = AXIS2_PLACEMENT_3D('',#144335,#111072,#111073) ;
#94235 = AXIS2_PLACEMENT_3D('',#144336,#111074,#111075) ;
#94236 = AXIS2_PLACEMENT_3D('',#144337,#111076,#111077) ;
#94237 = AXIS2_PLACEMENT_3D('',#144338,#111078,#111079) ;
#94238 = AXIS2_PLACEMENT_3D('',#144339,#111080,#111081) ;
#94239 = AXIS2_PLACEMENT_3D('',#144340,#111082,#111083) ;
#94240 = AXIS2_PLACEMENT_3D('',#144341,#111084,#111085) ;
#94241 = AXIS2_PLACEMENT_3D('',#144350,#111090,#111091) ;
#94242 = AXIS2_PLACEMENT_3D('',#144359,#111096,#111097) ;
#94243 = AXIS2_PLACEMENT_3D('',#144368,#111102,#111103) ;
#94244 = AXIS2_PLACEMENT_3D('',#144377,#111108,#111109) ;
#94245 = AXIS2_PLACEMENT_3D('',#144386,#111114,#111115) ;
#94246 = AXIS2_PLACEMENT_3D('',#144390,#111117,#111118) ;
#94247 = AXIS2_PLACEMENT_3D('',#144392,#111119,#111120) ;
#94248 = AXIS2_PLACEMENT_3D('',#144396,#111123,#111124) ;
#94249 = AXIS2_PLACEMENT_3D('',#144400,#111126,#111127) ;
#94250 = AXIS2_PLACEMENT_3D('',#144402,#111128,#111129) ;
#94251 = AXIS2_PLACEMENT_3D('',#144406,#111132,#111133) ;
#94252 = AXIS2_PLACEMENT_3D('',#144407,#111134,#111135) ;
#94253 = AXIS2_PLACEMENT_3D('',#144408,#111136,#111137) ;
#94254 = AXIS2_PLACEMENT_3D('',#144409,#111138,#111139) ;
#94255 = AXIS2_PLACEMENT_3D('',#144410,#111140,#111141) ;
#94256 = AXIS2_PLACEMENT_3D('',#144411,#111142,#111143) ;
#94257 = AXIS2_PLACEMENT_3D('',#144412,#111144,#111145) ;
#94258 = AXIS2_PLACEMENT_3D('',#144421,#111150,#111151) ;
#94259 = AXIS2_PLACEMENT_3D('',#144427,#111155,#111156) ;
#94260 = AXIS2_PLACEMENT_3D('',#144433,#111160,#111161) ;
#94261 = AXIS2_PLACEMENT_3D('',#144442,#111166,#111167) ;
#94262 = AXIS2_PLACEMENT_3D('',#144451,#111172,#111173) ;
#94263 = AXIS2_PLACEMENT_3D('',#144457,#111177,#111178) ;
#94264 = AXIS2_PLACEMENT_3D('',#144463,#111182,#111183) ;
#94265 = AXIS2_PLACEMENT_3D('',#144472,#111188,#111189) ;
#94266 = AXIS2_PLACEMENT_3D('',#144481,#111194,#111195) ;
#94267 = AXIS2_PLACEMENT_3D('',#144490,#111200,#111201) ;
#94268 = AXIS2_PLACEMENT_3D('',#144499,#111206,#111207) ;
#94269 = AXIS2_PLACEMENT_3D('',#144500,#111208,#111209) ;
#94270 = AXIS2_PLACEMENT_3D('',#144501,#111210,#111211) ;
#94271 = AXIS2_PLACEMENT_3D('',#144502,#111212,#111213) ;
#94272 = AXIS2_PLACEMENT_3D('',#144503,#111214,#111215) ;
#94273 = AXIS2_PLACEMENT_3D('',#144504,#111216,#111217) ;
#94274 = AXIS2_PLACEMENT_3D('',#144505,#111218,#111219) ;
#94275 = AXIS2_PLACEMENT_3D('',#144506,#111220,#111221) ;
#94276 = AXIS2_PLACEMENT_3D('',#144507,#111222,#111223) ;
#94277 = AXIS2_PLACEMENT_3D('',#144508,#111224,#111225) ;
#94278 = AXIS2_PLACEMENT_3D('',#144509,#111226,#111227) ;
#94279 = AXIS2_PLACEMENT_3D('',#144510,#111228,#111229) ;
#94280 = AXIS2_PLACEMENT_3D('',#144511,#111230,#111231) ;
#94281 = AXIS2_PLACEMENT_3D('',#144512,#111232,#111233) ;
#94282 = AXIS2_PLACEMENT_3D('',#144513,#111234,#111235) ;
#94283 = AXIS2_PLACEMENT_3D('',#144514,#111236,#111237) ;
#94284 = AXIS2_PLACEMENT_3D('',#144515,#111238,#111239) ;
#94285 = AXIS2_PLACEMENT_3D('',#144516,#111240,#111241) ;
#94286 = AXIS2_PLACEMENT_3D('',#144517,#111242,#111243) ;
#94287 = AXIS2_PLACEMENT_3D('',#144518,#111244,#111245) ;
#94288 = AXIS2_PLACEMENT_3D('',#144519,#111246,#111247) ;
#94289 = AXIS2_PLACEMENT_3D('',#144520,#111248,#111249) ;
#94290 = AXIS2_PLACEMENT_3D('',#144521,#111250,#111251) ;
#94291 = AXIS2_PLACEMENT_3D('',#144522,#111252,#111253) ;
#94292 = AXIS2_PLACEMENT_3D('',#144523,#111254,#111255) ;
#94293 = AXIS2_PLACEMENT_3D('',#144524,#111256,#111257) ;
#94294 = AXIS2_PLACEMENT_3D('',#144525,#111258,#111259) ;
#94295 = AXIS2_PLACEMENT_3D('',#144526,#111260,#111261) ;
#94296 = AXIS2_PLACEMENT_3D('',#144527,#111262,#111263) ;
#94297 = AXIS2_PLACEMENT_3D('',#144528,#111264,#111265) ;
#94298 = AXIS2_PLACEMENT_3D('',#144529,#111266,#111267) ;
#94299 = AXIS2_PLACEMENT_3D('',#144530,#111268,#111269) ;
#94300 = AXIS2_PLACEMENT_3D('',#144531,#111270,#111271) ;
#94301 = AXIS2_PLACEMENT_3D('',#144532,#111272,#111273) ;
#94302 = AXIS2_PLACEMENT_3D('',#144533,#111274,#111275) ;
#94303 = AXIS2_PLACEMENT_3D('',#144534,#111276,#111277) ;
#94304 = AXIS2_PLACEMENT_3D('',#144535,#111278,#111279) ;
#94305 = AXIS2_PLACEMENT_3D('',#144536,#111280,#111281) ;
#94306 = AXIS2_PLACEMENT_3D('',#144537,#111282,#111283) ;
#94307 = AXIS2_PLACEMENT_3D('',#144538,#111284,#111285) ;
#94308 = AXIS2_PLACEMENT_3D('',#144539,#111286,#111287) ;
#94309 = AXIS2_PLACEMENT_3D('',#144540,#111288,#111289) ;
#94310 = AXIS2_PLACEMENT_3D('',#144541,#111290,#111291) ;
#94311 = AXIS2_PLACEMENT_3D('',#144542,#111292,#111293) ;
#94312 = AXIS2_PLACEMENT_3D('',#144543,#111294,#111295) ;
#94313 = AXIS2_PLACEMENT_3D('',#144544,#111296,#111297) ;
#94314 = AXIS2_PLACEMENT_3D('',#144545,#111298,#111299) ;
#94315 = AXIS2_PLACEMENT_3D('',#144546,#111300,#111301) ;
#94316 = AXIS2_PLACEMENT_3D('',#144547,#111302,#111303) ;
#94317 = AXIS2_PLACEMENT_3D('',#144548,#111304,#111305) ;
#94318 = AXIS2_PLACEMENT_3D('',#144549,#111306,#111307) ;
#94319 = AXIS2_PLACEMENT_3D('',#144550,#111308,#111309) ;
#94320 = AXIS2_PLACEMENT_3D('',#144551,#111310,#111311) ;
#94321 = AXIS2_PLACEMENT_3D('',#144552,#111312,#111313) ;
#94322 = AXIS2_PLACEMENT_3D('',#144553,#111314,#111315) ;
#94323 = AXIS2_PLACEMENT_3D('',#144554,#111316,#111317) ;
#94324 = AXIS2_PLACEMENT_3D('',#144555,#111318,#111319) ;
#94325 = AXIS2_PLACEMENT_3D('',#144556,#111320,#111321) ;
#94326 = AXIS2_PLACEMENT_3D('',#144557,#111322,#111323) ;
#94327 = AXIS2_PLACEMENT_3D('',#144558,#111324,#111325) ;
#94328 = AXIS2_PLACEMENT_3D('',#144559,#111326,#111327) ;
#94329 = AXIS2_PLACEMENT_3D('',#144560,#111328,#111329) ;
#94330 = AXIS2_PLACEMENT_3D('',#144561,#111330,#111331) ;
#94331 = AXIS2_PLACEMENT_3D('',#144562,#111332,#111333) ;
#94332 = AXIS2_PLACEMENT_3D('',#144563,#111334,#111335) ;
#94333 = AXIS2_PLACEMENT_3D('',#144564,#111336,#111337) ;
#94334 = AXIS2_PLACEMENT_3D('',#144565,#111338,#111339) ;
#94335 = AXIS2_PLACEMENT_3D('',#144566,#111340,#111341) ;
#94336 = AXIS2_PLACEMENT_3D('',#144567,#111342,#111343) ;
#94337 = AXIS2_PLACEMENT_3D('',#144568,#111344,#111345) ;
#94338 = AXIS2_PLACEMENT_3D('',#144569,#111346,#111347) ;
#94339 = AXIS2_PLACEMENT_3D('',#144570,#111348,#111349) ;
#94340 = AXIS2_PLACEMENT_3D('',#144571,#111350,#111351) ;
#94341 = AXIS2_PLACEMENT_3D('',#144572,#111352,#111353) ;
#94342 = AXIS2_PLACEMENT_3D('',#144573,#111354,#111355) ;
#94343 = AXIS2_PLACEMENT_3D('',#144574,#111356,#111357) ;
#94344 = AXIS2_PLACEMENT_3D('',#144575,#111358,#111359) ;
#94345 = AXIS2_PLACEMENT_3D('',#144576,#111360,#111361) ;
#94346 = AXIS2_PLACEMENT_3D('',#144577,#111362,#111363) ;
#94347 = AXIS2_PLACEMENT_3D('',#144578,#111364,#111365) ;
#94348 = AXIS2_PLACEMENT_3D('',#144579,#111366,#111367) ;
#94349 = AXIS2_PLACEMENT_3D('',#144580,#111368,#111369) ;
#94350 = AXIS2_PLACEMENT_3D('',#144581,#111370,#111371) ;
#94351 = AXIS2_PLACEMENT_3D('',#144582,#111372,#111373) ;
#94352 = AXIS2_PLACEMENT_3D('',#144583,#111374,#111375) ;
#94353 = AXIS2_PLACEMENT_3D('',#144584,#111376,#111377) ;
#94354 = AXIS2_PLACEMENT_3D('',#144585,#111378,#111379) ;
#94355 = AXIS2_PLACEMENT_3D('',#144586,#111380,#111381) ;
#94356 = AXIS2_PLACEMENT_3D('',#144587,#111382,#111383) ;
#94357 = AXIS2_PLACEMENT_3D('',#144588,#111384,#111385) ;
#94358 = AXIS2_PLACEMENT_3D('',#144589,#111386,#111387) ;
#94359 = AXIS2_PLACEMENT_3D('',#144590,#111388,#111389) ;
#94360 = AXIS2_PLACEMENT_3D('',#144591,#111390,#111391) ;
#94361 = AXIS2_PLACEMENT_3D('',#144592,#111392,#111393) ;
#94362 = AXIS2_PLACEMENT_3D('',#144593,#111394,#111395) ;
#94363 = AXIS2_PLACEMENT_3D('',#144594,#111396,#111397) ;
#94364 = AXIS2_PLACEMENT_3D('',#144595,#111398,#111399) ;
#94365 = AXIS2_PLACEMENT_3D('',#144596,#111400,#111401) ;
#94366 = AXIS2_PLACEMENT_3D('',#144597,#111402,#111403) ;
#94367 = AXIS2_PLACEMENT_3D('',#144598,#111404,#111405) ;
#94368 = AXIS2_PLACEMENT_3D('',#144599,#111406,#111407) ;
#94369 = AXIS2_PLACEMENT_3D('',#144600,#111408,#111409) ;
#94370 = AXIS2_PLACEMENT_3D('',#144601,#111410,#111411) ;
#94371 = AXIS2_PLACEMENT_3D('',#144602,#111412,#111413) ;
#94372 = AXIS2_PLACEMENT_3D('',#144603,#111414,#111415) ;
#94373 = AXIS2_PLACEMENT_3D('',#144604,#111416,#111417) ;
#94374 = AXIS2_PLACEMENT_3D('',#144605,#111418,#111419) ;
#94375 = AXIS2_PLACEMENT_3D('',#144606,#111420,#111421) ;
#94376 = AXIS2_PLACEMENT_3D('',#144607,#111422,#111423) ;
#94377 = AXIS2_PLACEMENT_3D('',#144608,#111424,#111425) ;
#94378 = AXIS2_PLACEMENT_3D('',#144609,#111426,#111427) ;
#94379 = AXIS2_PLACEMENT_3D('',#144610,#111428,#111429) ;
#94380 = AXIS2_PLACEMENT_3D('',#144611,#111430,#111431) ;
#94381 = AXIS2_PLACEMENT_3D('',#144626,#111438,#111439) ;
#94382 = AXIS2_PLACEMENT_3D('',#144630,#111441,#111442) ;
#94383 = AXIS2_PLACEMENT_3D('',#144632,#111444,#111445) ;
#94384 = AXIS2_PLACEMENT_3D('',#144647,#111452,#111453) ;
#94385 = AXIS2_PLACEMENT_3D('',#144651,#111455,#111456) ;
#94386 = AXIS2_PLACEMENT_3D('',#144653,#111458,#111459) ;
#94387 = AXIS2_PLACEMENT_3D('',#144668,#111466,#111467) ;
#94388 = AXIS2_PLACEMENT_3D('',#144672,#111469,#111470) ;
#94389 = AXIS2_PLACEMENT_3D('',#144674,#111472,#111473) ;
#94390 = AXIS2_PLACEMENT_3D('',#144689,#111480,#111481) ;
#94391 = AXIS2_PLACEMENT_3D('',#144693,#111483,#111484) ;
#94392 = AXIS2_PLACEMENT_3D('',#144695,#111486,#111487) ;
#94393 = AXIS2_PLACEMENT_3D('',#144710,#111494,#111495) ;
#94394 = AXIS2_PLACEMENT_3D('',#144714,#111497,#111498) ;
#94395 = AXIS2_PLACEMENT_3D('',#144716,#111500,#111501) ;
#94396 = AXIS2_PLACEMENT_3D('',#144731,#111508,#111509) ;
#94397 = AXIS2_PLACEMENT_3D('',#144735,#111511,#111512) ;
#94398 = AXIS2_PLACEMENT_3D('',#144737,#111514,#111515) ;
#94399 = AXIS2_PLACEMENT_3D('',#144752,#111522,#111523) ;
#94400 = AXIS2_PLACEMENT_3D('',#144756,#111525,#111526) ;
#94401 = AXIS2_PLACEMENT_3D('',#144758,#111528,#111529) ;
#94402 = AXIS2_PLACEMENT_3D('',#144773,#111536,#111537) ;
#94403 = AXIS2_PLACEMENT_3D('',#144777,#111539,#111540) ;
#94404 = AXIS2_PLACEMENT_3D('',#144779,#111542,#111543) ;
#94405 = AXIS2_PLACEMENT_3D('',#144794,#111550,#111551) ;
#94406 = AXIS2_PLACEMENT_3D('',#144798,#111553,#111554) ;
#94407 = AXIS2_PLACEMENT_3D('',#144800,#111556,#111557) ;
#94408 = AXIS2_PLACEMENT_3D('',#144809,#111562,#111563) ;
#94409 = AXIS2_PLACEMENT_3D('',#144815,#111567,#111568) ;
#94410 = AXIS2_PLACEMENT_3D('',#144824,#111573,#111574) ;
#94411 = AXIS2_PLACEMENT_3D('',#144833,#111579,#111580) ;
#94412 = AXIS2_PLACEMENT_3D('',#144842,#111585,#111586) ;
#94413 = AXIS2_PLACEMENT_3D('',#144851,#111591,#111592) ;
#94414 = AXIS2_PLACEMENT_3D('',#144857,#111596,#111597) ;
#94415 = AXIS2_PLACEMENT_3D('',#144866,#111602,#111603) ;
#94416 = AXIS2_PLACEMENT_3D('',#144875,#111608,#111609) ;
#94417 = AXIS2_PLACEMENT_3D('',#144884,#111614,#111615) ;
#94418 = AXIS2_PLACEMENT_3D('',#144893,#111620,#111621) ;
#94419 = AXIS2_PLACEMENT_3D('',#144899,#111625,#111626) ;
#94420 = AXIS2_PLACEMENT_3D('',#144908,#111631,#111632) ;
#94421 = AXIS2_PLACEMENT_3D('',#144917,#111637,#111638) ;
#94422 = AXIS2_PLACEMENT_3D('',#144926,#111643,#111644) ;
#94423 = AXIS2_PLACEMENT_3D('',#144935,#111649,#111650) ;
#94424 = AXIS2_PLACEMENT_3D('',#144941,#111654,#111655) ;
#94425 = AXIS2_PLACEMENT_3D('',#144950,#111660,#111661) ;
#94426 = AXIS2_PLACEMENT_3D('',#144959,#111666,#111667) ;
#94427 = AXIS2_PLACEMENT_3D('',#144968,#111672,#111673) ;
#94428 = AXIS2_PLACEMENT_3D('',#144977,#111678,#111679) ;
#94429 = AXIS2_PLACEMENT_3D('',#144983,#111683,#111684) ;
#94430 = AXIS2_PLACEMENT_3D('',#144992,#111689,#111690) ;
#94431 = AXIS2_PLACEMENT_3D('',#145001,#111695,#111696) ;
#94432 = AXIS2_PLACEMENT_3D('',#145010,#111701,#111702) ;
#94433 = AXIS2_PLACEMENT_3D('',#145019,#111707,#111708) ;
#94434 = AXIS2_PLACEMENT_3D('',#145025,#111712,#111713) ;
#94435 = AXIS2_PLACEMENT_3D('',#145034,#111718,#111719) ;
#94436 = AXIS2_PLACEMENT_3D('',#145043,#111724,#111725) ;
#94437 = AXIS2_PLACEMENT_3D('',#145052,#111730,#111731) ;
#94438 = AXIS2_PLACEMENT_3D('',#145061,#111736,#111737) ;
#94439 = AXIS2_PLACEMENT_3D('',#145067,#111741,#111742) ;
#94440 = AXIS2_PLACEMENT_3D('',#145076,#111747,#111748) ;
#94441 = AXIS2_PLACEMENT_3D('',#145085,#111753,#111754) ;
#94442 = AXIS2_PLACEMENT_3D('',#145094,#111759,#111760) ;
#94443 = AXIS2_PLACEMENT_3D('',#145103,#111765,#111766) ;
#94444 = AXIS2_PLACEMENT_3D('',#145109,#111770,#111771) ;
#94445 = AXIS2_PLACEMENT_3D('',#145118,#111776,#111777) ;
#94446 = AXIS2_PLACEMENT_3D('',#145127,#111782,#111783) ;
#94447 = AXIS2_PLACEMENT_3D('',#145136,#111788,#111789) ;
#94448 = AXIS2_PLACEMENT_3D('',#145145,#111794,#111795) ;
#94449 = AXIS2_PLACEMENT_3D('',#145151,#111799,#111800) ;
#94450 = AXIS2_PLACEMENT_3D('',#145160,#111805,#111806) ;
#94451 = AXIS2_PLACEMENT_3D('',#145169,#111811,#111812) ;
#94452 = AXIS2_PLACEMENT_3D('',#145178,#111817,#111818) ;
#94453 = AXIS2_PLACEMENT_3D('',#145183,#111820,#111821) ;
#94454 = AXIS2_PLACEMENT_3D('',#145186,#111823,#111824) ;
#94455 = AXIS2_PLACEMENT_3D('',#145187,#111825,#111826) ;
#94456 = AXIS2_PLACEMENT_3D('',#145193,#111830,#111831) ;
#94457 = AXIS2_PLACEMENT_3D('',#145195,#111832,#111833) ;
#94458 = AXIS2_PLACEMENT_3D('',#145198,#111835,#111836) ;
#94459 = AXIS2_PLACEMENT_3D('',#145199,#111837,#111838) ;
#94460 = AXIS2_PLACEMENT_3D('',#145205,#111842,#111843) ;
#94461 = AXIS2_PLACEMENT_3D('',#145207,#111844,#111845) ;
#94462 = AXIS2_PLACEMENT_3D('',#145210,#111847,#111848) ;
#94463 = AXIS2_PLACEMENT_3D('',#145211,#111849,#111850) ;
#94464 = AXIS2_PLACEMENT_3D('',#145216,#111854,#111855) ;
#94465 = AXIS2_PLACEMENT_3D('',#145219,#111857,#111858) ;
#94466 = AXIS2_PLACEMENT_3D('',#145220,#111859,#111860) ;
#94467 = AXIS2_PLACEMENT_3D('',#145223,#111863,#111864) ;
#94468 = AXIS2_PLACEMENT_3D('',#145229,#111868,#111869) ;
#94469 = AXIS2_PLACEMENT_3D('',#145231,#111870,#111871) ;
#94470 = AXIS2_PLACEMENT_3D('',#145234,#111873,#111874) ;
#94471 = AXIS2_PLACEMENT_3D('',#145235,#111875,#111876) ;
#94472 = AXIS2_PLACEMENT_3D('',#145241,#111880,#111881) ;
#94473 = AXIS2_PLACEMENT_3D('',#145243,#111882,#111883) ;
#94474 = AXIS2_PLACEMENT_3D('',#145246,#111885,#111886) ;
#94475 = AXIS2_PLACEMENT_3D('',#145247,#111887,#111888) ;
#94476 = AXIS2_PLACEMENT_3D('',#145253,#111892,#111893) ;
#94477 = AXIS2_PLACEMENT_3D('',#145255,#111894,#111895) ;
#94478 = AXIS2_PLACEMENT_3D('',#145258,#111897,#111898) ;
#94479 = AXIS2_PLACEMENT_3D('',#145259,#111899,#111900) ;
#94480 = AXIS2_PLACEMENT_3D('',#145265,#111904,#111905) ;
#94481 = AXIS2_PLACEMENT_3D('',#145267,#111906,#111907) ;
#94482 = AXIS2_PLACEMENT_3D('',#145270,#111909,#111910) ;
#94483 = AXIS2_PLACEMENT_3D('',#145271,#111911,#111912) ;
#94484 = AXIS2_PLACEMENT_3D('',#145277,#111916,#111917) ;
#94485 = AXIS2_PLACEMENT_3D('',#145279,#111918,#111919) ;
#94486 = AXIS2_PLACEMENT_3D('',#145282,#111921,#111922) ;
#94487 = AXIS2_PLACEMENT_3D('',#145283,#111923,#111924) ;
#94488 = AXIS2_PLACEMENT_3D('',#145289,#111928,#111929) ;
#94489 = AXIS2_PLACEMENT_3D('',#145291,#111930,#111931) ;
#94490 = AXIS2_PLACEMENT_3D('',#145294,#111933,#111934) ;
#94491 = AXIS2_PLACEMENT_3D('',#145295,#111935,#111936) ;
#94492 = AXIS2_PLACEMENT_3D('',#145297,#111937,#111938) ;
#94493 = AXIS2_PLACEMENT_3D('',#145300,#111940,#111941) ;
#94494 = AXIS2_PLACEMENT_3D('',#145301,#111942,#111943) ;
#94495 = AXIS2_PLACEMENT_3D('',#145303,#111944,#111945) ;
#94496 = AXIS2_PLACEMENT_3D('',#145306,#111947,#111948) ;
#94497 = AXIS2_PLACEMENT_3D('',#145307,#111949,#111950) ;
#94498 = AXIS2_PLACEMENT_3D('',#145313,#111954,#111955) ;
#94499 = AXIS2_PLACEMENT_3D('',#145315,#111956,#111957) ;
#94500 = AXIS2_PLACEMENT_3D('',#145318,#111959,#111960) ;
#94501 = AXIS2_PLACEMENT_3D('',#145319,#111961,#111962) ;
#94502 = AXIS2_PLACEMENT_3D('',#145325,#111966,#111967) ;
#94503 = AXIS2_PLACEMENT_3D('',#145327,#111968,#111969) ;
#94504 = AXIS2_PLACEMENT_3D('',#145330,#111971,#111972) ;
#94505 = AXIS2_PLACEMENT_3D('',#145331,#111973,#111974) ;
#94506 = AXIS2_PLACEMENT_3D('',#145334,#111977,#111978) ;
#94507 = AXIS2_PLACEMENT_3D('',#145337,#111979,#111980) ;
#94508 = AXIS2_PLACEMENT_3D('',#145341,#111982,#111983) ;
#94509 = AXIS2_PLACEMENT_3D('',#145349,#111987,#111988) ;
#94510 = AXIS2_PLACEMENT_3D('',#145357,#111992,#111993) ;
#94511 = AXIS2_PLACEMENT_3D('',#145361,#111995,#111996) ;
#94512 = AXIS2_PLACEMENT_3D('',#145370,#112002,#112003) ;
#94513 = AXIS2_PLACEMENT_3D('',#145375,#112005,#112006) ;
#94514 = AXIS2_PLACEMENT_3D('',#145378,#112008,#112009) ;
#94515 = AXIS2_PLACEMENT_3D('',#145379,#112010,#112011) ;
#94516 = AXIS2_PLACEMENT_3D('',#145385,#112015,#112016) ;
#94517 = AXIS2_PLACEMENT_3D('',#145387,#112017,#112018) ;
#94518 = AXIS2_PLACEMENT_3D('',#145390,#112020,#112021) ;
#94519 = AXIS2_PLACEMENT_3D('',#145391,#112022,#112023) ;
#94520 = AXIS2_PLACEMENT_3D('',#145397,#112027,#112028) ;
#94521 = AXIS2_PLACEMENT_3D('',#145399,#112029,#112030) ;
#94522 = AXIS2_PLACEMENT_3D('',#145402,#112032,#112033) ;
#94523 = AXIS2_PLACEMENT_3D('',#145403,#112034,#112035) ;
#94524 = AXIS2_PLACEMENT_3D('',#145408,#112039,#112040) ;
#94525 = AXIS2_PLACEMENT_3D('',#145411,#112042,#112043) ;
#94526 = AXIS2_PLACEMENT_3D('',#145412,#112044,#112045) ;
#94527 = AXIS2_PLACEMENT_3D('',#145415,#112048,#112049) ;
#94528 = AXIS2_PLACEMENT_3D('',#145421,#112053,#112054) ;
#94529 = AXIS2_PLACEMENT_3D('',#145423,#112055,#112056) ;
#94530 = AXIS2_PLACEMENT_3D('',#145426,#112058,#112059) ;
#94531 = AXIS2_PLACEMENT_3D('',#145427,#112060,#112061) ;
#94532 = AXIS2_PLACEMENT_3D('',#145433,#112065,#112066) ;
#94533 = AXIS2_PLACEMENT_3D('',#145435,#112067,#112068) ;
#94534 = AXIS2_PLACEMENT_3D('',#145438,#112070,#112071) ;
#94535 = AXIS2_PLACEMENT_3D('',#145439,#112072,#112073) ;
#94536 = AXIS2_PLACEMENT_3D('',#145445,#112077,#112078) ;
#94537 = AXIS2_PLACEMENT_3D('',#145447,#112079,#112080) ;
#94538 = AXIS2_PLACEMENT_3D('',#145450,#112082,#112083) ;
#94539 = AXIS2_PLACEMENT_3D('',#145451,#112084,#112085) ;
#94540 = AXIS2_PLACEMENT_3D('',#145457,#112089,#112090) ;
#94541 = AXIS2_PLACEMENT_3D('',#145459,#112091,#112092) ;
#94542 = AXIS2_PLACEMENT_3D('',#145462,#112094,#112095) ;
#94543 = AXIS2_PLACEMENT_3D('',#145463,#112096,#112097) ;
#94544 = AXIS2_PLACEMENT_3D('',#145469,#112101,#112102) ;
#94545 = AXIS2_PLACEMENT_3D('',#145471,#112103,#112104) ;
#94546 = AXIS2_PLACEMENT_3D('',#145474,#112106,#112107) ;
#94547 = AXIS2_PLACEMENT_3D('',#145475,#112108,#112109) ;
#94548 = AXIS2_PLACEMENT_3D('',#145481,#112113,#112114) ;
#94549 = AXIS2_PLACEMENT_3D('',#145483,#112115,#112116) ;
#94550 = AXIS2_PLACEMENT_3D('',#145486,#112118,#112119) ;
#94551 = AXIS2_PLACEMENT_3D('',#145487,#112120,#112121) ;
#94552 = AXIS2_PLACEMENT_3D('',#145489,#112122,#112123) ;
#94553 = AXIS2_PLACEMENT_3D('',#145492,#112125,#112126) ;
#94554 = AXIS2_PLACEMENT_3D('',#145493,#112127,#112128) ;
#94555 = AXIS2_PLACEMENT_3D('',#145495,#112129,#112130) ;
#94556 = AXIS2_PLACEMENT_3D('',#145498,#112132,#112133) ;
#94557 = AXIS2_PLACEMENT_3D('',#145499,#112134,#112135) ;
#94558 = AXIS2_PLACEMENT_3D('',#145505,#112139,#112140) ;
#94559 = AXIS2_PLACEMENT_3D('',#145507,#112141,#112142) ;
#94560 = AXIS2_PLACEMENT_3D('',#145510,#112144,#112145) ;
#94561 = AXIS2_PLACEMENT_3D('',#145511,#112146,#112147) ;
#94562 = AXIS2_PLACEMENT_3D('',#145517,#112151,#112152) ;
#94563 = AXIS2_PLACEMENT_3D('',#145519,#112153,#112154) ;
#94564 = AXIS2_PLACEMENT_3D('',#145522,#112156,#112157) ;
#94565 = AXIS2_PLACEMENT_3D('',#145523,#112158,#112159) ;
#94566 = AXIS2_PLACEMENT_3D('',#145526,#112162,#112163) ;
#94567 = AXIS2_PLACEMENT_3D('',#145529,#112164,#112165) ;
#94568 = AXIS2_PLACEMENT_3D('',#145533,#112167,#112168) ;
#94569 = AXIS2_PLACEMENT_3D('',#145541,#112172,#112173) ;
#94570 = AXIS2_PLACEMENT_3D('',#145549,#112177,#112178) ;
#94571 = AXIS2_PLACEMENT_3D('',#145553,#112180,#112181) ;
#94572 = AXIS2_PLACEMENT_3D('',#145562,#112187,#112188) ;
#94573 = AXIS2_PLACEMENT_3D('',#145567,#112190,#112191) ;
#94574 = AXIS2_PLACEMENT_3D('',#145570,#112193,#112194) ;
#94575 = AXIS2_PLACEMENT_3D('',#145571,#112195,#112196) ;
#94576 = AXIS2_PLACEMENT_3D('',#145577,#112200,#112201) ;
#94577 = AXIS2_PLACEMENT_3D('',#145579,#112202,#112203) ;
#94578 = AXIS2_PLACEMENT_3D('',#145582,#112205,#112206) ;
#94579 = AXIS2_PLACEMENT_3D('',#145583,#112207,#112208) ;
#94580 = AXIS2_PLACEMENT_3D('',#145589,#112212,#112213) ;
#94581 = AXIS2_PLACEMENT_3D('',#145591,#112214,#112215) ;
#94582 = AXIS2_PLACEMENT_3D('',#145594,#112217,#112218) ;
#94583 = AXIS2_PLACEMENT_3D('',#145595,#112219,#112220) ;
#94584 = AXIS2_PLACEMENT_3D('',#145600,#112224,#112225) ;
#94585 = AXIS2_PLACEMENT_3D('',#145603,#112227,#112228) ;
#94586 = AXIS2_PLACEMENT_3D('',#145604,#112229,#112230) ;
#94587 = AXIS2_PLACEMENT_3D('',#145607,#112233,#112234) ;
#94588 = AXIS2_PLACEMENT_3D('',#145613,#112238,#112239) ;
#94589 = AXIS2_PLACEMENT_3D('',#145615,#112240,#112241) ;
#94590 = AXIS2_PLACEMENT_3D('',#145618,#112243,#112244) ;
#94591 = AXIS2_PLACEMENT_3D('',#145619,#112245,#112246) ;
#94592 = AXIS2_PLACEMENT_3D('',#145625,#112250,#112251) ;
#94593 = AXIS2_PLACEMENT_3D('',#145627,#112252,#112253) ;
#94594 = AXIS2_PLACEMENT_3D('',#145630,#112255,#112256) ;
#94595 = AXIS2_PLACEMENT_3D('',#145631,#112257,#112258) ;
#94596 = AXIS2_PLACEMENT_3D('',#145637,#112262,#112263) ;
#94597 = AXIS2_PLACEMENT_3D('',#145639,#112264,#112265) ;
#94598 = AXIS2_PLACEMENT_3D('',#145642,#112267,#112268) ;
#94599 = AXIS2_PLACEMENT_3D('',#145643,#112269,#112270) ;
#94600 = AXIS2_PLACEMENT_3D('',#145649,#112274,#112275) ;
#94601 = AXIS2_PLACEMENT_3D('',#145651,#112276,#112277) ;
#94602 = AXIS2_PLACEMENT_3D('',#145654,#112279,#112280) ;
#94603 = AXIS2_PLACEMENT_3D('',#145655,#112281,#112282) ;
#94604 = AXIS2_PLACEMENT_3D('',#145661,#112286,#112287) ;
#94605 = AXIS2_PLACEMENT_3D('',#145663,#112288,#112289) ;
#94606 = AXIS2_PLACEMENT_3D('',#145666,#112291,#112292) ;
#94607 = AXIS2_PLACEMENT_3D('',#145667,#112293,#112294) ;
#94608 = AXIS2_PLACEMENT_3D('',#145673,#112298,#112299) ;
#94609 = AXIS2_PLACEMENT_3D('',#145675,#112300,#112301) ;
#94610 = AXIS2_PLACEMENT_3D('',#145678,#112303,#112304) ;
#94611 = AXIS2_PLACEMENT_3D('',#145679,#112305,#112306) ;
#94612 = AXIS2_PLACEMENT_3D('',#145681,#112307,#112308) ;
#94613 = AXIS2_PLACEMENT_3D('',#145684,#112310,#112311) ;
#94614 = AXIS2_PLACEMENT_3D('',#145685,#112312,#112313) ;
#94615 = AXIS2_PLACEMENT_3D('',#145687,#112314,#112315) ;
#94616 = AXIS2_PLACEMENT_3D('',#145690,#112317,#112318) ;
#94617 = AXIS2_PLACEMENT_3D('',#145691,#112319,#112320) ;
#94618 = AXIS2_PLACEMENT_3D('',#145697,#112324,#112325) ;
#94619 = AXIS2_PLACEMENT_3D('',#145699,#112326,#112327) ;
#94620 = AXIS2_PLACEMENT_3D('',#145702,#112329,#112330) ;
#94621 = AXIS2_PLACEMENT_3D('',#145703,#112331,#112332) ;
#94622 = AXIS2_PLACEMENT_3D('',#145709,#112336,#112337) ;
#94623 = AXIS2_PLACEMENT_3D('',#145711,#112338,#112339) ;
#94624 = AXIS2_PLACEMENT_3D('',#145714,#112341,#112342) ;
#94625 = AXIS2_PLACEMENT_3D('',#145715,#112343,#112344) ;
#94626 = AXIS2_PLACEMENT_3D('',#145718,#112347,#112348) ;
#94627 = AXIS2_PLACEMENT_3D('',#145721,#112349,#112350) ;
#94628 = AXIS2_PLACEMENT_3D('',#145725,#112352,#112353) ;
#94629 = AXIS2_PLACEMENT_3D('',#145733,#112357,#112358) ;
#94630 = AXIS2_PLACEMENT_3D('',#145741,#112362,#112363) ;
#94631 = AXIS2_PLACEMENT_3D('',#145745,#112365,#112366) ;
#94632 = AXIS2_PLACEMENT_3D('',#145754,#112372,#112373) ;
#94633 = AXIS2_PLACEMENT_3D('',#145759,#112375,#112376) ;
#94634 = AXIS2_PLACEMENT_3D('',#145762,#112378,#112379) ;
#94635 = AXIS2_PLACEMENT_3D('',#145763,#112380,#112381) ;
#94636 = AXIS2_PLACEMENT_3D('',#145769,#112385,#112386) ;
#94637 = AXIS2_PLACEMENT_3D('',#145771,#112387,#112388) ;
#94638 = AXIS2_PLACEMENT_3D('',#145774,#112390,#112391) ;
#94639 = AXIS2_PLACEMENT_3D('',#145775,#112392,#112393) ;
#94640 = AXIS2_PLACEMENT_3D('',#145781,#112397,#112398) ;
#94641 = AXIS2_PLACEMENT_3D('',#145783,#112399,#112400) ;
#94642 = AXIS2_PLACEMENT_3D('',#145786,#112402,#112403) ;
#94643 = AXIS2_PLACEMENT_3D('',#145787,#112404,#112405) ;
#94644 = AXIS2_PLACEMENT_3D('',#145792,#112409,#112410) ;
#94645 = AXIS2_PLACEMENT_3D('',#145795,#112412,#112413) ;
#94646 = AXIS2_PLACEMENT_3D('',#145796,#112414,#112415) ;
#94647 = AXIS2_PLACEMENT_3D('',#145799,#112418,#112419) ;
#94648 = AXIS2_PLACEMENT_3D('',#145805,#112423,#112424) ;
#94649 = AXIS2_PLACEMENT_3D('',#145807,#112425,#112426) ;
#94650 = AXIS2_PLACEMENT_3D('',#145810,#112428,#112429) ;
#94651 = AXIS2_PLACEMENT_3D('',#145811,#112430,#112431) ;
#94652 = AXIS2_PLACEMENT_3D('',#145817,#112435,#112436) ;
#94653 = AXIS2_PLACEMENT_3D('',#145819,#112437,#112438) ;
#94654 = AXIS2_PLACEMENT_3D('',#145822,#112440,#112441) ;
#94655 = AXIS2_PLACEMENT_3D('',#145823,#112442,#112443) ;
#94656 = AXIS2_PLACEMENT_3D('',#145829,#112447,#112448) ;
#94657 = AXIS2_PLACEMENT_3D('',#145831,#112449,#112450) ;
#94658 = AXIS2_PLACEMENT_3D('',#145834,#112452,#112453) ;
#94659 = AXIS2_PLACEMENT_3D('',#145835,#112454,#112455) ;
#94660 = AXIS2_PLACEMENT_3D('',#145841,#112459,#112460) ;
#94661 = AXIS2_PLACEMENT_3D('',#145843,#112461,#112462) ;
#94662 = AXIS2_PLACEMENT_3D('',#145846,#112464,#112465) ;
#94663 = AXIS2_PLACEMENT_3D('',#145847,#112466,#112467) ;
#94664 = AXIS2_PLACEMENT_3D('',#145853,#112471,#112472) ;
#94665 = AXIS2_PLACEMENT_3D('',#145855,#112473,#112474) ;
#94666 = AXIS2_PLACEMENT_3D('',#145858,#112476,#112477) ;
#94667 = AXIS2_PLACEMENT_3D('',#145859,#112478,#112479) ;
#94668 = AXIS2_PLACEMENT_3D('',#145865,#112483,#112484) ;
#94669 = AXIS2_PLACEMENT_3D('',#145867,#112485,#112486) ;
#94670 = AXIS2_PLACEMENT_3D('',#145870,#112488,#112489) ;
#94671 = AXIS2_PLACEMENT_3D('',#145871,#112490,#112491) ;
#94672 = AXIS2_PLACEMENT_3D('',#145873,#112492,#112493) ;
#94673 = AXIS2_PLACEMENT_3D('',#145876,#112495,#112496) ;
#94674 = AXIS2_PLACEMENT_3D('',#145877,#112497,#112498) ;
#94675 = AXIS2_PLACEMENT_3D('',#145879,#112499,#112500) ;
#94676 = AXIS2_PLACEMENT_3D('',#145882,#112502,#112503) ;
#94677 = AXIS2_PLACEMENT_3D('',#145883,#112504,#112505) ;
#94678 = AXIS2_PLACEMENT_3D('',#145889,#112509,#112510) ;
#94679 = AXIS2_PLACEMENT_3D('',#145891,#112511,#112512) ;
#94680 = AXIS2_PLACEMENT_3D('',#145894,#112514,#112515) ;
#94681 = AXIS2_PLACEMENT_3D('',#145895,#112516,#112517) ;
#94682 = AXIS2_PLACEMENT_3D('',#145901,#112521,#112522) ;
#94683 = AXIS2_PLACEMENT_3D('',#145903,#112523,#112524) ;
#94684 = AXIS2_PLACEMENT_3D('',#145906,#112526,#112527) ;
#94685 = AXIS2_PLACEMENT_3D('',#145907,#112528,#112529) ;
#94686 = AXIS2_PLACEMENT_3D('',#145910,#112532,#112533) ;
#94687 = AXIS2_PLACEMENT_3D('',#145913,#112534,#112535) ;
#94688 = AXIS2_PLACEMENT_3D('',#145917,#112537,#112538) ;
#94689 = AXIS2_PLACEMENT_3D('',#145925,#112542,#112543) ;
#94690 = AXIS2_PLACEMENT_3D('',#145933,#112547,#112548) ;
#94691 = AXIS2_PLACEMENT_3D('',#145937,#112550,#112551) ;
#94692 = AXIS2_PLACEMENT_3D('',#145946,#112557,#112558) ;
#94693 = AXIS2_PLACEMENT_3D('',#145951,#112560,#112561) ;
#94694 = AXIS2_PLACEMENT_3D('',#145954,#112563,#112564) ;
#94695 = AXIS2_PLACEMENT_3D('',#145955,#112565,#112566) ;
#94696 = AXIS2_PLACEMENT_3D('',#145961,#112570,#112571) ;
#94697 = AXIS2_PLACEMENT_3D('',#145963,#112572,#112573) ;
#94698 = AXIS2_PLACEMENT_3D('',#145966,#112575,#112576) ;
#94699 = AXIS2_PLACEMENT_3D('',#145967,#112577,#112578) ;
#94700 = AXIS2_PLACEMENT_3D('',#145973,#112582,#112583) ;
#94701 = AXIS2_PLACEMENT_3D('',#145975,#112584,#112585) ;
#94702 = AXIS2_PLACEMENT_3D('',#145978,#112587,#112588) ;
#94703 = AXIS2_PLACEMENT_3D('',#145979,#112589,#112590) ;
#94704 = AXIS2_PLACEMENT_3D('',#145984,#112594,#112595) ;
#94705 = AXIS2_PLACEMENT_3D('',#145987,#112597,#112598) ;
#94706 = AXIS2_PLACEMENT_3D('',#145988,#112599,#112600) ;
#94707 = AXIS2_PLACEMENT_3D('',#145991,#112603,#112604) ;
#94708 = AXIS2_PLACEMENT_3D('',#145997,#112608,#112609) ;
#94709 = AXIS2_PLACEMENT_3D('',#145999,#112610,#112611) ;
#94710 = AXIS2_PLACEMENT_3D('',#146002,#112613,#112614) ;
#94711 = AXIS2_PLACEMENT_3D('',#146003,#112615,#112616) ;
#94712 = AXIS2_PLACEMENT_3D('',#146009,#112620,#112621) ;
#94713 = AXIS2_PLACEMENT_3D('',#146011,#112622,#112623) ;
#94714 = AXIS2_PLACEMENT_3D('',#146014,#112625,#112626) ;
#94715 = AXIS2_PLACEMENT_3D('',#146015,#112627,#112628) ;
#94716 = AXIS2_PLACEMENT_3D('',#146021,#112632,#112633) ;
#94717 = AXIS2_PLACEMENT_3D('',#146023,#112634,#112635) ;
#94718 = AXIS2_PLACEMENT_3D('',#146026,#112637,#112638) ;
#94719 = AXIS2_PLACEMENT_3D('',#146027,#112639,#112640) ;
#94720 = AXIS2_PLACEMENT_3D('',#146033,#112644,#112645) ;
#94721 = AXIS2_PLACEMENT_3D('',#146035,#112646,#112647) ;
#94722 = AXIS2_PLACEMENT_3D('',#146038,#112649,#112650) ;
#94723 = AXIS2_PLACEMENT_3D('',#146039,#112651,#112652) ;
#94724 = AXIS2_PLACEMENT_3D('',#146045,#112656,#112657) ;
#94725 = AXIS2_PLACEMENT_3D('',#146047,#112658,#112659) ;
#94726 = AXIS2_PLACEMENT_3D('',#146050,#112661,#112662) ;
#94727 = AXIS2_PLACEMENT_3D('',#146051,#112663,#112664) ;
#94728 = AXIS2_PLACEMENT_3D('',#146057,#112668,#112669) ;
#94729 = AXIS2_PLACEMENT_3D('',#146059,#112670,#112671) ;
#94730 = AXIS2_PLACEMENT_3D('',#146062,#112673,#112674) ;
#94731 = AXIS2_PLACEMENT_3D('',#146063,#112675,#112676) ;
#94732 = AXIS2_PLACEMENT_3D('',#146065,#112677,#112678) ;
#94733 = AXIS2_PLACEMENT_3D('',#146068,#112680,#112681) ;
#94734 = AXIS2_PLACEMENT_3D('',#146069,#112682,#112683) ;
#94735 = AXIS2_PLACEMENT_3D('',#146071,#112684,#112685) ;
#94736 = AXIS2_PLACEMENT_3D('',#146074,#112687,#112688) ;
#94737 = AXIS2_PLACEMENT_3D('',#146075,#112689,#112690) ;
#94738 = AXIS2_PLACEMENT_3D('',#146081,#112694,#112695) ;
#94739 = AXIS2_PLACEMENT_3D('',#146083,#112696,#112697) ;
#94740 = AXIS2_PLACEMENT_3D('',#146086,#112699,#112700) ;
#94741 = AXIS2_PLACEMENT_3D('',#146087,#112701,#112702) ;
#94742 = AXIS2_PLACEMENT_3D('',#146093,#112706,#112707) ;
#94743 = AXIS2_PLACEMENT_3D('',#146095,#112708,#112709) ;
#94744 = AXIS2_PLACEMENT_3D('',#146098,#112711,#112712) ;
#94745 = AXIS2_PLACEMENT_3D('',#146099,#112713,#112714) ;
#94746 = AXIS2_PLACEMENT_3D('',#146102,#112717,#112718) ;
#94747 = AXIS2_PLACEMENT_3D('',#146105,#112719,#112720) ;
#94748 = AXIS2_PLACEMENT_3D('',#146109,#112722,#112723) ;
#94749 = AXIS2_PLACEMENT_3D('',#146117,#112727,#112728) ;
#94750 = AXIS2_PLACEMENT_3D('',#146125,#112732,#112733) ;
#94751 = AXIS2_PLACEMENT_3D('',#146129,#112735,#112736) ;
#94752 = AXIS2_PLACEMENT_3D('',#146138,#112742,#112743) ;
#94753 = AXIS2_PLACEMENT_3D('',#146143,#112745,#112746) ;
#94754 = AXIS2_PLACEMENT_3D('',#146146,#112748,#112749) ;
#94755 = AXIS2_PLACEMENT_3D('',#146147,#112750,#112751) ;
#94756 = AXIS2_PLACEMENT_3D('',#146153,#112755,#112756) ;
#94757 = AXIS2_PLACEMENT_3D('',#146155,#112757,#112758) ;
#94758 = AXIS2_PLACEMENT_3D('',#146158,#112760,#112761) ;
#94759 = AXIS2_PLACEMENT_3D('',#146159,#112762,#112763) ;
#94760 = AXIS2_PLACEMENT_3D('',#146165,#112767,#112768) ;
#94761 = AXIS2_PLACEMENT_3D('',#146167,#112769,#112770) ;
#94762 = AXIS2_PLACEMENT_3D('',#146170,#112772,#112773) ;
#94763 = AXIS2_PLACEMENT_3D('',#146171,#112774,#112775) ;
#94764 = AXIS2_PLACEMENT_3D('',#146176,#112779,#112780) ;
#94765 = AXIS2_PLACEMENT_3D('',#146179,#112782,#112783) ;
#94766 = AXIS2_PLACEMENT_3D('',#146180,#112784,#112785) ;
#94767 = AXIS2_PLACEMENT_3D('',#146183,#112788,#112789) ;
#94768 = AXIS2_PLACEMENT_3D('',#146189,#112793,#112794) ;
#94769 = AXIS2_PLACEMENT_3D('',#146191,#112795,#112796) ;
#94770 = AXIS2_PLACEMENT_3D('',#146194,#112798,#112799) ;
#94771 = AXIS2_PLACEMENT_3D('',#146195,#112800,#112801) ;
#94772 = AXIS2_PLACEMENT_3D('',#146201,#112805,#112806) ;
#94773 = AXIS2_PLACEMENT_3D('',#146203,#112807,#112808) ;
#94774 = AXIS2_PLACEMENT_3D('',#146206,#112810,#112811) ;
#94775 = AXIS2_PLACEMENT_3D('',#146207,#112812,#112813) ;
#94776 = AXIS2_PLACEMENT_3D('',#146213,#112817,#112818) ;
#94777 = AXIS2_PLACEMENT_3D('',#146215,#112819,#112820) ;
#94778 = AXIS2_PLACEMENT_3D('',#146218,#112822,#112823) ;
#94779 = AXIS2_PLACEMENT_3D('',#146219,#112824,#112825) ;
#94780 = AXIS2_PLACEMENT_3D('',#146225,#112829,#112830) ;
#94781 = AXIS2_PLACEMENT_3D('',#146227,#112831,#112832) ;
#94782 = AXIS2_PLACEMENT_3D('',#146230,#112834,#112835) ;
#94783 = AXIS2_PLACEMENT_3D('',#146231,#112836,#112837) ;
#94784 = AXIS2_PLACEMENT_3D('',#146237,#112841,#112842) ;
#94785 = AXIS2_PLACEMENT_3D('',#146239,#112843,#112844) ;
#94786 = AXIS2_PLACEMENT_3D('',#146242,#112846,#112847) ;
#94787 = AXIS2_PLACEMENT_3D('',#146243,#112848,#112849) ;
#94788 = AXIS2_PLACEMENT_3D('',#146249,#112853,#112854) ;
#94789 = AXIS2_PLACEMENT_3D('',#146251,#112855,#112856) ;
#94790 = AXIS2_PLACEMENT_3D('',#146254,#112858,#112859) ;
#94791 = AXIS2_PLACEMENT_3D('',#146255,#112860,#112861) ;
#94792 = AXIS2_PLACEMENT_3D('',#146257,#112862,#112863) ;
#94793 = AXIS2_PLACEMENT_3D('',#146260,#112865,#112866) ;
#94794 = AXIS2_PLACEMENT_3D('',#146261,#112867,#112868) ;
#94795 = AXIS2_PLACEMENT_3D('',#146263,#112869,#112870) ;
#94796 = AXIS2_PLACEMENT_3D('',#146266,#112872,#112873) ;
#94797 = AXIS2_PLACEMENT_3D('',#146267,#112874,#112875) ;
#94798 = AXIS2_PLACEMENT_3D('',#146273,#112879,#112880) ;
#94799 = AXIS2_PLACEMENT_3D('',#146275,#112881,#112882) ;
#94800 = AXIS2_PLACEMENT_3D('',#146278,#112884,#112885) ;
#94801 = AXIS2_PLACEMENT_3D('',#146279,#112886,#112887) ;
#94802 = AXIS2_PLACEMENT_3D('',#146285,#112891,#112892) ;
#94803 = AXIS2_PLACEMENT_3D('',#146287,#112893,#112894) ;
#94804 = AXIS2_PLACEMENT_3D('',#146290,#112896,#112897) ;
#94805 = AXIS2_PLACEMENT_3D('',#146291,#112898,#112899) ;
#94806 = AXIS2_PLACEMENT_3D('',#146294,#112902,#112903) ;
#94807 = AXIS2_PLACEMENT_3D('',#146297,#112904,#112905) ;
#94808 = AXIS2_PLACEMENT_3D('',#146301,#112907,#112908) ;
#94809 = AXIS2_PLACEMENT_3D('',#146309,#112912,#112913) ;
#94810 = AXIS2_PLACEMENT_3D('',#146317,#112917,#112918) ;
#94811 = AXIS2_PLACEMENT_3D('',#146321,#112920,#112921) ;
#94812 = AXIS2_PLACEMENT_3D('',#146330,#112927,#112928) ;
#94813 = AXIS2_PLACEMENT_3D('',#146335,#112930,#112931) ;
#94814 = AXIS2_PLACEMENT_3D('',#146338,#112933,#112934) ;
#94815 = AXIS2_PLACEMENT_3D('',#146339,#112935,#112936) ;
#94816 = AXIS2_PLACEMENT_3D('',#146345,#112940,#112941) ;
#94817 = AXIS2_PLACEMENT_3D('',#146347,#112942,#112943) ;
#94818 = AXIS2_PLACEMENT_3D('',#146350,#112945,#112946) ;
#94819 = AXIS2_PLACEMENT_3D('',#146351,#112947,#112948) ;
#94820 = AXIS2_PLACEMENT_3D('',#146357,#112952,#112953) ;
#94821 = AXIS2_PLACEMENT_3D('',#146359,#112954,#112955) ;
#94822 = AXIS2_PLACEMENT_3D('',#146362,#112957,#112958) ;
#94823 = AXIS2_PLACEMENT_3D('',#146363,#112959,#112960) ;
#94824 = AXIS2_PLACEMENT_3D('',#146368,#112964,#112965) ;
#94825 = AXIS2_PLACEMENT_3D('',#146371,#112967,#112968) ;
#94826 = AXIS2_PLACEMENT_3D('',#146372,#112969,#112970) ;
#94827 = AXIS2_PLACEMENT_3D('',#146375,#112973,#112974) ;
#94828 = AXIS2_PLACEMENT_3D('',#146381,#112978,#112979) ;
#94829 = AXIS2_PLACEMENT_3D('',#146383,#112980,#112981) ;
#94830 = AXIS2_PLACEMENT_3D('',#146386,#112983,#112984) ;
#94831 = AXIS2_PLACEMENT_3D('',#146387,#112985,#112986) ;
#94832 = AXIS2_PLACEMENT_3D('',#146393,#112990,#112991) ;
#94833 = AXIS2_PLACEMENT_3D('',#146395,#112992,#112993) ;
#94834 = AXIS2_PLACEMENT_3D('',#146398,#112995,#112996) ;
#94835 = AXIS2_PLACEMENT_3D('',#146399,#112997,#112998) ;
#94836 = AXIS2_PLACEMENT_3D('',#146405,#113002,#113003) ;
#94837 = AXIS2_PLACEMENT_3D('',#146407,#113004,#113005) ;
#94838 = AXIS2_PLACEMENT_3D('',#146410,#113007,#113008) ;
#94839 = AXIS2_PLACEMENT_3D('',#146411,#113009,#113010) ;
#94840 = AXIS2_PLACEMENT_3D('',#146417,#113014,#113015) ;
#94841 = AXIS2_PLACEMENT_3D('',#146419,#113016,#113017) ;
#94842 = AXIS2_PLACEMENT_3D('',#146422,#113019,#113020) ;
#94843 = AXIS2_PLACEMENT_3D('',#146423,#113021,#113022) ;
#94844 = AXIS2_PLACEMENT_3D('',#146429,#113026,#113027) ;
#94845 = AXIS2_PLACEMENT_3D('',#146431,#113028,#113029) ;
#94846 = AXIS2_PLACEMENT_3D('',#146434,#113031,#113032) ;
#94847 = AXIS2_PLACEMENT_3D('',#146435,#113033,#113034) ;
#94848 = AXIS2_PLACEMENT_3D('',#146441,#113038,#113039) ;
#94849 = AXIS2_PLACEMENT_3D('',#146443,#113040,#113041) ;
#94850 = AXIS2_PLACEMENT_3D('',#146446,#113043,#113044) ;
#94851 = AXIS2_PLACEMENT_3D('',#146447,#113045,#113046) ;
#94852 = AXIS2_PLACEMENT_3D('',#146449,#113047,#113048) ;
#94853 = AXIS2_PLACEMENT_3D('',#146452,#113050,#113051) ;
#94854 = AXIS2_PLACEMENT_3D('',#146453,#113052,#113053) ;
#94855 = AXIS2_PLACEMENT_3D('',#146455,#113054,#113055) ;
#94856 = AXIS2_PLACEMENT_3D('',#146458,#113057,#113058) ;
#94857 = AXIS2_PLACEMENT_3D('',#146459,#113059,#113060) ;
#94858 = AXIS2_PLACEMENT_3D('',#146465,#113064,#113065) ;
#94859 = AXIS2_PLACEMENT_3D('',#146467,#113066,#113067) ;
#94860 = AXIS2_PLACEMENT_3D('',#146470,#113069,#113070) ;
#94861 = AXIS2_PLACEMENT_3D('',#146471,#113071,#113072) ;
#94862 = AXIS2_PLACEMENT_3D('',#146477,#113076,#113077) ;
#94863 = AXIS2_PLACEMENT_3D('',#146479,#113078,#113079) ;
#94864 = AXIS2_PLACEMENT_3D('',#146482,#113081,#113082) ;
#94865 = AXIS2_PLACEMENT_3D('',#146483,#113083,#113084) ;
#94866 = AXIS2_PLACEMENT_3D('',#146486,#113087,#113088) ;
#94867 = AXIS2_PLACEMENT_3D('',#146489,#113089,#113090) ;
#94868 = AXIS2_PLACEMENT_3D('',#146493,#113092,#113093) ;
#94869 = AXIS2_PLACEMENT_3D('',#146501,#113097,#113098) ;
#94870 = AXIS2_PLACEMENT_3D('',#146509,#113102,#113103) ;
#94871 = AXIS2_PLACEMENT_3D('',#146513,#113105,#113106) ;
#94872 = AXIS2_PLACEMENT_3D('',#146522,#113112,#113113) ;
#94873 = AXIS2_PLACEMENT_3D('',#146527,#113115,#113116) ;
#94874 = AXIS2_PLACEMENT_3D('',#146530,#113118,#113119) ;
#94875 = AXIS2_PLACEMENT_3D('',#146531,#113120,#113121) ;
#94876 = AXIS2_PLACEMENT_3D('',#146537,#113125,#113126) ;
#94877 = AXIS2_PLACEMENT_3D('',#146539,#113127,#113128) ;
#94878 = AXIS2_PLACEMENT_3D('',#146542,#113130,#113131) ;
#94879 = AXIS2_PLACEMENT_3D('',#146543,#113132,#113133) ;
#94880 = AXIS2_PLACEMENT_3D('',#146549,#113137,#113138) ;
#94881 = AXIS2_PLACEMENT_3D('',#146551,#113139,#113140) ;
#94882 = AXIS2_PLACEMENT_3D('',#146554,#113142,#113143) ;
#94883 = AXIS2_PLACEMENT_3D('',#146555,#113144,#113145) ;
#94884 = AXIS2_PLACEMENT_3D('',#146560,#113149,#113150) ;
#94885 = AXIS2_PLACEMENT_3D('',#146563,#113152,#113153) ;
#94886 = AXIS2_PLACEMENT_3D('',#146564,#113154,#113155) ;
#94887 = AXIS2_PLACEMENT_3D('',#146567,#113158,#113159) ;
#94888 = AXIS2_PLACEMENT_3D('',#146573,#113163,#113164) ;
#94889 = AXIS2_PLACEMENT_3D('',#146575,#113165,#113166) ;
#94890 = AXIS2_PLACEMENT_3D('',#146578,#113168,#113169) ;
#94891 = AXIS2_PLACEMENT_3D('',#146579,#113170,#113171) ;
#94892 = AXIS2_PLACEMENT_3D('',#146585,#113175,#113176) ;
#94893 = AXIS2_PLACEMENT_3D('',#146587,#113177,#113178) ;
#94894 = AXIS2_PLACEMENT_3D('',#146590,#113180,#113181) ;
#94895 = AXIS2_PLACEMENT_3D('',#146591,#113182,#113183) ;
#94896 = AXIS2_PLACEMENT_3D('',#146597,#113187,#113188) ;
#94897 = AXIS2_PLACEMENT_3D('',#146599,#113189,#113190) ;
#94898 = AXIS2_PLACEMENT_3D('',#146602,#113192,#113193) ;
#94899 = AXIS2_PLACEMENT_3D('',#146603,#113194,#113195) ;
#94900 = AXIS2_PLACEMENT_3D('',#146609,#113199,#113200) ;
#94901 = AXIS2_PLACEMENT_3D('',#146611,#113201,#113202) ;
#94902 = AXIS2_PLACEMENT_3D('',#146614,#113204,#113205) ;
#94903 = AXIS2_PLACEMENT_3D('',#146615,#113206,#113207) ;
#94904 = AXIS2_PLACEMENT_3D('',#146621,#113211,#113212) ;
#94905 = AXIS2_PLACEMENT_3D('',#146623,#113213,#113214) ;
#94906 = AXIS2_PLACEMENT_3D('',#146626,#113216,#113217) ;
#94907 = AXIS2_PLACEMENT_3D('',#146627,#113218,#113219) ;
#94908 = AXIS2_PLACEMENT_3D('',#146633,#113223,#113224) ;
#94909 = AXIS2_PLACEMENT_3D('',#146635,#113225,#113226) ;
#94910 = AXIS2_PLACEMENT_3D('',#146638,#113228,#113229) ;
#94911 = AXIS2_PLACEMENT_3D('',#146639,#113230,#113231) ;
#94912 = AXIS2_PLACEMENT_3D('',#146641,#113232,#113233) ;
#94913 = AXIS2_PLACEMENT_3D('',#146644,#113235,#113236) ;
#94914 = AXIS2_PLACEMENT_3D('',#146645,#113237,#113238) ;
#94915 = AXIS2_PLACEMENT_3D('',#146647,#113239,#113240) ;
#94916 = AXIS2_PLACEMENT_3D('',#146650,#113242,#113243) ;
#94917 = AXIS2_PLACEMENT_3D('',#146651,#113244,#113245) ;
#94918 = AXIS2_PLACEMENT_3D('',#146657,#113249,#113250) ;
#94919 = AXIS2_PLACEMENT_3D('',#146659,#113251,#113252) ;
#94920 = AXIS2_PLACEMENT_3D('',#146662,#113254,#113255) ;
#94921 = AXIS2_PLACEMENT_3D('',#146663,#113256,#113257) ;
#94922 = AXIS2_PLACEMENT_3D('',#146669,#113261,#113262) ;
#94923 = AXIS2_PLACEMENT_3D('',#146671,#113263,#113264) ;
#94924 = AXIS2_PLACEMENT_3D('',#146674,#113266,#113267) ;
#94925 = AXIS2_PLACEMENT_3D('',#146675,#113268,#113269) ;
#94926 = AXIS2_PLACEMENT_3D('',#146678,#113272,#113273) ;
#94927 = AXIS2_PLACEMENT_3D('',#146681,#113274,#113275) ;
#94928 = AXIS2_PLACEMENT_3D('',#146685,#113277,#113278) ;
#94929 = AXIS2_PLACEMENT_3D('',#146693,#113282,#113283) ;
#94930 = AXIS2_PLACEMENT_3D('',#146701,#113287,#113288) ;
#94931 = AXIS2_PLACEMENT_3D('',#146705,#113290,#113291) ;
#94932 = AXIS2_PLACEMENT_3D('',#146714,#113297,#113298) ;
#94933 = AXIS2_PLACEMENT_3D('',#146719,#113300,#113301) ;
#94934 = AXIS2_PLACEMENT_3D('',#146722,#113303,#113304) ;
#94935 = AXIS2_PLACEMENT_3D('',#146723,#113305,#113306) ;
#94936 = AXIS2_PLACEMENT_3D('',#146729,#113310,#113311) ;
#94937 = AXIS2_PLACEMENT_3D('',#146731,#113312,#113313) ;
#94938 = AXIS2_PLACEMENT_3D('',#146734,#113315,#113316) ;
#94939 = AXIS2_PLACEMENT_3D('',#146735,#113317,#113318) ;
#94940 = AXIS2_PLACEMENT_3D('',#146741,#113322,#113323) ;
#94941 = AXIS2_PLACEMENT_3D('',#146743,#113324,#113325) ;
#94942 = AXIS2_PLACEMENT_3D('',#146746,#113327,#113328) ;
#94943 = AXIS2_PLACEMENT_3D('',#146747,#113329,#113330) ;
#94944 = AXIS2_PLACEMENT_3D('',#146752,#113334,#113335) ;
#94945 = AXIS2_PLACEMENT_3D('',#146755,#113337,#113338) ;
#94946 = AXIS2_PLACEMENT_3D('',#146756,#113339,#113340) ;
#94947 = AXIS2_PLACEMENT_3D('',#146759,#113343,#113344) ;
#94948 = AXIS2_PLACEMENT_3D('',#146765,#113348,#113349) ;
#94949 = AXIS2_PLACEMENT_3D('',#146767,#113350,#113351) ;
#94950 = AXIS2_PLACEMENT_3D('',#146770,#113353,#113354) ;
#94951 = AXIS2_PLACEMENT_3D('',#146771,#113355,#113356) ;
#94952 = AXIS2_PLACEMENT_3D('',#146777,#113360,#113361) ;
#94953 = AXIS2_PLACEMENT_3D('',#146779,#113362,#113363) ;
#94954 = AXIS2_PLACEMENT_3D('',#146782,#113365,#113366) ;
#94955 = AXIS2_PLACEMENT_3D('',#146783,#113367,#113368) ;
#94956 = AXIS2_PLACEMENT_3D('',#146789,#113372,#113373) ;
#94957 = AXIS2_PLACEMENT_3D('',#146791,#113374,#113375) ;
#94958 = AXIS2_PLACEMENT_3D('',#146794,#113377,#113378) ;
#94959 = AXIS2_PLACEMENT_3D('',#146795,#113379,#113380) ;
#94960 = AXIS2_PLACEMENT_3D('',#146801,#113384,#113385) ;
#94961 = AXIS2_PLACEMENT_3D('',#146803,#113386,#113387) ;
#94962 = AXIS2_PLACEMENT_3D('',#146806,#113389,#113390) ;
#94963 = AXIS2_PLACEMENT_3D('',#146807,#113391,#113392) ;
#94964 = AXIS2_PLACEMENT_3D('',#146813,#113396,#113397) ;
#94965 = AXIS2_PLACEMENT_3D('',#146815,#113398,#113399) ;
#94966 = AXIS2_PLACEMENT_3D('',#146818,#113401,#113402) ;
#94967 = AXIS2_PLACEMENT_3D('',#146819,#113403,#113404) ;
#94968 = AXIS2_PLACEMENT_3D('',#146825,#113408,#113409) ;
#94969 = AXIS2_PLACEMENT_3D('',#146827,#113410,#113411) ;
#94970 = AXIS2_PLACEMENT_3D('',#146830,#113413,#113414) ;
#94971 = AXIS2_PLACEMENT_3D('',#146831,#113415,#113416) ;
#94972 = AXIS2_PLACEMENT_3D('',#146833,#113417,#113418) ;
#94973 = AXIS2_PLACEMENT_3D('',#146836,#113420,#113421) ;
#94974 = AXIS2_PLACEMENT_3D('',#146837,#113422,#113423) ;
#94975 = AXIS2_PLACEMENT_3D('',#146839,#113424,#113425) ;
#94976 = AXIS2_PLACEMENT_3D('',#146842,#113427,#113428) ;
#94977 = AXIS2_PLACEMENT_3D('',#146843,#113429,#113430) ;
#94978 = AXIS2_PLACEMENT_3D('',#146849,#113434,#113435) ;
#94979 = AXIS2_PLACEMENT_3D('',#146851,#113436,#113437) ;
#94980 = AXIS2_PLACEMENT_3D('',#146854,#113439,#113440) ;
#94981 = AXIS2_PLACEMENT_3D('',#146855,#113441,#113442) ;
#94982 = AXIS2_PLACEMENT_3D('',#146861,#113446,#113447) ;
#94983 = AXIS2_PLACEMENT_3D('',#146863,#113448,#113449) ;
#94984 = AXIS2_PLACEMENT_3D('',#146866,#113451,#113452) ;
#94985 = AXIS2_PLACEMENT_3D('',#146867,#113453,#113454) ;
#94986 = AXIS2_PLACEMENT_3D('',#146870,#113457,#113458) ;
#94987 = AXIS2_PLACEMENT_3D('',#146873,#113459,#113460) ;
#94988 = AXIS2_PLACEMENT_3D('',#146877,#113462,#113463) ;
#94989 = AXIS2_PLACEMENT_3D('',#146885,#113467,#113468) ;
#94990 = AXIS2_PLACEMENT_3D('',#146893,#113472,#113473) ;
#94991 = AXIS2_PLACEMENT_3D('',#146897,#113475,#113476) ;
#94992 = AXIS2_PLACEMENT_3D('',#146906,#113482,#113483) ;
#94993 = AXIS2_PLACEMENT_3D('',#146911,#113485,#113486) ;
#94994 = AXIS2_PLACEMENT_3D('',#146915,#113488,#113489) ;
#94995 = AXIS2_PLACEMENT_3D('',#146919,#113491,#113492) ;
#94996 = AXIS2_PLACEMENT_3D('',#146922,#113494,#113495) ;
#94997 = AXIS2_PLACEMENT_3D('',#146923,#113496,#113497) ;
#94998 = AXIS2_PLACEMENT_3D('',#146928,#113499,#113500) ;
#94999 = AXIS2_PLACEMENT_3D('',#146932,#113502,#113503) ;
#95000 = AXIS2_PLACEMENT_3D('',#146936,#113505,#113506) ;
#95001 = AXIS2_PLACEMENT_3D('',#146939,#113508,#113509) ;
#95002 = AXIS2_PLACEMENT_3D('',#146940,#113510,#113511) ;
#95003 = AXIS2_PLACEMENT_3D('',#146945,#113513,#113514) ;
#95004 = AXIS2_PLACEMENT_3D('',#146949,#113516,#113517) ;
#95005 = AXIS2_PLACEMENT_3D('',#146953,#113519,#113520) ;
#95006 = AXIS2_PLACEMENT_3D('',#146956,#113522,#113523) ;
#95007 = AXIS2_PLACEMENT_3D('',#146957,#113524,#113525) ;
#95008 = AXIS2_PLACEMENT_3D('',#146962,#113527,#113528) ;
#95009 = AXIS2_PLACEMENT_3D('',#146966,#113530,#113531) ;
#95010 = AXIS2_PLACEMENT_3D('',#146970,#113533,#113534) ;
#95011 = AXIS2_PLACEMENT_3D('',#146973,#113536,#113537) ;
#95012 = AXIS2_PLACEMENT_3D('',#146974,#113538,#113539) ;
#95013 = AXIS2_PLACEMENT_3D('',#146979,#113541,#113542) ;
#95014 = AXIS2_PLACEMENT_3D('',#146983,#113544,#113545) ;
#95015 = AXIS2_PLACEMENT_3D('',#146987,#113547,#113548) ;
#95016 = AXIS2_PLACEMENT_3D('',#146990,#113550,#113551) ;
#95017 = AXIS2_PLACEMENT_3D('',#146991,#113552,#113553) ;
#95018 = AXIS2_PLACEMENT_3D('',#146996,#113555,#113556) ;
#95019 = AXIS2_PLACEMENT_3D('',#147000,#113558,#113559) ;
#95020 = AXIS2_PLACEMENT_3D('',#147004,#113561,#113562) ;
#95021 = AXIS2_PLACEMENT_3D('',#147007,#113564,#113565) ;
#95022 = AXIS2_PLACEMENT_3D('',#147008,#113566,#113567) ;
#95023 = AXIS2_PLACEMENT_3D('',#147013,#113569,#113570) ;
#95024 = AXIS2_PLACEMENT_3D('',#147017,#113572,#113573) ;
#95025 = AXIS2_PLACEMENT_3D('',#147021,#113575,#113576) ;
#95026 = AXIS2_PLACEMENT_3D('',#147024,#113578,#113579) ;
#95027 = AXIS2_PLACEMENT_3D('',#147025,#113580,#113581) ;
#95028 = AXIS2_PLACEMENT_3D('',#147030,#113583,#113584) ;
#95029 = AXIS2_PLACEMENT_3D('',#147034,#113586,#113587) ;
#95030 = AXIS2_PLACEMENT_3D('',#147038,#113589,#113590) ;
#95031 = AXIS2_PLACEMENT_3D('',#147041,#113592,#113593) ;
#95032 = AXIS2_PLACEMENT_3D('',#147042,#113594,#113595) ;
#95033 = AXIS2_PLACEMENT_3D('',#147047,#113597,#113598) ;
#95034 = AXIS2_PLACEMENT_3D('',#147051,#113600,#113601) ;
#95035 = AXIS2_PLACEMENT_3D('',#147055,#113603,#113604) ;
#95036 = AXIS2_PLACEMENT_3D('',#147058,#113606,#113607) ;
#95037 = AXIS2_PLACEMENT_3D('',#147059,#113608,#113609) ;
#95038 = AXIS2_PLACEMENT_3D('',#147060,#113610,#113611) ;
#95039 = AXIS2_PLACEMENT_3D('',#147061,#113612,#113613) ;
#95040 = AXIS2_PLACEMENT_3D('',#147062,#113614,#113615) ;
#95041 = AXIS2_PLACEMENT_3D('',#147063,#113616,#113617) ;
#95042 = AXIS2_PLACEMENT_3D('',#147064,#113618,#113619) ;
#95043 = AXIS2_PLACEMENT_3D('',#147065,#113620,#113621) ;
#95044 = AXIS2_PLACEMENT_3D('',#147067,#113622,#113623) ;
#95045 = AXIS2_PLACEMENT_3D('',#147068,#113624,#113625) ;
#95046 = AXIS2_PLACEMENT_3D('',#147069,#113626,#113627) ;
#95047 = AXIS2_PLACEMENT_3D('',#147070,#113628,#113629) ;
#95048 = AXIS2_PLACEMENT_3D('',#147071,#113630,#113631) ;
#95049 = AXIS2_PLACEMENT_3D('',#147072,#113632,#113633) ;
#95050 = AXIS2_PLACEMENT_3D('',#147073,#113634,#113635) ;
#95051 = AXIS2_PLACEMENT_3D('',#147074,#113636,#113637) ;
#95052 = AXIS2_PLACEMENT_3D('',#147075,#113638,#113639) ;
#95053 = AXIS2_PLACEMENT_3D('',#147086,#113641,#113642) ;
#95054 = AXIS2_PLACEMENT_3D('',#147143,#113644,#113645) ;
#95055 = AXIS2_PLACEMENT_3D('',#147144,#113646,#113647) ;
#95056 = AXIS2_PLACEMENT_3D('',#147145,#113648,#113649) ;
#95057 = AXIS2_PLACEMENT_3D('',#147146,#113650,#113651) ;
#95058 = AXIS2_PLACEMENT_3D('',#147147,#113652,#113653) ;
#95059 = AXIS2_PLACEMENT_3D('',#147148,#113654,#113655) ;
#95060 = AXIS2_PLACEMENT_3D('',#147149,#113656,#113657) ;
#95061 = AXIS2_PLACEMENT_3D('',#147150,#113658,#113659) ;
#95062 = AXIS2_PLACEMENT_3D('',#147151,#113660,#113661) ;
#95063 = AXIS2_PLACEMENT_3D('',#147152,#113662,#113663) ;
#95064 = AXIS2_PLACEMENT_3D('',#147153,#113664,#113665) ;
#95065 = AXIS2_PLACEMENT_3D('',#147154,#113666,#113667) ;
#95066 = AXIS2_PLACEMENT_3D('',#147155,#113668,#113669) ;
#95067 = AXIS2_PLACEMENT_3D('',#147156,#113670,#113671) ;
#95068 = AXIS2_PLACEMENT_3D('',#147157,#113672,#113673) ;
#95069 = AXIS2_PLACEMENT_3D('',#147158,#113674,#113675) ;
#95070 = AXIS2_PLACEMENT_3D('',#147159,#113676,#113677) ;
#95071 = AXIS2_PLACEMENT_3D('',#147160,#113678,#113679) ;
#95072 = AXIS2_PLACEMENT_3D('',#147161,#113680,#113681) ;
#95073 = AXIS2_PLACEMENT_3D('',#147162,#113682,#113683) ;
#95074 = AXIS2_PLACEMENT_3D('',#147163,#113684,#113685) ;
#95075 = AXIS2_PLACEMENT_3D('',#147164,#113686,#113687) ;
#95076 = AXIS2_PLACEMENT_3D('',#147165,#113688,#113689) ;
#95077 = AXIS2_PLACEMENT_3D('',#147168,#113691,#113692) ;
#95078 = AXIS2_PLACEMENT_3D('',#147169,#113693,#113694) ;
#95079 = AXIS2_PLACEMENT_3D('',#147170,#113695,#113696) ;
#95080 = AXIS2_PLACEMENT_3D('',#147171,#113697,#113698) ;
#95081 = AXIS2_PLACEMENT_3D('',#147172,#113699,#113700) ;
#95082 = AXIS2_PLACEMENT_3D('',#147173,#113701,#113702) ;
#95083 = AXIS2_PLACEMENT_3D('',#147174,#113703,#113704) ;
#95084 = AXIS2_PLACEMENT_3D('',#147175,#113705,#113706) ;
#95085 = AXIS2_PLACEMENT_3D('',#147176,#113707,#113708) ;
#95086 = AXIS2_PLACEMENT_3D('',#147177,#113709,#113710) ;
#95087 = AXIS2_PLACEMENT_3D('',#147178,#113711,#113712) ;
#95088 = AXIS2_PLACEMENT_3D('',#147179,#113713,#113714) ;
#95089 = AXIS2_PLACEMENT_3D('',#147180,#113715,#113716) ;
#95090 = AXIS2_PLACEMENT_3D('',#147181,#113717,#113718) ;
#95091 = AXIS2_PLACEMENT_3D('',#147182,#113719,#113720) ;
#95092 = AXIS2_PLACEMENT_3D('',#147183,#113721,#113722) ;
#95093 = AXIS2_PLACEMENT_3D('',#147185,#113723,#113724) ;
#95094 = AXIS2_PLACEMENT_3D('',#147186,#113725,#113726) ;
#95095 = AXIS2_PLACEMENT_3D('',#147187,#113727,#113728) ;
#95096 = AXIS2_PLACEMENT_3D('',#147188,#113729,#113730) ;
#95097 = AXIS2_PLACEMENT_3D('',#147189,#113731,#113732) ;
#95098 = AXIS2_PLACEMENT_3D('',#147190,#113733,#113734) ;
#95099 = AXIS2_PLACEMENT_3D('',#147191,#113735,#113736) ;
#95100 = AXIS2_PLACEMENT_3D('',#147192,#113737,#113738) ;
#95101 = AXIS2_PLACEMENT_3D('',#147193,#113739,#113740) ;
#95102 = AXIS2_PLACEMENT_3D('',#147194,#113741,#113742) ;
#95103 = AXIS2_PLACEMENT_3D('',#147195,#113743,#113744) ;
#95104 = AXIS2_PLACEMENT_3D('',#147196,#113745,#113746) ;
#95105 = AXIS2_PLACEMENT_3D('',#147197,#113747,#113748) ;
#95106 = AXIS2_PLACEMENT_3D('',#147200,#113750,#113751) ;
#95107 = AXIS2_PLACEMENT_3D('',#147201,#113752,#113753) ;
#95108 = AXIS2_PLACEMENT_3D('',#147202,#113754,#113755) ;
#95109 = AXIS2_PLACEMENT_3D('',#147203,#113756,#113757) ;
#95110 = AXIS2_PLACEMENT_3D('',#147204,#113758,#113759) ;
#95111 = AXIS2_PLACEMENT_3D('',#147205,#113760,#113761) ;
#95112 = AXIS2_PLACEMENT_3D('',#147206,#113762,#113763) ;
#95113 = AXIS2_PLACEMENT_3D('',#147207,#113764,#113765) ;
#95114 = AXIS2_PLACEMENT_3D('',#147208,#113766,#113767) ;
#95115 = AXIS2_PLACEMENT_3D('',#147209,#113768,#113769) ;
#95116 = AXIS2_PLACEMENT_3D('',#147210,#113770,#113771) ;
#95117 = AXIS2_PLACEMENT_3D('',#147211,#113772,#113773) ;
#95118 = AXIS2_PLACEMENT_3D('',#147212,#113774,#113775) ;
#95119 = AXIS2_PLACEMENT_3D('',#147214,#113776,#113777) ;
#95120 = AXIS2_PLACEMENT_3D('',#147215,#113778,#113779) ;
#95121 = AXIS2_PLACEMENT_3D('',#147216,#113780,#113781) ;
#95122 = AXIS2_PLACEMENT_3D('',#147217,#113782,#113783) ;
#95123 = AXIS2_PLACEMENT_3D('',#147218,#113784,#113785) ;
#95124 = AXIS2_PLACEMENT_3D('',#147219,#113786,#113787) ;
#95125 = AXIS2_PLACEMENT_3D('',#147220,#113788,#113789) ;
#95126 = AXIS2_PLACEMENT_3D('',#147221,#113790,#113791) ;
#95127 = AXIS2_PLACEMENT_3D('',#147222,#113792,#113793) ;
#95128 = AXIS2_PLACEMENT_3D('',#147223,#113794,#113795) ;
#95129 = AXIS2_PLACEMENT_3D('',#147224,#113796,#113797) ;
#95130 = AXIS2_PLACEMENT_3D('',#147226,#113799,#113800) ;
#95131 = AXIS2_PLACEMENT_3D('',#147227,#113801,#113802) ;
#95132 = AXIS2_PLACEMENT_3D('',#147228,#113803,#113804) ;
#95133 = AXIS2_PLACEMENT_3D('',#147229,#113805,#113806) ;
#95134 = AXIS2_PLACEMENT_3D('',#147230,#113807,#113808) ;
#95135 = AXIS2_PLACEMENT_3D('',#147231,#113809,#113810) ;
#95136 = AXIS2_PLACEMENT_3D('',#147232,#113811,#113812) ;
#95137 = AXIS2_PLACEMENT_3D('',#147233,#113813,#113814) ;
#95138 = AXIS2_PLACEMENT_3D('',#147234,#113815,#113816) ;
#95139 = AXIS2_PLACEMENT_3D('',#147235,#113817,#113818) ;
#95140 = AXIS2_PLACEMENT_3D('',#147236,#113819,#113820) ;
#95141 = AXIS2_PLACEMENT_3D('',#147237,#113821,#113822) ;
#95142 = AXIS2_PLACEMENT_3D('',#147238,#113823,#113824) ;
#95143 = AXIS2_PLACEMENT_3D('',#147239,#113825,#113826) ;
#95144 = AXIS2_PLACEMENT_3D('',#147240,#113827,#113828) ;
#95145 = AXIS2_PLACEMENT_3D('',#147241,#113829,#113830) ;
#95146 = AXIS2_PLACEMENT_3D('',#147242,#113831,#113832) ;
#95147 = AXIS2_PLACEMENT_3D('',#147243,#113833,#113834) ;
#95148 = AXIS2_PLACEMENT_3D('',#147244,#113835,#113836) ;
#95149 = AXIS2_PLACEMENT_3D('',#147245,#113837,#113838) ;
#95150 = AXIS2_PLACEMENT_3D('',#147246,#113839,#113840) ;
#95151 = AXIS2_PLACEMENT_3D('',#147247,#113841,#113842) ;
#95152 = AXIS2_PLACEMENT_3D('',#147248,#113843,#113844) ;
#95153 = AXIS2_PLACEMENT_3D('',#147249,#113845,#113846) ;
#95154 = AXIS2_PLACEMENT_3D('',#147250,#113847,#113848) ;
#95155 = AXIS2_PLACEMENT_3D('',#147251,#113849,#113850) ;
#95156 = AXIS2_PLACEMENT_3D('',#147252,#113851,#113852) ;
#95157 = AXIS2_PLACEMENT_3D('',#147253,#113853,#113854) ;
#95158 = AXIS2_PLACEMENT_3D('',#147254,#113855,#113856) ;
#95159 = AXIS2_PLACEMENT_3D('',#147255,#113857,#113858) ;
#95160 = AXIS2_PLACEMENT_3D('',#147256,#113859,#113860) ;
#95161 = AXIS2_PLACEMENT_3D('',#147257,#113861,#113862) ;
#95162 = AXIS2_PLACEMENT_3D('',#147258,#113863,#113864) ;
#95163 = AXIS2_PLACEMENT_3D('',#147259,#113865,#113866) ;
#95164 = AXIS2_PLACEMENT_3D('',#147260,#113867,#113868) ;
#95165 = AXIS2_PLACEMENT_3D('',#147261,#113869,#113870) ;
#95166 = AXIS2_PLACEMENT_3D('',#147262,#113871,#113872) ;
#95167 = AXIS2_PLACEMENT_3D('',#147263,#113873,#113874) ;
#95168 = AXIS2_PLACEMENT_3D('',#147264,#113875,#113876) ;
#95169 = AXIS2_PLACEMENT_3D('',#147265,#113877,#113878) ;
#95170 = AXIS2_PLACEMENT_3D('',#147266,#113879,#113880) ;
#95171 = AXIS2_PLACEMENT_3D('',#147267,#113881,#113882) ;
#95172 = AXIS2_PLACEMENT_3D('',#147268,#113883,#113884) ;
#95173 = AXIS2_PLACEMENT_3D('',#147269,#113885,#113886) ;
#95174 = AXIS2_PLACEMENT_3D('',#147270,#113887,#113888) ;
#95175 = AXIS2_PLACEMENT_3D('',#147271,#113889,#113890) ;
#95176 = AXIS2_PLACEMENT_3D('',#147272,#113891,#113892) ;
#95177 = AXIS2_PLACEMENT_3D('',#147273,#113893,#113894) ;
#95178 = AXIS2_PLACEMENT_3D('',#147274,#113895,#113896) ;
#95179 = AXIS2_PLACEMENT_3D('',#147275,#113897,#113898) ;
#95180 = AXIS2_PLACEMENT_3D('',#147276,#113899,#113900) ;
#95181 = AXIS2_PLACEMENT_3D('',#147277,#113901,#113902) ;
#95182 = AXIS2_PLACEMENT_3D('',#147278,#113903,#113904) ;
#95183 = AXIS2_PLACEMENT_3D('',#147279,#113905,#113906) ;
#95184 = AXIS2_PLACEMENT_3D('',#147280,#113907,#113908) ;
#95185 = AXIS2_PLACEMENT_3D('',#147281,#113909,#113910) ;
#95186 = AXIS2_PLACEMENT_3D('',#147282,#113911,#113912) ;
#95187 = AXIS2_PLACEMENT_3D('',#147283,#113913,#113914) ;
#95188 = AXIS2_PLACEMENT_3D('',#147284,#113915,#113916) ;
#95189 = AXIS2_PLACEMENT_3D('',#147285,#113917,#113918) ;
#95190 = AXIS2_PLACEMENT_3D('',#147286,#113919,#113920) ;
#95191 = AXIS2_PLACEMENT_3D('',#147287,#113921,#113922) ;
#95192 = AXIS2_PLACEMENT_3D('',#147288,#113923,#113924) ;
#95193 = AXIS2_PLACEMENT_3D('',#147289,#113925,#113926) ;
#95194 = AXIS2_PLACEMENT_3D('',#147290,#113927,#113928) ;
#95195 = AXIS2_PLACEMENT_3D('',#147291,#113929,#113930) ;
#95196 = AXIS2_PLACEMENT_3D('',#147292,#113931,#113932) ;
#95197 = AXIS2_PLACEMENT_3D('',#147293,#113933,#113934) ;
#95198 = AXIS2_PLACEMENT_3D('',#147294,#113935,#113936) ;
#95199 = AXIS2_PLACEMENT_3D('',#147295,#113937,#113938) ;
#95200 = AXIS2_PLACEMENT_3D('',#147296,#113939,#113940) ;
#95201 = AXIS2_PLACEMENT_3D('',#147297,#113941,#113942) ;
#95202 = AXIS2_PLACEMENT_3D('',#147298,#113943,#113944) ;
#95203 = AXIS2_PLACEMENT_3D('',#147299,#113945,#113946) ;
#95204 = AXIS2_PLACEMENT_3D('',#147300,#113947,#113948) ;
#95205 = AXIS2_PLACEMENT_3D('',#147301,#113949,#113950) ;
#95206 = AXIS2_PLACEMENT_3D('',#147302,#113951,#113952) ;
#95207 = AXIS2_PLACEMENT_3D('',#147303,#113953,#113954) ;
#95208 = AXIS2_PLACEMENT_3D('',#147304,#113955,#113956) ;
#95209 = AXIS2_PLACEMENT_3D('',#147305,#113957,#113958) ;
#95210 = AXIS2_PLACEMENT_3D('',#147306,#113959,#113960) ;
#95211 = AXIS2_PLACEMENT_3D('',#147307,#113961,#113962) ;
#95212 = AXIS2_PLACEMENT_3D('',#147308,#113963,#113964) ;
#95213 = AXIS2_PLACEMENT_3D('',#147309,#113965,#113966) ;
#95214 = AXIS2_PLACEMENT_3D('',#147310,#113967,#113968) ;
#95215 = AXIS2_PLACEMENT_3D('',#147311,#113969,#113970) ;
#95216 = AXIS2_PLACEMENT_3D('',#147312,#113971,#113972) ;
#95217 = AXIS2_PLACEMENT_3D('',#147313,#113973,#113974) ;
#95218 = AXIS2_PLACEMENT_3D('',#147314,#113975,#113976) ;
#95219 = AXIS2_PLACEMENT_3D('',#147315,#113977,#113978) ;
#95220 = AXIS2_PLACEMENT_3D('',#147316,#113979,#113980) ;
#95221 = AXIS2_PLACEMENT_3D('',#147317,#113981,#113982) ;
#95222 = AXIS2_PLACEMENT_3D('',#147318,#113983,#113984) ;
#95223 = AXIS2_PLACEMENT_3D('',#147319,#113985,#113986) ;
#95224 = AXIS2_PLACEMENT_3D('',#147320,#113987,#113988) ;
#95225 = AXIS2_PLACEMENT_3D('',#147321,#113989,#113990) ;
#95226 = AXIS2_PLACEMENT_3D('',#147322,#113991,#113992) ;
#95227 = AXIS2_PLACEMENT_3D('',#147323,#113993,#113994) ;
#95228 = AXIS2_PLACEMENT_3D('',#147324,#113995,#113996) ;
#95229 = AXIS2_PLACEMENT_3D('',#147325,#113997,#113998) ;
#95230 = AXIS2_PLACEMENT_3D('',#147326,#113999,#114000) ;
#95231 = AXIS2_PLACEMENT_3D('',#147327,#114001,#114002) ;
#95232 = AXIS2_PLACEMENT_3D('',#147328,#114003,#114004) ;
#95233 = AXIS2_PLACEMENT_3D('',#147329,#114005,#114006) ;
#95234 = AXIS2_PLACEMENT_3D('',#147330,#114007,#114008) ;
#95235 = AXIS2_PLACEMENT_3D('',#147331,#114009,#114010) ;
#95236 = AXIS2_PLACEMENT_3D('',#147332,#114011,#114012) ;
#95237 = AXIS2_PLACEMENT_3D('',#147333,#114013,#114014) ;
#95238 = AXIS2_PLACEMENT_3D('',#147334,#114015,#114016) ;
#95239 = AXIS2_PLACEMENT_3D('',#147335,#114017,#114018) ;
#95240 = AXIS2_PLACEMENT_3D('',#147336,#114019,#114020) ;
#95241 = AXIS2_PLACEMENT_3D('',#147337,#114021,#114022) ;
#95242 = AXIS2_PLACEMENT_3D('',#147338,#114023,#114024) ;
#95243 = AXIS2_PLACEMENT_3D('',#147339,#114025,#114026) ;
#95244 = AXIS2_PLACEMENT_3D('',#147340,#114027,#114028) ;
#95245 = AXIS2_PLACEMENT_3D('',#147341,#114029,#114030) ;
#95246 = AXIS2_PLACEMENT_3D('',#147342,#114031,#114032) ;
#95247 = AXIS2_PLACEMENT_3D('',#147343,#114033,#114034) ;
#95248 = AXIS2_PLACEMENT_3D('',#147344,#114035,#114036) ;
#95249 = AXIS2_PLACEMENT_3D('',#147345,#114037,#114038) ;
#95250 = AXIS2_PLACEMENT_3D('',#147346,#114039,#114040) ;
#95251 = AXIS2_PLACEMENT_3D('',#147347,#114041,#114042) ;
#95252 = AXIS2_PLACEMENT_3D('',#147348,#114043,#114044) ;
#95253 = AXIS2_PLACEMENT_3D('',#147349,#114045,#114046) ;
#95254 = AXIS2_PLACEMENT_3D('',#147350,#114047,#114048) ;
#95255 = AXIS2_PLACEMENT_3D('',#147351,#114049,#114050) ;
#95256 = AXIS2_PLACEMENT_3D('',#147352,#114051,#114052) ;
#95257 = AXIS2_PLACEMENT_3D('',#147353,#114053,#114054) ;
#95258 = AXIS2_PLACEMENT_3D('',#147354,#114055,#114056) ;
#95259 = AXIS2_PLACEMENT_3D('',#147355,#114057,#114058) ;
#95260 = AXIS2_PLACEMENT_3D('',#147356,#114059,#114060) ;
#95261 = AXIS2_PLACEMENT_3D('',#147357,#114061,#114062) ;
#95262 = AXIS2_PLACEMENT_3D('',#147358,#114063,#114064) ;
#95263 = AXIS2_PLACEMENT_3D('',#147359,#114065,#114066) ;
#95264 = AXIS2_PLACEMENT_3D('',#147360,#114067,#114068) ;
#95265 = AXIS2_PLACEMENT_3D('',#147361,#114069,#114070) ;
#95266 = AXIS2_PLACEMENT_3D('',#147362,#114071,#114072) ;
#95267 = AXIS2_PLACEMENT_3D('',#147363,#114073,#114074) ;
#95268 = AXIS2_PLACEMENT_3D('',#147364,#114075,#114076) ;
#95269 = AXIS2_PLACEMENT_3D('',#147365,#114077,#114078) ;
#95270 = AXIS2_PLACEMENT_3D('',#147366,#114079,#114080) ;
#95271 = AXIS2_PLACEMENT_3D('',#147367,#114081,#114082) ;
#95272 = AXIS2_PLACEMENT_3D('',#147368,#114083,#114084) ;
#95273 = AXIS2_PLACEMENT_3D('',#147369,#114085,#114086) ;
#95274 = AXIS2_PLACEMENT_3D('',#147370,#114087,#114088) ;
#95275 = AXIS2_PLACEMENT_3D('',#147371,#114089,#114090) ;
#95276 = AXIS2_PLACEMENT_3D('',#147372,#114091,#114092) ;
#95277 = AXIS2_PLACEMENT_3D('',#147373,#114093,#114094) ;
#95278 = AXIS2_PLACEMENT_3D('',#147374,#114095,#114096) ;
#95279 = AXIS2_PLACEMENT_3D('',#147375,#114097,#114098) ;
#95280 = AXIS2_PLACEMENT_3D('',#147376,#114099,#114100) ;
#95281 = AXIS2_PLACEMENT_3D('',#147377,#114101,#114102) ;
#95282 = AXIS2_PLACEMENT_3D('',#147378,#114103,#114104) ;
#95283 = AXIS2_PLACEMENT_3D('',#147379,#114105,#114106) ;
#95284 = AXIS2_PLACEMENT_3D('',#147380,#114107,#114108) ;
#95285 = AXIS2_PLACEMENT_3D('',#147381,#114109,#114110) ;
#95286 = AXIS2_PLACEMENT_3D('',#147382,#114111,#114112) ;
#95287 = AXIS2_PLACEMENT_3D('',#147383,#114113,#114114) ;
#95288 = AXIS2_PLACEMENT_3D('',#147384,#114115,#114116) ;
#95289 = AXIS2_PLACEMENT_3D('',#147385,#114117,#114118) ;
#95290 = AXIS2_PLACEMENT_3D('',#147386,#114119,#114120) ;
#95291 = AXIS2_PLACEMENT_3D('',#147387,#114121,#114122) ;
#95292 = AXIS2_PLACEMENT_3D('',#147388,#114123,#114124) ;
#95293 = AXIS2_PLACEMENT_3D('',#147389,#114125,#114126) ;
#95294 = AXIS2_PLACEMENT_3D('',#147390,#114127,#114128) ;
#95295 = AXIS2_PLACEMENT_3D('',#147391,#114129,#114130) ;
#95296 = AXIS2_PLACEMENT_3D('',#147392,#114131,#114132) ;
#95297 = AXIS2_PLACEMENT_3D('',#147393,#114133,#114134) ;
#95298 = AXIS2_PLACEMENT_3D('',#147394,#114135,#114136) ;
#95299 = AXIS2_PLACEMENT_3D('',#147395,#114137,#114138) ;
#95300 = AXIS2_PLACEMENT_3D('',#147396,#114139,#114140) ;
#95301 = AXIS2_PLACEMENT_3D('',#147397,#114141,#114142) ;
#95302 = AXIS2_PLACEMENT_3D('',#147398,#114143,#114144) ;
#95303 = AXIS2_PLACEMENT_3D('',#147399,#114145,#114146) ;
#95304 = AXIS2_PLACEMENT_3D('',#147400,#114147,#114148) ;
#95305 = AXIS2_PLACEMENT_3D('',#147401,#114149,#114150) ;
#95306 = AXIS2_PLACEMENT_3D('',#147402,#114151,#114152) ;
#95307 = AXIS2_PLACEMENT_3D('',#147403,#114153,#114154) ;
#95308 = AXIS2_PLACEMENT_3D('',#147404,#114155,#114156) ;
#95309 = AXIS2_PLACEMENT_3D('',#147405,#114157,#114158) ;
#95310 = AXIS2_PLACEMENT_3D('',#147406,#114159,#114160) ;
#95311 = AXIS2_PLACEMENT_3D('',#147407,#114161,#114162) ;
#95312 = AXIS2_PLACEMENT_3D('',#147408,#114163,#114164) ;
#95313 = AXIS2_PLACEMENT_3D('',#147409,#114165,#114166) ;
#95314 = AXIS2_PLACEMENT_3D('',#147410,#114167,#114168) ;
#95315 = AXIS2_PLACEMENT_3D('',#147411,#114169,#114170) ;
#95316 = AXIS2_PLACEMENT_3D('',#147412,#114171,#114172) ;
#95317 = AXIS2_PLACEMENT_3D('',#147413,#114173,#114174) ;
#95318 = AXIS2_PLACEMENT_3D('',#147414,#114175,#114176) ;
#95319 = AXIS2_PLACEMENT_3D('',#147415,#114177,#114178) ;
#95320 = AXIS2_PLACEMENT_3D('',#147416,#114179,#114180) ;
#95321 = AXIS2_PLACEMENT_3D('',#147417,#114181,#114182) ;
#95322 = AXIS2_PLACEMENT_3D('',#147418,#114183,#114184) ;
#95323 = AXIS2_PLACEMENT_3D('',#147419,#114185,#114186) ;
#95324 = AXIS2_PLACEMENT_3D('',#147420,#114187,#114188) ;
#95325 = AXIS2_PLACEMENT_3D('',#147421,#114189,#114190) ;
#95326 = AXIS2_PLACEMENT_3D('',#147422,#114191,#114192) ;
#95327 = AXIS2_PLACEMENT_3D('',#147423,#114193,#114194) ;
#95328 = AXIS2_PLACEMENT_3D('',#147424,#114195,#114196) ;
#95329 = AXIS2_PLACEMENT_3D('',#147425,#114197,#114198) ;
#95330 = AXIS2_PLACEMENT_3D('',#147426,#114199,#114200) ;
#95331 = AXIS2_PLACEMENT_3D('',#147427,#114201,#114202) ;
#95332 = AXIS2_PLACEMENT_3D('',#147428,#114203,#114204) ;
#95333 = AXIS2_PLACEMENT_3D('',#147429,#114205,#114206) ;
#95334 = AXIS2_PLACEMENT_3D('',#147430,#114207,#114208) ;
#95335 = AXIS2_PLACEMENT_3D('',#147431,#114209,#114210) ;
#95336 = AXIS2_PLACEMENT_3D('',#147432,#114211,#114212) ;
#95337 = AXIS2_PLACEMENT_3D('',#147433,#114213,#114214) ;
#95338 = AXIS2_PLACEMENT_3D('',#147434,#114215,#114216) ;
#95339 = AXIS2_PLACEMENT_3D('',#147435,#114217,#114218) ;
#95340 = AXIS2_PLACEMENT_3D('',#147436,#114219,#114220) ;
#95341 = AXIS2_PLACEMENT_3D('',#147437,#114221,#114222) ;
#95342 = AXIS2_PLACEMENT_3D('',#147438,#114223,#114224) ;
#95343 = AXIS2_PLACEMENT_3D('',#147439,#114225,#114226) ;
#95344 = AXIS2_PLACEMENT_3D('',#147440,#114227,#114228) ;
#95345 = AXIS2_PLACEMENT_3D('',#147441,#114229,#114230) ;
#95346 = AXIS2_PLACEMENT_3D('',#147442,#114231,#114232) ;
#95347 = AXIS2_PLACEMENT_3D('',#147443,#114233,#114234) ;
#95348 = AXIS2_PLACEMENT_3D('',#147444,#114235,#114236) ;
#95349 = AXIS2_PLACEMENT_3D('',#147445,#114237,#114238) ;
#95350 = AXIS2_PLACEMENT_3D('',#147446,#114239,#114240) ;
#95351 = AXIS2_PLACEMENT_3D('',#147447,#114241,#114242) ;
#95352 = AXIS2_PLACEMENT_3D('',#147448,#114243,#114244) ;
#95353 = AXIS2_PLACEMENT_3D('',#147449,#114245,#114246) ;
#95354 = AXIS2_PLACEMENT_3D('',#147450,#114247,#114248) ;
#95355 = AXIS2_PLACEMENT_3D('',#147451,#114249,#114250) ;
#95356 = AXIS2_PLACEMENT_3D('',#147452,#114251,#114252) ;
#95357 = AXIS2_PLACEMENT_3D('',#147453,#114253,#114254) ;
#95358 = AXIS2_PLACEMENT_3D('',#147454,#114255,#114256) ;
#95359 = AXIS2_PLACEMENT_3D('',#147455,#114257,#114258) ;
#95360 = AXIS2_PLACEMENT_3D('',#147456,#114259,#114260) ;
#95361 = AXIS2_PLACEMENT_3D('',#147457,#114261,#114262) ;
#95362 = AXIS2_PLACEMENT_3D('',#147458,#114263,#114264) ;
#95363 = AXIS2_PLACEMENT_3D('',#147459,#114265,#114266) ;
#95364 = AXIS2_PLACEMENT_3D('',#147460,#114267,#114268) ;
#95365 = AXIS2_PLACEMENT_3D('',#147461,#114269,#114270) ;
#95366 = AXIS2_PLACEMENT_3D('',#147462,#114271,#114272) ;
#95367 = AXIS2_PLACEMENT_3D('',#147463,#114273,#114274) ;
#95368 = AXIS2_PLACEMENT_3D('',#147464,#114275,#114276) ;
#95369 = AXIS2_PLACEMENT_3D('',#147465,#114277,#114278) ;
#95370 = AXIS2_PLACEMENT_3D('',#147466,#114279,#114280) ;
#95371 = AXIS2_PLACEMENT_3D('',#147467,#114281,#114282) ;
#95372 = AXIS2_PLACEMENT_3D('',#147468,#114283,#114284) ;
#95373 = AXIS2_PLACEMENT_3D('',#147469,#114285,#114286) ;
#95374 = AXIS2_PLACEMENT_3D('',#147470,#114287,#114288) ;
#95375 = AXIS2_PLACEMENT_3D('',#147471,#114289,#114290) ;
#95376 = AXIS2_PLACEMENT_3D('',#147472,#114291,#114292) ;
#95377 = AXIS2_PLACEMENT_3D('',#147473,#114293,#114294) ;
#95378 = AXIS2_PLACEMENT_3D('',#147474,#114295,#114296) ;
#95379 = AXIS2_PLACEMENT_3D('',#147475,#114297,#114298) ;
#95380 = AXIS2_PLACEMENT_3D('',#147476,#114299,#114300) ;
#95381 = AXIS2_PLACEMENT_3D('',#147477,#114301,#114302) ;
#95382 = AXIS2_PLACEMENT_3D('',#147478,#114303,#114304) ;
#95383 = AXIS2_PLACEMENT_3D('',#147479,#114305,#114306) ;
#95384 = AXIS2_PLACEMENT_3D('',#147480,#114307,#114308) ;
#95385 = AXIS2_PLACEMENT_3D('',#147481,#114309,#114310) ;
#95386 = AXIS2_PLACEMENT_3D('',#147482,#114311,#114312) ;
#95387 = AXIS2_PLACEMENT_3D('',#147483,#114313,#114314) ;
#95388 = AXIS2_PLACEMENT_3D('',#147484,#114315,#114316) ;
#95389 = AXIS2_PLACEMENT_3D('',#147485,#114317,#114318) ;
#95390 = AXIS2_PLACEMENT_3D('',#147486,#114319,#114320) ;
#95391 = AXIS2_PLACEMENT_3D('',#147487,#114321,#114322) ;
#95392 = AXIS2_PLACEMENT_3D('',#147488,#114323,#114324) ;
#95393 = AXIS2_PLACEMENT_3D('',#147489,#114325,#114326) ;
#95394 = AXIS2_PLACEMENT_3D('',#147490,#114327,#114328) ;
#95395 = AXIS2_PLACEMENT_3D('',#147491,#114329,#114330) ;
#95396 = AXIS2_PLACEMENT_3D('',#147492,#114331,#114332) ;
#95397 = AXIS2_PLACEMENT_3D('',#147493,#114333,#114334) ;
#95398 = AXIS2_PLACEMENT_3D('',#147494,#114335,#114336) ;
#95399 = AXIS2_PLACEMENT_3D('',#147495,#114337,#114338) ;
#95400 = AXIS2_PLACEMENT_3D('',#147496,#114339,#114340) ;
#95401 = AXIS2_PLACEMENT_3D('',#147497,#114341,#114342) ;
#95402 = AXIS2_PLACEMENT_3D('',#147498,#114343,#114344) ;
#95403 = AXIS2_PLACEMENT_3D('',#147499,#114345,#114346) ;
#95404 = AXIS2_PLACEMENT_3D('',#147500,#114347,#114348) ;
#95405 = AXIS2_PLACEMENT_3D('',#147501,#114349,#114350) ;
#95406 = AXIS2_PLACEMENT_3D('',#147502,#114351,#114352) ;
#95407 = AXIS2_PLACEMENT_3D('',#147503,#114353,#114354) ;
#95408 = AXIS2_PLACEMENT_3D('',#147504,#114355,#114356) ;
#95409 = AXIS2_PLACEMENT_3D('',#147505,#114357,#114358) ;
#95410 = AXIS2_PLACEMENT_3D('',#147506,#114359,#114360) ;
#95411 = AXIS2_PLACEMENT_3D('',#147507,#114361,#114362) ;
#95412 = AXIS2_PLACEMENT_3D('',#147508,#114363,#114364) ;
#95413 = AXIS2_PLACEMENT_3D('',#147509,#114365,#114366) ;
#95414 = AXIS2_PLACEMENT_3D('',#147510,#114367,#114368) ;
#95415 = AXIS2_PLACEMENT_3D('',#147511,#114369,#114370) ;
#95416 = AXIS2_PLACEMENT_3D('',#147512,#114371,#114372) ;
#95417 = AXIS2_PLACEMENT_3D('',#147513,#114373,#114374) ;
#95418 = AXIS2_PLACEMENT_3D('',#147514,#114375,#114376) ;
#95419 = AXIS2_PLACEMENT_3D('',#147515,#114377,#114378) ;
#95420 = AXIS2_PLACEMENT_3D('',#147516,#114379,#114380) ;
#95421 = AXIS2_PLACEMENT_3D('',#147517,#114381,#114382) ;
#95422 = AXIS2_PLACEMENT_3D('',#147518,#114383,#114384) ;
#95423 = AXIS2_PLACEMENT_3D('',#147519,#114385,#114386) ;
#95424 = AXIS2_PLACEMENT_3D('',#147520,#114387,#114388) ;
#95425 = AXIS2_PLACEMENT_3D('',#147521,#114389,#114390) ;
#95426 = AXIS2_PLACEMENT_3D('',#147522,#114391,#114392) ;
#95427 = AXIS2_PLACEMENT_3D('',#147523,#114393,#114394) ;
#95428 = AXIS2_PLACEMENT_3D('',#147524,#114395,#114396) ;
#95429 = AXIS2_PLACEMENT_3D('',#147525,#114397,#114398) ;
#95430 = AXIS2_PLACEMENT_3D('',#147526,#114399,#114400) ;
#95431 = AXIS2_PLACEMENT_3D('',#147527,#114401,#114402) ;
#95432 = AXIS2_PLACEMENT_3D('',#147528,#114403,#114404) ;
#95433 = AXIS2_PLACEMENT_3D('',#147529,#114405,#114406) ;
#95434 = AXIS2_PLACEMENT_3D('',#147530,#114407,#114408) ;
#95435 = AXIS2_PLACEMENT_3D('',#147531,#114409,#114410) ;
#95436 = AXIS2_PLACEMENT_3D('',#147532,#114411,#114412) ;
#95437 = AXIS2_PLACEMENT_3D('',#147533,#114413,#114414) ;
#95438 = AXIS2_PLACEMENT_3D('',#147534,#114415,#114416) ;
#95439 = AXIS2_PLACEMENT_3D('',#147535,#114417,#114418) ;
#95440 = AXIS2_PLACEMENT_3D('',#147536,#114419,#114420) ;
#95441 = AXIS2_PLACEMENT_3D('',#147537,#114421,#114422) ;
#95442 = AXIS2_PLACEMENT_3D('',#147538,#114423,#114424) ;
#95443 = AXIS2_PLACEMENT_3D('',#147539,#114425,#114426) ;
#95444 = AXIS2_PLACEMENT_3D('',#147540,#114427,#114428) ;
#95445 = AXIS2_PLACEMENT_3D('',#147541,#114429,#114430) ;
#95446 = AXIS2_PLACEMENT_3D('',#147542,#114431,#114432) ;
#95447 = AXIS2_PLACEMENT_3D('',#147543,#114433,#114434) ;
#95448 = AXIS2_PLACEMENT_3D('',#147544,#114435,#114436) ;
#95449 = AXIS2_PLACEMENT_3D('',#147545,#114437,#114438) ;
#95450 = AXIS2_PLACEMENT_3D('',#147546,#114439,#114440) ;
#95451 = AXIS2_PLACEMENT_3D('',#147547,#114441,#114442) ;
#95452 = AXIS2_PLACEMENT_3D('',#147548,#114443,#114444) ;
#95453 = AXIS2_PLACEMENT_3D('',#147549,#114445,#114446) ;
#95454 = AXIS2_PLACEMENT_3D('',#147550,#114447,#114448) ;
#95455 = AXIS2_PLACEMENT_3D('',#147551,#114449,#114450) ;
#95456 = AXIS2_PLACEMENT_3D('',#147552,#114451,#114452) ;
#95457 = AXIS2_PLACEMENT_3D('',#147553,#114453,#114454) ;
#95458 = AXIS2_PLACEMENT_3D('',#147554,#114455,#114456) ;
#95459 = AXIS2_PLACEMENT_3D('',#147555,#114457,#114458) ;
#95460 = AXIS2_PLACEMENT_3D('',#147556,#114459,#114460) ;
#95461 = AXIS2_PLACEMENT_3D('',#147557,#114461,#114462) ;
#95462 = AXIS2_PLACEMENT_3D('',#147558,#114463,#114464) ;
#95463 = AXIS2_PLACEMENT_3D('',#147559,#114465,#114466) ;
#95464 = AXIS2_PLACEMENT_3D('',#147560,#114467,#114468) ;
#95465 = AXIS2_PLACEMENT_3D('',#147561,#114469,#114470) ;
#95466 = AXIS2_PLACEMENT_3D('',#147562,#114471,#114472) ;
#95467 = AXIS2_PLACEMENT_3D('',#147563,#114473,#114474) ;
#95468 = AXIS2_PLACEMENT_3D('',#147564,#114475,#114476) ;
#95469 = AXIS2_PLACEMENT_3D('',#147565,#114477,#114478) ;
#95470 = AXIS2_PLACEMENT_3D('',#147566,#114479,#114480) ;
#95471 = AXIS2_PLACEMENT_3D('',#147567,#114481,#114482) ;
#95472 = AXIS2_PLACEMENT_3D('',#147568,#114483,#114484) ;
#95473 = AXIS2_PLACEMENT_3D('',#147569,#114485,#114486) ;
#95474 = AXIS2_PLACEMENT_3D('',#147570,#114487,#114488) ;
#95475 = AXIS2_PLACEMENT_3D('',#147571,#114489,#114490) ;
#95476 = AXIS2_PLACEMENT_3D('',#147572,#114491,#114492) ;
#95477 = AXIS2_PLACEMENT_3D('',#147573,#114493,#114494) ;
#95478 = AXIS2_PLACEMENT_3D('',#147574,#114495,#114496) ;
#95479 = AXIS2_PLACEMENT_3D('',#147575,#114497,#114498) ;
#95480 = AXIS2_PLACEMENT_3D('',#147576,#114499,#114500) ;
#95481 = AXIS2_PLACEMENT_3D('',#147577,#114501,#114502) ;
#95482 = AXIS2_PLACEMENT_3D('',#147578,#114503,#114504) ;
#95483 = AXIS2_PLACEMENT_3D('',#147579,#114505,#114506) ;
#95484 = AXIS2_PLACEMENT_3D('',#147580,#114507,#114508) ;
#95485 = AXIS2_PLACEMENT_3D('',#147581,#114509,#114510) ;
#95486 = AXIS2_PLACEMENT_3D('',#147582,#114511,#114512) ;
#95487 = AXIS2_PLACEMENT_3D('',#147583,#114513,#114514) ;
#95488 = AXIS2_PLACEMENT_3D('',#147584,#114515,#114516) ;
#95489 = AXIS2_PLACEMENT_3D('',#147585,#114517,#114518) ;
#95490 = AXIS2_PLACEMENT_3D('',#147586,#114519,#114520) ;
#95491 = AXIS2_PLACEMENT_3D('',#147587,#114521,#114522) ;
#95492 = AXIS2_PLACEMENT_3D('',#147588,#114523,#114524) ;
#95493 = AXIS2_PLACEMENT_3D('',#147589,#114525,#114526) ;
#95494 = AXIS2_PLACEMENT_3D('',#147590,#114527,#114528) ;
#95495 = AXIS2_PLACEMENT_3D('',#147591,#114529,#114530) ;
#95496 = AXIS2_PLACEMENT_3D('',#147592,#114531,#114532) ;
#95497 = AXIS2_PLACEMENT_3D('',#147593,#114533,#114534) ;
#95498 = AXIS2_PLACEMENT_3D('',#147594,#114535,#114536) ;
#95499 = AXIS2_PLACEMENT_3D('',#147595,#114537,#114538) ;
#95500 = AXIS2_PLACEMENT_3D('',#147596,#114539,#114540) ;
#95501 = AXIS2_PLACEMENT_3D('',#147597,#114541,#114542) ;
#95502 = AXIS2_PLACEMENT_3D('',#147598,#114543,#114544) ;
#95503 = AXIS2_PLACEMENT_3D('',#147599,#114545,#114546) ;
#95504 = AXIS2_PLACEMENT_3D('',#147600,#114547,#114548) ;
#95505 = AXIS2_PLACEMENT_3D('',#147601,#114549,#114550) ;
#95506 = AXIS2_PLACEMENT_3D('',#147602,#114551,#114552) ;
#95507 = AXIS2_PLACEMENT_3D('',#147603,#114553,#114554) ;
#95508 = AXIS2_PLACEMENT_3D('',#147604,#114555,#114556) ;
#95509 = AXIS2_PLACEMENT_3D('',#147605,#114557,#114558) ;
#95510 = AXIS2_PLACEMENT_3D('',#147606,#114559,#114560) ;
#95511 = AXIS2_PLACEMENT_3D('',#147607,#114561,#114562) ;
#95512 = AXIS2_PLACEMENT_3D('',#147608,#114563,#114564) ;
#95513 = AXIS2_PLACEMENT_3D('',#147609,#114565,#114566) ;
#95514 = AXIS2_PLACEMENT_3D('',#147610,#114567,#114568) ;
#95515 = AXIS2_PLACEMENT_3D('',#147611,#114569,#114570) ;
#95516 = AXIS2_PLACEMENT_3D('',#147612,#114571,#114572) ;
#95517 = AXIS2_PLACEMENT_3D('',#147613,#114573,#114574) ;
#95518 = AXIS2_PLACEMENT_3D('',#147614,#114575,#114576) ;
#95519 = AXIS2_PLACEMENT_3D('',#147615,#114577,#114578) ;
#95520 = AXIS2_PLACEMENT_3D('',#147616,#114579,#114580) ;
#95521 = AXIS2_PLACEMENT_3D('',#147617,#114581,#114582) ;
#95522 = AXIS2_PLACEMENT_3D('',#147618,#114583,#114584) ;
#95523 = AXIS2_PLACEMENT_3D('',#147619,#114585,#114586) ;
#95524 = AXIS2_PLACEMENT_3D('',#147620,#114587,#114588) ;
#95525 = AXIS2_PLACEMENT_3D('',#147621,#114589,#114590) ;
#95526 = AXIS2_PLACEMENT_3D('',#147622,#114591,#114592) ;
#95527 = AXIS2_PLACEMENT_3D('',#147623,#114593,#114594) ;
#95528 = AXIS2_PLACEMENT_3D('',#147624,#114595,#114596) ;
#95529 = AXIS2_PLACEMENT_3D('',#147625,#114597,#114598) ;
#95530 = AXIS2_PLACEMENT_3D('',#147626,#114599,#114600) ;
#95531 = AXIS2_PLACEMENT_3D('',#147627,#114601,#114602) ;
#95532 = AXIS2_PLACEMENT_3D('',#147628,#114603,#114604) ;
#95533 = AXIS2_PLACEMENT_3D('',#147629,#114605,#114606) ;
#95534 = AXIS2_PLACEMENT_3D('',#147630,#114607,#114608) ;
#95535 = AXIS2_PLACEMENT_3D('',#147631,#114609,#114610) ;
#95536 = AXIS2_PLACEMENT_3D('',#147632,#114611,#114612) ;
#95537 = AXIS2_PLACEMENT_3D('',#147633,#114613,#114614) ;
#95538 = AXIS2_PLACEMENT_3D('',#147634,#114615,#114616) ;
#95539 = AXIS2_PLACEMENT_3D('',#147635,#114617,#114618) ;
#95540 = AXIS2_PLACEMENT_3D('',#147636,#114619,#114620) ;
#95541 = AXIS2_PLACEMENT_3D('',#147637,#114621,#114622) ;
#95542 = AXIS2_PLACEMENT_3D('',#147638,#114623,#114624) ;
#95543 = AXIS2_PLACEMENT_3D('',#147639,#114625,#114626) ;
#95544 = AXIS2_PLACEMENT_3D('',#147640,#114627,#114628) ;
#95545 = AXIS2_PLACEMENT_3D('',#147641,#114629,#114630) ;
#95546 = AXIS2_PLACEMENT_3D('',#147642,#114631,#114632) ;
#95547 = AXIS2_PLACEMENT_3D('',#147643,#114633,#114634) ;
#95548 = AXIS2_PLACEMENT_3D('',#147644,#114635,#114636) ;
#95549 = AXIS2_PLACEMENT_3D('',#147645,#114637,#114638) ;
#95550 = AXIS2_PLACEMENT_3D('',#147646,#114639,#114640) ;
#95551 = AXIS2_PLACEMENT_3D('',#147647,#114641,#114642) ;
#95552 = AXIS2_PLACEMENT_3D('',#147648,#114643,#114644) ;
#95553 = AXIS2_PLACEMENT_3D('',#147649,#114645,#114646) ;
#95554 = AXIS2_PLACEMENT_3D('',#147650,#114647,#114648) ;
#95555 = AXIS2_PLACEMENT_3D('',#147651,#114649,#114650) ;
#95556 = AXIS2_PLACEMENT_3D('',#147652,#114651,#114652) ;
#95557 = AXIS2_PLACEMENT_3D('',#147653,#114653,#114654) ;
#95558 = AXIS2_PLACEMENT_3D('',#147654,#114655,#114656) ;
#95559 = AXIS2_PLACEMENT_3D('',#147655,#114657,#114658) ;
#95560 = AXIS2_PLACEMENT_3D('',#147656,#114659,#114660) ;
#95561 = AXIS2_PLACEMENT_3D('',#147657,#114661,#114662) ;
#95562 = AXIS2_PLACEMENT_3D('',#147658,#114663,#114664) ;
#95563 = AXIS2_PLACEMENT_3D('',#147659,#114665,#114666) ;
#95564 = AXIS2_PLACEMENT_3D('',#147660,#114667,#114668) ;
#95565 = AXIS2_PLACEMENT_3D('',#147661,#114669,#114670) ;
#95566 = AXIS2_PLACEMENT_3D('',#147662,#114671,#114672) ;
#95567 = AXIS2_PLACEMENT_3D('',#147663,#114673,#114674) ;
#95568 = AXIS2_PLACEMENT_3D('',#147664,#114675,#114676) ;
#95569 = AXIS2_PLACEMENT_3D('',#147665,#114677,#114678) ;
#95570 = AXIS2_PLACEMENT_3D('',#147666,#114679,#114680) ;
#95571 = AXIS2_PLACEMENT_3D('',#147667,#114681,#114682) ;
#95572 = AXIS2_PLACEMENT_3D('',#147668,#114683,#114684) ;
#95573 = AXIS2_PLACEMENT_3D('',#147669,#114685,#114686) ;
#95574 = AXIS2_PLACEMENT_3D('',#147670,#114687,#114688) ;
#95575 = AXIS2_PLACEMENT_3D('',#147671,#114689,#114690) ;
#95576 = AXIS2_PLACEMENT_3D('',#147672,#114691,#114692) ;
#95577 = AXIS2_PLACEMENT_3D('',#147673,#114693,#114694) ;
#95578 = AXIS2_PLACEMENT_3D('',#147674,#114695,#114696) ;
#95579 = AXIS2_PLACEMENT_3D('',#147675,#114697,#114698) ;
#95580 = AXIS2_PLACEMENT_3D('',#147676,#114699,#114700) ;
#95581 = AXIS2_PLACEMENT_3D('',#147677,#114701,#114702) ;
#95582 = AXIS2_PLACEMENT_3D('',#147678,#114703,#114704) ;
#95583 = AXIS2_PLACEMENT_3D('',#147679,#114705,#114706) ;
#95584 = AXIS2_PLACEMENT_3D('',#147680,#114707,#114708) ;
#95585 = AXIS2_PLACEMENT_3D('',#147681,#114709,#114710) ;
#95586 = AXIS2_PLACEMENT_3D('',#147682,#114711,#114712) ;
#95587 = AXIS2_PLACEMENT_3D('',#147683,#114713,#114714) ;
#95588 = AXIS2_PLACEMENT_3D('',#147684,#114715,#114716) ;
#95589 = AXIS2_PLACEMENT_3D('',#147685,#114717,#114718) ;
#95590 = AXIS2_PLACEMENT_3D('',#147686,#114719,#114720) ;
#95591 = AXIS2_PLACEMENT_3D('',#147687,#114721,#114722) ;
#95592 = AXIS2_PLACEMENT_3D('',#147688,#114723,#114724) ;
#95593 = AXIS2_PLACEMENT_3D('',#147689,#114725,#114726) ;
#95594 = AXIS2_PLACEMENT_3D('',#147690,#114727,#114728) ;
#95595 = AXIS2_PLACEMENT_3D('',#147691,#114729,#114730) ;
#95596 = AXIS2_PLACEMENT_3D('',#147692,#114731,#114732) ;
#95597 = AXIS2_PLACEMENT_3D('',#147693,#114733,#114734) ;
#95598 = AXIS2_PLACEMENT_3D('',#147694,#114735,#114736) ;
#95599 = AXIS2_PLACEMENT_3D('',#147695,#114737,#114738) ;
#95600 = AXIS2_PLACEMENT_3D('',#147696,#114739,#114740) ;
#95601 = AXIS2_PLACEMENT_3D('',#147697,#114741,#114742) ;
#95602 = AXIS2_PLACEMENT_3D('',#147698,#114743,#114744) ;
#95603 = AXIS2_PLACEMENT_3D('',#147699,#114745,#114746) ;
#95604 = AXIS2_PLACEMENT_3D('',#147700,#114747,#114748) ;
#95605 = AXIS2_PLACEMENT_3D('',#147701,#114749,#114750) ;
#95606 = AXIS2_PLACEMENT_3D('',#147702,#114751,#114752) ;
#95607 = AXIS2_PLACEMENT_3D('',#147703,#114753,#114754) ;
#95608 = AXIS2_PLACEMENT_3D('',#147704,#114755,#114756) ;
#95609 = AXIS2_PLACEMENT_3D('',#147705,#114757,#114758) ;
#95610 = AXIS2_PLACEMENT_3D('',#147706,#114759,#114760) ;
#95611 = AXIS2_PLACEMENT_3D('',#147707,#114761,#114762) ;
#95612 = AXIS2_PLACEMENT_3D('',#147708,#114763,#114764) ;
#95613 = AXIS2_PLACEMENT_3D('',#147709,#114765,#114766) ;
#95614 = AXIS2_PLACEMENT_3D('',#147710,#114767,#114768) ;
#95615 = AXIS2_PLACEMENT_3D('',#147711,#114769,#114770) ;
#95616 = AXIS2_PLACEMENT_3D('',#147712,#114771,#114772) ;
#95617 = AXIS2_PLACEMENT_3D('',#147713,#114773,#114774) ;
#95618 = AXIS2_PLACEMENT_3D('',#147714,#114775,#114776) ;
#95619 = AXIS2_PLACEMENT_3D('',#147715,#114777,#114778) ;
#95620 = AXIS2_PLACEMENT_3D('',#147716,#114779,#114780) ;
#95621 = AXIS2_PLACEMENT_3D('',#147717,#114781,#114782) ;
#95622 = AXIS2_PLACEMENT_3D('',#147718,#114783,#114784) ;
#95623 = AXIS2_PLACEMENT_3D('',#147719,#114785,#114786) ;
#95624 = AXIS2_PLACEMENT_3D('',#147720,#114787,#114788) ;
#95625 = AXIS2_PLACEMENT_3D('',#147721,#114789,#114790) ;
#95626 = AXIS2_PLACEMENT_3D('',#147722,#114791,#114792) ;
#95627 = AXIS2_PLACEMENT_3D('',#147723,#114793,#114794) ;
#95628 = AXIS2_PLACEMENT_3D('',#147724,#114795,#114796) ;
#95629 = AXIS2_PLACEMENT_3D('',#147725,#114797,#114798) ;
#95630 = AXIS2_PLACEMENT_3D('',#147726,#114799,#114800) ;
#95631 = AXIS2_PLACEMENT_3D('',#147727,#114801,#114802) ;
#95632 = AXIS2_PLACEMENT_3D('',#147728,#114803,#114804) ;
#95633 = AXIS2_PLACEMENT_3D('',#147729,#114805,#114806) ;
#95634 = AXIS2_PLACEMENT_3D('',#147730,#114807,#114808) ;
#95635 = AXIS2_PLACEMENT_3D('',#147731,#114809,#114810) ;
#95636 = AXIS2_PLACEMENT_3D('',#147732,#114811,#114812) ;
#95637 = AXIS2_PLACEMENT_3D('',#147733,#114813,#114814) ;
#95638 = AXIS2_PLACEMENT_3D('',#147734,#114815,#114816) ;
#95639 = AXIS2_PLACEMENT_3D('',#147735,#114817,#114818) ;
#95640 = AXIS2_PLACEMENT_3D('',#147736,#114819,#114820) ;
#95641 = AXIS2_PLACEMENT_3D('',#147737,#114821,#114822) ;
#95642 = AXIS2_PLACEMENT_3D('',#147738,#114823,#114824) ;
#95643 = AXIS2_PLACEMENT_3D('',#147739,#114825,#114826) ;
#95644 = AXIS2_PLACEMENT_3D('',#147740,#114827,#114828) ;
#95645 = AXIS2_PLACEMENT_3D('',#147741,#114829,#114830) ;
#95646 = AXIS2_PLACEMENT_3D('',#147742,#114831,#114832) ;
#95647 = AXIS2_PLACEMENT_3D('',#147743,#114833,#114834) ;
#95648 = AXIS2_PLACEMENT_3D('',#147744,#114835,#114836) ;
#95649 = AXIS2_PLACEMENT_3D('',#147745,#114837,#114838) ;
#95650 = AXIS2_PLACEMENT_3D('',#147746,#114839,#114840) ;
#95651 = AXIS2_PLACEMENT_3D('',#147747,#114841,#114842) ;
#95652 = AXIS2_PLACEMENT_3D('',#147748,#114843,#114844) ;
#95653 = AXIS2_PLACEMENT_3D('',#147749,#114845,#114846) ;
#95654 = AXIS2_PLACEMENT_3D('',#147750,#114847,#114848) ;
#95655 = AXIS2_PLACEMENT_3D('',#147751,#114849,#114850) ;
#95656 = AXIS2_PLACEMENT_3D('',#147752,#114851,#114852) ;
#95657 = AXIS2_PLACEMENT_3D('',#147753,#114853,#114854) ;
#95658 = AXIS2_PLACEMENT_3D('',#147754,#114855,#114856) ;
#95659 = AXIS2_PLACEMENT_3D('',#147755,#114857,#114858) ;
#95660 = AXIS2_PLACEMENT_3D('',#147756,#114859,#114860) ;
#95661 = AXIS2_PLACEMENT_3D('',#147757,#114861,#114862) ;
#95662 = AXIS2_PLACEMENT_3D('',#147758,#114863,#114864) ;
#95663 = AXIS2_PLACEMENT_3D('',#147759,#114865,#114866) ;
#95664 = AXIS2_PLACEMENT_3D('',#147760,#114867,#114868) ;
#95665 = AXIS2_PLACEMENT_3D('',#147761,#114869,#114870) ;
#95666 = AXIS2_PLACEMENT_3D('',#147762,#114871,#114872) ;
#95667 = AXIS2_PLACEMENT_3D('',#147763,#114873,#114874) ;
#95668 = AXIS2_PLACEMENT_3D('',#147764,#114875,#114876) ;
#95669 = AXIS2_PLACEMENT_3D('',#147765,#114877,#114878) ;
#95670 = AXIS2_PLACEMENT_3D('',#147766,#114879,#114880) ;
#95671 = AXIS2_PLACEMENT_3D('',#147767,#114881,#114882) ;
#95672 = AXIS2_PLACEMENT_3D('',#147768,#114883,#114884) ;
#95673 = AXIS2_PLACEMENT_3D('',#147769,#114885,#114886) ;
#95674 = AXIS2_PLACEMENT_3D('',#147771,#114887,#114888) ;
#95675 = AXIS2_PLACEMENT_3D('',#147772,#114889,#114890) ;
#95676 = AXIS2_PLACEMENT_3D('',#147773,#114891,#114892) ;
#95677 = AXIS2_PLACEMENT_3D('',#147774,#114893,#114894) ;
#95678 = AXIS2_PLACEMENT_3D('',#147775,#114895,#114896) ;
#95679 = AXIS2_PLACEMENT_3D('',#147776,#114897,#114898) ;
#95680 = AXIS2_PLACEMENT_3D('',#147777,#114899,#114900) ;
#95681 = AXIS2_PLACEMENT_3D('',#147778,#114901,#114902) ;
#95682 = AXIS2_PLACEMENT_3D('',#147779,#114903,#114904) ;
#95683 = AXIS2_PLACEMENT_3D('',#147790,#114906,#114907) ;
#95684 = AXIS2_PLACEMENT_3D('',#147847,#114909,#114910) ;
#95685 = AXIS2_PLACEMENT_3D('',#147848,#114911,#114912) ;
#95686 = AXIS2_PLACEMENT_3D('',#147849,#114913,#114914) ;
#95687 = AXIS2_PLACEMENT_3D('',#147850,#114915,#114916) ;
#95688 = AXIS2_PLACEMENT_3D('',#147851,#114917,#114918) ;
#95689 = AXIS2_PLACEMENT_3D('',#147852,#114919,#114920) ;
#95690 = AXIS2_PLACEMENT_3D('',#147853,#114921,#114922) ;
#95691 = AXIS2_PLACEMENT_3D('',#147854,#114923,#114924) ;
#95692 = AXIS2_PLACEMENT_3D('',#147855,#114925,#114926) ;
#95693 = AXIS2_PLACEMENT_3D('',#147856,#114927,#114928) ;
#95694 = AXIS2_PLACEMENT_3D('',#147857,#114929,#114930) ;
#95695 = AXIS2_PLACEMENT_3D('',#147858,#114931,#114932) ;
#95696 = AXIS2_PLACEMENT_3D('',#147859,#114933,#114934) ;
#95697 = AXIS2_PLACEMENT_3D('',#147860,#114935,#114936) ;
#95698 = AXIS2_PLACEMENT_3D('',#147861,#114937,#114938) ;
#95699 = AXIS2_PLACEMENT_3D('',#147862,#114939,#114940) ;
#95700 = AXIS2_PLACEMENT_3D('',#147863,#114941,#114942) ;
#95701 = AXIS2_PLACEMENT_3D('',#147864,#114943,#114944) ;
#95702 = AXIS2_PLACEMENT_3D('',#147865,#114945,#114946) ;
#95703 = AXIS2_PLACEMENT_3D('',#147866,#114947,#114948) ;
#95704 = AXIS2_PLACEMENT_3D('',#147867,#114949,#114950) ;
#95705 = AXIS2_PLACEMENT_3D('',#147868,#114951,#114952) ;
#95706 = AXIS2_PLACEMENT_3D('',#147869,#114953,#114954) ;
#95707 = AXIS2_PLACEMENT_3D('',#147872,#114956,#114957) ;
#95708 = AXIS2_PLACEMENT_3D('',#147873,#114958,#114959) ;
#95709 = AXIS2_PLACEMENT_3D('',#147874,#114960,#114961) ;
#95710 = AXIS2_PLACEMENT_3D('',#147875,#114962,#114963) ;
#95711 = AXIS2_PLACEMENT_3D('',#147876,#114964,#114965) ;
#95712 = AXIS2_PLACEMENT_3D('',#147877,#114966,#114967) ;
#95713 = AXIS2_PLACEMENT_3D('',#147878,#114968,#114969) ;
#95714 = AXIS2_PLACEMENT_3D('',#147879,#114970,#114971) ;
#95715 = AXIS2_PLACEMENT_3D('',#147880,#114972,#114973) ;
#95716 = AXIS2_PLACEMENT_3D('',#147881,#114974,#114975) ;
#95717 = AXIS2_PLACEMENT_3D('',#147882,#114976,#114977) ;
#95718 = AXIS2_PLACEMENT_3D('',#147883,#114978,#114979) ;
#95719 = AXIS2_PLACEMENT_3D('',#147884,#114980,#114981) ;
#95720 = AXIS2_PLACEMENT_3D('',#147885,#114982,#114983) ;
#95721 = AXIS2_PLACEMENT_3D('',#147886,#114984,#114985) ;
#95722 = AXIS2_PLACEMENT_3D('',#147887,#114986,#114987) ;
#95723 = AXIS2_PLACEMENT_3D('',#147889,#114988,#114989) ;
#95724 = AXIS2_PLACEMENT_3D('',#147890,#114990,#114991) ;
#95725 = AXIS2_PLACEMENT_3D('',#147891,#114992,#114993) ;
#95726 = AXIS2_PLACEMENT_3D('',#147892,#114994,#114995) ;
#95727 = AXIS2_PLACEMENT_3D('',#147893,#114996,#114997) ;
#95728 = AXIS2_PLACEMENT_3D('',#147894,#114998,#114999) ;
#95729 = AXIS2_PLACEMENT_3D('',#147895,#115000,#115001) ;
#95730 = AXIS2_PLACEMENT_3D('',#147896,#115002,#115003) ;
#95731 = AXIS2_PLACEMENT_3D('',#147897,#115004,#115005) ;
#95732 = AXIS2_PLACEMENT_3D('',#147898,#115006,#115007) ;
#95733 = AXIS2_PLACEMENT_3D('',#147899,#115008,#115009) ;
#95734 = AXIS2_PLACEMENT_3D('',#147900,#115010,#115011) ;
#95735 = AXIS2_PLACEMENT_3D('',#147901,#115012,#115013) ;
#95736 = AXIS2_PLACEMENT_3D('',#147904,#115015,#115016) ;
#95737 = AXIS2_PLACEMENT_3D('',#147905,#115017,#115018) ;
#95738 = AXIS2_PLACEMENT_3D('',#147906,#115019,#115020) ;
#95739 = AXIS2_PLACEMENT_3D('',#147907,#115021,#115022) ;
#95740 = AXIS2_PLACEMENT_3D('',#147908,#115023,#115024) ;
#95741 = AXIS2_PLACEMENT_3D('',#147909,#115025,#115026) ;
#95742 = AXIS2_PLACEMENT_3D('',#147910,#115027,#115028) ;
#95743 = AXIS2_PLACEMENT_3D('',#147911,#115029,#115030) ;
#95744 = AXIS2_PLACEMENT_3D('',#147912,#115031,#115032) ;
#95745 = AXIS2_PLACEMENT_3D('',#147913,#115033,#115034) ;
#95746 = AXIS2_PLACEMENT_3D('',#147914,#115035,#115036) ;
#95747 = AXIS2_PLACEMENT_3D('',#147915,#115037,#115038) ;
#95748 = AXIS2_PLACEMENT_3D('',#147916,#115039,#115040) ;
#95749 = AXIS2_PLACEMENT_3D('',#147918,#115041,#115042) ;
#95750 = AXIS2_PLACEMENT_3D('',#147919,#115043,#115044) ;
#95751 = AXIS2_PLACEMENT_3D('',#147920,#115045,#115046) ;
#95752 = AXIS2_PLACEMENT_3D('',#147921,#115047,#115048) ;
#95753 = AXIS2_PLACEMENT_3D('',#147922,#115049,#115050) ;
#95754 = AXIS2_PLACEMENT_3D('',#147923,#115051,#115052) ;
#95755 = AXIS2_PLACEMENT_3D('',#147924,#115053,#115054) ;
#95756 = AXIS2_PLACEMENT_3D('',#147925,#115055,#115056) ;
#95757 = AXIS2_PLACEMENT_3D('',#147926,#115057,#115058) ;
#95758 = AXIS2_PLACEMENT_3D('',#147927,#115059,#115060) ;
#95759 = AXIS2_PLACEMENT_3D('',#147928,#115061,#115062) ;
#95760 = AXIS2_PLACEMENT_3D('',#147930,#115064,#115065) ;
#95761 = AXIS2_PLACEMENT_3D('',#147931,#115066,#115067) ;
#95762 = AXIS2_PLACEMENT_3D('',#147932,#115068,#115069) ;
#95763 = AXIS2_PLACEMENT_3D('',#147933,#115070,#115071) ;
#95764 = AXIS2_PLACEMENT_3D('',#147934,#115072,#115073) ;
#95765 = AXIS2_PLACEMENT_3D('',#147935,#115074,#115075) ;
#95766 = AXIS2_PLACEMENT_3D('',#147936,#115076,#115077) ;
#95767 = AXIS2_PLACEMENT_3D('',#147937,#115078,#115079) ;
#95768 = AXIS2_PLACEMENT_3D('',#147938,#115080,#115081) ;
#95769 = AXIS2_PLACEMENT_3D('',#147939,#115082,#115083) ;
#95770 = AXIS2_PLACEMENT_3D('',#147940,#115084,#115085) ;
#95771 = AXIS2_PLACEMENT_3D('',#147941,#115086,#115087) ;
#95772 = AXIS2_PLACEMENT_3D('',#147942,#115088,#115089) ;
#95773 = AXIS2_PLACEMENT_3D('',#147943,#115090,#115091) ;
#95774 = AXIS2_PLACEMENT_3D('',#147944,#115092,#115093) ;
#95775 = AXIS2_PLACEMENT_3D('',#147945,#115094,#115095) ;
#95776 = AXIS2_PLACEMENT_3D('',#147946,#115096,#115097) ;
#95777 = AXIS2_PLACEMENT_3D('',#147947,#115098,#115099) ;
#95778 = AXIS2_PLACEMENT_3D('',#147948,#115100,#115101) ;
#95779 = AXIS2_PLACEMENT_3D('',#147949,#115102,#115103) ;
#95780 = AXIS2_PLACEMENT_3D('',#147950,#115104,#115105) ;
#95781 = AXIS2_PLACEMENT_3D('',#147951,#115106,#115107) ;
#95782 = AXIS2_PLACEMENT_3D('',#147952,#115108,#115109) ;
#95783 = AXIS2_PLACEMENT_3D('',#147953,#115110,#115111) ;
#95784 = AXIS2_PLACEMENT_3D('',#147954,#115112,#115113) ;
#95785 = AXIS2_PLACEMENT_3D('',#147955,#115114,#115115) ;
#95786 = AXIS2_PLACEMENT_3D('',#147956,#115116,#115117) ;
#95787 = AXIS2_PLACEMENT_3D('',#147957,#115118,#115119) ;
#95788 = AXIS2_PLACEMENT_3D('',#147958,#115120,#115121) ;
#95789 = AXIS2_PLACEMENT_3D('',#147959,#115122,#115123) ;
#95790 = AXIS2_PLACEMENT_3D('',#147960,#115124,#115125) ;
#95791 = AXIS2_PLACEMENT_3D('',#147961,#115126,#115127) ;
#95792 = AXIS2_PLACEMENT_3D('',#147962,#115128,#115129) ;
#95793 = AXIS2_PLACEMENT_3D('',#147963,#115130,#115131) ;
#95794 = AXIS2_PLACEMENT_3D('',#147964,#115132,#115133) ;
#95795 = AXIS2_PLACEMENT_3D('',#147965,#115134,#115135) ;
#95796 = AXIS2_PLACEMENT_3D('',#147966,#115136,#115137) ;
#95797 = AXIS2_PLACEMENT_3D('',#147967,#115138,#115139) ;
#95798 = AXIS2_PLACEMENT_3D('',#147968,#115140,#115141) ;
#95799 = AXIS2_PLACEMENT_3D('',#147969,#115142,#115143) ;
#95800 = AXIS2_PLACEMENT_3D('',#147970,#115144,#115145) ;
#95801 = AXIS2_PLACEMENT_3D('',#147971,#115146,#115147) ;
#95802 = AXIS2_PLACEMENT_3D('',#147972,#115148,#115149) ;
#95803 = AXIS2_PLACEMENT_3D('',#147973,#115150,#115151) ;
#95804 = AXIS2_PLACEMENT_3D('',#147974,#115152,#115153) ;
#95805 = AXIS2_PLACEMENT_3D('',#147975,#115154,#115155) ;
#95806 = AXIS2_PLACEMENT_3D('',#147976,#115156,#115157) ;
#95807 = AXIS2_PLACEMENT_3D('',#147977,#115158,#115159) ;
#95808 = AXIS2_PLACEMENT_3D('',#147978,#115160,#115161) ;
#95809 = AXIS2_PLACEMENT_3D('',#147979,#115162,#115163) ;
#95810 = AXIS2_PLACEMENT_3D('',#147980,#115164,#115165) ;
#95811 = AXIS2_PLACEMENT_3D('',#147981,#115166,#115167) ;
#95812 = AXIS2_PLACEMENT_3D('',#147982,#115168,#115169) ;
#95813 = AXIS2_PLACEMENT_3D('',#147983,#115170,#115171) ;
#95814 = AXIS2_PLACEMENT_3D('',#147984,#115172,#115173) ;
#95815 = AXIS2_PLACEMENT_3D('',#147985,#115174,#115175) ;
#95816 = AXIS2_PLACEMENT_3D('',#147986,#115176,#115177) ;
#95817 = AXIS2_PLACEMENT_3D('',#147987,#115178,#115179) ;
#95818 = AXIS2_PLACEMENT_3D('',#147988,#115180,#115181) ;
#95819 = AXIS2_PLACEMENT_3D('',#147989,#115182,#115183) ;
#95820 = AXIS2_PLACEMENT_3D('',#147990,#115184,#115185) ;
#95821 = AXIS2_PLACEMENT_3D('',#147991,#115186,#115187) ;
#95822 = AXIS2_PLACEMENT_3D('',#147992,#115188,#115189) ;
#95823 = AXIS2_PLACEMENT_3D('',#147993,#115190,#115191) ;
#95824 = AXIS2_PLACEMENT_3D('',#147994,#115192,#115193) ;
#95825 = AXIS2_PLACEMENT_3D('',#147995,#115194,#115195) ;
#95826 = AXIS2_PLACEMENT_3D('',#147996,#115196,#115197) ;
#95827 = AXIS2_PLACEMENT_3D('',#147998,#115198,#115199) ;
#95828 = AXIS2_PLACEMENT_3D('',#147999,#115200,#115201) ;
#95829 = AXIS2_PLACEMENT_3D('',#148000,#115202,#115203) ;
#95830 = AXIS2_PLACEMENT_3D('',#148001,#115204,#115205) ;
#95831 = AXIS2_PLACEMENT_3D('',#148002,#115206,#115207) ;
#95832 = AXIS2_PLACEMENT_3D('',#148003,#115208,#115209) ;
#95833 = AXIS2_PLACEMENT_3D('',#148004,#115210,#115211) ;
#95834 = AXIS2_PLACEMENT_3D('',#148005,#115212,#115213) ;
#95835 = AXIS2_PLACEMENT_3D('',#148006,#115214,#115215) ;
#95836 = AXIS2_PLACEMENT_3D('',#148017,#115217,#115218) ;
#95837 = AXIS2_PLACEMENT_3D('',#148074,#115220,#115221) ;
#95838 = AXIS2_PLACEMENT_3D('',#148075,#115222,#115223) ;
#95839 = AXIS2_PLACEMENT_3D('',#148076,#115224,#115225) ;
#95840 = AXIS2_PLACEMENT_3D('',#148077,#115226,#115227) ;
#95841 = AXIS2_PLACEMENT_3D('',#148078,#115228,#115229) ;
#95842 = AXIS2_PLACEMENT_3D('',#148079,#115230,#115231) ;
#95843 = AXIS2_PLACEMENT_3D('',#148080,#115232,#115233) ;
#95844 = AXIS2_PLACEMENT_3D('',#148081,#115234,#115235) ;
#95845 = AXIS2_PLACEMENT_3D('',#148082,#115236,#115237) ;
#95846 = AXIS2_PLACEMENT_3D('',#148083,#115238,#115239) ;
#95847 = AXIS2_PLACEMENT_3D('',#148084,#115240,#115241) ;
#95848 = AXIS2_PLACEMENT_3D('',#148085,#115242,#115243) ;
#95849 = AXIS2_PLACEMENT_3D('',#148086,#115244,#115245) ;
#95850 = AXIS2_PLACEMENT_3D('',#148087,#115246,#115247) ;
#95851 = AXIS2_PLACEMENT_3D('',#148088,#115248,#115249) ;
#95852 = AXIS2_PLACEMENT_3D('',#148089,#115250,#115251) ;
#95853 = AXIS2_PLACEMENT_3D('',#148090,#115252,#115253) ;
#95854 = AXIS2_PLACEMENT_3D('',#148091,#115254,#115255) ;
#95855 = AXIS2_PLACEMENT_3D('',#148092,#115256,#115257) ;
#95856 = AXIS2_PLACEMENT_3D('',#148093,#115258,#115259) ;
#95857 = AXIS2_PLACEMENT_3D('',#148094,#115260,#115261) ;
#95858 = AXIS2_PLACEMENT_3D('',#148095,#115262,#115263) ;
#95859 = AXIS2_PLACEMENT_3D('',#148096,#115264,#115265) ;
#95860 = AXIS2_PLACEMENT_3D('',#148099,#115267,#115268) ;
#95861 = AXIS2_PLACEMENT_3D('',#148100,#115269,#115270) ;
#95862 = AXIS2_PLACEMENT_3D('',#148101,#115271,#115272) ;
#95863 = AXIS2_PLACEMENT_3D('',#148102,#115273,#115274) ;
#95864 = AXIS2_PLACEMENT_3D('',#148103,#115275,#115276) ;
#95865 = AXIS2_PLACEMENT_3D('',#148104,#115277,#115278) ;
#95866 = AXIS2_PLACEMENT_3D('',#148105,#115279,#115280) ;
#95867 = AXIS2_PLACEMENT_3D('',#148106,#115281,#115282) ;
#95868 = AXIS2_PLACEMENT_3D('',#148107,#115283,#115284) ;
#95869 = AXIS2_PLACEMENT_3D('',#148108,#115285,#115286) ;
#95870 = AXIS2_PLACEMENT_3D('',#148109,#115287,#115288) ;
#95871 = AXIS2_PLACEMENT_3D('',#148110,#115289,#115290) ;
#95872 = AXIS2_PLACEMENT_3D('',#148111,#115291,#115292) ;
#95873 = AXIS2_PLACEMENT_3D('',#148112,#115293,#115294) ;
#95874 = AXIS2_PLACEMENT_3D('',#148113,#115295,#115296) ;
#95875 = AXIS2_PLACEMENT_3D('',#148114,#115297,#115298) ;
#95876 = AXIS2_PLACEMENT_3D('',#148116,#115299,#115300) ;
#95877 = AXIS2_PLACEMENT_3D('',#148117,#115301,#115302) ;
#95878 = AXIS2_PLACEMENT_3D('',#148118,#115303,#115304) ;
#95879 = AXIS2_PLACEMENT_3D('',#148119,#115305,#115306) ;
#95880 = AXIS2_PLACEMENT_3D('',#148120,#115307,#115308) ;
#95881 = AXIS2_PLACEMENT_3D('',#148121,#115309,#115310) ;
#95882 = AXIS2_PLACEMENT_3D('',#148122,#115311,#115312) ;
#95883 = AXIS2_PLACEMENT_3D('',#148123,#115313,#115314) ;
#95884 = AXIS2_PLACEMENT_3D('',#148124,#115315,#115316) ;
#95885 = AXIS2_PLACEMENT_3D('',#148125,#115317,#115318) ;
#95886 = AXIS2_PLACEMENT_3D('',#148126,#115319,#115320) ;
#95887 = AXIS2_PLACEMENT_3D('',#148127,#115321,#115322) ;
#95888 = AXIS2_PLACEMENT_3D('',#148128,#115323,#115324) ;
#95889 = AXIS2_PLACEMENT_3D('',#148131,#115326,#115327) ;
#95890 = AXIS2_PLACEMENT_3D('',#148132,#115328,#115329) ;
#95891 = AXIS2_PLACEMENT_3D('',#148133,#115330,#115331) ;
#95892 = AXIS2_PLACEMENT_3D('',#148134,#115332,#115333) ;
#95893 = AXIS2_PLACEMENT_3D('',#148135,#115334,#115335) ;
#95894 = AXIS2_PLACEMENT_3D('',#148136,#115336,#115337) ;
#95895 = AXIS2_PLACEMENT_3D('',#148137,#115338,#115339) ;
#95896 = AXIS2_PLACEMENT_3D('',#148138,#115340,#115341) ;
#95897 = AXIS2_PLACEMENT_3D('',#148139,#115342,#115343) ;
#95898 = AXIS2_PLACEMENT_3D('',#148140,#115344,#115345) ;
#95899 = AXIS2_PLACEMENT_3D('',#148141,#115346,#115347) ;
#95900 = AXIS2_PLACEMENT_3D('',#148142,#115348,#115349) ;
#95901 = AXIS2_PLACEMENT_3D('',#148143,#115350,#115351) ;
#95902 = AXIS2_PLACEMENT_3D('',#148145,#115352,#115353) ;
#95903 = AXIS2_PLACEMENT_3D('',#148146,#115354,#115355) ;
#95904 = AXIS2_PLACEMENT_3D('',#148147,#115356,#115357) ;
#95905 = AXIS2_PLACEMENT_3D('',#148148,#115358,#115359) ;
#95906 = AXIS2_PLACEMENT_3D('',#148149,#115360,#115361) ;
#95907 = AXIS2_PLACEMENT_3D('',#148150,#115362,#115363) ;
#95908 = AXIS2_PLACEMENT_3D('',#148151,#115364,#115365) ;
#95909 = AXIS2_PLACEMENT_3D('',#148152,#115366,#115367) ;
#95910 = AXIS2_PLACEMENT_3D('',#148153,#115368,#115369) ;
#95911 = AXIS2_PLACEMENT_3D('',#148154,#115370,#115371) ;
#95912 = AXIS2_PLACEMENT_3D('',#148155,#115372,#115373) ;
#95913 = AXIS2_PLACEMENT_3D('',#148157,#115375,#115376) ;
#95914 = AXIS2_PLACEMENT_3D('',#148158,#115377,#115378) ;
#95915 = AXIS2_PLACEMENT_3D('',#148159,#115379,#115380) ;
#95916 = AXIS2_PLACEMENT_3D('',#148160,#115381,#115382) ;
#95917 = AXIS2_PLACEMENT_3D('',#148161,#115383,#115384) ;
#95918 = AXIS2_PLACEMENT_3D('',#148162,#115385,#115386) ;
#95919 = AXIS2_PLACEMENT_3D('',#148163,#115387,#115388) ;
#95920 = AXIS2_PLACEMENT_3D('',#148164,#115389,#115390) ;
#95921 = AXIS2_PLACEMENT_3D('',#148165,#115391,#115392) ;
#95922 = AXIS2_PLACEMENT_3D('',#148166,#115393,#115394) ;
#95923 = AXIS2_PLACEMENT_3D('',#148167,#115395,#115396) ;
#95924 = AXIS2_PLACEMENT_3D('',#148168,#115397,#115398) ;
#95925 = AXIS2_PLACEMENT_3D('',#148169,#115399,#115400) ;
#95926 = AXIS2_PLACEMENT_3D('',#148170,#115401,#115402) ;
#95927 = AXIS2_PLACEMENT_3D('',#148171,#115403,#115404) ;
#95928 = AXIS2_PLACEMENT_3D('',#148172,#115405,#115406) ;
#95929 = AXIS2_PLACEMENT_3D('',#148173,#115407,#115408) ;
#95930 = AXIS2_PLACEMENT_3D('',#148174,#115409,#115410) ;
#95931 = AXIS2_PLACEMENT_3D('',#148175,#115411,#115412) ;
#95932 = AXIS2_PLACEMENT_3D('',#148176,#115413,#115414) ;
#95933 = AXIS2_PLACEMENT_3D('',#148177,#115415,#115416) ;
#95934 = AXIS2_PLACEMENT_3D('',#148178,#115417,#115418) ;
#95935 = AXIS2_PLACEMENT_3D('',#148179,#115419,#115420) ;
#95936 = AXIS2_PLACEMENT_3D('',#148180,#115421,#115422) ;
#95937 = AXIS2_PLACEMENT_3D('',#148181,#115423,#115424) ;
#95938 = AXIS2_PLACEMENT_3D('',#148182,#115425,#115426) ;
#95939 = AXIS2_PLACEMENT_3D('',#148183,#115427,#115428) ;
#95940 = AXIS2_PLACEMENT_3D('',#148184,#115429,#115430) ;
#95941 = AXIS2_PLACEMENT_3D('',#148185,#115431,#115432) ;
#95942 = AXIS2_PLACEMENT_3D('',#148186,#115433,#115434) ;
#95943 = AXIS2_PLACEMENT_3D('',#148187,#115435,#115436) ;
#95944 = AXIS2_PLACEMENT_3D('',#148188,#115437,#115438) ;
#95945 = AXIS2_PLACEMENT_3D('',#148189,#115439,#115440) ;
#95946 = AXIS2_PLACEMENT_3D('',#148190,#115441,#115442) ;
#95947 = AXIS2_PLACEMENT_3D('',#148191,#115443,#115444) ;
#95948 = AXIS2_PLACEMENT_3D('',#148192,#115445,#115446) ;
#95949 = AXIS2_PLACEMENT_3D('',#148193,#115447,#115448) ;
#95950 = AXIS2_PLACEMENT_3D('',#148194,#115449,#115450) ;
#95951 = AXIS2_PLACEMENT_3D('',#148195,#115451,#115452) ;
#95952 = AXIS2_PLACEMENT_3D('',#148196,#115453,#115454) ;
#95953 = AXIS2_PLACEMENT_3D('',#148197,#115455,#115456) ;
#95954 = AXIS2_PLACEMENT_3D('',#148198,#115457,#115458) ;
#95955 = AXIS2_PLACEMENT_3D('',#148199,#115459,#115460) ;
#95956 = AXIS2_PLACEMENT_3D('',#148200,#115461,#115462) ;
#95957 = AXIS2_PLACEMENT_3D('',#148201,#115463,#115464) ;
#95958 = AXIS2_PLACEMENT_3D('',#148202,#115465,#115466) ;
#95959 = AXIS2_PLACEMENT_3D('',#148203,#115467,#115468) ;
#95960 = AXIS2_PLACEMENT_3D('',#148204,#115469,#115470) ;
#95961 = AXIS2_PLACEMENT_3D('',#148205,#115471,#115472) ;
#95962 = AXIS2_PLACEMENT_3D('',#148206,#115473,#115474) ;
#95963 = AXIS2_PLACEMENT_3D('',#148207,#115475,#115476) ;
#95964 = AXIS2_PLACEMENT_3D('',#148208,#115477,#115478) ;
#95965 = AXIS2_PLACEMENT_3D('',#148209,#115479,#115480) ;
#95966 = AXIS2_PLACEMENT_3D('',#148210,#115481,#115482) ;
#95967 = AXIS2_PLACEMENT_3D('',#148211,#115483,#115484) ;
#95968 = AXIS2_PLACEMENT_3D('',#148212,#115485,#115486) ;
#95969 = AXIS2_PLACEMENT_3D('',#148213,#115487,#115488) ;
#95970 = AXIS2_PLACEMENT_3D('',#148214,#115489,#115490) ;
#95971 = AXIS2_PLACEMENT_3D('',#148215,#115491,#115492) ;
#95972 = AXIS2_PLACEMENT_3D('',#148216,#115493,#115494) ;
#95973 = AXIS2_PLACEMENT_3D('',#148217,#115495,#115496) ;
#95974 = AXIS2_PLACEMENT_3D('',#148218,#115497,#115498) ;
#95975 = AXIS2_PLACEMENT_3D('',#148219,#115499,#115500) ;
#95976 = AXIS2_PLACEMENT_3D('',#148220,#115501,#115502) ;
#95977 = AXIS2_PLACEMENT_3D('',#148221,#115503,#115504) ;
#95978 = AXIS2_PLACEMENT_3D('',#148222,#115505,#115506) ;
#95979 = AXIS2_PLACEMENT_3D('',#148223,#115507,#115508) ;
#95980 = AXIS2_PLACEMENT_3D('',#148225,#115509,#115510) ;
#95981 = AXIS2_PLACEMENT_3D('',#148226,#115511,#115512) ;
#95982 = AXIS2_PLACEMENT_3D('',#148227,#115513,#115514) ;
#95983 = AXIS2_PLACEMENT_3D('',#148228,#115515,#115516) ;
#95984 = AXIS2_PLACEMENT_3D('',#148229,#115517,#115518) ;
#95985 = AXIS2_PLACEMENT_3D('',#148230,#115519,#115520) ;
#95986 = AXIS2_PLACEMENT_3D('',#148231,#115521,#115522) ;
#95987 = AXIS2_PLACEMENT_3D('',#148232,#115523,#115524) ;
#95988 = AXIS2_PLACEMENT_3D('',#148233,#115525,#115526) ;
#95989 = AXIS2_PLACEMENT_3D('',#148244,#115528,#115529) ;
#95990 = AXIS2_PLACEMENT_3D('',#148301,#115531,#115532) ;
#95991 = AXIS2_PLACEMENT_3D('',#148302,#115533,#115534) ;
#95992 = AXIS2_PLACEMENT_3D('',#148303,#115535,#115536) ;
#95993 = AXIS2_PLACEMENT_3D('',#148304,#115537,#115538) ;
#95994 = AXIS2_PLACEMENT_3D('',#148305,#115539,#115540) ;
#95995 = AXIS2_PLACEMENT_3D('',#148306,#115541,#115542) ;
#95996 = AXIS2_PLACEMENT_3D('',#148307,#115543,#115544) ;
#95997 = AXIS2_PLACEMENT_3D('',#148308,#115545,#115546) ;
#95998 = AXIS2_PLACEMENT_3D('',#148309,#115547,#115548) ;
#95999 = AXIS2_PLACEMENT_3D('',#148310,#115549,#115550) ;
#96000 = AXIS2_PLACEMENT_3D('',#148311,#115551,#115552) ;
#96001 = AXIS2_PLACEMENT_3D('',#148312,#115553,#115554) ;
#96002 = AXIS2_PLACEMENT_3D('',#148313,#115555,#115556) ;
#96003 = AXIS2_PLACEMENT_3D('',#148314,#115557,#115558) ;
#96004 = AXIS2_PLACEMENT_3D('',#148315,#115559,#115560) ;
#96005 = AXIS2_PLACEMENT_3D('',#148316,#115561,#115562) ;
#96006 = AXIS2_PLACEMENT_3D('',#148317,#115563,#115564) ;
#96007 = AXIS2_PLACEMENT_3D('',#148318,#115565,#115566) ;
#96008 = AXIS2_PLACEMENT_3D('',#148319,#115567,#115568) ;
#96009 = AXIS2_PLACEMENT_3D('',#148320,#115569,#115570) ;
#96010 = AXIS2_PLACEMENT_3D('',#148321,#115571,#115572) ;
#96011 = AXIS2_PLACEMENT_3D('',#148322,#115573,#115574) ;
#96012 = AXIS2_PLACEMENT_3D('',#148323,#115575,#115576) ;
#96013 = AXIS2_PLACEMENT_3D('',#148326,#115578,#115579) ;
#96014 = AXIS2_PLACEMENT_3D('',#148327,#115580,#115581) ;
#96015 = AXIS2_PLACEMENT_3D('',#148328,#115582,#115583) ;
#96016 = AXIS2_PLACEMENT_3D('',#148329,#115584,#115585) ;
#96017 = AXIS2_PLACEMENT_3D('',#148330,#115586,#115587) ;
#96018 = AXIS2_PLACEMENT_3D('',#148331,#115588,#115589) ;
#96019 = AXIS2_PLACEMENT_3D('',#148332,#115590,#115591) ;
#96020 = AXIS2_PLACEMENT_3D('',#148333,#115592,#115593) ;
#96021 = AXIS2_PLACEMENT_3D('',#148334,#115594,#115595) ;
#96022 = AXIS2_PLACEMENT_3D('',#148335,#115596,#115597) ;
#96023 = AXIS2_PLACEMENT_3D('',#148336,#115598,#115599) ;
#96024 = AXIS2_PLACEMENT_3D('',#148337,#115600,#115601) ;
#96025 = AXIS2_PLACEMENT_3D('',#148338,#115602,#115603) ;
#96026 = AXIS2_PLACEMENT_3D('',#148339,#115604,#115605) ;
#96027 = AXIS2_PLACEMENT_3D('',#148340,#115606,#115607) ;
#96028 = AXIS2_PLACEMENT_3D('',#148341,#115608,#115609) ;
#96029 = AXIS2_PLACEMENT_3D('',#148343,#115610,#115611) ;
#96030 = AXIS2_PLACEMENT_3D('',#148344,#115612,#115613) ;
#96031 = AXIS2_PLACEMENT_3D('',#148345,#115614,#115615) ;
#96032 = AXIS2_PLACEMENT_3D('',#148346,#115616,#115617) ;
#96033 = AXIS2_PLACEMENT_3D('',#148347,#115618,#115619) ;
#96034 = AXIS2_PLACEMENT_3D('',#148348,#115620,#115621) ;
#96035 = AXIS2_PLACEMENT_3D('',#148349,#115622,#115623) ;
#96036 = AXIS2_PLACEMENT_3D('',#148350,#115624,#115625) ;
#96037 = AXIS2_PLACEMENT_3D('',#148351,#115626,#115627) ;
#96038 = AXIS2_PLACEMENT_3D('',#148352,#115628,#115629) ;
#96039 = AXIS2_PLACEMENT_3D('',#148353,#115630,#115631) ;
#96040 = AXIS2_PLACEMENT_3D('',#148354,#115632,#115633) ;
#96041 = AXIS2_PLACEMENT_3D('',#148355,#115634,#115635) ;
#96042 = AXIS2_PLACEMENT_3D('',#148358,#115637,#115638) ;
#96043 = AXIS2_PLACEMENT_3D('',#148359,#115639,#115640) ;
#96044 = AXIS2_PLACEMENT_3D('',#148360,#115641,#115642) ;
#96045 = AXIS2_PLACEMENT_3D('',#148361,#115643,#115644) ;
#96046 = AXIS2_PLACEMENT_3D('',#148362,#115645,#115646) ;
#96047 = AXIS2_PLACEMENT_3D('',#148363,#115647,#115648) ;
#96048 = AXIS2_PLACEMENT_3D('',#148364,#115649,#115650) ;
#96049 = AXIS2_PLACEMENT_3D('',#148365,#115651,#115652) ;
#96050 = AXIS2_PLACEMENT_3D('',#148366,#115653,#115654) ;
#96051 = AXIS2_PLACEMENT_3D('',#148367,#115655,#115656) ;
#96052 = AXIS2_PLACEMENT_3D('',#148368,#115657,#115658) ;
#96053 = AXIS2_PLACEMENT_3D('',#148369,#115659,#115660) ;
#96054 = AXIS2_PLACEMENT_3D('',#148370,#115661,#115662) ;
#96055 = AXIS2_PLACEMENT_3D('',#148372,#115663,#115664) ;
#96056 = AXIS2_PLACEMENT_3D('',#148373,#115665,#115666) ;
#96057 = AXIS2_PLACEMENT_3D('',#148374,#115667,#115668) ;
#96058 = AXIS2_PLACEMENT_3D('',#148375,#115669,#115670) ;
#96059 = AXIS2_PLACEMENT_3D('',#148376,#115671,#115672) ;
#96060 = AXIS2_PLACEMENT_3D('',#148377,#115673,#115674) ;
#96061 = AXIS2_PLACEMENT_3D('',#148378,#115675,#115676) ;
#96062 = AXIS2_PLACEMENT_3D('',#148379,#115677,#115678) ;
#96063 = AXIS2_PLACEMENT_3D('',#148380,#115679,#115680) ;
#96064 = AXIS2_PLACEMENT_3D('',#148381,#115681,#115682) ;
#96065 = AXIS2_PLACEMENT_3D('',#148382,#115683,#115684) ;
#96066 = AXIS2_PLACEMENT_3D('',#148384,#115686,#115687) ;
#96067 = AXIS2_PLACEMENT_3D('',#148385,#115688,#115689) ;
#96068 = AXIS2_PLACEMENT_3D('',#148386,#115690,#115691) ;
#96069 = AXIS2_PLACEMENT_3D('',#148387,#115692,#115693) ;
#96070 = AXIS2_PLACEMENT_3D('',#148388,#115694,#115695) ;
#96071 = AXIS2_PLACEMENT_3D('',#148389,#115696,#115697) ;
#96072 = AXIS2_PLACEMENT_3D('',#148390,#115698,#115699) ;
#96073 = AXIS2_PLACEMENT_3D('',#148391,#115700,#115701) ;
#96074 = AXIS2_PLACEMENT_3D('',#148392,#115702,#115703) ;
#96075 = AXIS2_PLACEMENT_3D('',#148393,#115704,#115705) ;
#96076 = AXIS2_PLACEMENT_3D('',#148394,#115706,#115707) ;
#96077 = AXIS2_PLACEMENT_3D('',#148395,#115708,#115709) ;
#96078 = AXIS2_PLACEMENT_3D('',#148396,#115710,#115711) ;
#96079 = AXIS2_PLACEMENT_3D('',#148397,#115712,#115713) ;
#96080 = AXIS2_PLACEMENT_3D('',#148398,#115714,#115715) ;
#96081 = AXIS2_PLACEMENT_3D('',#148399,#115716,#115717) ;
#96082 = AXIS2_PLACEMENT_3D('',#148400,#115718,#115719) ;
#96083 = AXIS2_PLACEMENT_3D('',#148401,#115720,#115721) ;
#96084 = AXIS2_PLACEMENT_3D('',#148402,#115722,#115723) ;
#96085 = AXIS2_PLACEMENT_3D('',#148403,#115724,#115725) ;
#96086 = AXIS2_PLACEMENT_3D('',#148404,#115726,#115727) ;
#96087 = AXIS2_PLACEMENT_3D('',#148405,#115728,#115729) ;
#96088 = AXIS2_PLACEMENT_3D('',#148406,#115730,#115731) ;
#96089 = AXIS2_PLACEMENT_3D('',#148407,#115732,#115733) ;
#96090 = AXIS2_PLACEMENT_3D('',#148408,#115734,#115735) ;
#96091 = AXIS2_PLACEMENT_3D('',#148409,#115736,#115737) ;
#96092 = AXIS2_PLACEMENT_3D('',#148410,#115738,#115739) ;
#96093 = AXIS2_PLACEMENT_3D('',#148411,#115740,#115741) ;
#96094 = AXIS2_PLACEMENT_3D('',#148412,#115742,#115743) ;
#96095 = AXIS2_PLACEMENT_3D('',#148413,#115744,#115745) ;
#96096 = AXIS2_PLACEMENT_3D('',#148414,#115746,#115747) ;
#96097 = AXIS2_PLACEMENT_3D('',#148415,#115748,#115749) ;
#96098 = AXIS2_PLACEMENT_3D('',#148416,#115750,#115751) ;
#96099 = AXIS2_PLACEMENT_3D('',#148417,#115752,#115753) ;
#96100 = AXIS2_PLACEMENT_3D('',#148418,#115754,#115755) ;
#96101 = AXIS2_PLACEMENT_3D('',#148419,#115756,#115757) ;
#96102 = AXIS2_PLACEMENT_3D('',#148420,#115758,#115759) ;
#96103 = AXIS2_PLACEMENT_3D('',#148421,#115760,#115761) ;
#96104 = AXIS2_PLACEMENT_3D('',#148422,#115762,#115763) ;
#96105 = AXIS2_PLACEMENT_3D('',#148423,#115764,#115765) ;
#96106 = AXIS2_PLACEMENT_3D('',#148424,#115766,#115767) ;
#96107 = AXIS2_PLACEMENT_3D('',#148425,#115768,#115769) ;
#96108 = AXIS2_PLACEMENT_3D('',#148426,#115770,#115771) ;
#96109 = AXIS2_PLACEMENT_3D('',#148427,#115772,#115773) ;
#96110 = AXIS2_PLACEMENT_3D('',#148428,#115774,#115775) ;
#96111 = AXIS2_PLACEMENT_3D('',#148429,#115776,#115777) ;
#96112 = AXIS2_PLACEMENT_3D('',#148430,#115778,#115779) ;
#96113 = AXIS2_PLACEMENT_3D('',#148431,#115780,#115781) ;
#96114 = AXIS2_PLACEMENT_3D('',#148432,#115782,#115783) ;
#96115 = AXIS2_PLACEMENT_3D('',#148433,#115784,#115785) ;
#96116 = AXIS2_PLACEMENT_3D('',#148434,#115786,#115787) ;
#96117 = AXIS2_PLACEMENT_3D('',#148435,#115788,#115789) ;
#96118 = AXIS2_PLACEMENT_3D('',#148436,#115790,#115791) ;
#96119 = AXIS2_PLACEMENT_3D('',#148437,#115792,#115793) ;
#96120 = AXIS2_PLACEMENT_3D('',#148438,#115794,#115795) ;
#96121 = AXIS2_PLACEMENT_3D('',#148439,#115796,#115797) ;
#96122 = AXIS2_PLACEMENT_3D('',#148440,#115798,#115799) ;
#96123 = AXIS2_PLACEMENT_3D('',#148441,#115800,#115801) ;
#96124 = AXIS2_PLACEMENT_3D('',#148442,#115802,#115803) ;
#96125 = AXIS2_PLACEMENT_3D('',#148443,#115804,#115805) ;
#96126 = AXIS2_PLACEMENT_3D('',#148444,#115806,#115807) ;
#96127 = AXIS2_PLACEMENT_3D('',#148445,#115808,#115809) ;
#96128 = AXIS2_PLACEMENT_3D('',#148446,#115810,#115811) ;
#96129 = AXIS2_PLACEMENT_3D('',#148447,#115812,#115813) ;
#96130 = AXIS2_PLACEMENT_3D('',#148448,#115814,#115815) ;
#96131 = AXIS2_PLACEMENT_3D('',#148449,#115816,#115817) ;
#96132 = AXIS2_PLACEMENT_3D('',#148450,#115818,#115819) ;
#96133 = AXIS2_PLACEMENT_3D('',#148452,#115820,#115821) ;
#96134 = AXIS2_PLACEMENT_3D('',#148453,#115822,#115823) ;
#96135 = AXIS2_PLACEMENT_3D('',#148454,#115824,#115825) ;
#96136 = AXIS2_PLACEMENT_3D('',#148455,#115826,#115827) ;
#96137 = AXIS2_PLACEMENT_3D('',#148456,#115828,#115829) ;
#96138 = AXIS2_PLACEMENT_3D('',#148457,#115830,#115831) ;
#96139 = AXIS2_PLACEMENT_3D('',#148458,#115832,#115833) ;
#96140 = AXIS2_PLACEMENT_3D('',#148459,#115834,#115835) ;
#96141 = AXIS2_PLACEMENT_3D('',#148460,#115836,#115837) ;
#96142 = AXIS2_PLACEMENT_3D('',#148471,#115839,#115840) ;
#96143 = AXIS2_PLACEMENT_3D('',#148528,#115842,#115843) ;
#96144 = AXIS2_PLACEMENT_3D('',#148529,#115844,#115845) ;
#96145 = AXIS2_PLACEMENT_3D('',#148530,#115846,#115847) ;
#96146 = AXIS2_PLACEMENT_3D('',#148531,#115848,#115849) ;
#96147 = AXIS2_PLACEMENT_3D('',#148532,#115850,#115851) ;
#96148 = AXIS2_PLACEMENT_3D('',#148533,#115852,#115853) ;
#96149 = AXIS2_PLACEMENT_3D('',#148534,#115854,#115855) ;
#96150 = AXIS2_PLACEMENT_3D('',#148535,#115856,#115857) ;
#96151 = AXIS2_PLACEMENT_3D('',#148536,#115858,#115859) ;
#96152 = AXIS2_PLACEMENT_3D('',#148537,#115860,#115861) ;
#96153 = AXIS2_PLACEMENT_3D('',#148538,#115862,#115863) ;
#96154 = AXIS2_PLACEMENT_3D('',#148539,#115864,#115865) ;
#96155 = AXIS2_PLACEMENT_3D('',#148540,#115866,#115867) ;
#96156 = AXIS2_PLACEMENT_3D('',#148541,#115868,#115869) ;
#96157 = AXIS2_PLACEMENT_3D('',#148542,#115870,#115871) ;
#96158 = AXIS2_PLACEMENT_3D('',#148543,#115872,#115873) ;
#96159 = AXIS2_PLACEMENT_3D('',#148544,#115874,#115875) ;
#96160 = AXIS2_PLACEMENT_3D('',#148545,#115876,#115877) ;
#96161 = AXIS2_PLACEMENT_3D('',#148546,#115878,#115879) ;
#96162 = AXIS2_PLACEMENT_3D('',#148547,#115880,#115881) ;
#96163 = AXIS2_PLACEMENT_3D('',#148548,#115882,#115883) ;
#96164 = AXIS2_PLACEMENT_3D('',#148549,#115884,#115885) ;
#96165 = AXIS2_PLACEMENT_3D('',#148550,#115886,#115887) ;
#96166 = AXIS2_PLACEMENT_3D('',#148553,#115889,#115890) ;
#96167 = AXIS2_PLACEMENT_3D('',#148554,#115891,#115892) ;
#96168 = AXIS2_PLACEMENT_3D('',#148555,#115893,#115894) ;
#96169 = AXIS2_PLACEMENT_3D('',#148556,#115895,#115896) ;
#96170 = AXIS2_PLACEMENT_3D('',#148557,#115897,#115898) ;
#96171 = AXIS2_PLACEMENT_3D('',#148558,#115899,#115900) ;
#96172 = AXIS2_PLACEMENT_3D('',#148559,#115901,#115902) ;
#96173 = AXIS2_PLACEMENT_3D('',#148560,#115903,#115904) ;
#96174 = AXIS2_PLACEMENT_3D('',#148561,#115905,#115906) ;
#96175 = AXIS2_PLACEMENT_3D('',#148562,#115907,#115908) ;
#96176 = AXIS2_PLACEMENT_3D('',#148563,#115909,#115910) ;
#96177 = AXIS2_PLACEMENT_3D('',#148564,#115911,#115912) ;
#96178 = AXIS2_PLACEMENT_3D('',#148565,#115913,#115914) ;
#96179 = AXIS2_PLACEMENT_3D('',#148566,#115915,#115916) ;
#96180 = AXIS2_PLACEMENT_3D('',#148567,#115917,#115918) ;
#96181 = AXIS2_PLACEMENT_3D('',#148568,#115919,#115920) ;
#96182 = AXIS2_PLACEMENT_3D('',#148570,#115921,#115922) ;
#96183 = AXIS2_PLACEMENT_3D('',#148571,#115923,#115924) ;
#96184 = AXIS2_PLACEMENT_3D('',#148572,#115925,#115926) ;
#96185 = AXIS2_PLACEMENT_3D('',#148573,#115927,#115928) ;
#96186 = AXIS2_PLACEMENT_3D('',#148574,#115929,#115930) ;
#96187 = AXIS2_PLACEMENT_3D('',#148575,#115931,#115932) ;
#96188 = AXIS2_PLACEMENT_3D('',#148576,#115933,#115934) ;
#96189 = AXIS2_PLACEMENT_3D('',#148577,#115935,#115936) ;
#96190 = AXIS2_PLACEMENT_3D('',#148578,#115937,#115938) ;
#96191 = AXIS2_PLACEMENT_3D('',#148579,#115939,#115940) ;
#96192 = AXIS2_PLACEMENT_3D('',#148580,#115941,#115942) ;
#96193 = AXIS2_PLACEMENT_3D('',#148581,#115943,#115944) ;
#96194 = AXIS2_PLACEMENT_3D('',#148582,#115945,#115946) ;
#96195 = AXIS2_PLACEMENT_3D('',#148585,#115948,#115949) ;
#96196 = AXIS2_PLACEMENT_3D('',#148586,#115950,#115951) ;
#96197 = AXIS2_PLACEMENT_3D('',#148587,#115952,#115953) ;
#96198 = AXIS2_PLACEMENT_3D('',#148588,#115954,#115955) ;
#96199 = AXIS2_PLACEMENT_3D('',#148589,#115956,#115957) ;
#96200 = AXIS2_PLACEMENT_3D('',#148590,#115958,#115959) ;
#96201 = AXIS2_PLACEMENT_3D('',#148591,#115960,#115961) ;
#96202 = AXIS2_PLACEMENT_3D('',#148592,#115962,#115963) ;
#96203 = AXIS2_PLACEMENT_3D('',#148593,#115964,#115965) ;
#96204 = AXIS2_PLACEMENT_3D('',#148594,#115966,#115967) ;
#96205 = AXIS2_PLACEMENT_3D('',#148595,#115968,#115969) ;
#96206 = AXIS2_PLACEMENT_3D('',#148596,#115970,#115971) ;
#96207 = AXIS2_PLACEMENT_3D('',#148597,#115972,#115973) ;
#96208 = AXIS2_PLACEMENT_3D('',#148599,#115974,#115975) ;
#96209 = AXIS2_PLACEMENT_3D('',#148600,#115976,#115977) ;
#96210 = AXIS2_PLACEMENT_3D('',#148601,#115978,#115979) ;
#96211 = AXIS2_PLACEMENT_3D('',#148602,#115980,#115981) ;
#96212 = AXIS2_PLACEMENT_3D('',#148603,#115982,#115983) ;
#96213 = AXIS2_PLACEMENT_3D('',#148604,#115984,#115985) ;
#96214 = AXIS2_PLACEMENT_3D('',#148605,#115986,#115987) ;
#96215 = AXIS2_PLACEMENT_3D('',#148606,#115988,#115989) ;
#96216 = AXIS2_PLACEMENT_3D('',#148607,#115990,#115991) ;
#96217 = AXIS2_PLACEMENT_3D('',#148608,#115992,#115993) ;
#96218 = AXIS2_PLACEMENT_3D('',#148609,#115994,#115995) ;
#96219 = AXIS2_PLACEMENT_3D('',#148611,#115997,#115998) ;
#96220 = AXIS2_PLACEMENT_3D('',#148612,#115999,#116000) ;
#96221 = AXIS2_PLACEMENT_3D('',#148613,#116001,#116002) ;
#96222 = AXIS2_PLACEMENT_3D('',#148614,#116003,#116004) ;
#96223 = AXIS2_PLACEMENT_3D('',#148615,#116005,#116006) ;
#96224 = AXIS2_PLACEMENT_3D('',#148616,#116007,#116008) ;
#96225 = AXIS2_PLACEMENT_3D('',#148617,#116009,#116010) ;
#96226 = AXIS2_PLACEMENT_3D('',#148618,#116011,#116012) ;
#96227 = AXIS2_PLACEMENT_3D('',#148619,#116013,#116014) ;
#96228 = AXIS2_PLACEMENT_3D('',#148620,#116015,#116016) ;
#96229 = AXIS2_PLACEMENT_3D('',#148621,#116017,#116018) ;
#96230 = AXIS2_PLACEMENT_3D('',#148622,#116019,#116020) ;
#96231 = AXIS2_PLACEMENT_3D('',#148623,#116021,#116022) ;
#96232 = AXIS2_PLACEMENT_3D('',#148624,#116023,#116024) ;
#96233 = AXIS2_PLACEMENT_3D('',#148625,#116025,#116026) ;
#96234 = AXIS2_PLACEMENT_3D('',#148626,#116027,#116028) ;
#96235 = AXIS2_PLACEMENT_3D('',#148627,#116029,#116030) ;
#96236 = AXIS2_PLACEMENT_3D('',#148628,#116031,#116032) ;
#96237 = AXIS2_PLACEMENT_3D('',#148629,#116033,#116034) ;
#96238 = AXIS2_PLACEMENT_3D('',#148630,#116035,#116036) ;
#96239 = AXIS2_PLACEMENT_3D('',#148631,#116037,#116038) ;
#96240 = AXIS2_PLACEMENT_3D('',#148632,#116039,#116040) ;
#96241 = AXIS2_PLACEMENT_3D('',#148633,#116041,#116042) ;
#96242 = AXIS2_PLACEMENT_3D('',#148634,#116043,#116044) ;
#96243 = AXIS2_PLACEMENT_3D('',#148635,#116045,#116046) ;
#96244 = AXIS2_PLACEMENT_3D('',#148636,#116047,#116048) ;
#96245 = AXIS2_PLACEMENT_3D('',#148637,#116049,#116050) ;
#96246 = AXIS2_PLACEMENT_3D('',#148638,#116051,#116052) ;
#96247 = AXIS2_PLACEMENT_3D('',#148639,#116053,#116054) ;
#96248 = AXIS2_PLACEMENT_3D('',#148640,#116055,#116056) ;
#96249 = AXIS2_PLACEMENT_3D('',#148641,#116057,#116058) ;
#96250 = AXIS2_PLACEMENT_3D('',#148642,#116059,#116060) ;
#96251 = AXIS2_PLACEMENT_3D('',#148643,#116061,#116062) ;
#96252 = AXIS2_PLACEMENT_3D('',#148644,#116063,#116064) ;
#96253 = AXIS2_PLACEMENT_3D('',#148645,#116065,#116066) ;
#96254 = AXIS2_PLACEMENT_3D('',#148646,#116067,#116068) ;
#96255 = AXIS2_PLACEMENT_3D('',#148647,#116069,#116070) ;
#96256 = AXIS2_PLACEMENT_3D('',#148648,#116071,#116072) ;
#96257 = AXIS2_PLACEMENT_3D('',#148649,#116073,#116074) ;
#96258 = AXIS2_PLACEMENT_3D('',#148650,#116075,#116076) ;
#96259 = AXIS2_PLACEMENT_3D('',#148651,#116077,#116078) ;
#96260 = AXIS2_PLACEMENT_3D('',#148652,#116079,#116080) ;
#96261 = AXIS2_PLACEMENT_3D('',#148653,#116081,#116082) ;
#96262 = AXIS2_PLACEMENT_3D('',#148654,#116083,#116084) ;
#96263 = AXIS2_PLACEMENT_3D('',#148655,#116085,#116086) ;
#96264 = AXIS2_PLACEMENT_3D('',#148656,#116087,#116088) ;
#96265 = AXIS2_PLACEMENT_3D('',#148657,#116089,#116090) ;
#96266 = AXIS2_PLACEMENT_3D('',#148658,#116091,#116092) ;
#96267 = AXIS2_PLACEMENT_3D('',#148659,#116093,#116094) ;
#96268 = AXIS2_PLACEMENT_3D('',#148660,#116095,#116096) ;
#96269 = AXIS2_PLACEMENT_3D('',#148661,#116097,#116098) ;
#96270 = AXIS2_PLACEMENT_3D('',#148662,#116099,#116100) ;
#96271 = AXIS2_PLACEMENT_3D('',#148663,#116101,#116102) ;
#96272 = AXIS2_PLACEMENT_3D('',#148664,#116103,#116104) ;
#96273 = AXIS2_PLACEMENT_3D('',#148665,#116105,#116106) ;
#96274 = AXIS2_PLACEMENT_3D('',#148666,#116107,#116108) ;
#96275 = AXIS2_PLACEMENT_3D('',#148667,#116109,#116110) ;
#96276 = AXIS2_PLACEMENT_3D('',#148668,#116111,#116112) ;
#96277 = AXIS2_PLACEMENT_3D('',#148669,#116113,#116114) ;
#96278 = AXIS2_PLACEMENT_3D('',#148670,#116115,#116116) ;
#96279 = AXIS2_PLACEMENT_3D('',#148671,#116117,#116118) ;
#96280 = AXIS2_PLACEMENT_3D('',#148672,#116119,#116120) ;
#96281 = AXIS2_PLACEMENT_3D('',#148673,#116121,#116122) ;
#96282 = AXIS2_PLACEMENT_3D('',#148674,#116123,#116124) ;
#96283 = AXIS2_PLACEMENT_3D('',#148675,#116125,#116126) ;
#96284 = AXIS2_PLACEMENT_3D('',#148676,#116127,#116128) ;
#96285 = AXIS2_PLACEMENT_3D('',#148677,#116129,#116130) ;
#96286 = AXIS2_PLACEMENT_3D('',#148679,#116131,#116132) ;
#96287 = AXIS2_PLACEMENT_3D('',#148680,#116133,#116134) ;
#96288 = AXIS2_PLACEMENT_3D('',#148681,#116135,#116136) ;
#96289 = AXIS2_PLACEMENT_3D('',#148682,#116137,#116138) ;
#96290 = AXIS2_PLACEMENT_3D('',#148683,#116139,#116140) ;
#96291 = AXIS2_PLACEMENT_3D('',#148684,#116141,#116142) ;
#96292 = AXIS2_PLACEMENT_3D('',#148685,#116143,#116144) ;
#96293 = AXIS2_PLACEMENT_3D('',#148686,#116145,#116146) ;
#96294 = AXIS2_PLACEMENT_3D('',#148687,#116147,#116148) ;
#96295 = AXIS2_PLACEMENT_3D('',#148698,#116150,#116151) ;
#96296 = AXIS2_PLACEMENT_3D('',#148755,#116153,#116154) ;
#96297 = AXIS2_PLACEMENT_3D('',#148756,#116155,#116156) ;
#96298 = AXIS2_PLACEMENT_3D('',#148757,#116157,#116158) ;
#96299 = AXIS2_PLACEMENT_3D('',#148758,#116159,#116160) ;
#96300 = AXIS2_PLACEMENT_3D('',#148759,#116161,#116162) ;
#96301 = AXIS2_PLACEMENT_3D('',#148760,#116163,#116164) ;
#96302 = AXIS2_PLACEMENT_3D('',#148761,#116165,#116166) ;
#96303 = AXIS2_PLACEMENT_3D('',#148762,#116167,#116168) ;
#96304 = AXIS2_PLACEMENT_3D('',#148763,#116169,#116170) ;
#96305 = AXIS2_PLACEMENT_3D('',#148764,#116171,#116172) ;
#96306 = AXIS2_PLACEMENT_3D('',#148765,#116173,#116174) ;
#96307 = AXIS2_PLACEMENT_3D('',#148766,#116175,#116176) ;
#96308 = AXIS2_PLACEMENT_3D('',#148767,#116177,#116178) ;
#96309 = AXIS2_PLACEMENT_3D('',#148768,#116179,#116180) ;
#96310 = AXIS2_PLACEMENT_3D('',#148769,#116181,#116182) ;
#96311 = AXIS2_PLACEMENT_3D('',#148770,#116183,#116184) ;
#96312 = AXIS2_PLACEMENT_3D('',#148771,#116185,#116186) ;
#96313 = AXIS2_PLACEMENT_3D('',#148772,#116187,#116188) ;
#96314 = AXIS2_PLACEMENT_3D('',#148773,#116189,#116190) ;
#96315 = AXIS2_PLACEMENT_3D('',#148774,#116191,#116192) ;
#96316 = AXIS2_PLACEMENT_3D('',#148775,#116193,#116194) ;
#96317 = AXIS2_PLACEMENT_3D('',#148776,#116195,#116196) ;
#96318 = AXIS2_PLACEMENT_3D('',#148777,#116197,#116198) ;
#96319 = AXIS2_PLACEMENT_3D('',#148780,#116200,#116201) ;
#96320 = AXIS2_PLACEMENT_3D('',#148781,#116202,#116203) ;
#96321 = AXIS2_PLACEMENT_3D('',#148782,#116204,#116205) ;
#96322 = AXIS2_PLACEMENT_3D('',#148783,#116206,#116207) ;
#96323 = AXIS2_PLACEMENT_3D('',#148784,#116208,#116209) ;
#96324 = AXIS2_PLACEMENT_3D('',#148785,#116210,#116211) ;
#96325 = AXIS2_PLACEMENT_3D('',#148786,#116212,#116213) ;
#96326 = AXIS2_PLACEMENT_3D('',#148787,#116214,#116215) ;
#96327 = AXIS2_PLACEMENT_3D('',#148788,#116216,#116217) ;
#96328 = AXIS2_PLACEMENT_3D('',#148789,#116218,#116219) ;
#96329 = AXIS2_PLACEMENT_3D('',#148790,#116220,#116221) ;
#96330 = AXIS2_PLACEMENT_3D('',#148791,#116222,#116223) ;
#96331 = AXIS2_PLACEMENT_3D('',#148792,#116224,#116225) ;
#96332 = AXIS2_PLACEMENT_3D('',#148793,#116226,#116227) ;
#96333 = AXIS2_PLACEMENT_3D('',#148794,#116228,#116229) ;
#96334 = AXIS2_PLACEMENT_3D('',#148795,#116230,#116231) ;
#96335 = AXIS2_PLACEMENT_3D('',#148797,#116232,#116233) ;
#96336 = AXIS2_PLACEMENT_3D('',#148798,#116234,#116235) ;
#96337 = AXIS2_PLACEMENT_3D('',#148799,#116236,#116237) ;
#96338 = AXIS2_PLACEMENT_3D('',#148800,#116238,#116239) ;
#96339 = AXIS2_PLACEMENT_3D('',#148801,#116240,#116241) ;
#96340 = AXIS2_PLACEMENT_3D('',#148802,#116242,#116243) ;
#96341 = AXIS2_PLACEMENT_3D('',#148803,#116244,#116245) ;
#96342 = AXIS2_PLACEMENT_3D('',#148804,#116246,#116247) ;
#96343 = AXIS2_PLACEMENT_3D('',#148805,#116248,#116249) ;
#96344 = AXIS2_PLACEMENT_3D('',#148806,#116250,#116251) ;
#96345 = AXIS2_PLACEMENT_3D('',#148807,#116252,#116253) ;
#96346 = AXIS2_PLACEMENT_3D('',#148808,#116254,#116255) ;
#96347 = AXIS2_PLACEMENT_3D('',#148809,#116256,#116257) ;
#96348 = AXIS2_PLACEMENT_3D('',#148812,#116259,#116260) ;
#96349 = AXIS2_PLACEMENT_3D('',#148813,#116261,#116262) ;
#96350 = AXIS2_PLACEMENT_3D('',#148814,#116263,#116264) ;
#96351 = AXIS2_PLACEMENT_3D('',#148815,#116265,#116266) ;
#96352 = AXIS2_PLACEMENT_3D('',#148816,#116267,#116268) ;
#96353 = AXIS2_PLACEMENT_3D('',#148817,#116269,#116270) ;
#96354 = AXIS2_PLACEMENT_3D('',#148818,#116271,#116272) ;
#96355 = AXIS2_PLACEMENT_3D('',#148819,#116273,#116274) ;
#96356 = AXIS2_PLACEMENT_3D('',#148820,#116275,#116276) ;
#96357 = AXIS2_PLACEMENT_3D('',#148821,#116277,#116278) ;
#96358 = AXIS2_PLACEMENT_3D('',#148822,#116279,#116280) ;
#96359 = AXIS2_PLACEMENT_3D('',#148823,#116281,#116282) ;
#96360 = AXIS2_PLACEMENT_3D('',#148824,#116283,#116284) ;
#96361 = AXIS2_PLACEMENT_3D('',#148826,#116285,#116286) ;
#96362 = AXIS2_PLACEMENT_3D('',#148827,#116287,#116288) ;
#96363 = AXIS2_PLACEMENT_3D('',#148828,#116289,#116290) ;
#96364 = AXIS2_PLACEMENT_3D('',#148829,#116291,#116292) ;
#96365 = AXIS2_PLACEMENT_3D('',#148830,#116293,#116294) ;
#96366 = AXIS2_PLACEMENT_3D('',#148831,#116295,#116296) ;
#96367 = AXIS2_PLACEMENT_3D('',#148832,#116297,#116298) ;
#96368 = AXIS2_PLACEMENT_3D('',#148833,#116299,#116300) ;
#96369 = AXIS2_PLACEMENT_3D('',#148834,#116301,#116302) ;
#96370 = AXIS2_PLACEMENT_3D('',#148835,#116303,#116304) ;
#96371 = AXIS2_PLACEMENT_3D('',#148836,#116305,#116306) ;
#96372 = AXIS2_PLACEMENT_3D('',#148838,#116308,#116309) ;
#96373 = AXIS2_PLACEMENT_3D('',#148839,#116310,#116311) ;
#96374 = AXIS2_PLACEMENT_3D('',#148840,#116312,#116313) ;
#96375 = AXIS2_PLACEMENT_3D('',#148841,#116314,#116315) ;
#96376 = AXIS2_PLACEMENT_3D('',#148842,#116316,#116317) ;
#96377 = AXIS2_PLACEMENT_3D('',#148843,#116318,#116319) ;
#96378 = AXIS2_PLACEMENT_3D('',#148844,#116320,#116321) ;
#96379 = AXIS2_PLACEMENT_3D('',#148845,#116322,#116323) ;
#96380 = AXIS2_PLACEMENT_3D('',#148846,#116324,#116325) ;
#96381 = AXIS2_PLACEMENT_3D('',#148847,#116326,#116327) ;
#96382 = AXIS2_PLACEMENT_3D('',#148848,#116328,#116329) ;
#96383 = AXIS2_PLACEMENT_3D('',#148849,#116330,#116331) ;
#96384 = AXIS2_PLACEMENT_3D('',#148850,#116332,#116333) ;
#96385 = AXIS2_PLACEMENT_3D('',#148851,#116334,#116335) ;
#96386 = AXIS2_PLACEMENT_3D('',#148852,#116336,#116337) ;
#96387 = AXIS2_PLACEMENT_3D('',#148853,#116338,#116339) ;
#96388 = AXIS2_PLACEMENT_3D('',#148854,#116340,#116341) ;
#96389 = AXIS2_PLACEMENT_3D('',#148855,#116342,#116343) ;
#96390 = AXIS2_PLACEMENT_3D('',#148856,#116344,#116345) ;
#96391 = AXIS2_PLACEMENT_3D('',#148857,#116346,#116347) ;
#96392 = AXIS2_PLACEMENT_3D('',#148858,#116348,#116349) ;
#96393 = AXIS2_PLACEMENT_3D('',#148859,#116350,#116351) ;
#96394 = AXIS2_PLACEMENT_3D('',#148860,#116352,#116353) ;
#96395 = AXIS2_PLACEMENT_3D('',#148861,#116354,#116355) ;
#96396 = AXIS2_PLACEMENT_3D('',#148862,#116356,#116357) ;
#96397 = AXIS2_PLACEMENT_3D('',#148863,#116358,#116359) ;
#96398 = AXIS2_PLACEMENT_3D('',#148864,#116360,#116361) ;
#96399 = AXIS2_PLACEMENT_3D('',#148865,#116362,#116363) ;
#96400 = AXIS2_PLACEMENT_3D('',#148866,#116364,#116365) ;
#96401 = AXIS2_PLACEMENT_3D('',#148867,#116366,#116367) ;
#96402 = AXIS2_PLACEMENT_3D('',#148868,#116368,#116369) ;
#96403 = AXIS2_PLACEMENT_3D('',#148869,#116370,#116371) ;
#96404 = AXIS2_PLACEMENT_3D('',#148870,#116372,#116373) ;
#96405 = AXIS2_PLACEMENT_3D('',#148871,#116374,#116375) ;
#96406 = AXIS2_PLACEMENT_3D('',#148872,#116376,#116377) ;
#96407 = AXIS2_PLACEMENT_3D('',#148873,#116378,#116379) ;
#96408 = AXIS2_PLACEMENT_3D('',#148874,#116380,#116381) ;
#96409 = AXIS2_PLACEMENT_3D('',#148875,#116382,#116383) ;
#96410 = AXIS2_PLACEMENT_3D('',#148876,#116384,#116385) ;
#96411 = AXIS2_PLACEMENT_3D('',#148877,#116386,#116387) ;
#96412 = AXIS2_PLACEMENT_3D('',#148878,#116388,#116389) ;
#96413 = AXIS2_PLACEMENT_3D('',#148879,#116390,#116391) ;
#96414 = AXIS2_PLACEMENT_3D('',#148880,#116392,#116393) ;
#96415 = AXIS2_PLACEMENT_3D('',#148881,#116394,#116395) ;
#96416 = AXIS2_PLACEMENT_3D('',#148882,#116396,#116397) ;
#96417 = AXIS2_PLACEMENT_3D('',#148883,#116398,#116399) ;
#96418 = AXIS2_PLACEMENT_3D('',#148884,#116400,#116401) ;
#96419 = AXIS2_PLACEMENT_3D('',#148885,#116402,#116403) ;
#96420 = AXIS2_PLACEMENT_3D('',#148886,#116404,#116405) ;
#96421 = AXIS2_PLACEMENT_3D('',#148887,#116406,#116407) ;
#96422 = AXIS2_PLACEMENT_3D('',#148888,#116408,#116409) ;
#96423 = AXIS2_PLACEMENT_3D('',#148889,#116410,#116411) ;
#96424 = AXIS2_PLACEMENT_3D('',#148890,#116412,#116413) ;
#96425 = AXIS2_PLACEMENT_3D('',#148891,#116414,#116415) ;
#96426 = AXIS2_PLACEMENT_3D('',#148892,#116416,#116417) ;
#96427 = AXIS2_PLACEMENT_3D('',#148893,#116418,#116419) ;
#96428 = AXIS2_PLACEMENT_3D('',#148894,#116420,#116421) ;
#96429 = AXIS2_PLACEMENT_3D('',#148895,#116422,#116423) ;
#96430 = AXIS2_PLACEMENT_3D('',#148896,#116424,#116425) ;
#96431 = AXIS2_PLACEMENT_3D('',#148897,#116426,#116427) ;
#96432 = AXIS2_PLACEMENT_3D('',#148898,#116428,#116429) ;
#96433 = AXIS2_PLACEMENT_3D('',#148899,#116430,#116431) ;
#96434 = AXIS2_PLACEMENT_3D('',#148900,#116432,#116433) ;
#96435 = AXIS2_PLACEMENT_3D('',#148901,#116434,#116435) ;
#96436 = AXIS2_PLACEMENT_3D('',#148902,#116436,#116437) ;
#96437 = AXIS2_PLACEMENT_3D('',#148903,#116438,#116439) ;
#96438 = AXIS2_PLACEMENT_3D('',#148904,#116440,#116441) ;
#96439 = AXIS2_PLACEMENT_3D('',#148906,#116442,#116443) ;
#96440 = AXIS2_PLACEMENT_3D('',#148907,#116444,#116445) ;
#96441 = AXIS2_PLACEMENT_3D('',#148908,#116446,#116447) ;
#96442 = AXIS2_PLACEMENT_3D('',#148909,#116448,#116449) ;
#96443 = AXIS2_PLACEMENT_3D('',#148910,#116450,#116451) ;
#96444 = AXIS2_PLACEMENT_3D('',#148911,#116452,#116453) ;
#96445 = AXIS2_PLACEMENT_3D('',#148912,#116454,#116455) ;
#96446 = AXIS2_PLACEMENT_3D('',#148913,#116456,#116457) ;
#96447 = AXIS2_PLACEMENT_3D('',#148914,#116458,#116459) ;
#96448 = AXIS2_PLACEMENT_3D('',#148925,#116461,#116462) ;
#96449 = AXIS2_PLACEMENT_3D('',#148982,#116464,#116465) ;
#96450 = AXIS2_PLACEMENT_3D('',#148983,#116466,#116467) ;
#96451 = AXIS2_PLACEMENT_3D('',#148984,#116468,#116469) ;
#96452 = AXIS2_PLACEMENT_3D('',#148985,#116470,#116471) ;
#96453 = AXIS2_PLACEMENT_3D('',#148986,#116472,#116473) ;
#96454 = AXIS2_PLACEMENT_3D('',#148987,#116474,#116475) ;
#96455 = AXIS2_PLACEMENT_3D('',#148988,#116476,#116477) ;
#96456 = AXIS2_PLACEMENT_3D('',#148989,#116478,#116479) ;
#96457 = AXIS2_PLACEMENT_3D('',#148990,#116480,#116481) ;
#96458 = AXIS2_PLACEMENT_3D('',#148991,#116482,#116483) ;
#96459 = AXIS2_PLACEMENT_3D('',#148992,#116484,#116485) ;
#96460 = AXIS2_PLACEMENT_3D('',#148993,#116486,#116487) ;
#96461 = AXIS2_PLACEMENT_3D('',#148994,#116488,#116489) ;
#96462 = AXIS2_PLACEMENT_3D('',#148995,#116490,#116491) ;
#96463 = AXIS2_PLACEMENT_3D('',#148996,#116492,#116493) ;
#96464 = AXIS2_PLACEMENT_3D('',#148997,#116494,#116495) ;
#96465 = AXIS2_PLACEMENT_3D('',#148998,#116496,#116497) ;
#96466 = AXIS2_PLACEMENT_3D('',#148999,#116498,#116499) ;
#96467 = AXIS2_PLACEMENT_3D('',#149000,#116500,#116501) ;
#96468 = AXIS2_PLACEMENT_3D('',#149001,#116502,#116503) ;
#96469 = AXIS2_PLACEMENT_3D('',#149002,#116504,#116505) ;
#96470 = AXIS2_PLACEMENT_3D('',#149003,#116506,#116507) ;
#96471 = AXIS2_PLACEMENT_3D('',#149004,#116508,#116509) ;
#96472 = AXIS2_PLACEMENT_3D('',#149007,#116511,#116512) ;
#96473 = AXIS2_PLACEMENT_3D('',#149008,#116513,#116514) ;
#96474 = AXIS2_PLACEMENT_3D('',#149009,#116515,#116516) ;
#96475 = AXIS2_PLACEMENT_3D('',#149010,#116517,#116518) ;
#96476 = AXIS2_PLACEMENT_3D('',#149011,#116519,#116520) ;
#96477 = AXIS2_PLACEMENT_3D('',#149012,#116521,#116522) ;
#96478 = AXIS2_PLACEMENT_3D('',#149013,#116523,#116524) ;
#96479 = AXIS2_PLACEMENT_3D('',#149014,#116525,#116526) ;
#96480 = AXIS2_PLACEMENT_3D('',#149015,#116527,#116528) ;
#96481 = AXIS2_PLACEMENT_3D('',#149016,#116529,#116530) ;
#96482 = AXIS2_PLACEMENT_3D('',#149017,#116531,#116532) ;
#96483 = AXIS2_PLACEMENT_3D('',#149018,#116533,#116534) ;
#96484 = AXIS2_PLACEMENT_3D('',#149019,#116535,#116536) ;
#96485 = AXIS2_PLACEMENT_3D('',#149020,#116537,#116538) ;
#96486 = AXIS2_PLACEMENT_3D('',#149021,#116539,#116540) ;
#96487 = AXIS2_PLACEMENT_3D('',#149022,#116541,#116542) ;
#96488 = AXIS2_PLACEMENT_3D('',#149024,#116543,#116544) ;
#96489 = AXIS2_PLACEMENT_3D('',#149025,#116545,#116546) ;
#96490 = AXIS2_PLACEMENT_3D('',#149026,#116547,#116548) ;
#96491 = AXIS2_PLACEMENT_3D('',#149027,#116549,#116550) ;
#96492 = AXIS2_PLACEMENT_3D('',#149028,#116551,#116552) ;
#96493 = AXIS2_PLACEMENT_3D('',#149029,#116553,#116554) ;
#96494 = AXIS2_PLACEMENT_3D('',#149030,#116555,#116556) ;
#96495 = AXIS2_PLACEMENT_3D('',#149031,#116557,#116558) ;
#96496 = AXIS2_PLACEMENT_3D('',#149032,#116559,#116560) ;
#96497 = AXIS2_PLACEMENT_3D('',#149033,#116561,#116562) ;
#96498 = AXIS2_PLACEMENT_3D('',#149034,#116563,#116564) ;
#96499 = AXIS2_PLACEMENT_3D('',#149035,#116565,#116566) ;
#96500 = AXIS2_PLACEMENT_3D('',#149036,#116567,#116568) ;
#96501 = AXIS2_PLACEMENT_3D('',#149039,#116570,#116571) ;
#96502 = AXIS2_PLACEMENT_3D('',#149040,#116572,#116573) ;
#96503 = AXIS2_PLACEMENT_3D('',#149041,#116574,#116575) ;
#96504 = AXIS2_PLACEMENT_3D('',#149042,#116576,#116577) ;
#96505 = AXIS2_PLACEMENT_3D('',#149043,#116578,#116579) ;
#96506 = AXIS2_PLACEMENT_3D('',#149044,#116580,#116581) ;
#96507 = AXIS2_PLACEMENT_3D('',#149045,#116582,#116583) ;
#96508 = AXIS2_PLACEMENT_3D('',#149046,#116584,#116585) ;
#96509 = AXIS2_PLACEMENT_3D('',#149047,#116586,#116587) ;
#96510 = AXIS2_PLACEMENT_3D('',#149048,#116588,#116589) ;
#96511 = AXIS2_PLACEMENT_3D('',#149049,#116590,#116591) ;
#96512 = AXIS2_PLACEMENT_3D('',#149050,#116592,#116593) ;
#96513 = AXIS2_PLACEMENT_3D('',#149051,#116594,#116595) ;
#96514 = AXIS2_PLACEMENT_3D('',#149053,#116596,#116597) ;
#96515 = AXIS2_PLACEMENT_3D('',#149054,#116598,#116599) ;
#96516 = AXIS2_PLACEMENT_3D('',#149055,#116600,#116601) ;
#96517 = AXIS2_PLACEMENT_3D('',#149056,#116602,#116603) ;
#96518 = AXIS2_PLACEMENT_3D('',#149057,#116604,#116605) ;
#96519 = AXIS2_PLACEMENT_3D('',#149058,#116606,#116607) ;
#96520 = AXIS2_PLACEMENT_3D('',#149059,#116608,#116609) ;
#96521 = AXIS2_PLACEMENT_3D('',#149060,#116610,#116611) ;
#96522 = AXIS2_PLACEMENT_3D('',#149061,#116612,#116613) ;
#96523 = AXIS2_PLACEMENT_3D('',#149062,#116614,#116615) ;
#96524 = AXIS2_PLACEMENT_3D('',#149063,#116616,#116617) ;
#96525 = AXIS2_PLACEMENT_3D('',#149065,#116619,#116620) ;
#96526 = AXIS2_PLACEMENT_3D('',#149066,#116621,#116622) ;
#96527 = AXIS2_PLACEMENT_3D('',#149067,#116623,#116624) ;
#96528 = AXIS2_PLACEMENT_3D('',#149068,#116625,#116626) ;
#96529 = AXIS2_PLACEMENT_3D('',#149069,#116627,#116628) ;
#96530 = AXIS2_PLACEMENT_3D('',#149070,#116629,#116630) ;
#96531 = AXIS2_PLACEMENT_3D('',#149071,#116631,#116632) ;
#96532 = AXIS2_PLACEMENT_3D('',#149072,#116633,#116634) ;
#96533 = AXIS2_PLACEMENT_3D('',#149073,#116635,#116636) ;
#96534 = AXIS2_PLACEMENT_3D('',#149074,#116637,#116638) ;
#96535 = AXIS2_PLACEMENT_3D('',#149075,#116639,#116640) ;
#96536 = AXIS2_PLACEMENT_3D('',#149076,#116641,#116642) ;
#96537 = AXIS2_PLACEMENT_3D('',#149077,#116643,#116644) ;
#96538 = AXIS2_PLACEMENT_3D('',#149078,#116645,#116646) ;
#96539 = AXIS2_PLACEMENT_3D('',#149079,#116647,#116648) ;
#96540 = AXIS2_PLACEMENT_3D('',#149080,#116649,#116650) ;
#96541 = AXIS2_PLACEMENT_3D('',#149081,#116651,#116652) ;
#96542 = AXIS2_PLACEMENT_3D('',#149082,#116653,#116654) ;
#96543 = AXIS2_PLACEMENT_3D('',#149083,#116655,#116656) ;
#96544 = AXIS2_PLACEMENT_3D('',#149084,#116657,#116658) ;
#96545 = AXIS2_PLACEMENT_3D('',#149085,#116659,#116660) ;
#96546 = AXIS2_PLACEMENT_3D('',#149086,#116661,#116662) ;
#96547 = AXIS2_PLACEMENT_3D('',#149087,#116663,#116664) ;
#96548 = AXIS2_PLACEMENT_3D('',#149088,#116665,#116666) ;
#96549 = AXIS2_PLACEMENT_3D('',#149089,#116667,#116668) ;
#96550 = AXIS2_PLACEMENT_3D('',#149090,#116669,#116670) ;
#96551 = AXIS2_PLACEMENT_3D('',#149091,#116671,#116672) ;
#96552 = AXIS2_PLACEMENT_3D('',#149092,#116673,#116674) ;
#96553 = AXIS2_PLACEMENT_3D('',#149093,#116675,#116676) ;
#96554 = AXIS2_PLACEMENT_3D('',#149094,#116677,#116678) ;
#96555 = AXIS2_PLACEMENT_3D('',#149095,#116679,#116680) ;
#96556 = AXIS2_PLACEMENT_3D('',#149096,#116681,#116682) ;
#96557 = AXIS2_PLACEMENT_3D('',#149097,#116683,#116684) ;
#96558 = AXIS2_PLACEMENT_3D('',#149098,#116685,#116686) ;
#96559 = AXIS2_PLACEMENT_3D('',#149099,#116687,#116688) ;
#96560 = AXIS2_PLACEMENT_3D('',#149100,#116689,#116690) ;
#96561 = AXIS2_PLACEMENT_3D('',#149101,#116691,#116692) ;
#96562 = AXIS2_PLACEMENT_3D('',#149102,#116693,#116694) ;
#96563 = AXIS2_PLACEMENT_3D('',#149103,#116695,#116696) ;
#96564 = AXIS2_PLACEMENT_3D('',#149104,#116697,#116698) ;
#96565 = AXIS2_PLACEMENT_3D('',#149105,#116699,#116700) ;
#96566 = AXIS2_PLACEMENT_3D('',#149106,#116701,#116702) ;
#96567 = AXIS2_PLACEMENT_3D('',#149107,#116703,#116704) ;
#96568 = AXIS2_PLACEMENT_3D('',#149108,#116705,#116706) ;
#96569 = AXIS2_PLACEMENT_3D('',#149109,#116707,#116708) ;
#96570 = AXIS2_PLACEMENT_3D('',#149110,#116709,#116710) ;
#96571 = AXIS2_PLACEMENT_3D('',#149111,#116711,#116712) ;
#96572 = AXIS2_PLACEMENT_3D('',#149112,#116713,#116714) ;
#96573 = AXIS2_PLACEMENT_3D('',#149113,#116715,#116716) ;
#96574 = AXIS2_PLACEMENT_3D('',#149114,#116717,#116718) ;
#96575 = AXIS2_PLACEMENT_3D('',#149115,#116719,#116720) ;
#96576 = AXIS2_PLACEMENT_3D('',#149116,#116721,#116722) ;
#96577 = AXIS2_PLACEMENT_3D('',#149117,#116723,#116724) ;
#96578 = AXIS2_PLACEMENT_3D('',#149118,#116725,#116726) ;
#96579 = AXIS2_PLACEMENT_3D('',#149119,#116727,#116728) ;
#96580 = AXIS2_PLACEMENT_3D('',#149120,#116729,#116730) ;
#96581 = AXIS2_PLACEMENT_3D('',#149121,#116731,#116732) ;
#96582 = AXIS2_PLACEMENT_3D('',#149122,#116733,#116734) ;
#96583 = AXIS2_PLACEMENT_3D('',#149123,#116735,#116736) ;
#96584 = AXIS2_PLACEMENT_3D('',#149124,#116737,#116738) ;
#96585 = AXIS2_PLACEMENT_3D('',#149125,#116739,#116740) ;
#96586 = AXIS2_PLACEMENT_3D('',#149126,#116741,#116742) ;
#96587 = AXIS2_PLACEMENT_3D('',#149127,#116743,#116744) ;
#96588 = AXIS2_PLACEMENT_3D('',#149128,#116745,#116746) ;
#96589 = AXIS2_PLACEMENT_3D('',#149129,#116747,#116748) ;
#96590 = AXIS2_PLACEMENT_3D('',#149130,#116749,#116750) ;
#96591 = AXIS2_PLACEMENT_3D('',#149131,#116751,#116752) ;
#96592 = AXIS2_PLACEMENT_3D('',#149133,#116753,#116754) ;
#96593 = AXIS2_PLACEMENT_3D('',#149134,#116755,#116756) ;
#96594 = AXIS2_PLACEMENT_3D('',#149135,#116757,#116758) ;
#96595 = AXIS2_PLACEMENT_3D('',#149136,#116759,#116760) ;
#96596 = AXIS2_PLACEMENT_3D('',#149137,#116761,#116762) ;
#96597 = AXIS2_PLACEMENT_3D('',#149138,#116763,#116764) ;
#96598 = AXIS2_PLACEMENT_3D('',#149139,#116765,#116766) ;
#96599 = AXIS2_PLACEMENT_3D('',#149140,#116767,#116768) ;
#96600 = AXIS2_PLACEMENT_3D('',#149141,#116769,#116770) ;
#96601 = AXIS2_PLACEMENT_3D('',#149152,#116772,#116773) ;
#96602 = AXIS2_PLACEMENT_3D('',#149209,#116775,#116776) ;
#96603 = AXIS2_PLACEMENT_3D('',#149210,#116777,#116778) ;
#96604 = AXIS2_PLACEMENT_3D('',#149211,#116779,#116780) ;
#96605 = AXIS2_PLACEMENT_3D('',#149212,#116781,#116782) ;
#96606 = AXIS2_PLACEMENT_3D('',#149213,#116783,#116784) ;
#96607 = AXIS2_PLACEMENT_3D('',#149214,#116785,#116786) ;
#96608 = AXIS2_PLACEMENT_3D('',#149215,#116787,#116788) ;
#96609 = AXIS2_PLACEMENT_3D('',#149216,#116789,#116790) ;
#96610 = AXIS2_PLACEMENT_3D('',#149217,#116791,#116792) ;
#96611 = AXIS2_PLACEMENT_3D('',#149218,#116793,#116794) ;
#96612 = AXIS2_PLACEMENT_3D('',#149219,#116795,#116796) ;
#96613 = AXIS2_PLACEMENT_3D('',#149220,#116797,#116798) ;
#96614 = AXIS2_PLACEMENT_3D('',#149221,#116799,#116800) ;
#96615 = AXIS2_PLACEMENT_3D('',#149222,#116801,#116802) ;
#96616 = AXIS2_PLACEMENT_3D('',#149223,#116803,#116804) ;
#96617 = AXIS2_PLACEMENT_3D('',#149224,#116805,#116806) ;
#96618 = AXIS2_PLACEMENT_3D('',#149225,#116807,#116808) ;
#96619 = AXIS2_PLACEMENT_3D('',#149226,#116809,#116810) ;
#96620 = AXIS2_PLACEMENT_3D('',#149227,#116811,#116812) ;
#96621 = AXIS2_PLACEMENT_3D('',#149228,#116813,#116814) ;
#96622 = AXIS2_PLACEMENT_3D('',#149229,#116815,#116816) ;
#96623 = AXIS2_PLACEMENT_3D('',#149230,#116817,#116818) ;
#96624 = AXIS2_PLACEMENT_3D('',#149231,#116819,#116820) ;
#96625 = AXIS2_PLACEMENT_3D('',#149234,#116822,#116823) ;
#96626 = AXIS2_PLACEMENT_3D('',#149235,#116824,#116825) ;
#96627 = AXIS2_PLACEMENT_3D('',#149236,#116826,#116827) ;
#96628 = AXIS2_PLACEMENT_3D('',#149237,#116828,#116829) ;
#96629 = AXIS2_PLACEMENT_3D('',#149238,#116830,#116831) ;
#96630 = AXIS2_PLACEMENT_3D('',#149239,#116832,#116833) ;
#96631 = AXIS2_PLACEMENT_3D('',#149240,#116834,#116835) ;
#96632 = AXIS2_PLACEMENT_3D('',#149241,#116836,#116837) ;
#96633 = AXIS2_PLACEMENT_3D('',#149242,#116838,#116839) ;
#96634 = AXIS2_PLACEMENT_3D('',#149243,#116840,#116841) ;
#96635 = AXIS2_PLACEMENT_3D('',#149244,#116842,#116843) ;
#96636 = AXIS2_PLACEMENT_3D('',#149245,#116844,#116845) ;
#96637 = AXIS2_PLACEMENT_3D('',#149246,#116846,#116847) ;
#96638 = AXIS2_PLACEMENT_3D('',#149247,#116848,#116849) ;
#96639 = AXIS2_PLACEMENT_3D('',#149248,#116850,#116851) ;
#96640 = AXIS2_PLACEMENT_3D('',#149249,#116852,#116853) ;
#96641 = AXIS2_PLACEMENT_3D('',#149251,#116854,#116855) ;
#96642 = AXIS2_PLACEMENT_3D('',#149252,#116856,#116857) ;
#96643 = AXIS2_PLACEMENT_3D('',#149253,#116858,#116859) ;
#96644 = AXIS2_PLACEMENT_3D('',#149254,#116860,#116861) ;
#96645 = AXIS2_PLACEMENT_3D('',#149255,#116862,#116863) ;
#96646 = AXIS2_PLACEMENT_3D('',#149256,#116864,#116865) ;
#96647 = AXIS2_PLACEMENT_3D('',#149257,#116866,#116867) ;
#96648 = AXIS2_PLACEMENT_3D('',#149258,#116868,#116869) ;
#96649 = AXIS2_PLACEMENT_3D('',#149259,#116870,#116871) ;
#96650 = AXIS2_PLACEMENT_3D('',#149260,#116872,#116873) ;
#96651 = AXIS2_PLACEMENT_3D('',#149261,#116874,#116875) ;
#96652 = AXIS2_PLACEMENT_3D('',#149262,#116876,#116877) ;
#96653 = AXIS2_PLACEMENT_3D('',#149263,#116878,#116879) ;
#96654 = AXIS2_PLACEMENT_3D('',#149266,#116881,#116882) ;
#96655 = AXIS2_PLACEMENT_3D('',#149267,#116883,#116884) ;
#96656 = AXIS2_PLACEMENT_3D('',#149268,#116885,#116886) ;
#96657 = AXIS2_PLACEMENT_3D('',#149269,#116887,#116888) ;
#96658 = AXIS2_PLACEMENT_3D('',#149270,#116889,#116890) ;
#96659 = AXIS2_PLACEMENT_3D('',#149271,#116891,#116892) ;
#96660 = AXIS2_PLACEMENT_3D('',#149272,#116893,#116894) ;
#96661 = AXIS2_PLACEMENT_3D('',#149273,#116895,#116896) ;
#96662 = AXIS2_PLACEMENT_3D('',#149274,#116897,#116898) ;
#96663 = AXIS2_PLACEMENT_3D('',#149275,#116899,#116900) ;
#96664 = AXIS2_PLACEMENT_3D('',#149276,#116901,#116902) ;
#96665 = AXIS2_PLACEMENT_3D('',#149277,#116903,#116904) ;
#96666 = AXIS2_PLACEMENT_3D('',#149278,#116905,#116906) ;
#96667 = AXIS2_PLACEMENT_3D('',#149280,#116907,#116908) ;
#96668 = AXIS2_PLACEMENT_3D('',#149281,#116909,#116910) ;
#96669 = AXIS2_PLACEMENT_3D('',#149282,#116911,#116912) ;
#96670 = AXIS2_PLACEMENT_3D('',#149283,#116913,#116914) ;
#96671 = AXIS2_PLACEMENT_3D('',#149284,#116915,#116916) ;
#96672 = AXIS2_PLACEMENT_3D('',#149285,#116917,#116918) ;
#96673 = AXIS2_PLACEMENT_3D('',#149286,#116919,#116920) ;
#96674 = AXIS2_PLACEMENT_3D('',#149287,#116921,#116922) ;
#96675 = AXIS2_PLACEMENT_3D('',#149288,#116923,#116924) ;
#96676 = AXIS2_PLACEMENT_3D('',#149289,#116925,#116926) ;
#96677 = AXIS2_PLACEMENT_3D('',#149290,#116927,#116928) ;
#96678 = AXIS2_PLACEMENT_3D('',#149292,#116930,#116931) ;
#96679 = AXIS2_PLACEMENT_3D('',#149293,#116932,#116933) ;
#96680 = AXIS2_PLACEMENT_3D('',#149294,#116934,#116935) ;
#96681 = AXIS2_PLACEMENT_3D('',#149295,#116936,#116937) ;
#96682 = AXIS2_PLACEMENT_3D('',#149296,#116938,#116939) ;
#96683 = AXIS2_PLACEMENT_3D('',#149297,#116940,#116941) ;
#96684 = AXIS2_PLACEMENT_3D('',#149298,#116942,#116943) ;
#96685 = AXIS2_PLACEMENT_3D('',#149299,#116944,#116945) ;
#96686 = AXIS2_PLACEMENT_3D('',#149300,#116946,#116947) ;
#96687 = AXIS2_PLACEMENT_3D('',#149301,#116948,#116949) ;
#96688 = AXIS2_PLACEMENT_3D('',#149302,#116950,#116951) ;
#96689 = AXIS2_PLACEMENT_3D('',#149303,#116952,#116953) ;
#96690 = AXIS2_PLACEMENT_3D('',#149304,#116954,#116955) ;
#96691 = AXIS2_PLACEMENT_3D('',#149305,#116956,#116957) ;
#96692 = AXIS2_PLACEMENT_3D('',#149306,#116958,#116959) ;
#96693 = AXIS2_PLACEMENT_3D('',#149307,#116960,#116961) ;
#96694 = AXIS2_PLACEMENT_3D('',#149308,#116962,#116963) ;
#96695 = AXIS2_PLACEMENT_3D('',#149309,#116964,#116965) ;
#96696 = AXIS2_PLACEMENT_3D('',#149310,#116966,#116967) ;
#96697 = AXIS2_PLACEMENT_3D('',#149311,#116968,#116969) ;
#96698 = AXIS2_PLACEMENT_3D('',#149312,#116970,#116971) ;
#96699 = AXIS2_PLACEMENT_3D('',#149313,#116972,#116973) ;
#96700 = AXIS2_PLACEMENT_3D('',#149314,#116974,#116975) ;
#96701 = AXIS2_PLACEMENT_3D('',#149315,#116976,#116977) ;
#96702 = AXIS2_PLACEMENT_3D('',#149316,#116978,#116979) ;
#96703 = AXIS2_PLACEMENT_3D('',#149317,#116980,#116981) ;
#96704 = AXIS2_PLACEMENT_3D('',#149318,#116982,#116983) ;
#96705 = AXIS2_PLACEMENT_3D('',#149319,#116984,#116985) ;
#96706 = AXIS2_PLACEMENT_3D('',#149320,#116986,#116987) ;
#96707 = AXIS2_PLACEMENT_3D('',#149321,#116988,#116989) ;
#96708 = AXIS2_PLACEMENT_3D('',#149322,#116990,#116991) ;
#96709 = AXIS2_PLACEMENT_3D('',#149323,#116992,#116993) ;
#96710 = AXIS2_PLACEMENT_3D('',#149324,#116994,#116995) ;
#96711 = AXIS2_PLACEMENT_3D('',#149325,#116996,#116997) ;
#96712 = AXIS2_PLACEMENT_3D('',#149326,#116998,#116999) ;
#96713 = AXIS2_PLACEMENT_3D('',#149327,#117000,#117001) ;
#96714 = AXIS2_PLACEMENT_3D('',#149328,#117002,#117003) ;
#96715 = AXIS2_PLACEMENT_3D('',#149329,#117004,#117005) ;
#96716 = AXIS2_PLACEMENT_3D('',#149330,#117006,#117007) ;
#96717 = AXIS2_PLACEMENT_3D('',#149331,#117008,#117009) ;
#96718 = AXIS2_PLACEMENT_3D('',#149332,#117010,#117011) ;
#96719 = AXIS2_PLACEMENT_3D('',#149333,#117012,#117013) ;
#96720 = AXIS2_PLACEMENT_3D('',#149334,#117014,#117015) ;
#96721 = AXIS2_PLACEMENT_3D('',#149335,#117016,#117017) ;
#96722 = AXIS2_PLACEMENT_3D('',#149336,#117018,#117019) ;
#96723 = AXIS2_PLACEMENT_3D('',#149337,#117020,#117021) ;
#96724 = AXIS2_PLACEMENT_3D('',#149338,#117022,#117023) ;
#96725 = AXIS2_PLACEMENT_3D('',#149339,#117024,#117025) ;
#96726 = AXIS2_PLACEMENT_3D('',#149340,#117026,#117027) ;
#96727 = AXIS2_PLACEMENT_3D('',#149341,#117028,#117029) ;
#96728 = AXIS2_PLACEMENT_3D('',#149342,#117030,#117031) ;
#96729 = AXIS2_PLACEMENT_3D('',#149343,#117032,#117033) ;
#96730 = AXIS2_PLACEMENT_3D('',#149344,#117034,#117035) ;
#96731 = AXIS2_PLACEMENT_3D('',#149345,#117036,#117037) ;
#96732 = AXIS2_PLACEMENT_3D('',#149346,#117038,#117039) ;
#96733 = AXIS2_PLACEMENT_3D('',#149347,#117040,#117041) ;
#96734 = AXIS2_PLACEMENT_3D('',#149348,#117042,#117043) ;
#96735 = AXIS2_PLACEMENT_3D('',#149349,#117044,#117045) ;
#96736 = AXIS2_PLACEMENT_3D('',#149350,#117046,#117047) ;
#96737 = AXIS2_PLACEMENT_3D('',#149351,#117048,#117049) ;
#96738 = AXIS2_PLACEMENT_3D('',#149352,#117050,#117051) ;
#96739 = AXIS2_PLACEMENT_3D('',#149353,#117052,#117053) ;
#96740 = AXIS2_PLACEMENT_3D('',#149354,#117054,#117055) ;
#96741 = AXIS2_PLACEMENT_3D('',#149355,#117056,#117057) ;
#96742 = AXIS2_PLACEMENT_3D('',#149356,#117058,#117059) ;
#96743 = AXIS2_PLACEMENT_3D('',#149357,#117060,#117061) ;
#96744 = AXIS2_PLACEMENT_3D('',#149358,#117062,#117063) ;
#96745 = AXIS2_PLACEMENT_3D('',#149360,#117064,#117065) ;
#96746 = AXIS2_PLACEMENT_3D('',#149361,#117066,#117067) ;
#96747 = AXIS2_PLACEMENT_3D('',#149362,#117068,#117069) ;
#96748 = AXIS2_PLACEMENT_3D('',#149363,#117070,#117071) ;
#96749 = AXIS2_PLACEMENT_3D('',#149364,#117072,#117073) ;
#96750 = AXIS2_PLACEMENT_3D('',#149365,#117074,#117075) ;
#96751 = AXIS2_PLACEMENT_3D('',#149366,#117076,#117077) ;
#96752 = AXIS2_PLACEMENT_3D('',#149367,#117078,#117079) ;
#96753 = AXIS2_PLACEMENT_3D('',#149368,#117080,#117081) ;
#96754 = AXIS2_PLACEMENT_3D('',#149379,#117083,#117084) ;
#96755 = AXIS2_PLACEMENT_3D('',#149436,#117086,#117087) ;
#96756 = AXIS2_PLACEMENT_3D('',#149437,#117088,#117089) ;
#96757 = AXIS2_PLACEMENT_3D('',#149438,#117090,#117091) ;
#96758 = AXIS2_PLACEMENT_3D('',#149439,#117092,#117093) ;
#96759 = AXIS2_PLACEMENT_3D('',#149440,#117094,#117095) ;
#96760 = AXIS2_PLACEMENT_3D('',#149441,#117096,#117097) ;
#96761 = AXIS2_PLACEMENT_3D('',#149442,#117098,#117099) ;
#96762 = AXIS2_PLACEMENT_3D('',#149443,#117100,#117101) ;
#96763 = AXIS2_PLACEMENT_3D('',#149444,#117102,#117103) ;
#96764 = AXIS2_PLACEMENT_3D('',#149445,#117104,#117105) ;
#96765 = AXIS2_PLACEMENT_3D('',#149446,#117106,#117107) ;
#96766 = AXIS2_PLACEMENT_3D('',#149447,#117108,#117109) ;
#96767 = AXIS2_PLACEMENT_3D('',#149448,#117110,#117111) ;
#96768 = AXIS2_PLACEMENT_3D('',#149449,#117112,#117113) ;
#96769 = AXIS2_PLACEMENT_3D('',#149450,#117114,#117115) ;
#96770 = AXIS2_PLACEMENT_3D('',#149451,#117116,#117117) ;
#96771 = AXIS2_PLACEMENT_3D('',#149452,#117118,#117119) ;
#96772 = AXIS2_PLACEMENT_3D('',#149453,#117120,#117121) ;
#96773 = AXIS2_PLACEMENT_3D('',#149454,#117122,#117123) ;
#96774 = AXIS2_PLACEMENT_3D('',#149455,#117124,#117125) ;
#96775 = AXIS2_PLACEMENT_3D('',#149456,#117126,#117127) ;
#96776 = AXIS2_PLACEMENT_3D('',#149457,#117128,#117129) ;
#96777 = AXIS2_PLACEMENT_3D('',#149458,#117130,#117131) ;
#96778 = AXIS2_PLACEMENT_3D('',#149461,#117133,#117134) ;
#96779 = AXIS2_PLACEMENT_3D('',#149462,#117135,#117136) ;
#96780 = AXIS2_PLACEMENT_3D('',#149463,#117137,#117138) ;
#96781 = AXIS2_PLACEMENT_3D('',#149464,#117139,#117140) ;
#96782 = AXIS2_PLACEMENT_3D('',#149465,#117141,#117142) ;
#96783 = AXIS2_PLACEMENT_3D('',#149466,#117143,#117144) ;
#96784 = AXIS2_PLACEMENT_3D('',#149467,#117145,#117146) ;
#96785 = AXIS2_PLACEMENT_3D('',#149468,#117147,#117148) ;
#96786 = AXIS2_PLACEMENT_3D('',#149469,#117149,#117150) ;
#96787 = AXIS2_PLACEMENT_3D('',#149470,#117151,#117152) ;
#96788 = AXIS2_PLACEMENT_3D('',#149471,#117153,#117154) ;
#96789 = AXIS2_PLACEMENT_3D('',#149472,#117155,#117156) ;
#96790 = AXIS2_PLACEMENT_3D('',#149473,#117157,#117158) ;
#96791 = AXIS2_PLACEMENT_3D('',#149474,#117159,#117160) ;
#96792 = AXIS2_PLACEMENT_3D('',#149475,#117161,#117162) ;
#96793 = AXIS2_PLACEMENT_3D('',#149476,#117163,#117164) ;
#96794 = AXIS2_PLACEMENT_3D('',#149478,#117165,#117166) ;
#96795 = AXIS2_PLACEMENT_3D('',#149479,#117167,#117168) ;
#96796 = AXIS2_PLACEMENT_3D('',#149480,#117169,#117170) ;
#96797 = AXIS2_PLACEMENT_3D('',#149481,#117171,#117172) ;
#96798 = AXIS2_PLACEMENT_3D('',#149482,#117173,#117174) ;
#96799 = AXIS2_PLACEMENT_3D('',#149483,#117175,#117176) ;
#96800 = AXIS2_PLACEMENT_3D('',#149484,#117177,#117178) ;
#96801 = AXIS2_PLACEMENT_3D('',#149485,#117179,#117180) ;
#96802 = AXIS2_PLACEMENT_3D('',#149486,#117181,#117182) ;
#96803 = AXIS2_PLACEMENT_3D('',#149487,#117183,#117184) ;
#96804 = AXIS2_PLACEMENT_3D('',#149488,#117185,#117186) ;
#96805 = AXIS2_PLACEMENT_3D('',#149489,#117187,#117188) ;
#96806 = AXIS2_PLACEMENT_3D('',#149490,#117189,#117190) ;
#96807 = AXIS2_PLACEMENT_3D('',#149493,#117192,#117193) ;
#96808 = AXIS2_PLACEMENT_3D('',#149494,#117194,#117195) ;
#96809 = AXIS2_PLACEMENT_3D('',#149495,#117196,#117197) ;
#96810 = AXIS2_PLACEMENT_3D('',#149496,#117198,#117199) ;
#96811 = AXIS2_PLACEMENT_3D('',#149497,#117200,#117201) ;
#96812 = AXIS2_PLACEMENT_3D('',#149498,#117202,#117203) ;
#96813 = AXIS2_PLACEMENT_3D('',#149499,#117204,#117205) ;
#96814 = AXIS2_PLACEMENT_3D('',#149500,#117206,#117207) ;
#96815 = AXIS2_PLACEMENT_3D('',#149501,#117208,#117209) ;
#96816 = AXIS2_PLACEMENT_3D('',#149502,#117210,#117211) ;
#96817 = AXIS2_PLACEMENT_3D('',#149503,#117212,#117213) ;
#96818 = AXIS2_PLACEMENT_3D('',#149504,#117214,#117215) ;
#96819 = AXIS2_PLACEMENT_3D('',#149505,#117216,#117217) ;
#96820 = AXIS2_PLACEMENT_3D('',#149507,#117218,#117219) ;
#96821 = AXIS2_PLACEMENT_3D('',#149508,#117220,#117221) ;
#96822 = AXIS2_PLACEMENT_3D('',#149509,#117222,#117223) ;
#96823 = AXIS2_PLACEMENT_3D('',#149510,#117224,#117225) ;
#96824 = AXIS2_PLACEMENT_3D('',#149511,#117226,#117227) ;
#96825 = AXIS2_PLACEMENT_3D('',#149512,#117228,#117229) ;
#96826 = AXIS2_PLACEMENT_3D('',#149513,#117230,#117231) ;
#96827 = AXIS2_PLACEMENT_3D('',#149514,#117232,#117233) ;
#96828 = AXIS2_PLACEMENT_3D('',#149515,#117234,#117235) ;
#96829 = AXIS2_PLACEMENT_3D('',#149516,#117236,#117237) ;
#96830 = AXIS2_PLACEMENT_3D('',#149517,#117238,#117239) ;
#96831 = AXIS2_PLACEMENT_3D('',#149519,#117241,#117242) ;
#96832 = AXIS2_PLACEMENT_3D('',#149520,#117243,#117244) ;
#96833 = AXIS2_PLACEMENT_3D('',#149521,#117245,#117246) ;
#96834 = AXIS2_PLACEMENT_3D('',#149522,#117247,#117248) ;
#96835 = AXIS2_PLACEMENT_3D('',#149523,#117249,#117250) ;
#96836 = AXIS2_PLACEMENT_3D('',#149524,#117251,#117252) ;
#96837 = AXIS2_PLACEMENT_3D('',#149525,#117253,#117254) ;
#96838 = AXIS2_PLACEMENT_3D('',#149526,#117255,#117256) ;
#96839 = AXIS2_PLACEMENT_3D('',#149527,#117257,#117258) ;
#96840 = AXIS2_PLACEMENT_3D('',#149528,#117259,#117260) ;
#96841 = AXIS2_PLACEMENT_3D('',#149529,#117261,#117262) ;
#96842 = AXIS2_PLACEMENT_3D('',#149530,#117263,#117264) ;
#96843 = AXIS2_PLACEMENT_3D('',#149531,#117265,#117266) ;
#96844 = AXIS2_PLACEMENT_3D('',#149532,#117267,#117268) ;
#96845 = AXIS2_PLACEMENT_3D('',#149533,#117269,#117270) ;
#96846 = AXIS2_PLACEMENT_3D('',#149534,#117271,#117272) ;
#96847 = AXIS2_PLACEMENT_3D('',#149535,#117273,#117274) ;
#96848 = AXIS2_PLACEMENT_3D('',#149536,#117275,#117276) ;
#96849 = AXIS2_PLACEMENT_3D('',#149537,#117277,#117278) ;
#96850 = AXIS2_PLACEMENT_3D('',#149538,#117279,#117280) ;
#96851 = AXIS2_PLACEMENT_3D('',#149539,#117281,#117282) ;
#96852 = AXIS2_PLACEMENT_3D('',#149540,#117283,#117284) ;
#96853 = AXIS2_PLACEMENT_3D('',#149541,#117285,#117286) ;
#96854 = AXIS2_PLACEMENT_3D('',#149542,#117287,#117288) ;
#96855 = AXIS2_PLACEMENT_3D('',#149543,#117289,#117290) ;
#96856 = AXIS2_PLACEMENT_3D('',#149544,#117291,#117292) ;
#96857 = AXIS2_PLACEMENT_3D('',#149545,#117293,#117294) ;
#96858 = AXIS2_PLACEMENT_3D('',#149546,#117295,#117296) ;
#96859 = AXIS2_PLACEMENT_3D('',#149547,#117297,#117298) ;
#96860 = AXIS2_PLACEMENT_3D('',#149548,#117299,#117300) ;
#96861 = AXIS2_PLACEMENT_3D('',#149549,#117301,#117302) ;
#96862 = AXIS2_PLACEMENT_3D('',#149550,#117303,#117304) ;
#96863 = AXIS2_PLACEMENT_3D('',#149551,#117305,#117306) ;
#96864 = AXIS2_PLACEMENT_3D('',#149552,#117307,#117308) ;
#96865 = AXIS2_PLACEMENT_3D('',#149553,#117309,#117310) ;
#96866 = AXIS2_PLACEMENT_3D('',#149554,#117311,#117312) ;
#96867 = AXIS2_PLACEMENT_3D('',#149555,#117313,#117314) ;
#96868 = AXIS2_PLACEMENT_3D('',#149556,#117315,#117316) ;
#96869 = AXIS2_PLACEMENT_3D('',#149557,#117317,#117318) ;
#96870 = AXIS2_PLACEMENT_3D('',#149558,#117319,#117320) ;
#96871 = AXIS2_PLACEMENT_3D('',#149559,#117321,#117322) ;
#96872 = AXIS2_PLACEMENT_3D('',#149560,#117323,#117324) ;
#96873 = AXIS2_PLACEMENT_3D('',#149561,#117325,#117326) ;
#96874 = AXIS2_PLACEMENT_3D('',#149562,#117327,#117328) ;
#96875 = AXIS2_PLACEMENT_3D('',#149563,#117329,#117330) ;
#96876 = AXIS2_PLACEMENT_3D('',#149564,#117331,#117332) ;
#96877 = AXIS2_PLACEMENT_3D('',#149565,#117333,#117334) ;
#96878 = AXIS2_PLACEMENT_3D('',#149566,#117335,#117336) ;
#96879 = AXIS2_PLACEMENT_3D('',#149567,#117337,#117338) ;
#96880 = AXIS2_PLACEMENT_3D('',#149568,#117339,#117340) ;
#96881 = AXIS2_PLACEMENT_3D('',#149569,#117341,#117342) ;
#96882 = AXIS2_PLACEMENT_3D('',#149570,#117343,#117344) ;
#96883 = AXIS2_PLACEMENT_3D('',#149571,#117345,#117346) ;
#96884 = AXIS2_PLACEMENT_3D('',#149572,#117347,#117348) ;
#96885 = AXIS2_PLACEMENT_3D('',#149573,#117349,#117350) ;
#96886 = AXIS2_PLACEMENT_3D('',#149574,#117351,#117352) ;
#96887 = AXIS2_PLACEMENT_3D('',#149575,#117353,#117354) ;
#96888 = AXIS2_PLACEMENT_3D('',#149576,#117355,#117356) ;
#96889 = AXIS2_PLACEMENT_3D('',#149577,#117357,#117358) ;
#96890 = AXIS2_PLACEMENT_3D('',#149578,#117359,#117360) ;
#96891 = AXIS2_PLACEMENT_3D('',#149579,#117361,#117362) ;
#96892 = AXIS2_PLACEMENT_3D('',#149588,#117367,#117368) ;
#96893 = AXIS2_PLACEMENT_3D('',#149597,#117373,#117374) ;
#96894 = AXIS2_PLACEMENT_3D('',#149606,#117379,#117380) ;
#96895 = AXIS2_PLACEMENT_3D('',#149615,#117385,#117386) ;
#96896 = AXIS2_PLACEMENT_3D('',#149624,#117391,#117392) ;
#96897 = AXIS2_PLACEMENT_3D('',#149628,#117394,#117395) ;
#96898 = AXIS2_PLACEMENT_3D('',#149630,#117396,#117397) ;
#96899 = AXIS2_PLACEMENT_3D('',#149634,#117400,#117401) ;
#96900 = AXIS2_PLACEMENT_3D('',#149638,#117403,#117404) ;
#96901 = AXIS2_PLACEMENT_3D('',#149640,#117405,#117406) ;
#96902 = AXIS2_PLACEMENT_3D('',#149644,#117409,#117410) ;
#96903 = AXIS2_PLACEMENT_3D('',#149645,#117411,#117412) ;
#96904 = AXIS2_PLACEMENT_3D('',#149646,#117413,#117414) ;
#96905 = AXIS2_PLACEMENT_3D('',#149647,#117415,#117416) ;
#96906 = AXIS2_PLACEMENT_3D('',#149648,#117417,#117418) ;
#96907 = AXIS2_PLACEMENT_3D('',#149649,#117419,#117420) ;
#96908 = AXIS2_PLACEMENT_3D('',#149650,#117421,#117422) ;
#96909 = AXIS2_PLACEMENT_3D('',#149659,#117427,#117428) ;
#96910 = AXIS2_PLACEMENT_3D('',#149665,#117432,#117433) ;
#96911 = AXIS2_PLACEMENT_3D('',#149671,#117437,#117438) ;
#96912 = AXIS2_PLACEMENT_3D('',#149680,#117443,#117444) ;
#96913 = AXIS2_PLACEMENT_3D('',#149689,#117449,#117450) ;
#96914 = AXIS2_PLACEMENT_3D('',#149695,#117454,#117455) ;
#96915 = AXIS2_PLACEMENT_3D('',#149701,#117459,#117460) ;
#96916 = AXIS2_PLACEMENT_3D('',#149710,#117465,#117466) ;
#96917 = AXIS2_PLACEMENT_3D('',#149719,#117471,#117472) ;
#96918 = AXIS2_PLACEMENT_3D('',#149728,#117477,#117478) ;
#96919 = AXIS2_PLACEMENT_3D('',#149737,#117483,#117484) ;
#96920 = AXIS2_PLACEMENT_3D('',#149746,#117489,#117490) ;
#96921 = AXIS2_PLACEMENT_3D('',#149750,#117492,#117493) ;
#96922 = AXIS2_PLACEMENT_3D('',#149752,#117494,#117495) ;
#96923 = AXIS2_PLACEMENT_3D('',#149756,#117498,#117499) ;
#96924 = AXIS2_PLACEMENT_3D('',#149760,#117501,#117502) ;
#96925 = AXIS2_PLACEMENT_3D('',#149762,#117503,#117504) ;
#96926 = AXIS2_PLACEMENT_3D('',#149766,#117507,#117508) ;
#96927 = AXIS2_PLACEMENT_3D('',#149767,#117509,#117510) ;
#96928 = AXIS2_PLACEMENT_3D('',#149768,#117511,#117512) ;
#96929 = AXIS2_PLACEMENT_3D('',#149769,#117513,#117514) ;
#96930 = AXIS2_PLACEMENT_3D('',#149770,#117515,#117516) ;
#96931 = AXIS2_PLACEMENT_3D('',#149771,#117517,#117518) ;
#96932 = AXIS2_PLACEMENT_3D('',#149772,#117519,#117520) ;
#96933 = AXIS2_PLACEMENT_3D('',#149781,#117525,#117526) ;
#96934 = AXIS2_PLACEMENT_3D('',#149787,#117530,#117531) ;
#96935 = AXIS2_PLACEMENT_3D('',#149793,#117535,#117536) ;
#96936 = AXIS2_PLACEMENT_3D('',#149802,#117541,#117542) ;
#96937 = AXIS2_PLACEMENT_3D('',#149811,#117547,#117548) ;
#96938 = AXIS2_PLACEMENT_3D('',#149817,#117552,#117553) ;
#96939 = AXIS2_PLACEMENT_3D('',#149823,#117557,#117558) ;
#96940 = AXIS2_PLACEMENT_3D('',#149832,#117563,#117564) ;
#96941 = AXIS2_PLACEMENT_3D('',#149841,#117569,#117570) ;
#96942 = AXIS2_PLACEMENT_3D('',#149850,#117575,#117576) ;
#96943 = AXIS2_PLACEMENT_3D('',#149859,#117581,#117582) ;
#96944 = AXIS2_PLACEMENT_3D('',#149868,#117587,#117588) ;
#96945 = AXIS2_PLACEMENT_3D('',#149872,#117590,#117591) ;
#96946 = AXIS2_PLACEMENT_3D('',#149874,#117592,#117593) ;
#96947 = AXIS2_PLACEMENT_3D('',#149878,#117596,#117597) ;
#96948 = AXIS2_PLACEMENT_3D('',#149882,#117599,#117600) ;
#96949 = AXIS2_PLACEMENT_3D('',#149884,#117601,#117602) ;
#96950 = AXIS2_PLACEMENT_3D('',#149888,#117605,#117606) ;
#96951 = AXIS2_PLACEMENT_3D('',#149889,#117607,#117608) ;
#96952 = AXIS2_PLACEMENT_3D('',#149890,#117609,#117610) ;
#96953 = AXIS2_PLACEMENT_3D('',#149891,#117611,#117612) ;
#96954 = AXIS2_PLACEMENT_3D('',#149892,#117613,#117614) ;
#96955 = AXIS2_PLACEMENT_3D('',#149893,#117615,#117616) ;
#96956 = AXIS2_PLACEMENT_3D('',#149894,#117617,#117618) ;
#96957 = AXIS2_PLACEMENT_3D('',#149903,#117623,#117624) ;
#96958 = AXIS2_PLACEMENT_3D('',#149909,#117628,#117629) ;
#96959 = AXIS2_PLACEMENT_3D('',#149915,#117633,#117634) ;
#96960 = AXIS2_PLACEMENT_3D('',#149924,#117639,#117640) ;
#96961 = AXIS2_PLACEMENT_3D('',#149933,#117645,#117646) ;
#96962 = AXIS2_PLACEMENT_3D('',#149939,#117650,#117651) ;
#96963 = AXIS2_PLACEMENT_3D('',#149945,#117655,#117656) ;
#96964 = AXIS2_PLACEMENT_3D('',#149954,#117661,#117662) ;
#96965 = AXIS2_PLACEMENT_3D('',#149963,#117667,#117668) ;
#96966 = AXIS2_PLACEMENT_3D('',#149972,#117673,#117674) ;
#96967 = AXIS2_PLACEMENT_3D('',#149981,#117679,#117680) ;
#96968 = AXIS2_PLACEMENT_3D('',#149990,#117685,#117686) ;
#96969 = AXIS2_PLACEMENT_3D('',#149994,#117688,#117689) ;
#96970 = AXIS2_PLACEMENT_3D('',#149996,#117690,#117691) ;
#96971 = AXIS2_PLACEMENT_3D('',#150000,#117694,#117695) ;
#96972 = AXIS2_PLACEMENT_3D('',#150004,#117697,#117698) ;
#96973 = AXIS2_PLACEMENT_3D('',#150006,#117699,#117700) ;
#96974 = AXIS2_PLACEMENT_3D('',#150010,#117703,#117704) ;
#96975 = AXIS2_PLACEMENT_3D('',#150011,#117705,#117706) ;
#96976 = AXIS2_PLACEMENT_3D('',#150012,#117707,#117708) ;
#96977 = AXIS2_PLACEMENT_3D('',#150013,#117709,#117710) ;
#96978 = AXIS2_PLACEMENT_3D('',#150014,#117711,#117712) ;
#96979 = AXIS2_PLACEMENT_3D('',#150015,#117713,#117714) ;
#96980 = AXIS2_PLACEMENT_3D('',#150016,#117715,#117716) ;
#96981 = AXIS2_PLACEMENT_3D('',#150025,#117721,#117722) ;
#96982 = AXIS2_PLACEMENT_3D('',#150031,#117726,#117727) ;
#96983 = AXIS2_PLACEMENT_3D('',#150037,#117731,#117732) ;
#96984 = AXIS2_PLACEMENT_3D('',#150046,#117737,#117738) ;
#96985 = AXIS2_PLACEMENT_3D('',#150055,#117743,#117744) ;
#96986 = AXIS2_PLACEMENT_3D('',#150061,#117748,#117749) ;
#96987 = AXIS2_PLACEMENT_3D('',#150067,#117753,#117754) ;
#96988 = AXIS2_PLACEMENT_3D('',#150076,#117759,#117760) ;
#96989 = AXIS2_PLACEMENT_3D('',#150085,#117765,#117766) ;
#96990 = AXIS2_PLACEMENT_3D('',#150094,#117771,#117772) ;
#96991 = AXIS2_PLACEMENT_3D('',#150103,#117777,#117778) ;
#96992 = AXIS2_PLACEMENT_3D('',#150112,#117783,#117784) ;
#96993 = AXIS2_PLACEMENT_3D('',#150116,#117786,#117787) ;
#96994 = AXIS2_PLACEMENT_3D('',#150118,#117788,#117789) ;
#96995 = AXIS2_PLACEMENT_3D('',#150122,#117792,#117793) ;
#96996 = AXIS2_PLACEMENT_3D('',#150126,#117795,#117796) ;
#96997 = AXIS2_PLACEMENT_3D('',#150128,#117797,#117798) ;
#96998 = AXIS2_PLACEMENT_3D('',#150132,#117801,#117802) ;
#96999 = AXIS2_PLACEMENT_3D('',#150133,#117803,#117804) ;
#97000 = AXIS2_PLACEMENT_3D('',#150134,#117805,#117806) ;
#97001 = AXIS2_PLACEMENT_3D('',#150135,#117807,#117808) ;
#97002 = AXIS2_PLACEMENT_3D('',#150136,#117809,#117810) ;
#97003 = AXIS2_PLACEMENT_3D('',#150137,#117811,#117812) ;
#97004 = AXIS2_PLACEMENT_3D('',#150138,#117813,#117814) ;
#97005 = AXIS2_PLACEMENT_3D('',#150147,#117819,#117820) ;
#97006 = AXIS2_PLACEMENT_3D('',#150153,#117824,#117825) ;
#97007 = AXIS2_PLACEMENT_3D('',#150159,#117829,#117830) ;
#97008 = AXIS2_PLACEMENT_3D('',#150168,#117835,#117836) ;
#97009 = AXIS2_PLACEMENT_3D('',#150177,#117841,#117842) ;
#97010 = AXIS2_PLACEMENT_3D('',#150183,#117846,#117847) ;
#97011 = AXIS2_PLACEMENT_3D('',#150189,#117851,#117852) ;
#97012 = AXIS2_PLACEMENT_3D('',#150198,#117857,#117858) ;
#97013 = AXIS2_PLACEMENT_3D('',#150207,#117863,#117864) ;
#97014 = AXIS2_PLACEMENT_3D('',#150216,#117869,#117870) ;
#97015 = AXIS2_PLACEMENT_3D('',#150225,#117875,#117876) ;
#97016 = AXIS2_PLACEMENT_3D('',#150234,#117881,#117882) ;
#97017 = AXIS2_PLACEMENT_3D('',#150238,#117884,#117885) ;
#97018 = AXIS2_PLACEMENT_3D('',#150240,#117886,#117887) ;
#97019 = AXIS2_PLACEMENT_3D('',#150244,#117890,#117891) ;
#97020 = AXIS2_PLACEMENT_3D('',#150248,#117893,#117894) ;
#97021 = AXIS2_PLACEMENT_3D('',#150250,#117895,#117896) ;
#97022 = AXIS2_PLACEMENT_3D('',#150254,#117899,#117900) ;
#97023 = AXIS2_PLACEMENT_3D('',#150255,#117901,#117902) ;
#97024 = AXIS2_PLACEMENT_3D('',#150256,#117903,#117904) ;
#97025 = AXIS2_PLACEMENT_3D('',#150257,#117905,#117906) ;
#97026 = AXIS2_PLACEMENT_3D('',#150258,#117907,#117908) ;
#97027 = AXIS2_PLACEMENT_3D('',#150259,#117909,#117910) ;
#97028 = AXIS2_PLACEMENT_3D('',#150260,#117911,#117912) ;
#97029 = AXIS2_PLACEMENT_3D('',#150269,#117917,#117918) ;
#97030 = AXIS2_PLACEMENT_3D('',#150275,#117922,#117923) ;
#97031 = AXIS2_PLACEMENT_3D('',#150281,#117927,#117928) ;
#97032 = AXIS2_PLACEMENT_3D('',#150290,#117933,#117934) ;
#97033 = AXIS2_PLACEMENT_3D('',#150299,#117939,#117940) ;
#97034 = AXIS2_PLACEMENT_3D('',#150305,#117944,#117945) ;
#97035 = AXIS2_PLACEMENT_3D('',#150311,#117949,#117950) ;
#97036 = AXIS2_PLACEMENT_3D('',#150320,#117955,#117956) ;
#97037 = AXIS2_PLACEMENT_3D('',#150329,#117961,#117962) ;
#97038 = AXIS2_PLACEMENT_3D('',#150338,#117967,#117968) ;
#97039 = AXIS2_PLACEMENT_3D('',#150347,#117973,#117974) ;
#97040 = AXIS2_PLACEMENT_3D('',#150356,#117979,#117980) ;
#97041 = AXIS2_PLACEMENT_3D('',#150360,#117982,#117983) ;
#97042 = AXIS2_PLACEMENT_3D('',#150362,#117984,#117985) ;
#97043 = AXIS2_PLACEMENT_3D('',#150366,#117988,#117989) ;
#97044 = AXIS2_PLACEMENT_3D('',#150370,#117991,#117992) ;
#97045 = AXIS2_PLACEMENT_3D('',#150372,#117993,#117994) ;
#97046 = AXIS2_PLACEMENT_3D('',#150376,#117997,#117998) ;
#97047 = AXIS2_PLACEMENT_3D('',#150377,#117999,#118000) ;
#97048 = AXIS2_PLACEMENT_3D('',#150378,#118001,#118002) ;
#97049 = AXIS2_PLACEMENT_3D('',#150379,#118003,#118004) ;
#97050 = AXIS2_PLACEMENT_3D('',#150380,#118005,#118006) ;
#97051 = AXIS2_PLACEMENT_3D('',#150381,#118007,#118008) ;
#97052 = AXIS2_PLACEMENT_3D('',#150382,#118009,#118010) ;
#97053 = AXIS2_PLACEMENT_3D('',#150391,#118015,#118016) ;
#97054 = AXIS2_PLACEMENT_3D('',#150397,#118020,#118021) ;
#97055 = AXIS2_PLACEMENT_3D('',#150403,#118025,#118026) ;
#97056 = AXIS2_PLACEMENT_3D('',#150412,#118031,#118032) ;
#97057 = AXIS2_PLACEMENT_3D('',#150421,#118037,#118038) ;
#97058 = AXIS2_PLACEMENT_3D('',#150427,#118042,#118043) ;
#97059 = AXIS2_PLACEMENT_3D('',#150433,#118047,#118048) ;
#97060 = AXIS2_PLACEMENT_3D('',#150442,#118053,#118054) ;
#97061 = AXIS2_PLACEMENT_3D('',#150451,#118059,#118060) ;
#97062 = AXIS2_PLACEMENT_3D('',#150460,#118065,#118066) ;
#97063 = AXIS2_PLACEMENT_3D('',#150469,#118071,#118072) ;
#97064 = AXIS2_PLACEMENT_3D('',#150478,#118077,#118078) ;
#97065 = AXIS2_PLACEMENT_3D('',#150482,#118080,#118081) ;
#97066 = AXIS2_PLACEMENT_3D('',#150484,#118082,#118083) ;
#97067 = AXIS2_PLACEMENT_3D('',#150488,#118086,#118087) ;
#97068 = AXIS2_PLACEMENT_3D('',#150492,#118089,#118090) ;
#97069 = AXIS2_PLACEMENT_3D('',#150494,#118091,#118092) ;
#97070 = AXIS2_PLACEMENT_3D('',#150498,#118095,#118096) ;
#97071 = AXIS2_PLACEMENT_3D('',#150499,#118097,#118098) ;
#97072 = AXIS2_PLACEMENT_3D('',#150500,#118099,#118100) ;
#97073 = AXIS2_PLACEMENT_3D('',#150501,#118101,#118102) ;
#97074 = AXIS2_PLACEMENT_3D('',#150502,#118103,#118104) ;
#97075 = AXIS2_PLACEMENT_3D('',#150503,#118105,#118106) ;
#97076 = AXIS2_PLACEMENT_3D('',#150504,#118107,#118108) ;
#97077 = AXIS2_PLACEMENT_3D('',#150513,#118113,#118114) ;
#97078 = AXIS2_PLACEMENT_3D('',#150519,#118118,#118119) ;
#97079 = AXIS2_PLACEMENT_3D('',#150525,#118123,#118124) ;
#97080 = AXIS2_PLACEMENT_3D('',#150534,#118129,#118130) ;
#97081 = AXIS2_PLACEMENT_3D('',#150543,#118135,#118136) ;
#97082 = AXIS2_PLACEMENT_3D('',#150549,#118140,#118141) ;
#97083 = AXIS2_PLACEMENT_3D('',#150555,#118145,#118146) ;
#97084 = AXIS2_PLACEMENT_3D('',#150564,#118151,#118152) ;
#97085 = AXIS2_PLACEMENT_3D('',#150573,#118157,#118158) ;
#97086 = AXIS2_PLACEMENT_3D('',#150582,#118163,#118164) ;
#97087 = AXIS2_PLACEMENT_3D('',#150591,#118169,#118170) ;
#97088 = AXIS2_PLACEMENT_3D('',#150600,#118175,#118176) ;
#97089 = AXIS2_PLACEMENT_3D('',#150604,#118178,#118179) ;
#97090 = AXIS2_PLACEMENT_3D('',#150606,#118180,#118181) ;
#97091 = AXIS2_PLACEMENT_3D('',#150610,#118184,#118185) ;
#97092 = AXIS2_PLACEMENT_3D('',#150614,#118187,#118188) ;
#97093 = AXIS2_PLACEMENT_3D('',#150616,#118189,#118190) ;
#97094 = AXIS2_PLACEMENT_3D('',#150620,#118193,#118194) ;
#97095 = AXIS2_PLACEMENT_3D('',#150621,#118195,#118196) ;
#97096 = AXIS2_PLACEMENT_3D('',#150622,#118197,#118198) ;
#97097 = AXIS2_PLACEMENT_3D('',#150623,#118199,#118200) ;
#97098 = AXIS2_PLACEMENT_3D('',#150624,#118201,#118202) ;
#97099 = AXIS2_PLACEMENT_3D('',#150625,#118203,#118204) ;
#97100 = AXIS2_PLACEMENT_3D('',#150626,#118205,#118206) ;
#97101 = AXIS2_PLACEMENT_3D('',#150635,#118211,#118212) ;
#97102 = AXIS2_PLACEMENT_3D('',#150641,#118216,#118217) ;
#97103 = AXIS2_PLACEMENT_3D('',#150647,#118221,#118222) ;
#97104 = AXIS2_PLACEMENT_3D('',#150656,#118227,#118228) ;
#97105 = AXIS2_PLACEMENT_3D('',#150665,#118233,#118234) ;
#97106 = AXIS2_PLACEMENT_3D('',#150671,#118238,#118239) ;
#97107 = AXIS2_PLACEMENT_3D('',#150677,#118243,#118244) ;
#97108 = AXIS2_PLACEMENT_3D('',#150686,#118249,#118250) ;
#97109 = AXIS2_PLACEMENT_3D('',#150695,#118255,#118256) ;
#97110 = AXIS2_PLACEMENT_3D('',#150704,#118261,#118262) ;
#97111 = AXIS2_PLACEMENT_3D('',#150713,#118267,#118268) ;
#97112 = AXIS2_PLACEMENT_3D('',#150722,#118273,#118274) ;
#97113 = AXIS2_PLACEMENT_3D('',#150731,#118279,#118280) ;
#97114 = AXIS2_PLACEMENT_3D('',#150740,#118285,#118286) ;
#97115 = AXIS2_PLACEMENT_3D('',#150749,#118291,#118292) ;
#97116 = AXIS2_PLACEMENT_3D('',#150758,#118297,#118298) ;
#97117 = AXIS2_PLACEMENT_3D('',#150767,#118303,#118304) ;
#97118 = AXIS2_PLACEMENT_3D('',#150776,#118309,#118310) ;
#97119 = AXIS2_PLACEMENT_3D('',#150785,#118315,#118316) ;
#97120 = AXIS2_PLACEMENT_3D('',#150794,#118321,#118322) ;
#97121 = AXIS2_PLACEMENT_3D('',#150803,#118327,#118328) ;
#97122 = AXIS2_PLACEMENT_3D('',#150812,#118333,#118334) ;
#97123 = AXIS2_PLACEMENT_3D('',#150821,#118339,#118340) ;
#97124 = AXIS2_PLACEMENT_3D('',#150830,#118345,#118346) ;
#97125 = AXIS2_PLACEMENT_3D('',#150839,#118351,#118352) ;
#97126 = AXIS2_PLACEMENT_3D('',#150848,#118357,#118358) ;
#97127 = AXIS2_PLACEMENT_3D('',#150857,#118363,#118364) ;
#97128 = AXIS2_PLACEMENT_3D('',#150866,#118369,#118370) ;
#97129 = AXIS2_PLACEMENT_3D('',#150875,#118375,#118376) ;
#97130 = AXIS2_PLACEMENT_3D('',#150884,#118381,#118382) ;
#97131 = AXIS2_PLACEMENT_3D('',#150893,#118387,#118388) ;
#97132 = AXIS2_PLACEMENT_3D('',#150902,#118393,#118394) ;
#97133 = AXIS2_PLACEMENT_3D('',#150911,#118399,#118400) ;
#97134 = AXIS2_PLACEMENT_3D('',#150920,#118405,#118406) ;
#97135 = AXIS2_PLACEMENT_3D('',#150929,#118411,#118412) ;
#97136 = AXIS2_PLACEMENT_3D('',#150938,#118417,#118418) ;
#97137 = AXIS2_PLACEMENT_3D('',#150947,#118423,#118424) ;
#97138 = AXIS2_PLACEMENT_3D('',#150956,#118429,#118430) ;
#97139 = AXIS2_PLACEMENT_3D('',#150965,#118435,#118436) ;
#97140 = AXIS2_PLACEMENT_3D('',#150974,#118441,#118442) ;
#97141 = AXIS2_PLACEMENT_3D('',#150983,#118447,#118448) ;
#97142 = AXIS2_PLACEMENT_3D('',#150992,#118453,#118454) ;
#97143 = AXIS2_PLACEMENT_3D('',#151001,#118459,#118460) ;
#97144 = AXIS2_PLACEMENT_3D('',#151002,#118461,#118462) ;
#97145 = AXIS2_PLACEMENT_3D('',#151003,#118463,#118464) ;
#97146 = AXIS2_PLACEMENT_3D('',#151004,#118465,#118466) ;
#97147 = AXIS2_PLACEMENT_3D('',#151005,#118467,#118468) ;
#97148 = AXIS2_PLACEMENT_3D('',#151006,#118469,#118470) ;
#97149 = AXIS2_PLACEMENT_3D('',#151007,#118471,#118472) ;
#97150 = AXIS2_PLACEMENT_3D('',#151008,#118473,#118474) ;
#97151 = AXIS2_PLACEMENT_3D('',#151009,#118475,#118476) ;
#97152 = AXIS2_PLACEMENT_3D('',#151010,#118477,#118478) ;
#97153 = AXIS2_PLACEMENT_3D('',#151011,#118479,#118480) ;
#97154 = AXIS2_PLACEMENT_3D('',#151012,#118481,#118482) ;
#97155 = AXIS2_PLACEMENT_3D('',#151013,#118483,#118484) ;
#97156 = AXIS2_PLACEMENT_3D('',#151014,#118485,#118486) ;
#97157 = AXIS2_PLACEMENT_3D('',#151015,#118487,#118488) ;
#97158 = AXIS2_PLACEMENT_3D('',#151016,#118489,#118490) ;
#97159 = AXIS2_PLACEMENT_3D('',#151017,#118491,#118492) ;
#97160 = AXIS2_PLACEMENT_3D('',#151018,#118493,#118494) ;
#97161 = AXIS2_PLACEMENT_3D('',#151019,#118495,#118496) ;
#97162 = AXIS2_PLACEMENT_3D('',#151020,#118497,#118498) ;
#97163 = AXIS2_PLACEMENT_3D('',#151021,#118499,#118500) ;
#97164 = AXIS2_PLACEMENT_3D('',#151022,#118501,#118502) ;
#97165 = AXIS2_PLACEMENT_3D('',#151023,#118503,#118504) ;
#97166 = AXIS2_PLACEMENT_3D('',#151024,#118505,#118506) ;
#97167 = AXIS2_PLACEMENT_3D('',#151025,#118507,#118508) ;
#97168 = AXIS2_PLACEMENT_3D('',#151026,#118509,#118510) ;
#97169 = AXIS2_PLACEMENT_3D('',#151027,#118511,#118512) ;
#97170 = AXIS2_PLACEMENT_3D('',#151028,#118513,#118514) ;
#97171 = AXIS2_PLACEMENT_3D('',#151029,#118515,#118516) ;
#97172 = AXIS2_PLACEMENT_3D('',#151030,#118517,#118518) ;
#97173 = AXIS2_PLACEMENT_3D('',#151031,#118519,#118520) ;
#97174 = AXIS2_PLACEMENT_3D('',#151032,#118521,#118522) ;
#97175 = AXIS2_PLACEMENT_3D('',#151033,#118523,#118524) ;
#97176 = AXIS2_PLACEMENT_3D('',#151034,#118525,#118526) ;
#97177 = AXIS2_PLACEMENT_3D('',#151035,#118527,#118528) ;
#97178 = AXIS2_PLACEMENT_3D('',#151036,#118529,#118530) ;
#97179 = AXIS2_PLACEMENT_3D('',#151037,#118531,#118532) ;
#97180 = AXIS2_PLACEMENT_3D('',#151038,#118533,#118534) ;
#97181 = AXIS2_PLACEMENT_3D('',#151039,#118535,#118536) ;
#97182 = AXIS2_PLACEMENT_3D('',#151040,#118537,#118538) ;
#97183 = AXIS2_PLACEMENT_3D('',#151041,#118539,#118540) ;
#97184 = AXIS2_PLACEMENT_3D('',#151042,#118541,#118542) ;
#97185 = AXIS2_PLACEMENT_3D('',#151043,#118543,#118544) ;
#97186 = AXIS2_PLACEMENT_3D('',#151044,#118545,#118546) ;
#97187 = AXIS2_PLACEMENT_3D('',#151045,#118547,#118548) ;
#97188 = AXIS2_PLACEMENT_3D('',#151046,#118549,#118550) ;
#97189 = AXIS2_PLACEMENT_3D('',#151047,#118551,#118552) ;
#97190 = AXIS2_PLACEMENT_3D('',#151048,#118553,#118554) ;
#97191 = AXIS2_PLACEMENT_3D('',#151049,#118555,#118556) ;
#97192 = AXIS2_PLACEMENT_3D('',#151050,#118557,#118558) ;
#97193 = AXIS2_PLACEMENT_3D('',#151051,#118559,#118560) ;
#97194 = AXIS2_PLACEMENT_3D('',#151052,#118561,#118562) ;
#97195 = AXIS2_PLACEMENT_3D('',#151053,#118563,#118564) ;
#97196 = AXIS2_PLACEMENT_3D('',#151054,#118565,#118566) ;
#97197 = AXIS2_PLACEMENT_3D('',#151055,#118567,#118568) ;
#97198 = AXIS2_PLACEMENT_3D('',#151056,#118569,#118570) ;
#97199 = AXIS2_PLACEMENT_3D('',#151057,#118571,#118572) ;
#97200 = AXIS2_PLACEMENT_3D('',#151058,#118573,#118574) ;
#97201 = AXIS2_PLACEMENT_3D('',#151059,#118575,#118576) ;
#97202 = AXIS2_PLACEMENT_3D('',#151060,#118577,#118578) ;
#97203 = AXIS2_PLACEMENT_3D('',#151061,#118579,#118580) ;
#97204 = AXIS2_PLACEMENT_3D('',#151062,#118581,#118582) ;
#97205 = AXIS2_PLACEMENT_3D('',#151063,#118583,#118584) ;
#97206 = AXIS2_PLACEMENT_3D('',#151064,#118585,#118586) ;
#97207 = AXIS2_PLACEMENT_3D('',#151065,#118587,#118588) ;
#97208 = AXIS2_PLACEMENT_3D('',#151066,#118589,#118590) ;
#97209 = AXIS2_PLACEMENT_3D('',#151067,#118591,#118592) ;
#97210 = AXIS2_PLACEMENT_3D('',#151068,#118593,#118594) ;
#97211 = AXIS2_PLACEMENT_3D('',#151069,#118595,#118596) ;
#97212 = AXIS2_PLACEMENT_3D('',#151070,#118597,#118598) ;
#97213 = AXIS2_PLACEMENT_3D('',#151071,#118599,#118600) ;
#97214 = AXIS2_PLACEMENT_3D('',#151072,#118601,#118602) ;
#97215 = AXIS2_PLACEMENT_3D('',#151073,#118603,#118604) ;
#97216 = AXIS2_PLACEMENT_3D('',#151074,#118605,#118606) ;
#97217 = AXIS2_PLACEMENT_3D('',#151075,#118607,#118608) ;
#97218 = AXIS2_PLACEMENT_3D('',#151076,#118609,#118610) ;
#97219 = AXIS2_PLACEMENT_3D('',#151077,#118611,#118612) ;
#97220 = AXIS2_PLACEMENT_3D('',#151078,#118613,#118614) ;
#97221 = AXIS2_PLACEMENT_3D('',#151079,#118615,#118616) ;
#97222 = AXIS2_PLACEMENT_3D('',#151080,#118617,#118618) ;
#97223 = AXIS2_PLACEMENT_3D('',#151081,#118619,#118620) ;
#97224 = AXIS2_PLACEMENT_3D('',#151082,#118621,#118622) ;
#97225 = AXIS2_PLACEMENT_3D('',#151083,#118623,#118624) ;
#97226 = AXIS2_PLACEMENT_3D('',#151084,#118625,#118626) ;
#97227 = AXIS2_PLACEMENT_3D('',#151085,#118627,#118628) ;
#97228 = AXIS2_PLACEMENT_3D('',#151086,#118629,#118630) ;
#97229 = AXIS2_PLACEMENT_3D('',#151087,#118631,#118632) ;
#97230 = AXIS2_PLACEMENT_3D('',#151088,#118633,#118634) ;
#97231 = AXIS2_PLACEMENT_3D('',#151089,#118635,#118636) ;
#97232 = AXIS2_PLACEMENT_3D('',#151090,#118637,#118638) ;
#97233 = AXIS2_PLACEMENT_3D('',#151091,#118639,#118640) ;
#97234 = AXIS2_PLACEMENT_3D('',#151092,#118641,#118642) ;
#97235 = AXIS2_PLACEMENT_3D('',#151093,#118643,#118644) ;
#97236 = AXIS2_PLACEMENT_3D('',#151094,#118645,#118646) ;
#97237 = AXIS2_PLACEMENT_3D('',#151095,#118647,#118648) ;
#97238 = AXIS2_PLACEMENT_3D('',#151096,#118649,#118650) ;
#97239 = AXIS2_PLACEMENT_3D('',#151097,#118651,#118652) ;
#97240 = AXIS2_PLACEMENT_3D('',#151098,#118653,#118654) ;
#97241 = AXIS2_PLACEMENT_3D('',#151099,#118655,#118656) ;
#97242 = AXIS2_PLACEMENT_3D('',#151100,#118657,#118658) ;
#97243 = AXIS2_PLACEMENT_3D('',#151101,#118659,#118660) ;
#97244 = AXIS2_PLACEMENT_3D('',#151102,#118661,#118662) ;
#97245 = AXIS2_PLACEMENT_3D('',#151103,#118663,#118664) ;
#97246 = AXIS2_PLACEMENT_3D('',#151104,#118665,#118666) ;
#97247 = AXIS2_PLACEMENT_3D('',#151105,#118667,#118668) ;
#97248 = AXIS2_PLACEMENT_3D('',#151106,#118669,#118670) ;
#97249 = AXIS2_PLACEMENT_3D('',#151107,#118671,#118672) ;
#97250 = AXIS2_PLACEMENT_3D('',#151108,#118673,#118674) ;
#97251 = AXIS2_PLACEMENT_3D('',#151109,#118675,#118676) ;
#97252 = AXIS2_PLACEMENT_3D('',#151110,#118677,#118678) ;
#97253 = AXIS2_PLACEMENT_3D('',#151111,#118679,#118680) ;
#97254 = AXIS2_PLACEMENT_3D('',#151112,#118681,#118682) ;
#97255 = AXIS2_PLACEMENT_3D('',#151113,#118683,#118684) ;
#97256 = AXIS2_PLACEMENT_3D('',#151114,#118685,#118686) ;
#97257 = AXIS2_PLACEMENT_3D('',#151115,#118687,#118688) ;
#97258 = AXIS2_PLACEMENT_3D('',#151116,#118689,#118690) ;
#97259 = AXIS2_PLACEMENT_3D('',#151117,#118691,#118692) ;
#97260 = AXIS2_PLACEMENT_3D('',#151118,#118693,#118694) ;
#97261 = AXIS2_PLACEMENT_3D('',#151119,#118695,#118696) ;
#97262 = AXIS2_PLACEMENT_3D('',#151120,#118697,#118698) ;
#97263 = AXIS2_PLACEMENT_3D('',#151121,#118699,#118700) ;
#97264 = AXIS2_PLACEMENT_3D('',#151122,#118701,#118702) ;
#97265 = AXIS2_PLACEMENT_3D('',#151123,#118703,#118704) ;
#97266 = AXIS2_PLACEMENT_3D('',#151124,#118705,#118706) ;
#97267 = AXIS2_PLACEMENT_3D('',#151125,#118707,#118708) ;
#97268 = AXIS2_PLACEMENT_3D('',#151126,#118709,#118710) ;
#97269 = AXIS2_PLACEMENT_3D('',#151127,#118711,#118712) ;
#97270 = AXIS2_PLACEMENT_3D('',#151128,#118713,#118714) ;
#97271 = AXIS2_PLACEMENT_3D('',#151129,#118715,#118716) ;
#97272 = AXIS2_PLACEMENT_3D('',#151130,#118717,#118718) ;
#97273 = AXIS2_PLACEMENT_3D('',#151131,#118719,#118720) ;
#97274 = AXIS2_PLACEMENT_3D('',#151132,#118721,#118722) ;
#97275 = AXIS2_PLACEMENT_3D('',#151133,#118723,#118724) ;
#97276 = AXIS2_PLACEMENT_3D('',#151134,#118725,#118726) ;
#97277 = AXIS2_PLACEMENT_3D('',#151135,#118727,#118728) ;
#97278 = AXIS2_PLACEMENT_3D('',#151136,#118729,#118730) ;
#97279 = AXIS2_PLACEMENT_3D('',#151137,#118731,#118732) ;
#97280 = AXIS2_PLACEMENT_3D('',#151138,#118733,#118734) ;
#97281 = AXIS2_PLACEMENT_3D('',#151139,#118735,#118736) ;
#97282 = AXIS2_PLACEMENT_3D('',#151140,#118737,#118738) ;
#97283 = AXIS2_PLACEMENT_3D('',#151141,#118739,#118740) ;
#97284 = AXIS2_PLACEMENT_3D('',#151142,#118741,#118742) ;
#97285 = AXIS2_PLACEMENT_3D('',#151143,#118743,#118744) ;
#97286 = AXIS2_PLACEMENT_3D('',#151144,#118745,#118746) ;
#97287 = AXIS2_PLACEMENT_3D('',#151145,#118747,#118748) ;
#97288 = AXIS2_PLACEMENT_3D('',#151146,#118749,#118750) ;
#97289 = AXIS2_PLACEMENT_3D('',#151147,#118751,#118752) ;
#97290 = AXIS2_PLACEMENT_3D('',#151148,#118753,#118754) ;
#97291 = AXIS2_PLACEMENT_3D('',#151149,#118755,#118756) ;
#97292 = AXIS2_PLACEMENT_3D('',#151150,#118757,#118758) ;
#97293 = AXIS2_PLACEMENT_3D('',#151151,#118759,#118760) ;
#97294 = AXIS2_PLACEMENT_3D('',#151152,#118761,#118762) ;
#97295 = AXIS2_PLACEMENT_3D('',#151153,#118763,#118764) ;
#97296 = AXIS2_PLACEMENT_3D('',#151154,#118765,#118766) ;
#97297 = AXIS2_PLACEMENT_3D('',#151155,#118767,#118768) ;
#97298 = AXIS2_PLACEMENT_3D('',#151156,#118769,#118770) ;
#97299 = AXIS2_PLACEMENT_3D('',#151157,#118771,#118772) ;
#97300 = AXIS2_PLACEMENT_3D('',#151158,#118773,#118774) ;
#97301 = AXIS2_PLACEMENT_3D('',#151159,#118775,#118776) ;
#97302 = AXIS2_PLACEMENT_3D('',#151160,#118777,#118778) ;
#97303 = AXIS2_PLACEMENT_3D('',#151161,#118779,#118780) ;
#97304 = AXIS2_PLACEMENT_3D('',#151162,#118781,#118782) ;
#97305 = AXIS2_PLACEMENT_3D('',#151163,#118783,#118784) ;
#97306 = AXIS2_PLACEMENT_3D('',#151164,#118785,#118786) ;
#97307 = AXIS2_PLACEMENT_3D('',#151165,#118787,#118788) ;
#97308 = AXIS2_PLACEMENT_3D('',#151166,#118789,#118790) ;
#97309 = AXIS2_PLACEMENT_3D('',#151167,#118791,#118792) ;
#97310 = AXIS2_PLACEMENT_3D('',#151168,#118793,#118794) ;
#97311 = AXIS2_PLACEMENT_3D('',#151169,#118795,#118796) ;
#97312 = AXIS2_PLACEMENT_3D('',#151170,#118797,#118798) ;
#97313 = AXIS2_PLACEMENT_3D('',#151171,#118799,#118800) ;
#97314 = AXIS2_PLACEMENT_3D('',#151172,#118801,#118802) ;
#97315 = AXIS2_PLACEMENT_3D('',#151173,#118803,#118804) ;
#97316 = AXIS2_PLACEMENT_3D('',#151174,#118805,#118806) ;
#97317 = AXIS2_PLACEMENT_3D('',#151175,#118807,#118808) ;
#97318 = AXIS2_PLACEMENT_3D('',#151176,#118809,#118810) ;
#97319 = AXIS2_PLACEMENT_3D('',#151177,#118811,#118812) ;
#97320 = AXIS2_PLACEMENT_3D('',#151178,#118813,#118814) ;
#97321 = AXIS2_PLACEMENT_3D('',#151179,#118815,#118816) ;
#97322 = AXIS2_PLACEMENT_3D('',#151180,#118817,#118818) ;
#97323 = AXIS2_PLACEMENT_3D('',#151181,#118819,#118820) ;
#97324 = AXIS2_PLACEMENT_3D('',#151182,#118821,#118822) ;
#97325 = AXIS2_PLACEMENT_3D('',#151183,#118823,#118824) ;
#97326 = AXIS2_PLACEMENT_3D('',#151184,#118825,#118826) ;
#97327 = AXIS2_PLACEMENT_3D('',#151185,#118827,#118828) ;
#97328 = AXIS2_PLACEMENT_3D('',#151186,#118829,#118830) ;
#97329 = AXIS2_PLACEMENT_3D('',#151187,#118831,#118832) ;
#97330 = AXIS2_PLACEMENT_3D('',#151188,#118833,#118834) ;
#97331 = AXIS2_PLACEMENT_3D('',#151189,#118835,#118836) ;
#97332 = AXIS2_PLACEMENT_3D('',#151190,#118837,#118838) ;
#97333 = AXIS2_PLACEMENT_3D('',#151191,#118839,#118840) ;
#97334 = AXIS2_PLACEMENT_3D('',#151192,#118841,#118842) ;
#97335 = AXIS2_PLACEMENT_3D('',#151193,#118843,#118844) ;
#97336 = AXIS2_PLACEMENT_3D('',#151194,#118845,#118846) ;
#97337 = AXIS2_PLACEMENT_3D('',#151195,#118847,#118848) ;
#97338 = AXIS2_PLACEMENT_3D('',#151196,#118849,#118850) ;
#97339 = AXIS2_PLACEMENT_3D('',#151197,#118851,#118852) ;
#97340 = AXIS2_PLACEMENT_3D('',#151198,#118853,#118854) ;
#97341 = AXIS2_PLACEMENT_3D('',#151199,#118855,#118856) ;
#97342 = AXIS2_PLACEMENT_3D('',#151200,#118857,#118858) ;
#97343 = AXIS2_PLACEMENT_3D('',#151201,#118859,#118860) ;
#97344 = AXIS2_PLACEMENT_3D('',#151202,#118861,#118862) ;
#97345 = AXIS2_PLACEMENT_3D('',#151203,#118863,#118864) ;
#97346 = AXIS2_PLACEMENT_3D('',#151204,#118865,#118866) ;
#97347 = AXIS2_PLACEMENT_3D('',#151205,#118867,#118868) ;
#97348 = AXIS2_PLACEMENT_3D('',#151206,#118869,#118870) ;
#97349 = AXIS2_PLACEMENT_3D('',#151207,#118871,#118872) ;
#97350 = AXIS2_PLACEMENT_3D('',#151208,#118873,#118874) ;
#97351 = AXIS2_PLACEMENT_3D('',#151209,#118875,#118876) ;
#97352 = AXIS2_PLACEMENT_3D('',#151210,#118877,#118878) ;
#97353 = AXIS2_PLACEMENT_3D('',#151211,#118879,#118880) ;
#97354 = AXIS2_PLACEMENT_3D('',#151212,#118881,#118882) ;
#97355 = AXIS2_PLACEMENT_3D('',#151213,#118883,#118884) ;
#97356 = AXIS2_PLACEMENT_3D('',#151214,#118885,#118886) ;
#97357 = AXIS2_PLACEMENT_3D('',#151215,#118887,#118888) ;
#97358 = AXIS2_PLACEMENT_3D('',#151216,#118889,#118890) ;
#97359 = AXIS2_PLACEMENT_3D('',#151217,#118891,#118892) ;
#97360 = AXIS2_PLACEMENT_3D('',#151218,#118893,#118894) ;
#97361 = AXIS2_PLACEMENT_3D('',#151219,#118895,#118896) ;
#97362 = AXIS2_PLACEMENT_3D('',#151220,#118897,#118898) ;
#97363 = AXIS2_PLACEMENT_3D('',#151221,#118899,#118900) ;
#97364 = AXIS2_PLACEMENT_3D('',#151222,#118901,#118902) ;
#97365 = AXIS2_PLACEMENT_3D('',#151223,#118903,#118904) ;
#97366 = AXIS2_PLACEMENT_3D('',#151224,#118905,#118906) ;
#97367 = AXIS2_PLACEMENT_3D('',#151225,#118907,#118908) ;
#97368 = AXIS2_PLACEMENT_3D('',#151226,#118909,#118910) ;
#97369 = AXIS2_PLACEMENT_3D('',#151227,#118911,#118912) ;
#97370 = AXIS2_PLACEMENT_3D('',#151228,#118913,#118914) ;
#97371 = AXIS2_PLACEMENT_3D('',#151229,#118915,#118916) ;
#97372 = AXIS2_PLACEMENT_3D('',#151230,#118917,#118918) ;
#97373 = AXIS2_PLACEMENT_3D('',#151231,#118919,#118920) ;
#97374 = AXIS2_PLACEMENT_3D('',#151232,#118921,#118922) ;
#97375 = AXIS2_PLACEMENT_3D('',#151233,#118923,#118924) ;
#97376 = AXIS2_PLACEMENT_3D('',#151234,#118925,#118926) ;
#97377 = AXIS2_PLACEMENT_3D('',#151235,#118927,#118928) ;
#97378 = AXIS2_PLACEMENT_3D('',#151236,#118929,#118930) ;
#97379 = AXIS2_PLACEMENT_3D('',#151237,#118931,#118932) ;
#97380 = AXIS2_PLACEMENT_3D('',#151238,#118933,#118934) ;
#97381 = AXIS2_PLACEMENT_3D('',#151239,#118935,#118936) ;
#97382 = AXIS2_PLACEMENT_3D('',#151240,#118937,#118938) ;
#97383 = AXIS2_PLACEMENT_3D('',#151241,#118939,#118940) ;
#97384 = AXIS2_PLACEMENT_3D('',#151242,#118941,#118942) ;
#97385 = AXIS2_PLACEMENT_3D('',#151243,#118943,#118944) ;
#97386 = AXIS2_PLACEMENT_3D('',#151244,#118945,#118946) ;
#97387 = AXIS2_PLACEMENT_3D('',#151245,#118947,#118948) ;
#97388 = AXIS2_PLACEMENT_3D('',#151246,#118949,#118950) ;
#97389 = AXIS2_PLACEMENT_3D('',#151247,#118951,#118952) ;
#97390 = AXIS2_PLACEMENT_3D('',#151248,#118953,#118954) ;
#97391 = AXIS2_PLACEMENT_3D('',#151249,#118955,#118956) ;
#97392 = AXIS2_PLACEMENT_3D('',#151250,#118957,#118958) ;
#97393 = AXIS2_PLACEMENT_3D('',#151251,#118959,#118960) ;
#97394 = AXIS2_PLACEMENT_3D('',#151252,#118961,#118962) ;
#97395 = AXIS2_PLACEMENT_3D('',#151253,#118963,#118964) ;
#97396 = AXIS2_PLACEMENT_3D('',#151254,#118965,#118966) ;
#97397 = AXIS2_PLACEMENT_3D('',#151255,#118967,#118968) ;
#97398 = AXIS2_PLACEMENT_3D('',#151256,#118969,#118970) ;
#97399 = AXIS2_PLACEMENT_3D('',#151257,#118971,#118972) ;
#97400 = AXIS2_PLACEMENT_3D('',#151258,#118973,#118974) ;
#97401 = AXIS2_PLACEMENT_3D('',#151259,#118975,#118976) ;
#97402 = AXIS2_PLACEMENT_3D('',#151260,#118977,#118978) ;
#97403 = AXIS2_PLACEMENT_3D('',#151261,#118979,#118980) ;
#97404 = AXIS2_PLACEMENT_3D('',#151262,#118981,#118982) ;
#97405 = AXIS2_PLACEMENT_3D('',#151263,#118983,#118984) ;
#97406 = AXIS2_PLACEMENT_3D('',#151264,#118985,#118986) ;
#97407 = AXIS2_PLACEMENT_3D('',#151265,#118987,#118988) ;
#97408 = AXIS2_PLACEMENT_3D('',#151266,#118989,#118990) ;
#97409 = AXIS2_PLACEMENT_3D('',#151267,#118991,#118992) ;
#97410 = AXIS2_PLACEMENT_3D('',#151268,#118993,#118994) ;
#97411 = AXIS2_PLACEMENT_3D('',#151269,#118995,#118996) ;
#97412 = AXIS2_PLACEMENT_3D('',#151270,#118997,#118998) ;
#97413 = AXIS2_PLACEMENT_3D('',#151271,#118999,#119000) ;
#97414 = AXIS2_PLACEMENT_3D('',#151272,#119001,#119002) ;
#97415 = AXIS2_PLACEMENT_3D('',#151273,#119003,#119004) ;
#97416 = AXIS2_PLACEMENT_3D('',#151274,#119005,#119006) ;
#97417 = AXIS2_PLACEMENT_3D('',#151275,#119007,#119008) ;
#97418 = AXIS2_PLACEMENT_3D('',#151276,#119009,#119010) ;
#97419 = AXIS2_PLACEMENT_3D('',#151277,#119011,#119012) ;
#97420 = AXIS2_PLACEMENT_3D('',#151278,#119013,#119014) ;
#97421 = AXIS2_PLACEMENT_3D('',#151279,#119015,#119016) ;
#97422 = AXIS2_PLACEMENT_3D('',#151280,#119017,#119018) ;
#97423 = AXIS2_PLACEMENT_3D('',#151281,#119019,#119020) ;
#97424 = AXIS2_PLACEMENT_3D('',#151282,#119021,#119022) ;
#97425 = AXIS2_PLACEMENT_3D('',#151283,#119023,#119024) ;
#97426 = AXIS2_PLACEMENT_3D('',#151284,#119025,#119026) ;
#97427 = AXIS2_PLACEMENT_3D('',#151285,#119027,#119028) ;
#97428 = AXIS2_PLACEMENT_3D('',#151286,#119029,#119030) ;
#97429 = AXIS2_PLACEMENT_3D('',#151287,#119031,#119032) ;
#97430 = AXIS2_PLACEMENT_3D('',#151288,#119033,#119034) ;
#97431 = AXIS2_PLACEMENT_3D('',#151289,#119035,#119036) ;
#97432 = AXIS2_PLACEMENT_3D('',#151290,#119037,#119038) ;
#97433 = AXIS2_PLACEMENT_3D('',#151291,#119039,#119040) ;
#97434 = AXIS2_PLACEMENT_3D('',#151292,#119041,#119042) ;
#97435 = AXIS2_PLACEMENT_3D('',#151293,#119043,#119044) ;
#97436 = AXIS2_PLACEMENT_3D('',#151294,#119045,#119046) ;
#97437 = AXIS2_PLACEMENT_3D('',#151295,#119047,#119048) ;
#97438 = AXIS2_PLACEMENT_3D('',#151296,#119049,#119050) ;
#97439 = AXIS2_PLACEMENT_3D('',#151297,#119051,#119052) ;
#97440 = AXIS2_PLACEMENT_3D('',#151298,#119053,#119054) ;
#97441 = AXIS2_PLACEMENT_3D('',#151299,#119055,#119056) ;
#97442 = AXIS2_PLACEMENT_3D('',#151300,#119057,#119058) ;
#97443 = AXIS2_PLACEMENT_3D('',#151301,#119059,#119060) ;
#97444 = AXIS2_PLACEMENT_3D('',#151302,#119061,#119062) ;
#97445 = AXIS2_PLACEMENT_3D('',#151303,#119063,#119064) ;
#97446 = AXIS2_PLACEMENT_3D('',#151304,#119065,#119066) ;
#97447 = AXIS2_PLACEMENT_3D('',#151305,#119067,#119068) ;
#97448 = AXIS2_PLACEMENT_3D('',#151306,#119069,#119070) ;
#97449 = AXIS2_PLACEMENT_3D('',#151307,#119071,#119072) ;
#97450 = AXIS2_PLACEMENT_3D('',#151308,#119073,#119074) ;
#97451 = AXIS2_PLACEMENT_3D('',#151309,#119075,#119076) ;
#97452 = AXIS2_PLACEMENT_3D('',#151310,#119077,#119078) ;
#97453 = AXIS2_PLACEMENT_3D('',#151311,#119079,#119080) ;
#97454 = AXIS2_PLACEMENT_3D('',#151312,#119081,#119082) ;
#97455 = AXIS2_PLACEMENT_3D('',#151313,#119083,#119084) ;
#97456 = AXIS2_PLACEMENT_3D('',#151314,#119085,#119086) ;
#97457 = AXIS2_PLACEMENT_3D('',#151315,#119087,#119088) ;
#97458 = AXIS2_PLACEMENT_3D('',#151316,#119089,#119090) ;
#97459 = AXIS2_PLACEMENT_3D('',#151317,#119091,#119092) ;
#97460 = AXIS2_PLACEMENT_3D('',#151318,#119093,#119094) ;
#97461 = AXIS2_PLACEMENT_3D('',#151319,#119095,#119096) ;
#97462 = AXIS2_PLACEMENT_3D('',#151320,#119097,#119098) ;
#97463 = AXIS2_PLACEMENT_3D('',#151321,#119099,#119100) ;
#97464 = AXIS2_PLACEMENT_3D('',#151322,#119101,#119102) ;
#97465 = AXIS2_PLACEMENT_3D('',#151323,#119103,#119104) ;
#97466 = AXIS2_PLACEMENT_3D('',#151324,#119105,#119106) ;
#97467 = AXIS2_PLACEMENT_3D('',#151325,#119107,#119108) ;
#97468 = AXIS2_PLACEMENT_3D('',#151326,#119109,#119110) ;
#97469 = AXIS2_PLACEMENT_3D('',#151327,#119111,#119112) ;
#97470 = AXIS2_PLACEMENT_3D('',#151328,#119113,#119114) ;
#97471 = AXIS2_PLACEMENT_3D('',#151329,#119115,#119116) ;
#97472 = AXIS2_PLACEMENT_3D('',#151330,#119117,#119118) ;
#97473 = AXIS2_PLACEMENT_3D('',#151331,#119119,#119120) ;
#97474 = AXIS2_PLACEMENT_3D('',#151332,#119121,#119122) ;
#97475 = AXIS2_PLACEMENT_3D('',#151333,#119123,#119124) ;
#97476 = AXIS2_PLACEMENT_3D('',#151334,#119125,#119126) ;
#97477 = AXIS2_PLACEMENT_3D('',#151335,#119127,#119128) ;
#97478 = AXIS2_PLACEMENT_3D('',#151336,#119129,#119130) ;
#97479 = AXIS2_PLACEMENT_3D('',#151337,#119131,#119132) ;
#97480 = AXIS2_PLACEMENT_3D('',#151338,#119133,#119134) ;
#97481 = AXIS2_PLACEMENT_3D('',#151339,#119135,#119136) ;
#97482 = AXIS2_PLACEMENT_3D('',#151340,#119137,#119138) ;
#97483 = AXIS2_PLACEMENT_3D('',#151341,#119139,#119140) ;
#97484 = AXIS2_PLACEMENT_3D('',#151342,#119141,#119142) ;
#97485 = AXIS2_PLACEMENT_3D('',#151343,#119143,#119144) ;
#97486 = AXIS2_PLACEMENT_3D('',#151344,#119145,#119146) ;
#97487 = AXIS2_PLACEMENT_3D('',#151345,#119147,#119148) ;
#97488 = AXIS2_PLACEMENT_3D('',#151346,#119149,#119150) ;
#97489 = AXIS2_PLACEMENT_3D('',#151347,#119151,#119152) ;
#97490 = AXIS2_PLACEMENT_3D('',#151348,#119153,#119154) ;
#97491 = AXIS2_PLACEMENT_3D('',#151349,#119155,#119156) ;
#97492 = AXIS2_PLACEMENT_3D('',#151350,#119157,#119158) ;
#97493 = AXIS2_PLACEMENT_3D('',#151351,#119159,#119160) ;
#97494 = AXIS2_PLACEMENT_3D('',#151352,#119161,#119162) ;
#97495 = AXIS2_PLACEMENT_3D('',#151353,#119163,#119164) ;
#97496 = AXIS2_PLACEMENT_3D('',#151354,#119165,#119166) ;
#97497 = AXIS2_PLACEMENT_3D('',#151355,#119167,#119168) ;
#97498 = AXIS2_PLACEMENT_3D('',#151356,#119169,#119170) ;
#97499 = AXIS2_PLACEMENT_3D('',#151357,#119171,#119172) ;
#97500 = AXIS2_PLACEMENT_3D('',#151358,#119173,#119174) ;
#97501 = AXIS2_PLACEMENT_3D('',#151359,#119175,#119176) ;
#97502 = AXIS2_PLACEMENT_3D('',#151360,#119177,#119178) ;
#97503 = AXIS2_PLACEMENT_3D('',#151361,#119179,#119180) ;
#97504 = AXIS2_PLACEMENT_3D('',#151362,#119181,#119182) ;
#97505 = AXIS2_PLACEMENT_3D('',#151363,#119183,#119184) ;
#97506 = AXIS2_PLACEMENT_3D('',#151364,#119185,#119186) ;
#97507 = AXIS2_PLACEMENT_3D('',#151365,#119187,#119188) ;
#97508 = AXIS2_PLACEMENT_3D('',#151366,#119189,#119190) ;
#97509 = AXIS2_PLACEMENT_3D('',#151367,#119191,#119192) ;
#97510 = AXIS2_PLACEMENT_3D('',#151368,#119193,#119194) ;
#97511 = AXIS2_PLACEMENT_3D('',#151369,#119195,#119196) ;
#97512 = AXIS2_PLACEMENT_3D('',#151370,#119197,#119198) ;
#97513 = AXIS2_PLACEMENT_3D('',#151371,#119199,#119200) ;
#97514 = AXIS2_PLACEMENT_3D('',#151372,#119201,#119202) ;
#97515 = AXIS2_PLACEMENT_3D('',#151373,#119203,#119204) ;
#97516 = AXIS2_PLACEMENT_3D('',#151374,#119205,#119206) ;
#97517 = AXIS2_PLACEMENT_3D('',#151375,#119207,#119208) ;
#97518 = AXIS2_PLACEMENT_3D('',#151376,#119209,#119210) ;
#97519 = AXIS2_PLACEMENT_3D('',#151377,#119211,#119212) ;
#97520 = AXIS2_PLACEMENT_3D('',#151378,#119213,#119214) ;
#97521 = AXIS2_PLACEMENT_3D('',#151379,#119215,#119216) ;
#97522 = AXIS2_PLACEMENT_3D('',#151380,#119217,#119218) ;
#97523 = AXIS2_PLACEMENT_3D('',#151381,#119219,#119220) ;
#97524 = AXIS2_PLACEMENT_3D('',#151382,#119221,#119222) ;
#97525 = AXIS2_PLACEMENT_3D('',#151383,#119223,#119224) ;
#97526 = AXIS2_PLACEMENT_3D('',#151384,#119225,#119226) ;
#97527 = AXIS2_PLACEMENT_3D('',#151385,#119227,#119228) ;
#97528 = AXIS2_PLACEMENT_3D('',#151386,#119229,#119230) ;
#97529 = AXIS2_PLACEMENT_3D('',#151387,#119231,#119232) ;
#97530 = AXIS2_PLACEMENT_3D('',#151388,#119233,#119234) ;
#97531 = AXIS2_PLACEMENT_3D('',#151389,#119235,#119236) ;
#97532 = AXIS2_PLACEMENT_3D('',#151390,#119237,#119238) ;
#97533 = AXIS2_PLACEMENT_3D('',#151391,#119239,#119240) ;
#97534 = AXIS2_PLACEMENT_3D('',#151392,#119241,#119242) ;
#97535 = AXIS2_PLACEMENT_3D('',#151393,#119243,#119244) ;
#97536 = AXIS2_PLACEMENT_3D('',#151394,#119245,#119246) ;
#97537 = AXIS2_PLACEMENT_3D('',#151395,#119247,#119248) ;
#97538 = AXIS2_PLACEMENT_3D('',#151396,#119249,#119250) ;
#97539 = AXIS2_PLACEMENT_3D('',#151397,#119251,#119252) ;
#97540 = AXIS2_PLACEMENT_3D('',#151398,#119253,#119254) ;
#97541 = AXIS2_PLACEMENT_3D('',#151399,#119255,#119256) ;
#97542 = AXIS2_PLACEMENT_3D('',#151400,#119257,#119258) ;
#97543 = AXIS2_PLACEMENT_3D('',#151401,#119259,#119260) ;
#97544 = AXIS2_PLACEMENT_3D('',#151402,#119261,#119262) ;
#97545 = AXIS2_PLACEMENT_3D('',#151403,#119263,#119264) ;
#97546 = AXIS2_PLACEMENT_3D('',#151404,#119265,#119266) ;
#97547 = AXIS2_PLACEMENT_3D('',#151405,#119267,#119268) ;
#97548 = AXIS2_PLACEMENT_3D('',#151406,#119269,#119270) ;
#97549 = AXIS2_PLACEMENT_3D('',#151407,#119271,#119272) ;
#97550 = AXIS2_PLACEMENT_3D('',#151408,#119273,#119274) ;
#97551 = AXIS2_PLACEMENT_3D('',#151409,#119275,#119276) ;
#97552 = AXIS2_PLACEMENT_3D('',#151410,#119277,#119278) ;
#97553 = AXIS2_PLACEMENT_3D('',#151411,#119279,#119280) ;
#97554 = AXIS2_PLACEMENT_3D('',#151412,#119281,#119282) ;
#97555 = AXIS2_PLACEMENT_3D('',#151413,#119283,#119284) ;
#97556 = AXIS2_PLACEMENT_3D('',#151414,#119285,#119286) ;
#97557 = AXIS2_PLACEMENT_3D('',#151415,#119287,#119288) ;
#97558 = AXIS2_PLACEMENT_3D('',#151416,#119289,#119290) ;
#97559 = AXIS2_PLACEMENT_3D('',#151417,#119291,#119292) ;
#97560 = AXIS2_PLACEMENT_3D('',#151418,#119293,#119294) ;
#97561 = AXIS2_PLACEMENT_3D('',#151419,#119295,#119296) ;
#97562 = AXIS2_PLACEMENT_3D('',#151420,#119297,#119298) ;
#97563 = AXIS2_PLACEMENT_3D('',#151421,#119299,#119300) ;
#97564 = AXIS2_PLACEMENT_3D('',#151422,#119301,#119302) ;
#97565 = AXIS2_PLACEMENT_3D('',#151423,#119303,#119304) ;
#97566 = AXIS2_PLACEMENT_3D('',#151424,#119305,#119306) ;
#97567 = AXIS2_PLACEMENT_3D('',#151425,#119307,#119308) ;
#97568 = AXIS2_PLACEMENT_3D('',#151426,#119309,#119310) ;
#97569 = AXIS2_PLACEMENT_3D('',#151427,#119311,#119312) ;
#97570 = AXIS2_PLACEMENT_3D('',#151428,#119313,#119314) ;
#97571 = AXIS2_PLACEMENT_3D('',#151429,#119315,#119316) ;
#97572 = AXIS2_PLACEMENT_3D('',#151430,#119317,#119318) ;
#97573 = AXIS2_PLACEMENT_3D('',#151431,#119319,#119320) ;
#97574 = AXIS2_PLACEMENT_3D('',#151432,#119321,#119322) ;
#97575 = AXIS2_PLACEMENT_3D('',#151433,#119323,#119324) ;
#97576 = AXIS2_PLACEMENT_3D('',#151434,#119325,#119326) ;
#97577 = AXIS2_PLACEMENT_3D('',#151435,#119327,#119328) ;
#97578 = AXIS2_PLACEMENT_3D('',#151436,#119329,#119330) ;
#97579 = AXIS2_PLACEMENT_3D('',#151437,#119331,#119332) ;
#97580 = AXIS2_PLACEMENT_3D('',#151438,#119333,#119334) ;
#97581 = AXIS2_PLACEMENT_3D('',#151439,#119335,#119336) ;
#97582 = AXIS2_PLACEMENT_3D('',#151440,#119337,#119338) ;
#97583 = AXIS2_PLACEMENT_3D('',#151441,#119339,#119340) ;
#97584 = AXIS2_PLACEMENT_3D('',#151442,#119341,#119342) ;
#97585 = AXIS2_PLACEMENT_3D('',#151443,#119343,#119344) ;
#97586 = AXIS2_PLACEMENT_3D('',#151444,#119345,#119346) ;
#97587 = AXIS2_PLACEMENT_3D('',#151445,#119347,#119348) ;
#97588 = AXIS2_PLACEMENT_3D('',#151446,#119349,#119350) ;
#97589 = AXIS2_PLACEMENT_3D('',#151447,#119351,#119352) ;
#97590 = AXIS2_PLACEMENT_3D('',#151448,#119353,#119354) ;
#97591 = AXIS2_PLACEMENT_3D('',#151449,#119355,#119356) ;
#97592 = AXIS2_PLACEMENT_3D('',#151450,#119357,#119358) ;
#97593 = AXIS2_PLACEMENT_3D('',#151451,#119359,#119360) ;
#97594 = AXIS2_PLACEMENT_3D('',#151452,#119361,#119362) ;
#97595 = AXIS2_PLACEMENT_3D('',#151453,#119363,#119364) ;
#97596 = AXIS2_PLACEMENT_3D('',#151454,#119365,#119366) ;
#97597 = AXIS2_PLACEMENT_3D('',#151455,#119367,#119368) ;
#97598 = AXIS2_PLACEMENT_3D('',#151456,#119369,#119370) ;
#97599 = AXIS2_PLACEMENT_3D('',#151457,#119371,#119372) ;
#97600 = AXIS2_PLACEMENT_3D('',#151458,#119373,#119374) ;
#97601 = AXIS2_PLACEMENT_3D('',#151459,#119375,#119376) ;
#97602 = AXIS2_PLACEMENT_3D('',#151460,#119377,#119378) ;
#97603 = AXIS2_PLACEMENT_3D('',#151461,#119379,#119380) ;
#97604 = AXIS2_PLACEMENT_3D('',#151462,#119381,#119382) ;
#97605 = AXIS2_PLACEMENT_3D('',#151463,#119383,#119384) ;
#97606 = AXIS2_PLACEMENT_3D('',#151464,#119385,#119386) ;
#97607 = AXIS2_PLACEMENT_3D('',#151465,#119387,#119388) ;
#97608 = AXIS2_PLACEMENT_3D('',#151466,#119389,#119390) ;
#97609 = AXIS2_PLACEMENT_3D('',#151467,#119391,#119392) ;
#97610 = AXIS2_PLACEMENT_3D('',#151468,#119393,#119394) ;
#97611 = AXIS2_PLACEMENT_3D('',#151469,#119395,#119396) ;
#97612 = AXIS2_PLACEMENT_3D('',#151470,#119397,#119398) ;
#97613 = AXIS2_PLACEMENT_3D('',#151471,#119399,#119400) ;
#97614 = AXIS2_PLACEMENT_3D('',#151472,#119401,#119402) ;
#97615 = AXIS2_PLACEMENT_3D('',#151473,#119403,#119404) ;
#97616 = AXIS2_PLACEMENT_3D('',#151474,#119405,#119406) ;
#97617 = AXIS2_PLACEMENT_3D('',#151475,#119407,#119408) ;
#97618 = AXIS2_PLACEMENT_3D('',#151476,#119409,#119410) ;
#97619 = AXIS2_PLACEMENT_3D('',#151477,#119411,#119412) ;
#97620 = AXIS2_PLACEMENT_3D('',#151478,#119413,#119414) ;
#97621 = AXIS2_PLACEMENT_3D('',#151479,#119415,#119416) ;
#97622 = AXIS2_PLACEMENT_3D('',#151480,#119417,#119418) ;
#97623 = AXIS2_PLACEMENT_3D('',#151481,#119419,#119420) ;
#97624 = AXIS2_PLACEMENT_3D('',#151482,#119421,#119422) ;
#97625 = AXIS2_PLACEMENT_3D('',#151483,#119423,#119424) ;
#97626 = AXIS2_PLACEMENT_3D('',#151484,#119425,#119426) ;
#97627 = AXIS2_PLACEMENT_3D('',#151485,#119427,#119428) ;
#97628 = AXIS2_PLACEMENT_3D('',#151486,#119429,#119430) ;
#97629 = AXIS2_PLACEMENT_3D('',#151487,#119431,#119432) ;
#97630 = AXIS2_PLACEMENT_3D('',#151488,#119433,#119434) ;
#97631 = AXIS2_PLACEMENT_3D('',#151489,#119435,#119436) ;
#97632 = AXIS2_PLACEMENT_3D('',#151490,#119437,#119438) ;
#97633 = AXIS2_PLACEMENT_3D('',#151491,#119439,#119440) ;
#97634 = AXIS2_PLACEMENT_3D('',#151492,#119441,#119442) ;
#97635 = AXIS2_PLACEMENT_3D('',#151493,#119443,#119444) ;
#97636 = AXIS2_PLACEMENT_3D('',#151494,#119445,#119446) ;
#97637 = AXIS2_PLACEMENT_3D('',#151495,#119447,#119448) ;
#97638 = AXIS2_PLACEMENT_3D('',#151496,#119449,#119450) ;
#97639 = AXIS2_PLACEMENT_3D('',#151497,#119451,#119452) ;
#97640 = AXIS2_PLACEMENT_3D('',#151498,#119453,#119454) ;
#97641 = AXIS2_PLACEMENT_3D('',#151499,#119455,#119456) ;
#97642 = AXIS2_PLACEMENT_3D('',#151500,#119457,#119458) ;
#97643 = AXIS2_PLACEMENT_3D('',#151501,#119459,#119460) ;
#97644 = AXIS2_PLACEMENT_3D('',#151502,#119461,#119462) ;
#97645 = AXIS2_PLACEMENT_3D('',#151503,#119463,#119464) ;
#97646 = AXIS2_PLACEMENT_3D('',#151504,#119465,#119466) ;
#97647 = AXIS2_PLACEMENT_3D('',#151505,#119467,#119468) ;
#97648 = AXIS2_PLACEMENT_3D('',#151506,#119469,#119470) ;
#97649 = AXIS2_PLACEMENT_3D('',#151507,#119471,#119472) ;
#97650 = AXIS2_PLACEMENT_3D('',#151508,#119473,#119474) ;
#97651 = AXIS2_PLACEMENT_3D('',#151509,#119475,#119476) ;
#97652 = AXIS2_PLACEMENT_3D('',#151510,#119477,#119478) ;
#97653 = AXIS2_PLACEMENT_3D('',#151511,#119479,#119480) ;
#97654 = AXIS2_PLACEMENT_3D('',#151512,#119481,#119482) ;
#97655 = AXIS2_PLACEMENT_3D('',#151513,#119483,#119484) ;
#97656 = AXIS2_PLACEMENT_3D('',#151514,#119485,#119486) ;
#97657 = AXIS2_PLACEMENT_3D('',#151515,#119487,#119488) ;
#97658 = AXIS2_PLACEMENT_3D('',#151516,#119489,#119490) ;
#97659 = AXIS2_PLACEMENT_3D('',#151517,#119491,#119492) ;
#97660 = AXIS2_PLACEMENT_3D('',#151518,#119493,#119494) ;
#97661 = AXIS2_PLACEMENT_3D('',#151519,#119495,#119496) ;
#97662 = AXIS2_PLACEMENT_3D('',#151520,#119497,#119498) ;
#97663 = AXIS2_PLACEMENT_3D('',#151521,#119499,#119500) ;
#97664 = AXIS2_PLACEMENT_3D('',#151522,#119501,#119502) ;
#97665 = AXIS2_PLACEMENT_3D('',#151523,#119503,#119504) ;
#97666 = AXIS2_PLACEMENT_3D('',#151524,#119505,#119506) ;
#97667 = AXIS2_PLACEMENT_3D('',#151525,#119507,#119508) ;
#97668 = AXIS2_PLACEMENT_3D('',#151526,#119509,#119510) ;
#97669 = AXIS2_PLACEMENT_3D('',#151527,#119511,#119512) ;
#97670 = AXIS2_PLACEMENT_3D('',#151528,#119513,#119514) ;
#97671 = AXIS2_PLACEMENT_3D('',#151529,#119515,#119516) ;
#97672 = AXIS2_PLACEMENT_3D('',#151530,#119517,#119518) ;
#97673 = AXIS2_PLACEMENT_3D('',#151531,#119519,#119520) ;
#97674 = AXIS2_PLACEMENT_3D('',#151532,#119521,#119522) ;
#97675 = AXIS2_PLACEMENT_3D('',#151533,#119523,#119524) ;
#97676 = AXIS2_PLACEMENT_3D('',#151534,#119525,#119526) ;
#97677 = AXIS2_PLACEMENT_3D('',#151535,#119527,#119528) ;
#97678 = AXIS2_PLACEMENT_3D('',#151536,#119529,#119530) ;
#97679 = AXIS2_PLACEMENT_3D('',#151537,#119531,#119532) ;
#97680 = AXIS2_PLACEMENT_3D('',#151538,#119533,#119534) ;
#97681 = AXIS2_PLACEMENT_3D('',#151539,#119535,#119536) ;
#97682 = AXIS2_PLACEMENT_3D('',#151540,#119537,#119538) ;
#97683 = AXIS2_PLACEMENT_3D('',#151541,#119539,#119540) ;
#97684 = AXIS2_PLACEMENT_3D('',#151542,#119541,#119542) ;
#97685 = AXIS2_PLACEMENT_3D('',#151543,#119543,#119544) ;
#97686 = AXIS2_PLACEMENT_3D('',#151544,#119545,#119546) ;
#97687 = AXIS2_PLACEMENT_3D('',#151545,#119547,#119548) ;
#97688 = AXIS2_PLACEMENT_3D('',#151546,#119549,#119550) ;
#97689 = AXIS2_PLACEMENT_3D('',#151547,#119551,#119552) ;
#97690 = AXIS2_PLACEMENT_3D('',#151548,#119553,#119554) ;
#97691 = AXIS2_PLACEMENT_3D('',#151549,#119555,#119556) ;
#97692 = AXIS2_PLACEMENT_3D('',#151550,#119557,#119558) ;
#97693 = AXIS2_PLACEMENT_3D('',#151551,#119559,#119560) ;
#97694 = AXIS2_PLACEMENT_3D('',#151552,#119561,#119562) ;
#97695 = AXIS2_PLACEMENT_3D('',#151553,#119563,#119564) ;
#97696 = AXIS2_PLACEMENT_3D('',#151554,#119565,#119566) ;
#97697 = AXIS2_PLACEMENT_3D('',#151555,#119567,#119568) ;
#97698 = AXIS2_PLACEMENT_3D('',#151556,#119569,#119570) ;
#97699 = AXIS2_PLACEMENT_3D('',#151557,#119571,#119572) ;
#97700 = AXIS2_PLACEMENT_3D('',#151558,#119573,#119574) ;
#97701 = AXIS2_PLACEMENT_3D('',#151559,#119575,#119576) ;
#97702 = AXIS2_PLACEMENT_3D('',#151560,#119577,#119578) ;
#97703 = AXIS2_PLACEMENT_3D('',#151561,#119579,#119580) ;
#97704 = AXIS2_PLACEMENT_3D('',#151562,#119581,#119582) ;
#97705 = AXIS2_PLACEMENT_3D('',#151563,#119583,#119584) ;
#97706 = AXIS2_PLACEMENT_3D('',#151564,#119585,#119586) ;
#97707 = AXIS2_PLACEMENT_3D('',#151565,#119587,#119588) ;
#97708 = AXIS2_PLACEMENT_3D('',#151566,#119589,#119590) ;
#97709 = AXIS2_PLACEMENT_3D('',#151567,#119591,#119592) ;
#97710 = AXIS2_PLACEMENT_3D('',#151568,#119593,#119594) ;
#97711 = AXIS2_PLACEMENT_3D('',#151569,#119595,#119596) ;
#97712 = AXIS2_PLACEMENT_3D('',#151570,#119597,#119598) ;
#97713 = AXIS2_PLACEMENT_3D('',#151571,#119599,#119600) ;
#97714 = AXIS2_PLACEMENT_3D('',#151572,#119601,#119602) ;
#97715 = AXIS2_PLACEMENT_3D('',#151573,#119603,#119604) ;
#97716 = AXIS2_PLACEMENT_3D('',#151574,#119605,#119606) ;
#97717 = AXIS2_PLACEMENT_3D('',#151575,#119607,#119608) ;
#97718 = AXIS2_PLACEMENT_3D('',#151576,#119609,#119610) ;
#97719 = AXIS2_PLACEMENT_3D('',#151577,#119611,#119612) ;
#97720 = AXIS2_PLACEMENT_3D('',#151578,#119613,#119614) ;
#97721 = AXIS2_PLACEMENT_3D('',#151579,#119615,#119616) ;
#97722 = AXIS2_PLACEMENT_3D('',#151580,#119617,#119618) ;
#97723 = AXIS2_PLACEMENT_3D('',#151581,#119619,#119620) ;
#97724 = AXIS2_PLACEMENT_3D('',#151582,#119621,#119622) ;
#97725 = AXIS2_PLACEMENT_3D('',#151583,#119623,#119624) ;
#97726 = AXIS2_PLACEMENT_3D('',#151584,#119625,#119626) ;
#97727 = AXIS2_PLACEMENT_3D('',#151585,#119627,#119628) ;
#97728 = AXIS2_PLACEMENT_3D('',#151586,#119629,#119630) ;
#97729 = AXIS2_PLACEMENT_3D('',#151587,#119631,#119632) ;
#97730 = AXIS2_PLACEMENT_3D('',#151588,#119633,#119634) ;
#97731 = AXIS2_PLACEMENT_3D('',#151589,#119635,#119636) ;
#97732 = AXIS2_PLACEMENT_3D('',#151590,#119637,#119638) ;
#97733 = AXIS2_PLACEMENT_3D('',#151591,#119639,#119640) ;
#97734 = AXIS2_PLACEMENT_3D('',#151592,#119641,#119642) ;
#97735 = AXIS2_PLACEMENT_3D('',#151593,#119643,#119644) ;
#97736 = AXIS2_PLACEMENT_3D('',#151594,#119645,#119646) ;
#97737 = AXIS2_PLACEMENT_3D('',#151595,#119647,#119648) ;
#97738 = AXIS2_PLACEMENT_3D('',#151596,#119649,#119650) ;
#97739 = AXIS2_PLACEMENT_3D('',#151597,#119651,#119652) ;
#97740 = AXIS2_PLACEMENT_3D('',#151598,#119653,#119654) ;
#97741 = AXIS2_PLACEMENT_3D('',#151599,#119655,#119656) ;
#97742 = AXIS2_PLACEMENT_3D('',#151600,#119657,#119658) ;
#97743 = AXIS2_PLACEMENT_3D('',#151601,#119659,#119660) ;
#97744 = AXIS2_PLACEMENT_3D('',#151602,#119661,#119662) ;
#97745 = AXIS2_PLACEMENT_3D('',#151603,#119663,#119664) ;
#97746 = AXIS2_PLACEMENT_3D('',#151604,#119665,#119666) ;
#97747 = AXIS2_PLACEMENT_3D('',#151605,#119667,#119668) ;
#97748 = AXIS2_PLACEMENT_3D('',#151606,#119669,#119670) ;
#97749 = AXIS2_PLACEMENT_3D('',#151607,#119671,#119672) ;
#97750 = AXIS2_PLACEMENT_3D('',#151608,#119673,#119674) ;
#97751 = AXIS2_PLACEMENT_3D('',#151609,#119675,#119676) ;
#97752 = AXIS2_PLACEMENT_3D('',#151610,#119677,#119678) ;
#97753 = AXIS2_PLACEMENT_3D('',#151611,#119679,#119680) ;
#97754 = AXIS2_PLACEMENT_3D('',#151612,#119681,#119682) ;
#97755 = AXIS2_PLACEMENT_3D('',#151613,#119683,#119684) ;
#97756 = AXIS2_PLACEMENT_3D('',#151614,#119685,#119686) ;
#97757 = AXIS2_PLACEMENT_3D('',#151615,#119687,#119688) ;
#97758 = AXIS2_PLACEMENT_3D('',#151616,#119689,#119690) ;
#97759 = AXIS2_PLACEMENT_3D('',#151617,#119691,#119692) ;
#97760 = AXIS2_PLACEMENT_3D('',#151618,#119693,#119694) ;
#97761 = AXIS2_PLACEMENT_3D('',#151619,#119695,#119696) ;
#97762 = AXIS2_PLACEMENT_3D('',#151620,#119697,#119698) ;
#97763 = AXIS2_PLACEMENT_3D('',#151621,#119699,#119700) ;
#97764 = AXIS2_PLACEMENT_3D('',#151622,#119701,#119702) ;
#97765 = AXIS2_PLACEMENT_3D('',#151623,#119703,#119704) ;
#97766 = AXIS2_PLACEMENT_3D('',#151624,#119705,#119706) ;
#97767 = AXIS2_PLACEMENT_3D('',#151625,#119707,#119708) ;
#97768 = AXIS2_PLACEMENT_3D('',#151626,#119709,#119710) ;
#97769 = AXIS2_PLACEMENT_3D('',#151627,#119711,#119712) ;
#97770 = AXIS2_PLACEMENT_3D('',#151628,#119713,#119714) ;
#97771 = AXIS2_PLACEMENT_3D('',#151629,#119715,#119716) ;
#97772 = AXIS2_PLACEMENT_3D('',#151630,#119717,#119718) ;
#97773 = AXIS2_PLACEMENT_3D('',#151631,#119719,#119720) ;
#97774 = AXIS2_PLACEMENT_3D('',#151632,#119721,#119722) ;
#97775 = AXIS2_PLACEMENT_3D('',#151633,#119723,#119724) ;
#97776 = AXIS2_PLACEMENT_3D('',#151634,#119725,#119726) ;
#97777 = AXIS2_PLACEMENT_3D('',#151635,#119727,#119728) ;
#97778 = AXIS2_PLACEMENT_3D('',#151636,#119729,#119730) ;
#97779 = AXIS2_PLACEMENT_3D('',#151637,#119731,#119732) ;
#97780 = AXIS2_PLACEMENT_3D('',#151638,#119733,#119734) ;
#97781 = AXIS2_PLACEMENT_3D('',#151639,#119735,#119736) ;
#97782 = AXIS2_PLACEMENT_3D('',#151640,#119737,#119738) ;
#97783 = AXIS2_PLACEMENT_3D('',#151641,#119739,#119740) ;
#97784 = AXIS2_PLACEMENT_3D('',#151642,#119741,#119742) ;
#97785 = AXIS2_PLACEMENT_3D('',#151643,#119743,#119744) ;
#97786 = AXIS2_PLACEMENT_3D('',#151644,#119745,#119746) ;
#97787 = AXIS2_PLACEMENT_3D('',#151645,#119747,#119748) ;
#97788 = AXIS2_PLACEMENT_3D('',#151646,#119749,#119750) ;
#97789 = AXIS2_PLACEMENT_3D('',#151647,#119751,#119752) ;
#97790 = AXIS2_PLACEMENT_3D('',#151648,#119753,#119754) ;
#97791 = AXIS2_PLACEMENT_3D('',#151649,#119755,#119756) ;
#97792 = AXIS2_PLACEMENT_3D('',#151650,#119757,#119758) ;
#97793 = AXIS2_PLACEMENT_3D('',#151651,#119759,#119760) ;
#97794 = AXIS2_PLACEMENT_3D('',#151652,#119761,#119762) ;
#97795 = AXIS2_PLACEMENT_3D('',#151653,#119763,#119764) ;
#97796 = AXIS2_PLACEMENT_3D('',#151654,#119765,#119766) ;
#97797 = AXIS2_PLACEMENT_3D('',#151655,#119767,#119768) ;
#97798 = AXIS2_PLACEMENT_3D('',#151656,#119769,#119770) ;
#97799 = AXIS2_PLACEMENT_3D('',#151657,#119771,#119772) ;
#97800 = AXIS2_PLACEMENT_3D('',#151658,#119773,#119774) ;
#97801 = AXIS2_PLACEMENT_3D('',#151659,#119775,#119776) ;
#97802 = AXIS2_PLACEMENT_3D('',#151660,#119777,#119778) ;
#97803 = AXIS2_PLACEMENT_3D('',#151661,#119779,#119780) ;
#97804 = AXIS2_PLACEMENT_3D('',#151662,#119781,#119782) ;
#97805 = AXIS2_PLACEMENT_3D('',#151663,#119783,#119784) ;
#97806 = AXIS2_PLACEMENT_3D('',#151664,#119785,#119786) ;
#97807 = AXIS2_PLACEMENT_3D('',#151665,#119787,#119788) ;
#97808 = AXIS2_PLACEMENT_3D('',#151666,#119789,#119790) ;
#97809 = AXIS2_PLACEMENT_3D('',#151667,#119791,#119792) ;
#97810 = AXIS2_PLACEMENT_3D('',#151668,#119793,#119794) ;
#97811 = AXIS2_PLACEMENT_3D('',#151669,#119795,#119796) ;
#97812 = AXIS2_PLACEMENT_3D('',#151670,#119797,#119798) ;
#97813 = AXIS2_PLACEMENT_3D('',#151671,#119799,#119800) ;
#97814 = AXIS2_PLACEMENT_3D('',#151672,#119801,#119802) ;
#97815 = AXIS2_PLACEMENT_3D('',#151673,#119803,#119804) ;
#97816 = AXIS2_PLACEMENT_3D('',#151674,#119805,#119806) ;
#97817 = AXIS2_PLACEMENT_3D('',#151675,#119807,#119808) ;
#97818 = AXIS2_PLACEMENT_3D('',#151676,#119809,#119810) ;
#97819 = AXIS2_PLACEMENT_3D('',#151677,#119811,#119812) ;
#97820 = AXIS2_PLACEMENT_3D('',#151678,#119813,#119814) ;
#97821 = AXIS2_PLACEMENT_3D('',#151679,#119815,#119816) ;
#97822 = AXIS2_PLACEMENT_3D('',#151680,#119817,#119818) ;
#97823 = AXIS2_PLACEMENT_3D('',#151681,#119819,#119820) ;
#97824 = AXIS2_PLACEMENT_3D('',#151682,#119821,#119822) ;
#97825 = AXIS2_PLACEMENT_3D('',#151683,#119823,#119824) ;
#97826 = AXIS2_PLACEMENT_3D('',#151684,#119825,#119826) ;
#97827 = AXIS2_PLACEMENT_3D('',#151685,#119827,#119828) ;
#97828 = AXIS2_PLACEMENT_3D('',#151686,#119829,#119830) ;
#97829 = AXIS2_PLACEMENT_3D('',#151687,#119831,#119832) ;
#97830 = AXIS2_PLACEMENT_3D('',#151688,#119833,#119834) ;
#97831 = AXIS2_PLACEMENT_3D('',#151689,#119835,#119836) ;
#97832 = AXIS2_PLACEMENT_3D('',#151690,#119837,#119838) ;
#97833 = AXIS2_PLACEMENT_3D('',#151691,#119839,#119840) ;
#97834 = AXIS2_PLACEMENT_3D('',#151692,#119841,#119842) ;
#97835 = AXIS2_PLACEMENT_3D('',#151693,#119843,#119844) ;
#97836 = AXIS2_PLACEMENT_3D('',#151694,#119845,#119846) ;
#97837 = AXIS2_PLACEMENT_3D('',#151695,#119847,#119848) ;
#97838 = AXIS2_PLACEMENT_3D('',#151696,#119849,#119850) ;
#97839 = AXIS2_PLACEMENT_3D('',#151697,#119851,#119852) ;
#97840 = AXIS2_PLACEMENT_3D('',#151698,#119853,#119854) ;
#97841 = AXIS2_PLACEMENT_3D('',#151699,#119855,#119856) ;
#97842 = AXIS2_PLACEMENT_3D('',#151700,#119857,#119858) ;
#97843 = AXIS2_PLACEMENT_3D('',#151701,#119859,#119860) ;
#97844 = AXIS2_PLACEMENT_3D('',#151702,#119861,#119862) ;
#97845 = AXIS2_PLACEMENT_3D('',#151703,#119863,#119864) ;
#97846 = AXIS2_PLACEMENT_3D('',#151704,#119865,#119866) ;
#97847 = AXIS2_PLACEMENT_3D('',#151705,#119867,#119868) ;
#97848 = AXIS2_PLACEMENT_3D('',#151706,#119869,#119870) ;
#97849 = AXIS2_PLACEMENT_3D('',#151707,#119871,#119872) ;
#97850 = AXIS2_PLACEMENT_3D('',#151708,#119873,#119874) ;
#97851 = AXIS2_PLACEMENT_3D('',#151709,#119875,#119876) ;
#97852 = AXIS2_PLACEMENT_3D('',#151710,#119877,#119878) ;
#97853 = AXIS2_PLACEMENT_3D('',#151711,#119879,#119880) ;
#97854 = AXIS2_PLACEMENT_3D('',#151712,#119881,#119882) ;
#97855 = AXIS2_PLACEMENT_3D('',#151713,#119883,#119884) ;
#97856 = AXIS2_PLACEMENT_3D('',#151714,#119885,#119886) ;
#97857 = AXIS2_PLACEMENT_3D('',#151715,#119887,#119888) ;
#97858 = AXIS2_PLACEMENT_3D('',#151716,#119889,#119890) ;
#97859 = AXIS2_PLACEMENT_3D('',#151717,#119891,#119892) ;
#97860 = AXIS2_PLACEMENT_3D('',#151718,#119893,#119894) ;
#97861 = AXIS2_PLACEMENT_3D('',#151719,#119895,#119896) ;
#97862 = AXIS2_PLACEMENT_3D('',#151720,#119897,#119898) ;
#97863 = AXIS2_PLACEMENT_3D('',#151721,#119899,#119900) ;
#97864 = AXIS2_PLACEMENT_3D('',#151722,#119901,#119902) ;
#97865 = AXIS2_PLACEMENT_3D('',#151723,#119903,#119904) ;
#97866 = AXIS2_PLACEMENT_3D('',#151724,#119905,#119906) ;
#97867 = AXIS2_PLACEMENT_3D('',#151725,#119907,#119908) ;
#97868 = AXIS2_PLACEMENT_3D('',#151726,#119909,#119910) ;
#97869 = AXIS2_PLACEMENT_3D('',#151727,#119911,#119912) ;
#97870 = AXIS2_PLACEMENT_3D('',#151728,#119913,#119914) ;
#97871 = AXIS2_PLACEMENT_3D('',#151729,#119915,#119916) ;
#97872 = AXIS2_PLACEMENT_3D('',#151730,#119917,#119918) ;
#97873 = AXIS2_PLACEMENT_3D('',#151731,#119919,#119920) ;
#97874 = AXIS2_PLACEMENT_3D('',#151732,#119921,#119922) ;
#97875 = AXIS2_PLACEMENT_3D('',#151733,#119923,#119924) ;
#97876 = AXIS2_PLACEMENT_3D('',#151734,#119925,#119926) ;
#97877 = AXIS2_PLACEMENT_3D('',#151735,#119927,#119928) ;
#97878 = AXIS2_PLACEMENT_3D('',#151736,#119929,#119930) ;
#97879 = AXIS2_PLACEMENT_3D('',#151737,#119931,#119932) ;
#97880 = AXIS2_PLACEMENT_3D('',#151738,#119933,#119934) ;
#97881 = AXIS2_PLACEMENT_3D('',#151739,#119935,#119936) ;
#97882 = AXIS2_PLACEMENT_3D('',#151740,#119937,#119938) ;
#97883 = AXIS2_PLACEMENT_3D('',#151741,#119939,#119940) ;
#97884 = AXIS2_PLACEMENT_3D('',#151742,#119941,#119942) ;
#97885 = AXIS2_PLACEMENT_3D('',#151743,#119943,#119944) ;
#97886 = AXIS2_PLACEMENT_3D('',#151744,#119945,#119946) ;
#97887 = AXIS2_PLACEMENT_3D('',#151745,#119947,#119948) ;
#97888 = AXIS2_PLACEMENT_3D('',#151746,#119949,#119950) ;
#97889 = AXIS2_PLACEMENT_3D('',#151747,#119951,#119952) ;
#97890 = AXIS2_PLACEMENT_3D('',#151748,#119953,#119954) ;
#97891 = AXIS2_PLACEMENT_3D('',#151749,#119955,#119956) ;
#97892 = AXIS2_PLACEMENT_3D('',#151750,#119957,#119958) ;
#97893 = AXIS2_PLACEMENT_3D('',#151751,#119959,#119960) ;
#97894 = AXIS2_PLACEMENT_3D('',#151752,#119961,#119962) ;
#97895 = AXIS2_PLACEMENT_3D('',#151753,#119963,#119964) ;
#97896 = AXIS2_PLACEMENT_3D('',#151754,#119965,#119966) ;
#97897 = AXIS2_PLACEMENT_3D('',#151755,#119967,#119968) ;
#97898 = AXIS2_PLACEMENT_3D('',#151756,#119969,#119970) ;
#97899 = AXIS2_PLACEMENT_3D('',#151757,#119971,#119972) ;
#97900 = AXIS2_PLACEMENT_3D('',#151758,#119973,#119974) ;
#97901 = AXIS2_PLACEMENT_3D('',#151759,#119975,#119976) ;
#97902 = AXIS2_PLACEMENT_3D('',#151760,#119977,#119978) ;
#97903 = AXIS2_PLACEMENT_3D('',#151761,#119979,#119980) ;
#97904 = AXIS2_PLACEMENT_3D('',#151762,#119981,#119982) ;
#97905 = AXIS2_PLACEMENT_3D('',#151763,#119983,#119984) ;
#97906 = AXIS2_PLACEMENT_3D('',#151764,#119985,#119986) ;
#97907 = AXIS2_PLACEMENT_3D('',#151765,#119987,#119988) ;
#97908 = AXIS2_PLACEMENT_3D('',#151766,#119989,#119990) ;
#97909 = AXIS2_PLACEMENT_3D('',#151767,#119991,#119992) ;
#97910 = AXIS2_PLACEMENT_3D('',#151768,#119993,#119994) ;
#97911 = AXIS2_PLACEMENT_3D('',#151769,#119995,#119996) ;
#97912 = AXIS2_PLACEMENT_3D('',#151770,#119997,#119998) ;
#97913 = AXIS2_PLACEMENT_3D('',#151771,#119999,#120000) ;
#97914 = AXIS2_PLACEMENT_3D('',#151772,#120001,#120002) ;
#97915 = AXIS2_PLACEMENT_3D('',#151773,#120003,#120004) ;
#97916 = AXIS2_PLACEMENT_3D('',#151774,#120005,#120006) ;
#97917 = AXIS2_PLACEMENT_3D('',#151775,#120007,#120008) ;
#97918 = AXIS2_PLACEMENT_3D('',#151776,#120009,#120010) ;
#97919 = AXIS2_PLACEMENT_3D('',#151777,#120011,#120012) ;
#97920 = AXIS2_PLACEMENT_3D('',#151778,#120013,#120014) ;
#97921 = AXIS2_PLACEMENT_3D('',#151779,#120015,#120016) ;
#97922 = AXIS2_PLACEMENT_3D('',#151780,#120017,#120018) ;
#97923 = AXIS2_PLACEMENT_3D('',#151781,#120019,#120020) ;
#97924 = AXIS2_PLACEMENT_3D('',#151782,#120021,#120022) ;
#97925 = AXIS2_PLACEMENT_3D('',#151783,#120023,#120024) ;
#97926 = AXIS2_PLACEMENT_3D('',#151784,#120025,#120026) ;
#97927 = AXIS2_PLACEMENT_3D('',#151785,#120027,#120028) ;
#97928 = AXIS2_PLACEMENT_3D('',#151786,#120029,#120030) ;
#97929 = AXIS2_PLACEMENT_3D('',#151787,#120031,#120032) ;
#97930 = AXIS2_PLACEMENT_3D('',#151788,#120033,#120034) ;
#97931 = AXIS2_PLACEMENT_3D('',#151789,#120035,#120036) ;
#97932 = AXIS2_PLACEMENT_3D('',#151790,#120037,#120038) ;
#97933 = AXIS2_PLACEMENT_3D('',#151791,#120039,#120040) ;
#97934 = AXIS2_PLACEMENT_3D('',#151792,#120041,#120042) ;
#97935 = AXIS2_PLACEMENT_3D('',#151793,#120043,#120044) ;
#97936 = AXIS2_PLACEMENT_3D('',#151794,#120045,#120046) ;
#97937 = AXIS2_PLACEMENT_3D('',#151795,#120047,#120048) ;
#97938 = AXIS2_PLACEMENT_3D('',#151796,#120049,#120050) ;
#97939 = AXIS2_PLACEMENT_3D('',#151797,#120051,#120052) ;
#97940 = AXIS2_PLACEMENT_3D('',#151798,#120053,#120054) ;
#97941 = AXIS2_PLACEMENT_3D('',#151799,#120055,#120056) ;
#97942 = AXIS2_PLACEMENT_3D('',#151800,#120057,#120058) ;
#97943 = AXIS2_PLACEMENT_3D('',#151801,#120059,#120060) ;
#97944 = AXIS2_PLACEMENT_3D('',#151802,#120061,#120062) ;
#97945 = AXIS2_PLACEMENT_3D('',#151803,#120063,#120064) ;
#97946 = AXIS2_PLACEMENT_3D('',#151804,#120065,#120066) ;
#97947 = AXIS2_PLACEMENT_3D('',#151805,#120067,#120068) ;
#97948 = AXIS2_PLACEMENT_3D('',#151806,#120069,#120070) ;
#97949 = AXIS2_PLACEMENT_3D('',#151807,#120071,#120072) ;
#97950 = AXIS2_PLACEMENT_3D('',#151808,#120073,#120074) ;
#97951 = AXIS2_PLACEMENT_3D('',#151809,#120075,#120076) ;
#97952 = AXIS2_PLACEMENT_3D('',#151810,#120077,#120078) ;
#97953 = AXIS2_PLACEMENT_3D('',#151811,#120079,#120080) ;
#97954 = AXIS2_PLACEMENT_3D('',#151812,#120081,#120082) ;
#97955 = AXIS2_PLACEMENT_3D('',#151813,#120083,#120084) ;
#97956 = AXIS2_PLACEMENT_3D('',#151814,#120085,#120086) ;
#97957 = AXIS2_PLACEMENT_3D('',#151815,#120087,#120088) ;
#97958 = AXIS2_PLACEMENT_3D('',#151816,#120089,#120090) ;
#97959 = AXIS2_PLACEMENT_3D('',#151817,#120091,#120092) ;
#97960 = AXIS2_PLACEMENT_3D('',#151818,#120093,#120094) ;
#97961 = AXIS2_PLACEMENT_3D('',#151819,#120095,#120096) ;
#97962 = AXIS2_PLACEMENT_3D('',#151820,#120097,#120098) ;
#97963 = AXIS2_PLACEMENT_3D('',#151821,#120099,#120100) ;
#97964 = AXIS2_PLACEMENT_3D('',#151822,#120101,#120102) ;
#97965 = AXIS2_PLACEMENT_3D('',#151823,#120103,#120104) ;
#97966 = AXIS2_PLACEMENT_3D('',#151824,#120105,#120106) ;
#97967 = AXIS2_PLACEMENT_3D('',#151825,#120107,#120108) ;
#97968 = AXIS2_PLACEMENT_3D('',#151826,#120109,#120110) ;
#97969 = AXIS2_PLACEMENT_3D('',#151827,#120111,#120112) ;
#97970 = AXIS2_PLACEMENT_3D('',#151828,#120113,#120114) ;
#97971 = AXIS2_PLACEMENT_3D('',#151829,#120115,#120116) ;
#97972 = AXIS2_PLACEMENT_3D('',#151830,#120117,#120118) ;
#97973 = AXIS2_PLACEMENT_3D('',#151831,#120119,#120120) ;
#97974 = AXIS2_PLACEMENT_3D('',#151832,#120121,#120122) ;
#97975 = AXIS2_PLACEMENT_3D('',#151833,#120123,#120124) ;
#97976 = AXIS2_PLACEMENT_3D('',#151834,#120125,#120126) ;
#97977 = AXIS2_PLACEMENT_3D('',#151835,#120127,#120128) ;
#97978 = AXIS2_PLACEMENT_3D('',#151836,#120129,#120130) ;
#97979 = AXIS2_PLACEMENT_3D('',#151837,#120131,#120132) ;
#97980 = AXIS2_PLACEMENT_3D('',#151838,#120133,#120134) ;
#97981 = AXIS2_PLACEMENT_3D('',#151839,#120135,#120136) ;
#97982 = AXIS2_PLACEMENT_3D('',#151840,#120137,#120138) ;
#97983 = AXIS2_PLACEMENT_3D('',#151841,#120139,#120140) ;
#97984 = AXIS2_PLACEMENT_3D('',#151842,#120141,#120142) ;
#97985 = AXIS2_PLACEMENT_3D('',#151843,#120143,#120144) ;
#97986 = AXIS2_PLACEMENT_3D('',#151844,#120145,#120146) ;
#97987 = AXIS2_PLACEMENT_3D('',#151845,#120147,#120148) ;
#97988 = AXIS2_PLACEMENT_3D('',#151846,#120149,#120150) ;
#97989 = AXIS2_PLACEMENT_3D('',#151847,#120151,#120152) ;
#97990 = AXIS2_PLACEMENT_3D('',#151848,#120153,#120154) ;
#97991 = AXIS2_PLACEMENT_3D('',#151849,#120155,#120156) ;
#97992 = AXIS2_PLACEMENT_3D('',#151850,#120157,#120158) ;
#97993 = AXIS2_PLACEMENT_3D('',#151851,#120159,#120160) ;
#97994 = AXIS2_PLACEMENT_3D('',#151852,#120161,#120162) ;
#97995 = AXIS2_PLACEMENT_3D('',#151853,#120163,#120164) ;
#97996 = AXIS2_PLACEMENT_3D('',#151854,#120165,#120166) ;
#97997 = AXIS2_PLACEMENT_3D('',#151855,#120167,#120168) ;
#97998 = AXIS2_PLACEMENT_3D('',#151856,#120169,#120170) ;
#97999 = AXIS2_PLACEMENT_3D('',#151857,#120171,#120172) ;
#98000 = AXIS2_PLACEMENT_3D('',#151858,#120173,#120174) ;
#98001 = AXIS2_PLACEMENT_3D('',#151859,#120175,#120176) ;
#98002 = AXIS2_PLACEMENT_3D('',#151860,#120177,#120178) ;
#98003 = AXIS2_PLACEMENT_3D('',#151861,#120179,#120180) ;
#98004 = AXIS2_PLACEMENT_3D('',#151862,#120181,#120182) ;
#98005 = AXIS2_PLACEMENT_3D('',#151863,#120183,#120184) ;
#98006 = AXIS2_PLACEMENT_3D('',#151864,#120185,#120186) ;
#98007 = AXIS2_PLACEMENT_3D('',#151865,#120187,#120188) ;
#98008 = AXIS2_PLACEMENT_3D('',#151866,#120189,#120190) ;
#98009 = AXIS2_PLACEMENT_3D('',#151867,#120191,#120192) ;
#98010 = AXIS2_PLACEMENT_3D('',#151868,#120193,#120194) ;
#98011 = AXIS2_PLACEMENT_3D('',#151869,#120195,#120196) ;
#98012 = AXIS2_PLACEMENT_3D('',#151870,#120197,#120198) ;
#98013 = AXIS2_PLACEMENT_3D('',#151871,#120199,#120200) ;
#98014 = AXIS2_PLACEMENT_3D('',#151872,#120201,#120202) ;
#98015 = AXIS2_PLACEMENT_3D('',#151873,#120203,#120204) ;
#98016 = AXIS2_PLACEMENT_3D('',#151874,#120205,#120206) ;
#98017 = AXIS2_PLACEMENT_3D('',#151875,#120207,#120208) ;
#98018 = AXIS2_PLACEMENT_3D('',#151876,#120209,#120210) ;
#98019 = AXIS2_PLACEMENT_3D('',#151877,#120211,#120212) ;
#98020 = AXIS2_PLACEMENT_3D('',#151878,#120213,#120214) ;
#98021 = AXIS2_PLACEMENT_3D('',#151879,#120215,#120216) ;
#98022 = AXIS2_PLACEMENT_3D('',#151880,#120217,#120218) ;
#98023 = AXIS2_PLACEMENT_3D('',#151881,#120219,#120220) ;
#98024 = AXIS2_PLACEMENT_3D('',#151882,#120221,#120222) ;
#98025 = AXIS2_PLACEMENT_3D('',#151883,#120223,#120224) ;
#98026 = AXIS2_PLACEMENT_3D('',#151884,#120225,#120226) ;
#98027 = AXIS2_PLACEMENT_3D('',#151885,#120227,#120228) ;
#98028 = AXIS2_PLACEMENT_3D('',#151886,#120229,#120230) ;
#98029 = AXIS2_PLACEMENT_3D('',#151887,#120231,#120232) ;
#98030 = AXIS2_PLACEMENT_3D('',#151888,#120233,#120234) ;
#98031 = AXIS2_PLACEMENT_3D('',#151889,#120235,#120236) ;
#98032 = AXIS2_PLACEMENT_3D('',#151890,#120237,#120238) ;
#98033 = AXIS2_PLACEMENT_3D('',#151891,#120239,#120240) ;
#98034 = AXIS2_PLACEMENT_3D('',#151892,#120241,#120242) ;
#98035 = AXIS2_PLACEMENT_3D('',#151893,#120243,#120244) ;
#98036 = AXIS2_PLACEMENT_3D('',#151894,#120245,#120246) ;
#98037 = AXIS2_PLACEMENT_3D('',#151895,#120247,#120248) ;
#98038 = AXIS2_PLACEMENT_3D('',#151896,#120249,#120250) ;
#98039 = AXIS2_PLACEMENT_3D('',#151897,#120251,#120252) ;
#98040 = AXIS2_PLACEMENT_3D('',#151898,#120253,#120254) ;
#98041 = AXIS2_PLACEMENT_3D('',#151899,#120255,#120256) ;
#98042 = AXIS2_PLACEMENT_3D('',#151900,#120257,#120258) ;
#98043 = AXIS2_PLACEMENT_3D('',#151901,#120259,#120260) ;
#98044 = AXIS2_PLACEMENT_3D('',#151902,#120261,#120262) ;
#98045 = AXIS2_PLACEMENT_3D('',#151903,#120263,#120264) ;
#98046 = AXIS2_PLACEMENT_3D('',#151904,#120265,#120266) ;
#98047 = AXIS2_PLACEMENT_3D('',#151905,#120267,#120268) ;
#98048 = AXIS2_PLACEMENT_3D('',#151906,#120269,#120270) ;
#98049 = AXIS2_PLACEMENT_3D('',#151907,#120271,#120272) ;
#98050 = AXIS2_PLACEMENT_3D('',#151908,#120273,#120274) ;
#98051 = AXIS2_PLACEMENT_3D('',#151909,#120275,#120276) ;
#98052 = AXIS2_PLACEMENT_3D('',#151910,#120277,#120278) ;
#98053 = AXIS2_PLACEMENT_3D('',#151911,#120279,#120280) ;
#98054 = AXIS2_PLACEMENT_3D('',#151912,#120281,#120282) ;
#98055 = AXIS2_PLACEMENT_3D('',#151913,#120283,#120284) ;
#98056 = AXIS2_PLACEMENT_3D('',#151914,#120285,#120286) ;
#98057 = AXIS2_PLACEMENT_3D('',#151915,#120287,#120288) ;
#98058 = AXIS2_PLACEMENT_3D('',#151916,#120289,#120290) ;
#98059 = AXIS2_PLACEMENT_3D('',#151917,#120291,#120292) ;
#98060 = AXIS2_PLACEMENT_3D('',#151918,#120293,#120294) ;
#98061 = AXIS2_PLACEMENT_3D('',#151919,#120295,#120296) ;
#98062 = AXIS2_PLACEMENT_3D('',#151920,#120297,#120298) ;
#98063 = AXIS2_PLACEMENT_3D('',#151921,#120299,#120300) ;
#98064 = AXIS2_PLACEMENT_3D('',#151922,#120301,#120302) ;
#98065 = AXIS2_PLACEMENT_3D('',#151923,#120303,#120304) ;
#98066 = AXIS2_PLACEMENT_3D('',#151924,#120305,#120306) ;
#98067 = AXIS2_PLACEMENT_3D('',#151925,#120307,#120308) ;
#98068 = AXIS2_PLACEMENT_3D('',#151926,#120309,#120310) ;
#98069 = AXIS2_PLACEMENT_3D('',#151927,#120311,#120312) ;
#98070 = AXIS2_PLACEMENT_3D('',#151928,#120313,#120314) ;
#98071 = AXIS2_PLACEMENT_3D('',#151929,#120315,#120316) ;
#98072 = AXIS2_PLACEMENT_3D('',#151930,#120317,#120318) ;
#98073 = AXIS2_PLACEMENT_3D('',#151931,#120319,#120320) ;
#98074 = AXIS2_PLACEMENT_3D('',#151932,#120321,#120322) ;
#98075 = AXIS2_PLACEMENT_3D('',#151933,#120323,#120324) ;
#98076 = AXIS2_PLACEMENT_3D('',#151934,#120325,#120326) ;
#98077 = AXIS2_PLACEMENT_3D('',#151935,#120327,#120328) ;
#98078 = AXIS2_PLACEMENT_3D('',#151936,#120329,#120330) ;
#98079 = AXIS2_PLACEMENT_3D('',#151937,#120331,#120332) ;
#98080 = AXIS2_PLACEMENT_3D('',#151938,#120333,#120334) ;
#98081 = AXIS2_PLACEMENT_3D('',#151939,#120335,#120336) ;
#98082 = AXIS2_PLACEMENT_3D('',#151940,#120337,#120338) ;
#98083 = AXIS2_PLACEMENT_3D('',#151941,#120339,#120340) ;
#98084 = AXIS2_PLACEMENT_3D('',#151942,#120341,#120342) ;
#98085 = AXIS2_PLACEMENT_3D('',#151943,#120343,#120344) ;
#98086 = AXIS2_PLACEMENT_3D('',#151944,#120345,#120346) ;
#98087 = AXIS2_PLACEMENT_3D('',#151945,#120347,#120348) ;
#98088 = AXIS2_PLACEMENT_3D('',#151946,#120349,#120350) ;
#98089 = AXIS2_PLACEMENT_3D('',#151947,#120351,#120352) ;
#98090 = AXIS2_PLACEMENT_3D('',#151948,#120353,#120354) ;
#98091 = AXIS2_PLACEMENT_3D('',#151949,#120355,#120356) ;
#98092 = AXIS2_PLACEMENT_3D('',#151950,#120357,#120358) ;
#98093 = AXIS2_PLACEMENT_3D('',#151951,#120359,#120360) ;
#98094 = AXIS2_PLACEMENT_3D('',#151952,#120361,#120362) ;
#98095 = AXIS2_PLACEMENT_3D('',#151953,#120363,#120364) ;
#98096 = AXIS2_PLACEMENT_3D('',#151954,#120365,#120366) ;
#98097 = AXIS2_PLACEMENT_3D('',#151955,#120367,#120368) ;
#98098 = AXIS2_PLACEMENT_3D('',#151956,#120369,#120370) ;
#98099 = AXIS2_PLACEMENT_3D('',#151957,#120371,#120372) ;
#98100 = AXIS2_PLACEMENT_3D('',#151958,#120373,#120374) ;
#98101 = AXIS2_PLACEMENT_3D('',#151959,#120375,#120376) ;
#98102 = AXIS2_PLACEMENT_3D('',#151960,#120377,#120378) ;
#98103 = AXIS2_PLACEMENT_3D('',#151961,#120379,#120380) ;
#98104 = AXIS2_PLACEMENT_3D('',#151962,#120381,#120382) ;
#98105 = AXIS2_PLACEMENT_3D('',#151963,#120383,#120384) ;
#98106 = AXIS2_PLACEMENT_3D('',#151964,#120385,#120386) ;
#98107 = AXIS2_PLACEMENT_3D('',#151965,#120387,#120388) ;
#98108 = AXIS2_PLACEMENT_3D('',#151966,#120389,#120390) ;
#98109 = AXIS2_PLACEMENT_3D('',#151967,#120391,#120392) ;
#98110 = AXIS2_PLACEMENT_3D('',#151968,#120393,#120394) ;
#98111 = AXIS2_PLACEMENT_3D('',#151969,#120395,#120396) ;
#98112 = AXIS2_PLACEMENT_3D('',#151970,#120397,#120398) ;
#98113 = AXIS2_PLACEMENT_3D('',#151971,#120399,#120400) ;
#98114 = AXIS2_PLACEMENT_3D('',#151972,#120401,#120402) ;
#98115 = AXIS2_PLACEMENT_3D('',#151973,#120403,#120404) ;
#98116 = AXIS2_PLACEMENT_3D('',#151974,#120405,#120406) ;
#98117 = AXIS2_PLACEMENT_3D('',#151975,#120407,#120408) ;
#98118 = AXIS2_PLACEMENT_3D('',#151976,#120409,#120410) ;
#98119 = AXIS2_PLACEMENT_3D('',#151977,#120411,#120412) ;
#98120 = AXIS2_PLACEMENT_3D('',#151978,#120413,#120414) ;
#98121 = AXIS2_PLACEMENT_3D('',#151979,#120415,#120416) ;
#98122 = AXIS2_PLACEMENT_3D('',#151980,#120417,#120418) ;
#98123 = AXIS2_PLACEMENT_3D('',#151981,#120419,#120420) ;
#98124 = AXIS2_PLACEMENT_3D('',#151982,#120421,#120422) ;
#98125 = AXIS2_PLACEMENT_3D('',#151983,#120423,#120424) ;
#98126 = AXIS2_PLACEMENT_3D('',#151984,#120425,#120426) ;
#98127 = AXIS2_PLACEMENT_3D('',#151985,#120427,#120428) ;
#98128 = AXIS2_PLACEMENT_3D('',#151986,#120429,#120430) ;
#98129 = AXIS2_PLACEMENT_3D('',#151987,#120431,#120432) ;
#98130 = AXIS2_PLACEMENT_3D('',#151988,#120433,#120434) ;
#98131 = AXIS2_PLACEMENT_3D('',#151989,#120435,#120436) ;
#98132 = AXIS2_PLACEMENT_3D('',#151990,#120437,#120438) ;
#98133 = AXIS2_PLACEMENT_3D('',#151991,#120439,#120440) ;
#98134 = AXIS2_PLACEMENT_3D('',#151992,#120441,#120442) ;
#98135 = AXIS2_PLACEMENT_3D('',#151993,#120443,#120444) ;
#98136 = AXIS2_PLACEMENT_3D('',#151994,#120445,#120446) ;
#98137 = AXIS2_PLACEMENT_3D('',#151995,#120447,#120448) ;
#98138 = AXIS2_PLACEMENT_3D('',#151996,#120449,#120450) ;
#98139 = AXIS2_PLACEMENT_3D('',#151997,#120451,#120452) ;
#98140 = AXIS2_PLACEMENT_3D('',#151998,#120453,#120454) ;
#98141 = AXIS2_PLACEMENT_3D('',#151999,#120455,#120456) ;
#98142 = AXIS2_PLACEMENT_3D('',#152000,#120457,#120458) ;
#98143 = AXIS2_PLACEMENT_3D('',#152001,#120459,#120460) ;
#98144 = AXIS2_PLACEMENT_3D('',#152002,#120461,#120462) ;
#98145 = AXIS2_PLACEMENT_3D('',#152003,#120463,#120464) ;
#98146 = AXIS2_PLACEMENT_3D('',#152004,#120465,#120466) ;
#98147 = AXIS2_PLACEMENT_3D('',#152005,#120467,#120468) ;
#98148 = AXIS2_PLACEMENT_3D('',#152006,#120469,#120470) ;
#98149 = AXIS2_PLACEMENT_3D('',#152007,#120471,#120472) ;
#98150 = AXIS2_PLACEMENT_3D('',#152008,#120473,#120474) ;
#98151 = AXIS2_PLACEMENT_3D('',#152009,#120475,#120476) ;
#98152 = AXIS2_PLACEMENT_3D('',#152010,#120477,#120478) ;
#98153 = AXIS2_PLACEMENT_3D('',#152013,#120479,#120480) ;
#98154 = AXIS2_PLACEMENT_3D('',#152017,#120482,#120483) ;
#98155 = AXIS2_PLACEMENT_3D('',#152019,#120485,#120486) ;
#98156 = AXIS2_PLACEMENT_3D('',#152022,#120487,#120488) ;
#98157 = AXIS2_PLACEMENT_3D('',#152024,#120489,#120490) ;
#98158 = AXIS2_PLACEMENT_3D('',#152026,#120491,#120492) ;
#98159 = AXIS2_PLACEMENT_3D('',#152027,#120493,#120494) ;
#98160 = AXIS2_PLACEMENT_3D('',#152028,#120495,#120496) ;
#98161 = AXIS2_PLACEMENT_3D('',#152031,#120497,#120498) ;
#98162 = AXIS2_PLACEMENT_3D('',#152033,#120499,#120500) ;
#98163 = AXIS2_PLACEMENT_3D('',#152035,#120501,#120502) ;
#98164 = AXIS2_PLACEMENT_3D('',#152036,#120503,#120504) ;
#98165 = AXIS2_PLACEMENT_3D('',#152037,#120505,#120506) ;
#98166 = AXIS2_PLACEMENT_3D('',#152040,#120507,#120508) ;
#98167 = AXIS2_PLACEMENT_3D('',#152122,#120509,#120510) ;
#98168 = AXIS2_PLACEMENT_3D('',#152173,#120511,#120512) ;
#98169 = AXIS2_PLACEMENT_3D('',#152176,#120513,#120514) ;
#98170 = AXIS2_PLACEMENT_3D('',#152178,#120515,#120516) ;
#98171 = AXIS2_PLACEMENT_3D('',#152180,#120517,#120518) ;
#98172 = AXIS2_PLACEMENT_3D('',#152181,#120519,#120520) ;
#98173 = AXIS2_PLACEMENT_3D('',#152182,#120521,#120522) ;
#98174 = AXIS2_PLACEMENT_3D('',#152184,#120523,#120524) ;
#98175 = AXIS2_PLACEMENT_3D('',#152266,#120525,#120526) ;
#98176 = AXIS2_PLACEMENT_3D('',#152348,#120527,#120528) ;
#98177 = AXIS2_PLACEMENT_3D('',#152351,#120529,#120530) ;
#98178 = AXIS2_PLACEMENT_3D('',#152353,#120531,#120532) ;
#98179 = AXIS2_PLACEMENT_3D('',#152355,#120533,#120534) ;
#98180 = AXIS2_PLACEMENT_3D('',#152356,#120535,#120536) ;
#98181 = AXIS2_PLACEMENT_3D('',#152357,#120537,#120538) ;
#98182 = AXIS2_PLACEMENT_3D('',#152359,#120539,#120540) ;
#98183 = AXIS2_PLACEMENT_3D('',#152444,#120541,#120542) ;
#98184 = AXIS2_PLACEMENT_3D('',#152524,#120543,#120544) ;
#98185 = AXIS2_PLACEMENT_3D('',#152527,#120545,#120546) ;
#98186 = AXIS2_PLACEMENT_3D('',#152529,#120547,#120548) ;
#98187 = AXIS2_PLACEMENT_3D('',#152531,#120549,#120550) ;
#98188 = AXIS2_PLACEMENT_3D('',#152532,#120551,#120552) ;
#98189 = AXIS2_PLACEMENT_3D('',#152533,#120553,#120554) ;
#98190 = AXIS2_PLACEMENT_3D('',#152535,#120555,#120556) ;
#98191 = AXIS2_PLACEMENT_3D('',#152618,#120557,#120558) ;
#98192 = AXIS2_PLACEMENT_3D('',#152700,#120559,#120560) ;
#98193 = AXIS2_PLACEMENT_3D('',#152703,#120561,#120562) ;
#98194 = AXIS2_PLACEMENT_3D('',#152705,#120563,#120564) ;
#98195 = AXIS2_PLACEMENT_3D('',#152707,#120565,#120566) ;
#98196 = AXIS2_PLACEMENT_3D('',#152708,#120567,#120568) ;
#98197 = AXIS2_PLACEMENT_3D('',#152709,#120569,#120570) ;
#98198 = AXIS2_PLACEMENT_3D('',#152711,#120571,#120572) ;
#98199 = AXIS2_PLACEMENT_3D('',#152793,#120573,#120574) ;
#98200 = AXIS2_PLACEMENT_3D('',#152875,#120575,#120576) ;
#98201 = AXIS2_PLACEMENT_3D('',#152878,#120577,#120578) ;
#98202 = AXIS2_PLACEMENT_3D('',#152880,#120579,#120580) ;
#98203 = AXIS2_PLACEMENT_3D('',#152882,#120581,#120582) ;
#98204 = AXIS2_PLACEMENT_3D('',#152883,#120583,#120584) ;
#98205 = AXIS2_PLACEMENT_3D('',#152884,#120585,#120586) ;
#98206 = AXIS2_PLACEMENT_3D('',#152886,#120587,#120588) ;
#98207 = AXIS2_PLACEMENT_3D('',#152968,#120589,#120590) ;
#98208 = AXIS2_PLACEMENT_3D('',#153050,#120591,#120592) ;
#98209 = AXIS2_PLACEMENT_3D('',#153053,#120593,#120594) ;
#98210 = AXIS2_PLACEMENT_3D('',#153055,#120595,#120596) ;
#98211 = AXIS2_PLACEMENT_3D('',#153057,#120597,#120598) ;
#98212 = AXIS2_PLACEMENT_3D('',#153058,#120599,#120600) ;
#98213 = AXIS2_PLACEMENT_3D('',#153059,#120601,#120602) ;
#98214 = AXIS2_PLACEMENT_3D('',#153061,#120603,#120604) ;
#98215 = AXIS2_PLACEMENT_3D('',#153143,#120605,#120606) ;
#98216 = AXIS2_PLACEMENT_3D('',#153225,#120607,#120608) ;
#98217 = AXIS2_PLACEMENT_3D('',#153228,#120609,#120610) ;
#98218 = AXIS2_PLACEMENT_3D('',#153230,#120611,#120612) ;
#98219 = AXIS2_PLACEMENT_3D('',#153232,#120613,#120614) ;
#98220 = AXIS2_PLACEMENT_3D('',#153233,#120615,#120616) ;
#98221 = AXIS2_PLACEMENT_3D('',#153234,#120617,#120618) ;
#98222 = AXIS2_PLACEMENT_3D('',#153236,#120619,#120620) ;
#98223 = AXIS2_PLACEMENT_3D('',#153320,#120621,#120622) ;
#98224 = AXIS2_PLACEMENT_3D('',#153401,#120623,#120624) ;
#98225 = AXIS2_PLACEMENT_3D('',#153404,#120625,#120626) ;
#98226 = AXIS2_PLACEMENT_3D('',#153406,#120627,#120628) ;
#98227 = AXIS2_PLACEMENT_3D('',#153408,#120629,#120630) ;
#98228 = AXIS2_PLACEMENT_3D('',#153409,#120631,#120632) ;
#98229 = AXIS2_PLACEMENT_3D('',#153410,#120633,#120634) ;
#98230 = AXIS2_PLACEMENT_3D('',#153412,#120635,#120636) ;
#98231 = AXIS2_PLACEMENT_3D('',#153495,#120637,#120638) ;
#98232 = AXIS2_PLACEMENT_3D('',#153575,#120639,#120640) ;
#98233 = AXIS2_PLACEMENT_3D('',#153578,#120641,#120642) ;
#98234 = AXIS2_PLACEMENT_3D('',#153580,#120643,#120644) ;
#98235 = AXIS2_PLACEMENT_3D('',#153582,#120645,#120646) ;
#98236 = AXIS2_PLACEMENT_3D('',#153583,#120647,#120648) ;
#98237 = AXIS2_PLACEMENT_3D('',#153584,#120649,#120650) ;
#98238 = AXIS2_PLACEMENT_3D('',#153586,#120651,#120652) ;
#98239 = AXIS2_PLACEMENT_3D('',#153639,#120653,#120654) ;
#98240 = AXIS2_PLACEMENT_3D('',#153719,#120655,#120656) ;
#98241 = AXIS2_PLACEMENT_3D('',#153720,#120657,#120658) ;
#98242 = AXIS2_PLACEMENT_3D('',#153723,#120661,#120662) ;
#98243 = AXIS2_PLACEMENT_3D('',#153724,#120663,#120664) ;
#98244 = AXIS2_PLACEMENT_3D('',#153727,#120667,#120668) ;
#98245 = AXIS2_PLACEMENT_3D('',#153728,#120669,#120670) ;
#98246 = AXIS2_PLACEMENT_3D('',#153731,#120673,#120674) ;
#98247 = AXIS2_PLACEMENT_3D('',#153732,#120675,#120676) ;
#98248 = AXIS2_PLACEMENT_3D('',#153735,#120679,#120680) ;
#98249 = AXIS2_PLACEMENT_3D('',#153736,#120681,#120682) ;
#98250 = AXIS2_PLACEMENT_3D('',#153739,#120685,#120686) ;
#98251 = AXIS2_PLACEMENT_3D('',#153740,#120687,#120688) ;
#98252 = AXIS2_PLACEMENT_3D('',#153743,#120691,#120692) ;
#98253 = AXIS2_PLACEMENT_3D('',#153744,#120693,#120694) ;
#98254 = AXIS2_PLACEMENT_3D('',#153747,#120697,#120698) ;
#98255 = AXIS2_PLACEMENT_3D('',#153749,#120699,#120700) ;
#98256 = AXIS2_PLACEMENT_3D('',#153751,#120701,#120702) ;
#98257 = AXIS2_PLACEMENT_3D('',#153752,#120703,#120704) ;
#98258 = AXIS2_PLACEMENT_3D('',#153753,#120705,#120706) ;
#98259 = AXIS2_PLACEMENT_3D('',#153755,#120707,#120708) ;
#98260 = AXIS2_PLACEMENT_3D('',#153757,#120709,#120710) ;
#98261 = AXIS2_PLACEMENT_3D('',#153758,#120711,#120712) ;
#98262 = AXIS2_PLACEMENT_3D('',#153759,#120713,#120714) ;
#98263 = AXIS2_PLACEMENT_3D('',#153761,#120715,#120716) ;
#98264 = AXIS2_PLACEMENT_3D('',#153763,#120717,#120718) ;
#98265 = AXIS2_PLACEMENT_3D('',#153764,#120719,#120720) ;
#98266 = AXIS2_PLACEMENT_3D('',#153765,#120721,#120722) ;
#98267 = AXIS2_PLACEMENT_3D('',#153767,#120723,#120724) ;
#98268 = AXIS2_PLACEMENT_3D('',#153769,#120725,#120726) ;
#98269 = AXIS2_PLACEMENT_3D('',#153770,#120727,#120728) ;
#98270 = AXIS2_PLACEMENT_3D('',#153771,#120729,#120730) ;
#98271 = AXIS2_PLACEMENT_3D('',#153773,#120731,#120732) ;
#98272 = AXIS2_PLACEMENT_3D('',#153775,#120733,#120734) ;
#98273 = AXIS2_PLACEMENT_3D('',#153776,#120735,#120736) ;
#98274 = AXIS2_PLACEMENT_3D('',#153777,#120737,#120738) ;
#98275 = AXIS2_PLACEMENT_3D('',#153779,#120739,#120740) ;
#98276 = AXIS2_PLACEMENT_3D('',#153781,#120741,#120742) ;
#98277 = AXIS2_PLACEMENT_3D('',#153782,#120743,#120744) ;
#98278 = AXIS2_PLACEMENT_3D('',#153783,#120745,#120746) ;
#98279 = AXIS2_PLACEMENT_3D('',#153785,#120747,#120748) ;
#98280 = AXIS2_PLACEMENT_3D('',#153787,#120749,#120750) ;
#98281 = AXIS2_PLACEMENT_3D('',#153788,#120751,#120752) ;
#98282 = AXIS2_PLACEMENT_3D('',#153789,#120753,#120754) ;
#98283 = AXIS2_PLACEMENT_3D('',#153791,#120755,#120756) ;
#98284 = AXIS2_PLACEMENT_3D('',#153793,#120757,#120758) ;
#98285 = AXIS2_PLACEMENT_3D('',#153794,#120759,#120760) ;
#98286 = AXIS2_PLACEMENT_3D('',#153795,#120761,#120762) ;
#98287 = AXIS2_PLACEMENT_3D('',#153797,#120763,#120764) ;
#98288 = AXIS2_PLACEMENT_3D('',#153799,#120765,#120766) ;
#98289 = AXIS2_PLACEMENT_3D('',#153800,#120767,#120768) ;
#98290 = AXIS2_PLACEMENT_3D('',#153801,#120769,#120770) ;
#98291 = AXIS2_PLACEMENT_3D('',#153803,#120771,#120772) ;
#98292 = AXIS2_PLACEMENT_3D('',#153805,#120773,#120774) ;
#98293 = AXIS2_PLACEMENT_3D('',#153806,#120775,#120776) ;
#98294 = AXIS2_PLACEMENT_3D('',#153807,#120777,#120778) ;
#98295 = AXIS2_PLACEMENT_3D('',#153809,#120779,#120780) ;
#98296 = AXIS2_PLACEMENT_3D('',#153811,#120781,#120782) ;
#98297 = AXIS2_PLACEMENT_3D('',#153812,#120783,#120784) ;
#98298 = AXIS2_PLACEMENT_3D('',#153813,#120785,#120786) ;
#98299 = AXIS2_PLACEMENT_3D('',#153815,#120787,#120788) ;
#98300 = AXIS2_PLACEMENT_3D('',#153817,#120789,#120790) ;
#98301 = AXIS2_PLACEMENT_3D('',#153818,#120791,#120792) ;
#98302 = AXIS2_PLACEMENT_3D('',#153819,#120793,#120794) ;
#98303 = AXIS2_PLACEMENT_3D('',#153821,#120795,#120796) ;
#98304 = AXIS2_PLACEMENT_3D('',#153823,#120797,#120798) ;
#98305 = AXIS2_PLACEMENT_3D('',#153824,#120799,#120800) ;
#98306 = AXIS2_PLACEMENT_3D('',#153825,#120801,#120802) ;
#98307 = AXIS2_PLACEMENT_3D('',#153827,#120803,#120804) ;
#98308 = AXIS2_PLACEMENT_3D('',#153829,#120805,#120806) ;
#98309 = AXIS2_PLACEMENT_3D('',#153830,#120807,#120808) ;
#98310 = AXIS2_PLACEMENT_3D('',#153831,#120809,#120810) ;
#98311 = AXIS2_PLACEMENT_3D('',#153833,#120811,#120812) ;
#98312 = AXIS2_PLACEMENT_3D('',#153835,#120813,#120814) ;
#98313 = AXIS2_PLACEMENT_3D('',#153836,#120815,#120816) ;
#98314 = AXIS2_PLACEMENT_3D('',#153837,#120817,#120818) ;
#98315 = AXIS2_PLACEMENT_3D('',#153839,#120819,#120820) ;
#98316 = AXIS2_PLACEMENT_3D('',#153841,#120821,#120822) ;
#98317 = AXIS2_PLACEMENT_3D('',#153842,#120823,#120824) ;
#98318 = AXIS2_PLACEMENT_3D('',#153843,#120825,#120826) ;
#98319 = AXIS2_PLACEMENT_3D('',#153845,#120827,#120828) ;
#98320 = AXIS2_PLACEMENT_3D('',#153847,#120829,#120830) ;
#98321 = AXIS2_PLACEMENT_3D('',#153848,#120831,#120832) ;
#98322 = AXIS2_PLACEMENT_3D('',#153849,#120833,#120834) ;
#98323 = AXIS2_PLACEMENT_3D('',#153851,#120835,#120836) ;
#98324 = AXIS2_PLACEMENT_3D('',#153853,#120837,#120838) ;
#98325 = AXIS2_PLACEMENT_3D('',#153854,#120839,#120840) ;
#98326 = AXIS2_PLACEMENT_3D('',#153855,#120841,#120842) ;
#98327 = AXIS2_PLACEMENT_3D('',#153857,#120843,#120844) ;
#98328 = AXIS2_PLACEMENT_3D('',#153859,#120845,#120846) ;
#98329 = AXIS2_PLACEMENT_3D('',#153860,#120847,#120848) ;
#98330 = AXIS2_PLACEMENT_3D('',#153861,#120849,#120850) ;
#98331 = AXIS2_PLACEMENT_3D('',#153863,#120851,#120852) ;
#98332 = AXIS2_PLACEMENT_3D('',#153865,#120853,#120854) ;
#98333 = AXIS2_PLACEMENT_3D('',#153866,#120855,#120856) ;
#98334 = AXIS2_PLACEMENT_3D('',#153867,#120857,#120858) ;
#98335 = AXIS2_PLACEMENT_3D('',#153869,#120859,#120860) ;
#98336 = AXIS2_PLACEMENT_3D('',#153871,#120861,#120862) ;
#98337 = AXIS2_PLACEMENT_3D('',#153872,#120863,#120864) ;
#98338 = AXIS2_PLACEMENT_3D('',#153873,#120865,#120866) ;
#98339 = AXIS2_PLACEMENT_3D('',#153875,#120867,#120868) ;
#98340 = AXIS2_PLACEMENT_3D('',#153877,#120869,#120870) ;
#98341 = AXIS2_PLACEMENT_3D('',#153878,#120871,#120872) ;
#98342 = AXIS2_PLACEMENT_3D('',#153879,#120873,#120874) ;
#98343 = AXIS2_PLACEMENT_3D('',#153881,#120875,#120876) ;
#98344 = AXIS2_PLACEMENT_3D('',#153883,#120877,#120878) ;
#98345 = AXIS2_PLACEMENT_3D('',#153884,#120879,#120880) ;
#98346 = AXIS2_PLACEMENT_3D('',#153885,#120881,#120882) ;
#98347 = AXIS2_PLACEMENT_3D('',#153887,#120883,#120884) ;
#98348 = AXIS2_PLACEMENT_3D('',#153889,#120885,#120886) ;
#98349 = AXIS2_PLACEMENT_3D('',#153890,#120887,#120888) ;
#98350 = AXIS2_PLACEMENT_3D('',#153891,#120889,#120890) ;
#98351 = AXIS2_PLACEMENT_3D('',#153893,#120891,#120892) ;
#98352 = AXIS2_PLACEMENT_3D('',#153895,#120893,#120894) ;
#98353 = AXIS2_PLACEMENT_3D('',#153896,#120895,#120896) ;
#98354 = AXIS2_PLACEMENT_3D('',#153897,#120897,#120898) ;
#98355 = AXIS2_PLACEMENT_3D('',#153899,#120899,#120900) ;
#98356 = AXIS2_PLACEMENT_3D('',#153901,#120901,#120902) ;
#98357 = AXIS2_PLACEMENT_3D('',#153902,#120903,#120904) ;
#98358 = AXIS2_PLACEMENT_3D('',#153903,#120905,#120906) ;
#98359 = AXIS2_PLACEMENT_3D('',#153905,#120907,#120908) ;
#98360 = AXIS2_PLACEMENT_3D('',#153907,#120909,#120910) ;
#98361 = AXIS2_PLACEMENT_3D('',#153908,#120911,#120912) ;
#98362 = AXIS2_PLACEMENT_3D('',#153909,#120913,#120914) ;
#98363 = AXIS2_PLACEMENT_3D('',#153912,#120915,#120916) ;
#98364 = AXIS2_PLACEMENT_3D('',#153938,#120918,#120919) ;
#98365 = AXIS2_PLACEMENT_3D('',#153985,#120921,#120922) ;
#98366 = AXIS2_PLACEMENT_3D('',#154011,#120924,#120925) ;
#98367 = AXIS2_PLACEMENT_3D('',#154057,#120927,#120928) ;
#98368 = AXIS2_PLACEMENT_3D('',#154059,#120930,#120931) ;
#98369 = AXIS2_PLACEMENT_3D('',#154062,#120932,#120933) ;
#98370 = AXIS2_PLACEMENT_3D('',#154088,#120935,#120936) ;
#98371 = AXIS2_PLACEMENT_3D('',#154135,#120938,#120939) ;
#98372 = AXIS2_PLACEMENT_3D('',#154161,#120941,#120942) ;
#98373 = AXIS2_PLACEMENT_3D('',#154207,#120944,#120945) ;
#98374 = AXIS2_PLACEMENT_3D('',#154209,#120947,#120948) ;
#98375 = AXIS2_PLACEMENT_3D('',#154212,#120949,#120950) ;
#98376 = AXIS2_PLACEMENT_3D('',#154238,#120952,#120953) ;
#98377 = AXIS2_PLACEMENT_3D('',#154285,#120955,#120956) ;
#98378 = AXIS2_PLACEMENT_3D('',#154311,#120958,#120959) ;
#98379 = AXIS2_PLACEMENT_3D('',#154357,#120961,#120962) ;
#98380 = AXIS2_PLACEMENT_3D('',#154359,#120964,#120965) ;
#98381 = AXIS2_PLACEMENT_3D('',#154362,#120966,#120967) ;
#98382 = AXIS2_PLACEMENT_3D('',#154388,#120969,#120970) ;
#98383 = AXIS2_PLACEMENT_3D('',#154435,#120972,#120973) ;
#98384 = AXIS2_PLACEMENT_3D('',#154461,#120975,#120976) ;
#98385 = AXIS2_PLACEMENT_3D('',#154507,#120978,#120979) ;
#98386 = AXIS2_PLACEMENT_3D('',#154509,#120981,#120982) ;
#98387 = AXIS2_PLACEMENT_3D('',#154512,#120983,#120984) ;
#98388 = AXIS2_PLACEMENT_3D('',#154538,#120986,#120987) ;
#98389 = AXIS2_PLACEMENT_3D('',#154585,#120989,#120990) ;
#98390 = AXIS2_PLACEMENT_3D('',#154611,#120992,#120993) ;
#98391 = AXIS2_PLACEMENT_3D('',#154657,#120995,#120996) ;
#98392 = AXIS2_PLACEMENT_3D('',#154659,#120998,#120999) ;
#98393 = AXIS2_PLACEMENT_3D('',#154662,#121000,#121001) ;
#98394 = AXIS2_PLACEMENT_3D('',#154688,#121003,#121004) ;
#98395 = AXIS2_PLACEMENT_3D('',#154735,#121006,#121007) ;
#98396 = AXIS2_PLACEMENT_3D('',#154761,#121009,#121010) ;
#98397 = AXIS2_PLACEMENT_3D('',#154807,#121012,#121013) ;
#98398 = AXIS2_PLACEMENT_3D('',#154809,#121015,#121016) ;
#98399 = AXIS2_PLACEMENT_3D('',#154812,#121017,#121018) ;
#98400 = AXIS2_PLACEMENT_3D('',#154838,#121020,#121021) ;
#98401 = AXIS2_PLACEMENT_3D('',#154885,#121023,#121024) ;
#98402 = AXIS2_PLACEMENT_3D('',#154911,#121026,#121027) ;
#98403 = AXIS2_PLACEMENT_3D('',#154957,#121029,#121030) ;
#98404 = AXIS2_PLACEMENT_3D('',#154959,#121032,#121033) ;
#98405 = AXIS2_PLACEMENT_3D('',#154962,#121034,#121035) ;
#98406 = AXIS2_PLACEMENT_3D('',#154988,#121037,#121038) ;
#98407 = AXIS2_PLACEMENT_3D('',#155035,#121040,#121041) ;
#98408 = AXIS2_PLACEMENT_3D('',#155061,#121043,#121044) ;
#98409 = AXIS2_PLACEMENT_3D('',#155107,#121046,#121047) ;
#98410 = AXIS2_PLACEMENT_3D('',#155109,#121049,#121050) ;
#98411 = AXIS2_PLACEMENT_3D('',#155112,#121051,#121052) ;
#98412 = AXIS2_PLACEMENT_3D('',#155138,#121054,#121055) ;
#98413 = AXIS2_PLACEMENT_3D('',#155185,#121057,#121058) ;
#98414 = AXIS2_PLACEMENT_3D('',#155211,#121060,#121061) ;
#98415 = AXIS2_PLACEMENT_3D('',#155257,#121063,#121064) ;
#98416 = AXIS2_PLACEMENT_3D('',#155259,#121066,#121067) ;
#98417 = AXIS2_PLACEMENT_3D('',#155261,#121068,#121069) ;
#98418 = AXIS2_PLACEMENT_3D('',#155263,#121071,#121072) ;
#98419 = AXIS2_PLACEMENT_3D('',#155265,#121073,#121074) ;
#98420 = AXIS2_PLACEMENT_3D('',#155267,#121076,#121077) ;
#98421 = AXIS2_PLACEMENT_3D('',#155269,#121078,#121079) ;
#98422 = AXIS2_PLACEMENT_3D('',#155271,#121081,#121082) ;
#98423 = AXIS2_PLACEMENT_3D('',#155273,#121083,#121084) ;
#98424 = AXIS2_PLACEMENT_3D('',#155275,#121086,#121087) ;
#98425 = AXIS2_PLACEMENT_3D('',#155277,#121088,#121089) ;
#98426 = AXIS2_PLACEMENT_3D('',#155279,#121091,#121092) ;
#98427 = AXIS2_PLACEMENT_3D('',#155281,#121093,#121094) ;
#98428 = AXIS2_PLACEMENT_3D('',#155283,#121096,#121097) ;
#98429 = AXIS2_PLACEMENT_3D('',#155285,#121098,#121099) ;
#98430 = AXIS2_PLACEMENT_3D('',#155287,#121101,#121102) ;
#98431 = AXIS2_PLACEMENT_3D('',#155289,#121103,#121104) ;
#98432 = AXIS2_PLACEMENT_3D('',#155291,#121106,#121107) ;
#98433 = AXIS2_PLACEMENT_3D('',#155293,#121108,#121109) ;
#98434 = AXIS2_PLACEMENT_3D('',#155295,#121111,#121112) ;
#98435 = AXIS2_PLACEMENT_3D('',#155297,#121114,#121115) ;
#98436 = AXIS2_PLACEMENT_3D('',#155299,#121117,#121118) ;
#98437 = AXIS2_PLACEMENT_3D('',#155301,#121120,#121121) ;
#98438 = AXIS2_PLACEMENT_3D('',#155303,#121123,#121124) ;
#98439 = AXIS2_PLACEMENT_3D('',#155305,#121126,#121127) ;
#98440 = AXIS2_PLACEMENT_3D('',#155307,#121129,#121130) ;
#98441 = AXIS2_PLACEMENT_3D('',#155309,#121132,#121133) ;
#98442 = AXIS2_PLACEMENT_3D('',#155311,#121135,#121136) ;
#98443 = AXIS2_PLACEMENT_3D('',#155313,#121138,#121139) ;
#98444 = AXIS2_PLACEMENT_3D('',#155315,#121140,#121141) ;
#98445 = AXIS2_PLACEMENT_3D('',#155317,#121142,#121143) ;
#98446 = AXIS2_PLACEMENT_3D('',#155318,#121144,#121145) ;
#98447 = AXIS2_PLACEMENT_3D('',#155319,#121146,#121147) ;
#98448 = AXIS2_PLACEMENT_3D('',#155321,#121148,#121149) ;
#98449 = AXIS2_PLACEMENT_3D('',#155323,#121150,#121151) ;
#98450 = AXIS2_PLACEMENT_3D('',#155324,#121152,#121153) ;
#98451 = AXIS2_PLACEMENT_3D('',#155325,#121154,#121155) ;
#98452 = AXIS2_PLACEMENT_3D('',#155327,#121156,#121157) ;
#98453 = AXIS2_PLACEMENT_3D('',#155329,#121158,#121159) ;
#98454 = AXIS2_PLACEMENT_3D('',#155330,#121160,#121161) ;
#98455 = AXIS2_PLACEMENT_3D('',#155331,#121162,#121163) ;
#98456 = AXIS2_PLACEMENT_3D('',#155332,#121164,#121165) ;
#98457 = AXIS2_PLACEMENT_3D('',#155335,#121168,#121169) ;
#98458 = AXIS2_PLACEMENT_3D('',#155337,#121170,#121171) ;
#98459 = AXIS2_PLACEMENT_3D('',#155340,#121174,#121175) ;
#98460 = AXIS2_PLACEMENT_3D('',#155342,#121176,#121177) ;
#98461 = AXIS2_PLACEMENT_3D('',#155345,#121180,#121181) ;
#98462 = AXIS2_PLACEMENT_3D('',#155346,#121182,#121183) ;
#98463 = AXIS2_PLACEMENT_3D('',#155349,#121186,#121187) ;
#98464 = AXIS2_PLACEMENT_3D('',#155352,#121188,#121189) ;
#98465 = AXIS2_PLACEMENT_3D('',#155378,#121191,#121192) ;
#98466 = AXIS2_PLACEMENT_3D('',#155425,#121194,#121195) ;
#98467 = AXIS2_PLACEMENT_3D('',#155451,#121197,#121198) ;
#98468 = AXIS2_PLACEMENT_3D('',#155497,#121200,#121201) ;
#98469 = AXIS2_PLACEMENT_3D('',#155499,#121203,#121204) ;
#98470 = AXIS2_PLACEMENT_3D('',#155501,#121205,#121206) ;
#98471 = AXIS2_PLACEMENT_3D('',#155503,#121208,#121209) ;
#98472 = AXIS2_PLACEMENT_3D('',#155505,#121211,#121212) ;
#98473 = AXIS2_PLACEMENT_3D('',#155514,#121217,#121218) ;
#98474 = AXIS2_PLACEMENT_3D('',#155515,#121219,#121220) ;
#98475 = AXIS2_PLACEMENT_3D('',#155516,#121221,#121222) ;
#98476 = AXIS2_PLACEMENT_3D('',#155517,#121223,#121224) ;
#98477 = AXIS2_PLACEMENT_3D('',#155518,#121225,#121226) ;
#98478 = AXIS2_PLACEMENT_3D('',#155519,#121227,#121228) ;
#98479 = AXIS2_PLACEMENT_3D('',#155520,#121229,#121230) ;
#98480 = AXIS2_PLACEMENT_3D('',#155521,#121231,#121232) ;
#98481 = AXIS2_PLACEMENT_3D('',#155522,#121233,#121234) ;
#98482 = AXIS2_PLACEMENT_3D('',#155523,#121235,#121236) ;
#98483 = AXIS2_PLACEMENT_3D('',#155531,#121240,#121241) ;
#98484 = AXIS2_PLACEMENT_3D('',#155535,#121243,#121244) ;
#98485 = AXIS2_PLACEMENT_3D('',#155539,#121246,#121247) ;
#98486 = AXIS2_PLACEMENT_3D('',#155543,#121249,#121250) ;
#98487 = AXIS2_PLACEMENT_3D('',#155547,#121252,#121253) ;
#98488 = AXIS2_PLACEMENT_3D('',#155551,#121255,#121256) ;
#98489 = AXIS2_PLACEMENT_3D('',#155555,#121258,#121259) ;
#98490 = AXIS2_PLACEMENT_3D('',#155559,#121261,#121262) ;
#98491 = AXIS2_PLACEMENT_3D('',#155563,#121264,#121265) ;
#98492 = AXIS2_PLACEMENT_3D('',#155567,#121267,#121268) ;
#98493 = AXIS2_PLACEMENT_3D('',#155571,#121270,#121271) ;
#98494 = AXIS2_PLACEMENT_3D('',#155575,#121273,#121274) ;
#98495 = AXIS2_PLACEMENT_3D('',#155579,#121276,#121277) ;
#98496 = AXIS2_PLACEMENT_3D('',#155583,#121279,#121280) ;
#98497 = AXIS2_PLACEMENT_3D('',#155587,#121282,#121283) ;
#98498 = AXIS2_PLACEMENT_3D('',#155591,#121285,#121286) ;
#98499 = AXIS2_PLACEMENT_3D('',#155595,#121288,#121289) ;
#98500 = AXIS2_PLACEMENT_3D('',#155599,#121291,#121292) ;
#98501 = AXIS2_PLACEMENT_3D('',#155603,#121294,#121295) ;
#98502 = AXIS2_PLACEMENT_3D('',#155607,#121297,#121298) ;
#98503 = AXIS2_PLACEMENT_3D('',#155611,#121300,#121301) ;
#98504 = AXIS2_PLACEMENT_3D('',#155615,#121303,#121304) ;
#98505 = AXIS2_PLACEMENT_3D('',#155619,#121306,#121307) ;
#98506 = AXIS2_PLACEMENT_3D('',#155623,#121309,#121310) ;
#98507 = AXIS2_PLACEMENT_3D('',#155627,#121312,#121313) ;
#98508 = AXIS2_PLACEMENT_3D('',#155631,#121315,#121316) ;
#98509 = AXIS2_PLACEMENT_3D('',#155635,#121318,#121319) ;
#98510 = AXIS2_PLACEMENT_3D('',#155639,#121321,#121322) ;
#98511 = AXIS2_PLACEMENT_3D('',#155643,#121324,#121325) ;
#98512 = AXIS2_PLACEMENT_3D('',#155647,#121327,#121328) ;
#98513 = AXIS2_PLACEMENT_3D('',#155651,#121330,#121331) ;
#98514 = AXIS2_PLACEMENT_3D('',#155655,#121333,#121334) ;
#98515 = AXIS2_PLACEMENT_3D('',#155659,#121336,#121337) ;
#98516 = AXIS2_PLACEMENT_3D('',#155663,#121339,#121340) ;
#98517 = AXIS2_PLACEMENT_3D('',#155667,#121342,#121343) ;
#98518 = AXIS2_PLACEMENT_3D('',#155671,#121345,#121346) ;
#98519 = AXIS2_PLACEMENT_3D('',#155675,#121348,#121349) ;
#98520 = AXIS2_PLACEMENT_3D('',#155679,#121351,#121352) ;
#98521 = AXIS2_PLACEMENT_3D('',#155683,#121354,#121355) ;
#98522 = AXIS2_PLACEMENT_3D('',#155687,#121357,#121358) ;
#98523 = AXIS2_PLACEMENT_3D('',#155689,#121360,#121361) ;
#98524 = AXIS2_PLACEMENT_3D('',#155702,#121367,#121368) ;
#98525 = AXIS2_PLACEMENT_3D('',#155706,#121370,#121371) ;
#98526 = AXIS2_PLACEMENT_3D('',#155710,#121373,#121374) ;
#98527 = AXIS2_PLACEMENT_3D('',#155713,#121376,#121377) ;
#98528 = AXIS2_PLACEMENT_3D('',#155714,#121378,#121379) ;
#98529 = AXIS2_PLACEMENT_3D('',#155727,#121385,#121386) ;
#98530 = AXIS2_PLACEMENT_3D('',#155731,#121388,#121389) ;
#98531 = AXIS2_PLACEMENT_3D('',#155735,#121391,#121392) ;
#98532 = AXIS2_PLACEMENT_3D('',#155738,#121394,#121395) ;
#98533 = AXIS2_PLACEMENT_3D('',#155739,#121396,#121397) ;
#98534 = AXIS2_PLACEMENT_3D('',#155752,#121403,#121404) ;
#98535 = AXIS2_PLACEMENT_3D('',#155756,#121406,#121407) ;
#98536 = AXIS2_PLACEMENT_3D('',#155760,#121409,#121410) ;
#98537 = AXIS2_PLACEMENT_3D('',#155763,#121412,#121413) ;
#98538 = AXIS2_PLACEMENT_3D('',#155764,#121414,#121415) ;
#98539 = AXIS2_PLACEMENT_3D('',#155777,#121421,#121422) ;
#98540 = AXIS2_PLACEMENT_3D('',#155781,#121424,#121425) ;
#98541 = AXIS2_PLACEMENT_3D('',#155785,#121427,#121428) ;
#98542 = AXIS2_PLACEMENT_3D('',#155788,#121430,#121431) ;
#98543 = AXIS2_PLACEMENT_3D('',#155789,#121432,#121433) ;
#98544 = AXIS2_PLACEMENT_3D('',#155802,#121439,#121440) ;
#98545 = AXIS2_PLACEMENT_3D('',#155806,#121442,#121443) ;
#98546 = AXIS2_PLACEMENT_3D('',#155810,#121445,#121446) ;
#98547 = AXIS2_PLACEMENT_3D('',#155813,#121448,#121449) ;
#98548 = AXIS2_PLACEMENT_3D('',#155814,#121450,#121451) ;
#98549 = AXIS2_PLACEMENT_3D('',#155827,#121457,#121458) ;
#98550 = AXIS2_PLACEMENT_3D('',#155831,#121460,#121461) ;
#98551 = AXIS2_PLACEMENT_3D('',#155835,#121463,#121464) ;
#98552 = AXIS2_PLACEMENT_3D('',#155838,#121466,#121467) ;
#98553 = AXIS2_PLACEMENT_3D('',#155839,#121468,#121469) ;
#98554 = AXIS2_PLACEMENT_3D('',#155852,#121475,#121476) ;
#98555 = AXIS2_PLACEMENT_3D('',#155856,#121478,#121479) ;
#98556 = AXIS2_PLACEMENT_3D('',#155860,#121481,#121482) ;
#98557 = AXIS2_PLACEMENT_3D('',#155863,#121484,#121485) ;
#98558 = AXIS2_PLACEMENT_3D('',#155864,#121486,#121487) ;
#98559 = AXIS2_PLACEMENT_3D('',#155877,#121493,#121494) ;
#98560 = AXIS2_PLACEMENT_3D('',#155881,#121496,#121497) ;
#98561 = AXIS2_PLACEMENT_3D('',#155885,#121499,#121500) ;
#98562 = AXIS2_PLACEMENT_3D('',#155888,#121502,#121503) ;
#98563 = AXIS2_PLACEMENT_3D('',#155889,#121504,#121505) ;
#98564 = AXIS2_PLACEMENT_3D('',#155902,#121511,#121512) ;
#98565 = AXIS2_PLACEMENT_3D('',#155906,#121514,#121515) ;
#98566 = AXIS2_PLACEMENT_3D('',#155910,#121517,#121518) ;
#98567 = AXIS2_PLACEMENT_3D('',#155913,#121520,#121521) ;
#98568 = AXIS2_PLACEMENT_3D('',#155914,#121522,#121523) ;
#98569 = AXIS2_PLACEMENT_3D('',#155916,#121525,#121526) ;
#98570 = AXIS2_PLACEMENT_3D('',#155918,#121528,#121529) ;
#98571 = AXIS2_PLACEMENT_3D('',#155920,#121531,#121532) ;
#98572 = AXIS2_PLACEMENT_3D('',#155922,#121534,#121535) ;
#98573 = AXIS2_PLACEMENT_3D('',#155924,#121537,#121538) ;
#98574 = AXIS2_PLACEMENT_3D('',#155926,#121540,#121541) ;
#98575 = AXIS2_PLACEMENT_3D('',#155928,#121543,#121544) ;
#98576 = AXIS2_PLACEMENT_3D('',#155930,#121546,#121547) ;
#98577 = AXIS2_PLACEMENT_3D('',#155932,#121549,#121550) ;
#98578 = AXIS2_PLACEMENT_3D('',#155945,#121556,#121557) ;
#98579 = AXIS2_PLACEMENT_3D('',#155947,#121558,#121559) ;
#98580 = AXIS2_PLACEMENT_3D('',#155951,#121561,#121562) ;
#98581 = AXIS2_PLACEMENT_3D('',#155953,#121563,#121564) ;
#98582 = AXIS2_PLACEMENT_3D('',#155957,#121566,#121567) ;
#98583 = AXIS2_PLACEMENT_3D('',#155959,#121568,#121569) ;
#98584 = AXIS2_PLACEMENT_3D('',#155963,#121571,#121572) ;
#98585 = AXIS2_PLACEMENT_3D('',#155965,#121573,#121574) ;
#98586 = AXIS2_PLACEMENT_3D('',#155969,#121576,#121577) ;
#98587 = AXIS2_PLACEMENT_3D('',#155971,#121578,#121579) ;
#98588 = AXIS2_PLACEMENT_3D('',#155975,#121581,#121582) ;
#98589 = AXIS2_PLACEMENT_3D('',#155977,#121583,#121584) ;
#98590 = AXIS2_PLACEMENT_3D('',#155981,#121586,#121587) ;
#98591 = AXIS2_PLACEMENT_3D('',#155983,#121588,#121589) ;
#98592 = AXIS2_PLACEMENT_3D('',#155987,#121591,#121592) ;
#98593 = AXIS2_PLACEMENT_3D('',#155989,#121593,#121594) ;
#98594 = AXIS2_PLACEMENT_3D('',#155993,#121596,#121597) ;
#98595 = AXIS2_PLACEMENT_3D('',#155995,#121598,#121599) ;
#98596 = AXIS2_PLACEMENT_3D('',#155999,#121601,#121602) ;
#98597 = AXIS2_PLACEMENT_3D('',#156001,#121603,#121604) ;
#98598 = AXIS2_PLACEMENT_3D('',#156005,#121606,#121607) ;
#98599 = AXIS2_PLACEMENT_3D('',#156007,#121608,#121609) ;
#98600 = AXIS2_PLACEMENT_3D('',#156011,#121611,#121612) ;
#98601 = AXIS2_PLACEMENT_3D('',#156013,#121613,#121614) ;
#98602 = AXIS2_PLACEMENT_3D('',#156017,#121616,#121617) ;
#98603 = AXIS2_PLACEMENT_3D('',#156019,#121618,#121619) ;
#98604 = AXIS2_PLACEMENT_3D('',#156023,#121621,#121622) ;
#98605 = AXIS2_PLACEMENT_3D('',#156025,#121623,#121624) ;
#98606 = AXIS2_PLACEMENT_3D('',#156029,#121626,#121627) ;
#98607 = AXIS2_PLACEMENT_3D('',#156031,#121628,#121629) ;
#98608 = AXIS2_PLACEMENT_3D('',#156035,#121631,#121632) ;
#98609 = AXIS2_PLACEMENT_3D('',#156037,#121633,#121634) ;
#98610 = AXIS2_PLACEMENT_3D('',#156041,#121636,#121637) ;
#98611 = AXIS2_PLACEMENT_3D('',#156043,#121638,#121639) ;
#98612 = AXIS2_PLACEMENT_3D('',#156047,#121641,#121642) ;
#98613 = AXIS2_PLACEMENT_3D('',#156049,#121643,#121644) ;
#98614 = AXIS2_PLACEMENT_3D('',#156053,#121646,#121647) ;
#98615 = AXIS2_PLACEMENT_3D('',#156055,#121648,#121649) ;
#98616 = AXIS2_PLACEMENT_3D('',#156059,#121651,#121652) ;
#98617 = AXIS2_PLACEMENT_3D('',#156060,#121653,#121654) ;
#98618 = AXIS2_PLACEMENT_3D('',#156061,#121655,#121656) ;
#98619 = AXIS2_PLACEMENT_3D('',#156064,#121657,#121658) ;
#98620 = AXIS2_PLACEMENT_3D('',#156076,#121664,#121665) ;
#98621 = AXIS2_PLACEMENT_3D('',#156077,#121666,#121667) ;
#98622 = AXIS2_PLACEMENT_3D('',#156078,#121668,#121669) ;
#98623 = AXIS2_PLACEMENT_3D('',#156081,#121670,#121671) ;
#98624 = AXIS2_PLACEMENT_3D('',#156093,#121677,#121678) ;
#98625 = AXIS2_PLACEMENT_3D('',#156094,#121679,#121680) ;
#98626 = AXIS2_PLACEMENT_3D('',#156095,#121681,#121682) ;
#98627 = AXIS2_PLACEMENT_3D('',#156098,#121683,#121684) ;
#98628 = AXIS2_PLACEMENT_3D('',#156110,#121690,#121691) ;
#98629 = AXIS2_PLACEMENT_3D('',#156111,#121692,#121693) ;
#98630 = AXIS2_PLACEMENT_3D('',#156112,#121694,#121695) ;
#98631 = AXIS2_PLACEMENT_3D('',#156115,#121696,#121697) ;
#98632 = AXIS2_PLACEMENT_3D('',#156127,#121703,#121704) ;
#98633 = AXIS2_PLACEMENT_3D('',#156128,#121705,#121706) ;
#98634 = AXIS2_PLACEMENT_3D('',#156129,#121707,#121708) ;
#98635 = AXIS2_PLACEMENT_3D('',#156132,#121709,#121710) ;
#98636 = AXIS2_PLACEMENT_3D('',#156144,#121716,#121717) ;
#98637 = AXIS2_PLACEMENT_3D('',#156145,#121718,#121719) ;
#98638 = AXIS2_PLACEMENT_3D('',#156146,#121720,#121721) ;
#98639 = AXIS2_PLACEMENT_3D('',#156149,#121722,#121723) ;
#98640 = AXIS2_PLACEMENT_3D('',#156161,#121729,#121730) ;
#98641 = AXIS2_PLACEMENT_3D('',#156162,#121731,#121732) ;
#98642 = AXIS2_PLACEMENT_3D('',#156163,#121733,#121734) ;
#98643 = AXIS2_PLACEMENT_3D('',#156166,#121735,#121736) ;
#98644 = AXIS2_PLACEMENT_3D('',#156178,#121742,#121743) ;
#98645 = AXIS2_PLACEMENT_3D('',#156179,#121744,#121745) ;
#98646 = AXIS2_PLACEMENT_3D('',#156180,#121746,#121747) ;
#98647 = AXIS2_PLACEMENT_3D('',#156183,#121748,#121749) ;
#98648 = AXIS2_PLACEMENT_3D('',#156195,#121755,#121756) ;
#98649 = AXIS2_PLACEMENT_3D('',#156196,#121757,#121758) ;
#98650 = AXIS2_PLACEMENT_3D('',#156197,#121759,#121760) ;
#98651 = AXIS2_PLACEMENT_3D('',#156200,#121761,#121762) ;
#98652 = AXIS2_PLACEMENT_3D('',#156212,#121768,#121769) ;
#98653 = AXIS2_PLACEMENT_3D('',#156213,#121770,#121771) ;
#98654 = AXIS2_PLACEMENT_3D('',#156214,#121772,#121773) ;
#98655 = AXIS2_PLACEMENT_3D('',#156223,#121778,#121779) ;
#98656 = AXIS2_PLACEMENT_3D('',#156234,#121784,#121785) ;
#98657 = AXIS2_PLACEMENT_3D('',#156238,#121787,#121788) ;
#98658 = AXIS2_PLACEMENT_3D('',#156246,#121792,#121793) ;
#98659 = AXIS2_PLACEMENT_3D('',#156250,#121795,#121796) ;
#98660 = AXIS2_PLACEMENT_3D('',#156258,#121800,#121801) ;
#98661 = AXIS2_PLACEMENT_3D('',#156262,#121803,#121804) ;
#98662 = AXIS2_PLACEMENT_3D('',#156270,#121808,#121809) ;
#98663 = AXIS2_PLACEMENT_3D('',#156274,#121811,#121812) ;
#98664 = AXIS2_PLACEMENT_3D('',#156282,#121816,#121817) ;
#98665 = AXIS2_PLACEMENT_3D('',#156286,#121819,#121820) ;
#98666 = AXIS2_PLACEMENT_3D('',#156294,#121824,#121825) ;
#98667 = AXIS2_PLACEMENT_3D('',#156298,#121827,#121828) ;
#98668 = AXIS2_PLACEMENT_3D('',#156306,#121832,#121833) ;
#98669 = AXIS2_PLACEMENT_3D('',#156310,#121835,#121836) ;
#98670 = AXIS2_PLACEMENT_3D('',#156318,#121840,#121841) ;
#98671 = AXIS2_PLACEMENT_3D('',#156322,#121843,#121844) ;
#98672 = AXIS2_PLACEMENT_3D('',#156330,#121848,#121849) ;
#98673 = AXIS2_PLACEMENT_3D('',#156334,#121851,#121852) ;
#98674 = AXIS2_PLACEMENT_3D('',#156342,#121856,#121857) ;
#98675 = AXIS2_PLACEMENT_3D('',#156346,#121859,#121860) ;
#98676 = AXIS2_PLACEMENT_3D('',#156352,#121864,#121865) ;
#98677 = AXIS2_PLACEMENT_3D('',#156356,#121867,#121868) ;
#98678 = AXIS2_PLACEMENT_3D('',#156357,#121869,#121870) ;
#98679 = AXIS2_PLACEMENT_3D('',#156358,#121871,#121872) ;
#98680 = AXIS2_PLACEMENT_3D('',#156363,#121874,#121875) ;
#98681 = AXIS2_PLACEMENT_3D('',#156364,#121876,#121877) ;
#98682 = AXIS2_PLACEMENT_3D('',#156366,#121878,#121879) ;
#98683 = AXIS2_PLACEMENT_3D('',#156367,#121880,#121881) ;
#98684 = AXIS2_PLACEMENT_3D('',#156368,#121882,#121883) ;
#98685 = AXIS2_PLACEMENT_3D('',#156513,#121928,#121929) ;
#98686 = AXIS2_PLACEMENT_3D('',#156526,#121935,#121936) ;
#98687 = AXIS2_PLACEMENT_3D('',#156530,#121938,#121939) ;
#98688 = AXIS2_PLACEMENT_3D('',#156534,#121941,#121942) ;
#98689 = AXIS2_PLACEMENT_3D('',#156537,#121944,#121945) ;
#98690 = AXIS2_PLACEMENT_3D('',#156538,#121946,#121947) ;
#98691 = AXIS2_PLACEMENT_3D('',#156547,#121952,#121953) ;
#98692 = AXIS2_PLACEMENT_3D('',#156549,#121955,#121956) ;
#98693 = AXIS2_PLACEMENT_3D('',#156560,#121961,#121962) ;
#98694 = AXIS2_PLACEMENT_3D('',#156562,#121963,#121964) ;
#98695 = AXIS2_PLACEMENT_3D('',#156564,#121965,#121966) ;
#98696 = AXIS2_PLACEMENT_3D('',#156566,#121968,#121969) ;
#98697 = AXIS2_PLACEMENT_3D('',#156575,#121974,#121975) ;
#98698 = AXIS2_PLACEMENT_3D('',#156581,#121979,#121980) ;
#98699 = AXIS2_PLACEMENT_3D('',#156590,#121985,#121986) ;
#98700 = AXIS2_PLACEMENT_3D('',#156665,#122023,#122024) ;
#98701 = AXIS2_PLACEMENT_3D('',#156669,#122026,#122027) ;
#98702 = AXIS2_PLACEMENT_3D('',#156673,#122029,#122030) ;
#98703 = AXIS2_PLACEMENT_3D('',#156677,#122032,#122033) ;
#98704 = AXIS2_PLACEMENT_3D('',#156681,#122035,#122036) ;
#98705 = AXIS2_PLACEMENT_3D('',#156685,#122038,#122039) ;
#98706 = AXIS2_PLACEMENT_3D('',#156689,#122041,#122042) ;
#98707 = AXIS2_PLACEMENT_3D('',#156693,#122044,#122045) ;
#98708 = AXIS2_PLACEMENT_3D('',#156695,#122047,#122048) ;
#98709 = AXIS2_PLACEMENT_3D('',#156704,#122052,#122053) ;
#98710 = AXIS2_PLACEMENT_3D('',#156712,#122057,#122058) ;
#98711 = AXIS2_PLACEMENT_3D('',#156722,#122063,#122064) ;
#98712 = AXIS2_PLACEMENT_3D('',#156726,#122067,#122068) ;
#98713 = AXIS2_PLACEMENT_3D('',#156739,#122074,#122075) ;
#98714 = AXIS2_PLACEMENT_3D('',#156749,#122080,#122081) ;
#98715 = AXIS2_PLACEMENT_3D('',#156756,#122085,#122086) ;
#98716 = AXIS2_PLACEMENT_3D('',#156757,#122087,#122088) ;
#98717 = AXIS2_PLACEMENT_3D('',#156766,#122093,#122094) ;
#98718 = AXIS2_PLACEMENT_3D('',#156775,#122099,#122100) ;
#98719 = AXIS2_PLACEMENT_3D('',#156780,#122102,#122103) ;
#98720 = AXIS2_PLACEMENT_3D('',#156784,#122105,#122106) ;
#98721 = AXIS2_PLACEMENT_3D('',#156787,#122108,#122109) ;
#98722 = AXIS2_PLACEMENT_3D('',#156788,#122110,#122111) ;
#98723 = AXIS2_PLACEMENT_3D('',#156789,#122112,#122113) ;
#98724 = AXIS2_PLACEMENT_3D('',#156795,#122117,#122118) ;
#98725 = AXIS2_PLACEMENT_3D('',#156804,#122123,#122124) ;
#98726 = AXIS2_PLACEMENT_3D('',#156814,#122130,#122131) ;
#98727 = AXIS2_PLACEMENT_3D('',#156824,#122137,#122138) ;
#98728 = AXIS2_PLACEMENT_3D('',#156833,#122143,#122144) ;
#98729 = AXIS2_PLACEMENT_3D('',#156842,#122149,#122150) ;
#98730 = AXIS2_PLACEMENT_3D('',#156851,#122155,#122156) ;
#98731 = AXIS2_PLACEMENT_3D('',#156860,#122161,#122162) ;
#98732 = AXIS2_PLACEMENT_3D('',#156873,#122168,#122169) ;
#98733 = AXIS2_PLACEMENT_3D('',#156877,#122171,#122172) ;
#98734 = AXIS2_PLACEMENT_3D('',#156881,#122174,#122175) ;
#98735 = AXIS2_PLACEMENT_3D('',#156884,#122177,#122178) ;
#98736 = AXIS2_PLACEMENT_3D('',#156885,#122179,#122180) ;
#98737 = AXIS2_PLACEMENT_3D('',#156891,#122184,#122185) ;
#98738 = AXIS2_PLACEMENT_3D('',#156897,#122189,#122190) ;
#98739 = AXIS2_PLACEMENT_3D('',#156903,#122194,#122195) ;
#98740 = AXIS2_PLACEMENT_3D('',#156909,#122199,#122200) ;
#98741 = AXIS2_PLACEMENT_3D('',#156918,#122205,#122206) ;
#98742 = AXIS2_PLACEMENT_3D('',#156924,#122209,#122210) ;
#98743 = AXIS2_PLACEMENT_3D('',#156929,#122213,#122214) ;
#98744 = AXIS2_PLACEMENT_3D('',#156933,#122217,#122218) ;
#98745 = AXIS2_PLACEMENT_3D('',#156942,#122223,#122224) ;
#98746 = AXIS2_PLACEMENT_3D('',#156945,#122225,#122226) ;
#98747 = AXIS2_PLACEMENT_3D('',#156947,#122227,#122228) ;
#98748 = AXIS2_PLACEMENT_3D('',#156957,#122233,#122234) ;
#98749 = AXIS2_PLACEMENT_3D('',#156963,#122238,#122239) ;
#98750 = AXIS2_PLACEMENT_3D('',#156972,#122244,#122245) ;
#98751 = AXIS2_PLACEMENT_3D('',#156977,#122247,#122248) ;
#98752 = AXIS2_PLACEMENT_3D('',#156979,#122249,#122250) ;
#98753 = AXIS2_PLACEMENT_3D('',#156987,#122254,#122255) ;
#98754 = AXIS2_PLACEMENT_3D('',#156993,#122259,#122260) ;
#98755 = AXIS2_PLACEMENT_3D('',#156999,#122264,#122265) ;
#98756 = AXIS2_PLACEMENT_3D('',#157008,#122270,#122271) ;
#98757 = AXIS2_PLACEMENT_3D('',#157017,#122276,#122277) ;
#98758 = AXIS2_PLACEMENT_3D('',#157022,#122279,#122280) ;
#98759 = AXIS2_PLACEMENT_3D('',#157025,#122282,#122283) ;
#98760 = AXIS2_PLACEMENT_3D('',#157026,#122284,#122285) ;
#98761 = AXIS2_PLACEMENT_3D('',#157031,#122287,#122288) ;
#98762 = AXIS2_PLACEMENT_3D('',#157039,#122293,#122294) ;
#98763 = AXIS2_PLACEMENT_3D('',#157040,#122295,#122296) ;
#98764 = AXIS2_PLACEMENT_3D('',#157049,#122301,#122302) ;
#98765 = AXIS2_PLACEMENT_3D('',#157058,#122307,#122308) ;
#98766 = AXIS2_PLACEMENT_3D('',#157067,#122313,#122314) ;
#98767 = AXIS2_PLACEMENT_3D('',#157076,#122319,#122320) ;
#98768 = AXIS2_PLACEMENT_3D('',#157089,#122326,#122327) ;
#98769 = AXIS2_PLACEMENT_3D('',#157093,#122329,#122330) ;
#98770 = AXIS2_PLACEMENT_3D('',#157097,#122332,#122333) ;
#98771 = AXIS2_PLACEMENT_3D('',#157100,#122335,#122336) ;
#98772 = AXIS2_PLACEMENT_3D('',#157101,#122337,#122338) ;
#98773 = AXIS2_PLACEMENT_3D('',#157107,#122342,#122343) ;
#98774 = AXIS2_PLACEMENT_3D('',#157113,#122347,#122348) ;
#98775 = AXIS2_PLACEMENT_3D('',#157119,#122352,#122353) ;
#98776 = AXIS2_PLACEMENT_3D('',#157125,#122357,#122358) ;
#98777 = AXIS2_PLACEMENT_3D('',#157134,#122363,#122364) ;
#98778 = AXIS2_PLACEMENT_3D('',#157136,#122366,#122367) ;
#98779 = AXIS2_PLACEMENT_3D('',#157139,#122370,#122371) ;
#98780 = AXIS2_PLACEMENT_3D('',#157142,#122374,#122375) ;
#98781 = AXIS2_PLACEMENT_3D('',#157145,#122378,#122379) ;
#98782 = AXIS2_PLACEMENT_3D('',#157146,#122380,#122381) ;
#98783 = AXIS2_PLACEMENT_3D('',#157147,#122382,#122383) ;
#98784 = AXIS2_PLACEMENT_3D('',#157148,#122384,#122385) ;
#98785 = AXIS2_PLACEMENT_3D('',#157149,#122386,#122387) ;
#98786 = AXIS2_PLACEMENT_3D('',#157155,#122391,#122392) ;
#98787 = AXIS2_PLACEMENT_3D('',#157161,#122396,#122397) ;
#98788 = AXIS2_PLACEMENT_3D('',#157162,#122398,#122399) ;
#98789 = AXIS2_PLACEMENT_3D('',#157163,#122400,#122401) ;
#98790 = AXIS2_PLACEMENT_3D('',#157164,#122402,#122403) ;
#98791 = AXIS2_PLACEMENT_3D('',#157165,#122404,#122405) ;
#98792 = AXIS2_PLACEMENT_3D('',#157170,#122407,#122408) ;
#98793 = AXIS2_PLACEMENT_3D('',#157173,#122410,#122411) ;
#98794 = AXIS2_PLACEMENT_3D('',#157174,#122412,#122413) ;
#98795 = AXIS2_PLACEMENT_3D('',#157180,#122417,#122418) ;
#98796 = AXIS2_PLACEMENT_3D('',#157182,#122419,#122420) ;
#98797 = AXIS2_PLACEMENT_3D('',#157185,#122422,#122423) ;
#98798 = AXIS2_PLACEMENT_3D('',#157186,#122424,#122425) ;
#98799 = AXIS2_PLACEMENT_3D('',#157192,#122429,#122430) ;
#98800 = AXIS2_PLACEMENT_3D('',#157194,#122431,#122432) ;
#98801 = AXIS2_PLACEMENT_3D('',#157197,#122434,#122435) ;
#98802 = AXIS2_PLACEMENT_3D('',#157198,#122436,#122437) ;
#98803 = AXIS2_PLACEMENT_3D('',#157204,#122441,#122442) ;
#98804 = AXIS2_PLACEMENT_3D('',#157206,#122443,#122444) ;
#98805 = AXIS2_PLACEMENT_3D('',#157209,#122446,#122447) ;
#98806 = AXIS2_PLACEMENT_3D('',#157210,#122448,#122449) ;
#98807 = AXIS2_PLACEMENT_3D('',#157213,#122452,#122453) ;
#98808 = AXIS2_PLACEMENT_3D('',#157222,#122458,#122459) ;
#98809 = AXIS2_PLACEMENT_3D('',#157223,#122460,#122461) ;
#98810 = AXIS2_PLACEMENT_3D('',#157224,#122462,#122463) ;
#98811 = AXIS2_PLACEMENT_3D('',#157225,#122464,#122465) ;
#98812 = AXIS2_PLACEMENT_3D('',#157226,#122466,#122467) ;
#98813 = AXIS2_PLACEMENT_3D('',#157227,#122468,#122469) ;
#98814 = AXIS2_PLACEMENT_3D('',#157228,#122470,#122471) ;
#98815 = AXIS2_PLACEMENT_3D('',#157229,#122472,#122473) ;
#98816 = AXIS2_PLACEMENT_3D('',#157230,#122474,#122475) ;
#98817 = AXIS2_PLACEMENT_3D('',#157231,#122476,#122477) ;
#98818 = AXIS2_PLACEMENT_3D('',#157232,#122478,#122479) ;
#98819 = AXIS2_PLACEMENT_3D('',#157233,#122480,#122481) ;
#98820 = AXIS2_PLACEMENT_3D('',#157234,#122482,#122483) ;
#98821 = AXIS2_PLACEMENT_3D('',#157235,#122484,#122485) ;
#98822 = AXIS2_PLACEMENT_3D('',#157236,#122486,#122487) ;
#98823 = AXIS2_PLACEMENT_3D('',#157237,#122488,#122489) ;
#98824 = AXIS2_PLACEMENT_3D('',#157238,#122490,#122491) ;
#98825 = AXIS2_PLACEMENT_3D('',#157239,#122492,#122493) ;
#98826 = AXIS2_PLACEMENT_3D('',#157240,#122494,#122495) ;
#98827 = AXIS2_PLACEMENT_3D('',#157241,#122496,#122497) ;
#98828 = AXIS2_PLACEMENT_3D('',#157243,#122498,#122499) ;
#98829 = AXIS2_PLACEMENT_3D('',#157245,#122500,#122501) ;
#98830 = AXIS2_PLACEMENT_3D('',#157246,#122502,#122503) ;
#98831 = AXIS2_PLACEMENT_3D('',#157247,#122504,#122505) ;
#98832 = AXIS2_PLACEMENT_3D('',#157248,#122506,#122507) ;
#98833 = AXIS2_PLACEMENT_3D('',#157249,#122508,#122509) ;
#98834 = AXIS2_PLACEMENT_3D('',#157250,#122510,#122511) ;
#98835 = AXIS2_PLACEMENT_3D('',#157251,#122512,#122513) ;
#98836 = AXIS2_PLACEMENT_3D('',#157252,#122514,#122515) ;
#98837 = AXIS2_PLACEMENT_3D('',#157253,#122516,#122517) ;
#98838 = AXIS2_PLACEMENT_3D('',#157254,#122518,#122519) ;
#98839 = AXIS2_PLACEMENT_3D('',#157255,#122520,#122521) ;
#98840 = AXIS2_PLACEMENT_3D('',#157256,#122522,#122523) ;
#98841 = AXIS2_PLACEMENT_3D('',#157257,#122524,#122525) ;
#98842 = AXIS2_PLACEMENT_3D('',#157258,#122526,#122527) ;
#98843 = AXIS2_PLACEMENT_3D('',#157260,#122528,#122529) ;
#98844 = AXIS2_PLACEMENT_3D('',#157262,#122530,#122531) ;
#98845 = AXIS2_PLACEMENT_3D('',#157263,#122532,#122533) ;
#98846 = AXIS2_PLACEMENT_3D('',#157264,#122534,#122535) ;
#98847 = AXIS2_PLACEMENT_3D('',#157265,#122536,#122537) ;
#98848 = AXIS2_PLACEMENT_3D('',#157266,#122538,#122539) ;
#98849 = AXIS2_PLACEMENT_3D('',#157267,#122540,#122541) ;
#98850 = AXIS2_PLACEMENT_3D('',#157268,#122542,#122543) ;
#98851 = AXIS2_PLACEMENT_3D('',#157269,#122544,#122545) ;
#98852 = AXIS2_PLACEMENT_3D('',#157270,#122546,#122547) ;
#98853 = AXIS2_PLACEMENT_3D('',#157271,#122548,#122549) ;
#98854 = AXIS2_PLACEMENT_3D('',#157272,#122550,#122551) ;
#98855 = AXIS2_PLACEMENT_3D('',#157273,#122552,#122553) ;
#98856 = AXIS2_PLACEMENT_3D('',#157274,#122554,#122555) ;
#98857 = AXIS2_PLACEMENT_3D('',#157275,#122556,#122557) ;
#98858 = AXIS2_PLACEMENT_3D('',#157276,#122558,#122559) ;
#98859 = AXIS2_PLACEMENT_3D('',#157277,#122560,#122561) ;
#98860 = AXIS2_PLACEMENT_3D('',#157278,#122562,#122563) ;
#98861 = AXIS2_PLACEMENT_3D('',#157279,#122564,#122565) ;
#98862 = AXIS2_PLACEMENT_3D('',#157280,#122566,#122567) ;
#98863 = AXIS2_PLACEMENT_3D('',#157282,#122568,#122569) ;
#98864 = AXIS2_PLACEMENT_3D('',#157283,#122570,#122571) ;
#98865 = AXIS2_PLACEMENT_3D('',#157284,#122572,#122573) ;
#98866 = AXIS2_PLACEMENT_3D('',#157285,#122574,#122575) ;
#98867 = AXIS2_PLACEMENT_3D('',#157286,#122576,#122577) ;
#98868 = AXIS2_PLACEMENT_3D('',#157287,#122578,#122579) ;
#98869 = AXIS2_PLACEMENT_3D('',#157288,#122580,#122581) ;
#98870 = AXIS2_PLACEMENT_3D('',#157290,#122582,#122583) ;
#98871 = AXIS2_PLACEMENT_3D('',#157291,#122584,#122585) ;
#98872 = AXIS2_PLACEMENT_3D('',#157292,#122586,#122587) ;
#98873 = AXIS2_PLACEMENT_3D('',#157293,#122588,#122589) ;
#98874 = AXIS2_PLACEMENT_3D('',#157294,#122590,#122591) ;
#98875 = AXIS2_PLACEMENT_3D('',#157296,#122592,#122593) ;
#98876 = AXIS2_PLACEMENT_3D('',#157298,#122594,#122595) ;
#98877 = AXIS2_PLACEMENT_3D('',#157299,#122596,#122597) ;
#98878 = AXIS2_PLACEMENT_3D('',#157300,#122598,#122599) ;
#98879 = AXIS2_PLACEMENT_3D('',#157301,#122600,#122601) ;
#98880 = AXIS2_PLACEMENT_3D('',#157302,#122602,#122603) ;
#98881 = AXIS2_PLACEMENT_3D('',#157303,#122604,#122605) ;
#98882 = AXIS2_PLACEMENT_3D('',#157304,#122606,#122607) ;
#98883 = AXIS2_PLACEMENT_3D('',#157305,#122608,#122609) ;
#98884 = AXIS2_PLACEMENT_3D('',#157306,#122610,#122611) ;
#98885 = AXIS2_PLACEMENT_3D('',#157307,#122612,#122613) ;
#98886 = AXIS2_PLACEMENT_3D('',#157308,#122614,#122615) ;
#98887 = AXIS2_PLACEMENT_3D('',#157309,#122616,#122617) ;
#98888 = AXIS2_PLACEMENT_3D('',#157310,#122618,#122619) ;
#98889 = AXIS2_PLACEMENT_3D('',#157311,#122620,#122621) ;
#98890 = AXIS2_PLACEMENT_3D('',#157312,#122622,#122623) ;
#98891 = AXIS2_PLACEMENT_3D('',#157313,#122624,#122625) ;
#98892 = AXIS2_PLACEMENT_3D('',#157314,#122626,#122627) ;
#98893 = AXIS2_PLACEMENT_3D('',#157315,#122628,#122629) ;
#98894 = AXIS2_PLACEMENT_3D('',#157316,#122630,#122631) ;
#98895 = AXIS2_PLACEMENT_3D('',#157317,#122632,#122633) ;
#98896 = AXIS2_PLACEMENT_3D('',#157318,#122634,#122635) ;
#98897 = AXIS2_PLACEMENT_3D('',#157319,#122636,#122637) ;
#98898 = AXIS2_PLACEMENT_3D('',#157320,#122638,#122639) ;
#98899 = AXIS2_PLACEMENT_3D('',#157321,#122640,#122641) ;
#98900 = AXIS2_PLACEMENT_3D('',#157322,#122642,#122643) ;
#98901 = AXIS2_PLACEMENT_3D('',#157323,#122644,#122645) ;
#98902 = AXIS2_PLACEMENT_3D('',#157324,#122646,#122647) ;
#98903 = AXIS2_PLACEMENT_3D('',#157325,#122648,#122649) ;
#98904 = AXIS2_PLACEMENT_3D('',#157326,#122650,#122651) ;
#98905 = AXIS2_PLACEMENT_3D('',#157327,#122652,#122653) ;
#98906 = AXIS2_PLACEMENT_3D('',#157328,#122654,#122655) ;
#98907 = AXIS2_PLACEMENT_3D('',#157329,#122656,#122657) ;
#98908 = AXIS2_PLACEMENT_3D('',#157330,#122658,#122659) ;
#98909 = AXIS2_PLACEMENT_3D('',#157331,#122660,#122661) ;
#98910 = AXIS2_PLACEMENT_3D('',#157332,#122662,#122663) ;
#98911 = AXIS2_PLACEMENT_3D('',#157333,#122664,#122665) ;
#98912 = AXIS2_PLACEMENT_3D('',#157334,#122666,#122667) ;
#98913 = AXIS2_PLACEMENT_3D('',#157335,#122668,#122669) ;
#98914 = AXIS2_PLACEMENT_3D('',#157336,#122670,#122671) ;
#98915 = AXIS2_PLACEMENT_3D('',#157337,#122672,#122673) ;
#98916 = AXIS2_PLACEMENT_3D('',#157338,#122674,#122675) ;
#98917 = AXIS2_PLACEMENT_3D('',#157339,#122676,#122677) ;
#98918 = AXIS2_PLACEMENT_3D('',#157340,#122678,#122679) ;
#98919 = AXIS2_PLACEMENT_3D('',#157341,#122680,#122681) ;
#98920 = AXIS2_PLACEMENT_3D('',#157342,#122682,#122683) ;
#98921 = AXIS2_PLACEMENT_3D('',#157343,#122684,#122685) ;
#98922 = AXIS2_PLACEMENT_3D('',#157344,#122686,#122687) ;
#98923 = AXIS2_PLACEMENT_3D('',#157345,#122688,#122689) ;
#98924 = AXIS2_PLACEMENT_3D('',#157346,#122690,#122691) ;
#98925 = AXIS2_PLACEMENT_3D('',#157347,#122692,#122693) ;
#98926 = AXIS2_PLACEMENT_3D('',#157348,#122694,#122695) ;
#98927 = AXIS2_PLACEMENT_3D('',#157349,#122696,#122697) ;
#98928 = AXIS2_PLACEMENT_3D('',#157350,#122698,#122699) ;
#98929 = AXIS2_PLACEMENT_3D('',#157351,#122700,#122701) ;
#98930 = AXIS2_PLACEMENT_3D('',#157352,#122702,#122703) ;
#98931 = AXIS2_PLACEMENT_3D('',#157353,#122704,#122705) ;
#98932 = AXIS2_PLACEMENT_3D('',#157354,#122706,#122707) ;
#98933 = AXIS2_PLACEMENT_3D('',#157355,#122708,#122709) ;
#98934 = AXIS2_PLACEMENT_3D('',#157356,#122710,#122711) ;
#98935 = AXIS2_PLACEMENT_3D('',#157357,#122712,#122713) ;
#98936 = AXIS2_PLACEMENT_3D('',#157358,#122714,#122715) ;
#98937 = AXIS2_PLACEMENT_3D('',#157359,#122716,#122717) ;
#98938 = AXIS2_PLACEMENT_3D('',#157360,#122718,#122719) ;
#98939 = AXIS2_PLACEMENT_3D('',#157361,#122720,#122721) ;
#98940 = AXIS2_PLACEMENT_3D('',#157362,#122722,#122723) ;
#98941 = AXIS2_PLACEMENT_3D('',#157363,#122724,#122725) ;
#98942 = AXIS2_PLACEMENT_3D('',#157364,#122726,#122727) ;
#98943 = AXIS2_PLACEMENT_3D('',#157365,#122728,#122729) ;
#98944 = AXIS2_PLACEMENT_3D('',#157366,#122730,#122731) ;
#98945 = AXIS2_PLACEMENT_3D('',#157367,#122732,#122733) ;
#98946 = AXIS2_PLACEMENT_3D('',#157368,#122734,#122735) ;
#98947 = AXIS2_PLACEMENT_3D('',#157369,#122736,#122737) ;
#98948 = AXIS2_PLACEMENT_3D('',#157370,#122738,#122739) ;
#98949 = AXIS2_PLACEMENT_3D('',#157371,#122740,#122741) ;
#98950 = AXIS2_PLACEMENT_3D('',#157372,#122742,#122743) ;
#98951 = AXIS2_PLACEMENT_3D('',#157373,#122744,#122745) ;
#98952 = AXIS2_PLACEMENT_3D('',#157374,#122746,#122747) ;
#98953 = AXIS2_PLACEMENT_3D('',#157375,#122748,#122749) ;
#98954 = AXIS2_PLACEMENT_3D('',#157376,#122750,#122751) ;
#98955 = AXIS2_PLACEMENT_3D('',#157377,#122752,#122753) ;
#98956 = AXIS2_PLACEMENT_3D('',#157378,#122754,#122755) ;
#98957 = AXIS2_PLACEMENT_3D('',#157379,#122756,#122757) ;
#98958 = AXIS2_PLACEMENT_3D('',#157380,#122758,#122759) ;
#98959 = AXIS2_PLACEMENT_3D('',#157381,#122760,#122761) ;
#98960 = AXIS2_PLACEMENT_3D('',#157382,#122762,#122763) ;
#98961 = AXIS2_PLACEMENT_3D('',#157383,#122764,#122765) ;
#98962 = AXIS2_PLACEMENT_3D('',#157384,#122766,#122767) ;
#98963 = AXIS2_PLACEMENT_3D('',#157385,#122768,#122769) ;
#98964 = AXIS2_PLACEMENT_3D('',#157386,#122770,#122771) ;
#98965 = AXIS2_PLACEMENT_3D('',#157387,#122772,#122773) ;
#98966 = AXIS2_PLACEMENT_3D('',#157388,#122774,#122775) ;
#98967 = AXIS2_PLACEMENT_3D('',#157389,#122776,#122777) ;
#98968 = AXIS2_PLACEMENT_3D('',#157390,#122778,#122779) ;
#98969 = AXIS2_PLACEMENT_3D('',#157391,#122780,#122781) ;
#98970 = AXIS2_PLACEMENT_3D('',#157392,#122782,#122783) ;
#98971 = AXIS2_PLACEMENT_3D('',#157393,#122784,#122785) ;
#98972 = AXIS2_PLACEMENT_3D('',#157394,#122786,#122787) ;
#98973 = AXIS2_PLACEMENT_3D('',#157395,#122788,#122789) ;
#98974 = AXIS2_PLACEMENT_3D('',#157396,#122790,#122791) ;
#98975 = AXIS2_PLACEMENT_3D('',#157397,#122792,#122793) ;
#98976 = AXIS2_PLACEMENT_3D('',#157398,#122794,#122795) ;
#98977 = AXIS2_PLACEMENT_3D('',#157399,#122796,#122797) ;
#98978 = AXIS2_PLACEMENT_3D('',#157400,#122798,#122799) ;
#98979 = AXIS2_PLACEMENT_3D('',#157401,#122800,#122801) ;
#98980 = AXIS2_PLACEMENT_3D('',#157402,#122802,#122803) ;
#98981 = AXIS2_PLACEMENT_3D('',#157403,#122804,#122805) ;
#98982 = AXIS2_PLACEMENT_3D('',#157404,#122806,#122807) ;
#98983 = AXIS2_PLACEMENT_3D('',#157405,#122808,#122809) ;
#98984 = AXIS2_PLACEMENT_3D('',#157406,#122810,#122811) ;
#98985 = AXIS2_PLACEMENT_3D('',#157407,#122812,#122813) ;
#98986 = AXIS2_PLACEMENT_3D('',#157408,#122814,#122815) ;
#98987 = AXIS2_PLACEMENT_3D('',#157409,#122816,#122817) ;
#98988 = AXIS2_PLACEMENT_3D('',#157410,#122818,#122819) ;
#98989 = AXIS2_PLACEMENT_3D('',#157411,#122820,#122821) ;
#98990 = AXIS2_PLACEMENT_3D('',#157412,#122822,#122823) ;
#98991 = AXIS2_PLACEMENT_3D('',#157413,#122824,#122825) ;
#98992 = AXIS2_PLACEMENT_3D('',#157414,#122826,#122827) ;
#98993 = AXIS2_PLACEMENT_3D('',#157415,#122828,#122829) ;
#98994 = AXIS2_PLACEMENT_3D('',#157416,#122830,#122831) ;
#98995 = AXIS2_PLACEMENT_3D('',#157417,#122832,#122833) ;
#98996 = AXIS2_PLACEMENT_3D('',#157418,#122834,#122835) ;
#98997 = AXIS2_PLACEMENT_3D('',#157419,#122836,#122837) ;
#98998 = AXIS2_PLACEMENT_3D('',#157420,#122838,#122839) ;
#98999 = AXIS2_PLACEMENT_3D('',#157421,#122840,#122841) ;
#99000 = AXIS2_PLACEMENT_3D('',#157422,#122842,#122843) ;
#99001 = AXIS2_PLACEMENT_3D('',#157423,#122844,#122845) ;
#99002 = AXIS2_PLACEMENT_3D('',#157424,#122846,#122847) ;
#99003 = AXIS2_PLACEMENT_3D('',#157425,#122848,#122849) ;
#99004 = AXIS2_PLACEMENT_3D('',#157426,#122850,#122851) ;
#99005 = AXIS2_PLACEMENT_3D('',#157427,#122852,#122853) ;
#99006 = AXIS2_PLACEMENT_3D('',#157428,#122854,#122855) ;
#99007 = AXIS2_PLACEMENT_3D('',#157429,#122856,#122857) ;
#99008 = AXIS2_PLACEMENT_3D('',#157430,#122858,#122859) ;
#99009 = AXIS2_PLACEMENT_3D('',#157431,#122860,#122861) ;
#99010 = AXIS2_PLACEMENT_3D('',#157432,#122862,#122863) ;
#99011 = AXIS2_PLACEMENT_3D('',#157433,#122864,#122865) ;
#99012 = AXIS2_PLACEMENT_3D('',#157434,#122866,#122867) ;
#99013 = AXIS2_PLACEMENT_3D('',#157435,#122868,#122869) ;
#99014 = AXIS2_PLACEMENT_3D('',#157436,#122870,#122871) ;
#99015 = AXIS2_PLACEMENT_3D('',#157437,#122872,#122873) ;
#99016 = AXIS2_PLACEMENT_3D('',#157438,#122874,#122875) ;
#99017 = AXIS2_PLACEMENT_3D('',#157439,#122876,#122877) ;
#99018 = AXIS2_PLACEMENT_3D('',#157440,#122878,#122879) ;
#99019 = AXIS2_PLACEMENT_3D('',#157441,#122880,#122881) ;
#99020 = AXIS2_PLACEMENT_3D('',#157442,#122882,#122883) ;
#99021 = AXIS2_PLACEMENT_3D('',#157443,#122884,#122885) ;
#99022 = AXIS2_PLACEMENT_3D('',#157444,#122886,#122887) ;
#99023 = AXIS2_PLACEMENT_3D('',#157445,#122888,#122889) ;
#99024 = AXIS2_PLACEMENT_3D('',#157446,#122890,#122891) ;
#99025 = AXIS2_PLACEMENT_3D('',#157447,#122892,#122893) ;
#99026 = AXIS2_PLACEMENT_3D('',#157448,#122894,#122895) ;
#99027 = AXIS2_PLACEMENT_3D('',#157449,#122896,#122897) ;
#99028 = AXIS2_PLACEMENT_3D('',#157450,#122898,#122899) ;
#99029 = AXIS2_PLACEMENT_3D('',#157451,#122900,#122901) ;
#99030 = AXIS2_PLACEMENT_3D('',#157452,#122902,#122903) ;
#99031 = AXIS2_PLACEMENT_3D('',#157453,#122904,#122905) ;
#99032 = AXIS2_PLACEMENT_3D('',#157454,#122906,#122907) ;
#99033 = AXIS2_PLACEMENT_3D('',#157455,#122908,#122909) ;
#99034 = AXIS2_PLACEMENT_3D('',#157456,#122910,#122911) ;
#99035 = AXIS2_PLACEMENT_3D('',#157457,#122912,#122913) ;
#99036 = AXIS2_PLACEMENT_3D('',#157458,#122914,#122915) ;
#99037 = AXIS2_PLACEMENT_3D('',#157459,#122916,#122917) ;
#99038 = AXIS2_PLACEMENT_3D('',#157460,#122918,#122919) ;
#99039 = AXIS2_PLACEMENT_3D('',#157461,#122920,#122921) ;
#99040 = AXIS2_PLACEMENT_3D('',#157462,#122922,#122923) ;
#99041 = AXIS2_PLACEMENT_3D('',#157463,#122924,#122925) ;
#99042 = AXIS2_PLACEMENT_3D('',#157464,#122926,#122927) ;
#99043 = AXIS2_PLACEMENT_3D('',#157465,#122928,#122929) ;
#99044 = AXIS2_PLACEMENT_3D('',#157466,#122930,#122931) ;
#99045 = AXIS2_PLACEMENT_3D('',#157467,#122932,#122933) ;
#99046 = AXIS2_PLACEMENT_3D('',#157468,#122934,#122935) ;
#99047 = AXIS2_PLACEMENT_3D('',#157469,#122936,#122937) ;
#99048 = AXIS2_PLACEMENT_3D('',#157470,#122938,#122939) ;
#99049 = AXIS2_PLACEMENT_3D('',#157471,#122940,#122941) ;
#99050 = AXIS2_PLACEMENT_3D('',#157472,#122942,#122943) ;
#99051 = AXIS2_PLACEMENT_3D('',#157473,#122944,#122945) ;
#99052 = AXIS2_PLACEMENT_3D('',#157474,#122946,#122947) ;
#99053 = AXIS2_PLACEMENT_3D('',#157475,#122948,#122949) ;
#99054 = AXIS2_PLACEMENT_3D('',#157476,#122950,#122951) ;
#99055 = AXIS2_PLACEMENT_3D('',#157477,#122952,#122953) ;
#99056 = AXIS2_PLACEMENT_3D('',#157478,#122954,#122955) ;
#99057 = AXIS2_PLACEMENT_3D('',#157485,#122956,#122957) ;
#99058 = AXIS2_PLACEMENT_3D('',#157486,#122958,#122959) ;
#99059 = AXIS2_PLACEMENT_3D('',#157487,#122960,#122961) ;
#99060 = AXIS2_PLACEMENT_3D('',#157488,#122962,#122963) ;
#99061 = AXIS2_PLACEMENT_3D('',#157507,#122964,#122965) ;
#99062 = AXIS2_PLACEMENT_3D('',#157508,#122966,#122967) ;
#99063 = AXIS2_PLACEMENT_3D('',#157509,#122968,#122969) ;
#99064 = AXIS2_PLACEMENT_3D('',#157510,#122970,#122971) ;
#99065 = AXIS2_PLACEMENT_3D('',#157511,#122972,#122973) ;
#99066 = AXIS2_PLACEMENT_3D('',#157512,#122974,#122975) ;
#99067 = AXIS2_PLACEMENT_3D('',#157513,#122976,#122977) ;
#99068 = AXIS2_PLACEMENT_3D('',#157520,#122978,#122979) ;
#99069 = AXIS2_PLACEMENT_3D('',#157521,#122980,#122981) ;
#99070 = AXIS2_PLACEMENT_3D('',#157522,#122982,#122983) ;
#99071 = AXIS2_PLACEMENT_3D('',#157523,#122984,#122985) ;
#99072 = AXIS2_PLACEMENT_3D('',#157524,#122986,#122987) ;
#99073 = AXIS2_PLACEMENT_3D('',#157525,#122988,#122989) ;
#99074 = AXIS2_PLACEMENT_3D('',#157526,#122990,#122991) ;
#99075 = AXIS2_PLACEMENT_3D('',#157527,#122992,#122993) ;
#99076 = AXIS2_PLACEMENT_3D('',#157528,#122994,#122995) ;
#99077 = AXIS2_PLACEMENT_3D('',#157547,#122996,#122997) ;
#99078 = AXIS2_PLACEMENT_3D('',#157566,#122998,#122999) ;
#99079 = AXIS2_PLACEMENT_3D('',#157567,#123000,#123001) ;
#99080 = AXIS2_PLACEMENT_3D('',#157568,#123002,#123003) ;
#99081 = AXIS2_PLACEMENT_3D('',#157569,#123004,#123005) ;
#99082 = AXIS2_PLACEMENT_3D('',#157570,#123006,#123007) ;
#99083 = AXIS2_PLACEMENT_3D('',#157571,#123008,#123009) ;
#99084 = AXIS2_PLACEMENT_3D('',#157572,#123010,#123011) ;
#99085 = AXIS2_PLACEMENT_3D('',#157573,#123012,#123013) ;
#99086 = AXIS2_PLACEMENT_3D('',#157574,#123014,#123015) ;
#99087 = AXIS2_PLACEMENT_3D('',#157575,#123016,#123017) ;
#99088 = AXIS2_PLACEMENT_3D('',#157576,#123018,#123019) ;
#99089 = AXIS2_PLACEMENT_3D('',#157595,#123020,#123021) ;
#99090 = AXIS2_PLACEMENT_3D('',#157596,#123022,#123023) ;
#99091 = AXIS2_PLACEMENT_3D('',#157597,#123024,#123025) ;
#99092 = AXIS2_PLACEMENT_3D('',#157598,#123026,#123027) ;
#99093 = AXIS2_PLACEMENT_3D('',#157599,#123028,#123029) ;
#99094 = AXIS2_PLACEMENT_3D('',#157600,#123030,#123031) ;
#99095 = AXIS2_PLACEMENT_3D('',#157601,#123032,#123033) ;
#99096 = AXIS2_PLACEMENT_3D('',#157602,#123034,#123035) ;
#99097 = AXIS2_PLACEMENT_3D('',#157603,#123036,#123037) ;
#99098 = AXIS2_PLACEMENT_3D('',#157604,#123038,#123039) ;
#99099 = AXIS2_PLACEMENT_3D('',#157605,#123040,#123041) ;
#99100 = AXIS2_PLACEMENT_3D('',#157606,#123042,#123043) ;
#99101 = AXIS2_PLACEMENT_3D('',#157607,#123044,#123045) ;
#99102 = AXIS2_PLACEMENT_3D('',#157608,#123046,#123047) ;
#99103 = AXIS2_PLACEMENT_3D('',#157609,#123048,#123049) ;
#99104 = AXIS2_PLACEMENT_3D('',#157610,#123050,#123051) ;
#99105 = AXIS2_PLACEMENT_3D('',#157611,#123052,#123053) ;
#99106 = AXIS2_PLACEMENT_3D('',#157612,#123054,#123055) ;
#99107 = AXIS2_PLACEMENT_3D('',#157613,#123056,#123057) ;
#99108 = AXIS2_PLACEMENT_3D('',#157614,#123058,#123059) ;
#99109 = AXIS2_PLACEMENT_3D('',#157615,#123060,#123061) ;
#99110 = AXIS2_PLACEMENT_3D('',#157616,#123062,#123063) ;
#99111 = AXIS2_PLACEMENT_3D('',#157617,#123064,#123065) ;
#99112 = AXIS2_PLACEMENT_3D('',#157618,#123066,#123067) ;
#99113 = AXIS2_PLACEMENT_3D('',#157619,#123068,#123069) ;
#99114 = AXIS2_PLACEMENT_3D('',#157620,#123070,#123071) ;
#99115 = AXIS2_PLACEMENT_3D('',#157621,#123072,#123073) ;
#99116 = AXIS2_PLACEMENT_3D('',#157622,#123074,#123075) ;
#99117 = AXIS2_PLACEMENT_3D('',#157623,#123076,#123077) ;
#99118 = AXIS2_PLACEMENT_3D('',#157624,#123078,#123079) ;
#99119 = AXIS2_PLACEMENT_3D('',#157625,#123080,#123081) ;
#99120 = AXIS2_PLACEMENT_3D('',#157626,#123082,#123083) ;
#99121 = AXIS2_PLACEMENT_3D('',#157627,#123084,#123085) ;
#99122 = AXIS2_PLACEMENT_3D('',#157628,#123086,#123087) ;
#99123 = AXIS2_PLACEMENT_3D('',#157629,#123088,#123089) ;
#99124 = AXIS2_PLACEMENT_3D('',#157630,#123090,#123091) ;
#99125 = AXIS2_PLACEMENT_3D('',#157631,#123092,#123093) ;
#99126 = AXIS2_PLACEMENT_3D('',#157632,#123094,#123095) ;
#99127 = AXIS2_PLACEMENT_3D('',#157633,#123096,#123097) ;
#99128 = AXIS2_PLACEMENT_3D('',#157634,#123098,#123099) ;
#99129 = AXIS2_PLACEMENT_3D('',#157635,#123100,#123101) ;
#99130 = AXIS2_PLACEMENT_3D('',#157636,#123102,#123103) ;
#99131 = AXIS2_PLACEMENT_3D('',#157637,#123104,#123105) ;
#99132 = AXIS2_PLACEMENT_3D('',#157638,#123106,#123107) ;
#99133 = AXIS2_PLACEMENT_3D('',#157639,#123108,#123109) ;
#99134 = AXIS2_PLACEMENT_3D('',#157640,#123110,#123111) ;
#99135 = AXIS2_PLACEMENT_3D('',#157641,#123112,#123113) ;
#99136 = AXIS2_PLACEMENT_3D('',#157642,#123114,#123115) ;
#99137 = AXIS2_PLACEMENT_3D('',#157643,#123116,#123117) ;
#99138 = AXIS2_PLACEMENT_3D('',#157644,#123118,#123119) ;
#99139 = AXIS2_PLACEMENT_3D('',#157645,#123120,#123121) ;
#99140 = AXIS2_PLACEMENT_3D('',#157646,#123122,#123123) ;
#99141 = AXIS2_PLACEMENT_3D('',#157647,#123124,#123125) ;
#99142 = AXIS2_PLACEMENT_3D('',#157648,#123126,#123127) ;
#99143 = AXIS2_PLACEMENT_3D('',#157649,#123128,#123129) ;
#99144 = AXIS2_PLACEMENT_3D('',#157650,#123130,#123131) ;
#99145 = AXIS2_PLACEMENT_3D('',#157651,#123132,#123133) ;
#99146 = AXIS2_PLACEMENT_3D('',#157652,#123134,#123135) ;
#99147 = AXIS2_PLACEMENT_3D('',#157653,#123136,#123137) ;
#99148 = AXIS2_PLACEMENT_3D('',#157654,#123138,#123139) ;
#99149 = AXIS2_PLACEMENT_3D('',#157655,#123140,#123141) ;
#99150 = AXIS2_PLACEMENT_3D('',#157656,#123142,#123143) ;
#99151 = AXIS2_PLACEMENT_3D('',#157657,#123144,#123145) ;
#99152 = AXIS2_PLACEMENT_3D('',#157658,#123146,#123147) ;
#99153 = AXIS2_PLACEMENT_3D('',#157659,#123148,#123149) ;
#99154 = AXIS2_PLACEMENT_3D('',#157660,#123150,#123151) ;
#99155 = AXIS2_PLACEMENT_3D('',#157661,#123152,#123153) ;
#99156 = AXIS2_PLACEMENT_3D('',#157662,#123154,#123155) ;
#99157 = AXIS2_PLACEMENT_3D('',#157663,#123156,#123157) ;
#99158 = AXIS2_PLACEMENT_3D('',#157664,#123158,#123159) ;
#99159 = AXIS2_PLACEMENT_3D('',#157665,#123160,#123161) ;
#99160 = AXIS2_PLACEMENT_3D('',#157666,#123162,#123163) ;
#99161 = AXIS2_PLACEMENT_3D('',#157667,#123164,#123165) ;
#99162 = AXIS2_PLACEMENT_3D('',#157668,#123166,#123167) ;
#99163 = AXIS2_PLACEMENT_3D('',#157669,#123168,#123169) ;
#99164 = AXIS2_PLACEMENT_3D('',#157670,#123170,#123171) ;
#99165 = AXIS2_PLACEMENT_3D('',#157671,#123172,#123173) ;
#99166 = AXIS2_PLACEMENT_3D('',#157672,#123174,#123175) ;
#99167 = AXIS2_PLACEMENT_3D('',#157673,#123176,#123177) ;
#99168 = AXIS2_PLACEMENT_3D('',#157674,#123178,#123179) ;
#99169 = AXIS2_PLACEMENT_3D('',#157675,#123180,#123181) ;
#99170 = AXIS2_PLACEMENT_3D('',#157676,#123182,#123183) ;
#99171 = AXIS2_PLACEMENT_3D('',#157677,#123184,#123185) ;
#99172 = AXIS2_PLACEMENT_3D('',#157678,#123186,#123187) ;
#99173 = AXIS2_PLACEMENT_3D('',#157679,#123188,#123189) ;
#99174 = AXIS2_PLACEMENT_3D('',#157680,#123190,#123191) ;
#99175 = AXIS2_PLACEMENT_3D('',#157681,#123192,#123193) ;
#99176 = AXIS2_PLACEMENT_3D('',#157682,#123194,#123195) ;
#99177 = AXIS2_PLACEMENT_3D('',#157683,#123196,#123197) ;
#99178 = AXIS2_PLACEMENT_3D('',#157684,#123198,#123199) ;
#99179 = AXIS2_PLACEMENT_3D('',#157685,#123200,#123201) ;
#99180 = AXIS2_PLACEMENT_3D('',#157686,#123202,#123203) ;
#99181 = AXIS2_PLACEMENT_3D('',#157687,#123204,#123205) ;
#99182 = AXIS2_PLACEMENT_3D('',#157688,#123206,#123207) ;
#99183 = AXIS2_PLACEMENT_3D('',#157723,#123208,#123209) ;
#99184 = AXIS2_PLACEMENT_3D('',#157724,#123210,#123211) ;
#99185 = AXIS2_PLACEMENT_3D('',#157726,#123212,#123213) ;
#99186 = AXIS2_PLACEMENT_3D('',#157727,#123214,#123215) ;
#99187 = AXIS2_PLACEMENT_3D('',#157728,#123216,#123217) ;
#99188 = AXIS2_PLACEMENT_3D('',#157755,#123218,#123219) ;
#99189 = AXIS2_PLACEMENT_3D('',#157812,#123220,#123221) ;
#99190 = AXIS2_PLACEMENT_3D('',#157813,#123222,#123223) ;
#99191 = AXIS2_PLACEMENT_3D('',#157814,#123224,#123225) ;
#99192 = AXIS2_PLACEMENT_3D('',#157815,#123226,#123227) ;
#99193 = AXIS2_PLACEMENT_3D('',#157816,#123228,#123229) ;
#99194 = AXIS2_PLACEMENT_3D('',#157817,#123230,#123231) ;
#99195 = AXIS2_PLACEMENT_3D('',#157819,#123232,#123233) ;
#99196 = AXIS2_PLACEMENT_3D('',#157846,#123234,#123235) ;
#99197 = AXIS2_PLACEMENT_3D('',#157847,#123236,#123237) ;
#99198 = AXIS2_PLACEMENT_3D('',#157848,#123238,#123239) ;
#99199 = AXIS2_PLACEMENT_3D('',#157849,#123240,#123241) ;
#99200 = AXIS2_PLACEMENT_3D('',#157850,#123242,#123243) ;
#99201 = AXIS2_PLACEMENT_3D('',#157851,#123244,#123245) ;
#99202 = AXIS2_PLACEMENT_3D('',#157882,#123246,#123247) ;
#99203 = AXIS2_PLACEMENT_3D('',#157883,#123248,#123249) ;
#99204 = AXIS2_PLACEMENT_3D('',#157884,#123250,#123251) ;
#99205 = AXIS2_PLACEMENT_3D('',#157885,#123252,#123253) ;
#99206 = AXIS2_PLACEMENT_3D('',#157916,#123254,#123255) ;
#99207 = AXIS2_PLACEMENT_3D('',#157917,#123256,#123257) ;
#99208 = AXIS2_PLACEMENT_3D('',#157918,#123258,#123259) ;
#99209 = AXIS2_PLACEMENT_3D('',#157927,#123264,#123265) ;
#99210 = AXIS2_PLACEMENT_3D('',#157936,#123270,#123271) ;
#99211 = AXIS2_PLACEMENT_3D('',#157941,#123273,#123274) ;
#99212 = AXIS2_PLACEMENT_3D('',#157945,#123276,#123277) ;
#99213 = AXIS2_PLACEMENT_3D('',#157948,#123279,#123280) ;
#99214 = AXIS2_PLACEMENT_3D('',#157949,#123281,#123282) ;
#99215 = AXIS2_PLACEMENT_3D('',#157950,#123283,#123284) ;
#99216 = AXIS2_PLACEMENT_3D('',#157956,#123288,#123289) ;
#99217 = AXIS2_PLACEMENT_3D('',#157965,#123294,#123295) ;
#99218 = AXIS2_PLACEMENT_3D('',#157974,#123300,#123301) ;
#99219 = AXIS2_PLACEMENT_3D('',#157983,#123306,#123307) ;
#99220 = AXIS2_PLACEMENT_3D('',#157988,#123309,#123310) ;
#99221 = AXIS2_PLACEMENT_3D('',#157992,#123312,#123313) ;
#99222 = AXIS2_PLACEMENT_3D('',#157995,#123315,#123316) ;
#99223 = AXIS2_PLACEMENT_3D('',#157996,#123317,#123318) ;
#99224 = AXIS2_PLACEMENT_3D('',#157997,#123319,#123320) ;
#99225 = AXIS2_PLACEMENT_3D('',#158003,#123324,#123325) ;
#99226 = AXIS2_PLACEMENT_3D('',#158012,#123330,#123331) ;
#99227 = AXIS2_PLACEMENT_3D('',#158021,#123336,#123337) ;
#99228 = AXIS2_PLACEMENT_3D('',#158030,#123342,#123343) ;
#99229 = AXIS2_PLACEMENT_3D('',#158035,#123345,#123346) ;
#99230 = AXIS2_PLACEMENT_3D('',#158039,#123348,#123349) ;
#99231 = AXIS2_PLACEMENT_3D('',#158042,#123351,#123352) ;
#99232 = AXIS2_PLACEMENT_3D('',#158043,#123353,#123354) ;
#99233 = AXIS2_PLACEMENT_3D('',#158044,#123355,#123356) ;
#99234 = AXIS2_PLACEMENT_3D('',#158050,#123360,#123361) ;
#99235 = AXIS2_PLACEMENT_3D('',#158059,#123366,#123367) ;
#99236 = AXIS2_PLACEMENT_3D('',#158068,#123372,#123373) ;
#99237 = AXIS2_PLACEMENT_3D('',#158077,#123378,#123379) ;
#99238 = AXIS2_PLACEMENT_3D('',#158082,#123381,#123382) ;
#99239 = AXIS2_PLACEMENT_3D('',#158086,#123384,#123385) ;
#99240 = AXIS2_PLACEMENT_3D('',#158089,#123387,#123388) ;
#99241 = AXIS2_PLACEMENT_3D('',#158090,#123389,#123390) ;
#99242 = AXIS2_PLACEMENT_3D('',#158091,#123391,#123392) ;
#99243 = AXIS2_PLACEMENT_3D('',#158097,#123396,#123397) ;
#99244 = AXIS2_PLACEMENT_3D('',#158106,#123402,#123403) ;
#99245 = AXIS2_PLACEMENT_3D('',#158115,#123408,#123409) ;
#99246 = AXIS2_PLACEMENT_3D('',#158124,#123414,#123415) ;
#99247 = AXIS2_PLACEMENT_3D('',#158129,#123417,#123418) ;
#99248 = AXIS2_PLACEMENT_3D('',#158133,#123420,#123421) ;
#99249 = AXIS2_PLACEMENT_3D('',#158136,#123423,#123424) ;
#99250 = AXIS2_PLACEMENT_3D('',#158137,#123425,#123426) ;
#99251 = AXIS2_PLACEMENT_3D('',#158138,#123427,#123428) ;
#99252 = AXIS2_PLACEMENT_3D('',#158144,#123432,#123433) ;
#99253 = AXIS2_PLACEMENT_3D('',#158153,#123438,#123439) ;
#99254 = AXIS2_PLACEMENT_3D('',#158162,#123444,#123445) ;
#99255 = AXIS2_PLACEMENT_3D('',#158171,#123450,#123451) ;
#99256 = AXIS2_PLACEMENT_3D('',#158176,#123453,#123454) ;
#99257 = AXIS2_PLACEMENT_3D('',#158180,#123456,#123457) ;
#99258 = AXIS2_PLACEMENT_3D('',#158183,#123459,#123460) ;
#99259 = AXIS2_PLACEMENT_3D('',#158184,#123461,#123462) ;
#99260 = AXIS2_PLACEMENT_3D('',#158185,#123463,#123464) ;
#99261 = AXIS2_PLACEMENT_3D('',#158191,#123468,#123469) ;
#99262 = AXIS2_PLACEMENT_3D('',#158200,#123474,#123475) ;
#99263 = AXIS2_PLACEMENT_3D('',#158209,#123480,#123481) ;
#99264 = AXIS2_PLACEMENT_3D('',#158218,#123486,#123487) ;
#99265 = AXIS2_PLACEMENT_3D('',#158223,#123489,#123490) ;
#99266 = AXIS2_PLACEMENT_3D('',#158227,#123492,#123493) ;
#99267 = AXIS2_PLACEMENT_3D('',#158230,#123495,#123496) ;
#99268 = AXIS2_PLACEMENT_3D('',#158231,#123497,#123498) ;
#99269 = AXIS2_PLACEMENT_3D('',#158232,#123499,#123500) ;
#99270 = AXIS2_PLACEMENT_3D('',#158238,#123504,#123505) ;
#99271 = AXIS2_PLACEMENT_3D('',#158247,#123510,#123511) ;
#99272 = AXIS2_PLACEMENT_3D('',#158256,#123516,#123517) ;
#99273 = AXIS2_PLACEMENT_3D('',#158265,#123522,#123523) ;
#99274 = AXIS2_PLACEMENT_3D('',#158270,#123525,#123526) ;
#99275 = AXIS2_PLACEMENT_3D('',#158274,#123528,#123529) ;
#99276 = AXIS2_PLACEMENT_3D('',#158277,#123531,#123532) ;
#99277 = AXIS2_PLACEMENT_3D('',#158278,#123533,#123534) ;
#99278 = AXIS2_PLACEMENT_3D('',#158279,#123535,#123536) ;
#99279 = AXIS2_PLACEMENT_3D('',#158285,#123540,#123541) ;
#99280 = AXIS2_PLACEMENT_3D('',#158294,#123546,#123547) ;
#99281 = AXIS2_PLACEMENT_3D('',#158303,#123552,#123553) ;
#99282 = AXIS2_PLACEMENT_3D('',#158312,#123558,#123559) ;
#99283 = AXIS2_PLACEMENT_3D('',#158317,#123561,#123562) ;
#99284 = AXIS2_PLACEMENT_3D('',#158321,#123564,#123565) ;
#99285 = AXIS2_PLACEMENT_3D('',#158324,#123567,#123568) ;
#99286 = AXIS2_PLACEMENT_3D('',#158325,#123569,#123570) ;
#99287 = AXIS2_PLACEMENT_3D('',#158326,#123571,#123572) ;
#99288 = AXIS2_PLACEMENT_3D('',#158332,#123576,#123577) ;
#99289 = AXIS2_PLACEMENT_3D('',#158341,#123582,#123583) ;
#99290 = AXIS2_PLACEMENT_3D('',#158351,#123589,#123590) ;
#99291 = AXIS2_PLACEMENT_3D('',#158356,#123592,#123593) ;
#99292 = AXIS2_PLACEMENT_3D('',#158364,#123598,#123599) ;
#99293 = AXIS2_PLACEMENT_3D('',#158365,#123600,#123601) ;
#99294 = AXIS2_PLACEMENT_3D('',#158370,#123603,#123604) ;
#99295 = AXIS2_PLACEMENT_3D('',#158378,#123609,#123610) ;
#99296 = AXIS2_PLACEMENT_3D('',#158379,#123611,#123612) ;
#99297 = AXIS2_PLACEMENT_3D('',#158384,#123614,#123615) ;
#99298 = AXIS2_PLACEMENT_3D('',#158392,#123620,#123621) ;
#99299 = AXIS2_PLACEMENT_3D('',#158393,#123622,#123623) ;
#99300 = AXIS2_PLACEMENT_3D('',#158398,#123625,#123626) ;
#99301 = AXIS2_PLACEMENT_3D('',#158406,#123631,#123632) ;
#99302 = AXIS2_PLACEMENT_3D('',#158407,#123633,#123634) ;
#99303 = AXIS2_PLACEMENT_3D('',#158412,#123636,#123637) ;
#99304 = AXIS2_PLACEMENT_3D('',#158420,#123642,#123643) ;
#99305 = AXIS2_PLACEMENT_3D('',#158421,#123644,#123645) ;
#99306 = AXIS2_PLACEMENT_3D('',#158426,#123647,#123648) ;
#99307 = AXIS2_PLACEMENT_3D('',#158434,#123653,#123654) ;
#99308 = AXIS2_PLACEMENT_3D('',#158435,#123655,#123656) ;
#99309 = AXIS2_PLACEMENT_3D('',#158440,#123658,#123659) ;
#99310 = AXIS2_PLACEMENT_3D('',#158448,#123664,#123665) ;
#99311 = AXIS2_PLACEMENT_3D('',#158449,#123666,#123667) ;
#99312 = AXIS2_PLACEMENT_3D('',#158454,#123669,#123670) ;
#99313 = AXIS2_PLACEMENT_3D('',#158462,#123675,#123676) ;
#99314 = AXIS2_PLACEMENT_3D('',#158463,#123677,#123678) ;
#99315 = AXIS2_PLACEMENT_3D('',#158473,#123684,#123685) ;
#99316 = AXIS2_PLACEMENT_3D('',#158478,#123687,#123688) ;
#99317 = AXIS2_PLACEMENT_3D('',#158486,#123693,#123694) ;
#99318 = AXIS2_PLACEMENT_3D('',#158487,#123695,#123696) ;
#99319 = AXIS2_PLACEMENT_3D('',#158492,#123698,#123699) ;
#99320 = AXIS2_PLACEMENT_3D('',#158500,#123704,#123705) ;
#99321 = AXIS2_PLACEMENT_3D('',#158501,#123706,#123707) ;
#99322 = AXIS2_PLACEMENT_3D('',#158506,#123709,#123710) ;
#99323 = AXIS2_PLACEMENT_3D('',#158514,#123715,#123716) ;
#99324 = AXIS2_PLACEMENT_3D('',#158515,#123717,#123718) ;
#99325 = AXIS2_PLACEMENT_3D('',#158520,#123720,#123721) ;
#99326 = AXIS2_PLACEMENT_3D('',#158528,#123726,#123727) ;
#99327 = AXIS2_PLACEMENT_3D('',#158529,#123728,#123729) ;
#99328 = AXIS2_PLACEMENT_3D('',#158534,#123731,#123732) ;
#99329 = AXIS2_PLACEMENT_3D('',#158542,#123737,#123738) ;
#99330 = AXIS2_PLACEMENT_3D('',#158543,#123739,#123740) ;
#99331 = AXIS2_PLACEMENT_3D('',#158548,#123742,#123743) ;
#99332 = AXIS2_PLACEMENT_3D('',#158556,#123748,#123749) ;
#99333 = AXIS2_PLACEMENT_3D('',#158557,#123750,#123751) ;
#99334 = AXIS2_PLACEMENT_3D('',#158562,#123753,#123754) ;
#99335 = AXIS2_PLACEMENT_3D('',#158570,#123759,#123760) ;
#99336 = AXIS2_PLACEMENT_3D('',#158571,#123761,#123762) ;
#99337 = AXIS2_PLACEMENT_3D('',#158576,#123764,#123765) ;
#99338 = AXIS2_PLACEMENT_3D('',#158584,#123770,#123771) ;
#99339 = AXIS2_PLACEMENT_3D('',#158585,#123772,#123773) ;
#99340 = AXIS2_PLACEMENT_3D('',#158594,#123778,#123779) ;
#99341 = AXIS2_PLACEMENT_3D('',#158603,#123784,#123785) ;
#99342 = AXIS2_PLACEMENT_3D('',#158612,#123790,#123791) ;
#99343 = AXIS2_PLACEMENT_3D('',#158621,#123796,#123797) ;
#99344 = AXIS2_PLACEMENT_3D('',#158630,#123802,#123803) ;
#99345 = AXIS2_PLACEMENT_3D('',#158639,#123808,#123809) ;
#99346 = AXIS2_PLACEMENT_3D('',#158648,#123814,#123815) ;
#99347 = AXIS2_PLACEMENT_3D('',#158657,#123820,#123821) ;
#99348 = AXIS2_PLACEMENT_3D('',#158666,#123826,#123827) ;
#99349 = AXIS2_PLACEMENT_3D('',#158675,#123832,#123833) ;
#99350 = AXIS2_PLACEMENT_3D('',#158684,#123838,#123839) ;
#99351 = AXIS2_PLACEMENT_3D('',#158693,#123844,#123845) ;
#99352 = AXIS2_PLACEMENT_3D('',#158702,#123850,#123851) ;
#99353 = AXIS2_PLACEMENT_3D('',#158711,#123856,#123857) ;
#99354 = AXIS2_PLACEMENT_3D('',#158720,#123862,#123863) ;
#99355 = AXIS2_PLACEMENT_3D('',#158729,#123868,#123869) ;
#99356 = AXIS2_PLACEMENT_3D('',#158738,#123874,#123875) ;
#99357 = AXIS2_PLACEMENT_3D('',#158747,#123880,#123881) ;
#99358 = AXIS2_PLACEMENT_3D('',#158756,#123886,#123887) ;
#99359 = AXIS2_PLACEMENT_3D('',#158765,#123892,#123893) ;
#99360 = AXIS2_PLACEMENT_3D('',#158774,#123898,#123899) ;
#99361 = AXIS2_PLACEMENT_3D('',#158783,#123904,#123905) ;
#99362 = AXIS2_PLACEMENT_3D('',#158792,#123910,#123911) ;
#99363 = AXIS2_PLACEMENT_3D('',#158801,#123916,#123917) ;
#99364 = AXIS2_PLACEMENT_3D('',#158810,#123922,#123923) ;
#99365 = AXIS2_PLACEMENT_3D('',#158819,#123928,#123929) ;
#99366 = AXIS2_PLACEMENT_3D('',#158828,#123934,#123935) ;
#99367 = AXIS2_PLACEMENT_3D('',#158837,#123940,#123941) ;
#99368 = AXIS2_PLACEMENT_3D('',#158846,#123946,#123947) ;
#99369 = AXIS2_PLACEMENT_3D('',#158855,#123952,#123953) ;
#99370 = AXIS2_PLACEMENT_3D('',#158864,#123958,#123959) ;
#99371 = AXIS2_PLACEMENT_3D('',#158873,#123964,#123965) ;
#99372 = AXIS2_PLACEMENT_3D('',#158882,#123970,#123971) ;
#99373 = AXIS2_PLACEMENT_3D('',#158891,#123976,#123977) ;
#99374 = AXIS2_PLACEMENT_3D('',#158900,#123982,#123983) ;
#99375 = AXIS2_PLACEMENT_3D('',#158909,#123988,#123989) ;
#99376 = AXIS2_PLACEMENT_3D('',#158922,#123995,#123996) ;
#99377 = AXIS2_PLACEMENT_3D('',#158926,#123998,#123999) ;
#99378 = AXIS2_PLACEMENT_3D('',#158930,#124001,#124002) ;
#99379 = AXIS2_PLACEMENT_3D('',#158933,#124004,#124005) ;
#99380 = AXIS2_PLACEMENT_3D('',#158934,#124006,#124007) ;
#99381 = AXIS2_PLACEMENT_3D('',#158940,#124011,#124012) ;
#99382 = AXIS2_PLACEMENT_3D('',#158946,#124016,#124017) ;
#99383 = AXIS2_PLACEMENT_3D('',#158952,#124021,#124022) ;
#99384 = AXIS2_PLACEMENT_3D('',#158958,#124026,#124027) ;
#99385 = AXIS2_PLACEMENT_3D('',#158971,#124033,#124034) ;
#99386 = AXIS2_PLACEMENT_3D('',#158975,#124036,#124037) ;
#99387 = AXIS2_PLACEMENT_3D('',#158979,#124039,#124040) ;
#99388 = AXIS2_PLACEMENT_3D('',#158982,#124042,#124043) ;
#99389 = AXIS2_PLACEMENT_3D('',#158983,#124044,#124045) ;
#99390 = AXIS2_PLACEMENT_3D('',#158989,#124049,#124050) ;
#99391 = AXIS2_PLACEMENT_3D('',#158995,#124054,#124055) ;
#99392 = AXIS2_PLACEMENT_3D('',#159001,#124059,#124060) ;
#99393 = AXIS2_PLACEMENT_3D('',#159007,#124064,#124065) ;
#99394 = AXIS2_PLACEMENT_3D('',#159020,#124071,#124072) ;
#99395 = AXIS2_PLACEMENT_3D('',#159024,#124074,#124075) ;
#99396 = AXIS2_PLACEMENT_3D('',#159028,#124077,#124078) ;
#99397 = AXIS2_PLACEMENT_3D('',#159031,#124080,#124081) ;
#99398 = AXIS2_PLACEMENT_3D('',#159032,#124082,#124083) ;
#99399 = AXIS2_PLACEMENT_3D('',#159038,#124087,#124088) ;
#99400 = AXIS2_PLACEMENT_3D('',#159044,#124092,#124093) ;
#99401 = AXIS2_PLACEMENT_3D('',#159050,#124097,#124098) ;
#99402 = AXIS2_PLACEMENT_3D('',#159056,#124102,#124103) ;
#99403 = AXIS2_PLACEMENT_3D('',#159069,#124109,#124110) ;
#99404 = AXIS2_PLACEMENT_3D('',#159073,#124112,#124113) ;
#99405 = AXIS2_PLACEMENT_3D('',#159077,#124115,#124116) ;
#99406 = AXIS2_PLACEMENT_3D('',#159080,#124118,#124119) ;
#99407 = AXIS2_PLACEMENT_3D('',#159081,#124120,#124121) ;
#99408 = AXIS2_PLACEMENT_3D('',#159087,#124125,#124126) ;
#99409 = AXIS2_PLACEMENT_3D('',#159093,#124130,#124131) ;
#99410 = AXIS2_PLACEMENT_3D('',#159099,#124135,#124136) ;
#99411 = AXIS2_PLACEMENT_3D('',#159105,#124140,#124141) ;
#99412 = AXIS2_PLACEMENT_3D('',#159118,#124147,#124148) ;
#99413 = AXIS2_PLACEMENT_3D('',#159122,#124150,#124151) ;
#99414 = AXIS2_PLACEMENT_3D('',#159126,#124153,#124154) ;
#99415 = AXIS2_PLACEMENT_3D('',#159129,#124156,#124157) ;
#99416 = AXIS2_PLACEMENT_3D('',#159130,#124158,#124159) ;
#99417 = AXIS2_PLACEMENT_3D('',#159136,#124163,#124164) ;
#99418 = AXIS2_PLACEMENT_3D('',#159142,#124168,#124169) ;
#99419 = AXIS2_PLACEMENT_3D('',#159148,#124173,#124174) ;
#99420 = AXIS2_PLACEMENT_3D('',#159154,#124178,#124179) ;
#99421 = AXIS2_PLACEMENT_3D('',#159167,#124185,#124186) ;
#99422 = AXIS2_PLACEMENT_3D('',#159171,#124188,#124189) ;
#99423 = AXIS2_PLACEMENT_3D('',#159175,#124191,#124192) ;
#99424 = AXIS2_PLACEMENT_3D('',#159178,#124194,#124195) ;
#99425 = AXIS2_PLACEMENT_3D('',#159179,#124196,#124197) ;
#99426 = AXIS2_PLACEMENT_3D('',#159185,#124201,#124202) ;
#99427 = AXIS2_PLACEMENT_3D('',#159191,#124206,#124207) ;
#99428 = AXIS2_PLACEMENT_3D('',#159197,#124211,#124212) ;
#99429 = AXIS2_PLACEMENT_3D('',#159203,#124216,#124217) ;
#99430 = AXIS2_PLACEMENT_3D('',#159216,#124223,#124224) ;
#99431 = AXIS2_PLACEMENT_3D('',#159220,#124226,#124227) ;
#99432 = AXIS2_PLACEMENT_3D('',#159224,#124229,#124230) ;
#99433 = AXIS2_PLACEMENT_3D('',#159227,#124232,#124233) ;
#99434 = AXIS2_PLACEMENT_3D('',#159228,#124234,#124235) ;
#99435 = AXIS2_PLACEMENT_3D('',#159234,#124239,#124240) ;
#99436 = AXIS2_PLACEMENT_3D('',#159240,#124244,#124245) ;
#99437 = AXIS2_PLACEMENT_3D('',#159246,#124249,#124250) ;
#99438 = AXIS2_PLACEMENT_3D('',#159252,#124254,#124255) ;
#99439 = AXIS2_PLACEMENT_3D('',#159265,#124261,#124262) ;
#99440 = AXIS2_PLACEMENT_3D('',#159269,#124264,#124265) ;
#99441 = AXIS2_PLACEMENT_3D('',#159273,#124267,#124268) ;
#99442 = AXIS2_PLACEMENT_3D('',#159276,#124270,#124271) ;
#99443 = AXIS2_PLACEMENT_3D('',#159277,#124272,#124273) ;
#99444 = AXIS2_PLACEMENT_3D('',#159283,#124277,#124278) ;
#99445 = AXIS2_PLACEMENT_3D('',#159289,#124282,#124283) ;
#99446 = AXIS2_PLACEMENT_3D('',#159295,#124287,#124288) ;
#99447 = AXIS2_PLACEMENT_3D('',#159301,#124292,#124293) ;
#99448 = AXIS2_PLACEMENT_3D('',#159314,#124299,#124300) ;
#99449 = AXIS2_PLACEMENT_3D('',#159318,#124302,#124303) ;
#99450 = AXIS2_PLACEMENT_3D('',#159322,#124305,#124306) ;
#99451 = AXIS2_PLACEMENT_3D('',#159325,#124308,#124309) ;
#99452 = AXIS2_PLACEMENT_3D('',#159326,#124310,#124311) ;
#99453 = AXIS2_PLACEMENT_3D('',#159332,#124315,#124316) ;
#99454 = AXIS2_PLACEMENT_3D('',#159338,#124320,#124321) ;
#99455 = AXIS2_PLACEMENT_3D('',#159344,#124325,#124326) ;
#99456 = AXIS2_PLACEMENT_3D('',#159350,#124330,#124331) ;
#99457 = AXIS2_PLACEMENT_3D('',#159359,#124336,#124337) ;
#99458 = AXIS2_PLACEMENT_3D('',#159368,#124342,#124343) ;
#99459 = AXIS2_PLACEMENT_3D('',#159377,#124348,#124349) ;
#99460 = AXIS2_PLACEMENT_3D('',#159386,#124354,#124355) ;
#99461 = AXIS2_PLACEMENT_3D('',#159395,#124360,#124361) ;
#99462 = AXIS2_PLACEMENT_3D('',#159404,#124366,#124367) ;
#99463 = AXIS2_PLACEMENT_3D('',#159413,#124372,#124373) ;
#99464 = AXIS2_PLACEMENT_3D('',#159422,#124378,#124379) ;
#99465 = AXIS2_PLACEMENT_3D('',#159431,#124384,#124385) ;
#99466 = AXIS2_PLACEMENT_3D('',#159434,#124386,#124387) ;
#99467 = AXIS2_PLACEMENT_3D('',#159436,#124388,#124389) ;
#99468 = AXIS2_PLACEMENT_3D('',#159446,#124394,#124395) ;
#99469 = AXIS2_PLACEMENT_3D('',#159452,#124399,#124400) ;
#99470 = AXIS2_PLACEMENT_3D('',#159461,#124405,#124406) ;
#99471 = AXIS2_PLACEMENT_3D('',#159466,#124408,#124409) ;
#99472 = AXIS2_PLACEMENT_3D('',#159468,#124410,#124411) ;
#99473 = AXIS2_PLACEMENT_3D('',#159476,#124415,#124416) ;
#99474 = AXIS2_PLACEMENT_3D('',#159482,#124420,#124421) ;
#99475 = AXIS2_PLACEMENT_3D('',#159491,#124426,#124427) ;
#99476 = AXIS2_PLACEMENT_3D('',#159494,#124428,#124429) ;
#99477 = AXIS2_PLACEMENT_3D('',#159496,#124430,#124431) ;
#99478 = AXIS2_PLACEMENT_3D('',#159506,#124436,#124437) ;
#99479 = AXIS2_PLACEMENT_3D('',#159512,#124441,#124442) ;
#99480 = AXIS2_PLACEMENT_3D('',#159521,#124447,#124448) ;
#99481 = AXIS2_PLACEMENT_3D('',#159526,#124450,#124451) ;
#99482 = AXIS2_PLACEMENT_3D('',#159528,#124452,#124453) ;
#99483 = AXIS2_PLACEMENT_3D('',#159536,#124457,#124458) ;
#99484 = AXIS2_PLACEMENT_3D('',#159542,#124462,#124463) ;
#99485 = AXIS2_PLACEMENT_3D('',#159551,#124468,#124469) ;
#99486 = AXIS2_PLACEMENT_3D('',#159554,#124470,#124471) ;
#99487 = AXIS2_PLACEMENT_3D('',#159556,#124472,#124473) ;
#99488 = AXIS2_PLACEMENT_3D('',#159566,#124478,#124479) ;
#99489 = AXIS2_PLACEMENT_3D('',#159572,#124483,#124484) ;
#99490 = AXIS2_PLACEMENT_3D('',#159581,#124489,#124490) ;
#99491 = AXIS2_PLACEMENT_3D('',#159586,#124492,#124493) ;
#99492 = AXIS2_PLACEMENT_3D('',#159588,#124494,#124495) ;
#99493 = AXIS2_PLACEMENT_3D('',#159596,#124499,#124500) ;
#99494 = AXIS2_PLACEMENT_3D('',#159602,#124504,#124505) ;
#99495 = AXIS2_PLACEMENT_3D('',#159611,#124510,#124511) ;
#99496 = AXIS2_PLACEMENT_3D('',#159614,#124512,#124513) ;
#99497 = AXIS2_PLACEMENT_3D('',#159616,#124514,#124515) ;
#99498 = AXIS2_PLACEMENT_3D('',#159626,#124520,#124521) ;
#99499 = AXIS2_PLACEMENT_3D('',#159632,#124525,#124526) ;
#99500 = AXIS2_PLACEMENT_3D('',#159641,#124531,#124532) ;
#99501 = AXIS2_PLACEMENT_3D('',#159646,#124534,#124535) ;
#99502 = AXIS2_PLACEMENT_3D('',#159648,#124536,#124537) ;
#99503 = AXIS2_PLACEMENT_3D('',#159656,#124541,#124542) ;
#99504 = AXIS2_PLACEMENT_3D('',#159662,#124546,#124547) ;
#99505 = AXIS2_PLACEMENT_3D('',#159671,#124552,#124553) ;
#99506 = AXIS2_PLACEMENT_3D('',#159674,#124554,#124555) ;
#99507 = AXIS2_PLACEMENT_3D('',#159676,#124556,#124557) ;
#99508 = AXIS2_PLACEMENT_3D('',#159686,#124562,#124563) ;
#99509 = AXIS2_PLACEMENT_3D('',#159692,#124567,#124568) ;
#99510 = AXIS2_PLACEMENT_3D('',#159701,#124573,#124574) ;
#99511 = AXIS2_PLACEMENT_3D('',#159706,#124576,#124577) ;
#99512 = AXIS2_PLACEMENT_3D('',#159708,#124578,#124579) ;
#99513 = AXIS2_PLACEMENT_3D('',#159716,#124583,#124584) ;
#99514 = AXIS2_PLACEMENT_3D('',#159722,#124588,#124589) ;
#99515 = AXIS2_PLACEMENT_3D('',#159731,#124594,#124595) ;
#99516 = AXIS2_PLACEMENT_3D('',#159734,#124596,#124597) ;
#99517 = AXIS2_PLACEMENT_3D('',#159736,#124598,#124599) ;
#99518 = AXIS2_PLACEMENT_3D('',#159746,#124604,#124605) ;
#99519 = AXIS2_PLACEMENT_3D('',#159752,#124609,#124610) ;
#99520 = AXIS2_PLACEMENT_3D('',#159761,#124615,#124616) ;
#99521 = AXIS2_PLACEMENT_3D('',#159766,#124618,#124619) ;
#99522 = AXIS2_PLACEMENT_3D('',#159768,#124620,#124621) ;
#99523 = AXIS2_PLACEMENT_3D('',#159776,#124625,#124626) ;
#99524 = AXIS2_PLACEMENT_3D('',#159782,#124630,#124631) ;
#99525 = AXIS2_PLACEMENT_3D('',#159791,#124636,#124637) ;
#99526 = AXIS2_PLACEMENT_3D('',#159794,#124638,#124639) ;
#99527 = AXIS2_PLACEMENT_3D('',#159796,#124640,#124641) ;
#99528 = AXIS2_PLACEMENT_3D('',#159806,#124646,#124647) ;
#99529 = AXIS2_PLACEMENT_3D('',#159812,#124651,#124652) ;
#99530 = AXIS2_PLACEMENT_3D('',#159821,#124657,#124658) ;
#99531 = AXIS2_PLACEMENT_3D('',#159826,#124660,#124661) ;
#99532 = AXIS2_PLACEMENT_3D('',#159828,#124662,#124663) ;
#99533 = AXIS2_PLACEMENT_3D('',#159836,#124667,#124668) ;
#99534 = AXIS2_PLACEMENT_3D('',#159842,#124672,#124673) ;
#99535 = AXIS2_PLACEMENT_3D('',#159851,#124678,#124679) ;
#99536 = AXIS2_PLACEMENT_3D('',#159854,#124680,#124681) ;
#99537 = AXIS2_PLACEMENT_3D('',#159856,#124682,#124683) ;
#99538 = AXIS2_PLACEMENT_3D('',#159866,#124688,#124689) ;
#99539 = AXIS2_PLACEMENT_3D('',#159872,#124693,#124694) ;
#99540 = AXIS2_PLACEMENT_3D('',#159881,#124699,#124700) ;
#99541 = AXIS2_PLACEMENT_3D('',#159886,#124702,#124703) ;
#99542 = AXIS2_PLACEMENT_3D('',#159888,#124704,#124705) ;
#99543 = AXIS2_PLACEMENT_3D('',#159896,#124709,#124710) ;
#99544 = AXIS2_PLACEMENT_3D('',#159902,#124714,#124715) ;
#99545 = AXIS2_PLACEMENT_3D('',#159911,#124720,#124721) ;
#99546 = AXIS2_PLACEMENT_3D('',#159914,#124722,#124723) ;
#99547 = AXIS2_PLACEMENT_3D('',#159916,#124724,#124725) ;
#99548 = AXIS2_PLACEMENT_3D('',#159926,#124730,#124731) ;
#99549 = AXIS2_PLACEMENT_3D('',#159932,#124735,#124736) ;
#99550 = AXIS2_PLACEMENT_3D('',#159941,#124741,#124742) ;
#99551 = AXIS2_PLACEMENT_3D('',#159946,#124744,#124745) ;
#99552 = AXIS2_PLACEMENT_3D('',#159948,#124746,#124747) ;
#99553 = AXIS2_PLACEMENT_3D('',#159956,#124751,#124752) ;
#99554 = AXIS2_PLACEMENT_3D('',#159962,#124756,#124757) ;
#99555 = AXIS2_PLACEMENT_3D('',#159971,#124762,#124763) ;
#99556 = AXIS2_PLACEMENT_3D('',#159980,#124768,#124769) ;
#99557 = AXIS2_PLACEMENT_3D('',#159989,#124774,#124775) ;
#99558 = AXIS2_PLACEMENT_3D('',#159994,#124777,#124778) ;
#99559 = AXIS2_PLACEMENT_3D('',#159997,#124780,#124781) ;
#99560 = AXIS2_PLACEMENT_3D('',#159998,#124782,#124783) ;
#99561 = AXIS2_PLACEMENT_3D('',#160003,#124785,#124786) ;
#99562 = AXIS2_PLACEMENT_3D('',#160011,#124791,#124792) ;
#99563 = AXIS2_PLACEMENT_3D('',#160020,#124797,#124798) ;
#99564 = AXIS2_PLACEMENT_3D('',#160029,#124803,#124804) ;
#99565 = AXIS2_PLACEMENT_3D('',#160034,#124806,#124807) ;
#99566 = AXIS2_PLACEMENT_3D('',#160037,#124809,#124810) ;
#99567 = AXIS2_PLACEMENT_3D('',#160038,#124811,#124812) ;
#99568 = AXIS2_PLACEMENT_3D('',#160043,#124814,#124815) ;
#99569 = AXIS2_PLACEMENT_3D('',#160051,#124820,#124821) ;
#99570 = AXIS2_PLACEMENT_3D('',#160060,#124826,#124827) ;
#99571 = AXIS2_PLACEMENT_3D('',#160069,#124832,#124833) ;
#99572 = AXIS2_PLACEMENT_3D('',#160074,#124835,#124836) ;
#99573 = AXIS2_PLACEMENT_3D('',#160077,#124838,#124839) ;
#99574 = AXIS2_PLACEMENT_3D('',#160078,#124840,#124841) ;
#99575 = AXIS2_PLACEMENT_3D('',#160083,#124843,#124844) ;
#99576 = AXIS2_PLACEMENT_3D('',#160091,#124849,#124850) ;
#99577 = AXIS2_PLACEMENT_3D('',#160100,#124855,#124856) ;
#99578 = AXIS2_PLACEMENT_3D('',#160109,#124861,#124862) ;
#99579 = AXIS2_PLACEMENT_3D('',#160114,#124864,#124865) ;
#99580 = AXIS2_PLACEMENT_3D('',#160117,#124867,#124868) ;
#99581 = AXIS2_PLACEMENT_3D('',#160118,#124869,#124870) ;
#99582 = AXIS2_PLACEMENT_3D('',#160123,#124872,#124873) ;
#99583 = AXIS2_PLACEMENT_3D('',#160131,#124878,#124879) ;
#99584 = AXIS2_PLACEMENT_3D('',#160140,#124884,#124885) ;
#99585 = AXIS2_PLACEMENT_3D('',#160149,#124890,#124891) ;
#99586 = AXIS2_PLACEMENT_3D('',#160154,#124893,#124894) ;
#99587 = AXIS2_PLACEMENT_3D('',#160157,#124896,#124897) ;
#99588 = AXIS2_PLACEMENT_3D('',#160158,#124898,#124899) ;
#99589 = AXIS2_PLACEMENT_3D('',#160163,#124901,#124902) ;
#99590 = AXIS2_PLACEMENT_3D('',#160171,#124907,#124908) ;
#99591 = AXIS2_PLACEMENT_3D('',#160180,#124913,#124914) ;
#99592 = AXIS2_PLACEMENT_3D('',#160189,#124919,#124920) ;
#99593 = AXIS2_PLACEMENT_3D('',#160194,#124922,#124923) ;
#99594 = AXIS2_PLACEMENT_3D('',#160197,#124925,#124926) ;
#99595 = AXIS2_PLACEMENT_3D('',#160198,#124927,#124928) ;
#99596 = AXIS2_PLACEMENT_3D('',#160203,#124930,#124931) ;
#99597 = AXIS2_PLACEMENT_3D('',#160211,#124936,#124937) ;
#99598 = AXIS2_PLACEMENT_3D('',#160220,#124942,#124943) ;
#99599 = AXIS2_PLACEMENT_3D('',#160229,#124948,#124949) ;
#99600 = AXIS2_PLACEMENT_3D('',#160234,#124951,#124952) ;
#99601 = AXIS2_PLACEMENT_3D('',#160237,#124954,#124955) ;
#99602 = AXIS2_PLACEMENT_3D('',#160238,#124956,#124957) ;
#99603 = AXIS2_PLACEMENT_3D('',#160243,#124959,#124960) ;
#99604 = AXIS2_PLACEMENT_3D('',#160251,#124965,#124966) ;
#99605 = AXIS2_PLACEMENT_3D('',#160260,#124971,#124972) ;
#99606 = AXIS2_PLACEMENT_3D('',#160269,#124977,#124978) ;
#99607 = AXIS2_PLACEMENT_3D('',#160274,#124980,#124981) ;
#99608 = AXIS2_PLACEMENT_3D('',#160277,#124983,#124984) ;
#99609 = AXIS2_PLACEMENT_3D('',#160278,#124985,#124986) ;
#99610 = AXIS2_PLACEMENT_3D('',#160283,#124988,#124989) ;
#99611 = AXIS2_PLACEMENT_3D('',#160291,#124994,#124995) ;
#99612 = AXIS2_PLACEMENT_3D('',#160300,#125000,#125001) ;
#99613 = AXIS2_PLACEMENT_3D('',#160309,#125006,#125007) ;
#99614 = AXIS2_PLACEMENT_3D('',#160314,#125009,#125010) ;
#99615 = AXIS2_PLACEMENT_3D('',#160317,#125012,#125013) ;
#99616 = AXIS2_PLACEMENT_3D('',#160318,#125014,#125015) ;
#99617 = AXIS2_PLACEMENT_3D('',#160323,#125017,#125018) ;
#99618 = AXIS2_PLACEMENT_3D('',#160331,#125023,#125024) ;
#99619 = AXIS2_PLACEMENT_3D('',#160332,#125025,#125026) ;
#99620 = AXIS2_PLACEMENT_3D('',#160333,#125027,#125028) ;
#99621 = AXIS2_PLACEMENT_3D('',#160334,#125029,#125030) ;
#99622 = AXIS2_PLACEMENT_3D('',#160335,#125031,#125032) ;
#99623 = AXIS2_PLACEMENT_3D('',#160336,#125033,#125034) ;
#99624 = AXIS2_PLACEMENT_3D('',#160337,#125035,#125036) ;
#99625 = AXIS2_PLACEMENT_3D('',#160338,#125037,#125038) ;
#99626 = AXIS2_PLACEMENT_3D('',#160339,#125039,#125040) ;
#99627 = AXIS2_PLACEMENT_3D('',#160340,#125041,#125042) ;
#99628 = AXIS2_PLACEMENT_3D('',#160349,#125047,#125048) ;
#99629 = AXIS2_PLACEMENT_3D('',#160358,#125053,#125054) ;
#99630 = AXIS2_PLACEMENT_3D('',#160367,#125059,#125060) ;
#99631 = AXIS2_PLACEMENT_3D('',#160376,#125065,#125066) ;
#99632 = AXIS2_PLACEMENT_3D('',#160385,#125071,#125072) ;
#99633 = AXIS2_PLACEMENT_3D('',#160394,#125077,#125078) ;
#99634 = AXIS2_PLACEMENT_3D('',#160403,#125083,#125084) ;
#99635 = AXIS2_PLACEMENT_3D('',#160412,#125089,#125090) ;
#99636 = AXIS2_PLACEMENT_3D('',#160421,#125095,#125096) ;
#99637 = AXIS2_PLACEMENT_3D('',#160430,#125101,#125102) ;
#99638 = AXIS2_PLACEMENT_3D('',#160439,#125107,#125108) ;
#99639 = AXIS2_PLACEMENT_3D('',#160448,#125113,#125114) ;
#99640 = AXIS2_PLACEMENT_3D('',#160457,#125119,#125120) ;
#99641 = AXIS2_PLACEMENT_3D('',#160466,#125125,#125126) ;
#99642 = AXIS2_PLACEMENT_3D('',#160475,#125131,#125132) ;
#99643 = AXIS2_PLACEMENT_3D('',#160484,#125137,#125138) ;
#99644 = AXIS2_PLACEMENT_3D('',#160493,#125143,#125144) ;
#99645 = AXIS2_PLACEMENT_3D('',#160502,#125149,#125150) ;
#99646 = AXIS2_PLACEMENT_3D('',#160511,#125155,#125156) ;
#99647 = AXIS2_PLACEMENT_3D('',#160520,#125161,#125162) ;
#99648 = AXIS2_PLACEMENT_3D('',#160529,#125167,#125168) ;
#99649 = AXIS2_PLACEMENT_3D('',#160538,#125173,#125174) ;
#99650 = AXIS2_PLACEMENT_3D('',#160547,#125179,#125180) ;
#99651 = AXIS2_PLACEMENT_3D('',#160556,#125185,#125186) ;
#99652 = AXIS2_PLACEMENT_3D('',#160565,#125191,#125192) ;
#99653 = AXIS2_PLACEMENT_3D('',#160574,#125197,#125198) ;
#99654 = AXIS2_PLACEMENT_3D('',#160583,#125203,#125204) ;
#99655 = AXIS2_PLACEMENT_3D('',#160592,#125209,#125210) ;
#99656 = AXIS2_PLACEMENT_3D('',#160601,#125215,#125216) ;
#99657 = AXIS2_PLACEMENT_3D('',#160610,#125221,#125222) ;
#99658 = AXIS2_PLACEMENT_3D('',#160619,#125227,#125228) ;
#99659 = AXIS2_PLACEMENT_3D('',#160628,#125233,#125234) ;
#99660 = AXIS2_PLACEMENT_3D('',#160637,#125239,#125240) ;
#99661 = AXIS2_PLACEMENT_3D('',#160646,#125245,#125246) ;
#99662 = AXIS2_PLACEMENT_3D('',#160655,#125251,#125252) ;
#99663 = AXIS2_PLACEMENT_3D('',#160664,#125257,#125258) ;
#99664 = AXIS2_PLACEMENT_3D('',#160677,#125264,#125265) ;
#99665 = AXIS2_PLACEMENT_3D('',#160681,#125267,#125268) ;
#99666 = AXIS2_PLACEMENT_3D('',#160685,#125270,#125271) ;
#99667 = AXIS2_PLACEMENT_3D('',#160688,#125273,#125274) ;
#99668 = AXIS2_PLACEMENT_3D('',#160689,#125275,#125276) ;
#99669 = AXIS2_PLACEMENT_3D('',#160695,#125280,#125281) ;
#99670 = AXIS2_PLACEMENT_3D('',#160701,#125285,#125286) ;
#99671 = AXIS2_PLACEMENT_3D('',#160707,#125290,#125291) ;
#99672 = AXIS2_PLACEMENT_3D('',#160713,#125295,#125296) ;
#99673 = AXIS2_PLACEMENT_3D('',#160726,#125302,#125303) ;
#99674 = AXIS2_PLACEMENT_3D('',#160730,#125305,#125306) ;
#99675 = AXIS2_PLACEMENT_3D('',#160734,#125308,#125309) ;
#99676 = AXIS2_PLACEMENT_3D('',#160737,#125311,#125312) ;
#99677 = AXIS2_PLACEMENT_3D('',#160738,#125313,#125314) ;
#99678 = AXIS2_PLACEMENT_3D('',#160744,#125318,#125319) ;
#99679 = AXIS2_PLACEMENT_3D('',#160750,#125323,#125324) ;
#99680 = AXIS2_PLACEMENT_3D('',#160756,#125328,#125329) ;
#99681 = AXIS2_PLACEMENT_3D('',#160762,#125333,#125334) ;
#99682 = AXIS2_PLACEMENT_3D('',#160775,#125340,#125341) ;
#99683 = AXIS2_PLACEMENT_3D('',#160779,#125343,#125344) ;
#99684 = AXIS2_PLACEMENT_3D('',#160783,#125346,#125347) ;
#99685 = AXIS2_PLACEMENT_3D('',#160786,#125349,#125350) ;
#99686 = AXIS2_PLACEMENT_3D('',#160787,#125351,#125352) ;
#99687 = AXIS2_PLACEMENT_3D('',#160793,#125356,#125357) ;
#99688 = AXIS2_PLACEMENT_3D('',#160799,#125361,#125362) ;
#99689 = AXIS2_PLACEMENT_3D('',#160805,#125366,#125367) ;
#99690 = AXIS2_PLACEMENT_3D('',#160811,#125371,#125372) ;
#99691 = AXIS2_PLACEMENT_3D('',#160824,#125378,#125379) ;
#99692 = AXIS2_PLACEMENT_3D('',#160828,#125381,#125382) ;
#99693 = AXIS2_PLACEMENT_3D('',#160832,#125384,#125385) ;
#99694 = AXIS2_PLACEMENT_3D('',#160835,#125387,#125388) ;
#99695 = AXIS2_PLACEMENT_3D('',#160836,#125389,#125390) ;
#99696 = AXIS2_PLACEMENT_3D('',#160842,#125394,#125395) ;
#99697 = AXIS2_PLACEMENT_3D('',#160848,#125399,#125400) ;
#99698 = AXIS2_PLACEMENT_3D('',#160854,#125404,#125405) ;
#99699 = AXIS2_PLACEMENT_3D('',#160860,#125409,#125410) ;
#99700 = AXIS2_PLACEMENT_3D('',#160873,#125416,#125417) ;
#99701 = AXIS2_PLACEMENT_3D('',#160877,#125419,#125420) ;
#99702 = AXIS2_PLACEMENT_3D('',#160881,#125422,#125423) ;
#99703 = AXIS2_PLACEMENT_3D('',#160884,#125425,#125426) ;
#99704 = AXIS2_PLACEMENT_3D('',#160885,#125427,#125428) ;
#99705 = AXIS2_PLACEMENT_3D('',#160891,#125432,#125433) ;
#99706 = AXIS2_PLACEMENT_3D('',#160897,#125437,#125438) ;
#99707 = AXIS2_PLACEMENT_3D('',#160903,#125442,#125443) ;
#99708 = AXIS2_PLACEMENT_3D('',#160909,#125447,#125448) ;
#99709 = AXIS2_PLACEMENT_3D('',#160922,#125454,#125455) ;
#99710 = AXIS2_PLACEMENT_3D('',#160926,#125457,#125458) ;
#99711 = AXIS2_PLACEMENT_3D('',#160930,#125460,#125461) ;
#99712 = AXIS2_PLACEMENT_3D('',#160933,#125463,#125464) ;
#99713 = AXIS2_PLACEMENT_3D('',#160934,#125465,#125466) ;
#99714 = AXIS2_PLACEMENT_3D('',#160940,#125470,#125471) ;
#99715 = AXIS2_PLACEMENT_3D('',#160946,#125475,#125476) ;
#99716 = AXIS2_PLACEMENT_3D('',#160952,#125480,#125481) ;
#99717 = AXIS2_PLACEMENT_3D('',#160958,#125485,#125486) ;
#99718 = AXIS2_PLACEMENT_3D('',#160971,#125492,#125493) ;
#99719 = AXIS2_PLACEMENT_3D('',#160975,#125495,#125496) ;
#99720 = AXIS2_PLACEMENT_3D('',#160979,#125498,#125499) ;
#99721 = AXIS2_PLACEMENT_3D('',#160982,#125501,#125502) ;
#99722 = AXIS2_PLACEMENT_3D('',#160983,#125503,#125504) ;
#99723 = AXIS2_PLACEMENT_3D('',#160989,#125508,#125509) ;
#99724 = AXIS2_PLACEMENT_3D('',#160995,#125513,#125514) ;
#99725 = AXIS2_PLACEMENT_3D('',#161001,#125518,#125519) ;
#99726 = AXIS2_PLACEMENT_3D('',#161007,#125523,#125524) ;
#99727 = AXIS2_PLACEMENT_3D('',#161020,#125530,#125531) ;
#99728 = AXIS2_PLACEMENT_3D('',#161024,#125533,#125534) ;
#99729 = AXIS2_PLACEMENT_3D('',#161028,#125536,#125537) ;
#99730 = AXIS2_PLACEMENT_3D('',#161031,#125539,#125540) ;
#99731 = AXIS2_PLACEMENT_3D('',#161032,#125541,#125542) ;
#99732 = AXIS2_PLACEMENT_3D('',#161038,#125546,#125547) ;
#99733 = AXIS2_PLACEMENT_3D('',#161044,#125551,#125552) ;
#99734 = AXIS2_PLACEMENT_3D('',#161050,#125556,#125557) ;
#99735 = AXIS2_PLACEMENT_3D('',#161056,#125561,#125562) ;
#99736 = AXIS2_PLACEMENT_3D('',#161069,#125568,#125569) ;
#99737 = AXIS2_PLACEMENT_3D('',#161073,#125571,#125572) ;
#99738 = AXIS2_PLACEMENT_3D('',#161077,#125574,#125575) ;
#99739 = AXIS2_PLACEMENT_3D('',#161080,#125577,#125578) ;
#99740 = AXIS2_PLACEMENT_3D('',#161081,#125579,#125580) ;
#99741 = AXIS2_PLACEMENT_3D('',#161087,#125584,#125585) ;
#99742 = AXIS2_PLACEMENT_3D('',#161093,#125589,#125590) ;
#99743 = AXIS2_PLACEMENT_3D('',#161099,#125594,#125595) ;
#99744 = AXIS2_PLACEMENT_3D('',#161105,#125599,#125600) ;
#99745 = AXIS2_PLACEMENT_3D('',#161114,#125605,#125606) ;
#99746 = AXIS2_PLACEMENT_3D('',#161123,#125611,#125612) ;
#99747 = AXIS2_PLACEMENT_3D('',#161132,#125617,#125618) ;
#99748 = AXIS2_PLACEMENT_3D('',#161141,#125623,#125624) ;
#99749 = AXIS2_PLACEMENT_3D('',#161150,#125629,#125630) ;
#99750 = AXIS2_PLACEMENT_3D('',#161159,#125635,#125636) ;
#99751 = AXIS2_PLACEMENT_3D('',#161168,#125641,#125642) ;
#99752 = AXIS2_PLACEMENT_3D('',#161177,#125647,#125648) ;
#99753 = AXIS2_PLACEMENT_3D('',#161186,#125653,#125654) ;
#99754 = AXIS2_PLACEMENT_3D('',#161188,#125656,#125657) ;
#99755 = AXIS2_PLACEMENT_3D('',#161190,#125659,#125660) ;
#99756 = AXIS2_PLACEMENT_3D('',#161192,#125662,#125663) ;
#99757 = AXIS2_PLACEMENT_3D('',#161194,#125665,#125666) ;
#99758 = AXIS2_PLACEMENT_3D('',#161196,#125668,#125669) ;
#99759 = AXIS2_PLACEMENT_3D('',#161198,#125671,#125672) ;
#99760 = AXIS2_PLACEMENT_3D('',#161200,#125674,#125675) ;
#99761 = AXIS2_PLACEMENT_3D('',#161202,#125677,#125678) ;
#99762 = AXIS2_PLACEMENT_3D('',#161204,#125680,#125681) ;
#99763 = AXIS2_PLACEMENT_3D('',#161207,#125684,#125685) ;
#99764 = AXIS2_PLACEMENT_3D('',#161210,#125688,#125689) ;
#99765 = AXIS2_PLACEMENT_3D('',#161213,#125692,#125693) ;
#99766 = AXIS2_PLACEMENT_3D('',#161216,#125696,#125697) ;
#99767 = AXIS2_PLACEMENT_3D('',#161219,#125700,#125701) ;
#99768 = AXIS2_PLACEMENT_3D('',#161222,#125704,#125705) ;
#99769 = AXIS2_PLACEMENT_3D('',#161225,#125708,#125709) ;
#99770 = AXIS2_PLACEMENT_3D('',#161228,#125712,#125713) ;
#99771 = AXIS2_PLACEMENT_3D('',#161231,#125716,#125717) ;
#99772 = AXIS2_PLACEMENT_3D('',#161234,#125720,#125721) ;
#99773 = AXIS2_PLACEMENT_3D('',#161237,#125724,#125725) ;
#99774 = AXIS2_PLACEMENT_3D('',#161240,#125728,#125729) ;
#99775 = AXIS2_PLACEMENT_3D('',#161243,#125732,#125733) ;
#99776 = AXIS2_PLACEMENT_3D('',#161246,#125736,#125737) ;
#99777 = AXIS2_PLACEMENT_3D('',#161249,#125740,#125741) ;
#99778 = AXIS2_PLACEMENT_3D('',#161252,#125744,#125745) ;
#99779 = AXIS2_PLACEMENT_3D('',#161255,#125748,#125749) ;
#99780 = AXIS2_PLACEMENT_3D('',#161258,#125752,#125753) ;
#99781 = AXIS2_PLACEMENT_3D('',#161261,#125756,#125757) ;
#99782 = AXIS2_PLACEMENT_3D('',#161264,#125760,#125761) ;
#99783 = AXIS2_PLACEMENT_3D('',#161267,#125764,#125765) ;
#99784 = AXIS2_PLACEMENT_3D('',#161270,#125768,#125769) ;
#99785 = AXIS2_PLACEMENT_3D('',#161273,#125772,#125773) ;
#99786 = AXIS2_PLACEMENT_3D('',#161276,#125776,#125777) ;
#99787 = AXIS2_PLACEMENT_3D('',#161279,#125780,#125781) ;
#99788 = AXIS2_PLACEMENT_3D('',#161282,#125784,#125785) ;
#99789 = AXIS2_PLACEMENT_3D('',#161285,#125788,#125789) ;
#99790 = AXIS2_PLACEMENT_3D('',#161290,#125791,#125792) ;
#99791 = AXIS2_PLACEMENT_3D('',#161293,#125794,#125795) ;
#99792 = AXIS2_PLACEMENT_3D('',#161294,#125796,#125797) ;
#99793 = AXIS2_PLACEMENT_3D('',#161300,#125801,#125802) ;
#99794 = AXIS2_PLACEMENT_3D('',#161302,#125803,#125804) ;
#99795 = AXIS2_PLACEMENT_3D('',#161305,#125806,#125807) ;
#99796 = AXIS2_PLACEMENT_3D('',#161306,#125808,#125809) ;
#99797 = AXIS2_PLACEMENT_3D('',#161312,#125813,#125814) ;
#99798 = AXIS2_PLACEMENT_3D('',#161314,#125815,#125816) ;
#99799 = AXIS2_PLACEMENT_3D('',#161317,#125818,#125819) ;
#99800 = AXIS2_PLACEMENT_3D('',#161318,#125820,#125821) ;
#99801 = AXIS2_PLACEMENT_3D('',#161324,#125825,#125826) ;
#99802 = AXIS2_PLACEMENT_3D('',#161326,#125827,#125828) ;
#99803 = AXIS2_PLACEMENT_3D('',#161329,#125830,#125831) ;
#99804 = AXIS2_PLACEMENT_3D('',#161330,#125832,#125833) ;
#99805 = AXIS2_PLACEMENT_3D('',#161333,#125836,#125837) ;
#99806 = AXIS2_PLACEMENT_3D('',#161342,#125842,#125843) ;
#99807 = AXIS2_PLACEMENT_3D('',#161347,#125845,#125846) ;
#99808 = AXIS2_PLACEMENT_3D('',#161350,#125848,#125849) ;
#99809 = AXIS2_PLACEMENT_3D('',#161351,#125850,#125851) ;
#99810 = AXIS2_PLACEMENT_3D('',#161357,#125855,#125856) ;
#99811 = AXIS2_PLACEMENT_3D('',#161359,#125857,#125858) ;
#99812 = AXIS2_PLACEMENT_3D('',#161362,#125860,#125861) ;
#99813 = AXIS2_PLACEMENT_3D('',#161363,#125862,#125863) ;
#99814 = AXIS2_PLACEMENT_3D('',#161369,#125867,#125868) ;
#99815 = AXIS2_PLACEMENT_3D('',#161371,#125869,#125870) ;
#99816 = AXIS2_PLACEMENT_3D('',#161374,#125872,#125873) ;
#99817 = AXIS2_PLACEMENT_3D('',#161375,#125874,#125875) ;
#99818 = AXIS2_PLACEMENT_3D('',#161381,#125879,#125880) ;
#99819 = AXIS2_PLACEMENT_3D('',#161383,#125881,#125882) ;
#99820 = AXIS2_PLACEMENT_3D('',#161386,#125884,#125885) ;
#99821 = AXIS2_PLACEMENT_3D('',#161387,#125886,#125887) ;
#99822 = AXIS2_PLACEMENT_3D('',#161390,#125890,#125891) ;
#99823 = AXIS2_PLACEMENT_3D('',#161399,#125896,#125897) ;
#99824 = AXIS2_PLACEMENT_3D('',#161404,#125899,#125900) ;
#99825 = AXIS2_PLACEMENT_3D('',#161407,#125902,#125903) ;
#99826 = AXIS2_PLACEMENT_3D('',#161408,#125904,#125905) ;
#99827 = AXIS2_PLACEMENT_3D('',#161414,#125909,#125910) ;
#99828 = AXIS2_PLACEMENT_3D('',#161416,#125911,#125912) ;
#99829 = AXIS2_PLACEMENT_3D('',#161419,#125914,#125915) ;
#99830 = AXIS2_PLACEMENT_3D('',#161420,#125916,#125917) ;
#99831 = AXIS2_PLACEMENT_3D('',#161426,#125921,#125922) ;
#99832 = AXIS2_PLACEMENT_3D('',#161428,#125923,#125924) ;
#99833 = AXIS2_PLACEMENT_3D('',#161431,#125926,#125927) ;
#99834 = AXIS2_PLACEMENT_3D('',#161432,#125928,#125929) ;
#99835 = AXIS2_PLACEMENT_3D('',#161438,#125933,#125934) ;
#99836 = AXIS2_PLACEMENT_3D('',#161440,#125935,#125936) ;
#99837 = AXIS2_PLACEMENT_3D('',#161443,#125938,#125939) ;
#99838 = AXIS2_PLACEMENT_3D('',#161444,#125940,#125941) ;
#99839 = AXIS2_PLACEMENT_3D('',#161447,#125944,#125945) ;
#99840 = AXIS2_PLACEMENT_3D('',#161456,#125950,#125951) ;
#99841 = AXIS2_PLACEMENT_3D('',#161461,#125953,#125954) ;
#99842 = AXIS2_PLACEMENT_3D('',#161464,#125956,#125957) ;
#99843 = AXIS2_PLACEMENT_3D('',#161465,#125958,#125959) ;
#99844 = AXIS2_PLACEMENT_3D('',#161471,#125963,#125964) ;
#99845 = AXIS2_PLACEMENT_3D('',#161473,#125965,#125966) ;
#99846 = AXIS2_PLACEMENT_3D('',#161476,#125968,#125969) ;
#99847 = AXIS2_PLACEMENT_3D('',#161477,#125970,#125971) ;
#99848 = AXIS2_PLACEMENT_3D('',#161483,#125975,#125976) ;
#99849 = AXIS2_PLACEMENT_3D('',#161485,#125977,#125978) ;
#99850 = AXIS2_PLACEMENT_3D('',#161488,#125980,#125981) ;
#99851 = AXIS2_PLACEMENT_3D('',#161489,#125982,#125983) ;
#99852 = AXIS2_PLACEMENT_3D('',#161495,#125987,#125988) ;
#99853 = AXIS2_PLACEMENT_3D('',#161497,#125989,#125990) ;
#99854 = AXIS2_PLACEMENT_3D('',#161500,#125992,#125993) ;
#99855 = AXIS2_PLACEMENT_3D('',#161501,#125994,#125995) ;
#99856 = AXIS2_PLACEMENT_3D('',#161504,#125998,#125999) ;
#99857 = AXIS2_PLACEMENT_3D('',#161513,#126004,#126005) ;
#99858 = AXIS2_PLACEMENT_3D('',#161518,#126007,#126008) ;
#99859 = AXIS2_PLACEMENT_3D('',#161521,#126010,#126011) ;
#99860 = AXIS2_PLACEMENT_3D('',#161522,#126012,#126013) ;
#99861 = AXIS2_PLACEMENT_3D('',#161528,#126017,#126018) ;
#99862 = AXIS2_PLACEMENT_3D('',#161530,#126019,#126020) ;
#99863 = AXIS2_PLACEMENT_3D('',#161533,#126022,#126023) ;
#99864 = AXIS2_PLACEMENT_3D('',#161534,#126024,#126025) ;
#99865 = AXIS2_PLACEMENT_3D('',#161540,#126029,#126030) ;
#99866 = AXIS2_PLACEMENT_3D('',#161542,#126031,#126032) ;
#99867 = AXIS2_PLACEMENT_3D('',#161545,#126034,#126035) ;
#99868 = AXIS2_PLACEMENT_3D('',#161546,#126036,#126037) ;
#99869 = AXIS2_PLACEMENT_3D('',#161552,#126041,#126042) ;
#99870 = AXIS2_PLACEMENT_3D('',#161554,#126043,#126044) ;
#99871 = AXIS2_PLACEMENT_3D('',#161557,#126046,#126047) ;
#99872 = AXIS2_PLACEMENT_3D('',#161558,#126048,#126049) ;
#99873 = AXIS2_PLACEMENT_3D('',#161561,#126052,#126053) ;
#99874 = AXIS2_PLACEMENT_3D('',#161570,#126058,#126059) ;
#99875 = AXIS2_PLACEMENT_3D('',#161575,#126061,#126062) ;
#99876 = AXIS2_PLACEMENT_3D('',#161578,#126064,#126065) ;
#99877 = AXIS2_PLACEMENT_3D('',#161579,#126066,#126067) ;
#99878 = AXIS2_PLACEMENT_3D('',#161585,#126071,#126072) ;
#99879 = AXIS2_PLACEMENT_3D('',#161587,#126073,#126074) ;
#99880 = AXIS2_PLACEMENT_3D('',#161590,#126076,#126077) ;
#99881 = AXIS2_PLACEMENT_3D('',#161591,#126078,#126079) ;
#99882 = AXIS2_PLACEMENT_3D('',#161597,#126083,#126084) ;
#99883 = AXIS2_PLACEMENT_3D('',#161599,#126085,#126086) ;
#99884 = AXIS2_PLACEMENT_3D('',#161602,#126088,#126089) ;
#99885 = AXIS2_PLACEMENT_3D('',#161603,#126090,#126091) ;
#99886 = AXIS2_PLACEMENT_3D('',#161609,#126095,#126096) ;
#99887 = AXIS2_PLACEMENT_3D('',#161611,#126097,#126098) ;
#99888 = AXIS2_PLACEMENT_3D('',#161614,#126100,#126101) ;
#99889 = AXIS2_PLACEMENT_3D('',#161615,#126102,#126103) ;
#99890 = AXIS2_PLACEMENT_3D('',#161618,#126106,#126107) ;
#99891 = AXIS2_PLACEMENT_3D('',#161627,#126112,#126113) ;
#99892 = AXIS2_PLACEMENT_3D('',#161632,#126115,#126116) ;
#99893 = AXIS2_PLACEMENT_3D('',#161635,#126118,#126119) ;
#99894 = AXIS2_PLACEMENT_3D('',#161636,#126120,#126121) ;
#99895 = AXIS2_PLACEMENT_3D('',#161642,#126125,#126126) ;
#99896 = AXIS2_PLACEMENT_3D('',#161644,#126127,#126128) ;
#99897 = AXIS2_PLACEMENT_3D('',#161647,#126130,#126131) ;
#99898 = AXIS2_PLACEMENT_3D('',#161648,#126132,#126133) ;
#99899 = AXIS2_PLACEMENT_3D('',#161654,#126137,#126138) ;
#99900 = AXIS2_PLACEMENT_3D('',#161656,#126139,#126140) ;
#99901 = AXIS2_PLACEMENT_3D('',#161659,#126142,#126143) ;
#99902 = AXIS2_PLACEMENT_3D('',#161660,#126144,#126145) ;
#99903 = AXIS2_PLACEMENT_3D('',#161666,#126149,#126150) ;
#99904 = AXIS2_PLACEMENT_3D('',#161668,#126151,#126152) ;
#99905 = AXIS2_PLACEMENT_3D('',#161671,#126154,#126155) ;
#99906 = AXIS2_PLACEMENT_3D('',#161672,#126156,#126157) ;
#99907 = AXIS2_PLACEMENT_3D('',#161675,#126160,#126161) ;
#99908 = AXIS2_PLACEMENT_3D('',#161684,#126166,#126167) ;
#99909 = AXIS2_PLACEMENT_3D('',#161689,#126169,#126170) ;
#99910 = AXIS2_PLACEMENT_3D('',#161692,#126172,#126173) ;
#99911 = AXIS2_PLACEMENT_3D('',#161693,#126174,#126175) ;
#99912 = AXIS2_PLACEMENT_3D('',#161699,#126179,#126180) ;
#99913 = AXIS2_PLACEMENT_3D('',#161701,#126181,#126182) ;
#99914 = AXIS2_PLACEMENT_3D('',#161704,#126184,#126185) ;
#99915 = AXIS2_PLACEMENT_3D('',#161705,#126186,#126187) ;
#99916 = AXIS2_PLACEMENT_3D('',#161711,#126191,#126192) ;
#99917 = AXIS2_PLACEMENT_3D('',#161713,#126193,#126194) ;
#99918 = AXIS2_PLACEMENT_3D('',#161716,#126196,#126197) ;
#99919 = AXIS2_PLACEMENT_3D('',#161717,#126198,#126199) ;
#99920 = AXIS2_PLACEMENT_3D('',#161723,#126203,#126204) ;
#99921 = AXIS2_PLACEMENT_3D('',#161725,#126205,#126206) ;
#99922 = AXIS2_PLACEMENT_3D('',#161728,#126208,#126209) ;
#99923 = AXIS2_PLACEMENT_3D('',#161729,#126210,#126211) ;
#99924 = AXIS2_PLACEMENT_3D('',#161732,#126214,#126215) ;
#99925 = AXIS2_PLACEMENT_3D('',#161741,#126220,#126221) ;
#99926 = AXIS2_PLACEMENT_3D('',#161746,#126223,#126224) ;
#99927 = AXIS2_PLACEMENT_3D('',#161749,#126226,#126227) ;
#99928 = AXIS2_PLACEMENT_3D('',#161750,#126228,#126229) ;
#99929 = AXIS2_PLACEMENT_3D('',#161756,#126233,#126234) ;
#99930 = AXIS2_PLACEMENT_3D('',#161758,#126235,#126236) ;
#99931 = AXIS2_PLACEMENT_3D('',#161761,#126238,#126239) ;
#99932 = AXIS2_PLACEMENT_3D('',#161762,#126240,#126241) ;
#99933 = AXIS2_PLACEMENT_3D('',#161768,#126245,#126246) ;
#99934 = AXIS2_PLACEMENT_3D('',#161770,#126247,#126248) ;
#99935 = AXIS2_PLACEMENT_3D('',#161773,#126250,#126251) ;
#99936 = AXIS2_PLACEMENT_3D('',#161774,#126252,#126253) ;
#99937 = AXIS2_PLACEMENT_3D('',#161780,#126257,#126258) ;
#99938 = AXIS2_PLACEMENT_3D('',#161782,#126259,#126260) ;
#99939 = AXIS2_PLACEMENT_3D('',#161785,#126262,#126263) ;
#99940 = AXIS2_PLACEMENT_3D('',#161786,#126264,#126265) ;
#99941 = AXIS2_PLACEMENT_3D('',#161789,#126268,#126269) ;
#99942 = AXIS2_PLACEMENT_3D('',#161798,#126274,#126275) ;
#99943 = AXIS2_PLACEMENT_3D('',#161799,#126276,#126277) ;
#99944 = AXIS2_PLACEMENT_3D('',#161800,#126278,#126279) ;
#99945 = AXIS2_PLACEMENT_3D('',#161801,#126280,#126281) ;
#99946 = AXIS2_PLACEMENT_3D('',#161802,#126282,#126283) ;
#99947 = AXIS2_PLACEMENT_3D('',#161803,#126284,#126285) ;
#99948 = AXIS2_PLACEMENT_3D('',#161804,#126286,#126287) ;
#99949 = AXIS2_PLACEMENT_3D('',#161805,#126288,#126289) ;
#99950 = AXIS2_PLACEMENT_3D('',#161806,#126290,#126291) ;
#99951 = AXIS2_PLACEMENT_3D('',#161807,#126292,#126293) ;
#99952 = AXIS2_PLACEMENT_3D('',#161808,#126294,#126295) ;
#99953 = AXIS2_PLACEMENT_3D('',#161809,#126296,#126297) ;
#99954 = AXIS2_PLACEMENT_3D('',#161810,#126298,#126299) ;
#99955 = AXIS2_PLACEMENT_3D('',#161811,#126300,#126301) ;
#99956 = AXIS2_PLACEMENT_3D('',#161812,#126302,#126303) ;
#99957 = AXIS2_PLACEMENT_3D('',#161813,#126304,#126305) ;
#99958 = AXIS2_PLACEMENT_3D('',#161814,#126306,#126307) ;
#99959 = AXIS2_PLACEMENT_3D('',#161815,#126308,#126309) ;
#99960 = AXIS2_PLACEMENT_3D('',#161816,#126310,#126311) ;
#99961 = AXIS2_PLACEMENT_3D('',#161817,#126312,#126313) ;
#99962 = AXIS2_PLACEMENT_3D('',#161818,#126314,#126315) ;
#99963 = AXIS2_PLACEMENT_3D('',#161819,#126316,#126317) ;
#99964 = AXIS2_PLACEMENT_3D('',#161820,#126318,#126319) ;
#99965 = AXIS2_PLACEMENT_3D('',#161821,#126320,#126321) ;
#99966 = AXIS2_PLACEMENT_3D('',#161822,#126322,#126323) ;
#99967 = AXIS2_PLACEMENT_3D('',#161823,#126324,#126325) ;
#99968 = AXIS2_PLACEMENT_3D('',#161824,#126326,#126327) ;
#99969 = AXIS2_PLACEMENT_3D('',#161825,#126328,#126329) ;
#99970 = AXIS2_PLACEMENT_3D('',#161826,#126330,#126331) ;
#99971 = AXIS2_PLACEMENT_3D('',#161827,#126332,#126333) ;
#99972 = AXIS2_PLACEMENT_3D('',#161828,#126334,#126335) ;
#99973 = AXIS2_PLACEMENT_3D('',#161829,#126336,#126337) ;
#99974 = AXIS2_PLACEMENT_3D('',#161830,#126338,#126339) ;
#99975 = AXIS2_PLACEMENT_3D('',#161831,#126340,#126341) ;
#99976 = AXIS2_PLACEMENT_3D('',#161832,#126342,#126343) ;
#99977 = AXIS2_PLACEMENT_3D('',#161833,#126344,#126345) ;
#99978 = AXIS2_PLACEMENT_3D('',#161834,#126346,#126347) ;
#99979 = AXIS2_PLACEMENT_3D('',#161835,#126348,#126349) ;
#99980 = AXIS2_PLACEMENT_3D('',#161836,#126350,#126351) ;
#99981 = AXIS2_PLACEMENT_3D('',#161837,#126352,#126353) ;
#99982 = AXIS2_PLACEMENT_3D('',#161838,#126354,#126355) ;
#99983 = AXIS2_PLACEMENT_3D('',#161839,#126356,#126357) ;
#99984 = AXIS2_PLACEMENT_3D('',#161840,#126358,#126359) ;
#99985 = AXIS2_PLACEMENT_3D('',#161841,#126360,#126361) ;
#99986 = AXIS2_PLACEMENT_3D('',#161842,#126362,#126363) ;
#99987 = AXIS2_PLACEMENT_3D('',#161843,#126364,#126365) ;
#99988 = AXIS2_PLACEMENT_3D('',#161844,#126366,#126367) ;
#99989 = AXIS2_PLACEMENT_3D('',#161845,#126368,#126369) ;
#99990 = AXIS2_PLACEMENT_3D('',#161846,#126370,#126371) ;
#99991 = AXIS2_PLACEMENT_3D('',#161847,#126372,#126373) ;
#99992 = AXIS2_PLACEMENT_3D('',#161848,#126374,#126375) ;
#99993 = AXIS2_PLACEMENT_3D('',#161849,#126376,#126377) ;
#99994 = AXIS2_PLACEMENT_3D('',#161850,#126378,#126379) ;
#99995 = AXIS2_PLACEMENT_3D('',#161851,#126380,#126381) ;
#99996 = AXIS2_PLACEMENT_3D('',#161852,#126382,#126383) ;
#99997 = AXIS2_PLACEMENT_3D('',#161853,#126384,#126385) ;
#99998 = AXIS2_PLACEMENT_3D('',#161854,#126386,#126387) ;
#99999 = AXIS2_PLACEMENT_3D('',#161855,#126388,#126389) ;
#100000 = AXIS2_PLACEMENT_3D('',#161856,#126390,#126391) ;
#100001 = AXIS2_PLACEMENT_3D('',#161857,#126392,#126393) ;
#100002 = AXIS2_PLACEMENT_3D('',#161858,#126394,#126395) ;
#100003 = AXIS2_PLACEMENT_3D('',#161859,#126396,#126397) ;
#100004 = AXIS2_PLACEMENT_3D('',#161860,#126398,#126399) ;
#100005 = AXIS2_PLACEMENT_3D('',#161861,#126400,#126401) ;
#100006 = AXIS2_PLACEMENT_3D('',#161862,#126402,#126403) ;
#100007 = AXIS2_PLACEMENT_3D('',#161863,#126404,#126405) ;
#100008 = AXIS2_PLACEMENT_3D('',#161864,#126406,#126407) ;
#100009 = AXIS2_PLACEMENT_3D('',#161865,#126408,#126409) ;
#100010 = AXIS2_PLACEMENT_3D('',#161866,#126410,#126411) ;
#100011 = AXIS2_PLACEMENT_3D('',#161867,#126412,#126413) ;
#100012 = AXIS2_PLACEMENT_3D('',#161868,#126414,#126415) ;
#100013 = AXIS2_PLACEMENT_3D('',#161869,#126416,#126417) ;
#100014 = AXIS2_PLACEMENT_3D('',#161870,#126418,#126419) ;
#100015 = AXIS2_PLACEMENT_3D('',#161871,#126420,#126421) ;
#100016 = AXIS2_PLACEMENT_3D('',#161872,#126422,#126423) ;
#100017 = AXIS2_PLACEMENT_3D('',#161873,#126424,#126425) ;
#100018 = AXIS2_PLACEMENT_3D('',#161874,#126426,#126427) ;
#100019 = AXIS2_PLACEMENT_3D('',#161875,#126428,#126429) ;
#100020 = AXIS2_PLACEMENT_3D('',#161876,#126430,#126431) ;
#100021 = AXIS2_PLACEMENT_3D('',#161877,#126432,#126433) ;
#100022 = AXIS2_PLACEMENT_3D('',#161878,#126434,#126435) ;
#100023 = AXIS2_PLACEMENT_3D('',#161879,#126436,#126437) ;
#100024 = AXIS2_PLACEMENT_3D('',#161880,#126438,#126439) ;
#100025 = AXIS2_PLACEMENT_3D('',#161881,#126440,#126441) ;
#100026 = AXIS2_PLACEMENT_3D('',#161882,#126442,#126443) ;
#100027 = AXIS2_PLACEMENT_3D('',#161883,#126444,#126445) ;
#100028 = AXIS2_PLACEMENT_3D('',#161884,#126446,#126447) ;
#100029 = AXIS2_PLACEMENT_3D('',#161885,#126448,#126449) ;
#100030 = AXIS2_PLACEMENT_3D('',#161886,#126450,#126451) ;
#100031 = AXIS2_PLACEMENT_3D('',#161887,#126452,#126453) ;
#100032 = AXIS2_PLACEMENT_3D('',#161888,#126454,#126455) ;
#100033 = AXIS2_PLACEMENT_3D('',#161889,#126456,#126457) ;
#100034 = AXIS2_PLACEMENT_3D('',#161890,#126458,#126459) ;
#100035 = AXIS2_PLACEMENT_3D('',#161891,#126460,#126461) ;
#100036 = AXIS2_PLACEMENT_3D('',#161892,#126462,#126463) ;
#100037 = AXIS2_PLACEMENT_3D('',#161893,#126464,#126465) ;
#100038 = AXIS2_PLACEMENT_3D('',#161894,#126466,#126467) ;
#100039 = AXIS2_PLACEMENT_3D('',#161895,#126468,#126469) ;
#100040 = AXIS2_PLACEMENT_3D('',#161896,#126470,#126471) ;
#100041 = AXIS2_PLACEMENT_3D('',#161897,#126472,#126473) ;
#100042 = AXIS2_PLACEMENT_3D('',#161898,#126474,#126475) ;
#100043 = AXIS2_PLACEMENT_3D('',#161899,#126476,#126477) ;
#100044 = AXIS2_PLACEMENT_3D('',#161900,#126478,#126479) ;
#100045 = AXIS2_PLACEMENT_3D('',#161902,#126480,#126481) ;
#100046 = AXIS2_PLACEMENT_3D('',#161932,#126482,#126483) ;
#100047 = AXIS2_PLACEMENT_3D('',#161933,#126484,#126485) ;
#100048 = AXIS2_PLACEMENT_3D('',#161949,#126486,#126487) ;
#100049 = AXIS2_PLACEMENT_3D('',#161951,#126488,#126489) ;
#100050 = AXIS2_PLACEMENT_3D('',#161966,#126490,#126491) ;
#100051 = AXIS2_PLACEMENT_3D('',#161982,#126492,#126493) ;
#100052 = AXIS2_PLACEMENT_3D('',#161984,#126494,#126495) ;
#100053 = AXIS2_PLACEMENT_3D('',#161999,#126496,#126497) ;
#100054 = AXIS2_PLACEMENT_3D('',#162015,#126498,#126499) ;
#100055 = AXIS2_PLACEMENT_3D('',#162017,#126500,#126501) ;
#100056 = AXIS2_PLACEMENT_3D('',#162032,#126502,#126503) ;
#100057 = AXIS2_PLACEMENT_3D('',#162034,#126504,#126505) ;
#100058 = AXIS2_PLACEMENT_3D('',#162064,#126506,#126507) ;
#100059 = AXIS2_PLACEMENT_3D('',#162065,#126508,#126509) ;
#100060 = AXIS2_PLACEMENT_3D('',#162081,#126510,#126511) ;
#100061 = AXIS2_PLACEMENT_3D('',#162083,#126512,#126513) ;
#100062 = AXIS2_PLACEMENT_3D('',#162098,#126514,#126515) ;
#100063 = AXIS2_PLACEMENT_3D('',#162114,#126516,#126517) ;
#100064 = AXIS2_PLACEMENT_3D('',#162116,#126518,#126519) ;
#100065 = AXIS2_PLACEMENT_3D('',#162131,#126520,#126521) ;
#100066 = AXIS2_PLACEMENT_3D('',#162147,#126522,#126523) ;
#100067 = AXIS2_PLACEMENT_3D('',#162149,#126524,#126525) ;
#100068 = AXIS2_PLACEMENT_3D('',#162164,#126526,#126527) ;
#100069 = AXIS2_PLACEMENT_3D('',#162166,#126528,#126529) ;
#100070 = AXIS2_PLACEMENT_3D('',#162196,#126530,#126531) ;
#100071 = AXIS2_PLACEMENT_3D('',#162197,#126532,#126533) ;
#100072 = AXIS2_PLACEMENT_3D('',#162213,#126534,#126535) ;
#100073 = AXIS2_PLACEMENT_3D('',#162215,#126536,#126537) ;
#100074 = AXIS2_PLACEMENT_3D('',#162230,#126538,#126539) ;
#100075 = AXIS2_PLACEMENT_3D('',#162246,#126540,#126541) ;
#100076 = AXIS2_PLACEMENT_3D('',#162248,#126542,#126543) ;
#100077 = AXIS2_PLACEMENT_3D('',#162263,#126544,#126545) ;
#100078 = AXIS2_PLACEMENT_3D('',#162279,#126546,#126547) ;
#100079 = AXIS2_PLACEMENT_3D('',#162281,#126548,#126549) ;
#100080 = AXIS2_PLACEMENT_3D('',#162296,#126550,#126551) ;
#100081 = AXIS2_PLACEMENT_3D('',#162298,#126552,#126553) ;
#100082 = AXIS2_PLACEMENT_3D('',#162328,#126554,#126555) ;
#100083 = AXIS2_PLACEMENT_3D('',#162329,#126556,#126557) ;
#100084 = AXIS2_PLACEMENT_3D('',#162345,#126558,#126559) ;
#100085 = AXIS2_PLACEMENT_3D('',#162347,#126560,#126561) ;
#100086 = AXIS2_PLACEMENT_3D('',#162362,#126562,#126563) ;
#100087 = AXIS2_PLACEMENT_3D('',#162378,#126564,#126565) ;
#100088 = AXIS2_PLACEMENT_3D('',#162380,#126566,#126567) ;
#100089 = AXIS2_PLACEMENT_3D('',#162395,#126568,#126569) ;
#100090 = AXIS2_PLACEMENT_3D('',#162411,#126570,#126571) ;
#100091 = AXIS2_PLACEMENT_3D('',#162413,#126572,#126573) ;
#100092 = AXIS2_PLACEMENT_3D('',#162428,#126574,#126575) ;
#100093 = AXIS2_PLACEMENT_3D('',#162430,#126576,#126577) ;
#100094 = AXIS2_PLACEMENT_3D('',#162460,#126578,#126579) ;
#100095 = AXIS2_PLACEMENT_3D('',#162461,#126580,#126581) ;
#100096 = AXIS2_PLACEMENT_3D('',#162477,#126582,#126583) ;
#100097 = AXIS2_PLACEMENT_3D('',#162479,#126584,#126585) ;
#100098 = AXIS2_PLACEMENT_3D('',#162494,#126586,#126587) ;
#100099 = AXIS2_PLACEMENT_3D('',#162510,#126588,#126589) ;
#100100 = AXIS2_PLACEMENT_3D('',#162512,#126590,#126591) ;
#100101 = AXIS2_PLACEMENT_3D('',#162527,#126592,#126593) ;
#100102 = AXIS2_PLACEMENT_3D('',#162543,#126594,#126595) ;
#100103 = AXIS2_PLACEMENT_3D('',#162545,#126596,#126597) ;
#100104 = AXIS2_PLACEMENT_3D('',#162560,#126598,#126599) ;
#100105 = AXIS2_PLACEMENT_3D('',#162562,#126600,#126601) ;
#100106 = AXIS2_PLACEMENT_3D('',#162592,#126602,#126603) ;
#100107 = AXIS2_PLACEMENT_3D('',#162593,#126604,#126605) ;
#100108 = AXIS2_PLACEMENT_3D('',#162609,#126606,#126607) ;
#100109 = AXIS2_PLACEMENT_3D('',#162611,#126608,#126609) ;
#100110 = AXIS2_PLACEMENT_3D('',#162626,#126610,#126611) ;
#100111 = AXIS2_PLACEMENT_3D('',#162642,#126612,#126613) ;
#100112 = AXIS2_PLACEMENT_3D('',#162644,#126614,#126615) ;
#100113 = AXIS2_PLACEMENT_3D('',#162659,#126616,#126617) ;
#100114 = AXIS2_PLACEMENT_3D('',#162675,#126618,#126619) ;
#100115 = AXIS2_PLACEMENT_3D('',#162677,#126620,#126621) ;
#100116 = AXIS2_PLACEMENT_3D('',#162692,#126622,#126623) ;
#100117 = AXIS2_PLACEMENT_3D('',#162694,#126624,#126625) ;
#100118 = AXIS2_PLACEMENT_3D('',#162724,#126626,#126627) ;
#100119 = AXIS2_PLACEMENT_3D('',#162725,#126628,#126629) ;
#100120 = AXIS2_PLACEMENT_3D('',#162741,#126630,#126631) ;
#100121 = AXIS2_PLACEMENT_3D('',#162743,#126632,#126633) ;
#100122 = AXIS2_PLACEMENT_3D('',#162758,#126634,#126635) ;
#100123 = AXIS2_PLACEMENT_3D('',#162774,#126636,#126637) ;
#100124 = AXIS2_PLACEMENT_3D('',#162776,#126638,#126639) ;
#100125 = AXIS2_PLACEMENT_3D('',#162791,#126640,#126641) ;
#100126 = AXIS2_PLACEMENT_3D('',#162807,#126642,#126643) ;
#100127 = AXIS2_PLACEMENT_3D('',#162809,#126644,#126645) ;
#100128 = AXIS2_PLACEMENT_3D('',#162824,#126646,#126647) ;
#100129 = AXIS2_PLACEMENT_3D('',#162826,#126648,#126649) ;
#100130 = AXIS2_PLACEMENT_3D('',#162856,#126650,#126651) ;
#100131 = AXIS2_PLACEMENT_3D('',#162857,#126652,#126653) ;
#100132 = AXIS2_PLACEMENT_3D('',#162873,#126654,#126655) ;
#100133 = AXIS2_PLACEMENT_3D('',#162875,#126656,#126657) ;
#100134 = AXIS2_PLACEMENT_3D('',#162890,#126658,#126659) ;
#100135 = AXIS2_PLACEMENT_3D('',#162906,#126660,#126661) ;
#100136 = AXIS2_PLACEMENT_3D('',#162908,#126662,#126663) ;
#100137 = AXIS2_PLACEMENT_3D('',#162923,#126664,#126665) ;
#100138 = AXIS2_PLACEMENT_3D('',#162939,#126666,#126667) ;
#100139 = AXIS2_PLACEMENT_3D('',#162941,#126668,#126669) ;
#100140 = AXIS2_PLACEMENT_3D('',#162956,#126670,#126671) ;
#100141 = AXIS2_PLACEMENT_3D('',#162957,#126672,#126673) ;
#100142 = AXIS2_PLACEMENT_3D('',#162958,#126674,#126675) ;
#100143 = AXIS2_PLACEMENT_3D('',#162959,#126676,#126677) ;
#100144 = AXIS2_PLACEMENT_3D('',#162960,#126678,#126679) ;
#100145 = AXIS2_PLACEMENT_3D('',#162961,#126680,#126681) ;
#100146 = AXIS2_PLACEMENT_3D('',#162962,#126682,#126683) ;
#100147 = AXIS2_PLACEMENT_3D('',#162963,#126684,#126685) ;
#100148 = AXIS2_PLACEMENT_3D('',#162964,#126686,#126687) ;
#100149 = AXIS2_PLACEMENT_3D('',#162965,#126688,#126689) ;
#100150 = AXIS2_PLACEMENT_3D('',#162966,#126690,#126691) ;
#100151 = AXIS2_PLACEMENT_3D('',#162967,#126692,#126693) ;
#100152 = AXIS2_PLACEMENT_3D('',#162968,#126694,#126695) ;
#100153 = AXIS2_PLACEMENT_3D('',#162969,#126696,#126697) ;
#100154 = AXIS2_PLACEMENT_3D('',#162970,#126698,#126699) ;
#100155 = AXIS2_PLACEMENT_3D('',#162971,#126700,#126701) ;
#100156 = AXIS2_PLACEMENT_3D('',#162972,#126702,#126703) ;
#100157 = AXIS2_PLACEMENT_3D('',#162973,#126704,#126705) ;
#100158 = AXIS2_PLACEMENT_3D('',#162974,#126706,#126707) ;
#100159 = AXIS2_PLACEMENT_3D('',#162975,#126708,#126709) ;
#100160 = AXIS2_PLACEMENT_3D('',#162976,#126710,#126711) ;
#100161 = AXIS2_PLACEMENT_3D('',#162977,#126712,#126713) ;
#100162 = AXIS2_PLACEMENT_3D('',#162978,#126714,#126715) ;
#100163 = AXIS2_PLACEMENT_3D('',#162979,#126716,#126717) ;
#100164 = AXIS2_PLACEMENT_3D('',#162980,#126718,#126719) ;
#100165 = AXIS2_PLACEMENT_3D('',#162981,#126720,#126721) ;
#100166 = AXIS2_PLACEMENT_3D('',#162982,#126722,#126723) ;
#100167 = AXIS2_PLACEMENT_3D('',#162983,#126724,#126725) ;
#100168 = AXIS2_PLACEMENT_3D('',#162984,#126726,#126727) ;
#100169 = AXIS2_PLACEMENT_3D('',#162985,#126728,#126729) ;
#100170 = AXIS2_PLACEMENT_3D('',#162986,#126730,#126731) ;
#100171 = AXIS2_PLACEMENT_3D('',#162987,#126732,#126733) ;
#100172 = AXIS2_PLACEMENT_3D('',#162988,#126734,#126735) ;
#100173 = AXIS2_PLACEMENT_3D('',#162989,#126736,#126737) ;
#100174 = AXIS2_PLACEMENT_3D('',#162990,#126738,#126739) ;
#100175 = AXIS2_PLACEMENT_3D('',#162991,#126740,#126741) ;
#100176 = AXIS2_PLACEMENT_3D('',#162992,#126742,#126743) ;
#100177 = AXIS2_PLACEMENT_3D('',#162993,#126744,#126745) ;
#100178 = AXIS2_PLACEMENT_3D('',#162994,#126746,#126747) ;
#100179 = AXIS2_PLACEMENT_3D('',#162995,#126748,#126749) ;
#100180 = AXIS2_PLACEMENT_3D('',#162996,#126750,#126751) ;
#100181 = AXIS2_PLACEMENT_3D('',#162997,#126752,#126753) ;
#100182 = AXIS2_PLACEMENT_3D('',#162998,#126754,#126755) ;
#100183 = AXIS2_PLACEMENT_3D('',#162999,#126756,#126757) ;
#100184 = AXIS2_PLACEMENT_3D('',#163000,#126758,#126759) ;
#100185 = AXIS2_PLACEMENT_3D('',#163001,#126760,#126761) ;
#100186 = AXIS2_PLACEMENT_3D('',#163002,#126762,#126763) ;
#100187 = AXIS2_PLACEMENT_3D('',#163003,#126764,#126765) ;
#100188 = AXIS2_PLACEMENT_3D('',#163004,#126766,#126767) ;
#100189 = AXIS2_PLACEMENT_3D('',#163005,#126768,#126769) ;
#100190 = AXIS2_PLACEMENT_3D('',#163006,#126770,#126771) ;
#100191 = AXIS2_PLACEMENT_3D('',#163007,#126772,#126773) ;
#100192 = AXIS2_PLACEMENT_3D('',#163008,#126774,#126775) ;
#100193 = AXIS2_PLACEMENT_3D('',#163009,#126776,#126777) ;
#100194 = AXIS2_PLACEMENT_3D('',#163010,#126778,#126779) ;
#100195 = AXIS2_PLACEMENT_3D('',#163011,#126780,#126781) ;
#100196 = AXIS2_PLACEMENT_3D('',#163012,#126782,#126783) ;
#100197 = AXIS2_PLACEMENT_3D('',#163013,#126784,#126785) ;
#100198 = AXIS2_PLACEMENT_3D('',#163014,#126786,#126787) ;
#100199 = AXIS2_PLACEMENT_3D('',#163015,#126788,#126789) ;
#100200 = AXIS2_PLACEMENT_3D('',#163016,#126790,#126791) ;
#100201 = AXIS2_PLACEMENT_3D('',#163017,#126792,#126793) ;
#100202 = AXIS2_PLACEMENT_3D('',#163018,#126794,#126795) ;
#100203 = AXIS2_PLACEMENT_3D('',#163019,#126796,#126797) ;
#100204 = AXIS2_PLACEMENT_3D('',#163020,#126798,#126799) ;
#100205 = AXIS2_PLACEMENT_3D('',#163021,#126800,#126801) ;
#100206 = AXIS2_PLACEMENT_3D('',#163022,#126802,#126803) ;
#100207 = AXIS2_PLACEMENT_3D('',#163023,#126804,#126805) ;
#100208 = AXIS2_PLACEMENT_3D('',#163024,#126806,#126807) ;
#100209 = AXIS2_PLACEMENT_3D('',#163025,#126808,#126809) ;
#100210 = AXIS2_PLACEMENT_3D('',#163026,#126810,#126811) ;
#100211 = AXIS2_PLACEMENT_3D('',#163027,#126812,#126813) ;
#100212 = AXIS2_PLACEMENT_3D('',#163028,#126814,#126815) ;
#100213 = AXIS2_PLACEMENT_3D('',#163029,#126816,#126817) ;
#100214 = AXIS2_PLACEMENT_3D('',#163036,#126818,#126819) ;
#100215 = AXIS2_PLACEMENT_3D('',#163037,#126820,#126821) ;
#100216 = AXIS2_PLACEMENT_3D('',#163038,#126822,#126823) ;
#100217 = AXIS2_PLACEMENT_3D('',#163039,#126824,#126825) ;
#100218 = AXIS2_PLACEMENT_3D('',#163058,#126826,#126827) ;
#100219 = AXIS2_PLACEMENT_3D('',#163059,#126828,#126829) ;
#100220 = AXIS2_PLACEMENT_3D('',#163060,#126830,#126831) ;
#100221 = AXIS2_PLACEMENT_3D('',#163061,#126832,#126833) ;
#100222 = AXIS2_PLACEMENT_3D('',#163062,#126834,#126835) ;
#100223 = AXIS2_PLACEMENT_3D('',#163063,#126836,#126837) ;
#100224 = AXIS2_PLACEMENT_3D('',#163064,#126838,#126839) ;
#100225 = AXIS2_PLACEMENT_3D('',#163071,#126840,#126841) ;
#100226 = AXIS2_PLACEMENT_3D('',#163072,#126842,#126843) ;
#100227 = AXIS2_PLACEMENT_3D('',#163073,#126844,#126845) ;
#100228 = AXIS2_PLACEMENT_3D('',#163074,#126846,#126847) ;
#100229 = AXIS2_PLACEMENT_3D('',#163075,#126848,#126849) ;
#100230 = AXIS2_PLACEMENT_3D('',#163076,#126850,#126851) ;
#100231 = AXIS2_PLACEMENT_3D('',#163077,#126852,#126853) ;
#100232 = AXIS2_PLACEMENT_3D('',#163078,#126854,#126855) ;
#100233 = AXIS2_PLACEMENT_3D('',#163079,#126856,#126857) ;
#100234 = AXIS2_PLACEMENT_3D('',#163098,#126858,#126859) ;
#100235 = AXIS2_PLACEMENT_3D('',#163117,#126860,#126861) ;
#100236 = AXIS2_PLACEMENT_3D('',#163118,#126862,#126863) ;
#100237 = AXIS2_PLACEMENT_3D('',#163119,#126864,#126865) ;
#100238 = AXIS2_PLACEMENT_3D('',#163120,#126866,#126867) ;
#100239 = AXIS2_PLACEMENT_3D('',#163121,#126868,#126869) ;
#100240 = AXIS2_PLACEMENT_3D('',#163122,#126870,#126871) ;
#100241 = AXIS2_PLACEMENT_3D('',#163123,#126872,#126873) ;
#100242 = AXIS2_PLACEMENT_3D('',#163124,#126874,#126875) ;
#100243 = AXIS2_PLACEMENT_3D('',#163125,#126876,#126877) ;
#100244 = AXIS2_PLACEMENT_3D('',#163126,#126878,#126879) ;
#100245 = AXIS2_PLACEMENT_3D('',#163127,#126880,#126881) ;
#100246 = AXIS2_PLACEMENT_3D('',#163146,#126882,#126883) ;
#100247 = AXIS2_PLACEMENT_3D('',#163147,#126884,#126885) ;
#100248 = AXIS2_PLACEMENT_3D('',#163148,#126886,#126887) ;
#100249 = AXIS2_PLACEMENT_3D('',#163150,#126888,#126889) ;
#100250 = AXIS2_PLACEMENT_3D('',#163151,#126890,#126891) ;
#100251 = AXIS2_PLACEMENT_3D('',#163153,#126892,#126893) ;
#100252 = AXIS2_PLACEMENT_3D('',#163155,#126894,#126895) ;
#100253 = AXIS2_PLACEMENT_3D('',#163156,#126896,#126897) ;
#100254 = AXIS2_PLACEMENT_3D('',#163157,#126898,#126899) ;
#100255 = AXIS2_PLACEMENT_3D('',#163159,#126900,#126901) ;
#100256 = AXIS2_PLACEMENT_3D('',#163160,#126902,#126903) ;
#100257 = AXIS2_PLACEMENT_3D('',#163162,#126904,#126905) ;
#100258 = AXIS2_PLACEMENT_3D('',#163163,#126906,#126907) ;
#100259 = AXIS2_PLACEMENT_3D('',#163164,#126908,#126909) ;
#100260 = AXIS2_PLACEMENT_3D('',#163165,#126910,#126911) ;
#100261 = AXIS2_PLACEMENT_3D('',#163166,#126912,#126913) ;
#100262 = AXIS2_PLACEMENT_3D('',#163167,#126914,#126915) ;
#100263 = AXIS2_PLACEMENT_3D('',#163169,#126916,#126917) ;
#100264 = AXIS2_PLACEMENT_3D('',#163171,#126918,#126919) ;
#100265 = AXIS2_PLACEMENT_3D('',#163172,#126920,#126921) ;
#100266 = AXIS2_PLACEMENT_3D('',#163174,#126922,#126923) ;
#100267 = AXIS2_PLACEMENT_3D('',#163175,#126924,#126925) ;
#100268 = AXIS2_PLACEMENT_3D('',#163176,#126926,#126927) ;
#100269 = AXIS2_PLACEMENT_3D('',#163178,#126928,#126929) ;
#100270 = AXIS2_PLACEMENT_3D('',#163179,#126930,#126931) ;
#100271 = AXIS2_PLACEMENT_3D('',#163181,#126932,#126933) ;
#100272 = AXIS2_PLACEMENT_3D('',#163183,#126934,#126935) ;
#100273 = AXIS2_PLACEMENT_3D('',#163184,#126936,#126937) ;
#100274 = AXIS2_PLACEMENT_3D('',#163185,#126938,#126939) ;
#100275 = AXIS2_PLACEMENT_3D('',#163187,#126940,#126941) ;
#100276 = AXIS2_PLACEMENT_3D('',#163188,#126942,#126943) ;
#100277 = AXIS2_PLACEMENT_3D('',#163190,#126944,#126945) ;
#100278 = AXIS2_PLACEMENT_3D('',#163191,#126946,#126947) ;
#100279 = AXIS2_PLACEMENT_3D('',#163192,#126948,#126949) ;
#100280 = AXIS2_PLACEMENT_3D('',#163193,#126950,#126951) ;
#100281 = AXIS2_PLACEMENT_3D('',#163194,#126952,#126953) ;
#100282 = AXIS2_PLACEMENT_3D('',#163195,#126954,#126955) ;
#100283 = AXIS2_PLACEMENT_3D('',#163197,#126956,#126957) ;
#100284 = AXIS2_PLACEMENT_3D('',#163199,#126958,#126959) ;
#100285 = AXIS2_PLACEMENT_3D('',#163200,#126960,#126961) ;
#100286 = AXIS2_PLACEMENT_3D('',#163202,#126962,#126963) ;
#100287 = AXIS2_PLACEMENT_3D('',#163203,#126964,#126965) ;
#100288 = AXIS2_PLACEMENT_3D('',#163204,#126966,#126967) ;
#100289 = AXIS2_PLACEMENT_3D('',#163206,#126968,#126969) ;
#100290 = AXIS2_PLACEMENT_3D('',#163207,#126970,#126971) ;
#100291 = AXIS2_PLACEMENT_3D('',#163209,#126972,#126973) ;
#100292 = AXIS2_PLACEMENT_3D('',#163211,#126974,#126975) ;
#100293 = AXIS2_PLACEMENT_3D('',#163212,#126976,#126977) ;
#100294 = AXIS2_PLACEMENT_3D('',#163213,#126978,#126979) ;
#100295 = AXIS2_PLACEMENT_3D('',#163215,#126980,#126981) ;
#100296 = AXIS2_PLACEMENT_3D('',#163216,#126982,#126983) ;
#100297 = AXIS2_PLACEMENT_3D('',#163218,#126984,#126985) ;
#100298 = AXIS2_PLACEMENT_3D('',#163219,#126986,#126987) ;
#100299 = AXIS2_PLACEMENT_3D('',#163220,#126988,#126989) ;
#100300 = AXIS2_PLACEMENT_3D('',#163221,#126990,#126991) ;
#100301 = AXIS2_PLACEMENT_3D('',#163222,#126992,#126993) ;
#100302 = AXIS2_PLACEMENT_3D('',#163223,#126994,#126995) ;
#100303 = AXIS2_PLACEMENT_3D('',#163225,#126996,#126997) ;
#100304 = AXIS2_PLACEMENT_3D('',#163227,#126998,#126999) ;
#100305 = AXIS2_PLACEMENT_3D('',#163228,#127000,#127001) ;
#100306 = AXIS2_PLACEMENT_3D('',#163230,#127002,#127003) ;
#100307 = AXIS2_PLACEMENT_3D('',#163231,#127004,#127005) ;
#100308 = AXIS2_PLACEMENT_3D('',#163232,#127006,#127007) ;
#100309 = AXIS2_PLACEMENT_3D('',#163234,#127008,#127009) ;
#100310 = AXIS2_PLACEMENT_3D('',#163235,#127010,#127011) ;
#100311 = AXIS2_PLACEMENT_3D('',#163237,#127012,#127013) ;
#100312 = AXIS2_PLACEMENT_3D('',#163239,#127014,#127015) ;
#100313 = AXIS2_PLACEMENT_3D('',#163240,#127016,#127017) ;
#100314 = AXIS2_PLACEMENT_3D('',#163241,#127018,#127019) ;
#100315 = AXIS2_PLACEMENT_3D('',#163243,#127020,#127021) ;
#100316 = AXIS2_PLACEMENT_3D('',#163244,#127022,#127023) ;
#100317 = AXIS2_PLACEMENT_3D('',#163246,#127024,#127025) ;
#100318 = AXIS2_PLACEMENT_3D('',#163247,#127026,#127027) ;
#100319 = AXIS2_PLACEMENT_3D('',#163248,#127028,#127029) ;
#100320 = AXIS2_PLACEMENT_3D('',#163249,#127030,#127031) ;
#100321 = AXIS2_PLACEMENT_3D('',#163250,#127032,#127033) ;
#100322 = AXIS2_PLACEMENT_3D('',#163251,#127034,#127035) ;
#100323 = AXIS2_PLACEMENT_3D('',#163253,#127036,#127037) ;
#100324 = AXIS2_PLACEMENT_3D('',#163255,#127038,#127039) ;
#100325 = AXIS2_PLACEMENT_3D('',#163256,#127040,#127041) ;
#100326 = AXIS2_PLACEMENT_3D('',#163258,#127042,#127043) ;
#100327 = AXIS2_PLACEMENT_3D('',#163259,#127044,#127045) ;
#100328 = AXIS2_PLACEMENT_3D('',#163260,#127046,#127047) ;
#100329 = AXIS2_PLACEMENT_3D('',#163262,#127048,#127049) ;
#100330 = AXIS2_PLACEMENT_3D('',#163263,#127050,#127051) ;
#100331 = AXIS2_PLACEMENT_3D('',#163265,#127052,#127053) ;
#100332 = AXIS2_PLACEMENT_3D('',#163267,#127054,#127055) ;
#100333 = AXIS2_PLACEMENT_3D('',#163268,#127056,#127057) ;
#100334 = AXIS2_PLACEMENT_3D('',#163269,#127058,#127059) ;
#100335 = AXIS2_PLACEMENT_3D('',#163271,#127060,#127061) ;
#100336 = AXIS2_PLACEMENT_3D('',#163272,#127062,#127063) ;
#100337 = AXIS2_PLACEMENT_3D('',#163274,#127064,#127065) ;
#100338 = AXIS2_PLACEMENT_3D('',#163275,#127066,#127067) ;
#100339 = AXIS2_PLACEMENT_3D('',#163276,#127068,#127069) ;
#100340 = AXIS2_PLACEMENT_3D('',#163277,#127070,#127071) ;
#100341 = AXIS2_PLACEMENT_3D('',#163278,#127072,#127073) ;
#100342 = AXIS2_PLACEMENT_3D('',#163279,#127074,#127075) ;
#100343 = AXIS2_PLACEMENT_3D('',#163281,#127076,#127077) ;
#100344 = AXIS2_PLACEMENT_3D('',#163283,#127078,#127079) ;
#100345 = AXIS2_PLACEMENT_3D('',#163284,#127080,#127081) ;
#100346 = AXIS2_PLACEMENT_3D('',#163286,#127082,#127083) ;
#100347 = AXIS2_PLACEMENT_3D('',#163287,#127084,#127085) ;
#100348 = AXIS2_PLACEMENT_3D('',#163288,#127086,#127087) ;
#100349 = AXIS2_PLACEMENT_3D('',#163290,#127088,#127089) ;
#100350 = AXIS2_PLACEMENT_3D('',#163291,#127090,#127091) ;
#100351 = AXIS2_PLACEMENT_3D('',#163293,#127092,#127093) ;
#100352 = AXIS2_PLACEMENT_3D('',#163295,#127094,#127095) ;
#100353 = AXIS2_PLACEMENT_3D('',#163296,#127096,#127097) ;
#100354 = AXIS2_PLACEMENT_3D('',#163297,#127098,#127099) ;
#100355 = AXIS2_PLACEMENT_3D('',#163299,#127100,#127101) ;
#100356 = AXIS2_PLACEMENT_3D('',#163300,#127102,#127103) ;
#100357 = AXIS2_PLACEMENT_3D('',#163302,#127104,#127105) ;
#100358 = AXIS2_PLACEMENT_3D('',#163303,#127106,#127107) ;
#100359 = AXIS2_PLACEMENT_3D('',#163304,#127108,#127109) ;
#100360 = AXIS2_PLACEMENT_3D('',#163305,#127110,#127111) ;
#100361 = AXIS2_PLACEMENT_3D('',#163306,#127112,#127113) ;
#100362 = AXIS2_PLACEMENT_3D('',#163307,#127114,#127115) ;
#100363 = AXIS2_PLACEMENT_3D('',#163309,#127116,#127117) ;
#100364 = AXIS2_PLACEMENT_3D('',#163311,#127118,#127119) ;
#100365 = AXIS2_PLACEMENT_3D('',#163312,#127120,#127121) ;
#100366 = AXIS2_PLACEMENT_3D('',#163314,#127122,#127123) ;
#100367 = AXIS2_PLACEMENT_3D('',#163315,#127124,#127125) ;
#100368 = AXIS2_PLACEMENT_3D('',#163316,#127126,#127127) ;
#100369 = AXIS2_PLACEMENT_3D('',#163318,#127128,#127129) ;
#100370 = AXIS2_PLACEMENT_3D('',#163319,#127130,#127131) ;
#100371 = AXIS2_PLACEMENT_3D('',#163321,#127132,#127133) ;
#100372 = AXIS2_PLACEMENT_3D('',#163323,#127134,#127135) ;
#100373 = AXIS2_PLACEMENT_3D('',#163324,#127136,#127137) ;
#100374 = AXIS2_PLACEMENT_3D('',#163325,#127138,#127139) ;
#100375 = AXIS2_PLACEMENT_3D('',#163327,#127140,#127141) ;
#100376 = AXIS2_PLACEMENT_3D('',#163328,#127142,#127143) ;
#100377 = AXIS2_PLACEMENT_3D('',#163330,#127144,#127145) ;
#100378 = AXIS2_PLACEMENT_3D('',#163331,#127146,#127147) ;
#100379 = AXIS2_PLACEMENT_3D('',#163332,#127148,#127149) ;
#100380 = AXIS2_PLACEMENT_3D('',#163333,#127150,#127151) ;
#100381 = AXIS2_PLACEMENT_3D('',#163334,#127152,#127153) ;
#100382 = AXIS2_PLACEMENT_3D('',#163335,#127154,#127155) ;
#100383 = AXIS2_PLACEMENT_3D('',#163337,#127156,#127157) ;
#100384 = AXIS2_PLACEMENT_3D('',#163339,#127158,#127159) ;
#100385 = AXIS2_PLACEMENT_3D('',#163340,#127160,#127161) ;
#100386 = AXIS2_PLACEMENT_3D('',#163342,#127162,#127163) ;
#100387 = AXIS2_PLACEMENT_3D('',#163343,#127164,#127165) ;
#100388 = AXIS2_PLACEMENT_3D('',#163344,#127166,#127167) ;
#100389 = AXIS2_PLACEMENT_3D('',#163346,#127168,#127169) ;
#100390 = AXIS2_PLACEMENT_3D('',#163347,#127170,#127171) ;
#100391 = AXIS2_PLACEMENT_3D('',#163349,#127172,#127173) ;
#100392 = AXIS2_PLACEMENT_3D('',#163351,#127174,#127175) ;
#100393 = AXIS2_PLACEMENT_3D('',#163352,#127176,#127177) ;
#100394 = AXIS2_PLACEMENT_3D('',#163353,#127178,#127179) ;
#100395 = AXIS2_PLACEMENT_3D('',#163355,#127180,#127181) ;
#100396 = AXIS2_PLACEMENT_3D('',#163356,#127182,#127183) ;
#100397 = AXIS2_PLACEMENT_3D('',#163358,#127184,#127185) ;
#100398 = AXIS2_PLACEMENT_3D('',#163359,#127186,#127187) ;
#100399 = AXIS2_PLACEMENT_3D('',#163360,#127188,#127189) ;
#100400 = AXIS2_PLACEMENT_3D('',#163361,#127190,#127191) ;
#100401 = AXIS2_PLACEMENT_3D('',#163362,#127192,#127193) ;
#100402 = AXIS2_PLACEMENT_3D('',#163363,#127194,#127195) ;
#100403 = AXIS2_PLACEMENT_3D('',#163365,#127196,#127197) ;
#100404 = AXIS2_PLACEMENT_3D('',#163367,#127198,#127199) ;
#100405 = AXIS2_PLACEMENT_3D('',#163368,#127200,#127201) ;
#100406 = AXIS2_PLACEMENT_3D('',#163370,#127202,#127203) ;
#100407 = AXIS2_PLACEMENT_3D('',#163371,#127204,#127205) ;
#100408 = AXIS2_PLACEMENT_3D('',#163372,#127206,#127207) ;
#100409 = AXIS2_PLACEMENT_3D('',#163373,#127208,#127209) ;
#100410 = AXIS2_PLACEMENT_3D('',#163374,#127210,#127211) ;
#100411 = AXIS2_PLACEMENT_3D('',#163375,#127212,#127213) ;
#100412 = AXIS2_PLACEMENT_3D('',#163376,#127214,#127215) ;
#100413 = AXIS2_PLACEMENT_3D('',#163377,#127216,#127217) ;
#100414 = AXIS2_PLACEMENT_3D('',#163378,#127218,#127219) ;
#100415 = AXIS2_PLACEMENT_3D('',#163379,#127220,#127221) ;
#100416 = AXIS2_PLACEMENT_3D('',#163380,#127222,#127223) ;
#100417 = AXIS2_PLACEMENT_3D('',#163381,#127224,#127225) ;
#100418 = AXIS2_PLACEMENT_3D('',#163382,#127226,#127227) ;
#100419 = AXIS2_PLACEMENT_3D('',#163383,#127228,#127229) ;
#100420 = AXIS2_PLACEMENT_3D('',#163384,#127230,#127231) ;
#100421 = AXIS2_PLACEMENT_3D('',#163385,#127232,#127233) ;
#100422 = AXIS2_PLACEMENT_3D('',#163386,#127234,#127235) ;
#100423 = AXIS2_PLACEMENT_3D('',#163387,#127236,#127237) ;
#100424 = AXIS2_PLACEMENT_3D('',#163388,#127238,#127239) ;
#100425 = AXIS2_PLACEMENT_3D('',#163389,#127240,#127241) ;
#100426 = AXIS2_PLACEMENT_3D('',#163390,#127242,#127243) ;
#100427 = AXIS2_PLACEMENT_3D('',#163391,#127244,#127245) ;
#100428 = AXIS2_PLACEMENT_3D('',#163392,#127246,#127247) ;
#100429 = AXIS2_PLACEMENT_3D('',#163393,#127248,#127249) ;
#100430 = AXIS2_PLACEMENT_3D('',#163394,#127250,#127251) ;
#100431 = AXIS2_PLACEMENT_3D('',#163395,#127252,#127253) ;
#100432 = AXIS2_PLACEMENT_3D('',#163396,#127254,#127255) ;
#100433 = AXIS2_PLACEMENT_3D('',#163397,#127256,#127257) ;
#100434 = AXIS2_PLACEMENT_3D('',#163398,#127258,#127259) ;
#100435 = AXIS2_PLACEMENT_3D('',#163399,#127260,#127261) ;
#100436 = AXIS2_PLACEMENT_3D('',#163400,#127262,#127263) ;
#100437 = AXIS2_PLACEMENT_3D('',#163401,#127264,#127265) ;
#100438 = AXIS2_PLACEMENT_3D('',#163402,#127266,#127267) ;
#100439 = AXIS2_PLACEMENT_3D('',#163403,#127268,#127269) ;
#100440 = AXIS2_PLACEMENT_3D('',#163404,#127270,#127271) ;
#100441 = AXIS2_PLACEMENT_3D('',#163405,#127272,#127273) ;
#100442 = AXIS2_PLACEMENT_3D('',#163406,#127274,#127275) ;
#100443 = AXIS2_PLACEMENT_3D('',#163407,#127276,#127277) ;
#100444 = AXIS2_PLACEMENT_3D('',#163408,#127278,#127279) ;
#100445 = AXIS2_PLACEMENT_3D('',#163409,#127280,#127281) ;
#100446 = AXIS2_PLACEMENT_3D('',#163410,#127282,#127283) ;
#100447 = AXIS2_PLACEMENT_3D('',#163411,#127284,#127285) ;
#100448 = AXIS2_PLACEMENT_3D('',#163412,#127286,#127287) ;
#100449 = AXIS2_PLACEMENT_3D('',#163413,#127288,#127289) ;
#100450 = AXIS2_PLACEMENT_3D('',#163414,#127290,#127291) ;
#100451 = AXIS2_PLACEMENT_3D('',#163415,#127292,#127293) ;
#100452 = AXIS2_PLACEMENT_3D('',#163416,#127294,#127295) ;
#100453 = AXIS2_PLACEMENT_3D('',#163417,#127296,#127297) ;
#100454 = AXIS2_PLACEMENT_3D('',#163418,#127298,#127299) ;
#100455 = AXIS2_PLACEMENT_3D('',#163419,#127300,#127301) ;
#100456 = AXIS2_PLACEMENT_3D('',#163420,#127302,#127303) ;
#100457 = AXIS2_PLACEMENT_3D('',#163421,#127304,#127305) ;
#100458 = AXIS2_PLACEMENT_3D('',#163422,#127306,#127307) ;
#100459 = AXIS2_PLACEMENT_3D('',#163423,#127308,#127309) ;
#100460 = AXIS2_PLACEMENT_3D('',#163424,#127310,#127311) ;
#100461 = AXIS2_PLACEMENT_3D('',#163425,#127312,#127313) ;
#100462 = AXIS2_PLACEMENT_3D('',#163426,#127314,#127315) ;
#100463 = AXIS2_PLACEMENT_3D('',#163427,#127316,#127317) ;
#100464 = AXIS2_PLACEMENT_3D('',#163428,#127318,#127319) ;
#100465 = AXIS2_PLACEMENT_3D('',#163429,#127320,#127321) ;
#100466 = AXIS2_PLACEMENT_3D('',#163430,#127322,#127323) ;
#100467 = AXIS2_PLACEMENT_3D('',#163431,#127324,#127325) ;
#100468 = AXIS2_PLACEMENT_3D('',#163432,#127326,#127327) ;
#100469 = AXIS2_PLACEMENT_3D('',#163433,#127328,#127329) ;
#100470 = AXIS2_PLACEMENT_3D('',#163434,#127330,#127331) ;
#100471 = AXIS2_PLACEMENT_3D('',#163435,#127332,#127333) ;
#100472 = AXIS2_PLACEMENT_3D('',#163436,#127334,#127335) ;
#100473 = AXIS2_PLACEMENT_3D('',#163437,#127336,#127337) ;
#100474 = AXIS2_PLACEMENT_3D('',#163438,#127338,#127339) ;
#100475 = AXIS2_PLACEMENT_3D('',#163439,#127340,#127341) ;
#100476 = AXIS2_PLACEMENT_3D('',#163440,#127342,#127343) ;
#100477 = AXIS2_PLACEMENT_3D('',#163441,#127344,#127345) ;
#100478 = AXIS2_PLACEMENT_3D('',#163442,#127346,#127347) ;
#100479 = AXIS2_PLACEMENT_3D('',#163443,#127348,#127349) ;
#100480 = AXIS2_PLACEMENT_3D('',#163444,#127350,#127351) ;
#100481 = AXIS2_PLACEMENT_3D('',#163445,#127352,#127353) ;
#100482 = AXIS2_PLACEMENT_3D('',#163446,#127354,#127355) ;
#100483 = AXIS2_PLACEMENT_3D('',#163447,#127356,#127357) ;
#100484 = AXIS2_PLACEMENT_3D('',#163448,#127358,#127359) ;
#100485 = AXIS2_PLACEMENT_3D('',#163449,#127360,#127361) ;
#100486 = AXIS2_PLACEMENT_3D('',#163450,#127362,#127363) ;
#100487 = AXIS2_PLACEMENT_3D('',#163451,#127364,#127365) ;
#100488 = AXIS2_PLACEMENT_3D('',#163452,#127366,#127367) ;
#100489 = AXIS2_PLACEMENT_3D('',#163453,#127368,#127369) ;
#100490 = AXIS2_PLACEMENT_3D('',#163454,#127370,#127371) ;
#100491 = AXIS2_PLACEMENT_3D('',#163455,#127372,#127373) ;
#100492 = AXIS2_PLACEMENT_3D('',#163456,#127374,#127375) ;
#100493 = AXIS2_PLACEMENT_3D('',#163457,#127376,#127377) ;
#100494 = AXIS2_PLACEMENT_3D('',#163458,#127378,#127379) ;
#100495 = AXIS2_PLACEMENT_3D('',#163459,#127380,#127381) ;
#100496 = AXIS2_PLACEMENT_3D('',#163460,#127382,#127383) ;
#100497 = AXIS2_PLACEMENT_3D('',#163461,#127384,#127385) ;
#100498 = AXIS2_PLACEMENT_3D('',#163462,#127386,#127387) ;
#100499 = AXIS2_PLACEMENT_3D('',#163463,#127388,#127389) ;
#100500 = AXIS2_PLACEMENT_3D('',#163464,#127390,#127391) ;
#100501 = AXIS2_PLACEMENT_3D('',#163465,#127392,#127393) ;
#100502 = AXIS2_PLACEMENT_3D('',#163466,#127394,#127395) ;
#100503 = AXIS2_PLACEMENT_3D('',#163467,#127396,#127397) ;
#100504 = AXIS2_PLACEMENT_3D('',#163468,#127398,#127399) ;
#100505 = AXIS2_PLACEMENT_3D('',#163469,#127400,#127401) ;
#100506 = AXIS2_PLACEMENT_3D('',#163470,#127402,#127403) ;
#100507 = AXIS2_PLACEMENT_3D('',#163471,#127404,#127405) ;
#100508 = AXIS2_PLACEMENT_3D('',#163472,#127406,#127407) ;
#100509 = AXIS2_PLACEMENT_3D('',#163473,#127408,#127409) ;
#100510 = AXIS2_PLACEMENT_3D('',#163474,#127410,#127411) ;
#100511 = AXIS2_PLACEMENT_3D('',#163475,#127412,#127413) ;
#100512 = AXIS2_PLACEMENT_3D('',#163476,#127414,#127415) ;
#100513 = AXIS2_PLACEMENT_3D('',#163477,#127416,#127417) ;
#100514 = AXIS2_PLACEMENT_3D('',#163478,#127418,#127419) ;
#100515 = AXIS2_PLACEMENT_3D('',#163479,#127420,#127421) ;
#100516 = AXIS2_PLACEMENT_3D('',#163480,#127422,#127423) ;
#100517 = AXIS2_PLACEMENT_3D('',#163481,#127424,#127425) ;
#100518 = AXIS2_PLACEMENT_3D('',#163482,#127426,#127427) ;
#100519 = AXIS2_PLACEMENT_3D('',#163483,#127428,#127429) ;
#100520 = AXIS2_PLACEMENT_3D('',#163484,#127430,#127431) ;
#100521 = AXIS2_PLACEMENT_3D('',#163485,#127432,#127433) ;
#100522 = AXIS2_PLACEMENT_3D('',#163486,#127434,#127435) ;
#100523 = AXIS2_PLACEMENT_3D('',#163487,#127436,#127437) ;
#100524 = AXIS2_PLACEMENT_3D('',#163488,#127438,#127439) ;
#100525 = AXIS2_PLACEMENT_3D('',#163489,#127440,#127441) ;
#100526 = AXIS2_PLACEMENT_3D('',#163490,#127442,#127443) ;
#100527 = AXIS2_PLACEMENT_3D('',#163491,#127444,#127445) ;
#100528 = AXIS2_PLACEMENT_3D('',#163492,#127446,#127447) ;
#100529 = AXIS2_PLACEMENT_3D('',#163493,#127448,#127449) ;
#100530 = AXIS2_PLACEMENT_3D('',#163494,#127450,#127451) ;
#100531 = AXIS2_PLACEMENT_3D('',#163495,#127452,#127453) ;
#100532 = AXIS2_PLACEMENT_3D('',#163496,#127454,#127455) ;
#100533 = AXIS2_PLACEMENT_3D('',#163497,#127456,#127457) ;
#100534 = AXIS2_PLACEMENT_3D('',#163498,#127458,#127459) ;
#100535 = AXIS2_PLACEMENT_3D('',#163499,#127460,#127461) ;
#100536 = AXIS2_PLACEMENT_3D('',#163500,#127462,#127463) ;
#100537 = AXIS2_PLACEMENT_3D('',#163501,#127464,#127465) ;
#100538 = AXIS2_PLACEMENT_3D('',#163502,#127466,#127467) ;
#100539 = AXIS2_PLACEMENT_3D('',#163503,#127468,#127469) ;
#100540 = AXIS2_PLACEMENT_3D('',#163504,#127470,#127471) ;
#100541 = AXIS2_PLACEMENT_3D('',#163505,#127472,#127473) ;
#100542 = AXIS2_PLACEMENT_3D('',#163506,#127474,#127475) ;
#100543 = AXIS2_PLACEMENT_3D('',#163507,#127476,#127477) ;
#100544 = AXIS2_PLACEMENT_3D('',#163508,#127478,#127479) ;
#100545 = AXIS2_PLACEMENT_3D('',#163509,#127480,#127481) ;
#100546 = AXIS2_PLACEMENT_3D('',#163510,#127482,#127483) ;
#100547 = AXIS2_PLACEMENT_3D('',#163511,#127484,#127485) ;
#100548 = AXIS2_PLACEMENT_3D('',#163512,#127486,#127487) ;
#100549 = AXIS2_PLACEMENT_3D('',#163513,#127488,#127489) ;
#100550 = AXIS2_PLACEMENT_3D('',#163514,#127490,#127491) ;
#100551 = AXIS2_PLACEMENT_3D('',#163515,#127492,#127493) ;
#100552 = AXIS2_PLACEMENT_3D('',#163516,#127494,#127495) ;
#100553 = AXIS2_PLACEMENT_3D('',#163517,#127496,#127497) ;
#100554 = AXIS2_PLACEMENT_3D('',#163518,#127498,#127499) ;
#100555 = AXIS2_PLACEMENT_3D('',#163519,#127500,#127501) ;
#100556 = AXIS2_PLACEMENT_3D('',#163520,#127502,#127503) ;
#100557 = AXIS2_PLACEMENT_3D('',#163521,#127504,#127505) ;
#100558 = AXIS2_PLACEMENT_3D('',#163522,#127506,#127507) ;
#100559 = AXIS2_PLACEMENT_3D('',#163523,#127508,#127509) ;
#100560 = AXIS2_PLACEMENT_3D('',#163524,#127510,#127511) ;
#100561 = AXIS2_PLACEMENT_3D('',#163525,#127512,#127513) ;
#100562 = AXIS2_PLACEMENT_3D('',#163526,#127514,#127515) ;
#100563 = AXIS2_PLACEMENT_3D('',#163527,#127516,#127517) ;
#100564 = AXIS2_PLACEMENT_3D('',#163528,#127518,#127519) ;
#100565 = AXIS2_PLACEMENT_3D('',#163529,#127520,#127521) ;
#100566 = AXIS2_PLACEMENT_3D('',#163530,#127522,#127523) ;
#100567 = AXIS2_PLACEMENT_3D('',#163531,#127524,#127525) ;
#100568 = AXIS2_PLACEMENT_3D('',#163532,#127526,#127527) ;
#100569 = AXIS2_PLACEMENT_3D('',#163533,#127528,#127529) ;
#100570 = AXIS2_PLACEMENT_3D('',#163534,#127530,#127531) ;
#100571 = AXIS2_PLACEMENT_3D('',#163535,#127532,#127533) ;
#100572 = AXIS2_PLACEMENT_3D('',#163536,#127534,#127535) ;
#100573 = AXIS2_PLACEMENT_3D('',#163537,#127536,#127537) ;
#100574 = AXIS2_PLACEMENT_3D('',#163538,#127538,#127539) ;
#100575 = AXIS2_PLACEMENT_3D('',#163539,#127540,#127541) ;
#100576 = AXIS2_PLACEMENT_3D('',#163540,#127542,#127543) ;
#100577 = AXIS2_PLACEMENT_3D('',#163541,#127544,#127545) ;
#100578 = AXIS2_PLACEMENT_3D('',#163542,#127546,#127547) ;
#100579 = AXIS2_PLACEMENT_3D('',#163543,#127548,#127549) ;
#100580 = AXIS2_PLACEMENT_3D('',#163544,#127550,#127551) ;
#100581 = AXIS2_PLACEMENT_3D('',#163545,#127552,#127553) ;
#100582 = AXIS2_PLACEMENT_3D('',#163570,#127554,#127555) ;
#100583 = AXIS2_PLACEMENT_3D('',#163571,#127556,#127557) ;
#100584 = AXIS2_PLACEMENT_3D('',#163572,#127558,#127559) ;
#100585 = AXIS2_PLACEMENT_3D('',#163597,#127560,#127561) ;
#100586 = AXIS2_PLACEMENT_3D('',#163598,#127562,#127563) ;
#100587 = AXIS2_PLACEMENT_3D('',#163599,#127564,#127565) ;
#100588 = AXIS2_PLACEMENT_3D('',#163600,#127566,#127567) ;
#100589 = AXIS2_PLACEMENT_3D('',#163625,#127568,#127569) ;
#100590 = AXIS2_PLACEMENT_3D('',#163626,#127570,#127571) ;
#100591 = AXIS2_PLACEMENT_3D('',#163627,#127572,#127573) ;
#100592 = AXIS2_PLACEMENT_3D('',#163628,#127574,#127575) ;
#100593 = AXIS2_PLACEMENT_3D('',#163629,#127576,#127577) ;
#100594 = AXIS2_PLACEMENT_3D('',#163630,#127578,#127579) ;
#100595 = AXIS2_PLACEMENT_3D('',#163631,#127580,#127581) ;
#100596 = AXIS2_PLACEMENT_3D('',#163632,#127582,#127583) ;
#100597 = AXIS2_PLACEMENT_3D('',#163633,#127584,#127585) ;
#100598 = AXIS2_PLACEMENT_3D('',#163634,#127586,#127587) ;
#100599 = AXIS2_PLACEMENT_3D('',#163635,#127588,#127589) ;
#100600 = AXIS2_PLACEMENT_3D('',#163636,#127590,#127591) ;
#100601 = AXIS2_PLACEMENT_3D('',#163637,#127592,#127593) ;
#100602 = AXIS2_PLACEMENT_3D('',#163638,#127594,#127595) ;
#100603 = AXIS2_PLACEMENT_3D('',#163639,#127596,#127597) ;
#100604 = AXIS2_PLACEMENT_3D('',#163640,#127598,#127599) ;
#100605 = AXIS2_PLACEMENT_3D('',#163641,#127600,#127601) ;
#100606 = AXIS2_PLACEMENT_3D('',#163642,#127602,#127603) ;
#100607 = AXIS2_PLACEMENT_3D('',#163643,#127604,#127605) ;
#100608 = AXIS2_PLACEMENT_3D('',#163644,#127606,#127607) ;
#100609 = AXIS2_PLACEMENT_3D('',#163645,#127608,#127609) ;
#100610 = AXIS2_PLACEMENT_3D('',#163694,#127610,#127611) ;
#100611 = AXIS2_PLACEMENT_3D('',#163707,#127612,#127613) ;
#100612 = AXIS2_PLACEMENT_3D('',#163708,#127614,#127615) ;
#100613 = AXIS2_PLACEMENT_3D('',#163709,#127616,#127617) ;
#100614 = AXIS2_PLACEMENT_3D('',#163710,#127618,#127619) ;
#100615 = AXIS2_PLACEMENT_3D('',#163711,#127620,#127621) ;
#100616 = AXIS2_PLACEMENT_3D('',#163712,#127622,#127623) ;
#100617 = AXIS2_PLACEMENT_3D('',#163713,#127624,#127625) ;
#100618 = AXIS2_PLACEMENT_3D('',#163714,#127626,#127627) ;
#100619 = AXIS2_PLACEMENT_3D('',#163715,#127628,#127629) ;
#100620 = AXIS2_PLACEMENT_3D('',#163716,#127630,#127631) ;
#100621 = AXIS2_PLACEMENT_3D('',#163717,#127632,#127633) ;
#100622 = AXIS2_PLACEMENT_3D('',#163718,#127634,#127635) ;
#100623 = AXIS2_PLACEMENT_3D('',#163719,#127636,#127637) ;
#100624 = AXIS2_PLACEMENT_3D('',#163720,#127638,#127639) ;
#100625 = AXIS2_PLACEMENT_3D('',#163721,#127640,#127641) ;
#100626 = AXIS2_PLACEMENT_3D('',#163734,#127642,#127643) ;
#100627 = AXIS2_PLACEMENT_3D('',#163759,#127644,#127645) ;
#100628 = AXIS2_PLACEMENT_3D('',#163772,#127646,#127647) ;
#100629 = AXIS2_PLACEMENT_3D('',#163773,#127648,#127649) ;
#100630 = AXIS2_PLACEMENT_3D('',#163774,#127650,#127651) ;
#100631 = AXIS2_PLACEMENT_3D('',#163775,#127652,#127653) ;
#100632 = AXIS2_PLACEMENT_3D('',#163776,#127654,#127655) ;
#100633 = AXIS2_PLACEMENT_3D('',#163777,#127656,#127657) ;
#100634 = AXIS2_PLACEMENT_3D('',#163778,#127658,#127659) ;
#100635 = AXIS2_PLACEMENT_3D('',#163779,#127660,#127661) ;
#100636 = AXIS2_PLACEMENT_3D('',#163780,#127662,#127663) ;
#100637 = AXIS2_PLACEMENT_3D('',#163781,#127664,#127665) ;
#100638 = AXIS2_PLACEMENT_3D('',#163782,#127666,#127667) ;
#100639 = AXIS2_PLACEMENT_3D('',#163783,#127668,#127669) ;
#100640 = AXIS2_PLACEMENT_3D('',#163784,#127670,#127671) ;
#100641 = AXIS2_PLACEMENT_3D('',#163785,#127672,#127673) ;
#100642 = AXIS2_PLACEMENT_3D('',#163786,#127674,#127675) ;
#100643 = AXIS2_PLACEMENT_3D('',#163799,#127676,#127677) ;
#100644 = AXIS2_PLACEMENT_3D('',#163824,#127678,#127679) ;
#100645 = AXIS2_PLACEMENT_3D('',#163825,#127680,#127681) ;
#100646 = AXIS2_PLACEMENT_3D('',#163826,#127682,#127683) ;
#100647 = AXIS2_PLACEMENT_3D('',#163827,#127684,#127685) ;
#100648 = AXIS2_PLACEMENT_3D('',#163828,#127686,#127687) ;
#100649 = AXIS2_PLACEMENT_3D('',#163829,#127688,#127689) ;
#100650 = AXIS2_PLACEMENT_3D('',#163830,#127690,#127691) ;
#100651 = AXIS2_PLACEMENT_3D('',#163831,#127692,#127693) ;
#100652 = AXIS2_PLACEMENT_3D('',#163832,#127694,#127695) ;
#100653 = AXIS2_PLACEMENT_3D('',#163833,#127696,#127697) ;
#100654 = AXIS2_PLACEMENT_3D('',#163834,#127698,#127699) ;
#100655 = AXIS2_PLACEMENT_3D('',#163835,#127700,#127701) ;
#100656 = AXIS2_PLACEMENT_3D('',#163836,#127702,#127703) ;
#100657 = AXIS2_PLACEMENT_3D('',#163837,#127704,#127705) ;
#100658 = AXIS2_PLACEMENT_3D('',#163838,#127706,#127707) ;
#100659 = AXIS2_PLACEMENT_3D('',#163839,#127708,#127709) ;
#100660 = AXIS2_PLACEMENT_3D('',#163840,#127710,#127711) ;
#100661 = AXIS2_PLACEMENT_3D('',#163841,#127712,#127713) ;
#100662 = AXIS2_PLACEMENT_3D('',#163842,#127714,#127715) ;
#100663 = AXIS2_PLACEMENT_3D('',#163843,#127716,#127717) ;
#100664 = AXIS2_PLACEMENT_3D('',#163844,#127718,#127719) ;
#100665 = AXIS2_PLACEMENT_3D('',#163845,#127720,#127721) ;
#100666 = AXIS2_PLACEMENT_3D('',#163846,#127722,#127723) ;
#100667 = AXIS2_PLACEMENT_3D('',#163847,#127724,#127725) ;
#100668 = AXIS2_PLACEMENT_3D('',#163848,#127726,#127727) ;
#100669 = AXIS2_PLACEMENT_3D('',#163849,#127728,#127729) ;
#100670 = AXIS2_PLACEMENT_3D('',#163850,#127730,#127731) ;
#100671 = AXIS2_PLACEMENT_3D('',#163851,#127732,#127733) ;
#100672 = AXIS2_PLACEMENT_3D('',#163852,#127734,#127735) ;
#100673 = AXIS2_PLACEMENT_3D('',#163853,#127736,#127737) ;
#100674 = AXIS2_PLACEMENT_3D('',#163854,#127738,#127739) ;
#100675 = AXIS2_PLACEMENT_3D('',#163855,#127740,#127741) ;
#100676 = AXIS2_PLACEMENT_3D('',#163856,#127742,#127743) ;
#100677 = AXIS2_PLACEMENT_3D('',#163857,#127744,#127745) ;
#100678 = AXIS2_PLACEMENT_3D('',#163858,#127746,#127747) ;
#100679 = AXIS2_PLACEMENT_3D('',#163859,#127748,#127749) ;
#100680 = AXIS2_PLACEMENT_3D('',#163860,#127750,#127751) ;
#100681 = AXIS2_PLACEMENT_3D('',#163861,#127752,#127753) ;
#100682 = AXIS2_PLACEMENT_3D('',#163862,#127754,#127755) ;
#100683 = AXIS2_PLACEMENT_3D('',#163863,#127756,#127757) ;
#100684 = AXIS2_PLACEMENT_3D('',#163864,#127758,#127759) ;
#100685 = AXIS2_PLACEMENT_3D('',#163865,#127760,#127761) ;
#100686 = AXIS2_PLACEMENT_3D('',#163866,#127762,#127763) ;
#100687 = AXIS2_PLACEMENT_3D('',#163867,#127764,#127765) ;
#100688 = AXIS2_PLACEMENT_3D('',#163868,#127766,#127767) ;
#100689 = AXIS2_PLACEMENT_3D('',#163869,#127768,#127769) ;
#100690 = AXIS2_PLACEMENT_3D('',#163870,#127770,#127771) ;
#100691 = AXIS2_PLACEMENT_3D('',#163871,#127772,#127773) ;
#100692 = AXIS2_PLACEMENT_3D('',#163872,#127774,#127775) ;
#100693 = AXIS2_PLACEMENT_3D('',#163873,#127776,#127777) ;
#100694 = AXIS2_PLACEMENT_3D('',#163874,#127778,#127779) ;
#100695 = AXIS2_PLACEMENT_3D('',#163875,#127780,#127781) ;
#100696 = AXIS2_PLACEMENT_3D('',#163876,#127782,#127783) ;
#100697 = AXIS2_PLACEMENT_3D('',#163877,#127784,#127785) ;
#100698 = AXIS2_PLACEMENT_3D('',#163878,#127786,#127787) ;
#100699 = AXIS2_PLACEMENT_3D('',#163879,#127788,#127789) ;
#100700 = AXIS2_PLACEMENT_3D('',#163880,#127790,#127791) ;
#100701 = AXIS2_PLACEMENT_3D('',#163881,#127792,#127793) ;
#100702 = AXIS2_PLACEMENT_3D('',#163882,#127794,#127795) ;
#100703 = AXIS2_PLACEMENT_3D('',#163883,#127796,#127797) ;
#100704 = AXIS2_PLACEMENT_3D('',#163884,#127798,#127799) ;
#100705 = AXIS2_PLACEMENT_3D('',#163885,#127800,#127801) ;
#100706 = AXIS2_PLACEMENT_3D('',#163886,#127802,#127803) ;
#100707 = AXIS2_PLACEMENT_3D('',#163887,#127804,#127805) ;
#100708 = AXIS2_PLACEMENT_3D('',#163888,#127806,#127807) ;
#100709 = AXIS2_PLACEMENT_3D('',#163889,#127808,#127809) ;
#100710 = AXIS2_PLACEMENT_3D('',#163890,#127810,#127811) ;
#100711 = AXIS2_PLACEMENT_3D('',#163891,#127812,#127813) ;
#100712 = AXIS2_PLACEMENT_3D('',#163892,#127814,#127815) ;
#100713 = AXIS2_PLACEMENT_3D('',#163893,#127816,#127817) ;
#100714 = AXIS2_PLACEMENT_3D('',#163894,#127818,#127819) ;
#100715 = AXIS2_PLACEMENT_3D('',#163895,#127820,#127821) ;
#100716 = AXIS2_PLACEMENT_3D('',#163896,#127822,#127823) ;
#100717 = AXIS2_PLACEMENT_3D('',#163897,#127824,#127825) ;
#100718 = AXIS2_PLACEMENT_3D('',#163898,#127826,#127827) ;
#100719 = AXIS2_PLACEMENT_3D('',#163899,#127828,#127829) ;
#100720 = AXIS2_PLACEMENT_3D('',#163900,#127830,#127831) ;
#100721 = AXIS2_PLACEMENT_3D('',#163901,#127832,#127833) ;
#100722 = AXIS2_PLACEMENT_3D('',#163902,#127834,#127835) ;
#100723 = AXIS2_PLACEMENT_3D('',#163903,#127836,#127837) ;
#100724 = AXIS2_PLACEMENT_3D('',#163904,#127838,#127839) ;
#100725 = AXIS2_PLACEMENT_3D('',#163905,#127840,#127841) ;
#100726 = AXIS2_PLACEMENT_3D('',#163906,#127842,#127843) ;
#100727 = AXIS2_PLACEMENT_3D('',#163907,#127844,#127845) ;
#100728 = AXIS2_PLACEMENT_3D('',#163908,#127846,#127847) ;
#100729 = AXIS2_PLACEMENT_3D('',#163909,#127848,#127849) ;
#100730 = AXIS2_PLACEMENT_3D('',#163910,#127850,#127851) ;
#100731 = AXIS2_PLACEMENT_3D('',#163911,#127852,#127853) ;
#100732 = AXIS2_PLACEMENT_3D('',#163912,#127854,#127855) ;
#100733 = AXIS2_PLACEMENT_3D('',#163913,#127856,#127857) ;
#100734 = AXIS2_PLACEMENT_3D('',#163914,#127858,#127859) ;
#100735 = AXIS2_PLACEMENT_3D('',#163915,#127860,#127861) ;
#100736 = AXIS2_PLACEMENT_3D('',#163916,#127862,#127863) ;
#100737 = AXIS2_PLACEMENT_3D('',#163917,#127864,#127865) ;
#100738 = AXIS2_PLACEMENT_3D('',#163918,#127866,#127867) ;
#100739 = AXIS2_PLACEMENT_3D('',#163919,#127868,#127869) ;
#100740 = AXIS2_PLACEMENT_3D('',#163920,#127870,#127871) ;
#100741 = AXIS2_PLACEMENT_3D('',#163921,#127872,#127873) ;
#100742 = AXIS2_PLACEMENT_3D('',#163922,#127874,#127875) ;
#100743 = AXIS2_PLACEMENT_3D('',#163923,#127876,#127877) ;
#100744 = AXIS2_PLACEMENT_3D('',#163924,#127878,#127879) ;
#100745 = AXIS2_PLACEMENT_3D('',#163925,#127880,#127881) ;
#100746 = AXIS2_PLACEMENT_3D('',#163926,#127882,#127883) ;
#100747 = AXIS2_PLACEMENT_3D('',#163927,#127884,#127885) ;
#100748 = AXIS2_PLACEMENT_3D('',#163928,#127886,#127887) ;
#100749 = AXIS2_PLACEMENT_3D('',#163929,#127888,#127889) ;
#100750 = AXIS2_PLACEMENT_3D('',#163930,#127890,#127891) ;
#100751 = AXIS2_PLACEMENT_3D('',#163931,#127892,#127893) ;
#100752 = AXIS2_PLACEMENT_3D('',#163932,#127894,#127895) ;
#100753 = AXIS2_PLACEMENT_3D('',#163933,#127896,#127897) ;
#100754 = AXIS2_PLACEMENT_3D('',#163934,#127898,#127899) ;
#100755 = AXIS2_PLACEMENT_3D('',#163935,#127900,#127901) ;
#100756 = AXIS2_PLACEMENT_3D('',#163936,#127902,#127903) ;
#100757 = AXIS2_PLACEMENT_3D('',#163937,#127904,#127905) ;
#100758 = AXIS2_PLACEMENT_3D('',#163938,#127906,#127907) ;
#100759 = AXIS2_PLACEMENT_3D('',#163939,#127908,#127909) ;
#100760 = AXIS2_PLACEMENT_3D('',#163940,#127910,#127911) ;
#100761 = AXIS2_PLACEMENT_3D('',#163941,#127912,#127913) ;
#100762 = AXIS2_PLACEMENT_3D('',#163942,#127914,#127915) ;
#100763 = AXIS2_PLACEMENT_3D('',#163943,#127916,#127917) ;
#100764 = AXIS2_PLACEMENT_3D('',#163944,#127918,#127919) ;
#100765 = AXIS2_PLACEMENT_3D('',#163945,#127920,#127921) ;
#100766 = AXIS2_PLACEMENT_3D('',#163946,#127922,#127923) ;
#100767 = AXIS2_PLACEMENT_3D('',#163947,#127924,#127925) ;
#100768 = AXIS2_PLACEMENT_3D('',#163948,#127926,#127927) ;
#100769 = AXIS2_PLACEMENT_3D('',#163949,#127928,#127929) ;
#100770 = AXIS2_PLACEMENT_3D('',#163950,#127930,#127931) ;
#100771 = AXIS2_PLACEMENT_3D('',#163951,#127932,#127933) ;
#100772 = AXIS2_PLACEMENT_3D('',#163952,#127934,#127935) ;
#100773 = AXIS2_PLACEMENT_3D('',#163953,#127936,#127937) ;
#100774 = AXIS2_PLACEMENT_3D('',#163954,#127938,#127939) ;
#100775 = AXIS2_PLACEMENT_3D('',#163955,#127940,#127941) ;
#100776 = AXIS2_PLACEMENT_3D('',#163956,#127942,#127943) ;
#100777 = AXIS2_PLACEMENT_3D('',#163957,#127944,#127945) ;
#100778 = AXIS2_PLACEMENT_3D('',#163958,#127946,#127947) ;
#100779 = AXIS2_PLACEMENT_3D('',#163959,#127948,#127949) ;
#100780 = AXIS2_PLACEMENT_3D('',#163960,#127950,#127951) ;
#100781 = AXIS2_PLACEMENT_3D('',#163961,#127952,#127953) ;
#100782 = AXIS2_PLACEMENT_3D('',#163962,#127954,#127955) ;
#100783 = AXIS2_PLACEMENT_3D('',#163963,#127956,#127957) ;
#100784 = AXIS2_PLACEMENT_3D('',#163964,#127958,#127959) ;
#100785 = AXIS2_PLACEMENT_3D('',#163965,#127960,#127961) ;
#100786 = AXIS2_PLACEMENT_3D('',#163966,#127962,#127963) ;
#100787 = AXIS2_PLACEMENT_3D('',#163967,#127964,#127965) ;
#100788 = AXIS2_PLACEMENT_3D('',#163968,#127966,#127967) ;
#100789 = AXIS2_PLACEMENT_3D('',#163969,#127968,#127969) ;
#100790 = AXIS2_PLACEMENT_3D('',#163970,#127970,#127971) ;
#100791 = AXIS2_PLACEMENT_3D('',#163971,#127972,#127973) ;
#100792 = AXIS2_PLACEMENT_3D('',#163972,#127974,#127975) ;
#100793 = AXIS2_PLACEMENT_3D('',#163973,#127976,#127977) ;
#100794 = AXIS2_PLACEMENT_3D('',#163974,#127978,#127979) ;
#100795 = AXIS2_PLACEMENT_3D('',#163975,#127980,#127981) ;
#100796 = AXIS2_PLACEMENT_3D('',#163976,#127982,#127983) ;
#100797 = AXIS2_PLACEMENT_3D('',#163977,#127984,#127985) ;
#100798 = AXIS2_PLACEMENT_3D('',#163978,#127986,#127987) ;
#100799 = AXIS2_PLACEMENT_3D('',#163979,#127988,#127989) ;
#100800 = AXIS2_PLACEMENT_3D('',#163980,#127990,#127991) ;
#100801 = AXIS2_PLACEMENT_3D('',#163981,#127992,#127993) ;
#100802 = AXIS2_PLACEMENT_3D('',#163982,#127994,#127995) ;
#100803 = AXIS2_PLACEMENT_3D('',#163983,#127996,#127997) ;
#100804 = AXIS2_PLACEMENT_3D('',#163984,#127998,#127999) ;
#100805 = AXIS2_PLACEMENT_3D('',#163985,#128000,#128001) ;
#100806 = AXIS2_PLACEMENT_3D('',#163986,#128002,#128003) ;
#100807 = AXIS2_PLACEMENT_3D('',#163987,#128004,#128005) ;
#100808 = AXIS2_PLACEMENT_3D('',#163988,#128006,#128007) ;
#100809 = AXIS2_PLACEMENT_3D('',#163989,#128008,#128009) ;
#100810 = AXIS2_PLACEMENT_3D('',#163990,#128010,#128011) ;
#100811 = AXIS2_PLACEMENT_3D('',#163991,#128012,#128013) ;
#100812 = AXIS2_PLACEMENT_3D('',#163992,#128014,#128015) ;
#100813 = AXIS2_PLACEMENT_3D('',#163993,#128016,#128017) ;
#100814 = AXIS2_PLACEMENT_3D('',#163994,#128018,#128019) ;
#100815 = AXIS2_PLACEMENT_3D('',#163995,#128020,#128021) ;
#100816 = AXIS2_PLACEMENT_3D('',#163996,#128022,#128023) ;
#100817 = AXIS2_PLACEMENT_3D('',#163997,#128024,#128025) ;
#100818 = AXIS2_PLACEMENT_3D('',#163998,#128026,#128027) ;
#100819 = AXIS2_PLACEMENT_3D('',#163999,#128028,#128029) ;
#100820 = AXIS2_PLACEMENT_3D('',#164000,#128030,#128031) ;
#100821 = AXIS2_PLACEMENT_3D('',#164001,#128032,#128033) ;
#100822 = AXIS2_PLACEMENT_3D('',#164002,#128034,#128035) ;
#100823 = AXIS2_PLACEMENT_3D('',#164003,#128036,#128037) ;
#100824 = AXIS2_PLACEMENT_3D('',#164004,#128038,#128039) ;
#100825 = AXIS2_PLACEMENT_3D('',#164005,#128040,#128041) ;
#100826 = AXIS2_PLACEMENT_3D('',#164006,#128042,#128043) ;
#100827 = AXIS2_PLACEMENT_3D('',#164007,#128044,#128045) ;
#100828 = AXIS2_PLACEMENT_3D('',#164008,#128046,#128047) ;
#100829 = AXIS2_PLACEMENT_3D('',#164009,#128048,#128049) ;
#100830 = AXIS2_PLACEMENT_3D('',#164010,#128050,#128051) ;
#100831 = AXIS2_PLACEMENT_3D('',#164011,#128052,#128053) ;
#100832 = AXIS2_PLACEMENT_3D('',#164012,#128054,#128055) ;
#100833 = AXIS2_PLACEMENT_3D('',#164013,#128056,#128057) ;
#100834 = AXIS2_PLACEMENT_3D('',#164014,#128058,#128059) ;
#100835 = AXIS2_PLACEMENT_3D('',#164015,#128060,#128061) ;
#100836 = AXIS2_PLACEMENT_3D('',#164016,#128062,#128063) ;
#100837 = AXIS2_PLACEMENT_3D('',#164017,#128064,#128065) ;
#100838 = AXIS2_PLACEMENT_3D('',#164018,#128066,#128067) ;
#100839 = AXIS2_PLACEMENT_3D('',#164019,#128068,#128069) ;
#100840 = AXIS2_PLACEMENT_3D('',#164020,#128070,#128071) ;
#100841 = AXIS2_PLACEMENT_3D('',#164021,#128072,#128073) ;
#100842 = AXIS2_PLACEMENT_3D('',#164022,#128074,#128075) ;
#100843 = AXIS2_PLACEMENT_3D('',#164023,#128076,#128077) ;
#100844 = AXIS2_PLACEMENT_3D('',#164024,#128078,#128079) ;
#100845 = AXIS2_PLACEMENT_3D('',#164025,#128080,#128081) ;
#100846 = AXIS2_PLACEMENT_3D('',#164026,#128082,#128083) ;
#100847 = AXIS2_PLACEMENT_3D('',#164027,#128084,#128085) ;
#100848 = AXIS2_PLACEMENT_3D('',#164028,#128086,#128087) ;
#100849 = AXIS2_PLACEMENT_3D('',#164029,#128088,#128089) ;
#100850 = AXIS2_PLACEMENT_3D('',#164030,#128090,#128091) ;
#100851 = AXIS2_PLACEMENT_3D('',#164031,#128092,#128093) ;
#100852 = AXIS2_PLACEMENT_3D('',#164032,#128094,#128095) ;
#100853 = AXIS2_PLACEMENT_3D('',#164033,#128096,#128097) ;
#100854 = AXIS2_PLACEMENT_3D('',#164034,#128098,#128099) ;
#100855 = AXIS2_PLACEMENT_3D('',#164035,#128100,#128101) ;
#100856 = AXIS2_PLACEMENT_3D('',#164036,#128102,#128103) ;
#100857 = AXIS2_PLACEMENT_3D('',#164037,#128104,#128105) ;
#100858 = AXIS2_PLACEMENT_3D('',#164062,#128106,#128107) ;
#100859 = AXIS2_PLACEMENT_3D('',#164063,#128108,#128109) ;
#100860 = AXIS2_PLACEMENT_3D('',#164064,#128110,#128111) ;
#100861 = AXIS2_PLACEMENT_3D('',#164089,#128112,#128113) ;
#100862 = AXIS2_PLACEMENT_3D('',#164090,#128114,#128115) ;
#100863 = AXIS2_PLACEMENT_3D('',#164091,#128116,#128117) ;
#100864 = AXIS2_PLACEMENT_3D('',#164092,#128118,#128119) ;
#100865 = AXIS2_PLACEMENT_3D('',#164117,#128120,#128121) ;
#100866 = AXIS2_PLACEMENT_3D('',#164118,#128122,#128123) ;
#100867 = AXIS2_PLACEMENT_3D('',#164119,#128124,#128125) ;
#100868 = AXIS2_PLACEMENT_3D('',#164120,#128126,#128127) ;
#100869 = AXIS2_PLACEMENT_3D('',#164121,#128128,#128129) ;
#100870 = AXIS2_PLACEMENT_3D('',#164122,#128130,#128131) ;
#100871 = AXIS2_PLACEMENT_3D('',#164123,#128132,#128133) ;
#100872 = AXIS2_PLACEMENT_3D('',#164124,#128134,#128135) ;
#100873 = AXIS2_PLACEMENT_3D('',#164125,#128136,#128137) ;
#100874 = AXIS2_PLACEMENT_3D('',#164126,#128138,#128139) ;
#100875 = AXIS2_PLACEMENT_3D('',#164127,#128140,#128141) ;
#100876 = AXIS2_PLACEMENT_3D('',#164128,#128142,#128143) ;
#100877 = AXIS2_PLACEMENT_3D('',#164129,#128144,#128145) ;
#100878 = AXIS2_PLACEMENT_3D('',#164130,#128146,#128147) ;
#100879 = AXIS2_PLACEMENT_3D('',#164131,#128148,#128149) ;
#100880 = AXIS2_PLACEMENT_3D('',#164132,#128150,#128151) ;
#100881 = AXIS2_PLACEMENT_3D('',#164133,#128152,#128153) ;
#100882 = AXIS2_PLACEMENT_3D('',#164134,#128154,#128155) ;
#100883 = AXIS2_PLACEMENT_3D('',#164135,#128156,#128157) ;
#100884 = AXIS2_PLACEMENT_3D('',#164136,#128158,#128159) ;
#100885 = AXIS2_PLACEMENT_3D('',#164137,#128160,#128161) ;
#100886 = AXIS2_PLACEMENT_3D('',#164186,#128162,#128163) ;
#100887 = AXIS2_PLACEMENT_3D('',#164199,#128164,#128165) ;
#100888 = AXIS2_PLACEMENT_3D('',#164200,#128166,#128167) ;
#100889 = AXIS2_PLACEMENT_3D('',#164201,#128168,#128169) ;
#100890 = AXIS2_PLACEMENT_3D('',#164202,#128170,#128171) ;
#100891 = AXIS2_PLACEMENT_3D('',#164203,#128172,#128173) ;
#100892 = AXIS2_PLACEMENT_3D('',#164204,#128174,#128175) ;
#100893 = AXIS2_PLACEMENT_3D('',#164205,#128176,#128177) ;
#100894 = AXIS2_PLACEMENT_3D('',#164206,#128178,#128179) ;
#100895 = AXIS2_PLACEMENT_3D('',#164207,#128180,#128181) ;
#100896 = AXIS2_PLACEMENT_3D('',#164208,#128182,#128183) ;
#100897 = AXIS2_PLACEMENT_3D('',#164209,#128184,#128185) ;
#100898 = AXIS2_PLACEMENT_3D('',#164210,#128186,#128187) ;
#100899 = AXIS2_PLACEMENT_3D('',#164211,#128188,#128189) ;
#100900 = AXIS2_PLACEMENT_3D('',#164212,#128190,#128191) ;
#100901 = AXIS2_PLACEMENT_3D('',#164213,#128192,#128193) ;
#100902 = AXIS2_PLACEMENT_3D('',#164226,#128194,#128195) ;
#100903 = AXIS2_PLACEMENT_3D('',#164251,#128196,#128197) ;
#100904 = AXIS2_PLACEMENT_3D('',#164264,#128198,#128199) ;
#100905 = AXIS2_PLACEMENT_3D('',#164265,#128200,#128201) ;
#100906 = AXIS2_PLACEMENT_3D('',#164266,#128202,#128203) ;
#100907 = AXIS2_PLACEMENT_3D('',#164267,#128204,#128205) ;
#100908 = AXIS2_PLACEMENT_3D('',#164268,#128206,#128207) ;
#100909 = AXIS2_PLACEMENT_3D('',#164269,#128208,#128209) ;
#100910 = AXIS2_PLACEMENT_3D('',#164270,#128210,#128211) ;
#100911 = AXIS2_PLACEMENT_3D('',#164271,#128212,#128213) ;
#100912 = AXIS2_PLACEMENT_3D('',#164272,#128214,#128215) ;
#100913 = AXIS2_PLACEMENT_3D('',#164273,#128216,#128217) ;
#100914 = AXIS2_PLACEMENT_3D('',#164274,#128218,#128219) ;
#100915 = AXIS2_PLACEMENT_3D('',#164275,#128220,#128221) ;
#100916 = AXIS2_PLACEMENT_3D('',#164276,#128222,#128223) ;
#100917 = AXIS2_PLACEMENT_3D('',#164277,#128224,#128225) ;
#100918 = AXIS2_PLACEMENT_3D('',#164278,#128226,#128227) ;
#100919 = AXIS2_PLACEMENT_3D('',#164291,#128228,#128229) ;
#100920 = AXIS2_PLACEMENT_3D('',#164316,#128230,#128231) ;
#100921 = AXIS2_PLACEMENT_3D('',#164317,#128232,#128233) ;
#100922 = AXIS2_PLACEMENT_3D('',#164318,#128234,#128235) ;
#100923 = AXIS2_PLACEMENT_3D('',#164319,#128236,#128237) ;
#100924 = AXIS2_PLACEMENT_3D('',#164320,#128238,#128239) ;
#100925 = AXIS2_PLACEMENT_3D('',#164321,#128240,#128241) ;
#100926 = AXIS2_PLACEMENT_3D('',#164322,#128242,#128243) ;
#100927 = AXIS2_PLACEMENT_3D('',#164323,#128244,#128245) ;
#100928 = AXIS2_PLACEMENT_3D('',#164324,#128246,#128247) ;
#100929 = AXIS2_PLACEMENT_3D('',#164325,#128248,#128249) ;
#100930 = AXIS2_PLACEMENT_3D('',#164326,#128250,#128251) ;
#100931 = AXIS2_PLACEMENT_3D('',#164327,#128252,#128253) ;
#100932 = AXIS2_PLACEMENT_3D('',#164328,#128254,#128255) ;
#100933 = AXIS2_PLACEMENT_3D('',#164329,#128256,#128257) ;
#100934 = AXIS2_PLACEMENT_3D('',#164330,#128258,#128259) ;
#100935 = AXIS2_PLACEMENT_3D('',#164331,#128260,#128261) ;
#100936 = AXIS2_PLACEMENT_3D('',#164332,#128262,#128263) ;
#100937 = AXIS2_PLACEMENT_3D('',#164333,#128264,#128265) ;
#100938 = AXIS2_PLACEMENT_3D('',#164334,#128266,#128267) ;
#100939 = AXIS2_PLACEMENT_3D('',#164335,#128268,#128269) ;
#100940 = AXIS2_PLACEMENT_3D('',#164336,#128270,#128271) ;
#100941 = AXIS2_PLACEMENT_3D('',#164337,#128272,#128273) ;
#100942 = AXIS2_PLACEMENT_3D('',#164338,#128274,#128275) ;
#100943 = AXIS2_PLACEMENT_3D('',#164339,#128276,#128277) ;
#100944 = AXIS2_PLACEMENT_3D('',#164340,#128278,#128279) ;
#100945 = AXIS2_PLACEMENT_3D('',#164341,#128280,#128281) ;
#100946 = AXIS2_PLACEMENT_3D('',#164342,#128282,#128283) ;
#100947 = AXIS2_PLACEMENT_3D('',#164343,#128284,#128285) ;
#100948 = AXIS2_PLACEMENT_3D('',#164344,#128286,#128287) ;
#100949 = AXIS2_PLACEMENT_3D('',#164345,#128288,#128289) ;
#100950 = AXIS2_PLACEMENT_3D('',#164346,#128290,#128291) ;
#100951 = AXIS2_PLACEMENT_3D('',#164347,#128292,#128293) ;
#100952 = AXIS2_PLACEMENT_3D('',#164348,#128294,#128295) ;
#100953 = AXIS2_PLACEMENT_3D('',#164349,#128296,#128297) ;
#100954 = AXIS2_PLACEMENT_3D('',#164350,#128298,#128299) ;
#100955 = AXIS2_PLACEMENT_3D('',#164351,#128300,#128301) ;
#100956 = AXIS2_PLACEMENT_3D('',#164352,#128302,#128303) ;
#100957 = AXIS2_PLACEMENT_3D('',#164353,#128304,#128305) ;
#100958 = AXIS2_PLACEMENT_3D('',#164354,#128306,#128307) ;
#100959 = AXIS2_PLACEMENT_3D('',#164355,#128308,#128309) ;
#100960 = AXIS2_PLACEMENT_3D('',#164356,#128310,#128311) ;
#100961 = AXIS2_PLACEMENT_3D('',#164357,#128312,#128313) ;
#100962 = AXIS2_PLACEMENT_3D('',#164358,#128314,#128315) ;
#100963 = AXIS2_PLACEMENT_3D('',#164359,#128316,#128317) ;
#100964 = AXIS2_PLACEMENT_3D('',#164360,#128318,#128319) ;
#100965 = AXIS2_PLACEMENT_3D('',#164361,#128320,#128321) ;
#100966 = AXIS2_PLACEMENT_3D('',#164362,#128322,#128323) ;
#100967 = AXIS2_PLACEMENT_3D('',#164363,#128324,#128325) ;
#100968 = AXIS2_PLACEMENT_3D('',#164364,#128326,#128327) ;
#100969 = AXIS2_PLACEMENT_3D('',#164365,#128328,#128329) ;
#100970 = AXIS2_PLACEMENT_3D('',#164366,#128330,#128331) ;
#100971 = AXIS2_PLACEMENT_3D('',#164367,#128332,#128333) ;
#100972 = AXIS2_PLACEMENT_3D('',#164368,#128334,#128335) ;
#100973 = AXIS2_PLACEMENT_3D('',#164369,#128336,#128337) ;
#100974 = AXIS2_PLACEMENT_3D('',#164370,#128338,#128339) ;
#100975 = AXIS2_PLACEMENT_3D('',#164371,#128340,#128341) ;
#100976 = AXIS2_PLACEMENT_3D('',#164372,#128342,#128343) ;
#100977 = AXIS2_PLACEMENT_3D('',#164373,#128344,#128345) ;
#100978 = AXIS2_PLACEMENT_3D('',#164374,#128346,#128347) ;
#100979 = AXIS2_PLACEMENT_3D('',#164375,#128348,#128349) ;
#100980 = AXIS2_PLACEMENT_3D('',#164376,#128350,#128351) ;
#100981 = AXIS2_PLACEMENT_3D('',#164377,#128352,#128353) ;
#100982 = AXIS2_PLACEMENT_3D('',#164378,#128354,#128355) ;
#100983 = AXIS2_PLACEMENT_3D('',#164379,#128356,#128357) ;
#100984 = AXIS2_PLACEMENT_3D('',#164380,#128358,#128359) ;
#100985 = AXIS2_PLACEMENT_3D('',#164381,#128360,#128361) ;
#100986 = AXIS2_PLACEMENT_3D('',#164382,#128362,#128363) ;
#100987 = AXIS2_PLACEMENT_3D('',#164383,#128364,#128365) ;
#100988 = AXIS2_PLACEMENT_3D('',#164384,#128366,#128367) ;
#100989 = AXIS2_PLACEMENT_3D('',#164385,#128368,#128369) ;
#100990 = AXIS2_PLACEMENT_3D('',#164386,#128370,#128371) ;
#100991 = AXIS2_PLACEMENT_3D('',#164387,#128372,#128373) ;
#100992 = AXIS2_PLACEMENT_3D('',#164388,#128374,#128375) ;
#100993 = AXIS2_PLACEMENT_3D('',#164389,#128376,#128377) ;
#100994 = AXIS2_PLACEMENT_3D('',#164390,#128378,#128379) ;
#100995 = AXIS2_PLACEMENT_3D('',#164391,#128380,#128381) ;
#100996 = AXIS2_PLACEMENT_3D('',#164392,#128382,#128383) ;
#100997 = AXIS2_PLACEMENT_3D('',#164393,#128384,#128385) ;
#100998 = AXIS2_PLACEMENT_3D('',#164394,#128386,#128387) ;
#100999 = AXIS2_PLACEMENT_3D('',#164395,#128388,#128389) ;
#101000 = AXIS2_PLACEMENT_3D('',#164396,#128390,#128391) ;
#101001 = AXIS2_PLACEMENT_3D('',#164397,#128392,#128393) ;
#101002 = AXIS2_PLACEMENT_3D('',#164398,#128394,#128395) ;
#101003 = AXIS2_PLACEMENT_3D('',#164399,#128396,#128397) ;
#101004 = AXIS2_PLACEMENT_3D('',#164400,#128398,#128399) ;
#101005 = AXIS2_PLACEMENT_3D('',#164401,#128400,#128401) ;
#101006 = AXIS2_PLACEMENT_3D('',#164402,#128402,#128403) ;
#101007 = AXIS2_PLACEMENT_3D('',#164403,#128404,#128405) ;
#101008 = AXIS2_PLACEMENT_3D('',#164404,#128406,#128407) ;
#101009 = AXIS2_PLACEMENT_3D('',#164405,#128408,#128409) ;
#101010 = AXIS2_PLACEMENT_3D('',#164406,#128410,#128411) ;
#101011 = AXIS2_PLACEMENT_3D('',#164407,#128412,#128413) ;
#101012 = AXIS2_PLACEMENT_3D('',#164408,#128414,#128415) ;
#101013 = AXIS2_PLACEMENT_3D('',#164409,#128416,#128417) ;
#101014 = AXIS2_PLACEMENT_3D('',#164410,#128418,#128419) ;
#101015 = AXIS2_PLACEMENT_3D('',#164411,#128420,#128421) ;
#101016 = AXIS2_PLACEMENT_3D('',#164412,#128422,#128423) ;
#101017 = AXIS2_PLACEMENT_3D('',#164413,#128424,#128425) ;
#101018 = AXIS2_PLACEMENT_3D('',#164414,#128426,#128427) ;
#101019 = AXIS2_PLACEMENT_3D('',#164415,#128428,#128429) ;
#101020 = AXIS2_PLACEMENT_3D('',#164416,#128430,#128431) ;
#101021 = AXIS2_PLACEMENT_3D('',#164417,#128432,#128433) ;
#101022 = AXIS2_PLACEMENT_3D('',#164418,#128434,#128435) ;
#101023 = AXIS2_PLACEMENT_3D('',#164419,#128436,#128437) ;
#101024 = AXIS2_PLACEMENT_3D('',#164420,#128438,#128439) ;
#101025 = AXIS2_PLACEMENT_3D('',#164421,#128440,#128441) ;
#101026 = AXIS2_PLACEMENT_3D('',#164422,#128442,#128443) ;
#101027 = AXIS2_PLACEMENT_3D('',#164423,#128444,#128445) ;
#101028 = AXIS2_PLACEMENT_3D('',#164424,#128446,#128447) ;
#101029 = AXIS2_PLACEMENT_3D('',#164425,#128448,#128449) ;
#101030 = AXIS2_PLACEMENT_3D('',#164426,#128450,#128451) ;
#101031 = AXIS2_PLACEMENT_3D('',#164427,#128452,#128453) ;
#101032 = AXIS2_PLACEMENT_3D('',#164428,#128454,#128455) ;
#101033 = AXIS2_PLACEMENT_3D('',#164429,#128456,#128457) ;
#101034 = AXIS2_PLACEMENT_3D('',#164430,#128458,#128459) ;
#101035 = AXIS2_PLACEMENT_3D('',#164431,#128460,#128461) ;
#101036 = AXIS2_PLACEMENT_3D('',#164432,#128462,#128463) ;
#101037 = AXIS2_PLACEMENT_3D('',#164433,#128464,#128465) ;
#101038 = AXIS2_PLACEMENT_3D('',#164434,#128466,#128467) ;
#101039 = AXIS2_PLACEMENT_3D('',#164435,#128468,#128469) ;
#101040 = AXIS2_PLACEMENT_3D('',#164436,#128470,#128471) ;
#101041 = AXIS2_PLACEMENT_3D('',#164437,#128472,#128473) ;
#101042 = AXIS2_PLACEMENT_3D('',#164438,#128474,#128475) ;
#101043 = AXIS2_PLACEMENT_3D('',#164439,#128476,#128477) ;
#101044 = AXIS2_PLACEMENT_3D('',#164440,#128478,#128479) ;
#101045 = AXIS2_PLACEMENT_3D('',#164441,#128480,#128481) ;
#101046 = AXIS2_PLACEMENT_3D('',#164442,#128482,#128483) ;
#101047 = AXIS2_PLACEMENT_3D('',#164443,#128484,#128485) ;
#101048 = AXIS2_PLACEMENT_3D('',#164444,#128486,#128487) ;
#101049 = AXIS2_PLACEMENT_3D('',#164445,#128488,#128489) ;
#101050 = AXIS2_PLACEMENT_3D('',#164446,#128490,#128491) ;
#101051 = AXIS2_PLACEMENT_3D('',#164447,#128492,#128493) ;
#101052 = AXIS2_PLACEMENT_3D('',#164448,#128494,#128495) ;
#101053 = AXIS2_PLACEMENT_3D('',#164449,#128496,#128497) ;
#101054 = AXIS2_PLACEMENT_3D('',#164450,#128498,#128499) ;
#101055 = AXIS2_PLACEMENT_3D('',#164451,#128500,#128501) ;
#101056 = AXIS2_PLACEMENT_3D('',#164452,#128502,#128503) ;
#101057 = AXIS2_PLACEMENT_3D('',#164453,#128504,#128505) ;
#101058 = AXIS2_PLACEMENT_3D('',#164454,#128506,#128507) ;
#101059 = AXIS2_PLACEMENT_3D('',#164455,#128508,#128509) ;
#101060 = AXIS2_PLACEMENT_3D('',#164456,#128510,#128511) ;
#101061 = AXIS2_PLACEMENT_3D('',#164457,#128512,#128513) ;
#101062 = AXIS2_PLACEMENT_3D('',#164458,#128514,#128515) ;
#101063 = AXIS2_PLACEMENT_3D('',#164459,#128516,#128517) ;
#101064 = AXIS2_PLACEMENT_3D('',#164460,#128518,#128519) ;
#101065 = AXIS2_PLACEMENT_3D('',#164461,#128520,#128521) ;
#101066 = AXIS2_PLACEMENT_3D('',#164462,#128522,#128523) ;
#101067 = AXIS2_PLACEMENT_3D('',#164463,#128524,#128525) ;
#101068 = AXIS2_PLACEMENT_3D('',#164464,#128526,#128527) ;
#101069 = AXIS2_PLACEMENT_3D('',#164465,#128528,#128529) ;
#101070 = AXIS2_PLACEMENT_3D('',#164466,#128530,#128531) ;
#101071 = AXIS2_PLACEMENT_3D('',#164467,#128532,#128533) ;
#101072 = AXIS2_PLACEMENT_3D('',#164468,#128534,#128535) ;
#101073 = AXIS2_PLACEMENT_3D('',#164469,#128536,#128537) ;
#101074 = AXIS2_PLACEMENT_3D('',#164470,#128538,#128539) ;
#101075 = AXIS2_PLACEMENT_3D('',#164471,#128540,#128541) ;
#101076 = AXIS2_PLACEMENT_3D('',#164472,#128542,#128543) ;
#101077 = AXIS2_PLACEMENT_3D('',#164473,#128544,#128545) ;
#101078 = AXIS2_PLACEMENT_3D('',#164474,#128546,#128547) ;
#101079 = AXIS2_PLACEMENT_3D('',#164475,#128548,#128549) ;
#101080 = AXIS2_PLACEMENT_3D('',#164476,#128550,#128551) ;
#101081 = AXIS2_PLACEMENT_3D('',#164477,#128552,#128553) ;
#101082 = AXIS2_PLACEMENT_3D('',#164478,#128554,#128555) ;
#101083 = AXIS2_PLACEMENT_3D('',#164479,#128556,#128557) ;
#101084 = AXIS2_PLACEMENT_3D('',#164480,#128558,#128559) ;
#101085 = AXIS2_PLACEMENT_3D('',#164481,#128560,#128561) ;
#101086 = AXIS2_PLACEMENT_3D('',#164482,#128562,#128563) ;
#101087 = AXIS2_PLACEMENT_3D('',#164483,#128564,#128565) ;
#101088 = AXIS2_PLACEMENT_3D('',#164484,#128566,#128567) ;
#101089 = AXIS2_PLACEMENT_3D('',#164485,#128568,#128569) ;
#101090 = AXIS2_PLACEMENT_3D('',#164486,#128570,#128571) ;
#101091 = AXIS2_PLACEMENT_3D('',#164487,#128572,#128573) ;
#101092 = AXIS2_PLACEMENT_3D('',#164488,#128574,#128575) ;
#101093 = AXIS2_PLACEMENT_3D('',#164489,#128576,#128577) ;
#101094 = AXIS2_PLACEMENT_3D('',#164490,#128578,#128579) ;
#101095 = AXIS2_PLACEMENT_3D('',#164491,#128580,#128581) ;
#101096 = AXIS2_PLACEMENT_3D('',#164492,#128582,#128583) ;
#101097 = AXIS2_PLACEMENT_3D('',#164493,#128584,#128585) ;
#101098 = AXIS2_PLACEMENT_3D('',#164494,#128586,#128587) ;
#101099 = AXIS2_PLACEMENT_3D('',#164495,#128588,#128589) ;
#101100 = AXIS2_PLACEMENT_3D('',#164496,#128590,#128591) ;
#101101 = AXIS2_PLACEMENT_3D('',#164497,#128592,#128593) ;
#101102 = AXIS2_PLACEMENT_3D('',#164498,#128594,#128595) ;
#101103 = AXIS2_PLACEMENT_3D('',#164499,#128596,#128597) ;
#101104 = AXIS2_PLACEMENT_3D('',#164500,#128598,#128599) ;
#101105 = AXIS2_PLACEMENT_3D('',#164501,#128600,#128601) ;
#101106 = AXIS2_PLACEMENT_3D('',#164502,#128602,#128603) ;
#101107 = AXIS2_PLACEMENT_3D('',#164503,#128604,#128605) ;
#101108 = AXIS2_PLACEMENT_3D('',#164504,#128606,#128607) ;
#101109 = AXIS2_PLACEMENT_3D('',#164505,#128608,#128609) ;
#101110 = AXIS2_PLACEMENT_3D('',#164506,#128610,#128611) ;
#101111 = AXIS2_PLACEMENT_3D('',#164507,#128612,#128613) ;
#101112 = AXIS2_PLACEMENT_3D('',#164508,#128614,#128615) ;
#101113 = AXIS2_PLACEMENT_3D('',#164509,#128616,#128617) ;
#101114 = AXIS2_PLACEMENT_3D('',#164510,#128618,#128619) ;
#101115 = AXIS2_PLACEMENT_3D('',#164511,#128620,#128621) ;
#101116 = AXIS2_PLACEMENT_3D('',#164512,#128622,#128623) ;
#101117 = AXIS2_PLACEMENT_3D('',#164513,#128624,#128625) ;
#101118 = AXIS2_PLACEMENT_3D('',#164514,#128626,#128627) ;
#101119 = AXIS2_PLACEMENT_3D('',#164515,#128628,#128629) ;
#101120 = AXIS2_PLACEMENT_3D('',#164516,#128630,#128631) ;
#101121 = AXIS2_PLACEMENT_3D('',#164517,#128632,#128633) ;
#101122 = AXIS2_PLACEMENT_3D('',#164518,#128634,#128635) ;
#101123 = AXIS2_PLACEMENT_3D('',#164519,#128636,#128637) ;
#101124 = AXIS2_PLACEMENT_3D('',#164520,#128638,#128639) ;
#101125 = AXIS2_PLACEMENT_3D('',#164521,#128640,#128641) ;
#101126 = AXIS2_PLACEMENT_3D('',#164522,#128642,#128643) ;
#101127 = AXIS2_PLACEMENT_3D('',#164523,#128644,#128645) ;
#101128 = AXIS2_PLACEMENT_3D('',#164524,#128646,#128647) ;
#101129 = AXIS2_PLACEMENT_3D('',#164525,#128648,#128649) ;
#101130 = AXIS2_PLACEMENT_3D('',#164526,#128650,#128651) ;
#101131 = AXIS2_PLACEMENT_3D('',#164527,#128652,#128653) ;
#101132 = AXIS2_PLACEMENT_3D('',#164528,#128654,#128655) ;
#101133 = AXIS2_PLACEMENT_3D('',#164529,#128656,#128657) ;
#101134 = AXIS2_PLACEMENT_3D('',#164554,#128658,#128659) ;
#101135 = AXIS2_PLACEMENT_3D('',#164555,#128660,#128661) ;
#101136 = AXIS2_PLACEMENT_3D('',#164556,#128662,#128663) ;
#101137 = AXIS2_PLACEMENT_3D('',#164581,#128664,#128665) ;
#101138 = AXIS2_PLACEMENT_3D('',#164582,#128666,#128667) ;
#101139 = AXIS2_PLACEMENT_3D('',#164583,#128668,#128669) ;
#101140 = AXIS2_PLACEMENT_3D('',#164584,#128670,#128671) ;
#101141 = AXIS2_PLACEMENT_3D('',#164609,#128672,#128673) ;
#101142 = AXIS2_PLACEMENT_3D('',#164610,#128674,#128675) ;
#101143 = AXIS2_PLACEMENT_3D('',#164611,#128676,#128677) ;
#101144 = AXIS2_PLACEMENT_3D('',#164612,#128678,#128679) ;
#101145 = AXIS2_PLACEMENT_3D('',#164613,#128680,#128681) ;
#101146 = AXIS2_PLACEMENT_3D('',#164614,#128682,#128683) ;
#101147 = AXIS2_PLACEMENT_3D('',#164615,#128684,#128685) ;
#101148 = AXIS2_PLACEMENT_3D('',#164616,#128686,#128687) ;
#101149 = AXIS2_PLACEMENT_3D('',#164617,#128688,#128689) ;
#101150 = AXIS2_PLACEMENT_3D('',#164618,#128690,#128691) ;
#101151 = AXIS2_PLACEMENT_3D('',#164619,#128692,#128693) ;
#101152 = AXIS2_PLACEMENT_3D('',#164620,#128694,#128695) ;
#101153 = AXIS2_PLACEMENT_3D('',#164621,#128696,#128697) ;
#101154 = AXIS2_PLACEMENT_3D('',#164622,#128698,#128699) ;
#101155 = AXIS2_PLACEMENT_3D('',#164623,#128700,#128701) ;
#101156 = AXIS2_PLACEMENT_3D('',#164624,#128702,#128703) ;
#101157 = AXIS2_PLACEMENT_3D('',#164625,#128704,#128705) ;
#101158 = AXIS2_PLACEMENT_3D('',#164626,#128706,#128707) ;
#101159 = AXIS2_PLACEMENT_3D('',#164627,#128708,#128709) ;
#101160 = AXIS2_PLACEMENT_3D('',#164628,#128710,#128711) ;
#101161 = AXIS2_PLACEMENT_3D('',#164629,#128712,#128713) ;
#101162 = AXIS2_PLACEMENT_3D('',#164678,#128714,#128715) ;
#101163 = AXIS2_PLACEMENT_3D('',#164691,#128716,#128717) ;
#101164 = AXIS2_PLACEMENT_3D('',#164692,#128718,#128719) ;
#101165 = AXIS2_PLACEMENT_3D('',#164693,#128720,#128721) ;
#101166 = AXIS2_PLACEMENT_3D('',#164694,#128722,#128723) ;
#101167 = AXIS2_PLACEMENT_3D('',#164695,#128724,#128725) ;
#101168 = AXIS2_PLACEMENT_3D('',#164696,#128726,#128727) ;
#101169 = AXIS2_PLACEMENT_3D('',#164697,#128728,#128729) ;
#101170 = AXIS2_PLACEMENT_3D('',#164698,#128730,#128731) ;
#101171 = AXIS2_PLACEMENT_3D('',#164699,#128732,#128733) ;
#101172 = AXIS2_PLACEMENT_3D('',#164700,#128734,#128735) ;
#101173 = AXIS2_PLACEMENT_3D('',#164701,#128736,#128737) ;
#101174 = AXIS2_PLACEMENT_3D('',#164702,#128738,#128739) ;
#101175 = AXIS2_PLACEMENT_3D('',#164703,#128740,#128741) ;
#101176 = AXIS2_PLACEMENT_3D('',#164704,#128742,#128743) ;
#101177 = AXIS2_PLACEMENT_3D('',#164705,#128744,#128745) ;
#101178 = AXIS2_PLACEMENT_3D('',#164718,#128746,#128747) ;
#101179 = AXIS2_PLACEMENT_3D('',#164743,#128748,#128749) ;
#101180 = AXIS2_PLACEMENT_3D('',#164756,#128750,#128751) ;
#101181 = AXIS2_PLACEMENT_3D('',#164757,#128752,#128753) ;
#101182 = AXIS2_PLACEMENT_3D('',#164758,#128754,#128755) ;
#101183 = AXIS2_PLACEMENT_3D('',#164759,#128756,#128757) ;
#101184 = AXIS2_PLACEMENT_3D('',#164760,#128758,#128759) ;
#101185 = AXIS2_PLACEMENT_3D('',#164761,#128760,#128761) ;
#101186 = AXIS2_PLACEMENT_3D('',#164762,#128762,#128763) ;
#101187 = AXIS2_PLACEMENT_3D('',#164763,#128764,#128765) ;
#101188 = AXIS2_PLACEMENT_3D('',#164764,#128766,#128767) ;
#101189 = AXIS2_PLACEMENT_3D('',#164765,#128768,#128769) ;
#101190 = AXIS2_PLACEMENT_3D('',#164766,#128770,#128771) ;
#101191 = AXIS2_PLACEMENT_3D('',#164767,#128772,#128773) ;
#101192 = AXIS2_PLACEMENT_3D('',#164768,#128774,#128775) ;
#101193 = AXIS2_PLACEMENT_3D('',#164769,#128776,#128777) ;
#101194 = AXIS2_PLACEMENT_3D('',#164770,#128778,#128779) ;
#101195 = AXIS2_PLACEMENT_3D('',#164783,#128780,#128781) ;
#101196 = AXIS2_PLACEMENT_3D('',#164808,#128782,#128783) ;
#101197 = AXIS2_PLACEMENT_3D('',#164809,#128784,#128785) ;
#101198 = AXIS2_PLACEMENT_3D('',#164810,#128786,#128787) ;
#101199 = AXIS2_PLACEMENT_3D('',#164811,#128788,#128789) ;
#101200 = AXIS2_PLACEMENT_3D('',#164812,#128790,#128791) ;
#101201 = AXIS2_PLACEMENT_3D('',#164813,#128792,#128793) ;
#101202 = AXIS2_PLACEMENT_3D('',#164814,#128794,#128795) ;
#101203 = AXIS2_PLACEMENT_3D('',#164815,#128796,#128797) ;
#101204 = AXIS2_PLACEMENT_3D('',#164816,#128798,#128799) ;
#101205 = AXIS2_PLACEMENT_3D('',#164817,#128800,#128801) ;
#101206 = AXIS2_PLACEMENT_3D('',#164818,#128802,#128803) ;
#101207 = AXIS2_PLACEMENT_3D('',#164819,#128804,#128805) ;
#101208 = AXIS2_PLACEMENT_3D('',#164820,#128806,#128807) ;
#101209 = AXIS2_PLACEMENT_3D('',#164821,#128808,#128809) ;
#101210 = AXIS2_PLACEMENT_3D('',#164822,#128810,#128811) ;
#101211 = AXIS2_PLACEMENT_3D('',#164823,#128812,#128813) ;
#101212 = AXIS2_PLACEMENT_3D('',#164824,#128814,#128815) ;
#101213 = AXIS2_PLACEMENT_3D('',#164825,#128816,#128817) ;
#101214 = AXIS2_PLACEMENT_3D('',#164826,#128818,#128819) ;
#101215 = AXIS2_PLACEMENT_3D('',#164827,#128820,#128821) ;
#101216 = AXIS2_PLACEMENT_3D('',#164828,#128822,#128823) ;
#101217 = AXIS2_PLACEMENT_3D('',#164829,#128824,#128825) ;
#101218 = AXIS2_PLACEMENT_3D('',#164830,#128826,#128827) ;
#101219 = AXIS2_PLACEMENT_3D('',#164831,#128828,#128829) ;
#101220 = AXIS2_PLACEMENT_3D('',#164832,#128830,#128831) ;
#101221 = AXIS2_PLACEMENT_3D('',#164833,#128832,#128833) ;
#101222 = AXIS2_PLACEMENT_3D('',#164834,#128834,#128835) ;
#101223 = AXIS2_PLACEMENT_3D('',#164835,#128836,#128837) ;
#101224 = AXIS2_PLACEMENT_3D('',#164836,#128838,#128839) ;
#101225 = AXIS2_PLACEMENT_3D('',#164837,#128840,#128841) ;
#101226 = AXIS2_PLACEMENT_3D('',#164838,#128842,#128843) ;
#101227 = AXIS2_PLACEMENT_3D('',#164839,#128844,#128845) ;
#101228 = AXIS2_PLACEMENT_3D('',#164840,#128846,#128847) ;
#101229 = AXIS2_PLACEMENT_3D('',#164841,#128848,#128849) ;
#101230 = AXIS2_PLACEMENT_3D('',#164842,#128850,#128851) ;
#101231 = AXIS2_PLACEMENT_3D('',#164843,#128852,#128853) ;
#101232 = AXIS2_PLACEMENT_3D('',#164844,#128854,#128855) ;
#101233 = AXIS2_PLACEMENT_3D('',#164845,#128856,#128857) ;
#101234 = AXIS2_PLACEMENT_3D('',#164846,#128858,#128859) ;
#101235 = AXIS2_PLACEMENT_3D('',#164847,#128860,#128861) ;
#101236 = AXIS2_PLACEMENT_3D('',#164848,#128862,#128863) ;
#101237 = AXIS2_PLACEMENT_3D('',#164849,#128864,#128865) ;
#101238 = AXIS2_PLACEMENT_3D('',#164850,#128866,#128867) ;
#101239 = AXIS2_PLACEMENT_3D('',#164851,#128868,#128869) ;
#101240 = AXIS2_PLACEMENT_3D('',#164852,#128870,#128871) ;
#101241 = AXIS2_PLACEMENT_3D('',#164853,#128872,#128873) ;
#101242 = AXIS2_PLACEMENT_3D('',#164854,#128874,#128875) ;
#101243 = AXIS2_PLACEMENT_3D('',#164855,#128876,#128877) ;
#101244 = AXIS2_PLACEMENT_3D('',#164856,#128878,#128879) ;
#101245 = AXIS2_PLACEMENT_3D('',#164857,#128880,#128881) ;
#101246 = AXIS2_PLACEMENT_3D('',#164858,#128882,#128883) ;
#101247 = AXIS2_PLACEMENT_3D('',#164859,#128884,#128885) ;
#101248 = AXIS2_PLACEMENT_3D('',#164860,#128886,#128887) ;
#101249 = AXIS2_PLACEMENT_3D('',#164861,#128888,#128889) ;
#101250 = AXIS2_PLACEMENT_3D('',#164862,#128890,#128891) ;
#101251 = AXIS2_PLACEMENT_3D('',#164863,#128892,#128893) ;
#101252 = AXIS2_PLACEMENT_3D('',#164864,#128894,#128895) ;
#101253 = AXIS2_PLACEMENT_3D('',#164865,#128896,#128897) ;
#101254 = AXIS2_PLACEMENT_3D('',#164866,#128898,#128899) ;
#101255 = AXIS2_PLACEMENT_3D('',#164867,#128900,#128901) ;
#101256 = AXIS2_PLACEMENT_3D('',#164868,#128902,#128903) ;
#101257 = AXIS2_PLACEMENT_3D('',#164869,#128904,#128905) ;
#101258 = AXIS2_PLACEMENT_3D('',#164870,#128906,#128907) ;
#101259 = AXIS2_PLACEMENT_3D('',#164871,#128908,#128909) ;
#101260 = AXIS2_PLACEMENT_3D('',#164872,#128910,#128911) ;
#101261 = AXIS2_PLACEMENT_3D('',#164873,#128912,#128913) ;
#101262 = AXIS2_PLACEMENT_3D('',#164874,#128914,#128915) ;
#101263 = AXIS2_PLACEMENT_3D('',#164875,#128916,#128917) ;
#101264 = AXIS2_PLACEMENT_3D('',#164876,#128918,#128919) ;
#101265 = AXIS2_PLACEMENT_3D('',#164877,#128920,#128921) ;
#101266 = AXIS2_PLACEMENT_3D('',#164878,#128922,#128923) ;
#101267 = AXIS2_PLACEMENT_3D('',#164879,#128924,#128925) ;
#101268 = AXIS2_PLACEMENT_3D('',#164880,#128926,#128927) ;
#101269 = AXIS2_PLACEMENT_3D('',#164881,#128928,#128929) ;
#101270 = AXIS2_PLACEMENT_3D('',#164882,#128930,#128931) ;
#101271 = AXIS2_PLACEMENT_3D('',#164883,#128932,#128933) ;
#101272 = AXIS2_PLACEMENT_3D('',#164884,#128934,#128935) ;
#101273 = AXIS2_PLACEMENT_3D('',#164885,#128936,#128937) ;
#101274 = AXIS2_PLACEMENT_3D('',#164886,#128938,#128939) ;
#101275 = AXIS2_PLACEMENT_3D('',#164887,#128940,#128941) ;
#101276 = AXIS2_PLACEMENT_3D('',#164888,#128942,#128943) ;
#101277 = AXIS2_PLACEMENT_3D('',#164889,#128944,#128945) ;
#101278 = AXIS2_PLACEMENT_3D('',#164890,#128946,#128947) ;
#101279 = AXIS2_PLACEMENT_3D('',#164891,#128948,#128949) ;
#101280 = AXIS2_PLACEMENT_3D('',#164892,#128950,#128951) ;
#101281 = AXIS2_PLACEMENT_3D('',#164893,#128952,#128953) ;
#101282 = AXIS2_PLACEMENT_3D('',#164894,#128954,#128955) ;
#101283 = AXIS2_PLACEMENT_3D('',#164895,#128956,#128957) ;
#101284 = AXIS2_PLACEMENT_3D('',#164896,#128958,#128959) ;
#101285 = AXIS2_PLACEMENT_3D('',#164897,#128960,#128961) ;
#101286 = AXIS2_PLACEMENT_3D('',#164898,#128962,#128963) ;
#101287 = AXIS2_PLACEMENT_3D('',#164899,#128964,#128965) ;
#101288 = AXIS2_PLACEMENT_3D('',#164900,#128966,#128967) ;
#101289 = AXIS2_PLACEMENT_3D('',#164901,#128968,#128969) ;
#101290 = AXIS2_PLACEMENT_3D('',#164902,#128970,#128971) ;
#101291 = AXIS2_PLACEMENT_3D('',#164903,#128972,#128973) ;
#101292 = AXIS2_PLACEMENT_3D('',#164904,#128974,#128975) ;
#101293 = AXIS2_PLACEMENT_3D('',#164905,#128976,#128977) ;
#101294 = AXIS2_PLACEMENT_3D('',#164906,#128978,#128979) ;
#101295 = AXIS2_PLACEMENT_3D('',#164907,#128980,#128981) ;
#101296 = AXIS2_PLACEMENT_3D('',#164908,#128982,#128983) ;
#101297 = AXIS2_PLACEMENT_3D('',#164909,#128984,#128985) ;
#101298 = AXIS2_PLACEMENT_3D('',#164910,#128986,#128987) ;
#101299 = AXIS2_PLACEMENT_3D('',#164911,#128988,#128989) ;
#101300 = AXIS2_PLACEMENT_3D('',#164912,#128990,#128991) ;
#101301 = AXIS2_PLACEMENT_3D('',#164913,#128992,#128993) ;
#101302 = AXIS2_PLACEMENT_3D('',#164914,#128994,#128995) ;
#101303 = AXIS2_PLACEMENT_3D('',#164915,#128996,#128997) ;
#101304 = AXIS2_PLACEMENT_3D('',#164916,#128998,#128999) ;
#101305 = AXIS2_PLACEMENT_3D('',#164917,#129000,#129001) ;
#101306 = AXIS2_PLACEMENT_3D('',#164918,#129002,#129003) ;
#101307 = AXIS2_PLACEMENT_3D('',#164919,#129004,#129005) ;
#101308 = AXIS2_PLACEMENT_3D('',#164920,#129006,#129007) ;
#101309 = AXIS2_PLACEMENT_3D('',#164921,#129008,#129009) ;
#101310 = AXIS2_PLACEMENT_3D('',#164922,#129010,#129011) ;
#101311 = AXIS2_PLACEMENT_3D('',#164923,#129012,#129013) ;
#101312 = AXIS2_PLACEMENT_3D('',#164924,#129014,#129015) ;
#101313 = AXIS2_PLACEMENT_3D('',#164925,#129016,#129017) ;
#101314 = AXIS2_PLACEMENT_3D('',#164926,#129018,#129019) ;
#101315 = AXIS2_PLACEMENT_3D('',#164927,#129020,#129021) ;
#101316 = AXIS2_PLACEMENT_3D('',#164928,#129022,#129023) ;
#101317 = AXIS2_PLACEMENT_3D('',#164929,#129024,#129025) ;
#101318 = AXIS2_PLACEMENT_3D('',#164930,#129026,#129027) ;
#101319 = AXIS2_PLACEMENT_3D('',#164931,#129028,#129029) ;
#101320 = AXIS2_PLACEMENT_3D('',#164932,#129030,#129031) ;
#101321 = AXIS2_PLACEMENT_3D('',#164933,#129032,#129033) ;
#101322 = AXIS2_PLACEMENT_3D('',#164934,#129034,#129035) ;
#101323 = AXIS2_PLACEMENT_3D('',#164935,#129036,#129037) ;
#101324 = AXIS2_PLACEMENT_3D('',#164936,#129038,#129039) ;
#101325 = AXIS2_PLACEMENT_3D('',#164937,#129040,#129041) ;
#101326 = AXIS2_PLACEMENT_3D('',#164938,#129042,#129043) ;
#101327 = AXIS2_PLACEMENT_3D('',#164939,#129044,#129045) ;
#101328 = AXIS2_PLACEMENT_3D('',#164940,#129046,#129047) ;
#101329 = AXIS2_PLACEMENT_3D('',#164941,#129048,#129049) ;
#101330 = AXIS2_PLACEMENT_3D('',#164942,#129050,#129051) ;
#101331 = AXIS2_PLACEMENT_3D('',#164943,#129052,#129053) ;
#101332 = AXIS2_PLACEMENT_3D('',#164944,#129054,#129055) ;
#101333 = AXIS2_PLACEMENT_3D('',#164945,#129056,#129057) ;
#101334 = AXIS2_PLACEMENT_3D('',#164946,#129058,#129059) ;
#101335 = AXIS2_PLACEMENT_3D('',#164947,#129060,#129061) ;
#101336 = AXIS2_PLACEMENT_3D('',#164948,#129062,#129063) ;
#101337 = AXIS2_PLACEMENT_3D('',#164949,#129064,#129065) ;
#101338 = AXIS2_PLACEMENT_3D('',#164950,#129066,#129067) ;
#101339 = AXIS2_PLACEMENT_3D('',#164951,#129068,#129069) ;
#101340 = AXIS2_PLACEMENT_3D('',#164952,#129070,#129071) ;
#101341 = AXIS2_PLACEMENT_3D('',#164953,#129072,#129073) ;
#101342 = AXIS2_PLACEMENT_3D('',#164954,#129074,#129075) ;
#101343 = AXIS2_PLACEMENT_3D('',#164955,#129076,#129077) ;
#101344 = AXIS2_PLACEMENT_3D('',#164956,#129078,#129079) ;
#101345 = AXIS2_PLACEMENT_3D('',#164957,#129080,#129081) ;
#101346 = AXIS2_PLACEMENT_3D('',#164958,#129082,#129083) ;
#101347 = AXIS2_PLACEMENT_3D('',#164959,#129084,#129085) ;
#101348 = AXIS2_PLACEMENT_3D('',#164960,#129086,#129087) ;
#101349 = AXIS2_PLACEMENT_3D('',#164961,#129088,#129089) ;
#101350 = AXIS2_PLACEMENT_3D('',#164962,#129090,#129091) ;
#101351 = AXIS2_PLACEMENT_3D('',#164963,#129092,#129093) ;
#101352 = AXIS2_PLACEMENT_3D('',#164964,#129094,#129095) ;
#101353 = AXIS2_PLACEMENT_3D('',#164965,#129096,#129097) ;
#101354 = AXIS2_PLACEMENT_3D('',#164966,#129098,#129099) ;
#101355 = AXIS2_PLACEMENT_3D('',#164967,#129100,#129101) ;
#101356 = AXIS2_PLACEMENT_3D('',#164968,#129102,#129103) ;
#101357 = AXIS2_PLACEMENT_3D('',#164969,#129104,#129105) ;
#101358 = AXIS2_PLACEMENT_3D('',#164970,#129106,#129107) ;
#101359 = AXIS2_PLACEMENT_3D('',#164971,#129108,#129109) ;
#101360 = AXIS2_PLACEMENT_3D('',#164972,#129110,#129111) ;
#101361 = AXIS2_PLACEMENT_3D('',#164973,#129112,#129113) ;
#101362 = AXIS2_PLACEMENT_3D('',#164974,#129114,#129115) ;
#101363 = AXIS2_PLACEMENT_3D('',#164975,#129116,#129117) ;
#101364 = AXIS2_PLACEMENT_3D('',#164976,#129118,#129119) ;
#101365 = AXIS2_PLACEMENT_3D('',#164977,#129120,#129121) ;
#101366 = AXIS2_PLACEMENT_3D('',#164978,#129122,#129123) ;
#101367 = AXIS2_PLACEMENT_3D('',#164979,#129124,#129125) ;
#101368 = AXIS2_PLACEMENT_3D('',#164980,#129126,#129127) ;
#101369 = AXIS2_PLACEMENT_3D('',#164981,#129128,#129129) ;
#101370 = AXIS2_PLACEMENT_3D('',#164982,#129130,#129131) ;
#101371 = AXIS2_PLACEMENT_3D('',#164983,#129132,#129133) ;
#101372 = AXIS2_PLACEMENT_3D('',#164984,#129134,#129135) ;
#101373 = AXIS2_PLACEMENT_3D('',#164985,#129136,#129137) ;
#101374 = AXIS2_PLACEMENT_3D('',#164986,#129138,#129139) ;
#101375 = AXIS2_PLACEMENT_3D('',#164987,#129140,#129141) ;
#101376 = AXIS2_PLACEMENT_3D('',#164988,#129142,#129143) ;
#101377 = AXIS2_PLACEMENT_3D('',#164989,#129144,#129145) ;
#101378 = AXIS2_PLACEMENT_3D('',#164990,#129146,#129147) ;
#101379 = AXIS2_PLACEMENT_3D('',#164991,#129148,#129149) ;
#101380 = AXIS2_PLACEMENT_3D('',#164992,#129150,#129151) ;
#101381 = AXIS2_PLACEMENT_3D('',#164993,#129152,#129153) ;
#101382 = AXIS2_PLACEMENT_3D('',#164994,#129154,#129155) ;
#101383 = AXIS2_PLACEMENT_3D('',#164995,#129156,#129157) ;
#101384 = AXIS2_PLACEMENT_3D('',#164996,#129158,#129159) ;
#101385 = AXIS2_PLACEMENT_3D('',#164997,#129160,#129161) ;
#101386 = AXIS2_PLACEMENT_3D('',#164998,#129162,#129163) ;
#101387 = AXIS2_PLACEMENT_3D('',#164999,#129164,#129165) ;
#101388 = AXIS2_PLACEMENT_3D('',#165000,#129166,#129167) ;
#101389 = AXIS2_PLACEMENT_3D('',#165001,#129168,#129169) ;
#101390 = AXIS2_PLACEMENT_3D('',#165002,#129170,#129171) ;
#101391 = AXIS2_PLACEMENT_3D('',#165003,#129172,#129173) ;
#101392 = AXIS2_PLACEMENT_3D('',#165004,#129174,#129175) ;
#101393 = AXIS2_PLACEMENT_3D('',#165005,#129176,#129177) ;
#101394 = AXIS2_PLACEMENT_3D('',#165006,#129178,#129179) ;
#101395 = AXIS2_PLACEMENT_3D('',#165007,#129180,#129181) ;
#101396 = AXIS2_PLACEMENT_3D('',#165008,#129182,#129183) ;
#101397 = AXIS2_PLACEMENT_3D('',#165009,#129184,#129185) ;
#101398 = AXIS2_PLACEMENT_3D('',#165010,#129186,#129187) ;
#101399 = AXIS2_PLACEMENT_3D('',#165011,#129188,#129189) ;
#101400 = AXIS2_PLACEMENT_3D('',#165012,#129190,#129191) ;
#101401 = AXIS2_PLACEMENT_3D('',#165013,#129192,#129193) ;
#101402 = AXIS2_PLACEMENT_3D('',#165014,#129194,#129195) ;
#101403 = AXIS2_PLACEMENT_3D('',#165015,#129196,#129197) ;
#101404 = AXIS2_PLACEMENT_3D('',#165016,#129198,#129199) ;
#101405 = AXIS2_PLACEMENT_3D('',#165017,#129200,#129201) ;
#101406 = AXIS2_PLACEMENT_3D('',#165018,#129202,#129203) ;
#101407 = AXIS2_PLACEMENT_3D('',#165019,#129204,#129205) ;
#101408 = AXIS2_PLACEMENT_3D('',#165020,#129206,#129207) ;
#101409 = AXIS2_PLACEMENT_3D('',#165021,#129208,#129209) ;
#101410 = AXIS2_PLACEMENT_3D('',#165046,#129210,#129211) ;
#101411 = AXIS2_PLACEMENT_3D('',#165047,#129212,#129213) ;
#101412 = AXIS2_PLACEMENT_3D('',#165048,#129214,#129215) ;
#101413 = AXIS2_PLACEMENT_3D('',#165073,#129216,#129217) ;
#101414 = AXIS2_PLACEMENT_3D('',#165074,#129218,#129219) ;
#101415 = AXIS2_PLACEMENT_3D('',#165075,#129220,#129221) ;
#101416 = AXIS2_PLACEMENT_3D('',#165076,#129222,#129223) ;
#101417 = AXIS2_PLACEMENT_3D('',#165101,#129224,#129225) ;
#101418 = AXIS2_PLACEMENT_3D('',#165102,#129226,#129227) ;
#101419 = AXIS2_PLACEMENT_3D('',#165103,#129228,#129229) ;
#101420 = AXIS2_PLACEMENT_3D('',#165104,#129230,#129231) ;
#101421 = AXIS2_PLACEMENT_3D('',#165105,#129232,#129233) ;
#101422 = AXIS2_PLACEMENT_3D('',#165106,#129234,#129235) ;
#101423 = AXIS2_PLACEMENT_3D('',#165107,#129236,#129237) ;
#101424 = AXIS2_PLACEMENT_3D('',#165108,#129238,#129239) ;
#101425 = AXIS2_PLACEMENT_3D('',#165109,#129240,#129241) ;
#101426 = AXIS2_PLACEMENT_3D('',#165110,#129242,#129243) ;
#101427 = AXIS2_PLACEMENT_3D('',#165111,#129244,#129245) ;
#101428 = AXIS2_PLACEMENT_3D('',#165112,#129246,#129247) ;
#101429 = AXIS2_PLACEMENT_3D('',#165113,#129248,#129249) ;
#101430 = AXIS2_PLACEMENT_3D('',#165114,#129250,#129251) ;
#101431 = AXIS2_PLACEMENT_3D('',#165115,#129252,#129253) ;
#101432 = AXIS2_PLACEMENT_3D('',#165116,#129254,#129255) ;
#101433 = AXIS2_PLACEMENT_3D('',#165117,#129256,#129257) ;
#101434 = AXIS2_PLACEMENT_3D('',#165118,#129258,#129259) ;
#101435 = AXIS2_PLACEMENT_3D('',#165119,#129260,#129261) ;
#101436 = AXIS2_PLACEMENT_3D('',#165120,#129262,#129263) ;
#101437 = AXIS2_PLACEMENT_3D('',#165121,#129264,#129265) ;
#101438 = AXIS2_PLACEMENT_3D('',#165170,#129266,#129267) ;
#101439 = AXIS2_PLACEMENT_3D('',#165183,#129268,#129269) ;
#101440 = AXIS2_PLACEMENT_3D('',#165184,#129270,#129271) ;
#101441 = AXIS2_PLACEMENT_3D('',#165185,#129272,#129273) ;
#101442 = AXIS2_PLACEMENT_3D('',#165186,#129274,#129275) ;
#101443 = AXIS2_PLACEMENT_3D('',#165187,#129276,#129277) ;
#101444 = AXIS2_PLACEMENT_3D('',#165188,#129278,#129279) ;
#101445 = AXIS2_PLACEMENT_3D('',#165189,#129280,#129281) ;
#101446 = AXIS2_PLACEMENT_3D('',#165190,#129282,#129283) ;
#101447 = AXIS2_PLACEMENT_3D('',#165191,#129284,#129285) ;
#101448 = AXIS2_PLACEMENT_3D('',#165192,#129286,#129287) ;
#101449 = AXIS2_PLACEMENT_3D('',#165193,#129288,#129289) ;
#101450 = AXIS2_PLACEMENT_3D('',#165194,#129290,#129291) ;
#101451 = AXIS2_PLACEMENT_3D('',#165195,#129292,#129293) ;
#101452 = AXIS2_PLACEMENT_3D('',#165196,#129294,#129295) ;
#101453 = AXIS2_PLACEMENT_3D('',#165197,#129296,#129297) ;
#101454 = AXIS2_PLACEMENT_3D('',#165210,#129298,#129299) ;
#101455 = AXIS2_PLACEMENT_3D('',#165235,#129300,#129301) ;
#101456 = AXIS2_PLACEMENT_3D('',#165248,#129302,#129303) ;
#101457 = AXIS2_PLACEMENT_3D('',#165249,#129304,#129305) ;
#101458 = AXIS2_PLACEMENT_3D('',#165250,#129306,#129307) ;
#101459 = AXIS2_PLACEMENT_3D('',#165251,#129308,#129309) ;
#101460 = AXIS2_PLACEMENT_3D('',#165252,#129310,#129311) ;
#101461 = AXIS2_PLACEMENT_3D('',#165253,#129312,#129313) ;
#101462 = AXIS2_PLACEMENT_3D('',#165254,#129314,#129315) ;
#101463 = AXIS2_PLACEMENT_3D('',#165255,#129316,#129317) ;
#101464 = AXIS2_PLACEMENT_3D('',#165256,#129318,#129319) ;
#101465 = AXIS2_PLACEMENT_3D('',#165257,#129320,#129321) ;
#101466 = AXIS2_PLACEMENT_3D('',#165258,#129322,#129323) ;
#101467 = AXIS2_PLACEMENT_3D('',#165259,#129324,#129325) ;
#101468 = AXIS2_PLACEMENT_3D('',#165260,#129326,#129327) ;
#101469 = AXIS2_PLACEMENT_3D('',#165261,#129328,#129329) ;
#101470 = AXIS2_PLACEMENT_3D('',#165262,#129330,#129331) ;
#101471 = AXIS2_PLACEMENT_3D('',#165275,#129332,#129333) ;
#101472 = AXIS2_PLACEMENT_3D('',#165300,#129334,#129335) ;
#101473 = AXIS2_PLACEMENT_3D('',#165301,#129336,#129337) ;
#101474 = AXIS2_PLACEMENT_3D('',#165302,#129338,#129339) ;
#101475 = AXIS2_PLACEMENT_3D('',#165303,#129340,#129341) ;
#101476 = AXIS2_PLACEMENT_3D('',#165304,#129342,#129343) ;
#101477 = AXIS2_PLACEMENT_3D('',#165305,#129344,#129345) ;
#101478 = AXIS2_PLACEMENT_3D('',#165306,#129346,#129347) ;
#101479 = AXIS2_PLACEMENT_3D('',#165307,#129348,#129349) ;
#101480 = AXIS2_PLACEMENT_3D('',#165308,#129350,#129351) ;
#101481 = AXIS2_PLACEMENT_3D('',#165309,#129352,#129353) ;
#101482 = AXIS2_PLACEMENT_3D('',#165310,#129354,#129355) ;
#101483 = AXIS2_PLACEMENT_3D('',#165311,#129356,#129357) ;
#101484 = AXIS2_PLACEMENT_3D('',#165312,#129358,#129359) ;
#101485 = AXIS2_PLACEMENT_3D('',#165313,#129360,#129361) ;
#101486 = AXIS2_PLACEMENT_3D('',#165314,#129362,#129363) ;
#101487 = AXIS2_PLACEMENT_3D('',#165315,#129364,#129365) ;
#101488 = AXIS2_PLACEMENT_3D('',#165316,#129366,#129367) ;
#101489 = AXIS2_PLACEMENT_3D('',#165317,#129368,#129369) ;
#101490 = AXIS2_PLACEMENT_3D('',#165318,#129370,#129371) ;
#101491 = AXIS2_PLACEMENT_3D('',#165319,#129372,#129373) ;
#101492 = AXIS2_PLACEMENT_3D('',#165320,#129374,#129375) ;
#101493 = AXIS2_PLACEMENT_3D('',#165321,#129376,#129377) ;
#101494 = AXIS2_PLACEMENT_3D('',#165322,#129378,#129379) ;
#101495 = AXIS2_PLACEMENT_3D('',#165323,#129380,#129381) ;
#101496 = AXIS2_PLACEMENT_3D('',#165324,#129382,#129383) ;
#101497 = AXIS2_PLACEMENT_3D('',#165325,#129384,#129385) ;
#101498 = AXIS2_PLACEMENT_3D('',#165326,#129386,#129387) ;
#101499 = AXIS2_PLACEMENT_3D('',#165327,#129388,#129389) ;
#101500 = AXIS2_PLACEMENT_3D('',#165328,#129390,#129391) ;
#101501 = AXIS2_PLACEMENT_3D('',#165329,#129392,#129393) ;
#101502 = AXIS2_PLACEMENT_3D('',#165330,#129394,#129395) ;
#101503 = AXIS2_PLACEMENT_3D('',#165331,#129396,#129397) ;
#101504 = AXIS2_PLACEMENT_3D('',#165332,#129398,#129399) ;
#101505 = AXIS2_PLACEMENT_3D('',#165333,#129400,#129401) ;
#101506 = AXIS2_PLACEMENT_3D('',#165334,#129402,#129403) ;
#101507 = AXIS2_PLACEMENT_3D('',#165335,#129404,#129405) ;
#101508 = AXIS2_PLACEMENT_3D('',#165336,#129406,#129407) ;
#101509 = AXIS2_PLACEMENT_3D('',#165337,#129408,#129409) ;
#101510 = AXIS2_PLACEMENT_3D('',#165338,#129410,#129411) ;
#101511 = AXIS2_PLACEMENT_3D('',#165339,#129412,#129413) ;
#101512 = AXIS2_PLACEMENT_3D('',#165340,#129414,#129415) ;
#101513 = AXIS2_PLACEMENT_3D('',#165341,#129416,#129417) ;
#101514 = AXIS2_PLACEMENT_3D('',#165342,#129418,#129419) ;
#101515 = AXIS2_PLACEMENT_3D('',#165343,#129420,#129421) ;
#101516 = AXIS2_PLACEMENT_3D('',#165344,#129422,#129423) ;
#101517 = AXIS2_PLACEMENT_3D('',#165345,#129424,#129425) ;
#101518 = AXIS2_PLACEMENT_3D('',#165346,#129426,#129427) ;
#101519 = AXIS2_PLACEMENT_3D('',#165347,#129428,#129429) ;
#101520 = AXIS2_PLACEMENT_3D('',#165348,#129430,#129431) ;
#101521 = AXIS2_PLACEMENT_3D('',#165349,#129432,#129433) ;
#101522 = AXIS2_PLACEMENT_3D('',#165350,#129434,#129435) ;
#101523 = AXIS2_PLACEMENT_3D('',#165351,#129436,#129437) ;
#101524 = AXIS2_PLACEMENT_3D('',#165352,#129438,#129439) ;
#101525 = AXIS2_PLACEMENT_3D('',#165353,#129440,#129441) ;
#101526 = AXIS2_PLACEMENT_3D('',#165354,#129442,#129443) ;
#101527 = AXIS2_PLACEMENT_3D('',#165355,#129444,#129445) ;
#101528 = AXIS2_PLACEMENT_3D('',#165356,#129446,#129447) ;
#101529 = AXIS2_PLACEMENT_3D('',#165357,#129448,#129449) ;
#101530 = AXIS2_PLACEMENT_3D('',#165358,#129450,#129451) ;
#101531 = AXIS2_PLACEMENT_3D('',#165359,#129452,#129453) ;
#101532 = AXIS2_PLACEMENT_3D('',#165360,#129454,#129455) ;
#101533 = AXIS2_PLACEMENT_3D('',#165361,#129456,#129457) ;
#101534 = AXIS2_PLACEMENT_3D('',#165362,#129458,#129459) ;
#101535 = AXIS2_PLACEMENT_3D('',#165363,#129460,#129461) ;
#101536 = AXIS2_PLACEMENT_3D('',#165364,#129462,#129463) ;
#101537 = AXIS2_PLACEMENT_3D('',#165365,#129464,#129465) ;
#101538 = AXIS2_PLACEMENT_3D('',#165366,#129466,#129467) ;
#101539 = AXIS2_PLACEMENT_3D('',#165367,#129468,#129469) ;
#101540 = AXIS2_PLACEMENT_3D('',#165368,#129470,#129471) ;
#101541 = AXIS2_PLACEMENT_3D('',#165369,#129472,#129473) ;
#101542 = AXIS2_PLACEMENT_3D('',#165370,#129474,#129475) ;
#101543 = AXIS2_PLACEMENT_3D('',#165371,#129476,#129477) ;
#101544 = AXIS2_PLACEMENT_3D('',#165372,#129478,#129479) ;
#101545 = AXIS2_PLACEMENT_3D('',#165373,#129480,#129481) ;
#101546 = AXIS2_PLACEMENT_3D('',#165374,#129482,#129483) ;
#101547 = AXIS2_PLACEMENT_3D('',#165375,#129484,#129485) ;
#101548 = AXIS2_PLACEMENT_3D('',#165376,#129486,#129487) ;
#101549 = AXIS2_PLACEMENT_3D('',#165377,#129488,#129489) ;
#101550 = AXIS2_PLACEMENT_3D('',#165378,#129490,#129491) ;
#101551 = AXIS2_PLACEMENT_3D('',#165379,#129492,#129493) ;
#101552 = AXIS2_PLACEMENT_3D('',#165380,#129494,#129495) ;
#101553 = AXIS2_PLACEMENT_3D('',#165381,#129496,#129497) ;
#101554 = AXIS2_PLACEMENT_3D('',#165382,#129498,#129499) ;
#101555 = AXIS2_PLACEMENT_3D('',#165383,#129500,#129501) ;
#101556 = AXIS2_PLACEMENT_3D('',#165384,#129502,#129503) ;
#101557 = AXIS2_PLACEMENT_3D('',#165385,#129504,#129505) ;
#101558 = AXIS2_PLACEMENT_3D('',#165386,#129506,#129507) ;
#101559 = AXIS2_PLACEMENT_3D('',#165387,#129508,#129509) ;
#101560 = AXIS2_PLACEMENT_3D('',#165388,#129510,#129511) ;
#101561 = AXIS2_PLACEMENT_3D('',#165389,#129512,#129513) ;
#101562 = AXIS2_PLACEMENT_3D('',#165390,#129514,#129515) ;
#101563 = AXIS2_PLACEMENT_3D('',#165391,#129516,#129517) ;
#101564 = AXIS2_PLACEMENT_3D('',#165392,#129518,#129519) ;
#101565 = AXIS2_PLACEMENT_3D('',#165393,#129520,#129521) ;
#101566 = AXIS2_PLACEMENT_3D('',#165394,#129522,#129523) ;
#101567 = AXIS2_PLACEMENT_3D('',#165395,#129524,#129525) ;
#101568 = AXIS2_PLACEMENT_3D('',#165396,#129526,#129527) ;
#101569 = AXIS2_PLACEMENT_3D('',#165397,#129528,#129529) ;
#101570 = AXIS2_PLACEMENT_3D('',#165398,#129530,#129531) ;
#101571 = AXIS2_PLACEMENT_3D('',#165399,#129532,#129533) ;
#101572 = AXIS2_PLACEMENT_3D('',#165400,#129534,#129535) ;
#101573 = AXIS2_PLACEMENT_3D('',#165401,#129536,#129537) ;
#101574 = AXIS2_PLACEMENT_3D('',#165402,#129538,#129539) ;
#101575 = AXIS2_PLACEMENT_3D('',#165403,#129540,#129541) ;
#101576 = AXIS2_PLACEMENT_3D('',#165404,#129542,#129543) ;
#101577 = AXIS2_PLACEMENT_3D('',#165405,#129544,#129545) ;
#101578 = AXIS2_PLACEMENT_3D('',#165406,#129546,#129547) ;
#101579 = AXIS2_PLACEMENT_3D('',#165407,#129548,#129549) ;
#101580 = AXIS2_PLACEMENT_3D('',#165408,#129550,#129551) ;
#101581 = AXIS2_PLACEMENT_3D('',#165409,#129552,#129553) ;
#101582 = AXIS2_PLACEMENT_3D('',#165410,#129554,#129555) ;
#101583 = AXIS2_PLACEMENT_3D('',#165411,#129556,#129557) ;
#101584 = AXIS2_PLACEMENT_3D('',#165412,#129558,#129559) ;
#101585 = AXIS2_PLACEMENT_3D('',#165413,#129560,#129561) ;
#101586 = AXIS2_PLACEMENT_3D('',#165414,#129562,#129563) ;
#101587 = AXIS2_PLACEMENT_3D('',#165415,#129564,#129565) ;
#101588 = AXIS2_PLACEMENT_3D('',#165416,#129566,#129567) ;
#101589 = AXIS2_PLACEMENT_3D('',#165417,#129568,#129569) ;
#101590 = AXIS2_PLACEMENT_3D('',#165418,#129570,#129571) ;
#101591 = AXIS2_PLACEMENT_3D('',#165419,#129572,#129573) ;
#101592 = AXIS2_PLACEMENT_3D('',#165420,#129574,#129575) ;
#101593 = AXIS2_PLACEMENT_3D('',#165421,#129576,#129577) ;
#101594 = AXIS2_PLACEMENT_3D('',#165422,#129578,#129579) ;
#101595 = AXIS2_PLACEMENT_3D('',#165423,#129580,#129581) ;
#101596 = AXIS2_PLACEMENT_3D('',#165424,#129582,#129583) ;
#101597 = AXIS2_PLACEMENT_3D('',#165425,#129584,#129585) ;
#101598 = AXIS2_PLACEMENT_3D('',#165426,#129586,#129587) ;
#101599 = AXIS2_PLACEMENT_3D('',#165427,#129588,#129589) ;
#101600 = AXIS2_PLACEMENT_3D('',#165428,#129590,#129591) ;
#101601 = AXIS2_PLACEMENT_3D('',#165429,#129592,#129593) ;
#101602 = AXIS2_PLACEMENT_3D('',#165430,#129594,#129595) ;
#101603 = AXIS2_PLACEMENT_3D('',#165431,#129596,#129597) ;
#101604 = AXIS2_PLACEMENT_3D('',#165432,#129598,#129599) ;
#101605 = AXIS2_PLACEMENT_3D('',#165433,#129600,#129601) ;
#101606 = AXIS2_PLACEMENT_3D('',#165434,#129602,#129603) ;
#101607 = AXIS2_PLACEMENT_3D('',#165435,#129604,#129605) ;
#101608 = AXIS2_PLACEMENT_3D('',#165436,#129606,#129607) ;
#101609 = AXIS2_PLACEMENT_3D('',#165437,#129608,#129609) ;
#101610 = AXIS2_PLACEMENT_3D('',#165438,#129610,#129611) ;
#101611 = AXIS2_PLACEMENT_3D('',#165439,#129612,#129613) ;
#101612 = AXIS2_PLACEMENT_3D('',#165440,#129614,#129615) ;
#101613 = AXIS2_PLACEMENT_3D('',#165441,#129616,#129617) ;
#101614 = AXIS2_PLACEMENT_3D('',#165442,#129618,#129619) ;
#101615 = AXIS2_PLACEMENT_3D('',#165443,#129620,#129621) ;
#101616 = AXIS2_PLACEMENT_3D('',#165444,#129622,#129623) ;
#101617 = AXIS2_PLACEMENT_3D('',#165445,#129624,#129625) ;
#101618 = AXIS2_PLACEMENT_3D('',#165446,#129626,#129627) ;
#101619 = AXIS2_PLACEMENT_3D('',#165447,#129628,#129629) ;
#101620 = AXIS2_PLACEMENT_3D('',#165448,#129630,#129631) ;
#101621 = AXIS2_PLACEMENT_3D('',#165449,#129632,#129633) ;
#101622 = AXIS2_PLACEMENT_3D('',#165450,#129634,#129635) ;
#101623 = AXIS2_PLACEMENT_3D('',#165451,#129636,#129637) ;
#101624 = AXIS2_PLACEMENT_3D('',#165452,#129638,#129639) ;
#101625 = AXIS2_PLACEMENT_3D('',#165453,#129640,#129641) ;
#101626 = AXIS2_PLACEMENT_3D('',#165454,#129642,#129643) ;
#101627 = AXIS2_PLACEMENT_3D('',#165455,#129644,#129645) ;
#101628 = AXIS2_PLACEMENT_3D('',#165456,#129646,#129647) ;
#101629 = AXIS2_PLACEMENT_3D('',#165457,#129648,#129649) ;
#101630 = AXIS2_PLACEMENT_3D('',#165458,#129650,#129651) ;
#101631 = AXIS2_PLACEMENT_3D('',#165459,#129652,#129653) ;
#101632 = AXIS2_PLACEMENT_3D('',#165460,#129654,#129655) ;
#101633 = AXIS2_PLACEMENT_3D('',#165461,#129656,#129657) ;
#101634 = AXIS2_PLACEMENT_3D('',#165462,#129658,#129659) ;
#101635 = AXIS2_PLACEMENT_3D('',#165463,#129660,#129661) ;
#101636 = AXIS2_PLACEMENT_3D('',#165464,#129662,#129663) ;
#101637 = AXIS2_PLACEMENT_3D('',#165465,#129664,#129665) ;
#101638 = AXIS2_PLACEMENT_3D('',#165466,#129666,#129667) ;
#101639 = AXIS2_PLACEMENT_3D('',#165467,#129668,#129669) ;
#101640 = AXIS2_PLACEMENT_3D('',#165468,#129670,#129671) ;
#101641 = AXIS2_PLACEMENT_3D('',#165469,#129672,#129673) ;
#101642 = AXIS2_PLACEMENT_3D('',#165470,#129674,#129675) ;
#101643 = AXIS2_PLACEMENT_3D('',#165471,#129676,#129677) ;
#101644 = AXIS2_PLACEMENT_3D('',#165472,#129678,#129679) ;
#101645 = AXIS2_PLACEMENT_3D('',#165473,#129680,#129681) ;
#101646 = AXIS2_PLACEMENT_3D('',#165474,#129682,#129683) ;
#101647 = AXIS2_PLACEMENT_3D('',#165475,#129684,#129685) ;
#101648 = AXIS2_PLACEMENT_3D('',#165476,#129686,#129687) ;
#101649 = AXIS2_PLACEMENT_3D('',#165477,#129688,#129689) ;
#101650 = AXIS2_PLACEMENT_3D('',#165478,#129690,#129691) ;
#101651 = AXIS2_PLACEMENT_3D('',#165479,#129692,#129693) ;
#101652 = AXIS2_PLACEMENT_3D('',#165480,#129694,#129695) ;
#101653 = AXIS2_PLACEMENT_3D('',#165481,#129696,#129697) ;
#101654 = AXIS2_PLACEMENT_3D('',#165482,#129698,#129699) ;
#101655 = AXIS2_PLACEMENT_3D('',#165483,#129700,#129701) ;
#101656 = AXIS2_PLACEMENT_3D('',#165484,#129702,#129703) ;
#101657 = AXIS2_PLACEMENT_3D('',#165485,#129704,#129705) ;
#101658 = AXIS2_PLACEMENT_3D('',#165486,#129706,#129707) ;
#101659 = AXIS2_PLACEMENT_3D('',#165487,#129708,#129709) ;
#101660 = AXIS2_PLACEMENT_3D('',#165488,#129710,#129711) ;
#101661 = AXIS2_PLACEMENT_3D('',#165489,#129712,#129713) ;
#101662 = AXIS2_PLACEMENT_3D('',#165490,#129714,#129715) ;
#101663 = AXIS2_PLACEMENT_3D('',#165491,#129716,#129717) ;
#101664 = AXIS2_PLACEMENT_3D('',#165492,#129718,#129719) ;
#101665 = AXIS2_PLACEMENT_3D('',#165493,#129720,#129721) ;
#101666 = AXIS2_PLACEMENT_3D('',#165494,#129722,#129723) ;
#101667 = AXIS2_PLACEMENT_3D('',#165495,#129724,#129725) ;
#101668 = AXIS2_PLACEMENT_3D('',#165496,#129726,#129727) ;
#101669 = AXIS2_PLACEMENT_3D('',#165497,#129728,#129729) ;
#101670 = AXIS2_PLACEMENT_3D('',#165498,#129730,#129731) ;
#101671 = AXIS2_PLACEMENT_3D('',#165499,#129732,#129733) ;
#101672 = AXIS2_PLACEMENT_3D('',#165500,#129734,#129735) ;
#101673 = AXIS2_PLACEMENT_3D('',#165501,#129736,#129737) ;
#101674 = AXIS2_PLACEMENT_3D('',#165502,#129738,#129739) ;
#101675 = AXIS2_PLACEMENT_3D('',#165503,#129740,#129741) ;
#101676 = AXIS2_PLACEMENT_3D('',#165504,#129742,#129743) ;
#101677 = AXIS2_PLACEMENT_3D('',#165505,#129744,#129745) ;
#101678 = AXIS2_PLACEMENT_3D('',#165506,#129746,#129747) ;
#101679 = AXIS2_PLACEMENT_3D('',#165507,#129748,#129749) ;
#101680 = AXIS2_PLACEMENT_3D('',#165508,#129750,#129751) ;
#101681 = AXIS2_PLACEMENT_3D('',#165509,#129752,#129753) ;
#101682 = AXIS2_PLACEMENT_3D('',#165510,#129754,#129755) ;
#101683 = AXIS2_PLACEMENT_3D('',#165511,#129756,#129757) ;
#101684 = AXIS2_PLACEMENT_3D('',#165512,#129758,#129759) ;
#101685 = AXIS2_PLACEMENT_3D('',#165513,#129760,#129761) ;
#101686 = AXIS2_PLACEMENT_3D('',#165538,#129762,#129763) ;
#101687 = AXIS2_PLACEMENT_3D('',#165539,#129764,#129765) ;
#101688 = AXIS2_PLACEMENT_3D('',#165540,#129766,#129767) ;
#101689 = AXIS2_PLACEMENT_3D('',#165565,#129768,#129769) ;
#101690 = AXIS2_PLACEMENT_3D('',#165566,#129770,#129771) ;
#101691 = AXIS2_PLACEMENT_3D('',#165567,#129772,#129773) ;
#101692 = AXIS2_PLACEMENT_3D('',#165568,#129774,#129775) ;
#101693 = AXIS2_PLACEMENT_3D('',#165593,#129776,#129777) ;
#101694 = AXIS2_PLACEMENT_3D('',#165594,#129778,#129779) ;
#101695 = AXIS2_PLACEMENT_3D('',#165595,#129780,#129781) ;
#101696 = AXIS2_PLACEMENT_3D('',#165596,#129782,#129783) ;
#101697 = AXIS2_PLACEMENT_3D('',#165597,#129784,#129785) ;
#101698 = AXIS2_PLACEMENT_3D('',#165598,#129786,#129787) ;
#101699 = AXIS2_PLACEMENT_3D('',#165599,#129788,#129789) ;
#101700 = AXIS2_PLACEMENT_3D('',#165600,#129790,#129791) ;
#101701 = AXIS2_PLACEMENT_3D('',#165601,#129792,#129793) ;
#101702 = AXIS2_PLACEMENT_3D('',#165602,#129794,#129795) ;
#101703 = AXIS2_PLACEMENT_3D('',#165603,#129796,#129797) ;
#101704 = AXIS2_PLACEMENT_3D('',#165604,#129798,#129799) ;
#101705 = AXIS2_PLACEMENT_3D('',#165605,#129800,#129801) ;
#101706 = AXIS2_PLACEMENT_3D('',#165606,#129802,#129803) ;
#101707 = AXIS2_PLACEMENT_3D('',#165607,#129804,#129805) ;
#101708 = AXIS2_PLACEMENT_3D('',#165608,#129806,#129807) ;
#101709 = AXIS2_PLACEMENT_3D('',#165609,#129808,#129809) ;
#101710 = AXIS2_PLACEMENT_3D('',#165610,#129810,#129811) ;
#101711 = AXIS2_PLACEMENT_3D('',#165611,#129812,#129813) ;
#101712 = AXIS2_PLACEMENT_3D('',#165612,#129814,#129815) ;
#101713 = AXIS2_PLACEMENT_3D('',#165613,#129816,#129817) ;
#101714 = AXIS2_PLACEMENT_3D('',#165662,#129818,#129819) ;
#101715 = AXIS2_PLACEMENT_3D('',#165675,#129820,#129821) ;
#101716 = AXIS2_PLACEMENT_3D('',#165676,#129822,#129823) ;
#101717 = AXIS2_PLACEMENT_3D('',#165677,#129824,#129825) ;
#101718 = AXIS2_PLACEMENT_3D('',#165678,#129826,#129827) ;
#101719 = AXIS2_PLACEMENT_3D('',#165679,#129828,#129829) ;
#101720 = AXIS2_PLACEMENT_3D('',#165680,#129830,#129831) ;
#101721 = AXIS2_PLACEMENT_3D('',#165681,#129832,#129833) ;
#101722 = AXIS2_PLACEMENT_3D('',#165682,#129834,#129835) ;
#101723 = AXIS2_PLACEMENT_3D('',#165683,#129836,#129837) ;
#101724 = AXIS2_PLACEMENT_3D('',#165684,#129838,#129839) ;
#101725 = AXIS2_PLACEMENT_3D('',#165685,#129840,#129841) ;
#101726 = AXIS2_PLACEMENT_3D('',#165686,#129842,#129843) ;
#101727 = AXIS2_PLACEMENT_3D('',#165687,#129844,#129845) ;
#101728 = AXIS2_PLACEMENT_3D('',#165688,#129846,#129847) ;
#101729 = AXIS2_PLACEMENT_3D('',#165689,#129848,#129849) ;
#101730 = AXIS2_PLACEMENT_3D('',#165702,#129850,#129851) ;
#101731 = AXIS2_PLACEMENT_3D('',#165727,#129852,#129853) ;
#101732 = AXIS2_PLACEMENT_3D('',#165740,#129854,#129855) ;
#101733 = AXIS2_PLACEMENT_3D('',#165741,#129856,#129857) ;
#101734 = AXIS2_PLACEMENT_3D('',#165742,#129858,#129859) ;
#101735 = AXIS2_PLACEMENT_3D('',#165743,#129860,#129861) ;
#101736 = AXIS2_PLACEMENT_3D('',#165744,#129862,#129863) ;
#101737 = AXIS2_PLACEMENT_3D('',#165745,#129864,#129865) ;
#101738 = AXIS2_PLACEMENT_3D('',#165746,#129866,#129867) ;
#101739 = AXIS2_PLACEMENT_3D('',#165747,#129868,#129869) ;
#101740 = AXIS2_PLACEMENT_3D('',#165748,#129870,#129871) ;
#101741 = AXIS2_PLACEMENT_3D('',#165749,#129872,#129873) ;
#101742 = AXIS2_PLACEMENT_3D('',#165750,#129874,#129875) ;
#101743 = AXIS2_PLACEMENT_3D('',#165751,#129876,#129877) ;
#101744 = AXIS2_PLACEMENT_3D('',#165752,#129878,#129879) ;
#101745 = AXIS2_PLACEMENT_3D('',#165753,#129880,#129881) ;
#101746 = AXIS2_PLACEMENT_3D('',#165754,#129882,#129883) ;
#101747 = AXIS2_PLACEMENT_3D('',#165767,#129884,#129885) ;
#101748 = AXIS2_PLACEMENT_3D('',#165792,#129886,#129887) ;
#101749 = AXIS2_PLACEMENT_3D('',#165793,#129888,#129889) ;
#101750 = AXIS2_PLACEMENT_3D('',#165794,#129890,#129891) ;
#101751 = AXIS2_PLACEMENT_3D('',#165795,#129892,#129893) ;
#101752 = AXIS2_PLACEMENT_3D('',#165796,#129894,#129895) ;
#101753 = AXIS2_PLACEMENT_3D('',#165797,#129896,#129897) ;
#101754 = AXIS2_PLACEMENT_3D('',#165798,#129898,#129899) ;
#101755 = AXIS2_PLACEMENT_3D('',#165799,#129900,#129901) ;
#101756 = AXIS2_PLACEMENT_3D('',#165800,#129902,#129903) ;
#101757 = AXIS2_PLACEMENT_3D('',#165801,#129904,#129905) ;
#101758 = AXIS2_PLACEMENT_3D('',#165802,#129906,#129907) ;
#101759 = AXIS2_PLACEMENT_3D('',#165803,#129908,#129909) ;
#101760 = AXIS2_PLACEMENT_3D('',#165804,#129910,#129911) ;
#101761 = AXIS2_PLACEMENT_3D('',#165805,#129912,#129913) ;
#101762 = AXIS2_PLACEMENT_3D('',#165806,#129914,#129915) ;
#101763 = AXIS2_PLACEMENT_3D('',#165807,#129916,#129917) ;
#101764 = AXIS2_PLACEMENT_3D('',#165808,#129918,#129919) ;
#101765 = AXIS2_PLACEMENT_3D('',#165809,#129920,#129921) ;
#101766 = AXIS2_PLACEMENT_3D('',#165810,#129922,#129923) ;
#101767 = AXIS2_PLACEMENT_3D('',#165811,#129924,#129925) ;
#101768 = AXIS2_PLACEMENT_3D('',#165812,#129926,#129927) ;
#101769 = AXIS2_PLACEMENT_3D('',#165813,#129928,#129929) ;
#101770 = AXIS2_PLACEMENT_3D('',#165814,#129930,#129931) ;
#101771 = AXIS2_PLACEMENT_3D('',#165815,#129932,#129933) ;
#101772 = AXIS2_PLACEMENT_3D('',#165816,#129934,#129935) ;
#101773 = AXIS2_PLACEMENT_3D('',#165817,#129936,#129937) ;
#101774 = AXIS2_PLACEMENT_3D('',#165818,#129938,#129939) ;
#101775 = AXIS2_PLACEMENT_3D('',#165819,#129940,#129941) ;
#101776 = AXIS2_PLACEMENT_3D('',#165820,#129942,#129943) ;
#101777 = AXIS2_PLACEMENT_3D('',#165821,#129944,#129945) ;
#101778 = AXIS2_PLACEMENT_3D('',#165822,#129946,#129947) ;
#101779 = AXIS2_PLACEMENT_3D('',#165823,#129948,#129949) ;
#101780 = AXIS2_PLACEMENT_3D('',#165824,#129950,#129951) ;
#101781 = AXIS2_PLACEMENT_3D('',#165825,#129952,#129953) ;
#101782 = AXIS2_PLACEMENT_3D('',#165826,#129954,#129955) ;
#101783 = AXIS2_PLACEMENT_3D('',#165827,#129956,#129957) ;
#101784 = AXIS2_PLACEMENT_3D('',#165828,#129958,#129959) ;
#101785 = AXIS2_PLACEMENT_3D('',#165829,#129960,#129961) ;
#101786 = AXIS2_PLACEMENT_3D('',#165830,#129962,#129963) ;
#101787 = AXIS2_PLACEMENT_3D('',#165831,#129964,#129965) ;
#101788 = AXIS2_PLACEMENT_3D('',#165832,#129966,#129967) ;
#101789 = AXIS2_PLACEMENT_3D('',#165833,#129968,#129969) ;
#101790 = AXIS2_PLACEMENT_3D('',#165834,#129970,#129971) ;
#101791 = AXIS2_PLACEMENT_3D('',#165835,#129972,#129973) ;
#101792 = AXIS2_PLACEMENT_3D('',#165836,#129974,#129975) ;
#101793 = AXIS2_PLACEMENT_3D('',#165837,#129976,#129977) ;
#101794 = AXIS2_PLACEMENT_3D('',#165838,#129978,#129979) ;
#101795 = AXIS2_PLACEMENT_3D('',#165839,#129980,#129981) ;
#101796 = AXIS2_PLACEMENT_3D('',#165840,#129982,#129983) ;
#101797 = AXIS2_PLACEMENT_3D('',#165841,#129984,#129985) ;
#101798 = AXIS2_PLACEMENT_3D('',#165842,#129986,#129987) ;
#101799 = AXIS2_PLACEMENT_3D('',#165843,#129988,#129989) ;
#101800 = AXIS2_PLACEMENT_3D('',#165844,#129990,#129991) ;
#101801 = AXIS2_PLACEMENT_3D('',#165845,#129992,#129993) ;
#101802 = AXIS2_PLACEMENT_3D('',#165846,#129994,#129995) ;
#101803 = AXIS2_PLACEMENT_3D('',#165847,#129996,#129997) ;
#101804 = AXIS2_PLACEMENT_3D('',#165848,#129998,#129999) ;
#101805 = AXIS2_PLACEMENT_3D('',#165849,#130000,#130001) ;
#101806 = AXIS2_PLACEMENT_3D('',#165850,#130002,#130003) ;
#101807 = AXIS2_PLACEMENT_3D('',#165851,#130004,#130005) ;
#101808 = AXIS2_PLACEMENT_3D('',#165852,#130006,#130007) ;
#101809 = AXIS2_PLACEMENT_3D('',#165853,#130008,#130009) ;
#101810 = AXIS2_PLACEMENT_3D('',#165854,#130010,#130011) ;
#101811 = AXIS2_PLACEMENT_3D('',#165855,#130012,#130013) ;
#101812 = AXIS2_PLACEMENT_3D('',#165856,#130014,#130015) ;
#101813 = AXIS2_PLACEMENT_3D('',#165857,#130016,#130017) ;
#101814 = AXIS2_PLACEMENT_3D('',#165858,#130018,#130019) ;
#101815 = AXIS2_PLACEMENT_3D('',#165859,#130020,#130021) ;
#101816 = AXIS2_PLACEMENT_3D('',#165860,#130022,#130023) ;
#101817 = AXIS2_PLACEMENT_3D('',#165861,#130024,#130025) ;
#101818 = AXIS2_PLACEMENT_3D('',#165862,#130026,#130027) ;
#101819 = AXIS2_PLACEMENT_3D('',#165863,#130028,#130029) ;
#101820 = AXIS2_PLACEMENT_3D('',#165864,#130030,#130031) ;
#101821 = AXIS2_PLACEMENT_3D('',#165865,#130032,#130033) ;
#101822 = AXIS2_PLACEMENT_3D('',#165866,#130034,#130035) ;
#101823 = AXIS2_PLACEMENT_3D('',#165867,#130036,#130037) ;
#101824 = AXIS2_PLACEMENT_3D('',#165868,#130038,#130039) ;
#101825 = AXIS2_PLACEMENT_3D('',#165869,#130040,#130041) ;
#101826 = AXIS2_PLACEMENT_3D('',#165870,#130042,#130043) ;
#101827 = AXIS2_PLACEMENT_3D('',#165871,#130044,#130045) ;
#101828 = AXIS2_PLACEMENT_3D('',#165872,#130046,#130047) ;
#101829 = AXIS2_PLACEMENT_3D('',#165873,#130048,#130049) ;
#101830 = AXIS2_PLACEMENT_3D('',#165874,#130050,#130051) ;
#101831 = AXIS2_PLACEMENT_3D('',#165875,#130052,#130053) ;
#101832 = AXIS2_PLACEMENT_3D('',#165876,#130054,#130055) ;
#101833 = AXIS2_PLACEMENT_3D('',#165877,#130056,#130057) ;
#101834 = AXIS2_PLACEMENT_3D('',#165878,#130058,#130059) ;
#101835 = AXIS2_PLACEMENT_3D('',#165879,#130060,#130061) ;
#101836 = AXIS2_PLACEMENT_3D('',#165880,#130062,#130063) ;
#101837 = AXIS2_PLACEMENT_3D('',#165881,#130064,#130065) ;
#101838 = AXIS2_PLACEMENT_3D('',#165882,#130066,#130067) ;
#101839 = AXIS2_PLACEMENT_3D('',#165883,#130068,#130069) ;
#101840 = AXIS2_PLACEMENT_3D('',#165884,#130070,#130071) ;
#101841 = AXIS2_PLACEMENT_3D('',#165885,#130072,#130073) ;
#101842 = AXIS2_PLACEMENT_3D('',#165886,#130074,#130075) ;
#101843 = AXIS2_PLACEMENT_3D('',#165887,#130076,#130077) ;
#101844 = AXIS2_PLACEMENT_3D('',#165888,#130078,#130079) ;
#101845 = AXIS2_PLACEMENT_3D('',#165889,#130080,#130081) ;
#101846 = AXIS2_PLACEMENT_3D('',#165890,#130082,#130083) ;
#101847 = AXIS2_PLACEMENT_3D('',#165891,#130084,#130085) ;
#101848 = AXIS2_PLACEMENT_3D('',#165892,#130086,#130087) ;
#101849 = AXIS2_PLACEMENT_3D('',#165893,#130088,#130089) ;
#101850 = AXIS2_PLACEMENT_3D('',#165894,#130090,#130091) ;
#101851 = AXIS2_PLACEMENT_3D('',#165895,#130092,#130093) ;
#101852 = AXIS2_PLACEMENT_3D('',#165896,#130094,#130095) ;
#101853 = AXIS2_PLACEMENT_3D('',#165897,#130096,#130097) ;
#101854 = AXIS2_PLACEMENT_3D('',#165898,#130098,#130099) ;
#101855 = AXIS2_PLACEMENT_3D('',#165899,#130100,#130101) ;
#101856 = AXIS2_PLACEMENT_3D('',#165900,#130102,#130103) ;
#101857 = AXIS2_PLACEMENT_3D('',#165901,#130104,#130105) ;
#101858 = AXIS2_PLACEMENT_3D('',#165902,#130106,#130107) ;
#101859 = AXIS2_PLACEMENT_3D('',#165903,#130108,#130109) ;
#101860 = AXIS2_PLACEMENT_3D('',#165904,#130110,#130111) ;
#101861 = AXIS2_PLACEMENT_3D('',#165905,#130112,#130113) ;
#101862 = AXIS2_PLACEMENT_3D('',#165906,#130114,#130115) ;
#101863 = AXIS2_PLACEMENT_3D('',#165907,#130116,#130117) ;
#101864 = AXIS2_PLACEMENT_3D('',#165908,#130118,#130119) ;
#101865 = AXIS2_PLACEMENT_3D('',#165909,#130120,#130121) ;
#101866 = AXIS2_PLACEMENT_3D('',#165910,#130122,#130123) ;
#101867 = AXIS2_PLACEMENT_3D('',#165911,#130124,#130125) ;
#101868 = AXIS2_PLACEMENT_3D('',#165912,#130126,#130127) ;
#101869 = AXIS2_PLACEMENT_3D('',#165913,#130128,#130129) ;
#101870 = AXIS2_PLACEMENT_3D('',#165914,#130130,#130131) ;
#101871 = AXIS2_PLACEMENT_3D('',#165915,#130132,#130133) ;
#101872 = AXIS2_PLACEMENT_3D('',#165916,#130134,#130135) ;
#101873 = AXIS2_PLACEMENT_3D('',#165917,#130136,#130137) ;
#101874 = AXIS2_PLACEMENT_3D('',#165918,#130138,#130139) ;
#101875 = AXIS2_PLACEMENT_3D('',#165919,#130140,#130141) ;
#101876 = AXIS2_PLACEMENT_3D('',#165920,#130142,#130143) ;
#101877 = AXIS2_PLACEMENT_3D('',#165921,#130144,#130145) ;
#101878 = AXIS2_PLACEMENT_3D('',#165922,#130146,#130147) ;
#101879 = AXIS2_PLACEMENT_3D('',#165923,#130148,#130149) ;
#101880 = AXIS2_PLACEMENT_3D('',#165924,#130150,#130151) ;
#101881 = AXIS2_PLACEMENT_3D('',#165925,#130152,#130153) ;
#101882 = AXIS2_PLACEMENT_3D('',#165926,#130154,#130155) ;
#101883 = AXIS2_PLACEMENT_3D('',#165927,#130156,#130157) ;
#101884 = AXIS2_PLACEMENT_3D('',#165928,#130158,#130159) ;
#101885 = AXIS2_PLACEMENT_3D('',#165929,#130160,#130161) ;
#101886 = AXIS2_PLACEMENT_3D('',#165930,#130162,#130163) ;
#101887 = AXIS2_PLACEMENT_3D('',#165931,#130164,#130165) ;
#101888 = AXIS2_PLACEMENT_3D('',#165932,#130166,#130167) ;
#101889 = AXIS2_PLACEMENT_3D('',#165933,#130168,#130169) ;
#101890 = AXIS2_PLACEMENT_3D('',#165934,#130170,#130171) ;
#101891 = AXIS2_PLACEMENT_3D('',#165935,#130172,#130173) ;
#101892 = AXIS2_PLACEMENT_3D('',#165936,#130174,#130175) ;
#101893 = AXIS2_PLACEMENT_3D('',#165937,#130176,#130177) ;
#101894 = AXIS2_PLACEMENT_3D('',#165938,#130178,#130179) ;
#101895 = AXIS2_PLACEMENT_3D('',#165939,#130180,#130181) ;
#101896 = AXIS2_PLACEMENT_3D('',#165940,#130182,#130183) ;
#101897 = AXIS2_PLACEMENT_3D('',#165941,#130184,#130185) ;
#101898 = AXIS2_PLACEMENT_3D('',#165942,#130186,#130187) ;
#101899 = AXIS2_PLACEMENT_3D('',#165943,#130188,#130189) ;
#101900 = AXIS2_PLACEMENT_3D('',#165944,#130190,#130191) ;
#101901 = AXIS2_PLACEMENT_3D('',#165945,#130192,#130193) ;
#101902 = AXIS2_PLACEMENT_3D('',#165946,#130194,#130195) ;
#101903 = AXIS2_PLACEMENT_3D('',#165947,#130196,#130197) ;
#101904 = AXIS2_PLACEMENT_3D('',#165948,#130198,#130199) ;
#101905 = AXIS2_PLACEMENT_3D('',#165949,#130200,#130201) ;
#101906 = AXIS2_PLACEMENT_3D('',#165950,#130202,#130203) ;
#101907 = AXIS2_PLACEMENT_3D('',#165951,#130204,#130205) ;
#101908 = AXIS2_PLACEMENT_3D('',#165952,#130206,#130207) ;
#101909 = AXIS2_PLACEMENT_3D('',#165953,#130208,#130209) ;
#101910 = AXIS2_PLACEMENT_3D('',#165954,#130210,#130211) ;
#101911 = AXIS2_PLACEMENT_3D('',#165955,#130212,#130213) ;
#101912 = AXIS2_PLACEMENT_3D('',#165956,#130214,#130215) ;
#101913 = AXIS2_PLACEMENT_3D('',#165957,#130216,#130217) ;
#101914 = AXIS2_PLACEMENT_3D('',#165958,#130218,#130219) ;
#101915 = AXIS2_PLACEMENT_3D('',#165959,#130220,#130221) ;
#101916 = AXIS2_PLACEMENT_3D('',#165960,#130222,#130223) ;
#101917 = AXIS2_PLACEMENT_3D('',#165961,#130224,#130225) ;
#101918 = AXIS2_PLACEMENT_3D('',#165962,#130226,#130227) ;
#101919 = AXIS2_PLACEMENT_3D('',#165963,#130228,#130229) ;
#101920 = AXIS2_PLACEMENT_3D('',#165964,#130230,#130231) ;
#101921 = AXIS2_PLACEMENT_3D('',#165965,#130232,#130233) ;
#101922 = AXIS2_PLACEMENT_3D('',#165966,#130234,#130235) ;
#101923 = AXIS2_PLACEMENT_3D('',#165967,#130236,#130237) ;
#101924 = AXIS2_PLACEMENT_3D('',#165968,#130238,#130239) ;
#101925 = AXIS2_PLACEMENT_3D('',#165969,#130240,#130241) ;
#101926 = AXIS2_PLACEMENT_3D('',#165970,#130242,#130243) ;
#101927 = AXIS2_PLACEMENT_3D('',#165971,#130244,#130245) ;
#101928 = AXIS2_PLACEMENT_3D('',#165972,#130246,#130247) ;
#101929 = AXIS2_PLACEMENT_3D('',#165973,#130248,#130249) ;
#101930 = AXIS2_PLACEMENT_3D('',#165974,#130250,#130251) ;
#101931 = AXIS2_PLACEMENT_3D('',#165975,#130252,#130253) ;
#101932 = AXIS2_PLACEMENT_3D('',#165976,#130254,#130255) ;
#101933 = AXIS2_PLACEMENT_3D('',#165977,#130256,#130257) ;
#101934 = AXIS2_PLACEMENT_3D('',#165978,#130258,#130259) ;
#101935 = AXIS2_PLACEMENT_3D('',#165979,#130260,#130261) ;
#101936 = AXIS2_PLACEMENT_3D('',#165980,#130262,#130263) ;
#101937 = AXIS2_PLACEMENT_3D('',#165981,#130264,#130265) ;
#101938 = AXIS2_PLACEMENT_3D('',#165982,#130266,#130267) ;
#101939 = AXIS2_PLACEMENT_3D('',#165983,#130268,#130269) ;
#101940 = AXIS2_PLACEMENT_3D('',#165984,#130270,#130271) ;
#101941 = AXIS2_PLACEMENT_3D('',#165985,#130272,#130273) ;
#101942 = AXIS2_PLACEMENT_3D('',#165986,#130274,#130275) ;
#101943 = AXIS2_PLACEMENT_3D('',#165987,#130276,#130277) ;
#101944 = AXIS2_PLACEMENT_3D('',#165988,#130278,#130279) ;
#101945 = AXIS2_PLACEMENT_3D('',#165989,#130280,#130281) ;
#101946 = AXIS2_PLACEMENT_3D('',#165990,#130282,#130283) ;
#101947 = AXIS2_PLACEMENT_3D('',#165991,#130284,#130285) ;
#101948 = AXIS2_PLACEMENT_3D('',#165992,#130286,#130287) ;
#101949 = AXIS2_PLACEMENT_3D('',#165993,#130288,#130289) ;
#101950 = AXIS2_PLACEMENT_3D('',#165994,#130290,#130291) ;
#101951 = AXIS2_PLACEMENT_3D('',#165995,#130292,#130293) ;
#101952 = AXIS2_PLACEMENT_3D('',#165996,#130294,#130295) ;
#101953 = AXIS2_PLACEMENT_3D('',#165997,#130296,#130297) ;
#101954 = AXIS2_PLACEMENT_3D('',#165998,#130298,#130299) ;
#101955 = AXIS2_PLACEMENT_3D('',#165999,#130300,#130301) ;
#101956 = AXIS2_PLACEMENT_3D('',#166000,#130302,#130303) ;
#101957 = AXIS2_PLACEMENT_3D('',#166001,#130304,#130305) ;
#101958 = AXIS2_PLACEMENT_3D('',#166002,#130306,#130307) ;
#101959 = AXIS2_PLACEMENT_3D('',#166003,#130308,#130309) ;
#101960 = AXIS2_PLACEMENT_3D('',#166004,#130310,#130311) ;
#101961 = AXIS2_PLACEMENT_3D('',#166005,#130312,#130313) ;
#101962 = AXIS2_PLACEMENT_3D('',#166030,#130314,#130315) ;
#101963 = AXIS2_PLACEMENT_3D('',#166031,#130316,#130317) ;
#101964 = AXIS2_PLACEMENT_3D('',#166032,#130318,#130319) ;
#101965 = AXIS2_PLACEMENT_3D('',#166057,#130320,#130321) ;
#101966 = AXIS2_PLACEMENT_3D('',#166058,#130322,#130323) ;
#101967 = AXIS2_PLACEMENT_3D('',#166059,#130324,#130325) ;
#101968 = AXIS2_PLACEMENT_3D('',#166060,#130326,#130327) ;
#101969 = AXIS2_PLACEMENT_3D('',#166085,#130328,#130329) ;
#101970 = AXIS2_PLACEMENT_3D('',#166086,#130330,#130331) ;
#101971 = AXIS2_PLACEMENT_3D('',#166087,#130332,#130333) ;
#101972 = AXIS2_PLACEMENT_3D('',#166088,#130334,#130335) ;
#101973 = AXIS2_PLACEMENT_3D('',#166089,#130336,#130337) ;
#101974 = AXIS2_PLACEMENT_3D('',#166090,#130338,#130339) ;
#101975 = AXIS2_PLACEMENT_3D('',#166091,#130340,#130341) ;
#101976 = AXIS2_PLACEMENT_3D('',#166092,#130342,#130343) ;
#101977 = AXIS2_PLACEMENT_3D('',#166093,#130344,#130345) ;
#101978 = AXIS2_PLACEMENT_3D('',#166094,#130346,#130347) ;
#101979 = AXIS2_PLACEMENT_3D('',#166095,#130348,#130349) ;
#101980 = AXIS2_PLACEMENT_3D('',#166096,#130350,#130351) ;
#101981 = AXIS2_PLACEMENT_3D('',#166097,#130352,#130353) ;
#101982 = AXIS2_PLACEMENT_3D('',#166098,#130354,#130355) ;
#101983 = AXIS2_PLACEMENT_3D('',#166099,#130356,#130357) ;
#101984 = AXIS2_PLACEMENT_3D('',#166100,#130358,#130359) ;
#101985 = AXIS2_PLACEMENT_3D('',#166101,#130360,#130361) ;
#101986 = AXIS2_PLACEMENT_3D('',#166102,#130362,#130363) ;
#101987 = AXIS2_PLACEMENT_3D('',#166103,#130364,#130365) ;
#101988 = AXIS2_PLACEMENT_3D('',#166104,#130366,#130367) ;
#101989 = AXIS2_PLACEMENT_3D('',#166105,#130368,#130369) ;
#101990 = AXIS2_PLACEMENT_3D('',#166154,#130370,#130371) ;
#101991 = AXIS2_PLACEMENT_3D('',#166167,#130372,#130373) ;
#101992 = AXIS2_PLACEMENT_3D('',#166168,#130374,#130375) ;
#101993 = AXIS2_PLACEMENT_3D('',#166169,#130376,#130377) ;
#101994 = AXIS2_PLACEMENT_3D('',#166170,#130378,#130379) ;
#101995 = AXIS2_PLACEMENT_3D('',#166171,#130380,#130381) ;
#101996 = AXIS2_PLACEMENT_3D('',#166172,#130382,#130383) ;
#101997 = AXIS2_PLACEMENT_3D('',#166173,#130384,#130385) ;
#101998 = AXIS2_PLACEMENT_3D('',#166174,#130386,#130387) ;
#101999 = AXIS2_PLACEMENT_3D('',#166175,#130388,#130389) ;
#102000 = AXIS2_PLACEMENT_3D('',#166176,#130390,#130391) ;
#102001 = AXIS2_PLACEMENT_3D('',#166177,#130392,#130393) ;
#102002 = AXIS2_PLACEMENT_3D('',#166178,#130394,#130395) ;
#102003 = AXIS2_PLACEMENT_3D('',#166179,#130396,#130397) ;
#102004 = AXIS2_PLACEMENT_3D('',#166180,#130398,#130399) ;
#102005 = AXIS2_PLACEMENT_3D('',#166181,#130400,#130401) ;
#102006 = AXIS2_PLACEMENT_3D('',#166194,#130402,#130403) ;
#102007 = AXIS2_PLACEMENT_3D('',#166219,#130404,#130405) ;
#102008 = AXIS2_PLACEMENT_3D('',#166232,#130406,#130407) ;
#102009 = AXIS2_PLACEMENT_3D('',#166233,#130408,#130409) ;
#102010 = AXIS2_PLACEMENT_3D('',#166234,#130410,#130411) ;
#102011 = AXIS2_PLACEMENT_3D('',#166235,#130412,#130413) ;
#102012 = AXIS2_PLACEMENT_3D('',#166236,#130414,#130415) ;
#102013 = AXIS2_PLACEMENT_3D('',#166237,#130416,#130417) ;
#102014 = AXIS2_PLACEMENT_3D('',#166238,#130418,#130419) ;
#102015 = AXIS2_PLACEMENT_3D('',#166239,#130420,#130421) ;
#102016 = AXIS2_PLACEMENT_3D('',#166240,#130422,#130423) ;
#102017 = AXIS2_PLACEMENT_3D('',#166241,#130424,#130425) ;
#102018 = AXIS2_PLACEMENT_3D('',#166242,#130426,#130427) ;
#102019 = AXIS2_PLACEMENT_3D('',#166243,#130428,#130429) ;
#102020 = AXIS2_PLACEMENT_3D('',#166244,#130430,#130431) ;
#102021 = AXIS2_PLACEMENT_3D('',#166245,#130432,#130433) ;
#102022 = AXIS2_PLACEMENT_3D('',#166246,#130434,#130435) ;
#102023 = AXIS2_PLACEMENT_3D('',#166259,#130436,#130437) ;
#102024 = AXIS2_PLACEMENT_3D('',#166284,#130438,#130439) ;
#102025 = AXIS2_PLACEMENT_3D('',#166285,#130440,#130441) ;
#102026 = AXIS2_PLACEMENT_3D('',#166286,#130442,#130443) ;
#102027 = AXIS2_PLACEMENT_3D('',#166287,#130444,#130445) ;
#102028 = AXIS2_PLACEMENT_3D('',#166288,#130446,#130447) ;
#102029 = AXIS2_PLACEMENT_3D('',#166289,#130448,#130449) ;
#102030 = AXIS2_PLACEMENT_3D('',#166290,#130450,#130451) ;
#102031 = AXIS2_PLACEMENT_3D('',#166291,#130452,#130453) ;
#102032 = AXIS2_PLACEMENT_3D('',#166292,#130454,#130455) ;
#102033 = AXIS2_PLACEMENT_3D('',#166293,#130456,#130457) ;
#102034 = AXIS2_PLACEMENT_3D('',#166294,#130458,#130459) ;
#102035 = AXIS2_PLACEMENT_3D('',#166295,#130460,#130461) ;
#102036 = AXIS2_PLACEMENT_3D('',#166296,#130462,#130463) ;
#102037 = AXIS2_PLACEMENT_3D('',#166297,#130464,#130465) ;
#102038 = AXIS2_PLACEMENT_3D('',#166298,#130466,#130467) ;
#102039 = AXIS2_PLACEMENT_3D('',#166299,#130468,#130469) ;
#102040 = AXIS2_PLACEMENT_3D('',#166300,#130470,#130471) ;
#102041 = AXIS2_PLACEMENT_3D('',#166301,#130472,#130473) ;
#102042 = AXIS2_PLACEMENT_3D('',#166302,#130474,#130475) ;
#102043 = AXIS2_PLACEMENT_3D('',#166303,#130476,#130477) ;
#102044 = AXIS2_PLACEMENT_3D('',#166304,#130478,#130479) ;
#102045 = AXIS2_PLACEMENT_3D('',#166305,#130480,#130481) ;
#102046 = AXIS2_PLACEMENT_3D('',#166306,#130482,#130483) ;
#102047 = AXIS2_PLACEMENT_3D('',#166307,#130484,#130485) ;
#102048 = AXIS2_PLACEMENT_3D('',#166308,#130486,#130487) ;
#102049 = AXIS2_PLACEMENT_3D('',#166309,#130488,#130489) ;
#102050 = AXIS2_PLACEMENT_3D('',#166310,#130490,#130491) ;
#102051 = AXIS2_PLACEMENT_3D('',#166311,#130492,#130493) ;
#102052 = AXIS2_PLACEMENT_3D('',#166312,#130494,#130495) ;
#102053 = AXIS2_PLACEMENT_3D('',#166313,#130496,#130497) ;
#102054 = AXIS2_PLACEMENT_3D('',#166314,#130498,#130499) ;
#102055 = AXIS2_PLACEMENT_3D('',#166315,#130500,#130501) ;
#102056 = AXIS2_PLACEMENT_3D('',#166316,#130502,#130503) ;
#102057 = AXIS2_PLACEMENT_3D('',#166317,#130504,#130505) ;
#102058 = AXIS2_PLACEMENT_3D('',#166318,#130506,#130507) ;
#102059 = AXIS2_PLACEMENT_3D('',#166319,#130508,#130509) ;
#102060 = AXIS2_PLACEMENT_3D('',#166320,#130510,#130511) ;
#102061 = AXIS2_PLACEMENT_3D('',#166321,#130512,#130513) ;
#102062 = AXIS2_PLACEMENT_3D('',#166322,#130514,#130515) ;
#102063 = AXIS2_PLACEMENT_3D('',#166323,#130516,#130517) ;
#102064 = AXIS2_PLACEMENT_3D('',#166324,#130518,#130519) ;
#102065 = AXIS2_PLACEMENT_3D('',#166325,#130520,#130521) ;
#102066 = AXIS2_PLACEMENT_3D('',#166326,#130522,#130523) ;
#102067 = AXIS2_PLACEMENT_3D('',#166327,#130524,#130525) ;
#102068 = AXIS2_PLACEMENT_3D('',#166328,#130526,#130527) ;
#102069 = AXIS2_PLACEMENT_3D('',#166329,#130528,#130529) ;
#102070 = AXIS2_PLACEMENT_3D('',#166330,#130530,#130531) ;
#102071 = AXIS2_PLACEMENT_3D('',#166331,#130532,#130533) ;
#102072 = AXIS2_PLACEMENT_3D('',#166332,#130534,#130535) ;
#102073 = AXIS2_PLACEMENT_3D('',#166333,#130536,#130537) ;
#102074 = AXIS2_PLACEMENT_3D('',#166334,#130538,#130539) ;
#102075 = AXIS2_PLACEMENT_3D('',#166335,#130540,#130541) ;
#102076 = AXIS2_PLACEMENT_3D('',#166336,#130542,#130543) ;
#102077 = AXIS2_PLACEMENT_3D('',#166337,#130544,#130545) ;
#102078 = AXIS2_PLACEMENT_3D('',#166338,#130546,#130547) ;
#102079 = AXIS2_PLACEMENT_3D('',#166339,#130548,#130549) ;
#102080 = AXIS2_PLACEMENT_3D('',#166340,#130550,#130551) ;
#102081 = AXIS2_PLACEMENT_3D('',#166341,#130552,#130553) ;
#102082 = AXIS2_PLACEMENT_3D('',#166342,#130554,#130555) ;
#102083 = AXIS2_PLACEMENT_3D('',#166343,#130556,#130557) ;
#102084 = AXIS2_PLACEMENT_3D('',#166344,#130558,#130559) ;
#102085 = AXIS2_PLACEMENT_3D('',#166345,#130560,#130561) ;
#102086 = AXIS2_PLACEMENT_3D('',#166346,#130562,#130563) ;
#102087 = AXIS2_PLACEMENT_3D('',#166347,#130564,#130565) ;
#102088 = AXIS2_PLACEMENT_3D('',#166348,#130566,#130567) ;
#102089 = AXIS2_PLACEMENT_3D('',#166349,#130568,#130569) ;
#102090 = AXIS2_PLACEMENT_3D('',#166350,#130570,#130571) ;
#102091 = AXIS2_PLACEMENT_3D('',#166351,#130572,#130573) ;
#102092 = AXIS2_PLACEMENT_3D('',#166352,#130574,#130575) ;
#102093 = AXIS2_PLACEMENT_3D('',#166353,#130576,#130577) ;
#102094 = AXIS2_PLACEMENT_3D('',#166354,#130578,#130579) ;
#102095 = AXIS2_PLACEMENT_3D('',#166355,#130580,#130581) ;
#102096 = AXIS2_PLACEMENT_3D('',#166356,#130582,#130583) ;
#102097 = AXIS2_PLACEMENT_3D('',#166357,#130584,#130585) ;
#102098 = AXIS2_PLACEMENT_3D('',#166358,#130586,#130587) ;
#102099 = AXIS2_PLACEMENT_3D('',#166359,#130588,#130589) ;
#102100 = AXIS2_PLACEMENT_3D('',#166360,#130590,#130591) ;
#102101 = AXIS2_PLACEMENT_3D('',#166361,#130592,#130593) ;
#102102 = AXIS2_PLACEMENT_3D('',#166362,#130594,#130595) ;
#102103 = AXIS2_PLACEMENT_3D('',#166363,#130596,#130597) ;
#102104 = AXIS2_PLACEMENT_3D('',#166364,#130598,#130599) ;
#102105 = AXIS2_PLACEMENT_3D('',#166365,#130600,#130601) ;
#102106 = AXIS2_PLACEMENT_3D('',#166366,#130602,#130603) ;
#102107 = AXIS2_PLACEMENT_3D('',#166367,#130604,#130605) ;
#102108 = AXIS2_PLACEMENT_3D('',#166368,#130606,#130607) ;
#102109 = AXIS2_PLACEMENT_3D('',#166369,#130608,#130609) ;
#102110 = AXIS2_PLACEMENT_3D('',#166370,#130610,#130611) ;
#102111 = AXIS2_PLACEMENT_3D('',#166371,#130612,#130613) ;
#102112 = AXIS2_PLACEMENT_3D('',#166372,#130614,#130615) ;
#102113 = AXIS2_PLACEMENT_3D('',#166373,#130616,#130617) ;
#102114 = AXIS2_PLACEMENT_3D('',#166374,#130618,#130619) ;
#102115 = AXIS2_PLACEMENT_3D('',#166375,#130620,#130621) ;
#102116 = AXIS2_PLACEMENT_3D('',#166376,#130622,#130623) ;
#102117 = AXIS2_PLACEMENT_3D('',#166377,#130624,#130625) ;
#102118 = AXIS2_PLACEMENT_3D('',#166378,#130626,#130627) ;
#102119 = AXIS2_PLACEMENT_3D('',#166379,#130628,#130629) ;
#102120 = AXIS2_PLACEMENT_3D('',#166380,#130630,#130631) ;
#102121 = AXIS2_PLACEMENT_3D('',#166381,#130632,#130633) ;
#102122 = AXIS2_PLACEMENT_3D('',#166382,#130634,#130635) ;
#102123 = AXIS2_PLACEMENT_3D('',#166383,#130636,#130637) ;
#102124 = AXIS2_PLACEMENT_3D('',#166384,#130638,#130639) ;
#102125 = AXIS2_PLACEMENT_3D('',#166385,#130640,#130641) ;
#102126 = AXIS2_PLACEMENT_3D('',#166386,#130642,#130643) ;
#102127 = AXIS2_PLACEMENT_3D('',#166387,#130644,#130645) ;
#102128 = AXIS2_PLACEMENT_3D('',#166388,#130646,#130647) ;
#102129 = AXIS2_PLACEMENT_3D('',#166389,#130648,#130649) ;
#102130 = AXIS2_PLACEMENT_3D('',#166390,#130650,#130651) ;
#102131 = AXIS2_PLACEMENT_3D('',#166391,#130652,#130653) ;
#102132 = AXIS2_PLACEMENT_3D('',#166392,#130654,#130655) ;
#102133 = AXIS2_PLACEMENT_3D('',#166393,#130656,#130657) ;
#102134 = AXIS2_PLACEMENT_3D('',#166394,#130658,#130659) ;
#102135 = AXIS2_PLACEMENT_3D('',#166395,#130660,#130661) ;
#102136 = AXIS2_PLACEMENT_3D('',#166396,#130662,#130663) ;
#102137 = AXIS2_PLACEMENT_3D('',#166397,#130664,#130665) ;
#102138 = AXIS2_PLACEMENT_3D('',#166398,#130666,#130667) ;
#102139 = AXIS2_PLACEMENT_3D('',#166399,#130668,#130669) ;
#102140 = AXIS2_PLACEMENT_3D('',#166400,#130670,#130671) ;
#102141 = AXIS2_PLACEMENT_3D('',#166401,#130672,#130673) ;
#102142 = AXIS2_PLACEMENT_3D('',#166402,#130674,#130675) ;
#102143 = AXIS2_PLACEMENT_3D('',#166403,#130676,#130677) ;
#102144 = AXIS2_PLACEMENT_3D('',#166404,#130678,#130679) ;
#102145 = AXIS2_PLACEMENT_3D('',#166405,#130680,#130681) ;
#102146 = AXIS2_PLACEMENT_3D('',#166406,#130682,#130683) ;
#102147 = AXIS2_PLACEMENT_3D('',#166407,#130684,#130685) ;
#102148 = AXIS2_PLACEMENT_3D('',#166408,#130686,#130687) ;
#102149 = AXIS2_PLACEMENT_3D('',#166409,#130688,#130689) ;
#102150 = AXIS2_PLACEMENT_3D('',#166410,#130690,#130691) ;
#102151 = AXIS2_PLACEMENT_3D('',#166411,#130692,#130693) ;
#102152 = AXIS2_PLACEMENT_3D('',#166412,#130694,#130695) ;
#102153 = AXIS2_PLACEMENT_3D('',#166413,#130696,#130697) ;
#102154 = AXIS2_PLACEMENT_3D('',#166414,#130698,#130699) ;
#102155 = AXIS2_PLACEMENT_3D('',#166415,#130700,#130701) ;
#102156 = AXIS2_PLACEMENT_3D('',#166416,#130702,#130703) ;
#102157 = AXIS2_PLACEMENT_3D('',#166417,#130704,#130705) ;
#102158 = AXIS2_PLACEMENT_3D('',#166418,#130706,#130707) ;
#102159 = AXIS2_PLACEMENT_3D('',#166419,#130708,#130709) ;
#102160 = AXIS2_PLACEMENT_3D('',#166420,#130710,#130711) ;
#102161 = AXIS2_PLACEMENT_3D('',#166421,#130712,#130713) ;
#102162 = AXIS2_PLACEMENT_3D('',#166422,#130714,#130715) ;
#102163 = AXIS2_PLACEMENT_3D('',#166423,#130716,#130717) ;
#102164 = AXIS2_PLACEMENT_3D('',#166424,#130718,#130719) ;
#102165 = AXIS2_PLACEMENT_3D('',#166425,#130720,#130721) ;
#102166 = AXIS2_PLACEMENT_3D('',#166426,#130722,#130723) ;
#102167 = AXIS2_PLACEMENT_3D('',#166427,#130724,#130725) ;
#102168 = AXIS2_PLACEMENT_3D('',#166428,#130726,#130727) ;
#102169 = AXIS2_PLACEMENT_3D('',#166429,#130728,#130729) ;
#102170 = AXIS2_PLACEMENT_3D('',#166430,#130730,#130731) ;
#102171 = AXIS2_PLACEMENT_3D('',#166431,#130732,#130733) ;
#102172 = AXIS2_PLACEMENT_3D('',#166432,#130734,#130735) ;
#102173 = AXIS2_PLACEMENT_3D('',#166433,#130736,#130737) ;
#102174 = AXIS2_PLACEMENT_3D('',#166434,#130738,#130739) ;
#102175 = AXIS2_PLACEMENT_3D('',#166435,#130740,#130741) ;
#102176 = AXIS2_PLACEMENT_3D('',#166436,#130742,#130743) ;
#102177 = AXIS2_PLACEMENT_3D('',#166437,#130744,#130745) ;
#102178 = AXIS2_PLACEMENT_3D('',#166438,#130746,#130747) ;
#102179 = AXIS2_PLACEMENT_3D('',#166439,#130748,#130749) ;
#102180 = AXIS2_PLACEMENT_3D('',#166440,#130750,#130751) ;
#102181 = AXIS2_PLACEMENT_3D('',#166441,#130752,#130753) ;
#102182 = AXIS2_PLACEMENT_3D('',#166442,#130754,#130755) ;
#102183 = AXIS2_PLACEMENT_3D('',#166443,#130756,#130757) ;
#102184 = AXIS2_PLACEMENT_3D('',#166444,#130758,#130759) ;
#102185 = AXIS2_PLACEMENT_3D('',#166445,#130760,#130761) ;
#102186 = AXIS2_PLACEMENT_3D('',#166446,#130762,#130763) ;
#102187 = AXIS2_PLACEMENT_3D('',#166447,#130764,#130765) ;
#102188 = AXIS2_PLACEMENT_3D('',#166448,#130766,#130767) ;
#102189 = AXIS2_PLACEMENT_3D('',#166449,#130768,#130769) ;
#102190 = AXIS2_PLACEMENT_3D('',#166450,#130770,#130771) ;
#102191 = AXIS2_PLACEMENT_3D('',#166451,#130772,#130773) ;
#102192 = AXIS2_PLACEMENT_3D('',#166452,#130774,#130775) ;
#102193 = AXIS2_PLACEMENT_3D('',#166453,#130776,#130777) ;
#102194 = AXIS2_PLACEMENT_3D('',#166454,#130778,#130779) ;
#102195 = AXIS2_PLACEMENT_3D('',#166455,#130780,#130781) ;
#102196 = AXIS2_PLACEMENT_3D('',#166456,#130782,#130783) ;
#102197 = AXIS2_PLACEMENT_3D('',#166457,#130784,#130785) ;
#102198 = AXIS2_PLACEMENT_3D('',#166458,#130786,#130787) ;
#102199 = AXIS2_PLACEMENT_3D('',#166459,#130788,#130789) ;
#102200 = AXIS2_PLACEMENT_3D('',#166460,#130790,#130791) ;
#102201 = AXIS2_PLACEMENT_3D('',#166461,#130792,#130793) ;
#102202 = AXIS2_PLACEMENT_3D('',#166462,#130794,#130795) ;
#102203 = AXIS2_PLACEMENT_3D('',#166463,#130796,#130797) ;
#102204 = AXIS2_PLACEMENT_3D('',#166464,#130798,#130799) ;
#102205 = AXIS2_PLACEMENT_3D('',#166465,#130800,#130801) ;
#102206 = AXIS2_PLACEMENT_3D('',#166466,#130802,#130803) ;
#102207 = AXIS2_PLACEMENT_3D('',#166467,#130804,#130805) ;
#102208 = AXIS2_PLACEMENT_3D('',#166468,#130806,#130807) ;
#102209 = AXIS2_PLACEMENT_3D('',#166469,#130808,#130809) ;
#102210 = AXIS2_PLACEMENT_3D('',#166470,#130810,#130811) ;
#102211 = AXIS2_PLACEMENT_3D('',#166471,#130812,#130813) ;
#102212 = AXIS2_PLACEMENT_3D('',#166472,#130814,#130815) ;
#102213 = AXIS2_PLACEMENT_3D('',#166473,#130816,#130817) ;
#102214 = AXIS2_PLACEMENT_3D('',#166474,#130818,#130819) ;
#102215 = AXIS2_PLACEMENT_3D('',#166475,#130820,#130821) ;
#102216 = AXIS2_PLACEMENT_3D('',#166476,#130822,#130823) ;
#102217 = AXIS2_PLACEMENT_3D('',#166477,#130824,#130825) ;
#102218 = AXIS2_PLACEMENT_3D('',#166478,#130826,#130827) ;
#102219 = AXIS2_PLACEMENT_3D('',#166479,#130828,#130829) ;
#102220 = AXIS2_PLACEMENT_3D('',#166480,#130830,#130831) ;
#102221 = AXIS2_PLACEMENT_3D('',#166481,#130832,#130833) ;
#102222 = AXIS2_PLACEMENT_3D('',#166482,#130834,#130835) ;
#102223 = AXIS2_PLACEMENT_3D('',#166483,#130836,#130837) ;
#102224 = AXIS2_PLACEMENT_3D('',#166484,#130838,#130839) ;
#102225 = AXIS2_PLACEMENT_3D('',#166485,#130840,#130841) ;
#102226 = AXIS2_PLACEMENT_3D('',#166486,#130842,#130843) ;
#102227 = AXIS2_PLACEMENT_3D('',#166487,#130844,#130845) ;
#102228 = AXIS2_PLACEMENT_3D('',#166488,#130846,#130847) ;
#102229 = AXIS2_PLACEMENT_3D('',#166489,#130848,#130849) ;
#102230 = AXIS2_PLACEMENT_3D('',#166490,#130850,#130851) ;
#102231 = AXIS2_PLACEMENT_3D('',#166491,#130852,#130853) ;
#102232 = AXIS2_PLACEMENT_3D('',#166492,#130854,#130855) ;
#102233 = AXIS2_PLACEMENT_3D('',#166493,#130856,#130857) ;
#102234 = AXIS2_PLACEMENT_3D('',#166494,#130858,#130859) ;
#102235 = AXIS2_PLACEMENT_3D('',#166495,#130860,#130861) ;
#102236 = AXIS2_PLACEMENT_3D('',#166496,#130862,#130863) ;
#102237 = AXIS2_PLACEMENT_3D('',#166497,#130864,#130865) ;
#102238 = AXIS2_PLACEMENT_3D('',#166522,#130866,#130867) ;
#102239 = AXIS2_PLACEMENT_3D('',#166523,#130868,#130869) ;
#102240 = AXIS2_PLACEMENT_3D('',#166524,#130870,#130871) ;
#102241 = AXIS2_PLACEMENT_3D('',#166549,#130872,#130873) ;
#102242 = AXIS2_PLACEMENT_3D('',#166550,#130874,#130875) ;
#102243 = AXIS2_PLACEMENT_3D('',#166551,#130876,#130877) ;
#102244 = AXIS2_PLACEMENT_3D('',#166552,#130878,#130879) ;
#102245 = AXIS2_PLACEMENT_3D('',#166577,#130880,#130881) ;
#102246 = AXIS2_PLACEMENT_3D('',#166578,#130882,#130883) ;
#102247 = AXIS2_PLACEMENT_3D('',#166579,#130884,#130885) ;
#102248 = AXIS2_PLACEMENT_3D('',#166580,#130886,#130887) ;
#102249 = AXIS2_PLACEMENT_3D('',#166581,#130888,#130889) ;
#102250 = AXIS2_PLACEMENT_3D('',#166582,#130890,#130891) ;
#102251 = AXIS2_PLACEMENT_3D('',#166583,#130892,#130893) ;
#102252 = AXIS2_PLACEMENT_3D('',#166584,#130894,#130895) ;
#102253 = AXIS2_PLACEMENT_3D('',#166585,#130896,#130897) ;
#102254 = AXIS2_PLACEMENT_3D('',#166586,#130898,#130899) ;
#102255 = AXIS2_PLACEMENT_3D('',#166587,#130900,#130901) ;
#102256 = AXIS2_PLACEMENT_3D('',#166588,#130902,#130903) ;
#102257 = AXIS2_PLACEMENT_3D('',#166589,#130904,#130905) ;
#102258 = AXIS2_PLACEMENT_3D('',#166590,#130906,#130907) ;
#102259 = AXIS2_PLACEMENT_3D('',#166591,#130908,#130909) ;
#102260 = AXIS2_PLACEMENT_3D('',#166592,#130910,#130911) ;
#102261 = AXIS2_PLACEMENT_3D('',#166593,#130912,#130913) ;
#102262 = AXIS2_PLACEMENT_3D('',#166594,#130914,#130915) ;
#102263 = AXIS2_PLACEMENT_3D('',#166595,#130916,#130917) ;
#102264 = AXIS2_PLACEMENT_3D('',#166596,#130918,#130919) ;
#102265 = AXIS2_PLACEMENT_3D('',#166597,#130920,#130921) ;
#102266 = AXIS2_PLACEMENT_3D('',#166646,#130922,#130923) ;
#102267 = AXIS2_PLACEMENT_3D('',#166659,#130924,#130925) ;
#102268 = AXIS2_PLACEMENT_3D('',#166660,#130926,#130927) ;
#102269 = AXIS2_PLACEMENT_3D('',#166661,#130928,#130929) ;
#102270 = AXIS2_PLACEMENT_3D('',#166662,#130930,#130931) ;
#102271 = AXIS2_PLACEMENT_3D('',#166663,#130932,#130933) ;
#102272 = AXIS2_PLACEMENT_3D('',#166664,#130934,#130935) ;
#102273 = AXIS2_PLACEMENT_3D('',#166665,#130936,#130937) ;
#102274 = AXIS2_PLACEMENT_3D('',#166666,#130938,#130939) ;
#102275 = AXIS2_PLACEMENT_3D('',#166667,#130940,#130941) ;
#102276 = AXIS2_PLACEMENT_3D('',#166668,#130942,#130943) ;
#102277 = AXIS2_PLACEMENT_3D('',#166669,#130944,#130945) ;
#102278 = AXIS2_PLACEMENT_3D('',#166670,#130946,#130947) ;
#102279 = AXIS2_PLACEMENT_3D('',#166671,#130948,#130949) ;
#102280 = AXIS2_PLACEMENT_3D('',#166672,#130950,#130951) ;
#102281 = AXIS2_PLACEMENT_3D('',#166673,#130952,#130953) ;
#102282 = AXIS2_PLACEMENT_3D('',#166686,#130954,#130955) ;
#102283 = AXIS2_PLACEMENT_3D('',#166711,#130956,#130957) ;
#102284 = AXIS2_PLACEMENT_3D('',#166724,#130958,#130959) ;
#102285 = AXIS2_PLACEMENT_3D('',#166725,#130960,#130961) ;
#102286 = AXIS2_PLACEMENT_3D('',#166726,#130962,#130963) ;
#102287 = AXIS2_PLACEMENT_3D('',#166727,#130964,#130965) ;
#102288 = AXIS2_PLACEMENT_3D('',#166728,#130966,#130967) ;
#102289 = AXIS2_PLACEMENT_3D('',#166729,#130968,#130969) ;
#102290 = AXIS2_PLACEMENT_3D('',#166730,#130970,#130971) ;
#102291 = AXIS2_PLACEMENT_3D('',#166731,#130972,#130973) ;
#102292 = AXIS2_PLACEMENT_3D('',#166732,#130974,#130975) ;
#102293 = AXIS2_PLACEMENT_3D('',#166733,#130976,#130977) ;
#102294 = AXIS2_PLACEMENT_3D('',#166734,#130978,#130979) ;
#102295 = AXIS2_PLACEMENT_3D('',#166735,#130980,#130981) ;
#102296 = AXIS2_PLACEMENT_3D('',#166736,#130982,#130983) ;
#102297 = AXIS2_PLACEMENT_3D('',#166737,#130984,#130985) ;
#102298 = AXIS2_PLACEMENT_3D('',#166738,#130986,#130987) ;
#102299 = AXIS2_PLACEMENT_3D('',#166751,#130988,#130989) ;
#102300 = AXIS2_PLACEMENT_3D('',#166776,#130990,#130991) ;
#102301 = AXIS2_PLACEMENT_3D('',#166777,#130992,#130993) ;
#102302 = AXIS2_PLACEMENT_3D('',#166778,#130994,#130995) ;
#102303 = AXIS2_PLACEMENT_3D('',#166779,#130996,#130997) ;
#102304 = AXIS2_PLACEMENT_3D('',#166780,#130998,#130999) ;
#102305 = AXIS2_PLACEMENT_3D('',#166781,#131000,#131001) ;
#102306 = AXIS2_PLACEMENT_3D('',#166782,#131002,#131003) ;
#102307 = AXIS2_PLACEMENT_3D('',#166783,#131004,#131005) ;
#102308 = AXIS2_PLACEMENT_3D('',#166784,#131006,#131007) ;
#102309 = AXIS2_PLACEMENT_3D('',#166785,#131008,#131009) ;
#102310 = AXIS2_PLACEMENT_3D('',#166786,#131010,#131011) ;
#102311 = AXIS2_PLACEMENT_3D('',#166787,#131012,#131013) ;
#102312 = AXIS2_PLACEMENT_3D('',#166788,#131014,#131015) ;
#102313 = AXIS2_PLACEMENT_3D('',#166789,#131016,#131017) ;
#102314 = AXIS2_PLACEMENT_3D('',#166790,#131018,#131019) ;
#102315 = AXIS2_PLACEMENT_3D('',#166791,#131020,#131021) ;
#102316 = AXIS2_PLACEMENT_3D('',#166792,#131022,#131023) ;
#102317 = AXIS2_PLACEMENT_3D('',#166793,#131024,#131025) ;
#102318 = AXIS2_PLACEMENT_3D('',#166794,#131026,#131027) ;
#102319 = AXIS2_PLACEMENT_3D('',#166795,#131028,#131029) ;
#102320 = AXIS2_PLACEMENT_3D('',#166796,#131030,#131031) ;
#102321 = AXIS2_PLACEMENT_3D('',#166797,#131032,#131033) ;
#102322 = AXIS2_PLACEMENT_3D('',#166798,#131034,#131035) ;
#102323 = AXIS2_PLACEMENT_3D('',#166799,#131036,#131037) ;
#102324 = AXIS2_PLACEMENT_3D('',#166800,#131038,#131039) ;
#102325 = AXIS2_PLACEMENT_3D('',#166801,#131040,#131041) ;
#102326 = AXIS2_PLACEMENT_3D('',#166802,#131042,#131043) ;
#102327 = AXIS2_PLACEMENT_3D('',#166803,#131044,#131045) ;
#102328 = AXIS2_PLACEMENT_3D('',#166804,#131046,#131047) ;
#102329 = AXIS2_PLACEMENT_3D('',#166805,#131048,#131049) ;
#102330 = AXIS2_PLACEMENT_3D('',#166806,#131050,#131051) ;
#102331 = AXIS2_PLACEMENT_3D('',#166807,#131052,#131053) ;
#102332 = AXIS2_PLACEMENT_3D('',#166808,#131054,#131055) ;
#102333 = AXIS2_PLACEMENT_3D('',#166809,#131056,#131057) ;
#102334 = AXIS2_PLACEMENT_3D('',#166810,#131058,#131059) ;
#102335 = AXIS2_PLACEMENT_3D('',#166811,#131060,#131061) ;
#102336 = AXIS2_PLACEMENT_3D('',#166812,#131062,#131063) ;
#102337 = AXIS2_PLACEMENT_3D('',#166813,#131064,#131065) ;
#102338 = AXIS2_PLACEMENT_3D('',#166814,#131066,#131067) ;
#102339 = AXIS2_PLACEMENT_3D('',#166815,#131068,#131069) ;
#102340 = AXIS2_PLACEMENT_3D('',#166816,#131070,#131071) ;
#102341 = AXIS2_PLACEMENT_3D('',#166817,#131072,#131073) ;
#102342 = AXIS2_PLACEMENT_3D('',#166818,#131074,#131075) ;
#102343 = AXIS2_PLACEMENT_3D('',#166819,#131076,#131077) ;
#102344 = AXIS2_PLACEMENT_3D('',#166820,#131078,#131079) ;
#102345 = AXIS2_PLACEMENT_3D('',#166821,#131080,#131081) ;
#102346 = AXIS2_PLACEMENT_3D('',#166822,#131082,#131083) ;
#102347 = AXIS2_PLACEMENT_3D('',#166823,#131084,#131085) ;
#102348 = AXIS2_PLACEMENT_3D('',#166824,#131086,#131087) ;
#102349 = AXIS2_PLACEMENT_3D('',#166825,#131088,#131089) ;
#102350 = AXIS2_PLACEMENT_3D('',#166826,#131090,#131091) ;
#102351 = AXIS2_PLACEMENT_3D('',#166827,#131092,#131093) ;
#102352 = AXIS2_PLACEMENT_3D('',#166828,#131094,#131095) ;
#102353 = AXIS2_PLACEMENT_3D('',#166829,#131096,#131097) ;
#102354 = AXIS2_PLACEMENT_3D('',#166830,#131098,#131099) ;
#102355 = AXIS2_PLACEMENT_3D('',#166831,#131100,#131101) ;
#102356 = AXIS2_PLACEMENT_3D('',#166832,#131102,#131103) ;
#102357 = AXIS2_PLACEMENT_3D('',#166833,#131104,#131105) ;
#102358 = AXIS2_PLACEMENT_3D('',#166834,#131106,#131107) ;
#102359 = AXIS2_PLACEMENT_3D('',#166835,#131108,#131109) ;
#102360 = AXIS2_PLACEMENT_3D('',#166836,#131110,#131111) ;
#102361 = AXIS2_PLACEMENT_3D('',#166837,#131112,#131113) ;
#102362 = AXIS2_PLACEMENT_3D('',#166838,#131114,#131115) ;
#102363 = AXIS2_PLACEMENT_3D('',#166839,#131116,#131117) ;
#102364 = AXIS2_PLACEMENT_3D('',#166840,#131118,#131119) ;
#102365 = AXIS2_PLACEMENT_3D('',#166841,#131120,#131121) ;
#102366 = AXIS2_PLACEMENT_3D('',#166842,#131122,#131123) ;
#102367 = AXIS2_PLACEMENT_3D('',#166843,#131124,#131125) ;
#102368 = AXIS2_PLACEMENT_3D('',#166844,#131126,#131127) ;
#102369 = AXIS2_PLACEMENT_3D('',#166845,#131128,#131129) ;
#102370 = AXIS2_PLACEMENT_3D('',#166846,#131130,#131131) ;
#102371 = AXIS2_PLACEMENT_3D('',#166847,#131132,#131133) ;
#102372 = AXIS2_PLACEMENT_3D('',#166848,#131134,#131135) ;
#102373 = AXIS2_PLACEMENT_3D('',#166849,#131136,#131137) ;
#102374 = AXIS2_PLACEMENT_3D('',#166850,#131138,#131139) ;
#102375 = AXIS2_PLACEMENT_3D('',#166851,#131140,#131141) ;
#102376 = AXIS2_PLACEMENT_3D('',#166852,#131142,#131143) ;
#102377 = AXIS2_PLACEMENT_3D('',#166853,#131144,#131145) ;
#102378 = AXIS2_PLACEMENT_3D('',#166854,#131146,#131147) ;
#102379 = AXIS2_PLACEMENT_3D('',#166855,#131148,#131149) ;
#102380 = AXIS2_PLACEMENT_3D('',#166856,#131150,#131151) ;
#102381 = AXIS2_PLACEMENT_3D('',#166857,#131152,#131153) ;
#102382 = AXIS2_PLACEMENT_3D('',#166858,#131154,#131155) ;
#102383 = AXIS2_PLACEMENT_3D('',#166859,#131156,#131157) ;
#102384 = AXIS2_PLACEMENT_3D('',#166860,#131158,#131159) ;
#102385 = AXIS2_PLACEMENT_3D('',#166861,#131160,#131161) ;
#102386 = AXIS2_PLACEMENT_3D('',#166862,#131162,#131163) ;
#102387 = AXIS2_PLACEMENT_3D('',#166863,#131164,#131165) ;
#102388 = AXIS2_PLACEMENT_3D('',#166864,#131166,#131167) ;
#102389 = AXIS2_PLACEMENT_3D('',#166865,#131168,#131169) ;
#102390 = AXIS2_PLACEMENT_3D('',#166866,#131170,#131171) ;
#102391 = AXIS2_PLACEMENT_3D('',#166867,#131172,#131173) ;
#102392 = AXIS2_PLACEMENT_3D('',#166868,#131174,#131175) ;
#102393 = AXIS2_PLACEMENT_3D('',#166869,#131176,#131177) ;
#102394 = AXIS2_PLACEMENT_3D('',#166870,#131178,#131179) ;
#102395 = AXIS2_PLACEMENT_3D('',#166871,#131180,#131181) ;
#102396 = AXIS2_PLACEMENT_3D('',#166872,#131182,#131183) ;
#102397 = AXIS2_PLACEMENT_3D('',#166873,#131184,#131185) ;
#102398 = AXIS2_PLACEMENT_3D('',#166874,#131186,#131187) ;
#102399 = AXIS2_PLACEMENT_3D('',#166875,#131188,#131189) ;
#102400 = AXIS2_PLACEMENT_3D('',#166876,#131190,#131191) ;
#102401 = AXIS2_PLACEMENT_3D('',#166877,#131192,#131193) ;
#102402 = AXIS2_PLACEMENT_3D('',#166878,#131194,#131195) ;
#102403 = AXIS2_PLACEMENT_3D('',#166879,#131196,#131197) ;
#102404 = AXIS2_PLACEMENT_3D('',#166880,#131198,#131199) ;
#102405 = AXIS2_PLACEMENT_3D('',#166881,#131200,#131201) ;
#102406 = AXIS2_PLACEMENT_3D('',#166882,#131202,#131203) ;
#102407 = AXIS2_PLACEMENT_3D('',#166883,#131204,#131205) ;
#102408 = AXIS2_PLACEMENT_3D('',#166884,#131206,#131207) ;
#102409 = AXIS2_PLACEMENT_3D('',#166885,#131208,#131209) ;
#102410 = AXIS2_PLACEMENT_3D('',#166886,#131210,#131211) ;
#102411 = AXIS2_PLACEMENT_3D('',#166887,#131212,#131213) ;
#102412 = AXIS2_PLACEMENT_3D('',#166888,#131214,#131215) ;
#102413 = AXIS2_PLACEMENT_3D('',#166889,#131216,#131217) ;
#102414 = AXIS2_PLACEMENT_3D('',#166890,#131218,#131219) ;
#102415 = AXIS2_PLACEMENT_3D('',#166891,#131220,#131221) ;
#102416 = AXIS2_PLACEMENT_3D('',#166892,#131222,#131223) ;
#102417 = AXIS2_PLACEMENT_3D('',#166893,#131224,#131225) ;
#102418 = AXIS2_PLACEMENT_3D('',#166894,#131226,#131227) ;
#102419 = AXIS2_PLACEMENT_3D('',#166895,#131228,#131229) ;
#102420 = AXIS2_PLACEMENT_3D('',#166896,#131230,#131231) ;
#102421 = AXIS2_PLACEMENT_3D('',#166897,#131232,#131233) ;
#102422 = AXIS2_PLACEMENT_3D('',#166898,#131234,#131235) ;
#102423 = AXIS2_PLACEMENT_3D('',#166899,#131236,#131237) ;
#102424 = AXIS2_PLACEMENT_3D('',#166900,#131238,#131239) ;
#102425 = AXIS2_PLACEMENT_3D('',#166901,#131240,#131241) ;
#102426 = AXIS2_PLACEMENT_3D('',#166902,#131242,#131243) ;
#102427 = AXIS2_PLACEMENT_3D('',#166903,#131244,#131245) ;
#102428 = AXIS2_PLACEMENT_3D('',#166904,#131246,#131247) ;
#102429 = AXIS2_PLACEMENT_3D('',#166905,#131248,#131249) ;
#102430 = AXIS2_PLACEMENT_3D('',#166906,#131250,#131251) ;
#102431 = AXIS2_PLACEMENT_3D('',#166907,#131252,#131253) ;
#102432 = AXIS2_PLACEMENT_3D('',#166908,#131254,#131255) ;
#102433 = AXIS2_PLACEMENT_3D('',#166909,#131256,#131257) ;
#102434 = AXIS2_PLACEMENT_3D('',#166910,#131258,#131259) ;
#102435 = AXIS2_PLACEMENT_3D('',#166911,#131260,#131261) ;
#102436 = AXIS2_PLACEMENT_3D('',#166912,#131262,#131263) ;
#102437 = AXIS2_PLACEMENT_3D('',#166913,#131264,#131265) ;
#102438 = AXIS2_PLACEMENT_3D('',#166914,#131266,#131267) ;
#102439 = AXIS2_PLACEMENT_3D('',#166915,#131268,#131269) ;
#102440 = AXIS2_PLACEMENT_3D('',#166916,#131270,#131271) ;
#102441 = AXIS2_PLACEMENT_3D('',#166917,#131272,#131273) ;
#102442 = AXIS2_PLACEMENT_3D('',#166918,#131274,#131275) ;
#102443 = AXIS2_PLACEMENT_3D('',#166919,#131276,#131277) ;
#102444 = AXIS2_PLACEMENT_3D('',#166920,#131278,#131279) ;
#102445 = AXIS2_PLACEMENT_3D('',#166921,#131280,#131281) ;
#102446 = AXIS2_PLACEMENT_3D('',#166922,#131282,#131283) ;
#102447 = AXIS2_PLACEMENT_3D('',#166923,#131284,#131285) ;
#102448 = AXIS2_PLACEMENT_3D('',#166924,#131286,#131287) ;
#102449 = AXIS2_PLACEMENT_3D('',#166925,#131288,#131289) ;
#102450 = AXIS2_PLACEMENT_3D('',#166926,#131290,#131291) ;
#102451 = AXIS2_PLACEMENT_3D('',#166927,#131292,#131293) ;
#102452 = AXIS2_PLACEMENT_3D('',#166928,#131294,#131295) ;
#102453 = AXIS2_PLACEMENT_3D('',#166929,#131296,#131297) ;
#102454 = AXIS2_PLACEMENT_3D('',#166930,#131298,#131299) ;
#102455 = AXIS2_PLACEMENT_3D('',#166931,#131300,#131301) ;
#102456 = AXIS2_PLACEMENT_3D('',#166932,#131302,#131303) ;
#102457 = AXIS2_PLACEMENT_3D('',#166933,#131304,#131305) ;
#102458 = AXIS2_PLACEMENT_3D('',#166934,#131306,#131307) ;
#102459 = AXIS2_PLACEMENT_3D('',#166935,#131308,#131309) ;
#102460 = AXIS2_PLACEMENT_3D('',#166936,#131310,#131311) ;
#102461 = AXIS2_PLACEMENT_3D('',#166937,#131312,#131313) ;
#102462 = AXIS2_PLACEMENT_3D('',#166938,#131314,#131315) ;
#102463 = AXIS2_PLACEMENT_3D('',#166939,#131316,#131317) ;
#102464 = AXIS2_PLACEMENT_3D('',#166940,#131318,#131319) ;
#102465 = AXIS2_PLACEMENT_3D('',#166941,#131320,#131321) ;
#102466 = AXIS2_PLACEMENT_3D('',#166942,#131322,#131323) ;
#102467 = AXIS2_PLACEMENT_3D('',#166943,#131324,#131325) ;
#102468 = AXIS2_PLACEMENT_3D('',#166944,#131326,#131327) ;
#102469 = AXIS2_PLACEMENT_3D('',#166945,#131328,#131329) ;
#102470 = AXIS2_PLACEMENT_3D('',#166946,#131330,#131331) ;
#102471 = AXIS2_PLACEMENT_3D('',#166947,#131332,#131333) ;
#102472 = AXIS2_PLACEMENT_3D('',#166948,#131334,#131335) ;
#102473 = AXIS2_PLACEMENT_3D('',#166949,#131336,#131337) ;
#102474 = AXIS2_PLACEMENT_3D('',#166950,#131338,#131339) ;
#102475 = AXIS2_PLACEMENT_3D('',#166951,#131340,#131341) ;
#102476 = AXIS2_PLACEMENT_3D('',#166952,#131342,#131343) ;
#102477 = AXIS2_PLACEMENT_3D('',#166953,#131344,#131345) ;
#102478 = AXIS2_PLACEMENT_3D('',#166954,#131346,#131347) ;
#102479 = AXIS2_PLACEMENT_3D('',#166955,#131348,#131349) ;
#102480 = AXIS2_PLACEMENT_3D('',#166956,#131350,#131351) ;
#102481 = AXIS2_PLACEMENT_3D('',#166957,#131352,#131353) ;
#102482 = AXIS2_PLACEMENT_3D('',#166958,#131354,#131355) ;
#102483 = AXIS2_PLACEMENT_3D('',#166959,#131356,#131357) ;
#102484 = AXIS2_PLACEMENT_3D('',#166960,#131358,#131359) ;
#102485 = AXIS2_PLACEMENT_3D('',#166961,#131360,#131361) ;
#102486 = AXIS2_PLACEMENT_3D('',#166962,#131362,#131363) ;
#102487 = AXIS2_PLACEMENT_3D('',#166963,#131364,#131365) ;
#102488 = AXIS2_PLACEMENT_3D('',#166964,#131366,#131367) ;
#102489 = AXIS2_PLACEMENT_3D('',#166965,#131368,#131369) ;
#102490 = AXIS2_PLACEMENT_3D('',#166966,#131370,#131371) ;
#102491 = AXIS2_PLACEMENT_3D('',#166967,#131372,#131373) ;
#102492 = AXIS2_PLACEMENT_3D('',#166968,#131374,#131375) ;
#102493 = AXIS2_PLACEMENT_3D('',#166969,#131376,#131377) ;
#102494 = AXIS2_PLACEMENT_3D('',#166970,#131378,#131379) ;
#102495 = AXIS2_PLACEMENT_3D('',#166971,#131380,#131381) ;
#102496 = AXIS2_PLACEMENT_3D('',#166972,#131382,#131383) ;
#102497 = AXIS2_PLACEMENT_3D('',#166973,#131384,#131385) ;
#102498 = AXIS2_PLACEMENT_3D('',#166974,#131386,#131387) ;
#102499 = AXIS2_PLACEMENT_3D('',#166975,#131388,#131389) ;
#102500 = AXIS2_PLACEMENT_3D('',#166976,#131390,#131391) ;
#102501 = AXIS2_PLACEMENT_3D('',#166977,#131392,#131393) ;
#102502 = AXIS2_PLACEMENT_3D('',#166978,#131394,#131395) ;
#102503 = AXIS2_PLACEMENT_3D('',#166979,#131396,#131397) ;
#102504 = AXIS2_PLACEMENT_3D('',#166980,#131398,#131399) ;
#102505 = AXIS2_PLACEMENT_3D('',#166981,#131400,#131401) ;
#102506 = AXIS2_PLACEMENT_3D('',#166982,#131402,#131403) ;
#102507 = AXIS2_PLACEMENT_3D('',#166983,#131404,#131405) ;
#102508 = AXIS2_PLACEMENT_3D('',#166984,#131406,#131407) ;
#102509 = AXIS2_PLACEMENT_3D('',#166985,#131408,#131409) ;
#102510 = AXIS2_PLACEMENT_3D('',#166986,#131410,#131411) ;
#102511 = AXIS2_PLACEMENT_3D('',#166987,#131412,#131413) ;
#102512 = AXIS2_PLACEMENT_3D('',#166988,#131414,#131415) ;
#102513 = AXIS2_PLACEMENT_3D('',#166989,#131416,#131417) ;
#102514 = AXIS2_PLACEMENT_3D('',#167014,#131418,#131419) ;
#102515 = AXIS2_PLACEMENT_3D('',#167015,#131420,#131421) ;
#102516 = AXIS2_PLACEMENT_3D('',#167016,#131422,#131423) ;
#102517 = AXIS2_PLACEMENT_3D('',#167041,#131424,#131425) ;
#102518 = AXIS2_PLACEMENT_3D('',#167042,#131426,#131427) ;
#102519 = AXIS2_PLACEMENT_3D('',#167043,#131428,#131429) ;
#102520 = AXIS2_PLACEMENT_3D('',#167044,#131430,#131431) ;
#102521 = AXIS2_PLACEMENT_3D('',#167069,#131432,#131433) ;
#102522 = AXIS2_PLACEMENT_3D('',#167070,#131434,#131435) ;
#102523 = AXIS2_PLACEMENT_3D('',#167071,#131436,#131437) ;
#102524 = AXIS2_PLACEMENT_3D('',#167072,#131438,#131439) ;
#102525 = AXIS2_PLACEMENT_3D('',#167073,#131440,#131441) ;
#102526 = AXIS2_PLACEMENT_3D('',#167074,#131442,#131443) ;
#102527 = AXIS2_PLACEMENT_3D('',#167075,#131444,#131445) ;
#102528 = AXIS2_PLACEMENT_3D('',#167076,#131446,#131447) ;
#102529 = AXIS2_PLACEMENT_3D('',#167077,#131448,#131449) ;
#102530 = AXIS2_PLACEMENT_3D('',#167078,#131450,#131451) ;
#102531 = AXIS2_PLACEMENT_3D('',#167079,#131452,#131453) ;
#102532 = AXIS2_PLACEMENT_3D('',#167080,#131454,#131455) ;
#102533 = AXIS2_PLACEMENT_3D('',#167081,#131456,#131457) ;
#102534 = AXIS2_PLACEMENT_3D('',#167082,#131458,#131459) ;
#102535 = AXIS2_PLACEMENT_3D('',#167083,#131460,#131461) ;
#102536 = AXIS2_PLACEMENT_3D('',#167084,#131462,#131463) ;
#102537 = AXIS2_PLACEMENT_3D('',#167085,#131464,#131465) ;
#102538 = AXIS2_PLACEMENT_3D('',#167086,#131466,#131467) ;
#102539 = AXIS2_PLACEMENT_3D('',#167087,#131468,#131469) ;
#102540 = AXIS2_PLACEMENT_3D('',#167088,#131470,#131471) ;
#102541 = AXIS2_PLACEMENT_3D('',#167089,#131472,#131473) ;
#102542 = AXIS2_PLACEMENT_3D('',#167138,#131474,#131475) ;
#102543 = AXIS2_PLACEMENT_3D('',#167151,#131476,#131477) ;
#102544 = AXIS2_PLACEMENT_3D('',#167152,#131478,#131479) ;
#102545 = AXIS2_PLACEMENT_3D('',#167153,#131480,#131481) ;
#102546 = AXIS2_PLACEMENT_3D('',#167154,#131482,#131483) ;
#102547 = AXIS2_PLACEMENT_3D('',#167155,#131484,#131485) ;
#102548 = AXIS2_PLACEMENT_3D('',#167156,#131486,#131487) ;
#102549 = AXIS2_PLACEMENT_3D('',#167157,#131488,#131489) ;
#102550 = AXIS2_PLACEMENT_3D('',#167158,#131490,#131491) ;
#102551 = AXIS2_PLACEMENT_3D('',#167159,#131492,#131493) ;
#102552 = AXIS2_PLACEMENT_3D('',#167160,#131494,#131495) ;
#102553 = AXIS2_PLACEMENT_3D('',#167161,#131496,#131497) ;
#102554 = AXIS2_PLACEMENT_3D('',#167162,#131498,#131499) ;
#102555 = AXIS2_PLACEMENT_3D('',#167163,#131500,#131501) ;
#102556 = AXIS2_PLACEMENT_3D('',#167164,#131502,#131503) ;
#102557 = AXIS2_PLACEMENT_3D('',#167165,#131504,#131505) ;
#102558 = AXIS2_PLACEMENT_3D('',#167178,#131506,#131507) ;
#102559 = AXIS2_PLACEMENT_3D('',#167203,#131508,#131509) ;
#102560 = AXIS2_PLACEMENT_3D('',#167216,#131510,#131511) ;
#102561 = AXIS2_PLACEMENT_3D('',#167217,#131512,#131513) ;
#102562 = AXIS2_PLACEMENT_3D('',#167218,#131514,#131515) ;
#102563 = AXIS2_PLACEMENT_3D('',#167219,#131516,#131517) ;
#102564 = AXIS2_PLACEMENT_3D('',#167220,#131518,#131519) ;
#102565 = AXIS2_PLACEMENT_3D('',#167221,#131520,#131521) ;
#102566 = AXIS2_PLACEMENT_3D('',#167222,#131522,#131523) ;
#102567 = AXIS2_PLACEMENT_3D('',#167223,#131524,#131525) ;
#102568 = AXIS2_PLACEMENT_3D('',#167224,#131526,#131527) ;
#102569 = AXIS2_PLACEMENT_3D('',#167225,#131528,#131529) ;
#102570 = AXIS2_PLACEMENT_3D('',#167226,#131530,#131531) ;
#102571 = AXIS2_PLACEMENT_3D('',#167227,#131532,#131533) ;
#102572 = AXIS2_PLACEMENT_3D('',#167228,#131534,#131535) ;
#102573 = AXIS2_PLACEMENT_3D('',#167229,#131536,#131537) ;
#102574 = AXIS2_PLACEMENT_3D('',#167230,#131538,#131539) ;
#102575 = AXIS2_PLACEMENT_3D('',#167243,#131540,#131541) ;
#102576 = AXIS2_PLACEMENT_3D('',#167268,#131542,#131543) ;
#102577 = AXIS2_PLACEMENT_3D('',#167269,#131544,#131545) ;
#102578 = AXIS2_PLACEMENT_3D('',#167270,#131546,#131547) ;
#102579 = AXIS2_PLACEMENT_3D('',#167271,#131548,#131549) ;
#102580 = AXIS2_PLACEMENT_3D('',#167272,#131550,#131551) ;
#102581 = AXIS2_PLACEMENT_3D('',#167273,#131552,#131553) ;
#102582 = AXIS2_PLACEMENT_3D('',#167274,#131554,#131555) ;
#102583 = AXIS2_PLACEMENT_3D('',#167275,#131556,#131557) ;
#102584 = AXIS2_PLACEMENT_3D('',#167276,#131558,#131559) ;
#102585 = AXIS2_PLACEMENT_3D('',#167277,#131560,#131561) ;
#102586 = AXIS2_PLACEMENT_3D('',#167278,#131562,#131563) ;
#102587 = AXIS2_PLACEMENT_3D('',#167279,#131564,#131565) ;
#102588 = AXIS2_PLACEMENT_3D('',#167280,#131566,#131567) ;
#102589 = AXIS2_PLACEMENT_3D('',#167281,#131568,#131569) ;
#102590 = AXIS2_PLACEMENT_3D('',#167282,#131570,#131571) ;
#102591 = AXIS2_PLACEMENT_3D('',#167283,#131572,#131573) ;
#102592 = AXIS2_PLACEMENT_3D('',#167284,#131574,#131575) ;
#102593 = AXIS2_PLACEMENT_3D('',#167285,#131576,#131577) ;
#102594 = AXIS2_PLACEMENT_3D('',#167286,#131578,#131579) ;
#102595 = AXIS2_PLACEMENT_3D('',#167287,#131580,#131581) ;
#102596 = AXIS2_PLACEMENT_3D('',#167288,#131582,#131583) ;
#102597 = AXIS2_PLACEMENT_3D('',#167289,#131584,#131585) ;
#102598 = AXIS2_PLACEMENT_3D('',#167290,#131586,#131587) ;
#102599 = AXIS2_PLACEMENT_3D('',#167291,#131588,#131589) ;
#102600 = AXIS2_PLACEMENT_3D('',#167292,#131590,#131591) ;
#102601 = AXIS2_PLACEMENT_3D('',#167293,#131592,#131593) ;
#102602 = AXIS2_PLACEMENT_3D('',#167294,#131594,#131595) ;
#102603 = AXIS2_PLACEMENT_3D('',#167295,#131596,#131597) ;
#102604 = AXIS2_PLACEMENT_3D('',#167296,#131598,#131599) ;
#102605 = AXIS2_PLACEMENT_3D('',#167297,#131600,#131601) ;
#102606 = AXIS2_PLACEMENT_3D('',#167298,#131602,#131603) ;
#102607 = AXIS2_PLACEMENT_3D('',#167299,#131604,#131605) ;
#102608 = AXIS2_PLACEMENT_3D('',#167300,#131606,#131607) ;
#102609 = AXIS2_PLACEMENT_3D('',#167301,#131608,#131609) ;
#102610 = AXIS2_PLACEMENT_3D('',#167302,#131610,#131611) ;
#102611 = AXIS2_PLACEMENT_3D('',#167303,#131612,#131613) ;
#102612 = AXIS2_PLACEMENT_3D('',#167304,#131614,#131615) ;
#102613 = AXIS2_PLACEMENT_3D('',#167305,#131616,#131617) ;
#102614 = AXIS2_PLACEMENT_3D('',#167306,#131618,#131619) ;
#102615 = AXIS2_PLACEMENT_3D('',#167307,#131620,#131621) ;
#102616 = AXIS2_PLACEMENT_3D('',#167308,#131622,#131623) ;
#102617 = AXIS2_PLACEMENT_3D('',#167309,#131624,#131625) ;
#102618 = AXIS2_PLACEMENT_3D('',#167310,#131626,#131627) ;
#102619 = AXIS2_PLACEMENT_3D('',#167311,#131628,#131629) ;
#102620 = AXIS2_PLACEMENT_3D('',#167312,#131630,#131631) ;
#102621 = AXIS2_PLACEMENT_3D('',#167313,#131632,#131633) ;
#102622 = AXIS2_PLACEMENT_3D('',#167314,#131634,#131635) ;
#102623 = AXIS2_PLACEMENT_3D('',#167315,#131636,#131637) ;
#102624 = AXIS2_PLACEMENT_3D('',#167316,#131638,#131639) ;
#102625 = AXIS2_PLACEMENT_3D('',#167317,#131640,#131641) ;
#102626 = AXIS2_PLACEMENT_3D('',#167318,#131642,#131643) ;
#102627 = AXIS2_PLACEMENT_3D('',#167319,#131644,#131645) ;
#102628 = AXIS2_PLACEMENT_3D('',#167320,#131646,#131647) ;
#102629 = AXIS2_PLACEMENT_3D('',#167321,#131648,#131649) ;
#102630 = AXIS2_PLACEMENT_3D('',#167322,#131650,#131651) ;
#102631 = AXIS2_PLACEMENT_3D('',#167323,#131652,#131653) ;
#102632 = AXIS2_PLACEMENT_3D('',#167324,#131654,#131655) ;
#102633 = AXIS2_PLACEMENT_3D('',#167325,#131656,#131657) ;
#102634 = AXIS2_PLACEMENT_3D('',#167326,#131658,#131659) ;
#102635 = AXIS2_PLACEMENT_3D('',#167327,#131660,#131661) ;
#102636 = AXIS2_PLACEMENT_3D('',#167328,#131662,#131663) ;
#102637 = AXIS2_PLACEMENT_3D('',#167329,#131664,#131665) ;
#102638 = AXIS2_PLACEMENT_3D('',#167330,#131666,#131667) ;
#102639 = AXIS2_PLACEMENT_3D('',#167331,#131668,#131669) ;
#102640 = AXIS2_PLACEMENT_3D('',#167332,#131670,#131671) ;
#102641 = AXIS2_PLACEMENT_3D('',#167333,#131672,#131673) ;
#102642 = AXIS2_PLACEMENT_3D('',#167334,#131674,#131675) ;
#102643 = AXIS2_PLACEMENT_3D('',#167335,#131676,#131677) ;
#102644 = AXIS2_PLACEMENT_3D('',#167336,#131678,#131679) ;
#102645 = AXIS2_PLACEMENT_3D('',#167337,#131680,#131681) ;
#102646 = AXIS2_PLACEMENT_3D('',#167338,#131682,#131683) ;
#102647 = AXIS2_PLACEMENT_3D('',#167339,#131684,#131685) ;
#102648 = AXIS2_PLACEMENT_3D('',#167340,#131686,#131687) ;
#102649 = AXIS2_PLACEMENT_3D('',#167341,#131688,#131689) ;
#102650 = AXIS2_PLACEMENT_3D('',#167342,#131690,#131691) ;
#102651 = AXIS2_PLACEMENT_3D('',#167343,#131692,#131693) ;
#102652 = AXIS2_PLACEMENT_3D('',#167344,#131694,#131695) ;
#102653 = AXIS2_PLACEMENT_3D('',#167345,#131696,#131697) ;
#102654 = AXIS2_PLACEMENT_3D('',#167346,#131698,#131699) ;
#102655 = AXIS2_PLACEMENT_3D('',#167347,#131700,#131701) ;
#102656 = AXIS2_PLACEMENT_3D('',#167348,#131702,#131703) ;
#102657 = AXIS2_PLACEMENT_3D('',#167349,#131704,#131705) ;
#102658 = AXIS2_PLACEMENT_3D('',#167350,#131706,#131707) ;
#102659 = AXIS2_PLACEMENT_3D('',#167351,#131708,#131709) ;
#102660 = AXIS2_PLACEMENT_3D('',#167352,#131710,#131711) ;
#102661 = AXIS2_PLACEMENT_3D('',#167353,#131712,#131713) ;
#102662 = AXIS2_PLACEMENT_3D('',#167354,#131714,#131715) ;
#102663 = AXIS2_PLACEMENT_3D('',#167355,#131716,#131717) ;
#102664 = AXIS2_PLACEMENT_3D('',#167356,#131718,#131719) ;
#102665 = AXIS2_PLACEMENT_3D('',#167357,#131720,#131721) ;
#102666 = AXIS2_PLACEMENT_3D('',#167358,#131722,#131723) ;
#102667 = AXIS2_PLACEMENT_3D('',#167359,#131724,#131725) ;
#102668 = AXIS2_PLACEMENT_3D('',#167360,#131726,#131727) ;
#102669 = AXIS2_PLACEMENT_3D('',#167361,#131728,#131729) ;
#102670 = AXIS2_PLACEMENT_3D('',#167362,#131730,#131731) ;
#102671 = AXIS2_PLACEMENT_3D('',#167363,#131732,#131733) ;
#102672 = AXIS2_PLACEMENT_3D('',#167364,#131734,#131735) ;
#102673 = AXIS2_PLACEMENT_3D('',#167365,#131736,#131737) ;
#102674 = AXIS2_PLACEMENT_3D('',#167366,#131738,#131739) ;
#102675 = AXIS2_PLACEMENT_3D('',#167367,#131740,#131741) ;
#102676 = AXIS2_PLACEMENT_3D('',#167368,#131742,#131743) ;
#102677 = AXIS2_PLACEMENT_3D('',#167369,#131744,#131745) ;
#102678 = AXIS2_PLACEMENT_3D('',#167370,#131746,#131747) ;
#102679 = AXIS2_PLACEMENT_3D('',#167371,#131748,#131749) ;
#102680 = AXIS2_PLACEMENT_3D('',#167372,#131750,#131751) ;
#102681 = AXIS2_PLACEMENT_3D('',#167373,#131752,#131753) ;
#102682 = AXIS2_PLACEMENT_3D('',#167374,#131754,#131755) ;
#102683 = AXIS2_PLACEMENT_3D('',#167375,#131756,#131757) ;
#102684 = AXIS2_PLACEMENT_3D('',#167376,#131758,#131759) ;
#102685 = AXIS2_PLACEMENT_3D('',#167377,#131760,#131761) ;
#102686 = AXIS2_PLACEMENT_3D('',#167378,#131762,#131763) ;
#102687 = AXIS2_PLACEMENT_3D('',#167379,#131764,#131765) ;
#102688 = AXIS2_PLACEMENT_3D('',#167380,#131766,#131767) ;
#102689 = AXIS2_PLACEMENT_3D('',#167381,#131768,#131769) ;
#102690 = AXIS2_PLACEMENT_3D('',#167382,#131770,#131771) ;
#102691 = AXIS2_PLACEMENT_3D('',#167383,#131772,#131773) ;
#102692 = AXIS2_PLACEMENT_3D('',#167384,#131774,#131775) ;
#102693 = AXIS2_PLACEMENT_3D('',#167385,#131776,#131777) ;
#102694 = AXIS2_PLACEMENT_3D('',#167386,#131778,#131779) ;
#102695 = AXIS2_PLACEMENT_3D('',#167387,#131780,#131781) ;
#102696 = AXIS2_PLACEMENT_3D('',#167388,#131782,#131783) ;
#102697 = AXIS2_PLACEMENT_3D('',#167389,#131784,#131785) ;
#102698 = AXIS2_PLACEMENT_3D('',#167390,#131786,#131787) ;
#102699 = AXIS2_PLACEMENT_3D('',#167391,#131788,#131789) ;
#102700 = AXIS2_PLACEMENT_3D('',#167392,#131790,#131791) ;
#102701 = AXIS2_PLACEMENT_3D('',#167393,#131792,#131793) ;
#102702 = AXIS2_PLACEMENT_3D('',#167394,#131794,#131795) ;
#102703 = AXIS2_PLACEMENT_3D('',#167395,#131796,#131797) ;
#102704 = AXIS2_PLACEMENT_3D('',#167396,#131798,#131799) ;
#102705 = AXIS2_PLACEMENT_3D('',#167397,#131800,#131801) ;
#102706 = AXIS2_PLACEMENT_3D('',#167398,#131802,#131803) ;
#102707 = AXIS2_PLACEMENT_3D('',#167399,#131804,#131805) ;
#102708 = AXIS2_PLACEMENT_3D('',#167400,#131806,#131807) ;
#102709 = AXIS2_PLACEMENT_3D('',#167401,#131808,#131809) ;
#102710 = AXIS2_PLACEMENT_3D('',#167402,#131810,#131811) ;
#102711 = AXIS2_PLACEMENT_3D('',#167403,#131812,#131813) ;
#102712 = AXIS2_PLACEMENT_3D('',#167404,#131814,#131815) ;
#102713 = AXIS2_PLACEMENT_3D('',#167405,#131816,#131817) ;
#102714 = AXIS2_PLACEMENT_3D('',#167406,#131818,#131819) ;
#102715 = AXIS2_PLACEMENT_3D('',#167407,#131820,#131821) ;
#102716 = AXIS2_PLACEMENT_3D('',#167408,#131822,#131823) ;
#102717 = AXIS2_PLACEMENT_3D('',#167409,#131824,#131825) ;
#102718 = AXIS2_PLACEMENT_3D('',#167410,#131826,#131827) ;
#102719 = AXIS2_PLACEMENT_3D('',#167411,#131828,#131829) ;
#102720 = AXIS2_PLACEMENT_3D('',#167412,#131830,#131831) ;
#102721 = AXIS2_PLACEMENT_3D('',#167413,#131832,#131833) ;
#102722 = AXIS2_PLACEMENT_3D('',#167414,#131834,#131835) ;
#102723 = AXIS2_PLACEMENT_3D('',#167415,#131836,#131837) ;
#102724 = AXIS2_PLACEMENT_3D('',#167416,#131838,#131839) ;
#102725 = AXIS2_PLACEMENT_3D('',#167417,#131840,#131841) ;
#102726 = AXIS2_PLACEMENT_3D('',#167418,#131842,#131843) ;
#102727 = AXIS2_PLACEMENT_3D('',#167419,#131844,#131845) ;
#102728 = AXIS2_PLACEMENT_3D('',#167420,#131846,#131847) ;
#102729 = AXIS2_PLACEMENT_3D('',#167421,#131848,#131849) ;
#102730 = AXIS2_PLACEMENT_3D('',#167422,#131850,#131851) ;
#102731 = AXIS2_PLACEMENT_3D('',#167423,#131852,#131853) ;
#102732 = AXIS2_PLACEMENT_3D('',#167425,#131854,#131855) ;
#102733 = AXIS2_PLACEMENT_3D('',#167452,#131856,#131857) ;
#102734 = AXIS2_PLACEMENT_3D('',#167453,#131858,#131859) ;
#102735 = AXIS2_PLACEMENT_3D('',#167455,#131860,#131861) ;
#102736 = AXIS2_PLACEMENT_3D('',#167456,#131862,#131863) ;
#102737 = AXIS2_PLACEMENT_3D('',#167457,#131864,#131865) ;
#102738 = AXIS2_PLACEMENT_3D('',#167492,#131866,#131867) ;
#102739 = AXIS2_PLACEMENT_3D('',#167519,#131868,#131869) ;
#102740 = AXIS2_PLACEMENT_3D('',#167521,#131870,#131871) ;
#102741 = AXIS2_PLACEMENT_3D('',#167548,#131872,#131873) ;
#102742 = AXIS2_PLACEMENT_3D('',#167549,#131874,#131875) ;
#102743 = AXIS2_PLACEMENT_3D('',#167551,#131876,#131877) ;
#102744 = AXIS2_PLACEMENT_3D('',#167552,#131878,#131879) ;
#102745 = AXIS2_PLACEMENT_3D('',#167553,#131880,#131881) ;
#102746 = AXIS2_PLACEMENT_3D('',#167588,#131882,#131883) ;
#102747 = AXIS2_PLACEMENT_3D('',#167590,#131884,#131885) ;
#102748 = AXIS2_PLACEMENT_3D('',#167617,#131886,#131887) ;
#102749 = AXIS2_PLACEMENT_3D('',#167618,#131888,#131889) ;
#102750 = AXIS2_PLACEMENT_3D('',#167620,#131890,#131891) ;
#102751 = AXIS2_PLACEMENT_3D('',#167621,#131892,#131893) ;
#102752 = AXIS2_PLACEMENT_3D('',#167622,#131894,#131895) ;
#102753 = AXIS2_PLACEMENT_3D('',#167657,#131896,#131897) ;
#102754 = AXIS2_PLACEMENT_3D('',#167659,#131898,#131899) ;
#102755 = AXIS2_PLACEMENT_3D('',#167686,#131900,#131901) ;
#102756 = AXIS2_PLACEMENT_3D('',#167687,#131902,#131903) ;
#102757 = AXIS2_PLACEMENT_3D('',#167689,#131904,#131905) ;
#102758 = AXIS2_PLACEMENT_3D('',#167690,#131906,#131907) ;
#102759 = AXIS2_PLACEMENT_3D('',#167691,#131908,#131909) ;
#102760 = AXIS2_PLACEMENT_3D('',#167726,#131910,#131911) ;
#102761 = AXIS2_PLACEMENT_3D('',#167728,#131912,#131913) ;
#102762 = AXIS2_PLACEMENT_3D('',#167755,#131914,#131915) ;
#102763 = AXIS2_PLACEMENT_3D('',#167756,#131916,#131917) ;
#102764 = AXIS2_PLACEMENT_3D('',#167758,#131918,#131919) ;
#102765 = AXIS2_PLACEMENT_3D('',#167759,#131920,#131921) ;
#102766 = AXIS2_PLACEMENT_3D('',#167760,#131922,#131923) ;
#102767 = AXIS2_PLACEMENT_3D('',#167795,#131924,#131925) ;
#102768 = AXIS2_PLACEMENT_3D('',#167797,#131926,#131927) ;
#102769 = AXIS2_PLACEMENT_3D('',#167824,#131928,#131929) ;
#102770 = AXIS2_PLACEMENT_3D('',#167825,#131930,#131931) ;
#102771 = AXIS2_PLACEMENT_3D('',#167827,#131932,#131933) ;
#102772 = AXIS2_PLACEMENT_3D('',#167828,#131934,#131935) ;
#102773 = AXIS2_PLACEMENT_3D('',#167829,#131936,#131937) ;
#102774 = AXIS2_PLACEMENT_3D('',#167864,#131938,#131939) ;
#102775 = AXIS2_PLACEMENT_3D('',#167866,#131940,#131941) ;
#102776 = AXIS2_PLACEMENT_3D('',#167893,#131942,#131943) ;
#102777 = AXIS2_PLACEMENT_3D('',#167894,#131944,#131945) ;
#102778 = AXIS2_PLACEMENT_3D('',#167896,#131946,#131947) ;
#102779 = AXIS2_PLACEMENT_3D('',#167897,#131948,#131949) ;
#102780 = AXIS2_PLACEMENT_3D('',#167898,#131950,#131951) ;
#102781 = AXIS2_PLACEMENT_3D('',#167933,#131952,#131953) ;
#102782 = AXIS2_PLACEMENT_3D('',#167935,#131954,#131955) ;
#102783 = AXIS2_PLACEMENT_3D('',#167962,#131956,#131957) ;
#102784 = AXIS2_PLACEMENT_3D('',#167963,#131958,#131959) ;
#102785 = AXIS2_PLACEMENT_3D('',#167965,#131960,#131961) ;
#102786 = AXIS2_PLACEMENT_3D('',#167966,#131962,#131963) ;
#102787 = AXIS2_PLACEMENT_3D('',#167967,#131964,#131965) ;
#102788 = AXIS2_PLACEMENT_3D('',#168002,#131966,#131967) ;
#102789 = AXIS2_PLACEMENT_3D('',#168003,#131968,#131969) ;
#102790 = AXIS2_PLACEMENT_3D('',#168005,#131970,#131971) ;
#102791 = AXIS2_PLACEMENT_3D('',#168006,#131972,#131973) ;
#102792 = AXIS2_PLACEMENT_3D('',#168007,#131974,#131975) ;
#102793 = AXIS2_PLACEMENT_3D('',#168042,#131976,#131977) ;
#102794 = AXIS2_PLACEMENT_3D('',#168099,#131978,#131979) ;
#102795 = AXIS2_PLACEMENT_3D('',#168100,#131980,#131981) ;
#102796 = AXIS2_PLACEMENT_3D('',#168101,#131982,#131983) ;
#102797 = AXIS2_PLACEMENT_3D('',#168102,#131984,#131985) ;
#102798 = AXIS2_PLACEMENT_3D('',#168103,#131986,#131987) ;
#102799 = AXIS2_PLACEMENT_3D('',#168104,#131988,#131989) ;
#102800 = AXIS2_PLACEMENT_3D('',#168106,#131990,#131991) ;
#102801 = AXIS2_PLACEMENT_3D('',#168133,#131992,#131993) ;
#102802 = AXIS2_PLACEMENT_3D('',#168134,#131994,#131995) ;
#102803 = AXIS2_PLACEMENT_3D('',#168135,#131996,#131997) ;
#102804 = AXIS2_PLACEMENT_3D('',#168136,#131998,#131999) ;
#102805 = AXIS2_PLACEMENT_3D('',#168137,#132000,#132001) ;
#102806 = AXIS2_PLACEMENT_3D('',#168194,#132002,#132003) ;
#102807 = AXIS2_PLACEMENT_3D('',#168195,#132004,#132005) ;
#102808 = AXIS2_PLACEMENT_3D('',#168196,#132006,#132007) ;
#102809 = AXIS2_PLACEMENT_3D('',#168197,#132008,#132009) ;
#102810 = AXIS2_PLACEMENT_3D('',#168198,#132010,#132011) ;
#102811 = AXIS2_PLACEMENT_3D('',#168199,#132012,#132013) ;
#102812 = AXIS2_PLACEMENT_3D('',#168201,#132014,#132015) ;
#102813 = AXIS2_PLACEMENT_3D('',#168228,#132016,#132017) ;
#102814 = AXIS2_PLACEMENT_3D('',#168229,#132018,#132019) ;
#102815 = AXIS2_PLACEMENT_3D('',#168230,#132020,#132021) ;
#102816 = AXIS2_PLACEMENT_3D('',#168231,#132022,#132023) ;
#102817 = AXIS2_PLACEMENT_3D('',#168232,#132024,#132025) ;
#102818 = AXIS2_PLACEMENT_3D('',#168289,#132026,#132027) ;
#102819 = AXIS2_PLACEMENT_3D('',#168290,#132028,#132029) ;
#102820 = AXIS2_PLACEMENT_3D('',#168291,#132030,#132031) ;
#102821 = AXIS2_PLACEMENT_3D('',#168292,#132032,#132033) ;
#102822 = AXIS2_PLACEMENT_3D('',#168293,#132034,#132035) ;
#102823 = AXIS2_PLACEMENT_3D('',#168294,#132036,#132037) ;
#102824 = AXIS2_PLACEMENT_3D('',#168296,#132038,#132039) ;
#102825 = AXIS2_PLACEMENT_3D('',#168323,#132040,#132041) ;
#102826 = AXIS2_PLACEMENT_3D('',#168324,#132042,#132043) ;
#102827 = AXIS2_PLACEMENT_3D('',#168325,#132044,#132045) ;
#102828 = AXIS2_PLACEMENT_3D('',#168326,#132046,#132047) ;
#102829 = AXIS2_PLACEMENT_3D('',#168327,#132048,#132049) ;
#102830 = AXIS2_PLACEMENT_3D('',#168384,#132050,#132051) ;
#102831 = AXIS2_PLACEMENT_3D('',#168385,#132052,#132053) ;
#102832 = AXIS2_PLACEMENT_3D('',#168386,#132054,#132055) ;
#102833 = AXIS2_PLACEMENT_3D('',#168387,#132056,#132057) ;
#102834 = AXIS2_PLACEMENT_3D('',#168388,#132058,#132059) ;
#102835 = AXIS2_PLACEMENT_3D('',#168389,#132060,#132061) ;
#102836 = AXIS2_PLACEMENT_3D('',#168391,#132062,#132063) ;
#102837 = AXIS2_PLACEMENT_3D('',#168418,#132064,#132065) ;
#102838 = AXIS2_PLACEMENT_3D('',#168419,#132066,#132067) ;
#102839 = AXIS2_PLACEMENT_3D('',#168420,#132068,#132069) ;
#102840 = AXIS2_PLACEMENT_3D('',#168421,#132070,#132071) ;
#102841 = AXIS2_PLACEMENT_3D('',#168422,#132072,#132073) ;
#102842 = AXIS2_PLACEMENT_3D('',#168479,#132074,#132075) ;
#102843 = AXIS2_PLACEMENT_3D('',#168480,#132076,#132077) ;
#102844 = AXIS2_PLACEMENT_3D('',#168481,#132078,#132079) ;
#102845 = AXIS2_PLACEMENT_3D('',#168482,#132080,#132081) ;
#102846 = AXIS2_PLACEMENT_3D('',#168483,#132082,#132083) ;
#102847 = AXIS2_PLACEMENT_3D('',#168484,#132084,#132085) ;
#102848 = AXIS2_PLACEMENT_3D('',#168486,#132086,#132087) ;
#102849 = AXIS2_PLACEMENT_3D('',#168513,#132088,#132089) ;
#102850 = AXIS2_PLACEMENT_3D('',#168514,#132090,#132091) ;
#102851 = AXIS2_PLACEMENT_3D('',#168515,#132092,#132093) ;
#102852 = AXIS2_PLACEMENT_3D('',#168516,#132094,#132095) ;
#102853 = AXIS2_PLACEMENT_3D('',#168517,#132096,#132097) ;
#102854 = AXIS2_PLACEMENT_3D('',#168574,#132098,#132099) ;
#102855 = AXIS2_PLACEMENT_3D('',#168575,#132100,#132101) ;
#102856 = AXIS2_PLACEMENT_3D('',#168576,#132102,#132103) ;
#102857 = AXIS2_PLACEMENT_3D('',#168577,#132104,#132105) ;
#102858 = AXIS2_PLACEMENT_3D('',#168578,#132106,#132107) ;
#102859 = AXIS2_PLACEMENT_3D('',#168579,#132108,#132109) ;
#102860 = AXIS2_PLACEMENT_3D('',#168581,#132110,#132111) ;
#102861 = AXIS2_PLACEMENT_3D('',#168608,#132112,#132113) ;
#102862 = AXIS2_PLACEMENT_3D('',#168609,#132114,#132115) ;
#102863 = AXIS2_PLACEMENT_3D('',#168610,#132116,#132117) ;
#102864 = AXIS2_PLACEMENT_3D('',#168611,#132118,#132119) ;
#102865 = AXIS2_PLACEMENT_3D('',#168612,#132120,#132121) ;
#102866 = AXIS2_PLACEMENT_3D('',#168669,#132122,#132123) ;
#102867 = AXIS2_PLACEMENT_3D('',#168670,#132124,#132125) ;
#102868 = AXIS2_PLACEMENT_3D('',#168671,#132126,#132127) ;
#102869 = AXIS2_PLACEMENT_3D('',#168672,#132128,#132129) ;
#102870 = AXIS2_PLACEMENT_3D('',#168673,#132130,#132131) ;
#102871 = AXIS2_PLACEMENT_3D('',#168674,#132132,#132133) ;
#102872 = AXIS2_PLACEMENT_3D('',#168676,#132134,#132135) ;
#102873 = AXIS2_PLACEMENT_3D('',#168703,#132136,#132137) ;
#102874 = AXIS2_PLACEMENT_3D('',#168704,#132138,#132139) ;
#102875 = AXIS2_PLACEMENT_3D('',#168705,#132140,#132141) ;
#102876 = AXIS2_PLACEMENT_3D('',#168706,#132142,#132143) ;
#102877 = AXIS2_PLACEMENT_3D('',#168707,#132144,#132145) ;
#102878 = AXIS2_PLACEMENT_3D('',#168764,#132146,#132147) ;
#102879 = AXIS2_PLACEMENT_3D('',#168765,#132148,#132149) ;
#102880 = AXIS2_PLACEMENT_3D('',#168766,#132150,#132151) ;
#102881 = AXIS2_PLACEMENT_3D('',#168767,#132152,#132153) ;
#102882 = AXIS2_PLACEMENT_3D('',#168768,#132154,#132155) ;
#102883 = AXIS2_PLACEMENT_3D('',#168769,#132156,#132157) ;
#102884 = AXIS2_PLACEMENT_3D('',#168771,#132158,#132159) ;
#102885 = AXIS2_PLACEMENT_3D('',#168798,#132160,#132161) ;
#102886 = AXIS2_PLACEMENT_3D('',#168799,#132162,#132163) ;
#102887 = AXIS2_PLACEMENT_3D('',#168800,#132164,#132165) ;
#102888 = AXIS2_PLACEMENT_3D('',#168801,#132166,#132167) ;
#102889 = AXIS2_PLACEMENT_3D('',#168802,#132168,#132169) ;
#102890 = AXIS2_PLACEMENT_3D('',#168859,#132170,#132171) ;
#102891 = AXIS2_PLACEMENT_3D('',#168860,#132172,#132173) ;
#102892 = AXIS2_PLACEMENT_3D('',#168861,#132174,#132175) ;
#102893 = AXIS2_PLACEMENT_3D('',#168862,#132176,#132177) ;
#102894 = AXIS2_PLACEMENT_3D('',#168863,#132178,#132179) ;
#102895 = AXIS2_PLACEMENT_3D('',#168864,#132180,#132181) ;
#102896 = AXIS2_PLACEMENT_3D('',#168866,#132182,#132183) ;
#102897 = AXIS2_PLACEMENT_3D('',#168893,#132184,#132185) ;
#102898 = AXIS2_PLACEMENT_3D('',#168894,#132186,#132187) ;
#102899 = AXIS2_PLACEMENT_3D('',#168895,#132188,#132189) ;
#102900 = AXIS2_PLACEMENT_3D('',#168896,#132190,#132191) ;
#102901 = AXIS2_PLACEMENT_3D('',#168897,#132192,#132193) ;
#102902 = AXIS2_PLACEMENT_3D('',#168898,#132194,#132195) ;
#102903 = AXIS2_PLACEMENT_3D('',#168929,#132196,#132197) ;
#102904 = AXIS2_PLACEMENT_3D('',#168930,#132198,#132199) ;
#102905 = AXIS2_PLACEMENT_3D('',#168931,#132200,#132201) ;
#102906 = AXIS2_PLACEMENT_3D('',#168932,#132202,#132203) ;
#102907 = AXIS2_PLACEMENT_3D('',#168963,#132204,#132205) ;
#102908 = AXIS2_PLACEMENT_3D('',#168964,#132206,#132207) ;
#102909 = AXIS2_PLACEMENT_3D('',#168965,#132208,#132209) ;
#102910 = AXIS2_PLACEMENT_3D('',#168966,#132210,#132211) ;
#102911 = AXIS2_PLACEMENT_3D('',#168997,#132212,#132213) ;
#102912 = AXIS2_PLACEMENT_3D('',#168998,#132214,#132215) ;
#102913 = AXIS2_PLACEMENT_3D('',#168999,#132216,#132217) ;
#102914 = AXIS2_PLACEMENT_3D('',#169000,#132218,#132219) ;
#102915 = AXIS2_PLACEMENT_3D('',#169031,#132220,#132221) ;
#102916 = AXIS2_PLACEMENT_3D('',#169032,#132222,#132223) ;
#102917 = AXIS2_PLACEMENT_3D('',#169033,#132224,#132225) ;
#102918 = AXIS2_PLACEMENT_3D('',#169034,#132226,#132227) ;
#102919 = AXIS2_PLACEMENT_3D('',#169065,#132228,#132229) ;
#102920 = AXIS2_PLACEMENT_3D('',#169066,#132230,#132231) ;
#102921 = AXIS2_PLACEMENT_3D('',#169067,#132232,#132233) ;
#102922 = AXIS2_PLACEMENT_3D('',#169068,#132234,#132235) ;
#102923 = AXIS2_PLACEMENT_3D('',#169099,#132236,#132237) ;
#102924 = AXIS2_PLACEMENT_3D('',#169100,#132238,#132239) ;
#102925 = AXIS2_PLACEMENT_3D('',#169101,#132240,#132241) ;
#102926 = AXIS2_PLACEMENT_3D('',#169102,#132242,#132243) ;
#102927 = AXIS2_PLACEMENT_3D('',#169133,#132244,#132245) ;
#102928 = AXIS2_PLACEMENT_3D('',#169134,#132246,#132247) ;
#102929 = AXIS2_PLACEMENT_3D('',#169135,#132248,#132249) ;
#102930 = AXIS2_PLACEMENT_3D('',#169136,#132250,#132251) ;
#102931 = AXIS2_PLACEMENT_3D('',#169167,#132252,#132253) ;
#102932 = AXIS2_PLACEMENT_3D('',#169168,#132254,#132255) ;
#102933 = AXIS2_PLACEMENT_3D('',#169169,#132256,#132257) ;
#102934 = AXIS2_PLACEMENT_3D('',#169170,#132258,#132259) ;
#102935 = AXIS2_PLACEMENT_3D('',#169201,#132260,#132261) ;
#102936 = AXIS2_PLACEMENT_3D('',#169202,#132262,#132263) ;
#102937 = AXIS2_PLACEMENT_3D('',#169203,#132264,#132265) ;
#102938 = AXIS2_PLACEMENT_3D('',#169204,#132266,#132267) ;
#102939 = AXIS2_PLACEMENT_3D('',#169235,#132268,#132269) ;
#102940 = AXIS2_PLACEMENT_3D('',#169236,#132270,#132271) ;
#102941 = AXIS2_PLACEMENT_3D('',#169237,#132272,#132273) ;
#102942 = AXIS2_PLACEMENT_3D('',#169238,#132274,#132275) ;
#102943 = AXIS2_PLACEMENT_3D('',#169269,#132276,#132277) ;
#102944 = AXIS2_PLACEMENT_3D('',#169270,#132278,#132279) ;
#102945 = AXIS2_PLACEMENT_3D('',#169271,#132280,#132281) ;
#102946 = AXIS2_PLACEMENT_3D('',#169272,#132282,#132283) ;
#102947 = AXIS2_PLACEMENT_3D('',#169303,#132284,#132285) ;
#102948 = AXIS2_PLACEMENT_3D('',#169304,#132286,#132287) ;
#102949 = AXIS2_PLACEMENT_3D('',#169305,#132288,#132289) ;
#102950 = AXIS2_PLACEMENT_3D('',#169306,#132290,#132291) ;
#102951 = AXIS2_PLACEMENT_3D('',#169337,#132292,#132293) ;
#102952 = AXIS2_PLACEMENT_3D('',#169338,#132294,#132295) ;
#102953 = AXIS2_PLACEMENT_3D('',#169339,#132296,#132297) ;
#102954 = AXIS2_PLACEMENT_3D('',#169340,#132298,#132299) ;
#102955 = AXIS2_PLACEMENT_3D('',#169371,#132300,#132301) ;
#102956 = AXIS2_PLACEMENT_3D('',#169372,#132302,#132303) ;
#102957 = AXIS2_PLACEMENT_3D('',#169373,#132304,#132305) ;
#102958 = AXIS2_PLACEMENT_3D('',#169374,#132306,#132307) ;
#102959 = AXIS2_PLACEMENT_3D('',#169405,#132308,#132309) ;
#102960 = AXIS2_PLACEMENT_3D('',#169406,#132310,#132311) ;
#102961 = AXIS2_PLACEMENT_3D('',#169407,#132312,#132313) ;
#102962 = AXIS2_PLACEMENT_3D('',#169408,#132314,#132315) ;
#102963 = AXIS2_PLACEMENT_3D('',#169439,#132316,#132317) ;
#102964 = AXIS2_PLACEMENT_3D('',#169440,#132318,#132319) ;
#102965 = AXIS2_PLACEMENT_3D('',#169441,#132320,#132321) ;
#102966 = AXIS2_PLACEMENT_3D('',#169442,#132322,#132323) ;
#102967 = AXIS2_PLACEMENT_3D('',#169473,#132324,#132325) ;
#102968 = AXIS2_PLACEMENT_3D('',#169474,#132326,#132327) ;
#102969 = AXIS2_PLACEMENT_3D('',#169475,#132328,#132329) ;
#102970 = AXIS2_PLACEMENT_3D('',#169476,#132330,#132331) ;
#102971 = AXIS2_PLACEMENT_3D('',#169507,#132332,#132333) ;
#102972 = AXIS2_PLACEMENT_3D('',#169508,#132334,#132335) ;
#102973 = AXIS2_PLACEMENT_3D('',#169509,#132336,#132337) ;
#102974 = AXIS2_PLACEMENT_3D('',#169510,#132338,#132339) ;
#102975 = AXIS2_PLACEMENT_3D('',#169511,#132340,#132341) ;
#102976 = AXIS2_PLACEMENT_3D('',#169512,#132342,#132343) ;
#102977 = AXIS2_PLACEMENT_3D('',#169513,#132344,#132345) ;
#102978 = AXIS2_PLACEMENT_3D('',#169514,#132346,#132347) ;
#102979 = AXIS2_PLACEMENT_3D('',#169515,#132348,#132349) ;
#102980 = AXIS2_PLACEMENT_3D('',#169516,#132350,#132351) ;
#102981 = AXIS2_PLACEMENT_3D('',#169517,#132352,#132353) ;
#102982 = AXIS2_PLACEMENT_3D('',#169518,#132354,#132355) ;
#102983 = AXIS2_PLACEMENT_3D('',#169519,#132356,#132357) ;
#102984 = AXIS2_PLACEMENT_3D('',#169520,#132358,#132359) ;
#102985 = AXIS2_PLACEMENT_3D('',#169521,#132360,#132361) ;
#102986 = AXIS2_PLACEMENT_3D('',#169522,#132362,#132363) ;
#102987 = AXIS2_PLACEMENT_3D('',#169523,#132364,#132365) ;
#102988 = AXIS2_PLACEMENT_3D('',#169524,#132366,#132367) ;
#102989 = AXIS2_PLACEMENT_3D('',#169525,#132368,#132369) ;
#102990 = AXIS2_PLACEMENT_3D('',#169526,#132370,#132371) ;
#102991 = AXIS2_PLACEMENT_3D('',#169527,#132372,#132373) ;
#102992 = AXIS2_PLACEMENT_3D('',#169528,#132374,#132375) ;
#102993 = AXIS2_PLACEMENT_3D('',#169529,#132376,#132377) ;
#102994 = AXIS2_PLACEMENT_3D('',#169530,#132378,#132379) ;
#102995 = AXIS2_PLACEMENT_3D('',#169531,#132380,#132381) ;
#102996 = AXIS2_PLACEMENT_3D('',#169532,#132382,#132383) ;
#102997 = AXIS2_PLACEMENT_3D('',#169533,#132384,#132385) ;
#102998 = AXIS2_PLACEMENT_3D('',#169534,#132386,#132387) ;
#102999 = AXIS2_PLACEMENT_3D('',#169535,#132388,#132389) ;
#103000 = AXIS2_PLACEMENT_3D('',#169536,#132390,#132391) ;
#103001 = AXIS2_PLACEMENT_3D('',#169537,#132392,#132393) ;
#103002 = AXIS2_PLACEMENT_3D('',#169538,#132394,#132395) ;
#103003 = AXIS2_PLACEMENT_3D('',#169539,#132396,#132397) ;
#103004 = AXIS2_PLACEMENT_3D('',#169540,#132398,#132399) ;
#103005 = AXIS2_PLACEMENT_3D('',#169541,#132400,#132401) ;
#103006 = AXIS2_PLACEMENT_3D('',#169542,#132402,#132403) ;
#103007 = AXIS2_PLACEMENT_3D('',#169543,#132404,#132405) ;
#103008 = AXIS2_PLACEMENT_3D('',#169544,#132406,#132407) ;
#103009 = AXIS2_PLACEMENT_3D('',#169545,#132408,#132409) ;
#103010 = AXIS2_PLACEMENT_3D('',#169546,#132410,#132411) ;
#103011 = AXIS2_PLACEMENT_3D('',#169547,#132412,#132413) ;
#103012 = AXIS2_PLACEMENT_3D('',#169548,#132414,#132415) ;
#103013 = AXIS2_PLACEMENT_3D('',#169549,#132416,#132417) ;
#103014 = AXIS2_PLACEMENT_3D('',#169550,#132418,#132419) ;
#103015 = AXIS2_PLACEMENT_3D('',#169551,#132420,#132421) ;
#103016 = AXIS2_PLACEMENT_3D('',#169552,#132422,#132423) ;
#103017 = AXIS2_PLACEMENT_3D('',#169553,#132424,#132425) ;
#103018 = AXIS2_PLACEMENT_3D('',#169554,#132426,#132427) ;
#103019 = AXIS2_PLACEMENT_3D('',#169555,#132428,#132429) ;
#103020 = AXIS2_PLACEMENT_3D('',#169556,#132430,#132431) ;
#103021 = AXIS2_PLACEMENT_3D('',#169557,#132432,#132433) ;
#103022 = AXIS2_PLACEMENT_3D('',#169608,#132434,#132435) ;
#103023 = AXIS2_PLACEMENT_3D('',#169609,#132436,#132437) ;
#103024 = AXIS2_PLACEMENT_3D('',#169640,#132438,#132439) ;
#103025 = AXIS2_PLACEMENT_3D('',#169671,#132440,#132441) ;
#103026 = AXIS2_PLACEMENT_3D('',#169702,#132442,#132443) ;
#103027 = AXIS2_PLACEMENT_3D('',#169733,#132444,#132445) ;
#103028 = AXIS2_PLACEMENT_3D('',#169764,#132446,#132447) ;
#103029 = AXIS2_PLACEMENT_3D('',#169795,#132448,#132449) ;
#103030 = AXIS2_PLACEMENT_3D('',#169826,#132450,#132451) ;
#103031 = AXIS2_PLACEMENT_3D('',#169857,#132452,#132453) ;
#103032 = AXIS2_PLACEMENT_3D('',#169888,#132454,#132455) ;
#103033 = AXIS2_PLACEMENT_3D('',#169889,#132456,#132457) ;
#103034 = AXIS2_PLACEMENT_3D('',#169890,#132458,#132459) ;
#103035 = AXIS2_PLACEMENT_3D('',#169891,#132460,#132461) ;
#103036 = AXIS2_PLACEMENT_3D('',#169892,#132462,#132463) ;
#103037 = AXIS2_PLACEMENT_3D('',#169923,#132464,#132465) ;
#103038 = AXIS2_PLACEMENT_3D('',#169924,#132466,#132467) ;
#103039 = AXIS2_PLACEMENT_3D('',#169925,#132468,#132469) ;
#103040 = AXIS2_PLACEMENT_3D('',#169926,#132470,#132471) ;
#103041 = AXIS2_PLACEMENT_3D('',#169927,#132472,#132473) ;
#103042 = AXIS2_PLACEMENT_3D('',#170008,#132474,#132475) ;
#103043 = AXIS2_PLACEMENT_3D('',#170009,#132476,#132477) ;
#103044 = AXIS2_PLACEMENT_3D('',#170010,#132478,#132479) ;
#103045 = AXIS2_PLACEMENT_3D('',#170011,#132480,#132481) ;
#103046 = AXIS2_PLACEMENT_3D('',#170012,#132482,#132483) ;
#103047 = AXIS2_PLACEMENT_3D('',#170013,#132484,#132485) ;
#103048 = AXIS2_PLACEMENT_3D('',#170014,#132486,#132487) ;
#103049 = AXIS2_PLACEMENT_3D('',#170015,#132488,#132489) ;
#103050 = AXIS2_PLACEMENT_3D('',#170016,#132490,#132491) ;
#103051 = AXIS2_PLACEMENT_3D('',#170017,#132492,#132493) ;
#103052 = AXIS2_PLACEMENT_3D('',#170018,#132494,#132495) ;
#103053 = AXIS2_PLACEMENT_3D('',#170019,#132496,#132497) ;
#103054 = AXIS2_PLACEMENT_3D('',#170020,#132498,#132499) ;
#103055 = AXIS2_PLACEMENT_3D('',#170021,#132500,#132501) ;
#103056 = AXIS2_PLACEMENT_3D('',#170022,#132502,#132503) ;
#103057 = AXIS2_PLACEMENT_3D('',#170023,#132504,#132505) ;
#103058 = AXIS2_PLACEMENT_3D('',#170024,#132506,#132507) ;
#103059 = AXIS2_PLACEMENT_3D('',#170025,#132508,#132509) ;
#103060 = AXIS2_PLACEMENT_3D('',#170026,#132510,#132511) ;
#103061 = AXIS2_PLACEMENT_3D('',#170027,#132512,#132513) ;
#103062 = AXIS2_PLACEMENT_3D('',#170028,#132514,#132515) ;
#103063 = AXIS2_PLACEMENT_3D('',#170029,#132516,#132517) ;
#103064 = AXIS2_PLACEMENT_3D('',#170030,#132518,#132519) ;
#103065 = AXIS2_PLACEMENT_3D('',#170031,#132520,#132521) ;
#103066 = AXIS2_PLACEMENT_3D('',#170032,#132522,#132523) ;
#103067 = AXIS2_PLACEMENT_3D('',#170033,#132524,#132525) ;
#103068 = AXIS2_PLACEMENT_3D('',#170034,#132526,#132527) ;
#103069 = AXIS2_PLACEMENT_3D('',#170035,#132528,#132529) ;
#103070 = AXIS2_PLACEMENT_3D('',#170036,#132530,#132531) ;
#103071 = AXIS2_PLACEMENT_3D('',#170037,#132532,#132533) ;
#103072 = AXIS2_PLACEMENT_3D('',#170038,#132534,#132535) ;
#103073 = AXIS2_PLACEMENT_3D('',#170039,#132536,#132537) ;
#103074 = AXIS2_PLACEMENT_3D('',#170040,#132538,#132539) ;
#103075 = AXIS2_PLACEMENT_3D('',#170065,#132540,#132541) ;
#103076 = AXIS2_PLACEMENT_3D('',#170102,#132542,#132543) ;
#103077 = AXIS2_PLACEMENT_3D('',#170115,#132544,#132545) ;
#103078 = AXIS2_PLACEMENT_3D('',#170116,#132546,#132547) ;
#103079 = AXIS2_PLACEMENT_3D('',#170117,#132548,#132549) ;
#103080 = DIRECTION('axis',(0.,0.,1.)) ;
#103081 = DIRECTION('refdir',(1.,0.,0.)) ;
#103082 = DIRECTION('axis',(0.,0.,1.)) ;
#103083 = DIRECTION('refdir',(1.,0.,0.)) ;
#103084 = DIRECTION('center_axis',(-1.,0.,0.)) ;
#103085 = DIRECTION('ref_axis',(0.,0.,1.)) ;
#103086 = DIRECTION('center_axis',(-1.,0.,0.)) ;
#103087 = DIRECTION('ref_axis',(0.,0.,1.)) ;
#103088 = DIRECTION('center_axis',(-3.56483478381767E-16,0.986393923832144,
0.164398987305358)) ;
#103089 = DIRECTION('ref_axis',(1.28176283288123E-31,-0.164398987305358,0.986393923832144)) ;
#103090 = DIRECTION('center_axis',(1.,0.,0.)) ;
#103091 = DIRECTION('ref_axis',(0.,0.,1.)) ;
#103092 = DIRECTION('center_axis',(-4.02631181035926E-15,0.928404294083138,
-0.371571617226061)) ;
#103093 = DIRECTION('ref_axis',(1.34987128984705E-31,0.371571617226061,0.928404294083138)) ;
#103094 = DIRECTION('center_axis',(0.,-1.,0.)) ;
#103095 = DIRECTION('ref_axis',(0.,0.,-1.)) ;
#103096 = DIRECTION('center_axis',(0.,-1.,0.)) ;
#103097 = DIRECTION('ref_axis',(0.,0.,-1.)) ;
#103098 = DIRECTION('center_axis',(-1.,0.,-1.22464679914735E-16)) ;
#103099 = DIRECTION('ref_axis',(-1.22464679914735E-16,0.,1.)) ;
#103100 = DIRECTION('center_axis',(0.,1.,0.)) ;
#103101 = DIRECTION('ref_axis',(0.,0.,-1.)) ;
#103102 = DIRECTION('center_axis',(0.,1.,0.)) ;
#103103 = DIRECTION('ref_axis',(0.,0.,-1.)) ;
#103104 = DIRECTION('center_axis',(1.,0.,0.)) ;
#103105 = DIRECTION('ref_axis',(0.,0.,-1.)) ;
#103106 = DIRECTION('center_axis',(1.,0.,0.)) ;
#103107 = DIRECTION('ref_axis',(0.,0.,-1.)) ;
#103108 = DIRECTION('center_axis',(0.,1.,1.22464679914735E-16)) ;
#103109 = DIRECTION('ref_axis',(0.,-1.22464679914735E-16,1.)) ;
#103110 = DIRECTION('center_axis',(-1.,0.,0.)) ;
#103111 = DIRECTION('ref_axis',(0.,0.,-1.)) ;
#103112 = DIRECTION('center_axis',(-1.,0.,0.)) ;
#103113 = DIRECTION('ref_axis',(0.,0.,1.)) ;
#103114 = DIRECTION('center_axis',(-1.,0.,0.)) ;
#103115 = DIRECTION('ref_axis',(0.,0.,1.)) ;
#103116 = DIRECTION('center_axis',(0.,-1.,1.22464679914735E-16)) ;
#103117 = DIRECTION('ref_axis',(0.,-1.22464679914735E-16,-1.)) ;
#103118 = DIRECTION('center_axis',(1.,0.,0.)) ;
#103119 = DIRECTION('ref_axis',(0.,0.,1.)) ;
#103120 = DIRECTION('center_axis',(1.,0.,0.)) ;
#103121 = DIRECTION('ref_axis',(0.,0.,1.)) ;
#103122 = DIRECTION('center_axis',(-1.,0.,0.)) ;
#103123 = DIRECTION('ref_axis',(0.,0.,1.)) ;
#103124 = DIRECTION('center_axis',(-1.,0.,0.)) ;
#103125 = DIRECTION('ref_axis',(0.,0.,1.)) ;
#103126 = DIRECTION('center_axis',(0.,0.986393923832144,-0.164398987305358)) ;
#103127 = DIRECTION('ref_axis',(0.,-0.164398987305358,-0.986393923832144)) ;
#103128 = DIRECTION('center_axis',(1.,0.,0.)) ;
#103129 = DIRECTION('ref_axis',(0.,0.,1.)) ;
#103130 = DIRECTION('center_axis',(0.,0.,1.)) ;
#103131 = DIRECTION('ref_axis',(1.,0.,0.)) ;
#103132 = DIRECTION('center_axis',(0.,1.,0.)) ;
#103133 = DIRECTION('ref_axis',(1.,0.,0.)) ;
#103134 = DIRECTION('center_axis',(1.,0.,0.)) ;
#103135 = DIRECTION('ref_axis',(0.,0.,-1.)) ;
#103136 = DIRECTION('center_axis',(0.,0.,-1.)) ;
#103137 = DIRECTION('ref_axis',(-1.,0.,0.)) ;
#103138 = DIRECTION('center_axis',(0.,-0.986393923832144,0.164398987305358)) ;
#103139 = DIRECTION('ref_axis',(0.,0.164398987305358,0.986393923832144)) ;
#103140 = DIRECTION('center_axis',(-1.,0.,0.)) ;
#103141 = DIRECTION('ref_axis',(0.,0.,1.)) ;
#103142 = DIRECTION('',(1.,0.,0.)) ;
#103143 = DIRECTION('center_axis',(-1.,0.,0.)) ;
#103144 = DIRECTION('ref_axis',(0.,0.,1.)) ;
#103145 = DIRECTION('',(-1.,0.,0.)) ;
#103146 = DIRECTION('center_axis',(0.,1.,0.)) ;
#103147 = DIRECTION('ref_axis',(1.,0.,0.)) ;
#103148 = DIRECTION('center_axis',(0.,-0.986393923832144,-0.164398987305358)) ;
#103149 = DIRECTION('ref_axis',(0.,-0.164398987305358,0.986393923832144)) ;
#103150 = DIRECTION('center_axis',(0.,0.,1.)) ;
#103151 = DIRECTION('ref_axis',(1.,0.,0.)) ;
#103152 = DIRECTION('center_axis',(-1.,0.,0.)) ;
#103153 = DIRECTION('ref_axis',(0.,2.6020852139652E-14,-1.)) ;
#103154 = DIRECTION('center_axis',(1.,0.,0.)) ;
#103155 = DIRECTION('ref_axis',(0.,0.,-1.)) ;
#103156 = DIRECTION('center_axis',(1.,0.,0.)) ;
#103157 = DIRECTION('ref_axis',(0.,0.,-1.)) ;
#103158 = DIRECTION('',(0.707106781186546,-8.65956056235495E-17,0.707106781186549)) ;
#103159 = DIRECTION('center_axis',(1.,0.,0.)) ;
#103160 = DIRECTION('ref_axis',(0.,0.,-1.)) ;
#103161 = DIRECTION('',(1.,0.,0.)) ;
#103162 = DIRECTION('center_axis',(0.,1.,0.)) ;
#103163 = DIRECTION('ref_axis',(0.,0.,1.)) ;
#103164 = DIRECTION('center_axis',(0.,1.,0.)) ;
#103165 = DIRECTION('ref_axis',(0.,0.,1.)) ;
#103166 = DIRECTION('',(0.,1.,0.)) ;
#103167 = DIRECTION('center_axis',(0.,1.,0.)) ;
#103168 = DIRECTION('ref_axis',(0.,0.,1.)) ;
#103169 = DIRECTION('',(0.,1.,0.)) ;
#103170 = DIRECTION('center_axis',(0.,1.,0.)) ;
#103171 = DIRECTION('ref_axis',(0.,0.,1.)) ;
#103172 = DIRECTION('',(0.,1.,0.)) ;
#103173 = DIRECTION('center_axis',(0.,1.,0.)) ;
#103174 = DIRECTION('ref_axis',(0.,0.,1.)) ;
#103175 = DIRECTION('',(0.,1.,0.)) ;
#103176 = DIRECTION('center_axis',(0.,1.,0.)) ;
#103177 = DIRECTION('ref_axis',(0.,0.,1.)) ;
#103178 = DIRECTION('',(0.,1.,0.)) ;
#103179 = DIRECTION('center_axis',(-1.,0.,0.)) ;
#103180 = DIRECTION('ref_axis',(0.,0.,1.)) ;
#103181 = DIRECTION('center_axis',(-1.,0.,0.)) ;
#103182 = DIRECTION('ref_axis',(0.,0.,1.)) ;
#103183 = DIRECTION('center_axis',(-3.56483478381767E-16,0.986393923832144,
0.164398987305358)) ;
#103184 = DIRECTION('ref_axis',(4.9167668473396E-33,-0.164398987305358,0.986393923832144)) ;
#103185 = DIRECTION('center_axis',(1.,0.,0.)) ;
#103186 = DIRECTION('ref_axis',(0.,0.,1.)) ;
#103187 = DIRECTION('center_axis',(-4.02631181035926E-15,0.928404294083138,
-0.371571617226061)) ;
#103188 = DIRECTION('ref_axis',(1.34987128984705E-31,0.371571617226061,0.928404294083138)) ;
#103189 = DIRECTION('center_axis',(0.,0.,1.)) ;
#103190 = DIRECTION('ref_axis',(1.,0.,0.)) ;
#103191 = DIRECTION('center_axis',(0.,0.,1.)) ;
#103192 = DIRECTION('ref_axis',(1.,0.,0.)) ;
#103193 = DIRECTION('',(0.,0.,-1.)) ;
#103194 = DIRECTION('center_axis',(0.,0.,-1.)) ;
#103195 = DIRECTION('ref_axis',(1.,0.,0.)) ;
#103196 = DIRECTION('',(0.,0.,1.)) ;
#103197 = DIRECTION('center_axis',(0.,-1.,0.)) ;
#103198 = DIRECTION('ref_axis',(0.,0.,-1.)) ;
#103199 = DIRECTION('center_axis',(0.,-1.,0.)) ;
#103200 = DIRECTION('ref_axis',(0.,0.,-1.)) ;
#103201 = DIRECTION('center_axis',(-1.,0.,-1.22464679914735E-16)) ;
#103202 = DIRECTION('ref_axis',(-1.22464679914735E-16,0.,1.)) ;
#103203 = DIRECTION('center_axis',(0.,1.,0.)) ;
#103204 = DIRECTION('ref_axis',(0.,0.,-1.)) ;
#103205 = DIRECTION('center_axis',(0.,1.,0.)) ;
#103206 = DIRECTION('ref_axis',(0.,0.,-1.)) ;
#103207 = DIRECTION('center_axis',(1.,0.,0.)) ;
#103208 = DIRECTION('ref_axis',(0.,0.,-1.)) ;
#103209 = DIRECTION('center_axis',(1.,0.,0.)) ;
#103210 = DIRECTION('ref_axis',(0.,0.,-1.)) ;
#103211 = DIRECTION('center_axis',(0.,1.,1.22464679914735E-16)) ;
#103212 = DIRECTION('ref_axis',(0.,-1.22464679914735E-16,1.)) ;
#103213 = DIRECTION('center_axis',(-1.,0.,0.)) ;
#103214 = DIRECTION('ref_axis',(0.,0.,-1.)) ;
#103215 = DIRECTION('center_axis',(-1.,0.,0.)) ;
#103216 = DIRECTION('ref_axis',(0.,0.,1.)) ;
#103217 = DIRECTION('center_axis',(-1.,0.,0.)) ;
#103218 = DIRECTION('ref_axis',(0.,0.,1.)) ;
#103219 = DIRECTION('center_axis',(0.,-1.,1.22464679914735E-16)) ;
#103220 = DIRECTION('ref_axis',(0.,-1.22464679914735E-16,-1.)) ;
#103221 = DIRECTION('center_axis',(1.,0.,0.)) ;
#103222 = DIRECTION('ref_axis',(0.,0.,1.)) ;
#103223 = DIRECTION('center_axis',(1.,0.,0.)) ;
#103224 = DIRECTION('ref_axis',(0.,0.,1.)) ;
#103225 = DIRECTION('center_axis',(-1.,0.,0.)) ;
#103226 = DIRECTION('ref_axis',(0.,0.,1.)) ;
#103227 = DIRECTION('center_axis',(-1.,0.,0.)) ;
#103228 = DIRECTION('ref_axis',(0.,0.,1.)) ;
#103229 = DIRECTION('center_axis',(0.,0.986393923832144,-0.164398987305358)) ;
#103230 = DIRECTION('ref_axis',(0.,-0.164398987305358,-0.986393923832144)) ;
#103231 = DIRECTION('center_axis',(1.,0.,0.)) ;
#103232 = DIRECTION('ref_axis',(0.,0.,1.)) ;
#103233 = DIRECTION('center_axis',(0.,0.,1.)) ;
#103234 = DIRECTION('ref_axis',(1.,0.,0.)) ;
#103235 = DIRECTION('center_axis',(0.,1.,0.)) ;
#103236 = DIRECTION('ref_axis',(1.,0.,0.)) ;
#103237 = DIRECTION('center_axis',(1.,0.,0.)) ;
#103238 = DIRECTION('ref_axis',(0.,0.,-1.)) ;
#103239 = DIRECTION('center_axis',(0.,0.,-1.)) ;
#103240 = DIRECTION('ref_axis',(-1.,0.,0.)) ;
#103241 = DIRECTION('center_axis',(0.,-0.986393923832144,0.164398987305358)) ;
#103242 = DIRECTION('ref_axis',(0.,0.164398987305358,0.986393923832144)) ;
#103243 = DIRECTION('center_axis',(-1.,0.,0.)) ;
#103244 = DIRECTION('ref_axis',(0.,0.,1.)) ;
#103245 = DIRECTION('',(1.,0.,0.)) ;
#103246 = DIRECTION('center_axis',(-1.,0.,0.)) ;
#103247 = DIRECTION('ref_axis',(0.,0.,1.)) ;
#103248 = DIRECTION('',(-1.,0.,0.)) ;
#103249 = DIRECTION('center_axis',(0.,1.,0.)) ;
#103250 = DIRECTION('ref_axis',(1.,0.,0.)) ;
#103251 = DIRECTION('center_axis',(0.,-0.986393923832144,-0.164398987305358)) ;
#103252 = DIRECTION('ref_axis',(0.,-0.164398987305358,0.986393923832144)) ;
#103253 = DIRECTION('center_axis',(0.,0.,1.)) ;
#103254 = DIRECTION('ref_axis',(1.,0.,0.)) ;
#103255 = DIRECTION('center_axis',(-1.,0.,0.)) ;
#103256 = DIRECTION('ref_axis',(0.,0.,-1.)) ;
#103257 = DIRECTION('center_axis',(1.,0.,0.)) ;
#103258 = DIRECTION('ref_axis',(0.,0.,-1.)) ;
#103259 = DIRECTION('center_axis',(1.,0.,0.)) ;
#103260 = DIRECTION('ref_axis',(0.,0.,-1.)) ;
#103261 = DIRECTION('',(0.707106781186546,-8.65956056235495E-17,0.707106781186549)) ;
#103262 = DIRECTION('center_axis',(1.,0.,0.)) ;
#103263 = DIRECTION('ref_axis',(0.,0.,-1.)) ;
#103264 = DIRECTION('',(1.,0.,0.)) ;
#103265 = DIRECTION('center_axis',(0.,1.,0.)) ;
#103266 = DIRECTION('ref_axis',(0.,0.,1.)) ;
#103267 = DIRECTION('center_axis',(0.,1.,0.)) ;
#103268 = DIRECTION('ref_axis',(0.,0.,1.)) ;
#103269 = DIRECTION('',(0.,1.,0.)) ;
#103270 = DIRECTION('center_axis',(0.,1.,0.)) ;
#103271 = DIRECTION('ref_axis',(0.,0.,1.)) ;
#103272 = DIRECTION('',(0.,1.,0.)) ;
#103273 = DIRECTION('center_axis',(0.,1.,0.)) ;
#103274 = DIRECTION('ref_axis',(0.,0.,1.)) ;
#103275 = DIRECTION('',(0.,1.,0.)) ;
#103276 = DIRECTION('center_axis',(0.,1.,0.)) ;
#103277 = DIRECTION('ref_axis',(0.,0.,1.)) ;
#103278 = DIRECTION('',(0.,1.,0.)) ;
#103279 = DIRECTION('center_axis',(0.,1.,0.)) ;
#103280 = DIRECTION('ref_axis',(0.,0.,1.)) ;
#103281 = DIRECTION('',(0.,1.,0.)) ;
#103282 = DIRECTION('center_axis',(-1.,0.,0.)) ;
#103283 = DIRECTION('ref_axis',(0.,0.,1.)) ;
#103284 = DIRECTION('',(0.,1.,0.)) ;
#103285 = DIRECTION('',(0.,0.,1.)) ;
#103286 = DIRECTION('',(0.,1.,0.)) ;
#103287 = DIRECTION('',(0.,0.,-1.)) ;
#103288 = DIRECTION('center_axis',(1.,0.,0.)) ;
#103289 = DIRECTION('ref_axis',(0.,0.,1.)) ;
#103290 = DIRECTION('',(0.,1.,0.)) ;
#103291 = DIRECTION('',(0.,0.,-1.)) ;
#103292 = DIRECTION('',(0.,-1.,0.)) ;
#103293 = DIRECTION('center_axis',(1.,0.,0.)) ;
#103294 = DIRECTION('ref_axis',(0.,0.,1.)) ;
#103295 = DIRECTION('',(0.,0.,1.)) ;
#103296 = DIRECTION('center_axis',(-3.46944695195361E-15,-1.,0.)) ;
#103297 = DIRECTION('ref_axis',(1.,-3.46944695195361E-15,0.)) ;
#103298 = DIRECTION('',(-1.,3.46944695195361E-15,1.36784797186593E-30)) ;
#103299 = DIRECTION('',(0.,0.,-1.)) ;
#103300 = DIRECTION('',(-1.,3.46944695195361E-15,0.)) ;
#103301 = DIRECTION('',(0.,0.,1.)) ;
#103302 = DIRECTION('center_axis',(-1.,0.,0.)) ;
#103303 = DIRECTION('ref_axis',(0.,0.,1.)) ;
#103304 = DIRECTION('',(0.,1.,3.94255335449274E-16)) ;
#103305 = DIRECTION('',(0.,0.,-1.)) ;
#103306 = DIRECTION('',(0.,1.,0.)) ;
#103307 = DIRECTION('',(0.,0.,1.)) ;
#103308 = DIRECTION('center_axis',(0.,1.,0.)) ;
#103309 = DIRECTION('ref_axis',(0.,0.,1.)) ;
#103310 = DIRECTION('',(1.,0.,0.)) ;
#103311 = DIRECTION('',(0.,0.,-1.)) ;
#103312 = DIRECTION('',(1.,0.,0.)) ;
#103313 = DIRECTION('',(0.,0.,1.)) ;
#103314 = DIRECTION('center_axis',(0.,0.,-1.)) ;
#103315 = DIRECTION('ref_axis',(-1.,0.,0.)) ;
#103316 = DIRECTION('',(0.,0.,-1.)) ;
#103317 = DIRECTION('center_axis',(0.,3.94255335449274E-16,-1.)) ;
#103318 = DIRECTION('ref_axis',(0.,-1.,-3.94255335449274E-16)) ;
#103319 = DIRECTION('center_axis',(0.,0.,-1.)) ;
#103320 = DIRECTION('ref_axis',(1.,0.,0.)) ;
#103321 = DIRECTION('center_axis',(0.,0.,1.)) ;
#103322 = DIRECTION('ref_axis',(1.,0.,0.)) ;
#103323 = DIRECTION('center_axis',(0.,3.94255335449274E-16,-1.)) ;
#103324 = DIRECTION('ref_axis',(0.,-1.,-3.94255335449274E-16)) ;
#103325 = DIRECTION('center_axis',(0.,0.,1.)) ;
#103326 = DIRECTION('ref_axis',(1.,0.,0.)) ;
#103327 = DIRECTION('center_axis',(0.,0.,1.)) ;
#103328 = DIRECTION('ref_axis',(1.,0.,0.)) ;
#103329 = DIRECTION('center_axis',(0.,3.94255335449274E-16,-1.)) ;
#103330 = DIRECTION('ref_axis',(-4.33680868994204E-15,-1.,-3.94255335449274E-16)) ;
#103331 = DIRECTION('center_axis',(0.,0.,1.)) ;
#103332 = DIRECTION('ref_axis',(1.,0.,0.)) ;
#103333 = DIRECTION('center_axis',(0.,0.,-1.)) ;
#103334 = DIRECTION('ref_axis',(-1.,0.,0.)) ;
#103335 = DIRECTION('center_axis',(0.,3.94255335449274E-16,-1.)) ;
#103336 = DIRECTION('ref_axis',(3.46944695195361E-14,-1.,-3.94255335449274E-16)) ;
#103337 = DIRECTION('',(0.,0.,1.)) ;
#103338 = DIRECTION('center_axis',(0.,0.,1.)) ;
#103339 = DIRECTION('ref_axis',(1.,0.,0.)) ;
#103340 = DIRECTION('',(0.,0.,1.)) ;
#103341 = DIRECTION('center_axis',(0.,0.,-1.)) ;
#103342 = DIRECTION('ref_axis',(1.,0.,0.)) ;
#103343 = DIRECTION('center_axis',(-1.,0.,0.)) ;
#103344 = DIRECTION('ref_axis',(0.,0.,1.)) ;
#103345 = DIRECTION('center_axis',(-1.,0.,0.)) ;
#103346 = DIRECTION('ref_axis',(0.,0.,1.)) ;
#103347 = DIRECTION('',(0.,0.,-1.)) ;
#103348 = DIRECTION('center_axis',(-1.,0.,0.)) ;
#103349 = DIRECTION('ref_axis',(0.,0.,1.)) ;
#103350 = DIRECTION('',(0.,0.,1.)) ;
#103351 = DIRECTION('center_axis',(-2.09002828430941E-16,1.,0.)) ;
#103352 = DIRECTION('ref_axis',(-1.,-2.09002828430941E-16,0.)) ;
#103353 = DIRECTION('',(1.,2.09002828430941E-16,0.)) ;
#103354 = DIRECTION('',(0.,0.,-1.)) ;
#103355 = DIRECTION('',(1.,2.09002828430941E-16,0.)) ;
#103356 = DIRECTION('',(0.,0.,1.)) ;
#103357 = DIRECTION('center_axis',(1.0450141421547E-16,-1.,0.)) ;
#103358 = DIRECTION('ref_axis',(1.,1.0450141421547E-16,0.)) ;
#103359 = DIRECTION('',(0.,0.,-1.)) ;
#103360 = DIRECTION('',(-1.,-1.0450141421547E-16,1.7416902369245E-17)) ;
#103361 = DIRECTION('',(0.,0.,1.)) ;
#103362 = DIRECTION('',(1.,1.0450141421547E-16,1.7416902369245E-17)) ;
#103363 = DIRECTION('center_axis',(0.,1.,0.)) ;
#103364 = DIRECTION('ref_axis',(0.,0.,1.)) ;
#103365 = DIRECTION('',(0.422618261740697,0.,-0.906307787036651)) ;
#103366 = DIRECTION('center_axis',(-1.,0.,0.)) ;
#103367 = DIRECTION('ref_axis',(0.,0.,1.)) ;
#103368 = DIRECTION('',(0.,0.986393923832144,-0.164398987305357)) ;
#103369 = DIRECTION('',(0.,0.,1.)) ;
#103370 = DIRECTION('',(0.,1.,0.)) ;
#103371 = DIRECTION('',(0.,0.,-1.)) ;
#103372 = DIRECTION('center_axis',(1.,0.,0.)) ;
#103373 = DIRECTION('ref_axis',(0.,4.33680868994202E-15,1.)) ;
#103374 = DIRECTION('center_axis',(1.,0.,0.)) ;
#103375 = DIRECTION('ref_axis',(0.,0.,1.)) ;
#103376 = DIRECTION('center_axis',(1.,0.,0.)) ;
#103377 = DIRECTION('ref_axis',(0.,0.,1.)) ;
#103378 = DIRECTION('',(0.,0.,-1.)) ;
#103379 = DIRECTION('center_axis',(1.,0.,0.)) ;
#103380 = DIRECTION('ref_axis',(0.,-4.33680868994202E-15,1.)) ;
#103381 = DIRECTION('center_axis',(1.,0.,0.)) ;
#103382 = DIRECTION('ref_axis',(0.,8.88178419700125E-16,1.)) ;
#103383 = DIRECTION('center_axis',(1.,0.,0.)) ;
#103384 = DIRECTION('ref_axis',(0.,6.50521303491304E-15,1.)) ;
#103385 = DIRECTION('',(0.,0.,-1.)) ;
#103386 = DIRECTION('',(0.,1.,0.)) ;
#103387 = DIRECTION('',(0.,0.,1.)) ;
#103388 = DIRECTION('',(0.,-0.986393923832144,-0.164398987305357)) ;
#103389 = DIRECTION('center_axis',(1.,0.,0.)) ;
#103390 = DIRECTION('ref_axis',(0.,0.,1.)) ;
#103391 = DIRECTION('',(0.,0.,1.)) ;
#103392 = DIRECTION('',(0.,0.986393923832144,-0.164398987305357)) ;
#103393 = DIRECTION('',(0.,0.,1.)) ;
#103394 = DIRECTION('',(0.,-0.986393923832144,-0.164398987305357)) ;
#103395 = DIRECTION('center_axis',(1.,0.,0.)) ;
#103396 = DIRECTION('ref_axis',(0.,0.,1.)) ;
#103397 = DIRECTION('',(0.,0.,1.)) ;
#103398 = DIRECTION('center_axis',(1.0450141421547E-16,-1.,0.)) ;
#103399 = DIRECTION('ref_axis',(1.,1.0450141421547E-16,0.)) ;
#103400 = DIRECTION('',(-1.,-1.0450141421547E-16,1.7416902369245E-17)) ;
#103401 = DIRECTION('',(0.,0.,1.)) ;
#103402 = DIRECTION('',(-1.,-1.0450141421547E-16,0.)) ;
#103403 = DIRECTION('',(0.,0.,-1.)) ;
#103404 = DIRECTION('center_axis',(-0.876215908676647,-0.481918749772156,
0.)) ;
#103405 = DIRECTION('ref_axis',(0.481918749772156,-0.876215908676647,0.)) ;
#103406 = DIRECTION('',(-0.481918749772156,0.876215908676647,0.)) ;
#103407 = DIRECTION('',(0.,0.,-1.)) ;
#103408 = DIRECTION('center_axis',(-0.87621590867663,-0.481918749772186,-1.71185066180799E-15)) ;
#103409 = DIRECTION('ref_axis',(0.436954455877847,-0.794462647050564,-0.421781822664167)) ;
#103410 = DIRECTION('',(0.,0.,-1.)) ;
#103411 = DIRECTION('center_axis',(-0.876215908676628,-0.48191874977219,-1.569734757823E-14)) ;
#103412 = DIRECTION('ref_axis',(0.436954455972081,-0.794462647221906,0.421781822243805)) ;
#103413 = DIRECTION('',(0.,0.,-1.)) ;
#103414 = DIRECTION('center_axis',(-0.876215908676574,-0.481918749772289,
3.39624711488767E-14)) ;
#103415 = DIRECTION('ref_axis',(0.436954455864899,-0.794462647026833,-0.421781822722279)) ;
#103416 = DIRECTION('',(0.,0.,-1.)) ;
#103417 = DIRECTION('center_axis',(-0.87621590867663,-0.481918749772186,-9.62512258910975E-15)) ;
#103418 = DIRECTION('ref_axis',(0.436954455963938,-0.794462647207104,0.421781822280121)) ;
#103419 = DIRECTION('',(0.,0.,-1.)) ;
#103420 = DIRECTION('',(-0.481918749772156,0.876215908676647,0.)) ;
#103421 = DIRECTION('',(0.,0.,1.)) ;
#103422 = DIRECTION('center_axis',(-0.876215908676647,-0.481918749772156,
0.)) ;
#103423 = DIRECTION('ref_axis',(0.481918749772156,-0.876215908676647,0.)) ;
#103424 = DIRECTION('',(0.,0.,-1.)) ;
#103425 = DIRECTION('',(-0.481918749772156,0.876215908676647,0.)) ;
#103426 = DIRECTION('',(-0.481918749772156,0.876215908676647,0.)) ;
#103427 = DIRECTION('center_axis',(-1.,0.,0.)) ;
#103428 = DIRECTION('ref_axis',(0.,0.,1.)) ;
#103429 = DIRECTION('',(0.,1.,0.)) ;
#103430 = DIRECTION('',(0.,0.,1.)) ;
#103431 = DIRECTION('',(0.,1.,0.)) ;
#103432 = DIRECTION('',(0.,-1.,-3.94255335449274E-16)) ;
#103433 = DIRECTION('center_axis',(0.,-1.,0.)) ;
#103434 = DIRECTION('ref_axis',(0.,0.,-1.)) ;
#103435 = DIRECTION('',(0.,0.,-1.)) ;
#103436 = DIRECTION('',(-1.,0.,0.)) ;
#103437 = DIRECTION('',(0.,0.,1.)) ;
#103438 = DIRECTION('',(-1.,0.,0.)) ;
#103439 = DIRECTION('center_axis',(0.,1.,0.)) ;
#103440 = DIRECTION('ref_axis',(0.,0.,-1.)) ;
#103441 = DIRECTION('',(2.16840434497101E-16,0.,1.)) ;
#103442 = DIRECTION('center_axis',(0.,1.,0.)) ;
#103443 = DIRECTION('ref_axis',(0.,0.,-1.)) ;
#103444 = DIRECTION('',(-1.,0.,1.73472347597681E-16)) ;
#103445 = DIRECTION('center_axis',(0.,1.,0.)) ;
#103446 = DIRECTION('ref_axis',(0.,0.,-1.)) ;
#103447 = DIRECTION('',(-2.16840434497101E-16,0.,-1.)) ;
#103448 = DIRECTION('center_axis',(0.,1.,0.)) ;
#103449 = DIRECTION('ref_axis',(0.,0.,-1.)) ;
#103450 = DIRECTION('',(1.,0.,-1.73472347597681E-16)) ;
#103451 = DIRECTION('center_axis',(0.,1.,0.)) ;
#103452 = DIRECTION('ref_axis',(0.,0.,-1.)) ;
#103453 = DIRECTION('',(2.16840434497101E-16,0.,1.)) ;
#103454 = DIRECTION('center_axis',(0.,1.,0.)) ;
#103455 = DIRECTION('ref_axis',(0.,0.,-1.)) ;
#103456 = DIRECTION('',(-1.,0.,1.73472347597681E-16)) ;
#103457 = DIRECTION('center_axis',(0.,1.,0.)) ;
#103458 = DIRECTION('ref_axis',(0.,0.,-1.)) ;
#103459 = DIRECTION('',(-2.16840434497101E-16,0.,-1.)) ;
#103460 = DIRECTION('center_axis',(0.,1.,0.)) ;
#103461 = DIRECTION('ref_axis',(0.,0.,-1.)) ;
#103462 = DIRECTION('',(1.,0.,-1.73472347597681E-16)) ;
#103463 = DIRECTION('center_axis',(1.,0.,0.)) ;
#103464 = DIRECTION('ref_axis',(0.,0.,-1.)) ;
#103465 = DIRECTION('',(0.,0.,-1.)) ;
#103466 = DIRECTION('',(0.,-1.,0.)) ;
#103467 = DIRECTION('',(0.,0.,1.)) ;
#103468 = DIRECTION('',(0.,-1.,0.)) ;
#103469 = DIRECTION('center_axis',(0.,1.,0.)) ;
#103470 = DIRECTION('ref_axis',(0.,0.,1.)) ;
#103471 = DIRECTION('',(0.,0.,-1.)) ;
#103472 = DIRECTION('',(1.,0.,0.)) ;
#103473 = DIRECTION('',(1.,0.,0.)) ;
#103474 = DIRECTION('center_axis',(0.98058067569092,-0.196116135138184,0.)) ;
#103475 = DIRECTION('ref_axis',(0.196116135138184,0.98058067569092,0.)) ;
#103476 = DIRECTION('',(-0.196116135138184,-0.98058067569092,0.)) ;
#103477 = DIRECTION('',(0.,0.,1.)) ;
#103478 = DIRECTION('',(-0.196116135138184,-0.98058067569092,0.)) ;
#103479 = DIRECTION('center_axis',(1.,0.,0.)) ;
#103480 = DIRECTION('ref_axis',(0.,0.,-1.)) ;
#103481 = DIRECTION('',(0.,0.,-1.)) ;
#103482 = DIRECTION('',(0.,-1.,0.)) ;
#103483 = DIRECTION('',(0.,0.,1.)) ;
#103484 = DIRECTION('',(0.,-1.,0.)) ;
#103485 = DIRECTION('',(0.,0.,1.)) ;
#103486 = DIRECTION('',(0.,-1.,0.)) ;
#103487 = DIRECTION('',(0.,0.,-1.)) ;
#103488 = DIRECTION('',(0.,1.,0.)) ;
#103489 = DIRECTION('',(0.,0.,1.)) ;
#103490 = DIRECTION('',(0.,-1.,0.)) ;
#103491 = DIRECTION('',(0.,0.,-1.)) ;
#103492 = DIRECTION('',(0.,1.,0.)) ;
#103493 = DIRECTION('center_axis',(0.,1.,0.)) ;
#103494 = DIRECTION('ref_axis',(0.,0.,1.)) ;
#103495 = DIRECTION('',(0.,0.,-1.)) ;
#103496 = DIRECTION('',(1.,0.,0.)) ;
#103497 = DIRECTION('',(0.,0.,1.)) ;
#103498 = DIRECTION('',(1.,0.,0.)) ;
#103499 = DIRECTION('center_axis',(0.,-1.,0.)) ;
#103500 = DIRECTION('ref_axis',(0.,0.,1.)) ;
#103501 = DIRECTION('',(0.,0.,1.)) ;
#103502 = DIRECTION('center_axis',(0.,-1.,0.)) ;
#103503 = DIRECTION('ref_axis',(0.,0.,1.)) ;
#103504 = DIRECTION('',(1.,0.,1.73472347597681E-16)) ;
#103505 = DIRECTION('center_axis',(0.,-1.,0.)) ;
#103506 = DIRECTION('ref_axis',(0.,0.,1.)) ;
#103507 = DIRECTION('',(4.33680868994202E-16,0.,-1.)) ;
#103508 = DIRECTION('center_axis',(0.,-1.,0.)) ;
#103509 = DIRECTION('ref_axis',(0.,0.,1.)) ;
#103510 = DIRECTION('',(-1.,0.,1.73472347597681E-16)) ;
#103511 = DIRECTION('center_axis',(0.,-1.,0.)) ;
#103512 = DIRECTION('ref_axis',(0.,0.,1.)) ;
#103513 = DIRECTION('',(0.,0.,1.)) ;
#103514 = DIRECTION('center_axis',(0.,-1.,0.)) ;
#103515 = DIRECTION('ref_axis',(0.,0.,1.)) ;
#103516 = DIRECTION('',(1.,0.,1.73472347597681E-16)) ;
#103517 = DIRECTION('center_axis',(0.,-1.,0.)) ;
#103518 = DIRECTION('ref_axis',(0.,0.,1.)) ;
#103519 = DIRECTION('',(4.33680868994202E-16,0.,-1.)) ;
#103520 = DIRECTION('center_axis',(0.,-1.,0.)) ;
#103521 = DIRECTION('ref_axis',(0.,0.,1.)) ;
#103522 = DIRECTION('',(-1.,0.,1.73472347597681E-16)) ;
#103523 = DIRECTION('center_axis',(-1.,6.93889390390723E-16,0.)) ;
#103524 = DIRECTION('ref_axis',(-6.93889390390723E-16,-1.,0.)) ;
#103525 = DIRECTION('',(0.,0.,-1.)) ;
#103526 = DIRECTION('',(6.93889390390723E-16,1.,0.)) ;
#103527 = DIRECTION('',(0.,0.,1.)) ;
#103528 = DIRECTION('',(6.93889390390723E-16,1.,0.)) ;
#103529 = DIRECTION('center_axis',(0.,1.,0.)) ;
#103530 = DIRECTION('ref_axis',(0.,0.,1.)) ;
#103531 = DIRECTION('',(0.,0.,1.)) ;
#103532 = DIRECTION('',(1.,0.,0.)) ;
#103533 = DIRECTION('',(0.,0.,-1.)) ;
#103534 = DIRECTION('',(1.,0.,0.)) ;
#103535 = DIRECTION('',(0.,0.,1.)) ;
#103536 = DIRECTION('',(0.,0.,1.)) ;
#103537 = DIRECTION('center_axis',(-1.,0.,0.)) ;
#103538 = DIRECTION('ref_axis',(0.,0.,1.)) ;
#103539 = DIRECTION('',(0.,1.,0.)) ;
#103540 = DIRECTION('',(0.,0.,-1.)) ;
#103541 = DIRECTION('center_axis',(-1.,0.,0.)) ;
#103542 = DIRECTION('ref_axis',(0.,0.,1.)) ;
#103543 = DIRECTION('',(0.,0.,1.)) ;
#103544 = DIRECTION('center_axis',(-2.09002828430941E-16,1.,0.)) ;
#103545 = DIRECTION('ref_axis',(-1.,-2.09002828430941E-16,0.)) ;
#103546 = DIRECTION('',(-1.,-2.09002828430941E-16,0.)) ;
#103547 = DIRECTION('',(0.,0.,-1.)) ;
#103548 = DIRECTION('',(1.,2.09002828430941E-16,0.)) ;
#103549 = DIRECTION('',(0.,0.,1.)) ;
#103550 = DIRECTION('center_axis',(0.,0.,1.)) ;
#103551 = DIRECTION('ref_axis',(1.,0.,0.)) ;
#103552 = DIRECTION('center_axis',(0.,0.,1.)) ;
#103553 = DIRECTION('ref_axis',(1.,0.,0.)) ;
#103554 = DIRECTION('center_axis',(0.,0.,1.)) ;
#103555 = DIRECTION('ref_axis',(1.,0.,0.)) ;
#103556 = DIRECTION('center_axis',(0.,0.,1.)) ;
#103557 = DIRECTION('ref_axis',(1.,0.,0.)) ;
#103558 = DIRECTION('center_axis',(0.,0.,1.)) ;
#103559 = DIRECTION('ref_axis',(1.,0.,0.)) ;
#103560 = DIRECTION('center_axis',(0.,0.,1.)) ;
#103561 = DIRECTION('ref_axis',(1.,0.,0.)) ;
#103562 = DIRECTION('center_axis',(0.,0.,1.)) ;
#103563 = DIRECTION('ref_axis',(1.,0.,0.)) ;
#103564 = DIRECTION('center_axis',(0.,0.,-1.)) ;
#103565 = DIRECTION('ref_axis',(1.,0.,0.)) ;
#103566 = DIRECTION('center_axis',(0.,0.,1.)) ;
#103567 = DIRECTION('ref_axis',(1.,0.,0.)) ;
#103568 = DIRECTION('center_axis',(0.,0.,-1.)) ;
#103569 = DIRECTION('ref_axis',(1.,0.,0.)) ;
#103570 = DIRECTION('center_axis',(0.,0.,1.)) ;
#103571 = DIRECTION('ref_axis',(1.,0.,0.)) ;
#103572 = DIRECTION('center_axis',(0.,0.,1.)) ;
#103573 = DIRECTION('ref_axis',(1.,0.,0.)) ;
#103574 = DIRECTION('center_axis',(0.,0.,-1.)) ;
#103575 = DIRECTION('ref_axis',(1.,0.,0.)) ;
#103576 = DIRECTION('center_axis',(0.,0.,-1.)) ;
#103577 = DIRECTION('ref_axis',(1.,0.,0.)) ;
#103578 = DIRECTION('center_axis',(0.,0.,1.)) ;
#103579 = DIRECTION('ref_axis',(1.,0.,0.)) ;
#103580 = DIRECTION('center_axis',(0.,0.,1.)) ;
#103581 = DIRECTION('ref_axis',(1.,0.,0.)) ;
#103582 = DIRECTION('',(-0.664363838829919,0.74740931868366,0.)) ;
#103583 = DIRECTION('',(0.,-1.,0.)) ;
#103584 = DIRECTION('',(0.894427190999917,0.447213595499956,0.)) ;
#103585 = DIRECTION('',(0.,1.,0.)) ;
#103586 = DIRECTION('center_axis',(0.,0.,-1.)) ;
#103587 = DIRECTION('ref_axis',(-1.,0.,0.)) ;
#103588 = DIRECTION('',(-0.894427190999917,-0.447213595499956,0.)) ;
#103589 = DIRECTION('',(0.,1.,0.)) ;
#103590 = DIRECTION('',(0.664363838829919,-0.74740931868366,0.)) ;
#103591 = DIRECTION('',(0.,-1.,0.)) ;
#103592 = DIRECTION('center_axis',(-0.23745309047699,0.,-0.971399006496778)) ;
#103593 = DIRECTION('ref_axis',(-0.971399006496778,0.,0.23745309047699)) ;
#103594 = DIRECTION('center_axis',(-0.237453090476991,1.73471514883906E-15,
-0.971399006496777)) ;
#103595 = DIRECTION('ref_axis',(0.921799787670948,-0.315455332293223,-0.225328836986233)) ;
#103596 = DIRECTION('',(0.971399006496777,0.,-0.23745309047699)) ;
#103597 = DIRECTION('',(0.,-1.,0.)) ;
#103598 = DIRECTION('',(-0.971399006496777,0.,0.23745309047699)) ;
#103599 = DIRECTION('center_axis',(-0.237453090476988,-5.68535949803261E-15,
-0.971399006496778)) ;
#103600 = DIRECTION('ref_axis',(0.954559354253041,0.18539258117777,-0.233336731039631)) ;
#103601 = DIRECTION('',(-0.873786407766991,-0.436893203883493,0.213592233009709)) ;
#103602 = DIRECTION('',(0.,1.,0.)) ;
#103603 = DIRECTION('',(0.655772517804503,-0.737744082530068,-0.160299948796656)) ;
#103604 = DIRECTION('center_axis',(-1.,0.,0.)) ;
#103605 = DIRECTION('ref_axis',(0.,0.,1.)) ;
#103606 = DIRECTION('',(0.,-1.,0.)) ;
#103607 = DIRECTION('center_axis',(-1.,-6.70078870827233E-15,-6.50913949396058E-15)) ;
#103608 = DIRECTION('ref_axis',(6.50913949395829E-15,3.4174057398699E-13,
-1.)) ;
#103609 = DIRECTION('',(0.,0.,-1.)) ;
#103610 = DIRECTION('center_axis',(-1.,6.70078870827231E-15,-6.50913949396055E-15)) ;
#103611 = DIRECTION('ref_axis',(6.50913949394042E-15,-3.00413806900314E-12,
-1.)) ;
#103612 = DIRECTION('center_axis',(-1.,6.70078870827234E-15,6.50913949396058E-15)) ;
#103613 = DIRECTION('ref_axis',(-6.50913949393696E-15,3.524696385192E-12,
-1.)) ;
#103614 = DIRECTION('',(0.,0.,-1.)) ;
#103615 = DIRECTION('center_axis',(-1.,6.70078870827234E-15,-6.50913949396058E-15)) ;
#103616 = DIRECTION('ref_axis',(6.50913949393646E-15,-3.60019720967755E-12,
-1.)) ;
#103617 = DIRECTION('center_axis',(-0.23745309047699,0.,0.971399006496778)) ;
#103618 = DIRECTION('ref_axis',(0.971399006496778,0.,0.23745309047699)) ;
#103619 = DIRECTION('center_axis',(-0.237453090476982,-3.00511859181728E-14,
0.971399006496779)) ;
#103620 = DIRECTION('ref_axis',(0.954559354252495,0.185392581180749,0.233336731039496)) ;
#103621 = DIRECTION('',(0.971399006496777,0.,0.23745309047699)) ;
#103622 = DIRECTION('',(-0.971399006496777,0.,-0.23745309047699)) ;
#103623 = DIRECTION('center_axis',(-0.237453090476993,-4.21287964718113E-15,
0.971399006496777)) ;
#103624 = DIRECTION('ref_axis',(0.921799787669916,-0.315455332296417,0.225328836985981)) ;
#103625 = DIRECTION('',(-0.655772517804503,0.737744082530068,-0.160299948796656)) ;
#103626 = DIRECTION('',(0.,-1.,0.)) ;
#103627 = DIRECTION('',(0.873786407766991,0.436893203883493,0.213592233009709)) ;
#103628 = DIRECTION('center_axis',(0.,1.,0.)) ;
#103629 = DIRECTION('ref_axis',(0.,0.,1.)) ;
#103630 = DIRECTION('',(-0.971399006496777,0.,0.23745309047699)) ;
#103631 = DIRECTION('',(0.,0.,-1.)) ;
#103632 = DIRECTION('',(0.971399006496777,0.,0.23745309047699)) ;
#103633 = DIRECTION('center_axis',(0.,1.,0.)) ;
#103634 = DIRECTION('ref_axis',(0.,0.,1.)) ;
#103635 = DIRECTION('',(-0.971399006496777,0.,-0.23745309047699)) ;
#103636 = DIRECTION('',(0.,0.,1.)) ;
#103637 = DIRECTION('',(0.971399006496777,0.,-0.23745309047699)) ;
#103638 = DIRECTION('center_axis',(-0.447213595499956,0.894427190999917,0.)) ;
#103639 = DIRECTION('ref_axis',(0.,0.,-1.)) ;
#103640 = DIRECTION('',(0.,0.,-1.)) ;
#103641 = DIRECTION('',(-0.873786407766991,-0.436893203883493,-0.213592233009709)) ;
#103642 = DIRECTION('',(-0.894427190999917,-0.447213595499956,0.)) ;
#103643 = DIRECTION('',(0.,0.,1.)) ;
#103644 = DIRECTION('',(0.894427190999917,0.447213595499956,0.)) ;
#103645 = DIRECTION('',(0.873786407766991,0.436893203883493,-0.213592233009709)) ;
#103646 = DIRECTION('center_axis',(0.74740931868366,0.664363838829919,0.)) ;
#103647 = DIRECTION('ref_axis',(0.,0.,1.)) ;
#103648 = DIRECTION('',(0.,0.,-1.)) ;
#103649 = DIRECTION('',(0.664363838829919,-0.74740931868366,0.)) ;
#103650 = DIRECTION('',(0.655772517804503,-0.737744082530068,0.160299948796656)) ;
#103651 = DIRECTION('',(0.,0.,1.)) ;
#103652 = DIRECTION('',(-0.655772517804503,0.737744082530068,0.160299948796656)) ;
#103653 = DIRECTION('',(-0.664363838829919,0.74740931868366,0.)) ;
#103654 = DIRECTION('center_axis',(1.,0.,4.33680868994202E-16)) ;
#103655 = DIRECTION('ref_axis',(4.33680868994202E-16,0.,-1.)) ;
#103656 = DIRECTION('',(0.,1.,0.)) ;
#103657 = DIRECTION('',(4.33680868994202E-16,0.,-1.)) ;
#103658 = DIRECTION('',(0.,-1.,0.)) ;
#103659 = DIRECTION('',(-4.33680868994202E-16,0.,1.)) ;
#103660 = DIRECTION('center_axis',(-1.73472347597681E-16,0.,-1.)) ;
#103661 = DIRECTION('ref_axis',(-1.,0.,1.73472347597681E-16)) ;
#103662 = DIRECTION('',(-1.,0.,1.73472347597681E-16)) ;
#103663 = DIRECTION('',(0.,-1.,0.)) ;
#103664 = DIRECTION('',(1.,0.,-1.73472347597681E-16)) ;
#103665 = DIRECTION('',(0.,1.,0.)) ;
#103666 = DIRECTION('center_axis',(-1.,0.,0.)) ;
#103667 = DIRECTION('ref_axis',(0.,0.,1.)) ;
#103668 = DIRECTION('',(0.,0.,1.)) ;
#103669 = DIRECTION('',(0.,-1.,0.)) ;
#103670 = DIRECTION('',(0.,0.,-1.)) ;
#103671 = DIRECTION('',(0.,1.,0.)) ;
#103672 = DIRECTION('center_axis',(-1.73472347597681E-16,0.,1.)) ;
#103673 = DIRECTION('ref_axis',(1.,0.,1.73472347597681E-16)) ;
#103674 = DIRECTION('',(0.,1.,0.)) ;
#103675 = DIRECTION('',(1.,0.,1.73472347597681E-16)) ;
#103676 = DIRECTION('',(0.,-1.,0.)) ;
#103677 = DIRECTION('',(-1.,0.,-1.73472347597681E-16)) ;
#103678 = DIRECTION('center_axis',(0.,-1.,0.)) ;
#103679 = DIRECTION('ref_axis',(0.,0.,-1.)) ;
#103680 = DIRECTION('',(-1.,0.,-1.73472347597681E-16)) ;
#103681 = DIRECTION('',(0.,0.,-1.)) ;
#103682 = DIRECTION('',(1.,0.,-1.73472347597681E-16)) ;
#103683 = DIRECTION('',(-4.33680868994202E-16,0.,1.)) ;
#103684 = DIRECTION('',(1.,0.,0.)) ;
#103685 = DIRECTION('center_axis',(0.,-1.,0.)) ;
#103686 = DIRECTION('ref_axis',(0.,0.,-1.)) ;
#103687 = DIRECTION('',(0.,0.,-1.)) ;
#103688 = DIRECTION('center_axis',(0.,-1.,0.)) ;
#103689 = DIRECTION('ref_axis',(0.,0.,-1.)) ;
#103690 = DIRECTION('',(-1.,0.,0.)) ;
#103691 = DIRECTION('center_axis',(0.,-1.,0.)) ;
#103692 = DIRECTION('ref_axis',(0.,0.,1.)) ;
#103693 = DIRECTION('',(0.,0.,1.)) ;
#103694 = DIRECTION('center_axis',(0.,-1.,0.)) ;
#103695 = DIRECTION('ref_axis',(0.,0.,-1.)) ;
#103696 = DIRECTION('center_axis',(0.,-1.,0.)) ;
#103697 = DIRECTION('ref_axis',(0.,0.,-1.)) ;
#103698 = DIRECTION('center_axis',(0.,-1.,0.)) ;
#103699 = DIRECTION('ref_axis',(0.,0.,-1.)) ;
#103700 = DIRECTION('',(0.,-1.,0.)) ;
#103701 = DIRECTION('',(0.,-1.,0.)) ;
#103702 = DIRECTION('center_axis',(0.,0.,-1.)) ;
#103703 = DIRECTION('ref_axis',(-1.,0.,0.)) ;
#103704 = DIRECTION('',(1.,0.,0.)) ;
#103705 = DIRECTION('',(0.,-1.,0.)) ;
#103706 = DIRECTION('center_axis',(0.,-1.,0.)) ;
#103707 = DIRECTION('ref_axis',(0.,0.,-1.)) ;
#103708 = DIRECTION('center_axis',(0.,-1.,0.)) ;
#103709 = DIRECTION('ref_axis',(0.,0.,-1.)) ;
#103710 = DIRECTION('',(0.,-1.,0.)) ;
#103711 = DIRECTION('center_axis',(-1.,0.,0.)) ;
#103712 = DIRECTION('ref_axis',(0.,0.,1.)) ;
#103713 = DIRECTION('',(0.,0.,-1.)) ;
#103714 = DIRECTION('',(0.,-1.,0.)) ;
#103715 = DIRECTION('center_axis',(0.,-1.,0.)) ;
#103716 = DIRECTION('ref_axis',(0.,0.,-1.)) ;
#103717 = DIRECTION('center_axis',(0.,-1.,0.)) ;
#103718 = DIRECTION('ref_axis',(0.,0.,-1.)) ;
#103719 = DIRECTION('',(0.,-1.,0.)) ;
#103720 = DIRECTION('center_axis',(0.,0.,1.)) ;
#103721 = DIRECTION('ref_axis',(1.,0.,0.)) ;
#103722 = DIRECTION('',(-1.,0.,0.)) ;
#103723 = DIRECTION('',(0.,-1.,0.)) ;
#103724 = DIRECTION('center_axis',(0.,-1.,0.)) ;
#103725 = DIRECTION('ref_axis',(0.,0.,-1.)) ;
#103726 = DIRECTION('center_axis',(0.,-1.,0.)) ;
#103727 = DIRECTION('ref_axis',(0.,0.,1.)) ;
#103728 = DIRECTION('',(0.,-1.,0.)) ;
#103729 = DIRECTION('center_axis',(1.,0.,0.)) ;
#103730 = DIRECTION('ref_axis',(0.,0.,-1.)) ;
#103731 = DIRECTION('',(0.,0.,1.)) ;
#103732 = DIRECTION('center_axis',(0.,-1.,0.)) ;
#103733 = DIRECTION('ref_axis',(0.,0.,-1.)) ;
#103734 = DIRECTION('center_axis',(0.,1.,0.)) ;
#103735 = DIRECTION('ref_axis',(0.,0.,1.)) ;
#103736 = DIRECTION('',(-0.422618261740697,0.,0.906307787036651)) ;
#103737 = DIRECTION('center_axis',(0.906307787036651,0.,0.422618261740697)) ;
#103738 = DIRECTION('ref_axis',(0.422618261740697,0.,-0.906307787036651)) ;
#103739 = DIRECTION('',(-0.422618261740697,0.,0.906307787036651)) ;
#103740 = DIRECTION('',(0.422618261740697,0.,-0.906307787036651)) ;
#103741 = DIRECTION('center_axis',(-0.906307787036651,0.,-0.422618261740697)) ;
#103742 = DIRECTION('ref_axis',(-0.422618261740697,0.,0.906307787036651)) ;
#103743 = DIRECTION('',(0.422618261740697,0.,-0.906307787036651)) ;
#103744 = DIRECTION('',(-0.422618261740697,0.,0.906307787036651)) ;
#103745 = DIRECTION('center_axis',(0.,1.,0.)) ;
#103746 = DIRECTION('ref_axis',(0.,0.,1.)) ;
#103747 = DIRECTION('',(-0.422618261740697,0.,0.906307787036651)) ;
#103748 = DIRECTION('',(0.422618261740697,0.,-0.906307787036651)) ;
#103749 = DIRECTION('center_axis',(1.,0.,-2.16840434497101E-16)) ;
#103750 = DIRECTION('ref_axis',(-2.16840434497101E-16,0.,-1.)) ;
#103751 = DIRECTION('',(2.16840434497101E-16,0.,1.)) ;
#103752 = DIRECTION('',(0.,1.,0.)) ;
#103753 = DIRECTION('',(-2.16840434497101E-16,0.,-1.)) ;
#103754 = DIRECTION('',(0.,-1.,0.)) ;
#103755 = DIRECTION('center_axis',(1.73472347597681E-16,0.,1.)) ;
#103756 = DIRECTION('ref_axis',(1.,0.,-1.73472347597681E-16)) ;
#103757 = DIRECTION('',(0.,-1.,0.)) ;
#103758 = DIRECTION('',(-1.,0.,1.73472347597681E-16)) ;
#103759 = DIRECTION('',(0.,1.,0.)) ;
#103760 = DIRECTION('',(1.,0.,-1.73472347597681E-16)) ;
#103761 = DIRECTION('center_axis',(-1.,0.,2.16840434497101E-16)) ;
#103762 = DIRECTION('ref_axis',(2.16840434497101E-16,0.,1.)) ;
#103763 = DIRECTION('',(0.,-1.,0.)) ;
#103764 = DIRECTION('',(-2.16840434497101E-16,0.,-1.)) ;
#103765 = DIRECTION('',(0.,1.,0.)) ;
#103766 = DIRECTION('',(2.16840434497101E-16,0.,1.)) ;
#103767 = DIRECTION('center_axis',(-1.73472347597681E-16,0.,-1.)) ;
#103768 = DIRECTION('ref_axis',(-1.,0.,1.73472347597681E-16)) ;
#103769 = DIRECTION('',(1.,0.,-1.73472347597681E-16)) ;
#103770 = DIRECTION('',(0.,1.,0.)) ;
#103771 = DIRECTION('',(-1.,0.,1.73472347597681E-16)) ;
#103772 = DIRECTION('',(0.,-1.,0.)) ;
#103773 = DIRECTION('center_axis',(0.,1.,0.)) ;
#103774 = DIRECTION('ref_axis',(0.,0.,1.)) ;
#103775 = DIRECTION('',(1.,0.,-1.73472347597681E-16)) ;
#103776 = DIRECTION('',(-2.16840434497101E-16,0.,-1.)) ;
#103777 = DIRECTION('',(-1.,0.,1.73472347597681E-16)) ;
#103778 = DIRECTION('',(2.16840434497101E-16,0.,1.)) ;
#103779 = DIRECTION('',(1.,0.,0.)) ;
#103780 = DIRECTION('center_axis',(0.,1.,0.)) ;
#103781 = DIRECTION('ref_axis',(0.,0.,1.)) ;
#103782 = DIRECTION('',(0.,0.,1.)) ;
#103783 = DIRECTION('center_axis',(0.,1.,0.)) ;
#103784 = DIRECTION('ref_axis',(0.,0.,1.)) ;
#103785 = DIRECTION('',(-1.,0.,0.)) ;
#103786 = DIRECTION('center_axis',(0.,1.,0.)) ;
#103787 = DIRECTION('ref_axis',(0.,0.,-1.)) ;
#103788 = DIRECTION('',(0.,0.,-1.)) ;
#103789 = DIRECTION('center_axis',(0.,1.,0.)) ;
#103790 = DIRECTION('ref_axis',(0.,0.,1.)) ;
#103791 = DIRECTION('center_axis',(0.,1.,0.)) ;
#103792 = DIRECTION('ref_axis',(0.,0.,1.)) ;
#103793 = DIRECTION('',(0.,1.,0.)) ;
#103794 = DIRECTION('center_axis',(0.,-1.,0.)) ;
#103795 = DIRECTION('ref_axis',(2.60208521396521E-14,0.,1.)) ;
#103796 = DIRECTION('',(0.,1.,0.)) ;
#103797 = DIRECTION('center_axis',(0.,0.,1.)) ;
#103798 = DIRECTION('ref_axis',(1.,0.,0.)) ;
#103799 = DIRECTION('',(-1.,0.,0.)) ;
#103800 = DIRECTION('',(0.,1.,0.)) ;
#103801 = DIRECTION('center_axis',(0.,1.,0.)) ;
#103802 = DIRECTION('ref_axis',(0.,0.,1.)) ;
#103803 = DIRECTION('center_axis',(0.,-1.,0.)) ;
#103804 = DIRECTION('ref_axis',(0.,0.,1.)) ;
#103805 = DIRECTION('',(0.,1.,0.)) ;
#103806 = DIRECTION('center_axis',(-1.,0.,0.)) ;
#103807 = DIRECTION('ref_axis',(0.,0.,1.)) ;
#103808 = DIRECTION('',(0.,0.,-1.)) ;
#103809 = DIRECTION('',(0.,1.,0.)) ;
#103810 = DIRECTION('center_axis',(0.,1.,0.)) ;
#103811 = DIRECTION('ref_axis',(0.,0.,1.)) ;
#103812 = DIRECTION('center_axis',(0.,-1.,0.)) ;
#103813 = DIRECTION('ref_axis',(0.,0.,1.)) ;
#103814 = DIRECTION('',(0.,1.,0.)) ;
#103815 = DIRECTION('center_axis',(0.,0.,-1.)) ;
#103816 = DIRECTION('ref_axis',(-1.,0.,0.)) ;
#103817 = DIRECTION('',(1.,0.,0.)) ;
#103818 = DIRECTION('',(0.,1.,0.)) ;
#103819 = DIRECTION('center_axis',(0.,1.,0.)) ;
#103820 = DIRECTION('ref_axis',(0.,0.,1.)) ;
#103821 = DIRECTION('center_axis',(0.,-1.,0.)) ;
#103822 = DIRECTION('ref_axis',(0.,0.,1.)) ;
#103823 = DIRECTION('',(0.,1.,0.)) ;
#103824 = DIRECTION('center_axis',(1.,0.,0.)) ;
#103825 = DIRECTION('ref_axis',(0.,0.,-1.)) ;
#103826 = DIRECTION('',(0.,0.,1.)) ;
#103827 = DIRECTION('center_axis',(0.,1.,0.)) ;
#103828 = DIRECTION('ref_axis',(0.,0.,1.)) ;
#103829 = DIRECTION('',(1.,0.,0.)) ;
#103830 = DIRECTION('',(0.,0.,-1.)) ;
#103831 = DIRECTION('',(-1.,0.,0.)) ;
#103832 = DIRECTION('',(0.,0.,1.)) ;
#103833 = DIRECTION('center_axis',(0.,0.164398987305357,-0.986393923832144)) ;
#103834 = DIRECTION('ref_axis',(0.,0.986393923832144,0.164398987305357)) ;
#103835 = DIRECTION('',(-1.,-1.0450141421547E-16,-1.7416902369245E-17)) ;
#103836 = DIRECTION('',(0.,-0.986393923832144,-0.164398987305357)) ;
#103837 = DIRECTION('',(1.,0.,0.)) ;
#103838 = DIRECTION('',(0.,0.986393923832144,0.164398987305357)) ;
#103839 = DIRECTION('center_axis',(0.,-1.,0.)) ;
#103840 = DIRECTION('ref_axis',(0.,0.,-1.)) ;
#103841 = DIRECTION('',(0.,0.,1.)) ;
#103842 = DIRECTION('',(0.,0.,-1.)) ;
#103843 = DIRECTION('',(-1.,0.,0.)) ;
#103844 = DIRECTION('center_axis',(0.,0.164398987305357,0.986393923832144)) ;
#103845 = DIRECTION('ref_axis',(0.,-0.986393923832144,0.164398987305357)) ;
#103846 = DIRECTION('',(0.,0.986393923832144,-0.164398987305357)) ;
#103847 = DIRECTION('',(1.,1.0450141421547E-16,-1.7416902369245E-17)) ;
#103848 = DIRECTION('',(0.,-0.986393923832144,0.164398987305357)) ;
#103849 = DIRECTION('center_axis',(-1.,0.,0.)) ;
#103850 = DIRECTION('ref_axis',(0.,0.,1.)) ;
#103851 = DIRECTION('',(0.,0.,1.)) ;
#103852 = DIRECTION('center_axis',(-1.,0.,0.)) ;
#103853 = DIRECTION('ref_axis',(0.,0.,1.)) ;
#103854 = DIRECTION('',(0.,-0.986393923832144,0.164398987305357)) ;
#103855 = DIRECTION('',(0.,0.,-1.)) ;
#103856 = DIRECTION('',(0.,0.986393923832144,0.164398987305357)) ;
#103857 = DIRECTION('center_axis',(1.,0.,0.)) ;
#103858 = DIRECTION('ref_axis',(0.,0.,-1.)) ;
#103859 = DIRECTION('center_axis',(1.,0.,0.)) ;
#103860 = DIRECTION('ref_axis',(0.,0.,-1.)) ;
#103861 = DIRECTION('center_axis',(1.,0.,0.)) ;
#103862 = DIRECTION('ref_axis',(0.,0.,1.)) ;
#103863 = DIRECTION('center_axis',(1.,0.,0.)) ;
#103864 = DIRECTION('ref_axis',(0.,0.,1.)) ;
#103865 = DIRECTION('center_axis',(1.,0.,0.)) ;
#103866 = DIRECTION('ref_axis',(0.,-8.88178419700125E-16,1.)) ;
#103867 = DIRECTION('',(1.,0.,0.)) ;
#103868 = DIRECTION('center_axis',(-1.,0.,0.)) ;
#103869 = DIRECTION('ref_axis',(0.,0.,1.)) ;
#103870 = DIRECTION('',(-1.,0.,0.)) ;
#103871 = DIRECTION('center_axis',(0.,0.,-1.)) ;
#103872 = DIRECTION('ref_axis',(1.,0.,0.)) ;
#103873 = DIRECTION('center_axis',(0.,-1.,0.)) ;
#103874 = DIRECTION('ref_axis',(0.,0.,1.)) ;
#103875 = DIRECTION('center_axis',(0.971399006496778,0.,-0.23745309047699)) ;
#103876 = DIRECTION('ref_axis',(-0.23745309047699,0.,-0.971399006496778)) ;
#103877 = DIRECTION('center_axis',(0.971399006496778,0.,-0.237453090476989)) ;
#103878 = DIRECTION('ref_axis',(-0.237453090476989,0.,-0.971399006496778)) ;
#103879 = DIRECTION('center_axis',(0.655772517804501,-0.73774408253007,-0.160299948796655)) ;
#103880 = DIRECTION('ref_axis',(-0.747409318683662,-0.664363838829917,2.67307565105543E-16)) ;
#103881 = DIRECTION('center_axis',(-0.439210132175304,-4.70034527894889E-10,
-0.898384360835913)) ;
#103882 = DIRECTION('ref_axis',(0.882040291645493,-0.189880214237367,-0.431219698245691)) ;
#103883 = DIRECTION('center_axis',(0.655772517804504,-0.737744082530068,-0.160299948796656)) ;
#103884 = DIRECTION('ref_axis',(0.74740931868366,0.664363838829919,-2.08334010827303E-16)) ;
#103885 = DIRECTION('center_axis',(0.655772517804505,-0.737744082530068,-0.16029994879665)) ;
#103886 = DIRECTION('ref_axis',(0.74740931868366,0.66436383882992,-5.75609428574487E-16)) ;
#103887 = DIRECTION('center_axis',(0.664363838829919,-0.74740931868366,0.)) ;
#103888 = DIRECTION('ref_axis',(0.74740931868366,0.664363838829919,0.)) ;
#103889 = DIRECTION('center_axis',(-0.664363838829918,0.747409318683661,0.)) ;
#103890 = DIRECTION('ref_axis',(-0.747409318683661,-0.664363838829918,0.)) ;
#103891 = DIRECTION('center_axis',(0.,1.,0.)) ;
#103892 = DIRECTION('ref_axis',(0.,0.,1.)) ;
#103893 = DIRECTION('center_axis',(0.,-1.,0.)) ;
#103894 = DIRECTION('ref_axis',(0.,0.,-1.)) ;
#103895 = DIRECTION('center_axis',(0.,0.,1.)) ;
#103896 = DIRECTION('ref_axis',(1.,0.,0.)) ;
#103897 = DIRECTION('center_axis',(0.,0.,-1.)) ;
#103898 = DIRECTION('ref_axis',(-1.,0.,0.)) ;
#103899 = DIRECTION('center_axis',(0.,0.,-1.)) ;
#103900 = DIRECTION('ref_axis',(-1.,0.,0.)) ;
#103901 = DIRECTION('center_axis',(0.439210132175297,4.70023746982989E-10,
-0.898384360835917)) ;
#103902 = DIRECTION('ref_axis',(0.882040291644911,-0.189880214240733,0.4312196982454)) ;
#103903 = DIRECTION('center_axis',(-0.971399006496778,0.,-0.23745309047699)) ;
#103904 = DIRECTION('ref_axis',(-0.23745309047699,0.,0.971399006496777)) ;
#103905 = DIRECTION('center_axis',(0.971399006496778,0.,0.237453090476989)) ;
#103906 = DIRECTION('ref_axis',(0.237453090476989,0.,-0.971399006496778)) ;
#103907 = DIRECTION('center_axis',(0.,1.,0.)) ;
#103908 = DIRECTION('ref_axis',(1.,0.,0.)) ;
#103909 = DIRECTION('center_axis',(-3.54829801904343E-14,1.,8.67361737988405E-15)) ;
#103910 = DIRECTION('ref_axis',(1.,3.54829801904343E-14,6.83923985932746E-30)) ;
#103911 = DIRECTION('center_axis',(-0.948683298050516,0.316227766016832,4.6163005901636E-15)) ;
#103912 = DIRECTION('ref_axis',(0.316227766016832,0.948683298050516,5.23037330488368E-13)) ;
#103913 = DIRECTION('center_axis',(0.,0.,-1.)) ;
#103914 = DIRECTION('ref_axis',(1.,0.,0.)) ;
#103915 = DIRECTION('center_axis',(0.,-1.,0.)) ;
#103916 = DIRECTION('ref_axis',(0.,0.,1.)) ;
#103917 = DIRECTION('center_axis',(0.655772517804503,-0.737744082530069,0.160299948796655)) ;
#103918 = DIRECTION('ref_axis',(-0.747409318683661,-0.664363838829918,1.99521945175207E-17)) ;
#103919 = DIRECTION('center_axis',(0.,1.,0.)) ;
#103920 = DIRECTION('ref_axis',(0.,0.,1.)) ;
#103921 = DIRECTION('center_axis',(2.73957817177508E-14,1.,0.)) ;
#103922 = DIRECTION('ref_axis',(-1.,2.73957817177508E-14,0.)) ;
#103923 = DIRECTION('center_axis',(0.894427190999917,0.447213595499956,0.)) ;
#103924 = DIRECTION('ref_axis',(-0.447213595499956,0.894427190999917,0.)) ;
#103925 = DIRECTION('center_axis',(-0.894427190999916,-0.447213595499958,
0.)) ;
#103926 = DIRECTION('ref_axis',(0.447213595499958,-0.894427190999916,0.)) ;
#103927 = DIRECTION('center_axis',(0.,0.,1.)) ;
#103928 = DIRECTION('ref_axis',(1.,0.,0.)) ;
#103929 = DIRECTION('center_axis',(0.,0.,-1.)) ;
#103930 = DIRECTION('ref_axis',(-1.,0.,0.)) ;
#103931 = DIRECTION('center_axis',(0.,1.,0.)) ;
#103932 = DIRECTION('ref_axis',(0.,0.,1.)) ;
#103933 = DIRECTION('center_axis',(0.,-1.,0.)) ;
#103934 = DIRECTION('ref_axis',(0.,0.,-1.)) ;
#103935 = DIRECTION('center_axis',(-0.664363838829919,0.74740931868366,0.)) ;
#103936 = DIRECTION('ref_axis',(-0.74740931868366,-0.664363838829919,0.)) ;
#103937 = DIRECTION('center_axis',(-0.66436383882992,0.747409318683659,2.52106651083074E-15)) ;
#103938 = DIRECTION('ref_axis',(-0.747409318683659,-0.66436383882992,7.82575143531171E-30)) ;
#103939 = DIRECTION('center_axis',(-0.655772517804504,0.737744082530068,-0.160299948796656)) ;
#103940 = DIRECTION('ref_axis',(-0.74740931868366,-0.664363838829919,2.31673158493852E-16)) ;
#103941 = DIRECTION('center_axis',(0.655772517804496,-0.737744082530075,0.160299948796656)) ;
#103942 = DIRECTION('ref_axis',(0.747409318683667,0.664363838829911,-2.10122272487167E-17)) ;
#103943 = DIRECTION('center_axis',(0.,1.,0.)) ;
#103944 = DIRECTION('ref_axis',(1.,0.,0.)) ;
#103945 = DIRECTION('center_axis',(-0.873786407766988,-0.436893203883498,
0.213592233009711)) ;
#103946 = DIRECTION('ref_axis',(-0.447213595499961,0.894427190999914,-1.41283224420644E-15)) ;
#103947 = DIRECTION('center_axis',(-0.948683298050516,0.316227766016832,-3.71868658652068E-15)) ;
#103948 = DIRECTION('ref_axis',(0.316227766016832,0.948683298050516,-5.15504951476798E-13)) ;
#103949 = DIRECTION('center_axis',(0.,1.,0.)) ;
#103950 = DIRECTION('ref_axis',(1.,0.,0.)) ;
#103951 = DIRECTION('center_axis',(-5.47915634355017E-14,1.,0.)) ;
#103952 = DIRECTION('ref_axis',(1.,5.47915634355017E-14,8.67361737988401E-15)) ;
#103953 = DIRECTION('center_axis',(-0.971399006496778,0.,0.23745309047699)) ;
#103954 = DIRECTION('ref_axis',(0.23745309047699,0.,0.971399006496778)) ;
#103955 = DIRECTION('center_axis',(0.971399006496778,-3.69787733965917E-15,
-0.237453090476989)) ;
#103956 = DIRECTION('ref_axis',(-0.237453090476989,1.76125929374961E-30,-0.971399006496778)) ;
#103957 = DIRECTION('center_axis',(0.873786407766991,0.436893203883493,-0.213592233009709)) ;
#103958 = DIRECTION('ref_axis',(-0.447213595499956,0.894427190999917,2.83414331365695E-16)) ;
#103959 = DIRECTION('center_axis',(-0.873786407766992,-0.436893203883492,
0.21359223300971)) ;
#103960 = DIRECTION('ref_axis',(0.447213595499955,-0.894427190999918,-1.48231119036019E-16)) ;
#103961 = DIRECTION('center_axis',(-0.894427190999917,-0.447213595499956,
0.)) ;
#103962 = DIRECTION('ref_axis',(0.447213595499956,-0.894427190999917,0.)) ;
#103963 = DIRECTION('center_axis',(-0.894427190999917,-0.447213595499955,
0.)) ;
#103964 = DIRECTION('ref_axis',(0.447213595499955,-0.894427190999917,0.)) ;
#103965 = DIRECTION('center_axis',(0.,1.,0.)) ;
#103966 = DIRECTION('ref_axis',(0.,0.,1.)) ;
#103967 = DIRECTION('center_axis',(2.66122351428257E-14,1.,6.50521303491301E-15)) ;
#103968 = DIRECTION('ref_axis',(-1.,2.66122351428257E-14,3.84707242087163E-30)) ;
#103969 = DIRECTION('center_axis',(-0.439210132004928,-6.77418203687457E-14,
-0.898384360919208)) ;
#103970 = DIRECTION('ref_axis',(0.898384360919208,9.23120187976291E-12,-0.439210132004928)) ;
#103971 = DIRECTION('center_axis',(0.,1.,0.)) ;
#103972 = DIRECTION('ref_axis',(1.,0.,0.)) ;
#103973 = DIRECTION('center_axis',(-0.87378640776699,-0.436893203883495,-0.213592233009712)) ;
#103974 = DIRECTION('ref_axis',(-0.447213595499958,0.894427190999916,-1.87666485977959E-15)) ;
#103975 = DIRECTION('center_axis',(0.,0.,1.)) ;
#103976 = DIRECTION('ref_axis',(1.,0.,0.)) ;
#103977 = DIRECTION('center_axis',(0.439210132004928,6.77418203687389E-14,
-0.898384360919208)) ;
#103978 = DIRECTION('ref_axis',(0.898384360919208,-4.19790080461511E-11,0.439210132004928)) ;
#103979 = DIRECTION('center_axis',(-0.873786407766991,-0.436893203883493,
-0.213592233009709)) ;
#103980 = DIRECTION('ref_axis',(0.447213595499956,-0.894427190999917,-1.06780556900622E-16)) ;
#103981 = DIRECTION('center_axis',(-0.873786407766992,-0.436893203883492,
-0.213592233009707)) ;
#103982 = DIRECTION('ref_axis',(0.447213595499955,-0.894427190999918,-7.04543255365314E-18)) ;
#103983 = DIRECTION('center_axis',(-0.971399006496778,0.,-0.237453090476989)) ;
#103984 = DIRECTION('ref_axis',(0.237453090476989,0.,-0.971399006496778)) ;
#103985 = DIRECTION('center_axis',(0.971399006496778,0.,0.23745309047699)) ;
#103986 = DIRECTION('ref_axis',(0.23745309047699,0.,-0.971399006496778)) ;
#103987 = DIRECTION('center_axis',(0.,0.,-1.)) ;
#103988 = DIRECTION('ref_axis',(-1.,0.,0.)) ;
#103989 = DIRECTION('center_axis',(1.,1.0450141421547E-16,1.7416902369245E-17)) ;
#103990 = DIRECTION('ref_axis',(-1.0450141421547E-16,1.,-1.82009092883888E-33)) ;
#103991 = DIRECTION('center_axis',(0.672672795322926,0.739940072189931,-7.49337348295411E-10)) ;
#103992 = DIRECTION('ref_axis',(0.738044870608594,-0.670949884715798,0.0715263669439543)) ;
#103993 = DIRECTION('center_axis',(-1.,0.,0.)) ;
#103994 = DIRECTION('ref_axis',(0.,-0.646374896130195,-0.763019982472726)) ;
#103995 = DIRECTION('center_axis',(-1.,0.,0.)) ;
#103996 = DIRECTION('ref_axis',(0.,0.,1.)) ;
#103997 = DIRECTION('center_axis',(-1.,0.,0.)) ;
#103998 = DIRECTION('ref_axis',(0.,0.,1.)) ;
#103999 = DIRECTION('center_axis',(0.,0.986393923832144,0.164398987305357)) ;
#104000 = DIRECTION('ref_axis',(0.,-0.164398987305357,0.986393923832144)) ;
#104001 = DIRECTION('center_axis',(0.,-0.986393923832144,-0.164398987305358)) ;
#104002 = DIRECTION('ref_axis',(0.,0.164398987305358,-0.986393923832144)) ;
#104003 = DIRECTION('center_axis',(0.,0.,1.)) ;
#104004 = DIRECTION('ref_axis',(1.,0.,0.)) ;
#104005 = DIRECTION('center_axis',(0.,0.,1.)) ;
#104006 = DIRECTION('ref_axis',(1.,0.,0.)) ;
#104007 = DIRECTION('center_axis',(0.,0.,1.)) ;
#104008 = DIRECTION('ref_axis',(1.,0.,0.)) ;
#104009 = DIRECTION('center_axis',(0.,0.,-1.)) ;
#104010 = DIRECTION('ref_axis',(1.,0.,0.)) ;
#104011 = DIRECTION('center_axis',(-1.,0.,0.)) ;
#104012 = DIRECTION('ref_axis',(0.,-0.646374896130195,-0.763019982472726)) ;
#104013 = DIRECTION('center_axis',(0.,0.,1.)) ;
#104014 = DIRECTION('ref_axis',(-1.,0.,0.)) ;
#104015 = DIRECTION('center_axis',(0.,0.,-1.)) ;
#104016 = DIRECTION('ref_axis',(-1.,0.,0.)) ;
#104017 = DIRECTION('center_axis',(1.,1.0450141421547E-16,-1.7416902369245E-17)) ;
#104018 = DIRECTION('ref_axis',(-1.0450141421547E-16,1.,1.82009092883888E-33)) ;
#104019 = DIRECTION('center_axis',(0.672672795322883,0.73994007218997,7.49325583516064E-10)) ;
#104020 = DIRECTION('ref_axis',(0.738044870607526,-0.67094988471475,-0.071526366964805)) ;
#104021 = DIRECTION('center_axis',(1.,0.,0.)) ;
#104022 = DIRECTION('ref_axis',(0.,0.,1.)) ;
#104023 = DIRECTION('center_axis',(0.,0.,-1.)) ;
#104024 = DIRECTION('ref_axis',(-1.,0.,0.)) ;
#104025 = DIRECTION('center_axis',(0.,-0.986393923832144,0.164398987305357)) ;
#104026 = DIRECTION('ref_axis',(0.,-0.164398987305357,-0.986393923832144)) ;
#104027 = DIRECTION('center_axis',(1.,0.,0.)) ;
#104028 = DIRECTION('ref_axis',(0.,0.,1.)) ;
#104029 = DIRECTION('center_axis',(7.58941520739854E-15,0.,-1.)) ;
#104030 = DIRECTION('ref_axis',(-1.,0.,-7.58941520739854E-15)) ;
#104031 = DIRECTION('center_axis',(1.,0.,-8.67361737988404E-15)) ;
#104032 = DIRECTION('ref_axis',(-8.67361737988404E-15,0.,-1.)) ;
#104033 = DIRECTION('center_axis',(1.,0.,0.)) ;
#104034 = DIRECTION('ref_axis',(0.,0.,-1.)) ;
#104035 = DIRECTION('center_axis',(1.,0.,8.67361737988403E-15)) ;
#104036 = DIRECTION('ref_axis',(8.67361737988403E-15,0.,-1.)) ;
#104037 = DIRECTION('center_axis',(0.,0.,1.)) ;
#104038 = DIRECTION('ref_axis',(1.,0.,0.)) ;
#104039 = DIRECTION('center_axis',(0.,0.,-1.)) ;
#104040 = DIRECTION('ref_axis',(-1.,0.,0.)) ;
#104041 = DIRECTION('center_axis',(1.,0.,0.)) ;
#104042 = DIRECTION('ref_axis',(0.,0.,1.)) ;
#104043 = DIRECTION('center_axis',(-6.50521303491304E-15,0.,-1.)) ;
#104044 = DIRECTION('ref_axis',(-1.,0.,6.50521303491304E-15)) ;
#104045 = DIRECTION('center_axis',(1.,0.,0.)) ;
#104046 = DIRECTION('ref_axis',(0.,0.,1.)) ;
#104047 = DIRECTION('center_axis',(1.,9.40395480657835E-30,8.67361737988403E-15)) ;
#104048 = DIRECTION('ref_axis',(8.67361737988403E-15,9.95682444457783E-60,
-1.)) ;
#104049 = DIRECTION('center_axis',(0.,0.,-1.)) ;
#104050 = DIRECTION('ref_axis',(-1.,0.,0.)) ;
#104051 = DIRECTION('center_axis',(6.50521303491304E-15,0.,-1.)) ;
#104052 = DIRECTION('ref_axis',(-1.,0.,-6.50521303491304E-15)) ;
#104053 = DIRECTION('center_axis',(-1.,0.,0.)) ;
#104054 = DIRECTION('ref_axis',(0.,0.,1.)) ;
#104055 = DIRECTION('center_axis',(1.,-8.67361737988409E-15,0.)) ;
#104056 = DIRECTION('ref_axis',(8.67361737988409E-15,1.,0.)) ;
#104057 = DIRECTION('center_axis',(1.,0.,0.)) ;
#104058 = DIRECTION('ref_axis',(0.,0.,1.)) ;
#104059 = DIRECTION('center_axis',(-4.33680868994202E-16,0.,1.)) ;
#104060 = DIRECTION('ref_axis',(1.,0.,4.33680868994202E-16)) ;
#104061 = DIRECTION('center_axis',(0.,0.,-1.)) ;
#104062 = DIRECTION('ref_axis',(-1.,0.,0.)) ;
#104063 = DIRECTION('center_axis',(0.,0.,1.)) ;
#104064 = DIRECTION('ref_axis',(1.,0.,0.)) ;
#104065 = DIRECTION('center_axis',(0.,1.,0.)) ;
#104066 = DIRECTION('ref_axis',(0.,0.,1.)) ;
#104067 = DIRECTION('center_axis',(-1.,0.,0.)) ;
#104068 = DIRECTION('ref_axis',(0.,0.,-1.)) ;
#104069 = DIRECTION('center_axis',(0.,-1.,0.)) ;
#104070 = DIRECTION('ref_axis',(0.,0.,1.)) ;
#104071 = DIRECTION('center_axis',(0.,1.,0.)) ;
#104072 = DIRECTION('ref_axis',(0.,0.,1.)) ;
#104073 = DIRECTION('center_axis',(0.,-1.,0.)) ;
#104074 = DIRECTION('ref_axis',(0.,0.,1.)) ;
#104075 = DIRECTION('center_axis',(-1.,0.,0.)) ;
#104076 = DIRECTION('ref_axis',(0.,0.,-1.)) ;
#104077 = DIRECTION('center_axis',(-1.,0.,-1.73472347597681E-16)) ;
#104078 = DIRECTION('ref_axis',(-1.73472347597681E-16,0.,1.)) ;
#104079 = DIRECTION('center_axis',(-1.,0.,0.)) ;
#104080 = DIRECTION('ref_axis',(0.,0.,1.)) ;
#104081 = DIRECTION('center_axis',(0.,1.,0.)) ;
#104082 = DIRECTION('ref_axis',(0.,0.,1.)) ;
#104083 = DIRECTION('center_axis',(0.,-1.,0.)) ;
#104084 = DIRECTION('ref_axis',(0.,0.,-1.)) ;
#104085 = DIRECTION('center_axis',(-4.33680868994202E-16,0.,1.)) ;
#104086 = DIRECTION('ref_axis',(1.,0.,4.33680868994202E-16)) ;
#104087 = DIRECTION('center_axis',(0.,0.,1.)) ;
#104088 = DIRECTION('ref_axis',(1.,0.,0.)) ;
#104089 = DIRECTION('center_axis',(0.,0.,-1.)) ;
#104090 = DIRECTION('ref_axis',(-1.,0.,0.)) ;
#104091 = DIRECTION('center_axis',(0.,1.,0.)) ;
#104092 = DIRECTION('ref_axis',(0.,0.,1.)) ;
#104093 = DIRECTION('center_axis',(0.,-1.,0.)) ;
#104094 = DIRECTION('ref_axis',(0.,0.,-1.)) ;
#104095 = DIRECTION('center_axis',(1.,0.,-1.73472347597681E-16)) ;
#104096 = DIRECTION('ref_axis',(-1.73472347597681E-16,0.,-1.)) ;
#104097 = DIRECTION('center_axis',(-1.,0.,0.)) ;
#104098 = DIRECTION('ref_axis',(0.,0.,1.)) ;
#104099 = DIRECTION('center_axis',(0.,0.,-1.)) ;
#104100 = DIRECTION('ref_axis',(-1.,0.,0.)) ;
#104101 = DIRECTION('center_axis',(0.,0.,1.)) ;
#104102 = DIRECTION('ref_axis',(1.,0.,0.)) ;
#104103 = DIRECTION('center_axis',(0.,0.,-1.)) ;
#104104 = DIRECTION('ref_axis',(-1.,0.,0.)) ;
#104105 = DIRECTION('center_axis',(0.,1.,0.)) ;
#104106 = DIRECTION('ref_axis',(0.,0.,1.)) ;
#104107 = DIRECTION('center_axis',(0.,-1.,0.)) ;
#104108 = DIRECTION('ref_axis',(0.,0.,1.)) ;
#104109 = DIRECTION('center_axis',(0.,1.,0.)) ;
#104110 = DIRECTION('ref_axis',(1.,0.,0.)) ;
#104111 = DIRECTION('center_axis',(1.,0.,0.)) ;
#104112 = DIRECTION('ref_axis',(0.,0.,1.)) ;
#104113 = DIRECTION('center_axis',(0.,1.,0.)) ;
#104114 = DIRECTION('ref_axis',(1.,0.,0.)) ;
#104115 = DIRECTION('center_axis',(1.,0.,0.)) ;
#104116 = DIRECTION('ref_axis',(0.,0.,1.)) ;
#104117 = DIRECTION('center_axis',(0.,1.,0.)) ;
#104118 = DIRECTION('ref_axis',(0.,0.,1.)) ;
#104119 = DIRECTION('center_axis',(0.,-1.,0.)) ;
#104120 = DIRECTION('ref_axis',(0.,0.,1.)) ;
#104121 = DIRECTION('center_axis',(0.,1.,0.)) ;
#104122 = DIRECTION('ref_axis',(0.,0.,1.)) ;
#104123 = DIRECTION('center_axis',(0.,-1.,0.)) ;
#104124 = DIRECTION('ref_axis',(0.,0.,-1.)) ;
#104125 = DIRECTION('center_axis',(-1.,0.,-1.73472347597681E-16)) ;
#104126 = DIRECTION('ref_axis',(-1.73472347597681E-16,0.,1.)) ;
#104127 = DIRECTION('center_axis',(1.,0.,0.)) ;
#104128 = DIRECTION('ref_axis',(0.,0.,-1.)) ;
#104129 = DIRECTION('center_axis',(1.,0.,-1.73472347597681E-16)) ;
#104130 = DIRECTION('ref_axis',(-1.73472347597681E-16,0.,-1.)) ;
#104131 = DIRECTION('center_axis',(1.,0.,0.)) ;
#104132 = DIRECTION('ref_axis',(0.,0.,-1.)) ;
#104133 = DIRECTION('center_axis',(0.,1.,0.)) ;
#104134 = DIRECTION('ref_axis',(0.,0.,1.)) ;
#104135 = DIRECTION('center_axis',(0.,-1.,0.)) ;
#104136 = DIRECTION('ref_axis',(0.,0.,-1.)) ;
#104137 = DIRECTION('center_axis',(0.,1.,0.)) ;
#104138 = DIRECTION('ref_axis',(1.,0.,0.)) ;
#104139 = DIRECTION('center_axis',(0.,0.,1.)) ;
#104140 = DIRECTION('ref_axis',(-1.,0.,0.)) ;
#104141 = DIRECTION('center_axis',(0.,1.,0.)) ;
#104142 = DIRECTION('ref_axis',(1.,0.,0.)) ;
#104143 = DIRECTION('center_axis',(0.,0.,-1.)) ;
#104144 = DIRECTION('ref_axis',(1.,0.,0.)) ;
#104145 = DIRECTION('center_axis',(0.,0.,-1.)) ;
#104146 = DIRECTION('ref_axis',(-1.,0.,0.)) ;
#104147 = DIRECTION('center_axis',(2.16840434497101E-16,0.,1.)) ;
#104148 = DIRECTION('ref_axis',(1.,0.,-2.16840434497101E-16)) ;
#104149 = DIRECTION('center_axis',(0.,0.,-1.)) ;
#104150 = DIRECTION('ref_axis',(-1.,0.,0.)) ;
#104151 = DIRECTION('center_axis',(0.,0.,1.)) ;
#104152 = DIRECTION('ref_axis',(1.,0.,0.)) ;
#104153 = DIRECTION('center_axis',(0.,-1.,0.)) ;
#104154 = DIRECTION('ref_axis',(0.,0.,-1.)) ;
#104155 = DIRECTION('center_axis',(1.,0.,0.)) ;
#104156 = DIRECTION('ref_axis',(0.,0.,1.)) ;
#104157 = DIRECTION('center_axis',(0.,1.,0.)) ;
#104158 = DIRECTION('ref_axis',(0.,0.,-1.)) ;
#104159 = DIRECTION('center_axis',(0.,-1.,0.)) ;
#104160 = DIRECTION('ref_axis',(0.,0.,-1.)) ;
#104161 = DIRECTION('center_axis',(0.,1.,0.)) ;
#104162 = DIRECTION('ref_axis',(0.,0.,-1.)) ;
#104163 = DIRECTION('center_axis',(1.,0.,0.)) ;
#104164 = DIRECTION('ref_axis',(0.,0.,1.)) ;
#104165 = DIRECTION('center_axis',(1.,0.,-1.73472347597681E-16)) ;
#104166 = DIRECTION('ref_axis',(-1.73472347597681E-16,0.,-1.)) ;
#104167 = DIRECTION('center_axis',(1.,0.,0.)) ;
#104168 = DIRECTION('ref_axis',(0.,0.,-1.)) ;
#104169 = DIRECTION('center_axis',(0.,-1.,0.)) ;
#104170 = DIRECTION('ref_axis',(0.,0.,-1.)) ;
#104171 = DIRECTION('center_axis',(0.,1.,0.)) ;
#104172 = DIRECTION('ref_axis',(0.,0.,1.)) ;
#104173 = DIRECTION('center_axis',(2.16840434497101E-16,0.,1.)) ;
#104174 = DIRECTION('ref_axis',(1.,0.,-2.16840434497101E-16)) ;
#104175 = DIRECTION('center_axis',(0.,0.,1.)) ;
#104176 = DIRECTION('ref_axis',(1.,0.,0.)) ;
#104177 = DIRECTION('center_axis',(0.,0.,-1.)) ;
#104178 = DIRECTION('ref_axis',(-1.,0.,0.)) ;
#104179 = DIRECTION('center_axis',(0.,-1.,0.)) ;
#104180 = DIRECTION('ref_axis',(0.,0.,-1.)) ;
#104181 = DIRECTION('center_axis',(0.,1.,0.)) ;
#104182 = DIRECTION('ref_axis',(0.,0.,1.)) ;
#104183 = DIRECTION('center_axis',(-1.,0.,1.73472347597681E-16)) ;
#104184 = DIRECTION('ref_axis',(1.73472347597681E-16,0.,1.)) ;
#104185 = DIRECTION('center_axis',(1.,0.,0.)) ;
#104186 = DIRECTION('ref_axis',(0.,0.,-1.)) ;
#104187 = DIRECTION('center_axis',(-2.16840434497101E-16,0.,-1.)) ;
#104188 = DIRECTION('ref_axis',(-1.,0.,2.16840434497101E-16)) ;
#104189 = DIRECTION('center_axis',(0.,0.,1.)) ;
#104190 = DIRECTION('ref_axis',(1.,0.,0.)) ;
#104191 = DIRECTION('center_axis',(0.,0.,-1.)) ;
#104192 = DIRECTION('ref_axis',(-1.,0.,0.)) ;
#104193 = DIRECTION('center_axis',(0.,-1.,0.)) ;
#104194 = DIRECTION('ref_axis',(0.,0.,-1.)) ;
#104195 = DIRECTION('center_axis',(0.,1.,0.)) ;
#104196 = DIRECTION('ref_axis',(0.,0.,-1.)) ;
#104197 = DIRECTION('center_axis',(0.,1.,0.)) ;
#104198 = DIRECTION('ref_axis',(1.,0.,0.)) ;
#104199 = DIRECTION('center_axis',(-1.,0.,0.)) ;
#104200 = DIRECTION('ref_axis',(0.,0.,-1.)) ;
#104201 = DIRECTION('center_axis',(0.,1.,0.)) ;
#104202 = DIRECTION('ref_axis',(1.,0.,0.)) ;
#104203 = DIRECTION('center_axis',(-1.,0.,0.)) ;
#104204 = DIRECTION('ref_axis',(0.,0.,-1.)) ;
#104205 = DIRECTION('center_axis',(0.,-1.,0.)) ;
#104206 = DIRECTION('ref_axis',(0.,0.,-1.)) ;
#104207 = DIRECTION('center_axis',(0.,1.,0.)) ;
#104208 = DIRECTION('ref_axis',(0.,0.,-1.)) ;
#104209 = DIRECTION('center_axis',(0.,-1.,0.)) ;
#104210 = DIRECTION('ref_axis',(0.,0.,-1.)) ;
#104211 = DIRECTION('center_axis',(0.,1.,0.)) ;
#104212 = DIRECTION('ref_axis',(0.,0.,1.)) ;
#104213 = DIRECTION('center_axis',(1.,0.,-1.73472347597681E-16)) ;
#104214 = DIRECTION('ref_axis',(-1.73472347597681E-16,0.,-1.)) ;
#104215 = DIRECTION('center_axis',(-1.,0.,0.)) ;
#104216 = DIRECTION('ref_axis',(0.,0.,1.)) ;
#104217 = DIRECTION('center_axis',(-1.,0.,1.73472347597681E-16)) ;
#104218 = DIRECTION('ref_axis',(1.73472347597681E-16,0.,1.)) ;
#104219 = DIRECTION('center_axis',(-1.,0.,0.)) ;
#104220 = DIRECTION('ref_axis',(0.,0.,1.)) ;
#104221 = DIRECTION('center_axis',(0.,-1.,0.)) ;
#104222 = DIRECTION('ref_axis',(0.,0.,-1.)) ;
#104223 = DIRECTION('center_axis',(0.,1.,0.)) ;
#104224 = DIRECTION('ref_axis',(0.,0.,1.)) ;
#104225 = DIRECTION('center_axis',(0.,1.,0.)) ;
#104226 = DIRECTION('ref_axis',(1.,0.,0.)) ;
#104227 = DIRECTION('center_axis',(0.,0.,1.)) ;
#104228 = DIRECTION('ref_axis',(-1.,0.,0.)) ;
#104229 = DIRECTION('center_axis',(0.,1.,0.)) ;
#104230 = DIRECTION('ref_axis',(1.,0.,0.)) ;
#104231 = DIRECTION('center_axis',(0.,0.,-1.)) ;
#104232 = DIRECTION('ref_axis',(1.,0.,0.)) ;
#104233 = DIRECTION('center_axis',(-2.16840434497101E-16,0.,-1.)) ;
#104234 = DIRECTION('ref_axis',(-1.,0.,2.16840434497101E-16)) ;
#104235 = DIRECTION('center_axis',(-1.,0.,0.)) ;
#104236 = DIRECTION('ref_axis',(0.,0.,1.)) ;
#104237 = DIRECTION('center_axis',(0.,-0.632948931301575,-0.774193548387091)) ;
#104238 = DIRECTION('ref_axis',(0.,0.774193548387091,-0.632948931301575)) ;
#104239 = DIRECTION('center_axis',(0.,0.,1.)) ;
#104240 = DIRECTION('ref_axis',(1.,0.,0.)) ;
#104241 = DIRECTION('center_axis',(8.67361737988401E-15,0.,1.)) ;
#104242 = DIRECTION('ref_axis',(1.,0.,-8.67361737988401E-15)) ;
#104243 = DIRECTION('center_axis',(0.,1.,0.)) ;
#104244 = DIRECTION('ref_axis',(1.,0.,0.)) ;
#104245 = DIRECTION('center_axis',(-1.,0.,0.)) ;
#104246 = DIRECTION('ref_axis',(0.,0.,-1.)) ;
#104247 = DIRECTION('center_axis',(1.,0.,0.)) ;
#104248 = DIRECTION('ref_axis',(0.,0.,-1.)) ;
#104249 = DIRECTION('center_axis',(-1.,0.,0.)) ;
#104250 = DIRECTION('ref_axis',(0.,0.,1.)) ;
#104251 = DIRECTION('center_axis',(0.,0.,-1.)) ;
#104252 = DIRECTION('ref_axis',(-1.,0.,0.)) ;
#104253 = DIRECTION('center_axis',(0.,0.,-1.)) ;
#104254 = DIRECTION('ref_axis',(-1.,0.,0.)) ;
#104255 = DIRECTION('center_axis',(-1.,0.,0.)) ;
#104256 = DIRECTION('ref_axis',(0.,0.,1.)) ;
#104257 = DIRECTION('center_axis',(0.,-0.632948931301567,-0.774193548387097)) ;
#104258 = DIRECTION('ref_axis',(0.,-0.774193548387097,0.632948931301567)) ;
#104259 = DIRECTION('center_axis',(-1.,0.,0.)) ;
#104260 = DIRECTION('ref_axis',(0.,0.,1.)) ;
#104261 = DIRECTION('center_axis',(0.,0.632948931301567,-0.774193548387097)) ;
#104262 = DIRECTION('ref_axis',(0.,0.774193548387097,0.632948931301567)) ;
#104263 = DIRECTION('center_axis',(0.,0.,-1.)) ;
#104264 = DIRECTION('ref_axis',(-1.,0.,0.)) ;
#104265 = DIRECTION('center_axis',(0.,0.,-1.)) ;
#104266 = DIRECTION('ref_axis',(-1.,0.,0.)) ;
#104267 = DIRECTION('center_axis',(0.,0.,1.)) ;
#104268 = DIRECTION('ref_axis',(1.,0.,0.)) ;
#104269 = DIRECTION('center_axis',(-1.,0.,0.)) ;
#104270 = DIRECTION('ref_axis',(0.,0.,1.)) ;
#104271 = DIRECTION('center_axis',(1.,0.,0.)) ;
#104272 = DIRECTION('ref_axis',(0.,-8.67361737988403E-15,1.)) ;
#104273 = DIRECTION('center_axis',(1.,0.,0.)) ;
#104274 = DIRECTION('ref_axis',(0.,0.,-1.)) ;
#104275 = DIRECTION('center_axis',(1.,0.,0.)) ;
#104276 = DIRECTION('ref_axis',(0.,0.,-1.)) ;
#104277 = DIRECTION('center_axis',(0.,0.,1.)) ;
#104278 = DIRECTION('ref_axis',(1.,0.,0.)) ;
#104279 = DIRECTION('center_axis',(8.67361737988401E-15,0.,1.)) ;
#104280 = DIRECTION('ref_axis',(1.,0.,-8.67361737988401E-15)) ;
#104281 = DIRECTION('center_axis',(0.,8.67361737988405E-15,-1.)) ;
#104282 = DIRECTION('ref_axis',(0.,1.,8.67361737988405E-15)) ;
#104283 = DIRECTION('center_axis',(0.,1.,0.)) ;
#104284 = DIRECTION('ref_axis',(1.,0.,0.)) ;
#104285 = DIRECTION('center_axis',(1.22050154678007E-14,0.632948931301567,
-0.774193548387097)) ;
#104286 = DIRECTION('ref_axis',(-2.03293076771647E-29,-0.774193548387097,
-0.632948931301567)) ;
#104287 = DIRECTION('center_axis',(-1.,0.,0.)) ;
#104288 = DIRECTION('ref_axis',(0.,0.,1.)) ;
#104289 = DIRECTION('center_axis',(0.,0.,1.)) ;
#104290 = DIRECTION('ref_axis',(1.,0.,0.)) ;
#104291 = DIRECTION('center_axis',(0.,0.,1.)) ;
#104292 = DIRECTION('ref_axis',(1.,0.,0.)) ;
#104293 = DIRECTION('center_axis',(0.,0.,-1.)) ;
#104294 = DIRECTION('ref_axis',(-1.,0.,0.)) ;
#104295 = DIRECTION('center_axis',(0.,0.,-1.)) ;
#104296 = DIRECTION('ref_axis',(1.,0.,0.)) ;
#104297 = DIRECTION('center_axis',(0.,0.,-1.)) ;
#104298 = DIRECTION('ref_axis',(-1.,0.,0.)) ;
#104299 = DIRECTION('center_axis',(0.,0.,-1.)) ;
#104300 = DIRECTION('ref_axis',(1.,0.,0.)) ;
#104301 = DIRECTION('center_axis',(0.,0.,-1.)) ;
#104302 = DIRECTION('ref_axis',(-1.,0.,0.)) ;
#104303 = DIRECTION('center_axis',(0.,0.,-1.)) ;
#104304 = DIRECTION('ref_axis',(1.,2.6020852139652E-14,0.)) ;
#104305 = DIRECTION('center_axis',(0.,0.,-1.)) ;
#104306 = DIRECTION('ref_axis',(-1.,0.,0.)) ;
#104307 = DIRECTION('center_axis',(0.,0.,-1.)) ;
#104308 = DIRECTION('ref_axis',(1.,0.,0.)) ;
#104309 = DIRECTION('center_axis',(0.,0.,-1.)) ;
#104310 = DIRECTION('ref_axis',(-1.,0.,0.)) ;
#104311 = DIRECTION('center_axis',(0.,0.,-1.)) ;
#104312 = DIRECTION('ref_axis',(1.,0.,0.)) ;
#104313 = DIRECTION('center_axis',(-0.422618261740697,0.,0.906307787036651)) ;
#104314 = DIRECTION('ref_axis',(0.906307787036651,0.,0.422618261740697)) ;
#104315 = DIRECTION('center_axis',(0.422618261740697,0.,-0.906307787036651)) ;
#104316 = DIRECTION('ref_axis',(-0.906307787036651,0.,-0.422618261740697)) ;
#104317 = DIRECTION('center_axis',(0.422618261740697,0.,-0.906307787036651)) ;
#104318 = DIRECTION('ref_axis',(-0.906307787036651,0.,-0.422618261740697)) ;
#104319 = DIRECTION('center_axis',(-0.422618261740697,0.,0.906307787036651)) ;
#104320 = DIRECTION('ref_axis',(0.906307787036651,0.,0.422618261740697)) ;
#104321 = DIRECTION('center_axis',(0.,0.,-1.)) ;
#104322 = DIRECTION('ref_axis',(-1.,0.,0.)) ;
#104323 = DIRECTION('center_axis',(0.,0.,-1.)) ;
#104324 = DIRECTION('ref_axis',(1.,0.,0.)) ;
#104325 = DIRECTION('center_axis',(0.,0.,-1.)) ;
#104326 = DIRECTION('ref_axis',(-1.,0.,0.)) ;
#104327 = DIRECTION('center_axis',(0.,0.,-1.)) ;
#104328 = DIRECTION('ref_axis',(1.,1.04083408558609E-13,0.)) ;
#104329 = DIRECTION('center_axis',(0.,0.,1.)) ;
#104330 = DIRECTION('ref_axis',(1.,0.,0.)) ;
#104331 = DIRECTION('center_axis',(0.,0.,1.)) ;
#104332 = DIRECTION('ref_axis',(1.,0.,0.)) ;
#104333 = DIRECTION('center_axis',(0.,1.,0.)) ;
#104334 = DIRECTION('ref_axis',(1.,0.,0.)) ;
#104335 = DIRECTION('center_axis',(0.,-0.986393923832144,0.164398987305358)) ;
#104336 = DIRECTION('ref_axis',(0.,-0.164398987305358,-0.986393923832144)) ;
#104337 = DIRECTION('center_axis',(0.,0.986393923832144,-0.164398987305357)) ;
#104338 = DIRECTION('ref_axis',(0.,0.164398987305357,0.986393923832144)) ;
#104339 = DIRECTION('center_axis',(0.,-0.986393923832144,0.164398987305358)) ;
#104340 = DIRECTION('ref_axis',(0.,-0.164398987305358,-0.986393923832144)) ;
#104341 = DIRECTION('center_axis',(-1.,0.,0.)) ;
#104342 = DIRECTION('ref_axis',(0.,0.107567764393763,-0.994197755008192)) ;
#104343 = DIRECTION('center_axis',(4.02631181035923E-15,-0.928404294083138,
-0.371571617226061)) ;
#104344 = DIRECTION('ref_axis',(-2.55493810320452E-31,0.371571617226061,-0.928404294083138)) ;
#104345 = DIRECTION('center_axis',(0.275516865537137,-0.50093975551097,-0.820457078800105)) ;
#104346 = DIRECTION('ref_axis',(-8.25573355829978E-17,0.853490367006418,-0.521108619605597)) ;
#104347 = DIRECTION('center_axis',(0.,0.,-1.)) ;
#104348 = DIRECTION('ref_axis',(-1.,0.,0.)) ;
#104349 = DIRECTION('center_axis',(0.,0.,-1.)) ;
#104350 = DIRECTION('ref_axis',(-1.,0.,0.)) ;
#104351 = DIRECTION('center_axis',(0.,0.,-1.)) ;
#104352 = DIRECTION('ref_axis',(-1.,0.,0.)) ;
#104353 = DIRECTION('center_axis',(0.,0.,-1.)) ;
#104354 = DIRECTION('ref_axis',(-1.,0.,0.)) ;
#104355 = DIRECTION('center_axis',(0.,0.,-1.)) ;
#104356 = DIRECTION('ref_axis',(-1.,0.,0.)) ;
#104357 = DIRECTION('center_axis',(-0.275516865538071,0.500939755523742,-0.820457078791993)) ;
#104358 = DIRECTION('ref_axis',(7.85941951813298E-17,0.853490366998217,0.521108619619028)) ;
#104359 = DIRECTION('center_axis',(0.,-0.986393923832144,-0.164398987305357)) ;
#104360 = DIRECTION('ref_axis',(0.,0.164398987305357,-0.986393923832144)) ;
#104361 = DIRECTION('center_axis',(3.5648347838177E-16,0.986393923832144,
0.164398987305358)) ;
#104362 = DIRECTION('ref_axis',(-2.28603566590726E-32,-0.164398987305358,
0.986393923832144)) ;
#104363 = DIRECTION('center_axis',(0.,1.,0.)) ;
#104364 = DIRECTION('ref_axis',(1.,0.,0.)) ;
#104365 = DIRECTION('center_axis',(-1.,0.,0.)) ;
#104366 = DIRECTION('ref_axis',(0.,0.,1.)) ;
#104367 = DIRECTION('center_axis',(0.,0.,-1.)) ;
#104368 = DIRECTION('ref_axis',(-1.,0.,0.)) ;
#104369 = DIRECTION('center_axis',(0.,0.,-1.)) ;
#104370 = DIRECTION('ref_axis',(-1.,0.,0.)) ;
#104371 = DIRECTION('center_axis',(0.,0.,-1.)) ;
#104372 = DIRECTION('ref_axis',(-1.,0.,0.)) ;
#104373 = DIRECTION('center_axis',(0.,0.,-1.)) ;
#104374 = DIRECTION('ref_axis',(-1.,0.,0.)) ;
#104375 = DIRECTION('center_axis',(2.168404344971E-15,0.,1.)) ;
#104376 = DIRECTION('ref_axis',(1.,0.,-2.168404344971E-15)) ;
#104377 = DIRECTION('center_axis',(0.795723237447208,-7.53302716311723E-12,
0.605660407643206)) ;
#104378 = DIRECTION('ref_axis',(0.605660407643206,-1.05709445921463E-26,-0.795723237447208)) ;
#104379 = DIRECTION('center_axis',(1.57772181044204E-26,2.36658271566302E-26,
1.)) ;
#104380 = DIRECTION('ref_axis',(-3.78339027370117E-66,-1.,2.36658271566302E-26)) ;
#104381 = DIRECTION('center_axis',(-0.795723237415222,-2.11663082418553E-11,
0.605660407685229)) ;
#104382 = DIRECTION('ref_axis',(0.605660407685229,9.32717726754359E-27,0.795723237415222)) ;
#104383 = DIRECTION('center_axis',(0.,-3.94255335449274E-16,1.)) ;
#104384 = DIRECTION('ref_axis',(0.,-1.,-3.94255335449274E-16)) ;
#104385 = DIRECTION('center_axis',(0.147618562252691,0.989044367093028,0.)) ;
#104386 = DIRECTION('ref_axis',(-0.989044367093028,0.147618562252691,0.)) ;
#104387 = DIRECTION('',(0.,0.,1.)) ;
#104388 = DIRECTION('',(0.989044367093028,-0.147618562252691,0.)) ;
#104389 = DIRECTION('',(0.,0.,1.)) ;
#104390 = DIRECTION('',(-0.989044367093028,0.147618562252691,0.)) ;
#104391 = DIRECTION('center_axis',(0.,0.,1.)) ;
#104392 = DIRECTION('ref_axis',(1.,0.,0.)) ;
#104393 = DIRECTION('center_axis',(0.,0.,-1.)) ;
#104394 = DIRECTION('ref_axis',(1.,0.,0.)) ;
#104395 = DIRECTION('',(0.,0.,1.)) ;
#104396 = DIRECTION('center_axis',(0.,0.,1.)) ;
#104397 = DIRECTION('ref_axis',(1.,0.,0.)) ;
#104398 = DIRECTION('center_axis',(0.697619267438899,0.716468671818953,0.)) ;
#104399 = DIRECTION('ref_axis',(-0.716468671818953,0.697619267438899,0.)) ;
#104400 = DIRECTION('',(0.716468671818953,-0.697619267438899,0.)) ;
#104401 = DIRECTION('',(0.,0.,1.)) ;
#104402 = DIRECTION('',(-0.716468671818953,0.697619267438899,0.)) ;
#104403 = DIRECTION('center_axis',(0.,0.,1.)) ;
#104404 = DIRECTION('ref_axis',(1.,0.,0.)) ;
#104405 = DIRECTION('center_axis',(0.,0.,-1.)) ;
#104406 = DIRECTION('ref_axis',(1.,0.,0.)) ;
#104407 = DIRECTION('',(0.,0.,1.)) ;
#104408 = DIRECTION('center_axis',(0.,0.,1.)) ;
#104409 = DIRECTION('ref_axis',(1.,0.,0.)) ;
#104410 = DIRECTION('center_axis',(1.,0.,0.)) ;
#104411 = DIRECTION('ref_axis',(0.,0.,-1.)) ;
#104412 = DIRECTION('',(0.,-1.,0.)) ;
#104413 = DIRECTION('',(0.,0.,1.)) ;
#104414 = DIRECTION('',(0.,1.,0.)) ;
#104415 = DIRECTION('center_axis',(0.,0.,1.)) ;
#104416 = DIRECTION('ref_axis',(1.,0.,0.)) ;
#104417 = DIRECTION('center_axis',(0.,0.,-1.)) ;
#104418 = DIRECTION('ref_axis',(1.,0.,0.)) ;
#104419 = DIRECTION('',(0.,0.,1.)) ;
#104420 = DIRECTION('center_axis',(0.,0.,1.)) ;
#104421 = DIRECTION('ref_axis',(1.,0.,0.)) ;
#104422 = DIRECTION('center_axis',(-0.453905661840943,-0.891049746169503,
0.)) ;
#104423 = DIRECTION('ref_axis',(0.891049746169503,-0.453905661840943,0.)) ;
#104424 = DIRECTION('',(-0.891049746169503,0.453905661840943,0.)) ;
#104425 = DIRECTION('',(0.,0.,1.)) ;
#104426 = DIRECTION('',(0.891049746169503,-0.453905661840943,0.)) ;
#104427 = DIRECTION('center_axis',(0.,0.,1.)) ;
#104428 = DIRECTION('ref_axis',(1.,0.,0.)) ;
#104429 = DIRECTION('center_axis',(0.,0.,1.)) ;
#104430 = DIRECTION('ref_axis',(1.,0.,0.)) ;
#104431 = DIRECTION('',(0.,0.,1.)) ;
#104432 = DIRECTION('center_axis',(0.,0.,-1.)) ;
#104433 = DIRECTION('ref_axis',(1.,0.,0.)) ;
#104434 = DIRECTION('center_axis',(-2.60782465076463E-16,-1.,0.)) ;
#104435 = DIRECTION('ref_axis',(1.,-2.60782465076463E-16,0.)) ;
#104436 = DIRECTION('',(-1.,2.60782465076463E-16,0.)) ;
#104437 = DIRECTION('',(0.,0.,-1.)) ;
#104438 = DIRECTION('',(1.,-2.60782465076463E-16,0.)) ;
#104439 = DIRECTION('center_axis',(0.,0.,1.)) ;
#104440 = DIRECTION('ref_axis',(1.,0.,0.)) ;
#104441 = DIRECTION('center_axis',(0.,0.,1.)) ;
#104442 = DIRECTION('ref_axis',(1.,0.,0.)) ;
#104443 = DIRECTION('',(-1.,2.60782465076463E-16,0.)) ;
#104444 = DIRECTION('',(0.,1.,0.)) ;
#104445 = DIRECTION('',(0.989044367093028,-0.147618562252691,0.)) ;
#104446 = DIRECTION('',(0.716468671818953,-0.697619267438899,0.)) ;
#104447 = DIRECTION('',(0.,-1.,0.)) ;
#104448 = DIRECTION('',(-0.891049746169503,0.453905661840943,0.)) ;
#104449 = DIRECTION('center_axis',(0.,0.,1.)) ;
#104450 = DIRECTION('ref_axis',(1.,0.,0.)) ;
#104451 = DIRECTION('',(-0.716468671818953,0.697619267438899,0.)) ;
#104452 = DIRECTION('',(-0.989044367093028,0.147618562252691,0.)) ;
#104453 = DIRECTION('',(0.,-1.,0.)) ;
#104454 = DIRECTION('',(1.,-2.60782465076463E-16,0.)) ;
#104455 = DIRECTION('center_axis',(0.,0.,-1.)) ;
#104456 = DIRECTION('ref_axis',(1.,0.,0.)) ;
#104457 = DIRECTION('',(0.891049746169503,-0.453905661840943,0.)) ;
#104458 = DIRECTION('',(0.,1.,0.)) ;
#104459 = DIRECTION('center_axis',(-1.,0.,0.)) ;
#104460 = DIRECTION('ref_axis',(0.,0.,1.)) ;
#104461 = DIRECTION('center_axis',(-1.,0.,0.)) ;
#104462 = DIRECTION('ref_axis',(0.,0.,1.)) ;
#104463 = DIRECTION('',(0.,0.,-1.)) ;
#104464 = DIRECTION('',(0.,1.,0.)) ;
#104465 = DIRECTION('',(0.,0.,1.)) ;
#104466 = DIRECTION('center_axis',(1.0450141421547E-16,-1.,0.)) ;
#104467 = DIRECTION('ref_axis',(1.,1.0450141421547E-16,0.)) ;
#104468 = DIRECTION('',(-1.,-1.0450141421547E-16,0.)) ;
#104469 = DIRECTION('',(0.,0.,1.)) ;
#104470 = DIRECTION('',(1.,1.0450141421547E-16,1.7416902369245E-17)) ;
#104471 = DIRECTION('',(0.,0.,-1.)) ;
#104472 = DIRECTION('center_axis',(0.,1.,0.)) ;
#104473 = DIRECTION('ref_axis',(0.,0.,1.)) ;
#104474 = DIRECTION('',(0.422618261740697,0.,-0.906307787036651)) ;
#104475 = DIRECTION('center_axis',(-2.09002828430941E-16,1.,0.)) ;
#104476 = DIRECTION('ref_axis',(-1.,-2.09002828430941E-16,0.)) ;
#104477 = DIRECTION('',(-1.,-2.09002828430941E-16,0.)) ;
#104478 = DIRECTION('',(0.,0.,-1.)) ;
#104479 = DIRECTION('',(1.,2.09002828430941E-16,0.)) ;
#104480 = DIRECTION('',(0.,0.,1.)) ;
#104481 = DIRECTION('center_axis',(0.,0.,1.)) ;
#104482 = DIRECTION('ref_axis',(1.,0.,0.)) ;
#104483 = DIRECTION('center_axis',(0.,0.,-1.)) ;
#104484 = DIRECTION('ref_axis',(1.,0.,0.)) ;
#104485 = DIRECTION('center_axis',(0.,0.,1.)) ;
#104486 = DIRECTION('ref_axis',(1.,0.,0.)) ;
#104487 = DIRECTION('center_axis',(0.,0.,-1.)) ;
#104488 = DIRECTION('ref_axis',(1.,1.30104260698261E-14,0.)) ;
#104489 = DIRECTION('center_axis',(0.,0.,-1.)) ;
#104490 = DIRECTION('ref_axis',(1.,0.,0.)) ;
#104491 = DIRECTION('center_axis',(0.,0.,1.)) ;
#104492 = DIRECTION('ref_axis',(1.,0.,0.)) ;
#104493 = DIRECTION('center_axis',(0.,0.,1.)) ;
#104494 = DIRECTION('ref_axis',(1.,0.,0.)) ;
#104495 = DIRECTION('',(-0.664363838829919,0.74740931868366,0.)) ;
#104496 = DIRECTION('',(0.,-1.,0.)) ;
#104497 = DIRECTION('',(0.894427190999917,0.447213595499956,0.)) ;
#104498 = DIRECTION('',(0.,1.,0.)) ;
#104499 = DIRECTION('center_axis',(0.,0.,-1.)) ;
#104500 = DIRECTION('ref_axis',(-1.,0.,0.)) ;
#104501 = DIRECTION('',(-0.894427190999917,-0.447213595499956,0.)) ;
#104502 = DIRECTION('',(0.,1.,0.)) ;
#104503 = DIRECTION('',(0.664363838829919,-0.74740931868366,0.)) ;
#104504 = DIRECTION('',(0.,-1.,0.)) ;
#104505 = DIRECTION('center_axis',(-0.23745309047699,0.,-0.971399006496778)) ;
#104506 = DIRECTION('ref_axis',(-0.971399006496778,0.,0.23745309047699)) ;
#104507 = DIRECTION('center_axis',(-0.237453090476989,4.46069609701422E-15,
-0.971399006496778)) ;
#104508 = DIRECTION('ref_axis',(0.921799787671161,-0.315455332292563,-0.225328836986284)) ;
#104509 = DIRECTION('',(0.971399006496777,0.,-0.23745309047699)) ;
#104510 = DIRECTION('',(0.,-1.,0.)) ;
#104511 = DIRECTION('',(-0.971399006496777,0.,0.23745309047699)) ;
#104512 = DIRECTION('center_axis',(-0.237453090476974,-7.91889358654166E-14,
-0.971399006496781)) ;
#104513 = DIRECTION('ref_axis',(0.954559354254046,0.185392581172289,-0.233336731039876)) ;
#104514 = DIRECTION('',(-0.873786407766991,-0.436893203883493,0.213592233009709)) ;
#104515 = DIRECTION('',(0.,1.,0.)) ;
#104516 = DIRECTION('',(0.655772517804503,-0.737744082530068,-0.160299948796656)) ;
#104517 = DIRECTION('center_axis',(-1.,0.,0.)) ;
#104518 = DIRECTION('ref_axis',(0.,0.,1.)) ;
#104519 = DIRECTION('',(0.,-1.,0.)) ;
#104520 = DIRECTION('center_axis',(-1.,-6.70078870827235E-15,-6.50913949396064E-15)) ;
#104521 = DIRECTION('ref_axis',(6.50913949395814E-15,3.73530394823002E-13,
-1.)) ;
#104522 = DIRECTION('',(0.,0.,-1.)) ;
#104523 = DIRECTION('center_axis',(-1.,0.,0.)) ;
#104524 = DIRECTION('ref_axis',(0.,1.52591140012917E-12,-1.)) ;
#104525 = DIRECTION('center_axis',(-1.,6.70078870827225E-15,6.5091394939605E-15)) ;
#104526 = DIRECTION('ref_axis',(-6.5091394939748E-15,-2.1338917236146E-12,
-1.)) ;
#104527 = DIRECTION('',(0.,0.,-1.)) ;
#104528 = DIRECTION('center_axis',(-1.,6.70078870827219E-15,-6.50913949396048E-15)) ;
#104529 = DIRECTION('ref_axis',(6.50913949391343E-15,-7.02157667714827E-12,
-1.)) ;
#104530 = DIRECTION('center_axis',(-0.23745309047699,0.,0.971399006496778)) ;
#104531 = DIRECTION('ref_axis',(0.971399006496778,0.,0.23745309047699)) ;
#104532 = DIRECTION('center_axis',(-0.237453090476981,-4.06097107001983E-14,
0.97139900649678)) ;
#104533 = DIRECTION('ref_axis',(0.95455935425498,0.185392581167189,0.233336731040105)) ;
#104534 = DIRECTION('',(0.971399006496777,0.,0.23745309047699)) ;
#104535 = DIRECTION('',(-0.971399006496777,0.,-0.23745309047699)) ;
#104536 = DIRECTION('center_axis',(-0.23745309047696,8.47532258432748E-14,
0.971399006496785)) ;
#104537 = DIRECTION('ref_axis',(0.921799787670825,-0.315455332293604,0.225328836986199)) ;
#104538 = DIRECTION('',(-0.655772517804503,0.737744082530068,-0.160299948796656)) ;
#104539 = DIRECTION('',(0.,-1.,0.)) ;
#104540 = DIRECTION('',(0.873786407766991,0.436893203883493,0.213592233009709)) ;
#104541 = DIRECTION('center_axis',(0.,1.,0.)) ;
#104542 = DIRECTION('ref_axis',(0.,0.,1.)) ;
#104543 = DIRECTION('',(-0.971399006496777,0.,0.23745309047699)) ;
#104544 = DIRECTION('',(0.,0.,-1.)) ;
#104545 = DIRECTION('',(0.971399006496777,0.,0.23745309047699)) ;
#104546 = DIRECTION('center_axis',(0.,1.,0.)) ;
#104547 = DIRECTION('ref_axis',(0.,0.,1.)) ;
#104548 = DIRECTION('',(-0.971399006496777,0.,-0.23745309047699)) ;
#104549 = DIRECTION('',(0.,0.,1.)) ;
#104550 = DIRECTION('',(0.971399006496777,0.,-0.23745309047699)) ;
#104551 = DIRECTION('center_axis',(-0.447213595499956,0.894427190999917,0.)) ;
#104552 = DIRECTION('ref_axis',(0.,0.,-1.)) ;
#104553 = DIRECTION('',(0.,0.,-1.)) ;
#104554 = DIRECTION('',(-0.873786407766991,-0.436893203883493,-0.213592233009709)) ;
#104555 = DIRECTION('',(-0.894427190999917,-0.447213595499956,0.)) ;
#104556 = DIRECTION('',(0.,0.,1.)) ;
#104557 = DIRECTION('',(0.894427190999917,0.447213595499956,0.)) ;
#104558 = DIRECTION('',(0.873786407766991,0.436893203883493,-0.213592233009709)) ;
#104559 = DIRECTION('center_axis',(0.74740931868366,0.664363838829919,0.)) ;
#104560 = DIRECTION('ref_axis',(0.,0.,1.)) ;
#104561 = DIRECTION('',(0.,0.,-1.)) ;
#104562 = DIRECTION('',(0.664363838829919,-0.74740931868366,0.)) ;
#104563 = DIRECTION('',(0.655772517804503,-0.737744082530068,0.160299948796656)) ;
#104564 = DIRECTION('',(0.,0.,1.)) ;
#104565 = DIRECTION('',(-0.655772517804503,0.737744082530068,0.160299948796656)) ;
#104566 = DIRECTION('',(-0.664363838829919,0.74740931868366,0.)) ;
#104567 = DIRECTION('center_axis',(1.,0.,4.33680868994202E-16)) ;
#104568 = DIRECTION('ref_axis',(4.33680868994202E-16,0.,-1.)) ;
#104569 = DIRECTION('',(0.,1.,0.)) ;
#104570 = DIRECTION('',(4.33680868994202E-16,0.,-1.)) ;
#104571 = DIRECTION('',(0.,-1.,0.)) ;
#104572 = DIRECTION('',(-4.33680868994202E-16,0.,1.)) ;
#104573 = DIRECTION('center_axis',(-1.73472347597681E-16,0.,-1.)) ;
#104574 = DIRECTION('ref_axis',(-1.,0.,1.73472347597681E-16)) ;
#104575 = DIRECTION('',(-1.,0.,1.73472347597681E-16)) ;
#104576 = DIRECTION('',(0.,-1.,0.)) ;
#104577 = DIRECTION('',(1.,0.,-1.73472347597681E-16)) ;
#104578 = DIRECTION('',(0.,1.,0.)) ;
#104579 = DIRECTION('center_axis',(-1.,0.,0.)) ;
#104580 = DIRECTION('ref_axis',(0.,0.,1.)) ;
#104581 = DIRECTION('',(0.,0.,1.)) ;
#104582 = DIRECTION('',(0.,-1.,0.)) ;
#104583 = DIRECTION('',(0.,0.,-1.)) ;
#104584 = DIRECTION('',(0.,1.,0.)) ;
#104585 = DIRECTION('center_axis',(-1.73472347597681E-16,0.,1.)) ;
#104586 = DIRECTION('ref_axis',(1.,0.,1.73472347597681E-16)) ;
#104587 = DIRECTION('',(0.,1.,0.)) ;
#104588 = DIRECTION('',(1.,0.,1.73472347597681E-16)) ;
#104589 = DIRECTION('',(0.,-1.,0.)) ;
#104590 = DIRECTION('',(-1.,0.,-1.73472347597681E-16)) ;
#104591 = DIRECTION('center_axis',(0.,-1.,0.)) ;
#104592 = DIRECTION('ref_axis',(0.,0.,-1.)) ;
#104593 = DIRECTION('',(-1.,0.,-1.73472347597681E-16)) ;
#104594 = DIRECTION('',(0.,0.,-1.)) ;
#104595 = DIRECTION('',(1.,0.,-1.73472347597681E-16)) ;
#104596 = DIRECTION('',(-4.33680868994202E-16,0.,1.)) ;
#104597 = DIRECTION('',(1.,0.,0.)) ;
#104598 = DIRECTION('center_axis',(0.,-1.,0.)) ;
#104599 = DIRECTION('ref_axis',(0.,0.,-1.)) ;
#104600 = DIRECTION('',(0.,0.,-1.)) ;
#104601 = DIRECTION('center_axis',(0.,-1.,0.)) ;
#104602 = DIRECTION('ref_axis',(0.,0.,-1.)) ;
#104603 = DIRECTION('',(-1.,0.,0.)) ;
#104604 = DIRECTION('center_axis',(0.,-1.,0.)) ;
#104605 = DIRECTION('ref_axis',(0.,0.,1.)) ;
#104606 = DIRECTION('',(0.,0.,1.)) ;
#104607 = DIRECTION('center_axis',(0.,-1.,0.)) ;
#104608 = DIRECTION('ref_axis',(0.,0.,-1.)) ;
#104609 = DIRECTION('center_axis',(0.,-1.,0.)) ;
#104610 = DIRECTION('ref_axis',(0.,0.,-1.)) ;
#104611 = DIRECTION('center_axis',(0.,-1.,0.)) ;
#104612 = DIRECTION('ref_axis',(0.,0.,-1.)) ;
#104613 = DIRECTION('',(0.,-1.,0.)) ;
#104614 = DIRECTION('',(0.,-1.,0.)) ;
#104615 = DIRECTION('center_axis',(0.,0.,-1.)) ;
#104616 = DIRECTION('ref_axis',(-1.,0.,0.)) ;
#104617 = DIRECTION('',(1.,0.,0.)) ;
#104618 = DIRECTION('',(0.,-1.,0.)) ;
#104619 = DIRECTION('center_axis',(0.,-1.,0.)) ;
#104620 = DIRECTION('ref_axis',(0.,0.,-1.)) ;
#104621 = DIRECTION('center_axis',(0.,-1.,0.)) ;
#104622 = DIRECTION('ref_axis',(0.,0.,-1.)) ;
#104623 = DIRECTION('',(0.,-1.,0.)) ;
#104624 = DIRECTION('center_axis',(-1.,0.,0.)) ;
#104625 = DIRECTION('ref_axis',(0.,0.,1.)) ;
#104626 = DIRECTION('',(0.,0.,-1.)) ;
#104627 = DIRECTION('',(0.,-1.,0.)) ;
#104628 = DIRECTION('center_axis',(0.,-1.,0.)) ;
#104629 = DIRECTION('ref_axis',(0.,0.,-1.)) ;
#104630 = DIRECTION('center_axis',(0.,-1.,0.)) ;
#104631 = DIRECTION('ref_axis',(0.,0.,-1.)) ;
#104632 = DIRECTION('',(0.,-1.,0.)) ;
#104633 = DIRECTION('center_axis',(0.,0.,1.)) ;
#104634 = DIRECTION('ref_axis',(1.,0.,0.)) ;
#104635 = DIRECTION('',(-1.,0.,0.)) ;
#104636 = DIRECTION('',(0.,-1.,0.)) ;
#104637 = DIRECTION('center_axis',(0.,-1.,0.)) ;
#104638 = DIRECTION('ref_axis',(0.,0.,-1.)) ;
#104639 = DIRECTION('center_axis',(0.,-1.,0.)) ;
#104640 = DIRECTION('ref_axis',(0.,0.,1.)) ;
#104641 = DIRECTION('',(0.,-1.,0.)) ;
#104642 = DIRECTION('center_axis',(1.,0.,0.)) ;
#104643 = DIRECTION('ref_axis',(0.,0.,-1.)) ;
#104644 = DIRECTION('',(0.,0.,1.)) ;
#104645 = DIRECTION('center_axis',(0.,-1.,0.)) ;
#104646 = DIRECTION('ref_axis',(0.,0.,-1.)) ;
#104647 = DIRECTION('center_axis',(0.,1.,0.)) ;
#104648 = DIRECTION('ref_axis',(0.,0.,1.)) ;
#104649 = DIRECTION('',(-0.422618261740697,0.,0.906307787036651)) ;
#104650 = DIRECTION('center_axis',(0.906307787036651,0.,0.422618261740697)) ;
#104651 = DIRECTION('ref_axis',(0.422618261740697,0.,-0.906307787036651)) ;
#104652 = DIRECTION('',(-0.422618261740697,0.,0.906307787036651)) ;
#104653 = DIRECTION('',(0.422618261740697,0.,-0.906307787036651)) ;
#104654 = DIRECTION('center_axis',(-0.906307787036651,0.,-0.422618261740697)) ;
#104655 = DIRECTION('ref_axis',(-0.422618261740697,0.,0.906307787036651)) ;
#104656 = DIRECTION('',(0.422618261740697,0.,-0.906307787036651)) ;
#104657 = DIRECTION('',(-0.422618261740697,0.,0.906307787036651)) ;
#104658 = DIRECTION('center_axis',(0.,1.,0.)) ;
#104659 = DIRECTION('ref_axis',(0.,0.,1.)) ;
#104660 = DIRECTION('',(-0.422618261740697,0.,0.906307787036651)) ;
#104661 = DIRECTION('',(0.422618261740697,0.,-0.906307787036651)) ;
#104662 = DIRECTION('center_axis',(1.,0.,-2.16840434497101E-16)) ;
#104663 = DIRECTION('ref_axis',(-2.16840434497101E-16,0.,-1.)) ;
#104664 = DIRECTION('',(2.16840434497101E-16,0.,1.)) ;
#104665 = DIRECTION('',(0.,1.,0.)) ;
#104666 = DIRECTION('',(-2.16840434497101E-16,0.,-1.)) ;
#104667 = DIRECTION('',(0.,-1.,0.)) ;
#104668 = DIRECTION('center_axis',(1.73472347597681E-16,0.,1.)) ;
#104669 = DIRECTION('ref_axis',(1.,0.,-1.73472347597681E-16)) ;
#104670 = DIRECTION('',(0.,-1.,0.)) ;
#104671 = DIRECTION('',(-1.,0.,1.73472347597681E-16)) ;
#104672 = DIRECTION('',(0.,1.,0.)) ;
#104673 = DIRECTION('',(1.,0.,-1.73472347597681E-16)) ;
#104674 = DIRECTION('center_axis',(-1.,0.,2.16840434497101E-16)) ;
#104675 = DIRECTION('ref_axis',(2.16840434497101E-16,0.,1.)) ;
#104676 = DIRECTION('',(0.,-1.,0.)) ;
#104677 = DIRECTION('',(-2.16840434497101E-16,0.,-1.)) ;
#104678 = DIRECTION('',(0.,1.,0.)) ;
#104679 = DIRECTION('',(2.16840434497101E-16,0.,1.)) ;
#104680 = DIRECTION('center_axis',(-1.73472347597681E-16,0.,-1.)) ;
#104681 = DIRECTION('ref_axis',(-1.,0.,1.73472347597681E-16)) ;
#104682 = DIRECTION('',(1.,0.,-1.73472347597681E-16)) ;
#104683 = DIRECTION('',(0.,1.,0.)) ;
#104684 = DIRECTION('',(-1.,0.,1.73472347597681E-16)) ;
#104685 = DIRECTION('',(0.,-1.,0.)) ;
#104686 = DIRECTION('center_axis',(0.,1.,0.)) ;
#104687 = DIRECTION('ref_axis',(0.,0.,1.)) ;
#104688 = DIRECTION('',(1.,0.,-1.73472347597681E-16)) ;
#104689 = DIRECTION('',(-2.16840434497101E-16,0.,-1.)) ;
#104690 = DIRECTION('',(-1.,0.,1.73472347597681E-16)) ;
#104691 = DIRECTION('',(2.16840434497101E-16,0.,1.)) ;
#104692 = DIRECTION('',(1.,0.,0.)) ;
#104693 = DIRECTION('center_axis',(0.,1.,0.)) ;
#104694 = DIRECTION('ref_axis',(0.,0.,1.)) ;
#104695 = DIRECTION('',(0.,0.,1.)) ;
#104696 = DIRECTION('center_axis',(0.,1.,0.)) ;
#104697 = DIRECTION('ref_axis',(0.,0.,1.)) ;
#104698 = DIRECTION('',(-1.,0.,0.)) ;
#104699 = DIRECTION('center_axis',(0.,1.,0.)) ;
#104700 = DIRECTION('ref_axis',(0.,0.,-1.)) ;
#104701 = DIRECTION('',(0.,0.,-1.)) ;
#104702 = DIRECTION('center_axis',(0.,1.,0.)) ;
#104703 = DIRECTION('ref_axis',(0.,0.,1.)) ;
#104704 = DIRECTION('center_axis',(0.,1.,0.)) ;
#104705 = DIRECTION('ref_axis',(0.,0.,1.)) ;
#104706 = DIRECTION('',(0.,1.,0.)) ;
#104707 = DIRECTION('center_axis',(0.,-1.,0.)) ;
#104708 = DIRECTION('ref_axis',(2.6020852139652E-14,0.,1.)) ;
#104709 = DIRECTION('',(0.,1.,0.)) ;
#104710 = DIRECTION('center_axis',(0.,0.,1.)) ;
#104711 = DIRECTION('ref_axis',(1.,0.,0.)) ;
#104712 = DIRECTION('',(-1.,0.,0.)) ;
#104713 = DIRECTION('',(0.,1.,0.)) ;
#104714 = DIRECTION('center_axis',(0.,1.,0.)) ;
#104715 = DIRECTION('ref_axis',(0.,0.,1.)) ;
#104716 = DIRECTION('center_axis',(0.,-1.,0.)) ;
#104717 = DIRECTION('ref_axis',(0.,0.,1.)) ;
#104718 = DIRECTION('',(0.,1.,0.)) ;
#104719 = DIRECTION('center_axis',(-1.,0.,0.)) ;
#104720 = DIRECTION('ref_axis',(0.,0.,1.)) ;
#104721 = DIRECTION('',(0.,0.,-1.)) ;
#104722 = DIRECTION('',(0.,1.,0.)) ;
#104723 = DIRECTION('center_axis',(0.,1.,0.)) ;
#104724 = DIRECTION('ref_axis',(0.,0.,1.)) ;
#104725 = DIRECTION('center_axis',(0.,-1.,0.)) ;
#104726 = DIRECTION('ref_axis',(0.,0.,1.)) ;
#104727 = DIRECTION('',(0.,1.,0.)) ;
#104728 = DIRECTION('center_axis',(0.,0.,-1.)) ;
#104729 = DIRECTION('ref_axis',(-1.,0.,0.)) ;
#104730 = DIRECTION('',(1.,0.,0.)) ;
#104731 = DIRECTION('',(0.,1.,0.)) ;
#104732 = DIRECTION('center_axis',(0.,1.,0.)) ;
#104733 = DIRECTION('ref_axis',(0.,0.,1.)) ;
#104734 = DIRECTION('center_axis',(0.,-1.,0.)) ;
#104735 = DIRECTION('ref_axis',(0.,0.,1.)) ;
#104736 = DIRECTION('',(0.,1.,0.)) ;
#104737 = DIRECTION('center_axis',(1.,0.,0.)) ;
#104738 = DIRECTION('ref_axis',(0.,0.,-1.)) ;
#104739 = DIRECTION('',(0.,0.,1.)) ;
#104740 = DIRECTION('center_axis',(0.,1.,0.)) ;
#104741 = DIRECTION('ref_axis',(0.,0.,1.)) ;
#104742 = DIRECTION('',(1.,0.,0.)) ;
#104743 = DIRECTION('',(0.,0.,-1.)) ;
#104744 = DIRECTION('',(-1.,0.,0.)) ;
#104745 = DIRECTION('',(0.,0.,1.)) ;
#104746 = DIRECTION('center_axis',(0.,0.164398987305357,-0.986393923832144)) ;
#104747 = DIRECTION('ref_axis',(0.,0.986393923832144,0.164398987305357)) ;
#104748 = DIRECTION('',(-1.,-1.0450141421547E-16,-1.7416902369245E-17)) ;
#104749 = DIRECTION('',(0.,-0.986393923832144,-0.164398987305357)) ;
#104750 = DIRECTION('',(1.,0.,0.)) ;
#104751 = DIRECTION('',(0.,0.986393923832144,0.164398987305357)) ;
#104752 = DIRECTION('center_axis',(0.,-1.,0.)) ;
#104753 = DIRECTION('ref_axis',(0.,0.,-1.)) ;
#104754 = DIRECTION('',(0.,0.,1.)) ;
#104755 = DIRECTION('',(0.,0.,-1.)) ;
#104756 = DIRECTION('',(-1.,0.,0.)) ;
#104757 = DIRECTION('center_axis',(0.,0.164398987305357,0.986393923832144)) ;
#104758 = DIRECTION('ref_axis',(0.,-0.986393923832144,0.164398987305357)) ;
#104759 = DIRECTION('',(0.,0.986393923832144,-0.164398987305357)) ;
#104760 = DIRECTION('',(1.,1.0450141421547E-16,-1.7416902369245E-17)) ;
#104761 = DIRECTION('',(0.,-0.986393923832144,0.164398987305357)) ;
#104762 = DIRECTION('center_axis',(-1.,0.,0.)) ;
#104763 = DIRECTION('ref_axis',(0.,0.,1.)) ;
#104764 = DIRECTION('',(0.,0.,1.)) ;
#104765 = DIRECTION('center_axis',(-1.,0.,0.)) ;
#104766 = DIRECTION('ref_axis',(0.,0.,1.)) ;
#104767 = DIRECTION('',(0.,-0.986393923832144,0.164398987305357)) ;
#104768 = DIRECTION('',(0.,0.,-1.)) ;
#104769 = DIRECTION('',(0.,0.986393923832144,0.164398987305357)) ;
#104770 = DIRECTION('center_axis',(1.,0.,0.)) ;
#104771 = DIRECTION('ref_axis',(0.,0.,-1.)) ;
#104772 = DIRECTION('center_axis',(1.,0.,0.)) ;
#104773 = DIRECTION('ref_axis',(0.,0.,-1.)) ;
#104774 = DIRECTION('center_axis',(1.,0.,0.)) ;
#104775 = DIRECTION('ref_axis',(0.,0.,1.)) ;
#104776 = DIRECTION('center_axis',(1.,0.,0.)) ;
#104777 = DIRECTION('ref_axis',(0.,0.,1.)) ;
#104778 = DIRECTION('center_axis',(1.,0.,0.)) ;
#104779 = DIRECTION('ref_axis',(0.,-8.88178419700125E-16,1.)) ;
#104780 = DIRECTION('',(1.,0.,0.)) ;
#104781 = DIRECTION('center_axis',(-1.,0.,0.)) ;
#104782 = DIRECTION('ref_axis',(0.,0.,1.)) ;
#104783 = DIRECTION('',(-1.,0.,0.)) ;
#104784 = DIRECTION('center_axis',(0.,0.,-1.)) ;
#104785 = DIRECTION('ref_axis',(1.,0.,0.)) ;
#104786 = DIRECTION('center_axis',(0.,-1.,0.)) ;
#104787 = DIRECTION('ref_axis',(0.,0.,1.)) ;
#104788 = DIRECTION('center_axis',(0.971399006496778,0.,-0.23745309047699)) ;
#104789 = DIRECTION('ref_axis',(-0.23745309047699,0.,-0.971399006496778)) ;
#104790 = DIRECTION('center_axis',(0.971399006496778,0.,-0.237453090476989)) ;
#104791 = DIRECTION('ref_axis',(-0.237453090476989,0.,-0.971399006496778)) ;
#104792 = DIRECTION('center_axis',(0.655772517804501,-0.73774408253007,-0.160299948796655)) ;
#104793 = DIRECTION('ref_axis',(-0.747409318683662,-0.664363838829917,2.67307565105543E-16)) ;
#104794 = DIRECTION('center_axis',(-0.439210132175389,-4.7027023783242E-10,
-0.898384360835871)) ;
#104795 = DIRECTION('ref_axis',(0.882040291645213,-0.189880214238859,-0.431219698245608)) ;
#104796 = DIRECTION('center_axis',(0.655772517804504,-0.737744082530068,-0.160299948796656)) ;
#104797 = DIRECTION('ref_axis',(0.74740931868366,0.664363838829919,-2.08334010827303E-16)) ;
#104798 = DIRECTION('center_axis',(0.655772517804505,-0.737744082530068,-0.16029994879665)) ;
#104799 = DIRECTION('ref_axis',(0.74740931868366,0.66436383882992,-5.75609428574487E-16)) ;
#104800 = DIRECTION('center_axis',(0.664363838829919,-0.74740931868366,0.)) ;
#104801 = DIRECTION('ref_axis',(0.74740931868366,0.664363838829919,0.)) ;
#104802 = DIRECTION('center_axis',(-0.664363838829918,0.747409318683661,0.)) ;
#104803 = DIRECTION('ref_axis',(-0.747409318683661,-0.664363838829918,0.)) ;
#104804 = DIRECTION('center_axis',(0.,1.,0.)) ;
#104805 = DIRECTION('ref_axis',(0.,0.,1.)) ;
#104806 = DIRECTION('center_axis',(0.,-1.,0.)) ;
#104807 = DIRECTION('ref_axis',(0.,0.,-1.)) ;
#104808 = DIRECTION('center_axis',(0.,0.,1.)) ;
#104809 = DIRECTION('ref_axis',(1.,0.,0.)) ;
#104810 = DIRECTION('center_axis',(0.,0.,-1.)) ;
#104811 = DIRECTION('ref_axis',(-1.,0.,0.)) ;
#104812 = DIRECTION('center_axis',(0.,0.,-1.)) ;
#104813 = DIRECTION('ref_axis',(-1.,0.,0.)) ;
#104814 = DIRECTION('center_axis',(0.439210132175242,4.69850272309497E-10,
-0.898384360835943)) ;
#104815 = DIRECTION('ref_axis',(0.882040291645527,-0.189880214237253,0.431219698245671)) ;
#104816 = DIRECTION('center_axis',(-0.971399006496778,0.,-0.23745309047699)) ;
#104817 = DIRECTION('ref_axis',(-0.23745309047699,0.,0.971399006496777)) ;
#104818 = DIRECTION('center_axis',(0.971399006496778,0.,0.237453090476989)) ;
#104819 = DIRECTION('ref_axis',(0.237453090476989,0.,-0.971399006496778)) ;
#104820 = DIRECTION('center_axis',(0.,1.,0.)) ;
#104821 = DIRECTION('ref_axis',(1.,0.,0.)) ;
#104822 = DIRECTION('center_axis',(-3.54829801904343E-14,1.,8.67361737988405E-15)) ;
#104823 = DIRECTION('ref_axis',(1.,3.54829801904343E-14,6.83923985932746E-30)) ;
#104824 = DIRECTION('center_axis',(-0.948683298050516,0.316227766016833,4.61630059016351E-15)) ;
#104825 = DIRECTION('ref_axis',(0.316227766016833,0.948683298050516,-2.58893576341231E-13)) ;
#104826 = DIRECTION('center_axis',(0.,0.,-1.)) ;
#104827 = DIRECTION('ref_axis',(1.,0.,0.)) ;
#104828 = DIRECTION('center_axis',(0.,-1.,0.)) ;
#104829 = DIRECTION('ref_axis',(0.,0.,1.)) ;
#104830 = DIRECTION('center_axis',(0.655772517804503,-0.737744082530069,0.160299948796655)) ;
#104831 = DIRECTION('ref_axis',(-0.747409318683661,-0.664363838829918,1.99521945175207E-17)) ;
#104832 = DIRECTION('center_axis',(0.,1.,0.)) ;
#104833 = DIRECTION('ref_axis',(0.,0.,1.)) ;
#104834 = DIRECTION('center_axis',(2.73957817177508E-14,1.,0.)) ;
#104835 = DIRECTION('ref_axis',(-1.,2.73957817177508E-14,0.)) ;
#104836 = DIRECTION('center_axis',(0.894427190999917,0.447213595499956,0.)) ;
#104837 = DIRECTION('ref_axis',(-0.447213595499956,0.894427190999917,0.)) ;
#104838 = DIRECTION('center_axis',(-0.894427190999916,-0.447213595499958,
0.)) ;
#104839 = DIRECTION('ref_axis',(0.447213595499958,-0.894427190999916,0.)) ;
#104840 = DIRECTION('center_axis',(0.,0.,1.)) ;
#104841 = DIRECTION('ref_axis',(1.,0.,0.)) ;
#104842 = DIRECTION('center_axis',(0.,0.,-1.)) ;
#104843 = DIRECTION('ref_axis',(-1.,0.,0.)) ;
#104844 = DIRECTION('center_axis',(0.,1.,0.)) ;
#104845 = DIRECTION('ref_axis',(0.,0.,1.)) ;
#104846 = DIRECTION('center_axis',(0.,-1.,0.)) ;
#104847 = DIRECTION('ref_axis',(0.,0.,-1.)) ;
#104848 = DIRECTION('center_axis',(-0.664363838829919,0.74740931868366,0.)) ;
#104849 = DIRECTION('ref_axis',(-0.74740931868366,-0.664363838829919,0.)) ;
#104850 = DIRECTION('center_axis',(-0.66436383882992,0.747409318683659,2.52106651083074E-15)) ;
#104851 = DIRECTION('ref_axis',(-0.747409318683659,-0.66436383882992,7.82575143531171E-30)) ;
#104852 = DIRECTION('center_axis',(-0.655772517804504,0.737744082530068,-0.160299948796656)) ;
#104853 = DIRECTION('ref_axis',(-0.74740931868366,-0.664363838829919,2.31673158493852E-16)) ;
#104854 = DIRECTION('center_axis',(0.655772517804496,-0.737744082530075,0.160299948796656)) ;
#104855 = DIRECTION('ref_axis',(0.747409318683667,0.664363838829911,-2.10122272487167E-17)) ;
#104856 = DIRECTION('center_axis',(0.,1.,0.)) ;
#104857 = DIRECTION('ref_axis',(1.,0.,0.)) ;
#104858 = DIRECTION('center_axis',(-0.873786407766988,-0.436893203883498,
0.213592233009711)) ;
#104859 = DIRECTION('ref_axis',(-0.447213595499961,0.894427190999914,5.03515095507592E-16)) ;
#104860 = DIRECTION('center_axis',(-0.948683298050516,0.316227766016832,-3.71868658652085E-15)) ;
#104861 = DIRECTION('ref_axis',(0.316227766016832,0.948683298050516,-1.82909356595573E-12)) ;
#104862 = DIRECTION('center_axis',(0.,1.,0.)) ;
#104863 = DIRECTION('ref_axis',(1.,0.,0.)) ;
#104864 = DIRECTION('center_axis',(-5.47915634355017E-14,1.,0.)) ;
#104865 = DIRECTION('ref_axis',(1.,5.47915634355017E-14,0.)) ;
#104866 = DIRECTION('center_axis',(-0.971399006496778,0.,0.23745309047699)) ;
#104867 = DIRECTION('ref_axis',(0.23745309047699,0.,0.971399006496777)) ;
#104868 = DIRECTION('center_axis',(0.971399006496778,-3.69787733965917E-15,
-0.237453090476989)) ;
#104869 = DIRECTION('ref_axis',(-0.237453090476989,3.58403898099287E-30,-0.971399006496778)) ;
#104870 = DIRECTION('center_axis',(0.873786407766991,0.436893203883493,-0.213592233009709)) ;
#104871 = DIRECTION('ref_axis',(-0.447213595499956,0.894427190999917,2.83414331365695E-16)) ;
#104872 = DIRECTION('center_axis',(-0.873786407766992,-0.436893203883492,
0.21359223300971)) ;
#104873 = DIRECTION('ref_axis',(0.447213595499955,-0.894427190999918,-1.48231119036019E-16)) ;
#104874 = DIRECTION('center_axis',(-0.894427190999917,-0.447213595499956,
0.)) ;
#104875 = DIRECTION('ref_axis',(0.447213595499956,-0.894427190999917,0.)) ;
#104876 = DIRECTION('center_axis',(-0.894427190999917,-0.447213595499955,
0.)) ;
#104877 = DIRECTION('ref_axis',(0.447213595499955,-0.894427190999917,0.)) ;
#104878 = DIRECTION('center_axis',(0.,1.,0.)) ;
#104879 = DIRECTION('ref_axis',(0.,0.,1.)) ;
#104880 = DIRECTION('center_axis',(2.66122351428257E-14,1.,6.50521303491301E-15)) ;
#104881 = DIRECTION('ref_axis',(-1.,2.66122351428257E-14,3.84707242087163E-30)) ;
#104882 = DIRECTION('center_axis',(-0.439210132004996,2.91128537537112E-13,
-0.898384360919175)) ;
#104883 = DIRECTION('ref_axis',(0.898384360919175,-2.87197520732744E-11,-0.439210132004996)) ;
#104884 = DIRECTION('center_axis',(0.,1.,0.)) ;
#104885 = DIRECTION('ref_axis',(1.,0.,0.)) ;
#104886 = DIRECTION('center_axis',(-0.87378640776699,-0.436893203883495,-0.213592233009712)) ;
#104887 = DIRECTION('ref_axis',(-0.447213595499958,0.894427190999916,1.8708344946598E-16)) ;
#104888 = DIRECTION('center_axis',(0.,0.,1.)) ;
#104889 = DIRECTION('ref_axis',(1.,0.,0.)) ;
#104890 = DIRECTION('center_axis',(0.439210132004893,2.5322537614034E-13,
-0.898384360919225)) ;
#104891 = DIRECTION('ref_axis',(0.898384360919225,-2.39002175271898E-11,0.439210132004893)) ;
#104892 = DIRECTION('center_axis',(-0.873786407766991,-0.436893203883493,
-0.213592233009709)) ;
#104893 = DIRECTION('ref_axis',(0.447213595499956,-0.894427190999917,-1.06780556900622E-16)) ;
#104894 = DIRECTION('center_axis',(-0.873786407766992,-0.436893203883492,
-0.213592233009707)) ;
#104895 = DIRECTION('ref_axis',(0.447213595499955,-0.894427190999918,-7.04543255365314E-18)) ;
#104896 = DIRECTION('center_axis',(-0.971399006496778,0.,-0.237453090476989)) ;
#104897 = DIRECTION('ref_axis',(0.237453090476989,0.,-0.971399006496778)) ;
#104898 = DIRECTION('center_axis',(0.971399006496778,0.,0.23745309047699)) ;
#104899 = DIRECTION('ref_axis',(0.23745309047699,0.,-0.971399006496777)) ;
#104900 = DIRECTION('center_axis',(0.,0.,-1.)) ;
#104901 = DIRECTION('ref_axis',(-1.,0.,0.)) ;
#104902 = DIRECTION('center_axis',(1.,1.0450141421547E-16,1.7416902369245E-17)) ;
#104903 = DIRECTION('ref_axis',(-1.0450141421547E-16,1.,-1.82009092883888E-33)) ;
#104904 = DIRECTION('center_axis',(0.672672795322785,0.73994007219006,-7.49271823359204E-10)) ;
#104905 = DIRECTION('ref_axis',(0.738044870607466,-0.670949884714521,0.0715263669675738)) ;
#104906 = DIRECTION('center_axis',(-1.,0.,0.)) ;
#104907 = DIRECTION('ref_axis',(0.,-0.646374896130196,-0.763019982472726)) ;
#104908 = DIRECTION('center_axis',(-1.,0.,0.)) ;
#104909 = DIRECTION('ref_axis',(0.,0.,1.)) ;
#104910 = DIRECTION('center_axis',(-1.,0.,0.)) ;
#104911 = DIRECTION('ref_axis',(0.,0.,1.)) ;
#104912 = DIRECTION('center_axis',(0.,0.986393923832144,0.164398987305357)) ;
#104913 = DIRECTION('ref_axis',(0.,-0.164398987305357,0.986393923832144)) ;
#104914 = DIRECTION('center_axis',(0.,-0.986393923832144,-0.164398987305358)) ;
#104915 = DIRECTION('ref_axis',(0.,0.164398987305358,-0.986393923832144)) ;
#104916 = DIRECTION('center_axis',(0.,0.,1.)) ;
#104917 = DIRECTION('ref_axis',(1.,0.,0.)) ;
#104918 = DIRECTION('center_axis',(0.,0.,1.)) ;
#104919 = DIRECTION('ref_axis',(1.,0.,0.)) ;
#104920 = DIRECTION('center_axis',(0.,0.,1.)) ;
#104921 = DIRECTION('ref_axis',(1.,0.,0.)) ;
#104922 = DIRECTION('center_axis',(0.,0.,-1.)) ;
#104923 = DIRECTION('ref_axis',(1.,0.,0.)) ;
#104924 = DIRECTION('center_axis',(-1.,0.,0.)) ;
#104925 = DIRECTION('ref_axis',(0.,-0.646374896130195,-0.763019982472726)) ;
#104926 = DIRECTION('center_axis',(0.,0.,1.)) ;
#104927 = DIRECTION('ref_axis',(-1.,0.,0.)) ;
#104928 = DIRECTION('center_axis',(1.,1.0450141421547E-16,-1.7416902369245E-17)) ;
#104929 = DIRECTION('ref_axis',(-1.0450141421547E-16,1.,1.82009092883888E-33)) ;
#104930 = DIRECTION('center_axis',(0.67267279532264,0.739940072190192,7.49194226733993E-10)) ;
#104931 = DIRECTION('ref_axis',(0.738044870608016,-0.670949884714764,-0.0715263669596091)) ;
#104932 = DIRECTION('center_axis',(1.,0.,0.)) ;
#104933 = DIRECTION('ref_axis',(0.,-4.33680868994203E-15,1.)) ;
#104934 = DIRECTION('center_axis',(0.,0.,-1.)) ;
#104935 = DIRECTION('ref_axis',(-1.,0.,0.)) ;
#104936 = DIRECTION('center_axis',(0.,-0.986393923832144,0.164398987305357)) ;
#104937 = DIRECTION('ref_axis',(0.,-0.164398987305357,-0.986393923832144)) ;
#104938 = DIRECTION('center_axis',(1.,0.,0.)) ;
#104939 = DIRECTION('ref_axis',(0.,0.,1.)) ;
#104940 = DIRECTION('center_axis',(7.58941520739854E-15,0.,-1.)) ;
#104941 = DIRECTION('ref_axis',(-1.,0.,-7.58941520739854E-15)) ;
#104942 = DIRECTION('center_axis',(1.,0.,-8.67361737988404E-15)) ;
#104943 = DIRECTION('ref_axis',(-8.67361737988404E-15,0.,-1.)) ;
#104944 = DIRECTION('center_axis',(1.,0.,0.)) ;
#104945 = DIRECTION('ref_axis',(0.,0.,-1.)) ;
#104946 = DIRECTION('center_axis',(1.,0.,8.67361737988403E-15)) ;
#104947 = DIRECTION('ref_axis',(8.67361737988403E-15,0.,-1.)) ;
#104948 = DIRECTION('center_axis',(0.,0.,1.)) ;
#104949 = DIRECTION('ref_axis',(1.,0.,0.)) ;
#104950 = DIRECTION('center_axis',(0.,0.,-1.)) ;
#104951 = DIRECTION('ref_axis',(-1.,0.,0.)) ;
#104952 = DIRECTION('center_axis',(1.,0.,0.)) ;
#104953 = DIRECTION('ref_axis',(0.,0.,1.)) ;
#104954 = DIRECTION('center_axis',(-6.50521303491304E-15,0.,-1.)) ;
#104955 = DIRECTION('ref_axis',(-1.,0.,6.50521303491304E-15)) ;
#104956 = DIRECTION('center_axis',(1.,0.,0.)) ;
#104957 = DIRECTION('ref_axis',(0.,0.,1.)) ;
#104958 = DIRECTION('center_axis',(1.,9.40395480657835E-30,8.67361737988403E-15)) ;
#104959 = DIRECTION('ref_axis',(8.67361737988403E-15,1.69266015557823E-58,
-1.)) ;
#104960 = DIRECTION('center_axis',(0.,0.,-1.)) ;
#104961 = DIRECTION('ref_axis',(-1.,0.,0.)) ;
#104962 = DIRECTION('center_axis',(6.50521303491304E-15,0.,-1.)) ;
#104963 = DIRECTION('ref_axis',(-1.,0.,-6.50521303491304E-15)) ;
#104964 = DIRECTION('center_axis',(-1.,0.,0.)) ;
#104965 = DIRECTION('ref_axis',(0.,0.,1.)) ;
#104966 = DIRECTION('center_axis',(1.,-8.67361737988409E-15,0.)) ;
#104967 = DIRECTION('ref_axis',(8.67361737988409E-15,1.,0.)) ;
#104968 = DIRECTION('center_axis',(1.,0.,0.)) ;
#104969 = DIRECTION('ref_axis',(0.,0.,1.)) ;
#104970 = DIRECTION('center_axis',(-4.33680868994202E-16,0.,1.)) ;
#104971 = DIRECTION('ref_axis',(1.,0.,4.33680868994202E-16)) ;
#104972 = DIRECTION('center_axis',(0.,0.,-1.)) ;
#104973 = DIRECTION('ref_axis',(-1.,0.,0.)) ;
#104974 = DIRECTION('center_axis',(0.,0.,1.)) ;
#104975 = DIRECTION('ref_axis',(1.,0.,0.)) ;
#104976 = DIRECTION('center_axis',(0.,1.,0.)) ;
#104977 = DIRECTION('ref_axis',(0.,0.,1.)) ;
#104978 = DIRECTION('center_axis',(-1.,0.,0.)) ;
#104979 = DIRECTION('ref_axis',(0.,0.,-1.)) ;
#104980 = DIRECTION('center_axis',(0.,-1.,0.)) ;
#104981 = DIRECTION('ref_axis',(0.,0.,1.)) ;
#104982 = DIRECTION('center_axis',(0.,1.,0.)) ;
#104983 = DIRECTION('ref_axis',(0.,0.,1.)) ;
#104984 = DIRECTION('center_axis',(0.,-1.,0.)) ;
#104985 = DIRECTION('ref_axis',(0.,0.,1.)) ;
#104986 = DIRECTION('center_axis',(-1.,0.,0.)) ;
#104987 = DIRECTION('ref_axis',(0.,0.,-1.)) ;
#104988 = DIRECTION('center_axis',(-1.,0.,-1.73472347597681E-16)) ;
#104989 = DIRECTION('ref_axis',(-1.73472347597681E-16,0.,1.)) ;
#104990 = DIRECTION('center_axis',(-1.,0.,0.)) ;
#104991 = DIRECTION('ref_axis',(0.,0.,1.)) ;
#104992 = DIRECTION('center_axis',(0.,1.,0.)) ;
#104993 = DIRECTION('ref_axis',(0.,0.,1.)) ;
#104994 = DIRECTION('center_axis',(0.,-1.,0.)) ;
#104995 = DIRECTION('ref_axis',(0.,0.,-1.)) ;
#104996 = DIRECTION('center_axis',(-4.33680868994202E-16,0.,1.)) ;
#104997 = DIRECTION('ref_axis',(1.,0.,4.33680868994202E-16)) ;
#104998 = DIRECTION('center_axis',(0.,0.,1.)) ;
#104999 = DIRECTION('ref_axis',(1.,0.,0.)) ;
#105000 = DIRECTION('center_axis',(0.,0.,-1.)) ;
#105001 = DIRECTION('ref_axis',(-1.,0.,0.)) ;
#105002 = DIRECTION('center_axis',(0.,1.,0.)) ;
#105003 = DIRECTION('ref_axis',(0.,0.,1.)) ;
#105004 = DIRECTION('center_axis',(0.,-1.,0.)) ;
#105005 = DIRECTION('ref_axis',(0.,0.,-1.)) ;
#105006 = DIRECTION('center_axis',(1.,0.,-1.73472347597681E-16)) ;
#105007 = DIRECTION('ref_axis',(-1.73472347597681E-16,0.,-1.)) ;
#105008 = DIRECTION('center_axis',(-1.,0.,0.)) ;
#105009 = DIRECTION('ref_axis',(0.,0.,1.)) ;
#105010 = DIRECTION('center_axis',(0.,0.,-1.)) ;
#105011 = DIRECTION('ref_axis',(-1.,0.,0.)) ;
#105012 = DIRECTION('center_axis',(0.,0.,1.)) ;
#105013 = DIRECTION('ref_axis',(1.,0.,0.)) ;
#105014 = DIRECTION('center_axis',(0.,0.,-1.)) ;
#105015 = DIRECTION('ref_axis',(-1.,0.,0.)) ;
#105016 = DIRECTION('center_axis',(0.,1.,0.)) ;
#105017 = DIRECTION('ref_axis',(0.,0.,1.)) ;
#105018 = DIRECTION('center_axis',(0.,-1.,0.)) ;
#105019 = DIRECTION('ref_axis',(0.,0.,1.)) ;
#105020 = DIRECTION('center_axis',(0.,1.,0.)) ;
#105021 = DIRECTION('ref_axis',(1.,0.,0.)) ;
#105022 = DIRECTION('center_axis',(1.,0.,0.)) ;
#105023 = DIRECTION('ref_axis',(0.,0.,1.)) ;
#105024 = DIRECTION('center_axis',(0.,1.,0.)) ;
#105025 = DIRECTION('ref_axis',(1.,0.,0.)) ;
#105026 = DIRECTION('center_axis',(1.,0.,0.)) ;
#105027 = DIRECTION('ref_axis',(0.,0.,1.)) ;
#105028 = DIRECTION('center_axis',(0.,1.,0.)) ;
#105029 = DIRECTION('ref_axis',(0.,0.,1.)) ;
#105030 = DIRECTION('center_axis',(0.,-1.,0.)) ;
#105031 = DIRECTION('ref_axis',(0.,0.,1.)) ;
#105032 = DIRECTION('center_axis',(0.,1.,0.)) ;
#105033 = DIRECTION('ref_axis',(0.,0.,1.)) ;
#105034 = DIRECTION('center_axis',(0.,-1.,0.)) ;
#105035 = DIRECTION('ref_axis',(0.,0.,-1.)) ;
#105036 = DIRECTION('center_axis',(-1.,0.,-1.73472347597681E-16)) ;
#105037 = DIRECTION('ref_axis',(-1.73472347597681E-16,0.,1.)) ;
#105038 = DIRECTION('center_axis',(1.,0.,0.)) ;
#105039 = DIRECTION('ref_axis',(0.,0.,-1.)) ;
#105040 = DIRECTION('center_axis',(1.,0.,-1.73472347597681E-16)) ;
#105041 = DIRECTION('ref_axis',(-1.73472347597681E-16,0.,-1.)) ;
#105042 = DIRECTION('center_axis',(1.,0.,0.)) ;
#105043 = DIRECTION('ref_axis',(0.,0.,-1.)) ;
#105044 = DIRECTION('center_axis',(0.,1.,0.)) ;
#105045 = DIRECTION('ref_axis',(0.,0.,1.)) ;
#105046 = DIRECTION('center_axis',(0.,-1.,0.)) ;
#105047 = DIRECTION('ref_axis',(0.,0.,-1.)) ;
#105048 = DIRECTION('center_axis',(0.,1.,0.)) ;
#105049 = DIRECTION('ref_axis',(1.,0.,0.)) ;
#105050 = DIRECTION('center_axis',(0.,0.,1.)) ;
#105051 = DIRECTION('ref_axis',(-1.,0.,0.)) ;
#105052 = DIRECTION('center_axis',(0.,1.,0.)) ;
#105053 = DIRECTION('ref_axis',(1.,0.,0.)) ;
#105054 = DIRECTION('center_axis',(0.,0.,-1.)) ;
#105055 = DIRECTION('ref_axis',(1.,0.,0.)) ;
#105056 = DIRECTION('center_axis',(0.,0.,-1.)) ;
#105057 = DIRECTION('ref_axis',(-1.,0.,0.)) ;
#105058 = DIRECTION('center_axis',(2.16840434497101E-16,0.,1.)) ;
#105059 = DIRECTION('ref_axis',(1.,0.,-2.16840434497101E-16)) ;
#105060 = DIRECTION('center_axis',(0.,0.,-1.)) ;
#105061 = DIRECTION('ref_axis',(-1.,0.,0.)) ;
#105062 = DIRECTION('center_axis',(0.,0.,1.)) ;
#105063 = DIRECTION('ref_axis',(1.,0.,0.)) ;
#105064 = DIRECTION('center_axis',(0.,-1.,0.)) ;
#105065 = DIRECTION('ref_axis',(0.,0.,-1.)) ;
#105066 = DIRECTION('center_axis',(1.,0.,0.)) ;
#105067 = DIRECTION('ref_axis',(0.,0.,1.)) ;
#105068 = DIRECTION('center_axis',(0.,1.,0.)) ;
#105069 = DIRECTION('ref_axis',(0.,0.,-1.)) ;
#105070 = DIRECTION('center_axis',(0.,-1.,0.)) ;
#105071 = DIRECTION('ref_axis',(0.,0.,-1.)) ;
#105072 = DIRECTION('center_axis',(0.,1.,0.)) ;
#105073 = DIRECTION('ref_axis',(0.,0.,-1.)) ;
#105074 = DIRECTION('center_axis',(1.,0.,0.)) ;
#105075 = DIRECTION('ref_axis',(0.,0.,1.)) ;
#105076 = DIRECTION('center_axis',(1.,0.,-1.73472347597681E-16)) ;
#105077 = DIRECTION('ref_axis',(-1.73472347597681E-16,0.,-1.)) ;
#105078 = DIRECTION('center_axis',(1.,0.,0.)) ;
#105079 = DIRECTION('ref_axis',(0.,0.,-1.)) ;
#105080 = DIRECTION('center_axis',(0.,-1.,0.)) ;
#105081 = DIRECTION('ref_axis',(0.,0.,-1.)) ;
#105082 = DIRECTION('center_axis',(0.,1.,0.)) ;
#105083 = DIRECTION('ref_axis',(0.,0.,1.)) ;
#105084 = DIRECTION('center_axis',(2.16840434497101E-16,0.,1.)) ;
#105085 = DIRECTION('ref_axis',(1.,0.,-2.16840434497101E-16)) ;
#105086 = DIRECTION('center_axis',(0.,0.,1.)) ;
#105087 = DIRECTION('ref_axis',(1.,0.,0.)) ;
#105088 = DIRECTION('center_axis',(0.,0.,-1.)) ;
#105089 = DIRECTION('ref_axis',(-1.,0.,0.)) ;
#105090 = DIRECTION('center_axis',(0.,-1.,0.)) ;
#105091 = DIRECTION('ref_axis',(0.,0.,-1.)) ;
#105092 = DIRECTION('center_axis',(0.,1.,0.)) ;
#105093 = DIRECTION('ref_axis',(0.,0.,1.)) ;
#105094 = DIRECTION('center_axis',(-1.,0.,1.73472347597681E-16)) ;
#105095 = DIRECTION('ref_axis',(1.73472347597681E-16,0.,1.)) ;
#105096 = DIRECTION('center_axis',(1.,0.,0.)) ;
#105097 = DIRECTION('ref_axis',(0.,0.,-1.)) ;
#105098 = DIRECTION('center_axis',(-2.16840434497101E-16,0.,-1.)) ;
#105099 = DIRECTION('ref_axis',(-1.,0.,2.16840434497101E-16)) ;
#105100 = DIRECTION('center_axis',(0.,0.,1.)) ;
#105101 = DIRECTION('ref_axis',(1.,0.,0.)) ;
#105102 = DIRECTION('center_axis',(0.,0.,-1.)) ;
#105103 = DIRECTION('ref_axis',(-1.,0.,0.)) ;
#105104 = DIRECTION('center_axis',(0.,-1.,0.)) ;
#105105 = DIRECTION('ref_axis',(0.,0.,-1.)) ;
#105106 = DIRECTION('center_axis',(0.,1.,0.)) ;
#105107 = DIRECTION('ref_axis',(0.,0.,-1.)) ;
#105108 = DIRECTION('center_axis',(0.,1.,0.)) ;
#105109 = DIRECTION('ref_axis',(1.,0.,0.)) ;
#105110 = DIRECTION('center_axis',(-1.,0.,0.)) ;
#105111 = DIRECTION('ref_axis',(0.,0.,-1.)) ;
#105112 = DIRECTION('center_axis',(0.,1.,0.)) ;
#105113 = DIRECTION('ref_axis',(1.,0.,0.)) ;
#105114 = DIRECTION('center_axis',(-1.,0.,0.)) ;
#105115 = DIRECTION('ref_axis',(0.,0.,-1.)) ;
#105116 = DIRECTION('center_axis',(0.,-1.,0.)) ;
#105117 = DIRECTION('ref_axis',(0.,0.,-1.)) ;
#105118 = DIRECTION('center_axis',(0.,1.,0.)) ;
#105119 = DIRECTION('ref_axis',(0.,0.,-1.)) ;
#105120 = DIRECTION('center_axis',(0.,-1.,0.)) ;
#105121 = DIRECTION('ref_axis',(0.,0.,-1.)) ;
#105122 = DIRECTION('center_axis',(0.,1.,0.)) ;
#105123 = DIRECTION('ref_axis',(0.,0.,1.)) ;
#105124 = DIRECTION('center_axis',(1.,0.,-1.73472347597681E-16)) ;
#105125 = DIRECTION('ref_axis',(-1.73472347597681E-16,0.,-1.)) ;
#105126 = DIRECTION('center_axis',(-1.,0.,0.)) ;
#105127 = DIRECTION('ref_axis',(0.,0.,1.)) ;
#105128 = DIRECTION('center_axis',(-1.,0.,1.73472347597681E-16)) ;
#105129 = DIRECTION('ref_axis',(1.73472347597681E-16,0.,1.)) ;
#105130 = DIRECTION('center_axis',(-1.,0.,0.)) ;
#105131 = DIRECTION('ref_axis',(0.,0.,1.)) ;
#105132 = DIRECTION('center_axis',(0.,-1.,0.)) ;
#105133 = DIRECTION('ref_axis',(0.,0.,-1.)) ;
#105134 = DIRECTION('center_axis',(0.,1.,0.)) ;
#105135 = DIRECTION('ref_axis',(0.,0.,1.)) ;
#105136 = DIRECTION('center_axis',(0.,1.,0.)) ;
#105137 = DIRECTION('ref_axis',(1.,0.,0.)) ;
#105138 = DIRECTION('center_axis',(0.,0.,1.)) ;
#105139 = DIRECTION('ref_axis',(-1.,0.,0.)) ;
#105140 = DIRECTION('center_axis',(0.,1.,0.)) ;
#105141 = DIRECTION('ref_axis',(1.,0.,0.)) ;
#105142 = DIRECTION('center_axis',(0.,0.,-1.)) ;
#105143 = DIRECTION('ref_axis',(1.,0.,0.)) ;
#105144 = DIRECTION('center_axis',(-2.16840434497101E-16,0.,-1.)) ;
#105145 = DIRECTION('ref_axis',(-1.,0.,2.16840434497101E-16)) ;
#105146 = DIRECTION('center_axis',(-1.,0.,0.)) ;
#105147 = DIRECTION('ref_axis',(0.,0.,1.)) ;
#105148 = DIRECTION('center_axis',(0.,-0.632948931301575,-0.774193548387091)) ;
#105149 = DIRECTION('ref_axis',(0.,0.774193548387091,-0.632948931301575)) ;
#105150 = DIRECTION('center_axis',(0.,1.,0.)) ;
#105151 = DIRECTION('ref_axis',(1.,0.,0.)) ;
#105152 = DIRECTION('center_axis',(-1.,0.,0.)) ;
#105153 = DIRECTION('ref_axis',(0.,0.,-1.)) ;
#105154 = DIRECTION('center_axis',(1.,0.,0.)) ;
#105155 = DIRECTION('ref_axis',(0.,0.,-1.)) ;
#105156 = DIRECTION('center_axis',(-1.,0.,0.)) ;
#105157 = DIRECTION('ref_axis',(0.,0.,1.)) ;
#105158 = DIRECTION('center_axis',(-1.,0.,0.)) ;
#105159 = DIRECTION('ref_axis',(0.,0.,1.)) ;
#105160 = DIRECTION('center_axis',(0.,-0.632948931301567,-0.774193548387097)) ;
#105161 = DIRECTION('ref_axis',(0.,-0.774193548387097,0.632948931301567)) ;
#105162 = DIRECTION('center_axis',(-1.,0.,0.)) ;
#105163 = DIRECTION('ref_axis',(0.,0.,1.)) ;
#105164 = DIRECTION('center_axis',(0.,0.632948931301567,-0.774193548387097)) ;
#105165 = DIRECTION('ref_axis',(0.,0.774193548387097,0.632948931301567)) ;
#105166 = DIRECTION('center_axis',(0.,0.,-1.)) ;
#105167 = DIRECTION('ref_axis',(-1.,0.,0.)) ;
#105168 = DIRECTION('center_axis',(0.,0.,1.)) ;
#105169 = DIRECTION('ref_axis',(1.,0.,0.)) ;
#105170 = DIRECTION('center_axis',(-1.,0.,0.)) ;
#105171 = DIRECTION('ref_axis',(0.,0.,1.)) ;
#105172 = DIRECTION('center_axis',(1.,0.,0.)) ;
#105173 = DIRECTION('ref_axis',(0.,0.,1.)) ;
#105174 = DIRECTION('center_axis',(1.,0.,0.)) ;
#105175 = DIRECTION('ref_axis',(0.,0.,-1.)) ;
#105176 = DIRECTION('center_axis',(1.,0.,0.)) ;
#105177 = DIRECTION('ref_axis',(0.,0.,-1.)) ;
#105178 = DIRECTION('center_axis',(0.,0.,1.)) ;
#105179 = DIRECTION('ref_axis',(1.,0.,0.)) ;
#105180 = DIRECTION('center_axis',(0.,8.67361737988405E-15,-1.)) ;
#105181 = DIRECTION('ref_axis',(0.,1.,8.67361737988405E-15)) ;
#105182 = DIRECTION('center_axis',(0.,1.,0.)) ;
#105183 = DIRECTION('ref_axis',(1.,0.,0.)) ;
#105184 = DIRECTION('center_axis',(1.22050154678007E-14,0.632948931301567,
-0.774193548387097)) ;
#105185 = DIRECTION('ref_axis',(-2.03293076771647E-29,-0.774193548387097,
-0.632948931301567)) ;
#105186 = DIRECTION('center_axis',(-1.,0.,0.)) ;
#105187 = DIRECTION('ref_axis',(0.,0.,1.)) ;
#105188 = DIRECTION('center_axis',(-0.422618261740697,0.,0.906307787036651)) ;
#105189 = DIRECTION('ref_axis',(0.906307787036651,0.,0.422618261740697)) ;
#105190 = DIRECTION('center_axis',(0.422618261740697,0.,-0.906307787036651)) ;
#105191 = DIRECTION('ref_axis',(-0.906307787036651,0.,-0.422618261740697)) ;
#105192 = DIRECTION('center_axis',(0.422618261740697,0.,-0.906307787036651)) ;
#105193 = DIRECTION('ref_axis',(-0.906307787036651,0.,-0.422618261740697)) ;
#105194 = DIRECTION('center_axis',(-0.422618261740697,0.,0.906307787036651)) ;
#105195 = DIRECTION('ref_axis',(0.906307787036651,0.,0.422618261740697)) ;
#105196 = DIRECTION('center_axis',(0.,1.,0.)) ;
#105197 = DIRECTION('ref_axis',(1.,0.,0.)) ;
#105198 = DIRECTION('center_axis',(0.,-0.986393923832144,0.164398987305358)) ;
#105199 = DIRECTION('ref_axis',(0.,-0.164398987305358,-0.986393923832144)) ;
#105200 = DIRECTION('center_axis',(0.,0.986393923832144,-0.164398987305357)) ;
#105201 = DIRECTION('ref_axis',(0.,0.164398987305357,0.986393923832144)) ;
#105202 = DIRECTION('center_axis',(0.,-0.986393923832144,0.164398987305358)) ;
#105203 = DIRECTION('ref_axis',(0.,-0.164398987305358,-0.986393923832144)) ;
#105204 = DIRECTION('center_axis',(-1.,0.,0.)) ;
#105205 = DIRECTION('ref_axis',(0.,0.107567764393761,-0.994197755008192)) ;
#105206 = DIRECTION('center_axis',(4.02631181035923E-15,-0.928404294083138,
-0.371571617226061)) ;
#105207 = DIRECTION('ref_axis',(-2.55493810320452E-31,0.371571617226061,-0.928404294083138)) ;
#105208 = DIRECTION('center_axis',(0.275516865537137,-0.50093975551097,-0.820457078800105)) ;
#105209 = DIRECTION('ref_axis',(3.47276585739718E-16,0.853490367006418,-0.521108619605597)) ;
#105210 = DIRECTION('center_axis',(0.,0.,-1.)) ;
#105211 = DIRECTION('ref_axis',(-1.,0.,0.)) ;
#105212 = DIRECTION('center_axis',(0.,0.,-1.)) ;
#105213 = DIRECTION('ref_axis',(-1.,0.,0.)) ;
#105214 = DIRECTION('center_axis',(-0.275516865538071,0.500939755523742,-0.820457078791993)) ;
#105215 = DIRECTION('ref_axis',(-3.28467467648445E-16,0.853490366998217,0.521108619619028)) ;
#105216 = DIRECTION('center_axis',(0.,-0.986393923832144,-0.164398987305357)) ;
#105217 = DIRECTION('ref_axis',(0.,0.164398987305357,-0.986393923832144)) ;
#105218 = DIRECTION('center_axis',(3.5648347838177E-16,0.986393923832144,
0.164398987305358)) ;
#105219 = DIRECTION('ref_axis',(-1.58445824743934E-31,-0.164398987305358,
0.986393923832144)) ;
#105220 = DIRECTION('center_axis',(0.,1.,0.)) ;
#105221 = DIRECTION('ref_axis',(1.,0.,0.)) ;
#105222 = DIRECTION('center_axis',(-1.,0.,0.)) ;
#105223 = DIRECTION('ref_axis',(0.,0.,1.)) ;
#105224 = DIRECTION('center_axis',(0.,0.,-1.)) ;
#105225 = DIRECTION('ref_axis',(-1.,0.,0.)) ;
#105226 = DIRECTION('center_axis',(2.168404344971E-15,0.,1.)) ;
#105227 = DIRECTION('ref_axis',(1.,0.,-2.168404344971E-15)) ;
#105228 = DIRECTION('center_axis',(0.795723237447208,-7.53302716311723E-12,
0.605660407643206)) ;
#105229 = DIRECTION('ref_axis',(0.605660407643206,-1.95871398704475E-26,-0.795723237447208)) ;
#105230 = DIRECTION('center_axis',(1.57772181044204E-26,2.36658271566302E-26,
1.)) ;
#105231 = DIRECTION('ref_axis',(3.73380916671669E-52,-1.,2.36658271566302E-26)) ;
#105232 = DIRECTION('center_axis',(-0.795723237415222,-2.11663082418553E-11,
0.605660407685229)) ;
#105233 = DIRECTION('ref_axis',(0.605660407685229,9.32717726754359E-27,0.795723237415222)) ;
#105234 = DIRECTION('center_axis',(0.,1.,0.)) ;
#105235 = DIRECTION('ref_axis',(1.,0.,0.)) ;
#105236 = DIRECTION('center_axis',(-0.716468671818951,0.697619267438901,0.)) ;
#105237 = DIRECTION('ref_axis',(-0.697619267438901,-0.716468671818951,0.)) ;
#105238 = DIRECTION('center_axis',(0.,-1.,0.)) ;
#105239 = DIRECTION('ref_axis',(0.,0.,-1.)) ;
#105240 = DIRECTION('center_axis',(0.,1.,0.)) ;
#105241 = DIRECTION('ref_axis',(1.,0.,0.)) ;
#105242 = DIRECTION('center_axis',(0.,-1.,0.)) ;
#105243 = DIRECTION('ref_axis',(0.,0.,-1.)) ;
#105244 = DIRECTION('center_axis',(-0.716468671818951,0.697619267438901,0.)) ;
#105245 = DIRECTION('ref_axis',(-0.697619267438901,-0.716468671818951,0.)) ;
#105246 = DIRECTION('center_axis',(0.,-1.,0.)) ;
#105247 = DIRECTION('ref_axis',(0.,0.,-1.)) ;
#105248 = DIRECTION('center_axis',(0.,-1.,0.)) ;
#105249 = DIRECTION('ref_axis',(0.,0.,-1.)) ;
#105250 = DIRECTION('center_axis',(0.716468671818953,-0.697619267438899,0.)) ;
#105251 = DIRECTION('ref_axis',(0.697619267438899,0.716468671818953,0.)) ;
#105252 = DIRECTION('center_axis',(-0.716468671818955,0.697619267438896,0.)) ;
#105253 = DIRECTION('ref_axis',(-0.697619267438896,-0.716468671818955,0.)) ;
#105254 = DIRECTION('center_axis',(-0.716468671818953,0.697619267438899,0.)) ;
#105255 = DIRECTION('ref_axis',(-0.697619267438899,-0.716468671818953,0.)) ;
#105256 = DIRECTION('center_axis',(-0.716468671818955,0.697619267438897,0.)) ;
#105257 = DIRECTION('ref_axis',(-0.697619267438897,-0.716468671818955,0.)) ;
#105258 = DIRECTION('center_axis',(0.,1.,0.)) ;
#105259 = DIRECTION('ref_axis',(0.,0.,1.)) ;
#105260 = DIRECTION('center_axis',(0.,-1.,0.)) ;
#105261 = DIRECTION('ref_axis',(0.,0.,-1.)) ;
#105262 = DIRECTION('center_axis',(0.,0.,1.)) ;
#105263 = DIRECTION('ref_axis',(1.,0.,0.)) ;
#105264 = DIRECTION('center_axis',(-0.891049746169499,0.453905661840951,0.)) ;
#105265 = DIRECTION('ref_axis',(-0.453905661840951,-0.891049746169499,0.)) ;
#105266 = DIRECTION('center_axis',(0.,1.,0.)) ;
#105267 = DIRECTION('ref_axis',(1.,0.,0.)) ;
#105268 = DIRECTION('center_axis',(-0.989044367093028,0.147618562252689,-1.28038692714842E-15)) ;
#105269 = DIRECTION('ref_axis',(-0.147618562252689,-0.989044367093028,-5.00003579437924E-32)) ;
#105270 = DIRECTION('center_axis',(0.,1.,0.)) ;
#105271 = DIRECTION('ref_axis',(1.,0.,0.)) ;
#105272 = DIRECTION('center_axis',(-0.989044367093028,0.147618562252688,0.)) ;
#105273 = DIRECTION('ref_axis',(-0.147618562252688,-0.989044367093028,0.)) ;
#105274 = DIRECTION('center_axis',(0.,0.,1.)) ;
#105275 = DIRECTION('ref_axis',(1.,0.,0.)) ;
#105276 = DIRECTION('center_axis',(-0.891049746169497,0.453905661840955,-3.93700403737147E-15)) ;
#105277 = DIRECTION('ref_axis',(-0.453905661840955,-0.891049746169497,3.34787224203447E-31)) ;
#105278 = DIRECTION('center_axis',(-0.891049746169503,0.453905661840943,0.)) ;
#105279 = DIRECTION('ref_axis',(-0.453905661840943,-0.891049746169503,0.)) ;
#105280 = DIRECTION('center_axis',(-0.891049746169501,0.453905661840946,0.)) ;
#105281 = DIRECTION('ref_axis',(-0.453905661840946,-0.891049746169501,0.)) ;
#105282 = DIRECTION('center_axis',(0.989044367093028,-0.147618562252691,0.)) ;
#105283 = DIRECTION('ref_axis',(0.147618562252691,0.989044367093028,0.)) ;
#105284 = DIRECTION('center_axis',(0.,0.,1.)) ;
#105285 = DIRECTION('ref_axis',(1.,0.,0.)) ;
#105286 = DIRECTION('center_axis',(0.,0.,-1.)) ;
#105287 = DIRECTION('ref_axis',(-1.,0.,0.)) ;
#105288 = DIRECTION('center_axis',(0.,0.,1.)) ;
#105289 = DIRECTION('ref_axis',(1.,0.,0.)) ;
#105290 = DIRECTION('center_axis',(-0.989044367093028,0.147618562252691,0.)) ;
#105291 = DIRECTION('ref_axis',(-0.147618562252691,-0.989044367093028,0.)) ;
#105292 = DIRECTION('center_axis',(0.891049746169503,-0.453905661840943,0.)) ;
#105293 = DIRECTION('ref_axis',(0.453905661840943,0.891049746169503,0.)) ;
#105294 = DIRECTION('center_axis',(-0.891049746169501,0.453905661840946,0.)) ;
#105295 = DIRECTION('ref_axis',(-0.453905661840946,-0.891049746169501,0.)) ;
#105296 = DIRECTION('center_axis',(0.,0.,1.)) ;
#105297 = DIRECTION('ref_axis',(1.,0.,0.)) ;
#105298 = DIRECTION('center_axis',(-1.,0.,0.)) ;
#105299 = DIRECTION('ref_axis',(0.,0.,1.)) ;
#105300 = DIRECTION('center_axis',(0.,1.,0.)) ;
#105301 = DIRECTION('ref_axis',(0.,0.,-1.)) ;
#105302 = DIRECTION('center_axis',(0.,1.,0.)) ;
#105303 = DIRECTION('ref_axis',(0.,0.,-1.)) ;
#105304 = DIRECTION('center_axis',(0.,0.,1.)) ;
#105305 = DIRECTION('ref_axis',(1.,0.,0.)) ;
#105306 = DIRECTION('center_axis',(-1.,0.,0.)) ;
#105307 = DIRECTION('ref_axis',(0.,0.,1.)) ;
#105308 = DIRECTION('center_axis',(-1.,2.60782465076463E-16,0.)) ;
#105309 = DIRECTION('ref_axis',(-2.60782465076463E-16,-1.,0.)) ;
#105310 = DIRECTION('center_axis',(-1.,0.,0.)) ;
#105311 = DIRECTION('ref_axis',(0.,0.,1.)) ;
#105312 = DIRECTION('center_axis',(0.,1.,0.)) ;
#105313 = DIRECTION('ref_axis',(0.,0.,1.)) ;
#105314 = DIRECTION('center_axis',(0.,1.,0.)) ;
#105315 = DIRECTION('ref_axis',(0.,0.,1.)) ;
#105316 = DIRECTION('center_axis',(0.,-1.,0.)) ;
#105317 = DIRECTION('ref_axis',(0.,0.,-1.)) ;
#105318 = DIRECTION('center_axis',(0.,1.,0.)) ;
#105319 = DIRECTION('ref_axis',(0.,0.,1.)) ;
#105320 = DIRECTION('center_axis',(1.,-2.60782465076463E-16,0.)) ;
#105321 = DIRECTION('ref_axis',(2.60782465076463E-16,1.,0.)) ;
#105322 = DIRECTION('center_axis',(-1.,0.,0.)) ;
#105323 = DIRECTION('ref_axis',(0.,0.,1.)) ;
#105324 = DIRECTION('center_axis',(-1.,0.,0.)) ;
#105325 = DIRECTION('ref_axis',(0.,0.,1.)) ;
#105326 = DIRECTION('center_axis',(0.,0.,-1.)) ;
#105327 = DIRECTION('ref_axis',(1.,0.,0.)) ;
#105328 = DIRECTION('center_axis',(-1.,0.,0.)) ;
#105329 = DIRECTION('ref_axis',(0.,0.,1.)) ;
#105330 = DIRECTION('center_axis',(0.,0.,1.)) ;
#105331 = DIRECTION('ref_axis',(-1.,0.,0.)) ;
#105332 = DIRECTION('center_axis',(0.,0.,1.)) ;
#105333 = DIRECTION('ref_axis',(1.,0.,0.)) ;
#105334 = DIRECTION('center_axis',(-1.,0.,0.)) ;
#105335 = DIRECTION('ref_axis',(0.,0.,1.)) ;
#105336 = DIRECTION('center_axis',(-1.,0.,0.)) ;
#105337 = DIRECTION('ref_axis',(0.,0.,1.)) ;
#105338 = DIRECTION('center_axis',(-3.56483478381767E-16,0.986393923832144,
0.164398987305358)) ;
#105339 = DIRECTION('ref_axis',(-3.72967278346455E-31,-0.164398987305358,
0.986393923832144)) ;
#105340 = DIRECTION('center_axis',(1.,0.,0.)) ;
#105341 = DIRECTION('ref_axis',(0.,1.43114686768087E-13,1.)) ;
#105342 = DIRECTION('center_axis',(-4.02631181035926E-15,0.928404294083138,
-0.371571617226061)) ;
#105343 = DIRECTION('ref_axis',(-1.2864990704331E-29,0.371571617226061,0.928404294083138)) ;
#105344 = DIRECTION('center_axis',(0.,-1.,0.)) ;
#105345 = DIRECTION('ref_axis',(0.,0.,-1.)) ;
#105346 = DIRECTION('center_axis',(0.,-1.,0.)) ;
#105347 = DIRECTION('ref_axis',(0.,0.,-1.)) ;
#105348 = DIRECTION('center_axis',(-1.,0.,-1.22464679914735E-16)) ;
#105349 = DIRECTION('ref_axis',(-1.22464679914735E-16,0.,1.)) ;
#105350 = DIRECTION('center_axis',(0.,1.,0.)) ;
#105351 = DIRECTION('ref_axis',(0.,0.,-1.)) ;
#105352 = DIRECTION('center_axis',(0.,1.,0.)) ;
#105353 = DIRECTION('ref_axis',(0.,0.,-1.)) ;
#105354 = DIRECTION('center_axis',(1.,0.,0.)) ;
#105355 = DIRECTION('ref_axis',(0.,0.,-1.)) ;
#105356 = DIRECTION('center_axis',(1.,0.,0.)) ;
#105357 = DIRECTION('ref_axis',(0.,0.,-1.)) ;
#105358 = DIRECTION('center_axis',(0.,1.,1.22464679914735E-16)) ;
#105359 = DIRECTION('ref_axis',(0.,-1.22464679914735E-16,1.)) ;
#105360 = DIRECTION('center_axis',(-1.,0.,0.)) ;
#105361 = DIRECTION('ref_axis',(0.,0.,-1.)) ;
#105362 = DIRECTION('center_axis',(-1.,0.,0.)) ;
#105363 = DIRECTION('ref_axis',(0.,0.,1.)) ;
#105364 = DIRECTION('center_axis',(-1.,0.,0.)) ;
#105365 = DIRECTION('ref_axis',(0.,0.,1.)) ;
#105366 = DIRECTION('center_axis',(0.,-1.,1.22464679914735E-16)) ;
#105367 = DIRECTION('ref_axis',(0.,-1.22464679914735E-16,-1.)) ;
#105368 = DIRECTION('center_axis',(1.,0.,0.)) ;
#105369 = DIRECTION('ref_axis',(0.,0.,1.)) ;
#105370 = DIRECTION('center_axis',(1.,0.,0.)) ;
#105371 = DIRECTION('ref_axis',(0.,0.,1.)) ;
#105372 = DIRECTION('center_axis',(-1.,0.,0.)) ;
#105373 = DIRECTION('ref_axis',(0.,0.,1.)) ;
#105374 = DIRECTION('center_axis',(-1.,0.,0.)) ;
#105375 = DIRECTION('ref_axis',(0.,0.,1.)) ;
#105376 = DIRECTION('center_axis',(0.,0.986393923832144,-0.164398987305358)) ;
#105377 = DIRECTION('ref_axis',(0.,-0.164398987305358,-0.986393923832144)) ;
#105378 = DIRECTION('center_axis',(1.,0.,0.)) ;
#105379 = DIRECTION('ref_axis',(0.,0.,1.)) ;
#105380 = DIRECTION('center_axis',(0.,0.,1.)) ;
#105381 = DIRECTION('ref_axis',(1.,0.,0.)) ;
#105382 = DIRECTION('center_axis',(0.,1.,0.)) ;
#105383 = DIRECTION('ref_axis',(1.,0.,0.)) ;
#105384 = DIRECTION('center_axis',(1.,0.,0.)) ;
#105385 = DIRECTION('ref_axis',(0.,0.,-1.)) ;
#105386 = DIRECTION('center_axis',(0.,0.,-1.)) ;
#105387 = DIRECTION('ref_axis',(-1.,0.,0.)) ;
#105388 = DIRECTION('center_axis',(0.,-0.986393923832144,0.164398987305358)) ;
#105389 = DIRECTION('ref_axis',(0.,0.164398987305358,0.986393923832144)) ;
#105390 = DIRECTION('center_axis',(-1.,0.,0.)) ;
#105391 = DIRECTION('ref_axis',(0.,0.,1.)) ;
#105392 = DIRECTION('',(1.,0.,0.)) ;
#105393 = DIRECTION('center_axis',(-1.,0.,0.)) ;
#105394 = DIRECTION('ref_axis',(0.,0.,1.)) ;
#105395 = DIRECTION('',(-1.,0.,0.)) ;
#105396 = DIRECTION('center_axis',(0.,1.,0.)) ;
#105397 = DIRECTION('ref_axis',(1.,0.,0.)) ;
#105398 = DIRECTION('center_axis',(0.,-0.986393923832144,-0.164398987305358)) ;
#105399 = DIRECTION('ref_axis',(0.,-0.164398987305358,0.986393923832144)) ;
#105400 = DIRECTION('center_axis',(0.,0.,1.)) ;
#105401 = DIRECTION('ref_axis',(1.,0.,0.)) ;
#105402 = DIRECTION('center_axis',(-1.,0.,0.)) ;
#105403 = DIRECTION('ref_axis',(0.,0.,-1.)) ;
#105404 = DIRECTION('center_axis',(1.,0.,0.)) ;
#105405 = DIRECTION('ref_axis',(0.,0.,-1.)) ;
#105406 = DIRECTION('center_axis',(1.,0.,0.)) ;
#105407 = DIRECTION('ref_axis',(0.,0.,-1.)) ;
#105408 = DIRECTION('',(0.707106781186546,-8.65956056235495E-17,0.707106781186549)) ;
#105409 = DIRECTION('center_axis',(1.,0.,0.)) ;
#105410 = DIRECTION('ref_axis',(0.,0.,-1.)) ;
#105411 = DIRECTION('',(1.,0.,0.)) ;
#105412 = DIRECTION('center_axis',(0.,1.,0.)) ;
#105413 = DIRECTION('ref_axis',(0.,0.,1.)) ;
#105414 = DIRECTION('center_axis',(0.,1.,0.)) ;
#105415 = DIRECTION('ref_axis',(0.,0.,1.)) ;
#105416 = DIRECTION('',(0.,1.,0.)) ;
#105417 = DIRECTION('center_axis',(0.,1.,0.)) ;
#105418 = DIRECTION('ref_axis',(0.,0.,1.)) ;
#105419 = DIRECTION('',(0.,1.,0.)) ;
#105420 = DIRECTION('center_axis',(0.,1.,0.)) ;
#105421 = DIRECTION('ref_axis',(0.,0.,1.)) ;
#105422 = DIRECTION('',(0.,1.,0.)) ;
#105423 = DIRECTION('center_axis',(0.,1.,0.)) ;
#105424 = DIRECTION('ref_axis',(0.,0.,1.)) ;
#105425 = DIRECTION('',(0.,1.,0.)) ;
#105426 = DIRECTION('center_axis',(0.,1.,0.)) ;
#105427 = DIRECTION('ref_axis',(0.,0.,1.)) ;
#105428 = DIRECTION('',(0.,1.,0.)) ;
#105429 = DIRECTION('center_axis',(-1.,0.,0.)) ;
#105430 = DIRECTION('ref_axis',(0.,0.,1.)) ;
#105431 = DIRECTION('center_axis',(-1.,0.,0.)) ;
#105432 = DIRECTION('ref_axis',(0.,0.,1.)) ;
#105433 = DIRECTION('center_axis',(-3.56483478381767E-16,0.986393923832144,
0.164398987305358)) ;
#105434 = DIRECTION('ref_axis',(-3.72967278346455E-31,-0.164398987305358,
0.986393923832144)) ;
#105435 = DIRECTION('center_axis',(1.,0.,0.)) ;
#105436 = DIRECTION('ref_axis',(0.,1.43114686768087E-13,1.)) ;
#105437 = DIRECTION('center_axis',(-4.02631181035926E-15,0.928404294083138,
-0.371571617226061)) ;
#105438 = DIRECTION('ref_axis',(-1.2864990704331E-29,0.371571617226061,0.928404294083138)) ;
#105439 = DIRECTION('center_axis',(0.,0.,1.)) ;
#105440 = DIRECTION('ref_axis',(1.,0.,0.)) ;
#105441 = DIRECTION('center_axis',(0.,0.,1.)) ;
#105442 = DIRECTION('ref_axis',(1.,0.,0.)) ;
#105443 = DIRECTION('',(0.,0.,-1.)) ;
#105444 = DIRECTION('center_axis',(0.,0.,-1.)) ;
#105445 = DIRECTION('ref_axis',(1.,0.,0.)) ;
#105446 = DIRECTION('',(0.,0.,1.)) ;
#105447 = DIRECTION('center_axis',(0.,-1.,0.)) ;
#105448 = DIRECTION('ref_axis',(0.,0.,-1.)) ;
#105449 = DIRECTION('center_axis',(0.,-1.,0.)) ;
#105450 = DIRECTION('ref_axis',(0.,0.,-1.)) ;
#105451 = DIRECTION('center_axis',(-1.,0.,-1.22464679914735E-16)) ;
#105452 = DIRECTION('ref_axis',(-1.22464679914735E-16,0.,1.)) ;
#105453 = DIRECTION('center_axis',(0.,1.,0.)) ;
#105454 = DIRECTION('ref_axis',(0.,0.,-1.)) ;
#105455 = DIRECTION('center_axis',(0.,1.,0.)) ;
#105456 = DIRECTION('ref_axis',(0.,0.,-1.)) ;
#105457 = DIRECTION('center_axis',(1.,0.,0.)) ;
#105458 = DIRECTION('ref_axis',(0.,0.,-1.)) ;
#105459 = DIRECTION('center_axis',(1.,0.,0.)) ;
#105460 = DIRECTION('ref_axis',(0.,0.,-1.)) ;
#105461 = DIRECTION('center_axis',(0.,1.,1.22464679914735E-16)) ;
#105462 = DIRECTION('ref_axis',(0.,-1.22464679914735E-16,1.)) ;
#105463 = DIRECTION('center_axis',(-1.,0.,0.)) ;
#105464 = DIRECTION('ref_axis',(0.,0.,-1.)) ;
#105465 = DIRECTION('center_axis',(-1.,0.,0.)) ;
#105466 = DIRECTION('ref_axis',(0.,0.,1.)) ;
#105467 = DIRECTION('center_axis',(-1.,0.,0.)) ;
#105468 = DIRECTION('ref_axis',(0.,0.,1.)) ;
#105469 = DIRECTION('center_axis',(0.,-1.,1.22464679914735E-16)) ;
#105470 = DIRECTION('ref_axis',(0.,-1.22464679914735E-16,-1.)) ;
#105471 = DIRECTION('center_axis',(1.,0.,0.)) ;
#105472 = DIRECTION('ref_axis',(0.,0.,1.)) ;
#105473 = DIRECTION('center_axis',(1.,0.,0.)) ;
#105474 = DIRECTION('ref_axis',(0.,0.,1.)) ;
#105475 = DIRECTION('center_axis',(-1.,0.,0.)) ;
#105476 = DIRECTION('ref_axis',(0.,0.,1.)) ;
#105477 = DIRECTION('center_axis',(-1.,0.,0.)) ;
#105478 = DIRECTION('ref_axis',(0.,0.,1.)) ;
#105479 = DIRECTION('center_axis',(0.,0.986393923832144,-0.164398987305358)) ;
#105480 = DIRECTION('ref_axis',(0.,-0.164398987305358,-0.986393923832144)) ;
#105481 = DIRECTION('center_axis',(1.,0.,0.)) ;
#105482 = DIRECTION('ref_axis',(0.,0.,1.)) ;
#105483 = DIRECTION('center_axis',(0.,0.,1.)) ;
#105484 = DIRECTION('ref_axis',(1.,0.,0.)) ;
#105485 = DIRECTION('center_axis',(0.,1.,0.)) ;
#105486 = DIRECTION('ref_axis',(1.,0.,0.)) ;
#105487 = DIRECTION('center_axis',(1.,0.,0.)) ;
#105488 = DIRECTION('ref_axis',(0.,0.,-1.)) ;
#105489 = DIRECTION('center_axis',(0.,0.,-1.)) ;
#105490 = DIRECTION('ref_axis',(-1.,0.,0.)) ;
#105491 = DIRECTION('center_axis',(0.,-0.986393923832144,0.164398987305358)) ;
#105492 = DIRECTION('ref_axis',(0.,0.164398987305358,0.986393923832144)) ;
#105493 = DIRECTION('center_axis',(-1.,0.,0.)) ;
#105494 = DIRECTION('ref_axis',(0.,0.,1.)) ;
#105495 = DIRECTION('',(1.,0.,0.)) ;
#105496 = DIRECTION('center_axis',(-1.,0.,0.)) ;
#105497 = DIRECTION('ref_axis',(0.,0.,1.)) ;
#105498 = DIRECTION('',(-1.,0.,0.)) ;
#105499 = DIRECTION('center_axis',(0.,1.,0.)) ;
#105500 = DIRECTION('ref_axis',(1.,0.,0.)) ;
#105501 = DIRECTION('center_axis',(0.,-0.986393923832144,-0.164398987305358)) ;
#105502 = DIRECTION('ref_axis',(0.,-0.164398987305358,0.986393923832144)) ;
#105503 = DIRECTION('center_axis',(0.,0.,1.)) ;
#105504 = DIRECTION('ref_axis',(1.,0.,0.)) ;
#105505 = DIRECTION('center_axis',(-1.,0.,0.)) ;
#105506 = DIRECTION('ref_axis',(0.,0.,-1.)) ;
#105507 = DIRECTION('center_axis',(1.,0.,0.)) ;
#105508 = DIRECTION('ref_axis',(0.,0.,-1.)) ;
#105509 = DIRECTION('center_axis',(1.,0.,0.)) ;
#105510 = DIRECTION('ref_axis',(0.,0.,-1.)) ;
#105511 = DIRECTION('',(0.707106781186546,-8.65956056235495E-17,0.707106781186549)) ;
#105512 = DIRECTION('center_axis',(1.,0.,0.)) ;
#105513 = DIRECTION('ref_axis',(0.,0.,-1.)) ;
#105514 = DIRECTION('',(1.,0.,0.)) ;
#105515 = DIRECTION('center_axis',(0.,1.,0.)) ;
#105516 = DIRECTION('ref_axis',(0.,0.,1.)) ;
#105517 = DIRECTION('center_axis',(0.,1.,0.)) ;
#105518 = DIRECTION('ref_axis',(0.,0.,1.)) ;
#105519 = DIRECTION('',(0.,1.,0.)) ;
#105520 = DIRECTION('center_axis',(0.,1.,0.)) ;
#105521 = DIRECTION('ref_axis',(0.,0.,1.)) ;
#105522 = DIRECTION('',(0.,1.,0.)) ;
#105523 = DIRECTION('center_axis',(0.,1.,0.)) ;
#105524 = DIRECTION('ref_axis',(0.,0.,1.)) ;
#105525 = DIRECTION('',(0.,1.,0.)) ;
#105526 = DIRECTION('center_axis',(0.,1.,0.)) ;
#105527 = DIRECTION('ref_axis',(0.,0.,1.)) ;
#105528 = DIRECTION('',(0.,1.,0.)) ;
#105529 = DIRECTION('center_axis',(0.,1.,0.)) ;
#105530 = DIRECTION('ref_axis',(0.,0.,1.)) ;
#105531 = DIRECTION('',(0.,1.,0.)) ;
#105532 = DIRECTION('center_axis',(-1.,0.,0.)) ;
#105533 = DIRECTION('ref_axis',(0.,0.,1.)) ;
#105534 = DIRECTION('',(0.,0.,1.)) ;
#105535 = DIRECTION('',(0.,1.,0.)) ;
#105536 = DIRECTION('',(0.,0.,-1.)) ;
#105537 = DIRECTION('',(0.,1.,0.)) ;
#105538 = DIRECTION('center_axis',(1.,0.,0.)) ;
#105539 = DIRECTION('ref_axis',(0.,0.,1.)) ;
#105540 = DIRECTION('',(0.,1.,0.)) ;
#105541 = DIRECTION('',(0.,0.,-1.)) ;
#105542 = DIRECTION('',(0.,-1.,0.)) ;
#105543 = DIRECTION('center_axis',(1.,0.,0.)) ;
#105544 = DIRECTION('ref_axis',(0.,0.,1.)) ;
#105545 = DIRECTION('',(0.,0.,1.)) ;
#105546 = DIRECTION('center_axis',(-3.46944695195361E-15,-1.,0.)) ;
#105547 = DIRECTION('ref_axis',(1.,-3.46944695195361E-15,0.)) ;
#105548 = DIRECTION('',(1.,-3.46944695195361E-15,0.)) ;
#105549 = DIRECTION('',(0.,0.,1.)) ;
#105550 = DIRECTION('',(-1.,3.46944695195361E-15,0.)) ;
#105551 = DIRECTION('',(0.,0.,-1.)) ;
#105552 = DIRECTION('center_axis',(-1.,0.,0.)) ;
#105553 = DIRECTION('ref_axis',(0.,0.,1.)) ;
#105554 = DIRECTION('',(0.,-1.,0.)) ;
#105555 = DIRECTION('',(0.,0.,1.)) ;
#105556 = DIRECTION('',(0.,1.,0.)) ;
#105557 = DIRECTION('',(0.,0.,-1.)) ;
#105558 = DIRECTION('center_axis',(0.,1.,0.)) ;
#105559 = DIRECTION('ref_axis',(0.,0.,1.)) ;
#105560 = DIRECTION('',(-1.,0.,0.)) ;
#105561 = DIRECTION('',(0.,0.,1.)) ;
#105562 = DIRECTION('',(1.,0.,0.)) ;
#105563 = DIRECTION('',(0.,0.,-1.)) ;
#105564 = DIRECTION('center_axis',(0.,0.,-1.)) ;
#105565 = DIRECTION('ref_axis',(-1.,0.,0.)) ;
#105566 = DIRECTION('center_axis',(0.,0.,1.)) ;
#105567 = DIRECTION('ref_axis',(-1.,0.,0.)) ;
#105568 = DIRECTION('',(0.,0.,-1.)) ;
#105569 = DIRECTION('center_axis',(0.,0.,1.)) ;
#105570 = DIRECTION('ref_axis',(1.,0.,0.)) ;
#105571 = DIRECTION('center_axis',(0.,0.,1.)) ;
#105572 = DIRECTION('ref_axis',(1.,0.,0.)) ;
#105573 = DIRECTION('center_axis',(0.,0.,1.)) ;
#105574 = DIRECTION('ref_axis',(-1.,0.,0.)) ;
#105575 = DIRECTION('center_axis',(0.,0.,-1.)) ;
#105576 = DIRECTION('ref_axis',(1.,0.,0.)) ;
#105577 = DIRECTION('center_axis',(0.,0.,1.)) ;
#105578 = DIRECTION('ref_axis',(1.,0.,0.)) ;
#105579 = DIRECTION('center_axis',(0.,0.,1.)) ;
#105580 = DIRECTION('ref_axis',(-1.,0.,0.)) ;
#105581 = DIRECTION('center_axis',(0.,0.,-1.)) ;
#105582 = DIRECTION('ref_axis',(1.,0.,0.)) ;
#105583 = DIRECTION('center_axis',(0.,0.,-1.)) ;
#105584 = DIRECTION('ref_axis',(-1.,0.,0.)) ;
#105585 = DIRECTION('center_axis',(0.,0.,-1.)) ;
#105586 = DIRECTION('ref_axis',(1.,0.,0.)) ;
#105587 = DIRECTION('',(0.,0.,1.)) ;
#105588 = DIRECTION('center_axis',(0.,0.,1.)) ;
#105589 = DIRECTION('ref_axis',(-1.,3.46944695195362E-14,0.)) ;
#105590 = DIRECTION('center_axis',(0.,0.,1.)) ;
#105591 = DIRECTION('ref_axis',(1.,0.,0.)) ;
#105592 = DIRECTION('',(0.,0.,1.)) ;
#105593 = DIRECTION('center_axis',(-1.,0.,0.)) ;
#105594 = DIRECTION('ref_axis',(0.,0.,1.)) ;
#105595 = DIRECTION('center_axis',(-1.,0.,0.)) ;
#105596 = DIRECTION('ref_axis',(0.,0.,1.)) ;
#105597 = DIRECTION('',(0.,0.,-1.)) ;
#105598 = DIRECTION('',(0.,1.,0.)) ;
#105599 = DIRECTION('',(0.,0.,1.)) ;
#105600 = DIRECTION('center_axis',(-2.09002828430941E-16,1.,0.)) ;
#105601 = DIRECTION('ref_axis',(-1.,-2.09002828430941E-16,0.)) ;
#105602 = DIRECTION('',(0.,0.,1.)) ;
#105603 = DIRECTION('',(-1.,-2.09002828430941E-16,0.)) ;
#105604 = DIRECTION('',(0.,0.,-1.)) ;
#105605 = DIRECTION('',(1.,2.09002828430941E-16,0.)) ;
#105606 = DIRECTION('center_axis',(1.0450141421547E-16,-1.,0.)) ;
#105607 = DIRECTION('ref_axis',(1.,1.0450141421547E-16,0.)) ;
#105608 = DIRECTION('',(-1.,-1.0450141421547E-16,0.)) ;
#105609 = DIRECTION('',(0.,0.,1.)) ;
#105610 = DIRECTION('',(1.,1.0450141421547E-16,1.7416902369245E-17)) ;
#105611 = DIRECTION('',(0.,0.,-1.)) ;
#105612 = DIRECTION('center_axis',(0.,1.,0.)) ;
#105613 = DIRECTION('ref_axis',(0.,0.,1.)) ;
#105614 = DIRECTION('',(0.422618261740697,0.,-0.906307787036651)) ;
#105615 = DIRECTION('center_axis',(-1.,0.,0.)) ;
#105616 = DIRECTION('ref_axis',(0.,0.,1.)) ;
#105617 = DIRECTION('',(0.,0.986393923832144,-0.164398987305357)) ;
#105618 = DIRECTION('',(0.,0.,1.)) ;
#105619 = DIRECTION('',(0.,-0.986393923832144,-0.164398987305357)) ;
#105620 = DIRECTION('center_axis',(1.,0.,0.)) ;
#105621 = DIRECTION('ref_axis',(0.,0.,1.)) ;
#105622 = DIRECTION('',(0.,0.,1.)) ;
#105623 = DIRECTION('',(0.,0.986393923832144,-0.164398987305357)) ;
#105624 = DIRECTION('',(0.,0.,1.)) ;
#105625 = DIRECTION('',(0.,1.,0.)) ;
#105626 = DIRECTION('',(0.,0.,-1.)) ;
#105627 = DIRECTION('center_axis',(1.,0.,0.)) ;
#105628 = DIRECTION('ref_axis',(0.,2.6020852139652E-14,1.)) ;
#105629 = DIRECTION('center_axis',(1.,0.,0.)) ;
#105630 = DIRECTION('ref_axis',(0.,8.88178419700125E-16,1.)) ;
#105631 = DIRECTION('center_axis',(1.,0.,0.)) ;
#105632 = DIRECTION('ref_axis',(0.,0.,1.)) ;
#105633 = DIRECTION('',(0.,0.,-1.)) ;
#105634 = DIRECTION('center_axis',(1.,0.,0.)) ;
#105635 = DIRECTION('ref_axis',(0.,0.,1.)) ;
#105636 = DIRECTION('center_axis',(1.,0.,0.)) ;
#105637 = DIRECTION('ref_axis',(0.,0.,1.)) ;
#105638 = DIRECTION('center_axis',(1.,0.,0.)) ;
#105639 = DIRECTION('ref_axis',(0.,0.,1.)) ;
#105640 = DIRECTION('',(0.,0.,-1.)) ;
#105641 = DIRECTION('',(0.,1.,0.)) ;
#105642 = DIRECTION('',(0.,0.,1.)) ;
#105643 = DIRECTION('',(0.,-0.986393923832144,-0.164398987305357)) ;
#105644 = DIRECTION('center_axis',(1.,0.,0.)) ;
#105645 = DIRECTION('ref_axis',(0.,0.,1.)) ;
#105646 = DIRECTION('',(0.,0.,1.)) ;
#105647 = DIRECTION('center_axis',(1.0450141421547E-16,-1.,0.)) ;
#105648 = DIRECTION('ref_axis',(1.,1.0450141421547E-16,0.)) ;
#105649 = DIRECTION('',(-1.,-1.0450141421547E-16,1.7416902369245E-17)) ;
#105650 = DIRECTION('',(0.,0.,1.)) ;
#105651 = DIRECTION('',(1.,1.0450141421547E-16,1.7416902369245E-17)) ;
#105652 = DIRECTION('',(0.,0.,-1.)) ;
#105653 = DIRECTION('center_axis',(-0.876215908676647,-0.481918749772156,
0.)) ;
#105654 = DIRECTION('ref_axis',(0.481918749772156,-0.876215908676647,0.)) ;
#105655 = DIRECTION('',(0.,0.,1.)) ;
#105656 = DIRECTION('',(-0.481918749772156,0.876215908676647,0.)) ;
#105657 = DIRECTION('',(0.,0.,-1.)) ;
#105658 = DIRECTION('center_axis',(-0.87621590867669,-0.481918749772079,-2.87461714907713E-14)) ;
#105659 = DIRECTION('ref_axis',(0.436954455884537,-0.794462647062935,-0.421781822633934)) ;
#105660 = DIRECTION('',(0.,0.,-1.)) ;
#105661 = DIRECTION('center_axis',(-0.876215908676657,-0.481918749772137,
4.26347712001692E-15)) ;
#105662 = DIRECTION('ref_axis',(0.436954455989552,-0.794462647253768,0.421781822165689)) ;
#105663 = DIRECTION('',(0.,0.,-1.)) ;
#105664 = DIRECTION('center_axis',(-0.876215908676638,-0.481918749772173,
5.32934639996306E-15)) ;
#105665 = DIRECTION('ref_axis',(0.436954455831528,-0.794462646966382,-0.421781822870715)) ;
#105666 = DIRECTION('',(0.,0.,-1.)) ;
#105667 = DIRECTION('center_axis',(-0.876215908676651,-0.481918749772149,
9.43132817458479E-15)) ;
#105668 = DIRECTION('ref_axis',(0.436954455977753,-0.794462647232284,0.42178182221838)) ;
#105669 = DIRECTION('',(0.,0.,-1.)) ;
#105670 = DIRECTION('',(-0.481918749772156,0.876215908676647,0.)) ;
#105671 = DIRECTION('center_axis',(-0.876215908676647,-0.481918749772156,
0.)) ;
#105672 = DIRECTION('ref_axis',(0.481918749772156,-0.876215908676647,0.)) ;
#105673 = DIRECTION('',(-0.481918749772156,0.876215908676647,0.)) ;
#105674 = DIRECTION('',(-0.481918749772156,0.876215908676647,0.)) ;
#105675 = DIRECTION('',(0.,0.,-1.)) ;
#105676 = DIRECTION('center_axis',(-1.,0.,0.)) ;
#105677 = DIRECTION('ref_axis',(0.,0.,1.)) ;
#105678 = DIRECTION('',(0.,1.,0.)) ;
#105679 = DIRECTION('',(0.,0.,1.)) ;
#105680 = DIRECTION('',(0.,1.,0.)) ;
#105681 = DIRECTION('',(0.,1.,0.)) ;
#105682 = DIRECTION('center_axis',(0.,-1.,0.)) ;
#105683 = DIRECTION('ref_axis',(0.,0.,-1.)) ;
#105684 = DIRECTION('',(-1.,0.,0.)) ;
#105685 = DIRECTION('',(0.,0.,1.)) ;
#105686 = DIRECTION('',(-1.,0.,0.)) ;
#105687 = DIRECTION('',(0.,0.,-1.)) ;
#105688 = DIRECTION('center_axis',(0.,1.,0.)) ;
#105689 = DIRECTION('ref_axis',(0.,0.,-1.)) ;
#105690 = DIRECTION('',(2.16840434497101E-16,0.,1.)) ;
#105691 = DIRECTION('center_axis',(0.,1.,0.)) ;
#105692 = DIRECTION('ref_axis',(0.,0.,-1.)) ;
#105693 = DIRECTION('',(-1.,0.,1.73472347597681E-16)) ;
#105694 = DIRECTION('center_axis',(0.,1.,0.)) ;
#105695 = DIRECTION('ref_axis',(0.,0.,-1.)) ;
#105696 = DIRECTION('',(-2.16840434497101E-16,0.,-1.)) ;
#105697 = DIRECTION('center_axis',(0.,1.,0.)) ;
#105698 = DIRECTION('ref_axis',(0.,0.,-1.)) ;
#105699 = DIRECTION('',(1.,0.,-1.73472347597681E-16)) ;
#105700 = DIRECTION('center_axis',(0.,1.,0.)) ;
#105701 = DIRECTION('ref_axis',(0.,0.,-1.)) ;
#105702 = DIRECTION('',(2.16840434497101E-16,0.,1.)) ;
#105703 = DIRECTION('center_axis',(0.,1.,0.)) ;
#105704 = DIRECTION('ref_axis',(0.,0.,-1.)) ;
#105705 = DIRECTION('',(-1.,0.,1.73472347597681E-16)) ;
#105706 = DIRECTION('center_axis',(0.,1.,0.)) ;
#105707 = DIRECTION('ref_axis',(0.,0.,-1.)) ;
#105708 = DIRECTION('',(-2.16840434497101E-16,0.,-1.)) ;
#105709 = DIRECTION('center_axis',(0.,1.,0.)) ;
#105710 = DIRECTION('ref_axis',(0.,0.,-1.)) ;
#105711 = DIRECTION('',(1.,0.,-1.73472347597681E-16)) ;
#105712 = DIRECTION('center_axis',(1.,0.,0.)) ;
#105713 = DIRECTION('ref_axis',(0.,0.,-1.)) ;
#105714 = DIRECTION('',(0.,-1.,0.)) ;
#105715 = DIRECTION('',(0.,0.,1.)) ;
#105716 = DIRECTION('',(0.,-1.,0.)) ;
#105717 = DIRECTION('',(0.,0.,-1.)) ;
#105718 = DIRECTION('center_axis',(0.,1.,0.)) ;
#105719 = DIRECTION('ref_axis',(0.,0.,1.)) ;
#105720 = DIRECTION('',(1.,0.,0.)) ;
#105721 = DIRECTION('',(1.,0.,0.)) ;
#105722 = DIRECTION('',(0.,0.,-1.)) ;
#105723 = DIRECTION('center_axis',(0.98058067569092,-0.196116135138184,0.)) ;
#105724 = DIRECTION('ref_axis',(0.196116135138184,0.98058067569092,0.)) ;
#105725 = DIRECTION('',(-0.196116135138184,-0.98058067569092,0.)) ;
#105726 = DIRECTION('',(0.,0.,1.)) ;
#105727 = DIRECTION('',(-0.196116135138184,-0.98058067569092,0.)) ;
#105728 = DIRECTION('center_axis',(1.,0.,0.)) ;
#105729 = DIRECTION('ref_axis',(0.,0.,-1.)) ;
#105730 = DIRECTION('',(0.,-1.,0.)) ;
#105731 = DIRECTION('',(0.,0.,1.)) ;
#105732 = DIRECTION('',(0.,-1.,0.)) ;
#105733 = DIRECTION('',(0.,0.,-1.)) ;
#105734 = DIRECTION('',(0.,0.,1.)) ;
#105735 = DIRECTION('',(0.,-1.,0.)) ;
#105736 = DIRECTION('',(0.,0.,-1.)) ;
#105737 = DIRECTION('',(0.,1.,0.)) ;
#105738 = DIRECTION('',(0.,0.,1.)) ;
#105739 = DIRECTION('',(0.,-1.,0.)) ;
#105740 = DIRECTION('',(0.,0.,-1.)) ;
#105741 = DIRECTION('',(0.,1.,0.)) ;
#105742 = DIRECTION('center_axis',(0.,1.,0.)) ;
#105743 = DIRECTION('ref_axis',(0.,0.,1.)) ;
#105744 = DIRECTION('',(1.,0.,0.)) ;
#105745 = DIRECTION('',(0.,0.,1.)) ;
#105746 = DIRECTION('',(1.,0.,0.)) ;
#105747 = DIRECTION('',(0.,0.,-1.)) ;
#105748 = DIRECTION('center_axis',(0.,-1.,0.)) ;
#105749 = DIRECTION('ref_axis',(0.,0.,1.)) ;
#105750 = DIRECTION('',(0.,0.,1.)) ;
#105751 = DIRECTION('center_axis',(0.,-1.,0.)) ;
#105752 = DIRECTION('ref_axis',(0.,0.,1.)) ;
#105753 = DIRECTION('',(1.,0.,1.73472347597681E-16)) ;
#105754 = DIRECTION('center_axis',(0.,-1.,0.)) ;
#105755 = DIRECTION('ref_axis',(0.,0.,1.)) ;
#105756 = DIRECTION('',(4.33680868994202E-16,0.,-1.)) ;
#105757 = DIRECTION('center_axis',(0.,-1.,0.)) ;
#105758 = DIRECTION('ref_axis',(0.,0.,1.)) ;
#105759 = DIRECTION('',(-1.,0.,1.73472347597681E-16)) ;
#105760 = DIRECTION('center_axis',(0.,-1.,0.)) ;
#105761 = DIRECTION('ref_axis',(0.,0.,1.)) ;
#105762 = DIRECTION('',(0.,0.,1.)) ;
#105763 = DIRECTION('center_axis',(0.,-1.,0.)) ;
#105764 = DIRECTION('ref_axis',(0.,0.,1.)) ;
#105765 = DIRECTION('',(1.,0.,1.73472347597681E-16)) ;
#105766 = DIRECTION('center_axis',(0.,-1.,0.)) ;
#105767 = DIRECTION('ref_axis',(0.,0.,1.)) ;
#105768 = DIRECTION('',(4.33680868994202E-16,0.,-1.)) ;
#105769 = DIRECTION('center_axis',(0.,-1.,0.)) ;
#105770 = DIRECTION('ref_axis',(0.,0.,1.)) ;
#105771 = DIRECTION('',(-1.,0.,1.73472347597681E-16)) ;
#105772 = DIRECTION('center_axis',(-1.,6.93889390390723E-16,0.)) ;
#105773 = DIRECTION('ref_axis',(-6.93889390390723E-16,-1.,0.)) ;
#105774 = DIRECTION('',(6.93889390390723E-16,1.,0.)) ;
#105775 = DIRECTION('',(0.,0.,1.)) ;
#105776 = DIRECTION('',(6.93889390390723E-16,1.,0.)) ;
#105777 = DIRECTION('',(0.,0.,-1.)) ;
#105778 = DIRECTION('center_axis',(0.,1.,0.)) ;
#105779 = DIRECTION('ref_axis',(0.,0.,1.)) ;
#105780 = DIRECTION('',(0.,0.,1.)) ;
#105781 = DIRECTION('',(0.,0.,1.)) ;
#105782 = DIRECTION('',(1.,0.,0.)) ;
#105783 = DIRECTION('',(0.,0.,-1.)) ;
#105784 = DIRECTION('',(1.,0.,0.)) ;
#105785 = DIRECTION('',(0.,0.,1.)) ;
#105786 = DIRECTION('center_axis',(-1.,0.,0.)) ;
#105787 = DIRECTION('ref_axis',(0.,0.,1.)) ;
#105788 = DIRECTION('',(0.,0.,1.)) ;
#105789 = DIRECTION('center_axis',(-1.,0.,0.)) ;
#105790 = DIRECTION('ref_axis',(0.,0.,1.)) ;
#105791 = DIRECTION('',(0.,0.,-1.)) ;
#105792 = DIRECTION('center_axis',(-1.,0.,0.)) ;
#105793 = DIRECTION('ref_axis',(0.,0.,1.)) ;
#105794 = DIRECTION('center_axis',(-2.09002828430941E-16,1.,0.)) ;
#105795 = DIRECTION('ref_axis',(-1.,-2.09002828430941E-16,0.)) ;
#105796 = DIRECTION('',(-1.,-2.09002828430941E-16,0.)) ;
#105797 = DIRECTION('',(0.,0.,-1.)) ;
#105798 = DIRECTION('',(1.,2.09002828430941E-16,0.)) ;
#105799 = DIRECTION('',(0.,0.,1.)) ;
#105800 = DIRECTION('center_axis',(0.,0.,1.)) ;
#105801 = DIRECTION('ref_axis',(1.,0.,0.)) ;
#105802 = DIRECTION('center_axis',(0.,0.,-1.)) ;
#105803 = DIRECTION('ref_axis',(1.,0.,0.)) ;
#105804 = DIRECTION('center_axis',(0.,0.,-1.)) ;
#105805 = DIRECTION('ref_axis',(1.,1.04083408558609E-13,0.)) ;
#105806 = DIRECTION('center_axis',(0.,0.,1.)) ;
#105807 = DIRECTION('ref_axis',(1.,0.,0.)) ;
#105808 = DIRECTION('center_axis',(0.,0.,1.)) ;
#105809 = DIRECTION('ref_axis',(1.,0.,0.)) ;
#105810 = DIRECTION('center_axis',(0.,0.,-1.)) ;
#105811 = DIRECTION('ref_axis',(1.,1.30104260698261E-14,0.)) ;
#105812 = DIRECTION('center_axis',(0.,0.,-1.)) ;
#105813 = DIRECTION('ref_axis',(1.,0.,0.)) ;
#105814 = DIRECTION('center_axis',(0.,0.,1.)) ;
#105815 = DIRECTION('ref_axis',(1.,0.,0.)) ;
#105816 = DIRECTION('center_axis',(0.,0.,-1.)) ;
#105817 = DIRECTION('ref_axis',(1.,0.,0.)) ;
#105818 = DIRECTION('center_axis',(0.,0.,1.)) ;
#105819 = DIRECTION('ref_axis',(1.,0.,0.)) ;
#105820 = DIRECTION('center_axis',(0.,0.,-1.)) ;
#105821 = DIRECTION('ref_axis',(1.,0.,0.)) ;
#105822 = DIRECTION('center_axis',(0.,0.,-1.)) ;
#105823 = DIRECTION('ref_axis',(1.,0.,0.)) ;
#105824 = DIRECTION('center_axis',(0.,0.,-1.)) ;
#105825 = DIRECTION('ref_axis',(1.,2.6020852139652E-14,0.)) ;
#105826 = DIRECTION('center_axis',(0.,0.,-1.)) ;
#105827 = DIRECTION('ref_axis',(1.,0.,0.)) ;
#105828 = DIRECTION('center_axis',(0.,0.,-1.)) ;
#105829 = DIRECTION('ref_axis',(1.,0.,0.)) ;
#105830 = DIRECTION('center_axis',(0.,0.,1.)) ;
#105831 = DIRECTION('ref_axis',(1.,0.,0.)) ;
#105832 = DIRECTION('',(-0.664363838829919,0.74740931868366,0.)) ;
#105833 = DIRECTION('',(0.,-1.,0.)) ;
#105834 = DIRECTION('',(0.894427190999917,0.447213595499956,0.)) ;
#105835 = DIRECTION('',(0.,1.,0.)) ;
#105836 = DIRECTION('center_axis',(0.,0.,-1.)) ;
#105837 = DIRECTION('ref_axis',(-1.,0.,0.)) ;
#105838 = DIRECTION('',(-0.894427190999917,-0.447213595499956,0.)) ;
#105839 = DIRECTION('',(0.,1.,0.)) ;
#105840 = DIRECTION('',(0.664363838829919,-0.74740931868366,0.)) ;
#105841 = DIRECTION('',(0.,-1.,0.)) ;
#105842 = DIRECTION('center_axis',(-0.23745309047699,0.,-0.971399006496778)) ;
#105843 = DIRECTION('ref_axis',(-0.971399006496778,0.,0.23745309047699)) ;
#105844 = DIRECTION('center_axis',(-0.237453090476988,5.12980051156625E-14,
-0.971399006496778)) ;
#105845 = DIRECTION('ref_axis',(0.921799787670952,-0.315455332293199,-0.225328836986247)) ;
#105846 = DIRECTION('',(0.971399006496777,0.,-0.23745309047699)) ;
#105847 = DIRECTION('',(0.,-1.,0.)) ;
#105848 = DIRECTION('',(-0.971399006496777,0.,0.23745309047699)) ;
#105849 = DIRECTION('center_axis',(-0.23745309047692,-4.15843437570133E-13,
-0.971399006496795)) ;
#105850 = DIRECTION('ref_axis',(0.9545593542551,0.185392581166527,-0.233336731040142)) ;
#105851 = DIRECTION('',(-0.873786407766991,-0.436893203883493,0.213592233009709)) ;
#105852 = DIRECTION('',(0.,1.,0.)) ;
#105853 = DIRECTION('',(0.655772517804503,-0.737744082530068,-0.160299948796656)) ;
#105854 = DIRECTION('center_axis',(-1.,0.,0.)) ;
#105855 = DIRECTION('ref_axis',(0.,0.,1.)) ;
#105856 = DIRECTION('',(0.,-1.,0.)) ;
#105857 = DIRECTION('center_axis',(-1.,-6.70078870827245E-15,-6.50913949396088E-15)) ;
#105858 = DIRECTION('ref_axis',(6.50913949389232E-15,1.02323485816278E-11,
-1.)) ;
#105859 = DIRECTION('',(0.,0.,-1.)) ;
#105860 = DIRECTION('center_axis',(-1.,-6.70078870827188E-15,6.50913949396004E-15)) ;
#105861 = DIRECTION('ref_axis',(-6.5091394941529E-15,2.87817090394427E-11,
-1.)) ;
#105862 = DIRECTION('center_axis',(-1.,6.70078870827192E-15,6.50913949396007E-15)) ;
#105863 = DIRECTION('ref_axis',(-6.50913949414225E-15,-2.71882442700375E-11,
-1.)) ;
#105864 = DIRECTION('',(0.,0.,-1.)) ;
#105865 = DIRECTION('center_axis',(-1.,6.70078870827247E-15,-6.50913949396088E-15)) ;
#105866 = DIRECTION('ref_axis',(6.50913949373767E-15,-3.33117585083476E-11,
-1.)) ;
#105867 = DIRECTION('center_axis',(-0.23745309047699,0.,0.971399006496778)) ;
#105868 = DIRECTION('ref_axis',(0.971399006496778,0.,0.23745309047699)) ;
#105869 = DIRECTION('center_axis',(-0.237453090476876,-4.17061728891309E-13,
0.971399006496805)) ;
#105870 = DIRECTION('ref_axis',(0.954559354253017,0.185392581177947,0.233336731039587)) ;
#105871 = DIRECTION('',(0.971399006496777,0.,0.23745309047699)) ;
#105872 = DIRECTION('',(-0.971399006496777,0.,-0.23745309047699)) ;
#105873 = DIRECTION('center_axis',(-0.237453090476943,1.57363445644675E-13,
0.971399006496789)) ;
#105874 = DIRECTION('ref_axis',(0.921799787671554,-0.315455332291342,0.225328836986384)) ;
#105875 = DIRECTION('',(-0.655772517804503,0.737744082530068,-0.160299948796656)) ;
#105876 = DIRECTION('',(0.,-1.,0.)) ;
#105877 = DIRECTION('',(0.873786407766991,0.436893203883493,0.213592233009709)) ;
#105878 = DIRECTION('center_axis',(0.,1.,0.)) ;
#105879 = DIRECTION('ref_axis',(0.,0.,1.)) ;
#105880 = DIRECTION('',(-0.971399006496777,0.,0.23745309047699)) ;
#105881 = DIRECTION('',(0.,0.,-1.)) ;
#105882 = DIRECTION('',(0.971399006496777,0.,0.23745309047699)) ;
#105883 = DIRECTION('center_axis',(0.,1.,0.)) ;
#105884 = DIRECTION('ref_axis',(0.,0.,1.)) ;
#105885 = DIRECTION('',(-0.971399006496777,0.,-0.23745309047699)) ;
#105886 = DIRECTION('',(0.,0.,1.)) ;
#105887 = DIRECTION('',(0.971399006496777,0.,-0.23745309047699)) ;
#105888 = DIRECTION('center_axis',(-0.447213595499956,0.894427190999917,0.)) ;
#105889 = DIRECTION('ref_axis',(0.,0.,-1.)) ;
#105890 = DIRECTION('',(0.,0.,-1.)) ;
#105891 = DIRECTION('',(-0.873786407766991,-0.436893203883493,-0.213592233009709)) ;
#105892 = DIRECTION('',(-0.894427190999917,-0.447213595499956,0.)) ;
#105893 = DIRECTION('',(0.,0.,1.)) ;
#105894 = DIRECTION('',(0.894427190999917,0.447213595499956,0.)) ;
#105895 = DIRECTION('',(0.873786407766991,0.436893203883493,-0.213592233009709)) ;
#105896 = DIRECTION('center_axis',(0.74740931868366,0.664363838829919,0.)) ;
#105897 = DIRECTION('ref_axis',(0.,0.,1.)) ;
#105898 = DIRECTION('',(0.,0.,-1.)) ;
#105899 = DIRECTION('',(0.664363838829919,-0.74740931868366,0.)) ;
#105900 = DIRECTION('',(0.655772517804503,-0.737744082530068,0.160299948796656)) ;
#105901 = DIRECTION('',(0.,0.,1.)) ;
#105902 = DIRECTION('',(-0.655772517804503,0.737744082530068,0.160299948796656)) ;
#105903 = DIRECTION('',(-0.664363838829919,0.74740931868366,0.)) ;
#105904 = DIRECTION('center_axis',(1.,0.,4.33680868994202E-16)) ;
#105905 = DIRECTION('ref_axis',(4.33680868994202E-16,0.,-1.)) ;
#105906 = DIRECTION('',(0.,1.,0.)) ;
#105907 = DIRECTION('',(4.33680868994202E-16,0.,-1.)) ;
#105908 = DIRECTION('',(0.,-1.,0.)) ;
#105909 = DIRECTION('',(-4.33680868994202E-16,0.,1.)) ;
#105910 = DIRECTION('center_axis',(-1.73472347597681E-16,0.,-1.)) ;
#105911 = DIRECTION('ref_axis',(-1.,0.,1.73472347597681E-16)) ;
#105912 = DIRECTION('',(-1.,0.,1.73472347597681E-16)) ;
#105913 = DIRECTION('',(0.,-1.,0.)) ;
#105914 = DIRECTION('',(1.,0.,-1.73472347597681E-16)) ;
#105915 = DIRECTION('',(0.,1.,0.)) ;
#105916 = DIRECTION('center_axis',(-1.,0.,0.)) ;
#105917 = DIRECTION('ref_axis',(0.,0.,1.)) ;
#105918 = DIRECTION('',(0.,0.,1.)) ;
#105919 = DIRECTION('',(0.,-1.,0.)) ;
#105920 = DIRECTION('',(0.,0.,-1.)) ;
#105921 = DIRECTION('',(0.,1.,0.)) ;
#105922 = DIRECTION('center_axis',(-1.73472347597681E-16,0.,1.)) ;
#105923 = DIRECTION('ref_axis',(1.,0.,1.73472347597681E-16)) ;
#105924 = DIRECTION('',(0.,1.,0.)) ;
#105925 = DIRECTION('',(1.,0.,1.73472347597681E-16)) ;
#105926 = DIRECTION('',(0.,-1.,0.)) ;
#105927 = DIRECTION('',(-1.,0.,-1.73472347597681E-16)) ;
#105928 = DIRECTION('center_axis',(0.,-1.,0.)) ;
#105929 = DIRECTION('ref_axis',(0.,0.,-1.)) ;
#105930 = DIRECTION('',(-1.,0.,-1.73472347597681E-16)) ;
#105931 = DIRECTION('',(0.,0.,-1.)) ;
#105932 = DIRECTION('',(1.,0.,-1.73472347597681E-16)) ;
#105933 = DIRECTION('',(-4.33680868994202E-16,0.,1.)) ;
#105934 = DIRECTION('',(1.,0.,0.)) ;
#105935 = DIRECTION('center_axis',(0.,-1.,0.)) ;
#105936 = DIRECTION('ref_axis',(0.,0.,-1.)) ;
#105937 = DIRECTION('',(0.,0.,-1.)) ;
#105938 = DIRECTION('center_axis',(0.,-1.,0.)) ;
#105939 = DIRECTION('ref_axis',(0.,0.,-1.)) ;
#105940 = DIRECTION('',(-1.,0.,0.)) ;
#105941 = DIRECTION('center_axis',(0.,-1.,0.)) ;
#105942 = DIRECTION('ref_axis',(0.,0.,1.)) ;
#105943 = DIRECTION('',(0.,0.,1.)) ;
#105944 = DIRECTION('center_axis',(0.,-1.,0.)) ;
#105945 = DIRECTION('ref_axis',(0.,0.,-1.)) ;
#105946 = DIRECTION('center_axis',(0.,-1.,0.)) ;
#105947 = DIRECTION('ref_axis',(0.,0.,-1.)) ;
#105948 = DIRECTION('center_axis',(0.,-1.,0.)) ;
#105949 = DIRECTION('ref_axis',(0.,0.,-1.)) ;
#105950 = DIRECTION('',(0.,-1.,0.)) ;
#105951 = DIRECTION('',(0.,-1.,0.)) ;
#105952 = DIRECTION('center_axis',(0.,0.,-1.)) ;
#105953 = DIRECTION('ref_axis',(-1.,0.,0.)) ;
#105954 = DIRECTION('',(1.,0.,0.)) ;
#105955 = DIRECTION('',(0.,-1.,0.)) ;
#105956 = DIRECTION('center_axis',(0.,-1.,0.)) ;
#105957 = DIRECTION('ref_axis',(0.,0.,-1.)) ;
#105958 = DIRECTION('center_axis',(0.,-1.,0.)) ;
#105959 = DIRECTION('ref_axis',(0.,0.,-1.)) ;
#105960 = DIRECTION('',(0.,-1.,0.)) ;
#105961 = DIRECTION('center_axis',(-1.,0.,0.)) ;
#105962 = DIRECTION('ref_axis',(0.,0.,1.)) ;
#105963 = DIRECTION('',(0.,0.,-1.)) ;
#105964 = DIRECTION('',(0.,-1.,0.)) ;
#105965 = DIRECTION('center_axis',(0.,-1.,0.)) ;
#105966 = DIRECTION('ref_axis',(0.,0.,-1.)) ;
#105967 = DIRECTION('center_axis',(0.,-1.,0.)) ;
#105968 = DIRECTION('ref_axis',(0.,0.,-1.)) ;
#105969 = DIRECTION('',(0.,-1.,0.)) ;
#105970 = DIRECTION('center_axis',(0.,0.,1.)) ;
#105971 = DIRECTION('ref_axis',(1.,0.,0.)) ;
#105972 = DIRECTION('',(-1.,0.,0.)) ;
#105973 = DIRECTION('',(0.,-1.,0.)) ;
#105974 = DIRECTION('center_axis',(0.,-1.,0.)) ;
#105975 = DIRECTION('ref_axis',(0.,0.,-1.)) ;
#105976 = DIRECTION('center_axis',(0.,-1.,0.)) ;
#105977 = DIRECTION('ref_axis',(0.,0.,1.)) ;
#105978 = DIRECTION('',(0.,-1.,0.)) ;
#105979 = DIRECTION('center_axis',(1.,0.,0.)) ;
#105980 = DIRECTION('ref_axis',(0.,0.,-1.)) ;
#105981 = DIRECTION('',(0.,0.,1.)) ;
#105982 = DIRECTION('center_axis',(0.,-1.,0.)) ;
#105983 = DIRECTION('ref_axis',(0.,0.,-1.)) ;
#105984 = DIRECTION('center_axis',(0.,1.,0.)) ;
#105985 = DIRECTION('ref_axis',(0.,0.,1.)) ;
#105986 = DIRECTION('',(-0.422618261740697,0.,0.906307787036651)) ;
#105987 = DIRECTION('center_axis',(0.906307787036651,0.,0.422618261740697)) ;
#105988 = DIRECTION('ref_axis',(0.422618261740697,0.,-0.906307787036651)) ;
#105989 = DIRECTION('',(-0.422618261740697,0.,0.906307787036651)) ;
#105990 = DIRECTION('',(0.422618261740697,0.,-0.906307787036651)) ;
#105991 = DIRECTION('center_axis',(-0.906307787036651,0.,-0.422618261740697)) ;
#105992 = DIRECTION('ref_axis',(-0.422618261740697,0.,0.906307787036651)) ;
#105993 = DIRECTION('',(0.422618261740697,0.,-0.906307787036651)) ;
#105994 = DIRECTION('',(-0.422618261740697,0.,0.906307787036651)) ;
#105995 = DIRECTION('center_axis',(0.,1.,0.)) ;
#105996 = DIRECTION('ref_axis',(0.,0.,1.)) ;
#105997 = DIRECTION('',(-0.422618261740697,0.,0.906307787036651)) ;
#105998 = DIRECTION('',(0.422618261740697,0.,-0.906307787036651)) ;
#105999 = DIRECTION('center_axis',(1.,0.,-2.16840434497101E-16)) ;
#106000 = DIRECTION('ref_axis',(-2.16840434497101E-16,0.,-1.)) ;
#106001 = DIRECTION('',(2.16840434497101E-16,0.,1.)) ;
#106002 = DIRECTION('',(0.,1.,0.)) ;
#106003 = DIRECTION('',(-2.16840434497101E-16,0.,-1.)) ;
#106004 = DIRECTION('',(0.,-1.,0.)) ;
#106005 = DIRECTION('center_axis',(1.73472347597681E-16,0.,1.)) ;
#106006 = DIRECTION('ref_axis',(1.,0.,-1.73472347597681E-16)) ;
#106007 = DIRECTION('',(0.,-1.,0.)) ;
#106008 = DIRECTION('',(-1.,0.,1.73472347597681E-16)) ;
#106009 = DIRECTION('',(0.,1.,0.)) ;
#106010 = DIRECTION('',(1.,0.,-1.73472347597681E-16)) ;
#106011 = DIRECTION('center_axis',(-1.,0.,2.16840434497101E-16)) ;
#106012 = DIRECTION('ref_axis',(2.16840434497101E-16,0.,1.)) ;
#106013 = DIRECTION('',(0.,-1.,0.)) ;
#106014 = DIRECTION('',(-2.16840434497101E-16,0.,-1.)) ;
#106015 = DIRECTION('',(0.,1.,0.)) ;
#106016 = DIRECTION('',(2.16840434497101E-16,0.,1.)) ;
#106017 = DIRECTION('center_axis',(-1.73472347597681E-16,0.,-1.)) ;
#106018 = DIRECTION('ref_axis',(-1.,0.,1.73472347597681E-16)) ;
#106019 = DIRECTION('',(1.,0.,-1.73472347597681E-16)) ;
#106020 = DIRECTION('',(0.,1.,0.)) ;
#106021 = DIRECTION('',(-1.,0.,1.73472347597681E-16)) ;
#106022 = DIRECTION('',(0.,-1.,0.)) ;
#106023 = DIRECTION('center_axis',(0.,1.,0.)) ;
#106024 = DIRECTION('ref_axis',(0.,0.,1.)) ;
#106025 = DIRECTION('',(1.,0.,-1.73472347597681E-16)) ;
#106026 = DIRECTION('',(-2.16840434497101E-16,0.,-1.)) ;
#106027 = DIRECTION('',(-1.,0.,1.73472347597681E-16)) ;
#106028 = DIRECTION('',(2.16840434497101E-16,0.,1.)) ;
#106029 = DIRECTION('',(1.,0.,0.)) ;
#106030 = DIRECTION('center_axis',(0.,1.,0.)) ;
#106031 = DIRECTION('ref_axis',(0.,0.,1.)) ;
#106032 = DIRECTION('',(0.,0.,1.)) ;
#106033 = DIRECTION('center_axis',(0.,1.,0.)) ;
#106034 = DIRECTION('ref_axis',(0.,0.,1.)) ;
#106035 = DIRECTION('',(-1.,0.,0.)) ;
#106036 = DIRECTION('center_axis',(0.,1.,0.)) ;
#106037 = DIRECTION('ref_axis',(0.,0.,-1.)) ;
#106038 = DIRECTION('',(0.,0.,-1.)) ;
#106039 = DIRECTION('center_axis',(0.,1.,0.)) ;
#106040 = DIRECTION('ref_axis',(0.,0.,1.)) ;
#106041 = DIRECTION('center_axis',(0.,1.,0.)) ;
#106042 = DIRECTION('ref_axis',(0.,0.,1.)) ;
#106043 = DIRECTION('',(0.,1.,0.)) ;
#106044 = DIRECTION('center_axis',(0.,-1.,0.)) ;
#106045 = DIRECTION('ref_axis',(2.60208521396523E-14,0.,1.)) ;
#106046 = DIRECTION('',(0.,1.,0.)) ;
#106047 = DIRECTION('center_axis',(0.,0.,1.)) ;
#106048 = DIRECTION('ref_axis',(1.,0.,0.)) ;
#106049 = DIRECTION('',(-1.,0.,0.)) ;
#106050 = DIRECTION('',(0.,1.,0.)) ;
#106051 = DIRECTION('center_axis',(0.,1.,0.)) ;
#106052 = DIRECTION('ref_axis',(0.,0.,1.)) ;
#106053 = DIRECTION('center_axis',(0.,-1.,0.)) ;
#106054 = DIRECTION('ref_axis',(0.,0.,1.)) ;
#106055 = DIRECTION('',(0.,1.,0.)) ;
#106056 = DIRECTION('center_axis',(-1.,0.,0.)) ;
#106057 = DIRECTION('ref_axis',(0.,0.,1.)) ;
#106058 = DIRECTION('',(0.,0.,-1.)) ;
#106059 = DIRECTION('',(0.,1.,0.)) ;
#106060 = DIRECTION('center_axis',(0.,1.,0.)) ;
#106061 = DIRECTION('ref_axis',(0.,0.,1.)) ;
#106062 = DIRECTION('center_axis',(0.,-1.,0.)) ;
#106063 = DIRECTION('ref_axis',(0.,0.,1.)) ;
#106064 = DIRECTION('',(0.,1.,0.)) ;
#106065 = DIRECTION('center_axis',(0.,0.,-1.)) ;
#106066 = DIRECTION('ref_axis',(-1.,0.,0.)) ;
#106067 = DIRECTION('',(1.,0.,0.)) ;
#106068 = DIRECTION('',(0.,1.,0.)) ;
#106069 = DIRECTION('center_axis',(0.,1.,0.)) ;
#106070 = DIRECTION('ref_axis',(0.,0.,1.)) ;
#106071 = DIRECTION('center_axis',(0.,-1.,0.)) ;
#106072 = DIRECTION('ref_axis',(0.,0.,1.)) ;
#106073 = DIRECTION('',(0.,1.,0.)) ;
#106074 = DIRECTION('center_axis',(1.,0.,0.)) ;
#106075 = DIRECTION('ref_axis',(0.,0.,-1.)) ;
#106076 = DIRECTION('',(0.,0.,1.)) ;
#106077 = DIRECTION('center_axis',(0.,1.,0.)) ;
#106078 = DIRECTION('ref_axis',(0.,0.,1.)) ;
#106079 = DIRECTION('',(1.,0.,0.)) ;
#106080 = DIRECTION('',(0.,0.,-1.)) ;
#106081 = DIRECTION('',(-1.,0.,0.)) ;
#106082 = DIRECTION('',(0.,0.,1.)) ;
#106083 = DIRECTION('center_axis',(0.,0.164398987305357,-0.986393923832144)) ;
#106084 = DIRECTION('ref_axis',(0.,0.986393923832144,0.164398987305357)) ;
#106085 = DIRECTION('',(-1.,-1.0450141421547E-16,-1.7416902369245E-17)) ;
#106086 = DIRECTION('',(0.,-0.986393923832144,-0.164398987305357)) ;
#106087 = DIRECTION('',(1.,0.,0.)) ;
#106088 = DIRECTION('',(0.,0.986393923832144,0.164398987305357)) ;
#106089 = DIRECTION('center_axis',(0.,-1.,0.)) ;
#106090 = DIRECTION('ref_axis',(0.,0.,-1.)) ;
#106091 = DIRECTION('',(0.,0.,1.)) ;
#106092 = DIRECTION('',(0.,0.,-1.)) ;
#106093 = DIRECTION('',(-1.,0.,0.)) ;
#106094 = DIRECTION('center_axis',(0.,0.164398987305357,0.986393923832144)) ;
#106095 = DIRECTION('ref_axis',(0.,-0.986393923832144,0.164398987305357)) ;
#106096 = DIRECTION('',(0.,0.986393923832144,-0.164398987305357)) ;
#106097 = DIRECTION('',(1.,1.0450141421547E-16,-1.7416902369245E-17)) ;
#106098 = DIRECTION('',(0.,-0.986393923832144,0.164398987305357)) ;
#106099 = DIRECTION('center_axis',(-1.,0.,0.)) ;
#106100 = DIRECTION('ref_axis',(0.,0.,1.)) ;
#106101 = DIRECTION('',(0.,0.,1.)) ;
#106102 = DIRECTION('center_axis',(-1.,0.,0.)) ;
#106103 = DIRECTION('ref_axis',(0.,0.,1.)) ;
#106104 = DIRECTION('',(0.,-0.986393923832144,0.164398987305357)) ;
#106105 = DIRECTION('',(0.,0.,-1.)) ;
#106106 = DIRECTION('',(0.,0.986393923832144,0.164398987305357)) ;
#106107 = DIRECTION('center_axis',(1.,0.,0.)) ;
#106108 = DIRECTION('ref_axis',(0.,0.,-1.)) ;
#106109 = DIRECTION('center_axis',(1.,0.,0.)) ;
#106110 = DIRECTION('ref_axis',(0.,0.,-1.)) ;
#106111 = DIRECTION('center_axis',(1.,0.,0.)) ;
#106112 = DIRECTION('ref_axis',(0.,0.,1.)) ;
#106113 = DIRECTION('center_axis',(1.,0.,0.)) ;
#106114 = DIRECTION('ref_axis',(0.,1.77635683940025E-15,1.)) ;
#106115 = DIRECTION('center_axis',(1.,0.,0.)) ;
#106116 = DIRECTION('ref_axis',(0.,-3.5527136788005E-15,1.)) ;
#106117 = DIRECTION('',(1.,0.,0.)) ;
#106118 = DIRECTION('center_axis',(-1.,0.,0.)) ;
#106119 = DIRECTION('ref_axis',(0.,0.,1.)) ;
#106120 = DIRECTION('',(-1.,0.,0.)) ;
#106121 = DIRECTION('center_axis',(0.,0.,-1.)) ;
#106122 = DIRECTION('ref_axis',(1.,0.,0.)) ;
#106123 = DIRECTION('center_axis',(0.,-1.,0.)) ;
#106124 = DIRECTION('ref_axis',(0.,0.,1.)) ;
#106125 = DIRECTION('center_axis',(0.971399006496778,0.,-0.23745309047699)) ;
#106126 = DIRECTION('ref_axis',(-0.23745309047699,0.,-0.971399006496778)) ;
#106127 = DIRECTION('center_axis',(0.971399006496778,0.,-0.237453090476989)) ;
#106128 = DIRECTION('ref_axis',(-0.237453090476989,0.,-0.971399006496778)) ;
#106129 = DIRECTION('center_axis',(0.655772517804501,-0.73774408253007,-0.160299948796655)) ;
#106130 = DIRECTION('ref_axis',(-0.747409318683663,-0.664363838829916,-3.82464933042368E-16)) ;
#106131 = DIRECTION('center_axis',(-0.439210132175037,-4.69342344346061E-10,
-0.898384360836044)) ;
#106132 = DIRECTION('ref_axis',(0.882040291646593,-0.189880214231443,-0.43121969824605)) ;
#106133 = DIRECTION('center_axis',(0.655772517804504,-0.737744082530068,-0.160299948796656)) ;
#106134 = DIRECTION('ref_axis',(0.74740931868366,0.664363838829919,-2.08334010827303E-16)) ;
#106135 = DIRECTION('center_axis',(0.655772517804505,-0.737744082530068,-0.16029994879665)) ;
#106136 = DIRECTION('ref_axis',(0.74740931868366,0.66436383882992,-5.75609428574487E-16)) ;
#106137 = DIRECTION('center_axis',(0.664363838829919,-0.74740931868366,0.)) ;
#106138 = DIRECTION('ref_axis',(0.74740931868366,0.664363838829919,0.)) ;
#106139 = DIRECTION('center_axis',(-0.664363838829918,0.747409318683661,0.)) ;
#106140 = DIRECTION('ref_axis',(-0.747409318683661,-0.664363838829918,0.)) ;
#106141 = DIRECTION('center_axis',(0.,1.,0.)) ;
#106142 = DIRECTION('ref_axis',(0.,0.,1.)) ;
#106143 = DIRECTION('center_axis',(0.,-1.,0.)) ;
#106144 = DIRECTION('ref_axis',(0.,0.,-1.)) ;
#106145 = DIRECTION('center_axis',(0.,0.,1.)) ;
#106146 = DIRECTION('ref_axis',(1.,0.,0.)) ;
#106147 = DIRECTION('center_axis',(0.,0.,-1.)) ;
#106148 = DIRECTION('ref_axis',(-1.,0.,0.)) ;
#106149 = DIRECTION('center_axis',(0.,0.,-1.)) ;
#106150 = DIRECTION('ref_axis',(-1.,0.,0.)) ;
#106151 = DIRECTION('center_axis',(0.439210132174959,4.69119130465546E-10,
-0.898384360836082)) ;
#106152 = DIRECTION('ref_axis',(0.882040291646776,-0.189880214230495,0.431219698246092)) ;
#106153 = DIRECTION('center_axis',(-0.971399006496778,0.,-0.23745309047699)) ;
#106154 = DIRECTION('ref_axis',(-0.23745309047699,0.,0.971399006496778)) ;
#106155 = DIRECTION('center_axis',(0.971399006496778,0.,0.237453090476989)) ;
#106156 = DIRECTION('ref_axis',(0.237453090476989,0.,-0.971399006496778)) ;
#106157 = DIRECTION('center_axis',(0.,1.,0.)) ;
#106158 = DIRECTION('ref_axis',(1.,0.,0.)) ;
#106159 = DIRECTION('center_axis',(-3.54829801904343E-14,1.,8.67361737988405E-15)) ;
#106160 = DIRECTION('ref_axis',(1.,3.54829801904343E-14,6.83923985932746E-30)) ;
#106161 = DIRECTION('center_axis',(-0.948683298050516,0.316227766016833,4.68041587613745E-15)) ;
#106162 = DIRECTION('ref_axis',(0.316227766016833,0.948683298050516,-2.29441790171558E-12)) ;
#106163 = DIRECTION('center_axis',(0.,0.,-1.)) ;
#106164 = DIRECTION('ref_axis',(1.,0.,0.)) ;
#106165 = DIRECTION('center_axis',(0.,-1.,0.)) ;
#106166 = DIRECTION('ref_axis',(0.,0.,1.)) ;
#106167 = DIRECTION('center_axis',(0.655772517804503,-0.737744082530069,0.160299948796655)) ;
#106168 = DIRECTION('ref_axis',(-0.747409318683661,-0.664363838829918,2.39955779178099E-16)) ;
#106169 = DIRECTION('center_axis',(0.,1.,0.)) ;
#106170 = DIRECTION('ref_axis',(0.,0.,1.)) ;
#106171 = DIRECTION('center_axis',(2.73957817177508E-14,1.,0.)) ;
#106172 = DIRECTION('ref_axis',(-1.,2.73957817177508E-14,0.)) ;
#106173 = DIRECTION('center_axis',(0.894427190999917,0.447213595499956,0.)) ;
#106174 = DIRECTION('ref_axis',(-0.447213595499956,0.894427190999917,0.)) ;
#106175 = DIRECTION('center_axis',(-0.894427190999916,-0.447213595499958,
0.)) ;
#106176 = DIRECTION('ref_axis',(0.447213595499958,-0.894427190999916,0.)) ;
#106177 = DIRECTION('center_axis',(0.,0.,1.)) ;
#106178 = DIRECTION('ref_axis',(1.,0.,0.)) ;
#106179 = DIRECTION('center_axis',(0.,0.,-1.)) ;
#106180 = DIRECTION('ref_axis',(-1.,0.,0.)) ;
#106181 = DIRECTION('center_axis',(0.,1.,0.)) ;
#106182 = DIRECTION('ref_axis',(0.,0.,1.)) ;
#106183 = DIRECTION('center_axis',(0.,-1.,0.)) ;
#106184 = DIRECTION('ref_axis',(0.,0.,-1.)) ;
#106185 = DIRECTION('center_axis',(-0.664363838829919,0.74740931868366,0.)) ;
#106186 = DIRECTION('ref_axis',(-0.74740931868366,-0.664363838829919,0.)) ;
#106187 = DIRECTION('center_axis',(-0.66436383882992,0.747409318683659,2.52106651083074E-15)) ;
#106188 = DIRECTION('ref_axis',(-0.747409318683659,-0.66436383882992,7.82575143531171E-30)) ;
#106189 = DIRECTION('center_axis',(-0.655772517804504,0.737744082530068,-0.160299948796656)) ;
#106190 = DIRECTION('ref_axis',(-0.74740931868366,-0.664363838829919,2.31673158493852E-16)) ;
#106191 = DIRECTION('center_axis',(0.655772517804496,-0.737744082530075,0.160299948796656)) ;
#106192 = DIRECTION('ref_axis',(0.747409318683667,0.664363838829911,-2.10122272487167E-17)) ;
#106193 = DIRECTION('center_axis',(0.,1.,0.)) ;
#106194 = DIRECTION('ref_axis',(1.,0.,0.)) ;
#106195 = DIRECTION('center_axis',(-0.873786407766988,-0.436893203883498,
0.213592233009711)) ;
#106196 = DIRECTION('ref_axis',(-0.447213595499961,0.894427190999914,3.0060297474479E-16)) ;
#106197 = DIRECTION('center_axis',(-0.948683298050516,0.316227766016832,-3.84691715846994E-15)) ;
#106198 = DIRECTION('ref_axis',(0.316227766016832,0.948683298050516,-1.68048965429074E-12)) ;
#106199 = DIRECTION('center_axis',(0.,1.,0.)) ;
#106200 = DIRECTION('ref_axis',(1.,0.,0.)) ;
#106201 = DIRECTION('center_axis',(-5.47915634355017E-14,1.,0.)) ;
#106202 = DIRECTION('ref_axis',(1.,5.47915634355017E-14,6.93889390390721E-14)) ;
#106203 = DIRECTION('center_axis',(-0.971399006496778,0.,0.23745309047699)) ;
#106204 = DIRECTION('ref_axis',(0.23745309047699,0.,0.971399006496778)) ;
#106205 = DIRECTION('center_axis',(0.971399006496778,-3.69787733965917E-15,
-0.237453090476989)) ;
#106206 = DIRECTION('ref_axis',(-0.237453090476989,1.87410005036359E-29,-0.971399006496778)) ;
#106207 = DIRECTION('center_axis',(0.873786407766991,0.436893203883493,-0.213592233009709)) ;
#106208 = DIRECTION('ref_axis',(-0.447213595499956,0.894427190999917,2.83414331365695E-16)) ;
#106209 = DIRECTION('center_axis',(-0.873786407766992,-0.436893203883492,
0.21359223300971)) ;
#106210 = DIRECTION('ref_axis',(0.447213595499955,-0.894427190999918,-1.48231119036019E-16)) ;
#106211 = DIRECTION('center_axis',(-0.894427190999917,-0.447213595499956,
0.)) ;
#106212 = DIRECTION('ref_axis',(0.447213595499956,-0.894427190999917,0.)) ;
#106213 = DIRECTION('center_axis',(-0.894427190999917,-0.447213595499955,
0.)) ;
#106214 = DIRECTION('ref_axis',(0.447213595499955,-0.894427190999917,0.)) ;
#106215 = DIRECTION('center_axis',(0.,1.,0.)) ;
#106216 = DIRECTION('ref_axis',(0.,0.,1.)) ;
#106217 = DIRECTION('center_axis',(2.66122351428257E-14,1.,6.50521303491301E-15)) ;
#106218 = DIRECTION('ref_axis',(-1.,2.66122351428257E-14,3.84707242087163E-30)) ;
#106219 = DIRECTION('center_axis',(-0.439210132005065,2.74999532687384E-13,
-0.898384360919141)) ;
#106220 = DIRECTION('ref_axis',(0.898384360919141,-1.32695180921442E-11,-0.439210132005065)) ;
#106221 = DIRECTION('center_axis',(0.,1.,0.)) ;
#106222 = DIRECTION('ref_axis',(1.,0.,0.)) ;
#106223 = DIRECTION('center_axis',(-0.87378640776699,-0.436893203883495,-0.213592233009712)) ;
#106224 = DIRECTION('ref_axis',(-0.447213595499958,0.894427190999916,-1.950883489007E-18)) ;
#106225 = DIRECTION('center_axis',(0.,0.,1.)) ;
#106226 = DIRECTION('ref_axis',(1.,0.,0.)) ;
#106227 = DIRECTION('center_axis',(0.4392101320051,-6.47579544715494E-13,
-0.898384360919124)) ;
#106228 = DIRECTION('ref_axis',(0.898384360919124,-3.722424582079E-12,0.4392101320051)) ;
#106229 = DIRECTION('center_axis',(-0.873786407766991,-0.436893203883493,
-0.213592233009709)) ;
#106230 = DIRECTION('ref_axis',(0.447213595499956,-0.894427190999917,-1.06780556900622E-16)) ;
#106231 = DIRECTION('center_axis',(-0.873786407766992,-0.436893203883492,
-0.213592233009707)) ;
#106232 = DIRECTION('ref_axis',(0.447213595499955,-0.894427190999918,-7.04543255365314E-18)) ;
#106233 = DIRECTION('center_axis',(-0.971399006496778,0.,-0.237453090476989)) ;
#106234 = DIRECTION('ref_axis',(0.237453090476989,0.,-0.971399006496778)) ;
#106235 = DIRECTION('center_axis',(0.971399006496778,0.,0.23745309047699)) ;
#106236 = DIRECTION('ref_axis',(0.23745309047699,0.,-0.971399006496778)) ;
#106237 = DIRECTION('center_axis',(0.,0.,-1.)) ;
#106238 = DIRECTION('ref_axis',(-1.,0.,0.)) ;
#106239 = DIRECTION('center_axis',(1.,1.0450141421547E-16,1.7416902369245E-17)) ;
#106240 = DIRECTION('ref_axis',(-1.0450141421547E-16,1.,-1.82009092883888E-33)) ;
#106241 = DIRECTION('center_axis',(0.672672795323067,0.739940072189803,-7.49424791604764E-10)) ;
#106242 = DIRECTION('ref_axis',(0.738044870610434,-0.670949884717718,0.0715263669069537)) ;
#106243 = DIRECTION('center_axis',(-1.,0.,0.)) ;
#106244 = DIRECTION('ref_axis',(0.,-0.646374896130193,-0.763019982472728)) ;
#106245 = DIRECTION('center_axis',(-1.,0.,0.)) ;
#106246 = DIRECTION('ref_axis',(0.,0.,1.)) ;
#106247 = DIRECTION('center_axis',(-1.,0.,0.)) ;
#106248 = DIRECTION('ref_axis',(0.,0.,1.)) ;
#106249 = DIRECTION('center_axis',(0.,0.986393923832144,0.164398987305357)) ;
#106250 = DIRECTION('ref_axis',(0.,-0.164398987305357,0.986393923832144)) ;
#106251 = DIRECTION('center_axis',(0.,-0.986393923832144,-0.164398987305358)) ;
#106252 = DIRECTION('ref_axis',(0.,0.164398987305358,-0.986393923832144)) ;
#106253 = DIRECTION('center_axis',(0.,0.,1.)) ;
#106254 = DIRECTION('ref_axis',(1.,0.,0.)) ;
#106255 = DIRECTION('center_axis',(0.,0.,1.)) ;
#106256 = DIRECTION('ref_axis',(1.,0.,0.)) ;
#106257 = DIRECTION('center_axis',(0.,0.,1.)) ;
#106258 = DIRECTION('ref_axis',(1.,0.,0.)) ;
#106259 = DIRECTION('center_axis',(0.,0.,-1.)) ;
#106260 = DIRECTION('ref_axis',(1.,0.,0.)) ;
#106261 = DIRECTION('center_axis',(-1.,0.,0.)) ;
#106262 = DIRECTION('ref_axis',(0.,-0.646374896130191,-0.76301998247273)) ;
#106263 = DIRECTION('center_axis',(0.,0.,1.)) ;
#106264 = DIRECTION('ref_axis',(-1.,0.,0.)) ;
#106265 = DIRECTION('center_axis',(0.,0.,-1.)) ;
#106266 = DIRECTION('ref_axis',(-1.,0.,0.)) ;
#106267 = DIRECTION('center_axis',(1.,1.0450141421547E-16,-1.7416902369245E-17)) ;
#106268 = DIRECTION('ref_axis',(-1.0450141421547E-16,1.,1.82009092883888E-33)) ;
#106269 = DIRECTION('center_axis',(0.672672795322483,0.739940072190334,7.49091207824656E-10)) ;
#106270 = DIRECTION('ref_axis',(0.738044870606418,-0.670949884713036,-0.0715263669923128)) ;
#106271 = DIRECTION('center_axis',(1.,0.,0.)) ;
#106272 = DIRECTION('ref_axis',(0.,4.77048955893625E-14,1.)) ;
#106273 = DIRECTION('center_axis',(0.,0.,-1.)) ;
#106274 = DIRECTION('ref_axis',(-1.,0.,0.)) ;
#106275 = DIRECTION('center_axis',(0.,-0.986393923832144,0.164398987305357)) ;
#106276 = DIRECTION('ref_axis',(0.,-0.164398987305357,-0.986393923832144)) ;
#106277 = DIRECTION('center_axis',(1.,0.,0.)) ;
#106278 = DIRECTION('ref_axis',(0.,0.,1.)) ;
#106279 = DIRECTION('center_axis',(7.58941520739854E-15,0.,-1.)) ;
#106280 = DIRECTION('ref_axis',(-1.,0.,-7.58941520739854E-15)) ;
#106281 = DIRECTION('center_axis',(1.,0.,-8.67361737988404E-15)) ;
#106282 = DIRECTION('ref_axis',(-8.67361737988404E-15,0.,-1.)) ;
#106283 = DIRECTION('center_axis',(1.,0.,0.)) ;
#106284 = DIRECTION('ref_axis',(0.,0.,-1.)) ;
#106285 = DIRECTION('center_axis',(1.,0.,8.67361737988403E-15)) ;
#106286 = DIRECTION('ref_axis',(8.67361737988403E-15,0.,-1.)) ;
#106287 = DIRECTION('center_axis',(0.,0.,1.)) ;
#106288 = DIRECTION('ref_axis',(1.,0.,0.)) ;
#106289 = DIRECTION('center_axis',(0.,0.,-1.)) ;
#106290 = DIRECTION('ref_axis',(-1.,0.,0.)) ;
#106291 = DIRECTION('center_axis',(1.,0.,0.)) ;
#106292 = DIRECTION('ref_axis',(0.,0.,1.)) ;
#106293 = DIRECTION('center_axis',(-6.50521303491304E-15,0.,-1.)) ;
#106294 = DIRECTION('ref_axis',(-1.,0.,6.50521303491304E-15)) ;
#106295 = DIRECTION('center_axis',(1.,0.,0.)) ;
#106296 = DIRECTION('ref_axis',(0.,0.,1.)) ;
#106297 = DIRECTION('center_axis',(1.,9.40395480657835E-30,8.67361737988403E-15)) ;
#106298 = DIRECTION('ref_axis',(8.67361737988403E-15,-5.27711695562625E-58,
-1.)) ;
#106299 = DIRECTION('center_axis',(0.,0.,-1.)) ;
#106300 = DIRECTION('ref_axis',(-1.,0.,0.)) ;
#106301 = DIRECTION('center_axis',(6.50521303491304E-15,0.,-1.)) ;
#106302 = DIRECTION('ref_axis',(-1.,0.,-6.50521303491304E-15)) ;
#106303 = DIRECTION('center_axis',(-1.,0.,0.)) ;
#106304 = DIRECTION('ref_axis',(0.,0.,1.)) ;
#106305 = DIRECTION('center_axis',(1.,-8.67361737988409E-15,0.)) ;
#106306 = DIRECTION('ref_axis',(8.67361737988409E-15,1.,0.)) ;
#106307 = DIRECTION('center_axis',(1.,0.,0.)) ;
#106308 = DIRECTION('ref_axis',(0.,0.,1.)) ;
#106309 = DIRECTION('center_axis',(-4.33680868994202E-16,0.,1.)) ;
#106310 = DIRECTION('ref_axis',(1.,0.,4.33680868994202E-16)) ;
#106311 = DIRECTION('center_axis',(0.,0.,-1.)) ;
#106312 = DIRECTION('ref_axis',(-1.,0.,0.)) ;
#106313 = DIRECTION('center_axis',(0.,0.,1.)) ;
#106314 = DIRECTION('ref_axis',(1.,0.,0.)) ;
#106315 = DIRECTION('center_axis',(0.,1.,0.)) ;
#106316 = DIRECTION('ref_axis',(0.,0.,1.)) ;
#106317 = DIRECTION('center_axis',(-1.,0.,0.)) ;
#106318 = DIRECTION('ref_axis',(0.,0.,-1.)) ;
#106319 = DIRECTION('center_axis',(0.,-1.,0.)) ;
#106320 = DIRECTION('ref_axis',(0.,0.,1.)) ;
#106321 = DIRECTION('center_axis',(0.,1.,0.)) ;
#106322 = DIRECTION('ref_axis',(0.,0.,1.)) ;
#106323 = DIRECTION('center_axis',(0.,-1.,0.)) ;
#106324 = DIRECTION('ref_axis',(0.,0.,1.)) ;
#106325 = DIRECTION('center_axis',(-1.,0.,0.)) ;
#106326 = DIRECTION('ref_axis',(0.,0.,-1.)) ;
#106327 = DIRECTION('center_axis',(-1.,0.,-1.73472347597681E-16)) ;
#106328 = DIRECTION('ref_axis',(-1.73472347597681E-16,0.,1.)) ;
#106329 = DIRECTION('center_axis',(-1.,0.,0.)) ;
#106330 = DIRECTION('ref_axis',(0.,0.,1.)) ;
#106331 = DIRECTION('center_axis',(0.,1.,0.)) ;
#106332 = DIRECTION('ref_axis',(0.,0.,1.)) ;
#106333 = DIRECTION('center_axis',(0.,-1.,0.)) ;
#106334 = DIRECTION('ref_axis',(0.,0.,-1.)) ;
#106335 = DIRECTION('center_axis',(-4.33680868994202E-16,0.,1.)) ;
#106336 = DIRECTION('ref_axis',(1.,0.,4.33680868994202E-16)) ;
#106337 = DIRECTION('center_axis',(0.,0.,1.)) ;
#106338 = DIRECTION('ref_axis',(1.,0.,0.)) ;
#106339 = DIRECTION('center_axis',(0.,0.,-1.)) ;
#106340 = DIRECTION('ref_axis',(-1.,0.,0.)) ;
#106341 = DIRECTION('center_axis',(0.,1.,0.)) ;
#106342 = DIRECTION('ref_axis',(0.,0.,1.)) ;
#106343 = DIRECTION('center_axis',(0.,-1.,0.)) ;
#106344 = DIRECTION('ref_axis',(0.,0.,-1.)) ;
#106345 = DIRECTION('center_axis',(1.,0.,-1.73472347597681E-16)) ;
#106346 = DIRECTION('ref_axis',(-1.73472347597681E-16,0.,-1.)) ;
#106347 = DIRECTION('center_axis',(-1.,0.,0.)) ;
#106348 = DIRECTION('ref_axis',(0.,0.,1.)) ;
#106349 = DIRECTION('center_axis',(0.,0.,-1.)) ;
#106350 = DIRECTION('ref_axis',(-1.,0.,0.)) ;
#106351 = DIRECTION('center_axis',(0.,0.,1.)) ;
#106352 = DIRECTION('ref_axis',(1.,0.,0.)) ;
#106353 = DIRECTION('center_axis',(0.,0.,-1.)) ;
#106354 = DIRECTION('ref_axis',(-1.,0.,0.)) ;
#106355 = DIRECTION('center_axis',(0.,1.,0.)) ;
#106356 = DIRECTION('ref_axis',(0.,0.,1.)) ;
#106357 = DIRECTION('center_axis',(0.,-1.,0.)) ;
#106358 = DIRECTION('ref_axis',(0.,0.,1.)) ;
#106359 = DIRECTION('center_axis',(0.,1.,0.)) ;
#106360 = DIRECTION('ref_axis',(1.,0.,0.)) ;
#106361 = DIRECTION('center_axis',(1.,0.,0.)) ;
#106362 = DIRECTION('ref_axis',(0.,0.,1.)) ;
#106363 = DIRECTION('center_axis',(0.,1.,0.)) ;
#106364 = DIRECTION('ref_axis',(1.,0.,0.)) ;
#106365 = DIRECTION('center_axis',(1.,0.,0.)) ;
#106366 = DIRECTION('ref_axis',(0.,0.,1.)) ;
#106367 = DIRECTION('center_axis',(0.,1.,0.)) ;
#106368 = DIRECTION('ref_axis',(0.,0.,1.)) ;
#106369 = DIRECTION('center_axis',(0.,-1.,0.)) ;
#106370 = DIRECTION('ref_axis',(0.,0.,1.)) ;
#106371 = DIRECTION('center_axis',(0.,1.,0.)) ;
#106372 = DIRECTION('ref_axis',(0.,0.,1.)) ;
#106373 = DIRECTION('center_axis',(0.,-1.,0.)) ;
#106374 = DIRECTION('ref_axis',(0.,0.,-1.)) ;
#106375 = DIRECTION('center_axis',(-1.,0.,-1.73472347597681E-16)) ;
#106376 = DIRECTION('ref_axis',(-1.73472347597681E-16,0.,1.)) ;
#106377 = DIRECTION('center_axis',(1.,0.,0.)) ;
#106378 = DIRECTION('ref_axis',(0.,0.,-1.)) ;
#106379 = DIRECTION('center_axis',(1.,0.,-1.73472347597681E-16)) ;
#106380 = DIRECTION('ref_axis',(-1.73472347597681E-16,0.,-1.)) ;
#106381 = DIRECTION('center_axis',(1.,0.,0.)) ;
#106382 = DIRECTION('ref_axis',(0.,0.,-1.)) ;
#106383 = DIRECTION('center_axis',(0.,1.,0.)) ;
#106384 = DIRECTION('ref_axis',(0.,0.,1.)) ;
#106385 = DIRECTION('center_axis',(0.,-1.,0.)) ;
#106386 = DIRECTION('ref_axis',(0.,0.,-1.)) ;
#106387 = DIRECTION('center_axis',(0.,1.,0.)) ;
#106388 = DIRECTION('ref_axis',(1.,0.,0.)) ;
#106389 = DIRECTION('center_axis',(0.,0.,1.)) ;
#106390 = DIRECTION('ref_axis',(-1.,0.,0.)) ;
#106391 = DIRECTION('center_axis',(0.,1.,0.)) ;
#106392 = DIRECTION('ref_axis',(1.,0.,0.)) ;
#106393 = DIRECTION('center_axis',(0.,0.,-1.)) ;
#106394 = DIRECTION('ref_axis',(1.,0.,0.)) ;
#106395 = DIRECTION('center_axis',(0.,0.,-1.)) ;
#106396 = DIRECTION('ref_axis',(-1.,0.,0.)) ;
#106397 = DIRECTION('center_axis',(2.16840434497101E-16,0.,1.)) ;
#106398 = DIRECTION('ref_axis',(1.,0.,-2.16840434497101E-16)) ;
#106399 = DIRECTION('center_axis',(0.,0.,-1.)) ;
#106400 = DIRECTION('ref_axis',(-1.,0.,0.)) ;
#106401 = DIRECTION('center_axis',(0.,0.,1.)) ;
#106402 = DIRECTION('ref_axis',(1.,0.,0.)) ;
#106403 = DIRECTION('center_axis',(0.,-1.,0.)) ;
#106404 = DIRECTION('ref_axis',(0.,0.,-1.)) ;
#106405 = DIRECTION('center_axis',(1.,0.,0.)) ;
#106406 = DIRECTION('ref_axis',(0.,0.,1.)) ;
#106407 = DIRECTION('center_axis',(0.,1.,0.)) ;
#106408 = DIRECTION('ref_axis',(0.,0.,-1.)) ;
#106409 = DIRECTION('center_axis',(0.,-1.,0.)) ;
#106410 = DIRECTION('ref_axis',(0.,0.,-1.)) ;
#106411 = DIRECTION('center_axis',(0.,1.,0.)) ;
#106412 = DIRECTION('ref_axis',(0.,0.,-1.)) ;
#106413 = DIRECTION('center_axis',(1.,0.,0.)) ;
#106414 = DIRECTION('ref_axis',(0.,0.,1.)) ;
#106415 = DIRECTION('center_axis',(1.,0.,-1.73472347597681E-16)) ;
#106416 = DIRECTION('ref_axis',(-1.73472347597681E-16,0.,-1.)) ;
#106417 = DIRECTION('center_axis',(1.,0.,0.)) ;
#106418 = DIRECTION('ref_axis',(0.,0.,-1.)) ;
#106419 = DIRECTION('center_axis',(0.,-1.,0.)) ;
#106420 = DIRECTION('ref_axis',(0.,0.,-1.)) ;
#106421 = DIRECTION('center_axis',(0.,1.,0.)) ;
#106422 = DIRECTION('ref_axis',(0.,0.,1.)) ;
#106423 = DIRECTION('center_axis',(2.16840434497101E-16,0.,1.)) ;
#106424 = DIRECTION('ref_axis',(1.,0.,-2.16840434497101E-16)) ;
#106425 = DIRECTION('center_axis',(0.,0.,1.)) ;
#106426 = DIRECTION('ref_axis',(1.,0.,0.)) ;
#106427 = DIRECTION('center_axis',(0.,0.,-1.)) ;
#106428 = DIRECTION('ref_axis',(-1.,0.,0.)) ;
#106429 = DIRECTION('center_axis',(0.,-1.,0.)) ;
#106430 = DIRECTION('ref_axis',(0.,0.,-1.)) ;
#106431 = DIRECTION('center_axis',(0.,1.,0.)) ;
#106432 = DIRECTION('ref_axis',(0.,0.,1.)) ;
#106433 = DIRECTION('center_axis',(-1.,0.,1.73472347597681E-16)) ;
#106434 = DIRECTION('ref_axis',(1.73472347597681E-16,0.,1.)) ;
#106435 = DIRECTION('center_axis',(1.,0.,0.)) ;
#106436 = DIRECTION('ref_axis',(0.,0.,-1.)) ;
#106437 = DIRECTION('center_axis',(-2.16840434497101E-16,0.,-1.)) ;
#106438 = DIRECTION('ref_axis',(-1.,0.,2.16840434497101E-16)) ;
#106439 = DIRECTION('center_axis',(0.,0.,1.)) ;
#106440 = DIRECTION('ref_axis',(1.,0.,0.)) ;
#106441 = DIRECTION('center_axis',(0.,0.,-1.)) ;
#106442 = DIRECTION('ref_axis',(-1.,0.,0.)) ;
#106443 = DIRECTION('center_axis',(0.,-1.,0.)) ;
#106444 = DIRECTION('ref_axis',(0.,0.,-1.)) ;
#106445 = DIRECTION('center_axis',(0.,1.,0.)) ;
#106446 = DIRECTION('ref_axis',(0.,0.,-1.)) ;
#106447 = DIRECTION('center_axis',(0.,1.,0.)) ;
#106448 = DIRECTION('ref_axis',(1.,0.,0.)) ;
#106449 = DIRECTION('center_axis',(-1.,0.,0.)) ;
#106450 = DIRECTION('ref_axis',(0.,0.,-1.)) ;
#106451 = DIRECTION('center_axis',(0.,1.,0.)) ;
#106452 = DIRECTION('ref_axis',(1.,0.,0.)) ;
#106453 = DIRECTION('center_axis',(-1.,0.,0.)) ;
#106454 = DIRECTION('ref_axis',(0.,0.,-1.)) ;
#106455 = DIRECTION('center_axis',(0.,-1.,0.)) ;
#106456 = DIRECTION('ref_axis',(0.,0.,-1.)) ;
#106457 = DIRECTION('center_axis',(0.,1.,0.)) ;
#106458 = DIRECTION('ref_axis',(0.,0.,-1.)) ;
#106459 = DIRECTION('center_axis',(0.,-1.,0.)) ;
#106460 = DIRECTION('ref_axis',(0.,0.,-1.)) ;
#106461 = DIRECTION('center_axis',(0.,1.,0.)) ;
#106462 = DIRECTION('ref_axis',(0.,0.,1.)) ;
#106463 = DIRECTION('center_axis',(1.,0.,-1.73472347597681E-16)) ;
#106464 = DIRECTION('ref_axis',(-1.73472347597681E-16,0.,-1.)) ;
#106465 = DIRECTION('center_axis',(-1.,0.,0.)) ;
#106466 = DIRECTION('ref_axis',(0.,0.,1.)) ;
#106467 = DIRECTION('center_axis',(-1.,0.,1.73472347597681E-16)) ;
#106468 = DIRECTION('ref_axis',(1.73472347597681E-16,0.,1.)) ;
#106469 = DIRECTION('center_axis',(-1.,0.,0.)) ;
#106470 = DIRECTION('ref_axis',(0.,0.,1.)) ;
#106471 = DIRECTION('center_axis',(0.,-1.,0.)) ;
#106472 = DIRECTION('ref_axis',(0.,0.,-1.)) ;
#106473 = DIRECTION('center_axis',(0.,1.,0.)) ;
#106474 = DIRECTION('ref_axis',(0.,0.,1.)) ;
#106475 = DIRECTION('center_axis',(0.,1.,0.)) ;
#106476 = DIRECTION('ref_axis',(1.,0.,0.)) ;
#106477 = DIRECTION('center_axis',(0.,0.,1.)) ;
#106478 = DIRECTION('ref_axis',(-1.,0.,0.)) ;
#106479 = DIRECTION('center_axis',(0.,1.,0.)) ;
#106480 = DIRECTION('ref_axis',(1.,0.,0.)) ;
#106481 = DIRECTION('center_axis',(0.,0.,-1.)) ;
#106482 = DIRECTION('ref_axis',(1.,0.,0.)) ;
#106483 = DIRECTION('center_axis',(-2.16840434497101E-16,0.,-1.)) ;
#106484 = DIRECTION('ref_axis',(-1.,0.,2.16840434497101E-16)) ;
#106485 = DIRECTION('center_axis',(-1.,0.,0.)) ;
#106486 = DIRECTION('ref_axis',(0.,0.,1.)) ;
#106487 = DIRECTION('center_axis',(0.,-0.632948931301575,-0.774193548387091)) ;
#106488 = DIRECTION('ref_axis',(0.,0.774193548387091,-0.632948931301575)) ;
#106489 = DIRECTION('center_axis',(0.,0.,1.)) ;
#106490 = DIRECTION('ref_axis',(1.,0.,0.)) ;
#106491 = DIRECTION('center_axis',(0.,8.67361737988405E-15,-1.)) ;
#106492 = DIRECTION('ref_axis',(0.,1.,8.67361737988405E-15)) ;
#106493 = DIRECTION('center_axis',(8.67361737988401E-15,0.,1.)) ;
#106494 = DIRECTION('ref_axis',(1.,0.,-8.67361737988401E-15)) ;
#106495 = DIRECTION('center_axis',(0.,1.,0.)) ;
#106496 = DIRECTION('ref_axis',(1.,0.,0.)) ;
#106497 = DIRECTION('center_axis',(-1.,0.,0.)) ;
#106498 = DIRECTION('ref_axis',(0.,5.20417042793045E-14,-1.)) ;
#106499 = DIRECTION('center_axis',(1.,0.,0.)) ;
#106500 = DIRECTION('ref_axis',(0.,0.,-1.)) ;
#106501 = DIRECTION('center_axis',(-1.,0.,0.)) ;
#106502 = DIRECTION('ref_axis',(0.,0.,1.)) ;
#106503 = DIRECTION('center_axis',(0.,0.,-1.)) ;
#106504 = DIRECTION('ref_axis',(-1.,0.,0.)) ;
#106505 = DIRECTION('center_axis',(0.,0.,1.)) ;
#106506 = DIRECTION('ref_axis',(1.,0.,0.)) ;
#106507 = DIRECTION('center_axis',(0.,0.,-1.)) ;
#106508 = DIRECTION('ref_axis',(-1.,0.,0.)) ;
#106509 = DIRECTION('center_axis',(-1.,0.,0.)) ;
#106510 = DIRECTION('ref_axis',(0.,0.,1.)) ;
#106511 = DIRECTION('center_axis',(0.,-0.632948931301567,-0.774193548387097)) ;
#106512 = DIRECTION('ref_axis',(0.,-0.774193548387097,0.632948931301567)) ;
#106513 = DIRECTION('center_axis',(-1.,0.,0.)) ;
#106514 = DIRECTION('ref_axis',(0.,0.,1.)) ;
#106515 = DIRECTION('center_axis',(0.,0.632948931301567,-0.774193548387097)) ;
#106516 = DIRECTION('ref_axis',(0.,0.774193548387097,0.632948931301567)) ;
#106517 = DIRECTION('center_axis',(0.,0.,-1.)) ;
#106518 = DIRECTION('ref_axis',(-1.,0.,0.)) ;
#106519 = DIRECTION('center_axis',(0.,0.,1.)) ;
#106520 = DIRECTION('ref_axis',(1.,0.,0.)) ;
#106521 = DIRECTION('center_axis',(-1.,0.,0.)) ;
#106522 = DIRECTION('ref_axis',(0.,0.,1.)) ;
#106523 = DIRECTION('center_axis',(1.,0.,0.)) ;
#106524 = DIRECTION('ref_axis',(0.,5.20417042793045E-14,1.)) ;
#106525 = DIRECTION('center_axis',(1.,0.,0.)) ;
#106526 = DIRECTION('ref_axis',(0.,0.,-1.)) ;
#106527 = DIRECTION('center_axis',(1.,0.,0.)) ;
#106528 = DIRECTION('ref_axis',(0.,0.,-1.)) ;
#106529 = DIRECTION('center_axis',(0.,0.,1.)) ;
#106530 = DIRECTION('ref_axis',(1.,0.,0.)) ;
#106531 = DIRECTION('center_axis',(0.,8.67361737988405E-15,-1.)) ;
#106532 = DIRECTION('ref_axis',(0.,1.,8.67361737988405E-15)) ;
#106533 = DIRECTION('center_axis',(0.,1.,0.)) ;
#106534 = DIRECTION('ref_axis',(1.,0.,0.)) ;
#106535 = DIRECTION('center_axis',(1.22050154678007E-14,0.632948931301567,
-0.774193548387097)) ;
#106536 = DIRECTION('ref_axis',(1.73472347597684E-14,-0.774193548387097,-0.632948931301567)) ;
#106537 = DIRECTION('center_axis',(-1.,0.,0.)) ;
#106538 = DIRECTION('ref_axis',(0.,0.,1.)) ;
#106539 = DIRECTION('center_axis',(0.,0.,1.)) ;
#106540 = DIRECTION('ref_axis',(1.,0.,0.)) ;
#106541 = DIRECTION('center_axis',(0.,0.,-1.)) ;
#106542 = DIRECTION('ref_axis',(1.,0.,0.)) ;
#106543 = DIRECTION('center_axis',(0.,0.,-1.)) ;
#106544 = DIRECTION('ref_axis',(-1.,0.,0.)) ;
#106545 = DIRECTION('center_axis',(0.,0.,1.)) ;
#106546 = DIRECTION('ref_axis',(1.,0.,0.)) ;
#106547 = DIRECTION('center_axis',(0.,0.,-1.)) ;
#106548 = DIRECTION('ref_axis',(-1.,0.,0.)) ;
#106549 = DIRECTION('center_axis',(0.,0.,1.)) ;
#106550 = DIRECTION('ref_axis',(1.,0.,0.)) ;
#106551 = DIRECTION('center_axis',(0.,0.,-1.)) ;
#106552 = DIRECTION('ref_axis',(-1.,0.,0.)) ;
#106553 = DIRECTION('center_axis',(0.,0.,1.)) ;
#106554 = DIRECTION('ref_axis',(1.,0.,0.)) ;
#106555 = DIRECTION('center_axis',(0.,0.,-1.)) ;
#106556 = DIRECTION('ref_axis',(-1.,0.,0.)) ;
#106557 = DIRECTION('center_axis',(0.,0.,1.)) ;
#106558 = DIRECTION('ref_axis',(1.,0.,0.)) ;
#106559 = DIRECTION('center_axis',(0.,0.,-1.)) ;
#106560 = DIRECTION('ref_axis',(-1.,0.,0.)) ;
#106561 = DIRECTION('center_axis',(0.,0.,1.)) ;
#106562 = DIRECTION('ref_axis',(1.,0.,0.)) ;
#106563 = DIRECTION('center_axis',(-0.422618261740697,0.,0.906307787036651)) ;
#106564 = DIRECTION('ref_axis',(0.906307787036651,0.,0.422618261740697)) ;
#106565 = DIRECTION('center_axis',(0.422618261740697,0.,-0.906307787036651)) ;
#106566 = DIRECTION('ref_axis',(-0.906307787036651,0.,-0.422618261740697)) ;
#106567 = DIRECTION('center_axis',(0.422618261740697,0.,-0.906307787036651)) ;
#106568 = DIRECTION('ref_axis',(-0.906307787036651,0.,-0.422618261740697)) ;
#106569 = DIRECTION('center_axis',(-0.422618261740697,0.,0.906307787036651)) ;
#106570 = DIRECTION('ref_axis',(0.906307787036651,0.,0.422618261740697)) ;
#106571 = DIRECTION('center_axis',(0.,0.,-1.)) ;
#106572 = DIRECTION('ref_axis',(-1.,0.,0.)) ;
#106573 = DIRECTION('center_axis',(0.,0.,1.)) ;
#106574 = DIRECTION('ref_axis',(1.,0.,0.)) ;
#106575 = DIRECTION('center_axis',(0.,0.,-1.)) ;
#106576 = DIRECTION('ref_axis',(-1.,0.,0.)) ;
#106577 = DIRECTION('center_axis',(0.,0.,1.)) ;
#106578 = DIRECTION('ref_axis',(1.,0.,0.)) ;
#106579 = DIRECTION('center_axis',(0.,0.,1.)) ;
#106580 = DIRECTION('ref_axis',(1.,0.,0.)) ;
#106581 = DIRECTION('center_axis',(0.,0.,-1.)) ;
#106582 = DIRECTION('ref_axis',(1.,0.,0.)) ;
#106583 = DIRECTION('center_axis',(0.,1.,0.)) ;
#106584 = DIRECTION('ref_axis',(1.,0.,0.)) ;
#106585 = DIRECTION('center_axis',(0.,-0.986393923832144,0.164398987305358)) ;
#106586 = DIRECTION('ref_axis',(0.,-0.164398987305358,-0.986393923832144)) ;
#106587 = DIRECTION('center_axis',(0.,0.986393923832144,-0.164398987305357)) ;
#106588 = DIRECTION('ref_axis',(0.,0.164398987305357,0.986393923832144)) ;
#106589 = DIRECTION('center_axis',(0.,-0.986393923832144,0.164398987305358)) ;
#106590 = DIRECTION('ref_axis',(0.,-0.164398987305358,-0.986393923832144)) ;
#106591 = DIRECTION('center_axis',(-1.,0.,0.)) ;
#106592 = DIRECTION('ref_axis',(0.,0.107567764393767,-0.994197755008191)) ;
#106593 = DIRECTION('center_axis',(4.02631181035923E-15,-0.928404294083138,
-0.371571617226061)) ;
#106594 = DIRECTION('ref_axis',(-1.28610411910257E-29,0.371571617226061,-0.928404294083138)) ;
#106595 = DIRECTION('center_axis',(0.275516865537137,-0.50093975551097,-0.820457078800105)) ;
#106596 = DIRECTION('ref_axis',(3.47276585739718E-16,0.853490367006418,-0.521108619605597)) ;
#106597 = DIRECTION('center_axis',(0.,0.,-1.)) ;
#106598 = DIRECTION('ref_axis',(-1.,0.,0.)) ;
#106599 = DIRECTION('center_axis',(0.,0.,-1.)) ;
#106600 = DIRECTION('ref_axis',(-1.,0.,0.)) ;
#106601 = DIRECTION('center_axis',(0.,0.,-1.)) ;
#106602 = DIRECTION('ref_axis',(-1.,0.,0.)) ;
#106603 = DIRECTION('center_axis',(0.,0.,-1.)) ;
#106604 = DIRECTION('ref_axis',(-1.,0.,0.)) ;
#106605 = DIRECTION('center_axis',(0.,0.,-1.)) ;
#106606 = DIRECTION('ref_axis',(-1.,0.,0.)) ;
#106607 = DIRECTION('center_axis',(-0.275516865538071,0.500939755523742,-0.820457078791993)) ;
#106608 = DIRECTION('ref_axis',(1.34532370065023E-15,0.853490366998217,0.521108619619028)) ;
#106609 = DIRECTION('center_axis',(0.,-0.986393923832144,-0.164398987305357)) ;
#106610 = DIRECTION('ref_axis',(0.,0.164398987305357,-0.986393923832144)) ;
#106611 = DIRECTION('center_axis',(3.5648347838177E-16,0.986393923832144,
0.164398987305358)) ;
#106612 = DIRECTION('ref_axis',(3.79675591822878E-31,-0.164398987305358,0.986393923832144)) ;
#106613 = DIRECTION('center_axis',(0.,1.,0.)) ;
#106614 = DIRECTION('ref_axis',(1.,0.,0.)) ;
#106615 = DIRECTION('center_axis',(-1.,0.,0.)) ;
#106616 = DIRECTION('ref_axis',(0.,0.,1.)) ;
#106617 = DIRECTION('center_axis',(0.,0.,-1.)) ;
#106618 = DIRECTION('ref_axis',(-1.,0.,0.)) ;
#106619 = DIRECTION('center_axis',(2.168404344971E-15,0.,1.)) ;
#106620 = DIRECTION('ref_axis',(1.,0.,-2.168404344971E-15)) ;
#106621 = DIRECTION('center_axis',(0.,0.,-1.)) ;
#106622 = DIRECTION('ref_axis',(-1.,0.,0.)) ;
#106623 = DIRECTION('center_axis',(0.,0.,-1.)) ;
#106624 = DIRECTION('ref_axis',(-1.,0.,0.)) ;
#106625 = DIRECTION('center_axis',(2.168404344971E-15,0.,1.)) ;
#106626 = DIRECTION('ref_axis',(1.,0.,-2.168404344971E-15)) ;
#106627 = DIRECTION('center_axis',(0.795723237447208,-7.53302716311723E-12,
0.605660407643206)) ;
#106628 = DIRECTION('ref_axis',(0.605660407643206,-5.87919516709105E-26,-0.795723237447208)) ;
#106629 = DIRECTION('center_axis',(1.57772181044204E-26,2.36658271566302E-26,
1.)) ;
#106630 = DIRECTION('ref_axis',(3.73380916671669E-52,-1.,2.36658271566302E-26)) ;
#106631 = DIRECTION('center_axis',(-0.795723237415222,-2.11663082418553E-11,
0.605660407685229)) ;
#106632 = DIRECTION('ref_axis',(0.605660407685229,1.1913710773826E-25,0.795723237415222)) ;
#106633 = DIRECTION('center_axis',(0.,0.,-1.)) ;
#106634 = DIRECTION('ref_axis',(-1.,0.,0.)) ;
#106635 = DIRECTION('center_axis',(0.147618562252691,0.989044367093028,0.)) ;
#106636 = DIRECTION('ref_axis',(-0.989044367093028,0.147618562252691,0.)) ;
#106637 = DIRECTION('',(0.,0.,1.)) ;
#106638 = DIRECTION('',(0.989044367093028,-0.147618562252691,0.)) ;
#106639 = DIRECTION('',(0.,0.,1.)) ;
#106640 = DIRECTION('',(-0.989044367093028,0.147618562252691,0.)) ;
#106641 = DIRECTION('center_axis',(0.,0.,1.)) ;
#106642 = DIRECTION('ref_axis',(1.,0.,0.)) ;
#106643 = DIRECTION('center_axis',(0.,0.,-1.)) ;
#106644 = DIRECTION('ref_axis',(1.,0.,0.)) ;
#106645 = DIRECTION('',(0.,0.,1.)) ;
#106646 = DIRECTION('center_axis',(0.,0.,1.)) ;
#106647 = DIRECTION('ref_axis',(1.,0.,0.)) ;
#106648 = DIRECTION('center_axis',(0.697619267438899,0.716468671818953,0.)) ;
#106649 = DIRECTION('ref_axis',(-0.716468671818953,0.697619267438899,0.)) ;
#106650 = DIRECTION('',(0.716468671818953,-0.697619267438899,0.)) ;
#106651 = DIRECTION('',(0.,0.,1.)) ;
#106652 = DIRECTION('',(-0.716468671818953,0.697619267438899,0.)) ;
#106653 = DIRECTION('center_axis',(0.,0.,1.)) ;
#106654 = DIRECTION('ref_axis',(1.,0.,0.)) ;
#106655 = DIRECTION('center_axis',(0.,0.,-1.)) ;
#106656 = DIRECTION('ref_axis',(1.,0.,0.)) ;
#106657 = DIRECTION('',(0.,0.,1.)) ;
#106658 = DIRECTION('center_axis',(0.,0.,1.)) ;
#106659 = DIRECTION('ref_axis',(1.,0.,0.)) ;
#106660 = DIRECTION('center_axis',(1.,0.,0.)) ;
#106661 = DIRECTION('ref_axis',(0.,0.,-1.)) ;
#106662 = DIRECTION('',(0.,-1.,0.)) ;
#106663 = DIRECTION('',(0.,0.,1.)) ;
#106664 = DIRECTION('',(0.,1.,0.)) ;
#106665 = DIRECTION('center_axis',(0.,0.,1.)) ;
#106666 = DIRECTION('ref_axis',(1.,0.,0.)) ;
#106667 = DIRECTION('center_axis',(0.,0.,-1.)) ;
#106668 = DIRECTION('ref_axis',(1.,0.,0.)) ;
#106669 = DIRECTION('',(0.,0.,1.)) ;
#106670 = DIRECTION('center_axis',(0.,0.,1.)) ;
#106671 = DIRECTION('ref_axis',(1.,0.,0.)) ;
#106672 = DIRECTION('center_axis',(-0.453905661840943,-0.891049746169503,
0.)) ;
#106673 = DIRECTION('ref_axis',(0.891049746169503,-0.453905661840943,0.)) ;
#106674 = DIRECTION('',(-0.891049746169503,0.453905661840943,0.)) ;
#106675 = DIRECTION('',(0.,0.,1.)) ;
#106676 = DIRECTION('',(0.891049746169503,-0.453905661840943,0.)) ;
#106677 = DIRECTION('center_axis',(0.,0.,1.)) ;
#106678 = DIRECTION('ref_axis',(1.,0.,0.)) ;
#106679 = DIRECTION('center_axis',(0.,0.,1.)) ;
#106680 = DIRECTION('ref_axis',(1.,0.,0.)) ;
#106681 = DIRECTION('',(0.,0.,1.)) ;
#106682 = DIRECTION('center_axis',(0.,0.,-1.)) ;
#106683 = DIRECTION('ref_axis',(1.,0.,0.)) ;
#106684 = DIRECTION('center_axis',(-2.60782465076463E-16,-1.,0.)) ;
#106685 = DIRECTION('ref_axis',(1.,-2.60782465076463E-16,0.)) ;
#106686 = DIRECTION('',(-1.,2.60782465076463E-16,0.)) ;
#106687 = DIRECTION('',(0.,0.,-1.)) ;
#106688 = DIRECTION('',(1.,-2.60782465076463E-16,0.)) ;
#106689 = DIRECTION('center_axis',(0.,0.,1.)) ;
#106690 = DIRECTION('ref_axis',(1.,0.,0.)) ;
#106691 = DIRECTION('center_axis',(0.,0.,1.)) ;
#106692 = DIRECTION('ref_axis',(1.,0.,0.)) ;
#106693 = DIRECTION('',(-1.,2.60782465076463E-16,0.)) ;
#106694 = DIRECTION('',(0.,1.,0.)) ;
#106695 = DIRECTION('',(0.989044367093028,-0.147618562252691,0.)) ;
#106696 = DIRECTION('',(0.716468671818953,-0.697619267438899,0.)) ;
#106697 = DIRECTION('',(0.,-1.,0.)) ;
#106698 = DIRECTION('',(-0.891049746169503,0.453905661840943,0.)) ;
#106699 = DIRECTION('center_axis',(0.,0.,1.)) ;
#106700 = DIRECTION('ref_axis',(1.,0.,0.)) ;
#106701 = DIRECTION('',(-0.716468671818953,0.697619267438899,0.)) ;
#106702 = DIRECTION('',(-0.989044367093028,0.147618562252691,0.)) ;
#106703 = DIRECTION('',(0.,-1.,0.)) ;
#106704 = DIRECTION('',(1.,-2.60782465076463E-16,0.)) ;
#106705 = DIRECTION('center_axis',(0.,0.,-1.)) ;
#106706 = DIRECTION('ref_axis',(1.,0.,0.)) ;
#106707 = DIRECTION('',(0.891049746169503,-0.453905661840943,0.)) ;
#106708 = DIRECTION('',(0.,1.,0.)) ;
#106709 = DIRECTION('center_axis',(-2.09002828430941E-16,1.,0.)) ;
#106710 = DIRECTION('ref_axis',(-1.,-2.09002828430941E-16,0.)) ;
#106711 = DIRECTION('',(1.,2.09002828430941E-16,0.)) ;
#106712 = DIRECTION('',(0.,0.,-1.)) ;
#106713 = DIRECTION('',(1.,2.09002828430941E-16,0.)) ;
#106714 = DIRECTION('',(0.,0.,1.)) ;
#106715 = DIRECTION('center_axis',(0.,1.,0.)) ;
#106716 = DIRECTION('ref_axis',(0.,0.,1.)) ;
#106717 = DIRECTION('',(0.422618261740697,0.,-0.906307787036651)) ;
#106718 = DIRECTION('center_axis',(1.0450141421547E-16,-1.,0.)) ;
#106719 = DIRECTION('ref_axis',(1.,1.0450141421547E-16,0.)) ;
#106720 = DIRECTION('',(-1.,-1.0450141421547E-16,1.7416902369245E-17)) ;
#106721 = DIRECTION('',(0.,0.,1.)) ;
#106722 = DIRECTION('',(-1.,-1.0450141421547E-16,0.)) ;
#106723 = DIRECTION('',(0.,0.,-1.)) ;
#106724 = DIRECTION('center_axis',(-1.,0.,0.)) ;
#106725 = DIRECTION('ref_axis',(0.,0.,1.)) ;
#106726 = DIRECTION('',(0.,1.,0.)) ;
#106727 = DIRECTION('',(0.,0.,-1.)) ;
#106728 = DIRECTION('center_axis',(-1.,0.,0.)) ;
#106729 = DIRECTION('ref_axis',(0.,0.,1.)) ;
#106730 = DIRECTION('',(0.,0.,1.)) ;
#106731 = DIRECTION('center_axis',(0.,0.,1.)) ;
#106732 = DIRECTION('ref_axis',(1.,0.,0.)) ;
#106733 = DIRECTION('center_axis',(0.,0.,1.)) ;
#106734 = DIRECTION('ref_axis',(1.,0.,0.)) ;
#106735 = DIRECTION('center_axis',(0.,0.,-1.)) ;
#106736 = DIRECTION('ref_axis',(1.,0.,0.)) ;
#106737 = DIRECTION('center_axis',(0.,0.,1.)) ;
#106738 = DIRECTION('ref_axis',(1.,0.,0.)) ;
#106739 = DIRECTION('center_axis',(0.,0.,1.)) ;
#106740 = DIRECTION('ref_axis',(1.,0.,0.)) ;
#106741 = DIRECTION('center_axis',(0.,0.,-1.)) ;
#106742 = DIRECTION('ref_axis',(1.,0.,0.)) ;
#106743 = DIRECTION('center_axis',(0.,0.,1.)) ;
#106744 = DIRECTION('ref_axis',(1.,0.,0.)) ;
#106745 = DIRECTION('',(-0.664363838829919,0.74740931868366,0.)) ;
#106746 = DIRECTION('',(0.,-1.,0.)) ;
#106747 = DIRECTION('',(0.894427190999917,0.447213595499956,0.)) ;
#106748 = DIRECTION('',(0.,1.,0.)) ;
#106749 = DIRECTION('center_axis',(0.,0.,-1.)) ;
#106750 = DIRECTION('ref_axis',(-1.,0.,0.)) ;
#106751 = DIRECTION('',(-0.894427190999917,-0.447213595499956,0.)) ;
#106752 = DIRECTION('',(0.,1.,0.)) ;
#106753 = DIRECTION('',(0.664363838829919,-0.74740931868366,0.)) ;
#106754 = DIRECTION('',(0.,-1.,0.)) ;
#106755 = DIRECTION('center_axis',(-0.23745309047699,0.,-0.971399006496778)) ;
#106756 = DIRECTION('ref_axis',(-0.971399006496778,0.,0.23745309047699)) ;
#106757 = DIRECTION('center_axis',(-0.237453090476986,2.27991133847471E-14,
-0.971399006496778)) ;
#106758 = DIRECTION('ref_axis',(0.921799787669962,-0.315455332296274,-0.225328836985994)) ;
#106759 = DIRECTION('',(0.971399006496777,0.,-0.23745309047699)) ;
#106760 = DIRECTION('',(0.,-1.,0.)) ;
#106761 = DIRECTION('',(-0.971399006496777,0.,0.23745309047699)) ;
#106762 = DIRECTION('center_axis',(-0.237453090477116,4.55640954056451E-13,
-0.971399006496747)) ;
#106763 = DIRECTION('ref_axis',(0.954559354253584,0.18539258117475,-0.233336731039809)) ;
#106764 = DIRECTION('',(-0.873786407766991,-0.436893203883493,0.213592233009709)) ;
#106765 = DIRECTION('',(0.,1.,0.)) ;
#106766 = DIRECTION('',(0.655772517804503,-0.737744082530068,-0.160299948796656)) ;
#106767 = DIRECTION('center_axis',(-1.,0.,0.)) ;
#106768 = DIRECTION('ref_axis',(0.,0.,1.)) ;
#106769 = DIRECTION('',(0.,-1.,0.)) ;
#106770 = DIRECTION('center_axis',(-1.,-6.7007887082719E-15,-6.50913949396006E-15)) ;
#106771 = DIRECTION('ref_axis',(6.50913949401742E-15,-8.55940926010333E-12,
-1.)) ;
#106772 = DIRECTION('',(0.,0.,-1.)) ;
#106773 = DIRECTION('center_axis',(-1.,-6.70078870827233E-15,6.50913949396061E-15)) ;
#106774 = DIRECTION('ref_axis',(-6.50913949402726E-15,9.94624019410426E-12,
-1.)) ;
#106775 = DIRECTION('center_axis',(-1.,6.70078870827237E-15,6.50913949396064E-15)) ;
#106776 = DIRECTION('ref_axis',(-6.50913949394999E-15,1.589491041799E-12,
-1.)) ;
#106777 = DIRECTION('',(0.,0.,-1.)) ;
#106778 = DIRECTION('center_axis',(-1.,6.70078870827261E-15,-6.50913949396074E-15)) ;
#106779 = DIRECTION('ref_axis',(6.50913949379813E-15,-2.42675544807721E-11,
-1.)) ;
#106780 = DIRECTION('center_axis',(-0.23745309047699,0.,0.971399006496778)) ;
#106781 = DIRECTION('ref_axis',(0.971399006496778,0.,0.23745309047699)) ;
#106782 = DIRECTION('center_axis',(-0.237453090476854,-6.19298088178216E-13,
0.971399006496811)) ;
#106783 = DIRECTION('ref_axis',(0.954559354253699,0.185392581174206,0.23333673103977)) ;
#106784 = DIRECTION('',(0.971399006496777,0.,0.23745309047699)) ;
#106785 = DIRECTION('',(-0.971399006496777,0.,-0.23745309047699)) ;
#106786 = DIRECTION('center_axis',(-0.237453090477054,-1.72356340859612E-13,
0.971399006496762)) ;
#106787 = DIRECTION('ref_axis',(0.9217997876717,-0.315455332290889,0.225328836986424)) ;
#106788 = DIRECTION('',(-0.655772517804503,0.737744082530068,-0.160299948796656)) ;
#106789 = DIRECTION('',(0.,-1.,0.)) ;
#106790 = DIRECTION('',(0.873786407766991,0.436893203883493,0.213592233009709)) ;
#106791 = DIRECTION('center_axis',(0.,1.,0.)) ;
#106792 = DIRECTION('ref_axis',(0.,0.,1.)) ;
#106793 = DIRECTION('',(-0.971399006496777,0.,0.23745309047699)) ;
#106794 = DIRECTION('',(0.,0.,-1.)) ;
#106795 = DIRECTION('',(0.971399006496777,0.,0.23745309047699)) ;
#106796 = DIRECTION('center_axis',(0.,1.,0.)) ;
#106797 = DIRECTION('ref_axis',(0.,0.,1.)) ;
#106798 = DIRECTION('',(-0.971399006496777,0.,-0.23745309047699)) ;
#106799 = DIRECTION('',(0.,0.,1.)) ;
#106800 = DIRECTION('',(0.971399006496777,0.,-0.23745309047699)) ;
#106801 = DIRECTION('center_axis',(-0.447213595499956,0.894427190999917,0.)) ;
#106802 = DIRECTION('ref_axis',(0.,0.,-1.)) ;
#106803 = DIRECTION('',(0.,0.,-1.)) ;
#106804 = DIRECTION('',(-0.873786407766991,-0.436893203883493,-0.213592233009709)) ;
#106805 = DIRECTION('',(-0.894427190999917,-0.447213595499956,0.)) ;
#106806 = DIRECTION('',(0.,0.,1.)) ;
#106807 = DIRECTION('',(0.894427190999917,0.447213595499956,0.)) ;
#106808 = DIRECTION('',(0.873786407766991,0.436893203883493,-0.213592233009709)) ;
#106809 = DIRECTION('center_axis',(0.74740931868366,0.664363838829919,0.)) ;
#106810 = DIRECTION('ref_axis',(0.,0.,1.)) ;
#106811 = DIRECTION('',(0.,0.,-1.)) ;
#106812 = DIRECTION('',(0.664363838829919,-0.74740931868366,0.)) ;
#106813 = DIRECTION('',(0.655772517804503,-0.737744082530068,0.160299948796656)) ;
#106814 = DIRECTION('',(0.,0.,1.)) ;
#106815 = DIRECTION('',(-0.655772517804503,0.737744082530068,0.160299948796656)) ;
#106816 = DIRECTION('',(-0.664363838829919,0.74740931868366,0.)) ;
#106817 = DIRECTION('center_axis',(1.,0.,4.33680868994202E-16)) ;
#106818 = DIRECTION('ref_axis',(4.33680868994202E-16,0.,-1.)) ;
#106819 = DIRECTION('',(0.,1.,0.)) ;
#106820 = DIRECTION('',(4.33680868994202E-16,0.,-1.)) ;
#106821 = DIRECTION('',(0.,-1.,0.)) ;
#106822 = DIRECTION('',(-4.33680868994202E-16,0.,1.)) ;
#106823 = DIRECTION('center_axis',(-1.73472347597681E-16,0.,-1.)) ;
#106824 = DIRECTION('ref_axis',(-1.,0.,1.73472347597681E-16)) ;
#106825 = DIRECTION('',(-1.,0.,1.73472347597681E-16)) ;
#106826 = DIRECTION('',(0.,-1.,0.)) ;
#106827 = DIRECTION('',(1.,0.,-1.73472347597681E-16)) ;
#106828 = DIRECTION('',(0.,1.,0.)) ;
#106829 = DIRECTION('center_axis',(-1.,0.,0.)) ;
#106830 = DIRECTION('ref_axis',(0.,0.,1.)) ;
#106831 = DIRECTION('',(0.,0.,1.)) ;
#106832 = DIRECTION('',(0.,-1.,0.)) ;
#106833 = DIRECTION('',(0.,0.,-1.)) ;
#106834 = DIRECTION('',(0.,1.,0.)) ;
#106835 = DIRECTION('center_axis',(-1.73472347597681E-16,0.,1.)) ;
#106836 = DIRECTION('ref_axis',(1.,0.,1.73472347597681E-16)) ;
#106837 = DIRECTION('',(0.,1.,0.)) ;
#106838 = DIRECTION('',(1.,0.,1.73472347597681E-16)) ;
#106839 = DIRECTION('',(0.,-1.,0.)) ;
#106840 = DIRECTION('',(-1.,0.,-1.73472347597681E-16)) ;
#106841 = DIRECTION('center_axis',(0.,-1.,0.)) ;
#106842 = DIRECTION('ref_axis',(0.,0.,-1.)) ;
#106843 = DIRECTION('',(-1.,0.,-1.73472347597681E-16)) ;
#106844 = DIRECTION('',(0.,0.,-1.)) ;
#106845 = DIRECTION('',(1.,0.,-1.73472347597681E-16)) ;
#106846 = DIRECTION('',(-4.33680868994202E-16,0.,1.)) ;
#106847 = DIRECTION('',(1.,0.,0.)) ;
#106848 = DIRECTION('center_axis',(0.,-1.,0.)) ;
#106849 = DIRECTION('ref_axis',(0.,0.,-1.)) ;
#106850 = DIRECTION('',(0.,0.,-1.)) ;
#106851 = DIRECTION('center_axis',(0.,-1.,0.)) ;
#106852 = DIRECTION('ref_axis',(0.,0.,-1.)) ;
#106853 = DIRECTION('',(-1.,0.,0.)) ;
#106854 = DIRECTION('center_axis',(0.,-1.,0.)) ;
#106855 = DIRECTION('ref_axis',(0.,0.,1.)) ;
#106856 = DIRECTION('',(0.,0.,1.)) ;
#106857 = DIRECTION('center_axis',(0.,-1.,0.)) ;
#106858 = DIRECTION('ref_axis',(0.,0.,-1.)) ;
#106859 = DIRECTION('center_axis',(0.,-1.,0.)) ;
#106860 = DIRECTION('ref_axis',(0.,0.,-1.)) ;
#106861 = DIRECTION('center_axis',(0.,-1.,0.)) ;
#106862 = DIRECTION('ref_axis',(0.,0.,-1.)) ;
#106863 = DIRECTION('',(0.,-1.,0.)) ;
#106864 = DIRECTION('',(0.,-1.,0.)) ;
#106865 = DIRECTION('center_axis',(0.,0.,-1.)) ;
#106866 = DIRECTION('ref_axis',(-1.,0.,0.)) ;
#106867 = DIRECTION('',(1.,0.,0.)) ;
#106868 = DIRECTION('',(0.,-1.,0.)) ;
#106869 = DIRECTION('center_axis',(0.,-1.,0.)) ;
#106870 = DIRECTION('ref_axis',(0.,0.,-1.)) ;
#106871 = DIRECTION('center_axis',(0.,-1.,0.)) ;
#106872 = DIRECTION('ref_axis',(0.,0.,-1.)) ;
#106873 = DIRECTION('',(0.,-1.,0.)) ;
#106874 = DIRECTION('center_axis',(-1.,0.,0.)) ;
#106875 = DIRECTION('ref_axis',(0.,0.,1.)) ;
#106876 = DIRECTION('',(0.,0.,-1.)) ;
#106877 = DIRECTION('',(0.,-1.,0.)) ;
#106878 = DIRECTION('center_axis',(0.,-1.,0.)) ;
#106879 = DIRECTION('ref_axis',(0.,0.,-1.)) ;
#106880 = DIRECTION('center_axis',(0.,-1.,0.)) ;
#106881 = DIRECTION('ref_axis',(0.,0.,-1.)) ;
#106882 = DIRECTION('',(0.,-1.,0.)) ;
#106883 = DIRECTION('center_axis',(0.,0.,1.)) ;
#106884 = DIRECTION('ref_axis',(1.,0.,0.)) ;
#106885 = DIRECTION('',(-1.,0.,0.)) ;
#106886 = DIRECTION('',(0.,-1.,0.)) ;
#106887 = DIRECTION('center_axis',(0.,-1.,0.)) ;
#106888 = DIRECTION('ref_axis',(0.,0.,-1.)) ;
#106889 = DIRECTION('center_axis',(0.,-1.,0.)) ;
#106890 = DIRECTION('ref_axis',(0.,0.,1.)) ;
#106891 = DIRECTION('',(0.,-1.,0.)) ;
#106892 = DIRECTION('center_axis',(1.,0.,0.)) ;
#106893 = DIRECTION('ref_axis',(0.,0.,-1.)) ;
#106894 = DIRECTION('',(0.,0.,1.)) ;
#106895 = DIRECTION('center_axis',(0.,-1.,0.)) ;
#106896 = DIRECTION('ref_axis',(0.,0.,-1.)) ;
#106897 = DIRECTION('center_axis',(0.,1.,0.)) ;
#106898 = DIRECTION('ref_axis',(0.,0.,1.)) ;
#106899 = DIRECTION('',(-0.422618261740697,0.,0.906307787036651)) ;
#106900 = DIRECTION('center_axis',(0.906307787036651,0.,0.422618261740697)) ;
#106901 = DIRECTION('ref_axis',(0.422618261740697,0.,-0.906307787036651)) ;
#106902 = DIRECTION('',(-0.422618261740697,0.,0.906307787036651)) ;
#106903 = DIRECTION('',(0.422618261740697,0.,-0.906307787036651)) ;
#106904 = DIRECTION('center_axis',(-0.906307787036651,0.,-0.422618261740697)) ;
#106905 = DIRECTION('ref_axis',(-0.422618261740697,0.,0.906307787036651)) ;
#106906 = DIRECTION('',(0.422618261740697,0.,-0.906307787036651)) ;
#106907 = DIRECTION('',(-0.422618261740697,0.,0.906307787036651)) ;
#106908 = DIRECTION('center_axis',(0.,1.,0.)) ;
#106909 = DIRECTION('ref_axis',(0.,0.,1.)) ;
#106910 = DIRECTION('',(-0.422618261740697,0.,0.906307787036651)) ;
#106911 = DIRECTION('',(0.422618261740697,0.,-0.906307787036651)) ;
#106912 = DIRECTION('center_axis',(1.,0.,-2.16840434497101E-16)) ;
#106913 = DIRECTION('ref_axis',(-2.16840434497101E-16,0.,-1.)) ;
#106914 = DIRECTION('',(2.16840434497101E-16,0.,1.)) ;
#106915 = DIRECTION('',(0.,1.,0.)) ;
#106916 = DIRECTION('',(-2.16840434497101E-16,0.,-1.)) ;
#106917 = DIRECTION('',(0.,-1.,0.)) ;
#106918 = DIRECTION('center_axis',(1.73472347597681E-16,0.,1.)) ;
#106919 = DIRECTION('ref_axis',(1.,0.,-1.73472347597681E-16)) ;
#106920 = DIRECTION('',(0.,-1.,0.)) ;
#106921 = DIRECTION('',(-1.,0.,1.73472347597681E-16)) ;
#106922 = DIRECTION('',(0.,1.,0.)) ;
#106923 = DIRECTION('',(1.,0.,-1.73472347597681E-16)) ;
#106924 = DIRECTION('center_axis',(-1.,0.,2.16840434497101E-16)) ;
#106925 = DIRECTION('ref_axis',(2.16840434497101E-16,0.,1.)) ;
#106926 = DIRECTION('',(0.,-1.,0.)) ;
#106927 = DIRECTION('',(-2.16840434497101E-16,0.,-1.)) ;
#106928 = DIRECTION('',(0.,1.,0.)) ;
#106929 = DIRECTION('',(2.16840434497101E-16,0.,1.)) ;
#106930 = DIRECTION('center_axis',(-1.73472347597681E-16,0.,-1.)) ;
#106931 = DIRECTION('ref_axis',(-1.,0.,1.73472347597681E-16)) ;
#106932 = DIRECTION('',(1.,0.,-1.73472347597681E-16)) ;
#106933 = DIRECTION('',(0.,1.,0.)) ;
#106934 = DIRECTION('',(-1.,0.,1.73472347597681E-16)) ;
#106935 = DIRECTION('',(0.,-1.,0.)) ;
#106936 = DIRECTION('center_axis',(0.,1.,0.)) ;
#106937 = DIRECTION('ref_axis',(0.,0.,1.)) ;
#106938 = DIRECTION('',(1.,0.,-1.73472347597681E-16)) ;
#106939 = DIRECTION('',(-2.16840434497101E-16,0.,-1.)) ;
#106940 = DIRECTION('',(-1.,0.,1.73472347597681E-16)) ;
#106941 = DIRECTION('',(2.16840434497101E-16,0.,1.)) ;
#106942 = DIRECTION('',(1.,0.,0.)) ;
#106943 = DIRECTION('center_axis',(0.,1.,0.)) ;
#106944 = DIRECTION('ref_axis',(0.,0.,1.)) ;
#106945 = DIRECTION('',(0.,0.,1.)) ;
#106946 = DIRECTION('center_axis',(0.,1.,0.)) ;
#106947 = DIRECTION('ref_axis',(0.,0.,1.)) ;
#106948 = DIRECTION('',(-1.,0.,0.)) ;
#106949 = DIRECTION('center_axis',(0.,1.,0.)) ;
#106950 = DIRECTION('ref_axis',(0.,0.,-1.)) ;
#106951 = DIRECTION('',(0.,0.,-1.)) ;
#106952 = DIRECTION('center_axis',(0.,1.,0.)) ;
#106953 = DIRECTION('ref_axis',(0.,0.,1.)) ;
#106954 = DIRECTION('center_axis',(0.,1.,0.)) ;
#106955 = DIRECTION('ref_axis',(0.,0.,1.)) ;
#106956 = DIRECTION('',(0.,1.,0.)) ;
#106957 = DIRECTION('center_axis',(0.,-1.,0.)) ;
#106958 = DIRECTION('ref_axis',(2.60208521396523E-14,0.,1.)) ;
#106959 = DIRECTION('',(0.,1.,0.)) ;
#106960 = DIRECTION('center_axis',(0.,0.,1.)) ;
#106961 = DIRECTION('ref_axis',(1.,0.,0.)) ;
#106962 = DIRECTION('',(-1.,0.,0.)) ;
#106963 = DIRECTION('',(0.,1.,0.)) ;
#106964 = DIRECTION('center_axis',(0.,1.,0.)) ;
#106965 = DIRECTION('ref_axis',(0.,0.,1.)) ;
#106966 = DIRECTION('center_axis',(0.,-1.,0.)) ;
#106967 = DIRECTION('ref_axis',(0.,0.,1.)) ;
#106968 = DIRECTION('',(0.,1.,0.)) ;
#106969 = DIRECTION('center_axis',(-1.,0.,0.)) ;
#106970 = DIRECTION('ref_axis',(0.,0.,1.)) ;
#106971 = DIRECTION('',(0.,0.,-1.)) ;
#106972 = DIRECTION('',(0.,1.,0.)) ;
#106973 = DIRECTION('center_axis',(0.,1.,0.)) ;
#106974 = DIRECTION('ref_axis',(0.,0.,1.)) ;
#106975 = DIRECTION('center_axis',(0.,-1.,0.)) ;
#106976 = DIRECTION('ref_axis',(0.,0.,1.)) ;
#106977 = DIRECTION('',(0.,1.,0.)) ;
#106978 = DIRECTION('center_axis',(0.,0.,-1.)) ;
#106979 = DIRECTION('ref_axis',(-1.,0.,0.)) ;
#106980 = DIRECTION('',(1.,0.,0.)) ;
#106981 = DIRECTION('',(0.,1.,0.)) ;
#106982 = DIRECTION('center_axis',(0.,1.,0.)) ;
#106983 = DIRECTION('ref_axis',(0.,0.,1.)) ;
#106984 = DIRECTION('center_axis',(0.,-1.,0.)) ;
#106985 = DIRECTION('ref_axis',(0.,0.,1.)) ;
#106986 = DIRECTION('',(0.,1.,0.)) ;
#106987 = DIRECTION('center_axis',(1.,0.,0.)) ;
#106988 = DIRECTION('ref_axis',(0.,0.,-1.)) ;
#106989 = DIRECTION('',(0.,0.,1.)) ;
#106990 = DIRECTION('center_axis',(0.,1.,0.)) ;
#106991 = DIRECTION('ref_axis',(0.,0.,1.)) ;
#106992 = DIRECTION('',(1.,0.,0.)) ;
#106993 = DIRECTION('',(0.,0.,-1.)) ;
#106994 = DIRECTION('',(-1.,0.,0.)) ;
#106995 = DIRECTION('',(0.,0.,1.)) ;
#106996 = DIRECTION('center_axis',(0.,0.164398987305357,-0.986393923832144)) ;
#106997 = DIRECTION('ref_axis',(0.,0.986393923832144,0.164398987305357)) ;
#106998 = DIRECTION('',(-1.,-1.0450141421547E-16,-1.7416902369245E-17)) ;
#106999 = DIRECTION('',(0.,-0.986393923832144,-0.164398987305357)) ;
#107000 = DIRECTION('',(1.,0.,0.)) ;
#107001 = DIRECTION('',(0.,0.986393923832144,0.164398987305357)) ;
#107002 = DIRECTION('center_axis',(0.,-1.,0.)) ;
#107003 = DIRECTION('ref_axis',(0.,0.,-1.)) ;
#107004 = DIRECTION('',(0.,0.,1.)) ;
#107005 = DIRECTION('',(0.,0.,-1.)) ;
#107006 = DIRECTION('',(-1.,0.,0.)) ;
#107007 = DIRECTION('center_axis',(0.,0.164398987305357,0.986393923832144)) ;
#107008 = DIRECTION('ref_axis',(0.,-0.986393923832144,0.164398987305357)) ;
#107009 = DIRECTION('',(0.,0.986393923832144,-0.164398987305357)) ;
#107010 = DIRECTION('',(1.,1.0450141421547E-16,-1.7416902369245E-17)) ;
#107011 = DIRECTION('',(0.,-0.986393923832144,0.164398987305357)) ;
#107012 = DIRECTION('center_axis',(-1.,0.,0.)) ;
#107013 = DIRECTION('ref_axis',(0.,0.,1.)) ;
#107014 = DIRECTION('',(0.,0.,1.)) ;
#107015 = DIRECTION('center_axis',(-1.,0.,0.)) ;
#107016 = DIRECTION('ref_axis',(0.,0.,1.)) ;
#107017 = DIRECTION('',(0.,-0.986393923832144,0.164398987305357)) ;
#107018 = DIRECTION('',(0.,0.,-1.)) ;
#107019 = DIRECTION('',(0.,0.986393923832144,0.164398987305357)) ;
#107020 = DIRECTION('center_axis',(1.,0.,0.)) ;
#107021 = DIRECTION('ref_axis',(0.,0.,-1.)) ;
#107022 = DIRECTION('center_axis',(1.,0.,0.)) ;
#107023 = DIRECTION('ref_axis',(0.,0.,-1.)) ;
#107024 = DIRECTION('center_axis',(1.,0.,0.)) ;
#107025 = DIRECTION('ref_axis',(0.,0.,1.)) ;
#107026 = DIRECTION('center_axis',(1.,0.,0.)) ;
#107027 = DIRECTION('ref_axis',(0.,1.77635683940025E-15,1.)) ;
#107028 = DIRECTION('center_axis',(1.,0.,0.)) ;
#107029 = DIRECTION('ref_axis',(0.,-3.5527136788005E-15,1.)) ;
#107030 = DIRECTION('',(1.,0.,0.)) ;
#107031 = DIRECTION('center_axis',(-1.,0.,0.)) ;
#107032 = DIRECTION('ref_axis',(0.,0.,1.)) ;
#107033 = DIRECTION('',(-1.,0.,0.)) ;
#107034 = DIRECTION('center_axis',(0.,0.,-1.)) ;
#107035 = DIRECTION('ref_axis',(1.,0.,0.)) ;
#107036 = DIRECTION('center_axis',(0.,-1.,0.)) ;
#107037 = DIRECTION('ref_axis',(0.,0.,1.)) ;
#107038 = DIRECTION('center_axis',(0.971399006496778,0.,-0.23745309047699)) ;
#107039 = DIRECTION('ref_axis',(-0.23745309047699,0.,-0.971399006496778)) ;
#107040 = DIRECTION('center_axis',(0.971399006496778,0.,-0.237453090476989)) ;
#107041 = DIRECTION('ref_axis',(-0.237453090476989,0.,-0.971399006496778)) ;
#107042 = DIRECTION('center_axis',(0.655772517804501,-0.73774408253007,-0.160299948796655)) ;
#107043 = DIRECTION('ref_axis',(-0.747409318683662,-0.664363838829917,2.67307565105543E-16)) ;
#107044 = DIRECTION('center_axis',(-0.439210132176044,-4.72063789540106E-10,
-0.898384360835551)) ;
#107045 = DIRECTION('ref_axis',(0.882040291644445,-0.18988021424233,-0.43121969824565)) ;
#107046 = DIRECTION('center_axis',(0.655772517804504,-0.737744082530068,-0.160299948796656)) ;
#107047 = DIRECTION('ref_axis',(0.74740931868366,0.664363838829919,-2.08334010827303E-16)) ;
#107048 = DIRECTION('center_axis',(0.655772517804505,-0.737744082530068,-0.16029994879665)) ;
#107049 = DIRECTION('ref_axis',(0.74740931868366,0.66436383882992,-5.75609428574487E-16)) ;
#107050 = DIRECTION('center_axis',(0.664363838829919,-0.74740931868366,0.)) ;
#107051 = DIRECTION('ref_axis',(0.74740931868366,0.664363838829919,0.)) ;
#107052 = DIRECTION('center_axis',(-0.664363838829918,0.747409318683661,0.)) ;
#107053 = DIRECTION('ref_axis',(-0.747409318683661,-0.664363838829918,0.)) ;
#107054 = DIRECTION('center_axis',(0.,1.,0.)) ;
#107055 = DIRECTION('ref_axis',(0.,0.,1.)) ;
#107056 = DIRECTION('center_axis',(0.,-1.,0.)) ;
#107057 = DIRECTION('ref_axis',(0.,0.,-1.)) ;
#107058 = DIRECTION('center_axis',(0.,0.,1.)) ;
#107059 = DIRECTION('ref_axis',(1.,0.,0.)) ;
#107060 = DIRECTION('center_axis',(0.,0.,-1.)) ;
#107061 = DIRECTION('ref_axis',(-1.,0.,0.)) ;
#107062 = DIRECTION('center_axis',(0.,0.,-1.)) ;
#107063 = DIRECTION('ref_axis',(-1.,0.,0.)) ;
#107064 = DIRECTION('center_axis',(0.439210132175102,4.69462404501499E-10,
-0.898384360836012)) ;
#107065 = DIRECTION('ref_axis',(0.882040291646306,-0.189880214232972,0.431219698245964)) ;
#107066 = DIRECTION('center_axis',(-0.971399006496778,0.,-0.23745309047699)) ;
#107067 = DIRECTION('ref_axis',(-0.23745309047699,0.,0.971399006496778)) ;
#107068 = DIRECTION('center_axis',(0.971399006496778,0.,0.237453090476989)) ;
#107069 = DIRECTION('ref_axis',(0.237453090476989,0.,-0.971399006496778)) ;
#107070 = DIRECTION('center_axis',(0.,1.,0.)) ;
#107071 = DIRECTION('ref_axis',(1.,0.,0.)) ;
#107072 = DIRECTION('center_axis',(-3.54829801904343E-14,1.,8.67361737988405E-15)) ;
#107073 = DIRECTION('ref_axis',(1.,3.54829801904343E-14,6.83923985932746E-30)) ;
#107074 = DIRECTION('center_axis',(-0.948683298050516,0.316227766016833,4.61630059016332E-15)) ;
#107075 = DIRECTION('ref_axis',(0.316227766016833,0.948683298050516,2.49257808733912E-13)) ;
#107076 = DIRECTION('center_axis',(0.,0.,-1.)) ;
#107077 = DIRECTION('ref_axis',(1.,0.,0.)) ;
#107078 = DIRECTION('center_axis',(0.,-1.,0.)) ;
#107079 = DIRECTION('ref_axis',(0.,0.,1.)) ;
#107080 = DIRECTION('center_axis',(0.655772517804503,-0.737744082530069,0.160299948796655)) ;
#107081 = DIRECTION('ref_axis',(-0.747409318683661,-0.664363838829918,2.39955779178099E-16)) ;
#107082 = DIRECTION('center_axis',(0.,1.,0.)) ;
#107083 = DIRECTION('ref_axis',(0.,0.,1.)) ;
#107084 = DIRECTION('center_axis',(2.73957817177508E-14,1.,0.)) ;
#107085 = DIRECTION('ref_axis',(-1.,2.73957817177508E-14,0.)) ;
#107086 = DIRECTION('center_axis',(0.894427190999917,0.447213595499956,0.)) ;
#107087 = DIRECTION('ref_axis',(-0.447213595499956,0.894427190999917,0.)) ;
#107088 = DIRECTION('center_axis',(-0.894427190999916,-0.447213595499958,
0.)) ;
#107089 = DIRECTION('ref_axis',(0.447213595499958,-0.894427190999916,0.)) ;
#107090 = DIRECTION('center_axis',(0.,0.,1.)) ;
#107091 = DIRECTION('ref_axis',(1.,0.,0.)) ;
#107092 = DIRECTION('center_axis',(0.,0.,-1.)) ;
#107093 = DIRECTION('ref_axis',(-1.,0.,0.)) ;
#107094 = DIRECTION('center_axis',(0.,1.,0.)) ;
#107095 = DIRECTION('ref_axis',(0.,0.,1.)) ;
#107096 = DIRECTION('center_axis',(0.,-1.,0.)) ;
#107097 = DIRECTION('ref_axis',(0.,0.,-1.)) ;
#107098 = DIRECTION('center_axis',(-0.664363838829919,0.74740931868366,0.)) ;
#107099 = DIRECTION('ref_axis',(-0.74740931868366,-0.664363838829919,0.)) ;
#107100 = DIRECTION('center_axis',(-0.66436383882992,0.747409318683659,2.52106651083074E-15)) ;
#107101 = DIRECTION('ref_axis',(-0.747409318683659,-0.66436383882992,7.82575143531171E-30)) ;
#107102 = DIRECTION('center_axis',(-0.655772517804504,0.737744082530068,-0.160299948796656)) ;
#107103 = DIRECTION('ref_axis',(-0.74740931868366,-0.664363838829919,2.31673158493852E-16)) ;
#107104 = DIRECTION('center_axis',(0.655772517804496,-0.737744082530075,0.160299948796656)) ;
#107105 = DIRECTION('ref_axis',(0.747409318683667,0.664363838829911,-2.10122272487167E-17)) ;
#107106 = DIRECTION('center_axis',(0.,1.,0.)) ;
#107107 = DIRECTION('ref_axis',(1.,0.,0.)) ;
#107108 = DIRECTION('center_axis',(-0.873786407766988,-0.436893203883498,
0.213592233009711)) ;
#107109 = DIRECTION('ref_axis',(-0.447213595499961,0.894427190999914,5.03515095507592E-16)) ;
#107110 = DIRECTION('center_axis',(-0.948683298050516,0.316227766016832,-3.59045601457216E-15)) ;
#107111 = DIRECTION('ref_axis',(0.316227766016832,0.948683298050516,-1.73053540936819E-12)) ;
#107112 = DIRECTION('center_axis',(0.,1.,0.)) ;
#107113 = DIRECTION('ref_axis',(1.,0.,0.)) ;
#107114 = DIRECTION('center_axis',(-5.47915634355017E-14,1.,0.)) ;
#107115 = DIRECTION('ref_axis',(1.,5.47915634355017E-14,6.93889390390721E-14)) ;
#107116 = DIRECTION('center_axis',(-0.971399006496778,0.,0.23745309047699)) ;
#107117 = DIRECTION('ref_axis',(0.23745309047699,0.,0.971399006496777)) ;
#107118 = DIRECTION('center_axis',(0.971399006496778,-3.69787733965917E-15,
-0.237453090476989)) ;
#107119 = DIRECTION('ref_axis',(-0.237453090476989,3.58403898099287E-30,-0.971399006496778)) ;
#107120 = DIRECTION('center_axis',(0.873786407766991,0.436893203883493,-0.213592233009709)) ;
#107121 = DIRECTION('ref_axis',(-0.447213595499956,0.894427190999917,2.83414331365695E-16)) ;
#107122 = DIRECTION('center_axis',(-0.873786407766992,-0.436893203883492,
0.21359223300971)) ;
#107123 = DIRECTION('ref_axis',(0.447213595499955,-0.894427190999918,-1.48231119036019E-16)) ;
#107124 = DIRECTION('center_axis',(-0.894427190999917,-0.447213595499956,
0.)) ;
#107125 = DIRECTION('ref_axis',(0.447213595499956,-0.894427190999917,0.)) ;
#107126 = DIRECTION('center_axis',(-0.894427190999917,-0.447213595499955,
0.)) ;
#107127 = DIRECTION('ref_axis',(0.447213595499955,-0.894427190999917,0.)) ;
#107128 = DIRECTION('center_axis',(0.,1.,0.)) ;
#107129 = DIRECTION('ref_axis',(0.,0.,1.)) ;
#107130 = DIRECTION('center_axis',(2.66122351428257E-14,1.,6.50521303491301E-15)) ;
#107131 = DIRECTION('ref_axis',(-1.,2.66122351428257E-14,3.84707242087163E-30)) ;
#107132 = DIRECTION('center_axis',(-0.439210132004893,-2.53225376140315E-13,
-0.898384360919225)) ;
#107133 = DIRECTION('ref_axis',(0.898384360919225,-2.84946438885355E-11,-0.439210132004893)) ;
#107134 = DIRECTION('center_axis',(0.,1.,0.)) ;
#107135 = DIRECTION('ref_axis',(1.,0.,0.)) ;
#107136 = DIRECTION('center_axis',(-0.87378640776699,-0.436893203883495,-0.213592233009712)) ;
#107137 = DIRECTION('ref_axis',(-0.447213595499958,0.894427190999916,-1.950883489007E-18)) ;
#107138 = DIRECTION('center_axis',(0.,0.,1.)) ;
#107139 = DIRECTION('ref_axis',(1.,0.,0.)) ;
#107140 = DIRECTION('center_axis',(0.439210132005014,-3.83870315422912E-13,
-0.898384360919166)) ;
#107141 = DIRECTION('ref_axis',(0.898384360919166,1.69706610442857E-11,0.439210132005014)) ;
#107142 = DIRECTION('center_axis',(-0.873786407766991,-0.436893203883493,
-0.213592233009709)) ;
#107143 = DIRECTION('ref_axis',(0.447213595499956,-0.894427190999917,-1.06780556900622E-16)) ;
#107144 = DIRECTION('center_axis',(-0.873786407766992,-0.436893203883492,
-0.213592233009707)) ;
#107145 = DIRECTION('ref_axis',(0.447213595499955,-0.894427190999918,-7.04543255365314E-18)) ;
#107146 = DIRECTION('center_axis',(-0.971399006496778,0.,-0.237453090476989)) ;
#107147 = DIRECTION('ref_axis',(0.237453090476989,0.,-0.971399006496778)) ;
#107148 = DIRECTION('center_axis',(0.971399006496778,0.,0.23745309047699)) ;
#107149 = DIRECTION('ref_axis',(0.23745309047699,0.,-0.971399006496778)) ;
#107150 = DIRECTION('center_axis',(1.,1.0450141421547E-16,1.7416902369245E-17)) ;
#107151 = DIRECTION('ref_axis',(-1.0450141421547E-16,1.,-1.82009092883888E-33)) ;
#107152 = DIRECTION('center_axis',(0.672672795323245,0.739940072189642,-7.49525355246789E-10)) ;
#107153 = DIRECTION('ref_axis',(0.7380448706102,-0.670949884717819,0.0715263669084184)) ;
#107154 = DIRECTION('center_axis',(-1.,0.,0.)) ;
#107155 = DIRECTION('ref_axis',(0.,-0.646374896130194,-0.763019982472727)) ;
#107156 = DIRECTION('center_axis',(-1.,0.,0.)) ;
#107157 = DIRECTION('ref_axis',(0.,0.,1.)) ;
#107158 = DIRECTION('center_axis',(-1.,0.,0.)) ;
#107159 = DIRECTION('ref_axis',(0.,0.,1.)) ;
#107160 = DIRECTION('center_axis',(0.,0.986393923832144,0.164398987305357)) ;
#107161 = DIRECTION('ref_axis',(0.,-0.164398987305357,0.986393923832144)) ;
#107162 = DIRECTION('center_axis',(0.,-0.986393923832144,-0.164398987305358)) ;
#107163 = DIRECTION('ref_axis',(0.,0.164398987305358,-0.986393923832144)) ;
#107164 = DIRECTION('center_axis',(0.,0.,1.)) ;
#107165 = DIRECTION('ref_axis',(1.,0.,0.)) ;
#107166 = DIRECTION('center_axis',(0.,0.,1.)) ;
#107167 = DIRECTION('ref_axis',(1.,0.,0.)) ;
#107168 = DIRECTION('center_axis',(0.,0.,1.)) ;
#107169 = DIRECTION('ref_axis',(1.,0.,0.)) ;
#107170 = DIRECTION('center_axis',(0.,0.,-1.)) ;
#107171 = DIRECTION('ref_axis',(1.,0.,0.)) ;
#107172 = DIRECTION('center_axis',(-1.,0.,0.)) ;
#107173 = DIRECTION('ref_axis',(0.,-0.646374896130192,-0.763019982472729)) ;
#107174 = DIRECTION('center_axis',(0.,0.,1.)) ;
#107175 = DIRECTION('ref_axis',(-1.,0.,0.)) ;
#107176 = DIRECTION('center_axis',(0.,0.,-1.)) ;
#107177 = DIRECTION('ref_axis',(-1.,0.,0.)) ;
#107178 = DIRECTION('center_axis',(1.,1.0450141421547E-16,-1.7416902369245E-17)) ;
#107179 = DIRECTION('ref_axis',(-1.0450141421547E-16,1.,1.82009092883888E-33)) ;
#107180 = DIRECTION('center_axis',(0.672672795323166,0.739940072189713,7.49492439365374E-10)) ;
#107181 = DIRECTION('ref_axis',(0.738044870611677,-0.670949884719022,-0.0715263668818917)) ;
#107182 = DIRECTION('center_axis',(1.,0.,0.)) ;
#107183 = DIRECTION('ref_axis',(0.,5.20417042793045E-14,1.)) ;
#107184 = DIRECTION('center_axis',(0.,0.,-1.)) ;
#107185 = DIRECTION('ref_axis',(-1.,0.,0.)) ;
#107186 = DIRECTION('center_axis',(0.,-0.986393923832144,0.164398987305357)) ;
#107187 = DIRECTION('ref_axis',(0.,-0.164398987305357,-0.986393923832144)) ;
#107188 = DIRECTION('center_axis',(1.,0.,0.)) ;
#107189 = DIRECTION('ref_axis',(0.,0.,1.)) ;
#107190 = DIRECTION('center_axis',(7.58941520739854E-15,0.,-1.)) ;
#107191 = DIRECTION('ref_axis',(-1.,0.,-7.58941520739854E-15)) ;
#107192 = DIRECTION('center_axis',(1.,0.,-8.67361737988404E-15)) ;
#107193 = DIRECTION('ref_axis',(-8.67361737988404E-15,0.,-1.)) ;
#107194 = DIRECTION('center_axis',(1.,0.,0.)) ;
#107195 = DIRECTION('ref_axis',(0.,0.,-1.)) ;
#107196 = DIRECTION('center_axis',(1.,0.,8.67361737988403E-15)) ;
#107197 = DIRECTION('ref_axis',(8.67361737988403E-15,0.,-1.)) ;
#107198 = DIRECTION('center_axis',(0.,0.,1.)) ;
#107199 = DIRECTION('ref_axis',(1.,0.,0.)) ;
#107200 = DIRECTION('center_axis',(0.,0.,-1.)) ;
#107201 = DIRECTION('ref_axis',(-1.,0.,0.)) ;
#107202 = DIRECTION('center_axis',(1.,0.,0.)) ;
#107203 = DIRECTION('ref_axis',(0.,0.,1.)) ;
#107204 = DIRECTION('center_axis',(-6.50521303491304E-15,0.,-1.)) ;
#107205 = DIRECTION('ref_axis',(-1.,0.,6.50521303491304E-15)) ;
#107206 = DIRECTION('center_axis',(1.,0.,0.)) ;
#107207 = DIRECTION('ref_axis',(0.,0.,1.)) ;
#107208 = DIRECTION('center_axis',(1.,9.40395480657835E-30,8.67361737988403E-15)) ;
#107209 = DIRECTION('ref_axis',(8.67361737988403E-15,-5.27711695562625E-58,
-1.)) ;
#107210 = DIRECTION('center_axis',(0.,0.,-1.)) ;
#107211 = DIRECTION('ref_axis',(-1.,0.,0.)) ;
#107212 = DIRECTION('center_axis',(6.50521303491304E-15,0.,-1.)) ;
#107213 = DIRECTION('ref_axis',(-1.,0.,-6.50521303491304E-15)) ;
#107214 = DIRECTION('center_axis',(-1.,0.,0.)) ;
#107215 = DIRECTION('ref_axis',(0.,0.,1.)) ;
#107216 = DIRECTION('center_axis',(1.,-8.67361737988409E-15,0.)) ;
#107217 = DIRECTION('ref_axis',(8.67361737988409E-15,1.,0.)) ;
#107218 = DIRECTION('center_axis',(1.,0.,0.)) ;
#107219 = DIRECTION('ref_axis',(0.,0.,1.)) ;
#107220 = DIRECTION('center_axis',(-4.33680868994202E-16,0.,1.)) ;
#107221 = DIRECTION('ref_axis',(1.,0.,4.33680868994202E-16)) ;
#107222 = DIRECTION('center_axis',(0.,0.,-1.)) ;
#107223 = DIRECTION('ref_axis',(-1.,0.,0.)) ;
#107224 = DIRECTION('center_axis',(0.,0.,1.)) ;
#107225 = DIRECTION('ref_axis',(1.,0.,0.)) ;
#107226 = DIRECTION('center_axis',(0.,1.,0.)) ;
#107227 = DIRECTION('ref_axis',(0.,0.,1.)) ;
#107228 = DIRECTION('center_axis',(-1.,0.,0.)) ;
#107229 = DIRECTION('ref_axis',(0.,0.,-1.)) ;
#107230 = DIRECTION('center_axis',(0.,-1.,0.)) ;
#107231 = DIRECTION('ref_axis',(0.,0.,1.)) ;
#107232 = DIRECTION('center_axis',(0.,1.,0.)) ;
#107233 = DIRECTION('ref_axis',(0.,0.,1.)) ;
#107234 = DIRECTION('center_axis',(0.,-1.,0.)) ;
#107235 = DIRECTION('ref_axis',(0.,0.,1.)) ;
#107236 = DIRECTION('center_axis',(-1.,0.,0.)) ;
#107237 = DIRECTION('ref_axis',(0.,0.,-1.)) ;
#107238 = DIRECTION('center_axis',(-1.,0.,-1.73472347597681E-16)) ;
#107239 = DIRECTION('ref_axis',(-1.73472347597681E-16,0.,1.)) ;
#107240 = DIRECTION('center_axis',(-1.,0.,0.)) ;
#107241 = DIRECTION('ref_axis',(0.,0.,1.)) ;
#107242 = DIRECTION('center_axis',(0.,1.,0.)) ;
#107243 = DIRECTION('ref_axis',(0.,0.,1.)) ;
#107244 = DIRECTION('center_axis',(0.,-1.,0.)) ;
#107245 = DIRECTION('ref_axis',(0.,0.,-1.)) ;
#107246 = DIRECTION('center_axis',(-4.33680868994202E-16,0.,1.)) ;
#107247 = DIRECTION('ref_axis',(1.,0.,4.33680868994202E-16)) ;
#107248 = DIRECTION('center_axis',(0.,0.,1.)) ;
#107249 = DIRECTION('ref_axis',(1.,0.,0.)) ;
#107250 = DIRECTION('center_axis',(0.,0.,-1.)) ;
#107251 = DIRECTION('ref_axis',(-1.,0.,0.)) ;
#107252 = DIRECTION('center_axis',(0.,1.,0.)) ;
#107253 = DIRECTION('ref_axis',(0.,0.,1.)) ;
#107254 = DIRECTION('center_axis',(0.,-1.,0.)) ;
#107255 = DIRECTION('ref_axis',(0.,0.,-1.)) ;
#107256 = DIRECTION('center_axis',(1.,0.,-1.73472347597681E-16)) ;
#107257 = DIRECTION('ref_axis',(-1.73472347597681E-16,0.,-1.)) ;
#107258 = DIRECTION('center_axis',(-1.,0.,0.)) ;
#107259 = DIRECTION('ref_axis',(0.,0.,1.)) ;
#107260 = DIRECTION('center_axis',(0.,0.,-1.)) ;
#107261 = DIRECTION('ref_axis',(-1.,0.,0.)) ;
#107262 = DIRECTION('center_axis',(0.,0.,1.)) ;
#107263 = DIRECTION('ref_axis',(1.,0.,0.)) ;
#107264 = DIRECTION('center_axis',(0.,0.,-1.)) ;
#107265 = DIRECTION('ref_axis',(-1.,0.,0.)) ;
#107266 = DIRECTION('center_axis',(0.,1.,0.)) ;
#107267 = DIRECTION('ref_axis',(0.,0.,1.)) ;
#107268 = DIRECTION('center_axis',(0.,-1.,0.)) ;
#107269 = DIRECTION('ref_axis',(0.,0.,1.)) ;
#107270 = DIRECTION('center_axis',(0.,1.,0.)) ;
#107271 = DIRECTION('ref_axis',(1.,0.,0.)) ;
#107272 = DIRECTION('center_axis',(1.,0.,0.)) ;
#107273 = DIRECTION('ref_axis',(0.,0.,1.)) ;
#107274 = DIRECTION('center_axis',(0.,1.,0.)) ;
#107275 = DIRECTION('ref_axis',(1.,0.,0.)) ;
#107276 = DIRECTION('center_axis',(1.,0.,0.)) ;
#107277 = DIRECTION('ref_axis',(0.,0.,1.)) ;
#107278 = DIRECTION('center_axis',(0.,1.,0.)) ;
#107279 = DIRECTION('ref_axis',(0.,0.,1.)) ;
#107280 = DIRECTION('center_axis',(0.,-1.,0.)) ;
#107281 = DIRECTION('ref_axis',(0.,0.,1.)) ;
#107282 = DIRECTION('center_axis',(0.,1.,0.)) ;
#107283 = DIRECTION('ref_axis',(0.,0.,1.)) ;
#107284 = DIRECTION('center_axis',(0.,-1.,0.)) ;
#107285 = DIRECTION('ref_axis',(0.,0.,-1.)) ;
#107286 = DIRECTION('center_axis',(-1.,0.,-1.73472347597681E-16)) ;
#107287 = DIRECTION('ref_axis',(-1.73472347597681E-16,0.,1.)) ;
#107288 = DIRECTION('center_axis',(1.,0.,0.)) ;
#107289 = DIRECTION('ref_axis',(0.,0.,-1.)) ;
#107290 = DIRECTION('center_axis',(1.,0.,-1.73472347597681E-16)) ;
#107291 = DIRECTION('ref_axis',(-1.73472347597681E-16,0.,-1.)) ;
#107292 = DIRECTION('center_axis',(1.,0.,0.)) ;
#107293 = DIRECTION('ref_axis',(0.,0.,-1.)) ;
#107294 = DIRECTION('center_axis',(0.,1.,0.)) ;
#107295 = DIRECTION('ref_axis',(0.,0.,1.)) ;
#107296 = DIRECTION('center_axis',(0.,-1.,0.)) ;
#107297 = DIRECTION('ref_axis',(0.,0.,-1.)) ;
#107298 = DIRECTION('center_axis',(0.,1.,0.)) ;
#107299 = DIRECTION('ref_axis',(1.,0.,0.)) ;
#107300 = DIRECTION('center_axis',(0.,0.,1.)) ;
#107301 = DIRECTION('ref_axis',(-1.,0.,0.)) ;
#107302 = DIRECTION('center_axis',(0.,1.,0.)) ;
#107303 = DIRECTION('ref_axis',(1.,0.,0.)) ;
#107304 = DIRECTION('center_axis',(0.,0.,-1.)) ;
#107305 = DIRECTION('ref_axis',(1.,0.,0.)) ;
#107306 = DIRECTION('center_axis',(0.,0.,-1.)) ;
#107307 = DIRECTION('ref_axis',(-1.,0.,0.)) ;
#107308 = DIRECTION('center_axis',(2.16840434497101E-16,0.,1.)) ;
#107309 = DIRECTION('ref_axis',(1.,0.,-2.16840434497101E-16)) ;
#107310 = DIRECTION('center_axis',(0.,0.,-1.)) ;
#107311 = DIRECTION('ref_axis',(-1.,0.,0.)) ;
#107312 = DIRECTION('center_axis',(0.,0.,1.)) ;
#107313 = DIRECTION('ref_axis',(1.,0.,0.)) ;
#107314 = DIRECTION('center_axis',(0.,-1.,0.)) ;
#107315 = DIRECTION('ref_axis',(0.,0.,-1.)) ;
#107316 = DIRECTION('center_axis',(1.,0.,0.)) ;
#107317 = DIRECTION('ref_axis',(0.,0.,1.)) ;
#107318 = DIRECTION('center_axis',(0.,1.,0.)) ;
#107319 = DIRECTION('ref_axis',(0.,0.,-1.)) ;
#107320 = DIRECTION('center_axis',(0.,-1.,0.)) ;
#107321 = DIRECTION('ref_axis',(0.,0.,-1.)) ;
#107322 = DIRECTION('center_axis',(0.,1.,0.)) ;
#107323 = DIRECTION('ref_axis',(0.,0.,-1.)) ;
#107324 = DIRECTION('center_axis',(1.,0.,0.)) ;
#107325 = DIRECTION('ref_axis',(0.,0.,1.)) ;
#107326 = DIRECTION('center_axis',(1.,0.,-1.73472347597681E-16)) ;
#107327 = DIRECTION('ref_axis',(-1.73472347597681E-16,0.,-1.)) ;
#107328 = DIRECTION('center_axis',(1.,0.,0.)) ;
#107329 = DIRECTION('ref_axis',(0.,0.,-1.)) ;
#107330 = DIRECTION('center_axis',(0.,-1.,0.)) ;
#107331 = DIRECTION('ref_axis',(0.,0.,-1.)) ;
#107332 = DIRECTION('center_axis',(0.,1.,0.)) ;
#107333 = DIRECTION('ref_axis',(0.,0.,1.)) ;
#107334 = DIRECTION('center_axis',(2.16840434497101E-16,0.,1.)) ;
#107335 = DIRECTION('ref_axis',(1.,0.,-2.16840434497101E-16)) ;
#107336 = DIRECTION('center_axis',(0.,0.,1.)) ;
#107337 = DIRECTION('ref_axis',(1.,0.,0.)) ;
#107338 = DIRECTION('center_axis',(0.,0.,-1.)) ;
#107339 = DIRECTION('ref_axis',(-1.,0.,0.)) ;
#107340 = DIRECTION('center_axis',(0.,-1.,0.)) ;
#107341 = DIRECTION('ref_axis',(0.,0.,-1.)) ;
#107342 = DIRECTION('center_axis',(0.,1.,0.)) ;
#107343 = DIRECTION('ref_axis',(0.,0.,1.)) ;
#107344 = DIRECTION('center_axis',(-1.,0.,1.73472347597681E-16)) ;
#107345 = DIRECTION('ref_axis',(1.73472347597681E-16,0.,1.)) ;
#107346 = DIRECTION('center_axis',(1.,0.,0.)) ;
#107347 = DIRECTION('ref_axis',(0.,0.,-1.)) ;
#107348 = DIRECTION('center_axis',(-2.16840434497101E-16,0.,-1.)) ;
#107349 = DIRECTION('ref_axis',(-1.,0.,2.16840434497101E-16)) ;
#107350 = DIRECTION('center_axis',(0.,0.,1.)) ;
#107351 = DIRECTION('ref_axis',(1.,0.,0.)) ;
#107352 = DIRECTION('center_axis',(0.,0.,-1.)) ;
#107353 = DIRECTION('ref_axis',(-1.,0.,0.)) ;
#107354 = DIRECTION('center_axis',(0.,-1.,0.)) ;
#107355 = DIRECTION('ref_axis',(0.,0.,-1.)) ;
#107356 = DIRECTION('center_axis',(0.,1.,0.)) ;
#107357 = DIRECTION('ref_axis',(0.,0.,-1.)) ;
#107358 = DIRECTION('center_axis',(0.,1.,0.)) ;
#107359 = DIRECTION('ref_axis',(1.,0.,0.)) ;
#107360 = DIRECTION('center_axis',(-1.,0.,0.)) ;
#107361 = DIRECTION('ref_axis',(0.,0.,-1.)) ;
#107362 = DIRECTION('center_axis',(0.,1.,0.)) ;
#107363 = DIRECTION('ref_axis',(1.,0.,0.)) ;
#107364 = DIRECTION('center_axis',(-1.,0.,0.)) ;
#107365 = DIRECTION('ref_axis',(0.,0.,-1.)) ;
#107366 = DIRECTION('center_axis',(0.,-1.,0.)) ;
#107367 = DIRECTION('ref_axis',(0.,0.,-1.)) ;
#107368 = DIRECTION('center_axis',(0.,1.,0.)) ;
#107369 = DIRECTION('ref_axis',(0.,0.,-1.)) ;
#107370 = DIRECTION('center_axis',(0.,-1.,0.)) ;
#107371 = DIRECTION('ref_axis',(0.,0.,-1.)) ;
#107372 = DIRECTION('center_axis',(0.,1.,0.)) ;
#107373 = DIRECTION('ref_axis',(0.,0.,1.)) ;
#107374 = DIRECTION('center_axis',(1.,0.,-1.73472347597681E-16)) ;
#107375 = DIRECTION('ref_axis',(-1.73472347597681E-16,0.,-1.)) ;
#107376 = DIRECTION('center_axis',(-1.,0.,0.)) ;
#107377 = DIRECTION('ref_axis',(0.,0.,1.)) ;
#107378 = DIRECTION('center_axis',(-1.,0.,1.73472347597681E-16)) ;
#107379 = DIRECTION('ref_axis',(1.73472347597681E-16,0.,1.)) ;
#107380 = DIRECTION('center_axis',(-1.,0.,0.)) ;
#107381 = DIRECTION('ref_axis',(0.,0.,1.)) ;
#107382 = DIRECTION('center_axis',(0.,-1.,0.)) ;
#107383 = DIRECTION('ref_axis',(0.,0.,-1.)) ;
#107384 = DIRECTION('center_axis',(0.,1.,0.)) ;
#107385 = DIRECTION('ref_axis',(0.,0.,1.)) ;
#107386 = DIRECTION('center_axis',(0.,1.,0.)) ;
#107387 = DIRECTION('ref_axis',(1.,0.,0.)) ;
#107388 = DIRECTION('center_axis',(0.,0.,1.)) ;
#107389 = DIRECTION('ref_axis',(-1.,0.,0.)) ;
#107390 = DIRECTION('center_axis',(0.,1.,0.)) ;
#107391 = DIRECTION('ref_axis',(1.,0.,0.)) ;
#107392 = DIRECTION('center_axis',(0.,0.,-1.)) ;
#107393 = DIRECTION('ref_axis',(1.,0.,0.)) ;
#107394 = DIRECTION('center_axis',(-2.16840434497101E-16,0.,-1.)) ;
#107395 = DIRECTION('ref_axis',(-1.,0.,2.16840434497101E-16)) ;
#107396 = DIRECTION('center_axis',(-1.,0.,0.)) ;
#107397 = DIRECTION('ref_axis',(0.,0.,1.)) ;
#107398 = DIRECTION('center_axis',(0.,-0.632948931301575,-0.774193548387091)) ;
#107399 = DIRECTION('ref_axis',(0.,0.774193548387091,-0.632948931301575)) ;
#107400 = DIRECTION('center_axis',(0.,0.,1.)) ;
#107401 = DIRECTION('ref_axis',(1.,0.,0.)) ;
#107402 = DIRECTION('center_axis',(8.67361737988401E-15,0.,1.)) ;
#107403 = DIRECTION('ref_axis',(1.,0.,-8.67361737988401E-15)) ;
#107404 = DIRECTION('center_axis',(0.,1.,0.)) ;
#107405 = DIRECTION('ref_axis',(1.,0.,0.)) ;
#107406 = DIRECTION('center_axis',(-1.,0.,0.)) ;
#107407 = DIRECTION('ref_axis',(0.,4.33680868994204E-15,-1.)) ;
#107408 = DIRECTION('center_axis',(1.,0.,0.)) ;
#107409 = DIRECTION('ref_axis',(0.,0.,-1.)) ;
#107410 = DIRECTION('center_axis',(-1.,0.,0.)) ;
#107411 = DIRECTION('ref_axis',(0.,0.,1.)) ;
#107412 = DIRECTION('center_axis',(0.,0.,-1.)) ;
#107413 = DIRECTION('ref_axis',(-1.,0.,0.)) ;
#107414 = DIRECTION('center_axis',(0.,0.,-1.)) ;
#107415 = DIRECTION('ref_axis',(-1.,0.,0.)) ;
#107416 = DIRECTION('center_axis',(-1.,0.,0.)) ;
#107417 = DIRECTION('ref_axis',(0.,0.,1.)) ;
#107418 = DIRECTION('center_axis',(0.,-0.632948931301567,-0.774193548387097)) ;
#107419 = DIRECTION('ref_axis',(0.,-0.774193548387097,0.632948931301567)) ;
#107420 = DIRECTION('center_axis',(-1.,0.,0.)) ;
#107421 = DIRECTION('ref_axis',(0.,0.,1.)) ;
#107422 = DIRECTION('center_axis',(0.,0.632948931301567,-0.774193548387097)) ;
#107423 = DIRECTION('ref_axis',(0.,0.774193548387097,0.632948931301567)) ;
#107424 = DIRECTION('center_axis',(-1.,0.,0.)) ;
#107425 = DIRECTION('ref_axis',(0.,0.,1.)) ;
#107426 = DIRECTION('center_axis',(1.,0.,0.)) ;
#107427 = DIRECTION('ref_axis',(0.,5.20417042793045E-14,1.)) ;
#107428 = DIRECTION('center_axis',(1.,0.,0.)) ;
#107429 = DIRECTION('ref_axis',(0.,0.,-1.)) ;
#107430 = DIRECTION('center_axis',(1.,0.,0.)) ;
#107431 = DIRECTION('ref_axis',(0.,0.,-1.)) ;
#107432 = DIRECTION('center_axis',(0.,1.,0.)) ;
#107433 = DIRECTION('ref_axis',(1.,0.,0.)) ;
#107434 = DIRECTION('center_axis',(1.22050154678007E-14,0.632948931301567,
-0.774193548387097)) ;
#107435 = DIRECTION('ref_axis',(1.73472347597684E-14,-0.774193548387097,-0.632948931301567)) ;
#107436 = DIRECTION('center_axis',(-1.,0.,0.)) ;
#107437 = DIRECTION('ref_axis',(0.,0.,1.)) ;
#107438 = DIRECTION('center_axis',(-0.422618261740697,0.,0.906307787036651)) ;
#107439 = DIRECTION('ref_axis',(0.906307787036651,0.,0.422618261740697)) ;
#107440 = DIRECTION('center_axis',(0.422618261740697,0.,-0.906307787036651)) ;
#107441 = DIRECTION('ref_axis',(-0.906307787036651,0.,-0.422618261740697)) ;
#107442 = DIRECTION('center_axis',(0.422618261740697,0.,-0.906307787036651)) ;
#107443 = DIRECTION('ref_axis',(-0.906307787036651,0.,-0.422618261740697)) ;
#107444 = DIRECTION('center_axis',(-0.422618261740697,0.,0.906307787036651)) ;
#107445 = DIRECTION('ref_axis',(0.906307787036651,0.,0.422618261740697)) ;
#107446 = DIRECTION('center_axis',(0.,1.,0.)) ;
#107447 = DIRECTION('ref_axis',(1.,0.,0.)) ;
#107448 = DIRECTION('center_axis',(0.,-0.986393923832144,0.164398987305358)) ;
#107449 = DIRECTION('ref_axis',(0.,-0.164398987305358,-0.986393923832144)) ;
#107450 = DIRECTION('center_axis',(0.,0.986393923832144,-0.164398987305357)) ;
#107451 = DIRECTION('ref_axis',(0.,0.164398987305357,0.986393923832144)) ;
#107452 = DIRECTION('center_axis',(0.,-0.986393923832144,0.164398987305358)) ;
#107453 = DIRECTION('ref_axis',(0.,-0.164398987305358,-0.986393923832144)) ;
#107454 = DIRECTION('center_axis',(-1.,0.,0.)) ;
#107455 = DIRECTION('ref_axis',(0.,0.107567764393758,-0.994197755008192)) ;
#107456 = DIRECTION('center_axis',(4.02631181035923E-15,-0.928404294083138,
-0.371571617226061)) ;
#107457 = DIRECTION('ref_axis',(1.27444840229953E-29,0.371571617226061,-0.928404294083138)) ;
#107458 = DIRECTION('center_axis',(0.275516865537137,-0.50093975551097,-0.820457078800105)) ;
#107459 = DIRECTION('ref_axis',(3.47276585739718E-16,0.853490367006418,-0.521108619605597)) ;
#107460 = DIRECTION('center_axis',(0.,0.,-1.)) ;
#107461 = DIRECTION('ref_axis',(-1.,0.,0.)) ;
#107462 = DIRECTION('center_axis',(0.,0.,-1.)) ;
#107463 = DIRECTION('ref_axis',(-1.,0.,0.)) ;
#107464 = DIRECTION('center_axis',(-0.275516865538071,0.500939755523742,-0.820457078791993)) ;
#107465 = DIRECTION('ref_axis',(1.34532370065023E-15,0.853490366998217,0.521108619619028)) ;
#107466 = DIRECTION('center_axis',(0.,-0.986393923832144,-0.164398987305357)) ;
#107467 = DIRECTION('ref_axis',(0.,0.164398987305357,-0.986393923832144)) ;
#107468 = DIRECTION('center_axis',(3.5648347838177E-16,0.986393923832144,
0.164398987305358)) ;
#107469 = DIRECTION('ref_axis',(3.79675591822878E-31,-0.164398987305358,0.986393923832144)) ;
#107470 = DIRECTION('center_axis',(0.,1.,0.)) ;
#107471 = DIRECTION('ref_axis',(1.,0.,0.)) ;
#107472 = DIRECTION('center_axis',(-1.,0.,0.)) ;
#107473 = DIRECTION('ref_axis',(0.,0.,1.)) ;
#107474 = DIRECTION('center_axis',(0.,0.,-1.)) ;
#107475 = DIRECTION('ref_axis',(-1.,0.,0.)) ;
#107476 = DIRECTION('center_axis',(0.,0.,-1.)) ;
#107477 = DIRECTION('ref_axis',(-1.,0.,0.)) ;
#107478 = DIRECTION('center_axis',(0.795723237447208,-7.53302716311723E-12,
0.605660407643206)) ;
#107479 = DIRECTION('ref_axis',(0.605660407643206,2.00215687134887E-26,-0.795723237447208)) ;
#107480 = DIRECTION('center_axis',(1.57772181044204E-26,2.36658271566302E-26,
1.)) ;
#107481 = DIRECTION('ref_axis',(3.73380916671669E-52,-1.,2.36658271566302E-26)) ;
#107482 = DIRECTION('center_axis',(-0.795723237415222,-2.11663082418553E-11,
0.605660407685229)) ;
#107483 = DIRECTION('ref_axis',(0.605660407685229,1.1913710773826E-25,0.795723237415222)) ;
#107484 = DIRECTION('center_axis',(0.,1.,0.)) ;
#107485 = DIRECTION('ref_axis',(1.,0.,0.)) ;
#107486 = DIRECTION('center_axis',(-0.716468671818951,0.697619267438901,0.)) ;
#107487 = DIRECTION('ref_axis',(-0.697619267438901,-0.716468671818951,0.)) ;
#107488 = DIRECTION('center_axis',(0.,-1.,0.)) ;
#107489 = DIRECTION('ref_axis',(0.,0.,-1.)) ;
#107490 = DIRECTION('center_axis',(0.,1.,0.)) ;
#107491 = DIRECTION('ref_axis',(1.,0.,0.)) ;
#107492 = DIRECTION('center_axis',(0.,-1.,0.)) ;
#107493 = DIRECTION('ref_axis',(0.,0.,-1.)) ;
#107494 = DIRECTION('center_axis',(-0.716468671818951,0.697619267438901,0.)) ;
#107495 = DIRECTION('ref_axis',(-0.697619267438901,-0.716468671818951,0.)) ;
#107496 = DIRECTION('center_axis',(0.,-1.,0.)) ;
#107497 = DIRECTION('ref_axis',(0.,0.,-1.)) ;
#107498 = DIRECTION('center_axis',(0.,-1.,0.)) ;
#107499 = DIRECTION('ref_axis',(0.,0.,-1.)) ;
#107500 = DIRECTION('center_axis',(0.716468671818953,-0.697619267438899,0.)) ;
#107501 = DIRECTION('ref_axis',(0.697619267438899,0.716468671818953,0.)) ;
#107502 = DIRECTION('center_axis',(-0.716468671818955,0.697619267438896,0.)) ;
#107503 = DIRECTION('ref_axis',(-0.697619267438896,-0.716468671818955,0.)) ;
#107504 = DIRECTION('center_axis',(-0.716468671818953,0.697619267438899,0.)) ;
#107505 = DIRECTION('ref_axis',(-0.697619267438899,-0.716468671818953,0.)) ;
#107506 = DIRECTION('center_axis',(-0.716468671818955,0.697619267438896,0.)) ;
#107507 = DIRECTION('ref_axis',(-0.697619267438896,-0.716468671818955,0.)) ;
#107508 = DIRECTION('center_axis',(0.,1.,0.)) ;
#107509 = DIRECTION('ref_axis',(0.,0.,1.)) ;
#107510 = DIRECTION('center_axis',(0.,-1.,0.)) ;
#107511 = DIRECTION('ref_axis',(0.,0.,-1.)) ;
#107512 = DIRECTION('center_axis',(0.,0.,1.)) ;
#107513 = DIRECTION('ref_axis',(1.,0.,0.)) ;
#107514 = DIRECTION('center_axis',(-0.891049746169499,0.453905661840951,0.)) ;
#107515 = DIRECTION('ref_axis',(-0.453905661840951,-0.891049746169499,0.)) ;
#107516 = DIRECTION('center_axis',(0.,1.,0.)) ;
#107517 = DIRECTION('ref_axis',(1.,0.,0.)) ;
#107518 = DIRECTION('center_axis',(-0.989044367093028,0.147618562252689,-1.28038692714843E-15)) ;
#107519 = DIRECTION('ref_axis',(-0.147618562252689,-0.989044367093028,4.74381411340675E-32)) ;
#107520 = DIRECTION('center_axis',(0.,1.,0.)) ;
#107521 = DIRECTION('ref_axis',(1.,0.,0.)) ;
#107522 = DIRECTION('center_axis',(-0.989044367093028,0.147618562252688,0.)) ;
#107523 = DIRECTION('ref_axis',(-0.147618562252688,-0.989044367093028,0.)) ;
#107524 = DIRECTION('center_axis',(0.,0.,1.)) ;
#107525 = DIRECTION('ref_axis',(1.,0.,0.)) ;
#107526 = DIRECTION('center_axis',(-0.891049746169497,0.453905661840955,-3.93700403737149E-15)) ;
#107527 = DIRECTION('ref_axis',(-0.453905661840955,-0.891049746169497,6.00336752605965E-33)) ;
#107528 = DIRECTION('center_axis',(-0.891049746169503,0.453905661840943,0.)) ;
#107529 = DIRECTION('ref_axis',(-0.453905661840943,-0.891049746169503,0.)) ;
#107530 = DIRECTION('center_axis',(-0.891049746169501,0.453905661840946,0.)) ;
#107531 = DIRECTION('ref_axis',(-0.453905661840946,-0.891049746169501,0.)) ;
#107532 = DIRECTION('center_axis',(0.989044367093028,-0.147618562252691,0.)) ;
#107533 = DIRECTION('ref_axis',(0.147618562252691,0.989044367093028,0.)) ;
#107534 = DIRECTION('center_axis',(0.,0.,1.)) ;
#107535 = DIRECTION('ref_axis',(1.,0.,0.)) ;
#107536 = DIRECTION('center_axis',(0.,0.,-1.)) ;
#107537 = DIRECTION('ref_axis',(-1.,0.,0.)) ;
#107538 = DIRECTION('center_axis',(0.,0.,1.)) ;
#107539 = DIRECTION('ref_axis',(1.,0.,0.)) ;
#107540 = DIRECTION('center_axis',(-0.989044367093028,0.147618562252691,0.)) ;
#107541 = DIRECTION('ref_axis',(-0.147618562252691,-0.989044367093028,0.)) ;
#107542 = DIRECTION('center_axis',(0.891049746169503,-0.453905661840943,0.)) ;
#107543 = DIRECTION('ref_axis',(0.453905661840943,0.891049746169503,0.)) ;
#107544 = DIRECTION('center_axis',(-0.891049746169501,0.453905661840946,0.)) ;
#107545 = DIRECTION('ref_axis',(-0.453905661840946,-0.891049746169501,0.)) ;
#107546 = DIRECTION('center_axis',(0.,0.,1.)) ;
#107547 = DIRECTION('ref_axis',(1.,0.,0.)) ;
#107548 = DIRECTION('center_axis',(-1.,0.,0.)) ;
#107549 = DIRECTION('ref_axis',(0.,0.,1.)) ;
#107550 = DIRECTION('center_axis',(0.,1.,0.)) ;
#107551 = DIRECTION('ref_axis',(0.,0.,-1.)) ;
#107552 = DIRECTION('center_axis',(0.,1.,0.)) ;
#107553 = DIRECTION('ref_axis',(0.,0.,-1.)) ;
#107554 = DIRECTION('center_axis',(0.,0.,1.)) ;
#107555 = DIRECTION('ref_axis',(1.,0.,0.)) ;
#107556 = DIRECTION('center_axis',(-1.,0.,0.)) ;
#107557 = DIRECTION('ref_axis',(0.,0.,1.)) ;
#107558 = DIRECTION('center_axis',(-1.,2.60782465076463E-16,0.)) ;
#107559 = DIRECTION('ref_axis',(-2.60782465076463E-16,-1.,0.)) ;
#107560 = DIRECTION('center_axis',(-1.,0.,0.)) ;
#107561 = DIRECTION('ref_axis',(0.,0.,1.)) ;
#107562 = DIRECTION('center_axis',(0.,1.,0.)) ;
#107563 = DIRECTION('ref_axis',(0.,0.,1.)) ;
#107564 = DIRECTION('center_axis',(0.,1.,0.)) ;
#107565 = DIRECTION('ref_axis',(0.,0.,1.)) ;
#107566 = DIRECTION('center_axis',(0.,-1.,0.)) ;
#107567 = DIRECTION('ref_axis',(0.,0.,-1.)) ;
#107568 = DIRECTION('center_axis',(0.,1.,0.)) ;
#107569 = DIRECTION('ref_axis',(0.,0.,1.)) ;
#107570 = DIRECTION('center_axis',(1.,-2.60782465076463E-16,0.)) ;
#107571 = DIRECTION('ref_axis',(2.60782465076463E-16,1.,0.)) ;
#107572 = DIRECTION('center_axis',(-1.,0.,0.)) ;
#107573 = DIRECTION('ref_axis',(0.,0.,1.)) ;
#107574 = DIRECTION('center_axis',(-1.,0.,0.)) ;
#107575 = DIRECTION('ref_axis',(0.,0.,1.)) ;
#107576 = DIRECTION('center_axis',(0.,0.,-1.)) ;
#107577 = DIRECTION('ref_axis',(1.,0.,0.)) ;
#107578 = DIRECTION('center_axis',(-1.,0.,0.)) ;
#107579 = DIRECTION('ref_axis',(0.,0.,1.)) ;
#107580 = DIRECTION('center_axis',(0.,0.,1.)) ;
#107581 = DIRECTION('ref_axis',(-1.,0.,0.)) ;
#107582 = DIRECTION('center_axis',(0.,0.,1.)) ;
#107583 = DIRECTION('ref_axis',(1.,0.,0.)) ;
#107584 = DIRECTION('center_axis',(-1.,0.,0.)) ;
#107585 = DIRECTION('ref_axis',(0.,0.,1.)) ;
#107586 = DIRECTION('center_axis',(-1.,0.,0.)) ;
#107587 = DIRECTION('ref_axis',(0.,0.,1.)) ;
#107588 = DIRECTION('center_axis',(-3.56483478381767E-16,0.986393923832144,
0.164398987305358)) ;
#107589 = DIRECTION('ref_axis',(-3.72967278346455E-31,-0.164398987305358,
0.986393923832144)) ;
#107590 = DIRECTION('center_axis',(1.,0.,0.)) ;
#107591 = DIRECTION('ref_axis',(0.,1.38777878078145E-13,1.)) ;
#107592 = DIRECTION('center_axis',(-4.02631181035926E-15,0.928404294083138,
-0.371571617226061)) ;
#107593 = DIRECTION('ref_axis',(1.27405345096899E-29,0.371571617226061,0.928404294083138)) ;
#107594 = DIRECTION('center_axis',(0.,0.,1.)) ;
#107595 = DIRECTION('ref_axis',(1.,0.,0.)) ;
#107596 = DIRECTION('center_axis',(0.,0.,1.)) ;
#107597 = DIRECTION('ref_axis',(1.,0.,0.)) ;
#107598 = DIRECTION('',(0.,0.,-1.)) ;
#107599 = DIRECTION('center_axis',(0.,0.,-1.)) ;
#107600 = DIRECTION('ref_axis',(1.,0.,0.)) ;
#107601 = DIRECTION('',(0.,0.,1.)) ;
#107602 = DIRECTION('center_axis',(0.,-1.,0.)) ;
#107603 = DIRECTION('ref_axis',(0.,0.,-1.)) ;
#107604 = DIRECTION('center_axis',(0.,-1.,0.)) ;
#107605 = DIRECTION('ref_axis',(0.,0.,-1.)) ;
#107606 = DIRECTION('center_axis',(-1.,0.,-1.22464679914735E-16)) ;
#107607 = DIRECTION('ref_axis',(-1.22464679914735E-16,0.,1.)) ;
#107608 = DIRECTION('center_axis',(0.,1.,0.)) ;
#107609 = DIRECTION('ref_axis',(0.,0.,-1.)) ;
#107610 = DIRECTION('center_axis',(0.,1.,0.)) ;
#107611 = DIRECTION('ref_axis',(0.,0.,-1.)) ;
#107612 = DIRECTION('center_axis',(1.,0.,0.)) ;
#107613 = DIRECTION('ref_axis',(0.,0.,-1.)) ;
#107614 = DIRECTION('center_axis',(1.,0.,0.)) ;
#107615 = DIRECTION('ref_axis',(0.,0.,-1.)) ;
#107616 = DIRECTION('center_axis',(0.,1.,1.22464679914735E-16)) ;
#107617 = DIRECTION('ref_axis',(0.,-1.22464679914735E-16,1.)) ;
#107618 = DIRECTION('center_axis',(-1.,0.,0.)) ;
#107619 = DIRECTION('ref_axis',(0.,0.,-1.)) ;
#107620 = DIRECTION('center_axis',(-1.,0.,0.)) ;
#107621 = DIRECTION('ref_axis',(0.,0.,1.)) ;
#107622 = DIRECTION('center_axis',(-1.,0.,0.)) ;
#107623 = DIRECTION('ref_axis',(0.,0.,1.)) ;
#107624 = DIRECTION('center_axis',(0.,-1.,1.22464679914735E-16)) ;
#107625 = DIRECTION('ref_axis',(0.,-1.22464679914735E-16,-1.)) ;
#107626 = DIRECTION('center_axis',(1.,0.,0.)) ;
#107627 = DIRECTION('ref_axis',(0.,0.,1.)) ;
#107628 = DIRECTION('center_axis',(1.,0.,0.)) ;
#107629 = DIRECTION('ref_axis',(0.,0.,1.)) ;
#107630 = DIRECTION('center_axis',(-1.,0.,0.)) ;
#107631 = DIRECTION('ref_axis',(0.,0.,1.)) ;
#107632 = DIRECTION('center_axis',(-1.,0.,0.)) ;
#107633 = DIRECTION('ref_axis',(0.,0.,1.)) ;
#107634 = DIRECTION('center_axis',(0.,0.986393923832144,-0.164398987305358)) ;
#107635 = DIRECTION('ref_axis',(0.,-0.164398987305358,-0.986393923832144)) ;
#107636 = DIRECTION('center_axis',(1.,0.,0.)) ;
#107637 = DIRECTION('ref_axis',(0.,0.,1.)) ;
#107638 = DIRECTION('center_axis',(0.,0.,1.)) ;
#107639 = DIRECTION('ref_axis',(1.,0.,0.)) ;
#107640 = DIRECTION('center_axis',(0.,1.,0.)) ;
#107641 = DIRECTION('ref_axis',(1.,0.,0.)) ;
#107642 = DIRECTION('center_axis',(1.,0.,0.)) ;
#107643 = DIRECTION('ref_axis',(0.,0.,-1.)) ;
#107644 = DIRECTION('center_axis',(0.,0.,-1.)) ;
#107645 = DIRECTION('ref_axis',(-1.,0.,0.)) ;
#107646 = DIRECTION('center_axis',(0.,-0.986393923832144,0.164398987305358)) ;
#107647 = DIRECTION('ref_axis',(0.,0.164398987305358,0.986393923832144)) ;
#107648 = DIRECTION('center_axis',(-1.,0.,0.)) ;
#107649 = DIRECTION('ref_axis',(0.,0.,1.)) ;
#107650 = DIRECTION('',(1.,0.,0.)) ;
#107651 = DIRECTION('center_axis',(-1.,0.,0.)) ;
#107652 = DIRECTION('ref_axis',(0.,0.,1.)) ;
#107653 = DIRECTION('',(-1.,0.,0.)) ;
#107654 = DIRECTION('center_axis',(0.,1.,0.)) ;
#107655 = DIRECTION('ref_axis',(1.,0.,0.)) ;
#107656 = DIRECTION('center_axis',(0.,-0.986393923832144,-0.164398987305358)) ;
#107657 = DIRECTION('ref_axis',(0.,-0.164398987305358,0.986393923832144)) ;
#107658 = DIRECTION('center_axis',(0.,0.,1.)) ;
#107659 = DIRECTION('ref_axis',(1.,0.,0.)) ;
#107660 = DIRECTION('center_axis',(-1.,0.,0.)) ;
#107661 = DIRECTION('ref_axis',(0.,2.60208521396523E-14,-1.)) ;
#107662 = DIRECTION('center_axis',(1.,0.,0.)) ;
#107663 = DIRECTION('ref_axis',(0.,0.,-1.)) ;
#107664 = DIRECTION('center_axis',(1.,0.,0.)) ;
#107665 = DIRECTION('ref_axis',(0.,0.,-1.)) ;
#107666 = DIRECTION('',(0.707106781186546,-8.65956056235495E-17,0.707106781186549)) ;
#107667 = DIRECTION('center_axis',(1.,0.,0.)) ;
#107668 = DIRECTION('ref_axis',(0.,0.,-1.)) ;
#107669 = DIRECTION('',(1.,0.,0.)) ;
#107670 = DIRECTION('center_axis',(0.,1.,0.)) ;
#107671 = DIRECTION('ref_axis',(0.,0.,1.)) ;
#107672 = DIRECTION('center_axis',(0.,1.,0.)) ;
#107673 = DIRECTION('ref_axis',(0.,0.,1.)) ;
#107674 = DIRECTION('',(0.,1.,0.)) ;
#107675 = DIRECTION('center_axis',(0.,1.,0.)) ;
#107676 = DIRECTION('ref_axis',(0.,0.,1.)) ;
#107677 = DIRECTION('',(0.,1.,0.)) ;
#107678 = DIRECTION('center_axis',(0.,1.,0.)) ;
#107679 = DIRECTION('ref_axis',(0.,0.,1.)) ;
#107680 = DIRECTION('',(0.,1.,0.)) ;
#107681 = DIRECTION('center_axis',(0.,1.,0.)) ;
#107682 = DIRECTION('ref_axis',(0.,0.,1.)) ;
#107683 = DIRECTION('',(0.,1.,0.)) ;
#107684 = DIRECTION('center_axis',(0.,1.,0.)) ;
#107685 = DIRECTION('ref_axis',(0.,0.,1.)) ;
#107686 = DIRECTION('',(0.,1.,0.)) ;
#107687 = DIRECTION('center_axis',(-1.,0.,0.)) ;
#107688 = DIRECTION('ref_axis',(0.,0.,1.)) ;
#107689 = DIRECTION('center_axis',(-1.,0.,0.)) ;
#107690 = DIRECTION('ref_axis',(0.,0.,1.)) ;
#107691 = DIRECTION('',(0.,0.,-1.)) ;
#107692 = DIRECTION('',(0.,1.,0.)) ;
#107693 = DIRECTION('',(0.,0.,1.)) ;
#107694 = DIRECTION('center_axis',(-2.09002828430941E-16,1.,0.)) ;
#107695 = DIRECTION('ref_axis',(-1.,-2.09002828430941E-16,0.)) ;
#107696 = DIRECTION('',(1.,2.09002828430941E-16,0.)) ;
#107697 = DIRECTION('',(0.,0.,-1.)) ;
#107698 = DIRECTION('',(1.,2.09002828430941E-16,0.)) ;
#107699 = DIRECTION('',(0.,0.,1.)) ;
#107700 = DIRECTION('center_axis',(1.0450141421547E-16,-1.,0.)) ;
#107701 = DIRECTION('ref_axis',(1.,1.0450141421547E-16,0.)) ;
#107702 = DIRECTION('',(-1.,-1.0450141421547E-16,0.)) ;
#107703 = DIRECTION('',(0.,0.,1.)) ;
#107704 = DIRECTION('',(1.,1.0450141421547E-16,1.7416902369245E-17)) ;
#107705 = DIRECTION('',(0.,0.,-1.)) ;
#107706 = DIRECTION('center_axis',(0.,1.,0.)) ;
#107707 = DIRECTION('ref_axis',(0.,0.,1.)) ;
#107708 = DIRECTION('',(0.422618261740697,0.,-0.906307787036651)) ;
#107709 = DIRECTION('center_axis',(-1.,0.,0.)) ;
#107710 = DIRECTION('ref_axis',(0.,0.,1.)) ;
#107711 = DIRECTION('',(0.,0.986393923832144,-0.164398987305357)) ;
#107712 = DIRECTION('',(0.,0.,1.)) ;
#107713 = DIRECTION('',(0.,1.,0.)) ;
#107714 = DIRECTION('',(0.,0.,-1.)) ;
#107715 = DIRECTION('center_axis',(1.,0.,0.)) ;
#107716 = DIRECTION('ref_axis',(0.,0.,1.)) ;
#107717 = DIRECTION('center_axis',(1.,0.,0.)) ;
#107718 = DIRECTION('ref_axis',(0.,0.,1.)) ;
#107719 = DIRECTION('center_axis',(1.,0.,0.)) ;
#107720 = DIRECTION('ref_axis',(0.,0.,1.)) ;
#107721 = DIRECTION('',(0.,0.,-1.)) ;
#107722 = DIRECTION('',(0.,1.,0.)) ;
#107723 = DIRECTION('',(0.,0.,1.)) ;
#107724 = DIRECTION('',(0.,-0.986393923832144,-0.164398987305357)) ;
#107725 = DIRECTION('center_axis',(1.,0.,0.)) ;
#107726 = DIRECTION('ref_axis',(0.,0.,1.)) ;
#107727 = DIRECTION('',(0.,0.,1.)) ;
#107728 = DIRECTION('center_axis',(1.0450141421547E-16,-1.,0.)) ;
#107729 = DIRECTION('ref_axis',(1.,1.0450141421547E-16,0.)) ;
#107730 = DIRECTION('',(-1.,-1.0450141421547E-16,1.7416902369245E-17)) ;
#107731 = DIRECTION('',(0.,0.,1.)) ;
#107732 = DIRECTION('',(-1.,-1.0450141421547E-16,0.)) ;
#107733 = DIRECTION('',(0.,0.,-1.)) ;
#107734 = DIRECTION('center_axis',(-0.876215908676647,-0.481918749772156,
0.)) ;
#107735 = DIRECTION('ref_axis',(0.481918749772156,-0.876215908676647,0.)) ;
#107736 = DIRECTION('',(-0.481918749772156,0.876215908676647,0.)) ;
#107737 = DIRECTION('',(0.,0.,-1.)) ;
#107738 = DIRECTION('center_axis',(-0.876215908676613,-0.481918749772218,
1.02549544363153E-14)) ;
#107739 = DIRECTION('ref_axis',(0.43695445588893,-0.794462647070658,-0.421781822614834)) ;
#107740 = DIRECTION('',(0.,0.,-1.)) ;
#107741 = DIRECTION('center_axis',(-0.876215908676637,-0.481918749772175,
-7.94557099638636E-15)) ;
#107742 = DIRECTION('ref_axis',(0.436954455952196,-0.794462647185776,0.421781822332458)) ;
#107743 = DIRECTION('',(0.,0.,-1.)) ;
#107744 = DIRECTION('',(-0.481918749772156,0.876215908676647,0.)) ;
#107745 = DIRECTION('',(0.,0.,1.)) ;
#107746 = DIRECTION('center_axis',(-1.,0.,0.)) ;
#107747 = DIRECTION('ref_axis',(0.,0.,1.)) ;
#107748 = DIRECTION('',(0.,1.,0.)) ;
#107749 = DIRECTION('',(0.,0.,1.)) ;
#107750 = DIRECTION('',(0.,1.,0.)) ;
#107751 = DIRECTION('',(0.,0.,-1.)) ;
#107752 = DIRECTION('center_axis',(-0.876215908676647,-0.481918749772156,
0.)) ;
#107753 = DIRECTION('ref_axis',(0.481918749772156,-0.876215908676647,0.)) ;
#107754 = DIRECTION('',(-0.481918749772156,0.876215908676647,0.)) ;
#107755 = DIRECTION('',(0.,0.,1.)) ;
#107756 = DIRECTION('',(-0.481918749772156,0.876215908676647,0.)) ;
#107757 = DIRECTION('',(0.,0.,-1.)) ;
#107758 = DIRECTION('center_axis',(-3.46944695195361E-15,-1.,0.)) ;
#107759 = DIRECTION('ref_axis',(1.,-3.46944695195361E-15,0.)) ;
#107760 = DIRECTION('',(-1.,3.46944695195361E-15,0.)) ;
#107761 = DIRECTION('',(0.,0.,1.)) ;
#107762 = DIRECTION('',(-1.,3.46944695195361E-15,0.)) ;
#107763 = DIRECTION('',(0.,0.,-1.)) ;
#107764 = DIRECTION('center_axis',(-1.,0.,0.)) ;
#107765 = DIRECTION('ref_axis',(0.,0.,1.)) ;
#107766 = DIRECTION('',(0.,1.,0.)) ;
#107767 = DIRECTION('',(0.,0.,1.)) ;
#107768 = DIRECTION('',(0.,1.,0.)) ;
#107769 = DIRECTION('',(0.,0.,-1.)) ;
#107770 = DIRECTION('center_axis',(0.,1.,0.)) ;
#107771 = DIRECTION('ref_axis',(0.,0.,1.)) ;
#107772 = DIRECTION('',(1.,0.,0.)) ;
#107773 = DIRECTION('',(0.,0.,1.)) ;
#107774 = DIRECTION('',(1.,0.,0.)) ;
#107775 = DIRECTION('',(0.,0.,-1.)) ;
#107776 = DIRECTION('center_axis',(-1.,0.,0.)) ;
#107777 = DIRECTION('ref_axis',(0.,0.,1.)) ;
#107778 = DIRECTION('',(0.,1.,0.)) ;
#107779 = DIRECTION('',(0.,0.,1.)) ;
#107780 = DIRECTION('',(0.,1.,0.)) ;
#107781 = DIRECTION('',(0.,0.,-1.)) ;
#107782 = DIRECTION('center_axis',(0.,-1.,0.)) ;
#107783 = DIRECTION('ref_axis',(0.,0.,-1.)) ;
#107784 = DIRECTION('',(-1.,0.,0.)) ;
#107785 = DIRECTION('',(0.,0.,1.)) ;
#107786 = DIRECTION('',(-1.,0.,0.)) ;
#107787 = DIRECTION('',(0.,0.,-1.)) ;
#107788 = DIRECTION('center_axis',(0.,1.,0.)) ;
#107789 = DIRECTION('ref_axis',(0.,0.,-1.)) ;
#107790 = DIRECTION('',(2.16840434497101E-16,0.,1.)) ;
#107791 = DIRECTION('center_axis',(0.,1.,0.)) ;
#107792 = DIRECTION('ref_axis',(0.,0.,-1.)) ;
#107793 = DIRECTION('',(-1.,0.,1.73472347597681E-16)) ;
#107794 = DIRECTION('center_axis',(0.,1.,0.)) ;
#107795 = DIRECTION('ref_axis',(0.,0.,-1.)) ;
#107796 = DIRECTION('',(-2.16840434497101E-16,0.,-1.)) ;
#107797 = DIRECTION('center_axis',(0.,1.,0.)) ;
#107798 = DIRECTION('ref_axis',(0.,0.,-1.)) ;
#107799 = DIRECTION('',(1.,0.,-1.73472347597681E-16)) ;
#107800 = DIRECTION('center_axis',(1.,0.,0.)) ;
#107801 = DIRECTION('ref_axis',(0.,0.,-1.)) ;
#107802 = DIRECTION('',(0.,-1.,0.)) ;
#107803 = DIRECTION('',(0.,0.,1.)) ;
#107804 = DIRECTION('',(0.,-1.,0.)) ;
#107805 = DIRECTION('',(0.,0.,-1.)) ;
#107806 = DIRECTION('center_axis',(0.,1.,0.)) ;
#107807 = DIRECTION('ref_axis',(0.,0.,1.)) ;
#107808 = DIRECTION('',(1.,0.,0.)) ;
#107809 = DIRECTION('',(1.,0.,0.)) ;
#107810 = DIRECTION('',(0.,0.,-1.)) ;
#107811 = DIRECTION('center_axis',(0.98058067569092,-0.196116135138184,0.)) ;
#107812 = DIRECTION('ref_axis',(0.196116135138184,0.98058067569092,0.)) ;
#107813 = DIRECTION('',(-0.196116135138184,-0.98058067569092,0.)) ;
#107814 = DIRECTION('',(0.,0.,1.)) ;
#107815 = DIRECTION('',(-0.196116135138184,-0.98058067569092,0.)) ;
#107816 = DIRECTION('center_axis',(1.,0.,0.)) ;
#107817 = DIRECTION('ref_axis',(0.,0.,-1.)) ;
#107818 = DIRECTION('',(0.,-1.,0.)) ;
#107819 = DIRECTION('',(0.,0.,1.)) ;
#107820 = DIRECTION('',(0.,-1.,0.)) ;
#107821 = DIRECTION('',(0.,0.,-1.)) ;
#107822 = DIRECTION('',(0.,0.,1.)) ;
#107823 = DIRECTION('',(0.,-1.,0.)) ;
#107824 = DIRECTION('',(0.,0.,-1.)) ;
#107825 = DIRECTION('',(0.,1.,0.)) ;
#107826 = DIRECTION('center_axis',(0.,1.,0.)) ;
#107827 = DIRECTION('ref_axis',(0.,0.,1.)) ;
#107828 = DIRECTION('',(1.,0.,0.)) ;
#107829 = DIRECTION('',(0.,0.,1.)) ;
#107830 = DIRECTION('',(1.,0.,0.)) ;
#107831 = DIRECTION('',(0.,0.,-1.)) ;
#107832 = DIRECTION('center_axis',(0.,-1.,0.)) ;
#107833 = DIRECTION('ref_axis',(0.,0.,1.)) ;
#107834 = DIRECTION('',(0.,0.,1.)) ;
#107835 = DIRECTION('center_axis',(0.,-1.,0.)) ;
#107836 = DIRECTION('ref_axis',(0.,0.,1.)) ;
#107837 = DIRECTION('',(1.,0.,1.73472347597681E-16)) ;
#107838 = DIRECTION('center_axis',(0.,-1.,0.)) ;
#107839 = DIRECTION('ref_axis',(0.,0.,1.)) ;
#107840 = DIRECTION('',(4.33680868994202E-16,0.,-1.)) ;
#107841 = DIRECTION('center_axis',(0.,-1.,0.)) ;
#107842 = DIRECTION('ref_axis',(0.,0.,1.)) ;
#107843 = DIRECTION('',(-1.,0.,1.73472347597681E-16)) ;
#107844 = DIRECTION('center_axis',(-1.,6.93889390390723E-16,0.)) ;
#107845 = DIRECTION('ref_axis',(-6.93889390390723E-16,-1.,0.)) ;
#107846 = DIRECTION('',(6.93889390390723E-16,1.,0.)) ;
#107847 = DIRECTION('',(0.,0.,1.)) ;
#107848 = DIRECTION('',(6.93889390390723E-16,1.,0.)) ;
#107849 = DIRECTION('',(0.,0.,-1.)) ;
#107850 = DIRECTION('center_axis',(0.,1.,0.)) ;
#107851 = DIRECTION('ref_axis',(0.,0.,1.)) ;
#107852 = DIRECTION('',(0.,0.,1.)) ;
#107853 = DIRECTION('',(1.,0.,0.)) ;
#107854 = DIRECTION('',(0.,0.,-1.)) ;
#107855 = DIRECTION('',(1.,0.,0.)) ;
#107856 = DIRECTION('',(0.,0.,1.)) ;
#107857 = DIRECTION('center_axis',(-1.,0.,0.)) ;
#107858 = DIRECTION('ref_axis',(0.,0.,1.)) ;
#107859 = DIRECTION('',(0.,1.,0.)) ;
#107860 = DIRECTION('',(0.,0.,-1.)) ;
#107861 = DIRECTION('center_axis',(-1.,0.,0.)) ;
#107862 = DIRECTION('ref_axis',(0.,0.,1.)) ;
#107863 = DIRECTION('',(0.,0.,1.)) ;
#107864 = DIRECTION('center_axis',(-2.09002828430941E-16,1.,0.)) ;
#107865 = DIRECTION('ref_axis',(-1.,-2.09002828430941E-16,0.)) ;
#107866 = DIRECTION('',(-1.,-2.09002828430941E-16,0.)) ;
#107867 = DIRECTION('',(0.,0.,-1.)) ;
#107868 = DIRECTION('',(1.,2.09002828430941E-16,0.)) ;
#107869 = DIRECTION('',(0.,0.,1.)) ;
#107870 = DIRECTION('center_axis',(0.,0.,1.)) ;
#107871 = DIRECTION('ref_axis',(1.,0.,0.)) ;
#107872 = DIRECTION('center_axis',(0.,0.,1.)) ;
#107873 = DIRECTION('ref_axis',(1.,0.,0.)) ;
#107874 = DIRECTION('center_axis',(0.,0.,-1.)) ;
#107875 = DIRECTION('ref_axis',(1.,0.,0.)) ;
#107876 = DIRECTION('center_axis',(0.,0.,1.)) ;
#107877 = DIRECTION('ref_axis',(1.,0.,0.)) ;
#107878 = DIRECTION('center_axis',(0.,0.,1.)) ;
#107879 = DIRECTION('ref_axis',(1.,0.,0.)) ;
#107880 = DIRECTION('center_axis',(0.,0.,-1.)) ;
#107881 = DIRECTION('ref_axis',(1.,0.,0.)) ;
#107882 = DIRECTION('center_axis',(0.,0.,-1.)) ;
#107883 = DIRECTION('ref_axis',(1.,0.,0.)) ;
#107884 = DIRECTION('center_axis',(0.,0.,1.)) ;
#107885 = DIRECTION('ref_axis',(1.,0.,0.)) ;
#107886 = DIRECTION('center_axis',(0.,0.,1.)) ;
#107887 = DIRECTION('ref_axis',(1.,0.,0.)) ;
#107888 = DIRECTION('center_axis',(0.,0.,-1.)) ;
#107889 = DIRECTION('ref_axis',(1.,0.,0.)) ;
#107890 = DIRECTION('center_axis',(0.,0.,-1.)) ;
#107891 = DIRECTION('ref_axis',(1.,0.,0.)) ;
#107892 = DIRECTION('center_axis',(0.,0.,1.)) ;
#107893 = DIRECTION('ref_axis',(1.,0.,0.)) ;
#107894 = DIRECTION('center_axis',(0.,0.,1.)) ;
#107895 = DIRECTION('ref_axis',(1.,0.,0.)) ;
#107896 = DIRECTION('center_axis',(0.,0.,1.)) ;
#107897 = DIRECTION('ref_axis',(1.,0.,0.)) ;
#107898 = DIRECTION('center_axis',(0.,0.,1.)) ;
#107899 = DIRECTION('ref_axis',(1.,0.,0.)) ;
#107900 = DIRECTION('center_axis',(0.,0.,1.)) ;
#107901 = DIRECTION('ref_axis',(1.,0.,0.)) ;
#107902 = DIRECTION('center_axis',(0.,0.,1.)) ;
#107903 = DIRECTION('ref_axis',(1.,0.,0.)) ;
#107904 = DIRECTION('center_axis',(0.,0.,1.)) ;
#107905 = DIRECTION('ref_axis',(1.,0.,0.)) ;
#107906 = DIRECTION('center_axis',(0.,0.,-1.)) ;
#107907 = DIRECTION('ref_axis',(1.,0.,0.)) ;
#107908 = DIRECTION('center_axis',(0.,0.,1.)) ;
#107909 = DIRECTION('ref_axis',(1.,0.,0.)) ;
#107910 = DIRECTION('center_axis',(0.,0.,-1.)) ;
#107911 = DIRECTION('ref_axis',(1.,0.,0.)) ;
#107912 = DIRECTION('center_axis',(0.,0.,1.)) ;
#107913 = DIRECTION('ref_axis',(1.,0.,0.)) ;
#107914 = DIRECTION('center_axis',(0.,0.,-1.)) ;
#107915 = DIRECTION('ref_axis',(1.,0.,0.)) ;
#107916 = DIRECTION('center_axis',(0.,0.,-1.)) ;
#107917 = DIRECTION('ref_axis',(1.,0.,0.)) ;
#107918 = DIRECTION('center_axis',(0.,0.,-1.)) ;
#107919 = DIRECTION('ref_axis',(1.,2.6020852139652E-14,0.)) ;
#107920 = DIRECTION('center_axis',(0.,0.,-1.)) ;
#107921 = DIRECTION('ref_axis',(1.,0.,0.)) ;
#107922 = DIRECTION('center_axis',(0.,0.,-1.)) ;
#107923 = DIRECTION('ref_axis',(1.,0.,0.)) ;
#107924 = DIRECTION('center_axis',(0.,0.,-1.)) ;
#107925 = DIRECTION('ref_axis',(1.,0.,0.)) ;
#107926 = DIRECTION('center_axis',(0.,0.,-1.)) ;
#107927 = DIRECTION('ref_axis',(1.,0.,0.)) ;
#107928 = DIRECTION('center_axis',(0.,0.,1.)) ;
#107929 = DIRECTION('ref_axis',(1.,0.,0.)) ;
#107930 = DIRECTION('center_axis',(0.,0.,1.)) ;
#107931 = DIRECTION('ref_axis',(1.,0.,0.)) ;
#107932 = DIRECTION('center_axis',(0.,0.,-1.)) ;
#107933 = DIRECTION('ref_axis',(1.,0.,0.)) ;
#107934 = DIRECTION('center_axis',(0.,0.,-1.)) ;
#107935 = DIRECTION('ref_axis',(1.,1.04083408558609E-13,0.)) ;
#107936 = DIRECTION('center_axis',(0.,0.,1.)) ;
#107937 = DIRECTION('ref_axis',(1.,0.,0.)) ;
#107938 = DIRECTION('center_axis',(0.,0.,1.)) ;
#107939 = DIRECTION('ref_axis',(1.,0.,0.)) ;
#107940 = DIRECTION('center_axis',(0.,0.,-1.)) ;
#107941 = DIRECTION('ref_axis',(1.,1.30104260698261E-14,0.)) ;
#107942 = DIRECTION('center_axis',(0.,0.,-1.)) ;
#107943 = DIRECTION('ref_axis',(1.,0.,0.)) ;
#107944 = DIRECTION('center_axis',(0.,0.,1.)) ;
#107945 = DIRECTION('ref_axis',(1.,0.,0.)) ;
#107946 = DIRECTION('center_axis',(0.,0.,1.)) ;
#107947 = DIRECTION('ref_axis',(1.,0.,0.)) ;
#107948 = DIRECTION('',(-0.664363838829919,0.74740931868366,0.)) ;
#107949 = DIRECTION('',(0.,-1.,0.)) ;
#107950 = DIRECTION('',(0.894427190999917,0.447213595499956,0.)) ;
#107951 = DIRECTION('',(0.,1.,0.)) ;
#107952 = DIRECTION('center_axis',(0.,0.,-1.)) ;
#107953 = DIRECTION('ref_axis',(-1.,0.,0.)) ;
#107954 = DIRECTION('',(-0.894427190999917,-0.447213595499956,0.)) ;
#107955 = DIRECTION('',(0.,1.,0.)) ;
#107956 = DIRECTION('',(0.664363838829919,-0.74740931868366,0.)) ;
#107957 = DIRECTION('',(0.,-1.,0.)) ;
#107958 = DIRECTION('center_axis',(-0.23745309047699,0.,-0.971399006496778)) ;
#107959 = DIRECTION('ref_axis',(-0.971399006496778,0.,0.23745309047699)) ;
#107960 = DIRECTION('center_axis',(-0.237453090477004,-2.97379739801035E-15,
-0.971399006496774)) ;
#107961 = DIRECTION('ref_axis',(0.921799787670054,-0.315455332295983,-0.225328836986026)) ;
#107962 = DIRECTION('',(0.971399006496777,0.,-0.23745309047699)) ;
#107963 = DIRECTION('',(0.,-1.,0.)) ;
#107964 = DIRECTION('',(-0.971399006496777,0.,0.23745309047699)) ;
#107965 = DIRECTION('center_axis',(-0.237453090477001,4.30462933422326E-14,
-0.971399006496775)) ;
#107966 = DIRECTION('ref_axis',(0.954559354253683,0.185392581174263,-0.233336731039792)) ;
#107967 = DIRECTION('',(-0.873786407766991,-0.436893203883493,0.213592233009709)) ;
#107968 = DIRECTION('',(0.,1.,0.)) ;
#107969 = DIRECTION('',(0.655772517804503,-0.737744082530068,-0.160299948796656)) ;
#107970 = DIRECTION('center_axis',(-1.,0.,0.)) ;
#107971 = DIRECTION('ref_axis',(0.,0.,1.)) ;
#107972 = DIRECTION('',(0.,-1.,0.)) ;
#107973 = DIRECTION('center_axis',(-1.,-6.7007887082726E-15,-6.50913949396074E-15)) ;
#107974 = DIRECTION('ref_axis',(6.5091394940182E-15,-8.57530417051636E-12,
-1.)) ;
#107975 = DIRECTION('',(0.,0.,-1.)) ;
#107976 = DIRECTION('center_axis',(-1.,-6.70078870827228E-15,6.50913949396049E-15)) ;
#107977 = DIRECTION('ref_axis',(-6.50913949405411E-15,1.3971626257459E-11,
-1.)) ;
#107978 = DIRECTION('center_axis',(-1.,6.70078870827231E-15,6.50913949396052E-15)) ;
#107979 = DIRECTION('ref_axis',(-6.50913949404309E-15,-1.23225293015881E-11,
-1.)) ;
#107980 = DIRECTION('',(0.,0.,-1.)) ;
#107981 = DIRECTION('center_axis',(-1.,6.70078870827261E-15,-6.50913949396074E-15)) ;
#107982 = DIRECTION('ref_axis',(6.50913949382473E-15,-2.02978006038297E-11,
-1.)) ;
#107983 = DIRECTION('center_axis',(-0.23745309047699,0.,0.971399006496778)) ;
#107984 = DIRECTION('ref_axis',(0.971399006496778,0.,0.23745309047699)) ;
#107985 = DIRECTION('center_axis',(-0.237453090476854,-7.13106519896081E-13,
0.971399006496811)) ;
#107986 = DIRECTION('ref_axis',(0.954559354253092,0.185392581177496,0.233336731039639)) ;
#107987 = DIRECTION('',(0.971399006496777,0.,0.23745309047699)) ;
#107988 = DIRECTION('',(-0.971399006496777,0.,-0.23745309047699)) ;
#107989 = DIRECTION('center_axis',(-0.237453090476972,2.29230216096572E-14,
0.971399006496782)) ;
#107990 = DIRECTION('ref_axis',(0.921799787671121,-0.315455332292693,0.225328836986263)) ;
#107991 = DIRECTION('',(-0.655772517804503,0.737744082530068,-0.160299948796656)) ;
#107992 = DIRECTION('',(0.,-1.,0.)) ;
#107993 = DIRECTION('',(0.873786407766991,0.436893203883493,0.213592233009709)) ;
#107994 = DIRECTION('center_axis',(0.,1.,0.)) ;
#107995 = DIRECTION('ref_axis',(0.,0.,1.)) ;
#107996 = DIRECTION('',(-0.971399006496777,0.,0.23745309047699)) ;
#107997 = DIRECTION('',(0.,0.,-1.)) ;
#107998 = DIRECTION('',(0.971399006496777,0.,0.23745309047699)) ;
#107999 = DIRECTION('center_axis',(0.,1.,0.)) ;
#108000 = DIRECTION('ref_axis',(0.,0.,1.)) ;
#108001 = DIRECTION('',(-0.971399006496777,0.,-0.23745309047699)) ;
#108002 = DIRECTION('',(0.,0.,1.)) ;
#108003 = DIRECTION('',(0.971399006496777,0.,-0.23745309047699)) ;
#108004 = DIRECTION('center_axis',(-0.447213595499956,0.894427190999917,0.)) ;
#108005 = DIRECTION('ref_axis',(0.,0.,-1.)) ;
#108006 = DIRECTION('',(0.,0.,-1.)) ;
#108007 = DIRECTION('',(-0.873786407766991,-0.436893203883493,-0.213592233009709)) ;
#108008 = DIRECTION('',(-0.894427190999917,-0.447213595499956,0.)) ;
#108009 = DIRECTION('',(0.,0.,1.)) ;
#108010 = DIRECTION('',(0.894427190999917,0.447213595499956,0.)) ;
#108011 = DIRECTION('',(0.873786407766991,0.436893203883493,-0.213592233009709)) ;
#108012 = DIRECTION('center_axis',(0.74740931868366,0.664363838829919,0.)) ;
#108013 = DIRECTION('ref_axis',(0.,0.,1.)) ;
#108014 = DIRECTION('',(0.,0.,-1.)) ;
#108015 = DIRECTION('',(0.664363838829919,-0.74740931868366,0.)) ;
#108016 = DIRECTION('',(0.655772517804503,-0.737744082530068,0.160299948796656)) ;
#108017 = DIRECTION('',(0.,0.,1.)) ;
#108018 = DIRECTION('',(-0.655772517804503,0.737744082530068,0.160299948796656)) ;
#108019 = DIRECTION('',(-0.664363838829919,0.74740931868366,0.)) ;
#108020 = DIRECTION('center_axis',(1.,0.,4.33680868994202E-16)) ;
#108021 = DIRECTION('ref_axis',(4.33680868994202E-16,0.,-1.)) ;
#108022 = DIRECTION('',(0.,1.,0.)) ;
#108023 = DIRECTION('',(4.33680868994202E-16,0.,-1.)) ;
#108024 = DIRECTION('',(0.,-1.,0.)) ;
#108025 = DIRECTION('',(-4.33680868994202E-16,0.,1.)) ;
#108026 = DIRECTION('center_axis',(-1.73472347597681E-16,0.,-1.)) ;
#108027 = DIRECTION('ref_axis',(-1.,0.,1.73472347597681E-16)) ;
#108028 = DIRECTION('',(-1.,0.,1.73472347597681E-16)) ;
#108029 = DIRECTION('',(0.,-1.,0.)) ;
#108030 = DIRECTION('',(1.,0.,-1.73472347597681E-16)) ;
#108031 = DIRECTION('',(0.,1.,0.)) ;
#108032 = DIRECTION('center_axis',(-1.,0.,0.)) ;
#108033 = DIRECTION('ref_axis',(0.,0.,1.)) ;
#108034 = DIRECTION('',(0.,0.,1.)) ;
#108035 = DIRECTION('',(0.,-1.,0.)) ;
#108036 = DIRECTION('',(0.,0.,-1.)) ;
#108037 = DIRECTION('',(0.,1.,0.)) ;
#108038 = DIRECTION('center_axis',(-1.73472347597681E-16,0.,1.)) ;
#108039 = DIRECTION('ref_axis',(1.,0.,1.73472347597681E-16)) ;
#108040 = DIRECTION('',(0.,1.,0.)) ;
#108041 = DIRECTION('',(1.,0.,1.73472347597681E-16)) ;
#108042 = DIRECTION('',(0.,-1.,0.)) ;
#108043 = DIRECTION('',(-1.,0.,-1.73472347597681E-16)) ;
#108044 = DIRECTION('center_axis',(0.,-1.,0.)) ;
#108045 = DIRECTION('ref_axis',(0.,0.,-1.)) ;
#108046 = DIRECTION('',(-1.,0.,-1.73472347597681E-16)) ;
#108047 = DIRECTION('',(0.,0.,-1.)) ;
#108048 = DIRECTION('',(1.,0.,-1.73472347597681E-16)) ;
#108049 = DIRECTION('',(-4.33680868994202E-16,0.,1.)) ;
#108050 = DIRECTION('',(1.,0.,0.)) ;
#108051 = DIRECTION('center_axis',(0.,-1.,0.)) ;
#108052 = DIRECTION('ref_axis',(0.,0.,-1.)) ;
#108053 = DIRECTION('',(0.,0.,-1.)) ;
#108054 = DIRECTION('center_axis',(0.,-1.,0.)) ;
#108055 = DIRECTION('ref_axis',(0.,0.,-1.)) ;
#108056 = DIRECTION('',(-1.,0.,0.)) ;
#108057 = DIRECTION('center_axis',(0.,-1.,0.)) ;
#108058 = DIRECTION('ref_axis',(0.,0.,1.)) ;
#108059 = DIRECTION('',(0.,0.,1.)) ;
#108060 = DIRECTION('center_axis',(0.,-1.,0.)) ;
#108061 = DIRECTION('ref_axis',(0.,0.,-1.)) ;
#108062 = DIRECTION('center_axis',(0.,-1.,0.)) ;
#108063 = DIRECTION('ref_axis',(0.,0.,-1.)) ;
#108064 = DIRECTION('center_axis',(0.,-1.,0.)) ;
#108065 = DIRECTION('ref_axis',(0.,0.,-1.)) ;
#108066 = DIRECTION('',(0.,-1.,0.)) ;
#108067 = DIRECTION('',(0.,-1.,0.)) ;
#108068 = DIRECTION('center_axis',(0.,0.,-1.)) ;
#108069 = DIRECTION('ref_axis',(-1.,0.,0.)) ;
#108070 = DIRECTION('',(1.,0.,0.)) ;
#108071 = DIRECTION('',(0.,-1.,0.)) ;
#108072 = DIRECTION('center_axis',(0.,-1.,0.)) ;
#108073 = DIRECTION('ref_axis',(0.,0.,-1.)) ;
#108074 = DIRECTION('center_axis',(0.,-1.,0.)) ;
#108075 = DIRECTION('ref_axis',(0.,0.,-1.)) ;
#108076 = DIRECTION('',(0.,-1.,0.)) ;
#108077 = DIRECTION('center_axis',(-1.,0.,0.)) ;
#108078 = DIRECTION('ref_axis',(0.,0.,1.)) ;
#108079 = DIRECTION('',(0.,0.,-1.)) ;
#108080 = DIRECTION('',(0.,-1.,0.)) ;
#108081 = DIRECTION('center_axis',(0.,-1.,0.)) ;
#108082 = DIRECTION('ref_axis',(0.,0.,-1.)) ;
#108083 = DIRECTION('center_axis',(0.,-1.,0.)) ;
#108084 = DIRECTION('ref_axis',(0.,0.,-1.)) ;
#108085 = DIRECTION('',(0.,-1.,0.)) ;
#108086 = DIRECTION('center_axis',(0.,0.,1.)) ;
#108087 = DIRECTION('ref_axis',(1.,0.,0.)) ;
#108088 = DIRECTION('',(-1.,0.,0.)) ;
#108089 = DIRECTION('',(0.,-1.,0.)) ;
#108090 = DIRECTION('center_axis',(0.,-1.,0.)) ;
#108091 = DIRECTION('ref_axis',(0.,0.,-1.)) ;
#108092 = DIRECTION('center_axis',(0.,-1.,0.)) ;
#108093 = DIRECTION('ref_axis',(0.,0.,1.)) ;
#108094 = DIRECTION('',(0.,-1.,0.)) ;
#108095 = DIRECTION('center_axis',(1.,0.,0.)) ;
#108096 = DIRECTION('ref_axis',(0.,0.,-1.)) ;
#108097 = DIRECTION('',(0.,0.,1.)) ;
#108098 = DIRECTION('center_axis',(0.,-1.,0.)) ;
#108099 = DIRECTION('ref_axis',(0.,0.,-1.)) ;
#108100 = DIRECTION('center_axis',(0.,1.,0.)) ;
#108101 = DIRECTION('ref_axis',(0.,0.,1.)) ;
#108102 = DIRECTION('',(-0.422618261740697,0.,0.906307787036651)) ;
#108103 = DIRECTION('center_axis',(0.906307787036651,0.,0.422618261740697)) ;
#108104 = DIRECTION('ref_axis',(0.422618261740697,0.,-0.906307787036651)) ;
#108105 = DIRECTION('',(-0.422618261740697,0.,0.906307787036651)) ;
#108106 = DIRECTION('',(0.422618261740697,0.,-0.906307787036651)) ;
#108107 = DIRECTION('center_axis',(-0.906307787036651,0.,-0.422618261740697)) ;
#108108 = DIRECTION('ref_axis',(-0.422618261740697,0.,0.906307787036651)) ;
#108109 = DIRECTION('',(0.422618261740697,0.,-0.906307787036651)) ;
#108110 = DIRECTION('',(-0.422618261740697,0.,0.906307787036651)) ;
#108111 = DIRECTION('center_axis',(0.,1.,0.)) ;
#108112 = DIRECTION('ref_axis',(0.,0.,1.)) ;
#108113 = DIRECTION('',(-0.422618261740697,0.,0.906307787036651)) ;
#108114 = DIRECTION('',(0.422618261740697,0.,-0.906307787036651)) ;
#108115 = DIRECTION('center_axis',(1.,0.,-2.16840434497101E-16)) ;
#108116 = DIRECTION('ref_axis',(-2.16840434497101E-16,0.,-1.)) ;
#108117 = DIRECTION('',(2.16840434497101E-16,0.,1.)) ;
#108118 = DIRECTION('',(0.,1.,0.)) ;
#108119 = DIRECTION('',(-2.16840434497101E-16,0.,-1.)) ;
#108120 = DIRECTION('',(0.,-1.,0.)) ;
#108121 = DIRECTION('center_axis',(1.73472347597681E-16,0.,1.)) ;
#108122 = DIRECTION('ref_axis',(1.,0.,-1.73472347597681E-16)) ;
#108123 = DIRECTION('',(0.,-1.,0.)) ;
#108124 = DIRECTION('',(-1.,0.,1.73472347597681E-16)) ;
#108125 = DIRECTION('',(0.,1.,0.)) ;
#108126 = DIRECTION('',(1.,0.,-1.73472347597681E-16)) ;
#108127 = DIRECTION('center_axis',(-1.,0.,2.16840434497101E-16)) ;
#108128 = DIRECTION('ref_axis',(2.16840434497101E-16,0.,1.)) ;
#108129 = DIRECTION('',(0.,-1.,0.)) ;
#108130 = DIRECTION('',(-2.16840434497101E-16,0.,-1.)) ;
#108131 = DIRECTION('',(0.,1.,0.)) ;
#108132 = DIRECTION('',(2.16840434497101E-16,0.,1.)) ;
#108133 = DIRECTION('center_axis',(-1.73472347597681E-16,0.,-1.)) ;
#108134 = DIRECTION('ref_axis',(-1.,0.,1.73472347597681E-16)) ;
#108135 = DIRECTION('',(1.,0.,-1.73472347597681E-16)) ;
#108136 = DIRECTION('',(0.,1.,0.)) ;
#108137 = DIRECTION('',(-1.,0.,1.73472347597681E-16)) ;
#108138 = DIRECTION('',(0.,-1.,0.)) ;
#108139 = DIRECTION('center_axis',(0.,1.,0.)) ;
#108140 = DIRECTION('ref_axis',(0.,0.,1.)) ;
#108141 = DIRECTION('',(1.,0.,-1.73472347597681E-16)) ;
#108142 = DIRECTION('',(-2.16840434497101E-16,0.,-1.)) ;
#108143 = DIRECTION('',(-1.,0.,1.73472347597681E-16)) ;
#108144 = DIRECTION('',(2.16840434497101E-16,0.,1.)) ;
#108145 = DIRECTION('',(1.,0.,0.)) ;
#108146 = DIRECTION('center_axis',(0.,1.,0.)) ;
#108147 = DIRECTION('ref_axis',(0.,0.,1.)) ;
#108148 = DIRECTION('',(0.,0.,1.)) ;
#108149 = DIRECTION('center_axis',(0.,1.,0.)) ;
#108150 = DIRECTION('ref_axis',(0.,0.,1.)) ;
#108151 = DIRECTION('',(-1.,0.,0.)) ;
#108152 = DIRECTION('center_axis',(0.,1.,0.)) ;
#108153 = DIRECTION('ref_axis',(0.,0.,-1.)) ;
#108154 = DIRECTION('',(0.,0.,-1.)) ;
#108155 = DIRECTION('center_axis',(0.,1.,0.)) ;
#108156 = DIRECTION('ref_axis',(0.,0.,1.)) ;
#108157 = DIRECTION('center_axis',(0.,1.,0.)) ;
#108158 = DIRECTION('ref_axis',(0.,0.,1.)) ;
#108159 = DIRECTION('',(0.,1.,0.)) ;
#108160 = DIRECTION('center_axis',(0.,-1.,0.)) ;
#108161 = DIRECTION('ref_axis',(2.60208521396523E-14,0.,1.)) ;
#108162 = DIRECTION('',(0.,1.,0.)) ;
#108163 = DIRECTION('center_axis',(0.,0.,1.)) ;
#108164 = DIRECTION('ref_axis',(1.,0.,0.)) ;
#108165 = DIRECTION('',(-1.,0.,0.)) ;
#108166 = DIRECTION('',(0.,1.,0.)) ;
#108167 = DIRECTION('center_axis',(0.,1.,0.)) ;
#108168 = DIRECTION('ref_axis',(0.,0.,1.)) ;
#108169 = DIRECTION('center_axis',(0.,-1.,0.)) ;
#108170 = DIRECTION('ref_axis',(0.,0.,1.)) ;
#108171 = DIRECTION('',(0.,1.,0.)) ;
#108172 = DIRECTION('center_axis',(-1.,0.,0.)) ;
#108173 = DIRECTION('ref_axis',(0.,0.,1.)) ;
#108174 = DIRECTION('',(0.,0.,-1.)) ;
#108175 = DIRECTION('',(0.,1.,0.)) ;
#108176 = DIRECTION('center_axis',(0.,1.,0.)) ;
#108177 = DIRECTION('ref_axis',(0.,0.,1.)) ;
#108178 = DIRECTION('center_axis',(0.,-1.,0.)) ;
#108179 = DIRECTION('ref_axis',(0.,0.,1.)) ;
#108180 = DIRECTION('',(0.,1.,0.)) ;
#108181 = DIRECTION('center_axis',(0.,0.,-1.)) ;
#108182 = DIRECTION('ref_axis',(-1.,0.,0.)) ;
#108183 = DIRECTION('',(1.,0.,0.)) ;
#108184 = DIRECTION('',(0.,1.,0.)) ;
#108185 = DIRECTION('center_axis',(0.,1.,0.)) ;
#108186 = DIRECTION('ref_axis',(0.,0.,1.)) ;
#108187 = DIRECTION('center_axis',(0.,-1.,0.)) ;
#108188 = DIRECTION('ref_axis',(0.,0.,1.)) ;
#108189 = DIRECTION('',(0.,1.,0.)) ;
#108190 = DIRECTION('center_axis',(1.,0.,0.)) ;
#108191 = DIRECTION('ref_axis',(0.,0.,-1.)) ;
#108192 = DIRECTION('',(0.,0.,1.)) ;
#108193 = DIRECTION('center_axis',(0.,1.,0.)) ;
#108194 = DIRECTION('ref_axis',(0.,0.,1.)) ;
#108195 = DIRECTION('',(1.,0.,0.)) ;
#108196 = DIRECTION('',(0.,0.,-1.)) ;
#108197 = DIRECTION('',(-1.,0.,0.)) ;
#108198 = DIRECTION('',(0.,0.,1.)) ;
#108199 = DIRECTION('center_axis',(0.,0.164398987305357,-0.986393923832144)) ;
#108200 = DIRECTION('ref_axis',(0.,0.986393923832144,0.164398987305357)) ;
#108201 = DIRECTION('',(-1.,-1.0450141421547E-16,-1.7416902369245E-17)) ;
#108202 = DIRECTION('',(0.,-0.986393923832144,-0.164398987305357)) ;
#108203 = DIRECTION('',(1.,0.,0.)) ;
#108204 = DIRECTION('',(0.,0.986393923832144,0.164398987305357)) ;
#108205 = DIRECTION('center_axis',(0.,-1.,0.)) ;
#108206 = DIRECTION('ref_axis',(0.,0.,-1.)) ;
#108207 = DIRECTION('',(0.,0.,1.)) ;
#108208 = DIRECTION('',(0.,0.,-1.)) ;
#108209 = DIRECTION('',(-1.,0.,0.)) ;
#108210 = DIRECTION('center_axis',(0.,0.164398987305357,0.986393923832144)) ;
#108211 = DIRECTION('ref_axis',(0.,-0.986393923832144,0.164398987305357)) ;
#108212 = DIRECTION('',(0.,0.986393923832144,-0.164398987305357)) ;
#108213 = DIRECTION('',(1.,1.0450141421547E-16,-1.7416902369245E-17)) ;
#108214 = DIRECTION('',(0.,-0.986393923832144,0.164398987305357)) ;
#108215 = DIRECTION('center_axis',(-1.,0.,0.)) ;
#108216 = DIRECTION('ref_axis',(0.,0.,1.)) ;
#108217 = DIRECTION('',(0.,0.,1.)) ;
#108218 = DIRECTION('center_axis',(-1.,0.,0.)) ;
#108219 = DIRECTION('ref_axis',(0.,0.,1.)) ;
#108220 = DIRECTION('',(0.,-0.986393923832144,0.164398987305357)) ;
#108221 = DIRECTION('',(0.,0.,-1.)) ;
#108222 = DIRECTION('',(0.,0.986393923832144,0.164398987305357)) ;
#108223 = DIRECTION('center_axis',(1.,0.,0.)) ;
#108224 = DIRECTION('ref_axis',(0.,0.,-1.)) ;
#108225 = DIRECTION('center_axis',(1.,0.,0.)) ;
#108226 = DIRECTION('ref_axis',(0.,0.,-1.)) ;
#108227 = DIRECTION('center_axis',(1.,0.,0.)) ;
#108228 = DIRECTION('ref_axis',(0.,0.,1.)) ;
#108229 = DIRECTION('center_axis',(1.,0.,0.)) ;
#108230 = DIRECTION('ref_axis',(0.,8.88178419700125E-16,1.)) ;
#108231 = DIRECTION('center_axis',(1.,0.,0.)) ;
#108232 = DIRECTION('ref_axis',(0.,-1.77635683940025E-15,1.)) ;
#108233 = DIRECTION('',(1.,0.,0.)) ;
#108234 = DIRECTION('center_axis',(-1.,0.,0.)) ;
#108235 = DIRECTION('ref_axis',(0.,0.,1.)) ;
#108236 = DIRECTION('',(-1.,0.,0.)) ;
#108237 = DIRECTION('center_axis',(0.,0.,-1.)) ;
#108238 = DIRECTION('ref_axis',(1.,0.,0.)) ;
#108239 = DIRECTION('center_axis',(0.,-1.,0.)) ;
#108240 = DIRECTION('ref_axis',(0.,0.,1.)) ;
#108241 = DIRECTION('center_axis',(0.971399006496778,0.,-0.23745309047699)) ;
#108242 = DIRECTION('ref_axis',(-0.23745309047699,0.,-0.971399006496778)) ;
#108243 = DIRECTION('center_axis',(0.971399006496778,0.,-0.237453090476989)) ;
#108244 = DIRECTION('ref_axis',(-0.237453090476989,0.,-0.971399006496778)) ;
#108245 = DIRECTION('center_axis',(0.655772517804501,-0.73774408253007,-0.160299948796655)) ;
#108246 = DIRECTION('ref_axis',(-0.747409318683662,-0.664363838829917,4.77072893932298E-16)) ;
#108247 = DIRECTION('center_axis',(-0.439210132176035,-4.72038307384659E-10,
-0.898384360835556)) ;
#108248 = DIRECTION('ref_axis',(0.882040291644994,-0.189880214239185,-0.431219698245912)) ;
#108249 = DIRECTION('center_axis',(0.655772517804504,-0.737744082530068,-0.160299948796656)) ;
#108250 = DIRECTION('ref_axis',(0.74740931868366,0.664363838829919,-2.08334010827303E-16)) ;
#108251 = DIRECTION('center_axis',(0.655772517804505,-0.737744082530068,-0.16029994879665)) ;
#108252 = DIRECTION('ref_axis',(0.74740931868366,0.66436383882992,-5.75609428574487E-16)) ;
#108253 = DIRECTION('center_axis',(0.664363838829919,-0.74740931868366,0.)) ;
#108254 = DIRECTION('ref_axis',(0.74740931868366,0.664363838829919,0.)) ;
#108255 = DIRECTION('center_axis',(-0.664363838829918,0.747409318683661,0.)) ;
#108256 = DIRECTION('ref_axis',(-0.747409318683661,-0.664363838829918,0.)) ;
#108257 = DIRECTION('center_axis',(0.,1.,0.)) ;
#108258 = DIRECTION('ref_axis',(0.,0.,1.)) ;
#108259 = DIRECTION('center_axis',(0.,-1.,0.)) ;
#108260 = DIRECTION('ref_axis',(0.,0.,-1.)) ;
#108261 = DIRECTION('center_axis',(0.,0.,1.)) ;
#108262 = DIRECTION('ref_axis',(1.,0.,0.)) ;
#108263 = DIRECTION('center_axis',(0.,0.,-1.)) ;
#108264 = DIRECTION('ref_axis',(-1.,0.,0.)) ;
#108265 = DIRECTION('center_axis',(0.,0.,-1.)) ;
#108266 = DIRECTION('ref_axis',(-1.,0.,0.)) ;
#108267 = DIRECTION('center_axis',(0.439210132176171,4.7241906959143E-10,
-0.898384360835489)) ;
#108268 = DIRECTION('ref_axis',(0.882040291644681,-0.189880214240793,0.431219698245845)) ;
#108269 = DIRECTION('center_axis',(-0.971399006496778,0.,-0.23745309047699)) ;
#108270 = DIRECTION('ref_axis',(-0.23745309047699,0.,0.971399006496777)) ;
#108271 = DIRECTION('center_axis',(0.971399006496778,0.,0.237453090476989)) ;
#108272 = DIRECTION('ref_axis',(0.237453090476989,0.,-0.971399006496778)) ;
#108273 = DIRECTION('center_axis',(0.,1.,0.)) ;
#108274 = DIRECTION('ref_axis',(1.,0.,0.)) ;
#108275 = DIRECTION('center_axis',(-3.54829801904343E-14,1.,8.67361737988405E-15)) ;
#108276 = DIRECTION('ref_axis',(1.,3.54829801904343E-14,6.83923985932746E-30)) ;
#108277 = DIRECTION('center_axis',(-0.948683298050516,0.316227766016832,4.61630059016357E-15)) ;
#108278 = DIRECTION('ref_axis',(0.316227766016832,0.948683298050516,-4.49018244226562E-13)) ;
#108279 = DIRECTION('center_axis',(0.,0.,-1.)) ;
#108280 = DIRECTION('ref_axis',(1.,0.,0.)) ;
#108281 = DIRECTION('center_axis',(0.,-1.,0.)) ;
#108282 = DIRECTION('ref_axis',(0.,0.,1.)) ;
#108283 = DIRECTION('center_axis',(0.655772517804503,-0.737744082530069,0.160299948796655)) ;
#108284 = DIRECTION('ref_axis',(-0.747409318683661,-0.664363838829918,1.99521945175207E-17)) ;
#108285 = DIRECTION('center_axis',(0.,1.,0.)) ;
#108286 = DIRECTION('ref_axis',(0.,0.,1.)) ;
#108287 = DIRECTION('center_axis',(2.73957817177508E-14,1.,0.)) ;
#108288 = DIRECTION('ref_axis',(-1.,2.73957817177508E-14,0.)) ;
#108289 = DIRECTION('center_axis',(0.894427190999917,0.447213595499956,0.)) ;
#108290 = DIRECTION('ref_axis',(-0.447213595499956,0.894427190999917,0.)) ;
#108291 = DIRECTION('center_axis',(-0.894427190999916,-0.447213595499958,
0.)) ;
#108292 = DIRECTION('ref_axis',(0.447213595499958,-0.894427190999916,0.)) ;
#108293 = DIRECTION('center_axis',(0.,0.,1.)) ;
#108294 = DIRECTION('ref_axis',(1.,0.,0.)) ;
#108295 = DIRECTION('center_axis',(0.,0.,-1.)) ;
#108296 = DIRECTION('ref_axis',(-1.,0.,0.)) ;
#108297 = DIRECTION('center_axis',(0.,1.,0.)) ;
#108298 = DIRECTION('ref_axis',(0.,0.,1.)) ;
#108299 = DIRECTION('center_axis',(0.,-1.,0.)) ;
#108300 = DIRECTION('ref_axis',(0.,0.,-1.)) ;
#108301 = DIRECTION('center_axis',(-0.664363838829919,0.74740931868366,0.)) ;
#108302 = DIRECTION('ref_axis',(-0.74740931868366,-0.664363838829919,0.)) ;
#108303 = DIRECTION('center_axis',(-0.66436383882992,0.747409318683659,2.52106651083074E-15)) ;
#108304 = DIRECTION('ref_axis',(-0.747409318683659,-0.66436383882992,7.82575143531171E-30)) ;
#108305 = DIRECTION('center_axis',(-0.655772517804504,0.737744082530068,-0.160299948796656)) ;
#108306 = DIRECTION('ref_axis',(-0.74740931868366,-0.664363838829919,2.31673158493852E-16)) ;
#108307 = DIRECTION('center_axis',(0.655772517804496,-0.737744082530075,0.160299948796656)) ;
#108308 = DIRECTION('ref_axis',(0.747409318683667,0.664363838829911,-2.10122272487167E-17)) ;
#108309 = DIRECTION('center_axis',(0.,1.,0.)) ;
#108310 = DIRECTION('ref_axis',(1.,0.,0.)) ;
#108311 = DIRECTION('center_axis',(-0.873786407766988,-0.436893203883498,
0.213592233009711)) ;
#108312 = DIRECTION('ref_axis',(-0.447213595499961,0.894427190999914,5.03515095507592E-16)) ;
#108313 = DIRECTION('center_axis',(-0.948683298050516,0.316227766016832,-3.71868658652085E-15)) ;
#108314 = DIRECTION('ref_axis',(0.316227766016832,0.948683298050516,-1.37175731938863E-12)) ;
#108315 = DIRECTION('center_axis',(0.,1.,0.)) ;
#108316 = DIRECTION('ref_axis',(1.,0.,0.)) ;
#108317 = DIRECTION('center_axis',(-5.47915634355017E-14,1.,0.)) ;
#108318 = DIRECTION('ref_axis',(1.,5.47915634355017E-14,3.46944695195361E-14)) ;
#108319 = DIRECTION('center_axis',(-0.971399006496778,0.,0.23745309047699)) ;
#108320 = DIRECTION('ref_axis',(0.23745309047699,0.,0.971399006496777)) ;
#108321 = DIRECTION('center_axis',(0.971399006496778,-3.69787733965917E-15,
-0.237453090476989)) ;
#108322 = DIRECTION('ref_axis',(-0.237453090476989,3.58403898099287E-30,-0.971399006496778)) ;
#108323 = DIRECTION('center_axis',(0.873786407766991,0.436893203883493,-0.213592233009709)) ;
#108324 = DIRECTION('ref_axis',(-0.447213595499956,0.894427190999917,2.83414331365695E-16)) ;
#108325 = DIRECTION('center_axis',(-0.873786407766992,-0.436893203883492,
0.21359223300971)) ;
#108326 = DIRECTION('ref_axis',(0.447213595499955,-0.894427190999918,-1.48231119036019E-16)) ;
#108327 = DIRECTION('center_axis',(-0.894427190999917,-0.447213595499956,
0.)) ;
#108328 = DIRECTION('ref_axis',(0.447213595499956,-0.894427190999917,0.)) ;
#108329 = DIRECTION('center_axis',(-0.894427190999917,-0.447213595499955,
0.)) ;
#108330 = DIRECTION('ref_axis',(0.447213595499955,-0.894427190999917,0.)) ;
#108331 = DIRECTION('center_axis',(0.,1.,0.)) ;
#108332 = DIRECTION('ref_axis',(0.,0.,1.)) ;
#108333 = DIRECTION('center_axis',(2.66122351428257E-14,1.,6.50521303491301E-15)) ;
#108334 = DIRECTION('ref_axis',(-1.,2.66122351428257E-14,3.84707242087163E-30)) ;
#108335 = DIRECTION('center_axis',(-0.439210132004979,2.9556401387078E-13,
-0.898384360919183)) ;
#108336 = DIRECTION('ref_axis',(0.898384360919183,-2.12487583469939E-11,-0.439210132004979)) ;
#108337 = DIRECTION('center_axis',(0.,1.,0.)) ;
#108338 = DIRECTION('ref_axis',(1.,0.,0.)) ;
#108339 = DIRECTION('center_axis',(-0.87378640776699,-0.436893203883495,-0.213592233009712)) ;
#108340 = DIRECTION('ref_axis',(-0.447213595499958,0.894427190999916,1.8708344946598E-16)) ;
#108341 = DIRECTION('center_axis',(0.,0.,1.)) ;
#108342 = DIRECTION('ref_axis',(1.,0.,0.)) ;
#108343 = DIRECTION('center_axis',(0.439210132005031,-4.72579842096268E-13,
-0.898384360919158)) ;
#108344 = DIRECTION('ref_axis',(0.898384360919158,-2.70958403094291E-11,0.439210132005031)) ;
#108345 = DIRECTION('center_axis',(-0.873786407766991,-0.436893203883493,
-0.213592233009709)) ;
#108346 = DIRECTION('ref_axis',(0.447213595499956,-0.894427190999917,-1.06780556900622E-16)) ;
#108347 = DIRECTION('center_axis',(-0.873786407766992,-0.436893203883492,
-0.213592233009707)) ;
#108348 = DIRECTION('ref_axis',(0.447213595499955,-0.894427190999918,-7.04543255365314E-18)) ;
#108349 = DIRECTION('center_axis',(-0.971399006496778,0.,-0.237453090476989)) ;
#108350 = DIRECTION('ref_axis',(0.237453090476989,0.,-0.971399006496778)) ;
#108351 = DIRECTION('center_axis',(0.971399006496778,0.,0.23745309047699)) ;
#108352 = DIRECTION('ref_axis',(0.23745309047699,0.,-0.971399006496777)) ;
#108353 = DIRECTION('center_axis',(0.,0.,-1.)) ;
#108354 = DIRECTION('ref_axis',(-1.,0.,0.)) ;
#108355 = DIRECTION('center_axis',(1.,1.0450141421547E-16,1.7416902369245E-17)) ;
#108356 = DIRECTION('ref_axis',(-1.0450141421547E-16,1.,-1.82009092883888E-33)) ;
#108357 = DIRECTION('center_axis',(0.672672795322857,0.739940072189994,-7.49312539869347E-10)) ;
#108358 = DIRECTION('ref_axis',(0.738044870607246,-0.670949884714448,0.0715263669705305)) ;
#108359 = DIRECTION('center_axis',(-1.,0.,0.)) ;
#108360 = DIRECTION('ref_axis',(0.,-0.646374896130194,-0.763019982472727)) ;
#108361 = DIRECTION('center_axis',(-1.,0.,0.)) ;
#108362 = DIRECTION('ref_axis',(0.,0.,1.)) ;
#108363 = DIRECTION('center_axis',(-1.,0.,0.)) ;
#108364 = DIRECTION('ref_axis',(0.,0.,1.)) ;
#108365 = DIRECTION('center_axis',(0.,0.986393923832144,0.164398987305357)) ;
#108366 = DIRECTION('ref_axis',(0.,-0.164398987305357,0.986393923832144)) ;
#108367 = DIRECTION('center_axis',(0.,-0.986393923832144,-0.164398987305358)) ;
#108368 = DIRECTION('ref_axis',(0.,0.164398987305358,-0.986393923832144)) ;
#108369 = DIRECTION('center_axis',(0.,0.,1.)) ;
#108370 = DIRECTION('ref_axis',(1.,0.,0.)) ;
#108371 = DIRECTION('center_axis',(0.,0.,1.)) ;
#108372 = DIRECTION('ref_axis',(1.,0.,0.)) ;
#108373 = DIRECTION('center_axis',(0.,0.,1.)) ;
#108374 = DIRECTION('ref_axis',(1.,0.,0.)) ;
#108375 = DIRECTION('center_axis',(0.,0.,-1.)) ;
#108376 = DIRECTION('ref_axis',(1.,0.,0.)) ;
#108377 = DIRECTION('center_axis',(-1.,0.,0.)) ;
#108378 = DIRECTION('ref_axis',(0.,-0.646374896130192,-0.763019982472729)) ;
#108379 = DIRECTION('center_axis',(0.,0.,1.)) ;
#108380 = DIRECTION('ref_axis',(-1.,0.,0.)) ;
#108381 = DIRECTION('center_axis',(0.,0.,-1.)) ;
#108382 = DIRECTION('ref_axis',(-1.,0.,0.)) ;
#108383 = DIRECTION('center_axis',(1.,1.0450141421547E-16,-1.7416902369245E-17)) ;
#108384 = DIRECTION('ref_axis',(-1.0450141421547E-16,1.,1.82009092883888E-33)) ;
#108385 = DIRECTION('center_axis',(0.672672795323056,0.739940072189814,7.49430034663666E-10)) ;
#108386 = DIRECTION('ref_axis',(0.738044870609142,-0.670949884716522,-0.0715263669315059)) ;
#108387 = DIRECTION('center_axis',(1.,0.,0.)) ;
#108388 = DIRECTION('ref_axis',(0.,4.33680868994204E-14,1.)) ;
#108389 = DIRECTION('center_axis',(0.,0.,-1.)) ;
#108390 = DIRECTION('ref_axis',(-1.,0.,0.)) ;
#108391 = DIRECTION('center_axis',(0.,-0.986393923832144,0.164398987305357)) ;
#108392 = DIRECTION('ref_axis',(0.,-0.164398987305357,-0.986393923832144)) ;
#108393 = DIRECTION('center_axis',(1.,0.,0.)) ;
#108394 = DIRECTION('ref_axis',(0.,0.,1.)) ;
#108395 = DIRECTION('center_axis',(7.58941520739854E-15,0.,-1.)) ;
#108396 = DIRECTION('ref_axis',(-1.,0.,-7.58941520739854E-15)) ;
#108397 = DIRECTION('center_axis',(1.,0.,-8.67361737988404E-15)) ;
#108398 = DIRECTION('ref_axis',(-8.67361737988404E-15,0.,-1.)) ;
#108399 = DIRECTION('center_axis',(1.,0.,0.)) ;
#108400 = DIRECTION('ref_axis',(0.,0.,-1.)) ;
#108401 = DIRECTION('center_axis',(1.,0.,8.67361737988403E-15)) ;
#108402 = DIRECTION('ref_axis',(8.67361737988403E-15,0.,-1.)) ;
#108403 = DIRECTION('center_axis',(0.,0.,1.)) ;
#108404 = DIRECTION('ref_axis',(1.,0.,0.)) ;
#108405 = DIRECTION('center_axis',(0.,0.,-1.)) ;
#108406 = DIRECTION('ref_axis',(-1.,0.,0.)) ;
#108407 = DIRECTION('center_axis',(1.,0.,0.)) ;
#108408 = DIRECTION('ref_axis',(0.,0.,1.)) ;
#108409 = DIRECTION('center_axis',(-6.50521303491304E-15,0.,-1.)) ;
#108410 = DIRECTION('ref_axis',(-1.,0.,6.50521303491304E-15)) ;
#108411 = DIRECTION('center_axis',(1.,0.,0.)) ;
#108412 = DIRECTION('ref_axis',(0.,0.,1.)) ;
#108413 = DIRECTION('center_axis',(1.,9.40395480657835E-30,8.67361737988403E-15)) ;
#108414 = DIRECTION('ref_axis',(8.67361737988403E-15,-5.27711695562625E-58,
-1.)) ;
#108415 = DIRECTION('center_axis',(0.,0.,-1.)) ;
#108416 = DIRECTION('ref_axis',(-1.,0.,0.)) ;
#108417 = DIRECTION('center_axis',(6.50521303491304E-15,0.,-1.)) ;
#108418 = DIRECTION('ref_axis',(-1.,0.,-6.50521303491304E-15)) ;
#108419 = DIRECTION('center_axis',(-1.,0.,0.)) ;
#108420 = DIRECTION('ref_axis',(0.,0.,1.)) ;
#108421 = DIRECTION('center_axis',(1.,-8.67361737988409E-15,0.)) ;
#108422 = DIRECTION('ref_axis',(8.67361737988409E-15,1.,0.)) ;
#108423 = DIRECTION('center_axis',(1.,0.,0.)) ;
#108424 = DIRECTION('ref_axis',(0.,0.,1.)) ;
#108425 = DIRECTION('center_axis',(-4.33680868994202E-16,0.,1.)) ;
#108426 = DIRECTION('ref_axis',(1.,0.,4.33680868994202E-16)) ;
#108427 = DIRECTION('center_axis',(0.,0.,-1.)) ;
#108428 = DIRECTION('ref_axis',(-1.,0.,0.)) ;
#108429 = DIRECTION('center_axis',(0.,0.,1.)) ;
#108430 = DIRECTION('ref_axis',(1.,0.,0.)) ;
#108431 = DIRECTION('center_axis',(0.,1.,0.)) ;
#108432 = DIRECTION('ref_axis',(0.,0.,1.)) ;
#108433 = DIRECTION('center_axis',(-1.,0.,0.)) ;
#108434 = DIRECTION('ref_axis',(0.,0.,-1.)) ;
#108435 = DIRECTION('center_axis',(0.,-1.,0.)) ;
#108436 = DIRECTION('ref_axis',(0.,0.,1.)) ;
#108437 = DIRECTION('center_axis',(0.,1.,0.)) ;
#108438 = DIRECTION('ref_axis',(0.,0.,1.)) ;
#108439 = DIRECTION('center_axis',(0.,-1.,0.)) ;
#108440 = DIRECTION('ref_axis',(0.,0.,1.)) ;
#108441 = DIRECTION('center_axis',(-1.,0.,0.)) ;
#108442 = DIRECTION('ref_axis',(0.,0.,-1.)) ;
#108443 = DIRECTION('center_axis',(-1.,0.,-1.73472347597681E-16)) ;
#108444 = DIRECTION('ref_axis',(-1.73472347597681E-16,0.,1.)) ;
#108445 = DIRECTION('center_axis',(-1.,0.,0.)) ;
#108446 = DIRECTION('ref_axis',(0.,0.,1.)) ;
#108447 = DIRECTION('center_axis',(0.,1.,0.)) ;
#108448 = DIRECTION('ref_axis',(0.,0.,1.)) ;
#108449 = DIRECTION('center_axis',(0.,-1.,0.)) ;
#108450 = DIRECTION('ref_axis',(0.,0.,-1.)) ;
#108451 = DIRECTION('center_axis',(-4.33680868994202E-16,0.,1.)) ;
#108452 = DIRECTION('ref_axis',(1.,0.,4.33680868994202E-16)) ;
#108453 = DIRECTION('center_axis',(0.,0.,1.)) ;
#108454 = DIRECTION('ref_axis',(1.,0.,0.)) ;
#108455 = DIRECTION('center_axis',(0.,0.,-1.)) ;
#108456 = DIRECTION('ref_axis',(-1.,0.,0.)) ;
#108457 = DIRECTION('center_axis',(0.,1.,0.)) ;
#108458 = DIRECTION('ref_axis',(0.,0.,1.)) ;
#108459 = DIRECTION('center_axis',(0.,-1.,0.)) ;
#108460 = DIRECTION('ref_axis',(0.,0.,-1.)) ;
#108461 = DIRECTION('center_axis',(1.,0.,-1.73472347597681E-16)) ;
#108462 = DIRECTION('ref_axis',(-1.73472347597681E-16,0.,-1.)) ;
#108463 = DIRECTION('center_axis',(-1.,0.,0.)) ;
#108464 = DIRECTION('ref_axis',(0.,0.,1.)) ;
#108465 = DIRECTION('center_axis',(0.,0.,-1.)) ;
#108466 = DIRECTION('ref_axis',(-1.,0.,0.)) ;
#108467 = DIRECTION('center_axis',(0.,0.,1.)) ;
#108468 = DIRECTION('ref_axis',(1.,0.,0.)) ;
#108469 = DIRECTION('center_axis',(0.,0.,-1.)) ;
#108470 = DIRECTION('ref_axis',(-1.,0.,0.)) ;
#108471 = DIRECTION('center_axis',(0.,1.,0.)) ;
#108472 = DIRECTION('ref_axis',(0.,0.,1.)) ;
#108473 = DIRECTION('center_axis',(0.,-1.,0.)) ;
#108474 = DIRECTION('ref_axis',(0.,0.,1.)) ;
#108475 = DIRECTION('center_axis',(0.,1.,0.)) ;
#108476 = DIRECTION('ref_axis',(1.,0.,0.)) ;
#108477 = DIRECTION('center_axis',(1.,0.,0.)) ;
#108478 = DIRECTION('ref_axis',(0.,0.,1.)) ;
#108479 = DIRECTION('center_axis',(0.,1.,0.)) ;
#108480 = DIRECTION('ref_axis',(1.,0.,0.)) ;
#108481 = DIRECTION('center_axis',(1.,0.,0.)) ;
#108482 = DIRECTION('ref_axis',(0.,0.,1.)) ;
#108483 = DIRECTION('center_axis',(0.,1.,0.)) ;
#108484 = DIRECTION('ref_axis',(0.,0.,1.)) ;
#108485 = DIRECTION('center_axis',(0.,-1.,0.)) ;
#108486 = DIRECTION('ref_axis',(0.,0.,1.)) ;
#108487 = DIRECTION('center_axis',(0.,1.,0.)) ;
#108488 = DIRECTION('ref_axis',(0.,0.,1.)) ;
#108489 = DIRECTION('center_axis',(0.,-1.,0.)) ;
#108490 = DIRECTION('ref_axis',(0.,0.,-1.)) ;
#108491 = DIRECTION('center_axis',(-1.,0.,-1.73472347597681E-16)) ;
#108492 = DIRECTION('ref_axis',(-1.73472347597681E-16,0.,1.)) ;
#108493 = DIRECTION('center_axis',(1.,0.,0.)) ;
#108494 = DIRECTION('ref_axis',(0.,0.,-1.)) ;
#108495 = DIRECTION('center_axis',(1.,0.,-1.73472347597681E-16)) ;
#108496 = DIRECTION('ref_axis',(-1.73472347597681E-16,0.,-1.)) ;
#108497 = DIRECTION('center_axis',(1.,0.,0.)) ;
#108498 = DIRECTION('ref_axis',(0.,0.,-1.)) ;
#108499 = DIRECTION('center_axis',(0.,1.,0.)) ;
#108500 = DIRECTION('ref_axis',(0.,0.,1.)) ;
#108501 = DIRECTION('center_axis',(0.,-1.,0.)) ;
#108502 = DIRECTION('ref_axis',(0.,0.,-1.)) ;
#108503 = DIRECTION('center_axis',(0.,1.,0.)) ;
#108504 = DIRECTION('ref_axis',(1.,0.,0.)) ;
#108505 = DIRECTION('center_axis',(0.,0.,1.)) ;
#108506 = DIRECTION('ref_axis',(-1.,0.,0.)) ;
#108507 = DIRECTION('center_axis',(0.,1.,0.)) ;
#108508 = DIRECTION('ref_axis',(1.,0.,0.)) ;
#108509 = DIRECTION('center_axis',(0.,0.,-1.)) ;
#108510 = DIRECTION('ref_axis',(1.,0.,0.)) ;
#108511 = DIRECTION('center_axis',(0.,0.,-1.)) ;
#108512 = DIRECTION('ref_axis',(-1.,0.,0.)) ;
#108513 = DIRECTION('center_axis',(2.16840434497101E-16,0.,1.)) ;
#108514 = DIRECTION('ref_axis',(1.,0.,-2.16840434497101E-16)) ;
#108515 = DIRECTION('center_axis',(0.,0.,-1.)) ;
#108516 = DIRECTION('ref_axis',(-1.,0.,0.)) ;
#108517 = DIRECTION('center_axis',(0.,0.,1.)) ;
#108518 = DIRECTION('ref_axis',(1.,0.,0.)) ;
#108519 = DIRECTION('center_axis',(0.,-1.,0.)) ;
#108520 = DIRECTION('ref_axis',(0.,0.,-1.)) ;
#108521 = DIRECTION('center_axis',(1.,0.,0.)) ;
#108522 = DIRECTION('ref_axis',(0.,0.,1.)) ;
#108523 = DIRECTION('center_axis',(0.,1.,0.)) ;
#108524 = DIRECTION('ref_axis',(0.,0.,-1.)) ;
#108525 = DIRECTION('center_axis',(0.,-1.,0.)) ;
#108526 = DIRECTION('ref_axis',(0.,0.,-1.)) ;
#108527 = DIRECTION('center_axis',(0.,1.,0.)) ;
#108528 = DIRECTION('ref_axis',(0.,0.,-1.)) ;
#108529 = DIRECTION('center_axis',(1.,0.,0.)) ;
#108530 = DIRECTION('ref_axis',(0.,0.,1.)) ;
#108531 = DIRECTION('center_axis',(1.,0.,-1.73472347597681E-16)) ;
#108532 = DIRECTION('ref_axis',(-1.73472347597681E-16,0.,-1.)) ;
#108533 = DIRECTION('center_axis',(1.,0.,0.)) ;
#108534 = DIRECTION('ref_axis',(0.,0.,-1.)) ;
#108535 = DIRECTION('center_axis',(0.,-1.,0.)) ;
#108536 = DIRECTION('ref_axis',(0.,0.,-1.)) ;
#108537 = DIRECTION('center_axis',(0.,1.,0.)) ;
#108538 = DIRECTION('ref_axis',(0.,0.,1.)) ;
#108539 = DIRECTION('center_axis',(2.16840434497101E-16,0.,1.)) ;
#108540 = DIRECTION('ref_axis',(1.,0.,-2.16840434497101E-16)) ;
#108541 = DIRECTION('center_axis',(0.,0.,1.)) ;
#108542 = DIRECTION('ref_axis',(1.,0.,0.)) ;
#108543 = DIRECTION('center_axis',(0.,0.,-1.)) ;
#108544 = DIRECTION('ref_axis',(-1.,0.,0.)) ;
#108545 = DIRECTION('center_axis',(0.,-1.,0.)) ;
#108546 = DIRECTION('ref_axis',(0.,0.,-1.)) ;
#108547 = DIRECTION('center_axis',(0.,1.,0.)) ;
#108548 = DIRECTION('ref_axis',(0.,0.,1.)) ;
#108549 = DIRECTION('center_axis',(-1.,0.,1.73472347597681E-16)) ;
#108550 = DIRECTION('ref_axis',(1.73472347597681E-16,0.,1.)) ;
#108551 = DIRECTION('center_axis',(1.,0.,0.)) ;
#108552 = DIRECTION('ref_axis',(0.,0.,-1.)) ;
#108553 = DIRECTION('center_axis',(-2.16840434497101E-16,0.,-1.)) ;
#108554 = DIRECTION('ref_axis',(-1.,0.,2.16840434497101E-16)) ;
#108555 = DIRECTION('center_axis',(0.,0.,1.)) ;
#108556 = DIRECTION('ref_axis',(1.,0.,0.)) ;
#108557 = DIRECTION('center_axis',(0.,0.,-1.)) ;
#108558 = DIRECTION('ref_axis',(-1.,0.,0.)) ;
#108559 = DIRECTION('center_axis',(0.,-1.,0.)) ;
#108560 = DIRECTION('ref_axis',(0.,0.,-1.)) ;
#108561 = DIRECTION('center_axis',(0.,1.,0.)) ;
#108562 = DIRECTION('ref_axis',(0.,0.,-1.)) ;
#108563 = DIRECTION('center_axis',(0.,1.,0.)) ;
#108564 = DIRECTION('ref_axis',(1.,0.,0.)) ;
#108565 = DIRECTION('center_axis',(-1.,0.,0.)) ;
#108566 = DIRECTION('ref_axis',(0.,0.,-1.)) ;
#108567 = DIRECTION('center_axis',(0.,1.,0.)) ;
#108568 = DIRECTION('ref_axis',(1.,0.,0.)) ;
#108569 = DIRECTION('center_axis',(-1.,0.,0.)) ;
#108570 = DIRECTION('ref_axis',(0.,0.,-1.)) ;
#108571 = DIRECTION('center_axis',(0.,-1.,0.)) ;
#108572 = DIRECTION('ref_axis',(0.,0.,-1.)) ;
#108573 = DIRECTION('center_axis',(0.,1.,0.)) ;
#108574 = DIRECTION('ref_axis',(0.,0.,-1.)) ;
#108575 = DIRECTION('center_axis',(0.,-1.,0.)) ;
#108576 = DIRECTION('ref_axis',(0.,0.,-1.)) ;
#108577 = DIRECTION('center_axis',(0.,1.,0.)) ;
#108578 = DIRECTION('ref_axis',(0.,0.,1.)) ;
#108579 = DIRECTION('center_axis',(1.,0.,-1.73472347597681E-16)) ;
#108580 = DIRECTION('ref_axis',(-1.73472347597681E-16,0.,-1.)) ;
#108581 = DIRECTION('center_axis',(-1.,0.,0.)) ;
#108582 = DIRECTION('ref_axis',(0.,0.,1.)) ;
#108583 = DIRECTION('center_axis',(-1.,0.,1.73472347597681E-16)) ;
#108584 = DIRECTION('ref_axis',(1.73472347597681E-16,0.,1.)) ;
#108585 = DIRECTION('center_axis',(-1.,0.,0.)) ;
#108586 = DIRECTION('ref_axis',(0.,0.,1.)) ;
#108587 = DIRECTION('center_axis',(0.,-1.,0.)) ;
#108588 = DIRECTION('ref_axis',(0.,0.,-1.)) ;
#108589 = DIRECTION('center_axis',(0.,1.,0.)) ;
#108590 = DIRECTION('ref_axis',(0.,0.,1.)) ;
#108591 = DIRECTION('center_axis',(0.,1.,0.)) ;
#108592 = DIRECTION('ref_axis',(1.,0.,0.)) ;
#108593 = DIRECTION('center_axis',(0.,0.,1.)) ;
#108594 = DIRECTION('ref_axis',(-1.,0.,0.)) ;
#108595 = DIRECTION('center_axis',(0.,1.,0.)) ;
#108596 = DIRECTION('ref_axis',(1.,0.,0.)) ;
#108597 = DIRECTION('center_axis',(0.,0.,-1.)) ;
#108598 = DIRECTION('ref_axis',(1.,0.,0.)) ;
#108599 = DIRECTION('center_axis',(-2.16840434497101E-16,0.,-1.)) ;
#108600 = DIRECTION('ref_axis',(-1.,0.,2.16840434497101E-16)) ;
#108601 = DIRECTION('center_axis',(-1.,0.,0.)) ;
#108602 = DIRECTION('ref_axis',(0.,0.,1.)) ;
#108603 = DIRECTION('center_axis',(0.,-0.632948931301575,-0.774193548387091)) ;
#108604 = DIRECTION('ref_axis',(0.,0.774193548387091,-0.632948931301575)) ;
#108605 = DIRECTION('center_axis',(0.,0.,1.)) ;
#108606 = DIRECTION('ref_axis',(1.,0.,0.)) ;
#108607 = DIRECTION('center_axis',(8.67361737988401E-15,0.,1.)) ;
#108608 = DIRECTION('ref_axis',(1.,0.,-8.67361737988401E-15)) ;
#108609 = DIRECTION('center_axis',(0.,1.,0.)) ;
#108610 = DIRECTION('ref_axis',(1.,0.,0.)) ;
#108611 = DIRECTION('center_axis',(-1.,0.,0.)) ;
#108612 = DIRECTION('ref_axis',(0.,0.,-1.)) ;
#108613 = DIRECTION('center_axis',(1.,0.,0.)) ;
#108614 = DIRECTION('ref_axis',(0.,0.,-1.)) ;
#108615 = DIRECTION('center_axis',(-1.,0.,0.)) ;
#108616 = DIRECTION('ref_axis',(0.,0.,1.)) ;
#108617 = DIRECTION('center_axis',(0.,0.,-1.)) ;
#108618 = DIRECTION('ref_axis',(-1.,0.,0.)) ;
#108619 = DIRECTION('center_axis',(0.,0.,-1.)) ;
#108620 = DIRECTION('ref_axis',(-1.,0.,0.)) ;
#108621 = DIRECTION('center_axis',(-1.,0.,0.)) ;
#108622 = DIRECTION('ref_axis',(0.,0.,1.)) ;
#108623 = DIRECTION('center_axis',(0.,-0.632948931301567,-0.774193548387097)) ;
#108624 = DIRECTION('ref_axis',(0.,-0.774193548387097,0.632948931301567)) ;
#108625 = DIRECTION('center_axis',(-1.,0.,0.)) ;
#108626 = DIRECTION('ref_axis',(0.,0.,1.)) ;
#108627 = DIRECTION('center_axis',(0.,0.632948931301567,-0.774193548387097)) ;
#108628 = DIRECTION('ref_axis',(0.,0.774193548387097,0.632948931301567)) ;
#108629 = DIRECTION('center_axis',(0.,0.,-1.)) ;
#108630 = DIRECTION('ref_axis',(-1.,0.,0.)) ;
#108631 = DIRECTION('center_axis',(0.,0.,1.)) ;
#108632 = DIRECTION('ref_axis',(1.,0.,0.)) ;
#108633 = DIRECTION('center_axis',(-1.,0.,0.)) ;
#108634 = DIRECTION('ref_axis',(0.,0.,1.)) ;
#108635 = DIRECTION('center_axis',(1.,0.,0.)) ;
#108636 = DIRECTION('ref_axis',(0.,0.,1.)) ;
#108637 = DIRECTION('center_axis',(1.,0.,0.)) ;
#108638 = DIRECTION('ref_axis',(0.,0.,-1.)) ;
#108639 = DIRECTION('center_axis',(1.,0.,0.)) ;
#108640 = DIRECTION('ref_axis',(0.,0.,-1.)) ;
#108641 = DIRECTION('center_axis',(0.,0.,1.)) ;
#108642 = DIRECTION('ref_axis',(1.,0.,0.)) ;
#108643 = DIRECTION('center_axis',(0.,8.67361737988405E-15,-1.)) ;
#108644 = DIRECTION('ref_axis',(0.,1.,8.67361737988405E-15)) ;
#108645 = DIRECTION('center_axis',(0.,1.,0.)) ;
#108646 = DIRECTION('ref_axis',(1.,0.,0.)) ;
#108647 = DIRECTION('center_axis',(1.22050154678007E-14,0.632948931301567,
-0.774193548387097)) ;
#108648 = DIRECTION('ref_axis',(1.7347234759768E-14,-0.774193548387097,-0.632948931301567)) ;
#108649 = DIRECTION('center_axis',(-1.,0.,0.)) ;
#108650 = DIRECTION('ref_axis',(0.,0.,1.)) ;
#108651 = DIRECTION('center_axis',(0.,0.,1.)) ;
#108652 = DIRECTION('ref_axis',(1.,0.,0.)) ;
#108653 = DIRECTION('center_axis',(0.,0.,-1.)) ;
#108654 = DIRECTION('ref_axis',(-1.,0.,0.)) ;
#108655 = DIRECTION('center_axis',(0.,0.,-1.)) ;
#108656 = DIRECTION('ref_axis',(-1.,0.,0.)) ;
#108657 = DIRECTION('center_axis',(0.,0.,-1.)) ;
#108658 = DIRECTION('ref_axis',(-1.,0.,0.)) ;
#108659 = DIRECTION('center_axis',(0.,0.,-1.)) ;
#108660 = DIRECTION('ref_axis',(-1.,0.,0.)) ;
#108661 = DIRECTION('center_axis',(0.,0.,-1.)) ;
#108662 = DIRECTION('ref_axis',(-1.,0.,0.)) ;
#108663 = DIRECTION('center_axis',(-0.422618261740697,0.,0.906307787036651)) ;
#108664 = DIRECTION('ref_axis',(0.906307787036651,0.,0.422618261740697)) ;
#108665 = DIRECTION('center_axis',(0.422618261740697,0.,-0.906307787036651)) ;
#108666 = DIRECTION('ref_axis',(-0.906307787036651,0.,-0.422618261740697)) ;
#108667 = DIRECTION('center_axis',(0.422618261740697,0.,-0.906307787036651)) ;
#108668 = DIRECTION('ref_axis',(-0.906307787036651,0.,-0.422618261740697)) ;
#108669 = DIRECTION('center_axis',(-0.422618261740697,0.,0.906307787036651)) ;
#108670 = DIRECTION('ref_axis',(0.906307787036651,0.,0.422618261740697)) ;
#108671 = DIRECTION('center_axis',(0.,0.,-1.)) ;
#108672 = DIRECTION('ref_axis',(-1.,0.,0.)) ;
#108673 = DIRECTION('center_axis',(0.,0.,-1.)) ;
#108674 = DIRECTION('ref_axis',(-1.,0.,0.)) ;
#108675 = DIRECTION('center_axis',(0.,0.,1.)) ;
#108676 = DIRECTION('ref_axis',(1.,0.,0.)) ;
#108677 = DIRECTION('center_axis',(0.,0.,1.)) ;
#108678 = DIRECTION('ref_axis',(1.,0.,0.)) ;
#108679 = DIRECTION('center_axis',(0.,0.,-1.)) ;
#108680 = DIRECTION('ref_axis',(-1.,0.,0.)) ;
#108681 = DIRECTION('center_axis',(0.,0.,-1.)) ;
#108682 = DIRECTION('ref_axis',(-1.,0.,0.)) ;
#108683 = DIRECTION('center_axis',(0.,0.,1.)) ;
#108684 = DIRECTION('ref_axis',(1.,0.,0.)) ;
#108685 = DIRECTION('center_axis',(0.,1.,0.)) ;
#108686 = DIRECTION('ref_axis',(1.,0.,0.)) ;
#108687 = DIRECTION('center_axis',(0.,-0.986393923832144,0.164398987305358)) ;
#108688 = DIRECTION('ref_axis',(0.,-0.164398987305358,-0.986393923832144)) ;
#108689 = DIRECTION('center_axis',(0.,0.986393923832144,-0.164398987305357)) ;
#108690 = DIRECTION('ref_axis',(0.,0.164398987305357,0.986393923832144)) ;
#108691 = DIRECTION('center_axis',(0.,-0.986393923832144,0.164398987305358)) ;
#108692 = DIRECTION('ref_axis',(0.,-0.164398987305358,-0.986393923832144)) ;
#108693 = DIRECTION('center_axis',(-1.,0.,0.)) ;
#108694 = DIRECTION('ref_axis',(0.,0.107567764393764,-0.994197755008191)) ;
#108695 = DIRECTION('center_axis',(4.02631181035923E-15,-0.928404294083138,
-0.371571617226061)) ;
#108696 = DIRECTION('ref_axis',(1.27444840229953E-29,0.371571617226061,-0.928404294083138)) ;
#108697 = DIRECTION('center_axis',(0.275516865537137,-0.50093975551097,-0.820457078800105)) ;
#108698 = DIRECTION('ref_axis',(3.47276585739718E-16,0.853490367006418,-0.521108619605597)) ;
#108699 = DIRECTION('center_axis',(0.,0.,-1.)) ;
#108700 = DIRECTION('ref_axis',(-1.,0.,0.)) ;
#108701 = DIRECTION('center_axis',(0.,0.,-1.)) ;
#108702 = DIRECTION('ref_axis',(-1.,0.,0.)) ;
#108703 = DIRECTION('center_axis',(0.,0.,-1.)) ;
#108704 = DIRECTION('ref_axis',(-1.,0.,0.)) ;
#108705 = DIRECTION('center_axis',(0.,0.,-1.)) ;
#108706 = DIRECTION('ref_axis',(-1.,0.,0.)) ;
#108707 = DIRECTION('center_axis',(-0.275516865538071,0.500939755523742,-0.820457078791993)) ;
#108708 = DIRECTION('ref_axis',(1.34532370065023E-15,0.853490366998217,0.521108619619028)) ;
#108709 = DIRECTION('center_axis',(0.,-0.986393923832144,-0.164398987305357)) ;
#108710 = DIRECTION('ref_axis',(0.,0.164398987305357,-0.986393923832144)) ;
#108711 = DIRECTION('center_axis',(3.5648347838177E-16,0.986393923832144,
0.164398987305358)) ;
#108712 = DIRECTION('ref_axis',(3.79675591822878E-31,-0.164398987305358,0.986393923832144)) ;
#108713 = DIRECTION('center_axis',(0.,1.,0.)) ;
#108714 = DIRECTION('ref_axis',(1.,0.,0.)) ;
#108715 = DIRECTION('center_axis',(-1.,0.,0.)) ;
#108716 = DIRECTION('ref_axis',(0.,0.,1.)) ;
#108717 = DIRECTION('center_axis',(0.,0.,-1.)) ;
#108718 = DIRECTION('ref_axis',(-1.,0.,0.)) ;
#108719 = DIRECTION('center_axis',(0.,0.,-1.)) ;
#108720 = DIRECTION('ref_axis',(-1.,0.,0.)) ;
#108721 = DIRECTION('center_axis',(0.,0.,-1.)) ;
#108722 = DIRECTION('ref_axis',(-1.,0.,0.)) ;
#108723 = DIRECTION('center_axis',(2.168404344971E-15,0.,1.)) ;
#108724 = DIRECTION('ref_axis',(1.,0.,-2.168404344971E-15)) ;
#108725 = DIRECTION('center_axis',(0.795723237447208,-7.53302716311723E-12,
0.605660407643206)) ;
#108726 = DIRECTION('ref_axis',(0.605660407643206,2.00215687134887E-26,-0.795723237447208)) ;
#108727 = DIRECTION('center_axis',(1.57772181044204E-26,2.36658271566302E-26,
1.)) ;
#108728 = DIRECTION('ref_axis',(3.73380916671669E-52,-1.,2.36658271566302E-26)) ;
#108729 = DIRECTION('center_axis',(-0.795723237415222,-2.11663082418553E-11,
0.605660407685229)) ;
#108730 = DIRECTION('ref_axis',(0.605660407685229,-9.75816058447732E-26,0.795723237415222)) ;
#108731 = DIRECTION('axis',(0.,0.,1.)) ;
#108732 = DIRECTION('refdir',(1.,0.,0.)) ;
#108733 = DIRECTION('center_axis',(1.,0.,0.)) ;
#108734 = DIRECTION('ref_axis',(0.,0.,-1.)) ;
#108735 = DIRECTION('center_axis',(1.,0.,0.)) ;
#108736 = DIRECTION('ref_axis',(0.,0.,-1.)) ;
#108737 = DIRECTION('center_axis',(0.,-1.,-1.22464679914735E-16)) ;
#108738 = DIRECTION('ref_axis',(0.,-1.22464679914735E-16,1.)) ;
#108739 = DIRECTION('center_axis',(-1.,0.,0.)) ;
#108740 = DIRECTION('ref_axis',(0.,0.,-1.)) ;
#108741 = DIRECTION('center_axis',(-1.,0.,0.)) ;
#108742 = DIRECTION('ref_axis',(0.,0.,-1.)) ;
#108743 = DIRECTION('center_axis',(-1.,0.,0.)) ;
#108744 = DIRECTION('ref_axis',(0.,0.,1.)) ;
#108745 = DIRECTION('center_axis',(-1.,0.,0.)) ;
#108746 = DIRECTION('ref_axis',(0.,0.,1.)) ;
#108747 = DIRECTION('center_axis',(0.,1.,-1.22464679914735E-16)) ;
#108748 = DIRECTION('ref_axis',(0.,-1.22464679914735E-16,-1.)) ;
#108749 = DIRECTION('center_axis',(1.,0.,0.)) ;
#108750 = DIRECTION('ref_axis',(0.,0.,1.)) ;
#108751 = DIRECTION('center_axis',(0.,1.,0.)) ;
#108752 = DIRECTION('ref_axis',(0.,0.,1.)) ;
#108753 = DIRECTION('center_axis',(-1.,0.,0.)) ;
#108754 = DIRECTION('ref_axis',(0.,0.,-1.)) ;
#108755 = DIRECTION('center_axis',(0.,0.707106781186532,0.707106781186563)) ;
#108756 = DIRECTION('ref_axis',(0.,-0.707106781186563,0.707106781186532)) ;
#108757 = DIRECTION('center_axis',(0.,0.,-1.)) ;
#108758 = DIRECTION('ref_axis',(-1.,0.,0.)) ;
#108759 = DIRECTION('center_axis',(2.16840434497101E-16,-1.,1.30104260698261E-16)) ;
#108760 = DIRECTION('ref_axis',(1.,2.16840434497101E-16,-1.09476442525376E-47)) ;
#108761 = DIRECTION('center_axis',(-2.25262403289994E-12,-0.707106781186411,
-0.707106781186684)) ;
#108762 = DIRECTION('ref_axis',(2.77642807980434E-11,0.707106781186684,-0.707106781186411)) ;
#108763 = DIRECTION('center_axis',(-5.42101086242752E-16,1.,0.)) ;
#108764 = DIRECTION('ref_axis',(1.,5.42101086242752E-16,0.)) ;
#108765 = DIRECTION('',(-2.16840434497101E-16,1.,-1.30104260698261E-16)) ;
#108766 = DIRECTION('center_axis',(0.,1.,0.)) ;
#108767 = DIRECTION('ref_axis',(0.,0.,1.)) ;
#108768 = DIRECTION('',(2.16840434497101E-16,-1.,1.30104260698261E-16)) ;
#108769 = DIRECTION('',(2.16840434497101E-16,-1.,1.30104260698261E-16)) ;
#108770 = DIRECTION('center_axis',(1.,0.,0.)) ;
#108771 = DIRECTION('ref_axis',(0.,0.,-1.)) ;
#108772 = DIRECTION('center_axis',(1.,0.,0.)) ;
#108773 = DIRECTION('ref_axis',(0.,0.,-1.)) ;
#108774 = DIRECTION('center_axis',(0.,-1.,-1.22464679914735E-16)) ;
#108775 = DIRECTION('ref_axis',(0.,-1.22464679914735E-16,1.)) ;
#108776 = DIRECTION('center_axis',(-1.,0.,0.)) ;
#108777 = DIRECTION('ref_axis',(0.,0.,-1.)) ;
#108778 = DIRECTION('center_axis',(-1.,0.,0.)) ;
#108779 = DIRECTION('ref_axis',(0.,0.,-1.)) ;
#108780 = DIRECTION('center_axis',(-1.,0.,0.)) ;
#108781 = DIRECTION('ref_axis',(0.,0.,1.)) ;
#108782 = DIRECTION('center_axis',(-1.,0.,0.)) ;
#108783 = DIRECTION('ref_axis',(0.,0.,1.)) ;
#108784 = DIRECTION('center_axis',(0.,1.,-1.22464679914735E-16)) ;
#108785 = DIRECTION('ref_axis',(0.,-1.22464679914735E-16,-1.)) ;
#108786 = DIRECTION('center_axis',(1.,0.,0.)) ;
#108787 = DIRECTION('ref_axis',(0.,0.,1.)) ;
#108788 = DIRECTION('center_axis',(0.,1.,0.)) ;
#108789 = DIRECTION('ref_axis',(0.,0.,1.)) ;
#108790 = DIRECTION('center_axis',(-1.,0.,0.)) ;
#108791 = DIRECTION('ref_axis',(0.,0.,-1.)) ;
#108792 = DIRECTION('center_axis',(0.,0.707106781186558,0.707106781186537)) ;
#108793 = DIRECTION('ref_axis',(0.,-0.707106781186537,0.707106781186558)) ;
#108794 = DIRECTION('center_axis',(0.,0.,-1.)) ;
#108795 = DIRECTION('ref_axis',(-1.,0.,0.)) ;
#108796 = DIRECTION('center_axis',(2.16840434497101E-16,-1.,1.30104260698261E-16)) ;
#108797 = DIRECTION('ref_axis',(1.,2.16840434497101E-16,-1.09476442525376E-47)) ;
#108798 = DIRECTION('center_axis',(-2.85488809725132E-13,-0.707106781186525,
-0.70710678118657)) ;
#108799 = DIRECTION('ref_axis',(7.82804041694617E-11,0.70710678118657,-0.707106781186525)) ;
#108800 = DIRECTION('center_axis',(-5.42101086242752E-16,1.,0.)) ;
#108801 = DIRECTION('ref_axis',(1.,5.42101086242752E-16,0.)) ;
#108802 = DIRECTION('',(-2.16840434497101E-16,1.,-1.30104260698261E-16)) ;
#108803 = DIRECTION('center_axis',(0.,1.,0.)) ;
#108804 = DIRECTION('ref_axis',(0.,0.,1.)) ;
#108805 = DIRECTION('',(2.16840434497101E-16,-1.,1.30104260698261E-16)) ;
#108806 = DIRECTION('',(2.16840434497101E-16,-1.,1.30104260698261E-16)) ;
#108807 = DIRECTION('center_axis',(1.,0.,0.)) ;
#108808 = DIRECTION('ref_axis',(0.,0.,-1.)) ;
#108809 = DIRECTION('center_axis',(1.,0.,0.)) ;
#108810 = DIRECTION('ref_axis',(0.,0.,-1.)) ;
#108811 = DIRECTION('center_axis',(0.,-1.,-1.22464679914735E-16)) ;
#108812 = DIRECTION('ref_axis',(0.,-1.22464679914735E-16,1.)) ;
#108813 = DIRECTION('center_axis',(-1.,0.,0.)) ;
#108814 = DIRECTION('ref_axis',(0.,0.,-1.)) ;
#108815 = DIRECTION('center_axis',(-1.,0.,0.)) ;
#108816 = DIRECTION('ref_axis',(0.,0.,-1.)) ;
#108817 = DIRECTION('center_axis',(-1.,0.,0.)) ;
#108818 = DIRECTION('ref_axis',(0.,0.,1.)) ;
#108819 = DIRECTION('center_axis',(-1.,0.,0.)) ;
#108820 = DIRECTION('ref_axis',(0.,0.,1.)) ;
#108821 = DIRECTION('center_axis',(0.,1.,-1.22464679914735E-16)) ;
#108822 = DIRECTION('ref_axis',(0.,-1.22464679914735E-16,-1.)) ;
#108823 = DIRECTION('center_axis',(1.,0.,0.)) ;
#108824 = DIRECTION('ref_axis',(0.,0.,1.)) ;
#108825 = DIRECTION('center_axis',(0.,1.,0.)) ;
#108826 = DIRECTION('ref_axis',(0.,0.,1.)) ;
#108827 = DIRECTION('center_axis',(-1.,0.,0.)) ;
#108828 = DIRECTION('ref_axis',(0.,0.,-1.)) ;
#108829 = DIRECTION('center_axis',(0.,0.707106781186558,0.707106781186537)) ;
#108830 = DIRECTION('ref_axis',(0.,-0.707106781186537,0.707106781186558)) ;
#108831 = DIRECTION('center_axis',(0.,0.,-1.)) ;
#108832 = DIRECTION('ref_axis',(-1.,0.,0.)) ;
#108833 = DIRECTION('center_axis',(2.16840434497101E-16,-1.,1.30104260698261E-16)) ;
#108834 = DIRECTION('ref_axis',(1.,2.16840434497101E-16,-1.09476442525376E-47)) ;
#108835 = DIRECTION('center_axis',(-4.61475062295438E-13,-0.707106781186512,
-0.707106781186583)) ;
#108836 = DIRECTION('ref_axis',(8.02352901261504E-11,0.707106781186583,-0.707106781186512)) ;
#108837 = DIRECTION('center_axis',(-5.42101086242752E-16,1.,0.)) ;
#108838 = DIRECTION('ref_axis',(1.,5.42101086242752E-16,0.)) ;
#108839 = DIRECTION('',(-2.16840434497101E-16,1.,-1.30104260698261E-16)) ;
#108840 = DIRECTION('center_axis',(0.,1.,0.)) ;
#108841 = DIRECTION('ref_axis',(0.,0.,1.)) ;
#108842 = DIRECTION('',(2.16840434497101E-16,-1.,1.30104260698261E-16)) ;
#108843 = DIRECTION('',(2.16840434497101E-16,-1.,1.30104260698261E-16)) ;
#108844 = DIRECTION('center_axis',(1.,0.,0.)) ;
#108845 = DIRECTION('ref_axis',(0.,0.,-1.)) ;
#108846 = DIRECTION('center_axis',(1.,0.,0.)) ;
#108847 = DIRECTION('ref_axis',(0.,0.,-1.)) ;
#108848 = DIRECTION('center_axis',(0.,-1.,-1.22464679914735E-16)) ;
#108849 = DIRECTION('ref_axis',(0.,-1.22464679914735E-16,1.)) ;
#108850 = DIRECTION('center_axis',(-1.,0.,0.)) ;
#108851 = DIRECTION('ref_axis',(0.,0.,-1.)) ;
#108852 = DIRECTION('center_axis',(-1.,0.,0.)) ;
#108853 = DIRECTION('ref_axis',(0.,0.,-1.)) ;
#108854 = DIRECTION('center_axis',(-1.,0.,0.)) ;
#108855 = DIRECTION('ref_axis',(0.,0.,1.)) ;
#108856 = DIRECTION('center_axis',(-1.,0.,0.)) ;
#108857 = DIRECTION('ref_axis',(0.,0.,1.)) ;
#108858 = DIRECTION('center_axis',(0.,1.,-1.22464679914735E-16)) ;
#108859 = DIRECTION('ref_axis',(0.,-1.22464679914735E-16,-1.)) ;
#108860 = DIRECTION('center_axis',(1.,0.,0.)) ;
#108861 = DIRECTION('ref_axis',(0.,0.,1.)) ;
#108862 = DIRECTION('center_axis',(0.,1.,0.)) ;
#108863 = DIRECTION('ref_axis',(0.,0.,1.)) ;
#108864 = DIRECTION('center_axis',(-1.,0.,0.)) ;
#108865 = DIRECTION('ref_axis',(0.,0.,-1.)) ;
#108866 = DIRECTION('center_axis',(0.,0.707106781186558,0.707106781186537)) ;
#108867 = DIRECTION('ref_axis',(0.,-0.707106781186537,0.707106781186558)) ;
#108868 = DIRECTION('center_axis',(0.,0.,-1.)) ;
#108869 = DIRECTION('ref_axis',(-1.,0.,0.)) ;
#108870 = DIRECTION('center_axis',(2.16840434497101E-16,-1.,1.30104260698261E-16)) ;
#108871 = DIRECTION('ref_axis',(1.,2.16840434497101E-16,-1.09476442525376E-47)) ;
#108872 = DIRECTION('center_axis',(-5.4946818858058E-13,-0.707106781186505,
-0.70710678118659)) ;
#108873 = DIRECTION('ref_axis',(1.03835885983909E-10,0.70710678118659,-0.707106781186505)) ;
#108874 = DIRECTION('center_axis',(-5.42101086242752E-16,1.,0.)) ;
#108875 = DIRECTION('ref_axis',(1.,5.42101086242752E-16,0.)) ;
#108876 = DIRECTION('',(-2.16840434497101E-16,1.,-1.30104260698261E-16)) ;
#108877 = DIRECTION('center_axis',(0.,1.,0.)) ;
#108878 = DIRECTION('ref_axis',(0.,0.,1.)) ;
#108879 = DIRECTION('',(2.16840434497101E-16,-1.,1.30104260698261E-16)) ;
#108880 = DIRECTION('',(2.16840434497101E-16,-1.,1.30104260698261E-16)) ;
#108881 = DIRECTION('center_axis',(1.,0.,0.)) ;
#108882 = DIRECTION('ref_axis',(0.,0.,-1.)) ;
#108883 = DIRECTION('center_axis',(1.,0.,0.)) ;
#108884 = DIRECTION('ref_axis',(0.,0.,-1.)) ;
#108885 = DIRECTION('center_axis',(0.,-1.,-1.22464679914735E-16)) ;
#108886 = DIRECTION('ref_axis',(0.,-1.22464679914735E-16,1.)) ;
#108887 = DIRECTION('center_axis',(-1.,0.,0.)) ;
#108888 = DIRECTION('ref_axis',(0.,0.,-1.)) ;
#108889 = DIRECTION('center_axis',(-1.,0.,0.)) ;
#108890 = DIRECTION('ref_axis',(0.,0.,-1.)) ;
#108891 = DIRECTION('center_axis',(-1.,0.,0.)) ;
#108892 = DIRECTION('ref_axis',(0.,0.,1.)) ;
#108893 = DIRECTION('center_axis',(-1.,0.,0.)) ;
#108894 = DIRECTION('ref_axis',(0.,0.,1.)) ;
#108895 = DIRECTION('center_axis',(0.,1.,-1.22464679914735E-16)) ;
#108896 = DIRECTION('ref_axis',(0.,-1.22464679914735E-16,-1.)) ;
#108897 = DIRECTION('center_axis',(1.,0.,0.)) ;
#108898 = DIRECTION('ref_axis',(0.,0.,1.)) ;
#108899 = DIRECTION('center_axis',(0.,1.,0.)) ;
#108900 = DIRECTION('ref_axis',(0.,0.,1.)) ;
#108901 = DIRECTION('center_axis',(-1.,0.,0.)) ;
#108902 = DIRECTION('ref_axis',(0.,0.,-1.)) ;
#108903 = DIRECTION('center_axis',(0.,0.707106781186558,0.707106781186537)) ;
#108904 = DIRECTION('ref_axis',(0.,-0.707106781186537,0.707106781186558)) ;
#108905 = DIRECTION('center_axis',(0.,0.,-1.)) ;
#108906 = DIRECTION('ref_axis',(-1.,0.,0.)) ;
#108907 = DIRECTION('center_axis',(2.16840434497101E-16,-1.,1.30104260698261E-16)) ;
#108908 = DIRECTION('ref_axis',(1.,2.16840434497101E-16,-1.09476442525376E-47)) ;
#108909 = DIRECTION('center_axis',(-4.61475062295467E-13,-0.707106781186512,
-0.707106781186583)) ;
#108910 = DIRECTION('ref_axis',(8.2666922773353E-11,0.707106781186583,-0.707106781186512)) ;
#108911 = DIRECTION('center_axis',(-5.42101086242752E-16,1.,0.)) ;
#108912 = DIRECTION('ref_axis',(1.,5.42101086242752E-16,0.)) ;
#108913 = DIRECTION('',(-2.16840434497101E-16,1.,-1.30104260698261E-16)) ;
#108914 = DIRECTION('center_axis',(0.,1.,0.)) ;
#108915 = DIRECTION('ref_axis',(0.,0.,1.)) ;
#108916 = DIRECTION('',(2.16840434497101E-16,-1.,1.30104260698261E-16)) ;
#108917 = DIRECTION('',(2.16840434497101E-16,-1.,1.30104260698261E-16)) ;
#108918 = DIRECTION('center_axis',(1.,0.,0.)) ;
#108919 = DIRECTION('ref_axis',(0.,0.,-1.)) ;
#108920 = DIRECTION('center_axis',(1.,0.,0.)) ;
#108921 = DIRECTION('ref_axis',(0.,0.,-1.)) ;
#108922 = DIRECTION('center_axis',(0.,-1.,-1.22464679914735E-16)) ;
#108923 = DIRECTION('ref_axis',(0.,-1.22464679914735E-16,1.)) ;
#108924 = DIRECTION('center_axis',(-1.,0.,0.)) ;
#108925 = DIRECTION('ref_axis',(0.,0.,-1.)) ;
#108926 = DIRECTION('center_axis',(-1.,0.,0.)) ;
#108927 = DIRECTION('ref_axis',(0.,0.,-1.)) ;
#108928 = DIRECTION('center_axis',(-1.,0.,0.)) ;
#108929 = DIRECTION('ref_axis',(0.,0.,1.)) ;
#108930 = DIRECTION('center_axis',(-1.,0.,0.)) ;
#108931 = DIRECTION('ref_axis',(0.,0.,1.)) ;
#108932 = DIRECTION('center_axis',(0.,1.,-1.22464679914735E-16)) ;
#108933 = DIRECTION('ref_axis',(0.,-1.22464679914735E-16,-1.)) ;
#108934 = DIRECTION('center_axis',(1.,0.,0.)) ;
#108935 = DIRECTION('ref_axis',(0.,0.,1.)) ;
#108936 = DIRECTION('center_axis',(0.,1.,0.)) ;
#108937 = DIRECTION('ref_axis',(0.,0.,1.)) ;
#108938 = DIRECTION('center_axis',(-1.,0.,0.)) ;
#108939 = DIRECTION('ref_axis',(0.,0.,-1.)) ;
#108940 = DIRECTION('center_axis',(0.,0.707106781186545,0.70710678118655)) ;
#108941 = DIRECTION('ref_axis',(0.,-0.70710678118655,0.707106781186545)) ;
#108942 = DIRECTION('center_axis',(0.,0.,-1.)) ;
#108943 = DIRECTION('ref_axis',(-1.,0.,0.)) ;
#108944 = DIRECTION('center_axis',(2.16840434497101E-16,-1.,1.30104260698261E-16)) ;
#108945 = DIRECTION('ref_axis',(1.,2.16840434497101E-16,-1.09476442525376E-47)) ;
#108946 = DIRECTION('center_axis',(-6.37461314865721E-13,-0.707106781186499,
-0.707106781186596)) ;
#108947 = DIRECTION('ref_axis',(-7.23831307879934E-11,0.707106781186596,-0.707106781186499)) ;
#108948 = DIRECTION('center_axis',(-5.42101086242752E-16,1.,0.)) ;
#108949 = DIRECTION('ref_axis',(1.,5.42101086242752E-16,0.)) ;
#108950 = DIRECTION('',(-2.16840434497101E-16,1.,-1.30104260698261E-16)) ;
#108951 = DIRECTION('center_axis',(0.,1.,0.)) ;
#108952 = DIRECTION('ref_axis',(0.,0.,1.)) ;
#108953 = DIRECTION('',(2.16840434497101E-16,-1.,1.30104260698261E-16)) ;
#108954 = DIRECTION('',(2.16840434497101E-16,-1.,1.30104260698261E-16)) ;
#108955 = DIRECTION('center_axis',(1.,0.,0.)) ;
#108956 = DIRECTION('ref_axis',(0.,0.,-1.)) ;
#108957 = DIRECTION('center_axis',(1.,0.,0.)) ;
#108958 = DIRECTION('ref_axis',(0.,0.,-1.)) ;
#108959 = DIRECTION('center_axis',(0.,-1.,-1.22464679914735E-16)) ;
#108960 = DIRECTION('ref_axis',(0.,-1.22464679914735E-16,1.)) ;
#108961 = DIRECTION('center_axis',(-1.,0.,0.)) ;
#108962 = DIRECTION('ref_axis',(0.,0.,-1.)) ;
#108963 = DIRECTION('center_axis',(-1.,0.,0.)) ;
#108964 = DIRECTION('ref_axis',(0.,0.,-1.)) ;
#108965 = DIRECTION('center_axis',(-1.,0.,0.)) ;
#108966 = DIRECTION('ref_axis',(0.,0.,1.)) ;
#108967 = DIRECTION('center_axis',(-1.,0.,0.)) ;
#108968 = DIRECTION('ref_axis',(0.,0.,1.)) ;
#108969 = DIRECTION('center_axis',(0.,1.,-1.22464679914735E-16)) ;
#108970 = DIRECTION('ref_axis',(0.,-1.22464679914735E-16,-1.)) ;
#108971 = DIRECTION('center_axis',(1.,0.,0.)) ;
#108972 = DIRECTION('ref_axis',(0.,0.,1.)) ;
#108973 = DIRECTION('center_axis',(0.,1.,0.)) ;
#108974 = DIRECTION('ref_axis',(0.,0.,1.)) ;
#108975 = DIRECTION('center_axis',(-1.,0.,0.)) ;
#108976 = DIRECTION('ref_axis',(0.,0.,-1.)) ;
#108977 = DIRECTION('center_axis',(0.,0.707106781186545,0.70710678118655)) ;
#108978 = DIRECTION('ref_axis',(0.,-0.70710678118655,0.707106781186545)) ;
#108979 = DIRECTION('center_axis',(0.,0.,-1.)) ;
#108980 = DIRECTION('ref_axis',(-1.,0.,0.)) ;
#108981 = DIRECTION('center_axis',(2.16840434497101E-16,-1.,1.30104260698261E-16)) ;
#108982 = DIRECTION('ref_axis',(1.,2.16840434497101E-16,-1.09476442525376E-47)) ;
#108983 = DIRECTION('center_axis',(-2.04144052981523E-12,-0.707106781186384,
-0.707106781186711)) ;
#108984 = DIRECTION('ref_axis',(3.79286005912221E-12,0.707106781186711,-0.707106781186384)) ;
#108985 = DIRECTION('center_axis',(-5.42101086242752E-16,1.,0.)) ;
#108986 = DIRECTION('ref_axis',(1.,5.42101086242752E-16,0.)) ;
#108987 = DIRECTION('',(-2.16840434497101E-16,1.,-1.30104260698261E-16)) ;
#108988 = DIRECTION('center_axis',(0.,1.,0.)) ;
#108989 = DIRECTION('ref_axis',(0.,0.,1.)) ;
#108990 = DIRECTION('',(2.16840434497101E-16,-1.,1.30104260698261E-16)) ;
#108991 = DIRECTION('',(2.16840434497101E-16,-1.,1.30104260698261E-16)) ;
#108992 = DIRECTION('center_axis',(1.,0.,0.)) ;
#108993 = DIRECTION('ref_axis',(0.,0.,-1.)) ;
#108994 = DIRECTION('center_axis',(1.,0.,0.)) ;
#108995 = DIRECTION('ref_axis',(0.,0.,-1.)) ;
#108996 = DIRECTION('center_axis',(0.,-1.,-1.22464679914735E-16)) ;
#108997 = DIRECTION('ref_axis',(0.,-1.22464679914735E-16,1.)) ;
#108998 = DIRECTION('center_axis',(-1.,0.,0.)) ;
#108999 = DIRECTION('ref_axis',(0.,0.,-1.)) ;
#109000 = DIRECTION('center_axis',(-1.,0.,0.)) ;
#109001 = DIRECTION('ref_axis',(0.,0.,-1.)) ;
#109002 = DIRECTION('center_axis',(-1.,0.,0.)) ;
#109003 = DIRECTION('ref_axis',(0.,0.,1.)) ;
#109004 = DIRECTION('center_axis',(-1.,0.,0.)) ;
#109005 = DIRECTION('ref_axis',(0.,0.,1.)) ;
#109006 = DIRECTION('center_axis',(0.,1.,-1.22464679914735E-16)) ;
#109007 = DIRECTION('ref_axis',(0.,-1.22464679914735E-16,-1.)) ;
#109008 = DIRECTION('center_axis',(1.,0.,0.)) ;
#109009 = DIRECTION('ref_axis',(0.,0.,1.)) ;
#109010 = DIRECTION('center_axis',(0.,1.,0.)) ;
#109011 = DIRECTION('ref_axis',(0.,0.,1.)) ;
#109012 = DIRECTION('center_axis',(-1.,0.,0.)) ;
#109013 = DIRECTION('ref_axis',(0.,0.,-1.)) ;
#109014 = DIRECTION('center_axis',(0.,0.707106781186545,0.70710678118655)) ;
#109015 = DIRECTION('ref_axis',(0.,-0.70710678118655,0.707106781186545)) ;
#109016 = DIRECTION('center_axis',(0.,0.,-1.)) ;
#109017 = DIRECTION('ref_axis',(-1.,0.,0.)) ;
#109018 = DIRECTION('center_axis',(2.16840434497101E-16,-1.,1.30104260698261E-16)) ;
#109019 = DIRECTION('ref_axis',(1.,2.16840434497101E-16,-1.09476442525376E-47)) ;
#109020 = DIRECTION('center_axis',(-1.65035996854789E-12,-0.707106781186426,
-0.707106781186669)) ;
#109021 = DIRECTION('ref_axis',(-9.42995735618098E-12,0.707106781186669,-0.707106781186426)) ;
#109022 = DIRECTION('center_axis',(-5.42101086242752E-16,1.,0.)) ;
#109023 = DIRECTION('ref_axis',(1.,5.42101086242752E-16,0.)) ;
#109024 = DIRECTION('',(-2.16840434497101E-16,1.,-1.30104260698261E-16)) ;
#109025 = DIRECTION('center_axis',(0.,1.,0.)) ;
#109026 = DIRECTION('ref_axis',(0.,0.,1.)) ;
#109027 = DIRECTION('',(2.16840434497101E-16,-1.,1.30104260698261E-16)) ;
#109028 = DIRECTION('',(2.16840434497101E-16,-1.,1.30104260698261E-16)) ;
#109029 = DIRECTION('center_axis',(1.,0.,0.)) ;
#109030 = DIRECTION('ref_axis',(0.,0.,-1.)) ;
#109031 = DIRECTION('center_axis',(1.,0.,0.)) ;
#109032 = DIRECTION('ref_axis',(0.,0.,-1.)) ;
#109033 = DIRECTION('center_axis',(0.,-1.,-1.22464679914735E-16)) ;
#109034 = DIRECTION('ref_axis',(0.,-1.22464679914735E-16,1.)) ;
#109035 = DIRECTION('center_axis',(-1.,0.,0.)) ;
#109036 = DIRECTION('ref_axis',(0.,0.,-1.)) ;
#109037 = DIRECTION('center_axis',(-1.,0.,0.)) ;
#109038 = DIRECTION('ref_axis',(0.,0.,-1.)) ;
#109039 = DIRECTION('center_axis',(1.,0.,0.)) ;
#109040 = DIRECTION('ref_axis',(0.,0.,-1.)) ;
#109041 = DIRECTION('center_axis',(-1.,0.,0.)) ;
#109042 = DIRECTION('ref_axis',(0.,0.,-1.)) ;
#109043 = DIRECTION('center_axis',(0.,0.,1.)) ;
#109044 = DIRECTION('ref_axis',(1.,0.,0.)) ;
#109045 = DIRECTION('center_axis',(1.,0.,0.)) ;
#109046 = DIRECTION('ref_axis',(0.,0.,-1.)) ;
#109047 = DIRECTION('center_axis',(0.,0.707106781186548,-0.707106781186548)) ;
#109048 = DIRECTION('ref_axis',(0.,0.707106781186548,0.707106781186548)) ;
#109049 = DIRECTION('center_axis',(1.,0.,0.)) ;
#109050 = DIRECTION('ref_axis',(0.,0.,-1.)) ;
#109051 = DIRECTION('center_axis',(-1.,0.,0.)) ;
#109052 = DIRECTION('ref_axis',(0.,0.,-1.)) ;
#109053 = DIRECTION('center_axis',(0.,0.,1.)) ;
#109054 = DIRECTION('ref_axis',(1.,0.,0.)) ;
#109055 = DIRECTION('center_axis',(1.,0.,0.)) ;
#109056 = DIRECTION('ref_axis',(0.,0.,-1.)) ;
#109057 = DIRECTION('center_axis',(0.,0.707106781186548,-0.707106781186548)) ;
#109058 = DIRECTION('ref_axis',(0.,0.707106781186548,0.707106781186548)) ;
#109059 = DIRECTION('center_axis',(1.,0.,0.)) ;
#109060 = DIRECTION('ref_axis',(0.,0.,-1.)) ;
#109061 = DIRECTION('center_axis',(-1.,0.,0.)) ;
#109062 = DIRECTION('ref_axis',(0.,0.,-1.)) ;
#109063 = DIRECTION('center_axis',(0.,0.,1.)) ;
#109064 = DIRECTION('ref_axis',(1.,0.,0.)) ;
#109065 = DIRECTION('center_axis',(1.,0.,0.)) ;
#109066 = DIRECTION('ref_axis',(0.,0.,-1.)) ;
#109067 = DIRECTION('center_axis',(0.,0.707106781186548,-0.707106781186548)) ;
#109068 = DIRECTION('ref_axis',(0.,0.707106781186548,0.707106781186548)) ;
#109069 = DIRECTION('center_axis',(1.,0.,0.)) ;
#109070 = DIRECTION('ref_axis',(0.,0.,-1.)) ;
#109071 = DIRECTION('center_axis',(-1.,0.,0.)) ;
#109072 = DIRECTION('ref_axis',(0.,0.,-1.)) ;
#109073 = DIRECTION('center_axis',(0.,0.,1.)) ;
#109074 = DIRECTION('ref_axis',(1.,0.,0.)) ;
#109075 = DIRECTION('center_axis',(1.,0.,0.)) ;
#109076 = DIRECTION('ref_axis',(0.,0.,-1.)) ;
#109077 = DIRECTION('center_axis',(0.,0.707106781186539,-0.707106781186556)) ;
#109078 = DIRECTION('ref_axis',(0.,0.707106781186556,0.707106781186539)) ;
#109079 = DIRECTION('center_axis',(1.,0.,0.)) ;
#109080 = DIRECTION('ref_axis',(0.,0.,-1.)) ;
#109081 = DIRECTION('center_axis',(-1.,0.,0.)) ;
#109082 = DIRECTION('ref_axis',(0.,0.,-1.)) ;
#109083 = DIRECTION('center_axis',(0.,0.,1.)) ;
#109084 = DIRECTION('ref_axis',(1.,0.,0.)) ;
#109085 = DIRECTION('center_axis',(1.,0.,0.)) ;
#109086 = DIRECTION('ref_axis',(0.,0.,-1.)) ;
#109087 = DIRECTION('center_axis',(0.,0.707106781186539,-0.707106781186556)) ;
#109088 = DIRECTION('ref_axis',(0.,0.707106781186556,0.707106781186539)) ;
#109089 = DIRECTION('center_axis',(1.,0.,0.)) ;
#109090 = DIRECTION('ref_axis',(0.,0.,-1.)) ;
#109091 = DIRECTION('center_axis',(-1.,0.,0.)) ;
#109092 = DIRECTION('ref_axis',(0.,0.,-1.)) ;
#109093 = DIRECTION('center_axis',(0.,0.,1.)) ;
#109094 = DIRECTION('ref_axis',(1.,0.,0.)) ;
#109095 = DIRECTION('center_axis',(1.,0.,0.)) ;
#109096 = DIRECTION('ref_axis',(0.,0.,-1.)) ;
#109097 = DIRECTION('center_axis',(0.,0.707106781186539,-0.707106781186556)) ;
#109098 = DIRECTION('ref_axis',(0.,0.707106781186556,0.707106781186539)) ;
#109099 = DIRECTION('center_axis',(1.,0.,0.)) ;
#109100 = DIRECTION('ref_axis',(0.,0.,-1.)) ;
#109101 = DIRECTION('center_axis',(-1.,0.,0.)) ;
#109102 = DIRECTION('ref_axis',(0.,0.,-1.)) ;
#109103 = DIRECTION('center_axis',(0.,0.,1.)) ;
#109104 = DIRECTION('ref_axis',(1.,0.,0.)) ;
#109105 = DIRECTION('center_axis',(1.,0.,0.)) ;
#109106 = DIRECTION('ref_axis',(0.,0.,-1.)) ;
#109107 = DIRECTION('center_axis',(0.,0.707106781186539,-0.707106781186556)) ;
#109108 = DIRECTION('ref_axis',(0.,0.707106781186556,0.707106781186539)) ;
#109109 = DIRECTION('center_axis',(1.,0.,0.)) ;
#109110 = DIRECTION('ref_axis',(0.,0.,-1.)) ;
#109111 = DIRECTION('center_axis',(-1.,0.,0.)) ;
#109112 = DIRECTION('ref_axis',(0.,0.,-1.)) ;
#109113 = DIRECTION('center_axis',(0.,0.,1.)) ;
#109114 = DIRECTION('ref_axis',(1.,0.,0.)) ;
#109115 = DIRECTION('center_axis',(1.,0.,0.)) ;
#109116 = DIRECTION('ref_axis',(0.,0.,-1.)) ;
#109117 = DIRECTION('center_axis',(-6.13317366673346E-15,0.707106781186539,
-0.707106781186556)) ;
#109118 = DIRECTION('ref_axis',(3.80912633391397E-29,0.707106781186556,0.707106781186539)) ;
#109119 = DIRECTION('center_axis',(1.,0.,0.)) ;
#109120 = DIRECTION('ref_axis',(0.,0.,-1.)) ;
#109121 = DIRECTION('center_axis',(-1.,0.,0.)) ;
#109122 = DIRECTION('ref_axis',(0.,0.,-1.)) ;
#109123 = DIRECTION('center_axis',(0.,0.,1.)) ;
#109124 = DIRECTION('ref_axis',(1.,0.,0.)) ;
#109125 = DIRECTION('center_axis',(1.,0.,0.)) ;
#109126 = DIRECTION('ref_axis',(0.,0.,-1.)) ;
#109127 = DIRECTION('center_axis',(-6.13317366673346E-15,0.707106781186539,
-0.707106781186556)) ;
#109128 = DIRECTION('ref_axis',(3.80912633391397E-29,0.707106781186556,0.707106781186539)) ;
#109129 = DIRECTION('center_axis',(-1.,0.,0.)) ;
#109130 = DIRECTION('ref_axis',(0.,0.,1.)) ;
#109131 = DIRECTION('center_axis',(-1.,0.,0.)) ;
#109132 = DIRECTION('ref_axis',(0.,0.,1.)) ;
#109133 = DIRECTION('center_axis',(0.,1.,-1.22464679914735E-16)) ;
#109134 = DIRECTION('ref_axis',(0.,-1.22464679914735E-16,-1.)) ;
#109135 = DIRECTION('center_axis',(1.,0.,0.)) ;
#109136 = DIRECTION('ref_axis',(0.,0.,1.)) ;
#109137 = DIRECTION('center_axis',(0.,1.,0.)) ;
#109138 = DIRECTION('ref_axis',(0.,0.,1.)) ;
#109139 = DIRECTION('center_axis',(-1.,0.,0.)) ;
#109140 = DIRECTION('ref_axis',(0.,0.,-1.)) ;
#109141 = DIRECTION('center_axis',(0.,0.70710678118655,0.707106781186545)) ;
#109142 = DIRECTION('ref_axis',(0.,-0.707106781186545,0.70710678118655)) ;
#109143 = DIRECTION('center_axis',(0.,0.,-1.)) ;
#109144 = DIRECTION('ref_axis',(-1.,0.,0.)) ;
#109145 = DIRECTION('center_axis',(2.16840434497101E-16,-1.,1.30104260698261E-16)) ;
#109146 = DIRECTION('ref_axis',(1.,2.16840434497101E-16,-1.09476442525376E-47)) ;
#109147 = DIRECTION('center_axis',(6.64836954154425E-14,-0.707106781186552,
-0.707106781186543)) ;
#109148 = DIRECTION('ref_axis',(-1.70648371771735E-11,0.707106781186543,-0.707106781186552)) ;
#109149 = DIRECTION('center_axis',(-5.42101086242752E-16,1.,0.)) ;
#109150 = DIRECTION('ref_axis',(1.,5.42101086242752E-16,0.)) ;
#109151 = DIRECTION('',(-2.16840434497101E-16,1.,-1.30104260698261E-16)) ;
#109152 = DIRECTION('center_axis',(0.,1.,0.)) ;
#109153 = DIRECTION('ref_axis',(0.,0.,1.)) ;
#109154 = DIRECTION('',(2.16840434497101E-16,-1.,1.30104260698261E-16)) ;
#109155 = DIRECTION('',(2.16840434497101E-16,-1.,1.30104260698261E-16)) ;
#109156 = DIRECTION('center_axis',(-1.,0.,0.)) ;
#109157 = DIRECTION('ref_axis',(0.,0.,1.)) ;
#109158 = DIRECTION('',(1.,0.,0.)) ;
#109159 = DIRECTION('center_axis',(-1.,0.,0.)) ;
#109160 = DIRECTION('ref_axis',(0.,0.,1.)) ;
#109161 = DIRECTION('',(1.,0.,0.)) ;
#109162 = DIRECTION('center_axis',(-1.,0.,0.)) ;
#109163 = DIRECTION('ref_axis',(0.,0.,1.)) ;
#109164 = DIRECTION('',(1.,0.,0.)) ;
#109165 = DIRECTION('center_axis',(-1.,0.,0.)) ;
#109166 = DIRECTION('ref_axis',(0.,0.,1.)) ;
#109167 = DIRECTION('',(1.,0.,0.)) ;
#109168 = DIRECTION('center_axis',(-1.,0.,0.)) ;
#109169 = DIRECTION('ref_axis',(0.,0.,1.)) ;
#109170 = DIRECTION('',(1.,0.,0.)) ;
#109171 = DIRECTION('center_axis',(-1.,0.,0.)) ;
#109172 = DIRECTION('ref_axis',(0.,0.,1.)) ;
#109173 = DIRECTION('',(1.,0.,0.)) ;
#109174 = DIRECTION('center_axis',(-1.,0.,0.)) ;
#109175 = DIRECTION('ref_axis',(0.,0.,1.)) ;
#109176 = DIRECTION('',(1.,0.,0.)) ;
#109177 = DIRECTION('center_axis',(-1.,0.,0.)) ;
#109178 = DIRECTION('ref_axis',(0.,0.,1.)) ;
#109179 = DIRECTION('',(1.,0.,0.)) ;
#109180 = DIRECTION('center_axis',(-1.,0.,0.)) ;
#109181 = DIRECTION('ref_axis',(0.,0.,1.)) ;
#109182 = DIRECTION('',(1.,0.,0.)) ;
#109183 = DIRECTION('center_axis',(1.,0.,0.)) ;
#109184 = DIRECTION('ref_axis',(0.,0.,-1.)) ;
#109185 = DIRECTION('center_axis',(-1.,0.,0.)) ;
#109186 = DIRECTION('ref_axis',(0.,0.,-1.)) ;
#109187 = DIRECTION('',(1.,0.,0.)) ;
#109188 = DIRECTION('',(1.,0.,0.)) ;
#109189 = DIRECTION('center_axis',(1.,0.,0.)) ;
#109190 = DIRECTION('ref_axis',(0.,0.,-1.)) ;
#109191 = DIRECTION('center_axis',(-1.,0.,0.)) ;
#109192 = DIRECTION('ref_axis',(0.,0.,-1.)) ;
#109193 = DIRECTION('',(1.,0.,0.)) ;
#109194 = DIRECTION('',(1.,0.,0.)) ;
#109195 = DIRECTION('center_axis',(1.,0.,0.)) ;
#109196 = DIRECTION('ref_axis',(0.,0.,-1.)) ;
#109197 = DIRECTION('center_axis',(-1.,0.,0.)) ;
#109198 = DIRECTION('ref_axis',(0.,0.,-1.)) ;
#109199 = DIRECTION('',(1.,0.,0.)) ;
#109200 = DIRECTION('',(1.,0.,0.)) ;
#109201 = DIRECTION('center_axis',(1.,0.,0.)) ;
#109202 = DIRECTION('ref_axis',(0.,0.,-1.)) ;
#109203 = DIRECTION('center_axis',(-1.,0.,0.)) ;
#109204 = DIRECTION('ref_axis',(0.,0.,-1.)) ;
#109205 = DIRECTION('',(1.,0.,0.)) ;
#109206 = DIRECTION('',(1.,0.,0.)) ;
#109207 = DIRECTION('center_axis',(1.,0.,0.)) ;
#109208 = DIRECTION('ref_axis',(0.,0.,-1.)) ;
#109209 = DIRECTION('center_axis',(-1.,0.,0.)) ;
#109210 = DIRECTION('ref_axis',(0.,0.,-1.)) ;
#109211 = DIRECTION('',(1.,0.,0.)) ;
#109212 = DIRECTION('',(1.,0.,0.)) ;
#109213 = DIRECTION('center_axis',(1.,0.,0.)) ;
#109214 = DIRECTION('ref_axis',(0.,0.,-1.)) ;
#109215 = DIRECTION('center_axis',(-1.,0.,0.)) ;
#109216 = DIRECTION('ref_axis',(0.,0.,-1.)) ;
#109217 = DIRECTION('',(1.,0.,0.)) ;
#109218 = DIRECTION('',(1.,0.,0.)) ;
#109219 = DIRECTION('center_axis',(1.,0.,0.)) ;
#109220 = DIRECTION('ref_axis',(0.,0.,-1.)) ;
#109221 = DIRECTION('center_axis',(-1.,0.,0.)) ;
#109222 = DIRECTION('ref_axis',(0.,0.,-1.)) ;
#109223 = DIRECTION('',(1.,0.,0.)) ;
#109224 = DIRECTION('',(1.,0.,0.)) ;
#109225 = DIRECTION('center_axis',(1.,0.,0.)) ;
#109226 = DIRECTION('ref_axis',(0.,0.,-1.)) ;
#109227 = DIRECTION('center_axis',(-1.,0.,0.)) ;
#109228 = DIRECTION('ref_axis',(0.,0.,-1.)) ;
#109229 = DIRECTION('',(1.,0.,0.)) ;
#109230 = DIRECTION('',(1.,0.,0.)) ;
#109231 = DIRECTION('center_axis',(1.,0.,0.)) ;
#109232 = DIRECTION('ref_axis',(0.,0.,-1.)) ;
#109233 = DIRECTION('center_axis',(-1.,0.,0.)) ;
#109234 = DIRECTION('ref_axis',(0.,0.,-1.)) ;
#109235 = DIRECTION('',(1.,0.,0.)) ;
#109236 = DIRECTION('',(1.,0.,0.)) ;
#109237 = DIRECTION('center_axis',(1.,0.,0.)) ;
#109238 = DIRECTION('ref_axis',(0.,0.,-1.)) ;
#109239 = DIRECTION('center_axis',(1.,0.,0.)) ;
#109240 = DIRECTION('ref_axis',(0.,0.,-1.)) ;
#109241 = DIRECTION('center_axis',(0.,-1.,-1.22464679914735E-16)) ;
#109242 = DIRECTION('ref_axis',(0.,-1.22464679914735E-16,1.)) ;
#109243 = DIRECTION('center_axis',(-1.,0.,0.)) ;
#109244 = DIRECTION('ref_axis',(0.,0.,-1.)) ;
#109245 = DIRECTION('center_axis',(-1.,0.,0.)) ;
#109246 = DIRECTION('ref_axis',(0.,0.,-1.)) ;
#109247 = DIRECTION('center_axis',(1.,0.,0.)) ;
#109248 = DIRECTION('ref_axis',(0.,0.,-1.)) ;
#109249 = DIRECTION('center_axis',(-1.,0.,0.)) ;
#109250 = DIRECTION('ref_axis',(0.,0.,-1.)) ;
#109251 = DIRECTION('center_axis',(0.,0.,1.)) ;
#109252 = DIRECTION('ref_axis',(1.,0.,0.)) ;
#109253 = DIRECTION('center_axis',(1.,0.,0.)) ;
#109254 = DIRECTION('ref_axis',(0.,0.,-1.)) ;
#109255 = DIRECTION('center_axis',(0.,0.707106781186548,-0.707106781186548)) ;
#109256 = DIRECTION('ref_axis',(0.,0.707106781186548,0.707106781186548)) ;
#109257 = DIRECTION('center_axis',(-1.,0.,0.)) ;
#109258 = DIRECTION('ref_axis',(0.,0.,1.)) ;
#109259 = DIRECTION('center_axis',(-1.,0.,0.)) ;
#109260 = DIRECTION('ref_axis',(0.,0.,1.)) ;
#109261 = DIRECTION('center_axis',(0.,1.,-1.22464679914735E-16)) ;
#109262 = DIRECTION('ref_axis',(0.,-1.22464679914735E-16,-1.)) ;
#109263 = DIRECTION('center_axis',(1.,0.,0.)) ;
#109264 = DIRECTION('ref_axis',(0.,0.,1.)) ;
#109265 = DIRECTION('center_axis',(0.,1.,0.)) ;
#109266 = DIRECTION('ref_axis',(0.,0.,1.)) ;
#109267 = DIRECTION('center_axis',(-1.,0.,0.)) ;
#109268 = DIRECTION('ref_axis',(0.,0.,-1.)) ;
#109269 = DIRECTION('center_axis',(0.,0.70710678118655,0.707106781186545)) ;
#109270 = DIRECTION('ref_axis',(0.,-0.707106781186545,0.70710678118655)) ;
#109271 = DIRECTION('center_axis',(0.,0.,-1.)) ;
#109272 = DIRECTION('ref_axis',(-1.,0.,0.)) ;
#109273 = DIRECTION('center_axis',(2.16840434497101E-16,-1.,1.30104260698261E-16)) ;
#109274 = DIRECTION('ref_axis',(1.,2.16840434497101E-16,-1.09476442525376E-47)) ;
#109275 = DIRECTION('center_axis',(-1.95540280633655E-15,-0.707106781186549,
-0.707106781186546)) ;
#109276 = DIRECTION('ref_axis',(-2.18299406319968E-11,0.707106781186546,-0.707106781186549)) ;
#109277 = DIRECTION('center_axis',(-5.42101086242752E-16,1.,0.)) ;
#109278 = DIRECTION('ref_axis',(1.,5.42101086242752E-16,0.)) ;
#109279 = DIRECTION('',(-2.16840434497101E-16,1.,-1.30104260698261E-16)) ;
#109280 = DIRECTION('center_axis',(0.,1.,0.)) ;
#109281 = DIRECTION('ref_axis',(0.,0.,1.)) ;
#109282 = DIRECTION('',(2.16840434497101E-16,-1.,1.30104260698261E-16)) ;
#109283 = DIRECTION('',(2.16840434497101E-16,-1.,1.30104260698261E-16)) ;
#109284 = DIRECTION('center_axis',(-1.,0.,0.)) ;
#109285 = DIRECTION('ref_axis',(0.,0.,1.)) ;
#109286 = DIRECTION('',(1.,0.,0.)) ;
#109287 = DIRECTION('center_axis',(1.,0.,0.)) ;
#109288 = DIRECTION('ref_axis',(0.,0.,-1.)) ;
#109289 = DIRECTION('center_axis',(-1.,0.,0.)) ;
#109290 = DIRECTION('ref_axis',(0.,0.,-1.)) ;
#109291 = DIRECTION('',(1.,0.,0.)) ;
#109292 = DIRECTION('',(1.,0.,0.)) ;
#109293 = DIRECTION('center_axis',(-1.,-2.16840434497101E-16,0.)) ;
#109294 = DIRECTION('ref_axis',(2.16840434497101E-16,-1.,0.)) ;
#109295 = DIRECTION('',(-2.16840434497101E-16,1.,1.30104260698261E-16)) ;
#109296 = DIRECTION('center_axis',(1.,2.16840434497101E-16,0.)) ;
#109297 = DIRECTION('ref_axis',(2.16840434497101E-16,-1.,0.)) ;
#109298 = DIRECTION('',(0.,0.,-1.)) ;
#109299 = DIRECTION('center_axis',(1.,2.16840434497101E-16,0.)) ;
#109300 = DIRECTION('ref_axis',(2.16840434497101E-16,-1.,0.)) ;
#109301 = DIRECTION('center_axis',(-1.,-2.16840434497101E-16,0.)) ;
#109302 = DIRECTION('ref_axis',(2.16840434497101E-16,-1.,0.)) ;
#109303 = DIRECTION('',(0.,0.,-1.)) ;
#109304 = DIRECTION('',(2.16840434497101E-16,-1.,5.10212787052002E-17)) ;
#109305 = DIRECTION('',(0.,0.,1.)) ;
#109306 = DIRECTION('',(-2.16840434497101E-16,1.,-1.020425574104E-16)) ;
#109307 = DIRECTION('',(0.,0.,-1.)) ;
#109308 = DIRECTION('center_axis',(-1.,-2.16840434497101E-16,0.)) ;
#109309 = DIRECTION('ref_axis',(2.16840434497101E-16,-1.,0.)) ;
#109310 = DIRECTION('center_axis',(-1.,-2.16840434497101E-16,0.)) ;
#109311 = DIRECTION('ref_axis',(2.16840434497101E-16,-1.,0.)) ;
#109312 = DIRECTION('',(-2.16840434497101E-16,1.,1.30104260698261E-16)) ;
#109313 = DIRECTION('center_axis',(1.,2.16840434497101E-16,0.)) ;
#109314 = DIRECTION('ref_axis',(2.16840434497101E-16,-1.,0.)) ;
#109315 = DIRECTION('',(0.,0.,-1.)) ;
#109316 = DIRECTION('center_axis',(1.,2.16840434497101E-16,0.)) ;
#109317 = DIRECTION('ref_axis',(2.16840434497101E-16,-1.,0.)) ;
#109318 = DIRECTION('center_axis',(-1.,-2.16840434497101E-16,0.)) ;
#109319 = DIRECTION('ref_axis',(2.16840434497101E-16,-1.,0.)) ;
#109320 = DIRECTION('',(0.,0.,-1.)) ;
#109321 = DIRECTION('',(2.16840434497101E-16,-1.,5.10212787052002E-17)) ;
#109322 = DIRECTION('',(0.,0.,1.)) ;
#109323 = DIRECTION('',(-2.16840434497101E-16,1.,-1.020425574104E-16)) ;
#109324 = DIRECTION('',(0.,0.,-1.)) ;
#109325 = DIRECTION('center_axis',(-1.,-2.16840434497101E-16,0.)) ;
#109326 = DIRECTION('ref_axis',(2.16840434497101E-16,-1.,0.)) ;
#109327 = DIRECTION('center_axis',(-1.,-2.16840434497101E-16,0.)) ;
#109328 = DIRECTION('ref_axis',(2.16840434497101E-16,-1.,0.)) ;
#109329 = DIRECTION('',(-2.16840434497101E-16,1.,1.30104260698261E-16)) ;
#109330 = DIRECTION('center_axis',(1.,2.16840434497101E-16,0.)) ;
#109331 = DIRECTION('ref_axis',(2.16840434497101E-16,-1.,0.)) ;
#109332 = DIRECTION('',(0.,0.,-1.)) ;
#109333 = DIRECTION('center_axis',(1.,2.16840434497101E-16,0.)) ;
#109334 = DIRECTION('ref_axis',(2.16840434497101E-16,-1.,0.)) ;
#109335 = DIRECTION('center_axis',(-1.,-2.16840434497101E-16,0.)) ;
#109336 = DIRECTION('ref_axis',(2.16840434497101E-16,-1.,0.)) ;
#109337 = DIRECTION('',(0.,0.,-1.)) ;
#109338 = DIRECTION('',(2.16840434497101E-16,-1.,5.10212787052002E-17)) ;
#109339 = DIRECTION('',(0.,0.,1.)) ;
#109340 = DIRECTION('',(-2.16840434497101E-16,1.,-1.020425574104E-16)) ;
#109341 = DIRECTION('',(0.,0.,-1.)) ;
#109342 = DIRECTION('center_axis',(-1.,-2.16840434497101E-16,0.)) ;
#109343 = DIRECTION('ref_axis',(2.16840434497101E-16,-1.,0.)) ;
#109344 = DIRECTION('center_axis',(-1.,-2.16840434497101E-16,0.)) ;
#109345 = DIRECTION('ref_axis',(2.16840434497101E-16,-1.,0.)) ;
#109346 = DIRECTION('',(-2.16840434497101E-16,1.,1.30104260698261E-16)) ;
#109347 = DIRECTION('center_axis',(1.,2.16840434497101E-16,0.)) ;
#109348 = DIRECTION('ref_axis',(2.16840434497101E-16,-1.,0.)) ;
#109349 = DIRECTION('',(0.,0.,-1.)) ;
#109350 = DIRECTION('center_axis',(1.,2.16840434497101E-16,0.)) ;
#109351 = DIRECTION('ref_axis',(2.16840434497101E-16,-1.,0.)) ;
#109352 = DIRECTION('center_axis',(-1.,-2.16840434497101E-16,0.)) ;
#109353 = DIRECTION('ref_axis',(2.16840434497101E-16,-1.,0.)) ;
#109354 = DIRECTION('',(0.,0.,-1.)) ;
#109355 = DIRECTION('',(2.16840434497101E-16,-1.,5.10212787052002E-17)) ;
#109356 = DIRECTION('',(0.,0.,1.)) ;
#109357 = DIRECTION('',(-2.16840434497101E-16,1.,-1.020425574104E-16)) ;
#109358 = DIRECTION('',(0.,0.,-1.)) ;
#109359 = DIRECTION('center_axis',(-1.,-2.16840434497101E-16,0.)) ;
#109360 = DIRECTION('ref_axis',(2.16840434497101E-16,-1.,0.)) ;
#109361 = DIRECTION('center_axis',(-1.,-2.16840434497101E-16,0.)) ;
#109362 = DIRECTION('ref_axis',(2.16840434497101E-16,-1.,0.)) ;
#109363 = DIRECTION('',(-2.16840434497101E-16,1.,1.30104260698261E-16)) ;
#109364 = DIRECTION('center_axis',(1.,2.16840434497101E-16,0.)) ;
#109365 = DIRECTION('ref_axis',(2.16840434497101E-16,-1.,0.)) ;
#109366 = DIRECTION('',(0.,0.,-1.)) ;
#109367 = DIRECTION('center_axis',(1.,2.16840434497101E-16,0.)) ;
#109368 = DIRECTION('ref_axis',(2.16840434497101E-16,-1.,0.)) ;
#109369 = DIRECTION('center_axis',(-1.,-2.16840434497101E-16,0.)) ;
#109370 = DIRECTION('ref_axis',(2.16840434497101E-16,-1.,0.)) ;
#109371 = DIRECTION('',(0.,0.,-1.)) ;
#109372 = DIRECTION('',(2.16840434497101E-16,-1.,5.10212787052002E-17)) ;
#109373 = DIRECTION('',(0.,0.,1.)) ;
#109374 = DIRECTION('',(-2.16840434497101E-16,1.,-1.020425574104E-16)) ;
#109375 = DIRECTION('',(0.,0.,-1.)) ;
#109376 = DIRECTION('center_axis',(-1.,-2.16840434497101E-16,0.)) ;
#109377 = DIRECTION('ref_axis',(2.16840434497101E-16,-1.,0.)) ;
#109378 = DIRECTION('center_axis',(-1.,-2.16840434497101E-16,0.)) ;
#109379 = DIRECTION('ref_axis',(2.16840434497101E-16,-1.,0.)) ;
#109380 = DIRECTION('',(-2.16840434497101E-16,1.,1.30104260698261E-16)) ;
#109381 = DIRECTION('center_axis',(1.,2.16840434497101E-16,0.)) ;
#109382 = DIRECTION('ref_axis',(2.16840434497101E-16,-1.,0.)) ;
#109383 = DIRECTION('',(0.,0.,-1.)) ;
#109384 = DIRECTION('center_axis',(1.,2.16840434497101E-16,0.)) ;
#109385 = DIRECTION('ref_axis',(2.16840434497101E-16,-1.,0.)) ;
#109386 = DIRECTION('center_axis',(-1.,-2.16840434497101E-16,0.)) ;
#109387 = DIRECTION('ref_axis',(2.16840434497101E-16,-1.,0.)) ;
#109388 = DIRECTION('',(0.,0.,-1.)) ;
#109389 = DIRECTION('',(2.16840434497101E-16,-1.,5.10212787052002E-17)) ;
#109390 = DIRECTION('',(0.,0.,1.)) ;
#109391 = DIRECTION('',(-2.16840434497101E-16,1.,-1.020425574104E-16)) ;
#109392 = DIRECTION('',(0.,0.,-1.)) ;
#109393 = DIRECTION('center_axis',(-1.,-2.16840434497101E-16,0.)) ;
#109394 = DIRECTION('ref_axis',(2.16840434497101E-16,-1.,0.)) ;
#109395 = DIRECTION('center_axis',(-1.,-2.16840434497101E-16,0.)) ;
#109396 = DIRECTION('ref_axis',(2.16840434497101E-16,-1.,0.)) ;
#109397 = DIRECTION('',(-2.16840434497101E-16,1.,1.30104260698261E-16)) ;
#109398 = DIRECTION('center_axis',(1.,2.16840434497101E-16,0.)) ;
#109399 = DIRECTION('ref_axis',(2.16840434497101E-16,-1.,0.)) ;
#109400 = DIRECTION('',(0.,0.,-1.)) ;
#109401 = DIRECTION('center_axis',(1.,2.16840434497101E-16,0.)) ;
#109402 = DIRECTION('ref_axis',(2.16840434497101E-16,-1.,0.)) ;
#109403 = DIRECTION('center_axis',(-1.,-2.16840434497101E-16,0.)) ;
#109404 = DIRECTION('ref_axis',(2.16840434497101E-16,-1.,0.)) ;
#109405 = DIRECTION('',(0.,0.,-1.)) ;
#109406 = DIRECTION('',(2.16840434497101E-16,-1.,5.10212787052002E-17)) ;
#109407 = DIRECTION('',(0.,0.,1.)) ;
#109408 = DIRECTION('',(-2.16840434497101E-16,1.,-1.020425574104E-16)) ;
#109409 = DIRECTION('',(0.,0.,-1.)) ;
#109410 = DIRECTION('center_axis',(-1.,-2.16840434497101E-16,0.)) ;
#109411 = DIRECTION('ref_axis',(2.16840434497101E-16,-1.,0.)) ;
#109412 = DIRECTION('center_axis',(-1.,-2.16840434497101E-16,0.)) ;
#109413 = DIRECTION('ref_axis',(2.16840434497101E-16,-1.,0.)) ;
#109414 = DIRECTION('',(-2.16840434497101E-16,1.,1.30104260698261E-16)) ;
#109415 = DIRECTION('center_axis',(1.,2.16840434497101E-16,0.)) ;
#109416 = DIRECTION('ref_axis',(2.16840434497101E-16,-1.,0.)) ;
#109417 = DIRECTION('',(0.,0.,-1.)) ;
#109418 = DIRECTION('center_axis',(1.,2.16840434497101E-16,0.)) ;
#109419 = DIRECTION('ref_axis',(2.16840434497101E-16,-1.,0.)) ;
#109420 = DIRECTION('center_axis',(-1.,-2.16840434497101E-16,0.)) ;
#109421 = DIRECTION('ref_axis',(2.16840434497101E-16,-1.,0.)) ;
#109422 = DIRECTION('',(0.,0.,-1.)) ;
#109423 = DIRECTION('',(2.16840434497101E-16,-1.,5.10212787052002E-17)) ;
#109424 = DIRECTION('',(0.,0.,1.)) ;
#109425 = DIRECTION('',(-2.16840434497101E-16,1.,-1.020425574104E-16)) ;
#109426 = DIRECTION('',(0.,0.,-1.)) ;
#109427 = DIRECTION('center_axis',(-1.,-2.16840434497101E-16,0.)) ;
#109428 = DIRECTION('ref_axis',(2.16840434497101E-16,-1.,0.)) ;
#109429 = DIRECTION('center_axis',(-1.,-2.16840434497101E-16,0.)) ;
#109430 = DIRECTION('ref_axis',(2.16840434497101E-16,-1.,0.)) ;
#109431 = DIRECTION('',(-2.16840434497101E-16,1.,1.30104260698261E-16)) ;
#109432 = DIRECTION('center_axis',(1.,2.16840434497101E-16,0.)) ;
#109433 = DIRECTION('ref_axis',(2.16840434497101E-16,-1.,0.)) ;
#109434 = DIRECTION('',(0.,0.,-1.)) ;
#109435 = DIRECTION('center_axis',(1.,2.16840434497101E-16,0.)) ;
#109436 = DIRECTION('ref_axis',(2.16840434497101E-16,-1.,0.)) ;
#109437 = DIRECTION('center_axis',(-1.,-2.16840434497101E-16,0.)) ;
#109438 = DIRECTION('ref_axis',(2.16840434497101E-16,-1.,0.)) ;
#109439 = DIRECTION('',(0.,0.,-1.)) ;
#109440 = DIRECTION('',(2.16840434497101E-16,-1.,5.10212787052002E-17)) ;
#109441 = DIRECTION('',(0.,0.,1.)) ;
#109442 = DIRECTION('',(-2.16840434497101E-16,1.,-1.020425574104E-16)) ;
#109443 = DIRECTION('',(0.,0.,-1.)) ;
#109444 = DIRECTION('center_axis',(-1.,-2.16840434497101E-16,0.)) ;
#109445 = DIRECTION('ref_axis',(2.16840434497101E-16,-1.,0.)) ;
#109446 = DIRECTION('center_axis',(6.27714964143733E-33,-5.10212787052002E-17,
-1.)) ;
#109447 = DIRECTION('ref_axis',(0.,1.,-5.10212787052002E-17)) ;
#109448 = DIRECTION('center_axis',(-6.27714964143733E-33,5.10212787052002E-17,
1.)) ;
#109449 = DIRECTION('ref_axis',(3.20268201330022E-49,1.,-5.10212787052002E-17)) ;
#109450 = DIRECTION('',(1.2303003375722E-16,-1.,5.10212787052002E-17)) ;
#109451 = DIRECTION('',(1.,0.,6.27714964143733E-33)) ;
#109452 = DIRECTION('',(-2.16840434497101E-16,1.,-5.10212787052002E-17)) ;
#109453 = DIRECTION('',(-1.,-1.53063836115601E-16,1.53236300070382E-33)) ;
#109454 = DIRECTION('center_axis',(-1.25542992828747E-32,1.020425574104E-16,
1.)) ;
#109455 = DIRECTION('ref_axis',(0.,-1.,1.020425574104E-16)) ;
#109456 = DIRECTION('center_axis',(1.25542992828747E-32,-1.020425574104E-16,
-1.)) ;
#109457 = DIRECTION('ref_axis',(-1.28107280532009E-48,-1.,1.020425574104E-16)) ;
#109458 = DIRECTION('',(1.,1.53063836115601E-16,-3.06472600140763E-33)) ;
#109459 = DIRECTION('',(2.16840434497101E-16,-1.,1.020425574104E-16)) ;
#109460 = DIRECTION('',(-1.,0.,-1.25542992828747E-32)) ;
#109461 = DIRECTION('',(-1.2303003375722E-16,1.,-1.020425574104E-16)) ;
#109462 = DIRECTION('center_axis',(6.27714964143733E-33,-5.10212787052002E-17,
-1.)) ;
#109463 = DIRECTION('ref_axis',(0.,1.,-5.10212787052002E-17)) ;
#109464 = DIRECTION('center_axis',(-6.27714964143733E-33,5.10212787052002E-17,
1.)) ;
#109465 = DIRECTION('ref_axis',(3.20268201330022E-49,1.,-5.10212787052002E-17)) ;
#109466 = DIRECTION('',(1.2303003375722E-16,-1.,5.10212787052002E-17)) ;
#109467 = DIRECTION('',(1.,0.,6.27714964143733E-33)) ;
#109468 = DIRECTION('',(-2.16840434497101E-16,1.,-5.10212787052002E-17)) ;
#109469 = DIRECTION('',(-1.,-1.53063836115601E-16,1.53236300070382E-33)) ;
#109470 = DIRECTION('center_axis',(-1.25542992828747E-32,1.020425574104E-16,
1.)) ;
#109471 = DIRECTION('ref_axis',(0.,-1.,1.020425574104E-16)) ;
#109472 = DIRECTION('center_axis',(1.25542992828747E-32,-1.020425574104E-16,
-1.)) ;
#109473 = DIRECTION('ref_axis',(-1.28107280532009E-48,-1.,1.020425574104E-16)) ;
#109474 = DIRECTION('',(1.,1.53063836115601E-16,-3.06472600140763E-33)) ;
#109475 = DIRECTION('',(2.16840434497101E-16,-1.,1.020425574104E-16)) ;
#109476 = DIRECTION('',(-1.,0.,-1.25542992828747E-32)) ;
#109477 = DIRECTION('',(-1.2303003375722E-16,1.,-1.020425574104E-16)) ;
#109478 = DIRECTION('center_axis',(6.27714964143733E-33,-5.10212787052002E-17,
-1.)) ;
#109479 = DIRECTION('ref_axis',(0.,1.,-5.10212787052002E-17)) ;
#109480 = DIRECTION('center_axis',(-6.27714964143733E-33,5.10212787052002E-17,
1.)) ;
#109481 = DIRECTION('ref_axis',(3.20268201330022E-49,1.,-5.10212787052002E-17)) ;
#109482 = DIRECTION('',(1.2303003375722E-16,-1.,5.10212787052002E-17)) ;
#109483 = DIRECTION('',(1.,0.,6.27714964143733E-33)) ;
#109484 = DIRECTION('',(-2.16840434497101E-16,1.,-5.10212787052002E-17)) ;
#109485 = DIRECTION('',(-1.,-1.53063836115601E-16,1.53236300070382E-33)) ;
#109486 = DIRECTION('center_axis',(-1.25542992828747E-32,1.020425574104E-16,
1.)) ;
#109487 = DIRECTION('ref_axis',(0.,-1.,1.020425574104E-16)) ;
#109488 = DIRECTION('center_axis',(1.25542992828747E-32,-1.020425574104E-16,
-1.)) ;
#109489 = DIRECTION('ref_axis',(-1.28107280532009E-48,-1.,1.020425574104E-16)) ;
#109490 = DIRECTION('',(1.,1.53063836115601E-16,-3.06472600140763E-33)) ;
#109491 = DIRECTION('',(2.16840434497101E-16,-1.,1.020425574104E-16)) ;
#109492 = DIRECTION('',(-1.,0.,-1.25542992828747E-32)) ;
#109493 = DIRECTION('',(-1.2303003375722E-16,1.,-1.020425574104E-16)) ;
#109494 = DIRECTION('center_axis',(6.27714964143733E-33,-5.10212787052002E-17,
-1.)) ;
#109495 = DIRECTION('ref_axis',(0.,1.,-5.10212787052002E-17)) ;
#109496 = DIRECTION('center_axis',(-6.27714964143733E-33,5.10212787052002E-17,
1.)) ;
#109497 = DIRECTION('ref_axis',(3.20268201330022E-49,1.,-5.10212787052002E-17)) ;
#109498 = DIRECTION('',(1.2303003375722E-16,-1.,5.10212787052002E-17)) ;
#109499 = DIRECTION('',(1.,0.,6.27714964143733E-33)) ;
#109500 = DIRECTION('',(-2.16840434497101E-16,1.,-5.10212787052002E-17)) ;
#109501 = DIRECTION('',(-1.,-1.53063836115601E-16,1.53236300070382E-33)) ;
#109502 = DIRECTION('center_axis',(-1.25542992828747E-32,1.020425574104E-16,
1.)) ;
#109503 = DIRECTION('ref_axis',(0.,-1.,1.020425574104E-16)) ;
#109504 = DIRECTION('center_axis',(1.25542992828747E-32,-1.020425574104E-16,
-1.)) ;
#109505 = DIRECTION('ref_axis',(-1.28107280532009E-48,-1.,1.020425574104E-16)) ;
#109506 = DIRECTION('',(1.,1.53063836115601E-16,-3.06472600140763E-33)) ;
#109507 = DIRECTION('',(2.16840434497101E-16,-1.,1.020425574104E-16)) ;
#109508 = DIRECTION('',(-1.,0.,-1.25542992828747E-32)) ;
#109509 = DIRECTION('',(-1.2303003375722E-16,1.,-1.020425574104E-16)) ;
#109510 = DIRECTION('center_axis',(6.27714964143733E-33,-5.10212787052002E-17,
-1.)) ;
#109511 = DIRECTION('ref_axis',(0.,1.,-5.10212787052002E-17)) ;
#109512 = DIRECTION('center_axis',(-6.27714964143733E-33,5.10212787052002E-17,
1.)) ;
#109513 = DIRECTION('ref_axis',(3.20268201330022E-49,1.,-5.10212787052002E-17)) ;
#109514 = DIRECTION('',(1.2303003375722E-16,-1.,5.10212787052002E-17)) ;
#109515 = DIRECTION('',(1.,0.,6.27714964143733E-33)) ;
#109516 = DIRECTION('',(-2.16840434497101E-16,1.,-5.10212787052002E-17)) ;
#109517 = DIRECTION('',(-1.,-1.53063836115601E-16,1.53236300070382E-33)) ;
#109518 = DIRECTION('center_axis',(-1.25542992828747E-32,1.020425574104E-16,
1.)) ;
#109519 = DIRECTION('ref_axis',(0.,-1.,1.020425574104E-16)) ;
#109520 = DIRECTION('center_axis',(1.25542992828747E-32,-1.020425574104E-16,
-1.)) ;
#109521 = DIRECTION('ref_axis',(-1.28107280532009E-48,-1.,1.020425574104E-16)) ;
#109522 = DIRECTION('',(1.,1.53063836115601E-16,-3.06472600140763E-33)) ;
#109523 = DIRECTION('',(2.16840434497101E-16,-1.,1.020425574104E-16)) ;
#109524 = DIRECTION('',(-1.,0.,-1.25542992828747E-32)) ;
#109525 = DIRECTION('',(-1.2303003375722E-16,1.,-1.020425574104E-16)) ;
#109526 = DIRECTION('center_axis',(6.27714964143733E-33,-5.10212787052002E-17,
-1.)) ;
#109527 = DIRECTION('ref_axis',(0.,1.,-5.10212787052002E-17)) ;
#109528 = DIRECTION('center_axis',(-6.27714964143733E-33,5.10212787052002E-17,
1.)) ;
#109529 = DIRECTION('ref_axis',(3.20268201330022E-49,1.,-5.10212787052002E-17)) ;
#109530 = DIRECTION('',(1.2303003375722E-16,-1.,5.10212787052002E-17)) ;
#109531 = DIRECTION('',(1.,0.,6.27714964143733E-33)) ;
#109532 = DIRECTION('',(-2.16840434497101E-16,1.,-5.10212787052002E-17)) ;
#109533 = DIRECTION('',(-1.,-1.53063836115601E-16,1.53236300070382E-33)) ;
#109534 = DIRECTION('center_axis',(-1.25542992828747E-32,1.020425574104E-16,
1.)) ;
#109535 = DIRECTION('ref_axis',(0.,-1.,1.020425574104E-16)) ;
#109536 = DIRECTION('center_axis',(1.25542992828747E-32,-1.020425574104E-16,
-1.)) ;
#109537 = DIRECTION('ref_axis',(-1.28107280532009E-48,-1.,1.020425574104E-16)) ;
#109538 = DIRECTION('',(1.,1.53063836115601E-16,-3.06472600140763E-33)) ;
#109539 = DIRECTION('',(2.16840434497101E-16,-1.,1.020425574104E-16)) ;
#109540 = DIRECTION('',(-1.,0.,-1.25542992828747E-32)) ;
#109541 = DIRECTION('',(-1.2303003375722E-16,1.,-1.020425574104E-16)) ;
#109542 = DIRECTION('center_axis',(6.27714964143733E-33,-5.10212787052002E-17,
-1.)) ;
#109543 = DIRECTION('ref_axis',(0.,1.,-5.10212787052002E-17)) ;
#109544 = DIRECTION('center_axis',(-6.27714964143733E-33,5.10212787052002E-17,
1.)) ;
#109545 = DIRECTION('ref_axis',(3.20268201330022E-49,1.,-5.10212787052002E-17)) ;
#109546 = DIRECTION('',(1.2303003375722E-16,-1.,5.10212787052002E-17)) ;
#109547 = DIRECTION('',(1.,0.,6.27714964143733E-33)) ;
#109548 = DIRECTION('',(-2.16840434497101E-16,1.,-5.10212787052002E-17)) ;
#109549 = DIRECTION('',(-1.,-1.53063836115601E-16,1.53236300070382E-33)) ;
#109550 = DIRECTION('center_axis',(-1.25542992828747E-32,1.020425574104E-16,
1.)) ;
#109551 = DIRECTION('ref_axis',(0.,-1.,1.020425574104E-16)) ;
#109552 = DIRECTION('center_axis',(1.25542992828747E-32,-1.020425574104E-16,
-1.)) ;
#109553 = DIRECTION('ref_axis',(-1.28107280532009E-48,-1.,1.020425574104E-16)) ;
#109554 = DIRECTION('',(1.,1.53063836115601E-16,-3.06472600140763E-33)) ;
#109555 = DIRECTION('',(2.16840434497101E-16,-1.,1.020425574104E-16)) ;
#109556 = DIRECTION('',(-1.,0.,-1.25542992828747E-32)) ;
#109557 = DIRECTION('',(-1.2303003375722E-16,1.,-1.020425574104E-16)) ;
#109558 = DIRECTION('center_axis',(6.27714964143733E-33,-5.10212787052002E-17,
-1.)) ;
#109559 = DIRECTION('ref_axis',(0.,1.,-5.10212787052002E-17)) ;
#109560 = DIRECTION('center_axis',(-6.27714964143733E-33,5.10212787052002E-17,
1.)) ;
#109561 = DIRECTION('ref_axis',(3.20268201330022E-49,1.,-5.10212787052002E-17)) ;
#109562 = DIRECTION('',(1.2303003375722E-16,-1.,5.10212787052002E-17)) ;
#109563 = DIRECTION('',(1.,0.,6.27714964143733E-33)) ;
#109564 = DIRECTION('',(-2.16840434497101E-16,1.,-5.10212787052002E-17)) ;
#109565 = DIRECTION('',(-1.,-1.53063836115601E-16,1.53236300070382E-33)) ;
#109566 = DIRECTION('center_axis',(-1.25542992828747E-32,1.020425574104E-16,
1.)) ;
#109567 = DIRECTION('ref_axis',(0.,-1.,1.020425574104E-16)) ;
#109568 = DIRECTION('center_axis',(1.25542992828747E-32,-1.020425574104E-16,
-1.)) ;
#109569 = DIRECTION('ref_axis',(-1.28107280532009E-48,-1.,1.020425574104E-16)) ;
#109570 = DIRECTION('',(1.,1.53063836115601E-16,-3.06472600140763E-33)) ;
#109571 = DIRECTION('',(2.16840434497101E-16,-1.,1.020425574104E-16)) ;
#109572 = DIRECTION('',(-1.,0.,-1.25542992828747E-32)) ;
#109573 = DIRECTION('',(-1.2303003375722E-16,1.,-1.020425574104E-16)) ;
#109574 = DIRECTION('center_axis',(6.27714964143733E-33,-5.10212787052002E-17,
-1.)) ;
#109575 = DIRECTION('ref_axis',(0.,1.,-5.10212787052002E-17)) ;
#109576 = DIRECTION('center_axis',(-6.27714964143733E-33,5.10212787052002E-17,
1.)) ;
#109577 = DIRECTION('ref_axis',(3.20268201330022E-49,1.,-5.10212787052002E-17)) ;
#109578 = DIRECTION('',(1.2303003375722E-16,-1.,5.10212787052002E-17)) ;
#109579 = DIRECTION('',(1.,0.,6.27714964143733E-33)) ;
#109580 = DIRECTION('',(-2.16840434497101E-16,1.,-5.10212787052002E-17)) ;
#109581 = DIRECTION('',(-1.,-1.53063836115601E-16,1.53236300070382E-33)) ;
#109582 = DIRECTION('center_axis',(-1.25542992828747E-32,1.020425574104E-16,
1.)) ;
#109583 = DIRECTION('ref_axis',(0.,-1.,1.020425574104E-16)) ;
#109584 = DIRECTION('center_axis',(1.25542992828747E-32,-1.020425574104E-16,
-1.)) ;
#109585 = DIRECTION('ref_axis',(-1.28107280532009E-48,-1.,1.020425574104E-16)) ;
#109586 = DIRECTION('',(1.,1.53063836115601E-16,-3.06472600140763E-33)) ;
#109587 = DIRECTION('',(2.16840434497101E-16,-1.,1.020425574104E-16)) ;
#109588 = DIRECTION('',(-1.,0.,-1.25542992828747E-32)) ;
#109589 = DIRECTION('',(-1.2303003375722E-16,1.,-1.020425574104E-16)) ;
#109590 = DIRECTION('center_axis',(0.,0.,1.)) ;
#109591 = DIRECTION('ref_axis',(1.,0.,0.)) ;
#109592 = DIRECTION('',(0.,0.,1.)) ;
#109593 = DIRECTION('center_axis',(0.,0.,1.)) ;
#109594 = DIRECTION('ref_axis',(1.,0.,0.)) ;
#109595 = DIRECTION('',(0.,0.,1.)) ;
#109596 = DIRECTION('center_axis',(0.,0.,-1.)) ;
#109597 = DIRECTION('ref_axis',(1.,0.,0.)) ;
#109598 = DIRECTION('center_axis',(0.,0.,1.)) ;
#109599 = DIRECTION('ref_axis',(1.,0.,0.)) ;
#109600 = DIRECTION('',(0.,0.,1.)) ;
#109601 = DIRECTION('center_axis',(0.,0.,1.)) ;
#109602 = DIRECTION('ref_axis',(1.,0.,0.)) ;
#109603 = DIRECTION('',(0.,0.,1.)) ;
#109604 = DIRECTION('center_axis',(0.,0.,-1.)) ;
#109605 = DIRECTION('ref_axis',(1.,0.,0.)) ;
#109606 = DIRECTION('center_axis',(0.,0.,1.)) ;
#109607 = DIRECTION('ref_axis',(1.,0.,0.)) ;
#109608 = DIRECTION('',(0.,0.,1.)) ;
#109609 = DIRECTION('center_axis',(0.,0.,1.)) ;
#109610 = DIRECTION('ref_axis',(1.,0.,0.)) ;
#109611 = DIRECTION('',(0.,0.,1.)) ;
#109612 = DIRECTION('center_axis',(0.,0.,-1.)) ;
#109613 = DIRECTION('ref_axis',(1.,0.,0.)) ;
#109614 = DIRECTION('center_axis',(0.,0.,1.)) ;
#109615 = DIRECTION('ref_axis',(1.,0.,0.)) ;
#109616 = DIRECTION('',(0.,0.,1.)) ;
#109617 = DIRECTION('center_axis',(0.,0.,1.)) ;
#109618 = DIRECTION('ref_axis',(1.,0.,0.)) ;
#109619 = DIRECTION('',(0.,0.,1.)) ;
#109620 = DIRECTION('center_axis',(0.,0.,-1.)) ;
#109621 = DIRECTION('ref_axis',(1.,0.,0.)) ;
#109622 = DIRECTION('center_axis',(0.,0.,1.)) ;
#109623 = DIRECTION('ref_axis',(1.,0.,0.)) ;
#109624 = DIRECTION('',(0.,0.,1.)) ;
#109625 = DIRECTION('center_axis',(0.,0.,1.)) ;
#109626 = DIRECTION('ref_axis',(1.,0.,0.)) ;
#109627 = DIRECTION('',(0.,0.,1.)) ;
#109628 = DIRECTION('center_axis',(0.,0.,-1.)) ;
#109629 = DIRECTION('ref_axis',(1.,0.,0.)) ;
#109630 = DIRECTION('center_axis',(0.,0.,1.)) ;
#109631 = DIRECTION('ref_axis',(1.,0.,0.)) ;
#109632 = DIRECTION('',(0.,0.,1.)) ;
#109633 = DIRECTION('center_axis',(0.,0.,1.)) ;
#109634 = DIRECTION('ref_axis',(1.,0.,0.)) ;
#109635 = DIRECTION('',(0.,0.,1.)) ;
#109636 = DIRECTION('center_axis',(0.,0.,-1.)) ;
#109637 = DIRECTION('ref_axis',(1.,0.,0.)) ;
#109638 = DIRECTION('center_axis',(0.,0.,1.)) ;
#109639 = DIRECTION('ref_axis',(1.,0.,0.)) ;
#109640 = DIRECTION('',(0.,0.,1.)) ;
#109641 = DIRECTION('center_axis',(0.,0.,1.)) ;
#109642 = DIRECTION('ref_axis',(1.,0.,0.)) ;
#109643 = DIRECTION('',(0.,0.,1.)) ;
#109644 = DIRECTION('center_axis',(0.,0.,-1.)) ;
#109645 = DIRECTION('ref_axis',(1.,0.,0.)) ;
#109646 = DIRECTION('center_axis',(0.,0.,1.)) ;
#109647 = DIRECTION('ref_axis',(1.,0.,0.)) ;
#109648 = DIRECTION('',(0.,0.,1.)) ;
#109649 = DIRECTION('center_axis',(0.,0.,1.)) ;
#109650 = DIRECTION('ref_axis',(1.,0.,0.)) ;
#109651 = DIRECTION('',(0.,0.,1.)) ;
#109652 = DIRECTION('center_axis',(0.,0.,-1.)) ;
#109653 = DIRECTION('ref_axis',(1.,0.,0.)) ;
#109654 = DIRECTION('center_axis',(0.,0.,1.)) ;
#109655 = DIRECTION('ref_axis',(1.,0.,0.)) ;
#109656 = DIRECTION('',(0.,0.,1.)) ;
#109657 = DIRECTION('center_axis',(0.,0.,1.)) ;
#109658 = DIRECTION('ref_axis',(1.,0.,0.)) ;
#109659 = DIRECTION('',(0.,0.,1.)) ;
#109660 = DIRECTION('center_axis',(0.,0.,-1.)) ;
#109661 = DIRECTION('ref_axis',(1.,0.,0.)) ;
#109662 = DIRECTION('center_axis',(-1.,-2.16840434497101E-16,0.)) ;
#109663 = DIRECTION('ref_axis',(2.16840434497101E-16,-1.,0.)) ;
#109664 = DIRECTION('',(-2.16840434497101E-16,1.,1.30104260698261E-16)) ;
#109665 = DIRECTION('center_axis',(1.,2.16840434497101E-16,0.)) ;
#109666 = DIRECTION('ref_axis',(2.16840434497101E-16,-1.,0.)) ;
#109667 = DIRECTION('',(0.,0.,-1.)) ;
#109668 = DIRECTION('center_axis',(1.,2.16840434497101E-16,0.)) ;
#109669 = DIRECTION('ref_axis',(2.16840434497101E-16,-1.,0.)) ;
#109670 = DIRECTION('center_axis',(-1.,-2.16840434497101E-16,0.)) ;
#109671 = DIRECTION('ref_axis',(2.16840434497101E-16,-1.,0.)) ;
#109672 = DIRECTION('',(0.,0.,-1.)) ;
#109673 = DIRECTION('',(2.16840434497101E-16,-1.,5.10212787052002E-17)) ;
#109674 = DIRECTION('',(0.,0.,1.)) ;
#109675 = DIRECTION('',(-2.16840434497101E-16,1.,-1.020425574104E-16)) ;
#109676 = DIRECTION('',(0.,0.,-1.)) ;
#109677 = DIRECTION('center_axis',(-1.,-2.16840434497101E-16,0.)) ;
#109678 = DIRECTION('ref_axis',(2.16840434497101E-16,-1.,0.)) ;
#109679 = DIRECTION('center_axis',(6.27714964143733E-33,-5.10212787052002E-17,
-1.)) ;
#109680 = DIRECTION('ref_axis',(0.,1.,-5.10212787052002E-17)) ;
#109681 = DIRECTION('center_axis',(-6.27714964143733E-33,5.10212787052002E-17,
1.)) ;
#109682 = DIRECTION('ref_axis',(3.20268201330022E-49,1.,-5.10212787052002E-17)) ;
#109683 = DIRECTION('',(1.2303003375722E-16,-1.,5.10212787052002E-17)) ;
#109684 = DIRECTION('',(1.,0.,6.27714964143733E-33)) ;
#109685 = DIRECTION('',(-2.16840434497101E-16,1.,-5.10212787052002E-17)) ;
#109686 = DIRECTION('',(-1.,-1.53063836115601E-16,1.53236300070382E-33)) ;
#109687 = DIRECTION('center_axis',(-1.25542992828747E-32,1.020425574104E-16,
1.)) ;
#109688 = DIRECTION('ref_axis',(0.,-1.,1.020425574104E-16)) ;
#109689 = DIRECTION('center_axis',(1.25542992828747E-32,-1.020425574104E-16,
-1.)) ;
#109690 = DIRECTION('ref_axis',(-1.28107280532009E-48,-1.,1.020425574104E-16)) ;
#109691 = DIRECTION('',(1.,1.53063836115601E-16,-3.06472600140763E-33)) ;
#109692 = DIRECTION('',(2.16840434497101E-16,-1.,1.020425574104E-16)) ;
#109693 = DIRECTION('',(-1.,0.,-1.25542992828747E-32)) ;
#109694 = DIRECTION('',(-1.2303003375722E-16,1.,-1.020425574104E-16)) ;
#109695 = DIRECTION('center_axis',(0.,0.,1.)) ;
#109696 = DIRECTION('ref_axis',(1.,0.,0.)) ;
#109697 = DIRECTION('',(0.,0.,1.)) ;
#109698 = DIRECTION('center_axis',(0.,0.,1.)) ;
#109699 = DIRECTION('ref_axis',(1.,0.,0.)) ;
#109700 = DIRECTION('',(0.,0.,1.)) ;
#109701 = DIRECTION('center_axis',(0.,0.,-1.)) ;
#109702 = DIRECTION('ref_axis',(1.,0.,0.)) ;
#109703 = DIRECTION('center_axis',(0.,0.,1.)) ;
#109704 = DIRECTION('ref_axis',(1.,0.,0.)) ;
#109705 = DIRECTION('',(0.,0.,1.)) ;
#109706 = DIRECTION('center_axis',(0.,0.,1.)) ;
#109707 = DIRECTION('ref_axis',(1.,0.,0.)) ;
#109708 = DIRECTION('',(0.,0.,1.)) ;
#109709 = DIRECTION('center_axis',(0.,0.,-1.)) ;
#109710 = DIRECTION('ref_axis',(1.,0.,0.)) ;
#109711 = DIRECTION('center_axis',(0.,-1.,0.)) ;
#109712 = DIRECTION('ref_axis',(0.,0.,-1.)) ;
#109713 = DIRECTION('center_axis',(0.,-1.,0.)) ;
#109714 = DIRECTION('ref_axis',(0.,0.,-1.)) ;
#109715 = DIRECTION('',(-1.,0.,-6.27714964143733E-33)) ;
#109716 = DIRECTION('',(0.,0.,1.)) ;
#109717 = DIRECTION('',(1.,0.,0.)) ;
#109718 = DIRECTION('',(-1.,0.,0.)) ;
#109719 = DIRECTION('',(1.,0.,1.25542992828747E-32)) ;
#109720 = DIRECTION('center_axis',(0.,-1.,0.)) ;
#109721 = DIRECTION('ref_axis',(0.,0.,-1.)) ;
#109722 = DIRECTION('',(0.,0.,-1.)) ;
#109723 = DIRECTION('center_axis',(0.,-1.,0.)) ;
#109724 = DIRECTION('ref_axis',(0.,0.,-1.)) ;
#109725 = DIRECTION('',(-1.,0.,-6.27714964143733E-33)) ;
#109726 = DIRECTION('',(1.,0.,1.25542992828747E-32)) ;
#109727 = DIRECTION('center_axis',(0.,-1.,0.)) ;
#109728 = DIRECTION('ref_axis',(0.,0.,-1.)) ;
#109729 = DIRECTION('',(0.,0.,-1.)) ;
#109730 = DIRECTION('center_axis',(0.,-1.,0.)) ;
#109731 = DIRECTION('ref_axis',(0.,0.,-1.)) ;
#109732 = DIRECTION('',(-1.,0.,-6.27714964143733E-33)) ;
#109733 = DIRECTION('',(1.,0.,1.25542992828747E-32)) ;
#109734 = DIRECTION('center_axis',(0.,-1.,0.)) ;
#109735 = DIRECTION('ref_axis',(0.,0.,-1.)) ;
#109736 = DIRECTION('',(0.,0.,-1.)) ;
#109737 = DIRECTION('center_axis',(0.,-1.,0.)) ;
#109738 = DIRECTION('ref_axis',(0.,0.,-1.)) ;
#109739 = DIRECTION('',(-1.,0.,-6.27714964143733E-33)) ;
#109740 = DIRECTION('',(1.,0.,1.25542992828747E-32)) ;
#109741 = DIRECTION('center_axis',(0.,-1.,0.)) ;
#109742 = DIRECTION('ref_axis',(0.,0.,-1.)) ;
#109743 = DIRECTION('',(0.,0.,-1.)) ;
#109744 = DIRECTION('center_axis',(0.,-1.,0.)) ;
#109745 = DIRECTION('ref_axis',(0.,0.,-1.)) ;
#109746 = DIRECTION('',(-1.,0.,-6.27714964143733E-33)) ;
#109747 = DIRECTION('',(1.,0.,1.25542992828747E-32)) ;
#109748 = DIRECTION('center_axis',(0.,-1.,0.)) ;
#109749 = DIRECTION('ref_axis',(0.,0.,-1.)) ;
#109750 = DIRECTION('',(0.,0.,-1.)) ;
#109751 = DIRECTION('center_axis',(0.,-1.,0.)) ;
#109752 = DIRECTION('ref_axis',(0.,0.,-1.)) ;
#109753 = DIRECTION('',(-1.,0.,-6.27714964143733E-33)) ;
#109754 = DIRECTION('',(1.,0.,1.25542992828747E-32)) ;
#109755 = DIRECTION('center_axis',(0.,-1.,0.)) ;
#109756 = DIRECTION('ref_axis',(0.,0.,-1.)) ;
#109757 = DIRECTION('',(0.,0.,-1.)) ;
#109758 = DIRECTION('center_axis',(0.,-1.,0.)) ;
#109759 = DIRECTION('ref_axis',(0.,0.,-1.)) ;
#109760 = DIRECTION('',(-1.,0.,-6.27714964143733E-33)) ;
#109761 = DIRECTION('',(1.,0.,1.25542992828747E-32)) ;
#109762 = DIRECTION('center_axis',(0.,-1.,0.)) ;
#109763 = DIRECTION('ref_axis',(0.,0.,-1.)) ;
#109764 = DIRECTION('',(0.,0.,-1.)) ;
#109765 = DIRECTION('center_axis',(0.,-1.,0.)) ;
#109766 = DIRECTION('ref_axis',(0.,0.,-1.)) ;
#109767 = DIRECTION('',(-1.,0.,-6.27714964143733E-33)) ;
#109768 = DIRECTION('',(1.,0.,1.25542992828747E-32)) ;
#109769 = DIRECTION('center_axis',(0.,-1.,0.)) ;
#109770 = DIRECTION('ref_axis',(0.,0.,-1.)) ;
#109771 = DIRECTION('',(0.,0.,-1.)) ;
#109772 = DIRECTION('center_axis',(0.,-1.,0.)) ;
#109773 = DIRECTION('ref_axis',(0.,0.,-1.)) ;
#109774 = DIRECTION('',(-1.,0.,-6.27714964143733E-33)) ;
#109775 = DIRECTION('',(1.,0.,1.25542992828747E-32)) ;
#109776 = DIRECTION('center_axis',(0.,-1.,0.)) ;
#109777 = DIRECTION('ref_axis',(0.,0.,-1.)) ;
#109778 = DIRECTION('',(0.,0.,-1.)) ;
#109779 = DIRECTION('center_axis',(0.,-1.,0.)) ;
#109780 = DIRECTION('ref_axis',(0.,0.,-1.)) ;
#109781 = DIRECTION('',(-1.,0.,-6.27714964143733E-33)) ;
#109782 = DIRECTION('',(1.,0.,1.25542992828747E-32)) ;
#109783 = DIRECTION('center_axis',(0.,-1.,0.)) ;
#109784 = DIRECTION('ref_axis',(0.,0.,-1.)) ;
#109785 = DIRECTION('',(0.,0.,-1.)) ;
#109786 = DIRECTION('center_axis',(0.,0.,1.)) ;
#109787 = DIRECTION('ref_axis',(1.,0.,0.)) ;
#109788 = DIRECTION('center_axis',(0.,0.,-1.)) ;
#109789 = DIRECTION('ref_axis',(1.,0.,0.)) ;
#109790 = DIRECTION('',(0.,0.,1.)) ;
#109791 = DIRECTION('center_axis',(0.,0.,1.)) ;
#109792 = DIRECTION('ref_axis',(1.,0.,0.)) ;
#109793 = DIRECTION('center_axis',(-1.,-1.2303003375722E-16,0.)) ;
#109794 = DIRECTION('ref_axis',(1.2303003375722E-16,-1.,0.)) ;
#109795 = DIRECTION('center_axis',(-1.,-1.2303003375722E-16,0.)) ;
#109796 = DIRECTION('ref_axis',(1.2303003375722E-16,-1.,0.)) ;
#109797 = DIRECTION('',(1.2303003375722E-16,-1.,1.020425574104E-16)) ;
#109798 = DIRECTION('',(-1.2303003375722E-16,1.,-5.10212787052002E-17)) ;
#109799 = DIRECTION('center_axis',(-1.,-1.2303003375722E-16,0.)) ;
#109800 = DIRECTION('ref_axis',(1.2303003375722E-16,-1.,0.)) ;
#109801 = DIRECTION('',(0.,0.,1.)) ;
#109802 = DIRECTION('center_axis',(-1.,-1.2303003375722E-16,0.)) ;
#109803 = DIRECTION('ref_axis',(1.2303003375722E-16,-1.,0.)) ;
#109804 = DIRECTION('',(1.2303003375722E-16,-1.,1.020425574104E-16)) ;
#109805 = DIRECTION('',(-1.2303003375722E-16,1.,-5.10212787052002E-17)) ;
#109806 = DIRECTION('center_axis',(-1.,-1.2303003375722E-16,0.)) ;
#109807 = DIRECTION('ref_axis',(1.2303003375722E-16,-1.,0.)) ;
#109808 = DIRECTION('',(0.,0.,1.)) ;
#109809 = DIRECTION('center_axis',(-1.,-1.2303003375722E-16,0.)) ;
#109810 = DIRECTION('ref_axis',(1.2303003375722E-16,-1.,0.)) ;
#109811 = DIRECTION('',(1.2303003375722E-16,-1.,1.020425574104E-16)) ;
#109812 = DIRECTION('',(-1.2303003375722E-16,1.,-5.10212787052002E-17)) ;
#109813 = DIRECTION('center_axis',(-1.,-1.2303003375722E-16,0.)) ;
#109814 = DIRECTION('ref_axis',(1.2303003375722E-16,-1.,0.)) ;
#109815 = DIRECTION('',(0.,0.,1.)) ;
#109816 = DIRECTION('center_axis',(-1.,-1.2303003375722E-16,0.)) ;
#109817 = DIRECTION('ref_axis',(1.2303003375722E-16,-1.,0.)) ;
#109818 = DIRECTION('',(1.2303003375722E-16,-1.,1.020425574104E-16)) ;
#109819 = DIRECTION('',(-1.2303003375722E-16,1.,-5.10212787052002E-17)) ;
#109820 = DIRECTION('center_axis',(-1.,-1.2303003375722E-16,0.)) ;
#109821 = DIRECTION('ref_axis',(1.2303003375722E-16,-1.,0.)) ;
#109822 = DIRECTION('',(0.,0.,1.)) ;
#109823 = DIRECTION('center_axis',(-1.,-1.2303003375722E-16,0.)) ;
#109824 = DIRECTION('ref_axis',(1.2303003375722E-16,-1.,0.)) ;
#109825 = DIRECTION('',(1.2303003375722E-16,-1.,1.020425574104E-16)) ;
#109826 = DIRECTION('',(-1.2303003375722E-16,1.,-5.10212787052002E-17)) ;
#109827 = DIRECTION('center_axis',(-1.,-1.2303003375722E-16,0.)) ;
#109828 = DIRECTION('ref_axis',(1.2303003375722E-16,-1.,0.)) ;
#109829 = DIRECTION('',(0.,0.,1.)) ;
#109830 = DIRECTION('center_axis',(-1.,-1.2303003375722E-16,0.)) ;
#109831 = DIRECTION('ref_axis',(1.2303003375722E-16,-1.,0.)) ;
#109832 = DIRECTION('',(1.2303003375722E-16,-1.,1.020425574104E-16)) ;
#109833 = DIRECTION('',(-1.2303003375722E-16,1.,-5.10212787052002E-17)) ;
#109834 = DIRECTION('center_axis',(-1.,-1.2303003375722E-16,0.)) ;
#109835 = DIRECTION('ref_axis',(1.2303003375722E-16,-1.,0.)) ;
#109836 = DIRECTION('',(0.,0.,1.)) ;
#109837 = DIRECTION('center_axis',(-1.,-1.2303003375722E-16,0.)) ;
#109838 = DIRECTION('ref_axis',(1.2303003375722E-16,-1.,0.)) ;
#109839 = DIRECTION('',(1.2303003375722E-16,-1.,1.020425574104E-16)) ;
#109840 = DIRECTION('',(-1.2303003375722E-16,1.,-5.10212787052002E-17)) ;
#109841 = DIRECTION('center_axis',(-1.,-1.2303003375722E-16,0.)) ;
#109842 = DIRECTION('ref_axis',(1.2303003375722E-16,-1.,0.)) ;
#109843 = DIRECTION('',(0.,0.,1.)) ;
#109844 = DIRECTION('center_axis',(-1.,-1.2303003375722E-16,0.)) ;
#109845 = DIRECTION('ref_axis',(1.2303003375722E-16,-1.,0.)) ;
#109846 = DIRECTION('',(1.2303003375722E-16,-1.,1.020425574104E-16)) ;
#109847 = DIRECTION('',(-1.2303003375722E-16,1.,-5.10212787052002E-17)) ;
#109848 = DIRECTION('center_axis',(-1.,-1.2303003375722E-16,0.)) ;
#109849 = DIRECTION('ref_axis',(1.2303003375722E-16,-1.,0.)) ;
#109850 = DIRECTION('',(0.,0.,1.)) ;
#109851 = DIRECTION('center_axis',(-1.,-1.2303003375722E-16,0.)) ;
#109852 = DIRECTION('ref_axis',(1.2303003375722E-16,-1.,0.)) ;
#109853 = DIRECTION('',(1.2303003375722E-16,-1.,1.020425574104E-16)) ;
#109854 = DIRECTION('',(-1.2303003375722E-16,1.,-5.10212787052002E-17)) ;
#109855 = DIRECTION('center_axis',(-1.,-1.2303003375722E-16,0.)) ;
#109856 = DIRECTION('ref_axis',(1.2303003375722E-16,-1.,0.)) ;
#109857 = DIRECTION('',(0.,0.,1.)) ;
#109858 = DIRECTION('center_axis',(-1.,-1.2303003375722E-16,0.)) ;
#109859 = DIRECTION('ref_axis',(1.2303003375722E-16,-1.,0.)) ;
#109860 = DIRECTION('',(1.2303003375722E-16,-1.,1.020425574104E-16)) ;
#109861 = DIRECTION('',(-1.2303003375722E-16,1.,0.)) ;
#109862 = DIRECTION('',(0.,0.,1.)) ;
#109863 = DIRECTION('',(1.2303003375722E-16,-1.,0.)) ;
#109864 = DIRECTION('',(-1.2303003375722E-16,1.,-5.10212787052002E-17)) ;
#109865 = DIRECTION('center_axis',(-1.,-1.2303003375722E-16,0.)) ;
#109866 = DIRECTION('ref_axis',(1.2303003375722E-16,-1.,0.)) ;
#109867 = DIRECTION('',(0.,0.,1.)) ;
#109868 = DIRECTION('center_axis',(0.,0.,1.)) ;
#109869 = DIRECTION('ref_axis',(1.,0.,0.)) ;
#109870 = DIRECTION('',(0.,0.,1.)) ;
#109871 = DIRECTION('center_axis',(0.,0.,1.)) ;
#109872 = DIRECTION('ref_axis',(1.,0.,0.)) ;
#109873 = DIRECTION('center_axis',(0.,0.,-1.)) ;
#109874 = DIRECTION('ref_axis',(1.,0.,0.)) ;
#109875 = DIRECTION('center_axis',(-1.59148942750166E-16,1.,0.)) ;
#109876 = DIRECTION('ref_axis',(-1.,-1.59148942750166E-16,0.)) ;
#109877 = DIRECTION('',(0.,0.,1.)) ;
#109878 = DIRECTION('',(-1.,-1.59148942750166E-16,0.)) ;
#109879 = DIRECTION('',(1.,1.59148942750166E-16,0.)) ;
#109880 = DIRECTION('center_axis',(0.,0.,1.)) ;
#109881 = DIRECTION('ref_axis',(1.,0.,0.)) ;
#109882 = DIRECTION('',(0.,0.,1.)) ;
#109883 = DIRECTION('center_axis',(0.,0.,-1.)) ;
#109884 = DIRECTION('ref_axis',(1.,0.,0.)) ;
#109885 = DIRECTION('center_axis',(0.,0.,1.)) ;
#109886 = DIRECTION('ref_axis',(1.,0.,0.)) ;
#109887 = DIRECTION('center_axis',(-1.,0.,0.)) ;
#109888 = DIRECTION('ref_axis',(0.,0.,1.)) ;
#109889 = DIRECTION('',(0.,0.,1.)) ;
#109890 = DIRECTION('',(0.,-1.,0.)) ;
#109891 = DIRECTION('',(0.,1.,0.)) ;
#109892 = DIRECTION('center_axis',(0.,0.,1.)) ;
#109893 = DIRECTION('ref_axis',(1.,0.,0.)) ;
#109894 = DIRECTION('',(0.,0.,1.)) ;
#109895 = DIRECTION('center_axis',(0.,0.,1.)) ;
#109896 = DIRECTION('ref_axis',(1.,0.,0.)) ;
#109897 = DIRECTION('center_axis',(0.,0.,-1.)) ;
#109898 = DIRECTION('ref_axis',(1.,0.,0.)) ;
#109899 = DIRECTION('center_axis',(0.,1.,0.)) ;
#109900 = DIRECTION('ref_axis',(0.,0.,1.)) ;
#109901 = DIRECTION('',(0.,0.,1.)) ;
#109902 = DIRECTION('',(-1.,0.,0.)) ;
#109903 = DIRECTION('',(1.,0.,0.)) ;
#109904 = DIRECTION('center_axis',(0.,0.,1.)) ;
#109905 = DIRECTION('ref_axis',(1.,0.,0.)) ;
#109906 = DIRECTION('',(0.,0.,1.)) ;
#109907 = DIRECTION('center_axis',(0.,0.,1.)) ;
#109908 = DIRECTION('ref_axis',(1.,0.,0.)) ;
#109909 = DIRECTION('center_axis',(0.,0.,-1.)) ;
#109910 = DIRECTION('ref_axis',(1.,0.,0.)) ;
#109911 = DIRECTION('center_axis',(1.,-4.33680868994203E-15,0.)) ;
#109912 = DIRECTION('ref_axis',(4.33680868994203E-15,1.,0.)) ;
#109913 = DIRECTION('',(0.,0.,1.)) ;
#109914 = DIRECTION('',(4.33680868994203E-15,1.,0.)) ;
#109915 = DIRECTION('',(-4.33680868994203E-15,-1.,0.)) ;
#109916 = DIRECTION('center_axis',(0.,0.,1.)) ;
#109917 = DIRECTION('ref_axis',(1.,0.,0.)) ;
#109918 = DIRECTION('',(0.,0.,1.)) ;
#109919 = DIRECTION('center_axis',(0.,0.,-1.)) ;
#109920 = DIRECTION('ref_axis',(1.,0.,0.)) ;
#109921 = DIRECTION('center_axis',(0.,0.,1.)) ;
#109922 = DIRECTION('ref_axis',(1.,0.,0.)) ;
#109923 = DIRECTION('center_axis',(5.88041856263325E-16,1.,0.)) ;
#109924 = DIRECTION('ref_axis',(-1.,5.88041856263325E-16,0.)) ;
#109925 = DIRECTION('',(0.,0.,1.)) ;
#109926 = DIRECTION('',(-1.,5.88041856263325E-16,0.)) ;
#109927 = DIRECTION('',(1.,-5.88041856263325E-16,0.)) ;
#109928 = DIRECTION('center_axis',(0.,0.,1.)) ;
#109929 = DIRECTION('ref_axis',(1.,0.,0.)) ;
#109930 = DIRECTION('',(0.,0.,1.)) ;
#109931 = DIRECTION('center_axis',(0.,0.,1.)) ;
#109932 = DIRECTION('ref_axis',(1.,0.,0.)) ;
#109933 = DIRECTION('center_axis',(0.,0.,-1.)) ;
#109934 = DIRECTION('ref_axis',(1.,0.,0.)) ;
#109935 = DIRECTION('center_axis',(1.,0.,0.)) ;
#109936 = DIRECTION('ref_axis',(0.,0.,-1.)) ;
#109937 = DIRECTION('',(0.,1.,0.)) ;
#109938 = DIRECTION('',(0.,-1.,0.)) ;
#109939 = DIRECTION('center_axis',(-1.,0.,0.)) ;
#109940 = DIRECTION('ref_axis',(0.,0.,-1.)) ;
#109941 = DIRECTION('',(0.,0.,-1.)) ;
#109942 = DIRECTION('',(0.,1.,0.)) ;
#109943 = DIRECTION('',(0.,3.99416362155027E-15,1.)) ;
#109944 = DIRECTION('center_axis',(-1.,0.,0.)) ;
#109945 = DIRECTION('ref_axis',(0.,6.50521303491307E-15,-1.)) ;
#109946 = DIRECTION('',(0.,0.707106781186546,0.707106781186549)) ;
#109947 = DIRECTION('center_axis',(-1.,0.,0.)) ;
#109948 = DIRECTION('ref_axis',(0.,-1.51788304147972E-14,-1.)) ;
#109949 = DIRECTION('',(0.,0.,-1.)) ;
#109950 = DIRECTION('',(0.,-0.707106781186548,0.707106781186547)) ;
#109951 = DIRECTION('center_axis',(-1.,0.,0.)) ;
#109952 = DIRECTION('ref_axis',(0.,1.30104260698261E-14,-1.)) ;
#109953 = DIRECTION('',(0.,0.,1.)) ;
#109954 = DIRECTION('',(0.,-1.,0.)) ;
#109955 = DIRECTION('',(0.,0.,-1.)) ;
#109956 = DIRECTION('center_axis',(-1.,0.,0.)) ;
#109957 = DIRECTION('ref_axis',(0.,1.19262238973406E-14,-1.)) ;
#109958 = DIRECTION('',(0.,-1.,-1.07081696047951E-16)) ;
#109959 = DIRECTION('center_axis',(-1.,0.,0.)) ;
#109960 = DIRECTION('ref_axis',(0.,0.,-1.)) ;
#109961 = DIRECTION('',(0.,0.,1.)) ;
#109962 = DIRECTION('center_axis',(-1.,0.,0.)) ;
#109963 = DIRECTION('ref_axis',(0.,4.33680868994204E-15,-1.)) ;
#109964 = DIRECTION('center_axis',(1.,0.,0.)) ;
#109965 = DIRECTION('ref_axis',(0.,0.,-1.)) ;
#109966 = DIRECTION('center_axis',(-1.,0.,0.)) ;
#109967 = DIRECTION('ref_axis',(0.,8.67361737988409E-15,-1.)) ;
#109968 = DIRECTION('',(0.,0.,1.)) ;
#109969 = DIRECTION('center_axis',(-1.,0.,0.)) ;
#109970 = DIRECTION('ref_axis',(0.,0.,-1.)) ;
#109971 = DIRECTION('',(0.,1.,1.07081696047951E-16)) ;
#109972 = DIRECTION('center_axis',(-1.,0.,0.)) ;
#109973 = DIRECTION('ref_axis',(0.,0.,-1.)) ;
#109974 = DIRECTION('',(0.,0.,-1.)) ;
#109975 = DIRECTION('',(0.,1.,0.)) ;
#109976 = DIRECTION('',(0.,3.99416362155027E-15,1.)) ;
#109977 = DIRECTION('center_axis',(-1.,0.,0.)) ;
#109978 = DIRECTION('ref_axis',(0.,6.50521303491307E-15,-1.)) ;
#109979 = DIRECTION('',(0.,0.707106781186546,0.707106781186549)) ;
#109980 = DIRECTION('center_axis',(-1.,0.,0.)) ;
#109981 = DIRECTION('ref_axis',(0.,0.,-1.)) ;
#109982 = DIRECTION('',(0.,0.,-1.)) ;
#109983 = DIRECTION('',(0.,-0.707106781186548,0.707106781186547)) ;
#109984 = DIRECTION('center_axis',(-1.,0.,0.)) ;
#109985 = DIRECTION('ref_axis',(0.,1.30104260698261E-14,-1.)) ;
#109986 = DIRECTION('',(0.,0.,1.)) ;
#109987 = DIRECTION('',(0.,-1.,0.)) ;
#109988 = DIRECTION('',(0.,0.,-1.)) ;
#109989 = DIRECTION('center_axis',(-1.,0.,0.)) ;
#109990 = DIRECTION('ref_axis',(0.,1.08420217248551E-14,-1.)) ;
#109991 = DIRECTION('',(0.,-1.,-1.07081696047951E-16)) ;
#109992 = DIRECTION('center_axis',(-1.,0.,0.)) ;
#109993 = DIRECTION('ref_axis',(0.,0.,-1.)) ;
#109994 = DIRECTION('',(0.,0.,1.)) ;
#109995 = DIRECTION('center_axis',(-1.,0.,0.)) ;
#109996 = DIRECTION('ref_axis',(0.,4.33680868994204E-15,-1.)) ;
#109997 = DIRECTION('center_axis',(1.,0.,0.)) ;
#109998 = DIRECTION('ref_axis',(0.,0.,-1.)) ;
#109999 = DIRECTION('center_axis',(-1.,0.,0.)) ;
#110000 = DIRECTION('ref_axis',(0.,-2.16840434497102E-15,-1.)) ;
#110001 = DIRECTION('',(0.,0.,1.)) ;
#110002 = DIRECTION('center_axis',(-1.,0.,0.)) ;
#110003 = DIRECTION('ref_axis',(0.,0.,-1.)) ;
#110004 = DIRECTION('',(0.,1.,1.07081696047951E-16)) ;
#110005 = DIRECTION('center_axis',(-1.,0.,0.)) ;
#110006 = DIRECTION('ref_axis',(0.,0.,-1.)) ;
#110007 = DIRECTION('',(0.,0.,-1.)) ;
#110008 = DIRECTION('',(0.,1.,0.)) ;
#110009 = DIRECTION('',(0.,3.99416362155027E-15,1.)) ;
#110010 = DIRECTION('center_axis',(-1.,0.,0.)) ;
#110011 = DIRECTION('ref_axis',(0.,6.50521303491307E-15,-1.)) ;
#110012 = DIRECTION('',(0.,0.707106781186546,0.707106781186549)) ;
#110013 = DIRECTION('center_axis',(-1.,0.,0.)) ;
#110014 = DIRECTION('ref_axis',(0.,0.,-1.)) ;
#110015 = DIRECTION('',(0.,0.,-1.)) ;
#110016 = DIRECTION('',(0.,-0.707106781186548,0.707106781186547)) ;
#110017 = DIRECTION('center_axis',(-1.,0.,0.)) ;
#110018 = DIRECTION('ref_axis',(0.,0.,-1.)) ;
#110019 = DIRECTION('',(0.,0.,1.)) ;
#110020 = DIRECTION('',(0.,-1.,0.)) ;
#110021 = DIRECTION('',(0.,0.,-1.)) ;
#110022 = DIRECTION('center_axis',(-1.,0.,0.)) ;
#110023 = DIRECTION('ref_axis',(0.,1.08420217248551E-14,-1.)) ;
#110024 = DIRECTION('',(0.,-1.,-1.07081696047951E-16)) ;
#110025 = DIRECTION('center_axis',(-1.,0.,0.)) ;
#110026 = DIRECTION('ref_axis',(0.,0.,-1.)) ;
#110027 = DIRECTION('',(0.,0.,1.)) ;
#110028 = DIRECTION('center_axis',(-1.,0.,0.)) ;
#110029 = DIRECTION('ref_axis',(0.,0.,-1.)) ;
#110030 = DIRECTION('center_axis',(1.,0.,0.)) ;
#110031 = DIRECTION('ref_axis',(0.,0.,-1.)) ;
#110032 = DIRECTION('center_axis',(-1.,0.,0.)) ;
#110033 = DIRECTION('ref_axis',(0.,-2.16840434497102E-15,-1.)) ;
#110034 = DIRECTION('',(0.,0.,1.)) ;
#110035 = DIRECTION('center_axis',(-1.,0.,0.)) ;
#110036 = DIRECTION('ref_axis',(0.,0.,-1.)) ;
#110037 = DIRECTION('',(0.,1.,1.07081696047951E-16)) ;
#110038 = DIRECTION('center_axis',(-1.,0.,0.)) ;
#110039 = DIRECTION('ref_axis',(0.,0.,-1.)) ;
#110040 = DIRECTION('',(0.,0.,-1.)) ;
#110041 = DIRECTION('',(0.,1.,0.)) ;
#110042 = DIRECTION('',(0.,3.99416362155027E-15,1.)) ;
#110043 = DIRECTION('center_axis',(-1.,0.,0.)) ;
#110044 = DIRECTION('ref_axis',(0.,6.50521303491307E-15,-1.)) ;
#110045 = DIRECTION('',(0.,0.707106781186546,0.707106781186549)) ;
#110046 = DIRECTION('center_axis',(-1.,0.,0.)) ;
#110047 = DIRECTION('ref_axis',(0.,0.,-1.)) ;
#110048 = DIRECTION('',(0.,0.,-1.)) ;
#110049 = DIRECTION('',(0.,-0.707106781186548,0.707106781186547)) ;
#110050 = DIRECTION('center_axis',(-1.,0.,0.)) ;
#110051 = DIRECTION('ref_axis',(0.,0.,-1.)) ;
#110052 = DIRECTION('',(0.,0.,1.)) ;
#110053 = DIRECTION('',(0.,-1.,0.)) ;
#110054 = DIRECTION('',(0.,0.,-1.)) ;
#110055 = DIRECTION('center_axis',(-1.,0.,0.)) ;
#110056 = DIRECTION('ref_axis',(0.,1.08420217248551E-14,-1.)) ;
#110057 = DIRECTION('',(0.,-1.,-1.07081696047951E-16)) ;
#110058 = DIRECTION('center_axis',(-1.,0.,0.)) ;
#110059 = DIRECTION('ref_axis',(0.,0.,-1.)) ;
#110060 = DIRECTION('',(0.,0.,1.)) ;
#110061 = DIRECTION('center_axis',(-1.,0.,0.)) ;
#110062 = DIRECTION('ref_axis',(0.,0.,-1.)) ;
#110063 = DIRECTION('center_axis',(1.,0.,0.)) ;
#110064 = DIRECTION('ref_axis',(0.,0.,-1.)) ;
#110065 = DIRECTION('center_axis',(-1.,0.,0.)) ;
#110066 = DIRECTION('ref_axis',(0.,-2.16840434497102E-15,-1.)) ;
#110067 = DIRECTION('',(0.,0.,1.)) ;
#110068 = DIRECTION('center_axis',(-1.,0.,0.)) ;
#110069 = DIRECTION('ref_axis',(0.,0.,-1.)) ;
#110070 = DIRECTION('',(0.,1.,1.07081696047951E-16)) ;
#110071 = DIRECTION('center_axis',(-1.,0.,0.)) ;
#110072 = DIRECTION('ref_axis',(0.,0.,-1.)) ;
#110073 = DIRECTION('',(0.,0.,-1.)) ;
#110074 = DIRECTION('',(0.,1.,0.)) ;
#110075 = DIRECTION('',(0.,3.99416362155027E-15,1.)) ;
#110076 = DIRECTION('center_axis',(-1.,0.,0.)) ;
#110077 = DIRECTION('ref_axis',(0.,6.50521303491307E-15,-1.)) ;
#110078 = DIRECTION('',(0.,0.707106781186546,0.707106781186549)) ;
#110079 = DIRECTION('center_axis',(-1.,0.,0.)) ;
#110080 = DIRECTION('ref_axis',(0.,0.,-1.)) ;
#110081 = DIRECTION('',(0.,0.,-1.)) ;
#110082 = DIRECTION('',(0.,-0.707106781186548,0.707106781186547)) ;
#110083 = DIRECTION('center_axis',(-1.,0.,0.)) ;
#110084 = DIRECTION('ref_axis',(0.,0.,-1.)) ;
#110085 = DIRECTION('',(0.,0.,1.)) ;
#110086 = DIRECTION('',(0.,-1.,0.)) ;
#110087 = DIRECTION('',(0.,0.,-1.)) ;
#110088 = DIRECTION('center_axis',(-1.,0.,0.)) ;
#110089 = DIRECTION('ref_axis',(0.,1.08420217248551E-14,-1.)) ;
#110090 = DIRECTION('',(0.,-1.,-1.07081696047951E-16)) ;
#110091 = DIRECTION('center_axis',(-1.,0.,0.)) ;
#110092 = DIRECTION('ref_axis',(0.,0.,-1.)) ;
#110093 = DIRECTION('',(0.,0.,1.)) ;
#110094 = DIRECTION('center_axis',(-1.,0.,0.)) ;
#110095 = DIRECTION('ref_axis',(0.,0.,-1.)) ;
#110096 = DIRECTION('center_axis',(1.,0.,0.)) ;
#110097 = DIRECTION('ref_axis',(0.,0.,-1.)) ;
#110098 = DIRECTION('center_axis',(-1.,0.,0.)) ;
#110099 = DIRECTION('ref_axis',(0.,-2.16840434497102E-15,-1.)) ;
#110100 = DIRECTION('',(0.,0.,1.)) ;
#110101 = DIRECTION('center_axis',(-1.,0.,0.)) ;
#110102 = DIRECTION('ref_axis',(0.,0.,-1.)) ;
#110103 = DIRECTION('',(0.,1.,1.07081696047951E-16)) ;
#110104 = DIRECTION('center_axis',(-1.,0.,0.)) ;
#110105 = DIRECTION('ref_axis',(0.,0.,-1.)) ;
#110106 = DIRECTION('',(0.,0.,-1.)) ;
#110107 = DIRECTION('',(0.,1.,0.)) ;
#110108 = DIRECTION('',(0.,3.99416362155027E-15,1.)) ;
#110109 = DIRECTION('center_axis',(-1.,0.,0.)) ;
#110110 = DIRECTION('ref_axis',(0.,2.16840434497102E-15,-1.)) ;
#110111 = DIRECTION('',(0.,0.707106781186546,0.707106781186549)) ;
#110112 = DIRECTION('center_axis',(-1.,0.,0.)) ;
#110113 = DIRECTION('ref_axis',(0.,0.,-1.)) ;
#110114 = DIRECTION('',(0.,0.,-1.)) ;
#110115 = DIRECTION('',(0.,-0.707106781186548,0.707106781186547)) ;
#110116 = DIRECTION('center_axis',(-1.,0.,0.)) ;
#110117 = DIRECTION('ref_axis',(0.,0.,-1.)) ;
#110118 = DIRECTION('',(0.,0.,1.)) ;
#110119 = DIRECTION('',(0.,-1.,0.)) ;
#110120 = DIRECTION('',(0.,0.,-1.)) ;
#110121 = DIRECTION('center_axis',(-1.,0.,0.)) ;
#110122 = DIRECTION('ref_axis',(0.,1.08420217248551E-14,-1.)) ;
#110123 = DIRECTION('',(0.,-1.,-1.07081696047951E-16)) ;
#110124 = DIRECTION('center_axis',(-1.,0.,0.)) ;
#110125 = DIRECTION('ref_axis',(0.,0.,-1.)) ;
#110126 = DIRECTION('',(0.,0.,1.)) ;
#110127 = DIRECTION('center_axis',(-1.,0.,0.)) ;
#110128 = DIRECTION('ref_axis',(0.,0.,-1.)) ;
#110129 = DIRECTION('center_axis',(1.,0.,0.)) ;
#110130 = DIRECTION('ref_axis',(0.,0.,-1.)) ;
#110131 = DIRECTION('center_axis',(-1.,0.,0.)) ;
#110132 = DIRECTION('ref_axis',(0.,-2.168404344971E-15,-1.)) ;
#110133 = DIRECTION('',(0.,0.,1.)) ;
#110134 = DIRECTION('center_axis',(-1.,0.,0.)) ;
#110135 = DIRECTION('ref_axis',(0.,0.,-1.)) ;
#110136 = DIRECTION('',(0.,1.,1.07081696047951E-16)) ;
#110137 = DIRECTION('center_axis',(-1.,0.,0.)) ;
#110138 = DIRECTION('ref_axis',(0.,0.,-1.)) ;
#110139 = DIRECTION('',(0.,0.,-1.)) ;
#110140 = DIRECTION('',(0.,1.,0.)) ;
#110141 = DIRECTION('',(0.,3.99416362155027E-15,1.)) ;
#110142 = DIRECTION('center_axis',(-1.,0.,0.)) ;
#110143 = DIRECTION('ref_axis',(0.,2.16840434497102E-15,-1.)) ;
#110144 = DIRECTION('',(0.,0.707106781186546,0.707106781186549)) ;
#110145 = DIRECTION('center_axis',(-1.,0.,0.)) ;
#110146 = DIRECTION('ref_axis',(0.,0.,-1.)) ;
#110147 = DIRECTION('',(0.,0.,-1.)) ;
#110148 = DIRECTION('',(0.,-0.707106781186548,0.707106781186547)) ;
#110149 = DIRECTION('center_axis',(-1.,0.,0.)) ;
#110150 = DIRECTION('ref_axis',(0.,0.,-1.)) ;
#110151 = DIRECTION('',(0.,0.,1.)) ;
#110152 = DIRECTION('',(0.,-1.,0.)) ;
#110153 = DIRECTION('',(0.,0.,-1.)) ;
#110154 = DIRECTION('center_axis',(-1.,0.,0.)) ;
#110155 = DIRECTION('ref_axis',(0.,1.0842021724855E-14,-1.)) ;
#110156 = DIRECTION('',(0.,-1.,-1.07081696047951E-16)) ;
#110157 = DIRECTION('center_axis',(-1.,0.,0.)) ;
#110158 = DIRECTION('ref_axis',(0.,0.,-1.)) ;
#110159 = DIRECTION('',(0.,0.,1.)) ;
#110160 = DIRECTION('center_axis',(-1.,0.,0.)) ;
#110161 = DIRECTION('ref_axis',(0.,-2.168404344971E-15,-1.)) ;
#110162 = DIRECTION('center_axis',(1.,0.,0.)) ;
#110163 = DIRECTION('ref_axis',(0.,0.,-1.)) ;
#110164 = DIRECTION('center_axis',(-1.,0.,0.)) ;
#110165 = DIRECTION('ref_axis',(0.,-2.168404344971E-15,-1.)) ;
#110166 = DIRECTION('',(0.,0.,1.)) ;
#110167 = DIRECTION('center_axis',(-1.,0.,0.)) ;
#110168 = DIRECTION('ref_axis',(0.,0.,-1.)) ;
#110169 = DIRECTION('',(0.,1.,1.07081696047951E-16)) ;
#110170 = DIRECTION('center_axis',(-1.,0.,0.)) ;
#110171 = DIRECTION('ref_axis',(0.,0.,-1.)) ;
#110172 = DIRECTION('',(0.,0.,-1.)) ;
#110173 = DIRECTION('',(0.,1.,0.)) ;
#110174 = DIRECTION('',(0.,3.99416362155027E-15,1.)) ;
#110175 = DIRECTION('center_axis',(-1.,0.,0.)) ;
#110176 = DIRECTION('ref_axis',(0.,0.,-1.)) ;
#110177 = DIRECTION('',(0.,0.707106781186546,0.707106781186549)) ;
#110178 = DIRECTION('center_axis',(-1.,0.,0.)) ;
#110179 = DIRECTION('ref_axis',(0.,0.,-1.)) ;
#110180 = DIRECTION('',(0.,0.,-1.)) ;
#110181 = DIRECTION('',(0.,-0.707106781186548,0.707106781186547)) ;
#110182 = DIRECTION('center_axis',(-1.,0.,0.)) ;
#110183 = DIRECTION('ref_axis',(0.,0.,-1.)) ;
#110184 = DIRECTION('',(0.,0.,1.)) ;
#110185 = DIRECTION('',(0.,-1.,0.)) ;
#110186 = DIRECTION('',(0.,0.,-1.)) ;
#110187 = DIRECTION('center_axis',(-1.,0.,0.)) ;
#110188 = DIRECTION('ref_axis',(0.,1.0842021724855E-14,-1.)) ;
#110189 = DIRECTION('',(0.,-1.,-1.07081696047951E-16)) ;
#110190 = DIRECTION('center_axis',(-1.,0.,0.)) ;
#110191 = DIRECTION('ref_axis',(0.,0.,-1.)) ;
#110192 = DIRECTION('',(0.,0.,1.)) ;
#110193 = DIRECTION('center_axis',(-1.,0.,0.)) ;
#110194 = DIRECTION('ref_axis',(0.,-2.168404344971E-15,-1.)) ;
#110195 = DIRECTION('center_axis',(1.,0.,0.)) ;
#110196 = DIRECTION('ref_axis',(0.,0.,-1.)) ;
#110197 = DIRECTION('center_axis',(-1.,0.,0.)) ;
#110198 = DIRECTION('ref_axis',(0.,0.,-1.)) ;
#110199 = DIRECTION('',(0.,0.,1.)) ;
#110200 = DIRECTION('center_axis',(-1.,0.,0.)) ;
#110201 = DIRECTION('ref_axis',(0.,0.,-1.)) ;
#110202 = DIRECTION('',(0.,1.,1.07081696047951E-16)) ;
#110203 = DIRECTION('center_axis',(-1.,0.,0.)) ;
#110204 = DIRECTION('ref_axis',(0.,0.,-1.)) ;
#110205 = DIRECTION('',(0.,0.,-1.)) ;
#110206 = DIRECTION('',(0.,1.,0.)) ;
#110207 = DIRECTION('',(0.,3.99416362155027E-15,1.)) ;
#110208 = DIRECTION('center_axis',(-1.,0.,0.)) ;
#110209 = DIRECTION('ref_axis',(0.,0.,-1.)) ;
#110210 = DIRECTION('',(0.,0.707106781186546,0.707106781186549)) ;
#110211 = DIRECTION('center_axis',(-1.,0.,0.)) ;
#110212 = DIRECTION('ref_axis',(0.,0.,-1.)) ;
#110213 = DIRECTION('',(0.,0.,-1.)) ;
#110214 = DIRECTION('',(0.,-0.707106781186548,0.707106781186547)) ;
#110215 = DIRECTION('center_axis',(-1.,0.,0.)) ;
#110216 = DIRECTION('ref_axis',(0.,0.,-1.)) ;
#110217 = DIRECTION('',(0.,0.,1.)) ;
#110218 = DIRECTION('',(0.,-1.,0.)) ;
#110219 = DIRECTION('',(0.,0.,-1.)) ;
#110220 = DIRECTION('center_axis',(-1.,0.,0.)) ;
#110221 = DIRECTION('ref_axis',(0.,9.75781955236956E-15,-1.)) ;
#110222 = DIRECTION('',(0.,-1.,-1.07081696047951E-16)) ;
#110223 = DIRECTION('center_axis',(-1.,0.,0.)) ;
#110224 = DIRECTION('ref_axis',(0.,0.,-1.)) ;
#110225 = DIRECTION('',(0.,0.,1.)) ;
#110226 = DIRECTION('center_axis',(-1.,0.,0.)) ;
#110227 = DIRECTION('ref_axis',(0.,-2.16840434497101E-15,-1.)) ;
#110228 = DIRECTION('center_axis',(1.,0.,0.)) ;
#110229 = DIRECTION('ref_axis',(0.,0.,-1.)) ;
#110230 = DIRECTION('center_axis',(-1.,0.,0.)) ;
#110231 = DIRECTION('ref_axis',(0.,0.,-1.)) ;
#110232 = DIRECTION('',(0.,0.,1.)) ;
#110233 = DIRECTION('center_axis',(-1.,0.,0.)) ;
#110234 = DIRECTION('ref_axis',(0.,0.,-1.)) ;
#110235 = DIRECTION('',(0.,1.,1.07081696047951E-16)) ;
#110236 = DIRECTION('center_axis',(-1.,0.,0.)) ;
#110237 = DIRECTION('ref_axis',(0.,-1.0842021724855E-15,-1.)) ;
#110238 = DIRECTION('',(0.,0.,-1.)) ;
#110239 = DIRECTION('',(0.,1.,0.)) ;
#110240 = DIRECTION('',(0.,3.99416362155027E-15,1.)) ;
#110241 = DIRECTION('center_axis',(-1.,0.,0.)) ;
#110242 = DIRECTION('ref_axis',(0.,2.16840434497101E-15,-1.)) ;
#110243 = DIRECTION('',(0.,0.707106781186546,0.707106781186549)) ;
#110244 = DIRECTION('center_axis',(-1.,0.,0.)) ;
#110245 = DIRECTION('ref_axis',(0.,0.,-1.)) ;
#110246 = DIRECTION('',(0.,0.,-1.)) ;
#110247 = DIRECTION('',(0.,-0.707106781186548,0.707106781186547)) ;
#110248 = DIRECTION('center_axis',(-1.,0.,0.)) ;
#110249 = DIRECTION('ref_axis',(0.,0.,-1.)) ;
#110250 = DIRECTION('',(0.,0.,1.)) ;
#110251 = DIRECTION('',(0.,-1.,0.)) ;
#110252 = DIRECTION('',(0.,0.,-1.)) ;
#110253 = DIRECTION('center_axis',(-1.,0.,0.)) ;
#110254 = DIRECTION('ref_axis',(0.,8.67361737988403E-15,-1.)) ;
#110255 = DIRECTION('',(0.,-1.,-1.07081696047951E-16)) ;
#110256 = DIRECTION('center_axis',(-1.,0.,0.)) ;
#110257 = DIRECTION('ref_axis',(0.,0.,-1.)) ;
#110258 = DIRECTION('',(0.,0.,1.)) ;
#110259 = DIRECTION('center_axis',(-1.,0.,0.)) ;
#110260 = DIRECTION('ref_axis',(0.,2.16840434497101E-15,-1.)) ;
#110261 = DIRECTION('center_axis',(1.,0.,0.)) ;
#110262 = DIRECTION('ref_axis',(0.,0.,-1.)) ;
#110263 = DIRECTION('center_axis',(-1.,0.,0.)) ;
#110264 = DIRECTION('ref_axis',(0.,0.,-1.)) ;
#110265 = DIRECTION('',(0.,0.,1.)) ;
#110266 = DIRECTION('center_axis',(-1.,0.,0.)) ;
#110267 = DIRECTION('ref_axis',(0.,0.,-1.)) ;
#110268 = DIRECTION('',(0.,1.,1.07081696047951E-16)) ;
#110269 = DIRECTION('center_axis',(0.,0.,1.)) ;
#110270 = DIRECTION('ref_axis',(1.,0.,0.)) ;
#110271 = DIRECTION('',(0.,-1.,0.)) ;
#110272 = DIRECTION('',(-1.,0.,0.)) ;
#110273 = DIRECTION('',(-1.2303003375722E-16,1.,0.)) ;
#110274 = DIRECTION('',(1.,1.59148942750166E-16,0.)) ;
#110275 = DIRECTION('center_axis',(0.,0.,1.)) ;
#110276 = DIRECTION('ref_axis',(1.,0.,0.)) ;
#110277 = DIRECTION('',(0.,1.,0.)) ;
#110278 = DIRECTION('',(1.,0.,0.)) ;
#110279 = DIRECTION('',(-4.33680868994203E-15,-1.,0.)) ;
#110280 = DIRECTION('center_axis',(0.,0.,1.)) ;
#110281 = DIRECTION('ref_axis',(1.,0.,0.)) ;
#110282 = DIRECTION('',(1.,-5.88041856263325E-16,0.)) ;
#110283 = DIRECTION('center_axis',(0.,0.,1.)) ;
#110284 = DIRECTION('ref_axis',(1.,0.,0.)) ;
#110285 = DIRECTION('',(1.2303003375722E-16,-1.,0.)) ;
#110286 = DIRECTION('',(1.,0.,0.)) ;
#110287 = DIRECTION('',(0.,1.,0.)) ;
#110288 = DIRECTION('',(-1.,5.88041856263325E-16,0.)) ;
#110289 = DIRECTION('center_axis',(0.,0.,-1.)) ;
#110290 = DIRECTION('ref_axis',(1.,0.,0.)) ;
#110291 = DIRECTION('',(4.33680868994203E-15,1.,0.)) ;
#110292 = DIRECTION('',(-1.,0.,0.)) ;
#110293 = DIRECTION('',(0.,-1.,0.)) ;
#110294 = DIRECTION('center_axis',(0.,0.,-1.)) ;
#110295 = DIRECTION('ref_axis',(1.,0.,0.)) ;
#110296 = DIRECTION('',(-1.,-1.59148942750166E-16,0.)) ;
#110297 = DIRECTION('center_axis',(-1.,-1.53063836115601E-16,0.)) ;
#110298 = DIRECTION('ref_axis',(1.53063836115601E-16,-1.,0.)) ;
#110299 = DIRECTION('',(0.,0.,1.)) ;
#110300 = DIRECTION('',(-1.53063836115601E-16,1.,-1.020425574104E-16)) ;
#110301 = DIRECTION('',(0.,0.,-1.)) ;
#110302 = DIRECTION('',(1.53063836115601E-16,-1.,5.10212787052002E-17)) ;
#110303 = DIRECTION('',(0.,0.,1.)) ;
#110304 = DIRECTION('',(-1.53063836115601E-16,1.,-1.30104260698261E-16)) ;
#110305 = DIRECTION('center_axis',(-1.,-1.53063836115601E-16,0.)) ;
#110306 = DIRECTION('ref_axis',(1.53063836115601E-16,-1.,0.)) ;
#110307 = DIRECTION('',(0.,0.,1.)) ;
#110308 = DIRECTION('center_axis',(-1.,-1.53063836115601E-16,0.)) ;
#110309 = DIRECTION('ref_axis',(1.53063836115601E-16,-1.,0.)) ;
#110310 = DIRECTION('',(1.53063836115601E-16,-1.,-1.30104260698261E-16)) ;
#110311 = DIRECTION('center_axis',(-1.53063836115601E-16,1.,0.)) ;
#110312 = DIRECTION('ref_axis',(-1.,-1.53063836115601E-16,0.)) ;
#110313 = DIRECTION('',(-1.,-1.53063836115601E-16,2.73691106313441E-48)) ;
#110314 = DIRECTION('',(0.,0.,-1.)) ;
#110315 = DIRECTION('',(1.,1.53063836115601E-16,-1.53236300070382E-33)) ;
#110316 = DIRECTION('',(0.,0.,1.)) ;
#110317 = DIRECTION('center_axis',(1.99142572374599E-32,-1.30104260698261E-16,
-1.)) ;
#110318 = DIRECTION('ref_axis',(0.,1.,-1.30104260698261E-16)) ;
#110319 = DIRECTION('',(-1.,-1.53063836115601E-16,2.73691106313441E-48)) ;
#110320 = DIRECTION('',(1.53063836115601E-16,-1.,1.30104260698261E-16)) ;
#110321 = DIRECTION('',(1.,1.53063836115601E-16,-2.73691106313441E-48)) ;
#110322 = DIRECTION('center_axis',(-1.53063836115601E-16,1.,0.)) ;
#110323 = DIRECTION('ref_axis',(-1.,-1.53063836115601E-16,0.)) ;
#110324 = DIRECTION('',(-1.,-1.53063836115601E-16,-2.73691106313441E-48)) ;
#110325 = DIRECTION('',(0.,0.,-1.)) ;
#110326 = DIRECTION('',(1.,1.53063836115601E-16,-2.73691106313441E-48)) ;
#110327 = DIRECTION('',(0.,0.,1.)) ;
#110328 = DIRECTION('center_axis',(1.99142572374599E-32,-1.30104260698261E-16,
1.)) ;
#110329 = DIRECTION('ref_axis',(0.,-1.,-1.30104260698261E-16)) ;
#110330 = DIRECTION('',(-1.,-1.53063836115601E-16,-2.73691106313441E-48)) ;
#110331 = DIRECTION('',(-1.53063836115601E-16,1.,1.30104260698261E-16)) ;
#110332 = DIRECTION('',(1.,1.53063836115601E-16,2.73691106313441E-48)) ;
#110333 = DIRECTION('',(2.16840434497101E-16,-1.,-1.30104260698261E-16)) ;
#110334 = DIRECTION('center_axis',(-1.53063836115601E-16,1.,0.)) ;
#110335 = DIRECTION('ref_axis',(-1.,-1.53063836115601E-16,0.)) ;
#110336 = DIRECTION('',(-1.,-1.53063836115601E-16,3.06472600140763E-33)) ;
#110337 = DIRECTION('',(0.,0.,-1.)) ;
#110338 = DIRECTION('',(1.,1.53063836115601E-16,2.73691106313441E-48)) ;
#110339 = DIRECTION('',(0.,0.,1.)) ;
#110340 = DIRECTION('center_axis',(1.,0.,0.)) ;
#110341 = DIRECTION('ref_axis',(0.,0.,-1.)) ;
#110342 = DIRECTION('',(1.,0.,0.)) ;
#110343 = DIRECTION('center_axis',(1.,0.,0.)) ;
#110344 = DIRECTION('ref_axis',(0.,0.,1.)) ;
#110345 = DIRECTION('',(1.,0.,0.)) ;
#110346 = DIRECTION('center_axis',(-1.,0.,0.)) ;
#110347 = DIRECTION('ref_axis',(0.,0.,-1.)) ;
#110348 = DIRECTION('center_axis',(0.,0.,1.)) ;
#110349 = DIRECTION('ref_axis',(1.,0.,0.)) ;
#110350 = DIRECTION('',(0.,1.,0.)) ;
#110351 = DIRECTION('',(1.,0.,0.)) ;
#110352 = DIRECTION('',(0.,-1.,0.)) ;
#110353 = DIRECTION('center_axis',(1.,0.,0.)) ;
#110354 = DIRECTION('ref_axis',(0.,0.,-1.)) ;
#110355 = DIRECTION('center_axis',(1.,0.,0.)) ;
#110356 = DIRECTION('ref_axis',(0.,0.,1.)) ;
#110357 = DIRECTION('',(1.,0.,0.)) ;
#110358 = DIRECTION('center_axis',(-1.,0.,0.)) ;
#110359 = DIRECTION('ref_axis',(0.,0.,-1.)) ;
#110360 = DIRECTION('center_axis',(0.,-1.,3.99416362155027E-15)) ;
#110361 = DIRECTION('ref_axis',(0.,-3.99416362155027E-15,-1.)) ;
#110362 = DIRECTION('',(0.,3.99416362155027E-15,1.)) ;
#110363 = DIRECTION('',(1.,0.,0.)) ;
#110364 = DIRECTION('',(0.,-3.99416362155027E-15,-1.)) ;
#110365 = DIRECTION('center_axis',(1.,0.,0.)) ;
#110366 = DIRECTION('ref_axis',(0.,0.,-1.)) ;
#110367 = DIRECTION('center_axis',(-1.,0.,0.)) ;
#110368 = DIRECTION('ref_axis',(0.,0.,-1.)) ;
#110369 = DIRECTION('',(1.,0.,0.)) ;
#110370 = DIRECTION('center_axis',(1.,0.,0.)) ;
#110371 = DIRECTION('ref_axis',(0.,0.,-1.)) ;
#110372 = DIRECTION('center_axis',(0.,-0.707106781186549,0.707106781186546)) ;
#110373 = DIRECTION('ref_axis',(0.,-0.707106781186546,-0.707106781186549)) ;
#110374 = DIRECTION('',(0.,0.707106781186546,0.707106781186549)) ;
#110375 = DIRECTION('',(1.,0.,0.)) ;
#110376 = DIRECTION('',(0.,-0.707106781186546,-0.707106781186549)) ;
#110377 = DIRECTION('center_axis',(1.,0.,0.)) ;
#110378 = DIRECTION('ref_axis',(0.,0.382683432365091,0.923879532511286)) ;
#110379 = DIRECTION('',(1.,0.,0.)) ;
#110380 = DIRECTION('center_axis',(1.,0.,0.)) ;
#110381 = DIRECTION('ref_axis',(0.,0.,-1.)) ;
#110382 = DIRECTION('center_axis',(0.,1.,0.)) ;
#110383 = DIRECTION('ref_axis',(0.,0.,1.)) ;
#110384 = DIRECTION('',(0.,0.,-1.)) ;
#110385 = DIRECTION('',(0.,0.,1.)) ;
#110386 = DIRECTION('center_axis',(0.,-0.707106781186547,-0.707106781186548)) ;
#110387 = DIRECTION('ref_axis',(0.,0.707106781186548,-0.707106781186547)) ;
#110388 = DIRECTION('',(0.,-0.707106781186548,0.707106781186547)) ;
#110389 = DIRECTION('',(1.,0.,0.)) ;
#110390 = DIRECTION('',(0.,0.707106781186548,-0.707106781186547)) ;
#110391 = DIRECTION('center_axis',(1.,0.,0.)) ;
#110392 = DIRECTION('ref_axis',(0.,0.,-1.)) ;
#110393 = DIRECTION('center_axis',(-1.,0.,0.)) ;
#110394 = DIRECTION('ref_axis',(0.,0.,-1.)) ;
#110395 = DIRECTION('',(1.,0.,0.)) ;
#110396 = DIRECTION('center_axis',(1.,0.,0.)) ;
#110397 = DIRECTION('ref_axis',(0.,0.,-1.)) ;
#110398 = DIRECTION('center_axis',(0.,-1.,0.)) ;
#110399 = DIRECTION('ref_axis',(0.,0.,-1.)) ;
#110400 = DIRECTION('',(0.,0.,1.)) ;
#110401 = DIRECTION('',(1.,0.,0.)) ;
#110402 = DIRECTION('',(0.,0.,-1.)) ;
#110403 = DIRECTION('center_axis',(1.,0.,0.)) ;
#110404 = DIRECTION('ref_axis',(0.,0.,-1.)) ;
#110405 = DIRECTION('center_axis',(1.,0.,0.)) ;
#110406 = DIRECTION('ref_axis',(0.,0.,1.)) ;
#110407 = DIRECTION('',(1.,0.,0.)) ;
#110408 = DIRECTION('center_axis',(-1.,0.,0.)) ;
#110409 = DIRECTION('ref_axis',(0.,0.,-1.)) ;
#110410 = DIRECTION('center_axis',(0.,0.,-1.)) ;
#110411 = DIRECTION('ref_axis',(-1.,0.,0.)) ;
#110412 = DIRECTION('',(0.,-1.,0.)) ;
#110413 = DIRECTION('',(1.,0.,0.)) ;
#110414 = DIRECTION('',(0.,1.,0.)) ;
#110415 = DIRECTION('center_axis',(1.,0.,0.)) ;
#110416 = DIRECTION('ref_axis',(0.,0.,-1.)) ;
#110417 = DIRECTION('center_axis',(1.,0.,0.)) ;
#110418 = DIRECTION('ref_axis',(0.,0.,1.)) ;
#110419 = DIRECTION('',(1.,0.,0.)) ;
#110420 = DIRECTION('center_axis',(-1.,0.,0.)) ;
#110421 = DIRECTION('ref_axis',(0.,0.,-1.)) ;
#110422 = DIRECTION('center_axis',(0.,1.,0.)) ;
#110423 = DIRECTION('ref_axis',(0.,0.,1.)) ;
#110424 = DIRECTION('',(0.,0.,-1.)) ;
#110425 = DIRECTION('',(1.,0.,0.)) ;
#110426 = DIRECTION('',(0.,0.,1.)) ;
#110427 = DIRECTION('center_axis',(1.,0.,0.)) ;
#110428 = DIRECTION('ref_axis',(0.,0.,-1.)) ;
#110429 = DIRECTION('center_axis',(-1.,0.,0.)) ;
#110430 = DIRECTION('ref_axis',(0.,1.51788304147971E-14,-1.)) ;
#110431 = DIRECTION('',(1.,0.,0.)) ;
#110432 = DIRECTION('center_axis',(1.,0.,0.)) ;
#110433 = DIRECTION('ref_axis',(0.,0.,-1.)) ;
#110434 = DIRECTION('center_axis',(0.,1.07081696047951E-16,-1.)) ;
#110435 = DIRECTION('ref_axis',(0.,1.,1.07081696047951E-16)) ;
#110436 = DIRECTION('',(0.,-1.,-1.07081696047951E-16)) ;
#110437 = DIRECTION('',(1.,0.,0.)) ;
#110438 = DIRECTION('',(0.,1.,1.07081696047951E-16)) ;
#110439 = DIRECTION('center_axis',(1.,0.,0.)) ;
#110440 = DIRECTION('ref_axis',(0.,0.,-1.)) ;
#110441 = DIRECTION('center_axis',(-1.,0.,0.)) ;
#110442 = DIRECTION('ref_axis',(0.,0.,-1.)) ;
#110443 = DIRECTION('',(1.,0.,0.)) ;
#110444 = DIRECTION('center_axis',(1.,0.,0.)) ;
#110445 = DIRECTION('ref_axis',(0.,0.,-1.)) ;
#110446 = DIRECTION('center_axis',(0.,-1.,0.)) ;
#110447 = DIRECTION('ref_axis',(0.,0.,-1.)) ;
#110448 = DIRECTION('',(0.,0.,1.)) ;
#110449 = DIRECTION('',(1.,0.,0.)) ;
#110450 = DIRECTION('',(0.,0.,-1.)) ;
#110451 = DIRECTION('center_axis',(1.,0.,0.)) ;
#110452 = DIRECTION('ref_axis',(0.,0.,-1.)) ;
#110453 = DIRECTION('center_axis',(-1.,0.,0.)) ;
#110454 = DIRECTION('ref_axis',(0.,0.,-1.)) ;
#110455 = DIRECTION('',(1.,0.,0.)) ;
#110456 = DIRECTION('center_axis',(1.,0.,0.)) ;
#110457 = DIRECTION('ref_axis',(0.,0.,-1.)) ;
#110458 = DIRECTION('center_axis',(1.,0.,0.)) ;
#110459 = DIRECTION('ref_axis',(0.,0.,-1.)) ;
#110460 = DIRECTION('center_axis',(1.,0.,0.)) ;
#110461 = DIRECTION('ref_axis',(0.,0.,1.)) ;
#110462 = DIRECTION('',(1.,0.,0.)) ;
#110463 = DIRECTION('center_axis',(-1.,0.,0.)) ;
#110464 = DIRECTION('ref_axis',(0.,0.,-1.)) ;
#110465 = DIRECTION('center_axis',(1.,0.,0.)) ;
#110466 = DIRECTION('ref_axis',(0.,0.,-1.)) ;
#110467 = DIRECTION('center_axis',(-1.,0.,0.)) ;
#110468 = DIRECTION('ref_axis',(0.,0.,-1.)) ;
#110469 = DIRECTION('',(1.,0.,0.)) ;
#110470 = DIRECTION('center_axis',(1.,0.,0.)) ;
#110471 = DIRECTION('ref_axis',(0.,0.,-1.)) ;
#110472 = DIRECTION('center_axis',(0.,-1.,0.)) ;
#110473 = DIRECTION('ref_axis',(0.,0.,-1.)) ;
#110474 = DIRECTION('',(0.,0.,1.)) ;
#110475 = DIRECTION('',(1.,0.,0.)) ;
#110476 = DIRECTION('',(0.,0.,-1.)) ;
#110477 = DIRECTION('center_axis',(1.,0.,0.)) ;
#110478 = DIRECTION('ref_axis',(0.,0.,-1.)) ;
#110479 = DIRECTION('center_axis',(-1.,0.,0.)) ;
#110480 = DIRECTION('ref_axis',(0.,0.,-1.)) ;
#110481 = DIRECTION('',(1.,0.,0.)) ;
#110482 = DIRECTION('center_axis',(1.,0.,0.)) ;
#110483 = DIRECTION('ref_axis',(0.,0.,-1.)) ;
#110484 = DIRECTION('center_axis',(0.,-1.07081696047951E-16,1.)) ;
#110485 = DIRECTION('ref_axis',(0.,-1.,-1.07081696047951E-16)) ;
#110486 = DIRECTION('',(0.,1.,1.07081696047951E-16)) ;
#110487 = DIRECTION('',(1.,0.,0.)) ;
#110488 = DIRECTION('',(0.,-1.,-1.07081696047951E-16)) ;
#110489 = DIRECTION('center_axis',(1.,0.,0.)) ;
#110490 = DIRECTION('ref_axis',(0.,0.,-1.)) ;
#110491 = DIRECTION('center_axis',(-1.,0.,0.)) ;
#110492 = DIRECTION('ref_axis',(0.,0.,-1.)) ;
#110493 = DIRECTION('',(1.,0.,0.)) ;
#110494 = DIRECTION('center_axis',(1.,0.,0.)) ;
#110495 = DIRECTION('ref_axis',(0.,0.,-1.)) ;
#110496 = DIRECTION('center_axis',(0.,1.,0.)) ;
#110497 = DIRECTION('ref_axis',(0.,0.,1.)) ;
#110498 = DIRECTION('',(0.,0.,-1.)) ;
#110499 = DIRECTION('',(0.,0.,1.)) ;
#110500 = DIRECTION('center_axis',(-1.,0.,0.)) ;
#110501 = DIRECTION('ref_axis',(0.,0.,1.)) ;
#110502 = DIRECTION('center_axis',(-1.,0.,0.)) ;
#110503 = DIRECTION('ref_axis',(0.,0.,1.)) ;
#110504 = DIRECTION('',(0.,-1.,0.)) ;
#110505 = DIRECTION('center_axis',(-1.,0.,0.)) ;
#110506 = DIRECTION('ref_axis',(0.,0.,1.)) ;
#110507 = DIRECTION('',(0.,0.,1.)) ;
#110508 = DIRECTION('',(0.,-1.,-1.07081696047951E-16)) ;
#110509 = DIRECTION('',(0.,0.,-1.)) ;
#110510 = DIRECTION('center_axis',(-1.,0.,0.)) ;
#110511 = DIRECTION('ref_axis',(0.,0.,1.)) ;
#110512 = DIRECTION('',(0.,0.,-1.)) ;
#110513 = DIRECTION('',(0.,1.,1.07081696047951E-16)) ;
#110514 = DIRECTION('',(0.,0.,1.)) ;
#110515 = DIRECTION('center_axis',(-1.,0.,0.)) ;
#110516 = DIRECTION('ref_axis',(0.,0.,1.)) ;
#110517 = DIRECTION('',(0.,1.,0.)) ;
#110518 = DIRECTION('center_axis',(-1.,0.,0.)) ;
#110519 = DIRECTION('ref_axis',(0.,0.,1.)) ;
#110520 = DIRECTION('',(0.,0.,-1.)) ;
#110521 = DIRECTION('',(0.,0.707106781186548,-0.707106781186547)) ;
#110522 = DIRECTION('',(0.,0.,1.)) ;
#110523 = DIRECTION('',(0.,-0.707106781186546,-0.707106781186549)) ;
#110524 = DIRECTION('',(0.,-3.99416362155027E-15,-1.)) ;
#110525 = DIRECTION('center_axis',(1.,0.,0.)) ;
#110526 = DIRECTION('ref_axis',(0.,0.,-1.)) ;
#110527 = DIRECTION('',(0.,-1.,0.)) ;
#110528 = DIRECTION('center_axis',(-1.,0.,0.)) ;
#110529 = DIRECTION('ref_axis',(0.,0.,-1.)) ;
#110530 = DIRECTION('',(0.,0.,-1.)) ;
#110531 = DIRECTION('center_axis',(-1.,0.,0.)) ;
#110532 = DIRECTION('ref_axis',(0.,-1.0842021724855E-15,-1.)) ;
#110533 = DIRECTION('',(0.,-1.,0.)) ;
#110534 = DIRECTION('center_axis',(-1.,0.,0.)) ;
#110535 = DIRECTION('ref_axis',(0.,0.,-1.)) ;
#110536 = DIRECTION('',(0.,0.,1.)) ;
#110537 = DIRECTION('center_axis',(-1.,0.,0.)) ;
#110538 = DIRECTION('ref_axis',(0.,0.,-1.)) ;
#110539 = DIRECTION('center_axis',(1.53063836115601E-16,-1.,-1.30104260698261E-16)) ;
#110540 = DIRECTION('ref_axis',(1.,1.53063836115601E-16,1.99142572374599E-32)) ;
#110541 = DIRECTION('center_axis',(0.,1.,0.)) ;
#110542 = DIRECTION('ref_axis',(0.,0.,1.)) ;
#110543 = DIRECTION('center_axis',(0.,-1.,0.)) ;
#110544 = DIRECTION('ref_axis',(0.,0.,-1.)) ;
#110545 = DIRECTION('center_axis',(1.,1.53063836115601E-16,2.73691106313441E-48)) ;
#110546 = DIRECTION('ref_axis',(-1.53063836115601E-16,1.,-4.18922106430579E-64)) ;
#110547 = DIRECTION('center_axis',(-1.,0.,0.)) ;
#110548 = DIRECTION('ref_axis',(0.,0.,1.)) ;
#110549 = DIRECTION('center_axis',(1.,1.53063836115601E-16,0.)) ;
#110550 = DIRECTION('ref_axis',(1.53063836115601E-16,-1.,0.)) ;
#110551 = DIRECTION('center_axis',(0.,1.,0.)) ;
#110552 = DIRECTION('ref_axis',(1.,0.,0.)) ;
#110553 = DIRECTION('center_axis',(0.,1.,0.)) ;
#110554 = DIRECTION('ref_axis',(0.,0.,-1.)) ;
#110555 = DIRECTION('center_axis',(0.,0.,1.)) ;
#110556 = DIRECTION('ref_axis',(-1.,0.,0.)) ;
#110557 = DIRECTION('center_axis',(0.,1.,0.)) ;
#110558 = DIRECTION('ref_axis',(1.,0.,0.)) ;
#110559 = DIRECTION('center_axis',(0.,0.,1.)) ;
#110560 = DIRECTION('ref_axis',(-1.,0.,0.)) ;
#110561 = DIRECTION('center_axis',(1.,1.0842021724855E-15,0.)) ;
#110562 = DIRECTION('ref_axis',(1.0842021724855E-15,-1.,0.)) ;
#110563 = DIRECTION('center_axis',(-1.,-1.53063836115601E-16,0.)) ;
#110564 = DIRECTION('ref_axis',(0.,-1.,0.)) ;
#110565 = DIRECTION('center_axis',(0.,0.,-1.)) ;
#110566 = DIRECTION('ref_axis',(1.,0.,0.)) ;
#110567 = DIRECTION('center_axis',(0.,0.,-1.)) ;
#110568 = DIRECTION('ref_axis',(0.804034447892617,0.594582716366709,0.)) ;
#110569 = DIRECTION('center_axis',(0.,0.,1.)) ;
#110570 = DIRECTION('ref_axis',(1.,0.,0.)) ;
#110571 = DIRECTION('',(0.,0.,-1.)) ;
#110572 = DIRECTION('center_axis',(-2.16840434497101E-16,1.,1.30104260698261E-16)) ;
#110573 = DIRECTION('ref_axis',(1.,2.16840434497101E-16,1.22464679914735E-16)) ;
#110574 = DIRECTION('',(-2.16840434497101E-16,1.,1.30104260698261E-16)) ;
#110575 = DIRECTION('center_axis',(0.,1.,0.)) ;
#110576 = DIRECTION('ref_axis',(0.,0.,1.)) ;
#110577 = DIRECTION('center_axis',(-1.,-1.53063836115601E-16,-2.73691106313441E-48)) ;
#110578 = DIRECTION('ref_axis',(1.53063836115601E-16,-1.,4.18922106430579E-64)) ;
#110579 = DIRECTION('center_axis',(1.,2.16840434497101E-16,0.)) ;
#110580 = DIRECTION('ref_axis',(2.16840434497101E-16,-1.,0.)) ;
#110581 = DIRECTION('center_axis',(0.,0.,1.)) ;
#110582 = DIRECTION('ref_axis',(1.,0.,0.)) ;
#110583 = DIRECTION('center_axis',(-1.25542992828747E-32,1.020425574104E-16,
1.)) ;
#110584 = DIRECTION('ref_axis',(-1.28107280532009E-48,-1.,1.020425574104E-16)) ;
#110585 = DIRECTION('center_axis',(0.,0.,1.)) ;
#110586 = DIRECTION('ref_axis',(1.,0.,0.)) ;
#110587 = DIRECTION('center_axis',(0.,0.,-1.)) ;
#110588 = DIRECTION('ref_axis',(-1.,0.,0.)) ;
#110589 = DIRECTION('center_axis',(1.,1.53063836115601E-16,-2.73691106313441E-48)) ;
#110590 = DIRECTION('ref_axis',(-1.53063836115601E-16,1.,4.18922106430579E-64)) ;
#110591 = DIRECTION('center_axis',(-1.,0.,0.)) ;
#110592 = DIRECTION('ref_axis',(0.,0.,1.)) ;
#110593 = DIRECTION('center_axis',(1.,1.53063836115601E-16,0.)) ;
#110594 = DIRECTION('ref_axis',(1.53063836115601E-16,-1.,0.)) ;
#110595 = DIRECTION('center_axis',(0.,1.,0.)) ;
#110596 = DIRECTION('ref_axis',(1.,0.,0.)) ;
#110597 = DIRECTION('center_axis',(-1.,-2.16840434497101E-16,0.)) ;
#110598 = DIRECTION('ref_axis',(0.,-1.,0.)) ;
#110599 = DIRECTION('center_axis',(0.,0.,-1.)) ;
#110600 = DIRECTION('ref_axis',(1.,0.,0.)) ;
#110601 = DIRECTION('center_axis',(-1.25542992828747E-32,1.020425574104E-16,
1.)) ;
#110602 = DIRECTION('ref_axis',(0.,-1.,0.)) ;
#110603 = DIRECTION('center_axis',(0.,-1.,0.)) ;
#110604 = DIRECTION('ref_axis',(-6.50521303491302E-15,0.,1.)) ;
#110605 = DIRECTION('center_axis',(-1.,0.,0.)) ;
#110606 = DIRECTION('ref_axis',(0.,0.,-1.)) ;
#110607 = DIRECTION('center_axis',(-1.,-1.53063836115601E-16,0.)) ;
#110608 = DIRECTION('ref_axis',(0.,-1.,0.)) ;
#110609 = DIRECTION('center_axis',(0.,-1.,0.)) ;
#110610 = DIRECTION('ref_axis',(0.,0.,1.)) ;
#110611 = DIRECTION('center_axis',(0.,0.,-1.)) ;
#110612 = DIRECTION('ref_axis',(-1.,0.,0.)) ;
#110613 = DIRECTION('center_axis',(0.,0.,-1.)) ;
#110614 = DIRECTION('ref_axis',(-1.,0.,0.)) ;
#110615 = DIRECTION('center_axis',(1.,1.53063836115601E-16,-3.06472600140763E-33)) ;
#110616 = DIRECTION('ref_axis',(-1.53063836115601E-16,1.,4.69098718418678E-49)) ;
#110617 = DIRECTION('center_axis',(-1.,0.,0.)) ;
#110618 = DIRECTION('ref_axis',(0.,0.,1.)) ;
#110619 = DIRECTION('center_axis',(-1.53063836115601E-16,1.,-1.020425574104E-16)) ;
#110620 = DIRECTION('ref_axis',(-1.,-1.53063836115601E-16,1.3684555315672E-47)) ;
#110621 = DIRECTION('',(1.53063836115601E-16,-1.,1.020425574104E-16)) ;
#110622 = DIRECTION('center_axis',(0.,-1.,0.)) ;
#110623 = DIRECTION('ref_axis',(0.,0.,-1.)) ;
#110624 = DIRECTION('center_axis',(-1.53063836115601E-16,1.,-1.30104260698261E-16)) ;
#110625 = DIRECTION('ref_axis',(-1.,-1.53063836115601E-16,1.99142572374599E-32)) ;
#110626 = DIRECTION('center_axis',(0.,-1.,0.)) ;
#110627 = DIRECTION('ref_axis',(0.,0.,-1.)) ;
#110628 = DIRECTION('center_axis',(-1.,-1.53063836115601E-16,2.73691106313441E-48)) ;
#110629 = DIRECTION('ref_axis',(1.53063836115601E-16,-1.,-4.18922106430579E-64)) ;
#110630 = DIRECTION('center_axis',(1.,2.16840434497101E-16,0.)) ;
#110631 = DIRECTION('ref_axis',(2.16840434497101E-16,-1.,0.)) ;
#110632 = DIRECTION('center_axis',(-1.,0.,2.16840434497101E-15)) ;
#110633 = DIRECTION('ref_axis',(2.16840434497101E-15,0.,1.)) ;
#110634 = DIRECTION('center_axis',(-1.,-2.16840434497101E-16,0.)) ;
#110635 = DIRECTION('ref_axis',(0.,-1.,0.)) ;
#110636 = DIRECTION('center_axis',(0.,0.,1.)) ;
#110637 = DIRECTION('ref_axis',(-1.,0.,0.)) ;
#110638 = DIRECTION('center_axis',(0.,1.,0.)) ;
#110639 = DIRECTION('ref_axis',(1.,0.,0.)) ;
#110640 = DIRECTION('center_axis',(0.,1.,0.)) ;
#110641 = DIRECTION('ref_axis',(0.,0.,-1.)) ;
#110642 = DIRECTION('center_axis',(1.,0.,0.)) ;
#110643 = DIRECTION('ref_axis',(0.,-1.,0.)) ;
#110644 = DIRECTION('center_axis',(1.,6.50521303491304E-15,0.)) ;
#110645 = DIRECTION('ref_axis',(-6.50521303491304E-15,1.,0.)) ;
#110646 = DIRECTION('center_axis',(8.67361737988403E-15,1.,0.)) ;
#110647 = DIRECTION('ref_axis',(-1.,8.67361737988403E-15,0.)) ;
#110648 = DIRECTION('center_axis',(1.2303003375722E-16,-1.,1.020425574104E-16)) ;
#110649 = DIRECTION('ref_axis',(1.,1.2303003375722E-16,-1.25542992828747E-32)) ;
#110650 = DIRECTION('center_axis',(0.,1.,0.)) ;
#110651 = DIRECTION('ref_axis',(0.,0.,1.)) ;
#110652 = DIRECTION('center_axis',(0.,1.,0.)) ;
#110653 = DIRECTION('ref_axis',(1.,0.,0.)) ;
#110654 = DIRECTION('center_axis',(1.,1.2303003375722E-16,0.)) ;
#110655 = DIRECTION('ref_axis',(1.2303003375722E-16,-1.,0.)) ;
#110656 = DIRECTION('center_axis',(-2.16840434497101E-15,0.,1.)) ;
#110657 = DIRECTION('ref_axis',(-1.,0.,-2.16840434497101E-15)) ;
#110658 = DIRECTION('center_axis',(0.,1.,0.)) ;
#110659 = DIRECTION('ref_axis',(1.,0.,0.)) ;
#110660 = DIRECTION('center_axis',(0.,0.,-1.)) ;
#110661 = DIRECTION('ref_axis',(1.,0.,0.)) ;
#110662 = DIRECTION('center_axis',(0.,0.,-1.)) ;
#110663 = DIRECTION('ref_axis',(-1.,0.,0.)) ;
#110664 = DIRECTION('center_axis',(0.,0.,1.)) ;
#110665 = DIRECTION('ref_axis',(1.,0.,0.)) ;
#110666 = DIRECTION('center_axis',(-2.16840434497101E-16,1.,-1.020425574104E-16)) ;
#110667 = DIRECTION('ref_axis',(-1.,-2.16840434497101E-16,5.47382212626882E-48)) ;
#110668 = DIRECTION('center_axis',(0.,1.,0.)) ;
#110669 = DIRECTION('ref_axis',(0.,0.,-1.)) ;
#110670 = DIRECTION('center_axis',(1.,0.,1.25542992828747E-32)) ;
#110671 = DIRECTION('ref_axis',(1.25542992828747E-32,0.,-1.)) ;
#110672 = DIRECTION('center_axis',(1.,0.,0.)) ;
#110673 = DIRECTION('ref_axis',(0.,0.,-1.)) ;
#110674 = DIRECTION('center_axis',(-1.,-1.2303003375722E-16,0.)) ;
#110675 = DIRECTION('ref_axis',(0.,-1.,0.)) ;
#110676 = DIRECTION('center_axis',(0.,0.,-1.)) ;
#110677 = DIRECTION('ref_axis',(1.,0.,0.)) ;
#110678 = DIRECTION('center_axis',(0.,0.,-1.)) ;
#110679 = DIRECTION('ref_axis',(-1.,0.,0.)) ;
#110680 = DIRECTION('',(0.,0.,1.)) ;
#110681 = DIRECTION('center_axis',(0.,-2.16840434497101E-15,1.)) ;
#110682 = DIRECTION('ref_axis',(0.,-1.,-2.16840434497101E-15)) ;
#110683 = DIRECTION('center_axis',(0.,0.,1.)) ;
#110684 = DIRECTION('ref_axis',(1.,0.,0.)) ;
#110685 = DIRECTION('center_axis',(6.27714964143733E-33,-5.10212787052002E-17,
-1.)) ;
#110686 = DIRECTION('ref_axis',(3.20268201330022E-49,1.,-5.10212787052002E-17)) ;
#110687 = DIRECTION('center_axis',(1.,1.53063836115601E-16,-1.53236300070382E-33)) ;
#110688 = DIRECTION('ref_axis',(-1.53063836115601E-16,1.,2.34549359209339E-49)) ;
#110689 = DIRECTION('center_axis',(-1.,0.,0.)) ;
#110690 = DIRECTION('ref_axis',(0.,0.,1.)) ;
#110691 = DIRECTION('center_axis',(1.,0.,0.)) ;
#110692 = DIRECTION('ref_axis',(0.,0.,-1.)) ;
#110693 = DIRECTION('center_axis',(0.,1.,0.)) ;
#110694 = DIRECTION('ref_axis',(1.,0.,0.)) ;
#110695 = DIRECTION('center_axis',(-4.33680868994202E-15,1.,0.)) ;
#110696 = DIRECTION('ref_axis',(1.,4.33680868994202E-15,0.)) ;
#110697 = DIRECTION('center_axis',(0.,-1.,0.)) ;
#110698 = DIRECTION('ref_axis',(0.,0.,-1.)) ;
#110699 = DIRECTION('center_axis',(0.,0.,-1.)) ;
#110700 = DIRECTION('ref_axis',(1.,0.,0.)) ;
#110701 = DIRECTION('center_axis',(0.,0.,1.)) ;
#110702 = DIRECTION('ref_axis',(1.,0.,0.)) ;
#110703 = DIRECTION('center_axis',(0.,0.,-1.)) ;
#110704 = DIRECTION('ref_axis',(-1.,0.,0.)) ;
#110705 = DIRECTION('center_axis',(0.,1.,0.)) ;
#110706 = DIRECTION('ref_axis',(1.,0.,0.)) ;
#110707 = DIRECTION('center_axis',(1.,1.2303003375722E-16,0.)) ;
#110708 = DIRECTION('ref_axis',(1.2303003375722E-16,-1.,0.)) ;
#110709 = DIRECTION('center_axis',(0.,1.,0.)) ;
#110710 = DIRECTION('ref_axis',(-6.50521303491302E-15,0.,-1.)) ;
#110711 = DIRECTION('center_axis',(6.27714964143733E-33,-5.10212787052002E-17,
-1.)) ;
#110712 = DIRECTION('ref_axis',(0.,1.,0.)) ;
#110713 = DIRECTION('center_axis',(0.,-1.,0.)) ;
#110714 = DIRECTION('ref_axis',(0.,0.,1.)) ;
#110715 = DIRECTION('center_axis',(2.16840434497101E-16,-1.,5.10212787052002E-17)) ;
#110716 = DIRECTION('ref_axis',(1.,2.16840434497101E-16,-5.47382212626882E-48)) ;
#110717 = DIRECTION('center_axis',(0.,1.,0.)) ;
#110718 = DIRECTION('ref_axis',(0.,0.,-1.)) ;
#110719 = DIRECTION('center_axis',(0.,0.,1.)) ;
#110720 = DIRECTION('ref_axis',(1.,0.,0.)) ;
#110721 = DIRECTION('center_axis',(0.,0.,-1.)) ;
#110722 = DIRECTION('ref_axis',(-1.,0.,0.)) ;
#110723 = DIRECTION('center_axis',(-1.,-1.2303003375722E-16,0.)) ;
#110724 = DIRECTION('ref_axis',(0.,-1.,0.)) ;
#110725 = DIRECTION('center_axis',(0.,-1.,0.)) ;
#110726 = DIRECTION('ref_axis',(0.,0.,1.)) ;
#110727 = DIRECTION('center_axis',(1.53063836115601E-16,-1.,5.10212787052002E-17)) ;
#110728 = DIRECTION('ref_axis',(1.,1.53063836115601E-16,-6.84227765783602E-48)) ;
#110729 = DIRECTION('',(-1.53063836115601E-16,1.,-5.10212787052002E-17)) ;
#110730 = DIRECTION('center_axis',(0.,-1.,0.)) ;
#110731 = DIRECTION('ref_axis',(0.,0.,-1.)) ;
#110732 = DIRECTION('center_axis',(-1.,0.,0.)) ;
#110733 = DIRECTION('ref_axis',(0.,0.,-1.)) ;
#110734 = DIRECTION('center_axis',(-1.2303003375722E-16,1.,-5.10212787052002E-17)) ;
#110735 = DIRECTION('ref_axis',(-1.,-1.2303003375722E-16,6.27714964143733E-33)) ;
#110736 = DIRECTION('center_axis',(-8.67361737988403E-15,-1.,0.)) ;
#110737 = DIRECTION('ref_axis',(1.,-8.67361737988403E-15,0.)) ;
#110738 = DIRECTION('center_axis',(1.,0.,6.27714964143733E-33)) ;
#110739 = DIRECTION('ref_axis',(6.27714964143733E-33,0.,-1.)) ;
#110740 = DIRECTION('center_axis',(-1.,0.,-6.5052130349128E-15)) ;
#110741 = DIRECTION('ref_axis',(-6.5052130349128E-15,0.,1.)) ;
#110742 = DIRECTION('center_axis',(1.,0.,0.)) ;
#110743 = DIRECTION('ref_axis',(0.,1.,0.)) ;
#110744 = DIRECTION('center_axis',(0.,1.,0.)) ;
#110745 = DIRECTION('ref_axis',(1.,0.,0.)) ;
#110746 = DIRECTION('center_axis',(1.,0.,0.)) ;
#110747 = DIRECTION('ref_axis',(0.,0.,-1.)) ;
#110748 = DIRECTION('center_axis',(0.,-1.,0.)) ;
#110749 = DIRECTION('ref_axis',(0.,0.,-1.)) ;
#110750 = DIRECTION('center_axis',(0.,1.,0.)) ;
#110751 = DIRECTION('ref_axis',(0.,0.,1.)) ;
#110752 = DIRECTION('center_axis',(0.,-1.,0.)) ;
#110753 = DIRECTION('ref_axis',(0.,0.,-1.)) ;
#110754 = DIRECTION('center_axis',(1.,0.,0.)) ;
#110755 = DIRECTION('ref_axis',(0.,0.,-1.)) ;
#110756 = DIRECTION('center_axis',(1.,0.,0.)) ;
#110757 = DIRECTION('ref_axis',(0.,0.,-1.)) ;
#110758 = DIRECTION('center_axis',(0.,0.,1.)) ;
#110759 = DIRECTION('ref_axis',(1.,0.,0.)) ;
#110760 = DIRECTION('center_axis',(-1.,8.67361737988401E-15,-8.67361737988379E-15)) ;
#110761 = DIRECTION('ref_axis',(-8.67361737988401E-15,-1.,1.07724819444908E-44)) ;
#110762 = DIRECTION('center_axis',(0.,1.,0.)) ;
#110763 = DIRECTION('ref_axis',(1.,0.,0.)) ;
#110764 = DIRECTION('center_axis',(0.,-1.,0.)) ;
#110765 = DIRECTION('ref_axis',(0.,0.,-1.)) ;
#110766 = DIRECTION('center_axis',(1.,1.59148942750166E-16,0.)) ;
#110767 = DIRECTION('ref_axis',(-1.59148942750166E-16,1.,0.)) ;
#110768 = DIRECTION('center_axis',(-1.,0.,6.50521303491284E-15)) ;
#110769 = DIRECTION('ref_axis',(6.50521303491284E-15,0.,1.)) ;
#110770 = DIRECTION('center_axis',(-4.33680868994203E-15,-1.,0.)) ;
#110771 = DIRECTION('ref_axis',(1.,-4.33680868994203E-15,0.)) ;
#110772 = DIRECTION('center_axis',(-8.67361737988401E-15,-1.,0.)) ;
#110773 = DIRECTION('ref_axis',(1.,-8.67361737988401E-15,0.)) ;
#110774 = DIRECTION('center_axis',(0.,1.,0.)) ;
#110775 = DIRECTION('ref_axis',(1.,0.,0.)) ;
#110776 = DIRECTION('center_axis',(8.67361737988403E-15,-1.,0.)) ;
#110777 = DIRECTION('ref_axis',(1.,8.67361737988403E-15,0.)) ;
#110778 = DIRECTION('center_axis',(0.,0.,1.)) ;
#110779 = DIRECTION('ref_axis',(1.,0.,0.)) ;
#110780 = DIRECTION('center_axis',(1.,8.67361737988401E-15,0.)) ;
#110781 = DIRECTION('ref_axis',(-8.67361737988401E-15,1.,0.)) ;
#110782 = DIRECTION('center_axis',(-1.2303003375722E-16,1.,0.)) ;
#110783 = DIRECTION('ref_axis',(-1.,-1.2303003375722E-16,0.)) ;
#110784 = DIRECTION('center_axis',(0.,-1.,8.67361737988379E-15)) ;
#110785 = DIRECTION('ref_axis',(0.,-8.67361737988379E-15,-1.)) ;
#110786 = DIRECTION('center_axis',(1.,-5.88041856263325E-16,0.)) ;
#110787 = DIRECTION('ref_axis',(5.88041856263325E-16,1.,0.)) ;
#110788 = DIRECTION('center_axis',(1.,0.,0.)) ;
#110789 = DIRECTION('ref_axis',(0.,0.,-1.)) ;
#110790 = DIRECTION('center_axis',(0.,1.,0.)) ;
#110791 = DIRECTION('ref_axis',(1.,0.,0.)) ;
#110792 = DIRECTION('center_axis',(1.,6.50521303491304E-15,0.)) ;
#110793 = DIRECTION('ref_axis',(-6.50521303491304E-15,1.,0.)) ;
#110794 = DIRECTION('center_axis',(0.,1.,0.)) ;
#110795 = DIRECTION('ref_axis',(1.,0.,0.)) ;
#110796 = DIRECTION('center_axis',(0.,-1.,0.)) ;
#110797 = DIRECTION('ref_axis',(0.,0.,-1.)) ;
#110798 = DIRECTION('center_axis',(-1.,0.,0.)) ;
#110799 = DIRECTION('ref_axis',(0.,0.,1.)) ;
#110800 = DIRECTION('center_axis',(1.,0.,1.73472347597676E-14)) ;
#110801 = DIRECTION('ref_axis',(1.73472347597676E-14,0.,-1.)) ;
#110802 = DIRECTION('center_axis',(0.,-1.,0.)) ;
#110803 = DIRECTION('ref_axis',(0.,0.,-1.)) ;
#110804 = DIRECTION('center_axis',(8.67361737988409E-15,-1.,0.)) ;
#110805 = DIRECTION('ref_axis',(1.,8.67361737988409E-15,0.)) ;
#110806 = DIRECTION('center_axis',(0.,1.,0.)) ;
#110807 = DIRECTION('ref_axis',(1.,0.,0.)) ;
#110808 = DIRECTION('center_axis',(0.,1.,0.)) ;
#110809 = DIRECTION('ref_axis',(1.,0.,0.)) ;
#110810 = DIRECTION('center_axis',(1.,0.,0.)) ;
#110811 = DIRECTION('ref_axis',(0.,0.,-1.)) ;
#110812 = DIRECTION('center_axis',(0.,-1.,0.)) ;
#110813 = DIRECTION('ref_axis',(0.,0.,-1.)) ;
#110814 = DIRECTION('center_axis',(0.,-1.,0.)) ;
#110815 = DIRECTION('ref_axis',(0.,0.,-1.)) ;
#110816 = DIRECTION('center_axis',(0.,-1.,0.)) ;
#110817 = DIRECTION('ref_axis',(0.,0.,-1.)) ;
#110818 = DIRECTION('center_axis',(-1.,0.,0.)) ;
#110819 = DIRECTION('ref_axis',(0.,0.,1.)) ;
#110820 = DIRECTION('center_axis',(1.,0.,0.)) ;
#110821 = DIRECTION('ref_axis',(0.,0.,-1.)) ;
#110822 = DIRECTION('center_axis',(0.,0.,1.)) ;
#110823 = DIRECTION('ref_axis',(1.,0.,0.)) ;
#110824 = DIRECTION('center_axis',(-1.,0.,0.)) ;
#110825 = DIRECTION('ref_axis',(0.,0.,1.)) ;
#110826 = DIRECTION('center_axis',(0.,1.,0.)) ;
#110827 = DIRECTION('ref_axis',(1.,0.,0.)) ;
#110828 = DIRECTION('center_axis',(0.,-1.,0.)) ;
#110829 = DIRECTION('ref_axis',(0.,0.,-1.)) ;
#110830 = DIRECTION('center_axis',(-1.,-1.59148942750166E-16,0.)) ;
#110831 = DIRECTION('ref_axis',(1.59148942750166E-16,-1.,0.)) ;
#110832 = DIRECTION('center_axis',(-1.,6.50521303491307E-15,0.)) ;
#110833 = DIRECTION('ref_axis',(-6.50521303491307E-15,-1.,0.)) ;
#110834 = DIRECTION('center_axis',(4.33680868994203E-15,1.,0.)) ;
#110835 = DIRECTION('ref_axis',(-1.,4.33680868994203E-15,0.)) ;
#110836 = DIRECTION('center_axis',(-8.67361737988401E-15,-1.,0.)) ;
#110837 = DIRECTION('ref_axis',(1.,-8.67361737988401E-15,0.)) ;
#110838 = DIRECTION('center_axis',(0.,1.,0.)) ;
#110839 = DIRECTION('ref_axis',(1.,0.,0.)) ;
#110840 = DIRECTION('center_axis',(8.67361737988403E-15,-1.,0.)) ;
#110841 = DIRECTION('ref_axis',(1.,8.67361737988403E-15,0.)) ;
#110842 = DIRECTION('center_axis',(0.,0.,1.)) ;
#110843 = DIRECTION('ref_axis',(1.,0.,0.)) ;
#110844 = DIRECTION('center_axis',(1.,8.67361737988401E-15,0.)) ;
#110845 = DIRECTION('ref_axis',(-8.67361737988401E-15,1.,0.)) ;
#110846 = DIRECTION('center_axis',(1.2303003375722E-16,-1.,0.)) ;
#110847 = DIRECTION('ref_axis',(1.,1.2303003375722E-16,0.)) ;
#110848 = DIRECTION('center_axis',(-8.67361737988416E-15,-1.,0.)) ;
#110849 = DIRECTION('ref_axis',(1.,-8.67361737988416E-15,0.)) ;
#110850 = DIRECTION('center_axis',(-1.,5.88041856263325E-16,0.)) ;
#110851 = DIRECTION('ref_axis',(-5.88041856263325E-16,-1.,0.)) ;
#110852 = DIRECTION('center_axis',(1.,0.,0.)) ;
#110853 = DIRECTION('ref_axis',(0.,0.,-1.)) ;
#110854 = DIRECTION('center_axis',(0.,1.,0.)) ;
#110855 = DIRECTION('ref_axis',(1.,0.,0.)) ;
#110856 = DIRECTION('center_axis',(1.,6.50521303491304E-15,0.)) ;
#110857 = DIRECTION('ref_axis',(-6.50521303491304E-15,1.,0.)) ;
#110858 = DIRECTION('center_axis',(0.,1.,0.)) ;
#110859 = DIRECTION('ref_axis',(1.,0.,0.)) ;
#110860 = DIRECTION('center_axis',(0.,-1.,0.)) ;
#110861 = DIRECTION('ref_axis',(0.,0.,-1.)) ;
#110862 = DIRECTION('center_axis',(1.,0.,0.)) ;
#110863 = DIRECTION('ref_axis',(0.,0.,-1.)) ;
#110864 = DIRECTION('center_axis',(1.,-1.73472347597681E-14,0.)) ;
#110865 = DIRECTION('ref_axis',(1.73472347597681E-14,1.,0.)) ;
#110866 = DIRECTION('center_axis',(0.,1.,0.)) ;
#110867 = DIRECTION('ref_axis',(0.,0.,1.)) ;
#110868 = DIRECTION('center_axis',(0.,-1.,-8.67361737988405E-15)) ;
#110869 = DIRECTION('ref_axis',(0.,8.67361737988405E-15,-1.)) ;
#110870 = DIRECTION('center_axis',(0.,1.,0.)) ;
#110871 = DIRECTION('ref_axis',(1.,0.,0.)) ;
#110872 = DIRECTION('center_axis',(0.,0.,-1.)) ;
#110873 = DIRECTION('ref_axis',(-1.,0.,0.)) ;
#110874 = DIRECTION('center_axis',(0.,0.,1.)) ;
#110875 = DIRECTION('ref_axis',(1.,0.,0.)) ;
#110876 = DIRECTION('center_axis',(0.,0.,-1.)) ;
#110877 = DIRECTION('ref_axis',(-1.,0.,0.)) ;
#110878 = DIRECTION('center_axis',(-1.,0.,0.)) ;
#110879 = DIRECTION('ref_axis',(0.,0.,1.)) ;
#110880 = DIRECTION('center_axis',(0.,-1.,0.)) ;
#110881 = DIRECTION('ref_axis',(0.,0.,-1.)) ;
#110882 = DIRECTION('center_axis',(0.,1.,0.)) ;
#110883 = DIRECTION('ref_axis',(0.,0.,1.)) ;
#110884 = DIRECTION('center_axis',(0.,1.,-6.50521303491302E-15)) ;
#110885 = DIRECTION('ref_axis',(0.,6.50521303491302E-15,1.)) ;
#110886 = DIRECTION('center_axis',(0.,-1.,0.)) ;
#110887 = DIRECTION('ref_axis',(0.,0.,-1.)) ;
#110888 = DIRECTION('center_axis',(0.,-1.,0.)) ;
#110889 = DIRECTION('ref_axis',(0.,0.,-1.)) ;
#110890 = DIRECTION('center_axis',(0.,-1.,-1.07081696047951E-16)) ;
#110891 = DIRECTION('ref_axis',(0.,1.07081696047951E-16,-1.)) ;
#110892 = DIRECTION('center_axis',(0.,1.,0.)) ;
#110893 = DIRECTION('ref_axis',(0.,0.,1.)) ;
#110894 = DIRECTION('center_axis',(-1.,0.,0.)) ;
#110895 = DIRECTION('ref_axis',(0.,0.,1.)) ;
#110896 = DIRECTION('center_axis',(0.,0.,1.)) ;
#110897 = DIRECTION('ref_axis',(1.,0.,0.)) ;
#110898 = DIRECTION('center_axis',(0.,1.,0.)) ;
#110899 = DIRECTION('ref_axis',(0.,0.,1.)) ;
#110900 = DIRECTION('center_axis',(0.,-6.50521303491304E-15,-1.)) ;
#110901 = DIRECTION('ref_axis',(0.,1.,-6.50521303491304E-15)) ;
#110902 = DIRECTION('center_axis',(0.,0.,1.)) ;
#110903 = DIRECTION('ref_axis',(1.,0.,0.)) ;
#110904 = DIRECTION('center_axis',(0.,-1.08420217248551E-15,1.)) ;
#110905 = DIRECTION('ref_axis',(0.,-1.,-1.08420217248551E-15)) ;
#110906 = DIRECTION('center_axis',(0.,0.,1.)) ;
#110907 = DIRECTION('ref_axis',(1.,0.,0.)) ;
#110908 = DIRECTION('center_axis',(0.,0.,-1.)) ;
#110909 = DIRECTION('ref_axis',(-1.,0.,0.)) ;
#110910 = DIRECTION('center_axis',(0.,1.,0.)) ;
#110911 = DIRECTION('ref_axis',(0.,0.,1.)) ;
#110912 = DIRECTION('center_axis',(0.,-0.707106781186548,0.707106781186547)) ;
#110913 = DIRECTION('ref_axis',(0.,-0.707106781186547,-0.707106781186548)) ;
#110914 = DIRECTION('center_axis',(0.,1.,0.)) ;
#110915 = DIRECTION('ref_axis',(0.,0.,1.)) ;
#110916 = DIRECTION('center_axis',(0.,-0.5142317969591,-0.857651245551602)) ;
#110917 = DIRECTION('ref_axis',(0.,0.857651245551602,-0.5142317969591)) ;
#110918 = DIRECTION('center_axis',(0.,-0.707106781186548,0.707106781186547)) ;
#110919 = DIRECTION('ref_axis',(0.,-0.707106781186547,-0.707106781186548)) ;
#110920 = DIRECTION('center_axis',(0.,-0.70710678118655,0.707106781186545)) ;
#110921 = DIRECTION('ref_axis',(0.,-0.707106781186545,-0.70710678118655)) ;
#110922 = DIRECTION('center_axis',(-1.,0.,0.)) ;
#110923 = DIRECTION('ref_axis',(0.,0.,1.)) ;
#110924 = DIRECTION('center_axis',(0.,0.514231796959101,-0.857651245551602)) ;
#110925 = DIRECTION('ref_axis',(0.,0.857651245551602,0.514231796959101)) ;
#110926 = DIRECTION('center_axis',(0.,1.,0.)) ;
#110927 = DIRECTION('ref_axis',(0.,0.,1.)) ;
#110928 = DIRECTION('center_axis',(0.,0.,-1.)) ;
#110929 = DIRECTION('ref_axis',(-1.,0.,0.)) ;
#110930 = DIRECTION('center_axis',(0.,1.,0.)) ;
#110931 = DIRECTION('ref_axis',(0.,0.,1.)) ;
#110932 = DIRECTION('center_axis',(0.,0.,-1.)) ;
#110933 = DIRECTION('ref_axis',(-1.,0.,0.)) ;
#110934 = DIRECTION('center_axis',(0.,0.,-1.)) ;
#110935 = DIRECTION('ref_axis',(-1.,0.,0.)) ;
#110936 = DIRECTION('center_axis',(0.,0.,1.)) ;
#110937 = DIRECTION('ref_axis',(1.,0.,0.)) ;
#110938 = DIRECTION('center_axis',(0.,0.,-1.)) ;
#110939 = DIRECTION('ref_axis',(-1.,0.,0.)) ;
#110940 = DIRECTION('center_axis',(0.,1.,0.)) ;
#110941 = DIRECTION('ref_axis',(0.,0.,1.)) ;
#110942 = DIRECTION('center_axis',(0.,-1.,8.67361737988403E-15)) ;
#110943 = DIRECTION('ref_axis',(0.,-8.67361737988403E-15,-1.)) ;
#110944 = DIRECTION('center_axis',(0.,0.707106781186546,0.707106781186549)) ;
#110945 = DIRECTION('ref_axis',(0.,-0.707106781186549,0.707106781186546)) ;
#110946 = DIRECTION('center_axis',(0.,0.707106781186547,0.707106781186548)) ;
#110947 = DIRECTION('ref_axis',(0.,-0.707106781186548,0.707106781186547)) ;
#110948 = DIRECTION('center_axis',(0.,1.,1.07081696047951E-16)) ;
#110949 = DIRECTION('ref_axis',(0.,-1.07081696047951E-16,1.)) ;
#110950 = DIRECTION('center_axis',(0.,-1.,0.)) ;
#110951 = DIRECTION('ref_axis',(0.,0.,-1.)) ;
#110952 = DIRECTION('center_axis',(0.,1.,0.)) ;
#110953 = DIRECTION('ref_axis',(0.,0.,1.)) ;
#110954 = DIRECTION('center_axis',(0.,-1.08420217248551E-15,1.)) ;
#110955 = DIRECTION('ref_axis',(0.,-1.,-1.08420217248551E-15)) ;
#110956 = DIRECTION('center_axis',(0.,1.,0.)) ;
#110957 = DIRECTION('ref_axis',(0.,0.,1.)) ;
#110958 = DIRECTION('center_axis',(0.,6.50521303491302E-15,1.)) ;
#110959 = DIRECTION('ref_axis',(0.,-1.,6.50521303491302E-15)) ;
#110960 = DIRECTION('center_axis',(0.,3.99416362155027E-15,1.)) ;
#110961 = DIRECTION('ref_axis',(0.,-1.,3.99416362155027E-15)) ;
#110962 = DIRECTION('center_axis',(0.,0.,1.)) ;
#110963 = DIRECTION('ref_axis',(1.,0.,0.)) ;
#110964 = DIRECTION('center_axis',(0.,0.,-1.)) ;
#110965 = DIRECTION('ref_axis',(-1.,0.,0.)) ;
#110966 = DIRECTION('center_axis',(0.,0.,1.)) ;
#110967 = DIRECTION('ref_axis',(1.,0.,0.)) ;
#110968 = DIRECTION('center_axis',(-1.,0.,0.)) ;
#110969 = DIRECTION('ref_axis',(0.,0.,1.)) ;
#110970 = DIRECTION('center_axis',(0.,1.,0.)) ;
#110971 = DIRECTION('ref_axis',(0.,0.,1.)) ;
#110972 = DIRECTION('center_axis',(-1.,0.,0.)) ;
#110973 = DIRECTION('ref_axis',(0.,0.,1.)) ;
#110974 = DIRECTION('center_axis',(0.,-1.,0.)) ;
#110975 = DIRECTION('ref_axis',(0.,0.,-1.)) ;
#110976 = DIRECTION('center_axis',(0.,1.,0.)) ;
#110977 = DIRECTION('ref_axis',(0.,0.,1.)) ;
#110978 = DIRECTION('center_axis',(0.,-1.,0.)) ;
#110979 = DIRECTION('ref_axis',(0.,0.,-1.)) ;
#110980 = DIRECTION('center_axis',(0.,1.,0.)) ;
#110981 = DIRECTION('ref_axis',(0.,0.,1.)) ;
#110982 = DIRECTION('center_axis',(0.,-1.,0.)) ;
#110983 = DIRECTION('ref_axis',(0.,0.,-1.)) ;
#110984 = DIRECTION('center_axis',(0.,1.,0.)) ;
#110985 = DIRECTION('ref_axis',(0.,0.,-1.)) ;
#110986 = DIRECTION('center_axis',(-4.70197740328919E-30,-1.08420217248551E-15,
-1.)) ;
#110987 = DIRECTION('ref_axis',(6.22301527786114E-61,1.,-1.08420217248551E-15)) ;
#110988 = DIRECTION('center_axis',(0.,1.,0.)) ;
#110989 = DIRECTION('ref_axis',(0.,0.,-1.)) ;
#110990 = DIRECTION('center_axis',(0.,0.,-1.)) ;
#110991 = DIRECTION('ref_axis',(-1.,0.,0.)) ;
#110992 = DIRECTION('center_axis',(0.,0.,1.)) ;
#110993 = DIRECTION('ref_axis',(1.,0.,0.)) ;
#110994 = DIRECTION('center_axis',(0.,0.,-1.)) ;
#110995 = DIRECTION('ref_axis',(-1.,0.,0.)) ;
#110996 = DIRECTION('center_axis',(0.,0.,-1.)) ;
#110997 = DIRECTION('ref_axis',(-1.,0.,0.)) ;
#110998 = DIRECTION('center_axis',(0.,6.50521303491304E-15,-1.)) ;
#110999 = DIRECTION('ref_axis',(0.,1.,6.50521303491304E-15)) ;
#111000 = DIRECTION('center_axis',(1.,0.,0.)) ;
#111001 = DIRECTION('ref_axis',(0.,0.,-1.)) ;
#111002 = DIRECTION('center_axis',(0.,0.707106781186548,-0.707106781186548)) ;
#111003 = DIRECTION('ref_axis',(0.,0.707106781186548,0.707106781186548)) ;
#111004 = DIRECTION('center_axis',(1.,0.,0.)) ;
#111005 = DIRECTION('ref_axis',(0.,0.,-1.)) ;
#111006 = DIRECTION('center_axis',(0.,-1.,0.)) ;
#111007 = DIRECTION('ref_axis',(0.,0.,-1.)) ;
#111008 = DIRECTION('center_axis',(0.,-0.707106781186548,0.707106781186547)) ;
#111009 = DIRECTION('ref_axis',(0.,-0.707106781186547,-0.707106781186548)) ;
#111010 = DIRECTION('center_axis',(0.,-1.,-1.07081696047951E-16)) ;
#111011 = DIRECTION('ref_axis',(0.,1.07081696047951E-16,-1.)) ;
#111012 = DIRECTION('center_axis',(0.,-1.,-8.67361737988403E-15)) ;
#111013 = DIRECTION('ref_axis',(0.,8.67361737988403E-15,-1.)) ;
#111014 = DIRECTION('center_axis',(1.,0.,0.)) ;
#111015 = DIRECTION('ref_axis',(0.,0.,-1.)) ;
#111016 = DIRECTION('center_axis',(0.,0.,1.)) ;
#111017 = DIRECTION('ref_axis',(1.,0.,0.)) ;
#111018 = DIRECTION('center_axis',(0.,0.,-1.)) ;
#111019 = DIRECTION('ref_axis',(-1.,0.,0.)) ;
#111020 = DIRECTION('center_axis',(0.,0.,1.)) ;
#111021 = DIRECTION('ref_axis',(1.,0.,0.)) ;
#111022 = DIRECTION('center_axis',(0.,0.,1.)) ;
#111023 = DIRECTION('ref_axis',(1.,0.,0.)) ;
#111024 = DIRECTION('center_axis',(0.,0.,1.)) ;
#111025 = DIRECTION('ref_axis',(1.,0.,0.)) ;
#111026 = DIRECTION('center_axis',(1.,0.,0.)) ;
#111027 = DIRECTION('ref_axis',(0.,0.382683432365091,0.923879532511286)) ;
#111028 = DIRECTION('center_axis',(0.,-0.707106781186551,-0.707106781186544)) ;
#111029 = DIRECTION('ref_axis',(0.,0.707106781186544,-0.707106781186551)) ;
#111030 = DIRECTION('center_axis',(1.,0.,0.)) ;
#111031 = DIRECTION('ref_axis',(0.,0.,-1.)) ;
#111032 = DIRECTION('center_axis',(0.,0.5142317969591,0.857651245551602)) ;
#111033 = DIRECTION('ref_axis',(0.,-0.857651245551602,0.5142317969591)) ;
#111034 = DIRECTION('center_axis',(0.,0.707106781186546,0.707106781186549)) ;
#111035 = DIRECTION('ref_axis',(0.,-0.707106781186549,0.707106781186546)) ;
#111036 = DIRECTION('center_axis',(0.,-0.707106781186546,-0.707106781186549)) ;
#111037 = DIRECTION('ref_axis',(0.,0.707106781186549,-0.707106781186546)) ;
#111038 = DIRECTION('center_axis',(1.,0.,0.)) ;
#111039 = DIRECTION('ref_axis',(0.,0.,-1.)) ;
#111040 = DIRECTION('center_axis',(0.,-0.514231796959099,0.857651245551603)) ;
#111041 = DIRECTION('ref_axis',(0.,-0.857651245551603,-0.514231796959099)) ;
#111042 = DIRECTION('center_axis',(1.,0.,0.)) ;
#111043 = DIRECTION('ref_axis',(0.,0.,-1.)) ;
#111044 = DIRECTION('center_axis',(0.,1.08420217248551E-15,-1.)) ;
#111045 = DIRECTION('ref_axis',(0.,1.,1.08420217248551E-15)) ;
#111046 = DIRECTION('center_axis',(1.,0.,0.)) ;
#111047 = DIRECTION('ref_axis',(0.,0.,-1.)) ;
#111048 = DIRECTION('center_axis',(0.,0.,1.)) ;
#111049 = DIRECTION('ref_axis',(1.,0.,0.)) ;
#111050 = DIRECTION('center_axis',(0.,3.99416362155027E-15,1.)) ;
#111051 = DIRECTION('ref_axis',(0.,-1.,3.99416362155027E-15)) ;
#111052 = DIRECTION('center_axis',(0.,-4.33680868994202E-15,-1.)) ;
#111053 = DIRECTION('ref_axis',(0.,1.,-4.33680868994202E-15)) ;
#111054 = DIRECTION('center_axis',(0.,0.,1.)) ;
#111055 = DIRECTION('ref_axis',(1.,0.,0.)) ;
#111056 = DIRECTION('center_axis',(0.,-6.50521303491304E-15,1.)) ;
#111057 = DIRECTION('ref_axis',(0.,-1.,-6.50521303491304E-15)) ;
#111058 = DIRECTION('center_axis',(0.,1.,0.)) ;
#111059 = DIRECTION('ref_axis',(0.,0.,-1.)) ;
#111060 = DIRECTION('center_axis',(0.,-1.,0.)) ;
#111061 = DIRECTION('ref_axis',(0.,0.,-1.)) ;
#111062 = DIRECTION('center_axis',(1.,0.,0.)) ;
#111063 = DIRECTION('ref_axis',(0.,0.,-1.)) ;
#111064 = DIRECTION('center_axis',(0.,1.,0.)) ;
#111065 = DIRECTION('ref_axis',(0.,0.,1.)) ;
#111066 = DIRECTION('center_axis',(0.,1.,0.)) ;
#111067 = DIRECTION('ref_axis',(0.,0.,1.)) ;
#111068 = DIRECTION('center_axis',(0.,-1.,0.)) ;
#111069 = DIRECTION('ref_axis',(0.,0.,-1.)) ;
#111070 = DIRECTION('center_axis',(0.,1.,1.07081696047951E-16)) ;
#111071 = DIRECTION('ref_axis',(0.,-1.07081696047951E-16,1.)) ;
#111072 = DIRECTION('center_axis',(0.,1.,6.50521303491302E-15)) ;
#111073 = DIRECTION('ref_axis',(0.,-6.50521303491302E-15,1.)) ;
#111074 = DIRECTION('center_axis',(0.,1.,0.)) ;
#111075 = DIRECTION('ref_axis',(0.,0.,-1.)) ;
#111076 = DIRECTION('center_axis',(0.,0.,1.)) ;
#111077 = DIRECTION('ref_axis',(1.,0.,0.)) ;
#111078 = DIRECTION('center_axis',(1.,0.,0.)) ;
#111079 = DIRECTION('ref_axis',(0.,0.,-1.)) ;
#111080 = DIRECTION('center_axis',(0.,0.,-1.)) ;
#111081 = DIRECTION('ref_axis',(-1.,0.,0.)) ;
#111082 = DIRECTION('center_axis',(0.,0.,-1.)) ;
#111083 = DIRECTION('ref_axis',(-1.,0.,0.)) ;
#111084 = DIRECTION('center_axis',(1.,-9.85638338623186E-18,0.)) ;
#111085 = DIRECTION('ref_axis',(9.85638338623186E-18,1.,0.)) ;
#111086 = DIRECTION('',(0.,0.,-1.)) ;
#111087 = DIRECTION('',(-9.85638338623186E-18,-1.,0.)) ;
#111088 = DIRECTION('',(0.,0.,1.)) ;
#111089 = DIRECTION('',(9.85638338623186E-18,1.,0.)) ;
#111090 = DIRECTION('center_axis',(0.707106781186548,0.707106781186548,0.)) ;
#111091 = DIRECTION('ref_axis',(-0.707106781186548,0.707106781186548,0.)) ;
#111092 = DIRECTION('',(0.,0.,1.)) ;
#111093 = DIRECTION('',(-0.577350269189625,0.577350269189625,0.577350269189627)) ;
#111094 = DIRECTION('',(0.,0.,-1.)) ;
#111095 = DIRECTION('',(0.577350269189625,-0.577350269189625,0.577350269189627)) ;
#111096 = DIRECTION('center_axis',(0.,1.,0.)) ;
#111097 = DIRECTION('ref_axis',(0.,0.,1.)) ;
#111098 = DIRECTION('',(0.,0.,1.)) ;
#111099 = DIRECTION('',(-1.,0.,-9.8563833862319E-18)) ;
#111100 = DIRECTION('',(0.,0.,-1.)) ;
#111101 = DIRECTION('',(1.,0.,-9.8563833862319E-18)) ;
#111102 = DIRECTION('center_axis',(-0.707106781186548,0.707106781186548,0.)) ;
#111103 = DIRECTION('ref_axis',(-0.707106781186548,-0.707106781186548,0.)) ;
#111104 = DIRECTION('',(0.,0.,1.)) ;
#111105 = DIRECTION('',(-0.577350269189625,-0.577350269189625,-0.577350269189627)) ;
#111106 = DIRECTION('',(0.,0.,-1.)) ;
#111107 = DIRECTION('',(0.577350269189625,0.577350269189625,-0.577350269189627)) ;
#111108 = DIRECTION('center_axis',(-1.,9.85638338623186E-18,0.)) ;
#111109 = DIRECTION('ref_axis',(-9.85638338623186E-18,-1.,0.)) ;
#111110 = DIRECTION('',(0.,0.,-1.)) ;
#111111 = DIRECTION('',(9.85638338623186E-18,1.,0.)) ;
#111112 = DIRECTION('',(0.,0.,-1.)) ;
#111113 = DIRECTION('',(-9.85638338623186E-18,-1.,0.)) ;
#111114 = DIRECTION('center_axis',(0.,0.,1.)) ;
#111115 = DIRECTION('ref_axis',(1.,0.,0.)) ;
#111116 = DIRECTION('',(9.85638338623186E-18,1.,0.)) ;
#111117 = DIRECTION('center_axis',(0.,0.,-1.)) ;
#111118 = DIRECTION('ref_axis',(1.,0.,0.)) ;
#111119 = DIRECTION('center_axis',(0.,0.,1.)) ;
#111120 = DIRECTION('ref_axis',(1.,0.,0.)) ;
#111121 = DIRECTION('',(-9.85638338623186E-18,-1.,0.)) ;
#111122 = DIRECTION('',(1.,-9.85638338623186E-18,0.)) ;
#111123 = DIRECTION('center_axis',(0.,0.,1.)) ;
#111124 = DIRECTION('ref_axis',(1.,0.,0.)) ;
#111125 = DIRECTION('',(9.85638338623186E-18,1.,0.)) ;
#111126 = DIRECTION('center_axis',(0.,0.,-1.)) ;
#111127 = DIRECTION('ref_axis',(1.,0.,0.)) ;
#111128 = DIRECTION('center_axis',(0.,0.,1.)) ;
#111129 = DIRECTION('ref_axis',(1.,0.,0.)) ;
#111130 = DIRECTION('',(-9.85638338623186E-18,-1.,0.)) ;
#111131 = DIRECTION('',(-1.,9.85638338623186E-18,0.)) ;
#111132 = DIRECTION('center_axis',(0.,0.,-1.)) ;
#111133 = DIRECTION('ref_axis',(-1.,0.,0.)) ;
#111134 = DIRECTION('center_axis',(0.,0.,1.)) ;
#111135 = DIRECTION('ref_axis',(1.,0.,0.)) ;
#111136 = DIRECTION('center_axis',(0.,0.,-1.)) ;
#111137 = DIRECTION('ref_axis',(1.,0.,0.)) ;
#111138 = DIRECTION('center_axis',(0.,0.,-1.)) ;
#111139 = DIRECTION('ref_axis',(-1.,0.,0.)) ;
#111140 = DIRECTION('center_axis',(0.,0.,-1.)) ;
#111141 = DIRECTION('ref_axis',(1.,0.,0.)) ;
#111142 = DIRECTION('center_axis',(0.,0.,1.)) ;
#111143 = DIRECTION('ref_axis',(1.,0.,0.)) ;
#111144 = DIRECTION('center_axis',(-0.707106781186548,-0.707106781186547,
0.)) ;
#111145 = DIRECTION('ref_axis',(0.707106781186547,-0.707106781186548,0.)) ;
#111146 = DIRECTION('',(0.,0.,1.)) ;
#111147 = DIRECTION('',(0.577350269189625,-0.577350269189626,-0.577350269189626)) ;
#111148 = DIRECTION('',(0.,0.,-1.)) ;
#111149 = DIRECTION('',(-0.577350269189625,0.577350269189626,-0.577350269189626)) ;
#111150 = DIRECTION('center_axis',(1.95511867169517E-16,-1.,0.)) ;
#111151 = DIRECTION('ref_axis',(1.,1.95511867169517E-16,0.)) ;
#111152 = DIRECTION('',(0.,0.,-1.)) ;
#111153 = DIRECTION('',(-1.,-1.95511867169517E-16,0.)) ;
#111154 = DIRECTION('',(1.,1.95511867169517E-16,0.)) ;
#111155 = DIRECTION('center_axis',(1.06642836637918E-16,1.,0.)) ;
#111156 = DIRECTION('ref_axis',(-1.,1.06642836637918E-16,0.)) ;
#111157 = DIRECTION('',(1.,-1.06642836637919E-16,0.)) ;
#111158 = DIRECTION('',(0.,0.,1.)) ;
#111159 = DIRECTION('',(-1.,1.06642836637919E-16,0.)) ;
#111160 = DIRECTION('center_axis',(-0.707106781186548,0.707106781186547,0.)) ;
#111161 = DIRECTION('ref_axis',(-0.707106781186547,-0.707106781186548,0.)) ;
#111162 = DIRECTION('',(0.,0.,1.)) ;
#111163 = DIRECTION('',(-0.577350269189625,-0.577350269189626,0.577350269189627)) ;
#111164 = DIRECTION('',(0.,0.,-1.)) ;
#111165 = DIRECTION('',(0.577350269189625,0.577350269189626,0.577350269189627)) ;
#111166 = DIRECTION('center_axis',(-1.,0.,0.)) ;
#111167 = DIRECTION('ref_axis',(0.,0.,1.)) ;
#111168 = DIRECTION('',(0.,0.,-1.)) ;
#111169 = DIRECTION('',(0.,1.,1.95511867169518E-16)) ;
#111170 = DIRECTION('',(0.,0.,1.)) ;
#111171 = DIRECTION('',(0.,-1.,1.95511867169518E-16)) ;
#111172 = DIRECTION('center_axis',(0.,0.,1.)) ;
#111173 = DIRECTION('ref_axis',(1.,0.,0.)) ;
#111174 = DIRECTION('',(-1.95511867169517E-16,1.,0.)) ;
#111175 = DIRECTION('',(-1.,-1.95511867169517E-16,0.)) ;
#111176 = DIRECTION('',(1.,-1.06642836637919E-16,0.)) ;
#111177 = DIRECTION('center_axis',(0.,0.,1.)) ;
#111178 = DIRECTION('ref_axis',(1.,0.,0.)) ;
#111179 = DIRECTION('',(1.,1.95511867169517E-16,0.)) ;
#111180 = DIRECTION('',(1.95511867169517E-16,-1.,0.)) ;
#111181 = DIRECTION('',(-1.,1.06642836637919E-16,0.)) ;
#111182 = DIRECTION('center_axis',(6.96951553037899E-18,0.707106781186549,
0.707106781186546)) ;
#111183 = DIRECTION('ref_axis',(-8.6424177776148E-34,-0.707106781186546,0.707106781186549)) ;
#111184 = DIRECTION('',(-0.577350269189625,0.577350269189625,-0.577350269189627)) ;
#111185 = DIRECTION('',(1.,-9.85638338623186E-18,0.)) ;
#111186 = DIRECTION('',(-0.577350269189625,-0.577350269189625,0.577350269189627)) ;
#111187 = DIRECTION('',(-1.,7.70371977754894E-34,9.8563833862319E-18)) ;
#111188 = DIRECTION('center_axis',(6.96951553037899E-18,0.707106781186549,
-0.707106781186546)) ;
#111189 = DIRECTION('ref_axis',(8.6424177776148E-34,0.707106781186546,0.707106781186549)) ;
#111190 = DIRECTION('',(0.577350269189625,0.577350269189625,0.577350269189627)) ;
#111191 = DIRECTION('',(-1.,9.85638338623186E-18,0.)) ;
#111192 = DIRECTION('',(0.577350269189625,-0.577350269189625,-0.577350269189627)) ;
#111193 = DIRECTION('',(1.,-7.70371977754894E-34,9.8563833862319E-18)) ;
#111194 = DIRECTION('center_axis',(-0.707106781186548,-1.38247767078009E-16,
0.707106781186547)) ;
#111195 = DIRECTION('ref_axis',(0.707106781186547,8.815972061965E-34,0.707106781186548)) ;
#111196 = DIRECTION('',(-0.577350269189625,-0.577350269189626,-0.577350269189626)) ;
#111197 = DIRECTION('',(-1.95511867169517E-16,1.,0.)) ;
#111198 = DIRECTION('',(0.577350269189625,-0.577350269189626,0.577350269189626)) ;
#111199 = DIRECTION('',(0.,-1.,-1.95511867169518E-16)) ;
#111200 = DIRECTION('center_axis',(-0.707106781186548,-1.38247767078009E-16,
-0.707106781186547)) ;
#111201 = DIRECTION('ref_axis',(-0.707106781186547,-8.815972061965E-34,0.707106781186548)) ;
#111202 = DIRECTION('',(-0.577350269189625,0.577350269189626,0.577350269189626)) ;
#111203 = DIRECTION('',(1.95511867169517E-16,-1.,0.)) ;
#111204 = DIRECTION('',(0.577350269189625,0.577350269189626,-0.577350269189626)) ;
#111205 = DIRECTION('',(0.,1.,-1.95511867169518E-16)) ;
#111206 = DIRECTION('center_axis',(0.577350269189625,0.577350269189625,-0.577350269189628)) ;
#111207 = DIRECTION('ref_axis',(-0.707106781186549,-3.37019869349033E-16,
-0.707106781186546)) ;
#111208 = DIRECTION('center_axis',(-0.577350269189625,-0.577350269189625,
0.577350269189628)) ;
#111209 = DIRECTION('ref_axis',(-0.707106781186549,-5.7623968423712E-16,-0.707106781186546)) ;
#111210 = DIRECTION('center_axis',(-0.577350269189625,-0.577350269189625,
0.577350269189627)) ;
#111211 = DIRECTION('ref_axis',(0.707106781186549,-3.64954285315842E-16,0.707106781186546)) ;
#111212 = DIRECTION('center_axis',(0.,0.,-1.)) ;
#111213 = DIRECTION('ref_axis',(-1.,0.,0.)) ;
#111214 = DIRECTION('center_axis',(0.,0.,1.)) ;
#111215 = DIRECTION('ref_axis',(-1.,0.,0.)) ;
#111216 = DIRECTION('center_axis',(0.,0.,-1.)) ;
#111217 = DIRECTION('ref_axis',(-1.,0.,0.)) ;
#111218 = DIRECTION('center_axis',(2.08166817117218E-16,1.,0.)) ;
#111219 = DIRECTION('ref_axis',(1.,0.,0.)) ;
#111220 = DIRECTION('center_axis',(-1.,0.,-3.25824851045218E-15)) ;
#111221 = DIRECTION('ref_axis',(3.25824851045218E-15,0.,-1.)) ;
#111222 = DIRECTION('center_axis',(2.71050543121376E-15,2.71050543121375E-15,
1.)) ;
#111223 = DIRECTION('ref_axis',(-1.,-1.07215069759461E-44,2.71050543121376E-15)) ;
#111224 = DIRECTION('center_axis',(-0.577350269189625,-0.577350269189625,
-0.577350269189628)) ;
#111225 = DIRECTION('ref_axis',(-0.707106781186549,-3.37019869349033E-16,
0.707106781186546)) ;
#111226 = DIRECTION('center_axis',(-0.577350269189625,-0.577350269189625,
-0.577350269189628)) ;
#111227 = DIRECTION('ref_axis',(-0.707106781186549,-3.64775444964662E-16,
0.707106781186546)) ;
#111228 = DIRECTION('center_axis',(-0.577350269189625,-0.577350269189625,
-0.577350269189628)) ;
#111229 = DIRECTION('ref_axis',(-0.707106781186549,-3.37019869349033E-16,
0.707106781186546)) ;
#111230 = DIRECTION('center_axis',(0.,0.,-1.)) ;
#111231 = DIRECTION('ref_axis',(-1.,0.,0.)) ;
#111232 = DIRECTION('center_axis',(6.99565121361789E-15,0.,1.)) ;
#111233 = DIRECTION('ref_axis',(1.,0.,-6.99565121361789E-15)) ;
#111234 = DIRECTION('center_axis',(-1.,0.,9.8563833862319E-18)) ;
#111235 = DIRECTION('ref_axis',(9.8563833862319E-18,0.,1.)) ;
#111236 = DIRECTION('center_axis',(-1.,-1.62630325872825E-15,1.62630325872826E-15)) ;
#111237 = DIRECTION('ref_axis',(1.62630325872826E-15,2.45227231256843E-45,
1.)) ;
#111238 = DIRECTION('center_axis',(2.08166817117218E-16,1.,0.)) ;
#111239 = DIRECTION('ref_axis',(1.,0.,0.)) ;
#111240 = DIRECTION('center_axis',(-1.,-5.82758667710957E-15,-5.82758667710959E-15)) ;
#111241 = DIRECTION('ref_axis',(5.82758667710959E-15,3.92363570010949E-44,
-1.)) ;
#111242 = DIRECTION('center_axis',(2.08166817117218E-16,1.,0.)) ;
#111243 = DIRECTION('ref_axis',(1.,0.,0.)) ;
#111244 = DIRECTION('center_axis',(-0.577350269189626,0.577350269189625,-0.577350269189627)) ;
#111245 = DIRECTION('ref_axis',(0.707106781186548,-3.45739798078984E-16,-0.707106781186547)) ;
#111246 = DIRECTION('center_axis',(-1.91661677085422E-15,0.,1.)) ;
#111247 = DIRECTION('ref_axis',(-1.,0.,-1.91661677085422E-15)) ;
#111248 = DIRECTION('center_axis',(-1.,0.,-9.8563833862319E-18)) ;
#111249 = DIRECTION('ref_axis',(-9.8563833862319E-18,0.,1.)) ;
#111250 = DIRECTION('center_axis',(-1.,0.,-2.77909431773862E-15)) ;
#111251 = DIRECTION('ref_axis',(-2.77909431773862E-15,0.,1.)) ;
#111252 = DIRECTION('center_axis',(0.,0.,-1.)) ;
#111253 = DIRECTION('ref_axis',(-1.,0.,0.)) ;
#111254 = DIRECTION('center_axis',(1.49077798716757E-15,-1.49077798716756E-15,
1.)) ;
#111255 = DIRECTION('ref_axis',(1.,-2.47036158412635E-45,-1.49077798716757E-15)) ;
#111256 = DIRECTION('center_axis',(0.577350269189625,-0.577350269189625,0.577350269189628)) ;
#111257 = DIRECTION('ref_axis',(0.707106781186549,-3.37019869349033E-16,-0.707106781186546)) ;
#111258 = DIRECTION('center_axis',(0.577350269189625,-0.577350269189625,0.577350269189628)) ;
#111259 = DIRECTION('ref_axis',(0.707106781186549,-3.64775444964662E-16,-0.707106781186546)) ;
#111260 = DIRECTION('center_axis',(2.08166817117218E-16,1.,0.)) ;
#111261 = DIRECTION('ref_axis',(1.,0.,0.)) ;
#111262 = DIRECTION('center_axis',(-0.577350269189626,0.577350269189625,0.577350269189627)) ;
#111263 = DIRECTION('ref_axis',(-0.707106781186549,-1.20060139371205E-15,
-0.707106781186546)) ;
#111264 = DIRECTION('center_axis',(0.,0.,-1.)) ;
#111265 = DIRECTION('ref_axis',(-1.,0.,0.)) ;
#111266 = DIRECTION('center_axis',(0.,0.,1.)) ;
#111267 = DIRECTION('ref_axis',(-1.,0.,0.)) ;
#111268 = DIRECTION('center_axis',(0.,0.,-1.)) ;
#111269 = DIRECTION('ref_axis',(-1.,0.,0.)) ;
#111270 = DIRECTION('center_axis',(-0.577350269189625,0.577350269189625,0.577350269189628)) ;
#111271 = DIRECTION('ref_axis',(0.707106781186549,-3.64775444964662E-16,0.707106781186546)) ;
#111272 = DIRECTION('center_axis',(0.577350269189625,-0.577350269189625,-0.577350269189628)) ;
#111273 = DIRECTION('ref_axis',(0.707106781186549,-4.84385352408706E-16,0.707106781186546)) ;
#111274 = DIRECTION('center_axis',(-0.577350269189625,0.577350269189626,-0.577350269189626)) ;
#111275 = DIRECTION('ref_axis',(5.0289788758123E-16,0.707106781186548,0.707106781186547)) ;
#111276 = DIRECTION('center_axis',(0.577350269189625,-0.577350269189626,0.577350269189626)) ;
#111277 = DIRECTION('ref_axis',(5.0289788758123E-16,0.707106781186548,0.707106781186547)) ;
#111278 = DIRECTION('center_axis',(0.577350269189625,-0.577350269189627,0.577350269189626)) ;
#111279 = DIRECTION('ref_axis',(-1.3856936129729E-16,-0.707106781186547,-0.707106781186548)) ;
#111280 = DIRECTION('center_axis',(0.,0.,-1.)) ;
#111281 = DIRECTION('ref_axis',(-1.,0.,0.)) ;
#111282 = DIRECTION('center_axis',(0.,0.,1.)) ;
#111283 = DIRECTION('ref_axis',(-1.,-5.42101086242751E-15,0.)) ;
#111284 = DIRECTION('center_axis',(0.,0.,-1.)) ;
#111285 = DIRECTION('ref_axis',(-1.,0.,0.)) ;
#111286 = DIRECTION('center_axis',(0.,1.,0.)) ;
#111287 = DIRECTION('ref_axis',(1.,0.,0.)) ;
#111288 = DIRECTION('center_axis',(0.,-1.,-4.79154192713555E-15)) ;
#111289 = DIRECTION('ref_axis',(0.,-4.79154192713555E-15,1.)) ;
#111290 = DIRECTION('center_axis',(-3.18484388167616E-15,3.18484388167617E-15,
1.)) ;
#111291 = DIRECTION('ref_axis',(-4.20389539297445E-45,1.,-3.18484388167617E-15)) ;
#111292 = DIRECTION('center_axis',(0.577350269189625,-0.577350269189626,-0.577350269189626)) ;
#111293 = DIRECTION('ref_axis',(5.0289788758123E-16,0.707106781186548,-0.707106781186547)) ;
#111294 = DIRECTION('center_axis',(0.577350269189625,-0.577350269189626,-0.577350269189626)) ;
#111295 = DIRECTION('ref_axis',(5.0289788758123E-16,0.707106781186548,-0.707106781186547)) ;
#111296 = DIRECTION('center_axis',(0.577350269189625,-0.577350269189626,-0.577350269189626)) ;
#111297 = DIRECTION('ref_axis',(5.0289788758123E-16,0.707106781186548,-0.707106781186547)) ;
#111298 = DIRECTION('center_axis',(0.,0.,-1.)) ;
#111299 = DIRECTION('ref_axis',(-1.,0.,0.)) ;
#111300 = DIRECTION('center_axis',(0.,-2.87492515628133E-15,1.)) ;
#111301 = DIRECTION('ref_axis',(0.,-1.,-2.87492515628133E-15)) ;
#111302 = DIRECTION('center_axis',(0.,1.,1.95511867169518E-16)) ;
#111303 = DIRECTION('ref_axis',(0.,-1.95511867169518E-16,1.)) ;
#111304 = DIRECTION('center_axis',(2.71050543121375E-15,-1.,2.51884375412834E-15)) ;
#111305 = DIRECTION('ref_axis',(1.,2.71050543121375E-15,2.80259692864963E-45)) ;
#111306 = DIRECTION('center_axis',(0.,1.,0.)) ;
#111307 = DIRECTION('ref_axis',(1.,0.,0.)) ;
#111308 = DIRECTION('center_axis',(-2.30392961653169E-15,-1.,2.49559129361712E-15)) ;
#111309 = DIRECTION('ref_axis',(-2.67860162145163E-32,2.49559129361712E-15,
1.)) ;
#111310 = DIRECTION('center_axis',(0.,1.,0.)) ;
#111311 = DIRECTION('ref_axis',(1.,0.,0.)) ;
#111312 = DIRECTION('center_axis',(-0.577350269189625,-0.577350269189626,
-0.577350269189627)) ;
#111313 = DIRECTION('ref_axis',(-8.18676000863892E-15,-0.707106781186544,
0.707106781186551)) ;
#111314 = DIRECTION('center_axis',(0.,-4.50404941150742E-15,1.)) ;
#111315 = DIRECTION('ref_axis',(0.,1.,4.50404941150742E-15)) ;
#111316 = DIRECTION('center_axis',(0.,1.,-1.95511867169518E-16)) ;
#111317 = DIRECTION('ref_axis',(0.,1.95511867169518E-16,1.)) ;
#111318 = DIRECTION('center_axis',(0.,-1.,-2.10827844793964E-15)) ;
#111319 = DIRECTION('ref_axis',(0.,2.10827844793964E-15,-1.)) ;
#111320 = DIRECTION('center_axis',(0.,0.,-1.)) ;
#111321 = DIRECTION('ref_axis',(-1.,0.,0.)) ;
#111322 = DIRECTION('center_axis',(-6.77626357803439E-17,-6.7762635780344E-17,
1.)) ;
#111323 = DIRECTION('ref_axis',(-1.3684555315672E-48,-1.,-6.7762635780344E-17)) ;
#111324 = DIRECTION('center_axis',(0.577350269189625,0.577350269189626,0.577350269189627)) ;
#111325 = DIRECTION('ref_axis',(-9.19305248608458E-17,-0.707106781186548,
0.707106781186547)) ;
#111326 = DIRECTION('center_axis',(0.577350269189625,0.577350269189626,0.577350269189627)) ;
#111327 = DIRECTION('ref_axis',(-9.19305248608458E-17,-0.707106781186548,
0.707106781186547)) ;
#111328 = DIRECTION('center_axis',(0.,1.,0.)) ;
#111329 = DIRECTION('ref_axis',(1.,0.,0.)) ;
#111330 = DIRECTION('center_axis',(-0.577350269189624,-0.577350269189627,
0.577350269189626)) ;
#111331 = DIRECTION('ref_axis',(-1.46369207068818E-16,0.707106781186547,0.707106781186548)) ;
#111332 = DIRECTION('center_axis',(0.,0.,-1.)) ;
#111333 = DIRECTION('ref_axis',(-1.,0.,0.)) ;
#111334 = DIRECTION('center_axis',(0.,0.,1.)) ;
#111335 = DIRECTION('ref_axis',(-1.,1.0842021724855E-15,0.)) ;
#111336 = DIRECTION('center_axis',(0.,0.,-1.)) ;
#111337 = DIRECTION('ref_axis',(-1.,0.,0.)) ;
#111338 = DIRECTION('center_axis',(-0.577350269189625,-0.577350269189626,
0.577350269189627)) ;
#111339 = DIRECTION('ref_axis',(-1.51735478582867E-16,-0.707106781186548,
-0.707106781186547)) ;
#111340 = DIRECTION('center_axis',(0.577350269189625,0.577350269189626,-0.577350269189627)) ;
#111341 = DIRECTION('ref_axis',(-8.00734514747286E-15,-0.707106781186544,
-0.707106781186551)) ;
#111342 = DIRECTION('center_axis',(0.,0.,1.)) ;
#111343 = DIRECTION('ref_axis',(1.,0.,0.)) ;
#111344 = DIRECTION('center_axis',(0.,-1.,0.)) ;
#111345 = DIRECTION('ref_axis',(0.,0.,-1.)) ;
#111346 = DIRECTION('center_axis',(9.85638338623186E-18,1.,0.)) ;
#111347 = DIRECTION('ref_axis',(-1.,9.85638338623186E-18,0.)) ;
#111348 = DIRECTION('center_axis',(0.,-1.,0.)) ;
#111349 = DIRECTION('ref_axis',(0.,0.,-1.)) ;
#111350 = DIRECTION('center_axis',(0.,1.,0.)) ;
#111351 = DIRECTION('ref_axis',(1.,0.,0.)) ;
#111352 = DIRECTION('center_axis',(-1.,0.,0.)) ;
#111353 = DIRECTION('ref_axis',(0.,0.,1.)) ;
#111354 = DIRECTION('center_axis',(1.,-9.85638338623186E-18,0.)) ;
#111355 = DIRECTION('ref_axis',(9.85638338623186E-18,1.,0.)) ;
#111356 = DIRECTION('center_axis',(-1.,0.,0.)) ;
#111357 = DIRECTION('ref_axis',(0.,0.,1.)) ;
#111358 = DIRECTION('center_axis',(0.,1.,0.)) ;
#111359 = DIRECTION('ref_axis',(1.,0.,0.)) ;
#111360 = DIRECTION('center_axis',(0.,1.,0.)) ;
#111361 = DIRECTION('ref_axis',(0.,0.,1.)) ;
#111362 = DIRECTION('center_axis',(-9.85638338623186E-18,-1.,0.)) ;
#111363 = DIRECTION('ref_axis',(1.,-9.85638338623186E-18,0.)) ;
#111364 = DIRECTION('center_axis',(0.,1.,0.)) ;
#111365 = DIRECTION('ref_axis',(0.,0.,1.)) ;
#111366 = DIRECTION('center_axis',(0.,0.,1.)) ;
#111367 = DIRECTION('ref_axis',(1.,0.,0.)) ;
#111368 = DIRECTION('center_axis',(0.,0.,1.)) ;
#111369 = DIRECTION('ref_axis',(1.,0.,0.)) ;
#111370 = DIRECTION('center_axis',(0.,-1.,0.)) ;
#111371 = DIRECTION('ref_axis',(0.,0.,-1.)) ;
#111372 = DIRECTION('center_axis',(-9.85638338623186E-18,-1.,0.)) ;
#111373 = DIRECTION('ref_axis',(1.,-9.85638338623186E-18,0.)) ;
#111374 = DIRECTION('center_axis',(0.,-1.,0.)) ;
#111375 = DIRECTION('ref_axis',(0.,0.,-1.)) ;
#111376 = DIRECTION('center_axis',(0.,1.,0.)) ;
#111377 = DIRECTION('ref_axis',(1.,0.,0.)) ;
#111378 = DIRECTION('center_axis',(1.,-7.66646708341686E-16,0.)) ;
#111379 = DIRECTION('ref_axis',(7.66646708341686E-16,1.,0.)) ;
#111380 = DIRECTION('center_axis',(1.,-9.85638338623186E-18,0.)) ;
#111381 = DIRECTION('ref_axis',(9.85638338623186E-18,1.,0.)) ;
#111382 = DIRECTION('center_axis',(1.,0.,0.)) ;
#111383 = DIRECTION('ref_axis',(0.,0.,-1.)) ;
#111384 = DIRECTION('center_axis',(0.,1.,0.)) ;
#111385 = DIRECTION('ref_axis',(1.,0.,0.)) ;
#111386 = DIRECTION('center_axis',(0.,1.,0.)) ;
#111387 = DIRECTION('ref_axis',(0.,0.,1.)) ;
#111388 = DIRECTION('center_axis',(-9.85638338623186E-18,-1.,0.)) ;
#111389 = DIRECTION('ref_axis',(1.,-9.85638338623186E-18,0.)) ;
#111390 = DIRECTION('center_axis',(0.,1.,0.)) ;
#111391 = DIRECTION('ref_axis',(0.,0.,1.)) ;
#111392 = DIRECTION('center_axis',(0.,0.,1.)) ;
#111393 = DIRECTION('ref_axis',(1.,0.,0.)) ;
#111394 = DIRECTION('center_axis',(-1.,-1.95511867169517E-16,0.)) ;
#111395 = DIRECTION('ref_axis',(1.95511867169517E-16,-1.,0.)) ;
#111396 = DIRECTION('center_axis',(1.,0.,0.)) ;
#111397 = DIRECTION('ref_axis',(0.,0.,-1.)) ;
#111398 = DIRECTION('center_axis',(0.,1.,0.)) ;
#111399 = DIRECTION('ref_axis',(1.,0.,0.)) ;
#111400 = DIRECTION('center_axis',(-2.29994012502506E-15,-1.,0.)) ;
#111401 = DIRECTION('ref_axis',(1.,-2.29994012502506E-15,0.)) ;
#111402 = DIRECTION('center_axis',(-1.95511867169517E-16,1.,0.)) ;
#111403 = DIRECTION('ref_axis',(-1.,-1.95511867169517E-16,0.)) ;
#111404 = DIRECTION('center_axis',(0.,-1.,0.)) ;
#111405 = DIRECTION('ref_axis',(0.,0.,-1.)) ;
#111406 = DIRECTION('center_axis',(0.,1.,0.)) ;
#111407 = DIRECTION('ref_axis',(1.,0.,0.)) ;
#111408 = DIRECTION('center_axis',(-1.,0.,0.)) ;
#111409 = DIRECTION('ref_axis',(0.,0.,1.)) ;
#111410 = DIRECTION('center_axis',(1.,-1.06642836637918E-16,0.)) ;
#111411 = DIRECTION('ref_axis',(1.06642836637918E-16,1.,0.)) ;
#111412 = DIRECTION('center_axis',(1.,1.95511867169517E-16,0.)) ;
#111413 = DIRECTION('ref_axis',(-1.95511867169517E-16,1.,0.)) ;
#111414 = DIRECTION('center_axis',(1.,0.,0.)) ;
#111415 = DIRECTION('ref_axis',(0.,0.,-1.)) ;
#111416 = DIRECTION('center_axis',(0.,1.,0.)) ;
#111417 = DIRECTION('ref_axis',(1.,0.,0.)) ;
#111418 = DIRECTION('center_axis',(2.29994012502506E-15,-1.,0.)) ;
#111419 = DIRECTION('ref_axis',(1.,2.29994012502506E-15,0.)) ;
#111420 = DIRECTION('center_axis',(-1.95511867169517E-16,1.,0.)) ;
#111421 = DIRECTION('ref_axis',(-1.,-1.95511867169517E-16,0.)) ;
#111422 = DIRECTION('center_axis',(0.,-1.,0.)) ;
#111423 = DIRECTION('ref_axis',(0.,0.,-1.)) ;
#111424 = DIRECTION('center_axis',(-1.,1.06642836637918E-16,0.)) ;
#111425 = DIRECTION('ref_axis',(-1.06642836637918E-16,-1.,0.)) ;
#111426 = DIRECTION('center_axis',(1.,0.,0.)) ;
#111427 = DIRECTION('ref_axis',(0.,0.,-1.)) ;
#111428 = DIRECTION('center_axis',(0.,1.,0.)) ;
#111429 = DIRECTION('ref_axis',(1.,0.,0.)) ;
#111430 = DIRECTION('center_axis',(-1.,-1.53063836115601E-16,0.)) ;
#111431 = DIRECTION('ref_axis',(1.53063836115601E-16,-1.,0.)) ;
#111432 = DIRECTION('',(0.,0.,1.)) ;
#111433 = DIRECTION('',(-1.53063836115601E-16,1.,-1.020425574104E-16)) ;
#111434 = DIRECTION('',(0.,0.,-1.)) ;
#111435 = DIRECTION('',(1.53063836115601E-16,-1.,5.10212787052002E-17)) ;
#111436 = DIRECTION('',(0.,0.,1.)) ;
#111437 = DIRECTION('',(-1.53063836115601E-16,1.,-1.30104260698261E-16)) ;
#111438 = DIRECTION('center_axis',(-1.,-1.53063836115601E-16,0.)) ;
#111439 = DIRECTION('ref_axis',(1.53063836115601E-16,-1.,0.)) ;
#111440 = DIRECTION('',(0.,0.,1.)) ;
#111441 = DIRECTION('center_axis',(-1.,-1.53063836115601E-16,0.)) ;
#111442 = DIRECTION('ref_axis',(1.53063836115601E-16,-1.,0.)) ;
#111443 = DIRECTION('',(1.53063836115601E-16,-1.,-1.30104260698261E-16)) ;
#111444 = DIRECTION('center_axis',(-1.,-1.53063836115601E-16,0.)) ;
#111445 = DIRECTION('ref_axis',(1.53063836115601E-16,-1.,0.)) ;
#111446 = DIRECTION('',(0.,0.,1.)) ;
#111447 = DIRECTION('',(-1.53063836115601E-16,1.,-1.020425574104E-16)) ;
#111448 = DIRECTION('',(0.,0.,-1.)) ;
#111449 = DIRECTION('',(1.53063836115601E-16,-1.,5.10212787052002E-17)) ;
#111450 = DIRECTION('',(0.,0.,1.)) ;
#111451 = DIRECTION('',(-1.53063836115601E-16,1.,-1.30104260698261E-16)) ;
#111452 = DIRECTION('center_axis',(-1.,-1.53063836115601E-16,0.)) ;
#111453 = DIRECTION('ref_axis',(1.53063836115601E-16,-1.,0.)) ;
#111454 = DIRECTION('',(0.,0.,1.)) ;
#111455 = DIRECTION('center_axis',(-1.,-1.53063836115601E-16,0.)) ;
#111456 = DIRECTION('ref_axis',(1.53063836115601E-16,-1.,0.)) ;
#111457 = DIRECTION('',(1.53063836115601E-16,-1.,-1.30104260698261E-16)) ;
#111458 = DIRECTION('center_axis',(-1.,-1.53063836115601E-16,0.)) ;
#111459 = DIRECTION('ref_axis',(1.53063836115601E-16,-1.,0.)) ;
#111460 = DIRECTION('',(0.,0.,1.)) ;
#111461 = DIRECTION('',(-1.53063836115601E-16,1.,-1.020425574104E-16)) ;
#111462 = DIRECTION('',(0.,0.,-1.)) ;
#111463 = DIRECTION('',(1.53063836115601E-16,-1.,5.10212787052002E-17)) ;
#111464 = DIRECTION('',(0.,0.,1.)) ;
#111465 = DIRECTION('',(-1.53063836115601E-16,1.,-1.30104260698261E-16)) ;
#111466 = DIRECTION('center_axis',(-1.,-1.53063836115601E-16,0.)) ;
#111467 = DIRECTION('ref_axis',(1.53063836115601E-16,-1.,0.)) ;
#111468 = DIRECTION('',(0.,0.,1.)) ;
#111469 = DIRECTION('center_axis',(-1.,-1.53063836115601E-16,0.)) ;
#111470 = DIRECTION('ref_axis',(1.53063836115601E-16,-1.,0.)) ;
#111471 = DIRECTION('',(1.53063836115601E-16,-1.,-1.30104260698261E-16)) ;
#111472 = DIRECTION('center_axis',(-1.,-1.53063836115601E-16,0.)) ;
#111473 = DIRECTION('ref_axis',(1.53063836115601E-16,-1.,0.)) ;
#111474 = DIRECTION('',(0.,0.,1.)) ;
#111475 = DIRECTION('',(-1.53063836115601E-16,1.,-1.020425574104E-16)) ;
#111476 = DIRECTION('',(0.,0.,-1.)) ;
#111477 = DIRECTION('',(1.53063836115601E-16,-1.,5.10212787052002E-17)) ;
#111478 = DIRECTION('',(0.,0.,1.)) ;
#111479 = DIRECTION('',(-1.53063836115601E-16,1.,-1.30104260698261E-16)) ;
#111480 = DIRECTION('center_axis',(-1.,-1.53063836115601E-16,0.)) ;
#111481 = DIRECTION('ref_axis',(1.53063836115601E-16,-1.,0.)) ;
#111482 = DIRECTION('',(0.,0.,1.)) ;
#111483 = DIRECTION('center_axis',(-1.,-1.53063836115601E-16,0.)) ;
#111484 = DIRECTION('ref_axis',(1.53063836115601E-16,-1.,0.)) ;
#111485 = DIRECTION('',(1.53063836115601E-16,-1.,-1.30104260698261E-16)) ;
#111486 = DIRECTION('center_axis',(-1.,-1.53063836115601E-16,0.)) ;
#111487 = DIRECTION('ref_axis',(1.53063836115601E-16,-1.,0.)) ;
#111488 = DIRECTION('',(0.,0.,1.)) ;
#111489 = DIRECTION('',(-1.53063836115601E-16,1.,-1.020425574104E-16)) ;
#111490 = DIRECTION('',(0.,0.,-1.)) ;
#111491 = DIRECTION('',(1.53063836115601E-16,-1.,5.10212787052002E-17)) ;
#111492 = DIRECTION('',(0.,0.,1.)) ;
#111493 = DIRECTION('',(-1.53063836115601E-16,1.,-1.30104260698261E-16)) ;
#111494 = DIRECTION('center_axis',(-1.,-1.53063836115601E-16,0.)) ;
#111495 = DIRECTION('ref_axis',(1.53063836115601E-16,-1.,0.)) ;
#111496 = DIRECTION('',(0.,0.,1.)) ;
#111497 = DIRECTION('center_axis',(-1.,-1.53063836115601E-16,0.)) ;
#111498 = DIRECTION('ref_axis',(1.53063836115601E-16,-1.,0.)) ;
#111499 = DIRECTION('',(1.53063836115601E-16,-1.,-1.30104260698261E-16)) ;
#111500 = DIRECTION('center_axis',(-1.,-1.53063836115601E-16,0.)) ;
#111501 = DIRECTION('ref_axis',(1.53063836115601E-16,-1.,0.)) ;
#111502 = DIRECTION('',(0.,0.,1.)) ;
#111503 = DIRECTION('',(-1.53063836115601E-16,1.,-1.020425574104E-16)) ;
#111504 = DIRECTION('',(0.,0.,-1.)) ;
#111505 = DIRECTION('',(1.53063836115601E-16,-1.,5.10212787052002E-17)) ;
#111506 = DIRECTION('',(0.,0.,1.)) ;
#111507 = DIRECTION('',(-1.53063836115601E-16,1.,-1.30104260698261E-16)) ;
#111508 = DIRECTION('center_axis',(-1.,-1.53063836115601E-16,0.)) ;
#111509 = DIRECTION('ref_axis',(1.53063836115601E-16,-1.,0.)) ;
#111510 = DIRECTION('',(0.,0.,1.)) ;
#111511 = DIRECTION('center_axis',(-1.,-1.53063836115601E-16,0.)) ;
#111512 = DIRECTION('ref_axis',(1.53063836115601E-16,-1.,0.)) ;
#111513 = DIRECTION('',(1.53063836115601E-16,-1.,-1.30104260698261E-16)) ;
#111514 = DIRECTION('center_axis',(-1.,-1.53063836115601E-16,0.)) ;
#111515 = DIRECTION('ref_axis',(1.53063836115601E-16,-1.,0.)) ;
#111516 = DIRECTION('',(0.,0.,1.)) ;
#111517 = DIRECTION('',(-1.53063836115601E-16,1.,-1.020425574104E-16)) ;
#111518 = DIRECTION('',(0.,0.,-1.)) ;
#111519 = DIRECTION('',(1.53063836115601E-16,-1.,5.10212787052002E-17)) ;
#111520 = DIRECTION('',(0.,0.,1.)) ;
#111521 = DIRECTION('',(-1.53063836115601E-16,1.,-1.30104260698261E-16)) ;
#111522 = DIRECTION('center_axis',(-1.,-1.53063836115601E-16,0.)) ;
#111523 = DIRECTION('ref_axis',(1.53063836115601E-16,-1.,0.)) ;
#111524 = DIRECTION('',(0.,0.,1.)) ;
#111525 = DIRECTION('center_axis',(-1.,-1.53063836115601E-16,0.)) ;
#111526 = DIRECTION('ref_axis',(1.53063836115601E-16,-1.,0.)) ;
#111527 = DIRECTION('',(1.53063836115601E-16,-1.,-1.30104260698261E-16)) ;
#111528 = DIRECTION('center_axis',(-1.,-1.53063836115601E-16,0.)) ;
#111529 = DIRECTION('ref_axis',(1.53063836115601E-16,-1.,0.)) ;
#111530 = DIRECTION('',(0.,0.,1.)) ;
#111531 = DIRECTION('',(-1.53063836115601E-16,1.,-1.020425574104E-16)) ;
#111532 = DIRECTION('',(0.,0.,-1.)) ;
#111533 = DIRECTION('',(1.53063836115601E-16,-1.,5.10212787052002E-17)) ;
#111534 = DIRECTION('',(0.,0.,1.)) ;
#111535 = DIRECTION('',(-1.53063836115601E-16,1.,-1.30104260698261E-16)) ;
#111536 = DIRECTION('center_axis',(-1.,-1.53063836115601E-16,0.)) ;
#111537 = DIRECTION('ref_axis',(1.53063836115601E-16,-1.,0.)) ;
#111538 = DIRECTION('',(0.,0.,1.)) ;
#111539 = DIRECTION('center_axis',(-1.,-1.53063836115601E-16,0.)) ;
#111540 = DIRECTION('ref_axis',(1.53063836115601E-16,-1.,0.)) ;
#111541 = DIRECTION('',(1.53063836115601E-16,-1.,-1.30104260698261E-16)) ;
#111542 = DIRECTION('center_axis',(-1.,-1.53063836115601E-16,0.)) ;
#111543 = DIRECTION('ref_axis',(1.53063836115601E-16,-1.,0.)) ;
#111544 = DIRECTION('',(0.,0.,1.)) ;
#111545 = DIRECTION('',(-1.53063836115601E-16,1.,-1.020425574104E-16)) ;
#111546 = DIRECTION('',(0.,0.,-1.)) ;
#111547 = DIRECTION('',(1.53063836115601E-16,-1.,5.10212787052002E-17)) ;
#111548 = DIRECTION('',(0.,0.,1.)) ;
#111549 = DIRECTION('',(-1.53063836115601E-16,1.,-1.30104260698261E-16)) ;
#111550 = DIRECTION('center_axis',(-1.,-1.53063836115601E-16,0.)) ;
#111551 = DIRECTION('ref_axis',(1.53063836115601E-16,-1.,0.)) ;
#111552 = DIRECTION('',(0.,0.,1.)) ;
#111553 = DIRECTION('center_axis',(-1.,-1.53063836115601E-16,0.)) ;
#111554 = DIRECTION('ref_axis',(1.53063836115601E-16,-1.,0.)) ;
#111555 = DIRECTION('',(1.53063836115601E-16,-1.,-1.30104260698261E-16)) ;
#111556 = DIRECTION('center_axis',(-1.53063836115601E-16,1.,0.)) ;
#111557 = DIRECTION('ref_axis',(-1.,-1.53063836115601E-16,0.)) ;
#111558 = DIRECTION('',(-1.,-1.53063836115601E-16,2.73691106313441E-48)) ;
#111559 = DIRECTION('',(0.,0.,-1.)) ;
#111560 = DIRECTION('',(1.,1.53063836115601E-16,-1.53236300070382E-33)) ;
#111561 = DIRECTION('',(0.,0.,1.)) ;
#111562 = DIRECTION('center_axis',(1.99142572374599E-32,-1.30104260698261E-16,
-1.)) ;
#111563 = DIRECTION('ref_axis',(0.,1.,-1.30104260698261E-16)) ;
#111564 = DIRECTION('',(-1.,-1.53063836115601E-16,2.73691106313441E-48)) ;
#111565 = DIRECTION('',(1.53063836115601E-16,-1.,1.30104260698261E-16)) ;
#111566 = DIRECTION('',(1.,1.53063836115601E-16,-2.73691106313441E-48)) ;
#111567 = DIRECTION('center_axis',(-1.53063836115601E-16,1.,0.)) ;
#111568 = DIRECTION('ref_axis',(-1.,-1.53063836115601E-16,0.)) ;
#111569 = DIRECTION('',(-1.,-1.53063836115601E-16,-2.73691106313441E-48)) ;
#111570 = DIRECTION('',(0.,0.,-1.)) ;
#111571 = DIRECTION('',(1.,1.53063836115601E-16,-2.73691106313441E-48)) ;
#111572 = DIRECTION('',(0.,0.,1.)) ;
#111573 = DIRECTION('center_axis',(1.99142572374599E-32,-1.30104260698261E-16,
1.)) ;
#111574 = DIRECTION('ref_axis',(0.,-1.,-1.30104260698261E-16)) ;
#111575 = DIRECTION('',(-1.,-1.53063836115601E-16,-2.73691106313441E-48)) ;
#111576 = DIRECTION('',(-1.53063836115601E-16,1.,1.30104260698261E-16)) ;
#111577 = DIRECTION('',(1.,1.53063836115601E-16,2.73691106313441E-48)) ;
#111578 = DIRECTION('',(2.16840434497101E-16,-1.,-1.30104260698261E-16)) ;
#111579 = DIRECTION('center_axis',(-1.53063836115601E-16,1.,0.)) ;
#111580 = DIRECTION('ref_axis',(-1.,-1.53063836115601E-16,0.)) ;
#111581 = DIRECTION('',(-1.,-1.53063836115601E-16,3.06472600140763E-33)) ;
#111582 = DIRECTION('',(0.,0.,-1.)) ;
#111583 = DIRECTION('',(1.,1.53063836115601E-16,2.73691106313441E-48)) ;
#111584 = DIRECTION('',(0.,0.,1.)) ;
#111585 = DIRECTION('center_axis',(-1.53063836115601E-16,1.,0.)) ;
#111586 = DIRECTION('ref_axis',(-1.,-1.53063836115601E-16,0.)) ;
#111587 = DIRECTION('',(-1.,-1.53063836115601E-16,2.73691106313441E-48)) ;
#111588 = DIRECTION('',(0.,0.,-1.)) ;
#111589 = DIRECTION('',(1.,1.53063836115601E-16,-1.53236300070382E-33)) ;
#111590 = DIRECTION('',(0.,0.,1.)) ;
#111591 = DIRECTION('center_axis',(1.99142572374599E-32,-1.30104260698261E-16,
-1.)) ;
#111592 = DIRECTION('ref_axis',(0.,1.,-1.30104260698261E-16)) ;
#111593 = DIRECTION('',(-1.,-1.53063836115601E-16,2.73691106313441E-48)) ;
#111594 = DIRECTION('',(1.53063836115601E-16,-1.,1.30104260698261E-16)) ;
#111595 = DIRECTION('',(1.,1.53063836115601E-16,-2.73691106313441E-48)) ;
#111596 = DIRECTION('center_axis',(-1.53063836115601E-16,1.,0.)) ;
#111597 = DIRECTION('ref_axis',(-1.,-1.53063836115601E-16,0.)) ;
#111598 = DIRECTION('',(-1.,-1.53063836115601E-16,-2.73691106313441E-48)) ;
#111599 = DIRECTION('',(0.,0.,-1.)) ;
#111600 = DIRECTION('',(1.,1.53063836115601E-16,-2.73691106313441E-48)) ;
#111601 = DIRECTION('',(0.,0.,1.)) ;
#111602 = DIRECTION('center_axis',(1.99142572374599E-32,-1.30104260698261E-16,
1.)) ;
#111603 = DIRECTION('ref_axis',(0.,-1.,-1.30104260698261E-16)) ;
#111604 = DIRECTION('',(-1.,-1.53063836115601E-16,-2.73691106313441E-48)) ;
#111605 = DIRECTION('',(-1.53063836115601E-16,1.,1.30104260698261E-16)) ;
#111606 = DIRECTION('',(1.,1.53063836115601E-16,2.73691106313441E-48)) ;
#111607 = DIRECTION('',(2.16840434497101E-16,-1.,-1.30104260698261E-16)) ;
#111608 = DIRECTION('center_axis',(-1.53063836115601E-16,1.,0.)) ;
#111609 = DIRECTION('ref_axis',(-1.,-1.53063836115601E-16,0.)) ;
#111610 = DIRECTION('',(-1.,-1.53063836115601E-16,3.06472600140763E-33)) ;
#111611 = DIRECTION('',(0.,0.,-1.)) ;
#111612 = DIRECTION('',(1.,1.53063836115601E-16,2.73691106313441E-48)) ;
#111613 = DIRECTION('',(0.,0.,1.)) ;
#111614 = DIRECTION('center_axis',(-1.53063836115601E-16,1.,0.)) ;
#111615 = DIRECTION('ref_axis',(-1.,-1.53063836115601E-16,0.)) ;
#111616 = DIRECTION('',(-1.,-1.53063836115601E-16,2.73691106313441E-48)) ;
#111617 = DIRECTION('',(0.,0.,-1.)) ;
#111618 = DIRECTION('',(1.,1.53063836115601E-16,-1.53236300070382E-33)) ;
#111619 = DIRECTION('',(0.,0.,1.)) ;
#111620 = DIRECTION('center_axis',(1.99142572374599E-32,-1.30104260698261E-16,
-1.)) ;
#111621 = DIRECTION('ref_axis',(0.,1.,-1.30104260698261E-16)) ;
#111622 = DIRECTION('',(-1.,-1.53063836115601E-16,2.73691106313441E-48)) ;
#111623 = DIRECTION('',(1.53063836115601E-16,-1.,1.30104260698261E-16)) ;
#111624 = DIRECTION('',(1.,1.53063836115601E-16,-2.73691106313441E-48)) ;
#111625 = DIRECTION('center_axis',(-1.53063836115601E-16,1.,0.)) ;
#111626 = DIRECTION('ref_axis',(-1.,-1.53063836115601E-16,0.)) ;
#111627 = DIRECTION('',(-1.,-1.53063836115601E-16,-2.73691106313441E-48)) ;
#111628 = DIRECTION('',(0.,0.,-1.)) ;
#111629 = DIRECTION('',(1.,1.53063836115601E-16,-2.73691106313441E-48)) ;
#111630 = DIRECTION('',(0.,0.,1.)) ;
#111631 = DIRECTION('center_axis',(1.99142572374599E-32,-1.30104260698261E-16,
1.)) ;
#111632 = DIRECTION('ref_axis',(0.,-1.,-1.30104260698261E-16)) ;
#111633 = DIRECTION('',(-1.,-1.53063836115601E-16,-2.73691106313441E-48)) ;
#111634 = DIRECTION('',(-1.53063836115601E-16,1.,1.30104260698261E-16)) ;
#111635 = DIRECTION('',(1.,1.53063836115601E-16,2.73691106313441E-48)) ;
#111636 = DIRECTION('',(2.16840434497101E-16,-1.,-1.30104260698261E-16)) ;
#111637 = DIRECTION('center_axis',(-1.53063836115601E-16,1.,0.)) ;
#111638 = DIRECTION('ref_axis',(-1.,-1.53063836115601E-16,0.)) ;
#111639 = DIRECTION('',(-1.,-1.53063836115601E-16,3.06472600140763E-33)) ;
#111640 = DIRECTION('',(0.,0.,-1.)) ;
#111641 = DIRECTION('',(1.,1.53063836115601E-16,2.73691106313441E-48)) ;
#111642 = DIRECTION('',(0.,0.,1.)) ;
#111643 = DIRECTION('center_axis',(-1.53063836115601E-16,1.,0.)) ;
#111644 = DIRECTION('ref_axis',(-1.,-1.53063836115601E-16,0.)) ;
#111645 = DIRECTION('',(-1.,-1.53063836115601E-16,2.73691106313441E-48)) ;
#111646 = DIRECTION('',(0.,0.,-1.)) ;
#111647 = DIRECTION('',(1.,1.53063836115601E-16,-1.53236300070382E-33)) ;
#111648 = DIRECTION('',(0.,0.,1.)) ;
#111649 = DIRECTION('center_axis',(1.99142572374599E-32,-1.30104260698261E-16,
-1.)) ;
#111650 = DIRECTION('ref_axis',(0.,1.,-1.30104260698261E-16)) ;
#111651 = DIRECTION('',(-1.,-1.53063836115601E-16,2.73691106313441E-48)) ;
#111652 = DIRECTION('',(1.53063836115601E-16,-1.,1.30104260698261E-16)) ;
#111653 = DIRECTION('',(1.,1.53063836115601E-16,-2.73691106313441E-48)) ;
#111654 = DIRECTION('center_axis',(-1.53063836115601E-16,1.,0.)) ;
#111655 = DIRECTION('ref_axis',(-1.,-1.53063836115601E-16,0.)) ;
#111656 = DIRECTION('',(-1.,-1.53063836115601E-16,-2.73691106313441E-48)) ;
#111657 = DIRECTION('',(0.,0.,-1.)) ;
#111658 = DIRECTION('',(1.,1.53063836115601E-16,-2.73691106313441E-48)) ;
#111659 = DIRECTION('',(0.,0.,1.)) ;
#111660 = DIRECTION('center_axis',(1.99142572374599E-32,-1.30104260698261E-16,
1.)) ;
#111661 = DIRECTION('ref_axis',(0.,-1.,-1.30104260698261E-16)) ;
#111662 = DIRECTION('',(-1.,-1.53063836115601E-16,-2.73691106313441E-48)) ;
#111663 = DIRECTION('',(-1.53063836115601E-16,1.,1.30104260698261E-16)) ;
#111664 = DIRECTION('',(1.,1.53063836115601E-16,2.73691106313441E-48)) ;
#111665 = DIRECTION('',(2.16840434497101E-16,-1.,-1.30104260698261E-16)) ;
#111666 = DIRECTION('center_axis',(-1.53063836115601E-16,1.,0.)) ;
#111667 = DIRECTION('ref_axis',(-1.,-1.53063836115601E-16,0.)) ;
#111668 = DIRECTION('',(-1.,-1.53063836115601E-16,3.06472600140763E-33)) ;
#111669 = DIRECTION('',(0.,0.,-1.)) ;
#111670 = DIRECTION('',(1.,1.53063836115601E-16,2.73691106313441E-48)) ;
#111671 = DIRECTION('',(0.,0.,1.)) ;
#111672 = DIRECTION('center_axis',(-1.53063836115601E-16,1.,0.)) ;
#111673 = DIRECTION('ref_axis',(-1.,-1.53063836115601E-16,0.)) ;
#111674 = DIRECTION('',(-1.,-1.53063836115601E-16,2.73691106313441E-48)) ;
#111675 = DIRECTION('',(0.,0.,-1.)) ;
#111676 = DIRECTION('',(1.,1.53063836115601E-16,-1.53236300070382E-33)) ;
#111677 = DIRECTION('',(0.,0.,1.)) ;
#111678 = DIRECTION('center_axis',(1.99142572374599E-32,-1.30104260698261E-16,
-1.)) ;
#111679 = DIRECTION('ref_axis',(0.,1.,-1.30104260698261E-16)) ;
#111680 = DIRECTION('',(-1.,-1.53063836115601E-16,2.73691106313441E-48)) ;
#111681 = DIRECTION('',(1.53063836115601E-16,-1.,1.30104260698261E-16)) ;
#111682 = DIRECTION('',(1.,1.53063836115601E-16,-2.73691106313441E-48)) ;
#111683 = DIRECTION('center_axis',(-1.53063836115601E-16,1.,0.)) ;
#111684 = DIRECTION('ref_axis',(-1.,-1.53063836115601E-16,0.)) ;
#111685 = DIRECTION('',(-1.,-1.53063836115601E-16,-2.73691106313441E-48)) ;
#111686 = DIRECTION('',(0.,0.,-1.)) ;
#111687 = DIRECTION('',(1.,1.53063836115601E-16,-2.73691106313441E-48)) ;
#111688 = DIRECTION('',(0.,0.,1.)) ;
#111689 = DIRECTION('center_axis',(1.99142572374599E-32,-1.30104260698261E-16,
1.)) ;
#111690 = DIRECTION('ref_axis',(0.,-1.,-1.30104260698261E-16)) ;
#111691 = DIRECTION('',(-1.,-1.53063836115601E-16,-2.73691106313441E-48)) ;
#111692 = DIRECTION('',(-1.53063836115601E-16,1.,1.30104260698261E-16)) ;
#111693 = DIRECTION('',(1.,1.53063836115601E-16,2.73691106313441E-48)) ;
#111694 = DIRECTION('',(2.16840434497101E-16,-1.,-1.30104260698261E-16)) ;
#111695 = DIRECTION('center_axis',(-1.53063836115601E-16,1.,0.)) ;
#111696 = DIRECTION('ref_axis',(-1.,-1.53063836115601E-16,0.)) ;
#111697 = DIRECTION('',(-1.,-1.53063836115601E-16,3.06472600140763E-33)) ;
#111698 = DIRECTION('',(0.,0.,-1.)) ;
#111699 = DIRECTION('',(1.,1.53063836115601E-16,2.73691106313441E-48)) ;
#111700 = DIRECTION('',(0.,0.,1.)) ;
#111701 = DIRECTION('center_axis',(-1.53063836115601E-16,1.,0.)) ;
#111702 = DIRECTION('ref_axis',(-1.,-1.53063836115601E-16,0.)) ;
#111703 = DIRECTION('',(-1.,-1.53063836115601E-16,2.73691106313441E-48)) ;
#111704 = DIRECTION('',(0.,0.,-1.)) ;
#111705 = DIRECTION('',(1.,1.53063836115601E-16,-1.53236300070382E-33)) ;
#111706 = DIRECTION('',(0.,0.,1.)) ;
#111707 = DIRECTION('center_axis',(1.99142572374599E-32,-1.30104260698261E-16,
-1.)) ;
#111708 = DIRECTION('ref_axis',(0.,1.,-1.30104260698261E-16)) ;
#111709 = DIRECTION('',(-1.,-1.53063836115601E-16,2.73691106313441E-48)) ;
#111710 = DIRECTION('',(1.53063836115601E-16,-1.,1.30104260698261E-16)) ;
#111711 = DIRECTION('',(1.,1.53063836115601E-16,-2.73691106313441E-48)) ;
#111712 = DIRECTION('center_axis',(-1.53063836115601E-16,1.,0.)) ;
#111713 = DIRECTION('ref_axis',(-1.,-1.53063836115601E-16,0.)) ;
#111714 = DIRECTION('',(-1.,-1.53063836115601E-16,-2.73691106313441E-48)) ;
#111715 = DIRECTION('',(0.,0.,-1.)) ;
#111716 = DIRECTION('',(1.,1.53063836115601E-16,-2.73691106313441E-48)) ;
#111717 = DIRECTION('',(0.,0.,1.)) ;
#111718 = DIRECTION('center_axis',(1.99142572374599E-32,-1.30104260698261E-16,
1.)) ;
#111719 = DIRECTION('ref_axis',(0.,-1.,-1.30104260698261E-16)) ;
#111720 = DIRECTION('',(-1.,-1.53063836115601E-16,-2.73691106313441E-48)) ;
#111721 = DIRECTION('',(-1.53063836115601E-16,1.,1.30104260698261E-16)) ;
#111722 = DIRECTION('',(1.,1.53063836115601E-16,2.73691106313441E-48)) ;
#111723 = DIRECTION('',(2.16840434497101E-16,-1.,-1.30104260698261E-16)) ;
#111724 = DIRECTION('center_axis',(-1.53063836115601E-16,1.,0.)) ;
#111725 = DIRECTION('ref_axis',(-1.,-1.53063836115601E-16,0.)) ;
#111726 = DIRECTION('',(-1.,-1.53063836115601E-16,3.06472600140763E-33)) ;
#111727 = DIRECTION('',(0.,0.,-1.)) ;
#111728 = DIRECTION('',(1.,1.53063836115601E-16,2.73691106313441E-48)) ;
#111729 = DIRECTION('',(0.,0.,1.)) ;
#111730 = DIRECTION('center_axis',(-1.53063836115601E-16,1.,0.)) ;
#111731 = DIRECTION('ref_axis',(-1.,-1.53063836115601E-16,0.)) ;
#111732 = DIRECTION('',(-1.,-1.53063836115601E-16,2.73691106313441E-48)) ;
#111733 = DIRECTION('',(0.,0.,-1.)) ;
#111734 = DIRECTION('',(1.,1.53063836115601E-16,-1.53236300070382E-33)) ;
#111735 = DIRECTION('',(0.,0.,1.)) ;
#111736 = DIRECTION('center_axis',(1.99142572374599E-32,-1.30104260698261E-16,
-1.)) ;
#111737 = DIRECTION('ref_axis',(0.,1.,-1.30104260698261E-16)) ;
#111738 = DIRECTION('',(-1.,-1.53063836115601E-16,2.73691106313441E-48)) ;
#111739 = DIRECTION('',(1.53063836115601E-16,-1.,1.30104260698261E-16)) ;
#111740 = DIRECTION('',(1.,1.53063836115601E-16,-2.73691106313441E-48)) ;
#111741 = DIRECTION('center_axis',(-1.53063836115601E-16,1.,0.)) ;
#111742 = DIRECTION('ref_axis',(-1.,-1.53063836115601E-16,0.)) ;
#111743 = DIRECTION('',(-1.,-1.53063836115601E-16,-2.73691106313441E-48)) ;
#111744 = DIRECTION('',(0.,0.,-1.)) ;
#111745 = DIRECTION('',(1.,1.53063836115601E-16,-2.73691106313441E-48)) ;
#111746 = DIRECTION('',(0.,0.,1.)) ;
#111747 = DIRECTION('center_axis',(1.99142572374599E-32,-1.30104260698261E-16,
1.)) ;
#111748 = DIRECTION('ref_axis',(0.,-1.,-1.30104260698261E-16)) ;
#111749 = DIRECTION('',(-1.,-1.53063836115601E-16,-2.73691106313441E-48)) ;
#111750 = DIRECTION('',(-1.53063836115601E-16,1.,1.30104260698261E-16)) ;
#111751 = DIRECTION('',(1.,1.53063836115601E-16,2.73691106313441E-48)) ;
#111752 = DIRECTION('',(2.16840434497101E-16,-1.,-1.30104260698261E-16)) ;
#111753 = DIRECTION('center_axis',(-1.53063836115601E-16,1.,0.)) ;
#111754 = DIRECTION('ref_axis',(-1.,-1.53063836115601E-16,0.)) ;
#111755 = DIRECTION('',(-1.,-1.53063836115601E-16,3.06472600140763E-33)) ;
#111756 = DIRECTION('',(0.,0.,-1.)) ;
#111757 = DIRECTION('',(1.,1.53063836115601E-16,2.73691106313441E-48)) ;
#111758 = DIRECTION('',(0.,0.,1.)) ;
#111759 = DIRECTION('center_axis',(-1.53063836115601E-16,1.,0.)) ;
#111760 = DIRECTION('ref_axis',(-1.,-1.53063836115601E-16,0.)) ;
#111761 = DIRECTION('',(-1.,-1.53063836115601E-16,2.73691106313441E-48)) ;
#111762 = DIRECTION('',(0.,0.,-1.)) ;
#111763 = DIRECTION('',(1.,1.53063836115601E-16,-1.53236300070382E-33)) ;
#111764 = DIRECTION('',(0.,0.,1.)) ;
#111765 = DIRECTION('center_axis',(1.99142572374599E-32,-1.30104260698261E-16,
-1.)) ;
#111766 = DIRECTION('ref_axis',(0.,1.,-1.30104260698261E-16)) ;
#111767 = DIRECTION('',(-1.,-1.53063836115601E-16,2.73691106313441E-48)) ;
#111768 = DIRECTION('',(1.53063836115601E-16,-1.,1.30104260698261E-16)) ;
#111769 = DIRECTION('',(1.,1.53063836115601E-16,-2.73691106313441E-48)) ;
#111770 = DIRECTION('center_axis',(-1.53063836115601E-16,1.,0.)) ;
#111771 = DIRECTION('ref_axis',(-1.,-1.53063836115601E-16,0.)) ;
#111772 = DIRECTION('',(-1.,-1.53063836115601E-16,-2.73691106313441E-48)) ;
#111773 = DIRECTION('',(0.,0.,-1.)) ;
#111774 = DIRECTION('',(1.,1.53063836115601E-16,-2.73691106313441E-48)) ;
#111775 = DIRECTION('',(0.,0.,1.)) ;
#111776 = DIRECTION('center_axis',(1.99142572374599E-32,-1.30104260698261E-16,
1.)) ;
#111777 = DIRECTION('ref_axis',(0.,-1.,-1.30104260698261E-16)) ;
#111778 = DIRECTION('',(-1.,-1.53063836115601E-16,-2.73691106313441E-48)) ;
#111779 = DIRECTION('',(-1.53063836115601E-16,1.,1.30104260698261E-16)) ;
#111780 = DIRECTION('',(1.,1.53063836115601E-16,2.73691106313441E-48)) ;
#111781 = DIRECTION('',(2.16840434497101E-16,-1.,-1.30104260698261E-16)) ;
#111782 = DIRECTION('center_axis',(-1.53063836115601E-16,1.,0.)) ;
#111783 = DIRECTION('ref_axis',(-1.,-1.53063836115601E-16,0.)) ;
#111784 = DIRECTION('',(-1.,-1.53063836115601E-16,3.06472600140763E-33)) ;
#111785 = DIRECTION('',(0.,0.,-1.)) ;
#111786 = DIRECTION('',(1.,1.53063836115601E-16,2.73691106313441E-48)) ;
#111787 = DIRECTION('',(0.,0.,1.)) ;
#111788 = DIRECTION('center_axis',(-1.53063836115601E-16,1.,0.)) ;
#111789 = DIRECTION('ref_axis',(-1.,-1.53063836115601E-16,0.)) ;
#111790 = DIRECTION('',(-1.,-1.53063836115601E-16,2.73691106313441E-48)) ;
#111791 = DIRECTION('',(0.,0.,-1.)) ;
#111792 = DIRECTION('',(1.,1.53063836115601E-16,-1.53236300070382E-33)) ;
#111793 = DIRECTION('',(0.,0.,1.)) ;
#111794 = DIRECTION('center_axis',(1.99142572374599E-32,-1.30104260698261E-16,
-1.)) ;
#111795 = DIRECTION('ref_axis',(0.,1.,-1.30104260698261E-16)) ;
#111796 = DIRECTION('',(-1.,-1.53063836115601E-16,2.73691106313441E-48)) ;
#111797 = DIRECTION('',(1.53063836115601E-16,-1.,1.30104260698261E-16)) ;
#111798 = DIRECTION('',(1.,1.53063836115601E-16,-2.73691106313441E-48)) ;
#111799 = DIRECTION('center_axis',(-1.53063836115601E-16,1.,0.)) ;
#111800 = DIRECTION('ref_axis',(-1.,-1.53063836115601E-16,0.)) ;
#111801 = DIRECTION('',(-1.,-1.53063836115601E-16,-2.73691106313441E-48)) ;
#111802 = DIRECTION('',(0.,0.,-1.)) ;
#111803 = DIRECTION('',(1.,1.53063836115601E-16,-2.73691106313441E-48)) ;
#111804 = DIRECTION('',(0.,0.,1.)) ;
#111805 = DIRECTION('center_axis',(1.99142572374599E-32,-1.30104260698261E-16,
1.)) ;
#111806 = DIRECTION('ref_axis',(0.,-1.,-1.30104260698261E-16)) ;
#111807 = DIRECTION('',(-1.,-1.53063836115601E-16,-2.73691106313441E-48)) ;
#111808 = DIRECTION('',(-1.53063836115601E-16,1.,1.30104260698261E-16)) ;
#111809 = DIRECTION('',(1.,1.53063836115601E-16,2.73691106313441E-48)) ;
#111810 = DIRECTION('',(2.16840434497101E-16,-1.,-1.30104260698261E-16)) ;
#111811 = DIRECTION('center_axis',(-1.53063836115601E-16,1.,0.)) ;
#111812 = DIRECTION('ref_axis',(-1.,-1.53063836115601E-16,0.)) ;
#111813 = DIRECTION('',(-1.,-1.53063836115601E-16,3.06472600140763E-33)) ;
#111814 = DIRECTION('',(0.,0.,-1.)) ;
#111815 = DIRECTION('',(1.,1.53063836115601E-16,2.73691106313441E-48)) ;
#111816 = DIRECTION('',(0.,0.,1.)) ;
#111817 = DIRECTION('center_axis',(1.,0.,0.)) ;
#111818 = DIRECTION('ref_axis',(0.,0.,-1.)) ;
#111819 = DIRECTION('',(1.,0.,0.)) ;
#111820 = DIRECTION('center_axis',(1.,0.,0.)) ;
#111821 = DIRECTION('ref_axis',(0.,0.,1.)) ;
#111822 = DIRECTION('',(1.,0.,0.)) ;
#111823 = DIRECTION('center_axis',(-1.,0.,0.)) ;
#111824 = DIRECTION('ref_axis',(0.,0.,-1.)) ;
#111825 = DIRECTION('center_axis',(0.,0.,1.)) ;
#111826 = DIRECTION('ref_axis',(1.,0.,0.)) ;
#111827 = DIRECTION('',(0.,1.,0.)) ;
#111828 = DIRECTION('',(1.,0.,0.)) ;
#111829 = DIRECTION('',(0.,-1.,0.)) ;
#111830 = DIRECTION('center_axis',(1.,0.,0.)) ;
#111831 = DIRECTION('ref_axis',(0.,0.,-1.)) ;
#111832 = DIRECTION('center_axis',(1.,0.,0.)) ;
#111833 = DIRECTION('ref_axis',(0.,0.,1.)) ;
#111834 = DIRECTION('',(1.,0.,0.)) ;
#111835 = DIRECTION('center_axis',(-1.,0.,0.)) ;
#111836 = DIRECTION('ref_axis',(0.,0.,-1.)) ;
#111837 = DIRECTION('center_axis',(0.,-1.,3.99416362155027E-15)) ;
#111838 = DIRECTION('ref_axis',(0.,-3.99416362155027E-15,-1.)) ;
#111839 = DIRECTION('',(0.,3.99416362155027E-15,1.)) ;
#111840 = DIRECTION('',(1.,0.,0.)) ;
#111841 = DIRECTION('',(0.,-3.99416362155027E-15,-1.)) ;
#111842 = DIRECTION('center_axis',(1.,0.,0.)) ;
#111843 = DIRECTION('ref_axis',(0.,0.,-1.)) ;
#111844 = DIRECTION('center_axis',(-1.,0.,0.)) ;
#111845 = DIRECTION('ref_axis',(0.,1.30104260698266E-14,-1.)) ;
#111846 = DIRECTION('',(1.,0.,0.)) ;
#111847 = DIRECTION('center_axis',(1.,0.,0.)) ;
#111848 = DIRECTION('ref_axis',(0.,0.,-1.)) ;
#111849 = DIRECTION('center_axis',(0.,-0.707106781186549,0.707106781186546)) ;
#111850 = DIRECTION('ref_axis',(0.,-0.707106781186546,-0.707106781186549)) ;
#111851 = DIRECTION('',(0.,0.707106781186546,0.707106781186549)) ;
#111852 = DIRECTION('',(1.,0.,0.)) ;
#111853 = DIRECTION('',(0.,-0.707106781186546,-0.707106781186549)) ;
#111854 = DIRECTION('center_axis',(1.,0.,0.)) ;
#111855 = DIRECTION('ref_axis',(0.,0.382683432365084,0.923879532511289)) ;
#111856 = DIRECTION('',(1.,0.,0.)) ;
#111857 = DIRECTION('center_axis',(1.,0.,0.)) ;
#111858 = DIRECTION('ref_axis',(0.,0.,-1.)) ;
#111859 = DIRECTION('center_axis',(0.,1.,0.)) ;
#111860 = DIRECTION('ref_axis',(0.,0.,1.)) ;
#111861 = DIRECTION('',(0.,0.,-1.)) ;
#111862 = DIRECTION('',(0.,0.,1.)) ;
#111863 = DIRECTION('center_axis',(0.,-0.707106781186547,-0.707106781186548)) ;
#111864 = DIRECTION('ref_axis',(0.,0.707106781186548,-0.707106781186547)) ;
#111865 = DIRECTION('',(0.,-0.707106781186548,0.707106781186547)) ;
#111866 = DIRECTION('',(1.,0.,0.)) ;
#111867 = DIRECTION('',(0.,0.707106781186548,-0.707106781186547)) ;
#111868 = DIRECTION('center_axis',(1.,0.,0.)) ;
#111869 = DIRECTION('ref_axis',(0.,0.,-1.)) ;
#111870 = DIRECTION('center_axis',(-1.,0.,0.)) ;
#111871 = DIRECTION('ref_axis',(0.,1.73472347597676E-14,-1.)) ;
#111872 = DIRECTION('',(1.,0.,0.)) ;
#111873 = DIRECTION('center_axis',(1.,0.,0.)) ;
#111874 = DIRECTION('ref_axis',(0.,0.,-1.)) ;
#111875 = DIRECTION('center_axis',(0.,-1.,0.)) ;
#111876 = DIRECTION('ref_axis',(0.,0.,-1.)) ;
#111877 = DIRECTION('',(0.,0.,1.)) ;
#111878 = DIRECTION('',(1.,0.,0.)) ;
#111879 = DIRECTION('',(0.,0.,-1.)) ;
#111880 = DIRECTION('center_axis',(1.,0.,0.)) ;
#111881 = DIRECTION('ref_axis',(0.,0.,-1.)) ;
#111882 = DIRECTION('center_axis',(1.,0.,0.)) ;
#111883 = DIRECTION('ref_axis',(0.,0.,1.)) ;
#111884 = DIRECTION('',(1.,0.,0.)) ;
#111885 = DIRECTION('center_axis',(-1.,0.,0.)) ;
#111886 = DIRECTION('ref_axis',(0.,0.,-1.)) ;
#111887 = DIRECTION('center_axis',(0.,0.,-1.)) ;
#111888 = DIRECTION('ref_axis',(-1.,0.,0.)) ;
#111889 = DIRECTION('',(0.,-1.,0.)) ;
#111890 = DIRECTION('',(1.,0.,0.)) ;
#111891 = DIRECTION('',(0.,1.,0.)) ;
#111892 = DIRECTION('center_axis',(1.,0.,0.)) ;
#111893 = DIRECTION('ref_axis',(0.,0.,-1.)) ;
#111894 = DIRECTION('center_axis',(1.,0.,0.)) ;
#111895 = DIRECTION('ref_axis',(0.,0.,1.)) ;
#111896 = DIRECTION('',(1.,0.,0.)) ;
#111897 = DIRECTION('center_axis',(-1.,0.,0.)) ;
#111898 = DIRECTION('ref_axis',(0.,0.,-1.)) ;
#111899 = DIRECTION('center_axis',(0.,1.,0.)) ;
#111900 = DIRECTION('ref_axis',(0.,0.,1.)) ;
#111901 = DIRECTION('',(0.,0.,-1.)) ;
#111902 = DIRECTION('',(1.,0.,0.)) ;
#111903 = DIRECTION('',(0.,0.,1.)) ;
#111904 = DIRECTION('center_axis',(1.,0.,0.)) ;
#111905 = DIRECTION('ref_axis',(0.,0.,-1.)) ;
#111906 = DIRECTION('center_axis',(-1.,0.,0.)) ;
#111907 = DIRECTION('ref_axis',(0.,1.95156391047385E-14,-1.)) ;
#111908 = DIRECTION('',(1.,0.,0.)) ;
#111909 = DIRECTION('center_axis',(1.,0.,0.)) ;
#111910 = DIRECTION('ref_axis',(0.,0.,-1.)) ;
#111911 = DIRECTION('center_axis',(0.,1.07081696047951E-16,-1.)) ;
#111912 = DIRECTION('ref_axis',(0.,1.,1.07081696047951E-16)) ;
#111913 = DIRECTION('',(0.,-1.,-1.07081696047951E-16)) ;
#111914 = DIRECTION('',(1.,0.,0.)) ;
#111915 = DIRECTION('',(0.,1.,1.07081696047951E-16)) ;
#111916 = DIRECTION('center_axis',(1.,0.,0.)) ;
#111917 = DIRECTION('ref_axis',(0.,0.,-1.)) ;
#111918 = DIRECTION('center_axis',(-1.,0.,0.)) ;
#111919 = DIRECTION('ref_axis',(0.,0.,-1.)) ;
#111920 = DIRECTION('',(1.,0.,0.)) ;
#111921 = DIRECTION('center_axis',(1.,0.,0.)) ;
#111922 = DIRECTION('ref_axis',(0.,0.,-1.)) ;
#111923 = DIRECTION('center_axis',(0.,-1.,0.)) ;
#111924 = DIRECTION('ref_axis',(0.,0.,-1.)) ;
#111925 = DIRECTION('',(0.,0.,1.)) ;
#111926 = DIRECTION('',(1.,0.,0.)) ;
#111927 = DIRECTION('',(0.,0.,-1.)) ;
#111928 = DIRECTION('center_axis',(1.,0.,0.)) ;
#111929 = DIRECTION('ref_axis',(0.,0.,-1.)) ;
#111930 = DIRECTION('center_axis',(-1.,0.,0.)) ;
#111931 = DIRECTION('ref_axis',(0.,3.03576608295933E-14,-1.)) ;
#111932 = DIRECTION('',(1.,0.,0.)) ;
#111933 = DIRECTION('center_axis',(1.,0.,0.)) ;
#111934 = DIRECTION('ref_axis',(0.,0.,-1.)) ;
#111935 = DIRECTION('center_axis',(1.,0.,0.)) ;
#111936 = DIRECTION('ref_axis',(0.,0.,-1.)) ;
#111937 = DIRECTION('center_axis',(1.,0.,0.)) ;
#111938 = DIRECTION('ref_axis',(0.,-7.85535158932895E-16,1.)) ;
#111939 = DIRECTION('',(1.,0.,0.)) ;
#111940 = DIRECTION('center_axis',(-1.,0.,0.)) ;
#111941 = DIRECTION('ref_axis',(0.,-7.85535158932895E-16,-1.)) ;
#111942 = DIRECTION('center_axis',(1.,0.,0.)) ;
#111943 = DIRECTION('ref_axis',(0.,0.,-1.)) ;
#111944 = DIRECTION('center_axis',(-1.,0.,0.)) ;
#111945 = DIRECTION('ref_axis',(0.,3.46944695195352E-14,-1.)) ;
#111946 = DIRECTION('',(1.,0.,0.)) ;
#111947 = DIRECTION('center_axis',(1.,0.,0.)) ;
#111948 = DIRECTION('ref_axis',(0.,0.,-1.)) ;
#111949 = DIRECTION('center_axis',(0.,-1.,0.)) ;
#111950 = DIRECTION('ref_axis',(0.,0.,-1.)) ;
#111951 = DIRECTION('',(0.,0.,1.)) ;
#111952 = DIRECTION('',(1.,0.,0.)) ;
#111953 = DIRECTION('',(0.,0.,-1.)) ;
#111954 = DIRECTION('center_axis',(1.,0.,0.)) ;
#111955 = DIRECTION('ref_axis',(0.,0.,-1.)) ;
#111956 = DIRECTION('center_axis',(-1.,0.,0.)) ;
#111957 = DIRECTION('ref_axis',(0.,0.,-1.)) ;
#111958 = DIRECTION('',(1.,0.,0.)) ;
#111959 = DIRECTION('center_axis',(1.,0.,0.)) ;
#111960 = DIRECTION('ref_axis',(0.,0.,-1.)) ;
#111961 = DIRECTION('center_axis',(0.,-1.07081696047951E-16,1.)) ;
#111962 = DIRECTION('ref_axis',(0.,-1.,-1.07081696047951E-16)) ;
#111963 = DIRECTION('',(0.,1.,1.07081696047951E-16)) ;
#111964 = DIRECTION('',(1.,0.,0.)) ;
#111965 = DIRECTION('',(0.,-1.,-1.07081696047951E-16)) ;
#111966 = DIRECTION('center_axis',(1.,0.,0.)) ;
#111967 = DIRECTION('ref_axis',(0.,0.,-1.)) ;
#111968 = DIRECTION('center_axis',(-1.,0.,0.)) ;
#111969 = DIRECTION('ref_axis',(0.,0.,-1.)) ;
#111970 = DIRECTION('',(1.,0.,0.)) ;
#111971 = DIRECTION('center_axis',(1.,0.,0.)) ;
#111972 = DIRECTION('ref_axis',(0.,0.,-1.)) ;
#111973 = DIRECTION('center_axis',(0.,1.,0.)) ;
#111974 = DIRECTION('ref_axis',(0.,0.,1.)) ;
#111975 = DIRECTION('',(0.,0.,-1.)) ;
#111976 = DIRECTION('',(0.,0.,1.)) ;
#111977 = DIRECTION('center_axis',(-1.,0.,0.)) ;
#111978 = DIRECTION('ref_axis',(0.,0.,1.)) ;
#111979 = DIRECTION('center_axis',(-1.,0.,0.)) ;
#111980 = DIRECTION('ref_axis',(0.,0.,1.)) ;
#111981 = DIRECTION('',(0.,-1.,0.)) ;
#111982 = DIRECTION('center_axis',(-1.,0.,0.)) ;
#111983 = DIRECTION('ref_axis',(0.,0.,1.)) ;
#111984 = DIRECTION('',(0.,0.,1.)) ;
#111985 = DIRECTION('',(0.,-1.,-1.07081696047951E-16)) ;
#111986 = DIRECTION('',(0.,0.,-1.)) ;
#111987 = DIRECTION('center_axis',(-1.,0.,0.)) ;
#111988 = DIRECTION('ref_axis',(0.,0.,1.)) ;
#111989 = DIRECTION('',(0.,0.,-1.)) ;
#111990 = DIRECTION('',(0.,1.,1.07081696047951E-16)) ;
#111991 = DIRECTION('',(0.,0.,1.)) ;
#111992 = DIRECTION('center_axis',(-1.,0.,0.)) ;
#111993 = DIRECTION('ref_axis',(0.,0.,1.)) ;
#111994 = DIRECTION('',(0.,1.,0.)) ;
#111995 = DIRECTION('center_axis',(-1.,0.,0.)) ;
#111996 = DIRECTION('ref_axis',(0.,0.,1.)) ;
#111997 = DIRECTION('',(0.,0.,-1.)) ;
#111998 = DIRECTION('',(0.,0.707106781186548,-0.707106781186547)) ;
#111999 = DIRECTION('',(0.,0.,1.)) ;
#112000 = DIRECTION('',(0.,-0.707106781186546,-0.707106781186549)) ;
#112001 = DIRECTION('',(0.,-3.99416362155027E-15,-1.)) ;
#112002 = DIRECTION('center_axis',(1.,0.,0.)) ;
#112003 = DIRECTION('ref_axis',(0.,0.,-1.)) ;
#112004 = DIRECTION('',(1.,0.,0.)) ;
#112005 = DIRECTION('center_axis',(1.,0.,0.)) ;
#112006 = DIRECTION('ref_axis',(0.,0.,1.)) ;
#112007 = DIRECTION('',(1.,0.,0.)) ;
#112008 = DIRECTION('center_axis',(-1.,0.,0.)) ;
#112009 = DIRECTION('ref_axis',(0.,0.,-1.)) ;
#112010 = DIRECTION('center_axis',(0.,0.,1.)) ;
#112011 = DIRECTION('ref_axis',(1.,0.,0.)) ;
#112012 = DIRECTION('',(0.,1.,0.)) ;
#112013 = DIRECTION('',(1.,0.,0.)) ;
#112014 = DIRECTION('',(0.,-1.,0.)) ;
#112015 = DIRECTION('center_axis',(1.,0.,0.)) ;
#112016 = DIRECTION('ref_axis',(0.,0.,-1.)) ;
#112017 = DIRECTION('center_axis',(1.,0.,0.)) ;
#112018 = DIRECTION('ref_axis',(0.,0.,1.)) ;
#112019 = DIRECTION('',(1.,0.,0.)) ;
#112020 = DIRECTION('center_axis',(-1.,0.,0.)) ;
#112021 = DIRECTION('ref_axis',(0.,0.,-1.)) ;
#112022 = DIRECTION('center_axis',(0.,-1.,3.99416362155027E-15)) ;
#112023 = DIRECTION('ref_axis',(0.,-3.99416362155027E-15,-1.)) ;
#112024 = DIRECTION('',(0.,3.99416362155027E-15,1.)) ;
#112025 = DIRECTION('',(1.,0.,0.)) ;
#112026 = DIRECTION('',(0.,-3.99416362155027E-15,-1.)) ;
#112027 = DIRECTION('center_axis',(1.,0.,0.)) ;
#112028 = DIRECTION('ref_axis',(0.,0.,-1.)) ;
#112029 = DIRECTION('center_axis',(-1.,0.,0.)) ;
#112030 = DIRECTION('ref_axis',(0.,1.30104260698261E-14,-1.)) ;
#112031 = DIRECTION('',(1.,0.,0.)) ;
#112032 = DIRECTION('center_axis',(1.,0.,0.)) ;
#112033 = DIRECTION('ref_axis',(0.,0.,-1.)) ;
#112034 = DIRECTION('center_axis',(0.,-0.707106781186549,0.707106781186546)) ;
#112035 = DIRECTION('ref_axis',(0.,-0.707106781186546,-0.707106781186549)) ;
#112036 = DIRECTION('',(0.,0.707106781186546,0.707106781186549)) ;
#112037 = DIRECTION('',(1.,0.,0.)) ;
#112038 = DIRECTION('',(0.,-0.707106781186546,-0.707106781186549)) ;
#112039 = DIRECTION('center_axis',(1.,0.,0.)) ;
#112040 = DIRECTION('ref_axis',(0.,0.382683432365098,0.923879532511283)) ;
#112041 = DIRECTION('',(1.,0.,0.)) ;
#112042 = DIRECTION('center_axis',(1.,0.,0.)) ;
#112043 = DIRECTION('ref_axis',(0.,0.,-1.)) ;
#112044 = DIRECTION('center_axis',(0.,1.,0.)) ;
#112045 = DIRECTION('ref_axis',(0.,0.,1.)) ;
#112046 = DIRECTION('',(0.,0.,-1.)) ;
#112047 = DIRECTION('',(0.,0.,1.)) ;
#112048 = DIRECTION('center_axis',(0.,-0.707106781186547,-0.707106781186548)) ;
#112049 = DIRECTION('ref_axis',(0.,0.707106781186548,-0.707106781186547)) ;
#112050 = DIRECTION('',(0.,-0.707106781186548,0.707106781186547)) ;
#112051 = DIRECTION('',(1.,0.,0.)) ;
#112052 = DIRECTION('',(0.,0.707106781186548,-0.707106781186547)) ;
#112053 = DIRECTION('center_axis',(1.,0.,0.)) ;
#112054 = DIRECTION('ref_axis',(0.,0.,-1.)) ;
#112055 = DIRECTION('center_axis',(-1.,0.,0.)) ;
#112056 = DIRECTION('ref_axis',(0.,1.73472347597676E-14,-1.)) ;
#112057 = DIRECTION('',(1.,0.,0.)) ;
#112058 = DIRECTION('center_axis',(1.,0.,0.)) ;
#112059 = DIRECTION('ref_axis',(0.,0.,-1.)) ;
#112060 = DIRECTION('center_axis',(0.,-1.,0.)) ;
#112061 = DIRECTION('ref_axis',(0.,0.,-1.)) ;
#112062 = DIRECTION('',(0.,0.,1.)) ;
#112063 = DIRECTION('',(1.,0.,0.)) ;
#112064 = DIRECTION('',(0.,0.,-1.)) ;
#112065 = DIRECTION('center_axis',(1.,0.,0.)) ;
#112066 = DIRECTION('ref_axis',(0.,0.,-1.)) ;
#112067 = DIRECTION('center_axis',(1.,0.,0.)) ;
#112068 = DIRECTION('ref_axis',(0.,0.,1.)) ;
#112069 = DIRECTION('',(1.,0.,0.)) ;
#112070 = DIRECTION('center_axis',(-1.,0.,0.)) ;
#112071 = DIRECTION('ref_axis',(0.,0.,-1.)) ;
#112072 = DIRECTION('center_axis',(0.,0.,-1.)) ;
#112073 = DIRECTION('ref_axis',(-1.,0.,0.)) ;
#112074 = DIRECTION('',(0.,-1.,0.)) ;
#112075 = DIRECTION('',(1.,0.,0.)) ;
#112076 = DIRECTION('',(0.,1.,0.)) ;
#112077 = DIRECTION('center_axis',(1.,0.,0.)) ;
#112078 = DIRECTION('ref_axis',(0.,0.,-1.)) ;
#112079 = DIRECTION('center_axis',(1.,0.,0.)) ;
#112080 = DIRECTION('ref_axis',(0.,0.,1.)) ;
#112081 = DIRECTION('',(1.,0.,0.)) ;
#112082 = DIRECTION('center_axis',(-1.,0.,0.)) ;
#112083 = DIRECTION('ref_axis',(0.,0.,-1.)) ;
#112084 = DIRECTION('center_axis',(0.,1.,0.)) ;
#112085 = DIRECTION('ref_axis',(0.,0.,1.)) ;
#112086 = DIRECTION('',(0.,0.,-1.)) ;
#112087 = DIRECTION('',(1.,0.,0.)) ;
#112088 = DIRECTION('',(0.,0.,1.)) ;
#112089 = DIRECTION('center_axis',(1.,0.,0.)) ;
#112090 = DIRECTION('ref_axis',(0.,0.,-1.)) ;
#112091 = DIRECTION('center_axis',(-1.,0.,0.)) ;
#112092 = DIRECTION('ref_axis',(0.,1.95156391047385E-14,-1.)) ;
#112093 = DIRECTION('',(1.,0.,0.)) ;
#112094 = DIRECTION('center_axis',(1.,0.,0.)) ;
#112095 = DIRECTION('ref_axis',(0.,0.,-1.)) ;
#112096 = DIRECTION('center_axis',(0.,1.07081696047951E-16,-1.)) ;
#112097 = DIRECTION('ref_axis',(0.,1.,1.07081696047951E-16)) ;
#112098 = DIRECTION('',(0.,-1.,-1.07081696047951E-16)) ;
#112099 = DIRECTION('',(1.,0.,0.)) ;
#112100 = DIRECTION('',(0.,1.,1.07081696047951E-16)) ;
#112101 = DIRECTION('center_axis',(1.,0.,0.)) ;
#112102 = DIRECTION('ref_axis',(0.,0.,-1.)) ;
#112103 = DIRECTION('center_axis',(-1.,0.,0.)) ;
#112104 = DIRECTION('ref_axis',(0.,0.,-1.)) ;
#112105 = DIRECTION('',(1.,0.,0.)) ;
#112106 = DIRECTION('center_axis',(1.,0.,0.)) ;
#112107 = DIRECTION('ref_axis',(0.,0.,-1.)) ;
#112108 = DIRECTION('center_axis',(0.,-1.,0.)) ;
#112109 = DIRECTION('ref_axis',(0.,0.,-1.)) ;
#112110 = DIRECTION('',(0.,0.,1.)) ;
#112111 = DIRECTION('',(1.,0.,0.)) ;
#112112 = DIRECTION('',(0.,0.,-1.)) ;
#112113 = DIRECTION('center_axis',(1.,0.,0.)) ;
#112114 = DIRECTION('ref_axis',(0.,0.,-1.)) ;
#112115 = DIRECTION('center_axis',(-1.,0.,0.)) ;
#112116 = DIRECTION('ref_axis',(0.,3.03576608295933E-14,-1.)) ;
#112117 = DIRECTION('',(1.,0.,0.)) ;
#112118 = DIRECTION('center_axis',(1.,0.,0.)) ;
#112119 = DIRECTION('ref_axis',(0.,0.,-1.)) ;
#112120 = DIRECTION('center_axis',(1.,0.,0.)) ;
#112121 = DIRECTION('ref_axis',(0.,0.,-1.)) ;
#112122 = DIRECTION('center_axis',(1.,0.,0.)) ;
#112123 = DIRECTION('ref_axis',(0.,-7.85535158932895E-16,1.)) ;
#112124 = DIRECTION('',(1.,0.,0.)) ;
#112125 = DIRECTION('center_axis',(-1.,0.,0.)) ;
#112126 = DIRECTION('ref_axis',(0.,-7.85535158932895E-16,-1.)) ;
#112127 = DIRECTION('center_axis',(1.,0.,0.)) ;
#112128 = DIRECTION('ref_axis',(0.,0.,-1.)) ;
#112129 = DIRECTION('center_axis',(-1.,0.,0.)) ;
#112130 = DIRECTION('ref_axis',(0.,4.33680868994204E-15,-1.)) ;
#112131 = DIRECTION('',(1.,0.,0.)) ;
#112132 = DIRECTION('center_axis',(1.,0.,0.)) ;
#112133 = DIRECTION('ref_axis',(0.,0.,-1.)) ;
#112134 = DIRECTION('center_axis',(0.,-1.,0.)) ;
#112135 = DIRECTION('ref_axis',(0.,0.,-1.)) ;
#112136 = DIRECTION('',(0.,0.,1.)) ;
#112137 = DIRECTION('',(1.,0.,0.)) ;
#112138 = DIRECTION('',(0.,0.,-1.)) ;
#112139 = DIRECTION('center_axis',(1.,0.,0.)) ;
#112140 = DIRECTION('ref_axis',(0.,0.,-1.)) ;
#112141 = DIRECTION('center_axis',(-1.,0.,0.)) ;
#112142 = DIRECTION('ref_axis',(0.,0.,-1.)) ;
#112143 = DIRECTION('',(1.,0.,0.)) ;
#112144 = DIRECTION('center_axis',(1.,0.,0.)) ;
#112145 = DIRECTION('ref_axis',(0.,0.,-1.)) ;
#112146 = DIRECTION('center_axis',(0.,-1.07081696047951E-16,1.)) ;
#112147 = DIRECTION('ref_axis',(0.,-1.,-1.07081696047951E-16)) ;
#112148 = DIRECTION('',(0.,1.,1.07081696047951E-16)) ;
#112149 = DIRECTION('',(1.,0.,0.)) ;
#112150 = DIRECTION('',(0.,-1.,-1.07081696047951E-16)) ;
#112151 = DIRECTION('center_axis',(1.,0.,0.)) ;
#112152 = DIRECTION('ref_axis',(0.,0.,-1.)) ;
#112153 = DIRECTION('center_axis',(-1.,0.,0.)) ;
#112154 = DIRECTION('ref_axis',(0.,0.,-1.)) ;
#112155 = DIRECTION('',(1.,0.,0.)) ;
#112156 = DIRECTION('center_axis',(1.,0.,0.)) ;
#112157 = DIRECTION('ref_axis',(0.,0.,-1.)) ;
#112158 = DIRECTION('center_axis',(0.,1.,0.)) ;
#112159 = DIRECTION('ref_axis',(0.,0.,1.)) ;
#112160 = DIRECTION('',(0.,0.,-1.)) ;
#112161 = DIRECTION('',(0.,0.,1.)) ;
#112162 = DIRECTION('center_axis',(-1.,0.,0.)) ;
#112163 = DIRECTION('ref_axis',(0.,0.,1.)) ;
#112164 = DIRECTION('center_axis',(-1.,0.,0.)) ;
#112165 = DIRECTION('ref_axis',(0.,0.,1.)) ;
#112166 = DIRECTION('',(0.,-1.,0.)) ;
#112167 = DIRECTION('center_axis',(-1.,0.,0.)) ;
#112168 = DIRECTION('ref_axis',(0.,0.,1.)) ;
#112169 = DIRECTION('',(0.,0.,1.)) ;
#112170 = DIRECTION('',(0.,-1.,-1.07081696047951E-16)) ;
#112171 = DIRECTION('',(0.,0.,-1.)) ;
#112172 = DIRECTION('center_axis',(-1.,0.,0.)) ;
#112173 = DIRECTION('ref_axis',(0.,0.,1.)) ;
#112174 = DIRECTION('',(0.,0.,-1.)) ;
#112175 = DIRECTION('',(0.,1.,1.07081696047951E-16)) ;
#112176 = DIRECTION('',(0.,0.,1.)) ;
#112177 = DIRECTION('center_axis',(-1.,0.,0.)) ;
#112178 = DIRECTION('ref_axis',(0.,0.,1.)) ;
#112179 = DIRECTION('',(0.,1.,0.)) ;
#112180 = DIRECTION('center_axis',(-1.,0.,0.)) ;
#112181 = DIRECTION('ref_axis',(0.,0.,1.)) ;
#112182 = DIRECTION('',(0.,0.,-1.)) ;
#112183 = DIRECTION('',(0.,0.707106781186548,-0.707106781186547)) ;
#112184 = DIRECTION('',(0.,0.,1.)) ;
#112185 = DIRECTION('',(0.,-0.707106781186546,-0.707106781186549)) ;
#112186 = DIRECTION('',(0.,-3.99416362155027E-15,-1.)) ;
#112187 = DIRECTION('center_axis',(1.,0.,0.)) ;
#112188 = DIRECTION('ref_axis',(0.,0.,-1.)) ;
#112189 = DIRECTION('',(1.,0.,0.)) ;
#112190 = DIRECTION('center_axis',(1.,0.,0.)) ;
#112191 = DIRECTION('ref_axis',(0.,0.,1.)) ;
#112192 = DIRECTION('',(1.,0.,0.)) ;
#112193 = DIRECTION('center_axis',(-1.,0.,0.)) ;
#112194 = DIRECTION('ref_axis',(0.,0.,-1.)) ;
#112195 = DIRECTION('center_axis',(0.,0.,1.)) ;
#112196 = DIRECTION('ref_axis',(1.,0.,0.)) ;
#112197 = DIRECTION('',(0.,1.,0.)) ;
#112198 = DIRECTION('',(1.,0.,0.)) ;
#112199 = DIRECTION('',(0.,-1.,0.)) ;
#112200 = DIRECTION('center_axis',(1.,0.,0.)) ;
#112201 = DIRECTION('ref_axis',(0.,0.,-1.)) ;
#112202 = DIRECTION('center_axis',(1.,0.,0.)) ;
#112203 = DIRECTION('ref_axis',(0.,0.,1.)) ;
#112204 = DIRECTION('',(1.,0.,0.)) ;
#112205 = DIRECTION('center_axis',(-1.,0.,0.)) ;
#112206 = DIRECTION('ref_axis',(0.,0.,-1.)) ;
#112207 = DIRECTION('center_axis',(0.,-1.,3.99416362155027E-15)) ;
#112208 = DIRECTION('ref_axis',(0.,-3.99416362155027E-15,-1.)) ;
#112209 = DIRECTION('',(0.,3.99416362155027E-15,1.)) ;
#112210 = DIRECTION('',(1.,0.,0.)) ;
#112211 = DIRECTION('',(0.,-3.99416362155027E-15,-1.)) ;
#112212 = DIRECTION('center_axis',(1.,0.,0.)) ;
#112213 = DIRECTION('ref_axis',(0.,0.,-1.)) ;
#112214 = DIRECTION('center_axis',(-1.,0.,0.)) ;
#112215 = DIRECTION('ref_axis',(0.,1.30104260698261E-14,-1.)) ;
#112216 = DIRECTION('',(1.,0.,0.)) ;
#112217 = DIRECTION('center_axis',(1.,0.,0.)) ;
#112218 = DIRECTION('ref_axis',(0.,0.,-1.)) ;
#112219 = DIRECTION('center_axis',(0.,-0.707106781186549,0.707106781186546)) ;
#112220 = DIRECTION('ref_axis',(0.,-0.707106781186546,-0.707106781186549)) ;
#112221 = DIRECTION('',(0.,0.707106781186546,0.707106781186549)) ;
#112222 = DIRECTION('',(1.,0.,0.)) ;
#112223 = DIRECTION('',(0.,-0.707106781186546,-0.707106781186549)) ;
#112224 = DIRECTION('center_axis',(1.,0.,0.)) ;
#112225 = DIRECTION('ref_axis',(0.,0.382683432365098,0.923879532511283)) ;
#112226 = DIRECTION('',(1.,0.,0.)) ;
#112227 = DIRECTION('center_axis',(1.,0.,0.)) ;
#112228 = DIRECTION('ref_axis',(0.,0.,-1.)) ;
#112229 = DIRECTION('center_axis',(0.,1.,0.)) ;
#112230 = DIRECTION('ref_axis',(0.,0.,1.)) ;
#112231 = DIRECTION('',(0.,0.,-1.)) ;
#112232 = DIRECTION('',(0.,0.,1.)) ;
#112233 = DIRECTION('center_axis',(0.,-0.707106781186547,-0.707106781186548)) ;
#112234 = DIRECTION('ref_axis',(0.,0.707106781186548,-0.707106781186547)) ;
#112235 = DIRECTION('',(0.,-0.707106781186548,0.707106781186547)) ;
#112236 = DIRECTION('',(1.,0.,0.)) ;
#112237 = DIRECTION('',(0.,0.707106781186548,-0.707106781186547)) ;
#112238 = DIRECTION('center_axis',(1.,0.,0.)) ;
#112239 = DIRECTION('ref_axis',(0.,0.,-1.)) ;
#112240 = DIRECTION('center_axis',(-1.,0.,0.)) ;
#112241 = DIRECTION('ref_axis',(0.,-1.73472347597682E-14,-1.)) ;
#112242 = DIRECTION('',(1.,0.,0.)) ;
#112243 = DIRECTION('center_axis',(1.,0.,0.)) ;
#112244 = DIRECTION('ref_axis',(0.,0.,-1.)) ;
#112245 = DIRECTION('center_axis',(0.,-1.,0.)) ;
#112246 = DIRECTION('ref_axis',(0.,0.,-1.)) ;
#112247 = DIRECTION('',(0.,0.,1.)) ;
#112248 = DIRECTION('',(1.,0.,0.)) ;
#112249 = DIRECTION('',(0.,0.,-1.)) ;
#112250 = DIRECTION('center_axis',(1.,0.,0.)) ;
#112251 = DIRECTION('ref_axis',(0.,0.,-1.)) ;
#112252 = DIRECTION('center_axis',(1.,0.,0.)) ;
#112253 = DIRECTION('ref_axis',(0.,0.,1.)) ;
#112254 = DIRECTION('',(1.,0.,0.)) ;
#112255 = DIRECTION('center_axis',(-1.,0.,0.)) ;
#112256 = DIRECTION('ref_axis',(0.,0.,-1.)) ;
#112257 = DIRECTION('center_axis',(0.,0.,-1.)) ;
#112258 = DIRECTION('ref_axis',(-1.,0.,0.)) ;
#112259 = DIRECTION('',(0.,-1.,0.)) ;
#112260 = DIRECTION('',(1.,0.,0.)) ;
#112261 = DIRECTION('',(0.,1.,0.)) ;
#112262 = DIRECTION('center_axis',(1.,0.,0.)) ;
#112263 = DIRECTION('ref_axis',(0.,0.,-1.)) ;
#112264 = DIRECTION('center_axis',(1.,0.,0.)) ;
#112265 = DIRECTION('ref_axis',(0.,0.,1.)) ;
#112266 = DIRECTION('',(1.,0.,0.)) ;
#112267 = DIRECTION('center_axis',(-1.,0.,0.)) ;
#112268 = DIRECTION('ref_axis',(0.,0.,-1.)) ;
#112269 = DIRECTION('center_axis',(0.,1.,0.)) ;
#112270 = DIRECTION('ref_axis',(0.,0.,1.)) ;
#112271 = DIRECTION('',(0.,0.,-1.)) ;
#112272 = DIRECTION('',(1.,0.,0.)) ;
#112273 = DIRECTION('',(0.,0.,1.)) ;
#112274 = DIRECTION('center_axis',(1.,0.,0.)) ;
#112275 = DIRECTION('ref_axis',(0.,0.,-1.)) ;
#112276 = DIRECTION('center_axis',(-1.,0.,0.)) ;
#112277 = DIRECTION('ref_axis',(0.,1.95156391047392E-14,-1.)) ;
#112278 = DIRECTION('',(1.,0.,0.)) ;
#112279 = DIRECTION('center_axis',(1.,0.,0.)) ;
#112280 = DIRECTION('ref_axis',(0.,0.,-1.)) ;
#112281 = DIRECTION('center_axis',(0.,1.07081696047951E-16,-1.)) ;
#112282 = DIRECTION('ref_axis',(0.,1.,1.07081696047951E-16)) ;
#112283 = DIRECTION('',(0.,-1.,-1.07081696047951E-16)) ;
#112284 = DIRECTION('',(1.,0.,0.)) ;
#112285 = DIRECTION('',(0.,1.,1.07081696047951E-16)) ;
#112286 = DIRECTION('center_axis',(1.,0.,0.)) ;
#112287 = DIRECTION('ref_axis',(0.,0.,-1.)) ;
#112288 = DIRECTION('center_axis',(-1.,0.,0.)) ;
#112289 = DIRECTION('ref_axis',(0.,0.,-1.)) ;
#112290 = DIRECTION('',(1.,0.,0.)) ;
#112291 = DIRECTION('center_axis',(1.,0.,0.)) ;
#112292 = DIRECTION('ref_axis',(0.,0.,-1.)) ;
#112293 = DIRECTION('center_axis',(0.,-1.,0.)) ;
#112294 = DIRECTION('ref_axis',(0.,0.,-1.)) ;
#112295 = DIRECTION('',(0.,0.,1.)) ;
#112296 = DIRECTION('',(1.,0.,0.)) ;
#112297 = DIRECTION('',(0.,0.,-1.)) ;
#112298 = DIRECTION('center_axis',(1.,0.,0.)) ;
#112299 = DIRECTION('ref_axis',(0.,0.,-1.)) ;
#112300 = DIRECTION('center_axis',(-1.,0.,0.)) ;
#112301 = DIRECTION('ref_axis',(0.,4.33680868994204E-15,-1.)) ;
#112302 = DIRECTION('',(1.,0.,0.)) ;
#112303 = DIRECTION('center_axis',(1.,0.,0.)) ;
#112304 = DIRECTION('ref_axis',(0.,0.,-1.)) ;
#112305 = DIRECTION('center_axis',(1.,0.,0.)) ;
#112306 = DIRECTION('ref_axis',(0.,0.,-1.)) ;
#112307 = DIRECTION('center_axis',(1.,0.,0.)) ;
#112308 = DIRECTION('ref_axis',(0.,-7.85535158932895E-16,1.)) ;
#112309 = DIRECTION('',(1.,0.,0.)) ;
#112310 = DIRECTION('center_axis',(-1.,0.,0.)) ;
#112311 = DIRECTION('ref_axis',(0.,-7.85535158932895E-16,-1.)) ;
#112312 = DIRECTION('center_axis',(1.,0.,0.)) ;
#112313 = DIRECTION('ref_axis',(0.,0.,-1.)) ;
#112314 = DIRECTION('center_axis',(-1.,0.,0.)) ;
#112315 = DIRECTION('ref_axis',(0.,4.33680868994204E-15,-1.)) ;
#112316 = DIRECTION('',(1.,0.,0.)) ;
#112317 = DIRECTION('center_axis',(1.,0.,0.)) ;
#112318 = DIRECTION('ref_axis',(0.,0.,-1.)) ;
#112319 = DIRECTION('center_axis',(0.,-1.,0.)) ;
#112320 = DIRECTION('ref_axis',(0.,0.,-1.)) ;
#112321 = DIRECTION('',(0.,0.,1.)) ;
#112322 = DIRECTION('',(1.,0.,0.)) ;
#112323 = DIRECTION('',(0.,0.,-1.)) ;
#112324 = DIRECTION('center_axis',(1.,0.,0.)) ;
#112325 = DIRECTION('ref_axis',(0.,0.,-1.)) ;
#112326 = DIRECTION('center_axis',(-1.,0.,0.)) ;
#112327 = DIRECTION('ref_axis',(0.,0.,-1.)) ;
#112328 = DIRECTION('',(1.,0.,0.)) ;
#112329 = DIRECTION('center_axis',(1.,0.,0.)) ;
#112330 = DIRECTION('ref_axis',(0.,0.,-1.)) ;
#112331 = DIRECTION('center_axis',(0.,-1.07081696047951E-16,1.)) ;
#112332 = DIRECTION('ref_axis',(0.,-1.,-1.07081696047951E-16)) ;
#112333 = DIRECTION('',(0.,1.,1.07081696047951E-16)) ;
#112334 = DIRECTION('',(1.,0.,0.)) ;
#112335 = DIRECTION('',(0.,-1.,-1.07081696047951E-16)) ;
#112336 = DIRECTION('center_axis',(1.,0.,0.)) ;
#112337 = DIRECTION('ref_axis',(0.,0.,-1.)) ;
#112338 = DIRECTION('center_axis',(-1.,0.,0.)) ;
#112339 = DIRECTION('ref_axis',(0.,0.,-1.)) ;
#112340 = DIRECTION('',(1.,0.,0.)) ;
#112341 = DIRECTION('center_axis',(1.,0.,0.)) ;
#112342 = DIRECTION('ref_axis',(0.,0.,-1.)) ;
#112343 = DIRECTION('center_axis',(0.,1.,0.)) ;
#112344 = DIRECTION('ref_axis',(0.,0.,1.)) ;
#112345 = DIRECTION('',(0.,0.,-1.)) ;
#112346 = DIRECTION('',(0.,0.,1.)) ;
#112347 = DIRECTION('center_axis',(-1.,0.,0.)) ;
#112348 = DIRECTION('ref_axis',(0.,0.,1.)) ;
#112349 = DIRECTION('center_axis',(-1.,0.,0.)) ;
#112350 = DIRECTION('ref_axis',(0.,0.,1.)) ;
#112351 = DIRECTION('',(0.,-1.,0.)) ;
#112352 = DIRECTION('center_axis',(-1.,0.,0.)) ;
#112353 = DIRECTION('ref_axis',(0.,0.,1.)) ;
#112354 = DIRECTION('',(0.,0.,1.)) ;
#112355 = DIRECTION('',(0.,-1.,-1.07081696047951E-16)) ;
#112356 = DIRECTION('',(0.,0.,-1.)) ;
#112357 = DIRECTION('center_axis',(-1.,0.,0.)) ;
#112358 = DIRECTION('ref_axis',(0.,0.,1.)) ;
#112359 = DIRECTION('',(0.,0.,-1.)) ;
#112360 = DIRECTION('',(0.,1.,1.07081696047951E-16)) ;
#112361 = DIRECTION('',(0.,0.,1.)) ;
#112362 = DIRECTION('center_axis',(-1.,0.,0.)) ;
#112363 = DIRECTION('ref_axis',(0.,0.,1.)) ;
#112364 = DIRECTION('',(0.,1.,0.)) ;
#112365 = DIRECTION('center_axis',(-1.,0.,0.)) ;
#112366 = DIRECTION('ref_axis',(0.,0.,1.)) ;
#112367 = DIRECTION('',(0.,0.,-1.)) ;
#112368 = DIRECTION('',(0.,0.707106781186548,-0.707106781186547)) ;
#112369 = DIRECTION('',(0.,0.,1.)) ;
#112370 = DIRECTION('',(0.,-0.707106781186546,-0.707106781186549)) ;
#112371 = DIRECTION('',(0.,-3.99416362155027E-15,-1.)) ;
#112372 = DIRECTION('center_axis',(1.,0.,0.)) ;
#112373 = DIRECTION('ref_axis',(0.,0.,-1.)) ;
#112374 = DIRECTION('',(1.,0.,0.)) ;
#112375 = DIRECTION('center_axis',(1.,0.,0.)) ;
#112376 = DIRECTION('ref_axis',(0.,0.,1.)) ;
#112377 = DIRECTION('',(1.,0.,0.)) ;
#112378 = DIRECTION('center_axis',(-1.,0.,0.)) ;
#112379 = DIRECTION('ref_axis',(0.,0.,-1.)) ;
#112380 = DIRECTION('center_axis',(0.,0.,1.)) ;
#112381 = DIRECTION('ref_axis',(1.,0.,0.)) ;
#112382 = DIRECTION('',(0.,1.,0.)) ;
#112383 = DIRECTION('',(1.,0.,0.)) ;
#112384 = DIRECTION('',(0.,-1.,0.)) ;
#112385 = DIRECTION('center_axis',(1.,0.,0.)) ;
#112386 = DIRECTION('ref_axis',(0.,0.,-1.)) ;
#112387 = DIRECTION('center_axis',(1.,0.,0.)) ;
#112388 = DIRECTION('ref_axis',(0.,0.,1.)) ;
#112389 = DIRECTION('',(1.,0.,0.)) ;
#112390 = DIRECTION('center_axis',(-1.,0.,0.)) ;
#112391 = DIRECTION('ref_axis',(0.,0.,-1.)) ;
#112392 = DIRECTION('center_axis',(0.,-1.,3.99416362155027E-15)) ;
#112393 = DIRECTION('ref_axis',(0.,-3.99416362155027E-15,-1.)) ;
#112394 = DIRECTION('',(0.,3.99416362155027E-15,1.)) ;
#112395 = DIRECTION('',(1.,0.,0.)) ;
#112396 = DIRECTION('',(0.,-3.99416362155027E-15,-1.)) ;
#112397 = DIRECTION('center_axis',(1.,0.,0.)) ;
#112398 = DIRECTION('ref_axis',(0.,0.,-1.)) ;
#112399 = DIRECTION('center_axis',(-1.,0.,0.)) ;
#112400 = DIRECTION('ref_axis',(0.,1.30104260698261E-14,-1.)) ;
#112401 = DIRECTION('',(1.,0.,0.)) ;
#112402 = DIRECTION('center_axis',(1.,0.,0.)) ;
#112403 = DIRECTION('ref_axis',(0.,0.,-1.)) ;
#112404 = DIRECTION('center_axis',(0.,-0.707106781186549,0.707106781186546)) ;
#112405 = DIRECTION('ref_axis',(0.,-0.707106781186546,-0.707106781186549)) ;
#112406 = DIRECTION('',(0.,0.707106781186546,0.707106781186549)) ;
#112407 = DIRECTION('',(1.,0.,0.)) ;
#112408 = DIRECTION('',(0.,-0.707106781186546,-0.707106781186549)) ;
#112409 = DIRECTION('center_axis',(1.,0.,0.)) ;
#112410 = DIRECTION('ref_axis',(0.,0.382683432365098,0.923879532511283)) ;
#112411 = DIRECTION('',(1.,0.,0.)) ;
#112412 = DIRECTION('center_axis',(1.,0.,0.)) ;
#112413 = DIRECTION('ref_axis',(0.,0.,-1.)) ;
#112414 = DIRECTION('center_axis',(0.,1.,0.)) ;
#112415 = DIRECTION('ref_axis',(0.,0.,1.)) ;
#112416 = DIRECTION('',(0.,0.,-1.)) ;
#112417 = DIRECTION('',(0.,0.,1.)) ;
#112418 = DIRECTION('center_axis',(0.,-0.707106781186547,-0.707106781186548)) ;
#112419 = DIRECTION('ref_axis',(0.,0.707106781186548,-0.707106781186547)) ;
#112420 = DIRECTION('',(0.,-0.707106781186548,0.707106781186547)) ;
#112421 = DIRECTION('',(1.,0.,0.)) ;
#112422 = DIRECTION('',(0.,0.707106781186548,-0.707106781186547)) ;
#112423 = DIRECTION('center_axis',(1.,0.,0.)) ;
#112424 = DIRECTION('ref_axis',(0.,0.,-1.)) ;
#112425 = DIRECTION('center_axis',(-1.,0.,0.)) ;
#112426 = DIRECTION('ref_axis',(0.,-1.73472347597682E-14,-1.)) ;
#112427 = DIRECTION('',(1.,0.,0.)) ;
#112428 = DIRECTION('center_axis',(1.,0.,0.)) ;
#112429 = DIRECTION('ref_axis',(0.,0.,-1.)) ;
#112430 = DIRECTION('center_axis',(0.,-1.,0.)) ;
#112431 = DIRECTION('ref_axis',(0.,0.,-1.)) ;
#112432 = DIRECTION('',(0.,0.,1.)) ;
#112433 = DIRECTION('',(1.,0.,0.)) ;
#112434 = DIRECTION('',(0.,0.,-1.)) ;
#112435 = DIRECTION('center_axis',(1.,0.,0.)) ;
#112436 = DIRECTION('ref_axis',(0.,0.,-1.)) ;
#112437 = DIRECTION('center_axis',(1.,0.,0.)) ;
#112438 = DIRECTION('ref_axis',(0.,0.,1.)) ;
#112439 = DIRECTION('',(1.,0.,0.)) ;
#112440 = DIRECTION('center_axis',(-1.,0.,0.)) ;
#112441 = DIRECTION('ref_axis',(0.,0.,-1.)) ;
#112442 = DIRECTION('center_axis',(0.,0.,-1.)) ;
#112443 = DIRECTION('ref_axis',(-1.,0.,0.)) ;
#112444 = DIRECTION('',(0.,-1.,0.)) ;
#112445 = DIRECTION('',(1.,0.,0.)) ;
#112446 = DIRECTION('',(0.,1.,0.)) ;
#112447 = DIRECTION('center_axis',(1.,0.,0.)) ;
#112448 = DIRECTION('ref_axis',(0.,0.,-1.)) ;
#112449 = DIRECTION('center_axis',(1.,0.,0.)) ;
#112450 = DIRECTION('ref_axis',(0.,0.,1.)) ;
#112451 = DIRECTION('',(1.,0.,0.)) ;
#112452 = DIRECTION('center_axis',(-1.,0.,0.)) ;
#112453 = DIRECTION('ref_axis',(0.,0.,-1.)) ;
#112454 = DIRECTION('center_axis',(0.,1.,0.)) ;
#112455 = DIRECTION('ref_axis',(0.,0.,1.)) ;
#112456 = DIRECTION('',(0.,0.,-1.)) ;
#112457 = DIRECTION('',(1.,0.,0.)) ;
#112458 = DIRECTION('',(0.,0.,1.)) ;
#112459 = DIRECTION('center_axis',(1.,0.,0.)) ;
#112460 = DIRECTION('ref_axis',(0.,0.,-1.)) ;
#112461 = DIRECTION('center_axis',(-1.,0.,0.)) ;
#112462 = DIRECTION('ref_axis',(0.,1.95156391047392E-14,-1.)) ;
#112463 = DIRECTION('',(1.,0.,0.)) ;
#112464 = DIRECTION('center_axis',(1.,0.,0.)) ;
#112465 = DIRECTION('ref_axis',(0.,0.,-1.)) ;
#112466 = DIRECTION('center_axis',(0.,1.07081696047951E-16,-1.)) ;
#112467 = DIRECTION('ref_axis',(0.,1.,1.07081696047951E-16)) ;
#112468 = DIRECTION('',(0.,-1.,-1.07081696047951E-16)) ;
#112469 = DIRECTION('',(1.,0.,0.)) ;
#112470 = DIRECTION('',(0.,1.,1.07081696047951E-16)) ;
#112471 = DIRECTION('center_axis',(1.,0.,0.)) ;
#112472 = DIRECTION('ref_axis',(0.,0.,-1.)) ;
#112473 = DIRECTION('center_axis',(-1.,0.,0.)) ;
#112474 = DIRECTION('ref_axis',(0.,0.,-1.)) ;
#112475 = DIRECTION('',(1.,0.,0.)) ;
#112476 = DIRECTION('center_axis',(1.,0.,0.)) ;
#112477 = DIRECTION('ref_axis',(0.,0.,-1.)) ;
#112478 = DIRECTION('center_axis',(0.,-1.,0.)) ;
#112479 = DIRECTION('ref_axis',(0.,0.,-1.)) ;
#112480 = DIRECTION('',(0.,0.,1.)) ;
#112481 = DIRECTION('',(1.,0.,0.)) ;
#112482 = DIRECTION('',(0.,0.,-1.)) ;
#112483 = DIRECTION('center_axis',(1.,0.,0.)) ;
#112484 = DIRECTION('ref_axis',(0.,0.,-1.)) ;
#112485 = DIRECTION('center_axis',(-1.,0.,0.)) ;
#112486 = DIRECTION('ref_axis',(0.,4.33680868994204E-15,-1.)) ;
#112487 = DIRECTION('',(1.,0.,0.)) ;
#112488 = DIRECTION('center_axis',(1.,0.,0.)) ;
#112489 = DIRECTION('ref_axis',(0.,0.,-1.)) ;
#112490 = DIRECTION('center_axis',(1.,0.,0.)) ;
#112491 = DIRECTION('ref_axis',(0.,0.,-1.)) ;
#112492 = DIRECTION('center_axis',(1.,0.,0.)) ;
#112493 = DIRECTION('ref_axis',(0.,-7.85535158932895E-16,1.)) ;
#112494 = DIRECTION('',(1.,0.,0.)) ;
#112495 = DIRECTION('center_axis',(-1.,0.,0.)) ;
#112496 = DIRECTION('ref_axis',(0.,-7.85535158932895E-16,-1.)) ;
#112497 = DIRECTION('center_axis',(1.,0.,0.)) ;
#112498 = DIRECTION('ref_axis',(0.,0.,-1.)) ;
#112499 = DIRECTION('center_axis',(-1.,0.,0.)) ;
#112500 = DIRECTION('ref_axis',(0.,4.33680868994204E-15,-1.)) ;
#112501 = DIRECTION('',(1.,0.,0.)) ;
#112502 = DIRECTION('center_axis',(1.,0.,0.)) ;
#112503 = DIRECTION('ref_axis',(0.,0.,-1.)) ;
#112504 = DIRECTION('center_axis',(0.,-1.,0.)) ;
#112505 = DIRECTION('ref_axis',(0.,0.,-1.)) ;
#112506 = DIRECTION('',(0.,0.,1.)) ;
#112507 = DIRECTION('',(1.,0.,0.)) ;
#112508 = DIRECTION('',(0.,0.,-1.)) ;
#112509 = DIRECTION('center_axis',(1.,0.,0.)) ;
#112510 = DIRECTION('ref_axis',(0.,0.,-1.)) ;
#112511 = DIRECTION('center_axis',(-1.,0.,0.)) ;
#112512 = DIRECTION('ref_axis',(0.,0.,-1.)) ;
#112513 = DIRECTION('',(1.,0.,0.)) ;
#112514 = DIRECTION('center_axis',(1.,0.,0.)) ;
#112515 = DIRECTION('ref_axis',(0.,0.,-1.)) ;
#112516 = DIRECTION('center_axis',(0.,-1.07081696047951E-16,1.)) ;
#112517 = DIRECTION('ref_axis',(0.,-1.,-1.07081696047951E-16)) ;
#112518 = DIRECTION('',(0.,1.,1.07081696047951E-16)) ;
#112519 = DIRECTION('',(1.,0.,0.)) ;
#112520 = DIRECTION('',(0.,-1.,-1.07081696047951E-16)) ;
#112521 = DIRECTION('center_axis',(1.,0.,0.)) ;
#112522 = DIRECTION('ref_axis',(0.,0.,-1.)) ;
#112523 = DIRECTION('center_axis',(-1.,0.,0.)) ;
#112524 = DIRECTION('ref_axis',(0.,0.,-1.)) ;
#112525 = DIRECTION('',(1.,0.,0.)) ;
#112526 = DIRECTION('center_axis',(1.,0.,0.)) ;
#112527 = DIRECTION('ref_axis',(0.,0.,-1.)) ;
#112528 = DIRECTION('center_axis',(0.,1.,0.)) ;
#112529 = DIRECTION('ref_axis',(0.,0.,1.)) ;
#112530 = DIRECTION('',(0.,0.,-1.)) ;
#112531 = DIRECTION('',(0.,0.,1.)) ;
#112532 = DIRECTION('center_axis',(-1.,0.,0.)) ;
#112533 = DIRECTION('ref_axis',(0.,0.,1.)) ;
#112534 = DIRECTION('center_axis',(-1.,0.,0.)) ;
#112535 = DIRECTION('ref_axis',(0.,0.,1.)) ;
#112536 = DIRECTION('',(0.,-1.,0.)) ;
#112537 = DIRECTION('center_axis',(-1.,0.,0.)) ;
#112538 = DIRECTION('ref_axis',(0.,0.,1.)) ;
#112539 = DIRECTION('',(0.,0.,1.)) ;
#112540 = DIRECTION('',(0.,-1.,-1.07081696047951E-16)) ;
#112541 = DIRECTION('',(0.,0.,-1.)) ;
#112542 = DIRECTION('center_axis',(-1.,0.,0.)) ;
#112543 = DIRECTION('ref_axis',(0.,0.,1.)) ;
#112544 = DIRECTION('',(0.,0.,-1.)) ;
#112545 = DIRECTION('',(0.,1.,1.07081696047951E-16)) ;
#112546 = DIRECTION('',(0.,0.,1.)) ;
#112547 = DIRECTION('center_axis',(-1.,0.,0.)) ;
#112548 = DIRECTION('ref_axis',(0.,0.,1.)) ;
#112549 = DIRECTION('',(0.,1.,0.)) ;
#112550 = DIRECTION('center_axis',(-1.,0.,0.)) ;
#112551 = DIRECTION('ref_axis',(0.,0.,1.)) ;
#112552 = DIRECTION('',(0.,0.,-1.)) ;
#112553 = DIRECTION('',(0.,0.707106781186548,-0.707106781186547)) ;
#112554 = DIRECTION('',(0.,0.,1.)) ;
#112555 = DIRECTION('',(0.,-0.707106781186546,-0.707106781186549)) ;
#112556 = DIRECTION('',(0.,-3.99416362155027E-15,-1.)) ;
#112557 = DIRECTION('center_axis',(1.,0.,0.)) ;
#112558 = DIRECTION('ref_axis',(0.,0.,-1.)) ;
#112559 = DIRECTION('',(1.,0.,0.)) ;
#112560 = DIRECTION('center_axis',(1.,0.,0.)) ;
#112561 = DIRECTION('ref_axis',(0.,0.,1.)) ;
#112562 = DIRECTION('',(1.,0.,0.)) ;
#112563 = DIRECTION('center_axis',(-1.,0.,0.)) ;
#112564 = DIRECTION('ref_axis',(0.,0.,-1.)) ;
#112565 = DIRECTION('center_axis',(0.,0.,1.)) ;
#112566 = DIRECTION('ref_axis',(1.,0.,0.)) ;
#112567 = DIRECTION('',(0.,1.,0.)) ;
#112568 = DIRECTION('',(1.,0.,0.)) ;
#112569 = DIRECTION('',(0.,-1.,0.)) ;
#112570 = DIRECTION('center_axis',(1.,0.,0.)) ;
#112571 = DIRECTION('ref_axis',(0.,0.,-1.)) ;
#112572 = DIRECTION('center_axis',(1.,0.,0.)) ;
#112573 = DIRECTION('ref_axis',(0.,0.,1.)) ;
#112574 = DIRECTION('',(1.,0.,0.)) ;
#112575 = DIRECTION('center_axis',(-1.,0.,0.)) ;
#112576 = DIRECTION('ref_axis',(0.,0.,-1.)) ;
#112577 = DIRECTION('center_axis',(0.,-1.,3.99416362155027E-15)) ;
#112578 = DIRECTION('ref_axis',(0.,-3.99416362155027E-15,-1.)) ;
#112579 = DIRECTION('',(0.,3.99416362155027E-15,1.)) ;
#112580 = DIRECTION('',(1.,0.,0.)) ;
#112581 = DIRECTION('',(0.,-3.99416362155027E-15,-1.)) ;
#112582 = DIRECTION('center_axis',(1.,0.,0.)) ;
#112583 = DIRECTION('ref_axis',(0.,0.,-1.)) ;
#112584 = DIRECTION('center_axis',(-1.,0.,0.)) ;
#112585 = DIRECTION('ref_axis',(0.,1.30104260698261E-14,-1.)) ;
#112586 = DIRECTION('',(1.,0.,0.)) ;
#112587 = DIRECTION('center_axis',(1.,0.,0.)) ;
#112588 = DIRECTION('ref_axis',(0.,0.,-1.)) ;
#112589 = DIRECTION('center_axis',(0.,-0.707106781186549,0.707106781186546)) ;
#112590 = DIRECTION('ref_axis',(0.,-0.707106781186546,-0.707106781186549)) ;
#112591 = DIRECTION('',(0.,0.707106781186546,0.707106781186549)) ;
#112592 = DIRECTION('',(1.,0.,0.)) ;
#112593 = DIRECTION('',(0.,-0.707106781186546,-0.707106781186549)) ;
#112594 = DIRECTION('center_axis',(1.,0.,0.)) ;
#112595 = DIRECTION('ref_axis',(0.,0.38268343236508,0.923879532511291)) ;
#112596 = DIRECTION('',(1.,0.,0.)) ;
#112597 = DIRECTION('center_axis',(1.,0.,0.)) ;
#112598 = DIRECTION('ref_axis',(0.,0.,-1.)) ;
#112599 = DIRECTION('center_axis',(0.,1.,0.)) ;
#112600 = DIRECTION('ref_axis',(0.,0.,1.)) ;
#112601 = DIRECTION('',(0.,0.,-1.)) ;
#112602 = DIRECTION('',(0.,0.,1.)) ;
#112603 = DIRECTION('center_axis',(0.,-0.707106781186547,-0.707106781186548)) ;
#112604 = DIRECTION('ref_axis',(0.,0.707106781186548,-0.707106781186547)) ;
#112605 = DIRECTION('',(0.,-0.707106781186548,0.707106781186547)) ;
#112606 = DIRECTION('',(1.,0.,0.)) ;
#112607 = DIRECTION('',(0.,0.707106781186548,-0.707106781186547)) ;
#112608 = DIRECTION('center_axis',(1.,0.,0.)) ;
#112609 = DIRECTION('ref_axis',(0.,0.,-1.)) ;
#112610 = DIRECTION('center_axis',(-1.,0.,0.)) ;
#112611 = DIRECTION('ref_axis',(0.,-1.73472347597682E-14,-1.)) ;
#112612 = DIRECTION('',(1.,0.,0.)) ;
#112613 = DIRECTION('center_axis',(1.,0.,0.)) ;
#112614 = DIRECTION('ref_axis',(0.,0.,-1.)) ;
#112615 = DIRECTION('center_axis',(0.,-1.,0.)) ;
#112616 = DIRECTION('ref_axis',(0.,0.,-1.)) ;
#112617 = DIRECTION('',(0.,0.,1.)) ;
#112618 = DIRECTION('',(1.,0.,0.)) ;
#112619 = DIRECTION('',(0.,0.,-1.)) ;
#112620 = DIRECTION('center_axis',(1.,0.,0.)) ;
#112621 = DIRECTION('ref_axis',(0.,0.,-1.)) ;
#112622 = DIRECTION('center_axis',(1.,0.,0.)) ;
#112623 = DIRECTION('ref_axis',(0.,0.,1.)) ;
#112624 = DIRECTION('',(1.,0.,0.)) ;
#112625 = DIRECTION('center_axis',(-1.,0.,0.)) ;
#112626 = DIRECTION('ref_axis',(0.,0.,-1.)) ;
#112627 = DIRECTION('center_axis',(0.,0.,-1.)) ;
#112628 = DIRECTION('ref_axis',(-1.,0.,0.)) ;
#112629 = DIRECTION('',(0.,-1.,0.)) ;
#112630 = DIRECTION('',(1.,0.,0.)) ;
#112631 = DIRECTION('',(0.,1.,0.)) ;
#112632 = DIRECTION('center_axis',(1.,0.,0.)) ;
#112633 = DIRECTION('ref_axis',(0.,0.,-1.)) ;
#112634 = DIRECTION('center_axis',(1.,0.,0.)) ;
#112635 = DIRECTION('ref_axis',(0.,0.,1.)) ;
#112636 = DIRECTION('',(1.,0.,0.)) ;
#112637 = DIRECTION('center_axis',(-1.,0.,0.)) ;
#112638 = DIRECTION('ref_axis',(0.,0.,-1.)) ;
#112639 = DIRECTION('center_axis',(0.,1.,0.)) ;
#112640 = DIRECTION('ref_axis',(0.,0.,1.)) ;
#112641 = DIRECTION('',(0.,0.,-1.)) ;
#112642 = DIRECTION('',(1.,0.,0.)) ;
#112643 = DIRECTION('',(0.,0.,1.)) ;
#112644 = DIRECTION('center_axis',(1.,0.,0.)) ;
#112645 = DIRECTION('ref_axis',(0.,0.,-1.)) ;
#112646 = DIRECTION('center_axis',(-1.,0.,0.)) ;
#112647 = DIRECTION('ref_axis',(0.,1.95156391047392E-14,-1.)) ;
#112648 = DIRECTION('',(1.,0.,0.)) ;
#112649 = DIRECTION('center_axis',(1.,0.,0.)) ;
#112650 = DIRECTION('ref_axis',(0.,0.,-1.)) ;
#112651 = DIRECTION('center_axis',(0.,1.07081696047951E-16,-1.)) ;
#112652 = DIRECTION('ref_axis',(0.,1.,1.07081696047951E-16)) ;
#112653 = DIRECTION('',(0.,-1.,-1.07081696047951E-16)) ;
#112654 = DIRECTION('',(1.,0.,0.)) ;
#112655 = DIRECTION('',(0.,1.,1.07081696047951E-16)) ;
#112656 = DIRECTION('center_axis',(1.,0.,0.)) ;
#112657 = DIRECTION('ref_axis',(0.,0.,-1.)) ;
#112658 = DIRECTION('center_axis',(-1.,0.,0.)) ;
#112659 = DIRECTION('ref_axis',(0.,0.,-1.)) ;
#112660 = DIRECTION('',(1.,0.,0.)) ;
#112661 = DIRECTION('center_axis',(1.,0.,0.)) ;
#112662 = DIRECTION('ref_axis',(0.,0.,-1.)) ;
#112663 = DIRECTION('center_axis',(0.,-1.,0.)) ;
#112664 = DIRECTION('ref_axis',(0.,0.,-1.)) ;
#112665 = DIRECTION('',(0.,0.,1.)) ;
#112666 = DIRECTION('',(1.,0.,0.)) ;
#112667 = DIRECTION('',(0.,0.,-1.)) ;
#112668 = DIRECTION('center_axis',(1.,0.,0.)) ;
#112669 = DIRECTION('ref_axis',(0.,0.,-1.)) ;
#112670 = DIRECTION('center_axis',(-1.,0.,0.)) ;
#112671 = DIRECTION('ref_axis',(0.,4.33680868994204E-15,-1.)) ;
#112672 = DIRECTION('',(1.,0.,0.)) ;
#112673 = DIRECTION('center_axis',(1.,0.,0.)) ;
#112674 = DIRECTION('ref_axis',(0.,0.,-1.)) ;
#112675 = DIRECTION('center_axis',(1.,0.,0.)) ;
#112676 = DIRECTION('ref_axis',(0.,0.,-1.)) ;
#112677 = DIRECTION('center_axis',(1.,0.,0.)) ;
#112678 = DIRECTION('ref_axis',(0.,-7.85535158932895E-16,1.)) ;
#112679 = DIRECTION('',(1.,0.,0.)) ;
#112680 = DIRECTION('center_axis',(-1.,0.,0.)) ;
#112681 = DIRECTION('ref_axis',(0.,-7.85535158932895E-16,-1.)) ;
#112682 = DIRECTION('center_axis',(1.,0.,0.)) ;
#112683 = DIRECTION('ref_axis',(0.,0.,-1.)) ;
#112684 = DIRECTION('center_axis',(-1.,0.,0.)) ;
#112685 = DIRECTION('ref_axis',(0.,4.33680868994204E-15,-1.)) ;
#112686 = DIRECTION('',(1.,0.,0.)) ;
#112687 = DIRECTION('center_axis',(1.,0.,0.)) ;
#112688 = DIRECTION('ref_axis',(0.,0.,-1.)) ;
#112689 = DIRECTION('center_axis',(0.,-1.,0.)) ;
#112690 = DIRECTION('ref_axis',(0.,0.,-1.)) ;
#112691 = DIRECTION('',(0.,0.,1.)) ;
#112692 = DIRECTION('',(1.,0.,0.)) ;
#112693 = DIRECTION('',(0.,0.,-1.)) ;
#112694 = DIRECTION('center_axis',(1.,0.,0.)) ;
#112695 = DIRECTION('ref_axis',(0.,0.,-1.)) ;
#112696 = DIRECTION('center_axis',(-1.,0.,0.)) ;
#112697 = DIRECTION('ref_axis',(0.,0.,-1.)) ;
#112698 = DIRECTION('',(1.,0.,0.)) ;
#112699 = DIRECTION('center_axis',(1.,0.,0.)) ;
#112700 = DIRECTION('ref_axis',(0.,0.,-1.)) ;
#112701 = DIRECTION('center_axis',(0.,-1.07081696047951E-16,1.)) ;
#112702 = DIRECTION('ref_axis',(0.,-1.,-1.07081696047951E-16)) ;
#112703 = DIRECTION('',(0.,1.,1.07081696047951E-16)) ;
#112704 = DIRECTION('',(1.,0.,0.)) ;
#112705 = DIRECTION('',(0.,-1.,-1.07081696047951E-16)) ;
#112706 = DIRECTION('center_axis',(1.,0.,0.)) ;
#112707 = DIRECTION('ref_axis',(0.,0.,-1.)) ;
#112708 = DIRECTION('center_axis',(-1.,0.,0.)) ;
#112709 = DIRECTION('ref_axis',(0.,0.,-1.)) ;
#112710 = DIRECTION('',(1.,0.,0.)) ;
#112711 = DIRECTION('center_axis',(1.,0.,0.)) ;
#112712 = DIRECTION('ref_axis',(0.,0.,-1.)) ;
#112713 = DIRECTION('center_axis',(0.,1.,0.)) ;
#112714 = DIRECTION('ref_axis',(0.,0.,1.)) ;
#112715 = DIRECTION('',(0.,0.,-1.)) ;
#112716 = DIRECTION('',(0.,0.,1.)) ;
#112717 = DIRECTION('center_axis',(-1.,0.,0.)) ;
#112718 = DIRECTION('ref_axis',(0.,0.,1.)) ;
#112719 = DIRECTION('center_axis',(-1.,0.,0.)) ;
#112720 = DIRECTION('ref_axis',(0.,0.,1.)) ;
#112721 = DIRECTION('',(0.,-1.,0.)) ;
#112722 = DIRECTION('center_axis',(-1.,0.,0.)) ;
#112723 = DIRECTION('ref_axis',(0.,0.,1.)) ;
#112724 = DIRECTION('',(0.,0.,1.)) ;
#112725 = DIRECTION('',(0.,-1.,-1.07081696047951E-16)) ;
#112726 = DIRECTION('',(0.,0.,-1.)) ;
#112727 = DIRECTION('center_axis',(-1.,0.,0.)) ;
#112728 = DIRECTION('ref_axis',(0.,0.,1.)) ;
#112729 = DIRECTION('',(0.,0.,-1.)) ;
#112730 = DIRECTION('',(0.,1.,1.07081696047951E-16)) ;
#112731 = DIRECTION('',(0.,0.,1.)) ;
#112732 = DIRECTION('center_axis',(-1.,0.,0.)) ;
#112733 = DIRECTION('ref_axis',(0.,0.,1.)) ;
#112734 = DIRECTION('',(0.,1.,0.)) ;
#112735 = DIRECTION('center_axis',(-1.,0.,0.)) ;
#112736 = DIRECTION('ref_axis',(0.,0.,1.)) ;
#112737 = DIRECTION('',(0.,0.,-1.)) ;
#112738 = DIRECTION('',(0.,0.707106781186548,-0.707106781186547)) ;
#112739 = DIRECTION('',(0.,0.,1.)) ;
#112740 = DIRECTION('',(0.,-0.707106781186546,-0.707106781186549)) ;
#112741 = DIRECTION('',(0.,-3.99416362155027E-15,-1.)) ;
#112742 = DIRECTION('center_axis',(1.,0.,0.)) ;
#112743 = DIRECTION('ref_axis',(0.,0.,-1.)) ;
#112744 = DIRECTION('',(1.,0.,0.)) ;
#112745 = DIRECTION('center_axis',(1.,0.,0.)) ;
#112746 = DIRECTION('ref_axis',(0.,0.,1.)) ;
#112747 = DIRECTION('',(1.,0.,0.)) ;
#112748 = DIRECTION('center_axis',(-1.,0.,0.)) ;
#112749 = DIRECTION('ref_axis',(0.,0.,-1.)) ;
#112750 = DIRECTION('center_axis',(0.,0.,1.)) ;
#112751 = DIRECTION('ref_axis',(1.,0.,0.)) ;
#112752 = DIRECTION('',(0.,1.,0.)) ;
#112753 = DIRECTION('',(1.,0.,0.)) ;
#112754 = DIRECTION('',(0.,-1.,0.)) ;
#112755 = DIRECTION('center_axis',(1.,0.,0.)) ;
#112756 = DIRECTION('ref_axis',(0.,0.,-1.)) ;
#112757 = DIRECTION('center_axis',(1.,0.,0.)) ;
#112758 = DIRECTION('ref_axis',(0.,0.,1.)) ;
#112759 = DIRECTION('',(1.,0.,0.)) ;
#112760 = DIRECTION('center_axis',(-1.,0.,0.)) ;
#112761 = DIRECTION('ref_axis',(0.,0.,-1.)) ;
#112762 = DIRECTION('center_axis',(0.,-1.,3.99416362155027E-15)) ;
#112763 = DIRECTION('ref_axis',(0.,-3.99416362155027E-15,-1.)) ;
#112764 = DIRECTION('',(0.,3.99416362155027E-15,1.)) ;
#112765 = DIRECTION('',(1.,0.,0.)) ;
#112766 = DIRECTION('',(0.,-3.99416362155027E-15,-1.)) ;
#112767 = DIRECTION('center_axis',(1.,0.,0.)) ;
#112768 = DIRECTION('ref_axis',(0.,0.,-1.)) ;
#112769 = DIRECTION('center_axis',(-1.,0.,0.)) ;
#112770 = DIRECTION('ref_axis',(0.,1.30104260698261E-14,-1.)) ;
#112771 = DIRECTION('',(1.,0.,0.)) ;
#112772 = DIRECTION('center_axis',(1.,0.,0.)) ;
#112773 = DIRECTION('ref_axis',(0.,0.,-1.)) ;
#112774 = DIRECTION('center_axis',(0.,-0.707106781186549,0.707106781186546)) ;
#112775 = DIRECTION('ref_axis',(0.,-0.707106781186546,-0.707106781186549)) ;
#112776 = DIRECTION('',(0.,0.707106781186546,0.707106781186549)) ;
#112777 = DIRECTION('',(1.,0.,0.)) ;
#112778 = DIRECTION('',(0.,-0.707106781186546,-0.707106781186549)) ;
#112779 = DIRECTION('center_axis',(1.,0.,0.)) ;
#112780 = DIRECTION('ref_axis',(0.,0.382683432365084,0.923879532511289)) ;
#112781 = DIRECTION('',(1.,0.,0.)) ;
#112782 = DIRECTION('center_axis',(1.,0.,0.)) ;
#112783 = DIRECTION('ref_axis',(0.,0.,-1.)) ;
#112784 = DIRECTION('center_axis',(0.,1.,0.)) ;
#112785 = DIRECTION('ref_axis',(0.,0.,1.)) ;
#112786 = DIRECTION('',(0.,0.,-1.)) ;
#112787 = DIRECTION('',(0.,0.,1.)) ;
#112788 = DIRECTION('center_axis',(0.,-0.707106781186547,-0.707106781186548)) ;
#112789 = DIRECTION('ref_axis',(0.,0.707106781186548,-0.707106781186547)) ;
#112790 = DIRECTION('',(0.,-0.707106781186548,0.707106781186547)) ;
#112791 = DIRECTION('',(1.,0.,0.)) ;
#112792 = DIRECTION('',(0.,0.707106781186548,-0.707106781186547)) ;
#112793 = DIRECTION('center_axis',(1.,0.,0.)) ;
#112794 = DIRECTION('ref_axis',(0.,0.,-1.)) ;
#112795 = DIRECTION('center_axis',(-1.,0.,0.)) ;
#112796 = DIRECTION('ref_axis',(0.,-1.73472347597682E-14,-1.)) ;
#112797 = DIRECTION('',(1.,0.,0.)) ;
#112798 = DIRECTION('center_axis',(1.,0.,0.)) ;
#112799 = DIRECTION('ref_axis',(0.,0.,-1.)) ;
#112800 = DIRECTION('center_axis',(0.,-1.,0.)) ;
#112801 = DIRECTION('ref_axis',(0.,0.,-1.)) ;
#112802 = DIRECTION('',(0.,0.,1.)) ;
#112803 = DIRECTION('',(1.,0.,0.)) ;
#112804 = DIRECTION('',(0.,0.,-1.)) ;
#112805 = DIRECTION('center_axis',(1.,0.,0.)) ;
#112806 = DIRECTION('ref_axis',(0.,0.,-1.)) ;
#112807 = DIRECTION('center_axis',(1.,0.,0.)) ;
#112808 = DIRECTION('ref_axis',(0.,0.,1.)) ;
#112809 = DIRECTION('',(1.,0.,0.)) ;
#112810 = DIRECTION('center_axis',(-1.,0.,0.)) ;
#112811 = DIRECTION('ref_axis',(0.,0.,-1.)) ;
#112812 = DIRECTION('center_axis',(0.,0.,-1.)) ;
#112813 = DIRECTION('ref_axis',(-1.,0.,0.)) ;
#112814 = DIRECTION('',(0.,-1.,0.)) ;
#112815 = DIRECTION('',(1.,0.,0.)) ;
#112816 = DIRECTION('',(0.,1.,0.)) ;
#112817 = DIRECTION('center_axis',(1.,0.,0.)) ;
#112818 = DIRECTION('ref_axis',(0.,0.,-1.)) ;
#112819 = DIRECTION('center_axis',(1.,0.,0.)) ;
#112820 = DIRECTION('ref_axis',(0.,0.,1.)) ;
#112821 = DIRECTION('',(1.,0.,0.)) ;
#112822 = DIRECTION('center_axis',(-1.,0.,0.)) ;
#112823 = DIRECTION('ref_axis',(0.,0.,-1.)) ;
#112824 = DIRECTION('center_axis',(0.,1.,0.)) ;
#112825 = DIRECTION('ref_axis',(0.,0.,1.)) ;
#112826 = DIRECTION('',(0.,0.,-1.)) ;
#112827 = DIRECTION('',(1.,0.,0.)) ;
#112828 = DIRECTION('',(0.,0.,1.)) ;
#112829 = DIRECTION('center_axis',(1.,0.,0.)) ;
#112830 = DIRECTION('ref_axis',(0.,0.,-1.)) ;
#112831 = DIRECTION('center_axis',(-1.,0.,0.)) ;
#112832 = DIRECTION('ref_axis',(0.,1.95156391047392E-14,-1.)) ;
#112833 = DIRECTION('',(1.,0.,0.)) ;
#112834 = DIRECTION('center_axis',(1.,0.,0.)) ;
#112835 = DIRECTION('ref_axis',(0.,0.,-1.)) ;
#112836 = DIRECTION('center_axis',(0.,1.07081696047951E-16,-1.)) ;
#112837 = DIRECTION('ref_axis',(0.,1.,1.07081696047951E-16)) ;
#112838 = DIRECTION('',(0.,-1.,-1.07081696047951E-16)) ;
#112839 = DIRECTION('',(1.,0.,0.)) ;
#112840 = DIRECTION('',(0.,1.,1.07081696047951E-16)) ;
#112841 = DIRECTION('center_axis',(1.,0.,0.)) ;
#112842 = DIRECTION('ref_axis',(0.,0.,-1.)) ;
#112843 = DIRECTION('center_axis',(-1.,0.,0.)) ;
#112844 = DIRECTION('ref_axis',(0.,0.,-1.)) ;
#112845 = DIRECTION('',(1.,0.,0.)) ;
#112846 = DIRECTION('center_axis',(1.,0.,0.)) ;
#112847 = DIRECTION('ref_axis',(0.,0.,-1.)) ;
#112848 = DIRECTION('center_axis',(0.,-1.,0.)) ;
#112849 = DIRECTION('ref_axis',(0.,0.,-1.)) ;
#112850 = DIRECTION('',(0.,0.,1.)) ;
#112851 = DIRECTION('',(1.,0.,0.)) ;
#112852 = DIRECTION('',(0.,0.,-1.)) ;
#112853 = DIRECTION('center_axis',(1.,0.,0.)) ;
#112854 = DIRECTION('ref_axis',(0.,0.,-1.)) ;
#112855 = DIRECTION('center_axis',(-1.,0.,0.)) ;
#112856 = DIRECTION('ref_axis',(0.,4.33680868994204E-15,-1.)) ;
#112857 = DIRECTION('',(1.,0.,0.)) ;
#112858 = DIRECTION('center_axis',(1.,0.,0.)) ;
#112859 = DIRECTION('ref_axis',(0.,0.,-1.)) ;
#112860 = DIRECTION('center_axis',(1.,0.,0.)) ;
#112861 = DIRECTION('ref_axis',(0.,0.,-1.)) ;
#112862 = DIRECTION('center_axis',(1.,0.,0.)) ;
#112863 = DIRECTION('ref_axis',(0.,-7.85535158932894E-16,1.)) ;
#112864 = DIRECTION('',(1.,0.,0.)) ;
#112865 = DIRECTION('center_axis',(-1.,0.,0.)) ;
#112866 = DIRECTION('ref_axis',(0.,-7.85535158932895E-16,-1.)) ;
#112867 = DIRECTION('center_axis',(1.,0.,0.)) ;
#112868 = DIRECTION('ref_axis',(0.,0.,-1.)) ;
#112869 = DIRECTION('center_axis',(-1.,0.,0.)) ;
#112870 = DIRECTION('ref_axis',(0.,-8.67361737988409E-15,-1.)) ;
#112871 = DIRECTION('',(1.,0.,0.)) ;
#112872 = DIRECTION('center_axis',(1.,0.,0.)) ;
#112873 = DIRECTION('ref_axis',(0.,0.,-1.)) ;
#112874 = DIRECTION('center_axis',(0.,-1.,0.)) ;
#112875 = DIRECTION('ref_axis',(0.,0.,-1.)) ;
#112876 = DIRECTION('',(0.,0.,1.)) ;
#112877 = DIRECTION('',(1.,0.,0.)) ;
#112878 = DIRECTION('',(0.,0.,-1.)) ;
#112879 = DIRECTION('center_axis',(1.,0.,0.)) ;
#112880 = DIRECTION('ref_axis',(0.,0.,-1.)) ;
#112881 = DIRECTION('center_axis',(-1.,0.,0.)) ;
#112882 = DIRECTION('ref_axis',(0.,0.,-1.)) ;
#112883 = DIRECTION('',(1.,0.,0.)) ;
#112884 = DIRECTION('center_axis',(1.,0.,0.)) ;
#112885 = DIRECTION('ref_axis',(0.,0.,-1.)) ;
#112886 = DIRECTION('center_axis',(0.,-1.07081696047951E-16,1.)) ;
#112887 = DIRECTION('ref_axis',(0.,-1.,-1.07081696047951E-16)) ;
#112888 = DIRECTION('',(0.,1.,1.07081696047951E-16)) ;
#112889 = DIRECTION('',(1.,0.,0.)) ;
#112890 = DIRECTION('',(0.,-1.,-1.07081696047951E-16)) ;
#112891 = DIRECTION('center_axis',(1.,0.,0.)) ;
#112892 = DIRECTION('ref_axis',(0.,0.,-1.)) ;
#112893 = DIRECTION('center_axis',(-1.,0.,0.)) ;
#112894 = DIRECTION('ref_axis',(0.,0.,-1.)) ;
#112895 = DIRECTION('',(1.,0.,0.)) ;
#112896 = DIRECTION('center_axis',(1.,0.,0.)) ;
#112897 = DIRECTION('ref_axis',(0.,0.,-1.)) ;
#112898 = DIRECTION('center_axis',(0.,1.,0.)) ;
#112899 = DIRECTION('ref_axis',(0.,0.,1.)) ;
#112900 = DIRECTION('',(0.,0.,-1.)) ;
#112901 = DIRECTION('',(0.,0.,1.)) ;
#112902 = DIRECTION('center_axis',(-1.,0.,0.)) ;
#112903 = DIRECTION('ref_axis',(0.,0.,1.)) ;
#112904 = DIRECTION('center_axis',(-1.,0.,0.)) ;
#112905 = DIRECTION('ref_axis',(0.,0.,1.)) ;
#112906 = DIRECTION('',(0.,-1.,0.)) ;
#112907 = DIRECTION('center_axis',(-1.,0.,0.)) ;
#112908 = DIRECTION('ref_axis',(0.,0.,1.)) ;
#112909 = DIRECTION('',(0.,0.,1.)) ;
#112910 = DIRECTION('',(0.,-1.,-1.07081696047951E-16)) ;
#112911 = DIRECTION('',(0.,0.,-1.)) ;
#112912 = DIRECTION('center_axis',(-1.,0.,0.)) ;
#112913 = DIRECTION('ref_axis',(0.,0.,1.)) ;
#112914 = DIRECTION('',(0.,0.,-1.)) ;
#112915 = DIRECTION('',(0.,1.,1.07081696047951E-16)) ;
#112916 = DIRECTION('',(0.,0.,1.)) ;
#112917 = DIRECTION('center_axis',(-1.,0.,0.)) ;
#112918 = DIRECTION('ref_axis',(0.,0.,1.)) ;
#112919 = DIRECTION('',(0.,1.,0.)) ;
#112920 = DIRECTION('center_axis',(-1.,0.,0.)) ;
#112921 = DIRECTION('ref_axis',(0.,0.,1.)) ;
#112922 = DIRECTION('',(0.,0.,-1.)) ;
#112923 = DIRECTION('',(0.,0.707106781186548,-0.707106781186547)) ;
#112924 = DIRECTION('',(0.,0.,1.)) ;
#112925 = DIRECTION('',(0.,-0.707106781186546,-0.707106781186549)) ;
#112926 = DIRECTION('',(0.,-3.99416362155027E-15,-1.)) ;
#112927 = DIRECTION('center_axis',(1.,0.,0.)) ;
#112928 = DIRECTION('ref_axis',(0.,0.,-1.)) ;
#112929 = DIRECTION('',(1.,0.,0.)) ;
#112930 = DIRECTION('center_axis',(1.,0.,0.)) ;
#112931 = DIRECTION('ref_axis',(0.,0.,1.)) ;
#112932 = DIRECTION('',(1.,0.,0.)) ;
#112933 = DIRECTION('center_axis',(-1.,0.,0.)) ;
#112934 = DIRECTION('ref_axis',(0.,0.,-1.)) ;
#112935 = DIRECTION('center_axis',(0.,0.,1.)) ;
#112936 = DIRECTION('ref_axis',(1.,0.,0.)) ;
#112937 = DIRECTION('',(0.,1.,0.)) ;
#112938 = DIRECTION('',(1.,0.,0.)) ;
#112939 = DIRECTION('',(0.,-1.,0.)) ;
#112940 = DIRECTION('center_axis',(1.,0.,0.)) ;
#112941 = DIRECTION('ref_axis',(0.,0.,-1.)) ;
#112942 = DIRECTION('center_axis',(1.,0.,0.)) ;
#112943 = DIRECTION('ref_axis',(0.,0.,1.)) ;
#112944 = DIRECTION('',(1.,0.,0.)) ;
#112945 = DIRECTION('center_axis',(-1.,0.,0.)) ;
#112946 = DIRECTION('ref_axis',(0.,0.,-1.)) ;
#112947 = DIRECTION('center_axis',(0.,-1.,3.99416362155027E-15)) ;
#112948 = DIRECTION('ref_axis',(0.,-3.99416362155027E-15,-1.)) ;
#112949 = DIRECTION('',(0.,3.99416362155027E-15,1.)) ;
#112950 = DIRECTION('',(1.,0.,0.)) ;
#112951 = DIRECTION('',(0.,-3.99416362155027E-15,-1.)) ;
#112952 = DIRECTION('center_axis',(1.,0.,0.)) ;
#112953 = DIRECTION('ref_axis',(0.,0.,-1.)) ;
#112954 = DIRECTION('center_axis',(-1.,0.,0.)) ;
#112955 = DIRECTION('ref_axis',(0.,1.30104260698261E-14,-1.)) ;
#112956 = DIRECTION('',(1.,0.,0.)) ;
#112957 = DIRECTION('center_axis',(1.,0.,0.)) ;
#112958 = DIRECTION('ref_axis',(0.,0.,-1.)) ;
#112959 = DIRECTION('center_axis',(0.,-0.707106781186549,0.707106781186546)) ;
#112960 = DIRECTION('ref_axis',(0.,-0.707106781186546,-0.707106781186549)) ;
#112961 = DIRECTION('',(0.,0.707106781186546,0.707106781186549)) ;
#112962 = DIRECTION('',(1.,0.,0.)) ;
#112963 = DIRECTION('',(0.,-0.707106781186546,-0.707106781186549)) ;
#112964 = DIRECTION('center_axis',(1.,0.,0.)) ;
#112965 = DIRECTION('ref_axis',(0.,0.382683432365088,0.923879532511288)) ;
#112966 = DIRECTION('',(1.,0.,0.)) ;
#112967 = DIRECTION('center_axis',(1.,0.,0.)) ;
#112968 = DIRECTION('ref_axis',(0.,0.,-1.)) ;
#112969 = DIRECTION('center_axis',(0.,1.,0.)) ;
#112970 = DIRECTION('ref_axis',(0.,0.,1.)) ;
#112971 = DIRECTION('',(0.,0.,-1.)) ;
#112972 = DIRECTION('',(0.,0.,1.)) ;
#112973 = DIRECTION('center_axis',(0.,-0.707106781186547,-0.707106781186548)) ;
#112974 = DIRECTION('ref_axis',(0.,0.707106781186548,-0.707106781186547)) ;
#112975 = DIRECTION('',(0.,-0.707106781186548,0.707106781186547)) ;
#112976 = DIRECTION('',(1.,0.,0.)) ;
#112977 = DIRECTION('',(0.,0.707106781186548,-0.707106781186547)) ;
#112978 = DIRECTION('center_axis',(1.,0.,0.)) ;
#112979 = DIRECTION('ref_axis',(0.,0.,-1.)) ;
#112980 = DIRECTION('center_axis',(-1.,0.,0.)) ;
#112981 = DIRECTION('ref_axis',(0.,0.,-1.)) ;
#112982 = DIRECTION('',(1.,0.,0.)) ;
#112983 = DIRECTION('center_axis',(1.,0.,0.)) ;
#112984 = DIRECTION('ref_axis',(0.,0.,-1.)) ;
#112985 = DIRECTION('center_axis',(0.,-1.,0.)) ;
#112986 = DIRECTION('ref_axis',(0.,0.,-1.)) ;
#112987 = DIRECTION('',(0.,0.,1.)) ;
#112988 = DIRECTION('',(1.,0.,0.)) ;
#112989 = DIRECTION('',(0.,0.,-1.)) ;
#112990 = DIRECTION('center_axis',(1.,0.,0.)) ;
#112991 = DIRECTION('ref_axis',(0.,0.,-1.)) ;
#112992 = DIRECTION('center_axis',(1.,0.,0.)) ;
#112993 = DIRECTION('ref_axis',(0.,0.,1.)) ;
#112994 = DIRECTION('',(1.,0.,0.)) ;
#112995 = DIRECTION('center_axis',(-1.,0.,0.)) ;
#112996 = DIRECTION('ref_axis',(0.,0.,-1.)) ;
#112997 = DIRECTION('center_axis',(0.,0.,-1.)) ;
#112998 = DIRECTION('ref_axis',(-1.,0.,0.)) ;
#112999 = DIRECTION('',(0.,-1.,0.)) ;
#113000 = DIRECTION('',(1.,0.,0.)) ;
#113001 = DIRECTION('',(0.,1.,0.)) ;
#113002 = DIRECTION('center_axis',(1.,0.,0.)) ;
#113003 = DIRECTION('ref_axis',(0.,0.,-1.)) ;
#113004 = DIRECTION('center_axis',(1.,0.,0.)) ;
#113005 = DIRECTION('ref_axis',(0.,0.,1.)) ;
#113006 = DIRECTION('',(1.,0.,0.)) ;
#113007 = DIRECTION('center_axis',(-1.,0.,0.)) ;
#113008 = DIRECTION('ref_axis',(0.,0.,-1.)) ;
#113009 = DIRECTION('center_axis',(0.,1.,0.)) ;
#113010 = DIRECTION('ref_axis',(0.,0.,1.)) ;
#113011 = DIRECTION('',(0.,0.,-1.)) ;
#113012 = DIRECTION('',(1.,0.,0.)) ;
#113013 = DIRECTION('',(0.,0.,1.)) ;
#113014 = DIRECTION('center_axis',(1.,0.,0.)) ;
#113015 = DIRECTION('ref_axis',(0.,0.,-1.)) ;
#113016 = DIRECTION('center_axis',(-1.,0.,0.)) ;
#113017 = DIRECTION('ref_axis',(0.,1.95156391047392E-14,-1.)) ;
#113018 = DIRECTION('',(1.,0.,0.)) ;
#113019 = DIRECTION('center_axis',(1.,0.,0.)) ;
#113020 = DIRECTION('ref_axis',(0.,0.,-1.)) ;
#113021 = DIRECTION('center_axis',(0.,1.07081696047951E-16,-1.)) ;
#113022 = DIRECTION('ref_axis',(0.,1.,1.07081696047951E-16)) ;
#113023 = DIRECTION('',(0.,-1.,-1.07081696047951E-16)) ;
#113024 = DIRECTION('',(1.,0.,0.)) ;
#113025 = DIRECTION('',(0.,1.,1.07081696047951E-16)) ;
#113026 = DIRECTION('center_axis',(1.,0.,0.)) ;
#113027 = DIRECTION('ref_axis',(0.,0.,-1.)) ;
#113028 = DIRECTION('center_axis',(-1.,0.,0.)) ;
#113029 = DIRECTION('ref_axis',(0.,0.,-1.)) ;
#113030 = DIRECTION('',(1.,0.,0.)) ;
#113031 = DIRECTION('center_axis',(1.,0.,0.)) ;
#113032 = DIRECTION('ref_axis',(0.,0.,-1.)) ;
#113033 = DIRECTION('center_axis',(0.,-1.,0.)) ;
#113034 = DIRECTION('ref_axis',(0.,0.,-1.)) ;
#113035 = DIRECTION('',(0.,0.,1.)) ;
#113036 = DIRECTION('',(1.,0.,0.)) ;
#113037 = DIRECTION('',(0.,0.,-1.)) ;
#113038 = DIRECTION('center_axis',(1.,0.,0.)) ;
#113039 = DIRECTION('ref_axis',(0.,0.,-1.)) ;
#113040 = DIRECTION('center_axis',(-1.,0.,0.)) ;
#113041 = DIRECTION('ref_axis',(0.,-4.33680868994204E-15,-1.)) ;
#113042 = DIRECTION('',(1.,0.,0.)) ;
#113043 = DIRECTION('center_axis',(1.,0.,0.)) ;
#113044 = DIRECTION('ref_axis',(0.,0.,-1.)) ;
#113045 = DIRECTION('center_axis',(1.,0.,0.)) ;
#113046 = DIRECTION('ref_axis',(0.,0.,-1.)) ;
#113047 = DIRECTION('center_axis',(1.,0.,0.)) ;
#113048 = DIRECTION('ref_axis',(0.,-7.85535158932894E-16,1.)) ;
#113049 = DIRECTION('',(1.,0.,0.)) ;
#113050 = DIRECTION('center_axis',(-1.,0.,0.)) ;
#113051 = DIRECTION('ref_axis',(0.,-7.85535158932894E-16,-1.)) ;
#113052 = DIRECTION('center_axis',(1.,0.,0.)) ;
#113053 = DIRECTION('ref_axis',(0.,0.,-1.)) ;
#113054 = DIRECTION('center_axis',(-1.,0.,0.)) ;
#113055 = DIRECTION('ref_axis',(0.,-8.67361737988409E-15,-1.)) ;
#113056 = DIRECTION('',(1.,0.,0.)) ;
#113057 = DIRECTION('center_axis',(1.,0.,0.)) ;
#113058 = DIRECTION('ref_axis',(0.,0.,-1.)) ;
#113059 = DIRECTION('center_axis',(0.,-1.,0.)) ;
#113060 = DIRECTION('ref_axis',(0.,0.,-1.)) ;
#113061 = DIRECTION('',(0.,0.,1.)) ;
#113062 = DIRECTION('',(1.,0.,0.)) ;
#113063 = DIRECTION('',(0.,0.,-1.)) ;
#113064 = DIRECTION('center_axis',(1.,0.,0.)) ;
#113065 = DIRECTION('ref_axis',(0.,0.,-1.)) ;
#113066 = DIRECTION('center_axis',(-1.,0.,0.)) ;
#113067 = DIRECTION('ref_axis',(0.,0.,-1.)) ;
#113068 = DIRECTION('',(1.,0.,0.)) ;
#113069 = DIRECTION('center_axis',(1.,0.,0.)) ;
#113070 = DIRECTION('ref_axis',(0.,0.,-1.)) ;
#113071 = DIRECTION('center_axis',(0.,-1.07081696047951E-16,1.)) ;
#113072 = DIRECTION('ref_axis',(0.,-1.,-1.07081696047951E-16)) ;
#113073 = DIRECTION('',(0.,1.,1.07081696047951E-16)) ;
#113074 = DIRECTION('',(1.,0.,0.)) ;
#113075 = DIRECTION('',(0.,-1.,-1.07081696047951E-16)) ;
#113076 = DIRECTION('center_axis',(1.,0.,0.)) ;
#113077 = DIRECTION('ref_axis',(0.,0.,-1.)) ;
#113078 = DIRECTION('center_axis',(-1.,0.,0.)) ;
#113079 = DIRECTION('ref_axis',(0.,0.,-1.)) ;
#113080 = DIRECTION('',(1.,0.,0.)) ;
#113081 = DIRECTION('center_axis',(1.,0.,0.)) ;
#113082 = DIRECTION('ref_axis',(0.,0.,-1.)) ;
#113083 = DIRECTION('center_axis',(0.,1.,0.)) ;
#113084 = DIRECTION('ref_axis',(0.,0.,1.)) ;
#113085 = DIRECTION('',(0.,0.,-1.)) ;
#113086 = DIRECTION('',(0.,0.,1.)) ;
#113087 = DIRECTION('center_axis',(-1.,0.,0.)) ;
#113088 = DIRECTION('ref_axis',(0.,0.,1.)) ;
#113089 = DIRECTION('center_axis',(-1.,0.,0.)) ;
#113090 = DIRECTION('ref_axis',(0.,0.,1.)) ;
#113091 = DIRECTION('',(0.,-1.,0.)) ;
#113092 = DIRECTION('center_axis',(-1.,0.,0.)) ;
#113093 = DIRECTION('ref_axis',(0.,0.,1.)) ;
#113094 = DIRECTION('',(0.,0.,1.)) ;
#113095 = DIRECTION('',(0.,-1.,-1.07081696047951E-16)) ;
#113096 = DIRECTION('',(0.,0.,-1.)) ;
#113097 = DIRECTION('center_axis',(-1.,0.,0.)) ;
#113098 = DIRECTION('ref_axis',(0.,0.,1.)) ;
#113099 = DIRECTION('',(0.,0.,-1.)) ;
#113100 = DIRECTION('',(0.,1.,1.07081696047951E-16)) ;
#113101 = DIRECTION('',(0.,0.,1.)) ;
#113102 = DIRECTION('center_axis',(-1.,0.,0.)) ;
#113103 = DIRECTION('ref_axis',(0.,0.,1.)) ;
#113104 = DIRECTION('',(0.,1.,0.)) ;
#113105 = DIRECTION('center_axis',(-1.,0.,0.)) ;
#113106 = DIRECTION('ref_axis',(0.,0.,1.)) ;
#113107 = DIRECTION('',(0.,0.,-1.)) ;
#113108 = DIRECTION('',(0.,0.707106781186548,-0.707106781186547)) ;
#113109 = DIRECTION('',(0.,0.,1.)) ;
#113110 = DIRECTION('',(0.,-0.707106781186546,-0.707106781186549)) ;
#113111 = DIRECTION('',(0.,-3.99416362155027E-15,-1.)) ;
#113112 = DIRECTION('center_axis',(1.,0.,0.)) ;
#113113 = DIRECTION('ref_axis',(0.,0.,-1.)) ;
#113114 = DIRECTION('',(1.,0.,0.)) ;
#113115 = DIRECTION('center_axis',(1.,0.,0.)) ;
#113116 = DIRECTION('ref_axis',(0.,0.,1.)) ;
#113117 = DIRECTION('',(1.,0.,0.)) ;
#113118 = DIRECTION('center_axis',(-1.,0.,0.)) ;
#113119 = DIRECTION('ref_axis',(0.,0.,-1.)) ;
#113120 = DIRECTION('center_axis',(0.,0.,1.)) ;
#113121 = DIRECTION('ref_axis',(1.,0.,0.)) ;
#113122 = DIRECTION('',(0.,1.,0.)) ;
#113123 = DIRECTION('',(1.,0.,0.)) ;
#113124 = DIRECTION('',(0.,-1.,0.)) ;
#113125 = DIRECTION('center_axis',(1.,0.,0.)) ;
#113126 = DIRECTION('ref_axis',(0.,0.,-1.)) ;
#113127 = DIRECTION('center_axis',(1.,0.,0.)) ;
#113128 = DIRECTION('ref_axis',(0.,0.,1.)) ;
#113129 = DIRECTION('',(1.,0.,0.)) ;
#113130 = DIRECTION('center_axis',(-1.,0.,0.)) ;
#113131 = DIRECTION('ref_axis',(0.,0.,-1.)) ;
#113132 = DIRECTION('center_axis',(0.,-1.,3.99416362155027E-15)) ;
#113133 = DIRECTION('ref_axis',(0.,-3.99416362155027E-15,-1.)) ;
#113134 = DIRECTION('',(0.,3.99416362155027E-15,1.)) ;
#113135 = DIRECTION('',(1.,0.,0.)) ;
#113136 = DIRECTION('',(0.,-3.99416362155027E-15,-1.)) ;
#113137 = DIRECTION('center_axis',(1.,0.,0.)) ;
#113138 = DIRECTION('ref_axis',(0.,0.,-1.)) ;
#113139 = DIRECTION('center_axis',(-1.,0.,0.)) ;
#113140 = DIRECTION('ref_axis',(0.,0.,-1.)) ;
#113141 = DIRECTION('',(1.,0.,0.)) ;
#113142 = DIRECTION('center_axis',(1.,0.,0.)) ;
#113143 = DIRECTION('ref_axis',(0.,0.,-1.)) ;
#113144 = DIRECTION('center_axis',(0.,-0.707106781186549,0.707106781186546)) ;
#113145 = DIRECTION('ref_axis',(0.,-0.707106781186546,-0.707106781186549)) ;
#113146 = DIRECTION('',(0.,0.707106781186546,0.707106781186549)) ;
#113147 = DIRECTION('',(1.,0.,0.)) ;
#113148 = DIRECTION('',(0.,-0.707106781186546,-0.707106781186549)) ;
#113149 = DIRECTION('center_axis',(1.,0.,0.)) ;
#113150 = DIRECTION('ref_axis',(0.,0.382683432365092,0.923879532511286)) ;
#113151 = DIRECTION('',(1.,0.,0.)) ;
#113152 = DIRECTION('center_axis',(1.,0.,0.)) ;
#113153 = DIRECTION('ref_axis',(0.,0.,-1.)) ;
#113154 = DIRECTION('center_axis',(0.,1.,0.)) ;
#113155 = DIRECTION('ref_axis',(0.,0.,1.)) ;
#113156 = DIRECTION('',(0.,0.,-1.)) ;
#113157 = DIRECTION('',(0.,0.,1.)) ;
#113158 = DIRECTION('center_axis',(0.,-0.707106781186547,-0.707106781186548)) ;
#113159 = DIRECTION('ref_axis',(0.,0.707106781186548,-0.707106781186547)) ;
#113160 = DIRECTION('',(0.,-0.707106781186548,0.707106781186547)) ;
#113161 = DIRECTION('',(1.,0.,0.)) ;
#113162 = DIRECTION('',(0.,0.707106781186548,-0.707106781186547)) ;
#113163 = DIRECTION('center_axis',(1.,0.,0.)) ;
#113164 = DIRECTION('ref_axis',(0.,0.,-1.)) ;
#113165 = DIRECTION('center_axis',(-1.,0.,0.)) ;
#113166 = DIRECTION('ref_axis',(0.,0.,-1.)) ;
#113167 = DIRECTION('',(1.,0.,0.)) ;
#113168 = DIRECTION('center_axis',(1.,0.,0.)) ;
#113169 = DIRECTION('ref_axis',(0.,0.,-1.)) ;
#113170 = DIRECTION('center_axis',(0.,-1.,0.)) ;
#113171 = DIRECTION('ref_axis',(0.,0.,-1.)) ;
#113172 = DIRECTION('',(0.,0.,1.)) ;
#113173 = DIRECTION('',(1.,0.,0.)) ;
#113174 = DIRECTION('',(0.,0.,-1.)) ;
#113175 = DIRECTION('center_axis',(1.,0.,0.)) ;
#113176 = DIRECTION('ref_axis',(0.,0.,-1.)) ;
#113177 = DIRECTION('center_axis',(1.,0.,0.)) ;
#113178 = DIRECTION('ref_axis',(0.,0.,1.)) ;
#113179 = DIRECTION('',(1.,0.,0.)) ;
#113180 = DIRECTION('center_axis',(-1.,0.,0.)) ;
#113181 = DIRECTION('ref_axis',(0.,0.,-1.)) ;
#113182 = DIRECTION('center_axis',(0.,0.,-1.)) ;
#113183 = DIRECTION('ref_axis',(-1.,0.,0.)) ;
#113184 = DIRECTION('',(0.,-1.,0.)) ;
#113185 = DIRECTION('',(1.,0.,0.)) ;
#113186 = DIRECTION('',(0.,1.,0.)) ;
#113187 = DIRECTION('center_axis',(1.,0.,0.)) ;
#113188 = DIRECTION('ref_axis',(0.,0.,-1.)) ;
#113189 = DIRECTION('center_axis',(1.,0.,0.)) ;
#113190 = DIRECTION('ref_axis',(0.,0.,1.)) ;
#113191 = DIRECTION('',(1.,0.,0.)) ;
#113192 = DIRECTION('center_axis',(-1.,0.,0.)) ;
#113193 = DIRECTION('ref_axis',(0.,0.,-1.)) ;
#113194 = DIRECTION('center_axis',(0.,1.,0.)) ;
#113195 = DIRECTION('ref_axis',(0.,0.,1.)) ;
#113196 = DIRECTION('',(0.,0.,-1.)) ;
#113197 = DIRECTION('',(1.,0.,0.)) ;
#113198 = DIRECTION('',(0.,0.,1.)) ;
#113199 = DIRECTION('center_axis',(1.,0.,0.)) ;
#113200 = DIRECTION('ref_axis',(0.,0.,-1.)) ;
#113201 = DIRECTION('center_axis',(-1.,0.,0.)) ;
#113202 = DIRECTION('ref_axis',(0.,1.95156391047392E-14,-1.)) ;
#113203 = DIRECTION('',(1.,0.,0.)) ;
#113204 = DIRECTION('center_axis',(1.,0.,0.)) ;
#113205 = DIRECTION('ref_axis',(0.,0.,-1.)) ;
#113206 = DIRECTION('center_axis',(0.,1.07081696047951E-16,-1.)) ;
#113207 = DIRECTION('ref_axis',(0.,1.,1.07081696047951E-16)) ;
#113208 = DIRECTION('',(0.,-1.,-1.07081696047951E-16)) ;
#113209 = DIRECTION('',(1.,0.,0.)) ;
#113210 = DIRECTION('',(0.,1.,1.07081696047951E-16)) ;
#113211 = DIRECTION('center_axis',(1.,0.,0.)) ;
#113212 = DIRECTION('ref_axis',(0.,0.,-1.)) ;
#113213 = DIRECTION('center_axis',(-1.,0.,0.)) ;
#113214 = DIRECTION('ref_axis',(0.,0.,-1.)) ;
#113215 = DIRECTION('',(1.,0.,0.)) ;
#113216 = DIRECTION('center_axis',(1.,0.,0.)) ;
#113217 = DIRECTION('ref_axis',(0.,0.,-1.)) ;
#113218 = DIRECTION('center_axis',(0.,-1.,0.)) ;
#113219 = DIRECTION('ref_axis',(0.,0.,-1.)) ;
#113220 = DIRECTION('',(0.,0.,1.)) ;
#113221 = DIRECTION('',(1.,0.,0.)) ;
#113222 = DIRECTION('',(0.,0.,-1.)) ;
#113223 = DIRECTION('center_axis',(1.,0.,0.)) ;
#113224 = DIRECTION('ref_axis',(0.,0.,-1.)) ;
#113225 = DIRECTION('center_axis',(-1.,0.,0.)) ;
#113226 = DIRECTION('ref_axis',(0.,-4.33680868994204E-15,-1.)) ;
#113227 = DIRECTION('',(1.,0.,0.)) ;
#113228 = DIRECTION('center_axis',(1.,0.,0.)) ;
#113229 = DIRECTION('ref_axis',(0.,0.,-1.)) ;
#113230 = DIRECTION('center_axis',(1.,0.,0.)) ;
#113231 = DIRECTION('ref_axis',(0.,0.,-1.)) ;
#113232 = DIRECTION('center_axis',(1.,0.,0.)) ;
#113233 = DIRECTION('ref_axis',(0.,-7.85535158932894E-16,1.)) ;
#113234 = DIRECTION('',(1.,0.,0.)) ;
#113235 = DIRECTION('center_axis',(-1.,0.,0.)) ;
#113236 = DIRECTION('ref_axis',(0.,-7.85535158932894E-16,-1.)) ;
#113237 = DIRECTION('center_axis',(1.,0.,0.)) ;
#113238 = DIRECTION('ref_axis',(0.,0.,-1.)) ;
#113239 = DIRECTION('center_axis',(-1.,0.,0.)) ;
#113240 = DIRECTION('ref_axis',(0.,0.,-1.)) ;
#113241 = DIRECTION('',(1.,0.,0.)) ;
#113242 = DIRECTION('center_axis',(1.,0.,0.)) ;
#113243 = DIRECTION('ref_axis',(0.,0.,-1.)) ;
#113244 = DIRECTION('center_axis',(0.,-1.,0.)) ;
#113245 = DIRECTION('ref_axis',(0.,0.,-1.)) ;
#113246 = DIRECTION('',(0.,0.,1.)) ;
#113247 = DIRECTION('',(1.,0.,0.)) ;
#113248 = DIRECTION('',(0.,0.,-1.)) ;
#113249 = DIRECTION('center_axis',(1.,0.,0.)) ;
#113250 = DIRECTION('ref_axis',(0.,0.,-1.)) ;
#113251 = DIRECTION('center_axis',(-1.,0.,0.)) ;
#113252 = DIRECTION('ref_axis',(0.,0.,-1.)) ;
#113253 = DIRECTION('',(1.,0.,0.)) ;
#113254 = DIRECTION('center_axis',(1.,0.,0.)) ;
#113255 = DIRECTION('ref_axis',(0.,0.,-1.)) ;
#113256 = DIRECTION('center_axis',(0.,-1.07081696047951E-16,1.)) ;
#113257 = DIRECTION('ref_axis',(0.,-1.,-1.07081696047951E-16)) ;
#113258 = DIRECTION('',(0.,1.,1.07081696047951E-16)) ;
#113259 = DIRECTION('',(1.,0.,0.)) ;
#113260 = DIRECTION('',(0.,-1.,-1.07081696047951E-16)) ;
#113261 = DIRECTION('center_axis',(1.,0.,0.)) ;
#113262 = DIRECTION('ref_axis',(0.,0.,-1.)) ;
#113263 = DIRECTION('center_axis',(-1.,0.,0.)) ;
#113264 = DIRECTION('ref_axis',(0.,0.,-1.)) ;
#113265 = DIRECTION('',(1.,0.,0.)) ;
#113266 = DIRECTION('center_axis',(1.,0.,0.)) ;
#113267 = DIRECTION('ref_axis',(0.,0.,-1.)) ;
#113268 = DIRECTION('center_axis',(0.,1.,0.)) ;
#113269 = DIRECTION('ref_axis',(0.,0.,1.)) ;
#113270 = DIRECTION('',(0.,0.,-1.)) ;
#113271 = DIRECTION('',(0.,0.,1.)) ;
#113272 = DIRECTION('center_axis',(-1.,0.,0.)) ;
#113273 = DIRECTION('ref_axis',(0.,0.,1.)) ;
#113274 = DIRECTION('center_axis',(-1.,0.,0.)) ;
#113275 = DIRECTION('ref_axis',(0.,0.,1.)) ;
#113276 = DIRECTION('',(0.,-1.,0.)) ;
#113277 = DIRECTION('center_axis',(-1.,0.,0.)) ;
#113278 = DIRECTION('ref_axis',(0.,0.,1.)) ;
#113279 = DIRECTION('',(0.,0.,1.)) ;
#113280 = DIRECTION('',(0.,-1.,-1.07081696047951E-16)) ;
#113281 = DIRECTION('',(0.,0.,-1.)) ;
#113282 = DIRECTION('center_axis',(-1.,0.,0.)) ;
#113283 = DIRECTION('ref_axis',(0.,0.,1.)) ;
#113284 = DIRECTION('',(0.,0.,-1.)) ;
#113285 = DIRECTION('',(0.,1.,1.07081696047951E-16)) ;
#113286 = DIRECTION('',(0.,0.,1.)) ;
#113287 = DIRECTION('center_axis',(-1.,0.,0.)) ;
#113288 = DIRECTION('ref_axis',(0.,0.,1.)) ;
#113289 = DIRECTION('',(0.,1.,0.)) ;
#113290 = DIRECTION('center_axis',(-1.,0.,0.)) ;
#113291 = DIRECTION('ref_axis',(0.,0.,1.)) ;
#113292 = DIRECTION('',(0.,0.,-1.)) ;
#113293 = DIRECTION('',(0.,0.707106781186548,-0.707106781186547)) ;
#113294 = DIRECTION('',(0.,0.,1.)) ;
#113295 = DIRECTION('',(0.,-0.707106781186546,-0.707106781186549)) ;
#113296 = DIRECTION('',(0.,-3.99416362155027E-15,-1.)) ;
#113297 = DIRECTION('center_axis',(1.,0.,0.)) ;
#113298 = DIRECTION('ref_axis',(0.,0.,-1.)) ;
#113299 = DIRECTION('',(1.,0.,0.)) ;
#113300 = DIRECTION('center_axis',(1.,0.,0.)) ;
#113301 = DIRECTION('ref_axis',(0.,0.,1.)) ;
#113302 = DIRECTION('',(1.,0.,0.)) ;
#113303 = DIRECTION('center_axis',(-1.,0.,0.)) ;
#113304 = DIRECTION('ref_axis',(0.,0.,-1.)) ;
#113305 = DIRECTION('center_axis',(0.,0.,1.)) ;
#113306 = DIRECTION('ref_axis',(1.,0.,0.)) ;
#113307 = DIRECTION('',(0.,1.,0.)) ;
#113308 = DIRECTION('',(1.,0.,0.)) ;
#113309 = DIRECTION('',(0.,-1.,0.)) ;
#113310 = DIRECTION('center_axis',(1.,0.,0.)) ;
#113311 = DIRECTION('ref_axis',(0.,0.,-1.)) ;
#113312 = DIRECTION('center_axis',(1.,0.,0.)) ;
#113313 = DIRECTION('ref_axis',(0.,0.,1.)) ;
#113314 = DIRECTION('',(1.,0.,0.)) ;
#113315 = DIRECTION('center_axis',(-1.,0.,0.)) ;
#113316 = DIRECTION('ref_axis',(0.,0.,-1.)) ;
#113317 = DIRECTION('center_axis',(0.,-1.,3.99416362155027E-15)) ;
#113318 = DIRECTION('ref_axis',(0.,-3.99416362155027E-15,-1.)) ;
#113319 = DIRECTION('',(0.,3.99416362155027E-15,1.)) ;
#113320 = DIRECTION('',(1.,0.,0.)) ;
#113321 = DIRECTION('',(0.,-3.99416362155027E-15,-1.)) ;
#113322 = DIRECTION('center_axis',(1.,0.,0.)) ;
#113323 = DIRECTION('ref_axis',(0.,0.,-1.)) ;
#113324 = DIRECTION('center_axis',(-1.,0.,0.)) ;
#113325 = DIRECTION('ref_axis',(0.,0.,-1.)) ;
#113326 = DIRECTION('',(1.,0.,0.)) ;
#113327 = DIRECTION('center_axis',(1.,0.,0.)) ;
#113328 = DIRECTION('ref_axis',(0.,0.,-1.)) ;
#113329 = DIRECTION('center_axis',(0.,-0.707106781186549,0.707106781186546)) ;
#113330 = DIRECTION('ref_axis',(0.,-0.707106781186546,-0.707106781186549)) ;
#113331 = DIRECTION('',(0.,0.707106781186546,0.707106781186549)) ;
#113332 = DIRECTION('',(1.,0.,0.)) ;
#113333 = DIRECTION('',(0.,-0.707106781186546,-0.707106781186549)) ;
#113334 = DIRECTION('center_axis',(1.,0.,0.)) ;
#113335 = DIRECTION('ref_axis',(0.,0.382683432365092,0.923879532511286)) ;
#113336 = DIRECTION('',(1.,0.,0.)) ;
#113337 = DIRECTION('center_axis',(1.,0.,0.)) ;
#113338 = DIRECTION('ref_axis',(0.,0.,-1.)) ;
#113339 = DIRECTION('center_axis',(0.,1.,0.)) ;
#113340 = DIRECTION('ref_axis',(0.,0.,1.)) ;
#113341 = DIRECTION('',(0.,0.,-1.)) ;
#113342 = DIRECTION('',(0.,0.,1.)) ;
#113343 = DIRECTION('center_axis',(0.,-0.707106781186547,-0.707106781186548)) ;
#113344 = DIRECTION('ref_axis',(0.,0.707106781186548,-0.707106781186547)) ;
#113345 = DIRECTION('',(0.,-0.707106781186548,0.707106781186547)) ;
#113346 = DIRECTION('',(1.,0.,0.)) ;
#113347 = DIRECTION('',(0.,0.707106781186548,-0.707106781186547)) ;
#113348 = DIRECTION('center_axis',(1.,0.,0.)) ;
#113349 = DIRECTION('ref_axis',(0.,0.,-1.)) ;
#113350 = DIRECTION('center_axis',(-1.,0.,0.)) ;
#113351 = DIRECTION('ref_axis',(0.,0.,-1.)) ;
#113352 = DIRECTION('',(1.,0.,0.)) ;
#113353 = DIRECTION('center_axis',(1.,0.,0.)) ;
#113354 = DIRECTION('ref_axis',(0.,0.,-1.)) ;
#113355 = DIRECTION('center_axis',(0.,-1.,0.)) ;
#113356 = DIRECTION('ref_axis',(0.,0.,-1.)) ;
#113357 = DIRECTION('',(0.,0.,1.)) ;
#113358 = DIRECTION('',(1.,0.,0.)) ;
#113359 = DIRECTION('',(0.,0.,-1.)) ;
#113360 = DIRECTION('center_axis',(1.,0.,0.)) ;
#113361 = DIRECTION('ref_axis',(0.,0.,-1.)) ;
#113362 = DIRECTION('center_axis',(1.,0.,0.)) ;
#113363 = DIRECTION('ref_axis',(0.,0.,1.)) ;
#113364 = DIRECTION('',(1.,0.,0.)) ;
#113365 = DIRECTION('center_axis',(-1.,0.,0.)) ;
#113366 = DIRECTION('ref_axis',(0.,0.,-1.)) ;
#113367 = DIRECTION('center_axis',(0.,0.,-1.)) ;
#113368 = DIRECTION('ref_axis',(-1.,0.,0.)) ;
#113369 = DIRECTION('',(0.,-1.,0.)) ;
#113370 = DIRECTION('',(1.,0.,0.)) ;
#113371 = DIRECTION('',(0.,1.,0.)) ;
#113372 = DIRECTION('center_axis',(1.,0.,0.)) ;
#113373 = DIRECTION('ref_axis',(0.,0.,-1.)) ;
#113374 = DIRECTION('center_axis',(1.,0.,0.)) ;
#113375 = DIRECTION('ref_axis',(0.,0.,1.)) ;
#113376 = DIRECTION('',(1.,0.,0.)) ;
#113377 = DIRECTION('center_axis',(-1.,0.,0.)) ;
#113378 = DIRECTION('ref_axis',(0.,0.,-1.)) ;
#113379 = DIRECTION('center_axis',(0.,1.,0.)) ;
#113380 = DIRECTION('ref_axis',(0.,0.,1.)) ;
#113381 = DIRECTION('',(0.,0.,-1.)) ;
#113382 = DIRECTION('',(1.,0.,0.)) ;
#113383 = DIRECTION('',(0.,0.,1.)) ;
#113384 = DIRECTION('center_axis',(1.,0.,0.)) ;
#113385 = DIRECTION('ref_axis',(0.,0.,-1.)) ;
#113386 = DIRECTION('center_axis',(-1.,0.,0.)) ;
#113387 = DIRECTION('ref_axis',(0.,1.7347234759768E-14,-1.)) ;
#113388 = DIRECTION('',(1.,0.,0.)) ;
#113389 = DIRECTION('center_axis',(1.,0.,0.)) ;
#113390 = DIRECTION('ref_axis',(0.,0.,-1.)) ;
#113391 = DIRECTION('center_axis',(0.,1.07081696047951E-16,-1.)) ;
#113392 = DIRECTION('ref_axis',(0.,1.,1.07081696047951E-16)) ;
#113393 = DIRECTION('',(0.,-1.,-1.07081696047951E-16)) ;
#113394 = DIRECTION('',(1.,0.,0.)) ;
#113395 = DIRECTION('',(0.,1.,1.07081696047951E-16)) ;
#113396 = DIRECTION('center_axis',(1.,0.,0.)) ;
#113397 = DIRECTION('ref_axis',(0.,0.,-1.)) ;
#113398 = DIRECTION('center_axis',(-1.,0.,0.)) ;
#113399 = DIRECTION('ref_axis',(0.,0.,-1.)) ;
#113400 = DIRECTION('',(1.,0.,0.)) ;
#113401 = DIRECTION('center_axis',(1.,0.,0.)) ;
#113402 = DIRECTION('ref_axis',(0.,0.,-1.)) ;
#113403 = DIRECTION('center_axis',(0.,-1.,0.)) ;
#113404 = DIRECTION('ref_axis',(0.,0.,-1.)) ;
#113405 = DIRECTION('',(0.,0.,1.)) ;
#113406 = DIRECTION('',(1.,0.,0.)) ;
#113407 = DIRECTION('',(0.,0.,-1.)) ;
#113408 = DIRECTION('center_axis',(1.,0.,0.)) ;
#113409 = DIRECTION('ref_axis',(0.,0.,-1.)) ;
#113410 = DIRECTION('center_axis',(-1.,0.,0.)) ;
#113411 = DIRECTION('ref_axis',(0.,0.,-1.)) ;
#113412 = DIRECTION('',(1.,0.,0.)) ;
#113413 = DIRECTION('center_axis',(1.,0.,0.)) ;
#113414 = DIRECTION('ref_axis',(0.,0.,-1.)) ;
#113415 = DIRECTION('center_axis',(1.,0.,0.)) ;
#113416 = DIRECTION('ref_axis',(0.,0.,-1.)) ;
#113417 = DIRECTION('center_axis',(1.,0.,0.)) ;
#113418 = DIRECTION('ref_axis',(0.,-7.85535158932894E-16,1.)) ;
#113419 = DIRECTION('',(1.,0.,0.)) ;
#113420 = DIRECTION('center_axis',(-1.,0.,0.)) ;
#113421 = DIRECTION('ref_axis',(0.,-7.85535158932894E-16,-1.)) ;
#113422 = DIRECTION('center_axis',(1.,0.,0.)) ;
#113423 = DIRECTION('ref_axis',(0.,0.,-1.)) ;
#113424 = DIRECTION('center_axis',(-1.,0.,0.)) ;
#113425 = DIRECTION('ref_axis',(0.,0.,-1.)) ;
#113426 = DIRECTION('',(1.,0.,0.)) ;
#113427 = DIRECTION('center_axis',(1.,0.,0.)) ;
#113428 = DIRECTION('ref_axis',(0.,0.,-1.)) ;
#113429 = DIRECTION('center_axis',(0.,-1.,0.)) ;
#113430 = DIRECTION('ref_axis',(0.,0.,-1.)) ;
#113431 = DIRECTION('',(0.,0.,1.)) ;
#113432 = DIRECTION('',(1.,0.,0.)) ;
#113433 = DIRECTION('',(0.,0.,-1.)) ;
#113434 = DIRECTION('center_axis',(1.,0.,0.)) ;
#113435 = DIRECTION('ref_axis',(0.,0.,-1.)) ;
#113436 = DIRECTION('center_axis',(-1.,0.,0.)) ;
#113437 = DIRECTION('ref_axis',(0.,0.,-1.)) ;
#113438 = DIRECTION('',(1.,0.,0.)) ;
#113439 = DIRECTION('center_axis',(1.,0.,0.)) ;
#113440 = DIRECTION('ref_axis',(0.,0.,-1.)) ;
#113441 = DIRECTION('center_axis',(0.,-1.07081696047951E-16,1.)) ;
#113442 = DIRECTION('ref_axis',(0.,-1.,-1.07081696047951E-16)) ;
#113443 = DIRECTION('',(0.,1.,1.07081696047951E-16)) ;
#113444 = DIRECTION('',(1.,0.,0.)) ;
#113445 = DIRECTION('',(0.,-1.,-1.07081696047951E-16)) ;
#113446 = DIRECTION('center_axis',(1.,0.,0.)) ;
#113447 = DIRECTION('ref_axis',(0.,0.,-1.)) ;
#113448 = DIRECTION('center_axis',(-1.,0.,0.)) ;
#113449 = DIRECTION('ref_axis',(0.,0.,-1.)) ;
#113450 = DIRECTION('',(1.,0.,0.)) ;
#113451 = DIRECTION('center_axis',(1.,0.,0.)) ;
#113452 = DIRECTION('ref_axis',(0.,0.,-1.)) ;
#113453 = DIRECTION('center_axis',(0.,1.,0.)) ;
#113454 = DIRECTION('ref_axis',(0.,0.,1.)) ;
#113455 = DIRECTION('',(0.,0.,-1.)) ;
#113456 = DIRECTION('',(0.,0.,1.)) ;
#113457 = DIRECTION('center_axis',(-1.,0.,0.)) ;
#113458 = DIRECTION('ref_axis',(0.,0.,1.)) ;
#113459 = DIRECTION('center_axis',(-1.,0.,0.)) ;
#113460 = DIRECTION('ref_axis',(0.,0.,1.)) ;
#113461 = DIRECTION('',(0.,-1.,0.)) ;
#113462 = DIRECTION('center_axis',(-1.,0.,0.)) ;
#113463 = DIRECTION('ref_axis',(0.,0.,1.)) ;
#113464 = DIRECTION('',(0.,0.,1.)) ;
#113465 = DIRECTION('',(0.,-1.,-1.07081696047951E-16)) ;
#113466 = DIRECTION('',(0.,0.,-1.)) ;
#113467 = DIRECTION('center_axis',(-1.,0.,0.)) ;
#113468 = DIRECTION('ref_axis',(0.,0.,1.)) ;
#113469 = DIRECTION('',(0.,0.,-1.)) ;
#113470 = DIRECTION('',(0.,1.,1.07081696047951E-16)) ;
#113471 = DIRECTION('',(0.,0.,1.)) ;
#113472 = DIRECTION('center_axis',(-1.,0.,0.)) ;
#113473 = DIRECTION('ref_axis',(0.,0.,1.)) ;
#113474 = DIRECTION('',(0.,1.,0.)) ;
#113475 = DIRECTION('center_axis',(-1.,0.,0.)) ;
#113476 = DIRECTION('ref_axis',(0.,0.,1.)) ;
#113477 = DIRECTION('',(0.,0.,-1.)) ;
#113478 = DIRECTION('',(0.,0.707106781186548,-0.707106781186547)) ;
#113479 = DIRECTION('',(0.,0.,1.)) ;
#113480 = DIRECTION('',(0.,-0.707106781186546,-0.707106781186549)) ;
#113481 = DIRECTION('',(0.,-3.99416362155027E-15,-1.)) ;
#113482 = DIRECTION('center_axis',(1.,0.,0.)) ;
#113483 = DIRECTION('ref_axis',(0.,0.,-1.)) ;
#113484 = DIRECTION('',(0.,-1.,0.)) ;
#113485 = DIRECTION('center_axis',(-1.,0.,0.)) ;
#113486 = DIRECTION('ref_axis',(0.,0.,-1.)) ;
#113487 = DIRECTION('',(0.,0.,-1.)) ;
#113488 = DIRECTION('center_axis',(-1.,0.,0.)) ;
#113489 = DIRECTION('ref_axis',(0.,1.0842021724855E-15,-1.)) ;
#113490 = DIRECTION('',(0.,-1.,0.)) ;
#113491 = DIRECTION('center_axis',(-1.,0.,0.)) ;
#113492 = DIRECTION('ref_axis',(0.,0.,-1.)) ;
#113493 = DIRECTION('',(0.,0.,1.)) ;
#113494 = DIRECTION('center_axis',(-1.,0.,0.)) ;
#113495 = DIRECTION('ref_axis',(0.,0.,-1.)) ;
#113496 = DIRECTION('center_axis',(1.,0.,0.)) ;
#113497 = DIRECTION('ref_axis',(0.,0.,-1.)) ;
#113498 = DIRECTION('',(0.,-1.,0.)) ;
#113499 = DIRECTION('center_axis',(-1.,0.,0.)) ;
#113500 = DIRECTION('ref_axis',(0.,0.,-1.)) ;
#113501 = DIRECTION('',(0.,0.,-1.)) ;
#113502 = DIRECTION('center_axis',(-1.,0.,0.)) ;
#113503 = DIRECTION('ref_axis',(0.,-1.62630325872827E-15,-1.)) ;
#113504 = DIRECTION('',(0.,-1.,0.)) ;
#113505 = DIRECTION('center_axis',(-1.,0.,0.)) ;
#113506 = DIRECTION('ref_axis',(0.,0.,-1.)) ;
#113507 = DIRECTION('',(0.,0.,1.)) ;
#113508 = DIRECTION('center_axis',(-1.,0.,0.)) ;
#113509 = DIRECTION('ref_axis',(0.,0.,-1.)) ;
#113510 = DIRECTION('center_axis',(1.,0.,0.)) ;
#113511 = DIRECTION('ref_axis',(0.,0.,-1.)) ;
#113512 = DIRECTION('',(0.,-1.,0.)) ;
#113513 = DIRECTION('center_axis',(-1.,0.,0.)) ;
#113514 = DIRECTION('ref_axis',(0.,0.,-1.)) ;
#113515 = DIRECTION('',(0.,0.,-1.)) ;
#113516 = DIRECTION('center_axis',(-1.,0.,0.)) ;
#113517 = DIRECTION('ref_axis',(0.,0.,-1.)) ;
#113518 = DIRECTION('',(0.,-1.,0.)) ;
#113519 = DIRECTION('center_axis',(-1.,0.,0.)) ;
#113520 = DIRECTION('ref_axis',(0.,0.,-1.)) ;
#113521 = DIRECTION('',(0.,0.,1.)) ;
#113522 = DIRECTION('center_axis',(-1.,0.,0.)) ;
#113523 = DIRECTION('ref_axis',(0.,0.,-1.)) ;
#113524 = DIRECTION('center_axis',(1.,0.,0.)) ;
#113525 = DIRECTION('ref_axis',(0.,0.,-1.)) ;
#113526 = DIRECTION('',(0.,-1.,0.)) ;
#113527 = DIRECTION('center_axis',(-1.,0.,0.)) ;
#113528 = DIRECTION('ref_axis',(0.,0.,-1.)) ;
#113529 = DIRECTION('',(0.,0.,-1.)) ;
#113530 = DIRECTION('center_axis',(-1.,0.,0.)) ;
#113531 = DIRECTION('ref_axis',(0.,-1.62630325872827E-15,-1.)) ;
#113532 = DIRECTION('',(0.,-1.,0.)) ;
#113533 = DIRECTION('center_axis',(-1.,0.,0.)) ;
#113534 = DIRECTION('ref_axis',(0.,0.,-1.)) ;
#113535 = DIRECTION('',(0.,0.,1.)) ;
#113536 = DIRECTION('center_axis',(-1.,0.,0.)) ;
#113537 = DIRECTION('ref_axis',(0.,0.,-1.)) ;
#113538 = DIRECTION('center_axis',(1.,0.,0.)) ;
#113539 = DIRECTION('ref_axis',(0.,0.,-1.)) ;
#113540 = DIRECTION('',(0.,-1.,0.)) ;
#113541 = DIRECTION('center_axis',(-1.,0.,0.)) ;
#113542 = DIRECTION('ref_axis',(0.,0.,-1.)) ;
#113543 = DIRECTION('',(0.,0.,-1.)) ;
#113544 = DIRECTION('center_axis',(-1.,0.,0.)) ;
#113545 = DIRECTION('ref_axis',(0.,0.,-1.)) ;
#113546 = DIRECTION('',(0.,-1.,0.)) ;
#113547 = DIRECTION('center_axis',(-1.,0.,0.)) ;
#113548 = DIRECTION('ref_axis',(0.,0.,-1.)) ;
#113549 = DIRECTION('',(0.,0.,1.)) ;
#113550 = DIRECTION('center_axis',(-1.,0.,0.)) ;
#113551 = DIRECTION('ref_axis',(0.,0.,-1.)) ;
#113552 = DIRECTION('center_axis',(1.,0.,0.)) ;
#113553 = DIRECTION('ref_axis',(0.,0.,-1.)) ;
#113554 = DIRECTION('',(0.,-1.,0.)) ;
#113555 = DIRECTION('center_axis',(-1.,0.,0.)) ;
#113556 = DIRECTION('ref_axis',(0.,0.,-1.)) ;
#113557 = DIRECTION('',(0.,0.,-1.)) ;
#113558 = DIRECTION('center_axis',(-1.,0.,0.)) ;
#113559 = DIRECTION('ref_axis',(0.,0.,-1.)) ;
#113560 = DIRECTION('',(0.,-1.,0.)) ;
#113561 = DIRECTION('center_axis',(-1.,0.,0.)) ;
#113562 = DIRECTION('ref_axis',(0.,0.,-1.)) ;
#113563 = DIRECTION('',(0.,0.,1.)) ;
#113564 = DIRECTION('center_axis',(-1.,0.,0.)) ;
#113565 = DIRECTION('ref_axis',(0.,0.,-1.)) ;
#113566 = DIRECTION('center_axis',(1.,0.,0.)) ;
#113567 = DIRECTION('ref_axis',(0.,0.,-1.)) ;
#113568 = DIRECTION('',(0.,-1.,0.)) ;
#113569 = DIRECTION('center_axis',(-1.,0.,0.)) ;
#113570 = DIRECTION('ref_axis',(0.,0.,-1.)) ;
#113571 = DIRECTION('',(0.,0.,-1.)) ;
#113572 = DIRECTION('center_axis',(-1.,0.,0.)) ;
#113573 = DIRECTION('ref_axis',(0.,0.,-1.)) ;
#113574 = DIRECTION('',(0.,-1.,0.)) ;
#113575 = DIRECTION('center_axis',(-1.,0.,0.)) ;
#113576 = DIRECTION('ref_axis',(0.,0.,-1.)) ;
#113577 = DIRECTION('',(0.,0.,1.)) ;
#113578 = DIRECTION('center_axis',(-1.,0.,0.)) ;
#113579 = DIRECTION('ref_axis',(0.,0.,-1.)) ;
#113580 = DIRECTION('center_axis',(1.,0.,0.)) ;
#113581 = DIRECTION('ref_axis',(0.,0.,-1.)) ;
#113582 = DIRECTION('',(0.,-1.,0.)) ;
#113583 = DIRECTION('center_axis',(-1.,0.,0.)) ;
#113584 = DIRECTION('ref_axis',(0.,0.,-1.)) ;
#113585 = DIRECTION('',(0.,0.,-1.)) ;
#113586 = DIRECTION('center_axis',(-1.,0.,0.)) ;
#113587 = DIRECTION('ref_axis',(0.,0.,-1.)) ;
#113588 = DIRECTION('',(0.,-1.,0.)) ;
#113589 = DIRECTION('center_axis',(-1.,0.,0.)) ;
#113590 = DIRECTION('ref_axis',(0.,0.,-1.)) ;
#113591 = DIRECTION('',(0.,0.,1.)) ;
#113592 = DIRECTION('center_axis',(-1.,0.,0.)) ;
#113593 = DIRECTION('ref_axis',(0.,0.,-1.)) ;
#113594 = DIRECTION('center_axis',(1.,0.,0.)) ;
#113595 = DIRECTION('ref_axis',(0.,0.,-1.)) ;
#113596 = DIRECTION('',(0.,-1.,0.)) ;
#113597 = DIRECTION('center_axis',(-1.,0.,0.)) ;
#113598 = DIRECTION('ref_axis',(0.,0.,-1.)) ;
#113599 = DIRECTION('',(0.,0.,-1.)) ;
#113600 = DIRECTION('center_axis',(-1.,0.,0.)) ;
#113601 = DIRECTION('ref_axis',(0.,0.,-1.)) ;
#113602 = DIRECTION('',(0.,-1.,0.)) ;
#113603 = DIRECTION('center_axis',(-1.,0.,0.)) ;
#113604 = DIRECTION('ref_axis',(0.,0.,-1.)) ;
#113605 = DIRECTION('',(0.,0.,1.)) ;
#113606 = DIRECTION('center_axis',(-1.,0.,0.)) ;
#113607 = DIRECTION('ref_axis',(0.,0.,-1.)) ;
#113608 = DIRECTION('center_axis',(1.53063836115601E-16,-1.,-1.30104260698261E-16)) ;
#113609 = DIRECTION('ref_axis',(1.,1.53063836115601E-16,1.99142572374599E-32)) ;
#113610 = DIRECTION('center_axis',(0.,1.,0.)) ;
#113611 = DIRECTION('ref_axis',(0.,0.,1.)) ;
#113612 = DIRECTION('center_axis',(0.,-1.,0.)) ;
#113613 = DIRECTION('ref_axis',(0.,0.,-1.)) ;
#113614 = DIRECTION('center_axis',(1.,1.53063836115601E-16,2.73691106313441E-48)) ;
#113615 = DIRECTION('ref_axis',(-1.53063836115601E-16,1.,-4.18922106430579E-64)) ;
#113616 = DIRECTION('center_axis',(-1.,0.,0.)) ;
#113617 = DIRECTION('ref_axis',(0.,0.,1.)) ;
#113618 = DIRECTION('center_axis',(1.,1.53063836115601E-16,0.)) ;
#113619 = DIRECTION('ref_axis',(1.53063836115601E-16,-1.,0.)) ;
#113620 = DIRECTION('center_axis',(0.,1.,0.)) ;
#113621 = DIRECTION('ref_axis',(1.,0.,0.)) ;
#113622 = DIRECTION('center_axis',(0.,1.,0.)) ;
#113623 = DIRECTION('ref_axis',(0.,0.,-1.)) ;
#113624 = DIRECTION('center_axis',(0.,0.,1.)) ;
#113625 = DIRECTION('ref_axis',(-1.,0.,0.)) ;
#113626 = DIRECTION('center_axis',(0.,1.,0.)) ;
#113627 = DIRECTION('ref_axis',(1.,0.,0.)) ;
#113628 = DIRECTION('center_axis',(0.,0.,1.)) ;
#113629 = DIRECTION('ref_axis',(-1.,0.,0.)) ;
#113630 = DIRECTION('center_axis',(1.,1.0842021724855E-15,0.)) ;
#113631 = DIRECTION('ref_axis',(1.0842021724855E-15,-1.,0.)) ;
#113632 = DIRECTION('center_axis',(-1.,-1.53063836115601E-16,0.)) ;
#113633 = DIRECTION('ref_axis',(0.,-1.,0.)) ;
#113634 = DIRECTION('center_axis',(0.,0.,-1.)) ;
#113635 = DIRECTION('ref_axis',(1.,0.,0.)) ;
#113636 = DIRECTION('center_axis',(0.,0.,-1.)) ;
#113637 = DIRECTION('ref_axis',(0.804034447892617,0.594582716366709,0.)) ;
#113638 = DIRECTION('center_axis',(0.,0.,1.)) ;
#113639 = DIRECTION('ref_axis',(1.,0.,0.)) ;
#113640 = DIRECTION('',(0.,0.,-1.)) ;
#113641 = DIRECTION('center_axis',(-2.16840434497101E-16,1.,1.30104260698261E-16)) ;
#113642 = DIRECTION('ref_axis',(1.,2.16840434497101E-16,1.22464679914735E-16)) ;
#113643 = DIRECTION('',(-2.16840434497101E-16,1.,1.30104260698261E-16)) ;
#113644 = DIRECTION('center_axis',(0.,1.,0.)) ;
#113645 = DIRECTION('ref_axis',(0.,0.,1.)) ;
#113646 = DIRECTION('center_axis',(-1.,-1.53063836115601E-16,-2.73691106313441E-48)) ;
#113647 = DIRECTION('ref_axis',(1.53063836115601E-16,-1.,4.18922106430579E-64)) ;
#113648 = DIRECTION('center_axis',(1.,2.16840434497101E-16,0.)) ;
#113649 = DIRECTION('ref_axis',(2.16840434497101E-16,-1.,0.)) ;
#113650 = DIRECTION('center_axis',(0.,0.,1.)) ;
#113651 = DIRECTION('ref_axis',(1.,0.,0.)) ;
#113652 = DIRECTION('center_axis',(-1.25542992828747E-32,1.020425574104E-16,
1.)) ;
#113653 = DIRECTION('ref_axis',(-1.28107280532009E-48,-1.,1.020425574104E-16)) ;
#113654 = DIRECTION('center_axis',(0.,0.,1.)) ;
#113655 = DIRECTION('ref_axis',(1.,0.,0.)) ;
#113656 = DIRECTION('center_axis',(0.,0.,-1.)) ;
#113657 = DIRECTION('ref_axis',(-1.,0.,0.)) ;
#113658 = DIRECTION('center_axis',(1.,1.53063836115601E-16,-2.73691106313441E-48)) ;
#113659 = DIRECTION('ref_axis',(-1.53063836115601E-16,1.,4.18922106430579E-64)) ;
#113660 = DIRECTION('center_axis',(-1.,0.,0.)) ;
#113661 = DIRECTION('ref_axis',(0.,0.,1.)) ;
#113662 = DIRECTION('center_axis',(1.,1.53063836115601E-16,0.)) ;
#113663 = DIRECTION('ref_axis',(1.53063836115601E-16,-1.,0.)) ;
#113664 = DIRECTION('center_axis',(0.,1.,0.)) ;
#113665 = DIRECTION('ref_axis',(1.,0.,0.)) ;
#113666 = DIRECTION('center_axis',(-1.,-2.16840434497101E-16,0.)) ;
#113667 = DIRECTION('ref_axis',(0.,-1.,0.)) ;
#113668 = DIRECTION('center_axis',(0.,0.,-1.)) ;
#113669 = DIRECTION('ref_axis',(1.,0.,0.)) ;
#113670 = DIRECTION('center_axis',(-1.25542992828747E-32,1.020425574104E-16,
1.)) ;
#113671 = DIRECTION('ref_axis',(0.,-1.,0.)) ;
#113672 = DIRECTION('center_axis',(0.,-1.,0.)) ;
#113673 = DIRECTION('ref_axis',(-6.50521303491304E-15,0.,1.)) ;
#113674 = DIRECTION('center_axis',(-1.,0.,0.)) ;
#113675 = DIRECTION('ref_axis',(0.,0.,-1.)) ;
#113676 = DIRECTION('center_axis',(-1.,-1.53063836115601E-16,0.)) ;
#113677 = DIRECTION('ref_axis',(0.,-1.,0.)) ;
#113678 = DIRECTION('center_axis',(0.,-1.,0.)) ;
#113679 = DIRECTION('ref_axis',(0.,0.,1.)) ;
#113680 = DIRECTION('center_axis',(0.,0.,-1.)) ;
#113681 = DIRECTION('ref_axis',(-1.,0.,0.)) ;
#113682 = DIRECTION('center_axis',(-4.33680868994202E-15,0.,-1.)) ;
#113683 = DIRECTION('ref_axis',(-1.,0.,4.33680868994202E-15)) ;
#113684 = DIRECTION('center_axis',(1.,1.53063836115601E-16,-3.06472600140763E-33)) ;
#113685 = DIRECTION('ref_axis',(-1.53063836115601E-16,1.,4.69098718418678E-49)) ;
#113686 = DIRECTION('center_axis',(-1.,0.,0.)) ;
#113687 = DIRECTION('ref_axis',(0.,0.,1.)) ;
#113688 = DIRECTION('center_axis',(-1.53063836115601E-16,1.,-1.020425574104E-16)) ;
#113689 = DIRECTION('ref_axis',(-1.,-1.53063836115601E-16,1.3684555315672E-47)) ;
#113690 = DIRECTION('',(1.53063836115601E-16,-1.,1.020425574104E-16)) ;
#113691 = DIRECTION('center_axis',(0.,-1.,0.)) ;
#113692 = DIRECTION('ref_axis',(0.,0.,-1.)) ;
#113693 = DIRECTION('center_axis',(-1.53063836115601E-16,1.,-1.30104260698261E-16)) ;
#113694 = DIRECTION('ref_axis',(-1.,-1.53063836115601E-16,1.99142572374599E-32)) ;
#113695 = DIRECTION('center_axis',(0.,-1.,0.)) ;
#113696 = DIRECTION('ref_axis',(0.,0.,-1.)) ;
#113697 = DIRECTION('center_axis',(-1.,-1.53063836115601E-16,2.73691106313441E-48)) ;
#113698 = DIRECTION('ref_axis',(1.53063836115601E-16,-1.,-4.18922106430579E-64)) ;
#113699 = DIRECTION('center_axis',(1.,2.16840434497101E-16,0.)) ;
#113700 = DIRECTION('ref_axis',(2.16840434497101E-16,-1.,0.)) ;
#113701 = DIRECTION('center_axis',(-1.,0.,2.168404344971E-15)) ;
#113702 = DIRECTION('ref_axis',(2.168404344971E-15,0.,1.)) ;
#113703 = DIRECTION('center_axis',(-1.,-2.16840434497101E-16,0.)) ;
#113704 = DIRECTION('ref_axis',(0.,-1.,0.)) ;
#113705 = DIRECTION('center_axis',(0.,0.,1.)) ;
#113706 = DIRECTION('ref_axis',(-1.,0.,0.)) ;
#113707 = DIRECTION('center_axis',(0.,1.,0.)) ;
#113708 = DIRECTION('ref_axis',(1.,0.,0.)) ;
#113709 = DIRECTION('center_axis',(0.,1.,0.)) ;
#113710 = DIRECTION('ref_axis',(0.,0.,-1.)) ;
#113711 = DIRECTION('center_axis',(1.,0.,0.)) ;
#113712 = DIRECTION('ref_axis',(0.,-1.,0.)) ;
#113713 = DIRECTION('center_axis',(1.,6.50521303491304E-15,0.)) ;
#113714 = DIRECTION('ref_axis',(-6.50521303491304E-15,1.,0.)) ;
#113715 = DIRECTION('center_axis',(8.67361737988403E-15,1.,0.)) ;
#113716 = DIRECTION('ref_axis',(-1.,8.67361737988403E-15,0.)) ;
#113717 = DIRECTION('center_axis',(1.2303003375722E-16,-1.,1.020425574104E-16)) ;
#113718 = DIRECTION('ref_axis',(1.,1.2303003375722E-16,-1.25542992828747E-32)) ;
#113719 = DIRECTION('center_axis',(0.,1.,0.)) ;
#113720 = DIRECTION('ref_axis',(0.,0.,1.)) ;
#113721 = DIRECTION('center_axis',(0.,1.,0.)) ;
#113722 = DIRECTION('ref_axis',(1.,0.,0.)) ;
#113723 = DIRECTION('center_axis',(1.,1.2303003375722E-16,0.)) ;
#113724 = DIRECTION('ref_axis',(1.2303003375722E-16,-1.,0.)) ;
#113725 = DIRECTION('center_axis',(0.,0.,1.)) ;
#113726 = DIRECTION('ref_axis',(-1.,0.,0.)) ;
#113727 = DIRECTION('center_axis',(0.,1.,0.)) ;
#113728 = DIRECTION('ref_axis',(1.,0.,0.)) ;
#113729 = DIRECTION('center_axis',(0.,0.,-1.)) ;
#113730 = DIRECTION('ref_axis',(1.,0.,0.)) ;
#113731 = DIRECTION('center_axis',(0.,0.,-1.)) ;
#113732 = DIRECTION('ref_axis',(-1.,0.,0.)) ;
#113733 = DIRECTION('center_axis',(0.,0.,1.)) ;
#113734 = DIRECTION('ref_axis',(1.,0.,0.)) ;
#113735 = DIRECTION('center_axis',(-2.16840434497101E-16,1.,-1.020425574104E-16)) ;
#113736 = DIRECTION('ref_axis',(-1.,-2.16840434497101E-16,5.47382212626882E-48)) ;
#113737 = DIRECTION('center_axis',(0.,1.,0.)) ;
#113738 = DIRECTION('ref_axis',(0.,0.,-1.)) ;
#113739 = DIRECTION('center_axis',(1.,0.,1.25542992828747E-32)) ;
#113740 = DIRECTION('ref_axis',(1.25542992828747E-32,0.,-1.)) ;
#113741 = DIRECTION('center_axis',(1.,0.,0.)) ;
#113742 = DIRECTION('ref_axis',(0.,0.,-1.)) ;
#113743 = DIRECTION('center_axis',(-1.,-1.2303003375722E-16,0.)) ;
#113744 = DIRECTION('ref_axis',(0.,-1.,0.)) ;
#113745 = DIRECTION('center_axis',(0.,0.,-1.)) ;
#113746 = DIRECTION('ref_axis',(1.,0.,0.)) ;
#113747 = DIRECTION('center_axis',(0.,0.,-1.)) ;
#113748 = DIRECTION('ref_axis',(-1.,0.,0.)) ;
#113749 = DIRECTION('',(0.,0.,1.)) ;
#113750 = DIRECTION('center_axis',(0.,0.,1.)) ;
#113751 = DIRECTION('ref_axis',(1.,0.,0.)) ;
#113752 = DIRECTION('center_axis',(0.,0.,1.)) ;
#113753 = DIRECTION('ref_axis',(1.,0.,0.)) ;
#113754 = DIRECTION('center_axis',(6.27714964143733E-33,-5.10212787052002E-17,
-1.)) ;
#113755 = DIRECTION('ref_axis',(3.20268201330022E-49,1.,-5.10212787052002E-17)) ;
#113756 = DIRECTION('center_axis',(1.,1.53063836115601E-16,-1.53236300070382E-33)) ;
#113757 = DIRECTION('ref_axis',(-1.53063836115601E-16,1.,2.34549359209339E-49)) ;
#113758 = DIRECTION('center_axis',(-1.,0.,0.)) ;
#113759 = DIRECTION('ref_axis',(0.,0.,1.)) ;
#113760 = DIRECTION('center_axis',(1.,0.,0.)) ;
#113761 = DIRECTION('ref_axis',(0.,0.,-1.)) ;
#113762 = DIRECTION('center_axis',(0.,1.,0.)) ;
#113763 = DIRECTION('ref_axis',(1.,0.,0.)) ;
#113764 = DIRECTION('center_axis',(-4.33680868994202E-15,1.,0.)) ;
#113765 = DIRECTION('ref_axis',(1.,4.33680868994202E-15,0.)) ;
#113766 = DIRECTION('center_axis',(0.,-1.,0.)) ;
#113767 = DIRECTION('ref_axis',(0.,0.,-1.)) ;
#113768 = DIRECTION('center_axis',(0.,0.,-1.)) ;
#113769 = DIRECTION('ref_axis',(1.,0.,0.)) ;
#113770 = DIRECTION('center_axis',(0.,0.,1.)) ;
#113771 = DIRECTION('ref_axis',(1.,0.,0.)) ;
#113772 = DIRECTION('center_axis',(0.,0.,-1.)) ;
#113773 = DIRECTION('ref_axis',(-1.,0.,0.)) ;
#113774 = DIRECTION('center_axis',(0.,1.,0.)) ;
#113775 = DIRECTION('ref_axis',(1.,0.,0.)) ;
#113776 = DIRECTION('center_axis',(1.,1.2303003375722E-16,0.)) ;
#113777 = DIRECTION('ref_axis',(1.2303003375722E-16,-1.,0.)) ;
#113778 = DIRECTION('center_axis',(0.,1.,0.)) ;
#113779 = DIRECTION('ref_axis',(-6.50521303491301E-15,0.,-1.)) ;
#113780 = DIRECTION('center_axis',(6.27714964143733E-33,-5.10212787052002E-17,
-1.)) ;
#113781 = DIRECTION('ref_axis',(0.,1.,0.)) ;
#113782 = DIRECTION('center_axis',(0.,-1.,0.)) ;
#113783 = DIRECTION('ref_axis',(0.,0.,1.)) ;
#113784 = DIRECTION('center_axis',(2.16840434497101E-16,-1.,5.10212787052002E-17)) ;
#113785 = DIRECTION('ref_axis',(1.,2.16840434497101E-16,-5.47382212626882E-48)) ;
#113786 = DIRECTION('center_axis',(0.,1.,0.)) ;
#113787 = DIRECTION('ref_axis',(0.,0.,-1.)) ;
#113788 = DIRECTION('center_axis',(0.,0.,1.)) ;
#113789 = DIRECTION('ref_axis',(1.,0.,0.)) ;
#113790 = DIRECTION('center_axis',(0.,0.,-1.)) ;
#113791 = DIRECTION('ref_axis',(-1.,0.,0.)) ;
#113792 = DIRECTION('center_axis',(-1.,-1.2303003375722E-16,0.)) ;
#113793 = DIRECTION('ref_axis',(0.,-1.,0.)) ;
#113794 = DIRECTION('center_axis',(0.,-1.,0.)) ;
#113795 = DIRECTION('ref_axis',(0.,0.,1.)) ;
#113796 = DIRECTION('center_axis',(1.53063836115601E-16,-1.,5.10212787052002E-17)) ;
#113797 = DIRECTION('ref_axis',(1.,1.53063836115601E-16,-6.84227765783602E-48)) ;
#113798 = DIRECTION('',(-1.53063836115601E-16,1.,-5.10212787052002E-17)) ;
#113799 = DIRECTION('center_axis',(0.,-1.,0.)) ;
#113800 = DIRECTION('ref_axis',(0.,0.,-1.)) ;
#113801 = DIRECTION('center_axis',(-1.,0.,0.)) ;
#113802 = DIRECTION('ref_axis',(0.,0.,-1.)) ;
#113803 = DIRECTION('center_axis',(-1.2303003375722E-16,1.,-5.10212787052002E-17)) ;
#113804 = DIRECTION('ref_axis',(-1.,-1.2303003375722E-16,6.27714964143733E-33)) ;
#113805 = DIRECTION('center_axis',(-8.67361737988403E-15,-1.,0.)) ;
#113806 = DIRECTION('ref_axis',(1.,-8.67361737988403E-15,0.)) ;
#113807 = DIRECTION('center_axis',(1.,0.,6.27714964143733E-33)) ;
#113808 = DIRECTION('ref_axis',(6.27714964143733E-33,0.,-1.)) ;
#113809 = DIRECTION('center_axis',(-1.,0.,-6.50521303491318E-15)) ;
#113810 = DIRECTION('ref_axis',(-6.50521303491318E-15,0.,1.)) ;
#113811 = DIRECTION('center_axis',(1.,0.,0.)) ;
#113812 = DIRECTION('ref_axis',(0.,1.,0.)) ;
#113813 = DIRECTION('center_axis',(0.,0.,-1.)) ;
#113814 = DIRECTION('ref_axis',(-1.,0.,0.)) ;
#113815 = DIRECTION('center_axis',(0.,0.,1.)) ;
#113816 = DIRECTION('ref_axis',(1.,0.,0.)) ;
#113817 = DIRECTION('center_axis',(0.,0.,-1.)) ;
#113818 = DIRECTION('ref_axis',(-1.,0.,0.)) ;
#113819 = DIRECTION('center_axis',(-1.,0.,0.)) ;
#113820 = DIRECTION('ref_axis',(0.,0.,1.)) ;
#113821 = DIRECTION('center_axis',(0.,-1.,0.)) ;
#113822 = DIRECTION('ref_axis',(0.,0.,-1.)) ;
#113823 = DIRECTION('center_axis',(0.,1.,0.)) ;
#113824 = DIRECTION('ref_axis',(0.,0.,1.)) ;
#113825 = DIRECTION('center_axis',(0.,1.,-6.50521303491301E-15)) ;
#113826 = DIRECTION('ref_axis',(0.,6.50521303491301E-15,1.)) ;
#113827 = DIRECTION('center_axis',(0.,-1.,0.)) ;
#113828 = DIRECTION('ref_axis',(0.,0.,-1.)) ;
#113829 = DIRECTION('center_axis',(0.,-1.,0.)) ;
#113830 = DIRECTION('ref_axis',(0.,0.,-1.)) ;
#113831 = DIRECTION('center_axis',(0.,-1.,-1.07081696047951E-16)) ;
#113832 = DIRECTION('ref_axis',(0.,1.07081696047951E-16,-1.)) ;
#113833 = DIRECTION('center_axis',(0.,1.,0.)) ;
#113834 = DIRECTION('ref_axis',(0.,0.,1.)) ;
#113835 = DIRECTION('center_axis',(-1.,0.,0.)) ;
#113836 = DIRECTION('ref_axis',(0.,0.,1.)) ;
#113837 = DIRECTION('center_axis',(0.,0.,1.)) ;
#113838 = DIRECTION('ref_axis',(1.,0.,0.)) ;
#113839 = DIRECTION('center_axis',(0.,1.,0.)) ;
#113840 = DIRECTION('ref_axis',(0.,0.,1.)) ;
#113841 = DIRECTION('center_axis',(0.,0.,-1.)) ;
#113842 = DIRECTION('ref_axis',(-1.,0.,0.)) ;
#113843 = DIRECTION('center_axis',(0.,0.,1.)) ;
#113844 = DIRECTION('ref_axis',(1.,0.,0.)) ;
#113845 = DIRECTION('center_axis',(0.,0.,1.)) ;
#113846 = DIRECTION('ref_axis',(1.,0.,0.)) ;
#113847 = DIRECTION('center_axis',(0.,0.,1.)) ;
#113848 = DIRECTION('ref_axis',(1.,0.,0.)) ;
#113849 = DIRECTION('center_axis',(0.,0.,-1.)) ;
#113850 = DIRECTION('ref_axis',(-1.,0.,0.)) ;
#113851 = DIRECTION('center_axis',(0.,1.,0.)) ;
#113852 = DIRECTION('ref_axis',(0.,0.,1.)) ;
#113853 = DIRECTION('center_axis',(0.,-0.707106781186545,0.70710678118655)) ;
#113854 = DIRECTION('ref_axis',(0.,-0.70710678118655,-0.707106781186545)) ;
#113855 = DIRECTION('center_axis',(0.,1.,0.)) ;
#113856 = DIRECTION('ref_axis',(0.,0.,1.)) ;
#113857 = DIRECTION('center_axis',(0.,-0.514231796959101,-0.857651245551602)) ;
#113858 = DIRECTION('ref_axis',(0.,0.857651245551602,-0.514231796959101)) ;
#113859 = DIRECTION('center_axis',(0.,-0.707106781186548,0.707106781186547)) ;
#113860 = DIRECTION('ref_axis',(0.,-0.707106781186547,-0.707106781186548)) ;
#113861 = DIRECTION('center_axis',(0.,-0.707106781186552,0.707106781186543)) ;
#113862 = DIRECTION('ref_axis',(0.,-0.707106781186543,-0.707106781186552)) ;
#113863 = DIRECTION('center_axis',(-1.,0.,0.)) ;
#113864 = DIRECTION('ref_axis',(0.,0.,1.)) ;
#113865 = DIRECTION('center_axis',(0.,0.514231796959101,-0.857651245551602)) ;
#113866 = DIRECTION('ref_axis',(0.,0.857651245551602,0.514231796959101)) ;
#113867 = DIRECTION('center_axis',(0.,1.,0.)) ;
#113868 = DIRECTION('ref_axis',(0.,0.,1.)) ;
#113869 = DIRECTION('center_axis',(0.,0.,-1.)) ;
#113870 = DIRECTION('ref_axis',(-1.,0.,0.)) ;
#113871 = DIRECTION('center_axis',(0.,1.,0.)) ;
#113872 = DIRECTION('ref_axis',(0.,0.,1.)) ;
#113873 = DIRECTION('center_axis',(0.,0.,-1.)) ;
#113874 = DIRECTION('ref_axis',(-1.,0.,0.)) ;
#113875 = DIRECTION('center_axis',(0.,0.,-1.)) ;
#113876 = DIRECTION('ref_axis',(-1.,0.,0.)) ;
#113877 = DIRECTION('center_axis',(0.,0.,1.)) ;
#113878 = DIRECTION('ref_axis',(1.,0.,0.)) ;
#113879 = DIRECTION('center_axis',(0.,0.,-1.)) ;
#113880 = DIRECTION('ref_axis',(-1.,0.,0.)) ;
#113881 = DIRECTION('center_axis',(0.,1.,0.)) ;
#113882 = DIRECTION('ref_axis',(0.,0.,1.)) ;
#113883 = DIRECTION('center_axis',(0.,-1.,8.67361737988405E-15)) ;
#113884 = DIRECTION('ref_axis',(0.,-8.67361737988405E-15,-1.)) ;
#113885 = DIRECTION('center_axis',(0.,0.707106781186546,0.707106781186549)) ;
#113886 = DIRECTION('ref_axis',(0.,-0.707106781186549,0.707106781186546)) ;
#113887 = DIRECTION('center_axis',(0.,0.707106781186545,0.70710678118655)) ;
#113888 = DIRECTION('ref_axis',(0.,-0.70710678118655,0.707106781186545)) ;
#113889 = DIRECTION('center_axis',(0.,1.,1.07081696047951E-16)) ;
#113890 = DIRECTION('ref_axis',(0.,-1.07081696047951E-16,1.)) ;
#113891 = DIRECTION('center_axis',(0.,-1.,0.)) ;
#113892 = DIRECTION('ref_axis',(0.,0.,-1.)) ;
#113893 = DIRECTION('center_axis',(0.,1.,0.)) ;
#113894 = DIRECTION('ref_axis',(0.,0.,1.)) ;
#113895 = DIRECTION('center_axis',(0.,0.,1.)) ;
#113896 = DIRECTION('ref_axis',(1.,0.,0.)) ;
#113897 = DIRECTION('center_axis',(0.,1.,0.)) ;
#113898 = DIRECTION('ref_axis',(0.,0.,1.)) ;
#113899 = DIRECTION('center_axis',(0.,8.67361737988403E-15,1.)) ;
#113900 = DIRECTION('ref_axis',(0.,-1.,8.67361737988403E-15)) ;
#113901 = DIRECTION('center_axis',(0.,3.99416362155027E-15,1.)) ;
#113902 = DIRECTION('ref_axis',(0.,-1.,3.99416362155027E-15)) ;
#113903 = DIRECTION('center_axis',(0.,0.,1.)) ;
#113904 = DIRECTION('ref_axis',(1.,0.,0.)) ;
#113905 = DIRECTION('center_axis',(0.,0.,-1.)) ;
#113906 = DIRECTION('ref_axis',(-1.,0.,0.)) ;
#113907 = DIRECTION('center_axis',(0.,0.,1.)) ;
#113908 = DIRECTION('ref_axis',(1.,0.,0.)) ;
#113909 = DIRECTION('center_axis',(-1.,0.,0.)) ;
#113910 = DIRECTION('ref_axis',(0.,0.,1.)) ;
#113911 = DIRECTION('center_axis',(0.,1.,0.)) ;
#113912 = DIRECTION('ref_axis',(0.,0.,1.)) ;
#113913 = DIRECTION('center_axis',(-1.,0.,0.)) ;
#113914 = DIRECTION('ref_axis',(0.,0.,1.)) ;
#113915 = DIRECTION('center_axis',(0.,-1.,0.)) ;
#113916 = DIRECTION('ref_axis',(0.,0.,-1.)) ;
#113917 = DIRECTION('center_axis',(0.,1.,0.)) ;
#113918 = DIRECTION('ref_axis',(0.,0.,1.)) ;
#113919 = DIRECTION('center_axis',(0.,-1.,0.)) ;
#113920 = DIRECTION('ref_axis',(0.,0.,-1.)) ;
#113921 = DIRECTION('center_axis',(0.,1.,0.)) ;
#113922 = DIRECTION('ref_axis',(0.,0.,1.)) ;
#113923 = DIRECTION('center_axis',(0.,-1.,0.)) ;
#113924 = DIRECTION('ref_axis',(0.,0.,-1.)) ;
#113925 = DIRECTION('center_axis',(0.,1.,0.)) ;
#113926 = DIRECTION('ref_axis',(0.,0.,-1.)) ;
#113927 = DIRECTION('center_axis',(0.,0.,-1.)) ;
#113928 = DIRECTION('ref_axis',(-1.,0.,0.)) ;
#113929 = DIRECTION('center_axis',(0.,1.,0.)) ;
#113930 = DIRECTION('ref_axis',(0.,0.,-1.)) ;
#113931 = DIRECTION('center_axis',(0.,0.,-1.)) ;
#113932 = DIRECTION('ref_axis',(-1.,0.,0.)) ;
#113933 = DIRECTION('center_axis',(0.,0.,1.)) ;
#113934 = DIRECTION('ref_axis',(1.,0.,0.)) ;
#113935 = DIRECTION('center_axis',(0.,0.,-1.)) ;
#113936 = DIRECTION('ref_axis',(-1.,0.,0.)) ;
#113937 = DIRECTION('center_axis',(0.,0.,-1.)) ;
#113938 = DIRECTION('ref_axis',(-1.,0.,0.)) ;
#113939 = DIRECTION('center_axis',(0.,6.93889390390724E-14,-1.)) ;
#113940 = DIRECTION('ref_axis',(0.,1.,6.93889390390724E-14)) ;
#113941 = DIRECTION('center_axis',(1.,0.,0.)) ;
#113942 = DIRECTION('ref_axis',(0.,0.,-1.)) ;
#113943 = DIRECTION('center_axis',(3.0665868333667E-15,0.707106781186532,
-0.707106781186563)) ;
#113944 = DIRECTION('ref_axis',(-5.39294103027656E-31,0.707106781186563,0.707106781186532)) ;
#113945 = DIRECTION('center_axis',(1.,0.,0.)) ;
#113946 = DIRECTION('ref_axis',(0.,0.,-1.)) ;
#113947 = DIRECTION('center_axis',(0.,-1.,0.)) ;
#113948 = DIRECTION('ref_axis',(0.,0.,-1.)) ;
#113949 = DIRECTION('center_axis',(0.,-0.707106781186548,0.707106781186547)) ;
#113950 = DIRECTION('ref_axis',(0.,-0.707106781186547,-0.707106781186548)) ;
#113951 = DIRECTION('center_axis',(0.,-1.,-1.07081696047951E-16)) ;
#113952 = DIRECTION('ref_axis',(0.,1.07081696047951E-16,-1.)) ;
#113953 = DIRECTION('center_axis',(0.,-1.,-8.67361737988379E-15)) ;
#113954 = DIRECTION('ref_axis',(0.,8.67361737988379E-15,-1.)) ;
#113955 = DIRECTION('center_axis',(1.,0.,0.)) ;
#113956 = DIRECTION('ref_axis',(0.,0.,-1.)) ;
#113957 = DIRECTION('center_axis',(0.,0.,1.)) ;
#113958 = DIRECTION('ref_axis',(1.,0.,0.)) ;
#113959 = DIRECTION('center_axis',(0.,0.,-1.)) ;
#113960 = DIRECTION('ref_axis',(-1.,0.,0.)) ;
#113961 = DIRECTION('center_axis',(0.,0.,1.)) ;
#113962 = DIRECTION('ref_axis',(1.,0.,0.)) ;
#113963 = DIRECTION('center_axis',(0.,0.,1.)) ;
#113964 = DIRECTION('ref_axis',(1.,0.,0.)) ;
#113965 = DIRECTION('center_axis',(0.,0.,1.)) ;
#113966 = DIRECTION('ref_axis',(1.,0.,0.)) ;
#113967 = DIRECTION('center_axis',(1.,0.,0.)) ;
#113968 = DIRECTION('ref_axis',(0.,0.382683432365085,0.923879532511289)) ;
#113969 = DIRECTION('center_axis',(-3.0665868333667E-15,-0.707106781186532,
-0.707106781186563)) ;
#113970 = DIRECTION('ref_axis',(-5.39294103027656E-31,0.707106781186563,-0.707106781186532)) ;
#113971 = DIRECTION('center_axis',(1.,0.,0.)) ;
#113972 = DIRECTION('ref_axis',(0.,0.,-1.)) ;
#113973 = DIRECTION('center_axis',(0.,0.514231796959126,0.857651245551587)) ;
#113974 = DIRECTION('ref_axis',(0.,-0.857651245551587,0.514231796959126)) ;
#113975 = DIRECTION('center_axis',(0.,0.707106781186546,0.707106781186549)) ;
#113976 = DIRECTION('ref_axis',(0.,-0.707106781186549,0.707106781186546)) ;
#113977 = DIRECTION('center_axis',(3.06658683336673E-15,-0.707106781186539,
-0.707106781186556)) ;
#113978 = DIRECTION('ref_axis',(1.90456316695698E-29,0.707106781186556,-0.707106781186539)) ;
#113979 = DIRECTION('center_axis',(1.,0.,0.)) ;
#113980 = DIRECTION('ref_axis',(0.,0.,-1.)) ;
#113981 = DIRECTION('center_axis',(0.,-0.514231796959058,0.857651245551628)) ;
#113982 = DIRECTION('ref_axis',(0.,-0.857651245551628,-0.514231796959058)) ;
#113983 = DIRECTION('center_axis',(1.,0.,0.)) ;
#113984 = DIRECTION('ref_axis',(0.,0.,-1.)) ;
#113985 = DIRECTION('center_axis',(0.,0.,-1.)) ;
#113986 = DIRECTION('ref_axis',(-1.,0.,0.)) ;
#113987 = DIRECTION('center_axis',(1.,0.,0.)) ;
#113988 = DIRECTION('ref_axis',(0.,0.,-1.)) ;
#113989 = DIRECTION('center_axis',(0.,0.,1.)) ;
#113990 = DIRECTION('ref_axis',(1.,0.,0.)) ;
#113991 = DIRECTION('center_axis',(0.,3.99416362155027E-15,1.)) ;
#113992 = DIRECTION('ref_axis',(0.,-1.,3.99416362155027E-15)) ;
#113993 = DIRECTION('center_axis',(0.,0.,-1.)) ;
#113994 = DIRECTION('ref_axis',(-1.,0.,0.)) ;
#113995 = DIRECTION('center_axis',(0.,0.,1.)) ;
#113996 = DIRECTION('ref_axis',(1.,0.,0.)) ;
#113997 = DIRECTION('center_axis',(0.,-6.93889390390724E-14,1.)) ;
#113998 = DIRECTION('ref_axis',(0.,-1.,-6.93889390390724E-14)) ;
#113999 = DIRECTION('center_axis',(0.,1.,0.)) ;
#114000 = DIRECTION('ref_axis',(0.,0.,-1.)) ;
#114001 = DIRECTION('center_axis',(0.,-1.,0.)) ;
#114002 = DIRECTION('ref_axis',(0.,0.,-1.)) ;
#114003 = DIRECTION('center_axis',(1.,0.,0.)) ;
#114004 = DIRECTION('ref_axis',(0.,0.,-1.)) ;
#114005 = DIRECTION('center_axis',(0.,1.,0.)) ;
#114006 = DIRECTION('ref_axis',(0.,0.,1.)) ;
#114007 = DIRECTION('center_axis',(0.,1.,0.)) ;
#114008 = DIRECTION('ref_axis',(0.,0.,1.)) ;
#114009 = DIRECTION('center_axis',(0.,-1.,0.)) ;
#114010 = DIRECTION('ref_axis',(0.,0.,-1.)) ;
#114011 = DIRECTION('center_axis',(0.,1.,1.07081696047951E-16)) ;
#114012 = DIRECTION('ref_axis',(0.,-1.07081696047951E-16,1.)) ;
#114013 = DIRECTION('center_axis',(0.,1.,6.50521303491284E-15)) ;
#114014 = DIRECTION('ref_axis',(0.,-6.50521303491284E-15,1.)) ;
#114015 = DIRECTION('center_axis',(0.,1.,0.)) ;
#114016 = DIRECTION('ref_axis',(0.,0.,-1.)) ;
#114017 = DIRECTION('center_axis',(0.,0.,1.)) ;
#114018 = DIRECTION('ref_axis',(1.,0.,0.)) ;
#114019 = DIRECTION('center_axis',(1.,0.,0.)) ;
#114020 = DIRECTION('ref_axis',(0.,0.,-1.)) ;
#114021 = DIRECTION('center_axis',(0.,0.,-1.)) ;
#114022 = DIRECTION('ref_axis',(-1.,0.,0.)) ;
#114023 = DIRECTION('center_axis',(0.,0.,-1.)) ;
#114024 = DIRECTION('ref_axis',(-1.,0.,0.)) ;
#114025 = DIRECTION('center_axis',(0.,-1.,0.)) ;
#114026 = DIRECTION('ref_axis',(0.,0.,-1.)) ;
#114027 = DIRECTION('center_axis',(0.,1.,0.)) ;
#114028 = DIRECTION('ref_axis',(0.,0.,1.)) ;
#114029 = DIRECTION('center_axis',(0.,-1.,0.)) ;
#114030 = DIRECTION('ref_axis',(0.,0.,-1.)) ;
#114031 = DIRECTION('center_axis',(0.,1.,0.)) ;
#114032 = DIRECTION('ref_axis',(0.,0.,-1.)) ;
#114033 = DIRECTION('center_axis',(0.,0.,-1.)) ;
#114034 = DIRECTION('ref_axis',(-1.,0.,0.)) ;
#114035 = DIRECTION('center_axis',(0.,1.,0.)) ;
#114036 = DIRECTION('ref_axis',(0.,0.,-1.)) ;
#114037 = DIRECTION('center_axis',(0.,0.,-1.)) ;
#114038 = DIRECTION('ref_axis',(-1.,0.,0.)) ;
#114039 = DIRECTION('center_axis',(0.,0.,1.)) ;
#114040 = DIRECTION('ref_axis',(1.,0.,0.)) ;
#114041 = DIRECTION('center_axis',(0.,0.,-1.)) ;
#114042 = DIRECTION('ref_axis',(-1.,0.,0.)) ;
#114043 = DIRECTION('center_axis',(0.,0.,-1.)) ;
#114044 = DIRECTION('ref_axis',(-1.,0.,0.)) ;
#114045 = DIRECTION('center_axis',(0.,0.,-1.)) ;
#114046 = DIRECTION('ref_axis',(-1.,0.,0.)) ;
#114047 = DIRECTION('center_axis',(1.,0.,0.)) ;
#114048 = DIRECTION('ref_axis',(0.,0.,-1.)) ;
#114049 = DIRECTION('center_axis',(3.0665868333667E-15,0.707106781186532,
-0.707106781186563)) ;
#114050 = DIRECTION('ref_axis',(-5.39294103027656E-31,0.707106781186563,0.707106781186532)) ;
#114051 = DIRECTION('center_axis',(1.,0.,0.)) ;
#114052 = DIRECTION('ref_axis',(0.,0.,-1.)) ;
#114053 = DIRECTION('center_axis',(0.,-1.,0.)) ;
#114054 = DIRECTION('ref_axis',(0.,0.,-1.)) ;
#114055 = DIRECTION('center_axis',(0.,-0.707106781186548,0.707106781186547)) ;
#114056 = DIRECTION('ref_axis',(0.,-0.707106781186547,-0.707106781186548)) ;
#114057 = DIRECTION('center_axis',(0.,-1.,-1.07081696047951E-16)) ;
#114058 = DIRECTION('ref_axis',(0.,1.07081696047951E-16,-1.)) ;
#114059 = DIRECTION('center_axis',(0.,-1.,-8.67361737988379E-15)) ;
#114060 = DIRECTION('ref_axis',(0.,8.67361737988379E-15,-1.)) ;
#114061 = DIRECTION('center_axis',(1.,0.,0.)) ;
#114062 = DIRECTION('ref_axis',(0.,0.,-1.)) ;
#114063 = DIRECTION('center_axis',(0.,0.,1.)) ;
#114064 = DIRECTION('ref_axis',(1.,0.,0.)) ;
#114065 = DIRECTION('center_axis',(0.,0.,-1.)) ;
#114066 = DIRECTION('ref_axis',(-1.,0.,0.)) ;
#114067 = DIRECTION('center_axis',(0.,0.,1.)) ;
#114068 = DIRECTION('ref_axis',(1.,0.,0.)) ;
#114069 = DIRECTION('center_axis',(0.,0.,1.)) ;
#114070 = DIRECTION('ref_axis',(1.,0.,0.)) ;
#114071 = DIRECTION('center_axis',(0.,0.,1.)) ;
#114072 = DIRECTION('ref_axis',(1.,0.,0.)) ;
#114073 = DIRECTION('center_axis',(1.,0.,0.)) ;
#114074 = DIRECTION('ref_axis',(0.,0.382683432365093,0.923879532511286)) ;
#114075 = DIRECTION('center_axis',(6.13317366673366E-15,-0.707106781186563,
-0.707106781186532)) ;
#114076 = DIRECTION('ref_axis',(-1.7381816909424E-29,0.707106781186532,-0.707106781186563)) ;
#114077 = DIRECTION('center_axis',(1.,0.,0.)) ;
#114078 = DIRECTION('ref_axis',(0.,0.,-1.)) ;
#114079 = DIRECTION('center_axis',(0.,0.514231796959126,0.857651245551587)) ;
#114080 = DIRECTION('ref_axis',(0.,-0.857651245551587,0.514231796959126)) ;
#114081 = DIRECTION('center_axis',(0.,0.707106781186546,0.707106781186549)) ;
#114082 = DIRECTION('ref_axis',(0.,-0.707106781186549,0.707106781186546)) ;
#114083 = DIRECTION('center_axis',(3.06658683336673E-15,-0.707106781186539,
-0.707106781186556)) ;
#114084 = DIRECTION('ref_axis',(1.90456316695698E-29,0.707106781186556,-0.707106781186539)) ;
#114085 = DIRECTION('center_axis',(1.,0.,0.)) ;
#114086 = DIRECTION('ref_axis',(0.,0.,-1.)) ;
#114087 = DIRECTION('center_axis',(0.,-0.514231796959091,0.857651245551608)) ;
#114088 = DIRECTION('ref_axis',(0.,-0.857651245551608,-0.514231796959091)) ;
#114089 = DIRECTION('center_axis',(1.,0.,0.)) ;
#114090 = DIRECTION('ref_axis',(0.,0.,-1.)) ;
#114091 = DIRECTION('center_axis',(0.,0.,-1.)) ;
#114092 = DIRECTION('ref_axis',(-1.,0.,0.)) ;
#114093 = DIRECTION('center_axis',(1.,0.,0.)) ;
#114094 = DIRECTION('ref_axis',(0.,0.,-1.)) ;
#114095 = DIRECTION('center_axis',(0.,0.,1.)) ;
#114096 = DIRECTION('ref_axis',(1.,0.,0.)) ;
#114097 = DIRECTION('center_axis',(0.,3.99416362155027E-15,1.)) ;
#114098 = DIRECTION('ref_axis',(0.,-1.,3.99416362155027E-15)) ;
#114099 = DIRECTION('center_axis',(0.,0.,-1.)) ;
#114100 = DIRECTION('ref_axis',(-1.,0.,0.)) ;
#114101 = DIRECTION('center_axis',(0.,0.,1.)) ;
#114102 = DIRECTION('ref_axis',(1.,0.,0.)) ;
#114103 = DIRECTION('center_axis',(0.,0.,1.)) ;
#114104 = DIRECTION('ref_axis',(1.,0.,0.)) ;
#114105 = DIRECTION('center_axis',(0.,1.,0.)) ;
#114106 = DIRECTION('ref_axis',(0.,0.,-1.)) ;
#114107 = DIRECTION('center_axis',(0.,-1.,0.)) ;
#114108 = DIRECTION('ref_axis',(0.,0.,-1.)) ;
#114109 = DIRECTION('center_axis',(1.,0.,0.)) ;
#114110 = DIRECTION('ref_axis',(0.,0.,-1.)) ;
#114111 = DIRECTION('center_axis',(0.,1.,0.)) ;
#114112 = DIRECTION('ref_axis',(0.,0.,1.)) ;
#114113 = DIRECTION('center_axis',(0.,1.,0.)) ;
#114114 = DIRECTION('ref_axis',(0.,0.,1.)) ;
#114115 = DIRECTION('center_axis',(0.,-1.,0.)) ;
#114116 = DIRECTION('ref_axis',(0.,0.,-1.)) ;
#114117 = DIRECTION('center_axis',(0.,1.,1.07081696047951E-16)) ;
#114118 = DIRECTION('ref_axis',(0.,-1.07081696047951E-16,1.)) ;
#114119 = DIRECTION('center_axis',(0.,1.,6.50521303491307E-15)) ;
#114120 = DIRECTION('ref_axis',(0.,-6.50521303491307E-15,1.)) ;
#114121 = DIRECTION('center_axis',(0.,1.,0.)) ;
#114122 = DIRECTION('ref_axis',(0.,0.,-1.)) ;
#114123 = DIRECTION('center_axis',(0.,0.,1.)) ;
#114124 = DIRECTION('ref_axis',(1.,0.,0.)) ;
#114125 = DIRECTION('center_axis',(1.,0.,0.)) ;
#114126 = DIRECTION('ref_axis',(0.,0.,-1.)) ;
#114127 = DIRECTION('center_axis',(0.,0.,-1.)) ;
#114128 = DIRECTION('ref_axis',(-1.,0.,0.)) ;
#114129 = DIRECTION('center_axis',(0.,0.,-1.)) ;
#114130 = DIRECTION('ref_axis',(-1.,0.,0.)) ;
#114131 = DIRECTION('center_axis',(0.,-1.,0.)) ;
#114132 = DIRECTION('ref_axis',(0.,0.,-1.)) ;
#114133 = DIRECTION('center_axis',(0.,1.,0.)) ;
#114134 = DIRECTION('ref_axis',(0.,0.,1.)) ;
#114135 = DIRECTION('center_axis',(0.,-1.,0.)) ;
#114136 = DIRECTION('ref_axis',(0.,0.,-1.)) ;
#114137 = DIRECTION('center_axis',(0.,1.,0.)) ;
#114138 = DIRECTION('ref_axis',(0.,0.,-1.)) ;
#114139 = DIRECTION('center_axis',(0.,0.,-1.)) ;
#114140 = DIRECTION('ref_axis',(-1.,0.,0.)) ;
#114141 = DIRECTION('center_axis',(0.,1.,0.)) ;
#114142 = DIRECTION('ref_axis',(0.,0.,-1.)) ;
#114143 = DIRECTION('center_axis',(0.,0.,-1.)) ;
#114144 = DIRECTION('ref_axis',(-1.,0.,0.)) ;
#114145 = DIRECTION('center_axis',(0.,0.,1.)) ;
#114146 = DIRECTION('ref_axis',(1.,0.,0.)) ;
#114147 = DIRECTION('center_axis',(0.,0.,-1.)) ;
#114148 = DIRECTION('ref_axis',(-1.,0.,0.)) ;
#114149 = DIRECTION('center_axis',(0.,0.,-1.)) ;
#114150 = DIRECTION('ref_axis',(-1.,0.,0.)) ;
#114151 = DIRECTION('center_axis',(0.,0.,-1.)) ;
#114152 = DIRECTION('ref_axis',(-1.,0.,0.)) ;
#114153 = DIRECTION('center_axis',(1.,0.,0.)) ;
#114154 = DIRECTION('ref_axis',(0.,0.,-1.)) ;
#114155 = DIRECTION('center_axis',(-6.13317366673366E-15,0.707106781186563,
-0.707106781186532)) ;
#114156 = DIRECTION('ref_axis',(-1.7381816909424E-29,0.707106781186532,0.707106781186563)) ;
#114157 = DIRECTION('center_axis',(1.,0.,0.)) ;
#114158 = DIRECTION('ref_axis',(0.,0.,-1.)) ;
#114159 = DIRECTION('center_axis',(0.,-1.,0.)) ;
#114160 = DIRECTION('ref_axis',(0.,0.,-1.)) ;
#114161 = DIRECTION('center_axis',(0.,-0.707106781186548,0.707106781186547)) ;
#114162 = DIRECTION('ref_axis',(0.,-0.707106781186547,-0.707106781186548)) ;
#114163 = DIRECTION('center_axis',(0.,-1.,-1.07081696047951E-16)) ;
#114164 = DIRECTION('ref_axis',(0.,1.07081696047951E-16,-1.)) ;
#114165 = DIRECTION('center_axis',(0.,-1.,-8.67361737988409E-15)) ;
#114166 = DIRECTION('ref_axis',(0.,8.67361737988409E-15,-1.)) ;
#114167 = DIRECTION('center_axis',(1.,0.,0.)) ;
#114168 = DIRECTION('ref_axis',(0.,0.,-1.)) ;
#114169 = DIRECTION('center_axis',(0.,0.,1.)) ;
#114170 = DIRECTION('ref_axis',(1.,0.,0.)) ;
#114171 = DIRECTION('center_axis',(0.,0.,-1.)) ;
#114172 = DIRECTION('ref_axis',(-1.,0.,0.)) ;
#114173 = DIRECTION('center_axis',(0.,0.,1.)) ;
#114174 = DIRECTION('ref_axis',(1.,0.,0.)) ;
#114175 = DIRECTION('center_axis',(0.,0.,1.)) ;
#114176 = DIRECTION('ref_axis',(1.,0.,0.)) ;
#114177 = DIRECTION('center_axis',(0.,0.,1.)) ;
#114178 = DIRECTION('ref_axis',(1.,0.,0.)) ;
#114179 = DIRECTION('center_axis',(1.,0.,0.)) ;
#114180 = DIRECTION('ref_axis',(0.,0.382683432365093,0.923879532511286)) ;
#114181 = DIRECTION('center_axis',(6.13317366673366E-15,-0.707106781186563,
-0.707106781186532)) ;
#114182 = DIRECTION('ref_axis',(-1.7381816909424E-29,0.707106781186532,-0.707106781186563)) ;
#114183 = DIRECTION('center_axis',(1.,0.,0.)) ;
#114184 = DIRECTION('ref_axis',(0.,0.,-1.)) ;
#114185 = DIRECTION('center_axis',(0.,0.514231796959093,0.857651245551607)) ;
#114186 = DIRECTION('ref_axis',(0.,-0.857651245551607,0.514231796959093)) ;
#114187 = DIRECTION('center_axis',(0.,0.707106781186546,0.707106781186549)) ;
#114188 = DIRECTION('ref_axis',(0.,-0.707106781186549,0.707106781186546)) ;
#114189 = DIRECTION('center_axis',(3.06658683336673E-15,-0.707106781186539,
-0.707106781186556)) ;
#114190 = DIRECTION('ref_axis',(1.90456316695698E-29,0.707106781186556,-0.707106781186539)) ;
#114191 = DIRECTION('center_axis',(1.,0.,0.)) ;
#114192 = DIRECTION('ref_axis',(0.,0.,-1.)) ;
#114193 = DIRECTION('center_axis',(0.,-0.514231796959091,0.857651245551608)) ;
#114194 = DIRECTION('ref_axis',(0.,-0.857651245551608,-0.514231796959091)) ;
#114195 = DIRECTION('center_axis',(1.,0.,0.)) ;
#114196 = DIRECTION('ref_axis',(0.,0.,-1.)) ;
#114197 = DIRECTION('center_axis',(0.,0.,-1.)) ;
#114198 = DIRECTION('ref_axis',(-1.,0.,0.)) ;
#114199 = DIRECTION('center_axis',(1.,0.,0.)) ;
#114200 = DIRECTION('ref_axis',(0.,0.,-1.)) ;
#114201 = DIRECTION('center_axis',(0.,0.,1.)) ;
#114202 = DIRECTION('ref_axis',(1.,0.,0.)) ;
#114203 = DIRECTION('center_axis',(0.,3.99416362155027E-15,1.)) ;
#114204 = DIRECTION('ref_axis',(0.,-1.,3.99416362155027E-15)) ;
#114205 = DIRECTION('center_axis',(0.,0.,-1.)) ;
#114206 = DIRECTION('ref_axis',(-1.,0.,0.)) ;
#114207 = DIRECTION('center_axis',(0.,0.,1.)) ;
#114208 = DIRECTION('ref_axis',(1.,0.,0.)) ;
#114209 = DIRECTION('center_axis',(0.,0.,1.)) ;
#114210 = DIRECTION('ref_axis',(1.,0.,0.)) ;
#114211 = DIRECTION('center_axis',(0.,1.,0.)) ;
#114212 = DIRECTION('ref_axis',(0.,0.,-1.)) ;
#114213 = DIRECTION('center_axis',(0.,-1.,0.)) ;
#114214 = DIRECTION('ref_axis',(0.,0.,-1.)) ;
#114215 = DIRECTION('center_axis',(1.,0.,0.)) ;
#114216 = DIRECTION('ref_axis',(0.,0.,-1.)) ;
#114217 = DIRECTION('center_axis',(0.,1.,0.)) ;
#114218 = DIRECTION('ref_axis',(0.,0.,1.)) ;
#114219 = DIRECTION('center_axis',(0.,1.,0.)) ;
#114220 = DIRECTION('ref_axis',(0.,0.,1.)) ;
#114221 = DIRECTION('center_axis',(0.,-1.,0.)) ;
#114222 = DIRECTION('ref_axis',(0.,0.,-1.)) ;
#114223 = DIRECTION('center_axis',(0.,1.,1.07081696047951E-16)) ;
#114224 = DIRECTION('ref_axis',(0.,-1.07081696047951E-16,1.)) ;
#114225 = DIRECTION('center_axis',(0.,1.,6.50521303491307E-15)) ;
#114226 = DIRECTION('ref_axis',(0.,-6.50521303491307E-15,1.)) ;
#114227 = DIRECTION('center_axis',(0.,1.,0.)) ;
#114228 = DIRECTION('ref_axis',(0.,0.,-1.)) ;
#114229 = DIRECTION('center_axis',(0.,0.,1.)) ;
#114230 = DIRECTION('ref_axis',(1.,0.,0.)) ;
#114231 = DIRECTION('center_axis',(1.,0.,0.)) ;
#114232 = DIRECTION('ref_axis',(0.,0.,-1.)) ;
#114233 = DIRECTION('center_axis',(0.,0.,-1.)) ;
#114234 = DIRECTION('ref_axis',(-1.,0.,0.)) ;
#114235 = DIRECTION('center_axis',(0.,0.,-1.)) ;
#114236 = DIRECTION('ref_axis',(-1.,0.,0.)) ;
#114237 = DIRECTION('center_axis',(0.,-1.,0.)) ;
#114238 = DIRECTION('ref_axis',(0.,0.,-1.)) ;
#114239 = DIRECTION('center_axis',(0.,1.,0.)) ;
#114240 = DIRECTION('ref_axis',(0.,0.,1.)) ;
#114241 = DIRECTION('center_axis',(0.,-1.,0.)) ;
#114242 = DIRECTION('ref_axis',(0.,0.,-1.)) ;
#114243 = DIRECTION('center_axis',(0.,1.,0.)) ;
#114244 = DIRECTION('ref_axis',(0.,0.,-1.)) ;
#114245 = DIRECTION('center_axis',(0.,0.,-1.)) ;
#114246 = DIRECTION('ref_axis',(-1.,0.,0.)) ;
#114247 = DIRECTION('center_axis',(0.,1.,0.)) ;
#114248 = DIRECTION('ref_axis',(0.,0.,-1.)) ;
#114249 = DIRECTION('center_axis',(0.,0.,-1.)) ;
#114250 = DIRECTION('ref_axis',(-1.,0.,0.)) ;
#114251 = DIRECTION('center_axis',(0.,0.,1.)) ;
#114252 = DIRECTION('ref_axis',(1.,0.,0.)) ;
#114253 = DIRECTION('center_axis',(0.,0.,-1.)) ;
#114254 = DIRECTION('ref_axis',(-1.,0.,0.)) ;
#114255 = DIRECTION('center_axis',(0.,0.,-1.)) ;
#114256 = DIRECTION('ref_axis',(-1.,0.,0.)) ;
#114257 = DIRECTION('center_axis',(0.,0.,-1.)) ;
#114258 = DIRECTION('ref_axis',(-1.,0.,0.)) ;
#114259 = DIRECTION('center_axis',(1.,0.,0.)) ;
#114260 = DIRECTION('ref_axis',(0.,0.,-1.)) ;
#114261 = DIRECTION('center_axis',(-6.13317366673366E-15,0.707106781186563,
-0.707106781186532)) ;
#114262 = DIRECTION('ref_axis',(-1.7381816909424E-29,0.707106781186532,0.707106781186563)) ;
#114263 = DIRECTION('center_axis',(1.,0.,0.)) ;
#114264 = DIRECTION('ref_axis',(0.,0.,-1.)) ;
#114265 = DIRECTION('center_axis',(0.,-1.,0.)) ;
#114266 = DIRECTION('ref_axis',(0.,0.,-1.)) ;
#114267 = DIRECTION('center_axis',(0.,-0.707106781186548,0.707106781186547)) ;
#114268 = DIRECTION('ref_axis',(0.,-0.707106781186547,-0.707106781186548)) ;
#114269 = DIRECTION('center_axis',(0.,-1.,-1.07081696047951E-16)) ;
#114270 = DIRECTION('ref_axis',(0.,1.07081696047951E-16,-1.)) ;
#114271 = DIRECTION('center_axis',(0.,-1.,-8.67361737988409E-15)) ;
#114272 = DIRECTION('ref_axis',(0.,8.67361737988409E-15,-1.)) ;
#114273 = DIRECTION('center_axis',(1.,0.,0.)) ;
#114274 = DIRECTION('ref_axis',(0.,0.,-1.)) ;
#114275 = DIRECTION('center_axis',(0.,0.,1.)) ;
#114276 = DIRECTION('ref_axis',(1.,0.,0.)) ;
#114277 = DIRECTION('center_axis',(0.,0.,-1.)) ;
#114278 = DIRECTION('ref_axis',(-1.,0.,0.)) ;
#114279 = DIRECTION('center_axis',(0.,0.,1.)) ;
#114280 = DIRECTION('ref_axis',(1.,0.,0.)) ;
#114281 = DIRECTION('center_axis',(0.,0.,1.)) ;
#114282 = DIRECTION('ref_axis',(1.,0.,0.)) ;
#114283 = DIRECTION('center_axis',(0.,0.,1.)) ;
#114284 = DIRECTION('ref_axis',(1.,0.,0.)) ;
#114285 = DIRECTION('center_axis',(1.,0.,0.)) ;
#114286 = DIRECTION('ref_axis',(0.,0.382683432365092,0.923879532511286)) ;
#114287 = DIRECTION('center_axis',(6.13317366673366E-15,-0.707106781186563,
-0.707106781186532)) ;
#114288 = DIRECTION('ref_axis',(-1.7381816909424E-29,0.707106781186532,-0.707106781186563)) ;
#114289 = DIRECTION('center_axis',(1.,0.,0.)) ;
#114290 = DIRECTION('ref_axis',(0.,0.,-1.)) ;
#114291 = DIRECTION('center_axis',(0.,0.514231796959093,0.857651245551607)) ;
#114292 = DIRECTION('ref_axis',(0.,-0.857651245551607,0.514231796959093)) ;
#114293 = DIRECTION('center_axis',(0.,0.707106781186546,0.707106781186549)) ;
#114294 = DIRECTION('ref_axis',(0.,-0.707106781186549,0.707106781186546)) ;
#114295 = DIRECTION('center_axis',(3.06658683336673E-15,-0.707106781186539,
-0.707106781186556)) ;
#114296 = DIRECTION('ref_axis',(1.90456316695698E-29,0.707106781186556,-0.707106781186539)) ;
#114297 = DIRECTION('center_axis',(1.,0.,0.)) ;
#114298 = DIRECTION('ref_axis',(0.,0.,-1.)) ;
#114299 = DIRECTION('center_axis',(0.,-0.514231796959091,0.857651245551608)) ;
#114300 = DIRECTION('ref_axis',(0.,-0.857651245551608,-0.514231796959091)) ;
#114301 = DIRECTION('center_axis',(1.,0.,0.)) ;
#114302 = DIRECTION('ref_axis',(0.,0.,-1.)) ;
#114303 = DIRECTION('center_axis',(0.,0.,-1.)) ;
#114304 = DIRECTION('ref_axis',(-1.,0.,0.)) ;
#114305 = DIRECTION('center_axis',(1.,0.,0.)) ;
#114306 = DIRECTION('ref_axis',(0.,0.,-1.)) ;
#114307 = DIRECTION('center_axis',(0.,0.,1.)) ;
#114308 = DIRECTION('ref_axis',(1.,0.,0.)) ;
#114309 = DIRECTION('center_axis',(0.,3.99416362155027E-15,1.)) ;
#114310 = DIRECTION('ref_axis',(0.,-1.,3.99416362155027E-15)) ;
#114311 = DIRECTION('center_axis',(0.,0.,-1.)) ;
#114312 = DIRECTION('ref_axis',(-1.,0.,0.)) ;
#114313 = DIRECTION('center_axis',(0.,0.,1.)) ;
#114314 = DIRECTION('ref_axis',(1.,0.,0.)) ;
#114315 = DIRECTION('center_axis',(0.,0.,1.)) ;
#114316 = DIRECTION('ref_axis',(1.,0.,0.)) ;
#114317 = DIRECTION('center_axis',(0.,1.,0.)) ;
#114318 = DIRECTION('ref_axis',(0.,0.,-1.)) ;
#114319 = DIRECTION('center_axis',(0.,-1.,0.)) ;
#114320 = DIRECTION('ref_axis',(0.,0.,-1.)) ;
#114321 = DIRECTION('center_axis',(1.,0.,0.)) ;
#114322 = DIRECTION('ref_axis',(0.,0.,-1.)) ;
#114323 = DIRECTION('center_axis',(0.,1.,0.)) ;
#114324 = DIRECTION('ref_axis',(0.,0.,1.)) ;
#114325 = DIRECTION('center_axis',(0.,1.,0.)) ;
#114326 = DIRECTION('ref_axis',(0.,0.,1.)) ;
#114327 = DIRECTION('center_axis',(0.,-1.,0.)) ;
#114328 = DIRECTION('ref_axis',(0.,0.,-1.)) ;
#114329 = DIRECTION('center_axis',(0.,1.,1.07081696047951E-16)) ;
#114330 = DIRECTION('ref_axis',(0.,-1.07081696047951E-16,1.)) ;
#114331 = DIRECTION('center_axis',(0.,1.,6.50521303491307E-15)) ;
#114332 = DIRECTION('ref_axis',(0.,-6.50521303491307E-15,1.)) ;
#114333 = DIRECTION('center_axis',(0.,1.,0.)) ;
#114334 = DIRECTION('ref_axis',(0.,0.,-1.)) ;
#114335 = DIRECTION('center_axis',(0.,0.,1.)) ;
#114336 = DIRECTION('ref_axis',(1.,0.,0.)) ;
#114337 = DIRECTION('center_axis',(1.,0.,0.)) ;
#114338 = DIRECTION('ref_axis',(0.,0.,-1.)) ;
#114339 = DIRECTION('center_axis',(0.,0.,-1.)) ;
#114340 = DIRECTION('ref_axis',(-1.,0.,0.)) ;
#114341 = DIRECTION('center_axis',(0.,0.,-1.)) ;
#114342 = DIRECTION('ref_axis',(-1.,0.,0.)) ;
#114343 = DIRECTION('center_axis',(0.,-1.,0.)) ;
#114344 = DIRECTION('ref_axis',(0.,0.,-1.)) ;
#114345 = DIRECTION('center_axis',(0.,1.,0.)) ;
#114346 = DIRECTION('ref_axis',(0.,0.,1.)) ;
#114347 = DIRECTION('center_axis',(0.,-1.,0.)) ;
#114348 = DIRECTION('ref_axis',(0.,0.,-1.)) ;
#114349 = DIRECTION('center_axis',(0.,1.,0.)) ;
#114350 = DIRECTION('ref_axis',(0.,0.,-1.)) ;
#114351 = DIRECTION('center_axis',(0.,0.,-1.)) ;
#114352 = DIRECTION('ref_axis',(-1.,0.,0.)) ;
#114353 = DIRECTION('center_axis',(0.,1.,0.)) ;
#114354 = DIRECTION('ref_axis',(0.,0.,-1.)) ;
#114355 = DIRECTION('center_axis',(0.,0.,-1.)) ;
#114356 = DIRECTION('ref_axis',(-1.,0.,0.)) ;
#114357 = DIRECTION('center_axis',(0.,0.,1.)) ;
#114358 = DIRECTION('ref_axis',(1.,0.,0.)) ;
#114359 = DIRECTION('center_axis',(0.,0.,-1.)) ;
#114360 = DIRECTION('ref_axis',(-1.,0.,0.)) ;
#114361 = DIRECTION('center_axis',(0.,0.,-1.)) ;
#114362 = DIRECTION('ref_axis',(-1.,0.,0.)) ;
#114363 = DIRECTION('center_axis',(0.,0.,-1.)) ;
#114364 = DIRECTION('ref_axis',(-1.,0.,0.)) ;
#114365 = DIRECTION('center_axis',(1.,0.,0.)) ;
#114366 = DIRECTION('ref_axis',(0.,0.,-1.)) ;
#114367 = DIRECTION('center_axis',(-6.13317366673366E-15,0.707106781186563,
-0.707106781186532)) ;
#114368 = DIRECTION('ref_axis',(-1.7381816909424E-29,0.707106781186532,0.707106781186563)) ;
#114369 = DIRECTION('center_axis',(1.,0.,0.)) ;
#114370 = DIRECTION('ref_axis',(0.,0.,-1.)) ;
#114371 = DIRECTION('center_axis',(0.,-1.,0.)) ;
#114372 = DIRECTION('ref_axis',(0.,0.,-1.)) ;
#114373 = DIRECTION('center_axis',(0.,-0.707106781186548,0.707106781186547)) ;
#114374 = DIRECTION('ref_axis',(0.,-0.707106781186547,-0.707106781186548)) ;
#114375 = DIRECTION('center_axis',(0.,-1.,-1.07081696047951E-16)) ;
#114376 = DIRECTION('ref_axis',(0.,1.07081696047951E-16,-1.)) ;
#114377 = DIRECTION('center_axis',(0.,-1.,-8.67361737988409E-15)) ;
#114378 = DIRECTION('ref_axis',(0.,8.67361737988409E-15,-1.)) ;
#114379 = DIRECTION('center_axis',(1.,0.,0.)) ;
#114380 = DIRECTION('ref_axis',(0.,0.,-1.)) ;
#114381 = DIRECTION('center_axis',(0.,0.,1.)) ;
#114382 = DIRECTION('ref_axis',(1.,0.,0.)) ;
#114383 = DIRECTION('center_axis',(0.,0.,-1.)) ;
#114384 = DIRECTION('ref_axis',(-1.,0.,0.)) ;
#114385 = DIRECTION('center_axis',(0.,0.,1.)) ;
#114386 = DIRECTION('ref_axis',(1.,0.,0.)) ;
#114387 = DIRECTION('center_axis',(0.,0.,1.)) ;
#114388 = DIRECTION('ref_axis',(1.,0.,0.)) ;
#114389 = DIRECTION('center_axis',(0.,0.,1.)) ;
#114390 = DIRECTION('ref_axis',(1.,0.,0.)) ;
#114391 = DIRECTION('center_axis',(1.,0.,0.)) ;
#114392 = DIRECTION('ref_axis',(0.,0.382683432365085,0.923879532511289)) ;
#114393 = DIRECTION('center_axis',(6.13317366673366E-15,-0.707106781186563,
-0.707106781186532)) ;
#114394 = DIRECTION('ref_axis',(-1.7381816909424E-29,0.707106781186532,-0.707106781186563)) ;
#114395 = DIRECTION('center_axis',(1.,0.,0.)) ;
#114396 = DIRECTION('ref_axis',(0.,0.,-1.)) ;
#114397 = DIRECTION('center_axis',(0.,0.514231796959093,0.857651245551607)) ;
#114398 = DIRECTION('ref_axis',(0.,-0.857651245551607,0.514231796959093)) ;
#114399 = DIRECTION('center_axis',(0.,0.707106781186546,0.707106781186549)) ;
#114400 = DIRECTION('ref_axis',(0.,-0.707106781186549,0.707106781186546)) ;
#114401 = DIRECTION('center_axis',(3.06658683336673E-15,-0.707106781186539,
-0.707106781186556)) ;
#114402 = DIRECTION('ref_axis',(1.90456316695698E-29,0.707106781186556,-0.707106781186539)) ;
#114403 = DIRECTION('center_axis',(1.,0.,0.)) ;
#114404 = DIRECTION('ref_axis',(0.,0.,-1.)) ;
#114405 = DIRECTION('center_axis',(0.,-0.514231796959091,0.857651245551608)) ;
#114406 = DIRECTION('ref_axis',(0.,-0.857651245551608,-0.514231796959091)) ;
#114407 = DIRECTION('center_axis',(1.,0.,0.)) ;
#114408 = DIRECTION('ref_axis',(0.,0.,-1.)) ;
#114409 = DIRECTION('center_axis',(0.,0.,-1.)) ;
#114410 = DIRECTION('ref_axis',(-1.,0.,0.)) ;
#114411 = DIRECTION('center_axis',(1.,0.,0.)) ;
#114412 = DIRECTION('ref_axis',(0.,0.,-1.)) ;
#114413 = DIRECTION('center_axis',(0.,0.,1.)) ;
#114414 = DIRECTION('ref_axis',(1.,0.,0.)) ;
#114415 = DIRECTION('center_axis',(0.,3.99416362155027E-15,1.)) ;
#114416 = DIRECTION('ref_axis',(0.,-1.,3.99416362155027E-15)) ;
#114417 = DIRECTION('center_axis',(0.,0.,-1.)) ;
#114418 = DIRECTION('ref_axis',(-1.,0.,0.)) ;
#114419 = DIRECTION('center_axis',(0.,0.,1.)) ;
#114420 = DIRECTION('ref_axis',(1.,0.,0.)) ;
#114421 = DIRECTION('center_axis',(0.,0.,1.)) ;
#114422 = DIRECTION('ref_axis',(1.,0.,0.)) ;
#114423 = DIRECTION('center_axis',(0.,1.,0.)) ;
#114424 = DIRECTION('ref_axis',(0.,0.,-1.)) ;
#114425 = DIRECTION('center_axis',(0.,-1.,0.)) ;
#114426 = DIRECTION('ref_axis',(0.,0.,-1.)) ;
#114427 = DIRECTION('center_axis',(1.,0.,0.)) ;
#114428 = DIRECTION('ref_axis',(0.,0.,-1.)) ;
#114429 = DIRECTION('center_axis',(0.,1.,0.)) ;
#114430 = DIRECTION('ref_axis',(0.,0.,1.)) ;
#114431 = DIRECTION('center_axis',(0.,1.,0.)) ;
#114432 = DIRECTION('ref_axis',(0.,0.,1.)) ;
#114433 = DIRECTION('center_axis',(0.,-1.,0.)) ;
#114434 = DIRECTION('ref_axis',(0.,0.,-1.)) ;
#114435 = DIRECTION('center_axis',(0.,1.,1.07081696047951E-16)) ;
#114436 = DIRECTION('ref_axis',(0.,-1.07081696047951E-16,1.)) ;
#114437 = DIRECTION('center_axis',(0.,1.,6.50521303491307E-15)) ;
#114438 = DIRECTION('ref_axis',(0.,-6.50521303491307E-15,1.)) ;
#114439 = DIRECTION('center_axis',(0.,1.,0.)) ;
#114440 = DIRECTION('ref_axis',(0.,0.,-1.)) ;
#114441 = DIRECTION('center_axis',(0.,0.,1.)) ;
#114442 = DIRECTION('ref_axis',(1.,0.,0.)) ;
#114443 = DIRECTION('center_axis',(1.,0.,0.)) ;
#114444 = DIRECTION('ref_axis',(0.,0.,-1.)) ;
#114445 = DIRECTION('center_axis',(0.,0.,-1.)) ;
#114446 = DIRECTION('ref_axis',(-1.,0.,0.)) ;
#114447 = DIRECTION('center_axis',(0.,0.,-1.)) ;
#114448 = DIRECTION('ref_axis',(-1.,0.,0.)) ;
#114449 = DIRECTION('center_axis',(0.,-1.,0.)) ;
#114450 = DIRECTION('ref_axis',(0.,0.,-1.)) ;
#114451 = DIRECTION('center_axis',(0.,1.,0.)) ;
#114452 = DIRECTION('ref_axis',(0.,0.,1.)) ;
#114453 = DIRECTION('center_axis',(0.,-1.,0.)) ;
#114454 = DIRECTION('ref_axis',(0.,0.,-1.)) ;
#114455 = DIRECTION('center_axis',(0.,1.,0.)) ;
#114456 = DIRECTION('ref_axis',(0.,0.,-1.)) ;
#114457 = DIRECTION('center_axis',(0.,0.,-1.)) ;
#114458 = DIRECTION('ref_axis',(-1.,0.,0.)) ;
#114459 = DIRECTION('center_axis',(0.,1.,0.)) ;
#114460 = DIRECTION('ref_axis',(0.,0.,-1.)) ;
#114461 = DIRECTION('center_axis',(0.,0.,-1.)) ;
#114462 = DIRECTION('ref_axis',(-1.,0.,0.)) ;
#114463 = DIRECTION('center_axis',(0.,0.,1.)) ;
#114464 = DIRECTION('ref_axis',(1.,0.,0.)) ;
#114465 = DIRECTION('center_axis',(0.,0.,-1.)) ;
#114466 = DIRECTION('ref_axis',(-1.,0.,0.)) ;
#114467 = DIRECTION('center_axis',(0.,0.,-1.)) ;
#114468 = DIRECTION('ref_axis',(-1.,0.,0.)) ;
#114469 = DIRECTION('center_axis',(0.,0.,-1.)) ;
#114470 = DIRECTION('ref_axis',(-1.,0.,0.)) ;
#114471 = DIRECTION('center_axis',(1.,0.,0.)) ;
#114472 = DIRECTION('ref_axis',(0.,0.,-1.)) ;
#114473 = DIRECTION('center_axis',(-6.13317366673366E-15,0.707106781186563,
-0.707106781186532)) ;
#114474 = DIRECTION('ref_axis',(-1.7381816909424E-29,0.707106781186532,0.707106781186563)) ;
#114475 = DIRECTION('center_axis',(1.,0.,0.)) ;
#114476 = DIRECTION('ref_axis',(0.,0.,-1.)) ;
#114477 = DIRECTION('center_axis',(0.,-1.,0.)) ;
#114478 = DIRECTION('ref_axis',(0.,0.,-1.)) ;
#114479 = DIRECTION('center_axis',(0.,-0.707106781186548,0.707106781186547)) ;
#114480 = DIRECTION('ref_axis',(0.,-0.707106781186547,-0.707106781186548)) ;
#114481 = DIRECTION('center_axis',(0.,-1.,-1.07081696047951E-16)) ;
#114482 = DIRECTION('ref_axis',(0.,1.07081696047951E-16,-1.)) ;
#114483 = DIRECTION('center_axis',(0.,-1.,-8.67361737988409E-15)) ;
#114484 = DIRECTION('ref_axis',(0.,8.67361737988409E-15,-1.)) ;
#114485 = DIRECTION('center_axis',(1.,0.,0.)) ;
#114486 = DIRECTION('ref_axis',(0.,0.,-1.)) ;
#114487 = DIRECTION('center_axis',(0.,0.,1.)) ;
#114488 = DIRECTION('ref_axis',(1.,0.,0.)) ;
#114489 = DIRECTION('center_axis',(0.,0.,-1.)) ;
#114490 = DIRECTION('ref_axis',(-1.,0.,0.)) ;
#114491 = DIRECTION('center_axis',(0.,0.,1.)) ;
#114492 = DIRECTION('ref_axis',(1.,0.,0.)) ;
#114493 = DIRECTION('center_axis',(0.,0.,1.)) ;
#114494 = DIRECTION('ref_axis',(1.,0.,0.)) ;
#114495 = DIRECTION('center_axis',(0.,0.,1.)) ;
#114496 = DIRECTION('ref_axis',(1.,0.,0.)) ;
#114497 = DIRECTION('center_axis',(1.,0.,0.)) ;
#114498 = DIRECTION('ref_axis',(0.,0.382683432365081,0.92387953251129)) ;
#114499 = DIRECTION('center_axis',(0.,-0.707106781186548,-0.707106781186548)) ;
#114500 = DIRECTION('ref_axis',(0.,0.707106781186548,-0.707106781186548)) ;
#114501 = DIRECTION('center_axis',(1.,0.,0.)) ;
#114502 = DIRECTION('ref_axis',(0.,0.,-1.)) ;
#114503 = DIRECTION('center_axis',(0.,0.514231796959093,0.857651245551607)) ;
#114504 = DIRECTION('ref_axis',(0.,-0.857651245551607,0.514231796959093)) ;
#114505 = DIRECTION('center_axis',(0.,0.707106781186546,0.707106781186549)) ;
#114506 = DIRECTION('ref_axis',(0.,-0.707106781186549,0.707106781186546)) ;
#114507 = DIRECTION('center_axis',(0.,-0.707106781186548,-0.707106781186548)) ;
#114508 = DIRECTION('ref_axis',(0.,0.707106781186548,-0.707106781186548)) ;
#114509 = DIRECTION('center_axis',(1.,0.,0.)) ;
#114510 = DIRECTION('ref_axis',(0.,0.,-1.)) ;
#114511 = DIRECTION('center_axis',(0.,-0.514231796959109,0.857651245551597)) ;
#114512 = DIRECTION('ref_axis',(0.,-0.857651245551597,-0.514231796959109)) ;
#114513 = DIRECTION('center_axis',(1.,0.,0.)) ;
#114514 = DIRECTION('ref_axis',(0.,0.,-1.)) ;
#114515 = DIRECTION('center_axis',(0.,0.,-1.)) ;
#114516 = DIRECTION('ref_axis',(-1.,0.,0.)) ;
#114517 = DIRECTION('center_axis',(1.,0.,0.)) ;
#114518 = DIRECTION('ref_axis',(0.,0.,-1.)) ;
#114519 = DIRECTION('center_axis',(0.,0.,1.)) ;
#114520 = DIRECTION('ref_axis',(1.,0.,0.)) ;
#114521 = DIRECTION('center_axis',(0.,3.99416362155027E-15,1.)) ;
#114522 = DIRECTION('ref_axis',(0.,-1.,3.99416362155027E-15)) ;
#114523 = DIRECTION('center_axis',(0.,0.,-1.)) ;
#114524 = DIRECTION('ref_axis',(-1.,0.,0.)) ;
#114525 = DIRECTION('center_axis',(0.,0.,1.)) ;
#114526 = DIRECTION('ref_axis',(1.,0.,0.)) ;
#114527 = DIRECTION('center_axis',(0.,0.,1.)) ;
#114528 = DIRECTION('ref_axis',(1.,0.,0.)) ;
#114529 = DIRECTION('center_axis',(0.,1.,0.)) ;
#114530 = DIRECTION('ref_axis',(0.,0.,-1.)) ;
#114531 = DIRECTION('center_axis',(0.,-1.,0.)) ;
#114532 = DIRECTION('ref_axis',(0.,0.,-1.)) ;
#114533 = DIRECTION('center_axis',(1.,0.,0.)) ;
#114534 = DIRECTION('ref_axis',(0.,0.,-1.)) ;
#114535 = DIRECTION('center_axis',(0.,1.,0.)) ;
#114536 = DIRECTION('ref_axis',(0.,0.,1.)) ;
#114537 = DIRECTION('center_axis',(0.,1.,0.)) ;
#114538 = DIRECTION('ref_axis',(0.,0.,1.)) ;
#114539 = DIRECTION('center_axis',(0.,-1.,0.)) ;
#114540 = DIRECTION('ref_axis',(0.,0.,-1.)) ;
#114541 = DIRECTION('center_axis',(0.,1.,1.07081696047951E-16)) ;
#114542 = DIRECTION('ref_axis',(0.,-1.07081696047951E-16,1.)) ;
#114543 = DIRECTION('center_axis',(0.,1.,6.50521303491307E-15)) ;
#114544 = DIRECTION('ref_axis',(0.,-6.50521303491307E-15,1.)) ;
#114545 = DIRECTION('center_axis',(0.,1.,0.)) ;
#114546 = DIRECTION('ref_axis',(0.,0.,-1.)) ;
#114547 = DIRECTION('center_axis',(0.,0.,1.)) ;
#114548 = DIRECTION('ref_axis',(1.,0.,0.)) ;
#114549 = DIRECTION('center_axis',(1.,0.,0.)) ;
#114550 = DIRECTION('ref_axis',(0.,0.,-1.)) ;
#114551 = DIRECTION('center_axis',(0.,0.,-1.)) ;
#114552 = DIRECTION('ref_axis',(-1.,0.,0.)) ;
#114553 = DIRECTION('center_axis',(0.,0.,-1.)) ;
#114554 = DIRECTION('ref_axis',(-1.,0.,0.)) ;
#114555 = DIRECTION('center_axis',(0.,-1.,0.)) ;
#114556 = DIRECTION('ref_axis',(0.,0.,-1.)) ;
#114557 = DIRECTION('center_axis',(0.,1.,0.)) ;
#114558 = DIRECTION('ref_axis',(0.,0.,1.)) ;
#114559 = DIRECTION('center_axis',(0.,-1.,0.)) ;
#114560 = DIRECTION('ref_axis',(0.,0.,-1.)) ;
#114561 = DIRECTION('center_axis',(0.,1.,0.)) ;
#114562 = DIRECTION('ref_axis',(0.,0.,-1.)) ;
#114563 = DIRECTION('center_axis',(0.,0.,-1.)) ;
#114564 = DIRECTION('ref_axis',(-1.,0.,0.)) ;
#114565 = DIRECTION('center_axis',(0.,1.,0.)) ;
#114566 = DIRECTION('ref_axis',(0.,0.,-1.)) ;
#114567 = DIRECTION('center_axis',(0.,0.,-1.)) ;
#114568 = DIRECTION('ref_axis',(-1.,0.,0.)) ;
#114569 = DIRECTION('center_axis',(0.,0.,1.)) ;
#114570 = DIRECTION('ref_axis',(1.,0.,0.)) ;
#114571 = DIRECTION('center_axis',(0.,0.,-1.)) ;
#114572 = DIRECTION('ref_axis',(-1.,0.,0.)) ;
#114573 = DIRECTION('center_axis',(0.,0.,-1.)) ;
#114574 = DIRECTION('ref_axis',(-1.,0.,0.)) ;
#114575 = DIRECTION('center_axis',(0.,0.,-1.)) ;
#114576 = DIRECTION('ref_axis',(-1.,0.,0.)) ;
#114577 = DIRECTION('center_axis',(1.,0.,0.)) ;
#114578 = DIRECTION('ref_axis',(0.,0.,-1.)) ;
#114579 = DIRECTION('center_axis',(0.,0.707106781186548,-0.707106781186548)) ;
#114580 = DIRECTION('ref_axis',(0.,0.707106781186548,0.707106781186548)) ;
#114581 = DIRECTION('center_axis',(1.,0.,0.)) ;
#114582 = DIRECTION('ref_axis',(0.,0.,-1.)) ;
#114583 = DIRECTION('center_axis',(0.,-1.,0.)) ;
#114584 = DIRECTION('ref_axis',(0.,0.,-1.)) ;
#114585 = DIRECTION('center_axis',(0.,-0.707106781186548,0.707106781186547)) ;
#114586 = DIRECTION('ref_axis',(0.,-0.707106781186547,-0.707106781186548)) ;
#114587 = DIRECTION('center_axis',(0.,-1.,-1.07081696047951E-16)) ;
#114588 = DIRECTION('ref_axis',(0.,1.07081696047951E-16,-1.)) ;
#114589 = DIRECTION('center_axis',(0.,-1.,-8.67361737988409E-15)) ;
#114590 = DIRECTION('ref_axis',(0.,8.67361737988409E-15,-1.)) ;
#114591 = DIRECTION('center_axis',(1.,0.,0.)) ;
#114592 = DIRECTION('ref_axis',(0.,0.,-1.)) ;
#114593 = DIRECTION('center_axis',(0.,0.,1.)) ;
#114594 = DIRECTION('ref_axis',(1.,0.,0.)) ;
#114595 = DIRECTION('center_axis',(0.,0.,-1.)) ;
#114596 = DIRECTION('ref_axis',(-1.,0.,0.)) ;
#114597 = DIRECTION('center_axis',(0.,0.,1.)) ;
#114598 = DIRECTION('ref_axis',(1.,0.,0.)) ;
#114599 = DIRECTION('center_axis',(0.,0.,1.)) ;
#114600 = DIRECTION('ref_axis',(1.,0.,0.)) ;
#114601 = DIRECTION('center_axis',(0.,0.,1.)) ;
#114602 = DIRECTION('ref_axis',(1.,0.,0.)) ;
#114603 = DIRECTION('center_axis',(1.,0.,0.)) ;
#114604 = DIRECTION('ref_axis',(0.,0.382683432365087,0.923879532511288)) ;
#114605 = DIRECTION('center_axis',(0.,-0.707106781186548,-0.707106781186548)) ;
#114606 = DIRECTION('ref_axis',(0.,0.707106781186548,-0.707106781186548)) ;
#114607 = DIRECTION('center_axis',(1.,0.,0.)) ;
#114608 = DIRECTION('ref_axis',(0.,0.,-1.)) ;
#114609 = DIRECTION('center_axis',(0.,0.514231796959109,0.857651245551597)) ;
#114610 = DIRECTION('ref_axis',(0.,-0.857651245551597,0.514231796959109)) ;
#114611 = DIRECTION('center_axis',(0.,0.707106781186546,0.707106781186549)) ;
#114612 = DIRECTION('ref_axis',(0.,-0.707106781186549,0.707106781186546)) ;
#114613 = DIRECTION('center_axis',(0.,-0.707106781186548,-0.707106781186548)) ;
#114614 = DIRECTION('ref_axis',(0.,0.707106781186548,-0.707106781186548)) ;
#114615 = DIRECTION('center_axis',(1.,0.,0.)) ;
#114616 = DIRECTION('ref_axis',(0.,0.,-1.)) ;
#114617 = DIRECTION('center_axis',(0.,-0.514231796959109,0.857651245551597)) ;
#114618 = DIRECTION('ref_axis',(0.,-0.857651245551597,-0.514231796959109)) ;
#114619 = DIRECTION('center_axis',(1.,0.,0.)) ;
#114620 = DIRECTION('ref_axis',(0.,0.,-1.)) ;
#114621 = DIRECTION('center_axis',(0.,0.,-1.)) ;
#114622 = DIRECTION('ref_axis',(-1.,0.,0.)) ;
#114623 = DIRECTION('center_axis',(1.,0.,0.)) ;
#114624 = DIRECTION('ref_axis',(0.,0.,-1.)) ;
#114625 = DIRECTION('center_axis',(0.,0.,1.)) ;
#114626 = DIRECTION('ref_axis',(1.,0.,0.)) ;
#114627 = DIRECTION('center_axis',(0.,3.99416362155027E-15,1.)) ;
#114628 = DIRECTION('ref_axis',(0.,-1.,3.99416362155027E-15)) ;
#114629 = DIRECTION('center_axis',(0.,0.,-1.)) ;
#114630 = DIRECTION('ref_axis',(-1.,0.,0.)) ;
#114631 = DIRECTION('center_axis',(0.,0.,1.)) ;
#114632 = DIRECTION('ref_axis',(1.,0.,0.)) ;
#114633 = DIRECTION('center_axis',(0.,0.,1.)) ;
#114634 = DIRECTION('ref_axis',(1.,0.,0.)) ;
#114635 = DIRECTION('center_axis',(0.,1.,0.)) ;
#114636 = DIRECTION('ref_axis',(0.,0.,-1.)) ;
#114637 = DIRECTION('center_axis',(0.,-1.,0.)) ;
#114638 = DIRECTION('ref_axis',(0.,0.,-1.)) ;
#114639 = DIRECTION('center_axis',(1.,0.,0.)) ;
#114640 = DIRECTION('ref_axis',(0.,0.,-1.)) ;
#114641 = DIRECTION('center_axis',(0.,1.,0.)) ;
#114642 = DIRECTION('ref_axis',(0.,0.,1.)) ;
#114643 = DIRECTION('center_axis',(0.,1.,0.)) ;
#114644 = DIRECTION('ref_axis',(0.,0.,1.)) ;
#114645 = DIRECTION('center_axis',(0.,-1.,0.)) ;
#114646 = DIRECTION('ref_axis',(0.,0.,-1.)) ;
#114647 = DIRECTION('center_axis',(0.,1.,1.07081696047951E-16)) ;
#114648 = DIRECTION('ref_axis',(0.,-1.07081696047951E-16,1.)) ;
#114649 = DIRECTION('center_axis',(0.,1.,6.50521303491307E-15)) ;
#114650 = DIRECTION('ref_axis',(0.,-6.50521303491307E-15,1.)) ;
#114651 = DIRECTION('center_axis',(0.,1.,0.)) ;
#114652 = DIRECTION('ref_axis',(0.,0.,-1.)) ;
#114653 = DIRECTION('center_axis',(0.,0.,1.)) ;
#114654 = DIRECTION('ref_axis',(1.,0.,0.)) ;
#114655 = DIRECTION('center_axis',(1.,0.,0.)) ;
#114656 = DIRECTION('ref_axis',(0.,0.,-1.)) ;
#114657 = DIRECTION('center_axis',(0.,0.,-1.)) ;
#114658 = DIRECTION('ref_axis',(-1.,0.,0.)) ;
#114659 = DIRECTION('center_axis',(0.,0.,-1.)) ;
#114660 = DIRECTION('ref_axis',(-1.,0.,0.)) ;
#114661 = DIRECTION('center_axis',(0.,-1.,0.)) ;
#114662 = DIRECTION('ref_axis',(0.,0.,-1.)) ;
#114663 = DIRECTION('center_axis',(0.,1.,0.)) ;
#114664 = DIRECTION('ref_axis',(0.,0.,1.)) ;
#114665 = DIRECTION('center_axis',(0.,-1.,0.)) ;
#114666 = DIRECTION('ref_axis',(0.,0.,-1.)) ;
#114667 = DIRECTION('center_axis',(0.,1.,0.)) ;
#114668 = DIRECTION('ref_axis',(0.,0.,-1.)) ;
#114669 = DIRECTION('center_axis',(0.,0.,-1.)) ;
#114670 = DIRECTION('ref_axis',(-1.,0.,0.)) ;
#114671 = DIRECTION('center_axis',(0.,1.,0.)) ;
#114672 = DIRECTION('ref_axis',(0.,0.,-1.)) ;
#114673 = DIRECTION('center_axis',(0.,0.,-1.)) ;
#114674 = DIRECTION('ref_axis',(-1.,0.,0.)) ;
#114675 = DIRECTION('center_axis',(0.,0.,1.)) ;
#114676 = DIRECTION('ref_axis',(1.,0.,0.)) ;
#114677 = DIRECTION('center_axis',(0.,0.,-1.)) ;
#114678 = DIRECTION('ref_axis',(-1.,0.,0.)) ;
#114679 = DIRECTION('center_axis',(0.,0.,-1.)) ;
#114680 = DIRECTION('ref_axis',(-1.,0.,0.)) ;
#114681 = DIRECTION('center_axis',(0.,0.,-1.)) ;
#114682 = DIRECTION('ref_axis',(-1.,0.,0.)) ;
#114683 = DIRECTION('center_axis',(1.,0.,0.)) ;
#114684 = DIRECTION('ref_axis',(0.,0.,-1.)) ;
#114685 = DIRECTION('center_axis',(0.,0.707106781186548,-0.707106781186548)) ;
#114686 = DIRECTION('ref_axis',(0.,0.707106781186548,0.707106781186548)) ;
#114687 = DIRECTION('center_axis',(1.,0.,0.)) ;
#114688 = DIRECTION('ref_axis',(0.,0.,-1.)) ;
#114689 = DIRECTION('center_axis',(0.,-1.,0.)) ;
#114690 = DIRECTION('ref_axis',(0.,0.,-1.)) ;
#114691 = DIRECTION('center_axis',(0.,-0.707106781186548,0.707106781186547)) ;
#114692 = DIRECTION('ref_axis',(0.,-0.707106781186547,-0.707106781186548)) ;
#114693 = DIRECTION('center_axis',(0.,-1.,-1.07081696047951E-16)) ;
#114694 = DIRECTION('ref_axis',(0.,1.07081696047951E-16,-1.)) ;
#114695 = DIRECTION('center_axis',(0.,-1.,-8.67361737988409E-15)) ;
#114696 = DIRECTION('ref_axis',(0.,8.67361737988409E-15,-1.)) ;
#114697 = DIRECTION('center_axis',(1.,0.,0.)) ;
#114698 = DIRECTION('ref_axis',(0.,0.,-1.)) ;
#114699 = DIRECTION('center_axis',(0.,0.,1.)) ;
#114700 = DIRECTION('ref_axis',(1.,0.,0.)) ;
#114701 = DIRECTION('center_axis',(0.,0.,-1.)) ;
#114702 = DIRECTION('ref_axis',(-1.,0.,0.)) ;
#114703 = DIRECTION('center_axis',(0.,0.,1.)) ;
#114704 = DIRECTION('ref_axis',(1.,0.,0.)) ;
#114705 = DIRECTION('center_axis',(0.,0.,1.)) ;
#114706 = DIRECTION('ref_axis',(1.,0.,0.)) ;
#114707 = DIRECTION('center_axis',(0.,0.,1.)) ;
#114708 = DIRECTION('ref_axis',(1.,0.,0.)) ;
#114709 = DIRECTION('center_axis',(1.,0.,0.)) ;
#114710 = DIRECTION('ref_axis',(0.,0.382683432365088,0.923879532511288)) ;
#114711 = DIRECTION('center_axis',(0.,-0.707106781186548,-0.707106781186548)) ;
#114712 = DIRECTION('ref_axis',(0.,0.707106781186548,-0.707106781186548)) ;
#114713 = DIRECTION('center_axis',(1.,0.,0.)) ;
#114714 = DIRECTION('ref_axis',(0.,0.,-1.)) ;
#114715 = DIRECTION('center_axis',(0.,0.514231796959109,0.857651245551597)) ;
#114716 = DIRECTION('ref_axis',(0.,-0.857651245551597,0.514231796959109)) ;
#114717 = DIRECTION('center_axis',(0.,0.707106781186546,0.707106781186549)) ;
#114718 = DIRECTION('ref_axis',(0.,-0.707106781186549,0.707106781186546)) ;
#114719 = DIRECTION('center_axis',(0.,-0.707106781186548,-0.707106781186548)) ;
#114720 = DIRECTION('ref_axis',(0.,0.707106781186548,-0.707106781186548)) ;
#114721 = DIRECTION('center_axis',(1.,0.,0.)) ;
#114722 = DIRECTION('ref_axis',(0.,0.,-1.)) ;
#114723 = DIRECTION('center_axis',(0.,-0.514231796959101,0.857651245551602)) ;
#114724 = DIRECTION('ref_axis',(0.,-0.857651245551602,-0.514231796959101)) ;
#114725 = DIRECTION('center_axis',(1.,0.,0.)) ;
#114726 = DIRECTION('ref_axis',(0.,0.,-1.)) ;
#114727 = DIRECTION('center_axis',(0.,8.67361737988405E-15,-1.)) ;
#114728 = DIRECTION('ref_axis',(0.,1.,8.67361737988405E-15)) ;
#114729 = DIRECTION('center_axis',(1.,0.,0.)) ;
#114730 = DIRECTION('ref_axis',(0.,0.,-1.)) ;
#114731 = DIRECTION('center_axis',(0.,0.,1.)) ;
#114732 = DIRECTION('ref_axis',(1.,0.,0.)) ;
#114733 = DIRECTION('center_axis',(0.,3.99416362155027E-15,1.)) ;
#114734 = DIRECTION('ref_axis',(0.,-1.,3.99416362155027E-15)) ;
#114735 = DIRECTION('center_axis',(0.,0.,-1.)) ;
#114736 = DIRECTION('ref_axis',(-1.,0.,0.)) ;
#114737 = DIRECTION('center_axis',(0.,0.,1.)) ;
#114738 = DIRECTION('ref_axis',(1.,0.,0.)) ;
#114739 = DIRECTION('center_axis',(0.,0.,1.)) ;
#114740 = DIRECTION('ref_axis',(1.,0.,0.)) ;
#114741 = DIRECTION('center_axis',(0.,1.,0.)) ;
#114742 = DIRECTION('ref_axis',(0.,0.,-1.)) ;
#114743 = DIRECTION('center_axis',(0.,-1.,0.)) ;
#114744 = DIRECTION('ref_axis',(0.,0.,-1.)) ;
#114745 = DIRECTION('center_axis',(1.,0.,0.)) ;
#114746 = DIRECTION('ref_axis',(0.,0.,-1.)) ;
#114747 = DIRECTION('center_axis',(0.,1.,0.)) ;
#114748 = DIRECTION('ref_axis',(0.,0.,1.)) ;
#114749 = DIRECTION('center_axis',(0.,1.,0.)) ;
#114750 = DIRECTION('ref_axis',(0.,0.,1.)) ;
#114751 = DIRECTION('center_axis',(0.,-1.,0.)) ;
#114752 = DIRECTION('ref_axis',(0.,0.,-1.)) ;
#114753 = DIRECTION('center_axis',(0.,1.,1.07081696047951E-16)) ;
#114754 = DIRECTION('ref_axis',(0.,-1.07081696047951E-16,1.)) ;
#114755 = DIRECTION('center_axis',(0.,1.,6.50521303491301E-15)) ;
#114756 = DIRECTION('ref_axis',(0.,-6.50521303491301E-15,1.)) ;
#114757 = DIRECTION('center_axis',(0.,1.,0.)) ;
#114758 = DIRECTION('ref_axis',(0.,0.,-1.)) ;
#114759 = DIRECTION('center_axis',(0.,0.,1.)) ;
#114760 = DIRECTION('ref_axis',(1.,0.,0.)) ;
#114761 = DIRECTION('center_axis',(1.,0.,0.)) ;
#114762 = DIRECTION('ref_axis',(0.,0.,-1.)) ;
#114763 = DIRECTION('center_axis',(0.,0.,-1.)) ;
#114764 = DIRECTION('ref_axis',(-1.,0.,0.)) ;
#114765 = DIRECTION('center_axis',(0.,0.,-1.)) ;
#114766 = DIRECTION('ref_axis',(-1.,0.,0.)) ;
#114767 = DIRECTION('center_axis',(0.,-1.,0.)) ;
#114768 = DIRECTION('ref_axis',(0.,0.,-1.)) ;
#114769 = DIRECTION('center_axis',(0.,1.,0.)) ;
#114770 = DIRECTION('ref_axis',(0.,0.,1.)) ;
#114771 = DIRECTION('center_axis',(0.,-1.,0.)) ;
#114772 = DIRECTION('ref_axis',(0.,0.,-1.)) ;
#114773 = DIRECTION('center_axis',(0.,1.,0.)) ;
#114774 = DIRECTION('ref_axis',(0.,0.,-1.)) ;
#114775 = DIRECTION('center_axis',(0.,0.,-1.)) ;
#114776 = DIRECTION('ref_axis',(-1.,0.,0.)) ;
#114777 = DIRECTION('center_axis',(0.,1.,0.)) ;
#114778 = DIRECTION('ref_axis',(0.,0.,-1.)) ;
#114779 = DIRECTION('center_axis',(0.,0.,-1.)) ;
#114780 = DIRECTION('ref_axis',(-1.,0.,0.)) ;
#114781 = DIRECTION('center_axis',(0.,0.,1.)) ;
#114782 = DIRECTION('ref_axis',(1.,0.,0.)) ;
#114783 = DIRECTION('center_axis',(0.,0.,-1.)) ;
#114784 = DIRECTION('ref_axis',(-1.,0.,0.)) ;
#114785 = DIRECTION('center_axis',(0.,0.,-1.)) ;
#114786 = DIRECTION('ref_axis',(-1.,0.,0.)) ;
#114787 = DIRECTION('center_axis',(0.,8.67361737988405E-15,-1.)) ;
#114788 = DIRECTION('ref_axis',(0.,1.,8.67361737988405E-15)) ;
#114789 = DIRECTION('center_axis',(1.,0.,0.)) ;
#114790 = DIRECTION('ref_axis',(0.,0.,-1.)) ;
#114791 = DIRECTION('center_axis',(0.,0.707106781186548,-0.707106781186548)) ;
#114792 = DIRECTION('ref_axis',(0.,0.707106781186548,0.707106781186548)) ;
#114793 = DIRECTION('center_axis',(1.,0.,0.)) ;
#114794 = DIRECTION('ref_axis',(0.,0.,-1.)) ;
#114795 = DIRECTION('center_axis',(0.,-1.,0.)) ;
#114796 = DIRECTION('ref_axis',(0.,0.,-1.)) ;
#114797 = DIRECTION('center_axis',(0.,-0.707106781186548,0.707106781186547)) ;
#114798 = DIRECTION('ref_axis',(0.,-0.707106781186547,-0.707106781186548)) ;
#114799 = DIRECTION('center_axis',(0.,-1.,-1.07081696047951E-16)) ;
#114800 = DIRECTION('ref_axis',(0.,1.07081696047951E-16,-1.)) ;
#114801 = DIRECTION('center_axis',(0.,-1.,-8.67361737988401E-15)) ;
#114802 = DIRECTION('ref_axis',(0.,8.67361737988401E-15,-1.)) ;
#114803 = DIRECTION('center_axis',(1.,0.,0.)) ;
#114804 = DIRECTION('ref_axis',(0.,0.,-1.)) ;
#114805 = DIRECTION('center_axis',(0.,0.,1.)) ;
#114806 = DIRECTION('ref_axis',(1.,0.,0.)) ;
#114807 = DIRECTION('center_axis',(0.,0.,-1.)) ;
#114808 = DIRECTION('ref_axis',(-1.,0.,0.)) ;
#114809 = DIRECTION('center_axis',(0.,0.,1.)) ;
#114810 = DIRECTION('ref_axis',(1.,0.,0.)) ;
#114811 = DIRECTION('center_axis',(0.,0.,1.)) ;
#114812 = DIRECTION('ref_axis',(1.,0.,0.)) ;
#114813 = DIRECTION('center_axis',(0.,0.,1.)) ;
#114814 = DIRECTION('ref_axis',(1.,0.,0.)) ;
#114815 = DIRECTION('center_axis',(1.,0.,0.)) ;
#114816 = DIRECTION('ref_axis',(0.,0.38268343236509,0.923879532511287)) ;
#114817 = DIRECTION('center_axis',(0.,-0.70710678118655,-0.707106781186545)) ;
#114818 = DIRECTION('ref_axis',(0.,0.707106781186545,-0.70710678118655)) ;
#114819 = DIRECTION('center_axis',(1.,0.,0.)) ;
#114820 = DIRECTION('ref_axis',(0.,0.,-1.)) ;
#114821 = DIRECTION('center_axis',(0.,0.514231796959101,0.857651245551602)) ;
#114822 = DIRECTION('ref_axis',(0.,-0.857651245551602,0.514231796959101)) ;
#114823 = DIRECTION('center_axis',(0.,0.707106781186546,0.707106781186549)) ;
#114824 = DIRECTION('ref_axis',(0.,-0.707106781186549,0.707106781186546)) ;
#114825 = DIRECTION('center_axis',(1.88079096131567E-29,-0.707106781186545,
-0.70710678118655)) ;
#114826 = DIRECTION('ref_axis',(7.62257770433106E-46,0.70710678118655,-0.707106781186545)) ;
#114827 = DIRECTION('center_axis',(1.,0.,0.)) ;
#114828 = DIRECTION('ref_axis',(0.,0.,-1.)) ;
#114829 = DIRECTION('center_axis',(0.,-0.514231796959101,0.857651245551602)) ;
#114830 = DIRECTION('ref_axis',(0.,-0.857651245551602,-0.514231796959101)) ;
#114831 = DIRECTION('center_axis',(1.,0.,0.)) ;
#114832 = DIRECTION('ref_axis',(0.,0.,-1.)) ;
#114833 = DIRECTION('center_axis',(0.,0.,-1.)) ;
#114834 = DIRECTION('ref_axis',(-1.,0.,0.)) ;
#114835 = DIRECTION('center_axis',(1.,0.,0.)) ;
#114836 = DIRECTION('ref_axis',(0.,0.,-1.)) ;
#114837 = DIRECTION('center_axis',(0.,0.,1.)) ;
#114838 = DIRECTION('ref_axis',(1.,0.,0.)) ;
#114839 = DIRECTION('center_axis',(0.,3.99416362155027E-15,1.)) ;
#114840 = DIRECTION('ref_axis',(0.,-1.,3.99416362155027E-15)) ;
#114841 = DIRECTION('center_axis',(0.,-4.33680868994202E-15,-1.)) ;
#114842 = DIRECTION('ref_axis',(0.,1.,-4.33680868994202E-15)) ;
#114843 = DIRECTION('center_axis',(0.,0.,1.)) ;
#114844 = DIRECTION('ref_axis',(1.,0.,0.)) ;
#114845 = DIRECTION('center_axis',(0.,-4.33680868994202E-15,1.)) ;
#114846 = DIRECTION('ref_axis',(0.,-1.,-4.33680868994202E-15)) ;
#114847 = DIRECTION('center_axis',(0.,1.,0.)) ;
#114848 = DIRECTION('ref_axis',(0.,0.,-1.)) ;
#114849 = DIRECTION('center_axis',(0.,-1.,0.)) ;
#114850 = DIRECTION('ref_axis',(0.,0.,-1.)) ;
#114851 = DIRECTION('center_axis',(1.,0.,0.)) ;
#114852 = DIRECTION('ref_axis',(0.,0.,-1.)) ;
#114853 = DIRECTION('center_axis',(0.,1.,0.)) ;
#114854 = DIRECTION('ref_axis',(0.,0.,1.)) ;
#114855 = DIRECTION('center_axis',(0.,1.,0.)) ;
#114856 = DIRECTION('ref_axis',(0.,0.,1.)) ;
#114857 = DIRECTION('center_axis',(0.,-1.,0.)) ;
#114858 = DIRECTION('ref_axis',(0.,0.,-1.)) ;
#114859 = DIRECTION('center_axis',(0.,1.,1.07081696047951E-16)) ;
#114860 = DIRECTION('ref_axis',(0.,-1.07081696047951E-16,1.)) ;
#114861 = DIRECTION('center_axis',(0.,1.,6.50521303491304E-15)) ;
#114862 = DIRECTION('ref_axis',(0.,-6.50521303491304E-15,1.)) ;
#114863 = DIRECTION('center_axis',(0.,1.,0.)) ;
#114864 = DIRECTION('ref_axis',(0.,0.,-1.)) ;
#114865 = DIRECTION('center_axis',(0.,0.,1.)) ;
#114866 = DIRECTION('ref_axis',(1.,0.,0.)) ;
#114867 = DIRECTION('center_axis',(1.,0.,0.)) ;
#114868 = DIRECTION('ref_axis',(0.,0.,-1.)) ;
#114869 = DIRECTION('center_axis',(0.,0.,-1.)) ;
#114870 = DIRECTION('ref_axis',(-1.,0.,0.)) ;
#114871 = DIRECTION('center_axis',(0.,0.,-1.)) ;
#114872 = DIRECTION('ref_axis',(-1.,0.,0.)) ;
#114873 = DIRECTION('center_axis',(1.53063836115601E-16,-1.,-1.30104260698261E-16)) ;
#114874 = DIRECTION('ref_axis',(1.,1.53063836115601E-16,1.99142572374599E-32)) ;
#114875 = DIRECTION('center_axis',(0.,1.,0.)) ;
#114876 = DIRECTION('ref_axis',(0.,0.,1.)) ;
#114877 = DIRECTION('center_axis',(0.,-1.,0.)) ;
#114878 = DIRECTION('ref_axis',(0.,0.,-1.)) ;
#114879 = DIRECTION('center_axis',(1.,1.53063836115601E-16,2.73691106313441E-48)) ;
#114880 = DIRECTION('ref_axis',(-1.53063836115601E-16,1.,-4.18922106430579E-64)) ;
#114881 = DIRECTION('center_axis',(-1.,0.,0.)) ;
#114882 = DIRECTION('ref_axis',(0.,0.,1.)) ;
#114883 = DIRECTION('center_axis',(1.,1.53063836115601E-16,0.)) ;
#114884 = DIRECTION('ref_axis',(1.53063836115601E-16,-1.,0.)) ;
#114885 = DIRECTION('center_axis',(0.,1.,0.)) ;
#114886 = DIRECTION('ref_axis',(1.,0.,0.)) ;
#114887 = DIRECTION('center_axis',(0.,1.,0.)) ;
#114888 = DIRECTION('ref_axis',(0.,0.,-1.)) ;
#114889 = DIRECTION('center_axis',(0.,0.,1.)) ;
#114890 = DIRECTION('ref_axis',(-1.,0.,0.)) ;
#114891 = DIRECTION('center_axis',(0.,1.,0.)) ;
#114892 = DIRECTION('ref_axis',(1.,0.,0.)) ;
#114893 = DIRECTION('center_axis',(0.,0.,1.)) ;
#114894 = DIRECTION('ref_axis',(-1.,0.,0.)) ;
#114895 = DIRECTION('center_axis',(1.,1.0842021724855E-15,0.)) ;
#114896 = DIRECTION('ref_axis',(1.0842021724855E-15,-1.,0.)) ;
#114897 = DIRECTION('center_axis',(-1.,-1.53063836115601E-16,0.)) ;
#114898 = DIRECTION('ref_axis',(0.,-1.,0.)) ;
#114899 = DIRECTION('center_axis',(0.,0.,-1.)) ;
#114900 = DIRECTION('ref_axis',(1.,0.,0.)) ;
#114901 = DIRECTION('center_axis',(0.,0.,-1.)) ;
#114902 = DIRECTION('ref_axis',(0.804034447892619,0.594582716366707,0.)) ;
#114903 = DIRECTION('center_axis',(0.,0.,1.)) ;
#114904 = DIRECTION('ref_axis',(1.,0.,0.)) ;
#114905 = DIRECTION('',(0.,0.,-1.)) ;
#114906 = DIRECTION('center_axis',(-2.16840434497101E-16,1.,1.30104260698261E-16)) ;
#114907 = DIRECTION('ref_axis',(1.,2.16840434497101E-16,1.22464679914735E-16)) ;
#114908 = DIRECTION('',(-2.16840434497101E-16,1.,1.30104260698261E-16)) ;
#114909 = DIRECTION('center_axis',(0.,1.,0.)) ;
#114910 = DIRECTION('ref_axis',(0.,0.,1.)) ;
#114911 = DIRECTION('center_axis',(-1.,-1.53063836115601E-16,-2.73691106313441E-48)) ;
#114912 = DIRECTION('ref_axis',(1.53063836115601E-16,-1.,4.18922106430579E-64)) ;
#114913 = DIRECTION('center_axis',(1.,2.16840434497101E-16,0.)) ;
#114914 = DIRECTION('ref_axis',(2.16840434497101E-16,-1.,0.)) ;
#114915 = DIRECTION('center_axis',(0.,0.,1.)) ;
#114916 = DIRECTION('ref_axis',(1.,0.,0.)) ;
#114917 = DIRECTION('center_axis',(-1.25542992828747E-32,1.020425574104E-16,
1.)) ;
#114918 = DIRECTION('ref_axis',(-1.28107280532009E-48,-1.,1.020425574104E-16)) ;
#114919 = DIRECTION('center_axis',(0.,0.,1.)) ;
#114920 = DIRECTION('ref_axis',(1.,0.,0.)) ;
#114921 = DIRECTION('center_axis',(0.,0.,-1.)) ;
#114922 = DIRECTION('ref_axis',(-1.,0.,0.)) ;
#114923 = DIRECTION('center_axis',(1.,1.53063836115601E-16,-2.73691106313441E-48)) ;
#114924 = DIRECTION('ref_axis',(-1.53063836115601E-16,1.,4.18922106430579E-64)) ;
#114925 = DIRECTION('center_axis',(-1.,0.,0.)) ;
#114926 = DIRECTION('ref_axis',(0.,0.,1.)) ;
#114927 = DIRECTION('center_axis',(1.,1.53063836115601E-16,0.)) ;
#114928 = DIRECTION('ref_axis',(1.53063836115601E-16,-1.,0.)) ;
#114929 = DIRECTION('center_axis',(0.,1.,0.)) ;
#114930 = DIRECTION('ref_axis',(1.,0.,0.)) ;
#114931 = DIRECTION('center_axis',(-1.,-2.16840434497101E-16,0.)) ;
#114932 = DIRECTION('ref_axis',(0.,-1.,0.)) ;
#114933 = DIRECTION('center_axis',(0.,0.,-1.)) ;
#114934 = DIRECTION('ref_axis',(1.,0.,0.)) ;
#114935 = DIRECTION('center_axis',(-1.25542992828747E-32,1.020425574104E-16,
1.)) ;
#114936 = DIRECTION('ref_axis',(0.,-1.,0.)) ;
#114937 = DIRECTION('center_axis',(0.,-1.,0.)) ;
#114938 = DIRECTION('ref_axis',(-6.50521303491301E-15,0.,1.)) ;
#114939 = DIRECTION('center_axis',(-1.,0.,0.)) ;
#114940 = DIRECTION('ref_axis',(0.,0.,-1.)) ;
#114941 = DIRECTION('center_axis',(-1.,-1.53063836115601E-16,0.)) ;
#114942 = DIRECTION('ref_axis',(0.,-1.,0.)) ;
#114943 = DIRECTION('center_axis',(0.,-1.,0.)) ;
#114944 = DIRECTION('ref_axis',(0.,0.,1.)) ;
#114945 = DIRECTION('center_axis',(0.,0.,-1.)) ;
#114946 = DIRECTION('ref_axis',(-1.,0.,0.)) ;
#114947 = DIRECTION('center_axis',(0.,0.,-1.)) ;
#114948 = DIRECTION('ref_axis',(-1.,0.,0.)) ;
#114949 = DIRECTION('center_axis',(1.,1.53063836115601E-16,-3.06472600140763E-33)) ;
#114950 = DIRECTION('ref_axis',(-1.53063836115601E-16,1.,4.69098718418678E-49)) ;
#114951 = DIRECTION('center_axis',(-1.,0.,0.)) ;
#114952 = DIRECTION('ref_axis',(0.,0.,1.)) ;
#114953 = DIRECTION('center_axis',(-1.53063836115601E-16,1.,-1.020425574104E-16)) ;
#114954 = DIRECTION('ref_axis',(-1.,-1.53063836115601E-16,1.3684555315672E-47)) ;
#114955 = DIRECTION('',(1.53063836115601E-16,-1.,1.020425574104E-16)) ;
#114956 = DIRECTION('center_axis',(0.,-1.,0.)) ;
#114957 = DIRECTION('ref_axis',(0.,0.,-1.)) ;
#114958 = DIRECTION('center_axis',(-1.53063836115601E-16,1.,-1.30104260698261E-16)) ;
#114959 = DIRECTION('ref_axis',(-1.,-1.53063836115601E-16,1.99142572374599E-32)) ;
#114960 = DIRECTION('center_axis',(0.,-1.,0.)) ;
#114961 = DIRECTION('ref_axis',(0.,0.,-1.)) ;
#114962 = DIRECTION('center_axis',(-1.,-1.53063836115601E-16,2.73691106313441E-48)) ;
#114963 = DIRECTION('ref_axis',(1.53063836115601E-16,-1.,-4.18922106430579E-64)) ;
#114964 = DIRECTION('center_axis',(1.,2.16840434497101E-16,0.)) ;
#114965 = DIRECTION('ref_axis',(2.16840434497101E-16,-1.,0.)) ;
#114966 = DIRECTION('center_axis',(-1.,0.,2.16840434497102E-15)) ;
#114967 = DIRECTION('ref_axis',(2.16840434497102E-15,0.,1.)) ;
#114968 = DIRECTION('center_axis',(-1.,-2.16840434497101E-16,0.)) ;
#114969 = DIRECTION('ref_axis',(0.,-1.,0.)) ;
#114970 = DIRECTION('center_axis',(0.,0.,1.)) ;
#114971 = DIRECTION('ref_axis',(-1.,0.,0.)) ;
#114972 = DIRECTION('center_axis',(0.,1.,0.)) ;
#114973 = DIRECTION('ref_axis',(1.,0.,0.)) ;
#114974 = DIRECTION('center_axis',(0.,1.,0.)) ;
#114975 = DIRECTION('ref_axis',(0.,0.,-1.)) ;
#114976 = DIRECTION('center_axis',(1.,0.,0.)) ;
#114977 = DIRECTION('ref_axis',(0.,-1.,0.)) ;
#114978 = DIRECTION('center_axis',(1.,6.50521303491304E-15,0.)) ;
#114979 = DIRECTION('ref_axis',(-6.50521303491304E-15,1.,0.)) ;
#114980 = DIRECTION('center_axis',(8.67361737988403E-15,1.,0.)) ;
#114981 = DIRECTION('ref_axis',(-1.,8.67361737988403E-15,0.)) ;
#114982 = DIRECTION('center_axis',(1.2303003375722E-16,-1.,1.020425574104E-16)) ;
#114983 = DIRECTION('ref_axis',(1.,1.2303003375722E-16,-1.25542992828747E-32)) ;
#114984 = DIRECTION('center_axis',(0.,1.,0.)) ;
#114985 = DIRECTION('ref_axis',(0.,0.,1.)) ;
#114986 = DIRECTION('center_axis',(0.,1.,0.)) ;
#114987 = DIRECTION('ref_axis',(1.,0.,0.)) ;
#114988 = DIRECTION('center_axis',(1.,1.2303003375722E-16,0.)) ;
#114989 = DIRECTION('ref_axis',(1.2303003375722E-16,-1.,0.)) ;
#114990 = DIRECTION('center_axis',(0.,0.,1.)) ;
#114991 = DIRECTION('ref_axis',(-1.,0.,0.)) ;
#114992 = DIRECTION('center_axis',(0.,1.,0.)) ;
#114993 = DIRECTION('ref_axis',(1.,0.,0.)) ;
#114994 = DIRECTION('center_axis',(0.,0.,-1.)) ;
#114995 = DIRECTION('ref_axis',(1.,0.,0.)) ;
#114996 = DIRECTION('center_axis',(0.,0.,-1.)) ;
#114997 = DIRECTION('ref_axis',(-1.,0.,0.)) ;
#114998 = DIRECTION('center_axis',(0.,0.,1.)) ;
#114999 = DIRECTION('ref_axis',(1.,0.,0.)) ;
#115000 = DIRECTION('center_axis',(-2.16840434497101E-16,1.,-1.020425574104E-16)) ;
#115001 = DIRECTION('ref_axis',(-1.,-2.16840434497101E-16,5.47382212626882E-48)) ;
#115002 = DIRECTION('center_axis',(0.,1.,0.)) ;
#115003 = DIRECTION('ref_axis',(0.,0.,-1.)) ;
#115004 = DIRECTION('center_axis',(1.,0.,1.25542992828747E-32)) ;
#115005 = DIRECTION('ref_axis',(1.25542992828747E-32,0.,-1.)) ;
#115006 = DIRECTION('center_axis',(1.,0.,0.)) ;
#115007 = DIRECTION('ref_axis',(0.,0.,-1.)) ;
#115008 = DIRECTION('center_axis',(-1.,-1.2303003375722E-16,0.)) ;
#115009 = DIRECTION('ref_axis',(0.,-1.,0.)) ;
#115010 = DIRECTION('center_axis',(0.,0.,-1.)) ;
#115011 = DIRECTION('ref_axis',(1.,0.,0.)) ;
#115012 = DIRECTION('center_axis',(0.,0.,-1.)) ;
#115013 = DIRECTION('ref_axis',(-1.,0.,0.)) ;
#115014 = DIRECTION('',(0.,0.,1.)) ;
#115015 = DIRECTION('center_axis',(0.,0.,1.)) ;
#115016 = DIRECTION('ref_axis',(1.,0.,0.)) ;
#115017 = DIRECTION('center_axis',(0.,0.,1.)) ;
#115018 = DIRECTION('ref_axis',(1.,0.,0.)) ;
#115019 = DIRECTION('center_axis',(6.27714964143733E-33,-5.10212787052002E-17,
-1.)) ;
#115020 = DIRECTION('ref_axis',(3.20268201330022E-49,1.,-5.10212787052002E-17)) ;
#115021 = DIRECTION('center_axis',(1.,1.53063836115601E-16,-1.53236300070382E-33)) ;
#115022 = DIRECTION('ref_axis',(-1.53063836115601E-16,1.,2.34549359209339E-49)) ;
#115023 = DIRECTION('center_axis',(-1.,0.,0.)) ;
#115024 = DIRECTION('ref_axis',(0.,0.,1.)) ;
#115025 = DIRECTION('center_axis',(1.,0.,0.)) ;
#115026 = DIRECTION('ref_axis',(0.,0.,-1.)) ;
#115027 = DIRECTION('center_axis',(0.,1.,0.)) ;
#115028 = DIRECTION('ref_axis',(1.,0.,0.)) ;
#115029 = DIRECTION('center_axis',(-4.33680868994202E-15,1.,0.)) ;
#115030 = DIRECTION('ref_axis',(1.,4.33680868994202E-15,0.)) ;
#115031 = DIRECTION('center_axis',(0.,-1.,0.)) ;
#115032 = DIRECTION('ref_axis',(0.,0.,-1.)) ;
#115033 = DIRECTION('center_axis',(0.,0.,-1.)) ;
#115034 = DIRECTION('ref_axis',(1.,0.,0.)) ;
#115035 = DIRECTION('center_axis',(0.,0.,1.)) ;
#115036 = DIRECTION('ref_axis',(1.,0.,0.)) ;
#115037 = DIRECTION('center_axis',(0.,0.,-1.)) ;
#115038 = DIRECTION('ref_axis',(-1.,0.,0.)) ;
#115039 = DIRECTION('center_axis',(0.,1.,0.)) ;
#115040 = DIRECTION('ref_axis',(1.,0.,0.)) ;
#115041 = DIRECTION('center_axis',(1.,1.2303003375722E-16,0.)) ;
#115042 = DIRECTION('ref_axis',(1.2303003375722E-16,-1.,0.)) ;
#115043 = DIRECTION('center_axis',(0.,1.,0.)) ;
#115044 = DIRECTION('ref_axis',(-6.50521303491307E-15,0.,-1.)) ;
#115045 = DIRECTION('center_axis',(6.27714964143733E-33,-5.10212787052002E-17,
-1.)) ;
#115046 = DIRECTION('ref_axis',(0.,1.,0.)) ;
#115047 = DIRECTION('center_axis',(0.,-1.,0.)) ;
#115048 = DIRECTION('ref_axis',(0.,0.,1.)) ;
#115049 = DIRECTION('center_axis',(2.16840434497101E-16,-1.,5.10212787052002E-17)) ;
#115050 = DIRECTION('ref_axis',(1.,2.16840434497101E-16,-5.47382212626882E-48)) ;
#115051 = DIRECTION('center_axis',(0.,1.,0.)) ;
#115052 = DIRECTION('ref_axis',(0.,0.,-1.)) ;
#115053 = DIRECTION('center_axis',(0.,0.,1.)) ;
#115054 = DIRECTION('ref_axis',(1.,0.,0.)) ;
#115055 = DIRECTION('center_axis',(0.,0.,-1.)) ;
#115056 = DIRECTION('ref_axis',(-1.,0.,0.)) ;
#115057 = DIRECTION('center_axis',(-1.,-1.2303003375722E-16,0.)) ;
#115058 = DIRECTION('ref_axis',(0.,-1.,0.)) ;
#115059 = DIRECTION('center_axis',(0.,-1.,0.)) ;
#115060 = DIRECTION('ref_axis',(0.,0.,1.)) ;
#115061 = DIRECTION('center_axis',(1.53063836115601E-16,-1.,5.10212787052002E-17)) ;
#115062 = DIRECTION('ref_axis',(1.,1.53063836115601E-16,-6.84227765783602E-48)) ;
#115063 = DIRECTION('',(-1.53063836115601E-16,1.,-5.10212787052002E-17)) ;
#115064 = DIRECTION('center_axis',(0.,-1.,0.)) ;
#115065 = DIRECTION('ref_axis',(0.,0.,-1.)) ;
#115066 = DIRECTION('center_axis',(-1.,0.,0.)) ;
#115067 = DIRECTION('ref_axis',(0.,0.,-1.)) ;
#115068 = DIRECTION('center_axis',(-1.2303003375722E-16,1.,-5.10212787052002E-17)) ;
#115069 = DIRECTION('ref_axis',(-1.,-1.2303003375722E-16,6.27714964143733E-33)) ;
#115070 = DIRECTION('center_axis',(-8.67361737988403E-15,-1.,0.)) ;
#115071 = DIRECTION('ref_axis',(1.,-8.67361737988403E-15,0.)) ;
#115072 = DIRECTION('center_axis',(1.,0.,6.27714964143733E-33)) ;
#115073 = DIRECTION('ref_axis',(6.27714964143733E-33,0.,-1.)) ;
#115074 = DIRECTION('center_axis',(-1.,0.,-6.50521303491318E-15)) ;
#115075 = DIRECTION('ref_axis',(-6.50521303491318E-15,0.,1.)) ;
#115076 = DIRECTION('center_axis',(1.,0.,0.)) ;
#115077 = DIRECTION('ref_axis',(0.,1.,0.)) ;
#115078 = DIRECTION('center_axis',(0.,0.,-1.)) ;
#115079 = DIRECTION('ref_axis',(-1.,0.,0.)) ;
#115080 = DIRECTION('center_axis',(0.,0.,1.)) ;
#115081 = DIRECTION('ref_axis',(1.,0.,0.)) ;
#115082 = DIRECTION('center_axis',(0.,0.,-1.)) ;
#115083 = DIRECTION('ref_axis',(-1.,0.,0.)) ;
#115084 = DIRECTION('center_axis',(-1.,0.,0.)) ;
#115085 = DIRECTION('ref_axis',(0.,0.,1.)) ;
#115086 = DIRECTION('center_axis',(0.,-1.,0.)) ;
#115087 = DIRECTION('ref_axis',(0.,0.,-1.)) ;
#115088 = DIRECTION('center_axis',(0.,1.,0.)) ;
#115089 = DIRECTION('ref_axis',(0.,0.,1.)) ;
#115090 = DIRECTION('center_axis',(0.,1.,-6.50521303491307E-15)) ;
#115091 = DIRECTION('ref_axis',(0.,6.50521303491307E-15,1.)) ;
#115092 = DIRECTION('center_axis',(0.,-1.,0.)) ;
#115093 = DIRECTION('ref_axis',(0.,0.,-1.)) ;
#115094 = DIRECTION('center_axis',(0.,-1.,0.)) ;
#115095 = DIRECTION('ref_axis',(0.,0.,-1.)) ;
#115096 = DIRECTION('center_axis',(0.,-1.,-1.07081696047951E-16)) ;
#115097 = DIRECTION('ref_axis',(0.,1.07081696047951E-16,-1.)) ;
#115098 = DIRECTION('center_axis',(0.,1.,0.)) ;
#115099 = DIRECTION('ref_axis',(0.,0.,1.)) ;
#115100 = DIRECTION('center_axis',(-1.,0.,0.)) ;
#115101 = DIRECTION('ref_axis',(0.,0.,1.)) ;
#115102 = DIRECTION('center_axis',(0.,0.,1.)) ;
#115103 = DIRECTION('ref_axis',(1.,0.,0.)) ;
#115104 = DIRECTION('center_axis',(0.,1.,0.)) ;
#115105 = DIRECTION('ref_axis',(0.,0.,1.)) ;
#115106 = DIRECTION('center_axis',(0.,-1.73472347597681E-14,-1.)) ;
#115107 = DIRECTION('ref_axis',(0.,1.,-1.73472347597681E-14)) ;
#115108 = DIRECTION('center_axis',(0.,0.,1.)) ;
#115109 = DIRECTION('ref_axis',(1.,0.,0.)) ;
#115110 = DIRECTION('center_axis',(0.,0.,1.)) ;
#115111 = DIRECTION('ref_axis',(1.,0.,0.)) ;
#115112 = DIRECTION('center_axis',(0.,0.,1.)) ;
#115113 = DIRECTION('ref_axis',(1.,0.,0.)) ;
#115114 = DIRECTION('center_axis',(0.,0.,-1.)) ;
#115115 = DIRECTION('ref_axis',(-1.,0.,0.)) ;
#115116 = DIRECTION('center_axis',(0.,1.,0.)) ;
#115117 = DIRECTION('ref_axis',(0.,0.,1.)) ;
#115118 = DIRECTION('center_axis',(0.,-0.707106781186545,0.70710678118655)) ;
#115119 = DIRECTION('ref_axis',(0.,-0.70710678118655,-0.707106781186545)) ;
#115120 = DIRECTION('center_axis',(0.,1.,0.)) ;
#115121 = DIRECTION('ref_axis',(0.,0.,1.)) ;
#115122 = DIRECTION('center_axis',(0.,-0.514231796959109,-0.857651245551597)) ;
#115123 = DIRECTION('ref_axis',(0.,0.857651245551597,-0.514231796959109)) ;
#115124 = DIRECTION('center_axis',(0.,-0.707106781186548,0.707106781186547)) ;
#115125 = DIRECTION('ref_axis',(0.,-0.707106781186547,-0.707106781186548)) ;
#115126 = DIRECTION('center_axis',(0.,-0.707106781186548,0.707106781186548)) ;
#115127 = DIRECTION('ref_axis',(0.,-0.707106781186548,-0.707106781186548)) ;
#115128 = DIRECTION('center_axis',(-1.,0.,0.)) ;
#115129 = DIRECTION('ref_axis',(0.,0.,1.)) ;
#115130 = DIRECTION('center_axis',(0.,0.514231796959101,-0.857651245551602)) ;
#115131 = DIRECTION('ref_axis',(0.,0.857651245551602,0.514231796959101)) ;
#115132 = DIRECTION('center_axis',(0.,1.,0.)) ;
#115133 = DIRECTION('ref_axis',(0.,0.,1.)) ;
#115134 = DIRECTION('center_axis',(0.,0.,-1.)) ;
#115135 = DIRECTION('ref_axis',(-1.,0.,0.)) ;
#115136 = DIRECTION('center_axis',(0.,1.,0.)) ;
#115137 = DIRECTION('ref_axis',(0.,0.,1.)) ;
#115138 = DIRECTION('center_axis',(0.,0.,-1.)) ;
#115139 = DIRECTION('ref_axis',(-1.,0.,0.)) ;
#115140 = DIRECTION('center_axis',(0.,0.,-1.)) ;
#115141 = DIRECTION('ref_axis',(-1.,0.,0.)) ;
#115142 = DIRECTION('center_axis',(0.,0.,1.)) ;
#115143 = DIRECTION('ref_axis',(1.,0.,0.)) ;
#115144 = DIRECTION('center_axis',(0.,0.,-1.)) ;
#115145 = DIRECTION('ref_axis',(-1.,0.,0.)) ;
#115146 = DIRECTION('center_axis',(0.,1.,0.)) ;
#115147 = DIRECTION('ref_axis',(0.,0.,1.)) ;
#115148 = DIRECTION('center_axis',(0.,-1.,8.67361737988401E-15)) ;
#115149 = DIRECTION('ref_axis',(0.,-8.67361737988401E-15,-1.)) ;
#115150 = DIRECTION('center_axis',(0.,0.707106781186546,0.707106781186549)) ;
#115151 = DIRECTION('ref_axis',(0.,-0.707106781186549,0.707106781186546)) ;
#115152 = DIRECTION('center_axis',(0.,0.707106781186548,0.707106781186548)) ;
#115153 = DIRECTION('ref_axis',(0.,-0.707106781186548,0.707106781186548)) ;
#115154 = DIRECTION('center_axis',(0.,1.,1.07081696047951E-16)) ;
#115155 = DIRECTION('ref_axis',(0.,-1.07081696047951E-16,1.)) ;
#115156 = DIRECTION('center_axis',(0.,-1.,0.)) ;
#115157 = DIRECTION('ref_axis',(0.,0.,-1.)) ;
#115158 = DIRECTION('center_axis',(0.,1.,0.)) ;
#115159 = DIRECTION('ref_axis',(0.,0.,1.)) ;
#115160 = DIRECTION('center_axis',(0.,-8.67361737988409E-15,1.)) ;
#115161 = DIRECTION('ref_axis',(0.,-1.,-8.67361737988409E-15)) ;
#115162 = DIRECTION('center_axis',(0.,1.,0.)) ;
#115163 = DIRECTION('ref_axis',(0.,0.,1.)) ;
#115164 = DIRECTION('center_axis',(0.,8.67361737988403E-15,1.)) ;
#115165 = DIRECTION('ref_axis',(0.,-1.,8.67361737988403E-15)) ;
#115166 = DIRECTION('center_axis',(0.,3.99416362155027E-15,1.)) ;
#115167 = DIRECTION('ref_axis',(0.,-1.,3.99416362155027E-15)) ;
#115168 = DIRECTION('center_axis',(0.,0.,1.)) ;
#115169 = DIRECTION('ref_axis',(1.,0.,0.)) ;
#115170 = DIRECTION('center_axis',(0.,0.,-1.)) ;
#115171 = DIRECTION('ref_axis',(-1.,0.,0.)) ;
#115172 = DIRECTION('center_axis',(0.,0.,1.)) ;
#115173 = DIRECTION('ref_axis',(1.,0.,0.)) ;
#115174 = DIRECTION('center_axis',(-1.,0.,0.)) ;
#115175 = DIRECTION('ref_axis',(0.,0.,1.)) ;
#115176 = DIRECTION('center_axis',(0.,1.,0.)) ;
#115177 = DIRECTION('ref_axis',(0.,0.,1.)) ;
#115178 = DIRECTION('center_axis',(-1.,0.,0.)) ;
#115179 = DIRECTION('ref_axis',(0.,0.,1.)) ;
#115180 = DIRECTION('center_axis',(0.,-1.,0.)) ;
#115181 = DIRECTION('ref_axis',(0.,0.,-1.)) ;
#115182 = DIRECTION('center_axis',(0.,1.,0.)) ;
#115183 = DIRECTION('ref_axis',(0.,0.,1.)) ;
#115184 = DIRECTION('center_axis',(1.53063836115601E-16,-1.,-1.30104260698261E-16)) ;
#115185 = DIRECTION('ref_axis',(1.,1.53063836115601E-16,1.99142572374599E-32)) ;
#115186 = DIRECTION('center_axis',(0.,1.,0.)) ;
#115187 = DIRECTION('ref_axis',(0.,0.,1.)) ;
#115188 = DIRECTION('center_axis',(0.,-1.,0.)) ;
#115189 = DIRECTION('ref_axis',(0.,0.,-1.)) ;
#115190 = DIRECTION('center_axis',(1.,1.53063836115601E-16,2.73691106313441E-48)) ;
#115191 = DIRECTION('ref_axis',(-1.53063836115601E-16,1.,-4.18922106430579E-64)) ;
#115192 = DIRECTION('center_axis',(-1.,0.,0.)) ;
#115193 = DIRECTION('ref_axis',(0.,0.,1.)) ;
#115194 = DIRECTION('center_axis',(1.,1.53063836115601E-16,0.)) ;
#115195 = DIRECTION('ref_axis',(1.53063836115601E-16,-1.,0.)) ;
#115196 = DIRECTION('center_axis',(0.,1.,0.)) ;
#115197 = DIRECTION('ref_axis',(1.,0.,0.)) ;
#115198 = DIRECTION('center_axis',(0.,1.,0.)) ;
#115199 = DIRECTION('ref_axis',(0.,0.,-1.)) ;
#115200 = DIRECTION('center_axis',(0.,0.,1.)) ;
#115201 = DIRECTION('ref_axis',(-1.,0.,0.)) ;
#115202 = DIRECTION('center_axis',(0.,1.,0.)) ;
#115203 = DIRECTION('ref_axis',(1.,0.,0.)) ;
#115204 = DIRECTION('center_axis',(0.,0.,1.)) ;
#115205 = DIRECTION('ref_axis',(-1.,0.,0.)) ;
#115206 = DIRECTION('center_axis',(1.,1.0842021724855E-15,0.)) ;
#115207 = DIRECTION('ref_axis',(1.0842021724855E-15,-1.,0.)) ;
#115208 = DIRECTION('center_axis',(-1.,-1.53063836115601E-16,0.)) ;
#115209 = DIRECTION('ref_axis',(0.,-1.,0.)) ;
#115210 = DIRECTION('center_axis',(0.,0.,-1.)) ;
#115211 = DIRECTION('ref_axis',(1.,0.,0.)) ;
#115212 = DIRECTION('center_axis',(0.,0.,-1.)) ;
#115213 = DIRECTION('ref_axis',(0.804034447892625,0.594582716366698,0.)) ;
#115214 = DIRECTION('center_axis',(0.,0.,1.)) ;
#115215 = DIRECTION('ref_axis',(1.,0.,0.)) ;
#115216 = DIRECTION('',(0.,0.,-1.)) ;
#115217 = DIRECTION('center_axis',(-2.16840434497101E-16,1.,1.30104260698261E-16)) ;
#115218 = DIRECTION('ref_axis',(1.,2.16840434497101E-16,1.22464679914735E-16)) ;
#115219 = DIRECTION('',(-2.16840434497101E-16,1.,1.30104260698261E-16)) ;
#115220 = DIRECTION('center_axis',(0.,1.,0.)) ;
#115221 = DIRECTION('ref_axis',(0.,0.,1.)) ;
#115222 = DIRECTION('center_axis',(-1.,-1.53063836115601E-16,-2.73691106313441E-48)) ;
#115223 = DIRECTION('ref_axis',(1.53063836115601E-16,-1.,4.18922106430579E-64)) ;
#115224 = DIRECTION('center_axis',(1.,2.16840434497101E-16,0.)) ;
#115225 = DIRECTION('ref_axis',(2.16840434497101E-16,-1.,0.)) ;
#115226 = DIRECTION('center_axis',(0.,0.,1.)) ;
#115227 = DIRECTION('ref_axis',(1.,0.,0.)) ;
#115228 = DIRECTION('center_axis',(-1.25542992828747E-32,1.020425574104E-16,
1.)) ;
#115229 = DIRECTION('ref_axis',(-1.28107280532009E-48,-1.,1.020425574104E-16)) ;
#115230 = DIRECTION('center_axis',(0.,0.,1.)) ;
#115231 = DIRECTION('ref_axis',(1.,0.,0.)) ;
#115232 = DIRECTION('center_axis',(0.,0.,-1.)) ;
#115233 = DIRECTION('ref_axis',(-1.,0.,0.)) ;
#115234 = DIRECTION('center_axis',(1.,1.53063836115601E-16,-2.73691106313441E-48)) ;
#115235 = DIRECTION('ref_axis',(-1.53063836115601E-16,1.,4.18922106430579E-64)) ;
#115236 = DIRECTION('center_axis',(-1.,0.,0.)) ;
#115237 = DIRECTION('ref_axis',(0.,0.,1.)) ;
#115238 = DIRECTION('center_axis',(1.,1.53063836115601E-16,0.)) ;
#115239 = DIRECTION('ref_axis',(1.53063836115601E-16,-1.,0.)) ;
#115240 = DIRECTION('center_axis',(0.,1.,0.)) ;
#115241 = DIRECTION('ref_axis',(1.,0.,0.)) ;
#115242 = DIRECTION('center_axis',(-1.,-2.16840434497101E-16,0.)) ;
#115243 = DIRECTION('ref_axis',(0.,-1.,0.)) ;
#115244 = DIRECTION('center_axis',(0.,0.,-1.)) ;
#115245 = DIRECTION('ref_axis',(1.,0.,0.)) ;
#115246 = DIRECTION('center_axis',(-1.25542992828747E-32,1.020425574104E-16,
1.)) ;
#115247 = DIRECTION('ref_axis',(0.,-1.,0.)) ;
#115248 = DIRECTION('center_axis',(0.,-1.,0.)) ;
#115249 = DIRECTION('ref_axis',(-6.50521303491307E-15,0.,1.)) ;
#115250 = DIRECTION('center_axis',(-1.,0.,0.)) ;
#115251 = DIRECTION('ref_axis',(0.,0.,-1.)) ;
#115252 = DIRECTION('center_axis',(-1.,-1.53063836115601E-16,0.)) ;
#115253 = DIRECTION('ref_axis',(0.,-1.,0.)) ;
#115254 = DIRECTION('center_axis',(0.,-1.,0.)) ;
#115255 = DIRECTION('ref_axis',(0.,0.,1.)) ;
#115256 = DIRECTION('center_axis',(0.,0.,-1.)) ;
#115257 = DIRECTION('ref_axis',(-1.,0.,0.)) ;
#115258 = DIRECTION('center_axis',(0.,0.,-1.)) ;
#115259 = DIRECTION('ref_axis',(-1.,0.,0.)) ;
#115260 = DIRECTION('center_axis',(1.,1.53063836115601E-16,-3.06472600140763E-33)) ;
#115261 = DIRECTION('ref_axis',(-1.53063836115601E-16,1.,4.69098718418678E-49)) ;
#115262 = DIRECTION('center_axis',(-1.,0.,0.)) ;
#115263 = DIRECTION('ref_axis',(0.,0.,1.)) ;
#115264 = DIRECTION('center_axis',(-1.53063836115601E-16,1.,-1.020425574104E-16)) ;
#115265 = DIRECTION('ref_axis',(-1.,-1.53063836115601E-16,1.3684555315672E-47)) ;
#115266 = DIRECTION('',(1.53063836115601E-16,-1.,1.020425574104E-16)) ;
#115267 = DIRECTION('center_axis',(0.,-1.,0.)) ;
#115268 = DIRECTION('ref_axis',(0.,0.,-1.)) ;
#115269 = DIRECTION('center_axis',(-1.53063836115601E-16,1.,-1.30104260698261E-16)) ;
#115270 = DIRECTION('ref_axis',(-1.,-1.53063836115601E-16,1.99142572374599E-32)) ;
#115271 = DIRECTION('center_axis',(0.,-1.,0.)) ;
#115272 = DIRECTION('ref_axis',(0.,0.,-1.)) ;
#115273 = DIRECTION('center_axis',(-1.,-1.53063836115601E-16,2.73691106313441E-48)) ;
#115274 = DIRECTION('ref_axis',(1.53063836115601E-16,-1.,-4.18922106430579E-64)) ;
#115275 = DIRECTION('center_axis',(1.,2.16840434497101E-16,0.)) ;
#115276 = DIRECTION('ref_axis',(2.16840434497101E-16,-1.,0.)) ;
#115277 = DIRECTION('center_axis',(-1.,0.,2.16840434497102E-15)) ;
#115278 = DIRECTION('ref_axis',(2.16840434497102E-15,0.,1.)) ;
#115279 = DIRECTION('center_axis',(-1.,-2.16840434497101E-16,0.)) ;
#115280 = DIRECTION('ref_axis',(0.,-1.,0.)) ;
#115281 = DIRECTION('center_axis',(0.,0.,1.)) ;
#115282 = DIRECTION('ref_axis',(-1.,0.,0.)) ;
#115283 = DIRECTION('center_axis',(0.,1.,0.)) ;
#115284 = DIRECTION('ref_axis',(1.,0.,0.)) ;
#115285 = DIRECTION('center_axis',(0.,1.,0.)) ;
#115286 = DIRECTION('ref_axis',(0.,0.,-1.)) ;
#115287 = DIRECTION('center_axis',(1.,0.,0.)) ;
#115288 = DIRECTION('ref_axis',(0.,-1.,0.)) ;
#115289 = DIRECTION('center_axis',(1.,6.50521303491304E-15,0.)) ;
#115290 = DIRECTION('ref_axis',(-6.50521303491304E-15,1.,0.)) ;
#115291 = DIRECTION('center_axis',(8.67361737988403E-15,1.,0.)) ;
#115292 = DIRECTION('ref_axis',(-1.,8.67361737988403E-15,0.)) ;
#115293 = DIRECTION('center_axis',(1.2303003375722E-16,-1.,1.020425574104E-16)) ;
#115294 = DIRECTION('ref_axis',(1.,1.2303003375722E-16,-1.25542992828747E-32)) ;
#115295 = DIRECTION('center_axis',(0.,1.,0.)) ;
#115296 = DIRECTION('ref_axis',(0.,0.,1.)) ;
#115297 = DIRECTION('center_axis',(0.,1.,0.)) ;
#115298 = DIRECTION('ref_axis',(1.,0.,0.)) ;
#115299 = DIRECTION('center_axis',(1.,1.2303003375722E-16,0.)) ;
#115300 = DIRECTION('ref_axis',(1.2303003375722E-16,-1.,0.)) ;
#115301 = DIRECTION('center_axis',(0.,0.,1.)) ;
#115302 = DIRECTION('ref_axis',(-1.,0.,0.)) ;
#115303 = DIRECTION('center_axis',(0.,1.,0.)) ;
#115304 = DIRECTION('ref_axis',(1.,0.,0.)) ;
#115305 = DIRECTION('center_axis',(0.,0.,-1.)) ;
#115306 = DIRECTION('ref_axis',(1.,0.,0.)) ;
#115307 = DIRECTION('center_axis',(0.,0.,-1.)) ;
#115308 = DIRECTION('ref_axis',(-1.,0.,0.)) ;
#115309 = DIRECTION('center_axis',(0.,0.,1.)) ;
#115310 = DIRECTION('ref_axis',(1.,0.,0.)) ;
#115311 = DIRECTION('center_axis',(-2.16840434497101E-16,1.,-1.020425574104E-16)) ;
#115312 = DIRECTION('ref_axis',(-1.,-2.16840434497101E-16,5.47382212626882E-48)) ;
#115313 = DIRECTION('center_axis',(0.,1.,0.)) ;
#115314 = DIRECTION('ref_axis',(0.,0.,-1.)) ;
#115315 = DIRECTION('center_axis',(1.,0.,1.25542992828747E-32)) ;
#115316 = DIRECTION('ref_axis',(1.25542992828747E-32,0.,-1.)) ;
#115317 = DIRECTION('center_axis',(1.,0.,0.)) ;
#115318 = DIRECTION('ref_axis',(0.,0.,-1.)) ;
#115319 = DIRECTION('center_axis',(-1.,-1.2303003375722E-16,0.)) ;
#115320 = DIRECTION('ref_axis',(0.,-1.,0.)) ;
#115321 = DIRECTION('center_axis',(0.,0.,-1.)) ;
#115322 = DIRECTION('ref_axis',(1.,0.,0.)) ;
#115323 = DIRECTION('center_axis',(0.,0.,-1.)) ;
#115324 = DIRECTION('ref_axis',(-1.,0.,0.)) ;
#115325 = DIRECTION('',(0.,0.,1.)) ;
#115326 = DIRECTION('center_axis',(0.,0.,1.)) ;
#115327 = DIRECTION('ref_axis',(1.,0.,0.)) ;
#115328 = DIRECTION('center_axis',(0.,0.,1.)) ;
#115329 = DIRECTION('ref_axis',(1.,0.,0.)) ;
#115330 = DIRECTION('center_axis',(6.27714964143733E-33,-5.10212787052002E-17,
-1.)) ;
#115331 = DIRECTION('ref_axis',(3.20268201330022E-49,1.,-5.10212787052002E-17)) ;
#115332 = DIRECTION('center_axis',(1.,1.53063836115601E-16,-1.53236300070382E-33)) ;
#115333 = DIRECTION('ref_axis',(-1.53063836115601E-16,1.,2.34549359209339E-49)) ;
#115334 = DIRECTION('center_axis',(-1.,0.,0.)) ;
#115335 = DIRECTION('ref_axis',(0.,0.,1.)) ;
#115336 = DIRECTION('center_axis',(1.,0.,0.)) ;
#115337 = DIRECTION('ref_axis',(0.,0.,-1.)) ;
#115338 = DIRECTION('center_axis',(0.,1.,0.)) ;
#115339 = DIRECTION('ref_axis',(1.,0.,0.)) ;
#115340 = DIRECTION('center_axis',(-4.33680868994202E-15,1.,0.)) ;
#115341 = DIRECTION('ref_axis',(1.,4.33680868994202E-15,0.)) ;
#115342 = DIRECTION('center_axis',(0.,-1.,0.)) ;
#115343 = DIRECTION('ref_axis',(0.,0.,-1.)) ;
#115344 = DIRECTION('center_axis',(0.,0.,-1.)) ;
#115345 = DIRECTION('ref_axis',(1.,0.,0.)) ;
#115346 = DIRECTION('center_axis',(0.,0.,1.)) ;
#115347 = DIRECTION('ref_axis',(1.,0.,0.)) ;
#115348 = DIRECTION('center_axis',(0.,0.,-1.)) ;
#115349 = DIRECTION('ref_axis',(-1.,0.,0.)) ;
#115350 = DIRECTION('center_axis',(0.,1.,0.)) ;
#115351 = DIRECTION('ref_axis',(1.,0.,0.)) ;
#115352 = DIRECTION('center_axis',(1.,1.2303003375722E-16,0.)) ;
#115353 = DIRECTION('ref_axis',(1.2303003375722E-16,-1.,0.)) ;
#115354 = DIRECTION('center_axis',(0.,1.,0.)) ;
#115355 = DIRECTION('ref_axis',(-6.50521303491307E-15,0.,-1.)) ;
#115356 = DIRECTION('center_axis',(6.27714964143733E-33,-5.10212787052002E-17,
-1.)) ;
#115357 = DIRECTION('ref_axis',(0.,1.,0.)) ;
#115358 = DIRECTION('center_axis',(0.,-1.,0.)) ;
#115359 = DIRECTION('ref_axis',(0.,0.,1.)) ;
#115360 = DIRECTION('center_axis',(2.16840434497101E-16,-1.,5.10212787052002E-17)) ;
#115361 = DIRECTION('ref_axis',(1.,2.16840434497101E-16,-5.47382212626882E-48)) ;
#115362 = DIRECTION('center_axis',(0.,1.,0.)) ;
#115363 = DIRECTION('ref_axis',(0.,0.,-1.)) ;
#115364 = DIRECTION('center_axis',(0.,0.,1.)) ;
#115365 = DIRECTION('ref_axis',(1.,0.,0.)) ;
#115366 = DIRECTION('center_axis',(0.,0.,-1.)) ;
#115367 = DIRECTION('ref_axis',(-1.,0.,0.)) ;
#115368 = DIRECTION('center_axis',(-1.,-1.2303003375722E-16,0.)) ;
#115369 = DIRECTION('ref_axis',(0.,-1.,0.)) ;
#115370 = DIRECTION('center_axis',(0.,-1.,0.)) ;
#115371 = DIRECTION('ref_axis',(0.,0.,1.)) ;
#115372 = DIRECTION('center_axis',(1.53063836115601E-16,-1.,5.10212787052002E-17)) ;
#115373 = DIRECTION('ref_axis',(1.,1.53063836115601E-16,-6.84227765783602E-48)) ;
#115374 = DIRECTION('',(-1.53063836115601E-16,1.,-5.10212787052002E-17)) ;
#115375 = DIRECTION('center_axis',(0.,-1.,0.)) ;
#115376 = DIRECTION('ref_axis',(0.,0.,-1.)) ;
#115377 = DIRECTION('center_axis',(-1.,0.,0.)) ;
#115378 = DIRECTION('ref_axis',(0.,0.,-1.)) ;
#115379 = DIRECTION('center_axis',(-1.2303003375722E-16,1.,-5.10212787052002E-17)) ;
#115380 = DIRECTION('ref_axis',(-1.,-1.2303003375722E-16,6.27714964143733E-33)) ;
#115381 = DIRECTION('center_axis',(-8.67361737988403E-15,-1.,0.)) ;
#115382 = DIRECTION('ref_axis',(1.,-8.67361737988403E-15,0.)) ;
#115383 = DIRECTION('center_axis',(1.,0.,6.27714964143733E-33)) ;
#115384 = DIRECTION('ref_axis',(6.27714964143733E-33,0.,-1.)) ;
#115385 = DIRECTION('center_axis',(-1.,0.,-6.50521303491307E-15)) ;
#115386 = DIRECTION('ref_axis',(-6.50521303491307E-15,0.,1.)) ;
#115387 = DIRECTION('center_axis',(1.,0.,0.)) ;
#115388 = DIRECTION('ref_axis',(0.,1.,0.)) ;
#115389 = DIRECTION('center_axis',(0.,0.,-1.)) ;
#115390 = DIRECTION('ref_axis',(-1.,0.,0.)) ;
#115391 = DIRECTION('center_axis',(0.,0.,1.)) ;
#115392 = DIRECTION('ref_axis',(1.,0.,0.)) ;
#115393 = DIRECTION('center_axis',(0.,0.,-1.)) ;
#115394 = DIRECTION('ref_axis',(-1.,0.,0.)) ;
#115395 = DIRECTION('center_axis',(-1.,0.,0.)) ;
#115396 = DIRECTION('ref_axis',(0.,0.,1.)) ;
#115397 = DIRECTION('center_axis',(0.,-1.,0.)) ;
#115398 = DIRECTION('ref_axis',(0.,0.,-1.)) ;
#115399 = DIRECTION('center_axis',(0.,1.,0.)) ;
#115400 = DIRECTION('ref_axis',(0.,0.,1.)) ;
#115401 = DIRECTION('center_axis',(0.,1.,-6.50521303491307E-15)) ;
#115402 = DIRECTION('ref_axis',(0.,6.50521303491307E-15,1.)) ;
#115403 = DIRECTION('center_axis',(0.,-1.,0.)) ;
#115404 = DIRECTION('ref_axis',(0.,0.,-1.)) ;
#115405 = DIRECTION('center_axis',(0.,-1.,0.)) ;
#115406 = DIRECTION('ref_axis',(0.,0.,-1.)) ;
#115407 = DIRECTION('center_axis',(0.,-1.,-1.07081696047951E-16)) ;
#115408 = DIRECTION('ref_axis',(0.,1.07081696047951E-16,-1.)) ;
#115409 = DIRECTION('center_axis',(0.,1.,0.)) ;
#115410 = DIRECTION('ref_axis',(0.,0.,1.)) ;
#115411 = DIRECTION('center_axis',(-1.,0.,0.)) ;
#115412 = DIRECTION('ref_axis',(0.,0.,1.)) ;
#115413 = DIRECTION('center_axis',(0.,0.,1.)) ;
#115414 = DIRECTION('ref_axis',(1.,0.,0.)) ;
#115415 = DIRECTION('center_axis',(0.,1.,0.)) ;
#115416 = DIRECTION('ref_axis',(0.,0.,1.)) ;
#115417 = DIRECTION('center_axis',(0.,-1.73472347597681E-14,-1.)) ;
#115418 = DIRECTION('ref_axis',(0.,1.,-1.73472347597681E-14)) ;
#115419 = DIRECTION('center_axis',(0.,0.,1.)) ;
#115420 = DIRECTION('ref_axis',(1.,0.,0.)) ;
#115421 = DIRECTION('center_axis',(0.,0.,1.)) ;
#115422 = DIRECTION('ref_axis',(1.,0.,0.)) ;
#115423 = DIRECTION('center_axis',(0.,0.,1.)) ;
#115424 = DIRECTION('ref_axis',(1.,0.,0.)) ;
#115425 = DIRECTION('center_axis',(0.,0.,-1.)) ;
#115426 = DIRECTION('ref_axis',(-1.,0.,0.)) ;
#115427 = DIRECTION('center_axis',(0.,1.,0.)) ;
#115428 = DIRECTION('ref_axis',(0.,0.,1.)) ;
#115429 = DIRECTION('center_axis',(0.,-0.707106781186545,0.70710678118655)) ;
#115430 = DIRECTION('ref_axis',(0.,-0.70710678118655,-0.707106781186545)) ;
#115431 = DIRECTION('center_axis',(0.,1.,0.)) ;
#115432 = DIRECTION('ref_axis',(0.,0.,1.)) ;
#115433 = DIRECTION('center_axis',(0.,-0.514231796959109,-0.857651245551597)) ;
#115434 = DIRECTION('ref_axis',(0.,0.857651245551597,-0.514231796959109)) ;
#115435 = DIRECTION('center_axis',(0.,-0.707106781186548,0.707106781186547)) ;
#115436 = DIRECTION('ref_axis',(0.,-0.707106781186547,-0.707106781186548)) ;
#115437 = DIRECTION('center_axis',(0.,-0.707106781186548,0.707106781186548)) ;
#115438 = DIRECTION('ref_axis',(0.,-0.707106781186548,-0.707106781186548)) ;
#115439 = DIRECTION('center_axis',(-1.,0.,0.)) ;
#115440 = DIRECTION('ref_axis',(0.,0.,1.)) ;
#115441 = DIRECTION('center_axis',(-2.23012492569676E-15,0.514231796959107,
-0.857651245551598)) ;
#115442 = DIRECTION('ref_axis',(-5.69910941180089E-30,0.857651245551598,0.514231796959107)) ;
#115443 = DIRECTION('center_axis',(0.,1.,0.)) ;
#115444 = DIRECTION('ref_axis',(0.,0.,1.)) ;
#115445 = DIRECTION('center_axis',(0.,0.,-1.)) ;
#115446 = DIRECTION('ref_axis',(-1.,0.,0.)) ;
#115447 = DIRECTION('center_axis',(0.,1.,0.)) ;
#115448 = DIRECTION('ref_axis',(0.,0.,1.)) ;
#115449 = DIRECTION('center_axis',(0.,0.,-1.)) ;
#115450 = DIRECTION('ref_axis',(-1.,0.,0.)) ;
#115451 = DIRECTION('center_axis',(0.,0.,-1.)) ;
#115452 = DIRECTION('ref_axis',(-1.,0.,0.)) ;
#115453 = DIRECTION('center_axis',(0.,0.,1.)) ;
#115454 = DIRECTION('ref_axis',(1.,0.,0.)) ;
#115455 = DIRECTION('center_axis',(0.,0.,-1.)) ;
#115456 = DIRECTION('ref_axis',(-1.,0.,0.)) ;
#115457 = DIRECTION('center_axis',(0.,1.,0.)) ;
#115458 = DIRECTION('ref_axis',(0.,0.,1.)) ;
#115459 = DIRECTION('center_axis',(0.,-1.,8.67361737988409E-15)) ;
#115460 = DIRECTION('ref_axis',(0.,-8.67361737988409E-15,-1.)) ;
#115461 = DIRECTION('center_axis',(0.,0.707106781186546,0.707106781186549)) ;
#115462 = DIRECTION('ref_axis',(0.,-0.707106781186549,0.707106781186546)) ;
#115463 = DIRECTION('center_axis',(0.,0.707106781186541,0.707106781186554)) ;
#115464 = DIRECTION('ref_axis',(0.,-0.707106781186554,0.707106781186541)) ;
#115465 = DIRECTION('center_axis',(0.,1.,1.07081696047951E-16)) ;
#115466 = DIRECTION('ref_axis',(0.,-1.07081696047951E-16,1.)) ;
#115467 = DIRECTION('center_axis',(0.,-1.,0.)) ;
#115468 = DIRECTION('ref_axis',(0.,0.,-1.)) ;
#115469 = DIRECTION('center_axis',(0.,1.,0.)) ;
#115470 = DIRECTION('ref_axis',(0.,0.,1.)) ;
#115471 = DIRECTION('center_axis',(0.,0.,1.)) ;
#115472 = DIRECTION('ref_axis',(1.,0.,0.)) ;
#115473 = DIRECTION('center_axis',(0.,1.,0.)) ;
#115474 = DIRECTION('ref_axis',(0.,0.,1.)) ;
#115475 = DIRECTION('center_axis',(0.,0.,1.)) ;
#115476 = DIRECTION('ref_axis',(1.,0.,0.)) ;
#115477 = DIRECTION('center_axis',(0.,3.99416362155027E-15,1.)) ;
#115478 = DIRECTION('ref_axis',(0.,-1.,3.99416362155027E-15)) ;
#115479 = DIRECTION('center_axis',(0.,0.,1.)) ;
#115480 = DIRECTION('ref_axis',(1.,0.,0.)) ;
#115481 = DIRECTION('center_axis',(0.,0.,-1.)) ;
#115482 = DIRECTION('ref_axis',(-1.,0.,0.)) ;
#115483 = DIRECTION('center_axis',(0.,0.,1.)) ;
#115484 = DIRECTION('ref_axis',(1.,0.,0.)) ;
#115485 = DIRECTION('center_axis',(-1.,0.,0.)) ;
#115486 = DIRECTION('ref_axis',(0.,0.,1.)) ;
#115487 = DIRECTION('center_axis',(0.,1.,0.)) ;
#115488 = DIRECTION('ref_axis',(0.,0.,1.)) ;
#115489 = DIRECTION('center_axis',(-1.,0.,0.)) ;
#115490 = DIRECTION('ref_axis',(0.,0.,1.)) ;
#115491 = DIRECTION('center_axis',(0.,-1.,0.)) ;
#115492 = DIRECTION('ref_axis',(0.,0.,-1.)) ;
#115493 = DIRECTION('center_axis',(0.,1.,0.)) ;
#115494 = DIRECTION('ref_axis',(0.,0.,1.)) ;
#115495 = DIRECTION('center_axis',(1.53063836115601E-16,-1.,-1.30104260698261E-16)) ;
#115496 = DIRECTION('ref_axis',(1.,1.53063836115601E-16,1.99142572374599E-32)) ;
#115497 = DIRECTION('center_axis',(0.,1.,0.)) ;
#115498 = DIRECTION('ref_axis',(0.,0.,1.)) ;
#115499 = DIRECTION('center_axis',(0.,-1.,0.)) ;
#115500 = DIRECTION('ref_axis',(0.,0.,-1.)) ;
#115501 = DIRECTION('center_axis',(1.,1.53063836115601E-16,2.73691106313441E-48)) ;
#115502 = DIRECTION('ref_axis',(-1.53063836115601E-16,1.,-4.18922106430579E-64)) ;
#115503 = DIRECTION('center_axis',(-1.,0.,0.)) ;
#115504 = DIRECTION('ref_axis',(0.,0.,1.)) ;
#115505 = DIRECTION('center_axis',(1.,1.53063836115601E-16,0.)) ;
#115506 = DIRECTION('ref_axis',(1.53063836115601E-16,-1.,0.)) ;
#115507 = DIRECTION('center_axis',(0.,1.,0.)) ;
#115508 = DIRECTION('ref_axis',(1.,0.,0.)) ;
#115509 = DIRECTION('center_axis',(0.,1.,0.)) ;
#115510 = DIRECTION('ref_axis',(0.,0.,-1.)) ;
#115511 = DIRECTION('center_axis',(0.,0.,1.)) ;
#115512 = DIRECTION('ref_axis',(-1.,0.,0.)) ;
#115513 = DIRECTION('center_axis',(0.,1.,0.)) ;
#115514 = DIRECTION('ref_axis',(1.,0.,0.)) ;
#115515 = DIRECTION('center_axis',(0.,0.,1.)) ;
#115516 = DIRECTION('ref_axis',(-1.,0.,0.)) ;
#115517 = DIRECTION('center_axis',(1.,1.0842021724855E-15,0.)) ;
#115518 = DIRECTION('ref_axis',(1.0842021724855E-15,-1.,0.)) ;
#115519 = DIRECTION('center_axis',(-1.,-1.53063836115601E-16,0.)) ;
#115520 = DIRECTION('ref_axis',(0.,-1.,0.)) ;
#115521 = DIRECTION('center_axis',(0.,0.,-1.)) ;
#115522 = DIRECTION('ref_axis',(1.,0.,0.)) ;
#115523 = DIRECTION('center_axis',(0.,0.,-1.)) ;
#115524 = DIRECTION('ref_axis',(0.804034447892618,0.594582716366708,0.)) ;
#115525 = DIRECTION('center_axis',(0.,0.,1.)) ;
#115526 = DIRECTION('ref_axis',(1.,0.,0.)) ;
#115527 = DIRECTION('',(0.,0.,-1.)) ;
#115528 = DIRECTION('center_axis',(-2.16840434497101E-16,1.,1.30104260698261E-16)) ;
#115529 = DIRECTION('ref_axis',(1.,2.16840434497101E-16,1.22464679914735E-16)) ;
#115530 = DIRECTION('',(-2.16840434497101E-16,1.,1.30104260698261E-16)) ;
#115531 = DIRECTION('center_axis',(0.,1.,0.)) ;
#115532 = DIRECTION('ref_axis',(0.,0.,1.)) ;
#115533 = DIRECTION('center_axis',(-1.,-1.53063836115601E-16,-2.73691106313441E-48)) ;
#115534 = DIRECTION('ref_axis',(1.53063836115601E-16,-1.,4.18922106430579E-64)) ;
#115535 = DIRECTION('center_axis',(1.,2.16840434497101E-16,0.)) ;
#115536 = DIRECTION('ref_axis',(2.16840434497101E-16,-1.,0.)) ;
#115537 = DIRECTION('center_axis',(0.,0.,1.)) ;
#115538 = DIRECTION('ref_axis',(1.,0.,0.)) ;
#115539 = DIRECTION('center_axis',(-1.25542992828747E-32,1.020425574104E-16,
1.)) ;
#115540 = DIRECTION('ref_axis',(-1.28107280532009E-48,-1.,1.020425574104E-16)) ;
#115541 = DIRECTION('center_axis',(0.,0.,1.)) ;
#115542 = DIRECTION('ref_axis',(1.,0.,0.)) ;
#115543 = DIRECTION('center_axis',(0.,0.,-1.)) ;
#115544 = DIRECTION('ref_axis',(-1.,0.,0.)) ;
#115545 = DIRECTION('center_axis',(1.,1.53063836115601E-16,-2.73691106313441E-48)) ;
#115546 = DIRECTION('ref_axis',(-1.53063836115601E-16,1.,4.18922106430579E-64)) ;
#115547 = DIRECTION('center_axis',(-1.,0.,0.)) ;
#115548 = DIRECTION('ref_axis',(0.,0.,1.)) ;
#115549 = DIRECTION('center_axis',(1.,1.53063836115601E-16,0.)) ;
#115550 = DIRECTION('ref_axis',(1.53063836115601E-16,-1.,0.)) ;
#115551 = DIRECTION('center_axis',(0.,1.,0.)) ;
#115552 = DIRECTION('ref_axis',(1.,0.,0.)) ;
#115553 = DIRECTION('center_axis',(-1.,-2.16840434497101E-16,0.)) ;
#115554 = DIRECTION('ref_axis',(0.,-1.,0.)) ;
#115555 = DIRECTION('center_axis',(0.,0.,-1.)) ;
#115556 = DIRECTION('ref_axis',(1.,0.,0.)) ;
#115557 = DIRECTION('center_axis',(-1.25542992828747E-32,1.020425574104E-16,
1.)) ;
#115558 = DIRECTION('ref_axis',(0.,-1.,0.)) ;
#115559 = DIRECTION('center_axis',(0.,-1.,0.)) ;
#115560 = DIRECTION('ref_axis',(-6.50521303491307E-15,0.,1.)) ;
#115561 = DIRECTION('center_axis',(-1.,0.,0.)) ;
#115562 = DIRECTION('ref_axis',(0.,0.,-1.)) ;
#115563 = DIRECTION('center_axis',(-1.,-1.53063836115601E-16,0.)) ;
#115564 = DIRECTION('ref_axis',(0.,-1.,0.)) ;
#115565 = DIRECTION('center_axis',(0.,-1.,0.)) ;
#115566 = DIRECTION('ref_axis',(0.,0.,1.)) ;
#115567 = DIRECTION('center_axis',(0.,0.,-1.)) ;
#115568 = DIRECTION('ref_axis',(-1.,0.,0.)) ;
#115569 = DIRECTION('center_axis',(0.,0.,-1.)) ;
#115570 = DIRECTION('ref_axis',(-1.,0.,0.)) ;
#115571 = DIRECTION('center_axis',(1.,1.53063836115601E-16,-3.06472600140763E-33)) ;
#115572 = DIRECTION('ref_axis',(-1.53063836115601E-16,1.,4.69098718418678E-49)) ;
#115573 = DIRECTION('center_axis',(-1.,0.,0.)) ;
#115574 = DIRECTION('ref_axis',(0.,0.,1.)) ;
#115575 = DIRECTION('center_axis',(-1.53063836115601E-16,1.,-1.020425574104E-16)) ;
#115576 = DIRECTION('ref_axis',(-1.,-1.53063836115601E-16,1.3684555315672E-47)) ;
#115577 = DIRECTION('',(1.53063836115601E-16,-1.,1.020425574104E-16)) ;
#115578 = DIRECTION('center_axis',(0.,-1.,0.)) ;
#115579 = DIRECTION('ref_axis',(0.,0.,-1.)) ;
#115580 = DIRECTION('center_axis',(-1.53063836115601E-16,1.,-1.30104260698261E-16)) ;
#115581 = DIRECTION('ref_axis',(-1.,-1.53063836115601E-16,1.99142572374599E-32)) ;
#115582 = DIRECTION('center_axis',(0.,-1.,0.)) ;
#115583 = DIRECTION('ref_axis',(0.,0.,-1.)) ;
#115584 = DIRECTION('center_axis',(-1.,-1.53063836115601E-16,2.73691106313441E-48)) ;
#115585 = DIRECTION('ref_axis',(1.53063836115601E-16,-1.,-4.18922106430579E-64)) ;
#115586 = DIRECTION('center_axis',(1.,2.16840434497101E-16,0.)) ;
#115587 = DIRECTION('ref_axis',(2.16840434497101E-16,-1.,0.)) ;
#115588 = DIRECTION('center_axis',(-1.,0.,2.16840434497102E-15)) ;
#115589 = DIRECTION('ref_axis',(2.16840434497102E-15,0.,1.)) ;
#115590 = DIRECTION('center_axis',(-1.,-2.16840434497101E-16,0.)) ;
#115591 = DIRECTION('ref_axis',(0.,-1.,0.)) ;
#115592 = DIRECTION('center_axis',(0.,0.,1.)) ;
#115593 = DIRECTION('ref_axis',(-1.,0.,0.)) ;
#115594 = DIRECTION('center_axis',(0.,1.,0.)) ;
#115595 = DIRECTION('ref_axis',(1.,0.,0.)) ;
#115596 = DIRECTION('center_axis',(0.,1.,0.)) ;
#115597 = DIRECTION('ref_axis',(0.,0.,-1.)) ;
#115598 = DIRECTION('center_axis',(1.,0.,0.)) ;
#115599 = DIRECTION('ref_axis',(0.,-1.,0.)) ;
#115600 = DIRECTION('center_axis',(1.,6.50521303491304E-15,0.)) ;
#115601 = DIRECTION('ref_axis',(-6.50521303491304E-15,1.,0.)) ;
#115602 = DIRECTION('center_axis',(8.67361737988403E-15,1.,0.)) ;
#115603 = DIRECTION('ref_axis',(-1.,8.67361737988403E-15,0.)) ;
#115604 = DIRECTION('center_axis',(1.2303003375722E-16,-1.,1.020425574104E-16)) ;
#115605 = DIRECTION('ref_axis',(1.,1.2303003375722E-16,-1.25542992828747E-32)) ;
#115606 = DIRECTION('center_axis',(0.,1.,0.)) ;
#115607 = DIRECTION('ref_axis',(0.,0.,1.)) ;
#115608 = DIRECTION('center_axis',(0.,1.,0.)) ;
#115609 = DIRECTION('ref_axis',(1.,0.,0.)) ;
#115610 = DIRECTION('center_axis',(1.,1.2303003375722E-16,0.)) ;
#115611 = DIRECTION('ref_axis',(1.2303003375722E-16,-1.,0.)) ;
#115612 = DIRECTION('center_axis',(0.,0.,1.)) ;
#115613 = DIRECTION('ref_axis',(-1.,0.,0.)) ;
#115614 = DIRECTION('center_axis',(0.,1.,0.)) ;
#115615 = DIRECTION('ref_axis',(1.,0.,0.)) ;
#115616 = DIRECTION('center_axis',(0.,0.,-1.)) ;
#115617 = DIRECTION('ref_axis',(1.,0.,0.)) ;
#115618 = DIRECTION('center_axis',(0.,0.,-1.)) ;
#115619 = DIRECTION('ref_axis',(-1.,0.,0.)) ;
#115620 = DIRECTION('center_axis',(0.,0.,1.)) ;
#115621 = DIRECTION('ref_axis',(1.,0.,0.)) ;
#115622 = DIRECTION('center_axis',(-2.16840434497101E-16,1.,-1.020425574104E-16)) ;
#115623 = DIRECTION('ref_axis',(-1.,-2.16840434497101E-16,5.47382212626882E-48)) ;
#115624 = DIRECTION('center_axis',(0.,1.,0.)) ;
#115625 = DIRECTION('ref_axis',(0.,0.,-1.)) ;
#115626 = DIRECTION('center_axis',(1.,0.,1.25542992828747E-32)) ;
#115627 = DIRECTION('ref_axis',(1.25542992828747E-32,0.,-1.)) ;
#115628 = DIRECTION('center_axis',(1.,0.,0.)) ;
#115629 = DIRECTION('ref_axis',(0.,0.,-1.)) ;
#115630 = DIRECTION('center_axis',(-1.,-1.2303003375722E-16,0.)) ;
#115631 = DIRECTION('ref_axis',(0.,-1.,0.)) ;
#115632 = DIRECTION('center_axis',(0.,0.,-1.)) ;
#115633 = DIRECTION('ref_axis',(1.,0.,0.)) ;
#115634 = DIRECTION('center_axis',(0.,0.,-1.)) ;
#115635 = DIRECTION('ref_axis',(-1.,0.,0.)) ;
#115636 = DIRECTION('',(0.,0.,1.)) ;
#115637 = DIRECTION('center_axis',(0.,0.,1.)) ;
#115638 = DIRECTION('ref_axis',(1.,0.,0.)) ;
#115639 = DIRECTION('center_axis',(0.,0.,1.)) ;
#115640 = DIRECTION('ref_axis',(1.,0.,0.)) ;
#115641 = DIRECTION('center_axis',(6.27714964143733E-33,-5.10212787052002E-17,
-1.)) ;
#115642 = DIRECTION('ref_axis',(3.20268201330022E-49,1.,-5.10212787052002E-17)) ;
#115643 = DIRECTION('center_axis',(1.,1.53063836115601E-16,-1.53236300070382E-33)) ;
#115644 = DIRECTION('ref_axis',(-1.53063836115601E-16,1.,2.34549359209339E-49)) ;
#115645 = DIRECTION('center_axis',(-1.,0.,0.)) ;
#115646 = DIRECTION('ref_axis',(0.,0.,1.)) ;
#115647 = DIRECTION('center_axis',(1.,0.,0.)) ;
#115648 = DIRECTION('ref_axis',(0.,0.,-1.)) ;
#115649 = DIRECTION('center_axis',(0.,1.,0.)) ;
#115650 = DIRECTION('ref_axis',(1.,0.,0.)) ;
#115651 = DIRECTION('center_axis',(-4.33680868994202E-15,1.,0.)) ;
#115652 = DIRECTION('ref_axis',(1.,4.33680868994202E-15,0.)) ;
#115653 = DIRECTION('center_axis',(0.,-1.,0.)) ;
#115654 = DIRECTION('ref_axis',(0.,0.,-1.)) ;
#115655 = DIRECTION('center_axis',(0.,0.,-1.)) ;
#115656 = DIRECTION('ref_axis',(1.,0.,0.)) ;
#115657 = DIRECTION('center_axis',(0.,0.,1.)) ;
#115658 = DIRECTION('ref_axis',(1.,0.,0.)) ;
#115659 = DIRECTION('center_axis',(0.,0.,-1.)) ;
#115660 = DIRECTION('ref_axis',(-1.,0.,0.)) ;
#115661 = DIRECTION('center_axis',(0.,1.,0.)) ;
#115662 = DIRECTION('ref_axis',(1.,0.,0.)) ;
#115663 = DIRECTION('center_axis',(1.,1.2303003375722E-16,0.)) ;
#115664 = DIRECTION('ref_axis',(1.2303003375722E-16,-1.,0.)) ;
#115665 = DIRECTION('center_axis',(0.,1.,0.)) ;
#115666 = DIRECTION('ref_axis',(-6.50521303491307E-15,0.,-1.)) ;
#115667 = DIRECTION('center_axis',(6.27714964143733E-33,-5.10212787052002E-17,
-1.)) ;
#115668 = DIRECTION('ref_axis',(0.,1.,0.)) ;
#115669 = DIRECTION('center_axis',(0.,-1.,0.)) ;
#115670 = DIRECTION('ref_axis',(0.,0.,1.)) ;
#115671 = DIRECTION('center_axis',(2.16840434497101E-16,-1.,5.10212787052002E-17)) ;
#115672 = DIRECTION('ref_axis',(1.,2.16840434497101E-16,-5.47382212626882E-48)) ;
#115673 = DIRECTION('center_axis',(0.,1.,0.)) ;
#115674 = DIRECTION('ref_axis',(0.,0.,-1.)) ;
#115675 = DIRECTION('center_axis',(0.,0.,1.)) ;
#115676 = DIRECTION('ref_axis',(1.,0.,0.)) ;
#115677 = DIRECTION('center_axis',(0.,0.,-1.)) ;
#115678 = DIRECTION('ref_axis',(-1.,0.,0.)) ;
#115679 = DIRECTION('center_axis',(-1.,-1.2303003375722E-16,0.)) ;
#115680 = DIRECTION('ref_axis',(0.,-1.,0.)) ;
#115681 = DIRECTION('center_axis',(0.,-1.,0.)) ;
#115682 = DIRECTION('ref_axis',(0.,0.,1.)) ;
#115683 = DIRECTION('center_axis',(1.53063836115601E-16,-1.,5.10212787052002E-17)) ;
#115684 = DIRECTION('ref_axis',(1.,1.53063836115601E-16,-6.84227765783602E-48)) ;
#115685 = DIRECTION('',(-1.53063836115601E-16,1.,-5.10212787052002E-17)) ;
#115686 = DIRECTION('center_axis',(0.,-1.,0.)) ;
#115687 = DIRECTION('ref_axis',(0.,0.,-1.)) ;
#115688 = DIRECTION('center_axis',(-1.,0.,0.)) ;
#115689 = DIRECTION('ref_axis',(0.,0.,-1.)) ;
#115690 = DIRECTION('center_axis',(-1.2303003375722E-16,1.,-5.10212787052002E-17)) ;
#115691 = DIRECTION('ref_axis',(-1.,-1.2303003375722E-16,6.27714964143733E-33)) ;
#115692 = DIRECTION('center_axis',(-8.67361737988403E-15,-1.,0.)) ;
#115693 = DIRECTION('ref_axis',(1.,-8.67361737988403E-15,0.)) ;
#115694 = DIRECTION('center_axis',(1.,0.,6.27714964143733E-33)) ;
#115695 = DIRECTION('ref_axis',(6.27714964143733E-33,0.,-1.)) ;
#115696 = DIRECTION('center_axis',(-1.,0.,-6.50521303491307E-15)) ;
#115697 = DIRECTION('ref_axis',(-6.50521303491307E-15,0.,1.)) ;
#115698 = DIRECTION('center_axis',(1.,0.,0.)) ;
#115699 = DIRECTION('ref_axis',(0.,1.,0.)) ;
#115700 = DIRECTION('center_axis',(0.,0.,-1.)) ;
#115701 = DIRECTION('ref_axis',(-1.,0.,0.)) ;
#115702 = DIRECTION('center_axis',(0.,0.,1.)) ;
#115703 = DIRECTION('ref_axis',(1.,0.,0.)) ;
#115704 = DIRECTION('center_axis',(0.,0.,-1.)) ;
#115705 = DIRECTION('ref_axis',(-1.,0.,0.)) ;
#115706 = DIRECTION('center_axis',(-1.,0.,0.)) ;
#115707 = DIRECTION('ref_axis',(0.,0.,1.)) ;
#115708 = DIRECTION('center_axis',(0.,-1.,0.)) ;
#115709 = DIRECTION('ref_axis',(0.,0.,-1.)) ;
#115710 = DIRECTION('center_axis',(0.,1.,0.)) ;
#115711 = DIRECTION('ref_axis',(0.,0.,1.)) ;
#115712 = DIRECTION('center_axis',(0.,1.,-6.50521303491307E-15)) ;
#115713 = DIRECTION('ref_axis',(0.,6.50521303491307E-15,1.)) ;
#115714 = DIRECTION('center_axis',(0.,-1.,0.)) ;
#115715 = DIRECTION('ref_axis',(0.,0.,-1.)) ;
#115716 = DIRECTION('center_axis',(0.,-1.,0.)) ;
#115717 = DIRECTION('ref_axis',(0.,0.,-1.)) ;
#115718 = DIRECTION('center_axis',(0.,-1.,-1.07081696047951E-16)) ;
#115719 = DIRECTION('ref_axis',(0.,1.07081696047951E-16,-1.)) ;
#115720 = DIRECTION('center_axis',(0.,1.,0.)) ;
#115721 = DIRECTION('ref_axis',(0.,0.,1.)) ;
#115722 = DIRECTION('center_axis',(-1.,0.,0.)) ;
#115723 = DIRECTION('ref_axis',(0.,0.,1.)) ;
#115724 = DIRECTION('center_axis',(0.,0.,1.)) ;
#115725 = DIRECTION('ref_axis',(1.,0.,0.)) ;
#115726 = DIRECTION('center_axis',(0.,1.,0.)) ;
#115727 = DIRECTION('ref_axis',(0.,0.,1.)) ;
#115728 = DIRECTION('center_axis',(0.,0.,-1.)) ;
#115729 = DIRECTION('ref_axis',(-1.,0.,0.)) ;
#115730 = DIRECTION('center_axis',(0.,0.,1.)) ;
#115731 = DIRECTION('ref_axis',(1.,0.,0.)) ;
#115732 = DIRECTION('center_axis',(0.,0.,1.)) ;
#115733 = DIRECTION('ref_axis',(1.,0.,0.)) ;
#115734 = DIRECTION('center_axis',(0.,0.,1.)) ;
#115735 = DIRECTION('ref_axis',(1.,0.,0.)) ;
#115736 = DIRECTION('center_axis',(0.,0.,-1.)) ;
#115737 = DIRECTION('ref_axis',(-1.,0.,0.)) ;
#115738 = DIRECTION('center_axis',(0.,1.,0.)) ;
#115739 = DIRECTION('ref_axis',(0.,0.,1.)) ;
#115740 = DIRECTION('center_axis',(0.,-0.707106781186558,0.707106781186537)) ;
#115741 = DIRECTION('ref_axis',(0.,-0.707106781186537,-0.707106781186558)) ;
#115742 = DIRECTION('center_axis',(0.,1.,0.)) ;
#115743 = DIRECTION('ref_axis',(0.,0.,1.)) ;
#115744 = DIRECTION('center_axis',(0.,-0.514231796959093,-0.857651245551607)) ;
#115745 = DIRECTION('ref_axis',(0.,0.857651245551607,-0.514231796959093)) ;
#115746 = DIRECTION('center_axis',(0.,-0.707106781186548,0.707106781186547)) ;
#115747 = DIRECTION('ref_axis',(0.,-0.707106781186547,-0.707106781186548)) ;
#115748 = DIRECTION('center_axis',(0.,-0.70710678118655,0.707106781186545)) ;
#115749 = DIRECTION('ref_axis',(0.,-0.707106781186545,-0.70710678118655)) ;
#115750 = DIRECTION('center_axis',(-1.,0.,0.)) ;
#115751 = DIRECTION('ref_axis',(0.,0.,1.)) ;
#115752 = DIRECTION('center_axis',(-2.23012492569676E-15,0.514231796959107,
-0.857651245551598)) ;
#115753 = DIRECTION('ref_axis',(-5.69910941180089E-30,0.857651245551598,0.514231796959107)) ;
#115754 = DIRECTION('center_axis',(0.,1.,0.)) ;
#115755 = DIRECTION('ref_axis',(0.,0.,1.)) ;
#115756 = DIRECTION('center_axis',(0.,0.,-1.)) ;
#115757 = DIRECTION('ref_axis',(-1.,0.,0.)) ;
#115758 = DIRECTION('center_axis',(0.,1.,0.)) ;
#115759 = DIRECTION('ref_axis',(0.,0.,1.)) ;
#115760 = DIRECTION('center_axis',(0.,0.,-1.)) ;
#115761 = DIRECTION('ref_axis',(-1.,0.,0.)) ;
#115762 = DIRECTION('center_axis',(0.,0.,-1.)) ;
#115763 = DIRECTION('ref_axis',(-1.,0.,0.)) ;
#115764 = DIRECTION('center_axis',(0.,0.,1.)) ;
#115765 = DIRECTION('ref_axis',(1.,0.,0.)) ;
#115766 = DIRECTION('center_axis',(0.,0.,-1.)) ;
#115767 = DIRECTION('ref_axis',(-1.,0.,0.)) ;
#115768 = DIRECTION('center_axis',(0.,1.,0.)) ;
#115769 = DIRECTION('ref_axis',(0.,0.,1.)) ;
#115770 = DIRECTION('center_axis',(0.,-1.,8.67361737988409E-15)) ;
#115771 = DIRECTION('ref_axis',(0.,-8.67361737988409E-15,-1.)) ;
#115772 = DIRECTION('center_axis',(0.,0.707106781186546,0.707106781186549)) ;
#115773 = DIRECTION('ref_axis',(0.,-0.707106781186549,0.707106781186546)) ;
#115774 = DIRECTION('center_axis',(0.,0.707106781186541,0.707106781186554)) ;
#115775 = DIRECTION('ref_axis',(0.,-0.707106781186554,0.707106781186541)) ;
#115776 = DIRECTION('center_axis',(0.,1.,1.07081696047951E-16)) ;
#115777 = DIRECTION('ref_axis',(0.,-1.07081696047951E-16,1.)) ;
#115778 = DIRECTION('center_axis',(0.,-1.,0.)) ;
#115779 = DIRECTION('ref_axis',(0.,0.,-1.)) ;
#115780 = DIRECTION('center_axis',(0.,1.,0.)) ;
#115781 = DIRECTION('ref_axis',(0.,0.,1.)) ;
#115782 = DIRECTION('center_axis',(0.,0.,1.)) ;
#115783 = DIRECTION('ref_axis',(1.,0.,0.)) ;
#115784 = DIRECTION('center_axis',(0.,1.,0.)) ;
#115785 = DIRECTION('ref_axis',(0.,0.,1.)) ;
#115786 = DIRECTION('center_axis',(0.,0.,1.)) ;
#115787 = DIRECTION('ref_axis',(1.,0.,0.)) ;
#115788 = DIRECTION('center_axis',(0.,3.99416362155027E-15,1.)) ;
#115789 = DIRECTION('ref_axis',(0.,-1.,3.99416362155027E-15)) ;
#115790 = DIRECTION('center_axis',(0.,0.,1.)) ;
#115791 = DIRECTION('ref_axis',(1.,0.,0.)) ;
#115792 = DIRECTION('center_axis',(0.,0.,-1.)) ;
#115793 = DIRECTION('ref_axis',(-1.,0.,0.)) ;
#115794 = DIRECTION('center_axis',(0.,0.,1.)) ;
#115795 = DIRECTION('ref_axis',(1.,0.,0.)) ;
#115796 = DIRECTION('center_axis',(-1.,0.,0.)) ;
#115797 = DIRECTION('ref_axis',(0.,0.,1.)) ;
#115798 = DIRECTION('center_axis',(0.,1.,0.)) ;
#115799 = DIRECTION('ref_axis',(0.,0.,1.)) ;
#115800 = DIRECTION('center_axis',(-1.,0.,0.)) ;
#115801 = DIRECTION('ref_axis',(0.,0.,1.)) ;
#115802 = DIRECTION('center_axis',(0.,-1.,0.)) ;
#115803 = DIRECTION('ref_axis',(0.,0.,-1.)) ;
#115804 = DIRECTION('center_axis',(0.,1.,0.)) ;
#115805 = DIRECTION('ref_axis',(0.,0.,1.)) ;
#115806 = DIRECTION('center_axis',(1.53063836115601E-16,-1.,-1.30104260698261E-16)) ;
#115807 = DIRECTION('ref_axis',(1.,1.53063836115601E-16,1.99142572374599E-32)) ;
#115808 = DIRECTION('center_axis',(0.,1.,0.)) ;
#115809 = DIRECTION('ref_axis',(0.,0.,1.)) ;
#115810 = DIRECTION('center_axis',(0.,-1.,0.)) ;
#115811 = DIRECTION('ref_axis',(0.,0.,-1.)) ;
#115812 = DIRECTION('center_axis',(1.,1.53063836115601E-16,2.73691106313441E-48)) ;
#115813 = DIRECTION('ref_axis',(-1.53063836115601E-16,1.,-4.18922106430579E-64)) ;
#115814 = DIRECTION('center_axis',(-1.,0.,0.)) ;
#115815 = DIRECTION('ref_axis',(0.,0.,1.)) ;
#115816 = DIRECTION('center_axis',(1.,1.53063836115601E-16,0.)) ;
#115817 = DIRECTION('ref_axis',(1.53063836115601E-16,-1.,0.)) ;
#115818 = DIRECTION('center_axis',(0.,1.,0.)) ;
#115819 = DIRECTION('ref_axis',(1.,0.,0.)) ;
#115820 = DIRECTION('center_axis',(0.,1.,0.)) ;
#115821 = DIRECTION('ref_axis',(0.,0.,-1.)) ;
#115822 = DIRECTION('center_axis',(0.,0.,1.)) ;
#115823 = DIRECTION('ref_axis',(-1.,0.,0.)) ;
#115824 = DIRECTION('center_axis',(0.,1.,0.)) ;
#115825 = DIRECTION('ref_axis',(1.,0.,0.)) ;
#115826 = DIRECTION('center_axis',(0.,0.,1.)) ;
#115827 = DIRECTION('ref_axis',(-1.,0.,0.)) ;
#115828 = DIRECTION('center_axis',(1.,1.0842021724855E-15,0.)) ;
#115829 = DIRECTION('ref_axis',(1.0842021724855E-15,-1.,0.)) ;
#115830 = DIRECTION('center_axis',(-1.,-1.53063836115601E-16,0.)) ;
#115831 = DIRECTION('ref_axis',(0.,-1.,0.)) ;
#115832 = DIRECTION('center_axis',(0.,0.,-1.)) ;
#115833 = DIRECTION('ref_axis',(1.,0.,0.)) ;
#115834 = DIRECTION('center_axis',(0.,0.,-1.)) ;
#115835 = DIRECTION('ref_axis',(0.804034447892622,0.594582716366702,0.)) ;
#115836 = DIRECTION('center_axis',(0.,0.,1.)) ;
#115837 = DIRECTION('ref_axis',(1.,0.,0.)) ;
#115838 = DIRECTION('',(0.,0.,-1.)) ;
#115839 = DIRECTION('center_axis',(-2.16840434497101E-16,1.,1.30104260698261E-16)) ;
#115840 = DIRECTION('ref_axis',(1.,2.16840434497101E-16,1.22464679914735E-16)) ;
#115841 = DIRECTION('',(-2.16840434497101E-16,1.,1.30104260698261E-16)) ;
#115842 = DIRECTION('center_axis',(0.,1.,0.)) ;
#115843 = DIRECTION('ref_axis',(0.,0.,1.)) ;
#115844 = DIRECTION('center_axis',(-1.,-1.53063836115601E-16,-2.73691106313441E-48)) ;
#115845 = DIRECTION('ref_axis',(1.53063836115601E-16,-1.,4.18922106430579E-64)) ;
#115846 = DIRECTION('center_axis',(1.,2.16840434497101E-16,0.)) ;
#115847 = DIRECTION('ref_axis',(2.16840434497101E-16,-1.,0.)) ;
#115848 = DIRECTION('center_axis',(0.,0.,1.)) ;
#115849 = DIRECTION('ref_axis',(1.,0.,0.)) ;
#115850 = DIRECTION('center_axis',(-1.25542992828747E-32,1.020425574104E-16,
1.)) ;
#115851 = DIRECTION('ref_axis',(-1.28107280532009E-48,-1.,1.020425574104E-16)) ;
#115852 = DIRECTION('center_axis',(0.,0.,1.)) ;
#115853 = DIRECTION('ref_axis',(1.,0.,0.)) ;
#115854 = DIRECTION('center_axis',(0.,0.,-1.)) ;
#115855 = DIRECTION('ref_axis',(-1.,0.,0.)) ;
#115856 = DIRECTION('center_axis',(1.,1.53063836115601E-16,-2.73691106313441E-48)) ;
#115857 = DIRECTION('ref_axis',(-1.53063836115601E-16,1.,4.18922106430579E-64)) ;
#115858 = DIRECTION('center_axis',(-1.,0.,0.)) ;
#115859 = DIRECTION('ref_axis',(0.,0.,1.)) ;
#115860 = DIRECTION('center_axis',(1.,1.53063836115601E-16,0.)) ;
#115861 = DIRECTION('ref_axis',(1.53063836115601E-16,-1.,0.)) ;
#115862 = DIRECTION('center_axis',(0.,1.,0.)) ;
#115863 = DIRECTION('ref_axis',(1.,0.,0.)) ;
#115864 = DIRECTION('center_axis',(-1.,-2.16840434497101E-16,0.)) ;
#115865 = DIRECTION('ref_axis',(0.,-1.,0.)) ;
#115866 = DIRECTION('center_axis',(0.,0.,-1.)) ;
#115867 = DIRECTION('ref_axis',(1.,0.,0.)) ;
#115868 = DIRECTION('center_axis',(-1.25542992828747E-32,1.020425574104E-16,
1.)) ;
#115869 = DIRECTION('ref_axis',(0.,-1.,0.)) ;
#115870 = DIRECTION('center_axis',(0.,-1.,0.)) ;
#115871 = DIRECTION('ref_axis',(-6.50521303491307E-15,0.,1.)) ;
#115872 = DIRECTION('center_axis',(-1.,0.,0.)) ;
#115873 = DIRECTION('ref_axis',(0.,0.,-1.)) ;
#115874 = DIRECTION('center_axis',(-1.,-1.53063836115601E-16,0.)) ;
#115875 = DIRECTION('ref_axis',(0.,-1.,0.)) ;
#115876 = DIRECTION('center_axis',(0.,-1.,0.)) ;
#115877 = DIRECTION('ref_axis',(0.,0.,1.)) ;
#115878 = DIRECTION('center_axis',(0.,0.,-1.)) ;
#115879 = DIRECTION('ref_axis',(-1.,0.,0.)) ;
#115880 = DIRECTION('center_axis',(0.,0.,-1.)) ;
#115881 = DIRECTION('ref_axis',(-1.,0.,0.)) ;
#115882 = DIRECTION('center_axis',(1.,1.53063836115601E-16,-3.06472600140763E-33)) ;
#115883 = DIRECTION('ref_axis',(-1.53063836115601E-16,1.,4.69098718418678E-49)) ;
#115884 = DIRECTION('center_axis',(-1.,0.,0.)) ;
#115885 = DIRECTION('ref_axis',(0.,0.,1.)) ;
#115886 = DIRECTION('center_axis',(-1.53063836115601E-16,1.,-1.020425574104E-16)) ;
#115887 = DIRECTION('ref_axis',(-1.,-1.53063836115601E-16,1.3684555315672E-47)) ;
#115888 = DIRECTION('',(1.53063836115601E-16,-1.,1.020425574104E-16)) ;
#115889 = DIRECTION('center_axis',(0.,-1.,0.)) ;
#115890 = DIRECTION('ref_axis',(0.,0.,-1.)) ;
#115891 = DIRECTION('center_axis',(-1.53063836115601E-16,1.,-1.30104260698261E-16)) ;
#115892 = DIRECTION('ref_axis',(-1.,-1.53063836115601E-16,1.99142572374599E-32)) ;
#115893 = DIRECTION('center_axis',(0.,-1.,0.)) ;
#115894 = DIRECTION('ref_axis',(0.,0.,-1.)) ;
#115895 = DIRECTION('center_axis',(-1.,-1.53063836115601E-16,2.73691106313441E-48)) ;
#115896 = DIRECTION('ref_axis',(1.53063836115601E-16,-1.,-4.18922106430579E-64)) ;
#115897 = DIRECTION('center_axis',(1.,2.16840434497101E-16,0.)) ;
#115898 = DIRECTION('ref_axis',(2.16840434497101E-16,-1.,0.)) ;
#115899 = DIRECTION('center_axis',(-1.,0.,2.16840434497102E-15)) ;
#115900 = DIRECTION('ref_axis',(2.16840434497102E-15,0.,1.)) ;
#115901 = DIRECTION('center_axis',(-1.,-2.16840434497101E-16,0.)) ;
#115902 = DIRECTION('ref_axis',(0.,-1.,0.)) ;
#115903 = DIRECTION('center_axis',(0.,0.,1.)) ;
#115904 = DIRECTION('ref_axis',(-1.,0.,0.)) ;
#115905 = DIRECTION('center_axis',(0.,1.,0.)) ;
#115906 = DIRECTION('ref_axis',(1.,0.,0.)) ;
#115907 = DIRECTION('center_axis',(0.,1.,0.)) ;
#115908 = DIRECTION('ref_axis',(0.,0.,-1.)) ;
#115909 = DIRECTION('center_axis',(1.,0.,0.)) ;
#115910 = DIRECTION('ref_axis',(0.,-1.,0.)) ;
#115911 = DIRECTION('center_axis',(1.,6.50521303491304E-15,0.)) ;
#115912 = DIRECTION('ref_axis',(-6.50521303491304E-15,1.,0.)) ;
#115913 = DIRECTION('center_axis',(8.67361737988403E-15,1.,0.)) ;
#115914 = DIRECTION('ref_axis',(-1.,8.67361737988403E-15,0.)) ;
#115915 = DIRECTION('center_axis',(1.2303003375722E-16,-1.,1.020425574104E-16)) ;
#115916 = DIRECTION('ref_axis',(1.,1.2303003375722E-16,-1.25542992828747E-32)) ;
#115917 = DIRECTION('center_axis',(0.,1.,0.)) ;
#115918 = DIRECTION('ref_axis',(0.,0.,1.)) ;
#115919 = DIRECTION('center_axis',(0.,1.,0.)) ;
#115920 = DIRECTION('ref_axis',(1.,0.,0.)) ;
#115921 = DIRECTION('center_axis',(1.,1.2303003375722E-16,0.)) ;
#115922 = DIRECTION('ref_axis',(1.2303003375722E-16,-1.,0.)) ;
#115923 = DIRECTION('center_axis',(0.,0.,1.)) ;
#115924 = DIRECTION('ref_axis',(-1.,0.,0.)) ;
#115925 = DIRECTION('center_axis',(0.,1.,0.)) ;
#115926 = DIRECTION('ref_axis',(1.,0.,0.)) ;
#115927 = DIRECTION('center_axis',(0.,0.,-1.)) ;
#115928 = DIRECTION('ref_axis',(1.,0.,0.)) ;
#115929 = DIRECTION('center_axis',(0.,0.,-1.)) ;
#115930 = DIRECTION('ref_axis',(-1.,0.,0.)) ;
#115931 = DIRECTION('center_axis',(0.,0.,1.)) ;
#115932 = DIRECTION('ref_axis',(1.,0.,0.)) ;
#115933 = DIRECTION('center_axis',(-2.16840434497101E-16,1.,-1.020425574104E-16)) ;
#115934 = DIRECTION('ref_axis',(-1.,-2.16840434497101E-16,5.47382212626882E-48)) ;
#115935 = DIRECTION('center_axis',(0.,1.,0.)) ;
#115936 = DIRECTION('ref_axis',(0.,0.,-1.)) ;
#115937 = DIRECTION('center_axis',(1.,0.,1.25542992828747E-32)) ;
#115938 = DIRECTION('ref_axis',(1.25542992828747E-32,0.,-1.)) ;
#115939 = DIRECTION('center_axis',(1.,0.,0.)) ;
#115940 = DIRECTION('ref_axis',(0.,0.,-1.)) ;
#115941 = DIRECTION('center_axis',(-1.,-1.2303003375722E-16,0.)) ;
#115942 = DIRECTION('ref_axis',(0.,-1.,0.)) ;
#115943 = DIRECTION('center_axis',(0.,0.,-1.)) ;
#115944 = DIRECTION('ref_axis',(1.,0.,0.)) ;
#115945 = DIRECTION('center_axis',(0.,0.,-1.)) ;
#115946 = DIRECTION('ref_axis',(-1.,0.,0.)) ;
#115947 = DIRECTION('',(0.,0.,1.)) ;
#115948 = DIRECTION('center_axis',(0.,0.,1.)) ;
#115949 = DIRECTION('ref_axis',(1.,0.,0.)) ;
#115950 = DIRECTION('center_axis',(0.,0.,1.)) ;
#115951 = DIRECTION('ref_axis',(1.,0.,0.)) ;
#115952 = DIRECTION('center_axis',(6.27714964143733E-33,-5.10212787052002E-17,
-1.)) ;
#115953 = DIRECTION('ref_axis',(3.20268201330022E-49,1.,-5.10212787052002E-17)) ;
#115954 = DIRECTION('center_axis',(1.,1.53063836115601E-16,-1.53236300070382E-33)) ;
#115955 = DIRECTION('ref_axis',(-1.53063836115601E-16,1.,2.34549359209339E-49)) ;
#115956 = DIRECTION('center_axis',(-1.,0.,0.)) ;
#115957 = DIRECTION('ref_axis',(0.,0.,1.)) ;
#115958 = DIRECTION('center_axis',(1.,0.,0.)) ;
#115959 = DIRECTION('ref_axis',(0.,0.,-1.)) ;
#115960 = DIRECTION('center_axis',(0.,1.,0.)) ;
#115961 = DIRECTION('ref_axis',(1.,0.,0.)) ;
#115962 = DIRECTION('center_axis',(-4.33680868994202E-15,1.,0.)) ;
#115963 = DIRECTION('ref_axis',(1.,4.33680868994202E-15,0.)) ;
#115964 = DIRECTION('center_axis',(0.,-1.,0.)) ;
#115965 = DIRECTION('ref_axis',(0.,0.,-1.)) ;
#115966 = DIRECTION('center_axis',(0.,0.,-1.)) ;
#115967 = DIRECTION('ref_axis',(1.,0.,0.)) ;
#115968 = DIRECTION('center_axis',(0.,0.,1.)) ;
#115969 = DIRECTION('ref_axis',(1.,0.,0.)) ;
#115970 = DIRECTION('center_axis',(0.,0.,-1.)) ;
#115971 = DIRECTION('ref_axis',(-1.,0.,0.)) ;
#115972 = DIRECTION('center_axis',(0.,1.,0.)) ;
#115973 = DIRECTION('ref_axis',(1.,0.,0.)) ;
#115974 = DIRECTION('center_axis',(1.,1.2303003375722E-16,0.)) ;
#115975 = DIRECTION('ref_axis',(1.2303003375722E-16,-1.,0.)) ;
#115976 = DIRECTION('center_axis',(0.,1.,0.)) ;
#115977 = DIRECTION('ref_axis',(-6.50521303491307E-15,0.,-1.)) ;
#115978 = DIRECTION('center_axis',(6.27714964143733E-33,-5.10212787052002E-17,
-1.)) ;
#115979 = DIRECTION('ref_axis',(0.,1.,0.)) ;
#115980 = DIRECTION('center_axis',(0.,-1.,0.)) ;
#115981 = DIRECTION('ref_axis',(0.,0.,1.)) ;
#115982 = DIRECTION('center_axis',(2.16840434497101E-16,-1.,5.10212787052002E-17)) ;
#115983 = DIRECTION('ref_axis',(1.,2.16840434497101E-16,-5.47382212626882E-48)) ;
#115984 = DIRECTION('center_axis',(0.,1.,0.)) ;
#115985 = DIRECTION('ref_axis',(0.,0.,-1.)) ;
#115986 = DIRECTION('center_axis',(0.,0.,1.)) ;
#115987 = DIRECTION('ref_axis',(1.,0.,0.)) ;
#115988 = DIRECTION('center_axis',(0.,0.,-1.)) ;
#115989 = DIRECTION('ref_axis',(-1.,0.,0.)) ;
#115990 = DIRECTION('center_axis',(-1.,-1.2303003375722E-16,0.)) ;
#115991 = DIRECTION('ref_axis',(0.,-1.,0.)) ;
#115992 = DIRECTION('center_axis',(0.,-1.,0.)) ;
#115993 = DIRECTION('ref_axis',(0.,0.,1.)) ;
#115994 = DIRECTION('center_axis',(1.53063836115601E-16,-1.,5.10212787052002E-17)) ;
#115995 = DIRECTION('ref_axis',(1.,1.53063836115601E-16,-6.84227765783602E-48)) ;
#115996 = DIRECTION('',(-1.53063836115601E-16,1.,-5.10212787052002E-17)) ;
#115997 = DIRECTION('center_axis',(0.,-1.,0.)) ;
#115998 = DIRECTION('ref_axis',(0.,0.,-1.)) ;
#115999 = DIRECTION('center_axis',(-1.,0.,0.)) ;
#116000 = DIRECTION('ref_axis',(0.,0.,-1.)) ;
#116001 = DIRECTION('center_axis',(-1.2303003375722E-16,1.,-5.10212787052002E-17)) ;
#116002 = DIRECTION('ref_axis',(-1.,-1.2303003375722E-16,6.27714964143733E-33)) ;
#116003 = DIRECTION('center_axis',(-8.67361737988403E-15,-1.,0.)) ;
#116004 = DIRECTION('ref_axis',(1.,-8.67361737988403E-15,0.)) ;
#116005 = DIRECTION('center_axis',(1.,0.,6.27714964143733E-33)) ;
#116006 = DIRECTION('ref_axis',(6.27714964143733E-33,0.,-1.)) ;
#116007 = DIRECTION('center_axis',(-1.,0.,-6.50521303491307E-15)) ;
#116008 = DIRECTION('ref_axis',(-6.50521303491307E-15,0.,1.)) ;
#116009 = DIRECTION('center_axis',(1.,0.,0.)) ;
#116010 = DIRECTION('ref_axis',(0.,1.,0.)) ;
#116011 = DIRECTION('center_axis',(0.,0.,-1.)) ;
#116012 = DIRECTION('ref_axis',(-1.,0.,0.)) ;
#116013 = DIRECTION('center_axis',(0.,0.,1.)) ;
#116014 = DIRECTION('ref_axis',(1.,0.,0.)) ;
#116015 = DIRECTION('center_axis',(0.,0.,-1.)) ;
#116016 = DIRECTION('ref_axis',(-1.,0.,0.)) ;
#116017 = DIRECTION('center_axis',(-1.,0.,0.)) ;
#116018 = DIRECTION('ref_axis',(0.,0.,1.)) ;
#116019 = DIRECTION('center_axis',(0.,-1.,0.)) ;
#116020 = DIRECTION('ref_axis',(0.,0.,-1.)) ;
#116021 = DIRECTION('center_axis',(0.,1.,0.)) ;
#116022 = DIRECTION('ref_axis',(0.,0.,1.)) ;
#116023 = DIRECTION('center_axis',(0.,1.,-6.50521303491307E-15)) ;
#116024 = DIRECTION('ref_axis',(0.,6.50521303491307E-15,1.)) ;
#116025 = DIRECTION('center_axis',(0.,-1.,0.)) ;
#116026 = DIRECTION('ref_axis',(0.,0.,-1.)) ;
#116027 = DIRECTION('center_axis',(0.,-1.,0.)) ;
#116028 = DIRECTION('ref_axis',(0.,0.,-1.)) ;
#116029 = DIRECTION('center_axis',(0.,-1.,-1.07081696047951E-16)) ;
#116030 = DIRECTION('ref_axis',(0.,1.07081696047951E-16,-1.)) ;
#116031 = DIRECTION('center_axis',(0.,1.,0.)) ;
#116032 = DIRECTION('ref_axis',(0.,0.,1.)) ;
#116033 = DIRECTION('center_axis',(-1.,0.,0.)) ;
#116034 = DIRECTION('ref_axis',(0.,0.,1.)) ;
#116035 = DIRECTION('center_axis',(0.,0.,1.)) ;
#116036 = DIRECTION('ref_axis',(1.,0.,0.)) ;
#116037 = DIRECTION('center_axis',(0.,1.,0.)) ;
#116038 = DIRECTION('ref_axis',(0.,0.,1.)) ;
#116039 = DIRECTION('center_axis',(0.,0.,-1.)) ;
#116040 = DIRECTION('ref_axis',(-1.,0.,0.)) ;
#116041 = DIRECTION('center_axis',(0.,0.,1.)) ;
#116042 = DIRECTION('ref_axis',(1.,0.,0.)) ;
#116043 = DIRECTION('center_axis',(0.,0.,1.)) ;
#116044 = DIRECTION('ref_axis',(1.,0.,0.)) ;
#116045 = DIRECTION('center_axis',(0.,0.,1.)) ;
#116046 = DIRECTION('ref_axis',(1.,0.,0.)) ;
#116047 = DIRECTION('center_axis',(0.,0.,-1.)) ;
#116048 = DIRECTION('ref_axis',(-1.,0.,0.)) ;
#116049 = DIRECTION('center_axis',(0.,1.,0.)) ;
#116050 = DIRECTION('ref_axis',(0.,0.,1.)) ;
#116051 = DIRECTION('center_axis',(0.,-0.707106781186558,0.707106781186537)) ;
#116052 = DIRECTION('ref_axis',(0.,-0.707106781186537,-0.707106781186558)) ;
#116053 = DIRECTION('center_axis',(0.,1.,0.)) ;
#116054 = DIRECTION('ref_axis',(0.,0.,1.)) ;
#116055 = DIRECTION('center_axis',(0.,-0.514231796959093,-0.857651245551607)) ;
#116056 = DIRECTION('ref_axis',(0.,0.857651245551607,-0.514231796959093)) ;
#116057 = DIRECTION('center_axis',(0.,-0.707106781186548,0.707106781186547)) ;
#116058 = DIRECTION('ref_axis',(0.,-0.707106781186547,-0.707106781186548)) ;
#116059 = DIRECTION('center_axis',(0.,-0.707106781186548,0.707106781186548)) ;
#116060 = DIRECTION('ref_axis',(0.,-0.707106781186548,-0.707106781186548)) ;
#116061 = DIRECTION('center_axis',(-1.,0.,0.)) ;
#116062 = DIRECTION('ref_axis',(0.,0.,1.)) ;
#116063 = DIRECTION('center_axis',(0.,0.514231796959095,-0.857651245551606)) ;
#116064 = DIRECTION('ref_axis',(0.,0.857651245551606,0.514231796959095)) ;
#116065 = DIRECTION('center_axis',(0.,1.,0.)) ;
#116066 = DIRECTION('ref_axis',(0.,0.,1.)) ;
#116067 = DIRECTION('center_axis',(0.,0.,-1.)) ;
#116068 = DIRECTION('ref_axis',(-1.,0.,0.)) ;
#116069 = DIRECTION('center_axis',(0.,1.,0.)) ;
#116070 = DIRECTION('ref_axis',(0.,0.,1.)) ;
#116071 = DIRECTION('center_axis',(0.,0.,-1.)) ;
#116072 = DIRECTION('ref_axis',(-1.,0.,0.)) ;
#116073 = DIRECTION('center_axis',(0.,0.,-1.)) ;
#116074 = DIRECTION('ref_axis',(-1.,0.,0.)) ;
#116075 = DIRECTION('center_axis',(0.,0.,1.)) ;
#116076 = DIRECTION('ref_axis',(1.,0.,0.)) ;
#116077 = DIRECTION('center_axis',(0.,0.,-1.)) ;
#116078 = DIRECTION('ref_axis',(-1.,0.,0.)) ;
#116079 = DIRECTION('center_axis',(0.,1.,0.)) ;
#116080 = DIRECTION('ref_axis',(0.,0.,1.)) ;
#116081 = DIRECTION('center_axis',(0.,-1.,8.67361737988409E-15)) ;
#116082 = DIRECTION('ref_axis',(0.,-8.67361737988409E-15,-1.)) ;
#116083 = DIRECTION('center_axis',(0.,0.707106781186546,0.707106781186549)) ;
#116084 = DIRECTION('ref_axis',(0.,-0.707106781186549,0.707106781186546)) ;
#116085 = DIRECTION('center_axis',(0.,0.707106781186537,0.707106781186558)) ;
#116086 = DIRECTION('ref_axis',(0.,-0.707106781186558,0.707106781186537)) ;
#116087 = DIRECTION('center_axis',(0.,1.,1.07081696047951E-16)) ;
#116088 = DIRECTION('ref_axis',(0.,-1.07081696047951E-16,1.)) ;
#116089 = DIRECTION('center_axis',(0.,-1.,0.)) ;
#116090 = DIRECTION('ref_axis',(0.,0.,-1.)) ;
#116091 = DIRECTION('center_axis',(0.,1.,0.)) ;
#116092 = DIRECTION('ref_axis',(0.,0.,1.)) ;
#116093 = DIRECTION('center_axis',(0.,0.,1.)) ;
#116094 = DIRECTION('ref_axis',(1.,0.,0.)) ;
#116095 = DIRECTION('center_axis',(0.,1.,0.)) ;
#116096 = DIRECTION('ref_axis',(0.,0.,1.)) ;
#116097 = DIRECTION('center_axis',(0.,0.,1.)) ;
#116098 = DIRECTION('ref_axis',(1.,0.,0.)) ;
#116099 = DIRECTION('center_axis',(0.,3.99416362155027E-15,1.)) ;
#116100 = DIRECTION('ref_axis',(0.,-1.,3.99416362155027E-15)) ;
#116101 = DIRECTION('center_axis',(0.,0.,1.)) ;
#116102 = DIRECTION('ref_axis',(1.,0.,0.)) ;
#116103 = DIRECTION('center_axis',(0.,0.,-1.)) ;
#116104 = DIRECTION('ref_axis',(-1.,0.,0.)) ;
#116105 = DIRECTION('center_axis',(0.,0.,1.)) ;
#116106 = DIRECTION('ref_axis',(1.,0.,0.)) ;
#116107 = DIRECTION('center_axis',(-1.,0.,0.)) ;
#116108 = DIRECTION('ref_axis',(0.,0.,1.)) ;
#116109 = DIRECTION('center_axis',(0.,1.,0.)) ;
#116110 = DIRECTION('ref_axis',(0.,0.,1.)) ;
#116111 = DIRECTION('center_axis',(-1.,0.,0.)) ;
#116112 = DIRECTION('ref_axis',(0.,0.,1.)) ;
#116113 = DIRECTION('center_axis',(0.,-1.,0.)) ;
#116114 = DIRECTION('ref_axis',(0.,0.,-1.)) ;
#116115 = DIRECTION('center_axis',(0.,1.,0.)) ;
#116116 = DIRECTION('ref_axis',(0.,0.,1.)) ;
#116117 = DIRECTION('center_axis',(1.53063836115601E-16,-1.,-1.30104260698261E-16)) ;
#116118 = DIRECTION('ref_axis',(1.,1.53063836115601E-16,1.99142572374599E-32)) ;
#116119 = DIRECTION('center_axis',(0.,1.,0.)) ;
#116120 = DIRECTION('ref_axis',(0.,0.,1.)) ;
#116121 = DIRECTION('center_axis',(0.,-1.,0.)) ;
#116122 = DIRECTION('ref_axis',(0.,0.,-1.)) ;
#116123 = DIRECTION('center_axis',(1.,1.53063836115601E-16,2.73691106313441E-48)) ;
#116124 = DIRECTION('ref_axis',(-1.53063836115601E-16,1.,-4.18922106430579E-64)) ;
#116125 = DIRECTION('center_axis',(-1.,0.,0.)) ;
#116126 = DIRECTION('ref_axis',(0.,0.,1.)) ;
#116127 = DIRECTION('center_axis',(1.,1.53063836115601E-16,0.)) ;
#116128 = DIRECTION('ref_axis',(1.53063836115601E-16,-1.,0.)) ;
#116129 = DIRECTION('center_axis',(0.,1.,0.)) ;
#116130 = DIRECTION('ref_axis',(1.,0.,0.)) ;
#116131 = DIRECTION('center_axis',(0.,1.,0.)) ;
#116132 = DIRECTION('ref_axis',(0.,0.,-1.)) ;
#116133 = DIRECTION('center_axis',(0.,0.,1.)) ;
#116134 = DIRECTION('ref_axis',(-1.,0.,0.)) ;
#116135 = DIRECTION('center_axis',(0.,1.,0.)) ;
#116136 = DIRECTION('ref_axis',(1.,0.,0.)) ;
#116137 = DIRECTION('center_axis',(0.,0.,1.)) ;
#116138 = DIRECTION('ref_axis',(-1.,0.,0.)) ;
#116139 = DIRECTION('center_axis',(1.,1.0842021724855E-15,0.)) ;
#116140 = DIRECTION('ref_axis',(1.0842021724855E-15,-1.,0.)) ;
#116141 = DIRECTION('center_axis',(-1.,-1.53063836115601E-16,0.)) ;
#116142 = DIRECTION('ref_axis',(0.,-1.,0.)) ;
#116143 = DIRECTION('center_axis',(0.,0.,-1.)) ;
#116144 = DIRECTION('ref_axis',(1.,0.,0.)) ;
#116145 = DIRECTION('center_axis',(0.,0.,-1.)) ;
#116146 = DIRECTION('ref_axis',(0.804034447892617,0.594582716366709,0.)) ;
#116147 = DIRECTION('center_axis',(0.,0.,1.)) ;
#116148 = DIRECTION('ref_axis',(1.,0.,0.)) ;
#116149 = DIRECTION('',(0.,0.,-1.)) ;
#116150 = DIRECTION('center_axis',(-2.16840434497101E-16,1.,1.30104260698261E-16)) ;
#116151 = DIRECTION('ref_axis',(1.,2.16840434497101E-16,1.22464679914735E-16)) ;
#116152 = DIRECTION('',(-2.16840434497101E-16,1.,1.30104260698261E-16)) ;
#116153 = DIRECTION('center_axis',(0.,1.,0.)) ;
#116154 = DIRECTION('ref_axis',(0.,0.,1.)) ;
#116155 = DIRECTION('center_axis',(-1.,-1.53063836115601E-16,-2.73691106313441E-48)) ;
#116156 = DIRECTION('ref_axis',(1.53063836115601E-16,-1.,4.18922106430579E-64)) ;
#116157 = DIRECTION('center_axis',(1.,2.16840434497101E-16,0.)) ;
#116158 = DIRECTION('ref_axis',(2.16840434497101E-16,-1.,0.)) ;
#116159 = DIRECTION('center_axis',(0.,0.,1.)) ;
#116160 = DIRECTION('ref_axis',(1.,0.,0.)) ;
#116161 = DIRECTION('center_axis',(-1.25542992828747E-32,1.020425574104E-16,
1.)) ;
#116162 = DIRECTION('ref_axis',(-1.28107280532009E-48,-1.,1.020425574104E-16)) ;
#116163 = DIRECTION('center_axis',(0.,0.,1.)) ;
#116164 = DIRECTION('ref_axis',(1.,0.,0.)) ;
#116165 = DIRECTION('center_axis',(0.,0.,-1.)) ;
#116166 = DIRECTION('ref_axis',(-1.,0.,0.)) ;
#116167 = DIRECTION('center_axis',(1.,1.53063836115601E-16,-2.73691106313441E-48)) ;
#116168 = DIRECTION('ref_axis',(-1.53063836115601E-16,1.,4.18922106430579E-64)) ;
#116169 = DIRECTION('center_axis',(-1.,0.,0.)) ;
#116170 = DIRECTION('ref_axis',(0.,0.,1.)) ;
#116171 = DIRECTION('center_axis',(1.,1.53063836115601E-16,0.)) ;
#116172 = DIRECTION('ref_axis',(1.53063836115601E-16,-1.,0.)) ;
#116173 = DIRECTION('center_axis',(0.,1.,0.)) ;
#116174 = DIRECTION('ref_axis',(1.,0.,0.)) ;
#116175 = DIRECTION('center_axis',(-1.,-2.16840434497101E-16,0.)) ;
#116176 = DIRECTION('ref_axis',(0.,-1.,0.)) ;
#116177 = DIRECTION('center_axis',(0.,0.,-1.)) ;
#116178 = DIRECTION('ref_axis',(1.,0.,0.)) ;
#116179 = DIRECTION('center_axis',(-1.25542992828747E-32,1.020425574104E-16,
1.)) ;
#116180 = DIRECTION('ref_axis',(0.,-1.,0.)) ;
#116181 = DIRECTION('center_axis',(0.,-1.,0.)) ;
#116182 = DIRECTION('ref_axis',(-6.50521303491307E-15,0.,1.)) ;
#116183 = DIRECTION('center_axis',(-1.,0.,0.)) ;
#116184 = DIRECTION('ref_axis',(0.,0.,-1.)) ;
#116185 = DIRECTION('center_axis',(-1.,-1.53063836115601E-16,0.)) ;
#116186 = DIRECTION('ref_axis',(0.,-1.,0.)) ;
#116187 = DIRECTION('center_axis',(0.,-1.,0.)) ;
#116188 = DIRECTION('ref_axis',(0.,0.,1.)) ;
#116189 = DIRECTION('center_axis',(0.,0.,-1.)) ;
#116190 = DIRECTION('ref_axis',(-1.,0.,0.)) ;
#116191 = DIRECTION('center_axis',(0.,0.,-1.)) ;
#116192 = DIRECTION('ref_axis',(-1.,0.,0.)) ;
#116193 = DIRECTION('center_axis',(1.,1.53063836115601E-16,-3.06472600140763E-33)) ;
#116194 = DIRECTION('ref_axis',(-1.53063836115601E-16,1.,4.69098718418678E-49)) ;
#116195 = DIRECTION('center_axis',(-1.,0.,0.)) ;
#116196 = DIRECTION('ref_axis',(0.,0.,1.)) ;
#116197 = DIRECTION('center_axis',(-1.53063836115601E-16,1.,-1.020425574104E-16)) ;
#116198 = DIRECTION('ref_axis',(-1.,-1.53063836115601E-16,1.3684555315672E-47)) ;
#116199 = DIRECTION('',(1.53063836115601E-16,-1.,1.020425574104E-16)) ;
#116200 = DIRECTION('center_axis',(0.,-1.,0.)) ;
#116201 = DIRECTION('ref_axis',(0.,0.,-1.)) ;
#116202 = DIRECTION('center_axis',(-1.53063836115601E-16,1.,-1.30104260698261E-16)) ;
#116203 = DIRECTION('ref_axis',(-1.,-1.53063836115601E-16,1.99142572374599E-32)) ;
#116204 = DIRECTION('center_axis',(0.,-1.,0.)) ;
#116205 = DIRECTION('ref_axis',(0.,0.,-1.)) ;
#116206 = DIRECTION('center_axis',(-1.,-1.53063836115601E-16,2.73691106313441E-48)) ;
#116207 = DIRECTION('ref_axis',(1.53063836115601E-16,-1.,-4.18922106430579E-64)) ;
#116208 = DIRECTION('center_axis',(1.,2.16840434497101E-16,0.)) ;
#116209 = DIRECTION('ref_axis',(2.16840434497101E-16,-1.,0.)) ;
#116210 = DIRECTION('center_axis',(-1.,0.,2.16840434497102E-15)) ;
#116211 = DIRECTION('ref_axis',(2.16840434497102E-15,0.,1.)) ;
#116212 = DIRECTION('center_axis',(-1.,-2.16840434497101E-16,0.)) ;
#116213 = DIRECTION('ref_axis',(0.,-1.,0.)) ;
#116214 = DIRECTION('center_axis',(0.,0.,1.)) ;
#116215 = DIRECTION('ref_axis',(-1.,0.,0.)) ;
#116216 = DIRECTION('center_axis',(0.,1.,0.)) ;
#116217 = DIRECTION('ref_axis',(1.,0.,0.)) ;
#116218 = DIRECTION('center_axis',(0.,1.,0.)) ;
#116219 = DIRECTION('ref_axis',(0.,0.,-1.)) ;
#116220 = DIRECTION('center_axis',(1.,0.,0.)) ;
#116221 = DIRECTION('ref_axis',(0.,-1.,0.)) ;
#116222 = DIRECTION('center_axis',(1.,6.50521303491304E-15,0.)) ;
#116223 = DIRECTION('ref_axis',(-6.50521303491304E-15,1.,0.)) ;
#116224 = DIRECTION('center_axis',(8.67361737988403E-15,1.,0.)) ;
#116225 = DIRECTION('ref_axis',(-1.,8.67361737988403E-15,0.)) ;
#116226 = DIRECTION('center_axis',(1.2303003375722E-16,-1.,1.020425574104E-16)) ;
#116227 = DIRECTION('ref_axis',(1.,1.2303003375722E-16,-1.25542992828747E-32)) ;
#116228 = DIRECTION('center_axis',(0.,1.,0.)) ;
#116229 = DIRECTION('ref_axis',(0.,0.,1.)) ;
#116230 = DIRECTION('center_axis',(0.,1.,0.)) ;
#116231 = DIRECTION('ref_axis',(1.,0.,0.)) ;
#116232 = DIRECTION('center_axis',(1.,1.2303003375722E-16,0.)) ;
#116233 = DIRECTION('ref_axis',(1.2303003375722E-16,-1.,0.)) ;
#116234 = DIRECTION('center_axis',(0.,0.,1.)) ;
#116235 = DIRECTION('ref_axis',(-1.,0.,0.)) ;
#116236 = DIRECTION('center_axis',(0.,1.,0.)) ;
#116237 = DIRECTION('ref_axis',(1.,0.,0.)) ;
#116238 = DIRECTION('center_axis',(0.,0.,-1.)) ;
#116239 = DIRECTION('ref_axis',(1.,0.,0.)) ;
#116240 = DIRECTION('center_axis',(0.,0.,-1.)) ;
#116241 = DIRECTION('ref_axis',(-1.,0.,0.)) ;
#116242 = DIRECTION('center_axis',(0.,0.,1.)) ;
#116243 = DIRECTION('ref_axis',(1.,0.,0.)) ;
#116244 = DIRECTION('center_axis',(-2.16840434497101E-16,1.,-1.020425574104E-16)) ;
#116245 = DIRECTION('ref_axis',(-1.,-2.16840434497101E-16,5.47382212626882E-48)) ;
#116246 = DIRECTION('center_axis',(0.,1.,0.)) ;
#116247 = DIRECTION('ref_axis',(0.,0.,-1.)) ;
#116248 = DIRECTION('center_axis',(1.,0.,1.25542992828747E-32)) ;
#116249 = DIRECTION('ref_axis',(1.25542992828747E-32,0.,-1.)) ;
#116250 = DIRECTION('center_axis',(1.,0.,0.)) ;
#116251 = DIRECTION('ref_axis',(0.,0.,-1.)) ;
#116252 = DIRECTION('center_axis',(-1.,-1.2303003375722E-16,0.)) ;
#116253 = DIRECTION('ref_axis',(0.,-1.,0.)) ;
#116254 = DIRECTION('center_axis',(0.,0.,-1.)) ;
#116255 = DIRECTION('ref_axis',(1.,0.,0.)) ;
#116256 = DIRECTION('center_axis',(0.,0.,-1.)) ;
#116257 = DIRECTION('ref_axis',(-1.,0.,0.)) ;
#116258 = DIRECTION('',(0.,0.,1.)) ;
#116259 = DIRECTION('center_axis',(0.,0.,1.)) ;
#116260 = DIRECTION('ref_axis',(1.,0.,0.)) ;
#116261 = DIRECTION('center_axis',(0.,0.,1.)) ;
#116262 = DIRECTION('ref_axis',(1.,0.,0.)) ;
#116263 = DIRECTION('center_axis',(6.27714964143733E-33,-5.10212787052002E-17,
-1.)) ;
#116264 = DIRECTION('ref_axis',(3.20268201330022E-49,1.,-5.10212787052002E-17)) ;
#116265 = DIRECTION('center_axis',(1.,1.53063836115601E-16,-1.53236300070382E-33)) ;
#116266 = DIRECTION('ref_axis',(-1.53063836115601E-16,1.,2.34549359209339E-49)) ;
#116267 = DIRECTION('center_axis',(-1.,0.,0.)) ;
#116268 = DIRECTION('ref_axis',(0.,0.,1.)) ;
#116269 = DIRECTION('center_axis',(1.,0.,0.)) ;
#116270 = DIRECTION('ref_axis',(0.,0.,-1.)) ;
#116271 = DIRECTION('center_axis',(0.,1.,0.)) ;
#116272 = DIRECTION('ref_axis',(1.,0.,0.)) ;
#116273 = DIRECTION('center_axis',(-4.33680868994202E-15,1.,0.)) ;
#116274 = DIRECTION('ref_axis',(1.,4.33680868994202E-15,0.)) ;
#116275 = DIRECTION('center_axis',(0.,-1.,0.)) ;
#116276 = DIRECTION('ref_axis',(0.,0.,-1.)) ;
#116277 = DIRECTION('center_axis',(0.,0.,-1.)) ;
#116278 = DIRECTION('ref_axis',(1.,0.,0.)) ;
#116279 = DIRECTION('center_axis',(0.,0.,1.)) ;
#116280 = DIRECTION('ref_axis',(1.,0.,0.)) ;
#116281 = DIRECTION('center_axis',(0.,0.,-1.)) ;
#116282 = DIRECTION('ref_axis',(-1.,0.,0.)) ;
#116283 = DIRECTION('center_axis',(0.,1.,0.)) ;
#116284 = DIRECTION('ref_axis',(1.,0.,0.)) ;
#116285 = DIRECTION('center_axis',(1.,1.2303003375722E-16,0.)) ;
#116286 = DIRECTION('ref_axis',(1.2303003375722E-16,-1.,0.)) ;
#116287 = DIRECTION('center_axis',(0.,1.,0.)) ;
#116288 = DIRECTION('ref_axis',(-6.50521303491307E-15,0.,-1.)) ;
#116289 = DIRECTION('center_axis',(6.27714964143733E-33,-5.10212787052002E-17,
-1.)) ;
#116290 = DIRECTION('ref_axis',(0.,1.,0.)) ;
#116291 = DIRECTION('center_axis',(0.,-1.,0.)) ;
#116292 = DIRECTION('ref_axis',(0.,0.,1.)) ;
#116293 = DIRECTION('center_axis',(2.16840434497101E-16,-1.,5.10212787052002E-17)) ;
#116294 = DIRECTION('ref_axis',(1.,2.16840434497101E-16,-5.47382212626882E-48)) ;
#116295 = DIRECTION('center_axis',(0.,1.,0.)) ;
#116296 = DIRECTION('ref_axis',(0.,0.,-1.)) ;
#116297 = DIRECTION('center_axis',(0.,0.,1.)) ;
#116298 = DIRECTION('ref_axis',(1.,0.,0.)) ;
#116299 = DIRECTION('center_axis',(0.,0.,-1.)) ;
#116300 = DIRECTION('ref_axis',(-1.,0.,0.)) ;
#116301 = DIRECTION('center_axis',(-1.,-1.2303003375722E-16,0.)) ;
#116302 = DIRECTION('ref_axis',(0.,-1.,0.)) ;
#116303 = DIRECTION('center_axis',(0.,-1.,0.)) ;
#116304 = DIRECTION('ref_axis',(0.,0.,1.)) ;
#116305 = DIRECTION('center_axis',(1.53063836115601E-16,-1.,5.10212787052002E-17)) ;
#116306 = DIRECTION('ref_axis',(1.,1.53063836115601E-16,-6.84227765783602E-48)) ;
#116307 = DIRECTION('',(-1.53063836115601E-16,1.,-5.10212787052002E-17)) ;
#116308 = DIRECTION('center_axis',(0.,-1.,0.)) ;
#116309 = DIRECTION('ref_axis',(0.,0.,-1.)) ;
#116310 = DIRECTION('center_axis',(-1.,0.,0.)) ;
#116311 = DIRECTION('ref_axis',(0.,0.,-1.)) ;
#116312 = DIRECTION('center_axis',(-1.2303003375722E-16,1.,-5.10212787052002E-17)) ;
#116313 = DIRECTION('ref_axis',(-1.,-1.2303003375722E-16,6.27714964143733E-33)) ;
#116314 = DIRECTION('center_axis',(-8.67361737988403E-15,-1.,0.)) ;
#116315 = DIRECTION('ref_axis',(1.,-8.67361737988403E-15,0.)) ;
#116316 = DIRECTION('center_axis',(1.,0.,6.27714964143733E-33)) ;
#116317 = DIRECTION('ref_axis',(6.27714964143733E-33,0.,-1.)) ;
#116318 = DIRECTION('center_axis',(-1.,0.,-6.50521303491307E-15)) ;
#116319 = DIRECTION('ref_axis',(-6.50521303491307E-15,0.,1.)) ;
#116320 = DIRECTION('center_axis',(1.,0.,0.)) ;
#116321 = DIRECTION('ref_axis',(0.,1.,0.)) ;
#116322 = DIRECTION('center_axis',(0.,0.,-1.)) ;
#116323 = DIRECTION('ref_axis',(-1.,0.,0.)) ;
#116324 = DIRECTION('center_axis',(0.,0.,1.)) ;
#116325 = DIRECTION('ref_axis',(1.,0.,0.)) ;
#116326 = DIRECTION('center_axis',(0.,0.,-1.)) ;
#116327 = DIRECTION('ref_axis',(-1.,0.,0.)) ;
#116328 = DIRECTION('center_axis',(-1.,0.,0.)) ;
#116329 = DIRECTION('ref_axis',(0.,0.,1.)) ;
#116330 = DIRECTION('center_axis',(0.,-1.,0.)) ;
#116331 = DIRECTION('ref_axis',(0.,0.,-1.)) ;
#116332 = DIRECTION('center_axis',(0.,1.,0.)) ;
#116333 = DIRECTION('ref_axis',(0.,0.,1.)) ;
#116334 = DIRECTION('center_axis',(0.,1.,-6.50521303491307E-15)) ;
#116335 = DIRECTION('ref_axis',(0.,6.50521303491307E-15,1.)) ;
#116336 = DIRECTION('center_axis',(0.,-1.,0.)) ;
#116337 = DIRECTION('ref_axis',(0.,0.,-1.)) ;
#116338 = DIRECTION('center_axis',(0.,-1.,0.)) ;
#116339 = DIRECTION('ref_axis',(0.,0.,-1.)) ;
#116340 = DIRECTION('center_axis',(0.,-1.,-1.07081696047951E-16)) ;
#116341 = DIRECTION('ref_axis',(0.,1.07081696047951E-16,-1.)) ;
#116342 = DIRECTION('center_axis',(0.,1.,0.)) ;
#116343 = DIRECTION('ref_axis',(0.,0.,1.)) ;
#116344 = DIRECTION('center_axis',(-1.,0.,0.)) ;
#116345 = DIRECTION('ref_axis',(0.,0.,1.)) ;
#116346 = DIRECTION('center_axis',(0.,0.,1.)) ;
#116347 = DIRECTION('ref_axis',(1.,0.,0.)) ;
#116348 = DIRECTION('center_axis',(0.,1.,0.)) ;
#116349 = DIRECTION('ref_axis',(0.,0.,1.)) ;
#116350 = DIRECTION('center_axis',(0.,0.,-1.)) ;
#116351 = DIRECTION('ref_axis',(-1.,0.,0.)) ;
#116352 = DIRECTION('center_axis',(0.,0.,1.)) ;
#116353 = DIRECTION('ref_axis',(1.,0.,0.)) ;
#116354 = DIRECTION('center_axis',(0.,0.,1.)) ;
#116355 = DIRECTION('ref_axis',(1.,0.,0.)) ;
#116356 = DIRECTION('center_axis',(0.,0.,1.)) ;
#116357 = DIRECTION('ref_axis',(1.,0.,0.)) ;
#116358 = DIRECTION('center_axis',(0.,0.,-1.)) ;
#116359 = DIRECTION('ref_axis',(-1.,0.,0.)) ;
#116360 = DIRECTION('center_axis',(0.,1.,0.)) ;
#116361 = DIRECTION('ref_axis',(0.,0.,1.)) ;
#116362 = DIRECTION('center_axis',(0.,-0.707106781186558,0.707106781186537)) ;
#116363 = DIRECTION('ref_axis',(0.,-0.707106781186537,-0.707106781186558)) ;
#116364 = DIRECTION('center_axis',(0.,1.,0.)) ;
#116365 = DIRECTION('ref_axis',(0.,0.,1.)) ;
#116366 = DIRECTION('center_axis',(0.,-0.514231796959093,-0.857651245551607)) ;
#116367 = DIRECTION('ref_axis',(0.,0.857651245551607,-0.514231796959093)) ;
#116368 = DIRECTION('center_axis',(0.,-0.707106781186548,0.707106781186547)) ;
#116369 = DIRECTION('ref_axis',(0.,-0.707106781186547,-0.707106781186548)) ;
#116370 = DIRECTION('center_axis',(0.,-0.707106781186548,0.707106781186548)) ;
#116371 = DIRECTION('ref_axis',(0.,-0.707106781186548,-0.707106781186548)) ;
#116372 = DIRECTION('center_axis',(-1.,0.,0.)) ;
#116373 = DIRECTION('ref_axis',(0.,0.,1.)) ;
#116374 = DIRECTION('center_axis',(0.,0.514231796959095,-0.857651245551606)) ;
#116375 = DIRECTION('ref_axis',(0.,0.857651245551606,0.514231796959095)) ;
#116376 = DIRECTION('center_axis',(0.,1.,0.)) ;
#116377 = DIRECTION('ref_axis',(0.,0.,1.)) ;
#116378 = DIRECTION('center_axis',(0.,0.,-1.)) ;
#116379 = DIRECTION('ref_axis',(-1.,0.,0.)) ;
#116380 = DIRECTION('center_axis',(0.,1.,0.)) ;
#116381 = DIRECTION('ref_axis',(0.,0.,1.)) ;
#116382 = DIRECTION('center_axis',(0.,0.,-1.)) ;
#116383 = DIRECTION('ref_axis',(-1.,0.,0.)) ;
#116384 = DIRECTION('center_axis',(0.,0.,-1.)) ;
#116385 = DIRECTION('ref_axis',(-1.,0.,0.)) ;
#116386 = DIRECTION('center_axis',(0.,0.,1.)) ;
#116387 = DIRECTION('ref_axis',(1.,0.,0.)) ;
#116388 = DIRECTION('center_axis',(0.,0.,-1.)) ;
#116389 = DIRECTION('ref_axis',(-1.,0.,0.)) ;
#116390 = DIRECTION('center_axis',(0.,1.,0.)) ;
#116391 = DIRECTION('ref_axis',(0.,0.,1.)) ;
#116392 = DIRECTION('center_axis',(0.,-1.,8.67361737988409E-15)) ;
#116393 = DIRECTION('ref_axis',(0.,-8.67361737988409E-15,-1.)) ;
#116394 = DIRECTION('center_axis',(0.,0.707106781186546,0.707106781186549)) ;
#116395 = DIRECTION('ref_axis',(0.,-0.707106781186549,0.707106781186546)) ;
#116396 = DIRECTION('center_axis',(0.,0.707106781186537,0.707106781186558)) ;
#116397 = DIRECTION('ref_axis',(0.,-0.707106781186558,0.707106781186537)) ;
#116398 = DIRECTION('center_axis',(0.,1.,1.07081696047951E-16)) ;
#116399 = DIRECTION('ref_axis',(0.,-1.07081696047951E-16,1.)) ;
#116400 = DIRECTION('center_axis',(0.,-1.,0.)) ;
#116401 = DIRECTION('ref_axis',(0.,0.,-1.)) ;
#116402 = DIRECTION('center_axis',(0.,1.,0.)) ;
#116403 = DIRECTION('ref_axis',(0.,0.,1.)) ;
#116404 = DIRECTION('center_axis',(0.,0.,1.)) ;
#116405 = DIRECTION('ref_axis',(1.,0.,0.)) ;
#116406 = DIRECTION('center_axis',(0.,1.,0.)) ;
#116407 = DIRECTION('ref_axis',(0.,0.,1.)) ;
#116408 = DIRECTION('center_axis',(0.,0.,1.)) ;
#116409 = DIRECTION('ref_axis',(1.,0.,0.)) ;
#116410 = DIRECTION('center_axis',(0.,3.99416362155027E-15,1.)) ;
#116411 = DIRECTION('ref_axis',(0.,-1.,3.99416362155027E-15)) ;
#116412 = DIRECTION('center_axis',(0.,0.,1.)) ;
#116413 = DIRECTION('ref_axis',(1.,0.,0.)) ;
#116414 = DIRECTION('center_axis',(0.,0.,-1.)) ;
#116415 = DIRECTION('ref_axis',(-1.,0.,0.)) ;
#116416 = DIRECTION('center_axis',(0.,0.,1.)) ;
#116417 = DIRECTION('ref_axis',(1.,0.,0.)) ;
#116418 = DIRECTION('center_axis',(-1.,0.,0.)) ;
#116419 = DIRECTION('ref_axis',(0.,0.,1.)) ;
#116420 = DIRECTION('center_axis',(0.,1.,0.)) ;
#116421 = DIRECTION('ref_axis',(0.,0.,1.)) ;
#116422 = DIRECTION('center_axis',(-1.,0.,0.)) ;
#116423 = DIRECTION('ref_axis',(0.,0.,1.)) ;
#116424 = DIRECTION('center_axis',(0.,-1.,0.)) ;
#116425 = DIRECTION('ref_axis',(0.,0.,-1.)) ;
#116426 = DIRECTION('center_axis',(0.,1.,0.)) ;
#116427 = DIRECTION('ref_axis',(0.,0.,1.)) ;
#116428 = DIRECTION('center_axis',(1.53063836115601E-16,-1.,-1.30104260698261E-16)) ;
#116429 = DIRECTION('ref_axis',(1.,1.53063836115601E-16,1.99142572374599E-32)) ;
#116430 = DIRECTION('center_axis',(0.,1.,0.)) ;
#116431 = DIRECTION('ref_axis',(0.,0.,1.)) ;
#116432 = DIRECTION('center_axis',(0.,-1.,0.)) ;
#116433 = DIRECTION('ref_axis',(0.,0.,-1.)) ;
#116434 = DIRECTION('center_axis',(1.,1.53063836115601E-16,2.73691106313441E-48)) ;
#116435 = DIRECTION('ref_axis',(-1.53063836115601E-16,1.,-4.18922106430579E-64)) ;
#116436 = DIRECTION('center_axis',(-1.,0.,0.)) ;
#116437 = DIRECTION('ref_axis',(0.,0.,1.)) ;
#116438 = DIRECTION('center_axis',(1.,1.53063836115601E-16,0.)) ;
#116439 = DIRECTION('ref_axis',(1.53063836115601E-16,-1.,0.)) ;
#116440 = DIRECTION('center_axis',(0.,1.,0.)) ;
#116441 = DIRECTION('ref_axis',(1.,0.,0.)) ;
#116442 = DIRECTION('center_axis',(0.,1.,0.)) ;
#116443 = DIRECTION('ref_axis',(0.,0.,-1.)) ;
#116444 = DIRECTION('center_axis',(0.,0.,1.)) ;
#116445 = DIRECTION('ref_axis',(-1.,0.,0.)) ;
#116446 = DIRECTION('center_axis',(0.,1.,0.)) ;
#116447 = DIRECTION('ref_axis',(1.,0.,0.)) ;
#116448 = DIRECTION('center_axis',(0.,0.,1.)) ;
#116449 = DIRECTION('ref_axis',(-1.,0.,0.)) ;
#116450 = DIRECTION('center_axis',(1.,1.0842021724855E-15,0.)) ;
#116451 = DIRECTION('ref_axis',(1.0842021724855E-15,-1.,0.)) ;
#116452 = DIRECTION('center_axis',(-1.,-1.53063836115601E-16,0.)) ;
#116453 = DIRECTION('ref_axis',(0.,-1.,0.)) ;
#116454 = DIRECTION('center_axis',(0.,0.,-1.)) ;
#116455 = DIRECTION('ref_axis',(1.,0.,0.)) ;
#116456 = DIRECTION('center_axis',(0.,0.,-1.)) ;
#116457 = DIRECTION('ref_axis',(0.804034447892626,0.594582716366697,0.)) ;
#116458 = DIRECTION('center_axis',(0.,0.,1.)) ;
#116459 = DIRECTION('ref_axis',(1.,0.,0.)) ;
#116460 = DIRECTION('',(0.,0.,-1.)) ;
#116461 = DIRECTION('center_axis',(-2.16840434497101E-16,1.,1.30104260698261E-16)) ;
#116462 = DIRECTION('ref_axis',(1.,2.16840434497101E-16,1.22464679914735E-16)) ;
#116463 = DIRECTION('',(-2.16840434497101E-16,1.,1.30104260698261E-16)) ;
#116464 = DIRECTION('center_axis',(0.,1.,0.)) ;
#116465 = DIRECTION('ref_axis',(0.,0.,1.)) ;
#116466 = DIRECTION('center_axis',(-1.,-1.53063836115601E-16,-2.73691106313441E-48)) ;
#116467 = DIRECTION('ref_axis',(1.53063836115601E-16,-1.,4.18922106430579E-64)) ;
#116468 = DIRECTION('center_axis',(1.,2.16840434497101E-16,0.)) ;
#116469 = DIRECTION('ref_axis',(2.16840434497101E-16,-1.,0.)) ;
#116470 = DIRECTION('center_axis',(0.,0.,1.)) ;
#116471 = DIRECTION('ref_axis',(1.,0.,0.)) ;
#116472 = DIRECTION('center_axis',(-1.25542992828747E-32,1.020425574104E-16,
1.)) ;
#116473 = DIRECTION('ref_axis',(-1.28107280532009E-48,-1.,1.020425574104E-16)) ;
#116474 = DIRECTION('center_axis',(0.,0.,1.)) ;
#116475 = DIRECTION('ref_axis',(1.,0.,0.)) ;
#116476 = DIRECTION('center_axis',(0.,0.,-1.)) ;
#116477 = DIRECTION('ref_axis',(-1.,0.,0.)) ;
#116478 = DIRECTION('center_axis',(1.,1.53063836115601E-16,-2.73691106313441E-48)) ;
#116479 = DIRECTION('ref_axis',(-1.53063836115601E-16,1.,4.18922106430579E-64)) ;
#116480 = DIRECTION('center_axis',(-1.,0.,0.)) ;
#116481 = DIRECTION('ref_axis',(0.,0.,1.)) ;
#116482 = DIRECTION('center_axis',(1.,1.53063836115601E-16,0.)) ;
#116483 = DIRECTION('ref_axis',(1.53063836115601E-16,-1.,0.)) ;
#116484 = DIRECTION('center_axis',(0.,1.,0.)) ;
#116485 = DIRECTION('ref_axis',(1.,0.,0.)) ;
#116486 = DIRECTION('center_axis',(-1.,-2.16840434497101E-16,0.)) ;
#116487 = DIRECTION('ref_axis',(0.,-1.,0.)) ;
#116488 = DIRECTION('center_axis',(0.,0.,-1.)) ;
#116489 = DIRECTION('ref_axis',(1.,0.,0.)) ;
#116490 = DIRECTION('center_axis',(-1.25542992828747E-32,1.020425574104E-16,
1.)) ;
#116491 = DIRECTION('ref_axis',(0.,-1.,0.)) ;
#116492 = DIRECTION('center_axis',(0.,-1.,0.)) ;
#116493 = DIRECTION('ref_axis',(-6.50521303491307E-15,0.,1.)) ;
#116494 = DIRECTION('center_axis',(-1.,0.,0.)) ;
#116495 = DIRECTION('ref_axis',(0.,0.,-1.)) ;
#116496 = DIRECTION('center_axis',(-1.,-1.53063836115601E-16,0.)) ;
#116497 = DIRECTION('ref_axis',(0.,-1.,0.)) ;
#116498 = DIRECTION('center_axis',(0.,-1.,0.)) ;
#116499 = DIRECTION('ref_axis',(0.,0.,1.)) ;
#116500 = DIRECTION('center_axis',(0.,0.,-1.)) ;
#116501 = DIRECTION('ref_axis',(-1.,0.,0.)) ;
#116502 = DIRECTION('center_axis',(0.,0.,-1.)) ;
#116503 = DIRECTION('ref_axis',(-1.,0.,0.)) ;
#116504 = DIRECTION('center_axis',(1.,1.53063836115601E-16,-3.06472600140763E-33)) ;
#116505 = DIRECTION('ref_axis',(-1.53063836115601E-16,1.,4.69098718418678E-49)) ;
#116506 = DIRECTION('center_axis',(-1.,0.,0.)) ;
#116507 = DIRECTION('ref_axis',(0.,0.,1.)) ;
#116508 = DIRECTION('center_axis',(-1.53063836115601E-16,1.,-1.020425574104E-16)) ;
#116509 = DIRECTION('ref_axis',(-1.,-1.53063836115601E-16,1.3684555315672E-47)) ;
#116510 = DIRECTION('',(1.53063836115601E-16,-1.,1.020425574104E-16)) ;
#116511 = DIRECTION('center_axis',(0.,-1.,0.)) ;
#116512 = DIRECTION('ref_axis',(0.,0.,-1.)) ;
#116513 = DIRECTION('center_axis',(-1.53063836115601E-16,1.,-1.30104260698261E-16)) ;
#116514 = DIRECTION('ref_axis',(-1.,-1.53063836115601E-16,1.99142572374599E-32)) ;
#116515 = DIRECTION('center_axis',(0.,-1.,0.)) ;
#116516 = DIRECTION('ref_axis',(0.,0.,-1.)) ;
#116517 = DIRECTION('center_axis',(-1.,-1.53063836115601E-16,2.73691106313441E-48)) ;
#116518 = DIRECTION('ref_axis',(1.53063836115601E-16,-1.,-4.18922106430579E-64)) ;
#116519 = DIRECTION('center_axis',(1.,2.16840434497101E-16,0.)) ;
#116520 = DIRECTION('ref_axis',(2.16840434497101E-16,-1.,0.)) ;
#116521 = DIRECTION('center_axis',(-1.,0.,2.16840434497102E-15)) ;
#116522 = DIRECTION('ref_axis',(2.16840434497102E-15,0.,1.)) ;
#116523 = DIRECTION('center_axis',(-1.,-2.16840434497101E-16,0.)) ;
#116524 = DIRECTION('ref_axis',(0.,-1.,0.)) ;
#116525 = DIRECTION('center_axis',(0.,0.,1.)) ;
#116526 = DIRECTION('ref_axis',(-1.,0.,0.)) ;
#116527 = DIRECTION('center_axis',(0.,1.,0.)) ;
#116528 = DIRECTION('ref_axis',(1.,0.,0.)) ;
#116529 = DIRECTION('center_axis',(0.,1.,0.)) ;
#116530 = DIRECTION('ref_axis',(0.,0.,-1.)) ;
#116531 = DIRECTION('center_axis',(1.,0.,0.)) ;
#116532 = DIRECTION('ref_axis',(0.,-1.,0.)) ;
#116533 = DIRECTION('center_axis',(1.,6.50521303491304E-15,0.)) ;
#116534 = DIRECTION('ref_axis',(-6.50521303491304E-15,1.,0.)) ;
#116535 = DIRECTION('center_axis',(8.67361737988403E-15,1.,0.)) ;
#116536 = DIRECTION('ref_axis',(-1.,8.67361737988403E-15,0.)) ;
#116537 = DIRECTION('center_axis',(1.2303003375722E-16,-1.,1.020425574104E-16)) ;
#116538 = DIRECTION('ref_axis',(1.,1.2303003375722E-16,-1.25542992828747E-32)) ;
#116539 = DIRECTION('center_axis',(0.,1.,0.)) ;
#116540 = DIRECTION('ref_axis',(0.,0.,1.)) ;
#116541 = DIRECTION('center_axis',(0.,1.,0.)) ;
#116542 = DIRECTION('ref_axis',(1.,0.,0.)) ;
#116543 = DIRECTION('center_axis',(1.,1.2303003375722E-16,0.)) ;
#116544 = DIRECTION('ref_axis',(1.2303003375722E-16,-1.,0.)) ;
#116545 = DIRECTION('center_axis',(0.,0.,1.)) ;
#116546 = DIRECTION('ref_axis',(-1.,0.,0.)) ;
#116547 = DIRECTION('center_axis',(0.,1.,0.)) ;
#116548 = DIRECTION('ref_axis',(1.,0.,0.)) ;
#116549 = DIRECTION('center_axis',(0.,0.,-1.)) ;
#116550 = DIRECTION('ref_axis',(1.,0.,0.)) ;
#116551 = DIRECTION('center_axis',(0.,0.,-1.)) ;
#116552 = DIRECTION('ref_axis',(-1.,0.,0.)) ;
#116553 = DIRECTION('center_axis',(0.,0.,1.)) ;
#116554 = DIRECTION('ref_axis',(1.,0.,0.)) ;
#116555 = DIRECTION('center_axis',(-2.16840434497101E-16,1.,-1.020425574104E-16)) ;
#116556 = DIRECTION('ref_axis',(-1.,-2.16840434497101E-16,5.47382212626882E-48)) ;
#116557 = DIRECTION('center_axis',(0.,1.,0.)) ;
#116558 = DIRECTION('ref_axis',(0.,0.,-1.)) ;
#116559 = DIRECTION('center_axis',(1.,0.,1.25542992828747E-32)) ;
#116560 = DIRECTION('ref_axis',(1.25542992828747E-32,0.,-1.)) ;
#116561 = DIRECTION('center_axis',(1.,0.,0.)) ;
#116562 = DIRECTION('ref_axis',(0.,0.,-1.)) ;
#116563 = DIRECTION('center_axis',(-1.,-1.2303003375722E-16,0.)) ;
#116564 = DIRECTION('ref_axis',(0.,-1.,0.)) ;
#116565 = DIRECTION('center_axis',(0.,0.,-1.)) ;
#116566 = DIRECTION('ref_axis',(1.,0.,0.)) ;
#116567 = DIRECTION('center_axis',(0.,0.,-1.)) ;
#116568 = DIRECTION('ref_axis',(-1.,0.,0.)) ;
#116569 = DIRECTION('',(0.,0.,1.)) ;
#116570 = DIRECTION('center_axis',(0.,0.,1.)) ;
#116571 = DIRECTION('ref_axis',(1.,0.,0.)) ;
#116572 = DIRECTION('center_axis',(0.,0.,1.)) ;
#116573 = DIRECTION('ref_axis',(1.,0.,0.)) ;
#116574 = DIRECTION('center_axis',(6.27714964143733E-33,-5.10212787052002E-17,
-1.)) ;
#116575 = DIRECTION('ref_axis',(3.20268201330022E-49,1.,-5.10212787052002E-17)) ;
#116576 = DIRECTION('center_axis',(1.,1.53063836115601E-16,-1.53236300070382E-33)) ;
#116577 = DIRECTION('ref_axis',(-1.53063836115601E-16,1.,2.34549359209339E-49)) ;
#116578 = DIRECTION('center_axis',(-1.,0.,0.)) ;
#116579 = DIRECTION('ref_axis',(0.,0.,1.)) ;
#116580 = DIRECTION('center_axis',(1.,0.,0.)) ;
#116581 = DIRECTION('ref_axis',(0.,0.,-1.)) ;
#116582 = DIRECTION('center_axis',(0.,1.,0.)) ;
#116583 = DIRECTION('ref_axis',(1.,0.,0.)) ;
#116584 = DIRECTION('center_axis',(-4.33680868994202E-15,1.,0.)) ;
#116585 = DIRECTION('ref_axis',(1.,4.33680868994202E-15,0.)) ;
#116586 = DIRECTION('center_axis',(0.,-1.,0.)) ;
#116587 = DIRECTION('ref_axis',(0.,0.,-1.)) ;
#116588 = DIRECTION('center_axis',(0.,0.,-1.)) ;
#116589 = DIRECTION('ref_axis',(1.,0.,0.)) ;
#116590 = DIRECTION('center_axis',(0.,0.,1.)) ;
#116591 = DIRECTION('ref_axis',(1.,0.,0.)) ;
#116592 = DIRECTION('center_axis',(0.,0.,-1.)) ;
#116593 = DIRECTION('ref_axis',(-1.,0.,0.)) ;
#116594 = DIRECTION('center_axis',(0.,1.,0.)) ;
#116595 = DIRECTION('ref_axis',(1.,0.,0.)) ;
#116596 = DIRECTION('center_axis',(1.,1.2303003375722E-16,0.)) ;
#116597 = DIRECTION('ref_axis',(1.2303003375722E-16,-1.,0.)) ;
#116598 = DIRECTION('center_axis',(0.,1.,0.)) ;
#116599 = DIRECTION('ref_axis',(-6.50521303491307E-15,0.,-1.)) ;
#116600 = DIRECTION('center_axis',(6.27714964143733E-33,-5.10212787052002E-17,
-1.)) ;
#116601 = DIRECTION('ref_axis',(0.,1.,0.)) ;
#116602 = DIRECTION('center_axis',(0.,-1.,0.)) ;
#116603 = DIRECTION('ref_axis',(0.,0.,1.)) ;
#116604 = DIRECTION('center_axis',(2.16840434497101E-16,-1.,5.10212787052002E-17)) ;
#116605 = DIRECTION('ref_axis',(1.,2.16840434497101E-16,-5.47382212626882E-48)) ;
#116606 = DIRECTION('center_axis',(0.,1.,0.)) ;
#116607 = DIRECTION('ref_axis',(0.,0.,-1.)) ;
#116608 = DIRECTION('center_axis',(0.,0.,1.)) ;
#116609 = DIRECTION('ref_axis',(1.,0.,0.)) ;
#116610 = DIRECTION('center_axis',(0.,0.,-1.)) ;
#116611 = DIRECTION('ref_axis',(-1.,0.,0.)) ;
#116612 = DIRECTION('center_axis',(-1.,-1.2303003375722E-16,0.)) ;
#116613 = DIRECTION('ref_axis',(0.,-1.,0.)) ;
#116614 = DIRECTION('center_axis',(0.,-1.,0.)) ;
#116615 = DIRECTION('ref_axis',(0.,0.,1.)) ;
#116616 = DIRECTION('center_axis',(1.53063836115601E-16,-1.,5.10212787052002E-17)) ;
#116617 = DIRECTION('ref_axis',(1.,1.53063836115601E-16,-6.84227765783602E-48)) ;
#116618 = DIRECTION('',(-1.53063836115601E-16,1.,-5.10212787052002E-17)) ;
#116619 = DIRECTION('center_axis',(0.,-1.,0.)) ;
#116620 = DIRECTION('ref_axis',(0.,0.,-1.)) ;
#116621 = DIRECTION('center_axis',(-1.,0.,0.)) ;
#116622 = DIRECTION('ref_axis',(0.,0.,-1.)) ;
#116623 = DIRECTION('center_axis',(-1.2303003375722E-16,1.,-5.10212787052002E-17)) ;
#116624 = DIRECTION('ref_axis',(-1.,-1.2303003375722E-16,6.27714964143733E-33)) ;
#116625 = DIRECTION('center_axis',(-8.67361737988403E-15,-1.,0.)) ;
#116626 = DIRECTION('ref_axis',(1.,-8.67361737988403E-15,0.)) ;
#116627 = DIRECTION('center_axis',(1.,0.,6.27714964143733E-33)) ;
#116628 = DIRECTION('ref_axis',(6.27714964143733E-33,0.,-1.)) ;
#116629 = DIRECTION('center_axis',(-1.,0.,-6.50521303491307E-15)) ;
#116630 = DIRECTION('ref_axis',(-6.50521303491307E-15,0.,1.)) ;
#116631 = DIRECTION('center_axis',(1.,0.,0.)) ;
#116632 = DIRECTION('ref_axis',(0.,1.,0.)) ;
#116633 = DIRECTION('center_axis',(0.,0.,-1.)) ;
#116634 = DIRECTION('ref_axis',(-1.,0.,0.)) ;
#116635 = DIRECTION('center_axis',(0.,0.,1.)) ;
#116636 = DIRECTION('ref_axis',(1.,0.,0.)) ;
#116637 = DIRECTION('center_axis',(0.,0.,-1.)) ;
#116638 = DIRECTION('ref_axis',(-1.,0.,0.)) ;
#116639 = DIRECTION('center_axis',(-1.,0.,0.)) ;
#116640 = DIRECTION('ref_axis',(0.,0.,1.)) ;
#116641 = DIRECTION('center_axis',(0.,-1.,0.)) ;
#116642 = DIRECTION('ref_axis',(0.,0.,-1.)) ;
#116643 = DIRECTION('center_axis',(0.,1.,0.)) ;
#116644 = DIRECTION('ref_axis',(0.,0.,1.)) ;
#116645 = DIRECTION('center_axis',(0.,1.,-6.50521303491307E-15)) ;
#116646 = DIRECTION('ref_axis',(0.,6.50521303491307E-15,1.)) ;
#116647 = DIRECTION('center_axis',(0.,-1.,0.)) ;
#116648 = DIRECTION('ref_axis',(0.,0.,-1.)) ;
#116649 = DIRECTION('center_axis',(0.,-1.,0.)) ;
#116650 = DIRECTION('ref_axis',(0.,0.,-1.)) ;
#116651 = DIRECTION('center_axis',(0.,-1.,-1.07081696047951E-16)) ;
#116652 = DIRECTION('ref_axis',(0.,1.07081696047951E-16,-1.)) ;
#116653 = DIRECTION('center_axis',(0.,1.,0.)) ;
#116654 = DIRECTION('ref_axis',(0.,0.,1.)) ;
#116655 = DIRECTION('center_axis',(-1.,0.,0.)) ;
#116656 = DIRECTION('ref_axis',(0.,0.,1.)) ;
#116657 = DIRECTION('center_axis',(0.,0.,1.)) ;
#116658 = DIRECTION('ref_axis',(1.,0.,0.)) ;
#116659 = DIRECTION('center_axis',(0.,1.,0.)) ;
#116660 = DIRECTION('ref_axis',(0.,0.,1.)) ;
#116661 = DIRECTION('center_axis',(0.,0.,-1.)) ;
#116662 = DIRECTION('ref_axis',(-1.,0.,0.)) ;
#116663 = DIRECTION('center_axis',(0.,0.,1.)) ;
#116664 = DIRECTION('ref_axis',(1.,0.,0.)) ;
#116665 = DIRECTION('center_axis',(0.,0.,1.)) ;
#116666 = DIRECTION('ref_axis',(1.,0.,0.)) ;
#116667 = DIRECTION('center_axis',(0.,0.,1.)) ;
#116668 = DIRECTION('ref_axis',(1.,0.,0.)) ;
#116669 = DIRECTION('center_axis',(0.,0.,-1.)) ;
#116670 = DIRECTION('ref_axis',(-1.,0.,0.)) ;
#116671 = DIRECTION('center_axis',(0.,1.,0.)) ;
#116672 = DIRECTION('ref_axis',(0.,0.,1.)) ;
#116673 = DIRECTION('center_axis',(0.,-0.707106781186558,0.707106781186537)) ;
#116674 = DIRECTION('ref_axis',(0.,-0.707106781186537,-0.707106781186558)) ;
#116675 = DIRECTION('center_axis',(0.,1.,0.)) ;
#116676 = DIRECTION('ref_axis',(0.,0.,1.)) ;
#116677 = DIRECTION('center_axis',(0.,-0.514231796959093,-0.857651245551607)) ;
#116678 = DIRECTION('ref_axis',(0.,0.857651245551607,-0.514231796959093)) ;
#116679 = DIRECTION('center_axis',(0.,-0.707106781186548,0.707106781186547)) ;
#116680 = DIRECTION('ref_axis',(0.,-0.707106781186547,-0.707106781186548)) ;
#116681 = DIRECTION('center_axis',(0.,-0.707106781186548,0.707106781186548)) ;
#116682 = DIRECTION('ref_axis',(0.,-0.707106781186548,-0.707106781186548)) ;
#116683 = DIRECTION('center_axis',(-1.,0.,0.)) ;
#116684 = DIRECTION('ref_axis',(0.,0.,1.)) ;
#116685 = DIRECTION('center_axis',(0.,0.514231796959095,-0.857651245551606)) ;
#116686 = DIRECTION('ref_axis',(0.,0.857651245551606,0.514231796959095)) ;
#116687 = DIRECTION('center_axis',(0.,1.,0.)) ;
#116688 = DIRECTION('ref_axis',(0.,0.,1.)) ;
#116689 = DIRECTION('center_axis',(0.,0.,-1.)) ;
#116690 = DIRECTION('ref_axis',(-1.,0.,0.)) ;
#116691 = DIRECTION('center_axis',(0.,1.,0.)) ;
#116692 = DIRECTION('ref_axis',(0.,0.,1.)) ;
#116693 = DIRECTION('center_axis',(0.,0.,-1.)) ;
#116694 = DIRECTION('ref_axis',(-1.,0.,0.)) ;
#116695 = DIRECTION('center_axis',(0.,0.,-1.)) ;
#116696 = DIRECTION('ref_axis',(-1.,0.,0.)) ;
#116697 = DIRECTION('center_axis',(0.,0.,1.)) ;
#116698 = DIRECTION('ref_axis',(1.,0.,0.)) ;
#116699 = DIRECTION('center_axis',(0.,0.,-1.)) ;
#116700 = DIRECTION('ref_axis',(-1.,0.,0.)) ;
#116701 = DIRECTION('center_axis',(0.,1.,0.)) ;
#116702 = DIRECTION('ref_axis',(0.,0.,1.)) ;
#116703 = DIRECTION('center_axis',(0.,-1.,8.67361737988409E-15)) ;
#116704 = DIRECTION('ref_axis',(0.,-8.67361737988409E-15,-1.)) ;
#116705 = DIRECTION('center_axis',(0.,0.707106781186546,0.707106781186549)) ;
#116706 = DIRECTION('ref_axis',(0.,-0.707106781186549,0.707106781186546)) ;
#116707 = DIRECTION('center_axis',(0.,0.707106781186537,0.707106781186558)) ;
#116708 = DIRECTION('ref_axis',(0.,-0.707106781186558,0.707106781186537)) ;
#116709 = DIRECTION('center_axis',(0.,1.,1.07081696047951E-16)) ;
#116710 = DIRECTION('ref_axis',(0.,-1.07081696047951E-16,1.)) ;
#116711 = DIRECTION('center_axis',(0.,-1.,0.)) ;
#116712 = DIRECTION('ref_axis',(0.,0.,-1.)) ;
#116713 = DIRECTION('center_axis',(0.,1.,0.)) ;
#116714 = DIRECTION('ref_axis',(0.,0.,1.)) ;
#116715 = DIRECTION('center_axis',(0.,0.,1.)) ;
#116716 = DIRECTION('ref_axis',(1.,0.,0.)) ;
#116717 = DIRECTION('center_axis',(0.,1.,0.)) ;
#116718 = DIRECTION('ref_axis',(0.,0.,1.)) ;
#116719 = DIRECTION('center_axis',(0.,0.,1.)) ;
#116720 = DIRECTION('ref_axis',(1.,0.,0.)) ;
#116721 = DIRECTION('center_axis',(0.,3.99416362155027E-15,1.)) ;
#116722 = DIRECTION('ref_axis',(0.,-1.,3.99416362155027E-15)) ;
#116723 = DIRECTION('center_axis',(0.,0.,1.)) ;
#116724 = DIRECTION('ref_axis',(1.,0.,0.)) ;
#116725 = DIRECTION('center_axis',(0.,0.,-1.)) ;
#116726 = DIRECTION('ref_axis',(-1.,0.,0.)) ;
#116727 = DIRECTION('center_axis',(0.,0.,1.)) ;
#116728 = DIRECTION('ref_axis',(1.,0.,0.)) ;
#116729 = DIRECTION('center_axis',(-1.,0.,0.)) ;
#116730 = DIRECTION('ref_axis',(0.,0.,1.)) ;
#116731 = DIRECTION('center_axis',(0.,1.,0.)) ;
#116732 = DIRECTION('ref_axis',(0.,0.,1.)) ;
#116733 = DIRECTION('center_axis',(-1.,0.,0.)) ;
#116734 = DIRECTION('ref_axis',(0.,0.,1.)) ;
#116735 = DIRECTION('center_axis',(0.,-1.,0.)) ;
#116736 = DIRECTION('ref_axis',(0.,0.,-1.)) ;
#116737 = DIRECTION('center_axis',(0.,1.,0.)) ;
#116738 = DIRECTION('ref_axis',(0.,0.,1.)) ;
#116739 = DIRECTION('center_axis',(1.53063836115601E-16,-1.,-1.30104260698261E-16)) ;
#116740 = DIRECTION('ref_axis',(1.,1.53063836115601E-16,1.99142572374599E-32)) ;
#116741 = DIRECTION('center_axis',(0.,1.,0.)) ;
#116742 = DIRECTION('ref_axis',(0.,0.,1.)) ;
#116743 = DIRECTION('center_axis',(0.,-1.,0.)) ;
#116744 = DIRECTION('ref_axis',(0.,0.,-1.)) ;
#116745 = DIRECTION('center_axis',(1.,1.53063836115601E-16,2.73691106313441E-48)) ;
#116746 = DIRECTION('ref_axis',(-1.53063836115601E-16,1.,-4.18922106430579E-64)) ;
#116747 = DIRECTION('center_axis',(-1.,0.,0.)) ;
#116748 = DIRECTION('ref_axis',(0.,0.,1.)) ;
#116749 = DIRECTION('center_axis',(1.,1.53063836115601E-16,0.)) ;
#116750 = DIRECTION('ref_axis',(1.53063836115601E-16,-1.,0.)) ;
#116751 = DIRECTION('center_axis',(0.,1.,0.)) ;
#116752 = DIRECTION('ref_axis',(1.,0.,0.)) ;
#116753 = DIRECTION('center_axis',(0.,1.,0.)) ;
#116754 = DIRECTION('ref_axis',(0.,0.,-1.)) ;
#116755 = DIRECTION('center_axis',(0.,0.,1.)) ;
#116756 = DIRECTION('ref_axis',(-1.,0.,0.)) ;
#116757 = DIRECTION('center_axis',(0.,1.,0.)) ;
#116758 = DIRECTION('ref_axis',(1.,0.,0.)) ;
#116759 = DIRECTION('center_axis',(0.,0.,1.)) ;
#116760 = DIRECTION('ref_axis',(-1.,0.,0.)) ;
#116761 = DIRECTION('center_axis',(1.,1.0842021724855E-15,0.)) ;
#116762 = DIRECTION('ref_axis',(1.0842021724855E-15,-1.,0.)) ;
#116763 = DIRECTION('center_axis',(-1.,-1.53063836115601E-16,0.)) ;
#116764 = DIRECTION('ref_axis',(0.,-1.,0.)) ;
#116765 = DIRECTION('center_axis',(0.,0.,-1.)) ;
#116766 = DIRECTION('ref_axis',(1.,0.,0.)) ;
#116767 = DIRECTION('center_axis',(0.,0.,-1.)) ;
#116768 = DIRECTION('ref_axis',(0.804034447892627,0.594582716366695,0.)) ;
#116769 = DIRECTION('center_axis',(0.,0.,1.)) ;
#116770 = DIRECTION('ref_axis',(1.,0.,0.)) ;
#116771 = DIRECTION('',(0.,0.,-1.)) ;
#116772 = DIRECTION('center_axis',(-2.16840434497101E-16,1.,1.30104260698261E-16)) ;
#116773 = DIRECTION('ref_axis',(1.,2.16840434497101E-16,1.22464679914735E-16)) ;
#116774 = DIRECTION('',(-2.16840434497101E-16,1.,1.30104260698261E-16)) ;
#116775 = DIRECTION('center_axis',(0.,1.,0.)) ;
#116776 = DIRECTION('ref_axis',(0.,0.,1.)) ;
#116777 = DIRECTION('center_axis',(-1.,-1.53063836115601E-16,-2.73691106313441E-48)) ;
#116778 = DIRECTION('ref_axis',(1.53063836115601E-16,-1.,4.18922106430579E-64)) ;
#116779 = DIRECTION('center_axis',(1.,2.16840434497101E-16,0.)) ;
#116780 = DIRECTION('ref_axis',(2.16840434497101E-16,-1.,0.)) ;
#116781 = DIRECTION('center_axis',(0.,0.,1.)) ;
#116782 = DIRECTION('ref_axis',(1.,0.,0.)) ;
#116783 = DIRECTION('center_axis',(-1.25542992828747E-32,1.020425574104E-16,
1.)) ;
#116784 = DIRECTION('ref_axis',(-1.28107280532009E-48,-1.,1.020425574104E-16)) ;
#116785 = DIRECTION('center_axis',(0.,0.,1.)) ;
#116786 = DIRECTION('ref_axis',(1.,0.,0.)) ;
#116787 = DIRECTION('center_axis',(0.,0.,-1.)) ;
#116788 = DIRECTION('ref_axis',(-1.,0.,0.)) ;
#116789 = DIRECTION('center_axis',(1.,1.53063836115601E-16,-2.73691106313441E-48)) ;
#116790 = DIRECTION('ref_axis',(-1.53063836115601E-16,1.,4.18922106430579E-64)) ;
#116791 = DIRECTION('center_axis',(-1.,0.,0.)) ;
#116792 = DIRECTION('ref_axis',(0.,0.,1.)) ;
#116793 = DIRECTION('center_axis',(1.,1.53063836115601E-16,0.)) ;
#116794 = DIRECTION('ref_axis',(1.53063836115601E-16,-1.,0.)) ;
#116795 = DIRECTION('center_axis',(0.,1.,0.)) ;
#116796 = DIRECTION('ref_axis',(1.,0.,0.)) ;
#116797 = DIRECTION('center_axis',(-1.,-2.16840434497101E-16,0.)) ;
#116798 = DIRECTION('ref_axis',(0.,-1.,0.)) ;
#116799 = DIRECTION('center_axis',(0.,0.,-1.)) ;
#116800 = DIRECTION('ref_axis',(1.,0.,0.)) ;
#116801 = DIRECTION('center_axis',(-1.25542992828747E-32,1.020425574104E-16,
1.)) ;
#116802 = DIRECTION('ref_axis',(0.,-1.,0.)) ;
#116803 = DIRECTION('center_axis',(0.,-1.,0.)) ;
#116804 = DIRECTION('ref_axis',(-6.50521303491307E-15,0.,1.)) ;
#116805 = DIRECTION('center_axis',(-1.,0.,0.)) ;
#116806 = DIRECTION('ref_axis',(0.,0.,-1.)) ;
#116807 = DIRECTION('center_axis',(-1.,-1.53063836115601E-16,0.)) ;
#116808 = DIRECTION('ref_axis',(0.,-1.,0.)) ;
#116809 = DIRECTION('center_axis',(0.,-1.,0.)) ;
#116810 = DIRECTION('ref_axis',(0.,0.,1.)) ;
#116811 = DIRECTION('center_axis',(0.,0.,-1.)) ;
#116812 = DIRECTION('ref_axis',(-1.,0.,0.)) ;
#116813 = DIRECTION('center_axis',(0.,0.,-1.)) ;
#116814 = DIRECTION('ref_axis',(-1.,0.,0.)) ;
#116815 = DIRECTION('center_axis',(1.,1.53063836115601E-16,-3.06472600140763E-33)) ;
#116816 = DIRECTION('ref_axis',(-1.53063836115601E-16,1.,4.69098718418678E-49)) ;
#116817 = DIRECTION('center_axis',(-1.,0.,0.)) ;
#116818 = DIRECTION('ref_axis',(0.,0.,1.)) ;
#116819 = DIRECTION('center_axis',(-1.53063836115601E-16,1.,-1.020425574104E-16)) ;
#116820 = DIRECTION('ref_axis',(-1.,-1.53063836115601E-16,1.3684555315672E-47)) ;
#116821 = DIRECTION('',(1.53063836115601E-16,-1.,1.020425574104E-16)) ;
#116822 = DIRECTION('center_axis',(0.,-1.,0.)) ;
#116823 = DIRECTION('ref_axis',(0.,0.,-1.)) ;
#116824 = DIRECTION('center_axis',(-1.53063836115601E-16,1.,-1.30104260698261E-16)) ;
#116825 = DIRECTION('ref_axis',(-1.,-1.53063836115601E-16,1.99142572374599E-32)) ;
#116826 = DIRECTION('center_axis',(0.,-1.,0.)) ;
#116827 = DIRECTION('ref_axis',(0.,0.,-1.)) ;
#116828 = DIRECTION('center_axis',(-1.,-1.53063836115601E-16,2.73691106313441E-48)) ;
#116829 = DIRECTION('ref_axis',(1.53063836115601E-16,-1.,-4.18922106430579E-64)) ;
#116830 = DIRECTION('center_axis',(1.,2.16840434497101E-16,0.)) ;
#116831 = DIRECTION('ref_axis',(2.16840434497101E-16,-1.,0.)) ;
#116832 = DIRECTION('center_axis',(-1.,0.,2.16840434497102E-15)) ;
#116833 = DIRECTION('ref_axis',(2.16840434497102E-15,0.,1.)) ;
#116834 = DIRECTION('center_axis',(-1.,-2.16840434497101E-16,0.)) ;
#116835 = DIRECTION('ref_axis',(0.,-1.,0.)) ;
#116836 = DIRECTION('center_axis',(0.,0.,1.)) ;
#116837 = DIRECTION('ref_axis',(-1.,0.,0.)) ;
#116838 = DIRECTION('center_axis',(0.,1.,0.)) ;
#116839 = DIRECTION('ref_axis',(1.,0.,0.)) ;
#116840 = DIRECTION('center_axis',(0.,1.,0.)) ;
#116841 = DIRECTION('ref_axis',(0.,0.,-1.)) ;
#116842 = DIRECTION('center_axis',(1.,0.,0.)) ;
#116843 = DIRECTION('ref_axis',(0.,-1.,0.)) ;
#116844 = DIRECTION('center_axis',(1.,6.50521303491304E-15,0.)) ;
#116845 = DIRECTION('ref_axis',(-6.50521303491304E-15,1.,0.)) ;
#116846 = DIRECTION('center_axis',(8.67361737988403E-15,1.,0.)) ;
#116847 = DIRECTION('ref_axis',(-1.,8.67361737988403E-15,0.)) ;
#116848 = DIRECTION('center_axis',(1.2303003375722E-16,-1.,1.020425574104E-16)) ;
#116849 = DIRECTION('ref_axis',(1.,1.2303003375722E-16,-1.25542992828747E-32)) ;
#116850 = DIRECTION('center_axis',(0.,1.,0.)) ;
#116851 = DIRECTION('ref_axis',(0.,0.,1.)) ;
#116852 = DIRECTION('center_axis',(0.,1.,0.)) ;
#116853 = DIRECTION('ref_axis',(1.,0.,0.)) ;
#116854 = DIRECTION('center_axis',(1.,1.2303003375722E-16,0.)) ;
#116855 = DIRECTION('ref_axis',(1.2303003375722E-16,-1.,0.)) ;
#116856 = DIRECTION('center_axis',(0.,0.,1.)) ;
#116857 = DIRECTION('ref_axis',(-1.,0.,0.)) ;
#116858 = DIRECTION('center_axis',(0.,1.,0.)) ;
#116859 = DIRECTION('ref_axis',(1.,0.,0.)) ;
#116860 = DIRECTION('center_axis',(0.,0.,-1.)) ;
#116861 = DIRECTION('ref_axis',(1.,0.,0.)) ;
#116862 = DIRECTION('center_axis',(0.,0.,-1.)) ;
#116863 = DIRECTION('ref_axis',(-1.,0.,0.)) ;
#116864 = DIRECTION('center_axis',(0.,0.,1.)) ;
#116865 = DIRECTION('ref_axis',(1.,0.,0.)) ;
#116866 = DIRECTION('center_axis',(-2.16840434497101E-16,1.,-1.020425574104E-16)) ;
#116867 = DIRECTION('ref_axis',(-1.,-2.16840434497101E-16,5.47382212626882E-48)) ;
#116868 = DIRECTION('center_axis',(0.,1.,0.)) ;
#116869 = DIRECTION('ref_axis',(0.,0.,-1.)) ;
#116870 = DIRECTION('center_axis',(1.,0.,1.25542992828747E-32)) ;
#116871 = DIRECTION('ref_axis',(1.25542992828747E-32,0.,-1.)) ;
#116872 = DIRECTION('center_axis',(1.,0.,0.)) ;
#116873 = DIRECTION('ref_axis',(0.,0.,-1.)) ;
#116874 = DIRECTION('center_axis',(-1.,-1.2303003375722E-16,0.)) ;
#116875 = DIRECTION('ref_axis',(0.,-1.,0.)) ;
#116876 = DIRECTION('center_axis',(0.,0.,-1.)) ;
#116877 = DIRECTION('ref_axis',(1.,0.,0.)) ;
#116878 = DIRECTION('center_axis',(0.,0.,-1.)) ;
#116879 = DIRECTION('ref_axis',(-1.,0.,0.)) ;
#116880 = DIRECTION('',(0.,0.,1.)) ;
#116881 = DIRECTION('center_axis',(0.,0.,1.)) ;
#116882 = DIRECTION('ref_axis',(1.,0.,0.)) ;
#116883 = DIRECTION('center_axis',(0.,0.,1.)) ;
#116884 = DIRECTION('ref_axis',(1.,0.,0.)) ;
#116885 = DIRECTION('center_axis',(6.27714964143733E-33,-5.10212787052002E-17,
-1.)) ;
#116886 = DIRECTION('ref_axis',(3.20268201330022E-49,1.,-5.10212787052002E-17)) ;
#116887 = DIRECTION('center_axis',(1.,1.53063836115601E-16,-1.53236300070382E-33)) ;
#116888 = DIRECTION('ref_axis',(-1.53063836115601E-16,1.,2.34549359209339E-49)) ;
#116889 = DIRECTION('center_axis',(-1.,0.,0.)) ;
#116890 = DIRECTION('ref_axis',(0.,0.,1.)) ;
#116891 = DIRECTION('center_axis',(1.,0.,0.)) ;
#116892 = DIRECTION('ref_axis',(0.,0.,-1.)) ;
#116893 = DIRECTION('center_axis',(0.,1.,0.)) ;
#116894 = DIRECTION('ref_axis',(1.,0.,0.)) ;
#116895 = DIRECTION('center_axis',(-4.33680868994202E-15,1.,0.)) ;
#116896 = DIRECTION('ref_axis',(1.,4.33680868994202E-15,0.)) ;
#116897 = DIRECTION('center_axis',(0.,-1.,0.)) ;
#116898 = DIRECTION('ref_axis',(0.,0.,-1.)) ;
#116899 = DIRECTION('center_axis',(0.,0.,-1.)) ;
#116900 = DIRECTION('ref_axis',(1.,0.,0.)) ;
#116901 = DIRECTION('center_axis',(0.,0.,1.)) ;
#116902 = DIRECTION('ref_axis',(1.,0.,0.)) ;
#116903 = DIRECTION('center_axis',(0.,0.,-1.)) ;
#116904 = DIRECTION('ref_axis',(-1.,0.,0.)) ;
#116905 = DIRECTION('center_axis',(0.,1.,0.)) ;
#116906 = DIRECTION('ref_axis',(1.,0.,0.)) ;
#116907 = DIRECTION('center_axis',(1.,1.2303003375722E-16,0.)) ;
#116908 = DIRECTION('ref_axis',(1.2303003375722E-16,-1.,0.)) ;
#116909 = DIRECTION('center_axis',(0.,1.,0.)) ;
#116910 = DIRECTION('ref_axis',(-6.50521303491284E-15,0.,-1.)) ;
#116911 = DIRECTION('center_axis',(6.27714964143733E-33,-5.10212787052002E-17,
-1.)) ;
#116912 = DIRECTION('ref_axis',(0.,1.,0.)) ;
#116913 = DIRECTION('center_axis',(0.,-1.,0.)) ;
#116914 = DIRECTION('ref_axis',(0.,0.,1.)) ;
#116915 = DIRECTION('center_axis',(2.16840434497101E-16,-1.,5.10212787052002E-17)) ;
#116916 = DIRECTION('ref_axis',(1.,2.16840434497101E-16,-5.47382212626882E-48)) ;
#116917 = DIRECTION('center_axis',(0.,1.,0.)) ;
#116918 = DIRECTION('ref_axis',(0.,0.,-1.)) ;
#116919 = DIRECTION('center_axis',(0.,0.,1.)) ;
#116920 = DIRECTION('ref_axis',(1.,0.,0.)) ;
#116921 = DIRECTION('center_axis',(0.,0.,-1.)) ;
#116922 = DIRECTION('ref_axis',(-1.,0.,0.)) ;
#116923 = DIRECTION('center_axis',(-1.,-1.2303003375722E-16,0.)) ;
#116924 = DIRECTION('ref_axis',(0.,-1.,0.)) ;
#116925 = DIRECTION('center_axis',(0.,-1.,0.)) ;
#116926 = DIRECTION('ref_axis',(0.,0.,1.)) ;
#116927 = DIRECTION('center_axis',(1.53063836115601E-16,-1.,5.10212787052002E-17)) ;
#116928 = DIRECTION('ref_axis',(1.,1.53063836115601E-16,-6.84227765783602E-48)) ;
#116929 = DIRECTION('',(-1.53063836115601E-16,1.,-5.10212787052002E-17)) ;
#116930 = DIRECTION('center_axis',(0.,-1.,0.)) ;
#116931 = DIRECTION('ref_axis',(0.,0.,-1.)) ;
#116932 = DIRECTION('center_axis',(-1.,0.,0.)) ;
#116933 = DIRECTION('ref_axis',(0.,0.,-1.)) ;
#116934 = DIRECTION('center_axis',(-1.2303003375722E-16,1.,-5.10212787052002E-17)) ;
#116935 = DIRECTION('ref_axis',(-1.,-1.2303003375722E-16,6.27714964143733E-33)) ;
#116936 = DIRECTION('center_axis',(-8.67361737988403E-15,-1.,0.)) ;
#116937 = DIRECTION('ref_axis',(1.,-8.67361737988403E-15,0.)) ;
#116938 = DIRECTION('center_axis',(1.,0.,6.27714964143733E-33)) ;
#116939 = DIRECTION('ref_axis',(6.27714964143733E-33,0.,-1.)) ;
#116940 = DIRECTION('center_axis',(-1.,0.,-6.50521303491284E-15)) ;
#116941 = DIRECTION('ref_axis',(-6.50521303491284E-15,0.,1.)) ;
#116942 = DIRECTION('center_axis',(1.,0.,0.)) ;
#116943 = DIRECTION('ref_axis',(0.,1.,0.)) ;
#116944 = DIRECTION('center_axis',(0.,0.,-1.)) ;
#116945 = DIRECTION('ref_axis',(-1.,0.,0.)) ;
#116946 = DIRECTION('center_axis',(0.,0.,1.)) ;
#116947 = DIRECTION('ref_axis',(1.,0.,0.)) ;
#116948 = DIRECTION('center_axis',(0.,0.,-1.)) ;
#116949 = DIRECTION('ref_axis',(-1.,0.,0.)) ;
#116950 = DIRECTION('center_axis',(-1.,0.,0.)) ;
#116951 = DIRECTION('ref_axis',(0.,0.,1.)) ;
#116952 = DIRECTION('center_axis',(0.,-1.,0.)) ;
#116953 = DIRECTION('ref_axis',(0.,0.,-1.)) ;
#116954 = DIRECTION('center_axis',(0.,1.,0.)) ;
#116955 = DIRECTION('ref_axis',(0.,0.,1.)) ;
#116956 = DIRECTION('center_axis',(0.,1.,-6.50521303491284E-15)) ;
#116957 = DIRECTION('ref_axis',(0.,6.50521303491284E-15,1.)) ;
#116958 = DIRECTION('center_axis',(0.,-1.,0.)) ;
#116959 = DIRECTION('ref_axis',(0.,0.,-1.)) ;
#116960 = DIRECTION('center_axis',(0.,-1.,0.)) ;
#116961 = DIRECTION('ref_axis',(0.,0.,-1.)) ;
#116962 = DIRECTION('center_axis',(0.,-1.,-1.07081696047951E-16)) ;
#116963 = DIRECTION('ref_axis',(0.,1.07081696047951E-16,-1.)) ;
#116964 = DIRECTION('center_axis',(0.,1.,0.)) ;
#116965 = DIRECTION('ref_axis',(0.,0.,1.)) ;
#116966 = DIRECTION('center_axis',(-1.,0.,0.)) ;
#116967 = DIRECTION('ref_axis',(0.,0.,1.)) ;
#116968 = DIRECTION('center_axis',(0.,0.,1.)) ;
#116969 = DIRECTION('ref_axis',(1.,0.,0.)) ;
#116970 = DIRECTION('center_axis',(0.,1.,0.)) ;
#116971 = DIRECTION('ref_axis',(0.,0.,1.)) ;
#116972 = DIRECTION('center_axis',(0.,0.,-1.)) ;
#116973 = DIRECTION('ref_axis',(-1.,0.,0.)) ;
#116974 = DIRECTION('center_axis',(0.,0.,1.)) ;
#116975 = DIRECTION('ref_axis',(1.,0.,0.)) ;
#116976 = DIRECTION('center_axis',(0.,0.,1.)) ;
#116977 = DIRECTION('ref_axis',(1.,0.,0.)) ;
#116978 = DIRECTION('center_axis',(0.,0.,1.)) ;
#116979 = DIRECTION('ref_axis',(1.,0.,0.)) ;
#116980 = DIRECTION('center_axis',(0.,0.,-1.)) ;
#116981 = DIRECTION('ref_axis',(-1.,0.,0.)) ;
#116982 = DIRECTION('center_axis',(0.,1.,0.)) ;
#116983 = DIRECTION('ref_axis',(0.,0.,1.)) ;
#116984 = DIRECTION('center_axis',(0.,-0.707106781186532,0.707106781186563)) ;
#116985 = DIRECTION('ref_axis',(0.,-0.707106781186563,-0.707106781186532)) ;
#116986 = DIRECTION('center_axis',(0.,1.,0.)) ;
#116987 = DIRECTION('ref_axis',(0.,0.,1.)) ;
#116988 = DIRECTION('center_axis',(2.23012492569655E-15,-0.51423179695906,
-0.857651245551627)) ;
#116989 = DIRECTION('ref_axis',(2.6714619735869E-30,0.857651245551626,-0.51423179695906)) ;
#116990 = DIRECTION('center_axis',(0.,-0.707106781186548,0.707106781186547)) ;
#116991 = DIRECTION('ref_axis',(0.,-0.707106781186547,-0.707106781186548)) ;
#116992 = DIRECTION('center_axis',(0.,-0.707106781186541,0.707106781186554)) ;
#116993 = DIRECTION('ref_axis',(0.,-0.707106781186554,-0.707106781186541)) ;
#116994 = DIRECTION('center_axis',(-1.,0.,0.)) ;
#116995 = DIRECTION('ref_axis',(0.,0.,1.)) ;
#116996 = DIRECTION('center_axis',(0.,0.514231796959095,-0.857651245551606)) ;
#116997 = DIRECTION('ref_axis',(0.,0.857651245551606,0.514231796959095)) ;
#116998 = DIRECTION('center_axis',(0.,1.,0.)) ;
#116999 = DIRECTION('ref_axis',(0.,0.,1.)) ;
#117000 = DIRECTION('center_axis',(0.,0.,-1.)) ;
#117001 = DIRECTION('ref_axis',(-1.,0.,0.)) ;
#117002 = DIRECTION('center_axis',(0.,1.,0.)) ;
#117003 = DIRECTION('ref_axis',(0.,0.,1.)) ;
#117004 = DIRECTION('center_axis',(0.,0.,-1.)) ;
#117005 = DIRECTION('ref_axis',(-1.,0.,0.)) ;
#117006 = DIRECTION('center_axis',(0.,0.,-1.)) ;
#117007 = DIRECTION('ref_axis',(-1.,0.,0.)) ;
#117008 = DIRECTION('center_axis',(0.,0.,1.)) ;
#117009 = DIRECTION('ref_axis',(1.,0.,0.)) ;
#117010 = DIRECTION('center_axis',(0.,0.,-1.)) ;
#117011 = DIRECTION('ref_axis',(-1.,0.,0.)) ;
#117012 = DIRECTION('center_axis',(0.,1.,0.)) ;
#117013 = DIRECTION('ref_axis',(0.,0.,1.)) ;
#117014 = DIRECTION('center_axis',(0.,-1.,8.67361737988409E-15)) ;
#117015 = DIRECTION('ref_axis',(0.,-8.67361737988409E-15,-1.)) ;
#117016 = DIRECTION('center_axis',(0.,0.707106781186546,0.707106781186549)) ;
#117017 = DIRECTION('ref_axis',(0.,-0.707106781186549,0.707106781186546)) ;
#117018 = DIRECTION('center_axis',(0.,0.707106781186537,0.707106781186558)) ;
#117019 = DIRECTION('ref_axis',(0.,-0.707106781186558,0.707106781186537)) ;
#117020 = DIRECTION('center_axis',(0.,1.,1.07081696047951E-16)) ;
#117021 = DIRECTION('ref_axis',(0.,-1.07081696047951E-16,1.)) ;
#117022 = DIRECTION('center_axis',(0.,-1.,0.)) ;
#117023 = DIRECTION('ref_axis',(0.,0.,-1.)) ;
#117024 = DIRECTION('center_axis',(0.,1.,0.)) ;
#117025 = DIRECTION('ref_axis',(0.,0.,1.)) ;
#117026 = DIRECTION('center_axis',(0.,0.,1.)) ;
#117027 = DIRECTION('ref_axis',(1.,0.,0.)) ;
#117028 = DIRECTION('center_axis',(0.,1.,0.)) ;
#117029 = DIRECTION('ref_axis',(0.,0.,1.)) ;
#117030 = DIRECTION('center_axis',(0.,0.,1.)) ;
#117031 = DIRECTION('ref_axis',(1.,0.,0.)) ;
#117032 = DIRECTION('center_axis',(0.,3.99416362155027E-15,1.)) ;
#117033 = DIRECTION('ref_axis',(0.,-1.,3.99416362155027E-15)) ;
#117034 = DIRECTION('center_axis',(0.,0.,1.)) ;
#117035 = DIRECTION('ref_axis',(1.,0.,0.)) ;
#117036 = DIRECTION('center_axis',(0.,0.,-1.)) ;
#117037 = DIRECTION('ref_axis',(-1.,0.,0.)) ;
#117038 = DIRECTION('center_axis',(0.,0.,1.)) ;
#117039 = DIRECTION('ref_axis',(1.,0.,0.)) ;
#117040 = DIRECTION('center_axis',(-1.,0.,0.)) ;
#117041 = DIRECTION('ref_axis',(0.,0.,1.)) ;
#117042 = DIRECTION('center_axis',(0.,1.,0.)) ;
#117043 = DIRECTION('ref_axis',(0.,0.,1.)) ;
#117044 = DIRECTION('center_axis',(-1.,0.,0.)) ;
#117045 = DIRECTION('ref_axis',(0.,0.,1.)) ;
#117046 = DIRECTION('center_axis',(0.,-1.,0.)) ;
#117047 = DIRECTION('ref_axis',(0.,0.,-1.)) ;
#117048 = DIRECTION('center_axis',(0.,1.,0.)) ;
#117049 = DIRECTION('ref_axis',(0.,0.,1.)) ;
#117050 = DIRECTION('center_axis',(1.53063836115601E-16,-1.,-1.30104260698261E-16)) ;
#117051 = DIRECTION('ref_axis',(1.,1.53063836115601E-16,1.99142572374599E-32)) ;
#117052 = DIRECTION('center_axis',(0.,1.,0.)) ;
#117053 = DIRECTION('ref_axis',(0.,0.,1.)) ;
#117054 = DIRECTION('center_axis',(0.,-1.,0.)) ;
#117055 = DIRECTION('ref_axis',(0.,0.,-1.)) ;
#117056 = DIRECTION('center_axis',(1.,1.53063836115601E-16,2.73691106313441E-48)) ;
#117057 = DIRECTION('ref_axis',(-1.53063836115601E-16,1.,-4.18922106430579E-64)) ;
#117058 = DIRECTION('center_axis',(-1.,0.,0.)) ;
#117059 = DIRECTION('ref_axis',(0.,0.,1.)) ;
#117060 = DIRECTION('center_axis',(1.,1.53063836115601E-16,0.)) ;
#117061 = DIRECTION('ref_axis',(1.53063836115601E-16,-1.,0.)) ;
#117062 = DIRECTION('center_axis',(0.,1.,0.)) ;
#117063 = DIRECTION('ref_axis',(1.,0.,0.)) ;
#117064 = DIRECTION('center_axis',(0.,1.,0.)) ;
#117065 = DIRECTION('ref_axis',(0.,0.,-1.)) ;
#117066 = DIRECTION('center_axis',(0.,0.,1.)) ;
#117067 = DIRECTION('ref_axis',(-1.,0.,0.)) ;
#117068 = DIRECTION('center_axis',(0.,1.,0.)) ;
#117069 = DIRECTION('ref_axis',(1.,0.,0.)) ;
#117070 = DIRECTION('center_axis',(0.,0.,1.)) ;
#117071 = DIRECTION('ref_axis',(-1.,0.,0.)) ;
#117072 = DIRECTION('center_axis',(1.,1.0842021724855E-15,0.)) ;
#117073 = DIRECTION('ref_axis',(1.0842021724855E-15,-1.,0.)) ;
#117074 = DIRECTION('center_axis',(-1.,-1.53063836115601E-16,0.)) ;
#117075 = DIRECTION('ref_axis',(0.,-1.,0.)) ;
#117076 = DIRECTION('center_axis',(0.,0.,-1.)) ;
#117077 = DIRECTION('ref_axis',(1.,0.,0.)) ;
#117078 = DIRECTION('center_axis',(0.,0.,-1.)) ;
#117079 = DIRECTION('ref_axis',(0.804034447892622,0.594582716366703,0.)) ;
#117080 = DIRECTION('center_axis',(0.,0.,1.)) ;
#117081 = DIRECTION('ref_axis',(1.,0.,0.)) ;
#117082 = DIRECTION('',(0.,0.,-1.)) ;
#117083 = DIRECTION('center_axis',(-2.16840434497101E-16,1.,1.30104260698261E-16)) ;
#117084 = DIRECTION('ref_axis',(1.,2.16840434497101E-16,1.22464679914735E-16)) ;
#117085 = DIRECTION('',(-2.16840434497101E-16,1.,1.30104260698261E-16)) ;
#117086 = DIRECTION('center_axis',(0.,1.,0.)) ;
#117087 = DIRECTION('ref_axis',(0.,0.,1.)) ;
#117088 = DIRECTION('center_axis',(-1.,-1.53063836115601E-16,-2.73691106313441E-48)) ;
#117089 = DIRECTION('ref_axis',(1.53063836115601E-16,-1.,4.18922106430579E-64)) ;
#117090 = DIRECTION('center_axis',(1.,2.16840434497101E-16,0.)) ;
#117091 = DIRECTION('ref_axis',(2.16840434497101E-16,-1.,0.)) ;
#117092 = DIRECTION('center_axis',(0.,0.,1.)) ;
#117093 = DIRECTION('ref_axis',(1.,0.,0.)) ;
#117094 = DIRECTION('center_axis',(-1.25542992828747E-32,1.020425574104E-16,
1.)) ;
#117095 = DIRECTION('ref_axis',(-1.28107280532009E-48,-1.,1.020425574104E-16)) ;
#117096 = DIRECTION('center_axis',(0.,0.,1.)) ;
#117097 = DIRECTION('ref_axis',(1.,0.,0.)) ;
#117098 = DIRECTION('center_axis',(0.,0.,-1.)) ;
#117099 = DIRECTION('ref_axis',(-1.,0.,0.)) ;
#117100 = DIRECTION('center_axis',(1.,1.53063836115601E-16,-2.73691106313441E-48)) ;
#117101 = DIRECTION('ref_axis',(-1.53063836115601E-16,1.,4.18922106430579E-64)) ;
#117102 = DIRECTION('center_axis',(-1.,0.,0.)) ;
#117103 = DIRECTION('ref_axis',(0.,0.,1.)) ;
#117104 = DIRECTION('center_axis',(1.,1.53063836115601E-16,0.)) ;
#117105 = DIRECTION('ref_axis',(1.53063836115601E-16,-1.,0.)) ;
#117106 = DIRECTION('center_axis',(0.,1.,0.)) ;
#117107 = DIRECTION('ref_axis',(1.,0.,0.)) ;
#117108 = DIRECTION('center_axis',(-1.,-2.16840434497101E-16,0.)) ;
#117109 = DIRECTION('ref_axis',(0.,-1.,0.)) ;
#117110 = DIRECTION('center_axis',(0.,0.,-1.)) ;
#117111 = DIRECTION('ref_axis',(1.,0.,0.)) ;
#117112 = DIRECTION('center_axis',(-1.25542992828747E-32,1.020425574104E-16,
1.)) ;
#117113 = DIRECTION('ref_axis',(0.,-1.,0.)) ;
#117114 = DIRECTION('center_axis',(0.,-1.,0.)) ;
#117115 = DIRECTION('ref_axis',(-6.50521303491284E-15,0.,1.)) ;
#117116 = DIRECTION('center_axis',(-1.,0.,0.)) ;
#117117 = DIRECTION('ref_axis',(0.,0.,-1.)) ;
#117118 = DIRECTION('center_axis',(-1.,-1.53063836115601E-16,0.)) ;
#117119 = DIRECTION('ref_axis',(0.,-1.,0.)) ;
#117120 = DIRECTION('center_axis',(0.,-1.,0.)) ;
#117121 = DIRECTION('ref_axis',(0.,0.,1.)) ;
#117122 = DIRECTION('center_axis',(0.,0.,-1.)) ;
#117123 = DIRECTION('ref_axis',(-1.,0.,0.)) ;
#117124 = DIRECTION('center_axis',(0.,0.,-1.)) ;
#117125 = DIRECTION('ref_axis',(-1.,0.,0.)) ;
#117126 = DIRECTION('center_axis',(1.,1.53063836115601E-16,-3.06472600140763E-33)) ;
#117127 = DIRECTION('ref_axis',(-1.53063836115601E-16,1.,4.69098718418678E-49)) ;
#117128 = DIRECTION('center_axis',(-1.,0.,0.)) ;
#117129 = DIRECTION('ref_axis',(0.,0.,1.)) ;
#117130 = DIRECTION('center_axis',(-1.53063836115601E-16,1.,-1.020425574104E-16)) ;
#117131 = DIRECTION('ref_axis',(-1.,-1.53063836115601E-16,1.3684555315672E-47)) ;
#117132 = DIRECTION('',(1.53063836115601E-16,-1.,1.020425574104E-16)) ;
#117133 = DIRECTION('center_axis',(0.,-1.,0.)) ;
#117134 = DIRECTION('ref_axis',(0.,0.,-1.)) ;
#117135 = DIRECTION('center_axis',(-1.53063836115601E-16,1.,-1.30104260698261E-16)) ;
#117136 = DIRECTION('ref_axis',(-1.,-1.53063836115601E-16,1.99142572374599E-32)) ;
#117137 = DIRECTION('center_axis',(0.,-1.,0.)) ;
#117138 = DIRECTION('ref_axis',(0.,0.,-1.)) ;
#117139 = DIRECTION('center_axis',(-1.,-1.53063836115601E-16,2.73691106313441E-48)) ;
#117140 = DIRECTION('ref_axis',(1.53063836115601E-16,-1.,-4.18922106430579E-64)) ;
#117141 = DIRECTION('center_axis',(1.,2.16840434497101E-16,0.)) ;
#117142 = DIRECTION('ref_axis',(2.16840434497101E-16,-1.,0.)) ;
#117143 = DIRECTION('center_axis',(-1.,0.,2.16840434497095E-15)) ;
#117144 = DIRECTION('ref_axis',(2.16840434497095E-15,0.,1.)) ;
#117145 = DIRECTION('center_axis',(-1.,-2.16840434497101E-16,0.)) ;
#117146 = DIRECTION('ref_axis',(0.,-1.,0.)) ;
#117147 = DIRECTION('center_axis',(0.,0.,1.)) ;
#117148 = DIRECTION('ref_axis',(-1.,0.,0.)) ;
#117149 = DIRECTION('center_axis',(0.,1.,0.)) ;
#117150 = DIRECTION('ref_axis',(1.,0.,0.)) ;
#117151 = DIRECTION('center_axis',(0.,1.,0.)) ;
#117152 = DIRECTION('ref_axis',(0.,0.,-1.)) ;
#117153 = DIRECTION('center_axis',(1.,0.,0.)) ;
#117154 = DIRECTION('ref_axis',(0.,-1.,0.)) ;
#117155 = DIRECTION('center_axis',(1.,6.50521303491304E-15,0.)) ;
#117156 = DIRECTION('ref_axis',(-6.50521303491304E-15,1.,0.)) ;
#117157 = DIRECTION('center_axis',(8.67361737988403E-15,1.,0.)) ;
#117158 = DIRECTION('ref_axis',(-1.,8.67361737988403E-15,0.)) ;
#117159 = DIRECTION('center_axis',(1.2303003375722E-16,-1.,1.020425574104E-16)) ;
#117160 = DIRECTION('ref_axis',(1.,1.2303003375722E-16,-1.25542992828747E-32)) ;
#117161 = DIRECTION('center_axis',(0.,1.,0.)) ;
#117162 = DIRECTION('ref_axis',(0.,0.,1.)) ;
#117163 = DIRECTION('center_axis',(0.,1.,0.)) ;
#117164 = DIRECTION('ref_axis',(1.,0.,0.)) ;
#117165 = DIRECTION('center_axis',(1.,1.2303003375722E-16,0.)) ;
#117166 = DIRECTION('ref_axis',(1.2303003375722E-16,-1.,0.)) ;
#117167 = DIRECTION('center_axis',(0.,0.,1.)) ;
#117168 = DIRECTION('ref_axis',(-1.,0.,0.)) ;
#117169 = DIRECTION('center_axis',(0.,1.,0.)) ;
#117170 = DIRECTION('ref_axis',(1.,0.,0.)) ;
#117171 = DIRECTION('center_axis',(0.,0.,-1.)) ;
#117172 = DIRECTION('ref_axis',(1.,0.,0.)) ;
#117173 = DIRECTION('center_axis',(0.,0.,-1.)) ;
#117174 = DIRECTION('ref_axis',(-1.,0.,0.)) ;
#117175 = DIRECTION('center_axis',(0.,0.,1.)) ;
#117176 = DIRECTION('ref_axis',(1.,0.,0.)) ;
#117177 = DIRECTION('center_axis',(-2.16840434497101E-16,1.,-1.020425574104E-16)) ;
#117178 = DIRECTION('ref_axis',(-1.,-2.16840434497101E-16,5.47382212626882E-48)) ;
#117179 = DIRECTION('center_axis',(0.,1.,0.)) ;
#117180 = DIRECTION('ref_axis',(0.,0.,-1.)) ;
#117181 = DIRECTION('center_axis',(1.,0.,1.25542992828747E-32)) ;
#117182 = DIRECTION('ref_axis',(1.25542992828747E-32,0.,-1.)) ;
#117183 = DIRECTION('center_axis',(1.,0.,0.)) ;
#117184 = DIRECTION('ref_axis',(0.,0.,-1.)) ;
#117185 = DIRECTION('center_axis',(-1.,-1.2303003375722E-16,0.)) ;
#117186 = DIRECTION('ref_axis',(0.,-1.,0.)) ;
#117187 = DIRECTION('center_axis',(0.,0.,-1.)) ;
#117188 = DIRECTION('ref_axis',(1.,0.,0.)) ;
#117189 = DIRECTION('center_axis',(0.,0.,-1.)) ;
#117190 = DIRECTION('ref_axis',(-1.,0.,0.)) ;
#117191 = DIRECTION('',(0.,0.,1.)) ;
#117192 = DIRECTION('center_axis',(0.,0.,1.)) ;
#117193 = DIRECTION('ref_axis',(1.,0.,0.)) ;
#117194 = DIRECTION('center_axis',(0.,0.,1.)) ;
#117195 = DIRECTION('ref_axis',(1.,0.,0.)) ;
#117196 = DIRECTION('center_axis',(6.27714964143733E-33,-5.10212787052002E-17,
-1.)) ;
#117197 = DIRECTION('ref_axis',(3.20268201330022E-49,1.,-5.10212787052002E-17)) ;
#117198 = DIRECTION('center_axis',(1.,1.53063836115601E-16,-1.53236300070382E-33)) ;
#117199 = DIRECTION('ref_axis',(-1.53063836115601E-16,1.,2.34549359209339E-49)) ;
#117200 = DIRECTION('center_axis',(-1.,0.,0.)) ;
#117201 = DIRECTION('ref_axis',(0.,0.,1.)) ;
#117202 = DIRECTION('center_axis',(1.,0.,0.)) ;
#117203 = DIRECTION('ref_axis',(0.,0.,-1.)) ;
#117204 = DIRECTION('center_axis',(0.,1.,0.)) ;
#117205 = DIRECTION('ref_axis',(1.,0.,0.)) ;
#117206 = DIRECTION('center_axis',(-4.33680868994202E-15,1.,0.)) ;
#117207 = DIRECTION('ref_axis',(1.,4.33680868994202E-15,0.)) ;
#117208 = DIRECTION('center_axis',(0.,-1.,0.)) ;
#117209 = DIRECTION('ref_axis',(0.,0.,-1.)) ;
#117210 = DIRECTION('center_axis',(0.,0.,-1.)) ;
#117211 = DIRECTION('ref_axis',(1.,0.,0.)) ;
#117212 = DIRECTION('center_axis',(0.,0.,1.)) ;
#117213 = DIRECTION('ref_axis',(1.,0.,0.)) ;
#117214 = DIRECTION('center_axis',(0.,0.,-1.)) ;
#117215 = DIRECTION('ref_axis',(-1.,0.,0.)) ;
#117216 = DIRECTION('center_axis',(0.,1.,0.)) ;
#117217 = DIRECTION('ref_axis',(1.,0.,0.)) ;
#117218 = DIRECTION('center_axis',(1.,1.2303003375722E-16,0.)) ;
#117219 = DIRECTION('ref_axis',(1.2303003375722E-16,-1.,0.)) ;
#117220 = DIRECTION('center_axis',(0.,1.,0.)) ;
#117221 = DIRECTION('ref_axis',(-6.50521303491284E-15,0.,-1.)) ;
#117222 = DIRECTION('center_axis',(6.27714964143733E-33,-5.10212787052002E-17,
-1.)) ;
#117223 = DIRECTION('ref_axis',(0.,1.,0.)) ;
#117224 = DIRECTION('center_axis',(0.,-1.,0.)) ;
#117225 = DIRECTION('ref_axis',(0.,0.,1.)) ;
#117226 = DIRECTION('center_axis',(2.16840434497101E-16,-1.,5.10212787052002E-17)) ;
#117227 = DIRECTION('ref_axis',(1.,2.16840434497101E-16,-5.47382212626882E-48)) ;
#117228 = DIRECTION('center_axis',(0.,1.,0.)) ;
#117229 = DIRECTION('ref_axis',(0.,0.,-1.)) ;
#117230 = DIRECTION('center_axis',(0.,0.,1.)) ;
#117231 = DIRECTION('ref_axis',(1.,0.,0.)) ;
#117232 = DIRECTION('center_axis',(0.,0.,-1.)) ;
#117233 = DIRECTION('ref_axis',(-1.,0.,0.)) ;
#117234 = DIRECTION('center_axis',(-1.,-1.2303003375722E-16,0.)) ;
#117235 = DIRECTION('ref_axis',(0.,-1.,0.)) ;
#117236 = DIRECTION('center_axis',(0.,-1.,0.)) ;
#117237 = DIRECTION('ref_axis',(0.,0.,1.)) ;
#117238 = DIRECTION('center_axis',(1.53063836115601E-16,-1.,5.10212787052002E-17)) ;
#117239 = DIRECTION('ref_axis',(1.,1.53063836115601E-16,-6.84227765783602E-48)) ;
#117240 = DIRECTION('',(-1.53063836115601E-16,1.,-5.10212787052002E-17)) ;
#117241 = DIRECTION('center_axis',(0.,-1.,0.)) ;
#117242 = DIRECTION('ref_axis',(0.,0.,-1.)) ;
#117243 = DIRECTION('center_axis',(-1.,0.,0.)) ;
#117244 = DIRECTION('ref_axis',(0.,0.,-1.)) ;
#117245 = DIRECTION('center_axis',(-1.2303003375722E-16,1.,-5.10212787052002E-17)) ;
#117246 = DIRECTION('ref_axis',(-1.,-1.2303003375722E-16,6.27714964143733E-33)) ;
#117247 = DIRECTION('center_axis',(-8.67361737988403E-15,-1.,0.)) ;
#117248 = DIRECTION('ref_axis',(1.,-8.67361737988403E-15,0.)) ;
#117249 = DIRECTION('center_axis',(1.,0.,6.27714964143733E-33)) ;
#117250 = DIRECTION('ref_axis',(6.27714964143733E-33,0.,-1.)) ;
#117251 = DIRECTION('center_axis',(-1.,0.,-6.50521303491284E-15)) ;
#117252 = DIRECTION('ref_axis',(-6.50521303491284E-15,0.,1.)) ;
#117253 = DIRECTION('center_axis',(1.,0.,0.)) ;
#117254 = DIRECTION('ref_axis',(0.,1.,0.)) ;
#117255 = DIRECTION('center_axis',(0.,0.,-1.)) ;
#117256 = DIRECTION('ref_axis',(-1.,0.,0.)) ;
#117257 = DIRECTION('center_axis',(0.,0.,1.)) ;
#117258 = DIRECTION('ref_axis',(1.,0.,0.)) ;
#117259 = DIRECTION('center_axis',(0.,0.,-1.)) ;
#117260 = DIRECTION('ref_axis',(-1.,0.,0.)) ;
#117261 = DIRECTION('center_axis',(-1.,0.,0.)) ;
#117262 = DIRECTION('ref_axis',(0.,0.,1.)) ;
#117263 = DIRECTION('center_axis',(0.,-1.,0.)) ;
#117264 = DIRECTION('ref_axis',(0.,0.,-1.)) ;
#117265 = DIRECTION('center_axis',(0.,1.,0.)) ;
#117266 = DIRECTION('ref_axis',(0.,0.,1.)) ;
#117267 = DIRECTION('center_axis',(0.,1.,-6.50521303491284E-15)) ;
#117268 = DIRECTION('ref_axis',(0.,6.50521303491284E-15,1.)) ;
#117269 = DIRECTION('center_axis',(0.,-1.,0.)) ;
#117270 = DIRECTION('ref_axis',(0.,0.,-1.)) ;
#117271 = DIRECTION('center_axis',(0.,-1.,0.)) ;
#117272 = DIRECTION('ref_axis',(0.,0.,-1.)) ;
#117273 = DIRECTION('center_axis',(0.,-1.,-1.07081696047951E-16)) ;
#117274 = DIRECTION('ref_axis',(0.,1.07081696047951E-16,-1.)) ;
#117275 = DIRECTION('center_axis',(0.,1.,0.)) ;
#117276 = DIRECTION('ref_axis',(0.,0.,1.)) ;
#117277 = DIRECTION('center_axis',(-1.,0.,0.)) ;
#117278 = DIRECTION('ref_axis',(0.,0.,1.)) ;
#117279 = DIRECTION('center_axis',(0.,0.,1.)) ;
#117280 = DIRECTION('ref_axis',(1.,0.,0.)) ;
#117281 = DIRECTION('center_axis',(0.,1.,0.)) ;
#117282 = DIRECTION('ref_axis',(0.,0.,1.)) ;
#117283 = DIRECTION('center_axis',(0.,0.,-1.)) ;
#117284 = DIRECTION('ref_axis',(-1.,0.,0.)) ;
#117285 = DIRECTION('center_axis',(0.,0.,1.)) ;
#117286 = DIRECTION('ref_axis',(1.,0.,0.)) ;
#117287 = DIRECTION('center_axis',(0.,0.,1.)) ;
#117288 = DIRECTION('ref_axis',(1.,0.,0.)) ;
#117289 = DIRECTION('center_axis',(0.,0.,1.)) ;
#117290 = DIRECTION('ref_axis',(1.,0.,0.)) ;
#117291 = DIRECTION('center_axis',(0.,0.,-1.)) ;
#117292 = DIRECTION('ref_axis',(-1.,0.,0.)) ;
#117293 = DIRECTION('center_axis',(0.,1.,0.)) ;
#117294 = DIRECTION('ref_axis',(0.,0.,1.)) ;
#117295 = DIRECTION('center_axis',(0.,-0.707106781186532,0.707106781186563)) ;
#117296 = DIRECTION('ref_axis',(0.,-0.707106781186563,-0.707106781186532)) ;
#117297 = DIRECTION('center_axis',(0.,1.,0.)) ;
#117298 = DIRECTION('ref_axis',(0.,0.,1.)) ;
#117299 = DIRECTION('center_axis',(2.23012492569655E-15,-0.51423179695906,
-0.857651245551627)) ;
#117300 = DIRECTION('ref_axis',(2.6714619735869E-30,0.857651245551626,-0.51423179695906)) ;
#117301 = DIRECTION('center_axis',(0.,-0.707106781186548,0.707106781186547)) ;
#117302 = DIRECTION('ref_axis',(0.,-0.707106781186547,-0.707106781186548)) ;
#117303 = DIRECTION('center_axis',(0.,-0.707106781186543,0.707106781186552)) ;
#117304 = DIRECTION('ref_axis',(0.,-0.707106781186552,-0.707106781186543)) ;
#117305 = DIRECTION('center_axis',(-1.,0.,0.)) ;
#117306 = DIRECTION('ref_axis',(0.,0.,1.)) ;
#117307 = DIRECTION('center_axis',(-6.69037477709043E-15,0.51423179695912,
-0.85765124555159)) ;
#117308 = DIRECTION('ref_axis',(-4.44487660401203E-29,0.85765124555159,0.51423179695912)) ;
#117309 = DIRECTION('center_axis',(0.,1.,0.)) ;
#117310 = DIRECTION('ref_axis',(0.,0.,1.)) ;
#117311 = DIRECTION('center_axis',(0.,0.,-1.)) ;
#117312 = DIRECTION('ref_axis',(-1.,0.,0.)) ;
#117313 = DIRECTION('center_axis',(0.,1.,0.)) ;
#117314 = DIRECTION('ref_axis',(0.,0.,1.)) ;
#117315 = DIRECTION('center_axis',(0.,0.,-1.)) ;
#117316 = DIRECTION('ref_axis',(-1.,0.,0.)) ;
#117317 = DIRECTION('center_axis',(0.,0.,-1.)) ;
#117318 = DIRECTION('ref_axis',(-1.,0.,0.)) ;
#117319 = DIRECTION('center_axis',(0.,0.,1.)) ;
#117320 = DIRECTION('ref_axis',(1.,0.,0.)) ;
#117321 = DIRECTION('center_axis',(0.,0.,-1.)) ;
#117322 = DIRECTION('ref_axis',(-1.,0.,0.)) ;
#117323 = DIRECTION('center_axis',(0.,1.,0.)) ;
#117324 = DIRECTION('ref_axis',(0.,0.,1.)) ;
#117325 = DIRECTION('center_axis',(0.,-1.,8.67361737988379E-15)) ;
#117326 = DIRECTION('ref_axis',(0.,-8.67361737988379E-15,-1.)) ;
#117327 = DIRECTION('center_axis',(0.,0.707106781186546,0.707106781186549)) ;
#117328 = DIRECTION('ref_axis',(0.,-0.707106781186549,0.707106781186546)) ;
#117329 = DIRECTION('center_axis',(0.,0.707106781186534,0.707106781186561)) ;
#117330 = DIRECTION('ref_axis',(0.,-0.707106781186561,0.707106781186534)) ;
#117331 = DIRECTION('center_axis',(0.,1.,1.07081696047951E-16)) ;
#117332 = DIRECTION('ref_axis',(0.,-1.07081696047951E-16,1.)) ;
#117333 = DIRECTION('center_axis',(0.,-1.,0.)) ;
#117334 = DIRECTION('ref_axis',(0.,0.,-1.)) ;
#117335 = DIRECTION('center_axis',(0.,1.,0.)) ;
#117336 = DIRECTION('ref_axis',(0.,0.,1.)) ;
#117337 = DIRECTION('center_axis',(0.,0.,1.)) ;
#117338 = DIRECTION('ref_axis',(1.,0.,0.)) ;
#117339 = DIRECTION('center_axis',(0.,1.,0.)) ;
#117340 = DIRECTION('ref_axis',(0.,0.,1.)) ;
#117341 = DIRECTION('center_axis',(0.,6.93889390390723E-14,1.)) ;
#117342 = DIRECTION('ref_axis',(0.,-1.,6.93889390390723E-14)) ;
#117343 = DIRECTION('center_axis',(0.,3.99416362155027E-15,1.)) ;
#117344 = DIRECTION('ref_axis',(0.,-1.,3.99416362155027E-15)) ;
#117345 = DIRECTION('center_axis',(0.,0.,1.)) ;
#117346 = DIRECTION('ref_axis',(1.,0.,0.)) ;
#117347 = DIRECTION('center_axis',(0.,0.,-1.)) ;
#117348 = DIRECTION('ref_axis',(-1.,0.,0.)) ;
#117349 = DIRECTION('center_axis',(0.,0.,1.)) ;
#117350 = DIRECTION('ref_axis',(1.,0.,0.)) ;
#117351 = DIRECTION('center_axis',(-1.,0.,0.)) ;
#117352 = DIRECTION('ref_axis',(0.,0.,1.)) ;
#117353 = DIRECTION('center_axis',(0.,1.,0.)) ;
#117354 = DIRECTION('ref_axis',(0.,0.,1.)) ;
#117355 = DIRECTION('center_axis',(-1.,0.,0.)) ;
#117356 = DIRECTION('ref_axis',(0.,0.,1.)) ;
#117357 = DIRECTION('center_axis',(0.,-1.,0.)) ;
#117358 = DIRECTION('ref_axis',(0.,0.,-1.)) ;
#117359 = DIRECTION('center_axis',(0.,1.,0.)) ;
#117360 = DIRECTION('ref_axis',(0.,0.,1.)) ;
#117361 = DIRECTION('center_axis',(1.,-9.85638338623186E-18,0.)) ;
#117362 = DIRECTION('ref_axis',(9.85638338623186E-18,1.,0.)) ;
#117363 = DIRECTION('',(0.,0.,-1.)) ;
#117364 = DIRECTION('',(-9.85638338623186E-18,-1.,0.)) ;
#117365 = DIRECTION('',(0.,0.,1.)) ;
#117366 = DIRECTION('',(9.85638338623186E-18,1.,0.)) ;
#117367 = DIRECTION('center_axis',(0.707106781186548,0.707106781186548,0.)) ;
#117368 = DIRECTION('ref_axis',(-0.707106781186548,0.707106781186548,0.)) ;
#117369 = DIRECTION('',(0.,0.,1.)) ;
#117370 = DIRECTION('',(-0.577350269189625,0.577350269189625,0.577350269189627)) ;
#117371 = DIRECTION('',(0.,0.,-1.)) ;
#117372 = DIRECTION('',(0.577350269189625,-0.577350269189625,0.577350269189627)) ;
#117373 = DIRECTION('center_axis',(0.,1.,0.)) ;
#117374 = DIRECTION('ref_axis',(0.,0.,1.)) ;
#117375 = DIRECTION('',(0.,0.,1.)) ;
#117376 = DIRECTION('',(-1.,0.,-9.8563833862319E-18)) ;
#117377 = DIRECTION('',(0.,0.,-1.)) ;
#117378 = DIRECTION('',(1.,0.,-9.8563833862319E-18)) ;
#117379 = DIRECTION('center_axis',(-0.707106781186548,0.707106781186548,0.)) ;
#117380 = DIRECTION('ref_axis',(-0.707106781186548,-0.707106781186548,0.)) ;
#117381 = DIRECTION('',(0.,0.,1.)) ;
#117382 = DIRECTION('',(-0.577350269189625,-0.577350269189625,-0.577350269189627)) ;
#117383 = DIRECTION('',(0.,0.,-1.)) ;
#117384 = DIRECTION('',(0.577350269189625,0.577350269189625,-0.577350269189627)) ;
#117385 = DIRECTION('center_axis',(-1.,9.85638338623186E-18,0.)) ;
#117386 = DIRECTION('ref_axis',(-9.85638338623186E-18,-1.,0.)) ;
#117387 = DIRECTION('',(0.,0.,-1.)) ;
#117388 = DIRECTION('',(9.85638338623186E-18,1.,0.)) ;
#117389 = DIRECTION('',(0.,0.,-1.)) ;
#117390 = DIRECTION('',(-9.85638338623186E-18,-1.,0.)) ;
#117391 = DIRECTION('center_axis',(0.,0.,1.)) ;
#117392 = DIRECTION('ref_axis',(1.,0.,0.)) ;
#117393 = DIRECTION('',(9.85638338623186E-18,1.,0.)) ;
#117394 = DIRECTION('center_axis',(0.,0.,-1.)) ;
#117395 = DIRECTION('ref_axis',(1.,0.,0.)) ;
#117396 = DIRECTION('center_axis',(0.,0.,1.)) ;
#117397 = DIRECTION('ref_axis',(1.,0.,0.)) ;
#117398 = DIRECTION('',(-9.85638338623186E-18,-1.,0.)) ;
#117399 = DIRECTION('',(1.,-9.85638338623186E-18,0.)) ;
#117400 = DIRECTION('center_axis',(0.,0.,1.)) ;
#117401 = DIRECTION('ref_axis',(1.,0.,0.)) ;
#117402 = DIRECTION('',(9.85638338623186E-18,1.,0.)) ;
#117403 = DIRECTION('center_axis',(0.,0.,-1.)) ;
#117404 = DIRECTION('ref_axis',(1.,0.,0.)) ;
#117405 = DIRECTION('center_axis',(0.,0.,1.)) ;
#117406 = DIRECTION('ref_axis',(1.,0.,0.)) ;
#117407 = DIRECTION('',(-9.85638338623186E-18,-1.,0.)) ;
#117408 = DIRECTION('',(-1.,9.85638338623186E-18,0.)) ;
#117409 = DIRECTION('center_axis',(0.,0.,-1.)) ;
#117410 = DIRECTION('ref_axis',(-1.,0.,0.)) ;
#117411 = DIRECTION('center_axis',(0.,0.,1.)) ;
#117412 = DIRECTION('ref_axis',(1.,0.,0.)) ;
#117413 = DIRECTION('center_axis',(0.,0.,-1.)) ;
#117414 = DIRECTION('ref_axis',(1.,0.,0.)) ;
#117415 = DIRECTION('center_axis',(0.,0.,-1.)) ;
#117416 = DIRECTION('ref_axis',(-1.,0.,0.)) ;
#117417 = DIRECTION('center_axis',(0.,0.,-1.)) ;
#117418 = DIRECTION('ref_axis',(1.,0.,0.)) ;
#117419 = DIRECTION('center_axis',(0.,0.,1.)) ;
#117420 = DIRECTION('ref_axis',(1.,0.,0.)) ;
#117421 = DIRECTION('center_axis',(-0.707106781186548,-0.707106781186547,
0.)) ;
#117422 = DIRECTION('ref_axis',(0.707106781186547,-0.707106781186548,0.)) ;
#117423 = DIRECTION('',(0.,0.,1.)) ;
#117424 = DIRECTION('',(0.577350269189625,-0.577350269189626,-0.577350269189626)) ;
#117425 = DIRECTION('',(0.,0.,-1.)) ;
#117426 = DIRECTION('',(-0.577350269189625,0.577350269189626,-0.577350269189626)) ;
#117427 = DIRECTION('center_axis',(1.95511867169517E-16,-1.,0.)) ;
#117428 = DIRECTION('ref_axis',(1.,1.95511867169517E-16,0.)) ;
#117429 = DIRECTION('',(0.,0.,-1.)) ;
#117430 = DIRECTION('',(-1.,-1.95511867169517E-16,0.)) ;
#117431 = DIRECTION('',(1.,1.95511867169517E-16,0.)) ;
#117432 = DIRECTION('center_axis',(1.06642836637918E-16,1.,0.)) ;
#117433 = DIRECTION('ref_axis',(-1.,1.06642836637918E-16,0.)) ;
#117434 = DIRECTION('',(1.,-1.06642836637919E-16,0.)) ;
#117435 = DIRECTION('',(0.,0.,1.)) ;
#117436 = DIRECTION('',(-1.,1.06642836637919E-16,0.)) ;
#117437 = DIRECTION('center_axis',(-0.707106781186548,0.707106781186547,0.)) ;
#117438 = DIRECTION('ref_axis',(-0.707106781186547,-0.707106781186548,0.)) ;
#117439 = DIRECTION('',(0.,0.,1.)) ;
#117440 = DIRECTION('',(-0.577350269189625,-0.577350269189626,0.577350269189627)) ;
#117441 = DIRECTION('',(0.,0.,-1.)) ;
#117442 = DIRECTION('',(0.577350269189625,0.577350269189626,0.577350269189627)) ;
#117443 = DIRECTION('center_axis',(-1.,0.,0.)) ;
#117444 = DIRECTION('ref_axis',(0.,0.,1.)) ;
#117445 = DIRECTION('',(0.,0.,-1.)) ;
#117446 = DIRECTION('',(0.,1.,1.95511867169518E-16)) ;
#117447 = DIRECTION('',(0.,0.,1.)) ;
#117448 = DIRECTION('',(0.,-1.,1.95511867169518E-16)) ;
#117449 = DIRECTION('center_axis',(0.,0.,1.)) ;
#117450 = DIRECTION('ref_axis',(1.,0.,0.)) ;
#117451 = DIRECTION('',(-1.95511867169517E-16,1.,0.)) ;
#117452 = DIRECTION('',(-1.,-1.95511867169517E-16,0.)) ;
#117453 = DIRECTION('',(1.,-1.06642836637919E-16,0.)) ;
#117454 = DIRECTION('center_axis',(0.,0.,1.)) ;
#117455 = DIRECTION('ref_axis',(1.,0.,0.)) ;
#117456 = DIRECTION('',(1.,1.95511867169517E-16,0.)) ;
#117457 = DIRECTION('',(1.95511867169517E-16,-1.,0.)) ;
#117458 = DIRECTION('',(-1.,1.06642836637919E-16,0.)) ;
#117459 = DIRECTION('center_axis',(1.,-9.85638338623186E-18,0.)) ;
#117460 = DIRECTION('ref_axis',(9.85638338623186E-18,1.,0.)) ;
#117461 = DIRECTION('',(0.,0.,-1.)) ;
#117462 = DIRECTION('',(-9.85638338623186E-18,-1.,0.)) ;
#117463 = DIRECTION('',(0.,0.,1.)) ;
#117464 = DIRECTION('',(9.85638338623186E-18,1.,0.)) ;
#117465 = DIRECTION('center_axis',(0.707106781186548,0.707106781186548,0.)) ;
#117466 = DIRECTION('ref_axis',(-0.707106781186548,0.707106781186548,0.)) ;
#117467 = DIRECTION('',(0.,0.,1.)) ;
#117468 = DIRECTION('',(-0.577350269189625,0.577350269189625,0.577350269189627)) ;
#117469 = DIRECTION('',(0.,0.,-1.)) ;
#117470 = DIRECTION('',(0.577350269189625,-0.577350269189625,0.577350269189627)) ;
#117471 = DIRECTION('center_axis',(0.,1.,0.)) ;
#117472 = DIRECTION('ref_axis',(0.,0.,1.)) ;
#117473 = DIRECTION('',(0.,0.,1.)) ;
#117474 = DIRECTION('',(-1.,0.,-9.8563833862319E-18)) ;
#117475 = DIRECTION('',(0.,0.,-1.)) ;
#117476 = DIRECTION('',(1.,0.,-9.8563833862319E-18)) ;
#117477 = DIRECTION('center_axis',(-0.707106781186548,0.707106781186548,0.)) ;
#117478 = DIRECTION('ref_axis',(-0.707106781186548,-0.707106781186548,0.)) ;
#117479 = DIRECTION('',(0.,0.,1.)) ;
#117480 = DIRECTION('',(-0.577350269189625,-0.577350269189625,-0.577350269189627)) ;
#117481 = DIRECTION('',(0.,0.,-1.)) ;
#117482 = DIRECTION('',(0.577350269189625,0.577350269189625,-0.577350269189627)) ;
#117483 = DIRECTION('center_axis',(-1.,9.85638338623186E-18,0.)) ;
#117484 = DIRECTION('ref_axis',(-9.85638338623186E-18,-1.,0.)) ;
#117485 = DIRECTION('',(0.,0.,-1.)) ;
#117486 = DIRECTION('',(9.85638338623186E-18,1.,0.)) ;
#117487 = DIRECTION('',(0.,0.,-1.)) ;
#117488 = DIRECTION('',(-9.85638338623186E-18,-1.,0.)) ;
#117489 = DIRECTION('center_axis',(0.,0.,1.)) ;
#117490 = DIRECTION('ref_axis',(1.,0.,0.)) ;
#117491 = DIRECTION('',(9.85638338623186E-18,1.,0.)) ;
#117492 = DIRECTION('center_axis',(0.,0.,-1.)) ;
#117493 = DIRECTION('ref_axis',(1.,0.,0.)) ;
#117494 = DIRECTION('center_axis',(0.,0.,1.)) ;
#117495 = DIRECTION('ref_axis',(1.,0.,0.)) ;
#117496 = DIRECTION('',(-9.85638338623186E-18,-1.,0.)) ;
#117497 = DIRECTION('',(1.,-9.85638338623186E-18,0.)) ;
#117498 = DIRECTION('center_axis',(0.,0.,1.)) ;
#117499 = DIRECTION('ref_axis',(1.,0.,0.)) ;
#117500 = DIRECTION('',(9.85638338623186E-18,1.,0.)) ;
#117501 = DIRECTION('center_axis',(0.,0.,-1.)) ;
#117502 = DIRECTION('ref_axis',(1.,0.,0.)) ;
#117503 = DIRECTION('center_axis',(0.,0.,1.)) ;
#117504 = DIRECTION('ref_axis',(1.,0.,0.)) ;
#117505 = DIRECTION('',(-9.85638338623186E-18,-1.,0.)) ;
#117506 = DIRECTION('',(-1.,9.85638338623186E-18,0.)) ;
#117507 = DIRECTION('center_axis',(0.,0.,-1.)) ;
#117508 = DIRECTION('ref_axis',(-1.,0.,0.)) ;
#117509 = DIRECTION('center_axis',(0.,0.,1.)) ;
#117510 = DIRECTION('ref_axis',(1.,0.,0.)) ;
#117511 = DIRECTION('center_axis',(0.,0.,-1.)) ;
#117512 = DIRECTION('ref_axis',(1.,0.,0.)) ;
#117513 = DIRECTION('center_axis',(0.,0.,-1.)) ;
#117514 = DIRECTION('ref_axis',(-1.,0.,0.)) ;
#117515 = DIRECTION('center_axis',(0.,0.,-1.)) ;
#117516 = DIRECTION('ref_axis',(1.,0.,0.)) ;
#117517 = DIRECTION('center_axis',(0.,0.,1.)) ;
#117518 = DIRECTION('ref_axis',(1.,0.,0.)) ;
#117519 = DIRECTION('center_axis',(-0.707106781186548,-0.707106781186547,
0.)) ;
#117520 = DIRECTION('ref_axis',(0.707106781186547,-0.707106781186548,0.)) ;
#117521 = DIRECTION('',(0.,0.,1.)) ;
#117522 = DIRECTION('',(0.577350269189625,-0.577350269189626,-0.577350269189626)) ;
#117523 = DIRECTION('',(0.,0.,-1.)) ;
#117524 = DIRECTION('',(-0.577350269189625,0.577350269189626,-0.577350269189626)) ;
#117525 = DIRECTION('center_axis',(1.95511867169517E-16,-1.,0.)) ;
#117526 = DIRECTION('ref_axis',(1.,1.95511867169517E-16,0.)) ;
#117527 = DIRECTION('',(0.,0.,-1.)) ;
#117528 = DIRECTION('',(-1.,-1.95511867169517E-16,0.)) ;
#117529 = DIRECTION('',(1.,1.95511867169517E-16,0.)) ;
#117530 = DIRECTION('center_axis',(1.06642836637918E-16,1.,0.)) ;
#117531 = DIRECTION('ref_axis',(-1.,1.06642836637918E-16,0.)) ;
#117532 = DIRECTION('',(1.,-1.06642836637919E-16,0.)) ;
#117533 = DIRECTION('',(0.,0.,1.)) ;
#117534 = DIRECTION('',(-1.,1.06642836637919E-16,0.)) ;
#117535 = DIRECTION('center_axis',(-0.707106781186548,0.707106781186547,0.)) ;
#117536 = DIRECTION('ref_axis',(-0.707106781186547,-0.707106781186548,0.)) ;
#117537 = DIRECTION('',(0.,0.,1.)) ;
#117538 = DIRECTION('',(-0.577350269189625,-0.577350269189626,0.577350269189627)) ;
#117539 = DIRECTION('',(0.,0.,-1.)) ;
#117540 = DIRECTION('',(0.577350269189625,0.577350269189626,0.577350269189627)) ;
#117541 = DIRECTION('center_axis',(-1.,0.,0.)) ;
#117542 = DIRECTION('ref_axis',(0.,0.,1.)) ;
#117543 = DIRECTION('',(0.,0.,-1.)) ;
#117544 = DIRECTION('',(0.,1.,1.95511867169518E-16)) ;
#117545 = DIRECTION('',(0.,0.,1.)) ;
#117546 = DIRECTION('',(0.,-1.,1.95511867169518E-16)) ;
#117547 = DIRECTION('center_axis',(0.,0.,1.)) ;
#117548 = DIRECTION('ref_axis',(1.,0.,0.)) ;
#117549 = DIRECTION('',(-1.95511867169517E-16,1.,0.)) ;
#117550 = DIRECTION('',(-1.,-1.95511867169517E-16,0.)) ;
#117551 = DIRECTION('',(1.,-1.06642836637919E-16,0.)) ;
#117552 = DIRECTION('center_axis',(0.,0.,1.)) ;
#117553 = DIRECTION('ref_axis',(1.,0.,0.)) ;
#117554 = DIRECTION('',(1.,1.95511867169517E-16,0.)) ;
#117555 = DIRECTION('',(1.95511867169517E-16,-1.,0.)) ;
#117556 = DIRECTION('',(-1.,1.06642836637919E-16,0.)) ;
#117557 = DIRECTION('center_axis',(1.,-9.85638338623186E-18,0.)) ;
#117558 = DIRECTION('ref_axis',(9.85638338623186E-18,1.,0.)) ;
#117559 = DIRECTION('',(0.,0.,-1.)) ;
#117560 = DIRECTION('',(-9.85638338623186E-18,-1.,0.)) ;
#117561 = DIRECTION('',(0.,0.,1.)) ;
#117562 = DIRECTION('',(9.85638338623186E-18,1.,0.)) ;
#117563 = DIRECTION('center_axis',(0.707106781186548,0.707106781186548,0.)) ;
#117564 = DIRECTION('ref_axis',(-0.707106781186548,0.707106781186548,0.)) ;
#117565 = DIRECTION('',(0.,0.,1.)) ;
#117566 = DIRECTION('',(-0.577350269189625,0.577350269189625,0.577350269189627)) ;
#117567 = DIRECTION('',(0.,0.,-1.)) ;
#117568 = DIRECTION('',(0.577350269189625,-0.577350269189625,0.577350269189627)) ;
#117569 = DIRECTION('center_axis',(0.,1.,0.)) ;
#117570 = DIRECTION('ref_axis',(0.,0.,1.)) ;
#117571 = DIRECTION('',(0.,0.,1.)) ;
#117572 = DIRECTION('',(-1.,0.,-9.8563833862319E-18)) ;
#117573 = DIRECTION('',(0.,0.,-1.)) ;
#117574 = DIRECTION('',(1.,0.,-9.8563833862319E-18)) ;
#117575 = DIRECTION('center_axis',(-0.707106781186548,0.707106781186548,0.)) ;
#117576 = DIRECTION('ref_axis',(-0.707106781186548,-0.707106781186548,0.)) ;
#117577 = DIRECTION('',(0.,0.,1.)) ;
#117578 = DIRECTION('',(-0.577350269189625,-0.577350269189625,-0.577350269189627)) ;
#117579 = DIRECTION('',(0.,0.,-1.)) ;
#117580 = DIRECTION('',(0.577350269189625,0.577350269189625,-0.577350269189627)) ;
#117581 = DIRECTION('center_axis',(-1.,9.85638338623186E-18,0.)) ;
#117582 = DIRECTION('ref_axis',(-9.85638338623186E-18,-1.,0.)) ;
#117583 = DIRECTION('',(0.,0.,-1.)) ;
#117584 = DIRECTION('',(9.85638338623186E-18,1.,0.)) ;
#117585 = DIRECTION('',(0.,0.,-1.)) ;
#117586 = DIRECTION('',(-9.85638338623186E-18,-1.,0.)) ;
#117587 = DIRECTION('center_axis',(0.,0.,1.)) ;
#117588 = DIRECTION('ref_axis',(1.,0.,0.)) ;
#117589 = DIRECTION('',(9.85638338623186E-18,1.,0.)) ;
#117590 = DIRECTION('center_axis',(0.,0.,-1.)) ;
#117591 = DIRECTION('ref_axis',(1.,0.,0.)) ;
#117592 = DIRECTION('center_axis',(0.,0.,1.)) ;
#117593 = DIRECTION('ref_axis',(1.,0.,0.)) ;
#117594 = DIRECTION('',(-9.85638338623186E-18,-1.,0.)) ;
#117595 = DIRECTION('',(1.,-9.85638338623186E-18,0.)) ;
#117596 = DIRECTION('center_axis',(0.,0.,1.)) ;
#117597 = DIRECTION('ref_axis',(1.,0.,0.)) ;
#117598 = DIRECTION('',(9.85638338623186E-18,1.,0.)) ;
#117599 = DIRECTION('center_axis',(0.,0.,-1.)) ;
#117600 = DIRECTION('ref_axis',(1.,0.,0.)) ;
#117601 = DIRECTION('center_axis',(0.,0.,1.)) ;
#117602 = DIRECTION('ref_axis',(1.,0.,0.)) ;
#117603 = DIRECTION('',(-9.85638338623186E-18,-1.,0.)) ;
#117604 = DIRECTION('',(-1.,9.85638338623186E-18,0.)) ;
#117605 = DIRECTION('center_axis',(0.,0.,-1.)) ;
#117606 = DIRECTION('ref_axis',(-1.,0.,0.)) ;
#117607 = DIRECTION('center_axis',(0.,0.,1.)) ;
#117608 = DIRECTION('ref_axis',(1.,0.,0.)) ;
#117609 = DIRECTION('center_axis',(0.,0.,-1.)) ;
#117610 = DIRECTION('ref_axis',(1.,0.,0.)) ;
#117611 = DIRECTION('center_axis',(0.,0.,-1.)) ;
#117612 = DIRECTION('ref_axis',(-1.,0.,0.)) ;
#117613 = DIRECTION('center_axis',(0.,0.,-1.)) ;
#117614 = DIRECTION('ref_axis',(1.,0.,0.)) ;
#117615 = DIRECTION('center_axis',(0.,0.,1.)) ;
#117616 = DIRECTION('ref_axis',(1.,0.,0.)) ;
#117617 = DIRECTION('center_axis',(-0.707106781186548,-0.707106781186547,
0.)) ;
#117618 = DIRECTION('ref_axis',(0.707106781186547,-0.707106781186548,0.)) ;
#117619 = DIRECTION('',(0.,0.,1.)) ;
#117620 = DIRECTION('',(0.577350269189625,-0.577350269189626,-0.577350269189626)) ;
#117621 = DIRECTION('',(0.,0.,-1.)) ;
#117622 = DIRECTION('',(-0.577350269189625,0.577350269189626,-0.577350269189626)) ;
#117623 = DIRECTION('center_axis',(1.95511867169517E-16,-1.,0.)) ;
#117624 = DIRECTION('ref_axis',(1.,1.95511867169517E-16,0.)) ;
#117625 = DIRECTION('',(0.,0.,-1.)) ;
#117626 = DIRECTION('',(-1.,-1.95511867169517E-16,0.)) ;
#117627 = DIRECTION('',(1.,1.95511867169517E-16,0.)) ;
#117628 = DIRECTION('center_axis',(1.06642836637918E-16,1.,0.)) ;
#117629 = DIRECTION('ref_axis',(-1.,1.06642836637918E-16,0.)) ;
#117630 = DIRECTION('',(1.,-1.06642836637919E-16,0.)) ;
#117631 = DIRECTION('',(0.,0.,1.)) ;
#117632 = DIRECTION('',(-1.,1.06642836637919E-16,0.)) ;
#117633 = DIRECTION('center_axis',(-0.707106781186548,0.707106781186547,0.)) ;
#117634 = DIRECTION('ref_axis',(-0.707106781186547,-0.707106781186548,0.)) ;
#117635 = DIRECTION('',(0.,0.,1.)) ;
#117636 = DIRECTION('',(-0.577350269189625,-0.577350269189626,0.577350269189627)) ;
#117637 = DIRECTION('',(0.,0.,-1.)) ;
#117638 = DIRECTION('',(0.577350269189625,0.577350269189626,0.577350269189627)) ;
#117639 = DIRECTION('center_axis',(-1.,0.,0.)) ;
#117640 = DIRECTION('ref_axis',(0.,0.,1.)) ;
#117641 = DIRECTION('',(0.,0.,-1.)) ;
#117642 = DIRECTION('',(0.,1.,1.95511867169518E-16)) ;
#117643 = DIRECTION('',(0.,0.,1.)) ;
#117644 = DIRECTION('',(0.,-1.,1.95511867169518E-16)) ;
#117645 = DIRECTION('center_axis',(0.,0.,1.)) ;
#117646 = DIRECTION('ref_axis',(1.,0.,0.)) ;
#117647 = DIRECTION('',(-1.95511867169517E-16,1.,0.)) ;
#117648 = DIRECTION('',(-1.,-1.95511867169517E-16,0.)) ;
#117649 = DIRECTION('',(1.,-1.06642836637919E-16,0.)) ;
#117650 = DIRECTION('center_axis',(0.,0.,1.)) ;
#117651 = DIRECTION('ref_axis',(1.,0.,0.)) ;
#117652 = DIRECTION('',(1.,1.95511867169517E-16,0.)) ;
#117653 = DIRECTION('',(1.95511867169517E-16,-1.,0.)) ;
#117654 = DIRECTION('',(-1.,1.06642836637919E-16,0.)) ;
#117655 = DIRECTION('center_axis',(1.,-9.85638338623186E-18,0.)) ;
#117656 = DIRECTION('ref_axis',(9.85638338623186E-18,1.,0.)) ;
#117657 = DIRECTION('',(0.,0.,-1.)) ;
#117658 = DIRECTION('',(-9.85638338623186E-18,-1.,0.)) ;
#117659 = DIRECTION('',(0.,0.,1.)) ;
#117660 = DIRECTION('',(9.85638338623186E-18,1.,0.)) ;
#117661 = DIRECTION('center_axis',(0.707106781186548,0.707106781186548,0.)) ;
#117662 = DIRECTION('ref_axis',(-0.707106781186548,0.707106781186548,0.)) ;
#117663 = DIRECTION('',(0.,0.,1.)) ;
#117664 = DIRECTION('',(-0.577350269189625,0.577350269189625,0.577350269189627)) ;
#117665 = DIRECTION('',(0.,0.,-1.)) ;
#117666 = DIRECTION('',(0.577350269189625,-0.577350269189625,0.577350269189627)) ;
#117667 = DIRECTION('center_axis',(0.,1.,0.)) ;
#117668 = DIRECTION('ref_axis',(0.,0.,1.)) ;
#117669 = DIRECTION('',(0.,0.,1.)) ;
#117670 = DIRECTION('',(-1.,0.,-9.8563833862319E-18)) ;
#117671 = DIRECTION('',(0.,0.,-1.)) ;
#117672 = DIRECTION('',(1.,0.,-9.8563833862319E-18)) ;
#117673 = DIRECTION('center_axis',(-0.707106781186548,0.707106781186548,0.)) ;
#117674 = DIRECTION('ref_axis',(-0.707106781186548,-0.707106781186548,0.)) ;
#117675 = DIRECTION('',(0.,0.,1.)) ;
#117676 = DIRECTION('',(-0.577350269189625,-0.577350269189625,-0.577350269189627)) ;
#117677 = DIRECTION('',(0.,0.,-1.)) ;
#117678 = DIRECTION('',(0.577350269189625,0.577350269189625,-0.577350269189627)) ;
#117679 = DIRECTION('center_axis',(-1.,9.85638338623186E-18,0.)) ;
#117680 = DIRECTION('ref_axis',(-9.85638338623186E-18,-1.,0.)) ;
#117681 = DIRECTION('',(0.,0.,-1.)) ;
#117682 = DIRECTION('',(9.85638338623186E-18,1.,0.)) ;
#117683 = DIRECTION('',(0.,0.,-1.)) ;
#117684 = DIRECTION('',(-9.85638338623186E-18,-1.,0.)) ;
#117685 = DIRECTION('center_axis',(0.,0.,1.)) ;
#117686 = DIRECTION('ref_axis',(1.,0.,0.)) ;
#117687 = DIRECTION('',(9.85638338623186E-18,1.,0.)) ;
#117688 = DIRECTION('center_axis',(0.,0.,-1.)) ;
#117689 = DIRECTION('ref_axis',(1.,0.,0.)) ;
#117690 = DIRECTION('center_axis',(0.,0.,1.)) ;
#117691 = DIRECTION('ref_axis',(1.,0.,0.)) ;
#117692 = DIRECTION('',(-9.85638338623186E-18,-1.,0.)) ;
#117693 = DIRECTION('',(1.,-9.85638338623186E-18,0.)) ;
#117694 = DIRECTION('center_axis',(0.,0.,1.)) ;
#117695 = DIRECTION('ref_axis',(1.,0.,0.)) ;
#117696 = DIRECTION('',(9.85638338623186E-18,1.,0.)) ;
#117697 = DIRECTION('center_axis',(0.,0.,-1.)) ;
#117698 = DIRECTION('ref_axis',(1.,0.,0.)) ;
#117699 = DIRECTION('center_axis',(0.,0.,1.)) ;
#117700 = DIRECTION('ref_axis',(1.,0.,0.)) ;
#117701 = DIRECTION('',(-9.85638338623186E-18,-1.,0.)) ;
#117702 = DIRECTION('',(-1.,9.85638338623186E-18,0.)) ;
#117703 = DIRECTION('center_axis',(0.,0.,-1.)) ;
#117704 = DIRECTION('ref_axis',(-1.,0.,0.)) ;
#117705 = DIRECTION('center_axis',(0.,0.,1.)) ;
#117706 = DIRECTION('ref_axis',(1.,0.,0.)) ;
#117707 = DIRECTION('center_axis',(0.,0.,-1.)) ;
#117708 = DIRECTION('ref_axis',(1.,0.,0.)) ;
#117709 = DIRECTION('center_axis',(0.,0.,-1.)) ;
#117710 = DIRECTION('ref_axis',(-1.,0.,0.)) ;
#117711 = DIRECTION('center_axis',(0.,0.,-1.)) ;
#117712 = DIRECTION('ref_axis',(1.,0.,0.)) ;
#117713 = DIRECTION('center_axis',(0.,0.,1.)) ;
#117714 = DIRECTION('ref_axis',(1.,0.,0.)) ;
#117715 = DIRECTION('center_axis',(-0.707106781186548,-0.707106781186547,
0.)) ;
#117716 = DIRECTION('ref_axis',(0.707106781186547,-0.707106781186548,0.)) ;
#117717 = DIRECTION('',(0.,0.,1.)) ;
#117718 = DIRECTION('',(0.577350269189625,-0.577350269189626,-0.577350269189626)) ;
#117719 = DIRECTION('',(0.,0.,-1.)) ;
#117720 = DIRECTION('',(-0.577350269189625,0.577350269189626,-0.577350269189626)) ;
#117721 = DIRECTION('center_axis',(1.95511867169517E-16,-1.,0.)) ;
#117722 = DIRECTION('ref_axis',(1.,1.95511867169517E-16,0.)) ;
#117723 = DIRECTION('',(0.,0.,-1.)) ;
#117724 = DIRECTION('',(-1.,-1.95511867169517E-16,0.)) ;
#117725 = DIRECTION('',(1.,1.95511867169517E-16,0.)) ;
#117726 = DIRECTION('center_axis',(1.06642836637918E-16,1.,0.)) ;
#117727 = DIRECTION('ref_axis',(-1.,1.06642836637918E-16,0.)) ;
#117728 = DIRECTION('',(1.,-1.06642836637919E-16,0.)) ;
#117729 = DIRECTION('',(0.,0.,1.)) ;
#117730 = DIRECTION('',(-1.,1.06642836637919E-16,0.)) ;
#117731 = DIRECTION('center_axis',(-0.707106781186548,0.707106781186547,0.)) ;
#117732 = DIRECTION('ref_axis',(-0.707106781186547,-0.707106781186548,0.)) ;
#117733 = DIRECTION('',(0.,0.,1.)) ;
#117734 = DIRECTION('',(-0.577350269189625,-0.577350269189626,0.577350269189627)) ;
#117735 = DIRECTION('',(0.,0.,-1.)) ;
#117736 = DIRECTION('',(0.577350269189625,0.577350269189626,0.577350269189627)) ;
#117737 = DIRECTION('center_axis',(-1.,0.,0.)) ;
#117738 = DIRECTION('ref_axis',(0.,0.,1.)) ;
#117739 = DIRECTION('',(0.,0.,-1.)) ;
#117740 = DIRECTION('',(0.,1.,1.95511867169518E-16)) ;
#117741 = DIRECTION('',(0.,0.,1.)) ;
#117742 = DIRECTION('',(0.,-1.,1.95511867169518E-16)) ;
#117743 = DIRECTION('center_axis',(0.,0.,1.)) ;
#117744 = DIRECTION('ref_axis',(1.,0.,0.)) ;
#117745 = DIRECTION('',(-1.95511867169517E-16,1.,0.)) ;
#117746 = DIRECTION('',(-1.,-1.95511867169517E-16,0.)) ;
#117747 = DIRECTION('',(1.,-1.06642836637919E-16,0.)) ;
#117748 = DIRECTION('center_axis',(0.,0.,1.)) ;
#117749 = DIRECTION('ref_axis',(1.,0.,0.)) ;
#117750 = DIRECTION('',(1.,1.95511867169517E-16,0.)) ;
#117751 = DIRECTION('',(1.95511867169517E-16,-1.,0.)) ;
#117752 = DIRECTION('',(-1.,1.06642836637919E-16,0.)) ;
#117753 = DIRECTION('center_axis',(1.,-9.85638338623186E-18,0.)) ;
#117754 = DIRECTION('ref_axis',(9.85638338623186E-18,1.,0.)) ;
#117755 = DIRECTION('',(0.,0.,-1.)) ;
#117756 = DIRECTION('',(-9.85638338623186E-18,-1.,0.)) ;
#117757 = DIRECTION('',(0.,0.,1.)) ;
#117758 = DIRECTION('',(9.85638338623186E-18,1.,0.)) ;
#117759 = DIRECTION('center_axis',(0.707106781186548,0.707106781186548,0.)) ;
#117760 = DIRECTION('ref_axis',(-0.707106781186548,0.707106781186548,0.)) ;
#117761 = DIRECTION('',(0.,0.,1.)) ;
#117762 = DIRECTION('',(-0.577350269189625,0.577350269189625,0.577350269189627)) ;
#117763 = DIRECTION('',(0.,0.,-1.)) ;
#117764 = DIRECTION('',(0.577350269189625,-0.577350269189625,0.577350269189627)) ;
#117765 = DIRECTION('center_axis',(0.,1.,0.)) ;
#117766 = DIRECTION('ref_axis',(0.,0.,1.)) ;
#117767 = DIRECTION('',(0.,0.,1.)) ;
#117768 = DIRECTION('',(-1.,0.,-9.8563833862319E-18)) ;
#117769 = DIRECTION('',(0.,0.,-1.)) ;
#117770 = DIRECTION('',(1.,0.,-9.8563833862319E-18)) ;
#117771 = DIRECTION('center_axis',(-0.707106781186548,0.707106781186548,0.)) ;
#117772 = DIRECTION('ref_axis',(-0.707106781186548,-0.707106781186548,0.)) ;
#117773 = DIRECTION('',(0.,0.,1.)) ;
#117774 = DIRECTION('',(-0.577350269189625,-0.577350269189625,-0.577350269189627)) ;
#117775 = DIRECTION('',(0.,0.,-1.)) ;
#117776 = DIRECTION('',(0.577350269189625,0.577350269189625,-0.577350269189627)) ;
#117777 = DIRECTION('center_axis',(-1.,9.85638338623186E-18,0.)) ;
#117778 = DIRECTION('ref_axis',(-9.85638338623186E-18,-1.,0.)) ;
#117779 = DIRECTION('',(0.,0.,-1.)) ;
#117780 = DIRECTION('',(9.85638338623186E-18,1.,0.)) ;
#117781 = DIRECTION('',(0.,0.,-1.)) ;
#117782 = DIRECTION('',(-9.85638338623186E-18,-1.,0.)) ;
#117783 = DIRECTION('center_axis',(0.,0.,1.)) ;
#117784 = DIRECTION('ref_axis',(1.,0.,0.)) ;
#117785 = DIRECTION('',(9.85638338623186E-18,1.,0.)) ;
#117786 = DIRECTION('center_axis',(0.,0.,-1.)) ;
#117787 = DIRECTION('ref_axis',(1.,0.,0.)) ;
#117788 = DIRECTION('center_axis',(0.,0.,1.)) ;
#117789 = DIRECTION('ref_axis',(1.,0.,0.)) ;
#117790 = DIRECTION('',(-9.85638338623186E-18,-1.,0.)) ;
#117791 = DIRECTION('',(1.,-9.85638338623186E-18,0.)) ;
#117792 = DIRECTION('center_axis',(0.,0.,1.)) ;
#117793 = DIRECTION('ref_axis',(1.,0.,0.)) ;
#117794 = DIRECTION('',(9.85638338623186E-18,1.,0.)) ;
#117795 = DIRECTION('center_axis',(0.,0.,-1.)) ;
#117796 = DIRECTION('ref_axis',(1.,0.,0.)) ;
#117797 = DIRECTION('center_axis',(0.,0.,1.)) ;
#117798 = DIRECTION('ref_axis',(1.,0.,0.)) ;
#117799 = DIRECTION('',(-9.85638338623186E-18,-1.,0.)) ;
#117800 = DIRECTION('',(-1.,9.85638338623186E-18,0.)) ;
#117801 = DIRECTION('center_axis',(0.,0.,-1.)) ;
#117802 = DIRECTION('ref_axis',(-1.,0.,0.)) ;
#117803 = DIRECTION('center_axis',(0.,0.,1.)) ;
#117804 = DIRECTION('ref_axis',(1.,0.,0.)) ;
#117805 = DIRECTION('center_axis',(0.,0.,-1.)) ;
#117806 = DIRECTION('ref_axis',(1.,0.,0.)) ;
#117807 = DIRECTION('center_axis',(0.,0.,-1.)) ;
#117808 = DIRECTION('ref_axis',(-1.,0.,0.)) ;
#117809 = DIRECTION('center_axis',(0.,0.,-1.)) ;
#117810 = DIRECTION('ref_axis',(1.,0.,0.)) ;
#117811 = DIRECTION('center_axis',(0.,0.,1.)) ;
#117812 = DIRECTION('ref_axis',(1.,0.,0.)) ;
#117813 = DIRECTION('center_axis',(-0.707106781186548,-0.707106781186547,
0.)) ;
#117814 = DIRECTION('ref_axis',(0.707106781186547,-0.707106781186548,0.)) ;
#117815 = DIRECTION('',(0.,0.,1.)) ;
#117816 = DIRECTION('',(0.577350269189625,-0.577350269189626,-0.577350269189626)) ;
#117817 = DIRECTION('',(0.,0.,-1.)) ;
#117818 = DIRECTION('',(-0.577350269189625,0.577350269189626,-0.577350269189626)) ;
#117819 = DIRECTION('center_axis',(1.95511867169517E-16,-1.,0.)) ;
#117820 = DIRECTION('ref_axis',(1.,1.95511867169517E-16,0.)) ;
#117821 = DIRECTION('',(0.,0.,-1.)) ;
#117822 = DIRECTION('',(-1.,-1.95511867169517E-16,0.)) ;
#117823 = DIRECTION('',(1.,1.95511867169517E-16,0.)) ;
#117824 = DIRECTION('center_axis',(1.06642836637918E-16,1.,0.)) ;
#117825 = DIRECTION('ref_axis',(-1.,1.06642836637918E-16,0.)) ;
#117826 = DIRECTION('',(1.,-1.06642836637919E-16,0.)) ;
#117827 = DIRECTION('',(0.,0.,1.)) ;
#117828 = DIRECTION('',(-1.,1.06642836637919E-16,0.)) ;
#117829 = DIRECTION('center_axis',(-0.707106781186548,0.707106781186547,0.)) ;
#117830 = DIRECTION('ref_axis',(-0.707106781186547,-0.707106781186548,0.)) ;
#117831 = DIRECTION('',(0.,0.,1.)) ;
#117832 = DIRECTION('',(-0.577350269189625,-0.577350269189626,0.577350269189627)) ;
#117833 = DIRECTION('',(0.,0.,-1.)) ;
#117834 = DIRECTION('',(0.577350269189625,0.577350269189626,0.577350269189627)) ;
#117835 = DIRECTION('center_axis',(-1.,0.,0.)) ;
#117836 = DIRECTION('ref_axis',(0.,0.,1.)) ;
#117837 = DIRECTION('',(0.,0.,-1.)) ;
#117838 = DIRECTION('',(0.,1.,1.95511867169518E-16)) ;
#117839 = DIRECTION('',(0.,0.,1.)) ;
#117840 = DIRECTION('',(0.,-1.,1.95511867169518E-16)) ;
#117841 = DIRECTION('center_axis',(0.,0.,1.)) ;
#117842 = DIRECTION('ref_axis',(1.,0.,0.)) ;
#117843 = DIRECTION('',(-1.95511867169517E-16,1.,0.)) ;
#117844 = DIRECTION('',(-1.,-1.95511867169517E-16,0.)) ;
#117845 = DIRECTION('',(1.,-1.06642836637919E-16,0.)) ;
#117846 = DIRECTION('center_axis',(0.,0.,1.)) ;
#117847 = DIRECTION('ref_axis',(1.,0.,0.)) ;
#117848 = DIRECTION('',(1.,1.95511867169517E-16,0.)) ;
#117849 = DIRECTION('',(1.95511867169517E-16,-1.,0.)) ;
#117850 = DIRECTION('',(-1.,1.06642836637919E-16,0.)) ;
#117851 = DIRECTION('center_axis',(1.,-9.85638338623186E-18,0.)) ;
#117852 = DIRECTION('ref_axis',(9.85638338623186E-18,1.,0.)) ;
#117853 = DIRECTION('',(0.,0.,-1.)) ;
#117854 = DIRECTION('',(-9.85638338623186E-18,-1.,0.)) ;
#117855 = DIRECTION('',(0.,0.,1.)) ;
#117856 = DIRECTION('',(9.85638338623186E-18,1.,0.)) ;
#117857 = DIRECTION('center_axis',(0.707106781186548,0.707106781186548,0.)) ;
#117858 = DIRECTION('ref_axis',(-0.707106781186548,0.707106781186548,0.)) ;
#117859 = DIRECTION('',(0.,0.,1.)) ;
#117860 = DIRECTION('',(-0.577350269189625,0.577350269189625,0.577350269189627)) ;
#117861 = DIRECTION('',(0.,0.,-1.)) ;
#117862 = DIRECTION('',(0.577350269189625,-0.577350269189625,0.577350269189627)) ;
#117863 = DIRECTION('center_axis',(0.,1.,0.)) ;
#117864 = DIRECTION('ref_axis',(0.,0.,1.)) ;
#117865 = DIRECTION('',(0.,0.,1.)) ;
#117866 = DIRECTION('',(-1.,0.,-9.8563833862319E-18)) ;
#117867 = DIRECTION('',(0.,0.,-1.)) ;
#117868 = DIRECTION('',(1.,0.,-9.8563833862319E-18)) ;
#117869 = DIRECTION('center_axis',(-0.707106781186548,0.707106781186548,0.)) ;
#117870 = DIRECTION('ref_axis',(-0.707106781186548,-0.707106781186548,0.)) ;
#117871 = DIRECTION('',(0.,0.,1.)) ;
#117872 = DIRECTION('',(-0.577350269189625,-0.577350269189625,-0.577350269189627)) ;
#117873 = DIRECTION('',(0.,0.,-1.)) ;
#117874 = DIRECTION('',(0.577350269189625,0.577350269189625,-0.577350269189627)) ;
#117875 = DIRECTION('center_axis',(-1.,9.85638338623186E-18,0.)) ;
#117876 = DIRECTION('ref_axis',(-9.85638338623186E-18,-1.,0.)) ;
#117877 = DIRECTION('',(0.,0.,-1.)) ;
#117878 = DIRECTION('',(9.85638338623186E-18,1.,0.)) ;
#117879 = DIRECTION('',(0.,0.,-1.)) ;
#117880 = DIRECTION('',(-9.85638338623186E-18,-1.,0.)) ;
#117881 = DIRECTION('center_axis',(0.,0.,1.)) ;
#117882 = DIRECTION('ref_axis',(1.,0.,0.)) ;
#117883 = DIRECTION('',(9.85638338623186E-18,1.,0.)) ;
#117884 = DIRECTION('center_axis',(0.,0.,-1.)) ;
#117885 = DIRECTION('ref_axis',(1.,0.,0.)) ;
#117886 = DIRECTION('center_axis',(0.,0.,1.)) ;
#117887 = DIRECTION('ref_axis',(1.,0.,0.)) ;
#117888 = DIRECTION('',(-9.85638338623186E-18,-1.,0.)) ;
#117889 = DIRECTION('',(1.,-9.85638338623186E-18,0.)) ;
#117890 = DIRECTION('center_axis',(0.,0.,1.)) ;
#117891 = DIRECTION('ref_axis',(1.,0.,0.)) ;
#117892 = DIRECTION('',(9.85638338623186E-18,1.,0.)) ;
#117893 = DIRECTION('center_axis',(0.,0.,-1.)) ;
#117894 = DIRECTION('ref_axis',(1.,0.,0.)) ;
#117895 = DIRECTION('center_axis',(0.,0.,1.)) ;
#117896 = DIRECTION('ref_axis',(1.,0.,0.)) ;
#117897 = DIRECTION('',(-9.85638338623186E-18,-1.,0.)) ;
#117898 = DIRECTION('',(-1.,9.85638338623186E-18,0.)) ;
#117899 = DIRECTION('center_axis',(0.,0.,-1.)) ;
#117900 = DIRECTION('ref_axis',(-1.,0.,0.)) ;
#117901 = DIRECTION('center_axis',(0.,0.,1.)) ;
#117902 = DIRECTION('ref_axis',(1.,0.,0.)) ;
#117903 = DIRECTION('center_axis',(0.,0.,-1.)) ;
#117904 = DIRECTION('ref_axis',(1.,0.,0.)) ;
#117905 = DIRECTION('center_axis',(0.,0.,-1.)) ;
#117906 = DIRECTION('ref_axis',(-1.,0.,0.)) ;
#117907 = DIRECTION('center_axis',(0.,0.,-1.)) ;
#117908 = DIRECTION('ref_axis',(1.,0.,0.)) ;
#117909 = DIRECTION('center_axis',(0.,0.,1.)) ;
#117910 = DIRECTION('ref_axis',(1.,0.,0.)) ;
#117911 = DIRECTION('center_axis',(-0.707106781186548,-0.707106781186547,
0.)) ;
#117912 = DIRECTION('ref_axis',(0.707106781186547,-0.707106781186548,0.)) ;
#117913 = DIRECTION('',(0.,0.,1.)) ;
#117914 = DIRECTION('',(0.577350269189625,-0.577350269189626,-0.577350269189626)) ;
#117915 = DIRECTION('',(0.,0.,-1.)) ;
#117916 = DIRECTION('',(-0.577350269189625,0.577350269189626,-0.577350269189626)) ;
#117917 = DIRECTION('center_axis',(1.95511867169517E-16,-1.,0.)) ;
#117918 = DIRECTION('ref_axis',(1.,1.95511867169517E-16,0.)) ;
#117919 = DIRECTION('',(0.,0.,-1.)) ;
#117920 = DIRECTION('',(-1.,-1.95511867169517E-16,0.)) ;
#117921 = DIRECTION('',(1.,1.95511867169517E-16,0.)) ;
#117922 = DIRECTION('center_axis',(1.06642836637918E-16,1.,0.)) ;
#117923 = DIRECTION('ref_axis',(-1.,1.06642836637918E-16,0.)) ;
#117924 = DIRECTION('',(1.,-1.06642836637919E-16,0.)) ;
#117925 = DIRECTION('',(0.,0.,1.)) ;
#117926 = DIRECTION('',(-1.,1.06642836637919E-16,0.)) ;
#117927 = DIRECTION('center_axis',(-0.707106781186548,0.707106781186547,0.)) ;
#117928 = DIRECTION('ref_axis',(-0.707106781186547,-0.707106781186548,0.)) ;
#117929 = DIRECTION('',(0.,0.,1.)) ;
#117930 = DIRECTION('',(-0.577350269189625,-0.577350269189626,0.577350269189627)) ;
#117931 = DIRECTION('',(0.,0.,-1.)) ;
#117932 = DIRECTION('',(0.577350269189625,0.577350269189626,0.577350269189627)) ;
#117933 = DIRECTION('center_axis',(-1.,0.,0.)) ;
#117934 = DIRECTION('ref_axis',(0.,0.,1.)) ;
#117935 = DIRECTION('',(0.,0.,-1.)) ;
#117936 = DIRECTION('',(0.,1.,1.95511867169518E-16)) ;
#117937 = DIRECTION('',(0.,0.,1.)) ;
#117938 = DIRECTION('',(0.,-1.,1.95511867169518E-16)) ;
#117939 = DIRECTION('center_axis',(0.,0.,1.)) ;
#117940 = DIRECTION('ref_axis',(1.,0.,0.)) ;
#117941 = DIRECTION('',(-1.95511867169517E-16,1.,0.)) ;
#117942 = DIRECTION('',(-1.,-1.95511867169517E-16,0.)) ;
#117943 = DIRECTION('',(1.,-1.06642836637919E-16,0.)) ;
#117944 = DIRECTION('center_axis',(0.,0.,1.)) ;
#117945 = DIRECTION('ref_axis',(1.,0.,0.)) ;
#117946 = DIRECTION('',(1.,1.95511867169517E-16,0.)) ;
#117947 = DIRECTION('',(1.95511867169517E-16,-1.,0.)) ;
#117948 = DIRECTION('',(-1.,1.06642836637919E-16,0.)) ;
#117949 = DIRECTION('center_axis',(1.,-9.85638338623186E-18,0.)) ;
#117950 = DIRECTION('ref_axis',(9.85638338623186E-18,1.,0.)) ;
#117951 = DIRECTION('',(0.,0.,-1.)) ;
#117952 = DIRECTION('',(-9.85638338623186E-18,-1.,0.)) ;
#117953 = DIRECTION('',(0.,0.,1.)) ;
#117954 = DIRECTION('',(9.85638338623186E-18,1.,0.)) ;
#117955 = DIRECTION('center_axis',(0.707106781186548,0.707106781186548,0.)) ;
#117956 = DIRECTION('ref_axis',(-0.707106781186548,0.707106781186548,0.)) ;
#117957 = DIRECTION('',(0.,0.,1.)) ;
#117958 = DIRECTION('',(-0.577350269189625,0.577350269189625,0.577350269189627)) ;
#117959 = DIRECTION('',(0.,0.,-1.)) ;
#117960 = DIRECTION('',(0.577350269189625,-0.577350269189625,0.577350269189627)) ;
#117961 = DIRECTION('center_axis',(0.,1.,0.)) ;
#117962 = DIRECTION('ref_axis',(0.,0.,1.)) ;
#117963 = DIRECTION('',(0.,0.,1.)) ;
#117964 = DIRECTION('',(-1.,0.,-9.8563833862319E-18)) ;
#117965 = DIRECTION('',(0.,0.,-1.)) ;
#117966 = DIRECTION('',(1.,0.,-9.8563833862319E-18)) ;
#117967 = DIRECTION('center_axis',(-0.707106781186548,0.707106781186548,0.)) ;
#117968 = DIRECTION('ref_axis',(-0.707106781186548,-0.707106781186548,0.)) ;
#117969 = DIRECTION('',(0.,0.,1.)) ;
#117970 = DIRECTION('',(-0.577350269189625,-0.577350269189625,-0.577350269189627)) ;
#117971 = DIRECTION('',(0.,0.,-1.)) ;
#117972 = DIRECTION('',(0.577350269189625,0.577350269189625,-0.577350269189627)) ;
#117973 = DIRECTION('center_axis',(-1.,9.85638338623186E-18,0.)) ;
#117974 = DIRECTION('ref_axis',(-9.85638338623186E-18,-1.,0.)) ;
#117975 = DIRECTION('',(0.,0.,-1.)) ;
#117976 = DIRECTION('',(9.85638338623186E-18,1.,0.)) ;
#117977 = DIRECTION('',(0.,0.,-1.)) ;
#117978 = DIRECTION('',(-9.85638338623186E-18,-1.,0.)) ;
#117979 = DIRECTION('center_axis',(0.,0.,1.)) ;
#117980 = DIRECTION('ref_axis',(1.,0.,0.)) ;
#117981 = DIRECTION('',(9.85638338623186E-18,1.,0.)) ;
#117982 = DIRECTION('center_axis',(0.,0.,-1.)) ;
#117983 = DIRECTION('ref_axis',(1.,0.,0.)) ;
#117984 = DIRECTION('center_axis',(0.,0.,1.)) ;
#117985 = DIRECTION('ref_axis',(1.,0.,0.)) ;
#117986 = DIRECTION('',(-9.85638338623186E-18,-1.,0.)) ;
#117987 = DIRECTION('',(1.,-9.85638338623186E-18,0.)) ;
#117988 = DIRECTION('center_axis',(0.,0.,1.)) ;
#117989 = DIRECTION('ref_axis',(1.,0.,0.)) ;
#117990 = DIRECTION('',(9.85638338623186E-18,1.,0.)) ;
#117991 = DIRECTION('center_axis',(0.,0.,-1.)) ;
#117992 = DIRECTION('ref_axis',(1.,0.,0.)) ;
#117993 = DIRECTION('center_axis',(0.,0.,1.)) ;
#117994 = DIRECTION('ref_axis',(1.,0.,0.)) ;
#117995 = DIRECTION('',(-9.85638338623186E-18,-1.,0.)) ;
#117996 = DIRECTION('',(-1.,9.85638338623186E-18,0.)) ;
#117997 = DIRECTION('center_axis',(0.,0.,-1.)) ;
#117998 = DIRECTION('ref_axis',(-1.,0.,0.)) ;
#117999 = DIRECTION('center_axis',(0.,0.,1.)) ;
#118000 = DIRECTION('ref_axis',(1.,0.,0.)) ;
#118001 = DIRECTION('center_axis',(0.,0.,-1.)) ;
#118002 = DIRECTION('ref_axis',(1.,0.,0.)) ;
#118003 = DIRECTION('center_axis',(0.,0.,-1.)) ;
#118004 = DIRECTION('ref_axis',(-1.,0.,0.)) ;
#118005 = DIRECTION('center_axis',(0.,0.,-1.)) ;
#118006 = DIRECTION('ref_axis',(1.,0.,0.)) ;
#118007 = DIRECTION('center_axis',(0.,0.,1.)) ;
#118008 = DIRECTION('ref_axis',(1.,0.,0.)) ;
#118009 = DIRECTION('center_axis',(-0.707106781186548,-0.707106781186547,
0.)) ;
#118010 = DIRECTION('ref_axis',(0.707106781186547,-0.707106781186548,0.)) ;
#118011 = DIRECTION('',(0.,0.,1.)) ;
#118012 = DIRECTION('',(0.577350269189625,-0.577350269189626,-0.577350269189626)) ;
#118013 = DIRECTION('',(0.,0.,-1.)) ;
#118014 = DIRECTION('',(-0.577350269189625,0.577350269189626,-0.577350269189626)) ;
#118015 = DIRECTION('center_axis',(1.95511867169517E-16,-1.,0.)) ;
#118016 = DIRECTION('ref_axis',(1.,1.95511867169517E-16,0.)) ;
#118017 = DIRECTION('',(0.,0.,-1.)) ;
#118018 = DIRECTION('',(-1.,-1.95511867169517E-16,0.)) ;
#118019 = DIRECTION('',(1.,1.95511867169517E-16,0.)) ;
#118020 = DIRECTION('center_axis',(1.06642836637918E-16,1.,0.)) ;
#118021 = DIRECTION('ref_axis',(-1.,1.06642836637918E-16,0.)) ;
#118022 = DIRECTION('',(1.,-1.06642836637919E-16,0.)) ;
#118023 = DIRECTION('',(0.,0.,1.)) ;
#118024 = DIRECTION('',(-1.,1.06642836637919E-16,0.)) ;
#118025 = DIRECTION('center_axis',(-0.707106781186548,0.707106781186547,0.)) ;
#118026 = DIRECTION('ref_axis',(-0.707106781186547,-0.707106781186548,0.)) ;
#118027 = DIRECTION('',(0.,0.,1.)) ;
#118028 = DIRECTION('',(-0.577350269189625,-0.577350269189626,0.577350269189627)) ;
#118029 = DIRECTION('',(0.,0.,-1.)) ;
#118030 = DIRECTION('',(0.577350269189625,0.577350269189626,0.577350269189627)) ;
#118031 = DIRECTION('center_axis',(-1.,0.,0.)) ;
#118032 = DIRECTION('ref_axis',(0.,0.,1.)) ;
#118033 = DIRECTION('',(0.,0.,-1.)) ;
#118034 = DIRECTION('',(0.,1.,1.95511867169518E-16)) ;
#118035 = DIRECTION('',(0.,0.,1.)) ;
#118036 = DIRECTION('',(0.,-1.,1.95511867169518E-16)) ;
#118037 = DIRECTION('center_axis',(0.,0.,1.)) ;
#118038 = DIRECTION('ref_axis',(1.,0.,0.)) ;
#118039 = DIRECTION('',(-1.95511867169517E-16,1.,0.)) ;
#118040 = DIRECTION('',(-1.,-1.95511867169517E-16,0.)) ;
#118041 = DIRECTION('',(1.,-1.06642836637919E-16,0.)) ;
#118042 = DIRECTION('center_axis',(0.,0.,1.)) ;
#118043 = DIRECTION('ref_axis',(1.,0.,0.)) ;
#118044 = DIRECTION('',(1.,1.95511867169517E-16,0.)) ;
#118045 = DIRECTION('',(1.95511867169517E-16,-1.,0.)) ;
#118046 = DIRECTION('',(-1.,1.06642836637919E-16,0.)) ;
#118047 = DIRECTION('center_axis',(1.,-9.85638338623186E-18,0.)) ;
#118048 = DIRECTION('ref_axis',(9.85638338623186E-18,1.,0.)) ;
#118049 = DIRECTION('',(0.,0.,-1.)) ;
#118050 = DIRECTION('',(-9.85638338623186E-18,-1.,0.)) ;
#118051 = DIRECTION('',(0.,0.,1.)) ;
#118052 = DIRECTION('',(9.85638338623186E-18,1.,0.)) ;
#118053 = DIRECTION('center_axis',(0.707106781186548,0.707106781186548,0.)) ;
#118054 = DIRECTION('ref_axis',(-0.707106781186548,0.707106781186548,0.)) ;
#118055 = DIRECTION('',(0.,0.,1.)) ;
#118056 = DIRECTION('',(-0.577350269189625,0.577350269189625,0.577350269189627)) ;
#118057 = DIRECTION('',(0.,0.,-1.)) ;
#118058 = DIRECTION('',(0.577350269189625,-0.577350269189625,0.577350269189627)) ;
#118059 = DIRECTION('center_axis',(0.,1.,0.)) ;
#118060 = DIRECTION('ref_axis',(0.,0.,1.)) ;
#118061 = DIRECTION('',(0.,0.,1.)) ;
#118062 = DIRECTION('',(-1.,0.,-9.8563833862319E-18)) ;
#118063 = DIRECTION('',(0.,0.,-1.)) ;
#118064 = DIRECTION('',(1.,0.,-9.8563833862319E-18)) ;
#118065 = DIRECTION('center_axis',(-0.707106781186548,0.707106781186548,0.)) ;
#118066 = DIRECTION('ref_axis',(-0.707106781186548,-0.707106781186548,0.)) ;
#118067 = DIRECTION('',(0.,0.,1.)) ;
#118068 = DIRECTION('',(-0.577350269189625,-0.577350269189625,-0.577350269189627)) ;
#118069 = DIRECTION('',(0.,0.,-1.)) ;
#118070 = DIRECTION('',(0.577350269189625,0.577350269189625,-0.577350269189627)) ;
#118071 = DIRECTION('center_axis',(-1.,9.85638338623186E-18,0.)) ;
#118072 = DIRECTION('ref_axis',(-9.85638338623186E-18,-1.,0.)) ;
#118073 = DIRECTION('',(0.,0.,-1.)) ;
#118074 = DIRECTION('',(9.85638338623186E-18,1.,0.)) ;
#118075 = DIRECTION('',(0.,0.,-1.)) ;
#118076 = DIRECTION('',(-9.85638338623186E-18,-1.,0.)) ;
#118077 = DIRECTION('center_axis',(0.,0.,1.)) ;
#118078 = DIRECTION('ref_axis',(1.,0.,0.)) ;
#118079 = DIRECTION('',(9.85638338623186E-18,1.,0.)) ;
#118080 = DIRECTION('center_axis',(0.,0.,-1.)) ;
#118081 = DIRECTION('ref_axis',(1.,0.,0.)) ;
#118082 = DIRECTION('center_axis',(0.,0.,1.)) ;
#118083 = DIRECTION('ref_axis',(1.,0.,0.)) ;
#118084 = DIRECTION('',(-9.85638338623186E-18,-1.,0.)) ;
#118085 = DIRECTION('',(1.,-9.85638338623186E-18,0.)) ;
#118086 = DIRECTION('center_axis',(0.,0.,1.)) ;
#118087 = DIRECTION('ref_axis',(1.,0.,0.)) ;
#118088 = DIRECTION('',(9.85638338623186E-18,1.,0.)) ;
#118089 = DIRECTION('center_axis',(0.,0.,-1.)) ;
#118090 = DIRECTION('ref_axis',(1.,0.,0.)) ;
#118091 = DIRECTION('center_axis',(0.,0.,1.)) ;
#118092 = DIRECTION('ref_axis',(1.,0.,0.)) ;
#118093 = DIRECTION('',(-9.85638338623186E-18,-1.,0.)) ;
#118094 = DIRECTION('',(-1.,9.85638338623186E-18,0.)) ;
#118095 = DIRECTION('center_axis',(0.,0.,-1.)) ;
#118096 = DIRECTION('ref_axis',(-1.,0.,0.)) ;
#118097 = DIRECTION('center_axis',(0.,0.,1.)) ;
#118098 = DIRECTION('ref_axis',(1.,0.,0.)) ;
#118099 = DIRECTION('center_axis',(0.,0.,-1.)) ;
#118100 = DIRECTION('ref_axis',(1.,0.,0.)) ;
#118101 = DIRECTION('center_axis',(0.,0.,-1.)) ;
#118102 = DIRECTION('ref_axis',(-1.,0.,0.)) ;
#118103 = DIRECTION('center_axis',(0.,0.,-1.)) ;
#118104 = DIRECTION('ref_axis',(1.,0.,0.)) ;
#118105 = DIRECTION('center_axis',(0.,0.,1.)) ;
#118106 = DIRECTION('ref_axis',(1.,0.,0.)) ;
#118107 = DIRECTION('center_axis',(-0.707106781186548,-0.707106781186547,
0.)) ;
#118108 = DIRECTION('ref_axis',(0.707106781186547,-0.707106781186548,0.)) ;
#118109 = DIRECTION('',(0.,0.,1.)) ;
#118110 = DIRECTION('',(0.577350269189625,-0.577350269189626,-0.577350269189626)) ;
#118111 = DIRECTION('',(0.,0.,-1.)) ;
#118112 = DIRECTION('',(-0.577350269189625,0.577350269189626,-0.577350269189626)) ;
#118113 = DIRECTION('center_axis',(1.95511867169517E-16,-1.,0.)) ;
#118114 = DIRECTION('ref_axis',(1.,1.95511867169517E-16,0.)) ;
#118115 = DIRECTION('',(0.,0.,-1.)) ;
#118116 = DIRECTION('',(-1.,-1.95511867169517E-16,0.)) ;
#118117 = DIRECTION('',(1.,1.95511867169517E-16,0.)) ;
#118118 = DIRECTION('center_axis',(1.06642836637918E-16,1.,0.)) ;
#118119 = DIRECTION('ref_axis',(-1.,1.06642836637918E-16,0.)) ;
#118120 = DIRECTION('',(1.,-1.06642836637919E-16,0.)) ;
#118121 = DIRECTION('',(0.,0.,1.)) ;
#118122 = DIRECTION('',(-1.,1.06642836637919E-16,0.)) ;
#118123 = DIRECTION('center_axis',(-0.707106781186548,0.707106781186547,0.)) ;
#118124 = DIRECTION('ref_axis',(-0.707106781186547,-0.707106781186548,0.)) ;
#118125 = DIRECTION('',(0.,0.,1.)) ;
#118126 = DIRECTION('',(-0.577350269189625,-0.577350269189626,0.577350269189627)) ;
#118127 = DIRECTION('',(0.,0.,-1.)) ;
#118128 = DIRECTION('',(0.577350269189625,0.577350269189626,0.577350269189627)) ;
#118129 = DIRECTION('center_axis',(-1.,0.,0.)) ;
#118130 = DIRECTION('ref_axis',(0.,0.,1.)) ;
#118131 = DIRECTION('',(0.,0.,-1.)) ;
#118132 = DIRECTION('',(0.,1.,1.95511867169518E-16)) ;
#118133 = DIRECTION('',(0.,0.,1.)) ;
#118134 = DIRECTION('',(0.,-1.,1.95511867169518E-16)) ;
#118135 = DIRECTION('center_axis',(0.,0.,1.)) ;
#118136 = DIRECTION('ref_axis',(1.,0.,0.)) ;
#118137 = DIRECTION('',(-1.95511867169517E-16,1.,0.)) ;
#118138 = DIRECTION('',(-1.,-1.95511867169517E-16,0.)) ;
#118139 = DIRECTION('',(1.,-1.06642836637919E-16,0.)) ;
#118140 = DIRECTION('center_axis',(0.,0.,1.)) ;
#118141 = DIRECTION('ref_axis',(1.,0.,0.)) ;
#118142 = DIRECTION('',(1.,1.95511867169517E-16,0.)) ;
#118143 = DIRECTION('',(1.95511867169517E-16,-1.,0.)) ;
#118144 = DIRECTION('',(-1.,1.06642836637919E-16,0.)) ;
#118145 = DIRECTION('center_axis',(1.,-9.85638338623186E-18,0.)) ;
#118146 = DIRECTION('ref_axis',(9.85638338623186E-18,1.,0.)) ;
#118147 = DIRECTION('',(0.,0.,-1.)) ;
#118148 = DIRECTION('',(-9.85638338623186E-18,-1.,0.)) ;
#118149 = DIRECTION('',(0.,0.,1.)) ;
#118150 = DIRECTION('',(9.85638338623186E-18,1.,0.)) ;
#118151 = DIRECTION('center_axis',(0.707106781186548,0.707106781186548,0.)) ;
#118152 = DIRECTION('ref_axis',(-0.707106781186548,0.707106781186548,0.)) ;
#118153 = DIRECTION('',(0.,0.,1.)) ;
#118154 = DIRECTION('',(-0.577350269189625,0.577350269189625,0.577350269189627)) ;
#118155 = DIRECTION('',(0.,0.,-1.)) ;
#118156 = DIRECTION('',(0.577350269189625,-0.577350269189625,0.577350269189627)) ;
#118157 = DIRECTION('center_axis',(0.,1.,0.)) ;
#118158 = DIRECTION('ref_axis',(0.,0.,1.)) ;
#118159 = DIRECTION('',(0.,0.,1.)) ;
#118160 = DIRECTION('',(-1.,0.,-9.8563833862319E-18)) ;
#118161 = DIRECTION('',(0.,0.,-1.)) ;
#118162 = DIRECTION('',(1.,0.,-9.8563833862319E-18)) ;
#118163 = DIRECTION('center_axis',(-0.707106781186548,0.707106781186548,0.)) ;
#118164 = DIRECTION('ref_axis',(-0.707106781186548,-0.707106781186548,0.)) ;
#118165 = DIRECTION('',(0.,0.,1.)) ;
#118166 = DIRECTION('',(-0.577350269189625,-0.577350269189625,-0.577350269189627)) ;
#118167 = DIRECTION('',(0.,0.,-1.)) ;
#118168 = DIRECTION('',(0.577350269189625,0.577350269189625,-0.577350269189627)) ;
#118169 = DIRECTION('center_axis',(-1.,9.85638338623186E-18,0.)) ;
#118170 = DIRECTION('ref_axis',(-9.85638338623186E-18,-1.,0.)) ;
#118171 = DIRECTION('',(0.,0.,-1.)) ;
#118172 = DIRECTION('',(9.85638338623186E-18,1.,0.)) ;
#118173 = DIRECTION('',(0.,0.,-1.)) ;
#118174 = DIRECTION('',(-9.85638338623186E-18,-1.,0.)) ;
#118175 = DIRECTION('center_axis',(0.,0.,1.)) ;
#118176 = DIRECTION('ref_axis',(1.,0.,0.)) ;
#118177 = DIRECTION('',(9.85638338623186E-18,1.,0.)) ;
#118178 = DIRECTION('center_axis',(0.,0.,-1.)) ;
#118179 = DIRECTION('ref_axis',(1.,0.,0.)) ;
#118180 = DIRECTION('center_axis',(0.,0.,1.)) ;
#118181 = DIRECTION('ref_axis',(1.,0.,0.)) ;
#118182 = DIRECTION('',(-9.85638338623186E-18,-1.,0.)) ;
#118183 = DIRECTION('',(1.,-9.85638338623186E-18,0.)) ;
#118184 = DIRECTION('center_axis',(0.,0.,1.)) ;
#118185 = DIRECTION('ref_axis',(1.,0.,0.)) ;
#118186 = DIRECTION('',(9.85638338623186E-18,1.,0.)) ;
#118187 = DIRECTION('center_axis',(0.,0.,-1.)) ;
#118188 = DIRECTION('ref_axis',(1.,0.,0.)) ;
#118189 = DIRECTION('center_axis',(0.,0.,1.)) ;
#118190 = DIRECTION('ref_axis',(1.,0.,0.)) ;
#118191 = DIRECTION('',(-9.85638338623186E-18,-1.,0.)) ;
#118192 = DIRECTION('',(-1.,9.85638338623186E-18,0.)) ;
#118193 = DIRECTION('center_axis',(0.,0.,-1.)) ;
#118194 = DIRECTION('ref_axis',(-1.,0.,0.)) ;
#118195 = DIRECTION('center_axis',(0.,0.,1.)) ;
#118196 = DIRECTION('ref_axis',(1.,0.,0.)) ;
#118197 = DIRECTION('center_axis',(0.,0.,-1.)) ;
#118198 = DIRECTION('ref_axis',(1.,0.,0.)) ;
#118199 = DIRECTION('center_axis',(0.,0.,-1.)) ;
#118200 = DIRECTION('ref_axis',(-1.,0.,0.)) ;
#118201 = DIRECTION('center_axis',(0.,0.,-1.)) ;
#118202 = DIRECTION('ref_axis',(1.,0.,0.)) ;
#118203 = DIRECTION('center_axis',(0.,0.,1.)) ;
#118204 = DIRECTION('ref_axis',(1.,0.,0.)) ;
#118205 = DIRECTION('center_axis',(-0.707106781186548,-0.707106781186547,
0.)) ;
#118206 = DIRECTION('ref_axis',(0.707106781186547,-0.707106781186548,0.)) ;
#118207 = DIRECTION('',(0.,0.,1.)) ;
#118208 = DIRECTION('',(0.577350269189625,-0.577350269189626,-0.577350269189626)) ;
#118209 = DIRECTION('',(0.,0.,-1.)) ;
#118210 = DIRECTION('',(-0.577350269189625,0.577350269189626,-0.577350269189626)) ;
#118211 = DIRECTION('center_axis',(1.95511867169517E-16,-1.,0.)) ;
#118212 = DIRECTION('ref_axis',(1.,1.95511867169517E-16,0.)) ;
#118213 = DIRECTION('',(0.,0.,-1.)) ;
#118214 = DIRECTION('',(-1.,-1.95511867169517E-16,0.)) ;
#118215 = DIRECTION('',(1.,1.95511867169517E-16,0.)) ;
#118216 = DIRECTION('center_axis',(1.06642836637918E-16,1.,0.)) ;
#118217 = DIRECTION('ref_axis',(-1.,1.06642836637918E-16,0.)) ;
#118218 = DIRECTION('',(1.,-1.06642836637919E-16,0.)) ;
#118219 = DIRECTION('',(0.,0.,1.)) ;
#118220 = DIRECTION('',(-1.,1.06642836637919E-16,0.)) ;
#118221 = DIRECTION('center_axis',(-0.707106781186548,0.707106781186547,0.)) ;
#118222 = DIRECTION('ref_axis',(-0.707106781186547,-0.707106781186548,0.)) ;
#118223 = DIRECTION('',(0.,0.,1.)) ;
#118224 = DIRECTION('',(-0.577350269189625,-0.577350269189626,0.577350269189627)) ;
#118225 = DIRECTION('',(0.,0.,-1.)) ;
#118226 = DIRECTION('',(0.577350269189625,0.577350269189626,0.577350269189627)) ;
#118227 = DIRECTION('center_axis',(-1.,0.,0.)) ;
#118228 = DIRECTION('ref_axis',(0.,0.,1.)) ;
#118229 = DIRECTION('',(0.,0.,-1.)) ;
#118230 = DIRECTION('',(0.,1.,1.95511867169518E-16)) ;
#118231 = DIRECTION('',(0.,0.,1.)) ;
#118232 = DIRECTION('',(0.,-1.,1.95511867169518E-16)) ;
#118233 = DIRECTION('center_axis',(0.,0.,1.)) ;
#118234 = DIRECTION('ref_axis',(1.,0.,0.)) ;
#118235 = DIRECTION('',(-1.95511867169517E-16,1.,0.)) ;
#118236 = DIRECTION('',(-1.,-1.95511867169517E-16,0.)) ;
#118237 = DIRECTION('',(1.,-1.06642836637919E-16,0.)) ;
#118238 = DIRECTION('center_axis',(0.,0.,1.)) ;
#118239 = DIRECTION('ref_axis',(1.,0.,0.)) ;
#118240 = DIRECTION('',(1.,1.95511867169517E-16,0.)) ;
#118241 = DIRECTION('',(1.95511867169517E-16,-1.,0.)) ;
#118242 = DIRECTION('',(-1.,1.06642836637919E-16,0.)) ;
#118243 = DIRECTION('center_axis',(6.96951553037899E-18,0.707106781186549,
0.707106781186546)) ;
#118244 = DIRECTION('ref_axis',(-8.6424177776148E-34,-0.707106781186546,0.707106781186549)) ;
#118245 = DIRECTION('',(-0.577350269189625,0.577350269189625,-0.577350269189627)) ;
#118246 = DIRECTION('',(1.,-9.85638338623186E-18,0.)) ;
#118247 = DIRECTION('',(-0.577350269189625,-0.577350269189625,0.577350269189627)) ;
#118248 = DIRECTION('',(-1.,7.70371977754894E-34,9.8563833862319E-18)) ;
#118249 = DIRECTION('center_axis',(6.96951553037899E-18,0.707106781186549,
-0.707106781186546)) ;
#118250 = DIRECTION('ref_axis',(8.6424177776148E-34,0.707106781186546,0.707106781186549)) ;
#118251 = DIRECTION('',(0.577350269189625,0.577350269189625,0.577350269189627)) ;
#118252 = DIRECTION('',(-1.,9.85638338623186E-18,0.)) ;
#118253 = DIRECTION('',(0.577350269189625,-0.577350269189625,-0.577350269189627)) ;
#118254 = DIRECTION('',(1.,-7.70371977754894E-34,9.8563833862319E-18)) ;
#118255 = DIRECTION('center_axis',(6.96951553037899E-18,0.707106781186549,
0.707106781186546)) ;
#118256 = DIRECTION('ref_axis',(-8.6424177776148E-34,-0.707106781186546,0.707106781186549)) ;
#118257 = DIRECTION('',(-0.577350269189625,0.577350269189625,-0.577350269189627)) ;
#118258 = DIRECTION('',(1.,-9.85638338623186E-18,0.)) ;
#118259 = DIRECTION('',(-0.577350269189625,-0.577350269189625,0.577350269189627)) ;
#118260 = DIRECTION('',(-1.,7.70371977754894E-34,9.8563833862319E-18)) ;
#118261 = DIRECTION('center_axis',(6.96951553037899E-18,0.707106781186549,
-0.707106781186546)) ;
#118262 = DIRECTION('ref_axis',(8.6424177776148E-34,0.707106781186546,0.707106781186549)) ;
#118263 = DIRECTION('',(0.577350269189625,0.577350269189625,0.577350269189627)) ;
#118264 = DIRECTION('',(-1.,9.85638338623186E-18,0.)) ;
#118265 = DIRECTION('',(0.577350269189625,-0.577350269189625,-0.577350269189627)) ;
#118266 = DIRECTION('',(1.,-7.70371977754894E-34,9.8563833862319E-18)) ;
#118267 = DIRECTION('center_axis',(6.96951553037899E-18,0.707106781186549,
0.707106781186546)) ;
#118268 = DIRECTION('ref_axis',(-8.6424177776148E-34,-0.707106781186546,0.707106781186549)) ;
#118269 = DIRECTION('',(-0.577350269189625,0.577350269189625,-0.577350269189627)) ;
#118270 = DIRECTION('',(1.,-9.85638338623186E-18,0.)) ;
#118271 = DIRECTION('',(-0.577350269189625,-0.577350269189625,0.577350269189627)) ;
#118272 = DIRECTION('',(-1.,7.70371977754894E-34,9.8563833862319E-18)) ;
#118273 = DIRECTION('center_axis',(6.96951553037899E-18,0.707106781186549,
-0.707106781186546)) ;
#118274 = DIRECTION('ref_axis',(8.6424177776148E-34,0.707106781186546,0.707106781186549)) ;
#118275 = DIRECTION('',(0.577350269189625,0.577350269189625,0.577350269189627)) ;
#118276 = DIRECTION('',(-1.,9.85638338623186E-18,0.)) ;
#118277 = DIRECTION('',(0.577350269189625,-0.577350269189625,-0.577350269189627)) ;
#118278 = DIRECTION('',(1.,-7.70371977754894E-34,9.8563833862319E-18)) ;
#118279 = DIRECTION('center_axis',(6.96951553037899E-18,0.707106781186549,
0.707106781186546)) ;
#118280 = DIRECTION('ref_axis',(-8.6424177776148E-34,-0.707106781186546,0.707106781186549)) ;
#118281 = DIRECTION('',(-0.577350269189625,0.577350269189625,-0.577350269189627)) ;
#118282 = DIRECTION('',(1.,-9.85638338623186E-18,0.)) ;
#118283 = DIRECTION('',(-0.577350269189625,-0.577350269189625,0.577350269189627)) ;
#118284 = DIRECTION('',(-1.,7.70371977754894E-34,9.8563833862319E-18)) ;
#118285 = DIRECTION('center_axis',(6.96951553037899E-18,0.707106781186549,
-0.707106781186546)) ;
#118286 = DIRECTION('ref_axis',(8.6424177776148E-34,0.707106781186546,0.707106781186549)) ;
#118287 = DIRECTION('',(0.577350269189625,0.577350269189625,0.577350269189627)) ;
#118288 = DIRECTION('',(-1.,9.85638338623186E-18,0.)) ;
#118289 = DIRECTION('',(0.577350269189625,-0.577350269189625,-0.577350269189627)) ;
#118290 = DIRECTION('',(1.,-7.70371977754894E-34,9.8563833862319E-18)) ;
#118291 = DIRECTION('center_axis',(6.96951553037899E-18,0.707106781186549,
0.707106781186546)) ;
#118292 = DIRECTION('ref_axis',(-8.6424177776148E-34,-0.707106781186546,0.707106781186549)) ;
#118293 = DIRECTION('',(-0.577350269189625,0.577350269189625,-0.577350269189627)) ;
#118294 = DIRECTION('',(1.,-9.85638338623186E-18,0.)) ;
#118295 = DIRECTION('',(-0.577350269189625,-0.577350269189625,0.577350269189627)) ;
#118296 = DIRECTION('',(-1.,7.70371977754894E-34,9.8563833862319E-18)) ;
#118297 = DIRECTION('center_axis',(6.96951553037899E-18,0.707106781186549,
-0.707106781186546)) ;
#118298 = DIRECTION('ref_axis',(8.6424177776148E-34,0.707106781186546,0.707106781186549)) ;
#118299 = DIRECTION('',(0.577350269189625,0.577350269189625,0.577350269189627)) ;
#118300 = DIRECTION('',(-1.,9.85638338623186E-18,0.)) ;
#118301 = DIRECTION('',(0.577350269189625,-0.577350269189625,-0.577350269189627)) ;
#118302 = DIRECTION('',(1.,-7.70371977754894E-34,9.8563833862319E-18)) ;
#118303 = DIRECTION('center_axis',(6.96951553037899E-18,0.707106781186549,
0.707106781186546)) ;
#118304 = DIRECTION('ref_axis',(-8.6424177776148E-34,-0.707106781186546,0.707106781186549)) ;
#118305 = DIRECTION('',(-0.577350269189625,0.577350269189625,-0.577350269189627)) ;
#118306 = DIRECTION('',(1.,-9.85638338623186E-18,0.)) ;
#118307 = DIRECTION('',(-0.577350269189625,-0.577350269189625,0.577350269189627)) ;
#118308 = DIRECTION('',(-1.,7.70371977754894E-34,9.8563833862319E-18)) ;
#118309 = DIRECTION('center_axis',(6.96951553037899E-18,0.707106781186549,
-0.707106781186546)) ;
#118310 = DIRECTION('ref_axis',(8.6424177776148E-34,0.707106781186546,0.707106781186549)) ;
#118311 = DIRECTION('',(0.577350269189625,0.577350269189625,0.577350269189627)) ;
#118312 = DIRECTION('',(-1.,9.85638338623186E-18,0.)) ;
#118313 = DIRECTION('',(0.577350269189625,-0.577350269189625,-0.577350269189627)) ;
#118314 = DIRECTION('',(1.,-7.70371977754894E-34,9.8563833862319E-18)) ;
#118315 = DIRECTION('center_axis',(6.96951553037899E-18,0.707106781186549,
0.707106781186546)) ;
#118316 = DIRECTION('ref_axis',(-8.6424177776148E-34,-0.707106781186546,0.707106781186549)) ;
#118317 = DIRECTION('',(-0.577350269189625,0.577350269189625,-0.577350269189627)) ;
#118318 = DIRECTION('',(1.,-9.85638338623186E-18,0.)) ;
#118319 = DIRECTION('',(-0.577350269189625,-0.577350269189625,0.577350269189627)) ;
#118320 = DIRECTION('',(-1.,7.70371977754894E-34,9.8563833862319E-18)) ;
#118321 = DIRECTION('center_axis',(6.96951553037899E-18,0.707106781186549,
-0.707106781186546)) ;
#118322 = DIRECTION('ref_axis',(8.6424177776148E-34,0.707106781186546,0.707106781186549)) ;
#118323 = DIRECTION('',(0.577350269189625,0.577350269189625,0.577350269189627)) ;
#118324 = DIRECTION('',(-1.,9.85638338623186E-18,0.)) ;
#118325 = DIRECTION('',(0.577350269189625,-0.577350269189625,-0.577350269189627)) ;
#118326 = DIRECTION('',(1.,-7.70371977754894E-34,9.8563833862319E-18)) ;
#118327 = DIRECTION('center_axis',(6.96951553037899E-18,0.707106781186549,
0.707106781186546)) ;
#118328 = DIRECTION('ref_axis',(-8.6424177776148E-34,-0.707106781186546,0.707106781186549)) ;
#118329 = DIRECTION('',(-0.577350269189625,0.577350269189625,-0.577350269189627)) ;
#118330 = DIRECTION('',(1.,-9.85638338623186E-18,0.)) ;
#118331 = DIRECTION('',(-0.577350269189625,-0.577350269189625,0.577350269189627)) ;
#118332 = DIRECTION('',(-1.,7.70371977754894E-34,9.8563833862319E-18)) ;
#118333 = DIRECTION('center_axis',(6.96951553037899E-18,0.707106781186549,
-0.707106781186546)) ;
#118334 = DIRECTION('ref_axis',(8.6424177776148E-34,0.707106781186546,0.707106781186549)) ;
#118335 = DIRECTION('',(0.577350269189625,0.577350269189625,0.577350269189627)) ;
#118336 = DIRECTION('',(-1.,9.85638338623186E-18,0.)) ;
#118337 = DIRECTION('',(0.577350269189625,-0.577350269189625,-0.577350269189627)) ;
#118338 = DIRECTION('',(1.,-7.70371977754894E-34,9.8563833862319E-18)) ;
#118339 = DIRECTION('center_axis',(6.96951553037899E-18,0.707106781186549,
0.707106781186546)) ;
#118340 = DIRECTION('ref_axis',(-8.6424177776148E-34,-0.707106781186546,0.707106781186549)) ;
#118341 = DIRECTION('',(-0.577350269189625,0.577350269189625,-0.577350269189627)) ;
#118342 = DIRECTION('',(1.,-9.85638338623186E-18,0.)) ;
#118343 = DIRECTION('',(-0.577350269189625,-0.577350269189625,0.577350269189627)) ;
#118344 = DIRECTION('',(-1.,7.70371977754894E-34,9.8563833862319E-18)) ;
#118345 = DIRECTION('center_axis',(6.96951553037899E-18,0.707106781186549,
-0.707106781186546)) ;
#118346 = DIRECTION('ref_axis',(8.6424177776148E-34,0.707106781186546,0.707106781186549)) ;
#118347 = DIRECTION('',(0.577350269189625,0.577350269189625,0.577350269189627)) ;
#118348 = DIRECTION('',(-1.,9.85638338623186E-18,0.)) ;
#118349 = DIRECTION('',(0.577350269189625,-0.577350269189625,-0.577350269189627)) ;
#118350 = DIRECTION('',(1.,-7.70371977754894E-34,9.8563833862319E-18)) ;
#118351 = DIRECTION('center_axis',(-0.707106781186548,-1.38247767078009E-16,
0.707106781186547)) ;
#118352 = DIRECTION('ref_axis',(0.707106781186547,8.815972061965E-34,0.707106781186548)) ;
#118353 = DIRECTION('',(-0.577350269189625,-0.577350269189626,-0.577350269189626)) ;
#118354 = DIRECTION('',(-1.95511867169517E-16,1.,0.)) ;
#118355 = DIRECTION('',(0.577350269189625,-0.577350269189626,0.577350269189626)) ;
#118356 = DIRECTION('',(0.,-1.,-1.95511867169518E-16)) ;
#118357 = DIRECTION('center_axis',(-0.707106781186548,-1.38247767078009E-16,
-0.707106781186547)) ;
#118358 = DIRECTION('ref_axis',(-0.707106781186547,-8.815972061965E-34,0.707106781186548)) ;
#118359 = DIRECTION('',(-0.577350269189625,0.577350269189626,0.577350269189626)) ;
#118360 = DIRECTION('',(1.95511867169517E-16,-1.,0.)) ;
#118361 = DIRECTION('',(0.577350269189625,0.577350269189626,-0.577350269189626)) ;
#118362 = DIRECTION('',(0.,1.,-1.95511867169518E-16)) ;
#118363 = DIRECTION('center_axis',(-0.707106781186548,-1.38247767078009E-16,
0.707106781186547)) ;
#118364 = DIRECTION('ref_axis',(0.707106781186547,8.815972061965E-34,0.707106781186548)) ;
#118365 = DIRECTION('',(-0.577350269189625,-0.577350269189626,-0.577350269189626)) ;
#118366 = DIRECTION('',(-1.95511867169517E-16,1.,0.)) ;
#118367 = DIRECTION('',(0.577350269189625,-0.577350269189626,0.577350269189626)) ;
#118368 = DIRECTION('',(0.,-1.,-1.95511867169518E-16)) ;
#118369 = DIRECTION('center_axis',(-0.707106781186548,-1.38247767078009E-16,
-0.707106781186547)) ;
#118370 = DIRECTION('ref_axis',(-0.707106781186547,-8.815972061965E-34,0.707106781186548)) ;
#118371 = DIRECTION('',(-0.577350269189625,0.577350269189626,0.577350269189626)) ;
#118372 = DIRECTION('',(1.95511867169517E-16,-1.,0.)) ;
#118373 = DIRECTION('',(0.577350269189625,0.577350269189626,-0.577350269189626)) ;
#118374 = DIRECTION('',(0.,1.,-1.95511867169518E-16)) ;
#118375 = DIRECTION('center_axis',(-0.707106781186548,-1.38247767078009E-16,
0.707106781186547)) ;
#118376 = DIRECTION('ref_axis',(0.707106781186547,8.815972061965E-34,0.707106781186548)) ;
#118377 = DIRECTION('',(-0.577350269189625,-0.577350269189626,-0.577350269189626)) ;
#118378 = DIRECTION('',(-1.95511867169517E-16,1.,0.)) ;
#118379 = DIRECTION('',(0.577350269189625,-0.577350269189626,0.577350269189626)) ;
#118380 = DIRECTION('',(0.,-1.,-1.95511867169518E-16)) ;
#118381 = DIRECTION('center_axis',(-0.707106781186548,-1.38247767078009E-16,
-0.707106781186547)) ;
#118382 = DIRECTION('ref_axis',(-0.707106781186547,-8.815972061965E-34,0.707106781186548)) ;
#118383 = DIRECTION('',(-0.577350269189625,0.577350269189626,0.577350269189626)) ;
#118384 = DIRECTION('',(1.95511867169517E-16,-1.,0.)) ;
#118385 = DIRECTION('',(0.577350269189625,0.577350269189626,-0.577350269189626)) ;
#118386 = DIRECTION('',(0.,1.,-1.95511867169518E-16)) ;
#118387 = DIRECTION('center_axis',(-0.707106781186548,-1.38247767078009E-16,
0.707106781186547)) ;
#118388 = DIRECTION('ref_axis',(0.707106781186547,8.815972061965E-34,0.707106781186548)) ;
#118389 = DIRECTION('',(-0.577350269189625,-0.577350269189626,-0.577350269189626)) ;
#118390 = DIRECTION('',(-1.95511867169517E-16,1.,0.)) ;
#118391 = DIRECTION('',(0.577350269189625,-0.577350269189626,0.577350269189626)) ;
#118392 = DIRECTION('',(0.,-1.,-1.95511867169518E-16)) ;
#118393 = DIRECTION('center_axis',(-0.707106781186548,-1.38247767078009E-16,
-0.707106781186547)) ;
#118394 = DIRECTION('ref_axis',(-0.707106781186547,-8.815972061965E-34,0.707106781186548)) ;
#118395 = DIRECTION('',(-0.577350269189625,0.577350269189626,0.577350269189626)) ;
#118396 = DIRECTION('',(1.95511867169517E-16,-1.,0.)) ;
#118397 = DIRECTION('',(0.577350269189625,0.577350269189626,-0.577350269189626)) ;
#118398 = DIRECTION('',(0.,1.,-1.95511867169518E-16)) ;
#118399 = DIRECTION('center_axis',(-0.707106781186548,-1.38247767078009E-16,
0.707106781186547)) ;
#118400 = DIRECTION('ref_axis',(0.707106781186547,8.815972061965E-34,0.707106781186548)) ;
#118401 = DIRECTION('',(-0.577350269189625,-0.577350269189626,-0.577350269189626)) ;
#118402 = DIRECTION('',(-1.95511867169517E-16,1.,0.)) ;
#118403 = DIRECTION('',(0.577350269189625,-0.577350269189626,0.577350269189626)) ;
#118404 = DIRECTION('',(0.,-1.,-1.95511867169518E-16)) ;
#118405 = DIRECTION('center_axis',(-0.707106781186548,-1.38247767078009E-16,
-0.707106781186547)) ;
#118406 = DIRECTION('ref_axis',(-0.707106781186547,-8.815972061965E-34,0.707106781186548)) ;
#118407 = DIRECTION('',(-0.577350269189625,0.577350269189626,0.577350269189626)) ;
#118408 = DIRECTION('',(1.95511867169517E-16,-1.,0.)) ;
#118409 = DIRECTION('',(0.577350269189625,0.577350269189626,-0.577350269189626)) ;
#118410 = DIRECTION('',(0.,1.,-1.95511867169518E-16)) ;
#118411 = DIRECTION('center_axis',(-0.707106781186548,-1.38247767078009E-16,
0.707106781186547)) ;
#118412 = DIRECTION('ref_axis',(0.707106781186547,8.815972061965E-34,0.707106781186548)) ;
#118413 = DIRECTION('',(-0.577350269189625,-0.577350269189626,-0.577350269189626)) ;
#118414 = DIRECTION('',(-1.95511867169517E-16,1.,0.)) ;
#118415 = DIRECTION('',(0.577350269189625,-0.577350269189626,0.577350269189626)) ;
#118416 = DIRECTION('',(0.,-1.,-1.95511867169518E-16)) ;
#118417 = DIRECTION('center_axis',(-0.707106781186548,-1.38247767078009E-16,
-0.707106781186547)) ;
#118418 = DIRECTION('ref_axis',(-0.707106781186547,-8.815972061965E-34,0.707106781186548)) ;
#118419 = DIRECTION('',(-0.577350269189625,0.577350269189626,0.577350269189626)) ;
#118420 = DIRECTION('',(1.95511867169517E-16,-1.,0.)) ;
#118421 = DIRECTION('',(0.577350269189625,0.577350269189626,-0.577350269189626)) ;
#118422 = DIRECTION('',(0.,1.,-1.95511867169518E-16)) ;
#118423 = DIRECTION('center_axis',(-0.707106781186548,-1.38247767078009E-16,
0.707106781186547)) ;
#118424 = DIRECTION('ref_axis',(0.707106781186547,8.815972061965E-34,0.707106781186548)) ;
#118425 = DIRECTION('',(-0.577350269189625,-0.577350269189626,-0.577350269189626)) ;
#118426 = DIRECTION('',(-1.95511867169517E-16,1.,0.)) ;
#118427 = DIRECTION('',(0.577350269189625,-0.577350269189626,0.577350269189626)) ;
#118428 = DIRECTION('',(0.,-1.,-1.95511867169518E-16)) ;
#118429 = DIRECTION('center_axis',(-0.707106781186548,-1.38247767078009E-16,
-0.707106781186547)) ;
#118430 = DIRECTION('ref_axis',(-0.707106781186547,-8.815972061965E-34,0.707106781186548)) ;
#118431 = DIRECTION('',(-0.577350269189625,0.577350269189626,0.577350269189626)) ;
#118432 = DIRECTION('',(1.95511867169517E-16,-1.,0.)) ;
#118433 = DIRECTION('',(0.577350269189625,0.577350269189626,-0.577350269189626)) ;
#118434 = DIRECTION('',(0.,1.,-1.95511867169518E-16)) ;
#118435 = DIRECTION('center_axis',(-0.707106781186548,-1.38247767078009E-16,
0.707106781186547)) ;
#118436 = DIRECTION('ref_axis',(0.707106781186547,8.815972061965E-34,0.707106781186548)) ;
#118437 = DIRECTION('',(-0.577350269189625,-0.577350269189626,-0.577350269189626)) ;
#118438 = DIRECTION('',(-1.95511867169517E-16,1.,0.)) ;
#118439 = DIRECTION('',(0.577350269189625,-0.577350269189626,0.577350269189626)) ;
#118440 = DIRECTION('',(0.,-1.,-1.95511867169518E-16)) ;
#118441 = DIRECTION('center_axis',(-0.707106781186548,-1.38247767078009E-16,
-0.707106781186547)) ;
#118442 = DIRECTION('ref_axis',(-0.707106781186547,-8.815972061965E-34,0.707106781186548)) ;
#118443 = DIRECTION('',(-0.577350269189625,0.577350269189626,0.577350269189626)) ;
#118444 = DIRECTION('',(1.95511867169517E-16,-1.,0.)) ;
#118445 = DIRECTION('',(0.577350269189625,0.577350269189626,-0.577350269189626)) ;
#118446 = DIRECTION('',(0.,1.,-1.95511867169518E-16)) ;
#118447 = DIRECTION('center_axis',(-0.707106781186548,-1.38247767078009E-16,
0.707106781186547)) ;
#118448 = DIRECTION('ref_axis',(0.707106781186547,8.815972061965E-34,0.707106781186548)) ;
#118449 = DIRECTION('',(-0.577350269189625,-0.577350269189626,-0.577350269189626)) ;
#118450 = DIRECTION('',(-1.95511867169517E-16,1.,0.)) ;
#118451 = DIRECTION('',(0.577350269189625,-0.577350269189626,0.577350269189626)) ;
#118452 = DIRECTION('',(0.,-1.,-1.95511867169518E-16)) ;
#118453 = DIRECTION('center_axis',(-0.707106781186548,-1.38247767078009E-16,
-0.707106781186547)) ;
#118454 = DIRECTION('ref_axis',(-0.707106781186547,-8.815972061965E-34,0.707106781186548)) ;
#118455 = DIRECTION('',(-0.577350269189625,0.577350269189626,0.577350269189626)) ;
#118456 = DIRECTION('',(1.95511867169517E-16,-1.,0.)) ;
#118457 = DIRECTION('',(0.577350269189625,0.577350269189626,-0.577350269189626)) ;
#118458 = DIRECTION('',(0.,1.,-1.95511867169518E-16)) ;
#118459 = DIRECTION('center_axis',(0.577350269189625,0.577350269189625,-0.577350269189628)) ;
#118460 = DIRECTION('ref_axis',(-0.70710678118655,2.50449302218608E-16,-0.707106781186546)) ;
#118461 = DIRECTION('center_axis',(-0.577350269189625,-0.577350269189625,
0.577350269189628)) ;
#118462 = DIRECTION('ref_axis',(-0.707106781186548,-2.12258087602815E-15,
-0.707106781186547)) ;
#118463 = DIRECTION('center_axis',(-0.577350269189622,-0.577350269189626,
0.57735026918963)) ;
#118464 = DIRECTION('ref_axis',(4.78608867599257E-17,-0.70710678118655,-0.707106781186545)) ;
#118465 = DIRECTION('center_axis',(0.,0.,-1.)) ;
#118466 = DIRECTION('ref_axis',(-1.,0.,0.)) ;
#118467 = DIRECTION('center_axis',(0.,0.,1.)) ;
#118468 = DIRECTION('ref_axis',(-1.,-8.67361737988404E-15,0.)) ;
#118469 = DIRECTION('center_axis',(0.,0.,-1.)) ;
#118470 = DIRECTION('ref_axis',(-1.,0.,0.)) ;
#118471 = DIRECTION('center_axis',(2.08166817117218E-16,1.,0.)) ;
#118472 = DIRECTION('ref_axis',(1.,0.,0.)) ;
#118473 = DIRECTION('center_axis',(-1.,0.,-4.40821857296472E-15)) ;
#118474 = DIRECTION('ref_axis',(4.40821857296472E-15,0.,-1.)) ;
#118475 = DIRECTION('center_axis',(8.67361737988402E-15,8.67361737988401E-15,
1.)) ;
#118476 = DIRECTION('ref_axis',(-1.,-9.79595207717063E-44,8.67361737988402E-15)) ;
#118477 = DIRECTION('center_axis',(-0.577350269189625,-0.577350269189625,
-0.577350269189628)) ;
#118478 = DIRECTION('ref_axis',(-0.70710678118655,2.50449302218608E-16,0.707106781186546)) ;
#118479 = DIRECTION('center_axis',(-0.577350269189625,-0.577350269189625,
-0.577350269189628)) ;
#118480 = DIRECTION('ref_axis',(-0.70710678118655,2.22693726602979E-16,0.707106781186546)) ;
#118481 = DIRECTION('center_axis',(-0.577350269189624,-0.577350269189623,
-0.577350269189631)) ;
#118482 = DIRECTION('ref_axis',(-0.707106781186552,5.79770761800025E-17,0.707106781186543)) ;
#118483 = DIRECTION('center_axis',(0.,0.,-1.)) ;
#118484 = DIRECTION('ref_axis',(-1.,0.,0.)) ;
#118485 = DIRECTION('center_axis',(-6.1331736667335E-15,0.,1.)) ;
#118486 = DIRECTION('ref_axis',(1.,0.,6.1331736667335E-15)) ;
#118487 = DIRECTION('center_axis',(-1.,0.,9.8563833862319E-18)) ;
#118488 = DIRECTION('ref_axis',(9.8563833862319E-18,0.,1.)) ;
#118489 = DIRECTION('center_axis',(-1.,3.93023287525994E-15,-3.93023287525997E-15)) ;
#118490 = DIRECTION('ref_axis',(-3.93023287525997E-15,2.80259692864963E-44,
1.)) ;
#118491 = DIRECTION('center_axis',(2.08166817117218E-16,1.,0.)) ;
#118492 = DIRECTION('ref_axis',(1.,0.,0.)) ;
#118493 = DIRECTION('center_axis',(-1.,-8.13151629364126E-16,-8.13151629364131E-16)) ;
#118494 = DIRECTION('ref_axis',(8.13151629364131E-16,1.13855500226391E-45,
-1.)) ;
#118495 = DIRECTION('center_axis',(2.08166817117218E-16,1.,0.)) ;
#118496 = DIRECTION('ref_axis',(1.,0.,0.)) ;
#118497 = DIRECTION('center_axis',(-0.577350269189623,0.577350269189622,-0.577350269189633)) ;
#118498 = DIRECTION('ref_axis',(0.707106781186554,7.82055407754491E-16,-0.707106781186541)) ;
#118499 = DIRECTION('center_axis',(-6.1331736667335E-15,0.,1.)) ;
#118500 = DIRECTION('ref_axis',(-1.,0.,-6.1331736667335E-15)) ;
#118501 = DIRECTION('center_axis',(-1.,0.,-9.8563833862319E-18)) ;
#118502 = DIRECTION('ref_axis',(-9.8563833862319E-18,0.,1.)) ;
#118503 = DIRECTION('center_axis',(-1.,0.,-2.10827844793965E-15)) ;
#118504 = DIRECTION('ref_axis',(-2.10827844793965E-15,0.,1.)) ;
#118505 = DIRECTION('center_axis',(0.,0.,-1.)) ;
#118506 = DIRECTION('ref_axis',(-1.,0.,0.)) ;
#118507 = DIRECTION('center_axis',(0.,0.,1.)) ;
#118508 = DIRECTION('ref_axis',(1.,0.,0.)) ;
#118509 = DIRECTION('center_axis',(0.577350269189625,-0.577350269189625,0.577350269189628)) ;
#118510 = DIRECTION('ref_axis',(0.707106781186549,-7.23605167296792E-16,-0.707106781186546)) ;
#118511 = DIRECTION('center_axis',(0.577350269189625,-0.577350269189625,0.577350269189628)) ;
#118512 = DIRECTION('ref_axis',(0.707106781186549,-7.51360742912421E-16,-0.707106781186546)) ;
#118513 = DIRECTION('center_axis',(2.08166817117218E-16,1.,0.)) ;
#118514 = DIRECTION('ref_axis',(1.,0.,0.)) ;
#118515 = DIRECTION('center_axis',(-0.577350269189626,0.577350269189624,0.577350269189628)) ;
#118516 = DIRECTION('ref_axis',(-0.707106781186549,-7.24154524606924E-16,
-0.707106781186546)) ;
#118517 = DIRECTION('center_axis',(0.,0.,-1.)) ;
#118518 = DIRECTION('ref_axis',(-1.,0.,0.)) ;
#118519 = DIRECTION('center_axis',(0.,0.,1.)) ;
#118520 = DIRECTION('ref_axis',(-1.,0.,0.)) ;
#118521 = DIRECTION('center_axis',(0.,0.,-1.)) ;
#118522 = DIRECTION('ref_axis',(-1.,0.,0.)) ;
#118523 = DIRECTION('center_axis',(-0.577350269189625,0.577350269189625,0.577350269189628)) ;
#118524 = DIRECTION('ref_axis',(0.70710678118655,2.22693726602979E-16,0.707106781186546)) ;
#118525 = DIRECTION('center_axis',(0.577350269189625,-0.577350269189625,-0.577350269189628)) ;
#118526 = DIRECTION('ref_axis',(0.707106781186549,-8.43215074740835E-16,0.707106781186546)) ;
#118527 = DIRECTION('center_axis',(-0.577350269189625,0.577350269189626,-0.577350269189626)) ;
#118528 = DIRECTION('ref_axis',(6.27941990732594E-17,0.707106781186548,0.707106781186548)) ;
#118529 = DIRECTION('center_axis',(0.577350269189625,-0.577350269189626,0.577350269189626)) ;
#118530 = DIRECTION('ref_axis',(5.0289788758123E-16,0.707106781186548,0.707106781186547)) ;
#118531 = DIRECTION('center_axis',(0.577350269189624,-0.57735026918963,0.577350269189624)) ;
#118532 = DIRECTION('ref_axis',(0.707106781186551,0.707106781186544,6.33763658455854E-16)) ;
#118533 = DIRECTION('center_axis',(0.,0.,-1.)) ;
#118534 = DIRECTION('ref_axis',(-1.,0.,0.)) ;
#118535 = DIRECTION('center_axis',(0.,0.,1.)) ;
#118536 = DIRECTION('ref_axis',(-1.,2.71050543121375E-15,0.)) ;
#118537 = DIRECTION('center_axis',(0.,0.,-1.)) ;
#118538 = DIRECTION('ref_axis',(-1.,0.,0.)) ;
#118539 = DIRECTION('center_axis',(0.,1.,0.)) ;
#118540 = DIRECTION('ref_axis',(1.,0.,0.)) ;
#118541 = DIRECTION('center_axis',(0.,-1.,-3.25824851045217E-15)) ;
#118542 = DIRECTION('ref_axis',(0.,-3.25824851045217E-15,1.)) ;
#118543 = DIRECTION('center_axis',(4.33680868994201E-15,-4.33680868994202E-15,
1.)) ;
#118544 = DIRECTION('ref_axis',(3.0828566215146E-44,1.,4.33680868994202E-15)) ;
#118545 = DIRECTION('center_axis',(0.577350269189625,-0.577350269189626,-0.577350269189626)) ;
#118546 = DIRECTION('ref_axis',(6.27941990732594E-17,0.707106781186548,-0.707106781186548)) ;
#118547 = DIRECTION('center_axis',(0.577350269189625,-0.577350269189626,-0.577350269189626)) ;
#118548 = DIRECTION('ref_axis',(-7.7646791370609E-16,0.707106781186547,-0.707106781186548)) ;
#118549 = DIRECTION('center_axis',(0.577350269189625,-0.577350269189626,-0.577350269189627)) ;
#118550 = DIRECTION('ref_axis',(-3.31150339748933E-16,0.707106781186548,-0.707106781186547)) ;
#118551 = DIRECTION('center_axis',(0.,0.,-1.)) ;
#118552 = DIRECTION('ref_axis',(-1.,0.,0.)) ;
#118553 = DIRECTION('center_axis',(0.,-6.1331736667335E-15,1.)) ;
#118554 = DIRECTION('ref_axis',(0.,-1.,-6.1331736667335E-15)) ;
#118555 = DIRECTION('center_axis',(0.,1.,1.95511867169518E-16)) ;
#118556 = DIRECTION('ref_axis',(0.,-1.95511867169518E-16,1.)) ;
#118557 = DIRECTION('center_axis',(2.71050543121375E-16,-1.,7.93888660359539E-17)) ;
#118558 = DIRECTION('ref_axis',(1.,2.71050543121375E-16,0.)) ;
#118559 = DIRECTION('center_axis',(0.,1.,0.)) ;
#118560 = DIRECTION('ref_axis',(1.,0.,0.)) ;
#118561 = DIRECTION('center_axis',(-1.28749007982653E-15,-1.,1.47915175691195E-15)) ;
#118562 = DIRECTION('ref_axis',(-1.49686561198851E-32,1.47915175691195E-15,
1.)) ;
#118563 = DIRECTION('center_axis',(0.,1.,0.)) ;
#118564 = DIRECTION('ref_axis',(1.,0.,0.)) ;
#118565 = DIRECTION('center_axis',(-0.577350269189624,-0.577350269189626,
-0.577350269189628)) ;
#118566 = DIRECTION('ref_axis',(-1.24495925064522E-15,-0.707106781186548,
0.707106781186547)) ;
#118567 = DIRECTION('center_axis',(0.,-6.1331736667335E-15,1.)) ;
#118568 = DIRECTION('ref_axis',(0.,1.,6.1331736667335E-15)) ;
#118569 = DIRECTION('center_axis',(0.,1.,-1.95511867169518E-16)) ;
#118570 = DIRECTION('ref_axis',(0.,1.95511867169518E-16,1.)) ;
#118571 = DIRECTION('center_axis',(0.,-1.,-4.59988025005012E-15)) ;
#118572 = DIRECTION('ref_axis',(0.,4.59988025005012E-15,-1.)) ;
#118573 = DIRECTION('center_axis',(0.,0.,-1.)) ;
#118574 = DIRECTION('ref_axis',(-1.,0.,0.)) ;
#118575 = DIRECTION('center_axis',(0.,0.,1.)) ;
#118576 = DIRECTION('ref_axis',(1.,0.,0.)) ;
#118577 = DIRECTION('center_axis',(0.577350269189625,0.577350269189626,0.577350269189627)) ;
#118578 = DIRECTION('ref_axis',(-2.71345386026911E-16,-0.707106781186548,
0.707106781186547)) ;
#118579 = DIRECTION('center_axis',(0.577350269189625,0.577350269189626,0.577350269189627)) ;
#118580 = DIRECTION('ref_axis',(-2.71345386026911E-16,-0.707106781186548,
0.707106781186547)) ;
#118581 = DIRECTION('center_axis',(0.,1.,0.)) ;
#118582 = DIRECTION('ref_axis',(1.,0.,0.)) ;
#118583 = DIRECTION('center_axis',(-0.577350269189624,-0.577350269189628,
0.577350269189625)) ;
#118584 = DIRECTION('ref_axis',(-6.89490688817364E-15,0.707106781186549,0.707106781186546)) ;
#118585 = DIRECTION('center_axis',(0.,0.,-1.)) ;
#118586 = DIRECTION('ref_axis',(-1.,0.,0.)) ;
#118587 = DIRECTION('center_axis',(0.,0.,1.)) ;
#118588 = DIRECTION('ref_axis',(-1.,1.0842021724855E-15,0.)) ;
#118589 = DIRECTION('center_axis',(0.,0.,-1.)) ;
#118590 = DIRECTION('ref_axis',(-1.,0.,0.)) ;
#118591 = DIRECTION('center_axis',(-0.577350269189625,-0.577350269189626,
0.577350269189627)) ;
#118592 = DIRECTION('ref_axis',(-2.71345386026911E-16,-0.707106781186548,
-0.707106781186547)) ;
#118593 = DIRECTION('center_axis',(0.577350269189625,0.577350269189626,-0.577350269189627)) ;
#118594 = DIRECTION('ref_axis',(-9.76085677604559E-15,-0.707106781186543,
-0.707106781186552)) ;
#118595 = DIRECTION('center_axis',(0.577350269189625,0.577350269189625,-0.577350269189628)) ;
#118596 = DIRECTION('ref_axis',(-0.707106781186549,-7.23605167296792E-16,
-0.707106781186546)) ;
#118597 = DIRECTION('center_axis',(-0.577350269189625,-0.577350269189625,
0.577350269189628)) ;
#118598 = DIRECTION('ref_axis',(-0.707106781186542,-1.47047746496289E-14,
-0.707106781186553)) ;
#118599 = DIRECTION('center_axis',(-0.577350269189629,-0.577350269189624,
0.577350269189624)) ;
#118600 = DIRECTION('ref_axis',(0.707106781186545,-9.59471324968973E-16,0.70710678118655)) ;
#118601 = DIRECTION('center_axis',(0.,0.,-1.)) ;
#118602 = DIRECTION('ref_axis',(-1.,0.,0.)) ;
#118603 = DIRECTION('center_axis',(0.,0.,1.)) ;
#118604 = DIRECTION('ref_axis',(-1.,0.,0.)) ;
#118605 = DIRECTION('center_axis',(0.,0.,-1.)) ;
#118606 = DIRECTION('ref_axis',(-1.,0.,0.)) ;
#118607 = DIRECTION('center_axis',(2.08166817117218E-16,1.,0.)) ;
#118608 = DIRECTION('ref_axis',(1.,0.,0.)) ;
#118609 = DIRECTION('center_axis',(-1.,0.,-5.94151198964807E-15)) ;
#118610 = DIRECTION('ref_axis',(5.94151198964807E-15,0.,-1.)) ;
#118611 = DIRECTION('center_axis',(0.,0.,1.)) ;
#118612 = DIRECTION('ref_axis',(-1.,0.,0.)) ;
#118613 = DIRECTION('center_axis',(-0.577350269189625,-0.577350269189625,
-0.577350269189628)) ;
#118614 = DIRECTION('ref_axis',(-0.707106781186549,-7.23605167296792E-16,
0.707106781186546)) ;
#118615 = DIRECTION('center_axis',(-0.577350269189625,-0.577350269189625,
-0.577350269189628)) ;
#118616 = DIRECTION('ref_axis',(-0.707106781186549,-7.51360742912421E-16,
0.707106781186546)) ;
#118617 = DIRECTION('center_axis',(-0.577350269189629,-0.577350269189628,
-0.577350269189621)) ;
#118618 = DIRECTION('ref_axis',(0.707106781186547,-0.707106781186548,-9.25270248417546E-17)) ;
#118619 = DIRECTION('center_axis',(0.,0.,-1.)) ;
#118620 = DIRECTION('ref_axis',(-1.,0.,0.)) ;
#118621 = DIRECTION('center_axis',(1.2266347333467E-14,0.,1.)) ;
#118622 = DIRECTION('ref_axis',(1.,0.,-1.2266347333467E-14)) ;
#118623 = DIRECTION('center_axis',(-1.,0.,9.8563833862319E-18)) ;
#118624 = DIRECTION('ref_axis',(9.8563833862319E-18,0.,1.)) ;
#118625 = DIRECTION('center_axis',(-1.,1.62630325872825E-15,-1.62630325872825E-15)) ;
#118626 = DIRECTION('ref_axis',(-1.62630325872825E-15,0.,1.)) ;
#118627 = DIRECTION('center_axis',(2.08166817117218E-16,1.,0.)) ;
#118628 = DIRECTION('ref_axis',(1.,0.,0.)) ;
#118629 = DIRECTION('center_axis',(-1.,1.35525271560688E-16,1.35525271560688E-16)) ;
#118630 = DIRECTION('ref_axis',(-1.35525271560688E-16,0.,-1.)) ;
#118631 = DIRECTION('center_axis',(2.08166817117218E-16,1.,0.)) ;
#118632 = DIRECTION('ref_axis',(1.,0.,0.)) ;
#118633 = DIRECTION('center_axis',(-0.577350269189628,0.577350269189628,-0.577350269189621)) ;
#118634 = DIRECTION('ref_axis',(0.707106781186547,0.707106781186548,5.83290435273539E-16)) ;
#118635 = DIRECTION('center_axis',(1.2266347333467E-14,0.,1.)) ;
#118636 = DIRECTION('ref_axis',(-1.,0.,1.2266347333467E-14)) ;
#118637 = DIRECTION('center_axis',(-1.,0.,-9.8563833862319E-18)) ;
#118638 = DIRECTION('ref_axis',(-9.8563833862319E-18,0.,1.)) ;
#118639 = DIRECTION('center_axis',(-1.,0.,9.58308385427108E-16)) ;
#118640 = DIRECTION('ref_axis',(9.58308385427108E-16,0.,1.)) ;
#118641 = DIRECTION('center_axis',(0.,0.,-1.)) ;
#118642 = DIRECTION('ref_axis',(-1.,0.,0.)) ;
#118643 = DIRECTION('center_axis',(-8.67361737988402E-15,8.67361737988401E-15,
1.)) ;
#118644 = DIRECTION('ref_axis',(1.,-9.79595207717063E-44,8.67361737988402E-15)) ;
#118645 = DIRECTION('center_axis',(0.577350269189625,-0.577350269189625,0.577350269189628)) ;
#118646 = DIRECTION('ref_axis',(0.707106781186549,-7.23605167296792E-16,-0.707106781186546)) ;
#118647 = DIRECTION('center_axis',(0.577350269189625,-0.577350269189625,0.577350269189628)) ;
#118648 = DIRECTION('ref_axis',(0.707106781186549,-7.51360742912421E-16,-0.707106781186546)) ;
#118649 = DIRECTION('center_axis',(2.08166817117218E-16,1.,0.)) ;
#118650 = DIRECTION('ref_axis',(1.,0.,0.)) ;
#118651 = DIRECTION('center_axis',(-0.577350269189631,0.577350269189623,0.577350269189623)) ;
#118652 = DIRECTION('ref_axis',(-0.707106781186542,1.43689139429453E-15,-0.707106781186553)) ;
#118653 = DIRECTION('center_axis',(0.,0.,-1.)) ;
#118654 = DIRECTION('ref_axis',(-1.,0.,0.)) ;
#118655 = DIRECTION('center_axis',(0.,0.,1.)) ;
#118656 = DIRECTION('ref_axis',(-1.,0.,0.)) ;
#118657 = DIRECTION('center_axis',(0.,0.,-1.)) ;
#118658 = DIRECTION('ref_axis',(-1.,0.,0.)) ;
#118659 = DIRECTION('center_axis',(-0.577350269189625,0.577350269189625,0.577350269189628)) ;
#118660 = DIRECTION('ref_axis',(0.707106781186549,-7.51360742912421E-16,0.707106781186546)) ;
#118661 = DIRECTION('center_axis',(0.577350269189625,-0.577350269189625,-0.577350269189628)) ;
#118662 = DIRECTION('ref_axis',(0.707106781186549,-8.43215074740835E-16,0.707106781186546)) ;
#118663 = DIRECTION('center_axis',(-0.577350269189625,0.577350269189626,-0.577350269189626)) ;
#118664 = DIRECTION('ref_axis',(6.27941990732594E-17,0.707106781186548,0.707106781186548)) ;
#118665 = DIRECTION('center_axis',(0.577350269189625,-0.577350269189626,0.577350269189626)) ;
#118666 = DIRECTION('ref_axis',(-4.12932450763554E-14,0.707106781186527,0.707106781186568)) ;
#118667 = DIRECTION('center_axis',(0.577350269189626,-0.577350269189626,0.577350269189626)) ;
#118668 = DIRECTION('ref_axis',(0.707106781186548,0.707106781186547,-6.70219100485003E-16)) ;
#118669 = DIRECTION('center_axis',(0.,0.,-1.)) ;
#118670 = DIRECTION('ref_axis',(-1.,0.,0.)) ;
#118671 = DIRECTION('center_axis',(0.,0.,1.)) ;
#118672 = DIRECTION('ref_axis',(-1.,0.,0.)) ;
#118673 = DIRECTION('center_axis',(0.,0.,-1.)) ;
#118674 = DIRECTION('ref_axis',(-1.,0.,0.)) ;
#118675 = DIRECTION('center_axis',(0.,1.,0.)) ;
#118676 = DIRECTION('ref_axis',(1.,0.,0.)) ;
#118677 = DIRECTION('center_axis',(0.,-1.,-1.05413922396982E-14)) ;
#118678 = DIRECTION('ref_axis',(0.,-1.05413922396982E-14,1.)) ;
#118679 = DIRECTION('center_axis',(-8.67361737988401E-15,8.67361737988403E-15,
1.)) ;
#118680 = DIRECTION('ref_axis',(-4.48415508583941E-44,1.,-8.67361737988403E-15)) ;
#118681 = DIRECTION('center_axis',(0.577350269189625,-0.577350269189626,-0.577350269189626)) ;
#118682 = DIRECTION('ref_axis',(6.27941990732594E-17,0.707106781186548,-0.707106781186548)) ;
#118683 = DIRECTION('center_axis',(0.577350269189625,-0.577350269189626,-0.577350269189626)) ;
#118684 = DIRECTION('ref_axis',(-7.7646791370609E-16,0.707106781186547,-0.707106781186548)) ;
#118685 = DIRECTION('center_axis',(0.577350269189627,-0.577350269189628,-0.577350269189622)) ;
#118686 = DIRECTION('ref_axis',(0.707106781186548,0.707106781186547,-7.93962717014541E-17)) ;
#118687 = DIRECTION('center_axis',(0.,0.,-1.)) ;
#118688 = DIRECTION('ref_axis',(-1.,0.,0.)) ;
#118689 = DIRECTION('center_axis',(0.,1.2266347333467E-14,1.)) ;
#118690 = DIRECTION('ref_axis',(0.,-1.,1.2266347333467E-14)) ;
#118691 = DIRECTION('center_axis',(0.,1.,1.95511867169518E-16)) ;
#118692 = DIRECTION('ref_axis',(0.,-1.95511867169518E-16,1.)) ;
#118693 = DIRECTION('center_axis',(-1.42301535138722E-15,-1.,-1.61467702847264E-15)) ;
#118694 = DIRECTION('ref_axis',(-1.65443041324959E-32,1.61467702847264E-15,
-1.)) ;
#118695 = DIRECTION('center_axis',(0.,1.,0.)) ;
#118696 = DIRECTION('ref_axis',(1.,0.,0.)) ;
#118697 = DIRECTION('center_axis',(3.72694496791891E-15,-1.,-3.53528329083349E-15)) ;
#118698 = DIRECTION('ref_axis',(-1.,-3.72694496791891E-15,0.)) ;
#118699 = DIRECTION('center_axis',(0.,1.,0.)) ;
#118700 = DIRECTION('ref_axis',(1.,0.,0.)) ;
#118701 = DIRECTION('center_axis',(-0.577350269189623,-0.577350269189624,
-0.577350269189631)) ;
#118702 = DIRECTION('ref_axis',(1.89964573407132E-15,-0.707106781186553,0.707106781186542)) ;
#118703 = DIRECTION('center_axis',(0.,-1.2266347333467E-14,1.)) ;
#118704 = DIRECTION('ref_axis',(0.,1.,1.2266347333467E-14)) ;
#118705 = DIRECTION('center_axis',(0.,1.,-1.95511867169518E-16)) ;
#118706 = DIRECTION('ref_axis',(0.,1.95511867169518E-16,1.)) ;
#118707 = DIRECTION('center_axis',(0.,-1.,-7.66646708341686E-16)) ;
#118708 = DIRECTION('ref_axis',(0.,7.66646708341686E-16,-1.)) ;
#118709 = DIRECTION('center_axis',(0.,0.,-1.)) ;
#118710 = DIRECTION('ref_axis',(-1.,0.,0.)) ;
#118711 = DIRECTION('center_axis',(0.,0.,1.)) ;
#118712 = DIRECTION('ref_axis',(1.,0.,0.)) ;
#118713 = DIRECTION('center_axis',(0.577350269189625,0.577350269189626,0.577350269189627)) ;
#118714 = DIRECTION('ref_axis',(-2.71345386026911E-16,-0.707106781186548,
0.707106781186547)) ;
#118715 = DIRECTION('center_axis',(0.577350269189625,0.577350269189626,0.577350269189627)) ;
#118716 = DIRECTION('ref_axis',(-2.71345386026911E-16,-0.707106781186548,
0.707106781186547)) ;
#118717 = DIRECTION('center_axis',(0.,1.,0.)) ;
#118718 = DIRECTION('ref_axis',(1.,0.,0.)) ;
#118719 = DIRECTION('center_axis',(-0.577350269189625,-0.577350269189627,
0.577350269189625)) ;
#118720 = DIRECTION('ref_axis',(4.24759239037863E-16,0.707106781186546,0.707106781186549)) ;
#118721 = DIRECTION('center_axis',(0.,0.,-1.)) ;
#118722 = DIRECTION('ref_axis',(-1.,0.,0.)) ;
#118723 = DIRECTION('center_axis',(0.,0.,1.)) ;
#118724 = DIRECTION('ref_axis',(-1.,1.0842021724855E-15,0.)) ;
#118725 = DIRECTION('center_axis',(0.,0.,-1.)) ;
#118726 = DIRECTION('ref_axis',(-1.,0.,0.)) ;
#118727 = DIRECTION('center_axis',(-0.577350269189625,-0.577350269189626,
0.577350269189627)) ;
#118728 = DIRECTION('ref_axis',(-2.71345386026911E-16,-0.707106781186548,
-0.707106781186547)) ;
#118729 = DIRECTION('center_axis',(0.577350269189625,0.577350269189626,-0.577350269189627)) ;
#118730 = DIRECTION('ref_axis',(-8.1269550549169E-15,-0.707106781186544,-0.707106781186551)) ;
#118731 = DIRECTION('center_axis',(0.577350269189625,0.577350269189625,-0.577350269189628)) ;
#118732 = DIRECTION('ref_axis',(-0.707106781186549,-7.23605167296792E-16,
-0.707106781186546)) ;
#118733 = DIRECTION('center_axis',(-0.577350269189625,-0.577350269189625,
0.577350269189628)) ;
#118734 = DIRECTION('ref_axis',(-0.707106781186545,-8.33999502129868E-15,
-0.70710678118655)) ;
#118735 = DIRECTION('center_axis',(-0.577350269189627,-0.577350269189625,
0.577350269189625)) ;
#118736 = DIRECTION('ref_axis',(0.707106781186546,1.26631399429469E-16,0.707106781186549)) ;
#118737 = DIRECTION('center_axis',(0.,0.,-1.)) ;
#118738 = DIRECTION('ref_axis',(-1.,0.,0.)) ;
#118739 = DIRECTION('center_axis',(0.,0.,1.)) ;
#118740 = DIRECTION('ref_axis',(-1.,0.,0.)) ;
#118741 = DIRECTION('center_axis',(0.,0.,-1.)) ;
#118742 = DIRECTION('ref_axis',(-1.,0.,0.)) ;
#118743 = DIRECTION('center_axis',(2.08166817117218E-16,1.,0.)) ;
#118744 = DIRECTION('ref_axis',(1.,0.,0.)) ;
#118745 = DIRECTION('center_axis',(-1.,0.,9.58308385427108E-16)) ;
#118746 = DIRECTION('ref_axis',(-9.58308385427108E-16,0.,-1.)) ;
#118747 = DIRECTION('center_axis',(0.,0.,1.)) ;
#118748 = DIRECTION('ref_axis',(-1.,0.,0.)) ;
#118749 = DIRECTION('center_axis',(-0.577350269189625,-0.577350269189625,
-0.577350269189628)) ;
#118750 = DIRECTION('ref_axis',(-0.707106781186549,-7.23605167296792E-16,
0.707106781186546)) ;
#118751 = DIRECTION('center_axis',(-0.577350269189625,-0.577350269189625,
-0.577350269189628)) ;
#118752 = DIRECTION('ref_axis',(-0.707106781186549,-7.51360742912421E-16,
0.707106781186546)) ;
#118753 = DIRECTION('center_axis',(-0.577350269189633,-0.577350269189632,
-0.577350269189612)) ;
#118754 = DIRECTION('ref_axis',(0.707106781186547,-0.707106781186548,-7.39398349810839E-17)) ;
#118755 = DIRECTION('center_axis',(0.,0.,-1.)) ;
#118756 = DIRECTION('ref_axis',(-1.,0.,0.)) ;
#118757 = DIRECTION('center_axis',(2.4532694666934E-14,0.,1.)) ;
#118758 = DIRECTION('ref_axis',(1.,0.,-2.4532694666934E-14)) ;
#118759 = DIRECTION('center_axis',(-1.,0.,9.8563833862319E-18)) ;
#118760 = DIRECTION('ref_axis',(9.8563833862319E-18,0.,1.)) ;
#118761 = DIRECTION('center_axis',(-1.,-8.40256683676264E-15,8.40256683676264E-15)) ;
#118762 = DIRECTION('ref_axis',(8.40256683676264E-15,-6.05360936588321E-43,
1.)) ;
#118763 = DIRECTION('center_axis',(2.08166817117218E-16,1.,0.)) ;
#118764 = DIRECTION('ref_axis',(1.,0.,0.)) ;
#118765 = DIRECTION('center_axis',(-1.,4.9466724119651E-15,4.9466724119651E-15)) ;
#118766 = DIRECTION('ref_axis',(-4.9466724119651E-15,-2.12997366577372E-43,
-1.)) ;
#118767 = DIRECTION('center_axis',(2.08166817117218E-16,1.,0.)) ;
#118768 = DIRECTION('ref_axis',(1.,0.,0.)) ;
#118769 = DIRECTION('center_axis',(-0.577350269189629,0.577350269189628,-0.577350269189621)) ;
#118770 = DIRECTION('ref_axis',(0.707106781186547,0.707106781186548,-3.27220711197328E-17)) ;
#118771 = DIRECTION('center_axis',(0.,0.,1.)) ;
#118772 = DIRECTION('ref_axis',(-1.,0.,0.)) ;
#118773 = DIRECTION('center_axis',(-1.,0.,-9.8563833862319E-18)) ;
#118774 = DIRECTION('ref_axis',(-9.8563833862319E-18,0.,1.)) ;
#118775 = DIRECTION('center_axis',(-1.,0.,-1.05413922396982E-14)) ;
#118776 = DIRECTION('ref_axis',(-1.05413922396982E-14,0.,1.)) ;
#118777 = DIRECTION('center_axis',(0.,0.,-1.)) ;
#118778 = DIRECTION('ref_axis',(-1.,0.,0.)) ;
#118779 = DIRECTION('center_axis',(0.,0.,1.)) ;
#118780 = DIRECTION('ref_axis',(1.,0.,0.)) ;
#118781 = DIRECTION('center_axis',(0.577350269189625,-0.577350269189625,0.577350269189628)) ;
#118782 = DIRECTION('ref_axis',(0.707106781186549,-7.23605167296792E-16,-0.707106781186546)) ;
#118783 = DIRECTION('center_axis',(0.577350269189625,-0.577350269189625,0.577350269189628)) ;
#118784 = DIRECTION('ref_axis',(0.707106781186549,-7.51360742912421E-16,-0.707106781186546)) ;
#118785 = DIRECTION('center_axis',(2.08166817117218E-16,1.,0.)) ;
#118786 = DIRECTION('ref_axis',(1.,0.,0.)) ;
#118787 = DIRECTION('center_axis',(-0.577350269189631,0.577350269189623,0.577350269189623)) ;
#118788 = DIRECTION('ref_axis',(-0.707106781186544,-2.28159610212341E-15,
-0.707106781186551)) ;
#118789 = DIRECTION('center_axis',(0.,0.,-1.)) ;
#118790 = DIRECTION('ref_axis',(-1.,0.,0.)) ;
#118791 = DIRECTION('center_axis',(0.,0.,1.)) ;
#118792 = DIRECTION('ref_axis',(-1.,0.,0.)) ;
#118793 = DIRECTION('center_axis',(0.,0.,-1.)) ;
#118794 = DIRECTION('ref_axis',(-1.,0.,0.)) ;
#118795 = DIRECTION('center_axis',(-0.577350269189625,0.577350269189625,0.577350269189628)) ;
#118796 = DIRECTION('ref_axis',(0.707106781186549,-7.51360742912421E-16,0.707106781186546)) ;
#118797 = DIRECTION('center_axis',(0.577350269189625,-0.577350269189625,-0.577350269189628)) ;
#118798 = DIRECTION('ref_axis',(0.707106781186548,-2.12258087602815E-15,0.707106781186547)) ;
#118799 = DIRECTION('center_axis',(-0.577350269189625,0.577350269189626,-0.577350269189626)) ;
#118800 = DIRECTION('ref_axis',(6.27941990732594E-17,0.707106781186548,0.707106781186548)) ;
#118801 = DIRECTION('center_axis',(0.577350269189625,-0.577350269189626,0.577350269189626)) ;
#118802 = DIRECTION('ref_axis',(-2.74316855014674E-14,0.707106781186534,0.707106781186561)) ;
#118803 = DIRECTION('center_axis',(0.577350269189617,-0.577350269189643,0.577350269189617)) ;
#118804 = DIRECTION('ref_axis',(0.707106781186564,0.707106781186531,-7.69284786604672E-16)) ;
#118805 = DIRECTION('center_axis',(0.,0.,-1.)) ;
#118806 = DIRECTION('ref_axis',(-1.,0.,0.)) ;
#118807 = DIRECTION('center_axis',(0.,0.,1.)) ;
#118808 = DIRECTION('ref_axis',(-1.,0.,0.)) ;
#118809 = DIRECTION('center_axis',(0.,0.,-1.)) ;
#118810 = DIRECTION('ref_axis',(-1.,0.,0.)) ;
#118811 = DIRECTION('center_axis',(0.,1.,0.)) ;
#118812 = DIRECTION('ref_axis',(1.,0.,0.)) ;
#118813 = DIRECTION('center_axis',(0.,-1.,-1.39913024272358E-14)) ;
#118814 = DIRECTION('ref_axis',(0.,-1.39913024272358E-14,1.)) ;
#118815 = DIRECTION('center_axis',(1.7347234759768E-14,-1.73472347597681E-14,
1.)) ;
#118816 = DIRECTION('ref_axis',(-1.79366203433577E-43,1.,1.73472347597681E-14)) ;
#118817 = DIRECTION('center_axis',(0.577350269189625,-0.577350269189626,-0.577350269189626)) ;
#118818 = DIRECTION('ref_axis',(6.27941990732594E-17,0.707106781186548,-0.707106781186548)) ;
#118819 = DIRECTION('center_axis',(0.577350269189625,-0.577350269189626,-0.577350269189626)) ;
#118820 = DIRECTION('ref_axis',(-7.7646791370609E-16,0.707106781186547,-0.707106781186548)) ;
#118821 = DIRECTION('center_axis',(0.577350269189636,-0.577350269189637,-0.577350269189605)) ;
#118822 = DIRECTION('ref_axis',(0.707106781186548,0.707106781186547,-1.89650892222054E-16)) ;
#118823 = DIRECTION('center_axis',(0.,0.,-1.)) ;
#118824 = DIRECTION('ref_axis',(-1.,0.,0.)) ;
#118825 = DIRECTION('center_axis',(0.,2.4532694666934E-14,1.)) ;
#118826 = DIRECTION('ref_axis',(0.,-1.,2.4532694666934E-14)) ;
#118827 = DIRECTION('center_axis',(0.,1.,1.95511867169518E-16)) ;
#118828 = DIRECTION('ref_axis',(0.,-1.95511867169518E-16,1.)) ;
#118829 = DIRECTION('center_axis',(1.21972744404619E-15,-1.,1.02806576696077E-15)) ;
#118830 = DIRECTION('ref_axis',(1.,1.21972744404619E-15,0.)) ;
#118831 = DIRECTION('center_axis',(0.,1.,0.)) ;
#118832 = DIRECTION('ref_axis',(1.,0.,0.)) ;
#118833 = DIRECTION('center_axis',(-1.41623908780917E-14,-1.,1.43540525551772E-14)) ;
#118834 = DIRECTION('ref_axis',(-1.64655217322172E-31,1.43540525551772E-14,
1.)) ;
#118835 = DIRECTION('center_axis',(0.,1.,0.)) ;
#118836 = DIRECTION('ref_axis',(1.,0.,0.)) ;
#118837 = DIRECTION('center_axis',(-0.577350269189625,-0.577350269189626,
-0.577350269189626)) ;
#118838 = DIRECTION('ref_axis',(4.43092933859209E-16,-0.707106781186548,0.707106781186547)) ;
#118839 = DIRECTION('center_axis',(0.,0.,1.)) ;
#118840 = DIRECTION('ref_axis',(-1.,8.87690528722505E-15,0.)) ;
#118841 = DIRECTION('center_axis',(0.,1.,-1.95511867169518E-16)) ;
#118842 = DIRECTION('ref_axis',(0.,1.95511867169518E-16,1.)) ;
#118843 = DIRECTION('center_axis',(0.,-1.,-2.17536003491953E-14)) ;
#118844 = DIRECTION('ref_axis',(0.,2.17536003491953E-14,-1.)) ;
#118845 = DIRECTION('center_axis',(0.,0.,-1.)) ;
#118846 = DIRECTION('ref_axis',(-1.,0.,0.)) ;
#118847 = DIRECTION('center_axis',(-1.7347234759768E-14,-1.73472347597681E-14,
1.)) ;
#118848 = DIRECTION('ref_axis',(-8.96831017167883E-44,-1.,-1.73472347597681E-14)) ;
#118849 = DIRECTION('center_axis',(0.577350269189625,0.577350269189626,0.577350269189627)) ;
#118850 = DIRECTION('ref_axis',(-2.71345386026911E-16,-0.707106781186548,
0.707106781186547)) ;
#118851 = DIRECTION('center_axis',(0.577350269189625,0.577350269189626,0.577350269189627)) ;
#118852 = DIRECTION('ref_axis',(-2.71345386026911E-16,-0.707106781186548,
0.707106781186547)) ;
#118853 = DIRECTION('center_axis',(0.,1.,0.)) ;
#118854 = DIRECTION('ref_axis',(1.,0.,0.)) ;
#118855 = DIRECTION('center_axis',(-0.577350269189615,-0.577350269189648,
0.577350269189615)) ;
#118856 = DIRECTION('ref_axis',(-7.65039491896549E-15,0.707106781186531,0.707106781186564)) ;
#118857 = DIRECTION('center_axis',(0.,0.,-1.)) ;
#118858 = DIRECTION('ref_axis',(-1.,0.,0.)) ;
#118859 = DIRECTION('center_axis',(0.,0.,1.)) ;
#118860 = DIRECTION('ref_axis',(-1.,1.0842021724855E-15,0.)) ;
#118861 = DIRECTION('center_axis',(0.,0.,-1.)) ;
#118862 = DIRECTION('ref_axis',(-1.,0.,0.)) ;
#118863 = DIRECTION('center_axis',(-0.577350269189625,-0.577350269189626,
0.577350269189627)) ;
#118864 = DIRECTION('ref_axis',(-2.71345386026911E-16,-0.707106781186548,
-0.707106781186547)) ;
#118865 = DIRECTION('center_axis',(0.577350269189625,0.577350269189626,-0.577350269189627)) ;
#118866 = DIRECTION('ref_axis',(1.27552458785726E-14,-0.707106781186554,-0.707106781186541)) ;
#118867 = DIRECTION('center_axis',(0.577350269189625,0.577350269189625,-0.577350269189628)) ;
#118868 = DIRECTION('ref_axis',(-0.707106781186549,-7.23605167296792E-16,
-0.707106781186546)) ;
#118869 = DIRECTION('center_axis',(-0.577350269189625,-0.577350269189625,
0.577350269189628)) ;
#118870 = DIRECTION('ref_axis',(-0.707106781186545,-8.28019006757666E-15,
-0.70710678118655)) ;
#118871 = DIRECTION('center_axis',(-0.577350269189628,-0.577350269189625,
0.577350269189625)) ;
#118872 = DIRECTION('ref_axis',(0.707106781186546,1.58001979428239E-16,0.707106781186549)) ;
#118873 = DIRECTION('center_axis',(0.,0.,-1.)) ;
#118874 = DIRECTION('ref_axis',(-1.,0.,0.)) ;
#118875 = DIRECTION('center_axis',(0.,0.,1.)) ;
#118876 = DIRECTION('ref_axis',(-1.,-8.67361737988404E-15,0.)) ;
#118877 = DIRECTION('center_axis',(0.,0.,-1.)) ;
#118878 = DIRECTION('ref_axis',(-1.,0.,0.)) ;
#118879 = DIRECTION('center_axis',(2.08166817117218E-16,1.,0.)) ;
#118880 = DIRECTION('ref_axis',(1.,0.,0.)) ;
#118881 = DIRECTION('center_axis',(-1.,0.,-4.40821857296469E-15)) ;
#118882 = DIRECTION('ref_axis',(4.40821857296469E-15,0.,-1.)) ;
#118883 = DIRECTION('center_axis',(0.,0.,1.)) ;
#118884 = DIRECTION('ref_axis',(-1.,0.,0.)) ;
#118885 = DIRECTION('center_axis',(-0.577350269189625,-0.577350269189625,
-0.577350269189628)) ;
#118886 = DIRECTION('ref_axis',(-0.707106781186549,-7.23605167296792E-16,
0.707106781186546)) ;
#118887 = DIRECTION('center_axis',(-0.577350269189625,-0.577350269189625,
-0.577350269189628)) ;
#118888 = DIRECTION('ref_axis',(-0.707106781186549,-7.51360742912421E-16,
0.707106781186546)) ;
#118889 = DIRECTION('center_axis',(-0.577350269189624,-0.577350269189624,
-0.57735026918963)) ;
#118890 = DIRECTION('ref_axis',(-0.70710678118655,-1.90469774984546E-15,0.707106781186545)) ;
#118891 = DIRECTION('center_axis',(0.,0.,-1.)) ;
#118892 = DIRECTION('ref_axis',(-1.,0.,0.)) ;
#118893 = DIRECTION('center_axis',(0.,0.,1.)) ;
#118894 = DIRECTION('ref_axis',(1.,0.,0.)) ;
#118895 = DIRECTION('center_axis',(-1.,0.,9.8563833862319E-18)) ;
#118896 = DIRECTION('ref_axis',(9.8563833862319E-18,0.,1.)) ;
#118897 = DIRECTION('center_axis',(-1.,3.93023287525994E-15,-3.93023287525994E-15)) ;
#118898 = DIRECTION('ref_axis',(-3.93023287525994E-15,-1.34524652575182E-43,
1.)) ;
#118899 = DIRECTION('center_axis',(2.08166817117218E-16,1.,0.)) ;
#118900 = DIRECTION('ref_axis',(1.,0.,0.)) ;
#118901 = DIRECTION('center_axis',(-1.,-4.33680868994201E-15,-4.33680868994201E-15)) ;
#118902 = DIRECTION('ref_axis',(4.33680868994201E-15,-1.59748024933029E-43,
-1.)) ;
#118903 = DIRECTION('center_axis',(2.08166817117218E-16,1.,0.)) ;
#118904 = DIRECTION('ref_axis',(1.,0.,0.)) ;
#118905 = DIRECTION('center_axis',(-0.577350269189625,0.577350269189624,-0.577350269189628)) ;
#118906 = DIRECTION('ref_axis',(0.707106781186549,-6.77492742903108E-16,-0.707106781186546)) ;
#118907 = DIRECTION('center_axis',(0.,0.,1.)) ;
#118908 = DIRECTION('ref_axis',(-1.,0.,0.)) ;
#118909 = DIRECTION('center_axis',(-1.,0.,-9.8563833862319E-18)) ;
#118910 = DIRECTION('ref_axis',(-9.8563833862319E-18,0.,1.)) ;
#118911 = DIRECTION('center_axis',(-1.,0.,-9.00809882301481E-15)) ;
#118912 = DIRECTION('ref_axis',(-9.00809882301481E-15,0.,1.)) ;
#118913 = DIRECTION('center_axis',(0.,0.,-1.)) ;
#118914 = DIRECTION('ref_axis',(-1.,0.,0.)) ;
#118915 = DIRECTION('center_axis',(0.,0.,1.)) ;
#118916 = DIRECTION('ref_axis',(1.,0.,0.)) ;
#118917 = DIRECTION('center_axis',(0.577350269189625,-0.577350269189625,0.577350269189628)) ;
#118918 = DIRECTION('ref_axis',(0.707106781186549,-7.23605167296792E-16,-0.707106781186546)) ;
#118919 = DIRECTION('center_axis',(0.577350269189625,-0.577350269189625,0.577350269189628)) ;
#118920 = DIRECTION('ref_axis',(0.707106781186549,-7.51360742912421E-16,-0.707106781186546)) ;
#118921 = DIRECTION('center_axis',(2.08166817117218E-16,1.,0.)) ;
#118922 = DIRECTION('ref_axis',(1.,0.,0.)) ;
#118923 = DIRECTION('center_axis',(-0.57735026918963,0.577350269189624,0.577350269189624)) ;
#118924 = DIRECTION('ref_axis',(-0.707106781186544,-8.1317851962192E-16,-0.707106781186551)) ;
#118925 = DIRECTION('center_axis',(0.,0.,-1.)) ;
#118926 = DIRECTION('ref_axis',(-1.,0.,0.)) ;
#118927 = DIRECTION('center_axis',(0.,0.,1.)) ;
#118928 = DIRECTION('ref_axis',(-1.,0.,0.)) ;
#118929 = DIRECTION('center_axis',(0.,0.,-1.)) ;
#118930 = DIRECTION('ref_axis',(-1.,0.,0.)) ;
#118931 = DIRECTION('center_axis',(-0.577350269189625,0.577350269189625,0.577350269189628)) ;
#118932 = DIRECTION('ref_axis',(0.707106781186549,-7.51360742912421E-16,0.707106781186546)) ;
#118933 = DIRECTION('center_axis',(0.577350269189625,-0.577350269189625,-0.577350269189628)) ;
#118934 = DIRECTION('ref_axis',(0.707106781186545,-8.51940988246475E-15,0.70710678118655)) ;
#118935 = DIRECTION('center_axis',(-0.577350269189625,0.577350269189626,-0.577350269189626)) ;
#118936 = DIRECTION('ref_axis',(6.27941990732594E-17,0.707106781186548,0.707106781186548)) ;
#118937 = DIRECTION('center_axis',(0.577350269189625,-0.577350269189626,0.577350269189626)) ;
#118938 = DIRECTION('ref_axis',(-6.96183268087023E-15,0.707106781186544,0.707106781186551)) ;
#118939 = DIRECTION('center_axis',(0.577350269189619,-0.57735026918964,0.577350269189619)) ;
#118940 = DIRECTION('ref_axis',(0.70710678118656,0.707106781186535,9.56388759536482E-16)) ;
#118941 = DIRECTION('center_axis',(0.,0.,-1.)) ;
#118942 = DIRECTION('ref_axis',(-1.,0.,0.)) ;
#118943 = DIRECTION('center_axis',(0.,0.,1.)) ;
#118944 = DIRECTION('ref_axis',(-1.,0.,0.)) ;
#118945 = DIRECTION('center_axis',(0.,0.,-1.)) ;
#118946 = DIRECTION('ref_axis',(-1.,0.,0.)) ;
#118947 = DIRECTION('center_axis',(0.,1.,0.)) ;
#118948 = DIRECTION('ref_axis',(1.,0.,0.)) ;
#118949 = DIRECTION('center_axis',(0.,-1.,-5.94151198964807E-15)) ;
#118950 = DIRECTION('ref_axis',(0.,-5.94151198964807E-15,1.)) ;
#118951 = DIRECTION('center_axis',(1.7347234759768E-14,-1.73472347597681E-14,
1.)) ;
#118952 = DIRECTION('ref_axis',(-1.79366203433577E-43,1.,1.73472347597681E-14)) ;
#118953 = DIRECTION('center_axis',(0.577350269189625,-0.577350269189626,-0.577350269189626)) ;
#118954 = DIRECTION('ref_axis',(6.27941990732594E-17,0.707106781186548,-0.707106781186548)) ;
#118955 = DIRECTION('center_axis',(0.577350269189625,-0.577350269189626,-0.577350269189626)) ;
#118956 = DIRECTION('ref_axis',(3.83287980137187E-16,0.707106781186548,-0.707106781186547)) ;
#118957 = DIRECTION('center_axis',(0.57735026918963,-0.577350269189631,-0.577350269189617)) ;
#118958 = DIRECTION('ref_axis',(0.707106781186548,0.707106781186547,-9.21608659434825E-17)) ;
#118959 = DIRECTION('center_axis',(0.,0.,-1.)) ;
#118960 = DIRECTION('ref_axis',(-1.,0.,0.)) ;
#118961 = DIRECTION('center_axis',(0.,0.,1.)) ;
#118962 = DIRECTION('ref_axis',(1.,0.,0.)) ;
#118963 = DIRECTION('center_axis',(0.,1.,1.95511867169518E-16)) ;
#118964 = DIRECTION('ref_axis',(0.,-1.95511867169518E-16,1.)) ;
#118965 = DIRECTION('center_axis',(1.15196480826585E-15,-1.,9.60303131180424E-16)) ;
#118966 = DIRECTION('ref_axis',(1.,1.15196480826585E-15,0.)) ;
#118967 = DIRECTION('center_axis',(0.,1.,0.)) ;
#118968 = DIRECTION('ref_axis',(1.,0.,0.)) ;
#118969 = DIRECTION('center_axis',(-7.5216525716181E-15,-1.,7.71331424870352E-15)) ;
#118970 = DIRECTION('ref_axis',(-8.74484647013228E-32,7.71331424870352E-15,
1.)) ;
#118971 = DIRECTION('center_axis',(0.,1.,0.)) ;
#118972 = DIRECTION('ref_axis',(1.,0.,0.)) ;
#118973 = DIRECTION('center_axis',(-0.577350269189626,-0.577350269189627,
-0.577350269189625)) ;
#118974 = DIRECTION('ref_axis',(-0.707106781186548,0.707106781186547,-9.19305248608458E-17)) ;
#118975 = DIRECTION('center_axis',(0.,0.,1.)) ;
#118976 = DIRECTION('ref_axis',(-1.,1.76182853028894E-15,0.)) ;
#118977 = DIRECTION('center_axis',(0.,1.,-1.95511867169518E-16)) ;
#118978 = DIRECTION('ref_axis',(0.,1.95511867169518E-16,1.)) ;
#118979 = DIRECTION('center_axis',(0.,-1.,-7.95395959904499E-15)) ;
#118980 = DIRECTION('ref_axis',(0.,7.95395959904499E-15,-1.)) ;
#118981 = DIRECTION('center_axis',(0.,0.,-1.)) ;
#118982 = DIRECTION('ref_axis',(-1.,0.,0.)) ;
#118983 = DIRECTION('center_axis',(0.,0.,1.)) ;
#118984 = DIRECTION('ref_axis',(1.,0.,0.)) ;
#118985 = DIRECTION('center_axis',(0.577350269189625,0.577350269189626,0.577350269189627)) ;
#118986 = DIRECTION('ref_axis',(-2.71345386026911E-16,-0.707106781186548,
0.707106781186547)) ;
#118987 = DIRECTION('center_axis',(0.577350269189625,0.577350269189626,0.577350269189627)) ;
#118988 = DIRECTION('ref_axis',(-2.71345386026911E-16,-0.707106781186548,
0.707106781186547)) ;
#118989 = DIRECTION('center_axis',(0.,1.,0.)) ;
#118990 = DIRECTION('ref_axis',(1.,0.,0.)) ;
#118991 = DIRECTION('center_axis',(-0.577350269189622,-0.577350269189633,
0.577350269189622)) ;
#118992 = DIRECTION('ref_axis',(-1.42949951585321E-15,0.707106781186542,0.707106781186553)) ;
#118993 = DIRECTION('center_axis',(0.,0.,-1.)) ;
#118994 = DIRECTION('ref_axis',(-1.,0.,0.)) ;
#118995 = DIRECTION('center_axis',(0.,0.,1.)) ;
#118996 = DIRECTION('ref_axis',(-1.,1.0842021724855E-15,0.)) ;
#118997 = DIRECTION('center_axis',(0.,0.,-1.)) ;
#118998 = DIRECTION('ref_axis',(-1.,0.,0.)) ;
#118999 = DIRECTION('center_axis',(-0.577350269189625,-0.577350269189626,
0.577350269189627)) ;
#119000 = DIRECTION('ref_axis',(-2.71345386026911E-16,-0.707106781186548,
-0.707106781186547)) ;
#119001 = DIRECTION('center_axis',(0.577350269189625,0.577350269189626,-0.577350269189627)) ;
#119002 = DIRECTION('ref_axis',(-2.71345386026911E-16,-0.707106781186548,
-0.707106781186547)) ;
#119003 = DIRECTION('center_axis',(0.577350269189625,0.577350269189625,-0.577350269189628)) ;
#119004 = DIRECTION('ref_axis',(-0.707106781186552,5.19478420936363E-15,-0.707106781186543)) ;
#119005 = DIRECTION('center_axis',(-0.577350269189625,-0.577350269189625,
0.577350269189628)) ;
#119006 = DIRECTION('ref_axis',(-0.707106781186566,3.31891725521342E-14,-0.707106781186529)) ;
#119007 = DIRECTION('center_axis',(-0.577350269189652,-0.577350269189606,
0.57735026918962)) ;
#119008 = DIRECTION('ref_axis',(0.707106781186528,-3.96520952299298E-16,0.707106781186567)) ;
#119009 = DIRECTION('center_axis',(0.,0.,-1.)) ;
#119010 = DIRECTION('ref_axis',(-1.,0.,0.)) ;
#119011 = DIRECTION('center_axis',(0.,0.,1.)) ;
#119012 = DIRECTION('ref_axis',(-1.,-8.67361737988404E-15,0.)) ;
#119013 = DIRECTION('center_axis',(0.,0.,-1.)) ;
#119014 = DIRECTION('ref_axis',(-1.,0.,0.)) ;
#119015 = DIRECTION('center_axis',(2.08166817117218E-16,1.,0.)) ;
#119016 = DIRECTION('ref_axis',(1.,0.,0.)) ;
#119017 = DIRECTION('center_axis',(-1.,0.,-1.66745659064321E-14)) ;
#119018 = DIRECTION('ref_axis',(1.66745659064321E-14,2.60208521396523E-14,
-1.)) ;
#119019 = DIRECTION('center_axis',(-3.46944695195361E-14,-3.4694469519536E-14,
1.)) ;
#119020 = DIRECTION('ref_axis',(-1.,-1.68611237719883E-42,-3.46944695195361E-14)) ;
#119021 = DIRECTION('center_axis',(-0.577350269189625,-0.577350269189625,
-0.577350269189628)) ;
#119022 = DIRECTION('ref_axis',(-0.707106781186552,5.19478420936363E-15,0.707106781186543)) ;
#119023 = DIRECTION('center_axis',(-0.577350269189625,-0.577350269189625,
-0.577350269189628)) ;
#119024 = DIRECTION('ref_axis',(-0.707106781186552,5.1349792556416E-15,0.707106781186543)) ;
#119025 = DIRECTION('center_axis',(-0.577350269189626,-0.577350269189626,
-0.577350269189626)) ;
#119026 = DIRECTION('ref_axis',(0.707106781186547,-0.707106781186548,6.36902276417946E-16)) ;
#119027 = DIRECTION('center_axis',(0.,0.,-1.)) ;
#119028 = DIRECTION('ref_axis',(-1.,0.,0.)) ;
#119029 = DIRECTION('center_axis',(0.,0.,1.)) ;
#119030 = DIRECTION('ref_axis',(1.,0.,0.)) ;
#119031 = DIRECTION('center_axis',(-1.,0.,9.8563833862319E-18)) ;
#119032 = DIRECTION('ref_axis',(9.8563833862319E-18,0.,1.)) ;
#119033 = DIRECTION('center_axis',(-1.,8.87690528722497E-15,-8.87690528722518E-15)) ;
#119034 = DIRECTION('ref_axis',(-8.87690528722518E-15,4.48415508583942E-43,
1.)) ;
#119035 = DIRECTION('center_axis',(2.08166817117218E-16,1.,0.)) ;
#119036 = DIRECTION('ref_axis',(1.,0.,0.)) ;
#119037 = DIRECTION('center_axis',(-1.,8.53809210832325E-15,8.53809210832346E-15)) ;
#119038 = DIRECTION('ref_axis',(-8.53809210832339E-15,8.67361737988409E-15,
-1.)) ;
#119039 = DIRECTION('center_axis',(2.08166817117218E-16,1.,0.)) ;
#119040 = DIRECTION('ref_axis',(1.,0.,0.)) ;
#119041 = DIRECTION('center_axis',(-0.577350269189622,0.577350269189621,-0.577350269189634)) ;
#119042 = DIRECTION('ref_axis',(0.707106781186563,1.66970714627838E-14,-0.707106781186532)) ;
#119043 = DIRECTION('center_axis',(0.,0.,1.)) ;
#119044 = DIRECTION('ref_axis',(-1.,0.,0.)) ;
#119045 = DIRECTION('center_axis',(-1.,0.,-9.8563833862319E-18)) ;
#119046 = DIRECTION('ref_axis',(-9.8563833862319E-18,0.,1.)) ;
#119047 = DIRECTION('center_axis',(-1.,0.,-1.34163173959798E-15)) ;
#119048 = DIRECTION('ref_axis',(-1.34163173959798E-15,0.,1.)) ;
#119049 = DIRECTION('center_axis',(0.,0.,-1.)) ;
#119050 = DIRECTION('ref_axis',(-1.,0.,0.)) ;
#119051 = DIRECTION('center_axis',(-3.46944695195361E-14,3.4694469519536E-14,
1.)) ;
#119052 = DIRECTION('ref_axis',(1.,-1.68611237719883E-42,3.46944695195361E-14)) ;
#119053 = DIRECTION('center_axis',(0.577350269189625,-0.577350269189625,0.577350269189628)) ;
#119054 = DIRECTION('ref_axis',(0.707106781186552,5.19478420936363E-15,-0.707106781186543)) ;
#119055 = DIRECTION('center_axis',(0.577350269189625,-0.577350269189625,0.577350269189628)) ;
#119056 = DIRECTION('ref_axis',(0.707106781186552,5.1349792556416E-15,-0.707106781186543)) ;
#119057 = DIRECTION('center_axis',(2.08166817117218E-16,1.,0.)) ;
#119058 = DIRECTION('ref_axis',(1.,0.,0.)) ;
#119059 = DIRECTION('center_axis',(-0.577350269189646,0.577350269189609,0.577350269189623)) ;
#119060 = DIRECTION('ref_axis',(-0.707106781186529,8.66006384940495E-15,-0.707106781186566)) ;
#119061 = DIRECTION('center_axis',(0.,0.,-1.)) ;
#119062 = DIRECTION('ref_axis',(-1.,0.,0.)) ;
#119063 = DIRECTION('center_axis',(0.,0.,1.)) ;
#119064 = DIRECTION('ref_axis',(-1.,0.,0.)) ;
#119065 = DIRECTION('center_axis',(0.,0.,-1.)) ;
#119066 = DIRECTION('ref_axis',(-1.,0.,0.)) ;
#119067 = DIRECTION('center_axis',(-0.577350269189625,0.577350269189625,0.577350269189628)) ;
#119068 = DIRECTION('ref_axis',(0.707106781186552,5.1349792556416E-15,0.707106781186543)) ;
#119069 = DIRECTION('center_axis',(0.577350269189625,-0.577350269189625,-0.577350269189628)) ;
#119070 = DIRECTION('ref_axis',(0.707106781186559,1.92955635991398E-14,0.707106781186536)) ;
#119071 = DIRECTION('center_axis',(-0.577350269189625,0.577350269189626,-0.577350269189626)) ;
#119072 = DIRECTION('ref_axis',(5.20172641667636E-15,0.70710678118655,0.707106781186545)) ;
#119073 = DIRECTION('center_axis',(0.577350269189625,-0.577350269189626,0.577350269189626)) ;
#119074 = DIRECTION('ref_axis',(1.27903606950626E-14,0.707106781186554,0.707106781186541)) ;
#119075 = DIRECTION('center_axis',(0.577350269189636,-0.577350269189592,0.57735026918965)) ;
#119076 = DIRECTION('ref_axis',(0.707106781186558,3.40611850366138E-15,-0.707106781186537)) ;
#119077 = DIRECTION('center_axis',(0.,0.,-1.)) ;
#119078 = DIRECTION('ref_axis',(-1.,0.,0.)) ;
#119079 = DIRECTION('center_axis',(0.,0.,1.)) ;
#119080 = DIRECTION('ref_axis',(-1.,1.57209315010398E-14,0.)) ;
#119081 = DIRECTION('center_axis',(0.,0.,-1.)) ;
#119082 = DIRECTION('ref_axis',(-1.,0.,0.)) ;
#119083 = DIRECTION('center_axis',(0.,1.,0.)) ;
#119084 = DIRECTION('ref_axis',(1.,0.,0.)) ;
#119085 = DIRECTION('center_axis',(0.,-1.,7.76229792195976E-15)) ;
#119086 = DIRECTION('ref_axis',(3.46944695195364E-14,7.76229792195976E-15,
1.)) ;
#119087 = DIRECTION('center_axis',(-3.46944695195361E-14,3.46944695195361E-14,
1.)) ;
#119088 = DIRECTION('ref_axis',(-7.17464813734306E-43,1.,-3.46944695195361E-14)) ;
#119089 = DIRECTION('center_axis',(0.577350269189625,-0.577350269189626,-0.577350269189626)) ;
#119090 = DIRECTION('ref_axis',(5.20172641667636E-15,0.70710678118655,-0.707106781186545)) ;
#119091 = DIRECTION('center_axis',(0.577350269189625,-0.577350269189626,-0.577350269189626)) ;
#119092 = DIRECTION('ref_axis',(5.11416588733871E-15,0.70710678118655,-0.707106781186545)) ;
#119093 = DIRECTION('center_axis',(0.577350269189624,-0.577350269189625,-0.577350269189629)) ;
#119094 = DIRECTION('ref_axis',(4.29556475679742E-15,0.707106781186552,-0.707106781186543)) ;
#119095 = DIRECTION('center_axis',(0.,0.,-1.)) ;
#119096 = DIRECTION('ref_axis',(-1.,0.,0.)) ;
#119097 = DIRECTION('center_axis',(0.,0.,1.)) ;
#119098 = DIRECTION('ref_axis',(1.,0.,0.)) ;
#119099 = DIRECTION('center_axis',(0.,1.,1.95511867169518E-16)) ;
#119100 = DIRECTION('ref_axis',(0.,-1.95511867169518E-16,1.)) ;
#119101 = DIRECTION('center_axis',(-7.65717784317885E-15,-1.,-7.84883952026447E-15)) ;
#119102 = DIRECTION('ref_axis',(-8.90241127119925E-32,7.84883952026447E-15,
-1.)) ;
#119103 = DIRECTION('center_axis',(0.,1.,0.)) ;
#119104 = DIRECTION('ref_axis',(1.,0.,0.)) ;
#119105 = DIRECTION('center_axis',(-1.28749007982652E-15,-1.,1.47915175691198E-15)) ;
#119106 = DIRECTION('ref_axis',(3.46944695195364E-14,1.47915175691194E-15,
1.)) ;
#119107 = DIRECTION('center_axis',(0.,1.,0.)) ;
#119108 = DIRECTION('ref_axis',(1.,0.,0.)) ;
#119109 = DIRECTION('center_axis',(-0.577350269189619,-0.577350269189621,
-0.577350269189638)) ;
#119110 = DIRECTION('ref_axis',(1.66660234080318E-14,-0.707106781186566,0.707106781186529)) ;
#119111 = DIRECTION('center_axis',(0.,0.,1.)) ;
#119112 = DIRECTION('ref_axis',(-1.,-3.52365706057788E-15,0.)) ;
#119113 = DIRECTION('center_axis',(0.,1.,-1.95511867169518E-16)) ;
#119114 = DIRECTION('ref_axis',(0.,1.95511867169518E-16,1.)) ;
#119115 = DIRECTION('center_axis',(0.,-1.,3.06658683336682E-15)) ;
#119116 = DIRECTION('ref_axis',(0.,-3.06658683336682E-15,-1.)) ;
#119117 = DIRECTION('center_axis',(0.,0.,-1.)) ;
#119118 = DIRECTION('ref_axis',(-1.,0.,0.)) ;
#119119 = DIRECTION('center_axis',(-3.4694469519536E-14,-3.46944695195361E-14,
1.)) ;
#119120 = DIRECTION('ref_axis',(-8.96831017167883E-43,-1.,-3.46944695195361E-14)) ;
#119121 = DIRECTION('center_axis',(0.577350269189625,0.577350269189626,0.577350269189627)) ;
#119122 = DIRECTION('ref_axis',(5.35231302451417E-15,-0.707106781186551,0.707106781186544)) ;
#119123 = DIRECTION('center_axis',(0.577350269189625,0.577350269189626,0.577350269189627)) ;
#119124 = DIRECTION('ref_axis',(5.35231302451417E-15,-0.707106781186551,0.707106781186544)) ;
#119125 = DIRECTION('center_axis',(0.,1.,0.)) ;
#119126 = DIRECTION('ref_axis',(1.,0.,0.)) ;
#119127 = DIRECTION('center_axis',(-0.577350269189609,-0.577350269189646,
0.577350269189623)) ;
#119128 = DIRECTION('ref_axis',(8.91337114590872E-15,0.707106781186529,0.707106781186566)) ;
#119129 = DIRECTION('center_axis',(0.,0.,-1.)) ;
#119130 = DIRECTION('ref_axis',(-1.,0.,0.)) ;
#119131 = DIRECTION('center_axis',(0.,0.,1.)) ;
#119132 = DIRECTION('ref_axis',(-1.,1.0842021724855E-15,0.)) ;
#119133 = DIRECTION('center_axis',(0.,0.,-1.)) ;
#119134 = DIRECTION('ref_axis',(-1.,0.,0.)) ;
#119135 = DIRECTION('center_axis',(-0.577350269189625,-0.577350269189626,
0.577350269189627)) ;
#119136 = DIRECTION('ref_axis',(5.35231302451417E-15,-0.707106781186551,-0.707106781186544)) ;
#119137 = DIRECTION('center_axis',(0.577350269189625,0.577350269189626,-0.577350269189627)) ;
#119138 = DIRECTION('ref_axis',(-6.40836823623517E-14,-0.707106781186516,
-0.707106781186579)) ;
#119139 = DIRECTION('center_axis',(0.577350269189625,0.577350269189625,-0.577350269189628)) ;
#119140 = DIRECTION('ref_axis',(-0.707106781186552,5.19478420936363E-15,-0.707106781186543)) ;
#119141 = DIRECTION('center_axis',(-0.577350269189625,-0.577350269189625,
0.577350269189628)) ;
#119142 = DIRECTION('ref_axis',(-0.707106781186566,3.31891725521342E-14,-0.707106781186529)) ;
#119143 = DIRECTION('center_axis',(-0.577350269189652,-0.577350269189606,
0.57735026918962)) ;
#119144 = DIRECTION('ref_axis',(0.707106781186528,-3.96520952299298E-16,0.707106781186567)) ;
#119145 = DIRECTION('center_axis',(0.,0.,-1.)) ;
#119146 = DIRECTION('ref_axis',(-1.,0.,0.)) ;
#119147 = DIRECTION('center_axis',(0.,0.,1.)) ;
#119148 = DIRECTION('ref_axis',(-1.,-8.67361737988404E-15,0.)) ;
#119149 = DIRECTION('center_axis',(0.,0.,-1.)) ;
#119150 = DIRECTION('ref_axis',(-1.,0.,0.)) ;
#119151 = DIRECTION('center_axis',(2.08166817117218E-16,1.,0.)) ;
#119152 = DIRECTION('ref_axis',(1.,0.,0.)) ;
#119153 = DIRECTION('center_axis',(-1.,0.,-1.66745659064321E-14)) ;
#119154 = DIRECTION('ref_axis',(1.66745659064321E-14,2.60208521396523E-14,
-1.)) ;
#119155 = DIRECTION('center_axis',(-3.46944695195361E-14,-3.4694469519536E-14,
1.)) ;
#119156 = DIRECTION('ref_axis',(-1.,-1.68611237719883E-42,-3.46944695195361E-14)) ;
#119157 = DIRECTION('center_axis',(-0.577350269189625,-0.577350269189625,
-0.577350269189628)) ;
#119158 = DIRECTION('ref_axis',(-0.707106781186552,5.19478420936363E-15,0.707106781186543)) ;
#119159 = DIRECTION('center_axis',(-0.577350269189625,-0.577350269189625,
-0.577350269189628)) ;
#119160 = DIRECTION('ref_axis',(-0.707106781186552,5.1349792556416E-15,0.707106781186543)) ;
#119161 = DIRECTION('center_axis',(-0.577350269189626,-0.577350269189626,
-0.577350269189626)) ;
#119162 = DIRECTION('ref_axis',(0.707106781186547,-0.707106781186548,6.36902276417946E-16)) ;
#119163 = DIRECTION('center_axis',(0.,0.,-1.)) ;
#119164 = DIRECTION('ref_axis',(-1.,0.,0.)) ;
#119165 = DIRECTION('center_axis',(0.,0.,1.)) ;
#119166 = DIRECTION('ref_axis',(1.,0.,0.)) ;
#119167 = DIRECTION('center_axis',(-1.,0.,9.8563833862319E-18)) ;
#119168 = DIRECTION('ref_axis',(9.8563833862319E-18,0.,1.)) ;
#119169 = DIRECTION('center_axis',(-1.,8.87690528722497E-15,-8.87690528722518E-15)) ;
#119170 = DIRECTION('ref_axis',(-8.87690528722518E-15,4.48415508583942E-43,
1.)) ;
#119171 = DIRECTION('center_axis',(2.08166817117218E-16,1.,0.)) ;
#119172 = DIRECTION('ref_axis',(1.,0.,0.)) ;
#119173 = DIRECTION('center_axis',(-1.,8.53809210832325E-15,8.53809210832346E-15)) ;
#119174 = DIRECTION('ref_axis',(-8.53809210832339E-15,8.67361737988409E-15,
-1.)) ;
#119175 = DIRECTION('center_axis',(2.08166817117218E-16,1.,0.)) ;
#119176 = DIRECTION('ref_axis',(1.,0.,0.)) ;
#119177 = DIRECTION('center_axis',(-0.577350269189622,0.577350269189621,-0.577350269189634)) ;
#119178 = DIRECTION('ref_axis',(0.707106781186563,1.66970714627838E-14,-0.707106781186532)) ;
#119179 = DIRECTION('center_axis',(0.,0.,1.)) ;
#119180 = DIRECTION('ref_axis',(-1.,0.,0.)) ;
#119181 = DIRECTION('center_axis',(-1.,0.,-9.8563833862319E-18)) ;
#119182 = DIRECTION('ref_axis',(-9.8563833862319E-18,0.,1.)) ;
#119183 = DIRECTION('center_axis',(-1.,0.,-1.34163173959798E-15)) ;
#119184 = DIRECTION('ref_axis',(-1.34163173959798E-15,0.,1.)) ;
#119185 = DIRECTION('center_axis',(0.,0.,-1.)) ;
#119186 = DIRECTION('ref_axis',(-1.,0.,0.)) ;
#119187 = DIRECTION('center_axis',(-3.46944695195361E-14,3.4694469519536E-14,
1.)) ;
#119188 = DIRECTION('ref_axis',(1.,-1.68611237719883E-42,3.46944695195361E-14)) ;
#119189 = DIRECTION('center_axis',(0.577350269189625,-0.577350269189625,0.577350269189628)) ;
#119190 = DIRECTION('ref_axis',(0.707106781186552,5.19478420936363E-15,-0.707106781186543)) ;
#119191 = DIRECTION('center_axis',(0.577350269189625,-0.577350269189625,0.577350269189628)) ;
#119192 = DIRECTION('ref_axis',(0.707106781186552,5.1349792556416E-15,-0.707106781186543)) ;
#119193 = DIRECTION('center_axis',(2.08166817117218E-16,1.,0.)) ;
#119194 = DIRECTION('ref_axis',(1.,0.,0.)) ;
#119195 = DIRECTION('center_axis',(-0.577350269189646,0.577350269189609,0.577350269189623)) ;
#119196 = DIRECTION('ref_axis',(-0.707106781186529,8.66006384940495E-15,-0.707106781186566)) ;
#119197 = DIRECTION('center_axis',(0.,0.,-1.)) ;
#119198 = DIRECTION('ref_axis',(-1.,0.,0.)) ;
#119199 = DIRECTION('center_axis',(0.,0.,1.)) ;
#119200 = DIRECTION('ref_axis',(-1.,0.,0.)) ;
#119201 = DIRECTION('center_axis',(0.,0.,-1.)) ;
#119202 = DIRECTION('ref_axis',(-1.,0.,0.)) ;
#119203 = DIRECTION('center_axis',(-0.577350269189625,0.577350269189625,0.577350269189628)) ;
#119204 = DIRECTION('ref_axis',(0.707106781186552,5.1349792556416E-15,0.707106781186543)) ;
#119205 = DIRECTION('center_axis',(0.577350269189625,-0.577350269189625,-0.577350269189628)) ;
#119206 = DIRECTION('ref_axis',(0.707106781186559,1.92955635991398E-14,0.707106781186536)) ;
#119207 = DIRECTION('center_axis',(-0.577350269189625,0.577350269189626,-0.577350269189626)) ;
#119208 = DIRECTION('ref_axis',(5.20172641667636E-15,0.70710678118655,0.707106781186545)) ;
#119209 = DIRECTION('center_axis',(0.577350269189625,-0.577350269189626,0.577350269189626)) ;
#119210 = DIRECTION('ref_axis',(1.27903606950626E-14,0.707106781186554,0.707106781186541)) ;
#119211 = DIRECTION('center_axis',(0.577350269189636,-0.577350269189592,0.57735026918965)) ;
#119212 = DIRECTION('ref_axis',(0.707106781186558,3.40611850366138E-15,-0.707106781186537)) ;
#119213 = DIRECTION('center_axis',(0.,0.,-1.)) ;
#119214 = DIRECTION('ref_axis',(-1.,0.,0.)) ;
#119215 = DIRECTION('center_axis',(0.,0.,1.)) ;
#119216 = DIRECTION('ref_axis',(-1.,1.57209315010398E-14,0.)) ;
#119217 = DIRECTION('center_axis',(0.,0.,-1.)) ;
#119218 = DIRECTION('ref_axis',(-1.,0.,0.)) ;
#119219 = DIRECTION('center_axis',(0.,1.,0.)) ;
#119220 = DIRECTION('ref_axis',(1.,0.,0.)) ;
#119221 = DIRECTION('center_axis',(0.,-1.,7.76229792195976E-15)) ;
#119222 = DIRECTION('ref_axis',(3.46944695195364E-14,7.76229792195976E-15,
1.)) ;
#119223 = DIRECTION('center_axis',(-3.46944695195361E-14,3.46944695195361E-14,
1.)) ;
#119224 = DIRECTION('ref_axis',(-7.17464813734306E-43,1.,-3.46944695195361E-14)) ;
#119225 = DIRECTION('center_axis',(0.577350269189625,-0.577350269189626,-0.577350269189626)) ;
#119226 = DIRECTION('ref_axis',(5.20172641667636E-15,0.70710678118655,-0.707106781186545)) ;
#119227 = DIRECTION('center_axis',(0.577350269189625,-0.577350269189626,-0.577350269189626)) ;
#119228 = DIRECTION('ref_axis',(5.11416588733871E-15,0.70710678118655,-0.707106781186545)) ;
#119229 = DIRECTION('center_axis',(0.577350269189624,-0.577350269189625,-0.577350269189629)) ;
#119230 = DIRECTION('ref_axis',(4.29556475679742E-15,0.707106781186552,-0.707106781186543)) ;
#119231 = DIRECTION('center_axis',(0.,0.,-1.)) ;
#119232 = DIRECTION('ref_axis',(-1.,0.,0.)) ;
#119233 = DIRECTION('center_axis',(0.,0.,1.)) ;
#119234 = DIRECTION('ref_axis',(1.,0.,0.)) ;
#119235 = DIRECTION('center_axis',(0.,1.,1.95511867169518E-16)) ;
#119236 = DIRECTION('ref_axis',(0.,-1.95511867169518E-16,1.)) ;
#119237 = DIRECTION('center_axis',(-7.65717784317885E-15,-1.,-7.84883952026447E-15)) ;
#119238 = DIRECTION('ref_axis',(-8.90241127119925E-32,7.84883952026447E-15,
-1.)) ;
#119239 = DIRECTION('center_axis',(0.,1.,0.)) ;
#119240 = DIRECTION('ref_axis',(1.,0.,0.)) ;
#119241 = DIRECTION('center_axis',(-1.28749007982652E-15,-1.,1.47915175691198E-15)) ;
#119242 = DIRECTION('ref_axis',(3.46944695195364E-14,1.47915175691194E-15,
1.)) ;
#119243 = DIRECTION('center_axis',(0.,1.,0.)) ;
#119244 = DIRECTION('ref_axis',(1.,0.,0.)) ;
#119245 = DIRECTION('center_axis',(-0.577350269189619,-0.577350269189621,
-0.577350269189638)) ;
#119246 = DIRECTION('ref_axis',(1.66660234080318E-14,-0.707106781186566,0.707106781186529)) ;
#119247 = DIRECTION('center_axis',(0.,0.,1.)) ;
#119248 = DIRECTION('ref_axis',(-1.,-3.52365706057788E-15,0.)) ;
#119249 = DIRECTION('center_axis',(0.,1.,-1.95511867169518E-16)) ;
#119250 = DIRECTION('ref_axis',(0.,1.95511867169518E-16,1.)) ;
#119251 = DIRECTION('center_axis',(0.,-1.,3.06658683336682E-15)) ;
#119252 = DIRECTION('ref_axis',(0.,-3.06658683336682E-15,-1.)) ;
#119253 = DIRECTION('center_axis',(0.,0.,-1.)) ;
#119254 = DIRECTION('ref_axis',(-1.,0.,0.)) ;
#119255 = DIRECTION('center_axis',(-3.4694469519536E-14,-3.46944695195361E-14,
1.)) ;
#119256 = DIRECTION('ref_axis',(-8.96831017167883E-43,-1.,-3.46944695195361E-14)) ;
#119257 = DIRECTION('center_axis',(0.577350269189625,0.577350269189626,0.577350269189627)) ;
#119258 = DIRECTION('ref_axis',(5.35231302451417E-15,-0.707106781186551,0.707106781186544)) ;
#119259 = DIRECTION('center_axis',(0.577350269189625,0.577350269189626,0.577350269189627)) ;
#119260 = DIRECTION('ref_axis',(5.35231302451417E-15,-0.707106781186551,0.707106781186544)) ;
#119261 = DIRECTION('center_axis',(0.,1.,0.)) ;
#119262 = DIRECTION('ref_axis',(1.,0.,0.)) ;
#119263 = DIRECTION('center_axis',(-0.577350269189609,-0.577350269189646,
0.577350269189623)) ;
#119264 = DIRECTION('ref_axis',(8.91337114590872E-15,0.707106781186529,0.707106781186566)) ;
#119265 = DIRECTION('center_axis',(0.,0.,-1.)) ;
#119266 = DIRECTION('ref_axis',(-1.,0.,0.)) ;
#119267 = DIRECTION('center_axis',(0.,0.,1.)) ;
#119268 = DIRECTION('ref_axis',(-1.,1.0842021724855E-15,0.)) ;
#119269 = DIRECTION('center_axis',(0.,0.,-1.)) ;
#119270 = DIRECTION('ref_axis',(-1.,0.,0.)) ;
#119271 = DIRECTION('center_axis',(-0.577350269189625,-0.577350269189626,
0.577350269189627)) ;
#119272 = DIRECTION('ref_axis',(5.35231302451417E-15,-0.707106781186551,-0.707106781186544)) ;
#119273 = DIRECTION('center_axis',(0.577350269189625,0.577350269189626,-0.577350269189627)) ;
#119274 = DIRECTION('ref_axis',(-6.40836823623517E-14,-0.707106781186516,
-0.707106781186579)) ;
#119275 = DIRECTION('center_axis',(0.577350269189625,0.577350269189625,-0.577350269189628)) ;
#119276 = DIRECTION('ref_axis',(-0.707106781186552,5.19478420936363E-15,-0.707106781186543)) ;
#119277 = DIRECTION('center_axis',(-0.577350269189625,-0.577350269189625,
0.577350269189628)) ;
#119278 = DIRECTION('ref_axis',(-0.707106781186566,3.31891725521342E-14,-0.707106781186529)) ;
#119279 = DIRECTION('center_axis',(-0.577350269189652,-0.577350269189606,
0.57735026918962)) ;
#119280 = DIRECTION('ref_axis',(0.707106781186528,-3.96520952299298E-16,0.707106781186567)) ;
#119281 = DIRECTION('center_axis',(0.,0.,-1.)) ;
#119282 = DIRECTION('ref_axis',(-1.,0.,0.)) ;
#119283 = DIRECTION('center_axis',(0.,0.,1.)) ;
#119284 = DIRECTION('ref_axis',(-1.,-8.67361737988404E-15,0.)) ;
#119285 = DIRECTION('center_axis',(0.,0.,-1.)) ;
#119286 = DIRECTION('ref_axis',(-1.,0.,0.)) ;
#119287 = DIRECTION('center_axis',(2.08166817117218E-16,1.,0.)) ;
#119288 = DIRECTION('ref_axis',(1.,0.,0.)) ;
#119289 = DIRECTION('center_axis',(-1.,0.,-1.66745659064321E-14)) ;
#119290 = DIRECTION('ref_axis',(1.66745659064321E-14,2.60208521396523E-14,
-1.)) ;
#119291 = DIRECTION('center_axis',(-3.46944695195361E-14,-3.4694469519536E-14,
1.)) ;
#119292 = DIRECTION('ref_axis',(-1.,-1.68611237719883E-42,-3.46944695195361E-14)) ;
#119293 = DIRECTION('center_axis',(-0.577350269189625,-0.577350269189625,
-0.577350269189628)) ;
#119294 = DIRECTION('ref_axis',(-0.707106781186552,5.19478420936363E-15,0.707106781186543)) ;
#119295 = DIRECTION('center_axis',(-0.577350269189625,-0.577350269189625,
-0.577350269189628)) ;
#119296 = DIRECTION('ref_axis',(-0.707106781186552,5.1349792556416E-15,0.707106781186543)) ;
#119297 = DIRECTION('center_axis',(-0.577350269189626,-0.577350269189626,
-0.577350269189626)) ;
#119298 = DIRECTION('ref_axis',(0.707106781186547,-0.707106781186548,6.36902276417946E-16)) ;
#119299 = DIRECTION('center_axis',(0.,0.,-1.)) ;
#119300 = DIRECTION('ref_axis',(-1.,0.,0.)) ;
#119301 = DIRECTION('center_axis',(0.,0.,1.)) ;
#119302 = DIRECTION('ref_axis',(1.,0.,0.)) ;
#119303 = DIRECTION('center_axis',(-1.,0.,9.8563833862319E-18)) ;
#119304 = DIRECTION('ref_axis',(9.8563833862319E-18,0.,1.)) ;
#119305 = DIRECTION('center_axis',(-1.,8.87690528722497E-15,-8.87690528722518E-15)) ;
#119306 = DIRECTION('ref_axis',(-8.87690528722518E-15,4.48415508583942E-43,
1.)) ;
#119307 = DIRECTION('center_axis',(2.08166817117218E-16,1.,0.)) ;
#119308 = DIRECTION('ref_axis',(1.,0.,0.)) ;
#119309 = DIRECTION('center_axis',(-1.,8.53809210832325E-15,8.53809210832346E-15)) ;
#119310 = DIRECTION('ref_axis',(-8.53809210832339E-15,8.67361737988409E-15,
-1.)) ;
#119311 = DIRECTION('center_axis',(2.08166817117218E-16,1.,0.)) ;
#119312 = DIRECTION('ref_axis',(1.,0.,0.)) ;
#119313 = DIRECTION('center_axis',(-0.577350269189622,0.577350269189621,-0.577350269189634)) ;
#119314 = DIRECTION('ref_axis',(0.707106781186563,1.66970714627838E-14,-0.707106781186532)) ;
#119315 = DIRECTION('center_axis',(0.,0.,1.)) ;
#119316 = DIRECTION('ref_axis',(-1.,0.,0.)) ;
#119317 = DIRECTION('center_axis',(-1.,0.,-9.8563833862319E-18)) ;
#119318 = DIRECTION('ref_axis',(-9.8563833862319E-18,0.,1.)) ;
#119319 = DIRECTION('center_axis',(-1.,0.,-1.34163173959798E-15)) ;
#119320 = DIRECTION('ref_axis',(-1.34163173959798E-15,0.,1.)) ;
#119321 = DIRECTION('center_axis',(0.,0.,-1.)) ;
#119322 = DIRECTION('ref_axis',(-1.,0.,0.)) ;
#119323 = DIRECTION('center_axis',(-3.46944695195361E-14,3.4694469519536E-14,
1.)) ;
#119324 = DIRECTION('ref_axis',(1.,-1.68611237719883E-42,3.46944695195361E-14)) ;
#119325 = DIRECTION('center_axis',(0.577350269189625,-0.577350269189625,0.577350269189628)) ;
#119326 = DIRECTION('ref_axis',(0.707106781186552,5.19478420936363E-15,-0.707106781186543)) ;
#119327 = DIRECTION('center_axis',(0.577350269189625,-0.577350269189625,0.577350269189628)) ;
#119328 = DIRECTION('ref_axis',(0.707106781186552,5.1349792556416E-15,-0.707106781186543)) ;
#119329 = DIRECTION('center_axis',(2.08166817117218E-16,1.,0.)) ;
#119330 = DIRECTION('ref_axis',(1.,0.,0.)) ;
#119331 = DIRECTION('center_axis',(-0.577350269189646,0.577350269189609,0.577350269189623)) ;
#119332 = DIRECTION('ref_axis',(-0.707106781186529,8.66006384940495E-15,-0.707106781186566)) ;
#119333 = DIRECTION('center_axis',(0.,0.,-1.)) ;
#119334 = DIRECTION('ref_axis',(-1.,0.,0.)) ;
#119335 = DIRECTION('center_axis',(0.,0.,1.)) ;
#119336 = DIRECTION('ref_axis',(-1.,0.,0.)) ;
#119337 = DIRECTION('center_axis',(0.,0.,-1.)) ;
#119338 = DIRECTION('ref_axis',(-1.,0.,0.)) ;
#119339 = DIRECTION('center_axis',(-0.577350269189625,0.577350269189625,0.577350269189628)) ;
#119340 = DIRECTION('ref_axis',(0.707106781186552,5.1349792556416E-15,0.707106781186543)) ;
#119341 = DIRECTION('center_axis',(0.577350269189625,-0.577350269189625,-0.577350269189628)) ;
#119342 = DIRECTION('ref_axis',(0.707106781186559,1.92955635991398E-14,0.707106781186536)) ;
#119343 = DIRECTION('center_axis',(-0.577350269189625,0.577350269189626,-0.577350269189626)) ;
#119344 = DIRECTION('ref_axis',(5.20172641667636E-15,0.70710678118655,0.707106781186545)) ;
#119345 = DIRECTION('center_axis',(0.577350269189625,-0.577350269189626,0.577350269189626)) ;
#119346 = DIRECTION('ref_axis',(1.27903606950626E-14,0.707106781186554,0.707106781186541)) ;
#119347 = DIRECTION('center_axis',(0.577350269189636,-0.577350269189592,0.57735026918965)) ;
#119348 = DIRECTION('ref_axis',(0.707106781186558,3.40611850366138E-15,-0.707106781186537)) ;
#119349 = DIRECTION('center_axis',(0.,0.,-1.)) ;
#119350 = DIRECTION('ref_axis',(-1.,0.,0.)) ;
#119351 = DIRECTION('center_axis',(0.,0.,1.)) ;
#119352 = DIRECTION('ref_axis',(-1.,1.57209315010398E-14,0.)) ;
#119353 = DIRECTION('center_axis',(0.,0.,-1.)) ;
#119354 = DIRECTION('ref_axis',(-1.,0.,0.)) ;
#119355 = DIRECTION('center_axis',(0.,1.,0.)) ;
#119356 = DIRECTION('ref_axis',(1.,0.,0.)) ;
#119357 = DIRECTION('center_axis',(0.,-1.,7.76229792195976E-15)) ;
#119358 = DIRECTION('ref_axis',(3.46944695195364E-14,7.76229792195976E-15,
1.)) ;
#119359 = DIRECTION('center_axis',(-3.46944695195361E-14,3.46944695195361E-14,
1.)) ;
#119360 = DIRECTION('ref_axis',(-7.17464813734306E-43,1.,-3.46944695195361E-14)) ;
#119361 = DIRECTION('center_axis',(0.577350269189625,-0.577350269189626,-0.577350269189626)) ;
#119362 = DIRECTION('ref_axis',(5.20172641667636E-15,0.70710678118655,-0.707106781186545)) ;
#119363 = DIRECTION('center_axis',(0.577350269189625,-0.577350269189626,-0.577350269189626)) ;
#119364 = DIRECTION('ref_axis',(5.11416588733871E-15,0.70710678118655,-0.707106781186545)) ;
#119365 = DIRECTION('center_axis',(0.577350269189624,-0.577350269189625,-0.577350269189629)) ;
#119366 = DIRECTION('ref_axis',(4.29556475679742E-15,0.707106781186552,-0.707106781186543)) ;
#119367 = DIRECTION('center_axis',(0.,0.,-1.)) ;
#119368 = DIRECTION('ref_axis',(-1.,0.,0.)) ;
#119369 = DIRECTION('center_axis',(0.,0.,1.)) ;
#119370 = DIRECTION('ref_axis',(1.,0.,0.)) ;
#119371 = DIRECTION('center_axis',(0.,1.,1.95511867169518E-16)) ;
#119372 = DIRECTION('ref_axis',(0.,-1.95511867169518E-16,1.)) ;
#119373 = DIRECTION('center_axis',(-7.65717784317885E-15,-1.,-7.84883952026447E-15)) ;
#119374 = DIRECTION('ref_axis',(-8.90241127119925E-32,7.84883952026447E-15,
-1.)) ;
#119375 = DIRECTION('center_axis',(0.,1.,0.)) ;
#119376 = DIRECTION('ref_axis',(1.,0.,0.)) ;
#119377 = DIRECTION('center_axis',(-1.28749007982652E-15,-1.,1.47915175691198E-15)) ;
#119378 = DIRECTION('ref_axis',(3.46944695195364E-14,1.47915175691194E-15,
1.)) ;
#119379 = DIRECTION('center_axis',(0.,1.,0.)) ;
#119380 = DIRECTION('ref_axis',(1.,0.,0.)) ;
#119381 = DIRECTION('center_axis',(-0.577350269189619,-0.577350269189621,
-0.577350269189638)) ;
#119382 = DIRECTION('ref_axis',(1.66660234080318E-14,-0.707106781186566,0.707106781186529)) ;
#119383 = DIRECTION('center_axis',(0.,0.,1.)) ;
#119384 = DIRECTION('ref_axis',(-1.,-3.52365706057788E-15,0.)) ;
#119385 = DIRECTION('center_axis',(0.,1.,-1.95511867169518E-16)) ;
#119386 = DIRECTION('ref_axis',(0.,1.95511867169518E-16,1.)) ;
#119387 = DIRECTION('center_axis',(0.,-1.,3.06658683336682E-15)) ;
#119388 = DIRECTION('ref_axis',(0.,-3.06658683336682E-15,-1.)) ;
#119389 = DIRECTION('center_axis',(0.,0.,-1.)) ;
#119390 = DIRECTION('ref_axis',(-1.,0.,0.)) ;
#119391 = DIRECTION('center_axis',(-3.4694469519536E-14,-3.46944695195361E-14,
1.)) ;
#119392 = DIRECTION('ref_axis',(-8.96831017167883E-43,-1.,-3.46944695195361E-14)) ;
#119393 = DIRECTION('center_axis',(0.577350269189625,0.577350269189626,0.577350269189627)) ;
#119394 = DIRECTION('ref_axis',(5.35231302451417E-15,-0.707106781186551,0.707106781186544)) ;
#119395 = DIRECTION('center_axis',(0.577350269189625,0.577350269189626,0.577350269189627)) ;
#119396 = DIRECTION('ref_axis',(5.35231302451417E-15,-0.707106781186551,0.707106781186544)) ;
#119397 = DIRECTION('center_axis',(0.,1.,0.)) ;
#119398 = DIRECTION('ref_axis',(1.,0.,0.)) ;
#119399 = DIRECTION('center_axis',(-0.577350269189609,-0.577350269189646,
0.577350269189623)) ;
#119400 = DIRECTION('ref_axis',(8.91337114590872E-15,0.707106781186529,0.707106781186566)) ;
#119401 = DIRECTION('center_axis',(0.,0.,-1.)) ;
#119402 = DIRECTION('ref_axis',(-1.,0.,0.)) ;
#119403 = DIRECTION('center_axis',(0.,0.,1.)) ;
#119404 = DIRECTION('ref_axis',(-1.,1.0842021724855E-15,0.)) ;
#119405 = DIRECTION('center_axis',(0.,0.,-1.)) ;
#119406 = DIRECTION('ref_axis',(-1.,0.,0.)) ;
#119407 = DIRECTION('center_axis',(-0.577350269189625,-0.577350269189626,
0.577350269189627)) ;
#119408 = DIRECTION('ref_axis',(5.35231302451417E-15,-0.707106781186551,-0.707106781186544)) ;
#119409 = DIRECTION('center_axis',(0.577350269189625,0.577350269189626,-0.577350269189627)) ;
#119410 = DIRECTION('ref_axis',(-6.40836823623517E-14,-0.707106781186516,
-0.707106781186579)) ;
#119411 = DIRECTION('center_axis',(0.577350269189625,0.577350269189625,-0.577350269189628)) ;
#119412 = DIRECTION('ref_axis',(-0.707106781186552,5.19478420936363E-15,-0.707106781186543)) ;
#119413 = DIRECTION('center_axis',(-0.577350269189625,-0.577350269189625,
0.577350269189628)) ;
#119414 = DIRECTION('ref_axis',(-0.707106781186566,3.31891725521342E-14,-0.707106781186529)) ;
#119415 = DIRECTION('center_axis',(-0.577350269189652,-0.577350269189606,
0.57735026918962)) ;
#119416 = DIRECTION('ref_axis',(0.707106781186528,-3.96520952299298E-16,0.707106781186567)) ;
#119417 = DIRECTION('center_axis',(0.,0.,-1.)) ;
#119418 = DIRECTION('ref_axis',(-1.,0.,0.)) ;
#119419 = DIRECTION('center_axis',(0.,0.,1.)) ;
#119420 = DIRECTION('ref_axis',(-1.,-8.67361737988404E-15,0.)) ;
#119421 = DIRECTION('center_axis',(0.,0.,-1.)) ;
#119422 = DIRECTION('ref_axis',(-1.,0.,0.)) ;
#119423 = DIRECTION('center_axis',(2.08166817117218E-16,1.,0.)) ;
#119424 = DIRECTION('ref_axis',(1.,0.,0.)) ;
#119425 = DIRECTION('center_axis',(-1.,0.,-1.66745659064321E-14)) ;
#119426 = DIRECTION('ref_axis',(1.66745659064321E-14,2.60208521396523E-14,
-1.)) ;
#119427 = DIRECTION('center_axis',(-3.46944695195361E-14,-3.4694469519536E-14,
1.)) ;
#119428 = DIRECTION('ref_axis',(-1.,-1.68611237719883E-42,-3.46944695195361E-14)) ;
#119429 = DIRECTION('center_axis',(-0.577350269189625,-0.577350269189625,
-0.577350269189628)) ;
#119430 = DIRECTION('ref_axis',(-0.707106781186552,5.19478420936363E-15,0.707106781186543)) ;
#119431 = DIRECTION('center_axis',(-0.577350269189625,-0.577350269189625,
-0.577350269189628)) ;
#119432 = DIRECTION('ref_axis',(-0.707106781186552,5.1349792556416E-15,0.707106781186543)) ;
#119433 = DIRECTION('center_axis',(-0.577350269189626,-0.577350269189626,
-0.577350269189626)) ;
#119434 = DIRECTION('ref_axis',(0.707106781186547,-0.707106781186548,6.36902276417946E-16)) ;
#119435 = DIRECTION('center_axis',(0.,0.,-1.)) ;
#119436 = DIRECTION('ref_axis',(-1.,0.,0.)) ;
#119437 = DIRECTION('center_axis',(0.,0.,1.)) ;
#119438 = DIRECTION('ref_axis',(1.,0.,0.)) ;
#119439 = DIRECTION('center_axis',(-1.,0.,9.8563833862319E-18)) ;
#119440 = DIRECTION('ref_axis',(9.8563833862319E-18,0.,1.)) ;
#119441 = DIRECTION('center_axis',(-1.,8.87690528722497E-15,-8.87690528722518E-15)) ;
#119442 = DIRECTION('ref_axis',(-8.87690528722518E-15,4.48415508583942E-43,
1.)) ;
#119443 = DIRECTION('center_axis',(2.08166817117218E-16,1.,0.)) ;
#119444 = DIRECTION('ref_axis',(1.,0.,0.)) ;
#119445 = DIRECTION('center_axis',(-1.,8.53809210832325E-15,8.53809210832346E-15)) ;
#119446 = DIRECTION('ref_axis',(-8.53809210832339E-15,8.67361737988409E-15,
-1.)) ;
#119447 = DIRECTION('center_axis',(2.08166817117218E-16,1.,0.)) ;
#119448 = DIRECTION('ref_axis',(1.,0.,0.)) ;
#119449 = DIRECTION('center_axis',(-0.577350269189622,0.577350269189621,-0.577350269189634)) ;
#119450 = DIRECTION('ref_axis',(0.707106781186563,1.66970714627838E-14,-0.707106781186532)) ;
#119451 = DIRECTION('center_axis',(0.,0.,1.)) ;
#119452 = DIRECTION('ref_axis',(-1.,0.,0.)) ;
#119453 = DIRECTION('center_axis',(-1.,0.,-9.8563833862319E-18)) ;
#119454 = DIRECTION('ref_axis',(-9.8563833862319E-18,0.,1.)) ;
#119455 = DIRECTION('center_axis',(-1.,0.,-1.34163173959798E-15)) ;
#119456 = DIRECTION('ref_axis',(-1.34163173959798E-15,0.,1.)) ;
#119457 = DIRECTION('center_axis',(0.,0.,-1.)) ;
#119458 = DIRECTION('ref_axis',(-1.,0.,0.)) ;
#119459 = DIRECTION('center_axis',(-3.46944695195361E-14,3.4694469519536E-14,
1.)) ;
#119460 = DIRECTION('ref_axis',(1.,-1.68611237719883E-42,3.46944695195361E-14)) ;
#119461 = DIRECTION('center_axis',(0.577350269189625,-0.577350269189625,0.577350269189628)) ;
#119462 = DIRECTION('ref_axis',(0.707106781186552,5.19478420936363E-15,-0.707106781186543)) ;
#119463 = DIRECTION('center_axis',(0.577350269189625,-0.577350269189625,0.577350269189628)) ;
#119464 = DIRECTION('ref_axis',(0.707106781186552,5.1349792556416E-15,-0.707106781186543)) ;
#119465 = DIRECTION('center_axis',(2.08166817117218E-16,1.,0.)) ;
#119466 = DIRECTION('ref_axis',(1.,0.,0.)) ;
#119467 = DIRECTION('center_axis',(-0.577350269189646,0.577350269189609,0.577350269189623)) ;
#119468 = DIRECTION('ref_axis',(-0.707106781186529,8.66006384940495E-15,-0.707106781186566)) ;
#119469 = DIRECTION('center_axis',(0.,0.,-1.)) ;
#119470 = DIRECTION('ref_axis',(-1.,0.,0.)) ;
#119471 = DIRECTION('center_axis',(0.,0.,1.)) ;
#119472 = DIRECTION('ref_axis',(-1.,0.,0.)) ;
#119473 = DIRECTION('center_axis',(0.,0.,-1.)) ;
#119474 = DIRECTION('ref_axis',(-1.,0.,0.)) ;
#119475 = DIRECTION('center_axis',(-0.577350269189625,0.577350269189625,0.577350269189628)) ;
#119476 = DIRECTION('ref_axis',(0.707106781186552,5.1349792556416E-15,0.707106781186543)) ;
#119477 = DIRECTION('center_axis',(0.577350269189625,-0.577350269189625,-0.577350269189628)) ;
#119478 = DIRECTION('ref_axis',(0.707106781186559,1.92955635991398E-14,0.707106781186536)) ;
#119479 = DIRECTION('center_axis',(-0.577350269189625,0.577350269189626,-0.577350269189626)) ;
#119480 = DIRECTION('ref_axis',(5.20172641667636E-15,0.70710678118655,0.707106781186545)) ;
#119481 = DIRECTION('center_axis',(0.577350269189625,-0.577350269189626,0.577350269189626)) ;
#119482 = DIRECTION('ref_axis',(1.27903606950626E-14,0.707106781186554,0.707106781186541)) ;
#119483 = DIRECTION('center_axis',(0.577350269189636,-0.577350269189592,0.57735026918965)) ;
#119484 = DIRECTION('ref_axis',(0.707106781186558,3.40611850366138E-15,-0.707106781186537)) ;
#119485 = DIRECTION('center_axis',(0.,0.,-1.)) ;
#119486 = DIRECTION('ref_axis',(-1.,0.,0.)) ;
#119487 = DIRECTION('center_axis',(0.,0.,1.)) ;
#119488 = DIRECTION('ref_axis',(-1.,1.57209315010398E-14,0.)) ;
#119489 = DIRECTION('center_axis',(0.,0.,-1.)) ;
#119490 = DIRECTION('ref_axis',(-1.,0.,0.)) ;
#119491 = DIRECTION('center_axis',(0.,1.,0.)) ;
#119492 = DIRECTION('ref_axis',(1.,0.,0.)) ;
#119493 = DIRECTION('center_axis',(0.,-1.,7.76229792195976E-15)) ;
#119494 = DIRECTION('ref_axis',(3.46944695195364E-14,7.76229792195976E-15,
1.)) ;
#119495 = DIRECTION('center_axis',(-3.46944695195361E-14,3.46944695195361E-14,
1.)) ;
#119496 = DIRECTION('ref_axis',(-7.17464813734306E-43,1.,-3.46944695195361E-14)) ;
#119497 = DIRECTION('center_axis',(0.577350269189625,-0.577350269189626,-0.577350269189626)) ;
#119498 = DIRECTION('ref_axis',(5.20172641667636E-15,0.70710678118655,-0.707106781186545)) ;
#119499 = DIRECTION('center_axis',(0.577350269189625,-0.577350269189626,-0.577350269189626)) ;
#119500 = DIRECTION('ref_axis',(5.11416588733871E-15,0.70710678118655,-0.707106781186545)) ;
#119501 = DIRECTION('center_axis',(0.577350269189624,-0.577350269189625,-0.577350269189629)) ;
#119502 = DIRECTION('ref_axis',(4.29556475679742E-15,0.707106781186552,-0.707106781186543)) ;
#119503 = DIRECTION('center_axis',(0.,0.,-1.)) ;
#119504 = DIRECTION('ref_axis',(-1.,0.,0.)) ;
#119505 = DIRECTION('center_axis',(0.,0.,1.)) ;
#119506 = DIRECTION('ref_axis',(1.,0.,0.)) ;
#119507 = DIRECTION('center_axis',(0.,1.,1.95511867169518E-16)) ;
#119508 = DIRECTION('ref_axis',(0.,-1.95511867169518E-16,1.)) ;
#119509 = DIRECTION('center_axis',(-7.65717784317885E-15,-1.,-7.84883952026447E-15)) ;
#119510 = DIRECTION('ref_axis',(-8.90241127119925E-32,7.84883952026447E-15,
-1.)) ;
#119511 = DIRECTION('center_axis',(0.,1.,0.)) ;
#119512 = DIRECTION('ref_axis',(1.,0.,0.)) ;
#119513 = DIRECTION('center_axis',(-1.28749007982652E-15,-1.,1.47915175691198E-15)) ;
#119514 = DIRECTION('ref_axis',(3.46944695195364E-14,1.47915175691194E-15,
1.)) ;
#119515 = DIRECTION('center_axis',(0.,1.,0.)) ;
#119516 = DIRECTION('ref_axis',(1.,0.,0.)) ;
#119517 = DIRECTION('center_axis',(-0.577350269189619,-0.577350269189621,
-0.577350269189638)) ;
#119518 = DIRECTION('ref_axis',(1.66660234080318E-14,-0.707106781186566,0.707106781186529)) ;
#119519 = DIRECTION('center_axis',(0.,0.,1.)) ;
#119520 = DIRECTION('ref_axis',(-1.,-3.52365706057788E-15,0.)) ;
#119521 = DIRECTION('center_axis',(0.,1.,-1.95511867169518E-16)) ;
#119522 = DIRECTION('ref_axis',(0.,1.95511867169518E-16,1.)) ;
#119523 = DIRECTION('center_axis',(0.,-1.,3.06658683336682E-15)) ;
#119524 = DIRECTION('ref_axis',(0.,-3.06658683336682E-15,-1.)) ;
#119525 = DIRECTION('center_axis',(0.,0.,-1.)) ;
#119526 = DIRECTION('ref_axis',(-1.,0.,0.)) ;
#119527 = DIRECTION('center_axis',(-3.4694469519536E-14,-3.46944695195361E-14,
1.)) ;
#119528 = DIRECTION('ref_axis',(-8.96831017167883E-43,-1.,-3.46944695195361E-14)) ;
#119529 = DIRECTION('center_axis',(0.577350269189625,0.577350269189626,0.577350269189627)) ;
#119530 = DIRECTION('ref_axis',(5.35231302451417E-15,-0.707106781186551,0.707106781186544)) ;
#119531 = DIRECTION('center_axis',(0.577350269189625,0.577350269189626,0.577350269189627)) ;
#119532 = DIRECTION('ref_axis',(5.35231302451417E-15,-0.707106781186551,0.707106781186544)) ;
#119533 = DIRECTION('center_axis',(0.,1.,0.)) ;
#119534 = DIRECTION('ref_axis',(1.,0.,0.)) ;
#119535 = DIRECTION('center_axis',(-0.577350269189609,-0.577350269189646,
0.577350269189623)) ;
#119536 = DIRECTION('ref_axis',(8.91337114590872E-15,0.707106781186529,0.707106781186566)) ;
#119537 = DIRECTION('center_axis',(0.,0.,-1.)) ;
#119538 = DIRECTION('ref_axis',(-1.,0.,0.)) ;
#119539 = DIRECTION('center_axis',(0.,0.,1.)) ;
#119540 = DIRECTION('ref_axis',(-1.,1.0842021724855E-15,0.)) ;
#119541 = DIRECTION('center_axis',(0.,0.,-1.)) ;
#119542 = DIRECTION('ref_axis',(-1.,0.,0.)) ;
#119543 = DIRECTION('center_axis',(-0.577350269189625,-0.577350269189626,
0.577350269189627)) ;
#119544 = DIRECTION('ref_axis',(5.35231302451417E-15,-0.707106781186551,-0.707106781186544)) ;
#119545 = DIRECTION('center_axis',(0.577350269189625,0.577350269189626,-0.577350269189627)) ;
#119546 = DIRECTION('ref_axis',(-6.40836823623517E-14,-0.707106781186516,
-0.707106781186579)) ;
#119547 = DIRECTION('center_axis',(0.577350269189625,0.577350269189625,-0.577350269189628)) ;
#119548 = DIRECTION('ref_axis',(-0.707106781186552,5.19478420936363E-15,-0.707106781186543)) ;
#119549 = DIRECTION('center_axis',(-0.577350269189625,-0.577350269189625,
0.577350269189628)) ;
#119550 = DIRECTION('ref_axis',(-0.707106781186562,2.56048320762387E-14,-0.707106781186533)) ;
#119551 = DIRECTION('center_axis',(-0.577350269189542,-0.577350269189661,
0.577350269189675)) ;
#119552 = DIRECTION('ref_axis',(3.44881489367205E-15,-0.707106781186558,-0.707106781186537)) ;
#119553 = DIRECTION('center_axis',(0.,0.,-1.)) ;
#119554 = DIRECTION('ref_axis',(-1.,0.,0.)) ;
#119555 = DIRECTION('center_axis',(0.,0.,1.)) ;
#119556 = DIRECTION('ref_axis',(-1.,-8.67361737988404E-15,0.)) ;
#119557 = DIRECTION('center_axis',(0.,0.,-1.)) ;
#119558 = DIRECTION('ref_axis',(-1.,0.,0.)) ;
#119559 = DIRECTION('center_axis',(2.08166817117218E-16,1.,0.)) ;
#119560 = DIRECTION('ref_axis',(1.,0.,0.)) ;
#119561 = DIRECTION('center_axis',(-1.,0.,9.05601424228639E-14)) ;
#119562 = DIRECTION('ref_axis',(-9.05601424228639E-14,0.,-1.)) ;
#119563 = DIRECTION('center_axis',(6.93889390390722E-14,6.93889390390721E-14,
1.)) ;
#119564 = DIRECTION('ref_axis',(-1.,-6.3534872372487E-42,6.93889390390722E-14)) ;
#119565 = DIRECTION('center_axis',(-0.577350269189625,-0.577350269189625,
-0.577350269189628)) ;
#119566 = DIRECTION('ref_axis',(-0.707106781186552,5.19478420936363E-15,0.707106781186543)) ;
#119567 = DIRECTION('center_axis',(-0.577350269189625,-0.577350269189625,
-0.577350269189628)) ;
#119568 = DIRECTION('ref_axis',(-0.707106781186552,5.1349792556416E-15,0.707106781186543)) ;
#119569 = DIRECTION('center_axis',(-0.577350269189609,-0.577350269189608,
-0.57735026918966)) ;
#119570 = DIRECTION('ref_axis',(-0.707106781186576,-5.08171669240118E-15,
0.707106781186519)) ;
#119571 = DIRECTION('center_axis',(0.,0.,-1.)) ;
#119572 = DIRECTION('ref_axis',(-1.,0.,0.)) ;
#119573 = DIRECTION('center_axis',(0.,0.,1.)) ;
#119574 = DIRECTION('ref_axis',(1.,0.,0.)) ;
#119575 = DIRECTION('center_axis',(-1.,0.,9.8563833862319E-18)) ;
#119576 = DIRECTION('ref_axis',(9.8563833862319E-18,0.,1.)) ;
#119577 = DIRECTION('center_axis',(-1.,1.31459513413869E-14,-1.31459513413873E-14)) ;
#119578 = DIRECTION('ref_axis',(-1.31459513413873E-14,1.17484863248993E-41,
1.)) ;
#119579 = DIRECTION('center_axis',(2.08166817117218E-16,1.,0.)) ;
#119580 = DIRECTION('ref_axis',(1.,0.,0.)) ;
#119581 = DIRECTION('center_axis',(-1.,-1.77538105744504E-14,-1.77538105744508E-14)) ;
#119582 = DIRECTION('ref_axis',(1.77538105744506E-14,8.67361737988379E-15,
-1.)) ;
#119583 = DIRECTION('center_axis',(2.08166817117218E-16,1.,0.)) ;
#119584 = DIRECTION('ref_axis',(1.,0.,0.)) ;
#119585 = DIRECTION('center_axis',(-0.577350269189595,0.577350269189594,-0.577350269189688)) ;
#119586 = DIRECTION('ref_axis',(0.707106781186627,4.55186387217293E-14,-0.707106781186468)) ;
#119587 = DIRECTION('center_axis',(-9.81307786677359E-14,0.,1.)) ;
#119588 = DIRECTION('ref_axis',(-1.,0.,-9.81307786677359E-14)) ;
#119589 = DIRECTION('center_axis',(-1.,0.,-9.8563833862319E-18)) ;
#119590 = DIRECTION('ref_axis',(-9.8563833862319E-18,0.,1.)) ;
#119591 = DIRECTION('center_axis',(-1.,0.,8.71102322353262E-14)) ;
#119592 = DIRECTION('ref_axis',(8.71102322353262E-14,0.,1.)) ;
#119593 = DIRECTION('center_axis',(0.,0.,-1.)) ;
#119594 = DIRECTION('ref_axis',(-1.,0.,0.)) ;
#119595 = DIRECTION('center_axis',(6.93889390390722E-14,-6.93889390390721E-14,
1.)) ;
#119596 = DIRECTION('ref_axis',(1.,-6.3534872372487E-42,-6.93889390390722E-14)) ;
#119597 = DIRECTION('center_axis',(0.577350269189625,-0.577350269189625,0.577350269189628)) ;
#119598 = DIRECTION('ref_axis',(0.707106781186552,5.19478420936363E-15,-0.707106781186543)) ;
#119599 = DIRECTION('center_axis',(0.577350269189625,-0.577350269189625,0.577350269189628)) ;
#119600 = DIRECTION('ref_axis',(0.707106781186552,5.1349792556416E-15,-0.707106781186543)) ;
#119601 = DIRECTION('center_axis',(2.08166817117218E-16,1.,0.)) ;
#119602 = DIRECTION('ref_axis',(1.,0.,0.)) ;
#119603 = DIRECTION('center_axis',(-0.577350269189538,0.577350269189662,0.577350269189676)) ;
#119604 = DIRECTION('ref_axis',(1.74300544639431E-14,0.707106781186565,-0.70710678118653)) ;
#119605 = DIRECTION('center_axis',(0.,0.,-1.)) ;
#119606 = DIRECTION('ref_axis',(-1.,0.,0.)) ;
#119607 = DIRECTION('center_axis',(0.,0.,1.)) ;
#119608 = DIRECTION('ref_axis',(-1.,0.,0.)) ;
#119609 = DIRECTION('center_axis',(0.,0.,-1.)) ;
#119610 = DIRECTION('ref_axis',(-1.,0.,0.)) ;
#119611 = DIRECTION('center_axis',(-0.577350269189625,0.577350269189625,0.577350269189628)) ;
#119612 = DIRECTION('ref_axis',(0.707106781186552,5.1349792556416E-15,0.707106781186543)) ;
#119613 = DIRECTION('center_axis',(0.577350269189625,-0.577350269189625,-0.577350269189628)) ;
#119614 = DIRECTION('ref_axis',(0.707106781186562,2.5899563042358E-14,0.707106781186533)) ;
#119615 = DIRECTION('center_axis',(-0.577350269189625,0.577350269189626,-0.577350269189626)) ;
#119616 = DIRECTION('ref_axis',(5.20172641667636E-15,0.70710678118655,0.707106781186545)) ;
#119617 = DIRECTION('center_axis',(0.577350269189625,-0.577350269189626,0.577350269189626)) ;
#119618 = DIRECTION('ref_axis',(4.10196750502305E-14,0.707106781186568,0.707106781186527)) ;
#119619 = DIRECTION('center_axis',(0.577350269189612,-0.57735026918964,0.577350269189626)) ;
#119620 = DIRECTION('ref_axis',(-8.27428663398926E-15,-0.707106781186543,
-0.707106781186552)) ;
#119621 = DIRECTION('center_axis',(0.,0.,-1.)) ;
#119622 = DIRECTION('ref_axis',(-1.,0.,0.)) ;
#119623 = DIRECTION('center_axis',(0.,0.,1.)) ;
#119624 = DIRECTION('ref_axis',(-1.,1.35525271560688E-14,0.)) ;
#119625 = DIRECTION('center_axis',(0.,0.,-1.)) ;
#119626 = DIRECTION('ref_axis',(-1.,0.,0.)) ;
#119627 = DIRECTION('center_axis',(0.,1.,0.)) ;
#119628 = DIRECTION('ref_axis',(1.,0.,0.)) ;
#119629 = DIRECTION('center_axis',(0.,-1.,1.13080389480401E-14)) ;
#119630 = DIRECTION('ref_axis',(1.12757025938489E-13,1.13080389480401E-14,
1.)) ;
#119631 = DIRECTION('center_axis',(0.,0.,1.)) ;
#119632 = DIRECTION('ref_axis',(-1.,0.,0.)) ;
#119633 = DIRECTION('center_axis',(0.577350269189625,-0.577350269189626,-0.577350269189626)) ;
#119634 = DIRECTION('ref_axis',(5.20172641667636E-15,0.70710678118655,-0.707106781186545)) ;
#119635 = DIRECTION('center_axis',(0.577350269189625,-0.577350269189626,-0.577350269189626)) ;
#119636 = DIRECTION('ref_axis',(5.11416588733871E-15,0.70710678118655,-0.707106781186545)) ;
#119637 = DIRECTION('center_axis',(0.577350269189618,-0.577350269189619,-0.57735026918964)) ;
#119638 = DIRECTION('ref_axis',(1.15945863464918E-15,0.707106781186561,-0.707106781186534)) ;
#119639 = DIRECTION('center_axis',(0.,0.,-1.)) ;
#119640 = DIRECTION('ref_axis',(-1.,0.,0.)) ;
#119641 = DIRECTION('center_axis',(0.,0.,1.)) ;
#119642 = DIRECTION('ref_axis',(1.,0.,0.)) ;
#119643 = DIRECTION('center_axis',(0.,1.,1.95511867169518E-16)) ;
#119644 = DIRECTION('ref_axis',(0.,-1.95511867169518E-16,1.)) ;
#119645 = DIRECTION('center_axis',(4.26226979058352E-14,-1.,4.24310362287508E-14)) ;
#119646 = DIRECTION('ref_axis',(1.,4.26226979058352E-14,4.69939452995971E-41)) ;
#119647 = DIRECTION('center_axis',(0.,1.,0.)) ;
#119648 = DIRECTION('ref_axis',(1.,0.,0.)) ;
#119649 = DIRECTION('center_axis',(-1.00288700954911E-14,-1.,1.02205317725767E-14)) ;
#119650 = DIRECTION('ref_axis',(3.46944695195352E-14,1.02205317725764E-14,
1.)) ;
#119651 = DIRECTION('center_axis',(0.,1.,0.)) ;
#119652 = DIRECTION('ref_axis',(1.,0.,0.)) ;
#119653 = DIRECTION('center_axis',(-0.577350269189659,-0.57735026918966,-0.577350269189558)) ;
#119654 = DIRECTION('ref_axis',(-0.707106781186543,0.707106781186552,-1.03102727271032E-14)) ;
#119655 = DIRECTION('center_axis',(0.,9.8130778667736E-14,1.)) ;
#119656 = DIRECTION('ref_axis',(-8.67361737988403E-15,1.,-9.8130778667736E-14)) ;
#119657 = DIRECTION('center_axis',(0.,1.,-1.95511867169518E-16)) ;
#119658 = DIRECTION('ref_axis',(0.,1.95511867169518E-16,1.)) ;
#119659 = DIRECTION('center_axis',(0.,-1.,9.83224403448236E-14)) ;
#119660 = DIRECTION('ref_axis',(0.,-9.83224403448236E-14,-1.)) ;
#119661 = DIRECTION('center_axis',(0.,0.,-1.)) ;
#119662 = DIRECTION('ref_axis',(-1.,0.,0.)) ;
#119663 = DIRECTION('center_axis',(0.,0.,1.)) ;
#119664 = DIRECTION('ref_axis',(1.,0.,0.)) ;
#119665 = DIRECTION('center_axis',(0.577350269189625,0.577350269189626,0.577350269189627)) ;
#119666 = DIRECTION('ref_axis',(5.35231302451417E-15,-0.707106781186551,0.707106781186544)) ;
#119667 = DIRECTION('center_axis',(0.577350269189625,0.577350269189626,0.577350269189627)) ;
#119668 = DIRECTION('ref_axis',(5.35231302451417E-15,-0.707106781186551,0.707106781186544)) ;
#119669 = DIRECTION('center_axis',(0.,1.,0.)) ;
#119670 = DIRECTION('ref_axis',(1.,0.,0.)) ;
#119671 = DIRECTION('center_axis',(-0.57735026918964,-0.577350269189583,0.577350269189654)) ;
#119672 = DIRECTION('ref_axis',(-0.707106781186567,2.1970613508967E-14,-0.707106781186528)) ;
#119673 = DIRECTION('center_axis',(0.,0.,-1.)) ;
#119674 = DIRECTION('ref_axis',(-1.,0.,0.)) ;
#119675 = DIRECTION('center_axis',(0.,0.,1.)) ;
#119676 = DIRECTION('ref_axis',(-1.,1.0842021724855E-15,0.)) ;
#119677 = DIRECTION('center_axis',(0.,0.,-1.)) ;
#119678 = DIRECTION('ref_axis',(-1.,0.,0.)) ;
#119679 = DIRECTION('center_axis',(-0.577350269189625,-0.577350269189626,
0.577350269189627)) ;
#119680 = DIRECTION('ref_axis',(5.35231302451417E-15,-0.707106781186551,-0.707106781186544)) ;
#119681 = DIRECTION('center_axis',(0.577350269189625,0.577350269189626,-0.577350269189627)) ;
#119682 = DIRECTION('ref_axis',(4.8009187113684E-14,-0.707106781186572,-0.707106781186523)) ;
#119683 = DIRECTION('center_axis',(0.,0.,1.)) ;
#119684 = DIRECTION('ref_axis',(1.,0.,0.)) ;
#119685 = DIRECTION('center_axis',(0.,-1.,0.)) ;
#119686 = DIRECTION('ref_axis',(0.,0.,-1.)) ;
#119687 = DIRECTION('center_axis',(9.85638338623186E-18,1.,0.)) ;
#119688 = DIRECTION('ref_axis',(-1.,9.85638338623186E-18,0.)) ;
#119689 = DIRECTION('center_axis',(0.,-1.,0.)) ;
#119690 = DIRECTION('ref_axis',(0.,0.,-1.)) ;
#119691 = DIRECTION('center_axis',(0.,1.,0.)) ;
#119692 = DIRECTION('ref_axis',(1.,0.,0.)) ;
#119693 = DIRECTION('center_axis',(-1.,-7.66646708341686E-16,0.)) ;
#119694 = DIRECTION('ref_axis',(7.66646708341686E-16,-1.,0.)) ;
#119695 = DIRECTION('center_axis',(1.,-9.85638338623186E-18,0.)) ;
#119696 = DIRECTION('ref_axis',(9.85638338623186E-18,1.,0.)) ;
#119697 = DIRECTION('center_axis',(-1.,0.,0.)) ;
#119698 = DIRECTION('ref_axis',(0.,0.,1.)) ;
#119699 = DIRECTION('center_axis',(0.,1.,0.)) ;
#119700 = DIRECTION('ref_axis',(1.,0.,0.)) ;
#119701 = DIRECTION('center_axis',(0.,1.,0.)) ;
#119702 = DIRECTION('ref_axis',(0.,0.,1.)) ;
#119703 = DIRECTION('center_axis',(-9.85638338623186E-18,-1.,0.)) ;
#119704 = DIRECTION('ref_axis',(1.,-9.85638338623186E-18,0.)) ;
#119705 = DIRECTION('center_axis',(0.,1.,0.)) ;
#119706 = DIRECTION('ref_axis',(0.,0.,1.)) ;
#119707 = DIRECTION('center_axis',(0.,0.,1.)) ;
#119708 = DIRECTION('ref_axis',(1.,0.,0.)) ;
#119709 = DIRECTION('center_axis',(0.,0.,1.)) ;
#119710 = DIRECTION('ref_axis',(1.,0.,0.)) ;
#119711 = DIRECTION('center_axis',(0.,-1.,0.)) ;
#119712 = DIRECTION('ref_axis',(0.,0.,-1.)) ;
#119713 = DIRECTION('center_axis',(-9.85638338623186E-18,-1.,0.)) ;
#119714 = DIRECTION('ref_axis',(1.,-9.85638338623186E-18,0.)) ;
#119715 = DIRECTION('center_axis',(0.,-1.,0.)) ;
#119716 = DIRECTION('ref_axis',(0.,0.,-1.)) ;
#119717 = DIRECTION('center_axis',(0.,1.,0.)) ;
#119718 = DIRECTION('ref_axis',(1.,0.,0.)) ;
#119719 = DIRECTION('center_axis',(1.,-3.06658683336674E-15,0.)) ;
#119720 = DIRECTION('ref_axis',(3.06658683336674E-15,1.,0.)) ;
#119721 = DIRECTION('center_axis',(1.,-9.85638338623186E-18,0.)) ;
#119722 = DIRECTION('ref_axis',(9.85638338623186E-18,1.,0.)) ;
#119723 = DIRECTION('center_axis',(1.,0.,0.)) ;
#119724 = DIRECTION('ref_axis',(0.,0.,-1.)) ;
#119725 = DIRECTION('center_axis',(0.,1.,0.)) ;
#119726 = DIRECTION('ref_axis',(1.,0.,0.)) ;
#119727 = DIRECTION('center_axis',(0.,1.,0.)) ;
#119728 = DIRECTION('ref_axis',(0.,0.,1.)) ;
#119729 = DIRECTION('center_axis',(-9.85638338623186E-18,-1.,0.)) ;
#119730 = DIRECTION('ref_axis',(1.,-9.85638338623186E-18,0.)) ;
#119731 = DIRECTION('center_axis',(0.,1.,0.)) ;
#119732 = DIRECTION('ref_axis',(0.,0.,1.)) ;
#119733 = DIRECTION('center_axis',(0.,0.,1.)) ;
#119734 = DIRECTION('ref_axis',(1.,0.,0.)) ;
#119735 = DIRECTION('center_axis',(-1.,-1.95511867169517E-16,0.)) ;
#119736 = DIRECTION('ref_axis',(1.95511867169517E-16,-1.,0.)) ;
#119737 = DIRECTION('center_axis',(1.,0.,0.)) ;
#119738 = DIRECTION('ref_axis',(0.,0.,-1.)) ;
#119739 = DIRECTION('center_axis',(0.,1.,0.)) ;
#119740 = DIRECTION('ref_axis',(1.,0.,0.)) ;
#119741 = DIRECTION('center_axis',(7.66646708341686E-16,-1.,0.)) ;
#119742 = DIRECTION('ref_axis',(1.,7.66646708341686E-16,0.)) ;
#119743 = DIRECTION('center_axis',(-1.95511867169517E-16,1.,0.)) ;
#119744 = DIRECTION('ref_axis',(-1.,-1.95511867169517E-16,0.)) ;
#119745 = DIRECTION('center_axis',(0.,-1.,0.)) ;
#119746 = DIRECTION('ref_axis',(0.,0.,-1.)) ;
#119747 = DIRECTION('center_axis',(0.,1.,0.)) ;
#119748 = DIRECTION('ref_axis',(1.,0.,0.)) ;
#119749 = DIRECTION('center_axis',(-1.,0.,0.)) ;
#119750 = DIRECTION('ref_axis',(0.,0.,1.)) ;
#119751 = DIRECTION('center_axis',(1.,-1.06642836637918E-16,0.)) ;
#119752 = DIRECTION('ref_axis',(1.06642836637918E-16,1.,0.)) ;
#119753 = DIRECTION('center_axis',(1.,1.95511867169517E-16,0.)) ;
#119754 = DIRECTION('ref_axis',(-1.95511867169517E-16,1.,0.)) ;
#119755 = DIRECTION('center_axis',(1.,0.,0.)) ;
#119756 = DIRECTION('ref_axis',(0.,0.,-1.)) ;
#119757 = DIRECTION('center_axis',(0.,1.,0.)) ;
#119758 = DIRECTION('ref_axis',(1.,0.,0.)) ;
#119759 = DIRECTION('center_axis',(2.29994012502506E-15,-1.,0.)) ;
#119760 = DIRECTION('ref_axis',(1.,2.29994012502506E-15,0.)) ;
#119761 = DIRECTION('center_axis',(-1.95511867169517E-16,1.,0.)) ;
#119762 = DIRECTION('ref_axis',(-1.,-1.95511867169517E-16,0.)) ;
#119763 = DIRECTION('center_axis',(0.,-1.,0.)) ;
#119764 = DIRECTION('ref_axis',(0.,0.,-1.)) ;
#119765 = DIRECTION('center_axis',(-1.,1.06642836637918E-16,0.)) ;
#119766 = DIRECTION('ref_axis',(-1.06642836637918E-16,-1.,0.)) ;
#119767 = DIRECTION('center_axis',(1.,0.,0.)) ;
#119768 = DIRECTION('ref_axis',(0.,0.,-1.)) ;
#119769 = DIRECTION('center_axis',(0.,1.,0.)) ;
#119770 = DIRECTION('ref_axis',(1.,0.,0.)) ;
#119771 = DIRECTION('center_axis',(0.,0.,1.)) ;
#119772 = DIRECTION('ref_axis',(1.,0.,0.)) ;
#119773 = DIRECTION('center_axis',(0.,-1.,0.)) ;
#119774 = DIRECTION('ref_axis',(0.,0.,-1.)) ;
#119775 = DIRECTION('center_axis',(9.85638338623186E-18,1.,0.)) ;
#119776 = DIRECTION('ref_axis',(-1.,9.85638338623186E-18,0.)) ;
#119777 = DIRECTION('center_axis',(0.,-1.,0.)) ;
#119778 = DIRECTION('ref_axis',(0.,0.,-1.)) ;
#119779 = DIRECTION('center_axis',(0.,1.,0.)) ;
#119780 = DIRECTION('ref_axis',(1.,0.,0.)) ;
#119781 = DIRECTION('center_axis',(-1.,-1.14997006251252E-14,0.)) ;
#119782 = DIRECTION('ref_axis',(1.14997006251252E-14,-1.,0.)) ;
#119783 = DIRECTION('center_axis',(1.,-9.85638338623186E-18,0.)) ;
#119784 = DIRECTION('ref_axis',(9.85638338623186E-18,1.,0.)) ;
#119785 = DIRECTION('center_axis',(-1.,0.,0.)) ;
#119786 = DIRECTION('ref_axis',(0.,0.,1.)) ;
#119787 = DIRECTION('center_axis',(0.,1.,0.)) ;
#119788 = DIRECTION('ref_axis',(1.,0.,0.)) ;
#119789 = DIRECTION('center_axis',(0.,1.,0.)) ;
#119790 = DIRECTION('ref_axis',(0.,0.,1.)) ;
#119791 = DIRECTION('center_axis',(-9.85638338623186E-18,-1.,0.)) ;
#119792 = DIRECTION('ref_axis',(1.,-9.85638338623186E-18,0.)) ;
#119793 = DIRECTION('center_axis',(0.,1.,0.)) ;
#119794 = DIRECTION('ref_axis',(0.,0.,1.)) ;
#119795 = DIRECTION('center_axis',(0.,0.,1.)) ;
#119796 = DIRECTION('ref_axis',(1.,0.,0.)) ;
#119797 = DIRECTION('center_axis',(0.,0.,1.)) ;
#119798 = DIRECTION('ref_axis',(1.,0.,0.)) ;
#119799 = DIRECTION('center_axis',(0.,-1.,0.)) ;
#119800 = DIRECTION('ref_axis',(0.,0.,-1.)) ;
#119801 = DIRECTION('center_axis',(-9.85638338623186E-18,-1.,0.)) ;
#119802 = DIRECTION('ref_axis',(1.,-9.85638338623186E-18,0.)) ;
#119803 = DIRECTION('center_axis',(0.,-1.,0.)) ;
#119804 = DIRECTION('ref_axis',(0.,0.,-1.)) ;
#119805 = DIRECTION('center_axis',(0.,1.,0.)) ;
#119806 = DIRECTION('ref_axis',(1.,0.,0.)) ;
#119807 = DIRECTION('center_axis',(1.,3.83323354170843E-15,0.)) ;
#119808 = DIRECTION('ref_axis',(-3.83323354170843E-15,1.,0.)) ;
#119809 = DIRECTION('center_axis',(1.,-9.85638338623186E-18,0.)) ;
#119810 = DIRECTION('ref_axis',(9.85638338623186E-18,1.,0.)) ;
#119811 = DIRECTION('center_axis',(1.,0.,0.)) ;
#119812 = DIRECTION('ref_axis',(0.,0.,-1.)) ;
#119813 = DIRECTION('center_axis',(0.,1.,0.)) ;
#119814 = DIRECTION('ref_axis',(1.,0.,0.)) ;
#119815 = DIRECTION('center_axis',(0.,1.,0.)) ;
#119816 = DIRECTION('ref_axis',(0.,0.,1.)) ;
#119817 = DIRECTION('center_axis',(-9.85638338623186E-18,-1.,0.)) ;
#119818 = DIRECTION('ref_axis',(1.,-9.85638338623186E-18,0.)) ;
#119819 = DIRECTION('center_axis',(0.,1.,0.)) ;
#119820 = DIRECTION('ref_axis',(0.,0.,1.)) ;
#119821 = DIRECTION('center_axis',(0.,0.,1.)) ;
#119822 = DIRECTION('ref_axis',(1.,0.,0.)) ;
#119823 = DIRECTION('center_axis',(-1.,-1.95511867169517E-16,0.)) ;
#119824 = DIRECTION('ref_axis',(1.95511867169517E-16,-1.,0.)) ;
#119825 = DIRECTION('center_axis',(1.,0.,0.)) ;
#119826 = DIRECTION('ref_axis',(0.,0.,-1.)) ;
#119827 = DIRECTION('center_axis',(0.,1.,0.)) ;
#119828 = DIRECTION('ref_axis',(1.,0.,0.)) ;
#119829 = DIRECTION('center_axis',(4.59988025005012E-15,-1.,0.)) ;
#119830 = DIRECTION('ref_axis',(1.,4.59988025005012E-15,0.)) ;
#119831 = DIRECTION('center_axis',(-1.95511867169517E-16,1.,0.)) ;
#119832 = DIRECTION('ref_axis',(-1.,-1.95511867169517E-16,0.)) ;
#119833 = DIRECTION('center_axis',(0.,-1.,0.)) ;
#119834 = DIRECTION('ref_axis',(0.,0.,-1.)) ;
#119835 = DIRECTION('center_axis',(0.,1.,0.)) ;
#119836 = DIRECTION('ref_axis',(1.,0.,0.)) ;
#119837 = DIRECTION('center_axis',(-1.,0.,0.)) ;
#119838 = DIRECTION('ref_axis',(0.,0.,1.)) ;
#119839 = DIRECTION('center_axis',(1.,-1.06642836637918E-16,0.)) ;
#119840 = DIRECTION('ref_axis',(1.06642836637918E-16,1.,0.)) ;
#119841 = DIRECTION('center_axis',(1.,1.95511867169517E-16,0.)) ;
#119842 = DIRECTION('ref_axis',(-1.95511867169517E-16,1.,0.)) ;
#119843 = DIRECTION('center_axis',(1.,0.,0.)) ;
#119844 = DIRECTION('ref_axis',(0.,0.,-1.)) ;
#119845 = DIRECTION('center_axis',(0.,1.,0.)) ;
#119846 = DIRECTION('ref_axis',(1.,0.,0.)) ;
#119847 = DIRECTION('center_axis',(-1.53329341668337E-15,-1.,0.)) ;
#119848 = DIRECTION('ref_axis',(1.,-1.53329341668337E-15,0.)) ;
#119849 = DIRECTION('center_axis',(-1.95511867169517E-16,1.,0.)) ;
#119850 = DIRECTION('ref_axis',(-1.,-1.95511867169517E-16,0.)) ;
#119851 = DIRECTION('center_axis',(0.,-1.,0.)) ;
#119852 = DIRECTION('ref_axis',(0.,0.,-1.)) ;
#119853 = DIRECTION('center_axis',(-1.,1.06642836637918E-16,0.)) ;
#119854 = DIRECTION('ref_axis',(-1.06642836637918E-16,-1.,0.)) ;
#119855 = DIRECTION('center_axis',(1.,0.,0.)) ;
#119856 = DIRECTION('ref_axis',(0.,0.,-1.)) ;
#119857 = DIRECTION('center_axis',(0.,1.,0.)) ;
#119858 = DIRECTION('ref_axis',(1.,0.,0.)) ;
#119859 = DIRECTION('center_axis',(0.,0.,1.)) ;
#119860 = DIRECTION('ref_axis',(1.,0.,0.)) ;
#119861 = DIRECTION('center_axis',(0.,-1.,0.)) ;
#119862 = DIRECTION('ref_axis',(0.,0.,-1.)) ;
#119863 = DIRECTION('center_axis',(9.85638338623186E-18,1.,0.)) ;
#119864 = DIRECTION('ref_axis',(-1.,9.85638338623186E-18,0.)) ;
#119865 = DIRECTION('center_axis',(0.,-1.,0.)) ;
#119866 = DIRECTION('ref_axis',(0.,0.,-1.)) ;
#119867 = DIRECTION('center_axis',(0.,1.,0.)) ;
#119868 = DIRECTION('ref_axis',(1.,0.,0.)) ;
#119869 = DIRECTION('center_axis',(-1.,-2.29994012502506E-15,0.)) ;
#119870 = DIRECTION('ref_axis',(2.29994012502506E-15,-1.,0.)) ;
#119871 = DIRECTION('center_axis',(1.,-9.85638338623186E-18,0.)) ;
#119872 = DIRECTION('ref_axis',(9.85638338623186E-18,1.,0.)) ;
#119873 = DIRECTION('center_axis',(-1.,0.,0.)) ;
#119874 = DIRECTION('ref_axis',(0.,0.,1.)) ;
#119875 = DIRECTION('center_axis',(0.,1.,0.)) ;
#119876 = DIRECTION('ref_axis',(1.,0.,0.)) ;
#119877 = DIRECTION('center_axis',(0.,1.,0.)) ;
#119878 = DIRECTION('ref_axis',(0.,0.,1.)) ;
#119879 = DIRECTION('center_axis',(-9.85638338623186E-18,-1.,0.)) ;
#119880 = DIRECTION('ref_axis',(1.,-9.85638338623186E-18,0.)) ;
#119881 = DIRECTION('center_axis',(0.,1.,0.)) ;
#119882 = DIRECTION('ref_axis',(0.,0.,1.)) ;
#119883 = DIRECTION('center_axis',(0.,0.,1.)) ;
#119884 = DIRECTION('ref_axis',(1.,0.,0.)) ;
#119885 = DIRECTION('center_axis',(0.,0.,1.)) ;
#119886 = DIRECTION('ref_axis',(1.,0.,0.)) ;
#119887 = DIRECTION('center_axis',(0.,-1.,0.)) ;
#119888 = DIRECTION('ref_axis',(0.,0.,-1.)) ;
#119889 = DIRECTION('center_axis',(-9.85638338623186E-18,-1.,0.)) ;
#119890 = DIRECTION('ref_axis',(1.,-9.85638338623186E-18,0.)) ;
#119891 = DIRECTION('center_axis',(0.,-1.,0.)) ;
#119892 = DIRECTION('ref_axis',(0.,0.,-1.)) ;
#119893 = DIRECTION('center_axis',(0.,1.,0.)) ;
#119894 = DIRECTION('ref_axis',(1.,0.,0.)) ;
#119895 = DIRECTION('center_axis',(1.,-7.66646708341686E-15,0.)) ;
#119896 = DIRECTION('ref_axis',(7.66646708341686E-15,1.,0.)) ;
#119897 = DIRECTION('center_axis',(1.,-9.85638338623186E-18,0.)) ;
#119898 = DIRECTION('ref_axis',(9.85638338623186E-18,1.,0.)) ;
#119899 = DIRECTION('center_axis',(1.,0.,0.)) ;
#119900 = DIRECTION('ref_axis',(0.,0.,-1.)) ;
#119901 = DIRECTION('center_axis',(0.,1.,0.)) ;
#119902 = DIRECTION('ref_axis',(1.,0.,0.)) ;
#119903 = DIRECTION('center_axis',(0.,1.,0.)) ;
#119904 = DIRECTION('ref_axis',(0.,0.,1.)) ;
#119905 = DIRECTION('center_axis',(-9.85638338623186E-18,-1.,0.)) ;
#119906 = DIRECTION('ref_axis',(1.,-9.85638338623186E-18,0.)) ;
#119907 = DIRECTION('center_axis',(0.,1.,0.)) ;
#119908 = DIRECTION('ref_axis',(0.,0.,1.)) ;
#119909 = DIRECTION('center_axis',(0.,0.,1.)) ;
#119910 = DIRECTION('ref_axis',(1.,0.,0.)) ;
#119911 = DIRECTION('center_axis',(-1.,-1.95511867169517E-16,0.)) ;
#119912 = DIRECTION('ref_axis',(1.95511867169517E-16,-1.,0.)) ;
#119913 = DIRECTION('center_axis',(1.,0.,0.)) ;
#119914 = DIRECTION('ref_axis',(0.,0.,-1.)) ;
#119915 = DIRECTION('center_axis',(0.,1.,0.)) ;
#119916 = DIRECTION('ref_axis',(1.,0.,0.)) ;
#119917 = DIRECTION('center_axis',(9.9664072084418E-15,-1.,0.)) ;
#119918 = DIRECTION('ref_axis',(1.,9.9664072084418E-15,0.)) ;
#119919 = DIRECTION('center_axis',(-1.95511867169517E-16,1.,0.)) ;
#119920 = DIRECTION('ref_axis',(-1.,-1.95511867169517E-16,0.)) ;
#119921 = DIRECTION('center_axis',(0.,-1.,0.)) ;
#119922 = DIRECTION('ref_axis',(0.,0.,-1.)) ;
#119923 = DIRECTION('center_axis',(0.,1.,0.)) ;
#119924 = DIRECTION('ref_axis',(1.,0.,0.)) ;
#119925 = DIRECTION('center_axis',(-1.,0.,0.)) ;
#119926 = DIRECTION('ref_axis',(0.,0.,1.)) ;
#119927 = DIRECTION('center_axis',(1.,-1.06642836637918E-16,0.)) ;
#119928 = DIRECTION('ref_axis',(1.06642836637918E-16,1.,0.)) ;
#119929 = DIRECTION('center_axis',(1.,1.95511867169517E-16,0.)) ;
#119930 = DIRECTION('ref_axis',(-1.95511867169517E-16,1.,0.)) ;
#119931 = DIRECTION('center_axis',(1.,0.,0.)) ;
#119932 = DIRECTION('ref_axis',(0.,0.,-1.)) ;
#119933 = DIRECTION('center_axis',(0.,1.,0.)) ;
#119934 = DIRECTION('ref_axis',(1.,0.,0.)) ;
#119935 = DIRECTION('center_axis',(6.89982037507517E-15,-1.,0.)) ;
#119936 = DIRECTION('ref_axis',(1.,6.89982037507517E-15,0.)) ;
#119937 = DIRECTION('center_axis',(-1.95511867169517E-16,1.,0.)) ;
#119938 = DIRECTION('ref_axis',(-1.,-1.95511867169517E-16,0.)) ;
#119939 = DIRECTION('center_axis',(0.,-1.,0.)) ;
#119940 = DIRECTION('ref_axis',(0.,0.,-1.)) ;
#119941 = DIRECTION('center_axis',(-1.,1.06642836637918E-16,0.)) ;
#119942 = DIRECTION('ref_axis',(-1.06642836637918E-16,-1.,0.)) ;
#119943 = DIRECTION('center_axis',(1.,0.,0.)) ;
#119944 = DIRECTION('ref_axis',(0.,0.,-1.)) ;
#119945 = DIRECTION('center_axis',(0.,1.,0.)) ;
#119946 = DIRECTION('ref_axis',(1.,0.,0.)) ;
#119947 = DIRECTION('center_axis',(0.,0.,1.)) ;
#119948 = DIRECTION('ref_axis',(1.,0.,0.)) ;
#119949 = DIRECTION('center_axis',(0.,-1.,0.)) ;
#119950 = DIRECTION('ref_axis',(0.,0.,-1.)) ;
#119951 = DIRECTION('center_axis',(9.85638338623186E-18,1.,0.)) ;
#119952 = DIRECTION('ref_axis',(-1.,9.85638338623186E-18,0.)) ;
#119953 = DIRECTION('center_axis',(0.,-1.,0.)) ;
#119954 = DIRECTION('ref_axis',(0.,0.,-1.)) ;
#119955 = DIRECTION('center_axis',(0.,1.,0.)) ;
#119956 = DIRECTION('ref_axis',(1.,0.,0.)) ;
#119957 = DIRECTION('center_axis',(-1.,0.,0.)) ;
#119958 = DIRECTION('ref_axis',(0.,0.,1.)) ;
#119959 = DIRECTION('center_axis',(1.,-9.85638338623186E-18,0.)) ;
#119960 = DIRECTION('ref_axis',(9.85638338623186E-18,1.,0.)) ;
#119961 = DIRECTION('center_axis',(-1.,0.,0.)) ;
#119962 = DIRECTION('ref_axis',(0.,0.,1.)) ;
#119963 = DIRECTION('center_axis',(0.,1.,0.)) ;
#119964 = DIRECTION('ref_axis',(1.,0.,0.)) ;
#119965 = DIRECTION('center_axis',(0.,1.,0.)) ;
#119966 = DIRECTION('ref_axis',(0.,0.,1.)) ;
#119967 = DIRECTION('center_axis',(-9.85638338623186E-18,-1.,0.)) ;
#119968 = DIRECTION('ref_axis',(1.,-9.85638338623186E-18,0.)) ;
#119969 = DIRECTION('center_axis',(0.,1.,0.)) ;
#119970 = DIRECTION('ref_axis',(0.,0.,1.)) ;
#119971 = DIRECTION('center_axis',(0.,0.,1.)) ;
#119972 = DIRECTION('ref_axis',(1.,0.,0.)) ;
#119973 = DIRECTION('center_axis',(0.,0.,1.)) ;
#119974 = DIRECTION('ref_axis',(1.,0.,0.)) ;
#119975 = DIRECTION('center_axis',(0.,-1.,0.)) ;
#119976 = DIRECTION('ref_axis',(0.,0.,-1.)) ;
#119977 = DIRECTION('center_axis',(-9.85638338623186E-18,-1.,0.)) ;
#119978 = DIRECTION('ref_axis',(1.,-9.85638338623186E-18,0.)) ;
#119979 = DIRECTION('center_axis',(0.,-1.,0.)) ;
#119980 = DIRECTION('ref_axis',(0.,0.,-1.)) ;
#119981 = DIRECTION('center_axis',(0.,1.,0.)) ;
#119982 = DIRECTION('ref_axis',(1.,0.,0.)) ;
#119983 = DIRECTION('center_axis',(1.,-9.19976050010023E-15,0.)) ;
#119984 = DIRECTION('ref_axis',(9.19976050010023E-15,1.,0.)) ;
#119985 = DIRECTION('center_axis',(1.,-9.85638338623186E-18,0.)) ;
#119986 = DIRECTION('ref_axis',(9.85638338623186E-18,1.,0.)) ;
#119987 = DIRECTION('center_axis',(1.,0.,0.)) ;
#119988 = DIRECTION('ref_axis',(0.,0.,-1.)) ;
#119989 = DIRECTION('center_axis',(0.,1.,0.)) ;
#119990 = DIRECTION('ref_axis',(1.,0.,0.)) ;
#119991 = DIRECTION('center_axis',(0.,1.,0.)) ;
#119992 = DIRECTION('ref_axis',(0.,0.,1.)) ;
#119993 = DIRECTION('center_axis',(-9.85638338623186E-18,-1.,0.)) ;
#119994 = DIRECTION('ref_axis',(1.,-9.85638338623186E-18,0.)) ;
#119995 = DIRECTION('center_axis',(0.,1.,0.)) ;
#119996 = DIRECTION('ref_axis',(0.,0.,1.)) ;
#119997 = DIRECTION('center_axis',(0.,0.,1.)) ;
#119998 = DIRECTION('ref_axis',(1.,0.,0.)) ;
#119999 = DIRECTION('center_axis',(-1.,-1.95511867169517E-16,0.)) ;
#120000 = DIRECTION('ref_axis',(1.95511867169517E-16,-1.,0.)) ;
#120001 = DIRECTION('center_axis',(1.,0.,0.)) ;
#120002 = DIRECTION('ref_axis',(0.,0.,-1.)) ;
#120003 = DIRECTION('center_axis',(0.,1.,0.)) ;
#120004 = DIRECTION('ref_axis',(1.,0.,0.)) ;
#120005 = DIRECTION('center_axis',(-1.53329341668337E-15,-1.,0.)) ;
#120006 = DIRECTION('ref_axis',(1.,-1.53329341668337E-15,0.)) ;
#120007 = DIRECTION('center_axis',(-1.95511867169517E-16,1.,0.)) ;
#120008 = DIRECTION('ref_axis',(-1.,-1.95511867169517E-16,0.)) ;
#120009 = DIRECTION('center_axis',(0.,-1.,0.)) ;
#120010 = DIRECTION('ref_axis',(0.,0.,-1.)) ;
#120011 = DIRECTION('center_axis',(0.,1.,0.)) ;
#120012 = DIRECTION('ref_axis',(1.,0.,0.)) ;
#120013 = DIRECTION('center_axis',(-1.,0.,0.)) ;
#120014 = DIRECTION('ref_axis',(0.,0.,1.)) ;
#120015 = DIRECTION('center_axis',(1.,-1.06642836637918E-16,0.)) ;
#120016 = DIRECTION('ref_axis',(1.06642836637918E-16,1.,0.)) ;
#120017 = DIRECTION('center_axis',(1.,1.95511867169517E-16,0.)) ;
#120018 = DIRECTION('ref_axis',(-1.95511867169517E-16,1.,0.)) ;
#120019 = DIRECTION('center_axis',(1.,0.,0.)) ;
#120020 = DIRECTION('ref_axis',(0.,0.,-1.)) ;
#120021 = DIRECTION('center_axis',(0.,1.,0.)) ;
#120022 = DIRECTION('ref_axis',(1.,0.,0.)) ;
#120023 = DIRECTION('center_axis',(-3.06658683336674E-15,-1.,0.)) ;
#120024 = DIRECTION('ref_axis',(1.,-3.06658683336674E-15,0.)) ;
#120025 = DIRECTION('center_axis',(-1.95511867169517E-16,1.,0.)) ;
#120026 = DIRECTION('ref_axis',(-1.,-1.95511867169517E-16,0.)) ;
#120027 = DIRECTION('center_axis',(0.,-1.,0.)) ;
#120028 = DIRECTION('ref_axis',(0.,0.,-1.)) ;
#120029 = DIRECTION('center_axis',(-1.,1.06642836637918E-16,0.)) ;
#120030 = DIRECTION('ref_axis',(-1.06642836637918E-16,-1.,0.)) ;
#120031 = DIRECTION('center_axis',(1.,0.,0.)) ;
#120032 = DIRECTION('ref_axis',(0.,0.,-1.)) ;
#120033 = DIRECTION('center_axis',(0.,1.,0.)) ;
#120034 = DIRECTION('ref_axis',(1.,0.,0.)) ;
#120035 = DIRECTION('center_axis',(0.,0.,1.)) ;
#120036 = DIRECTION('ref_axis',(1.,0.,0.)) ;
#120037 = DIRECTION('center_axis',(0.,-1.,0.)) ;
#120038 = DIRECTION('ref_axis',(0.,0.,-1.)) ;
#120039 = DIRECTION('center_axis',(9.85638338623186E-18,1.,0.)) ;
#120040 = DIRECTION('ref_axis',(-1.,9.85638338623186E-18,0.)) ;
#120041 = DIRECTION('center_axis',(0.,-1.,0.)) ;
#120042 = DIRECTION('ref_axis',(0.,0.,-1.)) ;
#120043 = DIRECTION('center_axis',(0.,1.,0.)) ;
#120044 = DIRECTION('ref_axis',(1.,0.,0.)) ;
#120045 = DIRECTION('center_axis',(-1.,4.59988025005012E-15,0.)) ;
#120046 = DIRECTION('ref_axis',(-4.59988025005012E-15,-1.,0.)) ;
#120047 = DIRECTION('center_axis',(1.,-9.85638338623186E-18,0.)) ;
#120048 = DIRECTION('ref_axis',(9.85638338623186E-18,1.,0.)) ;
#120049 = DIRECTION('center_axis',(-1.,0.,0.)) ;
#120050 = DIRECTION('ref_axis',(0.,0.,1.)) ;
#120051 = DIRECTION('center_axis',(0.,1.,0.)) ;
#120052 = DIRECTION('ref_axis',(1.,0.,0.)) ;
#120053 = DIRECTION('center_axis',(0.,1.,0.)) ;
#120054 = DIRECTION('ref_axis',(0.,0.,1.)) ;
#120055 = DIRECTION('center_axis',(-9.85638338623186E-18,-1.,0.)) ;
#120056 = DIRECTION('ref_axis',(1.,-9.85638338623186E-18,0.)) ;
#120057 = DIRECTION('center_axis',(0.,1.,0.)) ;
#120058 = DIRECTION('ref_axis',(0.,0.,1.)) ;
#120059 = DIRECTION('center_axis',(0.,0.,1.)) ;
#120060 = DIRECTION('ref_axis',(1.,0.,0.)) ;
#120061 = DIRECTION('center_axis',(0.,0.,1.)) ;
#120062 = DIRECTION('ref_axis',(1.,0.,0.)) ;
#120063 = DIRECTION('center_axis',(0.,-1.,0.)) ;
#120064 = DIRECTION('ref_axis',(0.,0.,-1.)) ;
#120065 = DIRECTION('center_axis',(-9.85638338623186E-18,-1.,0.)) ;
#120066 = DIRECTION('ref_axis',(1.,-9.85638338623186E-18,0.)) ;
#120067 = DIRECTION('center_axis',(0.,-1.,0.)) ;
#120068 = DIRECTION('ref_axis',(0.,0.,-1.)) ;
#120069 = DIRECTION('center_axis',(0.,1.,0.)) ;
#120070 = DIRECTION('ref_axis',(1.,0.,0.)) ;
#120071 = DIRECTION('center_axis',(1.,-6.13317366673349E-15,0.)) ;
#120072 = DIRECTION('ref_axis',(6.13317366673349E-15,1.,0.)) ;
#120073 = DIRECTION('center_axis',(1.,-9.85638338623186E-18,0.)) ;
#120074 = DIRECTION('ref_axis',(9.85638338623186E-18,1.,0.)) ;
#120075 = DIRECTION('center_axis',(1.,0.,0.)) ;
#120076 = DIRECTION('ref_axis',(0.,0.,-1.)) ;
#120077 = DIRECTION('center_axis',(0.,1.,0.)) ;
#120078 = DIRECTION('ref_axis',(1.,0.,0.)) ;
#120079 = DIRECTION('center_axis',(0.,1.,0.)) ;
#120080 = DIRECTION('ref_axis',(0.,0.,1.)) ;
#120081 = DIRECTION('center_axis',(-9.85638338623186E-18,-1.,0.)) ;
#120082 = DIRECTION('ref_axis',(1.,-9.85638338623186E-18,0.)) ;
#120083 = DIRECTION('center_axis',(0.,1.,0.)) ;
#120084 = DIRECTION('ref_axis',(0.,0.,1.)) ;
#120085 = DIRECTION('center_axis',(0.,0.,1.)) ;
#120086 = DIRECTION('ref_axis',(1.,0.,0.)) ;
#120087 = DIRECTION('center_axis',(-1.,-1.95511867169517E-16,0.)) ;
#120088 = DIRECTION('ref_axis',(1.95511867169517E-16,-1.,0.)) ;
#120089 = DIRECTION('center_axis',(1.,0.,0.)) ;
#120090 = DIRECTION('ref_axis',(0.,0.,-1.)) ;
#120091 = DIRECTION('center_axis',(0.,1.,0.)) ;
#120092 = DIRECTION('ref_axis',(1.,0.,0.)) ;
#120093 = DIRECTION('center_axis',(1.22663473334668E-14,-1.,0.)) ;
#120094 = DIRECTION('ref_axis',(1.,1.22663473334668E-14,0.)) ;
#120095 = DIRECTION('center_axis',(-1.95511867169517E-16,1.,0.)) ;
#120096 = DIRECTION('ref_axis',(-1.,-1.95511867169517E-16,0.)) ;
#120097 = DIRECTION('center_axis',(0.,-1.,0.)) ;
#120098 = DIRECTION('ref_axis',(0.,0.,-1.)) ;
#120099 = DIRECTION('center_axis',(0.,1.,0.)) ;
#120100 = DIRECTION('ref_axis',(1.,0.,0.)) ;
#120101 = DIRECTION('center_axis',(-1.,0.,0.)) ;
#120102 = DIRECTION('ref_axis',(0.,0.,1.)) ;
#120103 = DIRECTION('center_axis',(1.,-1.06642836637918E-16,0.)) ;
#120104 = DIRECTION('ref_axis',(1.06642836637918E-16,1.,0.)) ;
#120105 = DIRECTION('center_axis',(1.,1.95511867169517E-16,0.)) ;
#120106 = DIRECTION('ref_axis',(-1.95511867169517E-16,1.,0.)) ;
#120107 = DIRECTION('center_axis',(1.,0.,0.)) ;
#120108 = DIRECTION('ref_axis',(0.,0.,-1.)) ;
#120109 = DIRECTION('center_axis',(0.,1.,0.)) ;
#120110 = DIRECTION('ref_axis',(1.,0.,0.)) ;
#120111 = DIRECTION('center_axis',(-8.43311379175855E-15,-1.,0.)) ;
#120112 = DIRECTION('ref_axis',(1.,-8.43311379175855E-15,0.)) ;
#120113 = DIRECTION('center_axis',(-1.95511867169517E-16,1.,0.)) ;
#120114 = DIRECTION('ref_axis',(-1.,-1.95511867169517E-16,0.)) ;
#120115 = DIRECTION('center_axis',(0.,-1.,0.)) ;
#120116 = DIRECTION('ref_axis',(0.,0.,-1.)) ;
#120117 = DIRECTION('center_axis',(-1.,1.06642836637918E-16,0.)) ;
#120118 = DIRECTION('ref_axis',(-1.06642836637918E-16,-1.,0.)) ;
#120119 = DIRECTION('center_axis',(1.,0.,0.)) ;
#120120 = DIRECTION('ref_axis',(0.,0.,-1.)) ;
#120121 = DIRECTION('center_axis',(0.,1.,0.)) ;
#120122 = DIRECTION('ref_axis',(1.,0.,0.)) ;
#120123 = DIRECTION('center_axis',(0.,0.,1.)) ;
#120124 = DIRECTION('ref_axis',(1.,0.,0.)) ;
#120125 = DIRECTION('center_axis',(0.,-1.,0.)) ;
#120126 = DIRECTION('ref_axis',(0.,0.,-1.)) ;
#120127 = DIRECTION('center_axis',(9.85638338623186E-18,1.,0.)) ;
#120128 = DIRECTION('ref_axis',(-1.,9.85638338623186E-18,0.)) ;
#120129 = DIRECTION('center_axis',(0.,-1.,0.)) ;
#120130 = DIRECTION('ref_axis',(0.,0.,-1.)) ;
#120131 = DIRECTION('center_axis',(0.,1.,0.)) ;
#120132 = DIRECTION('ref_axis',(1.,0.,0.)) ;
#120133 = DIRECTION('center_axis',(-1.,4.59988025005012E-15,0.)) ;
#120134 = DIRECTION('ref_axis',(-4.59988025005012E-15,-1.,0.)) ;
#120135 = DIRECTION('center_axis',(1.,-9.85638338623186E-18,0.)) ;
#120136 = DIRECTION('ref_axis',(9.85638338623186E-18,1.,0.)) ;
#120137 = DIRECTION('center_axis',(-1.,0.,0.)) ;
#120138 = DIRECTION('ref_axis',(0.,0.,1.)) ;
#120139 = DIRECTION('center_axis',(0.,1.,0.)) ;
#120140 = DIRECTION('ref_axis',(1.,0.,0.)) ;
#120141 = DIRECTION('center_axis',(0.,1.,0.)) ;
#120142 = DIRECTION('ref_axis',(0.,0.,1.)) ;
#120143 = DIRECTION('center_axis',(-9.85638338623186E-18,-1.,0.)) ;
#120144 = DIRECTION('ref_axis',(1.,-9.85638338623186E-18,0.)) ;
#120145 = DIRECTION('center_axis',(0.,1.,0.)) ;
#120146 = DIRECTION('ref_axis',(0.,0.,1.)) ;
#120147 = DIRECTION('center_axis',(0.,0.,1.)) ;
#120148 = DIRECTION('ref_axis',(1.,0.,0.)) ;
#120149 = DIRECTION('center_axis',(0.,0.,1.)) ;
#120150 = DIRECTION('ref_axis',(1.,0.,0.)) ;
#120151 = DIRECTION('center_axis',(0.,-1.,0.)) ;
#120152 = DIRECTION('ref_axis',(0.,0.,-1.)) ;
#120153 = DIRECTION('center_axis',(-9.85638338623186E-18,-1.,0.)) ;
#120154 = DIRECTION('ref_axis',(1.,-9.85638338623186E-18,0.)) ;
#120155 = DIRECTION('center_axis',(0.,-1.,0.)) ;
#120156 = DIRECTION('ref_axis',(0.,0.,-1.)) ;
#120157 = DIRECTION('center_axis',(0.,1.,0.)) ;
#120158 = DIRECTION('ref_axis',(1.,0.,0.)) ;
#120159 = DIRECTION('center_axis',(1.,-6.13317366673349E-15,0.)) ;
#120160 = DIRECTION('ref_axis',(6.13317366673349E-15,1.,0.)) ;
#120161 = DIRECTION('center_axis',(1.,-9.85638338623186E-18,0.)) ;
#120162 = DIRECTION('ref_axis',(9.85638338623186E-18,1.,0.)) ;
#120163 = DIRECTION('center_axis',(1.,0.,0.)) ;
#120164 = DIRECTION('ref_axis',(0.,0.,-1.)) ;
#120165 = DIRECTION('center_axis',(0.,1.,0.)) ;
#120166 = DIRECTION('ref_axis',(1.,0.,0.)) ;
#120167 = DIRECTION('center_axis',(0.,1.,0.)) ;
#120168 = DIRECTION('ref_axis',(0.,0.,1.)) ;
#120169 = DIRECTION('center_axis',(-9.85638338623186E-18,-1.,0.)) ;
#120170 = DIRECTION('ref_axis',(1.,-9.85638338623186E-18,0.)) ;
#120171 = DIRECTION('center_axis',(0.,1.,0.)) ;
#120172 = DIRECTION('ref_axis',(0.,0.,1.)) ;
#120173 = DIRECTION('center_axis',(0.,0.,1.)) ;
#120174 = DIRECTION('ref_axis',(1.,0.,0.)) ;
#120175 = DIRECTION('center_axis',(-1.,-1.95511867169517E-16,0.)) ;
#120176 = DIRECTION('ref_axis',(1.95511867169517E-16,-1.,0.)) ;
#120177 = DIRECTION('center_axis',(1.,0.,0.)) ;
#120178 = DIRECTION('ref_axis',(0.,0.,-1.)) ;
#120179 = DIRECTION('center_axis',(0.,1.,0.)) ;
#120180 = DIRECTION('ref_axis',(1.,0.,0.)) ;
#120181 = DIRECTION('center_axis',(1.22663473334668E-14,-1.,0.)) ;
#120182 = DIRECTION('ref_axis',(1.,1.22663473334668E-14,0.)) ;
#120183 = DIRECTION('center_axis',(-1.95511867169517E-16,1.,0.)) ;
#120184 = DIRECTION('ref_axis',(-1.,-1.95511867169517E-16,0.)) ;
#120185 = DIRECTION('center_axis',(0.,-1.,0.)) ;
#120186 = DIRECTION('ref_axis',(0.,0.,-1.)) ;
#120187 = DIRECTION('center_axis',(0.,1.,0.)) ;
#120188 = DIRECTION('ref_axis',(1.,0.,0.)) ;
#120189 = DIRECTION('center_axis',(-1.,0.,0.)) ;
#120190 = DIRECTION('ref_axis',(0.,0.,1.)) ;
#120191 = DIRECTION('center_axis',(1.,-1.06642836637918E-16,0.)) ;
#120192 = DIRECTION('ref_axis',(1.06642836637918E-16,1.,0.)) ;
#120193 = DIRECTION('center_axis',(1.,1.95511867169517E-16,0.)) ;
#120194 = DIRECTION('ref_axis',(-1.95511867169517E-16,1.,0.)) ;
#120195 = DIRECTION('center_axis',(1.,0.,0.)) ;
#120196 = DIRECTION('ref_axis',(0.,0.,-1.)) ;
#120197 = DIRECTION('center_axis',(0.,1.,0.)) ;
#120198 = DIRECTION('ref_axis',(1.,0.,0.)) ;
#120199 = DIRECTION('center_axis',(-8.43311379175855E-15,-1.,0.)) ;
#120200 = DIRECTION('ref_axis',(1.,-8.43311379175855E-15,0.)) ;
#120201 = DIRECTION('center_axis',(-1.95511867169517E-16,1.,0.)) ;
#120202 = DIRECTION('ref_axis',(-1.,-1.95511867169517E-16,0.)) ;
#120203 = DIRECTION('center_axis',(0.,-1.,0.)) ;
#120204 = DIRECTION('ref_axis',(0.,0.,-1.)) ;
#120205 = DIRECTION('center_axis',(-1.,1.06642836637918E-16,0.)) ;
#120206 = DIRECTION('ref_axis',(-1.06642836637918E-16,-1.,0.)) ;
#120207 = DIRECTION('center_axis',(1.,0.,0.)) ;
#120208 = DIRECTION('ref_axis',(0.,0.,-1.)) ;
#120209 = DIRECTION('center_axis',(0.,1.,0.)) ;
#120210 = DIRECTION('ref_axis',(1.,0.,0.)) ;
#120211 = DIRECTION('center_axis',(0.,0.,1.)) ;
#120212 = DIRECTION('ref_axis',(1.,0.,0.)) ;
#120213 = DIRECTION('center_axis',(0.,-1.,0.)) ;
#120214 = DIRECTION('ref_axis',(0.,0.,-1.)) ;
#120215 = DIRECTION('center_axis',(9.85638338623186E-18,1.,0.)) ;
#120216 = DIRECTION('ref_axis',(-1.,9.85638338623186E-18,0.)) ;
#120217 = DIRECTION('center_axis',(0.,-1.,0.)) ;
#120218 = DIRECTION('ref_axis',(0.,0.,-1.)) ;
#120219 = DIRECTION('center_axis',(0.,1.,0.)) ;
#120220 = DIRECTION('ref_axis',(1.,0.,0.)) ;
#120221 = DIRECTION('center_axis',(-1.,4.59988025005012E-15,0.)) ;
#120222 = DIRECTION('ref_axis',(-4.59988025005012E-15,-1.,0.)) ;
#120223 = DIRECTION('center_axis',(1.,-9.85638338623186E-18,0.)) ;
#120224 = DIRECTION('ref_axis',(9.85638338623186E-18,1.,0.)) ;
#120225 = DIRECTION('center_axis',(-1.,0.,0.)) ;
#120226 = DIRECTION('ref_axis',(0.,0.,1.)) ;
#120227 = DIRECTION('center_axis',(0.,1.,0.)) ;
#120228 = DIRECTION('ref_axis',(1.,0.,0.)) ;
#120229 = DIRECTION('center_axis',(0.,1.,0.)) ;
#120230 = DIRECTION('ref_axis',(0.,0.,1.)) ;
#120231 = DIRECTION('center_axis',(-9.85638338623186E-18,-1.,0.)) ;
#120232 = DIRECTION('ref_axis',(1.,-9.85638338623186E-18,0.)) ;
#120233 = DIRECTION('center_axis',(0.,1.,0.)) ;
#120234 = DIRECTION('ref_axis',(0.,0.,1.)) ;
#120235 = DIRECTION('center_axis',(0.,0.,1.)) ;
#120236 = DIRECTION('ref_axis',(1.,0.,0.)) ;
#120237 = DIRECTION('center_axis',(0.,0.,1.)) ;
#120238 = DIRECTION('ref_axis',(1.,0.,0.)) ;
#120239 = DIRECTION('center_axis',(0.,-1.,0.)) ;
#120240 = DIRECTION('ref_axis',(0.,0.,-1.)) ;
#120241 = DIRECTION('center_axis',(-9.85638338623186E-18,-1.,0.)) ;
#120242 = DIRECTION('ref_axis',(1.,-9.85638338623186E-18,0.)) ;
#120243 = DIRECTION('center_axis',(0.,-1.,0.)) ;
#120244 = DIRECTION('ref_axis',(0.,0.,-1.)) ;
#120245 = DIRECTION('center_axis',(0.,1.,0.)) ;
#120246 = DIRECTION('ref_axis',(1.,0.,0.)) ;
#120247 = DIRECTION('center_axis',(1.,-6.13317366673349E-15,0.)) ;
#120248 = DIRECTION('ref_axis',(6.13317366673349E-15,1.,0.)) ;
#120249 = DIRECTION('center_axis',(1.,-9.85638338623186E-18,0.)) ;
#120250 = DIRECTION('ref_axis',(9.85638338623186E-18,1.,0.)) ;
#120251 = DIRECTION('center_axis',(1.,0.,0.)) ;
#120252 = DIRECTION('ref_axis',(0.,0.,-1.)) ;
#120253 = DIRECTION('center_axis',(0.,1.,0.)) ;
#120254 = DIRECTION('ref_axis',(1.,0.,0.)) ;
#120255 = DIRECTION('center_axis',(0.,1.,0.)) ;
#120256 = DIRECTION('ref_axis',(0.,0.,1.)) ;
#120257 = DIRECTION('center_axis',(-9.85638338623186E-18,-1.,0.)) ;
#120258 = DIRECTION('ref_axis',(1.,-9.85638338623186E-18,0.)) ;
#120259 = DIRECTION('center_axis',(0.,1.,0.)) ;
#120260 = DIRECTION('ref_axis',(0.,0.,1.)) ;
#120261 = DIRECTION('center_axis',(0.,0.,1.)) ;
#120262 = DIRECTION('ref_axis',(1.,0.,0.)) ;
#120263 = DIRECTION('center_axis',(-1.,-1.95511867169517E-16,0.)) ;
#120264 = DIRECTION('ref_axis',(1.95511867169517E-16,-1.,0.)) ;
#120265 = DIRECTION('center_axis',(1.,0.,0.)) ;
#120266 = DIRECTION('ref_axis',(0.,0.,-1.)) ;
#120267 = DIRECTION('center_axis',(0.,1.,0.)) ;
#120268 = DIRECTION('ref_axis',(1.,0.,0.)) ;
#120269 = DIRECTION('center_axis',(1.22663473334668E-14,-1.,0.)) ;
#120270 = DIRECTION('ref_axis',(1.,1.22663473334668E-14,0.)) ;
#120271 = DIRECTION('center_axis',(-1.95511867169517E-16,1.,0.)) ;
#120272 = DIRECTION('ref_axis',(-1.,-1.95511867169517E-16,0.)) ;
#120273 = DIRECTION('center_axis',(0.,-1.,0.)) ;
#120274 = DIRECTION('ref_axis',(0.,0.,-1.)) ;
#120275 = DIRECTION('center_axis',(0.,1.,0.)) ;
#120276 = DIRECTION('ref_axis',(1.,0.,0.)) ;
#120277 = DIRECTION('center_axis',(-1.,0.,0.)) ;
#120278 = DIRECTION('ref_axis',(0.,0.,1.)) ;
#120279 = DIRECTION('center_axis',(1.,-1.06642836637918E-16,0.)) ;
#120280 = DIRECTION('ref_axis',(1.06642836637918E-16,1.,0.)) ;
#120281 = DIRECTION('center_axis',(1.,1.95511867169517E-16,0.)) ;
#120282 = DIRECTION('ref_axis',(-1.95511867169517E-16,1.,0.)) ;
#120283 = DIRECTION('center_axis',(1.,0.,0.)) ;
#120284 = DIRECTION('ref_axis',(0.,0.,-1.)) ;
#120285 = DIRECTION('center_axis',(0.,1.,0.)) ;
#120286 = DIRECTION('ref_axis',(1.,0.,0.)) ;
#120287 = DIRECTION('center_axis',(-8.43311379175855E-15,-1.,0.)) ;
#120288 = DIRECTION('ref_axis',(1.,-8.43311379175855E-15,0.)) ;
#120289 = DIRECTION('center_axis',(-1.95511867169517E-16,1.,0.)) ;
#120290 = DIRECTION('ref_axis',(-1.,-1.95511867169517E-16,0.)) ;
#120291 = DIRECTION('center_axis',(0.,-1.,0.)) ;
#120292 = DIRECTION('ref_axis',(0.,0.,-1.)) ;
#120293 = DIRECTION('center_axis',(-1.,1.06642836637918E-16,0.)) ;
#120294 = DIRECTION('ref_axis',(-1.06642836637918E-16,-1.,0.)) ;
#120295 = DIRECTION('center_axis',(1.,0.,0.)) ;
#120296 = DIRECTION('ref_axis',(0.,0.,-1.)) ;
#120297 = DIRECTION('center_axis',(0.,1.,0.)) ;
#120298 = DIRECTION('ref_axis',(1.,0.,0.)) ;
#120299 = DIRECTION('center_axis',(0.,0.,1.)) ;
#120300 = DIRECTION('ref_axis',(1.,0.,0.)) ;
#120301 = DIRECTION('center_axis',(0.,-1.,0.)) ;
#120302 = DIRECTION('ref_axis',(0.,0.,-1.)) ;
#120303 = DIRECTION('center_axis',(9.85638338623186E-18,1.,0.)) ;
#120304 = DIRECTION('ref_axis',(-1.,9.85638338623186E-18,0.)) ;
#120305 = DIRECTION('center_axis',(0.,-1.,0.)) ;
#120306 = DIRECTION('ref_axis',(0.,0.,-1.)) ;
#120307 = DIRECTION('center_axis',(0.,1.,0.)) ;
#120308 = DIRECTION('ref_axis',(1.,0.,0.)) ;
#120309 = DIRECTION('center_axis',(-1.,4.59988025005012E-15,0.)) ;
#120310 = DIRECTION('ref_axis',(-4.59988025005012E-15,-1.,0.)) ;
#120311 = DIRECTION('center_axis',(1.,-9.85638338623186E-18,0.)) ;
#120312 = DIRECTION('ref_axis',(9.85638338623186E-18,1.,0.)) ;
#120313 = DIRECTION('center_axis',(-1.,0.,0.)) ;
#120314 = DIRECTION('ref_axis',(0.,0.,1.)) ;
#120315 = DIRECTION('center_axis',(0.,1.,0.)) ;
#120316 = DIRECTION('ref_axis',(1.,0.,0.)) ;
#120317 = DIRECTION('center_axis',(0.,1.,0.)) ;
#120318 = DIRECTION('ref_axis',(0.,0.,1.)) ;
#120319 = DIRECTION('center_axis',(-9.85638338623186E-18,-1.,0.)) ;
#120320 = DIRECTION('ref_axis',(1.,-9.85638338623186E-18,0.)) ;
#120321 = DIRECTION('center_axis',(0.,1.,0.)) ;
#120322 = DIRECTION('ref_axis',(0.,0.,1.)) ;
#120323 = DIRECTION('center_axis',(0.,0.,1.)) ;
#120324 = DIRECTION('ref_axis',(1.,0.,0.)) ;
#120325 = DIRECTION('center_axis',(0.,0.,1.)) ;
#120326 = DIRECTION('ref_axis',(1.,0.,0.)) ;
#120327 = DIRECTION('center_axis',(0.,-1.,0.)) ;
#120328 = DIRECTION('ref_axis',(0.,0.,-1.)) ;
#120329 = DIRECTION('center_axis',(-9.85638338623186E-18,-1.,0.)) ;
#120330 = DIRECTION('ref_axis',(1.,-9.85638338623186E-18,0.)) ;
#120331 = DIRECTION('center_axis',(0.,-1.,0.)) ;
#120332 = DIRECTION('ref_axis',(0.,0.,-1.)) ;
#120333 = DIRECTION('center_axis',(0.,1.,0.)) ;
#120334 = DIRECTION('ref_axis',(1.,0.,0.)) ;
#120335 = DIRECTION('center_axis',(1.,-6.13317366673349E-15,0.)) ;
#120336 = DIRECTION('ref_axis',(6.13317366673349E-15,1.,0.)) ;
#120337 = DIRECTION('center_axis',(1.,-9.85638338623186E-18,0.)) ;
#120338 = DIRECTION('ref_axis',(9.85638338623186E-18,1.,0.)) ;
#120339 = DIRECTION('center_axis',(1.,0.,0.)) ;
#120340 = DIRECTION('ref_axis',(0.,0.,-1.)) ;
#120341 = DIRECTION('center_axis',(0.,1.,0.)) ;
#120342 = DIRECTION('ref_axis',(1.,0.,0.)) ;
#120343 = DIRECTION('center_axis',(0.,1.,0.)) ;
#120344 = DIRECTION('ref_axis',(0.,0.,1.)) ;
#120345 = DIRECTION('center_axis',(-9.85638338623186E-18,-1.,0.)) ;
#120346 = DIRECTION('ref_axis',(1.,-9.85638338623186E-18,0.)) ;
#120347 = DIRECTION('center_axis',(0.,1.,0.)) ;
#120348 = DIRECTION('ref_axis',(0.,0.,1.)) ;
#120349 = DIRECTION('center_axis',(0.,0.,1.)) ;
#120350 = DIRECTION('ref_axis',(1.,0.,0.)) ;
#120351 = DIRECTION('center_axis',(-1.,-1.95511867169517E-16,0.)) ;
#120352 = DIRECTION('ref_axis',(1.95511867169517E-16,-1.,0.)) ;
#120353 = DIRECTION('center_axis',(1.,0.,0.)) ;
#120354 = DIRECTION('ref_axis',(0.,0.,-1.)) ;
#120355 = DIRECTION('center_axis',(0.,1.,0.)) ;
#120356 = DIRECTION('ref_axis',(1.,0.,0.)) ;
#120357 = DIRECTION('center_axis',(1.22663473334668E-14,-1.,0.)) ;
#120358 = DIRECTION('ref_axis',(1.,1.22663473334668E-14,0.)) ;
#120359 = DIRECTION('center_axis',(-1.95511867169517E-16,1.,0.)) ;
#120360 = DIRECTION('ref_axis',(-1.,-1.95511867169517E-16,0.)) ;
#120361 = DIRECTION('center_axis',(0.,-1.,0.)) ;
#120362 = DIRECTION('ref_axis',(0.,0.,-1.)) ;
#120363 = DIRECTION('center_axis',(0.,1.,0.)) ;
#120364 = DIRECTION('ref_axis',(1.,0.,0.)) ;
#120365 = DIRECTION('center_axis',(-1.,0.,0.)) ;
#120366 = DIRECTION('ref_axis',(0.,0.,1.)) ;
#120367 = DIRECTION('center_axis',(1.,-1.06642836637918E-16,0.)) ;
#120368 = DIRECTION('ref_axis',(1.06642836637918E-16,1.,0.)) ;
#120369 = DIRECTION('center_axis',(1.,1.95511867169517E-16,0.)) ;
#120370 = DIRECTION('ref_axis',(-1.95511867169517E-16,1.,0.)) ;
#120371 = DIRECTION('center_axis',(1.,0.,0.)) ;
#120372 = DIRECTION('ref_axis',(0.,0.,-1.)) ;
#120373 = DIRECTION('center_axis',(0.,1.,0.)) ;
#120374 = DIRECTION('ref_axis',(1.,0.,0.)) ;
#120375 = DIRECTION('center_axis',(-8.43311379175855E-15,-1.,0.)) ;
#120376 = DIRECTION('ref_axis',(1.,-8.43311379175855E-15,0.)) ;
#120377 = DIRECTION('center_axis',(-1.95511867169517E-16,1.,0.)) ;
#120378 = DIRECTION('ref_axis',(-1.,-1.95511867169517E-16,0.)) ;
#120379 = DIRECTION('center_axis',(0.,-1.,0.)) ;
#120380 = DIRECTION('ref_axis',(0.,0.,-1.)) ;
#120381 = DIRECTION('center_axis',(-1.,1.06642836637918E-16,0.)) ;
#120382 = DIRECTION('ref_axis',(-1.06642836637918E-16,-1.,0.)) ;
#120383 = DIRECTION('center_axis',(1.,0.,0.)) ;
#120384 = DIRECTION('ref_axis',(0.,0.,-1.)) ;
#120385 = DIRECTION('center_axis',(0.,1.,0.)) ;
#120386 = DIRECTION('ref_axis',(1.,0.,0.)) ;
#120387 = DIRECTION('center_axis',(0.,0.,1.)) ;
#120388 = DIRECTION('ref_axis',(1.,0.,0.)) ;
#120389 = DIRECTION('center_axis',(0.,-1.,0.)) ;
#120390 = DIRECTION('ref_axis',(0.,0.,-1.)) ;
#120391 = DIRECTION('center_axis',(9.85638338623186E-18,1.,0.)) ;
#120392 = DIRECTION('ref_axis',(-1.,9.85638338623186E-18,0.)) ;
#120393 = DIRECTION('center_axis',(0.,-1.,0.)) ;
#120394 = DIRECTION('ref_axis',(0.,0.,-1.)) ;
#120395 = DIRECTION('center_axis',(0.,1.,0.)) ;
#120396 = DIRECTION('ref_axis',(1.,0.,0.)) ;
#120397 = DIRECTION('center_axis',(-1.,1.83995210002007E-14,0.)) ;
#120398 = DIRECTION('ref_axis',(-1.83995210002007E-14,-1.,0.)) ;
#120399 = DIRECTION('center_axis',(1.,-9.85638338623186E-18,0.)) ;
#120400 = DIRECTION('ref_axis',(9.85638338623186E-18,1.,0.)) ;
#120401 = DIRECTION('center_axis',(-1.,0.,0.)) ;
#120402 = DIRECTION('ref_axis',(0.,0.,1.)) ;
#120403 = DIRECTION('center_axis',(0.,1.,0.)) ;
#120404 = DIRECTION('ref_axis',(1.,0.,0.)) ;
#120405 = DIRECTION('center_axis',(0.,1.,0.)) ;
#120406 = DIRECTION('ref_axis',(0.,0.,1.)) ;
#120407 = DIRECTION('center_axis',(-9.85638338623186E-18,-1.,0.)) ;
#120408 = DIRECTION('ref_axis',(1.,-9.85638338623186E-18,0.)) ;
#120409 = DIRECTION('center_axis',(0.,1.,0.)) ;
#120410 = DIRECTION('ref_axis',(0.,0.,1.)) ;
#120411 = DIRECTION('center_axis',(0.,0.,1.)) ;
#120412 = DIRECTION('ref_axis',(1.,0.,0.)) ;
#120413 = DIRECTION('center_axis',(0.,0.,1.)) ;
#120414 = DIRECTION('ref_axis',(1.,0.,0.)) ;
#120415 = DIRECTION('center_axis',(0.,-1.,0.)) ;
#120416 = DIRECTION('ref_axis',(0.,0.,-1.)) ;
#120417 = DIRECTION('center_axis',(-9.85638338623186E-18,-1.,0.)) ;
#120418 = DIRECTION('ref_axis',(1.,-9.85638338623186E-18,0.)) ;
#120419 = DIRECTION('center_axis',(0.,-1.,0.)) ;
#120420 = DIRECTION('ref_axis',(0.,0.,-1.)) ;
#120421 = DIRECTION('center_axis',(0.,1.,0.)) ;
#120422 = DIRECTION('ref_axis',(1.,0.,0.)) ;
#120423 = DIRECTION('center_axis',(1.,2.22327545419092E-14,0.)) ;
#120424 = DIRECTION('ref_axis',(-2.22327545419092E-14,1.,0.)) ;
#120425 = DIRECTION('center_axis',(1.,-9.85638338623186E-18,0.)) ;
#120426 = DIRECTION('ref_axis',(9.85638338623186E-18,1.,0.)) ;
#120427 = DIRECTION('center_axis',(1.,0.,0.)) ;
#120428 = DIRECTION('ref_axis',(0.,0.,-1.)) ;
#120429 = DIRECTION('center_axis',(0.,1.,0.)) ;
#120430 = DIRECTION('ref_axis',(1.,0.,0.)) ;
#120431 = DIRECTION('center_axis',(0.,1.,0.)) ;
#120432 = DIRECTION('ref_axis',(0.,0.,1.)) ;
#120433 = DIRECTION('center_axis',(-9.85638338623186E-18,-1.,0.)) ;
#120434 = DIRECTION('ref_axis',(1.,-9.85638338623186E-18,0.)) ;
#120435 = DIRECTION('center_axis',(0.,1.,0.)) ;
#120436 = DIRECTION('ref_axis',(0.,0.,1.)) ;
#120437 = DIRECTION('center_axis',(0.,0.,1.)) ;
#120438 = DIRECTION('ref_axis',(1.,0.,0.)) ;
#120439 = DIRECTION('center_axis',(-1.,-1.95511867169517E-16,0.)) ;
#120440 = DIRECTION('ref_axis',(1.95511867169517E-16,-1.,0.)) ;
#120441 = DIRECTION('center_axis',(1.,0.,0.)) ;
#120442 = DIRECTION('ref_axis',(0.,0.,-1.)) ;
#120443 = DIRECTION('center_axis',(0.,1.,0.)) ;
#120444 = DIRECTION('ref_axis',(1.,0.,0.)) ;
#120445 = DIRECTION('center_axis',(-1.83995210002007E-14,-1.,0.)) ;
#120446 = DIRECTION('ref_axis',(1.,-1.83995210002007E-14,0.)) ;
#120447 = DIRECTION('center_axis',(-1.95511867169517E-16,1.,0.)) ;
#120448 = DIRECTION('ref_axis',(-1.,-1.95511867169517E-16,0.)) ;
#120449 = DIRECTION('center_axis',(0.,-1.,0.)) ;
#120450 = DIRECTION('ref_axis',(0.,0.,-1.)) ;
#120451 = DIRECTION('center_axis',(0.,1.,0.)) ;
#120452 = DIRECTION('ref_axis',(1.,0.,0.)) ;
#120453 = DIRECTION('center_axis',(-1.,0.,0.)) ;
#120454 = DIRECTION('ref_axis',(0.,0.,1.)) ;
#120455 = DIRECTION('center_axis',(1.,-1.06642836637918E-16,0.)) ;
#120456 = DIRECTION('ref_axis',(1.06642836637918E-16,1.,0.)) ;
#120457 = DIRECTION('center_axis',(1.,1.95511867169517E-16,0.)) ;
#120458 = DIRECTION('ref_axis',(-1.95511867169517E-16,1.,0.)) ;
#120459 = DIRECTION('center_axis',(1.,0.,0.)) ;
#120460 = DIRECTION('ref_axis',(0.,0.,-1.)) ;
#120461 = DIRECTION('center_axis',(0.,1.,0.)) ;
#120462 = DIRECTION('ref_axis',(1.,0.,0.)) ;
#120463 = DIRECTION('center_axis',(2.68326347919587E-14,-1.,0.)) ;
#120464 = DIRECTION('ref_axis',(1.,2.68326347919587E-14,0.)) ;
#120465 = DIRECTION('center_axis',(-1.95511867169517E-16,1.,0.)) ;
#120466 = DIRECTION('ref_axis',(-1.,-1.95511867169517E-16,0.)) ;
#120467 = DIRECTION('center_axis',(0.,-1.,0.)) ;
#120468 = DIRECTION('ref_axis',(0.,0.,-1.)) ;
#120469 = DIRECTION('center_axis',(-1.,1.06642836637918E-16,0.)) ;
#120470 = DIRECTION('ref_axis',(-1.06642836637918E-16,-1.,0.)) ;
#120471 = DIRECTION('center_axis',(1.,0.,0.)) ;
#120472 = DIRECTION('ref_axis',(0.,0.,-1.)) ;
#120473 = DIRECTION('center_axis',(0.,1.,0.)) ;
#120474 = DIRECTION('ref_axis',(1.,0.,0.)) ;
#120475 = DIRECTION('axis',(0.,0.,1.)) ;
#120476 = DIRECTION('refdir',(1.,0.,0.)) ;
#120477 = DIRECTION('center_axis',(0.,0.,1.)) ;
#120478 = DIRECTION('ref_axis',(1.,0.,0.)) ;
#120479 = DIRECTION('center_axis',(0.,0.,1.)) ;
#120480 = DIRECTION('ref_axis',(1.,0.,0.)) ;
#120481 = DIRECTION('',(0.,0.,-1.)) ;
#120482 = DIRECTION('center_axis',(0.,0.,1.)) ;
#120483 = DIRECTION('ref_axis',(1.,0.,0.)) ;
#120484 = DIRECTION('',(0.,0.,1.)) ;
#120485 = DIRECTION('center_axis',(-1.31418445149758E-16,1.,0.)) ;
#120486 = DIRECTION('ref_axis',(-1.,0.,0.)) ;
#120487 = DIRECTION('center_axis',(1.31418445149758E-16,-1.,0.)) ;
#120488 = DIRECTION('ref_axis',(-1.,-1.31418445149758E-16,0.)) ;
#120489 = DIRECTION('center_axis',(1.,0.,-2.16840434497101E-15)) ;
#120490 = DIRECTION('ref_axis',(-2.16840434497101E-15,0.,-1.)) ;
#120491 = DIRECTION('center_axis',(-1.31418445149758E-16,1.,0.)) ;
#120492 = DIRECTION('ref_axis',(-1.,-1.31418445149758E-16,0.)) ;
#120493 = DIRECTION('center_axis',(-0.641814420963378,0.,0.766859993117025)) ;
#120494 = DIRECTION('ref_axis',(0.766859993117025,0.,0.641814420963378)) ;
#120495 = DIRECTION('center_axis',(-1.31418445149758E-16,1.,0.)) ;
#120496 = DIRECTION('ref_axis',(-1.,0.,0.)) ;
#120497 = DIRECTION('center_axis',(1.31418445149758E-16,-1.,0.)) ;
#120498 = DIRECTION('ref_axis',(-1.,-1.31418445149758E-16,0.)) ;
#120499 = DIRECTION('center_axis',(0.823067492614529,0.,0.567943573430699)) ;
#120500 = DIRECTION('ref_axis',(0.567943573430699,0.,-0.823067492614529)) ;
#120501 = DIRECTION('center_axis',(-1.31418445149758E-16,1.,0.)) ;
#120502 = DIRECTION('ref_axis',(-1.,-1.31418445149758E-16,0.)) ;
#120503 = DIRECTION('center_axis',(-0.823067492614536,0.,0.56794357343069)) ;
#120504 = DIRECTION('ref_axis',(0.56794357343069,0.,0.823067492614536)) ;
#120505 = DIRECTION('center_axis',(7.81406971160724E-17,-1.,0.)) ;
#120506 = DIRECTION('ref_axis',(1.,0.,0.)) ;
#120507 = DIRECTION('center_axis',(7.81406971160724E-17,-1.,0.)) ;
#120508 = DIRECTION('ref_axis',(1.,7.81406971160724E-17,0.)) ;
#120509 = DIRECTION('center_axis',(-7.81406971160724E-17,1.,0.)) ;
#120510 = DIRECTION('ref_axis',(1.,7.81406971160724E-17,-2.66453525910038E-15)) ;
#120511 = DIRECTION('center_axis',(-1.31418445149758E-16,1.,0.)) ;
#120512 = DIRECTION('ref_axis',(-1.,0.,0.)) ;
#120513 = DIRECTION('center_axis',(1.31418445149758E-16,-1.,0.)) ;
#120514 = DIRECTION('ref_axis',(-1.,-1.31418445149758E-16,0.)) ;
#120515 = DIRECTION('center_axis',(0.823067492614528,-1.78474312718973E-15,
0.567943573430701)) ;
#120516 = DIRECTION('ref_axis',(0.567943573430701,-3.32899177295693E-30,-0.823067492614528)) ;
#120517 = DIRECTION('center_axis',(-1.31418445149758E-16,1.,0.)) ;
#120518 = DIRECTION('ref_axis',(-1.,-1.31418445149758E-16,0.)) ;
#120519 = DIRECTION('center_axis',(-0.823067492614537,0.,0.567943573430688)) ;
#120520 = DIRECTION('ref_axis',(0.567943573430688,0.,0.823067492614537)) ;
#120521 = DIRECTION('center_axis',(7.81406971160724E-17,-1.,0.)) ;
#120522 = DIRECTION('ref_axis',(1.,0.,0.)) ;
#120523 = DIRECTION('center_axis',(7.81406971160724E-17,-1.,0.)) ;
#120524 = DIRECTION('ref_axis',(1.,7.81406971160724E-17,0.)) ;
#120525 = DIRECTION('center_axis',(-7.81406971160724E-17,1.,0.)) ;
#120526 = DIRECTION('ref_axis',(1.,7.81406971160724E-17,-1.73472347597681E-15)) ;
#120527 = DIRECTION('center_axis',(-1.31418445149758E-16,1.,0.)) ;
#120528 = DIRECTION('ref_axis',(-1.,0.,0.)) ;
#120529 = DIRECTION('center_axis',(1.31418445149758E-16,-1.,0.)) ;
#120530 = DIRECTION('ref_axis',(-1.,-1.31418445149758E-16,0.)) ;
#120531 = DIRECTION('center_axis',(0.823067492614537,-3.5694862543795E-15,
0.567943573430688)) ;
#120532 = DIRECTION('ref_axis',(0.567943573430688,-6.20058923363573E-30,-0.823067492614537)) ;
#120533 = DIRECTION('center_axis',(-1.31418445149758E-16,1.,0.)) ;
#120534 = DIRECTION('ref_axis',(-1.,-1.31418445149758E-16,0.)) ;
#120535 = DIRECTION('center_axis',(-0.823067492614537,0.,0.567943573430688)) ;
#120536 = DIRECTION('ref_axis',(0.567943573430688,0.,0.823067492614537)) ;
#120537 = DIRECTION('center_axis',(7.81406971160724E-17,-1.,0.)) ;
#120538 = DIRECTION('ref_axis',(1.,0.,0.)) ;
#120539 = DIRECTION('center_axis',(7.81406971160724E-17,-1.,0.)) ;
#120540 = DIRECTION('ref_axis',(1.,7.81406971160724E-17,0.)) ;
#120541 = DIRECTION('center_axis',(-7.81406971160724E-17,1.,0.)) ;
#120542 = DIRECTION('ref_axis',(1.,7.81406971160724E-17,-1.92747052886312E-15)) ;
#120543 = DIRECTION('center_axis',(-1.31418445149758E-16,1.,0.)) ;
#120544 = DIRECTION('ref_axis',(-1.,0.,0.)) ;
#120545 = DIRECTION('center_axis',(1.31418445149758E-16,-1.,0.)) ;
#120546 = DIRECTION('ref_axis',(-1.,-1.31418445149758E-16,0.)) ;
#120547 = DIRECTION('center_axis',(0.823067492614537,-3.5694862543795E-15,
0.567943573430688)) ;
#120548 = DIRECTION('ref_axis',(0.567943573430688,-6.20058923363573E-30,-0.823067492614537)) ;
#120549 = DIRECTION('center_axis',(-1.31418445149758E-16,1.,0.)) ;
#120550 = DIRECTION('ref_axis',(-1.,-1.31418445149758E-16,0.)) ;
#120551 = DIRECTION('center_axis',(-0.823067492614537,0.,0.567943573430688)) ;
#120552 = DIRECTION('ref_axis',(0.567943573430688,0.,0.823067492614537)) ;
#120553 = DIRECTION('center_axis',(7.81406971160724E-17,-1.,0.)) ;
#120554 = DIRECTION('ref_axis',(1.,0.,0.)) ;
#120555 = DIRECTION('center_axis',(7.81406971160724E-17,-1.,0.)) ;
#120556 = DIRECTION('ref_axis',(1.,7.81406971160724E-17,0.)) ;
#120557 = DIRECTION('center_axis',(-7.81406971160724E-17,1.,0.)) ;
#120558 = DIRECTION('ref_axis',(1.,7.81406971160724E-17,-1.5419764230905E-15)) ;
#120559 = DIRECTION('center_axis',(-1.31418445149758E-16,1.,0.)) ;
#120560 = DIRECTION('ref_axis',(-1.,0.,0.)) ;
#120561 = DIRECTION('center_axis',(1.31418445149758E-16,-1.,0.)) ;
#120562 = DIRECTION('ref_axis',(-1.,-1.31418445149758E-16,0.)) ;
#120563 = DIRECTION('center_axis',(0.823067492614531,3.56948625437948E-15,
0.567943573430696)) ;
#120564 = DIRECTION('ref_axis',(0.567943573430696,-1.85164162127997E-29,-0.823067492614531)) ;
#120565 = DIRECTION('center_axis',(-1.31418445149758E-16,1.,0.)) ;
#120566 = DIRECTION('ref_axis',(-1.,-1.31418445149758E-16,0.)) ;
#120567 = DIRECTION('center_axis',(-0.823067492614531,-5.35422938156922E-15,
0.567943573430696)) ;
#120568 = DIRECTION('ref_axis',(0.567943573430696,-2.86909128817562E-29,0.823067492614531)) ;
#120569 = DIRECTION('center_axis',(7.81406971160724E-17,-1.,0.)) ;
#120570 = DIRECTION('ref_axis',(1.,0.,0.)) ;
#120571 = DIRECTION('center_axis',(7.81406971160724E-17,-1.,0.)) ;
#120572 = DIRECTION('ref_axis',(1.,7.81406971160724E-17,0.)) ;
#120573 = DIRECTION('center_axis',(-7.81406971160724E-17,1.,0.)) ;
#120574 = DIRECTION('ref_axis',(1.,7.81406971160724E-17,-1.5419764230905E-15)) ;
#120575 = DIRECTION('center_axis',(-1.31418445149758E-16,1.,0.)) ;
#120576 = DIRECTION('ref_axis',(-1.,0.,0.)) ;
#120577 = DIRECTION('center_axis',(1.31418445149758E-16,-1.,0.)) ;
#120578 = DIRECTION('ref_axis',(-1.,-1.31418445149758E-16,0.)) ;
#120579 = DIRECTION('center_axis',(0.823067492614531,3.56948625437948E-15,
0.567943573430696)) ;
#120580 = DIRECTION('ref_axis',(0.567943573430696,-1.85164162127997E-29,-0.823067492614531)) ;
#120581 = DIRECTION('center_axis',(-1.31418445149758E-16,1.,0.)) ;
#120582 = DIRECTION('ref_axis',(-1.,-1.31418445149758E-16,0.)) ;
#120583 = DIRECTION('center_axis',(-0.823067492614531,-5.35422938156922E-15,
0.567943573430696)) ;
#120584 = DIRECTION('ref_axis',(0.567943573430696,-2.86909128817562E-29,0.823067492614531)) ;
#120585 = DIRECTION('center_axis',(7.81406971160724E-17,-1.,0.)) ;
#120586 = DIRECTION('ref_axis',(1.,0.,0.)) ;
#120587 = DIRECTION('center_axis',(7.81406971160724E-17,-1.,0.)) ;
#120588 = DIRECTION('ref_axis',(1.,7.81406971160724E-17,0.)) ;
#120589 = DIRECTION('center_axis',(-7.81406971160724E-17,1.,0.)) ;
#120590 = DIRECTION('ref_axis',(1.,7.81406971160724E-17,-1.5419764230905E-15)) ;
#120591 = DIRECTION('center_axis',(-1.31418445149758E-16,1.,0.)) ;
#120592 = DIRECTION('ref_axis',(-1.,0.,0.)) ;
#120593 = DIRECTION('center_axis',(1.31418445149758E-16,-1.,0.)) ;
#120594 = DIRECTION('ref_axis',(-1.,-1.31418445149758E-16,0.)) ;
#120595 = DIRECTION('center_axis',(0.823067492614531,3.56948625437948E-15,
0.567943573430696)) ;
#120596 = DIRECTION('ref_axis',(0.567943573430696,-1.85164162127997E-29,-0.823067492614531)) ;
#120597 = DIRECTION('center_axis',(-1.31418445149758E-16,1.,0.)) ;
#120598 = DIRECTION('ref_axis',(-1.,-1.31418445149758E-16,0.)) ;
#120599 = DIRECTION('center_axis',(-0.823067492614531,-5.35422938156922E-15,
0.567943573430696)) ;
#120600 = DIRECTION('ref_axis',(0.567943573430696,-2.86909128817562E-29,0.823067492614531)) ;
#120601 = DIRECTION('center_axis',(7.81406971160724E-17,-1.,0.)) ;
#120602 = DIRECTION('ref_axis',(1.,0.,0.)) ;
#120603 = DIRECTION('center_axis',(7.81406971160724E-17,-1.,0.)) ;
#120604 = DIRECTION('ref_axis',(1.,7.81406971160724E-17,0.)) ;
#120605 = DIRECTION('center_axis',(-7.81406971160724E-17,1.,0.)) ;
#120606 = DIRECTION('ref_axis',(1.,7.81406971160724E-17,-1.5419764230905E-15)) ;
#120607 = DIRECTION('center_axis',(-1.31418445149758E-16,1.,0.)) ;
#120608 = DIRECTION('ref_axis',(-1.,0.,0.)) ;
#120609 = DIRECTION('center_axis',(1.31418445149758E-16,-1.,0.)) ;
#120610 = DIRECTION('ref_axis',(-1.,-1.31418445149758E-16,0.)) ;
#120611 = DIRECTION('center_axis',(0.823067492614531,3.56948625437948E-15,
0.567943573430696)) ;
#120612 = DIRECTION('ref_axis',(0.567943573430696,-1.85164162127997E-29,-0.823067492614531)) ;
#120613 = DIRECTION('center_axis',(-1.31418445149758E-16,1.,0.)) ;
#120614 = DIRECTION('ref_axis',(-1.,-1.31418445149758E-16,0.)) ;
#120615 = DIRECTION('center_axis',(-0.823067492614531,0.,0.567943573430696)) ;
#120616 = DIRECTION('ref_axis',(0.567943573430696,0.,0.823067492614531)) ;
#120617 = DIRECTION('center_axis',(7.81406971160724E-17,-1.,0.)) ;
#120618 = DIRECTION('ref_axis',(1.,0.,0.)) ;
#120619 = DIRECTION('center_axis',(7.81406971160724E-17,-1.,0.)) ;
#120620 = DIRECTION('ref_axis',(1.,7.81406971160724E-17,0.)) ;
#120621 = DIRECTION('center_axis',(-7.81406971160724E-17,1.,0.)) ;
#120622 = DIRECTION('ref_axis',(1.,7.81406971160724E-17,-1.5419764230905E-15)) ;
#120623 = DIRECTION('center_axis',(-1.31418445149758E-16,1.,0.)) ;
#120624 = DIRECTION('ref_axis',(-1.,0.,0.)) ;
#120625 = DIRECTION('center_axis',(1.31418445149758E-16,-1.,0.)) ;
#120626 = DIRECTION('ref_axis',(-1.,-1.31418445149758E-16,0.)) ;
#120627 = DIRECTION('center_axis',(0.823067492614489,5.35422938156894E-15,
0.567943573430758)) ;
#120628 = DIRECTION('ref_axis',(0.567943573430758,1.07515500753245E-30,-0.823067492614489)) ;
#120629 = DIRECTION('center_axis',(-1.31418445149758E-16,1.,0.)) ;
#120630 = DIRECTION('ref_axis',(-1.,-1.31418445149758E-16,0.)) ;
#120631 = DIRECTION('center_axis',(-0.823067492614541,1.24932018903283E-14,
0.567943573430683)) ;
#120632 = DIRECTION('ref_axis',(0.567943573430683,-1.12678102635321E-28,0.823067492614541)) ;
#120633 = DIRECTION('center_axis',(7.81406971160724E-17,-1.,0.)) ;
#120634 = DIRECTION('ref_axis',(1.,0.,0.)) ;
#120635 = DIRECTION('center_axis',(7.81406971160724E-17,-1.,0.)) ;
#120636 = DIRECTION('ref_axis',(1.,7.81406971160724E-17,0.)) ;
#120637 = DIRECTION('center_axis',(-7.81406971160724E-17,1.,0.)) ;
#120638 = DIRECTION('ref_axis',(1.,7.81406971160724E-17,4.62592926927148E-15)) ;
#120639 = DIRECTION('center_axis',(-1.31418445149758E-16,1.,0.)) ;
#120640 = DIRECTION('ref_axis',(-1.,0.,0.)) ;
#120641 = DIRECTION('center_axis',(1.31418445149758E-16,-1.,0.)) ;
#120642 = DIRECTION('ref_axis',(-1.,-1.31418445149758E-16,0.)) ;
#120643 = DIRECTION('center_axis',(0.641814420963294,9.74199225357299E-15,
0.766859993117096)) ;
#120644 = DIRECTION('ref_axis',(0.766859993117096,-8.05387548571638E-29,-0.641814420963294)) ;
#120645 = DIRECTION('center_axis',(-1.31418445149758E-16,1.,0.)) ;
#120646 = DIRECTION('ref_axis',(-1.,-1.31418445149758E-16,0.)) ;
#120647 = DIRECTION('center_axis',(-1.,0.,0.)) ;
#120648 = DIRECTION('ref_axis',(0.,0.,1.)) ;
#120649 = DIRECTION('center_axis',(7.81406971160724E-17,-1.,0.)) ;
#120650 = DIRECTION('ref_axis',(1.,0.,0.)) ;
#120651 = DIRECTION('center_axis',(7.81406971160724E-17,-1.,0.)) ;
#120652 = DIRECTION('ref_axis',(1.,7.81406971160724E-17,0.)) ;
#120653 = DIRECTION('center_axis',(-7.81406971160724E-17,1.,0.)) ;
#120654 = DIRECTION('ref_axis',(1.,7.81406971160724E-17,-3.08395284618099E-15)) ;
#120655 = DIRECTION('center_axis',(1.31418445149758E-16,1.,0.)) ;
#120656 = DIRECTION('ref_axis',(-1.,1.31418445149758E-16,0.)) ;
#120657 = DIRECTION('center_axis',(0.,-1.,0.)) ;
#120658 = DIRECTION('ref_axis',(0.,0.,-1.)) ;
#120659 = DIRECTION('',(1.31418445149758E-16,1.,0.)) ;
#120660 = DIRECTION('',(1.31418445149758E-16,1.,0.)) ;
#120661 = DIRECTION('center_axis',(1.31418445149758E-16,1.,0.)) ;
#120662 = DIRECTION('ref_axis',(-1.,1.31418445149758E-16,0.)) ;
#120663 = DIRECTION('center_axis',(0.,-1.,0.)) ;
#120664 = DIRECTION('ref_axis',(0.,0.,-1.)) ;
#120665 = DIRECTION('',(1.31418445149758E-16,1.,0.)) ;
#120666 = DIRECTION('',(1.31418445149758E-16,1.,0.)) ;
#120667 = DIRECTION('center_axis',(1.31418445149758E-16,1.,0.)) ;
#120668 = DIRECTION('ref_axis',(-1.,1.31418445149758E-16,0.)) ;
#120669 = DIRECTION('center_axis',(0.,-1.,0.)) ;
#120670 = DIRECTION('ref_axis',(0.,0.,-1.)) ;
#120671 = DIRECTION('',(1.31418445149758E-16,1.,0.)) ;
#120672 = DIRECTION('',(1.31418445149758E-16,1.,0.)) ;
#120673 = DIRECTION('center_axis',(1.31418445149758E-16,1.,0.)) ;
#120674 = DIRECTION('ref_axis',(-1.,1.31418445149758E-16,0.)) ;
#120675 = DIRECTION('center_axis',(0.,-1.,0.)) ;
#120676 = DIRECTION('ref_axis',(0.,0.,-1.)) ;
#120677 = DIRECTION('',(1.31418445149758E-16,1.,0.)) ;
#120678 = DIRECTION('',(1.31418445149758E-16,1.,0.)) ;
#120679 = DIRECTION('center_axis',(1.31418445149758E-16,1.,0.)) ;
#120680 = DIRECTION('ref_axis',(-1.,1.31418445149758E-16,0.)) ;
#120681 = DIRECTION('center_axis',(1.18364427747299E-14,-1.,8.16753384930027E-15)) ;
#120682 = DIRECTION('ref_axis',(1.,1.18364427747299E-14,1.31368283683801E-29)) ;
#120683 = DIRECTION('',(1.31418445149758E-16,1.,0.)) ;
#120684 = DIRECTION('',(1.31418445149758E-16,1.,0.)) ;
#120685 = DIRECTION('center_axis',(1.31418445149758E-16,1.,0.)) ;
#120686 = DIRECTION('ref_axis',(-1.,1.31418445149758E-16,0.)) ;
#120687 = DIRECTION('center_axis',(-1.18364427747301E-14,-1.,-8.16753384930045E-15)) ;
#120688 = DIRECTION('ref_axis',(1.,-1.18364427747301E-14,1.31368283683791E-29)) ;
#120689 = DIRECTION('',(1.31418445149758E-16,1.,0.)) ;
#120690 = DIRECTION('',(1.31418445149758E-16,1.,0.)) ;
#120691 = DIRECTION('center_axis',(1.31418445149758E-16,1.,0.)) ;
#120692 = DIRECTION('ref_axis',(-1.,1.31418445149758E-16,0.)) ;
#120693 = DIRECTION('center_axis',(0.,-1.,0.)) ;
#120694 = DIRECTION('ref_axis',(0.,0.,-1.)) ;
#120695 = DIRECTION('',(1.31418445149758E-16,1.,0.)) ;
#120696 = DIRECTION('',(1.31418445149758E-16,1.,0.)) ;
#120697 = DIRECTION('center_axis',(1.,0.,0.)) ;
#120698 = DIRECTION('ref_axis',(0.,0.,-1.)) ;
#120699 = DIRECTION('center_axis',(1.,0.,0.)) ;
#120700 = DIRECTION('ref_axis',(0.,0.,-1.)) ;
#120701 = DIRECTION('center_axis',(0.,1.,1.22464679914736E-16)) ;
#120702 = DIRECTION('ref_axis',(0.,-1.22464679914736E-16,1.)) ;
#120703 = DIRECTION('center_axis',(-1.,0.,0.)) ;
#120704 = DIRECTION('ref_axis',(0.,0.,-1.)) ;
#120705 = DIRECTION('center_axis',(-1.31418445149758E-16,1.,0.)) ;
#120706 = DIRECTION('ref_axis',(-1.,0.,0.)) ;
#120707 = DIRECTION('center_axis',(-1.31418445149758E-16,1.,0.)) ;
#120708 = DIRECTION('ref_axis',(-1.,-1.31418445149758E-16,0.)) ;
#120709 = DIRECTION('center_axis',(0.,0.,-1.)) ;
#120710 = DIRECTION('ref_axis',(1.,0.,0.)) ;
#120711 = DIRECTION('center_axis',(1.31418445149758E-16,-1.,0.)) ;
#120712 = DIRECTION('ref_axis',(-1.,-1.31418445149758E-16,0.)) ;
#120713 = DIRECTION('center_axis',(1.,0.,0.)) ;
#120714 = DIRECTION('ref_axis',(0.,0.,-1.)) ;
#120715 = DIRECTION('center_axis',(1.,0.,0.)) ;
#120716 = DIRECTION('ref_axis',(0.,0.,-1.)) ;
#120717 = DIRECTION('center_axis',(0.,-1.,-1.22464679914735E-16)) ;
#120718 = DIRECTION('ref_axis',(0.,-1.22464679914735E-16,1.)) ;
#120719 = DIRECTION('center_axis',(-1.,0.,0.)) ;
#120720 = DIRECTION('ref_axis',(0.,0.,-1.)) ;
#120721 = DIRECTION('center_axis',(1.,0.,0.)) ;
#120722 = DIRECTION('ref_axis',(0.,0.,-1.)) ;
#120723 = DIRECTION('center_axis',(1.,0.,0.)) ;
#120724 = DIRECTION('ref_axis',(0.,0.,-1.)) ;
#120725 = DIRECTION('center_axis',(0.,1.,1.22464679914735E-16)) ;
#120726 = DIRECTION('ref_axis',(0.,-1.22464679914735E-16,1.)) ;
#120727 = DIRECTION('center_axis',(-1.,0.,0.)) ;
#120728 = DIRECTION('ref_axis',(0.,0.,-1.)) ;
#120729 = DIRECTION('center_axis',(-1.31418445149758E-16,1.,0.)) ;
#120730 = DIRECTION('ref_axis',(-1.,0.,0.)) ;
#120731 = DIRECTION('center_axis',(-1.31418445149758E-16,1.,0.)) ;
#120732 = DIRECTION('ref_axis',(-1.,-1.31418445149758E-16,0.)) ;
#120733 = DIRECTION('center_axis',(0.,0.,-1.)) ;
#120734 = DIRECTION('ref_axis',(1.,0.,0.)) ;
#120735 = DIRECTION('center_axis',(1.31418445149758E-16,-1.,0.)) ;
#120736 = DIRECTION('ref_axis',(-1.,-1.31418445149758E-16,0.)) ;
#120737 = DIRECTION('center_axis',(1.,0.,0.)) ;
#120738 = DIRECTION('ref_axis',(0.,0.,-1.)) ;
#120739 = DIRECTION('center_axis',(1.,0.,0.)) ;
#120740 = DIRECTION('ref_axis',(0.,0.,-1.)) ;
#120741 = DIRECTION('center_axis',(0.,-1.,-1.22464679914735E-16)) ;
#120742 = DIRECTION('ref_axis',(0.,-1.22464679914735E-16,1.)) ;
#120743 = DIRECTION('center_axis',(-1.,0.,0.)) ;
#120744 = DIRECTION('ref_axis',(0.,0.,-1.)) ;
#120745 = DIRECTION('center_axis',(1.,0.,0.)) ;
#120746 = DIRECTION('ref_axis',(0.,0.,-1.)) ;
#120747 = DIRECTION('center_axis',(1.,0.,0.)) ;
#120748 = DIRECTION('ref_axis',(0.,0.,-1.)) ;
#120749 = DIRECTION('center_axis',(0.,1.,1.22464679914735E-16)) ;
#120750 = DIRECTION('ref_axis',(0.,-1.22464679914735E-16,1.)) ;
#120751 = DIRECTION('center_axis',(-1.,0.,0.)) ;
#120752 = DIRECTION('ref_axis',(0.,0.,-1.)) ;
#120753 = DIRECTION('center_axis',(-1.31418445149758E-16,1.,0.)) ;
#120754 = DIRECTION('ref_axis',(-1.,0.,0.)) ;
#120755 = DIRECTION('center_axis',(-1.31418445149758E-16,1.,0.)) ;
#120756 = DIRECTION('ref_axis',(-1.,-1.31418445149758E-16,0.)) ;
#120757 = DIRECTION('center_axis',(0.,0.,-1.)) ;
#120758 = DIRECTION('ref_axis',(1.,0.,0.)) ;
#120759 = DIRECTION('center_axis',(1.31418445149758E-16,-1.,0.)) ;
#120760 = DIRECTION('ref_axis',(-1.,-1.31418445149758E-16,0.)) ;
#120761 = DIRECTION('center_axis',(1.,0.,0.)) ;
#120762 = DIRECTION('ref_axis',(0.,0.,-1.)) ;
#120763 = DIRECTION('center_axis',(1.,0.,0.)) ;
#120764 = DIRECTION('ref_axis',(0.,0.,-1.)) ;
#120765 = DIRECTION('center_axis',(0.,-1.,-1.22464679914735E-16)) ;
#120766 = DIRECTION('ref_axis',(0.,-1.22464679914735E-16,1.)) ;
#120767 = DIRECTION('center_axis',(-1.,0.,0.)) ;
#120768 = DIRECTION('ref_axis',(0.,0.,-1.)) ;
#120769 = DIRECTION('center_axis',(1.,0.,0.)) ;
#120770 = DIRECTION('ref_axis',(0.,0.,-1.)) ;
#120771 = DIRECTION('center_axis',(1.,0.,0.)) ;
#120772 = DIRECTION('ref_axis',(0.,0.,-1.)) ;
#120773 = DIRECTION('center_axis',(0.,1.,1.22464679914735E-16)) ;
#120774 = DIRECTION('ref_axis',(0.,-1.22464679914735E-16,1.)) ;
#120775 = DIRECTION('center_axis',(-1.,0.,0.)) ;
#120776 = DIRECTION('ref_axis',(0.,0.,-1.)) ;
#120777 = DIRECTION('center_axis',(-1.31418445149758E-16,1.,0.)) ;
#120778 = DIRECTION('ref_axis',(-1.,0.,0.)) ;
#120779 = DIRECTION('center_axis',(-1.31418445149758E-16,1.,0.)) ;
#120780 = DIRECTION('ref_axis',(-1.,-1.31418445149758E-16,0.)) ;
#120781 = DIRECTION('center_axis',(0.,0.,-1.)) ;
#120782 = DIRECTION('ref_axis',(1.,0.,0.)) ;
#120783 = DIRECTION('center_axis',(1.31418445149758E-16,-1.,0.)) ;
#120784 = DIRECTION('ref_axis',(-1.,-1.31418445149758E-16,0.)) ;
#120785 = DIRECTION('center_axis',(1.,0.,0.)) ;
#120786 = DIRECTION('ref_axis',(0.,0.,-1.)) ;
#120787 = DIRECTION('center_axis',(1.,0.,0.)) ;
#120788 = DIRECTION('ref_axis',(0.,0.,-1.)) ;
#120789 = DIRECTION('center_axis',(0.,-1.,-1.22464679914735E-16)) ;
#120790 = DIRECTION('ref_axis',(0.,-1.22464679914735E-16,1.)) ;
#120791 = DIRECTION('center_axis',(-1.,0.,0.)) ;
#120792 = DIRECTION('ref_axis',(0.,0.,-1.)) ;
#120793 = DIRECTION('center_axis',(1.,0.,0.)) ;
#120794 = DIRECTION('ref_axis',(0.,0.,-1.)) ;
#120795 = DIRECTION('center_axis',(1.,0.,0.)) ;
#120796 = DIRECTION('ref_axis',(0.,0.,-1.)) ;
#120797 = DIRECTION('center_axis',(0.,1.,1.22464679914735E-16)) ;
#120798 = DIRECTION('ref_axis',(0.,-1.22464679914735E-16,1.)) ;
#120799 = DIRECTION('center_axis',(-1.,0.,0.)) ;
#120800 = DIRECTION('ref_axis',(0.,0.,-1.)) ;
#120801 = DIRECTION('center_axis',(-1.31418445149758E-16,1.,0.)) ;
#120802 = DIRECTION('ref_axis',(-1.,0.,0.)) ;
#120803 = DIRECTION('center_axis',(-1.31418445149758E-16,1.,0.)) ;
#120804 = DIRECTION('ref_axis',(-1.,-1.31418445149758E-16,0.)) ;
#120805 = DIRECTION('center_axis',(0.,0.,-1.)) ;
#120806 = DIRECTION('ref_axis',(1.,0.,0.)) ;
#120807 = DIRECTION('center_axis',(1.31418445149758E-16,-1.,0.)) ;
#120808 = DIRECTION('ref_axis',(-1.,-1.31418445149758E-16,0.)) ;
#120809 = DIRECTION('center_axis',(1.,0.,0.)) ;
#120810 = DIRECTION('ref_axis',(0.,0.,-1.)) ;
#120811 = DIRECTION('center_axis',(1.,0.,0.)) ;
#120812 = DIRECTION('ref_axis',(0.,0.,-1.)) ;
#120813 = DIRECTION('center_axis',(0.,-1.,-1.22464679914735E-16)) ;
#120814 = DIRECTION('ref_axis',(0.,-1.22464679914735E-16,1.)) ;
#120815 = DIRECTION('center_axis',(-1.,0.,0.)) ;
#120816 = DIRECTION('ref_axis',(0.,0.,-1.)) ;
#120817 = DIRECTION('center_axis',(1.,0.,0.)) ;
#120818 = DIRECTION('ref_axis',(0.,0.,-1.)) ;
#120819 = DIRECTION('center_axis',(1.,0.,0.)) ;
#120820 = DIRECTION('ref_axis',(0.,0.,-1.)) ;
#120821 = DIRECTION('center_axis',(0.,1.,1.22464679914735E-16)) ;
#120822 = DIRECTION('ref_axis',(0.,-1.22464679914735E-16,1.)) ;
#120823 = DIRECTION('center_axis',(-1.,0.,0.)) ;
#120824 = DIRECTION('ref_axis',(0.,0.,-1.)) ;
#120825 = DIRECTION('center_axis',(-1.31418445149758E-16,1.,0.)) ;
#120826 = DIRECTION('ref_axis',(-1.,0.,0.)) ;
#120827 = DIRECTION('center_axis',(-1.31418445149758E-16,1.,0.)) ;
#120828 = DIRECTION('ref_axis',(-1.,-1.31418445149758E-16,0.)) ;
#120829 = DIRECTION('center_axis',(0.,0.,-1.)) ;
#120830 = DIRECTION('ref_axis',(1.,0.,0.)) ;
#120831 = DIRECTION('center_axis',(1.31418445149758E-16,-1.,0.)) ;
#120832 = DIRECTION('ref_axis',(-1.,-1.31418445149758E-16,0.)) ;
#120833 = DIRECTION('center_axis',(1.,0.,0.)) ;
#120834 = DIRECTION('ref_axis',(0.,0.,-1.)) ;
#120835 = DIRECTION('center_axis',(1.,0.,0.)) ;
#120836 = DIRECTION('ref_axis',(0.,0.,-1.)) ;
#120837 = DIRECTION('center_axis',(0.,-1.,-1.22464679914735E-16)) ;
#120838 = DIRECTION('ref_axis',(0.,-1.22464679914735E-16,1.)) ;
#120839 = DIRECTION('center_axis',(-1.,0.,0.)) ;
#120840 = DIRECTION('ref_axis',(0.,0.,-1.)) ;
#120841 = DIRECTION('center_axis',(1.,0.,0.)) ;
#120842 = DIRECTION('ref_axis',(0.,0.,-1.)) ;
#120843 = DIRECTION('center_axis',(1.,0.,0.)) ;
#120844 = DIRECTION('ref_axis',(0.,0.,-1.)) ;
#120845 = DIRECTION('center_axis',(0.,1.,1.22464679914735E-16)) ;
#120846 = DIRECTION('ref_axis',(0.,-1.22464679914735E-16,1.)) ;
#120847 = DIRECTION('center_axis',(-1.,0.,0.)) ;
#120848 = DIRECTION('ref_axis',(0.,0.,-1.)) ;
#120849 = DIRECTION('center_axis',(-1.31418445149758E-16,1.,0.)) ;
#120850 = DIRECTION('ref_axis',(-1.,0.,0.)) ;
#120851 = DIRECTION('center_axis',(-1.31418445149758E-16,1.,0.)) ;
#120852 = DIRECTION('ref_axis',(-1.,-1.31418445149758E-16,0.)) ;
#120853 = DIRECTION('center_axis',(0.,0.,-1.)) ;
#120854 = DIRECTION('ref_axis',(1.,0.,0.)) ;
#120855 = DIRECTION('center_axis',(1.31418445149758E-16,-1.,0.)) ;
#120856 = DIRECTION('ref_axis',(-1.,-1.31418445149758E-16,0.)) ;
#120857 = DIRECTION('center_axis',(1.,0.,0.)) ;
#120858 = DIRECTION('ref_axis',(0.,0.,-1.)) ;
#120859 = DIRECTION('center_axis',(1.,0.,0.)) ;
#120860 = DIRECTION('ref_axis',(0.,0.,-1.)) ;
#120861 = DIRECTION('center_axis',(0.,-1.,-1.22464679914735E-16)) ;
#120862 = DIRECTION('ref_axis',(0.,-1.22464679914735E-16,1.)) ;
#120863 = DIRECTION('center_axis',(-1.,0.,0.)) ;
#120864 = DIRECTION('ref_axis',(0.,0.,-1.)) ;
#120865 = DIRECTION('center_axis',(1.,0.,0.)) ;
#120866 = DIRECTION('ref_axis',(0.,0.,-1.)) ;
#120867 = DIRECTION('center_axis',(1.,0.,0.)) ;
#120868 = DIRECTION('ref_axis',(0.,0.,-1.)) ;
#120869 = DIRECTION('center_axis',(0.,1.,1.22464679914735E-16)) ;
#120870 = DIRECTION('ref_axis',(0.,-1.22464679914735E-16,1.)) ;
#120871 = DIRECTION('center_axis',(-1.,0.,0.)) ;
#120872 = DIRECTION('ref_axis',(0.,0.,-1.)) ;
#120873 = DIRECTION('center_axis',(-1.31418445149758E-16,1.,0.)) ;
#120874 = DIRECTION('ref_axis',(-1.,0.,0.)) ;
#120875 = DIRECTION('center_axis',(-1.31418445149758E-16,1.,0.)) ;
#120876 = DIRECTION('ref_axis',(-1.,-1.31418445149758E-16,0.)) ;
#120877 = DIRECTION('center_axis',(0.,0.,-1.)) ;
#120878 = DIRECTION('ref_axis',(1.,0.,0.)) ;
#120879 = DIRECTION('center_axis',(1.31418445149758E-16,-1.,0.)) ;
#120880 = DIRECTION('ref_axis',(-1.,-1.31418445149758E-16,0.)) ;
#120881 = DIRECTION('center_axis',(1.,0.,0.)) ;
#120882 = DIRECTION('ref_axis',(0.,0.,-1.)) ;
#120883 = DIRECTION('center_axis',(1.,0.,0.)) ;
#120884 = DIRECTION('ref_axis',(0.,0.,-1.)) ;
#120885 = DIRECTION('center_axis',(0.,-1.,-1.22464679914735E-16)) ;
#120886 = DIRECTION('ref_axis',(0.,-1.22464679914735E-16,1.)) ;
#120887 = DIRECTION('center_axis',(-1.,0.,0.)) ;
#120888 = DIRECTION('ref_axis',(0.,0.,-1.)) ;
#120889 = DIRECTION('center_axis',(1.,0.,0.)) ;
#120890 = DIRECTION('ref_axis',(0.,0.,-1.)) ;
#120891 = DIRECTION('center_axis',(1.,0.,0.)) ;
#120892 = DIRECTION('ref_axis',(0.,0.,-1.)) ;
#120893 = DIRECTION('center_axis',(0.,1.,1.22464679914735E-16)) ;
#120894 = DIRECTION('ref_axis',(0.,-1.22464679914735E-16,1.)) ;
#120895 = DIRECTION('center_axis',(-1.,0.,0.)) ;
#120896 = DIRECTION('ref_axis',(0.,0.,-1.)) ;
#120897 = DIRECTION('center_axis',(-1.31418445149758E-16,1.,0.)) ;
#120898 = DIRECTION('ref_axis',(-1.,0.,0.)) ;
#120899 = DIRECTION('center_axis',(-1.31418445149758E-16,1.,0.)) ;
#120900 = DIRECTION('ref_axis',(-1.,-1.31418445149758E-16,0.)) ;
#120901 = DIRECTION('center_axis',(0.,0.,-1.)) ;
#120902 = DIRECTION('ref_axis',(1.,0.,0.)) ;
#120903 = DIRECTION('center_axis',(1.31418445149758E-16,-1.,0.)) ;
#120904 = DIRECTION('ref_axis',(-1.,-1.31418445149758E-16,0.)) ;
#120905 = DIRECTION('center_axis',(1.,0.,0.)) ;
#120906 = DIRECTION('ref_axis',(0.,0.,-1.)) ;
#120907 = DIRECTION('center_axis',(1.,0.,0.)) ;
#120908 = DIRECTION('ref_axis',(0.,0.,-1.)) ;
#120909 = DIRECTION('center_axis',(0.,-1.,-1.22464679914735E-16)) ;
#120910 = DIRECTION('ref_axis',(0.,-1.22464679914735E-16,1.)) ;
#120911 = DIRECTION('center_axis',(-1.,0.,0.)) ;
#120912 = DIRECTION('ref_axis',(0.,0.,-1.)) ;
#120913 = DIRECTION('center_axis',(1.31418445149758E-16,1.,0.)) ;
#120914 = DIRECTION('ref_axis',(-1.,1.31418445149758E-16,0.)) ;
#120915 = DIRECTION('center_axis',(1.31418445149758E-16,1.,0.)) ;
#120916 = DIRECTION('ref_axis',(-1.,1.31418445149758E-16,0.)) ;
#120917 = DIRECTION('',(1.31418445149758E-16,1.,0.)) ;
#120918 = DIRECTION('center_axis',(1.31418445149758E-16,1.,0.)) ;
#120919 = DIRECTION('ref_axis',(-1.,1.31418445149758E-16,0.)) ;
#120920 = DIRECTION('',(1.31418445149758E-16,1.,0.)) ;
#120921 = DIRECTION('center_axis',(1.31418445149758E-16,1.,0.)) ;
#120922 = DIRECTION('ref_axis',(-1.,1.31418445149758E-16,0.)) ;
#120923 = DIRECTION('',(1.31418445149758E-16,1.,0.)) ;
#120924 = DIRECTION('center_axis',(1.31418445149758E-16,1.,0.)) ;
#120925 = DIRECTION('ref_axis',(-1.,1.31418445149758E-16,0.)) ;
#120926 = DIRECTION('',(1.31418445149758E-16,1.,0.)) ;
#120927 = DIRECTION('center_axis',(1.31418445149758E-16,1.,0.)) ;
#120928 = DIRECTION('ref_axis',(-1.,1.31418445149758E-16,0.)) ;
#120929 = DIRECTION('',(1.31418445149758E-16,1.,0.)) ;
#120930 = DIRECTION('center_axis',(1.31418445149758E-16,1.,0.)) ;
#120931 = DIRECTION('ref_axis',(-1.,1.31418445149758E-16,0.)) ;
#120932 = DIRECTION('center_axis',(1.31418445149758E-16,1.,0.)) ;
#120933 = DIRECTION('ref_axis',(-1.,1.31418445149758E-16,0.)) ;
#120934 = DIRECTION('',(1.31418445149758E-16,1.,0.)) ;
#120935 = DIRECTION('center_axis',(1.31418445149758E-16,1.,0.)) ;
#120936 = DIRECTION('ref_axis',(-1.,1.31418445149758E-16,0.)) ;
#120937 = DIRECTION('',(1.31418445149758E-16,1.,0.)) ;
#120938 = DIRECTION('center_axis',(1.31418445149758E-16,1.,0.)) ;
#120939 = DIRECTION('ref_axis',(-1.,1.31418445149758E-16,0.)) ;
#120940 = DIRECTION('',(1.31418445149758E-16,1.,0.)) ;
#120941 = DIRECTION('center_axis',(1.31418445149758E-16,1.,0.)) ;
#120942 = DIRECTION('ref_axis',(-1.,1.31418445149758E-16,0.)) ;
#120943 = DIRECTION('',(1.31418445149758E-16,1.,0.)) ;
#120944 = DIRECTION('center_axis',(1.31418445149758E-16,1.,0.)) ;
#120945 = DIRECTION('ref_axis',(-1.,1.31418445149758E-16,0.)) ;
#120946 = DIRECTION('',(1.31418445149758E-16,1.,0.)) ;
#120947 = DIRECTION('center_axis',(1.31418445149758E-16,1.,0.)) ;
#120948 = DIRECTION('ref_axis',(-1.,1.31418445149758E-16,0.)) ;
#120949 = DIRECTION('center_axis',(1.31418445149758E-16,1.,0.)) ;
#120950 = DIRECTION('ref_axis',(-1.,1.31418445149758E-16,0.)) ;
#120951 = DIRECTION('',(1.31418445149758E-16,1.,0.)) ;
#120952 = DIRECTION('center_axis',(1.31418445149758E-16,1.,0.)) ;
#120953 = DIRECTION('ref_axis',(-1.,1.31418445149758E-16,0.)) ;
#120954 = DIRECTION('',(1.31418445149758E-16,1.,0.)) ;
#120955 = DIRECTION('center_axis',(1.31418445149758E-16,1.,0.)) ;
#120956 = DIRECTION('ref_axis',(-1.,1.31418445149758E-16,0.)) ;
#120957 = DIRECTION('',(1.31418445149758E-16,1.,0.)) ;
#120958 = DIRECTION('center_axis',(1.31418445149758E-16,1.,0.)) ;
#120959 = DIRECTION('ref_axis',(-1.,1.31418445149758E-16,0.)) ;
#120960 = DIRECTION('',(1.31418445149758E-16,1.,0.)) ;
#120961 = DIRECTION('center_axis',(1.31418445149758E-16,1.,0.)) ;
#120962 = DIRECTION('ref_axis',(-1.,1.31418445149758E-16,0.)) ;
#120963 = DIRECTION('',(1.31418445149758E-16,1.,0.)) ;
#120964 = DIRECTION('center_axis',(1.31418445149758E-16,1.,0.)) ;
#120965 = DIRECTION('ref_axis',(-1.,1.31418445149758E-16,0.)) ;
#120966 = DIRECTION('center_axis',(1.31418445149758E-16,1.,0.)) ;
#120967 = DIRECTION('ref_axis',(-1.,1.31418445149758E-16,0.)) ;
#120968 = DIRECTION('',(1.31418445149758E-16,1.,0.)) ;
#120969 = DIRECTION('center_axis',(1.31418445149758E-16,1.,0.)) ;
#120970 = DIRECTION('ref_axis',(-1.,1.31418445149758E-16,0.)) ;
#120971 = DIRECTION('',(1.31418445149758E-16,1.,0.)) ;
#120972 = DIRECTION('center_axis',(1.31418445149758E-16,1.,0.)) ;
#120973 = DIRECTION('ref_axis',(-1.,1.31418445149758E-16,0.)) ;
#120974 = DIRECTION('',(1.31418445149758E-16,1.,0.)) ;
#120975 = DIRECTION('center_axis',(1.31418445149758E-16,1.,0.)) ;
#120976 = DIRECTION('ref_axis',(-1.,1.31418445149758E-16,0.)) ;
#120977 = DIRECTION('',(1.31418445149758E-16,1.,0.)) ;
#120978 = DIRECTION('center_axis',(1.31418445149758E-16,1.,0.)) ;
#120979 = DIRECTION('ref_axis',(-1.,1.31418445149758E-16,0.)) ;
#120980 = DIRECTION('',(1.31418445149758E-16,1.,0.)) ;
#120981 = DIRECTION('center_axis',(1.31418445149758E-16,1.,0.)) ;
#120982 = DIRECTION('ref_axis',(-1.,1.31418445149758E-16,0.)) ;
#120983 = DIRECTION('center_axis',(1.31418445149758E-16,1.,0.)) ;
#120984 = DIRECTION('ref_axis',(-1.,1.31418445149758E-16,0.)) ;
#120985 = DIRECTION('',(1.31418445149758E-16,1.,0.)) ;
#120986 = DIRECTION('center_axis',(1.31418445149758E-16,1.,0.)) ;
#120987 = DIRECTION('ref_axis',(-1.,1.31418445149758E-16,0.)) ;
#120988 = DIRECTION('',(1.31418445149758E-16,1.,0.)) ;
#120989 = DIRECTION('center_axis',(1.31418445149758E-16,1.,0.)) ;
#120990 = DIRECTION('ref_axis',(-1.,1.31418445149758E-16,0.)) ;
#120991 = DIRECTION('',(1.31418445149758E-16,1.,0.)) ;
#120992 = DIRECTION('center_axis',(1.31418445149758E-16,1.,0.)) ;
#120993 = DIRECTION('ref_axis',(-1.,1.31418445149758E-16,0.)) ;
#120994 = DIRECTION('',(1.31418445149758E-16,1.,0.)) ;
#120995 = DIRECTION('center_axis',(1.31418445149758E-16,1.,0.)) ;
#120996 = DIRECTION('ref_axis',(-1.,1.31418445149758E-16,0.)) ;
#120997 = DIRECTION('',(1.31418445149758E-16,1.,0.)) ;
#120998 = DIRECTION('center_axis',(1.31418445149758E-16,1.,0.)) ;
#120999 = DIRECTION('ref_axis',(-1.,1.31418445149758E-16,0.)) ;
#121000 = DIRECTION('center_axis',(1.31418445149758E-16,1.,0.)) ;
#121001 = DIRECTION('ref_axis',(-1.,1.31418445149758E-16,0.)) ;
#121002 = DIRECTION('',(1.31418445149758E-16,1.,0.)) ;
#121003 = DIRECTION('center_axis',(1.31418445149758E-16,1.,0.)) ;
#121004 = DIRECTION('ref_axis',(-1.,1.31418445149758E-16,0.)) ;
#121005 = DIRECTION('',(1.31418445149758E-16,1.,0.)) ;
#121006 = DIRECTION('center_axis',(1.31418445149758E-16,1.,0.)) ;
#121007 = DIRECTION('ref_axis',(-1.,1.31418445149758E-16,0.)) ;
#121008 = DIRECTION('',(1.31418445149758E-16,1.,0.)) ;
#121009 = DIRECTION('center_axis',(1.31418445149758E-16,1.,0.)) ;
#121010 = DIRECTION('ref_axis',(-1.,1.31418445149758E-16,0.)) ;
#121011 = DIRECTION('',(1.31418445149758E-16,1.,0.)) ;
#121012 = DIRECTION('center_axis',(1.31418445149758E-16,1.,0.)) ;
#121013 = DIRECTION('ref_axis',(-1.,1.31418445149758E-16,0.)) ;
#121014 = DIRECTION('',(1.31418445149758E-16,1.,0.)) ;
#121015 = DIRECTION('center_axis',(1.31418445149758E-16,1.,0.)) ;
#121016 = DIRECTION('ref_axis',(-1.,1.31418445149758E-16,0.)) ;
#121017 = DIRECTION('center_axis',(1.31418445149758E-16,1.,0.)) ;
#121018 = DIRECTION('ref_axis',(-1.,1.31418445149758E-16,0.)) ;
#121019 = DIRECTION('',(1.31418445149758E-16,1.,0.)) ;
#121020 = DIRECTION('center_axis',(1.31418445149758E-16,1.,0.)) ;
#121021 = DIRECTION('ref_axis',(-1.,1.31418445149758E-16,0.)) ;
#121022 = DIRECTION('',(1.31418445149758E-16,1.,0.)) ;
#121023 = DIRECTION('center_axis',(1.31418445149758E-16,1.,0.)) ;
#121024 = DIRECTION('ref_axis',(-1.,1.31418445149758E-16,0.)) ;
#121025 = DIRECTION('',(1.31418445149758E-16,1.,0.)) ;
#121026 = DIRECTION('center_axis',(1.31418445149758E-16,1.,0.)) ;
#121027 = DIRECTION('ref_axis',(-1.,1.31418445149758E-16,0.)) ;
#121028 = DIRECTION('',(1.31418445149758E-16,1.,0.)) ;
#121029 = DIRECTION('center_axis',(1.31418445149758E-16,1.,0.)) ;
#121030 = DIRECTION('ref_axis',(-1.,1.31418445149758E-16,0.)) ;
#121031 = DIRECTION('',(1.31418445149758E-16,1.,0.)) ;
#121032 = DIRECTION('center_axis',(1.31418445149758E-16,1.,0.)) ;
#121033 = DIRECTION('ref_axis',(-1.,1.31418445149758E-16,0.)) ;
#121034 = DIRECTION('center_axis',(1.31418445149758E-16,1.,0.)) ;
#121035 = DIRECTION('ref_axis',(-1.,1.31418445149758E-16,0.)) ;
#121036 = DIRECTION('',(1.31418445149758E-16,1.,0.)) ;
#121037 = DIRECTION('center_axis',(1.31418445149758E-16,1.,0.)) ;
#121038 = DIRECTION('ref_axis',(-1.,1.31418445149758E-16,0.)) ;
#121039 = DIRECTION('',(1.31418445149758E-16,1.,0.)) ;
#121040 = DIRECTION('center_axis',(1.31418445149758E-16,1.,0.)) ;
#121041 = DIRECTION('ref_axis',(-1.,1.31418445149758E-16,0.)) ;
#121042 = DIRECTION('',(1.31418445149758E-16,1.,0.)) ;
#121043 = DIRECTION('center_axis',(1.31418445149758E-16,1.,0.)) ;
#121044 = DIRECTION('ref_axis',(-1.,1.31418445149758E-16,0.)) ;
#121045 = DIRECTION('',(1.31418445149758E-16,1.,0.)) ;
#121046 = DIRECTION('center_axis',(1.31418445149758E-16,1.,0.)) ;
#121047 = DIRECTION('ref_axis',(-1.,1.31418445149758E-16,0.)) ;
#121048 = DIRECTION('',(1.31418445149758E-16,1.,0.)) ;
#121049 = DIRECTION('center_axis',(1.31418445149758E-16,1.,0.)) ;
#121050 = DIRECTION('ref_axis',(-1.,1.31418445149758E-16,0.)) ;
#121051 = DIRECTION('center_axis',(1.31418445149758E-16,1.,0.)) ;
#121052 = DIRECTION('ref_axis',(-1.,1.31418445149758E-16,0.)) ;
#121053 = DIRECTION('',(1.31418445149758E-16,1.,0.)) ;
#121054 = DIRECTION('center_axis',(1.31418445149758E-16,1.,0.)) ;
#121055 = DIRECTION('ref_axis',(-1.,1.31418445149758E-16,0.)) ;
#121056 = DIRECTION('',(1.31418445149758E-16,1.,0.)) ;
#121057 = DIRECTION('center_axis',(1.31418445149758E-16,1.,0.)) ;
#121058 = DIRECTION('ref_axis',(-1.,1.31418445149758E-16,0.)) ;
#121059 = DIRECTION('',(1.31418445149758E-16,1.,0.)) ;
#121060 = DIRECTION('center_axis',(1.31418445149758E-16,1.,0.)) ;
#121061 = DIRECTION('ref_axis',(-1.,1.31418445149758E-16,0.)) ;
#121062 = DIRECTION('',(1.31418445149758E-16,1.,0.)) ;
#121063 = DIRECTION('center_axis',(1.31418445149758E-16,1.,0.)) ;
#121064 = DIRECTION('ref_axis',(-1.,1.31418445149758E-16,0.)) ;
#121065 = DIRECTION('',(1.31418445149758E-16,1.,0.)) ;
#121066 = DIRECTION('center_axis',(1.,0.,0.)) ;
#121067 = DIRECTION('ref_axis',(0.,0.,-1.)) ;
#121068 = DIRECTION('center_axis',(1.,0.,0.)) ;
#121069 = DIRECTION('ref_axis',(0.,0.,-1.)) ;
#121070 = DIRECTION('',(0.707106781186546,-8.65956056235495E-17,0.707106781186549)) ;
#121071 = DIRECTION('center_axis',(1.,0.,0.)) ;
#121072 = DIRECTION('ref_axis',(0.,0.,-1.)) ;
#121073 = DIRECTION('center_axis',(1.,0.,0.)) ;
#121074 = DIRECTION('ref_axis',(0.,0.,-1.)) ;
#121075 = DIRECTION('',(0.707106781186546,-8.65956056235495E-17,0.707106781186549)) ;
#121076 = DIRECTION('center_axis',(1.,0.,0.)) ;
#121077 = DIRECTION('ref_axis',(0.,0.,-1.)) ;
#121078 = DIRECTION('center_axis',(1.,0.,0.)) ;
#121079 = DIRECTION('ref_axis',(0.,0.,-1.)) ;
#121080 = DIRECTION('',(0.707106781186546,-8.65956056235495E-17,0.707106781186549)) ;
#121081 = DIRECTION('center_axis',(1.,0.,0.)) ;
#121082 = DIRECTION('ref_axis',(0.,0.,-1.)) ;
#121083 = DIRECTION('center_axis',(1.,0.,0.)) ;
#121084 = DIRECTION('ref_axis',(0.,0.,-1.)) ;
#121085 = DIRECTION('',(0.707106781186546,-8.65956056235495E-17,0.707106781186549)) ;
#121086 = DIRECTION('center_axis',(1.,0.,0.)) ;
#121087 = DIRECTION('ref_axis',(0.,0.,-1.)) ;
#121088 = DIRECTION('center_axis',(1.,0.,0.)) ;
#121089 = DIRECTION('ref_axis',(0.,0.,-1.)) ;
#121090 = DIRECTION('',(0.707106781186546,-8.65956056235495E-17,0.707106781186549)) ;
#121091 = DIRECTION('center_axis',(1.,0.,0.)) ;
#121092 = DIRECTION('ref_axis',(0.,0.,-1.)) ;
#121093 = DIRECTION('center_axis',(1.,0.,0.)) ;
#121094 = DIRECTION('ref_axis',(0.,0.,-1.)) ;
#121095 = DIRECTION('',(0.707106781186546,-8.65956056235495E-17,0.707106781186549)) ;
#121096 = DIRECTION('center_axis',(1.,0.,0.)) ;
#121097 = DIRECTION('ref_axis',(0.,0.,-1.)) ;
#121098 = DIRECTION('center_axis',(1.,0.,0.)) ;
#121099 = DIRECTION('ref_axis',(0.,0.,-1.)) ;
#121100 = DIRECTION('',(0.707106781186546,-8.65956056235495E-17,0.707106781186549)) ;
#121101 = DIRECTION('center_axis',(1.,0.,0.)) ;
#121102 = DIRECTION('ref_axis',(0.,0.,-1.)) ;
#121103 = DIRECTION('center_axis',(1.,0.,0.)) ;
#121104 = DIRECTION('ref_axis',(0.,0.,-1.)) ;
#121105 = DIRECTION('',(0.707106781186546,-8.65956056235495E-17,0.707106781186549)) ;
#121106 = DIRECTION('center_axis',(1.,0.,0.)) ;
#121107 = DIRECTION('ref_axis',(0.,0.,-1.)) ;
#121108 = DIRECTION('center_axis',(1.,0.,0.)) ;
#121109 = DIRECTION('ref_axis',(0.,0.,-1.)) ;
#121110 = DIRECTION('',(0.707106781186546,-8.65956056235495E-17,0.707106781186549)) ;
#121111 = DIRECTION('center_axis',(1.,0.,0.)) ;
#121112 = DIRECTION('ref_axis',(0.,0.,-1.)) ;
#121113 = DIRECTION('',(1.,0.,0.)) ;
#121114 = DIRECTION('center_axis',(1.,0.,0.)) ;
#121115 = DIRECTION('ref_axis',(0.,0.,-1.)) ;
#121116 = DIRECTION('',(1.,0.,0.)) ;
#121117 = DIRECTION('center_axis',(1.,0.,0.)) ;
#121118 = DIRECTION('ref_axis',(0.,0.,-1.)) ;
#121119 = DIRECTION('',(1.,0.,0.)) ;
#121120 = DIRECTION('center_axis',(1.,0.,0.)) ;
#121121 = DIRECTION('ref_axis',(0.,0.,-1.)) ;
#121122 = DIRECTION('',(1.,0.,0.)) ;
#121123 = DIRECTION('center_axis',(1.,0.,0.)) ;
#121124 = DIRECTION('ref_axis',(0.,0.,-1.)) ;
#121125 = DIRECTION('',(1.,0.,0.)) ;
#121126 = DIRECTION('center_axis',(1.,0.,0.)) ;
#121127 = DIRECTION('ref_axis',(0.,0.,-1.)) ;
#121128 = DIRECTION('',(1.,0.,0.)) ;
#121129 = DIRECTION('center_axis',(1.,0.,0.)) ;
#121130 = DIRECTION('ref_axis',(0.,0.,-1.)) ;
#121131 = DIRECTION('',(1.,0.,0.)) ;
#121132 = DIRECTION('center_axis',(1.,0.,0.)) ;
#121133 = DIRECTION('ref_axis',(0.,0.,-1.)) ;
#121134 = DIRECTION('',(1.,0.,0.)) ;
#121135 = DIRECTION('center_axis',(1.,0.,0.)) ;
#121136 = DIRECTION('ref_axis',(0.,0.,-1.)) ;
#121137 = DIRECTION('',(1.,0.,0.)) ;
#121138 = DIRECTION('center_axis',(1.,0.,0.)) ;
#121139 = DIRECTION('ref_axis',(0.,0.,-1.)) ;
#121140 = DIRECTION('center_axis',(1.,0.,0.)) ;
#121141 = DIRECTION('ref_axis',(0.,0.,-1.)) ;
#121142 = DIRECTION('center_axis',(0.,1.,1.22464679914735E-16)) ;
#121143 = DIRECTION('ref_axis',(0.,-1.22464679914735E-16,1.)) ;
#121144 = DIRECTION('center_axis',(-1.,0.,0.)) ;
#121145 = DIRECTION('ref_axis',(0.,0.,-1.)) ;
#121146 = DIRECTION('center_axis',(-1.31418445149758E-16,1.,0.)) ;
#121147 = DIRECTION('ref_axis',(-1.,0.,0.)) ;
#121148 = DIRECTION('center_axis',(-1.31418445149758E-16,1.,0.)) ;
#121149 = DIRECTION('ref_axis',(-1.,-1.31418445149758E-16,0.)) ;
#121150 = DIRECTION('center_axis',(-1.22464679914735E-16,-1.60941178201573E-32,
-1.)) ;
#121151 = DIRECTION('ref_axis',(1.,0.,-1.22464679914735E-16)) ;
#121152 = DIRECTION('center_axis',(1.31418445149758E-16,-1.,0.)) ;
#121153 = DIRECTION('ref_axis',(-1.,-1.31418445149758E-16,0.)) ;
#121154 = DIRECTION('center_axis',(1.,0.,0.)) ;
#121155 = DIRECTION('ref_axis',(0.,0.,-1.)) ;
#121156 = DIRECTION('center_axis',(1.,0.,0.)) ;
#121157 = DIRECTION('ref_axis',(0.,0.,-1.)) ;
#121158 = DIRECTION('center_axis',(0.,-1.,-1.22464679914735E-16)) ;
#121159 = DIRECTION('ref_axis',(0.,-1.22464679914735E-16,1.)) ;
#121160 = DIRECTION('center_axis',(-1.,0.,0.)) ;
#121161 = DIRECTION('ref_axis',(0.,0.,-1.)) ;
#121162 = DIRECTION('center_axis',(-1.31418445149758E-16,1.,0.)) ;
#121163 = DIRECTION('ref_axis',(-1.,-1.31418445149758E-16,0.)) ;
#121164 = DIRECTION('center_axis',(0.,-1.,0.)) ;
#121165 = DIRECTION('ref_axis',(0.,0.,-1.)) ;
#121166 = DIRECTION('',(-1.31418445149758E-16,1.,0.)) ;
#121167 = DIRECTION('',(-1.31418445149758E-16,1.,0.)) ;
#121168 = DIRECTION('center_axis',(-1.31418445149758E-16,1.,0.)) ;
#121169 = DIRECTION('ref_axis',(-1.,-1.31418445149758E-16,0.)) ;
#121170 = DIRECTION('center_axis',(-5.62625979646468E-15,-1.,-6.72243160618769E-15)) ;
#121171 = DIRECTION('ref_axis',(3.86570035924698E-42,6.72243160618769E-15,
-1.)) ;
#121172 = DIRECTION('',(-1.31418445149758E-16,1.,0.)) ;
#121173 = DIRECTION('',(-1.31418445149758E-16,1.,0.)) ;
#121174 = DIRECTION('center_axis',(1.31418445149758E-16,1.,0.)) ;
#121175 = DIRECTION('ref_axis',(-1.,1.31418445149758E-16,0.)) ;
#121176 = DIRECTION('center_axis',(8.7661785287084E-15,-1.,0.)) ;
#121177 = DIRECTION('ref_axis',(1.,8.7661785287084E-15,0.)) ;
#121178 = DIRECTION('',(1.31418445149758E-16,1.,0.)) ;
#121179 = DIRECTION('',(1.31418445149758E-16,1.,0.)) ;
#121180 = DIRECTION('center_axis',(1.31418445149758E-16,1.,0.)) ;
#121181 = DIRECTION('ref_axis',(-1.,1.31418445149758E-16,0.)) ;
#121182 = DIRECTION('center_axis',(0.,-1.,0.)) ;
#121183 = DIRECTION('ref_axis',(0.,0.,-1.)) ;
#121184 = DIRECTION('',(1.31418445149758E-16,1.,0.)) ;
#121185 = DIRECTION('',(1.31418445149758E-16,1.,0.)) ;
#121186 = DIRECTION('center_axis',(1.31418445149758E-16,1.,0.)) ;
#121187 = DIRECTION('ref_axis',(-1.,1.31418445149758E-16,0.)) ;
#121188 = DIRECTION('center_axis',(1.31418445149758E-16,1.,0.)) ;
#121189 = DIRECTION('ref_axis',(-1.,1.31418445149758E-16,0.)) ;
#121190 = DIRECTION('',(1.31418445149758E-16,1.,0.)) ;
#121191 = DIRECTION('center_axis',(1.31418445149758E-16,1.,0.)) ;
#121192 = DIRECTION('ref_axis',(-1.,1.31418445149758E-16,0.)) ;
#121193 = DIRECTION('',(1.31418445149758E-16,1.,0.)) ;
#121194 = DIRECTION('center_axis',(1.31418445149758E-16,1.,0.)) ;
#121195 = DIRECTION('ref_axis',(-1.,1.31418445149758E-16,0.)) ;
#121196 = DIRECTION('',(1.31418445149758E-16,1.,0.)) ;
#121197 = DIRECTION('center_axis',(1.31418445149758E-16,1.,0.)) ;
#121198 = DIRECTION('ref_axis',(-1.,1.31418445149758E-16,0.)) ;
#121199 = DIRECTION('',(1.31418445149758E-16,1.,0.)) ;
#121200 = DIRECTION('center_axis',(1.31418445149758E-16,1.,0.)) ;
#121201 = DIRECTION('ref_axis',(-1.,1.31418445149758E-16,0.)) ;
#121202 = DIRECTION('',(1.31418445149758E-16,1.,0.)) ;
#121203 = DIRECTION('center_axis',(1.,0.,0.)) ;
#121204 = DIRECTION('ref_axis',(0.,0.,-1.)) ;
#121205 = DIRECTION('center_axis',(1.,0.,0.)) ;
#121206 = DIRECTION('ref_axis',(0.,0.,-1.)) ;
#121207 = DIRECTION('',(0.707106781186546,-8.65956056235495E-17,0.707106781186549)) ;
#121208 = DIRECTION('center_axis',(1.,0.,0.)) ;
#121209 = DIRECTION('ref_axis',(0.,0.,-1.)) ;
#121210 = DIRECTION('',(1.,0.,0.)) ;
#121211 = DIRECTION('center_axis',(-1.31418445149758E-16,1.,0.)) ;
#121212 = DIRECTION('ref_axis',(-1.,-1.31418445149758E-16,0.)) ;
#121213 = DIRECTION('',(0.,0.,1.)) ;
#121214 = DIRECTION('',(1.,1.31418445149758E-16,0.)) ;
#121215 = DIRECTION('',(0.,0.,-1.)) ;
#121216 = DIRECTION('',(-1.,-1.31418445149758E-16,-5.2561455487295E-16)) ;
#121217 = DIRECTION('center_axis',(-1.31418445149758E-16,1.,0.)) ;
#121218 = DIRECTION('ref_axis',(-1.,-1.31418445149758E-16,0.)) ;
#121219 = DIRECTION('center_axis',(-1.31418445149758E-16,1.,0.)) ;
#121220 = DIRECTION('ref_axis',(-1.,-1.31418445149758E-16,0.)) ;
#121221 = DIRECTION('center_axis',(-1.31418445149758E-16,1.,0.)) ;
#121222 = DIRECTION('ref_axis',(-1.,-1.31418445149758E-16,0.)) ;
#121223 = DIRECTION('center_axis',(-1.31418445149758E-16,1.,0.)) ;
#121224 = DIRECTION('ref_axis',(-1.,-1.31418445149758E-16,0.)) ;
#121225 = DIRECTION('center_axis',(-1.31418445149758E-16,1.,0.)) ;
#121226 = DIRECTION('ref_axis',(-1.,-1.31418445149758E-16,0.)) ;
#121227 = DIRECTION('center_axis',(-1.31418445149758E-16,1.,0.)) ;
#121228 = DIRECTION('ref_axis',(-1.,-1.31418445149758E-16,0.)) ;
#121229 = DIRECTION('center_axis',(-1.31418445149758E-16,1.,0.)) ;
#121230 = DIRECTION('ref_axis',(-1.,-1.31418445149758E-16,0.)) ;
#121231 = DIRECTION('center_axis',(-1.31418445149758E-16,1.,0.)) ;
#121232 = DIRECTION('ref_axis',(-1.,-1.31418445149758E-16,0.)) ;
#121233 = DIRECTION('center_axis',(-1.31418445149758E-16,1.,0.)) ;
#121234 = DIRECTION('ref_axis',(-1.,-1.31418445149758E-16,0.)) ;
#121235 = DIRECTION('center_axis',(-1.31418445149758E-16,1.,0.)) ;
#121236 = DIRECTION('ref_axis',(-1.,-1.31418445149758E-16,0.)) ;
#121237 = DIRECTION('',(1.,1.31418445149758E-16,0.)) ;
#121238 = DIRECTION('',(0.,0.,-1.)) ;
#121239 = DIRECTION('',(-1.,-1.31418445149758E-16,0.)) ;
#121240 = DIRECTION('center_axis',(-1.31418445149758E-16,1.,0.)) ;
#121241 = DIRECTION('ref_axis',(-1.,-1.31418445149758E-16,0.)) ;
#121242 = DIRECTION('',(-1.,-1.31418445149758E-16,-2.16840434497101E-16)) ;
#121243 = DIRECTION('center_axis',(-1.31418445149758E-16,1.,0.)) ;
#121244 = DIRECTION('ref_axis',(-1.,-1.31418445149758E-16,0.)) ;
#121245 = DIRECTION('',(-4.33680868994202E-16,-5.69936654944139E-32,-1.)) ;
#121246 = DIRECTION('center_axis',(-1.31418445149758E-16,1.,0.)) ;
#121247 = DIRECTION('ref_axis',(-1.,-1.31418445149758E-16,0.)) ;
#121248 = DIRECTION('',(1.,1.31418445149758E-16,-2.16840434497101E-16)) ;
#121249 = DIRECTION('center_axis',(-1.31418445149758E-16,1.,0.)) ;
#121250 = DIRECTION('ref_axis',(-1.,-1.31418445149758E-16,0.)) ;
#121251 = DIRECTION('',(2.16840434497101E-16,2.8496832747207E-32,1.)) ;
#121252 = DIRECTION('center_axis',(-1.31418445149758E-16,1.,0.)) ;
#121253 = DIRECTION('ref_axis',(-1.,-1.31418445149758E-16,0.)) ;
#121254 = DIRECTION('',(-1.,-1.31418445149758E-16,-2.16840434497101E-16)) ;
#121255 = DIRECTION('center_axis',(-1.31418445149758E-16,1.,0.)) ;
#121256 = DIRECTION('ref_axis',(-1.,-1.31418445149758E-16,0.)) ;
#121257 = DIRECTION('',(-4.33680868994202E-16,-5.69936654944139E-32,-1.)) ;
#121258 = DIRECTION('center_axis',(-1.31418445149758E-16,1.,0.)) ;
#121259 = DIRECTION('ref_axis',(-1.,-1.31418445149758E-16,0.)) ;
#121260 = DIRECTION('',(1.,1.31418445149758E-16,-2.16840434497101E-16)) ;
#121261 = DIRECTION('center_axis',(-1.31418445149758E-16,1.,0.)) ;
#121262 = DIRECTION('ref_axis',(-1.,-1.31418445149758E-16,0.)) ;
#121263 = DIRECTION('',(2.16840434497101E-16,2.8496832747207E-32,1.)) ;
#121264 = DIRECTION('center_axis',(-1.31418445149758E-16,1.,0.)) ;
#121265 = DIRECTION('ref_axis',(-1.,-1.31418445149758E-16,0.)) ;
#121266 = DIRECTION('',(-1.,-1.31418445149758E-16,-2.16840434497101E-16)) ;
#121267 = DIRECTION('center_axis',(-1.31418445149758E-16,1.,0.)) ;
#121268 = DIRECTION('ref_axis',(-1.,-1.31418445149758E-16,0.)) ;
#121269 = DIRECTION('',(-4.33680868994202E-16,-5.69936654944139E-32,-1.)) ;
#121270 = DIRECTION('center_axis',(-1.31418445149758E-16,1.,0.)) ;
#121271 = DIRECTION('ref_axis',(-1.,-1.31418445149758E-16,0.)) ;
#121272 = DIRECTION('',(1.,1.31418445149758E-16,-2.16840434497101E-16)) ;
#121273 = DIRECTION('center_axis',(-1.31418445149758E-16,1.,0.)) ;
#121274 = DIRECTION('ref_axis',(-1.,-1.31418445149758E-16,0.)) ;
#121275 = DIRECTION('',(2.16840434497101E-16,2.8496832747207E-32,1.)) ;
#121276 = DIRECTION('center_axis',(-1.31418445149758E-16,1.,0.)) ;
#121277 = DIRECTION('ref_axis',(-1.,-1.31418445149758E-16,0.)) ;
#121278 = DIRECTION('',(-1.,-1.31418445149758E-16,-2.16840434497101E-16)) ;
#121279 = DIRECTION('center_axis',(-1.31418445149758E-16,1.,0.)) ;
#121280 = DIRECTION('ref_axis',(-1.,-1.31418445149758E-16,0.)) ;
#121281 = DIRECTION('',(-4.33680868994202E-16,-5.69936654944139E-32,-1.)) ;
#121282 = DIRECTION('center_axis',(-1.31418445149758E-16,1.,0.)) ;
#121283 = DIRECTION('ref_axis',(-1.,-1.31418445149758E-16,0.)) ;
#121284 = DIRECTION('',(1.,1.31418445149758E-16,-2.16840434497101E-16)) ;
#121285 = DIRECTION('center_axis',(-1.31418445149758E-16,1.,0.)) ;
#121286 = DIRECTION('ref_axis',(-1.,-1.31418445149758E-16,0.)) ;
#121287 = DIRECTION('',(2.16840434497101E-16,2.8496832747207E-32,1.)) ;
#121288 = DIRECTION('center_axis',(-1.31418445149758E-16,1.,0.)) ;
#121289 = DIRECTION('ref_axis',(-1.,-1.31418445149758E-16,0.)) ;
#121290 = DIRECTION('',(-1.,-1.31418445149758E-16,-2.16840434497101E-16)) ;
#121291 = DIRECTION('center_axis',(-1.31418445149758E-16,1.,0.)) ;
#121292 = DIRECTION('ref_axis',(-1.,-1.31418445149758E-16,0.)) ;
#121293 = DIRECTION('',(-4.33680868994202E-16,-5.69936654944139E-32,-1.)) ;
#121294 = DIRECTION('center_axis',(-1.31418445149758E-16,1.,0.)) ;
#121295 = DIRECTION('ref_axis',(-1.,-1.31418445149758E-16,0.)) ;
#121296 = DIRECTION('',(1.,1.31418445149758E-16,-2.16840434497101E-16)) ;
#121297 = DIRECTION('center_axis',(-1.31418445149758E-16,1.,0.)) ;
#121298 = DIRECTION('ref_axis',(-1.,-1.31418445149758E-16,0.)) ;
#121299 = DIRECTION('',(2.16840434497101E-16,2.8496832747207E-32,1.)) ;
#121300 = DIRECTION('center_axis',(-1.31418445149758E-16,1.,0.)) ;
#121301 = DIRECTION('ref_axis',(-1.,-1.31418445149758E-16,0.)) ;
#121302 = DIRECTION('',(-1.,-1.31418445149758E-16,-2.16840434497101E-16)) ;
#121303 = DIRECTION('center_axis',(-1.31418445149758E-16,1.,0.)) ;
#121304 = DIRECTION('ref_axis',(-1.,-1.31418445149758E-16,0.)) ;
#121305 = DIRECTION('',(-4.33680868994202E-16,-5.69936654944139E-32,-1.)) ;
#121306 = DIRECTION('center_axis',(-1.31418445149758E-16,1.,0.)) ;
#121307 = DIRECTION('ref_axis',(-1.,-1.31418445149758E-16,0.)) ;
#121308 = DIRECTION('',(1.,1.31418445149758E-16,-2.16840434497101E-16)) ;
#121309 = DIRECTION('center_axis',(-1.31418445149758E-16,1.,0.)) ;
#121310 = DIRECTION('ref_axis',(-1.,-1.31418445149758E-16,0.)) ;
#121311 = DIRECTION('',(2.16840434497101E-16,2.8496832747207E-32,1.)) ;
#121312 = DIRECTION('center_axis',(-1.31418445149758E-16,1.,0.)) ;
#121313 = DIRECTION('ref_axis',(-1.,-1.31418445149758E-16,0.)) ;
#121314 = DIRECTION('',(-1.,-1.31418445149758E-16,-2.16840434497101E-16)) ;
#121315 = DIRECTION('center_axis',(-1.31418445149758E-16,1.,0.)) ;
#121316 = DIRECTION('ref_axis',(-1.,-1.31418445149758E-16,0.)) ;
#121317 = DIRECTION('',(-4.33680868994202E-16,-5.69936654944139E-32,-1.)) ;
#121318 = DIRECTION('center_axis',(-1.31418445149758E-16,1.,0.)) ;
#121319 = DIRECTION('ref_axis',(-1.,-1.31418445149758E-16,0.)) ;
#121320 = DIRECTION('',(1.,1.31418445149758E-16,-2.16840434497101E-16)) ;
#121321 = DIRECTION('center_axis',(-1.31418445149758E-16,1.,0.)) ;
#121322 = DIRECTION('ref_axis',(-1.,-1.31418445149758E-16,0.)) ;
#121323 = DIRECTION('',(2.16840434497101E-16,2.8496832747207E-32,1.)) ;
#121324 = DIRECTION('center_axis',(-1.31418445149758E-16,1.,0.)) ;
#121325 = DIRECTION('ref_axis',(-1.,-1.31418445149758E-16,0.)) ;
#121326 = DIRECTION('',(-1.,-1.31418445149758E-16,-2.16840434497101E-16)) ;
#121327 = DIRECTION('center_axis',(-1.31418445149758E-16,1.,0.)) ;
#121328 = DIRECTION('ref_axis',(-1.,-1.31418445149758E-16,0.)) ;
#121329 = DIRECTION('',(-4.33680868994202E-16,-5.69936654944139E-32,-1.)) ;
#121330 = DIRECTION('center_axis',(-1.31418445149758E-16,1.,0.)) ;
#121331 = DIRECTION('ref_axis',(-1.,-1.31418445149758E-16,0.)) ;
#121332 = DIRECTION('',(1.,1.31418445149758E-16,-2.16840434497101E-16)) ;
#121333 = DIRECTION('center_axis',(-1.31418445149758E-16,1.,0.)) ;
#121334 = DIRECTION('ref_axis',(-1.,-1.31418445149758E-16,0.)) ;
#121335 = DIRECTION('',(2.16840434497101E-16,2.8496832747207E-32,1.)) ;
#121336 = DIRECTION('center_axis',(-1.31418445149758E-16,1.,0.)) ;
#121337 = DIRECTION('ref_axis',(-1.,-1.31418445149758E-16,0.)) ;
#121338 = DIRECTION('',(-1.,-1.31418445149758E-16,-2.16840434497101E-16)) ;
#121339 = DIRECTION('center_axis',(-1.31418445149758E-16,1.,0.)) ;
#121340 = DIRECTION('ref_axis',(-1.,-1.31418445149758E-16,0.)) ;
#121341 = DIRECTION('',(-4.33680868994202E-16,-5.69936654944139E-32,-1.)) ;
#121342 = DIRECTION('center_axis',(-1.31418445149758E-16,1.,0.)) ;
#121343 = DIRECTION('ref_axis',(-1.,-1.31418445149758E-16,0.)) ;
#121344 = DIRECTION('',(1.,1.31418445149758E-16,-2.16840434497101E-16)) ;
#121345 = DIRECTION('center_axis',(-1.31418445149758E-16,1.,0.)) ;
#121346 = DIRECTION('ref_axis',(-1.,-1.31418445149758E-16,0.)) ;
#121347 = DIRECTION('',(2.16840434497101E-16,2.8496832747207E-32,1.)) ;
#121348 = DIRECTION('center_axis',(-1.31418445149758E-16,1.,0.)) ;
#121349 = DIRECTION('ref_axis',(-1.,-1.31418445149758E-16,0.)) ;
#121350 = DIRECTION('',(-1.,-1.31418445149758E-16,-2.16840434497101E-16)) ;
#121351 = DIRECTION('center_axis',(-1.31418445149758E-16,1.,0.)) ;
#121352 = DIRECTION('ref_axis',(-1.,-1.31418445149758E-16,0.)) ;
#121353 = DIRECTION('',(-4.33680868994202E-16,-5.69936654944139E-32,-1.)) ;
#121354 = DIRECTION('center_axis',(-1.31418445149758E-16,1.,0.)) ;
#121355 = DIRECTION('ref_axis',(-1.,-1.31418445149758E-16,0.)) ;
#121356 = DIRECTION('',(1.,1.31418445149758E-16,-2.16840434497101E-16)) ;
#121357 = DIRECTION('center_axis',(-1.31418445149758E-16,1.,0.)) ;
#121358 = DIRECTION('ref_axis',(-1.,-1.31418445149758E-16,0.)) ;
#121359 = DIRECTION('',(2.16840434497101E-16,2.8496832747207E-32,1.)) ;
#121360 = DIRECTION('center_axis',(0.,-1.,0.)) ;
#121361 = DIRECTION('ref_axis',(0.,0.,-1.)) ;
#121362 = DIRECTION('',(0.,0.,-1.)) ;
#121363 = DIRECTION('',(-1.,0.,-7.01133629567814E-33)) ;
#121364 = DIRECTION('',(0.,0.,1.)) ;
#121365 = DIRECTION('',(1.,0.,-7.01133629567814E-33)) ;
#121366 = DIRECTION('',(0.,0.,1.)) ;
#121367 = DIRECTION('center_axis',(0.,-1.,0.)) ;
#121368 = DIRECTION('ref_axis',(0.,0.,-1.)) ;
#121369 = DIRECTION('',(-1.,0.,0.)) ;
#121370 = DIRECTION('center_axis',(0.,-1.,0.)) ;
#121371 = DIRECTION('ref_axis',(0.,0.,-1.)) ;
#121372 = DIRECTION('',(0.,0.,-1.)) ;
#121373 = DIRECTION('center_axis',(0.,-1.,0.)) ;
#121374 = DIRECTION('ref_axis',(0.,0.,-1.)) ;
#121375 = DIRECTION('',(1.,0.,0.)) ;
#121376 = DIRECTION('center_axis',(0.,-1.,0.)) ;
#121377 = DIRECTION('ref_axis',(0.,0.,-1.)) ;
#121378 = DIRECTION('center_axis',(0.,-1.,0.)) ;
#121379 = DIRECTION('ref_axis',(0.,0.,-1.)) ;
#121380 = DIRECTION('',(0.,0.,-1.)) ;
#121381 = DIRECTION('',(-1.,0.,-7.01133629567814E-33)) ;
#121382 = DIRECTION('',(0.,0.,1.)) ;
#121383 = DIRECTION('',(1.,0.,-7.01133629567814E-33)) ;
#121384 = DIRECTION('',(0.,0.,1.)) ;
#121385 = DIRECTION('center_axis',(0.,-1.,0.)) ;
#121386 = DIRECTION('ref_axis',(0.,0.,-1.)) ;
#121387 = DIRECTION('',(-1.,0.,0.)) ;
#121388 = DIRECTION('center_axis',(0.,-1.,0.)) ;
#121389 = DIRECTION('ref_axis',(0.,0.,-1.)) ;
#121390 = DIRECTION('',(0.,0.,-1.)) ;
#121391 = DIRECTION('center_axis',(0.,-1.,0.)) ;
#121392 = DIRECTION('ref_axis',(0.,0.,-1.)) ;
#121393 = DIRECTION('',(1.,0.,0.)) ;
#121394 = DIRECTION('center_axis',(0.,-1.,0.)) ;
#121395 = DIRECTION('ref_axis',(0.,0.,-1.)) ;
#121396 = DIRECTION('center_axis',(0.,-1.,0.)) ;
#121397 = DIRECTION('ref_axis',(0.,0.,-1.)) ;
#121398 = DIRECTION('',(0.,0.,-1.)) ;
#121399 = DIRECTION('',(-1.,0.,-7.01133629567814E-33)) ;
#121400 = DIRECTION('',(0.,0.,1.)) ;
#121401 = DIRECTION('',(1.,0.,-7.01133629567814E-33)) ;
#121402 = DIRECTION('',(0.,0.,1.)) ;
#121403 = DIRECTION('center_axis',(0.,-1.,0.)) ;
#121404 = DIRECTION('ref_axis',(0.,0.,-1.)) ;
#121405 = DIRECTION('',(-1.,0.,0.)) ;
#121406 = DIRECTION('center_axis',(0.,-1.,0.)) ;
#121407 = DIRECTION('ref_axis',(0.,0.,-1.)) ;
#121408 = DIRECTION('',(0.,0.,-1.)) ;
#121409 = DIRECTION('center_axis',(0.,-1.,0.)) ;
#121410 = DIRECTION('ref_axis',(0.,0.,-1.)) ;
#121411 = DIRECTION('',(1.,0.,0.)) ;
#121412 = DIRECTION('center_axis',(0.,-1.,0.)) ;
#121413 = DIRECTION('ref_axis',(0.,0.,-1.)) ;
#121414 = DIRECTION('center_axis',(0.,-1.,0.)) ;
#121415 = DIRECTION('ref_axis',(0.,0.,-1.)) ;
#121416 = DIRECTION('',(0.,0.,-1.)) ;
#121417 = DIRECTION('',(-1.,0.,-7.01133629567814E-33)) ;
#121418 = DIRECTION('',(0.,0.,1.)) ;
#121419 = DIRECTION('',(1.,0.,-7.01133629567814E-33)) ;
#121420 = DIRECTION('',(0.,0.,1.)) ;
#121421 = DIRECTION('center_axis',(0.,-1.,0.)) ;
#121422 = DIRECTION('ref_axis',(0.,0.,-1.)) ;
#121423 = DIRECTION('',(-1.,0.,0.)) ;
#121424 = DIRECTION('center_axis',(0.,-1.,0.)) ;
#121425 = DIRECTION('ref_axis',(0.,0.,-1.)) ;
#121426 = DIRECTION('',(0.,0.,-1.)) ;
#121427 = DIRECTION('center_axis',(0.,-1.,0.)) ;
#121428 = DIRECTION('ref_axis',(0.,0.,-1.)) ;
#121429 = DIRECTION('',(1.,0.,0.)) ;
#121430 = DIRECTION('center_axis',(0.,-1.,0.)) ;
#121431 = DIRECTION('ref_axis',(0.,0.,-1.)) ;
#121432 = DIRECTION('center_axis',(0.,-1.,0.)) ;
#121433 = DIRECTION('ref_axis',(0.,0.,-1.)) ;
#121434 = DIRECTION('',(0.,0.,-1.)) ;
#121435 = DIRECTION('',(-1.,0.,-7.01133629567814E-33)) ;
#121436 = DIRECTION('',(0.,0.,1.)) ;
#121437 = DIRECTION('',(1.,0.,-7.01133629567814E-33)) ;
#121438 = DIRECTION('',(0.,0.,1.)) ;
#121439 = DIRECTION('center_axis',(0.,-1.,0.)) ;
#121440 = DIRECTION('ref_axis',(0.,0.,-1.)) ;
#121441 = DIRECTION('',(-1.,0.,0.)) ;
#121442 = DIRECTION('center_axis',(0.,-1.,0.)) ;
#121443 = DIRECTION('ref_axis',(0.,0.,-1.)) ;
#121444 = DIRECTION('',(0.,0.,-1.)) ;
#121445 = DIRECTION('center_axis',(0.,-1.,0.)) ;
#121446 = DIRECTION('ref_axis',(0.,0.,-1.)) ;
#121447 = DIRECTION('',(1.,0.,0.)) ;
#121448 = DIRECTION('center_axis',(0.,-1.,0.)) ;
#121449 = DIRECTION('ref_axis',(0.,0.,-1.)) ;
#121450 = DIRECTION('center_axis',(0.,-1.,0.)) ;
#121451 = DIRECTION('ref_axis',(0.,0.,-1.)) ;
#121452 = DIRECTION('',(0.,0.,-1.)) ;
#121453 = DIRECTION('',(-1.,0.,-7.01133629567814E-33)) ;
#121454 = DIRECTION('',(0.,0.,1.)) ;
#121455 = DIRECTION('',(1.,0.,-7.01133629567814E-33)) ;
#121456 = DIRECTION('',(0.,0.,1.)) ;
#121457 = DIRECTION('center_axis',(0.,-1.,0.)) ;
#121458 = DIRECTION('ref_axis',(0.,0.,-1.)) ;
#121459 = DIRECTION('',(-1.,0.,0.)) ;
#121460 = DIRECTION('center_axis',(0.,-1.,0.)) ;
#121461 = DIRECTION('ref_axis',(0.,0.,-1.)) ;
#121462 = DIRECTION('',(0.,0.,-1.)) ;
#121463 = DIRECTION('center_axis',(0.,-1.,0.)) ;
#121464 = DIRECTION('ref_axis',(0.,0.,-1.)) ;
#121465 = DIRECTION('',(1.,0.,0.)) ;
#121466 = DIRECTION('center_axis',(0.,-1.,0.)) ;
#121467 = DIRECTION('ref_axis',(0.,0.,-1.)) ;
#121468 = DIRECTION('center_axis',(0.,-1.,0.)) ;
#121469 = DIRECTION('ref_axis',(0.,0.,-1.)) ;
#121470 = DIRECTION('',(0.,0.,-1.)) ;
#121471 = DIRECTION('',(-1.,0.,-7.01133629567814E-33)) ;
#121472 = DIRECTION('',(0.,0.,1.)) ;
#121473 = DIRECTION('',(1.,0.,-7.01133629567814E-33)) ;
#121474 = DIRECTION('',(0.,0.,1.)) ;
#121475 = DIRECTION('center_axis',(0.,-1.,0.)) ;
#121476 = DIRECTION('ref_axis',(0.,0.,-1.)) ;
#121477 = DIRECTION('',(-1.,0.,0.)) ;
#121478 = DIRECTION('center_axis',(0.,-1.,0.)) ;
#121479 = DIRECTION('ref_axis',(0.,0.,-1.)) ;
#121480 = DIRECTION('',(0.,0.,-1.)) ;
#121481 = DIRECTION('center_axis',(0.,-1.,0.)) ;
#121482 = DIRECTION('ref_axis',(0.,0.,-1.)) ;
#121483 = DIRECTION('',(1.,0.,0.)) ;
#121484 = DIRECTION('center_axis',(0.,-1.,0.)) ;
#121485 = DIRECTION('ref_axis',(0.,0.,-1.)) ;
#121486 = DIRECTION('center_axis',(0.,-1.,0.)) ;
#121487 = DIRECTION('ref_axis',(0.,0.,-1.)) ;
#121488 = DIRECTION('',(0.,0.,-1.)) ;
#121489 = DIRECTION('',(-1.,0.,-7.01133629567814E-33)) ;
#121490 = DIRECTION('',(0.,0.,1.)) ;
#121491 = DIRECTION('',(1.,0.,-7.01133629567814E-33)) ;
#121492 = DIRECTION('',(0.,0.,1.)) ;
#121493 = DIRECTION('center_axis',(0.,-1.,0.)) ;
#121494 = DIRECTION('ref_axis',(0.,0.,-1.)) ;
#121495 = DIRECTION('',(-1.,0.,0.)) ;
#121496 = DIRECTION('center_axis',(0.,-1.,0.)) ;
#121497 = DIRECTION('ref_axis',(0.,0.,-1.)) ;
#121498 = DIRECTION('',(0.,0.,-1.)) ;
#121499 = DIRECTION('center_axis',(0.,-1.,0.)) ;
#121500 = DIRECTION('ref_axis',(0.,0.,-1.)) ;
#121501 = DIRECTION('',(1.,0.,0.)) ;
#121502 = DIRECTION('center_axis',(0.,-1.,0.)) ;
#121503 = DIRECTION('ref_axis',(0.,0.,-1.)) ;
#121504 = DIRECTION('center_axis',(0.,-1.,0.)) ;
#121505 = DIRECTION('ref_axis',(0.,0.,-1.)) ;
#121506 = DIRECTION('',(0.,0.,-1.)) ;
#121507 = DIRECTION('',(-1.,0.,-7.01133629567814E-33)) ;
#121508 = DIRECTION('',(0.,0.,1.)) ;
#121509 = DIRECTION('',(1.,0.,-7.01133629567814E-33)) ;
#121510 = DIRECTION('',(0.,0.,1.)) ;
#121511 = DIRECTION('center_axis',(0.,-1.,0.)) ;
#121512 = DIRECTION('ref_axis',(0.,0.,-1.)) ;
#121513 = DIRECTION('',(-1.,0.,0.)) ;
#121514 = DIRECTION('center_axis',(0.,-1.,0.)) ;
#121515 = DIRECTION('ref_axis',(0.,0.,-1.)) ;
#121516 = DIRECTION('',(0.,0.,-1.)) ;
#121517 = DIRECTION('center_axis',(0.,-1.,0.)) ;
#121518 = DIRECTION('ref_axis',(0.,0.,-1.)) ;
#121519 = DIRECTION('',(1.,0.,0.)) ;
#121520 = DIRECTION('center_axis',(0.,-1.,0.)) ;
#121521 = DIRECTION('ref_axis',(0.,0.,-1.)) ;
#121522 = DIRECTION('center_axis',(1.31418445149758E-16,1.,0.)) ;
#121523 = DIRECTION('ref_axis',(-1.,1.31418445149758E-16,0.)) ;
#121524 = DIRECTION('',(0.422618261740697,-5.55398348498559E-17,-0.906307787036651)) ;
#121525 = DIRECTION('center_axis',(1.31418445149758E-16,1.,0.)) ;
#121526 = DIRECTION('ref_axis',(-1.,1.31418445149758E-16,0.)) ;
#121527 = DIRECTION('',(0.422618261740697,-5.55398348498559E-17,-0.906307787036651)) ;
#121528 = DIRECTION('center_axis',(1.31418445149758E-16,1.,0.)) ;
#121529 = DIRECTION('ref_axis',(-1.,1.31418445149758E-16,0.)) ;
#121530 = DIRECTION('',(0.422618261740697,-5.55398348498559E-17,-0.906307787036651)) ;
#121531 = DIRECTION('center_axis',(1.31418445149758E-16,1.,0.)) ;
#121532 = DIRECTION('ref_axis',(-1.,1.31418445149758E-16,0.)) ;
#121533 = DIRECTION('',(0.422618261740697,-5.55398348498559E-17,-0.906307787036651)) ;
#121534 = DIRECTION('center_axis',(1.31418445149758E-16,1.,0.)) ;
#121535 = DIRECTION('ref_axis',(-1.,1.31418445149758E-16,0.)) ;
#121536 = DIRECTION('',(0.422618261740697,-5.55398348498559E-17,-0.906307787036651)) ;
#121537 = DIRECTION('center_axis',(1.31418445149758E-16,1.,0.)) ;
#121538 = DIRECTION('ref_axis',(-1.,1.31418445149758E-16,0.)) ;
#121539 = DIRECTION('',(0.422618261740697,-5.55398348498559E-17,-0.906307787036651)) ;
#121540 = DIRECTION('center_axis',(1.31418445149758E-16,1.,0.)) ;
#121541 = DIRECTION('ref_axis',(-1.,1.31418445149758E-16,0.)) ;
#121542 = DIRECTION('',(0.422618261740697,-5.55398348498559E-17,-0.906307787036651)) ;
#121543 = DIRECTION('center_axis',(1.31418445149758E-16,1.,0.)) ;
#121544 = DIRECTION('ref_axis',(-1.,1.31418445149758E-16,0.)) ;
#121545 = DIRECTION('',(0.422618261740697,-5.55398348498559E-17,-0.906307787036651)) ;
#121546 = DIRECTION('center_axis',(1.31418445149758E-16,1.,0.)) ;
#121547 = DIRECTION('ref_axis',(-1.,1.31418445149758E-16,0.)) ;
#121548 = DIRECTION('',(0.422618261740697,-5.55398348498559E-17,-0.906307787036651)) ;
#121549 = DIRECTION('center_axis',(1.,0.,0.)) ;
#121550 = DIRECTION('ref_axis',(0.,0.,-1.)) ;
#121551 = DIRECTION('',(0.,-4.8455963016112E-16,-1.)) ;
#121552 = DIRECTION('',(0.,1.,0.)) ;
#121553 = DIRECTION('',(0.,0.,1.)) ;
#121554 = DIRECTION('',(0.,-1.,0.)) ;
#121555 = DIRECTION('',(0.,4.8455963016112E-16,-1.)) ;
#121556 = DIRECTION('center_axis',(-1.,0.,0.)) ;
#121557 = DIRECTION('ref_axis',(0.,2.16840434497101E-15,-1.)) ;
#121558 = DIRECTION('center_axis',(-1.,0.,0.)) ;
#121559 = DIRECTION('ref_axis',(0.,0.,-1.)) ;
#121560 = DIRECTION('',(0.,0.,-1.)) ;
#121561 = DIRECTION('center_axis',(-1.,0.,0.)) ;
#121562 = DIRECTION('ref_axis',(0.,-2.16840434497101E-15,-1.)) ;
#121563 = DIRECTION('center_axis',(-1.,0.,0.)) ;
#121564 = DIRECTION('ref_axis',(0.,-3.25260651745651E-15,-1.)) ;
#121565 = DIRECTION('',(0.,-4.8455963016112E-16,-1.)) ;
#121566 = DIRECTION('center_axis',(-1.,0.,0.)) ;
#121567 = DIRECTION('ref_axis',(0.,1.0842021724855E-15,-1.)) ;
#121568 = DIRECTION('center_axis',(-1.,0.,0.)) ;
#121569 = DIRECTION('ref_axis',(0.,0.,-1.)) ;
#121570 = DIRECTION('',(0.,0.,-1.)) ;
#121571 = DIRECTION('center_axis',(-1.,0.,0.)) ;
#121572 = DIRECTION('ref_axis',(0.,-2.16840434497101E-15,-1.)) ;
#121573 = DIRECTION('center_axis',(-1.,0.,0.)) ;
#121574 = DIRECTION('ref_axis',(0.,3.25260651745652E-15,-1.)) ;
#121575 = DIRECTION('',(0.,-4.8455963016112E-16,-1.)) ;
#121576 = DIRECTION('center_axis',(-1.,0.,0.)) ;
#121577 = DIRECTION('ref_axis',(0.,2.16840434497101E-15,-1.)) ;
#121578 = DIRECTION('center_axis',(-1.,0.,0.)) ;
#121579 = DIRECTION('ref_axis',(0.,0.,-1.)) ;
#121580 = DIRECTION('',(0.,0.,-1.)) ;
#121581 = DIRECTION('center_axis',(-1.,0.,0.)) ;
#121582 = DIRECTION('ref_axis',(0.,3.25260651745651E-15,-1.)) ;
#121583 = DIRECTION('center_axis',(-1.,0.,0.)) ;
#121584 = DIRECTION('ref_axis',(0.,-7.58941520739851E-15,-1.)) ;
#121585 = DIRECTION('',(0.,-4.8455963016112E-16,-1.)) ;
#121586 = DIRECTION('center_axis',(-1.,0.,0.)) ;
#121587 = DIRECTION('ref_axis',(0.,1.0842021724855E-15,-1.)) ;
#121588 = DIRECTION('center_axis',(-1.,0.,0.)) ;
#121589 = DIRECTION('ref_axis',(0.,1.19262238973405E-14,-1.)) ;
#121590 = DIRECTION('',(0.,0.,-1.)) ;
#121591 = DIRECTION('center_axis',(-1.,0.,0.)) ;
#121592 = DIRECTION('ref_axis',(0.,2.168404344971E-15,-1.)) ;
#121593 = DIRECTION('center_axis',(-1.,0.,0.)) ;
#121594 = DIRECTION('ref_axis',(0.,1.0842021724855E-15,-1.)) ;
#121595 = DIRECTION('',(0.,-4.8455963016112E-16,-1.)) ;
#121596 = DIRECTION('center_axis',(-1.,0.,0.)) ;
#121597 = DIRECTION('ref_axis',(0.,1.0842021724855E-15,-1.)) ;
#121598 = DIRECTION('center_axis',(-1.,0.,0.)) ;
#121599 = DIRECTION('ref_axis',(0.,1.19262238973405E-14,-1.)) ;
#121600 = DIRECTION('',(0.,0.,-1.)) ;
#121601 = DIRECTION('center_axis',(-1.,0.,0.)) ;
#121602 = DIRECTION('ref_axis',(0.,2.16840434497102E-15,-1.)) ;
#121603 = DIRECTION('center_axis',(-1.,0.,0.)) ;
#121604 = DIRECTION('ref_axis',(0.,1.08420217248551E-15,-1.)) ;
#121605 = DIRECTION('',(0.,-4.8455963016112E-16,-1.)) ;
#121606 = DIRECTION('center_axis',(-1.,0.,0.)) ;
#121607 = DIRECTION('ref_axis',(0.,1.08420217248551E-15,-1.)) ;
#121608 = DIRECTION('center_axis',(-1.,0.,0.)) ;
#121609 = DIRECTION('ref_axis',(0.,1.19262238973406E-14,-1.)) ;
#121610 = DIRECTION('',(0.,0.,-1.)) ;
#121611 = DIRECTION('center_axis',(-1.,0.,0.)) ;
#121612 = DIRECTION('ref_axis',(0.,2.16840434497102E-15,-1.)) ;
#121613 = DIRECTION('center_axis',(-1.,0.,0.)) ;
#121614 = DIRECTION('ref_axis',(0.,1.08420217248551E-15,-1.)) ;
#121615 = DIRECTION('',(0.,-4.8455963016112E-16,-1.)) ;
#121616 = DIRECTION('center_axis',(-1.,0.,0.)) ;
#121617 = DIRECTION('ref_axis',(0.,1.08420217248551E-15,-1.)) ;
#121618 = DIRECTION('center_axis',(-1.,0.,0.)) ;
#121619 = DIRECTION('ref_axis',(0.,1.19262238973406E-14,-1.)) ;
#121620 = DIRECTION('',(0.,0.,-1.)) ;
#121621 = DIRECTION('center_axis',(-1.,0.,0.)) ;
#121622 = DIRECTION('ref_axis',(0.,2.16840434497102E-15,-1.)) ;
#121623 = DIRECTION('center_axis',(-1.,0.,0.)) ;
#121624 = DIRECTION('ref_axis',(0.,1.08420217248551E-15,-1.)) ;
#121625 = DIRECTION('',(0.,-4.8455963016112E-16,-1.)) ;
#121626 = DIRECTION('center_axis',(-1.,0.,0.)) ;
#121627 = DIRECTION('ref_axis',(0.,1.08420217248551E-15,-1.)) ;
#121628 = DIRECTION('center_axis',(-1.,0.,0.)) ;
#121629 = DIRECTION('ref_axis',(0.,1.19262238973406E-14,-1.)) ;
#121630 = DIRECTION('',(0.,0.,-1.)) ;
#121631 = DIRECTION('center_axis',(-1.,0.,0.)) ;
#121632 = DIRECTION('ref_axis',(0.,2.16840434497102E-15,-1.)) ;
#121633 = DIRECTION('center_axis',(-1.,0.,0.)) ;
#121634 = DIRECTION('ref_axis',(0.,1.08420217248551E-15,-1.)) ;
#121635 = DIRECTION('',(0.,-4.8455963016112E-16,-1.)) ;
#121636 = DIRECTION('center_axis',(-1.,0.,0.)) ;
#121637 = DIRECTION('ref_axis',(0.,1.08420217248551E-15,-1.)) ;
#121638 = DIRECTION('center_axis',(-1.,0.,0.)) ;
#121639 = DIRECTION('ref_axis',(0.,1.19262238973406E-14,-1.)) ;
#121640 = DIRECTION('',(0.,0.,-1.)) ;
#121641 = DIRECTION('center_axis',(-1.,0.,0.)) ;
#121642 = DIRECTION('ref_axis',(0.,2.16840434497102E-15,-1.)) ;
#121643 = DIRECTION('center_axis',(-1.,0.,0.)) ;
#121644 = DIRECTION('ref_axis',(0.,0.,-1.)) ;
#121645 = DIRECTION('',(0.,-4.8455963016112E-16,-1.)) ;
#121646 = DIRECTION('center_axis',(-1.,0.,0.)) ;
#121647 = DIRECTION('ref_axis',(0.,-2.16840434497102E-15,-1.)) ;
#121648 = DIRECTION('center_axis',(-1.,0.,0.)) ;
#121649 = DIRECTION('ref_axis',(0.,-3.25260651745653E-15,-1.)) ;
#121650 = DIRECTION('',(0.,0.,-1.)) ;
#121651 = DIRECTION('center_axis',(-1.,0.,0.)) ;
#121652 = DIRECTION('ref_axis',(0.,2.16840434497102E-15,-1.)) ;
#121653 = DIRECTION('center_axis',(-1.,0.,0.)) ;
#121654 = DIRECTION('ref_axis',(0.,0.,-1.)) ;
#121655 = DIRECTION('center_axis',(1.,0.,0.)) ;
#121656 = DIRECTION('ref_axis',(0.,0.,-1.)) ;
#121657 = DIRECTION('center_axis',(1.,0.,0.)) ;
#121658 = DIRECTION('ref_axis',(0.,0.,-1.)) ;
#121659 = DIRECTION('',(0.,0.,1.)) ;
#121660 = DIRECTION('',(0.,-1.,-8.9727076343628E-17)) ;
#121661 = DIRECTION('',(0.,0.,-1.)) ;
#121662 = DIRECTION('',(0.,1.,-8.9727076343628E-17)) ;
#121663 = DIRECTION('',(0.,0.,1.)) ;
#121664 = DIRECTION('center_axis',(1.,0.,0.)) ;
#121665 = DIRECTION('ref_axis',(0.,0.,-1.)) ;
#121666 = DIRECTION('center_axis',(1.,0.,0.)) ;
#121667 = DIRECTION('ref_axis',(0.,0.,-1.)) ;
#121668 = DIRECTION('center_axis',(1.,0.,0.)) ;
#121669 = DIRECTION('ref_axis',(0.,0.,-1.)) ;
#121670 = DIRECTION('center_axis',(1.,0.,0.)) ;
#121671 = DIRECTION('ref_axis',(0.,0.,-1.)) ;
#121672 = DIRECTION('',(0.,0.,1.)) ;
#121673 = DIRECTION('',(0.,-1.,-8.9727076343628E-17)) ;
#121674 = DIRECTION('',(0.,0.,-1.)) ;
#121675 = DIRECTION('',(0.,1.,-8.9727076343628E-17)) ;
#121676 = DIRECTION('',(0.,0.,1.)) ;
#121677 = DIRECTION('center_axis',(1.,0.,0.)) ;
#121678 = DIRECTION('ref_axis',(0.,0.,-1.)) ;
#121679 = DIRECTION('center_axis',(1.,0.,0.)) ;
#121680 = DIRECTION('ref_axis',(0.,0.,-1.)) ;
#121681 = DIRECTION('center_axis',(1.,0.,0.)) ;
#121682 = DIRECTION('ref_axis',(0.,0.,-1.)) ;
#121683 = DIRECTION('center_axis',(1.,0.,0.)) ;
#121684 = DIRECTION('ref_axis',(0.,0.,-1.)) ;
#121685 = DIRECTION('',(0.,0.,1.)) ;
#121686 = DIRECTION('',(0.,-1.,-8.9727076343628E-17)) ;
#121687 = DIRECTION('',(0.,0.,-1.)) ;
#121688 = DIRECTION('',(0.,1.,-8.9727076343628E-17)) ;
#121689 = DIRECTION('',(0.,0.,1.)) ;
#121690 = DIRECTION('center_axis',(1.,0.,0.)) ;
#121691 = DIRECTION('ref_axis',(0.,0.,-1.)) ;
#121692 = DIRECTION('center_axis',(1.,0.,0.)) ;
#121693 = DIRECTION('ref_axis',(0.,0.,-1.)) ;
#121694 = DIRECTION('center_axis',(1.,0.,0.)) ;
#121695 = DIRECTION('ref_axis',(0.,0.,-1.)) ;
#121696 = DIRECTION('center_axis',(1.,0.,0.)) ;
#121697 = DIRECTION('ref_axis',(0.,0.,-1.)) ;
#121698 = DIRECTION('',(0.,0.,1.)) ;
#121699 = DIRECTION('',(0.,-1.,-8.9727076343628E-17)) ;
#121700 = DIRECTION('',(0.,0.,-1.)) ;
#121701 = DIRECTION('',(0.,1.,-8.9727076343628E-17)) ;
#121702 = DIRECTION('',(0.,0.,1.)) ;
#121703 = DIRECTION('center_axis',(1.,0.,0.)) ;
#121704 = DIRECTION('ref_axis',(0.,0.,-1.)) ;
#121705 = DIRECTION('center_axis',(1.,0.,0.)) ;
#121706 = DIRECTION('ref_axis',(0.,0.,-1.)) ;
#121707 = DIRECTION('center_axis',(1.,0.,0.)) ;
#121708 = DIRECTION('ref_axis',(0.,0.,-1.)) ;
#121709 = DIRECTION('center_axis',(1.,0.,0.)) ;
#121710 = DIRECTION('ref_axis',(0.,0.,-1.)) ;
#121711 = DIRECTION('',(0.,0.,1.)) ;
#121712 = DIRECTION('',(0.,-1.,-8.9727076343628E-17)) ;
#121713 = DIRECTION('',(0.,0.,-1.)) ;
#121714 = DIRECTION('',(0.,1.,-8.9727076343628E-17)) ;
#121715 = DIRECTION('',(0.,0.,1.)) ;
#121716 = DIRECTION('center_axis',(1.,0.,0.)) ;
#121717 = DIRECTION('ref_axis',(0.,0.,-1.)) ;
#121718 = DIRECTION('center_axis',(1.,0.,0.)) ;
#121719 = DIRECTION('ref_axis',(0.,0.,-1.)) ;
#121720 = DIRECTION('center_axis',(1.,0.,0.)) ;
#121721 = DIRECTION('ref_axis',(0.,0.,-1.)) ;
#121722 = DIRECTION('center_axis',(1.,0.,0.)) ;
#121723 = DIRECTION('ref_axis',(0.,0.,-1.)) ;
#121724 = DIRECTION('',(0.,0.,1.)) ;
#121725 = DIRECTION('',(0.,-1.,-8.9727076343628E-17)) ;
#121726 = DIRECTION('',(0.,0.,-1.)) ;
#121727 = DIRECTION('',(0.,1.,-8.9727076343628E-17)) ;
#121728 = DIRECTION('',(0.,0.,1.)) ;
#121729 = DIRECTION('center_axis',(1.,0.,0.)) ;
#121730 = DIRECTION('ref_axis',(0.,0.,-1.)) ;
#121731 = DIRECTION('center_axis',(1.,0.,0.)) ;
#121732 = DIRECTION('ref_axis',(0.,0.,-1.)) ;
#121733 = DIRECTION('center_axis',(1.,0.,0.)) ;
#121734 = DIRECTION('ref_axis',(0.,0.,-1.)) ;
#121735 = DIRECTION('center_axis',(1.,0.,0.)) ;
#121736 = DIRECTION('ref_axis',(0.,0.,-1.)) ;
#121737 = DIRECTION('',(0.,0.,1.)) ;
#121738 = DIRECTION('',(0.,-1.,-8.9727076343628E-17)) ;
#121739 = DIRECTION('',(0.,0.,-1.)) ;
#121740 = DIRECTION('',(0.,1.,-8.9727076343628E-17)) ;
#121741 = DIRECTION('',(0.,0.,1.)) ;
#121742 = DIRECTION('center_axis',(1.,0.,0.)) ;
#121743 = DIRECTION('ref_axis',(0.,0.,-1.)) ;
#121744 = DIRECTION('center_axis',(1.,0.,0.)) ;
#121745 = DIRECTION('ref_axis',(0.,0.,-1.)) ;
#121746 = DIRECTION('center_axis',(1.,0.,0.)) ;
#121747 = DIRECTION('ref_axis',(0.,0.,-1.)) ;
#121748 = DIRECTION('center_axis',(1.,0.,0.)) ;
#121749 = DIRECTION('ref_axis',(0.,0.,-1.)) ;
#121750 = DIRECTION('',(0.,0.,1.)) ;
#121751 = DIRECTION('',(0.,-1.,-8.9727076343628E-17)) ;
#121752 = DIRECTION('',(0.,0.,-1.)) ;
#121753 = DIRECTION('',(0.,1.,-8.9727076343628E-17)) ;
#121754 = DIRECTION('',(0.,0.,1.)) ;
#121755 = DIRECTION('center_axis',(1.,0.,0.)) ;
#121756 = DIRECTION('ref_axis',(0.,0.,-1.)) ;
#121757 = DIRECTION('center_axis',(1.,0.,0.)) ;
#121758 = DIRECTION('ref_axis',(0.,0.,-1.)) ;
#121759 = DIRECTION('center_axis',(1.,0.,0.)) ;
#121760 = DIRECTION('ref_axis',(0.,0.,-1.)) ;
#121761 = DIRECTION('center_axis',(1.,0.,0.)) ;
#121762 = DIRECTION('ref_axis',(0.,0.,-1.)) ;
#121763 = DIRECTION('',(0.,0.,1.)) ;
#121764 = DIRECTION('',(0.,-1.,-8.9727076343628E-17)) ;
#121765 = DIRECTION('',(0.,0.,-1.)) ;
#121766 = DIRECTION('',(0.,1.,-8.9727076343628E-17)) ;
#121767 = DIRECTION('',(0.,0.,1.)) ;
#121768 = DIRECTION('center_axis',(1.,0.,0.)) ;
#121769 = DIRECTION('ref_axis',(0.,0.,-1.)) ;
#121770 = DIRECTION('center_axis',(1.,0.,0.)) ;
#121771 = DIRECTION('ref_axis',(0.,0.,-1.)) ;
#121772 = DIRECTION('center_axis',(1.,7.81406971160724E-17,0.)) ;
#121773 = DIRECTION('ref_axis',(-7.81406971160724E-17,1.,0.)) ;
#121774 = DIRECTION('',(-7.81406971160724E-17,1.,0.)) ;
#121775 = DIRECTION('',(0.,0.,1.)) ;
#121776 = DIRECTION('',(7.81406971160724E-17,-1.,0.)) ;
#121777 = DIRECTION('',(0.,0.,-1.)) ;
#121778 = DIRECTION('center_axis',(1.,7.81406971160724E-17,0.)) ;
#121779 = DIRECTION('ref_axis',(-7.81406971160724E-17,1.,0.)) ;
#121780 = DIRECTION('',(0.,0.,-1.)) ;
#121781 = DIRECTION('',(-7.81406971160724E-17,1.,0.)) ;
#121782 = DIRECTION('',(-3.78638272950961E-32,4.8455963016112E-16,1.)) ;
#121783 = DIRECTION('',(7.81406971160724E-17,-1.,8.9727076343628E-17)) ;
#121784 = DIRECTION('center_axis',(1.,7.81406971160724E-17,0.)) ;
#121785 = DIRECTION('ref_axis',(-7.81406971160724E-17,1.,0.)) ;
#121786 = DIRECTION('',(0.,0.,1.)) ;
#121787 = DIRECTION('center_axis',(1.,7.81406971160724E-17,0.)) ;
#121788 = DIRECTION('ref_axis',(-7.81406971160724E-17,1.,0.)) ;
#121789 = DIRECTION('',(-7.81406971160724E-17,1.,8.9727076343628E-17)) ;
#121790 = DIRECTION('',(-3.78638272950961E-32,4.8455963016112E-16,1.)) ;
#121791 = DIRECTION('',(7.81406971160724E-17,-1.,8.9727076343628E-17)) ;
#121792 = DIRECTION('center_axis',(1.,7.81406971160724E-17,0.)) ;
#121793 = DIRECTION('ref_axis',(-7.81406971160724E-17,1.,0.)) ;
#121794 = DIRECTION('',(0.,0.,1.)) ;
#121795 = DIRECTION('center_axis',(1.,7.81406971160724E-17,0.)) ;
#121796 = DIRECTION('ref_axis',(-7.81406971160724E-17,1.,0.)) ;
#121797 = DIRECTION('',(-7.81406971160724E-17,1.,8.9727076343628E-17)) ;
#121798 = DIRECTION('',(-3.78638272950961E-32,4.8455963016112E-16,1.)) ;
#121799 = DIRECTION('',(7.81406971160724E-17,-1.,8.9727076343628E-17)) ;
#121800 = DIRECTION('center_axis',(1.,7.81406971160724E-17,0.)) ;
#121801 = DIRECTION('ref_axis',(-7.81406971160724E-17,1.,0.)) ;
#121802 = DIRECTION('',(0.,0.,1.)) ;
#121803 = DIRECTION('center_axis',(1.,7.81406971160724E-17,0.)) ;
#121804 = DIRECTION('ref_axis',(-7.81406971160724E-17,1.,0.)) ;
#121805 = DIRECTION('',(-7.81406971160724E-17,1.,8.9727076343628E-17)) ;
#121806 = DIRECTION('',(-3.78638272950961E-32,4.8455963016112E-16,1.)) ;
#121807 = DIRECTION('',(7.81406971160724E-17,-1.,8.9727076343628E-17)) ;
#121808 = DIRECTION('center_axis',(1.,7.81406971160724E-17,0.)) ;
#121809 = DIRECTION('ref_axis',(-7.81406971160724E-17,1.,0.)) ;
#121810 = DIRECTION('',(0.,0.,1.)) ;
#121811 = DIRECTION('center_axis',(1.,7.81406971160724E-17,0.)) ;
#121812 = DIRECTION('ref_axis',(-7.81406971160724E-17,1.,0.)) ;
#121813 = DIRECTION('',(-7.81406971160724E-17,1.,8.9727076343628E-17)) ;
#121814 = DIRECTION('',(-3.78638272950961E-32,4.8455963016112E-16,1.)) ;
#121815 = DIRECTION('',(7.81406971160724E-17,-1.,8.9727076343628E-17)) ;
#121816 = DIRECTION('center_axis',(1.,7.81406971160724E-17,0.)) ;
#121817 = DIRECTION('ref_axis',(-7.81406971160724E-17,1.,0.)) ;
#121818 = DIRECTION('',(0.,0.,1.)) ;
#121819 = DIRECTION('center_axis',(1.,7.81406971160724E-17,0.)) ;
#121820 = DIRECTION('ref_axis',(-7.81406971160724E-17,1.,0.)) ;
#121821 = DIRECTION('',(-7.81406971160724E-17,1.,8.9727076343628E-17)) ;
#121822 = DIRECTION('',(-3.78638272950961E-32,4.8455963016112E-16,1.)) ;
#121823 = DIRECTION('',(7.81406971160724E-17,-1.,8.9727076343628E-17)) ;
#121824 = DIRECTION('center_axis',(1.,7.81406971160724E-17,0.)) ;
#121825 = DIRECTION('ref_axis',(-7.81406971160724E-17,1.,0.)) ;
#121826 = DIRECTION('',(0.,0.,1.)) ;
#121827 = DIRECTION('center_axis',(1.,7.81406971160724E-17,0.)) ;
#121828 = DIRECTION('ref_axis',(-7.81406971160724E-17,1.,0.)) ;
#121829 = DIRECTION('',(-7.81406971160724E-17,1.,8.9727076343628E-17)) ;
#121830 = DIRECTION('',(-3.78638272950961E-32,4.8455963016112E-16,1.)) ;
#121831 = DIRECTION('',(7.81406971160724E-17,-1.,8.9727076343628E-17)) ;
#121832 = DIRECTION('center_axis',(1.,7.81406971160724E-17,0.)) ;
#121833 = DIRECTION('ref_axis',(-7.81406971160724E-17,1.,0.)) ;
#121834 = DIRECTION('',(0.,0.,1.)) ;
#121835 = DIRECTION('center_axis',(1.,7.81406971160724E-17,0.)) ;
#121836 = DIRECTION('ref_axis',(-7.81406971160724E-17,1.,0.)) ;
#121837 = DIRECTION('',(-7.81406971160724E-17,1.,8.9727076343628E-17)) ;
#121838 = DIRECTION('',(-3.78638272950961E-32,4.8455963016112E-16,1.)) ;
#121839 = DIRECTION('',(7.81406971160724E-17,-1.,8.9727076343628E-17)) ;
#121840 = DIRECTION('center_axis',(1.,7.81406971160724E-17,0.)) ;
#121841 = DIRECTION('ref_axis',(-7.81406971160724E-17,1.,0.)) ;
#121842 = DIRECTION('',(0.,0.,1.)) ;
#121843 = DIRECTION('center_axis',(1.,7.81406971160724E-17,0.)) ;
#121844 = DIRECTION('ref_axis',(-7.81406971160724E-17,1.,0.)) ;
#121845 = DIRECTION('',(-7.81406971160724E-17,1.,8.9727076343628E-17)) ;
#121846 = DIRECTION('',(-3.78638272950961E-32,4.8455963016112E-16,1.)) ;
#121847 = DIRECTION('',(7.81406971160724E-17,-1.,8.9727076343628E-17)) ;
#121848 = DIRECTION('center_axis',(1.,7.81406971160724E-17,0.)) ;
#121849 = DIRECTION('ref_axis',(-7.81406971160724E-17,1.,0.)) ;
#121850 = DIRECTION('',(0.,0.,1.)) ;
#121851 = DIRECTION('center_axis',(1.,7.81406971160724E-17,0.)) ;
#121852 = DIRECTION('ref_axis',(-7.81406971160724E-17,1.,0.)) ;
#121853 = DIRECTION('',(-7.81406971160724E-17,1.,8.9727076343628E-17)) ;
#121854 = DIRECTION('',(-3.78638272950961E-32,4.8455963016112E-16,1.)) ;
#121855 = DIRECTION('',(7.81406971160724E-17,-1.,8.9727076343628E-17)) ;
#121856 = DIRECTION('center_axis',(1.,7.81406971160724E-17,0.)) ;
#121857 = DIRECTION('ref_axis',(-7.81406971160724E-17,1.,0.)) ;
#121858 = DIRECTION('',(0.,0.,1.)) ;
#121859 = DIRECTION('center_axis',(1.,7.81406971160724E-17,0.)) ;
#121860 = DIRECTION('ref_axis',(-7.81406971160724E-17,1.,0.)) ;
#121861 = DIRECTION('',(-7.81406971160724E-17,1.,8.9727076343628E-17)) ;
#121862 = DIRECTION('',(3.78638272950961E-32,-4.8455963016112E-16,1.)) ;
#121863 = DIRECTION('',(7.81406971160724E-17,-1.,0.)) ;
#121864 = DIRECTION('center_axis',(0.,0.,-1.)) ;
#121865 = DIRECTION('ref_axis',(-1.,0.,0.)) ;
#121866 = DIRECTION('',(0.,0.,-1.)) ;
#121867 = DIRECTION('center_axis',(0.,0.,-1.)) ;
#121868 = DIRECTION('ref_axis',(-1.,0.,0.)) ;
#121869 = DIRECTION('center_axis',(0.,0.,1.)) ;
#121870 = DIRECTION('ref_axis',(-1.,0.,0.)) ;
#121871 = DIRECTION('center_axis',(0.,4.8455963016112E-16,1.)) ;
#121872 = DIRECTION('ref_axis',(0.,-1.,4.8455963016112E-16)) ;
#121873 = DIRECTION('',(0.,4.8455963016112E-16,1.)) ;
#121874 = DIRECTION('center_axis',(0.,0.,-1.)) ;
#121875 = DIRECTION('ref_axis',(-1.,0.,0.)) ;
#121876 = DIRECTION('center_axis',(0.,0.,-1.)) ;
#121877 = DIRECTION('ref_axis',(-1.,0.,0.)) ;
#121878 = DIRECTION('center_axis',(0.,0.,1.)) ;
#121879 = DIRECTION('ref_axis',(1.,0.,0.)) ;
#121880 = DIRECTION('center_axis',(0.,0.,1.)) ;
#121881 = DIRECTION('ref_axis',(1.,0.,0.)) ;
#121882 = DIRECTION('center_axis',(-1.,-2.47817639425258E-16,0.)) ;
#121883 = DIRECTION('ref_axis',(2.47817639425258E-16,-1.,0.)) ;
#121884 = DIRECTION('',(2.47817639425258E-16,-1.,0.)) ;
#121885 = DIRECTION('',(0.,0.,1.)) ;
#121886 = DIRECTION('',(-2.47817639425258E-16,1.,0.)) ;
#121887 = DIRECTION('',(0.,0.,-1.)) ;
#121888 = DIRECTION('',(0.,0.,-1.)) ;
#121889 = DIRECTION('',(-2.47817639425258E-16,1.,0.)) ;
#121890 = DIRECTION('',(0.,0.,1.)) ;
#121891 = DIRECTION('',(2.47817639425258E-16,-1.,0.)) ;
#121892 = DIRECTION('',(0.,0.,-1.)) ;
#121893 = DIRECTION('',(-2.47817639425258E-16,1.,0.)) ;
#121894 = DIRECTION('',(0.,0.,1.)) ;
#121895 = DIRECTION('',(2.47817639425258E-16,-1.,0.)) ;
#121896 = DIRECTION('',(0.,0.,-1.)) ;
#121897 = DIRECTION('',(-2.47817639425258E-16,1.,0.)) ;
#121898 = DIRECTION('',(0.,0.,1.)) ;
#121899 = DIRECTION('',(2.47817639425258E-16,-1.,0.)) ;
#121900 = DIRECTION('',(0.,0.,-1.)) ;
#121901 = DIRECTION('',(-2.47817639425258E-16,1.,0.)) ;
#121902 = DIRECTION('',(0.,0.,1.)) ;
#121903 = DIRECTION('',(2.47817639425258E-16,-1.,0.)) ;
#121904 = DIRECTION('',(0.,0.,-1.)) ;
#121905 = DIRECTION('',(-2.47817639425258E-16,1.,0.)) ;
#121906 = DIRECTION('',(0.,0.,1.)) ;
#121907 = DIRECTION('',(2.47817639425258E-16,-1.,0.)) ;
#121908 = DIRECTION('',(0.,0.,-1.)) ;
#121909 = DIRECTION('',(-2.47817639425258E-16,1.,0.)) ;
#121910 = DIRECTION('',(0.,0.,1.)) ;
#121911 = DIRECTION('',(2.47817639425258E-16,-1.,0.)) ;
#121912 = DIRECTION('',(0.,0.,-1.)) ;
#121913 = DIRECTION('',(-2.47817639425258E-16,1.,0.)) ;
#121914 = DIRECTION('',(0.,0.,1.)) ;
#121915 = DIRECTION('',(2.47817639425258E-16,-1.,0.)) ;
#121916 = DIRECTION('',(0.,0.,-1.)) ;
#121917 = DIRECTION('',(-2.47817639425258E-16,1.,0.)) ;
#121918 = DIRECTION('',(0.,0.,1.)) ;
#121919 = DIRECTION('',(2.47817639425258E-16,-1.,0.)) ;
#121920 = DIRECTION('',(0.,0.,-1.)) ;
#121921 = DIRECTION('',(-2.47817639425258E-16,1.,0.)) ;
#121922 = DIRECTION('',(0.,0.,1.)) ;
#121923 = DIRECTION('',(2.47817639425258E-16,-1.,0.)) ;
#121924 = DIRECTION('',(0.,0.,-1.)) ;
#121925 = DIRECTION('',(-2.47817639425258E-16,1.,0.)) ;
#121926 = DIRECTION('',(0.,0.,1.)) ;
#121927 = DIRECTION('',(2.47817639425258E-16,-1.,0.)) ;
#121928 = DIRECTION('center_axis',(0.,-1.,0.)) ;
#121929 = DIRECTION('ref_axis',(0.,0.,-1.)) ;
#121930 = DIRECTION('',(0.,0.,-1.)) ;
#121931 = DIRECTION('',(-1.,0.,-7.01133629567814E-33)) ;
#121932 = DIRECTION('',(0.,0.,1.)) ;
#121933 = DIRECTION('',(1.,0.,-7.01133629567814E-33)) ;
#121934 = DIRECTION('',(0.,0.,1.)) ;
#121935 = DIRECTION('center_axis',(0.,-1.,0.)) ;
#121936 = DIRECTION('ref_axis',(0.,0.,-1.)) ;
#121937 = DIRECTION('',(-1.,0.,0.)) ;
#121938 = DIRECTION('center_axis',(0.,-1.,0.)) ;
#121939 = DIRECTION('ref_axis',(0.,0.,-1.)) ;
#121940 = DIRECTION('',(0.,0.,-1.)) ;
#121941 = DIRECTION('center_axis',(0.,-1.,0.)) ;
#121942 = DIRECTION('ref_axis',(0.,0.,-1.)) ;
#121943 = DIRECTION('',(1.,0.,0.)) ;
#121944 = DIRECTION('center_axis',(0.,-1.,0.)) ;
#121945 = DIRECTION('ref_axis',(0.,0.,-1.)) ;
#121946 = DIRECTION('center_axis',(1.,7.81406971160724E-17,0.)) ;
#121947 = DIRECTION('ref_axis',(-7.81406971160724E-17,1.,0.)) ;
#121948 = DIRECTION('',(-7.81406971160724E-17,1.,-1.10147335281612E-31)) ;
#121949 = DIRECTION('',(0.,0.,1.)) ;
#121950 = DIRECTION('',(7.81406971160724E-17,-1.,0.)) ;
#121951 = DIRECTION('',(0.,0.,-1.)) ;
#121952 = DIRECTION('center_axis',(1.31418445149758E-16,1.,0.)) ;
#121953 = DIRECTION('ref_axis',(-1.,1.31418445149758E-16,0.)) ;
#121954 = DIRECTION('',(0.422618261740697,-5.55398348498559E-17,-0.906307787036651)) ;
#121955 = DIRECTION('center_axis',(1.,0.,0.)) ;
#121956 = DIRECTION('ref_axis',(0.,0.,-1.)) ;
#121957 = DIRECTION('',(0.,-1.,-8.9727076343628E-17)) ;
#121958 = DIRECTION('',(0.,0.,-1.)) ;
#121959 = DIRECTION('',(0.,1.,-8.9727076343628E-17)) ;
#121960 = DIRECTION('',(0.,0.,1.)) ;
#121961 = DIRECTION('center_axis',(1.,0.,0.)) ;
#121962 = DIRECTION('ref_axis',(0.,0.,-1.)) ;
#121963 = DIRECTION('center_axis',(1.,0.,0.)) ;
#121964 = DIRECTION('ref_axis',(0.,0.,-1.)) ;
#121965 = DIRECTION('center_axis',(1.,0.,0.)) ;
#121966 = DIRECTION('ref_axis',(0.,0.,-1.)) ;
#121967 = DIRECTION('',(0.,0.,1.)) ;
#121968 = DIRECTION('center_axis',(0.,1.,0.)) ;
#121969 = DIRECTION('ref_axis',(0.,0.,1.)) ;
#121970 = DIRECTION('',(0.,0.,-1.)) ;
#121971 = DIRECTION('',(-1.,0.,0.)) ;
#121972 = DIRECTION('',(0.,0.,1.)) ;
#121973 = DIRECTION('',(1.,0.,0.)) ;
#121974 = DIRECTION('center_axis',(-0.89708903366019,0.441849822549049,0.)) ;
#121975 = DIRECTION('ref_axis',(-0.441849822549049,-0.89708903366019,0.)) ;
#121976 = DIRECTION('',(0.441849822549049,0.89708903366019,0.)) ;
#121977 = DIRECTION('',(-0.441849822549049,-0.89708903366019,0.)) ;
#121978 = DIRECTION('',(0.,0.,1.)) ;
#121979 = DIRECTION('center_axis',(-1.,0.,0.)) ;
#121980 = DIRECTION('ref_axis',(0.,0.,1.)) ;
#121981 = DIRECTION('',(0.,-1.,0.)) ;
#121982 = DIRECTION('',(0.,0.,1.)) ;
#121983 = DIRECTION('',(0.,1.,0.)) ;
#121984 = DIRECTION('',(0.,0.,-1.)) ;
#121985 = DIRECTION('center_axis',(0.,-1.,0.)) ;
#121986 = DIRECTION('ref_axis',(0.,0.,-1.)) ;
#121987 = DIRECTION('',(1.,0.,0.)) ;
#121988 = DIRECTION('',(0.,0.,1.)) ;
#121989 = DIRECTION('',(-1.,0.,0.)) ;
#121990 = DIRECTION('',(0.,0.,-1.)) ;
#121991 = DIRECTION('',(0.,0.,1.)) ;
#121992 = DIRECTION('',(1.,0.,-2.16840434497101E-16)) ;
#121993 = DIRECTION('',(2.16840434497101E-16,0.,-1.)) ;
#121994 = DIRECTION('',(-1.,0.,-2.16840434497101E-16)) ;
#121995 = DIRECTION('',(0.,0.,1.)) ;
#121996 = DIRECTION('',(1.,0.,-2.16840434497101E-16)) ;
#121997 = DIRECTION('',(2.16840434497101E-16,0.,-1.)) ;
#121998 = DIRECTION('',(-1.,0.,-2.16840434497101E-16)) ;
#121999 = DIRECTION('',(0.,0.,1.)) ;
#122000 = DIRECTION('',(1.,0.,-2.16840434497101E-16)) ;
#122001 = DIRECTION('',(2.16840434497101E-16,0.,-1.)) ;
#122002 = DIRECTION('',(-1.,0.,-2.16840434497101E-16)) ;
#122003 = DIRECTION('',(0.,0.,1.)) ;
#122004 = DIRECTION('',(1.,0.,-2.16840434497101E-16)) ;
#122005 = DIRECTION('',(2.16840434497101E-16,0.,-1.)) ;
#122006 = DIRECTION('',(-1.,0.,-2.16840434497101E-16)) ;
#122007 = DIRECTION('',(0.,0.,1.)) ;
#122008 = DIRECTION('',(1.,0.,-2.16840434497101E-16)) ;
#122009 = DIRECTION('',(2.16840434497101E-16,0.,-1.)) ;
#122010 = DIRECTION('',(-1.,0.,-2.16840434497101E-16)) ;
#122011 = DIRECTION('',(0.,0.,1.)) ;
#122012 = DIRECTION('',(1.,0.,-2.16840434497101E-16)) ;
#122013 = DIRECTION('',(2.16840434497101E-16,0.,-1.)) ;
#122014 = DIRECTION('',(-1.,0.,-2.16840434497101E-16)) ;
#122015 = DIRECTION('',(0.,0.,1.)) ;
#122016 = DIRECTION('',(1.,0.,-2.16840434497101E-16)) ;
#122017 = DIRECTION('',(2.16840434497101E-16,0.,-1.)) ;
#122018 = DIRECTION('',(-1.,0.,-2.16840434497101E-16)) ;
#122019 = DIRECTION('',(0.,0.,1.)) ;
#122020 = DIRECTION('',(1.,0.,-2.16840434497101E-16)) ;
#122021 = DIRECTION('',(2.16840434497101E-16,0.,-1.)) ;
#122022 = DIRECTION('',(-1.,0.,-2.16840434497101E-16)) ;
#122023 = DIRECTION('center_axis',(0.,-1.,0.)) ;
#122024 = DIRECTION('ref_axis',(0.,0.,-1.)) ;
#122025 = DIRECTION('',(-1.,0.,-2.16840434497101E-16)) ;
#122026 = DIRECTION('center_axis',(0.,-1.,0.)) ;
#122027 = DIRECTION('ref_axis',(0.,0.,-1.)) ;
#122028 = DIRECTION('',(0.,0.,1.)) ;
#122029 = DIRECTION('center_axis',(0.,-1.,0.)) ;
#122030 = DIRECTION('ref_axis',(0.,0.,-1.)) ;
#122031 = DIRECTION('',(1.,0.,-2.16840434497101E-16)) ;
#122032 = DIRECTION('center_axis',(0.,-1.,0.)) ;
#122033 = DIRECTION('ref_axis',(0.,0.,-1.)) ;
#122034 = DIRECTION('',(2.16840434497101E-16,0.,-1.)) ;
#122035 = DIRECTION('center_axis',(0.,-1.,0.)) ;
#122036 = DIRECTION('ref_axis',(0.,0.,-1.)) ;
#122037 = DIRECTION('',(-1.,0.,-2.16840434497101E-16)) ;
#122038 = DIRECTION('center_axis',(0.,-1.,0.)) ;
#122039 = DIRECTION('ref_axis',(0.,0.,-1.)) ;
#122040 = DIRECTION('',(0.,0.,1.)) ;
#122041 = DIRECTION('center_axis',(0.,-1.,0.)) ;
#122042 = DIRECTION('ref_axis',(0.,0.,-1.)) ;
#122043 = DIRECTION('',(1.,0.,-2.16840434497101E-16)) ;
#122044 = DIRECTION('center_axis',(0.,-1.,0.)) ;
#122045 = DIRECTION('ref_axis',(0.,0.,-1.)) ;
#122046 = DIRECTION('',(2.16840434497101E-16,0.,-1.)) ;
#122047 = DIRECTION('center_axis',(0.,0.,-1.)) ;
#122048 = DIRECTION('ref_axis',(-1.,0.,0.)) ;
#122049 = DIRECTION('',(0.,1.,0.)) ;
#122050 = DIRECTION('',(1.,1.31418445149758E-16,0.)) ;
#122051 = DIRECTION('',(7.81406971160724E-17,-1.,0.)) ;
#122052 = DIRECTION('center_axis',(0.,0.,-1.)) ;
#122053 = DIRECTION('ref_axis',(-1.,0.,0.)) ;
#122054 = DIRECTION('',(1.,7.81406971160724E-17,0.)) ;
#122055 = DIRECTION('',(0.,-1.,0.)) ;
#122056 = DIRECTION('',(-1.,-7.81406971160724E-17,0.)) ;
#122057 = DIRECTION('center_axis',(0.,0.,1.)) ;
#122058 = DIRECTION('ref_axis',(-1.,-3.25260651745651E-15,0.)) ;
#122059 = DIRECTION('',(7.81406971160724E-17,-1.,0.)) ;
#122060 = DIRECTION('',(-1.,0.,0.)) ;
#122061 = DIRECTION('',(-2.47817639425258E-16,1.,0.)) ;
#122062 = DIRECTION('',(1.,0.,0.)) ;
#122063 = DIRECTION('center_axis',(0.,0.,-1.)) ;
#122064 = DIRECTION('ref_axis',(-1.,0.,0.)) ;
#122065 = DIRECTION('',(0.441849822549049,0.89708903366019,0.)) ;
#122066 = DIRECTION('',(-1.,0.,0.)) ;
#122067 = DIRECTION('center_axis',(0.,0.,-1.)) ;
#122068 = DIRECTION('ref_axis',(-1.,0.,0.)) ;
#122069 = DIRECTION('',(-7.81406971160724E-17,1.,0.)) ;
#122070 = DIRECTION('',(-1.,-1.31418445149758E-16,0.)) ;
#122071 = DIRECTION('',(0.,-1.,0.)) ;
#122072 = DIRECTION('',(1.,0.,0.)) ;
#122073 = DIRECTION('',(-0.441849822549049,-0.89708903366019,0.)) ;
#122074 = DIRECTION('center_axis',(0.,0.,1.)) ;
#122075 = DIRECTION('ref_axis',(-1.,0.,0.)) ;
#122076 = DIRECTION('',(-1.,0.,0.)) ;
#122077 = DIRECTION('',(2.47817639425258E-16,-1.,0.)) ;
#122078 = DIRECTION('',(1.,0.,0.)) ;
#122079 = DIRECTION('',(-7.81406971160724E-17,1.,0.)) ;
#122080 = DIRECTION('center_axis',(0.,0.,-1.)) ;
#122081 = DIRECTION('ref_axis',(-1.,0.,0.)) ;
#122082 = DIRECTION('',(1.,7.81406971160724E-17,0.)) ;
#122083 = DIRECTION('',(0.,1.,0.)) ;
#122084 = DIRECTION('',(-1.,-7.81406971160724E-17,0.)) ;
#122085 = DIRECTION('center_axis',(0.,0.,1.)) ;
#122086 = DIRECTION('ref_axis',(-1.,0.,0.)) ;
#122087 = DIRECTION('center_axis',(0.,0.,-1.)) ;
#122088 = DIRECTION('ref_axis',(-1.,0.,0.)) ;
#122089 = DIRECTION('',(0.970142500145333,0.24253562503633,0.)) ;
#122090 = DIRECTION('',(0.,1.,0.)) ;
#122091 = DIRECTION('',(-0.707106781186548,0.707106781186547,0.)) ;
#122092 = DIRECTION('',(2.47817639425258E-16,-1.,0.)) ;
#122093 = DIRECTION('center_axis',(0.432731067584771,0.,-0.901523057468274)) ;
#122094 = DIRECTION('ref_axis',(-0.901523057468274,0.,-0.432731067584771)) ;
#122095 = DIRECTION('',(0.,-1.,0.)) ;
#122096 = DIRECTION('',(0.879462917689188,0.219865729422294,0.42214220049081)) ;
#122097 = DIRECTION('',(0.,1.,0.)) ;
#122098 = DIRECTION('',(-0.669589480006975,0.669589480006975,-0.321402950403348)) ;
#122099 = DIRECTION('center_axis',(1.,0.,0.)) ;
#122100 = DIRECTION('ref_axis',(0.,0.,-1.)) ;
#122101 = DIRECTION('',(0.,0.,-1.)) ;
#122102 = DIRECTION('center_axis',(-1.,-1.41117851341148E-14,1.31136401905241E-14)) ;
#122103 = DIRECTION('ref_axis',(-1.81493914443541E-14,0.461934418837058,-0.886914084166933)) ;
#122104 = DIRECTION('',(0.,1.,0.)) ;
#122105 = DIRECTION('center_axis',(-1.,0.,0.)) ;
#122106 = DIRECTION('ref_axis',(0.,0.901523057468499,0.432731067584301)) ;
#122107 = DIRECTION('',(0.,0.,-1.)) ;
#122108 = DIRECTION('center_axis',(-1.,-1.26549640056948E-14,1.61343974433662E-14)) ;
#122109 = DIRECTION('ref_axis',(-1.83905968730662E-14,0.901523057468445,-0.432731067584414)) ;
#122110 = DIRECTION('center_axis',(-1.,-1.41117851341149E-14,-1.31136401905241E-14)) ;
#122111 = DIRECTION('ref_axis',(1.81493914443479E-14,-0.4619344188362,-0.88691408416738)) ;
#122112 = DIRECTION('center_axis',(0.432731067584771,0.,0.901523057468274)) ;
#122113 = DIRECTION('ref_axis',(0.901523057468274,0.,-0.432731067584771)) ;
#122114 = DIRECTION('',(-0.879462917689188,-0.219865729422294,0.42214220049081)) ;
#122115 = DIRECTION('',(0.,1.,0.)) ;
#122116 = DIRECTION('',(0.669589480006975,-0.669589480006975,-0.321402950403348)) ;
#122117 = DIRECTION('center_axis',(0.,0.,1.)) ;
#122118 = DIRECTION('ref_axis',(1.,0.,0.)) ;
#122119 = DIRECTION('',(0.,-1.,0.)) ;
#122120 = DIRECTION('',(-0.970142500145333,-0.24253562503633,0.)) ;
#122121 = DIRECTION('',(-2.47817639425258E-16,1.,0.)) ;
#122122 = DIRECTION('',(0.707106781186548,-0.707106781186547,0.)) ;
#122123 = DIRECTION('center_axis',(0.24253562503633,-0.970142500145333,0.)) ;
#122124 = DIRECTION('ref_axis',(0.,0.,1.)) ;
#122125 = DIRECTION('',(0.970142500145333,0.24253562503633,0.)) ;
#122126 = DIRECTION('',(0.879462917689188,0.219865729422294,-0.42214220049081)) ;
#122127 = DIRECTION('',(-0.879462917689188,-0.219865729422294,-0.42214220049081)) ;
#122128 = DIRECTION('',(-0.970142500145333,-0.24253562503633,0.)) ;
#122129 = DIRECTION('',(0.,0.,1.)) ;
#122130 = DIRECTION('center_axis',(-0.707106781186547,-0.707106781186548,
0.)) ;
#122131 = DIRECTION('ref_axis',(0.,0.,-1.)) ;
#122132 = DIRECTION('',(0.707106781186548,-0.707106781186547,0.)) ;
#122133 = DIRECTION('',(0.669589480006975,-0.669589480006975,0.321402950403348)) ;
#122134 = DIRECTION('',(-0.669589480006975,0.669589480006975,0.321402950403348)) ;
#122135 = DIRECTION('',(-0.707106781186548,0.707106781186547,0.)) ;
#122136 = DIRECTION('',(0.,0.,-1.)) ;
#122137 = DIRECTION('center_axis',(1.,0.,2.16840434497101E-16)) ;
#122138 = DIRECTION('ref_axis',(2.16840434497101E-16,0.,-1.)) ;
#122139 = DIRECTION('',(2.16840434497101E-16,0.,-1.)) ;
#122140 = DIRECTION('',(0.,-1.,0.)) ;
#122141 = DIRECTION('',(-2.16840434497101E-16,0.,1.)) ;
#122142 = DIRECTION('',(0.,1.,0.)) ;
#122143 = DIRECTION('center_axis',(2.16840434497101E-16,0.,-1.)) ;
#122144 = DIRECTION('ref_axis',(-1.,0.,-2.16840434497101E-16)) ;
#122145 = DIRECTION('',(-1.,0.,-2.16840434497101E-16)) ;
#122146 = DIRECTION('',(0.,-1.,0.)) ;
#122147 = DIRECTION('',(1.,0.,2.16840434497101E-16)) ;
#122148 = DIRECTION('',(0.,1.,0.)) ;
#122149 = DIRECTION('center_axis',(-1.,0.,0.)) ;
#122150 = DIRECTION('ref_axis',(0.,0.,1.)) ;
#122151 = DIRECTION('',(0.,1.,0.)) ;
#122152 = DIRECTION('',(0.,0.,1.)) ;
#122153 = DIRECTION('',(0.,-1.,0.)) ;
#122154 = DIRECTION('',(0.,0.,-1.)) ;
#122155 = DIRECTION('center_axis',(2.16840434497101E-16,0.,1.)) ;
#122156 = DIRECTION('ref_axis',(1.,0.,-2.16840434497101E-16)) ;
#122157 = DIRECTION('',(0.,1.,0.)) ;
#122158 = DIRECTION('',(1.,0.,-2.16840434497101E-16)) ;
#122159 = DIRECTION('',(0.,-1.,0.)) ;
#122160 = DIRECTION('',(-1.,0.,2.16840434497101E-16)) ;
#122161 = DIRECTION('center_axis',(0.,-1.,0.)) ;
#122162 = DIRECTION('ref_axis',(0.,0.,-1.)) ;
#122163 = DIRECTION('',(0.,0.,-1.)) ;
#122164 = DIRECTION('',(1.,0.,2.16840434497101E-16)) ;
#122165 = DIRECTION('',(-2.16840434497101E-16,0.,1.)) ;
#122166 = DIRECTION('',(-1.,0.,2.16840434497101E-16)) ;
#122167 = DIRECTION('',(1.,0.,0.)) ;
#122168 = DIRECTION('center_axis',(0.,1.,0.)) ;
#122169 = DIRECTION('ref_axis',(0.,0.,-1.)) ;
#122170 = DIRECTION('',(0.,0.,-1.)) ;
#122171 = DIRECTION('center_axis',(0.,1.,0.)) ;
#122172 = DIRECTION('ref_axis',(0.,0.,-1.)) ;
#122173 = DIRECTION('',(-1.,0.,0.)) ;
#122174 = DIRECTION('center_axis',(0.,1.,0.)) ;
#122175 = DIRECTION('ref_axis',(0.,0.,-1.)) ;
#122176 = DIRECTION('',(0.,0.,1.)) ;
#122177 = DIRECTION('center_axis',(0.,1.,0.)) ;
#122178 = DIRECTION('ref_axis',(0.,0.,-1.)) ;
#122179 = DIRECTION('center_axis',(1.,0.,0.)) ;
#122180 = DIRECTION('ref_axis',(0.,0.,-1.)) ;
#122181 = DIRECTION('',(0.,-1.,0.)) ;
#122182 = DIRECTION('',(0.,0.,-1.)) ;
#122183 = DIRECTION('',(0.,1.,0.)) ;
#122184 = DIRECTION('center_axis',(0.,0.,-1.)) ;
#122185 = DIRECTION('ref_axis',(-1.,0.,0.)) ;
#122186 = DIRECTION('',(0.,-1.,0.)) ;
#122187 = DIRECTION('',(-1.,0.,0.)) ;
#122188 = DIRECTION('',(0.,1.,0.)) ;
#122189 = DIRECTION('center_axis',(-1.,0.,0.)) ;
#122190 = DIRECTION('ref_axis',(0.,0.,1.)) ;
#122191 = DIRECTION('',(0.,0.,1.)) ;
#122192 = DIRECTION('',(0.,1.,0.)) ;
#122193 = DIRECTION('',(0.,-1.,0.)) ;
#122194 = DIRECTION('center_axis',(0.,0.,1.)) ;
#122195 = DIRECTION('ref_axis',(1.,0.,0.)) ;
#122196 = DIRECTION('',(0.,-1.,0.)) ;
#122197 = DIRECTION('',(1.,0.,0.)) ;
#122198 = DIRECTION('',(0.,1.,0.)) ;
#122199 = DIRECTION('center_axis',(0.,-1.,0.)) ;
#122200 = DIRECTION('ref_axis',(0.,0.,-1.)) ;
#122201 = DIRECTION('',(-1.,0.,0.)) ;
#122202 = DIRECTION('',(0.,0.,-1.)) ;
#122203 = DIRECTION('',(1.,0.,0.)) ;
#122204 = DIRECTION('',(0.,0.,1.)) ;
#122205 = DIRECTION('center_axis',(7.81406971160724E-17,-1.,0.)) ;
#122206 = DIRECTION('ref_axis',(1.,7.81406971160724E-17,0.)) ;
#122207 = DIRECTION('',(-1.,-7.81406971160724E-17,0.)) ;
#122208 = DIRECTION('',(0.,0.,1.)) ;
#122209 = DIRECTION('center_axis',(-7.81406971160724E-17,1.,0.)) ;
#122210 = DIRECTION('ref_axis',(1.,7.81406971160724E-17,0.)) ;
#122211 = DIRECTION('',(-1.,-7.81406971160724E-17,0.)) ;
#122212 = DIRECTION('',(1.,7.81406971160724E-17,5.2561455487295E-16)) ;
#122213 = DIRECTION('center_axis',(-7.81406971160724E-17,1.,0.)) ;
#122214 = DIRECTION('ref_axis',(1.,7.81406971160724E-17,0.)) ;
#122215 = DIRECTION('',(0.,0.,1.)) ;
#122216 = DIRECTION('',(1.,7.81406971160724E-17,0.)) ;
#122217 = DIRECTION('center_axis',(-7.81406971160724E-17,1.,4.8455963016112E-16)) ;
#122218 = DIRECTION('ref_axis',(-2.5241768025713E-48,-4.8455963016112E-16,
1.)) ;
#122219 = DIRECTION('',(0.,-4.8455963016112E-16,1.)) ;
#122220 = DIRECTION('',(-1.,-7.81406971160724E-17,0.)) ;
#122221 = DIRECTION('',(-3.78638272950961E-32,4.8455963016112E-16,-1.)) ;
#122222 = DIRECTION('',(1.,7.81406971160724E-17,0.)) ;
#122223 = DIRECTION('center_axis',(-7.01133629567814E-33,8.97270763436279E-17,
-1.)) ;
#122224 = DIRECTION('ref_axis',(-6.83680877694706E-64,1.,8.97270763436279E-17)) ;
#122225 = DIRECTION('center_axis',(-7.01133629567814E-33,8.97270763436279E-17,
-1.)) ;
#122226 = DIRECTION('ref_axis',(6.29106707073161E-49,1.,8.97270763436279E-17)) ;
#122227 = DIRECTION('center_axis',(-7.01133629567814E-33,8.97270763436279E-17,
-1.)) ;
#122228 = DIRECTION('ref_axis',(6.29106707073161E-49,1.,8.97270763436279E-17)) ;
#122229 = DIRECTION('',(-1.,-7.81406971160724E-17,0.)) ;
#122230 = DIRECTION('',(7.81406971160724E-17,-1.,-8.9727076343628E-17)) ;
#122231 = DIRECTION('',(1.,7.81406971160724E-17,0.)) ;
#122232 = DIRECTION('',(0.,1.,8.9727076343628E-17)) ;
#122233 = DIRECTION('center_axis',(7.01133629567814E-33,-8.97270763436279E-17,
1.)) ;
#122234 = DIRECTION('ref_axis',(6.29106707073161E-49,1.,8.97270763436279E-17)) ;
#122235 = DIRECTION('',(1.,0.,-7.01133629567814E-33)) ;
#122236 = DIRECTION('',(0.,1.,8.9727076343628E-17)) ;
#122237 = DIRECTION('',(-1.,0.,7.01133629567814E-33)) ;
#122238 = DIRECTION('center_axis',(-7.81406971160724E-17,1.,0.)) ;
#122239 = DIRECTION('ref_axis',(-1.,-7.81406971160724E-17,0.)) ;
#122240 = DIRECTION('',(-1.,-7.81406971160724E-17,0.)) ;
#122241 = DIRECTION('',(0.,0.,-1.)) ;
#122242 = DIRECTION('',(1.,7.81406971160724E-17,0.)) ;
#122243 = DIRECTION('',(0.,0.,1.)) ;
#122244 = DIRECTION('center_axis',(-7.01133629567814E-33,8.97270763436279E-17,
1.)) ;
#122245 = DIRECTION('ref_axis',(6.83680877694706E-64,-1.,8.97270763436279E-17)) ;
#122246 = DIRECTION('',(1.,7.81406971160724E-17,0.)) ;
#122247 = DIRECTION('center_axis',(-7.01133629567814E-33,8.97270763436279E-17,
1.)) ;
#122248 = DIRECTION('ref_axis',(-6.29106707073161E-49,-1.,8.97270763436279E-17)) ;
#122249 = DIRECTION('center_axis',(-7.01133629567814E-33,8.97270763436279E-17,
1.)) ;
#122250 = DIRECTION('ref_axis',(-6.29106707073161E-49,-1.,8.97270763436279E-17)) ;
#122251 = DIRECTION('',(1.,0.,7.01133629567814E-33)) ;
#122252 = DIRECTION('',(0.,-1.,8.9727076343628E-17)) ;
#122253 = DIRECTION('',(-1.,0.,-7.01133629567814E-33)) ;
#122254 = DIRECTION('center_axis',(7.01133629567814E-33,-8.97270763436279E-17,
-1.)) ;
#122255 = DIRECTION('ref_axis',(-6.29106707073161E-49,-1.,8.97270763436279E-17)) ;
#122256 = DIRECTION('',(0.,-1.,8.9727076343628E-17)) ;
#122257 = DIRECTION('',(-1.,-7.81406971160724E-17,0.)) ;
#122258 = DIRECTION('',(-7.81406971160724E-17,1.,-8.9727076343628E-17)) ;
#122259 = DIRECTION('center_axis',(-7.81406971160724E-17,1.,-4.8455963016112E-16)) ;
#122260 = DIRECTION('ref_axis',(2.5241768025713E-48,4.8455963016112E-16,1.)) ;
#122261 = DIRECTION('',(1.,7.81406971160724E-17,0.)) ;
#122262 = DIRECTION('',(-1.,-7.81406971160724E-17,0.)) ;
#122263 = DIRECTION('',(3.78638272950961E-32,-4.8455963016112E-16,-1.)) ;
#122264 = DIRECTION('center_axis',(0.,1.,0.)) ;
#122265 = DIRECTION('ref_axis',(0.,0.,1.)) ;
#122266 = DIRECTION('',(-1.,0.,0.)) ;
#122267 = DIRECTION('',(0.,0.,-1.)) ;
#122268 = DIRECTION('',(1.,0.,7.01133629567814E-33)) ;
#122269 = DIRECTION('',(0.,0.,1.)) ;
#122270 = DIRECTION('center_axis',(0.,1.,0.)) ;
#122271 = DIRECTION('ref_axis',(0.,0.,1.)) ;
#122272 = DIRECTION('',(-1.,0.,7.01133629567814E-33)) ;
#122273 = DIRECTION('',(0.,0.,-1.)) ;
#122274 = DIRECTION('',(1.,0.,0.)) ;
#122275 = DIRECTION('',(0.,0.,1.)) ;
#122276 = DIRECTION('center_axis',(-1.,0.,0.)) ;
#122277 = DIRECTION('ref_axis',(0.,0.,1.)) ;
#122278 = DIRECTION('',(-1.,0.,0.)) ;
#122279 = DIRECTION('center_axis',(-1.,0.,0.)) ;
#122280 = DIRECTION('ref_axis',(0.,0.,-1.)) ;
#122281 = DIRECTION('',(1.,0.,0.)) ;
#122282 = DIRECTION('center_axis',(1.,0.,0.)) ;
#122283 = DIRECTION('ref_axis',(0.,0.,-1.)) ;
#122284 = DIRECTION('center_axis',(1.,0.,0.)) ;
#122285 = DIRECTION('ref_axis',(0.,0.,-1.)) ;
#122286 = DIRECTION('',(0.,0.,-1.)) ;
#122287 = DIRECTION('center_axis',(-1.,0.,0.)) ;
#122288 = DIRECTION('ref_axis',(0.,0.,-1.)) ;
#122289 = DIRECTION('',(0.,0.,-1.)) ;
#122290 = DIRECTION('',(0.,1.,-8.9727076343628E-17)) ;
#122291 = DIRECTION('',(0.,0.,1.)) ;
#122292 = DIRECTION('',(0.,-1.,-8.9727076343628E-17)) ;
#122293 = DIRECTION('center_axis',(1.,0.,0.)) ;
#122294 = DIRECTION('ref_axis',(0.,0.,-1.)) ;
#122295 = DIRECTION('center_axis',(1.,-1.31418445149758E-16,-2.16840434497101E-16)) ;
#122296 = DIRECTION('ref_axis',(-2.16840434497101E-16,0.,-1.)) ;
#122297 = DIRECTION('',(2.16840434497101E-16,0.,1.)) ;
#122298 = DIRECTION('',(1.31418445149758E-16,1.,0.)) ;
#122299 = DIRECTION('',(-2.16840434497101E-16,-2.8496832747207E-32,-1.)) ;
#122300 = DIRECTION('',(-1.31418445149758E-16,-1.,0.)) ;
#122301 = DIRECTION('center_axis',(-2.16840434497101E-16,2.8496832747207E-32,
1.)) ;
#122302 = DIRECTION('ref_axis',(1.,4.92915281362991E-64,2.16840434497101E-16)) ;
#122303 = DIRECTION('',(1.,1.31418445149758E-16,2.16840434497101E-16)) ;
#122304 = DIRECTION('',(-1.31418445149758E-16,-1.,0.)) ;
#122305 = DIRECTION('',(-1.,0.,-2.16840434497101E-16)) ;
#122306 = DIRECTION('',(1.31418445149758E-16,1.,0.)) ;
#122307 = DIRECTION('center_axis',(-1.,1.31418445149758E-16,4.33680868994202E-16)) ;
#122308 = DIRECTION('ref_axis',(4.33680868994202E-16,0.,1.)) ;
#122309 = DIRECTION('',(-1.31418445149758E-16,-1.,0.)) ;
#122310 = DIRECTION('',(-4.33680868994202E-16,0.,-1.)) ;
#122311 = DIRECTION('',(1.31418445149758E-16,1.,0.)) ;
#122312 = DIRECTION('',(4.33680868994202E-16,5.69936654944139E-32,1.)) ;
#122313 = DIRECTION('center_axis',(-2.16840434497101E-16,2.8496832747207E-32,
-1.)) ;
#122314 = DIRECTION('ref_axis',(-1.,-4.92915281362991E-64,2.16840434497101E-16)) ;
#122315 = DIRECTION('',(1.,0.,-2.16840434497101E-16)) ;
#122316 = DIRECTION('',(1.31418445149758E-16,1.,0.)) ;
#122317 = DIRECTION('',(-1.,-1.31418445149758E-16,2.16840434497101E-16)) ;
#122318 = DIRECTION('',(-1.31418445149758E-16,-1.,0.)) ;
#122319 = DIRECTION('center_axis',(0.,1.,0.)) ;
#122320 = DIRECTION('ref_axis',(0.,0.,1.)) ;
#122321 = DIRECTION('',(4.33680868994202E-16,0.,1.)) ;
#122322 = DIRECTION('',(1.,0.,2.16840434497101E-16)) ;
#122323 = DIRECTION('',(-2.16840434497101E-16,0.,-1.)) ;
#122324 = DIRECTION('',(-1.,0.,2.16840434497101E-16)) ;
#122325 = DIRECTION('',(1.,0.,0.)) ;
#122326 = DIRECTION('center_axis',(0.,-1.,0.)) ;
#122327 = DIRECTION('ref_axis',(0.,0.,1.)) ;
#122328 = DIRECTION('',(0.,0.,1.)) ;
#122329 = DIRECTION('center_axis',(0.,-1.,0.)) ;
#122330 = DIRECTION('ref_axis',(0.,0.,1.)) ;
#122331 = DIRECTION('',(-1.,0.,0.)) ;
#122332 = DIRECTION('center_axis',(0.,-1.,0.)) ;
#122333 = DIRECTION('ref_axis',(0.,0.,1.)) ;
#122334 = DIRECTION('',(0.,0.,-1.)) ;
#122335 = DIRECTION('center_axis',(0.,-1.,0.)) ;
#122336 = DIRECTION('ref_axis',(0.,0.,1.)) ;
#122337 = DIRECTION('center_axis',(1.,0.,0.)) ;
#122338 = DIRECTION('ref_axis',(0.,0.,-1.)) ;
#122339 = DIRECTION('',(0.,0.,1.)) ;
#122340 = DIRECTION('',(0.,-1.,0.)) ;
#122341 = DIRECTION('',(0.,1.,0.)) ;
#122342 = DIRECTION('center_axis',(0.,0.,1.)) ;
#122343 = DIRECTION('ref_axis',(1.,0.,0.)) ;
#122344 = DIRECTION('',(-1.,0.,0.)) ;
#122345 = DIRECTION('',(0.,-1.,0.)) ;
#122346 = DIRECTION('',(0.,1.,0.)) ;
#122347 = DIRECTION('center_axis',(-1.,0.,0.)) ;
#122348 = DIRECTION('ref_axis',(0.,0.,1.)) ;
#122349 = DIRECTION('',(0.,1.,0.)) ;
#122350 = DIRECTION('',(0.,0.,-1.)) ;
#122351 = DIRECTION('',(0.,-1.,0.)) ;
#122352 = DIRECTION('center_axis',(0.,0.,-1.)) ;
#122353 = DIRECTION('ref_axis',(-1.,0.,0.)) ;
#122354 = DIRECTION('',(1.,0.,0.)) ;
#122355 = DIRECTION('',(0.,-1.,0.)) ;
#122356 = DIRECTION('',(0.,1.,0.)) ;
#122357 = DIRECTION('center_axis',(0.,1.,0.)) ;
#122358 = DIRECTION('ref_axis',(0.,0.,1.)) ;
#122359 = DIRECTION('',(-1.,0.,0.)) ;
#122360 = DIRECTION('',(0.,0.,1.)) ;
#122361 = DIRECTION('',(1.,0.,0.)) ;
#122362 = DIRECTION('',(0.,0.,-1.)) ;
#122363 = DIRECTION('center_axis',(1.31418445149758E-16,1.,0.)) ;
#122364 = DIRECTION('ref_axis',(-1.,1.31418445149758E-16,0.)) ;
#122365 = DIRECTION('',(-0.422618261740697,5.55398348498559E-17,0.906307787036651)) ;
#122366 = DIRECTION('center_axis',(0.906307787036651,-1.19105560199475E-16,
0.422618261740697)) ;
#122367 = DIRECTION('ref_axis',(0.422618261740697,-9.57222084411175E-33,-0.906307787036651)) ;
#122368 = DIRECTION('',(0.422618261740697,-5.55398348498559E-17,-0.906307787036651)) ;
#122369 = DIRECTION('',(-0.422618261740697,5.55398348498559E-17,0.906307787036651)) ;
#122370 = DIRECTION('center_axis',(-0.906307787036651,1.19105560199475E-16,
-0.422618261740697)) ;
#122371 = DIRECTION('ref_axis',(-0.422618261740697,9.57222084411175E-33,0.906307787036651)) ;
#122372 = DIRECTION('',(0.422618261740697,-5.55398348498559E-17,-0.906307787036651)) ;
#122373 = DIRECTION('',(-0.422618261740697,5.55398348498559E-17,0.906307787036651)) ;
#122374 = DIRECTION('center_axis',(1.31418445149758E-16,1.,0.)) ;
#122375 = DIRECTION('ref_axis',(-1.,1.31418445149758E-16,0.)) ;
#122376 = DIRECTION('',(0.422618261740697,-5.55398348498559E-17,-0.906307787036651)) ;
#122377 = DIRECTION('',(-0.422618261740697,5.55398348498559E-17,0.906307787036651)) ;
#122378 = DIRECTION('center_axis',(1.31418445149758E-16,1.,0.)) ;
#122379 = DIRECTION('ref_axis',(1.,-1.31418445149758E-16,-1.22464679914735E-16)) ;
#122380 = DIRECTION('center_axis',(1.31418445149758E-16,-1.,0.)) ;
#122381 = DIRECTION('ref_axis',(-1.,-1.31418445149758E-16,0.)) ;
#122382 = DIRECTION('center_axis',(1.31418445149758E-16,1.,0.)) ;
#122383 = DIRECTION('ref_axis',(0.990906098224775,-1.30223338718113E-16,-0.134555209861798)) ;
#122384 = DIRECTION('center_axis',(1.31418445149758E-16,-1.,0.)) ;
#122385 = DIRECTION('ref_axis',(-1.,-1.31418445149758E-16,8.88178419700125E-16)) ;
#122386 = DIRECTION('center_axis',(-5.2561455487295E-16,6.90754475494854E-32,
1.)) ;
#122387 = DIRECTION('ref_axis',(1.,-1.65558275742919E-64,5.2561455487295E-16)) ;
#122388 = DIRECTION('',(1.,1.31418445149758E-16,5.2561455487295E-16)) ;
#122389 = DIRECTION('',(7.81406971160724E-17,-1.,1.10147335281612E-31)) ;
#122390 = DIRECTION('',(-1.,-7.81406971160724E-17,-5.2561455487295E-16)) ;
#122391 = DIRECTION('center_axis',(0.,0.,-1.)) ;
#122392 = DIRECTION('ref_axis',(-1.,0.,0.)) ;
#122393 = DIRECTION('',(-7.81406971160724E-17,1.,0.)) ;
#122394 = DIRECTION('',(-1.,-1.31418445149758E-16,0.)) ;
#122395 = DIRECTION('',(1.,7.81406971160724E-17,0.)) ;
#122396 = DIRECTION('center_axis',(-1.31418445149758E-16,1.,0.)) ;
#122397 = DIRECTION('ref_axis',(0.990906098224775,1.30223338718113E-16,0.134555209861799)) ;
#122398 = DIRECTION('center_axis',(1.31418445149758E-16,-1.,0.)) ;
#122399 = DIRECTION('ref_axis',(-1.,-1.31418445149758E-16,0.)) ;
#122400 = DIRECTION('center_axis',(-1.31418445149758E-16,1.,0.)) ;
#122401 = DIRECTION('ref_axis',(1.,1.31418445149758E-16,7.6571373978539E-16)) ;
#122402 = DIRECTION('center_axis',(1.31418445149758E-16,-1.,0.)) ;
#122403 = DIRECTION('ref_axis',(-1.,-1.31418445149758E-16,-1.54197642309049E-15)) ;
#122404 = DIRECTION('center_axis',(0.,-1.,0.)) ;
#122405 = DIRECTION('ref_axis',(0.,0.,-1.)) ;
#122406 = DIRECTION('',(0.,-1.,0.)) ;
#122407 = DIRECTION('center_axis',(0.,1.,0.)) ;
#122408 = DIRECTION('ref_axis',(5.20417042793044E-14,0.,-1.)) ;
#122409 = DIRECTION('',(0.,-1.,0.)) ;
#122410 = DIRECTION('center_axis',(0.,-1.,0.)) ;
#122411 = DIRECTION('ref_axis',(0.,0.,-1.)) ;
#122412 = DIRECTION('center_axis',(0.,0.,1.)) ;
#122413 = DIRECTION('ref_axis',(1.,0.,0.)) ;
#122414 = DIRECTION('',(-1.,0.,0.)) ;
#122415 = DIRECTION('',(0.,-1.,0.)) ;
#122416 = DIRECTION('',(1.,0.,0.)) ;
#122417 = DIRECTION('center_axis',(0.,-1.,0.)) ;
#122418 = DIRECTION('ref_axis',(0.,0.,-1.)) ;
#122419 = DIRECTION('center_axis',(0.,1.,0.)) ;
#122420 = DIRECTION('ref_axis',(0.,0.,-1.)) ;
#122421 = DIRECTION('',(0.,-1.,0.)) ;
#122422 = DIRECTION('center_axis',(0.,-1.,0.)) ;
#122423 = DIRECTION('ref_axis',(0.,0.,-1.)) ;
#122424 = DIRECTION('center_axis',(1.,0.,0.)) ;
#122425 = DIRECTION('ref_axis',(0.,0.,-1.)) ;
#122426 = DIRECTION('',(0.,0.,1.)) ;
#122427 = DIRECTION('',(0.,-1.,0.)) ;
#122428 = DIRECTION('',(0.,0.,-1.)) ;
#122429 = DIRECTION('center_axis',(0.,-1.,0.)) ;
#122430 = DIRECTION('ref_axis',(0.,0.,-1.)) ;
#122431 = DIRECTION('center_axis',(0.,1.,0.)) ;
#122432 = DIRECTION('ref_axis',(0.,0.,-1.)) ;
#122433 = DIRECTION('',(0.,-1.,0.)) ;
#122434 = DIRECTION('center_axis',(0.,-1.,0.)) ;
#122435 = DIRECTION('ref_axis',(0.,0.,-1.)) ;
#122436 = DIRECTION('center_axis',(0.,0.,-1.)) ;
#122437 = DIRECTION('ref_axis',(-1.,0.,0.)) ;
#122438 = DIRECTION('',(1.,0.,0.)) ;
#122439 = DIRECTION('',(0.,-1.,0.)) ;
#122440 = DIRECTION('',(-1.,0.,0.)) ;
#122441 = DIRECTION('center_axis',(0.,-1.,0.)) ;
#122442 = DIRECTION('ref_axis',(0.,0.,-1.)) ;
#122443 = DIRECTION('center_axis',(0.,1.,0.)) ;
#122444 = DIRECTION('ref_axis',(0.,0.,-1.)) ;
#122445 = DIRECTION('',(0.,-1.,0.)) ;
#122446 = DIRECTION('center_axis',(0.,-1.,0.)) ;
#122447 = DIRECTION('ref_axis',(0.,0.,-1.)) ;
#122448 = DIRECTION('center_axis',(-1.,0.,0.)) ;
#122449 = DIRECTION('ref_axis',(0.,0.,1.)) ;
#122450 = DIRECTION('',(0.,0.,1.)) ;
#122451 = DIRECTION('',(0.,0.,-1.)) ;
#122452 = DIRECTION('center_axis',(0.,-1.,0.)) ;
#122453 = DIRECTION('ref_axis',(0.,0.,-1.)) ;
#122454 = DIRECTION('',(1.,0.,0.)) ;
#122455 = DIRECTION('',(0.,0.,-1.)) ;
#122456 = DIRECTION('',(-1.,0.,0.)) ;
#122457 = DIRECTION('',(0.,0.,1.)) ;
#122458 = DIRECTION('center_axis',(-1.,0.,0.)) ;
#122459 = DIRECTION('ref_axis',(0.,0.,1.)) ;
#122460 = DIRECTION('center_axis',(-1.,0.,0.)) ;
#122461 = DIRECTION('ref_axis',(0.,0.,1.)) ;
#122462 = DIRECTION('center_axis',(-1.,0.,0.)) ;
#122463 = DIRECTION('ref_axis',(0.,0.,1.)) ;
#122464 = DIRECTION('center_axis',(0.,1.,0.)) ;
#122465 = DIRECTION('ref_axis',(1.,0.,0.)) ;
#122466 = DIRECTION('center_axis',(0.,0.,-1.)) ;
#122467 = DIRECTION('ref_axis',(1.,0.,0.)) ;
#122468 = DIRECTION('center_axis',(0.,1.,0.)) ;
#122469 = DIRECTION('ref_axis',(0.,0.,-1.)) ;
#122470 = DIRECTION('center_axis',(0.,0.,1.)) ;
#122471 = DIRECTION('ref_axis',(1.,0.,0.)) ;
#122472 = DIRECTION('center_axis',(0.,0.,1.)) ;
#122473 = DIRECTION('ref_axis',(1.,0.,0.)) ;
#122474 = DIRECTION('center_axis',(0.,0.,-1.)) ;
#122475 = DIRECTION('ref_axis',(1.,0.,0.)) ;
#122476 = DIRECTION('center_axis',(-2.47817639425258E-16,1.,0.)) ;
#122477 = DIRECTION('ref_axis',(-1.,-2.47817639425258E-16,0.)) ;
#122478 = DIRECTION('center_axis',(0.,1.,0.)) ;
#122479 = DIRECTION('ref_axis',(0.,0.,1.)) ;
#122480 = DIRECTION('center_axis',(0.,0.,1.)) ;
#122481 = DIRECTION('ref_axis',(1.,0.,0.)) ;
#122482 = DIRECTION('center_axis',(0.,0.,-1.)) ;
#122483 = DIRECTION('ref_axis',(-1.,0.,0.)) ;
#122484 = DIRECTION('center_axis',(1.,0.,0.)) ;
#122485 = DIRECTION('ref_axis',(0.,0.,-1.)) ;
#122486 = DIRECTION('center_axis',(-1.,0.,0.)) ;
#122487 = DIRECTION('ref_axis',(0.,0.,-1.)) ;
#122488 = DIRECTION('center_axis',(-1.,0.,0.)) ;
#122489 = DIRECTION('ref_axis',(0.,0.,1.)) ;
#122490 = DIRECTION('center_axis',(0.,1.,0.)) ;
#122491 = DIRECTION('ref_axis',(0.,0.,1.)) ;
#122492 = DIRECTION('center_axis',(0.,-1.,0.)) ;
#122493 = DIRECTION('ref_axis',(0.,0.,1.)) ;
#122494 = DIRECTION('center_axis',(0.,-1.,0.)) ;
#122495 = DIRECTION('ref_axis',(0.,0.,-1.)) ;
#122496 = DIRECTION('center_axis',(-1.,0.,0.)) ;
#122497 = DIRECTION('ref_axis',(0.,0.,1.)) ;
#122498 = DIRECTION('center_axis',(-1.,0.,0.)) ;
#122499 = DIRECTION('ref_axis',(0.,0.,1.)) ;
#122500 = DIRECTION('center_axis',(-0.297047844549207,0.954862596423522,-1.49073359128363E-13)) ;
#122501 = DIRECTION('ref_axis',(0.954691435265115,0.296994598089069,-0.0189333604346236)) ;
#122502 = DIRECTION('center_axis',(-0.297047844549074,0.954862596423564,-1.68658673018685E-12)) ;
#122503 = DIRECTION('ref_axis',(0.95457509154025,0.296958404763534,0.0245377352504246)) ;
#122504 = DIRECTION('center_axis',(0.,1.,0.)) ;
#122505 = DIRECTION('ref_axis',(1.,0.,0.)) ;
#122506 = DIRECTION('center_axis',(0.,0.,-1.)) ;
#122507 = DIRECTION('ref_axis',(1.,0.,0.)) ;
#122508 = DIRECTION('center_axis',(1.,0.,0.)) ;
#122509 = DIRECTION('ref_axis',(0.,0.,1.)) ;
#122510 = DIRECTION('center_axis',(0.,1.,0.)) ;
#122511 = DIRECTION('ref_axis',(1.,0.,0.)) ;
#122512 = DIRECTION('center_axis',(0.,1.,0.)) ;
#122513 = DIRECTION('ref_axis',(0.,0.,-1.)) ;
#122514 = DIRECTION('center_axis',(0.,0.,1.)) ;
#122515 = DIRECTION('ref_axis',(1.,0.,0.)) ;
#122516 = DIRECTION('center_axis',(0.,0.,-1.)) ;
#122517 = DIRECTION('ref_axis',(1.,0.,0.)) ;
#122518 = DIRECTION('center_axis',(0.,0.,1.)) ;
#122519 = DIRECTION('ref_axis',(1.,0.,0.)) ;
#122520 = DIRECTION('center_axis',(0.,0.,1.)) ;
#122521 = DIRECTION('ref_axis',(1.,0.,0.)) ;
#122522 = DIRECTION('center_axis',(0.,0.,-1.)) ;
#122523 = DIRECTION('ref_axis',(1.,0.,0.)) ;
#122524 = DIRECTION('center_axis',(-0.527647792165807,0.849457787212664,0.00304551577146026)) ;
#122525 = DIRECTION('ref_axis',(0.709569539673246,0.438778321275517,0.551348032685832)) ;
#122526 = DIRECTION('center_axis',(0.441849822549049,0.89708903366019,0.)) ;
#122527 = DIRECTION('ref_axis',(-0.89708903366019,0.441849822549049,0.)) ;
#122528 = DIRECTION('center_axis',(0.725180709343317,-0.688554584578773,0.00235007486622799)) ;
#122529 = DIRECTION('ref_axis',(0.688552674549923,0.725184403719161,0.00167181716517875)) ;
#122530 = DIRECTION('center_axis',(0.725344906601501,-0.688385623360064,4.29369716312682E-6)) ;
#122531 = DIRECTION('ref_axis',(0.688335104937436,0.725291600262751,-0.0121193192493712)) ;
#122532 = DIRECTION('center_axis',(0.725299716569783,-0.688423829426493,-0.00359891949834901)) ;
#122533 = DIRECTION('ref_axis',(0.688175169518926,0.724874796156686,0.0311683485991717)) ;
#122534 = DIRECTION('center_axis',(-0.441849822549049,-0.89708903366019,0.)) ;
#122535 = DIRECTION('ref_axis',(0.89708903366019,-0.441849822549049,0.)) ;
#122536 = DIRECTION('center_axis',(1.,0.,0.)) ;
#122537 = DIRECTION('ref_axis',(0.,0.,-1.)) ;
#122538 = DIRECTION('center_axis',(1.,0.,0.)) ;
#122539 = DIRECTION('ref_axis',(0.,0.,-1.)) ;
#122540 = DIRECTION('center_axis',(0.,0.,1.)) ;
#122541 = DIRECTION('ref_axis',(1.,0.,0.)) ;
#122542 = DIRECTION('center_axis',(0.,0.,-1.)) ;
#122543 = DIRECTION('ref_axis',(-1.,0.,0.)) ;
#122544 = DIRECTION('center_axis',(2.47817639425258E-16,-1.,0.)) ;
#122545 = DIRECTION('ref_axis',(1.,2.47817639425258E-16,0.)) ;
#122546 = DIRECTION('center_axis',(0.,1.,0.)) ;
#122547 = DIRECTION('ref_axis',(0.,0.,1.)) ;
#122548 = DIRECTION('center_axis',(0.,-1.,0.)) ;
#122549 = DIRECTION('ref_axis',(0.,0.,-1.)) ;
#122550 = DIRECTION('center_axis',(0.,-1.,0.)) ;
#122551 = DIRECTION('ref_axis',(0.,0.,-1.)) ;
#122552 = DIRECTION('center_axis',(0.,-1.,0.)) ;
#122553 = DIRECTION('ref_axis',(0.,0.,-1.)) ;
#122554 = DIRECTION('center_axis',(0.,0.,1.)) ;
#122555 = DIRECTION('ref_axis',(1.,0.,0.)) ;
#122556 = DIRECTION('center_axis',(0.,0.,-1.)) ;
#122557 = DIRECTION('ref_axis',(-1.,0.,0.)) ;
#122558 = DIRECTION('center_axis',(0.,0.,-1.)) ;
#122559 = DIRECTION('ref_axis',(-1.,0.,0.)) ;
#122560 = DIRECTION('center_axis',(0.,0.,1.)) ;
#122561 = DIRECTION('ref_axis',(-1.,0.,0.)) ;
#122562 = DIRECTION('center_axis',(0.,1.,0.)) ;
#122563 = DIRECTION('ref_axis',(1.,0.,0.)) ;
#122564 = DIRECTION('center_axis',(1.,0.,0.)) ;
#122565 = DIRECTION('ref_axis',(0.,0.,1.)) ;
#122566 = DIRECTION('center_axis',(0.,0.,1.)) ;
#122567 = DIRECTION('ref_axis',(1.,0.,0.)) ;
#122568 = DIRECTION('center_axis',(1.,0.,0.)) ;
#122569 = DIRECTION('ref_axis',(0.,0.,1.)) ;
#122570 = DIRECTION('center_axis',(-0.527646808997082,0.849458398917494,-0.00304523623449406)) ;
#122571 = DIRECTION('ref_axis',(0.786342490392807,0.487079579861469,-0.380024960607608)) ;
#122572 = DIRECTION('center_axis',(0.,0.,-1.)) ;
#122573 = DIRECTION('ref_axis',(-1.,0.,0.)) ;
#122574 = DIRECTION('center_axis',(0.,0.,1.)) ;
#122575 = DIRECTION('ref_axis',(-1.,0.,0.)) ;
#122576 = DIRECTION('center_axis',(-1.,0.,0.)) ;
#122577 = DIRECTION('ref_axis',(0.,0.,1.)) ;
#122578 = DIRECTION('center_axis',(1.,0.,0.)) ;
#122579 = DIRECTION('ref_axis',(0.,0.,-1.)) ;
#122580 = DIRECTION('center_axis',(1.,0.,0.)) ;
#122581 = DIRECTION('ref_axis',(0.,0.,-1.)) ;
#122582 = DIRECTION('center_axis',(-0.297273799163877,0.954789382784888,-0.00235007487718195)) ;
#122583 = DIRECTION('ref_axis',(0.954791853023049,0.297270453338573,-0.00167181718241995)) ;
#122584 = DIRECTION('center_axis',(-0.297049675376424,0.954862026860596,-4.29369625967978E-6)) ;
#122585 = DIRECTION('ref_axis',(0.954791884772883,0.297027909249879,0.012119319225527)) ;
#122586 = DIRECTION('center_axis',(0.,0.,-1.)) ;
#122587 = DIRECTION('ref_axis',(-1.,0.,0.)) ;
#122588 = DIRECTION('center_axis',(0.441849822549049,0.89708903366019,-9.72625879207272E-16)) ;
#122589 = DIRECTION('ref_axis',(0.89708903366019,-0.441849822549049,3.9032054237323E-31)) ;
#122590 = DIRECTION('center_axis',(-0.441849822549049,-0.89708903366019,0.)) ;
#122591 = DIRECTION('ref_axis',(0.89708903366019,-0.441849822549049,0.)) ;
#122592 = DIRECTION('center_axis',(0.724093759486039,-0.689695657773317,0.00285081076274628)) ;
#122593 = DIRECTION('ref_axis',(0.681728923122044,0.715090798805641,-0.154566570908355)) ;
#122594 = DIRECTION('center_axis',(0.725345269034699,-0.688385241474045,-3.11468975456184E-6)) ;
#122595 = DIRECTION('ref_axis',(0.688334826632565,0.725292092601058,0.0121056538482987)) ;
#122596 = DIRECTION('center_axis',(0.725180989991168,-0.688554302427288,-0.0023461381674182)) ;
#122597 = DIRECTION('ref_axis',(0.688552456842981,0.725184663578072,-0.00164860142364575)) ;
#122598 = DIRECTION('center_axis',(0.,1.,0.)) ;
#122599 = DIRECTION('ref_axis',(1.,0.,0.)) ;
#122600 = DIRECTION('center_axis',(-2.05998412772247E-14,0.,-1.)) ;
#122601 = DIRECTION('ref_axis',(1.,0.,-2.05998412772247E-14)) ;
#122602 = DIRECTION('center_axis',(0.,0.514231796959122,0.857651245551589)) ;
#122603 = DIRECTION('ref_axis',(0.,0.857651245551589,-0.514231796959122)) ;
#122604 = DIRECTION('center_axis',(-1.,0.,0.)) ;
#122605 = DIRECTION('ref_axis',(0.,0.,-1.)) ;
#122606 = DIRECTION('center_axis',(1.,0.,0.)) ;
#122607 = DIRECTION('ref_axis',(0.,0.,-1.)) ;
#122608 = DIRECTION('center_axis',(-2.24981196193434E-14,-0.514231796959101,
0.857651245551602)) ;
#122609 = DIRECTION('ref_axis',(1.43956865771859E-30,-0.857651245551602,-0.514231796959101)) ;
#122610 = DIRECTION('center_axis',(-1.,0.,0.)) ;
#122611 = DIRECTION('ref_axis',(0.,0.,1.)) ;
#122612 = DIRECTION('center_axis',(-1.,0.,0.)) ;
#122613 = DIRECTION('ref_axis',(0.,0.,-1.)) ;
#122614 = DIRECTION('center_axis',(0.,0.,1.)) ;
#122615 = DIRECTION('ref_axis',(1.,0.,0.)) ;
#122616 = DIRECTION('center_axis',(0.,0.,-1.)) ;
#122617 = DIRECTION('ref_axis',(-1.,0.,0.)) ;
#122618 = DIRECTION('center_axis',(0.,-1.,8.97270763436279E-17)) ;
#122619 = DIRECTION('ref_axis',(0.,-8.97270763436279E-17,-1.)) ;
#122620 = DIRECTION('center_axis',(0.,-1.,8.97270763436279E-17)) ;
#122621 = DIRECTION('ref_axis',(0.,-8.97270763436279E-17,-1.)) ;
#122622 = DIRECTION('center_axis',(0.,-1.,0.)) ;
#122623 = DIRECTION('ref_axis',(0.,0.,-1.)) ;
#122624 = DIRECTION('center_axis',(0.,0.,-1.)) ;
#122625 = DIRECTION('ref_axis',(-1.,0.,0.)) ;
#122626 = DIRECTION('center_axis',(0.,0.,1.)) ;
#122627 = DIRECTION('ref_axis',(-1.,0.,0.)) ;
#122628 = DIRECTION('center_axis',(0.,0.,-1.)) ;
#122629 = DIRECTION('ref_axis',(-1.,0.,0.)) ;
#122630 = DIRECTION('center_axis',(0.,1.,0.)) ;
#122631 = DIRECTION('ref_axis',(1.,0.,0.)) ;
#122632 = DIRECTION('center_axis',(-1.,0.,0.)) ;
#122633 = DIRECTION('ref_axis',(0.,0.,-1.)) ;
#122634 = DIRECTION('center_axis',(0.,-1.84314369322536E-14,1.)) ;
#122635 = DIRECTION('ref_axis',(0.,1.,1.84314369322536E-14)) ;
#122636 = DIRECTION('center_axis',(1.,0.,0.)) ;
#122637 = DIRECTION('ref_axis',(0.,0.,-1.)) ;
#122638 = DIRECTION('center_axis',(0.,0.,1.)) ;
#122639 = DIRECTION('ref_axis',(-1.,0.,0.)) ;
#122640 = DIRECTION('center_axis',(0.,-0.514231796959101,-0.857651245551602)) ;
#122641 = DIRECTION('ref_axis',(0.,-0.857651245551602,0.514231796959101)) ;
#122642 = DIRECTION('center_axis',(0.,1.,0.)) ;
#122643 = DIRECTION('ref_axis',(1.,0.,0.)) ;
#122644 = DIRECTION('center_axis',(-1.,0.,0.)) ;
#122645 = DIRECTION('ref_axis',(0.,0.,-1.)) ;
#122646 = DIRECTION('center_axis',(0.,1.,8.97270763436279E-17)) ;
#122647 = DIRECTION('ref_axis',(0.,-8.97270763436279E-17,1.)) ;
#122648 = DIRECTION('center_axis',(0.,-1.,-8.97270763436279E-17)) ;
#122649 = DIRECTION('ref_axis',(0.,-8.97270763436279E-17,1.)) ;
#122650 = DIRECTION('center_axis',(0.,-1.,0.)) ;
#122651 = DIRECTION('ref_axis',(0.,0.,-1.)) ;
#122652 = DIRECTION('center_axis',(0.,0.,1.)) ;
#122653 = DIRECTION('ref_axis',(1.,0.,0.)) ;
#122654 = DIRECTION('center_axis',(-2.16840434497102E-15,0.,1.)) ;
#122655 = DIRECTION('ref_axis',(1.,0.,2.16840434497102E-15)) ;
#122656 = DIRECTION('center_axis',(-1.,0.,0.)) ;
#122657 = DIRECTION('ref_axis',(0.,0.,1.)) ;
#122658 = DIRECTION('center_axis',(-1.,0.,0.)) ;
#122659 = DIRECTION('ref_axis',(0.,0.,-1.)) ;
#122660 = DIRECTION('center_axis',(1.,0.,0.)) ;
#122661 = DIRECTION('ref_axis',(0.,0.,-1.)) ;
#122662 = DIRECTION('center_axis',(0.,0.514231796959101,-0.857651245551602)) ;
#122663 = DIRECTION('ref_axis',(0.,0.857651245551602,0.514231796959101)) ;
#122664 = DIRECTION('center_axis',(0.,0.,-1.)) ;
#122665 = DIRECTION('ref_axis',(-1.,0.,0.)) ;
#122666 = DIRECTION('center_axis',(-7.01133629567814E-33,8.97270763436279E-17,
1.)) ;
#122667 = DIRECTION('ref_axis',(-6.29106707073161E-49,-1.,8.97270763436279E-17)) ;
#122668 = DIRECTION('center_axis',(-1.,0.,-7.01133629567814E-33)) ;
#122669 = DIRECTION('ref_axis',(-7.01133629567814E-33,0.,1.)) ;
#122670 = DIRECTION('center_axis',(-1.,0.,0.)) ;
#122671 = DIRECTION('ref_axis',(0.,0.,1.)) ;
#122672 = DIRECTION('center_axis',(0.,1.,0.)) ;
#122673 = DIRECTION('ref_axis',(1.,0.,0.)) ;
#122674 = DIRECTION('center_axis',(-1.,0.,0.)) ;
#122675 = DIRECTION('ref_axis',(0.,0.,-1.)) ;
#122676 = DIRECTION('center_axis',(1.,0.,0.)) ;
#122677 = DIRECTION('ref_axis',(0.,0.,-1.)) ;
#122678 = DIRECTION('center_axis',(0.,0.,-1.)) ;
#122679 = DIRECTION('ref_axis',(1.,0.,0.)) ;
#122680 = DIRECTION('center_axis',(-7.01133629567814E-33,8.97270763436279E-17,
1.)) ;
#122681 = DIRECTION('ref_axis',(0.,-1.,0.)) ;
#122682 = DIRECTION('center_axis',(0.,-1.,0.)) ;
#122683 = DIRECTION('ref_axis',(0.,0.,1.)) ;
#122684 = DIRECTION('center_axis',(-1.,0.,7.01133629567814E-33)) ;
#122685 = DIRECTION('ref_axis',(7.01133629567814E-33,0.,1.)) ;
#122686 = DIRECTION('center_axis',(-1.,0.,0.)) ;
#122687 = DIRECTION('ref_axis',(0.,0.,1.)) ;
#122688 = DIRECTION('center_axis',(0.,0.,-1.)) ;
#122689 = DIRECTION('ref_axis',(-1.,0.,0.)) ;
#122690 = DIRECTION('center_axis',(-7.01133629567814E-33,8.97270763436279E-17,
-1.)) ;
#122691 = DIRECTION('ref_axis',(6.29106707073161E-49,1.,8.97270763436279E-17)) ;
#122692 = DIRECTION('center_axis',(0.,-1.,8.97270763436279E-17)) ;
#122693 = DIRECTION('ref_axis',(0.,-8.97270763436279E-17,-1.)) ;
#122694 = DIRECTION('center_axis',(0.,-1.,0.)) ;
#122695 = DIRECTION('ref_axis',(0.,0.,-1.)) ;
#122696 = DIRECTION('center_axis',(1.,7.81406971160724E-17,0.)) ;
#122697 = DIRECTION('ref_axis',(-7.81406971160724E-17,1.,0.)) ;
#122698 = DIRECTION('center_axis',(1.,0.,0.)) ;
#122699 = DIRECTION('ref_axis',(0.,0.,-1.)) ;
#122700 = DIRECTION('center_axis',(1.,0.,0.)) ;
#122701 = DIRECTION('ref_axis',(0.,0.,-1.)) ;
#122702 = DIRECTION('center_axis',(3.78638272950961E-32,-4.8455963016112E-16,
-1.)) ;
#122703 = DIRECTION('ref_axis',(1.83472821505963E-47,1.,-4.8455963016112E-16)) ;
#122704 = DIRECTION('center_axis',(0.,0.,-1.)) ;
#122705 = DIRECTION('ref_axis',(-1.,0.,0.)) ;
#122706 = DIRECTION('center_axis',(0.,0.,1.)) ;
#122707 = DIRECTION('ref_axis',(1.,0.,0.)) ;
#122708 = DIRECTION('center_axis',(-7.01133629567814E-33,8.97270763436279E-17,
-1.)) ;
#122709 = DIRECTION('ref_axis',(0.,1.,0.)) ;
#122710 = DIRECTION('center_axis',(0.,-1.,0.)) ;
#122711 = DIRECTION('ref_axis',(0.,0.,1.)) ;
#122712 = DIRECTION('center_axis',(0.,1.,0.)) ;
#122713 = DIRECTION('ref_axis',(1.,0.,0.)) ;
#122714 = DIRECTION('center_axis',(-1.,0.,0.)) ;
#122715 = DIRECTION('ref_axis',(0.,0.,-1.)) ;
#122716 = DIRECTION('center_axis',(0.,0.,1.)) ;
#122717 = DIRECTION('ref_axis',(-1.,0.,0.)) ;
#122718 = DIRECTION('center_axis',(0.,1.,0.)) ;
#122719 = DIRECTION('ref_axis',(1.,0.,0.)) ;
#122720 = DIRECTION('center_axis',(0.,1.,0.)) ;
#122721 = DIRECTION('ref_axis',(0.,0.,-1.)) ;
#122722 = DIRECTION('center_axis',(0.,1.,8.97270763436279E-17)) ;
#122723 = DIRECTION('ref_axis',(0.,-8.97270763436279E-17,1.)) ;
#122724 = DIRECTION('center_axis',(0.,-1.,0.)) ;
#122725 = DIRECTION('ref_axis',(0.,0.,-1.)) ;
#122726 = DIRECTION('center_axis',(0.,0.,1.)) ;
#122727 = DIRECTION('ref_axis',(1.,0.,0.)) ;
#122728 = DIRECTION('center_axis',(0.,0.,1.)) ;
#122729 = DIRECTION('ref_axis',(1.,0.,0.)) ;
#122730 = DIRECTION('center_axis',(-1.,-7.81406971160724E-17,0.)) ;
#122731 = DIRECTION('ref_axis',(7.81406971160724E-17,-1.,0.)) ;
#122732 = DIRECTION('center_axis',(-1.,-7.81406971160724E-17,0.)) ;
#122733 = DIRECTION('ref_axis',(-7.81406971160724E-17,1.,0.)) ;
#122734 = DIRECTION('center_axis',(-7.81406971160724E-17,1.,-8.97270763436279E-17)) ;
#122735 = DIRECTION('ref_axis',(-7.01133629567814E-33,8.97270763436279E-17,
1.)) ;
#122736 = DIRECTION('center_axis',(0.,1.,0.)) ;
#122737 = DIRECTION('ref_axis',(0.,0.,1.)) ;
#122738 = DIRECTION('center_axis',(0.,1.,0.)) ;
#122739 = DIRECTION('ref_axis',(1.,0.,0.)) ;
#122740 = DIRECTION('center_axis',(-1.,0.,0.)) ;
#122741 = DIRECTION('ref_axis',(0.,0.,-1.)) ;
#122742 = DIRECTION('center_axis',(1.,7.81406971160724E-17,0.)) ;
#122743 = DIRECTION('ref_axis',(0.,1.,0.)) ;
#122744 = DIRECTION('center_axis',(0.,0.,-1.)) ;
#122745 = DIRECTION('ref_axis',(1.,0.,0.)) ;
#122746 = DIRECTION('center_axis',(-3.78638272950961E-32,4.8455963016112E-16,
-1.)) ;
#122747 = DIRECTION('ref_axis',(1.83472821505963E-47,1.,4.8455963016112E-16)) ;
#122748 = DIRECTION('center_axis',(0.,0.,1.)) ;
#122749 = DIRECTION('ref_axis',(-1.,1.30104260698261E-14,0.)) ;
#122750 = DIRECTION('center_axis',(0.,0.,1.)) ;
#122751 = DIRECTION('ref_axis',(1.,0.,0.)) ;
#122752 = DIRECTION('center_axis',(1.,7.81406971160724E-17,0.)) ;
#122753 = DIRECTION('ref_axis',(-7.81406971160724E-17,1.,0.)) ;
#122754 = DIRECTION('center_axis',(1.,0.,0.)) ;
#122755 = DIRECTION('ref_axis',(0.,0.,-1.)) ;
#122756 = DIRECTION('center_axis',(1.,0.,0.)) ;
#122757 = DIRECTION('ref_axis',(0.,0.,-1.)) ;
#122758 = DIRECTION('center_axis',(-1.,-7.81406971160724E-17,0.)) ;
#122759 = DIRECTION('ref_axis',(7.81406971160724E-17,-1.,0.)) ;
#122760 = DIRECTION('center_axis',(-1.,-7.81406971160724E-17,0.)) ;
#122761 = DIRECTION('ref_axis',(-7.81406971160724E-17,1.,0.)) ;
#122762 = DIRECTION('center_axis',(0.,0.,-1.)) ;
#122763 = DIRECTION('ref_axis',(-1.,0.,0.)) ;
#122764 = DIRECTION('center_axis',(0.,0.,-1.)) ;
#122765 = DIRECTION('ref_axis',(-1.,0.,0.)) ;
#122766 = DIRECTION('center_axis',(0.,1.,0.)) ;
#122767 = DIRECTION('ref_axis',(1.,0.,0.)) ;
#122768 = DIRECTION('center_axis',(0.,1.,0.)) ;
#122769 = DIRECTION('ref_axis',(0.,0.,-1.)) ;
#122770 = DIRECTION('center_axis',(1.,7.81406971160724E-17,0.)) ;
#122771 = DIRECTION('ref_axis',(0.,1.,0.)) ;
#122772 = DIRECTION('center_axis',(0.,-1.,0.)) ;
#122773 = DIRECTION('ref_axis',(0.,0.,1.)) ;
#122774 = DIRECTION('center_axis',(7.81406971160724E-17,-1.,-8.97270763436279E-17)) ;
#122775 = DIRECTION('ref_axis',(-7.01133629567814E-33,8.97270763436279E-17,
-1.)) ;
#122776 = DIRECTION('center_axis',(0.,-1.,0.)) ;
#122777 = DIRECTION('ref_axis',(0.,0.,-1.)) ;
#122778 = DIRECTION('center_axis',(-1.,0.,-8.67361737988403E-15)) ;
#122779 = DIRECTION('ref_axis',(-8.67361737988403E-15,0.,1.)) ;
#122780 = DIRECTION('center_axis',(-5.96311194867026E-15,5.96311194867028E-15,
-1.)) ;
#122781 = DIRECTION('ref_axis',(0.,1.,5.96311194867028E-15)) ;
#122782 = DIRECTION('center_axis',(0.,0.,-1.)) ;
#122783 = DIRECTION('ref_axis',(-1.,0.,0.)) ;
#122784 = DIRECTION('center_axis',(0.,6.50521303491304E-15,-1.)) ;
#122785 = DIRECTION('ref_axis',(0.,1.,6.50521303491304E-15)) ;
#122786 = DIRECTION('center_axis',(1.,0.,0.)) ;
#122787 = DIRECTION('ref_axis',(0.,0.,-1.)) ;
#122788 = DIRECTION('center_axis',(-1.,0.,0.)) ;
#122789 = DIRECTION('ref_axis',(0.,0.,1.)) ;
#122790 = DIRECTION('center_axis',(0.,-1.,0.)) ;
#122791 = DIRECTION('ref_axis',(0.,0.,-1.)) ;
#122792 = DIRECTION('center_axis',(-1.,0.,0.)) ;
#122793 = DIRECTION('ref_axis',(0.,0.,1.)) ;
#122794 = DIRECTION('center_axis',(0.,-1.,0.)) ;
#122795 = DIRECTION('ref_axis',(0.,0.,-1.)) ;
#122796 = DIRECTION('center_axis',(6.50521303491295E-15,0.,-1.)) ;
#122797 = DIRECTION('ref_axis',(-1.,0.,-6.50521303491295E-15)) ;
#122798 = DIRECTION('center_axis',(-1.,0.,0.)) ;
#122799 = DIRECTION('ref_axis',(0.,0.,1.)) ;
#122800 = DIRECTION('center_axis',(-1.,1.73472347597681E-14,0.)) ;
#122801 = DIRECTION('ref_axis',(-1.73472347597681E-14,-1.,0.)) ;
#122802 = DIRECTION('center_axis',(0.,0.,1.)) ;
#122803 = DIRECTION('ref_axis',(1.,0.,0.)) ;
#122804 = DIRECTION('center_axis',(-7.04731412115582E-15,0.,-1.)) ;
#122805 = DIRECTION('ref_axis',(-1.,0.,7.04731412115582E-15)) ;
#122806 = DIRECTION('center_axis',(0.,-1.,0.)) ;
#122807 = DIRECTION('ref_axis',(0.,0.,-1.)) ;
#122808 = DIRECTION('center_axis',(1.,0.,-2.16840434497101E-16)) ;
#122809 = DIRECTION('ref_axis',(-2.16840434497101E-16,0.,-1.)) ;
#122810 = DIRECTION('center_axis',(1.,0.,0.)) ;
#122811 = DIRECTION('ref_axis',(0.,0.,-1.)) ;
#122812 = DIRECTION('center_axis',(-1.,0.,0.)) ;
#122813 = DIRECTION('ref_axis',(0.,0.,1.)) ;
#122814 = DIRECTION('center_axis',(0.,-1.,0.)) ;
#122815 = DIRECTION('ref_axis',(0.,0.,-1.)) ;
#122816 = DIRECTION('center_axis',(0.,0.,-1.)) ;
#122817 = DIRECTION('ref_axis',(1.,0.,0.)) ;
#122818 = DIRECTION('center_axis',(0.,-1.,0.)) ;
#122819 = DIRECTION('ref_axis',(0.,0.,-1.)) ;
#122820 = DIRECTION('center_axis',(0.,-1.,0.)) ;
#122821 = DIRECTION('ref_axis',(0.,0.,-1.)) ;
#122822 = DIRECTION('center_axis',(0.,-1.,0.)) ;
#122823 = DIRECTION('ref_axis',(0.,0.,-1.)) ;
#122824 = DIRECTION('center_axis',(0.,0.,-1.)) ;
#122825 = DIRECTION('ref_axis',(1.,0.,0.)) ;
#122826 = DIRECTION('center_axis',(0.,0.,1.)) ;
#122827 = DIRECTION('ref_axis',(1.,0.,0.)) ;
#122828 = DIRECTION('center_axis',(0.,0.,-1.)) ;
#122829 = DIRECTION('ref_axis',(-1.,0.,0.)) ;
#122830 = DIRECTION('center_axis',(0.,1.,0.)) ;
#122831 = DIRECTION('ref_axis',(0.,0.,1.)) ;
#122832 = DIRECTION('center_axis',(0.,-1.,0.)) ;
#122833 = DIRECTION('ref_axis',(0.,0.,-1.)) ;
#122834 = DIRECTION('center_axis',(-1.,0.,2.16840434497101E-16)) ;
#122835 = DIRECTION('ref_axis',(2.16840434497101E-16,0.,1.)) ;
#122836 = DIRECTION('center_axis',(-1.,0.,0.)) ;
#122837 = DIRECTION('ref_axis',(0.,0.,1.)) ;
#122838 = DIRECTION('center_axis',(1.,0.,0.)) ;
#122839 = DIRECTION('ref_axis',(0.,0.,-1.)) ;
#122840 = DIRECTION('center_axis',(0.,1.,0.)) ;
#122841 = DIRECTION('ref_axis',(0.,0.,1.)) ;
#122842 = DIRECTION('center_axis',(0.,-1.,0.)) ;
#122843 = DIRECTION('ref_axis',(0.,0.,-1.)) ;
#122844 = DIRECTION('center_axis',(2.16840434497101E-16,0.,-1.)) ;
#122845 = DIRECTION('ref_axis',(-1.,0.,-2.16840434497101E-16)) ;
#122846 = DIRECTION('center_axis',(0.,0.,-1.)) ;
#122847 = DIRECTION('ref_axis',(-1.,0.,0.)) ;
#122848 = DIRECTION('center_axis',(-1.,0.,-2.16840434497101E-16)) ;
#122849 = DIRECTION('ref_axis',(-2.16840434497101E-16,0.,1.)) ;
#122850 = DIRECTION('center_axis',(-1.,0.,0.)) ;
#122851 = DIRECTION('ref_axis',(0.,0.,1.)) ;
#122852 = DIRECTION('center_axis',(1.,0.,0.)) ;
#122853 = DIRECTION('ref_axis',(0.,0.,-1.)) ;
#122854 = DIRECTION('center_axis',(0.,-1.,0.)) ;
#122855 = DIRECTION('ref_axis',(0.,0.,-1.)) ;
#122856 = DIRECTION('center_axis',(0.,-1.,0.)) ;
#122857 = DIRECTION('ref_axis',(0.,0.,-1.)) ;
#122858 = DIRECTION('center_axis',(0.,1.,0.)) ;
#122859 = DIRECTION('ref_axis',(1.,0.,0.)) ;
#122860 = DIRECTION('center_axis',(0.,0.,1.)) ;
#122861 = DIRECTION('ref_axis',(-1.,0.,0.)) ;
#122862 = DIRECTION('center_axis',(0.,1.,0.)) ;
#122863 = DIRECTION('ref_axis',(1.,0.,0.)) ;
#122864 = DIRECTION('center_axis',(0.,0.,1.)) ;
#122865 = DIRECTION('ref_axis',(-1.,0.,0.)) ;
#122866 = DIRECTION('center_axis',(0.,-1.,0.)) ;
#122867 = DIRECTION('ref_axis',(0.,0.,-1.)) ;
#122868 = DIRECTION('center_axis',(0.,-1.,0.)) ;
#122869 = DIRECTION('ref_axis',(0.,0.,-1.)) ;
#122870 = DIRECTION('center_axis',(0.,1.,0.)) ;
#122871 = DIRECTION('ref_axis',(0.,0.,1.)) ;
#122872 = DIRECTION('center_axis',(0.,-1.,0.)) ;
#122873 = DIRECTION('ref_axis',(0.,0.,-1.)) ;
#122874 = DIRECTION('center_axis',(0.,0.,-1.)) ;
#122875 = DIRECTION('ref_axis',(-1.,0.,0.)) ;
#122876 = DIRECTION('center_axis',(0.,0.,1.)) ;
#122877 = DIRECTION('ref_axis',(1.,0.,0.)) ;
#122878 = DIRECTION('center_axis',(-2.16840434497101E-16,0.,1.)) ;
#122879 = DIRECTION('ref_axis',(1.,0.,2.16840434497101E-16)) ;
#122880 = DIRECTION('center_axis',(0.,0.,1.)) ;
#122881 = DIRECTION('ref_axis',(1.,0.,0.)) ;
#122882 = DIRECTION('center_axis',(0.,1.,0.)) ;
#122883 = DIRECTION('ref_axis',(0.,0.,1.)) ;
#122884 = DIRECTION('center_axis',(0.,-1.,0.)) ;
#122885 = DIRECTION('ref_axis',(0.,0.,-1.)) ;
#122886 = DIRECTION('center_axis',(0.,1.,0.)) ;
#122887 = DIRECTION('ref_axis',(1.,0.,0.)) ;
#122888 = DIRECTION('center_axis',(-1.,0.,0.)) ;
#122889 = DIRECTION('ref_axis',(0.,0.,-1.)) ;
#122890 = DIRECTION('center_axis',(0.,1.,0.)) ;
#122891 = DIRECTION('ref_axis',(1.,0.,0.)) ;
#122892 = DIRECTION('center_axis',(1.,0.,0.)) ;
#122893 = DIRECTION('ref_axis',(0.,0.,1.)) ;
#122894 = DIRECTION('center_axis',(1.,0.,2.16840434497101E-16)) ;
#122895 = DIRECTION('ref_axis',(2.16840434497101E-16,0.,-1.)) ;
#122896 = DIRECTION('center_axis',(0.,-1.,0.)) ;
#122897 = DIRECTION('ref_axis',(0.,0.,-1.)) ;
#122898 = DIRECTION('center_axis',(0.,-1.,0.)) ;
#122899 = DIRECTION('ref_axis',(0.,0.,-1.)) ;
#122900 = DIRECTION('center_axis',(0.,0.,1.)) ;
#122901 = DIRECTION('ref_axis',(1.,0.,0.)) ;
#122902 = DIRECTION('center_axis',(0.,0.,-1.)) ;
#122903 = DIRECTION('ref_axis',(-1.,0.,0.)) ;
#122904 = DIRECTION('center_axis',(0.,0.,1.)) ;
#122905 = DIRECTION('ref_axis',(1.,0.,0.)) ;
#122906 = DIRECTION('center_axis',(0.,-1.,0.)) ;
#122907 = DIRECTION('ref_axis',(0.,0.,-1.)) ;
#122908 = DIRECTION('center_axis',(0.,-1.,0.)) ;
#122909 = DIRECTION('ref_axis',(0.,0.,-1.)) ;
#122910 = DIRECTION('center_axis',(0.,1.,0.)) ;
#122911 = DIRECTION('ref_axis',(1.,0.,0.)) ;
#122912 = DIRECTION('center_axis',(-1.,0.,0.)) ;
#122913 = DIRECTION('ref_axis',(0.,0.,-1.)) ;
#122914 = DIRECTION('center_axis',(0.,1.,0.)) ;
#122915 = DIRECTION('ref_axis',(1.,0.,0.)) ;
#122916 = DIRECTION('center_axis',(-1.,0.,0.)) ;
#122917 = DIRECTION('ref_axis',(0.,0.,-1.)) ;
#122918 = DIRECTION('center_axis',(0.,-1.,0.)) ;
#122919 = DIRECTION('ref_axis',(0.,0.,-1.)) ;
#122920 = DIRECTION('center_axis',(0.,-1.,0.)) ;
#122921 = DIRECTION('ref_axis',(0.,0.,-1.)) ;
#122922 = DIRECTION('center_axis',(-1.,0.,0.)) ;
#122923 = DIRECTION('ref_axis',(0.,0.,1.)) ;
#122924 = DIRECTION('center_axis',(-1.,0.,0.)) ;
#122925 = DIRECTION('ref_axis',(0.,0.,1.)) ;
#122926 = DIRECTION('center_axis',(1.,0.,0.)) ;
#122927 = DIRECTION('ref_axis',(0.,0.,-1.)) ;
#122928 = DIRECTION('center_axis',(-1.,0.,0.)) ;
#122929 = DIRECTION('ref_axis',(0.,0.,1.)) ;
#122930 = DIRECTION('center_axis',(0.,-1.,0.)) ;
#122931 = DIRECTION('ref_axis',(0.,0.,-1.)) ;
#122932 = DIRECTION('center_axis',(0.,-1.,0.)) ;
#122933 = DIRECTION('ref_axis',(0.,0.,-1.)) ;
#122934 = DIRECTION('center_axis',(0.,1.,0.)) ;
#122935 = DIRECTION('ref_axis',(1.,0.,0.)) ;
#122936 = DIRECTION('center_axis',(0.,0.,-1.)) ;
#122937 = DIRECTION('ref_axis',(1.,0.,0.)) ;
#122938 = DIRECTION('center_axis',(0.,1.,0.)) ;
#122939 = DIRECTION('ref_axis',(1.,0.,0.)) ;
#122940 = DIRECTION('center_axis',(0.,0.,1.)) ;
#122941 = DIRECTION('ref_axis',(-1.,0.,0.)) ;
#122942 = DIRECTION('center_axis',(0.,0.,-1.)) ;
#122943 = DIRECTION('ref_axis',(-1.,0.,0.)) ;
#122944 = DIRECTION('center_axis',(-0.669589480006975,0.669589480006975,-0.321402950403348)) ;
#122945 = DIRECTION('ref_axis',(-0.707106781186547,-0.707106781186548,-3.60611190025948E-16)) ;
#122946 = DIRECTION('center_axis',(0.669589480006972,-0.66958948000698,0.321402950403345)) ;
#122947 = DIRECTION('ref_axis',(0.707106781186552,0.707106781186543,5.47414022772576E-16)) ;
#122948 = DIRECTION('center_axis',(0.,1.,0.)) ;
#122949 = DIRECTION('ref_axis',(1.,0.,0.)) ;
#122950 = DIRECTION('center_axis',(-5.0109744998751E-15,1.,0.)) ;
#122951 = DIRECTION('ref_axis',(1.,5.0109744998751E-15,-4.33680868994201E-15)) ;
#122952 = DIRECTION('center_axis',(0.707106781186548,-0.707106781186548,-4.59988025005012E-15)) ;
#122953 = DIRECTION('ref_axis',(-0.707106781186548,-0.707106781186548,-1.2354148483551E-31)) ;
#122954 = DIRECTION('center_axis',(-0.707106781186548,0.707106781186547,0.)) ;
#122955 = DIRECTION('ref_axis',(-0.707106781186547,-0.707106781186548,0.)) ;
#122956 = DIRECTION('center_axis',(0.,-1.,0.)) ;
#122957 = DIRECTION('ref_axis',(0.,0.,-1.)) ;
#122958 = DIRECTION('center_axis',(0.,1.,0.)) ;
#122959 = DIRECTION('ref_axis',(0.,0.,1.)) ;
#122960 = DIRECTION('center_axis',(-0.879462917689188,-0.219865729422294,
-0.42214220049081)) ;
#122961 = DIRECTION('ref_axis',(-0.432731067584771,-3.91091346796197E-16,
0.901523057468274)) ;
#122962 = DIRECTION('center_axis',(0.879462917689189,0.219865729422295,0.422142200490807)) ;
#122963 = DIRECTION('ref_axis',(0.432731067584768,-3.18283478174207E-16,-0.901523057468275)) ;
#122964 = DIRECTION('center_axis',(0.,-1.,0.)) ;
#122965 = DIRECTION('ref_axis',(0.,0.,1.)) ;
#122966 = DIRECTION('center_axis',(0.,0.,1.)) ;
#122967 = DIRECTION('ref_axis',(-1.,0.,0.)) ;
#122968 = DIRECTION('center_axis',(0.,1.,0.)) ;
#122969 = DIRECTION('ref_axis',(1.,0.,0.)) ;
#122970 = DIRECTION('center_axis',(0.970142500145333,0.242535625036331,0.)) ;
#122971 = DIRECTION('ref_axis',(0.242535625036331,-0.970142500145332,0.)) ;
#122972 = DIRECTION('center_axis',(0.669589480006975,-0.669589480006975,-0.321402950403348)) ;
#122973 = DIRECTION('ref_axis',(0.707106781186547,0.707106781186548,-3.60611190025948E-16)) ;
#122974 = DIRECTION('center_axis',(0.669589480006975,-0.669589480006975,-0.321402950403349)) ;
#122975 = DIRECTION('ref_axis',(0.707106781186548,0.707106781186547,2.25891969505504E-16)) ;
#122976 = DIRECTION('center_axis',(0.707106781186548,-0.707106781186547,0.)) ;
#122977 = DIRECTION('ref_axis',(0.707106781186547,0.707106781186548,0.)) ;
#122978 = DIRECTION('center_axis',(-0.707106781186542,0.707106781186553,0.)) ;
#122979 = DIRECTION('ref_axis',(-0.707106781186553,-0.707106781186542,0.)) ;
#122980 = DIRECTION('center_axis',(0.,0.,1.)) ;
#122981 = DIRECTION('ref_axis',(1.,0.,0.)) ;
#122982 = DIRECTION('center_axis',(0.,0.,1.)) ;
#122983 = DIRECTION('ref_axis',(1.,0.,0.)) ;
#122984 = DIRECTION('center_axis',(2.47817639425258E-16,-1.,0.)) ;
#122985 = DIRECTION('ref_axis',(1.,2.47817639425258E-16,0.)) ;
#122986 = DIRECTION('center_axis',(0.,-1.,0.)) ;
#122987 = DIRECTION('ref_axis',(0.,0.,-1.)) ;
#122988 = DIRECTION('center_axis',(-0.970142500145333,-0.24253562503633,0.)) ;
#122989 = DIRECTION('ref_axis',(0.24253562503633,-0.970142500145333,0.)) ;
#122990 = DIRECTION('center_axis',(0.976187060183959,-0.216930457818629,3.32210494350328E-14)) ;
#122991 = DIRECTION('ref_axis',(0.216930457818629,0.976187060183959,-2.9855370908175E-12)) ;
#122992 = DIRECTION('center_axis',(0.,1.,0.)) ;
#122993 = DIRECTION('ref_axis',(1.,0.,0.)) ;
#122994 = DIRECTION('center_axis',(2.71050543121376E-14,1.,-1.3010426069826E-14)) ;
#122995 = DIRECTION('ref_axis',(1.,-2.71050543121376E-14,2.16840434497099E-15)) ;
#122996 = DIRECTION('center_axis',(0.,-1.,0.)) ;
#122997 = DIRECTION('ref_axis',(0.,0.,1.)) ;
#122998 = DIRECTION('center_axis',(0.,0.,1.)) ;
#122999 = DIRECTION('ref_axis',(-1.,8.67361737988401E-15,0.)) ;
#123000 = DIRECTION('center_axis',(0.879462917689188,0.219865729422294,-0.42214220049081)) ;
#123001 = DIRECTION('ref_axis',(-0.432731067584771,-3.91091346796197E-16,
-0.901523057468274)) ;
#123002 = DIRECTION('center_axis',(0.879462917689188,0.219865729422296,-0.422142200490809)) ;
#123003 = DIRECTION('ref_axis',(-0.43273106758477,-9.90395117542237E-17,-0.901523057468274)) ;
#123004 = DIRECTION('center_axis',(0.,-1.,0.)) ;
#123005 = DIRECTION('ref_axis',(0.,0.,-1.)) ;
#123006 = DIRECTION('center_axis',(2.00438979995004E-14,1.,0.)) ;
#123007 = DIRECTION('ref_axis',(-1.,2.00438979995004E-14,0.)) ;
#123008 = DIRECTION('center_axis',(2.47817639425258E-16,-1.,0.)) ;
#123009 = DIRECTION('ref_axis',(1.,2.47817639425258E-16,0.)) ;
#123010 = DIRECTION('center_axis',(0.,-1.,0.)) ;
#123011 = DIRECTION('ref_axis',(0.,0.,-1.)) ;
#123012 = DIRECTION('center_axis',(0.,0.,1.)) ;
#123013 = DIRECTION('ref_axis',(1.,0.,0.)) ;
#123014 = DIRECTION('center_axis',(0.,0.,1.)) ;
#123015 = DIRECTION('ref_axis',(1.,0.,0.)) ;
#123016 = DIRECTION('center_axis',(0.,1.,0.)) ;
#123017 = DIRECTION('ref_axis',(1.,0.,0.)) ;
#123018 = DIRECTION('center_axis',(0.970142500145333,0.242535625036331,0.)) ;
#123019 = DIRECTION('ref_axis',(0.242535625036331,-0.970142500145332,0.)) ;
#123020 = DIRECTION('center_axis',(-0.97618706018396,0.216930457818626,3.48715666902613E-14)) ;
#123021 = DIRECTION('ref_axis',(0.216930457818626,0.97618706018396,1.89720090087137E-12)) ;
#123022 = DIRECTION('center_axis',(0.970142500145333,0.24253562503633,0.)) ;
#123023 = DIRECTION('ref_axis',(-0.24253562503633,0.970142500145333,0.)) ;
#123024 = DIRECTION('center_axis',(1.,1.31418445149758E-16,-2.16840434497101E-16)) ;
#123025 = DIRECTION('ref_axis',(-2.16840434497101E-16,-2.8496832747207E-32,
-1.)) ;
#123026 = DIRECTION('center_axis',(1.,0.,0.)) ;
#123027 = DIRECTION('ref_axis',(0.,0.,-1.)) ;
#123028 = DIRECTION('center_axis',(-1.,0.,0.)) ;
#123029 = DIRECTION('ref_axis',(0.,0.,1.)) ;
#123030 = DIRECTION('center_axis',(-1.31418445149758E-16,1.,0.)) ;
#123031 = DIRECTION('ref_axis',(-1.,0.,0.)) ;
#123032 = DIRECTION('center_axis',(0.,0.,1.)) ;
#123033 = DIRECTION('ref_axis',(-1.,0.,0.)) ;
#123034 = DIRECTION('center_axis',(-1.31418445149758E-16,1.,0.)) ;
#123035 = DIRECTION('ref_axis',(-1.,-1.31418445149758E-16,0.)) ;
#123036 = DIRECTION('center_axis',(-1.31418445149758E-16,1.,0.)) ;
#123037 = DIRECTION('ref_axis',(-1.,0.,0.)) ;
#123038 = DIRECTION('center_axis',(-1.31418445149758E-16,1.,0.)) ;
#123039 = DIRECTION('ref_axis',(-1.,-1.31418445149758E-16,0.)) ;
#123040 = DIRECTION('center_axis',(0.,0.,1.)) ;
#123041 = DIRECTION('ref_axis',(-1.,0.,0.)) ;
#123042 = DIRECTION('center_axis',(-4.33680868994202E-16,-5.69936654944139E-32,
-1.)) ;
#123043 = DIRECTION('ref_axis',(-1.,2.47170623787823E-47,4.33680868994202E-16)) ;
#123044 = DIRECTION('center_axis',(0.,0.,1.)) ;
#123045 = DIRECTION('ref_axis',(1.,0.,0.)) ;
#123046 = DIRECTION('center_axis',(-1.31418445149758E-16,-1.,0.)) ;
#123047 = DIRECTION('ref_axis',(1.,-1.31418445149758E-16,0.)) ;
#123048 = DIRECTION('center_axis',(0.,1.,0.)) ;
#123049 = DIRECTION('ref_axis',(0.,0.,1.)) ;
#123050 = DIRECTION('center_axis',(-1.,0.,2.16840434497101E-16)) ;
#123051 = DIRECTION('ref_axis',(2.16840434497101E-16,0.,1.)) ;
#123052 = DIRECTION('center_axis',(-1.,0.,0.)) ;
#123053 = DIRECTION('ref_axis',(0.,0.,1.)) ;
#123054 = DIRECTION('center_axis',(1.,0.,0.)) ;
#123055 = DIRECTION('ref_axis',(0.,0.,-1.)) ;
#123056 = DIRECTION('center_axis',(-1.31418445149758E-16,-1.,0.)) ;
#123057 = DIRECTION('ref_axis',(1.,-1.31418445149758E-16,0.)) ;
#123058 = DIRECTION('center_axis',(0.,1.,0.)) ;
#123059 = DIRECTION('ref_axis',(0.,0.,1.)) ;
#123060 = DIRECTION('center_axis',(2.16840434497101E-16,2.8496832747207E-32,
1.)) ;
#123061 = DIRECTION('ref_axis',(1.,-6.17926559469557E-48,-2.16840434497101E-16)) ;
#123062 = DIRECTION('center_axis',(0.,0.,1.)) ;
#123063 = DIRECTION('ref_axis',(1.,0.,0.)) ;
#123064 = DIRECTION('center_axis',(-1.,-1.31418445149758E-16,-2.16840434497101E-16)) ;
#123065 = DIRECTION('ref_axis',(-2.16840434497101E-16,-2.8496832747207E-32,
1.)) ;
#123066 = DIRECTION('center_axis',(-1.,0.,0.)) ;
#123067 = DIRECTION('ref_axis',(0.,0.,1.)) ;
#123068 = DIRECTION('center_axis',(1.,0.,0.)) ;
#123069 = DIRECTION('ref_axis',(0.,0.,-1.)) ;
#123070 = DIRECTION('center_axis',(-1.31418445149758E-16,1.,0.)) ;
#123071 = DIRECTION('ref_axis',(-1.,0.,0.)) ;
#123072 = DIRECTION('center_axis',(-1.31418445149758E-16,1.,0.)) ;
#123073 = DIRECTION('ref_axis',(-1.,-1.31418445149758E-16,0.)) ;
#123074 = DIRECTION('center_axis',(0.,1.,0.)) ;
#123075 = DIRECTION('ref_axis',(1.,0.,0.)) ;
#123076 = DIRECTION('center_axis',(0.,0.,-1.)) ;
#123077 = DIRECTION('ref_axis',(1.,0.,0.)) ;
#123078 = DIRECTION('center_axis',(0.,1.,0.)) ;
#123079 = DIRECTION('ref_axis',(1.,0.,0.)) ;
#123080 = DIRECTION('center_axis',(0.,0.,-1.)) ;
#123081 = DIRECTION('ref_axis',(1.,0.,0.)) ;
#123082 = DIRECTION('center_axis',(-1.31418445149758E-16,1.,0.)) ;
#123083 = DIRECTION('ref_axis',(-1.,0.,0.)) ;
#123084 = DIRECTION('center_axis',(-1.31418445149758E-16,1.,0.)) ;
#123085 = DIRECTION('ref_axis',(-1.,-1.31418445149758E-16,0.)) ;
#123086 = DIRECTION('center_axis',(-1.31418445149758E-16,-1.,0.)) ;
#123087 = DIRECTION('ref_axis',(1.,-1.31418445149758E-16,0.)) ;
#123088 = DIRECTION('center_axis',(0.,1.,0.)) ;
#123089 = DIRECTION('ref_axis',(0.,0.,1.)) ;
#123090 = DIRECTION('center_axis',(4.33680868994202E-16,0.,1.)) ;
#123091 = DIRECTION('ref_axis',(1.,0.,-4.33680868994202E-16)) ;
#123092 = DIRECTION('center_axis',(0.,0.,-1.)) ;
#123093 = DIRECTION('ref_axis',(-1.,0.,0.)) ;
#123094 = DIRECTION('center_axis',(-2.16840434497101E-16,0.,-1.)) ;
#123095 = DIRECTION('ref_axis',(-1.,0.,2.16840434497101E-16)) ;
#123096 = DIRECTION('center_axis',(0.,0.,-1.)) ;
#123097 = DIRECTION('ref_axis',(-1.,0.,0.)) ;
#123098 = DIRECTION('center_axis',(-1.31418445149758E-16,-1.,0.)) ;
#123099 = DIRECTION('ref_axis',(1.,-1.31418445149758E-16,0.)) ;
#123100 = DIRECTION('center_axis',(0.,1.,0.)) ;
#123101 = DIRECTION('ref_axis',(0.,0.,1.)) ;
#123102 = DIRECTION('center_axis',(0.,1.,0.)) ;
#123103 = DIRECTION('ref_axis',(1.,0.,0.)) ;
#123104 = DIRECTION('center_axis',(-1.,0.,0.)) ;
#123105 = DIRECTION('ref_axis',(0.,0.,-1.)) ;
#123106 = DIRECTION('center_axis',(0.,1.,0.)) ;
#123107 = DIRECTION('ref_axis',(1.,0.,0.)) ;
#123108 = DIRECTION('center_axis',(1.,0.,0.)) ;
#123109 = DIRECTION('ref_axis',(0.,0.,1.)) ;
#123110 = DIRECTION('center_axis',(1.,0.,2.16840434497101E-16)) ;
#123111 = DIRECTION('ref_axis',(2.16840434497101E-16,0.,-1.)) ;
#123112 = DIRECTION('center_axis',(0.,1.,0.)) ;
#123113 = DIRECTION('ref_axis',(0.,0.,1.)) ;
#123114 = DIRECTION('center_axis',(0.,1.,0.)) ;
#123115 = DIRECTION('ref_axis',(0.,0.,1.)) ;
#123116 = DIRECTION('center_axis',(0.,0.,-1.)) ;
#123117 = DIRECTION('ref_axis',(-1.,0.,0.)) ;
#123118 = DIRECTION('center_axis',(0.,0.,1.)) ;
#123119 = DIRECTION('ref_axis',(1.,0.,0.)) ;
#123120 = DIRECTION('center_axis',(0.,0.,-1.)) ;
#123121 = DIRECTION('ref_axis',(-1.,0.,0.)) ;
#123122 = DIRECTION('center_axis',(0.,1.,0.)) ;
#123123 = DIRECTION('ref_axis',(0.,0.,1.)) ;
#123124 = DIRECTION('center_axis',(0.,1.,0.)) ;
#123125 = DIRECTION('ref_axis',(0.,0.,1.)) ;
#123126 = DIRECTION('center_axis',(0.,1.,0.)) ;
#123127 = DIRECTION('ref_axis',(1.,0.,0.)) ;
#123128 = DIRECTION('center_axis',(-1.,0.,0.)) ;
#123129 = DIRECTION('ref_axis',(0.,0.,-1.)) ;
#123130 = DIRECTION('center_axis',(0.,1.,0.)) ;
#123131 = DIRECTION('ref_axis',(1.,0.,0.)) ;
#123132 = DIRECTION('center_axis',(-1.,0.,0.)) ;
#123133 = DIRECTION('ref_axis',(0.,0.,-1.)) ;
#123134 = DIRECTION('center_axis',(0.,1.,0.)) ;
#123135 = DIRECTION('ref_axis',(0.,0.,1.)) ;
#123136 = DIRECTION('center_axis',(0.,1.,0.)) ;
#123137 = DIRECTION('ref_axis',(0.,0.,1.)) ;
#123138 = DIRECTION('center_axis',(-1.,0.,0.)) ;
#123139 = DIRECTION('ref_axis',(0.,0.,1.)) ;
#123140 = DIRECTION('center_axis',(-1.,0.,0.)) ;
#123141 = DIRECTION('ref_axis',(0.,0.,1.)) ;
#123142 = DIRECTION('center_axis',(1.,0.,0.)) ;
#123143 = DIRECTION('ref_axis',(0.,0.,-1.)) ;
#123144 = DIRECTION('center_axis',(-1.,0.,0.)) ;
#123145 = DIRECTION('ref_axis',(0.,0.,1.)) ;
#123146 = DIRECTION('center_axis',(0.,1.,0.)) ;
#123147 = DIRECTION('ref_axis',(0.,0.,1.)) ;
#123148 = DIRECTION('center_axis',(0.,1.,0.)) ;
#123149 = DIRECTION('ref_axis',(0.,0.,1.)) ;
#123150 = DIRECTION('center_axis',(0.,1.,0.)) ;
#123151 = DIRECTION('ref_axis',(1.,0.,0.)) ;
#123152 = DIRECTION('center_axis',(0.,0.,1.)) ;
#123153 = DIRECTION('ref_axis',(-1.,0.,0.)) ;
#123154 = DIRECTION('center_axis',(0.,1.,0.)) ;
#123155 = DIRECTION('ref_axis',(1.,0.,0.)) ;
#123156 = DIRECTION('center_axis',(0.,0.,-1.)) ;
#123157 = DIRECTION('ref_axis',(1.,0.,0.)) ;
#123158 = DIRECTION('center_axis',(0.,0.,1.)) ;
#123159 = DIRECTION('ref_axis',(1.,0.,0.)) ;
#123160 = DIRECTION('center_axis',(0.,0.,1.)) ;
#123161 = DIRECTION('ref_axis',(1.,0.,0.)) ;
#123162 = DIRECTION('center_axis',(0.,0.,-1.)) ;
#123163 = DIRECTION('ref_axis',(-1.,0.,0.)) ;
#123164 = DIRECTION('center_axis',(-6.50521303491301E-15,0.,1.)) ;
#123165 = DIRECTION('ref_axis',(1.,0.,6.50521303491301E-15)) ;
#123166 = DIRECTION('center_axis',(1.,0.,0.)) ;
#123167 = DIRECTION('ref_axis',(0.,0.,-1.)) ;
#123168 = DIRECTION('center_axis',(1.,0.,0.)) ;
#123169 = DIRECTION('ref_axis',(0.,0.,-1.)) ;
#123170 = DIRECTION('center_axis',(1.,0.,0.)) ;
#123171 = DIRECTION('ref_axis',(0.,0.,-1.)) ;
#123172 = DIRECTION('center_axis',(1.,-1.41059322098675E-29,8.67361737988404E-15)) ;
#123173 = DIRECTION('ref_axis',(8.67361737988404E-15,0.,-1.)) ;
#123174 = DIRECTION('center_axis',(1.,0.,0.)) ;
#123175 = DIRECTION('ref_axis',(0.,0.,-1.)) ;
#123176 = DIRECTION('center_axis',(1.,0.,1.73472347597681E-14)) ;
#123177 = DIRECTION('ref_axis',(1.73472347597681E-14,0.,-1.)) ;
#123178 = DIRECTION('center_axis',(-1.,0.,0.)) ;
#123179 = DIRECTION('ref_axis',(0.,0.,1.)) ;
#123180 = DIRECTION('center_axis',(1.,0.,0.)) ;
#123181 = DIRECTION('ref_axis',(0.,0.,-1.)) ;
#123182 = DIRECTION('center_axis',(1.,0.,0.)) ;
#123183 = DIRECTION('ref_axis',(0.,0.,-1.)) ;
#123184 = DIRECTION('center_axis',(-7.04731412115582E-15,0.,-1.)) ;
#123185 = DIRECTION('ref_axis',(-1.,0.,7.04731412115582E-15)) ;
#123186 = DIRECTION('center_axis',(1.,0.,0.)) ;
#123187 = DIRECTION('ref_axis',(0.,0.,-1.)) ;
#123188 = DIRECTION('center_axis',(-6.50521303491307E-15,0.,1.)) ;
#123189 = DIRECTION('ref_axis',(1.,0.,6.50521303491307E-15)) ;
#123190 = DIRECTION('center_axis',(0.,0.,-1.)) ;
#123191 = DIRECTION('ref_axis',(-1.,0.,0.)) ;
#123192 = DIRECTION('center_axis',(-0.422618261740697,5.55398348498559E-17,
0.906307787036651)) ;
#123193 = DIRECTION('ref_axis',(0.906307787036651,-7.29829988871486E-33,0.422618261740697)) ;
#123194 = DIRECTION('center_axis',(0.422618261740697,-5.55398348498559E-17,
-0.906307787036651)) ;
#123195 = DIRECTION('ref_axis',(-0.906307787036651,1.61222584863515E-33,-0.422618261740697)) ;
#123196 = DIRECTION('center_axis',(-0.422618261740697,5.55398348498559E-17,
0.906307787036651)) ;
#123197 = DIRECTION('ref_axis',(0.906307787036651,-1.61222584863515E-33,0.422618261740697)) ;
#123198 = DIRECTION('center_axis',(0.422618261740697,-5.55398348498559E-17,
-0.906307787036651)) ;
#123199 = DIRECTION('ref_axis',(-0.906307787036651,1.03797877997344E-32,-0.422618261740697)) ;
#123200 = DIRECTION('center_axis',(0.,0.,1.)) ;
#123201 = DIRECTION('ref_axis',(1.,0.,0.)) ;
#123202 = DIRECTION('center_axis',(7.01133629567814E-33,-8.97270763436279E-17,
-1.)) ;
#123203 = DIRECTION('ref_axis',(-6.29106707073161E-49,-1.,8.97270763436279E-17)) ;
#123204 = DIRECTION('center_axis',(7.01133629567814E-33,-8.97270763436279E-17,
1.)) ;
#123205 = DIRECTION('ref_axis',(6.29106707073161E-49,1.,8.97270763436279E-17)) ;
#123206 = DIRECTION('center_axis',(1.,0.,0.)) ;
#123207 = DIRECTION('ref_axis',(0.,0.,-1.)) ;
#123208 = DIRECTION('center_axis',(0.,-4.8455963016112E-16,1.)) ;
#123209 = DIRECTION('ref_axis',(0.,-1.,-4.8455963016112E-16)) ;
#123210 = DIRECTION('center_axis',(0.,4.8455963016112E-16,-1.)) ;
#123211 = DIRECTION('ref_axis',(0.,-1.,-4.8455963016112E-16)) ;
#123212 = DIRECTION('center_axis',(0.,0.,-1.)) ;
#123213 = DIRECTION('ref_axis',(-1.,0.,0.)) ;
#123214 = DIRECTION('center_axis',(0.,0.,-1.)) ;
#123215 = DIRECTION('ref_axis',(-1.,0.,0.)) ;
#123216 = DIRECTION('center_axis',(1.,0.,0.)) ;
#123217 = DIRECTION('ref_axis',(0.,0.,-1.)) ;
#123218 = DIRECTION('center_axis',(-7.01133629567814E-33,8.97270763436279E-17,
1.)) ;
#123219 = DIRECTION('ref_axis',(0.,-1.,0.)) ;
#123220 = DIRECTION('center_axis',(1.,0.,0.)) ;
#123221 = DIRECTION('ref_axis',(0.,0.,-1.)) ;
#123222 = DIRECTION('center_axis',(-1.,0.,-7.01133629567814E-33)) ;
#123223 = DIRECTION('ref_axis',(-7.01133629567814E-33,0.,1.)) ;
#123224 = DIRECTION('center_axis',(1.,0.,0.)) ;
#123225 = DIRECTION('ref_axis',(0.,0.,-1.)) ;
#123226 = DIRECTION('center_axis',(1.,0.,0.)) ;
#123227 = DIRECTION('ref_axis',(0.,0.,-1.)) ;
#123228 = DIRECTION('center_axis',(0.,1.,0.)) ;
#123229 = DIRECTION('ref_axis',(1.,0.,0.)) ;
#123230 = DIRECTION('center_axis',(-7.01133629567814E-33,8.97270763436279E-17,
-1.)) ;
#123231 = DIRECTION('ref_axis',(0.,1.,0.)) ;
#123232 = DIRECTION('center_axis',(1.,0.,0.)) ;
#123233 = DIRECTION('ref_axis',(0.,0.,-1.)) ;
#123234 = DIRECTION('center_axis',(-1.,0.,7.01133629567814E-33)) ;
#123235 = DIRECTION('ref_axis',(7.01133629567814E-33,0.,1.)) ;
#123236 = DIRECTION('center_axis',(1.,0.,0.)) ;
#123237 = DIRECTION('ref_axis',(0.,0.,-1.)) ;
#123238 = DIRECTION('center_axis',(1.,0.,0.)) ;
#123239 = DIRECTION('ref_axis',(0.,0.,-1.)) ;
#123240 = DIRECTION('center_axis',(0.,1.,0.)) ;
#123241 = DIRECTION('ref_axis',(1.,0.,0.)) ;
#123242 = DIRECTION('center_axis',(1.,0.,0.)) ;
#123243 = DIRECTION('ref_axis',(0.,0.,-1.)) ;
#123244 = DIRECTION('center_axis',(0.,0.5,0.866025403784439)) ;
#123245 = DIRECTION('ref_axis',(0.,-0.866025403784439,0.5)) ;
#123246 = DIRECTION('center_axis',(0.866025403784441,0.499999999999997,-2.168404344971E-15)) ;
#123247 = DIRECTION('ref_axis',(-0.499999999999997,0.866025403784441,-1.29696145180704E-31)) ;
#123248 = DIRECTION('center_axis',(-7.01133629567814E-33,8.97270763436279E-17,
1.)) ;
#123249 = DIRECTION('ref_axis',(0.,-1.,0.)) ;
#123250 = DIRECTION('center_axis',(1.,0.,0.)) ;
#123251 = DIRECTION('ref_axis',(0.,0.,-1.)) ;
#123252 = DIRECTION('center_axis',(-2.16840434497101E-15,0.499999999999998,
-0.86602540378444)) ;
#123253 = DIRECTION('ref_axis',(-3.01985296231538E-32,0.86602540378444,0.499999999999998)) ;
#123254 = DIRECTION('center_axis',(0.866025403784439,0.5,0.)) ;
#123255 = DIRECTION('ref_axis',(-0.5,0.866025403784439,0.)) ;
#123256 = DIRECTION('center_axis',(-7.01133629567814E-33,8.97270763436279E-17,
-1.)) ;
#123257 = DIRECTION('ref_axis',(0.,1.,0.)) ;
#123258 = DIRECTION('center_axis',(0.,0.,-1.)) ;
#123259 = DIRECTION('ref_axis',(-1.,0.,0.)) ;
#123260 = DIRECTION('',(2.47817639425258E-16,-1.,0.)) ;
#123261 = DIRECTION('',(0.970142500145333,0.24253562503633,0.)) ;
#123262 = DIRECTION('',(0.,1.,0.)) ;
#123263 = DIRECTION('',(-0.707106781186549,0.707106781186546,0.)) ;
#123264 = DIRECTION('center_axis',(0.432731067584771,0.,-0.901523057468274)) ;
#123265 = DIRECTION('ref_axis',(-0.901523057468274,0.,-0.432731067584771)) ;
#123266 = DIRECTION('',(0.,-1.,0.)) ;
#123267 = DIRECTION('',(0.879462917689188,0.219865729422294,0.42214220049081)) ;
#123268 = DIRECTION('',(0.,1.,0.)) ;
#123269 = DIRECTION('',(-0.669589480006976,0.669589480006974,-0.321402950403348)) ;
#123270 = DIRECTION('center_axis',(1.,0.,0.)) ;
#123271 = DIRECTION('ref_axis',(0.,0.,-1.)) ;
#123272 = DIRECTION('',(0.,0.,-1.)) ;
#123273 = DIRECTION('center_axis',(-1.,0.,0.)) ;
#123274 = DIRECTION('ref_axis',(0.,0.461934418836862,-0.886914084167035)) ;
#123275 = DIRECTION('',(0.,1.,0.)) ;
#123276 = DIRECTION('center_axis',(-1.,-2.53099280113937E-14,-3.2268794886738E-14)) ;
#123277 = DIRECTION('ref_axis',(-3.67811937460755E-14,0.901523057469949,0.432731067581281)) ;
#123278 = DIRECTION('',(0.,0.,-1.)) ;
#123279 = DIRECTION('center_axis',(-1.,-2.53099280113875E-14,3.22687948867301E-14)) ;
#123280 = DIRECTION('ref_axis',(-3.67811937461193E-14,0.901523057468688,-0.432731067583908)) ;
#123281 = DIRECTION('center_axis',(-1.,2.82235702682257E-14,2.6227280381046E-14)) ;
#123282 = DIRECTION('ref_axis',(-3.62987828887412E-14,-0.461934418839581,
-0.886914084165619)) ;
#123283 = DIRECTION('center_axis',(0.432731067584771,0.,0.901523057468274)) ;
#123284 = DIRECTION('ref_axis',(0.901523057468274,0.,-0.432731067584771)) ;
#123285 = DIRECTION('',(-0.879462917689188,-0.219865729422294,0.42214220049081)) ;
#123286 = DIRECTION('',(0.,1.,0.)) ;
#123287 = DIRECTION('',(0.669589480006976,-0.669589480006974,-0.321402950403348)) ;
#123288 = DIRECTION('center_axis',(0.,0.,1.)) ;
#123289 = DIRECTION('ref_axis',(1.,0.,0.)) ;
#123290 = DIRECTION('',(-2.47817639425258E-16,1.,0.)) ;
#123291 = DIRECTION('',(0.707106781186549,-0.707106781186546,0.)) ;
#123292 = DIRECTION('',(0.,-1.,0.)) ;
#123293 = DIRECTION('',(-0.970142500145333,-0.24253562503633,0.)) ;
#123294 = DIRECTION('center_axis',(0.,0.,-1.)) ;
#123295 = DIRECTION('ref_axis',(-1.,0.,0.)) ;
#123296 = DIRECTION('',(2.47817639425258E-16,-1.,0.)) ;
#123297 = DIRECTION('',(0.970142500145333,0.24253562503633,0.)) ;
#123298 = DIRECTION('',(0.,1.,0.)) ;
#123299 = DIRECTION('',(-0.707106781186549,0.707106781186546,0.)) ;
#123300 = DIRECTION('center_axis',(0.432731067584771,0.,-0.901523057468274)) ;
#123301 = DIRECTION('ref_axis',(-0.901523057468274,0.,-0.432731067584771)) ;
#123302 = DIRECTION('',(0.,-1.,0.)) ;
#123303 = DIRECTION('',(0.879462917689188,0.219865729422294,0.42214220049081)) ;
#123304 = DIRECTION('',(0.,1.,0.)) ;
#123305 = DIRECTION('',(-0.669589480006976,0.669589480006974,-0.321402950403348)) ;
#123306 = DIRECTION('center_axis',(1.,0.,0.)) ;
#123307 = DIRECTION('ref_axis',(0.,0.,-1.)) ;
#123308 = DIRECTION('',(0.,0.,-1.)) ;
#123309 = DIRECTION('center_axis',(-1.,1.4111785134113E-14,-1.31136401905232E-14)) ;
#123310 = DIRECTION('ref_axis',(1.814939144438E-14,0.461934418840836,-0.886914084164965)) ;
#123311 = DIRECTION('',(0.,1.,0.)) ;
#123312 = DIRECTION('center_axis',(-1.,0.,0.)) ;
#123313 = DIRECTION('ref_axis',(0.,0.901523057470446,0.432731067580246)) ;
#123314 = DIRECTION('',(0.,0.,-1.)) ;
#123315 = DIRECTION('center_axis',(-1.,-2.53099280113875E-14,3.22687948867301E-14)) ;
#123316 = DIRECTION('ref_axis',(-3.6781193746113E-14,0.901523057468839,-0.432731067583594)) ;
#123317 = DIRECTION('center_axis',(-1.,2.82235702682248E-14,2.6227280381044E-14)) ;
#123318 = DIRECTION('ref_axis',(-3.62987828887609E-14,-0.46193441884108,-0.886914084164838)) ;
#123319 = DIRECTION('center_axis',(0.432731067584771,0.,0.901523057468274)) ;
#123320 = DIRECTION('ref_axis',(0.901523057468274,0.,-0.432731067584771)) ;
#123321 = DIRECTION('',(-0.879462917689188,-0.219865729422294,0.42214220049081)) ;
#123322 = DIRECTION('',(0.,1.,0.)) ;
#123323 = DIRECTION('',(0.669589480006976,-0.669589480006974,-0.321402950403348)) ;
#123324 = DIRECTION('center_axis',(0.,0.,1.)) ;
#123325 = DIRECTION('ref_axis',(1.,0.,0.)) ;
#123326 = DIRECTION('',(-2.47817639425258E-16,1.,0.)) ;
#123327 = DIRECTION('',(0.707106781186549,-0.707106781186546,0.)) ;
#123328 = DIRECTION('',(0.,-1.,0.)) ;
#123329 = DIRECTION('',(-0.970142500145333,-0.24253562503633,0.)) ;
#123330 = DIRECTION('center_axis',(0.,0.,-1.)) ;
#123331 = DIRECTION('ref_axis',(-1.,0.,0.)) ;
#123332 = DIRECTION('',(2.47817639425258E-16,-1.,0.)) ;
#123333 = DIRECTION('',(0.970142500145333,0.24253562503633,0.)) ;
#123334 = DIRECTION('',(0.,1.,0.)) ;
#123335 = DIRECTION('',(-0.707106781186549,0.707106781186546,0.)) ;
#123336 = DIRECTION('center_axis',(0.432731067584771,0.,-0.901523057468274)) ;
#123337 = DIRECTION('ref_axis',(-0.901523057468274,0.,-0.432731067584771)) ;
#123338 = DIRECTION('',(0.,-1.,0.)) ;
#123339 = DIRECTION('',(0.879462917689188,0.219865729422294,0.42214220049081)) ;
#123340 = DIRECTION('',(0.,1.,0.)) ;
#123341 = DIRECTION('',(-0.669589480006976,0.669589480006974,-0.321402950403348)) ;
#123342 = DIRECTION('center_axis',(1.,0.,0.)) ;
#123343 = DIRECTION('ref_axis',(0.,0.,-1.)) ;
#123344 = DIRECTION('',(0.,0.,-1.)) ;
#123345 = DIRECTION('center_axis',(-1.,1.4111785134113E-14,-1.31136401905232E-14)) ;
#123346 = DIRECTION('ref_axis',(1.81493914443659E-14,0.461934418838905,-0.886914084165971)) ;
#123347 = DIRECTION('',(0.,1.,0.)) ;
#123348 = DIRECTION('center_axis',(-1.,0.,0.)) ;
#123349 = DIRECTION('ref_axis',(0.,0.901523057469797,0.432731067581597)) ;
#123350 = DIRECTION('',(0.,0.,-1.)) ;
#123351 = DIRECTION('center_axis',(-1.,0.,0.)) ;
#123352 = DIRECTION('ref_axis',(0.,0.901523057468153,-0.432731067585023)) ;
#123353 = DIRECTION('center_axis',(-1.,1.41117851341127E-14,1.31136401905217E-14)) ;
#123354 = DIRECTION('ref_axis',(-1.8149391444346E-14,-0.461934418836372,-0.88691408416729)) ;
#123355 = DIRECTION('center_axis',(0.432731067584771,0.,0.901523057468274)) ;
#123356 = DIRECTION('ref_axis',(0.901523057468274,0.,-0.432731067584771)) ;
#123357 = DIRECTION('',(-0.879462917689188,-0.219865729422294,0.42214220049081)) ;
#123358 = DIRECTION('',(0.,1.,0.)) ;
#123359 = DIRECTION('',(0.669589480006976,-0.669589480006974,-0.321402950403348)) ;
#123360 = DIRECTION('center_axis',(0.,0.,1.)) ;
#123361 = DIRECTION('ref_axis',(1.,0.,0.)) ;
#123362 = DIRECTION('',(-2.47817639425258E-16,1.,0.)) ;
#123363 = DIRECTION('',(0.707106781186549,-0.707106781186546,0.)) ;
#123364 = DIRECTION('',(0.,-1.,0.)) ;
#123365 = DIRECTION('',(-0.970142500145333,-0.24253562503633,0.)) ;
#123366 = DIRECTION('center_axis',(0.,0.,-1.)) ;
#123367 = DIRECTION('ref_axis',(-1.,0.,0.)) ;
#123368 = DIRECTION('',(2.47817639425258E-16,-1.,0.)) ;
#123369 = DIRECTION('',(0.970142500145333,0.24253562503633,0.)) ;
#123370 = DIRECTION('',(0.,1.,0.)) ;
#123371 = DIRECTION('',(-0.707106781186549,0.707106781186546,0.)) ;
#123372 = DIRECTION('center_axis',(0.432731067584771,0.,-0.901523057468274)) ;
#123373 = DIRECTION('ref_axis',(-0.901523057468274,0.,-0.432731067584771)) ;
#123374 = DIRECTION('',(0.,-1.,0.)) ;
#123375 = DIRECTION('',(0.879462917689188,0.219865729422294,0.42214220049081)) ;
#123376 = DIRECTION('',(0.,1.,0.)) ;
#123377 = DIRECTION('',(-0.669589480006976,0.669589480006974,-0.321402950403348)) ;
#123378 = DIRECTION('center_axis',(1.,0.,0.)) ;
#123379 = DIRECTION('ref_axis',(0.,0.,-1.)) ;
#123380 = DIRECTION('',(0.,0.,-1.)) ;
#123381 = DIRECTION('center_axis',(-1.,1.41117851341151E-14,-1.3113640190524E-14)) ;
#123382 = DIRECTION('ref_axis',(1.81493914443558E-14,0.461934418837284,-0.886914084166815)) ;
#123383 = DIRECTION('',(0.,1.,0.)) ;
#123384 = DIRECTION('center_axis',(-1.,0.,0.)) ;
#123385 = DIRECTION('ref_axis',(0.,0.901523057469908,0.432731067581367)) ;
#123386 = DIRECTION('',(0.,0.,-1.)) ;
#123387 = DIRECTION('center_axis',(-1.,0.,0.)) ;
#123388 = DIRECTION('ref_axis',(0.,0.90152305746791,-0.432731067585528)) ;
#123389 = DIRECTION('center_axis',(-1.,1.41117851341131E-14,1.31136401905226E-14)) ;
#123390 = DIRECTION('ref_axis',(-1.8149391444372E-14,-0.461934418839798,-0.886914084165506)) ;
#123391 = DIRECTION('center_axis',(0.432731067584771,0.,0.901523057468274)) ;
#123392 = DIRECTION('ref_axis',(0.901523057468274,0.,-0.432731067584771)) ;
#123393 = DIRECTION('',(-0.879462917689188,-0.219865729422294,0.42214220049081)) ;
#123394 = DIRECTION('',(0.,1.,0.)) ;
#123395 = DIRECTION('',(0.669589480006976,-0.669589480006974,-0.321402950403348)) ;
#123396 = DIRECTION('center_axis',(0.,0.,1.)) ;
#123397 = DIRECTION('ref_axis',(1.,0.,0.)) ;
#123398 = DIRECTION('',(-2.47817639425258E-16,1.,0.)) ;
#123399 = DIRECTION('',(0.707106781186549,-0.707106781186546,0.)) ;
#123400 = DIRECTION('',(0.,-1.,0.)) ;
#123401 = DIRECTION('',(-0.970142500145333,-0.24253562503633,0.)) ;
#123402 = DIRECTION('center_axis',(0.,0.,-1.)) ;
#123403 = DIRECTION('ref_axis',(-1.,0.,0.)) ;
#123404 = DIRECTION('',(2.47817639425258E-16,-1.,0.)) ;
#123405 = DIRECTION('',(0.970142500145333,0.24253562503633,0.)) ;
#123406 = DIRECTION('',(0.,1.,0.)) ;
#123407 = DIRECTION('',(-0.707106781186549,0.707106781186546,0.)) ;
#123408 = DIRECTION('center_axis',(0.432731067584771,0.,-0.901523057468274)) ;
#123409 = DIRECTION('ref_axis',(-0.901523057468274,0.,-0.432731067584771)) ;
#123410 = DIRECTION('',(0.,-1.,0.)) ;
#123411 = DIRECTION('',(0.879462917689188,0.219865729422294,0.42214220049081)) ;
#123412 = DIRECTION('',(0.,1.,0.)) ;
#123413 = DIRECTION('',(-0.669589480006976,0.669589480006974,-0.321402950403348)) ;
#123414 = DIRECTION('center_axis',(1.,0.,0.)) ;
#123415 = DIRECTION('ref_axis',(0.,0.,-1.)) ;
#123416 = DIRECTION('',(0.,0.,-1.)) ;
#123417 = DIRECTION('center_axis',(-1.,1.4111785134114E-14,-1.31136401905236E-14)) ;
#123418 = DIRECTION('ref_axis',(1.81493914443555E-14,0.461934418837353,-0.886914084166779)) ;
#123419 = DIRECTION('',(0.,1.,0.)) ;
#123420 = DIRECTION('center_axis',(-1.,0.,0.)) ;
#123421 = DIRECTION('ref_axis',(0.,0.901523057469398,0.432731067582429)) ;
#123422 = DIRECTION('',(0.,0.,-1.)) ;
#123423 = DIRECTION('center_axis',(-1.,0.,0.)) ;
#123424 = DIRECTION('ref_axis',(0.,0.901523057469399,-0.432731067582427)) ;
#123425 = DIRECTION('center_axis',(-1.,2.82235702682282E-14,2.62272803810477E-14)) ;
#123426 = DIRECTION('ref_axis',(-3.62987828887127E-14,-0.461934418837437,
-0.886914084166736)) ;
#123427 = DIRECTION('center_axis',(0.432731067584771,0.,0.901523057468274)) ;
#123428 = DIRECTION('ref_axis',(0.901523057468274,0.,-0.432731067584771)) ;
#123429 = DIRECTION('',(-0.879462917689188,-0.219865729422294,0.42214220049081)) ;
#123430 = DIRECTION('',(0.,1.,0.)) ;
#123431 = DIRECTION('',(0.669589480006976,-0.669589480006974,-0.321402950403348)) ;
#123432 = DIRECTION('center_axis',(0.,0.,1.)) ;
#123433 = DIRECTION('ref_axis',(1.,0.,0.)) ;
#123434 = DIRECTION('',(-2.47817639425258E-16,1.,0.)) ;
#123435 = DIRECTION('',(0.707106781186549,-0.707106781186546,0.)) ;
#123436 = DIRECTION('',(0.,-1.,0.)) ;
#123437 = DIRECTION('',(-0.970142500145333,-0.24253562503633,0.)) ;
#123438 = DIRECTION('center_axis',(0.,0.,-1.)) ;
#123439 = DIRECTION('ref_axis',(-1.,0.,0.)) ;
#123440 = DIRECTION('',(2.47817639425258E-16,-1.,0.)) ;
#123441 = DIRECTION('',(0.970142500145333,0.24253562503633,0.)) ;
#123442 = DIRECTION('',(0.,1.,0.)) ;
#123443 = DIRECTION('',(-0.707106781186549,0.707106781186546,0.)) ;
#123444 = DIRECTION('center_axis',(0.432731067584771,0.,-0.901523057468274)) ;
#123445 = DIRECTION('ref_axis',(-0.901523057468274,0.,-0.432731067584771)) ;
#123446 = DIRECTION('',(0.,-1.,0.)) ;
#123447 = DIRECTION('',(0.879462917689188,0.219865729422294,0.42214220049081)) ;
#123448 = DIRECTION('',(0.,1.,0.)) ;
#123449 = DIRECTION('',(-0.669589480006976,0.669589480006974,-0.321402950403348)) ;
#123450 = DIRECTION('center_axis',(1.,0.,0.)) ;
#123451 = DIRECTION('ref_axis',(0.,0.,-1.)) ;
#123452 = DIRECTION('',(0.,0.,-1.)) ;
#123453 = DIRECTION('center_axis',(-1.,0.,0.)) ;
#123454 = DIRECTION('ref_axis',(0.,0.4619344188388,-0.886914084166026)) ;
#123455 = DIRECTION('',(0.,1.,0.)) ;
#123456 = DIRECTION('center_axis',(-1.,0.,0.)) ;
#123457 = DIRECTION('ref_axis',(0.,0.901523057467731,0.432731067585901)) ;
#123458 = DIRECTION('',(0.,0.,-1.)) ;
#123459 = DIRECTION('center_axis',(-1.,0.,0.)) ;
#123460 = DIRECTION('ref_axis',(0.,0.901523057469231,-0.432731067582777)) ;
#123461 = DIRECTION('center_axis',(-1.,2.82235702682263E-14,2.62272803810454E-14)) ;
#123462 = DIRECTION('ref_axis',(-3.62987828886724E-14,-0.461934418834871,
-0.886914084168072)) ;
#123463 = DIRECTION('center_axis',(0.432731067584771,0.,0.901523057468274)) ;
#123464 = DIRECTION('ref_axis',(0.901523057468274,0.,-0.432731067584771)) ;
#123465 = DIRECTION('',(-0.879462917689188,-0.219865729422294,0.42214220049081)) ;
#123466 = DIRECTION('',(0.,1.,0.)) ;
#123467 = DIRECTION('',(0.669589480006976,-0.669589480006974,-0.321402950403348)) ;
#123468 = DIRECTION('center_axis',(0.,0.,1.)) ;
#123469 = DIRECTION('ref_axis',(1.,0.,0.)) ;
#123470 = DIRECTION('',(-2.47817639425258E-16,1.,0.)) ;
#123471 = DIRECTION('',(0.707106781186549,-0.707106781186546,0.)) ;
#123472 = DIRECTION('',(0.,-1.,0.)) ;
#123473 = DIRECTION('',(-0.970142500145333,-0.24253562503633,0.)) ;
#123474 = DIRECTION('center_axis',(0.,0.,-1.)) ;
#123475 = DIRECTION('ref_axis',(-1.,0.,0.)) ;
#123476 = DIRECTION('',(2.47817639425258E-16,-1.,0.)) ;
#123477 = DIRECTION('',(0.970142500145333,0.24253562503633,0.)) ;
#123478 = DIRECTION('',(0.,1.,0.)) ;
#123479 = DIRECTION('',(-0.707106781186549,0.707106781186546,0.)) ;
#123480 = DIRECTION('center_axis',(0.432731067584771,0.,-0.901523057468274)) ;
#123481 = DIRECTION('ref_axis',(-0.901523057468274,0.,-0.432731067584771)) ;
#123482 = DIRECTION('',(0.,-1.,0.)) ;
#123483 = DIRECTION('',(0.879462917689188,0.219865729422294,0.42214220049081)) ;
#123484 = DIRECTION('',(0.,1.,0.)) ;
#123485 = DIRECTION('',(-0.669589480006976,0.669589480006974,-0.321402950403348)) ;
#123486 = DIRECTION('center_axis',(1.,0.,0.)) ;
#123487 = DIRECTION('ref_axis',(0.,0.,-1.)) ;
#123488 = DIRECTION('',(0.,0.,-1.)) ;
#123489 = DIRECTION('center_axis',(-1.,0.,0.)) ;
#123490 = DIRECTION('ref_axis',(0.,0.461934418836445,-0.886914084167252)) ;
#123491 = DIRECTION('',(0.,1.,0.)) ;
#123492 = DIRECTION('center_axis',(-1.,0.,0.)) ;
#123493 = DIRECTION('ref_axis',(0.,0.901523057468085,0.432731067585165)) ;
#123494 = DIRECTION('',(0.,0.,-1.)) ;
#123495 = DIRECTION('center_axis',(-1.,0.,0.)) ;
#123496 = DIRECTION('ref_axis',(0.,0.901523057468215,-0.432731067584893)) ;
#123497 = DIRECTION('center_axis',(-1.,2.82235702682288E-14,2.62272803810472E-14)) ;
#123498 = DIRECTION('ref_axis',(-3.62987828886828E-14,-0.461934418835395,
-0.886914084167799)) ;
#123499 = DIRECTION('center_axis',(0.432731067584771,0.,0.901523057468274)) ;
#123500 = DIRECTION('ref_axis',(0.901523057468274,0.,-0.432731067584771)) ;
#123501 = DIRECTION('',(-0.879462917689188,-0.219865729422294,0.42214220049081)) ;
#123502 = DIRECTION('',(0.,1.,0.)) ;
#123503 = DIRECTION('',(0.669589480006976,-0.669589480006974,-0.321402950403348)) ;
#123504 = DIRECTION('center_axis',(0.,0.,1.)) ;
#123505 = DIRECTION('ref_axis',(1.,0.,0.)) ;
#123506 = DIRECTION('',(-2.47817639425258E-16,1.,0.)) ;
#123507 = DIRECTION('',(0.707106781186549,-0.707106781186546,0.)) ;
#123508 = DIRECTION('',(0.,-1.,0.)) ;
#123509 = DIRECTION('',(-0.970142500145333,-0.24253562503633,0.)) ;
#123510 = DIRECTION('center_axis',(0.,0.,-1.)) ;
#123511 = DIRECTION('ref_axis',(-1.,0.,0.)) ;
#123512 = DIRECTION('',(2.47817639425258E-16,-1.,0.)) ;
#123513 = DIRECTION('',(0.970142500145333,0.24253562503633,0.)) ;
#123514 = DIRECTION('',(0.,1.,0.)) ;
#123515 = DIRECTION('',(-0.707106781186549,0.707106781186546,0.)) ;
#123516 = DIRECTION('center_axis',(0.432731067584771,0.,-0.901523057468274)) ;
#123517 = DIRECTION('ref_axis',(-0.901523057468274,0.,-0.432731067584771)) ;
#123518 = DIRECTION('',(0.,-1.,0.)) ;
#123519 = DIRECTION('',(0.879462917689188,0.219865729422294,0.42214220049081)) ;
#123520 = DIRECTION('',(0.,1.,0.)) ;
#123521 = DIRECTION('',(-0.669589480006976,0.669589480006974,-0.321402950403348)) ;
#123522 = DIRECTION('center_axis',(1.,0.,0.)) ;
#123523 = DIRECTION('ref_axis',(0.,0.,-1.)) ;
#123524 = DIRECTION('',(0.,0.,-1.)) ;
#123525 = DIRECTION('center_axis',(-1.,0.,0.)) ;
#123526 = DIRECTION('ref_axis',(0.,0.461934418837712,-0.886914084166592)) ;
#123527 = DIRECTION('',(0.,1.,0.)) ;
#123528 = DIRECTION('center_axis',(-1.,0.,0.)) ;
#123529 = DIRECTION('ref_axis',(0.,0.901523057468494,0.432731067584312)) ;
#123530 = DIRECTION('',(0.,0.,-1.)) ;
#123531 = DIRECTION('center_axis',(-1.,0.,0.)) ;
#123532 = DIRECTION('ref_axis',(0.,0.901523057467713,-0.43273106758594)) ;
#123533 = DIRECTION('center_axis',(-1.,2.82235702682276E-14,2.62272803810463E-14)) ;
#123534 = DIRECTION('ref_axis',(-3.62987828887053E-14,-0.461934418837035,
-0.886914084166945)) ;
#123535 = DIRECTION('center_axis',(0.432731067584771,0.,0.901523057468274)) ;
#123536 = DIRECTION('ref_axis',(0.901523057468274,0.,-0.432731067584771)) ;
#123537 = DIRECTION('',(-0.879462917689188,-0.219865729422294,0.42214220049081)) ;
#123538 = DIRECTION('',(0.,1.,0.)) ;
#123539 = DIRECTION('',(0.669589480006976,-0.669589480006974,-0.321402950403348)) ;
#123540 = DIRECTION('center_axis',(0.,0.,1.)) ;
#123541 = DIRECTION('ref_axis',(1.,0.,0.)) ;
#123542 = DIRECTION('',(-2.47817639425258E-16,1.,0.)) ;
#123543 = DIRECTION('',(0.707106781186549,-0.707106781186546,0.)) ;
#123544 = DIRECTION('',(0.,-1.,0.)) ;
#123545 = DIRECTION('',(-0.970142500145333,-0.24253562503633,0.)) ;
#123546 = DIRECTION('center_axis',(0.,0.,-1.)) ;
#123547 = DIRECTION('ref_axis',(-1.,0.,0.)) ;
#123548 = DIRECTION('',(0.970142500145333,0.24253562503633,0.)) ;
#123549 = DIRECTION('',(0.,1.,0.)) ;
#123550 = DIRECTION('',(-0.707106781186549,0.707106781186546,0.)) ;
#123551 = DIRECTION('',(2.47817639425258E-16,-1.,0.)) ;
#123552 = DIRECTION('center_axis',(0.432731067584771,0.,-0.901523057468274)) ;
#123553 = DIRECTION('ref_axis',(-0.901523057468274,0.,-0.432731067584771)) ;
#123554 = DIRECTION('',(0.,-1.,0.)) ;
#123555 = DIRECTION('',(0.879462917689188,0.219865729422294,0.42214220049081)) ;
#123556 = DIRECTION('',(0.,1.,0.)) ;
#123557 = DIRECTION('',(-0.669589480006976,0.669589480006974,-0.321402950403348)) ;
#123558 = DIRECTION('center_axis',(1.,0.,0.)) ;
#123559 = DIRECTION('ref_axis',(0.,0.,-1.)) ;
#123560 = DIRECTION('',(0.,0.,-1.)) ;
#123561 = DIRECTION('center_axis',(-1.,-1.41117851341144E-14,1.31136401905238E-14)) ;
#123562 = DIRECTION('ref_axis',(-1.81493914443513E-14,0.461934418836728,-0.886914084167105)) ;
#123563 = DIRECTION('',(0.,1.,0.)) ;
#123564 = DIRECTION('center_axis',(-1.,0.,0.)) ;
#123565 = DIRECTION('ref_axis',(0.,0.901523057468354,0.432731067584604)) ;
#123566 = DIRECTION('',(0.,0.,-1.)) ;
#123567 = DIRECTION('center_axis',(-1.,0.,0.)) ;
#123568 = DIRECTION('ref_axis',(0.,0.901523057468327,-0.43273106758466)) ;
#123569 = DIRECTION('center_axis',(-1.,0.,0.)) ;
#123570 = DIRECTION('ref_axis',(0.,-0.461934418836997,-0.886914084166965)) ;
#123571 = DIRECTION('center_axis',(0.432731067584771,0.,0.901523057468274)) ;
#123572 = DIRECTION('ref_axis',(0.901523057468274,0.,-0.432731067584771)) ;
#123573 = DIRECTION('',(-0.879462917689188,-0.219865729422294,0.42214220049081)) ;
#123574 = DIRECTION('',(0.,1.,0.)) ;
#123575 = DIRECTION('',(0.669589480006976,-0.669589480006974,-0.321402950403348)) ;
#123576 = DIRECTION('center_axis',(0.,0.,1.)) ;
#123577 = DIRECTION('ref_axis',(1.,0.,0.)) ;
#123578 = DIRECTION('',(0.,-1.,0.)) ;
#123579 = DIRECTION('',(-0.970142500145333,-0.24253562503633,0.)) ;
#123580 = DIRECTION('',(-2.47817639425258E-16,1.,0.)) ;
#123581 = DIRECTION('',(0.707106781186549,-0.707106781186546,0.)) ;
#123582 = DIRECTION('center_axis',(0.24253562503633,-0.970142500145333,0.)) ;
#123583 = DIRECTION('ref_axis',(0.,0.,1.)) ;
#123584 = DIRECTION('',(0.970142500145333,0.24253562503633,0.)) ;
#123585 = DIRECTION('',(0.879462917689188,0.219865729422294,-0.42214220049081)) ;
#123586 = DIRECTION('',(-0.879462917689188,-0.219865729422294,-0.42214220049081)) ;
#123587 = DIRECTION('',(-0.970142500145333,-0.24253562503633,0.)) ;
#123588 = DIRECTION('',(0.,0.,1.)) ;
#123589 = DIRECTION('center_axis',(0.24253562503633,-0.970142500145333,0.)) ;
#123590 = DIRECTION('ref_axis',(0.,0.,1.)) ;
#123591 = DIRECTION('',(0.,0.,1.)) ;
#123592 = DIRECTION('center_axis',(0.242535625036292,-0.970142500145342,-1.75219879118722E-13)) ;
#123593 = DIRECTION('ref_axis',(0.965295032173275,0.241323758043293,-0.0998415978711228)) ;
#123594 = DIRECTION('',(0.970142500145333,0.24253562503633,0.)) ;
#123595 = DIRECTION('',(0.879462917689188,0.219865729422294,-0.42214220049081)) ;
#123596 = DIRECTION('',(-0.879462917689188,-0.219865729422294,-0.42214220049081)) ;
#123597 = DIRECTION('',(-0.970142500145333,-0.24253562503633,0.)) ;
#123598 = DIRECTION('center_axis',(0.24253562503623,-0.970142500145358,7.11740252775332E-13)) ;
#123599 = DIRECTION('ref_axis',(0.965295032194209,0.241323758048516,0.0998415976561007)) ;
#123600 = DIRECTION('center_axis',(0.24253562503633,-0.970142500145333,0.)) ;
#123601 = DIRECTION('ref_axis',(0.,0.,1.)) ;
#123602 = DIRECTION('',(0.,0.,1.)) ;
#123603 = DIRECTION('center_axis',(0.242535625036328,-0.970142500145333,9.12301849944342E-14)) ;
#123604 = DIRECTION('ref_axis',(0.965295032195861,0.241323758048951,-0.0998415976390787)) ;
#123605 = DIRECTION('',(0.970142500145333,0.24253562503633,0.)) ;
#123606 = DIRECTION('',(0.879462917689188,0.219865729422294,-0.42214220049081)) ;
#123607 = DIRECTION('',(-0.879462917689188,-0.219865729422294,-0.42214220049081)) ;
#123608 = DIRECTION('',(-0.970142500145333,-0.24253562503633,0.)) ;
#123609 = DIRECTION('center_axis',(0.242535625036328,-0.970142500145333,-9.12301849944342E-14)) ;
#123610 = DIRECTION('ref_axis',(0.96529503220126,0.2413237580503,0.0998415975836097)) ;
#123611 = DIRECTION('center_axis',(0.24253562503633,-0.970142500145333,0.)) ;
#123612 = DIRECTION('ref_axis',(0.,0.,1.)) ;
#123613 = DIRECTION('',(0.,0.,1.)) ;
#123614 = DIRECTION('center_axis',(0.242535625036292,-0.970142500145342,-1.75943928203529E-13)) ;
#123615 = DIRECTION('ref_axis',(0.965295032208283,0.241323758052046,-0.0998415975114907)) ;
#123616 = DIRECTION('',(0.970142500145333,0.24253562503633,0.)) ;
#123617 = DIRECTION('',(0.879462917689188,0.219865729422294,-0.42214220049081)) ;
#123618 = DIRECTION('',(-0.879462917689188,-0.219865729422294,-0.42214220049081)) ;
#123619 = DIRECTION('',(-0.970142500145333,-0.24253562503633,0.)) ;
#123620 = DIRECTION('center_axis',(0.242535625036312,-0.970142500145337,-2.89619634903271E-15)) ;
#123621 = DIRECTION('ref_axis',(0.965295032130061,0.241323758032493,0.0998415983150268)) ;
#123622 = DIRECTION('center_axis',(0.24253562503633,-0.970142500145333,0.)) ;
#123623 = DIRECTION('ref_axis',(0.,0.,1.)) ;
#123624 = DIRECTION('',(0.,0.,1.)) ;
#123625 = DIRECTION('center_axis',(0.24253562503623,-0.970142500145358,-7.11016203688594E-13)) ;
#123626 = DIRECTION('ref_axis',(0.9652950321316,0.241323758032864,-0.0998415982992527)) ;
#123627 = DIRECTION('',(0.970142500145333,0.24253562503633,0.)) ;
#123628 = DIRECTION('',(0.879462917689188,0.219865729422294,-0.42214220049081)) ;
#123629 = DIRECTION('',(-0.879462917689188,-0.219865729422294,-0.42214220049081)) ;
#123630 = DIRECTION('',(-0.970142500145333,-0.24253562503633,0.)) ;
#123631 = DIRECTION('center_axis',(0.242535625036245,-0.970142500145354,6.23406264128872E-13)) ;
#123632 = DIRECTION('ref_axis',(0.965295032139512,0.241323758034849,0.0998415982179547)) ;
#123633 = DIRECTION('center_axis',(0.24253562503633,-0.970142500145333,0.)) ;
#123634 = DIRECTION('ref_axis',(0.,0.,1.)) ;
#123635 = DIRECTION('',(0.,0.,1.)) ;
#123636 = DIRECTION('center_axis',(0.24253562503623,-0.970142500145358,-7.11740252775329E-13)) ;
#123637 = DIRECTION('ref_axis',(0.965295032122132,0.241323758030497,-0.0998415983965105)) ;
#123638 = DIRECTION('',(0.970142500145333,0.24253562503633,0.)) ;
#123639 = DIRECTION('',(0.879462917689188,0.219865729422294,-0.42214220049081)) ;
#123640 = DIRECTION('',(-0.879462917689188,-0.219865729422294,-0.42214220049081)) ;
#123641 = DIRECTION('',(-0.970142500145333,-0.24253562503633,0.)) ;
#123642 = DIRECTION('center_axis',(0.242535625036312,-0.970142500145337,-2.89619634903485E-15)) ;
#123643 = DIRECTION('ref_axis',(0.965295032134543,0.241323758033613,0.099841598268988)) ;
#123644 = DIRECTION('center_axis',(0.24253562503633,-0.970142500145333,0.)) ;
#123645 = DIRECTION('ref_axis',(0.,0.,1.)) ;
#123646 = DIRECTION('',(0.,0.,1.)) ;
#123647 = DIRECTION('center_axis',(0.242535625036328,-0.970142500145333,2.72966505896118E-13)) ;
#123648 = DIRECTION('ref_axis',(0.965295032107306,0.241323758026793,-0.0998415985488062)) ;
#123649 = DIRECTION('',(0.970142500145333,0.24253562503633,0.)) ;
#123650 = DIRECTION('',(0.879462917689188,0.219865729422294,-0.42214220049081)) ;
#123651 = DIRECTION('',(-0.879462917689188,-0.219865729422294,-0.42214220049081)) ;
#123652 = DIRECTION('',(-0.970142500145333,-0.24253562503633,0.)) ;
#123653 = DIRECTION('center_axis',(0.242535625036224,-0.970142500145359,8.01522339595377E-13)) ;
#123654 = DIRECTION('ref_axis',(0.965295032121958,0.241323758030457,0.0998415983982931)) ;
#123655 = DIRECTION('center_axis',(0.24253562503633,-0.970142500145333,0.)) ;
#123656 = DIRECTION('ref_axis',(0.,0.,1.)) ;
#123657 = DIRECTION('',(0.,0.,1.)) ;
#123658 = DIRECTION('center_axis',(0.24253562503623,-0.970142500145358,-5.30003931873337E-13)) ;
#123659 = DIRECTION('ref_axis',(0.965295032137309,0.241323758034273,-0.0998415982406524)) ;
#123660 = DIRECTION('',(0.970142500145333,0.24253562503633,0.)) ;
#123661 = DIRECTION('',(0.879462917689188,0.219865729422294,-0.42214220049081)) ;
#123662 = DIRECTION('',(-0.879462917689188,-0.219865729422294,-0.42214220049081)) ;
#123663 = DIRECTION('',(-0.970142500145333,-0.24253562503633,0.)) ;
#123664 = DIRECTION('center_axis',(0.242535625036302,-0.97014250014534,-4.34429452349234E-15)) ;
#123665 = DIRECTION('ref_axis',(0.965295032195617,0.241323758048871,0.0998415976416312)) ;
#123666 = DIRECTION('center_axis',(0.24253562503633,-0.970142500145333,0.)) ;
#123667 = DIRECTION('ref_axis',(0.,0.,1.)) ;
#123668 = DIRECTION('',(0.,0.,1.)) ;
#123669 = DIRECTION('center_axis',(0.242535625036271,-0.970142500145347,-3.54784052751878E-13)) ;
#123670 = DIRECTION('ref_axis',(0.965295032201922,0.241323758050452,-0.0998415975768464)) ;
#123671 = DIRECTION('',(0.970142500145333,0.24253562503633,0.)) ;
#123672 = DIRECTION('',(0.879462917689188,0.219865729422294,-0.42214220049081)) ;
#123673 = DIRECTION('',(-0.879462917689188,-0.219865729422294,-0.42214220049081)) ;
#123674 = DIRECTION('',(-0.970142500145333,-0.24253562503633,0.)) ;
#123675 = DIRECTION('center_axis',(0.242535625036271,-0.970142500145347,3.54784052753445E-13)) ;
#123676 = DIRECTION('ref_axis',(0.965295032195717,0.2413237580489,0.0998415976405848)) ;
#123677 = DIRECTION('center_axis',(-0.707106781186546,-0.707106781186549,
0.)) ;
#123678 = DIRECTION('ref_axis',(0.,0.,-1.)) ;
#123679 = DIRECTION('',(0.707106781186549,-0.707106781186546,0.)) ;
#123680 = DIRECTION('',(0.669589480006976,-0.669589480006974,0.321402950403348)) ;
#123681 = DIRECTION('',(-0.669589480006976,0.669589480006974,0.321402950403348)) ;
#123682 = DIRECTION('',(-0.707106781186549,0.707106781186546,0.)) ;
#123683 = DIRECTION('',(0.,0.,-1.)) ;
#123684 = DIRECTION('center_axis',(-0.707106781186546,-0.707106781186549,
0.)) ;
#123685 = DIRECTION('ref_axis',(0.,0.,-1.)) ;
#123686 = DIRECTION('',(0.,0.,-1.)) ;
#123687 = DIRECTION('center_axis',(0.707106781186535,0.70710678118656,4.97855948833419E-14)) ;
#123688 = DIRECTION('ref_axis',(0.704497887013011,-0.704497887012992,0.0858222254921949)) ;
#123689 = DIRECTION('',(0.707106781186549,-0.707106781186546,0.)) ;
#123690 = DIRECTION('',(0.669589480006976,-0.669589480006974,0.321402950403348)) ;
#123691 = DIRECTION('',(-0.669589480006976,0.669589480006974,0.321402950403348)) ;
#123692 = DIRECTION('',(-0.707106781186549,0.707106781186546,0.)) ;
#123693 = DIRECTION('center_axis',(0.707106781186531,0.707106781186564,-8.40823380250688E-14)) ;
#123694 = DIRECTION('ref_axis',(0.704497887012093,-0.70449788701207,-0.0858222255072959)) ;
#123695 = DIRECTION('center_axis',(-0.707106781186546,-0.707106781186549,
0.)) ;
#123696 = DIRECTION('ref_axis',(0.,0.,-1.)) ;
#123697 = DIRECTION('',(0.,0.,-1.)) ;
#123698 = DIRECTION('center_axis',(0.707106781186544,0.707106781186551,7.74442587073954E-15)) ;
#123699 = DIRECTION('ref_axis',(0.70449788701354,-0.704497887013534,0.0858222254834004)) ;
#123700 = DIRECTION('',(0.707106781186549,-0.707106781186546,0.)) ;
#123701 = DIRECTION('',(0.669589480006976,-0.669589480006974,0.321402950403348)) ;
#123702 = DIRECTION('',(-0.669589480006976,0.669589480006974,0.321402950403348)) ;
#123703 = DIRECTION('',(-0.707106781186549,0.707106781186546,0.)) ;
#123704 = DIRECTION('center_axis',(0.707106781186537,0.707106781186558,-6.25085802423985E-14)) ;
#123705 = DIRECTION('ref_axis',(0.704497887013265,-0.704497887013252,-0.0858222254879714)) ;
#123706 = DIRECTION('center_axis',(-0.707106781186546,-0.707106781186549,
0.)) ;
#123707 = DIRECTION('ref_axis',(0.,0.,-1.)) ;
#123708 = DIRECTION('',(0.,0.,-1.)) ;
#123709 = DIRECTION('center_axis',(0.707106781186549,0.707106781186546,1.65951982944667E-15)) ;
#123710 = DIRECTION('ref_axis',(0.704497887013534,-0.704497887013537,0.0858222254834207)) ;
#123711 = DIRECTION('',(0.707106781186549,-0.707106781186546,0.)) ;
#123712 = DIRECTION('',(0.669589480006976,-0.669589480006974,0.321402950403348)) ;
#123713 = DIRECTION('',(-0.669589480006976,0.669589480006974,0.321402950403348)) ;
#123714 = DIRECTION('',(-0.707106781186549,0.707106781186546,0.)) ;
#123715 = DIRECTION('center_axis',(0.707106781186547,0.707106781186548,-7.1912525942593E-15)) ;
#123716 = DIRECTION('ref_axis',(0.704497887013064,-0.704497887013064,-0.0858222254911589)) ;
#123717 = DIRECTION('center_axis',(-0.707106781186546,-0.707106781186549,
0.)) ;
#123718 = DIRECTION('ref_axis',(0.,0.,-1.)) ;
#123719 = DIRECTION('',(0.,0.,-1.)) ;
#123720 = DIRECTION('center_axis',(0.707106781186549,0.707106781186546,4.42538621185838E-15)) ;
#123721 = DIRECTION('ref_axis',(0.70449788701323,-0.704497887013233,0.0858222254884169)) ;
#123722 = DIRECTION('',(0.707106781186549,-0.707106781186546,0.)) ;
#123723 = DIRECTION('',(0.669589480006976,-0.669589480006974,0.321402950403348)) ;
#123724 = DIRECTION('',(-0.669589480006976,0.669589480006974,0.321402950403348)) ;
#123725 = DIRECTION('',(-0.707106781186549,0.707106781186546,0.)) ;
#123726 = DIRECTION('center_axis',(0.707106781186555,0.70710678118654,3.31903965888224E-14)) ;
#123727 = DIRECTION('ref_axis',(0.704497887013092,-0.704497887013103,-0.0858222254906087)) ;
#123728 = DIRECTION('center_axis',(-0.707106781186546,-0.707106781186549,
0.)) ;
#123729 = DIRECTION('ref_axis',(0.,0.,-1.)) ;
#123730 = DIRECTION('',(0.,0.,-1.)) ;
#123731 = DIRECTION('center_axis',(0.707106781186558,0.707106781186537,-5.75300207541695E-14)) ;
#123732 = DIRECTION('ref_axis',(0.704497887013391,-0.704497887013405,0.0858222254856872)) ;
#123733 = DIRECTION('',(0.707106781186549,-0.707106781186546,0.)) ;
#123734 = DIRECTION('',(0.669589480006976,-0.669589480006974,0.321402950403348)) ;
#123735 = DIRECTION('',(-0.669589480006976,0.669589480006974,0.321402950403348)) ;
#123736 = DIRECTION('',(-0.707106781186549,0.707106781186546,0.)) ;
#123737 = DIRECTION('center_axis',(0.707106781186548,0.707106781186547,-3.87221293536151E-15)) ;
#123738 = DIRECTION('ref_axis',(0.704497887013335,-0.704497887013336,-0.0858222254867023)) ;
#123739 = DIRECTION('center_axis',(-0.707106781186546,-0.707106781186549,
0.)) ;
#123740 = DIRECTION('ref_axis',(0.,0.,-1.)) ;
#123741 = DIRECTION('',(0.,0.,-1.)) ;
#123742 = DIRECTION('center_axis',(0.707106781186543,0.707106781186552,1.7701544847441E-14)) ;
#123743 = DIRECTION('ref_axis',(0.704497887012761,-0.704497887012754,0.0858222254962028)) ;
#123744 = DIRECTION('',(0.707106781186549,-0.707106781186546,0.)) ;
#123745 = DIRECTION('',(0.669589480006976,-0.669589480006974,0.321402950403348)) ;
#123746 = DIRECTION('',(-0.669589480006976,0.669589480006974,0.321402950403348)) ;
#123747 = DIRECTION('',(-0.707106781186549,0.707106781186546,0.)) ;
#123748 = DIRECTION('center_axis',(0.707106781186551,0.707106781186544,1.82547181238502E-14)) ;
#123749 = DIRECTION('ref_axis',(0.704497887013145,-0.70449788701315,-0.0858222254897919)) ;
#123750 = DIRECTION('center_axis',(-0.707106781186546,-0.707106781186549,
0.)) ;
#123751 = DIRECTION('ref_axis',(0.,0.,-1.)) ;
#123752 = DIRECTION('',(0.,0.,-1.)) ;
#123753 = DIRECTION('center_axis',(0.707106781186541,0.707106781186554,2.26801043356451E-14)) ;
#123754 = DIRECTION('ref_axis',(0.704497887008924,-0.704497887008914,0.0858222255592156)) ;
#123755 = DIRECTION('',(0.707106781186549,-0.707106781186546,0.)) ;
#123756 = DIRECTION('',(0.669589480006976,-0.669589480006974,0.321402950403348)) ;
#123757 = DIRECTION('',(-0.669589480006976,0.669589480006974,0.321402950403348)) ;
#123758 = DIRECTION('',(-0.707106781186549,0.707106781186546,0.)) ;
#123759 = DIRECTION('center_axis',(0.707106781186548,0.707106781186547,6.63807931776562E-15)) ;
#123760 = DIRECTION('ref_axis',(0.704497887012742,-0.704497887012742,-0.0858222254964534)) ;
#123761 = DIRECTION('center_axis',(-0.707106781186546,-0.707106781186549,
0.)) ;
#123762 = DIRECTION('ref_axis',(0.,0.,-1.)) ;
#123763 = DIRECTION('',(0.,0.,-1.)) ;
#123764 = DIRECTION('center_axis',(0.707106781186546,0.707106781186549,-1.6595198294363E-15)) ;
#123765 = DIRECTION('ref_axis',(0.704497887009798,-0.704497887009795,0.0858222255448097)) ;
#123766 = DIRECTION('',(0.707106781186549,-0.707106781186546,0.)) ;
#123767 = DIRECTION('',(0.669589480006976,-0.669589480006974,0.321402950403348)) ;
#123768 = DIRECTION('',(-0.669589480006976,0.669589480006974,0.321402950403348)) ;
#123769 = DIRECTION('',(-0.707106781186549,0.707106781186546,0.)) ;
#123770 = DIRECTION('center_axis',(0.707106781186546,0.707106781186549,-9.40394570014366E-15)) ;
#123771 = DIRECTION('ref_axis',(0.704497887009107,-0.704497887009105,-0.0858222255561507)) ;
#123772 = DIRECTION('center_axis',(1.,0.,2.16840434497101E-16)) ;
#123773 = DIRECTION('ref_axis',(2.16840434497101E-16,0.,-1.)) ;
#123774 = DIRECTION('',(-2.16840434497101E-16,0.,1.)) ;
#123775 = DIRECTION('',(0.,1.,0.)) ;
#123776 = DIRECTION('',(2.16840434497101E-16,0.,-1.)) ;
#123777 = DIRECTION('',(0.,-1.,0.)) ;
#123778 = DIRECTION('center_axis',(2.16840434497101E-16,0.,-1.)) ;
#123779 = DIRECTION('ref_axis',(-1.,0.,-2.16840434497101E-16)) ;
#123780 = DIRECTION('',(-1.,0.,-2.16840434497101E-16)) ;
#123781 = DIRECTION('',(0.,-1.,0.)) ;
#123782 = DIRECTION('',(1.,0.,2.16840434497101E-16)) ;
#123783 = DIRECTION('',(0.,1.,0.)) ;
#123784 = DIRECTION('center_axis',(-1.,0.,0.)) ;
#123785 = DIRECTION('ref_axis',(0.,0.,1.)) ;
#123786 = DIRECTION('',(0.,0.,-1.)) ;
#123787 = DIRECTION('',(0.,1.,0.)) ;
#123788 = DIRECTION('',(0.,0.,1.)) ;
#123789 = DIRECTION('',(0.,-1.,0.)) ;
#123790 = DIRECTION('center_axis',(2.16840434497101E-16,0.,1.)) ;
#123791 = DIRECTION('ref_axis',(1.,0.,-2.16840434497101E-16)) ;
#123792 = DIRECTION('',(-1.,0.,2.16840434497101E-16)) ;
#123793 = DIRECTION('',(0.,1.,0.)) ;
#123794 = DIRECTION('',(1.,0.,-2.16840434497101E-16)) ;
#123795 = DIRECTION('',(0.,-1.,0.)) ;
#123796 = DIRECTION('center_axis',(1.,0.,2.16840434497101E-16)) ;
#123797 = DIRECTION('ref_axis',(2.16840434497101E-16,0.,-1.)) ;
#123798 = DIRECTION('',(-2.16840434497101E-16,0.,1.)) ;
#123799 = DIRECTION('',(0.,1.,0.)) ;
#123800 = DIRECTION('',(2.16840434497101E-16,0.,-1.)) ;
#123801 = DIRECTION('',(0.,-1.,0.)) ;
#123802 = DIRECTION('center_axis',(2.16840434497101E-16,0.,-1.)) ;
#123803 = DIRECTION('ref_axis',(-1.,0.,-2.16840434497101E-16)) ;
#123804 = DIRECTION('',(-1.,0.,-2.16840434497101E-16)) ;
#123805 = DIRECTION('',(0.,-1.,0.)) ;
#123806 = DIRECTION('',(1.,0.,2.16840434497101E-16)) ;
#123807 = DIRECTION('',(0.,1.,0.)) ;
#123808 = DIRECTION('center_axis',(-1.,0.,0.)) ;
#123809 = DIRECTION('ref_axis',(0.,0.,1.)) ;
#123810 = DIRECTION('',(0.,0.,-1.)) ;
#123811 = DIRECTION('',(0.,1.,0.)) ;
#123812 = DIRECTION('',(0.,0.,1.)) ;
#123813 = DIRECTION('',(0.,-1.,0.)) ;
#123814 = DIRECTION('center_axis',(2.16840434497101E-16,0.,1.)) ;
#123815 = DIRECTION('ref_axis',(1.,0.,-2.16840434497101E-16)) ;
#123816 = DIRECTION('',(-1.,0.,2.16840434497101E-16)) ;
#123817 = DIRECTION('',(0.,1.,0.)) ;
#123818 = DIRECTION('',(1.,0.,-2.16840434497101E-16)) ;
#123819 = DIRECTION('',(0.,-1.,0.)) ;
#123820 = DIRECTION('center_axis',(1.,0.,2.16840434497101E-16)) ;
#123821 = DIRECTION('ref_axis',(2.16840434497101E-16,0.,-1.)) ;
#123822 = DIRECTION('',(-2.16840434497101E-16,0.,1.)) ;
#123823 = DIRECTION('',(0.,1.,0.)) ;
#123824 = DIRECTION('',(2.16840434497101E-16,0.,-1.)) ;
#123825 = DIRECTION('',(0.,-1.,0.)) ;
#123826 = DIRECTION('center_axis',(2.16840434497101E-16,0.,-1.)) ;
#123827 = DIRECTION('ref_axis',(-1.,0.,-2.16840434497101E-16)) ;
#123828 = DIRECTION('',(-1.,0.,-2.16840434497101E-16)) ;
#123829 = DIRECTION('',(0.,-1.,0.)) ;
#123830 = DIRECTION('',(1.,0.,2.16840434497101E-16)) ;
#123831 = DIRECTION('',(0.,1.,0.)) ;
#123832 = DIRECTION('center_axis',(-1.,0.,0.)) ;
#123833 = DIRECTION('ref_axis',(0.,0.,1.)) ;
#123834 = DIRECTION('',(0.,0.,-1.)) ;
#123835 = DIRECTION('',(0.,1.,0.)) ;
#123836 = DIRECTION('',(0.,0.,1.)) ;
#123837 = DIRECTION('',(0.,-1.,0.)) ;
#123838 = DIRECTION('center_axis',(2.16840434497101E-16,0.,1.)) ;
#123839 = DIRECTION('ref_axis',(1.,0.,-2.16840434497101E-16)) ;
#123840 = DIRECTION('',(-1.,0.,2.16840434497101E-16)) ;
#123841 = DIRECTION('',(0.,1.,0.)) ;
#123842 = DIRECTION('',(1.,0.,-2.16840434497101E-16)) ;
#123843 = DIRECTION('',(0.,-1.,0.)) ;
#123844 = DIRECTION('center_axis',(1.,0.,2.16840434497101E-16)) ;
#123845 = DIRECTION('ref_axis',(2.16840434497101E-16,0.,-1.)) ;
#123846 = DIRECTION('',(-2.16840434497101E-16,0.,1.)) ;
#123847 = DIRECTION('',(0.,1.,0.)) ;
#123848 = DIRECTION('',(2.16840434497101E-16,0.,-1.)) ;
#123849 = DIRECTION('',(0.,-1.,0.)) ;
#123850 = DIRECTION('center_axis',(2.16840434497101E-16,0.,-1.)) ;
#123851 = DIRECTION('ref_axis',(-1.,0.,-2.16840434497101E-16)) ;
#123852 = DIRECTION('',(-1.,0.,-2.16840434497101E-16)) ;
#123853 = DIRECTION('',(0.,-1.,0.)) ;
#123854 = DIRECTION('',(1.,0.,2.16840434497101E-16)) ;
#123855 = DIRECTION('',(0.,1.,0.)) ;
#123856 = DIRECTION('center_axis',(-1.,0.,0.)) ;
#123857 = DIRECTION('ref_axis',(0.,0.,1.)) ;
#123858 = DIRECTION('',(0.,0.,-1.)) ;
#123859 = DIRECTION('',(0.,1.,0.)) ;
#123860 = DIRECTION('',(0.,0.,1.)) ;
#123861 = DIRECTION('',(0.,-1.,0.)) ;
#123862 = DIRECTION('center_axis',(2.16840434497101E-16,0.,1.)) ;
#123863 = DIRECTION('ref_axis',(1.,0.,-2.16840434497101E-16)) ;
#123864 = DIRECTION('',(-1.,0.,2.16840434497101E-16)) ;
#123865 = DIRECTION('',(0.,1.,0.)) ;
#123866 = DIRECTION('',(1.,0.,-2.16840434497101E-16)) ;
#123867 = DIRECTION('',(0.,-1.,0.)) ;
#123868 = DIRECTION('center_axis',(1.,0.,2.16840434497101E-16)) ;
#123869 = DIRECTION('ref_axis',(2.16840434497101E-16,0.,-1.)) ;
#123870 = DIRECTION('',(-2.16840434497101E-16,0.,1.)) ;
#123871 = DIRECTION('',(0.,1.,0.)) ;
#123872 = DIRECTION('',(2.16840434497101E-16,0.,-1.)) ;
#123873 = DIRECTION('',(0.,-1.,0.)) ;
#123874 = DIRECTION('center_axis',(2.16840434497101E-16,0.,-1.)) ;
#123875 = DIRECTION('ref_axis',(-1.,0.,-2.16840434497101E-16)) ;
#123876 = DIRECTION('',(-1.,0.,-2.16840434497101E-16)) ;
#123877 = DIRECTION('',(0.,-1.,0.)) ;
#123878 = DIRECTION('',(1.,0.,2.16840434497101E-16)) ;
#123879 = DIRECTION('',(0.,1.,0.)) ;
#123880 = DIRECTION('center_axis',(-1.,0.,0.)) ;
#123881 = DIRECTION('ref_axis',(0.,0.,1.)) ;
#123882 = DIRECTION('',(0.,0.,-1.)) ;
#123883 = DIRECTION('',(0.,1.,0.)) ;
#123884 = DIRECTION('',(0.,0.,1.)) ;
#123885 = DIRECTION('',(0.,-1.,0.)) ;
#123886 = DIRECTION('center_axis',(2.16840434497101E-16,0.,1.)) ;
#123887 = DIRECTION('ref_axis',(1.,0.,-2.16840434497101E-16)) ;
#123888 = DIRECTION('',(-1.,0.,2.16840434497101E-16)) ;
#123889 = DIRECTION('',(0.,1.,0.)) ;
#123890 = DIRECTION('',(1.,0.,-2.16840434497101E-16)) ;
#123891 = DIRECTION('',(0.,-1.,0.)) ;
#123892 = DIRECTION('center_axis',(1.,0.,2.16840434497101E-16)) ;
#123893 = DIRECTION('ref_axis',(2.16840434497101E-16,0.,-1.)) ;
#123894 = DIRECTION('',(-2.16840434497101E-16,0.,1.)) ;
#123895 = DIRECTION('',(0.,1.,0.)) ;
#123896 = DIRECTION('',(2.16840434497101E-16,0.,-1.)) ;
#123897 = DIRECTION('',(0.,-1.,0.)) ;
#123898 = DIRECTION('center_axis',(2.16840434497101E-16,0.,-1.)) ;
#123899 = DIRECTION('ref_axis',(-1.,0.,-2.16840434497101E-16)) ;
#123900 = DIRECTION('',(-1.,0.,-2.16840434497101E-16)) ;
#123901 = DIRECTION('',(0.,-1.,0.)) ;
#123902 = DIRECTION('',(1.,0.,2.16840434497101E-16)) ;
#123903 = DIRECTION('',(0.,1.,0.)) ;
#123904 = DIRECTION('center_axis',(-1.,0.,0.)) ;
#123905 = DIRECTION('ref_axis',(0.,0.,1.)) ;
#123906 = DIRECTION('',(0.,0.,-1.)) ;
#123907 = DIRECTION('',(0.,1.,0.)) ;
#123908 = DIRECTION('',(0.,0.,1.)) ;
#123909 = DIRECTION('',(0.,-1.,0.)) ;
#123910 = DIRECTION('center_axis',(2.16840434497101E-16,0.,1.)) ;
#123911 = DIRECTION('ref_axis',(1.,0.,-2.16840434497101E-16)) ;
#123912 = DIRECTION('',(-1.,0.,2.16840434497101E-16)) ;
#123913 = DIRECTION('',(0.,1.,0.)) ;
#123914 = DIRECTION('',(1.,0.,-2.16840434497101E-16)) ;
#123915 = DIRECTION('',(0.,-1.,0.)) ;
#123916 = DIRECTION('center_axis',(1.,0.,2.16840434497101E-16)) ;
#123917 = DIRECTION('ref_axis',(2.16840434497101E-16,0.,-1.)) ;
#123918 = DIRECTION('',(-2.16840434497101E-16,0.,1.)) ;
#123919 = DIRECTION('',(0.,1.,0.)) ;
#123920 = DIRECTION('',(2.16840434497101E-16,0.,-1.)) ;
#123921 = DIRECTION('',(0.,-1.,0.)) ;
#123922 = DIRECTION('center_axis',(2.16840434497101E-16,0.,-1.)) ;
#123923 = DIRECTION('ref_axis',(-1.,0.,-2.16840434497101E-16)) ;
#123924 = DIRECTION('',(-1.,0.,-2.16840434497101E-16)) ;
#123925 = DIRECTION('',(0.,-1.,0.)) ;
#123926 = DIRECTION('',(1.,0.,2.16840434497101E-16)) ;
#123927 = DIRECTION('',(0.,1.,0.)) ;
#123928 = DIRECTION('center_axis',(-1.,0.,0.)) ;
#123929 = DIRECTION('ref_axis',(0.,0.,1.)) ;
#123930 = DIRECTION('',(0.,0.,-1.)) ;
#123931 = DIRECTION('',(0.,1.,0.)) ;
#123932 = DIRECTION('',(0.,0.,1.)) ;
#123933 = DIRECTION('',(0.,-1.,0.)) ;
#123934 = DIRECTION('center_axis',(2.16840434497101E-16,0.,1.)) ;
#123935 = DIRECTION('ref_axis',(1.,0.,-2.16840434497101E-16)) ;
#123936 = DIRECTION('',(-1.,0.,2.16840434497101E-16)) ;
#123937 = DIRECTION('',(0.,1.,0.)) ;
#123938 = DIRECTION('',(1.,0.,-2.16840434497101E-16)) ;
#123939 = DIRECTION('',(0.,-1.,0.)) ;
#123940 = DIRECTION('center_axis',(1.,0.,2.16840434497101E-16)) ;
#123941 = DIRECTION('ref_axis',(2.16840434497101E-16,0.,-1.)) ;
#123942 = DIRECTION('',(-2.16840434497101E-16,0.,1.)) ;
#123943 = DIRECTION('',(0.,1.,0.)) ;
#123944 = DIRECTION('',(2.16840434497101E-16,0.,-1.)) ;
#123945 = DIRECTION('',(0.,-1.,0.)) ;
#123946 = DIRECTION('center_axis',(2.16840434497101E-16,0.,-1.)) ;
#123947 = DIRECTION('ref_axis',(-1.,0.,-2.16840434497101E-16)) ;
#123948 = DIRECTION('',(-1.,0.,-2.16840434497101E-16)) ;
#123949 = DIRECTION('',(0.,-1.,0.)) ;
#123950 = DIRECTION('',(1.,0.,2.16840434497101E-16)) ;
#123951 = DIRECTION('',(0.,1.,0.)) ;
#123952 = DIRECTION('center_axis',(-1.,0.,0.)) ;
#123953 = DIRECTION('ref_axis',(0.,0.,1.)) ;
#123954 = DIRECTION('',(0.,0.,-1.)) ;
#123955 = DIRECTION('',(0.,1.,0.)) ;
#123956 = DIRECTION('',(0.,0.,1.)) ;
#123957 = DIRECTION('',(0.,-1.,0.)) ;
#123958 = DIRECTION('center_axis',(2.16840434497101E-16,0.,1.)) ;
#123959 = DIRECTION('ref_axis',(1.,0.,-2.16840434497101E-16)) ;
#123960 = DIRECTION('',(-1.,0.,2.16840434497101E-16)) ;
#123961 = DIRECTION('',(0.,1.,0.)) ;
#123962 = DIRECTION('',(1.,0.,-2.16840434497101E-16)) ;
#123963 = DIRECTION('',(0.,-1.,0.)) ;
#123964 = DIRECTION('center_axis',(1.,0.,2.16840434497101E-16)) ;
#123965 = DIRECTION('ref_axis',(2.16840434497101E-16,0.,-1.)) ;
#123966 = DIRECTION('',(2.16840434497101E-16,0.,-1.)) ;
#123967 = DIRECTION('',(0.,-1.,0.)) ;
#123968 = DIRECTION('',(-2.16840434497101E-16,0.,1.)) ;
#123969 = DIRECTION('',(0.,1.,0.)) ;
#123970 = DIRECTION('center_axis',(2.16840434497101E-16,0.,-1.)) ;
#123971 = DIRECTION('ref_axis',(-1.,0.,-2.16840434497101E-16)) ;
#123972 = DIRECTION('',(-1.,0.,-2.16840434497101E-16)) ;
#123973 = DIRECTION('',(0.,-1.,0.)) ;
#123974 = DIRECTION('',(1.,0.,2.16840434497101E-16)) ;
#123975 = DIRECTION('',(0.,1.,0.)) ;
#123976 = DIRECTION('center_axis',(-1.,0.,0.)) ;
#123977 = DIRECTION('ref_axis',(0.,0.,1.)) ;
#123978 = DIRECTION('',(0.,1.,0.)) ;
#123979 = DIRECTION('',(0.,0.,1.)) ;
#123980 = DIRECTION('',(0.,-1.,0.)) ;
#123981 = DIRECTION('',(0.,0.,-1.)) ;
#123982 = DIRECTION('center_axis',(2.16840434497101E-16,0.,1.)) ;
#123983 = DIRECTION('ref_axis',(1.,0.,-2.16840434497101E-16)) ;
#123984 = DIRECTION('',(0.,1.,0.)) ;
#123985 = DIRECTION('',(1.,0.,-2.16840434497101E-16)) ;
#123986 = DIRECTION('',(0.,-1.,0.)) ;
#123987 = DIRECTION('',(-1.,0.,2.16840434497101E-16)) ;
#123988 = DIRECTION('center_axis',(0.,-1.,0.)) ;
#123989 = DIRECTION('ref_axis',(0.,0.,-1.)) ;
#123990 = DIRECTION('',(0.,0.,-1.)) ;
#123991 = DIRECTION('',(1.,0.,2.16840434497101E-16)) ;
#123992 = DIRECTION('',(-2.16840434497101E-16,0.,1.)) ;
#123993 = DIRECTION('',(-1.,0.,2.16840434497101E-16)) ;
#123994 = DIRECTION('',(1.,0.,0.)) ;
#123995 = DIRECTION('center_axis',(0.,1.,0.)) ;
#123996 = DIRECTION('ref_axis',(0.,0.,-1.)) ;
#123997 = DIRECTION('',(0.,0.,-1.)) ;
#123998 = DIRECTION('center_axis',(0.,1.,0.)) ;
#123999 = DIRECTION('ref_axis',(0.,0.,-1.)) ;
#124000 = DIRECTION('',(-1.,0.,0.)) ;
#124001 = DIRECTION('center_axis',(0.,1.,0.)) ;
#124002 = DIRECTION('ref_axis',(0.,0.,-1.)) ;
#124003 = DIRECTION('',(0.,0.,1.)) ;
#124004 = DIRECTION('center_axis',(0.,1.,0.)) ;
#124005 = DIRECTION('ref_axis',(0.,0.,-1.)) ;
#124006 = DIRECTION('center_axis',(1.,0.,0.)) ;
#124007 = DIRECTION('ref_axis',(0.,0.,-1.)) ;
#124008 = DIRECTION('',(0.,-1.,0.)) ;
#124009 = DIRECTION('',(0.,0.,-1.)) ;
#124010 = DIRECTION('',(0.,1.,0.)) ;
#124011 = DIRECTION('center_axis',(0.,0.,-1.)) ;
#124012 = DIRECTION('ref_axis',(-1.,0.,0.)) ;
#124013 = DIRECTION('',(0.,-1.,0.)) ;
#124014 = DIRECTION('',(-1.,0.,0.)) ;
#124015 = DIRECTION('',(0.,1.,0.)) ;
#124016 = DIRECTION('center_axis',(-1.,0.,0.)) ;
#124017 = DIRECTION('ref_axis',(0.,0.,1.)) ;
#124018 = DIRECTION('',(0.,0.,1.)) ;
#124019 = DIRECTION('',(0.,1.,0.)) ;
#124020 = DIRECTION('',(0.,-1.,0.)) ;
#124021 = DIRECTION('center_axis',(0.,0.,1.)) ;
#124022 = DIRECTION('ref_axis',(1.,0.,0.)) ;
#124023 = DIRECTION('',(0.,-1.,0.)) ;
#124024 = DIRECTION('',(1.,0.,0.)) ;
#124025 = DIRECTION('',(0.,1.,0.)) ;
#124026 = DIRECTION('center_axis',(0.,-1.,0.)) ;
#124027 = DIRECTION('ref_axis',(0.,0.,-1.)) ;
#124028 = DIRECTION('',(0.,0.,-1.)) ;
#124029 = DIRECTION('',(1.,0.,2.16840434497101E-16)) ;
#124030 = DIRECTION('',(-2.16840434497101E-16,0.,1.)) ;
#124031 = DIRECTION('',(-1.,0.,2.16840434497101E-16)) ;
#124032 = DIRECTION('',(1.,0.,0.)) ;
#124033 = DIRECTION('center_axis',(0.,1.,0.)) ;
#124034 = DIRECTION('ref_axis',(0.,0.,-1.)) ;
#124035 = DIRECTION('',(0.,0.,-1.)) ;
#124036 = DIRECTION('center_axis',(0.,1.,0.)) ;
#124037 = DIRECTION('ref_axis',(0.,0.,-1.)) ;
#124038 = DIRECTION('',(-1.,0.,0.)) ;
#124039 = DIRECTION('center_axis',(0.,1.,0.)) ;
#124040 = DIRECTION('ref_axis',(0.,0.,-1.)) ;
#124041 = DIRECTION('',(0.,0.,1.)) ;
#124042 = DIRECTION('center_axis',(0.,1.,0.)) ;
#124043 = DIRECTION('ref_axis',(0.,0.,-1.)) ;
#124044 = DIRECTION('center_axis',(1.,0.,0.)) ;
#124045 = DIRECTION('ref_axis',(0.,0.,-1.)) ;
#124046 = DIRECTION('',(0.,-1.,0.)) ;
#124047 = DIRECTION('',(0.,0.,-1.)) ;
#124048 = DIRECTION('',(0.,1.,0.)) ;
#124049 = DIRECTION('center_axis',(0.,0.,-1.)) ;
#124050 = DIRECTION('ref_axis',(-1.,0.,0.)) ;
#124051 = DIRECTION('',(0.,-1.,0.)) ;
#124052 = DIRECTION('',(-1.,0.,0.)) ;
#124053 = DIRECTION('',(0.,1.,0.)) ;
#124054 = DIRECTION('center_axis',(-1.,0.,0.)) ;
#124055 = DIRECTION('ref_axis',(0.,0.,1.)) ;
#124056 = DIRECTION('',(0.,0.,1.)) ;
#124057 = DIRECTION('',(0.,1.,0.)) ;
#124058 = DIRECTION('',(0.,-1.,0.)) ;
#124059 = DIRECTION('center_axis',(0.,0.,1.)) ;
#124060 = DIRECTION('ref_axis',(1.,0.,0.)) ;
#124061 = DIRECTION('',(0.,-1.,0.)) ;
#124062 = DIRECTION('',(1.,0.,0.)) ;
#124063 = DIRECTION('',(0.,1.,0.)) ;
#124064 = DIRECTION('center_axis',(0.,-1.,0.)) ;
#124065 = DIRECTION('ref_axis',(0.,0.,-1.)) ;
#124066 = DIRECTION('',(0.,0.,-1.)) ;
#124067 = DIRECTION('',(1.,0.,2.16840434497101E-16)) ;
#124068 = DIRECTION('',(-2.16840434497101E-16,0.,1.)) ;
#124069 = DIRECTION('',(-1.,0.,2.16840434497101E-16)) ;
#124070 = DIRECTION('',(1.,0.,0.)) ;
#124071 = DIRECTION('center_axis',(0.,1.,0.)) ;
#124072 = DIRECTION('ref_axis',(0.,0.,-1.)) ;
#124073 = DIRECTION('',(0.,0.,-1.)) ;
#124074 = DIRECTION('center_axis',(0.,1.,0.)) ;
#124075 = DIRECTION('ref_axis',(0.,0.,-1.)) ;
#124076 = DIRECTION('',(-1.,0.,0.)) ;
#124077 = DIRECTION('center_axis',(0.,1.,0.)) ;
#124078 = DIRECTION('ref_axis',(0.,0.,-1.)) ;
#124079 = DIRECTION('',(0.,0.,1.)) ;
#124080 = DIRECTION('center_axis',(0.,1.,0.)) ;
#124081 = DIRECTION('ref_axis',(0.,0.,-1.)) ;
#124082 = DIRECTION('center_axis',(1.,0.,0.)) ;
#124083 = DIRECTION('ref_axis',(0.,0.,-1.)) ;
#124084 = DIRECTION('',(0.,-1.,0.)) ;
#124085 = DIRECTION('',(0.,0.,-1.)) ;
#124086 = DIRECTION('',(0.,1.,0.)) ;
#124087 = DIRECTION('center_axis',(0.,0.,-1.)) ;
#124088 = DIRECTION('ref_axis',(-1.,0.,0.)) ;
#124089 = DIRECTION('',(0.,-1.,0.)) ;
#124090 = DIRECTION('',(-1.,0.,0.)) ;
#124091 = DIRECTION('',(0.,1.,0.)) ;
#124092 = DIRECTION('center_axis',(-1.,0.,0.)) ;
#124093 = DIRECTION('ref_axis',(0.,0.,1.)) ;
#124094 = DIRECTION('',(0.,0.,1.)) ;
#124095 = DIRECTION('',(0.,1.,0.)) ;
#124096 = DIRECTION('',(0.,-1.,0.)) ;
#124097 = DIRECTION('center_axis',(0.,0.,1.)) ;
#124098 = DIRECTION('ref_axis',(1.,0.,0.)) ;
#124099 = DIRECTION('',(0.,-1.,0.)) ;
#124100 = DIRECTION('',(1.,0.,0.)) ;
#124101 = DIRECTION('',(0.,1.,0.)) ;
#124102 = DIRECTION('center_axis',(0.,-1.,0.)) ;
#124103 = DIRECTION('ref_axis',(0.,0.,-1.)) ;
#124104 = DIRECTION('',(0.,0.,-1.)) ;
#124105 = DIRECTION('',(1.,0.,2.16840434497101E-16)) ;
#124106 = DIRECTION('',(-2.16840434497101E-16,0.,1.)) ;
#124107 = DIRECTION('',(-1.,0.,2.16840434497101E-16)) ;
#124108 = DIRECTION('',(1.,0.,0.)) ;
#124109 = DIRECTION('center_axis',(0.,1.,0.)) ;
#124110 = DIRECTION('ref_axis',(0.,0.,-1.)) ;
#124111 = DIRECTION('',(0.,0.,-1.)) ;
#124112 = DIRECTION('center_axis',(0.,1.,0.)) ;
#124113 = DIRECTION('ref_axis',(0.,0.,-1.)) ;
#124114 = DIRECTION('',(-1.,0.,0.)) ;
#124115 = DIRECTION('center_axis',(0.,1.,0.)) ;
#124116 = DIRECTION('ref_axis',(0.,0.,-1.)) ;
#124117 = DIRECTION('',(0.,0.,1.)) ;
#124118 = DIRECTION('center_axis',(0.,1.,0.)) ;
#124119 = DIRECTION('ref_axis',(0.,0.,-1.)) ;
#124120 = DIRECTION('center_axis',(1.,0.,0.)) ;
#124121 = DIRECTION('ref_axis',(0.,0.,-1.)) ;
#124122 = DIRECTION('',(0.,-1.,0.)) ;
#124123 = DIRECTION('',(0.,0.,-1.)) ;
#124124 = DIRECTION('',(0.,1.,0.)) ;
#124125 = DIRECTION('center_axis',(0.,0.,-1.)) ;
#124126 = DIRECTION('ref_axis',(-1.,0.,0.)) ;
#124127 = DIRECTION('',(0.,-1.,0.)) ;
#124128 = DIRECTION('',(-1.,0.,0.)) ;
#124129 = DIRECTION('',(0.,1.,0.)) ;
#124130 = DIRECTION('center_axis',(-1.,0.,0.)) ;
#124131 = DIRECTION('ref_axis',(0.,0.,1.)) ;
#124132 = DIRECTION('',(0.,0.,1.)) ;
#124133 = DIRECTION('',(0.,1.,0.)) ;
#124134 = DIRECTION('',(0.,-1.,0.)) ;
#124135 = DIRECTION('center_axis',(0.,0.,1.)) ;
#124136 = DIRECTION('ref_axis',(1.,0.,0.)) ;
#124137 = DIRECTION('',(0.,-1.,0.)) ;
#124138 = DIRECTION('',(1.,0.,0.)) ;
#124139 = DIRECTION('',(0.,1.,0.)) ;
#124140 = DIRECTION('center_axis',(0.,-1.,0.)) ;
#124141 = DIRECTION('ref_axis',(0.,0.,-1.)) ;
#124142 = DIRECTION('',(0.,0.,-1.)) ;
#124143 = DIRECTION('',(1.,0.,2.16840434497101E-16)) ;
#124144 = DIRECTION('',(-2.16840434497101E-16,0.,1.)) ;
#124145 = DIRECTION('',(-1.,0.,2.16840434497101E-16)) ;
#124146 = DIRECTION('',(1.,0.,0.)) ;
#124147 = DIRECTION('center_axis',(0.,1.,0.)) ;
#124148 = DIRECTION('ref_axis',(0.,0.,-1.)) ;
#124149 = DIRECTION('',(0.,0.,-1.)) ;
#124150 = DIRECTION('center_axis',(0.,1.,0.)) ;
#124151 = DIRECTION('ref_axis',(0.,0.,-1.)) ;
#124152 = DIRECTION('',(-1.,0.,0.)) ;
#124153 = DIRECTION('center_axis',(0.,1.,0.)) ;
#124154 = DIRECTION('ref_axis',(0.,0.,-1.)) ;
#124155 = DIRECTION('',(0.,0.,1.)) ;
#124156 = DIRECTION('center_axis',(0.,1.,0.)) ;
#124157 = DIRECTION('ref_axis',(0.,0.,-1.)) ;
#124158 = DIRECTION('center_axis',(1.,0.,0.)) ;
#124159 = DIRECTION('ref_axis',(0.,0.,-1.)) ;
#124160 = DIRECTION('',(0.,-1.,0.)) ;
#124161 = DIRECTION('',(0.,0.,-1.)) ;
#124162 = DIRECTION('',(0.,1.,0.)) ;
#124163 = DIRECTION('center_axis',(0.,0.,-1.)) ;
#124164 = DIRECTION('ref_axis',(-1.,0.,0.)) ;
#124165 = DIRECTION('',(0.,-1.,0.)) ;
#124166 = DIRECTION('',(-1.,0.,0.)) ;
#124167 = DIRECTION('',(0.,1.,0.)) ;
#124168 = DIRECTION('center_axis',(-1.,0.,0.)) ;
#124169 = DIRECTION('ref_axis',(0.,0.,1.)) ;
#124170 = DIRECTION('',(0.,0.,1.)) ;
#124171 = DIRECTION('',(0.,1.,0.)) ;
#124172 = DIRECTION('',(0.,-1.,0.)) ;
#124173 = DIRECTION('center_axis',(0.,0.,1.)) ;
#124174 = DIRECTION('ref_axis',(1.,0.,0.)) ;
#124175 = DIRECTION('',(0.,-1.,0.)) ;
#124176 = DIRECTION('',(1.,0.,0.)) ;
#124177 = DIRECTION('',(0.,1.,0.)) ;
#124178 = DIRECTION('center_axis',(0.,-1.,0.)) ;
#124179 = DIRECTION('ref_axis',(0.,0.,-1.)) ;
#124180 = DIRECTION('',(0.,0.,-1.)) ;
#124181 = DIRECTION('',(1.,0.,2.16840434497101E-16)) ;
#124182 = DIRECTION('',(-2.16840434497101E-16,0.,1.)) ;
#124183 = DIRECTION('',(-1.,0.,2.16840434497101E-16)) ;
#124184 = DIRECTION('',(1.,0.,0.)) ;
#124185 = DIRECTION('center_axis',(0.,1.,0.)) ;
#124186 = DIRECTION('ref_axis',(0.,0.,-1.)) ;
#124187 = DIRECTION('',(0.,0.,-1.)) ;
#124188 = DIRECTION('center_axis',(0.,1.,0.)) ;
#124189 = DIRECTION('ref_axis',(0.,0.,-1.)) ;
#124190 = DIRECTION('',(-1.,0.,0.)) ;
#124191 = DIRECTION('center_axis',(0.,1.,0.)) ;
#124192 = DIRECTION('ref_axis',(0.,0.,-1.)) ;
#124193 = DIRECTION('',(0.,0.,1.)) ;
#124194 = DIRECTION('center_axis',(0.,1.,0.)) ;
#124195 = DIRECTION('ref_axis',(0.,0.,-1.)) ;
#124196 = DIRECTION('center_axis',(1.,0.,0.)) ;
#124197 = DIRECTION('ref_axis',(0.,0.,-1.)) ;
#124198 = DIRECTION('',(0.,-1.,0.)) ;
#124199 = DIRECTION('',(0.,0.,-1.)) ;
#124200 = DIRECTION('',(0.,1.,0.)) ;
#124201 = DIRECTION('center_axis',(0.,0.,-1.)) ;
#124202 = DIRECTION('ref_axis',(-1.,0.,0.)) ;
#124203 = DIRECTION('',(0.,-1.,0.)) ;
#124204 = DIRECTION('',(-1.,0.,0.)) ;
#124205 = DIRECTION('',(0.,1.,0.)) ;
#124206 = DIRECTION('center_axis',(-1.,0.,0.)) ;
#124207 = DIRECTION('ref_axis',(0.,0.,1.)) ;
#124208 = DIRECTION('',(0.,0.,1.)) ;
#124209 = DIRECTION('',(0.,1.,0.)) ;
#124210 = DIRECTION('',(0.,-1.,0.)) ;
#124211 = DIRECTION('center_axis',(0.,0.,1.)) ;
#124212 = DIRECTION('ref_axis',(1.,0.,0.)) ;
#124213 = DIRECTION('',(0.,-1.,0.)) ;
#124214 = DIRECTION('',(1.,0.,0.)) ;
#124215 = DIRECTION('',(0.,1.,0.)) ;
#124216 = DIRECTION('center_axis',(0.,-1.,0.)) ;
#124217 = DIRECTION('ref_axis',(0.,0.,-1.)) ;
#124218 = DIRECTION('',(0.,0.,-1.)) ;
#124219 = DIRECTION('',(1.,0.,2.16840434497101E-16)) ;
#124220 = DIRECTION('',(-2.16840434497101E-16,0.,1.)) ;
#124221 = DIRECTION('',(-1.,0.,2.16840434497101E-16)) ;
#124222 = DIRECTION('',(1.,0.,0.)) ;
#124223 = DIRECTION('center_axis',(0.,1.,0.)) ;
#124224 = DIRECTION('ref_axis',(0.,0.,-1.)) ;
#124225 = DIRECTION('',(0.,0.,-1.)) ;
#124226 = DIRECTION('center_axis',(0.,1.,0.)) ;
#124227 = DIRECTION('ref_axis',(0.,0.,-1.)) ;
#124228 = DIRECTION('',(-1.,0.,0.)) ;
#124229 = DIRECTION('center_axis',(0.,1.,0.)) ;
#124230 = DIRECTION('ref_axis',(0.,0.,-1.)) ;
#124231 = DIRECTION('',(0.,0.,1.)) ;
#124232 = DIRECTION('center_axis',(0.,1.,0.)) ;
#124233 = DIRECTION('ref_axis',(0.,0.,-1.)) ;
#124234 = DIRECTION('center_axis',(1.,0.,0.)) ;
#124235 = DIRECTION('ref_axis',(0.,0.,-1.)) ;
#124236 = DIRECTION('',(0.,-1.,0.)) ;
#124237 = DIRECTION('',(0.,0.,-1.)) ;
#124238 = DIRECTION('',(0.,1.,0.)) ;
#124239 = DIRECTION('center_axis',(0.,0.,-1.)) ;
#124240 = DIRECTION('ref_axis',(-1.,0.,0.)) ;
#124241 = DIRECTION('',(0.,-1.,0.)) ;
#124242 = DIRECTION('',(-1.,0.,0.)) ;
#124243 = DIRECTION('',(0.,1.,0.)) ;
#124244 = DIRECTION('center_axis',(-1.,0.,0.)) ;
#124245 = DIRECTION('ref_axis',(0.,0.,1.)) ;
#124246 = DIRECTION('',(0.,0.,1.)) ;
#124247 = DIRECTION('',(0.,1.,0.)) ;
#124248 = DIRECTION('',(0.,-1.,0.)) ;
#124249 = DIRECTION('center_axis',(0.,0.,1.)) ;
#124250 = DIRECTION('ref_axis',(1.,0.,0.)) ;
#124251 = DIRECTION('',(0.,-1.,0.)) ;
#124252 = DIRECTION('',(1.,0.,0.)) ;
#124253 = DIRECTION('',(0.,1.,0.)) ;
#124254 = DIRECTION('center_axis',(0.,-1.,0.)) ;
#124255 = DIRECTION('ref_axis',(0.,0.,-1.)) ;
#124256 = DIRECTION('',(0.,0.,-1.)) ;
#124257 = DIRECTION('',(1.,0.,2.16840434497101E-16)) ;
#124258 = DIRECTION('',(-2.16840434497101E-16,0.,1.)) ;
#124259 = DIRECTION('',(-1.,0.,2.16840434497101E-16)) ;
#124260 = DIRECTION('',(1.,0.,0.)) ;
#124261 = DIRECTION('center_axis',(0.,1.,0.)) ;
#124262 = DIRECTION('ref_axis',(0.,0.,-1.)) ;
#124263 = DIRECTION('',(0.,0.,-1.)) ;
#124264 = DIRECTION('center_axis',(0.,1.,0.)) ;
#124265 = DIRECTION('ref_axis',(0.,0.,-1.)) ;
#124266 = DIRECTION('',(-1.,0.,0.)) ;
#124267 = DIRECTION('center_axis',(0.,1.,0.)) ;
#124268 = DIRECTION('ref_axis',(0.,0.,-1.)) ;
#124269 = DIRECTION('',(0.,0.,1.)) ;
#124270 = DIRECTION('center_axis',(0.,1.,0.)) ;
#124271 = DIRECTION('ref_axis',(0.,0.,-1.)) ;
#124272 = DIRECTION('center_axis',(1.,0.,0.)) ;
#124273 = DIRECTION('ref_axis',(0.,0.,-1.)) ;
#124274 = DIRECTION('',(0.,-1.,0.)) ;
#124275 = DIRECTION('',(0.,0.,-1.)) ;
#124276 = DIRECTION('',(0.,1.,0.)) ;
#124277 = DIRECTION('center_axis',(0.,0.,-1.)) ;
#124278 = DIRECTION('ref_axis',(-1.,0.,0.)) ;
#124279 = DIRECTION('',(0.,-1.,0.)) ;
#124280 = DIRECTION('',(-1.,0.,0.)) ;
#124281 = DIRECTION('',(0.,1.,0.)) ;
#124282 = DIRECTION('center_axis',(-1.,0.,0.)) ;
#124283 = DIRECTION('ref_axis',(0.,0.,1.)) ;
#124284 = DIRECTION('',(0.,0.,1.)) ;
#124285 = DIRECTION('',(0.,1.,0.)) ;
#124286 = DIRECTION('',(0.,-1.,0.)) ;
#124287 = DIRECTION('center_axis',(0.,0.,1.)) ;
#124288 = DIRECTION('ref_axis',(1.,0.,0.)) ;
#124289 = DIRECTION('',(0.,-1.,0.)) ;
#124290 = DIRECTION('',(1.,0.,0.)) ;
#124291 = DIRECTION('',(0.,1.,0.)) ;
#124292 = DIRECTION('center_axis',(0.,-1.,0.)) ;
#124293 = DIRECTION('ref_axis',(0.,0.,-1.)) ;
#124294 = DIRECTION('',(0.,0.,-1.)) ;
#124295 = DIRECTION('',(1.,0.,2.16840434497101E-16)) ;
#124296 = DIRECTION('',(-2.16840434497101E-16,0.,1.)) ;
#124297 = DIRECTION('',(-1.,0.,2.16840434497101E-16)) ;
#124298 = DIRECTION('',(1.,0.,0.)) ;
#124299 = DIRECTION('center_axis',(0.,1.,0.)) ;
#124300 = DIRECTION('ref_axis',(0.,0.,-1.)) ;
#124301 = DIRECTION('',(0.,0.,-1.)) ;
#124302 = DIRECTION('center_axis',(0.,1.,0.)) ;
#124303 = DIRECTION('ref_axis',(0.,0.,-1.)) ;
#124304 = DIRECTION('',(-1.,0.,0.)) ;
#124305 = DIRECTION('center_axis',(0.,1.,0.)) ;
#124306 = DIRECTION('ref_axis',(0.,0.,-1.)) ;
#124307 = DIRECTION('',(0.,0.,1.)) ;
#124308 = DIRECTION('center_axis',(0.,1.,0.)) ;
#124309 = DIRECTION('ref_axis',(0.,0.,-1.)) ;
#124310 = DIRECTION('center_axis',(1.,0.,0.)) ;
#124311 = DIRECTION('ref_axis',(0.,0.,-1.)) ;
#124312 = DIRECTION('',(0.,-1.,0.)) ;
#124313 = DIRECTION('',(0.,0.,-1.)) ;
#124314 = DIRECTION('',(0.,1.,0.)) ;
#124315 = DIRECTION('center_axis',(0.,0.,-1.)) ;
#124316 = DIRECTION('ref_axis',(-1.,0.,0.)) ;
#124317 = DIRECTION('',(0.,-1.,0.)) ;
#124318 = DIRECTION('',(-1.,0.,0.)) ;
#124319 = DIRECTION('',(0.,1.,0.)) ;
#124320 = DIRECTION('center_axis',(-1.,0.,0.)) ;
#124321 = DIRECTION('ref_axis',(0.,0.,1.)) ;
#124322 = DIRECTION('',(0.,0.,1.)) ;
#124323 = DIRECTION('',(0.,1.,0.)) ;
#124324 = DIRECTION('',(0.,-1.,0.)) ;
#124325 = DIRECTION('center_axis',(0.,0.,1.)) ;
#124326 = DIRECTION('ref_axis',(1.,0.,0.)) ;
#124327 = DIRECTION('',(0.,-1.,0.)) ;
#124328 = DIRECTION('',(1.,0.,0.)) ;
#124329 = DIRECTION('',(0.,1.,0.)) ;
#124330 = DIRECTION('center_axis',(0.,-1.,0.)) ;
#124331 = DIRECTION('ref_axis',(0.,0.,-1.)) ;
#124332 = DIRECTION('',(-1.,0.,0.)) ;
#124333 = DIRECTION('',(0.,0.,-1.)) ;
#124334 = DIRECTION('',(1.,0.,0.)) ;
#124335 = DIRECTION('',(0.,0.,1.)) ;
#124336 = DIRECTION('center_axis',(0.,-1.,0.)) ;
#124337 = DIRECTION('ref_axis',(0.,0.,-1.)) ;
#124338 = DIRECTION('',(-1.,0.,0.)) ;
#124339 = DIRECTION('',(0.,0.,-1.)) ;
#124340 = DIRECTION('',(1.,0.,0.)) ;
#124341 = DIRECTION('',(0.,0.,1.)) ;
#124342 = DIRECTION('center_axis',(0.,-1.,0.)) ;
#124343 = DIRECTION('ref_axis',(0.,0.,-1.)) ;
#124344 = DIRECTION('',(-1.,0.,0.)) ;
#124345 = DIRECTION('',(0.,0.,-1.)) ;
#124346 = DIRECTION('',(1.,0.,0.)) ;
#124347 = DIRECTION('',(0.,0.,1.)) ;
#124348 = DIRECTION('center_axis',(0.,-1.,0.)) ;
#124349 = DIRECTION('ref_axis',(0.,0.,-1.)) ;
#124350 = DIRECTION('',(-1.,0.,0.)) ;
#124351 = DIRECTION('',(0.,0.,-1.)) ;
#124352 = DIRECTION('',(1.,0.,0.)) ;
#124353 = DIRECTION('',(0.,0.,1.)) ;
#124354 = DIRECTION('center_axis',(0.,-1.,0.)) ;
#124355 = DIRECTION('ref_axis',(0.,0.,-1.)) ;
#124356 = DIRECTION('',(-1.,0.,0.)) ;
#124357 = DIRECTION('',(0.,0.,-1.)) ;
#124358 = DIRECTION('',(1.,0.,0.)) ;
#124359 = DIRECTION('',(0.,0.,1.)) ;
#124360 = DIRECTION('center_axis',(0.,-1.,0.)) ;
#124361 = DIRECTION('ref_axis',(0.,0.,-1.)) ;
#124362 = DIRECTION('',(-1.,0.,0.)) ;
#124363 = DIRECTION('',(0.,0.,-1.)) ;
#124364 = DIRECTION('',(1.,0.,0.)) ;
#124365 = DIRECTION('',(0.,0.,1.)) ;
#124366 = DIRECTION('center_axis',(0.,-1.,0.)) ;
#124367 = DIRECTION('ref_axis',(0.,0.,-1.)) ;
#124368 = DIRECTION('',(-1.,0.,0.)) ;
#124369 = DIRECTION('',(0.,0.,-1.)) ;
#124370 = DIRECTION('',(1.,0.,0.)) ;
#124371 = DIRECTION('',(0.,0.,1.)) ;
#124372 = DIRECTION('center_axis',(0.,-1.,0.)) ;
#124373 = DIRECTION('ref_axis',(0.,0.,-1.)) ;
#124374 = DIRECTION('',(-1.,0.,0.)) ;
#124375 = DIRECTION('',(0.,0.,-1.)) ;
#124376 = DIRECTION('',(1.,0.,0.)) ;
#124377 = DIRECTION('',(0.,0.,1.)) ;
#124378 = DIRECTION('center_axis',(0.,-1.,0.)) ;
#124379 = DIRECTION('ref_axis',(0.,0.,-1.)) ;
#124380 = DIRECTION('',(-1.,0.,0.)) ;
#124381 = DIRECTION('',(0.,0.,-1.)) ;
#124382 = DIRECTION('',(1.,0.,0.)) ;
#124383 = DIRECTION('',(0.,0.,1.)) ;
#124384 = DIRECTION('center_axis',(-7.01133629567814E-33,8.97270763436279E-17,
-1.)) ;
#124385 = DIRECTION('ref_axis',(-6.83680877694706E-64,1.,8.97270763436279E-17)) ;
#124386 = DIRECTION('center_axis',(-7.01133629567814E-33,8.97270763436279E-17,
-1.)) ;
#124387 = DIRECTION('ref_axis',(6.29106707073161E-49,1.,8.97270763436279E-17)) ;
#124388 = DIRECTION('center_axis',(-7.01133629567814E-33,8.97270763436279E-17,
-1.)) ;
#124389 = DIRECTION('ref_axis',(6.29106707073161E-49,1.,8.97270763436279E-17)) ;
#124390 = DIRECTION('',(-1.,-7.81406971160724E-17,0.)) ;
#124391 = DIRECTION('',(7.81406971160724E-17,-1.,-8.9727076343628E-17)) ;
#124392 = DIRECTION('',(1.,7.81406971160724E-17,0.)) ;
#124393 = DIRECTION('',(0.,1.,8.9727076343628E-17)) ;
#124394 = DIRECTION('center_axis',(7.01133629567814E-33,-8.97270763436279E-17,
1.)) ;
#124395 = DIRECTION('ref_axis',(6.29106707073161E-49,1.,8.97270763436279E-17)) ;
#124396 = DIRECTION('',(1.,0.,-7.01133629567814E-33)) ;
#124397 = DIRECTION('',(0.,1.,8.9727076343628E-17)) ;
#124398 = DIRECTION('',(-1.,0.,7.01133629567814E-33)) ;
#124399 = DIRECTION('center_axis',(-7.81406971160724E-17,1.,0.)) ;
#124400 = DIRECTION('ref_axis',(-1.,-7.81406971160724E-17,0.)) ;
#124401 = DIRECTION('',(-1.,-7.81406971160724E-17,0.)) ;
#124402 = DIRECTION('',(0.,0.,-1.)) ;
#124403 = DIRECTION('',(1.,7.81406971160724E-17,0.)) ;
#124404 = DIRECTION('',(0.,0.,1.)) ;
#124405 = DIRECTION('center_axis',(-7.01133629567814E-33,8.97270763436279E-17,
1.)) ;
#124406 = DIRECTION('ref_axis',(6.83680877694706E-64,-1.,8.97270763436279E-17)) ;
#124407 = DIRECTION('',(1.,7.81406971160724E-17,0.)) ;
#124408 = DIRECTION('center_axis',(-7.01133629567814E-33,8.97270763436279E-17,
1.)) ;
#124409 = DIRECTION('ref_axis',(-6.29106707073161E-49,-1.,8.97270763436279E-17)) ;
#124410 = DIRECTION('center_axis',(-7.01133629567814E-33,8.97270763436279E-17,
1.)) ;
#124411 = DIRECTION('ref_axis',(-6.29106707073161E-49,-1.,8.97270763436279E-17)) ;
#124412 = DIRECTION('',(1.,0.,7.01133629567814E-33)) ;
#124413 = DIRECTION('',(0.,-1.,8.9727076343628E-17)) ;
#124414 = DIRECTION('',(-1.,0.,-7.01133629567814E-33)) ;
#124415 = DIRECTION('center_axis',(7.01133629567814E-33,-8.97270763436279E-17,
-1.)) ;
#124416 = DIRECTION('ref_axis',(-6.29106707073161E-49,-1.,8.97270763436279E-17)) ;
#124417 = DIRECTION('',(0.,-1.,8.9727076343628E-17)) ;
#124418 = DIRECTION('',(-1.,-7.81406971160724E-17,0.)) ;
#124419 = DIRECTION('',(-7.81406971160724E-17,1.,-8.9727076343628E-17)) ;
#124420 = DIRECTION('center_axis',(-7.81406971160724E-17,1.,-4.8455963016112E-16)) ;
#124421 = DIRECTION('ref_axis',(2.5241768025713E-48,4.8455963016112E-16,1.)) ;
#124422 = DIRECTION('',(1.,7.81406971160724E-17,0.)) ;
#124423 = DIRECTION('',(0.,4.8455963016112E-16,1.)) ;
#124424 = DIRECTION('',(-1.,-7.81406971160724E-17,0.)) ;
#124425 = DIRECTION('',(3.78638272950961E-32,-4.8455963016112E-16,-1.)) ;
#124426 = DIRECTION('center_axis',(-7.01133629567814E-33,8.97270763436279E-17,
-1.)) ;
#124427 = DIRECTION('ref_axis',(-6.83680877694706E-64,1.,8.97270763436279E-17)) ;
#124428 = DIRECTION('center_axis',(-7.01133629567814E-33,8.97270763436279E-17,
-1.)) ;
#124429 = DIRECTION('ref_axis',(6.29106707073161E-49,1.,8.97270763436279E-17)) ;
#124430 = DIRECTION('center_axis',(-7.01133629567814E-33,8.97270763436279E-17,
-1.)) ;
#124431 = DIRECTION('ref_axis',(6.29106707073161E-49,1.,8.97270763436279E-17)) ;
#124432 = DIRECTION('',(-1.,-7.81406971160724E-17,0.)) ;
#124433 = DIRECTION('',(7.81406971160724E-17,-1.,-8.9727076343628E-17)) ;
#124434 = DIRECTION('',(1.,7.81406971160724E-17,0.)) ;
#124435 = DIRECTION('',(0.,1.,8.9727076343628E-17)) ;
#124436 = DIRECTION('center_axis',(7.01133629567814E-33,-8.97270763436279E-17,
1.)) ;
#124437 = DIRECTION('ref_axis',(6.29106707073161E-49,1.,8.97270763436279E-17)) ;
#124438 = DIRECTION('',(1.,0.,-7.01133629567814E-33)) ;
#124439 = DIRECTION('',(0.,1.,8.9727076343628E-17)) ;
#124440 = DIRECTION('',(-1.,0.,7.01133629567814E-33)) ;
#124441 = DIRECTION('center_axis',(-7.81406971160724E-17,1.,0.)) ;
#124442 = DIRECTION('ref_axis',(-1.,-7.81406971160724E-17,0.)) ;
#124443 = DIRECTION('',(-1.,-7.81406971160724E-17,0.)) ;
#124444 = DIRECTION('',(0.,0.,-1.)) ;
#124445 = DIRECTION('',(1.,7.81406971160724E-17,0.)) ;
#124446 = DIRECTION('',(0.,0.,1.)) ;
#124447 = DIRECTION('center_axis',(-7.01133629567814E-33,8.97270763436279E-17,
1.)) ;
#124448 = DIRECTION('ref_axis',(6.83680877694706E-64,-1.,8.97270763436279E-17)) ;
#124449 = DIRECTION('',(1.,7.81406971160724E-17,0.)) ;
#124450 = DIRECTION('center_axis',(-7.01133629567814E-33,8.97270763436279E-17,
1.)) ;
#124451 = DIRECTION('ref_axis',(-6.29106707073161E-49,-1.,8.97270763436279E-17)) ;
#124452 = DIRECTION('center_axis',(-7.01133629567814E-33,8.97270763436279E-17,
1.)) ;
#124453 = DIRECTION('ref_axis',(-6.29106707073161E-49,-1.,8.97270763436279E-17)) ;
#124454 = DIRECTION('',(1.,0.,7.01133629567814E-33)) ;
#124455 = DIRECTION('',(0.,-1.,8.9727076343628E-17)) ;
#124456 = DIRECTION('',(-1.,0.,-7.01133629567814E-33)) ;
#124457 = DIRECTION('center_axis',(7.01133629567814E-33,-8.97270763436279E-17,
-1.)) ;
#124458 = DIRECTION('ref_axis',(-6.29106707073161E-49,-1.,8.97270763436279E-17)) ;
#124459 = DIRECTION('',(0.,-1.,8.9727076343628E-17)) ;
#124460 = DIRECTION('',(-1.,-7.81406971160724E-17,0.)) ;
#124461 = DIRECTION('',(-7.81406971160724E-17,1.,-8.9727076343628E-17)) ;
#124462 = DIRECTION('center_axis',(-7.81406971160724E-17,1.,-4.8455963016112E-16)) ;
#124463 = DIRECTION('ref_axis',(2.5241768025713E-48,4.8455963016112E-16,1.)) ;
#124464 = DIRECTION('',(1.,7.81406971160724E-17,0.)) ;
#124465 = DIRECTION('',(0.,4.8455963016112E-16,1.)) ;
#124466 = DIRECTION('',(-1.,-7.81406971160724E-17,0.)) ;
#124467 = DIRECTION('',(3.78638272950961E-32,-4.8455963016112E-16,-1.)) ;
#124468 = DIRECTION('center_axis',(-7.01133629567814E-33,8.97270763436279E-17,
-1.)) ;
#124469 = DIRECTION('ref_axis',(-6.83680877694706E-64,1.,8.97270763436279E-17)) ;
#124470 = DIRECTION('center_axis',(-7.01133629567814E-33,8.97270763436279E-17,
-1.)) ;
#124471 = DIRECTION('ref_axis',(6.29106707073161E-49,1.,8.97270763436279E-17)) ;
#124472 = DIRECTION('center_axis',(-7.01133629567814E-33,8.97270763436279E-17,
-1.)) ;
#124473 = DIRECTION('ref_axis',(6.29106707073161E-49,1.,8.97270763436279E-17)) ;
#124474 = DIRECTION('',(-1.,-7.81406971160724E-17,0.)) ;
#124475 = DIRECTION('',(7.81406971160724E-17,-1.,-8.9727076343628E-17)) ;
#124476 = DIRECTION('',(1.,7.81406971160724E-17,0.)) ;
#124477 = DIRECTION('',(0.,1.,8.9727076343628E-17)) ;
#124478 = DIRECTION('center_axis',(7.01133629567814E-33,-8.97270763436279E-17,
1.)) ;
#124479 = DIRECTION('ref_axis',(6.29106707073161E-49,1.,8.97270763436279E-17)) ;
#124480 = DIRECTION('',(1.,0.,-7.01133629567814E-33)) ;
#124481 = DIRECTION('',(0.,1.,8.9727076343628E-17)) ;
#124482 = DIRECTION('',(-1.,0.,7.01133629567814E-33)) ;
#124483 = DIRECTION('center_axis',(-7.81406971160724E-17,1.,0.)) ;
#124484 = DIRECTION('ref_axis',(-1.,-7.81406971160724E-17,0.)) ;
#124485 = DIRECTION('',(-1.,-7.81406971160724E-17,0.)) ;
#124486 = DIRECTION('',(0.,0.,-1.)) ;
#124487 = DIRECTION('',(1.,7.81406971160724E-17,0.)) ;
#124488 = DIRECTION('',(0.,0.,1.)) ;
#124489 = DIRECTION('center_axis',(-7.01133629567814E-33,8.97270763436279E-17,
1.)) ;
#124490 = DIRECTION('ref_axis',(6.83680877694706E-64,-1.,8.97270763436279E-17)) ;
#124491 = DIRECTION('',(1.,7.81406971160724E-17,0.)) ;
#124492 = DIRECTION('center_axis',(-7.01133629567814E-33,8.97270763436279E-17,
1.)) ;
#124493 = DIRECTION('ref_axis',(-6.29106707073161E-49,-1.,8.97270763436279E-17)) ;
#124494 = DIRECTION('center_axis',(-7.01133629567814E-33,8.97270763436279E-17,
1.)) ;
#124495 = DIRECTION('ref_axis',(-6.29106707073161E-49,-1.,8.97270763436279E-17)) ;
#124496 = DIRECTION('',(1.,0.,7.01133629567814E-33)) ;
#124497 = DIRECTION('',(0.,-1.,8.9727076343628E-17)) ;
#124498 = DIRECTION('',(-1.,0.,-7.01133629567814E-33)) ;
#124499 = DIRECTION('center_axis',(7.01133629567814E-33,-8.97270763436279E-17,
-1.)) ;
#124500 = DIRECTION('ref_axis',(-6.29106707073161E-49,-1.,8.97270763436279E-17)) ;
#124501 = DIRECTION('',(0.,-1.,8.9727076343628E-17)) ;
#124502 = DIRECTION('',(-1.,-7.81406971160724E-17,0.)) ;
#124503 = DIRECTION('',(-7.81406971160724E-17,1.,-8.9727076343628E-17)) ;
#124504 = DIRECTION('center_axis',(-7.81406971160724E-17,1.,-4.8455963016112E-16)) ;
#124505 = DIRECTION('ref_axis',(2.5241768025713E-48,4.8455963016112E-16,1.)) ;
#124506 = DIRECTION('',(1.,7.81406971160724E-17,0.)) ;
#124507 = DIRECTION('',(0.,4.8455963016112E-16,1.)) ;
#124508 = DIRECTION('',(-1.,-7.81406971160724E-17,0.)) ;
#124509 = DIRECTION('',(3.78638272950961E-32,-4.8455963016112E-16,-1.)) ;
#124510 = DIRECTION('center_axis',(-7.01133629567814E-33,8.97270763436279E-17,
-1.)) ;
#124511 = DIRECTION('ref_axis',(-6.83680877694706E-64,1.,8.97270763436279E-17)) ;
#124512 = DIRECTION('center_axis',(-7.01133629567814E-33,8.97270763436279E-17,
-1.)) ;
#124513 = DIRECTION('ref_axis',(6.29106707073161E-49,1.,8.97270763436279E-17)) ;
#124514 = DIRECTION('center_axis',(-7.01133629567814E-33,8.97270763436279E-17,
-1.)) ;
#124515 = DIRECTION('ref_axis',(6.29106707073161E-49,1.,8.97270763436279E-17)) ;
#124516 = DIRECTION('',(-1.,-7.81406971160724E-17,0.)) ;
#124517 = DIRECTION('',(7.81406971160724E-17,-1.,-8.9727076343628E-17)) ;
#124518 = DIRECTION('',(1.,7.81406971160724E-17,0.)) ;
#124519 = DIRECTION('',(0.,1.,8.9727076343628E-17)) ;
#124520 = DIRECTION('center_axis',(7.01133629567814E-33,-8.97270763436279E-17,
1.)) ;
#124521 = DIRECTION('ref_axis',(6.29106707073161E-49,1.,8.97270763436279E-17)) ;
#124522 = DIRECTION('',(1.,0.,-7.01133629567814E-33)) ;
#124523 = DIRECTION('',(0.,1.,8.9727076343628E-17)) ;
#124524 = DIRECTION('',(-1.,0.,7.01133629567814E-33)) ;
#124525 = DIRECTION('center_axis',(-7.81406971160724E-17,1.,0.)) ;
#124526 = DIRECTION('ref_axis',(-1.,-7.81406971160724E-17,0.)) ;
#124527 = DIRECTION('',(-1.,-7.81406971160724E-17,0.)) ;
#124528 = DIRECTION('',(0.,0.,-1.)) ;
#124529 = DIRECTION('',(1.,7.81406971160724E-17,0.)) ;
#124530 = DIRECTION('',(0.,0.,1.)) ;
#124531 = DIRECTION('center_axis',(-7.01133629567814E-33,8.97270763436279E-17,
1.)) ;
#124532 = DIRECTION('ref_axis',(6.83680877694706E-64,-1.,8.97270763436279E-17)) ;
#124533 = DIRECTION('',(1.,7.81406971160724E-17,0.)) ;
#124534 = DIRECTION('center_axis',(-7.01133629567814E-33,8.97270763436279E-17,
1.)) ;
#124535 = DIRECTION('ref_axis',(-6.29106707073161E-49,-1.,8.97270763436279E-17)) ;
#124536 = DIRECTION('center_axis',(-7.01133629567814E-33,8.97270763436279E-17,
1.)) ;
#124537 = DIRECTION('ref_axis',(-6.29106707073161E-49,-1.,8.97270763436279E-17)) ;
#124538 = DIRECTION('',(1.,0.,7.01133629567814E-33)) ;
#124539 = DIRECTION('',(0.,-1.,8.9727076343628E-17)) ;
#124540 = DIRECTION('',(-1.,0.,-7.01133629567814E-33)) ;
#124541 = DIRECTION('center_axis',(7.01133629567814E-33,-8.97270763436279E-17,
-1.)) ;
#124542 = DIRECTION('ref_axis',(-6.29106707073161E-49,-1.,8.97270763436279E-17)) ;
#124543 = DIRECTION('',(0.,-1.,8.9727076343628E-17)) ;
#124544 = DIRECTION('',(-1.,-7.81406971160724E-17,0.)) ;
#124545 = DIRECTION('',(-7.81406971160724E-17,1.,-8.9727076343628E-17)) ;
#124546 = DIRECTION('center_axis',(-7.81406971160724E-17,1.,-4.8455963016112E-16)) ;
#124547 = DIRECTION('ref_axis',(2.5241768025713E-48,4.8455963016112E-16,1.)) ;
#124548 = DIRECTION('',(1.,7.81406971160724E-17,0.)) ;
#124549 = DIRECTION('',(0.,4.8455963016112E-16,1.)) ;
#124550 = DIRECTION('',(-1.,-7.81406971160724E-17,0.)) ;
#124551 = DIRECTION('',(3.78638272950961E-32,-4.8455963016112E-16,-1.)) ;
#124552 = DIRECTION('center_axis',(-7.01133629567814E-33,8.97270763436279E-17,
-1.)) ;
#124553 = DIRECTION('ref_axis',(-6.83680877694706E-64,1.,8.97270763436279E-17)) ;
#124554 = DIRECTION('center_axis',(-7.01133629567814E-33,8.97270763436279E-17,
-1.)) ;
#124555 = DIRECTION('ref_axis',(6.29106707073161E-49,1.,8.97270763436279E-17)) ;
#124556 = DIRECTION('center_axis',(-7.01133629567814E-33,8.97270763436279E-17,
-1.)) ;
#124557 = DIRECTION('ref_axis',(6.29106707073161E-49,1.,8.97270763436279E-17)) ;
#124558 = DIRECTION('',(-1.,-7.81406971160724E-17,0.)) ;
#124559 = DIRECTION('',(7.81406971160724E-17,-1.,-8.9727076343628E-17)) ;
#124560 = DIRECTION('',(1.,7.81406971160724E-17,0.)) ;
#124561 = DIRECTION('',(0.,1.,8.9727076343628E-17)) ;
#124562 = DIRECTION('center_axis',(7.01133629567814E-33,-8.97270763436279E-17,
1.)) ;
#124563 = DIRECTION('ref_axis',(6.29106707073161E-49,1.,8.97270763436279E-17)) ;
#124564 = DIRECTION('',(1.,0.,-7.01133629567814E-33)) ;
#124565 = DIRECTION('',(0.,1.,8.9727076343628E-17)) ;
#124566 = DIRECTION('',(-1.,0.,7.01133629567814E-33)) ;
#124567 = DIRECTION('center_axis',(-7.81406971160724E-17,1.,0.)) ;
#124568 = DIRECTION('ref_axis',(-1.,-7.81406971160724E-17,0.)) ;
#124569 = DIRECTION('',(-1.,-7.81406971160724E-17,0.)) ;
#124570 = DIRECTION('',(0.,0.,-1.)) ;
#124571 = DIRECTION('',(1.,7.81406971160724E-17,0.)) ;
#124572 = DIRECTION('',(0.,0.,1.)) ;
#124573 = DIRECTION('center_axis',(-7.01133629567814E-33,8.97270763436279E-17,
1.)) ;
#124574 = DIRECTION('ref_axis',(6.83680877694706E-64,-1.,8.97270763436279E-17)) ;
#124575 = DIRECTION('',(1.,7.81406971160724E-17,0.)) ;
#124576 = DIRECTION('center_axis',(-7.01133629567814E-33,8.97270763436279E-17,
1.)) ;
#124577 = DIRECTION('ref_axis',(-6.29106707073161E-49,-1.,8.97270763436279E-17)) ;
#124578 = DIRECTION('center_axis',(-7.01133629567814E-33,8.97270763436279E-17,
1.)) ;
#124579 = DIRECTION('ref_axis',(-6.29106707073161E-49,-1.,8.97270763436279E-17)) ;
#124580 = DIRECTION('',(1.,0.,7.01133629567814E-33)) ;
#124581 = DIRECTION('',(0.,-1.,8.9727076343628E-17)) ;
#124582 = DIRECTION('',(-1.,0.,-7.01133629567814E-33)) ;
#124583 = DIRECTION('center_axis',(7.01133629567814E-33,-8.97270763436279E-17,
-1.)) ;
#124584 = DIRECTION('ref_axis',(-6.29106707073161E-49,-1.,8.97270763436279E-17)) ;
#124585 = DIRECTION('',(0.,-1.,8.9727076343628E-17)) ;
#124586 = DIRECTION('',(-1.,-7.81406971160724E-17,0.)) ;
#124587 = DIRECTION('',(-7.81406971160724E-17,1.,-8.9727076343628E-17)) ;
#124588 = DIRECTION('center_axis',(-7.81406971160724E-17,1.,-4.8455963016112E-16)) ;
#124589 = DIRECTION('ref_axis',(2.5241768025713E-48,4.8455963016112E-16,1.)) ;
#124590 = DIRECTION('',(1.,7.81406971160724E-17,0.)) ;
#124591 = DIRECTION('',(0.,4.8455963016112E-16,1.)) ;
#124592 = DIRECTION('',(-1.,-7.81406971160724E-17,0.)) ;
#124593 = DIRECTION('',(3.78638272950961E-32,-4.8455963016112E-16,-1.)) ;
#124594 = DIRECTION('center_axis',(-7.01133629567814E-33,8.97270763436279E-17,
-1.)) ;
#124595 = DIRECTION('ref_axis',(-6.83680877694706E-64,1.,8.97270763436279E-17)) ;
#124596 = DIRECTION('center_axis',(-7.01133629567814E-33,8.97270763436279E-17,
-1.)) ;
#124597 = DIRECTION('ref_axis',(6.29106707073161E-49,1.,8.97270763436279E-17)) ;
#124598 = DIRECTION('center_axis',(-7.01133629567814E-33,8.97270763436279E-17,
-1.)) ;
#124599 = DIRECTION('ref_axis',(6.29106707073161E-49,1.,8.97270763436279E-17)) ;
#124600 = DIRECTION('',(-1.,-7.81406971160724E-17,0.)) ;
#124601 = DIRECTION('',(7.81406971160724E-17,-1.,-8.9727076343628E-17)) ;
#124602 = DIRECTION('',(1.,7.81406971160724E-17,0.)) ;
#124603 = DIRECTION('',(0.,1.,8.9727076343628E-17)) ;
#124604 = DIRECTION('center_axis',(7.01133629567814E-33,-8.97270763436279E-17,
1.)) ;
#124605 = DIRECTION('ref_axis',(6.29106707073161E-49,1.,8.97270763436279E-17)) ;
#124606 = DIRECTION('',(1.,0.,-7.01133629567814E-33)) ;
#124607 = DIRECTION('',(0.,1.,8.9727076343628E-17)) ;
#124608 = DIRECTION('',(-1.,0.,7.01133629567814E-33)) ;
#124609 = DIRECTION('center_axis',(-7.81406971160724E-17,1.,0.)) ;
#124610 = DIRECTION('ref_axis',(-1.,-7.81406971160724E-17,0.)) ;
#124611 = DIRECTION('',(-1.,-7.81406971160724E-17,0.)) ;
#124612 = DIRECTION('',(0.,0.,-1.)) ;
#124613 = DIRECTION('',(1.,7.81406971160724E-17,0.)) ;
#124614 = DIRECTION('',(0.,0.,1.)) ;
#124615 = DIRECTION('center_axis',(-7.01133629567814E-33,8.97270763436279E-17,
1.)) ;
#124616 = DIRECTION('ref_axis',(6.83680877694706E-64,-1.,8.97270763436279E-17)) ;
#124617 = DIRECTION('',(1.,7.81406971160724E-17,0.)) ;
#124618 = DIRECTION('center_axis',(-7.01133629567814E-33,8.97270763436279E-17,
1.)) ;
#124619 = DIRECTION('ref_axis',(-6.29106707073161E-49,-1.,8.97270763436279E-17)) ;
#124620 = DIRECTION('center_axis',(-7.01133629567814E-33,8.97270763436279E-17,
1.)) ;
#124621 = DIRECTION('ref_axis',(-6.29106707073161E-49,-1.,8.97270763436279E-17)) ;
#124622 = DIRECTION('',(1.,0.,7.01133629567814E-33)) ;
#124623 = DIRECTION('',(0.,-1.,8.9727076343628E-17)) ;
#124624 = DIRECTION('',(-1.,0.,-7.01133629567814E-33)) ;
#124625 = DIRECTION('center_axis',(7.01133629567814E-33,-8.97270763436279E-17,
-1.)) ;
#124626 = DIRECTION('ref_axis',(-6.29106707073161E-49,-1.,8.97270763436279E-17)) ;
#124627 = DIRECTION('',(0.,-1.,8.9727076343628E-17)) ;
#124628 = DIRECTION('',(-1.,-7.81406971160724E-17,0.)) ;
#124629 = DIRECTION('',(-7.81406971160724E-17,1.,-8.9727076343628E-17)) ;
#124630 = DIRECTION('center_axis',(-7.81406971160724E-17,1.,-4.8455963016112E-16)) ;
#124631 = DIRECTION('ref_axis',(2.5241768025713E-48,4.8455963016112E-16,1.)) ;
#124632 = DIRECTION('',(1.,7.81406971160724E-17,0.)) ;
#124633 = DIRECTION('',(0.,4.8455963016112E-16,1.)) ;
#124634 = DIRECTION('',(-1.,-7.81406971160724E-17,0.)) ;
#124635 = DIRECTION('',(3.78638272950961E-32,-4.8455963016112E-16,-1.)) ;
#124636 = DIRECTION('center_axis',(-7.01133629567814E-33,8.97270763436279E-17,
-1.)) ;
#124637 = DIRECTION('ref_axis',(-6.83680877694706E-64,1.,8.97270763436279E-17)) ;
#124638 = DIRECTION('center_axis',(-7.01133629567814E-33,8.97270763436279E-17,
-1.)) ;
#124639 = DIRECTION('ref_axis',(6.29106707073161E-49,1.,8.97270763436279E-17)) ;
#124640 = DIRECTION('center_axis',(-7.01133629567814E-33,8.97270763436279E-17,
-1.)) ;
#124641 = DIRECTION('ref_axis',(6.29106707073161E-49,1.,8.97270763436279E-17)) ;
#124642 = DIRECTION('',(-1.,-7.81406971160724E-17,0.)) ;
#124643 = DIRECTION('',(7.81406971160724E-17,-1.,-8.9727076343628E-17)) ;
#124644 = DIRECTION('',(1.,7.81406971160724E-17,0.)) ;
#124645 = DIRECTION('',(0.,1.,8.9727076343628E-17)) ;
#124646 = DIRECTION('center_axis',(7.01133629567814E-33,-8.97270763436279E-17,
1.)) ;
#124647 = DIRECTION('ref_axis',(6.29106707073161E-49,1.,8.97270763436279E-17)) ;
#124648 = DIRECTION('',(1.,0.,-7.01133629567814E-33)) ;
#124649 = DIRECTION('',(0.,1.,8.9727076343628E-17)) ;
#124650 = DIRECTION('',(-1.,0.,7.01133629567814E-33)) ;
#124651 = DIRECTION('center_axis',(-7.81406971160724E-17,1.,0.)) ;
#124652 = DIRECTION('ref_axis',(-1.,-7.81406971160724E-17,0.)) ;
#124653 = DIRECTION('',(-1.,-7.81406971160724E-17,0.)) ;
#124654 = DIRECTION('',(0.,0.,-1.)) ;
#124655 = DIRECTION('',(1.,7.81406971160724E-17,0.)) ;
#124656 = DIRECTION('',(0.,0.,1.)) ;
#124657 = DIRECTION('center_axis',(-7.01133629567814E-33,8.97270763436279E-17,
1.)) ;
#124658 = DIRECTION('ref_axis',(6.83680877694706E-64,-1.,8.97270763436279E-17)) ;
#124659 = DIRECTION('',(1.,7.81406971160724E-17,0.)) ;
#124660 = DIRECTION('center_axis',(-7.01133629567814E-33,8.97270763436279E-17,
1.)) ;
#124661 = DIRECTION('ref_axis',(-6.29106707073161E-49,-1.,8.97270763436279E-17)) ;
#124662 = DIRECTION('center_axis',(-7.01133629567814E-33,8.97270763436279E-17,
1.)) ;
#124663 = DIRECTION('ref_axis',(-6.29106707073161E-49,-1.,8.97270763436279E-17)) ;
#124664 = DIRECTION('',(1.,0.,7.01133629567814E-33)) ;
#124665 = DIRECTION('',(0.,-1.,8.9727076343628E-17)) ;
#124666 = DIRECTION('',(-1.,0.,-7.01133629567814E-33)) ;
#124667 = DIRECTION('center_axis',(7.01133629567814E-33,-8.97270763436279E-17,
-1.)) ;
#124668 = DIRECTION('ref_axis',(-6.29106707073161E-49,-1.,8.97270763436279E-17)) ;
#124669 = DIRECTION('',(0.,-1.,8.9727076343628E-17)) ;
#124670 = DIRECTION('',(-1.,-7.81406971160724E-17,0.)) ;
#124671 = DIRECTION('',(-7.81406971160724E-17,1.,-8.9727076343628E-17)) ;
#124672 = DIRECTION('center_axis',(-7.81406971160724E-17,1.,-4.8455963016112E-16)) ;
#124673 = DIRECTION('ref_axis',(2.5241768025713E-48,4.8455963016112E-16,1.)) ;
#124674 = DIRECTION('',(1.,7.81406971160724E-17,0.)) ;
#124675 = DIRECTION('',(0.,4.8455963016112E-16,1.)) ;
#124676 = DIRECTION('',(-1.,-7.81406971160724E-17,0.)) ;
#124677 = DIRECTION('',(3.78638272950961E-32,-4.8455963016112E-16,-1.)) ;
#124678 = DIRECTION('center_axis',(-7.01133629567814E-33,8.97270763436279E-17,
-1.)) ;
#124679 = DIRECTION('ref_axis',(-6.83680877694706E-64,1.,8.97270763436279E-17)) ;
#124680 = DIRECTION('center_axis',(-7.01133629567814E-33,8.97270763436279E-17,
-1.)) ;
#124681 = DIRECTION('ref_axis',(6.29106707073161E-49,1.,8.97270763436279E-17)) ;
#124682 = DIRECTION('center_axis',(-7.01133629567814E-33,8.97270763436279E-17,
-1.)) ;
#124683 = DIRECTION('ref_axis',(6.29106707073161E-49,1.,8.97270763436279E-17)) ;
#124684 = DIRECTION('',(-1.,-7.81406971160724E-17,0.)) ;
#124685 = DIRECTION('',(7.81406971160724E-17,-1.,-8.9727076343628E-17)) ;
#124686 = DIRECTION('',(1.,7.81406971160724E-17,0.)) ;
#124687 = DIRECTION('',(0.,1.,8.9727076343628E-17)) ;
#124688 = DIRECTION('center_axis',(7.01133629567814E-33,-8.97270763436279E-17,
1.)) ;
#124689 = DIRECTION('ref_axis',(6.29106707073161E-49,1.,8.97270763436279E-17)) ;
#124690 = DIRECTION('',(1.,0.,-7.01133629567814E-33)) ;
#124691 = DIRECTION('',(0.,1.,8.9727076343628E-17)) ;
#124692 = DIRECTION('',(-1.,0.,7.01133629567814E-33)) ;
#124693 = DIRECTION('center_axis',(-7.81406971160724E-17,1.,0.)) ;
#124694 = DIRECTION('ref_axis',(-1.,-7.81406971160724E-17,0.)) ;
#124695 = DIRECTION('',(-1.,-7.81406971160724E-17,0.)) ;
#124696 = DIRECTION('',(0.,0.,-1.)) ;
#124697 = DIRECTION('',(1.,7.81406971160724E-17,0.)) ;
#124698 = DIRECTION('',(0.,0.,1.)) ;
#124699 = DIRECTION('center_axis',(-7.01133629567814E-33,8.97270763436279E-17,
1.)) ;
#124700 = DIRECTION('ref_axis',(6.83680877694706E-64,-1.,8.97270763436279E-17)) ;
#124701 = DIRECTION('',(1.,7.81406971160724E-17,0.)) ;
#124702 = DIRECTION('center_axis',(-7.01133629567814E-33,8.97270763436279E-17,
1.)) ;
#124703 = DIRECTION('ref_axis',(-6.29106707073161E-49,-1.,8.97270763436279E-17)) ;
#124704 = DIRECTION('center_axis',(-7.01133629567814E-33,8.97270763436279E-17,
1.)) ;
#124705 = DIRECTION('ref_axis',(-6.29106707073161E-49,-1.,8.97270763436279E-17)) ;
#124706 = DIRECTION('',(1.,0.,7.01133629567814E-33)) ;
#124707 = DIRECTION('',(0.,-1.,8.9727076343628E-17)) ;
#124708 = DIRECTION('',(-1.,0.,-7.01133629567814E-33)) ;
#124709 = DIRECTION('center_axis',(7.01133629567814E-33,-8.97270763436279E-17,
-1.)) ;
#124710 = DIRECTION('ref_axis',(-6.29106707073161E-49,-1.,8.97270763436279E-17)) ;
#124711 = DIRECTION('',(0.,-1.,8.9727076343628E-17)) ;
#124712 = DIRECTION('',(-1.,-7.81406971160724E-17,0.)) ;
#124713 = DIRECTION('',(-7.81406971160724E-17,1.,-8.9727076343628E-17)) ;
#124714 = DIRECTION('center_axis',(-7.81406971160724E-17,1.,-4.8455963016112E-16)) ;
#124715 = DIRECTION('ref_axis',(2.5241768025713E-48,4.8455963016112E-16,1.)) ;
#124716 = DIRECTION('',(1.,7.81406971160724E-17,0.)) ;
#124717 = DIRECTION('',(0.,4.8455963016112E-16,1.)) ;
#124718 = DIRECTION('',(-1.,-7.81406971160724E-17,0.)) ;
#124719 = DIRECTION('',(3.78638272950961E-32,-4.8455963016112E-16,-1.)) ;
#124720 = DIRECTION('center_axis',(-7.01133629567814E-33,8.97270763436279E-17,
-1.)) ;
#124721 = DIRECTION('ref_axis',(-6.83680877694706E-64,1.,8.97270763436279E-17)) ;
#124722 = DIRECTION('center_axis',(-7.01133629567814E-33,8.97270763436279E-17,
-1.)) ;
#124723 = DIRECTION('ref_axis',(6.29106707073161E-49,1.,8.97270763436279E-17)) ;
#124724 = DIRECTION('center_axis',(-7.01133629567814E-33,8.97270763436279E-17,
-1.)) ;
#124725 = DIRECTION('ref_axis',(6.29106707073161E-49,1.,8.97270763436279E-17)) ;
#124726 = DIRECTION('',(-1.,-7.81406971160724E-17,0.)) ;
#124727 = DIRECTION('',(7.81406971160724E-17,-1.,-8.9727076343628E-17)) ;
#124728 = DIRECTION('',(1.,7.81406971160724E-17,0.)) ;
#124729 = DIRECTION('',(0.,1.,8.9727076343628E-17)) ;
#124730 = DIRECTION('center_axis',(7.01133629567814E-33,-8.97270763436279E-17,
1.)) ;
#124731 = DIRECTION('ref_axis',(6.29106707073161E-49,1.,8.97270763436279E-17)) ;
#124732 = DIRECTION('',(1.,0.,-7.01133629567814E-33)) ;
#124733 = DIRECTION('',(0.,1.,8.9727076343628E-17)) ;
#124734 = DIRECTION('',(-1.,0.,7.01133629567814E-33)) ;
#124735 = DIRECTION('center_axis',(-7.81406971160724E-17,1.,0.)) ;
#124736 = DIRECTION('ref_axis',(-1.,-7.81406971160724E-17,0.)) ;
#124737 = DIRECTION('',(-1.,-7.81406971160724E-17,0.)) ;
#124738 = DIRECTION('',(0.,0.,-1.)) ;
#124739 = DIRECTION('',(1.,7.81406971160724E-17,0.)) ;
#124740 = DIRECTION('',(0.,0.,1.)) ;
#124741 = DIRECTION('center_axis',(-7.01133629567814E-33,8.97270763436279E-17,
1.)) ;
#124742 = DIRECTION('ref_axis',(6.83680877694706E-64,-1.,8.97270763436279E-17)) ;
#124743 = DIRECTION('',(1.,7.81406971160724E-17,0.)) ;
#124744 = DIRECTION('center_axis',(-7.01133629567814E-33,8.97270763436279E-17,
1.)) ;
#124745 = DIRECTION('ref_axis',(-6.29106707073161E-49,-1.,8.97270763436279E-17)) ;
#124746 = DIRECTION('center_axis',(-7.01133629567814E-33,8.97270763436279E-17,
1.)) ;
#124747 = DIRECTION('ref_axis',(-6.29106707073161E-49,-1.,8.97270763436279E-17)) ;
#124748 = DIRECTION('',(1.,0.,7.01133629567814E-33)) ;
#124749 = DIRECTION('',(0.,-1.,8.9727076343628E-17)) ;
#124750 = DIRECTION('',(-1.,0.,-7.01133629567814E-33)) ;
#124751 = DIRECTION('center_axis',(7.01133629567814E-33,-8.97270763436279E-17,
-1.)) ;
#124752 = DIRECTION('ref_axis',(-6.29106707073161E-49,-1.,8.97270763436279E-17)) ;
#124753 = DIRECTION('',(0.,-1.,8.9727076343628E-17)) ;
#124754 = DIRECTION('',(-1.,-7.81406971160724E-17,0.)) ;
#124755 = DIRECTION('',(-7.81406971160724E-17,1.,-8.9727076343628E-17)) ;
#124756 = DIRECTION('center_axis',(-7.81406971160724E-17,1.,-4.8455963016112E-16)) ;
#124757 = DIRECTION('ref_axis',(2.5241768025713E-48,4.8455963016112E-16,1.)) ;
#124758 = DIRECTION('',(3.78638272950961E-32,-4.8455963016112E-16,-1.)) ;
#124759 = DIRECTION('',(1.,7.81406971160724E-17,0.)) ;
#124760 = DIRECTION('',(0.,4.8455963016112E-16,1.)) ;
#124761 = DIRECTION('',(-1.,-7.81406971160724E-17,0.)) ;
#124762 = DIRECTION('center_axis',(0.,1.,0.)) ;
#124763 = DIRECTION('ref_axis',(0.,0.,1.)) ;
#124764 = DIRECTION('',(-1.,0.,0.)) ;
#124765 = DIRECTION('',(0.,0.,-1.)) ;
#124766 = DIRECTION('',(1.,0.,7.01133629567814E-33)) ;
#124767 = DIRECTION('',(0.,0.,1.)) ;
#124768 = DIRECTION('center_axis',(0.,1.,0.)) ;
#124769 = DIRECTION('ref_axis',(0.,0.,1.)) ;
#124770 = DIRECTION('',(-1.,0.,7.01133629567814E-33)) ;
#124771 = DIRECTION('',(0.,0.,-1.)) ;
#124772 = DIRECTION('',(1.,0.,0.)) ;
#124773 = DIRECTION('',(0.,0.,1.)) ;
#124774 = DIRECTION('center_axis',(-1.,0.,0.)) ;
#124775 = DIRECTION('ref_axis',(0.,0.,1.)) ;
#124776 = DIRECTION('',(-1.,0.,0.)) ;
#124777 = DIRECTION('center_axis',(-1.,0.,0.)) ;
#124778 = DIRECTION('ref_axis',(0.,7.85535158932893E-16,-1.)) ;
#124779 = DIRECTION('',(1.,0.,0.)) ;
#124780 = DIRECTION('center_axis',(1.,0.,0.)) ;
#124781 = DIRECTION('ref_axis',(0.,0.,-1.)) ;
#124782 = DIRECTION('center_axis',(1.,0.,0.)) ;
#124783 = DIRECTION('ref_axis',(0.,0.,-1.)) ;
#124784 = DIRECTION('',(0.,0.,-1.)) ;
#124785 = DIRECTION('center_axis',(-1.,0.,0.)) ;
#124786 = DIRECTION('ref_axis',(0.,0.,-1.)) ;
#124787 = DIRECTION('',(0.,0.,-1.)) ;
#124788 = DIRECTION('',(0.,1.,-8.9727076343628E-17)) ;
#124789 = DIRECTION('',(0.,0.,1.)) ;
#124790 = DIRECTION('',(0.,-1.,-8.9727076343628E-17)) ;
#124791 = DIRECTION('center_axis',(0.,1.,0.)) ;
#124792 = DIRECTION('ref_axis',(0.,0.,1.)) ;
#124793 = DIRECTION('',(-1.,0.,0.)) ;
#124794 = DIRECTION('',(0.,0.,-1.)) ;
#124795 = DIRECTION('',(1.,0.,7.01133629567814E-33)) ;
#124796 = DIRECTION('',(0.,0.,1.)) ;
#124797 = DIRECTION('center_axis',(0.,1.,0.)) ;
#124798 = DIRECTION('ref_axis',(0.,0.,1.)) ;
#124799 = DIRECTION('',(-1.,0.,7.01133629567814E-33)) ;
#124800 = DIRECTION('',(0.,0.,-1.)) ;
#124801 = DIRECTION('',(1.,0.,0.)) ;
#124802 = DIRECTION('',(0.,0.,1.)) ;
#124803 = DIRECTION('center_axis',(-1.,0.,0.)) ;
#124804 = DIRECTION('ref_axis',(0.,0.,1.)) ;
#124805 = DIRECTION('',(-1.,0.,0.)) ;
#124806 = DIRECTION('center_axis',(-1.,0.,0.)) ;
#124807 = DIRECTION('ref_axis',(0.,0.,-1.)) ;
#124808 = DIRECTION('',(1.,0.,0.)) ;
#124809 = DIRECTION('center_axis',(1.,0.,0.)) ;
#124810 = DIRECTION('ref_axis',(0.,0.,-1.)) ;
#124811 = DIRECTION('center_axis',(1.,0.,0.)) ;
#124812 = DIRECTION('ref_axis',(0.,0.,-1.)) ;
#124813 = DIRECTION('',(0.,0.,-1.)) ;
#124814 = DIRECTION('center_axis',(-1.,0.,0.)) ;
#124815 = DIRECTION('ref_axis',(0.,9.87742904470778E-16,-1.)) ;
#124816 = DIRECTION('',(0.,0.,-1.)) ;
#124817 = DIRECTION('',(0.,1.,-8.9727076343628E-17)) ;
#124818 = DIRECTION('',(0.,0.,1.)) ;
#124819 = DIRECTION('',(0.,-1.,-8.9727076343628E-17)) ;
#124820 = DIRECTION('center_axis',(0.,1.,0.)) ;
#124821 = DIRECTION('ref_axis',(0.,0.,1.)) ;
#124822 = DIRECTION('',(-1.,0.,0.)) ;
#124823 = DIRECTION('',(0.,0.,-1.)) ;
#124824 = DIRECTION('',(1.,0.,7.01133629567814E-33)) ;
#124825 = DIRECTION('',(0.,0.,1.)) ;
#124826 = DIRECTION('center_axis',(0.,1.,0.)) ;
#124827 = DIRECTION('ref_axis',(0.,0.,1.)) ;
#124828 = DIRECTION('',(-1.,0.,7.01133629567814E-33)) ;
#124829 = DIRECTION('',(0.,0.,-1.)) ;
#124830 = DIRECTION('',(1.,0.,0.)) ;
#124831 = DIRECTION('',(0.,0.,1.)) ;
#124832 = DIRECTION('center_axis',(-1.,0.,0.)) ;
#124833 = DIRECTION('ref_axis',(0.,0.,1.)) ;
#124834 = DIRECTION('',(-1.,0.,0.)) ;
#124835 = DIRECTION('center_axis',(-1.,0.,0.)) ;
#124836 = DIRECTION('ref_axis',(0.,0.,-1.)) ;
#124837 = DIRECTION('',(1.,0.,0.)) ;
#124838 = DIRECTION('center_axis',(1.,0.,0.)) ;
#124839 = DIRECTION('ref_axis',(0.,0.,-1.)) ;
#124840 = DIRECTION('center_axis',(1.,0.,0.)) ;
#124841 = DIRECTION('ref_axis',(0.,0.,-1.)) ;
#124842 = DIRECTION('',(0.,0.,-1.)) ;
#124843 = DIRECTION('center_axis',(-1.,0.,0.)) ;
#124844 = DIRECTION('ref_axis',(0.,3.45710016564773E-15,-1.)) ;
#124845 = DIRECTION('',(0.,0.,-1.)) ;
#124846 = DIRECTION('',(0.,1.,-8.9727076343628E-17)) ;
#124847 = DIRECTION('',(0.,0.,1.)) ;
#124848 = DIRECTION('',(0.,-1.,-8.9727076343628E-17)) ;
#124849 = DIRECTION('center_axis',(0.,1.,0.)) ;
#124850 = DIRECTION('ref_axis',(0.,0.,1.)) ;
#124851 = DIRECTION('',(-1.,0.,0.)) ;
#124852 = DIRECTION('',(0.,0.,-1.)) ;
#124853 = DIRECTION('',(1.,0.,7.01133629567814E-33)) ;
#124854 = DIRECTION('',(0.,0.,1.)) ;
#124855 = DIRECTION('center_axis',(0.,1.,0.)) ;
#124856 = DIRECTION('ref_axis',(0.,0.,1.)) ;
#124857 = DIRECTION('',(-1.,0.,7.01133629567814E-33)) ;
#124858 = DIRECTION('',(0.,0.,-1.)) ;
#124859 = DIRECTION('',(1.,0.,0.)) ;
#124860 = DIRECTION('',(0.,0.,1.)) ;
#124861 = DIRECTION('center_axis',(-1.,0.,0.)) ;
#124862 = DIRECTION('ref_axis',(0.,0.,1.)) ;
#124863 = DIRECTION('',(-1.,0.,0.)) ;
#124864 = DIRECTION('center_axis',(-1.,0.,0.)) ;
#124865 = DIRECTION('ref_axis',(0.,7.85535158932893E-16,-1.)) ;
#124866 = DIRECTION('',(1.,0.,0.)) ;
#124867 = DIRECTION('center_axis',(1.,0.,0.)) ;
#124868 = DIRECTION('ref_axis',(0.,0.,-1.)) ;
#124869 = DIRECTION('center_axis',(1.,0.,0.)) ;
#124870 = DIRECTION('ref_axis',(0.,0.,-1.)) ;
#124871 = DIRECTION('',(0.,0.,-1.)) ;
#124872 = DIRECTION('center_axis',(-1.,0.,0.)) ;
#124873 = DIRECTION('ref_axis',(0.,0.,-1.)) ;
#124874 = DIRECTION('',(0.,0.,-1.)) ;
#124875 = DIRECTION('',(0.,1.,-8.9727076343628E-17)) ;
#124876 = DIRECTION('',(0.,0.,1.)) ;
#124877 = DIRECTION('',(0.,-1.,-8.9727076343628E-17)) ;
#124878 = DIRECTION('center_axis',(0.,1.,0.)) ;
#124879 = DIRECTION('ref_axis',(0.,0.,1.)) ;
#124880 = DIRECTION('',(-1.,0.,0.)) ;
#124881 = DIRECTION('',(0.,0.,-1.)) ;
#124882 = DIRECTION('',(1.,0.,7.01133629567814E-33)) ;
#124883 = DIRECTION('',(0.,0.,1.)) ;
#124884 = DIRECTION('center_axis',(0.,1.,0.)) ;
#124885 = DIRECTION('ref_axis',(0.,0.,1.)) ;
#124886 = DIRECTION('',(-1.,0.,7.01133629567814E-33)) ;
#124887 = DIRECTION('',(0.,0.,-1.)) ;
#124888 = DIRECTION('',(1.,0.,0.)) ;
#124889 = DIRECTION('',(0.,0.,1.)) ;
#124890 = DIRECTION('center_axis',(-1.,0.,0.)) ;
#124891 = DIRECTION('ref_axis',(0.,0.,1.)) ;
#124892 = DIRECTION('',(-1.,0.,0.)) ;
#124893 = DIRECTION('center_axis',(-1.,0.,0.)) ;
#124894 = DIRECTION('ref_axis',(0.,3.66583074168683E-15,-1.)) ;
#124895 = DIRECTION('',(1.,0.,0.)) ;
#124896 = DIRECTION('center_axis',(1.,0.,0.)) ;
#124897 = DIRECTION('ref_axis',(0.,0.,-1.)) ;
#124898 = DIRECTION('center_axis',(1.,0.,0.)) ;
#124899 = DIRECTION('ref_axis',(0.,0.,-1.)) ;
#124900 = DIRECTION('',(0.,0.,-1.)) ;
#124901 = DIRECTION('center_axis',(-1.,0.,0.)) ;
#124902 = DIRECTION('ref_axis',(0.,-5.43258597458929E-15,-1.)) ;
#124903 = DIRECTION('',(0.,0.,-1.)) ;
#124904 = DIRECTION('',(0.,1.,-8.9727076343628E-17)) ;
#124905 = DIRECTION('',(0.,0.,1.)) ;
#124906 = DIRECTION('',(0.,-1.,-8.9727076343628E-17)) ;
#124907 = DIRECTION('center_axis',(0.,1.,0.)) ;
#124908 = DIRECTION('ref_axis',(0.,0.,1.)) ;
#124909 = DIRECTION('',(-1.,0.,0.)) ;
#124910 = DIRECTION('',(0.,0.,-1.)) ;
#124911 = DIRECTION('',(1.,0.,7.01133629567814E-33)) ;
#124912 = DIRECTION('',(0.,0.,1.)) ;
#124913 = DIRECTION('center_axis',(0.,1.,0.)) ;
#124914 = DIRECTION('ref_axis',(0.,0.,1.)) ;
#124915 = DIRECTION('',(-1.,0.,7.01133629567814E-33)) ;
#124916 = DIRECTION('',(0.,0.,-1.)) ;
#124917 = DIRECTION('',(1.,0.,0.)) ;
#124918 = DIRECTION('',(0.,0.,1.)) ;
#124919 = DIRECTION('center_axis',(-1.,0.,0.)) ;
#124920 = DIRECTION('ref_axis',(0.,0.,1.)) ;
#124921 = DIRECTION('',(-1.,0.,0.)) ;
#124922 = DIRECTION('center_axis',(-1.,0.,0.)) ;
#124923 = DIRECTION('ref_axis',(0.,3.66583074168683E-15,-1.)) ;
#124924 = DIRECTION('',(1.,0.,0.)) ;
#124925 = DIRECTION('center_axis',(1.,0.,0.)) ;
#124926 = DIRECTION('ref_axis',(0.,0.,-1.)) ;
#124927 = DIRECTION('center_axis',(1.,0.,0.)) ;
#124928 = DIRECTION('ref_axis',(0.,0.,-1.)) ;
#124929 = DIRECTION('',(0.,0.,-1.)) ;
#124930 = DIRECTION('center_axis',(-1.,0.,0.)) ;
#124931 = DIRECTION('ref_axis',(0.,-5.43258597458929E-15,-1.)) ;
#124932 = DIRECTION('',(0.,0.,-1.)) ;
#124933 = DIRECTION('',(0.,1.,-8.9727076343628E-17)) ;
#124934 = DIRECTION('',(0.,0.,1.)) ;
#124935 = DIRECTION('',(0.,-1.,-8.9727076343628E-17)) ;
#124936 = DIRECTION('center_axis',(0.,1.,0.)) ;
#124937 = DIRECTION('ref_axis',(0.,0.,1.)) ;
#124938 = DIRECTION('',(-1.,0.,0.)) ;
#124939 = DIRECTION('',(0.,0.,-1.)) ;
#124940 = DIRECTION('',(1.,0.,7.01133629567814E-33)) ;
#124941 = DIRECTION('',(0.,0.,1.)) ;
#124942 = DIRECTION('center_axis',(0.,1.,0.)) ;
#124943 = DIRECTION('ref_axis',(0.,0.,1.)) ;
#124944 = DIRECTION('',(-1.,0.,7.01133629567814E-33)) ;
#124945 = DIRECTION('',(0.,0.,-1.)) ;
#124946 = DIRECTION('',(1.,0.,0.)) ;
#124947 = DIRECTION('',(0.,0.,1.)) ;
#124948 = DIRECTION('center_axis',(-1.,0.,0.)) ;
#124949 = DIRECTION('ref_axis',(0.,0.,1.)) ;
#124950 = DIRECTION('',(-1.,0.,0.)) ;
#124951 = DIRECTION('center_axis',(-1.,0.,0.)) ;
#124952 = DIRECTION('ref_axis',(0.,3.66583074168683E-15,-1.)) ;
#124953 = DIRECTION('',(1.,0.,0.)) ;
#124954 = DIRECTION('center_axis',(1.,0.,0.)) ;
#124955 = DIRECTION('ref_axis',(0.,0.,-1.)) ;
#124956 = DIRECTION('center_axis',(1.,0.,0.)) ;
#124957 = DIRECTION('ref_axis',(0.,0.,-1.)) ;
#124958 = DIRECTION('',(0.,0.,-1.)) ;
#124959 = DIRECTION('center_axis',(-1.,0.,0.)) ;
#124960 = DIRECTION('ref_axis',(0.,-5.43258597458929E-15,-1.)) ;
#124961 = DIRECTION('',(0.,0.,-1.)) ;
#124962 = DIRECTION('',(0.,1.,-8.9727076343628E-17)) ;
#124963 = DIRECTION('',(0.,0.,1.)) ;
#124964 = DIRECTION('',(0.,-1.,-8.9727076343628E-17)) ;
#124965 = DIRECTION('center_axis',(0.,1.,0.)) ;
#124966 = DIRECTION('ref_axis',(0.,0.,1.)) ;
#124967 = DIRECTION('',(-1.,0.,0.)) ;
#124968 = DIRECTION('',(0.,0.,-1.)) ;
#124969 = DIRECTION('',(1.,0.,7.01133629567814E-33)) ;
#124970 = DIRECTION('',(0.,0.,1.)) ;
#124971 = DIRECTION('center_axis',(0.,1.,0.)) ;
#124972 = DIRECTION('ref_axis',(0.,0.,1.)) ;
#124973 = DIRECTION('',(-1.,0.,7.01133629567814E-33)) ;
#124974 = DIRECTION('',(0.,0.,-1.)) ;
#124975 = DIRECTION('',(1.,0.,0.)) ;
#124976 = DIRECTION('',(0.,0.,1.)) ;
#124977 = DIRECTION('center_axis',(-1.,0.,0.)) ;
#124978 = DIRECTION('ref_axis',(0.,0.,1.)) ;
#124979 = DIRECTION('',(-1.,0.,0.)) ;
#124980 = DIRECTION('center_axis',(-1.,0.,0.)) ;
#124981 = DIRECTION('ref_axis',(0.,1.83291537084341E-15,-1.)) ;
#124982 = DIRECTION('',(1.,0.,0.)) ;
#124983 = DIRECTION('center_axis',(1.,0.,0.)) ;
#124984 = DIRECTION('ref_axis',(0.,0.,-1.)) ;
#124985 = DIRECTION('center_axis',(1.,0.,0.)) ;
#124986 = DIRECTION('ref_axis',(0.,0.,-1.)) ;
#124987 = DIRECTION('',(0.,0.,-1.)) ;
#124988 = DIRECTION('center_axis',(-1.,0.,0.)) ;
#124989 = DIRECTION('ref_axis',(0.,-5.43258597458929E-15,-1.)) ;
#124990 = DIRECTION('',(0.,0.,-1.)) ;
#124991 = DIRECTION('',(0.,1.,-8.9727076343628E-17)) ;
#124992 = DIRECTION('',(0.,0.,1.)) ;
#124993 = DIRECTION('',(0.,-1.,-8.9727076343628E-17)) ;
#124994 = DIRECTION('center_axis',(0.,1.,0.)) ;
#124995 = DIRECTION('ref_axis',(0.,0.,1.)) ;
#124996 = DIRECTION('',(-1.,0.,0.)) ;
#124997 = DIRECTION('',(0.,0.,-1.)) ;
#124998 = DIRECTION('',(1.,0.,7.01133629567814E-33)) ;
#124999 = DIRECTION('',(0.,0.,1.)) ;
#125000 = DIRECTION('center_axis',(0.,1.,0.)) ;
#125001 = DIRECTION('ref_axis',(0.,0.,1.)) ;
#125002 = DIRECTION('',(-1.,0.,7.01133629567814E-33)) ;
#125003 = DIRECTION('',(0.,0.,-1.)) ;
#125004 = DIRECTION('',(1.,0.,0.)) ;
#125005 = DIRECTION('',(0.,0.,1.)) ;
#125006 = DIRECTION('center_axis',(-1.,0.,0.)) ;
#125007 = DIRECTION('ref_axis',(0.,0.,1.)) ;
#125008 = DIRECTION('',(-1.,0.,0.)) ;
#125009 = DIRECTION('center_axis',(-1.,0.,0.)) ;
#125010 = DIRECTION('ref_axis',(0.,0.,-1.)) ;
#125011 = DIRECTION('',(1.,0.,0.)) ;
#125012 = DIRECTION('center_axis',(1.,0.,0.)) ;
#125013 = DIRECTION('ref_axis',(0.,0.,-1.)) ;
#125014 = DIRECTION('center_axis',(1.,0.,0.)) ;
#125015 = DIRECTION('ref_axis',(0.,0.,-1.)) ;
#125016 = DIRECTION('',(0.,0.,-1.)) ;
#125017 = DIRECTION('center_axis',(-1.,0.,0.)) ;
#125018 = DIRECTION('ref_axis',(0.,-5.43258597458929E-15,-1.)) ;
#125019 = DIRECTION('',(0.,0.,-1.)) ;
#125020 = DIRECTION('',(0.,1.,-8.9727076343628E-17)) ;
#125021 = DIRECTION('',(0.,0.,1.)) ;
#125022 = DIRECTION('',(0.,-1.,-8.9727076343628E-17)) ;
#125023 = DIRECTION('center_axis',(1.,0.,0.)) ;
#125024 = DIRECTION('ref_axis',(0.,0.,-1.)) ;
#125025 = DIRECTION('center_axis',(1.,0.,0.)) ;
#125026 = DIRECTION('ref_axis',(0.,0.,-1.)) ;
#125027 = DIRECTION('center_axis',(1.,0.,0.)) ;
#125028 = DIRECTION('ref_axis',(0.,0.,-1.)) ;
#125029 = DIRECTION('center_axis',(1.,0.,0.)) ;
#125030 = DIRECTION('ref_axis',(0.,0.,-1.)) ;
#125031 = DIRECTION('center_axis',(1.,0.,0.)) ;
#125032 = DIRECTION('ref_axis',(0.,0.,-1.)) ;
#125033 = DIRECTION('center_axis',(1.,0.,0.)) ;
#125034 = DIRECTION('ref_axis',(0.,0.,-1.)) ;
#125035 = DIRECTION('center_axis',(1.,0.,0.)) ;
#125036 = DIRECTION('ref_axis',(0.,0.,-1.)) ;
#125037 = DIRECTION('center_axis',(1.,0.,0.)) ;
#125038 = DIRECTION('ref_axis',(0.,0.,-1.)) ;
#125039 = DIRECTION('center_axis',(1.,0.,0.)) ;
#125040 = DIRECTION('ref_axis',(0.,0.,-1.)) ;
#125041 = DIRECTION('center_axis',(1.,-1.31418445149758E-16,-2.16840434497101E-16)) ;
#125042 = DIRECTION('ref_axis',(-2.16840434497101E-16,0.,-1.)) ;
#125043 = DIRECTION('',(2.16840434497101E-16,0.,1.)) ;
#125044 = DIRECTION('',(1.31418445149758E-16,1.,0.)) ;
#125045 = DIRECTION('',(-2.16840434497101E-16,-2.8496832747207E-32,-1.)) ;
#125046 = DIRECTION('',(-1.31418445149758E-16,-1.,0.)) ;
#125047 = DIRECTION('center_axis',(-2.16840434497101E-16,2.8496832747207E-32,
1.)) ;
#125048 = DIRECTION('ref_axis',(1.,4.92915281362991E-64,2.16840434497101E-16)) ;
#125049 = DIRECTION('',(1.,1.31418445149758E-16,2.16840434497101E-16)) ;
#125050 = DIRECTION('',(-1.31418445149758E-16,-1.,0.)) ;
#125051 = DIRECTION('',(-1.,0.,-2.16840434497101E-16)) ;
#125052 = DIRECTION('',(1.31418445149758E-16,1.,0.)) ;
#125053 = DIRECTION('center_axis',(-1.,1.31418445149758E-16,4.33680868994202E-16)) ;
#125054 = DIRECTION('ref_axis',(4.33680868994202E-16,0.,1.)) ;
#125055 = DIRECTION('',(-1.31418445149758E-16,-1.,0.)) ;
#125056 = DIRECTION('',(-4.33680868994202E-16,0.,-1.)) ;
#125057 = DIRECTION('',(1.31418445149758E-16,1.,0.)) ;
#125058 = DIRECTION('',(4.33680868994202E-16,5.69936654944139E-32,1.)) ;
#125059 = DIRECTION('center_axis',(-2.16840434497101E-16,2.8496832747207E-32,
-1.)) ;
#125060 = DIRECTION('ref_axis',(-1.,-4.92915281362991E-64,2.16840434497101E-16)) ;
#125061 = DIRECTION('',(1.,0.,-2.16840434497101E-16)) ;
#125062 = DIRECTION('',(1.31418445149758E-16,1.,0.)) ;
#125063 = DIRECTION('',(-1.,-1.31418445149758E-16,2.16840434497101E-16)) ;
#125064 = DIRECTION('',(-1.31418445149758E-16,-1.,0.)) ;
#125065 = DIRECTION('center_axis',(1.,-1.31418445149758E-16,-2.16840434497101E-16)) ;
#125066 = DIRECTION('ref_axis',(-2.16840434497101E-16,0.,-1.)) ;
#125067 = DIRECTION('',(2.16840434497101E-16,0.,1.)) ;
#125068 = DIRECTION('',(1.31418445149758E-16,1.,0.)) ;
#125069 = DIRECTION('',(-2.16840434497101E-16,-2.8496832747207E-32,-1.)) ;
#125070 = DIRECTION('',(-1.31418445149758E-16,-1.,0.)) ;
#125071 = DIRECTION('center_axis',(-2.16840434497101E-16,2.8496832747207E-32,
1.)) ;
#125072 = DIRECTION('ref_axis',(1.,4.92915281362991E-64,2.16840434497101E-16)) ;
#125073 = DIRECTION('',(1.,1.31418445149758E-16,2.16840434497101E-16)) ;
#125074 = DIRECTION('',(-1.31418445149758E-16,-1.,0.)) ;
#125075 = DIRECTION('',(-1.,0.,-2.16840434497101E-16)) ;
#125076 = DIRECTION('',(1.31418445149758E-16,1.,0.)) ;
#125077 = DIRECTION('center_axis',(-1.,1.31418445149758E-16,4.33680868994202E-16)) ;
#125078 = DIRECTION('ref_axis',(4.33680868994202E-16,0.,1.)) ;
#125079 = DIRECTION('',(-1.31418445149758E-16,-1.,0.)) ;
#125080 = DIRECTION('',(-4.33680868994202E-16,0.,-1.)) ;
#125081 = DIRECTION('',(1.31418445149758E-16,1.,0.)) ;
#125082 = DIRECTION('',(4.33680868994202E-16,5.69936654944139E-32,1.)) ;
#125083 = DIRECTION('center_axis',(-2.16840434497101E-16,2.8496832747207E-32,
-1.)) ;
#125084 = DIRECTION('ref_axis',(-1.,-4.92915281362991E-64,2.16840434497101E-16)) ;
#125085 = DIRECTION('',(1.,0.,-2.16840434497101E-16)) ;
#125086 = DIRECTION('',(1.31418445149758E-16,1.,0.)) ;
#125087 = DIRECTION('',(-1.,-1.31418445149758E-16,2.16840434497101E-16)) ;
#125088 = DIRECTION('',(-1.31418445149758E-16,-1.,0.)) ;
#125089 = DIRECTION('center_axis',(1.,-1.31418445149758E-16,-2.16840434497101E-16)) ;
#125090 = DIRECTION('ref_axis',(-2.16840434497101E-16,0.,-1.)) ;
#125091 = DIRECTION('',(2.16840434497101E-16,0.,1.)) ;
#125092 = DIRECTION('',(1.31418445149758E-16,1.,0.)) ;
#125093 = DIRECTION('',(-2.16840434497101E-16,-2.8496832747207E-32,-1.)) ;
#125094 = DIRECTION('',(-1.31418445149758E-16,-1.,0.)) ;
#125095 = DIRECTION('center_axis',(-2.16840434497101E-16,2.8496832747207E-32,
1.)) ;
#125096 = DIRECTION('ref_axis',(1.,4.92915281362991E-64,2.16840434497101E-16)) ;
#125097 = DIRECTION('',(1.,1.31418445149758E-16,2.16840434497101E-16)) ;
#125098 = DIRECTION('',(-1.31418445149758E-16,-1.,0.)) ;
#125099 = DIRECTION('',(-1.,0.,-2.16840434497101E-16)) ;
#125100 = DIRECTION('',(1.31418445149758E-16,1.,0.)) ;
#125101 = DIRECTION('center_axis',(-1.,1.31418445149758E-16,4.33680868994202E-16)) ;
#125102 = DIRECTION('ref_axis',(4.33680868994202E-16,0.,1.)) ;
#125103 = DIRECTION('',(-1.31418445149758E-16,-1.,0.)) ;
#125104 = DIRECTION('',(-4.33680868994202E-16,0.,-1.)) ;
#125105 = DIRECTION('',(1.31418445149758E-16,1.,0.)) ;
#125106 = DIRECTION('',(4.33680868994202E-16,5.69936654944139E-32,1.)) ;
#125107 = DIRECTION('center_axis',(-2.16840434497101E-16,2.8496832747207E-32,
-1.)) ;
#125108 = DIRECTION('ref_axis',(-1.,-4.92915281362991E-64,2.16840434497101E-16)) ;
#125109 = DIRECTION('',(1.,0.,-2.16840434497101E-16)) ;
#125110 = DIRECTION('',(1.31418445149758E-16,1.,0.)) ;
#125111 = DIRECTION('',(-1.,-1.31418445149758E-16,2.16840434497101E-16)) ;
#125112 = DIRECTION('',(-1.31418445149758E-16,-1.,0.)) ;
#125113 = DIRECTION('center_axis',(1.,-1.31418445149758E-16,-2.16840434497101E-16)) ;
#125114 = DIRECTION('ref_axis',(-2.16840434497101E-16,0.,-1.)) ;
#125115 = DIRECTION('',(2.16840434497101E-16,0.,1.)) ;
#125116 = DIRECTION('',(1.31418445149758E-16,1.,0.)) ;
#125117 = DIRECTION('',(-2.16840434497101E-16,-2.8496832747207E-32,-1.)) ;
#125118 = DIRECTION('',(-1.31418445149758E-16,-1.,0.)) ;
#125119 = DIRECTION('center_axis',(-2.16840434497101E-16,2.8496832747207E-32,
1.)) ;
#125120 = DIRECTION('ref_axis',(1.,4.92915281362991E-64,2.16840434497101E-16)) ;
#125121 = DIRECTION('',(1.,1.31418445149758E-16,2.16840434497101E-16)) ;
#125122 = DIRECTION('',(-1.31418445149758E-16,-1.,0.)) ;
#125123 = DIRECTION('',(-1.,0.,-2.16840434497101E-16)) ;
#125124 = DIRECTION('',(1.31418445149758E-16,1.,0.)) ;
#125125 = DIRECTION('center_axis',(-1.,1.31418445149758E-16,4.33680868994202E-16)) ;
#125126 = DIRECTION('ref_axis',(4.33680868994202E-16,0.,1.)) ;
#125127 = DIRECTION('',(-1.31418445149758E-16,-1.,0.)) ;
#125128 = DIRECTION('',(-4.33680868994202E-16,0.,-1.)) ;
#125129 = DIRECTION('',(1.31418445149758E-16,1.,0.)) ;
#125130 = DIRECTION('',(4.33680868994202E-16,5.69936654944139E-32,1.)) ;
#125131 = DIRECTION('center_axis',(-2.16840434497101E-16,2.8496832747207E-32,
-1.)) ;
#125132 = DIRECTION('ref_axis',(-1.,-4.92915281362991E-64,2.16840434497101E-16)) ;
#125133 = DIRECTION('',(1.,0.,-2.16840434497101E-16)) ;
#125134 = DIRECTION('',(1.31418445149758E-16,1.,0.)) ;
#125135 = DIRECTION('',(-1.,-1.31418445149758E-16,2.16840434497101E-16)) ;
#125136 = DIRECTION('',(-1.31418445149758E-16,-1.,0.)) ;
#125137 = DIRECTION('center_axis',(1.,-1.31418445149758E-16,-2.16840434497101E-16)) ;
#125138 = DIRECTION('ref_axis',(-2.16840434497101E-16,0.,-1.)) ;
#125139 = DIRECTION('',(2.16840434497101E-16,0.,1.)) ;
#125140 = DIRECTION('',(1.31418445149758E-16,1.,0.)) ;
#125141 = DIRECTION('',(-2.16840434497101E-16,-2.8496832747207E-32,-1.)) ;
#125142 = DIRECTION('',(-1.31418445149758E-16,-1.,0.)) ;
#125143 = DIRECTION('center_axis',(-2.16840434497101E-16,2.8496832747207E-32,
1.)) ;
#125144 = DIRECTION('ref_axis',(1.,4.92915281362991E-64,2.16840434497101E-16)) ;
#125145 = DIRECTION('',(1.,1.31418445149758E-16,2.16840434497101E-16)) ;
#125146 = DIRECTION('',(-1.31418445149758E-16,-1.,0.)) ;
#125147 = DIRECTION('',(-1.,0.,-2.16840434497101E-16)) ;
#125148 = DIRECTION('',(1.31418445149758E-16,1.,0.)) ;
#125149 = DIRECTION('center_axis',(-1.,1.31418445149758E-16,4.33680868994202E-16)) ;
#125150 = DIRECTION('ref_axis',(4.33680868994202E-16,0.,1.)) ;
#125151 = DIRECTION('',(-1.31418445149758E-16,-1.,0.)) ;
#125152 = DIRECTION('',(-4.33680868994202E-16,0.,-1.)) ;
#125153 = DIRECTION('',(1.31418445149758E-16,1.,0.)) ;
#125154 = DIRECTION('',(4.33680868994202E-16,5.69936654944139E-32,1.)) ;
#125155 = DIRECTION('center_axis',(-2.16840434497101E-16,2.8496832747207E-32,
-1.)) ;
#125156 = DIRECTION('ref_axis',(-1.,-4.92915281362991E-64,2.16840434497101E-16)) ;
#125157 = DIRECTION('',(1.,0.,-2.16840434497101E-16)) ;
#125158 = DIRECTION('',(1.31418445149758E-16,1.,0.)) ;
#125159 = DIRECTION('',(-1.,-1.31418445149758E-16,2.16840434497101E-16)) ;
#125160 = DIRECTION('',(-1.31418445149758E-16,-1.,0.)) ;
#125161 = DIRECTION('center_axis',(1.,-1.31418445149758E-16,-2.16840434497101E-16)) ;
#125162 = DIRECTION('ref_axis',(-2.16840434497101E-16,0.,-1.)) ;
#125163 = DIRECTION('',(2.16840434497101E-16,0.,1.)) ;
#125164 = DIRECTION('',(1.31418445149758E-16,1.,0.)) ;
#125165 = DIRECTION('',(-2.16840434497101E-16,-2.8496832747207E-32,-1.)) ;
#125166 = DIRECTION('',(-1.31418445149758E-16,-1.,0.)) ;
#125167 = DIRECTION('center_axis',(-2.16840434497101E-16,2.8496832747207E-32,
1.)) ;
#125168 = DIRECTION('ref_axis',(1.,4.92915281362991E-64,2.16840434497101E-16)) ;
#125169 = DIRECTION('',(1.,1.31418445149758E-16,2.16840434497101E-16)) ;
#125170 = DIRECTION('',(-1.31418445149758E-16,-1.,0.)) ;
#125171 = DIRECTION('',(-1.,0.,-2.16840434497101E-16)) ;
#125172 = DIRECTION('',(1.31418445149758E-16,1.,0.)) ;
#125173 = DIRECTION('center_axis',(-1.,1.31418445149758E-16,4.33680868994202E-16)) ;
#125174 = DIRECTION('ref_axis',(4.33680868994202E-16,0.,1.)) ;
#125175 = DIRECTION('',(-1.31418445149758E-16,-1.,0.)) ;
#125176 = DIRECTION('',(-4.33680868994202E-16,0.,-1.)) ;
#125177 = DIRECTION('',(1.31418445149758E-16,1.,0.)) ;
#125178 = DIRECTION('',(4.33680868994202E-16,5.69936654944139E-32,1.)) ;
#125179 = DIRECTION('center_axis',(-2.16840434497101E-16,2.8496832747207E-32,
-1.)) ;
#125180 = DIRECTION('ref_axis',(-1.,-4.92915281362991E-64,2.16840434497101E-16)) ;
#125181 = DIRECTION('',(1.,0.,-2.16840434497101E-16)) ;
#125182 = DIRECTION('',(1.31418445149758E-16,1.,0.)) ;
#125183 = DIRECTION('',(-1.,-1.31418445149758E-16,2.16840434497101E-16)) ;
#125184 = DIRECTION('',(-1.31418445149758E-16,-1.,0.)) ;
#125185 = DIRECTION('center_axis',(1.,-1.31418445149758E-16,-2.16840434497101E-16)) ;
#125186 = DIRECTION('ref_axis',(-2.16840434497101E-16,0.,-1.)) ;
#125187 = DIRECTION('',(2.16840434497101E-16,0.,1.)) ;
#125188 = DIRECTION('',(1.31418445149758E-16,1.,0.)) ;
#125189 = DIRECTION('',(-2.16840434497101E-16,-2.8496832747207E-32,-1.)) ;
#125190 = DIRECTION('',(-1.31418445149758E-16,-1.,0.)) ;
#125191 = DIRECTION('center_axis',(-2.16840434497101E-16,2.8496832747207E-32,
1.)) ;
#125192 = DIRECTION('ref_axis',(1.,4.92915281362991E-64,2.16840434497101E-16)) ;
#125193 = DIRECTION('',(1.,1.31418445149758E-16,2.16840434497101E-16)) ;
#125194 = DIRECTION('',(-1.31418445149758E-16,-1.,0.)) ;
#125195 = DIRECTION('',(-1.,0.,-2.16840434497101E-16)) ;
#125196 = DIRECTION('',(1.31418445149758E-16,1.,0.)) ;
#125197 = DIRECTION('center_axis',(-1.,1.31418445149758E-16,4.33680868994202E-16)) ;
#125198 = DIRECTION('ref_axis',(4.33680868994202E-16,0.,1.)) ;
#125199 = DIRECTION('',(-1.31418445149758E-16,-1.,0.)) ;
#125200 = DIRECTION('',(-4.33680868994202E-16,0.,-1.)) ;
#125201 = DIRECTION('',(1.31418445149758E-16,1.,0.)) ;
#125202 = DIRECTION('',(4.33680868994202E-16,5.69936654944139E-32,1.)) ;
#125203 = DIRECTION('center_axis',(-2.16840434497101E-16,2.8496832747207E-32,
-1.)) ;
#125204 = DIRECTION('ref_axis',(-1.,-4.92915281362991E-64,2.16840434497101E-16)) ;
#125205 = DIRECTION('',(1.,0.,-2.16840434497101E-16)) ;
#125206 = DIRECTION('',(1.31418445149758E-16,1.,0.)) ;
#125207 = DIRECTION('',(-1.,-1.31418445149758E-16,2.16840434497101E-16)) ;
#125208 = DIRECTION('',(-1.31418445149758E-16,-1.,0.)) ;
#125209 = DIRECTION('center_axis',(1.,-1.31418445149758E-16,-2.16840434497101E-16)) ;
#125210 = DIRECTION('ref_axis',(-2.16840434497101E-16,0.,-1.)) ;
#125211 = DIRECTION('',(2.16840434497101E-16,0.,1.)) ;
#125212 = DIRECTION('',(1.31418445149758E-16,1.,0.)) ;
#125213 = DIRECTION('',(-2.16840434497101E-16,-2.8496832747207E-32,-1.)) ;
#125214 = DIRECTION('',(-1.31418445149758E-16,-1.,0.)) ;
#125215 = DIRECTION('center_axis',(-2.16840434497101E-16,2.8496832747207E-32,
1.)) ;
#125216 = DIRECTION('ref_axis',(1.,4.92915281362991E-64,2.16840434497101E-16)) ;
#125217 = DIRECTION('',(1.,1.31418445149758E-16,2.16840434497101E-16)) ;
#125218 = DIRECTION('',(-1.31418445149758E-16,-1.,0.)) ;
#125219 = DIRECTION('',(-1.,0.,-2.16840434497101E-16)) ;
#125220 = DIRECTION('',(1.31418445149758E-16,1.,0.)) ;
#125221 = DIRECTION('center_axis',(-1.,1.31418445149758E-16,4.33680868994202E-16)) ;
#125222 = DIRECTION('ref_axis',(4.33680868994202E-16,0.,1.)) ;
#125223 = DIRECTION('',(-1.31418445149758E-16,-1.,0.)) ;
#125224 = DIRECTION('',(-4.33680868994202E-16,0.,-1.)) ;
#125225 = DIRECTION('',(1.31418445149758E-16,1.,0.)) ;
#125226 = DIRECTION('',(4.33680868994202E-16,5.69936654944139E-32,1.)) ;
#125227 = DIRECTION('center_axis',(-2.16840434497101E-16,2.8496832747207E-32,
-1.)) ;
#125228 = DIRECTION('ref_axis',(-1.,-4.92915281362991E-64,2.16840434497101E-16)) ;
#125229 = DIRECTION('',(1.,0.,-2.16840434497101E-16)) ;
#125230 = DIRECTION('',(1.31418445149758E-16,1.,0.)) ;
#125231 = DIRECTION('',(-1.,-1.31418445149758E-16,2.16840434497101E-16)) ;
#125232 = DIRECTION('',(-1.31418445149758E-16,-1.,0.)) ;
#125233 = DIRECTION('center_axis',(1.,-1.31418445149758E-16,-2.16840434497101E-16)) ;
#125234 = DIRECTION('ref_axis',(-2.16840434497101E-16,0.,-1.)) ;
#125235 = DIRECTION('',(2.16840434497101E-16,0.,1.)) ;
#125236 = DIRECTION('',(1.31418445149758E-16,1.,0.)) ;
#125237 = DIRECTION('',(-2.16840434497101E-16,-2.8496832747207E-32,-1.)) ;
#125238 = DIRECTION('',(-1.31418445149758E-16,-1.,0.)) ;
#125239 = DIRECTION('center_axis',(-2.16840434497101E-16,2.8496832747207E-32,
1.)) ;
#125240 = DIRECTION('ref_axis',(1.,4.92915281362991E-64,2.16840434497101E-16)) ;
#125241 = DIRECTION('',(1.,1.31418445149758E-16,2.16840434497101E-16)) ;
#125242 = DIRECTION('',(-1.31418445149758E-16,-1.,0.)) ;
#125243 = DIRECTION('',(-1.,0.,-2.16840434497101E-16)) ;
#125244 = DIRECTION('',(1.31418445149758E-16,1.,0.)) ;
#125245 = DIRECTION('center_axis',(-1.,1.31418445149758E-16,4.33680868994202E-16)) ;
#125246 = DIRECTION('ref_axis',(4.33680868994202E-16,0.,1.)) ;
#125247 = DIRECTION('',(-1.31418445149758E-16,-1.,0.)) ;
#125248 = DIRECTION('',(-4.33680868994202E-16,0.,-1.)) ;
#125249 = DIRECTION('',(1.31418445149758E-16,1.,0.)) ;
#125250 = DIRECTION('',(4.33680868994202E-16,5.69936654944139E-32,1.)) ;
#125251 = DIRECTION('center_axis',(-2.16840434497101E-16,2.8496832747207E-32,
-1.)) ;
#125252 = DIRECTION('ref_axis',(-1.,-4.92915281362991E-64,2.16840434497101E-16)) ;
#125253 = DIRECTION('',(1.,0.,-2.16840434497101E-16)) ;
#125254 = DIRECTION('',(1.31418445149758E-16,1.,0.)) ;
#125255 = DIRECTION('',(-1.,-1.31418445149758E-16,2.16840434497101E-16)) ;
#125256 = DIRECTION('',(-1.31418445149758E-16,-1.,0.)) ;
#125257 = DIRECTION('center_axis',(0.,1.,0.)) ;
#125258 = DIRECTION('ref_axis',(0.,0.,1.)) ;
#125259 = DIRECTION('',(4.33680868994202E-16,0.,1.)) ;
#125260 = DIRECTION('',(1.,0.,2.16840434497101E-16)) ;
#125261 = DIRECTION('',(-2.16840434497101E-16,0.,-1.)) ;
#125262 = DIRECTION('',(-1.,0.,2.16840434497101E-16)) ;
#125263 = DIRECTION('',(1.,0.,0.)) ;
#125264 = DIRECTION('center_axis',(0.,-1.,0.)) ;
#125265 = DIRECTION('ref_axis',(0.,0.,1.)) ;
#125266 = DIRECTION('',(0.,0.,1.)) ;
#125267 = DIRECTION('center_axis',(0.,-1.,0.)) ;
#125268 = DIRECTION('ref_axis',(0.,0.,1.)) ;
#125269 = DIRECTION('',(-1.,0.,0.)) ;
#125270 = DIRECTION('center_axis',(0.,-1.,0.)) ;
#125271 = DIRECTION('ref_axis',(0.,0.,1.)) ;
#125272 = DIRECTION('',(0.,0.,-1.)) ;
#125273 = DIRECTION('center_axis',(0.,-1.,0.)) ;
#125274 = DIRECTION('ref_axis',(0.,0.,1.)) ;
#125275 = DIRECTION('center_axis',(1.,0.,0.)) ;
#125276 = DIRECTION('ref_axis',(0.,0.,-1.)) ;
#125277 = DIRECTION('',(0.,0.,1.)) ;
#125278 = DIRECTION('',(0.,-1.,0.)) ;
#125279 = DIRECTION('',(0.,1.,0.)) ;
#125280 = DIRECTION('center_axis',(0.,0.,1.)) ;
#125281 = DIRECTION('ref_axis',(1.,0.,0.)) ;
#125282 = DIRECTION('',(-1.,0.,0.)) ;
#125283 = DIRECTION('',(0.,-1.,0.)) ;
#125284 = DIRECTION('',(0.,1.,0.)) ;
#125285 = DIRECTION('center_axis',(-1.,0.,0.)) ;
#125286 = DIRECTION('ref_axis',(0.,0.,1.)) ;
#125287 = DIRECTION('',(0.,1.,0.)) ;
#125288 = DIRECTION('',(0.,0.,-1.)) ;
#125289 = DIRECTION('',(0.,-1.,0.)) ;
#125290 = DIRECTION('center_axis',(0.,0.,-1.)) ;
#125291 = DIRECTION('ref_axis',(-1.,0.,0.)) ;
#125292 = DIRECTION('',(1.,0.,0.)) ;
#125293 = DIRECTION('',(0.,-1.,0.)) ;
#125294 = DIRECTION('',(0.,1.,0.)) ;
#125295 = DIRECTION('center_axis',(0.,1.,0.)) ;
#125296 = DIRECTION('ref_axis',(0.,0.,1.)) ;
#125297 = DIRECTION('',(4.33680868994202E-16,0.,1.)) ;
#125298 = DIRECTION('',(1.,0.,2.16840434497101E-16)) ;
#125299 = DIRECTION('',(-2.16840434497101E-16,0.,-1.)) ;
#125300 = DIRECTION('',(-1.,0.,2.16840434497101E-16)) ;
#125301 = DIRECTION('',(1.,0.,0.)) ;
#125302 = DIRECTION('center_axis',(0.,-1.,0.)) ;
#125303 = DIRECTION('ref_axis',(0.,0.,1.)) ;
#125304 = DIRECTION('',(0.,0.,1.)) ;
#125305 = DIRECTION('center_axis',(0.,-1.,0.)) ;
#125306 = DIRECTION('ref_axis',(0.,0.,1.)) ;
#125307 = DIRECTION('',(-1.,0.,0.)) ;
#125308 = DIRECTION('center_axis',(0.,-1.,0.)) ;
#125309 = DIRECTION('ref_axis',(0.,0.,1.)) ;
#125310 = DIRECTION('',(0.,0.,-1.)) ;
#125311 = DIRECTION('center_axis',(0.,-1.,0.)) ;
#125312 = DIRECTION('ref_axis',(0.,0.,1.)) ;
#125313 = DIRECTION('center_axis',(1.,0.,0.)) ;
#125314 = DIRECTION('ref_axis',(0.,0.,-1.)) ;
#125315 = DIRECTION('',(0.,0.,1.)) ;
#125316 = DIRECTION('',(0.,-1.,0.)) ;
#125317 = DIRECTION('',(0.,1.,0.)) ;
#125318 = DIRECTION('center_axis',(0.,0.,1.)) ;
#125319 = DIRECTION('ref_axis',(1.,0.,0.)) ;
#125320 = DIRECTION('',(-1.,0.,0.)) ;
#125321 = DIRECTION('',(0.,-1.,0.)) ;
#125322 = DIRECTION('',(0.,1.,0.)) ;
#125323 = DIRECTION('center_axis',(-1.,0.,0.)) ;
#125324 = DIRECTION('ref_axis',(0.,0.,1.)) ;
#125325 = DIRECTION('',(0.,1.,0.)) ;
#125326 = DIRECTION('',(0.,0.,-1.)) ;
#125327 = DIRECTION('',(0.,-1.,0.)) ;
#125328 = DIRECTION('center_axis',(0.,0.,-1.)) ;
#125329 = DIRECTION('ref_axis',(-1.,0.,0.)) ;
#125330 = DIRECTION('',(1.,0.,0.)) ;
#125331 = DIRECTION('',(0.,-1.,0.)) ;
#125332 = DIRECTION('',(0.,1.,0.)) ;
#125333 = DIRECTION('center_axis',(0.,1.,0.)) ;
#125334 = DIRECTION('ref_axis',(0.,0.,1.)) ;
#125335 = DIRECTION('',(4.33680868994202E-16,0.,1.)) ;
#125336 = DIRECTION('',(1.,0.,2.16840434497101E-16)) ;
#125337 = DIRECTION('',(-2.16840434497101E-16,0.,-1.)) ;
#125338 = DIRECTION('',(-1.,0.,2.16840434497101E-16)) ;
#125339 = DIRECTION('',(1.,0.,0.)) ;
#125340 = DIRECTION('center_axis',(0.,-1.,0.)) ;
#125341 = DIRECTION('ref_axis',(0.,0.,1.)) ;
#125342 = DIRECTION('',(0.,0.,1.)) ;
#125343 = DIRECTION('center_axis',(0.,-1.,0.)) ;
#125344 = DIRECTION('ref_axis',(0.,0.,1.)) ;
#125345 = DIRECTION('',(-1.,0.,0.)) ;
#125346 = DIRECTION('center_axis',(0.,-1.,0.)) ;
#125347 = DIRECTION('ref_axis',(0.,0.,1.)) ;
#125348 = DIRECTION('',(0.,0.,-1.)) ;
#125349 = DIRECTION('center_axis',(0.,-1.,0.)) ;
#125350 = DIRECTION('ref_axis',(0.,0.,1.)) ;
#125351 = DIRECTION('center_axis',(1.,0.,0.)) ;
#125352 = DIRECTION('ref_axis',(0.,0.,-1.)) ;
#125353 = DIRECTION('',(0.,0.,1.)) ;
#125354 = DIRECTION('',(0.,-1.,0.)) ;
#125355 = DIRECTION('',(0.,1.,0.)) ;
#125356 = DIRECTION('center_axis',(0.,0.,1.)) ;
#125357 = DIRECTION('ref_axis',(1.,0.,0.)) ;
#125358 = DIRECTION('',(-1.,0.,0.)) ;
#125359 = DIRECTION('',(0.,-1.,0.)) ;
#125360 = DIRECTION('',(0.,1.,0.)) ;
#125361 = DIRECTION('center_axis',(-1.,0.,0.)) ;
#125362 = DIRECTION('ref_axis',(0.,0.,1.)) ;
#125363 = DIRECTION('',(0.,1.,0.)) ;
#125364 = DIRECTION('',(0.,0.,-1.)) ;
#125365 = DIRECTION('',(0.,-1.,0.)) ;
#125366 = DIRECTION('center_axis',(0.,0.,-1.)) ;
#125367 = DIRECTION('ref_axis',(-1.,0.,0.)) ;
#125368 = DIRECTION('',(1.,0.,0.)) ;
#125369 = DIRECTION('',(0.,-1.,0.)) ;
#125370 = DIRECTION('',(0.,1.,0.)) ;
#125371 = DIRECTION('center_axis',(0.,1.,0.)) ;
#125372 = DIRECTION('ref_axis',(0.,0.,1.)) ;
#125373 = DIRECTION('',(4.33680868994202E-16,0.,1.)) ;
#125374 = DIRECTION('',(1.,0.,2.16840434497101E-16)) ;
#125375 = DIRECTION('',(-2.16840434497101E-16,0.,-1.)) ;
#125376 = DIRECTION('',(-1.,0.,2.16840434497101E-16)) ;
#125377 = DIRECTION('',(1.,0.,0.)) ;
#125378 = DIRECTION('center_axis',(0.,-1.,0.)) ;
#125379 = DIRECTION('ref_axis',(0.,0.,1.)) ;
#125380 = DIRECTION('',(0.,0.,1.)) ;
#125381 = DIRECTION('center_axis',(0.,-1.,0.)) ;
#125382 = DIRECTION('ref_axis',(0.,0.,1.)) ;
#125383 = DIRECTION('',(-1.,0.,0.)) ;
#125384 = DIRECTION('center_axis',(0.,-1.,0.)) ;
#125385 = DIRECTION('ref_axis',(0.,0.,1.)) ;
#125386 = DIRECTION('',(0.,0.,-1.)) ;
#125387 = DIRECTION('center_axis',(0.,-1.,0.)) ;
#125388 = DIRECTION('ref_axis',(0.,0.,1.)) ;
#125389 = DIRECTION('center_axis',(1.,0.,0.)) ;
#125390 = DIRECTION('ref_axis',(0.,0.,-1.)) ;
#125391 = DIRECTION('',(0.,0.,1.)) ;
#125392 = DIRECTION('',(0.,-1.,0.)) ;
#125393 = DIRECTION('',(0.,1.,0.)) ;
#125394 = DIRECTION('center_axis',(0.,0.,1.)) ;
#125395 = DIRECTION('ref_axis',(1.,0.,0.)) ;
#125396 = DIRECTION('',(-1.,0.,0.)) ;
#125397 = DIRECTION('',(0.,-1.,0.)) ;
#125398 = DIRECTION('',(0.,1.,0.)) ;
#125399 = DIRECTION('center_axis',(-1.,0.,0.)) ;
#125400 = DIRECTION('ref_axis',(0.,0.,1.)) ;
#125401 = DIRECTION('',(0.,1.,0.)) ;
#125402 = DIRECTION('',(0.,0.,-1.)) ;
#125403 = DIRECTION('',(0.,-1.,0.)) ;
#125404 = DIRECTION('center_axis',(0.,0.,-1.)) ;
#125405 = DIRECTION('ref_axis',(-1.,0.,0.)) ;
#125406 = DIRECTION('',(1.,0.,0.)) ;
#125407 = DIRECTION('',(0.,-1.,0.)) ;
#125408 = DIRECTION('',(0.,1.,0.)) ;
#125409 = DIRECTION('center_axis',(0.,1.,0.)) ;
#125410 = DIRECTION('ref_axis',(0.,0.,1.)) ;
#125411 = DIRECTION('',(4.33680868994202E-16,0.,1.)) ;
#125412 = DIRECTION('',(1.,0.,2.16840434497101E-16)) ;
#125413 = DIRECTION('',(-2.16840434497101E-16,0.,-1.)) ;
#125414 = DIRECTION('',(-1.,0.,2.16840434497101E-16)) ;
#125415 = DIRECTION('',(1.,0.,0.)) ;
#125416 = DIRECTION('center_axis',(0.,-1.,0.)) ;
#125417 = DIRECTION('ref_axis',(0.,0.,1.)) ;
#125418 = DIRECTION('',(0.,0.,1.)) ;
#125419 = DIRECTION('center_axis',(0.,-1.,0.)) ;
#125420 = DIRECTION('ref_axis',(0.,0.,1.)) ;
#125421 = DIRECTION('',(-1.,0.,0.)) ;
#125422 = DIRECTION('center_axis',(0.,-1.,0.)) ;
#125423 = DIRECTION('ref_axis',(0.,0.,1.)) ;
#125424 = DIRECTION('',(0.,0.,-1.)) ;
#125425 = DIRECTION('center_axis',(0.,-1.,0.)) ;
#125426 = DIRECTION('ref_axis',(0.,0.,1.)) ;
#125427 = DIRECTION('center_axis',(1.,0.,0.)) ;
#125428 = DIRECTION('ref_axis',(0.,0.,-1.)) ;
#125429 = DIRECTION('',(0.,0.,1.)) ;
#125430 = DIRECTION('',(0.,-1.,0.)) ;
#125431 = DIRECTION('',(0.,1.,0.)) ;
#125432 = DIRECTION('center_axis',(0.,0.,1.)) ;
#125433 = DIRECTION('ref_axis',(1.,0.,0.)) ;
#125434 = DIRECTION('',(-1.,0.,0.)) ;
#125435 = DIRECTION('',(0.,-1.,0.)) ;
#125436 = DIRECTION('',(0.,1.,0.)) ;
#125437 = DIRECTION('center_axis',(-1.,0.,0.)) ;
#125438 = DIRECTION('ref_axis',(0.,0.,1.)) ;
#125439 = DIRECTION('',(0.,1.,0.)) ;
#125440 = DIRECTION('',(0.,0.,-1.)) ;
#125441 = DIRECTION('',(0.,-1.,0.)) ;
#125442 = DIRECTION('center_axis',(0.,0.,-1.)) ;
#125443 = DIRECTION('ref_axis',(-1.,0.,0.)) ;
#125444 = DIRECTION('',(1.,0.,0.)) ;
#125445 = DIRECTION('',(0.,-1.,0.)) ;
#125446 = DIRECTION('',(0.,1.,0.)) ;
#125447 = DIRECTION('center_axis',(0.,1.,0.)) ;
#125448 = DIRECTION('ref_axis',(0.,0.,1.)) ;
#125449 = DIRECTION('',(4.33680868994202E-16,0.,1.)) ;
#125450 = DIRECTION('',(1.,0.,2.16840434497101E-16)) ;
#125451 = DIRECTION('',(-2.16840434497101E-16,0.,-1.)) ;
#125452 = DIRECTION('',(-1.,0.,2.16840434497101E-16)) ;
#125453 = DIRECTION('',(1.,0.,0.)) ;
#125454 = DIRECTION('center_axis',(0.,-1.,0.)) ;
#125455 = DIRECTION('ref_axis',(0.,0.,1.)) ;
#125456 = DIRECTION('',(0.,0.,1.)) ;
#125457 = DIRECTION('center_axis',(0.,-1.,0.)) ;
#125458 = DIRECTION('ref_axis',(0.,0.,1.)) ;
#125459 = DIRECTION('',(-1.,0.,0.)) ;
#125460 = DIRECTION('center_axis',(0.,-1.,0.)) ;
#125461 = DIRECTION('ref_axis',(0.,0.,1.)) ;
#125462 = DIRECTION('',(0.,0.,-1.)) ;
#125463 = DIRECTION('center_axis',(0.,-1.,0.)) ;
#125464 = DIRECTION('ref_axis',(0.,0.,1.)) ;
#125465 = DIRECTION('center_axis',(1.,0.,0.)) ;
#125466 = DIRECTION('ref_axis',(0.,0.,-1.)) ;
#125467 = DIRECTION('',(0.,0.,1.)) ;
#125468 = DIRECTION('',(0.,-1.,0.)) ;
#125469 = DIRECTION('',(0.,1.,0.)) ;
#125470 = DIRECTION('center_axis',(0.,0.,1.)) ;
#125471 = DIRECTION('ref_axis',(1.,0.,0.)) ;
#125472 = DIRECTION('',(-1.,0.,0.)) ;
#125473 = DIRECTION('',(0.,-1.,0.)) ;
#125474 = DIRECTION('',(0.,1.,0.)) ;
#125475 = DIRECTION('center_axis',(-1.,0.,0.)) ;
#125476 = DIRECTION('ref_axis',(0.,0.,1.)) ;
#125477 = DIRECTION('',(0.,1.,0.)) ;
#125478 = DIRECTION('',(0.,0.,-1.)) ;
#125479 = DIRECTION('',(0.,-1.,0.)) ;
#125480 = DIRECTION('center_axis',(0.,0.,-1.)) ;
#125481 = DIRECTION('ref_axis',(-1.,0.,0.)) ;
#125482 = DIRECTION('',(1.,0.,0.)) ;
#125483 = DIRECTION('',(0.,-1.,0.)) ;
#125484 = DIRECTION('',(0.,1.,0.)) ;
#125485 = DIRECTION('center_axis',(0.,1.,0.)) ;
#125486 = DIRECTION('ref_axis',(0.,0.,1.)) ;
#125487 = DIRECTION('',(4.33680868994202E-16,0.,1.)) ;
#125488 = DIRECTION('',(1.,0.,2.16840434497101E-16)) ;
#125489 = DIRECTION('',(-2.16840434497101E-16,0.,-1.)) ;
#125490 = DIRECTION('',(-1.,0.,2.16840434497101E-16)) ;
#125491 = DIRECTION('',(1.,0.,0.)) ;
#125492 = DIRECTION('center_axis',(0.,-1.,0.)) ;
#125493 = DIRECTION('ref_axis',(0.,0.,1.)) ;
#125494 = DIRECTION('',(0.,0.,1.)) ;
#125495 = DIRECTION('center_axis',(0.,-1.,0.)) ;
#125496 = DIRECTION('ref_axis',(0.,0.,1.)) ;
#125497 = DIRECTION('',(-1.,0.,0.)) ;
#125498 = DIRECTION('center_axis',(0.,-1.,0.)) ;
#125499 = DIRECTION('ref_axis',(0.,0.,1.)) ;
#125500 = DIRECTION('',(0.,0.,-1.)) ;
#125501 = DIRECTION('center_axis',(0.,-1.,0.)) ;
#125502 = DIRECTION('ref_axis',(0.,0.,1.)) ;
#125503 = DIRECTION('center_axis',(1.,0.,0.)) ;
#125504 = DIRECTION('ref_axis',(0.,0.,-1.)) ;
#125505 = DIRECTION('',(0.,0.,1.)) ;
#125506 = DIRECTION('',(0.,-1.,0.)) ;
#125507 = DIRECTION('',(0.,1.,0.)) ;
#125508 = DIRECTION('center_axis',(0.,0.,1.)) ;
#125509 = DIRECTION('ref_axis',(1.,0.,0.)) ;
#125510 = DIRECTION('',(-1.,0.,0.)) ;
#125511 = DIRECTION('',(0.,-1.,0.)) ;
#125512 = DIRECTION('',(0.,1.,0.)) ;
#125513 = DIRECTION('center_axis',(-1.,0.,0.)) ;
#125514 = DIRECTION('ref_axis',(0.,0.,1.)) ;
#125515 = DIRECTION('',(0.,1.,0.)) ;
#125516 = DIRECTION('',(0.,0.,-1.)) ;
#125517 = DIRECTION('',(0.,-1.,0.)) ;
#125518 = DIRECTION('center_axis',(0.,0.,-1.)) ;
#125519 = DIRECTION('ref_axis',(-1.,0.,0.)) ;
#125520 = DIRECTION('',(1.,0.,0.)) ;
#125521 = DIRECTION('',(0.,-1.,0.)) ;
#125522 = DIRECTION('',(0.,1.,0.)) ;
#125523 = DIRECTION('center_axis',(0.,1.,0.)) ;
#125524 = DIRECTION('ref_axis',(0.,0.,1.)) ;
#125525 = DIRECTION('',(4.33680868994202E-16,0.,1.)) ;
#125526 = DIRECTION('',(1.,0.,2.16840434497101E-16)) ;
#125527 = DIRECTION('',(-2.16840434497101E-16,0.,-1.)) ;
#125528 = DIRECTION('',(-1.,0.,2.16840434497101E-16)) ;
#125529 = DIRECTION('',(1.,0.,0.)) ;
#125530 = DIRECTION('center_axis',(0.,-1.,0.)) ;
#125531 = DIRECTION('ref_axis',(0.,0.,1.)) ;
#125532 = DIRECTION('',(0.,0.,1.)) ;
#125533 = DIRECTION('center_axis',(0.,-1.,0.)) ;
#125534 = DIRECTION('ref_axis',(0.,0.,1.)) ;
#125535 = DIRECTION('',(-1.,0.,0.)) ;
#125536 = DIRECTION('center_axis',(0.,-1.,0.)) ;
#125537 = DIRECTION('ref_axis',(0.,0.,1.)) ;
#125538 = DIRECTION('',(0.,0.,-1.)) ;
#125539 = DIRECTION('center_axis',(0.,-1.,0.)) ;
#125540 = DIRECTION('ref_axis',(0.,0.,1.)) ;
#125541 = DIRECTION('center_axis',(1.,0.,0.)) ;
#125542 = DIRECTION('ref_axis',(0.,0.,-1.)) ;
#125543 = DIRECTION('',(0.,0.,1.)) ;
#125544 = DIRECTION('',(0.,-1.,0.)) ;
#125545 = DIRECTION('',(0.,1.,0.)) ;
#125546 = DIRECTION('center_axis',(0.,0.,1.)) ;
#125547 = DIRECTION('ref_axis',(1.,0.,0.)) ;
#125548 = DIRECTION('',(-1.,0.,0.)) ;
#125549 = DIRECTION('',(0.,-1.,0.)) ;
#125550 = DIRECTION('',(0.,1.,0.)) ;
#125551 = DIRECTION('center_axis',(-1.,0.,0.)) ;
#125552 = DIRECTION('ref_axis',(0.,0.,1.)) ;
#125553 = DIRECTION('',(0.,1.,0.)) ;
#125554 = DIRECTION('',(0.,0.,-1.)) ;
#125555 = DIRECTION('',(0.,-1.,0.)) ;
#125556 = DIRECTION('center_axis',(0.,0.,-1.)) ;
#125557 = DIRECTION('ref_axis',(-1.,0.,0.)) ;
#125558 = DIRECTION('',(1.,0.,0.)) ;
#125559 = DIRECTION('',(0.,-1.,0.)) ;
#125560 = DIRECTION('',(0.,1.,0.)) ;
#125561 = DIRECTION('center_axis',(0.,1.,0.)) ;
#125562 = DIRECTION('ref_axis',(0.,0.,1.)) ;
#125563 = DIRECTION('',(4.33680868994202E-16,0.,1.)) ;
#125564 = DIRECTION('',(1.,0.,2.16840434497101E-16)) ;
#125565 = DIRECTION('',(-2.16840434497101E-16,0.,-1.)) ;
#125566 = DIRECTION('',(-1.,0.,2.16840434497101E-16)) ;
#125567 = DIRECTION('',(1.,0.,0.)) ;
#125568 = DIRECTION('center_axis',(0.,-1.,0.)) ;
#125569 = DIRECTION('ref_axis',(0.,0.,1.)) ;
#125570 = DIRECTION('',(0.,0.,1.)) ;
#125571 = DIRECTION('center_axis',(0.,-1.,0.)) ;
#125572 = DIRECTION('ref_axis',(0.,0.,1.)) ;
#125573 = DIRECTION('',(-1.,0.,0.)) ;
#125574 = DIRECTION('center_axis',(0.,-1.,0.)) ;
#125575 = DIRECTION('ref_axis',(0.,0.,1.)) ;
#125576 = DIRECTION('',(0.,0.,-1.)) ;
#125577 = DIRECTION('center_axis',(0.,-1.,0.)) ;
#125578 = DIRECTION('ref_axis',(0.,0.,1.)) ;
#125579 = DIRECTION('center_axis',(1.,0.,0.)) ;
#125580 = DIRECTION('ref_axis',(0.,0.,-1.)) ;
#125581 = DIRECTION('',(0.,0.,1.)) ;
#125582 = DIRECTION('',(0.,-1.,0.)) ;
#125583 = DIRECTION('',(0.,1.,0.)) ;
#125584 = DIRECTION('center_axis',(0.,0.,1.)) ;
#125585 = DIRECTION('ref_axis',(1.,0.,0.)) ;
#125586 = DIRECTION('',(-1.,0.,0.)) ;
#125587 = DIRECTION('',(0.,-1.,0.)) ;
#125588 = DIRECTION('',(0.,1.,0.)) ;
#125589 = DIRECTION('center_axis',(-1.,0.,0.)) ;
#125590 = DIRECTION('ref_axis',(0.,0.,1.)) ;
#125591 = DIRECTION('',(0.,1.,0.)) ;
#125592 = DIRECTION('',(0.,0.,-1.)) ;
#125593 = DIRECTION('',(0.,-1.,0.)) ;
#125594 = DIRECTION('center_axis',(0.,0.,-1.)) ;
#125595 = DIRECTION('ref_axis',(-1.,0.,0.)) ;
#125596 = DIRECTION('',(1.,0.,0.)) ;
#125597 = DIRECTION('',(0.,-1.,0.)) ;
#125598 = DIRECTION('',(0.,1.,0.)) ;
#125599 = DIRECTION('center_axis',(0.,1.,0.)) ;
#125600 = DIRECTION('ref_axis',(0.,0.,1.)) ;
#125601 = DIRECTION('',(-1.,0.,0.)) ;
#125602 = DIRECTION('',(0.,0.,1.)) ;
#125603 = DIRECTION('',(1.,0.,0.)) ;
#125604 = DIRECTION('',(0.,0.,-1.)) ;
#125605 = DIRECTION('center_axis',(0.,1.,0.)) ;
#125606 = DIRECTION('ref_axis',(0.,0.,1.)) ;
#125607 = DIRECTION('',(-1.,0.,0.)) ;
#125608 = DIRECTION('',(0.,0.,1.)) ;
#125609 = DIRECTION('',(1.,0.,0.)) ;
#125610 = DIRECTION('',(0.,0.,-1.)) ;
#125611 = DIRECTION('center_axis',(0.,1.,0.)) ;
#125612 = DIRECTION('ref_axis',(0.,0.,1.)) ;
#125613 = DIRECTION('',(-1.,0.,0.)) ;
#125614 = DIRECTION('',(0.,0.,1.)) ;
#125615 = DIRECTION('',(1.,0.,0.)) ;
#125616 = DIRECTION('',(0.,0.,-1.)) ;
#125617 = DIRECTION('center_axis',(0.,1.,0.)) ;
#125618 = DIRECTION('ref_axis',(0.,0.,1.)) ;
#125619 = DIRECTION('',(-1.,0.,0.)) ;
#125620 = DIRECTION('',(0.,0.,1.)) ;
#125621 = DIRECTION('',(1.,0.,0.)) ;
#125622 = DIRECTION('',(0.,0.,-1.)) ;
#125623 = DIRECTION('center_axis',(0.,1.,0.)) ;
#125624 = DIRECTION('ref_axis',(0.,0.,1.)) ;
#125625 = DIRECTION('',(-1.,0.,0.)) ;
#125626 = DIRECTION('',(0.,0.,1.)) ;
#125627 = DIRECTION('',(1.,0.,0.)) ;
#125628 = DIRECTION('',(0.,0.,-1.)) ;
#125629 = DIRECTION('center_axis',(0.,1.,0.)) ;
#125630 = DIRECTION('ref_axis',(0.,0.,1.)) ;
#125631 = DIRECTION('',(-1.,0.,0.)) ;
#125632 = DIRECTION('',(0.,0.,1.)) ;
#125633 = DIRECTION('',(1.,0.,0.)) ;
#125634 = DIRECTION('',(0.,0.,-1.)) ;
#125635 = DIRECTION('center_axis',(0.,1.,0.)) ;
#125636 = DIRECTION('ref_axis',(0.,0.,1.)) ;
#125637 = DIRECTION('',(-1.,0.,0.)) ;
#125638 = DIRECTION('',(0.,0.,1.)) ;
#125639 = DIRECTION('',(1.,0.,0.)) ;
#125640 = DIRECTION('',(0.,0.,-1.)) ;
#125641 = DIRECTION('center_axis',(0.,1.,0.)) ;
#125642 = DIRECTION('ref_axis',(0.,0.,1.)) ;
#125643 = DIRECTION('',(-1.,0.,0.)) ;
#125644 = DIRECTION('',(0.,0.,1.)) ;
#125645 = DIRECTION('',(1.,0.,0.)) ;
#125646 = DIRECTION('',(0.,0.,-1.)) ;
#125647 = DIRECTION('center_axis',(0.,1.,0.)) ;
#125648 = DIRECTION('ref_axis',(0.,0.,1.)) ;
#125649 = DIRECTION('',(-1.,0.,0.)) ;
#125650 = DIRECTION('',(0.,0.,1.)) ;
#125651 = DIRECTION('',(1.,0.,0.)) ;
#125652 = DIRECTION('',(0.,0.,-1.)) ;
#125653 = DIRECTION('center_axis',(1.31418445149758E-16,1.,0.)) ;
#125654 = DIRECTION('ref_axis',(-1.,1.31418445149758E-16,0.)) ;
#125655 = DIRECTION('',(-0.422618261740697,5.55398348498559E-17,0.906307787036651)) ;
#125656 = DIRECTION('center_axis',(1.31418445149758E-16,1.,0.)) ;
#125657 = DIRECTION('ref_axis',(-1.,1.31418445149758E-16,0.)) ;
#125658 = DIRECTION('',(-0.422618261740697,5.55398348498559E-17,0.906307787036651)) ;
#125659 = DIRECTION('center_axis',(1.31418445149758E-16,1.,0.)) ;
#125660 = DIRECTION('ref_axis',(-1.,1.31418445149758E-16,0.)) ;
#125661 = DIRECTION('',(-0.422618261740697,5.55398348498559E-17,0.906307787036651)) ;
#125662 = DIRECTION('center_axis',(1.31418445149758E-16,1.,0.)) ;
#125663 = DIRECTION('ref_axis',(-1.,1.31418445149758E-16,0.)) ;
#125664 = DIRECTION('',(-0.422618261740697,5.55398348498559E-17,0.906307787036651)) ;
#125665 = DIRECTION('center_axis',(1.31418445149758E-16,1.,0.)) ;
#125666 = DIRECTION('ref_axis',(-1.,1.31418445149758E-16,0.)) ;
#125667 = DIRECTION('',(-0.422618261740697,5.55398348498559E-17,0.906307787036651)) ;
#125668 = DIRECTION('center_axis',(1.31418445149758E-16,1.,0.)) ;
#125669 = DIRECTION('ref_axis',(-1.,1.31418445149758E-16,0.)) ;
#125670 = DIRECTION('',(-0.422618261740697,5.55398348498559E-17,0.906307787036651)) ;
#125671 = DIRECTION('center_axis',(1.31418445149758E-16,1.,0.)) ;
#125672 = DIRECTION('ref_axis',(-1.,1.31418445149758E-16,0.)) ;
#125673 = DIRECTION('',(-0.422618261740697,5.55398348498559E-17,0.906307787036651)) ;
#125674 = DIRECTION('center_axis',(1.31418445149758E-16,1.,0.)) ;
#125675 = DIRECTION('ref_axis',(-1.,1.31418445149758E-16,0.)) ;
#125676 = DIRECTION('',(-0.422618261740697,5.55398348498559E-17,0.906307787036651)) ;
#125677 = DIRECTION('center_axis',(1.31418445149758E-16,1.,0.)) ;
#125678 = DIRECTION('ref_axis',(-1.,1.31418445149758E-16,0.)) ;
#125679 = DIRECTION('',(-0.422618261740697,5.55398348498559E-17,0.906307787036651)) ;
#125680 = DIRECTION('center_axis',(0.906307787036651,-1.19105560199475E-16,
0.422618261740697)) ;
#125681 = DIRECTION('ref_axis',(0.422618261740697,-9.57222084411175E-33,-0.906307787036651)) ;
#125682 = DIRECTION('',(0.422618261740697,-5.55398348498559E-17,-0.906307787036651)) ;
#125683 = DIRECTION('',(-0.422618261740697,5.55398348498559E-17,0.906307787036651)) ;
#125684 = DIRECTION('center_axis',(-0.906307787036651,1.19105560199475E-16,
-0.422618261740697)) ;
#125685 = DIRECTION('ref_axis',(-0.422618261740697,9.57222084411175E-33,0.906307787036651)) ;
#125686 = DIRECTION('',(0.422618261740697,-5.55398348498559E-17,-0.906307787036651)) ;
#125687 = DIRECTION('',(-0.422618261740697,5.55398348498559E-17,0.906307787036651)) ;
#125688 = DIRECTION('center_axis',(1.31418445149758E-16,1.,0.)) ;
#125689 = DIRECTION('ref_axis',(-1.,1.31418445149758E-16,0.)) ;
#125690 = DIRECTION('',(0.422618261740697,-5.55398348498559E-17,-0.906307787036651)) ;
#125691 = DIRECTION('',(-0.422618261740697,5.55398348498559E-17,0.906307787036651)) ;
#125692 = DIRECTION('center_axis',(0.906307787036651,-1.19105560199475E-16,
0.422618261740697)) ;
#125693 = DIRECTION('ref_axis',(0.422618261740697,-9.57222084411175E-33,-0.906307787036651)) ;
#125694 = DIRECTION('',(0.422618261740697,-5.55398348498559E-17,-0.906307787036651)) ;
#125695 = DIRECTION('',(-0.422618261740697,5.55398348498559E-17,0.906307787036651)) ;
#125696 = DIRECTION('center_axis',(-0.906307787036651,1.19105560199475E-16,
-0.422618261740697)) ;
#125697 = DIRECTION('ref_axis',(-0.422618261740697,9.57222084411175E-33,0.906307787036651)) ;
#125698 = DIRECTION('',(0.422618261740697,-5.55398348498559E-17,-0.906307787036651)) ;
#125699 = DIRECTION('',(-0.422618261740697,5.55398348498559E-17,0.906307787036651)) ;
#125700 = DIRECTION('center_axis',(1.31418445149758E-16,1.,0.)) ;
#125701 = DIRECTION('ref_axis',(-1.,1.31418445149758E-16,0.)) ;
#125702 = DIRECTION('',(0.422618261740697,-5.55398348498559E-17,-0.906307787036651)) ;
#125703 = DIRECTION('',(-0.422618261740697,5.55398348498559E-17,0.906307787036651)) ;
#125704 = DIRECTION('center_axis',(0.906307787036651,-1.19105560199475E-16,
0.422618261740697)) ;
#125705 = DIRECTION('ref_axis',(0.422618261740697,-9.57222084411175E-33,-0.906307787036651)) ;
#125706 = DIRECTION('',(0.422618261740697,-5.55398348498559E-17,-0.906307787036651)) ;
#125707 = DIRECTION('',(-0.422618261740697,5.55398348498559E-17,0.906307787036651)) ;
#125708 = DIRECTION('center_axis',(-0.906307787036651,1.19105560199475E-16,
-0.422618261740697)) ;
#125709 = DIRECTION('ref_axis',(-0.422618261740697,9.57222084411175E-33,0.906307787036651)) ;
#125710 = DIRECTION('',(0.422618261740697,-5.55398348498559E-17,-0.906307787036651)) ;
#125711 = DIRECTION('',(-0.422618261740697,5.55398348498559E-17,0.906307787036651)) ;
#125712 = DIRECTION('center_axis',(1.31418445149758E-16,1.,0.)) ;
#125713 = DIRECTION('ref_axis',(-1.,1.31418445149758E-16,0.)) ;
#125714 = DIRECTION('',(0.422618261740697,-5.55398348498559E-17,-0.906307787036651)) ;
#125715 = DIRECTION('',(-0.422618261740697,5.55398348498559E-17,0.906307787036651)) ;
#125716 = DIRECTION('center_axis',(0.906307787036651,-1.19105560199475E-16,
0.422618261740697)) ;
#125717 = DIRECTION('ref_axis',(0.422618261740697,-9.57222084411175E-33,-0.906307787036651)) ;
#125718 = DIRECTION('',(0.422618261740697,-5.55398348498559E-17,-0.906307787036651)) ;
#125719 = DIRECTION('',(-0.422618261740697,5.55398348498559E-17,0.906307787036651)) ;
#125720 = DIRECTION('center_axis',(-0.906307787036651,1.19105560199475E-16,
-0.422618261740697)) ;
#125721 = DIRECTION('ref_axis',(-0.422618261740697,9.57222084411175E-33,0.906307787036651)) ;
#125722 = DIRECTION('',(0.422618261740697,-5.55398348498559E-17,-0.906307787036651)) ;
#125723 = DIRECTION('',(-0.422618261740697,5.55398348498559E-17,0.906307787036651)) ;
#125724 = DIRECTION('center_axis',(1.31418445149758E-16,1.,0.)) ;
#125725 = DIRECTION('ref_axis',(-1.,1.31418445149758E-16,0.)) ;
#125726 = DIRECTION('',(0.422618261740697,-5.55398348498559E-17,-0.906307787036651)) ;
#125727 = DIRECTION('',(-0.422618261740697,5.55398348498559E-17,0.906307787036651)) ;
#125728 = DIRECTION('center_axis',(0.906307787036651,-1.19105560199475E-16,
0.422618261740697)) ;
#125729 = DIRECTION('ref_axis',(0.422618261740697,-9.57222084411175E-33,-0.906307787036651)) ;
#125730 = DIRECTION('',(0.422618261740697,-5.55398348498559E-17,-0.906307787036651)) ;
#125731 = DIRECTION('',(-0.422618261740697,5.55398348498559E-17,0.906307787036651)) ;
#125732 = DIRECTION('center_axis',(-0.906307787036651,1.19105560199475E-16,
-0.422618261740697)) ;
#125733 = DIRECTION('ref_axis',(-0.422618261740697,9.57222084411175E-33,0.906307787036651)) ;
#125734 = DIRECTION('',(0.422618261740697,-5.55398348498559E-17,-0.906307787036651)) ;
#125735 = DIRECTION('',(-0.422618261740697,5.55398348498559E-17,0.906307787036651)) ;
#125736 = DIRECTION('center_axis',(1.31418445149758E-16,1.,0.)) ;
#125737 = DIRECTION('ref_axis',(-1.,1.31418445149758E-16,0.)) ;
#125738 = DIRECTION('',(0.422618261740697,-5.55398348498559E-17,-0.906307787036651)) ;
#125739 = DIRECTION('',(-0.422618261740697,5.55398348498559E-17,0.906307787036651)) ;
#125740 = DIRECTION('center_axis',(0.906307787036651,-1.19105560199475E-16,
0.422618261740697)) ;
#125741 = DIRECTION('ref_axis',(0.422618261740697,-9.57222084411175E-33,-0.906307787036651)) ;
#125742 = DIRECTION('',(0.422618261740697,-5.55398348498559E-17,-0.906307787036651)) ;
#125743 = DIRECTION('',(-0.422618261740697,5.55398348498559E-17,0.906307787036651)) ;
#125744 = DIRECTION('center_axis',(-0.906307787036651,1.19105560199475E-16,
-0.422618261740697)) ;
#125745 = DIRECTION('ref_axis',(-0.422618261740697,9.57222084411175E-33,0.906307787036651)) ;
#125746 = DIRECTION('',(0.422618261740697,-5.55398348498559E-17,-0.906307787036651)) ;
#125747 = DIRECTION('',(-0.422618261740697,5.55398348498559E-17,0.906307787036651)) ;
#125748 = DIRECTION('center_axis',(1.31418445149758E-16,1.,0.)) ;
#125749 = DIRECTION('ref_axis',(-1.,1.31418445149758E-16,0.)) ;
#125750 = DIRECTION('',(0.422618261740697,-5.55398348498559E-17,-0.906307787036651)) ;
#125751 = DIRECTION('',(-0.422618261740697,5.55398348498559E-17,0.906307787036651)) ;
#125752 = DIRECTION('center_axis',(0.906307787036651,-1.19105560199475E-16,
0.422618261740697)) ;
#125753 = DIRECTION('ref_axis',(0.422618261740697,-9.57222084411175E-33,-0.906307787036651)) ;
#125754 = DIRECTION('',(0.422618261740697,-5.55398348498559E-17,-0.906307787036651)) ;
#125755 = DIRECTION('',(-0.422618261740697,5.55398348498559E-17,0.906307787036651)) ;
#125756 = DIRECTION('center_axis',(-0.906307787036651,1.19105560199475E-16,
-0.422618261740697)) ;
#125757 = DIRECTION('ref_axis',(-0.422618261740697,9.57222084411175E-33,0.906307787036651)) ;
#125758 = DIRECTION('',(0.422618261740697,-5.55398348498559E-17,-0.906307787036651)) ;
#125759 = DIRECTION('',(-0.422618261740697,5.55398348498559E-17,0.906307787036651)) ;
#125760 = DIRECTION('center_axis',(1.31418445149758E-16,1.,0.)) ;
#125761 = DIRECTION('ref_axis',(-1.,1.31418445149758E-16,0.)) ;
#125762 = DIRECTION('',(0.422618261740697,-5.55398348498559E-17,-0.906307787036651)) ;
#125763 = DIRECTION('',(-0.422618261740697,5.55398348498559E-17,0.906307787036651)) ;
#125764 = DIRECTION('center_axis',(0.906307787036651,-1.19105560199475E-16,
0.422618261740697)) ;
#125765 = DIRECTION('ref_axis',(0.422618261740697,-9.57222084411175E-33,-0.906307787036651)) ;
#125766 = DIRECTION('',(0.422618261740697,-5.55398348498559E-17,-0.906307787036651)) ;
#125767 = DIRECTION('',(-0.422618261740697,5.55398348498559E-17,0.906307787036651)) ;
#125768 = DIRECTION('center_axis',(-0.906307787036651,1.19105560199475E-16,
-0.422618261740697)) ;
#125769 = DIRECTION('ref_axis',(-0.422618261740697,9.57222084411175E-33,0.906307787036651)) ;
#125770 = DIRECTION('',(0.422618261740697,-5.55398348498559E-17,-0.906307787036651)) ;
#125771 = DIRECTION('',(-0.422618261740697,5.55398348498559E-17,0.906307787036651)) ;
#125772 = DIRECTION('center_axis',(1.31418445149758E-16,1.,0.)) ;
#125773 = DIRECTION('ref_axis',(-1.,1.31418445149758E-16,0.)) ;
#125774 = DIRECTION('',(0.422618261740697,-5.55398348498559E-17,-0.906307787036651)) ;
#125775 = DIRECTION('',(-0.422618261740697,5.55398348498559E-17,0.906307787036651)) ;
#125776 = DIRECTION('center_axis',(0.906307787036651,-1.19105560199475E-16,
0.422618261740697)) ;
#125777 = DIRECTION('ref_axis',(0.422618261740697,-9.57222084411175E-33,-0.906307787036651)) ;
#125778 = DIRECTION('',(0.422618261740697,-5.55398348498559E-17,-0.906307787036651)) ;
#125779 = DIRECTION('',(-0.422618261740697,5.55398348498559E-17,0.906307787036651)) ;
#125780 = DIRECTION('center_axis',(-0.906307787036651,1.19105560199475E-16,
-0.422618261740697)) ;
#125781 = DIRECTION('ref_axis',(-0.422618261740697,9.57222084411175E-33,0.906307787036651)) ;
#125782 = DIRECTION('',(0.422618261740697,-5.55398348498559E-17,-0.906307787036651)) ;
#125783 = DIRECTION('',(-0.422618261740697,5.55398348498559E-17,0.906307787036651)) ;
#125784 = DIRECTION('center_axis',(1.31418445149758E-16,1.,0.)) ;
#125785 = DIRECTION('ref_axis',(-1.,1.31418445149758E-16,0.)) ;
#125786 = DIRECTION('',(0.422618261740697,-5.55398348498559E-17,-0.906307787036651)) ;
#125787 = DIRECTION('',(-0.422618261740697,5.55398348498559E-17,0.906307787036651)) ;
#125788 = DIRECTION('center_axis',(0.,-1.,0.)) ;
#125789 = DIRECTION('ref_axis',(0.,0.,-1.)) ;
#125790 = DIRECTION('',(0.,-1.,0.)) ;
#125791 = DIRECTION('center_axis',(0.,1.,0.)) ;
#125792 = DIRECTION('ref_axis',(5.20417042793045E-14,0.,-1.)) ;
#125793 = DIRECTION('',(0.,-1.,0.)) ;
#125794 = DIRECTION('center_axis',(0.,-1.,0.)) ;
#125795 = DIRECTION('ref_axis',(0.,0.,-1.)) ;
#125796 = DIRECTION('center_axis',(0.,0.,1.)) ;
#125797 = DIRECTION('ref_axis',(1.,0.,0.)) ;
#125798 = DIRECTION('',(-1.,0.,0.)) ;
#125799 = DIRECTION('',(0.,-1.,0.)) ;
#125800 = DIRECTION('',(1.,0.,0.)) ;
#125801 = DIRECTION('center_axis',(0.,-1.,0.)) ;
#125802 = DIRECTION('ref_axis',(0.,0.,-1.)) ;
#125803 = DIRECTION('center_axis',(0.,1.,0.)) ;
#125804 = DIRECTION('ref_axis',(0.,0.,-1.)) ;
#125805 = DIRECTION('',(0.,-1.,0.)) ;
#125806 = DIRECTION('center_axis',(0.,-1.,0.)) ;
#125807 = DIRECTION('ref_axis',(0.,0.,-1.)) ;
#125808 = DIRECTION('center_axis',(1.,0.,0.)) ;
#125809 = DIRECTION('ref_axis',(0.,0.,-1.)) ;
#125810 = DIRECTION('',(0.,0.,1.)) ;
#125811 = DIRECTION('',(0.,-1.,0.)) ;
#125812 = DIRECTION('',(0.,0.,-1.)) ;
#125813 = DIRECTION('center_axis',(0.,-1.,0.)) ;
#125814 = DIRECTION('ref_axis',(0.,0.,-1.)) ;
#125815 = DIRECTION('center_axis',(0.,1.,0.)) ;
#125816 = DIRECTION('ref_axis',(0.,0.,-1.)) ;
#125817 = DIRECTION('',(0.,-1.,0.)) ;
#125818 = DIRECTION('center_axis',(0.,-1.,0.)) ;
#125819 = DIRECTION('ref_axis',(0.,0.,-1.)) ;
#125820 = DIRECTION('center_axis',(0.,0.,-1.)) ;
#125821 = DIRECTION('ref_axis',(-1.,0.,0.)) ;
#125822 = DIRECTION('',(1.,0.,0.)) ;
#125823 = DIRECTION('',(0.,-1.,0.)) ;
#125824 = DIRECTION('',(-1.,0.,0.)) ;
#125825 = DIRECTION('center_axis',(0.,-1.,0.)) ;
#125826 = DIRECTION('ref_axis',(0.,0.,-1.)) ;
#125827 = DIRECTION('center_axis',(0.,1.,0.)) ;
#125828 = DIRECTION('ref_axis',(0.,0.,-1.)) ;
#125829 = DIRECTION('',(0.,-1.,0.)) ;
#125830 = DIRECTION('center_axis',(0.,-1.,0.)) ;
#125831 = DIRECTION('ref_axis',(0.,0.,-1.)) ;
#125832 = DIRECTION('center_axis',(-1.,0.,0.)) ;
#125833 = DIRECTION('ref_axis',(0.,0.,1.)) ;
#125834 = DIRECTION('',(0.,0.,1.)) ;
#125835 = DIRECTION('',(0.,0.,-1.)) ;
#125836 = DIRECTION('center_axis',(0.,-1.,0.)) ;
#125837 = DIRECTION('ref_axis',(0.,0.,-1.)) ;
#125838 = DIRECTION('',(1.,0.,0.)) ;
#125839 = DIRECTION('',(0.,0.,-1.)) ;
#125840 = DIRECTION('',(-1.,0.,0.)) ;
#125841 = DIRECTION('',(0.,0.,1.)) ;
#125842 = DIRECTION('center_axis',(0.,-1.,0.)) ;
#125843 = DIRECTION('ref_axis',(0.,0.,-1.)) ;
#125844 = DIRECTION('',(0.,-1.,0.)) ;
#125845 = DIRECTION('center_axis',(0.,1.,0.)) ;
#125846 = DIRECTION('ref_axis',(5.20417042793045E-14,0.,-1.)) ;
#125847 = DIRECTION('',(0.,-1.,0.)) ;
#125848 = DIRECTION('center_axis',(0.,-1.,0.)) ;
#125849 = DIRECTION('ref_axis',(0.,0.,-1.)) ;
#125850 = DIRECTION('center_axis',(0.,0.,1.)) ;
#125851 = DIRECTION('ref_axis',(1.,0.,0.)) ;
#125852 = DIRECTION('',(-1.,0.,0.)) ;
#125853 = DIRECTION('',(0.,-1.,0.)) ;
#125854 = DIRECTION('',(1.,0.,0.)) ;
#125855 = DIRECTION('center_axis',(0.,-1.,0.)) ;
#125856 = DIRECTION('ref_axis',(0.,0.,-1.)) ;
#125857 = DIRECTION('center_axis',(0.,1.,0.)) ;
#125858 = DIRECTION('ref_axis',(0.,0.,-1.)) ;
#125859 = DIRECTION('',(0.,-1.,0.)) ;
#125860 = DIRECTION('center_axis',(0.,-1.,0.)) ;
#125861 = DIRECTION('ref_axis',(0.,0.,-1.)) ;
#125862 = DIRECTION('center_axis',(1.,0.,0.)) ;
#125863 = DIRECTION('ref_axis',(0.,0.,-1.)) ;
#125864 = DIRECTION('',(0.,0.,1.)) ;
#125865 = DIRECTION('',(0.,-1.,0.)) ;
#125866 = DIRECTION('',(0.,0.,-1.)) ;
#125867 = DIRECTION('center_axis',(0.,-1.,0.)) ;
#125868 = DIRECTION('ref_axis',(0.,0.,-1.)) ;
#125869 = DIRECTION('center_axis',(0.,1.,0.)) ;
#125870 = DIRECTION('ref_axis',(0.,0.,-1.)) ;
#125871 = DIRECTION('',(0.,-1.,0.)) ;
#125872 = DIRECTION('center_axis',(0.,-1.,0.)) ;
#125873 = DIRECTION('ref_axis',(0.,0.,-1.)) ;
#125874 = DIRECTION('center_axis',(0.,0.,-1.)) ;
#125875 = DIRECTION('ref_axis',(-1.,0.,0.)) ;
#125876 = DIRECTION('',(1.,0.,0.)) ;
#125877 = DIRECTION('',(0.,-1.,0.)) ;
#125878 = DIRECTION('',(-1.,0.,0.)) ;
#125879 = DIRECTION('center_axis',(0.,-1.,0.)) ;
#125880 = DIRECTION('ref_axis',(0.,0.,-1.)) ;
#125881 = DIRECTION('center_axis',(0.,1.,0.)) ;
#125882 = DIRECTION('ref_axis',(0.,0.,-1.)) ;
#125883 = DIRECTION('',(0.,-1.,0.)) ;
#125884 = DIRECTION('center_axis',(0.,-1.,0.)) ;
#125885 = DIRECTION('ref_axis',(0.,0.,-1.)) ;
#125886 = DIRECTION('center_axis',(-1.,0.,0.)) ;
#125887 = DIRECTION('ref_axis',(0.,0.,1.)) ;
#125888 = DIRECTION('',(0.,0.,1.)) ;
#125889 = DIRECTION('',(0.,0.,-1.)) ;
#125890 = DIRECTION('center_axis',(0.,-1.,0.)) ;
#125891 = DIRECTION('ref_axis',(0.,0.,-1.)) ;
#125892 = DIRECTION('',(1.,0.,0.)) ;
#125893 = DIRECTION('',(0.,0.,-1.)) ;
#125894 = DIRECTION('',(-1.,0.,0.)) ;
#125895 = DIRECTION('',(0.,0.,1.)) ;
#125896 = DIRECTION('center_axis',(0.,-1.,0.)) ;
#125897 = DIRECTION('ref_axis',(0.,0.,-1.)) ;
#125898 = DIRECTION('',(0.,-1.,0.)) ;
#125899 = DIRECTION('center_axis',(0.,1.,0.)) ;
#125900 = DIRECTION('ref_axis',(5.20417042793045E-14,0.,-1.)) ;
#125901 = DIRECTION('',(0.,-1.,0.)) ;
#125902 = DIRECTION('center_axis',(0.,-1.,0.)) ;
#125903 = DIRECTION('ref_axis',(0.,0.,-1.)) ;
#125904 = DIRECTION('center_axis',(0.,0.,1.)) ;
#125905 = DIRECTION('ref_axis',(1.,0.,0.)) ;
#125906 = DIRECTION('',(-1.,0.,0.)) ;
#125907 = DIRECTION('',(0.,-1.,0.)) ;
#125908 = DIRECTION('',(1.,0.,0.)) ;
#125909 = DIRECTION('center_axis',(0.,-1.,0.)) ;
#125910 = DIRECTION('ref_axis',(0.,0.,-1.)) ;
#125911 = DIRECTION('center_axis',(0.,1.,0.)) ;
#125912 = DIRECTION('ref_axis',(0.,0.,-1.)) ;
#125913 = DIRECTION('',(0.,-1.,0.)) ;
#125914 = DIRECTION('center_axis',(0.,-1.,0.)) ;
#125915 = DIRECTION('ref_axis',(0.,0.,-1.)) ;
#125916 = DIRECTION('center_axis',(1.,0.,0.)) ;
#125917 = DIRECTION('ref_axis',(0.,0.,-1.)) ;
#125918 = DIRECTION('',(0.,0.,1.)) ;
#125919 = DIRECTION('',(0.,-1.,0.)) ;
#125920 = DIRECTION('',(0.,0.,-1.)) ;
#125921 = DIRECTION('center_axis',(0.,-1.,0.)) ;
#125922 = DIRECTION('ref_axis',(0.,0.,-1.)) ;
#125923 = DIRECTION('center_axis',(0.,1.,0.)) ;
#125924 = DIRECTION('ref_axis',(0.,0.,-1.)) ;
#125925 = DIRECTION('',(0.,-1.,0.)) ;
#125926 = DIRECTION('center_axis',(0.,-1.,0.)) ;
#125927 = DIRECTION('ref_axis',(0.,0.,-1.)) ;
#125928 = DIRECTION('center_axis',(0.,0.,-1.)) ;
#125929 = DIRECTION('ref_axis',(-1.,0.,0.)) ;
#125930 = DIRECTION('',(1.,0.,0.)) ;
#125931 = DIRECTION('',(0.,-1.,0.)) ;
#125932 = DIRECTION('',(-1.,0.,0.)) ;
#125933 = DIRECTION('center_axis',(0.,-1.,0.)) ;
#125934 = DIRECTION('ref_axis',(0.,0.,-1.)) ;
#125935 = DIRECTION('center_axis',(0.,1.,0.)) ;
#125936 = DIRECTION('ref_axis',(0.,0.,-1.)) ;
#125937 = DIRECTION('',(0.,-1.,0.)) ;
#125938 = DIRECTION('center_axis',(0.,-1.,0.)) ;
#125939 = DIRECTION('ref_axis',(0.,0.,-1.)) ;
#125940 = DIRECTION('center_axis',(-1.,0.,0.)) ;
#125941 = DIRECTION('ref_axis',(0.,0.,1.)) ;
#125942 = DIRECTION('',(0.,0.,1.)) ;
#125943 = DIRECTION('',(0.,0.,-1.)) ;
#125944 = DIRECTION('center_axis',(0.,-1.,0.)) ;
#125945 = DIRECTION('ref_axis',(0.,0.,-1.)) ;
#125946 = DIRECTION('',(1.,0.,0.)) ;
#125947 = DIRECTION('',(0.,0.,-1.)) ;
#125948 = DIRECTION('',(-1.,0.,0.)) ;
#125949 = DIRECTION('',(0.,0.,1.)) ;
#125950 = DIRECTION('center_axis',(0.,-1.,0.)) ;
#125951 = DIRECTION('ref_axis',(0.,0.,-1.)) ;
#125952 = DIRECTION('',(0.,-1.,0.)) ;
#125953 = DIRECTION('center_axis',(0.,1.,0.)) ;
#125954 = DIRECTION('ref_axis',(5.20417042793045E-14,0.,-1.)) ;
#125955 = DIRECTION('',(0.,-1.,0.)) ;
#125956 = DIRECTION('center_axis',(0.,-1.,0.)) ;
#125957 = DIRECTION('ref_axis',(0.,0.,-1.)) ;
#125958 = DIRECTION('center_axis',(0.,0.,1.)) ;
#125959 = DIRECTION('ref_axis',(1.,0.,0.)) ;
#125960 = DIRECTION('',(-1.,0.,0.)) ;
#125961 = DIRECTION('',(0.,-1.,0.)) ;
#125962 = DIRECTION('',(1.,0.,0.)) ;
#125963 = DIRECTION('center_axis',(0.,-1.,0.)) ;
#125964 = DIRECTION('ref_axis',(0.,0.,-1.)) ;
#125965 = DIRECTION('center_axis',(0.,1.,0.)) ;
#125966 = DIRECTION('ref_axis',(0.,0.,-1.)) ;
#125967 = DIRECTION('',(0.,-1.,0.)) ;
#125968 = DIRECTION('center_axis',(0.,-1.,0.)) ;
#125969 = DIRECTION('ref_axis',(0.,0.,-1.)) ;
#125970 = DIRECTION('center_axis',(1.,0.,0.)) ;
#125971 = DIRECTION('ref_axis',(0.,0.,-1.)) ;
#125972 = DIRECTION('',(0.,0.,1.)) ;
#125973 = DIRECTION('',(0.,-1.,0.)) ;
#125974 = DIRECTION('',(0.,0.,-1.)) ;
#125975 = DIRECTION('center_axis',(0.,-1.,0.)) ;
#125976 = DIRECTION('ref_axis',(0.,0.,-1.)) ;
#125977 = DIRECTION('center_axis',(0.,1.,0.)) ;
#125978 = DIRECTION('ref_axis',(0.,0.,-1.)) ;
#125979 = DIRECTION('',(0.,-1.,0.)) ;
#125980 = DIRECTION('center_axis',(0.,-1.,0.)) ;
#125981 = DIRECTION('ref_axis',(0.,0.,-1.)) ;
#125982 = DIRECTION('center_axis',(0.,0.,-1.)) ;
#125983 = DIRECTION('ref_axis',(-1.,0.,0.)) ;
#125984 = DIRECTION('',(1.,0.,0.)) ;
#125985 = DIRECTION('',(0.,-1.,0.)) ;
#125986 = DIRECTION('',(-1.,0.,0.)) ;
#125987 = DIRECTION('center_axis',(0.,-1.,0.)) ;
#125988 = DIRECTION('ref_axis',(0.,0.,-1.)) ;
#125989 = DIRECTION('center_axis',(0.,1.,0.)) ;
#125990 = DIRECTION('ref_axis',(0.,0.,-1.)) ;
#125991 = DIRECTION('',(0.,-1.,0.)) ;
#125992 = DIRECTION('center_axis',(0.,-1.,0.)) ;
#125993 = DIRECTION('ref_axis',(0.,0.,-1.)) ;
#125994 = DIRECTION('center_axis',(-1.,0.,0.)) ;
#125995 = DIRECTION('ref_axis',(0.,0.,1.)) ;
#125996 = DIRECTION('',(0.,0.,1.)) ;
#125997 = DIRECTION('',(0.,0.,-1.)) ;
#125998 = DIRECTION('center_axis',(0.,-1.,0.)) ;
#125999 = DIRECTION('ref_axis',(0.,0.,-1.)) ;
#126000 = DIRECTION('',(1.,0.,0.)) ;
#126001 = DIRECTION('',(0.,0.,-1.)) ;
#126002 = DIRECTION('',(-1.,0.,0.)) ;
#126003 = DIRECTION('',(0.,0.,1.)) ;
#126004 = DIRECTION('center_axis',(0.,-1.,0.)) ;
#126005 = DIRECTION('ref_axis',(0.,0.,-1.)) ;
#126006 = DIRECTION('',(0.,-1.,0.)) ;
#126007 = DIRECTION('center_axis',(0.,1.,0.)) ;
#126008 = DIRECTION('ref_axis',(5.20417042793045E-14,0.,-1.)) ;
#126009 = DIRECTION('',(0.,-1.,0.)) ;
#126010 = DIRECTION('center_axis',(0.,-1.,0.)) ;
#126011 = DIRECTION('ref_axis',(0.,0.,-1.)) ;
#126012 = DIRECTION('center_axis',(0.,0.,1.)) ;
#126013 = DIRECTION('ref_axis',(1.,0.,0.)) ;
#126014 = DIRECTION('',(-1.,0.,0.)) ;
#126015 = DIRECTION('',(0.,-1.,0.)) ;
#126016 = DIRECTION('',(1.,0.,0.)) ;
#126017 = DIRECTION('center_axis',(0.,-1.,0.)) ;
#126018 = DIRECTION('ref_axis',(0.,0.,-1.)) ;
#126019 = DIRECTION('center_axis',(0.,1.,0.)) ;
#126020 = DIRECTION('ref_axis',(0.,0.,-1.)) ;
#126021 = DIRECTION('',(0.,-1.,0.)) ;
#126022 = DIRECTION('center_axis',(0.,-1.,0.)) ;
#126023 = DIRECTION('ref_axis',(0.,0.,-1.)) ;
#126024 = DIRECTION('center_axis',(1.,0.,0.)) ;
#126025 = DIRECTION('ref_axis',(0.,0.,-1.)) ;
#126026 = DIRECTION('',(0.,0.,1.)) ;
#126027 = DIRECTION('',(0.,-1.,0.)) ;
#126028 = DIRECTION('',(0.,0.,-1.)) ;
#126029 = DIRECTION('center_axis',(0.,-1.,0.)) ;
#126030 = DIRECTION('ref_axis',(0.,0.,-1.)) ;
#126031 = DIRECTION('center_axis',(0.,1.,0.)) ;
#126032 = DIRECTION('ref_axis',(0.,0.,-1.)) ;
#126033 = DIRECTION('',(0.,-1.,0.)) ;
#126034 = DIRECTION('center_axis',(0.,-1.,0.)) ;
#126035 = DIRECTION('ref_axis',(0.,0.,-1.)) ;
#126036 = DIRECTION('center_axis',(0.,0.,-1.)) ;
#126037 = DIRECTION('ref_axis',(-1.,0.,0.)) ;
#126038 = DIRECTION('',(1.,0.,0.)) ;
#126039 = DIRECTION('',(0.,-1.,0.)) ;
#126040 = DIRECTION('',(-1.,0.,0.)) ;
#126041 = DIRECTION('center_axis',(0.,-1.,0.)) ;
#126042 = DIRECTION('ref_axis',(0.,0.,-1.)) ;
#126043 = DIRECTION('center_axis',(0.,1.,0.)) ;
#126044 = DIRECTION('ref_axis',(0.,0.,-1.)) ;
#126045 = DIRECTION('',(0.,-1.,0.)) ;
#126046 = DIRECTION('center_axis',(0.,-1.,0.)) ;
#126047 = DIRECTION('ref_axis',(0.,0.,-1.)) ;
#126048 = DIRECTION('center_axis',(-1.,0.,0.)) ;
#126049 = DIRECTION('ref_axis',(0.,0.,1.)) ;
#126050 = DIRECTION('',(0.,0.,1.)) ;
#126051 = DIRECTION('',(0.,0.,-1.)) ;
#126052 = DIRECTION('center_axis',(0.,-1.,0.)) ;
#126053 = DIRECTION('ref_axis',(0.,0.,-1.)) ;
#126054 = DIRECTION('',(1.,0.,0.)) ;
#126055 = DIRECTION('',(0.,0.,-1.)) ;
#126056 = DIRECTION('',(-1.,0.,0.)) ;
#126057 = DIRECTION('',(0.,0.,1.)) ;
#126058 = DIRECTION('center_axis',(0.,-1.,0.)) ;
#126059 = DIRECTION('ref_axis',(0.,0.,-1.)) ;
#126060 = DIRECTION('',(0.,-1.,0.)) ;
#126061 = DIRECTION('center_axis',(0.,1.,0.)) ;
#126062 = DIRECTION('ref_axis',(5.20417042793045E-14,0.,-1.)) ;
#126063 = DIRECTION('',(0.,-1.,0.)) ;
#126064 = DIRECTION('center_axis',(0.,-1.,0.)) ;
#126065 = DIRECTION('ref_axis',(0.,0.,-1.)) ;
#126066 = DIRECTION('center_axis',(0.,0.,1.)) ;
#126067 = DIRECTION('ref_axis',(1.,0.,0.)) ;
#126068 = DIRECTION('',(-1.,0.,0.)) ;
#126069 = DIRECTION('',(0.,-1.,0.)) ;
#126070 = DIRECTION('',(1.,0.,0.)) ;
#126071 = DIRECTION('center_axis',(0.,-1.,0.)) ;
#126072 = DIRECTION('ref_axis',(0.,0.,-1.)) ;
#126073 = DIRECTION('center_axis',(0.,1.,0.)) ;
#126074 = DIRECTION('ref_axis',(0.,0.,-1.)) ;
#126075 = DIRECTION('',(0.,-1.,0.)) ;
#126076 = DIRECTION('center_axis',(0.,-1.,0.)) ;
#126077 = DIRECTION('ref_axis',(0.,0.,-1.)) ;
#126078 = DIRECTION('center_axis',(1.,0.,0.)) ;
#126079 = DIRECTION('ref_axis',(0.,0.,-1.)) ;
#126080 = DIRECTION('',(0.,0.,1.)) ;
#126081 = DIRECTION('',(0.,-1.,0.)) ;
#126082 = DIRECTION('',(0.,0.,-1.)) ;
#126083 = DIRECTION('center_axis',(0.,-1.,0.)) ;
#126084 = DIRECTION('ref_axis',(0.,0.,-1.)) ;
#126085 = DIRECTION('center_axis',(0.,1.,0.)) ;
#126086 = DIRECTION('ref_axis',(0.,0.,-1.)) ;
#126087 = DIRECTION('',(0.,-1.,0.)) ;
#126088 = DIRECTION('center_axis',(0.,-1.,0.)) ;
#126089 = DIRECTION('ref_axis',(0.,0.,-1.)) ;
#126090 = DIRECTION('center_axis',(0.,0.,-1.)) ;
#126091 = DIRECTION('ref_axis',(-1.,0.,0.)) ;
#126092 = DIRECTION('',(1.,0.,0.)) ;
#126093 = DIRECTION('',(0.,-1.,0.)) ;
#126094 = DIRECTION('',(-1.,0.,0.)) ;
#126095 = DIRECTION('center_axis',(0.,-1.,0.)) ;
#126096 = DIRECTION('ref_axis',(0.,0.,-1.)) ;
#126097 = DIRECTION('center_axis',(0.,1.,0.)) ;
#126098 = DIRECTION('ref_axis',(0.,0.,-1.)) ;
#126099 = DIRECTION('',(0.,-1.,0.)) ;
#126100 = DIRECTION('center_axis',(0.,-1.,0.)) ;
#126101 = DIRECTION('ref_axis',(0.,0.,-1.)) ;
#126102 = DIRECTION('center_axis',(-1.,0.,0.)) ;
#126103 = DIRECTION('ref_axis',(0.,0.,1.)) ;
#126104 = DIRECTION('',(0.,0.,1.)) ;
#126105 = DIRECTION('',(0.,0.,-1.)) ;
#126106 = DIRECTION('center_axis',(0.,-1.,0.)) ;
#126107 = DIRECTION('ref_axis',(0.,0.,-1.)) ;
#126108 = DIRECTION('',(1.,0.,0.)) ;
#126109 = DIRECTION('',(0.,0.,-1.)) ;
#126110 = DIRECTION('',(-1.,0.,0.)) ;
#126111 = DIRECTION('',(0.,0.,1.)) ;
#126112 = DIRECTION('center_axis',(0.,-1.,0.)) ;
#126113 = DIRECTION('ref_axis',(0.,0.,-1.)) ;
#126114 = DIRECTION('',(0.,-1.,0.)) ;
#126115 = DIRECTION('center_axis',(0.,1.,0.)) ;
#126116 = DIRECTION('ref_axis',(5.20417042793045E-14,0.,-1.)) ;
#126117 = DIRECTION('',(0.,-1.,0.)) ;
#126118 = DIRECTION('center_axis',(0.,-1.,0.)) ;
#126119 = DIRECTION('ref_axis',(0.,0.,-1.)) ;
#126120 = DIRECTION('center_axis',(0.,0.,1.)) ;
#126121 = DIRECTION('ref_axis',(1.,0.,0.)) ;
#126122 = DIRECTION('',(-1.,0.,0.)) ;
#126123 = DIRECTION('',(0.,-1.,0.)) ;
#126124 = DIRECTION('',(1.,0.,0.)) ;
#126125 = DIRECTION('center_axis',(0.,-1.,0.)) ;
#126126 = DIRECTION('ref_axis',(0.,0.,-1.)) ;
#126127 = DIRECTION('center_axis',(0.,1.,0.)) ;
#126128 = DIRECTION('ref_axis',(0.,0.,-1.)) ;
#126129 = DIRECTION('',(0.,-1.,0.)) ;
#126130 = DIRECTION('center_axis',(0.,-1.,0.)) ;
#126131 = DIRECTION('ref_axis',(0.,0.,-1.)) ;
#126132 = DIRECTION('center_axis',(1.,0.,0.)) ;
#126133 = DIRECTION('ref_axis',(0.,0.,-1.)) ;
#126134 = DIRECTION('',(0.,0.,1.)) ;
#126135 = DIRECTION('',(0.,-1.,0.)) ;
#126136 = DIRECTION('',(0.,0.,-1.)) ;
#126137 = DIRECTION('center_axis',(0.,-1.,0.)) ;
#126138 = DIRECTION('ref_axis',(0.,0.,-1.)) ;
#126139 = DIRECTION('center_axis',(0.,1.,0.)) ;
#126140 = DIRECTION('ref_axis',(0.,0.,-1.)) ;
#126141 = DIRECTION('',(0.,-1.,0.)) ;
#126142 = DIRECTION('center_axis',(0.,-1.,0.)) ;
#126143 = DIRECTION('ref_axis',(0.,0.,-1.)) ;
#126144 = DIRECTION('center_axis',(0.,0.,-1.)) ;
#126145 = DIRECTION('ref_axis',(-1.,0.,0.)) ;
#126146 = DIRECTION('',(1.,0.,0.)) ;
#126147 = DIRECTION('',(0.,-1.,0.)) ;
#126148 = DIRECTION('',(-1.,0.,0.)) ;
#126149 = DIRECTION('center_axis',(0.,-1.,0.)) ;
#126150 = DIRECTION('ref_axis',(0.,0.,-1.)) ;
#126151 = DIRECTION('center_axis',(0.,1.,0.)) ;
#126152 = DIRECTION('ref_axis',(0.,0.,-1.)) ;
#126153 = DIRECTION('',(0.,-1.,0.)) ;
#126154 = DIRECTION('center_axis',(0.,-1.,0.)) ;
#126155 = DIRECTION('ref_axis',(0.,0.,-1.)) ;
#126156 = DIRECTION('center_axis',(-1.,0.,0.)) ;
#126157 = DIRECTION('ref_axis',(0.,0.,1.)) ;
#126158 = DIRECTION('',(0.,0.,1.)) ;
#126159 = DIRECTION('',(0.,0.,-1.)) ;
#126160 = DIRECTION('center_axis',(0.,-1.,0.)) ;
#126161 = DIRECTION('ref_axis',(0.,0.,-1.)) ;
#126162 = DIRECTION('',(1.,0.,0.)) ;
#126163 = DIRECTION('',(0.,0.,-1.)) ;
#126164 = DIRECTION('',(-1.,0.,0.)) ;
#126165 = DIRECTION('',(0.,0.,1.)) ;
#126166 = DIRECTION('center_axis',(0.,-1.,0.)) ;
#126167 = DIRECTION('ref_axis',(0.,0.,-1.)) ;
#126168 = DIRECTION('',(0.,-1.,0.)) ;
#126169 = DIRECTION('center_axis',(0.,1.,0.)) ;
#126170 = DIRECTION('ref_axis',(5.20417042793045E-14,0.,-1.)) ;
#126171 = DIRECTION('',(0.,-1.,0.)) ;
#126172 = DIRECTION('center_axis',(0.,-1.,0.)) ;
#126173 = DIRECTION('ref_axis',(0.,0.,-1.)) ;
#126174 = DIRECTION('center_axis',(0.,0.,1.)) ;
#126175 = DIRECTION('ref_axis',(1.,0.,0.)) ;
#126176 = DIRECTION('',(-1.,0.,0.)) ;
#126177 = DIRECTION('',(0.,-1.,0.)) ;
#126178 = DIRECTION('',(1.,0.,0.)) ;
#126179 = DIRECTION('center_axis',(0.,-1.,0.)) ;
#126180 = DIRECTION('ref_axis',(0.,0.,-1.)) ;
#126181 = DIRECTION('center_axis',(0.,1.,0.)) ;
#126182 = DIRECTION('ref_axis',(0.,0.,-1.)) ;
#126183 = DIRECTION('',(0.,-1.,0.)) ;
#126184 = DIRECTION('center_axis',(0.,-1.,0.)) ;
#126185 = DIRECTION('ref_axis',(0.,0.,-1.)) ;
#126186 = DIRECTION('center_axis',(1.,0.,0.)) ;
#126187 = DIRECTION('ref_axis',(0.,0.,-1.)) ;
#126188 = DIRECTION('',(0.,0.,1.)) ;
#126189 = DIRECTION('',(0.,-1.,0.)) ;
#126190 = DIRECTION('',(0.,0.,-1.)) ;
#126191 = DIRECTION('center_axis',(0.,-1.,0.)) ;
#126192 = DIRECTION('ref_axis',(0.,0.,-1.)) ;
#126193 = DIRECTION('center_axis',(0.,1.,0.)) ;
#126194 = DIRECTION('ref_axis',(0.,0.,-1.)) ;
#126195 = DIRECTION('',(0.,-1.,0.)) ;
#126196 = DIRECTION('center_axis',(0.,-1.,0.)) ;
#126197 = DIRECTION('ref_axis',(0.,0.,-1.)) ;
#126198 = DIRECTION('center_axis',(0.,0.,-1.)) ;
#126199 = DIRECTION('ref_axis',(-1.,0.,0.)) ;
#126200 = DIRECTION('',(1.,0.,0.)) ;
#126201 = DIRECTION('',(0.,-1.,0.)) ;
#126202 = DIRECTION('',(-1.,0.,0.)) ;
#126203 = DIRECTION('center_axis',(0.,-1.,0.)) ;
#126204 = DIRECTION('ref_axis',(0.,0.,-1.)) ;
#126205 = DIRECTION('center_axis',(0.,1.,0.)) ;
#126206 = DIRECTION('ref_axis',(0.,0.,-1.)) ;
#126207 = DIRECTION('',(0.,-1.,0.)) ;
#126208 = DIRECTION('center_axis',(0.,-1.,0.)) ;
#126209 = DIRECTION('ref_axis',(0.,0.,-1.)) ;
#126210 = DIRECTION('center_axis',(-1.,0.,0.)) ;
#126211 = DIRECTION('ref_axis',(0.,0.,1.)) ;
#126212 = DIRECTION('',(0.,0.,1.)) ;
#126213 = DIRECTION('',(0.,0.,-1.)) ;
#126214 = DIRECTION('center_axis',(0.,-1.,0.)) ;
#126215 = DIRECTION('ref_axis',(0.,0.,-1.)) ;
#126216 = DIRECTION('',(1.,0.,0.)) ;
#126217 = DIRECTION('',(0.,0.,-1.)) ;
#126218 = DIRECTION('',(-1.,0.,0.)) ;
#126219 = DIRECTION('',(0.,0.,1.)) ;
#126220 = DIRECTION('center_axis',(0.,-1.,0.)) ;
#126221 = DIRECTION('ref_axis',(0.,0.,-1.)) ;
#126222 = DIRECTION('',(0.,-1.,0.)) ;
#126223 = DIRECTION('center_axis',(0.,1.,0.)) ;
#126224 = DIRECTION('ref_axis',(5.20417042793027E-14,0.,-1.)) ;
#126225 = DIRECTION('',(0.,-1.,0.)) ;
#126226 = DIRECTION('center_axis',(0.,-1.,0.)) ;
#126227 = DIRECTION('ref_axis',(0.,0.,-1.)) ;
#126228 = DIRECTION('center_axis',(0.,0.,1.)) ;
#126229 = DIRECTION('ref_axis',(1.,0.,0.)) ;
#126230 = DIRECTION('',(-1.,0.,0.)) ;
#126231 = DIRECTION('',(0.,-1.,0.)) ;
#126232 = DIRECTION('',(1.,0.,0.)) ;
#126233 = DIRECTION('center_axis',(0.,-1.,0.)) ;
#126234 = DIRECTION('ref_axis',(0.,0.,-1.)) ;
#126235 = DIRECTION('center_axis',(0.,1.,0.)) ;
#126236 = DIRECTION('ref_axis',(0.,0.,-1.)) ;
#126237 = DIRECTION('',(0.,-1.,0.)) ;
#126238 = DIRECTION('center_axis',(0.,-1.,0.)) ;
#126239 = DIRECTION('ref_axis',(0.,0.,-1.)) ;
#126240 = DIRECTION('center_axis',(1.,0.,0.)) ;
#126241 = DIRECTION('ref_axis',(0.,0.,-1.)) ;
#126242 = DIRECTION('',(0.,0.,1.)) ;
#126243 = DIRECTION('',(0.,-1.,0.)) ;
#126244 = DIRECTION('',(0.,0.,-1.)) ;
#126245 = DIRECTION('center_axis',(0.,-1.,0.)) ;
#126246 = DIRECTION('ref_axis',(0.,0.,-1.)) ;
#126247 = DIRECTION('center_axis',(0.,1.,0.)) ;
#126248 = DIRECTION('ref_axis',(0.,0.,-1.)) ;
#126249 = DIRECTION('',(0.,-1.,0.)) ;
#126250 = DIRECTION('center_axis',(0.,-1.,0.)) ;
#126251 = DIRECTION('ref_axis',(0.,0.,-1.)) ;
#126252 = DIRECTION('center_axis',(0.,0.,-1.)) ;
#126253 = DIRECTION('ref_axis',(-1.,0.,0.)) ;
#126254 = DIRECTION('',(1.,0.,0.)) ;
#126255 = DIRECTION('',(0.,-1.,0.)) ;
#126256 = DIRECTION('',(-1.,0.,0.)) ;
#126257 = DIRECTION('center_axis',(0.,-1.,0.)) ;
#126258 = DIRECTION('ref_axis',(0.,0.,-1.)) ;
#126259 = DIRECTION('center_axis',(0.,1.,0.)) ;
#126260 = DIRECTION('ref_axis',(0.,0.,-1.)) ;
#126261 = DIRECTION('',(0.,-1.,0.)) ;
#126262 = DIRECTION('center_axis',(0.,-1.,0.)) ;
#126263 = DIRECTION('ref_axis',(0.,0.,-1.)) ;
#126264 = DIRECTION('center_axis',(-1.,0.,0.)) ;
#126265 = DIRECTION('ref_axis',(0.,0.,1.)) ;
#126266 = DIRECTION('',(0.,0.,1.)) ;
#126267 = DIRECTION('',(0.,0.,-1.)) ;
#126268 = DIRECTION('center_axis',(0.,-1.,0.)) ;
#126269 = DIRECTION('ref_axis',(0.,0.,-1.)) ;
#126270 = DIRECTION('',(1.,0.,0.)) ;
#126271 = DIRECTION('',(0.,0.,-1.)) ;
#126272 = DIRECTION('',(-1.,0.,0.)) ;
#126273 = DIRECTION('',(0.,0.,1.)) ;
#126274 = DIRECTION('center_axis',(0.,1.,0.)) ;
#126275 = DIRECTION('ref_axis',(1.,0.,0.)) ;
#126276 = DIRECTION('center_axis',(-1.73472347597682E-14,0.,-1.)) ;
#126277 = DIRECTION('ref_axis',(1.,0.,-1.73472347597682E-14)) ;
#126278 = DIRECTION('center_axis',(0.,0.514231796959119,0.857651245551591)) ;
#126279 = DIRECTION('ref_axis',(0.,0.857651245551591,-0.514231796959119)) ;
#126280 = DIRECTION('center_axis',(-1.,0.,0.)) ;
#126281 = DIRECTION('ref_axis',(0.,0.,-1.)) ;
#126282 = DIRECTION('center_axis',(1.,0.,0.)) ;
#126283 = DIRECTION('ref_axis',(0.,0.,-1.)) ;
#126284 = DIRECTION('center_axis',(-2.15682522756814E-14,-0.514231796959101,
0.857651245551602)) ;
#126285 = DIRECTION('ref_axis',(-4.48628358333197E-30,-0.857651245551602,
-0.514231796959101)) ;
#126286 = DIRECTION('center_axis',(-1.,0.,0.)) ;
#126287 = DIRECTION('ref_axis',(0.,0.,1.)) ;
#126288 = DIRECTION('center_axis',(-1.,0.,0.)) ;
#126289 = DIRECTION('ref_axis',(0.,0.,-1.)) ;
#126290 = DIRECTION('center_axis',(0.,0.,1.)) ;
#126291 = DIRECTION('ref_axis',(1.,0.,0.)) ;
#126292 = DIRECTION('center_axis',(0.,-8.67361737988405E-15,-1.)) ;
#126293 = DIRECTION('ref_axis',(0.,1.,-8.67361737988405E-15)) ;
#126294 = DIRECTION('center_axis',(0.,-1.,8.97270763436279E-17)) ;
#126295 = DIRECTION('ref_axis',(0.,-8.97270763436279E-17,-1.)) ;
#126296 = DIRECTION('center_axis',(0.,-1.,8.97270763436279E-17)) ;
#126297 = DIRECTION('ref_axis',(0.,-8.97270763436279E-17,-1.)) ;
#126298 = DIRECTION('center_axis',(0.,-1.,0.)) ;
#126299 = DIRECTION('ref_axis',(0.,0.,-1.)) ;
#126300 = DIRECTION('center_axis',(0.,0.,-1.)) ;
#126301 = DIRECTION('ref_axis',(-1.,0.,0.)) ;
#126302 = DIRECTION('center_axis',(0.,0.,1.)) ;
#126303 = DIRECTION('ref_axis',(-1.,0.,0.)) ;
#126304 = DIRECTION('center_axis',(0.,0.,-1.)) ;
#126305 = DIRECTION('ref_axis',(-1.,0.,0.)) ;
#126306 = DIRECTION('center_axis',(0.,1.,0.)) ;
#126307 = DIRECTION('ref_axis',(1.,0.,0.)) ;
#126308 = DIRECTION('center_axis',(-1.,0.,0.)) ;
#126309 = DIRECTION('ref_axis',(0.,0.,-1.)) ;
#126310 = DIRECTION('center_axis',(0.,-1.73472347597681E-14,1.)) ;
#126311 = DIRECTION('ref_axis',(0.,1.,1.73472347597681E-14)) ;
#126312 = DIRECTION('center_axis',(1.,0.,0.)) ;
#126313 = DIRECTION('ref_axis',(0.,0.,-1.)) ;
#126314 = DIRECTION('center_axis',(0.,0.,1.)) ;
#126315 = DIRECTION('ref_axis',(-1.,0.,0.)) ;
#126316 = DIRECTION('center_axis',(0.,-0.514231796959101,-0.857651245551602)) ;
#126317 = DIRECTION('ref_axis',(0.,-0.857651245551602,0.514231796959101)) ;
#126318 = DIRECTION('center_axis',(0.,1.,0.)) ;
#126319 = DIRECTION('ref_axis',(1.,0.,0.)) ;
#126320 = DIRECTION('center_axis',(-1.,0.,0.)) ;
#126321 = DIRECTION('ref_axis',(0.,0.,-1.)) ;
#126322 = DIRECTION('center_axis',(0.,1.,8.97270763436279E-17)) ;
#126323 = DIRECTION('ref_axis',(0.,-8.97270763436279E-17,1.)) ;
#126324 = DIRECTION('center_axis',(0.,-1.,-8.97270763436279E-17)) ;
#126325 = DIRECTION('ref_axis',(0.,-8.97270763436279E-17,1.)) ;
#126326 = DIRECTION('center_axis',(0.,-1.,0.)) ;
#126327 = DIRECTION('ref_axis',(0.,0.,-1.)) ;
#126328 = DIRECTION('center_axis',(0.,0.,1.)) ;
#126329 = DIRECTION('ref_axis',(1.,0.,0.)) ;
#126330 = DIRECTION('center_axis',(0.,0.,1.)) ;
#126331 = DIRECTION('ref_axis',(1.,0.,0.)) ;
#126332 = DIRECTION('center_axis',(-1.,0.,0.)) ;
#126333 = DIRECTION('ref_axis',(0.,0.,1.)) ;
#126334 = DIRECTION('center_axis',(-1.,0.,0.)) ;
#126335 = DIRECTION('ref_axis',(0.,0.,-1.)) ;
#126336 = DIRECTION('center_axis',(1.,0.,0.)) ;
#126337 = DIRECTION('ref_axis',(0.,0.,-1.)) ;
#126338 = DIRECTION('center_axis',(0.,0.514231796959101,-0.857651245551602)) ;
#126339 = DIRECTION('ref_axis',(0.,0.857651245551602,0.514231796959101)) ;
#126340 = DIRECTION('center_axis',(0.,0.,-1.)) ;
#126341 = DIRECTION('ref_axis',(-1.,0.,0.)) ;
#126342 = DIRECTION('center_axis',(-7.01133629567814E-33,8.97270763436279E-17,
1.)) ;
#126343 = DIRECTION('ref_axis',(-6.29106707073161E-49,-1.,8.97270763436279E-17)) ;
#126344 = DIRECTION('center_axis',(-1.,0.,-7.01133629567814E-33)) ;
#126345 = DIRECTION('ref_axis',(-7.01133629567814E-33,0.,1.)) ;
#126346 = DIRECTION('center_axis',(-1.,0.,0.)) ;
#126347 = DIRECTION('ref_axis',(0.,0.,1.)) ;
#126348 = DIRECTION('center_axis',(0.,1.,0.)) ;
#126349 = DIRECTION('ref_axis',(1.,0.,0.)) ;
#126350 = DIRECTION('center_axis',(-1.,0.,0.)) ;
#126351 = DIRECTION('ref_axis',(0.,0.,-1.)) ;
#126352 = DIRECTION('center_axis',(1.,0.,0.)) ;
#126353 = DIRECTION('ref_axis',(0.,0.,-1.)) ;
#126354 = DIRECTION('center_axis',(0.,0.,-1.)) ;
#126355 = DIRECTION('ref_axis',(1.,0.,0.)) ;
#126356 = DIRECTION('center_axis',(-7.01133629567814E-33,8.97270763436279E-17,
1.)) ;
#126357 = DIRECTION('ref_axis',(0.,-1.,0.)) ;
#126358 = DIRECTION('center_axis',(0.,-1.,0.)) ;
#126359 = DIRECTION('ref_axis',(0.,0.,1.)) ;
#126360 = DIRECTION('center_axis',(-1.,0.,7.01133629567814E-33)) ;
#126361 = DIRECTION('ref_axis',(7.01133629567814E-33,0.,1.)) ;
#126362 = DIRECTION('center_axis',(-1.,0.,0.)) ;
#126363 = DIRECTION('ref_axis',(0.,0.,1.)) ;
#126364 = DIRECTION('center_axis',(0.,0.,-1.)) ;
#126365 = DIRECTION('ref_axis',(-1.,0.,0.)) ;
#126366 = DIRECTION('center_axis',(-7.01133629567814E-33,8.97270763436279E-17,
-1.)) ;
#126367 = DIRECTION('ref_axis',(6.29106707073161E-49,1.,8.97270763436279E-17)) ;
#126368 = DIRECTION('center_axis',(0.,-1.,8.97270763436279E-17)) ;
#126369 = DIRECTION('ref_axis',(0.,-8.97270763436279E-17,-1.)) ;
#126370 = DIRECTION('center_axis',(0.,-1.,0.)) ;
#126371 = DIRECTION('ref_axis',(0.,0.,-1.)) ;
#126372 = DIRECTION('center_axis',(1.,7.81406971160724E-17,0.)) ;
#126373 = DIRECTION('ref_axis',(-7.81406971160724E-17,1.,0.)) ;
#126374 = DIRECTION('center_axis',(1.,0.,0.)) ;
#126375 = DIRECTION('ref_axis',(0.,0.,-1.)) ;
#126376 = DIRECTION('center_axis',(1.,0.,0.)) ;
#126377 = DIRECTION('ref_axis',(0.,0.,-1.)) ;
#126378 = DIRECTION('center_axis',(3.78638272950961E-32,-4.8455963016112E-16,
-1.)) ;
#126379 = DIRECTION('ref_axis',(1.83472821505963E-47,1.,-4.8455963016112E-16)) ;
#126380 = DIRECTION('center_axis',(3.78638272950961E-32,-4.8455963016112E-16,
-1.)) ;
#126381 = DIRECTION('ref_axis',(1.83472821505963E-47,1.,-4.8455963016112E-16)) ;
#126382 = DIRECTION('center_axis',(0.,0.,-1.)) ;
#126383 = DIRECTION('ref_axis',(-1.,0.,0.)) ;
#126384 = DIRECTION('center_axis',(-7.01133629567814E-33,8.97270763436279E-17,
-1.)) ;
#126385 = DIRECTION('ref_axis',(0.,1.,0.)) ;
#126386 = DIRECTION('center_axis',(0.,-1.,0.)) ;
#126387 = DIRECTION('ref_axis',(0.,0.,1.)) ;
#126388 = DIRECTION('center_axis',(0.,1.,0.)) ;
#126389 = DIRECTION('ref_axis',(1.,0.,0.)) ;
#126390 = DIRECTION('center_axis',(-1.,0.,0.)) ;
#126391 = DIRECTION('ref_axis',(0.,0.,-1.)) ;
#126392 = DIRECTION('center_axis',(0.,8.67361737988401E-15,1.)) ;
#126393 = DIRECTION('ref_axis',(0.,1.,-8.67361737988401E-15)) ;
#126394 = DIRECTION('center_axis',(0.,1.,0.)) ;
#126395 = DIRECTION('ref_axis',(1.,0.,0.)) ;
#126396 = DIRECTION('center_axis',(0.,1.,0.)) ;
#126397 = DIRECTION('ref_axis',(0.,0.,-1.)) ;
#126398 = DIRECTION('center_axis',(0.,1.,8.97270763436279E-17)) ;
#126399 = DIRECTION('ref_axis',(0.,-8.97270763436279E-17,1.)) ;
#126400 = DIRECTION('center_axis',(0.,-1.,0.)) ;
#126401 = DIRECTION('ref_axis',(0.,0.,-1.)) ;
#126402 = DIRECTION('center_axis',(0.,0.,1.)) ;
#126403 = DIRECTION('ref_axis',(1.,0.,0.)) ;
#126404 = DIRECTION('center_axis',(0.,0.,1.)) ;
#126405 = DIRECTION('ref_axis',(1.,0.,0.)) ;
#126406 = DIRECTION('center_axis',(-1.,-7.81406971160724E-17,0.)) ;
#126407 = DIRECTION('ref_axis',(7.81406971160724E-17,-1.,0.)) ;
#126408 = DIRECTION('center_axis',(-1.,-7.81406971160724E-17,0.)) ;
#126409 = DIRECTION('ref_axis',(-7.81406971160724E-17,1.,0.)) ;
#126410 = DIRECTION('center_axis',(-7.81406971160724E-17,1.,-8.97270763436279E-17)) ;
#126411 = DIRECTION('ref_axis',(-7.01133629567814E-33,8.97270763436279E-17,
1.)) ;
#126412 = DIRECTION('center_axis',(0.,1.,0.)) ;
#126413 = DIRECTION('ref_axis',(0.,0.,1.)) ;
#126414 = DIRECTION('center_axis',(0.,1.,0.)) ;
#126415 = DIRECTION('ref_axis',(1.,0.,0.)) ;
#126416 = DIRECTION('center_axis',(-1.,0.,0.)) ;
#126417 = DIRECTION('ref_axis',(0.,0.,-1.)) ;
#126418 = DIRECTION('center_axis',(1.,7.81406971160724E-17,0.)) ;
#126419 = DIRECTION('ref_axis',(0.,1.,0.)) ;
#126420 = DIRECTION('center_axis',(0.,0.,-1.)) ;
#126421 = DIRECTION('ref_axis',(1.,0.,0.)) ;
#126422 = DIRECTION('center_axis',(1.,7.81406971160724E-17,0.)) ;
#126423 = DIRECTION('ref_axis',(-7.81406971160724E-17,1.,0.)) ;
#126424 = DIRECTION('center_axis',(1.,0.,0.)) ;
#126425 = DIRECTION('ref_axis',(0.,0.,-1.)) ;
#126426 = DIRECTION('center_axis',(1.,0.,0.)) ;
#126427 = DIRECTION('ref_axis',(0.,0.,-1.)) ;
#126428 = DIRECTION('center_axis',(-1.,-7.81406971160724E-17,0.)) ;
#126429 = DIRECTION('ref_axis',(7.81406971160724E-17,-1.,0.)) ;
#126430 = DIRECTION('center_axis',(-1.,-7.81406971160724E-17,0.)) ;
#126431 = DIRECTION('ref_axis',(-7.81406971160724E-17,1.,0.)) ;
#126432 = DIRECTION('center_axis',(0.,0.,-1.)) ;
#126433 = DIRECTION('ref_axis',(-1.,0.,0.)) ;
#126434 = DIRECTION('center_axis',(0.,0.,-1.)) ;
#126435 = DIRECTION('ref_axis',(-1.,0.,0.)) ;
#126436 = DIRECTION('center_axis',(0.,1.,0.)) ;
#126437 = DIRECTION('ref_axis',(1.,0.,0.)) ;
#126438 = DIRECTION('center_axis',(0.,1.,0.)) ;
#126439 = DIRECTION('ref_axis',(0.,0.,-1.)) ;
#126440 = DIRECTION('center_axis',(1.,7.81406971160724E-17,0.)) ;
#126441 = DIRECTION('ref_axis',(0.,1.,0.)) ;
#126442 = DIRECTION('center_axis',(0.,-1.,0.)) ;
#126443 = DIRECTION('ref_axis',(0.,0.,1.)) ;
#126444 = DIRECTION('center_axis',(7.81406971160724E-17,-1.,-8.97270763436279E-17)) ;
#126445 = DIRECTION('ref_axis',(-7.01133629567814E-33,8.97270763436279E-17,
-1.)) ;
#126446 = DIRECTION('center_axis',(0.,-1.,0.)) ;
#126447 = DIRECTION('ref_axis',(0.,0.,-1.)) ;
#126448 = DIRECTION('center_axis',(-1.,0.,-8.67361737988401E-15)) ;
#126449 = DIRECTION('ref_axis',(-8.67361737988401E-15,0.,1.)) ;
#126450 = DIRECTION('center_axis',(-8.67361737988401E-15,8.67361737988405E-15,
-1.)) ;
#126451 = DIRECTION('ref_axis',(0.,1.,8.67361737988405E-15)) ;
#126452 = DIRECTION('center_axis',(0.,0.,-1.)) ;
#126453 = DIRECTION('ref_axis',(-1.,0.,0.)) ;
#126454 = DIRECTION('center_axis',(0.,8.67361737988405E-15,-1.)) ;
#126455 = DIRECTION('ref_axis',(0.,1.,8.67361737988405E-15)) ;
#126456 = DIRECTION('center_axis',(1.,0.,0.)) ;
#126457 = DIRECTION('ref_axis',(0.,0.,-1.)) ;
#126458 = DIRECTION('center_axis',(-1.,0.,0.)) ;
#126459 = DIRECTION('ref_axis',(0.,0.,1.)) ;
#126460 = DIRECTION('center_axis',(0.,-1.,0.)) ;
#126461 = DIRECTION('ref_axis',(0.,0.,-1.)) ;
#126462 = DIRECTION('center_axis',(-1.,0.,0.)) ;
#126463 = DIRECTION('ref_axis',(0.,0.,1.)) ;
#126464 = DIRECTION('center_axis',(0.,-1.,0.)) ;
#126465 = DIRECTION('ref_axis',(0.,0.,-1.)) ;
#126466 = DIRECTION('center_axis',(8.67361737988394E-15,0.,-1.)) ;
#126467 = DIRECTION('ref_axis',(-1.,0.,-8.67361737988394E-15)) ;
#126468 = DIRECTION('center_axis',(-1.,0.,0.)) ;
#126469 = DIRECTION('ref_axis',(0.,0.,1.)) ;
#126470 = DIRECTION('center_axis',(-1.,1.73472347597681E-14,0.)) ;
#126471 = DIRECTION('ref_axis',(-1.73472347597681E-14,-1.,0.)) ;
#126472 = DIRECTION('center_axis',(0.,0.,1.)) ;
#126473 = DIRECTION('ref_axis',(1.,0.,0.)) ;
#126474 = DIRECTION('center_axis',(-8.67361737988409E-15,0.,-1.)) ;
#126475 = DIRECTION('ref_axis',(-1.,0.,8.67361737988409E-15)) ;
#126476 = DIRECTION('center_axis',(0.,-1.,0.)) ;
#126477 = DIRECTION('ref_axis',(0.,0.,-1.)) ;
#126478 = DIRECTION('center_axis',(-1.,0.,-2.16840434497101E-16)) ;
#126479 = DIRECTION('ref_axis',(-2.16840434497101E-16,0.,1.)) ;
#126480 = DIRECTION('center_axis',(0.447219005481266,-5.60223447638367E-6,
-0.894424485971266)) ;
#126481 = DIRECTION('ref_axis',(0.894327914919435,-0.0146917039424838,0.447170811246801)) ;
#126482 = DIRECTION('center_axis',(-0.447220452186733,-7.1003629231252E-6,
-0.894423762595493)) ;
#126483 = DIRECTION('ref_axis',(0.894325663271496,0.0148067719247234,-0.447171519127916)) ;
#126484 = DIRECTION('center_axis',(2.16840434497101E-16,0.,-1.)) ;
#126485 = DIRECTION('ref_axis',(-1.,0.,-2.16840434497101E-16)) ;
#126486 = DIRECTION('center_axis',(0.894423762593898,-7.10036023719333E-6,
-0.447220452189923)) ;
#126487 = DIRECTION('ref_axis',(0.447171519131178,0.014806771908337,0.894325663270136)) ;
#126488 = DIRECTION('center_axis',(0.894424485971477,-5.6022343618357E-6,
0.447219005480843)) ;
#126489 = DIRECTION('ref_axis',(0.447170811246647,0.0146917039013095,-0.894327914920188)) ;
#126490 = DIRECTION('center_axis',(0.,0.,1.)) ;
#126491 = DIRECTION('ref_axis',(1.,0.,0.)) ;
#126492 = DIRECTION('center_axis',(-0.894423762593899,-7.10036026306032E-6,
0.447220452189921)) ;
#126493 = DIRECTION('ref_axis',(0.447171519131236,-0.0148067718993793,0.894325663270256)) ;
#126494 = DIRECTION('center_axis',(-0.894424485971371,-5.60223466451923E-6,
-0.447219005481054)) ;
#126495 = DIRECTION('ref_axis',(0.447170811246984,-0.0146917038828087,-0.894327914920324)) ;
#126496 = DIRECTION('center_axis',(1.,0.,-2.16840434497101E-16)) ;
#126497 = DIRECTION('ref_axis',(-2.16840434497101E-16,0.,-1.)) ;
#126498 = DIRECTION('center_axis',(0.447220452189006,-7.10035961013466E-6,
0.894423762594357)) ;
#126499 = DIRECTION('ref_axis',(0.894325663270134,-0.0148067719434002,-0.447171519130021)) ;
#126500 = DIRECTION('center_axis',(-0.447219005476855,-5.60223624898873E-6,
0.894424485973471)) ;
#126501 = DIRECTION('ref_axis',(0.894327914921509,0.0146917039515858,0.447170811242355)) ;
#126502 = DIRECTION('center_axis',(-1.,0.,-2.16840434497101E-16)) ;
#126503 = DIRECTION('ref_axis',(-2.16840434497101E-16,0.,1.)) ;
#126504 = DIRECTION('center_axis',(0.447219005481374,-5.60223458892711E-6,
-0.894424485971211)) ;
#126505 = DIRECTION('ref_axis',(0.894327914919542,-0.0146917039301271,0.447170811246992)) ;
#126506 = DIRECTION('center_axis',(-0.447220452186661,-7.10036284809686E-6,
-0.894423762595529)) ;
#126507 = DIRECTION('ref_axis',(0.894325663271462,0.0148067719300271,-0.447171519127808)) ;
#126508 = DIRECTION('center_axis',(2.16840434497101E-16,0.,-1.)) ;
#126509 = DIRECTION('ref_axis',(-1.,0.,-2.16840434497101E-16)) ;
#126510 = DIRECTION('center_axis',(0.8944237625938,-7.10036041135031E-6,-0.447220452190118)) ;
#126511 = DIRECTION('ref_axis',(0.447171519131424,0.0148067719010635,0.894325663270134)) ;
#126512 = DIRECTION('center_axis',(0.894424485971393,-5.60223456270103E-6,
0.44721900548101)) ;
#126513 = DIRECTION('ref_axis',(0.44717081124683,0.0146917038993221,-0.89432791492013)) ;
#126514 = DIRECTION('center_axis',(0.,0.,1.)) ;
#126515 = DIRECTION('ref_axis',(1.,0.,0.)) ;
#126516 = DIRECTION('center_axis',(-0.894423762593985,-7.10036011396666E-6,
0.44722045218975)) ;
#126517 = DIRECTION('ref_axis',(0.447171519131028,-0.0148067719045682,0.894325663270274)) ;
#126518 = DIRECTION('center_axis',(-0.894424485971438,-5.60223469492586E-6,
-0.447219005480921)) ;
#126519 = DIRECTION('ref_axis',(0.447170811246701,-0.0146917039057028,-0.894327914920089)) ;
#126520 = DIRECTION('center_axis',(1.,0.,-2.16840434497101E-16)) ;
#126521 = DIRECTION('ref_axis',(-2.16840434497101E-16,0.,-1.)) ;
#126522 = DIRECTION('center_axis',(0.447220452189581,-7.10036082007094E-6,
0.894423762594069)) ;
#126523 = DIRECTION('ref_axis',(0.894325663270147,-0.014806771920165,-0.447171519130766)) ;
#126524 = DIRECTION('center_axis',(-0.447219005480049,-5.60223383386894E-6,
0.894424485971874)) ;
#126525 = DIRECTION('ref_axis',(0.89432791492014,0.0146917039354466,0.447170811245622)) ;
#126526 = DIRECTION('center_axis',(-1.,0.,-2.16840434497101E-16)) ;
#126527 = DIRECTION('ref_axis',(-2.16840434497101E-16,0.,1.)) ;
#126528 = DIRECTION('center_axis',(0.447219005480065,-5.60223452105138E-6,
-0.894424485971866)) ;
#126529 = DIRECTION('ref_axis',(0.894327914920316,-0.0146917039210787,0.447170811245742)) ;
#126530 = DIRECTION('center_axis',(-0.447220452189082,-7.10035963327167E-6,
-0.894423762594318)) ;
#126531 = DIRECTION('ref_axis',(0.894325663270257,0.0148067719312621,-0.447171519130178)) ;
#126532 = DIRECTION('center_axis',(2.16840434497101E-16,0.,-1.)) ;
#126533 = DIRECTION('ref_axis',(-1.,0.,-2.16840434497101E-16)) ;
#126534 = DIRECTION('center_axis',(0.8944237625938,-7.10036041135031E-6,-0.447220452190118)) ;
#126535 = DIRECTION('ref_axis',(0.447171519131363,0.014806771910293,0.894325663270012)) ;
#126536 = DIRECTION('center_axis',(0.894424485971369,-5.60223461266618E-6,
0.447219005481058)) ;
#126537 = DIRECTION('ref_axis',(0.447170811246847,0.0146917039042423,-0.89432791492004)) ;
#126538 = DIRECTION('center_axis',(0.,0.,1.)) ;
#126539 = DIRECTION('ref_axis',(1.,0.,0.)) ;
#126540 = DIRECTION('center_axis',(-0.894423762593847,-7.10036059498734E-6,
0.447220452190025)) ;
#126541 = DIRECTION('ref_axis',(0.447171519131148,-0.0148067719290856,0.894325663269808)) ;
#126542 = DIRECTION('center_axis',(-0.894424485971523,-5.60223451992655E-6,
-0.447219005480752)) ;
#126543 = DIRECTION('ref_axis',(0.447170811246541,-0.0146917039039939,-0.894327914920198)) ;
#126544 = DIRECTION('center_axis',(1.,0.,-2.16840434497101E-16)) ;
#126545 = DIRECTION('ref_axis',(-2.16840434497101E-16,0.,-1.)) ;
#126546 = DIRECTION('center_axis',(0.447220452189557,-7.10036079532928E-6,
0.894423762594081)) ;
#126547 = DIRECTION('ref_axis',(0.894325663270269,-0.0148067719118157,-0.447171519130797)) ;
#126548 = DIRECTION('center_axis',(-0.447219005480149,-5.60223388206588E-6,
0.894424485971824)) ;
#126549 = DIRECTION('ref_axis',(0.894327914920146,0.0146917039311632,0.447170811245751)) ;
#126550 = DIRECTION('center_axis',(-1.,0.,-2.16840434497101E-16)) ;
#126551 = DIRECTION('ref_axis',(-2.16840434497101E-16,0.,1.)) ;
#126552 = DIRECTION('center_axis',(0.447219005480246,-5.60223470853928E-6,
-0.894424485971776)) ;
#126553 = DIRECTION('ref_axis',(0.894327914920193,-0.0146917039234679,0.447170811245909)) ;
#126554 = DIRECTION('center_axis',(-0.447220452189106,-7.10035965817415E-6,
-0.894423762594306)) ;
#126555 = DIRECTION('ref_axis',(0.894325663270211,0.014806771933774,-0.447171519130185)) ;
#126556 = DIRECTION('center_axis',(2.16840434497101E-16,0.,-1.)) ;
#126557 = DIRECTION('ref_axis',(-1.,0.,-2.16840434497101E-16)) ;
#126558 = DIRECTION('center_axis',(0.894423762593813,-7.10036038628687E-6,
-0.447220452190094)) ;
#126559 = DIRECTION('ref_axis',(0.447171519131279,0.0148067719193131,0.894325663269904)) ;
#126560 = DIRECTION('center_axis',(0.894424485972067,-5.60223311109745E-6,
0.447219005479663)) ;
#126561 = DIRECTION('ref_axis',(0.447170811245097,0.0146917039552028,-0.894327914920078)) ;
#126562 = DIRECTION('center_axis',(0.,0.,1.)) ;
#126563 = DIRECTION('ref_axis',(1.,0.,0.)) ;
#126564 = DIRECTION('center_axis',(-0.894423762593869,-7.10036049345021E-6,
0.447220452189981)) ;
#126565 = DIRECTION('ref_axis',(0.44717151913113,-0.0148067719249295,0.894325663269886)) ;
#126566 = DIRECTION('center_axis',(-0.89442448597151,-5.60223454494956E-6,
-0.447219005480776)) ;
#126567 = DIRECTION('ref_axis',(0.447170811246508,-0.0146917039126806,-0.894327914920071)) ;
#126568 = DIRECTION('center_axis',(1.,0.,-2.16840434497101E-16)) ;
#126569 = DIRECTION('ref_axis',(-2.16840434497101E-16,0.,-1.)) ;
#126570 = DIRECTION('center_axis',(0.447220452189376,-7.1003606078408E-6,
0.894423762594172)) ;
#126571 = DIRECTION('ref_axis',(0.894325663270274,-0.0148067719183669,-0.44717151913057)) ;
#126572 = DIRECTION('center_axis',(-0.447219005480174,-5.60223390704821E-6,
0.894424485971812)) ;
#126573 = DIRECTION('ref_axis',(0.894327914920086,0.0146917039347775,0.447170811245753)) ;
#126574 = DIRECTION('center_axis',(-1.,0.,-2.16840434497101E-16)) ;
#126575 = DIRECTION('ref_axis',(-2.16840434497101E-16,0.,1.)) ;
#126576 = DIRECTION('center_axis',(0.447219005480053,-5.60223450851907E-6,
-0.894424485971872)) ;
#126577 = DIRECTION('ref_axis',(0.894327914920194,-0.0146917039308781,0.447170811245665)) ;
#126578 = DIRECTION('center_axis',(-0.447220452189219,-7.10035971890228E-6,
-0.89442376259425)) ;
#126579 = DIRECTION('ref_axis',(0.894325663270168,0.0148067719327317,-0.447171519130306)) ;
#126580 = DIRECTION('center_axis',(2.16840434497101E-16,0.,-1.)) ;
#126581 = DIRECTION('ref_axis',(-1.,0.,-2.16840434497101E-16)) ;
#126582 = DIRECTION('center_axis',(0.894423762593776,-7.10036044814174E-6,
-0.447220452190168)) ;
#126583 = DIRECTION('ref_axis',(0.447171519131389,0.0148067719138353,0.894325663269939)) ;
#126584 = DIRECTION('center_axis',(0.894424485971344,-5.60223463676545E-6,
0.447219005481109)) ;
#126585 = DIRECTION('ref_axis',(0.447170811246964,0.0146917038941729,-0.894327914920147)) ;
#126586 = DIRECTION('center_axis',(0.,0.,1.)) ;
#126587 = DIRECTION('ref_axis',(1.,0.,0.)) ;
#126588 = DIRECTION('center_axis',(-0.89442376259387,-7.10036051931658E-6,
0.447220452189979)) ;
#126589 = DIRECTION('ref_axis',(0.447171519131125,-0.0148067719254494,0.89432566326988)) ;
#126590 = DIRECTION('center_axis',(-0.894424485971498,-5.60223455703937E-6,
-0.447219005480801)) ;
#126591 = DIRECTION('ref_axis',(0.447170811246509,-0.0146917039163654,-0.89432791492001)) ;
#126592 = DIRECTION('center_axis',(1.,0.,-2.16840434497101E-16)) ;
#126593 = DIRECTION('ref_axis',(-2.16840434497101E-16,0.,-1.)) ;
#126594 = DIRECTION('center_axis',(0.447220452189472,-7.10036070777138E-6,
0.894423762594123)) ;
#126595 = DIRECTION('ref_axis',(0.894325663270285,-0.0148067719138536,-0.447171519130697)) ;
#126596 = DIRECTION('center_axis',(-0.447219005479954,-5.60223370799162E-6,
0.894424485971921)) ;
#126597 = DIRECTION('ref_axis',(0.894327914920089,0.0146917039429744,0.447170811245477)) ;
#126598 = DIRECTION('center_axis',(-1.,0.,-2.16840434497101E-16)) ;
#126599 = DIRECTION('ref_axis',(-2.16840434497101E-16,0.,1.)) ;
#126600 = DIRECTION('center_axis',(0.44721900547998,-5.60223443353162E-6,
-0.894424485971908)) ;
#126601 = DIRECTION('ref_axis',(0.894327914920239,-0.0146917039302217,0.447170811245596)) ;
#126602 = DIRECTION('center_axis',(-0.44722045218906,-7.10035958218204E-6,
-0.894423762594329)) ;
#126603 = DIRECTION('ref_axis',(0.894325663270273,0.0148067719309328,-0.447171519130157)) ;
#126604 = DIRECTION('center_axis',(2.16840434497101E-16,0.,-1.)) ;
#126605 = DIRECTION('ref_axis',(-1.,0.,-2.16840434497101E-16)) ;
#126606 = DIRECTION('center_axis',(0.894423762593771,-7.10036080288375E-6,
-0.447220452190178)) ;
#126607 = DIRECTION('ref_axis',(0.447171519131049,0.0148067719675465,0.894325663269221)) ;
#126608 = DIRECTION('center_axis',(0.894424485971344,-5.60223464973865E-6,
0.447219005481108)) ;
#126609 = DIRECTION('ref_axis',(0.447170811246911,0.0146917039020779,-0.894327914920044)) ;
#126610 = DIRECTION('center_axis',(0.,0.,1.)) ;
#126611 = DIRECTION('ref_axis',(1.,0.,0.)) ;
#126612 = DIRECTION('center_axis',(-0.894423762593835,-7.10036060735852E-6,
0.44722045219005)) ;
#126613 = DIRECTION('ref_axis',(0.447171519131198,-0.0148067719252183,0.894325663269847)) ;
#126614 = DIRECTION('center_axis',(-0.894424485971953,-5.602234646445E-6,
-0.447219005479891)) ;
#126615 = DIRECTION('ref_axis',(0.447170811245515,-0.0146917039293451,-0.894327914920294)) ;
#126616 = DIRECTION('center_axis',(1.,0.,-2.16840434497101E-16)) ;
#126617 = DIRECTION('ref_axis',(-2.16840434497101E-16,0.,-1.)) ;
#126618 = DIRECTION('center_axis',(0.447220452189611,-7.10036020924201E-6,
0.894423762594054)) ;
#126619 = DIRECTION('ref_axis',(0.894325663270291,-0.0148067719084231,-0.447171519130865)) ;
#126620 = DIRECTION('center_axis',(-0.447219005479986,-5.60223428805301E-6,
0.894424485971906)) ;
#126621 = DIRECTION('ref_axis',(0.894327914919888,0.0146917039567803,0.447170811245425)) ;
#126622 = DIRECTION('center_axis',(-1.,0.,-2.16840434497101E-16)) ;
#126623 = DIRECTION('ref_axis',(-2.16840434497101E-16,0.,1.)) ;
#126624 = DIRECTION('center_axis',(0.447219005479986,-5.60223379723993E-6,
-0.894424485971905)) ;
#126625 = DIRECTION('ref_axis',(0.894327914920294,-0.0146917039261431,0.44717081124562)) ;
#126626 = DIRECTION('center_axis',(-0.447220452189224,-7.10036029985229E-6,
-0.894423762594247)) ;
#126627 = DIRECTION('ref_axis',(0.894325663270126,0.0148067719354631,-0.447171519130301)) ;
#126628 = DIRECTION('center_axis',(2.16840434497101E-16,0.,-1.)) ;
#126629 = DIRECTION('ref_axis',(-1.,0.,-2.16840434497101E-16)) ;
#126630 = DIRECTION('center_axis',(0.894423762593695,-7.10036088835547E-6,
-0.447220452190328)) ;
#126631 = DIRECTION('ref_axis',(0.447171519131228,0.0148067719634075,0.8943256632692)) ;
#126632 = DIRECTION('center_axis',(0.894424485971236,-5.60223487474278E-6,
0.447219005481325)) ;
#126633 = DIRECTION('ref_axis',(0.447170811247132,0.0146917039018784,-0.894327914919936)) ;
#126634 = DIRECTION('center_axis',(0.,0.,1.)) ;
#126635 = DIRECTION('ref_axis',(1.,0.,0.)) ;
#126636 = DIRECTION('center_axis',(-0.894423762594132,-7.10036099567427E-6,
0.447220452189455)) ;
#126637 = DIRECTION('ref_axis',(0.447171519130486,-0.0148067719437975,0.894325663269895)) ;
#126638 = DIRECTION('center_axis',(-0.894424485972025,-5.60223448349518E-6,
-0.447219005479747)) ;
#126639 = DIRECTION('ref_axis',(0.447170811245346,-0.0146917039328969,-0.89432791492032)) ;
#126640 = DIRECTION('center_axis',(1.,0.,-2.16840434497101E-16)) ;
#126641 = DIRECTION('ref_axis',(-2.16840434497101E-16,0.,-1.)) ;
#126642 = DIRECTION('center_axis',(0.447220452189153,-7.10035973416595E-6,
0.894423762594283)) ;
#126643 = DIRECTION('ref_axis',(0.894325663270205,-0.014806771932442,-0.447171519130242)) ;
#126644 = DIRECTION('center_axis',(-0.447219005479711,-5.60223412313625E-6,
0.894424485972043)) ;
#126645 = DIRECTION('ref_axis',(0.894327914920089,0.0146917039520517,0.447170811245179)) ;
#126646 = DIRECTION('center_axis',(-1.,0.,-2.16840434497101E-16)) ;
#126647 = DIRECTION('ref_axis',(-2.16840434497101E-16,0.,1.)) ;
#126648 = DIRECTION('center_axis',(0.447219005480528,-5.60223404983417E-6,
-0.894424485971634)) ;
#126649 = DIRECTION('ref_axis',(0.894327914919937,-0.0146917039325427,0.447170811246124)) ;
#126650 = DIRECTION('center_axis',(-0.447220452189473,-7.10036045906616E-6,
-0.894423762594123)) ;
#126651 = DIRECTION('ref_axis',(0.894325663270072,0.0148067719300326,-0.447171519130588)) ;
#126652 = DIRECTION('center_axis',(2.16840434497101E-16,0.,-1.)) ;
#126653 = DIRECTION('ref_axis',(-1.,0.,-2.16840434497101E-16)) ;
#126654 = DIRECTION('center_axis',(0.894423762593943,-7.10036005950268E-6,
-0.447220452189833)) ;
#126655 = DIRECTION('ref_axis',(0.44717151913091,0.0148067719349505,0.89432566326983)) ;
#126656 = DIRECTION('center_axis',(0.894424485971607,-5.60223403505354E-6,
0.447219005480582)) ;
#126657 = DIRECTION('ref_axis',(0.447170811245978,0.0146917039629369,-0.894327914919511)) ;
#126658 = DIRECTION('center_axis',(0.,0.,1.)) ;
#126659 = DIRECTION('ref_axis',(1.,0.,0.)) ;
#126660 = DIRECTION('center_axis',(-0.894423762594202,-7.10036078087079E-6,
0.447220452189316)) ;
#126661 = DIRECTION('ref_axis',(0.447171519130283,-0.0148067719529112,0.894325663269846)) ;
#126662 = DIRECTION('center_axis',(-0.894424485971881,-5.60223416366214E-6,
-0.447219005480035)) ;
#126663 = DIRECTION('ref_axis',(0.447170811245601,-0.014691703937177,-0.894327914920122)) ;
#126664 = DIRECTION('center_axis',(1.,0.,-2.16840434497101E-16)) ;
#126665 = DIRECTION('ref_axis',(-2.16840434497101E-16,0.,-1.)) ;
#126666 = DIRECTION('center_axis',(0.4472204521899,-7.10036019911746E-6,0.89442376259391)) ;
#126667 = DIRECTION('ref_axis',(0.89432566326982,-0.0148067719330621,-0.447171519130991)) ;
#126668 = DIRECTION('center_axis',(-0.447219005479637,-5.60223439043371E-6,
0.89442448597208)) ;
#126669 = DIRECTION('ref_axis',(0.894327914920201,0.0146917039462084,0.447170811245147)) ;
#126670 = DIRECTION('center_axis',(1.,0.,-2.16840434497101E-16)) ;
#126671 = DIRECTION('ref_axis',(-2.16840434497101E-16,0.,-1.)) ;
#126672 = DIRECTION('center_axis',(1.,0.,0.)) ;
#126673 = DIRECTION('ref_axis',(0.,0.,-1.)) ;
#126674 = DIRECTION('center_axis',(-1.,0.,0.)) ;
#126675 = DIRECTION('ref_axis',(0.,0.,1.)) ;
#126676 = DIRECTION('center_axis',(0.,-1.,0.)) ;
#126677 = DIRECTION('ref_axis',(0.,0.,-1.)) ;
#126678 = DIRECTION('center_axis',(0.,0.,-1.)) ;
#126679 = DIRECTION('ref_axis',(1.,0.,0.)) ;
#126680 = DIRECTION('center_axis',(0.,-1.,0.)) ;
#126681 = DIRECTION('ref_axis',(0.,0.,-1.)) ;
#126682 = DIRECTION('center_axis',(0.,-1.,0.)) ;
#126683 = DIRECTION('ref_axis',(0.,0.,-1.)) ;
#126684 = DIRECTION('center_axis',(0.,-1.,0.)) ;
#126685 = DIRECTION('ref_axis',(0.,0.,-1.)) ;
#126686 = DIRECTION('center_axis',(0.,0.,-1.)) ;
#126687 = DIRECTION('ref_axis',(1.,0.,0.)) ;
#126688 = DIRECTION('center_axis',(0.,0.,1.)) ;
#126689 = DIRECTION('ref_axis',(1.,0.,0.)) ;
#126690 = DIRECTION('center_axis',(0.,0.,-1.)) ;
#126691 = DIRECTION('ref_axis',(-1.,0.,0.)) ;
#126692 = DIRECTION('center_axis',(0.,1.,0.)) ;
#126693 = DIRECTION('ref_axis',(0.,0.,1.)) ;
#126694 = DIRECTION('center_axis',(0.,-1.,0.)) ;
#126695 = DIRECTION('ref_axis',(0.,0.,-1.)) ;
#126696 = DIRECTION('center_axis',(-1.,0.,2.16840434497101E-16)) ;
#126697 = DIRECTION('ref_axis',(2.16840434497101E-16,0.,1.)) ;
#126698 = DIRECTION('center_axis',(-1.,0.,0.)) ;
#126699 = DIRECTION('ref_axis',(0.,0.,1.)) ;
#126700 = DIRECTION('center_axis',(1.,0.,0.)) ;
#126701 = DIRECTION('ref_axis',(0.,0.,-1.)) ;
#126702 = DIRECTION('center_axis',(0.,1.,0.)) ;
#126703 = DIRECTION('ref_axis',(0.,0.,1.)) ;
#126704 = DIRECTION('center_axis',(0.,-1.,0.)) ;
#126705 = DIRECTION('ref_axis',(0.,0.,-1.)) ;
#126706 = DIRECTION('center_axis',(2.16840434497101E-16,0.,-1.)) ;
#126707 = DIRECTION('ref_axis',(-1.,0.,-2.16840434497101E-16)) ;
#126708 = DIRECTION('center_axis',(0.,0.,-1.)) ;
#126709 = DIRECTION('ref_axis',(-1.,0.,0.)) ;
#126710 = DIRECTION('center_axis',(-1.,0.,-2.16840434497101E-16)) ;
#126711 = DIRECTION('ref_axis',(-2.16840434497101E-16,0.,1.)) ;
#126712 = DIRECTION('center_axis',(-1.,0.,0.)) ;
#126713 = DIRECTION('ref_axis',(0.,0.,1.)) ;
#126714 = DIRECTION('center_axis',(1.,0.,0.)) ;
#126715 = DIRECTION('ref_axis',(0.,0.,-1.)) ;
#126716 = DIRECTION('center_axis',(0.,-1.,0.)) ;
#126717 = DIRECTION('ref_axis',(0.,0.,-1.)) ;
#126718 = DIRECTION('center_axis',(0.,-1.,0.)) ;
#126719 = DIRECTION('ref_axis',(0.,0.,-1.)) ;
#126720 = DIRECTION('center_axis',(0.,1.,0.)) ;
#126721 = DIRECTION('ref_axis',(1.,0.,0.)) ;
#126722 = DIRECTION('center_axis',(0.,0.,1.)) ;
#126723 = DIRECTION('ref_axis',(-1.,0.,0.)) ;
#126724 = DIRECTION('center_axis',(0.,1.,0.)) ;
#126725 = DIRECTION('ref_axis',(1.,0.,0.)) ;
#126726 = DIRECTION('center_axis',(0.,0.,1.)) ;
#126727 = DIRECTION('ref_axis',(-1.,0.,0.)) ;
#126728 = DIRECTION('center_axis',(0.,-1.,0.)) ;
#126729 = DIRECTION('ref_axis',(0.,0.,-1.)) ;
#126730 = DIRECTION('center_axis',(0.,-1.,0.)) ;
#126731 = DIRECTION('ref_axis',(0.,0.,-1.)) ;
#126732 = DIRECTION('center_axis',(0.,1.,0.)) ;
#126733 = DIRECTION('ref_axis',(0.,0.,1.)) ;
#126734 = DIRECTION('center_axis',(0.,-1.,0.)) ;
#126735 = DIRECTION('ref_axis',(0.,0.,-1.)) ;
#126736 = DIRECTION('center_axis',(0.,0.,-1.)) ;
#126737 = DIRECTION('ref_axis',(-1.,0.,0.)) ;
#126738 = DIRECTION('center_axis',(0.,0.,1.)) ;
#126739 = DIRECTION('ref_axis',(1.,0.,0.)) ;
#126740 = DIRECTION('center_axis',(-2.16840434497101E-16,0.,1.)) ;
#126741 = DIRECTION('ref_axis',(1.,0.,2.16840434497101E-16)) ;
#126742 = DIRECTION('center_axis',(0.,0.,1.)) ;
#126743 = DIRECTION('ref_axis',(1.,0.,0.)) ;
#126744 = DIRECTION('center_axis',(0.,1.,0.)) ;
#126745 = DIRECTION('ref_axis',(0.,0.,1.)) ;
#126746 = DIRECTION('center_axis',(0.,-1.,0.)) ;
#126747 = DIRECTION('ref_axis',(0.,0.,-1.)) ;
#126748 = DIRECTION('center_axis',(0.,1.,0.)) ;
#126749 = DIRECTION('ref_axis',(1.,0.,0.)) ;
#126750 = DIRECTION('center_axis',(-1.,0.,0.)) ;
#126751 = DIRECTION('ref_axis',(0.,0.,-1.)) ;
#126752 = DIRECTION('center_axis',(0.,1.,0.)) ;
#126753 = DIRECTION('ref_axis',(1.,0.,0.)) ;
#126754 = DIRECTION('center_axis',(1.,0.,0.)) ;
#126755 = DIRECTION('ref_axis',(0.,0.,1.)) ;
#126756 = DIRECTION('center_axis',(1.,0.,2.16840434497101E-16)) ;
#126757 = DIRECTION('ref_axis',(2.16840434497101E-16,0.,-1.)) ;
#126758 = DIRECTION('center_axis',(0.,-1.,0.)) ;
#126759 = DIRECTION('ref_axis',(0.,0.,-1.)) ;
#126760 = DIRECTION('center_axis',(0.,-1.,0.)) ;
#126761 = DIRECTION('ref_axis',(0.,0.,-1.)) ;
#126762 = DIRECTION('center_axis',(0.,0.,1.)) ;
#126763 = DIRECTION('ref_axis',(1.,0.,0.)) ;
#126764 = DIRECTION('center_axis',(0.,0.,-1.)) ;
#126765 = DIRECTION('ref_axis',(-1.,0.,0.)) ;
#126766 = DIRECTION('center_axis',(0.,0.,1.)) ;
#126767 = DIRECTION('ref_axis',(1.,0.,0.)) ;
#126768 = DIRECTION('center_axis',(0.,-1.,0.)) ;
#126769 = DIRECTION('ref_axis',(0.,0.,-1.)) ;
#126770 = DIRECTION('center_axis',(0.,-1.,0.)) ;
#126771 = DIRECTION('ref_axis',(0.,0.,-1.)) ;
#126772 = DIRECTION('center_axis',(0.,1.,0.)) ;
#126773 = DIRECTION('ref_axis',(1.,0.,0.)) ;
#126774 = DIRECTION('center_axis',(-1.,0.,0.)) ;
#126775 = DIRECTION('ref_axis',(0.,0.,-1.)) ;
#126776 = DIRECTION('center_axis',(0.,1.,0.)) ;
#126777 = DIRECTION('ref_axis',(1.,0.,0.)) ;
#126778 = DIRECTION('center_axis',(-1.,0.,0.)) ;
#126779 = DIRECTION('ref_axis',(0.,0.,-1.)) ;
#126780 = DIRECTION('center_axis',(0.,-1.,0.)) ;
#126781 = DIRECTION('ref_axis',(0.,0.,-1.)) ;
#126782 = DIRECTION('center_axis',(0.,-1.,0.)) ;
#126783 = DIRECTION('ref_axis',(0.,0.,-1.)) ;
#126784 = DIRECTION('center_axis',(-1.,0.,0.)) ;
#126785 = DIRECTION('ref_axis',(0.,0.,1.)) ;
#126786 = DIRECTION('center_axis',(-1.,0.,0.)) ;
#126787 = DIRECTION('ref_axis',(0.,0.,1.)) ;
#126788 = DIRECTION('center_axis',(1.,0.,0.)) ;
#126789 = DIRECTION('ref_axis',(0.,0.,-1.)) ;
#126790 = DIRECTION('center_axis',(-1.,0.,0.)) ;
#126791 = DIRECTION('ref_axis',(0.,0.,1.)) ;
#126792 = DIRECTION('center_axis',(0.,-1.,0.)) ;
#126793 = DIRECTION('ref_axis',(0.,0.,-1.)) ;
#126794 = DIRECTION('center_axis',(0.,-1.,0.)) ;
#126795 = DIRECTION('ref_axis',(0.,0.,-1.)) ;
#126796 = DIRECTION('center_axis',(0.,1.,0.)) ;
#126797 = DIRECTION('ref_axis',(1.,0.,0.)) ;
#126798 = DIRECTION('center_axis',(0.,0.,-1.)) ;
#126799 = DIRECTION('ref_axis',(1.,0.,0.)) ;
#126800 = DIRECTION('center_axis',(0.,1.,0.)) ;
#126801 = DIRECTION('ref_axis',(1.,0.,0.)) ;
#126802 = DIRECTION('center_axis',(0.,0.,1.)) ;
#126803 = DIRECTION('ref_axis',(-1.,0.,0.)) ;
#126804 = DIRECTION('center_axis',(0.,0.,-1.)) ;
#126805 = DIRECTION('ref_axis',(-1.,0.,0.)) ;
#126806 = DIRECTION('center_axis',(-0.669589480006976,0.669589480006974,-0.321402950403349)) ;
#126807 = DIRECTION('ref_axis',(-0.707106781186547,-0.707106781186548,5.45170614306381E-16)) ;
#126808 = DIRECTION('center_axis',(0.669589480006969,-0.669589480006984,0.321402950403343)) ;
#126809 = DIRECTION('ref_axis',(0.707106781186555,0.70710678118654,-2.64684135297117E-16)) ;
#126810 = DIRECTION('center_axis',(0.,1.,0.)) ;
#126811 = DIRECTION('ref_axis',(1.,0.,0.)) ;
#126812 = DIRECTION('center_axis',(0.,1.,0.)) ;
#126813 = DIRECTION('ref_axis',(0.,0.,-1.)) ;
#126814 = DIRECTION('center_axis',(0.707106781186548,-0.707106781186548,-1.07330539167836E-14)) ;
#126815 = DIRECTION('ref_axis',(-0.707106781186548,-0.707106781186548,3.64780758836058E-31)) ;
#126816 = DIRECTION('center_axis',(-0.707106781186549,0.707106781186546,0.)) ;
#126817 = DIRECTION('ref_axis',(-0.707106781186546,-0.707106781186549,0.)) ;
#126818 = DIRECTION('center_axis',(0.,-1.,0.)) ;
#126819 = DIRECTION('ref_axis',(0.,0.,-1.)) ;
#126820 = DIRECTION('center_axis',(0.,1.,0.)) ;
#126821 = DIRECTION('ref_axis',(0.,0.,1.)) ;
#126822 = DIRECTION('center_axis',(-0.879462917689188,-0.219865729422294,
-0.42214220049081)) ;
#126823 = DIRECTION('ref_axis',(-0.432731067584771,-5.39224131925863E-16,
0.901523057468274)) ;
#126824 = DIRECTION('center_axis',(0.879462917689189,0.219865729422295,0.422142200490806)) ;
#126825 = DIRECTION('ref_axis',(0.432731067584767,-3.28412466813249E-16,-0.901523057468275)) ;
#126826 = DIRECTION('center_axis',(0.,-1.,0.)) ;
#126827 = DIRECTION('ref_axis',(0.,0.,1.)) ;
#126828 = DIRECTION('center_axis',(0.,0.,1.)) ;
#126829 = DIRECTION('ref_axis',(-1.,0.,0.)) ;
#126830 = DIRECTION('center_axis',(0.,1.,0.)) ;
#126831 = DIRECTION('ref_axis',(1.,0.,0.)) ;
#126832 = DIRECTION('center_axis',(0.970142500145332,0.242535625036333,0.)) ;
#126833 = DIRECTION('ref_axis',(0.242535625036333,-0.970142500145332,0.)) ;
#126834 = DIRECTION('center_axis',(0.669589480006976,-0.669589480006974,-0.321402950403349)) ;
#126835 = DIRECTION('ref_axis',(0.707106781186547,0.707106781186548,5.45170614306381E-16)) ;
#126836 = DIRECTION('center_axis',(0.669589480006974,-0.669589480006974,-0.321402950403353)) ;
#126837 = DIRECTION('ref_axis',(0.707106781186548,0.707106781186548,1.13338310925322E-17)) ;
#126838 = DIRECTION('center_axis',(0.707106781186549,-0.707106781186546,0.)) ;
#126839 = DIRECTION('ref_axis',(0.707106781186546,0.707106781186549,0.)) ;
#126840 = DIRECTION('center_axis',(-0.70710678118655,0.707106781186545,0.)) ;
#126841 = DIRECTION('ref_axis',(-0.707106781186545,-0.70710678118655,0.)) ;
#126842 = DIRECTION('center_axis',(0.,0.,1.)) ;
#126843 = DIRECTION('ref_axis',(1.,0.,0.)) ;
#126844 = DIRECTION('center_axis',(0.,0.,1.)) ;
#126845 = DIRECTION('ref_axis',(1.,0.,0.)) ;
#126846 = DIRECTION('center_axis',(2.47817639425258E-16,-1.,0.)) ;
#126847 = DIRECTION('ref_axis',(1.,2.47817639425258E-16,0.)) ;
#126848 = DIRECTION('center_axis',(0.,-1.,0.)) ;
#126849 = DIRECTION('ref_axis',(0.,0.,-1.)) ;
#126850 = DIRECTION('center_axis',(-0.970142500145333,-0.24253562503633,0.)) ;
#126851 = DIRECTION('ref_axis',(0.24253562503633,-0.970142500145333,0.)) ;
#126852 = DIRECTION('center_axis',(0.976187060183959,-0.216930457818629,3.32210494350337E-14)) ;
#126853 = DIRECTION('ref_axis',(0.216930457818629,0.976187060183959,-2.98116453088841E-12)) ;
#126854 = DIRECTION('center_axis',(0.,1.,0.)) ;
#126855 = DIRECTION('ref_axis',(1.,0.,0.)) ;
#126856 = DIRECTION('center_axis',(9.0350181040459E-15,1.,-4.33680868994203E-15)) ;
#126857 = DIRECTION('ref_axis',(1.,-9.03501810404588E-15,4.33680868994201E-15)) ;
#126858 = DIRECTION('center_axis',(0.,-1.,0.)) ;
#126859 = DIRECTION('ref_axis',(0.,0.,1.)) ;
#126860 = DIRECTION('center_axis',(0.,0.,1.)) ;
#126861 = DIRECTION('ref_axis',(-1.,8.67361737988401E-15,0.)) ;
#126862 = DIRECTION('center_axis',(0.879462917689188,0.219865729422294,-0.42214220049081)) ;
#126863 = DIRECTION('ref_axis',(-0.432731067584771,-2.0299798629437E-16,-0.901523057468274)) ;
#126864 = DIRECTION('center_axis',(0.879462917689188,0.219865729422297,-0.422142200490809)) ;
#126865 = DIRECTION('ref_axis',(-0.43273106758477,8.71332159501362E-17,-0.901523057468274)) ;
#126866 = DIRECTION('center_axis',(0.,-1.,0.)) ;
#126867 = DIRECTION('ref_axis',(0.,0.,-1.)) ;
#126868 = DIRECTION('center_axis',(2.00438979995004E-14,1.,0.)) ;
#126869 = DIRECTION('ref_axis',(-1.,2.00438979995004E-14,0.)) ;
#126870 = DIRECTION('center_axis',(2.47817639425258E-16,-1.,0.)) ;
#126871 = DIRECTION('ref_axis',(1.,2.47817639425258E-16,0.)) ;
#126872 = DIRECTION('center_axis',(0.,-1.,0.)) ;
#126873 = DIRECTION('ref_axis',(0.,0.,-1.)) ;
#126874 = DIRECTION('center_axis',(0.,0.,1.)) ;
#126875 = DIRECTION('ref_axis',(1.,0.,0.)) ;
#126876 = DIRECTION('center_axis',(0.,0.,1.)) ;
#126877 = DIRECTION('ref_axis',(1.,0.,0.)) ;
#126878 = DIRECTION('center_axis',(0.,1.,0.)) ;
#126879 = DIRECTION('ref_axis',(1.,0.,0.)) ;
#126880 = DIRECTION('center_axis',(0.970142500145332,0.242535625036331,0.)) ;
#126881 = DIRECTION('ref_axis',(0.242535625036331,-0.970142500145332,0.)) ;
#126882 = DIRECTION('center_axis',(-0.97618706018396,0.216930457818626,3.48715666902615E-14)) ;
#126883 = DIRECTION('ref_axis',(0.216930457818626,0.976187060183959,-9.11731595942476E-13)) ;
#126884 = DIRECTION('center_axis',(0.970142500145333,0.24253562503633,0.)) ;
#126885 = DIRECTION('ref_axis',(-0.24253562503633,0.970142500145333,0.)) ;
#126886 = DIRECTION('center_axis',(2.47817639425258E-16,-1.,0.)) ;
#126887 = DIRECTION('ref_axis',(1.,2.47817639425258E-16,0.)) ;
#126888 = DIRECTION('center_axis',(-1.29658294628968E-8,-0.447213597648204,
0.894427189925793)) ;
#126889 = DIRECTION('ref_axis',(0.0446435808064758,-0.893535426885365,-0.446767715478149)) ;
#126890 = DIRECTION('center_axis',(-0.894427191461922,-0.447213594575946,
-5.57691505343739E-9)) ;
#126891 = DIRECTION('ref_axis',(0.446767713219253,-0.89353542818951,-0.0446435773099389)) ;
#126892 = DIRECTION('center_axis',(-0.447213595499893,0.894427190999948,6.57429044123456E-13)) ;
#126893 = DIRECTION('ref_axis',(0.894427190999948,0.447213595499893,6.87710394375266E-12)) ;
#126894 = DIRECTION('center_axis',(-2.76847490273994E-6,0.447215298958337,
0.894426339264414)) ;
#126895 = DIRECTION('ref_axis',(0.0170110523159659,-0.894296896128943,0.447150629735935)) ;
#126896 = DIRECTION('center_axis',(-0.00225743160624427,0.447523187701884,
0.894269478664953)) ;
#126897 = DIRECTION('ref_axis',(-0.0025523933809264,-0.894271422866288,0.44751771756293)) ;
#126898 = DIRECTION('center_axis',(0.,0.,1.)) ;
#126899 = DIRECTION('ref_axis',(1.,0.,0.)) ;
#126900 = DIRECTION('center_axis',(-0.00226103819060068,-0.894269222962555,
-0.44752368045529)) ;
#126901 = DIRECTION('ref_axis',(0.00257816448348457,0.447518124036693,-0.894271145529461)) ;
#126902 = DIRECTION('center_axis',(-4.29726983982175E-6,-0.894425868918636,
-0.447216239632101)) ;
#126903 = DIRECTION('ref_axis',(-0.016983449338369,0.447151803283565,-0.894296833981216)) ;
#126904 = DIRECTION('center_axis',(-2.76847487689518E-6,-0.894426339264826,
0.447215298957514)) ;
#126905 = DIRECTION('ref_axis',(0.0170110522878384,-0.447150629735325,-0.894296896129782)) ;
#126906 = DIRECTION('center_axis',(-0.00225743161331263,-0.894269478664216,
0.447523187703322)) ;
#126907 = DIRECTION('ref_axis',(-0.00255239338234728,-0.447517717564354,-0.894271422865571)) ;
#126908 = DIRECTION('center_axis',(0.,0.,1.)) ;
#126909 = DIRECTION('ref_axis',(1.,0.,0.)) ;
#126910 = DIRECTION('center_axis',(-1.29625486687073E-8,0.894427189926062,
-0.447213597647665)) ;
#126911 = DIRECTION('ref_axis',(-0.044643580803928,0.446767715477792,0.893535426885671)) ;
#126912 = DIRECTION('center_axis',(-1.2961187983127E-8,0.89442718992615,0.447213597647489)) ;
#126913 = DIRECTION('ref_axis',(0.0446435808019586,-0.44676771547771,0.89353542688581)) ;
#126914 = DIRECTION('center_axis',(2.47817639425258E-16,-1.,0.)) ;
#126915 = DIRECTION('ref_axis',(1.,2.47817639425258E-16,0.)) ;
#126916 = DIRECTION('center_axis',(-0.00226103817862702,0.447523680453237,
-0.894269222963613)) ;
#126917 = DIRECTION('ref_axis',(0.00257816447018989,0.894271145530498,0.447518124034698)) ;
#126918 = DIRECTION('center_axis',(-4.29727001441892E-6,0.447216239632936,
-0.894425868918218)) ;
#126919 = DIRECTION('ref_axis',(-0.0169834493203687,0.894296833981071,0.447151803284539)) ;
#126920 = DIRECTION('center_axis',(-0.447213595499861,0.894427190999964,-6.53094347128148E-13)) ;
#126921 = DIRECTION('ref_axis',(0.894427190999964,0.447213595499861,-1.04079071344172E-9)) ;
#126922 = DIRECTION('center_axis',(-0.894427191461906,-0.447213594575977,
5.57669377296248E-9)) ;
#126923 = DIRECTION('ref_axis',(0.446767713219282,-0.893535428189512,0.0446435773096007)) ;
#126924 = DIRECTION('center_axis',(-1.29699385710222E-8,-0.447213597648892,
-0.894427189925449)) ;
#126925 = DIRECTION('ref_axis',(-0.044643580804857,0.893535426885168,-0.446767715478704)) ;
#126926 = DIRECTION('center_axis',(2.47817639425258E-16,-1.,0.)) ;
#126927 = DIRECTION('ref_axis',(1.,2.47817639425258E-16,0.)) ;
#126928 = DIRECTION('center_axis',(-1.29715887066227E-8,-0.447213597649164,
0.894427189925313)) ;
#126929 = DIRECTION('ref_axis',(0.0446435808063265,-0.893535426885007,-0.446767715478881)) ;
#126930 = DIRECTION('center_axis',(-0.894427191462079,-0.447213594575632,
-5.57881081575365E-9)) ;
#126931 = DIRECTION('ref_axis',(0.446767713218975,-0.89353542818955,-0.0446435773119127)) ;
#126932 = DIRECTION('center_axis',(-0.447213595499893,0.894427190999948,6.57429044122489E-13)) ;
#126933 = DIRECTION('ref_axis',(0.894427190999948,0.447213595499893,-2.76140188029019E-10)) ;
#126934 = DIRECTION('center_axis',(-2.76847492423738E-6,0.447215298957762,
0.894426339264702)) ;
#126935 = DIRECTION('ref_axis',(0.0170110523543263,-0.894296896128646,0.447150629735068)) ;
#126936 = DIRECTION('center_axis',(-0.00225743161003937,0.447523187702742,
0.894269478664515)) ;
#126937 = DIRECTION('ref_axis',(-0.00255239339121028,-0.894271422865848,0.44751771756375)) ;
#126938 = DIRECTION('center_axis',(0.,0.,1.)) ;
#126939 = DIRECTION('ref_axis',(1.,0.,0.)) ;
#126940 = DIRECTION('center_axis',(-0.00226103819378627,-0.894269222962206,
-0.447523680455971)) ;
#126941 = DIRECTION('ref_axis',(0.00257816448755917,0.447518124037357,-0.894271145529117)) ;
#126942 = DIRECTION('center_axis',(-4.29727059150273E-6,-0.894425868918584,
-0.447216239632205)) ;
#126943 = DIRECTION('ref_axis',(-0.01698344924275,0.447151803284406,-0.894296833982612)) ;
#126944 = DIRECTION('center_axis',(-2.76847490340117E-6,-0.894426339264985,
0.447215298957195)) ;
#126945 = DIRECTION('ref_axis',(0.0170110522723741,-0.447150629735124,-0.894296896130177)) ;
#126946 = DIRECTION('center_axis',(-0.00225743161207314,-0.894269478664265,
0.447523187703229)) ;
#126947 = DIRECTION('ref_axis',(-0.00255239338700126,-0.447517717564248,-0.894271422865611)) ;
#126948 = DIRECTION('center_axis',(0.,0.,1.)) ;
#126949 = DIRECTION('ref_axis',(1.,0.,0.)) ;
#126950 = DIRECTION('center_axis',(-1.29671068301384E-8,0.894427189925688,
-0.447213597648414)) ;
#126951 = DIRECTION('ref_axis',(-0.0446435808024942,0.446767715478387,0.893535426885445)) ;
#126952 = DIRECTION('center_axis',(-1.29614141328542E-8,0.89442718992613,
0.447213597647529)) ;
#126953 = DIRECTION('ref_axis',(0.0446435808017462,-0.446767715477745,0.893535426885803)) ;
#126954 = DIRECTION('center_axis',(2.47817639425258E-16,-1.,0.)) ;
#126955 = DIRECTION('ref_axis',(1.,2.47817639425258E-16,0.)) ;
#126956 = DIRECTION('center_axis',(-0.00226103817312033,0.447523680452633,
-0.894269222963929)) ;
#126957 = DIRECTION('ref_axis',(0.00257816447255943,0.894271145530794,0.447518124034094)) ;
#126958 = DIRECTION('center_axis',(-4.2972691245385E-6,0.447216239632108,
-0.894425868918632)) ;
#126959 = DIRECTION('ref_axis',(-0.0169834493350175,0.894296833981269,0.447151803283587)) ;
#126960 = DIRECTION('center_axis',(-0.447213595499861,0.894427190999964,-6.53094347126708E-13)) ;
#126961 = DIRECTION('ref_axis',(0.894427190999964,0.447213595499861,-1.07153737410966E-9)) ;
#126962 = DIRECTION('center_axis',(-0.894427191461917,-0.447213594575955,
5.57686257371582E-9)) ;
#126963 = DIRECTION('ref_axis',(0.446767713219204,-0.893535428189395,0.0446435773127371)) ;
#126964 = DIRECTION('center_axis',(-1.2970065171587E-8,-0.447213597648908,
-0.894427189925441)) ;
#126965 = DIRECTION('ref_axis',(-0.0446435808026991,0.893535426885249,-0.446767715478758)) ;
#126966 = DIRECTION('center_axis',(2.47817639425258E-16,-1.,0.)) ;
#126967 = DIRECTION('ref_axis',(1.,2.47817639425258E-16,0.)) ;
#126968 = DIRECTION('center_axis',(-1.29716114298014E-8,-0.447213597649167,
0.894427189925311)) ;
#126969 = DIRECTION('ref_axis',(0.0446435808059489,-0.893535426885021,-0.446767715478891)) ;
#126970 = DIRECTION('center_axis',(-0.894427191462087,-0.447213594575616,
-5.57886600061672E-9)) ;
#126971 = DIRECTION('ref_axis',(0.446767713218963,-0.893535428189561,-0.0446435773118126)) ;
#126972 = DIRECTION('center_axis',(-0.447213595499893,0.894427190999948,6.57429044123457E-13)) ;
#126973 = DIRECTION('ref_axis',(0.894427190999948,0.447213595499893,2.28090461718898E-10)) ;
#126974 = DIRECTION('center_axis',(-2.76847537946315E-6,0.447215298958076,
0.894426339264545)) ;
#126975 = DIRECTION('ref_axis',(0.0170110523834622,-0.894296896128042,0.447150629735167)) ;
#126976 = DIRECTION('center_axis',(-0.0022574316137697,0.447523187703219,
0.894269478664266)) ;
#126977 = DIRECTION('ref_axis',(-0.00255239337889119,-0.894271422865627,0.447517717564262)) ;
#126978 = DIRECTION('center_axis',(0.,0.,1.)) ;
#126979 = DIRECTION('ref_axis',(1.,0.,0.)) ;
#126980 = DIRECTION('center_axis',(-0.00226103819029805,-0.894269222962415,
-0.447523680455572)) ;
#126981 = DIRECTION('ref_axis',(0.00257816448048495,0.447518124036985,-0.894271145529324)) ;
#126982 = DIRECTION('center_axis',(-4.29727144208701E-6,-0.894425868918501,
-0.44721623963237)) ;
#126983 = DIRECTION('ref_axis',(-0.0169834492064025,0.44715180328486,-0.894296833983075)) ;
#126984 = DIRECTION('center_axis',(-2.76847432632209E-6,-0.894426339264659,
0.447215298957848)) ;
#126985 = DIRECTION('ref_axis',(0.0170110525173505,-0.447150629733905,-0.894296896126127)) ;
#126986 = DIRECTION('center_axis',(-0.0022574316056552,-0.894269478665014,
0.447523187701765)) ;
#126987 = DIRECTION('ref_axis',(-0.00255239336525724,-0.447517717562861,-0.894271422866367)) ;
#126988 = DIRECTION('center_axis',(0.,0.,1.)) ;
#126989 = DIRECTION('ref_axis',(1.,0.,0.)) ;
#126990 = DIRECTION('center_axis',(-1.29670895172406E-8,0.894427189925688,
-0.447213597648414)) ;
#126991 = DIRECTION('ref_axis',(-0.0446435808044585,0.446767715478348,0.893535426885366)) ;
#126992 = DIRECTION('center_axis',(-1.29656779750599E-8,0.894427189925773,
0.447213597648244)) ;
#126993 = DIRECTION('ref_axis',(0.0446435808077213,-0.44676771547817,0.893535426885292)) ;
#126994 = DIRECTION('center_axis',(2.47817639425258E-16,-1.,0.)) ;
#126995 = DIRECTION('ref_axis',(1.,2.47817639425258E-16,0.)) ;
#126996 = DIRECTION('center_axis',(-0.00226103819750544,0.447523680456259,
-0.894269222962053)) ;
#126997 = DIRECTION('ref_axis',(0.00257816449032981,0.894271145528972,0.447518124037631)) ;
#126998 = DIRECTION('center_axis',(-4.29726910766065E-6,0.447216239631639,
-0.894425868918867)) ;
#126999 = DIRECTION('ref_axis',(-0.0169834493967404,0.894296833980566,0.447151803282649)) ;
#127000 = DIRECTION('center_axis',(-0.447213595499861,0.894427190999964,-6.5309434712767E-13)) ;
#127001 = DIRECTION('ref_axis',(0.894427190999964,0.447213595499861,-2.6192932457417E-9)) ;
#127002 = DIRECTION('center_axis',(-0.894427191462423,-0.447213594574943,
5.58297186255583E-9)) ;
#127003 = DIRECTION('ref_axis',(0.446767713218366,-0.893535428189637,0.0446435773162759)) ;
#127004 = DIRECTION('center_axis',(-1.29684675156914E-8,-0.447213597648659,
-0.894427189925565)) ;
#127005 = DIRECTION('ref_axis',(-0.0446435808033256,0.893535426885316,-0.446767715478561)) ;
#127006 = DIRECTION('center_axis',(2.47817639425258E-16,-1.,0.)) ;
#127007 = DIRECTION('ref_axis',(1.,2.47817639425258E-16,0.)) ;
#127008 = DIRECTION('center_axis',(-1.29625973612226E-8,-0.447213597647665,
0.894427189926062)) ;
#127009 = DIRECTION('ref_axis',(0.044643580802507,-0.893535426885728,-0.446767715477819)) ;
#127010 = DIRECTION('center_axis',(-0.894427191461881,-0.447213594576028,
-5.57641568453782E-9)) ;
#127011 = DIRECTION('ref_axis',(0.446767713219317,-0.893535428189484,-0.0446435773098233)) ;
#127012 = DIRECTION('center_axis',(-0.447213595499893,0.894427190999948,6.57429044120555E-13)) ;
#127013 = DIRECTION('ref_axis',(0.894427190999948,0.447213595499893,1.48077938673105E-9)) ;
#127014 = DIRECTION('center_axis',(-2.76847531827434E-6,0.447215298957909,
0.894426339264628)) ;
#127015 = DIRECTION('ref_axis',(0.0170110523648983,-0.894296896128409,0.447150629735141)) ;
#127016 = DIRECTION('center_axis',(-0.00225743160712761,0.447523187702386,
0.8942694786647)) ;
#127017 = DIRECTION('ref_axis',(-0.00255239337382405,-0.894271422866046,0.447517717563453)) ;
#127018 = DIRECTION('center_axis',(0.,0.,1.)) ;
#127019 = DIRECTION('ref_axis',(1.,0.,0.)) ;
#127020 = DIRECTION('center_axis',(-0.00226103819018861,-0.894269222962714,
-0.447523680454975)) ;
#127021 = DIRECTION('ref_axis',(0.00257816448743253,0.447518124036366,-0.894271145529614)) ;
#127022 = DIRECTION('center_axis',(-4.29726974249564E-6,-0.894425868918509,
-0.447216239632354)) ;
#127023 = DIRECTION('ref_axis',(-0.0169834493529471,0.447151803283706,-0.894296833980869)) ;
#127024 = DIRECTION('center_axis',(-2.76847442575453E-6,-0.894426339264628,
0.447215298957909)) ;
#127025 = DIRECTION('ref_axis',(0.0170110523617927,-0.447150629735151,-0.894296896128463)) ;
#127026 = DIRECTION('center_axis',(-0.0022574316083322,-0.894269478664822,
0.447523187702137)) ;
#127027 = DIRECTION('ref_axis',(-0.00255239338262315,-0.447517717563174,-0.89427142286616)) ;
#127028 = DIRECTION('center_axis',(0.,0.,1.)) ;
#127029 = DIRECTION('ref_axis',(1.,0.,0.)) ;
#127030 = DIRECTION('center_axis',(-1.29666123305221E-8,0.894427189925724,
-0.447213597648341)) ;
#127031 = DIRECTION('ref_axis',(-0.0446435808071081,0.446767715478242,0.893535426885287)) ;
#127032 = DIRECTION('center_axis',(-1.29660772537652E-8,0.894427189925737,
0.447213597648315)) ;
#127033 = DIRECTION('ref_axis',(0.0446435808082692,-0.446767715478214,0.893535426885243)) ;
#127034 = DIRECTION('center_axis',(2.47817639425258E-16,-1.,0.)) ;
#127035 = DIRECTION('ref_axis',(1.,2.47817639425258E-16,0.)) ;
#127036 = DIRECTION('center_axis',(-0.00226103819164361,0.447523680455419,
-0.894269222962488)) ;
#127037 = DIRECTION('ref_axis',(0.00257816448196719,0.894271145529399,0.447518124036826)) ;
#127038 = DIRECTION('center_axis',(-4.29726920049817E-6,0.447216239631741,
-0.894425868918816)) ;
#127039 = DIRECTION('ref_axis',(-0.0169834493771275,0.894296833980812,0.447151803282901)) ;
#127040 = DIRECTION('center_axis',(-0.447213595499861,0.894427190999964,-6.5309434712767E-13)) ;
#127041 = DIRECTION('ref_axis',(0.894427190999964,0.447213595499861,-5.78704355583638E-9)) ;
#127042 = DIRECTION('center_axis',(-0.894427191462433,-0.447213594574924,
5.58308656049955E-9)) ;
#127043 = DIRECTION('ref_axis',(0.446767713218432,-0.893535428189805,0.0446435773122526)) ;
#127044 = DIRECTION('center_axis',(-1.29685286518626E-8,-0.447213597648669,
-0.89442718992556)) ;
#127045 = DIRECTION('ref_axis',(-0.0446435808020355,0.893535426885364,-0.446767715478595)) ;
#127046 = DIRECTION('center_axis',(2.47817639425258E-16,-1.,0.)) ;
#127047 = DIRECTION('ref_axis',(1.,2.47817639425258E-16,0.)) ;
#127048 = DIRECTION('center_axis',(-1.29626249536512E-8,-0.447213597647691,
0.894427189926049)) ;
#127049 = DIRECTION('ref_axis',(0.0446435808039496,-0.893535426885658,-0.446767715477815)) ;
#127050 = DIRECTION('center_axis',(-0.894427191461901,-0.447213594575988,
-5.57661424183581E-9)) ;
#127051 = DIRECTION('ref_axis',(0.446767713219243,-0.893535428189416,-0.044643577311908)) ;
#127052 = DIRECTION('center_axis',(-0.447213595499893,0.894427190999948,6.57429044121523E-13)) ;
#127053 = DIRECTION('ref_axis',(0.894427190999948,0.447213595499893,4.15610219187823E-9)) ;
#127054 = DIRECTION('center_axis',(-2.7684747923646E-6,0.447215298957608,
0.894426339264779)) ;
#127055 = DIRECTION('ref_axis',(0.0170110524133555,-0.894296896127826,0.447150629734463)) ;
#127056 = DIRECTION('center_axis',(-0.00225743160937446,0.447523187702693,
0.894269478664541)) ;
#127057 = DIRECTION('ref_axis',(-0.00255239335690116,-0.894271422865916,0.44751771756381)) ;
#127058 = DIRECTION('center_axis',(0.,0.,1.)) ;
#127059 = DIRECTION('ref_axis',(1.,0.,0.)) ;
#127060 = DIRECTION('center_axis',(-0.00226103818966992,-0.894269222962751,
-0.447523680454904)) ;
#127061 = DIRECTION('ref_axis',(0.00257816448730185,0.447518124036296,-0.894271145529649)) ;
#127062 = DIRECTION('center_axis',(-4.29727242902498E-6,-0.894425868917683,
-0.447216239634007)) ;
#127063 = DIRECTION('ref_axis',(-0.0169834491710572,0.44715180328678,-0.894296833982786)) ;
#127064 = DIRECTION('center_axis',(-2.76847671454323E-6,-0.894426339263924,
0.447215298959317)) ;
#127065 = DIRECTION('ref_axis',(0.0170110522880356,-0.447150629737154,-0.894296896128864)) ;
#127066 = DIRECTION('center_axis',(-0.00225743160349176,-0.894269478665165,
0.447523187701476)) ;
#127067 = DIRECTION('ref_axis',(-0.0025523933684872,-0.447517717562564,-0.894271422866506)) ;
#127068 = DIRECTION('center_axis',(0.,0.,1.)) ;
#127069 = DIRECTION('ref_axis',(1.,0.,0.)) ;
#127070 = DIRECTION('center_axis',(-1.29665203557497E-8,0.89442718992574,
-0.447213597648309)) ;
#127071 = DIRECTION('ref_axis',(-0.0446435808065546,0.446767715478225,0.893535426885323)) ;
#127072 = DIRECTION('center_axis',(-1.29657120598193E-8,0.894427189925768,
0.447213597648254)) ;
#127073 = DIRECTION('ref_axis',(0.0446435808049235,-0.446767715478234,0.8935354268854)) ;
#127074 = DIRECTION('center_axis',(2.47817639425258E-16,-1.,0.)) ;
#127075 = DIRECTION('ref_axis',(1.,2.47817639425258E-16,0.)) ;
#127076 = DIRECTION('center_axis',(-0.00226103819699234,0.447523680456176,
-0.894269222962096)) ;
#127077 = DIRECTION('ref_axis',(0.00257816450066049,0.894271145529,0.447518124037516)) ;
#127078 = DIRECTION('center_axis',(-4.29727019561894E-6,0.447216239632353,
-0.89442586891851)) ;
#127079 = DIRECTION('ref_axis',(-0.01698344932343,0.894296833981315,0.447151803283936)) ;
#127080 = DIRECTION('center_axis',(-0.447213595499861,0.894427190999964,-6.53094347129588E-13)) ;
#127081 = DIRECTION('ref_axis',(0.894427190999964,0.447213595499861,-3.92952546747532E-9)) ;
#127082 = DIRECTION('center_axis',(-0.89442719146245,-0.447213594574889,5.58329918452941E-9)) ;
#127083 = DIRECTION('ref_axis',(0.446767713218494,-0.893535428189995,0.0446435773078344)) ;
#127084 = DIRECTION('center_axis',(-1.29683685075575E-8,-0.447213597648643,
-0.894427189925573)) ;
#127085 = DIRECTION('ref_axis',(-0.0446435808018708,0.89353542688538,-0.446767715478578)) ;
#127086 = DIRECTION('center_axis',(2.47817639425258E-16,-1.,0.)) ;
#127087 = DIRECTION('ref_axis',(1.,2.47817639425258E-16,0.)) ;
#127088 = DIRECTION('center_axis',(-1.29627337002934E-8,-0.447213597647736,
0.894427189926027)) ;
#127089 = DIRECTION('ref_axis',(0.0446435808020259,-0.893535426885715,-0.446767715477894)) ;
#127090 = DIRECTION('center_axis',(-0.894427191461892,-0.447213594576006,
-5.57650928239589E-9)) ;
#127091 = DIRECTION('ref_axis',(0.446767713219069,-0.893535428189034,-0.0446435773213116)) ;
#127092 = DIRECTION('center_axis',(-0.447213595499893,0.894427190999948,6.57429044123454E-13)) ;
#127093 = DIRECTION('ref_axis',(0.894427190999948,0.447213595499893,-1.55677214764901E-10)) ;
#127094 = DIRECTION('center_axis',(-2.76847529691129E-6,0.447215298957874,
0.894426339264646)) ;
#127095 = DIRECTION('ref_axis',(0.0170110523595498,-0.894296896128508,0.447150629735146)) ;
#127096 = DIRECTION('center_axis',(-0.00225743160737611,0.447523187702446,
0.894269478664669)) ;
#127097 = DIRECTION('ref_axis',(-0.00255239334383529,-0.894271422866054,0.447517717563608)) ;
#127098 = DIRECTION('center_axis',(0.,0.,1.)) ;
#127099 = DIRECTION('ref_axis',(1.,0.,0.)) ;
#127100 = DIRECTION('center_axis',(-0.0022610381865632,-0.894269222962977,
-0.447523680454467)) ;
#127101 = DIRECTION('ref_axis',(0.00257816448573324,0.447518124035868,-0.894271145529868)) ;
#127102 = DIRECTION('center_axis',(-4.29727033961916E-6,-0.894425868918326,
-0.447216239632722)) ;
#127103 = DIRECTION('ref_axis',(-0.0169834492560518,0.447151803284818,-0.894296833982153)) ;
#127104 = DIRECTION('center_axis',(-2.7684756198651E-6,-0.894426339264261,
0.447215298958644)) ;
#127105 = DIRECTION('ref_axis',(0.0170110523558667,-0.447150629735949,-0.894296896128176)) ;
#127106 = DIRECTION('center_axis',(-0.00225743160937456,-0.894269478664754,
0.447523187702266)) ;
#127107 = DIRECTION('ref_axis',(-0.0025523933836389,-0.447517717563299,-0.894271422866095)) ;
#127108 = DIRECTION('center_axis',(0.,0.,1.)) ;
#127109 = DIRECTION('ref_axis',(1.,0.,0.)) ;
#127110 = DIRECTION('center_axis',(-1.29663126009737E-8,0.894427189925752,
-0.447213597648286)) ;
#127111 = DIRECTION('ref_axis',(-0.0446435808089956,0.446767715478161,0.893535426885233)) ;
#127112 = DIRECTION('center_axis',(-1.29659598506744E-8,0.894427189925758,
0.447213597648273)) ;
#127113 = DIRECTION('ref_axis',(0.044643580808027,-0.446767715478182,0.893535426885271)) ;
#127114 = DIRECTION('center_axis',(2.47817639425258E-16,-1.,0.)) ;
#127115 = DIRECTION('ref_axis',(1.,2.47817639425258E-16,0.)) ;
#127116 = DIRECTION('center_axis',(-0.00226103819759674,0.447523680456259,
-0.894269222962053)) ;
#127117 = DIRECTION('ref_axis',(0.00257816448891836,0.894271145528974,0.447518124037636)) ;
#127118 = DIRECTION('center_axis',(-4.29726939936379E-6,0.447216239631863,
-0.894425868918755)) ;
#127119 = DIRECTION('ref_axis',(-0.0169834493845944,0.894296833980636,0.447151803282969)) ;
#127120 = DIRECTION('center_axis',(-0.447213595499861,0.894427190999964,-6.53094347125746E-13)) ;
#127121 = DIRECTION('ref_axis',(0.894427190999964,0.447213595499861,-1.24562590126493E-8)) ;
#127122 = DIRECTION('center_axis',(-0.894427191462441,-0.447213594574908,
5.58318556863866E-9)) ;
#127123 = DIRECTION('ref_axis',(0.446767713218345,-0.893535428189663,0.0446435773159677)) ;
#127124 = DIRECTION('center_axis',(-1.29684220693358E-8,-0.447213597648652,
-0.894427189925569)) ;
#127125 = DIRECTION('ref_axis',(-0.0446435808038521,0.893535426885298,-0.446767715478545)) ;
#127126 = DIRECTION('center_axis',(2.47817639425258E-16,-1.,0.)) ;
#127127 = DIRECTION('ref_axis',(1.,2.47817639425258E-16,0.)) ;
#127128 = DIRECTION('center_axis',(-1.2962669858985E-8,-0.447213597647703,
0.894427189926043)) ;
#127129 = DIRECTION('ref_axis',(0.0446435808048981,-0.893535426885615,-0.446767715477806)) ;
#127130 = DIRECTION('center_axis',(-0.894427191461877,-0.447213594576036,
-5.57636158173298E-9)) ;
#127131 = DIRECTION('ref_axis',(0.446767713219308,-0.893535428189452,-0.0446435773105443)) ;
#127132 = DIRECTION('center_axis',(-0.447213595499893,0.894427190999948,6.57429044121523E-13)) ;
#127133 = DIRECTION('ref_axis',(0.894427190999948,0.447213595499893,-2.24965278736678E-9)) ;
#127134 = DIRECTION('center_axis',(-2.76847551793095E-6,0.44721529895811,
0.894426339264528)) ;
#127135 = DIRECTION('ref_axis',(0.0170110523555864,-0.894296896128449,0.447150629735415)) ;
#127136 = DIRECTION('center_axis',(-0.00225743160765807,0.447523187702426,
0.894269478664679)) ;
#127137 = DIRECTION('ref_axis',(-0.00255239335397715,-0.894271422866052,0.447517717563555)) ;
#127138 = DIRECTION('center_axis',(0.,0.,1.)) ;
#127139 = DIRECTION('ref_axis',(1.,0.,0.)) ;
#127140 = DIRECTION('center_axis',(-0.00226103818742701,-0.894269222962916,
-0.447523680454585)) ;
#127141 = DIRECTION('ref_axis',(0.00257816448798919,0.447518124035978,-0.894271145529806)) ;
#127142 = DIRECTION('center_axis',(-4.29727014022669E-6,-0.894425868918387,
-0.447216239632599)) ;
#127143 = DIRECTION('ref_axis',(-0.0169834493651296,0.447151803283864,-0.894296833980558)) ;
#127144 = DIRECTION('center_axis',(-2.76847587648927E-6,-0.894426339264126,
0.447215298958913)) ;
#127145 = DIRECTION('ref_axis',(0.0170110521010361,-0.44715062973816,-0.894296896131918)) ;
#127146 = DIRECTION('center_axis',(-0.002257431604729,-0.894269478665109,
0.44752318770158)) ;
#127147 = DIRECTION('ref_axis',(-0.00255239336633799,-0.447517717562674,-0.894271422866457)) ;
#127148 = DIRECTION('center_axis',(0.,0.,1.)) ;
#127149 = DIRECTION('ref_axis',(1.,0.,0.)) ;
#127150 = DIRECTION('center_axis',(-1.29667389310869E-8,0.894427189925717,
-0.447213597648356)) ;
#127151 = DIRECTION('ref_axis',(-0.0446435808059711,0.446767715478274,0.893535426885327)) ;
#127152 = DIRECTION('center_axis',(-1.29552366744308E-8,0.89442718992664,
0.447213597646509)) ;
#127153 = DIRECTION('ref_axis',(0.044643580802271,-0.446767715476963,0.893535426886168)) ;
#127154 = DIRECTION('center_axis',(2.47817639425258E-16,-1.,0.)) ;
#127155 = DIRECTION('ref_axis',(1.,2.47817639425258E-16,0.)) ;
#127156 = DIRECTION('center_axis',(-0.00226103816569658,0.447523680451593,
-0.894269222964468)) ;
#127157 = DIRECTION('ref_axis',(0.00257816445059052,0.894271145531338,0.447518124033133)) ;
#127158 = DIRECTION('center_axis',(-4.297269498005E-6,0.447216239632456,-0.894425868918458)) ;
#127159 = DIRECTION('ref_axis',(-0.0169834493446286,0.894296833980946,0.447151803283867)) ;
#127160 = DIRECTION('center_axis',(-0.447213595499893,0.894427190999948,-6.57429044115844E-13)) ;
#127161 = DIRECTION('ref_axis',(0.894427190999948,0.447213595499893,-4.57322843461801E-9)) ;
#127162 = DIRECTION('center_axis',(-0.894427191462495,-0.4472135945748,5.5837520250107E-9)) ;
#127163 = DIRECTION('ref_axis',(0.446767713218335,-0.893535428189855,0.0446435773122149)) ;
#127164 = DIRECTION('center_axis',(-1.30106076504876E-8,-0.447213597655605,
-0.894427189922092)) ;
#127165 = DIRECTION('ref_axis',(-0.0446435808103084,0.893535426882409,-0.446767715483678)) ;
#127166 = DIRECTION('center_axis',(2.47817639425258E-16,-1.,0.)) ;
#127167 = DIRECTION('ref_axis',(1.,2.47817639425258E-16,0.)) ;
#127168 = DIRECTION('center_axis',(-1.29988256823834E-8,-0.447213597653671,
0.894427189923059)) ;
#127169 = DIRECTION('ref_axis',(0.0446435808102343,-0.893535426883143,-0.446767715482218)) ;
#127170 = DIRECTION('center_axis',(-0.894427191462464,-0.447213594574861,
-5.58340955425016E-9)) ;
#127171 = DIRECTION('ref_axis',(0.446767713218182,-0.89353542818943,-0.0446435773222543)) ;
#127172 = DIRECTION('center_axis',(-0.447213595500006,0.894427190999892,-3.26547173564688E-13)) ;
#127173 = DIRECTION('ref_axis',(0.894427190999892,0.447213595500006,-2.22301428109033E-9)) ;
#127174 = DIRECTION('center_axis',(-2.76847765482255E-6,0.447215298952696,
0.894426339267235)) ;
#127175 = DIRECTION('ref_axis',(0.0170110523220356,-0.894296896131649,0.44715062973029)) ;
#127176 = DIRECTION('center_axis',(-0.00225743165439838,0.447523187712696,
0.894269478659421)) ;
#127177 = DIRECTION('ref_axis',(-0.00255239347714828,-0.894271422860785,0.447517717573376)) ;
#127178 = DIRECTION('center_axis',(0.,0.,1.)) ;
#127179 = DIRECTION('ref_axis',(1.,0.,0.)) ;
#127180 = DIRECTION('center_axis',(-0.00226103818036704,-0.894269222963449,
-0.447523680453556)) ;
#127181 = DIRECTION('ref_axis',(0.00257816445525296,0.447518124035062,-0.894271145530359)) ;
#127182 = DIRECTION('center_axis',(-4.29726820748583E-6,-0.894425868918926,
-0.447216239631522)) ;
#127183 = DIRECTION('ref_axis',(-0.0169834493497015,0.447151803282875,-0.894296833981346)) ;
#127184 = DIRECTION('center_axis',(-2.7684764734789E-6,-0.894426339263942,
0.447215298959281)) ;
#127185 = DIRECTION('ref_axis',(0.0170110521812587,-0.447150629737927,-0.894296896130509)) ;
#127186 = DIRECTION('center_axis',(-0.0022574316061112,-0.894269478665011,
0.447523187701769)) ;
#127187 = DIRECTION('ref_axis',(-0.00255239340400457,-0.447517717562742,-0.894271422866316)) ;
#127188 = DIRECTION('center_axis',(0.,0.,1.)) ;
#127189 = DIRECTION('ref_axis',(1.,0.,0.)) ;
#127190 = DIRECTION('center_axis',(-1.29525055647508E-8,0.894427189926893,
-0.447213597646003)) ;
#127191 = DIRECTION('ref_axis',(-0.0446435807975522,0.44676771547666,0.893535426886555)) ;
#127192 = DIRECTION('center_axis',(-1.29551603894678E-8,0.894427189926646,
0.447213597646497)) ;
#127193 = DIRECTION('ref_axis',(0.0446435808026582,-0.446767715476946,0.893535426886157)) ;
#127194 = DIRECTION('center_axis',(2.47817639425258E-16,-1.,0.)) ;
#127195 = DIRECTION('ref_axis',(1.,2.47817639425258E-16,0.)) ;
#127196 = DIRECTION('center_axis',(-0.00226103816215286,0.447523680451109,
-0.894269222964719)) ;
#127197 = DIRECTION('ref_axis',(0.00257816445691698,0.89427114553157,0.447518124032634)) ;
#127198 = DIRECTION('center_axis',(-4.29726929913918E-6,0.447216239632333,
-0.89442586891852)) ;
#127199 = DIRECTION('ref_axis',(-0.0169834493712717,0.894296833980605,0.447151803283539)) ;
#127200 = DIRECTION('center_axis',(-0.447213595499893,0.894427190999948,-6.57429044119711E-13)) ;
#127201 = DIRECTION('ref_axis',(0.894427190999948,0.447213595499893,3.44653255660982E-9)) ;
#127202 = DIRECTION('center_axis',(-0.894427191462507,-0.447213594574776,
5.58399386455402E-9)) ;
#127203 = DIRECTION('ref_axis',(0.446767713218351,-0.893535428189922,0.0446435773107162)) ;
#127204 = DIRECTION('center_axis',(-1.30104853781452E-8,-0.447213597655585,
-0.894427189922102)) ;
#127205 = DIRECTION('ref_axis',(-0.0446435808113665,0.893535426882374,-0.446767715483642)) ;
#127206 = DIRECTION('center_axis',(1.,1.31418445149758E-16,-2.16840434497101E-16)) ;
#127207 = DIRECTION('ref_axis',(-2.16840434497101E-16,-2.8496832747207E-32,
-1.)) ;
#127208 = DIRECTION('center_axis',(1.,0.,0.)) ;
#127209 = DIRECTION('ref_axis',(0.,0.,-1.)) ;
#127210 = DIRECTION('center_axis',(-1.,0.,0.)) ;
#127211 = DIRECTION('ref_axis',(0.,0.,1.)) ;
#127212 = DIRECTION('center_axis',(-1.31418445149758E-16,1.,0.)) ;
#127213 = DIRECTION('ref_axis',(-1.,0.,0.)) ;
#127214 = DIRECTION('center_axis',(0.,0.,1.)) ;
#127215 = DIRECTION('ref_axis',(-1.,0.,0.)) ;
#127216 = DIRECTION('center_axis',(-1.31418445149758E-16,1.,0.)) ;
#127217 = DIRECTION('ref_axis',(-1.,-1.31418445149758E-16,0.)) ;
#127218 = DIRECTION('center_axis',(-1.31418445149758E-16,1.,0.)) ;
#127219 = DIRECTION('ref_axis',(-1.,0.,0.)) ;
#127220 = DIRECTION('center_axis',(-1.31418445149758E-16,1.,0.)) ;
#127221 = DIRECTION('ref_axis',(-1.,-1.31418445149758E-16,0.)) ;
#127222 = DIRECTION('center_axis',(0.,0.,1.)) ;
#127223 = DIRECTION('ref_axis',(-1.,0.,0.)) ;
#127224 = DIRECTION('center_axis',(-4.33680868994202E-16,-5.69936654944139E-32,
-1.)) ;
#127225 = DIRECTION('ref_axis',(-1.,2.47170623787823E-47,4.33680868994202E-16)) ;
#127226 = DIRECTION('center_axis',(0.,0.,1.)) ;
#127227 = DIRECTION('ref_axis',(1.,0.,0.)) ;
#127228 = DIRECTION('center_axis',(-1.31418445149758E-16,-1.,0.)) ;
#127229 = DIRECTION('ref_axis',(1.,-1.31418445149758E-16,0.)) ;
#127230 = DIRECTION('center_axis',(0.,1.,0.)) ;
#127231 = DIRECTION('ref_axis',(0.,0.,1.)) ;
#127232 = DIRECTION('center_axis',(-1.,0.,2.16840434497101E-16)) ;
#127233 = DIRECTION('ref_axis',(2.16840434497101E-16,0.,1.)) ;
#127234 = DIRECTION('center_axis',(-1.,4.33680868994201E-15,0.)) ;
#127235 = DIRECTION('ref_axis',(-4.33680868994201E-15,-1.,0.)) ;
#127236 = DIRECTION('center_axis',(1.,0.,0.)) ;
#127237 = DIRECTION('ref_axis',(0.,0.,-1.)) ;
#127238 = DIRECTION('center_axis',(-1.31418445149758E-16,-1.,0.)) ;
#127239 = DIRECTION('ref_axis',(1.,-1.31418445149758E-16,0.)) ;
#127240 = DIRECTION('center_axis',(0.,1.,0.)) ;
#127241 = DIRECTION('ref_axis',(0.,0.,1.)) ;
#127242 = DIRECTION('center_axis',(2.16840434497101E-16,2.8496832747207E-32,
1.)) ;
#127243 = DIRECTION('ref_axis',(1.,-6.17926559469557E-48,-2.16840434497101E-16)) ;
#127244 = DIRECTION('center_axis',(0.,0.,1.)) ;
#127245 = DIRECTION('ref_axis',(1.,0.,0.)) ;
#127246 = DIRECTION('center_axis',(-1.,-1.31418445149758E-16,-2.16840434497101E-16)) ;
#127247 = DIRECTION('ref_axis',(-2.16840434497101E-16,-2.8496832747207E-32,
1.)) ;
#127248 = DIRECTION('center_axis',(-1.,0.,0.)) ;
#127249 = DIRECTION('ref_axis',(0.,0.,1.)) ;
#127250 = DIRECTION('center_axis',(1.,0.,0.)) ;
#127251 = DIRECTION('ref_axis',(0.,0.,-1.)) ;
#127252 = DIRECTION('center_axis',(-1.31418445149758E-16,1.,0.)) ;
#127253 = DIRECTION('ref_axis',(-1.,0.,0.)) ;
#127254 = DIRECTION('center_axis',(-1.31418445149758E-16,1.,0.)) ;
#127255 = DIRECTION('ref_axis',(-1.,-1.31418445149758E-16,0.)) ;
#127256 = DIRECTION('center_axis',(0.,1.,0.)) ;
#127257 = DIRECTION('ref_axis',(1.,0.,0.)) ;
#127258 = DIRECTION('center_axis',(0.,0.,-1.)) ;
#127259 = DIRECTION('ref_axis',(1.,0.,0.)) ;
#127260 = DIRECTION('center_axis',(0.,1.,0.)) ;
#127261 = DIRECTION('ref_axis',(1.,0.,0.)) ;
#127262 = DIRECTION('center_axis',(0.,0.,-1.)) ;
#127263 = DIRECTION('ref_axis',(1.,0.,0.)) ;
#127264 = DIRECTION('center_axis',(-1.31418445149758E-16,1.,0.)) ;
#127265 = DIRECTION('ref_axis',(-1.,0.,0.)) ;
#127266 = DIRECTION('center_axis',(-1.31418445149758E-16,1.,0.)) ;
#127267 = DIRECTION('ref_axis',(-1.,-1.31418445149758E-16,0.)) ;
#127268 = DIRECTION('center_axis',(-1.31418445149758E-16,-1.,0.)) ;
#127269 = DIRECTION('ref_axis',(1.,-1.31418445149758E-16,0.)) ;
#127270 = DIRECTION('center_axis',(0.,1.,0.)) ;
#127271 = DIRECTION('ref_axis',(0.,0.,1.)) ;
#127272 = DIRECTION('center_axis',(4.33680868994202E-16,0.,1.)) ;
#127273 = DIRECTION('ref_axis',(1.,0.,-4.33680868994202E-16)) ;
#127274 = DIRECTION('center_axis',(0.,0.,-1.)) ;
#127275 = DIRECTION('ref_axis',(-1.,0.,0.)) ;
#127276 = DIRECTION('center_axis',(-2.16840434497101E-16,0.,-1.)) ;
#127277 = DIRECTION('ref_axis',(-1.,0.,2.16840434497101E-16)) ;
#127278 = DIRECTION('center_axis',(0.,4.33680868994201E-15,-1.)) ;
#127279 = DIRECTION('ref_axis',(0.,1.,4.33680868994201E-15)) ;
#127280 = DIRECTION('center_axis',(-1.31418445149758E-16,-1.,0.)) ;
#127281 = DIRECTION('ref_axis',(1.,-1.31418445149758E-16,0.)) ;
#127282 = DIRECTION('center_axis',(0.,1.,0.)) ;
#127283 = DIRECTION('ref_axis',(0.,0.,1.)) ;
#127284 = DIRECTION('center_axis',(0.,1.,0.)) ;
#127285 = DIRECTION('ref_axis',(1.,0.,0.)) ;
#127286 = DIRECTION('center_axis',(-1.,0.,0.)) ;
#127287 = DIRECTION('ref_axis',(0.,0.,-1.)) ;
#127288 = DIRECTION('center_axis',(0.,1.,0.)) ;
#127289 = DIRECTION('ref_axis',(1.,0.,0.)) ;
#127290 = DIRECTION('center_axis',(1.,0.,-4.33680868994203E-15)) ;
#127291 = DIRECTION('ref_axis',(4.33680868994203E-15,0.,1.)) ;
#127292 = DIRECTION('center_axis',(1.,0.,2.16840434497101E-16)) ;
#127293 = DIRECTION('ref_axis',(2.16840434497101E-16,0.,-1.)) ;
#127294 = DIRECTION('center_axis',(0.,1.,0.)) ;
#127295 = DIRECTION('ref_axis',(0.,0.,1.)) ;
#127296 = DIRECTION('center_axis',(0.,1.,0.)) ;
#127297 = DIRECTION('ref_axis',(0.,0.,1.)) ;
#127298 = DIRECTION('center_axis',(0.,0.,-1.)) ;
#127299 = DIRECTION('ref_axis',(-1.,0.,0.)) ;
#127300 = DIRECTION('center_axis',(0.,0.,1.)) ;
#127301 = DIRECTION('ref_axis',(1.,0.,0.)) ;
#127302 = DIRECTION('center_axis',(0.,0.,-1.)) ;
#127303 = DIRECTION('ref_axis',(-1.,0.,0.)) ;
#127304 = DIRECTION('center_axis',(0.,1.,0.)) ;
#127305 = DIRECTION('ref_axis',(0.,0.,1.)) ;
#127306 = DIRECTION('center_axis',(0.,1.,0.)) ;
#127307 = DIRECTION('ref_axis',(0.,0.,1.)) ;
#127308 = DIRECTION('center_axis',(0.,1.,0.)) ;
#127309 = DIRECTION('ref_axis',(1.,0.,0.)) ;
#127310 = DIRECTION('center_axis',(-1.,0.,0.)) ;
#127311 = DIRECTION('ref_axis',(0.,0.,-1.)) ;
#127312 = DIRECTION('center_axis',(0.,1.,0.)) ;
#127313 = DIRECTION('ref_axis',(1.,0.,0.)) ;
#127314 = DIRECTION('center_axis',(-1.,0.,0.)) ;
#127315 = DIRECTION('ref_axis',(0.,0.,-1.)) ;
#127316 = DIRECTION('center_axis',(0.,1.,0.)) ;
#127317 = DIRECTION('ref_axis',(0.,0.,1.)) ;
#127318 = DIRECTION('center_axis',(0.,1.,0.)) ;
#127319 = DIRECTION('ref_axis',(0.,0.,1.)) ;
#127320 = DIRECTION('center_axis',(-1.,0.,0.)) ;
#127321 = DIRECTION('ref_axis',(0.,0.,1.)) ;
#127322 = DIRECTION('center_axis',(-1.,0.,0.)) ;
#127323 = DIRECTION('ref_axis',(0.,0.,1.)) ;
#127324 = DIRECTION('center_axis',(1.,0.,0.)) ;
#127325 = DIRECTION('ref_axis',(0.,0.,-1.)) ;
#127326 = DIRECTION('center_axis',(-1.,0.,0.)) ;
#127327 = DIRECTION('ref_axis',(0.,0.,1.)) ;
#127328 = DIRECTION('center_axis',(0.,1.,0.)) ;
#127329 = DIRECTION('ref_axis',(0.,0.,1.)) ;
#127330 = DIRECTION('center_axis',(0.,1.,0.)) ;
#127331 = DIRECTION('ref_axis',(0.,0.,1.)) ;
#127332 = DIRECTION('center_axis',(0.,1.,0.)) ;
#127333 = DIRECTION('ref_axis',(1.,0.,0.)) ;
#127334 = DIRECTION('center_axis',(0.,0.,1.)) ;
#127335 = DIRECTION('ref_axis',(-1.,0.,0.)) ;
#127336 = DIRECTION('center_axis',(0.,1.,0.)) ;
#127337 = DIRECTION('ref_axis',(1.,0.,0.)) ;
#127338 = DIRECTION('center_axis',(0.,0.,-1.)) ;
#127339 = DIRECTION('ref_axis',(1.,0.,0.)) ;
#127340 = DIRECTION('center_axis',(0.,0.,1.)) ;
#127341 = DIRECTION('ref_axis',(1.,0.,0.)) ;
#127342 = DIRECTION('center_axis',(0.,0.,1.)) ;
#127343 = DIRECTION('ref_axis',(1.,0.,0.)) ;
#127344 = DIRECTION('center_axis',(0.,0.,-1.)) ;
#127345 = DIRECTION('ref_axis',(-1.,0.,0.)) ;
#127346 = DIRECTION('center_axis',(-8.67361737988401E-15,0.,1.)) ;
#127347 = DIRECTION('ref_axis',(1.,0.,8.67361737988401E-15)) ;
#127348 = DIRECTION('center_axis',(1.,0.,0.)) ;
#127349 = DIRECTION('ref_axis',(0.,0.,-1.)) ;
#127350 = DIRECTION('center_axis',(1.,0.,0.)) ;
#127351 = DIRECTION('ref_axis',(0.,0.,-1.)) ;
#127352 = DIRECTION('center_axis',(1.,0.,0.)) ;
#127353 = DIRECTION('ref_axis',(0.,0.,-1.)) ;
#127354 = DIRECTION('center_axis',(1.,0.,8.67361737988401E-15)) ;
#127355 = DIRECTION('ref_axis',(8.67361737988401E-15,0.,-1.)) ;
#127356 = DIRECTION('center_axis',(1.,0.,0.)) ;
#127357 = DIRECTION('ref_axis',(0.,0.,-1.)) ;
#127358 = DIRECTION('center_axis',(1.,0.,1.73472347597681E-14)) ;
#127359 = DIRECTION('ref_axis',(1.73472347597681E-14,0.,-1.)) ;
#127360 = DIRECTION('center_axis',(-1.,0.,0.)) ;
#127361 = DIRECTION('ref_axis',(0.,0.,1.)) ;
#127362 = DIRECTION('center_axis',(1.,0.,0.)) ;
#127363 = DIRECTION('ref_axis',(0.,0.,-1.)) ;
#127364 = DIRECTION('center_axis',(1.,0.,0.)) ;
#127365 = DIRECTION('ref_axis',(0.,0.,-1.)) ;
#127366 = DIRECTION('center_axis',(-8.67361737988409E-15,0.,-1.)) ;
#127367 = DIRECTION('ref_axis',(-1.,0.,8.67361737988409E-15)) ;
#127368 = DIRECTION('center_axis',(1.,0.,0.)) ;
#127369 = DIRECTION('ref_axis',(0.,0.,-1.)) ;
#127370 = DIRECTION('center_axis',(-8.67361737988409E-15,0.,1.)) ;
#127371 = DIRECTION('ref_axis',(1.,0.,8.67361737988409E-15)) ;
#127372 = DIRECTION('center_axis',(0.,0.,-1.)) ;
#127373 = DIRECTION('ref_axis',(-1.,0.,0.)) ;
#127374 = DIRECTION('center_axis',(-0.422618261740697,5.55398348498559E-17,
0.906307787036651)) ;
#127375 = DIRECTION('ref_axis',(0.906307787036651,-7.29829988871486E-33,0.422618261740697)) ;
#127376 = DIRECTION('center_axis',(0.422618261740697,-5.55398348498559E-17,
-0.906307787036651)) ;
#127377 = DIRECTION('ref_axis',(-0.906307787036651,1.03797877997344E-32,-0.422618261740697)) ;
#127378 = DIRECTION('center_axis',(-0.422618261740697,5.55398348498559E-17,
0.906307787036651)) ;
#127379 = DIRECTION('ref_axis',(0.906307787036651,-1.03797877997344E-32,0.422618261740697)) ;
#127380 = DIRECTION('center_axis',(0.422618261740697,-5.55398348498559E-17,
-0.906307787036651)) ;
#127381 = DIRECTION('ref_axis',(-0.906307787036651,1.03797877997344E-32,-0.422618261740697)) ;
#127382 = DIRECTION('center_axis',(0.,1.,0.)) ;
#127383 = DIRECTION('ref_axis',(1.,0.,0.)) ;
#127384 = DIRECTION('center_axis',(2.15682522756814E-14,0.514231796959101,
-0.857651245551602)) ;
#127385 = DIRECTION('ref_axis',(-4.48628358333197E-30,-0.857651245551602,
-0.514231796959101)) ;
#127386 = DIRECTION('center_axis',(0.,-1.73472347597681E-14,1.)) ;
#127387 = DIRECTION('ref_axis',(0.,1.,1.73472347597681E-14)) ;
#127388 = DIRECTION('center_axis',(-1.,0.,0.)) ;
#127389 = DIRECTION('ref_axis',(0.,0.,-1.)) ;
#127390 = DIRECTION('center_axis',(0.,0.,1.)) ;
#127391 = DIRECTION('ref_axis',(1.,0.,0.)) ;
#127392 = DIRECTION('center_axis',(0.,0.,1.)) ;
#127393 = DIRECTION('ref_axis',(1.,0.,0.)) ;
#127394 = DIRECTION('center_axis',(-1.,0.,0.)) ;
#127395 = DIRECTION('ref_axis',(0.,0.,1.)) ;
#127396 = DIRECTION('center_axis',(-1.,0.,0.)) ;
#127397 = DIRECTION('ref_axis',(0.,0.,-1.)) ;
#127398 = DIRECTION('center_axis',(1.,0.,0.)) ;
#127399 = DIRECTION('ref_axis',(0.,0.,-1.)) ;
#127400 = DIRECTION('center_axis',(0.,-0.514231796959126,-0.857651245551587)) ;
#127401 = DIRECTION('ref_axis',(0.,0.857651245551587,-0.514231796959126)) ;
#127402 = DIRECTION('center_axis',(0.,1.,8.97270763436279E-17)) ;
#127403 = DIRECTION('ref_axis',(0.,-8.97270763436279E-17,1.)) ;
#127404 = DIRECTION('center_axis',(0.,-1.,-8.97270763436279E-17)) ;
#127405 = DIRECTION('ref_axis',(0.,-8.97270763436279E-17,1.)) ;
#127406 = DIRECTION('center_axis',(0.,-1.,0.)) ;
#127407 = DIRECTION('ref_axis',(0.,0.,-1.)) ;
#127408 = DIRECTION('center_axis',(0.,1.,0.)) ;
#127409 = DIRECTION('ref_axis',(1.,0.,0.)) ;
#127410 = DIRECTION('center_axis',(-1.,0.,0.)) ;
#127411 = DIRECTION('ref_axis',(0.,0.,-1.)) ;
#127412 = DIRECTION('center_axis',(1.,0.,0.)) ;
#127413 = DIRECTION('ref_axis',(0.,0.,-1.)) ;
#127414 = DIRECTION('center_axis',(0.,-0.514231796959101,0.857651245551602)) ;
#127415 = DIRECTION('ref_axis',(0.,0.857651245551602,0.514231796959101)) ;
#127416 = DIRECTION('center_axis',(0.,0.,-1.)) ;
#127417 = DIRECTION('ref_axis',(1.,0.,0.)) ;
#127418 = DIRECTION('center_axis',(0.,1.,0.)) ;
#127419 = DIRECTION('ref_axis',(1.,0.,0.)) ;
#127420 = DIRECTION('center_axis',(-1.73472347597682E-14,0.,-1.)) ;
#127421 = DIRECTION('ref_axis',(1.,0.,-1.73472347597682E-14)) ;
#127422 = DIRECTION('center_axis',(-1.,0.,0.)) ;
#127423 = DIRECTION('ref_axis',(0.,8.67361737988409E-15,-1.)) ;
#127424 = DIRECTION('center_axis',(0.,0.,-1.)) ;
#127425 = DIRECTION('ref_axis',(-1.,0.,0.)) ;
#127426 = DIRECTION('center_axis',(0.,0.,1.)) ;
#127427 = DIRECTION('ref_axis',(-1.,0.,0.)) ;
#127428 = DIRECTION('center_axis',(0.,0.,-1.)) ;
#127429 = DIRECTION('ref_axis',(-1.,0.,0.)) ;
#127430 = DIRECTION('center_axis',(-1.,0.,7.01133629567814E-33)) ;
#127431 = DIRECTION('ref_axis',(7.01133629567814E-33,0.,1.)) ;
#127432 = DIRECTION('center_axis',(-1.,0.,0.)) ;
#127433 = DIRECTION('ref_axis',(0.,0.,1.)) ;
#127434 = DIRECTION('center_axis',(0.,0.,-1.)) ;
#127435 = DIRECTION('ref_axis',(-1.,0.,0.)) ;
#127436 = DIRECTION('center_axis',(-7.01133629567814E-33,8.97270763436279E-17,
-1.)) ;
#127437 = DIRECTION('ref_axis',(6.29106707073161E-49,1.,8.97270763436279E-17)) ;
#127438 = DIRECTION('center_axis',(1.,0.,0.)) ;
#127439 = DIRECTION('ref_axis',(0.,0.,-1.)) ;
#127440 = DIRECTION('center_axis',(0.,0.514231796959095,0.857651245551606)) ;
#127441 = DIRECTION('ref_axis',(0.,-0.857651245551606,0.514231796959095)) ;
#127442 = DIRECTION('center_axis',(-1.,0.,0.)) ;
#127443 = DIRECTION('ref_axis',(0.,0.,1.)) ;
#127444 = DIRECTION('center_axis',(-1.,0.,0.)) ;
#127445 = DIRECTION('ref_axis',(0.,-4.33680868994204E-15,-1.)) ;
#127446 = DIRECTION('center_axis',(0.,0.,1.)) ;
#127447 = DIRECTION('ref_axis',(1.,0.,0.)) ;
#127448 = DIRECTION('center_axis',(0.,0.,-1.)) ;
#127449 = DIRECTION('ref_axis',(-1.,0.,0.)) ;
#127450 = DIRECTION('center_axis',(0.,-1.,8.97270763436279E-17)) ;
#127451 = DIRECTION('ref_axis',(0.,-8.97270763436279E-17,-1.)) ;
#127452 = DIRECTION('center_axis',(0.,-1.,8.97270763436279E-17)) ;
#127453 = DIRECTION('ref_axis',(0.,-8.97270763436279E-17,-1.)) ;
#127454 = DIRECTION('center_axis',(0.,-1.,0.)) ;
#127455 = DIRECTION('ref_axis',(0.,0.,-1.)) ;
#127456 = DIRECTION('center_axis',(-7.01133629567814E-33,8.97270763436279E-17,
-1.)) ;
#127457 = DIRECTION('ref_axis',(0.,1.,0.)) ;
#127458 = DIRECTION('center_axis',(0.,-1.,0.)) ;
#127459 = DIRECTION('ref_axis',(0.,0.,1.)) ;
#127460 = DIRECTION('center_axis',(1.,0.,0.)) ;
#127461 = DIRECTION('ref_axis',(0.,0.,-1.)) ;
#127462 = DIRECTION('center_axis',(0.,0.,1.)) ;
#127463 = DIRECTION('ref_axis',(-1.,0.,0.)) ;
#127464 = DIRECTION('center_axis',(0.,1.,0.)) ;
#127465 = DIRECTION('ref_axis',(1.,0.,0.)) ;
#127466 = DIRECTION('center_axis',(-1.,0.,0.)) ;
#127467 = DIRECTION('ref_axis',(0.,0.,-1.)) ;
#127468 = DIRECTION('center_axis',(1.,7.81406971160724E-17,0.)) ;
#127469 = DIRECTION('ref_axis',(-7.81406971160724E-17,1.,0.)) ;
#127470 = DIRECTION('center_axis',(1.,0.,0.)) ;
#127471 = DIRECTION('ref_axis',(0.,0.,-1.)) ;
#127472 = DIRECTION('center_axis',(1.,0.,0.)) ;
#127473 = DIRECTION('ref_axis',(0.,0.,-1.)) ;
#127474 = DIRECTION('center_axis',(0.,1.,8.97270763436279E-17)) ;
#127475 = DIRECTION('ref_axis',(0.,-8.97270763436279E-17,1.)) ;
#127476 = DIRECTION('center_axis',(0.,-1.,0.)) ;
#127477 = DIRECTION('ref_axis',(0.,0.,-1.)) ;
#127478 = DIRECTION('center_axis',(0.,0.,-1.)) ;
#127479 = DIRECTION('ref_axis',(-1.,0.,0.)) ;
#127480 = DIRECTION('center_axis',(-7.01133629567814E-33,8.97270763436279E-17,
1.)) ;
#127481 = DIRECTION('ref_axis',(-6.29106707073161E-49,-1.,8.97270763436279E-17)) ;
#127482 = DIRECTION('center_axis',(-1.,0.,-7.01133629567814E-33)) ;
#127483 = DIRECTION('ref_axis',(-7.01133629567814E-33,0.,1.)) ;
#127484 = DIRECTION('center_axis',(-1.,0.,0.)) ;
#127485 = DIRECTION('ref_axis',(0.,0.,1.)) ;
#127486 = DIRECTION('center_axis',(1.,0.,0.)) ;
#127487 = DIRECTION('ref_axis',(0.,1.,0.)) ;
#127488 = DIRECTION('center_axis',(2.16840434497101E-15,1.,0.)) ;
#127489 = DIRECTION('ref_axis',(-1.,2.16840434497101E-15,0.)) ;
#127490 = DIRECTION('center_axis',(0.,1.,0.)) ;
#127491 = DIRECTION('ref_axis',(1.,0.,0.)) ;
#127492 = DIRECTION('center_axis',(0.,0.,-1.)) ;
#127493 = DIRECTION('ref_axis',(1.,0.,0.)) ;
#127494 = DIRECTION('center_axis',(-1.,0.,0.)) ;
#127495 = DIRECTION('ref_axis',(0.,0.,-1.)) ;
#127496 = DIRECTION('center_axis',(-7.01133629567814E-33,8.97270763436279E-17,
1.)) ;
#127497 = DIRECTION('ref_axis',(0.,-1.,0.)) ;
#127498 = DIRECTION('center_axis',(0.,-1.,0.)) ;
#127499 = DIRECTION('ref_axis',(0.,0.,1.)) ;
#127500 = DIRECTION('center_axis',(7.81406971160724E-17,-1.,-8.97270763436279E-17)) ;
#127501 = DIRECTION('ref_axis',(-7.01133629567814E-33,8.97270763436279E-17,
-1.)) ;
#127502 = DIRECTION('center_axis',(0.,1.,0.)) ;
#127503 = DIRECTION('ref_axis',(0.,0.,1.)) ;
#127504 = DIRECTION('center_axis',(-1.,-7.81406971160724E-17,0.)) ;
#127505 = DIRECTION('ref_axis',(7.81406971160724E-17,-1.,0.)) ;
#127506 = DIRECTION('center_axis',(-1.,-7.81406971160724E-17,0.)) ;
#127507 = DIRECTION('ref_axis',(-7.81406971160724E-17,1.,0.)) ;
#127508 = DIRECTION('center_axis',(0.,0.,1.)) ;
#127509 = DIRECTION('ref_axis',(1.,0.,0.)) ;
#127510 = DIRECTION('center_axis',(0.,0.,-1.)) ;
#127511 = DIRECTION('ref_axis',(-1.,0.,0.)) ;
#127512 = DIRECTION('center_axis',(0.,-1.,8.97270763436279E-17)) ;
#127513 = DIRECTION('ref_axis',(0.,-8.97270763436279E-17,-1.)) ;
#127514 = DIRECTION('center_axis',(0.,-1.,0.)) ;
#127515 = DIRECTION('ref_axis',(0.,0.,-1.)) ;
#127516 = DIRECTION('center_axis',(1.,7.81406971160724E-17,0.)) ;
#127517 = DIRECTION('ref_axis',(0.,1.,0.)) ;
#127518 = DIRECTION('center_axis',(0.,0.,1.)) ;
#127519 = DIRECTION('ref_axis',(-1.,0.,0.)) ;
#127520 = DIRECTION('center_axis',(0.,1.,0.)) ;
#127521 = DIRECTION('ref_axis',(1.,0.,0.)) ;
#127522 = DIRECTION('center_axis',(-1.,0.,0.)) ;
#127523 = DIRECTION('ref_axis',(0.,0.,-1.)) ;
#127524 = DIRECTION('center_axis',(0.,0.,-1.)) ;
#127525 = DIRECTION('ref_axis',(-1.,0.,0.)) ;
#127526 = DIRECTION('center_axis',(0.,0.,1.)) ;
#127527 = DIRECTION('ref_axis',(1.,0.,0.)) ;
#127528 = DIRECTION('center_axis',(-1.,-7.81406971160724E-17,0.)) ;
#127529 = DIRECTION('ref_axis',(7.81406971160724E-17,-1.,0.)) ;
#127530 = DIRECTION('center_axis',(-1.,-7.81406971160724E-17,0.)) ;
#127531 = DIRECTION('ref_axis',(-7.81406971160724E-17,1.,0.)) ;
#127532 = DIRECTION('center_axis',(1.,7.81406971160724E-17,0.)) ;
#127533 = DIRECTION('ref_axis',(-7.81406971160724E-17,1.,0.)) ;
#127534 = DIRECTION('center_axis',(1.,0.,0.)) ;
#127535 = DIRECTION('ref_axis',(0.,0.,-1.)) ;
#127536 = DIRECTION('center_axis',(1.,0.,0.)) ;
#127537 = DIRECTION('ref_axis',(0.,0.,-1.)) ;
#127538 = DIRECTION('center_axis',(3.78638272950961E-32,-4.8455963016112E-16,
-1.)) ;
#127539 = DIRECTION('ref_axis',(1.83472821505963E-47,1.,-4.8455963016112E-16)) ;
#127540 = DIRECTION('center_axis',(3.78638272950961E-32,-4.8455963016112E-16,
-1.)) ;
#127541 = DIRECTION('ref_axis',(1.83472821505963E-47,1.,-4.8455963016112E-16)) ;
#127542 = DIRECTION('center_axis',(0.,0.,-1.)) ;
#127543 = DIRECTION('ref_axis',(-1.,0.,0.)) ;
#127544 = DIRECTION('center_axis',(1.,7.81406971160724E-17,0.)) ;
#127545 = DIRECTION('ref_axis',(0.,1.,0.)) ;
#127546 = DIRECTION('center_axis',(0.,-1.,0.)) ;
#127547 = DIRECTION('ref_axis',(0.,0.,1.)) ;
#127548 = DIRECTION('center_axis',(0.,1.,0.)) ;
#127549 = DIRECTION('ref_axis',(1.,0.,0.)) ;
#127550 = DIRECTION('center_axis',(0.,1.,0.)) ;
#127551 = DIRECTION('ref_axis',(0.,0.,-1.)) ;
#127552 = DIRECTION('center_axis',(-7.81406971160724E-17,1.,-8.97270763436279E-17)) ;
#127553 = DIRECTION('ref_axis',(-7.01133629567814E-33,8.97270763436279E-17,
1.)) ;
#127554 = DIRECTION('center_axis',(0.,-1.,0.)) ;
#127555 = DIRECTION('ref_axis',(0.,0.,-1.)) ;
#127556 = DIRECTION('center_axis',(0.,1.,0.)) ;
#127557 = DIRECTION('ref_axis',(0.,0.,1.)) ;
#127558 = DIRECTION('center_axis',(0.,-1.,0.)) ;
#127559 = DIRECTION('ref_axis',(0.,0.,-1.)) ;
#127560 = DIRECTION('center_axis',(0.,-1.,0.)) ;
#127561 = DIRECTION('ref_axis',(0.,0.,-1.)) ;
#127562 = DIRECTION('center_axis',(0.,1.,0.)) ;
#127563 = DIRECTION('ref_axis',(1.,0.,0.)) ;
#127564 = DIRECTION('center_axis',(0.,0.,1.)) ;
#127565 = DIRECTION('ref_axis',(-1.,0.,0.)) ;
#127566 = DIRECTION('center_axis',(1.,0.,0.)) ;
#127567 = DIRECTION('ref_axis',(0.,0.,1.)) ;
#127568 = DIRECTION('center_axis',(0.,-1.,0.)) ;
#127569 = DIRECTION('ref_axis',(0.,0.,-1.)) ;
#127570 = DIRECTION('center_axis',(0.,1.,0.)) ;
#127571 = DIRECTION('ref_axis',(0.,0.,1.)) ;
#127572 = DIRECTION('center_axis',(0.,-1.,0.)) ;
#127573 = DIRECTION('ref_axis',(0.,0.,-1.)) ;
#127574 = DIRECTION('center_axis',(-1.,0.,2.16840434497101E-16)) ;
#127575 = DIRECTION('ref_axis',(2.16840434497101E-16,0.,1.)) ;
#127576 = DIRECTION('center_axis',(1.,0.,0.)) ;
#127577 = DIRECTION('ref_axis',(0.,0.,-1.)) ;
#127578 = DIRECTION('center_axis',(-2.16840434497101E-16,0.,1.)) ;
#127579 = DIRECTION('ref_axis',(1.,0.,2.16840434497101E-16)) ;
#127580 = DIRECTION('center_axis',(0.,-1.7347234759768E-14,1.)) ;
#127581 = DIRECTION('ref_axis',(0.,-1.,-1.7347234759768E-14)) ;
#127582 = DIRECTION('center_axis',(0.,1.,0.)) ;
#127583 = DIRECTION('ref_axis',(0.,0.,1.)) ;
#127584 = DIRECTION('center_axis',(0.,-1.,0.)) ;
#127585 = DIRECTION('ref_axis',(0.,0.,-1.)) ;
#127586 = DIRECTION('center_axis',(0.,1.,0.)) ;
#127587 = DIRECTION('ref_axis',(1.,0.,0.)) ;
#127588 = DIRECTION('center_axis',(0.,0.,1.)) ;
#127589 = DIRECTION('ref_axis',(-1.,0.,0.)) ;
#127590 = DIRECTION('center_axis',(0.,1.,0.)) ;
#127591 = DIRECTION('ref_axis',(1.,0.,0.)) ;
#127592 = DIRECTION('center_axis',(1.,0.,0.)) ;
#127593 = DIRECTION('ref_axis',(0.,0.,1.)) ;
#127594 = DIRECTION('center_axis',(0.,0.,-1.)) ;
#127595 = DIRECTION('ref_axis',(-1.,0.,0.)) ;
#127596 = DIRECTION('center_axis',(-1.7347234759768E-14,0.,1.)) ;
#127597 = DIRECTION('ref_axis',(1.,0.,1.7347234759768E-14)) ;
#127598 = DIRECTION('center_axis',(1.,0.,2.16840434497101E-16)) ;
#127599 = DIRECTION('ref_axis',(2.16840434497101E-16,0.,-1.)) ;
#127600 = DIRECTION('center_axis',(1.,0.,0.)) ;
#127601 = DIRECTION('ref_axis',(0.,0.,-1.)) ;
#127602 = DIRECTION('center_axis',(0.,1.,0.)) ;
#127603 = DIRECTION('ref_axis',(1.,0.,0.)) ;
#127604 = DIRECTION('center_axis',(0.,1.,0.)) ;
#127605 = DIRECTION('ref_axis',(0.,0.,-1.)) ;
#127606 = DIRECTION('center_axis',(0.,1.,0.)) ;
#127607 = DIRECTION('ref_axis',(0.,0.,1.)) ;
#127608 = DIRECTION('center_axis',(0.,1.,0.)) ;
#127609 = DIRECTION('ref_axis',(0.,0.,1.)) ;
#127610 = DIRECTION('center_axis',(-0.942809041582064,-0.235702260395514,
0.235702260395514)) ;
#127611 = DIRECTION('ref_axis',(0.242535625036331,-0.970142500145332,4.49011373492972E-16)) ;
#127612 = DIRECTION('center_axis',(-0.970142500145332,-0.242535625036331,
-2.10366121255617E-15)) ;
#127613 = DIRECTION('ref_axis',(0.242535625036331,-0.970142500145332,-4.47980524894761E-30)) ;
#127614 = DIRECTION('center_axis',(0.970142500145333,0.24253562503633,0.)) ;
#127615 = DIRECTION('ref_axis',(-0.24253562503633,0.970142500145333,0.)) ;
#127616 = DIRECTION('center_axis',(-0.970142500145333,-0.242535625036331,
-8.41464485022468E-15)) ;
#127617 = DIRECTION('ref_axis',(0.242535625036331,-0.970142500145332,-4.3372965844578E-30)) ;
#127618 = DIRECTION('center_axis',(0.879462917689188,0.219865729422294,-0.42214220049081)) ;
#127619 = DIRECTION('ref_axis',(-0.432731067584771,-5.39224131925863E-16,
-0.901523057468274)) ;
#127620 = DIRECTION('center_axis',(0.879462917689187,0.219865729422303,-0.422142200490807)) ;
#127621 = DIRECTION('ref_axis',(-0.432731067584769,-6.68249977502363E-17,
-0.901523057468275)) ;
#127622 = DIRECTION('center_axis',(0.,1.,0.)) ;
#127623 = DIRECTION('ref_axis',(1.,0.,0.)) ;
#127624 = DIRECTION('center_axis',(0.,-1.,0.)) ;
#127625 = DIRECTION('ref_axis',(0.,0.,1.)) ;
#127626 = DIRECTION('center_axis',(0.,-1.,0.)) ;
#127627 = DIRECTION('ref_axis',(0.,0.,-1.)) ;
#127628 = DIRECTION('center_axis',(-4.51750905202295E-15,-1.,2.168404344971E-15)) ;
#127629 = DIRECTION('ref_axis',(1.,-4.51750905202295E-15,3.91831450274155E-31)) ;
#127630 = DIRECTION('center_axis',(0.669589480006976,-0.669589480006974,-0.321402950403349)) ;
#127631 = DIRECTION('ref_axis',(0.707106781186547,0.707106781186548,5.45170614306381E-16)) ;
#127632 = DIRECTION('center_axis',(0.669589480006977,-0.669589480006977,-0.321402950403339)) ;
#127633 = DIRECTION('ref_axis',(0.707106781186548,0.707106781186548,1.13950759497276E-17)) ;
#127634 = DIRECTION('center_axis',(0.,1.,0.)) ;
#127635 = DIRECTION('ref_axis',(1.,0.,0.)) ;
#127636 = DIRECTION('center_axis',(0.707106781186541,-0.707106781186554,0.)) ;
#127637 = DIRECTION('ref_axis',(-0.707106781186554,-0.707106781186541,0.)) ;
#127638 = DIRECTION('center_axis',(0.707106781186549,-0.707106781186546,0.)) ;
#127639 = DIRECTION('ref_axis',(0.707106781186546,0.707106781186549,0.)) ;
#127640 = DIRECTION('center_axis',(0.707106781186548,-0.707106781186548,-1.53329341668337E-15)) ;
#127641 = DIRECTION('ref_axis',(0.707106781186548,0.707106781186548,5.40855345051871E-33)) ;
#127642 = DIRECTION('center_axis',(0.577350269189623,-0.577350269189623,-0.577350269189631)) ;
#127643 = DIRECTION('ref_axis',(-0.707106781186552,4.49290806924424E-16,-0.707106781186543)) ;
#127644 = DIRECTION('center_axis',(-0.577350269189344,0.577350269189586,-0.577350269189947)) ;
#127645 = DIRECTION('ref_axis',(1.30446081606812E-15,0.707106781186769,0.707106781186326)) ;
#127646 = DIRECTION('center_axis',(-0.707106781186548,0.707106781186548,7.66646708341679E-15)) ;
#127647 = DIRECTION('ref_axis',(-0.707106781186548,-0.707106781186548,-2.87534730433018E-31)) ;
#127648 = DIRECTION('center_axis',(-0.707106781186549,0.707106781186546,0.)) ;
#127649 = DIRECTION('ref_axis',(-0.707106781186546,-0.707106781186549,0.)) ;
#127650 = DIRECTION('center_axis',(-0.707106781186548,0.707106781186548,9.19976050010028E-15)) ;
#127651 = DIRECTION('ref_axis',(-0.707106781186548,-0.707106781186548,6.30681275467002E-31)) ;
#127652 = DIRECTION('center_axis',(-0.669589480006976,0.669589480006974,-0.321402950403349)) ;
#127653 = DIRECTION('ref_axis',(-0.707106781186547,-0.707106781186548,5.45170614306381E-16)) ;
#127654 = DIRECTION('center_axis',(0.669589480006969,-0.669589480006982,0.321402950403346)) ;
#127655 = DIRECTION('ref_axis',(0.707106781186554,0.707106781186541,-7.82217332695337E-17)) ;
#127656 = DIRECTION('center_axis',(0.,1.,0.)) ;
#127657 = DIRECTION('ref_axis',(1.,0.,0.)) ;
#127658 = DIRECTION('center_axis',(0.,1.,0.)) ;
#127659 = DIRECTION('ref_axis',(0.,0.,-1.)) ;
#127660 = DIRECTION('center_axis',(0.,-1.,0.)) ;
#127661 = DIRECTION('ref_axis',(0.,0.,-1.)) ;
#127662 = DIRECTION('center_axis',(0.,1.,0.)) ;
#127663 = DIRECTION('ref_axis',(0.,0.,1.)) ;
#127664 = DIRECTION('center_axis',(-0.879462917689188,-0.219865729422294,
-0.42214220049081)) ;
#127665 = DIRECTION('ref_axis',(-0.432731067584771,1.71515946658E-16,0.901523057468274)) ;
#127666 = DIRECTION('center_axis',(0.879462917689194,0.219865729422297,0.422142200490796)) ;
#127667 = DIRECTION('ref_axis',(0.432731067584757,1.37134448890593E-15,-0.901523057468281)) ;
#127668 = DIRECTION('center_axis',(0.,1.,0.)) ;
#127669 = DIRECTION('ref_axis',(1.,0.,0.)) ;
#127670 = DIRECTION('center_axis',(0.970142500145328,0.242535625036349,0.)) ;
#127671 = DIRECTION('ref_axis',(0.242535625036349,-0.970142500145328,0.)) ;
#127672 = DIRECTION('center_axis',(-0.970142500145333,-0.24253562503633,0.)) ;
#127673 = DIRECTION('ref_axis',(0.24253562503633,-0.970142500145333,0.)) ;
#127674 = DIRECTION('center_axis',(0.970142500145332,0.242535625036331,-2.10366121255617E-15)) ;
#127675 = DIRECTION('ref_axis',(-0.242535625036331,0.970142500145332,-4.47980524894761E-30)) ;
#127676 = DIRECTION('center_axis',(0.942809041582064,0.235702260395514,0.235702260395514)) ;
#127677 = DIRECTION('ref_axis',(-0.242535625036331,0.970142500145332,4.49011373492972E-16)) ;
#127678 = DIRECTION('center_axis',(0.,-1.,0.)) ;
#127679 = DIRECTION('ref_axis',(0.,0.,-1.)) ;
#127680 = DIRECTION('center_axis',(-1.,0.,-8.67361737988394E-15)) ;
#127681 = DIRECTION('ref_axis',(-8.67361737988394E-15,0.,1.)) ;
#127682 = DIRECTION('center_axis',(0.,0.,-1.)) ;
#127683 = DIRECTION('ref_axis',(-1.,0.,0.)) ;
#127684 = DIRECTION('center_axis',(0.,0.,-1.)) ;
#127685 = DIRECTION('ref_axis',(-1.,0.,0.)) ;
#127686 = DIRECTION('center_axis',(0.,8.67361737988405E-15,-1.)) ;
#127687 = DIRECTION('ref_axis',(0.,1.,8.67361737988405E-15)) ;
#127688 = DIRECTION('center_axis',(1.,0.,0.)) ;
#127689 = DIRECTION('ref_axis',(0.,0.,-1.)) ;
#127690 = DIRECTION('center_axis',(-1.,0.,0.)) ;
#127691 = DIRECTION('ref_axis',(0.,0.,1.)) ;
#127692 = DIRECTION('center_axis',(0.,-1.,0.)) ;
#127693 = DIRECTION('ref_axis',(0.,0.,-1.)) ;
#127694 = DIRECTION('center_axis',(-1.,0.,0.)) ;
#127695 = DIRECTION('ref_axis',(0.,0.,1.)) ;
#127696 = DIRECTION('center_axis',(0.,-1.,0.)) ;
#127697 = DIRECTION('ref_axis',(0.,0.,-1.)) ;
#127698 = DIRECTION('center_axis',(0.,0.,-1.)) ;
#127699 = DIRECTION('ref_axis',(-1.,0.,0.)) ;
#127700 = DIRECTION('center_axis',(-1.,0.,0.)) ;
#127701 = DIRECTION('ref_axis',(0.,0.,1.)) ;
#127702 = DIRECTION('center_axis',(-1.,1.73472347597681E-14,0.)) ;
#127703 = DIRECTION('ref_axis',(-1.73472347597681E-14,-1.,0.)) ;
#127704 = DIRECTION('center_axis',(0.,0.,1.)) ;
#127705 = DIRECTION('ref_axis',(1.,0.,0.)) ;
#127706 = DIRECTION('center_axis',(-8.67361737988409E-15,0.,-1.)) ;
#127707 = DIRECTION('ref_axis',(-1.,0.,8.67361737988409E-15)) ;
#127708 = DIRECTION('center_axis',(0.,-1.,0.)) ;
#127709 = DIRECTION('ref_axis',(0.,0.,-1.)) ;
#127710 = DIRECTION('center_axis',(0.,-1.,0.)) ;
#127711 = DIRECTION('ref_axis',(0.,0.,-1.)) ;
#127712 = DIRECTION('center_axis',(0.,-1.,0.)) ;
#127713 = DIRECTION('ref_axis',(0.,0.,-1.)) ;
#127714 = DIRECTION('center_axis',(0.,0.,1.)) ;
#127715 = DIRECTION('ref_axis',(1.,0.,0.)) ;
#127716 = DIRECTION('center_axis',(0.,0.,-1.)) ;
#127717 = DIRECTION('ref_axis',(-1.,0.,0.)) ;
#127718 = DIRECTION('center_axis',(0.,0.,1.)) ;
#127719 = DIRECTION('ref_axis',(1.,0.,0.)) ;
#127720 = DIRECTION('center_axis',(0.,-1.,0.)) ;
#127721 = DIRECTION('ref_axis',(0.,0.,-1.)) ;
#127722 = DIRECTION('center_axis',(0.,-1.,0.)) ;
#127723 = DIRECTION('ref_axis',(0.,0.,-1.)) ;
#127724 = DIRECTION('center_axis',(0.,1.,0.)) ;
#127725 = DIRECTION('ref_axis',(1.,0.,0.)) ;
#127726 = DIRECTION('center_axis',(-1.,0.,0.)) ;
#127727 = DIRECTION('ref_axis',(0.,0.,-1.)) ;
#127728 = DIRECTION('center_axis',(0.,1.,0.)) ;
#127729 = DIRECTION('ref_axis',(1.,0.,0.)) ;
#127730 = DIRECTION('center_axis',(-1.,0.,0.)) ;
#127731 = DIRECTION('ref_axis',(0.,0.,-1.)) ;
#127732 = DIRECTION('center_axis',(0.,-1.,0.)) ;
#127733 = DIRECTION('ref_axis',(0.,0.,-1.)) ;
#127734 = DIRECTION('center_axis',(0.,-1.,0.)) ;
#127735 = DIRECTION('ref_axis',(0.,0.,-1.)) ;
#127736 = DIRECTION('center_axis',(-1.,0.,0.)) ;
#127737 = DIRECTION('ref_axis',(0.,0.,1.)) ;
#127738 = DIRECTION('center_axis',(-1.,0.,0.)) ;
#127739 = DIRECTION('ref_axis',(0.,0.,1.)) ;
#127740 = DIRECTION('center_axis',(1.,0.,0.)) ;
#127741 = DIRECTION('ref_axis',(0.,0.,-1.)) ;
#127742 = DIRECTION('center_axis',(-1.,0.,0.)) ;
#127743 = DIRECTION('ref_axis',(0.,0.,1.)) ;
#127744 = DIRECTION('center_axis',(0.,-1.,0.)) ;
#127745 = DIRECTION('ref_axis',(0.,0.,-1.)) ;
#127746 = DIRECTION('center_axis',(0.,-1.,0.)) ;
#127747 = DIRECTION('ref_axis',(0.,0.,-1.)) ;
#127748 = DIRECTION('center_axis',(0.,1.,0.)) ;
#127749 = DIRECTION('ref_axis',(1.,0.,0.)) ;
#127750 = DIRECTION('center_axis',(0.,0.,-1.)) ;
#127751 = DIRECTION('ref_axis',(1.,0.,0.)) ;
#127752 = DIRECTION('center_axis',(0.,1.,0.)) ;
#127753 = DIRECTION('ref_axis',(1.,0.,0.)) ;
#127754 = DIRECTION('center_axis',(0.,0.,1.)) ;
#127755 = DIRECTION('ref_axis',(-1.,0.,0.)) ;
#127756 = DIRECTION('center_axis',(0.,0.,-1.)) ;
#127757 = DIRECTION('ref_axis',(-1.,0.,0.)) ;
#127758 = DIRECTION('center_axis',(1.,1.31418445149758E-16,-2.16840434497101E-16)) ;
#127759 = DIRECTION('ref_axis',(-2.16840434497101E-16,-2.8496832747207E-32,
-1.)) ;
#127760 = DIRECTION('center_axis',(1.,0.,0.)) ;
#127761 = DIRECTION('ref_axis',(0.,0.,-1.)) ;
#127762 = DIRECTION('center_axis',(-1.,0.,0.)) ;
#127763 = DIRECTION('ref_axis',(0.,0.,1.)) ;
#127764 = DIRECTION('center_axis',(-1.31418445149758E-16,1.,0.)) ;
#127765 = DIRECTION('ref_axis',(-1.,0.,0.)) ;
#127766 = DIRECTION('center_axis',(0.,0.,1.)) ;
#127767 = DIRECTION('ref_axis',(-1.,0.,0.)) ;
#127768 = DIRECTION('center_axis',(-1.31418445149758E-16,1.,0.)) ;
#127769 = DIRECTION('ref_axis',(-1.,-1.31418445149758E-16,0.)) ;
#127770 = DIRECTION('center_axis',(-1.31418445149758E-16,1.,0.)) ;
#127771 = DIRECTION('ref_axis',(-1.,0.,0.)) ;
#127772 = DIRECTION('center_axis',(-1.31418445149758E-16,1.,0.)) ;
#127773 = DIRECTION('ref_axis',(-1.,-1.31418445149758E-16,0.)) ;
#127774 = DIRECTION('center_axis',(0.,0.,1.)) ;
#127775 = DIRECTION('ref_axis',(-1.,0.,0.)) ;
#127776 = DIRECTION('center_axis',(-4.33680868994202E-16,-5.69936654944139E-32,
-1.)) ;
#127777 = DIRECTION('ref_axis',(-1.,2.47170623787823E-47,4.33680868994202E-16)) ;
#127778 = DIRECTION('center_axis',(0.,0.,1.)) ;
#127779 = DIRECTION('ref_axis',(1.,0.,0.)) ;
#127780 = DIRECTION('center_axis',(-1.31418445149758E-16,-1.,0.)) ;
#127781 = DIRECTION('ref_axis',(1.,-1.31418445149758E-16,0.)) ;
#127782 = DIRECTION('center_axis',(0.,1.,0.)) ;
#127783 = DIRECTION('ref_axis',(0.,0.,1.)) ;
#127784 = DIRECTION('center_axis',(-1.,0.,2.16840434497101E-16)) ;
#127785 = DIRECTION('ref_axis',(2.16840434497101E-16,0.,1.)) ;
#127786 = DIRECTION('center_axis',(-1.,0.,0.)) ;
#127787 = DIRECTION('ref_axis',(0.,0.,1.)) ;
#127788 = DIRECTION('center_axis',(1.,0.,0.)) ;
#127789 = DIRECTION('ref_axis',(0.,0.,-1.)) ;
#127790 = DIRECTION('center_axis',(-1.31418445149758E-16,-1.,0.)) ;
#127791 = DIRECTION('ref_axis',(1.,-1.31418445149758E-16,0.)) ;
#127792 = DIRECTION('center_axis',(0.,1.,0.)) ;
#127793 = DIRECTION('ref_axis',(0.,0.,1.)) ;
#127794 = DIRECTION('center_axis',(2.16840434497101E-16,2.8496832747207E-32,
1.)) ;
#127795 = DIRECTION('ref_axis',(1.,-6.17926559469557E-48,-2.16840434497101E-16)) ;
#127796 = DIRECTION('center_axis',(0.,0.,1.)) ;
#127797 = DIRECTION('ref_axis',(1.,0.,0.)) ;
#127798 = DIRECTION('center_axis',(-1.,-1.31418445149758E-16,-2.16840434497101E-16)) ;
#127799 = DIRECTION('ref_axis',(-2.16840434497101E-16,-2.8496832747207E-32,
1.)) ;
#127800 = DIRECTION('center_axis',(-1.,0.,0.)) ;
#127801 = DIRECTION('ref_axis',(0.,0.,1.)) ;
#127802 = DIRECTION('center_axis',(1.,0.,0.)) ;
#127803 = DIRECTION('ref_axis',(0.,0.,-1.)) ;
#127804 = DIRECTION('center_axis',(-1.31418445149758E-16,1.,0.)) ;
#127805 = DIRECTION('ref_axis',(-1.,0.,0.)) ;
#127806 = DIRECTION('center_axis',(-1.31418445149758E-16,1.,0.)) ;
#127807 = DIRECTION('ref_axis',(-1.,-1.31418445149758E-16,0.)) ;
#127808 = DIRECTION('center_axis',(0.,1.,0.)) ;
#127809 = DIRECTION('ref_axis',(1.,0.,0.)) ;
#127810 = DIRECTION('center_axis',(0.,0.,-1.)) ;
#127811 = DIRECTION('ref_axis',(1.,0.,0.)) ;
#127812 = DIRECTION('center_axis',(0.,1.,0.)) ;
#127813 = DIRECTION('ref_axis',(1.,0.,0.)) ;
#127814 = DIRECTION('center_axis',(0.,0.,-1.)) ;
#127815 = DIRECTION('ref_axis',(1.,0.,0.)) ;
#127816 = DIRECTION('center_axis',(-1.31418445149758E-16,1.,0.)) ;
#127817 = DIRECTION('ref_axis',(-1.,0.,0.)) ;
#127818 = DIRECTION('center_axis',(-1.31418445149758E-16,1.,0.)) ;
#127819 = DIRECTION('ref_axis',(-1.,-1.31418445149758E-16,0.)) ;
#127820 = DIRECTION('center_axis',(-1.31418445149758E-16,-1.,0.)) ;
#127821 = DIRECTION('ref_axis',(1.,-1.31418445149758E-16,0.)) ;
#127822 = DIRECTION('center_axis',(0.,1.,0.)) ;
#127823 = DIRECTION('ref_axis',(0.,0.,1.)) ;
#127824 = DIRECTION('center_axis',(4.33680868994202E-16,0.,1.)) ;
#127825 = DIRECTION('ref_axis',(1.,0.,-4.33680868994202E-16)) ;
#127826 = DIRECTION('center_axis',(0.,0.,-1.)) ;
#127827 = DIRECTION('ref_axis',(-1.,0.,0.)) ;
#127828 = DIRECTION('center_axis',(-2.16840434497101E-16,0.,-1.)) ;
#127829 = DIRECTION('ref_axis',(-1.,0.,2.16840434497101E-16)) ;
#127830 = DIRECTION('center_axis',(0.,0.,-1.)) ;
#127831 = DIRECTION('ref_axis',(-1.,0.,0.)) ;
#127832 = DIRECTION('center_axis',(-1.31418445149758E-16,-1.,0.)) ;
#127833 = DIRECTION('ref_axis',(1.,-1.31418445149758E-16,0.)) ;
#127834 = DIRECTION('center_axis',(0.,1.,0.)) ;
#127835 = DIRECTION('ref_axis',(0.,0.,1.)) ;
#127836 = DIRECTION('center_axis',(0.,1.,0.)) ;
#127837 = DIRECTION('ref_axis',(1.,0.,0.)) ;
#127838 = DIRECTION('center_axis',(-1.,0.,0.)) ;
#127839 = DIRECTION('ref_axis',(0.,0.,-1.)) ;
#127840 = DIRECTION('center_axis',(0.,1.,0.)) ;
#127841 = DIRECTION('ref_axis',(1.,0.,0.)) ;
#127842 = DIRECTION('center_axis',(1.,0.,0.)) ;
#127843 = DIRECTION('ref_axis',(0.,0.,1.)) ;
#127844 = DIRECTION('center_axis',(1.,0.,2.16840434497101E-16)) ;
#127845 = DIRECTION('ref_axis',(2.16840434497101E-16,0.,-1.)) ;
#127846 = DIRECTION('center_axis',(0.,1.,0.)) ;
#127847 = DIRECTION('ref_axis',(0.,0.,1.)) ;
#127848 = DIRECTION('center_axis',(0.,1.,0.)) ;
#127849 = DIRECTION('ref_axis',(0.,0.,1.)) ;
#127850 = DIRECTION('center_axis',(0.,0.,-1.)) ;
#127851 = DIRECTION('ref_axis',(-1.,0.,0.)) ;
#127852 = DIRECTION('center_axis',(0.,0.,1.)) ;
#127853 = DIRECTION('ref_axis',(1.,0.,0.)) ;
#127854 = DIRECTION('center_axis',(0.,0.,-1.)) ;
#127855 = DIRECTION('ref_axis',(-1.,0.,0.)) ;
#127856 = DIRECTION('center_axis',(0.,1.,0.)) ;
#127857 = DIRECTION('ref_axis',(0.,0.,1.)) ;
#127858 = DIRECTION('center_axis',(0.,1.,0.)) ;
#127859 = DIRECTION('ref_axis',(0.,0.,1.)) ;
#127860 = DIRECTION('center_axis',(0.,1.,0.)) ;
#127861 = DIRECTION('ref_axis',(1.,0.,0.)) ;
#127862 = DIRECTION('center_axis',(-1.,0.,0.)) ;
#127863 = DIRECTION('ref_axis',(0.,0.,-1.)) ;
#127864 = DIRECTION('center_axis',(0.,1.,0.)) ;
#127865 = DIRECTION('ref_axis',(1.,0.,0.)) ;
#127866 = DIRECTION('center_axis',(-1.,0.,0.)) ;
#127867 = DIRECTION('ref_axis',(0.,0.,-1.)) ;
#127868 = DIRECTION('center_axis',(0.,1.,0.)) ;
#127869 = DIRECTION('ref_axis',(0.,0.,1.)) ;
#127870 = DIRECTION('center_axis',(0.,1.,0.)) ;
#127871 = DIRECTION('ref_axis',(0.,0.,1.)) ;
#127872 = DIRECTION('center_axis',(-1.,0.,0.)) ;
#127873 = DIRECTION('ref_axis',(0.,0.,1.)) ;
#127874 = DIRECTION('center_axis',(-1.,0.,0.)) ;
#127875 = DIRECTION('ref_axis',(0.,0.,1.)) ;
#127876 = DIRECTION('center_axis',(1.,0.,0.)) ;
#127877 = DIRECTION('ref_axis',(0.,0.,-1.)) ;
#127878 = DIRECTION('center_axis',(-1.,0.,0.)) ;
#127879 = DIRECTION('ref_axis',(0.,0.,1.)) ;
#127880 = DIRECTION('center_axis',(0.,1.,0.)) ;
#127881 = DIRECTION('ref_axis',(0.,0.,1.)) ;
#127882 = DIRECTION('center_axis',(0.,1.,0.)) ;
#127883 = DIRECTION('ref_axis',(0.,0.,1.)) ;
#127884 = DIRECTION('center_axis',(0.,1.,0.)) ;
#127885 = DIRECTION('ref_axis',(1.,0.,0.)) ;
#127886 = DIRECTION('center_axis',(0.,0.,1.)) ;
#127887 = DIRECTION('ref_axis',(-1.,0.,0.)) ;
#127888 = DIRECTION('center_axis',(0.,1.,0.)) ;
#127889 = DIRECTION('ref_axis',(1.,0.,0.)) ;
#127890 = DIRECTION('center_axis',(0.,0.,-1.)) ;
#127891 = DIRECTION('ref_axis',(1.,0.,0.)) ;
#127892 = DIRECTION('center_axis',(0.,0.,1.)) ;
#127893 = DIRECTION('ref_axis',(1.,0.,0.)) ;
#127894 = DIRECTION('center_axis',(0.,0.,1.)) ;
#127895 = DIRECTION('ref_axis',(1.,0.,0.)) ;
#127896 = DIRECTION('center_axis',(0.,0.,-1.)) ;
#127897 = DIRECTION('ref_axis',(-1.,0.,0.)) ;
#127898 = DIRECTION('center_axis',(-8.67361737988401E-15,0.,1.)) ;
#127899 = DIRECTION('ref_axis',(1.,0.,8.67361737988401E-15)) ;
#127900 = DIRECTION('center_axis',(1.,0.,0.)) ;
#127901 = DIRECTION('ref_axis',(0.,0.,-1.)) ;
#127902 = DIRECTION('center_axis',(1.,0.,0.)) ;
#127903 = DIRECTION('ref_axis',(0.,0.,-1.)) ;
#127904 = DIRECTION('center_axis',(1.,0.,0.)) ;
#127905 = DIRECTION('ref_axis',(0.,0.,-1.)) ;
#127906 = DIRECTION('center_axis',(1.,0.,8.67361737988409E-15)) ;
#127907 = DIRECTION('ref_axis',(8.67361737988409E-15,0.,-1.)) ;
#127908 = DIRECTION('center_axis',(1.,0.,0.)) ;
#127909 = DIRECTION('ref_axis',(0.,0.,-1.)) ;
#127910 = DIRECTION('center_axis',(1.,0.,1.7347234759768E-14)) ;
#127911 = DIRECTION('ref_axis',(1.7347234759768E-14,0.,-1.)) ;
#127912 = DIRECTION('center_axis',(-1.,0.,0.)) ;
#127913 = DIRECTION('ref_axis',(0.,0.,1.)) ;
#127914 = DIRECTION('center_axis',(1.,0.,0.)) ;
#127915 = DIRECTION('ref_axis',(0.,0.,-1.)) ;
#127916 = DIRECTION('center_axis',(1.,0.,0.)) ;
#127917 = DIRECTION('ref_axis',(0.,0.,-1.)) ;
#127918 = DIRECTION('center_axis',(-8.67361737988409E-15,0.,-1.)) ;
#127919 = DIRECTION('ref_axis',(-1.,0.,8.67361737988409E-15)) ;
#127920 = DIRECTION('center_axis',(1.,0.,0.)) ;
#127921 = DIRECTION('ref_axis',(0.,0.,-1.)) ;
#127922 = DIRECTION('center_axis',(0.,0.,1.)) ;
#127923 = DIRECTION('ref_axis',(1.,0.,0.)) ;
#127924 = DIRECTION('center_axis',(0.,0.,-1.)) ;
#127925 = DIRECTION('ref_axis',(-1.,0.,0.)) ;
#127926 = DIRECTION('center_axis',(-0.422618261740697,5.55398348498559E-17,
0.906307787036651)) ;
#127927 = DIRECTION('ref_axis',(0.906307787036651,2.16182864926402E-31,0.422618261740697)) ;
#127928 = DIRECTION('center_axis',(0.422618261740697,-5.55398348498559E-17,
-0.906307787036651)) ;
#127929 = DIRECTION('ref_axis',(-0.906307787036651,-2.07415302975303E-31,
-0.422618261740697)) ;
#127930 = DIRECTION('center_axis',(-0.422618261740697,5.55398348498559E-17,
0.906307787036651)) ;
#127931 = DIRECTION('ref_axis',(0.906307787036651,2.07415302975303E-31,0.422618261740697)) ;
#127932 = DIRECTION('center_axis',(0.422618261740697,-5.55398348498559E-17,
-0.906307787036651)) ;
#127933 = DIRECTION('ref_axis',(-0.906307787036651,-2.07415302975303E-31,
-0.422618261740697)) ;
#127934 = DIRECTION('center_axis',(0.,1.,0.)) ;
#127935 = DIRECTION('ref_axis',(1.,0.,0.)) ;
#127936 = DIRECTION('center_axis',(3.64461297742727E-14,0.514231796959095,
-0.857651245551606)) ;
#127937 = DIRECTION('ref_axis',(3.46944695195362E-14,-0.857651245551606,-0.514231796959095)) ;
#127938 = DIRECTION('center_axis',(0.,-1.73472347597681E-14,1.)) ;
#127939 = DIRECTION('ref_axis',(0.,1.,1.73472347597681E-14)) ;
#127940 = DIRECTION('center_axis',(-1.,0.,0.)) ;
#127941 = DIRECTION('ref_axis',(0.,-8.67361737988409E-15,-1.)) ;
#127942 = DIRECTION('center_axis',(0.,0.,1.)) ;
#127943 = DIRECTION('ref_axis',(1.,0.,0.)) ;
#127944 = DIRECTION('center_axis',(0.,0.,1.)) ;
#127945 = DIRECTION('ref_axis',(1.,0.,0.)) ;
#127946 = DIRECTION('center_axis',(-1.,0.,0.)) ;
#127947 = DIRECTION('ref_axis',(0.,0.,1.)) ;
#127948 = DIRECTION('center_axis',(-1.,0.,0.)) ;
#127949 = DIRECTION('ref_axis',(0.,-8.67361737988409E-15,-1.)) ;
#127950 = DIRECTION('center_axis',(1.,0.,0.)) ;
#127951 = DIRECTION('ref_axis',(0.,0.,-1.)) ;
#127952 = DIRECTION('center_axis',(0.,-0.514231796959126,-0.857651245551587)) ;
#127953 = DIRECTION('ref_axis',(0.,0.857651245551587,-0.514231796959126)) ;
#127954 = DIRECTION('center_axis',(0.,1.,8.97270763436279E-17)) ;
#127955 = DIRECTION('ref_axis',(0.,-8.97270763436279E-17,1.)) ;
#127956 = DIRECTION('center_axis',(0.,-1.,-8.97270763436279E-17)) ;
#127957 = DIRECTION('ref_axis',(0.,-8.97270763436279E-17,1.)) ;
#127958 = DIRECTION('center_axis',(0.,-1.,0.)) ;
#127959 = DIRECTION('ref_axis',(0.,0.,-1.)) ;
#127960 = DIRECTION('center_axis',(0.,1.,0.)) ;
#127961 = DIRECTION('ref_axis',(1.,0.,0.)) ;
#127962 = DIRECTION('center_axis',(-1.,0.,0.)) ;
#127963 = DIRECTION('ref_axis',(0.,0.,-1.)) ;
#127964 = DIRECTION('center_axis',(1.,0.,0.)) ;
#127965 = DIRECTION('ref_axis',(0.,0.,-1.)) ;
#127966 = DIRECTION('center_axis',(0.,-0.514231796959095,0.857651245551606)) ;
#127967 = DIRECTION('ref_axis',(0.,0.857651245551606,0.514231796959095)) ;
#127968 = DIRECTION('center_axis',(0.,0.,-1.)) ;
#127969 = DIRECTION('ref_axis',(1.,0.,0.)) ;
#127970 = DIRECTION('center_axis',(0.,1.,0.)) ;
#127971 = DIRECTION('ref_axis',(1.,0.,0.)) ;
#127972 = DIRECTION('center_axis',(-1.73472347597682E-14,0.,-1.)) ;
#127973 = DIRECTION('ref_axis',(1.,0.,-1.73472347597682E-14)) ;
#127974 = DIRECTION('center_axis',(-1.,0.,0.)) ;
#127975 = DIRECTION('ref_axis',(0.,8.67361737988409E-15,-1.)) ;
#127976 = DIRECTION('center_axis',(0.,0.,-1.)) ;
#127977 = DIRECTION('ref_axis',(-1.,0.,0.)) ;
#127978 = DIRECTION('center_axis',(0.,0.,1.)) ;
#127979 = DIRECTION('ref_axis',(-1.,0.,0.)) ;
#127980 = DIRECTION('center_axis',(0.,0.,-1.)) ;
#127981 = DIRECTION('ref_axis',(-1.,0.,0.)) ;
#127982 = DIRECTION('center_axis',(-1.,0.,7.01133629567814E-33)) ;
#127983 = DIRECTION('ref_axis',(7.01133629567814E-33,0.,1.)) ;
#127984 = DIRECTION('center_axis',(-1.,0.,0.)) ;
#127985 = DIRECTION('ref_axis',(0.,0.,1.)) ;
#127986 = DIRECTION('center_axis',(0.,0.,-1.)) ;
#127987 = DIRECTION('ref_axis',(-1.,0.,0.)) ;
#127988 = DIRECTION('center_axis',(-7.01133629567814E-33,8.97270763436279E-17,
-1.)) ;
#127989 = DIRECTION('ref_axis',(6.29106707073161E-49,1.,8.97270763436279E-17)) ;
#127990 = DIRECTION('center_axis',(1.,0.,0.)) ;
#127991 = DIRECTION('ref_axis',(0.,0.,-1.)) ;
#127992 = DIRECTION('center_axis',(0.,0.514231796959095,0.857651245551606)) ;
#127993 = DIRECTION('ref_axis',(0.,-0.857651245551606,0.514231796959095)) ;
#127994 = DIRECTION('center_axis',(-1.,0.,0.)) ;
#127995 = DIRECTION('ref_axis',(0.,0.,1.)) ;
#127996 = DIRECTION('center_axis',(-1.,0.,0.)) ;
#127997 = DIRECTION('ref_axis',(0.,-4.33680868994204E-15,-1.)) ;
#127998 = DIRECTION('center_axis',(0.,0.,1.)) ;
#127999 = DIRECTION('ref_axis',(1.,0.,0.)) ;
#128000 = DIRECTION('center_axis',(0.,0.,-1.)) ;
#128001 = DIRECTION('ref_axis',(-1.,0.,0.)) ;
#128002 = DIRECTION('center_axis',(0.,-1.,8.97270763436279E-17)) ;
#128003 = DIRECTION('ref_axis',(0.,-8.97270763436279E-17,-1.)) ;
#128004 = DIRECTION('center_axis',(0.,-1.,8.97270763436279E-17)) ;
#128005 = DIRECTION('ref_axis',(0.,-8.97270763436279E-17,-1.)) ;
#128006 = DIRECTION('center_axis',(0.,-1.,0.)) ;
#128007 = DIRECTION('ref_axis',(0.,0.,-1.)) ;
#128008 = DIRECTION('center_axis',(-7.01133629567814E-33,8.97270763436279E-17,
-1.)) ;
#128009 = DIRECTION('ref_axis',(0.,1.,0.)) ;
#128010 = DIRECTION('center_axis',(0.,-1.,0.)) ;
#128011 = DIRECTION('ref_axis',(0.,0.,1.)) ;
#128012 = DIRECTION('center_axis',(1.,0.,0.)) ;
#128013 = DIRECTION('ref_axis',(0.,0.,-1.)) ;
#128014 = DIRECTION('center_axis',(0.,0.,1.)) ;
#128015 = DIRECTION('ref_axis',(-1.,0.,0.)) ;
#128016 = DIRECTION('center_axis',(0.,1.,0.)) ;
#128017 = DIRECTION('ref_axis',(1.,0.,0.)) ;
#128018 = DIRECTION('center_axis',(-1.,0.,0.)) ;
#128019 = DIRECTION('ref_axis',(0.,0.,-1.)) ;
#128020 = DIRECTION('center_axis',(1.,7.81406971160724E-17,0.)) ;
#128021 = DIRECTION('ref_axis',(-7.81406971160724E-17,1.,0.)) ;
#128022 = DIRECTION('center_axis',(1.,0.,0.)) ;
#128023 = DIRECTION('ref_axis',(0.,0.,-1.)) ;
#128024 = DIRECTION('center_axis',(1.,0.,0.)) ;
#128025 = DIRECTION('ref_axis',(0.,0.,-1.)) ;
#128026 = DIRECTION('center_axis',(0.,1.,8.97270763436279E-17)) ;
#128027 = DIRECTION('ref_axis',(0.,-8.97270763436279E-17,1.)) ;
#128028 = DIRECTION('center_axis',(0.,-1.,0.)) ;
#128029 = DIRECTION('ref_axis',(0.,0.,-1.)) ;
#128030 = DIRECTION('center_axis',(0.,0.,-1.)) ;
#128031 = DIRECTION('ref_axis',(-1.,0.,0.)) ;
#128032 = DIRECTION('center_axis',(-7.01133629567814E-33,8.97270763436279E-17,
1.)) ;
#128033 = DIRECTION('ref_axis',(-6.29106707073161E-49,-1.,8.97270763436279E-17)) ;
#128034 = DIRECTION('center_axis',(-1.,0.,-7.01133629567814E-33)) ;
#128035 = DIRECTION('ref_axis',(-7.01133629567814E-33,0.,1.)) ;
#128036 = DIRECTION('center_axis',(-1.,0.,0.)) ;
#128037 = DIRECTION('ref_axis',(0.,0.,1.)) ;
#128038 = DIRECTION('center_axis',(1.,0.,0.)) ;
#128039 = DIRECTION('ref_axis',(0.,1.,0.)) ;
#128040 = DIRECTION('center_axis',(2.16840434497101E-15,1.,0.)) ;
#128041 = DIRECTION('ref_axis',(-1.,2.16840434497101E-15,0.)) ;
#128042 = DIRECTION('center_axis',(0.,1.,0.)) ;
#128043 = DIRECTION('ref_axis',(1.,0.,0.)) ;
#128044 = DIRECTION('center_axis',(0.,0.,-1.)) ;
#128045 = DIRECTION('ref_axis',(1.,0.,0.)) ;
#128046 = DIRECTION('center_axis',(-1.,0.,0.)) ;
#128047 = DIRECTION('ref_axis',(0.,0.,-1.)) ;
#128048 = DIRECTION('center_axis',(-7.01133629567814E-33,8.97270763436279E-17,
1.)) ;
#128049 = DIRECTION('ref_axis',(0.,-1.,0.)) ;
#128050 = DIRECTION('center_axis',(0.,-1.,0.)) ;
#128051 = DIRECTION('ref_axis',(0.,0.,1.)) ;
#128052 = DIRECTION('center_axis',(7.81406971160724E-17,-1.,-8.97270763436279E-17)) ;
#128053 = DIRECTION('ref_axis',(-7.01133629567814E-33,8.97270763436279E-17,
-1.)) ;
#128054 = DIRECTION('center_axis',(0.,1.,0.)) ;
#128055 = DIRECTION('ref_axis',(0.,0.,1.)) ;
#128056 = DIRECTION('center_axis',(-1.,-7.81406971160724E-17,0.)) ;
#128057 = DIRECTION('ref_axis',(7.81406971160724E-17,-1.,0.)) ;
#128058 = DIRECTION('center_axis',(-1.,-7.81406971160724E-17,0.)) ;
#128059 = DIRECTION('ref_axis',(-7.81406971160724E-17,1.,0.)) ;
#128060 = DIRECTION('center_axis',(0.,0.,1.)) ;
#128061 = DIRECTION('ref_axis',(1.,0.,0.)) ;
#128062 = DIRECTION('center_axis',(0.,0.,-1.)) ;
#128063 = DIRECTION('ref_axis',(-1.,0.,0.)) ;
#128064 = DIRECTION('center_axis',(0.,-1.,8.97270763436279E-17)) ;
#128065 = DIRECTION('ref_axis',(0.,-8.97270763436279E-17,-1.)) ;
#128066 = DIRECTION('center_axis',(0.,-1.,0.)) ;
#128067 = DIRECTION('ref_axis',(0.,0.,-1.)) ;
#128068 = DIRECTION('center_axis',(1.,7.81406971160724E-17,0.)) ;
#128069 = DIRECTION('ref_axis',(0.,1.,0.)) ;
#128070 = DIRECTION('center_axis',(0.,0.,1.)) ;
#128071 = DIRECTION('ref_axis',(-1.,0.,0.)) ;
#128072 = DIRECTION('center_axis',(0.,1.,0.)) ;
#128073 = DIRECTION('ref_axis',(1.,0.,0.)) ;
#128074 = DIRECTION('center_axis',(-1.,0.,0.)) ;
#128075 = DIRECTION('ref_axis',(0.,0.,-1.)) ;
#128076 = DIRECTION('center_axis',(0.,0.,-1.)) ;
#128077 = DIRECTION('ref_axis',(-1.,0.,0.)) ;
#128078 = DIRECTION('center_axis',(0.,0.,1.)) ;
#128079 = DIRECTION('ref_axis',(1.,0.,0.)) ;
#128080 = DIRECTION('center_axis',(-1.,-7.81406971160724E-17,0.)) ;
#128081 = DIRECTION('ref_axis',(7.81406971160724E-17,-1.,0.)) ;
#128082 = DIRECTION('center_axis',(-1.,-7.81406971160724E-17,0.)) ;
#128083 = DIRECTION('ref_axis',(-7.81406971160724E-17,1.,0.)) ;
#128084 = DIRECTION('center_axis',(1.,7.81406971160724E-17,0.)) ;
#128085 = DIRECTION('ref_axis',(-7.81406971160724E-17,1.,0.)) ;
#128086 = DIRECTION('center_axis',(1.,0.,0.)) ;
#128087 = DIRECTION('ref_axis',(0.,0.,-1.)) ;
#128088 = DIRECTION('center_axis',(1.,0.,0.)) ;
#128089 = DIRECTION('ref_axis',(0.,0.,-1.)) ;
#128090 = DIRECTION('center_axis',(3.78638272950961E-32,-4.8455963016112E-16,
-1.)) ;
#128091 = DIRECTION('ref_axis',(1.83472821505963E-47,1.,-4.8455963016112E-16)) ;
#128092 = DIRECTION('center_axis',(3.78638272950961E-32,-4.8455963016112E-16,
-1.)) ;
#128093 = DIRECTION('ref_axis',(1.83472821505963E-47,1.,-4.8455963016112E-16)) ;
#128094 = DIRECTION('center_axis',(0.,0.,-1.)) ;
#128095 = DIRECTION('ref_axis',(-1.,0.,0.)) ;
#128096 = DIRECTION('center_axis',(1.,7.81406971160724E-17,0.)) ;
#128097 = DIRECTION('ref_axis',(0.,1.,0.)) ;
#128098 = DIRECTION('center_axis',(0.,-1.,0.)) ;
#128099 = DIRECTION('ref_axis',(0.,0.,1.)) ;
#128100 = DIRECTION('center_axis',(0.,1.,0.)) ;
#128101 = DIRECTION('ref_axis',(1.,0.,0.)) ;
#128102 = DIRECTION('center_axis',(0.,1.,0.)) ;
#128103 = DIRECTION('ref_axis',(0.,0.,-1.)) ;
#128104 = DIRECTION('center_axis',(-7.81406971160724E-17,1.,-8.97270763436279E-17)) ;
#128105 = DIRECTION('ref_axis',(-7.01133629567814E-33,8.97270763436279E-17,
1.)) ;
#128106 = DIRECTION('center_axis',(0.,-1.,0.)) ;
#128107 = DIRECTION('ref_axis',(0.,0.,-1.)) ;
#128108 = DIRECTION('center_axis',(0.,1.,0.)) ;
#128109 = DIRECTION('ref_axis',(0.,0.,1.)) ;
#128110 = DIRECTION('center_axis',(0.,-1.,0.)) ;
#128111 = DIRECTION('ref_axis',(0.,0.,-1.)) ;
#128112 = DIRECTION('center_axis',(0.,-1.,0.)) ;
#128113 = DIRECTION('ref_axis',(0.,0.,-1.)) ;
#128114 = DIRECTION('center_axis',(0.,1.,0.)) ;
#128115 = DIRECTION('ref_axis',(1.,0.,0.)) ;
#128116 = DIRECTION('center_axis',(0.,0.,1.)) ;
#128117 = DIRECTION('ref_axis',(-1.,0.,0.)) ;
#128118 = DIRECTION('center_axis',(1.,0.,0.)) ;
#128119 = DIRECTION('ref_axis',(0.,0.,1.)) ;
#128120 = DIRECTION('center_axis',(0.,-1.,0.)) ;
#128121 = DIRECTION('ref_axis',(0.,0.,-1.)) ;
#128122 = DIRECTION('center_axis',(0.,1.,0.)) ;
#128123 = DIRECTION('ref_axis',(0.,0.,1.)) ;
#128124 = DIRECTION('center_axis',(0.,-1.,0.)) ;
#128125 = DIRECTION('ref_axis',(0.,0.,-1.)) ;
#128126 = DIRECTION('center_axis',(-1.,0.,2.16840434497101E-16)) ;
#128127 = DIRECTION('ref_axis',(2.16840434497101E-16,0.,1.)) ;
#128128 = DIRECTION('center_axis',(1.,0.,0.)) ;
#128129 = DIRECTION('ref_axis',(0.,0.,-1.)) ;
#128130 = DIRECTION('center_axis',(-2.16840434497101E-16,0.,1.)) ;
#128131 = DIRECTION('ref_axis',(1.,0.,2.16840434497101E-16)) ;
#128132 = DIRECTION('center_axis',(0.,-1.7347234759768E-14,1.)) ;
#128133 = DIRECTION('ref_axis',(0.,-1.,-1.7347234759768E-14)) ;
#128134 = DIRECTION('center_axis',(0.,1.,0.)) ;
#128135 = DIRECTION('ref_axis',(0.,0.,1.)) ;
#128136 = DIRECTION('center_axis',(0.,-1.,0.)) ;
#128137 = DIRECTION('ref_axis',(0.,0.,-1.)) ;
#128138 = DIRECTION('center_axis',(0.,1.,0.)) ;
#128139 = DIRECTION('ref_axis',(1.,0.,0.)) ;
#128140 = DIRECTION('center_axis',(0.,0.,1.)) ;
#128141 = DIRECTION('ref_axis',(-1.,0.,0.)) ;
#128142 = DIRECTION('center_axis',(0.,1.,0.)) ;
#128143 = DIRECTION('ref_axis',(1.,0.,0.)) ;
#128144 = DIRECTION('center_axis',(1.,0.,0.)) ;
#128145 = DIRECTION('ref_axis',(0.,0.,1.)) ;
#128146 = DIRECTION('center_axis',(0.,0.,-1.)) ;
#128147 = DIRECTION('ref_axis',(-1.,0.,0.)) ;
#128148 = DIRECTION('center_axis',(-1.7347234759768E-14,0.,1.)) ;
#128149 = DIRECTION('ref_axis',(1.,0.,1.7347234759768E-14)) ;
#128150 = DIRECTION('center_axis',(1.,0.,2.16840434497101E-16)) ;
#128151 = DIRECTION('ref_axis',(2.16840434497101E-16,0.,-1.)) ;
#128152 = DIRECTION('center_axis',(1.,0.,0.)) ;
#128153 = DIRECTION('ref_axis',(0.,0.,-1.)) ;
#128154 = DIRECTION('center_axis',(0.,1.,0.)) ;
#128155 = DIRECTION('ref_axis',(1.,0.,0.)) ;
#128156 = DIRECTION('center_axis',(0.,1.,0.)) ;
#128157 = DIRECTION('ref_axis',(0.,0.,-1.)) ;
#128158 = DIRECTION('center_axis',(0.,1.,0.)) ;
#128159 = DIRECTION('ref_axis',(0.,0.,1.)) ;
#128160 = DIRECTION('center_axis',(0.,1.,0.)) ;
#128161 = DIRECTION('ref_axis',(0.,0.,1.)) ;
#128162 = DIRECTION('center_axis',(-0.942809041582063,-0.235702260395516,
0.235702260395518)) ;
#128163 = DIRECTION('ref_axis',(0.242535625036335,4.64743530723282E-16,0.970142500145331)) ;
#128164 = DIRECTION('center_axis',(-0.970142500145332,-0.242535625036331,
-2.10366121255613E-15)) ;
#128165 = DIRECTION('ref_axis',(0.242535625036331,-0.970142500145332,-4.48415458566342E-30)) ;
#128166 = DIRECTION('center_axis',(0.970142500145333,0.24253562503633,0.)) ;
#128167 = DIRECTION('ref_axis',(-0.24253562503633,0.970142500145333,0.)) ;
#128168 = DIRECTION('center_axis',(-0.970142500145332,-0.242535625036331,
-8.41464485022476E-15)) ;
#128169 = DIRECTION('ref_axis',(0.242535625036331,-0.970142500145332,-1.80900724878918E-29)) ;
#128170 = DIRECTION('center_axis',(0.879462917689188,0.219865729422294,-0.42214220049081)) ;
#128171 = DIRECTION('ref_axis',(-0.432731067584771,1.71515946658E-16,-0.901523057468274)) ;
#128172 = DIRECTION('center_axis',(0.879462917689185,0.219865729422304,-0.42214220049081)) ;
#128173 = DIRECTION('ref_axis',(-0.432731067584772,-1.04304727837597E-16,
-0.901523057468273)) ;
#128174 = DIRECTION('center_axis',(0.,1.,0.)) ;
#128175 = DIRECTION('ref_axis',(1.,0.,0.)) ;
#128176 = DIRECTION('center_axis',(-2.00438979995004E-14,-1.,0.)) ;
#128177 = DIRECTION('ref_axis',(-1.,2.00438979995004E-14,0.)) ;
#128178 = DIRECTION('center_axis',(0.,-1.,0.)) ;
#128179 = DIRECTION('ref_axis',(0.,0.,-1.)) ;
#128180 = DIRECTION('center_axis',(-4.51750905202295E-15,-1.,2.16840434497102E-15)) ;
#128181 = DIRECTION('ref_axis',(1.,-4.51750905202295E-15,3.91831450274151E-31)) ;
#128182 = DIRECTION('center_axis',(0.669589480006976,-0.669589480006974,-0.321402950403349)) ;
#128183 = DIRECTION('ref_axis',(0.707106781186547,0.707106781186548,5.45170614306381E-16)) ;
#128184 = DIRECTION('center_axis',(0.669589480006966,-0.669589480006966,-0.321402950403388)) ;
#128185 = DIRECTION('ref_axis',(0.707106781186547,0.707106781186547,-1.18959821530046E-17)) ;
#128186 = DIRECTION('center_axis',(0.,1.,0.)) ;
#128187 = DIRECTION('ref_axis',(1.,0.,0.)) ;
#128188 = DIRECTION('center_axis',(0.707106781186576,-0.707106781186519,0.)) ;
#128189 = DIRECTION('ref_axis',(-0.707106781186519,-0.707106781186576,0.)) ;
#128190 = DIRECTION('center_axis',(0.707106781186549,-0.707106781186546,0.)) ;
#128191 = DIRECTION('ref_axis',(0.707106781186546,0.707106781186549,0.)) ;
#128192 = DIRECTION('center_axis',(0.707106781186548,-0.707106781186548,-1.53329341668338E-15)) ;
#128193 = DIRECTION('ref_axis',(0.707106781186548,0.707106781186548,1.5356898865553E-31)) ;
#128194 = DIRECTION('center_axis',(0.577350269189622,-0.577350269189622,-0.577350269189634)) ;
#128195 = DIRECTION('ref_axis',(-0.707106781186554,1.85551679542784E-15,-0.707106781186541)) ;
#128196 = DIRECTION('center_axis',(-0.57735026918932,0.577350269189576,-0.577350269189982)) ;
#128197 = DIRECTION('ref_axis',(-2.21337158357689E-15,0.707106781186795,0.7071067811863)) ;
#128198 = DIRECTION('center_axis',(-0.707106781186548,0.707106781186548,7.66646708341679E-15)) ;
#128199 = DIRECTION('ref_axis',(-0.707106781186548,-0.707106781186548,-2.87534730433018E-31)) ;
#128200 = DIRECTION('center_axis',(-0.707106781186549,0.707106781186546,0.)) ;
#128201 = DIRECTION('ref_axis',(-0.707106781186546,-0.707106781186549,0.)) ;
#128202 = DIRECTION('center_axis',(-0.707106781186548,0.707106781186548,0.)) ;
#128203 = DIRECTION('ref_axis',(-0.707106781186548,-0.707106781186548,0.)) ;
#128204 = DIRECTION('center_axis',(-0.669589480006976,0.669589480006974,-0.321402950403349)) ;
#128205 = DIRECTION('ref_axis',(-0.707106781186547,-0.707106781186548,5.45170614306381E-16)) ;
#128206 = DIRECTION('center_axis',(0.669589480006977,-0.669589480006973,0.32140295040335)) ;
#128207 = DIRECTION('ref_axis',(0.707106781186545,0.70710678118655,-2.76381108894423E-16)) ;
#128208 = DIRECTION('center_axis',(0.,1.,0.)) ;
#128209 = DIRECTION('ref_axis',(1.,0.,0.)) ;
#128210 = DIRECTION('center_axis',(1.00219489997502E-14,1.,0.)) ;
#128211 = DIRECTION('ref_axis',(1.,-1.00219489997502E-14,0.)) ;
#128212 = DIRECTION('center_axis',(0.,-1.,0.)) ;
#128213 = DIRECTION('ref_axis',(0.,0.,-1.)) ;
#128214 = DIRECTION('center_axis',(0.,1.,0.)) ;
#128215 = DIRECTION('ref_axis',(0.,0.,1.)) ;
#128216 = DIRECTION('center_axis',(-0.879462917689188,-0.219865729422294,
-0.42214220049081)) ;
#128217 = DIRECTION('ref_axis',(-0.432731067584771,1.71515946658E-16,0.901523057468274)) ;
#128218 = DIRECTION('center_axis',(0.879462917689181,0.219865729422293,0.422142200490825)) ;
#128219 = DIRECTION('ref_axis',(0.432731067584786,8.68207988095619E-17,-0.901523057468266)) ;
#128220 = DIRECTION('center_axis',(0.,1.,0.)) ;
#128221 = DIRECTION('ref_axis',(1.,0.,0.)) ;
#128222 = DIRECTION('center_axis',(0.970142500145337,0.242535625036315,0.)) ;
#128223 = DIRECTION('ref_axis',(0.242535625036315,-0.970142500145336,0.)) ;
#128224 = DIRECTION('center_axis',(-0.970142500145333,-0.24253562503633,0.)) ;
#128225 = DIRECTION('ref_axis',(0.24253562503633,-0.970142500145333,0.)) ;
#128226 = DIRECTION('center_axis',(0.970142500145332,0.242535625036331,-2.10366121255617E-15)) ;
#128227 = DIRECTION('ref_axis',(-0.242535625036331,0.970142500145332,-4.47980524894761E-30)) ;
#128228 = DIRECTION('center_axis',(0.942809041582064,0.235702260395514,0.235702260395514)) ;
#128229 = DIRECTION('ref_axis',(-0.242535625036331,0.970142500145332,4.49011373492972E-16)) ;
#128230 = DIRECTION('center_axis',(0.,-1.,0.)) ;
#128231 = DIRECTION('ref_axis',(0.,0.,-1.)) ;
#128232 = DIRECTION('center_axis',(-1.,0.,-8.67361737988394E-15)) ;
#128233 = DIRECTION('ref_axis',(-8.67361737988394E-15,0.,1.)) ;
#128234 = DIRECTION('center_axis',(0.,0.,-1.)) ;
#128235 = DIRECTION('ref_axis',(-1.,0.,0.)) ;
#128236 = DIRECTION('center_axis',(0.,0.,-1.)) ;
#128237 = DIRECTION('ref_axis',(-1.,0.,0.)) ;
#128238 = DIRECTION('center_axis',(0.,0.,-1.)) ;
#128239 = DIRECTION('ref_axis',(-1.,0.,0.)) ;
#128240 = DIRECTION('center_axis',(1.,0.,0.)) ;
#128241 = DIRECTION('ref_axis',(0.,0.,-1.)) ;
#128242 = DIRECTION('center_axis',(-1.,0.,0.)) ;
#128243 = DIRECTION('ref_axis',(0.,0.,1.)) ;
#128244 = DIRECTION('center_axis',(0.,-1.,0.)) ;
#128245 = DIRECTION('ref_axis',(0.,0.,-1.)) ;
#128246 = DIRECTION('center_axis',(-1.,0.,0.)) ;
#128247 = DIRECTION('ref_axis',(0.,0.,1.)) ;
#128248 = DIRECTION('center_axis',(0.,-1.,0.)) ;
#128249 = DIRECTION('ref_axis',(0.,0.,-1.)) ;
#128250 = DIRECTION('center_axis',(0.,0.,-1.)) ;
#128251 = DIRECTION('ref_axis',(-1.,0.,0.)) ;
#128252 = DIRECTION('center_axis',(-1.,0.,0.)) ;
#128253 = DIRECTION('ref_axis',(0.,0.,1.)) ;
#128254 = DIRECTION('center_axis',(-1.,1.73472347597681E-14,0.)) ;
#128255 = DIRECTION('ref_axis',(-1.73472347597681E-14,-1.,0.)) ;
#128256 = DIRECTION('center_axis',(0.,0.,1.)) ;
#128257 = DIRECTION('ref_axis',(1.,0.,0.)) ;
#128258 = DIRECTION('center_axis',(0.,0.,-1.)) ;
#128259 = DIRECTION('ref_axis',(-1.,0.,0.)) ;
#128260 = DIRECTION('center_axis',(0.,-1.,0.)) ;
#128261 = DIRECTION('ref_axis',(0.,0.,-1.)) ;
#128262 = DIRECTION('center_axis',(0.,-1.,0.)) ;
#128263 = DIRECTION('ref_axis',(0.,0.,-1.)) ;
#128264 = DIRECTION('center_axis',(0.,-1.,0.)) ;
#128265 = DIRECTION('ref_axis',(0.,0.,-1.)) ;
#128266 = DIRECTION('center_axis',(0.,0.,1.)) ;
#128267 = DIRECTION('ref_axis',(1.,0.,0.)) ;
#128268 = DIRECTION('center_axis',(0.,0.,-1.)) ;
#128269 = DIRECTION('ref_axis',(-1.,0.,0.)) ;
#128270 = DIRECTION('center_axis',(0.,0.,1.)) ;
#128271 = DIRECTION('ref_axis',(1.,0.,0.)) ;
#128272 = DIRECTION('center_axis',(0.,-1.,0.)) ;
#128273 = DIRECTION('ref_axis',(0.,0.,-1.)) ;
#128274 = DIRECTION('center_axis',(0.,-1.,0.)) ;
#128275 = DIRECTION('ref_axis',(0.,0.,-1.)) ;
#128276 = DIRECTION('center_axis',(0.,1.,0.)) ;
#128277 = DIRECTION('ref_axis',(1.,0.,0.)) ;
#128278 = DIRECTION('center_axis',(-1.,0.,0.)) ;
#128279 = DIRECTION('ref_axis',(0.,0.,-1.)) ;
#128280 = DIRECTION('center_axis',(0.,1.,0.)) ;
#128281 = DIRECTION('ref_axis',(1.,0.,0.)) ;
#128282 = DIRECTION('center_axis',(-1.,0.,0.)) ;
#128283 = DIRECTION('ref_axis',(0.,0.,-1.)) ;
#128284 = DIRECTION('center_axis',(0.,-1.,0.)) ;
#128285 = DIRECTION('ref_axis',(0.,0.,-1.)) ;
#128286 = DIRECTION('center_axis',(0.,-1.,0.)) ;
#128287 = DIRECTION('ref_axis',(0.,0.,-1.)) ;
#128288 = DIRECTION('center_axis',(-1.,0.,0.)) ;
#128289 = DIRECTION('ref_axis',(0.,0.,1.)) ;
#128290 = DIRECTION('center_axis',(-1.,0.,0.)) ;
#128291 = DIRECTION('ref_axis',(0.,0.,1.)) ;
#128292 = DIRECTION('center_axis',(1.,0.,0.)) ;
#128293 = DIRECTION('ref_axis',(0.,0.,-1.)) ;
#128294 = DIRECTION('center_axis',(-1.,0.,0.)) ;
#128295 = DIRECTION('ref_axis',(0.,0.,1.)) ;
#128296 = DIRECTION('center_axis',(0.,-1.,0.)) ;
#128297 = DIRECTION('ref_axis',(0.,0.,-1.)) ;
#128298 = DIRECTION('center_axis',(0.,-1.,0.)) ;
#128299 = DIRECTION('ref_axis',(0.,0.,-1.)) ;
#128300 = DIRECTION('center_axis',(0.,1.,0.)) ;
#128301 = DIRECTION('ref_axis',(1.,0.,0.)) ;
#128302 = DIRECTION('center_axis',(0.,0.,-1.)) ;
#128303 = DIRECTION('ref_axis',(1.,0.,0.)) ;
#128304 = DIRECTION('center_axis',(0.,1.,0.)) ;
#128305 = DIRECTION('ref_axis',(1.,0.,0.)) ;
#128306 = DIRECTION('center_axis',(0.,0.,1.)) ;
#128307 = DIRECTION('ref_axis',(-1.,0.,0.)) ;
#128308 = DIRECTION('center_axis',(0.,0.,-1.)) ;
#128309 = DIRECTION('ref_axis',(-1.,0.,0.)) ;
#128310 = DIRECTION('center_axis',(1.,1.31418445149758E-16,-2.16840434497101E-16)) ;
#128311 = DIRECTION('ref_axis',(-2.16840434497101E-16,-2.8496832747207E-32,
-1.)) ;
#128312 = DIRECTION('center_axis',(1.,0.,0.)) ;
#128313 = DIRECTION('ref_axis',(0.,0.,-1.)) ;
#128314 = DIRECTION('center_axis',(-1.,0.,0.)) ;
#128315 = DIRECTION('ref_axis',(0.,0.,1.)) ;
#128316 = DIRECTION('center_axis',(-1.31418445149758E-16,1.,0.)) ;
#128317 = DIRECTION('ref_axis',(-1.,0.,0.)) ;
#128318 = DIRECTION('center_axis',(0.,0.,1.)) ;
#128319 = DIRECTION('ref_axis',(-1.,0.,0.)) ;
#128320 = DIRECTION('center_axis',(-1.31418445149758E-16,1.,0.)) ;
#128321 = DIRECTION('ref_axis',(-1.,-1.31418445149758E-16,0.)) ;
#128322 = DIRECTION('center_axis',(-1.31418445149758E-16,1.,0.)) ;
#128323 = DIRECTION('ref_axis',(-1.,0.,0.)) ;
#128324 = DIRECTION('center_axis',(-1.31418445149758E-16,1.,0.)) ;
#128325 = DIRECTION('ref_axis',(-1.,-1.31418445149758E-16,0.)) ;
#128326 = DIRECTION('center_axis',(0.,0.,1.)) ;
#128327 = DIRECTION('ref_axis',(-1.,0.,0.)) ;
#128328 = DIRECTION('center_axis',(-4.33680868994202E-16,-5.69936654944139E-32,
-1.)) ;
#128329 = DIRECTION('ref_axis',(-1.,2.47170623787823E-47,4.33680868994202E-16)) ;
#128330 = DIRECTION('center_axis',(0.,0.,1.)) ;
#128331 = DIRECTION('ref_axis',(1.,0.,0.)) ;
#128332 = DIRECTION('center_axis',(-1.31418445149758E-16,-1.,0.)) ;
#128333 = DIRECTION('ref_axis',(1.,-1.31418445149758E-16,0.)) ;
#128334 = DIRECTION('center_axis',(0.,1.,0.)) ;
#128335 = DIRECTION('ref_axis',(0.,0.,1.)) ;
#128336 = DIRECTION('center_axis',(-1.,0.,2.16840434497101E-16)) ;
#128337 = DIRECTION('ref_axis',(2.16840434497101E-16,0.,1.)) ;
#128338 = DIRECTION('center_axis',(-1.,0.,0.)) ;
#128339 = DIRECTION('ref_axis',(0.,0.,1.)) ;
#128340 = DIRECTION('center_axis',(1.,0.,0.)) ;
#128341 = DIRECTION('ref_axis',(0.,0.,-1.)) ;
#128342 = DIRECTION('center_axis',(-1.31418445149758E-16,-1.,0.)) ;
#128343 = DIRECTION('ref_axis',(1.,-1.31418445149758E-16,0.)) ;
#128344 = DIRECTION('center_axis',(0.,1.,0.)) ;
#128345 = DIRECTION('ref_axis',(0.,0.,1.)) ;
#128346 = DIRECTION('center_axis',(2.16840434497101E-16,2.8496832747207E-32,
1.)) ;
#128347 = DIRECTION('ref_axis',(1.,-6.17926559469557E-48,-2.16840434497101E-16)) ;
#128348 = DIRECTION('center_axis',(0.,0.,1.)) ;
#128349 = DIRECTION('ref_axis',(1.,0.,0.)) ;
#128350 = DIRECTION('center_axis',(-1.,-1.31418445149758E-16,-2.16840434497101E-16)) ;
#128351 = DIRECTION('ref_axis',(-2.16840434497101E-16,-2.8496832747207E-32,
1.)) ;
#128352 = DIRECTION('center_axis',(-1.,0.,0.)) ;
#128353 = DIRECTION('ref_axis',(0.,0.,1.)) ;
#128354 = DIRECTION('center_axis',(1.,0.,0.)) ;
#128355 = DIRECTION('ref_axis',(0.,0.,-1.)) ;
#128356 = DIRECTION('center_axis',(-1.31418445149758E-16,1.,0.)) ;
#128357 = DIRECTION('ref_axis',(-1.,0.,0.)) ;
#128358 = DIRECTION('center_axis',(-1.31418445149758E-16,1.,0.)) ;
#128359 = DIRECTION('ref_axis',(-1.,-1.31418445149758E-16,0.)) ;
#128360 = DIRECTION('center_axis',(0.,1.,0.)) ;
#128361 = DIRECTION('ref_axis',(1.,0.,0.)) ;
#128362 = DIRECTION('center_axis',(0.,0.,-1.)) ;
#128363 = DIRECTION('ref_axis',(1.,0.,0.)) ;
#128364 = DIRECTION('center_axis',(0.,1.,0.)) ;
#128365 = DIRECTION('ref_axis',(1.,0.,0.)) ;
#128366 = DIRECTION('center_axis',(0.,0.,-1.)) ;
#128367 = DIRECTION('ref_axis',(1.,0.,0.)) ;
#128368 = DIRECTION('center_axis',(-1.31418445149758E-16,1.,0.)) ;
#128369 = DIRECTION('ref_axis',(-1.,0.,0.)) ;
#128370 = DIRECTION('center_axis',(-1.31418445149758E-16,1.,0.)) ;
#128371 = DIRECTION('ref_axis',(-1.,-1.31418445149758E-16,0.)) ;
#128372 = DIRECTION('center_axis',(-1.31418445149758E-16,-1.,0.)) ;
#128373 = DIRECTION('ref_axis',(1.,-1.31418445149758E-16,0.)) ;
#128374 = DIRECTION('center_axis',(0.,1.,0.)) ;
#128375 = DIRECTION('ref_axis',(0.,0.,1.)) ;
#128376 = DIRECTION('center_axis',(4.33680868994202E-16,0.,1.)) ;
#128377 = DIRECTION('ref_axis',(1.,0.,-4.33680868994202E-16)) ;
#128378 = DIRECTION('center_axis',(0.,0.,-1.)) ;
#128379 = DIRECTION('ref_axis',(-1.,0.,0.)) ;
#128380 = DIRECTION('center_axis',(-2.16840434497101E-16,0.,-1.)) ;
#128381 = DIRECTION('ref_axis',(-1.,0.,2.16840434497101E-16)) ;
#128382 = DIRECTION('center_axis',(0.,0.,-1.)) ;
#128383 = DIRECTION('ref_axis',(-1.,0.,0.)) ;
#128384 = DIRECTION('center_axis',(-1.31418445149758E-16,-1.,0.)) ;
#128385 = DIRECTION('ref_axis',(1.,-1.31418445149758E-16,0.)) ;
#128386 = DIRECTION('center_axis',(0.,1.,0.)) ;
#128387 = DIRECTION('ref_axis',(0.,0.,1.)) ;
#128388 = DIRECTION('center_axis',(0.,1.,0.)) ;
#128389 = DIRECTION('ref_axis',(1.,0.,0.)) ;
#128390 = DIRECTION('center_axis',(-1.,0.,0.)) ;
#128391 = DIRECTION('ref_axis',(0.,0.,-1.)) ;
#128392 = DIRECTION('center_axis',(0.,1.,0.)) ;
#128393 = DIRECTION('ref_axis',(1.,0.,0.)) ;
#128394 = DIRECTION('center_axis',(1.,0.,0.)) ;
#128395 = DIRECTION('ref_axis',(0.,0.,1.)) ;
#128396 = DIRECTION('center_axis',(1.,0.,2.16840434497101E-16)) ;
#128397 = DIRECTION('ref_axis',(2.16840434497101E-16,0.,-1.)) ;
#128398 = DIRECTION('center_axis',(0.,1.,0.)) ;
#128399 = DIRECTION('ref_axis',(0.,0.,1.)) ;
#128400 = DIRECTION('center_axis',(0.,1.,0.)) ;
#128401 = DIRECTION('ref_axis',(0.,0.,1.)) ;
#128402 = DIRECTION('center_axis',(0.,0.,-1.)) ;
#128403 = DIRECTION('ref_axis',(-1.,0.,0.)) ;
#128404 = DIRECTION('center_axis',(0.,0.,1.)) ;
#128405 = DIRECTION('ref_axis',(1.,0.,0.)) ;
#128406 = DIRECTION('center_axis',(0.,0.,-1.)) ;
#128407 = DIRECTION('ref_axis',(-1.,0.,0.)) ;
#128408 = DIRECTION('center_axis',(0.,1.,0.)) ;
#128409 = DIRECTION('ref_axis',(0.,0.,1.)) ;
#128410 = DIRECTION('center_axis',(0.,1.,0.)) ;
#128411 = DIRECTION('ref_axis',(0.,0.,1.)) ;
#128412 = DIRECTION('center_axis',(0.,1.,0.)) ;
#128413 = DIRECTION('ref_axis',(1.,0.,0.)) ;
#128414 = DIRECTION('center_axis',(-1.,0.,0.)) ;
#128415 = DIRECTION('ref_axis',(0.,0.,-1.)) ;
#128416 = DIRECTION('center_axis',(0.,1.,0.)) ;
#128417 = DIRECTION('ref_axis',(1.,0.,0.)) ;
#128418 = DIRECTION('center_axis',(-1.,0.,0.)) ;
#128419 = DIRECTION('ref_axis',(0.,0.,-1.)) ;
#128420 = DIRECTION('center_axis',(0.,1.,0.)) ;
#128421 = DIRECTION('ref_axis',(0.,0.,1.)) ;
#128422 = DIRECTION('center_axis',(0.,1.,0.)) ;
#128423 = DIRECTION('ref_axis',(0.,0.,1.)) ;
#128424 = DIRECTION('center_axis',(-1.,0.,0.)) ;
#128425 = DIRECTION('ref_axis',(0.,0.,1.)) ;
#128426 = DIRECTION('center_axis',(-1.,0.,0.)) ;
#128427 = DIRECTION('ref_axis',(0.,0.,1.)) ;
#128428 = DIRECTION('center_axis',(1.,0.,0.)) ;
#128429 = DIRECTION('ref_axis',(0.,0.,-1.)) ;
#128430 = DIRECTION('center_axis',(-1.,0.,0.)) ;
#128431 = DIRECTION('ref_axis',(0.,0.,1.)) ;
#128432 = DIRECTION('center_axis',(0.,1.,0.)) ;
#128433 = DIRECTION('ref_axis',(0.,0.,1.)) ;
#128434 = DIRECTION('center_axis',(0.,1.,0.)) ;
#128435 = DIRECTION('ref_axis',(0.,0.,1.)) ;
#128436 = DIRECTION('center_axis',(0.,1.,0.)) ;
#128437 = DIRECTION('ref_axis',(1.,0.,0.)) ;
#128438 = DIRECTION('center_axis',(0.,0.,1.)) ;
#128439 = DIRECTION('ref_axis',(-1.,0.,0.)) ;
#128440 = DIRECTION('center_axis',(0.,1.,0.)) ;
#128441 = DIRECTION('ref_axis',(1.,0.,0.)) ;
#128442 = DIRECTION('center_axis',(0.,0.,-1.)) ;
#128443 = DIRECTION('ref_axis',(1.,0.,0.)) ;
#128444 = DIRECTION('center_axis',(0.,0.,1.)) ;
#128445 = DIRECTION('ref_axis',(1.,0.,0.)) ;
#128446 = DIRECTION('center_axis',(0.,0.,1.)) ;
#128447 = DIRECTION('ref_axis',(1.,0.,0.)) ;
#128448 = DIRECTION('center_axis',(0.,0.,-1.)) ;
#128449 = DIRECTION('ref_axis',(-1.,0.,0.)) ;
#128450 = DIRECTION('center_axis',(0.,0.,1.)) ;
#128451 = DIRECTION('ref_axis',(1.,0.,0.)) ;
#128452 = DIRECTION('center_axis',(1.,0.,0.)) ;
#128453 = DIRECTION('ref_axis',(0.,0.,-1.)) ;
#128454 = DIRECTION('center_axis',(1.,0.,0.)) ;
#128455 = DIRECTION('ref_axis',(0.,0.,-1.)) ;
#128456 = DIRECTION('center_axis',(1.,0.,0.)) ;
#128457 = DIRECTION('ref_axis',(0.,0.,-1.)) ;
#128458 = DIRECTION('center_axis',(1.,0.,8.67361737988409E-15)) ;
#128459 = DIRECTION('ref_axis',(8.67361737988409E-15,0.,-1.)) ;
#128460 = DIRECTION('center_axis',(1.,0.,0.)) ;
#128461 = DIRECTION('ref_axis',(0.,0.,-1.)) ;
#128462 = DIRECTION('center_axis',(1.,0.,1.73472347597682E-14)) ;
#128463 = DIRECTION('ref_axis',(1.73472347597682E-14,0.,-1.)) ;
#128464 = DIRECTION('center_axis',(-1.,0.,0.)) ;
#128465 = DIRECTION('ref_axis',(0.,0.,1.)) ;
#128466 = DIRECTION('center_axis',(1.,0.,0.)) ;
#128467 = DIRECTION('ref_axis',(0.,0.,-1.)) ;
#128468 = DIRECTION('center_axis',(1.,0.,0.)) ;
#128469 = DIRECTION('ref_axis',(0.,0.,-1.)) ;
#128470 = DIRECTION('center_axis',(0.,0.,-1.)) ;
#128471 = DIRECTION('ref_axis',(-1.,0.,0.)) ;
#128472 = DIRECTION('center_axis',(1.,0.,0.)) ;
#128473 = DIRECTION('ref_axis',(0.,0.,-1.)) ;
#128474 = DIRECTION('center_axis',(0.,0.,1.)) ;
#128475 = DIRECTION('ref_axis',(1.,0.,0.)) ;
#128476 = DIRECTION('center_axis',(0.,0.,-1.)) ;
#128477 = DIRECTION('ref_axis',(-1.,0.,0.)) ;
#128478 = DIRECTION('center_axis',(-0.422618261740697,5.55398348498559E-17,
0.906307787036651)) ;
#128479 = DIRECTION('ref_axis',(0.906307787036651,-2.19407316623673E-31,0.422618261740697)) ;
#128480 = DIRECTION('center_axis',(0.422618261740697,-5.55398348498559E-17,
-0.906307787036651)) ;
#128481 = DIRECTION('ref_axis',(-0.906307787036651,2.28174878574772E-31,-0.422618261740697)) ;
#128482 = DIRECTION('center_axis',(-0.422618261740697,5.55398348498559E-17,
0.906307787036651)) ;
#128483 = DIRECTION('ref_axis',(0.906307787036651,-2.28174878574772E-31,0.422618261740697)) ;
#128484 = DIRECTION('center_axis',(0.422618261740697,-5.55398348498559E-17,
-0.906307787036651)) ;
#128485 = DIRECTION('ref_axis',(-0.906307787036651,2.28174878574772E-31,-0.422618261740697)) ;
#128486 = DIRECTION('center_axis',(0.,1.,0.)) ;
#128487 = DIRECTION('ref_axis',(1.,0.,0.)) ;
#128488 = DIRECTION('center_axis',(3.64461297742727E-14,0.514231796959095,
-0.857651245551606)) ;
#128489 = DIRECTION('ref_axis',(3.46944695195362E-14,-0.857651245551606,-0.514231796959095)) ;
#128490 = DIRECTION('center_axis',(0.,-1.73472347597681E-14,1.)) ;
#128491 = DIRECTION('ref_axis',(0.,1.,1.73472347597681E-14)) ;
#128492 = DIRECTION('center_axis',(-1.,0.,0.)) ;
#128493 = DIRECTION('ref_axis',(0.,-8.67361737988409E-15,-1.)) ;
#128494 = DIRECTION('center_axis',(0.,0.,1.)) ;
#128495 = DIRECTION('ref_axis',(1.,0.,0.)) ;
#128496 = DIRECTION('center_axis',(0.,0.,1.)) ;
#128497 = DIRECTION('ref_axis',(1.,0.,0.)) ;
#128498 = DIRECTION('center_axis',(-1.,0.,0.)) ;
#128499 = DIRECTION('ref_axis',(0.,0.,1.)) ;
#128500 = DIRECTION('center_axis',(-1.,0.,0.)) ;
#128501 = DIRECTION('ref_axis',(0.,-8.67361737988409E-15,-1.)) ;
#128502 = DIRECTION('center_axis',(1.,0.,0.)) ;
#128503 = DIRECTION('ref_axis',(0.,0.,-1.)) ;
#128504 = DIRECTION('center_axis',(0.,-0.514231796959124,-0.857651245551588)) ;
#128505 = DIRECTION('ref_axis',(0.,0.857651245551588,-0.514231796959124)) ;
#128506 = DIRECTION('center_axis',(0.,1.,8.97270763436279E-17)) ;
#128507 = DIRECTION('ref_axis',(0.,-8.97270763436279E-17,1.)) ;
#128508 = DIRECTION('center_axis',(0.,-1.,-8.97270763436279E-17)) ;
#128509 = DIRECTION('ref_axis',(0.,-8.97270763436279E-17,1.)) ;
#128510 = DIRECTION('center_axis',(0.,-1.,0.)) ;
#128511 = DIRECTION('ref_axis',(0.,0.,-1.)) ;
#128512 = DIRECTION('center_axis',(0.,1.,0.)) ;
#128513 = DIRECTION('ref_axis',(1.,0.,0.)) ;
#128514 = DIRECTION('center_axis',(-1.,0.,0.)) ;
#128515 = DIRECTION('ref_axis',(0.,0.,-1.)) ;
#128516 = DIRECTION('center_axis',(1.,0.,0.)) ;
#128517 = DIRECTION('ref_axis',(0.,0.,-1.)) ;
#128518 = DIRECTION('center_axis',(0.,-0.514231796959095,0.857651245551606)) ;
#128519 = DIRECTION('ref_axis',(0.,0.857651245551606,0.514231796959095)) ;
#128520 = DIRECTION('center_axis',(0.,0.,-1.)) ;
#128521 = DIRECTION('ref_axis',(1.,0.,0.)) ;
#128522 = DIRECTION('center_axis',(0.,1.,0.)) ;
#128523 = DIRECTION('ref_axis',(1.,0.,0.)) ;
#128524 = DIRECTION('center_axis',(-3.46944695195364E-14,0.,-1.)) ;
#128525 = DIRECTION('ref_axis',(1.,0.,-3.46944695195364E-14)) ;
#128526 = DIRECTION('center_axis',(-1.,0.,0.)) ;
#128527 = DIRECTION('ref_axis',(0.,4.33680868994204E-15,-1.)) ;
#128528 = DIRECTION('center_axis',(0.,0.,-1.)) ;
#128529 = DIRECTION('ref_axis',(-1.,0.,0.)) ;
#128530 = DIRECTION('center_axis',(0.,0.,1.)) ;
#128531 = DIRECTION('ref_axis',(-1.,0.,0.)) ;
#128532 = DIRECTION('center_axis',(0.,0.,-1.)) ;
#128533 = DIRECTION('ref_axis',(-1.,0.,0.)) ;
#128534 = DIRECTION('center_axis',(-1.,0.,7.01133629567814E-33)) ;
#128535 = DIRECTION('ref_axis',(7.01133629567814E-33,0.,1.)) ;
#128536 = DIRECTION('center_axis',(-1.,0.,0.)) ;
#128537 = DIRECTION('ref_axis',(0.,0.,1.)) ;
#128538 = DIRECTION('center_axis',(0.,0.,-1.)) ;
#128539 = DIRECTION('ref_axis',(-1.,0.,0.)) ;
#128540 = DIRECTION('center_axis',(-7.01133629567814E-33,8.97270763436279E-17,
-1.)) ;
#128541 = DIRECTION('ref_axis',(6.29106707073161E-49,1.,8.97270763436279E-17)) ;
#128542 = DIRECTION('center_axis',(1.,0.,0.)) ;
#128543 = DIRECTION('ref_axis',(0.,0.,-1.)) ;
#128544 = DIRECTION('center_axis',(-2.2301249256967E-15,0.514231796959095,
0.857651245551606)) ;
#128545 = DIRECTION('ref_axis',(-4.79361507851841E-30,-0.857651245551606,
0.514231796959095)) ;
#128546 = DIRECTION('center_axis',(-1.,0.,0.)) ;
#128547 = DIRECTION('ref_axis',(0.,0.,1.)) ;
#128548 = DIRECTION('center_axis',(-1.,0.,0.)) ;
#128549 = DIRECTION('ref_axis',(0.,-4.33680868994204E-15,-1.)) ;
#128550 = DIRECTION('center_axis',(0.,0.,1.)) ;
#128551 = DIRECTION('ref_axis',(1.,0.,0.)) ;
#128552 = DIRECTION('center_axis',(0.,0.,-1.)) ;
#128553 = DIRECTION('ref_axis',(-1.,0.,0.)) ;
#128554 = DIRECTION('center_axis',(0.,-1.,8.97270763436279E-17)) ;
#128555 = DIRECTION('ref_axis',(0.,-8.97270763436279E-17,-1.)) ;
#128556 = DIRECTION('center_axis',(0.,-1.,8.97270763436279E-17)) ;
#128557 = DIRECTION('ref_axis',(0.,-8.97270763436279E-17,-1.)) ;
#128558 = DIRECTION('center_axis',(0.,-1.,0.)) ;
#128559 = DIRECTION('ref_axis',(0.,0.,-1.)) ;
#128560 = DIRECTION('center_axis',(-7.01133629567814E-33,8.97270763436279E-17,
-1.)) ;
#128561 = DIRECTION('ref_axis',(0.,1.,0.)) ;
#128562 = DIRECTION('center_axis',(0.,-1.,0.)) ;
#128563 = DIRECTION('ref_axis',(0.,0.,1.)) ;
#128564 = DIRECTION('center_axis',(1.,0.,0.)) ;
#128565 = DIRECTION('ref_axis',(0.,0.,-1.)) ;
#128566 = DIRECTION('center_axis',(0.,0.,1.)) ;
#128567 = DIRECTION('ref_axis',(-1.,0.,0.)) ;
#128568 = DIRECTION('center_axis',(0.,1.,0.)) ;
#128569 = DIRECTION('ref_axis',(1.,0.,0.)) ;
#128570 = DIRECTION('center_axis',(-1.,0.,0.)) ;
#128571 = DIRECTION('ref_axis',(0.,0.,-1.)) ;
#128572 = DIRECTION('center_axis',(1.,7.81406971160724E-17,0.)) ;
#128573 = DIRECTION('ref_axis',(-7.81406971160724E-17,1.,0.)) ;
#128574 = DIRECTION('center_axis',(1.,0.,0.)) ;
#128575 = DIRECTION('ref_axis',(0.,0.,-1.)) ;
#128576 = DIRECTION('center_axis',(1.,0.,0.)) ;
#128577 = DIRECTION('ref_axis',(0.,0.,-1.)) ;
#128578 = DIRECTION('center_axis',(0.,1.,8.97270763436279E-17)) ;
#128579 = DIRECTION('ref_axis',(0.,-8.97270763436279E-17,1.)) ;
#128580 = DIRECTION('center_axis',(0.,-1.,0.)) ;
#128581 = DIRECTION('ref_axis',(0.,0.,-1.)) ;
#128582 = DIRECTION('center_axis',(0.,0.,-1.)) ;
#128583 = DIRECTION('ref_axis',(-1.,0.,0.)) ;
#128584 = DIRECTION('center_axis',(-7.01133629567814E-33,8.97270763436279E-17,
1.)) ;
#128585 = DIRECTION('ref_axis',(-6.29106707073161E-49,-1.,8.97270763436279E-17)) ;
#128586 = DIRECTION('center_axis',(-1.,0.,-7.01133629567814E-33)) ;
#128587 = DIRECTION('ref_axis',(-7.01133629567814E-33,0.,1.)) ;
#128588 = DIRECTION('center_axis',(-1.,0.,0.)) ;
#128589 = DIRECTION('ref_axis',(0.,0.,1.)) ;
#128590 = DIRECTION('center_axis',(1.,0.,0.)) ;
#128591 = DIRECTION('ref_axis',(0.,1.,0.)) ;
#128592 = DIRECTION('center_axis',(0.,1.,0.)) ;
#128593 = DIRECTION('ref_axis',(0.,0.,1.)) ;
#128594 = DIRECTION('center_axis',(0.,1.,0.)) ;
#128595 = DIRECTION('ref_axis',(1.,0.,0.)) ;
#128596 = DIRECTION('center_axis',(0.,0.,-1.)) ;
#128597 = DIRECTION('ref_axis',(1.,0.,0.)) ;
#128598 = DIRECTION('center_axis',(-1.,0.,0.)) ;
#128599 = DIRECTION('ref_axis',(0.,0.,-1.)) ;
#128600 = DIRECTION('center_axis',(-7.01133629567814E-33,8.97270763436279E-17,
1.)) ;
#128601 = DIRECTION('ref_axis',(0.,-1.,0.)) ;
#128602 = DIRECTION('center_axis',(0.,-1.,0.)) ;
#128603 = DIRECTION('ref_axis',(0.,0.,1.)) ;
#128604 = DIRECTION('center_axis',(7.81406971160724E-17,-1.,-8.97270763436279E-17)) ;
#128605 = DIRECTION('ref_axis',(-7.01133629567814E-33,8.97270763436279E-17,
-1.)) ;
#128606 = DIRECTION('center_axis',(0.,1.,0.)) ;
#128607 = DIRECTION('ref_axis',(0.,0.,1.)) ;
#128608 = DIRECTION('center_axis',(-1.,-7.81406971160724E-17,0.)) ;
#128609 = DIRECTION('ref_axis',(7.81406971160724E-17,-1.,0.)) ;
#128610 = DIRECTION('center_axis',(-1.,-7.81406971160724E-17,0.)) ;
#128611 = DIRECTION('ref_axis',(-7.81406971160724E-17,1.,0.)) ;
#128612 = DIRECTION('center_axis',(0.,0.,1.)) ;
#128613 = DIRECTION('ref_axis',(1.,0.,0.)) ;
#128614 = DIRECTION('center_axis',(0.,0.,-1.)) ;
#128615 = DIRECTION('ref_axis',(-1.,0.,0.)) ;
#128616 = DIRECTION('center_axis',(0.,-1.,8.97270763436279E-17)) ;
#128617 = DIRECTION('ref_axis',(0.,-8.97270763436279E-17,-1.)) ;
#128618 = DIRECTION('center_axis',(0.,-1.,0.)) ;
#128619 = DIRECTION('ref_axis',(0.,0.,-1.)) ;
#128620 = DIRECTION('center_axis',(1.,7.81406971160724E-17,0.)) ;
#128621 = DIRECTION('ref_axis',(0.,1.,0.)) ;
#128622 = DIRECTION('center_axis',(0.,0.,1.)) ;
#128623 = DIRECTION('ref_axis',(-1.,0.,0.)) ;
#128624 = DIRECTION('center_axis',(0.,1.,0.)) ;
#128625 = DIRECTION('ref_axis',(1.,0.,0.)) ;
#128626 = DIRECTION('center_axis',(-1.,0.,0.)) ;
#128627 = DIRECTION('ref_axis',(0.,0.,-1.)) ;
#128628 = DIRECTION('center_axis',(0.,0.,-1.)) ;
#128629 = DIRECTION('ref_axis',(-1.,0.,0.)) ;
#128630 = DIRECTION('center_axis',(0.,0.,1.)) ;
#128631 = DIRECTION('ref_axis',(1.,0.,0.)) ;
#128632 = DIRECTION('center_axis',(-1.,-7.81406971160724E-17,0.)) ;
#128633 = DIRECTION('ref_axis',(7.81406971160724E-17,-1.,0.)) ;
#128634 = DIRECTION('center_axis',(-1.,-7.81406971160724E-17,0.)) ;
#128635 = DIRECTION('ref_axis',(-7.81406971160724E-17,1.,0.)) ;
#128636 = DIRECTION('center_axis',(1.,7.81406971160724E-17,0.)) ;
#128637 = DIRECTION('ref_axis',(-7.81406971160724E-17,1.,0.)) ;
#128638 = DIRECTION('center_axis',(1.,0.,0.)) ;
#128639 = DIRECTION('ref_axis',(0.,0.,-1.)) ;
#128640 = DIRECTION('center_axis',(1.,0.,0.)) ;
#128641 = DIRECTION('ref_axis',(0.,0.,-1.)) ;
#128642 = DIRECTION('center_axis',(3.78638272950961E-32,-4.8455963016112E-16,
-1.)) ;
#128643 = DIRECTION('ref_axis',(1.83472821505963E-47,1.,-4.8455963016112E-16)) ;
#128644 = DIRECTION('center_axis',(3.78638272950961E-32,-4.8455963016112E-16,
-1.)) ;
#128645 = DIRECTION('ref_axis',(1.83472821505963E-47,1.,-4.8455963016112E-16)) ;
#128646 = DIRECTION('center_axis',(0.,0.,-1.)) ;
#128647 = DIRECTION('ref_axis',(-1.,0.,0.)) ;
#128648 = DIRECTION('center_axis',(1.,7.81406971160724E-17,0.)) ;
#128649 = DIRECTION('ref_axis',(0.,1.,0.)) ;
#128650 = DIRECTION('center_axis',(0.,-1.,0.)) ;
#128651 = DIRECTION('ref_axis',(0.,0.,1.)) ;
#128652 = DIRECTION('center_axis',(0.,1.,0.)) ;
#128653 = DIRECTION('ref_axis',(1.,0.,0.)) ;
#128654 = DIRECTION('center_axis',(0.,1.,0.)) ;
#128655 = DIRECTION('ref_axis',(0.,0.,-1.)) ;
#128656 = DIRECTION('center_axis',(-7.81406971160724E-17,1.,-8.97270763436279E-17)) ;
#128657 = DIRECTION('ref_axis',(-7.01133629567814E-33,8.97270763436279E-17,
1.)) ;
#128658 = DIRECTION('center_axis',(0.,-1.,0.)) ;
#128659 = DIRECTION('ref_axis',(0.,0.,-1.)) ;
#128660 = DIRECTION('center_axis',(0.,1.,0.)) ;
#128661 = DIRECTION('ref_axis',(0.,0.,1.)) ;
#128662 = DIRECTION('center_axis',(0.,-1.,0.)) ;
#128663 = DIRECTION('ref_axis',(0.,0.,-1.)) ;
#128664 = DIRECTION('center_axis',(0.,-1.,0.)) ;
#128665 = DIRECTION('ref_axis',(0.,0.,-1.)) ;
#128666 = DIRECTION('center_axis',(0.,1.,0.)) ;
#128667 = DIRECTION('ref_axis',(1.,0.,0.)) ;
#128668 = DIRECTION('center_axis',(0.,0.,1.)) ;
#128669 = DIRECTION('ref_axis',(-1.,0.,0.)) ;
#128670 = DIRECTION('center_axis',(1.,0.,0.)) ;
#128671 = DIRECTION('ref_axis',(0.,0.,1.)) ;
#128672 = DIRECTION('center_axis',(0.,-1.,0.)) ;
#128673 = DIRECTION('ref_axis',(0.,0.,-1.)) ;
#128674 = DIRECTION('center_axis',(0.,1.,0.)) ;
#128675 = DIRECTION('ref_axis',(0.,0.,1.)) ;
#128676 = DIRECTION('center_axis',(0.,-1.,0.)) ;
#128677 = DIRECTION('ref_axis',(0.,0.,-1.)) ;
#128678 = DIRECTION('center_axis',(-1.,0.,2.16840434497101E-16)) ;
#128679 = DIRECTION('ref_axis',(2.16840434497101E-16,0.,1.)) ;
#128680 = DIRECTION('center_axis',(1.,0.,0.)) ;
#128681 = DIRECTION('ref_axis',(0.,0.,-1.)) ;
#128682 = DIRECTION('center_axis',(-2.16840434497101E-16,0.,1.)) ;
#128683 = DIRECTION('ref_axis',(1.,0.,2.16840434497101E-16)) ;
#128684 = DIRECTION('center_axis',(0.,0.,1.)) ;
#128685 = DIRECTION('ref_axis',(1.,0.,0.)) ;
#128686 = DIRECTION('center_axis',(0.,1.,0.)) ;
#128687 = DIRECTION('ref_axis',(0.,0.,1.)) ;
#128688 = DIRECTION('center_axis',(0.,-1.,0.)) ;
#128689 = DIRECTION('ref_axis',(0.,0.,-1.)) ;
#128690 = DIRECTION('center_axis',(0.,1.,0.)) ;
#128691 = DIRECTION('ref_axis',(1.,0.,0.)) ;
#128692 = DIRECTION('center_axis',(0.,0.,1.)) ;
#128693 = DIRECTION('ref_axis',(-1.,0.,0.)) ;
#128694 = DIRECTION('center_axis',(0.,1.,0.)) ;
#128695 = DIRECTION('ref_axis',(1.,0.,0.)) ;
#128696 = DIRECTION('center_axis',(1.,0.,0.)) ;
#128697 = DIRECTION('ref_axis',(0.,0.,1.)) ;
#128698 = DIRECTION('center_axis',(0.,0.,-1.)) ;
#128699 = DIRECTION('ref_axis',(-1.,0.,0.)) ;
#128700 = DIRECTION('center_axis',(0.,0.,1.)) ;
#128701 = DIRECTION('ref_axis',(1.,0.,0.)) ;
#128702 = DIRECTION('center_axis',(1.,0.,2.16840434497101E-16)) ;
#128703 = DIRECTION('ref_axis',(2.16840434497101E-16,0.,-1.)) ;
#128704 = DIRECTION('center_axis',(1.,0.,0.)) ;
#128705 = DIRECTION('ref_axis',(0.,0.,-1.)) ;
#128706 = DIRECTION('center_axis',(0.,1.,0.)) ;
#128707 = DIRECTION('ref_axis',(1.,0.,0.)) ;
#128708 = DIRECTION('center_axis',(0.,1.,0.)) ;
#128709 = DIRECTION('ref_axis',(0.,0.,-1.)) ;
#128710 = DIRECTION('center_axis',(0.,1.,0.)) ;
#128711 = DIRECTION('ref_axis',(0.,0.,1.)) ;
#128712 = DIRECTION('center_axis',(0.,1.,0.)) ;
#128713 = DIRECTION('ref_axis',(0.,0.,1.)) ;
#128714 = DIRECTION('center_axis',(-0.942809041582063,-0.235702260395516,
0.235702260395518)) ;
#128715 = DIRECTION('ref_axis',(0.242535625036335,4.64743530723282E-16,0.970142500145331)) ;
#128716 = DIRECTION('center_axis',(-0.970142500145332,-0.242535625036331,
-2.10366121255613E-15)) ;
#128717 = DIRECTION('ref_axis',(0.242535625036331,-0.970142500145332,-4.48415458566342E-30)) ;
#128718 = DIRECTION('center_axis',(0.970142500145333,0.24253562503633,0.)) ;
#128719 = DIRECTION('ref_axis',(-0.24253562503633,0.970142500145333,0.)) ;
#128720 = DIRECTION('center_axis',(-0.970142500145332,-0.242535625036331,
-8.41464485022476E-15)) ;
#128721 = DIRECTION('ref_axis',(0.242535625036331,-0.970142500145332,-1.80900724878918E-29)) ;
#128722 = DIRECTION('center_axis',(0.879462917689188,0.219865729422294,-0.42214220049081)) ;
#128723 = DIRECTION('ref_axis',(-0.432731067584771,1.71515946658E-16,-0.901523057468274)) ;
#128724 = DIRECTION('center_axis',(0.879462917689185,0.219865729422304,-0.42214220049081)) ;
#128725 = DIRECTION('ref_axis',(-0.432731067584772,-1.04304727837597E-16,
-0.901523057468273)) ;
#128726 = DIRECTION('center_axis',(0.,1.,0.)) ;
#128727 = DIRECTION('ref_axis',(1.,0.,0.)) ;
#128728 = DIRECTION('center_axis',(-2.00438979995004E-14,-1.,0.)) ;
#128729 = DIRECTION('ref_axis',(-1.,2.00438979995004E-14,0.)) ;
#128730 = DIRECTION('center_axis',(0.,-1.,0.)) ;
#128731 = DIRECTION('ref_axis',(0.,0.,-1.)) ;
#128732 = DIRECTION('center_axis',(-4.51750905202295E-15,-1.,2.16840434497102E-15)) ;
#128733 = DIRECTION('ref_axis',(1.,-4.51750905202295E-15,3.91831450274151E-31)) ;
#128734 = DIRECTION('center_axis',(0.669589480006976,-0.669589480006974,-0.321402950403349)) ;
#128735 = DIRECTION('ref_axis',(0.707106781186547,0.707106781186548,5.45170614306381E-16)) ;
#128736 = DIRECTION('center_axis',(0.669589480006966,-0.669589480006966,-0.321402950403388)) ;
#128737 = DIRECTION('ref_axis',(0.707106781186547,0.707106781186547,-1.18959821530046E-17)) ;
#128738 = DIRECTION('center_axis',(0.,1.,0.)) ;
#128739 = DIRECTION('ref_axis',(1.,0.,0.)) ;
#128740 = DIRECTION('center_axis',(0.707106781186576,-0.707106781186519,0.)) ;
#128741 = DIRECTION('ref_axis',(-0.707106781186519,-0.707106781186576,0.)) ;
#128742 = DIRECTION('center_axis',(0.707106781186549,-0.707106781186546,0.)) ;
#128743 = DIRECTION('ref_axis',(0.707106781186546,0.707106781186549,0.)) ;
#128744 = DIRECTION('center_axis',(0.707106781186548,-0.707106781186548,-1.53329341668338E-15)) ;
#128745 = DIRECTION('ref_axis',(0.707106781186548,0.707106781186548,1.5356898865553E-31)) ;
#128746 = DIRECTION('center_axis',(0.577350269189622,-0.577350269189622,-0.577350269189634)) ;
#128747 = DIRECTION('ref_axis',(-0.707106781186554,1.85551679542784E-15,-0.707106781186541)) ;
#128748 = DIRECTION('center_axis',(-0.577350269189329,0.577350269189586,-0.577350269189963)) ;
#128749 = DIRECTION('ref_axis',(-2.5143735500355E-15,0.707106781186777,0.707106781186318)) ;
#128750 = DIRECTION('center_axis',(-0.707106781186548,0.707106781186548,7.66646708341692E-15)) ;
#128751 = DIRECTION('ref_axis',(-0.707106781186548,-0.707106781186548,-2.68297081166629E-31)) ;
#128752 = DIRECTION('center_axis',(-0.707106781186549,0.707106781186546,0.)) ;
#128753 = DIRECTION('ref_axis',(-0.707106781186546,-0.707106781186549,0.)) ;
#128754 = DIRECTION('center_axis',(-0.707106781186548,0.707106781186548,-1.22663473334671E-14)) ;
#128755 = DIRECTION('ref_axis',(-0.707106781186548,-0.707106781186548,2.94725045705944E-31)) ;
#128756 = DIRECTION('center_axis',(-0.669589480006976,0.669589480006974,-0.321402950403349)) ;
#128757 = DIRECTION('ref_axis',(-0.707106781186547,-0.707106781186548,5.45170614306381E-16)) ;
#128758 = DIRECTION('center_axis',(0.669589480006982,-0.669589480006966,0.321402950403353)) ;
#128759 = DIRECTION('ref_axis',(0.707106781186539,0.707106781186556,5.77426876420606E-17)) ;
#128760 = DIRECTION('center_axis',(0.,1.,0.)) ;
#128761 = DIRECTION('ref_axis',(1.,0.,0.)) ;
#128762 = DIRECTION('center_axis',(0.,1.,0.)) ;
#128763 = DIRECTION('ref_axis',(0.,0.,-1.)) ;
#128764 = DIRECTION('center_axis',(0.,-1.,0.)) ;
#128765 = DIRECTION('ref_axis',(0.,0.,-1.)) ;
#128766 = DIRECTION('center_axis',(0.,1.,0.)) ;
#128767 = DIRECTION('ref_axis',(0.,0.,1.)) ;
#128768 = DIRECTION('center_axis',(-0.879462917689188,-0.219865729422294,
-0.42214220049081)) ;
#128769 = DIRECTION('ref_axis',(-0.432731067584771,1.71515946658E-16,0.901523057468274)) ;
#128770 = DIRECTION('center_axis',(0.879462917689201,0.219865729422298,0.42214220049078)) ;
#128771 = DIRECTION('ref_axis',(0.432731067584741,5.42470486237819E-16,-0.901523057468288)) ;
#128772 = DIRECTION('center_axis',(0.,1.,0.)) ;
#128773 = DIRECTION('ref_axis',(1.,0.,0.)) ;
#128774 = DIRECTION('center_axis',(0.970142500145323,0.242535625036368,0.)) ;
#128775 = DIRECTION('ref_axis',(0.242535625036368,-0.970142500145323,0.)) ;
#128776 = DIRECTION('center_axis',(-0.970142500145333,-0.24253562503633,0.)) ;
#128777 = DIRECTION('ref_axis',(0.24253562503633,-0.970142500145333,0.)) ;
#128778 = DIRECTION('center_axis',(0.970142500145332,0.242535625036331,-2.10366121255617E-15)) ;
#128779 = DIRECTION('ref_axis',(-0.242535625036331,0.970142500145332,-4.47980524894761E-30)) ;
#128780 = DIRECTION('center_axis',(0.942809041582064,0.235702260395514,0.235702260395514)) ;
#128781 = DIRECTION('ref_axis',(-0.242535625036331,0.970142500145332,4.49011373492972E-16)) ;
#128782 = DIRECTION('center_axis',(0.,-1.,0.)) ;
#128783 = DIRECTION('ref_axis',(0.,0.,-1.)) ;
#128784 = DIRECTION('center_axis',(-1.,0.,-8.67361737988409E-15)) ;
#128785 = DIRECTION('ref_axis',(-8.67361737988409E-15,0.,1.)) ;
#128786 = DIRECTION('center_axis',(0.,0.,-1.)) ;
#128787 = DIRECTION('ref_axis',(-1.,0.,0.)) ;
#128788 = DIRECTION('center_axis',(0.,0.,-1.)) ;
#128789 = DIRECTION('ref_axis',(-1.,0.,0.)) ;
#128790 = DIRECTION('center_axis',(0.,0.,-1.)) ;
#128791 = DIRECTION('ref_axis',(-1.,0.,0.)) ;
#128792 = DIRECTION('center_axis',(1.,0.,0.)) ;
#128793 = DIRECTION('ref_axis',(0.,0.,-1.)) ;
#128794 = DIRECTION('center_axis',(-1.,0.,0.)) ;
#128795 = DIRECTION('ref_axis',(0.,0.,1.)) ;
#128796 = DIRECTION('center_axis',(0.,-1.,0.)) ;
#128797 = DIRECTION('ref_axis',(0.,0.,-1.)) ;
#128798 = DIRECTION('center_axis',(-1.,0.,0.)) ;
#128799 = DIRECTION('ref_axis',(0.,0.,1.)) ;
#128800 = DIRECTION('center_axis',(0.,-1.,0.)) ;
#128801 = DIRECTION('ref_axis',(0.,0.,-1.)) ;
#128802 = DIRECTION('center_axis',(0.,0.,-1.)) ;
#128803 = DIRECTION('ref_axis',(-1.,0.,0.)) ;
#128804 = DIRECTION('center_axis',(-1.,0.,0.)) ;
#128805 = DIRECTION('ref_axis',(0.,0.,1.)) ;
#128806 = DIRECTION('center_axis',(-1.,1.73472347597681E-14,0.)) ;
#128807 = DIRECTION('ref_axis',(-1.73472347597681E-14,-1.,0.)) ;
#128808 = DIRECTION('center_axis',(0.,0.,1.)) ;
#128809 = DIRECTION('ref_axis',(1.,0.,0.)) ;
#128810 = DIRECTION('center_axis',(0.,0.,-1.)) ;
#128811 = DIRECTION('ref_axis',(-1.,0.,0.)) ;
#128812 = DIRECTION('center_axis',(0.,-1.,0.)) ;
#128813 = DIRECTION('ref_axis',(0.,0.,-1.)) ;
#128814 = DIRECTION('center_axis',(0.,-1.,0.)) ;
#128815 = DIRECTION('ref_axis',(0.,0.,-1.)) ;
#128816 = DIRECTION('center_axis',(0.,-1.,0.)) ;
#128817 = DIRECTION('ref_axis',(0.,0.,-1.)) ;
#128818 = DIRECTION('center_axis',(0.,0.,1.)) ;
#128819 = DIRECTION('ref_axis',(1.,0.,0.)) ;
#128820 = DIRECTION('center_axis',(0.,0.,-1.)) ;
#128821 = DIRECTION('ref_axis',(-1.,0.,0.)) ;
#128822 = DIRECTION('center_axis',(0.,0.,1.)) ;
#128823 = DIRECTION('ref_axis',(1.,0.,0.)) ;
#128824 = DIRECTION('center_axis',(0.,-1.,0.)) ;
#128825 = DIRECTION('ref_axis',(0.,0.,-1.)) ;
#128826 = DIRECTION('center_axis',(0.,-1.,0.)) ;
#128827 = DIRECTION('ref_axis',(0.,0.,-1.)) ;
#128828 = DIRECTION('center_axis',(0.,1.,0.)) ;
#128829 = DIRECTION('ref_axis',(1.,0.,0.)) ;
#128830 = DIRECTION('center_axis',(-1.,0.,0.)) ;
#128831 = DIRECTION('ref_axis',(0.,0.,-1.)) ;
#128832 = DIRECTION('center_axis',(0.,1.,0.)) ;
#128833 = DIRECTION('ref_axis',(1.,0.,0.)) ;
#128834 = DIRECTION('center_axis',(-1.,0.,0.)) ;
#128835 = DIRECTION('ref_axis',(0.,0.,-1.)) ;
#128836 = DIRECTION('center_axis',(0.,-1.,0.)) ;
#128837 = DIRECTION('ref_axis',(0.,0.,-1.)) ;
#128838 = DIRECTION('center_axis',(0.,-1.,0.)) ;
#128839 = DIRECTION('ref_axis',(0.,0.,-1.)) ;
#128840 = DIRECTION('center_axis',(-1.,0.,0.)) ;
#128841 = DIRECTION('ref_axis',(0.,0.,1.)) ;
#128842 = DIRECTION('center_axis',(-1.,0.,0.)) ;
#128843 = DIRECTION('ref_axis',(0.,0.,1.)) ;
#128844 = DIRECTION('center_axis',(1.,0.,0.)) ;
#128845 = DIRECTION('ref_axis',(0.,0.,-1.)) ;
#128846 = DIRECTION('center_axis',(-1.,0.,0.)) ;
#128847 = DIRECTION('ref_axis',(0.,0.,1.)) ;
#128848 = DIRECTION('center_axis',(0.,-1.,0.)) ;
#128849 = DIRECTION('ref_axis',(0.,0.,-1.)) ;
#128850 = DIRECTION('center_axis',(0.,-1.,0.)) ;
#128851 = DIRECTION('ref_axis',(0.,0.,-1.)) ;
#128852 = DIRECTION('center_axis',(0.,1.,0.)) ;
#128853 = DIRECTION('ref_axis',(1.,0.,0.)) ;
#128854 = DIRECTION('center_axis',(0.,0.,-1.)) ;
#128855 = DIRECTION('ref_axis',(1.,0.,0.)) ;
#128856 = DIRECTION('center_axis',(0.,1.,0.)) ;
#128857 = DIRECTION('ref_axis',(1.,0.,0.)) ;
#128858 = DIRECTION('center_axis',(0.,0.,1.)) ;
#128859 = DIRECTION('ref_axis',(-1.,0.,0.)) ;
#128860 = DIRECTION('center_axis',(0.,0.,-1.)) ;
#128861 = DIRECTION('ref_axis',(-1.,0.,0.)) ;
#128862 = DIRECTION('center_axis',(1.,1.31418445149758E-16,-2.16840434497101E-16)) ;
#128863 = DIRECTION('ref_axis',(-2.16840434497101E-16,-2.8496832747207E-32,
-1.)) ;
#128864 = DIRECTION('center_axis',(1.,0.,0.)) ;
#128865 = DIRECTION('ref_axis',(0.,0.,-1.)) ;
#128866 = DIRECTION('center_axis',(-1.,0.,0.)) ;
#128867 = DIRECTION('ref_axis',(0.,0.,1.)) ;
#128868 = DIRECTION('center_axis',(-1.31418445149758E-16,1.,0.)) ;
#128869 = DIRECTION('ref_axis',(-1.,0.,0.)) ;
#128870 = DIRECTION('center_axis',(0.,0.,1.)) ;
#128871 = DIRECTION('ref_axis',(-1.,0.,0.)) ;
#128872 = DIRECTION('center_axis',(-1.31418445149758E-16,1.,0.)) ;
#128873 = DIRECTION('ref_axis',(-1.,-1.31418445149758E-16,0.)) ;
#128874 = DIRECTION('center_axis',(-1.31418445149758E-16,1.,0.)) ;
#128875 = DIRECTION('ref_axis',(-1.,0.,0.)) ;
#128876 = DIRECTION('center_axis',(-1.31418445149758E-16,1.,0.)) ;
#128877 = DIRECTION('ref_axis',(-1.,-1.31418445149758E-16,0.)) ;
#128878 = DIRECTION('center_axis',(0.,0.,1.)) ;
#128879 = DIRECTION('ref_axis',(-1.,0.,0.)) ;
#128880 = DIRECTION('center_axis',(-4.33680868994202E-16,-5.69936654944139E-32,
-1.)) ;
#128881 = DIRECTION('ref_axis',(-1.,2.47170623787823E-47,4.33680868994202E-16)) ;
#128882 = DIRECTION('center_axis',(0.,0.,1.)) ;
#128883 = DIRECTION('ref_axis',(1.,0.,0.)) ;
#128884 = DIRECTION('center_axis',(-1.31418445149758E-16,-1.,0.)) ;
#128885 = DIRECTION('ref_axis',(1.,-1.31418445149758E-16,0.)) ;
#128886 = DIRECTION('center_axis',(0.,1.,0.)) ;
#128887 = DIRECTION('ref_axis',(0.,0.,1.)) ;
#128888 = DIRECTION('center_axis',(-1.,0.,2.16840434497101E-16)) ;
#128889 = DIRECTION('ref_axis',(2.16840434497101E-16,0.,1.)) ;
#128890 = DIRECTION('center_axis',(-1.,0.,0.)) ;
#128891 = DIRECTION('ref_axis',(0.,0.,1.)) ;
#128892 = DIRECTION('center_axis',(1.,0.,0.)) ;
#128893 = DIRECTION('ref_axis',(0.,0.,-1.)) ;
#128894 = DIRECTION('center_axis',(-1.31418445149758E-16,-1.,0.)) ;
#128895 = DIRECTION('ref_axis',(1.,-1.31418445149758E-16,0.)) ;
#128896 = DIRECTION('center_axis',(0.,1.,0.)) ;
#128897 = DIRECTION('ref_axis',(0.,0.,1.)) ;
#128898 = DIRECTION('center_axis',(2.16840434497101E-16,2.8496832747207E-32,
1.)) ;
#128899 = DIRECTION('ref_axis',(1.,-6.17926559469557E-48,-2.16840434497101E-16)) ;
#128900 = DIRECTION('center_axis',(0.,0.,1.)) ;
#128901 = DIRECTION('ref_axis',(1.,0.,0.)) ;
#128902 = DIRECTION('center_axis',(-1.,-1.31418445149758E-16,-2.16840434497101E-16)) ;
#128903 = DIRECTION('ref_axis',(-2.16840434497101E-16,-2.8496832747207E-32,
1.)) ;
#128904 = DIRECTION('center_axis',(-1.,0.,0.)) ;
#128905 = DIRECTION('ref_axis',(0.,0.,1.)) ;
#128906 = DIRECTION('center_axis',(1.,0.,0.)) ;
#128907 = DIRECTION('ref_axis',(0.,0.,-1.)) ;
#128908 = DIRECTION('center_axis',(-1.31418445149758E-16,1.,0.)) ;
#128909 = DIRECTION('ref_axis',(-1.,0.,0.)) ;
#128910 = DIRECTION('center_axis',(-1.31418445149758E-16,1.,0.)) ;
#128911 = DIRECTION('ref_axis',(-1.,-1.31418445149758E-16,0.)) ;
#128912 = DIRECTION('center_axis',(0.,1.,0.)) ;
#128913 = DIRECTION('ref_axis',(1.,0.,0.)) ;
#128914 = DIRECTION('center_axis',(0.,0.,-1.)) ;
#128915 = DIRECTION('ref_axis',(1.,0.,0.)) ;
#128916 = DIRECTION('center_axis',(0.,1.,0.)) ;
#128917 = DIRECTION('ref_axis',(1.,0.,0.)) ;
#128918 = DIRECTION('center_axis',(0.,0.,-1.)) ;
#128919 = DIRECTION('ref_axis',(1.,0.,0.)) ;
#128920 = DIRECTION('center_axis',(-1.31418445149758E-16,1.,0.)) ;
#128921 = DIRECTION('ref_axis',(-1.,0.,0.)) ;
#128922 = DIRECTION('center_axis',(-1.31418445149758E-16,1.,0.)) ;
#128923 = DIRECTION('ref_axis',(-1.,-1.31418445149758E-16,0.)) ;
#128924 = DIRECTION('center_axis',(-1.31418445149758E-16,-1.,0.)) ;
#128925 = DIRECTION('ref_axis',(1.,-1.31418445149758E-16,0.)) ;
#128926 = DIRECTION('center_axis',(0.,1.,0.)) ;
#128927 = DIRECTION('ref_axis',(0.,0.,1.)) ;
#128928 = DIRECTION('center_axis',(4.33680868994202E-16,0.,1.)) ;
#128929 = DIRECTION('ref_axis',(1.,0.,-4.33680868994202E-16)) ;
#128930 = DIRECTION('center_axis',(0.,0.,-1.)) ;
#128931 = DIRECTION('ref_axis',(-1.,0.,0.)) ;
#128932 = DIRECTION('center_axis',(-2.16840434497101E-16,0.,-1.)) ;
#128933 = DIRECTION('ref_axis',(-1.,0.,2.16840434497101E-16)) ;
#128934 = DIRECTION('center_axis',(0.,0.,-1.)) ;
#128935 = DIRECTION('ref_axis',(-1.,0.,0.)) ;
#128936 = DIRECTION('center_axis',(-1.31418445149758E-16,-1.,0.)) ;
#128937 = DIRECTION('ref_axis',(1.,-1.31418445149758E-16,0.)) ;
#128938 = DIRECTION('center_axis',(0.,1.,0.)) ;
#128939 = DIRECTION('ref_axis',(0.,0.,1.)) ;
#128940 = DIRECTION('center_axis',(0.,1.,0.)) ;
#128941 = DIRECTION('ref_axis',(1.,0.,0.)) ;
#128942 = DIRECTION('center_axis',(-1.,0.,0.)) ;
#128943 = DIRECTION('ref_axis',(0.,0.,-1.)) ;
#128944 = DIRECTION('center_axis',(0.,1.,0.)) ;
#128945 = DIRECTION('ref_axis',(1.,0.,0.)) ;
#128946 = DIRECTION('center_axis',(1.,0.,0.)) ;
#128947 = DIRECTION('ref_axis',(0.,0.,1.)) ;
#128948 = DIRECTION('center_axis',(1.,0.,2.16840434497101E-16)) ;
#128949 = DIRECTION('ref_axis',(2.16840434497101E-16,0.,-1.)) ;
#128950 = DIRECTION('center_axis',(0.,1.,0.)) ;
#128951 = DIRECTION('ref_axis',(0.,0.,1.)) ;
#128952 = DIRECTION('center_axis',(0.,1.,0.)) ;
#128953 = DIRECTION('ref_axis',(0.,0.,1.)) ;
#128954 = DIRECTION('center_axis',(0.,0.,-1.)) ;
#128955 = DIRECTION('ref_axis',(-1.,0.,0.)) ;
#128956 = DIRECTION('center_axis',(0.,0.,1.)) ;
#128957 = DIRECTION('ref_axis',(1.,0.,0.)) ;
#128958 = DIRECTION('center_axis',(0.,0.,-1.)) ;
#128959 = DIRECTION('ref_axis',(-1.,0.,0.)) ;
#128960 = DIRECTION('center_axis',(0.,1.,0.)) ;
#128961 = DIRECTION('ref_axis',(0.,0.,1.)) ;
#128962 = DIRECTION('center_axis',(0.,1.,0.)) ;
#128963 = DIRECTION('ref_axis',(0.,0.,1.)) ;
#128964 = DIRECTION('center_axis',(0.,1.,0.)) ;
#128965 = DIRECTION('ref_axis',(1.,0.,0.)) ;
#128966 = DIRECTION('center_axis',(-1.,0.,0.)) ;
#128967 = DIRECTION('ref_axis',(0.,0.,-1.)) ;
#128968 = DIRECTION('center_axis',(0.,1.,0.)) ;
#128969 = DIRECTION('ref_axis',(1.,0.,0.)) ;
#128970 = DIRECTION('center_axis',(-1.,0.,0.)) ;
#128971 = DIRECTION('ref_axis',(0.,0.,-1.)) ;
#128972 = DIRECTION('center_axis',(0.,1.,0.)) ;
#128973 = DIRECTION('ref_axis',(0.,0.,1.)) ;
#128974 = DIRECTION('center_axis',(0.,1.,0.)) ;
#128975 = DIRECTION('ref_axis',(0.,0.,1.)) ;
#128976 = DIRECTION('center_axis',(-1.,0.,0.)) ;
#128977 = DIRECTION('ref_axis',(0.,0.,1.)) ;
#128978 = DIRECTION('center_axis',(-1.,0.,0.)) ;
#128979 = DIRECTION('ref_axis',(0.,0.,1.)) ;
#128980 = DIRECTION('center_axis',(1.,0.,0.)) ;
#128981 = DIRECTION('ref_axis',(0.,0.,-1.)) ;
#128982 = DIRECTION('center_axis',(-1.,0.,0.)) ;
#128983 = DIRECTION('ref_axis',(0.,0.,1.)) ;
#128984 = DIRECTION('center_axis',(0.,1.,0.)) ;
#128985 = DIRECTION('ref_axis',(0.,0.,1.)) ;
#128986 = DIRECTION('center_axis',(0.,1.,0.)) ;
#128987 = DIRECTION('ref_axis',(0.,0.,1.)) ;
#128988 = DIRECTION('center_axis',(0.,1.,0.)) ;
#128989 = DIRECTION('ref_axis',(1.,0.,0.)) ;
#128990 = DIRECTION('center_axis',(0.,0.,1.)) ;
#128991 = DIRECTION('ref_axis',(-1.,0.,0.)) ;
#128992 = DIRECTION('center_axis',(0.,1.,0.)) ;
#128993 = DIRECTION('ref_axis',(1.,0.,0.)) ;
#128994 = DIRECTION('center_axis',(0.,0.,-1.)) ;
#128995 = DIRECTION('ref_axis',(1.,0.,0.)) ;
#128996 = DIRECTION('center_axis',(0.,0.,1.)) ;
#128997 = DIRECTION('ref_axis',(1.,0.,0.)) ;
#128998 = DIRECTION('center_axis',(0.,0.,1.)) ;
#128999 = DIRECTION('ref_axis',(1.,0.,0.)) ;
#129000 = DIRECTION('center_axis',(0.,0.,-1.)) ;
#129001 = DIRECTION('ref_axis',(-1.,0.,0.)) ;
#129002 = DIRECTION('center_axis',(0.,0.,1.)) ;
#129003 = DIRECTION('ref_axis',(1.,0.,0.)) ;
#129004 = DIRECTION('center_axis',(1.,0.,0.)) ;
#129005 = DIRECTION('ref_axis',(0.,0.,-1.)) ;
#129006 = DIRECTION('center_axis',(1.,0.,0.)) ;
#129007 = DIRECTION('ref_axis',(0.,0.,-1.)) ;
#129008 = DIRECTION('center_axis',(1.,0.,0.)) ;
#129009 = DIRECTION('ref_axis',(0.,0.,-1.)) ;
#129010 = DIRECTION('center_axis',(1.,0.,8.67361737988409E-15)) ;
#129011 = DIRECTION('ref_axis',(8.67361737988409E-15,0.,-1.)) ;
#129012 = DIRECTION('center_axis',(1.,0.,0.)) ;
#129013 = DIRECTION('ref_axis',(0.,0.,-1.)) ;
#129014 = DIRECTION('center_axis',(1.,0.,1.73472347597682E-14)) ;
#129015 = DIRECTION('ref_axis',(1.73472347597682E-14,0.,-1.)) ;
#129016 = DIRECTION('center_axis',(-1.,0.,0.)) ;
#129017 = DIRECTION('ref_axis',(0.,0.,1.)) ;
#129018 = DIRECTION('center_axis',(1.,0.,0.)) ;
#129019 = DIRECTION('ref_axis',(0.,0.,-1.)) ;
#129020 = DIRECTION('center_axis',(1.,0.,0.)) ;
#129021 = DIRECTION('ref_axis',(0.,0.,-1.)) ;
#129022 = DIRECTION('center_axis',(0.,0.,-1.)) ;
#129023 = DIRECTION('ref_axis',(-1.,0.,0.)) ;
#129024 = DIRECTION('center_axis',(1.,0.,0.)) ;
#129025 = DIRECTION('ref_axis',(0.,0.,-1.)) ;
#129026 = DIRECTION('center_axis',(0.,0.,1.)) ;
#129027 = DIRECTION('ref_axis',(1.,0.,0.)) ;
#129028 = DIRECTION('center_axis',(0.,0.,-1.)) ;
#129029 = DIRECTION('ref_axis',(-1.,0.,0.)) ;
#129030 = DIRECTION('center_axis',(-0.422618261740697,5.55398348498559E-17,
0.906307787036651)) ;
#129031 = DIRECTION('ref_axis',(0.906307787036651,-2.19407316623673E-31,0.422618261740697)) ;
#129032 = DIRECTION('center_axis',(0.422618261740697,-5.55398348498559E-17,
-0.906307787036651)) ;
#129033 = DIRECTION('ref_axis',(-0.906307787036651,2.28174878574772E-31,-0.422618261740697)) ;
#129034 = DIRECTION('center_axis',(-0.422618261740697,5.55398348498559E-17,
0.906307787036651)) ;
#129035 = DIRECTION('ref_axis',(0.906307787036651,-2.28174878574772E-31,0.422618261740697)) ;
#129036 = DIRECTION('center_axis',(0.422618261740697,-5.55398348498559E-17,
-0.906307787036651)) ;
#129037 = DIRECTION('ref_axis',(-0.906307787036651,2.28174878574772E-31,-0.422618261740697)) ;
#129038 = DIRECTION('center_axis',(0.,1.,0.)) ;
#129039 = DIRECTION('ref_axis',(1.,0.,0.)) ;
#129040 = DIRECTION('center_axis',(3.4216004848576E-14,0.514231796959095,
-0.857651245551606)) ;
#129041 = DIRECTION('ref_axis',(3.46944695195362E-14,-0.857651245551606,-0.514231796959095)) ;
#129042 = DIRECTION('center_axis',(0.,-3.46944695195362E-14,1.)) ;
#129043 = DIRECTION('ref_axis',(0.,1.,3.46944695195362E-14)) ;
#129044 = DIRECTION('center_axis',(-1.,0.,0.)) ;
#129045 = DIRECTION('ref_axis',(0.,-4.33680868994204E-15,-1.)) ;
#129046 = DIRECTION('center_axis',(0.,0.,1.)) ;
#129047 = DIRECTION('ref_axis',(1.,0.,0.)) ;
#129048 = DIRECTION('center_axis',(0.,0.,1.)) ;
#129049 = DIRECTION('ref_axis',(1.,0.,0.)) ;
#129050 = DIRECTION('center_axis',(-1.,0.,0.)) ;
#129051 = DIRECTION('ref_axis',(0.,0.,1.)) ;
#129052 = DIRECTION('center_axis',(-1.,0.,0.)) ;
#129053 = DIRECTION('ref_axis',(0.,-4.33680868994204E-15,-1.)) ;
#129054 = DIRECTION('center_axis',(1.,0.,0.)) ;
#129055 = DIRECTION('ref_axis',(0.,0.,-1.)) ;
#129056 = DIRECTION('center_axis',(0.,-0.514231796959124,-0.857651245551588)) ;
#129057 = DIRECTION('ref_axis',(0.,0.857651245551588,-0.514231796959124)) ;
#129058 = DIRECTION('center_axis',(0.,1.,8.97270763436279E-17)) ;
#129059 = DIRECTION('ref_axis',(0.,-8.97270763436279E-17,1.)) ;
#129060 = DIRECTION('center_axis',(0.,-1.,-8.97270763436279E-17)) ;
#129061 = DIRECTION('ref_axis',(0.,-8.97270763436279E-17,1.)) ;
#129062 = DIRECTION('center_axis',(0.,-1.,0.)) ;
#129063 = DIRECTION('ref_axis',(0.,0.,-1.)) ;
#129064 = DIRECTION('center_axis',(0.,1.,0.)) ;
#129065 = DIRECTION('ref_axis',(1.,0.,0.)) ;
#129066 = DIRECTION('center_axis',(-1.,0.,0.)) ;
#129067 = DIRECTION('ref_axis',(0.,0.,-1.)) ;
#129068 = DIRECTION('center_axis',(1.,0.,0.)) ;
#129069 = DIRECTION('ref_axis',(0.,0.,-1.)) ;
#129070 = DIRECTION('center_axis',(0.,-0.514231796959093,0.857651245551607)) ;
#129071 = DIRECTION('ref_axis',(0.,0.857651245551607,0.514231796959093)) ;
#129072 = DIRECTION('center_axis',(0.,0.,-1.)) ;
#129073 = DIRECTION('ref_axis',(1.,0.,0.)) ;
#129074 = DIRECTION('center_axis',(0.,1.,0.)) ;
#129075 = DIRECTION('ref_axis',(1.,0.,0.)) ;
#129076 = DIRECTION('center_axis',(-3.46944695195364E-14,0.,-1.)) ;
#129077 = DIRECTION('ref_axis',(1.,0.,-3.46944695195364E-14)) ;
#129078 = DIRECTION('center_axis',(-1.,0.,0.)) ;
#129079 = DIRECTION('ref_axis',(0.,4.33680868994204E-15,-1.)) ;
#129080 = DIRECTION('center_axis',(0.,0.,-1.)) ;
#129081 = DIRECTION('ref_axis',(-1.,0.,0.)) ;
#129082 = DIRECTION('center_axis',(0.,0.,1.)) ;
#129083 = DIRECTION('ref_axis',(-1.,0.,0.)) ;
#129084 = DIRECTION('center_axis',(0.,0.,-1.)) ;
#129085 = DIRECTION('ref_axis',(-1.,0.,0.)) ;
#129086 = DIRECTION('center_axis',(-1.,0.,7.01133629567814E-33)) ;
#129087 = DIRECTION('ref_axis',(7.01133629567814E-33,0.,1.)) ;
#129088 = DIRECTION('center_axis',(-1.,0.,0.)) ;
#129089 = DIRECTION('ref_axis',(0.,0.,1.)) ;
#129090 = DIRECTION('center_axis',(0.,0.,-1.)) ;
#129091 = DIRECTION('ref_axis',(-1.,0.,0.)) ;
#129092 = DIRECTION('center_axis',(-7.01133629567814E-33,8.97270763436279E-17,
-1.)) ;
#129093 = DIRECTION('ref_axis',(6.29106707073161E-49,1.,8.97270763436279E-17)) ;
#129094 = DIRECTION('center_axis',(1.,0.,0.)) ;
#129095 = DIRECTION('ref_axis',(0.,0.,-1.)) ;
#129096 = DIRECTION('center_axis',(-2.2301249256967E-15,0.514231796959095,
0.857651245551606)) ;
#129097 = DIRECTION('ref_axis',(-4.79361507851841E-30,-0.857651245551606,
0.514231796959095)) ;
#129098 = DIRECTION('center_axis',(-1.,0.,0.)) ;
#129099 = DIRECTION('ref_axis',(0.,0.,1.)) ;
#129100 = DIRECTION('center_axis',(-1.,0.,0.)) ;
#129101 = DIRECTION('ref_axis',(0.,-4.33680868994204E-15,-1.)) ;
#129102 = DIRECTION('center_axis',(0.,0.,1.)) ;
#129103 = DIRECTION('ref_axis',(1.,0.,0.)) ;
#129104 = DIRECTION('center_axis',(0.,0.,-1.)) ;
#129105 = DIRECTION('ref_axis',(-1.,0.,0.)) ;
#129106 = DIRECTION('center_axis',(0.,-1.,8.97270763436279E-17)) ;
#129107 = DIRECTION('ref_axis',(0.,-8.97270763436279E-17,-1.)) ;
#129108 = DIRECTION('center_axis',(0.,-1.,8.97270763436279E-17)) ;
#129109 = DIRECTION('ref_axis',(0.,-8.97270763436279E-17,-1.)) ;
#129110 = DIRECTION('center_axis',(0.,-1.,0.)) ;
#129111 = DIRECTION('ref_axis',(0.,0.,-1.)) ;
#129112 = DIRECTION('center_axis',(-7.01133629567814E-33,8.97270763436279E-17,
-1.)) ;
#129113 = DIRECTION('ref_axis',(0.,1.,0.)) ;
#129114 = DIRECTION('center_axis',(0.,-1.,0.)) ;
#129115 = DIRECTION('ref_axis',(0.,0.,1.)) ;
#129116 = DIRECTION('center_axis',(1.,0.,0.)) ;
#129117 = DIRECTION('ref_axis',(0.,0.,-1.)) ;
#129118 = DIRECTION('center_axis',(0.,0.,1.)) ;
#129119 = DIRECTION('ref_axis',(-1.,0.,0.)) ;
#129120 = DIRECTION('center_axis',(0.,1.,0.)) ;
#129121 = DIRECTION('ref_axis',(1.,0.,0.)) ;
#129122 = DIRECTION('center_axis',(-1.,0.,0.)) ;
#129123 = DIRECTION('ref_axis',(0.,0.,-1.)) ;
#129124 = DIRECTION('center_axis',(1.,7.81406971160724E-17,0.)) ;
#129125 = DIRECTION('ref_axis',(-7.81406971160724E-17,1.,0.)) ;
#129126 = DIRECTION('center_axis',(1.,0.,0.)) ;
#129127 = DIRECTION('ref_axis',(0.,0.,-1.)) ;
#129128 = DIRECTION('center_axis',(1.,0.,0.)) ;
#129129 = DIRECTION('ref_axis',(0.,0.,-1.)) ;
#129130 = DIRECTION('center_axis',(0.,1.,8.97270763436279E-17)) ;
#129131 = DIRECTION('ref_axis',(0.,-8.97270763436279E-17,1.)) ;
#129132 = DIRECTION('center_axis',(0.,-1.,0.)) ;
#129133 = DIRECTION('ref_axis',(0.,0.,-1.)) ;
#129134 = DIRECTION('center_axis',(0.,0.,-1.)) ;
#129135 = DIRECTION('ref_axis',(-1.,0.,0.)) ;
#129136 = DIRECTION('center_axis',(-7.01133629567814E-33,8.97270763436279E-17,
1.)) ;
#129137 = DIRECTION('ref_axis',(-6.29106707073161E-49,-1.,8.97270763436279E-17)) ;
#129138 = DIRECTION('center_axis',(-1.,0.,-7.01133629567814E-33)) ;
#129139 = DIRECTION('ref_axis',(-7.01133629567814E-33,0.,1.)) ;
#129140 = DIRECTION('center_axis',(-1.,0.,0.)) ;
#129141 = DIRECTION('ref_axis',(0.,0.,1.)) ;
#129142 = DIRECTION('center_axis',(1.,0.,0.)) ;
#129143 = DIRECTION('ref_axis',(0.,1.,0.)) ;
#129144 = DIRECTION('center_axis',(4.33680868994202E-15,1.,0.)) ;
#129145 = DIRECTION('ref_axis',(-1.,4.33680868994202E-15,0.)) ;
#129146 = DIRECTION('center_axis',(0.,1.,0.)) ;
#129147 = DIRECTION('ref_axis',(1.,0.,0.)) ;
#129148 = DIRECTION('center_axis',(0.,0.,-1.)) ;
#129149 = DIRECTION('ref_axis',(1.,0.,0.)) ;
#129150 = DIRECTION('center_axis',(-1.,0.,0.)) ;
#129151 = DIRECTION('ref_axis',(0.,0.,-1.)) ;
#129152 = DIRECTION('center_axis',(-7.01133629567814E-33,8.97270763436279E-17,
1.)) ;
#129153 = DIRECTION('ref_axis',(0.,-1.,0.)) ;
#129154 = DIRECTION('center_axis',(0.,-1.,0.)) ;
#129155 = DIRECTION('ref_axis',(0.,0.,1.)) ;
#129156 = DIRECTION('center_axis',(7.81406971160724E-17,-1.,-8.97270763436279E-17)) ;
#129157 = DIRECTION('ref_axis',(-7.01133629567814E-33,8.97270763436279E-17,
-1.)) ;
#129158 = DIRECTION('center_axis',(0.,1.,0.)) ;
#129159 = DIRECTION('ref_axis',(0.,0.,1.)) ;
#129160 = DIRECTION('center_axis',(-1.,-7.81406971160724E-17,0.)) ;
#129161 = DIRECTION('ref_axis',(7.81406971160724E-17,-1.,0.)) ;
#129162 = DIRECTION('center_axis',(-1.,-7.81406971160724E-17,0.)) ;
#129163 = DIRECTION('ref_axis',(-7.81406971160724E-17,1.,0.)) ;
#129164 = DIRECTION('center_axis',(0.,0.,1.)) ;
#129165 = DIRECTION('ref_axis',(1.,0.,0.)) ;
#129166 = DIRECTION('center_axis',(0.,0.,-1.)) ;
#129167 = DIRECTION('ref_axis',(-1.,0.,0.)) ;
#129168 = DIRECTION('center_axis',(0.,-1.,8.97270763436279E-17)) ;
#129169 = DIRECTION('ref_axis',(0.,-8.97270763436279E-17,-1.)) ;
#129170 = DIRECTION('center_axis',(0.,-1.,0.)) ;
#129171 = DIRECTION('ref_axis',(0.,0.,-1.)) ;
#129172 = DIRECTION('center_axis',(1.,7.81406971160724E-17,0.)) ;
#129173 = DIRECTION('ref_axis',(0.,1.,0.)) ;
#129174 = DIRECTION('center_axis',(0.,0.,1.)) ;
#129175 = DIRECTION('ref_axis',(-1.,0.,0.)) ;
#129176 = DIRECTION('center_axis',(0.,1.,0.)) ;
#129177 = DIRECTION('ref_axis',(1.,0.,0.)) ;
#129178 = DIRECTION('center_axis',(-1.,0.,0.)) ;
#129179 = DIRECTION('ref_axis',(0.,0.,-1.)) ;
#129180 = DIRECTION('center_axis',(0.,0.,-1.)) ;
#129181 = DIRECTION('ref_axis',(-1.,0.,0.)) ;
#129182 = DIRECTION('center_axis',(0.,0.,1.)) ;
#129183 = DIRECTION('ref_axis',(1.,0.,0.)) ;
#129184 = DIRECTION('center_axis',(-1.,-7.81406971160724E-17,0.)) ;
#129185 = DIRECTION('ref_axis',(7.81406971160724E-17,-1.,0.)) ;
#129186 = DIRECTION('center_axis',(-1.,-7.81406971160724E-17,0.)) ;
#129187 = DIRECTION('ref_axis',(-7.81406971160724E-17,1.,0.)) ;
#129188 = DIRECTION('center_axis',(1.,7.81406971160724E-17,0.)) ;
#129189 = DIRECTION('ref_axis',(-7.81406971160724E-17,1.,0.)) ;
#129190 = DIRECTION('center_axis',(1.,0.,0.)) ;
#129191 = DIRECTION('ref_axis',(0.,0.,-1.)) ;
#129192 = DIRECTION('center_axis',(1.,0.,0.)) ;
#129193 = DIRECTION('ref_axis',(0.,0.,-1.)) ;
#129194 = DIRECTION('center_axis',(3.78638272950961E-32,-4.8455963016112E-16,
-1.)) ;
#129195 = DIRECTION('ref_axis',(1.83472821505963E-47,1.,-4.8455963016112E-16)) ;
#129196 = DIRECTION('center_axis',(3.78638272950961E-32,-4.8455963016112E-16,
-1.)) ;
#129197 = DIRECTION('ref_axis',(1.83472821505963E-47,1.,-4.8455963016112E-16)) ;
#129198 = DIRECTION('center_axis',(0.,0.,-1.)) ;
#129199 = DIRECTION('ref_axis',(-1.,0.,0.)) ;
#129200 = DIRECTION('center_axis',(1.,7.81406971160724E-17,0.)) ;
#129201 = DIRECTION('ref_axis',(0.,1.,0.)) ;
#129202 = DIRECTION('center_axis',(0.,-1.,0.)) ;
#129203 = DIRECTION('ref_axis',(0.,0.,1.)) ;
#129204 = DIRECTION('center_axis',(0.,1.,0.)) ;
#129205 = DIRECTION('ref_axis',(1.,0.,0.)) ;
#129206 = DIRECTION('center_axis',(0.,1.,0.)) ;
#129207 = DIRECTION('ref_axis',(0.,0.,-1.)) ;
#129208 = DIRECTION('center_axis',(-7.81406971160724E-17,1.,-8.97270763436279E-17)) ;
#129209 = DIRECTION('ref_axis',(-7.01133629567814E-33,8.97270763436279E-17,
1.)) ;
#129210 = DIRECTION('center_axis',(0.,-1.,0.)) ;
#129211 = DIRECTION('ref_axis',(0.,0.,-1.)) ;
#129212 = DIRECTION('center_axis',(0.,1.,0.)) ;
#129213 = DIRECTION('ref_axis',(0.,0.,1.)) ;
#129214 = DIRECTION('center_axis',(0.,-1.,0.)) ;
#129215 = DIRECTION('ref_axis',(0.,0.,-1.)) ;
#129216 = DIRECTION('center_axis',(0.,-1.,0.)) ;
#129217 = DIRECTION('ref_axis',(0.,0.,-1.)) ;
#129218 = DIRECTION('center_axis',(0.,1.,0.)) ;
#129219 = DIRECTION('ref_axis',(1.,0.,0.)) ;
#129220 = DIRECTION('center_axis',(0.,0.,1.)) ;
#129221 = DIRECTION('ref_axis',(-1.,0.,0.)) ;
#129222 = DIRECTION('center_axis',(1.,0.,0.)) ;
#129223 = DIRECTION('ref_axis',(0.,0.,1.)) ;
#129224 = DIRECTION('center_axis',(0.,-1.,0.)) ;
#129225 = DIRECTION('ref_axis',(0.,0.,-1.)) ;
#129226 = DIRECTION('center_axis',(0.,1.,0.)) ;
#129227 = DIRECTION('ref_axis',(0.,0.,1.)) ;
#129228 = DIRECTION('center_axis',(0.,-1.,0.)) ;
#129229 = DIRECTION('ref_axis',(0.,0.,-1.)) ;
#129230 = DIRECTION('center_axis',(-1.,0.,2.16840434497101E-16)) ;
#129231 = DIRECTION('ref_axis',(2.16840434497101E-16,0.,1.)) ;
#129232 = DIRECTION('center_axis',(1.,0.,0.)) ;
#129233 = DIRECTION('ref_axis',(0.,0.,-1.)) ;
#129234 = DIRECTION('center_axis',(-2.16840434497101E-16,0.,1.)) ;
#129235 = DIRECTION('ref_axis',(1.,0.,2.16840434497101E-16)) ;
#129236 = DIRECTION('center_axis',(0.,0.,1.)) ;
#129237 = DIRECTION('ref_axis',(1.,0.,0.)) ;
#129238 = DIRECTION('center_axis',(0.,1.,0.)) ;
#129239 = DIRECTION('ref_axis',(0.,0.,1.)) ;
#129240 = DIRECTION('center_axis',(0.,-1.,0.)) ;
#129241 = DIRECTION('ref_axis',(0.,0.,-1.)) ;
#129242 = DIRECTION('center_axis',(0.,1.,0.)) ;
#129243 = DIRECTION('ref_axis',(1.,0.,0.)) ;
#129244 = DIRECTION('center_axis',(0.,0.,1.)) ;
#129245 = DIRECTION('ref_axis',(-1.,0.,0.)) ;
#129246 = DIRECTION('center_axis',(0.,1.,0.)) ;
#129247 = DIRECTION('ref_axis',(1.,0.,0.)) ;
#129248 = DIRECTION('center_axis',(1.,0.,0.)) ;
#129249 = DIRECTION('ref_axis',(0.,0.,1.)) ;
#129250 = DIRECTION('center_axis',(0.,0.,-1.)) ;
#129251 = DIRECTION('ref_axis',(-1.,0.,0.)) ;
#129252 = DIRECTION('center_axis',(0.,0.,1.)) ;
#129253 = DIRECTION('ref_axis',(1.,0.,0.)) ;
#129254 = DIRECTION('center_axis',(1.,0.,2.16840434497101E-16)) ;
#129255 = DIRECTION('ref_axis',(2.16840434497101E-16,0.,-1.)) ;
#129256 = DIRECTION('center_axis',(1.,0.,0.)) ;
#129257 = DIRECTION('ref_axis',(0.,0.,-1.)) ;
#129258 = DIRECTION('center_axis',(0.,1.,0.)) ;
#129259 = DIRECTION('ref_axis',(1.,0.,0.)) ;
#129260 = DIRECTION('center_axis',(0.,1.,0.)) ;
#129261 = DIRECTION('ref_axis',(0.,0.,-1.)) ;
#129262 = DIRECTION('center_axis',(0.,1.,0.)) ;
#129263 = DIRECTION('ref_axis',(0.,0.,1.)) ;
#129264 = DIRECTION('center_axis',(0.,1.,0.)) ;
#129265 = DIRECTION('ref_axis',(0.,0.,1.)) ;
#129266 = DIRECTION('center_axis',(-0.942809041582063,-0.235702260395516,
0.235702260395518)) ;
#129267 = DIRECTION('ref_axis',(0.242535625036335,4.64743530723282E-16,0.970142500145331)) ;
#129268 = DIRECTION('center_axis',(-0.970142500145332,-0.242535625036331,
-2.10366121255617E-15)) ;
#129269 = DIRECTION('ref_axis',(0.242535625036331,-0.970142500145332,-4.47980524894761E-30)) ;
#129270 = DIRECTION('center_axis',(0.970142500145333,0.24253562503633,0.)) ;
#129271 = DIRECTION('ref_axis',(-0.24253562503633,0.970142500145333,0.)) ;
#129272 = DIRECTION('center_axis',(-0.970142500145332,-0.242535625036331,
2.73475957632304E-14)) ;
#129273 = DIRECTION('ref_axis',(0.242535625036331,-0.970142500145332,1.1454669517322E-30)) ;
#129274 = DIRECTION('center_axis',(0.879462917689188,0.219865729422294,-0.42214220049081)) ;
#129275 = DIRECTION('ref_axis',(-0.432731067584771,1.71515946658E-16,-0.901523057468274)) ;
#129276 = DIRECTION('center_axis',(0.879462917689192,0.219865729422271,-0.422142200490814)) ;
#129277 = DIRECTION('ref_axis',(-0.432731067584773,-1.62351711522009E-16,
-0.901523057468273)) ;
#129278 = DIRECTION('center_axis',(0.,1.,0.)) ;
#129279 = DIRECTION('ref_axis',(1.,0.,0.)) ;
#129280 = DIRECTION('center_axis',(0.,-1.,0.)) ;
#129281 = DIRECTION('ref_axis',(0.,0.,1.)) ;
#129282 = DIRECTION('center_axis',(0.,-1.,0.)) ;
#129283 = DIRECTION('ref_axis',(0.,0.,-1.)) ;
#129284 = DIRECTION('center_axis',(-4.51750905202295E-15,-1.,2.16840434497102E-15)) ;
#129285 = DIRECTION('ref_axis',(1.,-4.51750905202295E-15,3.91831450274151E-31)) ;
#129286 = DIRECTION('center_axis',(0.669589480006976,-0.669589480006974,-0.321402950403349)) ;
#129287 = DIRECTION('ref_axis',(0.707106781186547,0.707106781186548,5.45170614306381E-16)) ;
#129288 = DIRECTION('center_axis',(0.669589480006977,-0.669589480006977,-0.321402950403342)) ;
#129289 = DIRECTION('ref_axis',(0.707106781186547,0.707106781186548,-1.94221176494188E-16)) ;
#129290 = DIRECTION('center_axis',(0.,1.,0.)) ;
#129291 = DIRECTION('ref_axis',(1.,0.,0.)) ;
#129292 = DIRECTION('center_axis',(0.707106781186541,-0.707106781186554,0.)) ;
#129293 = DIRECTION('ref_axis',(-0.707106781186554,-0.707106781186541,0.)) ;
#129294 = DIRECTION('center_axis',(0.707106781186549,-0.707106781186546,0.)) ;
#129295 = DIRECTION('ref_axis',(0.707106781186546,0.707106781186549,0.)) ;
#129296 = DIRECTION('center_axis',(0.707106781186548,-0.707106781186548,-1.53329341668338E-15)) ;
#129297 = DIRECTION('ref_axis',(0.707106781186548,0.707106781186548,1.5356898865553E-31)) ;
#129298 = DIRECTION('center_axis',(0.577350269189633,-0.577350269189633,-0.577350269189612)) ;
#129299 = DIRECTION('ref_axis',(0.707106781186548,0.707106781186548,1.34560831514457E-17)) ;
#129300 = DIRECTION('center_axis',(-0.577350269189344,0.577350269189586,-0.577350269189947)) ;
#129301 = DIRECTION('ref_axis',(1.30446081606812E-15,0.707106781186769,0.707106781186326)) ;
#129302 = DIRECTION('center_axis',(-0.707106781186548,0.707106781186548,7.66646708341692E-15)) ;
#129303 = DIRECTION('ref_axis',(-0.707106781186548,-0.707106781186548,-2.68297081166629E-31)) ;
#129304 = DIRECTION('center_axis',(-0.707106781186549,0.707106781186546,0.)) ;
#129305 = DIRECTION('ref_axis',(-0.707106781186546,-0.707106781186549,0.)) ;
#129306 = DIRECTION('center_axis',(-0.707106781186548,0.707106781186548,-1.22663473334671E-14)) ;
#129307 = DIRECTION('ref_axis',(-0.707106781186548,-0.707106781186548,2.94725045705944E-31)) ;
#129308 = DIRECTION('center_axis',(-0.669589480006976,0.669589480006974,-0.321402950403349)) ;
#129309 = DIRECTION('ref_axis',(-0.707106781186547,-0.707106781186548,5.45170614306381E-16)) ;
#129310 = DIRECTION('center_axis',(0.669589480006982,-0.669589480006966,0.321402950403353)) ;
#129311 = DIRECTION('ref_axis',(0.707106781186539,0.707106781186556,5.77426876420606E-17)) ;
#129312 = DIRECTION('center_axis',(0.,1.,0.)) ;
#129313 = DIRECTION('ref_axis',(1.,0.,0.)) ;
#129314 = DIRECTION('center_axis',(0.,1.,0.)) ;
#129315 = DIRECTION('ref_axis',(0.,0.,-1.)) ;
#129316 = DIRECTION('center_axis',(0.,-1.,0.)) ;
#129317 = DIRECTION('ref_axis',(0.,0.,-1.)) ;
#129318 = DIRECTION('center_axis',(0.,1.,0.)) ;
#129319 = DIRECTION('ref_axis',(0.,0.,1.)) ;
#129320 = DIRECTION('center_axis',(-0.879462917689188,-0.219865729422294,
-0.42214220049081)) ;
#129321 = DIRECTION('ref_axis',(-0.432731067584771,1.71515946658E-16,0.901523057468274)) ;
#129322 = DIRECTION('center_axis',(0.879462917689201,0.219865729422298,0.42214220049078)) ;
#129323 = DIRECTION('ref_axis',(0.432731067584741,5.42470486237819E-16,-0.901523057468288)) ;
#129324 = DIRECTION('center_axis',(0.,1.,0.)) ;
#129325 = DIRECTION('ref_axis',(1.,0.,0.)) ;
#129326 = DIRECTION('center_axis',(0.970142500145323,0.242535625036368,0.)) ;
#129327 = DIRECTION('ref_axis',(0.242535625036368,-0.970142500145323,0.)) ;
#129328 = DIRECTION('center_axis',(-0.970142500145333,-0.24253562503633,0.)) ;
#129329 = DIRECTION('ref_axis',(0.24253562503633,-0.970142500145333,0.)) ;
#129330 = DIRECTION('center_axis',(0.970142500145332,0.242535625036331,-2.10366121255617E-15)) ;
#129331 = DIRECTION('ref_axis',(-0.242535625036331,0.970142500145332,-4.47980524894761E-30)) ;
#129332 = DIRECTION('center_axis',(0.942809041582064,0.235702260395514,0.235702260395514)) ;
#129333 = DIRECTION('ref_axis',(-0.242535625036331,0.970142500145332,4.49011373492972E-16)) ;
#129334 = DIRECTION('center_axis',(0.,-1.,0.)) ;
#129335 = DIRECTION('ref_axis',(0.,0.,-1.)) ;
#129336 = DIRECTION('center_axis',(-1.,0.,-8.67361737988409E-15)) ;
#129337 = DIRECTION('ref_axis',(-8.67361737988409E-15,0.,1.)) ;
#129338 = DIRECTION('center_axis',(0.,0.,-1.)) ;
#129339 = DIRECTION('ref_axis',(-1.,0.,0.)) ;
#129340 = DIRECTION('center_axis',(0.,0.,-1.)) ;
#129341 = DIRECTION('ref_axis',(-1.,0.,0.)) ;
#129342 = DIRECTION('center_axis',(0.,0.,-1.)) ;
#129343 = DIRECTION('ref_axis',(-1.,0.,0.)) ;
#129344 = DIRECTION('center_axis',(1.,0.,0.)) ;
#129345 = DIRECTION('ref_axis',(0.,0.,-1.)) ;
#129346 = DIRECTION('center_axis',(-1.,0.,0.)) ;
#129347 = DIRECTION('ref_axis',(0.,0.,1.)) ;
#129348 = DIRECTION('center_axis',(0.,-1.,0.)) ;
#129349 = DIRECTION('ref_axis',(0.,0.,-1.)) ;
#129350 = DIRECTION('center_axis',(-1.,0.,0.)) ;
#129351 = DIRECTION('ref_axis',(0.,0.,1.)) ;
#129352 = DIRECTION('center_axis',(0.,-1.,0.)) ;
#129353 = DIRECTION('ref_axis',(0.,0.,-1.)) ;
#129354 = DIRECTION('center_axis',(0.,0.,-1.)) ;
#129355 = DIRECTION('ref_axis',(-1.,0.,0.)) ;
#129356 = DIRECTION('center_axis',(-1.,0.,0.)) ;
#129357 = DIRECTION('ref_axis',(0.,0.,1.)) ;
#129358 = DIRECTION('center_axis',(-1.,1.73472347597681E-14,0.)) ;
#129359 = DIRECTION('ref_axis',(-1.73472347597681E-14,-1.,0.)) ;
#129360 = DIRECTION('center_axis',(0.,0.,1.)) ;
#129361 = DIRECTION('ref_axis',(1.,0.,0.)) ;
#129362 = DIRECTION('center_axis',(-3.46944695195364E-14,0.,-1.)) ;
#129363 = DIRECTION('ref_axis',(-1.,0.,3.46944695195364E-14)) ;
#129364 = DIRECTION('center_axis',(0.,-1.,0.)) ;
#129365 = DIRECTION('ref_axis',(0.,0.,-1.)) ;
#129366 = DIRECTION('center_axis',(0.,-1.,0.)) ;
#129367 = DIRECTION('ref_axis',(0.,0.,-1.)) ;
#129368 = DIRECTION('center_axis',(0.,-1.,0.)) ;
#129369 = DIRECTION('ref_axis',(0.,0.,-1.)) ;
#129370 = DIRECTION('center_axis',(0.,0.,1.)) ;
#129371 = DIRECTION('ref_axis',(1.,0.,0.)) ;
#129372 = DIRECTION('center_axis',(0.,0.,-1.)) ;
#129373 = DIRECTION('ref_axis',(-1.,0.,0.)) ;
#129374 = DIRECTION('center_axis',(0.,0.,1.)) ;
#129375 = DIRECTION('ref_axis',(1.,0.,0.)) ;
#129376 = DIRECTION('center_axis',(0.,-1.,0.)) ;
#129377 = DIRECTION('ref_axis',(0.,0.,-1.)) ;
#129378 = DIRECTION('center_axis',(0.,-1.,0.)) ;
#129379 = DIRECTION('ref_axis',(0.,0.,-1.)) ;
#129380 = DIRECTION('center_axis',(0.,1.,0.)) ;
#129381 = DIRECTION('ref_axis',(1.,0.,0.)) ;
#129382 = DIRECTION('center_axis',(-1.,0.,0.)) ;
#129383 = DIRECTION('ref_axis',(0.,0.,-1.)) ;
#129384 = DIRECTION('center_axis',(0.,1.,0.)) ;
#129385 = DIRECTION('ref_axis',(1.,0.,0.)) ;
#129386 = DIRECTION('center_axis',(-1.,0.,0.)) ;
#129387 = DIRECTION('ref_axis',(0.,0.,-1.)) ;
#129388 = DIRECTION('center_axis',(0.,-1.,0.)) ;
#129389 = DIRECTION('ref_axis',(0.,0.,-1.)) ;
#129390 = DIRECTION('center_axis',(0.,-1.,0.)) ;
#129391 = DIRECTION('ref_axis',(0.,0.,-1.)) ;
#129392 = DIRECTION('center_axis',(-1.,0.,0.)) ;
#129393 = DIRECTION('ref_axis',(0.,0.,1.)) ;
#129394 = DIRECTION('center_axis',(-1.,0.,0.)) ;
#129395 = DIRECTION('ref_axis',(0.,0.,1.)) ;
#129396 = DIRECTION('center_axis',(1.,0.,0.)) ;
#129397 = DIRECTION('ref_axis',(0.,0.,-1.)) ;
#129398 = DIRECTION('center_axis',(-1.,0.,0.)) ;
#129399 = DIRECTION('ref_axis',(0.,0.,1.)) ;
#129400 = DIRECTION('center_axis',(0.,-1.,0.)) ;
#129401 = DIRECTION('ref_axis',(0.,0.,-1.)) ;
#129402 = DIRECTION('center_axis',(0.,-1.,0.)) ;
#129403 = DIRECTION('ref_axis',(0.,0.,-1.)) ;
#129404 = DIRECTION('center_axis',(0.,1.,0.)) ;
#129405 = DIRECTION('ref_axis',(1.,0.,0.)) ;
#129406 = DIRECTION('center_axis',(0.,0.,-1.)) ;
#129407 = DIRECTION('ref_axis',(1.,0.,0.)) ;
#129408 = DIRECTION('center_axis',(0.,1.,0.)) ;
#129409 = DIRECTION('ref_axis',(1.,0.,0.)) ;
#129410 = DIRECTION('center_axis',(0.,0.,1.)) ;
#129411 = DIRECTION('ref_axis',(-1.,0.,0.)) ;
#129412 = DIRECTION('center_axis',(0.,0.,-1.)) ;
#129413 = DIRECTION('ref_axis',(-1.,0.,0.)) ;
#129414 = DIRECTION('center_axis',(1.,1.31418445149758E-16,-2.16840434497101E-16)) ;
#129415 = DIRECTION('ref_axis',(-2.16840434497101E-16,-2.8496832747207E-32,
-1.)) ;
#129416 = DIRECTION('center_axis',(1.,0.,0.)) ;
#129417 = DIRECTION('ref_axis',(0.,0.,-1.)) ;
#129418 = DIRECTION('center_axis',(-1.,0.,0.)) ;
#129419 = DIRECTION('ref_axis',(0.,0.,1.)) ;
#129420 = DIRECTION('center_axis',(-1.31418445149758E-16,1.,0.)) ;
#129421 = DIRECTION('ref_axis',(-1.,0.,0.)) ;
#129422 = DIRECTION('center_axis',(0.,0.,1.)) ;
#129423 = DIRECTION('ref_axis',(-1.,0.,0.)) ;
#129424 = DIRECTION('center_axis',(-1.31418445149758E-16,1.,0.)) ;
#129425 = DIRECTION('ref_axis',(-1.,-1.31418445149758E-16,0.)) ;
#129426 = DIRECTION('center_axis',(-1.31418445149758E-16,1.,0.)) ;
#129427 = DIRECTION('ref_axis',(-1.,0.,0.)) ;
#129428 = DIRECTION('center_axis',(-1.31418445149758E-16,1.,0.)) ;
#129429 = DIRECTION('ref_axis',(-1.,-1.31418445149758E-16,0.)) ;
#129430 = DIRECTION('center_axis',(0.,0.,1.)) ;
#129431 = DIRECTION('ref_axis',(-1.,0.,0.)) ;
#129432 = DIRECTION('center_axis',(-4.33680868994202E-16,-5.69936654944139E-32,
-1.)) ;
#129433 = DIRECTION('ref_axis',(-1.,2.47170623787823E-47,4.33680868994202E-16)) ;
#129434 = DIRECTION('center_axis',(0.,0.,1.)) ;
#129435 = DIRECTION('ref_axis',(1.,0.,0.)) ;
#129436 = DIRECTION('center_axis',(-1.31418445149758E-16,-1.,0.)) ;
#129437 = DIRECTION('ref_axis',(1.,-1.31418445149758E-16,0.)) ;
#129438 = DIRECTION('center_axis',(0.,1.,0.)) ;
#129439 = DIRECTION('ref_axis',(0.,0.,1.)) ;
#129440 = DIRECTION('center_axis',(-1.,0.,2.16840434497101E-16)) ;
#129441 = DIRECTION('ref_axis',(2.16840434497101E-16,0.,1.)) ;
#129442 = DIRECTION('center_axis',(-1.,0.,0.)) ;
#129443 = DIRECTION('ref_axis',(0.,0.,1.)) ;
#129444 = DIRECTION('center_axis',(1.,0.,0.)) ;
#129445 = DIRECTION('ref_axis',(0.,0.,-1.)) ;
#129446 = DIRECTION('center_axis',(-1.31418445149758E-16,-1.,0.)) ;
#129447 = DIRECTION('ref_axis',(1.,-1.31418445149758E-16,0.)) ;
#129448 = DIRECTION('center_axis',(0.,1.,0.)) ;
#129449 = DIRECTION('ref_axis',(0.,0.,1.)) ;
#129450 = DIRECTION('center_axis',(2.16840434497101E-16,2.8496832747207E-32,
1.)) ;
#129451 = DIRECTION('ref_axis',(1.,-6.17926559469557E-48,-2.16840434497101E-16)) ;
#129452 = DIRECTION('center_axis',(0.,0.,1.)) ;
#129453 = DIRECTION('ref_axis',(1.,0.,0.)) ;
#129454 = DIRECTION('center_axis',(-1.,-1.31418445149758E-16,-2.16840434497101E-16)) ;
#129455 = DIRECTION('ref_axis',(-2.16840434497101E-16,-2.8496832747207E-32,
1.)) ;
#129456 = DIRECTION('center_axis',(-1.,0.,0.)) ;
#129457 = DIRECTION('ref_axis',(0.,0.,1.)) ;
#129458 = DIRECTION('center_axis',(1.,0.,0.)) ;
#129459 = DIRECTION('ref_axis',(0.,0.,-1.)) ;
#129460 = DIRECTION('center_axis',(-1.31418445149758E-16,1.,0.)) ;
#129461 = DIRECTION('ref_axis',(-1.,0.,0.)) ;
#129462 = DIRECTION('center_axis',(-1.31418445149758E-16,1.,0.)) ;
#129463 = DIRECTION('ref_axis',(-1.,-1.31418445149758E-16,0.)) ;
#129464 = DIRECTION('center_axis',(0.,1.,0.)) ;
#129465 = DIRECTION('ref_axis',(1.,0.,0.)) ;
#129466 = DIRECTION('center_axis',(0.,0.,-1.)) ;
#129467 = DIRECTION('ref_axis',(1.,0.,0.)) ;
#129468 = DIRECTION('center_axis',(0.,1.,0.)) ;
#129469 = DIRECTION('ref_axis',(1.,0.,0.)) ;
#129470 = DIRECTION('center_axis',(0.,0.,-1.)) ;
#129471 = DIRECTION('ref_axis',(1.,0.,0.)) ;
#129472 = DIRECTION('center_axis',(-1.31418445149758E-16,1.,0.)) ;
#129473 = DIRECTION('ref_axis',(-1.,0.,0.)) ;
#129474 = DIRECTION('center_axis',(-1.31418445149758E-16,1.,0.)) ;
#129475 = DIRECTION('ref_axis',(-1.,-1.31418445149758E-16,0.)) ;
#129476 = DIRECTION('center_axis',(-1.31418445149758E-16,-1.,0.)) ;
#129477 = DIRECTION('ref_axis',(1.,-1.31418445149758E-16,0.)) ;
#129478 = DIRECTION('center_axis',(0.,1.,0.)) ;
#129479 = DIRECTION('ref_axis',(0.,0.,1.)) ;
#129480 = DIRECTION('center_axis',(4.33680868994202E-16,0.,1.)) ;
#129481 = DIRECTION('ref_axis',(1.,0.,-4.33680868994202E-16)) ;
#129482 = DIRECTION('center_axis',(0.,0.,-1.)) ;
#129483 = DIRECTION('ref_axis',(-1.,0.,0.)) ;
#129484 = DIRECTION('center_axis',(-2.16840434497101E-16,0.,-1.)) ;
#129485 = DIRECTION('ref_axis',(-1.,0.,2.16840434497101E-16)) ;
#129486 = DIRECTION('center_axis',(0.,0.,-1.)) ;
#129487 = DIRECTION('ref_axis',(-1.,0.,0.)) ;
#129488 = DIRECTION('center_axis',(-1.31418445149758E-16,-1.,0.)) ;
#129489 = DIRECTION('ref_axis',(1.,-1.31418445149758E-16,0.)) ;
#129490 = DIRECTION('center_axis',(0.,1.,0.)) ;
#129491 = DIRECTION('ref_axis',(0.,0.,1.)) ;
#129492 = DIRECTION('center_axis',(0.,1.,0.)) ;
#129493 = DIRECTION('ref_axis',(1.,0.,0.)) ;
#129494 = DIRECTION('center_axis',(-1.,0.,0.)) ;
#129495 = DIRECTION('ref_axis',(0.,0.,-1.)) ;
#129496 = DIRECTION('center_axis',(0.,1.,0.)) ;
#129497 = DIRECTION('ref_axis',(1.,0.,0.)) ;
#129498 = DIRECTION('center_axis',(1.,0.,0.)) ;
#129499 = DIRECTION('ref_axis',(0.,0.,1.)) ;
#129500 = DIRECTION('center_axis',(1.,0.,2.16840434497101E-16)) ;
#129501 = DIRECTION('ref_axis',(2.16840434497101E-16,0.,-1.)) ;
#129502 = DIRECTION('center_axis',(0.,1.,0.)) ;
#129503 = DIRECTION('ref_axis',(0.,0.,1.)) ;
#129504 = DIRECTION('center_axis',(0.,1.,0.)) ;
#129505 = DIRECTION('ref_axis',(0.,0.,1.)) ;
#129506 = DIRECTION('center_axis',(0.,0.,-1.)) ;
#129507 = DIRECTION('ref_axis',(-1.,0.,0.)) ;
#129508 = DIRECTION('center_axis',(0.,0.,1.)) ;
#129509 = DIRECTION('ref_axis',(1.,0.,0.)) ;
#129510 = DIRECTION('center_axis',(0.,0.,-1.)) ;
#129511 = DIRECTION('ref_axis',(-1.,0.,0.)) ;
#129512 = DIRECTION('center_axis',(0.,1.,0.)) ;
#129513 = DIRECTION('ref_axis',(0.,0.,1.)) ;
#129514 = DIRECTION('center_axis',(0.,1.,0.)) ;
#129515 = DIRECTION('ref_axis',(0.,0.,1.)) ;
#129516 = DIRECTION('center_axis',(0.,1.,0.)) ;
#129517 = DIRECTION('ref_axis',(1.,0.,0.)) ;
#129518 = DIRECTION('center_axis',(-1.,0.,0.)) ;
#129519 = DIRECTION('ref_axis',(0.,0.,-1.)) ;
#129520 = DIRECTION('center_axis',(0.,1.,0.)) ;
#129521 = DIRECTION('ref_axis',(1.,0.,0.)) ;
#129522 = DIRECTION('center_axis',(-1.,0.,0.)) ;
#129523 = DIRECTION('ref_axis',(0.,0.,-1.)) ;
#129524 = DIRECTION('center_axis',(0.,1.,0.)) ;
#129525 = DIRECTION('ref_axis',(0.,0.,1.)) ;
#129526 = DIRECTION('center_axis',(0.,1.,0.)) ;
#129527 = DIRECTION('ref_axis',(0.,0.,1.)) ;
#129528 = DIRECTION('center_axis',(-1.,0.,0.)) ;
#129529 = DIRECTION('ref_axis',(0.,0.,1.)) ;
#129530 = DIRECTION('center_axis',(-1.,0.,0.)) ;
#129531 = DIRECTION('ref_axis',(0.,0.,1.)) ;
#129532 = DIRECTION('center_axis',(1.,0.,0.)) ;
#129533 = DIRECTION('ref_axis',(0.,0.,-1.)) ;
#129534 = DIRECTION('center_axis',(-1.,0.,0.)) ;
#129535 = DIRECTION('ref_axis',(0.,0.,1.)) ;
#129536 = DIRECTION('center_axis',(0.,1.,0.)) ;
#129537 = DIRECTION('ref_axis',(0.,0.,1.)) ;
#129538 = DIRECTION('center_axis',(0.,1.,0.)) ;
#129539 = DIRECTION('ref_axis',(0.,0.,1.)) ;
#129540 = DIRECTION('center_axis',(0.,1.,0.)) ;
#129541 = DIRECTION('ref_axis',(1.,0.,0.)) ;
#129542 = DIRECTION('center_axis',(0.,0.,1.)) ;
#129543 = DIRECTION('ref_axis',(-1.,0.,0.)) ;
#129544 = DIRECTION('center_axis',(0.,1.,0.)) ;
#129545 = DIRECTION('ref_axis',(1.,0.,0.)) ;
#129546 = DIRECTION('center_axis',(0.,0.,-1.)) ;
#129547 = DIRECTION('ref_axis',(1.,0.,0.)) ;
#129548 = DIRECTION('center_axis',(0.,0.,1.)) ;
#129549 = DIRECTION('ref_axis',(1.,0.,0.)) ;
#129550 = DIRECTION('center_axis',(0.,0.,1.)) ;
#129551 = DIRECTION('ref_axis',(1.,0.,0.)) ;
#129552 = DIRECTION('center_axis',(0.,0.,-1.)) ;
#129553 = DIRECTION('ref_axis',(-1.,0.,0.)) ;
#129554 = DIRECTION('center_axis',(0.,0.,1.)) ;
#129555 = DIRECTION('ref_axis',(1.,0.,0.)) ;
#129556 = DIRECTION('center_axis',(1.,0.,0.)) ;
#129557 = DIRECTION('ref_axis',(0.,0.,-1.)) ;
#129558 = DIRECTION('center_axis',(1.,0.,0.)) ;
#129559 = DIRECTION('ref_axis',(0.,0.,-1.)) ;
#129560 = DIRECTION('center_axis',(1.,0.,0.)) ;
#129561 = DIRECTION('ref_axis',(0.,0.,-1.)) ;
#129562 = DIRECTION('center_axis',(1.,0.,8.67361737988409E-15)) ;
#129563 = DIRECTION('ref_axis',(8.67361737988409E-15,0.,-1.)) ;
#129564 = DIRECTION('center_axis',(1.,0.,0.)) ;
#129565 = DIRECTION('ref_axis',(0.,0.,-1.)) ;
#129566 = DIRECTION('center_axis',(1.,0.,1.73472347597682E-14)) ;
#129567 = DIRECTION('ref_axis',(1.73472347597682E-14,0.,-1.)) ;
#129568 = DIRECTION('center_axis',(-1.,0.,0.)) ;
#129569 = DIRECTION('ref_axis',(0.,0.,1.)) ;
#129570 = DIRECTION('center_axis',(1.,0.,0.)) ;
#129571 = DIRECTION('ref_axis',(0.,0.,-1.)) ;
#129572 = DIRECTION('center_axis',(1.,0.,0.)) ;
#129573 = DIRECTION('ref_axis',(0.,0.,-1.)) ;
#129574 = DIRECTION('center_axis',(-3.46944695195364E-14,0.,-1.)) ;
#129575 = DIRECTION('ref_axis',(-1.,0.,3.46944695195364E-14)) ;
#129576 = DIRECTION('center_axis',(1.,0.,0.)) ;
#129577 = DIRECTION('ref_axis',(0.,0.,-1.)) ;
#129578 = DIRECTION('center_axis',(0.,0.,1.)) ;
#129579 = DIRECTION('ref_axis',(1.,0.,0.)) ;
#129580 = DIRECTION('center_axis',(0.,0.,-1.)) ;
#129581 = DIRECTION('ref_axis',(-1.,0.,0.)) ;
#129582 = DIRECTION('center_axis',(-0.422618261740697,5.55398348498559E-17,
0.906307787036651)) ;
#129583 = DIRECTION('ref_axis',(0.906307787036651,6.51773046476477E-31,0.422618261740697)) ;
#129584 = DIRECTION('center_axis',(0.422618261740697,-5.55398348498559E-17,
-0.906307787036651)) ;
#129585 = DIRECTION('ref_axis',(-0.906307787036651,-6.46086972436398E-31,
-0.422618261740697)) ;
#129586 = DIRECTION('center_axis',(-0.422618261740697,5.55398348498559E-17,
0.906307787036651)) ;
#129587 = DIRECTION('ref_axis',(0.906307787036651,6.46086972436398E-31,0.422618261740697)) ;
#129588 = DIRECTION('center_axis',(0.422618261740697,-5.55398348498559E-17,
-0.906307787036651)) ;
#129589 = DIRECTION('ref_axis',(-0.906307787036651,-6.46086972436398E-31,
-0.422618261740697)) ;
#129590 = DIRECTION('center_axis',(0.,1.,0.)) ;
#129591 = DIRECTION('ref_axis',(1.,0.,0.)) ;
#129592 = DIRECTION('center_axis',(3.4216004848576E-14,0.514231796959095,
-0.857651245551606)) ;
#129593 = DIRECTION('ref_axis',(3.46944695195362E-14,-0.857651245551606,-0.514231796959095)) ;
#129594 = DIRECTION('center_axis',(0.,-3.46944695195362E-14,1.)) ;
#129595 = DIRECTION('ref_axis',(0.,1.,3.46944695195362E-14)) ;
#129596 = DIRECTION('center_axis',(-1.,0.,0.)) ;
#129597 = DIRECTION('ref_axis',(0.,-4.33680868994204E-15,-1.)) ;
#129598 = DIRECTION('center_axis',(0.,0.,1.)) ;
#129599 = DIRECTION('ref_axis',(1.,0.,0.)) ;
#129600 = DIRECTION('center_axis',(0.,0.,1.)) ;
#129601 = DIRECTION('ref_axis',(1.,0.,0.)) ;
#129602 = DIRECTION('center_axis',(-1.,0.,0.)) ;
#129603 = DIRECTION('ref_axis',(0.,0.,1.)) ;
#129604 = DIRECTION('center_axis',(-1.,0.,0.)) ;
#129605 = DIRECTION('ref_axis',(0.,-4.33680868994204E-15,-1.)) ;
#129606 = DIRECTION('center_axis',(1.,0.,0.)) ;
#129607 = DIRECTION('ref_axis',(0.,0.,-1.)) ;
#129608 = DIRECTION('center_axis',(0.,-0.514231796959124,-0.857651245551588)) ;
#129609 = DIRECTION('ref_axis',(0.,0.857651245551588,-0.514231796959124)) ;
#129610 = DIRECTION('center_axis',(0.,1.,8.97270763436279E-17)) ;
#129611 = DIRECTION('ref_axis',(0.,-8.97270763436279E-17,1.)) ;
#129612 = DIRECTION('center_axis',(0.,-1.,-8.97270763436279E-17)) ;
#129613 = DIRECTION('ref_axis',(0.,-8.97270763436279E-17,1.)) ;
#129614 = DIRECTION('center_axis',(0.,-1.,0.)) ;
#129615 = DIRECTION('ref_axis',(0.,0.,-1.)) ;
#129616 = DIRECTION('center_axis',(0.,1.,0.)) ;
#129617 = DIRECTION('ref_axis',(1.,0.,0.)) ;
#129618 = DIRECTION('center_axis',(-1.,0.,0.)) ;
#129619 = DIRECTION('ref_axis',(0.,0.,-1.)) ;
#129620 = DIRECTION('center_axis',(1.,0.,0.)) ;
#129621 = DIRECTION('ref_axis',(0.,0.,-1.)) ;
#129622 = DIRECTION('center_axis',(0.,-0.514231796959093,0.857651245551607)) ;
#129623 = DIRECTION('ref_axis',(0.,0.857651245551607,0.514231796959093)) ;
#129624 = DIRECTION('center_axis',(0.,0.,-1.)) ;
#129625 = DIRECTION('ref_axis',(1.,0.,0.)) ;
#129626 = DIRECTION('center_axis',(0.,1.,0.)) ;
#129627 = DIRECTION('ref_axis',(1.,0.,0.)) ;
#129628 = DIRECTION('center_axis',(-3.46944695195364E-14,0.,-1.)) ;
#129629 = DIRECTION('ref_axis',(1.,0.,-3.46944695195364E-14)) ;
#129630 = DIRECTION('center_axis',(-1.,0.,0.)) ;
#129631 = DIRECTION('ref_axis',(0.,4.33680868994204E-15,-1.)) ;
#129632 = DIRECTION('center_axis',(0.,0.,-1.)) ;
#129633 = DIRECTION('ref_axis',(-1.,0.,0.)) ;
#129634 = DIRECTION('center_axis',(0.,0.,1.)) ;
#129635 = DIRECTION('ref_axis',(-1.,0.,0.)) ;
#129636 = DIRECTION('center_axis',(0.,0.,-1.)) ;
#129637 = DIRECTION('ref_axis',(-1.,0.,0.)) ;
#129638 = DIRECTION('center_axis',(-1.,0.,7.01133629567814E-33)) ;
#129639 = DIRECTION('ref_axis',(7.01133629567814E-33,0.,1.)) ;
#129640 = DIRECTION('center_axis',(-1.,0.,0.)) ;
#129641 = DIRECTION('ref_axis',(0.,0.,1.)) ;
#129642 = DIRECTION('center_axis',(0.,0.,-1.)) ;
#129643 = DIRECTION('ref_axis',(-1.,0.,0.)) ;
#129644 = DIRECTION('center_axis',(-7.01133629567814E-33,8.97270763436279E-17,
-1.)) ;
#129645 = DIRECTION('ref_axis',(6.29106707073161E-49,1.,8.97270763436279E-17)) ;
#129646 = DIRECTION('center_axis',(1.,0.,0.)) ;
#129647 = DIRECTION('ref_axis',(0.,0.,-1.)) ;
#129648 = DIRECTION('center_axis',(-2.2301249256967E-15,0.514231796959095,
0.857651245551606)) ;
#129649 = DIRECTION('ref_axis',(-4.79361507851841E-30,-0.857651245551606,
0.514231796959095)) ;
#129650 = DIRECTION('center_axis',(-1.,0.,0.)) ;
#129651 = DIRECTION('ref_axis',(0.,0.,1.)) ;
#129652 = DIRECTION('center_axis',(-1.,0.,0.)) ;
#129653 = DIRECTION('ref_axis',(0.,-4.33680868994204E-15,-1.)) ;
#129654 = DIRECTION('center_axis',(0.,0.,1.)) ;
#129655 = DIRECTION('ref_axis',(1.,0.,0.)) ;
#129656 = DIRECTION('center_axis',(0.,0.,-1.)) ;
#129657 = DIRECTION('ref_axis',(-1.,0.,0.)) ;
#129658 = DIRECTION('center_axis',(0.,-1.,8.97270763436279E-17)) ;
#129659 = DIRECTION('ref_axis',(0.,-8.97270763436279E-17,-1.)) ;
#129660 = DIRECTION('center_axis',(0.,-1.,8.97270763436279E-17)) ;
#129661 = DIRECTION('ref_axis',(0.,-8.97270763436279E-17,-1.)) ;
#129662 = DIRECTION('center_axis',(0.,-1.,0.)) ;
#129663 = DIRECTION('ref_axis',(0.,0.,-1.)) ;
#129664 = DIRECTION('center_axis',(-7.01133629567814E-33,8.97270763436279E-17,
-1.)) ;
#129665 = DIRECTION('ref_axis',(0.,1.,0.)) ;
#129666 = DIRECTION('center_axis',(0.,-1.,0.)) ;
#129667 = DIRECTION('ref_axis',(0.,0.,1.)) ;
#129668 = DIRECTION('center_axis',(1.,0.,0.)) ;
#129669 = DIRECTION('ref_axis',(0.,0.,-1.)) ;
#129670 = DIRECTION('center_axis',(0.,0.,1.)) ;
#129671 = DIRECTION('ref_axis',(-1.,0.,0.)) ;
#129672 = DIRECTION('center_axis',(0.,1.,0.)) ;
#129673 = DIRECTION('ref_axis',(1.,0.,0.)) ;
#129674 = DIRECTION('center_axis',(-1.,0.,0.)) ;
#129675 = DIRECTION('ref_axis',(0.,0.,-1.)) ;
#129676 = DIRECTION('center_axis',(1.,7.81406971160724E-17,0.)) ;
#129677 = DIRECTION('ref_axis',(-7.81406971160724E-17,1.,0.)) ;
#129678 = DIRECTION('center_axis',(1.,0.,0.)) ;
#129679 = DIRECTION('ref_axis',(0.,0.,-1.)) ;
#129680 = DIRECTION('center_axis',(1.,0.,0.)) ;
#129681 = DIRECTION('ref_axis',(0.,0.,-1.)) ;
#129682 = DIRECTION('center_axis',(0.,1.,8.97270763436279E-17)) ;
#129683 = DIRECTION('ref_axis',(0.,-8.97270763436279E-17,1.)) ;
#129684 = DIRECTION('center_axis',(0.,-1.,0.)) ;
#129685 = DIRECTION('ref_axis',(0.,0.,-1.)) ;
#129686 = DIRECTION('center_axis',(0.,0.,-1.)) ;
#129687 = DIRECTION('ref_axis',(-1.,0.,0.)) ;
#129688 = DIRECTION('center_axis',(-7.01133629567814E-33,8.97270763436279E-17,
1.)) ;
#129689 = DIRECTION('ref_axis',(-6.29106707073161E-49,-1.,8.97270763436279E-17)) ;
#129690 = DIRECTION('center_axis',(-1.,0.,-7.01133629567814E-33)) ;
#129691 = DIRECTION('ref_axis',(-7.01133629567814E-33,0.,1.)) ;
#129692 = DIRECTION('center_axis',(-1.,0.,0.)) ;
#129693 = DIRECTION('ref_axis',(0.,0.,1.)) ;
#129694 = DIRECTION('center_axis',(1.,0.,0.)) ;
#129695 = DIRECTION('ref_axis',(0.,1.,0.)) ;
#129696 = DIRECTION('center_axis',(2.16840434497101E-15,1.,0.)) ;
#129697 = DIRECTION('ref_axis',(-1.,2.16840434497101E-15,0.)) ;
#129698 = DIRECTION('center_axis',(0.,1.,0.)) ;
#129699 = DIRECTION('ref_axis',(1.,0.,0.)) ;
#129700 = DIRECTION('center_axis',(0.,0.,-1.)) ;
#129701 = DIRECTION('ref_axis',(1.,0.,0.)) ;
#129702 = DIRECTION('center_axis',(-1.,0.,0.)) ;
#129703 = DIRECTION('ref_axis',(0.,0.,-1.)) ;
#129704 = DIRECTION('center_axis',(-7.01133629567814E-33,8.97270763436279E-17,
1.)) ;
#129705 = DIRECTION('ref_axis',(0.,-1.,0.)) ;
#129706 = DIRECTION('center_axis',(0.,-1.,0.)) ;
#129707 = DIRECTION('ref_axis',(0.,0.,1.)) ;
#129708 = DIRECTION('center_axis',(7.81406971160724E-17,-1.,-8.97270763436279E-17)) ;
#129709 = DIRECTION('ref_axis',(-7.01133629567814E-33,8.97270763436279E-17,
-1.)) ;
#129710 = DIRECTION('center_axis',(0.,1.,0.)) ;
#129711 = DIRECTION('ref_axis',(0.,0.,1.)) ;
#129712 = DIRECTION('center_axis',(-1.,-7.81406971160724E-17,0.)) ;
#129713 = DIRECTION('ref_axis',(7.81406971160724E-17,-1.,0.)) ;
#129714 = DIRECTION('center_axis',(-1.,-7.81406971160724E-17,0.)) ;
#129715 = DIRECTION('ref_axis',(-7.81406971160724E-17,1.,0.)) ;
#129716 = DIRECTION('center_axis',(0.,0.,1.)) ;
#129717 = DIRECTION('ref_axis',(1.,0.,0.)) ;
#129718 = DIRECTION('center_axis',(0.,0.,-1.)) ;
#129719 = DIRECTION('ref_axis',(-1.,0.,0.)) ;
#129720 = DIRECTION('center_axis',(0.,-1.,8.97270763436279E-17)) ;
#129721 = DIRECTION('ref_axis',(0.,-8.97270763436279E-17,-1.)) ;
#129722 = DIRECTION('center_axis',(0.,-1.,0.)) ;
#129723 = DIRECTION('ref_axis',(0.,0.,-1.)) ;
#129724 = DIRECTION('center_axis',(1.,7.81406971160724E-17,0.)) ;
#129725 = DIRECTION('ref_axis',(0.,1.,0.)) ;
#129726 = DIRECTION('center_axis',(0.,0.,1.)) ;
#129727 = DIRECTION('ref_axis',(-1.,0.,0.)) ;
#129728 = DIRECTION('center_axis',(0.,1.,0.)) ;
#129729 = DIRECTION('ref_axis',(1.,0.,0.)) ;
#129730 = DIRECTION('center_axis',(-1.,0.,0.)) ;
#129731 = DIRECTION('ref_axis',(0.,0.,-1.)) ;
#129732 = DIRECTION('center_axis',(0.,0.,-1.)) ;
#129733 = DIRECTION('ref_axis',(-1.,0.,0.)) ;
#129734 = DIRECTION('center_axis',(0.,0.,1.)) ;
#129735 = DIRECTION('ref_axis',(1.,0.,0.)) ;
#129736 = DIRECTION('center_axis',(-1.,-7.81406971160724E-17,0.)) ;
#129737 = DIRECTION('ref_axis',(7.81406971160724E-17,-1.,0.)) ;
#129738 = DIRECTION('center_axis',(-1.,-7.81406971160724E-17,0.)) ;
#129739 = DIRECTION('ref_axis',(-7.81406971160724E-17,1.,0.)) ;
#129740 = DIRECTION('center_axis',(1.,7.81406971160724E-17,0.)) ;
#129741 = DIRECTION('ref_axis',(-7.81406971160724E-17,1.,0.)) ;
#129742 = DIRECTION('center_axis',(1.,0.,0.)) ;
#129743 = DIRECTION('ref_axis',(0.,0.,-1.)) ;
#129744 = DIRECTION('center_axis',(1.,0.,0.)) ;
#129745 = DIRECTION('ref_axis',(0.,0.,-1.)) ;
#129746 = DIRECTION('center_axis',(3.78638272950961E-32,-4.8455963016112E-16,
-1.)) ;
#129747 = DIRECTION('ref_axis',(1.83472821505963E-47,1.,-4.8455963016112E-16)) ;
#129748 = DIRECTION('center_axis',(3.78638272950961E-32,-4.8455963016112E-16,
-1.)) ;
#129749 = DIRECTION('ref_axis',(1.83472821505963E-47,1.,-4.8455963016112E-16)) ;
#129750 = DIRECTION('center_axis',(0.,0.,-1.)) ;
#129751 = DIRECTION('ref_axis',(-1.,0.,0.)) ;
#129752 = DIRECTION('center_axis',(1.,7.81406971160724E-17,0.)) ;
#129753 = DIRECTION('ref_axis',(0.,1.,0.)) ;
#129754 = DIRECTION('center_axis',(0.,-1.,0.)) ;
#129755 = DIRECTION('ref_axis',(0.,0.,1.)) ;
#129756 = DIRECTION('center_axis',(0.,1.,0.)) ;
#129757 = DIRECTION('ref_axis',(1.,0.,0.)) ;
#129758 = DIRECTION('center_axis',(0.,1.,0.)) ;
#129759 = DIRECTION('ref_axis',(0.,0.,-1.)) ;
#129760 = DIRECTION('center_axis',(-7.81406971160724E-17,1.,-8.97270763436279E-17)) ;
#129761 = DIRECTION('ref_axis',(-7.01133629567814E-33,8.97270763436279E-17,
1.)) ;
#129762 = DIRECTION('center_axis',(0.,-1.,0.)) ;
#129763 = DIRECTION('ref_axis',(0.,0.,-1.)) ;
#129764 = DIRECTION('center_axis',(0.,1.,0.)) ;
#129765 = DIRECTION('ref_axis',(0.,0.,1.)) ;
#129766 = DIRECTION('center_axis',(0.,-1.,0.)) ;
#129767 = DIRECTION('ref_axis',(0.,0.,-1.)) ;
#129768 = DIRECTION('center_axis',(0.,-1.,0.)) ;
#129769 = DIRECTION('ref_axis',(0.,0.,-1.)) ;
#129770 = DIRECTION('center_axis',(0.,1.,0.)) ;
#129771 = DIRECTION('ref_axis',(1.,0.,0.)) ;
#129772 = DIRECTION('center_axis',(0.,0.,1.)) ;
#129773 = DIRECTION('ref_axis',(-1.,0.,0.)) ;
#129774 = DIRECTION('center_axis',(1.,0.,0.)) ;
#129775 = DIRECTION('ref_axis',(0.,0.,1.)) ;
#129776 = DIRECTION('center_axis',(0.,-1.,0.)) ;
#129777 = DIRECTION('ref_axis',(0.,0.,-1.)) ;
#129778 = DIRECTION('center_axis',(0.,1.,0.)) ;
#129779 = DIRECTION('ref_axis',(0.,0.,1.)) ;
#129780 = DIRECTION('center_axis',(0.,-1.,0.)) ;
#129781 = DIRECTION('ref_axis',(0.,0.,-1.)) ;
#129782 = DIRECTION('center_axis',(-1.,0.,2.16840434497101E-16)) ;
#129783 = DIRECTION('ref_axis',(2.16840434497101E-16,0.,1.)) ;
#129784 = DIRECTION('center_axis',(1.,0.,0.)) ;
#129785 = DIRECTION('ref_axis',(0.,0.,-1.)) ;
#129786 = DIRECTION('center_axis',(-2.16840434497101E-16,0.,1.)) ;
#129787 = DIRECTION('ref_axis',(1.,0.,2.16840434497101E-16)) ;
#129788 = DIRECTION('center_axis',(0.,0.,1.)) ;
#129789 = DIRECTION('ref_axis',(1.,0.,0.)) ;
#129790 = DIRECTION('center_axis',(0.,1.,0.)) ;
#129791 = DIRECTION('ref_axis',(0.,0.,1.)) ;
#129792 = DIRECTION('center_axis',(0.,-1.,0.)) ;
#129793 = DIRECTION('ref_axis',(0.,0.,-1.)) ;
#129794 = DIRECTION('center_axis',(0.,1.,0.)) ;
#129795 = DIRECTION('ref_axis',(1.,0.,0.)) ;
#129796 = DIRECTION('center_axis',(0.,0.,1.)) ;
#129797 = DIRECTION('ref_axis',(-1.,0.,0.)) ;
#129798 = DIRECTION('center_axis',(0.,1.,0.)) ;
#129799 = DIRECTION('ref_axis',(1.,0.,0.)) ;
#129800 = DIRECTION('center_axis',(1.,0.,0.)) ;
#129801 = DIRECTION('ref_axis',(0.,0.,1.)) ;
#129802 = DIRECTION('center_axis',(0.,0.,-1.)) ;
#129803 = DIRECTION('ref_axis',(-1.,0.,0.)) ;
#129804 = DIRECTION('center_axis',(0.,0.,1.)) ;
#129805 = DIRECTION('ref_axis',(1.,0.,0.)) ;
#129806 = DIRECTION('center_axis',(1.,0.,2.16840434497101E-16)) ;
#129807 = DIRECTION('ref_axis',(2.16840434497101E-16,0.,-1.)) ;
#129808 = DIRECTION('center_axis',(1.,0.,0.)) ;
#129809 = DIRECTION('ref_axis',(0.,0.,-1.)) ;
#129810 = DIRECTION('center_axis',(0.,1.,0.)) ;
#129811 = DIRECTION('ref_axis',(1.,0.,0.)) ;
#129812 = DIRECTION('center_axis',(0.,1.,0.)) ;
#129813 = DIRECTION('ref_axis',(0.,0.,-1.)) ;
#129814 = DIRECTION('center_axis',(0.,1.,0.)) ;
#129815 = DIRECTION('ref_axis',(0.,0.,1.)) ;
#129816 = DIRECTION('center_axis',(0.,1.,0.)) ;
#129817 = DIRECTION('ref_axis',(0.,0.,1.)) ;
#129818 = DIRECTION('center_axis',(-0.942809041582063,-0.235702260395516,
0.235702260395518)) ;
#129819 = DIRECTION('ref_axis',(0.242535625036335,4.64743530723282E-16,0.970142500145331)) ;
#129820 = DIRECTION('center_axis',(-0.970142500145332,-0.242535625036331,
-2.10366121255617E-15)) ;
#129821 = DIRECTION('ref_axis',(0.242535625036331,-0.970142500145332,-4.47980524894761E-30)) ;
#129822 = DIRECTION('center_axis',(0.970142500145333,0.24253562503633,0.)) ;
#129823 = DIRECTION('ref_axis',(-0.24253562503633,0.970142500145333,0.)) ;
#129824 = DIRECTION('center_axis',(-0.970142500145332,-0.242535625036331,
2.73475957632304E-14)) ;
#129825 = DIRECTION('ref_axis',(0.242535625036331,-0.970142500145332,1.1454669517322E-30)) ;
#129826 = DIRECTION('center_axis',(0.879462917689188,0.219865729422294,-0.42214220049081)) ;
#129827 = DIRECTION('ref_axis',(-0.432731067584771,1.71515946658E-16,-0.901523057468274)) ;
#129828 = DIRECTION('center_axis',(0.879462917689192,0.219865729422271,-0.422142200490814)) ;
#129829 = DIRECTION('ref_axis',(-0.432731067584773,-1.62351711522009E-16,
-0.901523057468273)) ;
#129830 = DIRECTION('center_axis',(0.,1.,0.)) ;
#129831 = DIRECTION('ref_axis',(1.,0.,0.)) ;
#129832 = DIRECTION('center_axis',(0.,-1.,0.)) ;
#129833 = DIRECTION('ref_axis',(0.,0.,1.)) ;
#129834 = DIRECTION('center_axis',(0.,-1.,0.)) ;
#129835 = DIRECTION('ref_axis',(0.,0.,-1.)) ;
#129836 = DIRECTION('center_axis',(-4.51750905202295E-15,-1.,2.16840434497102E-15)) ;
#129837 = DIRECTION('ref_axis',(1.,-4.51750905202295E-15,3.91831450274151E-31)) ;
#129838 = DIRECTION('center_axis',(0.669589480006976,-0.669589480006974,-0.321402950403349)) ;
#129839 = DIRECTION('ref_axis',(0.707106781186547,0.707106781186548,5.45170614306381E-16)) ;
#129840 = DIRECTION('center_axis',(0.669589480006977,-0.669589480006977,-0.321402950403342)) ;
#129841 = DIRECTION('ref_axis',(0.707106781186547,0.707106781186548,-1.94221176494188E-16)) ;
#129842 = DIRECTION('center_axis',(0.,1.,0.)) ;
#129843 = DIRECTION('ref_axis',(1.,0.,0.)) ;
#129844 = DIRECTION('center_axis',(0.707106781186541,-0.707106781186554,0.)) ;
#129845 = DIRECTION('ref_axis',(-0.707106781186554,-0.707106781186541,0.)) ;
#129846 = DIRECTION('center_axis',(0.707106781186549,-0.707106781186546,0.)) ;
#129847 = DIRECTION('ref_axis',(0.707106781186546,0.707106781186549,0.)) ;
#129848 = DIRECTION('center_axis',(0.707106781186548,-0.707106781186548,-1.53329341668338E-15)) ;
#129849 = DIRECTION('ref_axis',(0.707106781186548,0.707106781186548,1.5356898865553E-31)) ;
#129850 = DIRECTION('center_axis',(0.577350269189633,-0.577350269189633,-0.577350269189612)) ;
#129851 = DIRECTION('ref_axis',(0.707106781186548,0.707106781186548,1.34560831514457E-17)) ;
#129852 = DIRECTION('center_axis',(-0.577350269189344,0.577350269189586,-0.577350269189947)) ;
#129853 = DIRECTION('ref_axis',(1.30446081606812E-15,0.707106781186769,0.707106781186326)) ;
#129854 = DIRECTION('center_axis',(-0.707106781186548,0.707106781186548,7.66646708341692E-15)) ;
#129855 = DIRECTION('ref_axis',(-0.707106781186548,-0.707106781186548,-2.68297081166629E-31)) ;
#129856 = DIRECTION('center_axis',(-0.707106781186549,0.707106781186546,0.)) ;
#129857 = DIRECTION('ref_axis',(-0.707106781186546,-0.707106781186549,0.)) ;
#129858 = DIRECTION('center_axis',(-0.707106781186548,0.707106781186548,-1.22663473334671E-14)) ;
#129859 = DIRECTION('ref_axis',(-0.707106781186548,-0.707106781186548,2.94725045705944E-31)) ;
#129860 = DIRECTION('center_axis',(-0.669589480006976,0.669589480006974,-0.321402950403349)) ;
#129861 = DIRECTION('ref_axis',(-0.707106781186547,-0.707106781186548,5.45170614306381E-16)) ;
#129862 = DIRECTION('center_axis',(0.669589480006982,-0.669589480006966,0.321402950403353)) ;
#129863 = DIRECTION('ref_axis',(0.707106781186539,0.707106781186556,5.77426876420606E-17)) ;
#129864 = DIRECTION('center_axis',(0.,1.,0.)) ;
#129865 = DIRECTION('ref_axis',(1.,0.,0.)) ;
#129866 = DIRECTION('center_axis',(0.,1.,0.)) ;
#129867 = DIRECTION('ref_axis',(0.,0.,-1.)) ;
#129868 = DIRECTION('center_axis',(0.,-1.,0.)) ;
#129869 = DIRECTION('ref_axis',(0.,0.,-1.)) ;
#129870 = DIRECTION('center_axis',(0.,1.,0.)) ;
#129871 = DIRECTION('ref_axis',(0.,0.,1.)) ;
#129872 = DIRECTION('center_axis',(-0.879462917689188,-0.219865729422294,
-0.42214220049081)) ;
#129873 = DIRECTION('ref_axis',(-0.432731067584771,1.71515946658E-16,0.901523057468274)) ;
#129874 = DIRECTION('center_axis',(0.879462917689201,0.219865729422298,0.42214220049078)) ;
#129875 = DIRECTION('ref_axis',(0.432731067584741,5.42470486237819E-16,-0.901523057468288)) ;
#129876 = DIRECTION('center_axis',(0.,1.,0.)) ;
#129877 = DIRECTION('ref_axis',(1.,0.,0.)) ;
#129878 = DIRECTION('center_axis',(0.970142500145323,0.242535625036368,0.)) ;
#129879 = DIRECTION('ref_axis',(0.242535625036368,-0.970142500145323,0.)) ;
#129880 = DIRECTION('center_axis',(-0.970142500145333,-0.24253562503633,0.)) ;
#129881 = DIRECTION('ref_axis',(0.24253562503633,-0.970142500145333,0.)) ;
#129882 = DIRECTION('center_axis',(0.970142500145332,0.242535625036331,-2.10366121255617E-15)) ;
#129883 = DIRECTION('ref_axis',(-0.242535625036331,0.970142500145332,-4.47980524894761E-30)) ;
#129884 = DIRECTION('center_axis',(0.942809041582064,0.235702260395514,0.235702260395514)) ;
#129885 = DIRECTION('ref_axis',(-0.242535625036331,0.970142500145332,4.49011373492972E-16)) ;
#129886 = DIRECTION('center_axis',(0.,-1.,0.)) ;
#129887 = DIRECTION('ref_axis',(0.,0.,-1.)) ;
#129888 = DIRECTION('center_axis',(-1.,0.,-8.67361737988409E-15)) ;
#129889 = DIRECTION('ref_axis',(-8.67361737988409E-15,0.,1.)) ;
#129890 = DIRECTION('center_axis',(0.,0.,-1.)) ;
#129891 = DIRECTION('ref_axis',(-1.,0.,0.)) ;
#129892 = DIRECTION('center_axis',(0.,0.,-1.)) ;
#129893 = DIRECTION('ref_axis',(-1.,0.,0.)) ;
#129894 = DIRECTION('center_axis',(0.,3.46944695195362E-14,-1.)) ;
#129895 = DIRECTION('ref_axis',(0.,1.,3.46944695195362E-14)) ;
#129896 = DIRECTION('center_axis',(1.,0.,0.)) ;
#129897 = DIRECTION('ref_axis',(0.,0.,-1.)) ;
#129898 = DIRECTION('center_axis',(-1.,0.,0.)) ;
#129899 = DIRECTION('ref_axis',(0.,0.,1.)) ;
#129900 = DIRECTION('center_axis',(0.,-1.,0.)) ;
#129901 = DIRECTION('ref_axis',(0.,0.,-1.)) ;
#129902 = DIRECTION('center_axis',(-1.,0.,0.)) ;
#129903 = DIRECTION('ref_axis',(0.,0.,1.)) ;
#129904 = DIRECTION('center_axis',(0.,-1.,0.)) ;
#129905 = DIRECTION('ref_axis',(0.,0.,-1.)) ;
#129906 = DIRECTION('center_axis',(3.46944695195358E-14,0.,-1.)) ;
#129907 = DIRECTION('ref_axis',(-1.,0.,-3.46944695195358E-14)) ;
#129908 = DIRECTION('center_axis',(-1.,0.,0.)) ;
#129909 = DIRECTION('ref_axis',(0.,0.,1.)) ;
#129910 = DIRECTION('center_axis',(-1.,1.73472347597681E-14,0.)) ;
#129911 = DIRECTION('ref_axis',(-1.73472347597681E-14,-1.,0.)) ;
#129912 = DIRECTION('center_axis',(0.,0.,1.)) ;
#129913 = DIRECTION('ref_axis',(1.,0.,0.)) ;
#129914 = DIRECTION('center_axis',(-3.46944695195364E-14,0.,-1.)) ;
#129915 = DIRECTION('ref_axis',(-1.,0.,3.46944695195364E-14)) ;
#129916 = DIRECTION('center_axis',(0.,-1.,0.)) ;
#129917 = DIRECTION('ref_axis',(0.,0.,-1.)) ;
#129918 = DIRECTION('center_axis',(0.,-1.,0.)) ;
#129919 = DIRECTION('ref_axis',(0.,0.,-1.)) ;
#129920 = DIRECTION('center_axis',(0.,-1.,0.)) ;
#129921 = DIRECTION('ref_axis',(0.,0.,-1.)) ;
#129922 = DIRECTION('center_axis',(0.,0.,1.)) ;
#129923 = DIRECTION('ref_axis',(1.,0.,0.)) ;
#129924 = DIRECTION('center_axis',(0.,0.,-1.)) ;
#129925 = DIRECTION('ref_axis',(-1.,0.,0.)) ;
#129926 = DIRECTION('center_axis',(0.,0.,1.)) ;
#129927 = DIRECTION('ref_axis',(1.,0.,0.)) ;
#129928 = DIRECTION('center_axis',(0.,-1.,0.)) ;
#129929 = DIRECTION('ref_axis',(0.,0.,-1.)) ;
#129930 = DIRECTION('center_axis',(0.,-1.,0.)) ;
#129931 = DIRECTION('ref_axis',(0.,0.,-1.)) ;
#129932 = DIRECTION('center_axis',(0.,1.,0.)) ;
#129933 = DIRECTION('ref_axis',(1.,0.,0.)) ;
#129934 = DIRECTION('center_axis',(-1.,0.,0.)) ;
#129935 = DIRECTION('ref_axis',(0.,0.,-1.)) ;
#129936 = DIRECTION('center_axis',(0.,1.,0.)) ;
#129937 = DIRECTION('ref_axis',(1.,0.,0.)) ;
#129938 = DIRECTION('center_axis',(-1.,0.,0.)) ;
#129939 = DIRECTION('ref_axis',(0.,0.,-1.)) ;
#129940 = DIRECTION('center_axis',(0.,-1.,0.)) ;
#129941 = DIRECTION('ref_axis',(0.,0.,-1.)) ;
#129942 = DIRECTION('center_axis',(0.,-1.,0.)) ;
#129943 = DIRECTION('ref_axis',(0.,0.,-1.)) ;
#129944 = DIRECTION('center_axis',(-1.,0.,0.)) ;
#129945 = DIRECTION('ref_axis',(0.,0.,1.)) ;
#129946 = DIRECTION('center_axis',(-1.,0.,0.)) ;
#129947 = DIRECTION('ref_axis',(0.,0.,1.)) ;
#129948 = DIRECTION('center_axis',(1.,0.,0.)) ;
#129949 = DIRECTION('ref_axis',(0.,0.,-1.)) ;
#129950 = DIRECTION('center_axis',(-1.,0.,0.)) ;
#129951 = DIRECTION('ref_axis',(0.,0.,1.)) ;
#129952 = DIRECTION('center_axis',(0.,-1.,0.)) ;
#129953 = DIRECTION('ref_axis',(0.,0.,-1.)) ;
#129954 = DIRECTION('center_axis',(0.,-1.,0.)) ;
#129955 = DIRECTION('ref_axis',(0.,0.,-1.)) ;
#129956 = DIRECTION('center_axis',(0.,1.,0.)) ;
#129957 = DIRECTION('ref_axis',(1.,0.,0.)) ;
#129958 = DIRECTION('center_axis',(0.,0.,-1.)) ;
#129959 = DIRECTION('ref_axis',(1.,0.,0.)) ;
#129960 = DIRECTION('center_axis',(0.,1.,0.)) ;
#129961 = DIRECTION('ref_axis',(1.,0.,0.)) ;
#129962 = DIRECTION('center_axis',(0.,0.,1.)) ;
#129963 = DIRECTION('ref_axis',(-1.,0.,0.)) ;
#129964 = DIRECTION('center_axis',(0.,0.,-1.)) ;
#129965 = DIRECTION('ref_axis',(-1.,0.,0.)) ;
#129966 = DIRECTION('center_axis',(1.,1.31418445149758E-16,-2.16840434497101E-16)) ;
#129967 = DIRECTION('ref_axis',(-2.16840434497101E-16,-2.8496832747207E-32,
-1.)) ;
#129968 = DIRECTION('center_axis',(1.,0.,0.)) ;
#129969 = DIRECTION('ref_axis',(0.,0.,-1.)) ;
#129970 = DIRECTION('center_axis',(-1.,0.,0.)) ;
#129971 = DIRECTION('ref_axis',(0.,0.,1.)) ;
#129972 = DIRECTION('center_axis',(-1.31418445149758E-16,1.,0.)) ;
#129973 = DIRECTION('ref_axis',(-1.,0.,0.)) ;
#129974 = DIRECTION('center_axis',(0.,0.,1.)) ;
#129975 = DIRECTION('ref_axis',(-1.,0.,0.)) ;
#129976 = DIRECTION('center_axis',(-1.31418445149758E-16,1.,0.)) ;
#129977 = DIRECTION('ref_axis',(-1.,-1.31418445149758E-16,0.)) ;
#129978 = DIRECTION('center_axis',(-1.31418445149758E-16,1.,0.)) ;
#129979 = DIRECTION('ref_axis',(-1.,0.,0.)) ;
#129980 = DIRECTION('center_axis',(-1.31418445149758E-16,1.,0.)) ;
#129981 = DIRECTION('ref_axis',(-1.,-1.31418445149758E-16,0.)) ;
#129982 = DIRECTION('center_axis',(0.,0.,1.)) ;
#129983 = DIRECTION('ref_axis',(-1.,0.,0.)) ;
#129984 = DIRECTION('center_axis',(-4.33680868994202E-16,-5.69936654944139E-32,
-1.)) ;
#129985 = DIRECTION('ref_axis',(-1.,2.47170623787823E-47,4.33680868994202E-16)) ;
#129986 = DIRECTION('center_axis',(0.,0.,1.)) ;
#129987 = DIRECTION('ref_axis',(1.,0.,0.)) ;
#129988 = DIRECTION('center_axis',(-1.31418445149758E-16,-1.,0.)) ;
#129989 = DIRECTION('ref_axis',(1.,-1.31418445149758E-16,0.)) ;
#129990 = DIRECTION('center_axis',(0.,1.,0.)) ;
#129991 = DIRECTION('ref_axis',(0.,0.,1.)) ;
#129992 = DIRECTION('center_axis',(-1.,0.,2.16840434497101E-16)) ;
#129993 = DIRECTION('ref_axis',(2.16840434497101E-16,0.,1.)) ;
#129994 = DIRECTION('center_axis',(-1.,0.,0.)) ;
#129995 = DIRECTION('ref_axis',(0.,0.,1.)) ;
#129996 = DIRECTION('center_axis',(1.,0.,0.)) ;
#129997 = DIRECTION('ref_axis',(0.,0.,-1.)) ;
#129998 = DIRECTION('center_axis',(-1.31418445149758E-16,-1.,0.)) ;
#129999 = DIRECTION('ref_axis',(1.,-1.31418445149758E-16,0.)) ;
#130000 = DIRECTION('center_axis',(0.,1.,0.)) ;
#130001 = DIRECTION('ref_axis',(0.,0.,1.)) ;
#130002 = DIRECTION('center_axis',(2.16840434497101E-16,2.8496832747207E-32,
1.)) ;
#130003 = DIRECTION('ref_axis',(1.,-6.17926559469557E-48,-2.16840434497101E-16)) ;
#130004 = DIRECTION('center_axis',(0.,0.,1.)) ;
#130005 = DIRECTION('ref_axis',(1.,0.,0.)) ;
#130006 = DIRECTION('center_axis',(-1.,-1.31418445149758E-16,-2.16840434497101E-16)) ;
#130007 = DIRECTION('ref_axis',(-2.16840434497101E-16,-2.8496832747207E-32,
1.)) ;
#130008 = DIRECTION('center_axis',(-1.,0.,0.)) ;
#130009 = DIRECTION('ref_axis',(0.,0.,1.)) ;
#130010 = DIRECTION('center_axis',(1.,0.,0.)) ;
#130011 = DIRECTION('ref_axis',(0.,0.,-1.)) ;
#130012 = DIRECTION('center_axis',(-1.31418445149758E-16,1.,0.)) ;
#130013 = DIRECTION('ref_axis',(-1.,0.,0.)) ;
#130014 = DIRECTION('center_axis',(-1.31418445149758E-16,1.,0.)) ;
#130015 = DIRECTION('ref_axis',(-1.,-1.31418445149758E-16,0.)) ;
#130016 = DIRECTION('center_axis',(0.,1.,0.)) ;
#130017 = DIRECTION('ref_axis',(1.,0.,0.)) ;
#130018 = DIRECTION('center_axis',(0.,0.,-1.)) ;
#130019 = DIRECTION('ref_axis',(1.,0.,0.)) ;
#130020 = DIRECTION('center_axis',(0.,1.,0.)) ;
#130021 = DIRECTION('ref_axis',(1.,0.,0.)) ;
#130022 = DIRECTION('center_axis',(0.,0.,-1.)) ;
#130023 = DIRECTION('ref_axis',(1.,0.,0.)) ;
#130024 = DIRECTION('center_axis',(-1.31418445149758E-16,1.,0.)) ;
#130025 = DIRECTION('ref_axis',(-1.,0.,0.)) ;
#130026 = DIRECTION('center_axis',(-1.31418445149758E-16,1.,0.)) ;
#130027 = DIRECTION('ref_axis',(-1.,-1.31418445149758E-16,0.)) ;
#130028 = DIRECTION('center_axis',(-1.31418445149758E-16,-1.,0.)) ;
#130029 = DIRECTION('ref_axis',(1.,-1.31418445149758E-16,0.)) ;
#130030 = DIRECTION('center_axis',(0.,1.,0.)) ;
#130031 = DIRECTION('ref_axis',(0.,0.,1.)) ;
#130032 = DIRECTION('center_axis',(4.33680868994202E-16,0.,1.)) ;
#130033 = DIRECTION('ref_axis',(1.,0.,-4.33680868994202E-16)) ;
#130034 = DIRECTION('center_axis',(0.,0.,-1.)) ;
#130035 = DIRECTION('ref_axis',(-1.,0.,0.)) ;
#130036 = DIRECTION('center_axis',(-2.16840434497101E-16,0.,-1.)) ;
#130037 = DIRECTION('ref_axis',(-1.,0.,2.16840434497101E-16)) ;
#130038 = DIRECTION('center_axis',(0.,0.,-1.)) ;
#130039 = DIRECTION('ref_axis',(-1.,0.,0.)) ;
#130040 = DIRECTION('center_axis',(-1.31418445149758E-16,-1.,0.)) ;
#130041 = DIRECTION('ref_axis',(1.,-1.31418445149758E-16,0.)) ;
#130042 = DIRECTION('center_axis',(0.,1.,0.)) ;
#130043 = DIRECTION('ref_axis',(0.,0.,1.)) ;
#130044 = DIRECTION('center_axis',(0.,1.,0.)) ;
#130045 = DIRECTION('ref_axis',(1.,0.,0.)) ;
#130046 = DIRECTION('center_axis',(-1.,0.,0.)) ;
#130047 = DIRECTION('ref_axis',(0.,0.,-1.)) ;
#130048 = DIRECTION('center_axis',(0.,1.,0.)) ;
#130049 = DIRECTION('ref_axis',(1.,0.,0.)) ;
#130050 = DIRECTION('center_axis',(1.,0.,0.)) ;
#130051 = DIRECTION('ref_axis',(0.,0.,1.)) ;
#130052 = DIRECTION('center_axis',(1.,0.,2.16840434497101E-16)) ;
#130053 = DIRECTION('ref_axis',(2.16840434497101E-16,0.,-1.)) ;
#130054 = DIRECTION('center_axis',(0.,1.,0.)) ;
#130055 = DIRECTION('ref_axis',(0.,0.,1.)) ;
#130056 = DIRECTION('center_axis',(0.,1.,0.)) ;
#130057 = DIRECTION('ref_axis',(0.,0.,1.)) ;
#130058 = DIRECTION('center_axis',(0.,0.,-1.)) ;
#130059 = DIRECTION('ref_axis',(-1.,0.,0.)) ;
#130060 = DIRECTION('center_axis',(0.,0.,1.)) ;
#130061 = DIRECTION('ref_axis',(1.,0.,0.)) ;
#130062 = DIRECTION('center_axis',(0.,0.,-1.)) ;
#130063 = DIRECTION('ref_axis',(-1.,0.,0.)) ;
#130064 = DIRECTION('center_axis',(0.,1.,0.)) ;
#130065 = DIRECTION('ref_axis',(0.,0.,1.)) ;
#130066 = DIRECTION('center_axis',(0.,1.,0.)) ;
#130067 = DIRECTION('ref_axis',(0.,0.,1.)) ;
#130068 = DIRECTION('center_axis',(0.,1.,0.)) ;
#130069 = DIRECTION('ref_axis',(1.,0.,0.)) ;
#130070 = DIRECTION('center_axis',(-1.,0.,0.)) ;
#130071 = DIRECTION('ref_axis',(0.,0.,-1.)) ;
#130072 = DIRECTION('center_axis',(0.,1.,0.)) ;
#130073 = DIRECTION('ref_axis',(1.,0.,0.)) ;
#130074 = DIRECTION('center_axis',(-1.,0.,0.)) ;
#130075 = DIRECTION('ref_axis',(0.,0.,-1.)) ;
#130076 = DIRECTION('center_axis',(0.,1.,0.)) ;
#130077 = DIRECTION('ref_axis',(0.,0.,1.)) ;
#130078 = DIRECTION('center_axis',(0.,1.,0.)) ;
#130079 = DIRECTION('ref_axis',(0.,0.,1.)) ;
#130080 = DIRECTION('center_axis',(-1.,0.,0.)) ;
#130081 = DIRECTION('ref_axis',(0.,0.,1.)) ;
#130082 = DIRECTION('center_axis',(-1.,0.,0.)) ;
#130083 = DIRECTION('ref_axis',(0.,0.,1.)) ;
#130084 = DIRECTION('center_axis',(1.,0.,0.)) ;
#130085 = DIRECTION('ref_axis',(0.,0.,-1.)) ;
#130086 = DIRECTION('center_axis',(-1.,0.,0.)) ;
#130087 = DIRECTION('ref_axis',(0.,0.,1.)) ;
#130088 = DIRECTION('center_axis',(0.,1.,0.)) ;
#130089 = DIRECTION('ref_axis',(0.,0.,1.)) ;
#130090 = DIRECTION('center_axis',(0.,1.,0.)) ;
#130091 = DIRECTION('ref_axis',(0.,0.,1.)) ;
#130092 = DIRECTION('center_axis',(0.,1.,0.)) ;
#130093 = DIRECTION('ref_axis',(1.,0.,0.)) ;
#130094 = DIRECTION('center_axis',(0.,0.,1.)) ;
#130095 = DIRECTION('ref_axis',(-1.,0.,0.)) ;
#130096 = DIRECTION('center_axis',(0.,1.,0.)) ;
#130097 = DIRECTION('ref_axis',(1.,0.,0.)) ;
#130098 = DIRECTION('center_axis',(0.,0.,-1.)) ;
#130099 = DIRECTION('ref_axis',(1.,0.,0.)) ;
#130100 = DIRECTION('center_axis',(0.,0.,1.)) ;
#130101 = DIRECTION('ref_axis',(1.,0.,0.)) ;
#130102 = DIRECTION('center_axis',(0.,0.,1.)) ;
#130103 = DIRECTION('ref_axis',(1.,0.,0.)) ;
#130104 = DIRECTION('center_axis',(0.,0.,-1.)) ;
#130105 = DIRECTION('ref_axis',(-1.,0.,0.)) ;
#130106 = DIRECTION('center_axis',(-3.46944695195361E-14,0.,1.)) ;
#130107 = DIRECTION('ref_axis',(1.,0.,3.46944695195361E-14)) ;
#130108 = DIRECTION('center_axis',(1.,0.,0.)) ;
#130109 = DIRECTION('ref_axis',(0.,0.,-1.)) ;
#130110 = DIRECTION('center_axis',(1.,0.,0.)) ;
#130111 = DIRECTION('ref_axis',(0.,0.,-1.)) ;
#130112 = DIRECTION('center_axis',(1.,0.,0.)) ;
#130113 = DIRECTION('ref_axis',(0.,0.,-1.)) ;
#130114 = DIRECTION('center_axis',(1.,0.,8.67361737988409E-15)) ;
#130115 = DIRECTION('ref_axis',(8.67361737988409E-15,0.,-1.)) ;
#130116 = DIRECTION('center_axis',(1.,0.,0.)) ;
#130117 = DIRECTION('ref_axis',(0.,0.,-1.)) ;
#130118 = DIRECTION('center_axis',(1.,0.,1.73472347597682E-14)) ;
#130119 = DIRECTION('ref_axis',(1.73472347597682E-14,0.,-1.)) ;
#130120 = DIRECTION('center_axis',(-1.,0.,0.)) ;
#130121 = DIRECTION('ref_axis',(0.,0.,1.)) ;
#130122 = DIRECTION('center_axis',(1.,0.,0.)) ;
#130123 = DIRECTION('ref_axis',(0.,0.,-1.)) ;
#130124 = DIRECTION('center_axis',(1.,0.,0.)) ;
#130125 = DIRECTION('ref_axis',(0.,0.,-1.)) ;
#130126 = DIRECTION('center_axis',(-3.46944695195364E-14,0.,-1.)) ;
#130127 = DIRECTION('ref_axis',(-1.,0.,3.46944695195364E-14)) ;
#130128 = DIRECTION('center_axis',(1.,0.,0.)) ;
#130129 = DIRECTION('ref_axis',(0.,0.,-1.)) ;
#130130 = DIRECTION('center_axis',(-3.46944695195364E-14,0.,1.)) ;
#130131 = DIRECTION('ref_axis',(1.,0.,3.46944695195364E-14)) ;
#130132 = DIRECTION('center_axis',(0.,0.,-1.)) ;
#130133 = DIRECTION('ref_axis',(-1.,0.,0.)) ;
#130134 = DIRECTION('center_axis',(-0.422618261740697,5.55398348498559E-17,
0.906307787036651)) ;
#130135 = DIRECTION('ref_axis',(0.906307787036651,6.51773046476477E-31,0.422618261740697)) ;
#130136 = DIRECTION('center_axis',(0.422618261740697,-5.55398348498559E-17,
-0.906307787036651)) ;
#130137 = DIRECTION('ref_axis',(-0.906307787036651,-6.46086972436398E-31,
-0.422618261740697)) ;
#130138 = DIRECTION('center_axis',(-0.422618261740697,5.55398348498559E-17,
0.906307787036651)) ;
#130139 = DIRECTION('ref_axis',(0.906307787036651,6.46086972436398E-31,0.422618261740697)) ;
#130140 = DIRECTION('center_axis',(0.422618261740697,-5.55398348498559E-17,
-0.906307787036651)) ;
#130141 = DIRECTION('ref_axis',(-0.906307787036651,-6.46086972436398E-31,
-0.422618261740697)) ;
#130142 = DIRECTION('center_axis',(0.,1.,0.)) ;
#130143 = DIRECTION('ref_axis',(1.,0.,0.)) ;
#130144 = DIRECTION('center_axis',(3.4216004848576E-14,0.514231796959095,
-0.857651245551606)) ;
#130145 = DIRECTION('ref_axis',(3.46944695195362E-14,-0.857651245551606,-0.514231796959095)) ;
#130146 = DIRECTION('center_axis',(0.,-3.46944695195362E-14,1.)) ;
#130147 = DIRECTION('ref_axis',(0.,1.,3.46944695195362E-14)) ;
#130148 = DIRECTION('center_axis',(-1.,0.,0.)) ;
#130149 = DIRECTION('ref_axis',(0.,-4.33680868994204E-15,-1.)) ;
#130150 = DIRECTION('center_axis',(0.,0.,1.)) ;
#130151 = DIRECTION('ref_axis',(1.,0.,0.)) ;
#130152 = DIRECTION('center_axis',(0.,0.,1.)) ;
#130153 = DIRECTION('ref_axis',(1.,0.,0.)) ;
#130154 = DIRECTION('center_axis',(-1.,0.,0.)) ;
#130155 = DIRECTION('ref_axis',(0.,0.,1.)) ;
#130156 = DIRECTION('center_axis',(-1.,0.,0.)) ;
#130157 = DIRECTION('ref_axis',(0.,-4.33680868994204E-15,-1.)) ;
#130158 = DIRECTION('center_axis',(1.,0.,0.)) ;
#130159 = DIRECTION('ref_axis',(0.,0.,-1.)) ;
#130160 = DIRECTION('center_axis',(0.,-0.514231796959124,-0.857651245551588)) ;
#130161 = DIRECTION('ref_axis',(0.,0.857651245551588,-0.514231796959124)) ;
#130162 = DIRECTION('center_axis',(0.,1.,8.97270763436279E-17)) ;
#130163 = DIRECTION('ref_axis',(0.,-8.97270763436279E-17,1.)) ;
#130164 = DIRECTION('center_axis',(0.,-1.,-8.97270763436279E-17)) ;
#130165 = DIRECTION('ref_axis',(0.,-8.97270763436279E-17,1.)) ;
#130166 = DIRECTION('center_axis',(0.,-1.,0.)) ;
#130167 = DIRECTION('ref_axis',(0.,0.,-1.)) ;
#130168 = DIRECTION('center_axis',(0.,1.,0.)) ;
#130169 = DIRECTION('ref_axis',(1.,0.,0.)) ;
#130170 = DIRECTION('center_axis',(-1.,0.,0.)) ;
#130171 = DIRECTION('ref_axis',(0.,0.,-1.)) ;
#130172 = DIRECTION('center_axis',(1.,0.,0.)) ;
#130173 = DIRECTION('ref_axis',(0.,0.,-1.)) ;
#130174 = DIRECTION('center_axis',(0.,-0.514231796959093,0.857651245551607)) ;
#130175 = DIRECTION('ref_axis',(0.,0.857651245551607,0.514231796959093)) ;
#130176 = DIRECTION('center_axis',(0.,0.,-1.)) ;
#130177 = DIRECTION('ref_axis',(1.,0.,0.)) ;
#130178 = DIRECTION('center_axis',(0.,1.,0.)) ;
#130179 = DIRECTION('ref_axis',(1.,0.,0.)) ;
#130180 = DIRECTION('center_axis',(-3.46944695195364E-14,0.,-1.)) ;
#130181 = DIRECTION('ref_axis',(1.,0.,-3.46944695195364E-14)) ;
#130182 = DIRECTION('center_axis',(-1.,0.,0.)) ;
#130183 = DIRECTION('ref_axis',(0.,4.33680868994204E-15,-1.)) ;
#130184 = DIRECTION('center_axis',(0.,0.,-1.)) ;
#130185 = DIRECTION('ref_axis',(-1.,0.,0.)) ;
#130186 = DIRECTION('center_axis',(0.,0.,1.)) ;
#130187 = DIRECTION('ref_axis',(-1.,0.,0.)) ;
#130188 = DIRECTION('center_axis',(0.,0.,-1.)) ;
#130189 = DIRECTION('ref_axis',(-1.,0.,0.)) ;
#130190 = DIRECTION('center_axis',(-1.,0.,7.01133629567814E-33)) ;
#130191 = DIRECTION('ref_axis',(7.01133629567814E-33,0.,1.)) ;
#130192 = DIRECTION('center_axis',(-1.,0.,0.)) ;
#130193 = DIRECTION('ref_axis',(0.,0.,1.)) ;
#130194 = DIRECTION('center_axis',(0.,0.,-1.)) ;
#130195 = DIRECTION('ref_axis',(-1.,0.,0.)) ;
#130196 = DIRECTION('center_axis',(-7.01133629567814E-33,8.97270763436279E-17,
-1.)) ;
#130197 = DIRECTION('ref_axis',(6.29106707073161E-49,1.,8.97270763436279E-17)) ;
#130198 = DIRECTION('center_axis',(1.,0.,0.)) ;
#130199 = DIRECTION('ref_axis',(0.,0.,-1.)) ;
#130200 = DIRECTION('center_axis',(-2.2301249256967E-15,0.514231796959095,
0.857651245551606)) ;
#130201 = DIRECTION('ref_axis',(-4.79361507851841E-30,-0.857651245551606,
0.514231796959095)) ;
#130202 = DIRECTION('center_axis',(-1.,0.,0.)) ;
#130203 = DIRECTION('ref_axis',(0.,0.,1.)) ;
#130204 = DIRECTION('center_axis',(-1.,0.,0.)) ;
#130205 = DIRECTION('ref_axis',(0.,-4.33680868994204E-15,-1.)) ;
#130206 = DIRECTION('center_axis',(0.,0.,1.)) ;
#130207 = DIRECTION('ref_axis',(1.,0.,0.)) ;
#130208 = DIRECTION('center_axis',(0.,0.,-1.)) ;
#130209 = DIRECTION('ref_axis',(-1.,0.,0.)) ;
#130210 = DIRECTION('center_axis',(0.,-1.,8.97270763436279E-17)) ;
#130211 = DIRECTION('ref_axis',(0.,-8.97270763436279E-17,-1.)) ;
#130212 = DIRECTION('center_axis',(0.,-1.,8.97270763436279E-17)) ;
#130213 = DIRECTION('ref_axis',(0.,-8.97270763436279E-17,-1.)) ;
#130214 = DIRECTION('center_axis',(0.,-1.,0.)) ;
#130215 = DIRECTION('ref_axis',(0.,0.,-1.)) ;
#130216 = DIRECTION('center_axis',(-7.01133629567814E-33,8.97270763436279E-17,
-1.)) ;
#130217 = DIRECTION('ref_axis',(0.,1.,0.)) ;
#130218 = DIRECTION('center_axis',(0.,-1.,0.)) ;
#130219 = DIRECTION('ref_axis',(0.,0.,1.)) ;
#130220 = DIRECTION('center_axis',(1.,0.,0.)) ;
#130221 = DIRECTION('ref_axis',(0.,0.,-1.)) ;
#130222 = DIRECTION('center_axis',(0.,0.,1.)) ;
#130223 = DIRECTION('ref_axis',(-1.,0.,0.)) ;
#130224 = DIRECTION('center_axis',(0.,1.,0.)) ;
#130225 = DIRECTION('ref_axis',(1.,0.,0.)) ;
#130226 = DIRECTION('center_axis',(-1.,0.,0.)) ;
#130227 = DIRECTION('ref_axis',(0.,0.,-1.)) ;
#130228 = DIRECTION('center_axis',(1.,7.81406971160724E-17,0.)) ;
#130229 = DIRECTION('ref_axis',(-7.81406971160724E-17,1.,0.)) ;
#130230 = DIRECTION('center_axis',(1.,0.,0.)) ;
#130231 = DIRECTION('ref_axis',(0.,0.,-1.)) ;
#130232 = DIRECTION('center_axis',(1.,0.,0.)) ;
#130233 = DIRECTION('ref_axis',(0.,0.,-1.)) ;
#130234 = DIRECTION('center_axis',(0.,1.,8.97270763436279E-17)) ;
#130235 = DIRECTION('ref_axis',(0.,-8.97270763436279E-17,1.)) ;
#130236 = DIRECTION('center_axis',(0.,-1.,0.)) ;
#130237 = DIRECTION('ref_axis',(0.,0.,-1.)) ;
#130238 = DIRECTION('center_axis',(0.,0.,-1.)) ;
#130239 = DIRECTION('ref_axis',(-1.,0.,0.)) ;
#130240 = DIRECTION('center_axis',(-7.01133629567814E-33,8.97270763436279E-17,
1.)) ;
#130241 = DIRECTION('ref_axis',(-6.29106707073161E-49,-1.,8.97270763436279E-17)) ;
#130242 = DIRECTION('center_axis',(-1.,0.,-7.01133629567814E-33)) ;
#130243 = DIRECTION('ref_axis',(-7.01133629567814E-33,0.,1.)) ;
#130244 = DIRECTION('center_axis',(-1.,0.,0.)) ;
#130245 = DIRECTION('ref_axis',(0.,0.,1.)) ;
#130246 = DIRECTION('center_axis',(1.,0.,0.)) ;
#130247 = DIRECTION('ref_axis',(0.,1.,0.)) ;
#130248 = DIRECTION('center_axis',(2.16840434497101E-15,1.,0.)) ;
#130249 = DIRECTION('ref_axis',(-1.,2.16840434497101E-15,0.)) ;
#130250 = DIRECTION('center_axis',(0.,1.,0.)) ;
#130251 = DIRECTION('ref_axis',(1.,0.,0.)) ;
#130252 = DIRECTION('center_axis',(0.,0.,-1.)) ;
#130253 = DIRECTION('ref_axis',(1.,0.,0.)) ;
#130254 = DIRECTION('center_axis',(-1.,0.,0.)) ;
#130255 = DIRECTION('ref_axis',(0.,0.,-1.)) ;
#130256 = DIRECTION('center_axis',(-7.01133629567814E-33,8.97270763436279E-17,
1.)) ;
#130257 = DIRECTION('ref_axis',(0.,-1.,0.)) ;
#130258 = DIRECTION('center_axis',(0.,-1.,0.)) ;
#130259 = DIRECTION('ref_axis',(0.,0.,1.)) ;
#130260 = DIRECTION('center_axis',(7.81406971160724E-17,-1.,-8.97270763436279E-17)) ;
#130261 = DIRECTION('ref_axis',(-7.01133629567814E-33,8.97270763436279E-17,
-1.)) ;
#130262 = DIRECTION('center_axis',(0.,1.,0.)) ;
#130263 = DIRECTION('ref_axis',(0.,0.,1.)) ;
#130264 = DIRECTION('center_axis',(-1.,-7.81406971160724E-17,0.)) ;
#130265 = DIRECTION('ref_axis',(7.81406971160724E-17,-1.,0.)) ;
#130266 = DIRECTION('center_axis',(-1.,-7.81406971160724E-17,0.)) ;
#130267 = DIRECTION('ref_axis',(-7.81406971160724E-17,1.,0.)) ;
#130268 = DIRECTION('center_axis',(0.,0.,1.)) ;
#130269 = DIRECTION('ref_axis',(1.,0.,0.)) ;
#130270 = DIRECTION('center_axis',(0.,0.,-1.)) ;
#130271 = DIRECTION('ref_axis',(-1.,0.,0.)) ;
#130272 = DIRECTION('center_axis',(0.,-1.,8.97270763436279E-17)) ;
#130273 = DIRECTION('ref_axis',(0.,-8.97270763436279E-17,-1.)) ;
#130274 = DIRECTION('center_axis',(0.,-1.,0.)) ;
#130275 = DIRECTION('ref_axis',(0.,0.,-1.)) ;
#130276 = DIRECTION('center_axis',(1.,7.81406971160724E-17,0.)) ;
#130277 = DIRECTION('ref_axis',(0.,1.,0.)) ;
#130278 = DIRECTION('center_axis',(0.,0.,1.)) ;
#130279 = DIRECTION('ref_axis',(-1.,0.,0.)) ;
#130280 = DIRECTION('center_axis',(0.,1.,0.)) ;
#130281 = DIRECTION('ref_axis',(1.,0.,0.)) ;
#130282 = DIRECTION('center_axis',(-1.,0.,0.)) ;
#130283 = DIRECTION('ref_axis',(0.,0.,-1.)) ;
#130284 = DIRECTION('center_axis',(0.,0.,-1.)) ;
#130285 = DIRECTION('ref_axis',(-1.,0.,0.)) ;
#130286 = DIRECTION('center_axis',(0.,0.,1.)) ;
#130287 = DIRECTION('ref_axis',(1.,0.,0.)) ;
#130288 = DIRECTION('center_axis',(-1.,-7.81406971160724E-17,0.)) ;
#130289 = DIRECTION('ref_axis',(7.81406971160724E-17,-1.,0.)) ;
#130290 = DIRECTION('center_axis',(-1.,-7.81406971160724E-17,0.)) ;
#130291 = DIRECTION('ref_axis',(-7.81406971160724E-17,1.,0.)) ;
#130292 = DIRECTION('center_axis',(1.,7.81406971160724E-17,0.)) ;
#130293 = DIRECTION('ref_axis',(-7.81406971160724E-17,1.,0.)) ;
#130294 = DIRECTION('center_axis',(1.,0.,0.)) ;
#130295 = DIRECTION('ref_axis',(0.,0.,-1.)) ;
#130296 = DIRECTION('center_axis',(1.,0.,0.)) ;
#130297 = DIRECTION('ref_axis',(0.,0.,-1.)) ;
#130298 = DIRECTION('center_axis',(3.78638272950961E-32,-4.8455963016112E-16,
-1.)) ;
#130299 = DIRECTION('ref_axis',(1.83472821505963E-47,1.,-4.8455963016112E-16)) ;
#130300 = DIRECTION('center_axis',(3.78638272950961E-32,-4.8455963016112E-16,
-1.)) ;
#130301 = DIRECTION('ref_axis',(1.83472821505963E-47,1.,-4.8455963016112E-16)) ;
#130302 = DIRECTION('center_axis',(0.,0.,-1.)) ;
#130303 = DIRECTION('ref_axis',(-1.,0.,0.)) ;
#130304 = DIRECTION('center_axis',(1.,7.81406971160724E-17,0.)) ;
#130305 = DIRECTION('ref_axis',(0.,1.,0.)) ;
#130306 = DIRECTION('center_axis',(0.,-1.,0.)) ;
#130307 = DIRECTION('ref_axis',(0.,0.,1.)) ;
#130308 = DIRECTION('center_axis',(0.,1.,0.)) ;
#130309 = DIRECTION('ref_axis',(1.,0.,0.)) ;
#130310 = DIRECTION('center_axis',(0.,1.,0.)) ;
#130311 = DIRECTION('ref_axis',(0.,0.,-1.)) ;
#130312 = DIRECTION('center_axis',(-7.81406971160724E-17,1.,-8.97270763436279E-17)) ;
#130313 = DIRECTION('ref_axis',(-7.01133629567814E-33,8.97270763436279E-17,
1.)) ;
#130314 = DIRECTION('center_axis',(0.,-1.,0.)) ;
#130315 = DIRECTION('ref_axis',(0.,0.,-1.)) ;
#130316 = DIRECTION('center_axis',(0.,1.,0.)) ;
#130317 = DIRECTION('ref_axis',(0.,0.,1.)) ;
#130318 = DIRECTION('center_axis',(0.,-1.,0.)) ;
#130319 = DIRECTION('ref_axis',(0.,0.,-1.)) ;
#130320 = DIRECTION('center_axis',(0.,-1.,0.)) ;
#130321 = DIRECTION('ref_axis',(0.,0.,-1.)) ;
#130322 = DIRECTION('center_axis',(0.,1.,0.)) ;
#130323 = DIRECTION('ref_axis',(1.,0.,0.)) ;
#130324 = DIRECTION('center_axis',(0.,0.,1.)) ;
#130325 = DIRECTION('ref_axis',(-1.,0.,0.)) ;
#130326 = DIRECTION('center_axis',(1.,0.,0.)) ;
#130327 = DIRECTION('ref_axis',(0.,0.,1.)) ;
#130328 = DIRECTION('center_axis',(0.,-1.,0.)) ;
#130329 = DIRECTION('ref_axis',(0.,0.,-1.)) ;
#130330 = DIRECTION('center_axis',(0.,1.,0.)) ;
#130331 = DIRECTION('ref_axis',(0.,0.,1.)) ;
#130332 = DIRECTION('center_axis',(0.,-1.,0.)) ;
#130333 = DIRECTION('ref_axis',(0.,0.,-1.)) ;
#130334 = DIRECTION('center_axis',(-1.,0.,2.16840434497101E-16)) ;
#130335 = DIRECTION('ref_axis',(2.16840434497101E-16,0.,1.)) ;
#130336 = DIRECTION('center_axis',(1.,0.,0.)) ;
#130337 = DIRECTION('ref_axis',(0.,0.,-1.)) ;
#130338 = DIRECTION('center_axis',(-2.16840434497101E-16,0.,1.)) ;
#130339 = DIRECTION('ref_axis',(1.,0.,2.16840434497101E-16)) ;
#130340 = DIRECTION('center_axis',(0.,0.,1.)) ;
#130341 = DIRECTION('ref_axis',(1.,0.,0.)) ;
#130342 = DIRECTION('center_axis',(0.,1.,0.)) ;
#130343 = DIRECTION('ref_axis',(0.,0.,1.)) ;
#130344 = DIRECTION('center_axis',(0.,-1.,0.)) ;
#130345 = DIRECTION('ref_axis',(0.,0.,-1.)) ;
#130346 = DIRECTION('center_axis',(0.,1.,0.)) ;
#130347 = DIRECTION('ref_axis',(1.,0.,0.)) ;
#130348 = DIRECTION('center_axis',(0.,0.,1.)) ;
#130349 = DIRECTION('ref_axis',(-1.,0.,0.)) ;
#130350 = DIRECTION('center_axis',(0.,1.,0.)) ;
#130351 = DIRECTION('ref_axis',(1.,0.,0.)) ;
#130352 = DIRECTION('center_axis',(1.,0.,0.)) ;
#130353 = DIRECTION('ref_axis',(0.,0.,1.)) ;
#130354 = DIRECTION('center_axis',(0.,0.,-1.)) ;
#130355 = DIRECTION('ref_axis',(-1.,0.,0.)) ;
#130356 = DIRECTION('center_axis',(0.,0.,1.)) ;
#130357 = DIRECTION('ref_axis',(1.,0.,0.)) ;
#130358 = DIRECTION('center_axis',(1.,0.,2.16840434497101E-16)) ;
#130359 = DIRECTION('ref_axis',(2.16840434497101E-16,0.,-1.)) ;
#130360 = DIRECTION('center_axis',(1.,0.,0.)) ;
#130361 = DIRECTION('ref_axis',(0.,0.,-1.)) ;
#130362 = DIRECTION('center_axis',(0.,1.,0.)) ;
#130363 = DIRECTION('ref_axis',(1.,0.,0.)) ;
#130364 = DIRECTION('center_axis',(0.,1.,0.)) ;
#130365 = DIRECTION('ref_axis',(0.,0.,-1.)) ;
#130366 = DIRECTION('center_axis',(0.,1.,0.)) ;
#130367 = DIRECTION('ref_axis',(0.,0.,1.)) ;
#130368 = DIRECTION('center_axis',(0.,1.,0.)) ;
#130369 = DIRECTION('ref_axis',(0.,0.,1.)) ;
#130370 = DIRECTION('center_axis',(-0.942809041582063,-0.235702260395516,
0.235702260395518)) ;
#130371 = DIRECTION('ref_axis',(0.242535625036335,4.64743530723282E-16,0.970142500145331)) ;
#130372 = DIRECTION('center_axis',(-0.970142500145332,-0.242535625036331,
-2.10366121255617E-15)) ;
#130373 = DIRECTION('ref_axis',(0.242535625036331,-0.970142500145332,-4.47980524894761E-30)) ;
#130374 = DIRECTION('center_axis',(0.970142500145333,0.24253562503633,0.)) ;
#130375 = DIRECTION('ref_axis',(-0.24253562503633,0.970142500145333,0.)) ;
#130376 = DIRECTION('center_axis',(-0.970142500145332,-0.242535625036331,
2.73475957632304E-14)) ;
#130377 = DIRECTION('ref_axis',(0.242535625036331,-0.970142500145332,1.1454669517322E-30)) ;
#130378 = DIRECTION('center_axis',(0.879462917689188,0.219865729422294,-0.42214220049081)) ;
#130379 = DIRECTION('ref_axis',(-0.432731067584771,1.71515946658E-16,-0.901523057468274)) ;
#130380 = DIRECTION('center_axis',(0.879462917689192,0.219865729422271,-0.422142200490814)) ;
#130381 = DIRECTION('ref_axis',(-0.432731067584773,-1.62351711522009E-16,
-0.901523057468273)) ;
#130382 = DIRECTION('center_axis',(0.,1.,0.)) ;
#130383 = DIRECTION('ref_axis',(1.,0.,0.)) ;
#130384 = DIRECTION('center_axis',(0.,-1.,0.)) ;
#130385 = DIRECTION('ref_axis',(0.,0.,1.)) ;
#130386 = DIRECTION('center_axis',(0.,-1.,0.)) ;
#130387 = DIRECTION('ref_axis',(0.,0.,-1.)) ;
#130388 = DIRECTION('center_axis',(-4.51750905202295E-15,-1.,2.16840434497102E-15)) ;
#130389 = DIRECTION('ref_axis',(1.,-4.51750905202295E-15,3.91831450274151E-31)) ;
#130390 = DIRECTION('center_axis',(0.669589480006976,-0.669589480006974,-0.321402950403349)) ;
#130391 = DIRECTION('ref_axis',(0.707106781186547,0.707106781186548,5.45170614306381E-16)) ;
#130392 = DIRECTION('center_axis',(0.669589480006977,-0.669589480006977,-0.321402950403342)) ;
#130393 = DIRECTION('ref_axis',(0.707106781186547,0.707106781186548,-1.94221176494188E-16)) ;
#130394 = DIRECTION('center_axis',(0.,1.,0.)) ;
#130395 = DIRECTION('ref_axis',(1.,0.,0.)) ;
#130396 = DIRECTION('center_axis',(0.707106781186541,-0.707106781186554,0.)) ;
#130397 = DIRECTION('ref_axis',(-0.707106781186554,-0.707106781186541,0.)) ;
#130398 = DIRECTION('center_axis',(0.707106781186549,-0.707106781186546,0.)) ;
#130399 = DIRECTION('ref_axis',(0.707106781186546,0.707106781186549,0.)) ;
#130400 = DIRECTION('center_axis',(0.707106781186548,-0.707106781186548,-1.53329341668338E-15)) ;
#130401 = DIRECTION('ref_axis',(0.707106781186548,0.707106781186548,1.5356898865553E-31)) ;
#130402 = DIRECTION('center_axis',(0.577350269189633,-0.577350269189633,-0.577350269189612)) ;
#130403 = DIRECTION('ref_axis',(0.707106781186548,0.707106781186548,1.34560831514457E-17)) ;
#130404 = DIRECTION('center_axis',(-0.577350269189344,0.577350269189586,-0.577350269189947)) ;
#130405 = DIRECTION('ref_axis',(1.30446081606812E-15,0.707106781186769,0.707106781186326)) ;
#130406 = DIRECTION('center_axis',(-0.707106781186548,0.707106781186548,7.66646708341692E-15)) ;
#130407 = DIRECTION('ref_axis',(-0.707106781186548,-0.707106781186548,-2.68297081166629E-31)) ;
#130408 = DIRECTION('center_axis',(-0.707106781186549,0.707106781186546,0.)) ;
#130409 = DIRECTION('ref_axis',(-0.707106781186546,-0.707106781186549,0.)) ;
#130410 = DIRECTION('center_axis',(-0.707106781186548,0.707106781186548,-1.22663473334671E-14)) ;
#130411 = DIRECTION('ref_axis',(-0.707106781186548,-0.707106781186548,2.94725045705944E-31)) ;
#130412 = DIRECTION('center_axis',(-0.669589480006976,0.669589480006974,-0.321402950403349)) ;
#130413 = DIRECTION('ref_axis',(-0.707106781186547,-0.707106781186548,5.45170614306381E-16)) ;
#130414 = DIRECTION('center_axis',(0.669589480006982,-0.669589480006966,0.321402950403353)) ;
#130415 = DIRECTION('ref_axis',(0.707106781186539,0.707106781186556,5.77426876420606E-17)) ;
#130416 = DIRECTION('center_axis',(0.,1.,0.)) ;
#130417 = DIRECTION('ref_axis',(1.,0.,0.)) ;
#130418 = DIRECTION('center_axis',(0.,1.,0.)) ;
#130419 = DIRECTION('ref_axis',(0.,0.,-1.)) ;
#130420 = DIRECTION('center_axis',(0.,-1.,0.)) ;
#130421 = DIRECTION('ref_axis',(0.,0.,-1.)) ;
#130422 = DIRECTION('center_axis',(0.,1.,0.)) ;
#130423 = DIRECTION('ref_axis',(0.,0.,1.)) ;
#130424 = DIRECTION('center_axis',(-0.879462917689188,-0.219865729422294,
-0.42214220049081)) ;
#130425 = DIRECTION('ref_axis',(-0.432731067584771,1.71515946658E-16,0.901523057468274)) ;
#130426 = DIRECTION('center_axis',(0.879462917689201,0.219865729422298,0.42214220049078)) ;
#130427 = DIRECTION('ref_axis',(0.432731067584741,5.42470486237819E-16,-0.901523057468288)) ;
#130428 = DIRECTION('center_axis',(0.,1.,0.)) ;
#130429 = DIRECTION('ref_axis',(1.,0.,0.)) ;
#130430 = DIRECTION('center_axis',(0.970142500145323,0.242535625036368,0.)) ;
#130431 = DIRECTION('ref_axis',(0.242535625036368,-0.970142500145323,0.)) ;
#130432 = DIRECTION('center_axis',(-0.970142500145333,-0.24253562503633,0.)) ;
#130433 = DIRECTION('ref_axis',(0.24253562503633,-0.970142500145333,0.)) ;
#130434 = DIRECTION('center_axis',(0.970142500145332,0.242535625036331,-2.10366121255617E-15)) ;
#130435 = DIRECTION('ref_axis',(-0.242535625036331,0.970142500145332,-4.47980524894761E-30)) ;
#130436 = DIRECTION('center_axis',(0.942809041582064,0.235702260395514,0.235702260395514)) ;
#130437 = DIRECTION('ref_axis',(-0.242535625036331,0.970142500145332,4.49011373492972E-16)) ;
#130438 = DIRECTION('center_axis',(0.,-1.,0.)) ;
#130439 = DIRECTION('ref_axis',(0.,0.,-1.)) ;
#130440 = DIRECTION('center_axis',(-1.,0.,-8.67361737988409E-15)) ;
#130441 = DIRECTION('ref_axis',(-8.67361737988409E-15,0.,1.)) ;
#130442 = DIRECTION('center_axis',(0.,0.,-1.)) ;
#130443 = DIRECTION('ref_axis',(-1.,0.,0.)) ;
#130444 = DIRECTION('center_axis',(0.,0.,-1.)) ;
#130445 = DIRECTION('ref_axis',(-1.,0.,0.)) ;
#130446 = DIRECTION('center_axis',(0.,3.46944695195362E-14,-1.)) ;
#130447 = DIRECTION('ref_axis',(0.,1.,3.46944695195362E-14)) ;
#130448 = DIRECTION('center_axis',(1.,0.,0.)) ;
#130449 = DIRECTION('ref_axis',(0.,0.,-1.)) ;
#130450 = DIRECTION('center_axis',(-1.,0.,0.)) ;
#130451 = DIRECTION('ref_axis',(0.,0.,1.)) ;
#130452 = DIRECTION('center_axis',(0.,-1.,0.)) ;
#130453 = DIRECTION('ref_axis',(0.,0.,-1.)) ;
#130454 = DIRECTION('center_axis',(-1.,0.,0.)) ;
#130455 = DIRECTION('ref_axis',(0.,0.,1.)) ;
#130456 = DIRECTION('center_axis',(0.,-1.,0.)) ;
#130457 = DIRECTION('ref_axis',(0.,0.,-1.)) ;
#130458 = DIRECTION('center_axis',(3.46944695195358E-14,0.,-1.)) ;
#130459 = DIRECTION('ref_axis',(-1.,0.,-3.46944695195358E-14)) ;
#130460 = DIRECTION('center_axis',(-1.,0.,0.)) ;
#130461 = DIRECTION('ref_axis',(0.,0.,1.)) ;
#130462 = DIRECTION('center_axis',(-1.,1.73472347597681E-14,0.)) ;
#130463 = DIRECTION('ref_axis',(-1.73472347597681E-14,-1.,0.)) ;
#130464 = DIRECTION('center_axis',(0.,0.,1.)) ;
#130465 = DIRECTION('ref_axis',(1.,0.,0.)) ;
#130466 = DIRECTION('center_axis',(-3.46944695195364E-14,0.,-1.)) ;
#130467 = DIRECTION('ref_axis',(-1.,0.,3.46944695195364E-14)) ;
#130468 = DIRECTION('center_axis',(0.,-1.,0.)) ;
#130469 = DIRECTION('ref_axis',(0.,0.,-1.)) ;
#130470 = DIRECTION('center_axis',(0.,-1.,0.)) ;
#130471 = DIRECTION('ref_axis',(0.,0.,-1.)) ;
#130472 = DIRECTION('center_axis',(0.,-1.,0.)) ;
#130473 = DIRECTION('ref_axis',(0.,0.,-1.)) ;
#130474 = DIRECTION('center_axis',(0.,0.,1.)) ;
#130475 = DIRECTION('ref_axis',(1.,0.,0.)) ;
#130476 = DIRECTION('center_axis',(0.,0.,-1.)) ;
#130477 = DIRECTION('ref_axis',(-1.,0.,0.)) ;
#130478 = DIRECTION('center_axis',(0.,0.,1.)) ;
#130479 = DIRECTION('ref_axis',(1.,0.,0.)) ;
#130480 = DIRECTION('center_axis',(0.,-1.,0.)) ;
#130481 = DIRECTION('ref_axis',(0.,0.,-1.)) ;
#130482 = DIRECTION('center_axis',(0.,-1.,0.)) ;
#130483 = DIRECTION('ref_axis',(0.,0.,-1.)) ;
#130484 = DIRECTION('center_axis',(0.,1.,0.)) ;
#130485 = DIRECTION('ref_axis',(1.,0.,0.)) ;
#130486 = DIRECTION('center_axis',(-1.,0.,0.)) ;
#130487 = DIRECTION('ref_axis',(0.,0.,-1.)) ;
#130488 = DIRECTION('center_axis',(0.,1.,0.)) ;
#130489 = DIRECTION('ref_axis',(1.,0.,0.)) ;
#130490 = DIRECTION('center_axis',(-1.,0.,0.)) ;
#130491 = DIRECTION('ref_axis',(0.,0.,-1.)) ;
#130492 = DIRECTION('center_axis',(0.,-1.,0.)) ;
#130493 = DIRECTION('ref_axis',(0.,0.,-1.)) ;
#130494 = DIRECTION('center_axis',(0.,-1.,0.)) ;
#130495 = DIRECTION('ref_axis',(0.,0.,-1.)) ;
#130496 = DIRECTION('center_axis',(-1.,0.,0.)) ;
#130497 = DIRECTION('ref_axis',(0.,0.,1.)) ;
#130498 = DIRECTION('center_axis',(-1.,0.,0.)) ;
#130499 = DIRECTION('ref_axis',(0.,0.,1.)) ;
#130500 = DIRECTION('center_axis',(1.,0.,0.)) ;
#130501 = DIRECTION('ref_axis',(0.,0.,-1.)) ;
#130502 = DIRECTION('center_axis',(-1.,0.,0.)) ;
#130503 = DIRECTION('ref_axis',(0.,0.,1.)) ;
#130504 = DIRECTION('center_axis',(0.,-1.,0.)) ;
#130505 = DIRECTION('ref_axis',(0.,0.,-1.)) ;
#130506 = DIRECTION('center_axis',(0.,-1.,0.)) ;
#130507 = DIRECTION('ref_axis',(0.,0.,-1.)) ;
#130508 = DIRECTION('center_axis',(0.,1.,0.)) ;
#130509 = DIRECTION('ref_axis',(1.,0.,0.)) ;
#130510 = DIRECTION('center_axis',(0.,0.,-1.)) ;
#130511 = DIRECTION('ref_axis',(1.,0.,0.)) ;
#130512 = DIRECTION('center_axis',(0.,1.,0.)) ;
#130513 = DIRECTION('ref_axis',(1.,0.,0.)) ;
#130514 = DIRECTION('center_axis',(0.,0.,1.)) ;
#130515 = DIRECTION('ref_axis',(-1.,0.,0.)) ;
#130516 = DIRECTION('center_axis',(0.,0.,-1.)) ;
#130517 = DIRECTION('ref_axis',(-1.,0.,0.)) ;
#130518 = DIRECTION('center_axis',(1.,1.31418445149758E-16,-2.16840434497101E-16)) ;
#130519 = DIRECTION('ref_axis',(-2.16840434497101E-16,-2.8496832747207E-32,
-1.)) ;
#130520 = DIRECTION('center_axis',(1.,0.,0.)) ;
#130521 = DIRECTION('ref_axis',(0.,0.,-1.)) ;
#130522 = DIRECTION('center_axis',(-1.,0.,0.)) ;
#130523 = DIRECTION('ref_axis',(0.,0.,1.)) ;
#130524 = DIRECTION('center_axis',(-1.31418445149758E-16,1.,0.)) ;
#130525 = DIRECTION('ref_axis',(-1.,0.,0.)) ;
#130526 = DIRECTION('center_axis',(0.,0.,1.)) ;
#130527 = DIRECTION('ref_axis',(-1.,0.,0.)) ;
#130528 = DIRECTION('center_axis',(-1.31418445149758E-16,1.,0.)) ;
#130529 = DIRECTION('ref_axis',(-1.,-1.31418445149758E-16,0.)) ;
#130530 = DIRECTION('center_axis',(-1.31418445149758E-16,1.,0.)) ;
#130531 = DIRECTION('ref_axis',(-1.,0.,0.)) ;
#130532 = DIRECTION('center_axis',(-1.31418445149758E-16,1.,0.)) ;
#130533 = DIRECTION('ref_axis',(-1.,-1.31418445149758E-16,0.)) ;
#130534 = DIRECTION('center_axis',(0.,0.,1.)) ;
#130535 = DIRECTION('ref_axis',(-1.,0.,0.)) ;
#130536 = DIRECTION('center_axis',(-4.33680868994202E-16,-5.69936654944139E-32,
-1.)) ;
#130537 = DIRECTION('ref_axis',(-1.,2.47170623787823E-47,4.33680868994202E-16)) ;
#130538 = DIRECTION('center_axis',(0.,0.,1.)) ;
#130539 = DIRECTION('ref_axis',(1.,0.,0.)) ;
#130540 = DIRECTION('center_axis',(-1.31418445149758E-16,-1.,0.)) ;
#130541 = DIRECTION('ref_axis',(1.,-1.31418445149758E-16,0.)) ;
#130542 = DIRECTION('center_axis',(0.,1.,0.)) ;
#130543 = DIRECTION('ref_axis',(0.,0.,1.)) ;
#130544 = DIRECTION('center_axis',(-1.,0.,2.16840434497101E-16)) ;
#130545 = DIRECTION('ref_axis',(2.16840434497101E-16,0.,1.)) ;
#130546 = DIRECTION('center_axis',(-1.,0.,0.)) ;
#130547 = DIRECTION('ref_axis',(0.,0.,1.)) ;
#130548 = DIRECTION('center_axis',(1.,0.,0.)) ;
#130549 = DIRECTION('ref_axis',(0.,0.,-1.)) ;
#130550 = DIRECTION('center_axis',(-1.31418445149758E-16,-1.,0.)) ;
#130551 = DIRECTION('ref_axis',(1.,-1.31418445149758E-16,0.)) ;
#130552 = DIRECTION('center_axis',(0.,1.,0.)) ;
#130553 = DIRECTION('ref_axis',(0.,0.,1.)) ;
#130554 = DIRECTION('center_axis',(2.16840434497101E-16,2.8496832747207E-32,
1.)) ;
#130555 = DIRECTION('ref_axis',(1.,-6.17926559469557E-48,-2.16840434497101E-16)) ;
#130556 = DIRECTION('center_axis',(0.,0.,1.)) ;
#130557 = DIRECTION('ref_axis',(1.,0.,0.)) ;
#130558 = DIRECTION('center_axis',(-1.,-1.31418445149758E-16,-2.16840434497101E-16)) ;
#130559 = DIRECTION('ref_axis',(-2.16840434497101E-16,-2.8496832747207E-32,
1.)) ;
#130560 = DIRECTION('center_axis',(-1.,0.,0.)) ;
#130561 = DIRECTION('ref_axis',(0.,0.,1.)) ;
#130562 = DIRECTION('center_axis',(1.,0.,0.)) ;
#130563 = DIRECTION('ref_axis',(0.,0.,-1.)) ;
#130564 = DIRECTION('center_axis',(-1.31418445149758E-16,1.,0.)) ;
#130565 = DIRECTION('ref_axis',(-1.,0.,0.)) ;
#130566 = DIRECTION('center_axis',(-1.31418445149758E-16,1.,0.)) ;
#130567 = DIRECTION('ref_axis',(-1.,-1.31418445149758E-16,0.)) ;
#130568 = DIRECTION('center_axis',(0.,1.,0.)) ;
#130569 = DIRECTION('ref_axis',(1.,0.,0.)) ;
#130570 = DIRECTION('center_axis',(0.,0.,-1.)) ;
#130571 = DIRECTION('ref_axis',(1.,0.,0.)) ;
#130572 = DIRECTION('center_axis',(0.,1.,0.)) ;
#130573 = DIRECTION('ref_axis',(1.,0.,0.)) ;
#130574 = DIRECTION('center_axis',(0.,0.,-1.)) ;
#130575 = DIRECTION('ref_axis',(1.,0.,0.)) ;
#130576 = DIRECTION('center_axis',(-1.31418445149758E-16,1.,0.)) ;
#130577 = DIRECTION('ref_axis',(-1.,0.,0.)) ;
#130578 = DIRECTION('center_axis',(-1.31418445149758E-16,1.,0.)) ;
#130579 = DIRECTION('ref_axis',(-1.,-1.31418445149758E-16,0.)) ;
#130580 = DIRECTION('center_axis',(-1.31418445149758E-16,-1.,0.)) ;
#130581 = DIRECTION('ref_axis',(1.,-1.31418445149758E-16,0.)) ;
#130582 = DIRECTION('center_axis',(0.,1.,0.)) ;
#130583 = DIRECTION('ref_axis',(0.,0.,1.)) ;
#130584 = DIRECTION('center_axis',(4.33680868994202E-16,0.,1.)) ;
#130585 = DIRECTION('ref_axis',(1.,0.,-4.33680868994202E-16)) ;
#130586 = DIRECTION('center_axis',(0.,0.,-1.)) ;
#130587 = DIRECTION('ref_axis',(-1.,0.,0.)) ;
#130588 = DIRECTION('center_axis',(-2.16840434497101E-16,0.,-1.)) ;
#130589 = DIRECTION('ref_axis',(-1.,0.,2.16840434497101E-16)) ;
#130590 = DIRECTION('center_axis',(0.,0.,-1.)) ;
#130591 = DIRECTION('ref_axis',(-1.,0.,0.)) ;
#130592 = DIRECTION('center_axis',(-1.31418445149758E-16,-1.,0.)) ;
#130593 = DIRECTION('ref_axis',(1.,-1.31418445149758E-16,0.)) ;
#130594 = DIRECTION('center_axis',(0.,1.,0.)) ;
#130595 = DIRECTION('ref_axis',(0.,0.,1.)) ;
#130596 = DIRECTION('center_axis',(0.,1.,0.)) ;
#130597 = DIRECTION('ref_axis',(1.,0.,0.)) ;
#130598 = DIRECTION('center_axis',(-1.,0.,0.)) ;
#130599 = DIRECTION('ref_axis',(0.,0.,-1.)) ;
#130600 = DIRECTION('center_axis',(0.,1.,0.)) ;
#130601 = DIRECTION('ref_axis',(1.,0.,0.)) ;
#130602 = DIRECTION('center_axis',(1.,0.,0.)) ;
#130603 = DIRECTION('ref_axis',(0.,0.,1.)) ;
#130604 = DIRECTION('center_axis',(1.,0.,2.16840434497101E-16)) ;
#130605 = DIRECTION('ref_axis',(2.16840434497101E-16,0.,-1.)) ;
#130606 = DIRECTION('center_axis',(0.,1.,0.)) ;
#130607 = DIRECTION('ref_axis',(0.,0.,1.)) ;
#130608 = DIRECTION('center_axis',(0.,1.,0.)) ;
#130609 = DIRECTION('ref_axis',(0.,0.,1.)) ;
#130610 = DIRECTION('center_axis',(0.,0.,-1.)) ;
#130611 = DIRECTION('ref_axis',(-1.,0.,0.)) ;
#130612 = DIRECTION('center_axis',(0.,0.,1.)) ;
#130613 = DIRECTION('ref_axis',(1.,0.,0.)) ;
#130614 = DIRECTION('center_axis',(0.,0.,-1.)) ;
#130615 = DIRECTION('ref_axis',(-1.,0.,0.)) ;
#130616 = DIRECTION('center_axis',(0.,1.,0.)) ;
#130617 = DIRECTION('ref_axis',(0.,0.,1.)) ;
#130618 = DIRECTION('center_axis',(0.,1.,0.)) ;
#130619 = DIRECTION('ref_axis',(0.,0.,1.)) ;
#130620 = DIRECTION('center_axis',(0.,1.,0.)) ;
#130621 = DIRECTION('ref_axis',(1.,0.,0.)) ;
#130622 = DIRECTION('center_axis',(-1.,0.,0.)) ;
#130623 = DIRECTION('ref_axis',(0.,0.,-1.)) ;
#130624 = DIRECTION('center_axis',(0.,1.,0.)) ;
#130625 = DIRECTION('ref_axis',(1.,0.,0.)) ;
#130626 = DIRECTION('center_axis',(-1.,0.,0.)) ;
#130627 = DIRECTION('ref_axis',(0.,0.,-1.)) ;
#130628 = DIRECTION('center_axis',(0.,1.,0.)) ;
#130629 = DIRECTION('ref_axis',(0.,0.,1.)) ;
#130630 = DIRECTION('center_axis',(0.,1.,0.)) ;
#130631 = DIRECTION('ref_axis',(0.,0.,1.)) ;
#130632 = DIRECTION('center_axis',(-1.,0.,0.)) ;
#130633 = DIRECTION('ref_axis',(0.,0.,1.)) ;
#130634 = DIRECTION('center_axis',(-1.,0.,0.)) ;
#130635 = DIRECTION('ref_axis',(0.,0.,1.)) ;
#130636 = DIRECTION('center_axis',(1.,0.,0.)) ;
#130637 = DIRECTION('ref_axis',(0.,0.,-1.)) ;
#130638 = DIRECTION('center_axis',(-1.,0.,0.)) ;
#130639 = DIRECTION('ref_axis',(0.,0.,1.)) ;
#130640 = DIRECTION('center_axis',(0.,1.,0.)) ;
#130641 = DIRECTION('ref_axis',(0.,0.,1.)) ;
#130642 = DIRECTION('center_axis',(0.,1.,0.)) ;
#130643 = DIRECTION('ref_axis',(0.,0.,1.)) ;
#130644 = DIRECTION('center_axis',(0.,1.,0.)) ;
#130645 = DIRECTION('ref_axis',(1.,0.,0.)) ;
#130646 = DIRECTION('center_axis',(0.,0.,1.)) ;
#130647 = DIRECTION('ref_axis',(-1.,0.,0.)) ;
#130648 = DIRECTION('center_axis',(0.,1.,0.)) ;
#130649 = DIRECTION('ref_axis',(1.,0.,0.)) ;
#130650 = DIRECTION('center_axis',(0.,0.,-1.)) ;
#130651 = DIRECTION('ref_axis',(1.,0.,0.)) ;
#130652 = DIRECTION('center_axis',(0.,0.,1.)) ;
#130653 = DIRECTION('ref_axis',(1.,0.,0.)) ;
#130654 = DIRECTION('center_axis',(0.,0.,1.)) ;
#130655 = DIRECTION('ref_axis',(1.,0.,0.)) ;
#130656 = DIRECTION('center_axis',(0.,0.,-1.)) ;
#130657 = DIRECTION('ref_axis',(-1.,0.,0.)) ;
#130658 = DIRECTION('center_axis',(-3.46944695195361E-14,0.,1.)) ;
#130659 = DIRECTION('ref_axis',(1.,0.,3.46944695195361E-14)) ;
#130660 = DIRECTION('center_axis',(1.,0.,0.)) ;
#130661 = DIRECTION('ref_axis',(0.,0.,-1.)) ;
#130662 = DIRECTION('center_axis',(1.,0.,0.)) ;
#130663 = DIRECTION('ref_axis',(0.,0.,-1.)) ;
#130664 = DIRECTION('center_axis',(1.,0.,0.)) ;
#130665 = DIRECTION('ref_axis',(0.,0.,-1.)) ;
#130666 = DIRECTION('center_axis',(1.,0.,8.67361737988409E-15)) ;
#130667 = DIRECTION('ref_axis',(8.67361737988409E-15,0.,-1.)) ;
#130668 = DIRECTION('center_axis',(1.,0.,0.)) ;
#130669 = DIRECTION('ref_axis',(0.,0.,-1.)) ;
#130670 = DIRECTION('center_axis',(1.,0.,1.73472347597682E-14)) ;
#130671 = DIRECTION('ref_axis',(1.73472347597682E-14,0.,-1.)) ;
#130672 = DIRECTION('center_axis',(-1.,0.,0.)) ;
#130673 = DIRECTION('ref_axis',(0.,0.,1.)) ;
#130674 = DIRECTION('center_axis',(1.,0.,0.)) ;
#130675 = DIRECTION('ref_axis',(0.,0.,-1.)) ;
#130676 = DIRECTION('center_axis',(1.,0.,0.)) ;
#130677 = DIRECTION('ref_axis',(0.,0.,-1.)) ;
#130678 = DIRECTION('center_axis',(-3.46944695195364E-14,0.,-1.)) ;
#130679 = DIRECTION('ref_axis',(-1.,0.,3.46944695195364E-14)) ;
#130680 = DIRECTION('center_axis',(1.,0.,0.)) ;
#130681 = DIRECTION('ref_axis',(0.,0.,-1.)) ;
#130682 = DIRECTION('center_axis',(-3.46944695195364E-14,0.,1.)) ;
#130683 = DIRECTION('ref_axis',(1.,0.,3.46944695195364E-14)) ;
#130684 = DIRECTION('center_axis',(0.,0.,-1.)) ;
#130685 = DIRECTION('ref_axis',(-1.,0.,0.)) ;
#130686 = DIRECTION('center_axis',(-0.422618261740697,5.55398348498559E-17,
0.906307787036651)) ;
#130687 = DIRECTION('ref_axis',(0.906307787036651,6.51773046476477E-31,0.422618261740697)) ;
#130688 = DIRECTION('center_axis',(0.422618261740697,-5.55398348498559E-17,
-0.906307787036651)) ;
#130689 = DIRECTION('ref_axis',(-0.906307787036651,-6.46086972436398E-31,
-0.422618261740697)) ;
#130690 = DIRECTION('center_axis',(-0.422618261740697,5.55398348498559E-17,
0.906307787036651)) ;
#130691 = DIRECTION('ref_axis',(0.906307787036651,6.46086972436398E-31,0.422618261740697)) ;
#130692 = DIRECTION('center_axis',(0.422618261740697,-5.55398348498559E-17,
-0.906307787036651)) ;
#130693 = DIRECTION('ref_axis',(-0.906307787036651,-6.46086972436398E-31,
-0.422618261740697)) ;
#130694 = DIRECTION('center_axis',(0.,1.,0.)) ;
#130695 = DIRECTION('ref_axis',(1.,0.,0.)) ;
#130696 = DIRECTION('center_axis',(3.4216004848576E-14,0.514231796959095,
-0.857651245551606)) ;
#130697 = DIRECTION('ref_axis',(3.46944695195362E-14,-0.857651245551606,-0.514231796959095)) ;
#130698 = DIRECTION('center_axis',(0.,-3.46944695195362E-14,1.)) ;
#130699 = DIRECTION('ref_axis',(0.,1.,3.46944695195362E-14)) ;
#130700 = DIRECTION('center_axis',(-1.,0.,0.)) ;
#130701 = DIRECTION('ref_axis',(0.,-4.33680868994204E-15,-1.)) ;
#130702 = DIRECTION('center_axis',(0.,0.,1.)) ;
#130703 = DIRECTION('ref_axis',(1.,0.,0.)) ;
#130704 = DIRECTION('center_axis',(0.,0.,1.)) ;
#130705 = DIRECTION('ref_axis',(1.,0.,0.)) ;
#130706 = DIRECTION('center_axis',(-1.,0.,0.)) ;
#130707 = DIRECTION('ref_axis',(0.,0.,1.)) ;
#130708 = DIRECTION('center_axis',(-1.,0.,0.)) ;
#130709 = DIRECTION('ref_axis',(0.,-4.33680868994204E-15,-1.)) ;
#130710 = DIRECTION('center_axis',(1.,0.,0.)) ;
#130711 = DIRECTION('ref_axis',(0.,0.,-1.)) ;
#130712 = DIRECTION('center_axis',(0.,-0.514231796959124,-0.857651245551588)) ;
#130713 = DIRECTION('ref_axis',(0.,0.857651245551588,-0.514231796959124)) ;
#130714 = DIRECTION('center_axis',(0.,1.,8.97270763436279E-17)) ;
#130715 = DIRECTION('ref_axis',(0.,-8.97270763436279E-17,1.)) ;
#130716 = DIRECTION('center_axis',(0.,-1.,-8.97270763436279E-17)) ;
#130717 = DIRECTION('ref_axis',(0.,-8.97270763436279E-17,1.)) ;
#130718 = DIRECTION('center_axis',(0.,-1.,0.)) ;
#130719 = DIRECTION('ref_axis',(0.,0.,-1.)) ;
#130720 = DIRECTION('center_axis',(0.,1.,0.)) ;
#130721 = DIRECTION('ref_axis',(1.,0.,0.)) ;
#130722 = DIRECTION('center_axis',(-1.,0.,0.)) ;
#130723 = DIRECTION('ref_axis',(0.,0.,-1.)) ;
#130724 = DIRECTION('center_axis',(1.,0.,0.)) ;
#130725 = DIRECTION('ref_axis',(0.,0.,-1.)) ;
#130726 = DIRECTION('center_axis',(0.,-0.514231796959093,0.857651245551607)) ;
#130727 = DIRECTION('ref_axis',(0.,0.857651245551607,0.514231796959093)) ;
#130728 = DIRECTION('center_axis',(0.,0.,-1.)) ;
#130729 = DIRECTION('ref_axis',(1.,0.,0.)) ;
#130730 = DIRECTION('center_axis',(0.,1.,0.)) ;
#130731 = DIRECTION('ref_axis',(1.,0.,0.)) ;
#130732 = DIRECTION('center_axis',(-6.93889390390727E-14,0.,-1.)) ;
#130733 = DIRECTION('ref_axis',(1.,0.,-6.93889390390727E-14)) ;
#130734 = DIRECTION('center_axis',(-1.,0.,0.)) ;
#130735 = DIRECTION('ref_axis',(0.,-3.03576608295933E-14,-1.)) ;
#130736 = DIRECTION('center_axis',(0.,0.,-1.)) ;
#130737 = DIRECTION('ref_axis',(-1.,0.,0.)) ;
#130738 = DIRECTION('center_axis',(0.,0.,1.)) ;
#130739 = DIRECTION('ref_axis',(-1.,0.,0.)) ;
#130740 = DIRECTION('center_axis',(0.,0.,-1.)) ;
#130741 = DIRECTION('ref_axis',(-1.,0.,0.)) ;
#130742 = DIRECTION('center_axis',(-1.,0.,7.01133629567814E-33)) ;
#130743 = DIRECTION('ref_axis',(7.01133629567814E-33,0.,1.)) ;
#130744 = DIRECTION('center_axis',(-1.,0.,0.)) ;
#130745 = DIRECTION('ref_axis',(0.,0.,1.)) ;
#130746 = DIRECTION('center_axis',(0.,0.,-1.)) ;
#130747 = DIRECTION('ref_axis',(-1.,0.,0.)) ;
#130748 = DIRECTION('center_axis',(-7.01133629567814E-33,8.97270763436279E-17,
-1.)) ;
#130749 = DIRECTION('ref_axis',(6.29106707073161E-49,1.,8.97270763436279E-17)) ;
#130750 = DIRECTION('center_axis',(1.,0.,0.)) ;
#130751 = DIRECTION('ref_axis',(0.,0.,-1.)) ;
#130752 = DIRECTION('center_axis',(6.69037477709045E-15,0.51423179695912,
0.85765124555159)) ;
#130753 = DIRECTION('ref_axis',(-4.49049578447409E-29,-0.85765124555159,0.51423179695912)) ;
#130754 = DIRECTION('center_axis',(-1.,0.,0.)) ;
#130755 = DIRECTION('ref_axis',(0.,0.,1.)) ;
#130756 = DIRECTION('center_axis',(-1.,0.,0.)) ;
#130757 = DIRECTION('ref_axis',(0.,2.60208521396514E-14,-1.)) ;
#130758 = DIRECTION('center_axis',(0.,0.,1.)) ;
#130759 = DIRECTION('ref_axis',(1.,0.,0.)) ;
#130760 = DIRECTION('center_axis',(0.,0.,-1.)) ;
#130761 = DIRECTION('ref_axis',(-1.,0.,0.)) ;
#130762 = DIRECTION('center_axis',(0.,-1.,8.97270763436279E-17)) ;
#130763 = DIRECTION('ref_axis',(0.,-8.97270763436279E-17,-1.)) ;
#130764 = DIRECTION('center_axis',(0.,-1.,8.97270763436279E-17)) ;
#130765 = DIRECTION('ref_axis',(0.,-8.97270763436279E-17,-1.)) ;
#130766 = DIRECTION('center_axis',(0.,-1.,0.)) ;
#130767 = DIRECTION('ref_axis',(0.,0.,-1.)) ;
#130768 = DIRECTION('center_axis',(-7.01133629567814E-33,8.97270763436279E-17,
-1.)) ;
#130769 = DIRECTION('ref_axis',(0.,1.,0.)) ;
#130770 = DIRECTION('center_axis',(0.,-1.,0.)) ;
#130771 = DIRECTION('ref_axis',(0.,0.,1.)) ;
#130772 = DIRECTION('center_axis',(1.,0.,0.)) ;
#130773 = DIRECTION('ref_axis',(0.,0.,-1.)) ;
#130774 = DIRECTION('center_axis',(0.,0.,1.)) ;
#130775 = DIRECTION('ref_axis',(-1.,0.,0.)) ;
#130776 = DIRECTION('center_axis',(0.,1.,0.)) ;
#130777 = DIRECTION('ref_axis',(1.,0.,0.)) ;
#130778 = DIRECTION('center_axis',(-1.,0.,0.)) ;
#130779 = DIRECTION('ref_axis',(0.,0.,-1.)) ;
#130780 = DIRECTION('center_axis',(1.,7.81406971160724E-17,0.)) ;
#130781 = DIRECTION('ref_axis',(-7.81406971160724E-17,1.,0.)) ;
#130782 = DIRECTION('center_axis',(1.,0.,0.)) ;
#130783 = DIRECTION('ref_axis',(0.,0.,-1.)) ;
#130784 = DIRECTION('center_axis',(1.,0.,0.)) ;
#130785 = DIRECTION('ref_axis',(0.,0.,-1.)) ;
#130786 = DIRECTION('center_axis',(0.,1.,8.97270763436279E-17)) ;
#130787 = DIRECTION('ref_axis',(0.,-8.97270763436279E-17,1.)) ;
#130788 = DIRECTION('center_axis',(0.,-1.,0.)) ;
#130789 = DIRECTION('ref_axis',(0.,0.,-1.)) ;
#130790 = DIRECTION('center_axis',(0.,0.,-1.)) ;
#130791 = DIRECTION('ref_axis',(-1.,0.,0.)) ;
#130792 = DIRECTION('center_axis',(-7.01133629567814E-33,8.97270763436279E-17,
1.)) ;
#130793 = DIRECTION('ref_axis',(-6.29106707073161E-49,-1.,8.97270763436279E-17)) ;
#130794 = DIRECTION('center_axis',(-1.,0.,-7.01133629567814E-33)) ;
#130795 = DIRECTION('ref_axis',(-7.01133629567814E-33,0.,1.)) ;
#130796 = DIRECTION('center_axis',(-1.,0.,0.)) ;
#130797 = DIRECTION('ref_axis',(0.,0.,1.)) ;
#130798 = DIRECTION('center_axis',(1.,0.,0.)) ;
#130799 = DIRECTION('ref_axis',(0.,1.,0.)) ;
#130800 = DIRECTION('center_axis',(0.,1.,0.)) ;
#130801 = DIRECTION('ref_axis',(0.,0.,1.)) ;
#130802 = DIRECTION('center_axis',(0.,1.,0.)) ;
#130803 = DIRECTION('ref_axis',(1.,0.,0.)) ;
#130804 = DIRECTION('center_axis',(0.,0.,-1.)) ;
#130805 = DIRECTION('ref_axis',(1.,0.,0.)) ;
#130806 = DIRECTION('center_axis',(-1.,0.,0.)) ;
#130807 = DIRECTION('ref_axis',(0.,0.,-1.)) ;
#130808 = DIRECTION('center_axis',(-7.01133629567814E-33,8.97270763436279E-17,
1.)) ;
#130809 = DIRECTION('ref_axis',(0.,-1.,0.)) ;
#130810 = DIRECTION('center_axis',(0.,-1.,0.)) ;
#130811 = DIRECTION('ref_axis',(0.,0.,1.)) ;
#130812 = DIRECTION('center_axis',(7.81406971160724E-17,-1.,-8.97270763436279E-17)) ;
#130813 = DIRECTION('ref_axis',(-7.01133629567814E-33,8.97270763436279E-17,
-1.)) ;
#130814 = DIRECTION('center_axis',(0.,1.,0.)) ;
#130815 = DIRECTION('ref_axis',(0.,0.,1.)) ;
#130816 = DIRECTION('center_axis',(-1.,-7.81406971160724E-17,0.)) ;
#130817 = DIRECTION('ref_axis',(7.81406971160724E-17,-1.,0.)) ;
#130818 = DIRECTION('center_axis',(-1.,-7.81406971160724E-17,0.)) ;
#130819 = DIRECTION('ref_axis',(-7.81406971160724E-17,1.,0.)) ;
#130820 = DIRECTION('center_axis',(0.,0.,1.)) ;
#130821 = DIRECTION('ref_axis',(1.,0.,0.)) ;
#130822 = DIRECTION('center_axis',(0.,0.,-1.)) ;
#130823 = DIRECTION('ref_axis',(-1.,0.,0.)) ;
#130824 = DIRECTION('center_axis',(0.,-1.,8.97270763436279E-17)) ;
#130825 = DIRECTION('ref_axis',(0.,-8.97270763436279E-17,-1.)) ;
#130826 = DIRECTION('center_axis',(0.,-1.,0.)) ;
#130827 = DIRECTION('ref_axis',(0.,0.,-1.)) ;
#130828 = DIRECTION('center_axis',(1.,7.81406971160724E-17,0.)) ;
#130829 = DIRECTION('ref_axis',(0.,1.,0.)) ;
#130830 = DIRECTION('center_axis',(0.,0.,1.)) ;
#130831 = DIRECTION('ref_axis',(-1.,0.,0.)) ;
#130832 = DIRECTION('center_axis',(0.,1.,0.)) ;
#130833 = DIRECTION('ref_axis',(1.,0.,0.)) ;
#130834 = DIRECTION('center_axis',(-1.,0.,0.)) ;
#130835 = DIRECTION('ref_axis',(0.,0.,-1.)) ;
#130836 = DIRECTION('center_axis',(0.,0.,-1.)) ;
#130837 = DIRECTION('ref_axis',(-1.,0.,0.)) ;
#130838 = DIRECTION('center_axis',(0.,0.,1.)) ;
#130839 = DIRECTION('ref_axis',(1.,0.,0.)) ;
#130840 = DIRECTION('center_axis',(-1.,-7.81406971160724E-17,0.)) ;
#130841 = DIRECTION('ref_axis',(7.81406971160724E-17,-1.,0.)) ;
#130842 = DIRECTION('center_axis',(-1.,-7.81406971160724E-17,0.)) ;
#130843 = DIRECTION('ref_axis',(-7.81406971160724E-17,1.,0.)) ;
#130844 = DIRECTION('center_axis',(1.,7.81406971160724E-17,0.)) ;
#130845 = DIRECTION('ref_axis',(-7.81406971160724E-17,1.,0.)) ;
#130846 = DIRECTION('center_axis',(1.,0.,0.)) ;
#130847 = DIRECTION('ref_axis',(0.,0.,-1.)) ;
#130848 = DIRECTION('center_axis',(1.,0.,0.)) ;
#130849 = DIRECTION('ref_axis',(0.,0.,-1.)) ;
#130850 = DIRECTION('center_axis',(3.78638272950961E-32,-4.8455963016112E-16,
-1.)) ;
#130851 = DIRECTION('ref_axis',(1.83472821505963E-47,1.,-4.8455963016112E-16)) ;
#130852 = DIRECTION('center_axis',(3.78638272950961E-32,-4.8455963016112E-16,
-1.)) ;
#130853 = DIRECTION('ref_axis',(1.83472821505963E-47,1.,-4.8455963016112E-16)) ;
#130854 = DIRECTION('center_axis',(0.,0.,-1.)) ;
#130855 = DIRECTION('ref_axis',(-1.,0.,0.)) ;
#130856 = DIRECTION('center_axis',(1.,7.81406971160724E-17,0.)) ;
#130857 = DIRECTION('ref_axis',(0.,1.,0.)) ;
#130858 = DIRECTION('center_axis',(0.,-1.,0.)) ;
#130859 = DIRECTION('ref_axis',(0.,0.,1.)) ;
#130860 = DIRECTION('center_axis',(0.,1.,0.)) ;
#130861 = DIRECTION('ref_axis',(1.,0.,0.)) ;
#130862 = DIRECTION('center_axis',(0.,1.,0.)) ;
#130863 = DIRECTION('ref_axis',(0.,0.,-1.)) ;
#130864 = DIRECTION('center_axis',(-7.81406971160724E-17,1.,-8.97270763436279E-17)) ;
#130865 = DIRECTION('ref_axis',(-7.01133629567814E-33,8.97270763436279E-17,
1.)) ;
#130866 = DIRECTION('center_axis',(0.,-1.,0.)) ;
#130867 = DIRECTION('ref_axis',(0.,0.,-1.)) ;
#130868 = DIRECTION('center_axis',(0.,1.,0.)) ;
#130869 = DIRECTION('ref_axis',(0.,0.,1.)) ;
#130870 = DIRECTION('center_axis',(0.,-1.,0.)) ;
#130871 = DIRECTION('ref_axis',(0.,0.,-1.)) ;
#130872 = DIRECTION('center_axis',(0.,-1.,0.)) ;
#130873 = DIRECTION('ref_axis',(0.,0.,-1.)) ;
#130874 = DIRECTION('center_axis',(0.,1.,0.)) ;
#130875 = DIRECTION('ref_axis',(1.,0.,0.)) ;
#130876 = DIRECTION('center_axis',(0.,0.,1.)) ;
#130877 = DIRECTION('ref_axis',(-1.,0.,0.)) ;
#130878 = DIRECTION('center_axis',(1.,0.,0.)) ;
#130879 = DIRECTION('ref_axis',(0.,0.,1.)) ;
#130880 = DIRECTION('center_axis',(0.,-1.,0.)) ;
#130881 = DIRECTION('ref_axis',(0.,0.,-1.)) ;
#130882 = DIRECTION('center_axis',(0.,1.,0.)) ;
#130883 = DIRECTION('ref_axis',(0.,0.,1.)) ;
#130884 = DIRECTION('center_axis',(0.,-1.,0.)) ;
#130885 = DIRECTION('ref_axis',(0.,0.,-1.)) ;
#130886 = DIRECTION('center_axis',(-1.,0.,2.16840434497101E-16)) ;
#130887 = DIRECTION('ref_axis',(2.16840434497101E-16,0.,1.)) ;
#130888 = DIRECTION('center_axis',(1.,0.,0.)) ;
#130889 = DIRECTION('ref_axis',(0.,0.,-1.)) ;
#130890 = DIRECTION('center_axis',(-2.16840434497101E-16,0.,1.)) ;
#130891 = DIRECTION('ref_axis',(1.,0.,2.16840434497101E-16)) ;
#130892 = DIRECTION('center_axis',(0.,0.,1.)) ;
#130893 = DIRECTION('ref_axis',(1.,0.,0.)) ;
#130894 = DIRECTION('center_axis',(0.,1.,0.)) ;
#130895 = DIRECTION('ref_axis',(0.,0.,1.)) ;
#130896 = DIRECTION('center_axis',(0.,-1.,0.)) ;
#130897 = DIRECTION('ref_axis',(0.,0.,-1.)) ;
#130898 = DIRECTION('center_axis',(0.,1.,0.)) ;
#130899 = DIRECTION('ref_axis',(1.,0.,0.)) ;
#130900 = DIRECTION('center_axis',(0.,0.,1.)) ;
#130901 = DIRECTION('ref_axis',(-1.,0.,0.)) ;
#130902 = DIRECTION('center_axis',(0.,1.,0.)) ;
#130903 = DIRECTION('ref_axis',(1.,0.,0.)) ;
#130904 = DIRECTION('center_axis',(1.,0.,0.)) ;
#130905 = DIRECTION('ref_axis',(0.,0.,1.)) ;
#130906 = DIRECTION('center_axis',(0.,0.,-1.)) ;
#130907 = DIRECTION('ref_axis',(-1.,0.,0.)) ;
#130908 = DIRECTION('center_axis',(0.,0.,1.)) ;
#130909 = DIRECTION('ref_axis',(1.,0.,0.)) ;
#130910 = DIRECTION('center_axis',(1.,0.,2.16840434497101E-16)) ;
#130911 = DIRECTION('ref_axis',(2.16840434497101E-16,0.,-1.)) ;
#130912 = DIRECTION('center_axis',(1.,0.,0.)) ;
#130913 = DIRECTION('ref_axis',(0.,0.,-1.)) ;
#130914 = DIRECTION('center_axis',(0.,1.,0.)) ;
#130915 = DIRECTION('ref_axis',(1.,0.,0.)) ;
#130916 = DIRECTION('center_axis',(0.,1.,0.)) ;
#130917 = DIRECTION('ref_axis',(0.,0.,-1.)) ;
#130918 = DIRECTION('center_axis',(0.,1.,0.)) ;
#130919 = DIRECTION('ref_axis',(0.,0.,1.)) ;
#130920 = DIRECTION('center_axis',(0.,1.,0.)) ;
#130921 = DIRECTION('ref_axis',(0.,0.,1.)) ;
#130922 = DIRECTION('center_axis',(-0.942809041582063,-0.235702260395516,
0.235702260395518)) ;
#130923 = DIRECTION('ref_axis',(0.242535625036335,4.64743530723282E-16,0.970142500145331)) ;
#130924 = DIRECTION('center_axis',(-0.970142500145332,-0.242535625036331,
-2.10366121255617E-15)) ;
#130925 = DIRECTION('ref_axis',(0.242535625036331,-0.970142500145332,-4.47980524894761E-30)) ;
#130926 = DIRECTION('center_axis',(0.970142500145333,0.24253562503633,0.)) ;
#130927 = DIRECTION('ref_axis',(-0.24253562503633,0.970142500145333,0.)) ;
#130928 = DIRECTION('center_axis',(-0.970142500145332,-0.242535625036331,
2.73475957632304E-14)) ;
#130929 = DIRECTION('ref_axis',(0.242535625036331,-0.970142500145332,1.1454669517322E-30)) ;
#130930 = DIRECTION('center_axis',(0.879462917689188,0.219865729422294,-0.42214220049081)) ;
#130931 = DIRECTION('ref_axis',(-0.432731067584771,1.71515946658E-16,-0.901523057468274)) ;
#130932 = DIRECTION('center_axis',(0.879462917689192,0.219865729422271,-0.422142200490814)) ;
#130933 = DIRECTION('ref_axis',(-0.432731067584773,-1.62351711522009E-16,
-0.901523057468273)) ;
#130934 = DIRECTION('center_axis',(0.,1.,0.)) ;
#130935 = DIRECTION('ref_axis',(1.,0.,0.)) ;
#130936 = DIRECTION('center_axis',(0.,-1.,0.)) ;
#130937 = DIRECTION('ref_axis',(0.,0.,1.)) ;
#130938 = DIRECTION('center_axis',(0.,-1.,0.)) ;
#130939 = DIRECTION('ref_axis',(0.,0.,-1.)) ;
#130940 = DIRECTION('center_axis',(-4.51750905202295E-15,-1.,2.16840434497102E-15)) ;
#130941 = DIRECTION('ref_axis',(1.,-4.51750905202295E-15,3.91831450274151E-31)) ;
#130942 = DIRECTION('center_axis',(0.669589480006976,-0.669589480006974,-0.321402950403349)) ;
#130943 = DIRECTION('ref_axis',(0.707106781186547,0.707106781186548,5.45170614306381E-16)) ;
#130944 = DIRECTION('center_axis',(0.669589480006977,-0.669589480006977,-0.321402950403342)) ;
#130945 = DIRECTION('ref_axis',(0.707106781186547,0.707106781186548,-1.94221176494188E-16)) ;
#130946 = DIRECTION('center_axis',(0.,1.,0.)) ;
#130947 = DIRECTION('ref_axis',(1.,0.,0.)) ;
#130948 = DIRECTION('center_axis',(0.707106781186541,-0.707106781186554,0.)) ;
#130949 = DIRECTION('ref_axis',(-0.707106781186554,-0.707106781186541,0.)) ;
#130950 = DIRECTION('center_axis',(0.707106781186549,-0.707106781186546,0.)) ;
#130951 = DIRECTION('ref_axis',(0.707106781186546,0.707106781186549,0.)) ;
#130952 = DIRECTION('center_axis',(0.707106781186548,-0.707106781186548,-1.53329341668338E-15)) ;
#130953 = DIRECTION('ref_axis',(0.707106781186548,0.707106781186548,1.5356898865553E-31)) ;
#130954 = DIRECTION('center_axis',(0.577350269189633,-0.577350269189633,-0.577350269189612)) ;
#130955 = DIRECTION('ref_axis',(0.707106781186548,0.707106781186548,1.34560831514457E-17)) ;
#130956 = DIRECTION('center_axis',(-0.577350269189328,0.577350269189571,-0.577350269189978)) ;
#130957 = DIRECTION('ref_axis',(-7.61554280732519E-15,0.707106781186793,0.707106781186302)) ;
#130958 = DIRECTION('center_axis',(-0.707106781186548,0.707106781186548,7.66646708341718E-15)) ;
#130959 = DIRECTION('ref_axis',(-0.707106781186548,-0.707106781186548,3.27987112860885E-31)) ;
#130960 = DIRECTION('center_axis',(-0.707106781186549,0.707106781186546,0.)) ;
#130961 = DIRECTION('ref_axis',(-0.707106781186546,-0.707106781186549,0.)) ;
#130962 = DIRECTION('center_axis',(-0.707106781186548,0.707106781186548,-1.13463712834566E-13)) ;
#130963 = DIRECTION('ref_axis',(-0.707106781186548,-0.707106781186548,1.81538773348134E-28)) ;
#130964 = DIRECTION('center_axis',(-0.669589480006976,0.669589480006974,-0.321402950403349)) ;
#130965 = DIRECTION('ref_axis',(-0.707106781186547,-0.707106781186548,5.45170614306381E-16)) ;
#130966 = DIRECTION('center_axis',(0.66958948000704,-0.669589480006895,0.32140295040338)) ;
#130967 = DIRECTION('ref_axis',(0.707106781186471,0.707106781186624,1.36895061126305E-16)) ;
#130968 = DIRECTION('center_axis',(0.,1.,0.)) ;
#130969 = DIRECTION('ref_axis',(1.,0.,0.)) ;
#130970 = DIRECTION('center_axis',(-1.50329234996253E-14,1.,0.)) ;
#130971 = DIRECTION('ref_axis',(1.,1.50329234996253E-14,0.)) ;
#130972 = DIRECTION('center_axis',(0.,-1.,0.)) ;
#130973 = DIRECTION('ref_axis',(0.,0.,-1.)) ;
#130974 = DIRECTION('center_axis',(0.,1.,0.)) ;
#130975 = DIRECTION('ref_axis',(0.,0.,1.)) ;
#130976 = DIRECTION('center_axis',(-0.879462917689188,-0.219865729422294,
-0.42214220049081)) ;
#130977 = DIRECTION('ref_axis',(-0.432731067584771,1.71515946658E-16,0.901523057468274)) ;
#130978 = DIRECTION('center_axis',(0.879462917689201,0.219865729422298,0.42214220049078)) ;
#130979 = DIRECTION('ref_axis',(0.432731067584741,-2.36820597908546E-15,-0.901523057468288)) ;
#130980 = DIRECTION('center_axis',(0.,1.,0.)) ;
#130981 = DIRECTION('ref_axis',(1.,0.,0.)) ;
#130982 = DIRECTION('center_axis',(0.970142500145323,0.242535625036368,0.)) ;
#130983 = DIRECTION('ref_axis',(0.242535625036368,-0.970142500145323,0.)) ;
#130984 = DIRECTION('center_axis',(-0.970142500145333,-0.24253562503633,0.)) ;
#130985 = DIRECTION('ref_axis',(0.24253562503633,-0.970142500145333,0.)) ;
#130986 = DIRECTION('center_axis',(0.970142500145333,0.242535625036331,-2.1036612125561E-15)) ;
#130987 = DIRECTION('ref_axis',(-0.242535625036331,0.970142500145332,-1.06801962627779E-30)) ;
#130988 = DIRECTION('center_axis',(0.942809041582058,0.235702260395512,0.23570226039554)) ;
#130989 = DIRECTION('ref_axis',(0.242535625036358,-1.84667126758454E-15,-0.970142500145326)) ;
#130990 = DIRECTION('center_axis',(0.,-1.,0.)) ;
#130991 = DIRECTION('ref_axis',(0.,0.,-1.)) ;
#130992 = DIRECTION('center_axis',(-1.,0.,-8.67361737988409E-15)) ;
#130993 = DIRECTION('ref_axis',(-8.67361737988409E-15,0.,1.)) ;
#130994 = DIRECTION('center_axis',(0.,0.,-1.)) ;
#130995 = DIRECTION('ref_axis',(-1.,0.,0.)) ;
#130996 = DIRECTION('center_axis',(0.,0.,-1.)) ;
#130997 = DIRECTION('ref_axis',(-1.,0.,0.)) ;
#130998 = DIRECTION('center_axis',(0.,3.46944695195362E-14,-1.)) ;
#130999 = DIRECTION('ref_axis',(0.,1.,3.46944695195362E-14)) ;
#131000 = DIRECTION('center_axis',(1.,0.,0.)) ;
#131001 = DIRECTION('ref_axis',(0.,0.,-1.)) ;
#131002 = DIRECTION('center_axis',(-1.,0.,0.)) ;
#131003 = DIRECTION('ref_axis',(0.,0.,1.)) ;
#131004 = DIRECTION('center_axis',(0.,-1.,0.)) ;
#131005 = DIRECTION('ref_axis',(0.,0.,-1.)) ;
#131006 = DIRECTION('center_axis',(-1.,0.,0.)) ;
#131007 = DIRECTION('ref_axis',(0.,0.,1.)) ;
#131008 = DIRECTION('center_axis',(0.,-1.,0.)) ;
#131009 = DIRECTION('ref_axis',(0.,0.,-1.)) ;
#131010 = DIRECTION('center_axis',(3.46944695195358E-14,0.,-1.)) ;
#131011 = DIRECTION('ref_axis',(-1.,0.,-3.46944695195358E-14)) ;
#131012 = DIRECTION('center_axis',(-1.,0.,0.)) ;
#131013 = DIRECTION('ref_axis',(0.,0.,1.)) ;
#131014 = DIRECTION('center_axis',(-1.,1.73472347597681E-14,0.)) ;
#131015 = DIRECTION('ref_axis',(-1.73472347597681E-14,-1.,0.)) ;
#131016 = DIRECTION('center_axis',(0.,0.,1.)) ;
#131017 = DIRECTION('ref_axis',(1.,0.,0.)) ;
#131018 = DIRECTION('center_axis',(-3.46944695195364E-14,0.,-1.)) ;
#131019 = DIRECTION('ref_axis',(-1.,0.,3.46944695195364E-14)) ;
#131020 = DIRECTION('center_axis',(0.,-1.,0.)) ;
#131021 = DIRECTION('ref_axis',(0.,0.,-1.)) ;
#131022 = DIRECTION('center_axis',(0.,-1.,0.)) ;
#131023 = DIRECTION('ref_axis',(0.,0.,-1.)) ;
#131024 = DIRECTION('center_axis',(0.,-1.,0.)) ;
#131025 = DIRECTION('ref_axis',(0.,0.,-1.)) ;
#131026 = DIRECTION('center_axis',(0.,0.,1.)) ;
#131027 = DIRECTION('ref_axis',(1.,0.,0.)) ;
#131028 = DIRECTION('center_axis',(0.,0.,-1.)) ;
#131029 = DIRECTION('ref_axis',(-1.,0.,0.)) ;
#131030 = DIRECTION('center_axis',(0.,0.,1.)) ;
#131031 = DIRECTION('ref_axis',(1.,0.,0.)) ;
#131032 = DIRECTION('center_axis',(0.,-1.,0.)) ;
#131033 = DIRECTION('ref_axis',(0.,0.,-1.)) ;
#131034 = DIRECTION('center_axis',(0.,-1.,0.)) ;
#131035 = DIRECTION('ref_axis',(0.,0.,-1.)) ;
#131036 = DIRECTION('center_axis',(0.,1.,0.)) ;
#131037 = DIRECTION('ref_axis',(1.,0.,0.)) ;
#131038 = DIRECTION('center_axis',(-1.,0.,0.)) ;
#131039 = DIRECTION('ref_axis',(0.,0.,-1.)) ;
#131040 = DIRECTION('center_axis',(0.,1.,0.)) ;
#131041 = DIRECTION('ref_axis',(1.,0.,0.)) ;
#131042 = DIRECTION('center_axis',(-1.,0.,0.)) ;
#131043 = DIRECTION('ref_axis',(0.,0.,-1.)) ;
#131044 = DIRECTION('center_axis',(0.,-1.,0.)) ;
#131045 = DIRECTION('ref_axis',(0.,0.,-1.)) ;
#131046 = DIRECTION('center_axis',(0.,-1.,0.)) ;
#131047 = DIRECTION('ref_axis',(0.,0.,-1.)) ;
#131048 = DIRECTION('center_axis',(-1.,0.,0.)) ;
#131049 = DIRECTION('ref_axis',(0.,0.,1.)) ;
#131050 = DIRECTION('center_axis',(-1.,0.,0.)) ;
#131051 = DIRECTION('ref_axis',(0.,0.,1.)) ;
#131052 = DIRECTION('center_axis',(1.,0.,0.)) ;
#131053 = DIRECTION('ref_axis',(0.,0.,-1.)) ;
#131054 = DIRECTION('center_axis',(-1.,0.,0.)) ;
#131055 = DIRECTION('ref_axis',(0.,0.,1.)) ;
#131056 = DIRECTION('center_axis',(0.,-1.,0.)) ;
#131057 = DIRECTION('ref_axis',(0.,0.,-1.)) ;
#131058 = DIRECTION('center_axis',(0.,-1.,0.)) ;
#131059 = DIRECTION('ref_axis',(0.,0.,-1.)) ;
#131060 = DIRECTION('center_axis',(0.,1.,0.)) ;
#131061 = DIRECTION('ref_axis',(1.,0.,0.)) ;
#131062 = DIRECTION('center_axis',(0.,0.,-1.)) ;
#131063 = DIRECTION('ref_axis',(1.,0.,0.)) ;
#131064 = DIRECTION('center_axis',(0.,1.,0.)) ;
#131065 = DIRECTION('ref_axis',(1.,0.,0.)) ;
#131066 = DIRECTION('center_axis',(0.,0.,1.)) ;
#131067 = DIRECTION('ref_axis',(-1.,0.,0.)) ;
#131068 = DIRECTION('center_axis',(0.,0.,-1.)) ;
#131069 = DIRECTION('ref_axis',(-1.,0.,0.)) ;
#131070 = DIRECTION('center_axis',(1.,1.31418445149758E-16,-2.16840434497101E-16)) ;
#131071 = DIRECTION('ref_axis',(-2.16840434497101E-16,-2.8496832747207E-32,
-1.)) ;
#131072 = DIRECTION('center_axis',(1.,0.,0.)) ;
#131073 = DIRECTION('ref_axis',(0.,0.,-1.)) ;
#131074 = DIRECTION('center_axis',(-1.,0.,0.)) ;
#131075 = DIRECTION('ref_axis',(0.,0.,1.)) ;
#131076 = DIRECTION('center_axis',(-1.31418445149758E-16,1.,0.)) ;
#131077 = DIRECTION('ref_axis',(-1.,0.,0.)) ;
#131078 = DIRECTION('center_axis',(0.,0.,1.)) ;
#131079 = DIRECTION('ref_axis',(-1.,0.,0.)) ;
#131080 = DIRECTION('center_axis',(-1.31418445149758E-16,1.,0.)) ;
#131081 = DIRECTION('ref_axis',(-1.,-1.31418445149758E-16,0.)) ;
#131082 = DIRECTION('center_axis',(-1.31418445149758E-16,1.,0.)) ;
#131083 = DIRECTION('ref_axis',(-1.,0.,0.)) ;
#131084 = DIRECTION('center_axis',(-1.31418445149758E-16,1.,0.)) ;
#131085 = DIRECTION('ref_axis',(-1.,-1.31418445149758E-16,0.)) ;
#131086 = DIRECTION('center_axis',(0.,0.,1.)) ;
#131087 = DIRECTION('ref_axis',(-1.,0.,0.)) ;
#131088 = DIRECTION('center_axis',(-4.33680868994202E-16,-5.69936654944139E-32,
-1.)) ;
#131089 = DIRECTION('ref_axis',(-1.,2.47170623787823E-47,4.33680868994202E-16)) ;
#131090 = DIRECTION('center_axis',(0.,0.,1.)) ;
#131091 = DIRECTION('ref_axis',(1.,0.,0.)) ;
#131092 = DIRECTION('center_axis',(-1.31418445149758E-16,-1.,0.)) ;
#131093 = DIRECTION('ref_axis',(1.,-1.31418445149758E-16,0.)) ;
#131094 = DIRECTION('center_axis',(0.,1.,0.)) ;
#131095 = DIRECTION('ref_axis',(0.,0.,1.)) ;
#131096 = DIRECTION('center_axis',(-1.,0.,2.16840434497101E-16)) ;
#131097 = DIRECTION('ref_axis',(2.16840434497101E-16,0.,1.)) ;
#131098 = DIRECTION('center_axis',(-1.,0.,0.)) ;
#131099 = DIRECTION('ref_axis',(0.,0.,1.)) ;
#131100 = DIRECTION('center_axis',(1.,0.,0.)) ;
#131101 = DIRECTION('ref_axis',(0.,0.,-1.)) ;
#131102 = DIRECTION('center_axis',(-1.31418445149758E-16,-1.,0.)) ;
#131103 = DIRECTION('ref_axis',(1.,-1.31418445149758E-16,0.)) ;
#131104 = DIRECTION('center_axis',(0.,1.,0.)) ;
#131105 = DIRECTION('ref_axis',(0.,0.,1.)) ;
#131106 = DIRECTION('center_axis',(2.16840434497101E-16,2.8496832747207E-32,
1.)) ;
#131107 = DIRECTION('ref_axis',(1.,-6.17926559469557E-48,-2.16840434497101E-16)) ;
#131108 = DIRECTION('center_axis',(0.,0.,1.)) ;
#131109 = DIRECTION('ref_axis',(1.,0.,0.)) ;
#131110 = DIRECTION('center_axis',(-1.,-1.31418445149758E-16,-2.16840434497101E-16)) ;
#131111 = DIRECTION('ref_axis',(-2.16840434497101E-16,-2.8496832747207E-32,
1.)) ;
#131112 = DIRECTION('center_axis',(-1.,0.,0.)) ;
#131113 = DIRECTION('ref_axis',(0.,0.,1.)) ;
#131114 = DIRECTION('center_axis',(1.,0.,0.)) ;
#131115 = DIRECTION('ref_axis',(0.,0.,-1.)) ;
#131116 = DIRECTION('center_axis',(-1.31418445149758E-16,1.,0.)) ;
#131117 = DIRECTION('ref_axis',(-1.,0.,0.)) ;
#131118 = DIRECTION('center_axis',(-1.31418445149758E-16,1.,0.)) ;
#131119 = DIRECTION('ref_axis',(-1.,-1.31418445149758E-16,0.)) ;
#131120 = DIRECTION('center_axis',(0.,1.,0.)) ;
#131121 = DIRECTION('ref_axis',(1.,0.,0.)) ;
#131122 = DIRECTION('center_axis',(0.,0.,-1.)) ;
#131123 = DIRECTION('ref_axis',(1.,0.,0.)) ;
#131124 = DIRECTION('center_axis',(0.,1.,0.)) ;
#131125 = DIRECTION('ref_axis',(1.,0.,0.)) ;
#131126 = DIRECTION('center_axis',(0.,0.,-1.)) ;
#131127 = DIRECTION('ref_axis',(1.,0.,0.)) ;
#131128 = DIRECTION('center_axis',(-1.31418445149758E-16,1.,0.)) ;
#131129 = DIRECTION('ref_axis',(-1.,0.,0.)) ;
#131130 = DIRECTION('center_axis',(-1.31418445149758E-16,1.,0.)) ;
#131131 = DIRECTION('ref_axis',(-1.,-1.31418445149758E-16,0.)) ;
#131132 = DIRECTION('center_axis',(-1.31418445149758E-16,-1.,0.)) ;
#131133 = DIRECTION('ref_axis',(1.,-1.31418445149758E-16,0.)) ;
#131134 = DIRECTION('center_axis',(0.,1.,0.)) ;
#131135 = DIRECTION('ref_axis',(0.,0.,1.)) ;
#131136 = DIRECTION('center_axis',(4.33680868994202E-16,0.,1.)) ;
#131137 = DIRECTION('ref_axis',(1.,0.,-4.33680868994202E-16)) ;
#131138 = DIRECTION('center_axis',(0.,0.,-1.)) ;
#131139 = DIRECTION('ref_axis',(-1.,0.,0.)) ;
#131140 = DIRECTION('center_axis',(-2.16840434497101E-16,0.,-1.)) ;
#131141 = DIRECTION('ref_axis',(-1.,0.,2.16840434497101E-16)) ;
#131142 = DIRECTION('center_axis',(0.,0.,-1.)) ;
#131143 = DIRECTION('ref_axis',(-1.,0.,0.)) ;
#131144 = DIRECTION('center_axis',(-1.31418445149758E-16,-1.,0.)) ;
#131145 = DIRECTION('ref_axis',(1.,-1.31418445149758E-16,0.)) ;
#131146 = DIRECTION('center_axis',(0.,1.,0.)) ;
#131147 = DIRECTION('ref_axis',(0.,0.,1.)) ;
#131148 = DIRECTION('center_axis',(0.,1.,0.)) ;
#131149 = DIRECTION('ref_axis',(1.,0.,0.)) ;
#131150 = DIRECTION('center_axis',(-1.,0.,0.)) ;
#131151 = DIRECTION('ref_axis',(0.,0.,-1.)) ;
#131152 = DIRECTION('center_axis',(0.,1.,0.)) ;
#131153 = DIRECTION('ref_axis',(1.,0.,0.)) ;
#131154 = DIRECTION('center_axis',(1.,0.,0.)) ;
#131155 = DIRECTION('ref_axis',(0.,0.,1.)) ;
#131156 = DIRECTION('center_axis',(1.,0.,2.16840434497101E-16)) ;
#131157 = DIRECTION('ref_axis',(2.16840434497101E-16,0.,-1.)) ;
#131158 = DIRECTION('center_axis',(0.,1.,0.)) ;
#131159 = DIRECTION('ref_axis',(0.,0.,1.)) ;
#131160 = DIRECTION('center_axis',(0.,1.,0.)) ;
#131161 = DIRECTION('ref_axis',(0.,0.,1.)) ;
#131162 = DIRECTION('center_axis',(0.,0.,-1.)) ;
#131163 = DIRECTION('ref_axis',(-1.,0.,0.)) ;
#131164 = DIRECTION('center_axis',(0.,0.,1.)) ;
#131165 = DIRECTION('ref_axis',(1.,0.,0.)) ;
#131166 = DIRECTION('center_axis',(0.,0.,-1.)) ;
#131167 = DIRECTION('ref_axis',(-1.,0.,0.)) ;
#131168 = DIRECTION('center_axis',(0.,1.,0.)) ;
#131169 = DIRECTION('ref_axis',(0.,0.,1.)) ;
#131170 = DIRECTION('center_axis',(0.,1.,0.)) ;
#131171 = DIRECTION('ref_axis',(0.,0.,1.)) ;
#131172 = DIRECTION('center_axis',(0.,1.,0.)) ;
#131173 = DIRECTION('ref_axis',(1.,0.,0.)) ;
#131174 = DIRECTION('center_axis',(-1.,0.,0.)) ;
#131175 = DIRECTION('ref_axis',(0.,0.,-1.)) ;
#131176 = DIRECTION('center_axis',(0.,1.,0.)) ;
#131177 = DIRECTION('ref_axis',(1.,0.,0.)) ;
#131178 = DIRECTION('center_axis',(-1.,0.,0.)) ;
#131179 = DIRECTION('ref_axis',(0.,0.,-1.)) ;
#131180 = DIRECTION('center_axis',(0.,1.,0.)) ;
#131181 = DIRECTION('ref_axis',(0.,0.,1.)) ;
#131182 = DIRECTION('center_axis',(0.,1.,0.)) ;
#131183 = DIRECTION('ref_axis',(0.,0.,1.)) ;
#131184 = DIRECTION('center_axis',(-1.,0.,0.)) ;
#131185 = DIRECTION('ref_axis',(0.,0.,1.)) ;
#131186 = DIRECTION('center_axis',(-1.,0.,0.)) ;
#131187 = DIRECTION('ref_axis',(0.,0.,1.)) ;
#131188 = DIRECTION('center_axis',(1.,0.,0.)) ;
#131189 = DIRECTION('ref_axis',(0.,0.,-1.)) ;
#131190 = DIRECTION('center_axis',(-1.,0.,0.)) ;
#131191 = DIRECTION('ref_axis',(0.,0.,1.)) ;
#131192 = DIRECTION('center_axis',(0.,1.,0.)) ;
#131193 = DIRECTION('ref_axis',(0.,0.,1.)) ;
#131194 = DIRECTION('center_axis',(0.,1.,0.)) ;
#131195 = DIRECTION('ref_axis',(0.,0.,1.)) ;
#131196 = DIRECTION('center_axis',(0.,1.,0.)) ;
#131197 = DIRECTION('ref_axis',(1.,0.,0.)) ;
#131198 = DIRECTION('center_axis',(0.,0.,1.)) ;
#131199 = DIRECTION('ref_axis',(-1.,0.,0.)) ;
#131200 = DIRECTION('center_axis',(0.,1.,0.)) ;
#131201 = DIRECTION('ref_axis',(1.,0.,0.)) ;
#131202 = DIRECTION('center_axis',(0.,0.,-1.)) ;
#131203 = DIRECTION('ref_axis',(1.,0.,0.)) ;
#131204 = DIRECTION('center_axis',(0.,0.,1.)) ;
#131205 = DIRECTION('ref_axis',(1.,0.,0.)) ;
#131206 = DIRECTION('center_axis',(0.,0.,1.)) ;
#131207 = DIRECTION('ref_axis',(1.,0.,0.)) ;
#131208 = DIRECTION('center_axis',(0.,0.,-1.)) ;
#131209 = DIRECTION('ref_axis',(-1.,0.,0.)) ;
#131210 = DIRECTION('center_axis',(-3.46944695195361E-14,0.,1.)) ;
#131211 = DIRECTION('ref_axis',(1.,0.,3.46944695195361E-14)) ;
#131212 = DIRECTION('center_axis',(1.,0.,0.)) ;
#131213 = DIRECTION('ref_axis',(0.,0.,-1.)) ;
#131214 = DIRECTION('center_axis',(1.,0.,0.)) ;
#131215 = DIRECTION('ref_axis',(0.,0.,-1.)) ;
#131216 = DIRECTION('center_axis',(1.,0.,0.)) ;
#131217 = DIRECTION('ref_axis',(0.,0.,-1.)) ;
#131218 = DIRECTION('center_axis',(1.,0.,8.67361737988409E-15)) ;
#131219 = DIRECTION('ref_axis',(8.67361737988409E-15,0.,-1.)) ;
#131220 = DIRECTION('center_axis',(1.,0.,0.)) ;
#131221 = DIRECTION('ref_axis',(0.,0.,-1.)) ;
#131222 = DIRECTION('center_axis',(1.,0.,1.73472347597682E-14)) ;
#131223 = DIRECTION('ref_axis',(1.73472347597682E-14,0.,-1.)) ;
#131224 = DIRECTION('center_axis',(-1.,0.,0.)) ;
#131225 = DIRECTION('ref_axis',(0.,0.,1.)) ;
#131226 = DIRECTION('center_axis',(1.,0.,0.)) ;
#131227 = DIRECTION('ref_axis',(0.,0.,-1.)) ;
#131228 = DIRECTION('center_axis',(1.,0.,0.)) ;
#131229 = DIRECTION('ref_axis',(0.,0.,-1.)) ;
#131230 = DIRECTION('center_axis',(-3.46944695195364E-14,0.,-1.)) ;
#131231 = DIRECTION('ref_axis',(-1.,0.,3.46944695195364E-14)) ;
#131232 = DIRECTION('center_axis',(1.,0.,0.)) ;
#131233 = DIRECTION('ref_axis',(0.,0.,-1.)) ;
#131234 = DIRECTION('center_axis',(-3.46944695195364E-14,0.,1.)) ;
#131235 = DIRECTION('ref_axis',(1.,0.,3.46944695195364E-14)) ;
#131236 = DIRECTION('center_axis',(0.,0.,-1.)) ;
#131237 = DIRECTION('ref_axis',(-1.,0.,0.)) ;
#131238 = DIRECTION('center_axis',(-0.422618261740697,5.55398348498559E-17,
0.906307787036651)) ;
#131239 = DIRECTION('ref_axis',(0.906307787036651,6.51773046476477E-31,0.422618261740697)) ;
#131240 = DIRECTION('center_axis',(0.422618261740697,-5.55398348498559E-17,
-0.906307787036651)) ;
#131241 = DIRECTION('ref_axis',(-0.906307787036651,-6.46086972436398E-31,
-0.422618261740697)) ;
#131242 = DIRECTION('center_axis',(-0.422618261740697,5.55398348498559E-17,
0.906307787036651)) ;
#131243 = DIRECTION('ref_axis',(0.906307787036651,6.46086972436398E-31,0.422618261740697)) ;
#131244 = DIRECTION('center_axis',(0.422618261740697,-5.55398348498559E-17,
-0.906307787036651)) ;
#131245 = DIRECTION('ref_axis',(-0.906307787036651,-6.46086972436398E-31,
-0.422618261740697)) ;
#131246 = DIRECTION('center_axis',(0.,1.,0.)) ;
#131247 = DIRECTION('ref_axis',(1.,0.,0.)) ;
#131248 = DIRECTION('center_axis',(8.40428841770292E-14,0.51423179695912,
-0.85765124555159)) ;
#131249 = DIRECTION('ref_axis',(3.46944695195355E-14,-0.85765124555159,-0.51423179695912)) ;
#131250 = DIRECTION('center_axis',(0.,-6.93889390390724E-14,1.)) ;
#131251 = DIRECTION('ref_axis',(0.,1.,6.93889390390724E-14)) ;
#131252 = DIRECTION('center_axis',(-1.,0.,0.)) ;
#131253 = DIRECTION('ref_axis',(0.,2.16840434497095E-14,-1.)) ;
#131254 = DIRECTION('center_axis',(0.,0.,1.)) ;
#131255 = DIRECTION('ref_axis',(1.,0.,0.)) ;
#131256 = DIRECTION('center_axis',(0.,0.,1.)) ;
#131257 = DIRECTION('ref_axis',(1.,0.,0.)) ;
#131258 = DIRECTION('center_axis',(-1.,0.,0.)) ;
#131259 = DIRECTION('ref_axis',(0.,0.,1.)) ;
#131260 = DIRECTION('center_axis',(-1.,0.,0.)) ;
#131261 = DIRECTION('ref_axis',(0.,1.30104260698257E-14,-1.)) ;
#131262 = DIRECTION('center_axis',(1.,0.,0.)) ;
#131263 = DIRECTION('ref_axis',(0.,0.,-1.)) ;
#131264 = DIRECTION('center_axis',(0.,-0.514231796959192,-0.857651245551547)) ;
#131265 = DIRECTION('ref_axis',(0.,0.857651245551547,-0.514231796959192)) ;
#131266 = DIRECTION('center_axis',(0.,1.,8.97270763436279E-17)) ;
#131267 = DIRECTION('ref_axis',(0.,-8.97270763436279E-17,1.)) ;
#131268 = DIRECTION('center_axis',(0.,-1.,-8.97270763436279E-17)) ;
#131269 = DIRECTION('ref_axis',(0.,-8.97270763436279E-17,1.)) ;
#131270 = DIRECTION('center_axis',(0.,-1.,0.)) ;
#131271 = DIRECTION('ref_axis',(0.,0.,-1.)) ;
#131272 = DIRECTION('center_axis',(0.,1.,0.)) ;
#131273 = DIRECTION('ref_axis',(1.,0.,0.)) ;
#131274 = DIRECTION('center_axis',(-1.,0.,0.)) ;
#131275 = DIRECTION('ref_axis',(0.,0.,-1.)) ;
#131276 = DIRECTION('center_axis',(1.,0.,0.)) ;
#131277 = DIRECTION('ref_axis',(0.,0.,-1.)) ;
#131278 = DIRECTION('center_axis',(0.,-0.514231796959126,0.857651245551587)) ;
#131279 = DIRECTION('ref_axis',(0.,0.857651245551587,0.514231796959126)) ;
#131280 = DIRECTION('center_axis',(0.,0.,-1.)) ;
#131281 = DIRECTION('ref_axis',(1.,0.,0.)) ;
#131282 = DIRECTION('center_axis',(0.,1.,0.)) ;
#131283 = DIRECTION('ref_axis',(1.,0.,0.)) ;
#131284 = DIRECTION('center_axis',(-6.93889390390727E-14,0.,-1.)) ;
#131285 = DIRECTION('ref_axis',(1.,0.,-6.93889390390727E-14)) ;
#131286 = DIRECTION('center_axis',(-1.,0.,0.)) ;
#131287 = DIRECTION('ref_axis',(0.,-2.16840434497095E-14,-1.)) ;
#131288 = DIRECTION('center_axis',(0.,0.,-1.)) ;
#131289 = DIRECTION('ref_axis',(-1.,0.,0.)) ;
#131290 = DIRECTION('center_axis',(0.,0.,1.)) ;
#131291 = DIRECTION('ref_axis',(-1.,0.,0.)) ;
#131292 = DIRECTION('center_axis',(0.,0.,-1.)) ;
#131293 = DIRECTION('ref_axis',(-1.,0.,0.)) ;
#131294 = DIRECTION('center_axis',(-1.,0.,7.01133629567814E-33)) ;
#131295 = DIRECTION('ref_axis',(7.01133629567814E-33,0.,1.)) ;
#131296 = DIRECTION('center_axis',(-1.,0.,0.)) ;
#131297 = DIRECTION('ref_axis',(0.,0.,1.)) ;
#131298 = DIRECTION('center_axis',(0.,0.,-1.)) ;
#131299 = DIRECTION('ref_axis',(-1.,0.,0.)) ;
#131300 = DIRECTION('center_axis',(-7.01133629567814E-33,8.97270763436279E-17,
-1.)) ;
#131301 = DIRECTION('ref_axis',(6.29106707073161E-49,1.,8.97270763436279E-17)) ;
#131302 = DIRECTION('center_axis',(1.,0.,0.)) ;
#131303 = DIRECTION('ref_axis',(0.,0.,-1.)) ;
#131304 = DIRECTION('center_axis',(6.69037477709045E-15,0.51423179695912,
0.85765124555159)) ;
#131305 = DIRECTION('ref_axis',(-4.49049578447409E-29,-0.85765124555159,0.51423179695912)) ;
#131306 = DIRECTION('center_axis',(-1.,0.,0.)) ;
#131307 = DIRECTION('ref_axis',(0.,0.,1.)) ;
#131308 = DIRECTION('center_axis',(-1.,0.,0.)) ;
#131309 = DIRECTION('ref_axis',(0.,1.30104260698257E-14,-1.)) ;
#131310 = DIRECTION('center_axis',(0.,0.,1.)) ;
#131311 = DIRECTION('ref_axis',(1.,0.,0.)) ;
#131312 = DIRECTION('center_axis',(0.,0.,-1.)) ;
#131313 = DIRECTION('ref_axis',(-1.,0.,0.)) ;
#131314 = DIRECTION('center_axis',(0.,-1.,8.97270763436279E-17)) ;
#131315 = DIRECTION('ref_axis',(0.,-8.97270763436279E-17,-1.)) ;
#131316 = DIRECTION('center_axis',(0.,-1.,8.97270763436279E-17)) ;
#131317 = DIRECTION('ref_axis',(0.,-8.97270763436279E-17,-1.)) ;
#131318 = DIRECTION('center_axis',(0.,-1.,0.)) ;
#131319 = DIRECTION('ref_axis',(0.,0.,-1.)) ;
#131320 = DIRECTION('center_axis',(-7.01133629567814E-33,8.97270763436279E-17,
-1.)) ;
#131321 = DIRECTION('ref_axis',(0.,1.,0.)) ;
#131322 = DIRECTION('center_axis',(0.,-1.,0.)) ;
#131323 = DIRECTION('ref_axis',(0.,0.,1.)) ;
#131324 = DIRECTION('center_axis',(1.,0.,0.)) ;
#131325 = DIRECTION('ref_axis',(0.,0.,-1.)) ;
#131326 = DIRECTION('center_axis',(0.,0.,1.)) ;
#131327 = DIRECTION('ref_axis',(-1.,0.,0.)) ;
#131328 = DIRECTION('center_axis',(0.,1.,0.)) ;
#131329 = DIRECTION('ref_axis',(1.,0.,0.)) ;
#131330 = DIRECTION('center_axis',(-1.,0.,0.)) ;
#131331 = DIRECTION('ref_axis',(0.,0.,-1.)) ;
#131332 = DIRECTION('center_axis',(1.,7.81406971160724E-17,0.)) ;
#131333 = DIRECTION('ref_axis',(-7.81406971160724E-17,1.,0.)) ;
#131334 = DIRECTION('center_axis',(1.,0.,0.)) ;
#131335 = DIRECTION('ref_axis',(0.,0.,-1.)) ;
#131336 = DIRECTION('center_axis',(1.,0.,0.)) ;
#131337 = DIRECTION('ref_axis',(0.,0.,-1.)) ;
#131338 = DIRECTION('center_axis',(0.,1.,8.97270763436279E-17)) ;
#131339 = DIRECTION('ref_axis',(0.,-8.97270763436279E-17,1.)) ;
#131340 = DIRECTION('center_axis',(0.,-1.,0.)) ;
#131341 = DIRECTION('ref_axis',(0.,0.,-1.)) ;
#131342 = DIRECTION('center_axis',(0.,0.,-1.)) ;
#131343 = DIRECTION('ref_axis',(-1.,0.,0.)) ;
#131344 = DIRECTION('center_axis',(-7.01133629567814E-33,8.97270763436279E-17,
1.)) ;
#131345 = DIRECTION('ref_axis',(-6.29106707073161E-49,-1.,8.97270763436279E-17)) ;
#131346 = DIRECTION('center_axis',(-1.,0.,-7.01133629567814E-33)) ;
#131347 = DIRECTION('ref_axis',(-7.01133629567814E-33,0.,1.)) ;
#131348 = DIRECTION('center_axis',(-1.,0.,0.)) ;
#131349 = DIRECTION('ref_axis',(0.,0.,1.)) ;
#131350 = DIRECTION('center_axis',(1.,0.,0.)) ;
#131351 = DIRECTION('ref_axis',(0.,1.,0.)) ;
#131352 = DIRECTION('center_axis',(4.33680868994202E-15,1.,0.)) ;
#131353 = DIRECTION('ref_axis',(-1.,4.33680868994202E-15,0.)) ;
#131354 = DIRECTION('center_axis',(0.,1.,0.)) ;
#131355 = DIRECTION('ref_axis',(1.,0.,0.)) ;
#131356 = DIRECTION('center_axis',(0.,0.,-1.)) ;
#131357 = DIRECTION('ref_axis',(1.,0.,0.)) ;
#131358 = DIRECTION('center_axis',(-1.,0.,0.)) ;
#131359 = DIRECTION('ref_axis',(0.,0.,-1.)) ;
#131360 = DIRECTION('center_axis',(-7.01133629567814E-33,8.97270763436279E-17,
1.)) ;
#131361 = DIRECTION('ref_axis',(0.,-1.,0.)) ;
#131362 = DIRECTION('center_axis',(0.,-1.,0.)) ;
#131363 = DIRECTION('ref_axis',(0.,0.,1.)) ;
#131364 = DIRECTION('center_axis',(7.81406971160724E-17,-1.,-8.97270763436279E-17)) ;
#131365 = DIRECTION('ref_axis',(-7.01133629567814E-33,8.97270763436279E-17,
-1.)) ;
#131366 = DIRECTION('center_axis',(0.,1.,0.)) ;
#131367 = DIRECTION('ref_axis',(0.,0.,1.)) ;
#131368 = DIRECTION('center_axis',(-1.,-7.81406971160724E-17,0.)) ;
#131369 = DIRECTION('ref_axis',(7.81406971160724E-17,-1.,0.)) ;
#131370 = DIRECTION('center_axis',(-1.,-7.81406971160724E-17,0.)) ;
#131371 = DIRECTION('ref_axis',(-7.81406971160724E-17,1.,0.)) ;
#131372 = DIRECTION('center_axis',(0.,0.,1.)) ;
#131373 = DIRECTION('ref_axis',(1.,0.,0.)) ;
#131374 = DIRECTION('center_axis',(0.,0.,-1.)) ;
#131375 = DIRECTION('ref_axis',(-1.,0.,0.)) ;
#131376 = DIRECTION('center_axis',(0.,-1.,8.97270763436279E-17)) ;
#131377 = DIRECTION('ref_axis',(0.,-8.97270763436279E-17,-1.)) ;
#131378 = DIRECTION('center_axis',(0.,-1.,0.)) ;
#131379 = DIRECTION('ref_axis',(0.,0.,-1.)) ;
#131380 = DIRECTION('center_axis',(1.,7.81406971160724E-17,0.)) ;
#131381 = DIRECTION('ref_axis',(0.,1.,0.)) ;
#131382 = DIRECTION('center_axis',(0.,0.,1.)) ;
#131383 = DIRECTION('ref_axis',(-1.,0.,0.)) ;
#131384 = DIRECTION('center_axis',(0.,1.,0.)) ;
#131385 = DIRECTION('ref_axis',(1.,0.,0.)) ;
#131386 = DIRECTION('center_axis',(-1.,0.,0.)) ;
#131387 = DIRECTION('ref_axis',(0.,0.,-1.)) ;
#131388 = DIRECTION('center_axis',(0.,0.,-1.)) ;
#131389 = DIRECTION('ref_axis',(-1.,0.,0.)) ;
#131390 = DIRECTION('center_axis',(0.,0.,1.)) ;
#131391 = DIRECTION('ref_axis',(1.,0.,0.)) ;
#131392 = DIRECTION('center_axis',(-1.,-7.81406971160724E-17,0.)) ;
#131393 = DIRECTION('ref_axis',(7.81406971160724E-17,-1.,0.)) ;
#131394 = DIRECTION('center_axis',(-1.,-7.81406971160724E-17,0.)) ;
#131395 = DIRECTION('ref_axis',(-7.81406971160724E-17,1.,0.)) ;
#131396 = DIRECTION('center_axis',(1.,7.81406971160724E-17,0.)) ;
#131397 = DIRECTION('ref_axis',(-7.81406971160724E-17,1.,0.)) ;
#131398 = DIRECTION('center_axis',(1.,0.,0.)) ;
#131399 = DIRECTION('ref_axis',(0.,0.,-1.)) ;
#131400 = DIRECTION('center_axis',(1.,0.,0.)) ;
#131401 = DIRECTION('ref_axis',(0.,0.,-1.)) ;
#131402 = DIRECTION('center_axis',(3.78638272950961E-32,-4.8455963016112E-16,
-1.)) ;
#131403 = DIRECTION('ref_axis',(1.83472821505963E-47,1.,-4.8455963016112E-16)) ;
#131404 = DIRECTION('center_axis',(0.,0.,-1.)) ;
#131405 = DIRECTION('ref_axis',(-1.,0.,0.)) ;
#131406 = DIRECTION('center_axis',(0.,0.,-1.)) ;
#131407 = DIRECTION('ref_axis',(-1.,0.,0.)) ;
#131408 = DIRECTION('center_axis',(1.,7.81406971160724E-17,0.)) ;
#131409 = DIRECTION('ref_axis',(0.,1.,0.)) ;
#131410 = DIRECTION('center_axis',(0.,-1.,0.)) ;
#131411 = DIRECTION('ref_axis',(0.,0.,1.)) ;
#131412 = DIRECTION('center_axis',(0.,1.,0.)) ;
#131413 = DIRECTION('ref_axis',(1.,0.,0.)) ;
#131414 = DIRECTION('center_axis',(0.,1.,0.)) ;
#131415 = DIRECTION('ref_axis',(0.,0.,-1.)) ;
#131416 = DIRECTION('center_axis',(-7.81406971160724E-17,1.,-8.97270763436279E-17)) ;
#131417 = DIRECTION('ref_axis',(-7.01133629567814E-33,8.97270763436279E-17,
1.)) ;
#131418 = DIRECTION('center_axis',(0.,-1.,0.)) ;
#131419 = DIRECTION('ref_axis',(0.,0.,-1.)) ;
#131420 = DIRECTION('center_axis',(0.,1.,0.)) ;
#131421 = DIRECTION('ref_axis',(0.,0.,1.)) ;
#131422 = DIRECTION('center_axis',(0.,-1.,0.)) ;
#131423 = DIRECTION('ref_axis',(0.,0.,-1.)) ;
#131424 = DIRECTION('center_axis',(0.,-1.,0.)) ;
#131425 = DIRECTION('ref_axis',(0.,0.,-1.)) ;
#131426 = DIRECTION('center_axis',(0.,1.,0.)) ;
#131427 = DIRECTION('ref_axis',(1.,0.,0.)) ;
#131428 = DIRECTION('center_axis',(0.,0.,1.)) ;
#131429 = DIRECTION('ref_axis',(-1.,0.,0.)) ;
#131430 = DIRECTION('center_axis',(1.,0.,0.)) ;
#131431 = DIRECTION('ref_axis',(0.,0.,1.)) ;
#131432 = DIRECTION('center_axis',(0.,-1.,0.)) ;
#131433 = DIRECTION('ref_axis',(0.,0.,-1.)) ;
#131434 = DIRECTION('center_axis',(0.,1.,0.)) ;
#131435 = DIRECTION('ref_axis',(0.,0.,1.)) ;
#131436 = DIRECTION('center_axis',(0.,-1.,0.)) ;
#131437 = DIRECTION('ref_axis',(0.,0.,-1.)) ;
#131438 = DIRECTION('center_axis',(-1.,0.,2.16840434497101E-16)) ;
#131439 = DIRECTION('ref_axis',(2.16840434497101E-16,0.,1.)) ;
#131440 = DIRECTION('center_axis',(1.,0.,0.)) ;
#131441 = DIRECTION('ref_axis',(0.,0.,-1.)) ;
#131442 = DIRECTION('center_axis',(-2.16840434497101E-16,0.,1.)) ;
#131443 = DIRECTION('ref_axis',(1.,0.,2.16840434497101E-16)) ;
#131444 = DIRECTION('center_axis',(0.,0.,1.)) ;
#131445 = DIRECTION('ref_axis',(1.,0.,0.)) ;
#131446 = DIRECTION('center_axis',(0.,1.,0.)) ;
#131447 = DIRECTION('ref_axis',(0.,0.,1.)) ;
#131448 = DIRECTION('center_axis',(0.,-1.,0.)) ;
#131449 = DIRECTION('ref_axis',(0.,0.,-1.)) ;
#131450 = DIRECTION('center_axis',(0.,1.,0.)) ;
#131451 = DIRECTION('ref_axis',(1.,0.,0.)) ;
#131452 = DIRECTION('center_axis',(0.,0.,1.)) ;
#131453 = DIRECTION('ref_axis',(-1.,0.,0.)) ;
#131454 = DIRECTION('center_axis',(0.,1.,0.)) ;
#131455 = DIRECTION('ref_axis',(1.,0.,0.)) ;
#131456 = DIRECTION('center_axis',(1.,0.,0.)) ;
#131457 = DIRECTION('ref_axis',(0.,0.,1.)) ;
#131458 = DIRECTION('center_axis',(0.,0.,-1.)) ;
#131459 = DIRECTION('ref_axis',(-1.,0.,0.)) ;
#131460 = DIRECTION('center_axis',(0.,0.,1.)) ;
#131461 = DIRECTION('ref_axis',(1.,0.,0.)) ;
#131462 = DIRECTION('center_axis',(1.,0.,2.16840434497101E-16)) ;
#131463 = DIRECTION('ref_axis',(2.16840434497101E-16,0.,-1.)) ;
#131464 = DIRECTION('center_axis',(1.,0.,0.)) ;
#131465 = DIRECTION('ref_axis',(0.,0.,-1.)) ;
#131466 = DIRECTION('center_axis',(0.,1.,0.)) ;
#131467 = DIRECTION('ref_axis',(1.,0.,0.)) ;
#131468 = DIRECTION('center_axis',(0.,1.,0.)) ;
#131469 = DIRECTION('ref_axis',(0.,0.,-1.)) ;
#131470 = DIRECTION('center_axis',(0.,1.,0.)) ;
#131471 = DIRECTION('ref_axis',(0.,0.,1.)) ;
#131472 = DIRECTION('center_axis',(0.,1.,0.)) ;
#131473 = DIRECTION('ref_axis',(0.,0.,1.)) ;
#131474 = DIRECTION('center_axis',(-0.942809041582061,-0.235702260395515,
0.235702260395526)) ;
#131475 = DIRECTION('ref_axis',(0.242535625036343,2.28772620246771E-15,0.970142500145329)) ;
#131476 = DIRECTION('center_axis',(-0.970142500145332,-0.242535625036331,
-2.10366121255624E-15)) ;
#131477 = DIRECTION('ref_axis',(0.242535625036331,-0.970142500145332,-4.68743664149877E-30)) ;
#131478 = DIRECTION('center_axis',(0.970142500145333,0.24253562503633,0.)) ;
#131479 = DIRECTION('ref_axis',(-0.24253562503633,0.970142500145333,0.)) ;
#131480 = DIRECTION('center_axis',(-0.970142500145333,-0.242535625036331,
-2.73475957632295E-14)) ;
#131481 = DIRECTION('ref_axis',(0.242535625036331,-0.970142500145332,-1.21802906808468E-29)) ;
#131482 = DIRECTION('center_axis',(0.879462917689188,0.219865729422294,-0.42214220049081)) ;
#131483 = DIRECTION('ref_axis',(-0.432731067584771,1.71515946658E-16,-0.901523057468274)) ;
#131484 = DIRECTION('center_axis',(0.879462917689182,0.219865729422321,-0.422142200490809)) ;
#131485 = DIRECTION('ref_axis',(-0.432731067584773,-7.60553175829864E-17,
-0.901523057468273)) ;
#131486 = DIRECTION('center_axis',(0.,1.,0.)) ;
#131487 = DIRECTION('ref_axis',(1.,0.,0.)) ;
#131488 = DIRECTION('center_axis',(-2.00438979995004E-14,-1.,0.)) ;
#131489 = DIRECTION('ref_axis',(-1.,2.00438979995004E-14,0.)) ;
#131490 = DIRECTION('center_axis',(0.,-1.,0.)) ;
#131491 = DIRECTION('ref_axis',(0.,0.,-1.)) ;
#131492 = DIRECTION('center_axis',(0.,-1.,0.)) ;
#131493 = DIRECTION('ref_axis',(0.,0.,-1.)) ;
#131494 = DIRECTION('center_axis',(0.669589480006976,-0.669589480006974,-0.321402950403349)) ;
#131495 = DIRECTION('ref_axis',(0.707106781186547,0.707106781186548,5.45170614306381E-16)) ;
#131496 = DIRECTION('center_axis',(0.669589480006977,-0.669589480006977,-0.321402950403339)) ;
#131497 = DIRECTION('ref_axis',(0.707106781186548,0.707106781186548,1.13950759497276E-17)) ;
#131498 = DIRECTION('center_axis',(0.,1.,0.)) ;
#131499 = DIRECTION('ref_axis',(1.,0.,0.)) ;
#131500 = DIRECTION('center_axis',(0.70710678118654,-0.707106781186555,0.)) ;
#131501 = DIRECTION('ref_axis',(-0.707106781186555,-0.70710678118654,0.)) ;
#131502 = DIRECTION('center_axis',(0.707106781186549,-0.707106781186546,0.)) ;
#131503 = DIRECTION('ref_axis',(0.707106781186546,0.707106781186549,0.)) ;
#131504 = DIRECTION('center_axis',(0.707106781186548,-0.707106781186548,-1.53329341668333E-15)) ;
#131505 = DIRECTION('ref_axis',(0.707106781186548,0.707106781186548,-2.94242918747921E-32)) ;
#131506 = DIRECTION('center_axis',(0.57735026918962,-0.57735026918962,-0.577350269189638)) ;
#131507 = DIRECTION('ref_axis',(-0.707106781186559,-1.11282436496257E-15,
-0.707106781186536)) ;
#131508 = DIRECTION('center_axis',(-0.577350269189328,0.577350269189571,-0.577350269189978)) ;
#131509 = DIRECTION('ref_axis',(-7.61554280732519E-15,0.707106781186793,0.707106781186302)) ;
#131510 = DIRECTION('center_axis',(-0.707106781186548,0.707106781186548,7.66646708341718E-15)) ;
#131511 = DIRECTION('ref_axis',(-0.707106781186548,-0.707106781186548,3.27987112860885E-31)) ;
#131512 = DIRECTION('center_axis',(-0.707106781186549,0.707106781186546,0.)) ;
#131513 = DIRECTION('ref_axis',(-0.707106781186546,-0.707106781186549,0.)) ;
#131514 = DIRECTION('center_axis',(-0.707106781186548,0.707106781186548,-1.13463712834566E-13)) ;
#131515 = DIRECTION('ref_axis',(-0.707106781186548,-0.707106781186548,1.81538773348134E-28)) ;
#131516 = DIRECTION('center_axis',(-0.669589480006976,0.669589480006974,-0.321402950403349)) ;
#131517 = DIRECTION('ref_axis',(-0.707106781186547,-0.707106781186548,5.45170614306381E-16)) ;
#131518 = DIRECTION('center_axis',(0.66958948000704,-0.669589480006895,0.32140295040338)) ;
#131519 = DIRECTION('ref_axis',(0.707106781186471,0.707106781186624,1.36895061126305E-16)) ;
#131520 = DIRECTION('center_axis',(0.,1.,0.)) ;
#131521 = DIRECTION('ref_axis',(1.,0.,0.)) ;
#131522 = DIRECTION('center_axis',(-1.50329234996253E-14,1.,0.)) ;
#131523 = DIRECTION('ref_axis',(1.,1.50329234996253E-14,0.)) ;
#131524 = DIRECTION('center_axis',(0.,-1.,0.)) ;
#131525 = DIRECTION('ref_axis',(0.,0.,-1.)) ;
#131526 = DIRECTION('center_axis',(0.,1.,0.)) ;
#131527 = DIRECTION('ref_axis',(0.,0.,1.)) ;
#131528 = DIRECTION('center_axis',(-0.879462917689188,-0.219865729422294,
-0.42214220049081)) ;
#131529 = DIRECTION('ref_axis',(-0.432731067584771,1.71515946658E-16,0.901523057468274)) ;
#131530 = DIRECTION('center_axis',(0.879462917689201,0.219865729422298,0.42214220049078)) ;
#131531 = DIRECTION('ref_axis',(0.432731067584741,-2.36820597908546E-15,-0.901523057468288)) ;
#131532 = DIRECTION('center_axis',(0.,1.,0.)) ;
#131533 = DIRECTION('ref_axis',(1.,0.,0.)) ;
#131534 = DIRECTION('center_axis',(0.970142500145323,0.242535625036368,0.)) ;
#131535 = DIRECTION('ref_axis',(0.242535625036368,-0.970142500145323,0.)) ;
#131536 = DIRECTION('center_axis',(-0.970142500145333,-0.24253562503633,0.)) ;
#131537 = DIRECTION('ref_axis',(0.24253562503633,-0.970142500145333,0.)) ;
#131538 = DIRECTION('center_axis',(0.970142500145333,0.242535625036331,-2.1036612125561E-15)) ;
#131539 = DIRECTION('ref_axis',(-0.242535625036331,0.970142500145332,-1.06801962627779E-30)) ;
#131540 = DIRECTION('center_axis',(0.942809041582058,0.235702260395512,0.23570226039554)) ;
#131541 = DIRECTION('ref_axis',(0.242535625036358,-1.84667126758454E-15,-0.970142500145326)) ;
#131542 = DIRECTION('center_axis',(0.,-1.,0.)) ;
#131543 = DIRECTION('ref_axis',(0.,0.,-1.)) ;
#131544 = DIRECTION('center_axis',(-1.,0.,-8.67361737988439E-15)) ;
#131545 = DIRECTION('ref_axis',(-8.67361737988439E-15,0.,1.)) ;
#131546 = DIRECTION('center_axis',(0.,0.,-1.)) ;
#131547 = DIRECTION('ref_axis',(-1.,0.,0.)) ;
#131548 = DIRECTION('center_axis',(0.,0.,-1.)) ;
#131549 = DIRECTION('ref_axis',(-1.,0.,0.)) ;
#131550 = DIRECTION('center_axis',(0.,0.,-1.)) ;
#131551 = DIRECTION('ref_axis',(-1.,0.,0.)) ;
#131552 = DIRECTION('center_axis',(1.,0.,0.)) ;
#131553 = DIRECTION('ref_axis',(0.,0.,-1.)) ;
#131554 = DIRECTION('center_axis',(-1.,0.,0.)) ;
#131555 = DIRECTION('ref_axis',(0.,0.,1.)) ;
#131556 = DIRECTION('center_axis',(0.,-1.,0.)) ;
#131557 = DIRECTION('ref_axis',(0.,0.,-1.)) ;
#131558 = DIRECTION('center_axis',(-1.,0.,0.)) ;
#131559 = DIRECTION('ref_axis',(0.,0.,1.)) ;
#131560 = DIRECTION('center_axis',(0.,-1.,0.)) ;
#131561 = DIRECTION('ref_axis',(0.,0.,-1.)) ;
#131562 = DIRECTION('center_axis',(0.,0.,-1.)) ;
#131563 = DIRECTION('ref_axis',(-1.,0.,0.)) ;
#131564 = DIRECTION('center_axis',(-1.,0.,0.)) ;
#131565 = DIRECTION('ref_axis',(0.,0.,1.)) ;
#131566 = DIRECTION('center_axis',(-1.,1.73472347597681E-14,0.)) ;
#131567 = DIRECTION('ref_axis',(-1.73472347597681E-14,-1.,0.)) ;
#131568 = DIRECTION('center_axis',(0.,0.,1.)) ;
#131569 = DIRECTION('ref_axis',(1.,0.,0.)) ;
#131570 = DIRECTION('center_axis',(0.,0.,-1.)) ;
#131571 = DIRECTION('ref_axis',(-1.,0.,0.)) ;
#131572 = DIRECTION('center_axis',(0.,-1.,0.)) ;
#131573 = DIRECTION('ref_axis',(0.,0.,-1.)) ;
#131574 = DIRECTION('center_axis',(0.,-1.,0.)) ;
#131575 = DIRECTION('ref_axis',(0.,0.,-1.)) ;
#131576 = DIRECTION('center_axis',(0.,-1.,0.)) ;
#131577 = DIRECTION('ref_axis',(0.,0.,-1.)) ;
#131578 = DIRECTION('center_axis',(0.,0.,1.)) ;
#131579 = DIRECTION('ref_axis',(1.,0.,0.)) ;
#131580 = DIRECTION('center_axis',(0.,0.,-1.)) ;
#131581 = DIRECTION('ref_axis',(-1.,0.,0.)) ;
#131582 = DIRECTION('center_axis',(0.,0.,1.)) ;
#131583 = DIRECTION('ref_axis',(1.,0.,0.)) ;
#131584 = DIRECTION('center_axis',(0.,-1.,0.)) ;
#131585 = DIRECTION('ref_axis',(0.,0.,-1.)) ;
#131586 = DIRECTION('center_axis',(0.,-1.,0.)) ;
#131587 = DIRECTION('ref_axis',(0.,0.,-1.)) ;
#131588 = DIRECTION('center_axis',(0.,1.,0.)) ;
#131589 = DIRECTION('ref_axis',(1.,0.,0.)) ;
#131590 = DIRECTION('center_axis',(-1.,0.,0.)) ;
#131591 = DIRECTION('ref_axis',(0.,0.,-1.)) ;
#131592 = DIRECTION('center_axis',(0.,1.,0.)) ;
#131593 = DIRECTION('ref_axis',(1.,0.,0.)) ;
#131594 = DIRECTION('center_axis',(-1.,0.,0.)) ;
#131595 = DIRECTION('ref_axis',(0.,0.,-1.)) ;
#131596 = DIRECTION('center_axis',(0.,-1.,0.)) ;
#131597 = DIRECTION('ref_axis',(0.,0.,-1.)) ;
#131598 = DIRECTION('center_axis',(0.,-1.,0.)) ;
#131599 = DIRECTION('ref_axis',(0.,0.,-1.)) ;
#131600 = DIRECTION('center_axis',(-1.,0.,0.)) ;
#131601 = DIRECTION('ref_axis',(0.,0.,1.)) ;
#131602 = DIRECTION('center_axis',(-1.,0.,0.)) ;
#131603 = DIRECTION('ref_axis',(0.,0.,1.)) ;
#131604 = DIRECTION('center_axis',(1.,0.,0.)) ;
#131605 = DIRECTION('ref_axis',(0.,0.,-1.)) ;
#131606 = DIRECTION('center_axis',(-1.,0.,0.)) ;
#131607 = DIRECTION('ref_axis',(0.,0.,1.)) ;
#131608 = DIRECTION('center_axis',(0.,-1.,0.)) ;
#131609 = DIRECTION('ref_axis',(0.,0.,-1.)) ;
#131610 = DIRECTION('center_axis',(0.,-1.,0.)) ;
#131611 = DIRECTION('ref_axis',(0.,0.,-1.)) ;
#131612 = DIRECTION('center_axis',(0.,1.,0.)) ;
#131613 = DIRECTION('ref_axis',(1.,0.,0.)) ;
#131614 = DIRECTION('center_axis',(0.,0.,-1.)) ;
#131615 = DIRECTION('ref_axis',(1.,0.,0.)) ;
#131616 = DIRECTION('center_axis',(0.,1.,0.)) ;
#131617 = DIRECTION('ref_axis',(1.,0.,0.)) ;
#131618 = DIRECTION('center_axis',(0.,0.,1.)) ;
#131619 = DIRECTION('ref_axis',(-1.,0.,0.)) ;
#131620 = DIRECTION('center_axis',(0.,0.,-1.)) ;
#131621 = DIRECTION('ref_axis',(-1.,0.,0.)) ;
#131622 = DIRECTION('center_axis',(1.,1.31418445149758E-16,-2.16840434497101E-16)) ;
#131623 = DIRECTION('ref_axis',(-2.16840434497101E-16,-2.8496832747207E-32,
-1.)) ;
#131624 = DIRECTION('center_axis',(1.,0.,0.)) ;
#131625 = DIRECTION('ref_axis',(0.,0.,-1.)) ;
#131626 = DIRECTION('center_axis',(-1.,0.,0.)) ;
#131627 = DIRECTION('ref_axis',(0.,0.,1.)) ;
#131628 = DIRECTION('center_axis',(-1.31418445149758E-16,1.,0.)) ;
#131629 = DIRECTION('ref_axis',(-1.,0.,0.)) ;
#131630 = DIRECTION('center_axis',(0.,0.,1.)) ;
#131631 = DIRECTION('ref_axis',(-1.,0.,0.)) ;
#131632 = DIRECTION('center_axis',(-1.31418445149758E-16,1.,0.)) ;
#131633 = DIRECTION('ref_axis',(-1.,-1.31418445149758E-16,0.)) ;
#131634 = DIRECTION('center_axis',(-1.31418445149758E-16,1.,0.)) ;
#131635 = DIRECTION('ref_axis',(-1.,0.,0.)) ;
#131636 = DIRECTION('center_axis',(-1.31418445149758E-16,1.,0.)) ;
#131637 = DIRECTION('ref_axis',(-1.,-1.31418445149758E-16,0.)) ;
#131638 = DIRECTION('center_axis',(0.,0.,1.)) ;
#131639 = DIRECTION('ref_axis',(-1.,0.,0.)) ;
#131640 = DIRECTION('center_axis',(-4.33680868994202E-16,-5.69936654944139E-32,
-1.)) ;
#131641 = DIRECTION('ref_axis',(-1.,2.47170623787823E-47,4.33680868994202E-16)) ;
#131642 = DIRECTION('center_axis',(0.,0.,1.)) ;
#131643 = DIRECTION('ref_axis',(1.,0.,0.)) ;
#131644 = DIRECTION('center_axis',(-1.31418445149758E-16,-1.,0.)) ;
#131645 = DIRECTION('ref_axis',(1.,-1.31418445149758E-16,0.)) ;
#131646 = DIRECTION('center_axis',(0.,1.,0.)) ;
#131647 = DIRECTION('ref_axis',(0.,0.,1.)) ;
#131648 = DIRECTION('center_axis',(-1.,0.,2.16840434497101E-16)) ;
#131649 = DIRECTION('ref_axis',(2.16840434497101E-16,0.,1.)) ;
#131650 = DIRECTION('center_axis',(-1.,0.,0.)) ;
#131651 = DIRECTION('ref_axis',(0.,0.,1.)) ;
#131652 = DIRECTION('center_axis',(1.,0.,0.)) ;
#131653 = DIRECTION('ref_axis',(0.,0.,-1.)) ;
#131654 = DIRECTION('center_axis',(-1.31418445149758E-16,-1.,0.)) ;
#131655 = DIRECTION('ref_axis',(1.,-1.31418445149758E-16,0.)) ;
#131656 = DIRECTION('center_axis',(0.,1.,0.)) ;
#131657 = DIRECTION('ref_axis',(0.,0.,1.)) ;
#131658 = DIRECTION('center_axis',(2.16840434497101E-16,2.8496832747207E-32,
1.)) ;
#131659 = DIRECTION('ref_axis',(1.,-6.17926559469557E-48,-2.16840434497101E-16)) ;
#131660 = DIRECTION('center_axis',(0.,0.,1.)) ;
#131661 = DIRECTION('ref_axis',(1.,0.,0.)) ;
#131662 = DIRECTION('center_axis',(-1.,-1.31418445149758E-16,-2.16840434497101E-16)) ;
#131663 = DIRECTION('ref_axis',(-2.16840434497101E-16,-2.8496832747207E-32,
1.)) ;
#131664 = DIRECTION('center_axis',(-1.,0.,0.)) ;
#131665 = DIRECTION('ref_axis',(0.,0.,1.)) ;
#131666 = DIRECTION('center_axis',(1.,0.,0.)) ;
#131667 = DIRECTION('ref_axis',(0.,0.,-1.)) ;
#131668 = DIRECTION('center_axis',(-1.31418445149758E-16,1.,0.)) ;
#131669 = DIRECTION('ref_axis',(-1.,0.,0.)) ;
#131670 = DIRECTION('center_axis',(-1.31418445149758E-16,1.,0.)) ;
#131671 = DIRECTION('ref_axis',(-1.,-1.31418445149758E-16,0.)) ;
#131672 = DIRECTION('center_axis',(0.,1.,0.)) ;
#131673 = DIRECTION('ref_axis',(1.,0.,0.)) ;
#131674 = DIRECTION('center_axis',(0.,0.,-1.)) ;
#131675 = DIRECTION('ref_axis',(1.,0.,0.)) ;
#131676 = DIRECTION('center_axis',(0.,1.,0.)) ;
#131677 = DIRECTION('ref_axis',(1.,0.,0.)) ;
#131678 = DIRECTION('center_axis',(0.,0.,-1.)) ;
#131679 = DIRECTION('ref_axis',(1.,0.,0.)) ;
#131680 = DIRECTION('center_axis',(-1.31418445149758E-16,1.,0.)) ;
#131681 = DIRECTION('ref_axis',(-1.,0.,0.)) ;
#131682 = DIRECTION('center_axis',(-1.31418445149758E-16,1.,0.)) ;
#131683 = DIRECTION('ref_axis',(-1.,-1.31418445149758E-16,0.)) ;
#131684 = DIRECTION('center_axis',(-1.31418445149758E-16,-1.,0.)) ;
#131685 = DIRECTION('ref_axis',(1.,-1.31418445149758E-16,0.)) ;
#131686 = DIRECTION('center_axis',(0.,1.,0.)) ;
#131687 = DIRECTION('ref_axis',(0.,0.,1.)) ;
#131688 = DIRECTION('center_axis',(4.33680868994202E-16,0.,1.)) ;
#131689 = DIRECTION('ref_axis',(1.,0.,-4.33680868994202E-16)) ;
#131690 = DIRECTION('center_axis',(0.,0.,-1.)) ;
#131691 = DIRECTION('ref_axis',(-1.,0.,0.)) ;
#131692 = DIRECTION('center_axis',(-2.16840434497101E-16,0.,-1.)) ;
#131693 = DIRECTION('ref_axis',(-1.,0.,2.16840434497101E-16)) ;
#131694 = DIRECTION('center_axis',(0.,0.,-1.)) ;
#131695 = DIRECTION('ref_axis',(-1.,0.,0.)) ;
#131696 = DIRECTION('center_axis',(-1.31418445149758E-16,-1.,0.)) ;
#131697 = DIRECTION('ref_axis',(1.,-1.31418445149758E-16,0.)) ;
#131698 = DIRECTION('center_axis',(0.,1.,0.)) ;
#131699 = DIRECTION('ref_axis',(0.,0.,1.)) ;
#131700 = DIRECTION('center_axis',(0.,1.,0.)) ;
#131701 = DIRECTION('ref_axis',(1.,0.,0.)) ;
#131702 = DIRECTION('center_axis',(-1.,0.,0.)) ;
#131703 = DIRECTION('ref_axis',(0.,0.,-1.)) ;
#131704 = DIRECTION('center_axis',(0.,1.,0.)) ;
#131705 = DIRECTION('ref_axis',(1.,0.,0.)) ;
#131706 = DIRECTION('center_axis',(1.,0.,0.)) ;
#131707 = DIRECTION('ref_axis',(0.,0.,1.)) ;
#131708 = DIRECTION('center_axis',(1.,0.,2.16840434497101E-16)) ;
#131709 = DIRECTION('ref_axis',(2.16840434497101E-16,0.,-1.)) ;
#131710 = DIRECTION('center_axis',(0.,1.,0.)) ;
#131711 = DIRECTION('ref_axis',(0.,0.,1.)) ;
#131712 = DIRECTION('center_axis',(0.,1.,0.)) ;
#131713 = DIRECTION('ref_axis',(0.,0.,1.)) ;
#131714 = DIRECTION('center_axis',(0.,0.,-1.)) ;
#131715 = DIRECTION('ref_axis',(-1.,0.,0.)) ;
#131716 = DIRECTION('center_axis',(0.,0.,1.)) ;
#131717 = DIRECTION('ref_axis',(1.,0.,0.)) ;
#131718 = DIRECTION('center_axis',(0.,0.,-1.)) ;
#131719 = DIRECTION('ref_axis',(-1.,0.,0.)) ;
#131720 = DIRECTION('center_axis',(0.,1.,0.)) ;
#131721 = DIRECTION('ref_axis',(0.,0.,1.)) ;
#131722 = DIRECTION('center_axis',(0.,1.,0.)) ;
#131723 = DIRECTION('ref_axis',(0.,0.,1.)) ;
#131724 = DIRECTION('center_axis',(0.,1.,0.)) ;
#131725 = DIRECTION('ref_axis',(1.,0.,0.)) ;
#131726 = DIRECTION('center_axis',(-1.,0.,0.)) ;
#131727 = DIRECTION('ref_axis',(0.,0.,-1.)) ;
#131728 = DIRECTION('center_axis',(0.,1.,0.)) ;
#131729 = DIRECTION('ref_axis',(1.,0.,0.)) ;
#131730 = DIRECTION('center_axis',(-1.,0.,0.)) ;
#131731 = DIRECTION('ref_axis',(0.,0.,-1.)) ;
#131732 = DIRECTION('center_axis',(0.,1.,0.)) ;
#131733 = DIRECTION('ref_axis',(0.,0.,1.)) ;
#131734 = DIRECTION('center_axis',(0.,1.,0.)) ;
#131735 = DIRECTION('ref_axis',(0.,0.,1.)) ;
#131736 = DIRECTION('center_axis',(-1.,0.,0.)) ;
#131737 = DIRECTION('ref_axis',(0.,0.,1.)) ;
#131738 = DIRECTION('center_axis',(-1.,0.,0.)) ;
#131739 = DIRECTION('ref_axis',(0.,0.,1.)) ;
#131740 = DIRECTION('center_axis',(1.,0.,0.)) ;
#131741 = DIRECTION('ref_axis',(0.,0.,-1.)) ;
#131742 = DIRECTION('center_axis',(-1.,0.,0.)) ;
#131743 = DIRECTION('ref_axis',(0.,0.,1.)) ;
#131744 = DIRECTION('center_axis',(0.,1.,0.)) ;
#131745 = DIRECTION('ref_axis',(0.,0.,1.)) ;
#131746 = DIRECTION('center_axis',(0.,1.,0.)) ;
#131747 = DIRECTION('ref_axis',(0.,0.,1.)) ;
#131748 = DIRECTION('center_axis',(0.,1.,0.)) ;
#131749 = DIRECTION('ref_axis',(1.,0.,0.)) ;
#131750 = DIRECTION('center_axis',(0.,0.,1.)) ;
#131751 = DIRECTION('ref_axis',(-1.,0.,0.)) ;
#131752 = DIRECTION('center_axis',(0.,1.,0.)) ;
#131753 = DIRECTION('ref_axis',(1.,0.,0.)) ;
#131754 = DIRECTION('center_axis',(0.,0.,-1.)) ;
#131755 = DIRECTION('ref_axis',(1.,0.,0.)) ;
#131756 = DIRECTION('center_axis',(0.,0.,1.)) ;
#131757 = DIRECTION('ref_axis',(1.,0.,0.)) ;
#131758 = DIRECTION('center_axis',(0.,0.,1.)) ;
#131759 = DIRECTION('ref_axis',(1.,0.,0.)) ;
#131760 = DIRECTION('center_axis',(0.,0.,-1.)) ;
#131761 = DIRECTION('ref_axis',(-1.,0.,0.)) ;
#131762 = DIRECTION('center_axis',(0.,0.,1.)) ;
#131763 = DIRECTION('ref_axis',(1.,0.,0.)) ;
#131764 = DIRECTION('center_axis',(1.,0.,0.)) ;
#131765 = DIRECTION('ref_axis',(0.,0.,-1.)) ;
#131766 = DIRECTION('center_axis',(1.,0.,0.)) ;
#131767 = DIRECTION('ref_axis',(0.,0.,-1.)) ;
#131768 = DIRECTION('center_axis',(1.,0.,0.)) ;
#131769 = DIRECTION('ref_axis',(0.,0.,-1.)) ;
#131770 = DIRECTION('center_axis',(1.,0.,8.67361737988379E-15)) ;
#131771 = DIRECTION('ref_axis',(8.67361737988379E-15,0.,-1.)) ;
#131772 = DIRECTION('center_axis',(1.,0.,0.)) ;
#131773 = DIRECTION('ref_axis',(0.,0.,-1.)) ;
#131774 = DIRECTION('center_axis',(1.,0.,1.73472347597676E-14)) ;
#131775 = DIRECTION('ref_axis',(1.73472347597676E-14,0.,-1.)) ;
#131776 = DIRECTION('center_axis',(-1.,0.,0.)) ;
#131777 = DIRECTION('ref_axis',(0.,0.,1.)) ;
#131778 = DIRECTION('center_axis',(1.,0.,0.)) ;
#131779 = DIRECTION('ref_axis',(0.,0.,-1.)) ;
#131780 = DIRECTION('center_axis',(1.,0.,0.)) ;
#131781 = DIRECTION('ref_axis',(0.,0.,-1.)) ;
#131782 = DIRECTION('center_axis',(0.,0.,-1.)) ;
#131783 = DIRECTION('ref_axis',(-1.,0.,0.)) ;
#131784 = DIRECTION('center_axis',(1.,0.,0.)) ;
#131785 = DIRECTION('ref_axis',(0.,0.,-1.)) ;
#131786 = DIRECTION('center_axis',(0.,0.,1.)) ;
#131787 = DIRECTION('ref_axis',(1.,0.,0.)) ;
#131788 = DIRECTION('center_axis',(0.,0.,-1.)) ;
#131789 = DIRECTION('ref_axis',(-1.,0.,0.)) ;
#131790 = DIRECTION('center_axis',(-0.422618261740697,5.55398348498559E-17,
0.906307787036651)) ;
#131791 = DIRECTION('ref_axis',(0.906307787036651,6.51773046476477E-31,0.422618261740697)) ;
#131792 = DIRECTION('center_axis',(0.422618261740697,-5.55398348498559E-17,
-0.906307787036651)) ;
#131793 = DIRECTION('ref_axis',(-0.906307787036651,-6.46086972436398E-31,
-0.422618261740697)) ;
#131794 = DIRECTION('center_axis',(-0.422618261740697,5.55398348498559E-17,
0.906307787036651)) ;
#131795 = DIRECTION('ref_axis',(0.906307787036651,6.46086972436398E-31,0.422618261740697)) ;
#131796 = DIRECTION('center_axis',(0.422618261740697,-5.55398348498559E-17,
-0.906307787036651)) ;
#131797 = DIRECTION('ref_axis',(-0.906307787036651,-6.46086972436398E-31,
-0.422618261740697)) ;
#131798 = DIRECTION('center_axis',(0.,0.,1.)) ;
#131799 = DIRECTION('ref_axis',(1.,0.,0.)) ;
#131800 = DIRECTION('center_axis',(7.01133629567814E-33,-8.97270763436279E-17,
-1.)) ;
#131801 = DIRECTION('ref_axis',(-6.29106707073161E-49,-1.,8.97270763436279E-17)) ;
#131802 = DIRECTION('center_axis',(7.01133629567814E-33,-8.97270763436279E-17,
1.)) ;
#131803 = DIRECTION('ref_axis',(6.29106707073161E-49,1.,8.97270763436279E-17)) ;
#131804 = DIRECTION('center_axis',(0.,0.,1.)) ;
#131805 = DIRECTION('ref_axis',(1.,0.,0.)) ;
#131806 = DIRECTION('center_axis',(7.01133629567814E-33,-8.97270763436279E-17,
-1.)) ;
#131807 = DIRECTION('ref_axis',(-6.29106707073161E-49,-1.,8.97270763436279E-17)) ;
#131808 = DIRECTION('center_axis',(7.01133629567814E-33,-8.97270763436279E-17,
1.)) ;
#131809 = DIRECTION('ref_axis',(6.29106707073161E-49,1.,8.97270763436279E-17)) ;
#131810 = DIRECTION('center_axis',(0.,0.,1.)) ;
#131811 = DIRECTION('ref_axis',(1.,0.,0.)) ;
#131812 = DIRECTION('center_axis',(7.01133629567814E-33,-8.97270763436279E-17,
-1.)) ;
#131813 = DIRECTION('ref_axis',(-6.29106707073161E-49,-1.,8.97270763436279E-17)) ;
#131814 = DIRECTION('center_axis',(7.01133629567814E-33,-8.97270763436279E-17,
1.)) ;
#131815 = DIRECTION('ref_axis',(6.29106707073161E-49,1.,8.97270763436279E-17)) ;
#131816 = DIRECTION('center_axis',(0.,0.,1.)) ;
#131817 = DIRECTION('ref_axis',(1.,0.,0.)) ;
#131818 = DIRECTION('center_axis',(7.01133629567814E-33,-8.97270763436279E-17,
-1.)) ;
#131819 = DIRECTION('ref_axis',(-6.29106707073161E-49,-1.,8.97270763436279E-17)) ;
#131820 = DIRECTION('center_axis',(7.01133629567814E-33,-8.97270763436279E-17,
1.)) ;
#131821 = DIRECTION('ref_axis',(6.29106707073161E-49,1.,8.97270763436279E-17)) ;
#131822 = DIRECTION('center_axis',(0.,0.,1.)) ;
#131823 = DIRECTION('ref_axis',(1.,0.,0.)) ;
#131824 = DIRECTION('center_axis',(7.01133629567814E-33,-8.97270763436279E-17,
-1.)) ;
#131825 = DIRECTION('ref_axis',(-6.29106707073161E-49,-1.,8.97270763436279E-17)) ;
#131826 = DIRECTION('center_axis',(7.01133629567814E-33,-8.97270763436279E-17,
1.)) ;
#131827 = DIRECTION('ref_axis',(6.29106707073161E-49,1.,8.97270763436279E-17)) ;
#131828 = DIRECTION('center_axis',(0.,0.,1.)) ;
#131829 = DIRECTION('ref_axis',(1.,0.,0.)) ;
#131830 = DIRECTION('center_axis',(7.01133629567814E-33,-8.97270763436279E-17,
-1.)) ;
#131831 = DIRECTION('ref_axis',(-6.29106707073161E-49,-1.,8.97270763436279E-17)) ;
#131832 = DIRECTION('center_axis',(7.01133629567814E-33,-8.97270763436279E-17,
1.)) ;
#131833 = DIRECTION('ref_axis',(6.29106707073161E-49,1.,8.97270763436279E-17)) ;
#131834 = DIRECTION('center_axis',(0.,0.,1.)) ;
#131835 = DIRECTION('ref_axis',(1.,0.,0.)) ;
#131836 = DIRECTION('center_axis',(7.01133629567814E-33,-8.97270763436279E-17,
-1.)) ;
#131837 = DIRECTION('ref_axis',(-6.29106707073161E-49,-1.,8.97270763436279E-17)) ;
#131838 = DIRECTION('center_axis',(7.01133629567814E-33,-8.97270763436279E-17,
1.)) ;
#131839 = DIRECTION('ref_axis',(6.29106707073161E-49,1.,8.97270763436279E-17)) ;
#131840 = DIRECTION('center_axis',(0.,0.,1.)) ;
#131841 = DIRECTION('ref_axis',(1.,0.,0.)) ;
#131842 = DIRECTION('center_axis',(7.01133629567814E-33,-8.97270763436279E-17,
-1.)) ;
#131843 = DIRECTION('ref_axis',(-6.29106707073161E-49,-1.,8.97270763436279E-17)) ;
#131844 = DIRECTION('center_axis',(7.01133629567814E-33,-8.97270763436279E-17,
1.)) ;
#131845 = DIRECTION('ref_axis',(6.29106707073161E-49,1.,8.97270763436279E-17)) ;
#131846 = DIRECTION('center_axis',(0.,0.,1.)) ;
#131847 = DIRECTION('ref_axis',(1.,0.,0.)) ;
#131848 = DIRECTION('center_axis',(7.01133629567814E-33,-8.97270763436279E-17,
-1.)) ;
#131849 = DIRECTION('ref_axis',(-6.29106707073161E-49,-1.,8.97270763436279E-17)) ;
#131850 = DIRECTION('center_axis',(7.01133629567814E-33,-8.97270763436279E-17,
1.)) ;
#131851 = DIRECTION('ref_axis',(6.29106707073161E-49,1.,8.97270763436279E-17)) ;
#131852 = DIRECTION('center_axis',(1.,0.,0.)) ;
#131853 = DIRECTION('ref_axis',(0.,0.,-1.)) ;
#131854 = DIRECTION('center_axis',(0.,0.,1.)) ;
#131855 = DIRECTION('ref_axis',(1.,0.,0.)) ;
#131856 = DIRECTION('center_axis',(0.,4.8455963016112E-16,1.)) ;
#131857 = DIRECTION('ref_axis',(0.,-1.,4.8455963016112E-16)) ;
#131858 = DIRECTION('center_axis',(0.,0.,1.)) ;
#131859 = DIRECTION('ref_axis',(1.,0.,0.)) ;
#131860 = DIRECTION('center_axis',(0.,0.,1.)) ;
#131861 = DIRECTION('ref_axis',(1.,0.,0.)) ;
#131862 = DIRECTION('center_axis',(0.,0.,1.)) ;
#131863 = DIRECTION('ref_axis',(1.,0.,0.)) ;
#131864 = DIRECTION('center_axis',(1.,0.,0.)) ;
#131865 = DIRECTION('ref_axis',(0.,0.,-1.)) ;
#131866 = DIRECTION('center_axis',(1.,0.,0.)) ;
#131867 = DIRECTION('ref_axis',(0.,0.,-1.)) ;
#131868 = DIRECTION('center_axis',(1.,0.,0.)) ;
#131869 = DIRECTION('ref_axis',(0.,0.,-1.)) ;
#131870 = DIRECTION('center_axis',(0.,0.,1.)) ;
#131871 = DIRECTION('ref_axis',(1.,0.,0.)) ;
#131872 = DIRECTION('center_axis',(0.,4.8455963016112E-16,1.)) ;
#131873 = DIRECTION('ref_axis',(0.,-1.,4.8455963016112E-16)) ;
#131874 = DIRECTION('center_axis',(0.,0.,1.)) ;
#131875 = DIRECTION('ref_axis',(1.,0.,0.)) ;
#131876 = DIRECTION('center_axis',(0.,0.,1.)) ;
#131877 = DIRECTION('ref_axis',(1.,0.,0.)) ;
#131878 = DIRECTION('center_axis',(0.,0.,1.)) ;
#131879 = DIRECTION('ref_axis',(1.,0.,0.)) ;
#131880 = DIRECTION('center_axis',(1.,0.,0.)) ;
#131881 = DIRECTION('ref_axis',(0.,0.,-1.)) ;
#131882 = DIRECTION('center_axis',(1.,0.,0.)) ;
#131883 = DIRECTION('ref_axis',(0.,0.,-1.)) ;
#131884 = DIRECTION('center_axis',(0.,0.,1.)) ;
#131885 = DIRECTION('ref_axis',(1.,0.,0.)) ;
#131886 = DIRECTION('center_axis',(0.,4.8455963016112E-16,1.)) ;
#131887 = DIRECTION('ref_axis',(0.,-1.,4.8455963016112E-16)) ;
#131888 = DIRECTION('center_axis',(0.,0.,1.)) ;
#131889 = DIRECTION('ref_axis',(1.,0.,0.)) ;
#131890 = DIRECTION('center_axis',(0.,0.,1.)) ;
#131891 = DIRECTION('ref_axis',(1.,0.,0.)) ;
#131892 = DIRECTION('center_axis',(0.,0.,1.)) ;
#131893 = DIRECTION('ref_axis',(1.,0.,0.)) ;
#131894 = DIRECTION('center_axis',(1.,0.,0.)) ;
#131895 = DIRECTION('ref_axis',(0.,0.,-1.)) ;
#131896 = DIRECTION('center_axis',(1.,0.,0.)) ;
#131897 = DIRECTION('ref_axis',(0.,0.,-1.)) ;
#131898 = DIRECTION('center_axis',(0.,0.,1.)) ;
#131899 = DIRECTION('ref_axis',(1.,0.,0.)) ;
#131900 = DIRECTION('center_axis',(0.,4.8455963016112E-16,1.)) ;
#131901 = DIRECTION('ref_axis',(0.,-1.,4.8455963016112E-16)) ;
#131902 = DIRECTION('center_axis',(0.,0.,1.)) ;
#131903 = DIRECTION('ref_axis',(1.,0.,0.)) ;
#131904 = DIRECTION('center_axis',(0.,0.,1.)) ;
#131905 = DIRECTION('ref_axis',(1.,0.,0.)) ;
#131906 = DIRECTION('center_axis',(0.,0.,1.)) ;
#131907 = DIRECTION('ref_axis',(1.,0.,0.)) ;
#131908 = DIRECTION('center_axis',(1.,0.,0.)) ;
#131909 = DIRECTION('ref_axis',(0.,0.,-1.)) ;
#131910 = DIRECTION('center_axis',(1.,0.,0.)) ;
#131911 = DIRECTION('ref_axis',(0.,0.,-1.)) ;
#131912 = DIRECTION('center_axis',(0.,0.,1.)) ;
#131913 = DIRECTION('ref_axis',(1.,0.,0.)) ;
#131914 = DIRECTION('center_axis',(0.,4.8455963016112E-16,1.)) ;
#131915 = DIRECTION('ref_axis',(0.,-1.,4.8455963016112E-16)) ;
#131916 = DIRECTION('center_axis',(0.,0.,1.)) ;
#131917 = DIRECTION('ref_axis',(1.,0.,0.)) ;
#131918 = DIRECTION('center_axis',(0.,0.,1.)) ;
#131919 = DIRECTION('ref_axis',(1.,0.,0.)) ;
#131920 = DIRECTION('center_axis',(0.,0.,1.)) ;
#131921 = DIRECTION('ref_axis',(1.,0.,0.)) ;
#131922 = DIRECTION('center_axis',(1.,0.,0.)) ;
#131923 = DIRECTION('ref_axis',(0.,0.,-1.)) ;
#131924 = DIRECTION('center_axis',(1.,0.,0.)) ;
#131925 = DIRECTION('ref_axis',(0.,0.,-1.)) ;
#131926 = DIRECTION('center_axis',(0.,0.,1.)) ;
#131927 = DIRECTION('ref_axis',(1.,0.,0.)) ;
#131928 = DIRECTION('center_axis',(0.,4.8455963016112E-16,1.)) ;
#131929 = DIRECTION('ref_axis',(0.,-1.,4.8455963016112E-16)) ;
#131930 = DIRECTION('center_axis',(0.,0.,1.)) ;
#131931 = DIRECTION('ref_axis',(1.,0.,0.)) ;
#131932 = DIRECTION('center_axis',(0.,0.,1.)) ;
#131933 = DIRECTION('ref_axis',(1.,0.,0.)) ;
#131934 = DIRECTION('center_axis',(0.,0.,1.)) ;
#131935 = DIRECTION('ref_axis',(1.,0.,0.)) ;
#131936 = DIRECTION('center_axis',(1.,0.,0.)) ;
#131937 = DIRECTION('ref_axis',(0.,0.,-1.)) ;
#131938 = DIRECTION('center_axis',(1.,0.,0.)) ;
#131939 = DIRECTION('ref_axis',(0.,0.,-1.)) ;
#131940 = DIRECTION('center_axis',(0.,0.,1.)) ;
#131941 = DIRECTION('ref_axis',(1.,0.,0.)) ;
#131942 = DIRECTION('center_axis',(0.,4.8455963016112E-16,1.)) ;
#131943 = DIRECTION('ref_axis',(0.,-1.,4.8455963016112E-16)) ;
#131944 = DIRECTION('center_axis',(0.,0.,1.)) ;
#131945 = DIRECTION('ref_axis',(1.,0.,0.)) ;
#131946 = DIRECTION('center_axis',(0.,0.,1.)) ;
#131947 = DIRECTION('ref_axis',(1.,0.,0.)) ;
#131948 = DIRECTION('center_axis',(0.,0.,1.)) ;
#131949 = DIRECTION('ref_axis',(1.,0.,0.)) ;
#131950 = DIRECTION('center_axis',(1.,0.,0.)) ;
#131951 = DIRECTION('ref_axis',(0.,0.,-1.)) ;
#131952 = DIRECTION('center_axis',(1.,0.,0.)) ;
#131953 = DIRECTION('ref_axis',(0.,0.,-1.)) ;
#131954 = DIRECTION('center_axis',(0.,0.,1.)) ;
#131955 = DIRECTION('ref_axis',(1.,0.,0.)) ;
#131956 = DIRECTION('center_axis',(0.,4.8455963016112E-16,1.)) ;
#131957 = DIRECTION('ref_axis',(0.,-1.,4.8455963016112E-16)) ;
#131958 = DIRECTION('center_axis',(0.,0.,1.)) ;
#131959 = DIRECTION('ref_axis',(1.,0.,0.)) ;
#131960 = DIRECTION('center_axis',(0.,0.,1.)) ;
#131961 = DIRECTION('ref_axis',(1.,0.,0.)) ;
#131962 = DIRECTION('center_axis',(0.,0.,1.)) ;
#131963 = DIRECTION('ref_axis',(1.,0.,0.)) ;
#131964 = DIRECTION('center_axis',(1.,0.,0.)) ;
#131965 = DIRECTION('ref_axis',(0.,0.,-1.)) ;
#131966 = DIRECTION('center_axis',(0.,4.8455963016112E-16,1.)) ;
#131967 = DIRECTION('ref_axis',(0.,-1.,4.8455963016112E-16)) ;
#131968 = DIRECTION('center_axis',(0.,4.8455963016112E-16,1.)) ;
#131969 = DIRECTION('ref_axis',(0.,-1.,4.8455963016112E-16)) ;
#131970 = DIRECTION('center_axis',(0.,0.,1.)) ;
#131971 = DIRECTION('ref_axis',(1.,0.,0.)) ;
#131972 = DIRECTION('center_axis',(0.,0.,1.)) ;
#131973 = DIRECTION('ref_axis',(1.,0.,0.)) ;
#131974 = DIRECTION('center_axis',(1.,0.,0.)) ;
#131975 = DIRECTION('ref_axis',(0.,0.,-1.)) ;
#131976 = DIRECTION('center_axis',(-7.01133629567814E-33,8.97270763436279E-17,
1.)) ;
#131977 = DIRECTION('ref_axis',(0.,-1.,0.)) ;
#131978 = DIRECTION('center_axis',(1.,0.,0.)) ;
#131979 = DIRECTION('ref_axis',(0.,0.,-1.)) ;
#131980 = DIRECTION('center_axis',(-1.,0.,-7.01133629567814E-33)) ;
#131981 = DIRECTION('ref_axis',(-7.01133629567814E-33,0.,1.)) ;
#131982 = DIRECTION('center_axis',(1.,0.,0.)) ;
#131983 = DIRECTION('ref_axis',(0.,0.,-1.)) ;
#131984 = DIRECTION('center_axis',(1.,0.,0.)) ;
#131985 = DIRECTION('ref_axis',(0.,0.,-1.)) ;
#131986 = DIRECTION('center_axis',(0.,1.,0.)) ;
#131987 = DIRECTION('ref_axis',(1.,0.,0.)) ;
#131988 = DIRECTION('center_axis',(-7.01133629567814E-33,8.97270763436279E-17,
-1.)) ;
#131989 = DIRECTION('ref_axis',(0.,1.,0.)) ;
#131990 = DIRECTION('center_axis',(1.,0.,0.)) ;
#131991 = DIRECTION('ref_axis',(0.,0.,-1.)) ;
#131992 = DIRECTION('center_axis',(-1.,0.,7.01133629567814E-33)) ;
#131993 = DIRECTION('ref_axis',(7.01133629567814E-33,0.,1.)) ;
#131994 = DIRECTION('center_axis',(1.,0.,0.)) ;
#131995 = DIRECTION('ref_axis',(0.,0.,-1.)) ;
#131996 = DIRECTION('center_axis',(1.,0.,0.)) ;
#131997 = DIRECTION('ref_axis',(0.,0.,-1.)) ;
#131998 = DIRECTION('center_axis',(0.,1.,0.)) ;
#131999 = DIRECTION('ref_axis',(1.,0.,0.)) ;
#132000 = DIRECTION('center_axis',(-7.01133629567814E-33,8.97270763436279E-17,
1.)) ;
#132001 = DIRECTION('ref_axis',(0.,-1.,0.)) ;
#132002 = DIRECTION('center_axis',(1.,0.,0.)) ;
#132003 = DIRECTION('ref_axis',(0.,0.,-1.)) ;
#132004 = DIRECTION('center_axis',(-1.,0.,-7.01133629567814E-33)) ;
#132005 = DIRECTION('ref_axis',(-7.01133629567814E-33,0.,1.)) ;
#132006 = DIRECTION('center_axis',(1.,0.,0.)) ;
#132007 = DIRECTION('ref_axis',(0.,0.,-1.)) ;
#132008 = DIRECTION('center_axis',(1.,0.,0.)) ;
#132009 = DIRECTION('ref_axis',(0.,0.,-1.)) ;
#132010 = DIRECTION('center_axis',(0.,1.,0.)) ;
#132011 = DIRECTION('ref_axis',(1.,0.,0.)) ;
#132012 = DIRECTION('center_axis',(-7.01133629567814E-33,8.97270763436279E-17,
-1.)) ;
#132013 = DIRECTION('ref_axis',(0.,1.,0.)) ;
#132014 = DIRECTION('center_axis',(1.,0.,0.)) ;
#132015 = DIRECTION('ref_axis',(0.,0.,-1.)) ;
#132016 = DIRECTION('center_axis',(-1.,0.,7.01133629567814E-33)) ;
#132017 = DIRECTION('ref_axis',(7.01133629567814E-33,0.,1.)) ;
#132018 = DIRECTION('center_axis',(1.,0.,0.)) ;
#132019 = DIRECTION('ref_axis',(0.,0.,-1.)) ;
#132020 = DIRECTION('center_axis',(1.,0.,0.)) ;
#132021 = DIRECTION('ref_axis',(0.,0.,-1.)) ;
#132022 = DIRECTION('center_axis',(0.,1.,0.)) ;
#132023 = DIRECTION('ref_axis',(1.,0.,0.)) ;
#132024 = DIRECTION('center_axis',(-7.01133629567814E-33,8.97270763436279E-17,
1.)) ;
#132025 = DIRECTION('ref_axis',(0.,-1.,0.)) ;
#132026 = DIRECTION('center_axis',(1.,0.,0.)) ;
#132027 = DIRECTION('ref_axis',(0.,0.,-1.)) ;
#132028 = DIRECTION('center_axis',(-1.,0.,-7.01133629567814E-33)) ;
#132029 = DIRECTION('ref_axis',(-7.01133629567814E-33,0.,1.)) ;
#132030 = DIRECTION('center_axis',(1.,0.,0.)) ;
#132031 = DIRECTION('ref_axis',(0.,0.,-1.)) ;
#132032 = DIRECTION('center_axis',(1.,0.,0.)) ;
#132033 = DIRECTION('ref_axis',(0.,0.,-1.)) ;
#132034 = DIRECTION('center_axis',(0.,1.,0.)) ;
#132035 = DIRECTION('ref_axis',(1.,0.,0.)) ;
#132036 = DIRECTION('center_axis',(-7.01133629567814E-33,8.97270763436279E-17,
-1.)) ;
#132037 = DIRECTION('ref_axis',(0.,1.,0.)) ;
#132038 = DIRECTION('center_axis',(1.,0.,0.)) ;
#132039 = DIRECTION('ref_axis',(0.,0.,-1.)) ;
#132040 = DIRECTION('center_axis',(-1.,0.,7.01133629567814E-33)) ;
#132041 = DIRECTION('ref_axis',(7.01133629567814E-33,0.,1.)) ;
#132042 = DIRECTION('center_axis',(1.,0.,0.)) ;
#132043 = DIRECTION('ref_axis',(0.,0.,-1.)) ;
#132044 = DIRECTION('center_axis',(1.,0.,0.)) ;
#132045 = DIRECTION('ref_axis',(0.,0.,-1.)) ;
#132046 = DIRECTION('center_axis',(0.,1.,0.)) ;
#132047 = DIRECTION('ref_axis',(1.,0.,0.)) ;
#132048 = DIRECTION('center_axis',(-7.01133629567814E-33,8.97270763436279E-17,
1.)) ;
#132049 = DIRECTION('ref_axis',(0.,-1.,0.)) ;
#132050 = DIRECTION('center_axis',(1.,0.,0.)) ;
#132051 = DIRECTION('ref_axis',(0.,0.,-1.)) ;
#132052 = DIRECTION('center_axis',(-1.,0.,-7.01133629567814E-33)) ;
#132053 = DIRECTION('ref_axis',(-7.01133629567814E-33,0.,1.)) ;
#132054 = DIRECTION('center_axis',(1.,0.,0.)) ;
#132055 = DIRECTION('ref_axis',(0.,0.,-1.)) ;
#132056 = DIRECTION('center_axis',(1.,0.,0.)) ;
#132057 = DIRECTION('ref_axis',(0.,0.,-1.)) ;
#132058 = DIRECTION('center_axis',(0.,1.,0.)) ;
#132059 = DIRECTION('ref_axis',(1.,0.,0.)) ;
#132060 = DIRECTION('center_axis',(-7.01133629567814E-33,8.97270763436279E-17,
-1.)) ;
#132061 = DIRECTION('ref_axis',(0.,1.,0.)) ;
#132062 = DIRECTION('center_axis',(1.,0.,0.)) ;
#132063 = DIRECTION('ref_axis',(0.,0.,-1.)) ;
#132064 = DIRECTION('center_axis',(-1.,0.,7.01133629567814E-33)) ;
#132065 = DIRECTION('ref_axis',(7.01133629567814E-33,0.,1.)) ;
#132066 = DIRECTION('center_axis',(1.,0.,0.)) ;
#132067 = DIRECTION('ref_axis',(0.,0.,-1.)) ;
#132068 = DIRECTION('center_axis',(1.,0.,0.)) ;
#132069 = DIRECTION('ref_axis',(0.,0.,-1.)) ;
#132070 = DIRECTION('center_axis',(0.,1.,0.)) ;
#132071 = DIRECTION('ref_axis',(1.,0.,0.)) ;
#132072 = DIRECTION('center_axis',(-7.01133629567814E-33,8.97270763436279E-17,
1.)) ;
#132073 = DIRECTION('ref_axis',(0.,-1.,0.)) ;
#132074 = DIRECTION('center_axis',(1.,0.,0.)) ;
#132075 = DIRECTION('ref_axis',(0.,0.,-1.)) ;
#132076 = DIRECTION('center_axis',(-1.,0.,-7.01133629567814E-33)) ;
#132077 = DIRECTION('ref_axis',(-7.01133629567814E-33,0.,1.)) ;
#132078 = DIRECTION('center_axis',(1.,0.,0.)) ;
#132079 = DIRECTION('ref_axis',(0.,0.,-1.)) ;
#132080 = DIRECTION('center_axis',(1.,0.,0.)) ;
#132081 = DIRECTION('ref_axis',(0.,0.,-1.)) ;
#132082 = DIRECTION('center_axis',(0.,1.,0.)) ;
#132083 = DIRECTION('ref_axis',(1.,0.,0.)) ;
#132084 = DIRECTION('center_axis',(-7.01133629567814E-33,8.97270763436279E-17,
-1.)) ;
#132085 = DIRECTION('ref_axis',(0.,1.,0.)) ;
#132086 = DIRECTION('center_axis',(1.,0.,0.)) ;
#132087 = DIRECTION('ref_axis',(0.,0.,-1.)) ;
#132088 = DIRECTION('center_axis',(-1.,0.,7.01133629567814E-33)) ;
#132089 = DIRECTION('ref_axis',(7.01133629567814E-33,0.,1.)) ;
#132090 = DIRECTION('center_axis',(1.,0.,0.)) ;
#132091 = DIRECTION('ref_axis',(0.,0.,-1.)) ;
#132092 = DIRECTION('center_axis',(1.,0.,0.)) ;
#132093 = DIRECTION('ref_axis',(0.,0.,-1.)) ;
#132094 = DIRECTION('center_axis',(0.,1.,0.)) ;
#132095 = DIRECTION('ref_axis',(1.,0.,0.)) ;
#132096 = DIRECTION('center_axis',(-7.01133629567814E-33,8.97270763436279E-17,
1.)) ;
#132097 = DIRECTION('ref_axis',(0.,-1.,0.)) ;
#132098 = DIRECTION('center_axis',(1.,0.,0.)) ;
#132099 = DIRECTION('ref_axis',(0.,0.,-1.)) ;
#132100 = DIRECTION('center_axis',(-1.,0.,-7.01133629567814E-33)) ;
#132101 = DIRECTION('ref_axis',(-7.01133629567814E-33,0.,1.)) ;
#132102 = DIRECTION('center_axis',(1.,0.,0.)) ;
#132103 = DIRECTION('ref_axis',(0.,0.,-1.)) ;
#132104 = DIRECTION('center_axis',(1.,0.,0.)) ;
#132105 = DIRECTION('ref_axis',(0.,0.,-1.)) ;
#132106 = DIRECTION('center_axis',(0.,1.,0.)) ;
#132107 = DIRECTION('ref_axis',(1.,0.,0.)) ;
#132108 = DIRECTION('center_axis',(-7.01133629567814E-33,8.97270763436279E-17,
-1.)) ;
#132109 = DIRECTION('ref_axis',(0.,1.,0.)) ;
#132110 = DIRECTION('center_axis',(1.,0.,0.)) ;
#132111 = DIRECTION('ref_axis',(0.,0.,-1.)) ;
#132112 = DIRECTION('center_axis',(-1.,0.,7.01133629567814E-33)) ;
#132113 = DIRECTION('ref_axis',(7.01133629567814E-33,0.,1.)) ;
#132114 = DIRECTION('center_axis',(1.,0.,0.)) ;
#132115 = DIRECTION('ref_axis',(0.,0.,-1.)) ;
#132116 = DIRECTION('center_axis',(1.,0.,0.)) ;
#132117 = DIRECTION('ref_axis',(0.,0.,-1.)) ;
#132118 = DIRECTION('center_axis',(0.,1.,0.)) ;
#132119 = DIRECTION('ref_axis',(1.,0.,0.)) ;
#132120 = DIRECTION('center_axis',(-7.01133629567814E-33,8.97270763436279E-17,
1.)) ;
#132121 = DIRECTION('ref_axis',(0.,-1.,0.)) ;
#132122 = DIRECTION('center_axis',(1.,0.,0.)) ;
#132123 = DIRECTION('ref_axis',(0.,0.,-1.)) ;
#132124 = DIRECTION('center_axis',(-1.,0.,-7.01133629567814E-33)) ;
#132125 = DIRECTION('ref_axis',(-7.01133629567814E-33,0.,1.)) ;
#132126 = DIRECTION('center_axis',(1.,0.,0.)) ;
#132127 = DIRECTION('ref_axis',(0.,0.,-1.)) ;
#132128 = DIRECTION('center_axis',(1.,0.,0.)) ;
#132129 = DIRECTION('ref_axis',(0.,0.,-1.)) ;
#132130 = DIRECTION('center_axis',(0.,1.,0.)) ;
#132131 = DIRECTION('ref_axis',(1.,0.,0.)) ;
#132132 = DIRECTION('center_axis',(-7.01133629567814E-33,8.97270763436279E-17,
-1.)) ;
#132133 = DIRECTION('ref_axis',(0.,1.,0.)) ;
#132134 = DIRECTION('center_axis',(1.,0.,0.)) ;
#132135 = DIRECTION('ref_axis',(0.,0.,-1.)) ;
#132136 = DIRECTION('center_axis',(-1.,0.,7.01133629567814E-33)) ;
#132137 = DIRECTION('ref_axis',(7.01133629567814E-33,0.,1.)) ;
#132138 = DIRECTION('center_axis',(1.,0.,0.)) ;
#132139 = DIRECTION('ref_axis',(0.,0.,-1.)) ;
#132140 = DIRECTION('center_axis',(1.,0.,0.)) ;
#132141 = DIRECTION('ref_axis',(0.,0.,-1.)) ;
#132142 = DIRECTION('center_axis',(0.,1.,0.)) ;
#132143 = DIRECTION('ref_axis',(1.,0.,0.)) ;
#132144 = DIRECTION('center_axis',(-7.01133629567814E-33,8.97270763436279E-17,
1.)) ;
#132145 = DIRECTION('ref_axis',(0.,-1.,0.)) ;
#132146 = DIRECTION('center_axis',(1.,0.,0.)) ;
#132147 = DIRECTION('ref_axis',(0.,0.,-1.)) ;
#132148 = DIRECTION('center_axis',(-1.,0.,-7.01133629567814E-33)) ;
#132149 = DIRECTION('ref_axis',(-7.01133629567814E-33,0.,1.)) ;
#132150 = DIRECTION('center_axis',(1.,0.,0.)) ;
#132151 = DIRECTION('ref_axis',(0.,0.,-1.)) ;
#132152 = DIRECTION('center_axis',(1.,0.,0.)) ;
#132153 = DIRECTION('ref_axis',(0.,0.,-1.)) ;
#132154 = DIRECTION('center_axis',(0.,1.,0.)) ;
#132155 = DIRECTION('ref_axis',(1.,0.,0.)) ;
#132156 = DIRECTION('center_axis',(-7.01133629567814E-33,8.97270763436279E-17,
-1.)) ;
#132157 = DIRECTION('ref_axis',(0.,1.,0.)) ;
#132158 = DIRECTION('center_axis',(1.,0.,0.)) ;
#132159 = DIRECTION('ref_axis',(0.,0.,-1.)) ;
#132160 = DIRECTION('center_axis',(-1.,0.,7.01133629567814E-33)) ;
#132161 = DIRECTION('ref_axis',(7.01133629567814E-33,0.,1.)) ;
#132162 = DIRECTION('center_axis',(1.,0.,0.)) ;
#132163 = DIRECTION('ref_axis',(0.,0.,-1.)) ;
#132164 = DIRECTION('center_axis',(1.,0.,0.)) ;
#132165 = DIRECTION('ref_axis',(0.,0.,-1.)) ;
#132166 = DIRECTION('center_axis',(0.,1.,0.)) ;
#132167 = DIRECTION('ref_axis',(1.,0.,0.)) ;
#132168 = DIRECTION('center_axis',(-7.01133629567814E-33,8.97270763436279E-17,
1.)) ;
#132169 = DIRECTION('ref_axis',(0.,-1.,0.)) ;
#132170 = DIRECTION('center_axis',(1.,0.,0.)) ;
#132171 = DIRECTION('ref_axis',(0.,0.,-1.)) ;
#132172 = DIRECTION('center_axis',(-1.,0.,-7.01133629567814E-33)) ;
#132173 = DIRECTION('ref_axis',(-7.01133629567814E-33,0.,1.)) ;
#132174 = DIRECTION('center_axis',(1.,0.,0.)) ;
#132175 = DIRECTION('ref_axis',(0.,0.,-1.)) ;
#132176 = DIRECTION('center_axis',(1.,0.,0.)) ;
#132177 = DIRECTION('ref_axis',(0.,0.,-1.)) ;
#132178 = DIRECTION('center_axis',(0.,1.,0.)) ;
#132179 = DIRECTION('ref_axis',(1.,0.,0.)) ;
#132180 = DIRECTION('center_axis',(-7.01133629567814E-33,8.97270763436279E-17,
-1.)) ;
#132181 = DIRECTION('ref_axis',(0.,1.,0.)) ;
#132182 = DIRECTION('center_axis',(1.,0.,0.)) ;
#132183 = DIRECTION('ref_axis',(0.,0.,-1.)) ;
#132184 = DIRECTION('center_axis',(-1.,0.,7.01133629567814E-33)) ;
#132185 = DIRECTION('ref_axis',(7.01133629567814E-33,0.,1.)) ;
#132186 = DIRECTION('center_axis',(1.,0.,0.)) ;
#132187 = DIRECTION('ref_axis',(0.,0.,-1.)) ;
#132188 = DIRECTION('center_axis',(1.,0.,0.)) ;
#132189 = DIRECTION('ref_axis',(0.,0.,-1.)) ;
#132190 = DIRECTION('center_axis',(0.,1.,0.)) ;
#132191 = DIRECTION('ref_axis',(1.,0.,0.)) ;
#132192 = DIRECTION('center_axis',(1.,0.,0.)) ;
#132193 = DIRECTION('ref_axis',(0.,0.,-1.)) ;
#132194 = DIRECTION('center_axis',(0.,0.500000000000005,0.866025403784436)) ;
#132195 = DIRECTION('ref_axis',(0.,-0.866025403784436,0.500000000000005)) ;
#132196 = DIRECTION('center_axis',(0.866025403784441,0.499999999999997,-2.16840434497101E-15)) ;
#132197 = DIRECTION('ref_axis',(-0.499999999999997,0.866025403784441,-1.29696145180732E-31)) ;
#132198 = DIRECTION('center_axis',(-7.01133629567814E-33,8.97270763436279E-17,
1.)) ;
#132199 = DIRECTION('ref_axis',(0.,-1.,0.)) ;
#132200 = DIRECTION('center_axis',(1.,0.,0.)) ;
#132201 = DIRECTION('ref_axis',(0.,0.,-1.)) ;
#132202 = DIRECTION('center_axis',(2.16840434497102E-15,0.500000000000002,
-0.866025403784438)) ;
#132203 = DIRECTION('ref_axis',(8.79920118707553E-32,0.866025403784438,0.500000000000002)) ;
#132204 = DIRECTION('center_axis',(0.866025403784438,0.500000000000001,0.)) ;
#132205 = DIRECTION('ref_axis',(-0.500000000000001,0.866025403784438,0.)) ;
#132206 = DIRECTION('center_axis',(-7.01133629567814E-33,8.97270763436279E-17,
-1.)) ;
#132207 = DIRECTION('ref_axis',(0.,1.,0.)) ;
#132208 = DIRECTION('center_axis',(1.,0.,0.)) ;
#132209 = DIRECTION('ref_axis',(0.,0.,-1.)) ;
#132210 = DIRECTION('center_axis',(0.,0.49999999999998,0.86602540378445)) ;
#132211 = DIRECTION('ref_axis',(0.,-0.86602540378445,0.49999999999998)) ;
#132212 = DIRECTION('center_axis',(0.866025403784441,0.499999999999997,-2.16840434497097E-15)) ;
#132213 = DIRECTION('ref_axis',(-0.499999999999997,0.866025403784441,2.64734307429885E-31)) ;
#132214 = DIRECTION('center_axis',(-7.01133629567814E-33,8.97270763436279E-17,
1.)) ;
#132215 = DIRECTION('ref_axis',(0.,-1.,0.)) ;
#132216 = DIRECTION('center_axis',(1.,0.,0.)) ;
#132217 = DIRECTION('ref_axis',(0.,0.,-1.)) ;
#132218 = DIRECTION('center_axis',(7.51157299368579E-15,0.500000000000005,
-0.866025403784436)) ;
#132219 = DIRECTION('ref_axis',(8.84230252037551E-31,0.866025403784436,0.500000000000005)) ;
#132220 = DIRECTION('center_axis',(0.866025403784438,0.500000000000001,0.)) ;
#132221 = DIRECTION('ref_axis',(-0.500000000000001,0.866025403784438,0.)) ;
#132222 = DIRECTION('center_axis',(-7.01133629567814E-33,8.97270763436279E-17,
-1.)) ;
#132223 = DIRECTION('ref_axis',(0.,1.,0.)) ;
#132224 = DIRECTION('center_axis',(1.,0.,0.)) ;
#132225 = DIRECTION('ref_axis',(0.,0.,-1.)) ;
#132226 = DIRECTION('center_axis',(0.,0.499999999999997,0.866025403784441)) ;
#132227 = DIRECTION('ref_axis',(0.,-0.866025403784441,0.499999999999997)) ;
#132228 = DIRECTION('center_axis',(0.866025403784441,0.499999999999997,-2.16840434497097E-15)) ;
#132229 = DIRECTION('ref_axis',(-0.499999999999997,0.866025403784441,2.64734307429885E-31)) ;
#132230 = DIRECTION('center_axis',(-7.01133629567814E-33,8.97270763436279E-17,
1.)) ;
#132231 = DIRECTION('ref_axis',(0.,-1.,0.)) ;
#132232 = DIRECTION('center_axis',(1.,0.,0.)) ;
#132233 = DIRECTION('ref_axis',(0.,0.,-1.)) ;
#132234 = DIRECTION('center_axis',(0.,0.499999999999997,-0.866025403784441)) ;
#132235 = DIRECTION('ref_axis',(0.,0.866025403784441,0.499999999999997)) ;
#132236 = DIRECTION('center_axis',(0.866025403784438,0.500000000000001,0.)) ;
#132237 = DIRECTION('ref_axis',(-0.500000000000001,0.866025403784438,0.)) ;
#132238 = DIRECTION('center_axis',(-7.01133629567814E-33,8.97270763436279E-17,
-1.)) ;
#132239 = DIRECTION('ref_axis',(0.,1.,0.)) ;
#132240 = DIRECTION('center_axis',(1.,0.,0.)) ;
#132241 = DIRECTION('ref_axis',(0.,0.,-1.)) ;
#132242 = DIRECTION('center_axis',(0.,0.500000000000014,0.866025403784431)) ;
#132243 = DIRECTION('ref_axis',(0.,-0.866025403784431,0.500000000000014)) ;
#132244 = DIRECTION('center_axis',(0.866025403784441,0.499999999999997,-2.16840434497101E-15)) ;
#132245 = DIRECTION('ref_axis',(-0.499999999999997,0.866025403784441,-1.29696145180732E-31)) ;
#132246 = DIRECTION('center_axis',(-7.01133629567814E-33,8.97270763436279E-17,
1.)) ;
#132247 = DIRECTION('ref_axis',(0.,-1.,0.)) ;
#132248 = DIRECTION('center_axis',(1.,0.,0.)) ;
#132249 = DIRECTION('ref_axis',(0.,0.,-1.)) ;
#132250 = DIRECTION('center_axis',(0.,0.499999999999997,-0.866025403784441)) ;
#132251 = DIRECTION('ref_axis',(0.,0.866025403784441,0.499999999999997)) ;
#132252 = DIRECTION('center_axis',(0.866025403784438,0.500000000000001,0.)) ;
#132253 = DIRECTION('ref_axis',(-0.500000000000001,0.866025403784438,0.)) ;
#132254 = DIRECTION('center_axis',(-7.01133629567814E-33,8.97270763436279E-17,
-1.)) ;
#132255 = DIRECTION('ref_axis',(0.,1.,0.)) ;
#132256 = DIRECTION('center_axis',(1.,0.,0.)) ;
#132257 = DIRECTION('ref_axis',(0.,0.,-1.)) ;
#132258 = DIRECTION('center_axis',(0.,0.500000000000014,0.866025403784431)) ;
#132259 = DIRECTION('ref_axis',(0.,-0.866025403784431,0.500000000000014)) ;
#132260 = DIRECTION('center_axis',(0.866025403784441,0.499999999999997,-2.16840434497101E-15)) ;
#132261 = DIRECTION('ref_axis',(-0.499999999999997,0.866025403784441,-1.29696145180732E-31)) ;
#132262 = DIRECTION('center_axis',(-7.01133629567814E-33,8.97270763436279E-17,
1.)) ;
#132263 = DIRECTION('ref_axis',(0.,-1.,0.)) ;
#132264 = DIRECTION('center_axis',(1.,0.,0.)) ;
#132265 = DIRECTION('ref_axis',(0.,0.,-1.)) ;
#132266 = DIRECTION('center_axis',(3.87199093546273E-14,0.500000000000014,
-0.866025403784431)) ;
#132267 = DIRECTION('ref_axis',(-3.42439963206942E-29,0.866025403784431,0.500000000000014)) ;
#132268 = DIRECTION('center_axis',(0.866025403784438,0.500000000000001,0.)) ;
#132269 = DIRECTION('ref_axis',(-0.500000000000001,0.866025403784438,0.)) ;
#132270 = DIRECTION('center_axis',(-7.01133629567814E-33,8.97270763436279E-17,
-1.)) ;
#132271 = DIRECTION('ref_axis',(0.,1.,0.)) ;
#132272 = DIRECTION('center_axis',(1.,0.,0.)) ;
#132273 = DIRECTION('ref_axis',(0.,0.,-1.)) ;
#132274 = DIRECTION('center_axis',(0.,0.500000000000014,0.866025403784431)) ;
#132275 = DIRECTION('ref_axis',(0.,-0.866025403784431,0.500000000000014)) ;
#132276 = DIRECTION('center_axis',(0.866025403784441,0.499999999999997,-2.16840434497101E-15)) ;
#132277 = DIRECTION('ref_axis',(-0.499999999999997,0.866025403784441,-1.29696145180732E-31)) ;
#132278 = DIRECTION('center_axis',(-7.01133629567814E-33,8.97270763436279E-17,
1.)) ;
#132279 = DIRECTION('ref_axis',(0.,-1.,0.)) ;
#132280 = DIRECTION('center_axis',(1.,0.,0.)) ;
#132281 = DIRECTION('ref_axis',(0.,0.,-1.)) ;
#132282 = DIRECTION('center_axis',(3.87199093546273E-14,0.500000000000014,
-0.866025403784431)) ;
#132283 = DIRECTION('ref_axis',(-3.42439963206942E-29,0.866025403784431,0.500000000000014)) ;
#132284 = DIRECTION('center_axis',(0.866025403784438,0.500000000000001,0.)) ;
#132285 = DIRECTION('ref_axis',(-0.500000000000001,0.866025403784438,0.)) ;
#132286 = DIRECTION('center_axis',(-7.01133629567814E-33,8.97270763436279E-17,
-1.)) ;
#132287 = DIRECTION('ref_axis',(0.,1.,0.)) ;
#132288 = DIRECTION('center_axis',(1.,0.,0.)) ;
#132289 = DIRECTION('ref_axis',(0.,0.,-1.)) ;
#132290 = DIRECTION('center_axis',(0.,0.500000000000014,0.866025403784431)) ;
#132291 = DIRECTION('ref_axis',(0.,-0.866025403784431,0.500000000000014)) ;
#132292 = DIRECTION('center_axis',(0.866025403784441,0.499999999999997,-2.16840434497101E-15)) ;
#132293 = DIRECTION('ref_axis',(-0.499999999999997,0.866025403784441,-1.29696145180732E-31)) ;
#132294 = DIRECTION('center_axis',(-7.01133629567814E-33,8.97270763436279E-17,
1.)) ;
#132295 = DIRECTION('ref_axis',(0.,-1.,0.)) ;
#132296 = DIRECTION('center_axis',(1.,0.,0.)) ;
#132297 = DIRECTION('ref_axis',(0.,0.,-1.)) ;
#132298 = DIRECTION('center_axis',(3.87199093546273E-14,0.500000000000014,
-0.866025403784431)) ;
#132299 = DIRECTION('ref_axis',(-3.42439963206942E-29,0.866025403784431,0.500000000000014)) ;
#132300 = DIRECTION('center_axis',(0.866025403784438,0.500000000000001,0.)) ;
#132301 = DIRECTION('ref_axis',(-0.500000000000001,0.866025403784438,0.)) ;
#132302 = DIRECTION('center_axis',(-7.01133629567814E-33,8.97270763436279E-17,
-1.)) ;
#132303 = DIRECTION('ref_axis',(0.,1.,0.)) ;
#132304 = DIRECTION('center_axis',(1.,0.,0.)) ;
#132305 = DIRECTION('ref_axis',(0.,0.,-1.)) ;
#132306 = DIRECTION('center_axis',(0.,0.500000000000015,0.86602540378443)) ;
#132307 = DIRECTION('ref_axis',(0.,-0.86602540378443,0.500000000000015)) ;
#132308 = DIRECTION('center_axis',(0.866025403784441,0.499999999999997,-2.16840434497108E-15)) ;
#132309 = DIRECTION('ref_axis',(-0.499999999999997,0.866025403784441,-1.29696145180926E-31)) ;
#132310 = DIRECTION('center_axis',(-7.01133629567814E-33,8.97270763436279E-17,
1.)) ;
#132311 = DIRECTION('ref_axis',(0.,-1.,0.)) ;
#132312 = DIRECTION('center_axis',(1.,0.,0.)) ;
#132313 = DIRECTION('ref_axis',(0.,0.,-1.)) ;
#132314 = DIRECTION('center_axis',(3.87199093546273E-14,0.500000000000014,
-0.866025403784431)) ;
#132315 = DIRECTION('ref_axis',(-3.42439963206942E-29,0.866025403784431,0.500000000000014)) ;
#132316 = DIRECTION('center_axis',(0.866025403784438,0.500000000000001,0.)) ;
#132317 = DIRECTION('ref_axis',(-0.500000000000001,0.866025403784438,0.)) ;
#132318 = DIRECTION('center_axis',(-7.01133629567814E-33,8.97270763436279E-17,
-1.)) ;
#132319 = DIRECTION('ref_axis',(0.,1.,0.)) ;
#132320 = DIRECTION('center_axis',(1.,0.,0.)) ;
#132321 = DIRECTION('ref_axis',(0.,0.,-1.)) ;
#132322 = DIRECTION('center_axis',(0.,0.500000000000015,0.86602540378443)) ;
#132323 = DIRECTION('ref_axis',(0.,-0.86602540378443,0.500000000000015)) ;
#132324 = DIRECTION('center_axis',(0.866025403784441,0.499999999999997,-2.16840434497108E-15)) ;
#132325 = DIRECTION('ref_axis',(-0.499999999999997,0.866025403784441,-1.29696145180926E-31)) ;
#132326 = DIRECTION('center_axis',(-7.01133629567814E-33,8.97270763436279E-17,
1.)) ;
#132327 = DIRECTION('ref_axis',(0.,-1.,0.)) ;
#132328 = DIRECTION('center_axis',(1.,0.,0.)) ;
#132329 = DIRECTION('ref_axis',(0.,0.,-1.)) ;
#132330 = DIRECTION('center_axis',(-2.16840434497107E-15,0.500000000000014,
-0.866025403784431)) ;
#132331 = DIRECTION('ref_axis',(1.87347069118046E-30,0.866025403784431,0.500000000000014)) ;
#132332 = DIRECTION('center_axis',(0.866025403784438,0.500000000000001,0.)) ;
#132333 = DIRECTION('ref_axis',(-0.500000000000001,0.866025403784438,0.)) ;
#132334 = DIRECTION('center_axis',(-7.01133629567814E-33,8.97270763436279E-17,
-1.)) ;
#132335 = DIRECTION('ref_axis',(0.,1.,0.)) ;
#132336 = DIRECTION('center_axis',(1.31418445149758E-16,1.,0.)) ;
#132337 = DIRECTION('ref_axis',(1.,-1.31418445149758E-16,-1.22464679914735E-16)) ;
#132338 = DIRECTION('center_axis',(1.31418445149758E-16,-1.,0.)) ;
#132339 = DIRECTION('ref_axis',(-1.,-1.31418445149758E-16,0.)) ;
#132340 = DIRECTION('center_axis',(1.31418445149758E-16,1.,0.)) ;
#132341 = DIRECTION('ref_axis',(1.,-1.31418445149758E-16,-1.22464679914735E-16)) ;
#132342 = DIRECTION('center_axis',(1.31418445149758E-16,-1.,0.)) ;
#132343 = DIRECTION('ref_axis',(-1.,-1.31418445149758E-16,0.)) ;
#132344 = DIRECTION('center_axis',(1.31418445149758E-16,1.,0.)) ;
#132345 = DIRECTION('ref_axis',(1.,-1.31418445149758E-16,-1.22464679914735E-16)) ;
#132346 = DIRECTION('center_axis',(1.31418445149758E-16,-1.,0.)) ;
#132347 = DIRECTION('ref_axis',(-1.,-1.31418445149758E-16,0.)) ;
#132348 = DIRECTION('center_axis',(1.31418445149758E-16,1.,0.)) ;
#132349 = DIRECTION('ref_axis',(1.,-1.31418445149758E-16,-1.22464679914735E-16)) ;
#132350 = DIRECTION('center_axis',(1.31418445149758E-16,-1.,0.)) ;
#132351 = DIRECTION('ref_axis',(-1.,-1.31418445149758E-16,0.)) ;
#132352 = DIRECTION('center_axis',(1.31418445149758E-16,1.,0.)) ;
#132353 = DIRECTION('ref_axis',(1.,-1.31418445149758E-16,7.6571373978539E-16)) ;
#132354 = DIRECTION('center_axis',(1.31418445149758E-16,-1.,0.)) ;
#132355 = DIRECTION('ref_axis',(-1.,-1.31418445149758E-16,1.5419764230905E-15)) ;
#132356 = DIRECTION('center_axis',(1.31418445149758E-16,1.,0.)) ;
#132357 = DIRECTION('ref_axis',(1.,-1.31418445149758E-16,-1.22464679914735E-16)) ;
#132358 = DIRECTION('center_axis',(1.31418445149758E-16,-1.,0.)) ;
#132359 = DIRECTION('ref_axis',(-1.,-1.31418445149758E-16,0.)) ;
#132360 = DIRECTION('center_axis',(0.,1.,0.)) ;
#132361 = DIRECTION('ref_axis',(1.,0.,0.)) ;
#132362 = DIRECTION('center_axis',(-8.67361737988405E-15,1.,0.)) ;
#132363 = DIRECTION('ref_axis',(-1.,-8.67361737988405E-15,0.)) ;
#132364 = DIRECTION('center_axis',(-7.81406971160724E-17,1.,0.)) ;
#132365 = DIRECTION('ref_axis',(-1.,-7.81406971160724E-17,0.)) ;
#132366 = DIRECTION('center_axis',(0.,1.,0.)) ;
#132367 = DIRECTION('ref_axis',(0.,0.,1.)) ;
#132368 = DIRECTION('center_axis',(0.,0.,-1.)) ;
#132369 = DIRECTION('ref_axis',(-1.,0.,0.)) ;
#132370 = DIRECTION('center_axis',(1.,0.,0.)) ;
#132371 = DIRECTION('ref_axis',(0.,0.,-1.)) ;
#132372 = DIRECTION('center_axis',(1.,7.81406971160724E-17,0.)) ;
#132373 = DIRECTION('ref_axis',(-7.81406971160724E-17,1.,0.)) ;
#132374 = DIRECTION('center_axis',(1.,0.,0.)) ;
#132375 = DIRECTION('ref_axis',(0.,0.,-1.)) ;
#132376 = DIRECTION('center_axis',(0.,1.,0.)) ;
#132377 = DIRECTION('ref_axis',(-1.,0.,0.)) ;
#132378 = DIRECTION('center_axis',(0.,1.,0.)) ;
#132379 = DIRECTION('ref_axis',(0.,0.,1.)) ;
#132380 = DIRECTION('center_axis',(0.,1.,0.)) ;
#132381 = DIRECTION('ref_axis',(0.,0.,1.)) ;
#132382 = DIRECTION('center_axis',(0.,1.,0.)) ;
#132383 = DIRECTION('ref_axis',(0.,0.,1.)) ;
#132384 = DIRECTION('center_axis',(0.,1.,0.)) ;
#132385 = DIRECTION('ref_axis',(-1.,0.,0.)) ;
#132386 = DIRECTION('center_axis',(-1.,0.,0.)) ;
#132387 = DIRECTION('ref_axis',(0.,0.,1.)) ;
#132388 = DIRECTION('center_axis',(1.,7.81406971160724E-17,0.)) ;
#132389 = DIRECTION('ref_axis',(-7.81406971160724E-17,1.,0.)) ;
#132390 = DIRECTION('center_axis',(-1.,0.,0.)) ;
#132391 = DIRECTION('ref_axis',(0.,0.,1.)) ;
#132392 = DIRECTION('center_axis',(0.,1.,0.)) ;
#132393 = DIRECTION('ref_axis',(1.,0.,0.)) ;
#132394 = DIRECTION('center_axis',(1.,0.,0.)) ;
#132395 = DIRECTION('ref_axis',(0.,0.,-1.)) ;
#132396 = DIRECTION('center_axis',(0.,0.,-1.)) ;
#132397 = DIRECTION('ref_axis',(-1.,0.,0.)) ;
#132398 = DIRECTION('center_axis',(0.,1.,0.)) ;
#132399 = DIRECTION('ref_axis',(0.,0.,-1.)) ;
#132400 = DIRECTION('center_axis',(0.,0.,-1.)) ;
#132401 = DIRECTION('ref_axis',(-1.,0.,0.)) ;
#132402 = DIRECTION('center_axis',(-1.,-1.31418445149758E-16,0.)) ;
#132403 = DIRECTION('ref_axis',(1.31418445149758E-16,-1.,0.)) ;
#132404 = DIRECTION('center_axis',(1.,0.,0.)) ;
#132405 = DIRECTION('ref_axis',(0.,0.,-1.)) ;
#132406 = DIRECTION('center_axis',(-7.81406971160724E-17,1.,0.)) ;
#132407 = DIRECTION('ref_axis',(-1.,-7.81406971160724E-17,0.)) ;
#132408 = DIRECTION('center_axis',(0.,1.,0.)) ;
#132409 = DIRECTION('ref_axis',(0.,0.,1.)) ;
#132410 = DIRECTION('center_axis',(0.,0.,1.)) ;
#132411 = DIRECTION('ref_axis',(1.,0.,0.)) ;
#132412 = DIRECTION('center_axis',(0.,0.,-1.)) ;
#132413 = DIRECTION('ref_axis',(-1.,0.,0.)) ;
#132414 = DIRECTION('center_axis',(0.,1.,0.)) ;
#132415 = DIRECTION('ref_axis',(1.,0.,0.)) ;
#132416 = DIRECTION('center_axis',(0.,0.,1.)) ;
#132417 = DIRECTION('ref_axis',(-1.,0.,0.)) ;
#132418 = DIRECTION('center_axis',(7.81406971160724E-17,-1.,0.)) ;
#132419 = DIRECTION('ref_axis',(1.,0.,0.)) ;
#132420 = DIRECTION('center_axis',(-7.81406971160724E-17,1.,0.)) ;
#132421 = DIRECTION('ref_axis',(1.,7.81406971160724E-17,0.)) ;
#132422 = DIRECTION('center_axis',(1.,0.,0.)) ;
#132423 = DIRECTION('ref_axis',(0.,0.,1.)) ;
#132424 = DIRECTION('center_axis',(0.,0.,1.)) ;
#132425 = DIRECTION('ref_axis',(1.,0.,0.)) ;
#132426 = DIRECTION('center_axis',(0.,0.,1.)) ;
#132427 = DIRECTION('ref_axis',(1.,0.,0.)) ;
#132428 = DIRECTION('center_axis',(7.81406971160724E-17,-1.,0.)) ;
#132429 = DIRECTION('ref_axis',(1.,7.81406971160724E-17,0.)) ;
#132430 = DIRECTION('center_axis',(0.,1.,0.)) ;
#132431 = DIRECTION('ref_axis',(0.,0.,1.)) ;
#132432 = DIRECTION('center_axis',(1.,7.81406971160724E-17,0.)) ;
#132433 = DIRECTION('ref_axis',(-7.81406971160724E-17,1.,0.)) ;
#132434 = DIRECTION('center_axis',(0.,1.,0.)) ;
#132435 = DIRECTION('ref_axis',(1.,0.,0.)) ;
#132436 = DIRECTION('center_axis',(-1.,0.,0.)) ;
#132437 = DIRECTION('ref_axis',(0.,0.,-1.)) ;
#132438 = DIRECTION('center_axis',(1.,1.31418445149758E-16,0.)) ;
#132439 = DIRECTION('ref_axis',(-1.31418445149758E-16,1.,0.)) ;
#132440 = DIRECTION('center_axis',(-1.31418445149758E-16,1.,0.)) ;
#132441 = DIRECTION('ref_axis',(0.990906098224775,0.,0.134555209861797)) ;
#132442 = DIRECTION('center_axis',(-1.31418445149758E-16,1.,0.)) ;
#132443 = DIRECTION('ref_axis',(1.,0.,0.)) ;
#132444 = DIRECTION('center_axis',(-1.31418445149758E-16,1.,0.)) ;
#132445 = DIRECTION('ref_axis',(1.,0.,-1.57898385724467E-15)) ;
#132446 = DIRECTION('center_axis',(-1.31418445149758E-16,1.,0.)) ;
#132447 = DIRECTION('ref_axis',(1.,0.,0.)) ;
#132448 = DIRECTION('center_axis',(-1.31418445149758E-16,1.,0.)) ;
#132449 = DIRECTION('ref_axis',(1.,0.,0.)) ;
#132450 = DIRECTION('center_axis',(-1.31418445149758E-16,1.,0.)) ;
#132451 = DIRECTION('ref_axis',(1.,0.,0.)) ;
#132452 = DIRECTION('center_axis',(-1.31418445149758E-16,1.,0.)) ;
#132453 = DIRECTION('ref_axis',(1.,0.,0.)) ;
#132454 = DIRECTION('center_axis',(0.,1.,0.)) ;
#132455 = DIRECTION('ref_axis',(1.,0.,0.)) ;
#132456 = DIRECTION('center_axis',(-8.67361737988405E-15,1.,0.)) ;
#132457 = DIRECTION('ref_axis',(-1.,-8.67361737988405E-15,0.)) ;
#132458 = DIRECTION('center_axis',(-1.31418445149758E-16,1.,0.)) ;
#132459 = DIRECTION('ref_axis',(1.,0.,0.)) ;
#132460 = DIRECTION('center_axis',(7.81406971160724E-17,-1.,0.)) ;
#132461 = DIRECTION('ref_axis',(1.,7.81406971160724E-17,0.)) ;
#132462 = DIRECTION('center_axis',(0.,1.,0.)) ;
#132463 = DIRECTION('ref_axis',(0.,0.,1.)) ;
#132464 = DIRECTION('center_axis',(0.,0.,-1.)) ;
#132465 = DIRECTION('ref_axis',(-1.,0.,0.)) ;
#132466 = DIRECTION('center_axis',(1.,0.,0.)) ;
#132467 = DIRECTION('ref_axis',(0.,0.,-1.)) ;
#132468 = DIRECTION('center_axis',(-1.31418445149758E-16,1.,0.)) ;
#132469 = DIRECTION('ref_axis',(1.,0.,-1.97372982155583E-16)) ;
#132470 = DIRECTION('center_axis',(-1.,-7.81406971160724E-17,0.)) ;
#132471 = DIRECTION('ref_axis',(7.81406971160724E-17,-1.,0.)) ;
#132472 = DIRECTION('center_axis',(1.,0.,0.)) ;
#132473 = DIRECTION('ref_axis',(0.,0.,-1.)) ;
#132474 = DIRECTION('center_axis',(0.,1.,0.)) ;
#132475 = DIRECTION('ref_axis',(-1.,0.,0.)) ;
#132476 = DIRECTION('center_axis',(4.33680868994202E-15,1.,0.)) ;
#132477 = DIRECTION('ref_axis',(-1.,4.33680868994202E-15,0.)) ;
#132478 = DIRECTION('center_axis',(-1.31418445149758E-16,1.,0.)) ;
#132479 = DIRECTION('ref_axis',(0.990906098224775,0.,-0.134555209861799)) ;
#132480 = DIRECTION('center_axis',(-1.,-7.81406971160724E-17,-5.25614554872951E-16)) ;
#132481 = DIRECTION('ref_axis',(-5.25614554872951E-16,-4.10718877321264E-32,
1.)) ;
#132482 = DIRECTION('center_axis',(-1.,0.,0.)) ;
#132483 = DIRECTION('ref_axis',(0.,0.,1.)) ;
#132484 = DIRECTION('center_axis',(0.,1.,0.)) ;
#132485 = DIRECTION('ref_axis',(0.,0.,1.)) ;
#132486 = DIRECTION('center_axis',(0.,1.,0.)) ;
#132487 = DIRECTION('ref_axis',(0.,0.,1.)) ;
#132488 = DIRECTION('center_axis',(7.81406971160724E-17,-1.,0.)) ;
#132489 = DIRECTION('ref_axis',(1.,0.,0.)) ;
#132490 = DIRECTION('center_axis',(-7.81406971160724E-17,1.,0.)) ;
#132491 = DIRECTION('ref_axis',(1.,7.81406971160724E-17,0.)) ;
#132492 = DIRECTION('center_axis',(0.,0.,-1.)) ;
#132493 = DIRECTION('ref_axis',(1.,0.,0.)) ;
#132494 = DIRECTION('center_axis',(0.,1.,0.)) ;
#132495 = DIRECTION('ref_axis',(-1.,0.,0.)) ;
#132496 = DIRECTION('center_axis',(-1.,0.,0.)) ;
#132497 = DIRECTION('ref_axis',(0.,0.,1.)) ;
#132498 = DIRECTION('center_axis',(-1.,-1.31418445149758E-16,-5.25614554872951E-16)) ;
#132499 = DIRECTION('ref_axis',(-5.25614554872951E-16,-6.90754475494854E-32,
1.)) ;
#132500 = DIRECTION('center_axis',(1.,0.,0.)) ;
#132501 = DIRECTION('ref_axis',(0.,0.,-1.)) ;
#132502 = DIRECTION('center_axis',(7.81406971160724E-17,-1.,1.10147335281612E-31)) ;
#132503 = DIRECTION('ref_axis',(1.,7.81406971160724E-17,-8.6069895643829E-48)) ;
#132504 = DIRECTION('center_axis',(0.,1.,0.)) ;
#132505 = DIRECTION('ref_axis',(0.,0.,1.)) ;
#132506 = DIRECTION('center_axis',(0.,0.,1.)) ;
#132507 = DIRECTION('ref_axis',(1.,0.,0.)) ;
#132508 = DIRECTION('center_axis',(0.,0.,-1.)) ;
#132509 = DIRECTION('ref_axis',(-1.,0.,0.)) ;
#132510 = DIRECTION('center_axis',(-1.,-7.81406971160724E-17,0.)) ;
#132511 = DIRECTION('ref_axis',(7.81406971160724E-17,-1.,0.)) ;
#132512 = DIRECTION('center_axis',(-1.,0.,0.)) ;
#132513 = DIRECTION('ref_axis',(0.,0.,1.)) ;
#132514 = DIRECTION('center_axis',(0.,1.,0.)) ;
#132515 = DIRECTION('ref_axis',(1.,0.,0.)) ;
#132516 = DIRECTION('center_axis',(1.51788304147971E-14,0.,1.)) ;
#132517 = DIRECTION('ref_axis',(-1.,0.,1.51788304147971E-14)) ;
#132518 = DIRECTION('center_axis',(0.,0.,-1.)) ;
#132519 = DIRECTION('ref_axis',(-1.,0.,0.)) ;
#132520 = DIRECTION('center_axis',(0.,1.,0.)) ;
#132521 = DIRECTION('ref_axis',(0.,0.,-1.)) ;
#132522 = DIRECTION('center_axis',(0.,0.,1.)) ;
#132523 = DIRECTION('ref_axis',(1.,0.,0.)) ;
#132524 = DIRECTION('center_axis',(0.,0.,1.)) ;
#132525 = DIRECTION('ref_axis',(1.,0.,0.)) ;
#132526 = DIRECTION('center_axis',(7.81406971160724E-17,-1.,0.)) ;
#132527 = DIRECTION('ref_axis',(1.,7.81406971160724E-17,0.)) ;
#132528 = DIRECTION('center_axis',(0.,1.,0.)) ;
#132529 = DIRECTION('ref_axis',(0.,0.,1.)) ;
#132530 = DIRECTION('center_axis',(0.,1.,0.)) ;
#132531 = DIRECTION('ref_axis',(1.,0.,0.)) ;
#132532 = DIRECTION('center_axis',(-1.,0.,0.)) ;
#132533 = DIRECTION('ref_axis',(0.,0.,-1.)) ;
#132534 = DIRECTION('center_axis',(1.,1.31418445149758E-16,0.)) ;
#132535 = DIRECTION('ref_axis',(-1.31418445149758E-16,1.,0.)) ;
#132536 = DIRECTION('center_axis',(-1.,0.,0.)) ;
#132537 = DIRECTION('ref_axis',(0.,0.,1.)) ;
#132538 = DIRECTION('center_axis',(0.,1.,0.)) ;
#132539 = DIRECTION('ref_axis',(1.,0.,0.)) ;
#132540 = DIRECTION('center_axis',(0.380709651665466,0.236869643538635,0.893841671158063)) ;
#132541 = DIRECTION('ref_axis',(0.920024234945248,1.04575356953145E-17,-0.391861464185253)) ;
#132542 = DIRECTION('center_axis',(0.380709651731648,0.236869643589572,-0.893841671116377)) ;
#132543 = DIRECTION('ref_axis',(-0.9200242349141,-4.58748474863685E-15,-0.391861464258384)) ;
#132544 = DIRECTION('',(-1.03148349253124E-17,-1.11022302462516E-16,-1.)) ;
#132545 = DIRECTION('',(-1.,-1.25063945412672E-16,1.03148349253124E-17)) ;
#132546 = DIRECTION('',(0.,0.,1.)) ;
#132547 = DIRECTION('',(1.,0.,0.)) ;
#132548 = DIRECTION('',(2.17539629770119E-19,-1.73472347597681E-17,-1.)) ;
#132549 = DIRECTION('',(-1.,8.88779593930745E-18,-2.17539629770119E-19)) ;
#132550 = CARTESIAN_POINT('',(0.,0.,0.)) ;
#132551 = CARTESIAN_POINT('',(0.,0.,0.)) ;
#132552 = CARTESIAN_POINT('Origin',(4.6,2.65,-6.57304604217164)) ;
#132553 = CARTESIAN_POINT('',(4.5,2.61712020253893,-6.37576725740521)) ;
#132554 = CARTESIAN_POINT('',(4.5,2.72431432344521,-6.38736518335501)) ;
#132555 = CARTESIAN_POINT('Origin',(4.5,2.65,-6.57304604217164)) ;
#132556 = CARTESIAN_POINT('',(4.6,2.63356010126946,-6.47440664978842)) ;
#132557 = CARTESIAN_POINT('Origin',(4.6,2.61712020253893,-6.37576725740521)) ;
#132558 = CARTESIAN_POINT('',(4.6,2.68715716172261,-6.48020561276332)) ;
#132559 = CARTESIAN_POINT('Origin',(4.6,2.65,-6.57304604217164)) ;
#132560 = CARTESIAN_POINT('Origin',(4.6,2.72431432344521,-6.38736518335501)) ;
#132561 = CARTESIAN_POINT('Origin',(0.,10.85,-5.08)) ;
#132562 = CARTESIAN_POINT('',(-2.44929359829471E-16,10.95,-3.08)) ;
#132563 = CARTESIAN_POINT('Origin',(0.,10.95,-5.08)) ;
#132564 = CARTESIAN_POINT('',(-2.32682891837997E-16,10.85,-3.18)) ;
#132565 = CARTESIAN_POINT('Origin',(-2.44929359829471E-16,10.85,-3.08)) ;
#132566 = CARTESIAN_POINT('',(2.32682891837997E-16,10.85,-6.98)) ;
#132567 = CARTESIAN_POINT('Origin',(0.,10.85,-5.08)) ;
#132568 = CARTESIAN_POINT('Origin',(0.,10.85,-5.08)) ;
#132569 = CARTESIAN_POINT('Origin',(11.0914213562373,0.,-5.08)) ;
#132570 = CARTESIAN_POINT('',(11.0207106781187,-1.80110112442984E-16,-3.60928932188135)) ;
#132571 = CARTESIAN_POINT('Origin',(11.0207106781187,0.,-5.08)) ;
#132572 = CARTESIAN_POINT('',(11.0914213562373,-1.83697019872103E-16,-3.58)) ;
#132573 = CARTESIAN_POINT('Origin',(11.0914213562373,-1.71450551880629E-16,
-3.68)) ;
#132574 = CARTESIAN_POINT('Origin',(11.0914213562373,0.,-5.08)) ;
#132575 = CARTESIAN_POINT('Origin',(12.7,0.,-5.08)) ;
#132576 = CARTESIAN_POINT('',(12.8,-1.95943487863576E-16,-6.68)) ;
#132577 = CARTESIAN_POINT('Origin',(12.8,0.,-5.08)) ;
#132578 = CARTESIAN_POINT('',(12.7,-1.83697019872103E-16,-6.58)) ;
#132579 = CARTESIAN_POINT('Origin',(12.7,-1.95943487863577E-16,-6.68)) ;
#132580 = CARTESIAN_POINT('',(12.7,1.83697019872103E-16,-3.58)) ;
#132581 = CARTESIAN_POINT('Origin',(12.7,0.,-5.08)) ;
#132582 = CARTESIAN_POINT('Origin',(12.7,0.,-5.08)) ;
#132583 = CARTESIAN_POINT('Origin',(12.7,2.1,-3.69804604217164)) ;
#132584 = CARTESIAN_POINT('',(12.7,2.,-3.69804604217164)) ;
#132585 = CARTESIAN_POINT('',(12.7,2.11643989873054,-3.59940664978842)) ;
#132586 = CARTESIAN_POINT('Origin',(12.7,2.1,-3.69804604217164)) ;
#132587 = CARTESIAN_POINT('',(12.8,2.13287979746107,-3.50076725740521)) ;
#132588 = CARTESIAN_POINT('Origin',(12.7,2.13287979746107,-3.50076725740521)) ;
#132589 = CARTESIAN_POINT('',(12.8,1.9,-3.69804604217164)) ;
#132590 = CARTESIAN_POINT('Origin',(12.8,2.1,-3.69804604217164)) ;
#132591 = CARTESIAN_POINT('Origin',(12.7,1.9,-3.69804604217164)) ;
#132592 = CARTESIAN_POINT('Origin',(12.7,2.65,-3.58695395782836)) ;
#132593 = CARTESIAN_POINT('',(12.7,2.63356010126947,-3.68559335021158)) ;
#132594 = CARTESIAN_POINT('',(12.7,2.75,-3.58695395782836)) ;
#132595 = CARTESIAN_POINT('Origin',(12.7,2.65,-3.58695395782836)) ;
#132596 = CARTESIAN_POINT('',(12.8,2.65,-3.58695395782836)) ;
#132597 = CARTESIAN_POINT('Origin',(12.7,2.65,-3.58695395782836)) ;
#132598 = CARTESIAN_POINT('Origin',(12.7,2.65,-3.58695395782836)) ;
#132599 = CARTESIAN_POINT('Origin',(4.5,2.1,-3.69804604217164)) ;
#132600 = CARTESIAN_POINT('',(4.6,2.,-3.69804604217164)) ;
#132601 = CARTESIAN_POINT('',(12.8,2.,-3.69804604217164)) ;
#132602 = CARTESIAN_POINT('',(4.6,2.11643989873054,-3.59940664978842)) ;
#132603 = CARTESIAN_POINT('Origin',(4.6,2.1,-3.69804604217164)) ;
#132604 = CARTESIAN_POINT('',(4.5,2.11643989873054,-3.59940664978842)) ;
#132605 = CARTESIAN_POINT('Origin',(12.7,2.65,-6.57304604217164)) ;
#132606 = CARTESIAN_POINT('',(12.8,2.65,-6.57304604217164)) ;
#132607 = CARTESIAN_POINT('',(12.7,2.63356010126947,-6.47440664978842)) ;
#132608 = CARTESIAN_POINT('Origin',(12.7,2.65,-6.57304604217164)) ;
#132609 = CARTESIAN_POINT('',(12.7,2.75,-6.57304604217164)) ;
#132610 = CARTESIAN_POINT('Origin',(12.7,2.65,-6.57304604217164)) ;
#132611 = CARTESIAN_POINT('Origin',(12.7,2.65,-6.57304604217164)) ;
#132612 = CARTESIAN_POINT('Origin',(11.05,0.,-5.08)) ;
#132613 = CARTESIAN_POINT('',(10.3,-9.1848509936051E-17,-4.33)) ;
#132614 = CARTESIAN_POINT('Origin',(10.3,0.,-5.08)) ;
#132615 = CARTESIAN_POINT('',(11.05,-1.83697019872103E-16,-3.58)) ;
#132616 = CARTESIAN_POINT('Origin',(11.05,0.,-5.08)) ;
#132617 = CARTESIAN_POINT('',(11.05,-1.83697019872103E-16,-3.58)) ;
#132618 = CARTESIAN_POINT('Origin',(0.,9.95,-5.08)) ;
#132619 = CARTESIAN_POINT('',(0.218101234104781,9.95,-6.96744055580089)) ;
#132620 = CARTESIAN_POINT('',(-2.32682891837997E-16,9.95,-6.98)) ;
#132621 = CARTESIAN_POINT('Origin',(0.,9.95,-5.08)) ;
#132622 = CARTESIAN_POINT('',(0.321518176280636,9.85,-6.9525987456797)) ;
#132623 = CARTESIAN_POINT('Ctrl Pts',(0.218101234104783,9.95,-6.96744055580089)) ;
#132624 = CARTESIAN_POINT('Ctrl Pts',(0.231193919344581,9.95,-6.9659276441493)) ;
#132625 = CARTESIAN_POINT('Ctrl Pts',(0.245192892440024,9.94751445938575,
-6.96415658257392)) ;
#132626 = CARTESIAN_POINT('Ctrl Pts',(0.270990685773162,9.93716996065971,
-6.96062157894673)) ;
#132627 = CARTESIAN_POINT('Ctrl Pts',(0.282791986325045,9.92931613918426,
-6.95886070936675)) ;
#132628 = CARTESIAN_POINT('Ctrl Pts',(0.300953024019397,9.91135900604096,
-6.95603502666193)) ;
#132629 = CARTESIAN_POINT('Ctrl Pts',(0.308688523153916,9.90025653083842,
-6.95476256180095)) ;
#132630 = CARTESIAN_POINT('Ctrl Pts',(0.318969164829205,9.87583423571802,
-6.95304298667495)) ;
#132631 = CARTESIAN_POINT('Ctrl Pts',(0.321518176280638,9.86251584266313,
-6.9525987456797)) ;
#132632 = CARTESIAN_POINT('Ctrl Pts',(0.321518176280638,9.85,-6.9525987456797)) ;
#132633 = CARTESIAN_POINT('',(0.321518176280636,9.05,-6.9525987456797)) ;
#132634 = CARTESIAN_POINT('',(0.321518176280636,8.95,-6.9525987456797)) ;
#132635 = CARTESIAN_POINT('',(0.422455466606969,8.95,-6.93243930500675)) ;
#132636 = CARTESIAN_POINT('Ctrl Pts',(0.321518176280635,9.05,-6.9525987456797)) ;
#132637 = CARTESIAN_POINT('Ctrl Pts',(0.321518176280635,9.03744936090869,
-6.9525987456797)) ;
#132638 = CARTESIAN_POINT('Ctrl Pts',(0.324085473150911,9.02409774280079,
-6.95216456224267)) ;
#132639 = CARTESIAN_POINT('Ctrl Pts',(0.334387313650439,8.99960748025859,
-6.95034985790769)) ;
#132640 = CARTESIAN_POINT('Ctrl Pts',(0.342122499456567,8.98846937989492,
-6.94896564206148)) ;
#132641 = CARTESIAN_POINT('Ctrl Pts',(0.360004521225396,8.97064401154629,
-6.94560497807954)) ;
#132642 = CARTESIAN_POINT('Ctrl Pts',(0.37144710874947,8.96285745107738,-6.94338208404762)) ;
#132643 = CARTESIAN_POINT('Ctrl Pts',(0.396373979529697,8.95253508546271,
-6.93823730327889)) ;
#132644 = CARTESIAN_POINT('Ctrl Pts',(0.409857901997329,8.95,-6.93531222506459)) ;
#132645 = CARTESIAN_POINT('Ctrl Pts',(0.422455466606967,8.95,-6.93243930500675)) ;
#132646 = CARTESIAN_POINT('',(1.14750169623629,8.95,-6.59434469561419)) ;
#132647 = CARTESIAN_POINT('Origin',(0.,8.95,-5.08)) ;
#132648 = CARTESIAN_POINT('',(1.22782596331729,9.05,-6.529980483939)) ;
#132649 = CARTESIAN_POINT('Ctrl Pts',(1.14750169623629,8.95,-6.59434469561419)) ;
#132650 = CARTESIAN_POINT('Ctrl Pts',(1.15780003912542,8.95,-6.58654107866494)) ;
#132651 = CARTESIAN_POINT('Ctrl Pts',(1.16870807732935,8.95253508546271,-6.57809199882069)) ;
#132652 = CARTESIAN_POINT('Ctrl Pts',(1.18867189173408,8.96285745107738,-6.56230390930784)) ;
#132653 = CARTESIAN_POINT('Ctrl Pts',(1.19772988083811,8.97064401154629,-6.55496722746149)) ;
#132654 = CARTESIAN_POINT('Ctrl Pts',(1.21179864083581,8.98846937989492,-6.54342899722165)) ;
#132655 = CARTESIAN_POINT('Ctrl Pts',(1.21783109328768,8.99960748025859,-6.53839325791345)) ;
#132656 = CARTESIAN_POINT('Ctrl Pts',(1.22584313288946,9.02409774280079,-6.53166805970666)) ;
#132657 = CARTESIAN_POINT('Ctrl Pts',(1.22782596331729,9.03744936090869,-6.529980483939)) ;
#132658 = CARTESIAN_POINT('Ctrl Pts',(1.22782596331729,9.05,-6.529980483939)) ;
#132659 = CARTESIAN_POINT('',(1.22782596331729,9.85,-6.529980483939)) ;
#132660 = CARTESIAN_POINT('',(1.22782596331729,8.95,-6.529980483939)) ;
#132661 = CARTESIAN_POINT('',(1.30567057854876,9.95,-6.46029864171205)) ;
#132662 = CARTESIAN_POINT('Ctrl Pts',(1.22782596331729,9.85,-6.529980483939)) ;
#132663 = CARTESIAN_POINT('Ctrl Pts',(1.22782596331729,9.85579162428539,-6.529980483939)) ;
#132664 = CARTESIAN_POINT('Ctrl Pts',(1.22822745887816,9.86162764920015,-6.52964057146522)) ;
#132665 = CARTESIAN_POINT('Ctrl Pts',(1.22902753823169,9.86736607146313,-6.52896195467785)) ;
#132666 = CARTESIAN_POINT('Ctrl Pts',(1.22973095933684,9.87241123018669,-6.52836532214579)) ;
#132667 = CARTESIAN_POINT('Ctrl Pts',(1.23074168751918,9.87738020477702,-6.52750743025347)) ;
#132668 = CARTESIAN_POINT('Ctrl Pts',(1.23203099150182,9.88218322835582,-6.52640922147928)) ;
#132669 = CARTESIAN_POINT('Ctrl Pts',(1.23351897101726,9.88772637473068,-6.52514178402336)) ;
#132670 = CARTESIAN_POINT('Ctrl Pts',(1.2354014557903,9.89313280655103,-6.52353433657835)) ;
#132671 = CARTESIAN_POINT('Ctrl Pts',(1.23763252770622,9.89827011881554,-6.52161898274845)) ;
#132672 = CARTESIAN_POINT('Ctrl Pts',(1.23953000874363,9.90263929783465,-6.51999001348654)) ;
#132673 = CARTESIAN_POINT('Ctrl Pts',(1.24167862345459,9.90681364346946,-6.51813903119877)) ;
#132674 = CARTESIAN_POINT('Ctrl Pts',(1.24403025306866,9.91072825704926,-6.51610192167908)) ;
#132675 = CARTESIAN_POINT('Ctrl Pts',(1.24687926059923,9.91547082513966,-6.51363395634666)) ;
#132676 = CARTESIAN_POINT('Ctrl Pts',(1.25006974298106,9.91990270163235,-6.51085512653216)) ;
#132677 = CARTESIAN_POINT('Ctrl Pts',(1.25351940932651,9.92391762881324,-6.50782661463088)) ;
#132678 = CARTESIAN_POINT('Ctrl Pts',(1.25634620505523,9.92720762206753,-6.50534492983889)) ;
#132679 = CARTESIAN_POINT('Ctrl Pts',(1.25934609941474,9.93021806933733,-6.50269631015879)) ;
#132680 = CARTESIAN_POINT('Ctrl Pts',(1.26246241000317,9.93291206679729,-6.49992558372932)) ;
#132681 = CARTESIAN_POINT('Ctrl Pts',(1.2664914591119,9.93639511117204,-6.49634333718027)) ;
#132682 = CARTESIAN_POINT('Ctrl Pts',(1.27077652588472,9.93940081548805,-6.49250226252408)) ;
#132683 = CARTESIAN_POINT('Ctrl Pts',(1.27520851369616,9.94185862744775,-6.48848967391021)) ;
#132684 = CARTESIAN_POINT('Ctrl Pts',(1.27864718185097,9.9437655820866,-6.48537640707106)) ;
#132685 = CARTESIAN_POINT('Ctrl Pts',(1.28217366418729,9.94534362661778,-6.48216049976224)) ;
#132686 = CARTESIAN_POINT('Ctrl Pts',(1.28573335778225,9.94658081625577,-6.47888874922024)) ;
#132687 = CARTESIAN_POINT('Ctrl Pts',(1.29026904082682,9.94815721599755,-6.47471995686114)) ;
#132688 = CARTESIAN_POINT('Ctrl Pts',(1.29492021413416,9.9491996901822,-6.47040365182261)) ;
#132689 = CARTESIAN_POINT('Ctrl Pts',(1.29957290046267,9.9496832238817,-6.46604122438749)) ;
#132690 = CARTESIAN_POINT('Ctrl Pts',(1.30160833994479,9.94989475836166,-6.46413276625978)) ;
#132691 = CARTESIAN_POINT('Ctrl Pts',(1.30364403319566,9.95,-6.46221561863551)) ;
#132692 = CARTESIAN_POINT('Ctrl Pts',(1.30567057854876,9.95,-6.46029864171205)) ;
#132693 = CARTESIAN_POINT('',(-0.218101234104782,9.95,-3.19255944419911)) ;
#132694 = CARTESIAN_POINT('Origin',(0.,9.95,-5.08)) ;
#132695 = CARTESIAN_POINT('',(-0.321518176280637,9.85,-3.2074012543203)) ;
#132696 = CARTESIAN_POINT('Ctrl Pts',(-0.218101234104781,9.95,-3.19255944419911)) ;
#132697 = CARTESIAN_POINT('Ctrl Pts',(-0.231193919344579,9.95,-3.19407235585069)) ;
#132698 = CARTESIAN_POINT('Ctrl Pts',(-0.245192892440022,9.94751445938575,
-3.19584341742608)) ;
#132699 = CARTESIAN_POINT('Ctrl Pts',(-0.27099068577316,9.93716996065971,
-3.19937842105326)) ;
#132700 = CARTESIAN_POINT('Ctrl Pts',(-0.282791986325042,9.92931613918426,
-3.20113929063325)) ;
#132701 = CARTESIAN_POINT('Ctrl Pts',(-0.300953024019395,9.91135900604096,
-3.20396497333807)) ;
#132702 = CARTESIAN_POINT('Ctrl Pts',(-0.308688523153914,9.90025653083842,
-3.20523743819905)) ;
#132703 = CARTESIAN_POINT('Ctrl Pts',(-0.318969164829203,9.87583423571802,
-3.20695701332505)) ;
#132704 = CARTESIAN_POINT('Ctrl Pts',(-0.321518176280636,9.86251584266313,
-3.2074012543203)) ;
#132705 = CARTESIAN_POINT('Ctrl Pts',(-0.321518176280636,9.85,-3.2074012543203)) ;
#132706 = CARTESIAN_POINT('',(-0.321518176280637,9.05,-3.2074012543203)) ;
#132707 = CARTESIAN_POINT('',(-0.321518176280637,8.95,-3.2074012543203)) ;
#132708 = CARTESIAN_POINT('',(-0.422455466606969,8.95,-3.22756069499325)) ;
#132709 = CARTESIAN_POINT('Ctrl Pts',(-0.321518176280636,9.05,-3.2074012543203)) ;
#132710 = CARTESIAN_POINT('Ctrl Pts',(-0.321518176280636,9.03744936090869,
-3.2074012543203)) ;
#132711 = CARTESIAN_POINT('Ctrl Pts',(-0.324085473150912,9.02409774280079,
-3.20783543775733)) ;
#132712 = CARTESIAN_POINT('Ctrl Pts',(-0.334387313650441,8.99960748025859,
-3.20965014209231)) ;
#132713 = CARTESIAN_POINT('Ctrl Pts',(-0.342122499456569,8.98846937989492,
-3.21103435793852)) ;
#132714 = CARTESIAN_POINT('Ctrl Pts',(-0.360004521225397,8.97064401154629,
-3.21439502192046)) ;
#132715 = CARTESIAN_POINT('Ctrl Pts',(-0.371447108749472,8.96285745107738,
-3.21661791595238)) ;
#132716 = CARTESIAN_POINT('Ctrl Pts',(-0.396373979529699,8.95253508546271,
-3.22176269672111)) ;
#132717 = CARTESIAN_POINT('Ctrl Pts',(-0.409857901997331,8.95,-3.22468777493542)) ;
#132718 = CARTESIAN_POINT('Ctrl Pts',(-0.422455466606968,8.95,-3.22756069499325)) ;
#132719 = CARTESIAN_POINT('',(-1.14750169623629,8.95,-3.56565530438581)) ;
#132720 = CARTESIAN_POINT('Origin',(0.,8.95,-5.08)) ;
#132721 = CARTESIAN_POINT('',(-1.22782596331729,9.05,-3.630019516061)) ;
#132722 = CARTESIAN_POINT('Ctrl Pts',(-1.14750169623629,8.95,-3.56565530438581)) ;
#132723 = CARTESIAN_POINT('Ctrl Pts',(-1.15780003912542,8.95,-3.57345892133506)) ;
#132724 = CARTESIAN_POINT('Ctrl Pts',(-1.16870807732935,8.95253508546271,
-3.58190800117931)) ;
#132725 = CARTESIAN_POINT('Ctrl Pts',(-1.18867189173408,8.96285745107738,
-3.59769609069216)) ;
#132726 = CARTESIAN_POINT('Ctrl Pts',(-1.19772988083811,8.97064401154629,
-3.60503277253851)) ;
#132727 = CARTESIAN_POINT('Ctrl Pts',(-1.21179864083581,8.98846937989492,
-3.61657100277835)) ;
#132728 = CARTESIAN_POINT('Ctrl Pts',(-1.21783109328768,8.99960748025859,
-3.62160674208655)) ;
#132729 = CARTESIAN_POINT('Ctrl Pts',(-1.22584313288946,9.02409774280079,
-3.62833194029334)) ;
#132730 = CARTESIAN_POINT('Ctrl Pts',(-1.22782596331729,9.03744936090869,
-3.630019516061)) ;
#132731 = CARTESIAN_POINT('Ctrl Pts',(-1.22782596331729,9.05,-3.630019516061)) ;
#132732 = CARTESIAN_POINT('',(-1.22782596331729,9.85,-3.630019516061)) ;
#132733 = CARTESIAN_POINT('',(-1.22782596331729,8.95,-3.630019516061)) ;
#132734 = CARTESIAN_POINT('',(-1.30567057854876,9.95,-3.69970135828795)) ;
#132735 = CARTESIAN_POINT('Ctrl Pts',(-1.22782596331729,9.85,-3.630019516061)) ;
#132736 = CARTESIAN_POINT('Ctrl Pts',(-1.22782596331729,9.85579162428539,
-3.630019516061)) ;
#132737 = CARTESIAN_POINT('Ctrl Pts',(-1.22822745887816,9.86162764920015,
-3.63035942853478)) ;
#132738 = CARTESIAN_POINT('Ctrl Pts',(-1.22902753823169,9.86736607146313,
-3.63103804532216)) ;
#132739 = CARTESIAN_POINT('Ctrl Pts',(-1.22973095933683,9.87241123018669,
-3.63163467785421)) ;
#132740 = CARTESIAN_POINT('Ctrl Pts',(-1.23074168751918,9.87738020477703,
-3.63249256974653)) ;
#132741 = CARTESIAN_POINT('Ctrl Pts',(-1.23203099150181,9.88218322835582,
-3.63359077852072)) ;
#132742 = CARTESIAN_POINT('Ctrl Pts',(-1.23351897101725,9.88772637473068,
-3.63485821597664)) ;
#132743 = CARTESIAN_POINT('Ctrl Pts',(-1.2354014557903,9.89313280655104,-3.63646566342165)) ;
#132744 = CARTESIAN_POINT('Ctrl Pts',(-1.23763252770622,9.89827011881554,
-3.63838101725155)) ;
#132745 = CARTESIAN_POINT('Ctrl Pts',(-1.23953000874363,9.90263929783465,
-3.64000998651346)) ;
#132746 = CARTESIAN_POINT('Ctrl Pts',(-1.24167862345459,9.90681364346947,
-3.64186096880123)) ;
#132747 = CARTESIAN_POINT('Ctrl Pts',(-1.24403025306866,9.91072825704926,
-3.64389807832092)) ;
#132748 = CARTESIAN_POINT('Ctrl Pts',(-1.24687926059923,9.91547082513966,
-3.64636604365334)) ;
#132749 = CARTESIAN_POINT('Ctrl Pts',(-1.25006974298106,9.91990270163235,
-3.64914487346785)) ;
#132750 = CARTESIAN_POINT('Ctrl Pts',(-1.2535194093265,9.92391762881324,-3.65217338536913)) ;
#132751 = CARTESIAN_POINT('Ctrl Pts',(-1.25634620505523,9.92720762206753,
-3.65465507016111)) ;
#132752 = CARTESIAN_POINT('Ctrl Pts',(-1.25934609941474,9.93021806933733,
-3.65730368984121)) ;
#132753 = CARTESIAN_POINT('Ctrl Pts',(-1.26246241000317,9.9329120667973,-3.66007441627069)) ;
#132754 = CARTESIAN_POINT('Ctrl Pts',(-1.26649145911191,9.93639511117205,
-3.66365666281975)) ;
#132755 = CARTESIAN_POINT('Ctrl Pts',(-1.27077652588473,9.93940081548806,
-3.66749773747593)) ;
#132756 = CARTESIAN_POINT('Ctrl Pts',(-1.27520851369618,9.94185862744776,
-3.67151032608981)) ;
#132757 = CARTESIAN_POINT('Ctrl Pts',(-1.27864718185098,9.94376558208661,
-3.67462359292896)) ;
#132758 = CARTESIAN_POINT('Ctrl Pts',(-1.2821736641873,9.94534362661778,-3.67783950023776)) ;
#132759 = CARTESIAN_POINT('Ctrl Pts',(-1.28573335778225,9.94658081625577,
-3.68111125077976)) ;
#132760 = CARTESIAN_POINT('Ctrl Pts',(-1.29026904082681,9.94815721599755,
-3.68528004313886)) ;
#132761 = CARTESIAN_POINT('Ctrl Pts',(-1.29492021413415,9.9491996901822,-3.68959634817738)) ;
#132762 = CARTESIAN_POINT('Ctrl Pts',(-1.29957290046265,9.9496832238817,-3.6939587756125)) ;
#132763 = CARTESIAN_POINT('Ctrl Pts',(-1.30160833994478,9.94989475836166,
-3.69586723374022)) ;
#132764 = CARTESIAN_POINT('Ctrl Pts',(-1.30364403319566,9.95,-3.69778438136449)) ;
#132765 = CARTESIAN_POINT('Ctrl Pts',(-1.30567057854876,9.95,-3.69970135828795)) ;
#132766 = CARTESIAN_POINT('Origin',(0.,9.95,-5.08)) ;
#132767 = CARTESIAN_POINT('',(-2.32682891837997E-16,9.95,-6.98)) ;
#132768 = CARTESIAN_POINT('Origin',(4.6,2.65,-1.49304604217164)) ;
#132769 = CARTESIAN_POINT('',(4.5,2.61712020253893,-1.29576725740521)) ;
#132770 = CARTESIAN_POINT('',(4.5,2.72431432344521,-1.30736518335501)) ;
#132771 = CARTESIAN_POINT('Origin',(4.5,2.65,-1.49304604217164)) ;
#132772 = CARTESIAN_POINT('',(4.6,2.63356010126946,-1.39440664978842)) ;
#132773 = CARTESIAN_POINT('Origin',(4.6,2.61712020253893,-1.29576725740521)) ;
#132774 = CARTESIAN_POINT('',(4.6,2.68715716172261,-1.40020561276332)) ;
#132775 = CARTESIAN_POINT('Origin',(4.6,2.65,-1.49304604217164)) ;
#132776 = CARTESIAN_POINT('Origin',(4.6,2.72431432344521,-1.30736518335501)) ;
#132777 = CARTESIAN_POINT('Origin',(-4.52198039027186,10.1,2.54)) ;
#132778 = CARTESIAN_POINT('',(-4.42392232270277,10.0803883864862,-7.62)) ;
#132779 = CARTESIAN_POINT('',(-4.52198039027186,10.2,-7.62)) ;
#132780 = CARTESIAN_POINT('Origin',(-4.52198039027186,10.1,-7.62)) ;
#132781 = CARTESIAN_POINT('',(-4.42392232270277,10.0803883864862,2.54)) ;
#132782 = CARTESIAN_POINT('',(-4.42392232270277,10.0803883864862,-2.54)) ;
#132783 = CARTESIAN_POINT('',(-4.52198039027186,10.2,2.54)) ;
#132784 = CARTESIAN_POINT('Origin',(-4.52198039027186,10.1,2.54)) ;
#132785 = CARTESIAN_POINT('',(-4.52198039027186,10.2,2.54)) ;
#132786 = CARTESIAN_POINT('Origin',(0.,10.85,0.)) ;
#132787 = CARTESIAN_POINT('',(-2.44929359829471E-16,10.95,2.)) ;
#132788 = CARTESIAN_POINT('Origin',(0.,10.95,0.)) ;
#132789 = CARTESIAN_POINT('',(-2.32682891837997E-16,10.85,1.9)) ;
#132790 = CARTESIAN_POINT('Origin',(-2.44929359829471E-16,10.85,2.)) ;
#132791 = CARTESIAN_POINT('',(2.32682891837997E-16,10.85,-1.9)) ;
#132792 = CARTESIAN_POINT('Origin',(0.,10.85,0.)) ;
#132793 = CARTESIAN_POINT('Origin',(0.,10.85,0.)) ;
#132794 = CARTESIAN_POINT('Origin',(11.0914213562373,0.,0.)) ;
#132795 = CARTESIAN_POINT('',(11.0207106781187,-1.80110112442984E-16,1.47071067811866)) ;
#132796 = CARTESIAN_POINT('Origin',(11.0207106781187,0.,0.)) ;
#132797 = CARTESIAN_POINT('',(11.0914213562373,-1.83697019872103E-16,1.5)) ;
#132798 = CARTESIAN_POINT('Origin',(11.0914213562373,-1.71450551880629E-16,
1.4)) ;
#132799 = CARTESIAN_POINT('Origin',(11.0914213562373,0.,0.)) ;
#132800 = CARTESIAN_POINT('Origin',(12.7,0.,0.)) ;
#132801 = CARTESIAN_POINT('',(12.8,-1.95943487863577E-16,-1.6)) ;
#132802 = CARTESIAN_POINT('Origin',(12.8,0.,0.)) ;
#132803 = CARTESIAN_POINT('',(12.7,-1.83697019872103E-16,-1.5)) ;
#132804 = CARTESIAN_POINT('Origin',(12.7,-1.95943487863577E-16,-1.6)) ;
#132805 = CARTESIAN_POINT('',(12.7,1.83697019872103E-16,1.5)) ;
#132806 = CARTESIAN_POINT('Origin',(12.7,0.,0.)) ;
#132807 = CARTESIAN_POINT('Origin',(12.7,0.,0.)) ;
#132808 = CARTESIAN_POINT('Origin',(12.7,2.1,1.38195395782836)) ;
#132809 = CARTESIAN_POINT('',(12.7,2.,1.38195395782836)) ;
#132810 = CARTESIAN_POINT('',(12.7,2.11643989873054,1.48059335021158)) ;
#132811 = CARTESIAN_POINT('Origin',(12.7,2.1,1.38195395782836)) ;
#132812 = CARTESIAN_POINT('',(12.8,2.13287979746107,1.57923274259479)) ;
#132813 = CARTESIAN_POINT('Origin',(12.7,2.13287979746107,1.57923274259479)) ;
#132814 = CARTESIAN_POINT('',(12.8,1.9,1.38195395782836)) ;
#132815 = CARTESIAN_POINT('Origin',(12.8,2.1,1.38195395782836)) ;
#132816 = CARTESIAN_POINT('Origin',(12.7,1.9,1.38195395782836)) ;
#132817 = CARTESIAN_POINT('Origin',(12.7,2.65,1.49304604217164)) ;
#132818 = CARTESIAN_POINT('',(12.7,2.63356010126947,1.39440664978842)) ;
#132819 = CARTESIAN_POINT('',(12.7,2.75,1.49304604217164)) ;
#132820 = CARTESIAN_POINT('Origin',(12.7,2.65,1.49304604217164)) ;
#132821 = CARTESIAN_POINT('',(12.8,2.65,1.49304604217164)) ;
#132822 = CARTESIAN_POINT('Origin',(12.7,2.65,1.49304604217164)) ;
#132823 = CARTESIAN_POINT('Origin',(12.7,2.65,1.49304604217164)) ;
#132824 = CARTESIAN_POINT('Origin',(4.5,2.1,1.38195395782836)) ;
#132825 = CARTESIAN_POINT('',(4.6,2.,1.38195395782836)) ;
#132826 = CARTESIAN_POINT('',(12.8,2.,1.38195395782836)) ;
#132827 = CARTESIAN_POINT('',(4.6,2.11643989873054,1.48059335021158)) ;
#132828 = CARTESIAN_POINT('Origin',(4.6,2.1,1.38195395782836)) ;
#132829 = CARTESIAN_POINT('',(4.5,2.11643989873054,1.48059335021158)) ;
#132830 = CARTESIAN_POINT('Origin',(12.7,2.65,-1.49304604217164)) ;
#132831 = CARTESIAN_POINT('',(12.8,2.65,-1.49304604217164)) ;
#132832 = CARTESIAN_POINT('',(12.7,2.63356010126947,-1.39440664978842)) ;
#132833 = CARTESIAN_POINT('Origin',(12.7,2.65,-1.49304604217164)) ;
#132834 = CARTESIAN_POINT('',(12.7,2.75,-1.49304604217164)) ;
#132835 = CARTESIAN_POINT('Origin',(12.7,2.65,-1.49304604217164)) ;
#132836 = CARTESIAN_POINT('Origin',(12.7,2.65,-1.49304604217164)) ;
#132837 = CARTESIAN_POINT('Origin',(11.05,0.,0.)) ;
#132838 = CARTESIAN_POINT('',(10.3,-9.1848509936051E-17,0.749999999999996)) ;
#132839 = CARTESIAN_POINT('Origin',(10.3,0.,0.)) ;
#132840 = CARTESIAN_POINT('',(11.05,-1.83697019872103E-16,1.5)) ;
#132841 = CARTESIAN_POINT('Origin',(11.05,0.,0.)) ;
#132842 = CARTESIAN_POINT('',(11.05,-1.83697019872103E-16,1.5)) ;
#132843 = CARTESIAN_POINT('Origin',(0.,9.95,0.)) ;
#132844 = CARTESIAN_POINT('',(0.218101234104781,9.95,-1.88744055580089)) ;
#132845 = CARTESIAN_POINT('',(-2.32682891837997E-16,9.95,-1.9)) ;
#132846 = CARTESIAN_POINT('Origin',(0.,9.95,0.)) ;
#132847 = CARTESIAN_POINT('',(0.321518176280636,9.85,-1.8725987456797)) ;
#132848 = CARTESIAN_POINT('Ctrl Pts',(0.218101234104784,9.95,-1.88744055580089)) ;
#132849 = CARTESIAN_POINT('Ctrl Pts',(0.231193919344581,9.95,-1.8859276441493)) ;
#132850 = CARTESIAN_POINT('Ctrl Pts',(0.245192892440025,9.94751445938575,
-1.88415658257392)) ;
#132851 = CARTESIAN_POINT('Ctrl Pts',(0.270990685773162,9.93716996065971,
-1.88062157894673)) ;
#132852 = CARTESIAN_POINT('Ctrl Pts',(0.282791986325045,9.92931613918426,
-1.87886070936675)) ;
#132853 = CARTESIAN_POINT('Ctrl Pts',(0.300953024019397,9.91135900604096,
-1.87603502666193)) ;
#132854 = CARTESIAN_POINT('Ctrl Pts',(0.308688523153917,9.90025653083842,
-1.87476256180095)) ;
#132855 = CARTESIAN_POINT('Ctrl Pts',(0.318969164829205,9.87583423571802,
-1.87304298667494)) ;
#132856 = CARTESIAN_POINT('Ctrl Pts',(0.321518176280638,9.86251584266313,
-1.8725987456797)) ;
#132857 = CARTESIAN_POINT('Ctrl Pts',(0.321518176280638,9.85,-1.8725987456797)) ;
#132858 = CARTESIAN_POINT('',(0.321518176280636,9.05,-1.8725987456797)) ;
#132859 = CARTESIAN_POINT('',(0.321518176280636,8.95,-1.8725987456797)) ;
#132860 = CARTESIAN_POINT('',(0.422455466606969,8.95,-1.85243930500675)) ;
#132861 = CARTESIAN_POINT('Ctrl Pts',(0.321518176280636,9.05,-1.8725987456797)) ;
#132862 = CARTESIAN_POINT('Ctrl Pts',(0.321518176280636,9.03744936090869,
-1.8725987456797)) ;
#132863 = CARTESIAN_POINT('Ctrl Pts',(0.324085473150911,9.02409774280079,
-1.87216456224267)) ;
#132864 = CARTESIAN_POINT('Ctrl Pts',(0.33438731365044,8.99960748025859,-1.87034985790769)) ;
#132865 = CARTESIAN_POINT('Ctrl Pts',(0.342122499456568,8.98846937989492,
-1.86896564206148)) ;
#132866 = CARTESIAN_POINT('Ctrl Pts',(0.360004521225396,8.97064401154629,
-1.86560497807954)) ;
#132867 = CARTESIAN_POINT('Ctrl Pts',(0.371447108749471,8.96285745107738,
-1.86338208404762)) ;
#132868 = CARTESIAN_POINT('Ctrl Pts',(0.396373979529698,8.95253508546271,
-1.85823730327889)) ;
#132869 = CARTESIAN_POINT('Ctrl Pts',(0.40985790199733,8.95,-1.85531222506458)) ;
#132870 = CARTESIAN_POINT('Ctrl Pts',(0.422455466606968,8.95,-1.85243930500675)) ;
#132871 = CARTESIAN_POINT('',(1.14750169623629,8.95,-1.51434469561419)) ;
#132872 = CARTESIAN_POINT('Origin',(0.,8.95,0.)) ;
#132873 = CARTESIAN_POINT('',(1.22782596331729,9.05,-1.449980483939)) ;
#132874 = CARTESIAN_POINT('Ctrl Pts',(1.14750169623629,8.95,-1.51434469561419)) ;
#132875 = CARTESIAN_POINT('Ctrl Pts',(1.15780003912542,8.95,-1.50654107866494)) ;
#132876 = CARTESIAN_POINT('Ctrl Pts',(1.16870807732935,8.95253508546271,-1.49809199882069)) ;
#132877 = CARTESIAN_POINT('Ctrl Pts',(1.18867189173408,8.96285745107738,-1.48230390930784)) ;
#132878 = CARTESIAN_POINT('Ctrl Pts',(1.19772988083811,8.97064401154629,-1.47496722746149)) ;
#132879 = CARTESIAN_POINT('Ctrl Pts',(1.21179864083581,8.98846937989492,-1.46342899722165)) ;
#132880 = CARTESIAN_POINT('Ctrl Pts',(1.21783109328768,8.99960748025859,-1.45839325791345)) ;
#132881 = CARTESIAN_POINT('Ctrl Pts',(1.22584313288946,9.02409774280079,-1.45166805970666)) ;
#132882 = CARTESIAN_POINT('Ctrl Pts',(1.22782596331729,9.03744936090869,-1.449980483939)) ;
#132883 = CARTESIAN_POINT('Ctrl Pts',(1.22782596331729,9.05,-1.449980483939)) ;
#132884 = CARTESIAN_POINT('',(1.22782596331729,9.85,-1.449980483939)) ;
#132885 = CARTESIAN_POINT('',(1.22782596331729,8.95,-1.449980483939)) ;
#132886 = CARTESIAN_POINT('',(1.30567057854876,9.95,-1.38029864171205)) ;
#132887 = CARTESIAN_POINT('Ctrl Pts',(1.22782596331729,9.85,-1.449980483939)) ;
#132888 = CARTESIAN_POINT('Ctrl Pts',(1.22782596331729,9.85579162428539,-1.449980483939)) ;
#132889 = CARTESIAN_POINT('Ctrl Pts',(1.22822745887816,9.86162764920015,-1.44964057146522)) ;
#132890 = CARTESIAN_POINT('Ctrl Pts',(1.22902753823169,9.86736607146313,-1.44896195467784)) ;
#132891 = CARTESIAN_POINT('Ctrl Pts',(1.22973095933684,9.87241123018669,-1.44836532214579)) ;
#132892 = CARTESIAN_POINT('Ctrl Pts',(1.23074168751918,9.87738020477702,-1.44750743025347)) ;
#132893 = CARTESIAN_POINT('Ctrl Pts',(1.23203099150182,9.88218322835582,-1.44640922147928)) ;
#132894 = CARTESIAN_POINT('Ctrl Pts',(1.23351897101726,9.88772637473068,-1.44514178402336)) ;
#132895 = CARTESIAN_POINT('Ctrl Pts',(1.2354014557903,9.89313280655104,-1.44353433657835)) ;
#132896 = CARTESIAN_POINT('Ctrl Pts',(1.23763252770622,9.89827011881554,-1.44161898274845)) ;
#132897 = CARTESIAN_POINT('Ctrl Pts',(1.23953000874363,9.90263929783464,-1.43999001348654)) ;
#132898 = CARTESIAN_POINT('Ctrl Pts',(1.2416786234546,9.90681364346947,-1.43813903119877)) ;
#132899 = CARTESIAN_POINT('Ctrl Pts',(1.24403025306866,9.91072825704926,-1.43610192167909)) ;
#132900 = CARTESIAN_POINT('Ctrl Pts',(1.24687926059923,9.91547082513966,-1.43363395634667)) ;
#132901 = CARTESIAN_POINT('Ctrl Pts',(1.25006974298105,9.91990270163234,-1.43085512653216)) ;
#132902 = CARTESIAN_POINT('Ctrl Pts',(1.2535194093265,9.92391762881323,-1.42782661463089)) ;
#132903 = CARTESIAN_POINT('Ctrl Pts',(1.25634620505522,9.92720762206753,-1.4253449298389)) ;
#132904 = CARTESIAN_POINT('Ctrl Pts',(1.25934609941474,9.93021806933732,-1.4226963101588)) ;
#132905 = CARTESIAN_POINT('Ctrl Pts',(1.26246241000318,9.9329120667973,-1.41992558372932)) ;
#132906 = CARTESIAN_POINT('Ctrl Pts',(1.26649145911191,9.93639511117205,-1.41634333718026)) ;
#132907 = CARTESIAN_POINT('Ctrl Pts',(1.27077652588474,9.93940081548806,-1.41250226252407)) ;
#132908 = CARTESIAN_POINT('Ctrl Pts',(1.27520851369618,9.94185862744776,-1.40848967391019)) ;
#132909 = CARTESIAN_POINT('Ctrl Pts',(1.27864718185098,9.9437655820866,-1.40537640707105)) ;
#132910 = CARTESIAN_POINT('Ctrl Pts',(1.2821736641873,9.94534362661778,-1.40216049976224)) ;
#132911 = CARTESIAN_POINT('Ctrl Pts',(1.28573335778226,9.94658081625577,-1.39888874922024)) ;
#132912 = CARTESIAN_POINT('Ctrl Pts',(1.29026904082681,9.94815721599755,-1.39471995686114)) ;
#132913 = CARTESIAN_POINT('Ctrl Pts',(1.29492021413414,9.9491996901822,-1.39040365182263)) ;
#132914 = CARTESIAN_POINT('Ctrl Pts',(1.29957290046265,9.9496832238817,-1.38604122438751)) ;
#132915 = CARTESIAN_POINT('Ctrl Pts',(1.30160833994478,9.94989475836166,-1.3841327662598)) ;
#132916 = CARTESIAN_POINT('Ctrl Pts',(1.30364403319565,9.95,-1.38221561863552)) ;
#132917 = CARTESIAN_POINT('Ctrl Pts',(1.30567057854876,9.95,-1.38029864171205)) ;
#132918 = CARTESIAN_POINT('',(-0.218101234104782,9.95,1.88744055580089)) ;
#132919 = CARTESIAN_POINT('Origin',(0.,9.95,0.)) ;
#132920 = CARTESIAN_POINT('',(-0.321518176280637,9.85,1.8725987456797)) ;
#132921 = CARTESIAN_POINT('Ctrl Pts',(-0.218101234104781,9.95,1.88744055580089)) ;
#132922 = CARTESIAN_POINT('Ctrl Pts',(-0.231193919344579,9.95,1.88592764414931)) ;
#132923 = CARTESIAN_POINT('Ctrl Pts',(-0.245192892440022,9.94751445938575,
1.88415658257392)) ;
#132924 = CARTESIAN_POINT('Ctrl Pts',(-0.27099068577316,9.93716996065971,
1.88062157894673)) ;
#132925 = CARTESIAN_POINT('Ctrl Pts',(-0.282791986325042,9.92931613918426,
1.87886070936675)) ;
#132926 = CARTESIAN_POINT('Ctrl Pts',(-0.300953024019395,9.91135900604096,
1.87603502666193)) ;
#132927 = CARTESIAN_POINT('Ctrl Pts',(-0.308688523153914,9.90025653083842,
1.87476256180095)) ;
#132928 = CARTESIAN_POINT('Ctrl Pts',(-0.318969164829203,9.87583423571802,
1.87304298667495)) ;
#132929 = CARTESIAN_POINT('Ctrl Pts',(-0.321518176280635,9.86251584266313,
1.8725987456797)) ;
#132930 = CARTESIAN_POINT('Ctrl Pts',(-0.321518176280635,9.85,1.8725987456797)) ;
#132931 = CARTESIAN_POINT('',(-0.321518176280637,9.05,1.8725987456797)) ;
#132932 = CARTESIAN_POINT('',(-0.321518176280637,8.95,1.8725987456797)) ;
#132933 = CARTESIAN_POINT('',(-0.422455466606969,8.95,1.85243930500675)) ;
#132934 = CARTESIAN_POINT('Ctrl Pts',(-0.321518176280636,9.05,1.8725987456797)) ;
#132935 = CARTESIAN_POINT('Ctrl Pts',(-0.321518176280636,9.03744936090869,
1.8725987456797)) ;
#132936 = CARTESIAN_POINT('Ctrl Pts',(-0.324085473150912,9.02409774280079,
1.87216456224267)) ;
#132937 = CARTESIAN_POINT('Ctrl Pts',(-0.334387313650441,8.99960748025859,
1.87034985790769)) ;
#132938 = CARTESIAN_POINT('Ctrl Pts',(-0.342122499456569,8.98846937989492,
1.86896564206148)) ;
#132939 = CARTESIAN_POINT('Ctrl Pts',(-0.360004521225397,8.97064401154629,
1.86560497807954)) ;
#132940 = CARTESIAN_POINT('Ctrl Pts',(-0.371447108749472,8.96285745107738,
1.86338208404762)) ;
#132941 = CARTESIAN_POINT('Ctrl Pts',(-0.396373979529699,8.95253508546271,
1.85823730327889)) ;
#132942 = CARTESIAN_POINT('Ctrl Pts',(-0.409857901997331,8.95,1.85531222506458)) ;
#132943 = CARTESIAN_POINT('Ctrl Pts',(-0.422455466606969,8.95,1.85243930500675)) ;
#132944 = CARTESIAN_POINT('',(-1.14750169623629,8.95,1.51434469561419)) ;
#132945 = CARTESIAN_POINT('Origin',(0.,8.95,0.)) ;
#132946 = CARTESIAN_POINT('',(-1.22782596331729,9.05,1.449980483939)) ;
#132947 = CARTESIAN_POINT('Ctrl Pts',(-1.14750169623629,8.95,1.51434469561419)) ;
#132948 = CARTESIAN_POINT('Ctrl Pts',(-1.15780003912542,8.95,1.50654107866494)) ;
#132949 = CARTESIAN_POINT('Ctrl Pts',(-1.16870807732935,8.95253508546271,
1.49809199882069)) ;
#132950 = CARTESIAN_POINT('Ctrl Pts',(-1.18867189173408,8.96285745107738,
1.48230390930784)) ;
#132951 = CARTESIAN_POINT('Ctrl Pts',(-1.19772988083811,8.97064401154629,
1.47496722746149)) ;
#132952 = CARTESIAN_POINT('Ctrl Pts',(-1.21179864083581,8.98846937989492,
1.46342899722165)) ;
#132953 = CARTESIAN_POINT('Ctrl Pts',(-1.21783109328768,8.99960748025859,
1.45839325791345)) ;
#132954 = CARTESIAN_POINT('Ctrl Pts',(-1.22584313288946,9.02409774280079,
1.45166805970666)) ;
#132955 = CARTESIAN_POINT('Ctrl Pts',(-1.22782596331729,9.03744936090869,
1.449980483939)) ;
#132956 = CARTESIAN_POINT('Ctrl Pts',(-1.22782596331729,9.05,1.449980483939)) ;
#132957 = CARTESIAN_POINT('',(-1.22782596331729,9.85,1.449980483939)) ;
#132958 = CARTESIAN_POINT('',(-1.22782596331729,8.95,1.449980483939)) ;
#132959 = CARTESIAN_POINT('',(-1.30567057854876,9.95,1.38029864171205)) ;
#132960 = CARTESIAN_POINT('Ctrl Pts',(-1.22782596331729,9.85,1.449980483939)) ;
#132961 = CARTESIAN_POINT('Ctrl Pts',(-1.22782596331729,9.85579162428539,
1.449980483939)) ;
#132962 = CARTESIAN_POINT('Ctrl Pts',(-1.22822745887816,9.86162764920014,
1.44964057146522)) ;
#132963 = CARTESIAN_POINT('Ctrl Pts',(-1.22902753823169,9.86736607146313,
1.44896195467784)) ;
#132964 = CARTESIAN_POINT('Ctrl Pts',(-1.22973095933683,9.87241123018669,
1.44836532214579)) ;
#132965 = CARTESIAN_POINT('Ctrl Pts',(-1.23074168751918,9.87738020477702,
1.44750743025347)) ;
#132966 = CARTESIAN_POINT('Ctrl Pts',(-1.23203099150181,9.88218322835582,
1.44640922147928)) ;
#132967 = CARTESIAN_POINT('Ctrl Pts',(-1.23351897101725,9.88772637473068,
1.44514178402336)) ;
#132968 = CARTESIAN_POINT('Ctrl Pts',(-1.2354014557903,9.89313280655104,1.44353433657835)) ;
#132969 = CARTESIAN_POINT('Ctrl Pts',(-1.23763252770622,9.89827011881554,
1.44161898274845)) ;
#132970 = CARTESIAN_POINT('Ctrl Pts',(-1.23953000874363,9.90263929783465,
1.43999001348654)) ;
#132971 = CARTESIAN_POINT('Ctrl Pts',(-1.24167862345459,9.90681364346947,
1.43813903119877)) ;
#132972 = CARTESIAN_POINT('Ctrl Pts',(-1.24403025306866,9.91072825704926,
1.43610192167908)) ;
#132973 = CARTESIAN_POINT('Ctrl Pts',(-1.24687926059922,9.91547082513966,
1.43363395634666)) ;
#132974 = CARTESIAN_POINT('Ctrl Pts',(-1.25006974298106,9.91990270163235,
1.43085512653216)) ;
#132975 = CARTESIAN_POINT('Ctrl Pts',(-1.2535194093265,9.92391762881324,1.42782661463088)) ;
#132976 = CARTESIAN_POINT('Ctrl Pts',(-1.25634620505523,9.92720762206753,
1.42534492983889)) ;
#132977 = CARTESIAN_POINT('Ctrl Pts',(-1.25934609941474,9.93021806933733,
1.42269631015879)) ;
#132978 = CARTESIAN_POINT('Ctrl Pts',(-1.26246241000317,9.9329120667973,1.41992558372931)) ;
#132979 = CARTESIAN_POINT('Ctrl Pts',(-1.26649145911191,9.93639511117205,
1.41634333718025)) ;
#132980 = CARTESIAN_POINT('Ctrl Pts',(-1.27077652588474,9.93940081548806,
1.41250226252406)) ;
#132981 = CARTESIAN_POINT('Ctrl Pts',(-1.27520851369618,9.94185862744776,
1.40848967391019)) ;
#132982 = CARTESIAN_POINT('Ctrl Pts',(-1.27864718185098,9.94376558208661,
1.40537640707104)) ;
#132983 = CARTESIAN_POINT('Ctrl Pts',(-1.2821736641873,9.94534362661778,1.40216049976224)) ;
#132984 = CARTESIAN_POINT('Ctrl Pts',(-1.28573335778225,9.94658081625577,
1.39888874922024)) ;
#132985 = CARTESIAN_POINT('Ctrl Pts',(-1.29026904082681,9.94815721599755,
1.39471995686114)) ;
#132986 = CARTESIAN_POINT('Ctrl Pts',(-1.29492021413415,9.9491996901822,1.39040365182262)) ;
#132987 = CARTESIAN_POINT('Ctrl Pts',(-1.29957290046265,9.9496832238817,1.3860412243875)) ;
#132988 = CARTESIAN_POINT('Ctrl Pts',(-1.30160833994478,9.94989475836166,
1.38413276625978)) ;
#132989 = CARTESIAN_POINT('Ctrl Pts',(-1.30364403319566,9.95,1.38221561863551)) ;
#132990 = CARTESIAN_POINT('Ctrl Pts',(-1.30567057854876,9.95,1.38029864171205)) ;
#132991 = CARTESIAN_POINT('Origin',(0.,9.95,0.)) ;
#132992 = CARTESIAN_POINT('',(-2.32682891837997E-16,9.95,-1.9)) ;
#132993 = CARTESIAN_POINT('Origin',(3.95,3.75,2.54)) ;
#132994 = CARTESIAN_POINT('',(3.95,3.77568567655479,-7.62)) ;
#132995 = CARTESIAN_POINT('',(3.95,6.92431432344521,-7.62)) ;
#132996 = CARTESIAN_POINT('',(3.95,3.75,-7.62)) ;
#132997 = CARTESIAN_POINT('',(3.95,6.92431432344521,2.54)) ;
#132998 = CARTESIAN_POINT('',(3.95,6.92431432344521,2.54)) ;
#132999 = CARTESIAN_POINT('',(3.95,3.77568567655479,2.54)) ;
#133000 = CARTESIAN_POINT('',(3.95,3.75,2.54)) ;
#133001 = CARTESIAN_POINT('',(3.95,3.77568567655479,-2.54)) ;
#133002 = CARTESIAN_POINT('',(3.95,4.6,-1.275)) ;
#133003 = CARTESIAN_POINT('',(3.95,4.4,-1.475)) ;
#133004 = CARTESIAN_POINT('Origin',(3.95,4.6,-1.475)) ;
#133005 = CARTESIAN_POINT('',(3.95,5.88396692803319,-1.275)) ;
#133006 = CARTESIAN_POINT('',(3.95,3.75,-1.275)) ;
#133007 = CARTESIAN_POINT('',(3.95,6.08618232569815,-1.475)) ;
#133008 = CARTESIAN_POINT('Ctrl Pts',(3.95,6.08618232569815,-1.475)) ;
#133009 = CARTESIAN_POINT('Ctrl Pts',(3.95,6.08618232225605,-1.36605743722782)) ;
#133010 = CARTESIAN_POINT('Ctrl Pts',(3.95,5.99411624638819,-1.27500000329373)) ;
#133011 = CARTESIAN_POINT('Ctrl Pts',(3.95,5.88396692803319,-1.275)) ;
#133012 = CARTESIAN_POINT('',(3.95,6.08618232569815,-2.775)) ;
#133013 = CARTESIAN_POINT('',(3.95,6.08618232569815,2.54)) ;
#133014 = CARTESIAN_POINT('',(3.95,5.88396692803319,-2.975)) ;
#133015 = CARTESIAN_POINT('Ctrl Pts',(3.95,5.88396692803319,-2.975)) ;
#133016 = CARTESIAN_POINT('Ctrl Pts',(3.95,5.99411624638818,-2.97499999670621)) ;
#133017 = CARTESIAN_POINT('Ctrl Pts',(3.95,6.08618232225605,-2.88394256277222)) ;
#133018 = CARTESIAN_POINT('Ctrl Pts',(3.95,6.08618232569815,-2.775)) ;
#133019 = CARTESIAN_POINT('',(3.95,4.6,-2.975)) ;
#133020 = CARTESIAN_POINT('',(3.95,4.5,-2.975)) ;
#133021 = CARTESIAN_POINT('',(3.95,4.4,-2.775)) ;
#133022 = CARTESIAN_POINT('Origin',(3.95,4.6,-2.775)) ;
#133023 = CARTESIAN_POINT('',(3.95,4.4,2.54)) ;
#133024 = CARTESIAN_POINT('Origin',(3.4,7.95,2.54)) ;
#133025 = CARTESIAN_POINT('',(3.34087287789487,7.95,2.04)) ;
#133026 = CARTESIAN_POINT('',(3.,7.95,2.04)) ;
#133027 = CARTESIAN_POINT('',(3.4,7.95,2.04)) ;
#133028 = CARTESIAN_POINT('',(3.34087287789487,7.95,-7.62)) ;
#133029 = CARTESIAN_POINT('',(3.34087287789487,7.95,2.54)) ;
#133030 = CARTESIAN_POINT('',(3.,7.95,-7.62)) ;
#133031 = CARTESIAN_POINT('',(3.4,7.95,-7.62)) ;
#133032 = CARTESIAN_POINT('',(3.,7.95,2.54)) ;
#133033 = CARTESIAN_POINT('Origin',(2.9,7.95,2.54)) ;
#133034 = CARTESIAN_POINT('',(2.9,8.05,2.04)) ;
#133035 = CARTESIAN_POINT('',(2.9,9.85,2.04)) ;
#133036 = CARTESIAN_POINT('',(2.9,10.05,2.04)) ;
#133037 = CARTESIAN_POINT('',(2.9,8.05,-7.62)) ;
#133038 = CARTESIAN_POINT('',(2.9,8.05,-2.54)) ;
#133039 = CARTESIAN_POINT('',(2.9,9.85,-7.62)) ;
#133040 = CARTESIAN_POINT('',(2.9,7.95,-7.62)) ;
#133041 = CARTESIAN_POINT('',(2.9,9.85,2.54)) ;
#133042 = CARTESIAN_POINT('Origin',(2.9,9.95,2.54)) ;
#133043 = CARTESIAN_POINT('',(3.,9.95,2.04)) ;
#133044 = CARTESIAN_POINT('',(3.3,9.95,2.04)) ;
#133045 = CARTESIAN_POINT('',(2.9,9.95,2.04)) ;
#133046 = CARTESIAN_POINT('',(3.,9.95,-7.62)) ;
#133047 = CARTESIAN_POINT('',(3.,9.95,-2.54)) ;
#133048 = CARTESIAN_POINT('',(3.3,9.95,-7.62)) ;
#133049 = CARTESIAN_POINT('',(2.9,9.95,-7.62)) ;
#133050 = CARTESIAN_POINT('',(3.3,9.95,2.54)) ;
#133051 = CARTESIAN_POINT('Origin',(3.3,10.05,2.54)) ;
#133052 = CARTESIAN_POINT('',(3.4,10.05,2.04)) ;
#133053 = CARTESIAN_POINT('',(3.4,10.05,-7.62)) ;
#133054 = CARTESIAN_POINT('',(3.4,10.05,2.54)) ;
#133055 = CARTESIAN_POINT('Origin',(3.3,10.05,2.04)) ;
#133056 = CARTESIAN_POINT('Origin',(3.3,10.05,-7.62)) ;
#133057 = CARTESIAN_POINT('Origin',(3.,9.85,2.54)) ;
#133058 = CARTESIAN_POINT('Origin',(3.,9.85,2.04)) ;
#133059 = CARTESIAN_POINT('Origin',(3.,9.85,-7.62)) ;
#133060 = CARTESIAN_POINT('Origin',(3.,8.05,2.54)) ;
#133061 = CARTESIAN_POINT('Origin',(3.,8.05,2.04)) ;
#133062 = CARTESIAN_POINT('Origin',(3.,8.05,-7.62)) ;
#133063 = CARTESIAN_POINT('Origin',(3.34087287789487,7.85,2.54)) ;
#133064 = CARTESIAN_POINT('',(3.4,7.93064727789309,2.04)) ;
#133065 = CARTESIAN_POINT('Origin',(3.34087287789487,7.85,2.04)) ;
#133066 = CARTESIAN_POINT('',(3.4,7.93064727789309,2.54)) ;
#133067 = CARTESIAN_POINT('',(3.4,7.93064727789309,2.54)) ;
#133068 = CARTESIAN_POINT('',(3.42849446876253,7.89819187497721,2.54)) ;
#133069 = CARTESIAN_POINT('Origin',(3.34087287789487,7.85,2.54)) ;
#133070 = CARTESIAN_POINT('',(3.42849446876253,7.89819187497721,-7.62)) ;
#133071 = CARTESIAN_POINT('',(3.42849446876253,7.89819187497721,2.54)) ;
#133072 = CARTESIAN_POINT('Origin',(3.34087287789487,7.85,-7.62)) ;
#133073 = CARTESIAN_POINT('Origin',(4.5,-2.8,2.54)) ;
#133074 = CARTESIAN_POINT('',(4.5,-2.4,-1.96214168703486)) ;
#133075 = CARTESIAN_POINT('',(4.5,-2.7,-1.52315462117279)) ;
#133076 = CARTESIAN_POINT('Origin',(4.5,0.,0.)) ;
#133077 = CARTESIAN_POINT('',(4.5,-2.7,-3.55684537882722)) ;
#133078 = CARTESIAN_POINT('',(4.5,-2.7,2.54)) ;
#133079 = CARTESIAN_POINT('',(4.5,-2.4,-3.11785831296514)) ;
#133080 = CARTESIAN_POINT('Origin',(4.5,0.,-5.08)) ;
#133081 = CARTESIAN_POINT('',(4.5,-2.4,-1.92613602842582)) ;
#133082 = CARTESIAN_POINT('Origin',(4.5,-2.3,2.54)) ;
#133083 = CARTESIAN_POINT('',(4.6,-2.3,2.54)) ;
#133084 = CARTESIAN_POINT('',(12.7,-2.3,2.54)) ;
#133085 = CARTESIAN_POINT('',(4.5,-2.3,2.54)) ;
#133086 = CARTESIAN_POINT('',(4.6,-2.3,1.96214168703486)) ;
#133087 = CARTESIAN_POINT('',(4.6,-2.3,1.92613602842582)) ;
#133088 = CARTESIAN_POINT('',(12.7,-2.3,1.96214168703486)) ;
#133089 = CARTESIAN_POINT('',(4.5,-2.3,1.96214168703486)) ;
#133090 = CARTESIAN_POINT('',(12.7,-2.3,2.54)) ;
#133091 = CARTESIAN_POINT('Origin',(12.8,2.75,2.54)) ;
#133092 = CARTESIAN_POINT('',(12.7,2.75,2.54)) ;
#133093 = CARTESIAN_POINT('',(4.55912712210513,2.75,-3.58695395782836)) ;
#133094 = CARTESIAN_POINT('',(12.8,2.75,-3.58695395782836)) ;
#133095 = CARTESIAN_POINT('',(4.55912712210513,2.75,-1.49304604217164)) ;
#133096 = CARTESIAN_POINT('',(4.55912712210514,2.75,-1.49304604217164)) ;
#133097 = CARTESIAN_POINT('',(12.8,2.75,-1.49304604217164)) ;
#133098 = CARTESIAN_POINT('Origin',(0.,9.95,0.)) ;
#133099 = CARTESIAN_POINT('',(0.230887397576971,9.95,-1.91486057185377)) ;
#133100 = CARTESIAN_POINT('Origin',(12.8,-2.3,2.54)) ;
#133101 = CARTESIAN_POINT('',(12.8,-2.3359925337019,2.32404479778862)) ;
#133102 = CARTESIAN_POINT('',(12.8,2.65,2.54)) ;
#133103 = CARTESIAN_POINT('',(12.8,2.65,2.54)) ;
#133104 = CARTESIAN_POINT('',(12.8,-2.2,2.54)) ;
#133105 = CARTESIAN_POINT('',(12.8,-2.3,2.54)) ;
#133106 = CARTESIAN_POINT('',(12.8,-2.2,1.96214168703486)) ;
#133107 = CARTESIAN_POINT('',(12.8,-2.2,2.54)) ;
#133108 = CARTESIAN_POINT('',(12.8,-2.24516129032258,1.83555190077454)) ;
#133109 = CARTESIAN_POINT('Origin',(12.8,-2.4,1.96214168703486)) ;
#133110 = CARTESIAN_POINT('',(12.8,-2.24516129032258,-1.83555190077454)) ;
#133111 = CARTESIAN_POINT('Origin',(12.8,0.,0.)) ;
#133112 = CARTESIAN_POINT('',(12.8,-2.2,-1.96214168703486)) ;
#133113 = CARTESIAN_POINT('Origin',(12.8,-2.4,-1.96214168703486)) ;
#133114 = CARTESIAN_POINT('',(12.8,-2.2,-3.11785831296514)) ;
#133115 = CARTESIAN_POINT('',(12.8,-2.2,2.54)) ;
#133116 = CARTESIAN_POINT('',(12.8,-2.24516129032258,-3.24444809922546)) ;
#133117 = CARTESIAN_POINT('Origin',(12.8,-2.4,-3.11785831296514)) ;
#133118 = CARTESIAN_POINT('',(12.8,-2.24516129032258,-6.91555190077455)) ;
#133119 = CARTESIAN_POINT('Origin',(12.8,0.,-5.08)) ;
#133120 = CARTESIAN_POINT('',(12.8,-2.2,-7.04214168703486)) ;
#133121 = CARTESIAN_POINT('Origin',(12.8,-2.4,-7.04214168703486)) ;
#133122 = CARTESIAN_POINT('',(12.8,-2.2,-7.62)) ;
#133123 = CARTESIAN_POINT('',(12.8,-2.2,-2.54)) ;
#133124 = CARTESIAN_POINT('',(12.8,2.65,-7.62)) ;
#133125 = CARTESIAN_POINT('',(12.8,-2.3,-7.62)) ;
#133126 = CARTESIAN_POINT('',(12.8,2.65,-2.54)) ;
#133127 = CARTESIAN_POINT('',(12.8,2.13287979746107,-6.65923274259479)) ;
#133128 = CARTESIAN_POINT('',(12.8,-1.51220874991811,-7.26674750049132)) ;
#133129 = CARTESIAN_POINT('',(12.8,1.9,-6.46195395782836)) ;
#133130 = CARTESIAN_POINT('Origin',(12.8,2.1,-6.46195395782836)) ;
#133131 = CARTESIAN_POINT('',(12.8,1.9,-2.54)) ;
#133132 = CARTESIAN_POINT('',(12.8,-2.3359925337019,-2.75595520221138)) ;
#133133 = CARTESIAN_POINT('',(12.8,2.65,2.54)) ;
#133134 = CARTESIAN_POINT('',(12.8,2.13287979746107,-1.57923274259479)) ;
#133135 = CARTESIAN_POINT('',(12.8,-1.51220874991811,-2.18674750049132)) ;
#133136 = CARTESIAN_POINT('',(12.8,1.9,-1.38195395782836)) ;
#133137 = CARTESIAN_POINT('Origin',(12.8,2.1,-1.38195395782836)) ;
#133138 = CARTESIAN_POINT('',(12.8,1.9,2.54)) ;
#133139 = CARTESIAN_POINT('Origin',(12.8,2.75,2.54)) ;
#133140 = CARTESIAN_POINT('',(4.55912712210513,2.75,1.49304604217164)) ;
#133141 = CARTESIAN_POINT('',(12.8,2.75,1.49304604217164)) ;
#133142 = CARTESIAN_POINT('',(4.55912712210514,2.75,2.54)) ;
#133143 = CARTESIAN_POINT('',(4.55912712210514,2.75,2.54)) ;
#133144 = CARTESIAN_POINT('',(12.7,2.75,2.54)) ;
#133145 = CARTESIAN_POINT('',(12.8,2.75,2.54)) ;
#133146 = CARTESIAN_POINT('',(12.7,2.75,2.54)) ;
#133147 = CARTESIAN_POINT('Origin',(4.5,2.75,2.54)) ;
#133148 = CARTESIAN_POINT('',(4.47150553123747,2.80180812502278,2.54)) ;
#133149 = CARTESIAN_POINT('',(3.96237840913234,3.72749380157757,2.54)) ;
#133150 = CARTESIAN_POINT('',(4.5,2.75,2.54)) ;
#133151 = CARTESIAN_POINT('',(4.47150553123747,2.80180812502279,1.49304604217164)) ;
#133152 = CARTESIAN_POINT('',(4.47150553123747,2.80180812502278,1.49304604217164)) ;
#133153 = CARTESIAN_POINT('',(4.48762159086767,2.77250619842243,1.38882431825052)) ;
#133154 = CARTESIAN_POINT('Origin',(4.56263299594614,2.63612182555249,1.48339970590384)) ;
#133155 = CARTESIAN_POINT('',(4.48762159086767,2.77250619842243,-1.38882431824783)) ;
#133156 = CARTESIAN_POINT('',(4.48762159086767,2.77250619842243,2.54)) ;
#133157 = CARTESIAN_POINT('',(4.47150553123747,2.80180812502279,-1.49304604217164)) ;
#133158 = CARTESIAN_POINT('Origin',(4.5626329959691,2.63612182551074,-1.48339970589483)) ;
#133159 = CARTESIAN_POINT('',(4.47150553123747,2.80180812502279,-3.58695395782836)) ;
#133160 = CARTESIAN_POINT('',(4.47150553123747,2.80180812502278,-2.54)) ;
#133161 = CARTESIAN_POINT('',(4.48762159086767,2.77250619842243,-3.69117568174948)) ;
#133162 = CARTESIAN_POINT('Origin',(4.56263299594449,2.63612182555554,-3.59660029409665)) ;
#133163 = CARTESIAN_POINT('',(4.48762159086767,2.77250619842243,-6.46882431824783)) ;
#133164 = CARTESIAN_POINT('',(4.48762159086767,2.77250619842243,-2.54)) ;
#133165 = CARTESIAN_POINT('',(4.47150553123747,2.80180812502279,-6.57304604217164)) ;
#133166 = CARTESIAN_POINT('Origin',(4.56263299596772,2.63612182551324,-6.56339970589523)) ;
#133167 = CARTESIAN_POINT('',(4.47150553123747,2.80180812502278,-7.62)) ;
#133168 = CARTESIAN_POINT('',(4.47150553123747,2.80180812502278,-7.62)) ;
#133169 = CARTESIAN_POINT('',(3.96237840913234,3.72749380157757,-7.62)) ;
#133170 = CARTESIAN_POINT('',(4.5,2.75,-7.62)) ;
#133171 = CARTESIAN_POINT('',(3.96237840913234,3.72749380157757,2.54)) ;
#133172 = CARTESIAN_POINT('Origin',(3.95,6.95,2.54)) ;
#133173 = CARTESIAN_POINT('',(3.93762159086767,6.97250619842243,2.54)) ;
#133174 = CARTESIAN_POINT('',(3.93762159086767,6.97250619842243,-7.62)) ;
#133175 = CARTESIAN_POINT('',(3.93762159086767,6.97250619842243,2.54)) ;
#133176 = CARTESIAN_POINT('',(3.95,6.95,-7.62)) ;
#133177 = CARTESIAN_POINT('',(3.95,6.95,2.54)) ;
#133178 = CARTESIAN_POINT('Origin',(3.4,9.95,2.54)) ;
#133179 = CARTESIAN_POINT('',(3.4,10.85,-7.62)) ;
#133180 = CARTESIAN_POINT('',(3.4,9.95,-7.62)) ;
#133181 = CARTESIAN_POINT('',(3.4,10.85,2.54)) ;
#133182 = CARTESIAN_POINT('',(3.4,10.85,2.54)) ;
#133183 = CARTESIAN_POINT('',(3.4,9.95,2.54)) ;
#133184 = CARTESIAN_POINT('',(3.4,10.05,2.04)) ;
#133185 = CARTESIAN_POINT('Origin',(3.4,10.95,2.54)) ;
#133186 = CARTESIAN_POINT('',(3.3,10.95,2.54)) ;
#133187 = CARTESIAN_POINT('',(3.3,10.95,-7.62)) ;
#133188 = CARTESIAN_POINT('',(3.3,10.95,2.54)) ;
#133189 = CARTESIAN_POINT('',(-4.8,10.95,-7.62)) ;
#133190 = CARTESIAN_POINT('',(3.4,10.95,-7.62)) ;
#133191 = CARTESIAN_POINT('',(-4.8,10.95,2.54)) ;
#133192 = CARTESIAN_POINT('',(-4.8,10.95,2.54)) ;
#133193 = CARTESIAN_POINT('',(3.4,10.95,2.54)) ;
#133194 = CARTESIAN_POINT('',(-2.55,10.95,-5.98)) ;
#133195 = CARTESIAN_POINT('',(-2.75,10.95,-6.18)) ;
#133196 = CARTESIAN_POINT('Origin',(-2.75,10.95,-5.98)) ;
#133197 = CARTESIAN_POINT('',(-2.55,10.95,-4.18)) ;
#133198 = CARTESIAN_POINT('',(-2.55,10.95,-2.54)) ;
#133199 = CARTESIAN_POINT('',(-2.75,10.95,-3.98)) ;
#133200 = CARTESIAN_POINT('Origin',(-2.75,10.95,-4.18)) ;
#133201 = CARTESIAN_POINT('',(-3.8,10.95,-3.98)) ;
#133202 = CARTESIAN_POINT('',(3.4,10.95,-3.98)) ;
#133203 = CARTESIAN_POINT('',(-4.,10.95,-4.18)) ;
#133204 = CARTESIAN_POINT('Origin',(-3.8,10.95,-4.18)) ;
#133205 = CARTESIAN_POINT('',(-4.,10.95,-5.98)) ;
#133206 = CARTESIAN_POINT('',(-4.,10.95,-2.54)) ;
#133207 = CARTESIAN_POINT('',(-3.8,10.95,-6.18)) ;
#133208 = CARTESIAN_POINT('Origin',(-3.8,10.95,-5.98)) ;
#133209 = CARTESIAN_POINT('',(3.4,10.95,-6.18)) ;
#133210 = CARTESIAN_POINT('',(-2.55,10.95,-0.900000000000001)) ;
#133211 = CARTESIAN_POINT('',(-2.75,10.95,-1.1)) ;
#133212 = CARTESIAN_POINT('Origin',(-2.75,10.95,-0.900000000000001)) ;
#133213 = CARTESIAN_POINT('',(-2.55,10.95,0.899999999999999)) ;
#133214 = CARTESIAN_POINT('',(-2.55,10.95,2.54)) ;
#133215 = CARTESIAN_POINT('',(-2.75,10.95,1.1)) ;
#133216 = CARTESIAN_POINT('Origin',(-2.75,10.95,0.899999999999999)) ;
#133217 = CARTESIAN_POINT('',(-3.8,10.95,1.1)) ;
#133218 = CARTESIAN_POINT('',(3.4,10.95,1.1)) ;
#133219 = CARTESIAN_POINT('',(-4.,10.95,0.9)) ;
#133220 = CARTESIAN_POINT('Origin',(-3.8,10.95,0.9)) ;
#133221 = CARTESIAN_POINT('',(-4.,10.95,-0.9)) ;
#133222 = CARTESIAN_POINT('',(-4.,10.95,2.54)) ;
#133223 = CARTESIAN_POINT('',(-3.8,10.95,-1.1)) ;
#133224 = CARTESIAN_POINT('Origin',(-3.8,10.95,-0.9)) ;
#133225 = CARTESIAN_POINT('',(3.4,10.95,-1.1)) ;
#133226 = CARTESIAN_POINT('Origin',(-4.9,10.95,2.54)) ;
#133227 = CARTESIAN_POINT('',(-4.9,10.85,2.54)) ;
#133228 = CARTESIAN_POINT('',(-4.9,10.85,-7.62)) ;
#133229 = CARTESIAN_POINT('',(-4.9,10.85,2.54)) ;
#133230 = CARTESIAN_POINT('',(-4.9,10.3,-7.62)) ;
#133231 = CARTESIAN_POINT('',(-4.9,10.95,-7.62)) ;
#133232 = CARTESIAN_POINT('',(-4.9,10.3,2.54)) ;
#133233 = CARTESIAN_POINT('',(-4.9,10.3,2.54)) ;
#133234 = CARTESIAN_POINT('',(-4.9,10.95,2.54)) ;
#133235 = CARTESIAN_POINT('Origin',(-4.9,10.2,2.54)) ;
#133236 = CARTESIAN_POINT('',(-4.8,10.2,2.54)) ;
#133237 = CARTESIAN_POINT('',(-4.8,10.2,-7.62)) ;
#133238 = CARTESIAN_POINT('',(-4.8,10.2,2.54)) ;
#133239 = CARTESIAN_POINT('',(-4.9,10.2,-7.62)) ;
#133240 = CARTESIAN_POINT('',(-4.9,10.2,2.54)) ;
#133241 = CARTESIAN_POINT('Origin',(-4.4,10.2,2.54)) ;
#133242 = CARTESIAN_POINT('',(-5.39805806756909,5.20970966215454,-7.62)) ;
#133243 = CARTESIAN_POINT('',(-4.4,10.2,-7.62)) ;
#133244 = CARTESIAN_POINT('',(-5.39805806756909,5.20970966215454,2.54)) ;
#133245 = CARTESIAN_POINT('',(-5.39805806756909,5.20970966215454,2.54)) ;
#133246 = CARTESIAN_POINT('',(-4.4,10.2,2.54)) ;
#133247 = CARTESIAN_POINT('Origin',(-5.4,5.2,2.54)) ;
#133248 = CARTESIAN_POINT('',(-5.4,5.19009804864072,2.54)) ;
#133249 = CARTESIAN_POINT('',(-5.4,5.19009804864072,-7.62)) ;
#133250 = CARTESIAN_POINT('',(-5.4,5.19009804864072,2.54)) ;
#133251 = CARTESIAN_POINT('',(-5.4,-3.95,-7.62)) ;
#133252 = CARTESIAN_POINT('',(-5.4,5.2,-7.62)) ;
#133253 = CARTESIAN_POINT('',(-5.4,-3.95,2.54)) ;
#133254 = CARTESIAN_POINT('',(-5.4,-3.95,2.54)) ;
#133255 = CARTESIAN_POINT('',(-5.4,5.2,2.54)) ;
#133256 = CARTESIAN_POINT('',(-5.4,4.23801993223491,-6.98)) ;
#133257 = CARTESIAN_POINT('',(-5.4,4.23801993223491,-3.18)) ;
#133258 = CARTESIAN_POINT('',(-5.4,4.23801993223491,-3.08)) ;
#133259 = CARTESIAN_POINT('',(-5.4,3.9369800677651,-2.98)) ;
#133260 = CARTESIAN_POINT('Ctrl Pts',(-5.4,4.23801993223491,-3.18)) ;
#133261 = CARTESIAN_POINT('Ctrl Pts',(-5.4,4.23801992976516,-3.12749312809026)) ;
#133262 = CARTESIAN_POINT('Ctrl Pts',(-5.4,4.20557579169425,-3.07560257376825)) ;
#133263 = CARTESIAN_POINT('Ctrl Pts',(-5.4,4.09411900298411,-3.00155471375713)) ;
#133264 = CARTESIAN_POINT('Ctrl Pts',(-5.4,4.0160133758189,-2.98000000048114)) ;
#133265 = CARTESIAN_POINT('Ctrl Pts',(-5.4,3.9369800677651,-2.98)) ;
#133266 = CARTESIAN_POINT('',(-5.4,-1.88819660112502,-2.98)) ;
#133267 = CARTESIAN_POINT('',(-5.4,-2.05,-2.98)) ;
#133268 = CARTESIAN_POINT('',(-5.4,-2.11180339887499,-3.18)) ;
#133269 = CARTESIAN_POINT('Ctrl Pts',(-5.4,-2.11180339887499,-3.18)) ;
#133270 = CARTESIAN_POINT('Ctrl Pts',(-5.4,-2.11180339704051,-3.12749316010866)) ;
#133271 = CARTESIAN_POINT('Ctrl Pts',(-5.4,-2.0877044485962,-3.07560253112148)) ;
#133272 = CARTESIAN_POINT('Ctrl Pts',(-5.4,-2.00491651967066,-3.0015547564039)) ;
#133273 = CARTESIAN_POINT('Ctrl Pts',(-5.4,-1.946901032774,-2.98000000117411)) ;
#133274 = CARTESIAN_POINT('Ctrl Pts',(-5.4,-1.88819660112502,-2.98)) ;
#133275 = CARTESIAN_POINT('',(-5.4,-2.11180339887499,-6.98)) ;
#133276 = CARTESIAN_POINT('',(-5.4,-2.11180339887499,-7.08)) ;
#133277 = CARTESIAN_POINT('',(-5.4,-1.88819660112501,-7.18)) ;
#133278 = CARTESIAN_POINT('Ctrl Pts',(-5.4,-1.88819660112501,-7.18)) ;
#133279 = CARTESIAN_POINT('Ctrl Pts',(-5.4,-1.946901032774,-7.17999999882592)) ;
#133280 = CARTESIAN_POINT('Ctrl Pts',(-5.4,-2.00491651967066,-7.1584452435961)) ;
#133281 = CARTESIAN_POINT('Ctrl Pts',(-5.4,-2.0877044485962,-7.08439746887852)) ;
#133282 = CARTESIAN_POINT('Ctrl Pts',(-5.4,-2.11180339704051,-7.03250683989134)) ;
#133283 = CARTESIAN_POINT('Ctrl Pts',(-5.4,-2.11180339887499,-6.98)) ;
#133284 = CARTESIAN_POINT('',(-5.4,3.9369800677651,-7.18)) ;
#133285 = CARTESIAN_POINT('',(-5.4,4.20000000000001,-7.18)) ;
#133286 = CARTESIAN_POINT('Ctrl Pts',(-5.4,3.9369800677651,-7.18)) ;
#133287 = CARTESIAN_POINT('Ctrl Pts',(-5.4,4.01601337581889,-7.17999999951891)) ;
#133288 = CARTESIAN_POINT('Ctrl Pts',(-5.4,4.09411900298413,-7.15844528624287)) ;
#133289 = CARTESIAN_POINT('Ctrl Pts',(-5.4,4.20557579169423,-7.08439742623175)) ;
#133290 = CARTESIAN_POINT('Ctrl Pts',(-5.4,4.23801992976516,-7.03250687190974)) ;
#133291 = CARTESIAN_POINT('Ctrl Pts',(-5.4,4.23801993223491,-6.98)) ;
#133292 = CARTESIAN_POINT('',(-5.4,4.23801993223491,-1.9)) ;
#133293 = CARTESIAN_POINT('',(-5.4,4.23801993223491,1.9)) ;
#133294 = CARTESIAN_POINT('',(-5.4,4.23801993223491,2.)) ;
#133295 = CARTESIAN_POINT('',(-5.4,3.9369800677651,2.1)) ;
#133296 = CARTESIAN_POINT('Ctrl Pts',(-5.4,4.23801993223491,1.9)) ;
#133297 = CARTESIAN_POINT('Ctrl Pts',(-5.4,4.23801992976516,1.95250687190974)) ;
#133298 = CARTESIAN_POINT('Ctrl Pts',(-5.4,4.20557579169425,2.00439742623175)) ;
#133299 = CARTESIAN_POINT('Ctrl Pts',(-5.4,4.09411900298411,2.07844528624287)) ;
#133300 = CARTESIAN_POINT('Ctrl Pts',(-5.4,4.01601337581891,2.09999999951886)) ;
#133301 = CARTESIAN_POINT('Ctrl Pts',(-5.4,3.9369800677651,2.1)) ;
#133302 = CARTESIAN_POINT('',(-5.4,-1.88819660112502,2.1)) ;
#133303 = CARTESIAN_POINT('',(-5.4,-2.05,2.1)) ;
#133304 = CARTESIAN_POINT('',(-5.4,-2.11180339887499,1.9)) ;
#133305 = CARTESIAN_POINT('Ctrl Pts',(-5.4,-2.11180339887499,1.9)) ;
#133306 = CARTESIAN_POINT('Ctrl Pts',(-5.4,-2.11180339704051,1.95250683989134)) ;
#133307 = CARTESIAN_POINT('Ctrl Pts',(-5.4,-2.0877044485962,2.00439746887852)) ;
#133308 = CARTESIAN_POINT('Ctrl Pts',(-5.4,-2.00491651967066,2.0784452435961)) ;
#133309 = CARTESIAN_POINT('Ctrl Pts',(-5.4,-1.946901032774,2.09999999882593)) ;
#133310 = CARTESIAN_POINT('Ctrl Pts',(-5.4,-1.88819660112502,2.1)) ;
#133311 = CARTESIAN_POINT('',(-5.4,-2.11180339887499,-1.9)) ;
#133312 = CARTESIAN_POINT('',(-5.4,-2.11180339887499,-2.)) ;
#133313 = CARTESIAN_POINT('',(-5.4,-1.88819660112501,-2.1)) ;
#133314 = CARTESIAN_POINT('Ctrl Pts',(-5.4,-1.88819660112501,-2.1)) ;
#133315 = CARTESIAN_POINT('Ctrl Pts',(-5.4,-1.946901032774,-2.09999999882593)) ;
#133316 = CARTESIAN_POINT('Ctrl Pts',(-5.4,-2.00491651967066,-2.07844524359609)) ;
#133317 = CARTESIAN_POINT('Ctrl Pts',(-5.4,-2.0877044485962,-2.00439746887853)) ;
#133318 = CARTESIAN_POINT('Ctrl Pts',(-5.4,-2.11180339704051,-1.95250683989133)) ;
#133319 = CARTESIAN_POINT('Ctrl Pts',(-5.4,-2.11180339887499,-1.9)) ;
#133320 = CARTESIAN_POINT('',(-5.4,3.9369800677651,-2.1)) ;
#133321 = CARTESIAN_POINT('',(-5.4,4.20000000000001,-2.1)) ;
#133322 = CARTESIAN_POINT('Ctrl Pts',(-5.4,3.9369800677651,-2.1)) ;
#133323 = CARTESIAN_POINT('Ctrl Pts',(-5.4,4.01601337581889,-2.09999999951886)) ;
#133324 = CARTESIAN_POINT('Ctrl Pts',(-5.4,4.09411900298413,-2.07844528624287)) ;
#133325 = CARTESIAN_POINT('Ctrl Pts',(-5.4,4.20557579169423,-2.00439742623175)) ;
#133326 = CARTESIAN_POINT('Ctrl Pts',(-5.4,4.23801992976516,-1.95250687190974)) ;
#133327 = CARTESIAN_POINT('Ctrl Pts',(-5.4,4.23801993223491,-1.9)) ;
#133328 = CARTESIAN_POINT('Origin',(-5.4,-4.05,2.54)) ;
#133329 = CARTESIAN_POINT('',(-5.3,-4.05,2.54)) ;
#133330 = CARTESIAN_POINT('',(-5.3,-4.05,-7.62)) ;
#133331 = CARTESIAN_POINT('',(-5.3,-4.05,2.54)) ;
#133332 = CARTESIAN_POINT('',(3.5,-4.05,-7.62)) ;
#133333 = CARTESIAN_POINT('',(-5.4,-4.05,-7.62)) ;
#133334 = CARTESIAN_POINT('',(3.5,-4.05,2.54)) ;
#133335 = CARTESIAN_POINT('',(3.5,-4.05,2.54)) ;
#133336 = CARTESIAN_POINT('',(-5.4,-4.05,2.54)) ;
#133337 = CARTESIAN_POINT('',(-4.5,-4.05,-5.98)) ;
#133338 = CARTESIAN_POINT('',(-4.3,-4.05,-6.18)) ;
#133339 = CARTESIAN_POINT('Origin',(-4.3,-4.05,-5.98)) ;
#133340 = CARTESIAN_POINT('',(-4.5,-4.05,-4.18)) ;
#133341 = CARTESIAN_POINT('',(-4.5,-4.05,-2.54)) ;
#133342 = CARTESIAN_POINT('',(-4.3,-4.05,-3.98)) ;
#133343 = CARTESIAN_POINT('Origin',(-4.3,-4.05,-4.18)) ;
#133344 = CARTESIAN_POINT('',(-3.25,-4.05,-3.98)) ;
#133345 = CARTESIAN_POINT('',(-5.4,-4.05,-3.98)) ;
#133346 = CARTESIAN_POINT('',(-3.05,-4.05,-4.18)) ;
#133347 = CARTESIAN_POINT('Origin',(-3.25,-4.05,-4.18)) ;
#133348 = CARTESIAN_POINT('',(-3.05,-4.05,-5.98)) ;
#133349 = CARTESIAN_POINT('',(-3.05,-4.05,-2.54)) ;
#133350 = CARTESIAN_POINT('',(-3.25,-4.05,-6.18)) ;
#133351 = CARTESIAN_POINT('Origin',(-3.25,-4.05,-5.98)) ;
#133352 = CARTESIAN_POINT('',(-5.4,-4.05,-6.18)) ;
#133353 = CARTESIAN_POINT('',(-4.5,-4.05,-0.900000000000001)) ;
#133354 = CARTESIAN_POINT('',(-4.3,-4.05,-1.1)) ;
#133355 = CARTESIAN_POINT('Origin',(-4.3,-4.05,-0.900000000000001)) ;
#133356 = CARTESIAN_POINT('',(-4.5,-4.05,0.899999999999999)) ;
#133357 = CARTESIAN_POINT('',(-4.5,-4.05,2.54)) ;
#133358 = CARTESIAN_POINT('',(-4.3,-4.05,1.1)) ;
#133359 = CARTESIAN_POINT('Origin',(-4.3,-4.05,0.899999999999999)) ;
#133360 = CARTESIAN_POINT('',(-3.25,-4.05,1.1)) ;
#133361 = CARTESIAN_POINT('',(-5.4,-4.05,1.1)) ;
#133362 = CARTESIAN_POINT('',(-3.05,-4.05,0.9)) ;
#133363 = CARTESIAN_POINT('Origin',(-3.25,-4.05,0.9)) ;
#133364 = CARTESIAN_POINT('',(-3.05,-4.05,-0.900000000000001)) ;
#133365 = CARTESIAN_POINT('',(-3.05,-4.05,2.54)) ;
#133366 = CARTESIAN_POINT('',(-3.25,-4.05,-1.1)) ;
#133367 = CARTESIAN_POINT('Origin',(-3.25,-4.05,-0.900000000000001)) ;
#133368 = CARTESIAN_POINT('',(-5.4,-4.05,-1.1)) ;
#133369 = CARTESIAN_POINT('Origin',(3.6,-4.05,2.54)) ;
#133370 = CARTESIAN_POINT('',(3.6,-3.95,2.54)) ;
#133371 = CARTESIAN_POINT('',(3.6,-3.95,-7.62)) ;
#133372 = CARTESIAN_POINT('',(3.6,-3.95,2.54)) ;
#133373 = CARTESIAN_POINT('',(3.6,-2.9,-7.62)) ;
#133374 = CARTESIAN_POINT('',(3.6,-4.05,-7.62)) ;
#133375 = CARTESIAN_POINT('',(3.6,-2.9,2.54)) ;
#133376 = CARTESIAN_POINT('',(3.6,-2.9,2.54)) ;
#133377 = CARTESIAN_POINT('',(3.6,-4.05,2.54)) ;
#133378 = CARTESIAN_POINT('Origin',(3.6,-2.8,2.54)) ;
#133379 = CARTESIAN_POINT('',(4.4,-2.8,-1.52315462117279)) ;
#133380 = CARTESIAN_POINT('',(4.54880051362943,-2.79999999972164,-1.07643786073294)) ;
#133381 = CARTESIAN_POINT('Ctrl Pts',(4.4,-2.8,-1.52315462117279)) ;
#133382 = CARTESIAN_POINT('Ctrl Pts',(4.40001102013632,-2.8,-1.48644001985269)) ;
#133383 = CARTESIAN_POINT('Ctrl Pts',(4.40220140384615,-2.79999999812164,
-1.45006816610693)) ;
#133384 = CARTESIAN_POINT('Ctrl Pts',(4.40664174993564,-2.79999999722267,
-1.41407273800855)) ;
#133385 = CARTESIAN_POINT('Ctrl Pts',(4.41108209602513,-2.79999999632371,
-1.37807730991017)) ;
#133386 = CARTESIAN_POINT('Ctrl Pts',(4.41777240449452,-2.79999999692353,
-1.34245830745924)) ;
#133387 = CARTESIAN_POINT('Ctrl Pts',(4.42678327414915,-2.79999999844302,
-1.30724940872871)) ;
#133388 = CARTESIAN_POINT('Ctrl Pts',(4.42864654534902,-2.79999999875722,
-1.29996889868936)) ;
#133389 = CARTESIAN_POINT('Ctrl Pts',(4.43060908636007,-2.79999999907333,
-1.29270591711623)) ;
#133390 = CARTESIAN_POINT('Ctrl Pts',(4.43267155768737,-2.79999999933982,
-1.28546075906515)) ;
#133391 = CARTESIAN_POINT('Ctrl Pts',(4.4352900037877,-2.79999999967816,-1.27626254350986)) ;
#133392 = CARTESIAN_POINT('Ctrl Pts',(4.4380733085653,-2.79999999966608,-1.2670911025424)) ;
#133393 = CARTESIAN_POINT('Ctrl Pts',(4.44102157277561,-2.79999999954234,
-1.25794807820152)) ;
#133394 = CARTESIAN_POINT('Ctrl Pts',(4.45046499569138,-2.79999999914597,
-1.22866255986902)) ;
#133395 = CARTESIAN_POINT('Ctrl Pts',(4.46157908226632,-2.79999999505379,
-1.19972021349317)) ;
#133396 = CARTESIAN_POINT('Ctrl Pts',(4.47540732315415,-2.79999999166095,
-1.1722492625065)) ;
#133397 = CARTESIAN_POINT('Ctrl Pts',(4.47702479055525,-2.79999999126409,
-1.16903602894638)) ;
#133398 = CARTESIAN_POINT('Ctrl Pts',(4.47867903313992,-2.79999999107055,
-1.16584272212549)) ;
#133399 = CARTESIAN_POINT('Ctrl Pts',(4.48037187481471,-2.79999999105954,
-1.162671097194)) ;
#133400 = CARTESIAN_POINT('Ctrl Pts',(4.48545039983908,-2.79999999102651,
-1.15315622239953)) ;
#133401 = CARTESIAN_POINT('Ctrl Pts',(4.49087631667453,-2.79999999265304,
-1.14383648460966)) ;
#133402 = CARTESIAN_POINT('Ctrl Pts',(4.49669887079745,-2.79999999431461,
-1.13475927287888)) ;
#133403 = CARTESIAN_POINT('Ctrl Pts',(4.50888705006189,-2.79999999779274,
-1.11575821570355)) ;
#133404 = CARTESIAN_POINT('Ctrl Pts',(4.52313265843748,-2.79999999982394,
-1.09737449917999)) ;
#133405 = CARTESIAN_POINT('Ctrl Pts',(4.54066913339539,-2.79999999997241,
-1.08273042197106)) ;
#133406 = CARTESIAN_POINT('Ctrl Pts',(4.54329026609835,-2.7999999999946,-1.08054160866798)) ;
#133407 = CARTESIAN_POINT('Ctrl Pts',(4.5460045281952,-2.8,-1.07843934457872)) ;
#133408 = CARTESIAN_POINT('Ctrl Pts',(4.54880363749516,-2.8,-1.07645020604105)) ;
#133409 = CARTESIAN_POINT('',(4.4,-2.8,-3.84865454255039E-12)) ;
#133410 = CARTESIAN_POINT('Ctrl Pts',(4.54879236168152,-2.8,-1.07643444348001)) ;
#133411 = CARTESIAN_POINT('Ctrl Pts',(4.51096310105345,-2.8,-1.04764090781959)) ;
#133412 = CARTESIAN_POINT('Ctrl Pts',(4.49022331291407,-2.8,-1.00382911927614)) ;
#133413 = CARTESIAN_POINT('Ctrl Pts',(4.45698031182017,-2.8,-0.917623871395766)) ;
#133414 = CARTESIAN_POINT('Ctrl Pts',(4.44561000227039,-2.8,-0.872361144958552)) ;
#133415 = CARTESIAN_POINT('Ctrl Pts',(4.41911102299977,-2.8,-0.735880791656898)) ;
#133416 = CARTESIAN_POINT('Ctrl Pts',(4.41155688769424,-2.8,-0.644231375192043)) ;
#133417 = CARTESIAN_POINT('Ctrl Pts',(4.39763503647248,-2.8,-0.368710456932986)) ;
#133418 = CARTESIAN_POINT('Ctrl Pts',(4.4,-2.8,-0.184260662117819)) ;
#133419 = CARTESIAN_POINT('Ctrl Pts',(4.4,-2.8,-3.84865454255039E-12)) ;
#133420 = CARTESIAN_POINT('',(4.54879236179094,-2.79999999953044,1.07643444349586)) ;
#133421 = CARTESIAN_POINT('Ctrl Pts',(4.4,-2.8,-3.84865750380219E-12)) ;
#133422 = CARTESIAN_POINT('Ctrl Pts',(4.4,-2.8,0.184515281657094)) ;
#133423 = CARTESIAN_POINT('Ctrl Pts',(4.39760751905643,-2.8,0.369216326714866)) ;
#133424 = CARTESIAN_POINT('Ctrl Pts',(4.40696794948104,-2.8,0.553410676296662)) ;
#133425 = CARTESIAN_POINT('Ctrl Pts',(4.41164816469334,-2.8,0.645507851087552)) ;
#133426 = CARTESIAN_POINT('Ctrl Pts',(4.41940496802384,-2.80000000000001,
0.737842856499212)) ;
#133427 = CARTESIAN_POINT('Ctrl Pts',(4.43698455094237,-2.8,0.827933846251606)) ;
#133428 = CARTESIAN_POINT('Ctrl Pts',(4.44577434240165,-2.8,0.872979341127799)) ;
#133429 = CARTESIAN_POINT('Ctrl Pts',(4.456925956929,-2.80000000000001,0.917523082510354)) ;
#133430 = CARTESIAN_POINT('Ctrl Pts',(4.47366127850408,-2.8,0.960880593909591)) ;
#133431 = CARTESIAN_POINT('Ctrl Pts',(4.47575319370098,-2.8,0.966300282834483)) ;
#133432 = CARTESIAN_POINT('Ctrl Pts',(4.4779117359051,-2.79999999997843,0.971725845219423)) ;
#133433 = CARTESIAN_POINT('Ctrl Pts',(4.48016062485991,-2.80000000010461,
0.977126712477952)) ;
#133434 = CARTESIAN_POINT('Ctrl Pts',(4.48803173620173,-2.80000000054624,
0.996029747882805)) ;
#133435 = CARTESIAN_POINT('Ctrl Pts',(4.49700942865457,-2.80000000534986,
1.01463033418563)) ;
#133436 = CARTESIAN_POINT('Ctrl Pts',(4.50810946414921,-2.80000000469598,
1.03161833486068)) ;
#133437 = CARTESIAN_POINT('Ctrl Pts',(4.51435323411495,-2.80000000432818,
1.04117408524039)) ;
#133438 = CARTESIAN_POINT('Ctrl Pts',(4.52126852668377,-2.80000000204489,
1.05021960344861)) ;
#133439 = CARTESIAN_POINT('Ctrl Pts',(4.52903612565461,-2.80000000089509,
1.05852171333236)) ;
#133440 = CARTESIAN_POINT('Ctrl Pts',(4.5320568585877,-2.80000000044794,1.06175031162049)) ;
#133441 = CARTESIAN_POINT('Ctrl Pts',(4.53520648971123,-2.80000000018876,
1.06486648087189)) ;
#133442 = CARTESIAN_POINT('Ctrl Pts',(4.53849565154302,-2.80000000008376,
1.06785650719406)) ;
#133443 = CARTESIAN_POINT('Ctrl Pts',(4.54178481337482,-2.79999999997876,
1.07084653351624)) ;
#133444 = CARTESIAN_POINT('Ctrl Pts',(4.54521363891046,-2.8,1.07371024217815)) ;
#133445 = CARTESIAN_POINT('Ctrl Pts',(4.54879236168087,-2.8,1.07643444348047)) ;
#133446 = CARTESIAN_POINT('',(4.4,-2.8,1.52315462117279)) ;
#133447 = CARTESIAN_POINT('Ctrl Pts',(4.54879236168109,-2.79999999812176,
1.07643444348078)) ;
#133448 = CARTESIAN_POINT('Ctrl Pts',(4.54599316991904,-2.79999999835896,
1.07842438566453)) ;
#133449 = CARTESIAN_POINT('Ctrl Pts',(4.54327885465675,-2.7999999985882,1.08052734316011)) ;
#133450 = CARTESIAN_POINT('Ctrl Pts',(4.523116040633,-2.80000000023132,1.09736894030692)) ;
#133451 = CARTESIAN_POINT('Ctrl Pts',(4.50886780632328,-2.80000000100533,
1.11575780035687)) ;
#133452 = CARTESIAN_POINT('Ctrl Pts',(4.48892103801304,-2.79999999510252,
1.14687097816957)) ;
#133453 = CARTESIAN_POINT('Ctrl Pts',(4.4818652331329,-2.7999999909955,1.1594167949763)) ;
#133454 = CARTESIAN_POINT('Ctrl Pts',(4.46162186753408,-2.79999997126272,
1.19974328605816)) ;
#133455 = CARTESIAN_POINT('Ctrl Pts',(4.45052849087262,-2.7999999685384,1.2286810382908)) ;
#133456 = CARTESIAN_POINT('Ctrl Pts',(4.43813540717735,-2.79999997674815,
1.2670939408709)) ;
#133457 = CARTESIAN_POINT('Ctrl Pts',(4.43535270120343,-2.79999997903695,
1.27624973594923)) ;
#133458 = CARTESIAN_POINT('Ctrl Pts',(4.41677772588063,-2.79999999273252,
1.34133119849698)) ;
#133459 = CARTESIAN_POINT('Ctrl Pts',(4.40678488791375,-2.79999999887621,
1.39828048147345)) ;
#133460 = CARTESIAN_POINT('Ctrl Pts',(4.40081887576623,-2.80000000006435,
1.47838010320481)) ;
#133461 = CARTESIAN_POINT('Ctrl Pts',(4.4,-2.8,1.50069810180457)) ;
#133462 = CARTESIAN_POINT('Ctrl Pts',(4.4,-2.8,1.52315462117279)) ;
#133463 = CARTESIAN_POINT('',(4.4,-2.8,2.54)) ;
#133464 = CARTESIAN_POINT('',(4.4,-2.8,2.54)) ;
#133465 = CARTESIAN_POINT('',(3.7,-2.8,2.54)) ;
#133466 = CARTESIAN_POINT('',(3.6,-2.8,2.54)) ;
#133467 = CARTESIAN_POINT('',(3.7,-2.8,-7.62)) ;
#133468 = CARTESIAN_POINT('',(3.7,-2.8,-2.54)) ;
#133469 = CARTESIAN_POINT('',(4.4,-2.8,-7.62)) ;
#133470 = CARTESIAN_POINT('',(3.6,-2.8,-7.62)) ;
#133471 = CARTESIAN_POINT('',(4.4,-2.8,-6.60315462117279)) ;
#133472 = CARTESIAN_POINT('',(4.4,-2.8,-2.54)) ;
#133473 = CARTESIAN_POINT('',(4.54880051362943,-2.79999999972164,-6.15643786073294)) ;
#133474 = CARTESIAN_POINT('Ctrl Pts',(4.4,-2.8,-6.60315462117279)) ;
#133475 = CARTESIAN_POINT('Ctrl Pts',(4.40001102013632,-2.8,-6.56644001985245)) ;
#133476 = CARTESIAN_POINT('Ctrl Pts',(4.40220140384618,-2.79999999812164,
-6.53006816610646)) ;
#133477 = CARTESIAN_POINT('Ctrl Pts',(4.40664174993573,-2.79999999722267,
-6.49407273800786)) ;
#133478 = CARTESIAN_POINT('Ctrl Pts',(4.41108209602527,-2.79999999632371,
-6.45807730990925)) ;
#133479 = CARTESIAN_POINT('Ctrl Pts',(4.41777240449475,-2.79999999692353,
-6.42245830745811)) ;
#133480 = CARTESIAN_POINT('Ctrl Pts',(4.4267832741495,-2.79999999844302,-6.38724940872736)) ;
#133481 = CARTESIAN_POINT('Ctrl Pts',(4.42864654534927,-2.79999999875722,
-6.37996889868846)) ;
#133482 = CARTESIAN_POINT('Ctrl Pts',(4.4306090863602,-2.79999999907333,-6.37270591711578)) ;
#133483 = CARTESIAN_POINT('Ctrl Pts',(4.43267155768737,-2.79999999933982,
-6.36546075906515)) ;
#133484 = CARTESIAN_POINT('Ctrl Pts',(4.4352900037877,-2.79999999967816,-6.35626254350987)) ;
#133485 = CARTESIAN_POINT('Ctrl Pts',(4.4380733085653,-2.79999999966609,-6.3470911025424)) ;
#133486 = CARTESIAN_POINT('Ctrl Pts',(4.44102157277561,-2.79999999954234,
-6.33794807820151)) ;
#133487 = CARTESIAN_POINT('Ctrl Pts',(4.45046499569138,-2.79999999914597,
-6.30866255986902)) ;
#133488 = CARTESIAN_POINT('Ctrl Pts',(4.46157908226632,-2.79999999505379,
-6.27972021349316)) ;
#133489 = CARTESIAN_POINT('Ctrl Pts',(4.47540732315415,-2.79999999166095,
-6.2522492625065)) ;
#133490 = CARTESIAN_POINT('Ctrl Pts',(4.47702479055525,-2.79999999126409,
-6.24903602894638)) ;
#133491 = CARTESIAN_POINT('Ctrl Pts',(4.47867903313992,-2.79999999107055,
-6.24584272212549)) ;
#133492 = CARTESIAN_POINT('Ctrl Pts',(4.48037187481471,-2.79999999105954,
-6.242671097194)) ;
#133493 = CARTESIAN_POINT('Ctrl Pts',(4.48545039983908,-2.79999999102651,
-6.23315622239953)) ;
#133494 = CARTESIAN_POINT('Ctrl Pts',(4.49087631667453,-2.79999999265304,
-6.22383648460966)) ;
#133495 = CARTESIAN_POINT('Ctrl Pts',(4.49669887079746,-2.79999999431461,
-6.21475927287888)) ;
#133496 = CARTESIAN_POINT('Ctrl Pts',(4.50888705006191,-2.79999999779274,
-6.19575821570356)) ;
#133497 = CARTESIAN_POINT('Ctrl Pts',(4.52313265843748,-2.79999999982394,
-6.17737449917998)) ;
#133498 = CARTESIAN_POINT('Ctrl Pts',(4.54066913339539,-2.79999999997241,
-6.16273042197107)) ;
#133499 = CARTESIAN_POINT('Ctrl Pts',(4.54329026609835,-2.79999999999461,
-6.16054160866799)) ;
#133500 = CARTESIAN_POINT('Ctrl Pts',(4.5460045281952,-2.8,-6.15843934457872)) ;
#133501 = CARTESIAN_POINT('Ctrl Pts',(4.54880363749516,-2.8,-6.15645020604105)) ;
#133502 = CARTESIAN_POINT('',(4.4,-2.8,-5.08000000000385)) ;
#133503 = CARTESIAN_POINT('Ctrl Pts',(4.54879236168152,-2.8,-6.15643444348001)) ;
#133504 = CARTESIAN_POINT('Ctrl Pts',(4.51096310105345,-2.8,-6.1276409078196)) ;
#133505 = CARTESIAN_POINT('Ctrl Pts',(4.49022331291407,-2.8,-6.08382911927614)) ;
#133506 = CARTESIAN_POINT('Ctrl Pts',(4.45698031182017,-2.8,-5.99762387139577)) ;
#133507 = CARTESIAN_POINT('Ctrl Pts',(4.4456100022704,-2.8,-5.95236114495855)) ;
#133508 = CARTESIAN_POINT('Ctrl Pts',(4.41911102299977,-2.8,-5.8158807916569)) ;
#133509 = CARTESIAN_POINT('Ctrl Pts',(4.41155688769424,-2.8,-5.72423137519204)) ;
#133510 = CARTESIAN_POINT('Ctrl Pts',(4.39763503647248,-2.8,-5.44871045693299)) ;
#133511 = CARTESIAN_POINT('Ctrl Pts',(4.4,-2.8,-5.26426066211782)) ;
#133512 = CARTESIAN_POINT('Ctrl Pts',(4.4,-2.8,-5.08000000000385)) ;
#133513 = CARTESIAN_POINT('',(4.54879236179094,-2.79999999953044,-4.00356555650414)) ;
#133514 = CARTESIAN_POINT('Ctrl Pts',(4.4,-2.8,-5.08000000000385)) ;
#133515 = CARTESIAN_POINT('Ctrl Pts',(4.4,-2.8,-4.89548471834291)) ;
#133516 = CARTESIAN_POINT('Ctrl Pts',(4.39760751905643,-2.8,-4.71078367328513)) ;
#133517 = CARTESIAN_POINT('Ctrl Pts',(4.40696794948104,-2.8,-4.52658932370334)) ;
#133518 = CARTESIAN_POINT('Ctrl Pts',(4.41164816469334,-2.8,-4.43449214891245)) ;
#133519 = CARTESIAN_POINT('Ctrl Pts',(4.41940496802384,-2.80000000000001,
-4.34215714350079)) ;
#133520 = CARTESIAN_POINT('Ctrl Pts',(4.43698455094237,-2.8,-4.2520661537484)) ;
#133521 = CARTESIAN_POINT('Ctrl Pts',(4.44577434240163,-2.8,-4.2070206588722)) ;
#133522 = CARTESIAN_POINT('Ctrl Pts',(4.456925956929,-2.80000000000001,-4.16247691748965)) ;
#133523 = CARTESIAN_POINT('Ctrl Pts',(4.47366127850408,-2.8,-4.11911940609041)) ;
#133524 = CARTESIAN_POINT('Ctrl Pts',(4.47575319370098,-2.8,-4.11369971716551)) ;
#133525 = CARTESIAN_POINT('Ctrl Pts',(4.47791173590511,-2.79999999997843,
-4.10827415478058)) ;
#133526 = CARTESIAN_POINT('Ctrl Pts',(4.48016062485992,-2.80000000010461,
-4.10287328752205)) ;
#133527 = CARTESIAN_POINT('Ctrl Pts',(4.48803173620173,-2.80000000054624,
-4.08397025211719)) ;
#133528 = CARTESIAN_POINT('Ctrl Pts',(4.49700942865457,-2.80000000534986,
-4.06536966581437)) ;
#133529 = CARTESIAN_POINT('Ctrl Pts',(4.50810946414922,-2.80000000469598,
-4.04838166513932)) ;
#133530 = CARTESIAN_POINT('Ctrl Pts',(4.51435323411496,-2.80000000432818,
-4.03882591475961)) ;
#133531 = CARTESIAN_POINT('Ctrl Pts',(4.52126852668377,-2.80000000204489,
-4.02978039655139)) ;
#133532 = CARTESIAN_POINT('Ctrl Pts',(4.5290361256546,-2.80000000089509,-4.02147828666764)) ;
#133533 = CARTESIAN_POINT('Ctrl Pts',(4.5320568585877,-2.80000000044794,-4.01824968837951)) ;
#133534 = CARTESIAN_POINT('Ctrl Pts',(4.53520648971123,-2.80000000018876,
-4.01513351912811)) ;
#133535 = CARTESIAN_POINT('Ctrl Pts',(4.53849565154302,-2.80000000008376,
-4.01214349280594)) ;
#133536 = CARTESIAN_POINT('Ctrl Pts',(4.54178481337482,-2.79999999997876,
-4.00915346648376)) ;
#133537 = CARTESIAN_POINT('Ctrl Pts',(4.54521363891047,-2.8,-4.00628975782185)) ;
#133538 = CARTESIAN_POINT('Ctrl Pts',(4.54879236168087,-2.8,-4.00356555651953)) ;
#133539 = CARTESIAN_POINT('',(4.4,-2.8,-3.55684537882721)) ;
#133540 = CARTESIAN_POINT('Ctrl Pts',(4.54879236168109,-2.79999999812176,
-4.00356555651922)) ;
#133541 = CARTESIAN_POINT('Ctrl Pts',(4.54599316991904,-2.79999999835896,
-4.00157561433547)) ;
#133542 = CARTESIAN_POINT('Ctrl Pts',(4.54327885465675,-2.7999999985882,-3.99947265683989)) ;
#133543 = CARTESIAN_POINT('Ctrl Pts',(4.523116040633,-2.80000000023133,-3.98263105969307)) ;
#133544 = CARTESIAN_POINT('Ctrl Pts',(4.50886780632328,-2.80000000100533,
-3.96424219964312)) ;
#133545 = CARTESIAN_POINT('Ctrl Pts',(4.48892103801304,-2.79999999510252,
-3.93312902183043)) ;
#133546 = CARTESIAN_POINT('Ctrl Pts',(4.4818652331329,-2.7999999909955,-3.9205832050237)) ;
#133547 = CARTESIAN_POINT('Ctrl Pts',(4.46162186753408,-2.79999997126272,
-3.88025671394184)) ;
#133548 = CARTESIAN_POINT('Ctrl Pts',(4.45052849087262,-2.7999999685384,-3.85131896170919)) ;
#133549 = CARTESIAN_POINT('Ctrl Pts',(4.43813540717735,-2.79999997674815,
-3.8129060591291)) ;
#133550 = CARTESIAN_POINT('Ctrl Pts',(4.43535270120344,-2.79999997903695,
-3.80375026405077)) ;
#133551 = CARTESIAN_POINT('Ctrl Pts',(4.41677772588091,-2.79999999273252,
-3.738668801504)) ;
#133552 = CARTESIAN_POINT('Ctrl Pts',(4.4067848879141,-2.79999999887621,-3.68171951852853)) ;
#133553 = CARTESIAN_POINT('Ctrl Pts',(4.40081887576631,-2.80000000006435,
-3.60161989679722)) ;
#133554 = CARTESIAN_POINT('Ctrl Pts',(4.4,-2.8,-3.57930189819645)) ;
#133555 = CARTESIAN_POINT('Ctrl Pts',(4.4,-2.8,-3.55684537882721)) ;
#133556 = CARTESIAN_POINT('',(4.4,-2.8,2.54)) ;
#133557 = CARTESIAN_POINT('Origin',(4.5,-2.8,2.54)) ;
#133558 = CARTESIAN_POINT('',(4.5,-2.7,2.54)) ;
#133559 = CARTESIAN_POINT('',(4.5,-2.4,2.54)) ;
#133560 = CARTESIAN_POINT('',(4.5,-2.8,2.54)) ;
#133561 = CARTESIAN_POINT('',(4.5,-2.7,1.52315462117279)) ;
#133562 = CARTESIAN_POINT('',(4.5,-2.7,2.54)) ;
#133563 = CARTESIAN_POINT('',(4.5,-2.4,1.96214168703486)) ;
#133564 = CARTESIAN_POINT('Origin',(4.5,0.,0.)) ;
#133565 = CARTESIAN_POINT('',(4.5,-2.4,2.54)) ;
#133566 = CARTESIAN_POINT('Origin',(4.5,-2.3,2.54)) ;
#133567 = CARTESIAN_POINT('',(12.7,-2.3,-1.96214168703486)) ;
#133568 = CARTESIAN_POINT('',(4.6,-2.3,-1.96214168703486)) ;
#133569 = CARTESIAN_POINT('',(4.5,-2.3,-1.96214168703486)) ;
#133570 = CARTESIAN_POINT('',(4.6,-2.3,-3.11785831296514)) ;
#133571 = CARTESIAN_POINT('',(4.6,-2.3,-2.54)) ;
#133572 = CARTESIAN_POINT('',(12.7,-2.3,-3.11785831296514)) ;
#133573 = CARTESIAN_POINT('',(4.5,-2.3,-3.11785831296514)) ;
#133574 = CARTESIAN_POINT('',(12.7,-2.3,2.54)) ;
#133575 = CARTESIAN_POINT('Origin',(0.,0.,2.54)) ;
#133576 = CARTESIAN_POINT('Origin',(3.3,10.85,2.54)) ;
#133577 = CARTESIAN_POINT('Origin',(-4.8,10.85,2.54)) ;
#133578 = CARTESIAN_POINT('Origin',(-4.8,10.3,2.54)) ;
#133579 = CARTESIAN_POINT('Origin',(-5.3,5.19009804864072,2.54)) ;
#133580 = CARTESIAN_POINT('Origin',(-5.3,-3.95,2.54)) ;
#133581 = CARTESIAN_POINT('Origin',(3.5,-3.95,2.54)) ;
#133582 = CARTESIAN_POINT('Origin',(3.7,-2.9,2.54)) ;
#133583 = CARTESIAN_POINT('Origin',(4.4,-2.7,2.54)) ;
#133584 = CARTESIAN_POINT('Origin',(4.6,-2.4,2.54)) ;
#133585 = CARTESIAN_POINT('Origin',(12.7,-2.2,2.54)) ;
#133586 = CARTESIAN_POINT('Origin',(12.7,2.65,2.54)) ;
#133587 = CARTESIAN_POINT('Origin',(4.55912712210514,2.85,2.54)) ;
#133588 = CARTESIAN_POINT('Origin',(4.05,3.77568567655479,2.54)) ;
#133589 = CARTESIAN_POINT('Origin',(3.85,6.92431432344521,2.54)) ;
#133590 = CARTESIAN_POINT('Origin',(-4.65,1.95,-2.)) ;
#133591 = CARTESIAN_POINT('',(-4.66204490261456,3.21928058320648,-2.)) ;
#133592 = CARTESIAN_POINT('',(-5.3,3.9369800677651,-2.)) ;
#133593 = CARTESIAN_POINT('',(-5.47474093186837,4.13356361611701,-2.)) ;
#133594 = CARTESIAN_POINT('',(-5.3,-1.88819660112501,-2.)) ;
#133595 = CARTESIAN_POINT('',(-5.3,-2.05,-2.)) ;
#133596 = CARTESIAN_POINT('',(-4.66204490261456,-1.5692190524323,-2.)) ;
#133597 = CARTESIAN_POINT('',(-4.69472135955,-1.58555728090001,-2.)) ;
#133598 = CARTESIAN_POINT('',(-4.66204490261456,3.35625,-2.)) ;
#133599 = CARTESIAN_POINT('Origin',(-5.4,1.95,2.)) ;
#133600 = CARTESIAN_POINT('',(-4.66204490261456,-1.5692190524323,2.)) ;
#133601 = CARTESIAN_POINT('',(-5.3,-1.88819660112502,2.)) ;
#133602 = CARTESIAN_POINT('',(-5.44472135955,-1.96055728090001,2.)) ;
#133603 = CARTESIAN_POINT('',(-5.3,3.9369800677651,2.)) ;
#133604 = CARTESIAN_POINT('',(-5.3,4.20000000000001,2.)) ;
#133605 = CARTESIAN_POINT('',(-4.66204490261456,3.21928058320648,2.)) ;
#133606 = CARTESIAN_POINT('',(-4.72474093186837,3.28981361611701,2.)) ;
#133607 = CARTESIAN_POINT('',(-4.66204490261456,-1.67500000000001,2.)) ;
#133608 = CARTESIAN_POINT('Origin',(-4.65,1.95,2.)) ;
#133609 = CARTESIAN_POINT('',(-3.33134808452128,1.85,1.6776628651052)) ;
#133610 = CARTESIAN_POINT('',(-3.48082994825801,1.91712723223402,1.71420287624085)) ;
#133611 = CARTESIAN_POINT('Origin',(-3.343288636449,2.02341244982204,1.68058166668753)) ;
#133612 = CARTESIAN_POINT('',(-2.4,1.85,1.45)) ;
#133613 = CARTESIAN_POINT('',(-4.65,1.85,2.)) ;
#133614 = CARTESIAN_POINT('',(-2.4,-0.95,1.45)) ;
#133615 = CARTESIAN_POINT('',(-2.4,1.95,1.45)) ;
#133616 = CARTESIAN_POINT('',(-3.3526478932023,-0.95,1.68286948500501)) ;
#133617 = CARTESIAN_POINT('',(-3.39999999999998,-0.95,1.69444444444444)) ;
#133618 = CARTESIAN_POINT('',(-3.44209061230229,-0.971114561800017,1.70473326078501)) ;
#133619 = CARTESIAN_POINT('Origin',(-3.36201220558073,-1.11033257691858,1.68515853914196)) ;
#133620 = CARTESIAN_POINT('',(-4.63829959356686,-1.5692190524323,1.99713990064968)) ;
#133621 = CARTESIAN_POINT('',(-4.68814869588294,-1.59414360359034,2.00932523677139)) ;
#133622 = CARTESIAN_POINT('',(-4.63829959356686,3.21928058320648,1.99713990064968)) ;
#133623 = CARTESIAN_POINT('',(-4.63829959356686,3.35625,1.99713990064968)) ;
#133624 = CARTESIAN_POINT('',(-3.45989661114215,1.89357722797868,1.70908583827919)) ;
#133625 = CARTESIAN_POINT('Origin',(-2.4,1.95,1.45)) ;
#133626 = CARTESIAN_POINT('',(-2.4,1.85,-1.45)) ;
#133627 = CARTESIAN_POINT('',(-2.4,-0.95,-1.45)) ;
#133628 = CARTESIAN_POINT('',(-2.4,1.95,-1.45)) ;
#133629 = CARTESIAN_POINT('',(-2.4,-1.05,-1.347055690472)) ;
#133630 = CARTESIAN_POINT('Origin',(-2.4,-0.950000000000003,-1.347055690472)) ;
#133631 = CARTESIAN_POINT('',(-2.4,-1.05,1.347055690472)) ;
#133632 = CARTESIAN_POINT('',(-2.4,-1.05,1.45)) ;
#133633 = CARTESIAN_POINT('Origin',(-2.4,-0.950000000000021,1.34705569047202)) ;
#133634 = CARTESIAN_POINT('',(-2.4,1.95,1.347055690472)) ;
#133635 = CARTESIAN_POINT('Origin',(-2.4,1.85000000000002,1.34705569047202)) ;
#133636 = CARTESIAN_POINT('',(-2.4,1.95,-1.347055690472)) ;
#133637 = CARTESIAN_POINT('',(-2.4,1.95,1.45)) ;
#133638 = CARTESIAN_POINT('Origin',(-2.4,1.85000000000002,-1.34705569047202)) ;
#133639 = CARTESIAN_POINT('Origin',(-2.4,1.95,-1.45)) ;
#133640 = CARTESIAN_POINT('',(-3.3526478932023,-0.95,-1.68286948500501)) ;
#133641 = CARTESIAN_POINT('',(-3.44209061230229,-0.971114561800017,-1.70473326078501)) ;
#133642 = CARTESIAN_POINT('Origin',(-3.36201220558183,-1.11033257691343,-1.68515853914223)) ;
#133643 = CARTESIAN_POINT('',(-2.4,-0.95,-1.45)) ;
#133644 = CARTESIAN_POINT('',(-3.33134808452128,1.85,-1.6776628651052)) ;
#133645 = CARTESIAN_POINT('',(-2.4,1.85,-1.45)) ;
#133646 = CARTESIAN_POINT('',(-3.48082994825801,1.91712723223402,-1.71420287624085)) ;
#133647 = CARTESIAN_POINT('Origin',(-3.34328863644904,2.02341244982232,-1.68058166668754)) ;
#133648 = CARTESIAN_POINT('',(-4.63829959356686,3.21928058320648,-1.99713990064968)) ;
#133649 = CARTESIAN_POINT('',(-4.70989661114216,3.29982722797869,-2.01464139383475)) ;
#133650 = CARTESIAN_POINT('',(-4.63829959356686,-1.5692190524323,-1.99713990064968)) ;
#133651 = CARTESIAN_POINT('',(-4.63829959356686,-1.67500000000001,-1.99713990064968)) ;
#133652 = CARTESIAN_POINT('',(-3.43814869588292,-0.969143603590331,-1.70376968121583)) ;
#133653 = CARTESIAN_POINT('Origin',(0.,1.95,0.)) ;
#133654 = CARTESIAN_POINT('',(-3.35509339356897,1.95,1.58052296445552)) ;
#133655 = CARTESIAN_POINT('',(0.175392621986784,1.95,0.717515271764115)) ;
#133656 = CARTESIAN_POINT('',(-3.35509339356897,1.95,-1.58052296445552)) ;
#133657 = CARTESIAN_POINT('',(-3.35509339356897,1.95,-1.69444444444444)) ;
#133658 = CARTESIAN_POINT('',(0.175392621986784,1.95,-0.717515271764115)) ;
#133659 = CARTESIAN_POINT('Origin',(0.,-1.05,0.)) ;
#133660 = CARTESIAN_POINT('',(-3.37639320225,-1.05,-1.58572958435533)) ;
#133661 = CARTESIAN_POINT('',(-3.42374530904768,-1.05,-1.59730454379476)) ;
#133662 = CARTESIAN_POINT('',(-3.37639320225,-1.05,1.58572958435533)) ;
#133663 = CARTESIAN_POINT('',(-3.37639320225,-1.05,0.)) ;
#133664 = CARTESIAN_POINT('',(-2.4237453090477,-1.05,1.35286009935032)) ;
#133665 = CARTESIAN_POINT('Origin',(-3.39999999999998,-1.05,0.)) ;
#133666 = CARTESIAN_POINT('',(-3.4211145618,-1.06055728090001,1.60759336013533)) ;
#133667 = CARTESIAN_POINT('',(-3.4211145618,-1.06055728090001,-1.60759336013533)) ;
#133668 = CARTESIAN_POINT('',(-3.4211145618,-1.06055728090001,0.)) ;
#133669 = CARTESIAN_POINT('',(-4.61732354306457,-1.65866177153229,-1.9)) ;
#133670 = CARTESIAN_POINT('',(-4.66717264538064,-1.68358632269033,-1.91218533612171)) ;
#133671 = CARTESIAN_POINT('',(-5.34472135954999,-2.022360679775,-1.9)) ;
#133672 = CARTESIAN_POINT('',(-5.4,-2.05,-1.9)) ;
#133673 = CARTESIAN_POINT('',(-5.34472135954999,-2.022360679775,1.9)) ;
#133674 = CARTESIAN_POINT('',(-5.34472135954999,-2.022360679775,2.)) ;
#133675 = CARTESIAN_POINT('',(-4.61732354306457,-1.65866177153229,1.9)) ;
#133676 = CARTESIAN_POINT('',(-4.65,-1.67500000000001,1.9)) ;
#133677 = CARTESIAN_POINT('',(-3.41717264538063,-1.05858632269032,1.60662978056615)) ;
#133678 = CARTESIAN_POINT('Origin',(-5.4,4.20000000000001,2.54)) ;
#133679 = CARTESIAN_POINT('',(-5.37474093186837,4.17158354835192,1.9)) ;
#133680 = CARTESIAN_POINT('',(-5.37474093186837,4.17158354835192,-1.9)) ;
#133681 = CARTESIAN_POINT('',(-5.37474093186837,4.17158354835192,-2.)) ;
#133682 = CARTESIAN_POINT('',(-4.58730397074619,3.28571696708947,-1.9)) ;
#133683 = CARTESIAN_POINT('',(-4.65,3.35625,-1.9)) ;
#133684 = CARTESIAN_POINT('',(-3.42983432543734,1.98356361611701,-1.61706297559117)) ;
#133685 = CARTESIAN_POINT('',(-3.40890098832149,1.96001361186167,-1.61194593762952)) ;
#133686 = CARTESIAN_POINT('',(-3.42983432543734,1.98356361611701,1.61706297559117)) ;
#133687 = CARTESIAN_POINT('',(-3.42983432543734,1.98356361611701,1.69444444444444)) ;
#133688 = CARTESIAN_POINT('',(-4.58730397074619,3.28571696708947,1.9)) ;
#133689 = CARTESIAN_POINT('',(-4.65890098832149,3.36626361186168,1.91750149318507)) ;
#133690 = CARTESIAN_POINT('',(-5.4,4.20000000000001,1.9)) ;
#133691 = CARTESIAN_POINT('Origin',(-3.15,-3.9,1.)) ;
#133692 = CARTESIAN_POINT('',(-3.15,-3.95,0.9)) ;
#133693 = CARTESIAN_POINT('',(-3.15,-3.85,0.9)) ;
#133694 = CARTESIAN_POINT('',(-3.15,-3.75,0.9)) ;
#133695 = CARTESIAN_POINT('',(-3.15,-3.85,-0.900000000000001)) ;
#133696 = CARTESIAN_POINT('',(-3.15,-3.85,1.)) ;
#133697 = CARTESIAN_POINT('',(-3.15,-3.95,-0.900000000000001)) ;
#133698 = CARTESIAN_POINT('',(-3.15,-4.05,-0.900000000000001)) ;
#133699 = CARTESIAN_POINT('',(-3.15,-3.95,1.)) ;
#133700 = CARTESIAN_POINT('Origin',(-4.4,-3.9,-1.)) ;
#133701 = CARTESIAN_POINT('',(-3.25,-3.85,-1.)) ;
#133702 = CARTESIAN_POINT('',(-4.3,-3.85,-1.)) ;
#133703 = CARTESIAN_POINT('',(-4.4,-3.85,-1.)) ;
#133704 = CARTESIAN_POINT('',(-4.3,-3.95,-1.)) ;
#133705 = CARTESIAN_POINT('',(-4.3,-4.05,-1.)) ;
#133706 = CARTESIAN_POINT('',(-3.25,-3.95,-1.)) ;
#133707 = CARTESIAN_POINT('',(-4.4,-3.95,-1.)) ;
#133708 = CARTESIAN_POINT('',(-3.25,-3.75,-1.)) ;
#133709 = CARTESIAN_POINT('Origin',(-4.4,-3.9,0.999999999999999)) ;
#133710 = CARTESIAN_POINT('',(-4.4,-3.85,-0.900000000000001)) ;
#133711 = CARTESIAN_POINT('',(-4.4,-3.85,0.899999999999999)) ;
#133712 = CARTESIAN_POINT('',(-4.4,-3.85,0.999999999999999)) ;
#133713 = CARTESIAN_POINT('',(-4.4,-3.95,0.899999999999999)) ;
#133714 = CARTESIAN_POINT('',(-4.4,-4.05,0.899999999999999)) ;
#133715 = CARTESIAN_POINT('',(-4.4,-3.95,-0.900000000000001)) ;
#133716 = CARTESIAN_POINT('',(-4.4,-3.95,0.999999999999999)) ;
#133717 = CARTESIAN_POINT('',(-4.4,-3.75,-0.900000000000001)) ;
#133718 = CARTESIAN_POINT('Origin',(-4.4,-3.9,0.999999999999999)) ;
#133719 = CARTESIAN_POINT('',(-4.3,-3.95,0.999999999999999)) ;
#133720 = CARTESIAN_POINT('',(-4.3,-3.85,0.999999999999999)) ;
#133721 = CARTESIAN_POINT('',(-4.3,-3.75,0.999999999999999)) ;
#133722 = CARTESIAN_POINT('',(-3.25,-3.85,1.)) ;
#133723 = CARTESIAN_POINT('',(-4.4,-3.85,0.999999999999999)) ;
#133724 = CARTESIAN_POINT('',(-3.25,-3.95,1.)) ;
#133725 = CARTESIAN_POINT('',(-3.25,-4.05,1.)) ;
#133726 = CARTESIAN_POINT('',(-4.4,-3.95,0.999999999999999)) ;
#133727 = CARTESIAN_POINT('Origin',(0.,-3.75,0.)) ;
#133728 = CARTESIAN_POINT('',(-3.25,-3.75,0.9)) ;
#133729 = CARTESIAN_POINT('',(-4.3,-3.75,0.899999999999999)) ;
#133730 = CARTESIAN_POINT('',(-1.56125112837913E-16,-3.75,0.9)) ;
#133731 = CARTESIAN_POINT('',(-4.3,-3.75,-0.900000000000001)) ;
#133732 = CARTESIAN_POINT('',(-4.3,-3.75,0.)) ;
#133733 = CARTESIAN_POINT('',(-3.25,-3.75,-0.900000000000001)) ;
#133734 = CARTESIAN_POINT('',(-1.56125112837913E-16,-3.75,-0.900000000000001)) ;
#133735 = CARTESIAN_POINT('',(-3.25,-3.75,-1.40946282423115E-15)) ;
#133736 = CARTESIAN_POINT('',(-4.15,-3.75,-0.850000000000001)) ;
#133737 = CARTESIAN_POINT('',(-3.4,-3.75,-0.850000000000001)) ;
#133738 = CARTESIAN_POINT('',(-4.15,-3.75,-0.850000000000001)) ;
#133739 = CARTESIAN_POINT('',(-4.25,-3.75,-0.75)) ;
#133740 = CARTESIAN_POINT('Origin',(-4.15,-3.75,-0.750000000000001)) ;
#133741 = CARTESIAN_POINT('',(-4.25,-3.75,0.749999999999999)) ;
#133742 = CARTESIAN_POINT('',(-4.25,-3.75,0.749999999999999)) ;
#133743 = CARTESIAN_POINT('',(-4.15,-3.75,0.85)) ;
#133744 = CARTESIAN_POINT('Origin',(-4.15,-3.75,0.75)) ;
#133745 = CARTESIAN_POINT('',(-3.4,-3.75,0.85)) ;
#133746 = CARTESIAN_POINT('',(-3.4,-3.75,0.85)) ;
#133747 = CARTESIAN_POINT('',(-3.3,-3.75,0.749999999999999)) ;
#133748 = CARTESIAN_POINT('Origin',(-3.4,-3.75,0.75)) ;
#133749 = CARTESIAN_POINT('',(-3.3,-3.75,-0.75)) ;
#133750 = CARTESIAN_POINT('',(-3.3,-3.75,-0.75)) ;
#133751 = CARTESIAN_POINT('Origin',(-3.4,-3.75,-0.750000000000001)) ;
#133752 = CARTESIAN_POINT('Origin',(-3.4,-3.75,-0.750000000000001)) ;
#133753 = CARTESIAN_POINT('',(-3.4,-3.9,-0.850000000000001)) ;
#133754 = CARTESIAN_POINT('',(-3.3,-3.9,-0.75)) ;
#133755 = CARTESIAN_POINT('Origin',(-3.4,-3.9,-0.750000000000001)) ;
#133756 = CARTESIAN_POINT('',(-3.4,-3.75,-0.850000000000001)) ;
#133757 = CARTESIAN_POINT('',(-3.3,-3.75,-0.75)) ;
#133758 = CARTESIAN_POINT('Origin',(-4.15,-3.75,-0.850000000000001)) ;
#133759 = CARTESIAN_POINT('',(-4.15,-3.9,-0.850000000000001)) ;
#133760 = CARTESIAN_POINT('',(-4.15,-3.9,-0.850000000000001)) ;
#133761 = CARTESIAN_POINT('',(-4.15,-3.75,-0.850000000000001)) ;
#133762 = CARTESIAN_POINT('Origin',(-4.15,-3.75,-0.750000000000001)) ;
#133763 = CARTESIAN_POINT('',(-4.25,-3.9,-0.75)) ;
#133764 = CARTESIAN_POINT('Origin',(-4.15,-3.9,-0.750000000000001)) ;
#133765 = CARTESIAN_POINT('',(-4.25,-3.75,-0.75)) ;
#133766 = CARTESIAN_POINT('Origin',(-4.25,-3.75,0.749999999999999)) ;
#133767 = CARTESIAN_POINT('',(-4.25,-3.9,0.749999999999999)) ;
#133768 = CARTESIAN_POINT('',(-4.25,-3.9,0.749999999999999)) ;
#133769 = CARTESIAN_POINT('',(-4.25,-3.75,0.749999999999999)) ;
#133770 = CARTESIAN_POINT('Origin',(-4.15,-3.75,0.75)) ;
#133771 = CARTESIAN_POINT('',(-4.15,-3.9,0.85)) ;
#133772 = CARTESIAN_POINT('Origin',(-4.15,-3.9,0.75)) ;
#133773 = CARTESIAN_POINT('',(-4.15,-3.75,0.85)) ;
#133774 = CARTESIAN_POINT('Origin',(-3.4,-3.75,0.85)) ;
#133775 = CARTESIAN_POINT('',(-3.4,-3.9,0.85)) ;
#133776 = CARTESIAN_POINT('',(-3.4,-3.9,0.85)) ;
#133777 = CARTESIAN_POINT('',(-3.4,-3.75,0.85)) ;
#133778 = CARTESIAN_POINT('Origin',(-3.4,-3.75,0.75)) ;
#133779 = CARTESIAN_POINT('',(-3.3,-3.9,0.749999999999999)) ;
#133780 = CARTESIAN_POINT('Origin',(-3.4,-3.9,0.75)) ;
#133781 = CARTESIAN_POINT('',(-3.3,-3.75,0.749999999999999)) ;
#133782 = CARTESIAN_POINT('Origin',(-3.3,-3.75,-0.75)) ;
#133783 = CARTESIAN_POINT('',(-3.3,-3.9,-0.75)) ;
#133784 = CARTESIAN_POINT('Origin',(0.,-3.9,0.)) ;
#133785 = CARTESIAN_POINT('Origin',(0.,9.95,0.)) ;
#133786 = CARTESIAN_POINT('',(-0.230887397576972,9.95,1.91486057185377)) ;
#133787 = CARTESIAN_POINT('Origin',(-0.321518176280637,8.95,1.8725987456797)) ;
#133788 = CARTESIAN_POINT('',(-0.321518176280637,9.05,1.8725987456797)) ;
#133789 = CARTESIAN_POINT('',(1.22782596331729,9.85,-1.449980483939)) ;
#133790 = CARTESIAN_POINT('Origin',(-1.22782596331729,8.95,1.449980483939)) ;
#133791 = CARTESIAN_POINT('',(-1.22782596331729,9.05,1.449980483939)) ;
#133792 = CARTESIAN_POINT('',(-1.22782596331729,9.85,1.449980483939)) ;
#133793 = CARTESIAN_POINT('Origin',(0.,8.95,0.)) ;
#133794 = CARTESIAN_POINT('',(-0.362523114814661,8.95,-0.169047304696279)) ;
#133795 = CARTESIAN_POINT('',(0.36252311481466,8.95,0.169047304696279)) ;
#133796 = CARTESIAN_POINT('Origin',(-2.65,10.8,-1.)) ;
#133797 = CARTESIAN_POINT('',(-2.65,10.75,-0.900000000000001)) ;
#133798 = CARTESIAN_POINT('',(-2.65,10.75,0.899999999999999)) ;
#133799 = CARTESIAN_POINT('',(-2.65,10.75,-1.)) ;
#133800 = CARTESIAN_POINT('',(-2.65,10.85,0.899999999999999)) ;
#133801 = CARTESIAN_POINT('',(-2.65,10.95,0.899999999999999)) ;
#133802 = CARTESIAN_POINT('',(-2.65,10.85,-0.900000000000001)) ;
#133803 = CARTESIAN_POINT('',(-2.65,10.85,-1.)) ;
#133804 = CARTESIAN_POINT('',(-2.65,10.65,-0.900000000000001)) ;
#133805 = CARTESIAN_POINT('Origin',(-3.9,10.8,1.)) ;
#133806 = CARTESIAN_POINT('',(-2.75,10.85,0.999999999999999)) ;
#133807 = CARTESIAN_POINT('',(-2.75,10.75,0.999999999999999)) ;
#133808 = CARTESIAN_POINT('',(-2.75,10.65,0.999999999999999)) ;
#133809 = CARTESIAN_POINT('',(-3.8,10.75,1.)) ;
#133810 = CARTESIAN_POINT('',(-3.9,10.75,1.)) ;
#133811 = CARTESIAN_POINT('',(-3.8,10.85,1.)) ;
#133812 = CARTESIAN_POINT('',(-3.8,10.95,1.)) ;
#133813 = CARTESIAN_POINT('',(-3.9,10.85,1.)) ;
#133814 = CARTESIAN_POINT('Origin',(-3.9,10.8,-1.)) ;
#133815 = CARTESIAN_POINT('',(-3.9,10.85,0.9)) ;
#133816 = CARTESIAN_POINT('',(-3.9,10.75,0.9)) ;
#133817 = CARTESIAN_POINT('',(-3.9,10.65,0.9)) ;
#133818 = CARTESIAN_POINT('',(-3.9,10.75,-0.9)) ;
#133819 = CARTESIAN_POINT('',(-3.9,10.75,-1.)) ;
#133820 = CARTESIAN_POINT('',(-3.9,10.85,-0.9)) ;
#133821 = CARTESIAN_POINT('',(-3.9,10.95,-0.9)) ;
#133822 = CARTESIAN_POINT('',(-3.9,10.85,-1.)) ;
#133823 = CARTESIAN_POINT('Origin',(-3.9,10.8,-1.)) ;
#133824 = CARTESIAN_POINT('',(-3.8,10.75,-1.)) ;
#133825 = CARTESIAN_POINT('',(-2.75,10.75,-1.)) ;
#133826 = CARTESIAN_POINT('',(-3.9,10.75,-1.)) ;
#133827 = CARTESIAN_POINT('',(-2.75,10.85,-1.)) ;
#133828 = CARTESIAN_POINT('',(-2.75,10.95,-1.)) ;
#133829 = CARTESIAN_POINT('',(-3.8,10.85,-1.)) ;
#133830 = CARTESIAN_POINT('',(-3.9,10.85,-1.)) ;
#133831 = CARTESIAN_POINT('',(-3.8,10.65,-1.)) ;
#133832 = CARTESIAN_POINT('Origin',(0.,10.65,0.)) ;
#133833 = CARTESIAN_POINT('',(-3.8,10.65,0.9)) ;
#133834 = CARTESIAN_POINT('',(-2.75,10.65,0.899999999999999)) ;
#133835 = CARTESIAN_POINT('',(1.56125112837912E-16,10.65,0.899999999999999)) ;
#133836 = CARTESIAN_POINT('',(-2.75,10.65,-0.900000000000001)) ;
#133837 = CARTESIAN_POINT('',(-2.75,10.65,5.96311194867028E-16)) ;
#133838 = CARTESIAN_POINT('',(-3.8,10.65,-0.9)) ;
#133839 = CARTESIAN_POINT('',(-1.56125112837913E-16,10.65,-0.900000000000001)) ;
#133840 = CARTESIAN_POINT('',(-3.8,10.65,8.23993651088984E-16)) ;
#133841 = CARTESIAN_POINT('',(-3.65,10.65,0.85)) ;
#133842 = CARTESIAN_POINT('',(-2.9,10.65,0.85)) ;
#133843 = CARTESIAN_POINT('',(-3.65,10.65,0.85)) ;
#133844 = CARTESIAN_POINT('',(-3.75,10.65,0.749999999999999)) ;
#133845 = CARTESIAN_POINT('Origin',(-3.65,10.65,0.75)) ;
#133846 = CARTESIAN_POINT('',(-3.75,10.65,-0.75)) ;
#133847 = CARTESIAN_POINT('',(-3.75,10.65,-0.75)) ;
#133848 = CARTESIAN_POINT('',(-3.65,10.65,-0.850000000000001)) ;
#133849 = CARTESIAN_POINT('Origin',(-3.65,10.65,-0.750000000000001)) ;
#133850 = CARTESIAN_POINT('',(-2.9,10.65,-0.850000000000001)) ;
#133851 = CARTESIAN_POINT('',(-2.9,10.65,-0.850000000000001)) ;
#133852 = CARTESIAN_POINT('',(-2.8,10.65,-0.75)) ;
#133853 = CARTESIAN_POINT('Origin',(-2.9,10.65,-0.750000000000001)) ;
#133854 = CARTESIAN_POINT('',(-2.8,10.65,0.749999999999999)) ;
#133855 = CARTESIAN_POINT('',(-2.8,10.65,0.749999999999999)) ;
#133856 = CARTESIAN_POINT('Origin',(-2.9,10.65,0.75)) ;
#133857 = CARTESIAN_POINT('Origin',(-2.9,10.65,0.75)) ;
#133858 = CARTESIAN_POINT('',(-2.8,10.7,0.749999999999999)) ;
#133859 = CARTESIAN_POINT('',(-2.8,10.65,0.749999999999999)) ;
#133860 = CARTESIAN_POINT('',(-2.9,10.7,0.85)) ;
#133861 = CARTESIAN_POINT('Origin',(-2.9,10.7,0.75)) ;
#133862 = CARTESIAN_POINT('',(-2.9,10.65,0.85)) ;
#133863 = CARTESIAN_POINT('Origin',(-3.65,10.65,0.85)) ;
#133864 = CARTESIAN_POINT('',(-3.65,10.7,0.85)) ;
#133865 = CARTESIAN_POINT('',(-3.65,10.7,0.85)) ;
#133866 = CARTESIAN_POINT('',(-3.65,10.65,0.85)) ;
#133867 = CARTESIAN_POINT('Origin',(-3.65,10.65,0.75)) ;
#133868 = CARTESIAN_POINT('',(-3.75,10.7,0.749999999999999)) ;
#133869 = CARTESIAN_POINT('Origin',(-3.65,10.7,0.75)) ;
#133870 = CARTESIAN_POINT('',(-3.75,10.65,0.749999999999999)) ;
#133871 = CARTESIAN_POINT('Origin',(-3.75,10.65,-0.75)) ;
#133872 = CARTESIAN_POINT('',(-3.75,10.7,-0.75)) ;
#133873 = CARTESIAN_POINT('',(-3.75,10.7,-0.75)) ;
#133874 = CARTESIAN_POINT('',(-3.75,10.65,-0.75)) ;
#133875 = CARTESIAN_POINT('Origin',(-3.65,10.65,-0.750000000000001)) ;
#133876 = CARTESIAN_POINT('',(-3.65,10.7,-0.850000000000001)) ;
#133877 = CARTESIAN_POINT('Origin',(-3.65,10.7,-0.750000000000001)) ;
#133878 = CARTESIAN_POINT('',(-3.65,10.65,-0.850000000000001)) ;
#133879 = CARTESIAN_POINT('Origin',(-2.9,10.65,-0.850000000000001)) ;
#133880 = CARTESIAN_POINT('',(-2.9,10.7,-0.850000000000001)) ;
#133881 = CARTESIAN_POINT('',(-2.9,10.7,-0.850000000000001)) ;
#133882 = CARTESIAN_POINT('',(-2.9,10.65,-0.850000000000001)) ;
#133883 = CARTESIAN_POINT('Origin',(-2.9,10.65,-0.750000000000001)) ;
#133884 = CARTESIAN_POINT('',(-2.8,10.7,-0.75)) ;
#133885 = CARTESIAN_POINT('Origin',(-2.9,10.7,-0.750000000000001)) ;
#133886 = CARTESIAN_POINT('',(-2.8,10.65,-0.75)) ;
#133887 = CARTESIAN_POINT('Origin',(-2.8,10.65,0.749999999999999)) ;
#133888 = CARTESIAN_POINT('',(-2.8,10.7,0.749999999999999)) ;
#133889 = CARTESIAN_POINT('Origin',(0.,10.8,0.)) ;
#133890 = CARTESIAN_POINT('',(-3.65,10.8,0.75)) ;
#133891 = CARTESIAN_POINT('',(-2.9,10.8,0.75)) ;
#133892 = CARTESIAN_POINT('',(0.,10.8,0.75)) ;
#133893 = CARTESIAN_POINT('',(-2.9,10.8,-0.750000000000001)) ;
#133894 = CARTESIAN_POINT('',(-2.9,10.8,0.)) ;
#133895 = CARTESIAN_POINT('',(-3.65,10.8,-0.750000000000001)) ;
#133896 = CARTESIAN_POINT('',(0.,10.8,-0.750000000000001)) ;
#133897 = CARTESIAN_POINT('',(-3.65,10.8,0.)) ;
#133898 = CARTESIAN_POINT('Origin',(4.5,2.75,-1.375)) ;
#133899 = CARTESIAN_POINT('',(4.5,2.63356010126946,-1.39440664978842)) ;
#133900 = CARTESIAN_POINT('',(4.6,2.11643989873054,-1.48059335021158)) ;
#133901 = CARTESIAN_POINT('',(4.6,2.11643989873054,-1.48059335021158)) ;
#133902 = CARTESIAN_POINT('',(12.7,2.11643989873054,-1.48059335021158)) ;
#133903 = CARTESIAN_POINT('',(12.8,2.11643989873054,-1.48059335021158)) ;
#133904 = CARTESIAN_POINT('',(12.7,2.75,-1.375)) ;
#133905 = CARTESIAN_POINT('Origin',(4.5,2.,-1.5)) ;
#133906 = CARTESIAN_POINT('',(4.6,2.,-1.38195395782836)) ;
#133907 = CARTESIAN_POINT('',(4.6,2.,1.5)) ;
#133908 = CARTESIAN_POINT('',(12.7,2.,-1.38195395782836)) ;
#133909 = CARTESIAN_POINT('',(12.7,2.,-1.5)) ;
#133910 = CARTESIAN_POINT('',(4.5,2.,-1.38195395782836)) ;
#133911 = CARTESIAN_POINT('Origin',(4.5,2.,1.5)) ;
#133912 = CARTESIAN_POINT('',(4.6,2.63356010126946,1.39440664978842)) ;
#133913 = CARTESIAN_POINT('',(4.6,2.63356010126947,1.39440664978842)) ;
#133914 = CARTESIAN_POINT('',(4.5,2.63356010126946,1.39440664978842)) ;
#133915 = CARTESIAN_POINT('',(12.7,2.,1.5)) ;
#133916 = CARTESIAN_POINT('Origin',(4.5,0.,0.)) ;
#133917 = CARTESIAN_POINT('',(4.5,2.72431432344521,1.30736518335501)) ;
#133918 = CARTESIAN_POINT('',(4.5,2.72431432344521,0.)) ;
#133919 = CARTESIAN_POINT('',(4.5,2.61712020253893,1.29576725740521)) ;
#133920 = CARTESIAN_POINT('Origin',(4.5,2.65,1.49304604217164)) ;
#133921 = CARTESIAN_POINT('',(4.5,2.1,1.38195395782836)) ;
#133922 = CARTESIAN_POINT('',(4.5,2.1,1.38195395782836)) ;
#133923 = CARTESIAN_POINT('',(4.5,2.1,-1.38195395782836)) ;
#133924 = CARTESIAN_POINT('',(4.5,2.1,-1.5)) ;
#133925 = CARTESIAN_POINT('',(4.5,2.61712020253893,-1.29576725740521)) ;
#133926 = CARTESIAN_POINT('Origin',(10.3,0.,0.)) ;
#133927 = CARTESIAN_POINT('Origin',(0.584645609909621,0.,0.)) ;
#133928 = CARTESIAN_POINT('',(4.6,-2.32258064516129,1.8988467939047)) ;
#133929 = CARTESIAN_POINT('',(4.6,-2.79310344827574,1.09479364595807)) ;
#133930 = CARTESIAN_POINT('Origin',(4.6,0.,0.)) ;
#133931 = CARTESIAN_POINT('',(4.6,-2.79310344827574,-1.09479364595807)) ;
#133932 = CARTESIAN_POINT('Origin',(4.6,0.,0.)) ;
#133933 = CARTESIAN_POINT('',(4.6,-2.32258064516129,-1.8988467939047)) ;
#133934 = CARTESIAN_POINT('Origin',(4.6,0.,0.)) ;
#133935 = CARTESIAN_POINT('',(12.7,-2.32258064516129,-1.8988467939047)) ;
#133936 = CARTESIAN_POINT('',(0.584645609909621,-2.32258064516129,-1.8988467939047)) ;
#133937 = CARTESIAN_POINT('',(12.7,-2.32258064516129,1.8988467939047)) ;
#133938 = CARTESIAN_POINT('Origin',(12.7,0.,0.)) ;
#133939 = CARTESIAN_POINT('',(0.584645609909621,-2.32258064516129,1.8988467939047)) ;
#133940 = CARTESIAN_POINT('Ctrl Pts',(-5.37474093186837,4.17158354835192,
1.9)) ;
#133941 = CARTESIAN_POINT('Ctrl Pts',(-5.4,4.2,1.9)) ;
#133942 = CARTESIAN_POINT('Ctrl Pts',(-5.4,4.23801993223491,1.9)) ;
#133943 = CARTESIAN_POINT('Ctrl Pts',(-5.37474093064202,4.17158354697228,
1.92625343593895)) ;
#133944 = CARTESIAN_POINT('Ctrl Pts',(-5.4,4.19999999724801,1.93751858720109)) ;
#133945 = CARTESIAN_POINT('Ctrl Pts',(-5.4,4.23801992976516,1.95250687190974)) ;
#133946 = CARTESIAN_POINT('Ctrl Pts',(-5.36668583490655,4.14629949399955,
1.95219871311588)) ;
#133947 = CARTESIAN_POINT('Ctrl Pts',(-5.4,4.16739198385624,1.97533216493415)) ;
#133948 = CARTESIAN_POINT('Ctrl Pts',(-5.4,4.20557579169425,2.00439742623175)) ;
#133949 = CARTESIAN_POINT('Ctrl Pts',(-5.33901380460609,4.05944006555646,
1.98922264312143)) ;
#133950 = CARTESIAN_POINT('Ctrl Pts',(-5.4,4.06625640449639,2.01686736338588)) ;
#133951 = CARTESIAN_POINT('Ctrl Pts',(-5.4,4.09411900298411,2.07844528624287)) ;
#133952 = CARTESIAN_POINT('Ctrl Pts',(-5.31962206268973,3.99857154231912,
2.)) ;
#133953 = CARTESIAN_POINT('Ctrl Pts',(-5.4,3.99346933127513,2.01799649257355)) ;
#133954 = CARTESIAN_POINT('Ctrl Pts',(-5.4,4.01601337581891,2.09999999951886)) ;
#133955 = CARTESIAN_POINT('Ctrl Pts',(-5.3,3.9369800677651,2.)) ;
#133956 = CARTESIAN_POINT('Ctrl Pts',(-5.4,3.9369800677651,2.)) ;
#133957 = CARTESIAN_POINT('Ctrl Pts',(-5.4,3.9369800677651,2.1)) ;
#133958 = CARTESIAN_POINT('Origin',(-5.3,4.23801993223491,1.9)) ;
#133959 = CARTESIAN_POINT('Ctrl Pts',(-5.3,3.9369800677651,2.)) ;
#133960 = CARTESIAN_POINT('Ctrl Pts',(-5.31962206268973,3.99857154231912,
2.)) ;
#133961 = CARTESIAN_POINT('Ctrl Pts',(-5.33901380460609,4.05944006555646,
1.98922264312143)) ;
#133962 = CARTESIAN_POINT('Ctrl Pts',(-5.36668583490655,4.14629949399955,
1.95219871311588)) ;
#133963 = CARTESIAN_POINT('Ctrl Pts',(-5.37474093064202,4.17158354697228,
1.92625343593895)) ;
#133964 = CARTESIAN_POINT('Ctrl Pts',(-5.37474093186837,4.17158354835192,
1.9)) ;
#133965 = CARTESIAN_POINT('Origin',(-5.3,3.9369800677651,2.1)) ;
#133966 = CARTESIAN_POINT('Origin',(-4.6737453090477,1.85,1.90286009935032)) ;
#133967 = CARTESIAN_POINT('Origin',(-3.35509339356897,1.85,1.58052296445552)) ;
#133968 = CARTESIAN_POINT('Ctrl Pts',(-3.35509339356897,1.95,1.58052296445552)) ;
#133969 = CARTESIAN_POINT('Ctrl Pts',(-3.33134808452128,1.95,1.6776628651052)) ;
#133970 = CARTESIAN_POINT('Ctrl Pts',(-3.33134808452128,1.85,1.6776628651052)) ;
#133971 = CARTESIAN_POINT('Ctrl Pts',(-3.38343213690419,1.95,1.59437746119719)) ;
#133972 = CARTESIAN_POINT('Ctrl Pts',(-3.36046743872484,1.94345445676969,
1.68478092946605)) ;
#133973 = CARTESIAN_POINT('Ctrl Pts',(-3.38803897426452,1.85000000162387,
1.69152063815355)) ;
#133974 = CARTESIAN_POINT('Ctrl Pts',(-3.41101314049054,1.96238978305186,
1.60786150708384)) ;
#133975 = CARTESIAN_POINT('Ctrl Pts',(-3.39538881861724,1.95068928167334,
1.69331726677308)) ;
#133976 = CARTESIAN_POINT('Ctrl Pts',(-3.44316973238528,1.87475949194143,
1.70499704569418)) ;
#133977 = CARTESIAN_POINT('Ctrl Pts',(-3.42983432543734,1.98356361611701,
1.61706297559117)) ;
#133978 = CARTESIAN_POINT('Ctrl Pts',(-3.42093333711585,1.97355000425533,
1.6995614824061)) ;
#133979 = CARTESIAN_POINT('Ctrl Pts',(-3.48082994825801,1.91712723223402,
1.71420287624085)) ;
#133980 = CARTESIAN_POINT('Origin',(-3.50457525730571,1.91712723223402,1.61706297559117)) ;
#133981 = CARTESIAN_POINT('Origin',(-3.36128627567748,2.03621361435751,1.58355059566492)) ;
#133982 = CARTESIAN_POINT('Origin',(-4.05330900605469,2.53445269957662,1.75119789195203)) ;
#133983 = CARTESIAN_POINT('Origin',(-4.66204490261456,3.21928058320648,1.9)) ;
#133984 = CARTESIAN_POINT('Origin',(-4.35749955255802,2.87666706439287,1.9)) ;
#133985 = CARTESIAN_POINT('Origin',(-4.66204490261456,3.21928058320648,1.9)) ;
#133986 = CARTESIAN_POINT('Origin',(-5.3,5.2,2.1)) ;
#133987 = CARTESIAN_POINT('Origin',(-5.3,-1.88819660112502,2.1)) ;
#133988 = CARTESIAN_POINT('Origin',(-5.3,4.23801993223491,2.54)) ;
#133989 = CARTESIAN_POINT('Origin',(-5.3,4.23801993223491,-1.9)) ;
#133990 = CARTESIAN_POINT('Origin',(-3.35509339356897,2.05,0.)) ;
#133991 = CARTESIAN_POINT('Origin',(-3.36128627567765,2.03621361435713,-1.583550595665)) ;
#133992 = CARTESIAN_POINT('Origin',(-2.4237453090477,1.85,-1.35286009935032)) ;
#133993 = CARTESIAN_POINT('Origin',(-3.35509339356897,1.85,-1.58052296445552)) ;
#133994 = CARTESIAN_POINT('Origin',(-4.66204490261456,3.21928058320648,1.9)) ;
#133995 = CARTESIAN_POINT('Origin',(-4.66204490261456,3.21928058320648,1.9)) ;
#133996 = CARTESIAN_POINT('Ctrl Pts',(-5.29976814257746,-1.88802911972917,
2.00000017262218)) ;
#133997 = CARTESIAN_POINT('Ctrl Pts',(-5.4,-1.88802831720455,1.99976740645701)) ;
#133998 = CARTESIAN_POINT('Ctrl Pts',(-5.4,-1.8879174628307,2.09999983753763)) ;
#133999 = CARTESIAN_POINT('Ctrl Pts',(-5.31153957531162,-1.92331224822995,
2.00001353231107)) ;
#134000 = CARTESIAN_POINT('Ctrl Pts',(-5.4,-1.92148676945292,2.01102210746197)) ;
#134001 = CARTESIAN_POINT('Ctrl Pts',(-5.4,-1.94671708614656,2.10006828697156)) ;
#134002 = CARTESIAN_POINT('Ctrl Pts',(-5.32318090226696,-1.95817527052251,
1.98921550273188)) ;
#134003 = CARTESIAN_POINT('Ctrl Pts',(-5.4,-1.96527310172482,2.00783661624713)) ;
#134004 = CARTESIAN_POINT('Ctrl Pts',(-5.4,-2.00485091174287,2.07850392511067)) ;
#134005 = CARTESIAN_POINT('Ctrl Pts',(-5.33978950165953,-2.00789652656154,
1.95213503498037)) ;
#134006 = CARTESIAN_POINT('Ctrl Pts',(-5.4,-2.02908601268744,1.96863348546834)) ;
#134007 = CARTESIAN_POINT('Ctrl Pts',(-5.4,-2.087770056524,2.00433878736395)) ;
#134008 = CARTESIAN_POINT('Ctrl Pts',(-5.34461954754096,-2.02234798681675,
1.92615385528167)) ;
#134009 = CARTESIAN_POINT('Ctrl Pts',(-5.4,-2.04997459329993,1.93432433515997)) ;
#134010 = CARTESIAN_POINT('Ctrl Pts',(-5.4,-2.11187974550671,1.95234231302604)) ;
#134011 = CARTESIAN_POINT('Ctrl Pts',(-5.34460423617422,-2.02230212313482,
1.89987524812986)) ;
#134012 = CARTESIAN_POINT('Ctrl Pts',(-5.4,-2.0499093833863,1.89983624572346)) ;
#134013 = CARTESIAN_POINT('Ctrl Pts',(-5.4,-2.11180321723903,1.89975033111955)) ;
#134014 = CARTESIAN_POINT('Origin',(-5.30000000000002,-1.88819660112507,1.90000000000004)) ;
#134015 = CARTESIAN_POINT('Origin',(-5.3,-2.11180339887499,1.9)) ;
#134016 = CARTESIAN_POINT('Ctrl Pts',(-5.3,3.9369800677651,-2.)) ;
#134017 = CARTESIAN_POINT('Ctrl Pts',(-5.4,3.9369800677651,-2.)) ;
#134018 = CARTESIAN_POINT('Ctrl Pts',(-5.4,3.9369800677651,-2.1)) ;
#134019 = CARTESIAN_POINT('Ctrl Pts',(-5.31962206268973,3.9985715423191,-2.)) ;
#134020 = CARTESIAN_POINT('Ctrl Pts',(-5.4,3.99346933127511,-2.01799649257355)) ;
#134021 = CARTESIAN_POINT('Ctrl Pts',(-5.4,4.01601337581889,-2.09999999951886)) ;
#134022 = CARTESIAN_POINT('Ctrl Pts',(-5.3390138046061,4.05944006555648,-1.98922264312143)) ;
#134023 = CARTESIAN_POINT('Ctrl Pts',(-5.4,4.06625640449641,-2.01686736338588)) ;
#134024 = CARTESIAN_POINT('Ctrl Pts',(-5.4,4.09411900298413,-2.07844528624287)) ;
#134025 = CARTESIAN_POINT('Ctrl Pts',(-5.36668583490655,4.14629949399953,
-1.95219871311588)) ;
#134026 = CARTESIAN_POINT('Ctrl Pts',(-5.4,4.16739198385622,-1.97533216493415)) ;
#134027 = CARTESIAN_POINT('Ctrl Pts',(-5.4,4.20557579169423,-2.00439742623175)) ;
#134028 = CARTESIAN_POINT('Ctrl Pts',(-5.37474093064202,4.17158354697228,
-1.92625343593895)) ;
#134029 = CARTESIAN_POINT('Ctrl Pts',(-5.4,4.19999999724801,-1.93751858720109)) ;
#134030 = CARTESIAN_POINT('Ctrl Pts',(-5.4,4.23801992976516,-1.95250687190974)) ;
#134031 = CARTESIAN_POINT('Ctrl Pts',(-5.37474093186837,4.17158354835192,
-1.9)) ;
#134032 = CARTESIAN_POINT('Ctrl Pts',(-5.4,4.2,-1.9)) ;
#134033 = CARTESIAN_POINT('Ctrl Pts',(-5.4,4.23801993223491,-1.9)) ;
#134034 = CARTESIAN_POINT('Origin',(-5.3,3.9369800677651,-2.1)) ;
#134035 = CARTESIAN_POINT('Ctrl Pts',(-5.37474093186837,4.17158354835192,
-1.9)) ;
#134036 = CARTESIAN_POINT('Ctrl Pts',(-5.37474093064202,4.17158354697228,
-1.92625343593895)) ;
#134037 = CARTESIAN_POINT('Ctrl Pts',(-5.36668583490655,4.14629949399953,
-1.95219871311588)) ;
#134038 = CARTESIAN_POINT('Ctrl Pts',(-5.3390138046061,4.05944006555648,-1.98922264312143)) ;
#134039 = CARTESIAN_POINT('Ctrl Pts',(-5.31962206268973,3.9985715423191,-2.)) ;
#134040 = CARTESIAN_POINT('Ctrl Pts',(-5.3,3.9369800677651,-2.)) ;
#134041 = CARTESIAN_POINT('Ctrl Pts',(-3.42983432543734,1.98356361611701,
-1.61706297559117)) ;
#134042 = CARTESIAN_POINT('Ctrl Pts',(-3.42093333711585,1.97355000425533,
-1.6995614824061)) ;
#134043 = CARTESIAN_POINT('Ctrl Pts',(-3.48082994825801,1.91712723223402,
-1.71420287624085)) ;
#134044 = CARTESIAN_POINT('Ctrl Pts',(-3.41101314049054,1.96238978305185,
-1.60786150708389)) ;
#134045 = CARTESIAN_POINT('Ctrl Pts',(-3.39538881861726,1.95068928167333,
-1.69331726677314)) ;
#134046 = CARTESIAN_POINT('Ctrl Pts',(-3.44316973238526,1.87475949194143,
-1.70499704569417)) ;
#134047 = CARTESIAN_POINT('Ctrl Pts',(-3.38343213690418,1.95,-1.59437746119719)) ;
#134048 = CARTESIAN_POINT('Ctrl Pts',(-3.36046743872482,1.94345445676967,
-1.68478092946604)) ;
#134049 = CARTESIAN_POINT('Ctrl Pts',(-3.38803897426454,1.85000000162387,
-1.69152063815355)) ;
#134050 = CARTESIAN_POINT('Ctrl Pts',(-3.35509339356897,1.95,-1.58052296445552)) ;
#134051 = CARTESIAN_POINT('Ctrl Pts',(-3.33134808452127,1.95,-1.6776628651052)) ;
#134052 = CARTESIAN_POINT('Ctrl Pts',(-3.33134808452128,1.85,-1.6776628651052)) ;
#134053 = CARTESIAN_POINT('Origin',(-3.50457525730571,1.91712723223402,-1.61706297559117)) ;
#134054 = CARTESIAN_POINT('Origin',(-4.66204490261456,1.95,1.9)) ;
#134055 = CARTESIAN_POINT('Origin',(-4.66204490261456,-1.5692190524323,1.9)) ;
#134056 = CARTESIAN_POINT('Origin',(-3.84472135955,-1.16055728090002,1.9)) ;
#134057 = CARTESIAN_POINT('Origin',(-4.66204490261456,-1.5692190524323,1.9)) ;
#134058 = CARTESIAN_POINT('Origin',(-5.3,-2.11180339887499,2.54)) ;
#134059 = CARTESIAN_POINT('Origin',(-5.3,-2.11180339887499,-1.9)) ;
#134060 = CARTESIAN_POINT('Origin',(-5.3,1.95,-2.1)) ;
#134061 = CARTESIAN_POINT('Origin',(-5.3,-1.88819660112501,-2.1)) ;
#134062 = CARTESIAN_POINT('Origin',(-4.0264650697994,2.50425327128942,-1.9)) ;
#134063 = CARTESIAN_POINT('Origin',(-4.66204490261456,3.21928058320648,-1.9)) ;
#134064 = CARTESIAN_POINT('Origin',(-3.02790825149799,1.38087685070033,-1.5005443741715)) ;
#134065 = CARTESIAN_POINT('Origin',(-4.66204490261456,3.21928058320648,-1.9)) ;
#134066 = CARTESIAN_POINT('Origin',(-4.66204490261456,-1.5692190524323,1.9)) ;
#134067 = CARTESIAN_POINT('Origin',(-4.66204490261456,-1.5692190524323,1.9)) ;
#134068 = CARTESIAN_POINT('Ctrl Pts',(-5.34460423617422,-2.02230212313483,
-1.89987524812986)) ;
#134069 = CARTESIAN_POINT('Ctrl Pts',(-5.4,-2.0499093833863,-1.89983624572346)) ;
#134070 = CARTESIAN_POINT('Ctrl Pts',(-5.4,-2.11180321723903,-1.89975033111956)) ;
#134071 = CARTESIAN_POINT('Ctrl Pts',(-5.34461954754096,-2.02234798681675,
-1.92615385528167)) ;
#134072 = CARTESIAN_POINT('Ctrl Pts',(-5.4,-2.04997459329992,-1.93432433515996)) ;
#134073 = CARTESIAN_POINT('Ctrl Pts',(-5.4,-2.11187974550671,-1.95234231302603)) ;
#134074 = CARTESIAN_POINT('Ctrl Pts',(-5.33978950165954,-2.00789652656154,
-1.95213503498037)) ;
#134075 = CARTESIAN_POINT('Ctrl Pts',(-5.4,-2.02908601268745,-1.96863348546836)) ;
#134076 = CARTESIAN_POINT('Ctrl Pts',(-5.4,-2.087770056524,-2.00433878736397)) ;
#134077 = CARTESIAN_POINT('Ctrl Pts',(-5.32318090226696,-1.95817527052251,
-1.98921550273188)) ;
#134078 = CARTESIAN_POINT('Ctrl Pts',(-5.4,-1.96527310172481,-2.00783661624711)) ;
#134079 = CARTESIAN_POINT('Ctrl Pts',(-5.4,-2.00485091174287,-2.07850392511065)) ;
#134080 = CARTESIAN_POINT('Ctrl Pts',(-5.31153957531163,-1.92331224822995,
-2.00001353231107)) ;
#134081 = CARTESIAN_POINT('Ctrl Pts',(-5.4,-1.92148676945294,-2.01102210746198)) ;
#134082 = CARTESIAN_POINT('Ctrl Pts',(-5.4,-1.94671708614656,-2.10006828697156)) ;
#134083 = CARTESIAN_POINT('Ctrl Pts',(-5.29976814257746,-1.88802911972917,
-2.00000017262218)) ;
#134084 = CARTESIAN_POINT('Ctrl Pts',(-5.4,-1.88802831720455,-1.99976740645701)) ;
#134085 = CARTESIAN_POINT('Ctrl Pts',(-5.4,-1.8879174628307,-2.09999983753763)) ;
#134086 = CARTESIAN_POINT('Origin',(-5.30000000000002,-1.88819660112507,-1.90000000000004)) ;
#134087 = CARTESIAN_POINT('Origin',(-4.66204490261456,3.21928058320648,-1.9)) ;
#134088 = CARTESIAN_POINT('Origin',(-4.66204490261456,3.21928058320648,-1.9)) ;
#134089 = CARTESIAN_POINT('Origin',(0.175392621986784,-0.95,0.717515271764115)) ;
#134090 = CARTESIAN_POINT('Origin',(-3.37639320225,-0.95,1.58572958435533)) ;
#134091 = CARTESIAN_POINT('Origin',(-3.32804538583365,-0.902219294041845,
1.57391122923133)) ;
#134092 = CARTESIAN_POINT('Origin',(-3.46583592134999,-0.971114561800017,
1.60759336013533)) ;
#134093 = CARTESIAN_POINT('Origin',(-3.24472135955,-0.860557280900019,-1.9)) ;
#134094 = CARTESIAN_POINT('Origin',(-4.66204490261456,-1.5692190524323,-1.9)) ;
#134095 = CARTESIAN_POINT('Origin',(-4.66204490261456,1.95,-1.9)) ;
#134096 = CARTESIAN_POINT('Origin',(-4.66204490261456,-1.5692190524323,-1.9)) ;
#134097 = CARTESIAN_POINT('Ctrl Pts',(-3.4211145618,-1.06055728090001,1.60759336013533)) ;
#134098 = CARTESIAN_POINT('Ctrl Pts',(-3.40394191641935,-1.05197095820969,
1.69540802401362)) ;
#134099 = CARTESIAN_POINT('Ctrl Pts',(-3.44209061230229,-0.971114561800017,
1.70473326078501)) ;
#134100 = CARTESIAN_POINT('Ctrl Pts',(-3.40727897628736,-1.05363948814369,
1.6008292960084)) ;
#134101 = CARTESIAN_POINT('Ctrl Pts',(-3.38665319245547,-1.04670310838586,
1.69118189148914)) ;
#134102 = CARTESIAN_POINT('Ctrl Pts',(-3.41441594520969,-0.957277229261624,
1.69796834216237)) ;
#134103 = CARTESIAN_POINT('Ctrl Pts',(-3.3918627446443,-1.05,1.5932924717481)) ;
#134104 = CARTESIAN_POINT('Ctrl Pts',(-3.36870744055524,-1.04639008266723,
1.68679515213573)) ;
#134105 = CARTESIAN_POINT('Ctrl Pts',(-3.38358960366098,-0.950000000886305,
1.69043301422824)) ;
#134106 = CARTESIAN_POINT('Ctrl Pts',(-3.37639320225,-1.05,1.58572958435533)) ;
#134107 = CARTESIAN_POINT('Ctrl Pts',(-3.3526478932023,-1.05,1.68286948500501)) ;
#134108 = CARTESIAN_POINT('Ctrl Pts',(-3.3526478932023,-0.95,1.68286948500501)) ;
#134109 = CARTESIAN_POINT('Origin',(-3.3763932022502,-1.14999999999944,1.58572958435544)) ;
#134110 = CARTESIAN_POINT('Origin',(-4.66204490261456,-1.5692190524323,-1.9)) ;
#134111 = CARTESIAN_POINT('Origin',(-4.66204490261456,-1.5692190524323,-1.9)) ;
#134112 = CARTESIAN_POINT('Origin',(-3.37639320225,-1.15,0.)) ;
#134113 = CARTESIAN_POINT('Origin',(-3.37639320224909,-1.15000000000409,-1.58572958435489)) ;
#134114 = CARTESIAN_POINT('Origin',(-1.50751564693271,0.00804557540861825,
-1.1288928486111)) ;
#134115 = CARTESIAN_POINT('Origin',(-3.46583592134999,-0.971114561800017,
-1.60759336013533)) ;
#134116 = CARTESIAN_POINT('Ctrl Pts',(-3.37639320225,-1.05,-1.58572958435533)) ;
#134117 = CARTESIAN_POINT('Ctrl Pts',(-3.3526478932023,-1.05,-1.68286948500501)) ;
#134118 = CARTESIAN_POINT('Ctrl Pts',(-3.3526478932023,-0.95,-1.68286948500501)) ;
#134119 = CARTESIAN_POINT('Ctrl Pts',(-3.3918627446443,-1.05,-1.5932924717481)) ;
#134120 = CARTESIAN_POINT('Ctrl Pts',(-3.36870744055523,-1.04639008266724,
-1.68679515213575)) ;
#134121 = CARTESIAN_POINT('Ctrl Pts',(-3.38358960366098,-0.950000000886305,
-1.69043301422824)) ;
#134122 = CARTESIAN_POINT('Ctrl Pts',(-3.40727897628736,-1.05363948814369,
-1.6008292960084)) ;
#134123 = CARTESIAN_POINT('Ctrl Pts',(-3.38665319245549,-1.04670310838585,
-1.69118189148912)) ;
#134124 = CARTESIAN_POINT('Ctrl Pts',(-3.4144159452097,-0.957277229261623,
-1.69796834216237)) ;
#134125 = CARTESIAN_POINT('Ctrl Pts',(-3.4211145618,-1.06055728090001,-1.60759336013533)) ;
#134126 = CARTESIAN_POINT('Ctrl Pts',(-3.40394191641936,-1.05197095820969,
-1.69540802401362)) ;
#134127 = CARTESIAN_POINT('Ctrl Pts',(-3.4420906123023,-0.971114561800017,
-1.70473326078501)) ;
#134128 = CARTESIAN_POINT('Origin',(-3.37639320225,-0.95,-1.58572958435533)) ;
#134129 = CARTESIAN_POINT('Origin',(0.175392621986784,-0.95,-0.717515271764115)) ;
#134130 = CARTESIAN_POINT('Origin',(12.7,2.65,2.54)) ;
#134131 = CARTESIAN_POINT('Origin',(12.8,2.65,-1.49304604217164)) ;
#134132 = CARTESIAN_POINT('',(4.57524318173533,2.73534903669982,-1.44093518020973)) ;
#134133 = CARTESIAN_POINT('Origin',(4.65232986200348,2.66527023615519,-1.48875421118475)) ;
#134134 = CARTESIAN_POINT('Ctrl Pts',(4.57524318173533,2.73534903669982,-1.44093518020973)) ;
#134135 = CARTESIAN_POINT('Ctrl Pts',(4.5761458558036,2.73452842391049,-1.43959115118323)) ;
#134136 = CARTESIAN_POINT('Ctrl Pts',(4.57705238626145,2.73367683201792,-1.43826812933933)) ;
#134137 = CARTESIAN_POINT('Ctrl Pts',(4.5779495181309,2.73280244902547,-1.43697684888884)) ;
#134138 = CARTESIAN_POINT('Ctrl Pts',(4.58144263576937,2.72939790755538,-1.43194905456852)) ;
#134139 = CARTESIAN_POINT('Ctrl Pts',(4.58496694799988,2.72549786515178,-1.4271699445179)) ;
#134140 = CARTESIAN_POINT('Ctrl Pts',(4.58815670056909,2.72107165565041,-1.42269819385267)) ;
#134141 = CARTESIAN_POINT('Ctrl Pts',(4.59069123847476,2.71755464437251,-1.41914499612971)) ;
#134142 = CARTESIAN_POINT('Ctrl Pts',(4.59301454561855,2.71370459823904,-1.41578631272423)) ;
#134143 = CARTESIAN_POINT('Ctrl Pts',(4.5949431309995,2.70950205848693,-1.41267499616739)) ;
#134144 = CARTESIAN_POINT('Ctrl Pts',(4.59651854606292,2.70606910472949,-1.41013343642151)) ;
#134145 = CARTESIAN_POINT('Ctrl Pts',(4.59783685868317,2.70233705077434,-1.40771608615721)) ;
#134146 = CARTESIAN_POINT('Ctrl Pts',(4.5987311897142,2.69838744820012,-1.4055323012124)) ;
#134147 = CARTESIAN_POINT('Ctrl Pts',(4.59916508318196,2.69647125978917,-1.40447281653651)) ;
#134148 = CARTESIAN_POINT('Ctrl Pts',(4.59949917984822,2.69450444432192,-1.40346779888205)) ;
#134149 = CARTESIAN_POINT('Ctrl Pts',(4.5997144226265,2.69249922659198,-1.40252634409943)) ;
#134150 = CARTESIAN_POINT('Ctrl Pts',(4.59990113259977,2.6907598225955,-1.40170968953523)) ;
#134151 = CARTESIAN_POINT('Ctrl Pts',(4.6,2.68896788689974,-1.40093031221453)) ;
#134152 = CARTESIAN_POINT('Ctrl Pts',(4.6,2.68715716172261,-1.40020561276333)) ;
#134153 = CARTESIAN_POINT('Origin',(4.5,2.1,-1.38195395782836)) ;
#134154 = CARTESIAN_POINT('Origin',(4.6,2.1,-1.38195395782836)) ;
#134155 = CARTESIAN_POINT('Origin',(12.7,2.1,-1.38195395782836)) ;
#134156 = CARTESIAN_POINT('Origin',(12.7,2.76643989873054,-1.47363939238321)) ;
#134157 = CARTESIAN_POINT('Origin',(12.7,2.13287979746107,-1.57923274259479)) ;
#134158 = CARTESIAN_POINT('Origin',(4.4,2.72431432344521,0.)) ;
#134159 = CARTESIAN_POINT('Ctrl Pts',(4.48762159086959,2.77250619842349,1.38882431825052)) ;
#134160 = CARTESIAN_POINT('Ctrl Pts',(4.48806820038223,2.77169418112776,1.38616443291017)) ;
#134161 = CARTESIAN_POINT('Ctrl Pts',(4.48852084821546,2.77084293101113,1.38351728498153)) ;
#134162 = CARTESIAN_POINT('Ctrl Pts',(4.49012932137855,2.76769877392855,1.37423699047925)) ;
#134163 = CARTESIAN_POINT('Ctrl Pts',(4.49131046584975,2.76517764467227,1.36765586829652)) ;
#134164 = CARTESIAN_POINT('Ctrl Pts',(4.49351977821777,2.75978760391029,1.35536471983786)) ;
#134165 = CARTESIAN_POINT('Ctrl Pts',(4.49455195297829,2.75697653750121,1.34963225939859)) ;
#134166 = CARTESIAN_POINT('Ctrl Pts',(4.49620670090467,2.75163165728869,1.34005667839666)) ;
#134167 = CARTESIAN_POINT('Ctrl Pts',(4.49686252944493,2.74924176842721,1.33613597379662)) ;
#134168 = CARTESIAN_POINT('Ctrl Pts',(4.49822764032851,2.74331716058947,1.32735536836523)) ;
#134169 = CARTESIAN_POINT('Ctrl Pts',(4.49890203357906,2.73961076902699,1.32251349983941)) ;
#134170 = CARTESIAN_POINT('Ctrl Pts',(4.49975897856023,2.73206576252672,1.31417222156017)) ;
#134171 = CARTESIAN_POINT('Ctrl Pts',(4.5,2.72833175948612,1.31058099770818)) ;
#134172 = CARTESIAN_POINT('Ctrl Pts',(4.5,2.72431432344521,1.30736518335501)) ;
#134173 = CARTESIAN_POINT('Ctrl Pts',(4.5,2.72431432344521,-1.30736518335501)) ;
#134174 = CARTESIAN_POINT('Ctrl Pts',(4.5,2.72904669151435,-1.31115327531372)) ;
#134175 = CARTESIAN_POINT('Ctrl Pts',(4.49966645684473,2.73338556955569,-1.31546141017617)) ;
#134176 = CARTESIAN_POINT('Ctrl Pts',(4.49869539480391,2.74072289096386,-1.32398024143758)) ;
#134177 = CARTESIAN_POINT('Ctrl Pts',(4.49811062025686,2.74382502998089,-1.3281080596587)) ;
#134178 = CARTESIAN_POINT('Ctrl Pts',(4.49664125196625,2.75020211699688,-1.33755926494058)) ;
#134179 = CARTESIAN_POINT('Ctrl Pts',(4.4957072138971,2.75339870015142,-1.34301039031936)) ;
#134180 = CARTESIAN_POINT('Ctrl Pts',(4.49363760641476,2.7595286326395,-1.35475170518698)) ;
#134181 = CARTESIAN_POINT('Ctrl Pts',(4.49249077386341,2.76240287369075,-1.36107122583085)) ;
#134182 = CARTESIAN_POINT('Ctrl Pts',(4.49055019898871,2.7667775727014,-1.37191412562091)) ;
#134183 = CARTESIAN_POINT('Ctrl Pts',(4.48975662823143,2.76842729450635,-1.37638729192265)) ;
#134184 = CARTESIAN_POINT('Ctrl Pts',(4.4885208482156,2.77084293101086,-1.38351728498073)) ;
#134185 = CARTESIAN_POINT('Ctrl Pts',(4.48806820038252,2.77169418112725,-1.38616443290854)) ;
#134186 = CARTESIAN_POINT('Ctrl Pts',(4.48762159086959,2.77250619842348,-1.38882431824782)) ;
#134187 = CARTESIAN_POINT('Origin',(4.6,2.1,0.)) ;
#134188 = CARTESIAN_POINT('Origin',(4.6,2.1,1.38195395782836)) ;
#134189 = CARTESIAN_POINT('Origin',(4.6,2.1,-1.38195395782836)) ;
#134190 = CARTESIAN_POINT('Origin',(12.7,2.1,-1.38195395782836)) ;
#134191 = CARTESIAN_POINT('Origin',(12.7,1.9,-1.38195395782836)) ;
#134192 = CARTESIAN_POINT('Origin',(12.7,2.65,2.54)) ;
#134193 = CARTESIAN_POINT('Origin',(4.5,2.65,1.49304604217164)) ;
#134194 = CARTESIAN_POINT('',(4.6,2.68715716172261,1.40020561276332)) ;
#134195 = CARTESIAN_POINT('',(4.57524318173443,2.73534903670064,1.44093518021108)) ;
#134196 = CARTESIAN_POINT('Ctrl Pts',(4.6,2.68715716172261,1.40020561276333)) ;
#134197 = CARTESIAN_POINT('Ctrl Pts',(4.6,2.69106036671412,1.40176777722153)) ;
#134198 = CARTESIAN_POINT('Ctrl Pts',(4.59952510519173,2.69488861888988,1.4035902905253)) ;
#134199 = CARTESIAN_POINT('Ctrl Pts',(4.59869497748254,2.6985274364077,1.40560984877499)) ;
#134200 = CARTESIAN_POINT('Ctrl Pts',(4.59815316003464,2.70090246232127,1.40692799763887)) ;
#134201 = CARTESIAN_POINT('Ctrl Pts',(4.59746001108778,2.70319720658047,1.40832903195479)) ;
#134202 = CARTESIAN_POINT('Ctrl Pts',(4.59664880273703,2.7053865971179,1.40978545810151)) ;
#134203 = CARTESIAN_POINT('Ctrl Pts',(4.59612777291939,2.70679281754376,1.41072090390766)) ;
#134204 = CARTESIAN_POINT('Ctrl Pts',(4.59555051815356,2.70817855133085,1.41169507009278)) ;
#134205 = CARTESIAN_POINT('Ctrl Pts',(4.59494172533681,2.70950512149367,1.41267726393019)) ;
#134206 = CARTESIAN_POINT('Ctrl Pts',(4.59250947890865,2.71480502887008,1.4166013205009)) ;
#134207 = CARTESIAN_POINT('Ctrl Pts',(4.58944857812999,2.7195451700524,1.42091766241906)) ;
#134208 = CARTESIAN_POINT('Ctrl Pts',(4.58612768646826,2.72376361218902,1.42552619681616)) ;
#134209 = CARTESIAN_POINT('Ctrl Pts',(4.58350334758184,2.72709724148709,1.42916809702239)) ;
#134210 = CARTESIAN_POINT('Ctrl Pts',(4.58071664514667,2.73010548898771,1.43299400406844)) ;
#134211 = CARTESIAN_POINT('Ctrl Pts',(4.5779495181309,2.73280244902548,1.43697684888885)) ;
#134212 = CARTESIAN_POINT('Ctrl Pts',(4.57705238626115,2.73367683201822,1.43826812933977)) ;
#134213 = CARTESIAN_POINT('Ctrl Pts',(4.576145855803,2.73452842391106,1.43959115118411)) ;
#134214 = CARTESIAN_POINT('Ctrl Pts',(4.57524318173443,2.73534903670064,1.44093518021108)) ;
#134215 = CARTESIAN_POINT('Origin',(4.65232986199958,2.66527023615875,1.48875421118384)) ;
#134216 = CARTESIAN_POINT('Origin',(4.6,2.65,1.49304604217164)) ;
#134217 = CARTESIAN_POINT('Origin',(12.7,1.9,-1.5)) ;
#134218 = CARTESIAN_POINT('Origin',(12.7,2.01643989873054,1.59863939238321)) ;
#134219 = CARTESIAN_POINT('Origin',(-3.65,10.7,0.75)) ;
#134220 = CARTESIAN_POINT('Origin',(-3.65,10.7,0.75)) ;
#134221 = CARTESIAN_POINT('Origin',(-3.65,10.7,0.75)) ;
#134222 = CARTESIAN_POINT('Origin',(0.,10.7,0.75)) ;
#134223 = CARTESIAN_POINT('Origin',(-2.9,10.7,0.75)) ;
#134224 = CARTESIAN_POINT('Origin',(-3.65,10.7,0.)) ;
#134225 = CARTESIAN_POINT('Origin',(-3.65,10.7,-0.75)) ;
#134226 = CARTESIAN_POINT('Origin',(-2.9,10.7,0.75)) ;
#134227 = CARTESIAN_POINT('Origin',(-2.9,10.7,0.75)) ;
#134228 = CARTESIAN_POINT('Origin',(-3.65,10.7,-0.750000000000001)) ;
#134229 = CARTESIAN_POINT('Origin',(-3.65,10.7,-0.750000000000001)) ;
#134230 = CARTESIAN_POINT('Origin',(-2.9,10.7,0.)) ;
#134231 = CARTESIAN_POINT('Origin',(-2.9,10.7,-0.750000000000001)) ;
#134232 = CARTESIAN_POINT('Origin',(0.,10.7,-0.750000000000001)) ;
#134233 = CARTESIAN_POINT('Origin',(-2.9,10.7,-0.750000000000001)) ;
#134234 = CARTESIAN_POINT('Origin',(-2.9,10.7,-0.750000000000001)) ;
#134235 = CARTESIAN_POINT('Origin',(-3.05,-3.95,1.)) ;
#134236 = CARTESIAN_POINT('Origin',(-3.05,-3.95,-0.900000000000001)) ;
#134237 = CARTESIAN_POINT('Origin',(-3.05,-3.95,0.9)) ;
#134238 = CARTESIAN_POINT('Origin',(-3.25,-3.95,0.9)) ;
#134239 = CARTESIAN_POINT('Origin',(-3.25,-3.95,1.1)) ;
#134240 = CARTESIAN_POINT('Origin',(-3.25,-3.95,0.9)) ;
#134241 = CARTESIAN_POINT('Origin',(-3.25,-3.95,-0.900000000000001)) ;
#134242 = CARTESIAN_POINT('Origin',(-3.25,-3.95,-0.900000000000001)) ;
#134243 = CARTESIAN_POINT('Origin',(-3.25,-3.95,-1.1)) ;
#134244 = CARTESIAN_POINT('Origin',(-4.4,-3.95,1.1)) ;
#134245 = CARTESIAN_POINT('Origin',(-4.3,-3.95,1.1)) ;
#134246 = CARTESIAN_POINT('Origin',(-3.25,-3.9,0.9)) ;
#134247 = CARTESIAN_POINT('Origin',(-3.25,-3.85,0.9)) ;
#134248 = CARTESIAN_POINT('Origin',(-3.25,-3.85,-1.40946282423115E-15)) ;
#134249 = CARTESIAN_POINT('Origin',(-3.25,-3.85,-0.900000000000001)) ;
#134250 = CARTESIAN_POINT('Origin',(-3.25,-3.85,0.9)) ;
#134251 = CARTESIAN_POINT('Origin',(-3.25,-3.9,-0.900000000000001)) ;
#134252 = CARTESIAN_POINT('Origin',(-3.25,-3.85,-0.900000000000001)) ;
#134253 = CARTESIAN_POINT('Origin',(-4.4,-3.95,-1.1)) ;
#134254 = CARTESIAN_POINT('Origin',(-4.3,-3.95,-1.1)) ;
#134255 = CARTESIAN_POINT('Origin',(-4.5,-3.95,0.999999999999999)) ;
#134256 = CARTESIAN_POINT('Origin',(-4.5,-3.95,0.899999999999999)) ;
#134257 = CARTESIAN_POINT('Origin',(-4.5,-3.95,-0.900000000000001)) ;
#134258 = CARTESIAN_POINT('Origin',(-4.3,-3.95,0.899999999999999)) ;
#134259 = CARTESIAN_POINT('Origin',(-4.3,-3.95,0.899999999999999)) ;
#134260 = CARTESIAN_POINT('Origin',(-3.25,-3.85,0.9)) ;
#134261 = CARTESIAN_POINT('Origin',(-3.25,-3.85,0.9)) ;
#134262 = CARTESIAN_POINT('Origin',(-3.25,-3.85,-0.900000000000001)) ;
#134263 = CARTESIAN_POINT('Origin',(-3.25,-3.85,-0.900000000000001)) ;
#134264 = CARTESIAN_POINT('Origin',(-4.3,-3.95,-0.900000000000001)) ;
#134265 = CARTESIAN_POINT('Origin',(-4.3,-3.95,-0.900000000000001)) ;
#134266 = CARTESIAN_POINT('Origin',(-4.3,-3.9,0.899999999999999)) ;
#134267 = CARTESIAN_POINT('Origin',(-4.3,-3.85,0.899999999999999)) ;
#134268 = CARTESIAN_POINT('Origin',(-1.56125112837913E-16,-3.85,0.9)) ;
#134269 = CARTESIAN_POINT('Origin',(-4.3,-3.85,0.899999999999999)) ;
#134270 = CARTESIAN_POINT('Origin',(-1.56125112837913E-16,-3.85,-0.900000000000001)) ;
#134271 = CARTESIAN_POINT('Origin',(-4.3,-3.85,-0.900000000000001)) ;
#134272 = CARTESIAN_POINT('Origin',(-4.3,-3.9,-0.900000000000001)) ;
#134273 = CARTESIAN_POINT('Origin',(-4.3,-3.85,-0.900000000000001)) ;
#134274 = CARTESIAN_POINT('Origin',(-4.3,-3.85,0.899999999999999)) ;
#134275 = CARTESIAN_POINT('Origin',(-4.3,-3.85,0.899999999999999)) ;
#134276 = CARTESIAN_POINT('Origin',(-4.3,-3.85,-0.900000000000001)) ;
#134277 = CARTESIAN_POINT('Origin',(-4.3,-3.85,-0.900000000000001)) ;
#134278 = CARTESIAN_POINT('Origin',(-4.3,-3.85,0.)) ;
#134279 = CARTESIAN_POINT('Origin',(-4.,10.85,-1.)) ;
#134280 = CARTESIAN_POINT('Origin',(-4.,10.85,-0.9)) ;
#134281 = CARTESIAN_POINT('Origin',(-4.,10.85,0.9)) ;
#134282 = CARTESIAN_POINT('Origin',(-3.8,10.85,0.9)) ;
#134283 = CARTESIAN_POINT('Origin',(-3.8,10.85,1.1)) ;
#134284 = CARTESIAN_POINT('Origin',(-3.8,10.85,0.9)) ;
#134285 = CARTESIAN_POINT('Origin',(-3.8,10.85,-0.9)) ;
#134286 = CARTESIAN_POINT('Origin',(-3.8,10.85,-0.9)) ;
#134287 = CARTESIAN_POINT('Origin',(-3.8,10.85,-1.1)) ;
#134288 = CARTESIAN_POINT('Origin',(-3.9,10.85,1.1)) ;
#134289 = CARTESIAN_POINT('Origin',(-2.75,10.85,1.1)) ;
#134290 = CARTESIAN_POINT('Origin',(-3.8,10.8,0.9)) ;
#134291 = CARTESIAN_POINT('Origin',(-3.8,10.75,0.9)) ;
#134292 = CARTESIAN_POINT('Origin',(-3.8,10.75,8.23993651088984E-16)) ;
#134293 = CARTESIAN_POINT('Origin',(-3.8,10.75,-0.9)) ;
#134294 = CARTESIAN_POINT('Origin',(-3.8,10.75,0.9)) ;
#134295 = CARTESIAN_POINT('Origin',(-3.8,10.8,-0.9)) ;
#134296 = CARTESIAN_POINT('Origin',(-3.8,10.75,-0.9)) ;
#134297 = CARTESIAN_POINT('Origin',(-3.9,10.85,-1.1)) ;
#134298 = CARTESIAN_POINT('Origin',(-2.75,10.85,-1.1)) ;
#134299 = CARTESIAN_POINT('Origin',(-2.55,10.85,-1.)) ;
#134300 = CARTESIAN_POINT('Origin',(-2.55,10.85,0.899999999999999)) ;
#134301 = CARTESIAN_POINT('Origin',(-2.55,10.85,-0.900000000000001)) ;
#134302 = CARTESIAN_POINT('Origin',(-2.75,10.85,0.899999999999999)) ;
#134303 = CARTESIAN_POINT('Origin',(-2.75,10.85,0.899999999999999)) ;
#134304 = CARTESIAN_POINT('Origin',(-3.8,10.75,0.9)) ;
#134305 = CARTESIAN_POINT('Origin',(-3.8,10.75,0.9)) ;
#134306 = CARTESIAN_POINT('Origin',(-3.8,10.75,-0.9)) ;
#134307 = CARTESIAN_POINT('Origin',(-3.8,10.75,-0.9)) ;
#134308 = CARTESIAN_POINT('Origin',(-2.75,10.85,-0.900000000000001)) ;
#134309 = CARTESIAN_POINT('Origin',(-2.75,10.85,-0.900000000000001)) ;
#134310 = CARTESIAN_POINT('Origin',(-2.75,10.8,0.899999999999999)) ;
#134311 = CARTESIAN_POINT('Origin',(-2.75,10.75,0.899999999999999)) ;
#134312 = CARTESIAN_POINT('Origin',(1.56125112837912E-16,10.75,0.899999999999999)) ;
#134313 = CARTESIAN_POINT('Origin',(-2.75,10.75,0.899999999999999)) ;
#134314 = CARTESIAN_POINT('Origin',(-1.56125112837913E-16,10.75,-0.900000000000001)) ;
#134315 = CARTESIAN_POINT('Origin',(-2.75,10.75,-0.900000000000001)) ;
#134316 = CARTESIAN_POINT('Origin',(-2.75,10.8,-0.900000000000001)) ;
#134317 = CARTESIAN_POINT('Origin',(-2.75,10.75,-0.900000000000001)) ;
#134318 = CARTESIAN_POINT('Origin',(-2.75,10.75,0.899999999999999)) ;
#134319 = CARTESIAN_POINT('Origin',(-2.75,10.75,0.899999999999999)) ;
#134320 = CARTESIAN_POINT('Origin',(-2.75,10.75,-0.900000000000001)) ;
#134321 = CARTESIAN_POINT('Origin',(-2.75,10.75,-0.900000000000001)) ;
#134322 = CARTESIAN_POINT('Origin',(-2.75,10.75,5.96311194867028E-16)) ;
#134323 = CARTESIAN_POINT('Origin',(4.6,0.,0.)) ;
#134324 = CARTESIAN_POINT('Ctrl Pts',(4.5,-2.7,1.52315462117279)) ;
#134325 = CARTESIAN_POINT('Ctrl Pts',(4.5,-2.71827986285823,1.44803526082493)) ;
#134326 = CARTESIAN_POINT('Ctrl Pts',(4.50597963419107,-2.73556801027185,
1.37326013954719)) ;
#134327 = CARTESIAN_POINT('Ctrl Pts',(4.52394923367545,-2.75977758633329,
1.26156316597844)) ;
#134328 = CARTESIAN_POINT('Ctrl Pts',(4.53141024883993,-2.76757607569523,
1.22431671760971)) ;
#134329 = CARTESIAN_POINT('Ctrl Pts',(4.54734065524867,-2.77857284247615,
1.16983431041704)) ;
#134330 = CARTESIAN_POINT('Ctrl Pts',(4.55339248498575,-2.78214991573955,
1.15176172558506)) ;
#134331 = CARTESIAN_POINT('Ctrl Pts',(4.56567492147096,-2.787183259287,1.12585327813928)) ;
#134332 = CARTESIAN_POINT('Ctrl Pts',(4.57024691433051,-2.78880341224557,
1.11742739494919)) ;
#134333 = CARTESIAN_POINT('Ctrl Pts',(4.58215938980081,-2.79169669265294,
1.10225652011491)) ;
#134334 = CARTESIAN_POINT('Ctrl Pts',(4.59005470866978,-2.79310344827587,
1.09479364595774)) ;
#134335 = CARTESIAN_POINT('Ctrl Pts',(4.6,-2.79310344827586,1.09479364595777)) ;
#134336 = CARTESIAN_POINT('Origin',(4.6,-2.4,1.96214168703486)) ;
#134337 = CARTESIAN_POINT('Origin',(4.6,-2.4,2.54)) ;
#134338 = CARTESIAN_POINT('Origin',(4.6,-2.4,1.96214168703486)) ;
#134339 = CARTESIAN_POINT('Origin',(4.6,-2.4,1.96214168703486)) ;
#134340 = CARTESIAN_POINT('Origin',(4.6,-2.4,1.96214168703486)) ;
#134341 = CARTESIAN_POINT('Origin',(0.584645609909622,-2.4,1.96214168703486)) ;
#134342 = CARTESIAN_POINT('Origin',(12.7,-2.4,1.96214168703486)) ;
#134343 = CARTESIAN_POINT('Origin',(12.7,-2.2,2.54)) ;
#134344 = CARTESIAN_POINT('Origin',(12.7,-2.2,1.96214168703486)) ;
#134345 = CARTESIAN_POINT('Origin',(12.7,-2.4,1.96214168703486)) ;
#134346 = CARTESIAN_POINT('Origin',(12.7,-2.24516129032258,1.83555190077454)) ;
#134347 = CARTESIAN_POINT('Origin',(12.7,0.,0.)) ;
#134348 = CARTESIAN_POINT('Origin',(12.7,-2.24516129032258,-1.83555190077454)) ;
#134349 = CARTESIAN_POINT('Origin',(12.7,-2.2,2.54)) ;
#134350 = CARTESIAN_POINT('Origin',(12.7,-2.2,-3.11785831296514)) ;
#134351 = CARTESIAN_POINT('Origin',(12.7,-2.2,-1.96214168703486)) ;
#134352 = CARTESIAN_POINT('Origin',(12.7,-2.4,-1.96214168703486)) ;
#134353 = CARTESIAN_POINT('Origin',(12.7,-2.4,-1.96214168703486)) ;
#134354 = CARTESIAN_POINT('Origin',(0.584645609909622,-2.4,-1.96214168703486)) ;
#134355 = CARTESIAN_POINT('Origin',(4.6,-2.4,-1.96214168703486)) ;
#134356 = CARTESIAN_POINT('Origin',(4.6,-2.4,2.54)) ;
#134357 = CARTESIAN_POINT('Origin',(4.6,-2.4,-3.11785831296514)) ;
#134358 = CARTESIAN_POINT('Origin',(4.6,-2.4,-1.96214168703486)) ;
#134359 = CARTESIAN_POINT('Origin',(4.6,-2.4,-1.96214168703486)) ;
#134360 = CARTESIAN_POINT('Origin',(4.6,-2.4,-1.96214168703486)) ;
#134361 = CARTESIAN_POINT('Origin',(4.6,0.,0.)) ;
#134362 = CARTESIAN_POINT('Ctrl Pts',(4.6,-2.79310344827586,-1.09479364595777)) ;
#134363 = CARTESIAN_POINT('Ctrl Pts',(4.59007568892311,-2.79310344827586,
-1.09479364595777)) ;
#134364 = CARTESIAN_POINT('Ctrl Pts',(4.58219207637239,-2.79170232102182,
-1.10222674227604)) ;
#134365 = CARTESIAN_POINT('Ctrl Pts',(4.57028631514659,-2.78881527838255,
-1.11736543899001)) ;
#134366 = CARTESIAN_POINT('Ctrl Pts',(4.56571532154372,-2.78719767797524,
-1.12577848858352)) ;
#134367 = CARTESIAN_POINT('Ctrl Pts',(4.55343865632726,-2.78217307830036,
-1.15164363330887)) ;
#134368 = CARTESIAN_POINT('Ctrl Pts',(4.54738888873343,-2.77860151743012,
-1.16969008596606)) ;
#134369 = CARTESIAN_POINT('Ctrl Pts',(4.53146440752601,-2.76762263748298,
-1.2240903156831)) ;
#134370 = CARTESIAN_POINT('Ctrl Pts',(4.52400917967609,-2.75984503873828,
-1.26124550630579)) ;
#134371 = CARTESIAN_POINT('Ctrl Pts',(4.50599905604505,-2.7356206423885,-1.37303013546926)) ;
#134372 = CARTESIAN_POINT('Ctrl Pts',(4.5,-2.71826422026483,-1.4480995425769)) ;
#134373 = CARTESIAN_POINT('Ctrl Pts',(4.5,-2.7,-1.52315462117279)) ;
#134374 = CARTESIAN_POINT('Origin',(3.7,-2.9,2.54)) ;
#134375 = CARTESIAN_POINT('Origin',(3.7,-2.9,-7.62)) ;
#134376 = CARTESIAN_POINT('Origin',(3.5,-3.95,2.54)) ;
#134377 = CARTESIAN_POINT('Origin',(3.5,-3.95,-7.62)) ;
#134378 = CARTESIAN_POINT('Origin',(-5.3,-3.95,2.54)) ;
#134379 = CARTESIAN_POINT('Origin',(-5.3,-3.95,-7.62)) ;
#134380 = CARTESIAN_POINT('Origin',(-5.3,5.19009804864072,2.54)) ;
#134381 = CARTESIAN_POINT('Origin',(-5.3,5.19009804864072,-7.62)) ;
#134382 = CARTESIAN_POINT('Origin',(-4.8,10.3,2.54)) ;
#134383 = CARTESIAN_POINT('Origin',(-4.8,10.3,-7.62)) ;
#134384 = CARTESIAN_POINT('Origin',(-4.8,10.85,2.54)) ;
#134385 = CARTESIAN_POINT('Origin',(-4.8,10.85,-7.62)) ;
#134386 = CARTESIAN_POINT('Origin',(-0.362523114814661,9.05,-0.169047304696279)) ;
#134387 = CARTESIAN_POINT('Origin',(0.36252311481466,9.05,0.169047304696279)) ;
#134388 = CARTESIAN_POINT('Origin',(-1.31845674202095,9.85,1.40771865776493)) ;
#134389 = CARTESIAN_POINT('Origin',(-0.230887397576972,9.85,1.91486057185377)) ;
#134390 = CARTESIAN_POINT('Origin',(3.3,10.85,2.54)) ;
#134391 = CARTESIAN_POINT('Origin',(3.3,10.85,-7.62)) ;
#134392 = CARTESIAN_POINT('Origin',(3.85,6.92431432344521,2.54)) ;
#134393 = CARTESIAN_POINT('Origin',(3.85,6.92431432344521,-7.62)) ;
#134394 = CARTESIAN_POINT('Origin',(4.05,3.77568567655479,2.54)) ;
#134395 = CARTESIAN_POINT('Origin',(4.05,3.77568567655479,-7.62)) ;
#134396 = CARTESIAN_POINT('Origin',(4.6,2.1,1.38195395782836)) ;
#134397 = CARTESIAN_POINT('Origin',(4.6,2.1,1.38195395782836)) ;
#134398 = CARTESIAN_POINT('Origin',(4.6,0.280857398566761,1.68514439140057)) ;
#134399 = CARTESIAN_POINT('Origin',(4.6,2.61712020253893,1.29576725740521)) ;
#134400 = CARTESIAN_POINT('Origin',(4.6,2.65,1.49304604217164)) ;
#134401 = CARTESIAN_POINT('Origin',(4.6,2.72431432344521,1.30736518335501)) ;
#134402 = CARTESIAN_POINT('Ctrl Pts',(4.48762159086906,2.77250619842445,1.38882431825039)) ;
#134403 = CARTESIAN_POINT('Ctrl Pts',(4.51316716229104,2.72605970493114,1.42576120580283)) ;
#134404 = CARTESIAN_POINT('Ctrl Pts',(4.57527453405851,2.73535372386122,1.44094284680199)) ;
#134405 = CARTESIAN_POINT('Ctrl Pts',(4.49363662433156,2.76156977394745,1.3530004075283)) ;
#134406 = CARTESIAN_POINT('Ctrl Pts',(4.5146945995807,2.70766535161865,1.40379915260673)) ;
#134407 = CARTESIAN_POINT('Ctrl Pts',(4.58732693581885,2.72440392220678,1.42300495876594)) ;
#134408 = CARTESIAN_POINT('Ctrl Pts',(4.5,2.74488438438029,1.32383078393385)) ;
#134409 = CARTESIAN_POINT('Ctrl Pts',(4.50856472873626,2.69031482079672,1.40150888629529)) ;
#134410 = CARTESIAN_POINT('Ctrl Pts',(4.60003980620507,2.70775073269832,1.40844768862527)) ;
#134411 = CARTESIAN_POINT('Ctrl Pts',(4.5,2.72431432344521,1.30736518335501)) ;
#134412 = CARTESIAN_POINT('Ctrl Pts',(4.5,2.68714136424467,1.4002450841483)) ;
#134413 = CARTESIAN_POINT('Ctrl Pts',(4.60004250625997,2.68715716507935,1.4002056043762)) ;
#134414 = CARTESIAN_POINT('Origin',(4.57524318173443,2.82069807340128,1.38882431825052)) ;
#134415 = CARTESIAN_POINT('Ctrl Pts',(4.47150553123747,2.80180812502279,1.49304604217164)) ;
#134416 = CARTESIAN_POINT('Ctrl Pts',(4.5,2.75,1.49304604217164)) ;
#134417 = CARTESIAN_POINT('Ctrl Pts',(4.55912712210514,2.75,1.49304604217164)) ;
#134418 = CARTESIAN_POINT('Ctrl Pts',(4.47150553186688,2.8018081238784,1.45642552726532)) ;
#134419 = CARTESIAN_POINT('Ctrl Pts',(4.50000000073523,2.74999999866316,1.46874191573125)) ;
#134420 = CARTESIAN_POINT('Ctrl Pts',(4.5591271227348,2.75,1.47472795424071)) ;
#134421 = CARTESIAN_POINT('Ctrl Pts',(4.47712448971609,2.79159183687984,1.42008346264768)) ;
#134422 = CARTESIAN_POINT('Ctrl Pts',(4.50480340096852,2.74126654369362,1.44446204900192)) ;
#134423 = CARTESIAN_POINT('Ctrl Pts',(4.56473907811159,2.74489822224645,1.45657517841774)) ;
#134424 = CARTESIAN_POINT('Ctrl Pts',(4.48762159086676,2.77250619842407,1.38882431825052)) ;
#134425 = CARTESIAN_POINT('Ctrl Pts',(4.51315802400618,2.72607631998876,1.4257479925657)) ;
#134426 = CARTESIAN_POINT('Ctrl Pts',(4.57524318173443,2.73534903670064,1.44093518021108)) ;
#134427 = CARTESIAN_POINT('Origin',(4.55912712210513,2.85,1.49304604217164)) ;
#134428 = CARTESIAN_POINT('Origin',(4.55912712210514,2.85,2.54)) ;
#134429 = CARTESIAN_POINT('Origin',(4.55912712210514,2.85,2.54)) ;
#134430 = CARTESIAN_POINT('Origin',(4.55912712210513,2.85,-3.58695395782836)) ;
#134431 = CARTESIAN_POINT('Origin',(4.55912712210514,2.85,-1.49304604217164)) ;
#134432 = CARTESIAN_POINT('Ctrl Pts',(4.48762159086766,2.77250619842243,-1.38882431824783)) ;
#134433 = CARTESIAN_POINT('Ctrl Pts',(4.51315802400691,2.72607631998743,-1.42574799256407)) ;
#134434 = CARTESIAN_POINT('Ctrl Pts',(4.57524318173533,2.73534903669982,-1.44093518020973)) ;
#134435 = CARTESIAN_POINT('Ctrl Pts',(4.47712448971642,2.79159183687923,-1.42008346264562)) ;
#134436 = CARTESIAN_POINT('Ctrl Pts',(4.5048034009688,2.74126654369307,-1.44446204900057)) ;
#134437 = CARTESIAN_POINT('Ctrl Pts',(4.56473907811194,2.74489822224616,-1.45657517841671)) ;
#134438 = CARTESIAN_POINT('Ctrl Pts',(4.47150553186688,2.8018081238784,-1.45642552726424)) ;
#134439 = CARTESIAN_POINT('Ctrl Pts',(4.50000000073523,2.74999999866316,-1.46874191573051)) ;
#134440 = CARTESIAN_POINT('Ctrl Pts',(4.5591271227348,2.75,-1.47472795424017)) ;
#134441 = CARTESIAN_POINT('Ctrl Pts',(4.47150553123747,2.80180812502279,-1.49304604217164)) ;
#134442 = CARTESIAN_POINT('Ctrl Pts',(4.5,2.75,-1.49304604217164)) ;
#134443 = CARTESIAN_POINT('Ctrl Pts',(4.55912712210513,2.75,-1.49304604217164)) ;
#134444 = CARTESIAN_POINT('Origin',(4.57524318173533,2.82069807339964,-1.38882431824783)) ;
#134445 = CARTESIAN_POINT('Ctrl Pts',(4.57527448145476,2.73535371598842,-1.44094283394186)) ;
#134446 = CARTESIAN_POINT('Ctrl Pts',(4.51316714695682,2.72605973281052,-1.42576118362916)) ;
#134447 = CARTESIAN_POINT('Ctrl Pts',(4.48762159086951,2.77250619842363,-1.3888243182477)) ;
#134448 = CARTESIAN_POINT('Ctrl Pts',(4.58732687742634,2.72440390874891,-1.42300494332461)) ;
#134449 = CARTESIAN_POINT('Ctrl Pts',(4.51469458626358,2.70766538570651,-1.40379912048168)) ;
#134450 = CARTESIAN_POINT('Ctrl Pts',(4.49363662433186,2.76156977394666,-1.35300040752687)) ;
#134451 = CARTESIAN_POINT('Ctrl Pts',(4.60003973844306,2.70775071978181,-1.40844768348499)) ;
#134452 = CARTESIAN_POINT('Ctrl Pts',(4.50856472285792,2.69031485824818,-1.40150883298414)) ;
#134453 = CARTESIAN_POINT('Ctrl Pts',(4.5,2.74488438437976,-1.32383078393342)) ;
#134454 = CARTESIAN_POINT('Ctrl Pts',(4.60004243494348,2.6871571650681,-1.40020560440432)) ;
#134455 = CARTESIAN_POINT('Ctrl Pts',(4.5,2.68714139075512,-1.40024501790962)) ;
#134456 = CARTESIAN_POINT('Ctrl Pts',(4.5,2.72431432344521,-1.30736518335501)) ;
#134457 = CARTESIAN_POINT('Origin',(4.6,0.280857398566761,-1.68514439140057)) ;
#134458 = CARTESIAN_POINT('Origin',(4.6,2.1,-1.38195395782836)) ;
#134459 = CARTESIAN_POINT('Origin',(4.6,2.1,-1.38195395782836)) ;
#134460 = CARTESIAN_POINT('Origin',(4.6,0.,0.)) ;
#134461 = CARTESIAN_POINT('',(4.5,-2.9,-3.84865454255039E-12)) ;
#134462 = CARTESIAN_POINT('',(4.57439618084313,-2.80937499999937,-1.04279586712545)) ;
#134463 = CARTESIAN_POINT('Ctrl Pts',(4.5,-2.9,-3.84865454255039E-12)) ;
#134464 = CARTESIAN_POINT('Ctrl Pts',(4.5,-2.9000000234111,-0.176176262570291)) ;
#134465 = CARTESIAN_POINT('Ctrl Pts',(4.49893459747296,-2.89187728142186,
-0.352293822555195)) ;
#134466 = CARTESIAN_POINT('Ctrl Pts',(4.50498172725087,-2.86839426105774,
-0.614943276887172)) ;
#134467 = CARTESIAN_POINT('Ctrl Pts',(4.50826226558342,-2.85869729223562,
-0.702287027113486)) ;
#134468 = CARTESIAN_POINT('Ctrl Pts',(4.52028413974051,-2.84160518746962,
-0.832840965432797)) ;
#134469 = CARTESIAN_POINT('Ctrl Pts',(4.52545003690602,-2.8354696349403,-0.876363113622023)) ;
#134470 = CARTESIAN_POINT('Ctrl Pts',(4.53741870680498,-2.82581179679252,
-0.940639455010752)) ;
#134471 = CARTESIAN_POINT('Ctrl Pts',(4.54209540184575,-2.82251395224859,
-0.961920018260584)) ;
#134472 = CARTESIAN_POINT('Ctrl Pts',(4.55451190949429,-2.81582803324483,
-1.0038742105328)) ;
#134473 = CARTESIAN_POINT('Ctrl Pts',(4.56139306411848,-2.8124020390272,-1.02474353182486)) ;
#134474 = CARTESIAN_POINT('Ctrl Pts',(4.57439618084313,-2.80937499999937,
-1.04279586712545)) ;
#134475 = CARTESIAN_POINT('Ctrl Pts',(4.57439618084313,-2.80937499999937,
-1.04279586712545)) ;
#134476 = CARTESIAN_POINT('Ctrl Pts',(4.57788811720511,-2.80856205104935,
-1.0476438845913)) ;
#134477 = CARTESIAN_POINT('Ctrl Pts',(4.58132110715664,-2.80743849592503,
-1.05265431141975)) ;
#134478 = CARTESIAN_POINT('Ctrl Pts',(4.58591063786561,-2.80541025280316,
-1.0600683491598)) ;
#134479 = CARTESIAN_POINT('Ctrl Pts',(4.587216947305,-2.80476695238162,-1.06226832508373)) ;
#134480 = CARTESIAN_POINT('Ctrl Pts',(4.5887449802686,-2.80393035430395,-1.06497171464084)) ;
#134481 = CARTESIAN_POINT('Ctrl Pts',(4.58900094431508,-2.8037870887984,-1.06542942337304)) ;
#134482 = CARTESIAN_POINT('Ctrl Pts',(4.58924476828968,-2.80364801935069,
-1.06586949326004)) ;
#134483 = CARTESIAN_POINT('Ctrl Pts',(4.58924931741448,-2.80364542371033,
-1.0658777053493)) ;
#134484 = CARTESIAN_POINT('Ctrl Pts',(4.59158188358133,-2.80231401319274,
-1.07008924012213)) ;
#134485 = CARTESIAN_POINT('Ctrl Pts',(4.59377134212491,-2.800813098491,-1.07443839239641)) ;
#134486 = CARTESIAN_POINT('Ctrl Pts',(4.59570408210448,-2.79909049146271,
-1.0791378632085)) ;
#134487 = CARTESIAN_POINT('Ctrl Pts',(4.59570848738489,-2.79908656285628,
-1.07914857957787)) ;
#134488 = CARTESIAN_POINT('Ctrl Pts',(4.59603576097761,-2.79879453264351,
-1.07994507543617)) ;
#134489 = CARTESIAN_POINT('Ctrl Pts',(4.59633794834607,-2.79851279959495,
-1.08070652531885)) ;
#134490 = CARTESIAN_POINT('Ctrl Pts',(4.59727216584803,-2.79759800070515,
-1.08316063340996)) ;
#134491 = CARTESIAN_POINT('Ctrl Pts',(4.59785661125443,-2.79695684051616,
-1.08485291560937)) ;
#134492 = CARTESIAN_POINT('Ctrl Pts',(4.59875882816121,-2.7958009226755,-1.08786832422156)) ;
#134493 = CARTESIAN_POINT('Ctrl Pts',(4.59910960512328,-2.79529211440565,
-1.08918449921755)) ;
#134494 = CARTESIAN_POINT('Ctrl Pts',(4.59950074890552,-2.79458032370896,
-1.09101507841206)) ;
#134495 = CARTESIAN_POINT('Ctrl Pts',(4.59959271145697,-2.79439474074568,
-1.09149484058078)) ;
#134496 = CARTESIAN_POINT('Ctrl Pts',(4.59970479219924,-2.79411978912796,
-1.09220257104619)) ;
#134497 = CARTESIAN_POINT('Ctrl Pts',(4.59973686334512,-2.7940323188425,-1.09242726844519)) ;
#134498 = CARTESIAN_POINT('Ctrl Pts',(4.59980956306601,-2.79380428276742,
-1.09301082640206)) ;
#134499 = CARTESIAN_POINT('Ctrl Pts',(4.59984405921136,-2.79366555090846,
-1.09336897900421)) ;
#134500 = CARTESIAN_POINT('Ctrl Pts',(4.59992170638736,-2.79338632637293,
-1.0940824135446)) ;
#134501 = CARTESIAN_POINT('Ctrl Pts',(4.59995882625634,-2.79324305250059,
-1.09443747925646)) ;
#134502 = CARTESIAN_POINT('Ctrl Pts',(4.59999999999999,-2.79310344827586,
-1.09479364595777)) ;
#134503 = CARTESIAN_POINT('',(4.57439618084271,-2.80937499999947,1.04279586712486)) ;
#134504 = CARTESIAN_POINT('Ctrl Pts',(4.59999999999999,-2.79310344827586,
1.09479364595777)) ;
#134505 = CARTESIAN_POINT('Ctrl Pts',(4.59995895305209,-2.79324111387631,
1.09443799295581)) ;
#134506 = CARTESIAN_POINT('Ctrl Pts',(4.59992125133673,-2.79338175512528,
1.09408335000483)) ;
#134507 = CARTESIAN_POINT('Ctrl Pts',(4.59984242179761,-2.79365985893298,
1.09337278174528)) ;
#134508 = CARTESIAN_POINT('Ctrl Pts',(4.5998070294299,-2.79379858543765,1.09301809599704)) ;
#134509 = CARTESIAN_POINT('Ctrl Pts',(4.59973261548695,-2.79401893257626,
1.09245417872038)) ;
#134510 = CARTESIAN_POINT('Ctrl Pts',(4.59970092564442,-2.7941005010842,1.09224529554737)) ;
#134511 = CARTESIAN_POINT('Ctrl Pts',(4.59958060815602,-2.79437456977472,
1.09154292574229)) ;
#134512 = CARTESIAN_POINT('Ctrl Pts',(4.59947821517875,-2.79456857658396,
1.09104490461926)) ;
#134513 = CARTESIAN_POINT('Ctrl Pts',(4.5990597198479,-2.79527981802028,1.08921493561152)) ;
#134514 = CARTESIAN_POINT('Ctrl Pts',(4.59869396429225,-2.79579226918928,
1.08788859879992)) ;
#134515 = CARTESIAN_POINT('Ctrl Pts',(4.59768320083748,-2.79706868650734,
1.08455592610668)) ;
#134516 = CARTESIAN_POINT('Ctrl Pts',(4.59698254015873,-2.79783590182172,
1.08252680033734)) ;
#134517 = CARTESIAN_POINT('Ctrl Pts',(4.5959970522588,-2.79876532988112,1.08001531576155)) ;
#134518 = CARTESIAN_POINT('Ctrl Pts',(4.59580678362761,-2.79893964110239,
1.07954189499608)) ;
#134519 = CARTESIAN_POINT('Ctrl Pts',(4.59367882781299,-2.80083904916685,
1.0743550880029)) ;
#134520 = CARTESIAN_POINT('Ctrl Pts',(4.5915070708769,-2.80233337893514,1.07002067229589)) ;
#134521 = CARTESIAN_POINT('Ctrl Pts',(4.58628071719234,-2.80532570224271,
1.06054853257076)) ;
#134522 = CARTESIAN_POINT('Ctrl Pts',(4.58313959595707,-2.8067311076741,1.05548975193422)) ;
#134523 = CARTESIAN_POINT('Ctrl Pts',(4.57802611146331,-2.80844040952816,
1.04790364250821)) ;
#134524 = CARTESIAN_POINT('Ctrl Pts',(4.57624387811645,-2.80894486836997,
1.04536104065828)) ;
#134525 = CARTESIAN_POINT('Ctrl Pts',(4.57439618084271,-2.80937499999947,
1.04279586712486)) ;
#134526 = CARTESIAN_POINT('Ctrl Pts',(4.57439618084271,-2.80937499999947,
1.04279586712486)) ;
#134527 = CARTESIAN_POINT('Ctrl Pts',(4.56149777794589,-2.81237766235468,
1.0248889068332)) ;
#134528 = CARTESIAN_POINT('Ctrl Pts',(4.55451596106519,-2.81582788236477,
1.00387375770319)) ;
#134529 = CARTESIAN_POINT('Ctrl Pts',(4.54213610452188,-2.82249001163036,
0.962071640371718)) ;
#134530 = CARTESIAN_POINT('Ctrl Pts',(4.53742891479326,-2.82580422498964,
0.940689032764001)) ;
#134531 = CARTESIAN_POINT('Ctrl Pts',(4.525451614243,-2.8354670333868,0.876382056205111)) ;
#134532 = CARTESIAN_POINT('Ctrl Pts',(4.52032009146395,-2.84156292603926,
0.833143426521514)) ;
#134533 = CARTESIAN_POINT('Ctrl Pts',(4.50830110904356,-2.85862448221642,
0.70288357404262)) ;
#134534 = CARTESIAN_POINT('Ctrl Pts',(4.50499166750953,-2.86836219567853,
0.615269961417698)) ;
#134535 = CARTESIAN_POINT('Ctrl Pts',(4.49892845988062,-2.8918880660271,0.352237003162138)) ;
#134536 = CARTESIAN_POINT('Ctrl Pts',(4.49999999999475,-2.89999999999869,
0.176169909882234)) ;
#134537 = CARTESIAN_POINT('Ctrl Pts',(4.5,-2.9,-3.84865454255039E-12)) ;
#134538 = CARTESIAN_POINT('Origin',(4.4,-2.7,2.54)) ;
#134539 = CARTESIAN_POINT('Origin',(4.4,-2.7,1.52315462117279)) ;
#134540 = CARTESIAN_POINT('Ctrl Pts',(4.4022743508907,-2.79999990867355,1.59059930711805)) ;
#134541 = CARTESIAN_POINT('Ctrl Pts',(4.51828879250243,-2.80015667527383,
1.58121443320753)) ;
#134542 = CARTESIAN_POINT('Ctrl Pts',(4.50118227077258,-2.68533700727764,
1.58202889255053)) ;
#134543 = CARTESIAN_POINT('Ctrl Pts',(4.39419482113923,-2.79999992837382,
1.47631230033095)) ;
#134544 = CARTESIAN_POINT('Ctrl Pts',(4.48571792501718,-2.80010751836587,
1.49732863324935)) ;
#134545 = CARTESIAN_POINT('Ctrl Pts',(4.49717570077253,-2.71006921719245,
1.48296810178551)) ;
#134546 = CARTESIAN_POINT('Ctrl Pts',(4.40636790575266,-2.79999994706265,
1.36509109264564)) ;
#134547 = CARTESIAN_POINT('Ctrl Pts',(4.47481046024549,-2.80007242131916,
1.38667757220097)) ;
#134548 = CARTESIAN_POINT('Ctrl Pts',(4.50328131876403,-2.73353293829091,
1.38297412518993)) ;
#134549 = CARTESIAN_POINT('Ctrl Pts',(4.45479736994228,-2.79999997092221,
1.21492633452891)) ;
#134550 = CARTESIAN_POINT('Ctrl Pts',(4.49869786247047,-2.80003603117403,
1.23372075650421)) ;
#134551 = CARTESIAN_POINT('Ctrl Pts',(4.52748687875416,-2.76348976047506,
1.2437108271413)) ;
#134552 = CARTESIAN_POINT('Ctrl Pts',(4.47221929614095,-2.79999997745988,
1.17269593977674)) ;
#134553 = CARTESIAN_POINT('Ctrl Pts',(4.50880556767618,-2.8000272573648,1.19172515171411)) ;
#134554 = CARTESIAN_POINT('Ctrl Pts',(4.5361913779553,-2.77169834185701,1.20401631763245)) ;
#134555 = CARTESIAN_POINT('Ctrl Pts',(4.50882352800135,-2.7999999860536,1.11571565039093)) ;
#134556 = CARTESIAN_POINT('Ctrl Pts',(4.53367802911271,-2.80001636071785,
1.13464129757966)) ;
#134557 = CARTESIAN_POINT('Ctrl Pts',(4.55447319025664,-2.78248861123825,
1.14990431857449)) ;
#134558 = CARTESIAN_POINT('Ctrl Pts',(4.52308919141482,-2.79999998878206,
1.09733743830892)) ;
#134559 = CARTESIAN_POINT('Ctrl Pts',(4.54363962638621,-2.80001303821803,
1.11627384982833)) ;
#134560 = CARTESIAN_POINT('Ctrl Pts',(4.56159739427507,-2.78591449131412,
1.13234572910531)) ;
#134561 = CARTESIAN_POINT('Ctrl Pts',(4.57467506176496,-2.79999999510246,
1.05430349160064)) ;
#134562 = CARTESIAN_POINT('Ctrl Pts',(4.58062405303292,-2.80000557393877,
1.07366583672224)) ;
#134563 = CARTESIAN_POINT('Ctrl Pts',(4.58735613403295,-2.79385049254303,
1.09108018500675)) ;
#134564 = CARTESIAN_POINT('Ctrl Pts',(4.62437069655632,-2.79999999703807,
1.04046865694003)) ;
#134565 = CARTESIAN_POINT('Ctrl Pts',(4.61827372661881,-2.80000334969051,
1.05906595451277)) ;
#134566 = CARTESIAN_POINT('Ctrl Pts',(4.61212682540736,-2.79628090446616,
1.07759718578196)) ;
#134567 = CARTESIAN_POINT('Ctrl Pts',(4.6716136830205,-2.79999998860619,1.09921017323439)) ;
#134568 = CARTESIAN_POINT('Ctrl Pts',(4.6540701010266,-2.80001325705937,1.11953626041004)) ;
#134569 = CARTESIAN_POINT('Ctrl Pts',(4.63587130780629,-2.78569367459202,
1.13437187040551)) ;
#134570 = CARTESIAN_POINT('Ctrl Pts',(4.54879236204369,-2.8,1.0764344436325)) ;
#134571 = CARTESIAN_POINT('Ctrl Pts',(4.55448837802386,-2.7999999999815,1.07882117908632)) ;
#134572 = CARTESIAN_POINT('Ctrl Pts',(4.56021842726591,-2.7995915078324,1.08116045726579)) ;
#134573 = CARTESIAN_POINT('Ctrl Pts',(4.56730671984969,-2.79865167182177,
1.08402111613638)) ;
#134574 = CARTESIAN_POINT('Ctrl Pts',(4.56847770958262,-2.79848295770259,
1.08449267316523)) ;
#134575 = CARTESIAN_POINT('Ctrl Pts',(4.57107523099021,-2.79808046368154,
1.08553703710302)) ;
#134576 = CARTESIAN_POINT('Ctrl Pts',(4.5725009361248,-2.79784058543152,1.08611035697199)) ;
#134577 = CARTESIAN_POINT('Ctrl Pts',(4.5764383594612,-2.79713266293194,1.08768631353511)) ;
#134578 = CARTESIAN_POINT('Ctrl Pts',(4.57879956048961,-2.79666132938902,
1.08862419960307)) ;
#134579 = CARTESIAN_POINT('Ctrl Pts',(4.58293855712952,-2.79579586318667,
1.09023918407038)) ;
#134580 = CARTESIAN_POINT('Ctrl Pts',(4.58471363403685,-2.79540911153441,
1.09092538280881)) ;
#134581 = CARTESIAN_POINT('Ctrl Pts',(4.58699082729421,-2.7949269768198,1.09175547073797)) ;
#134582 = CARTESIAN_POINT('Ctrl Pts',(4.58739952300692,-2.79484234870239,
1.0918980731536)) ;
#134583 = CARTESIAN_POINT('Ctrl Pts',(4.58871515235486,-2.79457617288695,
1.09233887089915)) ;
#134584 = CARTESIAN_POINT('Ctrl Pts',(4.58961690596143,-2.7944024780556,1.09261501300051)) ;
#134585 = CARTESIAN_POINT('Ctrl Pts',(4.59105375065869,-2.79414748185764,
1.09301701818209)) ;
#134586 = CARTESIAN_POINT('Ctrl Pts',(4.5915530390955,-2.79406229662442,1.09315075649288)) ;
#134587 = CARTESIAN_POINT('Ctrl Pts',(4.5924596538567,-2.79391282221553,1.09338740588514)) ;
#134588 = CARTESIAN_POINT('Ctrl Pts',(4.59286388425105,-2.79384761399903,
1.09349157821548)) ;
#134589 = CARTESIAN_POINT('Ctrl Pts',(4.59368973959982,-2.79370598615371,
1.09373232734835)) ;
#134590 = CARTESIAN_POINT('Ctrl Pts',(4.59407665941124,-2.79363973714591,
1.09384847876684)) ;
#134591 = CARTESIAN_POINT('Ctrl Pts',(4.59444371287733,-2.79357284110655,
1.09397320727212)) ;
#134592 = CARTESIAN_POINT('Ctrl Pts',(4.5944889025916,-2.79356452972317,1.09398884180049)) ;
#134593 = CARTESIAN_POINT('Ctrl Pts',(4.59470842334912,-2.79352377141065,
1.09406617454783)) ;
#134594 = CARTESIAN_POINT('Ctrl Pts',(4.59483598733269,-2.79349361011836,
1.09412766851589)) ;
#134595 = CARTESIAN_POINT('Ctrl Pts',(4.59514620525223,-2.7934297131363,1.0942540599508)) ;
#134596 = CARTESIAN_POINT('Ctrl Pts',(4.59533334275101,-2.79339696908416,
1.0943161621466)) ;
#134597 = CARTESIAN_POINT('Ctrl Pts',(4.59563785533348,-2.79335634095568,
1.09438700965973)) ;
#134598 = CARTESIAN_POINT('Ctrl Pts',(4.59571710962763,-2.79334654412181,
1.09440360871235)) ;
#134599 = CARTESIAN_POINT('Ctrl Pts',(4.59594411915587,-2.79332043135007,
1.0944466503818)) ;
#134600 = CARTESIAN_POINT('Ctrl Pts',(4.59600288191153,-2.79330503361987,
1.09446604875921)) ;
#134601 = CARTESIAN_POINT('Ctrl Pts',(4.59613307952174,-2.79327450473786,
1.09450071948058)) ;
#134602 = CARTESIAN_POINT('Ctrl Pts',(4.59620389659312,-2.79325970788819,
1.09451499394145)) ;
#134603 = CARTESIAN_POINT('Ctrl Pts',(4.59651192984771,-2.79322709231927,
1.09454972213713)) ;
#134604 = CARTESIAN_POINT('Ctrl Pts',(4.59679543741296,-2.79320989448354,
1.09457065581759)) ;
#134605 = CARTESIAN_POINT('Ctrl Pts',(4.59784475938523,-2.793166495242,1.0946421164934)) ;
#134606 = CARTESIAN_POINT('Ctrl Pts',(4.59874915064779,-2.79313948637392,
1.09470073568925)) ;
#134607 = CARTESIAN_POINT('Ctrl Pts',(4.59999999999999,-2.79310344827586,
1.09479364595777)) ;
#134608 = CARTESIAN_POINT('Origin',(4.4,-2.7,2.54)) ;
#134609 = CARTESIAN_POINT('Origin',(4.4,-2.7,-3.55684537882721)) ;
#134610 = CARTESIAN_POINT('Origin',(4.4,-2.7,-1.52315462117279)) ;
#134611 = CARTESIAN_POINT('Ctrl Pts',(4.5011795914298,-2.68531903459927,-1.58202902017228)) ;
#134612 = CARTESIAN_POINT('Ctrl Pts',(4.51828670358939,-2.8,-1.58121382514056)) ;
#134613 = CARTESIAN_POINT('Ctrl Pts',(4.40240952225579,-2.8,-1.59058837211075)) ;
#134614 = CARTESIAN_POINT('Ctrl Pts',(4.49717774927193,-2.71005310920072,
-1.48296553236262)) ;
#134615 = CARTESIAN_POINT('Ctrl Pts',(4.48574628541085,-2.8,-1.49731485204045)) ;
#134616 = CARTESIAN_POINT('Ctrl Pts',(4.39431668173578,-2.8,-1.47634026950832)) ;
#134617 = CARTESIAN_POINT('Ctrl Pts',(4.50328690685191,-2.73351987602563,
-1.38297339786192)) ;
#134618 = CARTESIAN_POINT('Ctrl Pts',(4.47485145549547,-2.8,-1.3866766957413)) ;
#134619 = CARTESIAN_POINT('Ctrl Pts',(4.40646789472124,-2.8,-1.36512261863837)) ;
#134620 = CARTESIAN_POINT('Ctrl Pts',(4.5274931179709,-2.76348183928882,-1.2437129921595)) ;
#134621 = CARTESIAN_POINT('Ctrl Pts',(4.49873206155793,-2.8,-1.233733095307)) ;
#134622 = CARTESIAN_POINT('Ctrl Pts',(4.4548681704377,-2.8,-1.21495664336612)) ;
#134623 = CARTESIAN_POINT('Ctrl Pts',(4.53619745972498,-2.77169205010107,
-1.20401904718522)) ;
#134624 = CARTESIAN_POINT('Ctrl Pts',(4.50883664816668,-2.8,-1.19173943817213)) ;
#134625 = CARTESIAN_POINT('Ctrl Pts',(4.47227975612149,-2.8,-1.17272738460373)) ;
#134626 = CARTESIAN_POINT('Ctrl Pts',(4.55447795090009,-2.7824845983034,-1.14990781273337)) ;
#134627 = CARTESIAN_POINT('Ctrl Pts',(4.53370055749885,-2.8,-1.13465791836995)) ;
#134628 = CARTESIAN_POINT('Ctrl Pts',(4.50886586566853,-2.8,-1.11574788827223)) ;
#134629 = CARTESIAN_POINT('Ctrl Pts',(4.56160154376424,-2.78591123334062,
-1.13234944281567)) ;
#134630 = CARTESIAN_POINT('Ctrl Pts',(4.54365878772217,-2.8,-1.11629106645424)) ;
#134631 = CARTESIAN_POINT('Ctrl Pts',(4.52312452397684,-2.8,-1.09736999548674)) ;
#134632 = CARTESIAN_POINT('Ctrl Pts',(4.58735772267364,-2.79384903998488,
-1.09108429439848)) ;
#134633 = CARTESIAN_POINT('Ctrl Pts',(4.58063087367388,-2.8,-1.07368396338091)) ;
#134634 = CARTESIAN_POINT('Ctrl Pts',(4.57468550767192,-2.8,-1.05433748660568)) ;
#134635 = CARTESIAN_POINT('Ctrl Pts',(4.61212536563475,-2.79628002040279,
-1.07760158659545)) ;
#134636 = CARTESIAN_POINT('Ctrl Pts',(4.61826745782982,-2.8,-1.05908487937578)) ;
#134637 = CARTESIAN_POINT('Ctrl Pts',(4.62435992349564,-2.8,-1.04050151732138)) ;
#134638 = CARTESIAN_POINT('Ctrl Pts',(4.63586710715936,-2.78569036914655,
-1.13437529467537)) ;
#134639 = CARTESIAN_POINT('Ctrl Pts',(4.65405106945745,-2.8,-1.11955252388339)) ;
#134640 = CARTESIAN_POINT('Ctrl Pts',(4.67158355065754,-2.8,-1.09924507978095)) ;
#134641 = CARTESIAN_POINT('Ctrl Pts',(4.59999999999999,-2.79310344827586,
-1.09479364595777)) ;
#134642 = CARTESIAN_POINT('Ctrl Pts',(4.59840954578196,-2.79314968944989,
-1.09467567269119)) ;
#134643 = CARTESIAN_POINT('Ctrl Pts',(4.59737383489065,-2.79318159606221,
-1.09461332397165)) ;
#134644 = CARTESIAN_POINT('Ctrl Pts',(4.59650507521634,-2.79322931786013,
-1.09455037725996)) ;
#134645 = CARTESIAN_POINT('Ctrl Pts',(4.59632758424293,-2.79324472590583,
-1.09453457917666)) ;
#134646 = CARTESIAN_POINT('Ctrl Pts',(4.5961184721084,-2.79327477162037,-1.09450475657722)) ;
#134647 = CARTESIAN_POINT('Ctrl Pts',(4.59606489504922,-2.79328892979787,
-1.09449102658529)) ;
#134648 = CARTESIAN_POINT('Ctrl Pts',(4.5959460167769,-2.79331605564258,-1.09445911449494)) ;
#134649 = CARTESIAN_POINT('Ctrl Pts',(4.59588597444854,-2.7933285533825,-1.09444265618345)) ;
#134650 = CARTESIAN_POINT('Ctrl Pts',(4.59549967474363,-2.79337285752324,
-1.09437027876054)) ;
#134651 = CARTESIAN_POINT('Ctrl Pts',(4.59527331486237,-2.79340622385959,
-1.09431008070831)) ;
#134652 = CARTESIAN_POINT('Ctrl Pts',(4.5949320123953,-2.79346950514991,-1.09418704029369)) ;
#134653 = CARTESIAN_POINT('Ctrl Pts',(4.59480393230129,-2.79349821606422,
-1.09412847427896)) ;
#134654 = CARTESIAN_POINT('Ctrl Pts',(4.59460326813595,-2.79353924388982,
-1.09404763514903)) ;
#134655 = CARTESIAN_POINT('Ctrl Pts',(4.59455075953096,-2.7935496343265,-1.09402742767144)) ;
#134656 = CARTESIAN_POINT('Ctrl Pts',(4.59417008680874,-2.79361944405451,
-1.09389559371761)) ;
#134657 = CARTESIAN_POINT('Ctrl Pts',(4.5937774209655,-2.79368602572532,-1.09377734615547)) ;
#134658 = CARTESIAN_POINT('Ctrl Pts',(4.59289939109636,-2.7938335466559,-1.09352541902408)) ;
#134659 = CARTESIAN_POINT('Ctrl Pts',(4.59245006584788,-2.79390305456782,
-1.09341603619896)) ;
#134660 = CARTESIAN_POINT('Ctrl Pts',(4.5909955251919,-2.79413629528614,-1.09305685240916)) ;
#134661 = CARTESIAN_POINT('Ctrl Pts',(4.59002197881477,-2.79430302757335,
-1.0928063701757)) ;
#134662 = CARTESIAN_POINT('Ctrl Pts',(4.58861122644569,-2.79456793455722,
-1.0923921365665)) ;
#134663 = CARTESIAN_POINT('Ctrl Pts',(4.58817904894343,-2.79465210327465,
-1.09225852343037)) ;
#134664 = CARTESIAN_POINT('Ctrl Pts',(4.58736872283364,-2.79481449815582,
-1.09199418358962)) ;
#134665 = CARTESIAN_POINT('Ctrl Pts',(4.58699491219414,-2.79489135860975,
-1.09186658235812)) ;
#134666 = CARTESIAN_POINT('Ctrl Pts',(4.58468897497186,-2.79537899446709,
-1.09103519061959)) ;
#134667 = CARTESIAN_POINT('Ctrl Pts',(4.58290717718701,-2.79577019617637,
-1.09034206422841)) ;
#134668 = CARTESIAN_POINT('Ctrl Pts',(4.57867627871777,-2.79666451416568,
-1.08867078828749)) ;
#134669 = CARTESIAN_POINT('Ctrl Pts',(4.57626321554132,-2.79715040843618,
-1.08768776514286)) ;
#134670 = CARTESIAN_POINT('Ctrl Pts',(4.57243386308706,-2.79784156172336,
-1.0861367865103)) ;
#134671 = CARTESIAN_POINT('Ctrl Pts',(4.57107519984215,-2.79807176647234,
-1.08558402144498)) ;
#134672 = CARTESIAN_POINT('Ctrl Pts',(4.56513452430488,-2.79900074294388,
-1.0831693903581)) ;
#134673 = CARTESIAN_POINT('Ctrl Pts',(4.56062162665772,-2.79951267011375,
-1.08133092934958)) ;
#134674 = CARTESIAN_POINT('Ctrl Pts',(4.55365420596664,-2.79992470862866,
-1.07846103027848)) ;
#134675 = CARTESIAN_POINT('Ctrl Pts',(4.55124660967283,-2.79999983267432,
-1.07746323925077)) ;
#134676 = CARTESIAN_POINT('Ctrl Pts',(4.54880051362943,-2.79999999972164,
-1.07643786073294)) ;
#134677 = CARTESIAN_POINT('Ctrl Pts',(4.54879236166275,-2.8,1.07643444348484)) ;
#134678 = CARTESIAN_POINT('Ctrl Pts',(4.5622387183224,-2.79999999999679,1.05876847372513)) ;
#134679 = CARTESIAN_POINT('Ctrl Pts',(4.57442182196495,-2.80939476060286,
1.0427621795332)) ;
#134680 = CARTESIAN_POINT('Ctrl Pts',(4.55556842517599,-2.79999999999889,
1.07927493595118)) ;
#134681 = CARTESIAN_POINT('Ctrl Pts',(4.56783337210914,-2.80040661803735,
1.06381369844813)) ;
#134682 = CARTESIAN_POINT('Ctrl Pts',(4.57961823522366,-2.80818164104597,
1.04998165867271)) ;
#134683 = CARTESIAN_POINT('Ctrl Pts',(4.56238982831618,-2.79942602551759,
1.08204714848293)) ;
#134684 = CARTESIAN_POINT('Ctrl Pts',(4.57357810388181,-2.80014618986472,
1.06906892785879)) ;
#134685 = CARTESIAN_POINT('Ctrl Pts',(4.58462643299473,-2.80630261261111,
1.05747672883513)) ;
#134686 = CARTESIAN_POINT('Ctrl Pts',(4.57328757735259,-2.7977370397245,1.08643000204986)) ;
#134687 = CARTESIAN_POINT('Ctrl Pts',(4.58237922839515,-2.79856394574987,
1.07773359106864)) ;
#134688 = CARTESIAN_POINT('Ctrl Pts',(4.59151541127592,-2.80237286596198,
1.06991699711942)) ;
#134689 = CARTESIAN_POINT('Ctrl Pts',(4.57700059755676,-2.79703714667161,
1.08792392365797)) ;
#134690 = CARTESIAN_POINT('Ctrl Pts',(4.58532305318676,-2.79784352093717,
1.08073745699554)) ;
#134691 = CARTESIAN_POINT('Ctrl Pts',(4.59370961102545,-2.80088045369937,
1.07425448581055)) ;
#134692 = CARTESIAN_POINT('Ctrl Pts',(4.58319893207065,-2.79574016930783,
1.09034532947887)) ;
#134693 = CARTESIAN_POINT('Ctrl Pts',(4.58990416109239,-2.79637293360539,
1.08566964543776)) ;
#134694 = CARTESIAN_POINT('Ctrl Pts',(4.59665800356694,-2.79825577077759,
1.08141805513029)) ;
#134695 = CARTESIAN_POINT('Ctrl Pts',(4.58534994317985,-2.79526732601294,
1.09118113811282)) ;
#134696 = CARTESIAN_POINT('Ctrl Pts',(4.59144552977842,-2.79581844972912,
1.08737996338929)) ;
#134697 = CARTESIAN_POINT('Ctrl Pts',(4.59758018705035,-2.79731769672696,
1.08391141960612)) ;
#134698 = CARTESIAN_POINT('Ctrl Pts',(4.58899927751307,-2.79450268149332,
1.09248269873289)) ;
#134699 = CARTESIAN_POINT('Ctrl Pts',(4.59386223202755,-2.79488630507105,
1.09005048296971)) ;
#134700 = CARTESIAN_POINT('Ctrl Pts',(4.59874684688641,-2.79582009356912,
1.08781863475525)) ;
#134701 = CARTESIAN_POINT('Ctrl Pts',(4.59026755692873,-2.79423885380164,
1.09292560041996)) ;
#134702 = CARTESIAN_POINT('Ctrl Pts',(4.59467706068313,-2.79455862385203,
1.09095945666394)) ;
#134703 = CARTESIAN_POINT('Ctrl Pts',(4.59910266898803,-2.79530499526365,
1.08915136009784)) ;
#134704 = CARTESIAN_POINT('Ctrl Pts',(4.59257623319514,-2.79382131826659,
1.09361586855001)) ;
#134705 = CARTESIAN_POINT('Ctrl Pts',(4.59605751036345,-2.79403163929514,
1.09237723896638)) ;
#134706 = CARTESIAN_POINT('Ctrl Pts',(4.59954701072604,-2.79449510806573,
1.09123423318303)) ;
#134707 = CARTESIAN_POINT('Ctrl Pts',(4.59342976933297,-2.79367543507711,
1.09385546254663)) ;
#134708 = CARTESIAN_POINT('Ctrl Pts',(4.59655016100493,-2.79384713427255,
1.09286511046971)) ;
#134709 = CARTESIAN_POINT('Ctrl Pts',(4.59967640178298,-2.79421605292372,
1.09194978606297)) ;
#134710 = CARTESIAN_POINT('Ctrl Pts',(4.59428414179642,-2.79346156087783,
1.09429306381474)) ;
#134711 = CARTESIAN_POINT('Ctrl Pts',(4.59704519451433,-2.79355469746529,
1.09362636425205)) ;
#134712 = CARTESIAN_POINT('Ctrl Pts',(4.5998104157401,-2.79379877456676,1.09301762872931)) ;
#134713 = CARTESIAN_POINT('Ctrl Pts',(4.59432658472652,-2.7933916625364,1.09446618185051)) ;
#134714 = CARTESIAN_POINT('Ctrl Pts',(4.59708408719785,-2.79345234504013,
1.09389092335371)) ;
#134715 = CARTESIAN_POINT('Ctrl Pts',(4.59984563524626,-2.79366003518351,
1.09337234564734)) ;
#134716 = CARTESIAN_POINT('Ctrl Pts',(4.59537197237733,-2.79324260992761,
1.09471273840615)) ;
#134717 = CARTESIAN_POINT('Ctrl Pts',(4.59764722167537,-2.79326383513928,
1.094379038145)) ;
#134718 = CARTESIAN_POINT('Ctrl Pts',(4.59992475053754,-2.79338190759658,
1.09408296935242)) ;
#134719 = CARTESIAN_POINT('Ctrl Pts',(4.5936418339237,-2.79313407032025,1.09471552115488)) ;
#134720 = CARTESIAN_POINT('Ctrl Pts',(4.59684754854893,-2.79327107597597,
1.09436106895479)) ;
#134721 = CARTESIAN_POINT('Ctrl Pts',(4.59996664298755,-2.79324102308607,
1.09443822631848)) ;
#134722 = CARTESIAN_POINT('Ctrl Pts',(4.59999999999999,-2.79310344827586,
1.09479364595777)) ;
#134723 = CARTESIAN_POINT('Ctrl Pts',(4.59999999999999,-2.79310344827586,
1.09479364595777)) ;
#134724 = CARTESIAN_POINT('Ctrl Pts',(4.59999999999999,-2.79310344827586,
1.09479364595777)) ;
#134725 = CARTESIAN_POINT('Origin',(4.54879236168542,-2.9,1.07643444348393)) ;
#134726 = CARTESIAN_POINT('Ctrl Pts',(4.39959973407451,-2.8,-0.110592242802564)) ;
#134727 = CARTESIAN_POINT('Ctrl Pts',(4.49922290141881,-2.8,-0.110105248331461)) ;
#134728 = CARTESIAN_POINT('Ctrl Pts',(4.49980764094185,-2.89969504276377,
-0.11060804589506)) ;
#134729 = CARTESIAN_POINT('Ctrl Pts',(4.40142712570759,-2.8,0.110466103992318)) ;
#134730 = CARTESIAN_POINT('Ctrl Pts',(4.5059362211965,-2.8,0.113951986531775)) ;
#134731 = CARTESIAN_POINT('Ctrl Pts',(4.50067611734352,-2.90411960318539,
0.110349712874591)) ;
#134732 = CARTESIAN_POINT('Ctrl Pts',(4.39573539165433,-2.8,0.332377458211494)) ;
#134733 = CARTESIAN_POINT('Ctrl Pts',(4.49039105203445,-2.8,0.313555133991133)) ;
#134734 = CARTESIAN_POINT('Ctrl Pts',(4.49793210898571,-2.89506044297344,
0.333407164930358)) ;
#134735 = CARTESIAN_POINT('Ctrl Pts',(4.41164816536272,-2.8,0.645507851343547)) ;
#134736 = CARTESIAN_POINT('Ctrl Pts',(4.48203507549535,-2.8,0.636992461610863)) ;
#134737 = CARTESIAN_POINT('Ctrl Pts',(4.50604587949363,-2.86657833599731,
0.638208366544944)) ;
#134738 = CARTESIAN_POINT('Ctrl Pts',(4.41940490599909,-2.8,0.737842868001297)) ;
#134739 = CARTESIAN_POINT('Ctrl Pts',(4.48133975791567,-2.8,0.726672536261365)) ;
#134740 = CARTESIAN_POINT('Ctrl Pts',(4.50997623336226,-2.85625883833133,
0.726935356761025)) ;
#134741 = CARTESIAN_POINT('Ctrl Pts',(4.44577434373642,-2.8,0.872979341174024)) ;
#134742 = CARTESIAN_POINT('Ctrl Pts',(4.49360122670478,-2.8,0.860669412332162)) ;
#134743 = CARTESIAN_POINT('Ctrl Pts',(4.52318558604183,-2.83896465559564,
0.854514957562391)) ;
#134744 = CARTESIAN_POINT('Ctrl Pts',(4.45692583760035,-2.8,0.917523106947224)) ;
#134745 = CARTESIAN_POINT('Ctrl Pts',(4.49949391572667,-2.8,0.90394569735387)) ;
#134746 = CARTESIAN_POINT('Ctrl Pts',(4.52876348458384,-2.83289258157629,
0.896197011395723)) ;
#134747 = CARTESIAN_POINT('Ctrl Pts',(4.50378503771653,-2.8,1.03892408374168)) ;
#134748 = CARTESIAN_POINT('Ctrl Pts',(4.52873519606807,-2.8,1.02007465772522)) ;
#134749 = CARTESIAN_POINT('Ctrl Pts',(4.55214466721901,-2.81552005845342,
1.00877513019841)) ;
#134750 = CARTESIAN_POINT('Ctrl Pts',(4.5471442379017,-2.8,1.11773150495339)) ;
#134751 = CARTESIAN_POINT('Ctrl Pts',(4.55761617337306,-2.8,1.09679343581194)) ;
#134752 = CARTESIAN_POINT('Ctrl Pts',(4.57259584813394,-2.80338245043794,
1.07876140481136)) ;
#134753 = CARTESIAN_POINT('Ctrl Pts',(4.67762904165636,-2.8,1.10850495520363)) ;
#134754 = CARTESIAN_POINT('Ctrl Pts',(4.66093484724981,-2.8,1.09293293416154)) ;
#134755 = CARTESIAN_POINT('Ctrl Pts',(4.64133868807436,-2.80368623369345,
1.07531199361316)) ;
#134756 = CARTESIAN_POINT('Origin',(4.4,-2.9,-3.84865454255039E-12)) ;
#134757 = CARTESIAN_POINT('Ctrl Pts',(4.7217278356704,-2.8000000024879,-1.10036295491226)) ;
#134758 = CARTESIAN_POINT('Ctrl Pts',(4.69645430308005,-2.79999660525785,
-1.08707004730944)) ;
#134759 = CARTESIAN_POINT('Ctrl Pts',(4.66463283185041,-2.80454824226961,
-1.06949036829269)) ;
#134760 = CARTESIAN_POINT('Ctrl Pts',(4.55709227475145,-2.80000000030525,
-1.13599643631035)) ;
#134761 = CARTESIAN_POINT('Ctrl Pts',(4.56399237478695,-2.79999958643658,
-1.1139593792008)) ;
#134762 = CARTESIAN_POINT('Ctrl Pts',(4.57729370999483,-2.80055804294513,
-1.09517590508062)) ;
#134763 = CARTESIAN_POINT('Ctrl Pts',(4.50667826286324,-2.80000000784871,
-1.04661464799811)) ;
#134764 = CARTESIAN_POINT('Ctrl Pts',(4.53037382014986,-2.79998899178918,
-1.02708460011663)) ;
#134765 = CARTESIAN_POINT('Ctrl Pts',(4.55348183854655,-2.814346995092,-1.01594660411382)) ;
#134766 = CARTESIAN_POINT('Ctrl Pts',(4.45692280158728,-2.80000001789831,
-0.917642218287593)) ;
#134767 = CARTESIAN_POINT('Ctrl Pts',(4.49938029267387,-2.79997354447567,
-0.904099888009291)) ;
#134768 = CARTESIAN_POINT('Ctrl Pts',(4.5286414976122,-2.83271033979029,-0.896329062079886)) ;
#134769 = CARTESIAN_POINT('Ctrl Pts',(4.44554661086167,-2.80000002126189,
-0.872377440013972)) ;
#134770 = CARTESIAN_POINT('Ctrl Pts',(4.49333665154873,-2.79996797963652,
-0.86009693987387)) ;
#134771 = CARTESIAN_POINT('Ctrl Pts',(4.52295544156375,-2.83885474437148,
-0.853967858227963)) ;
#134772 = CARTESIAN_POINT('Ctrl Pts',(4.41903322104342,-2.8000000307772,-0.735894797577176)) ;
#134773 = CARTESIAN_POINT('Ctrl Pts',(4.48100616080269,-2.79995095769185,
-0.724730004020391)) ;
#134774 = CARTESIAN_POINT('Ctrl Pts',(4.50969337368917,-2.85623179093908,
-0.725069623608933)) ;
#134775 = CARTESIAN_POINT('Ctrl Pts',(4.41147189908676,-2.8000000363501,-0.64424159004353)) ;
#134776 = CARTESIAN_POINT('Ctrl Pts',(4.48178828424082,-2.79993989905032,
-0.635789149205618)) ;
#134777 = CARTESIAN_POINT('Ctrl Pts',(4.50589025525755,-2.86640526991179,
-0.636968151201155)) ;
#134778 = CARTESIAN_POINT('Ctrl Pts',(4.39523119070925,-2.80000005228414,
-0.32317951983275)) ;
#134779 = CARTESIAN_POINT('Ctrl Pts',(4.49033836345961,-2.79990261688309,
-0.303074131660309)) ;
#134780 = CARTESIAN_POINT('Ctrl Pts',(4.49769757367181,-2.89547737953052,
-0.32433321576161)) ;
#134781 = CARTESIAN_POINT('Ctrl Pts',(4.40178225889358,-2.80000005718968,
-0.092623978285313)) ;
#134782 = CARTESIAN_POINT('Ctrl Pts',(4.50681341018239,-2.7998878412185,-0.0970581988245104)) ;
#134783 = CARTESIAN_POINT('Ctrl Pts',(4.50092255053472,-2.90441958896148,
-0.0924406960392595)) ;
#134784 = CARTESIAN_POINT('Ctrl Pts',(4.39924589760313,-2.80000005405718,
0.13696883112012)) ;
#134785 = CARTESIAN_POINT('Ctrl Pts',(4.49795607191458,-2.79989746608223,
0.136077062504044)) ;
#134786 = CARTESIAN_POINT('Ctrl Pts',(4.49968270404899,-2.89870974459617,
0.136971505408573)) ;
#134787 = CARTESIAN_POINT('Origin',(4.54879236168626,-2.9,-1.07643444348457)) ;
#134788 = CARTESIAN_POINT('Ctrl Pts',(4.57442492185552,-2.80939715119899,
-1.04275810686208)) ;
#134789 = CARTESIAN_POINT('Ctrl Pts',(4.56210583156796,-2.79989612750329,
-1.05894306178873)) ;
#134790 = CARTESIAN_POINT('Ctrl Pts',(4.54850917782856,-2.80000109307748,
-1.07680649348805)) ;
#134791 = CARTESIAN_POINT('Ctrl Pts',(4.57959763980855,-2.80818914940071,
-1.04994530049547)) ;
#134792 = CARTESIAN_POINT('Ctrl Pts',(4.56768008075467,-2.80031924975226,
-1.06394104572908)) ;
#134793 = CARTESIAN_POINT('Ctrl Pts',(4.55527876038346,-2.79999229227378,
-1.07958997638678)) ;
#134794 = CARTESIAN_POINT('Ctrl Pts',(4.58464248447265,-2.80630474344638,
-1.05748431263834)) ;
#134795 = CARTESIAN_POINT('Ctrl Pts',(4.57346944634372,-2.80008318972135,
-1.06920129105218)) ;
#134796 = CARTESIAN_POINT('Ctrl Pts',(4.56216307187795,-2.79941338753917,
-1.08232809153345)) ;
#134797 = CARTESIAN_POINT('Ctrl Pts',(4.59159231899494,-2.80232720646228,
-1.07005636929591)) ;
#134798 = CARTESIAN_POINT('Ctrl Pts',(4.58237910662986,-2.79850221241048,
-1.07791493625778)) ;
#134799 = CARTESIAN_POINT('Ctrl Pts',(4.57321634584967,-2.79769868647539,
-1.08666448649469)) ;
#134800 = CARTESIAN_POINT('Ctrl Pts',(4.59378564167737,-2.8008235544484,-1.07441458376545)) ;
#134801 = CARTESIAN_POINT('Ctrl Pts',(4.58533966160572,-2.79778056279966,
-1.08091806944782)) ;
#134802 = CARTESIAN_POINT('Ctrl Pts',(4.5769613009382,-2.79699227428059,-1.08813207403617)) ;
#134803 = CARTESIAN_POINT('Ctrl Pts',(4.59669734138576,-2.79821861236081,
-1.08151744690911)) ;
#134804 = CARTESIAN_POINT('Ctrl Pts',(4.58989502505307,-2.7963307230051,-1.08578370298498)) ;
#134805 = CARTESIAN_POINT('Ctrl Pts',(4.58314295739387,-2.79570785369251,
-1.09047890318143)) ;
#134806 = CARTESIAN_POINT('Ctrl Pts',(4.59760632414569,-2.79728965034655,
-1.08398524662906)) ;
#134807 = CARTESIAN_POINT('Ctrl Pts',(4.59142619397024,-2.79578507327359,
-1.08746789372294)) ;
#134808 = CARTESIAN_POINT('Ctrl Pts',(4.58528630332434,-2.79524119148169,
-1.09128737837496)) ;
#134809 = CARTESIAN_POINT('Ctrl Pts',(4.59875741430932,-2.79580683383092,
-1.08785300449597)) ;
#134810 = CARTESIAN_POINT('Ctrl Pts',(4.59383193680337,-2.79486773439436,
-1.09009800553385)) ;
#134811 = CARTESIAN_POINT('Ctrl Pts',(4.58892874314202,-2.79448758877844,
-1.09254647301294)) ;
#134812 = CARTESIAN_POINT('Ctrl Pts',(4.59910834609947,-2.79529718130591,
-1.08917149930144)) ;
#134813 = CARTESIAN_POINT('Ctrl Pts',(4.59464343907623,-2.79454543406796,
-1.09099269585011)) ;
#134814 = CARTESIAN_POINT('Ctrl Pts',(4.59019511689903,-2.79422790851556,
-1.09297467120907)) ;
#134815 = CARTESIAN_POINT('Ctrl Pts',(4.59954688679867,-2.79449699552073,
-1.0912293846587)) ;
#134816 = CARTESIAN_POINT('Ctrl Pts',(4.59601732089136,-2.79402779797775,
-1.09238633635182)) ;
#134817 = CARTESIAN_POINT('Ctrl Pts',(4.59249627585272,-2.79381771894921,
-1.09364111416748)) ;
#134818 = CARTESIAN_POINT('Ctrl Pts',(4.59967529310588,-2.79422450025963,
-1.09193546456122)) ;
#134819 = CARTESIAN_POINT('Ctrl Pts',(4.59651100242293,-2.79384821317134,
-1.09286441087348)) ;
#134820 = CARTESIAN_POINT('Ctrl Pts',(4.59335287412398,-2.79367727499394,
-1.09387144765738)) ;
#134821 = CARTESIAN_POINT('Ctrl Pts',(4.59980981518572,-2.79380630943631,
-1.09300564521014)) ;
#134822 = CARTESIAN_POINT('Ctrl Pts',(4.59701056623719,-2.79355888022806,
-1.09362493503647)) ;
#134823 = CARTESIAN_POINT('Ctrl Pts',(4.59421559911327,-2.79346462438276,
-1.09430302898986)) ;
#134824 = CARTESIAN_POINT('Ctrl Pts',(4.59984534134842,-2.79366726490194,
-1.09336460674889)) ;
#134825 = CARTESIAN_POINT('Ctrl Pts',(4.59705039509826,-2.79345667046143,
-1.09389173939615)) ;
#134826 = CARTESIAN_POINT('Ctrl Pts',(4.59425962044003,-2.79339574833516,
-1.09447656370425)) ;
#134827 = CARTESIAN_POINT('Ctrl Pts',(4.59992484646001,-2.7933873519883,-1.09407980383996)) ;
#134828 = CARTESIAN_POINT('Ctrl Pts',(4.59761652863209,-2.7932668237374,-1.09438058953102)) ;
#134829 = CARTESIAN_POINT('Ctrl Pts',(4.59531061070856,-2.79324678512396,
-1.09472041373345)) ;
#134830 = CARTESIAN_POINT('Ctrl Pts',(4.59996721368508,-2.79324340897637,
-1.09443656979399)) ;
#134831 = CARTESIAN_POINT('Ctrl Pts',(4.59680854952868,-2.79327323421043,
-1.09436047786159)) ;
#134832 = CARTESIAN_POINT('Ctrl Pts',(4.59356174266139,-2.79313094944462,
-1.09472348332067)) ;
#134833 = CARTESIAN_POINT('Ctrl Pts',(4.59999999999999,-2.79310344827586,
-1.09479364595777)) ;
#134834 = CARTESIAN_POINT('Ctrl Pts',(4.59999999999999,-2.79310344827586,
-1.09479364595777)) ;
#134835 = CARTESIAN_POINT('Ctrl Pts',(4.59999999999999,-2.79310344827586,
-1.09479364595777)) ;
#134836 = CARTESIAN_POINT('Origin',(5.6561028345357,10.05,2.04)) ;
#134837 = CARTESIAN_POINT('Origin',(7.26810489940853,5.50476046277485,-2.875)) ;
#134838 = CARTESIAN_POINT('',(4.03523814377473,5.98727788898885,-2.775)) ;
#134839 = CARTESIAN_POINT('',(4.03523814377473,5.98727788898885,-1.475)) ;
#134840 = CARTESIAN_POINT('',(4.03523814377473,5.98727788898885,-2.875)) ;
#134841 = CARTESIAN_POINT('',(7.26810489940853,5.50476046277485,-1.475)) ;
#134842 = CARTESIAN_POINT('',(7.26810489940853,5.50476046277485,-1.475)) ;
#134843 = CARTESIAN_POINT('',(7.26810489940853,5.50476046277485,-2.775)) ;
#134844 = CARTESIAN_POINT('',(7.26810489940853,5.50476046277485,-2.875)) ;
#134845 = CARTESIAN_POINT('',(3.95,6.,-2.775)) ;
#134846 = CARTESIAN_POINT('Origin',(7.25334304318326,5.40585602606554,-2.875)) ;
#134847 = CARTESIAN_POINT('',(7.32310496992715,5.47750289324744,-1.475)) ;
#134848 = CARTESIAN_POINT('Origin',(7.25334304318326,5.40585602606554,-1.475)) ;
#134849 = CARTESIAN_POINT('',(7.32310496992715,5.47750289324744,-2.775)) ;
#134850 = CARTESIAN_POINT('',(7.32310496992715,5.47750289324744,-2.875)) ;
#134851 = CARTESIAN_POINT('Origin',(7.25334304318326,5.40585602606554,-2.775)) ;
#134852 = CARTESIAN_POINT('Origin',(8.66976192674389,4.16627481495487,-2.875)) ;
#134853 = CARTESIAN_POINT('',(8.66976192674389,4.16627481495487,-1.475)) ;
#134854 = CARTESIAN_POINT('',(8.66976192674389,4.16627481495487,-1.475)) ;
#134855 = CARTESIAN_POINT('',(8.66976192674389,4.16627481495487,-2.775)) ;
#134856 = CARTESIAN_POINT('',(8.66976192674389,4.16627481495487,-2.875)) ;
#134857 = CARTESIAN_POINT('',(7.32310496992715,5.47750289324744,-2.775)) ;
#134858 = CARTESIAN_POINT('Origin',(8.6,4.09462794777298,-2.875)) ;
#134859 = CARTESIAN_POINT('',(8.7,4.09462794777298,-1.475)) ;
#134860 = CARTESIAN_POINT('Origin',(8.6,4.09462794777298,-1.475)) ;
#134861 = CARTESIAN_POINT('',(8.7,4.09462794777298,-2.775)) ;
#134862 = CARTESIAN_POINT('',(8.7,4.09462794777298,-2.875)) ;
#134863 = CARTESIAN_POINT('Origin',(8.6,4.09462794777298,-2.775)) ;
#134864 = CARTESIAN_POINT('Origin',(8.7,3.95,-2.875)) ;
#134865 = CARTESIAN_POINT('',(8.7,3.95,-1.475)) ;
#134866 = CARTESIAN_POINT('',(8.7,3.95,-1.475)) ;
#134867 = CARTESIAN_POINT('',(8.7,3.95,-2.775)) ;
#134868 = CARTESIAN_POINT('',(8.7,3.95,-2.875)) ;
#134869 = CARTESIAN_POINT('',(8.7,4.09462794777298,-2.775)) ;
#134870 = CARTESIAN_POINT('Origin',(8.6,3.95,-2.875)) ;
#134871 = CARTESIAN_POINT('',(8.55460943381591,3.86089502538305,-1.475)) ;
#134872 = CARTESIAN_POINT('Origin',(8.6,3.95,-1.475)) ;
#134873 = CARTESIAN_POINT('',(8.55460943381591,3.86089502538305,-2.775)) ;
#134874 = CARTESIAN_POINT('',(8.55460943381591,3.86089502538305,-2.875)) ;
#134875 = CARTESIAN_POINT('Origin',(8.6,3.95,-2.775)) ;
#134876 = CARTESIAN_POINT('Origin',(7.3213877252879,4.48910497461695,-2.875)) ;
#134877 = CARTESIAN_POINT('',(7.3213877252879,4.48910497461695,-1.475)) ;
#134878 = CARTESIAN_POINT('',(7.3213877252879,4.48910497461695,-1.475)) ;
#134879 = CARTESIAN_POINT('',(7.3213877252879,4.48910497461695,-2.775)) ;
#134880 = CARTESIAN_POINT('',(7.3213877252879,4.48910497461695,-2.875)) ;
#134881 = CARTESIAN_POINT('',(8.55460943381591,3.86089502538305,-2.775)) ;
#134882 = CARTESIAN_POINT('Origin',(7.27599715910381,4.4,-2.875)) ;
#134883 = CARTESIAN_POINT('',(7.27599715910381,4.5,-1.475)) ;
#134884 = CARTESIAN_POINT('Origin',(7.27599715910381,4.4,-1.475)) ;
#134885 = CARTESIAN_POINT('',(7.27599715910381,4.5,-2.775)) ;
#134886 = CARTESIAN_POINT('',(7.27599715910381,4.5,-2.875)) ;
#134887 = CARTESIAN_POINT('Origin',(7.27599715910381,4.4,-2.775)) ;
#134888 = CARTESIAN_POINT('Origin',(3.95,4.5,-2.875)) ;
#134889 = CARTESIAN_POINT('',(4.05,4.5,-1.475)) ;
#134890 = CARTESIAN_POINT('',(3.95,4.5,-1.475)) ;
#134891 = CARTESIAN_POINT('',(4.05,4.5,-2.775)) ;
#134892 = CARTESIAN_POINT('',(4.05,4.5,-2.875)) ;
#134893 = CARTESIAN_POINT('',(7.27599715910381,4.5,-2.775)) ;
#134894 = CARTESIAN_POINT('Origin',(7.25334304318326,5.40585602606554,-2.875)) ;
#134895 = CARTESIAN_POINT('',(7.36677829147199,4.5782099492339,-2.875)) ;
#134896 = CARTESIAN_POINT('',(7.27599715910381,4.6,-2.875)) ;
#134897 = CARTESIAN_POINT('Origin',(7.27599715910381,4.4,-2.875)) ;
#134898 = CARTESIAN_POINT('',(4.05,4.6,-2.875)) ;
#134899 = CARTESIAN_POINT('',(3.95,4.6,-2.875)) ;
#134900 = CARTESIAN_POINT('',(4.05,5.88396692803319,-2.875)) ;
#134901 = CARTESIAN_POINT('',(4.05,6.,-2.875)) ;
#134902 = CARTESIAN_POINT('',(7.25334304318326,5.40585602606554,-2.875)) ;
#134903 = CARTESIAN_POINT('',(7.25334304318326,5.40585602606554,-2.875)) ;
#134904 = CARTESIAN_POINT('',(8.6,4.09462794777298,-2.875)) ;
#134905 = CARTESIAN_POINT('',(8.6,4.09462794777298,-2.875)) ;
#134906 = CARTESIAN_POINT('',(8.6,3.95,-2.875)) ;
#134907 = CARTESIAN_POINT('',(8.6,3.95,-2.875)) ;
#134908 = CARTESIAN_POINT('',(7.36677829147199,4.5782099492339,-2.875)) ;
#134909 = CARTESIAN_POINT('Origin',(7.25334304318326,5.40585602606554,-1.375)) ;
#134910 = CARTESIAN_POINT('',(8.6,4.09462794777298,-1.375)) ;
#134911 = CARTESIAN_POINT('',(7.25334304318326,5.40585602606554,-1.375)) ;
#134912 = CARTESIAN_POINT('',(7.25334304318326,5.40585602606554,-1.375)) ;
#134913 = CARTESIAN_POINT('',(4.05,5.88396692803319,-1.375)) ;
#134914 = CARTESIAN_POINT('',(7.25334304318326,5.40585602606554,-1.375)) ;
#134915 = CARTESIAN_POINT('',(4.05,4.6,-1.375)) ;
#134916 = CARTESIAN_POINT('',(4.05,5.40585602606554,-1.375)) ;
#134917 = CARTESIAN_POINT('',(7.27599715910381,4.6,-1.375)) ;
#134918 = CARTESIAN_POINT('',(7.25334304318326,4.6,-1.375)) ;
#134919 = CARTESIAN_POINT('',(7.36677829147199,4.5782099492339,-1.375)) ;
#134920 = CARTESIAN_POINT('Origin',(7.27599715910381,4.4,-1.375)) ;
#134921 = CARTESIAN_POINT('',(8.6,3.95,-1.375)) ;
#134922 = CARTESIAN_POINT('',(6.94197060168454,4.79460933256464,-1.375)) ;
#134923 = CARTESIAN_POINT('',(8.6,5.40585602606554,-1.375)) ;
#134924 = CARTESIAN_POINT('Origin',(4.5,-2.8,-2.54)) ;
#134925 = CARTESIAN_POINT('',(4.5,-2.4,-7.04214168703486)) ;
#134926 = CARTESIAN_POINT('',(4.5,-2.7,-6.60315462117279)) ;
#134927 = CARTESIAN_POINT('Origin',(4.5,0.,-5.08)) ;
#134928 = CARTESIAN_POINT('',(4.5,-2.7,-7.62)) ;
#134929 = CARTESIAN_POINT('',(4.5,-2.7,-2.54)) ;
#134930 = CARTESIAN_POINT('',(4.5,-2.4,-7.62)) ;
#134931 = CARTESIAN_POINT('',(4.5,-2.8,-7.62)) ;
#134932 = CARTESIAN_POINT('',(4.5,-2.4,-7.00613602842582)) ;
#134933 = CARTESIAN_POINT('Origin',(12.8,2.75,-2.54)) ;
#134934 = CARTESIAN_POINT('',(12.7,2.75,-7.62)) ;
#134935 = CARTESIAN_POINT('',(4.55912712210514,2.75,-7.62)) ;
#134936 = CARTESIAN_POINT('',(12.8,2.75,-7.62)) ;
#134937 = CARTESIAN_POINT('',(4.55912712210513,2.75,-6.57304604217164)) ;
#134938 = CARTESIAN_POINT('',(4.55912712210514,2.75,-6.57304604217164)) ;
#134939 = CARTESIAN_POINT('',(12.8,2.75,-6.57304604217164)) ;
#134940 = CARTESIAN_POINT('',(12.7,2.75,-2.54)) ;
#134941 = CARTESIAN_POINT('Origin',(0.,9.95,-5.08)) ;
#134942 = CARTESIAN_POINT('',(0.230887397576971,9.95,-6.99486057185377)) ;
#134943 = CARTESIAN_POINT('Origin',(4.5,-2.3,-2.54)) ;
#134944 = CARTESIAN_POINT('',(12.7,-2.3,-7.04214168703486)) ;
#134945 = CARTESIAN_POINT('',(4.6,-2.3,-7.04214168703486)) ;
#134946 = CARTESIAN_POINT('',(4.5,-2.3,-7.04214168703486)) ;
#134947 = CARTESIAN_POINT('',(4.6,-2.3,-7.62)) ;
#134948 = CARTESIAN_POINT('',(4.6,-2.3,-7.62)) ;
#134949 = CARTESIAN_POINT('',(12.7,-2.3,-7.62)) ;
#134950 = CARTESIAN_POINT('',(4.5,-2.3,-7.62)) ;
#134951 = CARTESIAN_POINT('',(12.7,-2.3,-2.54)) ;
#134952 = CARTESIAN_POINT('Origin',(0.,0.,-7.62)) ;
#134953 = CARTESIAN_POINT('Origin',(4.4,-2.7,-7.62)) ;
#134954 = CARTESIAN_POINT('Origin',(4.55912712210514,2.85,-7.62)) ;
#134955 = CARTESIAN_POINT('Origin',(12.7,2.65,-7.62)) ;
#134956 = CARTESIAN_POINT('Origin',(12.7,-2.2,-7.62)) ;
#134957 = CARTESIAN_POINT('Origin',(4.6,-2.4,-7.62)) ;
#134958 = CARTESIAN_POINT('Origin',(-4.65,1.95,-7.08)) ;
#134959 = CARTESIAN_POINT('',(-4.66204490261456,3.21928058320648,-7.08)) ;
#134960 = CARTESIAN_POINT('',(-5.3,3.9369800677651,-7.08)) ;
#134961 = CARTESIAN_POINT('',(-5.47474093186837,4.13356361611701,-7.08)) ;
#134962 = CARTESIAN_POINT('',(-5.3,-1.88819660112501,-7.08)) ;
#134963 = CARTESIAN_POINT('',(-5.3,-2.05,-7.08)) ;
#134964 = CARTESIAN_POINT('',(-4.66204490261456,-1.5692190524323,-7.08)) ;
#134965 = CARTESIAN_POINT('',(-4.69472135955,-1.58555728090001,-7.08)) ;
#134966 = CARTESIAN_POINT('',(-4.66204490261456,3.35625,-7.08)) ;
#134967 = CARTESIAN_POINT('Origin',(-5.4,1.95,-3.08)) ;
#134968 = CARTESIAN_POINT('',(-4.66204490261456,-1.5692190524323,-3.08)) ;
#134969 = CARTESIAN_POINT('',(-5.3,-1.88819660112502,-3.08)) ;
#134970 = CARTESIAN_POINT('',(-5.44472135955,-1.96055728090001,-3.08)) ;
#134971 = CARTESIAN_POINT('',(-5.3,3.9369800677651,-3.08)) ;
#134972 = CARTESIAN_POINT('',(-5.3,4.20000000000001,-3.08)) ;
#134973 = CARTESIAN_POINT('',(-4.66204490261456,3.21928058320648,-3.08)) ;
#134974 = CARTESIAN_POINT('',(-4.72474093186837,3.28981361611701,-3.08)) ;
#134975 = CARTESIAN_POINT('',(-4.66204490261456,-1.67500000000001,-3.08)) ;
#134976 = CARTESIAN_POINT('Origin',(-4.65,1.95,-3.08)) ;
#134977 = CARTESIAN_POINT('',(-3.33134808452128,1.85,-3.4023371348948)) ;
#134978 = CARTESIAN_POINT('',(-3.48082994825801,1.91712723223402,-3.36579712375915)) ;
#134979 = CARTESIAN_POINT('Origin',(-3.34328863644912,2.02341244982159,-3.39941833331244)) ;
#134980 = CARTESIAN_POINT('',(-2.4,1.85,-3.63)) ;
#134981 = CARTESIAN_POINT('',(-4.65,1.85,-3.08)) ;
#134982 = CARTESIAN_POINT('',(-2.4,-0.95,-3.63)) ;
#134983 = CARTESIAN_POINT('',(-2.4,1.95,-3.63)) ;
#134984 = CARTESIAN_POINT('',(-3.3526478932023,-0.95,-3.39713051499499)) ;
#134985 = CARTESIAN_POINT('',(-3.39999999999998,-0.95,-3.38555555555556)) ;
#134986 = CARTESIAN_POINT('',(-3.44209061230229,-0.971114561800017,-3.37526673921499)) ;
#134987 = CARTESIAN_POINT('Origin',(-3.3620122055811,-1.11033257691499,-3.39484146085794)) ;
#134988 = CARTESIAN_POINT('',(-4.63829959356686,-1.5692190524323,-3.08286009935032)) ;
#134989 = CARTESIAN_POINT('',(-4.68814869588294,-1.59414360359034,-3.07067476322862)) ;
#134990 = CARTESIAN_POINT('',(-4.63829959356686,3.21928058320648,-3.08286009935032)) ;
#134991 = CARTESIAN_POINT('',(-4.63829959356686,3.35625,-3.08286009935032)) ;
#134992 = CARTESIAN_POINT('',(-3.45989661114215,1.89357722797868,-3.37091416172081)) ;
#134993 = CARTESIAN_POINT('Origin',(-2.4,1.95,-3.63)) ;
#134994 = CARTESIAN_POINT('',(-2.4,1.85,-6.53)) ;
#134995 = CARTESIAN_POINT('',(-2.4,-0.95,-6.53)) ;
#134996 = CARTESIAN_POINT('',(-2.4,1.95,-6.53)) ;
#134997 = CARTESIAN_POINT('',(-2.4,-1.05,-6.427055690472)) ;
#134998 = CARTESIAN_POINT('Origin',(-2.4,-0.950000000000003,-6.427055690472)) ;
#134999 = CARTESIAN_POINT('',(-2.4,-1.05,-3.73294430952801)) ;
#135000 = CARTESIAN_POINT('',(-2.4,-1.05,-3.63)) ;
#135001 = CARTESIAN_POINT('Origin',(-2.4,-0.949999999999989,-3.73294430952802)) ;
#135002 = CARTESIAN_POINT('',(-2.4,1.95,-3.732944309528)) ;
#135003 = CARTESIAN_POINT('Origin',(-2.4,1.84999999999999,-3.73294430952802)) ;
#135004 = CARTESIAN_POINT('',(-2.4,1.95,-6.427055690472)) ;
#135005 = CARTESIAN_POINT('',(-2.4,1.95,-3.63)) ;
#135006 = CARTESIAN_POINT('Origin',(-2.4,1.85000000000005,-6.42705569047205)) ;
#135007 = CARTESIAN_POINT('Origin',(-2.4,1.95,-6.53)) ;
#135008 = CARTESIAN_POINT('',(-3.3526478932023,-0.95,-6.76286948500501)) ;
#135009 = CARTESIAN_POINT('',(-3.44209061230229,-0.971114561800017,-6.78473326078501)) ;
#135010 = CARTESIAN_POINT('Origin',(-3.3620122055812,-1.11033257691303,-6.76515853914208)) ;
#135011 = CARTESIAN_POINT('',(-2.4,-0.95,-6.53)) ;
#135012 = CARTESIAN_POINT('',(-3.33134808452128,1.85,-6.7576628651052)) ;
#135013 = CARTESIAN_POINT('',(-2.4,1.85,-6.53)) ;
#135014 = CARTESIAN_POINT('',(-3.48082994825801,1.91712723223402,-6.79420287624085)) ;
#135015 = CARTESIAN_POINT('Origin',(-3.34328863644907,2.02341244982186,-6.76058166668757)) ;
#135016 = CARTESIAN_POINT('',(-4.63829959356686,3.21928058320648,-7.07713990064968)) ;
#135017 = CARTESIAN_POINT('',(-4.70989661114216,3.29982722797869,-7.09464139383475)) ;
#135018 = CARTESIAN_POINT('',(-4.63829959356686,-1.5692190524323,-7.07713990064968)) ;
#135019 = CARTESIAN_POINT('',(-4.63829959356686,-1.67500000000001,-7.07713990064968)) ;
#135020 = CARTESIAN_POINT('',(-3.43814869588292,-0.969143603590331,-6.78376968121583)) ;
#135021 = CARTESIAN_POINT('Origin',(0.,1.95,-5.08)) ;
#135022 = CARTESIAN_POINT('',(-3.35509339356897,1.95,-3.49947703554448)) ;
#135023 = CARTESIAN_POINT('',(0.175392621986784,1.95,-4.36248472823589)) ;
#135024 = CARTESIAN_POINT('',(-3.35509339356897,1.95,-6.66052296445552)) ;
#135025 = CARTESIAN_POINT('',(-3.35509339356897,1.95,-6.77444444444444)) ;
#135026 = CARTESIAN_POINT('',(0.175392621986784,1.95,-5.79751527176412)) ;
#135027 = CARTESIAN_POINT('Origin',(0.,-1.05,-5.08)) ;
#135028 = CARTESIAN_POINT('',(-3.37639320225,-1.05,-6.66572958435533)) ;
#135029 = CARTESIAN_POINT('',(-3.42374530904768,-1.05,-6.67730454379476)) ;
#135030 = CARTESIAN_POINT('',(-3.37639320225,-1.05,-3.49427041564467)) ;
#135031 = CARTESIAN_POINT('',(-3.37639320225,-1.05,-5.08)) ;
#135032 = CARTESIAN_POINT('',(-2.4237453090477,-1.05,-3.72713990064968)) ;
#135033 = CARTESIAN_POINT('Origin',(-3.39999999999998,-1.05,-5.08)) ;
#135034 = CARTESIAN_POINT('',(-3.4211145618,-1.06055728090001,-3.47240663986467)) ;
#135035 = CARTESIAN_POINT('',(-3.4211145618,-1.06055728090001,-6.68759336013533)) ;
#135036 = CARTESIAN_POINT('',(-3.4211145618,-1.06055728090001,-5.08)) ;
#135037 = CARTESIAN_POINT('',(-4.61732354306457,-1.65866177153229,-6.98)) ;
#135038 = CARTESIAN_POINT('',(-4.66717264538064,-1.68358632269033,-6.99218533612171)) ;
#135039 = CARTESIAN_POINT('',(-5.34472135954999,-2.022360679775,-6.98)) ;
#135040 = CARTESIAN_POINT('',(-5.4,-2.05,-6.98)) ;
#135041 = CARTESIAN_POINT('',(-5.34472135954999,-2.022360679775,-3.18)) ;
#135042 = CARTESIAN_POINT('',(-5.34472135954999,-2.022360679775,-3.08)) ;
#135043 = CARTESIAN_POINT('',(-4.61732354306457,-1.65866177153229,-3.18)) ;
#135044 = CARTESIAN_POINT('',(-4.65,-1.67500000000001,-3.18)) ;
#135045 = CARTESIAN_POINT('',(-3.41717264538063,-1.05858632269032,-3.47337021943385)) ;
#135046 = CARTESIAN_POINT('Origin',(-5.4,4.20000000000001,-2.54)) ;
#135047 = CARTESIAN_POINT('',(-5.37474093186837,4.17158354835192,-3.18)) ;
#135048 = CARTESIAN_POINT('',(-5.37474093186837,4.17158354835192,-6.98)) ;
#135049 = CARTESIAN_POINT('',(-5.37474093186837,4.17158354835192,-7.08)) ;
#135050 = CARTESIAN_POINT('',(-4.58730397074619,3.28571696708947,-6.98)) ;
#135051 = CARTESIAN_POINT('',(-4.65,3.35625,-6.98)) ;
#135052 = CARTESIAN_POINT('',(-3.42983432543734,1.98356361611701,-6.69706297559117)) ;
#135053 = CARTESIAN_POINT('',(-3.40890098832149,1.96001361186167,-6.69194593762952)) ;
#135054 = CARTESIAN_POINT('',(-3.42983432543734,1.98356361611701,-3.46293702440883)) ;
#135055 = CARTESIAN_POINT('',(-3.42983432543734,1.98356361611701,-3.38555555555556)) ;
#135056 = CARTESIAN_POINT('',(-4.58730397074619,3.28571696708947,-3.18)) ;
#135057 = CARTESIAN_POINT('',(-4.65890098832149,3.36626361186168,-3.16249850681493)) ;
#135058 = CARTESIAN_POINT('',(-5.4,4.20000000000001,-3.18)) ;
#135059 = CARTESIAN_POINT('Origin',(-3.15,-3.9,-4.08)) ;
#135060 = CARTESIAN_POINT('',(-3.15,-3.95,-4.18)) ;
#135061 = CARTESIAN_POINT('',(-3.15,-3.85,-4.18)) ;
#135062 = CARTESIAN_POINT('',(-3.15,-3.75,-4.18)) ;
#135063 = CARTESIAN_POINT('',(-3.15,-3.85,-5.98)) ;
#135064 = CARTESIAN_POINT('',(-3.15,-3.85,-4.08)) ;
#135065 = CARTESIAN_POINT('',(-3.15,-3.95,-5.98)) ;
#135066 = CARTESIAN_POINT('',(-3.15,-4.05,-5.98)) ;
#135067 = CARTESIAN_POINT('',(-3.15,-3.95,-4.08)) ;
#135068 = CARTESIAN_POINT('Origin',(-4.4,-3.9,-6.08)) ;
#135069 = CARTESIAN_POINT('',(-3.25,-3.85,-6.08)) ;
#135070 = CARTESIAN_POINT('',(-4.3,-3.85,-6.08)) ;
#135071 = CARTESIAN_POINT('',(-4.4,-3.85,-6.08)) ;
#135072 = CARTESIAN_POINT('',(-4.3,-3.95,-6.08)) ;
#135073 = CARTESIAN_POINT('',(-4.3,-4.05,-6.08)) ;
#135074 = CARTESIAN_POINT('',(-3.25,-3.95,-6.08)) ;
#135075 = CARTESIAN_POINT('',(-4.4,-3.95,-6.08)) ;
#135076 = CARTESIAN_POINT('',(-3.25,-3.75,-6.08)) ;
#135077 = CARTESIAN_POINT('Origin',(-4.4,-3.9,-4.08)) ;
#135078 = CARTESIAN_POINT('',(-4.4,-3.85,-5.98)) ;
#135079 = CARTESIAN_POINT('',(-4.4,-3.85,-4.18)) ;
#135080 = CARTESIAN_POINT('',(-4.4,-3.85,-4.08)) ;
#135081 = CARTESIAN_POINT('',(-4.4,-3.95,-4.18)) ;
#135082 = CARTESIAN_POINT('',(-4.4,-4.05,-4.18)) ;
#135083 = CARTESIAN_POINT('',(-4.4,-3.95,-5.98)) ;
#135084 = CARTESIAN_POINT('',(-4.4,-3.95,-4.08)) ;
#135085 = CARTESIAN_POINT('',(-4.4,-3.75,-5.98)) ;
#135086 = CARTESIAN_POINT('Origin',(-4.4,-3.9,-4.08)) ;
#135087 = CARTESIAN_POINT('',(-4.3,-3.95,-4.08)) ;
#135088 = CARTESIAN_POINT('',(-4.3,-3.85,-4.08)) ;
#135089 = CARTESIAN_POINT('',(-4.3,-3.75,-4.08)) ;
#135090 = CARTESIAN_POINT('',(-3.25,-3.85,-4.08)) ;
#135091 = CARTESIAN_POINT('',(-4.4,-3.85,-4.08)) ;
#135092 = CARTESIAN_POINT('',(-3.25,-3.95,-4.08)) ;
#135093 = CARTESIAN_POINT('',(-3.25,-4.05,-4.08)) ;
#135094 = CARTESIAN_POINT('',(-4.4,-3.95,-4.08)) ;
#135095 = CARTESIAN_POINT('Origin',(0.,-3.75,-5.08)) ;
#135096 = CARTESIAN_POINT('',(-3.25,-3.75,-4.18)) ;
#135097 = CARTESIAN_POINT('',(-4.3,-3.75,-4.18)) ;
#135098 = CARTESIAN_POINT('',(-1.56125112837913E-16,-3.75,-4.18)) ;
#135099 = CARTESIAN_POINT('',(-4.3,-3.75,-5.98)) ;
#135100 = CARTESIAN_POINT('',(-4.3,-3.75,-5.08)) ;
#135101 = CARTESIAN_POINT('',(-3.25,-3.75,-5.98)) ;
#135102 = CARTESIAN_POINT('',(-1.56125112837913E-16,-3.75,-5.98)) ;
#135103 = CARTESIAN_POINT('',(-3.25,-3.75,-5.08)) ;
#135104 = CARTESIAN_POINT('',(-4.15,-3.75,-5.93)) ;
#135105 = CARTESIAN_POINT('',(-3.4,-3.75,-5.93)) ;
#135106 = CARTESIAN_POINT('',(-4.15,-3.75,-5.93)) ;
#135107 = CARTESIAN_POINT('',(-4.25,-3.75,-5.83)) ;
#135108 = CARTESIAN_POINT('Origin',(-4.15,-3.75,-5.83)) ;
#135109 = CARTESIAN_POINT('',(-4.25,-3.75,-4.33)) ;
#135110 = CARTESIAN_POINT('',(-4.25,-3.75,-4.33)) ;
#135111 = CARTESIAN_POINT('',(-4.15,-3.75,-4.23)) ;
#135112 = CARTESIAN_POINT('Origin',(-4.15,-3.75,-4.33)) ;
#135113 = CARTESIAN_POINT('',(-3.4,-3.75,-4.23)) ;
#135114 = CARTESIAN_POINT('',(-3.4,-3.75,-4.23)) ;
#135115 = CARTESIAN_POINT('',(-3.3,-3.75,-4.33)) ;
#135116 = CARTESIAN_POINT('Origin',(-3.4,-3.75,-4.33)) ;
#135117 = CARTESIAN_POINT('',(-3.3,-3.75,-5.83)) ;
#135118 = CARTESIAN_POINT('',(-3.3,-3.75,-5.83)) ;
#135119 = CARTESIAN_POINT('Origin',(-3.4,-3.75,-5.83)) ;
#135120 = CARTESIAN_POINT('Origin',(-3.4,-3.75,-5.83)) ;
#135121 = CARTESIAN_POINT('',(-3.4,-3.9,-5.93)) ;
#135122 = CARTESIAN_POINT('',(-3.3,-3.9,-5.83)) ;
#135123 = CARTESIAN_POINT('Origin',(-3.4,-3.9,-5.83)) ;
#135124 = CARTESIAN_POINT('',(-3.4,-3.75,-5.93)) ;
#135125 = CARTESIAN_POINT('',(-3.3,-3.75,-5.83)) ;
#135126 = CARTESIAN_POINT('Origin',(-4.15,-3.75,-5.93)) ;
#135127 = CARTESIAN_POINT('',(-4.15,-3.9,-5.93)) ;
#135128 = CARTESIAN_POINT('',(-4.15,-3.9,-5.93)) ;
#135129 = CARTESIAN_POINT('',(-4.15,-3.75,-5.93)) ;
#135130 = CARTESIAN_POINT('Origin',(-4.15,-3.75,-5.83)) ;
#135131 = CARTESIAN_POINT('',(-4.25,-3.9,-5.83)) ;
#135132 = CARTESIAN_POINT('Origin',(-4.15,-3.9,-5.83)) ;
#135133 = CARTESIAN_POINT('',(-4.25,-3.75,-5.83)) ;
#135134 = CARTESIAN_POINT('Origin',(-4.25,-3.75,-4.33)) ;
#135135 = CARTESIAN_POINT('',(-4.25,-3.9,-4.33)) ;
#135136 = CARTESIAN_POINT('',(-4.25,-3.9,-4.33)) ;
#135137 = CARTESIAN_POINT('',(-4.25,-3.75,-4.33)) ;
#135138 = CARTESIAN_POINT('Origin',(-4.15,-3.75,-4.33)) ;
#135139 = CARTESIAN_POINT('',(-4.15,-3.9,-4.23)) ;
#135140 = CARTESIAN_POINT('Origin',(-4.15,-3.9,-4.33)) ;
#135141 = CARTESIAN_POINT('',(-4.15,-3.75,-4.23)) ;
#135142 = CARTESIAN_POINT('Origin',(-3.4,-3.75,-4.23)) ;
#135143 = CARTESIAN_POINT('',(-3.4,-3.9,-4.23)) ;
#135144 = CARTESIAN_POINT('',(-3.4,-3.9,-4.23)) ;
#135145 = CARTESIAN_POINT('',(-3.4,-3.75,-4.23)) ;
#135146 = CARTESIAN_POINT('Origin',(-3.4,-3.75,-4.33)) ;
#135147 = CARTESIAN_POINT('',(-3.3,-3.9,-4.33)) ;
#135148 = CARTESIAN_POINT('Origin',(-3.4,-3.9,-4.33)) ;
#135149 = CARTESIAN_POINT('',(-3.3,-3.75,-4.33)) ;
#135150 = CARTESIAN_POINT('Origin',(-3.3,-3.75,-5.83)) ;
#135151 = CARTESIAN_POINT('',(-3.3,-3.9,-5.83)) ;
#135152 = CARTESIAN_POINT('Origin',(0.,-3.9,-5.08)) ;
#135153 = CARTESIAN_POINT('Origin',(0.,9.95,-5.08)) ;
#135154 = CARTESIAN_POINT('',(-0.230887397576972,9.95,-3.16513942814623)) ;
#135155 = CARTESIAN_POINT('Origin',(-0.321518176280637,8.95,-3.2074012543203)) ;
#135156 = CARTESIAN_POINT('',(-0.321518176280637,9.05,-3.2074012543203)) ;
#135157 = CARTESIAN_POINT('',(1.22782596331729,9.85,-6.529980483939)) ;
#135158 = CARTESIAN_POINT('Origin',(-1.22782596331729,8.95,-3.630019516061)) ;
#135159 = CARTESIAN_POINT('',(-1.22782596331729,9.05,-3.630019516061)) ;
#135160 = CARTESIAN_POINT('',(-1.22782596331729,9.85,-3.630019516061)) ;
#135161 = CARTESIAN_POINT('Origin',(0.,8.95,-5.08)) ;
#135162 = CARTESIAN_POINT('',(-0.362523114814661,8.95,-5.24904730469628)) ;
#135163 = CARTESIAN_POINT('',(0.36252311481466,8.95,-4.91095269530372)) ;
#135164 = CARTESIAN_POINT('Origin',(-2.65,10.8,-6.08)) ;
#135165 = CARTESIAN_POINT('',(-2.65,10.75,-5.98)) ;
#135166 = CARTESIAN_POINT('',(-2.65,10.75,-4.18)) ;
#135167 = CARTESIAN_POINT('',(-2.65,10.75,-6.08)) ;
#135168 = CARTESIAN_POINT('',(-2.65,10.85,-4.18)) ;
#135169 = CARTESIAN_POINT('',(-2.65,10.95,-4.18)) ;
#135170 = CARTESIAN_POINT('',(-2.65,10.85,-5.98)) ;
#135171 = CARTESIAN_POINT('',(-2.65,10.85,-6.08)) ;
#135172 = CARTESIAN_POINT('',(-2.65,10.65,-5.98)) ;
#135173 = CARTESIAN_POINT('Origin',(-3.9,10.8,-4.08)) ;
#135174 = CARTESIAN_POINT('',(-2.75,10.85,-4.08)) ;
#135175 = CARTESIAN_POINT('',(-2.75,10.75,-4.08)) ;
#135176 = CARTESIAN_POINT('',(-2.75,10.65,-4.08)) ;
#135177 = CARTESIAN_POINT('',(-3.8,10.75,-4.08)) ;
#135178 = CARTESIAN_POINT('',(-3.9,10.75,-4.08)) ;
#135179 = CARTESIAN_POINT('',(-3.8,10.85,-4.08)) ;
#135180 = CARTESIAN_POINT('',(-3.8,10.95,-4.08)) ;
#135181 = CARTESIAN_POINT('',(-3.9,10.85,-4.08)) ;
#135182 = CARTESIAN_POINT('Origin',(-3.9,10.8,-6.08)) ;
#135183 = CARTESIAN_POINT('',(-3.9,10.85,-4.18)) ;
#135184 = CARTESIAN_POINT('',(-3.9,10.75,-4.18)) ;
#135185 = CARTESIAN_POINT('',(-3.9,10.65,-4.18)) ;
#135186 = CARTESIAN_POINT('',(-3.9,10.75,-5.98)) ;
#135187 = CARTESIAN_POINT('',(-3.9,10.75,-6.08)) ;
#135188 = CARTESIAN_POINT('',(-3.9,10.85,-5.98)) ;
#135189 = CARTESIAN_POINT('',(-3.9,10.95,-5.98)) ;
#135190 = CARTESIAN_POINT('',(-3.9,10.85,-6.08)) ;
#135191 = CARTESIAN_POINT('Origin',(-3.9,10.8,-6.08)) ;
#135192 = CARTESIAN_POINT('',(-3.8,10.75,-6.08)) ;
#135193 = CARTESIAN_POINT('',(-2.75,10.75,-6.08)) ;
#135194 = CARTESIAN_POINT('',(-3.9,10.75,-6.08)) ;
#135195 = CARTESIAN_POINT('',(-2.75,10.85,-6.08)) ;
#135196 = CARTESIAN_POINT('',(-2.75,10.95,-6.08)) ;
#135197 = CARTESIAN_POINT('',(-3.8,10.85,-6.08)) ;
#135198 = CARTESIAN_POINT('',(-3.9,10.85,-6.08)) ;
#135199 = CARTESIAN_POINT('',(-3.8,10.65,-6.08)) ;
#135200 = CARTESIAN_POINT('Origin',(0.,10.65,-5.08)) ;
#135201 = CARTESIAN_POINT('',(-3.8,10.65,-4.18)) ;
#135202 = CARTESIAN_POINT('',(-2.75,10.65,-4.18)) ;
#135203 = CARTESIAN_POINT('',(1.56125112837912E-16,10.65,-4.18)) ;
#135204 = CARTESIAN_POINT('',(-2.75,10.65,-5.98)) ;
#135205 = CARTESIAN_POINT('',(-2.75,10.65,-5.08)) ;
#135206 = CARTESIAN_POINT('',(-3.8,10.65,-5.98)) ;
#135207 = CARTESIAN_POINT('',(-1.56125112837913E-16,10.65,-5.98)) ;
#135208 = CARTESIAN_POINT('',(-3.8,10.65,-5.08)) ;
#135209 = CARTESIAN_POINT('',(-3.65,10.65,-4.23)) ;
#135210 = CARTESIAN_POINT('',(-2.9,10.65,-4.23)) ;
#135211 = CARTESIAN_POINT('',(-3.65,10.65,-4.23)) ;
#135212 = CARTESIAN_POINT('',(-3.75,10.65,-4.33)) ;
#135213 = CARTESIAN_POINT('Origin',(-3.65,10.65,-4.33)) ;
#135214 = CARTESIAN_POINT('',(-3.75,10.65,-5.83)) ;
#135215 = CARTESIAN_POINT('',(-3.75,10.65,-5.83)) ;
#135216 = CARTESIAN_POINT('',(-3.65,10.65,-5.93)) ;
#135217 = CARTESIAN_POINT('Origin',(-3.65,10.65,-5.83)) ;
#135218 = CARTESIAN_POINT('',(-2.9,10.65,-5.93)) ;
#135219 = CARTESIAN_POINT('',(-2.9,10.65,-5.93)) ;
#135220 = CARTESIAN_POINT('',(-2.8,10.65,-5.83)) ;
#135221 = CARTESIAN_POINT('Origin',(-2.9,10.65,-5.83)) ;
#135222 = CARTESIAN_POINT('',(-2.8,10.65,-4.33)) ;
#135223 = CARTESIAN_POINT('',(-2.8,10.65,-4.33)) ;
#135224 = CARTESIAN_POINT('Origin',(-2.9,10.65,-4.33)) ;
#135225 = CARTESIAN_POINT('Origin',(-2.9,10.65,-4.33)) ;
#135226 = CARTESIAN_POINT('',(-2.8,10.7,-4.33)) ;
#135227 = CARTESIAN_POINT('',(-2.8,10.65,-4.33)) ;
#135228 = CARTESIAN_POINT('',(-2.9,10.7,-4.23)) ;
#135229 = CARTESIAN_POINT('Origin',(-2.9,10.7,-4.33)) ;
#135230 = CARTESIAN_POINT('',(-2.9,10.65,-4.23)) ;
#135231 = CARTESIAN_POINT('Origin',(-3.65,10.65,-4.23)) ;
#135232 = CARTESIAN_POINT('',(-3.65,10.7,-4.23)) ;
#135233 = CARTESIAN_POINT('',(-3.65,10.7,-4.23)) ;
#135234 = CARTESIAN_POINT('',(-3.65,10.65,-4.23)) ;
#135235 = CARTESIAN_POINT('Origin',(-3.65,10.65,-4.33)) ;
#135236 = CARTESIAN_POINT('',(-3.75,10.7,-4.33)) ;
#135237 = CARTESIAN_POINT('Origin',(-3.65,10.7,-4.33)) ;
#135238 = CARTESIAN_POINT('',(-3.75,10.65,-4.33)) ;
#135239 = CARTESIAN_POINT('Origin',(-3.75,10.65,-5.83)) ;
#135240 = CARTESIAN_POINT('',(-3.75,10.7,-5.83)) ;
#135241 = CARTESIAN_POINT('',(-3.75,10.7,-5.83)) ;
#135242 = CARTESIAN_POINT('',(-3.75,10.65,-5.83)) ;
#135243 = CARTESIAN_POINT('Origin',(-3.65,10.65,-5.83)) ;
#135244 = CARTESIAN_POINT('',(-3.65,10.7,-5.93)) ;
#135245 = CARTESIAN_POINT('Origin',(-3.65,10.7,-5.83)) ;
#135246 = CARTESIAN_POINT('',(-3.65,10.65,-5.93)) ;
#135247 = CARTESIAN_POINT('Origin',(-2.9,10.65,-5.93)) ;
#135248 = CARTESIAN_POINT('',(-2.9,10.7,-5.93)) ;
#135249 = CARTESIAN_POINT('',(-2.9,10.7,-5.93)) ;
#135250 = CARTESIAN_POINT('',(-2.9,10.65,-5.93)) ;
#135251 = CARTESIAN_POINT('Origin',(-2.9,10.65,-5.83)) ;
#135252 = CARTESIAN_POINT('',(-2.8,10.7,-5.83)) ;
#135253 = CARTESIAN_POINT('Origin',(-2.9,10.7,-5.83)) ;
#135254 = CARTESIAN_POINT('',(-2.8,10.65,-5.83)) ;
#135255 = CARTESIAN_POINT('Origin',(-2.8,10.65,-4.33)) ;
#135256 = CARTESIAN_POINT('',(-2.8,10.7,-4.33)) ;
#135257 = CARTESIAN_POINT('Origin',(0.,10.8,-5.08)) ;
#135258 = CARTESIAN_POINT('',(-3.65,10.8,-4.33)) ;
#135259 = CARTESIAN_POINT('',(-2.9,10.8,-4.33)) ;
#135260 = CARTESIAN_POINT('',(0.,10.8,-4.33)) ;
#135261 = CARTESIAN_POINT('',(-2.9,10.8,-5.83)) ;
#135262 = CARTESIAN_POINT('',(-2.9,10.8,-5.08)) ;
#135263 = CARTESIAN_POINT('',(-3.65,10.8,-5.83)) ;
#135264 = CARTESIAN_POINT('',(0.,10.8,-5.83)) ;
#135265 = CARTESIAN_POINT('',(-3.65,10.8,-5.08)) ;
#135266 = CARTESIAN_POINT('Origin',(4.5,2.75,-6.455)) ;
#135267 = CARTESIAN_POINT('',(4.5,2.63356010126946,-6.47440664978842)) ;
#135268 = CARTESIAN_POINT('',(4.6,2.11643989873054,-6.56059335021158)) ;
#135269 = CARTESIAN_POINT('',(4.6,2.11643989873054,-6.56059335021158)) ;
#135270 = CARTESIAN_POINT('',(12.7,2.11643989873054,-6.56059335021158)) ;
#135271 = CARTESIAN_POINT('',(12.8,2.11643989873054,-6.56059335021158)) ;
#135272 = CARTESIAN_POINT('',(12.7,2.75,-6.455)) ;
#135273 = CARTESIAN_POINT('Origin',(4.5,2.,-6.58)) ;
#135274 = CARTESIAN_POINT('',(4.6,2.,-6.46195395782836)) ;
#135275 = CARTESIAN_POINT('',(4.6,2.,-3.58)) ;
#135276 = CARTESIAN_POINT('',(12.7,2.,-6.46195395782836)) ;
#135277 = CARTESIAN_POINT('',(12.7,2.,-6.58)) ;
#135278 = CARTESIAN_POINT('',(4.5,2.,-6.46195395782836)) ;
#135279 = CARTESIAN_POINT('Origin',(4.5,2.,-3.58)) ;
#135280 = CARTESIAN_POINT('',(4.6,2.63356010126946,-3.68559335021158)) ;
#135281 = CARTESIAN_POINT('',(4.6,2.63356010126947,-3.68559335021158)) ;
#135282 = CARTESIAN_POINT('',(4.5,2.63356010126946,-3.68559335021158)) ;
#135283 = CARTESIAN_POINT('',(12.7,2.,-3.58)) ;
#135284 = CARTESIAN_POINT('Origin',(4.5,0.,-5.08)) ;
#135285 = CARTESIAN_POINT('',(4.5,2.72431432344521,-3.77263481664499)) ;
#135286 = CARTESIAN_POINT('',(4.5,2.72431432344521,-5.08)) ;
#135287 = CARTESIAN_POINT('',(4.5,2.61712020253893,-3.78423274259479)) ;
#135288 = CARTESIAN_POINT('Origin',(4.5,2.65,-3.58695395782836)) ;
#135289 = CARTESIAN_POINT('',(4.5,2.1,-3.69804604217164)) ;
#135290 = CARTESIAN_POINT('',(4.5,2.1,-3.69804604217164)) ;
#135291 = CARTESIAN_POINT('',(4.5,2.1,-6.46195395782836)) ;
#135292 = CARTESIAN_POINT('',(4.5,2.1,-6.58)) ;
#135293 = CARTESIAN_POINT('',(4.5,2.61712020253893,-6.37576725740521)) ;
#135294 = CARTESIAN_POINT('Origin',(10.3,0.,-5.08)) ;
#135295 = CARTESIAN_POINT('Origin',(0.584645609909621,0.,-5.08)) ;
#135296 = CARTESIAN_POINT('',(4.6,-2.32258064516129,-3.1811532060953)) ;
#135297 = CARTESIAN_POINT('',(4.6,-2.79310344827574,-3.98520635404193)) ;
#135298 = CARTESIAN_POINT('Origin',(4.6,0.,-5.08)) ;
#135299 = CARTESIAN_POINT('',(4.6,-2.79310344827574,-6.17479364595807)) ;
#135300 = CARTESIAN_POINT('Origin',(4.6,0.,-5.08)) ;
#135301 = CARTESIAN_POINT('',(4.6,-2.32258064516129,-6.9788467939047)) ;
#135302 = CARTESIAN_POINT('Origin',(4.6,0.,-5.08)) ;
#135303 = CARTESIAN_POINT('',(12.7,-2.32258064516129,-6.9788467939047)) ;
#135304 = CARTESIAN_POINT('',(0.584645609909621,-2.32258064516129,-6.9788467939047)) ;
#135305 = CARTESIAN_POINT('',(12.7,-2.32258064516129,-3.1811532060953)) ;
#135306 = CARTESIAN_POINT('Origin',(12.7,0.,-5.08)) ;
#135307 = CARTESIAN_POINT('',(0.584645609909621,-2.32258064516129,-3.1811532060953)) ;
#135308 = CARTESIAN_POINT('Ctrl Pts',(-5.37474093186837,4.17158354835192,
-3.18)) ;
#135309 = CARTESIAN_POINT('Ctrl Pts',(-5.4,4.2,-3.18)) ;
#135310 = CARTESIAN_POINT('Ctrl Pts',(-5.4,4.23801993223491,-3.18)) ;
#135311 = CARTESIAN_POINT('Ctrl Pts',(-5.37474093064202,4.17158354697228,
-3.15374656406104)) ;
#135312 = CARTESIAN_POINT('Ctrl Pts',(-5.4,4.19999999724801,-3.1424814127989)) ;
#135313 = CARTESIAN_POINT('Ctrl Pts',(-5.4,4.23801992976516,-3.12749312809026)) ;
#135314 = CARTESIAN_POINT('Ctrl Pts',(-5.36668583490655,4.14629949399955,
-3.12780128688412)) ;
#135315 = CARTESIAN_POINT('Ctrl Pts',(-5.4,4.16739198385624,-3.10466783506586)) ;
#135316 = CARTESIAN_POINT('Ctrl Pts',(-5.4,4.20557579169425,-3.07560257376825)) ;
#135317 = CARTESIAN_POINT('Ctrl Pts',(-5.33901380460609,4.05944006555646,
-3.09077735687857)) ;
#135318 = CARTESIAN_POINT('Ctrl Pts',(-5.4,4.06625640449639,-3.06313263661411)) ;
#135319 = CARTESIAN_POINT('Ctrl Pts',(-5.4,4.09411900298411,-3.00155471375713)) ;
#135320 = CARTESIAN_POINT('Ctrl Pts',(-5.31962206268973,3.99857154231911,
-3.08)) ;
#135321 = CARTESIAN_POINT('Ctrl Pts',(-5.39999999999997,3.99346933127512,
-3.06200350742645)) ;
#135322 = CARTESIAN_POINT('Ctrl Pts',(-5.4,4.0160133758189,-2.98000000048114)) ;
#135323 = CARTESIAN_POINT('Ctrl Pts',(-5.3,3.9369800677651,-3.08)) ;
#135324 = CARTESIAN_POINT('Ctrl Pts',(-5.4,3.9369800677651,-3.08)) ;
#135325 = CARTESIAN_POINT('Ctrl Pts',(-5.4,3.9369800677651,-2.98)) ;
#135326 = CARTESIAN_POINT('Origin',(-5.3,4.23801993223491,-3.18)) ;
#135327 = CARTESIAN_POINT('Ctrl Pts',(-5.3,3.9369800677651,-3.08)) ;
#135328 = CARTESIAN_POINT('Ctrl Pts',(-5.31962206268973,3.99857154231912,
-3.08)) ;
#135329 = CARTESIAN_POINT('Ctrl Pts',(-5.33901380460609,4.05944006555646,
-3.09077735687857)) ;
#135330 = CARTESIAN_POINT('Ctrl Pts',(-5.36668583490655,4.14629949399955,
-3.12780128688412)) ;
#135331 = CARTESIAN_POINT('Ctrl Pts',(-5.37474093064202,4.17158354697228,
-3.15374656406104)) ;
#135332 = CARTESIAN_POINT('Ctrl Pts',(-5.37474093186837,4.17158354835192,
-3.18)) ;
#135333 = CARTESIAN_POINT('Origin',(-5.3,3.9369800677651,-2.98)) ;
#135334 = CARTESIAN_POINT('Origin',(-4.6737453090477,1.85,-3.17713990064968)) ;
#135335 = CARTESIAN_POINT('Origin',(-3.35509339356897,1.85,-3.49947703554448)) ;
#135336 = CARTESIAN_POINT('Ctrl Pts',(-3.35509339356897,1.95,-3.49947703554448)) ;
#135337 = CARTESIAN_POINT('Ctrl Pts',(-3.33134808452128,1.95,-3.4023371348948)) ;
#135338 = CARTESIAN_POINT('Ctrl Pts',(-3.33134808452128,1.85,-3.4023371348948)) ;
#135339 = CARTESIAN_POINT('Ctrl Pts',(-3.38343213690418,1.95,-3.48562253880281)) ;
#135340 = CARTESIAN_POINT('Ctrl Pts',(-3.36046743872482,1.94345445676969,
-3.39521907053391)) ;
#135341 = CARTESIAN_POINT('Ctrl Pts',(-3.38803897426452,1.85000000162387,
-3.38847936184645)) ;
#135342 = CARTESIAN_POINT('Ctrl Pts',(-3.41101314049054,1.96238978305186,
-3.47213849291613)) ;
#135343 = CARTESIAN_POINT('Ctrl Pts',(-3.39538881861724,1.95068928167333,
-3.38668273322682)) ;
#135344 = CARTESIAN_POINT('Ctrl Pts',(-3.44316973238528,1.87475949194142,
-3.37500295430582)) ;
#135345 = CARTESIAN_POINT('Ctrl Pts',(-3.42983432543734,1.98356361611701,
-3.46293702440883)) ;
#135346 = CARTESIAN_POINT('Ctrl Pts',(-3.42093333711585,1.97355000425533,
-3.3804385175939)) ;
#135347 = CARTESIAN_POINT('Ctrl Pts',(-3.48082994825801,1.91712723223402,
-3.36579712375916)) ;
#135348 = CARTESIAN_POINT('Origin',(-3.50457525730571,1.91712723223402,-3.46293702440883)) ;
#135349 = CARTESIAN_POINT('Origin',(-3.36128627567757,2.03621361435731,-3.49644940433506)) ;
#135350 = CARTESIAN_POINT('Origin',(-4.05330900605469,2.53445269957662,-3.32880210804797)) ;
#135351 = CARTESIAN_POINT('Origin',(-4.66204490261456,3.21928058320648,-3.18)) ;
#135352 = CARTESIAN_POINT('Origin',(-4.35749955255802,2.87666706439287,-3.18)) ;
#135353 = CARTESIAN_POINT('Origin',(-4.66204490261456,3.21928058320648,-3.18)) ;
#135354 = CARTESIAN_POINT('Origin',(-5.3,5.2,-2.98)) ;
#135355 = CARTESIAN_POINT('Origin',(-5.3,-1.88819660112502,-2.98)) ;
#135356 = CARTESIAN_POINT('Origin',(-5.3,4.23801993223491,-2.54)) ;
#135357 = CARTESIAN_POINT('Origin',(-5.3,4.23801993223491,-6.98)) ;
#135358 = CARTESIAN_POINT('Origin',(-3.35509339356897,2.05,-5.08)) ;
#135359 = CARTESIAN_POINT('Origin',(-3.36128627567745,2.03621361435763,-6.66355059566492)) ;
#135360 = CARTESIAN_POINT('Origin',(-2.4237453090477,1.85,-6.43286009935032)) ;
#135361 = CARTESIAN_POINT('Origin',(-3.35509339356897,1.85,-6.66052296445552)) ;
#135362 = CARTESIAN_POINT('Origin',(-4.66204490261456,3.21928058320648,-3.18)) ;
#135363 = CARTESIAN_POINT('Origin',(-4.66204490261456,3.21928058320648,-3.18)) ;
#135364 = CARTESIAN_POINT('Ctrl Pts',(-5.29976814257747,-1.88802911972918,
-3.07999982737782)) ;
#135365 = CARTESIAN_POINT('Ctrl Pts',(-5.4,-1.88802831720456,-3.08023259354298)) ;
#135366 = CARTESIAN_POINT('Ctrl Pts',(-5.4,-1.88791746283071,-2.98000016246237)) ;
#135367 = CARTESIAN_POINT('Ctrl Pts',(-5.31153957531164,-1.92331224822996,
-3.07998646768893)) ;
#135368 = CARTESIAN_POINT('Ctrl Pts',(-5.4,-1.92148676945295,-3.06897789253806)) ;
#135369 = CARTESIAN_POINT('Ctrl Pts',(-5.4,-1.94671708614657,-2.97993171302848)) ;
#135370 = CARTESIAN_POINT('Ctrl Pts',(-5.32318090226695,-1.95817527052251,
-3.09078449726813)) ;
#135371 = CARTESIAN_POINT('Ctrl Pts',(-5.4,-1.96527310172481,-3.07216338375286)) ;
#135372 = CARTESIAN_POINT('Ctrl Pts',(-5.4,-2.00485091174287,-3.00149607488934)) ;
#135373 = CARTESIAN_POINT('Ctrl Pts',(-5.33978950165956,-2.00789652656154,
-3.12786496501963)) ;
#135374 = CARTESIAN_POINT('Ctrl Pts',(-5.4,-2.02908601268745,-3.11136651453166)) ;
#135375 = CARTESIAN_POINT('Ctrl Pts',(-5.4,-2.087770056524,-3.07566121263605)) ;
#135376 = CARTESIAN_POINT('Ctrl Pts',(-5.34461954754097,-2.02234798681675,
-3.15384614471832)) ;
#135377 = CARTESIAN_POINT('Ctrl Pts',(-5.4,-2.04997459329993,-3.14567566484002)) ;
#135378 = CARTESIAN_POINT('Ctrl Pts',(-5.4,-2.1118797455067,-3.12765768697395)) ;
#135379 = CARTESIAN_POINT('Ctrl Pts',(-5.34460423617422,-2.02230212313483,
-3.18012475187013)) ;
#135380 = CARTESIAN_POINT('Ctrl Pts',(-5.4,-2.04990938338631,-3.18016375427654)) ;
#135381 = CARTESIAN_POINT('Ctrl Pts',(-5.4,-2.11180321723903,-3.18024966888043)) ;
#135382 = CARTESIAN_POINT('Origin',(-5.29999999999999,-1.88819660112499,-3.18000000000002)) ;
#135383 = CARTESIAN_POINT('Origin',(-5.3,-2.11180339887499,-3.18)) ;
#135384 = CARTESIAN_POINT('Ctrl Pts',(-5.3,3.9369800677651,-7.08)) ;
#135385 = CARTESIAN_POINT('Ctrl Pts',(-5.4,3.9369800677651,-7.08)) ;
#135386 = CARTESIAN_POINT('Ctrl Pts',(-5.4,3.9369800677651,-7.18)) ;
#135387 = CARTESIAN_POINT('Ctrl Pts',(-5.31962206268973,3.99857154231911,
-7.08)) ;
#135388 = CARTESIAN_POINT('Ctrl Pts',(-5.4,3.99346933127505,-7.09799649257373)) ;
#135389 = CARTESIAN_POINT('Ctrl Pts',(-5.4,4.01601337581889,-7.17999999951891)) ;
#135390 = CARTESIAN_POINT('Ctrl Pts',(-5.3390138046061,4.05944006555648,-7.06922264312143)) ;
#135391 = CARTESIAN_POINT('Ctrl Pts',(-5.4,4.06625640449641,-7.09686736338591)) ;
#135392 = CARTESIAN_POINT('Ctrl Pts',(-5.4,4.09411900298413,-7.15844528624287)) ;
#135393 = CARTESIAN_POINT('Ctrl Pts',(-5.36668583490654,4.14629949399953,
-7.03219871311588)) ;
#135394 = CARTESIAN_POINT('Ctrl Pts',(-5.4,4.16739198385622,-7.05533216493412)) ;
#135395 = CARTESIAN_POINT('Ctrl Pts',(-5.4,4.20557579169423,-7.08439742623175)) ;
#135396 = CARTESIAN_POINT('Ctrl Pts',(-5.37474093064202,4.17158354697228,
-7.00625343593896)) ;
#135397 = CARTESIAN_POINT('Ctrl Pts',(-5.4,4.19999999724801,-7.01751858720111)) ;
#135398 = CARTESIAN_POINT('Ctrl Pts',(-5.4,4.23801992976516,-7.03250687190974)) ;
#135399 = CARTESIAN_POINT('Ctrl Pts',(-5.37474093186837,4.17158354835192,
-6.98)) ;
#135400 = CARTESIAN_POINT('Ctrl Pts',(-5.4,4.2,-6.98)) ;
#135401 = CARTESIAN_POINT('Ctrl Pts',(-5.4,4.23801993223491,-6.98)) ;
#135402 = CARTESIAN_POINT('Origin',(-5.3,3.9369800677651,-7.18)) ;
#135403 = CARTESIAN_POINT('Ctrl Pts',(-5.37474093186837,4.17158354835192,
-6.98)) ;
#135404 = CARTESIAN_POINT('Ctrl Pts',(-5.37474093064202,4.17158354697228,
-7.00625343593896)) ;
#135405 = CARTESIAN_POINT('Ctrl Pts',(-5.36668583490654,4.14629949399953,
-7.03219871311588)) ;
#135406 = CARTESIAN_POINT('Ctrl Pts',(-5.3390138046061,4.05944006555648,-7.06922264312143)) ;
#135407 = CARTESIAN_POINT('Ctrl Pts',(-5.31962206268973,3.99857154231911,
-7.08)) ;
#135408 = CARTESIAN_POINT('Ctrl Pts',(-5.3,3.9369800677651,-7.08)) ;
#135409 = CARTESIAN_POINT('Ctrl Pts',(-3.42983432543734,1.98356361611701,
-6.69706297559117)) ;
#135410 = CARTESIAN_POINT('Ctrl Pts',(-3.42093333711585,1.97355000425533,
-6.7795614824061)) ;
#135411 = CARTESIAN_POINT('Ctrl Pts',(-3.48082994825801,1.91712723223402,
-6.79420287624085)) ;
#135412 = CARTESIAN_POINT('Ctrl Pts',(-3.41101314049054,1.96238978305186,
-6.68786150708384)) ;
#135413 = CARTESIAN_POINT('Ctrl Pts',(-3.3953888186174,1.95068928167321,-6.77331726677318)) ;
#135414 = CARTESIAN_POINT('Ctrl Pts',(-3.44316973238528,1.87475949194143,
-6.78499704569418)) ;
#135415 = CARTESIAN_POINT('Ctrl Pts',(-3.38343213690421,1.95,-6.67437746119715)) ;
#135416 = CARTESIAN_POINT('Ctrl Pts',(-3.36046743872472,1.94345445676975,
-6.76478092946601)) ;
#135417 = CARTESIAN_POINT('Ctrl Pts',(-3.38803897426452,1.85000000162387,
-6.77152063815355)) ;
#135418 = CARTESIAN_POINT('Ctrl Pts',(-3.35509339356897,1.95,-6.66052296445552)) ;
#135419 = CARTESIAN_POINT('Ctrl Pts',(-3.33134808452127,1.95,-6.7576628651052)) ;
#135420 = CARTESIAN_POINT('Ctrl Pts',(-3.33134808452128,1.85,-6.7576628651052)) ;
#135421 = CARTESIAN_POINT('Origin',(-3.50457525730571,1.91712723223402,-6.69706297559117)) ;
#135422 = CARTESIAN_POINT('Origin',(-4.66204490261456,1.95,-3.18)) ;
#135423 = CARTESIAN_POINT('Origin',(-4.66204490261456,-1.5692190524323,-3.18)) ;
#135424 = CARTESIAN_POINT('Origin',(-3.84472135955,-1.16055728090002,-3.18)) ;
#135425 = CARTESIAN_POINT('Origin',(-4.66204490261456,-1.5692190524323,-3.18)) ;
#135426 = CARTESIAN_POINT('Origin',(-5.3,-2.11180339887499,-2.54)) ;
#135427 = CARTESIAN_POINT('Origin',(-5.3,-2.11180339887499,-6.98)) ;
#135428 = CARTESIAN_POINT('Origin',(-5.3,1.95,-7.18)) ;
#135429 = CARTESIAN_POINT('Origin',(-5.3,-1.88819660112501,-7.18)) ;
#135430 = CARTESIAN_POINT('Origin',(-4.0264650697994,2.50425327128942,-6.98)) ;
#135431 = CARTESIAN_POINT('Origin',(-4.66204490261456,3.21928058320648,-6.98)) ;
#135432 = CARTESIAN_POINT('Origin',(-3.02790825149799,1.38087685070033,-6.5805443741715)) ;
#135433 = CARTESIAN_POINT('Origin',(-4.66204490261456,3.21928058320648,-6.98)) ;
#135434 = CARTESIAN_POINT('Origin',(-4.66204490261456,-1.5692190524323,-3.18)) ;
#135435 = CARTESIAN_POINT('Origin',(-4.66204490261456,-1.5692190524323,-3.18)) ;
#135436 = CARTESIAN_POINT('Ctrl Pts',(-5.34460423617422,-2.02230212313483,
-6.97987524812987)) ;
#135437 = CARTESIAN_POINT('Ctrl Pts',(-5.4,-2.04990938338631,-6.97983624572347)) ;
#135438 = CARTESIAN_POINT('Ctrl Pts',(-5.4,-2.11180321723903,-6.97975033111957)) ;
#135439 = CARTESIAN_POINT('Ctrl Pts',(-5.34461954754097,-2.02234798681676,
-7.00615385528167)) ;
#135440 = CARTESIAN_POINT('Ctrl Pts',(-5.4,-2.04997459329993,-7.01432433515999)) ;
#135441 = CARTESIAN_POINT('Ctrl Pts',(-5.4,-2.1118797455067,-7.03234231302605)) ;
#135442 = CARTESIAN_POINT('Ctrl Pts',(-5.33978950165958,-2.00789652656155,
-7.03213503498038)) ;
#135443 = CARTESIAN_POINT('Ctrl Pts',(-5.4,-2.02908601268746,-7.04863348546835)) ;
#135444 = CARTESIAN_POINT('Ctrl Pts',(-5.4,-2.08777005652399,-7.08433878736396)) ;
#135445 = CARTESIAN_POINT('Ctrl Pts',(-5.32318090226693,-1.9581752705225,
-7.06921550273187)) ;
#135446 = CARTESIAN_POINT('Ctrl Pts',(-5.4,-1.9652731017248,-7.08783661624714)) ;
#135447 = CARTESIAN_POINT('Ctrl Pts',(-5.4,-2.00485091174287,-7.15850392511066)) ;
#135448 = CARTESIAN_POINT('Ctrl Pts',(-5.31153957531165,-1.92331224822997,
-7.08001353231107)) ;
#135449 = CARTESIAN_POINT('Ctrl Pts',(-5.39999999999998,-1.92148676945294,
-7.091022107462)) ;
#135450 = CARTESIAN_POINT('Ctrl Pts',(-5.4,-1.94671708614657,-7.18006828697155)) ;
#135451 = CARTESIAN_POINT('Ctrl Pts',(-5.29976814257747,-1.88802911972918,
-7.08000017262218)) ;
#135452 = CARTESIAN_POINT('Ctrl Pts',(-5.4,-1.88802831720456,-7.07976740645702)) ;
#135453 = CARTESIAN_POINT('Ctrl Pts',(-5.4,-1.88791746283072,-7.17999983753763)) ;
#135454 = CARTESIAN_POINT('Origin',(-5.30000000000007,-1.88819660112522,-6.98000000000015)) ;
#135455 = CARTESIAN_POINT('Origin',(-4.66204490261456,3.21928058320648,-6.98)) ;
#135456 = CARTESIAN_POINT('Origin',(-4.66204490261456,3.21928058320648,-6.98)) ;
#135457 = CARTESIAN_POINT('Origin',(0.175392621986784,-0.95,-4.36248472823589)) ;
#135458 = CARTESIAN_POINT('Origin',(-3.37639320225,-0.95,-3.49427041564467)) ;
#135459 = CARTESIAN_POINT('Origin',(-3.32804538583365,-0.902219294041845,
-3.50608877076867)) ;
#135460 = CARTESIAN_POINT('Origin',(-3.46583592134999,-0.971114561800017,
-3.47240663986467)) ;
#135461 = CARTESIAN_POINT('Origin',(-3.24472135955,-0.860557280900019,-6.98)) ;
#135462 = CARTESIAN_POINT('Origin',(-4.66204490261456,-1.5692190524323,-6.98)) ;
#135463 = CARTESIAN_POINT('Origin',(-4.66204490261456,1.95,-6.98)) ;
#135464 = CARTESIAN_POINT('Origin',(-4.66204490261456,-1.5692190524323,-6.98)) ;
#135465 = CARTESIAN_POINT('Ctrl Pts',(-3.4211145618,-1.06055728090001,-3.47240663986467)) ;
#135466 = CARTESIAN_POINT('Ctrl Pts',(-3.40394191641935,-1.05197095820969,
-3.38459197598638)) ;
#135467 = CARTESIAN_POINT('Ctrl Pts',(-3.44209061230229,-0.971114561800017,
-3.37526673921499)) ;
#135468 = CARTESIAN_POINT('Ctrl Pts',(-3.40727897628736,-1.05363948814369,
-3.47917070399162)) ;
#135469 = CARTESIAN_POINT('Ctrl Pts',(-3.38665319245547,-1.04670310838587,
-3.38881810851091)) ;
#135470 = CARTESIAN_POINT('Ctrl Pts',(-3.4144159452097,-0.957277229261617,
-3.38203165783763)) ;
#135471 = CARTESIAN_POINT('Ctrl Pts',(-3.3918627446443,-1.05,-3.4867075282519)) ;
#135472 = CARTESIAN_POINT('Ctrl Pts',(-3.36870744055525,-1.04639008266724,
-3.39320484786425)) ;
#135473 = CARTESIAN_POINT('Ctrl Pts',(-3.38358960366098,-0.950000000886305,
-3.38956698577176)) ;
#135474 = CARTESIAN_POINT('Ctrl Pts',(-3.37639320225,-1.05,-3.49427041564467)) ;
#135475 = CARTESIAN_POINT('Ctrl Pts',(-3.3526478932023,-1.05,-3.39713051499499)) ;
#135476 = CARTESIAN_POINT('Ctrl Pts',(-3.3526478932023,-0.95,-3.39713051499499)) ;
#135477 = CARTESIAN_POINT('Origin',(-3.37639320224939,-1.15000000000261,-3.494270415645)) ;
#135478 = CARTESIAN_POINT('Origin',(-4.66204490261456,-1.5692190524323,-6.98)) ;
#135479 = CARTESIAN_POINT('Origin',(-4.66204490261456,-1.5692190524323,-6.98)) ;
#135480 = CARTESIAN_POINT('Origin',(-3.37639320225,-1.15,-5.08)) ;
#135481 = CARTESIAN_POINT('Origin',(-3.37639320224947,-1.15000000000223,-6.6657295843551)) ;
#135482 = CARTESIAN_POINT('Origin',(-1.50751564693271,0.00804557540861825,
-6.2088928486111)) ;
#135483 = CARTESIAN_POINT('Origin',(-3.46583592134999,-0.971114561800017,
-6.68759336013533)) ;
#135484 = CARTESIAN_POINT('Ctrl Pts',(-3.37639320225,-1.05,-6.66572958435533)) ;
#135485 = CARTESIAN_POINT('Ctrl Pts',(-3.3526478932023,-1.05,-6.76286948500501)) ;
#135486 = CARTESIAN_POINT('Ctrl Pts',(-3.3526478932023,-0.95,-6.76286948500501)) ;
#135487 = CARTESIAN_POINT('Ctrl Pts',(-3.39186274464432,-1.05,-6.67329247174809)) ;
#135488 = CARTESIAN_POINT('Ctrl Pts',(-3.36870744055522,-1.04639008266724,
-6.76679515213572)) ;
#135489 = CARTESIAN_POINT('Ctrl Pts',(-3.38358960366098,-0.950000000886305,
-6.77043301422824)) ;
#135490 = CARTESIAN_POINT('Ctrl Pts',(-3.40727897628736,-1.05363948814369,
-6.68082929600838)) ;
#135491 = CARTESIAN_POINT('Ctrl Pts',(-3.38665319245551,-1.04670310838583,
-6.7711818914891)) ;
#135492 = CARTESIAN_POINT('Ctrl Pts',(-3.4144159452097,-0.957277229261612,
-6.77796834216237)) ;
#135493 = CARTESIAN_POINT('Ctrl Pts',(-3.4211145618,-1.06055728090001,-6.68759336013533)) ;
#135494 = CARTESIAN_POINT('Ctrl Pts',(-3.40394191641936,-1.05197095820969,
-6.77540802401362)) ;
#135495 = CARTESIAN_POINT('Ctrl Pts',(-3.4420906123023,-0.971114561800017,
-6.78473326078501)) ;
#135496 = CARTESIAN_POINT('Origin',(-3.37639320225,-0.95,-6.66572958435533)) ;
#135497 = CARTESIAN_POINT('Origin',(0.175392621986784,-0.95,-5.79751527176412)) ;
#135498 = CARTESIAN_POINT('Origin',(12.7,2.65,-2.54)) ;
#135499 = CARTESIAN_POINT('Origin',(12.8,2.65,-6.57304604217164)) ;
#135500 = CARTESIAN_POINT('',(4.57524318173533,2.73534903669982,-6.52093518020973)) ;
#135501 = CARTESIAN_POINT('Origin',(4.65232986199931,2.66527023615902,-6.56875421118371)) ;
#135502 = CARTESIAN_POINT('Ctrl Pts',(4.57524318173533,2.73534903669982,-6.52093518020973)) ;
#135503 = CARTESIAN_POINT('Ctrl Pts',(4.5761458558036,2.73452842391049,-6.51959115118323)) ;
#135504 = CARTESIAN_POINT('Ctrl Pts',(4.57705238626145,2.73367683201792,-6.51826812933933)) ;
#135505 = CARTESIAN_POINT('Ctrl Pts',(4.5779495181309,2.73280244902547,-6.51697684888884)) ;
#135506 = CARTESIAN_POINT('Ctrl Pts',(4.58144263576941,2.72939790755534,-6.51194905456846)) ;
#135507 = CARTESIAN_POINT('Ctrl Pts',(4.58496694799996,2.72549786515169,-6.50716994451779)) ;
#135508 = CARTESIAN_POINT('Ctrl Pts',(4.5881567005692,2.72107165565026,-6.50269819385252)) ;
#135509 = CARTESIAN_POINT('Ctrl Pts',(4.59069123847483,2.7175546443724,-6.49914499612962)) ;
#135510 = CARTESIAN_POINT('Ctrl Pts',(4.59301454561858,2.71370459823898,-6.49578631272419)) ;
#135511 = CARTESIAN_POINT('Ctrl Pts',(4.5949431309995,2.70950205848694,-6.49267499616739)) ;
#135512 = CARTESIAN_POINT('Ctrl Pts',(4.59651854606294,2.70606910472946,-6.49013343642149)) ;
#135513 = CARTESIAN_POINT('Ctrl Pts',(4.59783685868319,2.70233705077427,-6.48771608615717)) ;
#135514 = CARTESIAN_POINT('Ctrl Pts',(4.59873118971422,2.69838744820002,-6.48553230121235)) ;
#135515 = CARTESIAN_POINT('Ctrl Pts',(4.59916508318198,2.6964712597891,-6.48447281653647)) ;
#135516 = CARTESIAN_POINT('Ctrl Pts',(4.59949917984822,2.69450444432188,-6.48346779888203)) ;
#135517 = CARTESIAN_POINT('Ctrl Pts',(4.5997144226265,2.69249922659198,-6.48252634409943)) ;
#135518 = CARTESIAN_POINT('Ctrl Pts',(4.59990113259977,2.6907598225955,-6.48170968953523)) ;
#135519 = CARTESIAN_POINT('Ctrl Pts',(4.6,2.68896788689974,-6.48093031221453)) ;
#135520 = CARTESIAN_POINT('Ctrl Pts',(4.6,2.68715716172261,-6.48020561276333)) ;
#135521 = CARTESIAN_POINT('Origin',(4.5,2.1,-6.46195395782836)) ;
#135522 = CARTESIAN_POINT('Origin',(4.6,2.1,-6.46195395782836)) ;
#135523 = CARTESIAN_POINT('Origin',(12.7,2.1,-6.46195395782836)) ;
#135524 = CARTESIAN_POINT('Origin',(12.7,2.76643989873054,-6.55363939238321)) ;
#135525 = CARTESIAN_POINT('Origin',(12.7,2.13287979746107,-6.65923274259479)) ;
#135526 = CARTESIAN_POINT('Origin',(4.4,2.72431432344521,-5.08)) ;
#135527 = CARTESIAN_POINT('Ctrl Pts',(4.48762159086959,2.77250619842349,-3.69117568174948)) ;
#135528 = CARTESIAN_POINT('Ctrl Pts',(4.48806820038223,2.77169418112776,-3.69383556708983)) ;
#135529 = CARTESIAN_POINT('Ctrl Pts',(4.48852084821546,2.77084293101113,-3.69648271501847)) ;
#135530 = CARTESIAN_POINT('Ctrl Pts',(4.49012932137855,2.76769877392855,-3.70576300952075)) ;
#135531 = CARTESIAN_POINT('Ctrl Pts',(4.49131046584975,2.76517764467227,-3.71234413170349)) ;
#135532 = CARTESIAN_POINT('Ctrl Pts',(4.49351977821778,2.75978760391028,-3.72463528016215)) ;
#135533 = CARTESIAN_POINT('Ctrl Pts',(4.49455195297829,2.7569765375012,-3.73036774060142)) ;
#135534 = CARTESIAN_POINT('Ctrl Pts',(4.49620670090467,2.75163165728869,-3.73994332160334)) ;
#135535 = CARTESIAN_POINT('Ctrl Pts',(4.49686252944493,2.74924176842721,-3.74386402620338)) ;
#135536 = CARTESIAN_POINT('Ctrl Pts',(4.49822764032851,2.74331716058949,-3.75264463163475)) ;
#135537 = CARTESIAN_POINT('Ctrl Pts',(4.49890203357906,2.73961076902702,-3.75748650016056)) ;
#135538 = CARTESIAN_POINT('Ctrl Pts',(4.49975897856022,2.73206576252675,-3.7658277784398)) ;
#135539 = CARTESIAN_POINT('Ctrl Pts',(4.5,2.72833175948613,-3.76941900229181)) ;
#135540 = CARTESIAN_POINT('Ctrl Pts',(4.5,2.72431432344521,-3.77263481664499)) ;
#135541 = CARTESIAN_POINT('Ctrl Pts',(4.5,2.72431432344521,-6.38736518335501)) ;
#135542 = CARTESIAN_POINT('Ctrl Pts',(4.5,2.7290466915143,-6.39115327531367)) ;
#135543 = CARTESIAN_POINT('Ctrl Pts',(4.49966645684473,2.73338556955559,-6.39546141017606)) ;
#135544 = CARTESIAN_POINT('Ctrl Pts',(4.49869539480393,2.74072289096378,-6.40398024143747)) ;
#135545 = CARTESIAN_POINT('Ctrl Pts',(4.49811062025687,2.74382502998085,-6.40810805965865)) ;
#135546 = CARTESIAN_POINT('Ctrl Pts',(4.49664125196625,2.75020211699687,-6.41755926494058)) ;
#135547 = CARTESIAN_POINT('Ctrl Pts',(4.49570721389711,2.75339870015141,-6.42301039031934)) ;
#135548 = CARTESIAN_POINT('Ctrl Pts',(4.49363760641477,2.75952863263949,-6.43475170518696)) ;
#135549 = CARTESIAN_POINT('Ctrl Pts',(4.49249077386342,2.76240287369074,-6.44107122583083)) ;
#135550 = CARTESIAN_POINT('Ctrl Pts',(4.49055019898872,2.76677757270139,-6.45191412562089)) ;
#135551 = CARTESIAN_POINT('Ctrl Pts',(4.48975662823143,2.76842729450635,-6.45638729192264)) ;
#135552 = CARTESIAN_POINT('Ctrl Pts',(4.4885208482156,2.77084293101086,-6.46351728498073)) ;
#135553 = CARTESIAN_POINT('Ctrl Pts',(4.48806820038252,2.77169418112725,-6.46616443290854)) ;
#135554 = CARTESIAN_POINT('Ctrl Pts',(4.48762159086959,2.77250619842348,-6.46882431824782)) ;
#135555 = CARTESIAN_POINT('Origin',(4.6,2.1,-5.08)) ;
#135556 = CARTESIAN_POINT('Origin',(4.6,2.1,-3.69804604217164)) ;
#135557 = CARTESIAN_POINT('Origin',(4.6,2.1,-6.46195395782836)) ;
#135558 = CARTESIAN_POINT('Origin',(12.7,2.1,-6.46195395782836)) ;
#135559 = CARTESIAN_POINT('Origin',(12.7,1.9,-6.46195395782836)) ;
#135560 = CARTESIAN_POINT('Origin',(4.5,2.65,-3.58695395782836)) ;
#135561 = CARTESIAN_POINT('',(4.6,2.68715716172261,-3.67979438723668)) ;
#135562 = CARTESIAN_POINT('',(4.57524318173443,2.73534903670064,-3.63906481978892)) ;
#135563 = CARTESIAN_POINT('Ctrl Pts',(4.6,2.68715716172261,-3.67979438723667)) ;
#135564 = CARTESIAN_POINT('Ctrl Pts',(4.6,2.69106036671413,-3.67823222277847)) ;
#135565 = CARTESIAN_POINT('Ctrl Pts',(4.59952510519173,2.69488861888989,-3.67640970947469)) ;
#135566 = CARTESIAN_POINT('Ctrl Pts',(4.59869497748254,2.69852743640772,-3.674390151225)) ;
#135567 = CARTESIAN_POINT('Ctrl Pts',(4.59815316003464,2.70090246232129,-3.67307200236113)) ;
#135568 = CARTESIAN_POINT('Ctrl Pts',(4.59746001108778,2.70319720658047,-3.6716709680452)) ;
#135569 = CARTESIAN_POINT('Ctrl Pts',(4.59664880273703,2.70538659711789,-3.6702145418985)) ;
#135570 = CARTESIAN_POINT('Ctrl Pts',(4.59612777291939,2.70679281754376,-3.66927909609234)) ;
#135571 = CARTESIAN_POINT('Ctrl Pts',(4.59555051815356,2.70817855133085,-3.66830492990722)) ;
#135572 = CARTESIAN_POINT('Ctrl Pts',(4.59494172533681,2.70950512149367,-3.66732273606981)) ;
#135573 = CARTESIAN_POINT('Ctrl Pts',(4.59250947890861,2.71480502887016,-3.66339867949904)) ;
#135574 = CARTESIAN_POINT('Ctrl Pts',(4.5894485781299,2.71954517005253,-3.65908233758082)) ;
#135575 = CARTESIAN_POINT('Ctrl Pts',(4.58612768646811,2.7237636121892,-3.65447380318364)) ;
#135576 = CARTESIAN_POINT('Ctrl Pts',(4.58350334758173,2.7270972414872,-3.65083190297747)) ;
#135577 = CARTESIAN_POINT('Ctrl Pts',(4.58071664514661,2.73010548898776,-3.6470059959315)) ;
#135578 = CARTESIAN_POINT('Ctrl Pts',(4.5779495181309,2.73280244902547,-3.64302315111117)) ;
#135579 = CARTESIAN_POINT('Ctrl Pts',(4.57705238626115,2.73367683201821,-3.64173187066025)) ;
#135580 = CARTESIAN_POINT('Ctrl Pts',(4.576145855803,2.73452842391106,-3.64040884881589)) ;
#135581 = CARTESIAN_POINT('Ctrl Pts',(4.57524318173443,2.73534903670064,-3.63906481978892)) ;
#135582 = CARTESIAN_POINT('Origin',(4.65232986200049,2.66527023615798,-3.5912457888159)) ;
#135583 = CARTESIAN_POINT('Origin',(4.6,2.65,-3.58695395782836)) ;
#135584 = CARTESIAN_POINT('Origin',(12.7,1.9,-6.58)) ;
#135585 = CARTESIAN_POINT('Origin',(12.7,2.01643989873054,-3.48136060761679)) ;
#135586 = CARTESIAN_POINT('Origin',(-3.65,10.7,-4.33)) ;
#135587 = CARTESIAN_POINT('Origin',(-3.65,10.7,-4.33)) ;
#135588 = CARTESIAN_POINT('Origin',(-3.65,10.7,-4.33)) ;
#135589 = CARTESIAN_POINT('Origin',(0.,10.7,-4.33)) ;
#135590 = CARTESIAN_POINT('Origin',(-2.9,10.7,-4.33)) ;
#135591 = CARTESIAN_POINT('Origin',(-3.65,10.7,-5.08)) ;
#135592 = CARTESIAN_POINT('Origin',(-3.65,10.7,-5.83)) ;
#135593 = CARTESIAN_POINT('Origin',(-2.9,10.7,-4.33)) ;
#135594 = CARTESIAN_POINT('Origin',(-2.9,10.7,-4.33)) ;
#135595 = CARTESIAN_POINT('Origin',(-3.65,10.7,-5.83)) ;
#135596 = CARTESIAN_POINT('Origin',(-3.65,10.7,-5.83)) ;
#135597 = CARTESIAN_POINT('Origin',(-2.9,10.7,-5.08)) ;
#135598 = CARTESIAN_POINT('Origin',(-2.9,10.7,-5.83)) ;
#135599 = CARTESIAN_POINT('Origin',(0.,10.7,-5.83)) ;
#135600 = CARTESIAN_POINT('Origin',(-2.9,10.7,-5.83)) ;
#135601 = CARTESIAN_POINT('Origin',(-2.9,10.7,-5.83)) ;
#135602 = CARTESIAN_POINT('Origin',(-3.05,-3.95,-4.08)) ;
#135603 = CARTESIAN_POINT('Origin',(-3.05,-3.95,-5.98)) ;
#135604 = CARTESIAN_POINT('Origin',(-3.05,-3.95,-4.18)) ;
#135605 = CARTESIAN_POINT('Origin',(-3.25,-3.95,-4.18)) ;
#135606 = CARTESIAN_POINT('Origin',(-3.25,-3.95,-3.98)) ;
#135607 = CARTESIAN_POINT('Origin',(-3.25,-3.95,-4.18)) ;
#135608 = CARTESIAN_POINT('Origin',(-3.25,-3.95,-5.98)) ;
#135609 = CARTESIAN_POINT('Origin',(-3.25,-3.95,-5.98)) ;
#135610 = CARTESIAN_POINT('Origin',(-3.25,-3.95,-6.18)) ;
#135611 = CARTESIAN_POINT('Origin',(-4.4,-3.95,-3.98)) ;
#135612 = CARTESIAN_POINT('Origin',(-4.3,-3.95,-3.98)) ;
#135613 = CARTESIAN_POINT('Origin',(-3.25,-3.9,-4.18)) ;
#135614 = CARTESIAN_POINT('Origin',(-3.25,-3.85,-4.18)) ;
#135615 = CARTESIAN_POINT('Origin',(-3.25,-3.85,-5.08)) ;
#135616 = CARTESIAN_POINT('Origin',(-3.25,-3.85,-5.98)) ;
#135617 = CARTESIAN_POINT('Origin',(-3.25,-3.85,-4.18)) ;
#135618 = CARTESIAN_POINT('Origin',(-3.25,-3.9,-5.98)) ;
#135619 = CARTESIAN_POINT('Origin',(-3.25,-3.85,-5.98)) ;
#135620 = CARTESIAN_POINT('Origin',(-4.4,-3.95,-6.18)) ;
#135621 = CARTESIAN_POINT('Origin',(-4.3,-3.95,-6.18)) ;
#135622 = CARTESIAN_POINT('Origin',(-4.5,-3.95,-4.08)) ;
#135623 = CARTESIAN_POINT('Origin',(-4.5,-3.95,-4.18)) ;
#135624 = CARTESIAN_POINT('Origin',(-4.5,-3.95,-5.98)) ;
#135625 = CARTESIAN_POINT('Origin',(-4.3,-3.95,-4.18)) ;
#135626 = CARTESIAN_POINT('Origin',(-4.3,-3.95,-4.18)) ;
#135627 = CARTESIAN_POINT('Origin',(-3.25,-3.85,-4.18)) ;
#135628 = CARTESIAN_POINT('Origin',(-3.25,-3.85,-4.18)) ;
#135629 = CARTESIAN_POINT('Origin',(-3.25,-3.85,-5.98)) ;
#135630 = CARTESIAN_POINT('Origin',(-3.25,-3.85,-5.98)) ;
#135631 = CARTESIAN_POINT('Origin',(-4.3,-3.95,-5.98)) ;
#135632 = CARTESIAN_POINT('Origin',(-4.3,-3.95,-5.98)) ;
#135633 = CARTESIAN_POINT('Origin',(-4.3,-3.9,-4.18)) ;
#135634 = CARTESIAN_POINT('Origin',(-4.3,-3.85,-4.18)) ;
#135635 = CARTESIAN_POINT('Origin',(-1.56125112837913E-16,-3.85,-4.18)) ;
#135636 = CARTESIAN_POINT('Origin',(-4.3,-3.85,-4.18)) ;
#135637 = CARTESIAN_POINT('Origin',(-1.56125112837913E-16,-3.85,-5.98)) ;
#135638 = CARTESIAN_POINT('Origin',(-4.3,-3.85,-5.98)) ;
#135639 = CARTESIAN_POINT('Origin',(-4.3,-3.9,-5.98)) ;
#135640 = CARTESIAN_POINT('Origin',(-4.3,-3.85,-5.98)) ;
#135641 = CARTESIAN_POINT('Origin',(-4.3,-3.85,-4.18)) ;
#135642 = CARTESIAN_POINT('Origin',(-4.3,-3.85,-4.18)) ;
#135643 = CARTESIAN_POINT('Origin',(-4.3,-3.85,-5.98)) ;
#135644 = CARTESIAN_POINT('Origin',(-4.3,-3.85,-5.98)) ;
#135645 = CARTESIAN_POINT('Origin',(-4.3,-3.85,-5.08)) ;
#135646 = CARTESIAN_POINT('Origin',(-4.,10.85,-6.08)) ;
#135647 = CARTESIAN_POINT('Origin',(-4.,10.85,-5.98)) ;
#135648 = CARTESIAN_POINT('Origin',(-4.,10.85,-4.18)) ;
#135649 = CARTESIAN_POINT('Origin',(-3.8,10.85,-4.18)) ;
#135650 = CARTESIAN_POINT('Origin',(-3.8,10.85,-3.98)) ;
#135651 = CARTESIAN_POINT('Origin',(-3.8,10.85,-4.18)) ;
#135652 = CARTESIAN_POINT('Origin',(-3.8,10.85,-5.98)) ;
#135653 = CARTESIAN_POINT('Origin',(-3.8,10.85,-5.98)) ;
#135654 = CARTESIAN_POINT('Origin',(-3.8,10.85,-6.18)) ;
#135655 = CARTESIAN_POINT('Origin',(-3.9,10.85,-3.98)) ;
#135656 = CARTESIAN_POINT('Origin',(-2.75,10.85,-3.98)) ;
#135657 = CARTESIAN_POINT('Origin',(-3.8,10.8,-4.18)) ;
#135658 = CARTESIAN_POINT('Origin',(-3.8,10.75,-4.18)) ;
#135659 = CARTESIAN_POINT('Origin',(-3.8,10.75,-5.08)) ;
#135660 = CARTESIAN_POINT('Origin',(-3.8,10.75,-5.98)) ;
#135661 = CARTESIAN_POINT('Origin',(-3.8,10.75,-4.18)) ;
#135662 = CARTESIAN_POINT('Origin',(-3.8,10.8,-5.98)) ;
#135663 = CARTESIAN_POINT('Origin',(-3.8,10.75,-5.98)) ;
#135664 = CARTESIAN_POINT('Origin',(-3.9,10.85,-6.18)) ;
#135665 = CARTESIAN_POINT('Origin',(-2.75,10.85,-6.18)) ;
#135666 = CARTESIAN_POINT('Origin',(-2.55,10.85,-6.08)) ;
#135667 = CARTESIAN_POINT('Origin',(-2.55,10.85,-4.18)) ;
#135668 = CARTESIAN_POINT('Origin',(-2.55,10.85,-5.98)) ;
#135669 = CARTESIAN_POINT('Origin',(-2.75,10.85,-4.18)) ;
#135670 = CARTESIAN_POINT('Origin',(-2.75,10.85,-4.18)) ;
#135671 = CARTESIAN_POINT('Origin',(-3.8,10.75,-4.18)) ;
#135672 = CARTESIAN_POINT('Origin',(-3.8,10.75,-4.18)) ;
#135673 = CARTESIAN_POINT('Origin',(-3.8,10.75,-5.98)) ;
#135674 = CARTESIAN_POINT('Origin',(-3.8,10.75,-5.98)) ;
#135675 = CARTESIAN_POINT('Origin',(-2.75,10.85,-5.98)) ;
#135676 = CARTESIAN_POINT('Origin',(-2.75,10.85,-5.98)) ;
#135677 = CARTESIAN_POINT('Origin',(-2.75,10.8,-4.18)) ;
#135678 = CARTESIAN_POINT('Origin',(-2.75,10.75,-4.18)) ;
#135679 = CARTESIAN_POINT('Origin',(1.56125112837912E-16,10.75,-4.18)) ;
#135680 = CARTESIAN_POINT('Origin',(-2.75,10.75,-4.18)) ;
#135681 = CARTESIAN_POINT('Origin',(-1.56125112837913E-16,10.75,-5.98)) ;
#135682 = CARTESIAN_POINT('Origin',(-2.75,10.75,-5.98)) ;
#135683 = CARTESIAN_POINT('Origin',(-2.75,10.8,-5.98)) ;
#135684 = CARTESIAN_POINT('Origin',(-2.75,10.75,-5.98)) ;
#135685 = CARTESIAN_POINT('Origin',(-2.75,10.75,-4.18)) ;
#135686 = CARTESIAN_POINT('Origin',(-2.75,10.75,-4.18)) ;
#135687 = CARTESIAN_POINT('Origin',(-2.75,10.75,-5.98)) ;
#135688 = CARTESIAN_POINT('Origin',(-2.75,10.75,-5.98)) ;
#135689 = CARTESIAN_POINT('Origin',(-2.75,10.75,-5.08)) ;
#135690 = CARTESIAN_POINT('Origin',(4.6,0.,-5.08)) ;
#135691 = CARTESIAN_POINT('Ctrl Pts',(4.5,-2.7,-3.55684537882722)) ;
#135692 = CARTESIAN_POINT('Ctrl Pts',(4.5,-2.71827986285823,-3.63196473917507)) ;
#135693 = CARTESIAN_POINT('Ctrl Pts',(4.50597963419107,-2.73556801027185,
-3.70673986045281)) ;
#135694 = CARTESIAN_POINT('Ctrl Pts',(4.52394923367545,-2.75977758633329,
-3.81843683402156)) ;
#135695 = CARTESIAN_POINT('Ctrl Pts',(4.53141024883993,-2.76757607569523,
-3.85568328239029)) ;
#135696 = CARTESIAN_POINT('Ctrl Pts',(4.54734065524866,-2.77857284247615,
-3.91016568958296)) ;
#135697 = CARTESIAN_POINT('Ctrl Pts',(4.55339248498575,-2.78214991573955,
-3.92823827441494)) ;
#135698 = CARTESIAN_POINT('Ctrl Pts',(4.56567492147095,-2.787183259287,-3.95414672186072)) ;
#135699 = CARTESIAN_POINT('Ctrl Pts',(4.5702469143305,-2.78880341224557,-3.96257260505082)) ;
#135700 = CARTESIAN_POINT('Ctrl Pts',(4.58215938980081,-2.79169669265294,
-3.97774347988509)) ;
#135701 = CARTESIAN_POINT('Ctrl Pts',(4.59005470866978,-2.79310344827587,
-3.98520635404226)) ;
#135702 = CARTESIAN_POINT('Ctrl Pts',(4.6,-2.79310344827586,-3.98520635404223)) ;
#135703 = CARTESIAN_POINT('Origin',(4.6,-2.4,-3.11785831296514)) ;
#135704 = CARTESIAN_POINT('Origin',(4.6,-2.4,-3.11785831296514)) ;
#135705 = CARTESIAN_POINT('Origin',(4.6,-2.4,-3.11785831296514)) ;
#135706 = CARTESIAN_POINT('Origin',(0.584645609909622,-2.4,-3.11785831296514)) ;
#135707 = CARTESIAN_POINT('Origin',(12.7,-2.4,-3.11785831296514)) ;
#135708 = CARTESIAN_POINT('Origin',(12.7,-2.4,-3.11785831296514)) ;
#135709 = CARTESIAN_POINT('Origin',(12.7,-2.24516129032258,-3.24444809922546)) ;
#135710 = CARTESIAN_POINT('Origin',(12.7,0.,-5.08)) ;
#135711 = CARTESIAN_POINT('Origin',(12.7,-2.24516129032258,-6.91555190077455)) ;
#135712 = CARTESIAN_POINT('Origin',(12.7,-2.2,-2.54)) ;
#135713 = CARTESIAN_POINT('Origin',(12.7,-2.2,-7.04214168703486)) ;
#135714 = CARTESIAN_POINT('Origin',(12.7,-2.4,-7.04214168703486)) ;
#135715 = CARTESIAN_POINT('Origin',(12.7,-2.4,-7.04214168703486)) ;
#135716 = CARTESIAN_POINT('Origin',(0.584645609909622,-2.4,-7.04214168703486)) ;
#135717 = CARTESIAN_POINT('Origin',(4.6,-2.4,-7.04214168703486)) ;
#135718 = CARTESIAN_POINT('Origin',(4.6,-2.4,-2.54)) ;
#135719 = CARTESIAN_POINT('Origin',(4.6,-2.4,-7.04214168703486)) ;
#135720 = CARTESIAN_POINT('Origin',(4.6,-2.4,-7.04214168703486)) ;
#135721 = CARTESIAN_POINT('Origin',(4.6,-2.4,-7.04214168703486)) ;
#135722 = CARTESIAN_POINT('Origin',(4.6,0.,-5.08)) ;
#135723 = CARTESIAN_POINT('Ctrl Pts',(4.6,-2.79310344827586,-6.17479364595777)) ;
#135724 = CARTESIAN_POINT('Ctrl Pts',(4.59007568892311,-2.79310344827586,
-6.17479364595777)) ;
#135725 = CARTESIAN_POINT('Ctrl Pts',(4.5821920763724,-2.79170232102182,-6.18222674227604)) ;
#135726 = CARTESIAN_POINT('Ctrl Pts',(4.57028631514659,-2.78881527838255,
-6.19736543899001)) ;
#135727 = CARTESIAN_POINT('Ctrl Pts',(4.56571532154372,-2.78719767797524,
-6.20577848858353)) ;
#135728 = CARTESIAN_POINT('Ctrl Pts',(4.55343865632726,-2.78217307830036,
-6.23164363330887)) ;
#135729 = CARTESIAN_POINT('Ctrl Pts',(4.54738888873344,-2.77860151743012,
-6.24969008596606)) ;
#135730 = CARTESIAN_POINT('Ctrl Pts',(4.53146440752601,-2.76762263748299,
-6.3040903156831)) ;
#135731 = CARTESIAN_POINT('Ctrl Pts',(4.52400917967609,-2.75984503873828,
-6.34124550630579)) ;
#135732 = CARTESIAN_POINT('Ctrl Pts',(4.50599905604505,-2.7356206423885,-6.45303013546926)) ;
#135733 = CARTESIAN_POINT('Ctrl Pts',(4.5,-2.71826422026483,-6.5280995425769)) ;
#135734 = CARTESIAN_POINT('Ctrl Pts',(4.5,-2.7,-6.60315462117279)) ;
#135735 = CARTESIAN_POINT('Origin',(-0.362523114814661,9.05,-5.24904730469628)) ;
#135736 = CARTESIAN_POINT('Origin',(0.36252311481466,9.05,-4.91095269530372)) ;
#135737 = CARTESIAN_POINT('Origin',(-1.31845674202095,9.85,-3.67228134223507)) ;
#135738 = CARTESIAN_POINT('Origin',(-0.230887397576972,9.85,-3.16513942814623)) ;
#135739 = CARTESIAN_POINT('Origin',(4.6,2.1,-3.69804604217164)) ;
#135740 = CARTESIAN_POINT('Origin',(4.6,2.1,-3.69804604217164)) ;
#135741 = CARTESIAN_POINT('Origin',(4.6,0.280857398566761,-3.39485560859943)) ;
#135742 = CARTESIAN_POINT('Origin',(4.6,2.61712020253893,-3.78423274259479)) ;
#135743 = CARTESIAN_POINT('Origin',(4.6,2.65,-3.58695395782836)) ;
#135744 = CARTESIAN_POINT('Origin',(4.6,2.72431432344521,-3.77263481664499)) ;
#135745 = CARTESIAN_POINT('Ctrl Pts',(4.48762159086906,2.77250619842445,-3.69117568174961)) ;
#135746 = CARTESIAN_POINT('Ctrl Pts',(4.51316716229105,2.72605970493114,-3.65423879419716)) ;
#135747 = CARTESIAN_POINT('Ctrl Pts',(4.57527453405851,2.73535372386122,-3.63905715319801)) ;
#135748 = CARTESIAN_POINT('Ctrl Pts',(4.49363662433156,2.76156977394745,-3.72699959247169)) ;
#135749 = CARTESIAN_POINT('Ctrl Pts',(4.5146945995807,2.70766535161869,-3.67620084739329)) ;
#135750 = CARTESIAN_POINT('Ctrl Pts',(4.58732693581885,2.72440392220678,-3.65699504123406)) ;
#135751 = CARTESIAN_POINT('Ctrl Pts',(4.5,2.7448843843803,-3.75616921606616)) ;
#135752 = CARTESIAN_POINT('Ctrl Pts',(4.50856472873626,2.6903148207967,-3.67849111370471)) ;
#135753 = CARTESIAN_POINT('Ctrl Pts',(4.60003980620507,2.70775073269832,-3.67155231137473)) ;
#135754 = CARTESIAN_POINT('Ctrl Pts',(4.5,2.72431432344521,-3.77263481664499)) ;
#135755 = CARTESIAN_POINT('Ctrl Pts',(4.5,2.68714136424467,-3.6797549158517)) ;
#135756 = CARTESIAN_POINT('Ctrl Pts',(4.60004250625998,2.68715716507935,-3.6797943956238)) ;
#135757 = CARTESIAN_POINT('Origin',(4.57524318173443,2.82069807340128,-3.69117568174948)) ;
#135758 = CARTESIAN_POINT('Ctrl Pts',(4.47150553123747,2.80180812502279,-3.58695395782836)) ;
#135759 = CARTESIAN_POINT('Ctrl Pts',(4.5,2.75,-3.58695395782836)) ;
#135760 = CARTESIAN_POINT('Ctrl Pts',(4.55912712210514,2.75,-3.58695395782836)) ;
#135761 = CARTESIAN_POINT('Ctrl Pts',(4.47150553186688,2.8018081238784,-3.62357447273468)) ;
#135762 = CARTESIAN_POINT('Ctrl Pts',(4.50000000073523,2.74999999866316,-3.61125808426874)) ;
#135763 = CARTESIAN_POINT('Ctrl Pts',(4.5591271227348,2.75,-3.60527204575928)) ;
#135764 = CARTESIAN_POINT('Ctrl Pts',(4.47712448971608,2.79159183687985,-3.65991653735233)) ;
#135765 = CARTESIAN_POINT('Ctrl Pts',(4.50480340096852,2.74126654369363,-3.63553795099809)) ;
#135766 = CARTESIAN_POINT('Ctrl Pts',(4.56473907811158,2.74489822224645,-3.62342482158227)) ;
#135767 = CARTESIAN_POINT('Ctrl Pts',(4.48762159086676,2.77250619842407,-3.69117568174948)) ;
#135768 = CARTESIAN_POINT('Ctrl Pts',(4.51315802400618,2.72607631998876,-3.6542520074343)) ;
#135769 = CARTESIAN_POINT('Ctrl Pts',(4.57524318173443,2.73534903670064,-3.63906481978892)) ;
#135770 = CARTESIAN_POINT('Origin',(4.55912712210514,2.85,-2.54)) ;
#135771 = CARTESIAN_POINT('Origin',(4.55912712210514,2.85,-6.57304604217164)) ;
#135772 = CARTESIAN_POINT('Ctrl Pts',(4.48762159086767,2.77250619842243,-6.46882431824783)) ;
#135773 = CARTESIAN_POINT('Ctrl Pts',(4.51315802400691,2.72607631998743,-6.50574799256407)) ;
#135774 = CARTESIAN_POINT('Ctrl Pts',(4.57524318173533,2.73534903669982,-6.52093518020973)) ;
#135775 = CARTESIAN_POINT('Ctrl Pts',(4.47712448971641,2.79159183687925,-6.50008346264559)) ;
#135776 = CARTESIAN_POINT('Ctrl Pts',(4.50480340096881,2.74126654369309,-6.52446204900054)) ;
#135777 = CARTESIAN_POINT('Ctrl Pts',(4.5647390781119,2.74489822224615,-6.53657517841669)) ;
#135778 = CARTESIAN_POINT('Ctrl Pts',(4.47150553186688,2.8018081238784,-6.53642552726426)) ;
#135779 = CARTESIAN_POINT('Ctrl Pts',(4.50000000073523,2.74999999866316,-6.54874191573054)) ;
#135780 = CARTESIAN_POINT('Ctrl Pts',(4.5591271227348,2.75,-6.55472795424019)) ;
#135781 = CARTESIAN_POINT('Ctrl Pts',(4.47150553123747,2.80180812502279,-6.57304604217164)) ;
#135782 = CARTESIAN_POINT('Ctrl Pts',(4.5,2.75,-6.57304604217164)) ;
#135783 = CARTESIAN_POINT('Ctrl Pts',(4.55912712210513,2.75,-6.57304604217164)) ;
#135784 = CARTESIAN_POINT('Origin',(4.57524318173533,2.82069807339964,-6.46882431824783)) ;
#135785 = CARTESIAN_POINT('Ctrl Pts',(4.57527448145475,2.73535371598842,-6.52094283394186)) ;
#135786 = CARTESIAN_POINT('Ctrl Pts',(4.51316714695682,2.72605973281053,-6.50576118362915)) ;
#135787 = CARTESIAN_POINT('Ctrl Pts',(4.48762159086951,2.77250619842363,-6.4688243182477)) ;
#135788 = CARTESIAN_POINT('Ctrl Pts',(4.58732687742635,2.72440390874892,-6.50300494332462)) ;
#135789 = CARTESIAN_POINT('Ctrl Pts',(4.51469458626358,2.70766538570653,-6.48379912048174)) ;
#135790 = CARTESIAN_POINT('Ctrl Pts',(4.49363662433187,2.76156977394665,-6.4330004075269)) ;
#135791 = CARTESIAN_POINT('Ctrl Pts',(4.60003973844304,2.7077507197818,-6.48844768348498)) ;
#135792 = CARTESIAN_POINT('Ctrl Pts',(4.50856472285793,2.69031485824819,-6.48150883298403)) ;
#135793 = CARTESIAN_POINT('Ctrl Pts',(4.5,2.74488438437979,-6.40383078393338)) ;
#135794 = CARTESIAN_POINT('Ctrl Pts',(4.60004243494347,2.6871571650681,-6.48020560440432)) ;
#135795 = CARTESIAN_POINT('Ctrl Pts',(4.5,2.68714139075513,-6.48024501790961)) ;
#135796 = CARTESIAN_POINT('Ctrl Pts',(4.5,2.72431432344521,-6.38736518335501)) ;
#135797 = CARTESIAN_POINT('Origin',(4.6,0.280857398566761,-6.76514439140057)) ;
#135798 = CARTESIAN_POINT('Origin',(4.6,2.1,-6.46195395782836)) ;
#135799 = CARTESIAN_POINT('Origin',(4.6,2.1,-6.46195395782836)) ;
#135800 = CARTESIAN_POINT('Origin',(4.6,0.,-5.08)) ;
#135801 = CARTESIAN_POINT('',(4.5,-2.9,-5.08000000000385)) ;
#135802 = CARTESIAN_POINT('',(4.57439618084313,-2.80937499999937,-6.12279586712545)) ;
#135803 = CARTESIAN_POINT('Ctrl Pts',(4.5,-2.9,-5.08000000000385)) ;
#135804 = CARTESIAN_POINT('Ctrl Pts',(4.5,-2.9000000234111,-5.25617626257029)) ;
#135805 = CARTESIAN_POINT('Ctrl Pts',(4.49893459747296,-2.89187728142186,
-5.43229382255519)) ;
#135806 = CARTESIAN_POINT('Ctrl Pts',(4.50498172725087,-2.86839426105774,
-5.69494327688717)) ;
#135807 = CARTESIAN_POINT('Ctrl Pts',(4.50826226558342,-2.85869729223562,
-5.78228702711349)) ;
#135808 = CARTESIAN_POINT('Ctrl Pts',(4.52028413974051,-2.84160518746962,
-5.9128409654328)) ;
#135809 = CARTESIAN_POINT('Ctrl Pts',(4.52545003690602,-2.8354696349403,-5.95636311362202)) ;
#135810 = CARTESIAN_POINT('Ctrl Pts',(4.53741870680498,-2.82581179679252,
-6.02063945501075)) ;
#135811 = CARTESIAN_POINT('Ctrl Pts',(4.54209540184575,-2.82251395224859,
-6.04192001826058)) ;
#135812 = CARTESIAN_POINT('Ctrl Pts',(4.55451190949429,-2.81582803324483,
-6.0838742105328)) ;
#135813 = CARTESIAN_POINT('Ctrl Pts',(4.56139306411848,-2.8124020390272,-6.10474353182486)) ;
#135814 = CARTESIAN_POINT('Ctrl Pts',(4.57439618084313,-2.80937499999937,
-6.12279586712545)) ;
#135815 = CARTESIAN_POINT('Ctrl Pts',(4.57439618084313,-2.80937499999937,
-6.12279586712545)) ;
#135816 = CARTESIAN_POINT('Ctrl Pts',(4.57788811720513,-2.80856205104935,
-6.12764388459131)) ;
#135817 = CARTESIAN_POINT('Ctrl Pts',(4.58132110715667,-2.80743849592502,
-6.1326543114198)) ;
#135818 = CARTESIAN_POINT('Ctrl Pts',(4.58591063786564,-2.80541025280315,
-6.14006834915985)) ;
#135819 = CARTESIAN_POINT('Ctrl Pts',(4.58721694730501,-2.80476695238161,
-6.14226832508376)) ;
#135820 = CARTESIAN_POINT('Ctrl Pts',(4.5887449802686,-2.80393035430395,-6.14497171464085)) ;
#135821 = CARTESIAN_POINT('Ctrl Pts',(4.58900094431508,-2.8037870887984,-6.14542942337304)) ;
#135822 = CARTESIAN_POINT('Ctrl Pts',(4.58924476828968,-2.80364801935069,
-6.14586949326005)) ;
#135823 = CARTESIAN_POINT('Ctrl Pts',(4.58924931741448,-2.80364542371033,
-6.1458777053493)) ;
#135824 = CARTESIAN_POINT('Ctrl Pts',(4.59158188358133,-2.80231401319274,
-6.15008924012213)) ;
#135825 = CARTESIAN_POINT('Ctrl Pts',(4.59377134212491,-2.800813098491,-6.15443839239641)) ;
#135826 = CARTESIAN_POINT('Ctrl Pts',(4.59570408210448,-2.79909049146271,
-6.1591378632085)) ;
#135827 = CARTESIAN_POINT('Ctrl Pts',(4.59570848738489,-2.79908656285628,
-6.15914857957787)) ;
#135828 = CARTESIAN_POINT('Ctrl Pts',(4.59603576097761,-2.79879453264351,
-6.15994507543617)) ;
#135829 = CARTESIAN_POINT('Ctrl Pts',(4.59633794834607,-2.79851279959495,
-6.16070652531885)) ;
#135830 = CARTESIAN_POINT('Ctrl Pts',(4.59727216584803,-2.79759800070516,
-6.16316063340996)) ;
#135831 = CARTESIAN_POINT('Ctrl Pts',(4.59785661125443,-2.79695684051616,
-6.16485291560937)) ;
#135832 = CARTESIAN_POINT('Ctrl Pts',(4.59875882816121,-2.79580092267551,
-6.16786832422156)) ;
#135833 = CARTESIAN_POINT('Ctrl Pts',(4.59910960512328,-2.79529211440566,
-6.16918449921755)) ;
#135834 = CARTESIAN_POINT('Ctrl Pts',(4.59950074890552,-2.79458032370897,
-6.17101507841206)) ;
#135835 = CARTESIAN_POINT('Ctrl Pts',(4.59959271145697,-2.79439474074568,
-6.17149484058078)) ;
#135836 = CARTESIAN_POINT('Ctrl Pts',(4.59970479219924,-2.79411978912796,
-6.1722025710462)) ;
#135837 = CARTESIAN_POINT('Ctrl Pts',(4.59973686334512,-2.79403231884249,
-6.17242726844519)) ;
#135838 = CARTESIAN_POINT('Ctrl Pts',(4.59980956306601,-2.79380428276742,
-6.17301082640206)) ;
#135839 = CARTESIAN_POINT('Ctrl Pts',(4.59984405921136,-2.79366555090846,
-6.17336897900421)) ;
#135840 = CARTESIAN_POINT('Ctrl Pts',(4.59992170638736,-2.79338632637293,
-6.1740824135446)) ;
#135841 = CARTESIAN_POINT('Ctrl Pts',(4.59995882625634,-2.79324305250059,
-6.17443747925646)) ;
#135842 = CARTESIAN_POINT('Ctrl Pts',(4.59999999999999,-2.79310344827586,
-6.17479364595777)) ;
#135843 = CARTESIAN_POINT('',(4.57439618084271,-2.80937499999947,-4.03720413287514)) ;
#135844 = CARTESIAN_POINT('Ctrl Pts',(4.59999999999999,-2.79310344827586,
-3.98520635404223)) ;
#135845 = CARTESIAN_POINT('Ctrl Pts',(4.59995895305209,-2.79324111387631,
-3.98556200704419)) ;
#135846 = CARTESIAN_POINT('Ctrl Pts',(4.59992125133673,-2.79338175512528,
-3.98591664999517)) ;
#135847 = CARTESIAN_POINT('Ctrl Pts',(4.59984242179761,-2.79365985893298,
-3.98662721825472)) ;
#135848 = CARTESIAN_POINT('Ctrl Pts',(4.5998070294299,-2.79379858543765,-3.98698190400296)) ;
#135849 = CARTESIAN_POINT('Ctrl Pts',(4.59973261548695,-2.79401893257626,
-3.98754582127962)) ;
#135850 = CARTESIAN_POINT('Ctrl Pts',(4.59970092564442,-2.79410050108421,
-3.98775470445263)) ;
#135851 = CARTESIAN_POINT('Ctrl Pts',(4.59958060815603,-2.79437456977472,
-3.98845707425772)) ;
#135852 = CARTESIAN_POINT('Ctrl Pts',(4.59947821517875,-2.79456857658396,
-3.98895509538074)) ;
#135853 = CARTESIAN_POINT('Ctrl Pts',(4.5990597198479,-2.79527981802028,-3.99078506438848)) ;
#135854 = CARTESIAN_POINT('Ctrl Pts',(4.59869396429225,-2.79579226918927,
-3.99211140120008)) ;
#135855 = CARTESIAN_POINT('Ctrl Pts',(4.59768320083749,-2.79706868650734,
-3.99544407389333)) ;
#135856 = CARTESIAN_POINT('Ctrl Pts',(4.59698254015873,-2.79783590182173,
-3.99747319966267)) ;
#135857 = CARTESIAN_POINT('Ctrl Pts',(4.5959970522588,-2.79876532988113,-3.99998468423847)) ;
#135858 = CARTESIAN_POINT('Ctrl Pts',(4.59580678362761,-2.7989396411024,-4.00045810500393)) ;
#135859 = CARTESIAN_POINT('Ctrl Pts',(4.59367882781298,-2.80083904916685,
-4.00564491199709)) ;
#135860 = CARTESIAN_POINT('Ctrl Pts',(4.5915070708769,-2.80233337893514,-4.00997932770411)) ;
#135861 = CARTESIAN_POINT('Ctrl Pts',(4.58628071719241,-2.80532570224267,
-4.01945146742912)) ;
#135862 = CARTESIAN_POINT('Ctrl Pts',(4.58313959595723,-2.80673110767403,
-4.02451024806553)) ;
#135863 = CARTESIAN_POINT('Ctrl Pts',(4.57802611146349,-2.80844040952811,
-4.03209635749153)) ;
#135864 = CARTESIAN_POINT('Ctrl Pts',(4.57624387811654,-2.80894486836994,
-4.03463895934158)) ;
#135865 = CARTESIAN_POINT('Ctrl Pts',(4.57439618084271,-2.80937499999947,
-4.03720413287514)) ;
#135866 = CARTESIAN_POINT('Ctrl Pts',(4.57439618084271,-2.80937499999947,
-4.03720413287514)) ;
#135867 = CARTESIAN_POINT('Ctrl Pts',(4.56149777794589,-2.81237766235467,
-4.0551110931668)) ;
#135868 = CARTESIAN_POINT('Ctrl Pts',(4.55451596106519,-2.81582788236477,
-4.07612624229681)) ;
#135869 = CARTESIAN_POINT('Ctrl Pts',(4.54213610452188,-2.82249001163036,
-4.11792835962828)) ;
#135870 = CARTESIAN_POINT('Ctrl Pts',(4.53742891479326,-2.82580422498964,
-4.139310967236)) ;
#135871 = CARTESIAN_POINT('Ctrl Pts',(4.52545161424301,-2.8354670333868,-4.20361794379489)) ;
#135872 = CARTESIAN_POINT('Ctrl Pts',(4.52032009146395,-2.84156292603926,
-4.24685657347849)) ;
#135873 = CARTESIAN_POINT('Ctrl Pts',(4.50830110904356,-2.85862448221642,
-4.37711642595738)) ;
#135874 = CARTESIAN_POINT('Ctrl Pts',(4.50499166750953,-2.86836219567853,
-4.4647300385823)) ;
#135875 = CARTESIAN_POINT('Ctrl Pts',(4.49892845988062,-2.8918880660271,-4.72776299683786)) ;
#135876 = CARTESIAN_POINT('Ctrl Pts',(4.49999999999475,-2.89999999999869,
-4.90383009011776)) ;
#135877 = CARTESIAN_POINT('Ctrl Pts',(4.5,-2.9,-5.08000000000385)) ;
#135878 = CARTESIAN_POINT('Ctrl Pts',(4.40227435089071,-2.79999990867355,
-3.48940069288197)) ;
#135879 = CARTESIAN_POINT('Ctrl Pts',(4.51828879250213,-2.80015667527382,
-3.49878556679245)) ;
#135880 = CARTESIAN_POINT('Ctrl Pts',(4.50118227077258,-2.68533700727783,
-3.49797110744947)) ;
#135881 = CARTESIAN_POINT('Ctrl Pts',(4.39419482113924,-2.79999992837382,
-3.60368769966904)) ;
#135882 = CARTESIAN_POINT('Ctrl Pts',(4.48571792501736,-2.80010751836586,
-3.5826713667507)) ;
#135883 = CARTESIAN_POINT('Ctrl Pts',(4.49717570077251,-2.71006921719236,
-3.5970318982145)) ;
#135884 = CARTESIAN_POINT('Ctrl Pts',(4.40636790575267,-2.79999994706265,
-3.71490890735437)) ;
#135885 = CARTESIAN_POINT('Ctrl Pts',(4.47481046024545,-2.80007242131916,
-3.69332242779908)) ;
#135886 = CARTESIAN_POINT('Ctrl Pts',(4.50328131876401,-2.73353293829097,
-3.69702587481009)) ;
#135887 = CARTESIAN_POINT('Ctrl Pts',(4.45479736994228,-2.79999997092221,
-3.86507366547108)) ;
#135888 = CARTESIAN_POINT('Ctrl Pts',(4.49869786247045,-2.80003603117403,
-3.84627924349579)) ;
#135889 = CARTESIAN_POINT('Ctrl Pts',(4.52748687875413,-2.76348976047509,
-3.8362891728587)) ;
#135890 = CARTESIAN_POINT('Ctrl Pts',(4.47221929614095,-2.79999997745988,
-3.90730406022327)) ;
#135891 = CARTESIAN_POINT('Ctrl Pts',(4.50880556767615,-2.8000272573648,-3.88827484828593)) ;
#135892 = CARTESIAN_POINT('Ctrl Pts',(4.53619137795527,-2.77169834185705,
-3.87598368236757)) ;
#135893 = CARTESIAN_POINT('Ctrl Pts',(4.50882352800135,-2.7999999860536,-3.96428434960906)) ;
#135894 = CARTESIAN_POINT('Ctrl Pts',(4.53367802911271,-2.80001636071784,
-3.94535870242034)) ;
#135895 = CARTESIAN_POINT('Ctrl Pts',(4.55447319025662,-2.78248861123826,
-3.93009568142552)) ;
#135896 = CARTESIAN_POINT('Ctrl Pts',(4.52308919141482,-2.79999998878206,
-3.98266256169107)) ;
#135897 = CARTESIAN_POINT('Ctrl Pts',(4.5436396263862,-2.80001303821803,-3.96372615017167)) ;
#135898 = CARTESIAN_POINT('Ctrl Pts',(4.56159739427506,-2.78591449131414,
-3.9476542708947)) ;
#135899 = CARTESIAN_POINT('Ctrl Pts',(4.57467506176496,-2.79999999510246,
-4.02569650839937)) ;
#135900 = CARTESIAN_POINT('Ctrl Pts',(4.58062405303292,-2.80000557393877,
-4.0063341632778)) ;
#135901 = CARTESIAN_POINT('Ctrl Pts',(4.58735613403294,-2.79385049254304,
-3.98891981499328)) ;
#135902 = CARTESIAN_POINT('Ctrl Pts',(4.62437069655631,-2.79999999703807,
-4.03953134305988)) ;
#135903 = CARTESIAN_POINT('Ctrl Pts',(4.6182737266188,-2.80000334969057,-4.02093404548721)) ;
#135904 = CARTESIAN_POINT('Ctrl Pts',(4.61212682540737,-2.79628090446616,
-4.00240281421806)) ;
#135905 = CARTESIAN_POINT('Ctrl Pts',(4.67161368302049,-2.79999998860619,
-3.98078982676581)) ;
#135906 = CARTESIAN_POINT('Ctrl Pts',(4.6540701010266,-2.80001325705919,-3.96046373959001)) ;
#135907 = CARTESIAN_POINT('Ctrl Pts',(4.63587130780629,-2.78569367459204,
-3.94562812959451)) ;
#135908 = CARTESIAN_POINT('Ctrl Pts',(4.54879236204369,-2.8,-4.0035655563675)) ;
#135909 = CARTESIAN_POINT('Ctrl Pts',(4.55448837802407,-2.7999999999815,-4.00117882091359)) ;
#135910 = CARTESIAN_POINT('Ctrl Pts',(4.56021842726647,-2.79959150783236,
-3.998839542734)) ;
#135911 = CARTESIAN_POINT('Ctrl Pts',(4.56730671985029,-2.79865167182169,
-3.99597888386339)) ;
#135912 = CARTESIAN_POINT('Ctrl Pts',(4.56847770958292,-2.79848295770254,
-3.99550732683466)) ;
#135913 = CARTESIAN_POINT('Ctrl Pts',(4.57107523099021,-2.79808046368154,
-3.99446296289698)) ;
#135914 = CARTESIAN_POINT('Ctrl Pts',(4.5725009361248,-2.79784058543152,-3.99388964302801)) ;
#135915 = CARTESIAN_POINT('Ctrl Pts',(4.5764383594612,-2.79713266293194,-3.99231368646489)) ;
#135916 = CARTESIAN_POINT('Ctrl Pts',(4.57879956048961,-2.79666132938901,
-3.99137580039693)) ;
#135917 = CARTESIAN_POINT('Ctrl Pts',(4.58293855712953,-2.79579586318667,
-3.98976081592963)) ;
#135918 = CARTESIAN_POINT('Ctrl Pts',(4.58471363403686,-2.79540911153441,
-3.98907461719119)) ;
#135919 = CARTESIAN_POINT('Ctrl Pts',(4.58699082729421,-2.79492697681981,
-3.98824452926203)) ;
#135920 = CARTESIAN_POINT('Ctrl Pts',(4.58739952300692,-2.79484234870239,
-3.9881019268464)) ;
#135921 = CARTESIAN_POINT('Ctrl Pts',(4.58871515235486,-2.79457617288695,
-3.98766112910085)) ;
#135922 = CARTESIAN_POINT('Ctrl Pts',(4.58961690596145,-2.7944024780556,-3.98738498699949)) ;
#135923 = CARTESIAN_POINT('Ctrl Pts',(4.5910537506587,-2.79414748185764,-3.98698298181791)) ;
#135924 = CARTESIAN_POINT('Ctrl Pts',(4.5915530390955,-2.79406229662442,-3.98684924350712)) ;
#135925 = CARTESIAN_POINT('Ctrl Pts',(4.59245965385669,-2.79391282221553,
-3.98661259411486)) ;
#135926 = CARTESIAN_POINT('Ctrl Pts',(4.59286388425105,-2.79384761399903,
-3.98650842178452)) ;
#135927 = CARTESIAN_POINT('Ctrl Pts',(4.59368973959981,-2.79370598615371,
-3.98626767265165)) ;
#135928 = CARTESIAN_POINT('Ctrl Pts',(4.59407665941124,-2.79363973714592,
-3.98615152123316)) ;
#135929 = CARTESIAN_POINT('Ctrl Pts',(4.59444371287733,-2.79357284110655,
-3.98602679272788)) ;
#135930 = CARTESIAN_POINT('Ctrl Pts',(4.5944889025916,-2.79356452972317,-3.98601115819951)) ;
#135931 = CARTESIAN_POINT('Ctrl Pts',(4.59470842334911,-2.79352377141065,
-3.98593382545217)) ;
#135932 = CARTESIAN_POINT('Ctrl Pts',(4.59483598733269,-2.79349361011836,
-3.98587233148411)) ;
#135933 = CARTESIAN_POINT('Ctrl Pts',(4.59514620525224,-2.7934297131363,-3.9857459400492)) ;
#135934 = CARTESIAN_POINT('Ctrl Pts',(4.59533334275102,-2.79339696908416,
-3.9856838378534)) ;
#135935 = CARTESIAN_POINT('Ctrl Pts',(4.59563785533348,-2.79335634095568,
-3.98561299034027)) ;
#135936 = CARTESIAN_POINT('Ctrl Pts',(4.59571710962763,-2.79334654412182,
-3.98559639128765)) ;
#135937 = CARTESIAN_POINT('Ctrl Pts',(4.59594411915587,-2.79332043135007,
-3.9855533496182)) ;
#135938 = CARTESIAN_POINT('Ctrl Pts',(4.59600288191153,-2.79330503361987,
-3.98553395124079)) ;
#135939 = CARTESIAN_POINT('Ctrl Pts',(4.59613307952174,-2.79327450473787,
-3.98549928051942)) ;
#135940 = CARTESIAN_POINT('Ctrl Pts',(4.59620389659312,-2.7932597078882,-3.98548500605855)) ;
#135941 = CARTESIAN_POINT('Ctrl Pts',(4.59651192984772,-2.79322709231927,
-3.98545027786287)) ;
#135942 = CARTESIAN_POINT('Ctrl Pts',(4.59679543741297,-2.79320989448354,
-3.98542934418241)) ;
#135943 = CARTESIAN_POINT('Ctrl Pts',(4.59784475938523,-2.793166495242,-3.9853578835066)) ;
#135944 = CARTESIAN_POINT('Ctrl Pts',(4.59874915064779,-2.79313948637392,
-3.98529926431075)) ;
#135945 = CARTESIAN_POINT('Ctrl Pts',(4.59999999999999,-2.79310344827586,
-3.98520635404223)) ;
#135946 = CARTESIAN_POINT('Origin',(4.4,-2.7,-2.54)) ;
#135947 = CARTESIAN_POINT('Origin',(4.4,-2.7,-6.60315462117279)) ;
#135948 = CARTESIAN_POINT('Ctrl Pts',(4.5011795914298,-2.68531903459929,-6.66202902017229)) ;
#135949 = CARTESIAN_POINT('Ctrl Pts',(4.51828670358941,-2.8,-6.66121382514058)) ;
#135950 = CARTESIAN_POINT('Ctrl Pts',(4.40240952225579,-2.8,-6.67058837211076)) ;
#135951 = CARTESIAN_POINT('Ctrl Pts',(4.49717774927193,-2.71005310920068,
-6.56296553236259)) ;
#135952 = CARTESIAN_POINT('Ctrl Pts',(4.48574628541085,-2.8,-6.5773148520404)) ;
#135953 = CARTESIAN_POINT('Ctrl Pts',(4.39431668173578,-2.8,-6.5563402695083)) ;
#135954 = CARTESIAN_POINT('Ctrl Pts',(4.50328690685191,-2.73351987602563,
-6.46297339786193)) ;
#135955 = CARTESIAN_POINT('Ctrl Pts',(4.47485145549548,-2.8,-6.46667669574134)) ;
#135956 = CARTESIAN_POINT('Ctrl Pts',(4.40646789472124,-2.8,-6.44512261863839)) ;
#135957 = CARTESIAN_POINT('Ctrl Pts',(4.52749311797091,-2.76348183928881,
-6.3237129921595)) ;
#135958 = CARTESIAN_POINT('Ctrl Pts',(4.49873206155793,-2.8,-6.31373309530699)) ;
#135959 = CARTESIAN_POINT('Ctrl Pts',(4.4548681704377,-2.8,-6.29495664336612)) ;
#135960 = CARTESIAN_POINT('Ctrl Pts',(4.53619745972499,-2.77169205010107,
-6.28401904718521)) ;
#135961 = CARTESIAN_POINT('Ctrl Pts',(4.5088366481667,-2.79999999999999,-6.27173943817213)) ;
#135962 = CARTESIAN_POINT('Ctrl Pts',(4.47227975612147,-2.8,-6.25272738460372)) ;
#135963 = CARTESIAN_POINT('Ctrl Pts',(4.55447795090009,-2.78248459830339,
-6.22990781273338)) ;
#135964 = CARTESIAN_POINT('Ctrl Pts',(4.53370055749884,-2.8,-6.21465791836995)) ;
#135965 = CARTESIAN_POINT('Ctrl Pts',(4.50886586566854,-2.8,-6.19574788827224)) ;
#135966 = CARTESIAN_POINT('Ctrl Pts',(4.56160154376424,-2.78591123334062,
-6.21234944281567)) ;
#135967 = CARTESIAN_POINT('Ctrl Pts',(4.54365878772218,-2.8,-6.19629106645425)) ;
#135968 = CARTESIAN_POINT('Ctrl Pts',(4.52312452397684,-2.8,-6.17736999548674)) ;
#135969 = CARTESIAN_POINT('Ctrl Pts',(4.58735772267364,-2.79384903998488,
-6.17108429439849)) ;
#135970 = CARTESIAN_POINT('Ctrl Pts',(4.58063087367386,-2.8,-6.15368396338089)) ;
#135971 = CARTESIAN_POINT('Ctrl Pts',(4.57468550767192,-2.8,-6.13433748660569)) ;
#135972 = CARTESIAN_POINT('Ctrl Pts',(4.61212536563475,-2.79628002040286,
-6.15760158659528)) ;
#135973 = CARTESIAN_POINT('Ctrl Pts',(4.61826745782994,-2.80000000000005,
-6.13908487937516)) ;
#135974 = CARTESIAN_POINT('Ctrl Pts',(4.62435992349563,-2.8,-6.12050151732127)) ;
#135975 = CARTESIAN_POINT('Ctrl Pts',(4.63586710715934,-2.78569036914635,
-6.21437529467588)) ;
#135976 = CARTESIAN_POINT('Ctrl Pts',(4.65405106945717,-2.79999999999983,
-6.19955252388527)) ;
#135977 = CARTESIAN_POINT('Ctrl Pts',(4.67158355065755,-2.8,-6.17924507978128)) ;
#135978 = CARTESIAN_POINT('Ctrl Pts',(4.59999999999999,-2.79310344827586,
-6.17479364595777)) ;
#135979 = CARTESIAN_POINT('Ctrl Pts',(4.59840954578197,-2.79314968944989,
-6.17467567269119)) ;
#135980 = CARTESIAN_POINT('Ctrl Pts',(4.59737383489067,-2.79318159606221,
-6.17461332397164)) ;
#135981 = CARTESIAN_POINT('Ctrl Pts',(4.59650507521635,-2.79322931786013,
-6.17455037725996)) ;
#135982 = CARTESIAN_POINT('Ctrl Pts',(4.59632758424294,-2.79324472590583,
-6.17453457917666)) ;
#135983 = CARTESIAN_POINT('Ctrl Pts',(4.59611847210841,-2.79327477162037,
-6.17450475657722)) ;
#135984 = CARTESIAN_POINT('Ctrl Pts',(4.59606489504923,-2.79328892979787,
-6.17449102658529)) ;
#135985 = CARTESIAN_POINT('Ctrl Pts',(4.59594601677692,-2.79331605564258,
-6.17445911449494)) ;
#135986 = CARTESIAN_POINT('Ctrl Pts',(4.59588597444855,-2.7933285533825,-6.17444265618345)) ;
#135987 = CARTESIAN_POINT('Ctrl Pts',(4.59549967474364,-2.79337285752324,
-6.17437027876054)) ;
#135988 = CARTESIAN_POINT('Ctrl Pts',(4.59527331486237,-2.79340622385959,
-6.17431008070831)) ;
#135989 = CARTESIAN_POINT('Ctrl Pts',(4.59493201239529,-2.79346950514991,
-6.17418704029369)) ;
#135990 = CARTESIAN_POINT('Ctrl Pts',(4.59480393230128,-2.79349821606423,
-6.17412847427896)) ;
#135991 = CARTESIAN_POINT('Ctrl Pts',(4.59460326813595,-2.79353924388982,
-6.17404763514903)) ;
#135992 = CARTESIAN_POINT('Ctrl Pts',(4.59455075953096,-2.79354963432651,
-6.17402742767144)) ;
#135993 = CARTESIAN_POINT('Ctrl Pts',(4.59417008680874,-2.79361944405452,
-6.17389559371762)) ;
#135994 = CARTESIAN_POINT('Ctrl Pts',(4.5937774209655,-2.79368602572532,-6.17377734615548)) ;
#135995 = CARTESIAN_POINT('Ctrl Pts',(4.59289939109634,-2.7938335466559,-6.17352541902409)) ;
#135996 = CARTESIAN_POINT('Ctrl Pts',(4.59245006584786,-2.79390305456782,
-6.17341603619897)) ;
#135997 = CARTESIAN_POINT('Ctrl Pts',(4.59099552519191,-2.79413629528614,
-6.17305685240917)) ;
#135998 = CARTESIAN_POINT('Ctrl Pts',(4.5900219788148,-2.79430302757335,-6.17280637017571)) ;
#135999 = CARTESIAN_POINT('Ctrl Pts',(4.58861122644573,-2.79456793455722,
-6.17239213656651)) ;
#136000 = CARTESIAN_POINT('Ctrl Pts',(4.58817904894346,-2.79465210327464,
-6.17225852343037)) ;
#136001 = CARTESIAN_POINT('Ctrl Pts',(4.58736872283365,-2.79481449815582,
-6.17199418358962)) ;
#136002 = CARTESIAN_POINT('Ctrl Pts',(4.58699491219413,-2.79489135860975,
-6.17186658235812)) ;
#136003 = CARTESIAN_POINT('Ctrl Pts',(4.58468897497186,-2.79537899446709,
-6.17103519061958)) ;
#136004 = CARTESIAN_POINT('Ctrl Pts',(4.58290717718701,-2.79577019617637,
-6.1703420642284)) ;
#136005 = CARTESIAN_POINT('Ctrl Pts',(4.57867627871777,-2.79666451416568,
-6.16867078828749)) ;
#136006 = CARTESIAN_POINT('Ctrl Pts',(4.57626321554132,-2.79715040843618,
-6.16768776514285)) ;
#136007 = CARTESIAN_POINT('Ctrl Pts',(4.57243386308706,-2.79784156172336,
-6.1661367865103)) ;
#136008 = CARTESIAN_POINT('Ctrl Pts',(4.57107519984216,-2.79807176647234,
-6.16558402144498)) ;
#136009 = CARTESIAN_POINT('Ctrl Pts',(4.56513452430488,-2.79900074294388,
-6.16316939035812)) ;
#136010 = CARTESIAN_POINT('Ctrl Pts',(4.56062162665774,-2.79951267011375,
-6.1613309293496)) ;
#136011 = CARTESIAN_POINT('Ctrl Pts',(4.55365420596667,-2.79992470862866,
-6.1584610302785)) ;
#136012 = CARTESIAN_POINT('Ctrl Pts',(4.55124660967284,-2.79999983267432,
-6.15746323925077)) ;
#136013 = CARTESIAN_POINT('Ctrl Pts',(4.54880051362943,-2.79999999972164,
-6.15643786073294)) ;
#136014 = CARTESIAN_POINT('Ctrl Pts',(4.54879236166275,-2.8,-4.00356555651516)) ;
#136015 = CARTESIAN_POINT('Ctrl Pts',(4.5622387183224,-2.79999999999679,-4.02123152627487)) ;
#136016 = CARTESIAN_POINT('Ctrl Pts',(4.57442182196495,-2.80939476060287,
-4.03723782046681)) ;
#136017 = CARTESIAN_POINT('Ctrl Pts',(4.5555684251759,-2.79999999999889,-4.00072506404886)) ;
#136018 = CARTESIAN_POINT('Ctrl Pts',(4.56783337210915,-2.80040661803735,
-4.01618630155189)) ;
#136019 = CARTESIAN_POINT('Ctrl Pts',(4.5796182352237,-2.80818164104597,-4.03001834132724)) ;
#136020 = CARTESIAN_POINT('Ctrl Pts',(4.5623898283162,-2.79942602551759,-3.99795285151707)) ;
#136021 = CARTESIAN_POINT('Ctrl Pts',(4.57357810388183,-2.80014618986472,
-4.01093107214122)) ;
#136022 = CARTESIAN_POINT('Ctrl Pts',(4.58462643299474,-2.80630261261112,
-4.02252327116488)) ;
#136023 = CARTESIAN_POINT('Ctrl Pts',(4.57328757735257,-2.7977370397245,-3.99356999795014)) ;
#136024 = CARTESIAN_POINT('Ctrl Pts',(4.58237922839514,-2.79856394574987,
-4.00226640893136)) ;
#136025 = CARTESIAN_POINT('Ctrl Pts',(4.59151541127592,-2.80237286596199,
-4.01008300288058)) ;
#136026 = CARTESIAN_POINT('Ctrl Pts',(4.57700059755674,-2.7970371466716,-3.99207607634203)) ;
#136027 = CARTESIAN_POINT('Ctrl Pts',(4.58532305318676,-2.79784352093717,
-3.99926254300445)) ;
#136028 = CARTESIAN_POINT('Ctrl Pts',(4.59370961102545,-2.80088045369937,
-4.00574551418945)) ;
#136029 = CARTESIAN_POINT('Ctrl Pts',(4.58319893207066,-2.79574016930783,
-3.98965467052114)) ;
#136030 = CARTESIAN_POINT('Ctrl Pts',(4.5899041610924,-2.79637293360539,-3.99433035456225)) ;
#136031 = CARTESIAN_POINT('Ctrl Pts',(4.59665800356695,-2.79825577077759,
-3.99858194486972)) ;
#136032 = CARTESIAN_POINT('Ctrl Pts',(4.58534994317986,-2.79526732601294,
-3.98881886188718)) ;
#136033 = CARTESIAN_POINT('Ctrl Pts',(4.59144552977844,-2.79581844972913,
-3.99262003661071)) ;
#136034 = CARTESIAN_POINT('Ctrl Pts',(4.59758018705035,-2.79731769672697,
-3.99608858039389)) ;
#136035 = CARTESIAN_POINT('Ctrl Pts',(4.58899927751306,-2.79450268149332,
-3.98751730126711)) ;
#136036 = CARTESIAN_POINT('Ctrl Pts',(4.59386223202754,-2.79488630507105,
-3.98994951703029)) ;
#136037 = CARTESIAN_POINT('Ctrl Pts',(4.59874684688641,-2.79582009356912,
-3.99218136524475)) ;
#136038 = CARTESIAN_POINT('Ctrl Pts',(4.59026755692872,-2.79423885380164,
-3.98707439958004)) ;
#136039 = CARTESIAN_POINT('Ctrl Pts',(4.59467706068312,-2.79455862385202,
-3.98904054333606)) ;
#136040 = CARTESIAN_POINT('Ctrl Pts',(4.59910266898803,-2.79530499526365,
-3.99084863990216)) ;
#136041 = CARTESIAN_POINT('Ctrl Pts',(4.59257623319513,-2.79382131826659,
-3.98638413144999)) ;
#136042 = CARTESIAN_POINT('Ctrl Pts',(4.59605751036344,-2.79403163929513,
-3.98762276103362)) ;
#136043 = CARTESIAN_POINT('Ctrl Pts',(4.59954701072604,-2.79449510806573,
-3.98876576681697)) ;
#136044 = CARTESIAN_POINT('Ctrl Pts',(4.59342976933297,-2.79367543507711,
-3.98614453745337)) ;
#136045 = CARTESIAN_POINT('Ctrl Pts',(4.59655016100493,-2.79384713427256,
-3.98713488953029)) ;
#136046 = CARTESIAN_POINT('Ctrl Pts',(4.59967640178298,-2.79421605292372,
-3.98805021393703)) ;
#136047 = CARTESIAN_POINT('Ctrl Pts',(4.59428414179641,-2.79346156087783,
-3.98570693618526)) ;
#136048 = CARTESIAN_POINT('Ctrl Pts',(4.59704519451433,-2.79355469746529,
-3.98637363574795)) ;
#136049 = CARTESIAN_POINT('Ctrl Pts',(4.5998104157401,-2.79379877456676,-3.98698237127069)) ;
#136050 = CARTESIAN_POINT('Ctrl Pts',(4.59432658472652,-2.7933916625364,-3.98553381814949)) ;
#136051 = CARTESIAN_POINT('Ctrl Pts',(4.59708408719785,-2.79345234504014,
-3.98610907664628)) ;
#136052 = CARTESIAN_POINT('Ctrl Pts',(4.59984563524626,-2.79366003518351,
-3.98662765435266)) ;
#136053 = CARTESIAN_POINT('Ctrl Pts',(4.59537197237733,-2.79324260992761,
-3.98528726159385)) ;
#136054 = CARTESIAN_POINT('Ctrl Pts',(4.59764722167537,-2.79326383513929,
-3.985620961855)) ;
#136055 = CARTESIAN_POINT('Ctrl Pts',(4.59992475053754,-2.79338190759658,
-3.98591703064758)) ;
#136056 = CARTESIAN_POINT('Ctrl Pts',(4.59364183392371,-2.79313407032025,
-3.98528447884512)) ;
#136057 = CARTESIAN_POINT('Ctrl Pts',(4.59684754854893,-2.79327107597597,
-3.9856389310452)) ;
#136058 = CARTESIAN_POINT('Ctrl Pts',(4.59996664298755,-2.79324102308607,
-3.98556177368153)) ;
#136059 = CARTESIAN_POINT('Ctrl Pts',(4.59999999999999,-2.79310344827586,
-3.98520635404223)) ;
#136060 = CARTESIAN_POINT('Ctrl Pts',(4.59999999999999,-2.79310344827586,
-3.98520635404223)) ;
#136061 = CARTESIAN_POINT('Ctrl Pts',(4.59999999999999,-2.79310344827586,
-3.98520635404223)) ;
#136062 = CARTESIAN_POINT('Origin',(4.54879236168542,-2.9,-4.00356555651607)) ;
#136063 = CARTESIAN_POINT('Ctrl Pts',(4.39959973407451,-2.8,-5.19059224280254)) ;
#136064 = CARTESIAN_POINT('Ctrl Pts',(4.49922290141885,-2.8,-5.19010524833144)) ;
#136065 = CARTESIAN_POINT('Ctrl Pts',(4.49980764094185,-2.8996950427638,-5.19060804589504)) ;
#136066 = CARTESIAN_POINT('Ctrl Pts',(4.40142712570759,-2.8,-4.96953389600773)) ;
#136067 = CARTESIAN_POINT('Ctrl Pts',(4.50593622119654,-2.8,-4.96604801346827)) ;
#136068 = CARTESIAN_POINT('Ctrl Pts',(4.50067611734351,-2.90411960318543,
-4.96965028712544)) ;
#136069 = CARTESIAN_POINT('Ctrl Pts',(4.39573539165433,-2.8,-4.74762254178847)) ;
#136070 = CARTESIAN_POINT('Ctrl Pts',(4.49039105203448,-2.8,-4.76644486600883)) ;
#136071 = CARTESIAN_POINT('Ctrl Pts',(4.49793210898572,-2.89506044297348,
-4.74659283506961)) ;
#136072 = CARTESIAN_POINT('Ctrl Pts',(4.41164816536272,-2.8,-4.43449214865647)) ;
#136073 = CARTESIAN_POINT('Ctrl Pts',(4.48203507549538,-2.8,-4.44300753838916)) ;
#136074 = CARTESIAN_POINT('Ctrl Pts',(4.50604587949365,-2.86657833599734,
-4.44179163345507)) ;
#136075 = CARTESIAN_POINT('Ctrl Pts',(4.41940490599913,-2.8,-4.34215713199869)) ;
#136076 = CARTESIAN_POINT('Ctrl Pts',(4.48133975791573,-2.8,-4.35332746373866)) ;
#136077 = CARTESIAN_POINT('Ctrl Pts',(4.50997623336228,-2.85625883833136,
-4.35306464323898)) ;
#136078 = CARTESIAN_POINT('Ctrl Pts',(4.4457743437364,-2.8,-4.20702065882598)) ;
#136079 = CARTESIAN_POINT('Ctrl Pts',(4.49360122670478,-2.8,-4.21933058766783)) ;
#136080 = CARTESIAN_POINT('Ctrl Pts',(4.52318558604184,-2.83896465559566,
-4.22548504243761)) ;
#136081 = CARTESIAN_POINT('Ctrl Pts',(4.45692583760035,-2.8,-4.16247689305276)) ;
#136082 = CARTESIAN_POINT('Ctrl Pts',(4.49949391572668,-2.8,-4.17605430264613)) ;
#136083 = CARTESIAN_POINT('Ctrl Pts',(4.52876348458385,-2.8328925815763,-4.18380298860427)) ;
#136084 = CARTESIAN_POINT('Ctrl Pts',(4.50378503771654,-2.8,-4.04107591625834)) ;
#136085 = CARTESIAN_POINT('Ctrl Pts',(4.52873519606808,-2.8,-4.05992534227479)) ;
#136086 = CARTESIAN_POINT('Ctrl Pts',(4.55214466721903,-2.81552005845344,
-4.07122486980161)) ;
#136087 = CARTESIAN_POINT('Ctrl Pts',(4.5471442379016,-2.8,-3.9622684950464)) ;
#136088 = CARTESIAN_POINT('Ctrl Pts',(4.55761617337291,-2.8,-3.98320656418789)) ;
#136089 = CARTESIAN_POINT('Ctrl Pts',(4.5725958481338,-2.80338245043785,-4.00123859518852)) ;
#136090 = CARTESIAN_POINT('Ctrl Pts',(4.67762904165661,-2.8,-3.97149504479684)) ;
#136091 = CARTESIAN_POINT('Ctrl Pts',(4.66093484725016,-2.8,-3.98706706583889)) ;
#136092 = CARTESIAN_POINT('Ctrl Pts',(4.64133868807469,-2.80368623369366,
-4.00468800638713)) ;
#136093 = CARTESIAN_POINT('Origin',(4.4,-2.9,-5.08000000000385)) ;
#136094 = CARTESIAN_POINT('Ctrl Pts',(4.72172783566997,-2.8000000024879,-6.18036295491321)) ;
#136095 = CARTESIAN_POINT('Ctrl Pts',(4.69645430307969,-2.7999966052579,-6.16707004731005)) ;
#136096 = CARTESIAN_POINT('Ctrl Pts',(4.66463283185045,-2.80454824226947,
-6.14949036829302)) ;
#136097 = CARTESIAN_POINT('Ctrl Pts',(4.55709227475159,-2.80000000030524,
-6.21599643631003)) ;
#136098 = CARTESIAN_POINT('Ctrl Pts',(4.56399237478705,-2.79999958643656,
-6.19395937920066)) ;
#136099 = CARTESIAN_POINT('Ctrl Pts',(4.57729370999481,-2.80055804294518,
-6.1751759050806)) ;
#136100 = CARTESIAN_POINT('Ctrl Pts',(4.50667826286322,-2.80000000784871,
-6.12661464799816)) ;
#136101 = CARTESIAN_POINT('Ctrl Pts',(4.53037382014979,-2.79998899178918,
-6.1070846001167)) ;
#136102 = CARTESIAN_POINT('Ctrl Pts',(4.55348183854644,-2.81434699509192,
-6.09594660411389)) ;
#136103 = CARTESIAN_POINT('Ctrl Pts',(4.45692280158724,-2.80000001789831,
-5.99764221828758)) ;
#136104 = CARTESIAN_POINT('Ctrl Pts',(4.49938029267375,-2.79997354447564,
-5.98409988800932)) ;
#136105 = CARTESIAN_POINT('Ctrl Pts',(4.52864149761209,-2.83271033979016,
-5.9763290620799)) ;
#136106 = CARTESIAN_POINT('Ctrl Pts',(4.44554661086163,-2.80000002126189,
-5.95237744001399)) ;
#136107 = CARTESIAN_POINT('Ctrl Pts',(4.49333665154859,-2.7999679796365,-5.9400969398739)) ;
#136108 = CARTESIAN_POINT('Ctrl Pts',(4.52295544156363,-2.83885474437132,
-5.93396785822799)) ;
#136109 = CARTESIAN_POINT('Ctrl Pts',(4.41903322104337,-2.8000000307772,-5.81589479757718)) ;
#136110 = CARTESIAN_POINT('Ctrl Pts',(4.48100616080251,-2.79995095769182,
-5.80473000402043)) ;
#136111 = CARTESIAN_POINT('Ctrl Pts',(4.50969337368906,-2.85623179093886,
-5.80506962360893)) ;
#136112 = CARTESIAN_POINT('Ctrl Pts',(4.41147189908671,-2.8000000363501,-5.72424159004355)) ;
#136113 = CARTESIAN_POINT('Ctrl Pts',(4.48178828424061,-2.79993989905029,
-5.71578914920562)) ;
#136114 = CARTESIAN_POINT('Ctrl Pts',(4.50589025525746,-2.86640526991155,
-5.71696815120114)) ;
#136115 = CARTESIAN_POINT('Ctrl Pts',(4.39523119070919,-2.80000005228414,
-5.40317951983274)) ;
#136116 = CARTESIAN_POINT('Ctrl Pts',(4.4903383634593,-2.79990261688304,-5.38307413166043)) ;
#136117 = CARTESIAN_POINT('Ctrl Pts',(4.49769757367178,-2.8954773795302,-5.40433321576157)) ;
#136118 = CARTESIAN_POINT('Ctrl Pts',(4.40178225889351,-2.80000005718968,
-5.17262397828535)) ;
#136119 = CARTESIAN_POINT('Ctrl Pts',(4.50681341018205,-2.79988784121843,
-5.17705819882443)) ;
#136120 = CARTESIAN_POINT('Ctrl Pts',(4.50092255053473,-2.90441958896115,
-5.17244069603922)) ;
#136121 = CARTESIAN_POINT('Ctrl Pts',(4.39924589760307,-2.80000005405718,
-4.94303116887986)) ;
#136122 = CARTESIAN_POINT('Ctrl Pts',(4.49795607191426,-2.79989746608216,
-4.94392293749601)) ;
#136123 = CARTESIAN_POINT('Ctrl Pts',(4.49968270404899,-2.89870974459585,
-4.94302849459147)) ;
#136124 = CARTESIAN_POINT('Origin',(4.54879236168626,-2.9,-6.15643444348457)) ;
#136125 = CARTESIAN_POINT('Ctrl Pts',(4.57442492185553,-2.809397151199,-6.12275810686208)) ;
#136126 = CARTESIAN_POINT('Ctrl Pts',(4.56210583156796,-2.79989612750329,
-6.13894306178873)) ;
#136127 = CARTESIAN_POINT('Ctrl Pts',(4.54850917782856,-2.80000109307748,
-6.15680649348806)) ;
#136128 = CARTESIAN_POINT('Ctrl Pts',(4.57959763980855,-2.80818914940071,
-6.12994530049546)) ;
#136129 = CARTESIAN_POINT('Ctrl Pts',(4.56768008075465,-2.80031924975227,
-6.14394104572909)) ;
#136130 = CARTESIAN_POINT('Ctrl Pts',(4.55527876038347,-2.79999229227378,
-6.15958997638679)) ;
#136131 = CARTESIAN_POINT('Ctrl Pts',(4.58464248447265,-2.80630474344638,
-6.13748431263835)) ;
#136132 = CARTESIAN_POINT('Ctrl Pts',(4.57346944634371,-2.80008318972134,
-6.14920129105219)) ;
#136133 = CARTESIAN_POINT('Ctrl Pts',(4.56216307187793,-2.79941338753917,
-6.16232809153347)) ;
#136134 = CARTESIAN_POINT('Ctrl Pts',(4.59159231899494,-2.80232720646228,
-6.15005636929591)) ;
#136135 = CARTESIAN_POINT('Ctrl Pts',(4.58237910662986,-2.79850221241048,
-6.15791493625778)) ;
#136136 = CARTESIAN_POINT('Ctrl Pts',(4.57321634584968,-2.79769868647539,
-6.16666448649469)) ;
#136137 = CARTESIAN_POINT('Ctrl Pts',(4.59378564167737,-2.8008235544484,-6.15441458376545)) ;
#136138 = CARTESIAN_POINT('Ctrl Pts',(4.58533966160572,-2.79778056279966,
-6.16091806944782)) ;
#136139 = CARTESIAN_POINT('Ctrl Pts',(4.57696130093819,-2.79699227428059,
-6.16813207403618)) ;
#136140 = CARTESIAN_POINT('Ctrl Pts',(4.59669734138576,-2.79821861236081,
-6.16151744690911)) ;
#136141 = CARTESIAN_POINT('Ctrl Pts',(4.58989502505308,-2.79633072300511,
-6.16578370298497)) ;
#136142 = CARTESIAN_POINT('Ctrl Pts',(4.58314295739387,-2.79570785369251,
-6.17047890318142)) ;
#136143 = CARTESIAN_POINT('Ctrl Pts',(4.59760632414568,-2.79728965034655,
-6.16398524662906)) ;
#136144 = CARTESIAN_POINT('Ctrl Pts',(4.59142619397023,-2.79578507327358,
-6.16746789372295)) ;
#136145 = CARTESIAN_POINT('Ctrl Pts',(4.58528630332434,-2.79524119148169,
-6.17128737837496)) ;
#136146 = CARTESIAN_POINT('Ctrl Pts',(4.59875741430933,-2.79580683383093,
-6.16785300449597)) ;
#136147 = CARTESIAN_POINT('Ctrl Pts',(4.59383193680337,-2.79486773439436,
-6.17009800553386)) ;
#136148 = CARTESIAN_POINT('Ctrl Pts',(4.58892874314203,-2.79448758877844,
-6.17254647301294)) ;
#136149 = CARTESIAN_POINT('Ctrl Pts',(4.59910834609947,-2.79529718130591,
-6.16917149930145)) ;
#136150 = CARTESIAN_POINT('Ctrl Pts',(4.59464343907623,-2.79454543406795,
-6.17099269585011)) ;
#136151 = CARTESIAN_POINT('Ctrl Pts',(4.59019511689903,-2.79422790851556,
-6.17297467120907)) ;
#136152 = CARTESIAN_POINT('Ctrl Pts',(4.59954688679867,-2.79449699552073,
-6.17122938465871)) ;
#136153 = CARTESIAN_POINT('Ctrl Pts',(4.59601732089134,-2.79402779797774,
-6.17238633635183)) ;
#136154 = CARTESIAN_POINT('Ctrl Pts',(4.59249627585269,-2.79381771894921,
-6.17364111416749)) ;
#136155 = CARTESIAN_POINT('Ctrl Pts',(4.59967529310588,-2.79422450025963,
-6.17193546456122)) ;
#136156 = CARTESIAN_POINT('Ctrl Pts',(4.59651100242293,-2.79384821317134,
-6.17286441087348)) ;
#136157 = CARTESIAN_POINT('Ctrl Pts',(4.59335287412397,-2.79367727499394,
-6.17387144765739)) ;
#136158 = CARTESIAN_POINT('Ctrl Pts',(4.59980981518572,-2.79380630943631,
-6.17300564521014)) ;
#136159 = CARTESIAN_POINT('Ctrl Pts',(4.59701056623719,-2.79355888022806,
-6.17362493503647)) ;
#136160 = CARTESIAN_POINT('Ctrl Pts',(4.59421559911326,-2.79346462438277,
-6.17430302898986)) ;
#136161 = CARTESIAN_POINT('Ctrl Pts',(4.59984534134842,-2.79366726490194,
-6.17336460674889)) ;
#136162 = CARTESIAN_POINT('Ctrl Pts',(4.59705039509826,-2.79345667046144,
-6.17389173939615)) ;
#136163 = CARTESIAN_POINT('Ctrl Pts',(4.59425962044003,-2.79339574833516,
-6.17447656370425)) ;
#136164 = CARTESIAN_POINT('Ctrl Pts',(4.59992484646001,-2.7933873519883,-6.17407980383996)) ;
#136165 = CARTESIAN_POINT('Ctrl Pts',(4.5976165286321,-2.7932668237374,-6.17438058953102)) ;
#136166 = CARTESIAN_POINT('Ctrl Pts',(4.59531061070858,-2.79324678512396,
-6.17472041373345)) ;
#136167 = CARTESIAN_POINT('Ctrl Pts',(4.59996721368508,-2.79324340897637,
-6.17443656979399)) ;
#136168 = CARTESIAN_POINT('Ctrl Pts',(4.59680854952868,-2.79327323421044,
-6.17436047786158)) ;
#136169 = CARTESIAN_POINT('Ctrl Pts',(4.59356174266137,-2.79313094944462,
-6.17472348332067)) ;
#136170 = CARTESIAN_POINT('Ctrl Pts',(4.59999999999999,-2.79310344827586,
-6.17479364595777)) ;
#136171 = CARTESIAN_POINT('Ctrl Pts',(4.59999999999999,-2.79310344827586,
-6.17479364595777)) ;
#136172 = CARTESIAN_POINT('Ctrl Pts',(4.59999999999999,-2.79310344827586,
-6.17479364595777)) ;
#136173 = CARTESIAN_POINT('Origin',(8.6,4.09462794777298,-2.775)) ;
#136174 = CARTESIAN_POINT('Origin',(8.6,4.09462794777298,-2.775)) ;
#136175 = CARTESIAN_POINT('Origin',(8.6,4.09462794777298,-2.775)) ;
#136176 = CARTESIAN_POINT('Origin',(8.6,4.09462794777298,-1.475)) ;
#136177 = CARTESIAN_POINT('Origin',(8.6,4.09462794777298,-1.475)) ;
#136178 = CARTESIAN_POINT('Origin',(8.6,4.09462794777298,-1.475)) ;
#136179 = CARTESIAN_POINT('Origin',(8.6,3.95,-2.775)) ;
#136180 = CARTESIAN_POINT('Origin',(8.6,3.95,-2.775)) ;
#136181 = CARTESIAN_POINT('Origin',(8.6,4.09462794777298,-2.775)) ;
#136182 = CARTESIAN_POINT('Origin',(7.25334304318326,5.40585602606554,-2.775)) ;
#136183 = CARTESIAN_POINT('Origin',(7.25334304318326,5.40585602606554,-1.475)) ;
#136184 = CARTESIAN_POINT('Origin',(7.25334304318326,5.40585602606554,-1.475)) ;
#136185 = CARTESIAN_POINT('Origin',(8.6,5.40585602606554,-1.475)) ;
#136186 = CARTESIAN_POINT('Origin',(8.6,3.95,-1.475)) ;
#136187 = CARTESIAN_POINT('Origin',(8.6,3.95,-2.775)) ;
#136188 = CARTESIAN_POINT('Origin',(8.6,3.95,-2.775)) ;
#136189 = CARTESIAN_POINT('Origin',(7.25334304318326,5.40585602606554,-2.775)) ;
#136190 = CARTESIAN_POINT('Origin',(7.25334304318326,5.40585602606554,-2.775)) ;
#136191 = CARTESIAN_POINT('Origin',(7.25334304318326,5.40585602606554,-1.475)) ;
#136192 = CARTESIAN_POINT('Origin',(7.25334304318326,5.40585602606554,-1.475)) ;
#136193 = CARTESIAN_POINT('Origin',(8.6,3.95,-1.475)) ;
#136194 = CARTESIAN_POINT('Origin',(8.6,3.95,-1.475)) ;
#136195 = CARTESIAN_POINT('Origin',(7.36677829147199,4.5782099492339,-2.775)) ;
#136196 = CARTESIAN_POINT('Origin',(7.36677829147199,4.5782099492339,-2.775)) ;
#136197 = CARTESIAN_POINT('Origin',(7.25334304318326,5.40585602606554,-2.775)) ;
#136198 = CARTESIAN_POINT('Ctrl Pts',(4.03523814377473,5.98727788898885,-2.775)) ;
#136199 = CARTESIAN_POINT('Ctrl Pts',(4.03523814427722,5.98727788891385,-2.82947128016675)) ;
#136200 = CARTESIAN_POINT('Ctrl Pts',(4.04195902792202,5.94024173112809,-2.875)) ;
#136201 = CARTESIAN_POINT('Ctrl Pts',(4.05,5.88396692803319,-2.875)) ;
#136202 = CARTESIAN_POINT('Origin',(4.05,6.08618232569815,-2.875)) ;
#136203 = CARTESIAN_POINT('Origin',(4.05,6.08618232569815,-1.475)) ;
#136204 = CARTESIAN_POINT('Origin',(4.05,6.08618232569815,-2.775)) ;
#136205 = CARTESIAN_POINT('Origin',(7.25334304318326,5.40585602606554,-1.475)) ;
#136206 = CARTESIAN_POINT('Ctrl Pts',(4.05,5.88396692803319,-1.375)) ;
#136207 = CARTESIAN_POINT('Ctrl Pts',(4.04195902792202,5.94024173112809,-1.375)) ;
#136208 = CARTESIAN_POINT('Ctrl Pts',(4.03523814427722,5.98727788891385,-1.42052871983325)) ;
#136209 = CARTESIAN_POINT('Ctrl Pts',(4.03523814377473,5.98727788898885,-1.475)) ;
#136210 = CARTESIAN_POINT('Origin',(6.94197060168454,4.79460933256464,-1.475)) ;
#136211 = CARTESIAN_POINT('Origin',(7.36677829147199,4.5782099492339,-1.475)) ;
#136212 = CARTESIAN_POINT('Origin',(7.27599715910381,4.4,-2.775)) ;
#136213 = CARTESIAN_POINT('Origin',(7.27599715910381,4.6,-2.775)) ;
#136214 = CARTESIAN_POINT('Ctrl Pts',(3.95,6.08618232569815,-2.775)) ;
#136215 = CARTESIAN_POINT('Ctrl Pts',(3.95,6.,-2.775)) ;
#136216 = CARTESIAN_POINT('Ctrl Pts',(4.03523814377473,5.98727788898885,-2.775)) ;
#136217 = CARTESIAN_POINT('Ctrl Pts',(3.95,6.08618232225605,-2.88394256277222)) ;
#136218 = CARTESIAN_POINT('Ctrl Pts',(3.95,5.99999999675454,-2.838335940386)) ;
#136219 = CARTESIAN_POINT('Ctrl Pts',(4.03523814427722,5.98727788891385,-2.82947128016675)) ;
#136220 = CARTESIAN_POINT('Ctrl Pts',(3.95,5.99411624638818,-2.97499999670621)) ;
#136221 = CARTESIAN_POINT('Ctrl Pts',(3.94999999999981,5.93865134487241,-2.88281389783655)) ;
#136222 = CARTESIAN_POINT('Ctrl Pts',(4.04195902792202,5.94024173112809,-2.875)) ;
#136223 = CARTESIAN_POINT('Ctrl Pts',(3.95,5.88396692803319,-2.975)) ;
#136224 = CARTESIAN_POINT('Ctrl Pts',(3.95,5.8839669280332,-2.875)) ;
#136225 = CARTESIAN_POINT('Ctrl Pts',(4.05,5.88396692803319,-2.875)) ;
#136226 = CARTESIAN_POINT('Origin',(4.05,5.88396692803319,-2.975)) ;
#136227 = CARTESIAN_POINT('Ctrl Pts',(3.95,5.88396692803319,-1.275)) ;
#136228 = CARTESIAN_POINT('Ctrl Pts',(3.95,5.8839669280332,-1.375)) ;
#136229 = CARTESIAN_POINT('Ctrl Pts',(4.05,5.88396692803319,-1.375)) ;
#136230 = CARTESIAN_POINT('Ctrl Pts',(3.95,5.99411624638819,-1.27500000329373)) ;
#136231 = CARTESIAN_POINT('Ctrl Pts',(3.95,5.9386513448724,-1.36718610216324)) ;
#136232 = CARTESIAN_POINT('Ctrl Pts',(4.04195902792202,5.94024173112809,-1.375)) ;
#136233 = CARTESIAN_POINT('Ctrl Pts',(3.95,6.08618232225605,-1.36605743722782)) ;
#136234 = CARTESIAN_POINT('Ctrl Pts',(3.95,5.99999999675454,-1.41166405961416)) ;
#136235 = CARTESIAN_POINT('Ctrl Pts',(4.03523814427722,5.98727788891385,-1.42052871983325)) ;
#136236 = CARTESIAN_POINT('Ctrl Pts',(3.95,6.08618232569815,-1.475)) ;
#136237 = CARTESIAN_POINT('Ctrl Pts',(3.95,6.,-1.475)) ;
#136238 = CARTESIAN_POINT('Ctrl Pts',(4.03523814377473,5.98727788898885,-1.475)) ;
#136239 = CARTESIAN_POINT('Origin',(4.05,5.88396692803319,-1.275)) ;
#136240 = CARTESIAN_POINT('Origin',(7.27599715910381,4.4,-1.475)) ;
#136241 = CARTESIAN_POINT('Origin',(7.27599715910381,4.6,-1.475)) ;
#136242 = CARTESIAN_POINT('Origin',(3.95,4.6,-2.775)) ;
#136243 = CARTESIAN_POINT('Origin',(4.05,4.6,-2.775)) ;
#136244 = CARTESIAN_POINT('Origin',(4.05,3.75,-2.975)) ;
#136245 = CARTESIAN_POINT('Origin',(4.05,4.6,-2.975)) ;
#136246 = CARTESIAN_POINT('Origin',(4.05,5.40585602606554,-1.275)) ;
#136247 = CARTESIAN_POINT('Origin',(4.05,4.6,-1.275)) ;
#136248 = CARTESIAN_POINT('Origin',(7.25334304318326,4.6,-1.475)) ;
#136249 = CARTESIAN_POINT('Origin',(4.05,4.6,-1.475)) ;
#136250 = CARTESIAN_POINT('Origin',(4.05,4.6,-2.775)) ;
#136251 = CARTESIAN_POINT('Origin',(4.05,4.4,-2.775)) ;
#136252 = CARTESIAN_POINT('Origin',(4.05,4.6,-1.475)) ;
#136253 = CARTESIAN_POINT('Origin',(4.05,4.4,-1.475)) ;
#136254 = CARTESIAN_POINT('Origin',(4.05,4.4,2.54)) ;
#136255 = CARTESIAN_POINT('Origin',(4.6,2.65,-16.7330460421716)) ;
#136256 = CARTESIAN_POINT('',(4.5,2.61712020253893,-16.5357672574052)) ;
#136257 = CARTESIAN_POINT('',(4.5,2.72431432344521,-16.547365183355)) ;
#136258 = CARTESIAN_POINT('Origin',(4.5,2.65,-16.7330460421716)) ;
#136259 = CARTESIAN_POINT('',(4.6,2.63356010126946,-16.6344066497884)) ;
#136260 = CARTESIAN_POINT('Origin',(4.6,2.61712020253893,-16.5357672574052)) ;
#136261 = CARTESIAN_POINT('',(4.6,2.68715716172261,-16.6402056127633)) ;
#136262 = CARTESIAN_POINT('Origin',(4.6,2.65,-16.7330460421716)) ;
#136263 = CARTESIAN_POINT('Origin',(4.6,2.72431432344521,-16.547365183355)) ;
#136264 = CARTESIAN_POINT('Origin',(0.,10.85,-15.24)) ;
#136265 = CARTESIAN_POINT('',(-2.44929359829471E-16,10.95,-13.24)) ;
#136266 = CARTESIAN_POINT('Origin',(0.,10.95,-15.24)) ;
#136267 = CARTESIAN_POINT('',(-2.32682891837997E-16,10.85,-13.34)) ;
#136268 = CARTESIAN_POINT('Origin',(-2.44929359829471E-16,10.85,-13.24)) ;
#136269 = CARTESIAN_POINT('',(2.32682891837997E-16,10.85,-17.14)) ;
#136270 = CARTESIAN_POINT('Origin',(0.,10.85,-15.24)) ;
#136271 = CARTESIAN_POINT('Origin',(0.,10.85,-15.24)) ;
#136272 = CARTESIAN_POINT('Origin',(11.0914213562373,0.,-15.24)) ;
#136273 = CARTESIAN_POINT('',(11.0207106781187,-1.80110112442985E-16,-13.7692893218813)) ;
#136274 = CARTESIAN_POINT('Origin',(11.0207106781187,0.,-15.24)) ;
#136275 = CARTESIAN_POINT('',(11.0914213562373,-1.83697019872103E-16,-13.74)) ;
#136276 = CARTESIAN_POINT('Origin',(11.0914213562373,-1.7145055188063E-16,
-13.84)) ;
#136277 = CARTESIAN_POINT('Origin',(11.0914213562373,0.,-15.24)) ;
#136278 = CARTESIAN_POINT('Origin',(12.7,0.,-15.24)) ;
#136279 = CARTESIAN_POINT('',(12.8,-1.95943487863577E-16,-16.84)) ;
#136280 = CARTESIAN_POINT('Origin',(12.8,0.,-15.24)) ;
#136281 = CARTESIAN_POINT('',(12.7,-1.83697019872103E-16,-16.74)) ;
#136282 = CARTESIAN_POINT('Origin',(12.7,-1.95943487863577E-16,-16.84)) ;
#136283 = CARTESIAN_POINT('',(12.7,1.83697019872103E-16,-13.74)) ;
#136284 = CARTESIAN_POINT('Origin',(12.7,0.,-15.24)) ;
#136285 = CARTESIAN_POINT('Origin',(12.7,0.,-15.24)) ;
#136286 = CARTESIAN_POINT('Origin',(12.7,2.1,-13.8580460421716)) ;
#136287 = CARTESIAN_POINT('',(12.7,2.,-13.8580460421716)) ;
#136288 = CARTESIAN_POINT('',(12.7,2.11643989873054,-13.7594066497884)) ;
#136289 = CARTESIAN_POINT('Origin',(12.7,2.1,-13.8580460421716)) ;
#136290 = CARTESIAN_POINT('',(12.8,2.13287979746107,-13.6607672574052)) ;
#136291 = CARTESIAN_POINT('Origin',(12.7,2.13287979746107,-13.6607672574052)) ;
#136292 = CARTESIAN_POINT('',(12.8,1.9,-13.8580460421716)) ;
#136293 = CARTESIAN_POINT('Origin',(12.8,2.1,-13.8580460421716)) ;
#136294 = CARTESIAN_POINT('Origin',(12.7,1.9,-13.8580460421716)) ;
#136295 = CARTESIAN_POINT('Origin',(12.7,2.65,-13.7469539578284)) ;
#136296 = CARTESIAN_POINT('',(12.7,2.63356010126947,-13.8455933502116)) ;
#136297 = CARTESIAN_POINT('',(12.7,2.75,-13.7469539578284)) ;
#136298 = CARTESIAN_POINT('Origin',(12.7,2.65,-13.7469539578284)) ;
#136299 = CARTESIAN_POINT('',(12.8,2.65,-13.7469539578284)) ;
#136300 = CARTESIAN_POINT('Origin',(12.7,2.65,-13.7469539578284)) ;
#136301 = CARTESIAN_POINT('Origin',(12.7,2.65,-13.7469539578284)) ;
#136302 = CARTESIAN_POINT('Origin',(4.5,2.1,-13.8580460421716)) ;
#136303 = CARTESIAN_POINT('',(4.6,2.,-13.8580460421716)) ;
#136304 = CARTESIAN_POINT('',(12.8,2.,-13.8580460421716)) ;
#136305 = CARTESIAN_POINT('',(4.6,2.11643989873054,-13.7594066497884)) ;
#136306 = CARTESIAN_POINT('Origin',(4.6,2.1,-13.8580460421716)) ;
#136307 = CARTESIAN_POINT('',(4.5,2.11643989873054,-13.7594066497884)) ;
#136308 = CARTESIAN_POINT('Origin',(12.7,2.65,-16.7330460421716)) ;
#136309 = CARTESIAN_POINT('',(12.8,2.65,-16.7330460421716)) ;
#136310 = CARTESIAN_POINT('',(12.7,2.63356010126947,-16.6344066497884)) ;
#136311 = CARTESIAN_POINT('Origin',(12.7,2.65,-16.7330460421716)) ;
#136312 = CARTESIAN_POINT('',(12.7,2.75,-16.7330460421716)) ;
#136313 = CARTESIAN_POINT('Origin',(12.7,2.65,-16.7330460421716)) ;
#136314 = CARTESIAN_POINT('Origin',(12.7,2.65,-16.7330460421716)) ;
#136315 = CARTESIAN_POINT('Origin',(11.05,0.,-15.24)) ;
#136316 = CARTESIAN_POINT('',(10.3,-9.18485099360511E-17,-14.49)) ;
#136317 = CARTESIAN_POINT('Origin',(10.3,0.,-15.24)) ;
#136318 = CARTESIAN_POINT('',(11.05,-1.83697019872103E-16,-13.74)) ;
#136319 = CARTESIAN_POINT('Origin',(11.05,0.,-15.24)) ;
#136320 = CARTESIAN_POINT('',(11.05,-1.83697019872103E-16,-13.74)) ;
#136321 = CARTESIAN_POINT('Origin',(0.,9.95,-15.24)) ;
#136322 = CARTESIAN_POINT('',(0.218101234104781,9.95,-17.1274405558009)) ;
#136323 = CARTESIAN_POINT('',(-2.32682891837997E-16,9.95,-17.14)) ;
#136324 = CARTESIAN_POINT('Origin',(0.,9.95,-15.24)) ;
#136325 = CARTESIAN_POINT('',(0.321518176280636,9.85,-17.1125987456797)) ;
#136326 = CARTESIAN_POINT('Ctrl Pts',(0.21810123410477,9.95,-17.1274405558009)) ;
#136327 = CARTESIAN_POINT('Ctrl Pts',(0.231193919344567,9.95,-17.1259276441493)) ;
#136328 = CARTESIAN_POINT('Ctrl Pts',(0.245192892440011,9.94751445938575,
-17.1241565825739)) ;
#136329 = CARTESIAN_POINT('Ctrl Pts',(0.270990685773149,9.93716996065971,
-17.1206215789467)) ;
#136330 = CARTESIAN_POINT('Ctrl Pts',(0.282791986325031,9.92931613918426,
-17.1188607093668)) ;
#136331 = CARTESIAN_POINT('Ctrl Pts',(0.300953024019383,9.91135900604096,
-17.1160350266619)) ;
#136332 = CARTESIAN_POINT('Ctrl Pts',(0.308688523153902,9.90025653083842,
-17.114762561801)) ;
#136333 = CARTESIAN_POINT('Ctrl Pts',(0.318969164829191,9.87583423571802,
-17.1130429866749)) ;
#136334 = CARTESIAN_POINT('Ctrl Pts',(0.321518176280625,9.86251584266313,
-17.1125987456797)) ;
#136335 = CARTESIAN_POINT('Ctrl Pts',(0.321518176280625,9.85,-17.1125987456797)) ;
#136336 = CARTESIAN_POINT('',(0.321518176280636,9.05,-17.1125987456797)) ;
#136337 = CARTESIAN_POINT('',(0.321518176280636,8.95,-17.1125987456797)) ;
#136338 = CARTESIAN_POINT('',(0.422455466606969,8.95,-17.0924393050067)) ;
#136339 = CARTESIAN_POINT('Ctrl Pts',(0.321518176280627,9.05,-17.1125987456797)) ;
#136340 = CARTESIAN_POINT('Ctrl Pts',(0.321518176280627,9.03744936090869,
-17.1125987456797)) ;
#136341 = CARTESIAN_POINT('Ctrl Pts',(0.324085473150902,9.02409774280079,
-17.1121645622427)) ;
#136342 = CARTESIAN_POINT('Ctrl Pts',(0.334387313650431,8.99960748025859,
-17.1103498579077)) ;
#136343 = CARTESIAN_POINT('Ctrl Pts',(0.34212249945656,8.98846937989492,-17.1089656420615)) ;
#136344 = CARTESIAN_POINT('Ctrl Pts',(0.360004521225388,8.97064401154629,
-17.1056049780795)) ;
#136345 = CARTESIAN_POINT('Ctrl Pts',(0.371447108749463,8.96285745107738,
-17.1033820840476)) ;
#136346 = CARTESIAN_POINT('Ctrl Pts',(0.39637397952969,8.95253508546271,-17.0982373032789)) ;
#136347 = CARTESIAN_POINT('Ctrl Pts',(0.409857901997321,8.95,-17.0953122250646)) ;
#136348 = CARTESIAN_POINT('Ctrl Pts',(0.422455466606959,8.95,-17.0924393050067)) ;
#136349 = CARTESIAN_POINT('',(1.14750169623629,8.95,-16.7543446956142)) ;
#136350 = CARTESIAN_POINT('Origin',(0.,8.95,-15.24)) ;
#136351 = CARTESIAN_POINT('',(1.22782596331729,9.05,-16.689980483939)) ;
#136352 = CARTESIAN_POINT('Ctrl Pts',(1.1475016962363,8.95,-16.7543446956142)) ;
#136353 = CARTESIAN_POINT('Ctrl Pts',(1.15780003912543,8.95,-16.7465410786649)) ;
#136354 = CARTESIAN_POINT('Ctrl Pts',(1.16870807732935,8.95253508546271,-16.7380919988207)) ;
#136355 = CARTESIAN_POINT('Ctrl Pts',(1.18867189173409,8.96285745107738,-16.7223039093078)) ;
#136356 = CARTESIAN_POINT('Ctrl Pts',(1.19772988083811,8.97064401154629,-16.7149672274615)) ;
#136357 = CARTESIAN_POINT('Ctrl Pts',(1.21179864083582,8.98846937989492,-16.7034289972216)) ;
#136358 = CARTESIAN_POINT('Ctrl Pts',(1.21783109328768,8.99960748025859,-16.6983932579134)) ;
#136359 = CARTESIAN_POINT('Ctrl Pts',(1.22584313288947,9.02409774280079,-16.6916680597067)) ;
#136360 = CARTESIAN_POINT('Ctrl Pts',(1.22782596331729,9.03744936090869,-16.689980483939)) ;
#136361 = CARTESIAN_POINT('Ctrl Pts',(1.22782596331729,9.05,-16.689980483939)) ;
#136362 = CARTESIAN_POINT('',(1.22782596331729,9.85,-16.689980483939)) ;
#136363 = CARTESIAN_POINT('',(1.22782596331729,8.95,-16.689980483939)) ;
#136364 = CARTESIAN_POINT('',(1.30567057854876,9.95,-16.6202986417121)) ;
#136365 = CARTESIAN_POINT('Ctrl Pts',(1.2278259633173,9.85,-16.689980483939)) ;
#136366 = CARTESIAN_POINT('Ctrl Pts',(1.2278259633173,9.85579162428539,-16.689980483939)) ;
#136367 = CARTESIAN_POINT('Ctrl Pts',(1.22822745887819,9.86162764920013,-16.6896405714653)) ;
#136368 = CARTESIAN_POINT('Ctrl Pts',(1.22902753823172,9.86736607146311,-16.6889619546779)) ;
#136369 = CARTESIAN_POINT('Ctrl Pts',(1.22973095933686,9.87241123018667,-16.6883653221458)) ;
#136370 = CARTESIAN_POINT('Ctrl Pts',(1.23074168751921,9.87738020477702,-16.6875074302535)) ;
#136371 = CARTESIAN_POINT('Ctrl Pts',(1.23203099150183,9.88218322835582,-16.6864092214793)) ;
#136372 = CARTESIAN_POINT('Ctrl Pts',(1.23351897101726,9.88772637473068,-16.6851417840233)) ;
#136373 = CARTESIAN_POINT('Ctrl Pts',(1.2354014557903,9.89313280655104,-16.6835343365783)) ;
#136374 = CARTESIAN_POINT('Ctrl Pts',(1.23763252770622,9.89827011881554,-16.6816189827484)) ;
#136375 = CARTESIAN_POINT('Ctrl Pts',(1.23953000874363,9.90263929783464,-16.6799900134865)) ;
#136376 = CARTESIAN_POINT('Ctrl Pts',(1.24167862345461,9.90681364346946,-16.6781390311988)) ;
#136377 = CARTESIAN_POINT('Ctrl Pts',(1.24403025306867,9.91072825704925,-16.6761019216791)) ;
#136378 = CARTESIAN_POINT('Ctrl Pts',(1.24687926059923,9.91547082513965,-16.6736339563467)) ;
#136379 = CARTESIAN_POINT('Ctrl Pts',(1.25006974298106,9.91990270163234,-16.6708551265321)) ;
#136380 = CARTESIAN_POINT('Ctrl Pts',(1.2535194093265,9.92391762881321,-16.6678266146309)) ;
#136381 = CARTESIAN_POINT('Ctrl Pts',(1.25634620505522,9.92720762206749,-16.665344929839)) ;
#136382 = CARTESIAN_POINT('Ctrl Pts',(1.25934609941473,9.93021806933732,-16.6626963101588)) ;
#136383 = CARTESIAN_POINT('Ctrl Pts',(1.26246241000316,9.93291206679729,-16.6599255837293)) ;
#136384 = CARTESIAN_POINT('Ctrl Pts',(1.26649145911189,9.93639511117203,-16.6563433371803)) ;
#136385 = CARTESIAN_POINT('Ctrl Pts',(1.27077652588474,9.93940081548805,-16.6525022625241)) ;
#136386 = CARTESIAN_POINT('Ctrl Pts',(1.27520851369617,9.94185862744775,-16.6484896739102)) ;
#136387 = CARTESIAN_POINT('Ctrl Pts',(1.27864718185097,9.94376558208659,-16.6453764070711)) ;
#136388 = CARTESIAN_POINT('Ctrl Pts',(1.28217366418729,9.94534362661778,-16.6421604997622)) ;
#136389 = CARTESIAN_POINT('Ctrl Pts',(1.28573335778226,9.94658081625577,-16.6388887492202)) ;
#136390 = CARTESIAN_POINT('Ctrl Pts',(1.29026904082682,9.94815721599755,-16.6347199568611)) ;
#136391 = CARTESIAN_POINT('Ctrl Pts',(1.29492021413416,9.9491996901822,-16.6304036518226)) ;
#136392 = CARTESIAN_POINT('Ctrl Pts',(1.29957290046268,9.9496832238817,-16.6260412243875)) ;
#136393 = CARTESIAN_POINT('Ctrl Pts',(1.30160833994481,9.94989475836166,-16.6241327662598)) ;
#136394 = CARTESIAN_POINT('Ctrl Pts',(1.30364403319568,9.95,-16.6222156186355)) ;
#136395 = CARTESIAN_POINT('Ctrl Pts',(1.30567057854874,9.95,-16.6202986417121)) ;
#136396 = CARTESIAN_POINT('',(-0.218101234104782,9.95,-13.3525594441991)) ;
#136397 = CARTESIAN_POINT('Origin',(0.,9.95,-15.24)) ;
#136398 = CARTESIAN_POINT('',(-0.321518176280637,9.85,-13.3674012543203)) ;
#136399 = CARTESIAN_POINT('Ctrl Pts',(-0.218101234104768,9.95,-13.3525594441991)) ;
#136400 = CARTESIAN_POINT('Ctrl Pts',(-0.231193919344566,9.95,-13.3540723558507)) ;
#136401 = CARTESIAN_POINT('Ctrl Pts',(-0.245192892440009,9.94751445938575,
-13.3558434174261)) ;
#136402 = CARTESIAN_POINT('Ctrl Pts',(-0.270990685773146,9.93716996065971,
-13.3593784210533)) ;
#136403 = CARTESIAN_POINT('Ctrl Pts',(-0.282791986325029,9.92931613918426,
-13.3611392906332)) ;
#136404 = CARTESIAN_POINT('Ctrl Pts',(-0.300953024019382,9.91135900604096,
-13.3639649733381)) ;
#136405 = CARTESIAN_POINT('Ctrl Pts',(-0.308688523153901,9.90025653083842,
-13.365237438199)) ;
#136406 = CARTESIAN_POINT('Ctrl Pts',(-0.31896916482919,9.87583423571802,
-13.3669570133251)) ;
#136407 = CARTESIAN_POINT('Ctrl Pts',(-0.321518176280622,9.86251584266313,
-13.3674012543203)) ;
#136408 = CARTESIAN_POINT('Ctrl Pts',(-0.321518176280622,9.85,-13.3674012543203)) ;
#136409 = CARTESIAN_POINT('',(-0.321518176280637,9.05,-13.3674012543203)) ;
#136410 = CARTESIAN_POINT('',(-0.321518176280637,8.95,-13.3674012543203)) ;
#136411 = CARTESIAN_POINT('',(-0.422455466606969,8.95,-13.3875606949933)) ;
#136412 = CARTESIAN_POINT('Ctrl Pts',(-0.321518176280627,9.05,-13.3674012543203)) ;
#136413 = CARTESIAN_POINT('Ctrl Pts',(-0.321518176280627,9.03744936090869,
-13.3674012543203)) ;
#136414 = CARTESIAN_POINT('Ctrl Pts',(-0.324085473150903,9.02409774280079,
-13.3678354377573)) ;
#136415 = CARTESIAN_POINT('Ctrl Pts',(-0.334387313650432,8.99960748025859,
-13.3696501420923)) ;
#136416 = CARTESIAN_POINT('Ctrl Pts',(-0.342122499456561,8.98846937989492,
-13.3710343579385)) ;
#136417 = CARTESIAN_POINT('Ctrl Pts',(-0.360004521225389,8.97064401154629,
-13.3743950219205)) ;
#136418 = CARTESIAN_POINT('Ctrl Pts',(-0.371447108749464,8.96285745107738,
-13.3766179159524)) ;
#136419 = CARTESIAN_POINT('Ctrl Pts',(-0.396373979529691,8.95253508546271,
-13.3817626967211)) ;
#136420 = CARTESIAN_POINT('Ctrl Pts',(-0.409857901997322,8.95,-13.3846877749354)) ;
#136421 = CARTESIAN_POINT('Ctrl Pts',(-0.42245546660696,8.95,-13.3875606949933)) ;
#136422 = CARTESIAN_POINT('',(-1.14750169623629,8.95,-13.7256553043858)) ;
#136423 = CARTESIAN_POINT('Origin',(0.,8.95,-15.24)) ;
#136424 = CARTESIAN_POINT('',(-1.22782596331729,9.05,-13.790019516061)) ;
#136425 = CARTESIAN_POINT('Ctrl Pts',(-1.1475016962363,8.95,-13.7256553043858)) ;
#136426 = CARTESIAN_POINT('Ctrl Pts',(-1.15780003912543,8.95,-13.7334589213351)) ;
#136427 = CARTESIAN_POINT('Ctrl Pts',(-1.16870807732935,8.95253508546271,
-13.7419080011793)) ;
#136428 = CARTESIAN_POINT('Ctrl Pts',(-1.18867189173409,8.96285745107738,
-13.7576960906922)) ;
#136429 = CARTESIAN_POINT('Ctrl Pts',(-1.19772988083812,8.97064401154629,
-13.7650327725385)) ;
#136430 = CARTESIAN_POINT('Ctrl Pts',(-1.21179864083582,8.98846937989492,
-13.7765710027784)) ;
#136431 = CARTESIAN_POINT('Ctrl Pts',(-1.21783109328768,8.99960748025859,
-13.7816067420866)) ;
#136432 = CARTESIAN_POINT('Ctrl Pts',(-1.22584313288947,9.02409774280079,
-13.7883319402933)) ;
#136433 = CARTESIAN_POINT('Ctrl Pts',(-1.22782596331729,9.03744936090869,
-13.790019516061)) ;
#136434 = CARTESIAN_POINT('Ctrl Pts',(-1.22782596331729,9.05,-13.790019516061)) ;
#136435 = CARTESIAN_POINT('',(-1.22782596331729,9.85,-13.790019516061)) ;
#136436 = CARTESIAN_POINT('',(-1.22782596331729,8.95,-13.790019516061)) ;
#136437 = CARTESIAN_POINT('',(-1.30567057854876,9.95,-13.8597013582879)) ;
#136438 = CARTESIAN_POINT('Ctrl Pts',(-1.2278259633173,9.85,-13.790019516061)) ;
#136439 = CARTESIAN_POINT('Ctrl Pts',(-1.2278259633173,9.85579162428539,-13.790019516061)) ;
#136440 = CARTESIAN_POINT('Ctrl Pts',(-1.22822745887819,9.86162764920014,
-13.7903594285347)) ;
#136441 = CARTESIAN_POINT('Ctrl Pts',(-1.22902753823172,9.86736607146313,
-13.7910380453221)) ;
#136442 = CARTESIAN_POINT('Ctrl Pts',(-1.22973095933686,9.87241123018668,
-13.7916346778542)) ;
#136443 = CARTESIAN_POINT('Ctrl Pts',(-1.23074168751921,9.87738020477702,
-13.7924925697465)) ;
#136444 = CARTESIAN_POINT('Ctrl Pts',(-1.23203099150183,9.88218322835582,
-13.7935907785207)) ;
#136445 = CARTESIAN_POINT('Ctrl Pts',(-1.23351897101726,9.88772637473068,
-13.7948582159767)) ;
#136446 = CARTESIAN_POINT('Ctrl Pts',(-1.23540145579029,9.89313280655104,
-13.7964656634217)) ;
#136447 = CARTESIAN_POINT('Ctrl Pts',(-1.23763252770621,9.89827011881554,
-13.7983810172516)) ;
#136448 = CARTESIAN_POINT('Ctrl Pts',(-1.23953000874362,9.90263929783464,
-13.8000099865135)) ;
#136449 = CARTESIAN_POINT('Ctrl Pts',(-1.24167862345461,9.90681364346945,
-13.8018609688012)) ;
#136450 = CARTESIAN_POINT('Ctrl Pts',(-1.24403025306867,9.91072825704925,
-13.8038980783209)) ;
#136451 = CARTESIAN_POINT('Ctrl Pts',(-1.24687926059924,9.91547082513966,
-13.8063660436533)) ;
#136452 = CARTESIAN_POINT('Ctrl Pts',(-1.25006974298107,9.91990270163235,
-13.8091448734679)) ;
#136453 = CARTESIAN_POINT('Ctrl Pts',(-1.25351940932651,9.92391762881324,
-13.8121733853692)) ;
#136454 = CARTESIAN_POINT('Ctrl Pts',(-1.25634620505522,9.92720762206753,
-13.8146550701611)) ;
#136455 = CARTESIAN_POINT('Ctrl Pts',(-1.25934609941473,9.93021806933732,
-13.8173036898412)) ;
#136456 = CARTESIAN_POINT('Ctrl Pts',(-1.26246241000317,9.93291206679729,
-13.8200744162707)) ;
#136457 = CARTESIAN_POINT('Ctrl Pts',(-1.26649145911189,9.93639511117203,
-13.8236566628197)) ;
#136458 = CARTESIAN_POINT('Ctrl Pts',(-1.27077652588473,9.93940081548805,
-13.827497737476)) ;
#136459 = CARTESIAN_POINT('Ctrl Pts',(-1.27520851369616,9.94185862744775,
-13.8315103260898)) ;
#136460 = CARTESIAN_POINT('Ctrl Pts',(-1.27864718185096,9.94376558208659,
-13.8346235929289)) ;
#136461 = CARTESIAN_POINT('Ctrl Pts',(-1.28217366418729,9.94534362661778,
-13.8378395002378)) ;
#136462 = CARTESIAN_POINT('Ctrl Pts',(-1.28573335778226,9.94658081625577,
-13.8411112507798)) ;
#136463 = CARTESIAN_POINT('Ctrl Pts',(-1.29026904082682,9.94815721599755,
-13.8452800431389)) ;
#136464 = CARTESIAN_POINT('Ctrl Pts',(-1.29492021413416,9.9491996901822,-13.8495963481774)) ;
#136465 = CARTESIAN_POINT('Ctrl Pts',(-1.29957290046264,9.9496832238817,-13.8539587756125)) ;
#136466 = CARTESIAN_POINT('Ctrl Pts',(-1.30160833994476,9.94989475836165,
-13.8558672337401)) ;
#136467 = CARTESIAN_POINT('Ctrl Pts',(-1.30364403319568,9.95,-13.8577843813645)) ;
#136468 = CARTESIAN_POINT('Ctrl Pts',(-1.30567057854874,9.95,-13.8597013582879)) ;
#136469 = CARTESIAN_POINT('Origin',(0.,9.95,-15.24)) ;
#136470 = CARTESIAN_POINT('',(-2.32682891837997E-16,9.95,-17.14)) ;
#136471 = CARTESIAN_POINT('Origin',(4.6,2.65,-21.8130460421716)) ;
#136472 = CARTESIAN_POINT('',(4.5,2.61712020253893,-21.6157672574052)) ;
#136473 = CARTESIAN_POINT('',(4.5,2.72431432344521,-21.627365183355)) ;
#136474 = CARTESIAN_POINT('Origin',(4.5,2.65,-21.8130460421716)) ;
#136475 = CARTESIAN_POINT('',(4.6,2.63356010126946,-21.7144066497884)) ;
#136476 = CARTESIAN_POINT('Origin',(4.6,2.61712020253893,-21.6157672574052)) ;
#136477 = CARTESIAN_POINT('',(4.6,2.68715716172261,-21.7202056127633)) ;
#136478 = CARTESIAN_POINT('Origin',(4.6,2.65,-21.8130460421716)) ;
#136479 = CARTESIAN_POINT('Origin',(4.6,2.72431432344521,-21.627365183355)) ;
#136480 = CARTESIAN_POINT('Origin',(-4.52198039027186,10.1,-17.78)) ;
#136481 = CARTESIAN_POINT('',(-4.42392232270277,10.0803883864862,-22.86)) ;
#136482 = CARTESIAN_POINT('',(-4.52198039027186,10.2,-22.86)) ;
#136483 = CARTESIAN_POINT('Origin',(-4.52198039027186,10.1,-22.86)) ;
#136484 = CARTESIAN_POINT('',(-4.42392232270277,10.0803883864862,-12.7)) ;
#136485 = CARTESIAN_POINT('',(-4.42392232270277,10.0803883864862,-22.86)) ;
#136486 = CARTESIAN_POINT('',(-4.52198039027186,10.2,-12.7)) ;
#136487 = CARTESIAN_POINT('Origin',(-4.52198039027186,10.1,-12.7)) ;
#136488 = CARTESIAN_POINT('',(-4.52198039027186,10.2,-17.78)) ;
#136489 = CARTESIAN_POINT('Origin',(0.,10.85,-20.32)) ;
#136490 = CARTESIAN_POINT('',(-2.44929359829471E-16,10.95,-18.32)) ;
#136491 = CARTESIAN_POINT('Origin',(0.,10.95,-20.32)) ;
#136492 = CARTESIAN_POINT('',(-2.32682891837997E-16,10.85,-18.42)) ;
#136493 = CARTESIAN_POINT('Origin',(-2.44929359829471E-16,10.85,-18.32)) ;
#136494 = CARTESIAN_POINT('',(2.32682891837997E-16,10.85,-22.22)) ;
#136495 = CARTESIAN_POINT('Origin',(0.,10.85,-20.32)) ;
#136496 = CARTESIAN_POINT('Origin',(0.,10.85,-20.32)) ;
#136497 = CARTESIAN_POINT('Origin',(11.0914213562373,0.,-20.32)) ;
#136498 = CARTESIAN_POINT('',(11.0207106781187,-1.80110112442985E-16,-18.8492893218813)) ;
#136499 = CARTESIAN_POINT('Origin',(11.0207106781187,0.,-20.32)) ;
#136500 = CARTESIAN_POINT('',(11.0914213562373,-1.83697019872103E-16,-18.82)) ;
#136501 = CARTESIAN_POINT('Origin',(11.0914213562373,-1.7145055188063E-16,
-18.92)) ;
#136502 = CARTESIAN_POINT('Origin',(11.0914213562373,0.,-20.32)) ;
#136503 = CARTESIAN_POINT('Origin',(12.7,0.,-20.32)) ;
#136504 = CARTESIAN_POINT('',(12.8,-1.95943487863577E-16,-21.92)) ;
#136505 = CARTESIAN_POINT('Origin',(12.8,0.,-20.32)) ;
#136506 = CARTESIAN_POINT('',(12.7,-1.83697019872103E-16,-21.82)) ;
#136507 = CARTESIAN_POINT('Origin',(12.7,-1.95943487863577E-16,-21.92)) ;
#136508 = CARTESIAN_POINT('',(12.7,1.83697019872103E-16,-18.82)) ;
#136509 = CARTESIAN_POINT('Origin',(12.7,0.,-20.32)) ;
#136510 = CARTESIAN_POINT('Origin',(12.7,0.,-20.32)) ;
#136511 = CARTESIAN_POINT('Origin',(12.7,2.1,-18.9380460421716)) ;
#136512 = CARTESIAN_POINT('',(12.7,2.,-18.9380460421716)) ;
#136513 = CARTESIAN_POINT('',(12.7,2.11643989873054,-18.8394066497884)) ;
#136514 = CARTESIAN_POINT('Origin',(12.7,2.1,-18.9380460421716)) ;
#136515 = CARTESIAN_POINT('',(12.8,2.13287979746107,-18.7407672574052)) ;
#136516 = CARTESIAN_POINT('Origin',(12.7,2.13287979746107,-18.7407672574052)) ;
#136517 = CARTESIAN_POINT('',(12.8,1.9,-18.9380460421716)) ;
#136518 = CARTESIAN_POINT('Origin',(12.8,2.1,-18.9380460421716)) ;
#136519 = CARTESIAN_POINT('Origin',(12.7,1.9,-18.9380460421716)) ;
#136520 = CARTESIAN_POINT('Origin',(12.7,2.65,-18.8269539578284)) ;
#136521 = CARTESIAN_POINT('',(12.7,2.63356010126947,-18.9255933502116)) ;
#136522 = CARTESIAN_POINT('',(12.7,2.75,-18.8269539578284)) ;
#136523 = CARTESIAN_POINT('Origin',(12.7,2.65,-18.8269539578284)) ;
#136524 = CARTESIAN_POINT('',(12.8,2.65,-18.8269539578284)) ;
#136525 = CARTESIAN_POINT('Origin',(12.7,2.65,-18.8269539578284)) ;
#136526 = CARTESIAN_POINT('Origin',(12.7,2.65,-18.8269539578284)) ;
#136527 = CARTESIAN_POINT('Origin',(4.5,2.1,-18.9380460421716)) ;
#136528 = CARTESIAN_POINT('',(4.6,2.,-18.9380460421716)) ;
#136529 = CARTESIAN_POINT('',(12.8,2.,-18.9380460421716)) ;
#136530 = CARTESIAN_POINT('',(4.6,2.11643989873054,-18.8394066497884)) ;
#136531 = CARTESIAN_POINT('Origin',(4.6,2.1,-18.9380460421716)) ;
#136532 = CARTESIAN_POINT('',(4.5,2.11643989873054,-18.8394066497884)) ;
#136533 = CARTESIAN_POINT('Origin',(12.7,2.65,-21.8130460421716)) ;
#136534 = CARTESIAN_POINT('',(12.8,2.65,-21.8130460421716)) ;
#136535 = CARTESIAN_POINT('',(12.7,2.63356010126947,-21.7144066497884)) ;
#136536 = CARTESIAN_POINT('Origin',(12.7,2.65,-21.8130460421716)) ;
#136537 = CARTESIAN_POINT('',(12.7,2.75,-21.8130460421716)) ;
#136538 = CARTESIAN_POINT('Origin',(12.7,2.65,-21.8130460421716)) ;
#136539 = CARTESIAN_POINT('Origin',(12.7,2.65,-21.8130460421716)) ;
#136540 = CARTESIAN_POINT('Origin',(11.05,0.,-20.32)) ;
#136541 = CARTESIAN_POINT('',(10.3,-9.1848509936051E-17,-19.57)) ;
#136542 = CARTESIAN_POINT('Origin',(10.3,0.,-20.32)) ;
#136543 = CARTESIAN_POINT('',(11.05,-1.83697019872103E-16,-18.82)) ;
#136544 = CARTESIAN_POINT('Origin',(11.05,0.,-20.32)) ;
#136545 = CARTESIAN_POINT('',(11.05,-1.83697019872103E-16,-18.82)) ;
#136546 = CARTESIAN_POINT('Origin',(0.,9.95,-20.32)) ;
#136547 = CARTESIAN_POINT('',(0.218101234104781,9.95,-22.2074405558009)) ;
#136548 = CARTESIAN_POINT('',(-2.32682891837997E-16,9.95,-22.22)) ;
#136549 = CARTESIAN_POINT('Origin',(0.,9.95,-20.32)) ;
#136550 = CARTESIAN_POINT('',(0.321518176280636,9.85,-22.1925987456797)) ;
#136551 = CARTESIAN_POINT('Ctrl Pts',(0.21810123410477,9.95,-22.2074405558009)) ;
#136552 = CARTESIAN_POINT('Ctrl Pts',(0.231193919344568,9.95,-22.2059276441493)) ;
#136553 = CARTESIAN_POINT('Ctrl Pts',(0.245192892440011,9.94751445938575,
-22.2041565825739)) ;
#136554 = CARTESIAN_POINT('Ctrl Pts',(0.270990685773149,9.93716996065971,
-22.2006215789467)) ;
#136555 = CARTESIAN_POINT('Ctrl Pts',(0.282791986325031,9.92931613918426,
-22.1988607093667)) ;
#136556 = CARTESIAN_POINT('Ctrl Pts',(0.300953024019383,9.91135900604096,
-22.1960350266619)) ;
#136557 = CARTESIAN_POINT('Ctrl Pts',(0.308688523153903,9.90025653083842,
-22.1947625618009)) ;
#136558 = CARTESIAN_POINT('Ctrl Pts',(0.318969164829192,9.87583423571802,
-22.1930429866749)) ;
#136559 = CARTESIAN_POINT('Ctrl Pts',(0.321518176280625,9.86251584266313,
-22.1925987456797)) ;
#136560 = CARTESIAN_POINT('Ctrl Pts',(0.321518176280625,9.85,-22.1925987456797)) ;
#136561 = CARTESIAN_POINT('',(0.321518176280636,9.05,-22.1925987456797)) ;
#136562 = CARTESIAN_POINT('',(0.321518176280636,8.95,-22.1925987456797)) ;
#136563 = CARTESIAN_POINT('',(0.422455466606969,8.95,-22.1724393050068)) ;
#136564 = CARTESIAN_POINT('Ctrl Pts',(0.321518176280626,9.05,-22.1925987456797)) ;
#136565 = CARTESIAN_POINT('Ctrl Pts',(0.321518176280626,9.03744936090869,
-22.1925987456797)) ;
#136566 = CARTESIAN_POINT('Ctrl Pts',(0.324085473150903,9.02409774280079,
-22.1921645622427)) ;
#136567 = CARTESIAN_POINT('Ctrl Pts',(0.334387313650432,8.99960748025859,
-22.1903498579077)) ;
#136568 = CARTESIAN_POINT('Ctrl Pts',(0.342122499456559,8.98846937989492,
-22.1889656420615)) ;
#136569 = CARTESIAN_POINT('Ctrl Pts',(0.360004521225388,8.97064401154629,
-22.1856049780795)) ;
#136570 = CARTESIAN_POINT('Ctrl Pts',(0.371447108749463,8.96285745107738,
-22.1833820840476)) ;
#136571 = CARTESIAN_POINT('Ctrl Pts',(0.39637397952969,8.95253508546271,-22.1782373032789)) ;
#136572 = CARTESIAN_POINT('Ctrl Pts',(0.409857901997322,8.95,-22.1753122250646)) ;
#136573 = CARTESIAN_POINT('Ctrl Pts',(0.42245546660696,8.95,-22.1724393050068)) ;
#136574 = CARTESIAN_POINT('',(1.14750169623629,8.95,-21.8343446956142)) ;
#136575 = CARTESIAN_POINT('Origin',(0.,8.95,-20.32)) ;
#136576 = CARTESIAN_POINT('',(1.22782596331729,9.05,-21.769980483939)) ;
#136577 = CARTESIAN_POINT('Ctrl Pts',(1.1475016962363,8.95,-21.8343446956142)) ;
#136578 = CARTESIAN_POINT('Ctrl Pts',(1.15780003912543,8.95,-21.8265410786649)) ;
#136579 = CARTESIAN_POINT('Ctrl Pts',(1.16870807732935,8.95253508546271,-21.8180919988207)) ;
#136580 = CARTESIAN_POINT('Ctrl Pts',(1.18867189173409,8.96285745107738,-21.8023039093078)) ;
#136581 = CARTESIAN_POINT('Ctrl Pts',(1.19772988083812,8.97064401154629,-21.7949672274615)) ;
#136582 = CARTESIAN_POINT('Ctrl Pts',(1.21179864083582,8.98846937989492,-21.7834289972216)) ;
#136583 = CARTESIAN_POINT('Ctrl Pts',(1.21783109328768,8.99960748025859,-21.7783932579134)) ;
#136584 = CARTESIAN_POINT('Ctrl Pts',(1.22584313288947,9.02409774280079,-21.7716680597067)) ;
#136585 = CARTESIAN_POINT('Ctrl Pts',(1.22782596331729,9.03744936090869,-21.769980483939)) ;
#136586 = CARTESIAN_POINT('Ctrl Pts',(1.22782596331729,9.05,-21.769980483939)) ;
#136587 = CARTESIAN_POINT('',(1.22782596331729,9.85,-21.769980483939)) ;
#136588 = CARTESIAN_POINT('',(1.22782596331729,8.95,-21.769980483939)) ;
#136589 = CARTESIAN_POINT('',(1.30567057854876,9.95,-21.7002986417121)) ;
#136590 = CARTESIAN_POINT('Ctrl Pts',(1.2278259633173,9.85,-21.769980483939)) ;
#136591 = CARTESIAN_POINT('Ctrl Pts',(1.2278259633173,9.85579162428539,-21.769980483939)) ;
#136592 = CARTESIAN_POINT('Ctrl Pts',(1.22822745887819,9.86162764920014,-21.7696405714653)) ;
#136593 = CARTESIAN_POINT('Ctrl Pts',(1.22902753823172,9.86736607146312,-21.7689619546779)) ;
#136594 = CARTESIAN_POINT('Ctrl Pts',(1.22973095933686,9.87241123018668,-21.7683653221458)) ;
#136595 = CARTESIAN_POINT('Ctrl Pts',(1.23074168751921,9.87738020477702,-21.7675074302535)) ;
#136596 = CARTESIAN_POINT('Ctrl Pts',(1.23203099150183,9.88218322835581,-21.7664092214793)) ;
#136597 = CARTESIAN_POINT('Ctrl Pts',(1.23351897101726,9.88772637473068,-21.7651417840233)) ;
#136598 = CARTESIAN_POINT('Ctrl Pts',(1.23540145579029,9.89313280655103,-21.7635343365783)) ;
#136599 = CARTESIAN_POINT('Ctrl Pts',(1.23763252770622,9.89827011881554,-21.7616189827484)) ;
#136600 = CARTESIAN_POINT('Ctrl Pts',(1.23953000874363,9.90263929783464,-21.7599900134865)) ;
#136601 = CARTESIAN_POINT('Ctrl Pts',(1.24167862345461,9.90681364346946,-21.7581390311988)) ;
#136602 = CARTESIAN_POINT('Ctrl Pts',(1.24403025306867,9.91072825704926,-21.7561019216791)) ;
#136603 = CARTESIAN_POINT('Ctrl Pts',(1.24687926059923,9.91547082513965,-21.7536339563467)) ;
#136604 = CARTESIAN_POINT('Ctrl Pts',(1.25006974298107,9.91990270163235,-21.7508551265321)) ;
#136605 = CARTESIAN_POINT('Ctrl Pts',(1.2535194093265,9.92391762881322,-21.7478266146309)) ;
#136606 = CARTESIAN_POINT('Ctrl Pts',(1.25634620505521,9.92720762206752,-21.7453449298389)) ;
#136607 = CARTESIAN_POINT('Ctrl Pts',(1.25934609941473,9.93021806933731,-21.7426963101588)) ;
#136608 = CARTESIAN_POINT('Ctrl Pts',(1.26246241000317,9.93291206679729,-21.7399255837293)) ;
#136609 = CARTESIAN_POINT('Ctrl Pts',(1.26649145911189,9.93639511117203,-21.7363433371803)) ;
#136610 = CARTESIAN_POINT('Ctrl Pts',(1.27077652588473,9.93940081548805,-21.732502262524)) ;
#136611 = CARTESIAN_POINT('Ctrl Pts',(1.27520851369616,9.94185862744774,-21.7284896739102)) ;
#136612 = CARTESIAN_POINT('Ctrl Pts',(1.27864718185096,9.94376558208659,-21.7253764070711)) ;
#136613 = CARTESIAN_POINT('Ctrl Pts',(1.28217366418729,9.94534362661778,-21.7221604997622)) ;
#136614 = CARTESIAN_POINT('Ctrl Pts',(1.28573335778226,9.94658081625576,-21.7188887492202)) ;
#136615 = CARTESIAN_POINT('Ctrl Pts',(1.29026904082681,9.94815721599754,-21.7147199568612)) ;
#136616 = CARTESIAN_POINT('Ctrl Pts',(1.29492021413415,9.9491996901822,-21.7104036518226)) ;
#136617 = CARTESIAN_POINT('Ctrl Pts',(1.29957290046262,9.9496832238817,-21.7060412243876)) ;
#136618 = CARTESIAN_POINT('Ctrl Pts',(1.30160833994475,9.94989475836165,-21.7041327662599)) ;
#136619 = CARTESIAN_POINT('Ctrl Pts',(1.30364403319562,9.95,-21.7022156186355)) ;
#136620 = CARTESIAN_POINT('Ctrl Pts',(1.30567057854874,9.95,-21.7002986417121)) ;
#136621 = CARTESIAN_POINT('',(-0.218101234104782,9.95,-18.4325594441991)) ;
#136622 = CARTESIAN_POINT('Origin',(0.,9.95,-20.32)) ;
#136623 = CARTESIAN_POINT('',(-0.321518176280637,9.85,-18.4474012543203)) ;
#136624 = CARTESIAN_POINT('Ctrl Pts',(-0.218101234104768,9.95,-18.4325594441991)) ;
#136625 = CARTESIAN_POINT('Ctrl Pts',(-0.231193919344566,9.95,-18.4340723558507)) ;
#136626 = CARTESIAN_POINT('Ctrl Pts',(-0.245192892440009,9.94751445938575,
-18.4358434174261)) ;
#136627 = CARTESIAN_POINT('Ctrl Pts',(-0.270990685773147,9.93716996065971,
-18.4393784210533)) ;
#136628 = CARTESIAN_POINT('Ctrl Pts',(-0.282791986325029,9.92931613918426,
-18.4411392906332)) ;
#136629 = CARTESIAN_POINT('Ctrl Pts',(-0.300953024019382,9.91135900604096,
-18.4439649733381)) ;
#136630 = CARTESIAN_POINT('Ctrl Pts',(-0.308688523153901,9.90025653083842,
-18.445237438199)) ;
#136631 = CARTESIAN_POINT('Ctrl Pts',(-0.31896916482919,9.87583423571802,
-18.4469570133251)) ;
#136632 = CARTESIAN_POINT('Ctrl Pts',(-0.321518176280622,9.86251584266313,
-18.4474012543203)) ;
#136633 = CARTESIAN_POINT('Ctrl Pts',(-0.321518176280622,9.85,-18.4474012543203)) ;
#136634 = CARTESIAN_POINT('',(-0.321518176280637,9.05,-18.4474012543203)) ;
#136635 = CARTESIAN_POINT('',(-0.321518176280637,8.95,-18.4474012543203)) ;
#136636 = CARTESIAN_POINT('',(-0.422455466606969,8.95,-18.4675606949933)) ;
#136637 = CARTESIAN_POINT('Ctrl Pts',(-0.321518176280627,9.05,-18.4474012543203)) ;
#136638 = CARTESIAN_POINT('Ctrl Pts',(-0.321518176280627,9.03744936090869,
-18.4474012543203)) ;
#136639 = CARTESIAN_POINT('Ctrl Pts',(-0.324085473150904,9.02409774280079,
-18.4478354377573)) ;
#136640 = CARTESIAN_POINT('Ctrl Pts',(-0.334387313650432,8.99960748025859,
-18.4496501420923)) ;
#136641 = CARTESIAN_POINT('Ctrl Pts',(-0.34212249945656,8.98846937989492,
-18.4510343579385)) ;
#136642 = CARTESIAN_POINT('Ctrl Pts',(-0.360004521225388,8.97064401154629,
-18.4543950219205)) ;
#136643 = CARTESIAN_POINT('Ctrl Pts',(-0.371447108749464,8.96285745107739,
-18.4566179159524)) ;
#136644 = CARTESIAN_POINT('Ctrl Pts',(-0.39637397952969,8.95253508546271,
-18.4617626967211)) ;
#136645 = CARTESIAN_POINT('Ctrl Pts',(-0.409857901997323,8.95,-18.4646877749354)) ;
#136646 = CARTESIAN_POINT('Ctrl Pts',(-0.42245546660696,8.95,-18.4675606949932)) ;
#136647 = CARTESIAN_POINT('',(-1.14750169623629,8.95,-18.8056553043858)) ;
#136648 = CARTESIAN_POINT('Origin',(0.,8.95,-20.32)) ;
#136649 = CARTESIAN_POINT('',(-1.22782596331729,9.05,-18.870019516061)) ;
#136650 = CARTESIAN_POINT('Ctrl Pts',(-1.1475016962363,8.95,-18.8056553043858)) ;
#136651 = CARTESIAN_POINT('Ctrl Pts',(-1.15780003912543,8.95,-18.8134589213351)) ;
#136652 = CARTESIAN_POINT('Ctrl Pts',(-1.16870807732935,8.95253508546271,
-18.8219080011793)) ;
#136653 = CARTESIAN_POINT('Ctrl Pts',(-1.18867189173409,8.96285745107739,
-18.8376960906922)) ;
#136654 = CARTESIAN_POINT('Ctrl Pts',(-1.19772988083812,8.97064401154629,
-18.8450327725385)) ;
#136655 = CARTESIAN_POINT('Ctrl Pts',(-1.21179864083582,8.98846937989492,
-18.8565710027784)) ;
#136656 = CARTESIAN_POINT('Ctrl Pts',(-1.21783109328768,8.99960748025859,
-18.8616067420866)) ;
#136657 = CARTESIAN_POINT('Ctrl Pts',(-1.22584313288947,9.02409774280079,
-18.8683319402933)) ;
#136658 = CARTESIAN_POINT('Ctrl Pts',(-1.22782596331729,9.03744936090869,
-18.870019516061)) ;
#136659 = CARTESIAN_POINT('Ctrl Pts',(-1.22782596331729,9.05,-18.870019516061)) ;
#136660 = CARTESIAN_POINT('',(-1.22782596331729,9.85,-18.870019516061)) ;
#136661 = CARTESIAN_POINT('',(-1.22782596331729,8.95,-18.870019516061)) ;
#136662 = CARTESIAN_POINT('',(-1.30567057854876,9.95,-18.9397013582879)) ;
#136663 = CARTESIAN_POINT('Ctrl Pts',(-1.2278259633173,9.85,-18.870019516061)) ;
#136664 = CARTESIAN_POINT('Ctrl Pts',(-1.2278259633173,9.85579162428539,-18.870019516061)) ;
#136665 = CARTESIAN_POINT('Ctrl Pts',(-1.22822745887819,9.86162764920014,
-18.8703594285347)) ;
#136666 = CARTESIAN_POINT('Ctrl Pts',(-1.22902753823172,9.86736607146313,
-18.8710380453221)) ;
#136667 = CARTESIAN_POINT('Ctrl Pts',(-1.22973095933686,9.87241123018668,
-18.8716346778542)) ;
#136668 = CARTESIAN_POINT('Ctrl Pts',(-1.23074168751921,9.87738020477702,
-18.8724925697465)) ;
#136669 = CARTESIAN_POINT('Ctrl Pts',(-1.23203099150183,9.88218322835581,
-18.8735907785207)) ;
#136670 = CARTESIAN_POINT('Ctrl Pts',(-1.23351897101725,9.88772637473067,
-18.8748582159767)) ;
#136671 = CARTESIAN_POINT('Ctrl Pts',(-1.23540145579029,9.89313280655104,
-18.8764656634217)) ;
#136672 = CARTESIAN_POINT('Ctrl Pts',(-1.23763252770621,9.89827011881553,
-18.8783810172516)) ;
#136673 = CARTESIAN_POINT('Ctrl Pts',(-1.23953000874362,9.90263929783464,
-18.8800099865135)) ;
#136674 = CARTESIAN_POINT('Ctrl Pts',(-1.24167862345461,9.90681364346945,
-18.8818609688012)) ;
#136675 = CARTESIAN_POINT('Ctrl Pts',(-1.24403025306867,9.91072825704926,
-18.8838980783209)) ;
#136676 = CARTESIAN_POINT('Ctrl Pts',(-1.24687926059923,9.91547082513966,
-18.8863660436533)) ;
#136677 = CARTESIAN_POINT('Ctrl Pts',(-1.25006974298107,9.91990270163235,
-18.8891448734679)) ;
#136678 = CARTESIAN_POINT('Ctrl Pts',(-1.2535194093265,9.92391762881323,-18.8921733853691)) ;
#136679 = CARTESIAN_POINT('Ctrl Pts',(-1.25634620505522,9.92720762206752,
-18.8946550701611)) ;
#136680 = CARTESIAN_POINT('Ctrl Pts',(-1.25934609941473,9.93021806933732,
-18.8973036898412)) ;
#136681 = CARTESIAN_POINT('Ctrl Pts',(-1.26246241000317,9.93291206679729,
-18.9000744162707)) ;
#136682 = CARTESIAN_POINT('Ctrl Pts',(-1.26649145911189,9.93639511117203,
-18.9036566628197)) ;
#136683 = CARTESIAN_POINT('Ctrl Pts',(-1.27077652588473,9.93940081548805,
-18.907497737476)) ;
#136684 = CARTESIAN_POINT('Ctrl Pts',(-1.27520851369617,9.94185862744775,
-18.9115103260898)) ;
#136685 = CARTESIAN_POINT('Ctrl Pts',(-1.27864718185097,9.94376558208659,
-18.9146235929289)) ;
#136686 = CARTESIAN_POINT('Ctrl Pts',(-1.28217366418729,9.94534362661778,
-18.9178395002378)) ;
#136687 = CARTESIAN_POINT('Ctrl Pts',(-1.28573335778226,9.94658081625577,
-18.9211112507798)) ;
#136688 = CARTESIAN_POINT('Ctrl Pts',(-1.29026904082681,9.94815721599754,
-18.9252800431388)) ;
#136689 = CARTESIAN_POINT('Ctrl Pts',(-1.29492021413408,9.94919969018218,
-18.9295963481773)) ;
#136690 = CARTESIAN_POINT('Ctrl Pts',(-1.29957290046257,9.94968322388169,
-18.9339587756124)) ;
#136691 = CARTESIAN_POINT('Ctrl Pts',(-1.30160833994473,9.94989475836165,
-18.9358672337401)) ;
#136692 = CARTESIAN_POINT('Ctrl Pts',(-1.30364403319561,9.95,-18.9377843813644)) ;
#136693 = CARTESIAN_POINT('Ctrl Pts',(-1.30567057854874,9.95,-18.9397013582879)) ;
#136694 = CARTESIAN_POINT('Origin',(0.,9.95,-20.32)) ;
#136695 = CARTESIAN_POINT('',(-2.32682891837997E-16,9.95,-22.22)) ;
#136696 = CARTESIAN_POINT('Origin',(3.95,3.75,-17.78)) ;
#136697 = CARTESIAN_POINT('',(3.95,6.92431432344521,-22.86)) ;
#136698 = CARTESIAN_POINT('',(3.95,6.92431432344521,-12.7)) ;
#136699 = CARTESIAN_POINT('',(3.95,6.92431432344521,-17.78)) ;
#136700 = CARTESIAN_POINT('',(3.95,3.77568567655479,-12.7)) ;
#136701 = CARTESIAN_POINT('',(3.95,3.75,-12.7)) ;
#136702 = CARTESIAN_POINT('',(3.95,3.77568567655479,-22.86)) ;
#136703 = CARTESIAN_POINT('',(3.95,3.77568567655479,-22.86)) ;
#136704 = CARTESIAN_POINT('',(3.95,3.75,-22.86)) ;
#136705 = CARTESIAN_POINT('',(3.95,4.6,-17.345)) ;
#136706 = CARTESIAN_POINT('',(3.95,4.4,-17.545)) ;
#136707 = CARTESIAN_POINT('Origin',(3.95,4.6,-17.545)) ;
#136708 = CARTESIAN_POINT('',(3.95,5.88396692803319,-17.345)) ;
#136709 = CARTESIAN_POINT('',(3.95,3.75,-17.345)) ;
#136710 = CARTESIAN_POINT('',(3.95,6.08618232569815,-17.545)) ;
#136711 = CARTESIAN_POINT('Ctrl Pts',(3.95,6.08618232569815,-17.545)) ;
#136712 = CARTESIAN_POINT('Ctrl Pts',(3.95,6.08618232225605,-17.4360574372282)) ;
#136713 = CARTESIAN_POINT('Ctrl Pts',(3.95,5.9941162463882,-17.3450000032932)) ;
#136714 = CARTESIAN_POINT('Ctrl Pts',(3.95,5.88396692803319,-17.345)) ;
#136715 = CARTESIAN_POINT('',(3.95,6.08618232569815,-18.845)) ;
#136716 = CARTESIAN_POINT('',(3.95,6.08618232569815,-17.78)) ;
#136717 = CARTESIAN_POINT('',(3.95,5.88396692803319,-19.045)) ;
#136718 = CARTESIAN_POINT('Ctrl Pts',(3.95,5.88396692803319,-19.045)) ;
#136719 = CARTESIAN_POINT('Ctrl Pts',(3.95,5.9941162463882,-19.0449999967068)) ;
#136720 = CARTESIAN_POINT('Ctrl Pts',(3.95,6.08618232225605,-18.9539425627718)) ;
#136721 = CARTESIAN_POINT('Ctrl Pts',(3.95,6.08618232569815,-18.845)) ;
#136722 = CARTESIAN_POINT('',(3.95,4.6,-19.045)) ;
#136723 = CARTESIAN_POINT('',(3.95,4.5,-19.045)) ;
#136724 = CARTESIAN_POINT('',(3.95,4.4,-18.845)) ;
#136725 = CARTESIAN_POINT('Origin',(3.95,4.6,-18.845)) ;
#136726 = CARTESIAN_POINT('',(3.95,4.4,-17.78)) ;
#136727 = CARTESIAN_POINT('Origin',(3.4,7.95,-17.78)) ;
#136728 = CARTESIAN_POINT('',(3.,7.95,-22.36)) ;
#136729 = CARTESIAN_POINT('',(3.34087287789487,7.95,-22.36)) ;
#136730 = CARTESIAN_POINT('',(3.4,7.95,-22.36)) ;
#136731 = CARTESIAN_POINT('',(3.,7.95,-12.7)) ;
#136732 = CARTESIAN_POINT('',(3.,7.95,-17.78)) ;
#136733 = CARTESIAN_POINT('',(3.34087287789487,7.95,-12.7)) ;
#136734 = CARTESIAN_POINT('',(3.4,7.95,-12.7)) ;
#136735 = CARTESIAN_POINT('',(3.34087287789487,7.95,-17.78)) ;
#136736 = CARTESIAN_POINT('Origin',(2.9,7.95,-17.78)) ;
#136737 = CARTESIAN_POINT('',(2.9,9.85,-22.36)) ;
#136738 = CARTESIAN_POINT('',(2.9,8.05,-22.36)) ;
#136739 = CARTESIAN_POINT('',(2.9,7.825,-22.36)) ;
#136740 = CARTESIAN_POINT('',(2.9,9.85,-12.7)) ;
#136741 = CARTESIAN_POINT('',(2.9,9.85,-17.78)) ;
#136742 = CARTESIAN_POINT('',(2.9,8.05,-12.7)) ;
#136743 = CARTESIAN_POINT('',(2.9,7.95,-12.7)) ;
#136744 = CARTESIAN_POINT('',(2.9,8.05,-22.86)) ;
#136745 = CARTESIAN_POINT('Origin',(2.9,9.95,-17.78)) ;
#136746 = CARTESIAN_POINT('',(3.3,9.95,-22.36)) ;
#136747 = CARTESIAN_POINT('',(3.,9.95,-22.36)) ;
#136748 = CARTESIAN_POINT('',(2.9,9.95,-22.36)) ;
#136749 = CARTESIAN_POINT('',(3.3,9.95,-12.7)) ;
#136750 = CARTESIAN_POINT('',(3.3,9.95,-17.78)) ;
#136751 = CARTESIAN_POINT('',(3.,9.95,-12.7)) ;
#136752 = CARTESIAN_POINT('',(2.9,9.95,-12.7)) ;
#136753 = CARTESIAN_POINT('',(3.,9.95,-22.86)) ;
#136754 = CARTESIAN_POINT('Origin',(3.3,10.05,-17.78)) ;
#136755 = CARTESIAN_POINT('',(3.4,10.05,-22.36)) ;
#136756 = CARTESIAN_POINT('Origin',(3.3,10.05,-22.36)) ;
#136757 = CARTESIAN_POINT('',(3.4,10.05,-12.7)) ;
#136758 = CARTESIAN_POINT('',(3.4,10.05,-17.78)) ;
#136759 = CARTESIAN_POINT('Origin',(3.3,10.05,-12.7)) ;
#136760 = CARTESIAN_POINT('Origin',(3.,9.85,-17.78)) ;
#136761 = CARTESIAN_POINT('Origin',(3.,9.85,-22.36)) ;
#136762 = CARTESIAN_POINT('Origin',(3.,9.85,-12.7)) ;
#136763 = CARTESIAN_POINT('Origin',(3.,8.05,-17.78)) ;
#136764 = CARTESIAN_POINT('Origin',(3.,8.05,-22.36)) ;
#136765 = CARTESIAN_POINT('Origin',(3.,8.05,-12.7)) ;
#136766 = CARTESIAN_POINT('Origin',(3.34087287789487,7.85,-17.78)) ;
#136767 = CARTESIAN_POINT('',(3.4,7.93064727789309,-22.86)) ;
#136768 = CARTESIAN_POINT('',(3.42849446876253,7.89819187497721,-22.86)) ;
#136769 = CARTESIAN_POINT('Origin',(3.34087287789487,7.85,-22.86)) ;
#136770 = CARTESIAN_POINT('',(3.4,7.93064727789309,-22.36)) ;
#136771 = CARTESIAN_POINT('',(3.4,7.93064727789309,-17.78)) ;
#136772 = CARTESIAN_POINT('Origin',(3.34087287789487,7.85,-22.36)) ;
#136773 = CARTESIAN_POINT('',(3.42849446876253,7.89819187497721,-12.7)) ;
#136774 = CARTESIAN_POINT('Origin',(3.34087287789487,7.85,-12.7)) ;
#136775 = CARTESIAN_POINT('',(3.42849446876253,7.89819187497721,-17.78)) ;
#136776 = CARTESIAN_POINT('Origin',(4.5,-2.8,-17.78)) ;
#136777 = CARTESIAN_POINT('',(4.5,-2.4,-22.2821416870349)) ;
#136778 = CARTESIAN_POINT('',(4.5,-2.7,-21.8431546211728)) ;
#136779 = CARTESIAN_POINT('Origin',(4.5,0.,-20.32)) ;
#136780 = CARTESIAN_POINT('',(4.5,-2.7,-22.86)) ;
#136781 = CARTESIAN_POINT('',(4.5,-2.7,-17.78)) ;
#136782 = CARTESIAN_POINT('',(4.5,-2.4,-22.86)) ;
#136783 = CARTESIAN_POINT('',(4.5,-2.8,-22.86)) ;
#136784 = CARTESIAN_POINT('',(4.5,-2.4,-22.2461360284258)) ;
#136785 = CARTESIAN_POINT('Origin',(4.5,-2.3,-17.78)) ;
#136786 = CARTESIAN_POINT('',(12.7,-2.3,-18.3578583129651)) ;
#136787 = CARTESIAN_POINT('',(12.7,-2.3,-17.2021416870349)) ;
#136788 = CARTESIAN_POINT('',(12.7,-2.3,-17.78)) ;
#136789 = CARTESIAN_POINT('',(4.6,-2.3,-17.2021416870349)) ;
#136790 = CARTESIAN_POINT('',(4.5,-2.3,-17.2021416870349)) ;
#136791 = CARTESIAN_POINT('',(4.6,-2.3,-18.3578583129651)) ;
#136792 = CARTESIAN_POINT('',(4.6,-2.3,-18.3938639715742)) ;
#136793 = CARTESIAN_POINT('',(4.5,-2.3,-18.3578583129651)) ;
#136794 = CARTESIAN_POINT('Origin',(12.8,2.75,-17.78)) ;
#136795 = CARTESIAN_POINT('',(12.7,2.75,-22.86)) ;
#136796 = CARTESIAN_POINT('',(4.55912712210514,2.75,-22.86)) ;
#136797 = CARTESIAN_POINT('',(12.8,2.75,-22.86)) ;
#136798 = CARTESIAN_POINT('',(4.55912712210513,2.75,-21.8130460421716)) ;
#136799 = CARTESIAN_POINT('',(4.55912712210514,2.75,-21.8130460421716)) ;
#136800 = CARTESIAN_POINT('',(12.8,2.75,-21.8130460421716)) ;
#136801 = CARTESIAN_POINT('',(12.7,2.75,-17.78)) ;
#136802 = CARTESIAN_POINT('Origin',(0.,9.95,-20.32)) ;
#136803 = CARTESIAN_POINT('',(0.230887397576971,9.95,-22.2348605718538)) ;
#136804 = CARTESIAN_POINT('Origin',(12.8,-2.3,-17.78)) ;
#136805 = CARTESIAN_POINT('',(12.8,-2.3359925337019,-17.9959552022114)) ;
#136806 = CARTESIAN_POINT('',(12.8,2.65,-17.78)) ;
#136807 = CARTESIAN_POINT('',(12.8,2.13287979746107,-16.8192327425948)) ;
#136808 = CARTESIAN_POINT('',(12.8,-1.51220874991811,-17.4267475004913)) ;
#136809 = CARTESIAN_POINT('',(12.8,1.9,-16.6219539578284)) ;
#136810 = CARTESIAN_POINT('Origin',(12.8,2.1,-16.6219539578284)) ;
#136811 = CARTESIAN_POINT('',(12.8,1.9,-12.7)) ;
#136812 = CARTESIAN_POINT('',(12.8,-2.3359925337019,-12.9159552022114)) ;
#136813 = CARTESIAN_POINT('',(12.8,2.65,-12.7)) ;
#136814 = CARTESIAN_POINT('',(12.8,2.65,-12.7)) ;
#136815 = CARTESIAN_POINT('',(12.8,-2.2,-12.7)) ;
#136816 = CARTESIAN_POINT('',(12.8,-2.3,-12.7)) ;
#136817 = CARTESIAN_POINT('',(12.8,-2.2,-13.2778583129651)) ;
#136818 = CARTESIAN_POINT('',(12.8,-2.2,-12.7)) ;
#136819 = CARTESIAN_POINT('',(12.8,-2.24516129032258,-13.4044480992255)) ;
#136820 = CARTESIAN_POINT('Origin',(12.8,-2.4,-13.2778583129651)) ;
#136821 = CARTESIAN_POINT('',(12.8,-2.24516129032258,-17.0755519007745)) ;
#136822 = CARTESIAN_POINT('Origin',(12.8,0.,-15.24)) ;
#136823 = CARTESIAN_POINT('',(12.8,-2.2,-17.2021416870349)) ;
#136824 = CARTESIAN_POINT('Origin',(12.8,-2.4,-17.2021416870349)) ;
#136825 = CARTESIAN_POINT('',(12.8,-2.2,-18.3578583129651)) ;
#136826 = CARTESIAN_POINT('',(12.8,-2.2,-17.78)) ;
#136827 = CARTESIAN_POINT('',(12.8,-2.24516129032258,-18.4844480992255)) ;
#136828 = CARTESIAN_POINT('Origin',(12.8,-2.4,-18.3578583129651)) ;
#136829 = CARTESIAN_POINT('',(12.8,-2.24516129032258,-22.1555519007745)) ;
#136830 = CARTESIAN_POINT('Origin',(12.8,0.,-20.32)) ;
#136831 = CARTESIAN_POINT('',(12.8,-2.2,-22.2821416870349)) ;
#136832 = CARTESIAN_POINT('Origin',(12.8,-2.4,-22.2821416870349)) ;
#136833 = CARTESIAN_POINT('',(12.8,-2.2,-22.86)) ;
#136834 = CARTESIAN_POINT('',(12.8,-2.2,-17.78)) ;
#136835 = CARTESIAN_POINT('',(12.8,2.65,-22.86)) ;
#136836 = CARTESIAN_POINT('',(12.8,-2.3,-22.86)) ;
#136837 = CARTESIAN_POINT('',(12.8,2.65,-17.78)) ;
#136838 = CARTESIAN_POINT('',(12.8,2.13287979746107,-21.8992327425948)) ;
#136839 = CARTESIAN_POINT('',(12.8,-1.51220874991811,-22.5067475004913)) ;
#136840 = CARTESIAN_POINT('',(12.8,1.9,-21.7019539578284)) ;
#136841 = CARTESIAN_POINT('Origin',(12.8,2.1,-21.7019539578284)) ;
#136842 = CARTESIAN_POINT('',(12.8,1.9,-17.78)) ;
#136843 = CARTESIAN_POINT('Origin',(12.8,2.75,-17.78)) ;
#136844 = CARTESIAN_POINT('',(4.55912712210513,2.75,-18.8269539578284)) ;
#136845 = CARTESIAN_POINT('',(12.8,2.75,-18.8269539578284)) ;
#136846 = CARTESIAN_POINT('',(4.55912712210513,2.75,-16.7330460421716)) ;
#136847 = CARTESIAN_POINT('',(4.55912712210514,2.75,-17.78)) ;
#136848 = CARTESIAN_POINT('',(12.8,2.75,-16.7330460421716)) ;
#136849 = CARTESIAN_POINT('',(12.7,2.75,-17.78)) ;
#136850 = CARTESIAN_POINT('Origin',(4.5,2.75,-17.78)) ;
#136851 = CARTESIAN_POINT('',(3.96237840913234,3.72749380157757,-22.86)) ;
#136852 = CARTESIAN_POINT('',(3.96237840913234,3.72749380157757,-12.7)) ;
#136853 = CARTESIAN_POINT('',(3.96237840913234,3.72749380157757,-17.78)) ;
#136854 = CARTESIAN_POINT('',(4.47150553123747,2.80180812502278,-12.7)) ;
#136855 = CARTESIAN_POINT('',(4.5,2.75,-12.7)) ;
#136856 = CARTESIAN_POINT('',(4.47150553123747,2.80180812502279,-13.7469539578284)) ;
#136857 = CARTESIAN_POINT('',(4.47150553123747,2.80180812502278,-13.7469539578284)) ;
#136858 = CARTESIAN_POINT('',(4.48762159086767,2.77250619842243,-13.8511756817495)) ;
#136859 = CARTESIAN_POINT('Origin',(4.56263299594724,2.63612182555043,-13.7566002940964)) ;
#136860 = CARTESIAN_POINT('',(4.48762159086767,2.77250619842243,-16.6288243182478)) ;
#136861 = CARTESIAN_POINT('',(4.48762159086767,2.77250619842243,-12.7)) ;
#136862 = CARTESIAN_POINT('',(4.47150553123747,2.80180812502279,-16.7330460421716)) ;
#136863 = CARTESIAN_POINT('Origin',(4.56263299597154,2.63612182550629,-16.723399705895)) ;
#136864 = CARTESIAN_POINT('',(4.47150553123747,2.80180812502279,-18.8269539578284)) ;
#136865 = CARTESIAN_POINT('',(4.47150553123747,2.80180812502278,-18.8269539578284)) ;
#136866 = CARTESIAN_POINT('',(4.48762159086767,2.77250619842243,-18.9311756817495)) ;
#136867 = CARTESIAN_POINT('Origin',(4.56263299594023,2.63612182556322,-18.836600294098)) ;
#136868 = CARTESIAN_POINT('',(4.48762159086767,2.77250619842243,-21.7088243182478)) ;
#136869 = CARTESIAN_POINT('',(4.48762159086767,2.77250619842243,-17.78)) ;
#136870 = CARTESIAN_POINT('',(4.47150553123747,2.80180812502279,-21.8130460421716)) ;
#136871 = CARTESIAN_POINT('Origin',(4.56263299597011,2.63612182550888,-21.8033997058945)) ;
#136872 = CARTESIAN_POINT('',(4.47150553123747,2.80180812502278,-22.86)) ;
#136873 = CARTESIAN_POINT('',(4.47150553123747,2.80180812502278,-22.86)) ;
#136874 = CARTESIAN_POINT('',(4.5,2.75,-22.86)) ;
#136875 = CARTESIAN_POINT('Origin',(3.95,6.95,-17.78)) ;
#136876 = CARTESIAN_POINT('',(3.93762159086767,6.97250619842243,-22.86)) ;
#136877 = CARTESIAN_POINT('',(3.95,6.95,-22.86)) ;
#136878 = CARTESIAN_POINT('',(3.93762159086767,6.97250619842243,-12.7)) ;
#136879 = CARTESIAN_POINT('',(3.95,6.95,-12.7)) ;
#136880 = CARTESIAN_POINT('',(3.93762159086767,6.97250619842243,-17.78)) ;
#136881 = CARTESIAN_POINT('Origin',(3.4,9.95,-17.78)) ;
#136882 = CARTESIAN_POINT('',(3.4,10.85,-22.86)) ;
#136883 = CARTESIAN_POINT('',(3.4,9.95,-22.86)) ;
#136884 = CARTESIAN_POINT('',(3.4,10.85,-12.7)) ;
#136885 = CARTESIAN_POINT('',(3.4,10.85,-17.78)) ;
#136886 = CARTESIAN_POINT('',(3.4,9.95,-12.7)) ;
#136887 = CARTESIAN_POINT('',(3.4,7.825,-22.36)) ;
#136888 = CARTESIAN_POINT('Origin',(3.4,10.95,-17.78)) ;
#136889 = CARTESIAN_POINT('',(3.3,10.95,-22.86)) ;
#136890 = CARTESIAN_POINT('',(-4.8,10.95,-22.86)) ;
#136891 = CARTESIAN_POINT('',(3.4,10.95,-22.86)) ;
#136892 = CARTESIAN_POINT('',(-4.8,10.95,-12.7)) ;
#136893 = CARTESIAN_POINT('',(-4.8,10.95,-17.78)) ;
#136894 = CARTESIAN_POINT('',(3.3,10.95,-12.7)) ;
#136895 = CARTESIAN_POINT('',(3.4,10.95,-12.7)) ;
#136896 = CARTESIAN_POINT('',(3.3,10.95,-17.78)) ;
#136897 = CARTESIAN_POINT('',(-2.55,10.95,-16.14)) ;
#136898 = CARTESIAN_POINT('',(-2.75,10.95,-16.34)) ;
#136899 = CARTESIAN_POINT('Origin',(-2.75,10.95,-16.14)) ;
#136900 = CARTESIAN_POINT('',(-2.55,10.95,-14.34)) ;
#136901 = CARTESIAN_POINT('',(-2.55,10.95,-12.7)) ;
#136902 = CARTESIAN_POINT('',(-2.75,10.95,-14.14)) ;
#136903 = CARTESIAN_POINT('Origin',(-2.75,10.95,-14.34)) ;
#136904 = CARTESIAN_POINT('',(-3.8,10.95,-14.14)) ;
#136905 = CARTESIAN_POINT('',(3.4,10.95,-14.14)) ;
#136906 = CARTESIAN_POINT('',(-4.,10.95,-14.34)) ;
#136907 = CARTESIAN_POINT('Origin',(-3.8,10.95,-14.34)) ;
#136908 = CARTESIAN_POINT('',(-4.,10.95,-16.14)) ;
#136909 = CARTESIAN_POINT('',(-4.,10.95,-12.7)) ;
#136910 = CARTESIAN_POINT('',(-3.8,10.95,-16.34)) ;
#136911 = CARTESIAN_POINT('Origin',(-3.8,10.95,-16.14)) ;
#136912 = CARTESIAN_POINT('',(3.4,10.95,-16.34)) ;
#136913 = CARTESIAN_POINT('',(-2.55,10.95,-21.22)) ;
#136914 = CARTESIAN_POINT('',(-2.75,10.95,-21.42)) ;
#136915 = CARTESIAN_POINT('Origin',(-2.75,10.95,-21.22)) ;
#136916 = CARTESIAN_POINT('',(-2.55,10.95,-19.42)) ;
#136917 = CARTESIAN_POINT('',(-2.55,10.95,-17.78)) ;
#136918 = CARTESIAN_POINT('',(-2.75,10.95,-19.22)) ;
#136919 = CARTESIAN_POINT('Origin',(-2.75,10.95,-19.42)) ;
#136920 = CARTESIAN_POINT('',(-3.8,10.95,-19.22)) ;
#136921 = CARTESIAN_POINT('',(3.4,10.95,-19.22)) ;
#136922 = CARTESIAN_POINT('',(-4.,10.95,-19.42)) ;
#136923 = CARTESIAN_POINT('Origin',(-3.8,10.95,-19.42)) ;
#136924 = CARTESIAN_POINT('',(-4.,10.95,-21.22)) ;
#136925 = CARTESIAN_POINT('',(-4.,10.95,-17.78)) ;
#136926 = CARTESIAN_POINT('',(-3.8,10.95,-21.42)) ;
#136927 = CARTESIAN_POINT('Origin',(-3.8,10.95,-21.22)) ;
#136928 = CARTESIAN_POINT('',(3.4,10.95,-21.42)) ;
#136929 = CARTESIAN_POINT('Origin',(-4.9,10.95,-17.78)) ;
#136930 = CARTESIAN_POINT('',(-4.9,10.85,-22.86)) ;
#136931 = CARTESIAN_POINT('',(-4.9,10.3,-22.86)) ;
#136932 = CARTESIAN_POINT('',(-4.9,10.95,-22.86)) ;
#136933 = CARTESIAN_POINT('',(-4.9,10.3,-12.7)) ;
#136934 = CARTESIAN_POINT('',(-4.9,10.3,-17.78)) ;
#136935 = CARTESIAN_POINT('',(-4.9,10.85,-12.7)) ;
#136936 = CARTESIAN_POINT('',(-4.9,10.95,-12.7)) ;
#136937 = CARTESIAN_POINT('',(-4.9,10.85,-17.78)) ;
#136938 = CARTESIAN_POINT('Origin',(-4.9,10.2,-17.78)) ;
#136939 = CARTESIAN_POINT('',(-4.8,10.2,-22.86)) ;
#136940 = CARTESIAN_POINT('',(-4.9,10.2,-22.86)) ;
#136941 = CARTESIAN_POINT('',(-4.8,10.2,-12.7)) ;
#136942 = CARTESIAN_POINT('',(-4.9,10.2,-12.7)) ;
#136943 = CARTESIAN_POINT('',(-4.8,10.2,-17.78)) ;
#136944 = CARTESIAN_POINT('Origin',(-4.4,10.2,-17.78)) ;
#136945 = CARTESIAN_POINT('',(-5.39805806756909,5.20970966215454,-22.86)) ;
#136946 = CARTESIAN_POINT('',(-4.4,10.2,-22.86)) ;
#136947 = CARTESIAN_POINT('',(-5.39805806756909,5.20970966215454,-12.7)) ;
#136948 = CARTESIAN_POINT('',(-5.39805806756909,5.20970966215454,-17.78)) ;
#136949 = CARTESIAN_POINT('',(-4.4,10.2,-12.7)) ;
#136950 = CARTESIAN_POINT('Origin',(-5.4,5.2,-17.78)) ;
#136951 = CARTESIAN_POINT('',(-5.4,5.19009804864072,-22.86)) ;
#136952 = CARTESIAN_POINT('',(-5.4,-3.95,-22.86)) ;
#136953 = CARTESIAN_POINT('',(-5.4,5.2,-22.86)) ;
#136954 = CARTESIAN_POINT('',(-5.4,-3.95,-12.7)) ;
#136955 = CARTESIAN_POINT('',(-5.4,-3.95,-17.78)) ;
#136956 = CARTESIAN_POINT('',(-5.4,5.19009804864072,-12.7)) ;
#136957 = CARTESIAN_POINT('',(-5.4,5.2,-12.7)) ;
#136958 = CARTESIAN_POINT('',(-5.4,5.19009804864072,-17.78)) ;
#136959 = CARTESIAN_POINT('',(-5.4,4.23801993223491,-17.14)) ;
#136960 = CARTESIAN_POINT('',(-5.4,4.23801993223491,-13.34)) ;
#136961 = CARTESIAN_POINT('',(-5.4,4.23801993223491,-13.24)) ;
#136962 = CARTESIAN_POINT('',(-5.4,3.9369800677651,-13.14)) ;
#136963 = CARTESIAN_POINT('Ctrl Pts',(-5.4,4.23801993223491,-13.34)) ;
#136964 = CARTESIAN_POINT('Ctrl Pts',(-5.4,4.23801992976516,-13.2874931280902)) ;
#136965 = CARTESIAN_POINT('Ctrl Pts',(-5.4,4.20557579169425,-13.2356025737683)) ;
#136966 = CARTESIAN_POINT('Ctrl Pts',(-5.4,4.09411900298411,-13.1615547137571)) ;
#136967 = CARTESIAN_POINT('Ctrl Pts',(-5.4,4.0160133758189,-13.1400000004813)) ;
#136968 = CARTESIAN_POINT('Ctrl Pts',(-5.4,3.9369800677651,-13.14)) ;
#136969 = CARTESIAN_POINT('',(-5.4,-1.88819660112502,-13.14)) ;
#136970 = CARTESIAN_POINT('',(-5.4,-2.05,-13.14)) ;
#136971 = CARTESIAN_POINT('',(-5.4,-2.11180339887499,-13.34)) ;
#136972 = CARTESIAN_POINT('Ctrl Pts',(-5.4,-2.11180339887499,-13.34)) ;
#136973 = CARTESIAN_POINT('Ctrl Pts',(-5.4,-2.11180339704051,-13.2874931601087)) ;
#136974 = CARTESIAN_POINT('Ctrl Pts',(-5.4,-2.0877044485962,-13.2356025311215)) ;
#136975 = CARTESIAN_POINT('Ctrl Pts',(-5.4,-2.00491651967066,-13.1615547564039)) ;
#136976 = CARTESIAN_POINT('Ctrl Pts',(-5.4,-1.946901032774,-13.1400000011741)) ;
#136977 = CARTESIAN_POINT('Ctrl Pts',(-5.4,-1.88819660112501,-13.14)) ;
#136978 = CARTESIAN_POINT('',(-5.4,-2.11180339887499,-17.14)) ;
#136979 = CARTESIAN_POINT('',(-5.4,-2.11180339887499,-17.24)) ;
#136980 = CARTESIAN_POINT('',(-5.4,-1.88819660112501,-17.34)) ;
#136981 = CARTESIAN_POINT('Ctrl Pts',(-5.4,-1.88819660112501,-17.34)) ;
#136982 = CARTESIAN_POINT('Ctrl Pts',(-5.4,-1.946901032774,-17.3399999988261)) ;
#136983 = CARTESIAN_POINT('Ctrl Pts',(-5.4,-2.00491651967066,-17.3184452435961)) ;
#136984 = CARTESIAN_POINT('Ctrl Pts',(-5.4,-2.0877044485962,-17.2443974688785)) ;
#136985 = CARTESIAN_POINT('Ctrl Pts',(-5.4,-2.11180339704051,-17.1925068398913)) ;
#136986 = CARTESIAN_POINT('Ctrl Pts',(-5.4,-2.11180339887499,-17.14)) ;
#136987 = CARTESIAN_POINT('',(-5.4,3.9369800677651,-17.34)) ;
#136988 = CARTESIAN_POINT('',(-5.4,4.20000000000001,-17.34)) ;
#136989 = CARTESIAN_POINT('Ctrl Pts',(-5.4,3.9369800677651,-17.34)) ;
#136990 = CARTESIAN_POINT('Ctrl Pts',(-5.4,4.01601337581888,-17.3399999995189)) ;
#136991 = CARTESIAN_POINT('Ctrl Pts',(-5.4,4.09411900298413,-17.3184452862429)) ;
#136992 = CARTESIAN_POINT('Ctrl Pts',(-5.4,4.20557579169423,-17.2443974262317)) ;
#136993 = CARTESIAN_POINT('Ctrl Pts',(-5.4,4.23801992976516,-17.1925068719098)) ;
#136994 = CARTESIAN_POINT('Ctrl Pts',(-5.4,4.23801993223491,-17.14)) ;
#136995 = CARTESIAN_POINT('',(-5.4,4.23801993223491,-22.22)) ;
#136996 = CARTESIAN_POINT('',(-5.4,4.23801993223491,-18.42)) ;
#136997 = CARTESIAN_POINT('',(-5.4,4.23801993223491,-18.32)) ;
#136998 = CARTESIAN_POINT('',(-5.4,3.9369800677651,-18.22)) ;
#136999 = CARTESIAN_POINT('Ctrl Pts',(-5.4,4.23801993223491,-18.42)) ;
#137000 = CARTESIAN_POINT('Ctrl Pts',(-5.4,4.23801992976516,-18.3674931280903)) ;
#137001 = CARTESIAN_POINT('Ctrl Pts',(-5.4,4.20557579169425,-18.3156025737682)) ;
#137002 = CARTESIAN_POINT('Ctrl Pts',(-5.4,4.09411900298411,-18.2415547137572)) ;
#137003 = CARTESIAN_POINT('Ctrl Pts',(-5.4,4.0160133758189,-18.2200000004811)) ;
#137004 = CARTESIAN_POINT('Ctrl Pts',(-5.4,3.9369800677651,-18.22)) ;
#137005 = CARTESIAN_POINT('',(-5.4,-1.88819660112502,-18.22)) ;
#137006 = CARTESIAN_POINT('',(-5.4,-2.05,-18.22)) ;
#137007 = CARTESIAN_POINT('',(-5.4,-2.11180339887499,-18.42)) ;
#137008 = CARTESIAN_POINT('Ctrl Pts',(-5.4,-2.11180339887499,-18.42)) ;
#137009 = CARTESIAN_POINT('Ctrl Pts',(-5.4,-2.11180339704051,-18.3674931601087)) ;
#137010 = CARTESIAN_POINT('Ctrl Pts',(-5.4,-2.0877044485962,-18.3156025311215)) ;
#137011 = CARTESIAN_POINT('Ctrl Pts',(-5.4,-2.00491651967066,-18.2415547564039)) ;
#137012 = CARTESIAN_POINT('Ctrl Pts',(-5.4,-1.946901032774,-18.2200000011739)) ;
#137013 = CARTESIAN_POINT('Ctrl Pts',(-5.4,-1.88819660112502,-18.22)) ;
#137014 = CARTESIAN_POINT('',(-5.4,-2.11180339887499,-22.22)) ;
#137015 = CARTESIAN_POINT('',(-5.4,-2.11180339887499,-22.32)) ;
#137016 = CARTESIAN_POINT('',(-5.4,-1.88819660112501,-22.42)) ;
#137017 = CARTESIAN_POINT('Ctrl Pts',(-5.4,-1.88819660112501,-22.42)) ;
#137018 = CARTESIAN_POINT('Ctrl Pts',(-5.4,-1.946901032774,-22.4199999988261)) ;
#137019 = CARTESIAN_POINT('Ctrl Pts',(-5.4,-2.00491651967066,-22.3984452435961)) ;
#137020 = CARTESIAN_POINT('Ctrl Pts',(-5.4,-2.0877044485962,-22.3243974688785)) ;
#137021 = CARTESIAN_POINT('Ctrl Pts',(-5.4,-2.11180339704051,-22.2725068398913)) ;
#137022 = CARTESIAN_POINT('Ctrl Pts',(-5.4,-2.11180339887499,-22.22)) ;
#137023 = CARTESIAN_POINT('',(-5.4,3.9369800677651,-22.42)) ;
#137024 = CARTESIAN_POINT('',(-5.4,4.20000000000001,-22.42)) ;
#137025 = CARTESIAN_POINT('Ctrl Pts',(-5.4,3.9369800677651,-22.42)) ;
#137026 = CARTESIAN_POINT('Ctrl Pts',(-5.4,4.01601337581889,-22.4199999995189)) ;
#137027 = CARTESIAN_POINT('Ctrl Pts',(-5.4,4.09411900298413,-22.3984452862429)) ;
#137028 = CARTESIAN_POINT('Ctrl Pts',(-5.4,4.20557579169423,-22.3243974262317)) ;
#137029 = CARTESIAN_POINT('Ctrl Pts',(-5.4,4.23801992976516,-22.2725068719098)) ;
#137030 = CARTESIAN_POINT('Ctrl Pts',(-5.4,4.23801993223491,-22.22)) ;
#137031 = CARTESIAN_POINT('Origin',(-5.4,-4.05,-17.78)) ;
#137032 = CARTESIAN_POINT('',(-5.3,-4.05,-22.86)) ;
#137033 = CARTESIAN_POINT('',(3.5,-4.05,-22.86)) ;
#137034 = CARTESIAN_POINT('',(-5.4,-4.05,-22.86)) ;
#137035 = CARTESIAN_POINT('',(3.5,-4.05,-12.7)) ;
#137036 = CARTESIAN_POINT('',(3.5,-4.05,-17.78)) ;
#137037 = CARTESIAN_POINT('',(-5.3,-4.05,-12.7)) ;
#137038 = CARTESIAN_POINT('',(-5.4,-4.05,-12.7)) ;
#137039 = CARTESIAN_POINT('',(-5.3,-4.05,-17.78)) ;
#137040 = CARTESIAN_POINT('',(-4.5,-4.05,-16.14)) ;
#137041 = CARTESIAN_POINT('',(-4.3,-4.05,-16.34)) ;
#137042 = CARTESIAN_POINT('Origin',(-4.3,-4.05,-16.14)) ;
#137043 = CARTESIAN_POINT('',(-4.5,-4.05,-14.34)) ;
#137044 = CARTESIAN_POINT('',(-4.5,-4.05,-12.7)) ;
#137045 = CARTESIAN_POINT('',(-4.3,-4.05,-14.14)) ;
#137046 = CARTESIAN_POINT('Origin',(-4.3,-4.05,-14.34)) ;
#137047 = CARTESIAN_POINT('',(-3.25,-4.05,-14.14)) ;
#137048 = CARTESIAN_POINT('',(-5.4,-4.05,-14.14)) ;
#137049 = CARTESIAN_POINT('',(-3.05,-4.05,-14.34)) ;
#137050 = CARTESIAN_POINT('Origin',(-3.25,-4.05,-14.34)) ;
#137051 = CARTESIAN_POINT('',(-3.05,-4.05,-16.14)) ;
#137052 = CARTESIAN_POINT('',(-3.05,-4.05,-12.7)) ;
#137053 = CARTESIAN_POINT('',(-3.25,-4.05,-16.34)) ;
#137054 = CARTESIAN_POINT('Origin',(-3.25,-4.05,-16.14)) ;
#137055 = CARTESIAN_POINT('',(-5.4,-4.05,-16.34)) ;
#137056 = CARTESIAN_POINT('',(-4.5,-4.05,-21.22)) ;
#137057 = CARTESIAN_POINT('',(-4.3,-4.05,-21.42)) ;
#137058 = CARTESIAN_POINT('Origin',(-4.3,-4.05,-21.22)) ;
#137059 = CARTESIAN_POINT('',(-4.5,-4.05,-19.42)) ;
#137060 = CARTESIAN_POINT('',(-4.5,-4.05,-17.78)) ;
#137061 = CARTESIAN_POINT('',(-4.3,-4.05,-19.22)) ;
#137062 = CARTESIAN_POINT('Origin',(-4.3,-4.05,-19.42)) ;
#137063 = CARTESIAN_POINT('',(-3.25,-4.05,-19.22)) ;
#137064 = CARTESIAN_POINT('',(-5.4,-4.05,-19.22)) ;
#137065 = CARTESIAN_POINT('',(-3.05,-4.05,-19.42)) ;
#137066 = CARTESIAN_POINT('Origin',(-3.25,-4.05,-19.42)) ;
#137067 = CARTESIAN_POINT('',(-3.05,-4.05,-21.22)) ;
#137068 = CARTESIAN_POINT('',(-3.05,-4.05,-17.78)) ;
#137069 = CARTESIAN_POINT('',(-3.25,-4.05,-21.42)) ;
#137070 = CARTESIAN_POINT('Origin',(-3.25,-4.05,-21.22)) ;
#137071 = CARTESIAN_POINT('',(-5.4,-4.05,-21.42)) ;
#137072 = CARTESIAN_POINT('Origin',(3.6,-4.05,-17.78)) ;
#137073 = CARTESIAN_POINT('',(3.6,-3.95,-22.86)) ;
#137074 = CARTESIAN_POINT('',(3.6,-2.9,-22.86)) ;
#137075 = CARTESIAN_POINT('',(3.6,-4.05,-22.86)) ;
#137076 = CARTESIAN_POINT('',(3.6,-2.9,-12.7)) ;
#137077 = CARTESIAN_POINT('',(3.6,-2.9,-17.78)) ;
#137078 = CARTESIAN_POINT('',(3.6,-3.95,-12.7)) ;
#137079 = CARTESIAN_POINT('',(3.6,-4.05,-12.7)) ;
#137080 = CARTESIAN_POINT('',(3.6,-3.95,-17.78)) ;
#137081 = CARTESIAN_POINT('Origin',(3.6,-2.8,-17.78)) ;
#137082 = CARTESIAN_POINT('',(4.4,-2.8,-21.8431546211728)) ;
#137083 = CARTESIAN_POINT('',(4.54880051362942,-2.79999999972164,-21.3964378607329)) ;
#137084 = CARTESIAN_POINT('Ctrl Pts',(4.4,-2.8,-21.8431546211728)) ;
#137085 = CARTESIAN_POINT('Ctrl Pts',(4.40001102013631,-2.8,-21.8064400198503)) ;
#137086 = CARTESIAN_POINT('Ctrl Pts',(4.40220140384643,-2.79999999812164,
-21.7700681661022)) ;
#137087 = CARTESIAN_POINT('Ctrl Pts',(4.4066417499365,-2.79999999722267,-21.7340727380016)) ;
#137088 = CARTESIAN_POINT('Ctrl Pts',(4.41108209602656,-2.79999999632371,
-21.6980773099009)) ;
#137089 = CARTESIAN_POINT('Ctrl Pts',(4.41777240449682,-2.79999999692353,
-21.6624583074478)) ;
#137090 = CARTESIAN_POINT('Ctrl Pts',(4.42678327415264,-2.79999999844302,
-21.6272494087151)) ;
#137091 = CARTESIAN_POINT('Ctrl Pts',(4.42864654535147,-2.79999999875722,
-21.6199688986803)) ;
#137092 = CARTESIAN_POINT('Ctrl Pts',(4.43060908636135,-2.79999999907333,
-21.6127059171117)) ;
#137093 = CARTESIAN_POINT('Ctrl Pts',(4.43267155768737,-2.79999999933983,
-21.6054607590652)) ;
#137094 = CARTESIAN_POINT('Ctrl Pts',(4.4352900037877,-2.79999999967816,-21.5962625435099)) ;
#137095 = CARTESIAN_POINT('Ctrl Pts',(4.4380733085653,-2.79999999966609,-21.5870911025424)) ;
#137096 = CARTESIAN_POINT('Ctrl Pts',(4.44102157277561,-2.79999999954234,
-21.5779480782015)) ;
#137097 = CARTESIAN_POINT('Ctrl Pts',(4.45046499569139,-2.79999999914597,
-21.548662559869)) ;
#137098 = CARTESIAN_POINT('Ctrl Pts',(4.46157908226631,-2.7999999950538,-21.5197202134932)) ;
#137099 = CARTESIAN_POINT('Ctrl Pts',(4.47540732315414,-2.79999999166095,
-21.4922492625065)) ;
#137100 = CARTESIAN_POINT('Ctrl Pts',(4.47702479055524,-2.79999999126409,
-21.4890360289464)) ;
#137101 = CARTESIAN_POINT('Ctrl Pts',(4.47867903313991,-2.79999999107055,
-21.4858427221255)) ;
#137102 = CARTESIAN_POINT('Ctrl Pts',(4.4803718748147,-2.79999999105954,-21.482671097194)) ;
#137103 = CARTESIAN_POINT('Ctrl Pts',(4.48545039983907,-2.79999999102651,
-21.4731562223995)) ;
#137104 = CARTESIAN_POINT('Ctrl Pts',(4.49087631667452,-2.79999999265304,
-21.4638364846097)) ;
#137105 = CARTESIAN_POINT('Ctrl Pts',(4.49669887079745,-2.79999999431461,
-21.4547592728789)) ;
#137106 = CARTESIAN_POINT('Ctrl Pts',(4.50888705006192,-2.79999999779274,
-21.4357582157035)) ;
#137107 = CARTESIAN_POINT('Ctrl Pts',(4.52313265843749,-2.79999999982394,
-21.41737449918)) ;
#137108 = CARTESIAN_POINT('Ctrl Pts',(4.54066913339539,-2.79999999997241,
-21.4027304219711)) ;
#137109 = CARTESIAN_POINT('Ctrl Pts',(4.54329026609835,-2.79999999999461,
-21.400541608668)) ;
#137110 = CARTESIAN_POINT('Ctrl Pts',(4.5460045281952,-2.8,-21.3984393445787)) ;
#137111 = CARTESIAN_POINT('Ctrl Pts',(4.54880363749517,-2.8,-21.396450206041)) ;
#137112 = CARTESIAN_POINT('',(4.4,-2.8,-20.3200000000039)) ;
#137113 = CARTESIAN_POINT('Ctrl Pts',(4.54879236168152,-2.8,-21.39643444348)) ;
#137114 = CARTESIAN_POINT('Ctrl Pts',(4.51096310105345,-2.8,-21.3676409078196)) ;
#137115 = CARTESIAN_POINT('Ctrl Pts',(4.49022331291407,-2.8,-21.3238291192761)) ;
#137116 = CARTESIAN_POINT('Ctrl Pts',(4.45698031182017,-2.8,-21.2376238713958)) ;
#137117 = CARTESIAN_POINT('Ctrl Pts',(4.44561000227039,-2.8,-21.1923611449586)) ;
#137118 = CARTESIAN_POINT('Ctrl Pts',(4.41911102299977,-2.8,-21.0558807916569)) ;
#137119 = CARTESIAN_POINT('Ctrl Pts',(4.41155688769424,-2.8,-20.964231375192)) ;
#137120 = CARTESIAN_POINT('Ctrl Pts',(4.39763503647248,-2.8,-20.688710456933)) ;
#137121 = CARTESIAN_POINT('Ctrl Pts',(4.4,-2.8,-20.5042606621178)) ;
#137122 = CARTESIAN_POINT('Ctrl Pts',(4.4,-2.8,-20.3200000000039)) ;
#137123 = CARTESIAN_POINT('',(4.54879236179094,-2.79999999953044,-19.2435655565041)) ;
#137124 = CARTESIAN_POINT('Ctrl Pts',(4.4,-2.8,-20.3200000000039)) ;
#137125 = CARTESIAN_POINT('Ctrl Pts',(4.4,-2.8,-20.1354847183429)) ;
#137126 = CARTESIAN_POINT('Ctrl Pts',(4.39760751905643,-2.8,-19.9507836732851)) ;
#137127 = CARTESIAN_POINT('Ctrl Pts',(4.40696794948104,-2.8,-19.7665893237033)) ;
#137128 = CARTESIAN_POINT('Ctrl Pts',(4.41164816469334,-2.8,-19.6744921489124)) ;
#137129 = CARTESIAN_POINT('Ctrl Pts',(4.41940496802384,-2.80000000000001,
-19.5821571435008)) ;
#137130 = CARTESIAN_POINT('Ctrl Pts',(4.43698455094239,-2.8,-19.4920661537484)) ;
#137131 = CARTESIAN_POINT('Ctrl Pts',(4.44577434240167,-2.8,-19.4470206588722)) ;
#137132 = CARTESIAN_POINT('Ctrl Pts',(4.456925956929,-2.80000000000001,-19.4024769174896)) ;
#137133 = CARTESIAN_POINT('Ctrl Pts',(4.47366127850408,-2.8,-19.3591194060904)) ;
#137134 = CARTESIAN_POINT('Ctrl Pts',(4.47575319370098,-2.8,-19.3536997171655)) ;
#137135 = CARTESIAN_POINT('Ctrl Pts',(4.47791173590511,-2.79999999997843,
-19.3482741547806)) ;
#137136 = CARTESIAN_POINT('Ctrl Pts',(4.48016062485992,-2.80000000010461,
-19.3428732875221)) ;
#137137 = CARTESIAN_POINT('Ctrl Pts',(4.48803173620173,-2.80000000054624,
-19.3239702521172)) ;
#137138 = CARTESIAN_POINT('Ctrl Pts',(4.49700942865457,-2.80000000534986,
-19.3053696658144)) ;
#137139 = CARTESIAN_POINT('Ctrl Pts',(4.50810946414921,-2.80000000469598,
-19.2883816651393)) ;
#137140 = CARTESIAN_POINT('Ctrl Pts',(4.51435323411495,-2.80000000432818,
-19.2788259147596)) ;
#137141 = CARTESIAN_POINT('Ctrl Pts',(4.52126852668377,-2.80000000204489,
-19.2697803965514)) ;
#137142 = CARTESIAN_POINT('Ctrl Pts',(4.5290361256546,-2.80000000089509,-19.2614782866676)) ;
#137143 = CARTESIAN_POINT('Ctrl Pts',(4.5320568585877,-2.80000000044794,-19.2582496883795)) ;
#137144 = CARTESIAN_POINT('Ctrl Pts',(4.53520648971123,-2.80000000018876,
-19.2551335191281)) ;
#137145 = CARTESIAN_POINT('Ctrl Pts',(4.53849565154303,-2.80000000008376,
-19.252143492806)) ;
#137146 = CARTESIAN_POINT('Ctrl Pts',(4.54178481337482,-2.79999999997876,
-19.2491534664838)) ;
#137147 = CARTESIAN_POINT('Ctrl Pts',(4.54521363891049,-2.8,-19.2462897578219)) ;
#137148 = CARTESIAN_POINT('Ctrl Pts',(4.5487923616809,-2.8,-19.2435655565195)) ;
#137149 = CARTESIAN_POINT('',(4.4,-2.8,-18.7968453788272)) ;
#137150 = CARTESIAN_POINT('Ctrl Pts',(4.54879236168109,-2.79999999812176,
-19.2435655565192)) ;
#137151 = CARTESIAN_POINT('Ctrl Pts',(4.54599316991904,-2.79999999835896,
-19.2415756143354)) ;
#137152 = CARTESIAN_POINT('Ctrl Pts',(4.54327885465676,-2.7999999985882,-19.2394726568399)) ;
#137153 = CARTESIAN_POINT('Ctrl Pts',(4.52311604063302,-2.80000000023132,
-19.2226310596931)) ;
#137154 = CARTESIAN_POINT('Ctrl Pts',(4.5088678063233,-2.80000000100533,-19.2042421996431)) ;
#137155 = CARTESIAN_POINT('Ctrl Pts',(4.48892103801306,-2.79999999510252,
-19.1731290218304)) ;
#137156 = CARTESIAN_POINT('Ctrl Pts',(4.48186523313292,-2.7999999909955,-19.1605832050237)) ;
#137157 = CARTESIAN_POINT('Ctrl Pts',(4.46162186753409,-2.79999997126272,
-19.1202567139418)) ;
#137158 = CARTESIAN_POINT('Ctrl Pts',(4.45052849087263,-2.7999999685384,-19.0913189617092)) ;
#137159 = CARTESIAN_POINT('Ctrl Pts',(4.43813540717736,-2.79999997674815,
-19.0529060591291)) ;
#137160 = CARTESIAN_POINT('Ctrl Pts',(4.43535270120343,-2.79999997903695,
-19.0437502640508)) ;
#137161 = CARTESIAN_POINT('Ctrl Pts',(4.41677772587598,-2.79999999273252,
-18.9786688014867)) ;
#137162 = CARTESIAN_POINT('Ctrl Pts',(4.40678488790793,-2.79999999887621,
-18.9217195184934)) ;
#137163 = CARTESIAN_POINT('Ctrl Pts',(4.40081887576499,-2.80000000006435,
-18.8416198967613)) ;
#137164 = CARTESIAN_POINT('Ctrl Pts',(4.4,-2.8,-18.8193018981784)) ;
#137165 = CARTESIAN_POINT('Ctrl Pts',(4.4,-2.8,-18.7968453788272)) ;
#137166 = CARTESIAN_POINT('',(4.4,-2.8,-16.7631546211728)) ;
#137167 = CARTESIAN_POINT('',(4.4,-2.8,-17.78)) ;
#137168 = CARTESIAN_POINT('',(4.54880051362942,-2.79999999972164,-16.3164378607329)) ;
#137169 = CARTESIAN_POINT('Ctrl Pts',(4.4,-2.8,-16.7631546211728)) ;
#137170 = CARTESIAN_POINT('Ctrl Pts',(4.40001102013631,-2.8,-16.7264400198511)) ;
#137171 = CARTESIAN_POINT('Ctrl Pts',(4.40220140384633,-2.79999999812164,
-16.6900681661039)) ;
#137172 = CARTESIAN_POINT('Ctrl Pts',(4.40664174993619,-2.79999999722267,
-16.6540727380041)) ;
#137173 = CARTESIAN_POINT('Ctrl Pts',(4.41108209602605,-2.79999999632371,
-16.6180773099042)) ;
#137174 = CARTESIAN_POINT('Ctrl Pts',(4.41777240449601,-2.79999999692353,
-16.5824583074518)) ;
#137175 = CARTESIAN_POINT('Ctrl Pts',(4.42678327415141,-2.79999999844302,
-16.5472494087199)) ;
#137176 = CARTESIAN_POINT('Ctrl Pts',(4.42864654535061,-2.79999999875722,
-16.5399688986835)) ;
#137177 = CARTESIAN_POINT('Ctrl Pts',(4.4306090863609,-2.79999999907333,-16.5327059171133)) ;
#137178 = CARTESIAN_POINT('Ctrl Pts',(4.43267155768737,-2.79999999933982,
-16.5254607590652)) ;
#137179 = CARTESIAN_POINT('Ctrl Pts',(4.4352900037877,-2.79999999967816,-16.5162625435099)) ;
#137180 = CARTESIAN_POINT('Ctrl Pts',(4.4380733085653,-2.79999999966609,-16.5070911025424)) ;
#137181 = CARTESIAN_POINT('Ctrl Pts',(4.44102157277562,-2.79999999954234,
-16.4979480782015)) ;
#137182 = CARTESIAN_POINT('Ctrl Pts',(4.45046499569139,-2.79999999914597,
-16.468662559869)) ;
#137183 = CARTESIAN_POINT('Ctrl Pts',(4.46157908226631,-2.79999999505379,
-16.4397202134932)) ;
#137184 = CARTESIAN_POINT('Ctrl Pts',(4.47540732315414,-2.79999999166095,
-16.4122492625065)) ;
#137185 = CARTESIAN_POINT('Ctrl Pts',(4.47702479055524,-2.79999999126409,
-16.4090360289464)) ;
#137186 = CARTESIAN_POINT('Ctrl Pts',(4.47867903313991,-2.79999999107055,
-16.4058427221255)) ;
#137187 = CARTESIAN_POINT('Ctrl Pts',(4.4803718748147,-2.79999999105954,-16.402671097194)) ;
#137188 = CARTESIAN_POINT('Ctrl Pts',(4.48545039983907,-2.79999999102651,
-16.3931562223995)) ;
#137189 = CARTESIAN_POINT('Ctrl Pts',(4.49087631667452,-2.79999999265304,
-16.3838364846097)) ;
#137190 = CARTESIAN_POINT('Ctrl Pts',(4.49669887079745,-2.79999999431461,
-16.3747592728789)) ;
#137191 = CARTESIAN_POINT('Ctrl Pts',(4.50888705006192,-2.79999999779274,
-16.3557582157035)) ;
#137192 = CARTESIAN_POINT('Ctrl Pts',(4.52313265843749,-2.79999999982394,
-16.33737449918)) ;
#137193 = CARTESIAN_POINT('Ctrl Pts',(4.54066913339539,-2.79999999997241,
-16.3227304219711)) ;
#137194 = CARTESIAN_POINT('Ctrl Pts',(4.54329026609835,-2.7999999999946,-16.320541608668)) ;
#137195 = CARTESIAN_POINT('Ctrl Pts',(4.5460045281952,-2.8,-16.3184393445787)) ;
#137196 = CARTESIAN_POINT('Ctrl Pts',(4.54880363749517,-2.8,-16.316450206041)) ;
#137197 = CARTESIAN_POINT('',(4.4,-2.8,-15.2400000000038)) ;
#137198 = CARTESIAN_POINT('Ctrl Pts',(4.54879236168152,-2.8,-16.31643444348)) ;
#137199 = CARTESIAN_POINT('Ctrl Pts',(4.51096310105345,-2.8,-16.2876409078196)) ;
#137200 = CARTESIAN_POINT('Ctrl Pts',(4.49022331291407,-2.8,-16.2438291192761)) ;
#137201 = CARTESIAN_POINT('Ctrl Pts',(4.45698031182017,-2.8,-16.1576238713958)) ;
#137202 = CARTESIAN_POINT('Ctrl Pts',(4.44561000227039,-2.8,-16.1123611449586)) ;
#137203 = CARTESIAN_POINT('Ctrl Pts',(4.41911102299977,-2.8,-15.9758807916569)) ;
#137204 = CARTESIAN_POINT('Ctrl Pts',(4.41155688769424,-2.8,-15.8842313751921)) ;
#137205 = CARTESIAN_POINT('Ctrl Pts',(4.39763503647248,-2.8,-15.608710456933)) ;
#137206 = CARTESIAN_POINT('Ctrl Pts',(4.4,-2.8,-15.4242606621178)) ;
#137207 = CARTESIAN_POINT('Ctrl Pts',(4.4,-2.8,-15.2400000000038)) ;
#137208 = CARTESIAN_POINT('',(4.54879236179093,-2.79999999953044,-14.1635655565041)) ;
#137209 = CARTESIAN_POINT('Ctrl Pts',(4.4,-2.8,-15.2400000000038)) ;
#137210 = CARTESIAN_POINT('Ctrl Pts',(4.4,-2.8,-15.0554847183429)) ;
#137211 = CARTESIAN_POINT('Ctrl Pts',(4.39760751905643,-2.8,-14.8707836732851)) ;
#137212 = CARTESIAN_POINT('Ctrl Pts',(4.40696794948104,-2.8,-14.6865893237033)) ;
#137213 = CARTESIAN_POINT('Ctrl Pts',(4.41164816469334,-2.8,-14.5944921489124)) ;
#137214 = CARTESIAN_POINT('Ctrl Pts',(4.41940496802384,-2.80000000000001,
-14.5021571435008)) ;
#137215 = CARTESIAN_POINT('Ctrl Pts',(4.43698455094237,-2.8,-14.4120661537484)) ;
#137216 = CARTESIAN_POINT('Ctrl Pts',(4.44577434240165,-2.8,-14.3670206588722)) ;
#137217 = CARTESIAN_POINT('Ctrl Pts',(4.456925956929,-2.80000000000001,-14.3224769174896)) ;
#137218 = CARTESIAN_POINT('Ctrl Pts',(4.47366127850409,-2.8,-14.2791194060904)) ;
#137219 = CARTESIAN_POINT('Ctrl Pts',(4.47575319370098,-2.8,-14.2736997171655)) ;
#137220 = CARTESIAN_POINT('Ctrl Pts',(4.47791173590511,-2.79999999997843,
-14.2682741547806)) ;
#137221 = CARTESIAN_POINT('Ctrl Pts',(4.48016062485991,-2.80000000010461,
-14.2628732875221)) ;
#137222 = CARTESIAN_POINT('Ctrl Pts',(4.48803173620173,-2.80000000054624,
-14.2439702521172)) ;
#137223 = CARTESIAN_POINT('Ctrl Pts',(4.49700942865457,-2.80000000534986,
-14.2253696658144)) ;
#137224 = CARTESIAN_POINT('Ctrl Pts',(4.50810946414921,-2.80000000469598,
-14.2083816651393)) ;
#137225 = CARTESIAN_POINT('Ctrl Pts',(4.51435323411495,-2.80000000432818,
-14.1988259147596)) ;
#137226 = CARTESIAN_POINT('Ctrl Pts',(4.52126852668377,-2.80000000204489,
-14.1897803965514)) ;
#137227 = CARTESIAN_POINT('Ctrl Pts',(4.5290361256546,-2.80000000089509,-14.1814782866676)) ;
#137228 = CARTESIAN_POINT('Ctrl Pts',(4.5320568585877,-2.80000000044794,-14.1782496883795)) ;
#137229 = CARTESIAN_POINT('Ctrl Pts',(4.53520648971123,-2.80000000018876,
-14.1751335191281)) ;
#137230 = CARTESIAN_POINT('Ctrl Pts',(4.53849565154302,-2.80000000008376,
-14.1721434928059)) ;
#137231 = CARTESIAN_POINT('Ctrl Pts',(4.54178481337482,-2.79999999997876,
-14.1691534664838)) ;
#137232 = CARTESIAN_POINT('Ctrl Pts',(4.54521363891049,-2.8,-14.1662897578218)) ;
#137233 = CARTESIAN_POINT('Ctrl Pts',(4.54879236168087,-2.8,-14.1635655565195)) ;
#137234 = CARTESIAN_POINT('',(4.4,-2.8,-13.7168453788272)) ;
#137235 = CARTESIAN_POINT('Ctrl Pts',(4.54879236168109,-2.79999999812176,
-14.1635655565192)) ;
#137236 = CARTESIAN_POINT('Ctrl Pts',(4.54599316991904,-2.79999999835896,
-14.1615756143355)) ;
#137237 = CARTESIAN_POINT('Ctrl Pts',(4.54327885465676,-2.7999999985882,-14.1594726568399)) ;
#137238 = CARTESIAN_POINT('Ctrl Pts',(4.52311604063302,-2.80000000023133,
-14.1426310596931)) ;
#137239 = CARTESIAN_POINT('Ctrl Pts',(4.5088678063233,-2.80000000100534,-14.1242421996432)) ;
#137240 = CARTESIAN_POINT('Ctrl Pts',(4.48892103801306,-2.79999999510253,
-14.0931290218304)) ;
#137241 = CARTESIAN_POINT('Ctrl Pts',(4.48186523313291,-2.79999999099551,
-14.0805832050237)) ;
#137242 = CARTESIAN_POINT('Ctrl Pts',(4.46162186753409,-2.79999997126272,
-14.0402567139419)) ;
#137243 = CARTESIAN_POINT('Ctrl Pts',(4.45052849087263,-2.7999999685384,-14.0113189617092)) ;
#137244 = CARTESIAN_POINT('Ctrl Pts',(4.43813540717736,-2.79999997674815,
-13.9729060591291)) ;
#137245 = CARTESIAN_POINT('Ctrl Pts',(4.43535270120344,-2.79999997903695,
-13.9637502640508)) ;
#137246 = CARTESIAN_POINT('Ctrl Pts',(4.4167777258757,-2.79999999273252,-13.8986688014857)) ;
#137247 = CARTESIAN_POINT('Ctrl Pts',(4.40678488790757,-2.79999999887621,
-13.8417195184913)) ;
#137248 = CARTESIAN_POINT('Ctrl Pts',(4.40081887576491,-2.80000000006435,
-13.7616198967592)) ;
#137249 = CARTESIAN_POINT('Ctrl Pts',(4.4,-2.8,-13.7393018981773)) ;
#137250 = CARTESIAN_POINT('Ctrl Pts',(4.4,-2.8,-13.7168453788272)) ;
#137251 = CARTESIAN_POINT('',(4.4,-2.8,-12.7)) ;
#137252 = CARTESIAN_POINT('',(4.4,-2.8,-12.7)) ;
#137253 = CARTESIAN_POINT('',(3.7,-2.8,-12.7)) ;
#137254 = CARTESIAN_POINT('',(3.6,-2.8,-12.7)) ;
#137255 = CARTESIAN_POINT('',(3.7,-2.8,-22.86)) ;
#137256 = CARTESIAN_POINT('',(3.7,-2.8,-22.86)) ;
#137257 = CARTESIAN_POINT('',(4.4,-2.8,-22.86)) ;
#137258 = CARTESIAN_POINT('',(3.6,-2.8,-22.86)) ;
#137259 = CARTESIAN_POINT('',(4.4,-2.8,-17.78)) ;
#137260 = CARTESIAN_POINT('Origin',(4.5,-2.8,-17.78)) ;
#137261 = CARTESIAN_POINT('',(4.5,-2.4,-18.3578583129651)) ;
#137262 = CARTESIAN_POINT('',(4.5,-2.4,-17.2021416870349)) ;
#137263 = CARTESIAN_POINT('',(4.5,-2.4,-17.78)) ;
#137264 = CARTESIAN_POINT('',(4.5,-2.7,-16.7631546211728)) ;
#137265 = CARTESIAN_POINT('Origin',(4.5,0.,-15.24)) ;
#137266 = CARTESIAN_POINT('',(4.5,-2.7,-18.7968453788272)) ;
#137267 = CARTESIAN_POINT('',(4.5,-2.7,-17.78)) ;
#137268 = CARTESIAN_POINT('Origin',(4.5,0.,-20.32)) ;
#137269 = CARTESIAN_POINT('Origin',(4.5,-2.3,-17.78)) ;
#137270 = CARTESIAN_POINT('',(12.7,-2.3,-22.2821416870349)) ;
#137271 = CARTESIAN_POINT('',(4.6,-2.3,-22.2821416870349)) ;
#137272 = CARTESIAN_POINT('',(4.5,-2.3,-22.2821416870349)) ;
#137273 = CARTESIAN_POINT('',(4.6,-2.3,-22.86)) ;
#137274 = CARTESIAN_POINT('',(4.6,-2.3,-22.86)) ;
#137275 = CARTESIAN_POINT('',(12.7,-2.3,-22.86)) ;
#137276 = CARTESIAN_POINT('',(4.5,-2.3,-22.86)) ;
#137277 = CARTESIAN_POINT('',(12.7,-2.3,-17.78)) ;
#137278 = CARTESIAN_POINT('Origin',(0.,0.,-22.86)) ;
#137279 = CARTESIAN_POINT('Origin',(3.3,10.85,-22.86)) ;
#137280 = CARTESIAN_POINT('Origin',(3.85,6.92431432344521,-22.86)) ;
#137281 = CARTESIAN_POINT('Origin',(4.05,3.77568567655479,-22.86)) ;
#137282 = CARTESIAN_POINT('Origin',(4.55912712210514,2.85,-22.86)) ;
#137283 = CARTESIAN_POINT('Origin',(12.7,2.65,-22.86)) ;
#137284 = CARTESIAN_POINT('Origin',(12.7,-2.2,-22.86)) ;
#137285 = CARTESIAN_POINT('Origin',(4.6,-2.4,-22.86)) ;
#137286 = CARTESIAN_POINT('Origin',(4.4,-2.7,-22.86)) ;
#137287 = CARTESIAN_POINT('Origin',(3.7,-2.9,-22.86)) ;
#137288 = CARTESIAN_POINT('Origin',(3.5,-3.95,-22.86)) ;
#137289 = CARTESIAN_POINT('Origin',(-5.3,-3.95,-22.86)) ;
#137290 = CARTESIAN_POINT('Origin',(-5.3,5.19009804864072,-22.86)) ;
#137291 = CARTESIAN_POINT('Origin',(-4.8,10.3,-22.86)) ;
#137292 = CARTESIAN_POINT('Origin',(-4.8,10.85,-22.86)) ;
#137293 = CARTESIAN_POINT('Origin',(-4.65,1.95,-22.32)) ;
#137294 = CARTESIAN_POINT('',(-4.66204490261456,3.21928058320648,-22.32)) ;
#137295 = CARTESIAN_POINT('',(-5.3,3.9369800677651,-22.32)) ;
#137296 = CARTESIAN_POINT('',(-5.47474093186837,4.13356361611701,-22.32)) ;
#137297 = CARTESIAN_POINT('',(-5.3,-1.88819660112501,-22.32)) ;
#137298 = CARTESIAN_POINT('',(-5.3,-2.05,-22.32)) ;
#137299 = CARTESIAN_POINT('',(-4.66204490261456,-1.5692190524323,-22.32)) ;
#137300 = CARTESIAN_POINT('',(-4.69472135955,-1.58555728090001,-22.32)) ;
#137301 = CARTESIAN_POINT('',(-4.66204490261456,3.35625,-22.32)) ;
#137302 = CARTESIAN_POINT('Origin',(-5.4,1.95,-18.32)) ;
#137303 = CARTESIAN_POINT('',(-4.66204490261456,-1.5692190524323,-18.32)) ;
#137304 = CARTESIAN_POINT('',(-5.3,-1.88819660112502,-18.32)) ;
#137305 = CARTESIAN_POINT('',(-5.44472135955,-1.96055728090001,-18.32)) ;
#137306 = CARTESIAN_POINT('',(-5.3,3.9369800677651,-18.32)) ;
#137307 = CARTESIAN_POINT('',(-5.3,4.20000000000001,-18.32)) ;
#137308 = CARTESIAN_POINT('',(-4.66204490261456,3.21928058320648,-18.32)) ;
#137309 = CARTESIAN_POINT('',(-4.72474093186837,3.28981361611701,-18.32)) ;
#137310 = CARTESIAN_POINT('',(-4.66204490261456,-1.67500000000001,-18.32)) ;
#137311 = CARTESIAN_POINT('Origin',(-4.65,1.95,-18.32)) ;
#137312 = CARTESIAN_POINT('',(-3.33134808452128,1.85,-18.6423371348948)) ;
#137313 = CARTESIAN_POINT('',(-3.48082994825801,1.91712723223402,-18.6057971237592)) ;
#137314 = CARTESIAN_POINT('Origin',(-3.34328863644916,2.02341244982155,-18.6394183333124)) ;
#137315 = CARTESIAN_POINT('',(-2.4,1.85,-18.87)) ;
#137316 = CARTESIAN_POINT('',(-4.65,1.85,-18.32)) ;
#137317 = CARTESIAN_POINT('',(-2.4,-0.95,-18.87)) ;
#137318 = CARTESIAN_POINT('',(-2.4,1.95,-18.87)) ;
#137319 = CARTESIAN_POINT('',(-3.3526478932023,-0.95,-18.637130514995)) ;
#137320 = CARTESIAN_POINT('',(-3.39999999999998,-0.95,-18.6255555555556)) ;
#137321 = CARTESIAN_POINT('',(-3.44209061230229,-0.971114561800017,-18.615266739215)) ;
#137322 = CARTESIAN_POINT('Origin',(-3.36201220558082,-1.11033257691485,-18.634841460858)) ;
#137323 = CARTESIAN_POINT('',(-4.63829959356686,-1.5692190524323,-18.3228600993503)) ;
#137324 = CARTESIAN_POINT('',(-4.68814869588294,-1.59414360359034,-18.3106747632286)) ;
#137325 = CARTESIAN_POINT('',(-4.63829959356686,3.21928058320648,-18.3228600993503)) ;
#137326 = CARTESIAN_POINT('',(-4.63829959356686,3.35625,-18.3228600993503)) ;
#137327 = CARTESIAN_POINT('',(-3.45989661114215,1.89357722797868,-18.6109141617208)) ;
#137328 = CARTESIAN_POINT('Origin',(-2.4,1.95,-18.87)) ;
#137329 = CARTESIAN_POINT('',(-2.4,1.85,-21.77)) ;
#137330 = CARTESIAN_POINT('',(-2.4,-0.95,-21.77)) ;
#137331 = CARTESIAN_POINT('',(-2.4,1.95,-21.77)) ;
#137332 = CARTESIAN_POINT('',(-2.4,-1.05,-21.667055690472)) ;
#137333 = CARTESIAN_POINT('Origin',(-2.4,-0.950000000000066,-21.6670556904721)) ;
#137334 = CARTESIAN_POINT('',(-2.4,-1.05,-18.972944309528)) ;
#137335 = CARTESIAN_POINT('',(-2.4,-1.05,-18.87)) ;
#137336 = CARTESIAN_POINT('Origin',(-2.4,-0.949999999999802,-18.9729443095282)) ;
#137337 = CARTESIAN_POINT('',(-2.4,1.95,-18.972944309528)) ;
#137338 = CARTESIAN_POINT('Origin',(-2.4,1.84999999999981,-18.9729443095282)) ;
#137339 = CARTESIAN_POINT('',(-2.4,1.95,-21.667055690472)) ;
#137340 = CARTESIAN_POINT('',(-2.4,1.95,-18.87)) ;
#137341 = CARTESIAN_POINT('Origin',(-2.4,1.85000000000024,-21.6670556904722)) ;
#137342 = CARTESIAN_POINT('Origin',(-2.4,1.95,-21.77)) ;
#137343 = CARTESIAN_POINT('',(-3.3526478932023,-0.95,-22.002869485005)) ;
#137344 = CARTESIAN_POINT('',(-3.44209061230229,-0.971114561800017,-22.024733260785)) ;
#137345 = CARTESIAN_POINT('Origin',(-3.36201220558296,-1.11033257690641,-22.0051585391426)) ;
#137346 = CARTESIAN_POINT('',(-2.4,-0.95,-21.77)) ;
#137347 = CARTESIAN_POINT('',(-3.33134808452128,1.85,-21.9976628651052)) ;
#137348 = CARTESIAN_POINT('',(-2.4,1.85,-21.77)) ;
#137349 = CARTESIAN_POINT('',(-3.48082994825801,1.91712723223402,-22.0342028762408)) ;
#137350 = CARTESIAN_POINT('Origin',(-3.34328863644886,2.0234124498222,-22.0005816666875)) ;
#137351 = CARTESIAN_POINT('',(-4.63829959356686,3.21928058320648,-22.3171399006497)) ;
#137352 = CARTESIAN_POINT('',(-4.70989661114216,3.29982722797869,-22.3346413938348)) ;
#137353 = CARTESIAN_POINT('',(-4.63829959356686,-1.5692190524323,-22.3171399006497)) ;
#137354 = CARTESIAN_POINT('',(-4.63829959356686,-1.67500000000001,-22.3171399006497)) ;
#137355 = CARTESIAN_POINT('',(-3.43814869588292,-0.969143603590331,-22.0237696812158)) ;
#137356 = CARTESIAN_POINT('Origin',(0.,1.95,-20.32)) ;
#137357 = CARTESIAN_POINT('',(-3.35509339356897,1.95,-18.7394770355445)) ;
#137358 = CARTESIAN_POINT('',(0.175392621986784,1.95,-19.6024847282359)) ;
#137359 = CARTESIAN_POINT('',(-3.35509339356897,1.95,-21.9005229644555)) ;
#137360 = CARTESIAN_POINT('',(-3.35509339356897,1.95,-22.0144444444444)) ;
#137361 = CARTESIAN_POINT('',(0.175392621986784,1.95,-21.0375152717641)) ;
#137362 = CARTESIAN_POINT('Origin',(0.,-1.05,-20.32)) ;
#137363 = CARTESIAN_POINT('',(-3.37639320225,-1.05,-21.9057295843553)) ;
#137364 = CARTESIAN_POINT('',(-3.42374530904768,-1.05,-21.9173045437948)) ;
#137365 = CARTESIAN_POINT('',(-3.37639320225,-1.05,-18.7342704156447)) ;
#137366 = CARTESIAN_POINT('',(-3.37639320225,-1.05,-20.32)) ;
#137367 = CARTESIAN_POINT('',(-2.4237453090477,-1.05,-18.9671399006497)) ;
#137368 = CARTESIAN_POINT('Origin',(-3.39999999999998,-1.05,-20.32)) ;
#137369 = CARTESIAN_POINT('',(-3.4211145618,-1.06055728090001,-18.7124066398647)) ;
#137370 = CARTESIAN_POINT('',(-3.4211145618,-1.06055728090001,-21.9275933601353)) ;
#137371 = CARTESIAN_POINT('',(-3.4211145618,-1.06055728090001,-20.32)) ;
#137372 = CARTESIAN_POINT('',(-4.61732354306457,-1.65866177153229,-22.22)) ;
#137373 = CARTESIAN_POINT('',(-4.66717264538064,-1.68358632269033,-22.2321853361217)) ;
#137374 = CARTESIAN_POINT('',(-5.34472135954999,-2.022360679775,-22.22)) ;
#137375 = CARTESIAN_POINT('',(-5.4,-2.05,-22.22)) ;
#137376 = CARTESIAN_POINT('',(-5.34472135954999,-2.022360679775,-18.42)) ;
#137377 = CARTESIAN_POINT('',(-5.34472135954999,-2.022360679775,-18.32)) ;
#137378 = CARTESIAN_POINT('',(-4.61732354306457,-1.65866177153229,-18.42)) ;
#137379 = CARTESIAN_POINT('',(-4.65,-1.67500000000001,-18.42)) ;
#137380 = CARTESIAN_POINT('',(-3.41717264538063,-1.05858632269032,-18.7133702194339)) ;
#137381 = CARTESIAN_POINT('Origin',(-5.4,4.20000000000001,-17.78)) ;
#137382 = CARTESIAN_POINT('',(-5.37474093186837,4.17158354835192,-18.42)) ;
#137383 = CARTESIAN_POINT('',(-5.37474093186837,4.17158354835192,-22.22)) ;
#137384 = CARTESIAN_POINT('',(-5.37474093186837,4.17158354835192,-22.32)) ;
#137385 = CARTESIAN_POINT('',(-4.58730397074619,3.28571696708947,-22.22)) ;
#137386 = CARTESIAN_POINT('',(-4.65,3.35625,-22.22)) ;
#137387 = CARTESIAN_POINT('',(-3.42983432543734,1.98356361611701,-21.9370629755912)) ;
#137388 = CARTESIAN_POINT('',(-3.40890098832149,1.96001361186167,-21.9319459376295)) ;
#137389 = CARTESIAN_POINT('',(-3.42983432543734,1.98356361611701,-18.7029370244088)) ;
#137390 = CARTESIAN_POINT('',(-3.42983432543734,1.98356361611701,-18.6255555555556)) ;
#137391 = CARTESIAN_POINT('',(-4.58730397074619,3.28571696708947,-18.42)) ;
#137392 = CARTESIAN_POINT('',(-4.65890098832149,3.36626361186168,-18.4024985068149)) ;
#137393 = CARTESIAN_POINT('',(-5.4,4.20000000000001,-18.42)) ;
#137394 = CARTESIAN_POINT('Origin',(-3.15,-3.9,-19.32)) ;
#137395 = CARTESIAN_POINT('',(-3.15,-3.95,-19.42)) ;
#137396 = CARTESIAN_POINT('',(-3.15,-3.85,-19.42)) ;
#137397 = CARTESIAN_POINT('',(-3.15,-3.75,-19.42)) ;
#137398 = CARTESIAN_POINT('',(-3.15,-3.85,-21.22)) ;
#137399 = CARTESIAN_POINT('',(-3.15,-3.85,-19.32)) ;
#137400 = CARTESIAN_POINT('',(-3.15,-3.95,-21.22)) ;
#137401 = CARTESIAN_POINT('',(-3.15,-4.05,-21.22)) ;
#137402 = CARTESIAN_POINT('',(-3.15,-3.95,-19.32)) ;
#137403 = CARTESIAN_POINT('Origin',(-4.4,-3.9,-21.32)) ;
#137404 = CARTESIAN_POINT('',(-3.25,-3.85,-21.32)) ;
#137405 = CARTESIAN_POINT('',(-4.3,-3.85,-21.32)) ;
#137406 = CARTESIAN_POINT('',(-4.4,-3.85,-21.32)) ;
#137407 = CARTESIAN_POINT('',(-4.3,-3.95,-21.32)) ;
#137408 = CARTESIAN_POINT('',(-4.3,-4.05,-21.32)) ;
#137409 = CARTESIAN_POINT('',(-3.25,-3.95,-21.32)) ;
#137410 = CARTESIAN_POINT('',(-4.4,-3.95,-21.32)) ;
#137411 = CARTESIAN_POINT('',(-3.25,-3.75,-21.32)) ;
#137412 = CARTESIAN_POINT('Origin',(-4.4,-3.9,-19.32)) ;
#137413 = CARTESIAN_POINT('',(-4.4,-3.85,-21.22)) ;
#137414 = CARTESIAN_POINT('',(-4.4,-3.85,-19.42)) ;
#137415 = CARTESIAN_POINT('',(-4.4,-3.85,-19.32)) ;
#137416 = CARTESIAN_POINT('',(-4.4,-3.95,-19.42)) ;
#137417 = CARTESIAN_POINT('',(-4.4,-4.05,-19.42)) ;
#137418 = CARTESIAN_POINT('',(-4.4,-3.95,-21.22)) ;
#137419 = CARTESIAN_POINT('',(-4.4,-3.95,-19.32)) ;
#137420 = CARTESIAN_POINT('',(-4.4,-3.75,-21.22)) ;
#137421 = CARTESIAN_POINT('Origin',(-4.4,-3.9,-19.32)) ;
#137422 = CARTESIAN_POINT('',(-4.3,-3.95,-19.32)) ;
#137423 = CARTESIAN_POINT('',(-4.3,-3.85,-19.32)) ;
#137424 = CARTESIAN_POINT('',(-4.3,-3.75,-19.32)) ;
#137425 = CARTESIAN_POINT('',(-3.25,-3.85,-19.32)) ;
#137426 = CARTESIAN_POINT('',(-4.4,-3.85,-19.32)) ;
#137427 = CARTESIAN_POINT('',(-3.25,-3.95,-19.32)) ;
#137428 = CARTESIAN_POINT('',(-3.25,-4.05,-19.32)) ;
#137429 = CARTESIAN_POINT('',(-4.4,-3.95,-19.32)) ;
#137430 = CARTESIAN_POINT('Origin',(0.,-3.75,-20.32)) ;
#137431 = CARTESIAN_POINT('',(-3.25,-3.75,-19.42)) ;
#137432 = CARTESIAN_POINT('',(-4.3,-3.75,-19.42)) ;
#137433 = CARTESIAN_POINT('',(-1.56125112837913E-16,-3.75,-19.42)) ;
#137434 = CARTESIAN_POINT('',(-4.3,-3.75,-21.22)) ;
#137435 = CARTESIAN_POINT('',(-4.3,-3.75,-20.32)) ;
#137436 = CARTESIAN_POINT('',(-3.25,-3.75,-21.22)) ;
#137437 = CARTESIAN_POINT('',(-1.56125112837913E-16,-3.75,-21.22)) ;
#137438 = CARTESIAN_POINT('',(-3.25,-3.75,-20.32)) ;
#137439 = CARTESIAN_POINT('',(-4.15,-3.75,-21.17)) ;
#137440 = CARTESIAN_POINT('',(-3.4,-3.75,-21.17)) ;
#137441 = CARTESIAN_POINT('',(-4.15,-3.75,-21.17)) ;
#137442 = CARTESIAN_POINT('',(-4.25,-3.75,-21.07)) ;
#137443 = CARTESIAN_POINT('Origin',(-4.15,-3.75,-21.07)) ;
#137444 = CARTESIAN_POINT('',(-4.25,-3.75,-19.57)) ;
#137445 = CARTESIAN_POINT('',(-4.25,-3.75,-19.57)) ;
#137446 = CARTESIAN_POINT('',(-4.15,-3.75,-19.47)) ;
#137447 = CARTESIAN_POINT('Origin',(-4.15,-3.75,-19.57)) ;
#137448 = CARTESIAN_POINT('',(-3.4,-3.75,-19.47)) ;
#137449 = CARTESIAN_POINT('',(-3.4,-3.75,-19.47)) ;
#137450 = CARTESIAN_POINT('',(-3.3,-3.75,-19.57)) ;
#137451 = CARTESIAN_POINT('Origin',(-3.4,-3.75,-19.57)) ;
#137452 = CARTESIAN_POINT('',(-3.3,-3.75,-21.07)) ;
#137453 = CARTESIAN_POINT('',(-3.3,-3.75,-21.07)) ;
#137454 = CARTESIAN_POINT('Origin',(-3.4,-3.75,-21.07)) ;
#137455 = CARTESIAN_POINT('Origin',(-3.4,-3.75,-21.07)) ;
#137456 = CARTESIAN_POINT('',(-3.4,-3.9,-21.17)) ;
#137457 = CARTESIAN_POINT('',(-3.3,-3.9,-21.07)) ;
#137458 = CARTESIAN_POINT('Origin',(-3.4,-3.9,-21.07)) ;
#137459 = CARTESIAN_POINT('',(-3.4,-3.75,-21.17)) ;
#137460 = CARTESIAN_POINT('',(-3.3,-3.75,-21.07)) ;
#137461 = CARTESIAN_POINT('Origin',(-4.15,-3.75,-21.17)) ;
#137462 = CARTESIAN_POINT('',(-4.15,-3.9,-21.17)) ;
#137463 = CARTESIAN_POINT('',(-4.15,-3.9,-21.17)) ;
#137464 = CARTESIAN_POINT('',(-4.15,-3.75,-21.17)) ;
#137465 = CARTESIAN_POINT('Origin',(-4.15,-3.75,-21.07)) ;
#137466 = CARTESIAN_POINT('',(-4.25,-3.9,-21.07)) ;
#137467 = CARTESIAN_POINT('Origin',(-4.15,-3.9,-21.07)) ;
#137468 = CARTESIAN_POINT('',(-4.25,-3.75,-21.07)) ;
#137469 = CARTESIAN_POINT('Origin',(-4.25,-3.75,-19.57)) ;
#137470 = CARTESIAN_POINT('',(-4.25,-3.9,-19.57)) ;
#137471 = CARTESIAN_POINT('',(-4.25,-3.9,-19.57)) ;
#137472 = CARTESIAN_POINT('',(-4.25,-3.75,-19.57)) ;
#137473 = CARTESIAN_POINT('Origin',(-4.15,-3.75,-19.57)) ;
#137474 = CARTESIAN_POINT('',(-4.15,-3.9,-19.47)) ;
#137475 = CARTESIAN_POINT('Origin',(-4.15,-3.9,-19.57)) ;
#137476 = CARTESIAN_POINT('',(-4.15,-3.75,-19.47)) ;
#137477 = CARTESIAN_POINT('Origin',(-3.4,-3.75,-19.47)) ;
#137478 = CARTESIAN_POINT('',(-3.4,-3.9,-19.47)) ;
#137479 = CARTESIAN_POINT('',(-3.4,-3.9,-19.47)) ;
#137480 = CARTESIAN_POINT('',(-3.4,-3.75,-19.47)) ;
#137481 = CARTESIAN_POINT('Origin',(-3.4,-3.75,-19.57)) ;
#137482 = CARTESIAN_POINT('',(-3.3,-3.9,-19.57)) ;
#137483 = CARTESIAN_POINT('Origin',(-3.4,-3.9,-19.57)) ;
#137484 = CARTESIAN_POINT('',(-3.3,-3.75,-19.57)) ;
#137485 = CARTESIAN_POINT('Origin',(-3.3,-3.75,-21.07)) ;
#137486 = CARTESIAN_POINT('',(-3.3,-3.9,-21.07)) ;
#137487 = CARTESIAN_POINT('Origin',(0.,-3.9,-20.32)) ;
#137488 = CARTESIAN_POINT('Origin',(0.,9.95,-20.32)) ;
#137489 = CARTESIAN_POINT('',(-0.230887397576972,9.95,-18.4051394281462)) ;
#137490 = CARTESIAN_POINT('Origin',(-0.321518176280637,8.95,-18.4474012543203)) ;
#137491 = CARTESIAN_POINT('',(-0.321518176280637,9.05,-18.4474012543203)) ;
#137492 = CARTESIAN_POINT('',(1.22782596331729,9.85,-21.769980483939)) ;
#137493 = CARTESIAN_POINT('Origin',(-1.22782596331729,8.95,-18.870019516061)) ;
#137494 = CARTESIAN_POINT('',(-1.22782596331729,9.05,-18.870019516061)) ;
#137495 = CARTESIAN_POINT('',(-1.22782596331729,9.85,-18.870019516061)) ;
#137496 = CARTESIAN_POINT('Origin',(0.,8.95,-20.32)) ;
#137497 = CARTESIAN_POINT('',(-0.362523114814661,8.95,-20.4890473046963)) ;
#137498 = CARTESIAN_POINT('',(0.36252311481466,8.95,-20.1509526953037)) ;
#137499 = CARTESIAN_POINT('Origin',(-2.65,10.8,-21.32)) ;
#137500 = CARTESIAN_POINT('',(-2.65,10.75,-21.22)) ;
#137501 = CARTESIAN_POINT('',(-2.65,10.75,-19.42)) ;
#137502 = CARTESIAN_POINT('',(-2.65,10.75,-21.32)) ;
#137503 = CARTESIAN_POINT('',(-2.65,10.85,-19.42)) ;
#137504 = CARTESIAN_POINT('',(-2.65,10.95,-19.42)) ;
#137505 = CARTESIAN_POINT('',(-2.65,10.85,-21.22)) ;
#137506 = CARTESIAN_POINT('',(-2.65,10.85,-21.32)) ;
#137507 = CARTESIAN_POINT('',(-2.65,10.65,-21.22)) ;
#137508 = CARTESIAN_POINT('Origin',(-3.9,10.8,-19.32)) ;
#137509 = CARTESIAN_POINT('',(-2.75,10.85,-19.32)) ;
#137510 = CARTESIAN_POINT('',(-2.75,10.75,-19.32)) ;
#137511 = CARTESIAN_POINT('',(-2.75,10.65,-19.32)) ;
#137512 = CARTESIAN_POINT('',(-3.8,10.75,-19.32)) ;
#137513 = CARTESIAN_POINT('',(-3.9,10.75,-19.32)) ;
#137514 = CARTESIAN_POINT('',(-3.8,10.85,-19.32)) ;
#137515 = CARTESIAN_POINT('',(-3.8,10.95,-19.32)) ;
#137516 = CARTESIAN_POINT('',(-3.9,10.85,-19.32)) ;
#137517 = CARTESIAN_POINT('Origin',(-3.9,10.8,-21.32)) ;
#137518 = CARTESIAN_POINT('',(-3.9,10.85,-19.42)) ;
#137519 = CARTESIAN_POINT('',(-3.9,10.75,-19.42)) ;
#137520 = CARTESIAN_POINT('',(-3.9,10.65,-19.42)) ;
#137521 = CARTESIAN_POINT('',(-3.9,10.75,-21.22)) ;
#137522 = CARTESIAN_POINT('',(-3.9,10.75,-21.32)) ;
#137523 = CARTESIAN_POINT('',(-3.9,10.85,-21.22)) ;
#137524 = CARTESIAN_POINT('',(-3.9,10.95,-21.22)) ;
#137525 = CARTESIAN_POINT('',(-3.9,10.85,-21.32)) ;
#137526 = CARTESIAN_POINT('Origin',(-3.9,10.8,-21.32)) ;
#137527 = CARTESIAN_POINT('',(-3.8,10.75,-21.32)) ;
#137528 = CARTESIAN_POINT('',(-2.75,10.75,-21.32)) ;
#137529 = CARTESIAN_POINT('',(-3.9,10.75,-21.32)) ;
#137530 = CARTESIAN_POINT('',(-2.75,10.85,-21.32)) ;
#137531 = CARTESIAN_POINT('',(-2.75,10.95,-21.32)) ;
#137532 = CARTESIAN_POINT('',(-3.8,10.85,-21.32)) ;
#137533 = CARTESIAN_POINT('',(-3.9,10.85,-21.32)) ;
#137534 = CARTESIAN_POINT('',(-3.8,10.65,-21.32)) ;
#137535 = CARTESIAN_POINT('Origin',(0.,10.65,-20.32)) ;
#137536 = CARTESIAN_POINT('',(-3.8,10.65,-19.42)) ;
#137537 = CARTESIAN_POINT('',(-2.75,10.65,-19.42)) ;
#137538 = CARTESIAN_POINT('',(1.56125112837912E-16,10.65,-19.42)) ;
#137539 = CARTESIAN_POINT('',(-2.75,10.65,-21.22)) ;
#137540 = CARTESIAN_POINT('',(-2.75,10.65,-20.32)) ;
#137541 = CARTESIAN_POINT('',(-3.8,10.65,-21.22)) ;
#137542 = CARTESIAN_POINT('',(-1.56125112837913E-16,10.65,-21.22)) ;
#137543 = CARTESIAN_POINT('',(-3.8,10.65,-20.32)) ;
#137544 = CARTESIAN_POINT('',(-3.65,10.65,-19.47)) ;
#137545 = CARTESIAN_POINT('',(-2.9,10.65,-19.47)) ;
#137546 = CARTESIAN_POINT('',(-3.65,10.65,-19.47)) ;
#137547 = CARTESIAN_POINT('',(-3.75,10.65,-19.57)) ;
#137548 = CARTESIAN_POINT('Origin',(-3.65,10.65,-19.57)) ;
#137549 = CARTESIAN_POINT('',(-3.75,10.65,-21.07)) ;
#137550 = CARTESIAN_POINT('',(-3.75,10.65,-21.07)) ;
#137551 = CARTESIAN_POINT('',(-3.65,10.65,-21.17)) ;
#137552 = CARTESIAN_POINT('Origin',(-3.65,10.65,-21.07)) ;
#137553 = CARTESIAN_POINT('',(-2.9,10.65,-21.17)) ;
#137554 = CARTESIAN_POINT('',(-2.9,10.65,-21.17)) ;
#137555 = CARTESIAN_POINT('',(-2.8,10.65,-21.07)) ;
#137556 = CARTESIAN_POINT('Origin',(-2.9,10.65,-21.07)) ;
#137557 = CARTESIAN_POINT('',(-2.8,10.65,-19.57)) ;
#137558 = CARTESIAN_POINT('',(-2.8,10.65,-19.57)) ;
#137559 = CARTESIAN_POINT('Origin',(-2.9,10.65,-19.57)) ;
#137560 = CARTESIAN_POINT('Origin',(-2.9,10.65,-19.57)) ;
#137561 = CARTESIAN_POINT('',(-2.8,10.7,-19.57)) ;
#137562 = CARTESIAN_POINT('',(-2.8,10.65,-19.57)) ;
#137563 = CARTESIAN_POINT('',(-2.9,10.7,-19.47)) ;
#137564 = CARTESIAN_POINT('Origin',(-2.9,10.7,-19.57)) ;
#137565 = CARTESIAN_POINT('',(-2.9,10.65,-19.47)) ;
#137566 = CARTESIAN_POINT('Origin',(-3.65,10.65,-19.47)) ;
#137567 = CARTESIAN_POINT('',(-3.65,10.7,-19.47)) ;
#137568 = CARTESIAN_POINT('',(-3.65,10.7,-19.47)) ;
#137569 = CARTESIAN_POINT('',(-3.65,10.65,-19.47)) ;
#137570 = CARTESIAN_POINT('Origin',(-3.65,10.65,-19.57)) ;
#137571 = CARTESIAN_POINT('',(-3.75,10.7,-19.57)) ;
#137572 = CARTESIAN_POINT('Origin',(-3.65,10.7,-19.57)) ;
#137573 = CARTESIAN_POINT('',(-3.75,10.65,-19.57)) ;
#137574 = CARTESIAN_POINT('Origin',(-3.75,10.65,-21.07)) ;
#137575 = CARTESIAN_POINT('',(-3.75,10.7,-21.07)) ;
#137576 = CARTESIAN_POINT('',(-3.75,10.7,-21.07)) ;
#137577 = CARTESIAN_POINT('',(-3.75,10.65,-21.07)) ;
#137578 = CARTESIAN_POINT('Origin',(-3.65,10.65,-21.07)) ;
#137579 = CARTESIAN_POINT('',(-3.65,10.7,-21.17)) ;
#137580 = CARTESIAN_POINT('Origin',(-3.65,10.7,-21.07)) ;
#137581 = CARTESIAN_POINT('',(-3.65,10.65,-21.17)) ;
#137582 = CARTESIAN_POINT('Origin',(-2.9,10.65,-21.17)) ;
#137583 = CARTESIAN_POINT('',(-2.9,10.7,-21.17)) ;
#137584 = CARTESIAN_POINT('',(-2.9,10.7,-21.17)) ;
#137585 = CARTESIAN_POINT('',(-2.9,10.65,-21.17)) ;
#137586 = CARTESIAN_POINT('Origin',(-2.9,10.65,-21.07)) ;
#137587 = CARTESIAN_POINT('',(-2.8,10.7,-21.07)) ;
#137588 = CARTESIAN_POINT('Origin',(-2.9,10.7,-21.07)) ;
#137589 = CARTESIAN_POINT('',(-2.8,10.65,-21.07)) ;
#137590 = CARTESIAN_POINT('Origin',(-2.8,10.65,-19.57)) ;
#137591 = CARTESIAN_POINT('',(-2.8,10.7,-19.57)) ;
#137592 = CARTESIAN_POINT('Origin',(0.,10.8,-20.32)) ;
#137593 = CARTESIAN_POINT('',(-3.65,10.8,-19.57)) ;
#137594 = CARTESIAN_POINT('',(-2.9,10.8,-19.57)) ;
#137595 = CARTESIAN_POINT('',(0.,10.8,-19.57)) ;
#137596 = CARTESIAN_POINT('',(-2.9,10.8,-21.07)) ;
#137597 = CARTESIAN_POINT('',(-2.9,10.8,-20.32)) ;
#137598 = CARTESIAN_POINT('',(-3.65,10.8,-21.07)) ;
#137599 = CARTESIAN_POINT('',(0.,10.8,-21.07)) ;
#137600 = CARTESIAN_POINT('',(-3.65,10.8,-20.32)) ;
#137601 = CARTESIAN_POINT('Origin',(4.5,2.75,-21.695)) ;
#137602 = CARTESIAN_POINT('',(4.5,2.63356010126946,-21.7144066497884)) ;
#137603 = CARTESIAN_POINT('',(4.6,2.11643989873054,-21.8005933502116)) ;
#137604 = CARTESIAN_POINT('',(4.6,2.11643989873054,-21.8005933502116)) ;
#137605 = CARTESIAN_POINT('',(12.7,2.11643989873054,-21.8005933502116)) ;
#137606 = CARTESIAN_POINT('',(12.8,2.11643989873054,-21.8005933502116)) ;
#137607 = CARTESIAN_POINT('',(12.7,2.75,-21.695)) ;
#137608 = CARTESIAN_POINT('Origin',(4.5,2.,-21.82)) ;
#137609 = CARTESIAN_POINT('',(4.6,2.,-21.7019539578284)) ;
#137610 = CARTESIAN_POINT('',(4.6,2.,-18.82)) ;
#137611 = CARTESIAN_POINT('',(12.7,2.,-21.7019539578284)) ;
#137612 = CARTESIAN_POINT('',(12.7,2.,-21.82)) ;
#137613 = CARTESIAN_POINT('',(4.5,2.,-21.7019539578284)) ;
#137614 = CARTESIAN_POINT('Origin',(4.5,2.,-18.82)) ;
#137615 = CARTESIAN_POINT('',(4.6,2.63356010126946,-18.9255933502116)) ;
#137616 = CARTESIAN_POINT('',(4.6,2.63356010126947,-18.9255933502116)) ;
#137617 = CARTESIAN_POINT('',(4.5,2.63356010126946,-18.9255933502116)) ;
#137618 = CARTESIAN_POINT('',(12.7,2.,-18.82)) ;
#137619 = CARTESIAN_POINT('Origin',(4.5,0.,-20.32)) ;
#137620 = CARTESIAN_POINT('',(4.5,2.72431432344521,-19.012634816645)) ;
#137621 = CARTESIAN_POINT('',(4.5,2.72431432344521,-20.32)) ;
#137622 = CARTESIAN_POINT('',(4.5,2.61712020253893,-19.0242327425948)) ;
#137623 = CARTESIAN_POINT('Origin',(4.5,2.65,-18.8269539578284)) ;
#137624 = CARTESIAN_POINT('',(4.5,2.1,-18.9380460421716)) ;
#137625 = CARTESIAN_POINT('',(4.5,2.1,-18.9380460421716)) ;
#137626 = CARTESIAN_POINT('',(4.5,2.1,-21.7019539578284)) ;
#137627 = CARTESIAN_POINT('',(4.5,2.1,-21.82)) ;
#137628 = CARTESIAN_POINT('',(4.5,2.61712020253893,-21.6157672574052)) ;
#137629 = CARTESIAN_POINT('Origin',(10.3,0.,-20.32)) ;
#137630 = CARTESIAN_POINT('Origin',(0.584645609909621,0.,-20.32)) ;
#137631 = CARTESIAN_POINT('',(4.6,-2.32258064516129,-18.4211532060953)) ;
#137632 = CARTESIAN_POINT('',(4.6,-2.79310344827574,-19.2252063540419)) ;
#137633 = CARTESIAN_POINT('Origin',(4.6,0.,-20.32)) ;
#137634 = CARTESIAN_POINT('',(4.6,-2.79310344827574,-21.4147936459581)) ;
#137635 = CARTESIAN_POINT('Origin',(4.6,0.,-20.32)) ;
#137636 = CARTESIAN_POINT('',(4.6,-2.32258064516129,-22.2188467939047)) ;
#137637 = CARTESIAN_POINT('Origin',(4.6,0.,-20.32)) ;
#137638 = CARTESIAN_POINT('',(12.7,-2.32258064516129,-22.2188467939047)) ;
#137639 = CARTESIAN_POINT('',(0.584645609909621,-2.32258064516129,-22.2188467939047)) ;
#137640 = CARTESIAN_POINT('',(12.7,-2.32258064516129,-18.4211532060953)) ;
#137641 = CARTESIAN_POINT('Origin',(12.7,0.,-20.32)) ;
#137642 = CARTESIAN_POINT('',(0.584645609909621,-2.32258064516129,-18.4211532060953)) ;
#137643 = CARTESIAN_POINT('Ctrl Pts',(-5.37474093186837,4.17158354835192,
-18.42)) ;
#137644 = CARTESIAN_POINT('Ctrl Pts',(-5.4,4.2,-18.42)) ;
#137645 = CARTESIAN_POINT('Ctrl Pts',(-5.4,4.23801993223491,-18.42)) ;
#137646 = CARTESIAN_POINT('Ctrl Pts',(-5.37474093064202,4.17158354697228,
-18.3937465640611)) ;
#137647 = CARTESIAN_POINT('Ctrl Pts',(-5.4,4.19999999724801,-18.382481412799)) ;
#137648 = CARTESIAN_POINT('Ctrl Pts',(-5.4,4.23801992976516,-18.3674931280903)) ;
#137649 = CARTESIAN_POINT('Ctrl Pts',(-5.36668583490659,4.14629949399949,
-18.3678012868841)) ;
#137650 = CARTESIAN_POINT('Ctrl Pts',(-5.4,4.16739198385624,-18.3446678350657)) ;
#137651 = CARTESIAN_POINT('Ctrl Pts',(-5.4,4.20557579169425,-18.3156025737682)) ;
#137652 = CARTESIAN_POINT('Ctrl Pts',(-5.33901380460605,4.05944006555652,
-18.3307773568786)) ;
#137653 = CARTESIAN_POINT('Ctrl Pts',(-5.4,4.06625640449639,-18.3031326366143)) ;
#137654 = CARTESIAN_POINT('Ctrl Pts',(-5.4,4.09411900298411,-18.2415547137572)) ;
#137655 = CARTESIAN_POINT('Ctrl Pts',(-5.31962206268972,3.99857154231908,
-18.32)) ;
#137656 = CARTESIAN_POINT('Ctrl Pts',(-5.4,3.99346933127516,-18.3020035074265)) ;
#137657 = CARTESIAN_POINT('Ctrl Pts',(-5.4,4.0160133758189,-18.2200000004811)) ;
#137658 = CARTESIAN_POINT('Ctrl Pts',(-5.3,3.9369800677651,-18.32)) ;
#137659 = CARTESIAN_POINT('Ctrl Pts',(-5.4,3.9369800677651,-18.32)) ;
#137660 = CARTESIAN_POINT('Ctrl Pts',(-5.4,3.9369800677651,-18.22)) ;
#137661 = CARTESIAN_POINT('Origin',(-5.3,4.23801993223491,-18.42)) ;
#137662 = CARTESIAN_POINT('Ctrl Pts',(-5.3,3.9369800677651,-18.32)) ;
#137663 = CARTESIAN_POINT('Ctrl Pts',(-5.31962206268972,3.99857154231908,
-18.32)) ;
#137664 = CARTESIAN_POINT('Ctrl Pts',(-5.33901380460605,4.05944006555653,
-18.3307773568786)) ;
#137665 = CARTESIAN_POINT('Ctrl Pts',(-5.36668583490659,4.14629949399949,
-18.3678012868841)) ;
#137666 = CARTESIAN_POINT('Ctrl Pts',(-5.37474093064202,4.17158354697228,
-18.3937465640611)) ;
#137667 = CARTESIAN_POINT('Ctrl Pts',(-5.37474093186837,4.17158354835192,
-18.42)) ;
#137668 = CARTESIAN_POINT('Origin',(-5.3,3.9369800677651,-18.22)) ;
#137669 = CARTESIAN_POINT('Origin',(-4.6737453090477,1.85,-18.4171399006497)) ;
#137670 = CARTESIAN_POINT('Origin',(-3.35509339356897,1.85,-18.7394770355445)) ;
#137671 = CARTESIAN_POINT('Ctrl Pts',(-3.35509339356897,1.95,-18.7394770355445)) ;
#137672 = CARTESIAN_POINT('Ctrl Pts',(-3.33134808452128,1.95,-18.6423371348948)) ;
#137673 = CARTESIAN_POINT('Ctrl Pts',(-3.33134808452128,1.85,-18.6423371348948)) ;
#137674 = CARTESIAN_POINT('Ctrl Pts',(-3.38343213690424,1.95,-18.7256225388029)) ;
#137675 = CARTESIAN_POINT('Ctrl Pts',(-3.36046743872486,1.94345445676968,
-18.6352190705343)) ;
#137676 = CARTESIAN_POINT('Ctrl Pts',(-3.38803897426452,1.85000000162387,
-18.6284793618465)) ;
#137677 = CARTESIAN_POINT('Ctrl Pts',(-3.41101314049054,1.96238978305186,
-18.7121384929161)) ;
#137678 = CARTESIAN_POINT('Ctrl Pts',(-3.39538881861725,1.95068928167331,
-18.6266827332266)) ;
#137679 = CARTESIAN_POINT('Ctrl Pts',(-3.44316973238528,1.87475949194142,
-18.6150029543058)) ;
#137680 = CARTESIAN_POINT('Ctrl Pts',(-3.42983432543734,1.98356361611701,
-18.7029370244088)) ;
#137681 = CARTESIAN_POINT('Ctrl Pts',(-3.42093333711585,1.97355000425533,
-18.6204385175939)) ;
#137682 = CARTESIAN_POINT('Ctrl Pts',(-3.48082994825801,1.91712723223402,
-18.6057971237592)) ;
#137683 = CARTESIAN_POINT('Origin',(-3.50457525730571,1.91712723223402,-18.7029370244088)) ;
#137684 = CARTESIAN_POINT('Origin',(-3.36128627567715,2.03621361435819,-18.7364494043352)) ;
#137685 = CARTESIAN_POINT('Origin',(-4.05330900605469,2.53445269957662,-18.568802108048)) ;
#137686 = CARTESIAN_POINT('Origin',(-4.66204490261456,3.21928058320648,-18.42)) ;
#137687 = CARTESIAN_POINT('Origin',(-4.35749955255802,2.87666706439287,-18.42)) ;
#137688 = CARTESIAN_POINT('Origin',(-4.66204490261456,3.21928058320648,-18.42)) ;
#137689 = CARTESIAN_POINT('Origin',(-5.3,5.2,-18.22)) ;
#137690 = CARTESIAN_POINT('Origin',(-5.3,-1.88819660112502,-18.22)) ;
#137691 = CARTESIAN_POINT('Origin',(-5.3,4.23801993223491,-17.78)) ;
#137692 = CARTESIAN_POINT('Origin',(-5.3,4.23801993223491,-22.22)) ;
#137693 = CARTESIAN_POINT('Origin',(-3.35509339356897,2.05,-20.32)) ;
#137694 = CARTESIAN_POINT('Origin',(-3.36128627567707,2.03621361435845,-21.9035505956648)) ;
#137695 = CARTESIAN_POINT('Origin',(-2.4237453090477,1.85,-21.6728600993503)) ;
#137696 = CARTESIAN_POINT('Origin',(-3.35509339356897,1.85,-21.9005229644555)) ;
#137697 = CARTESIAN_POINT('Origin',(-4.66204490261456,3.21928058320648,-18.42)) ;
#137698 = CARTESIAN_POINT('Origin',(-4.66204490261456,3.21928058320648,-18.42)) ;
#137699 = CARTESIAN_POINT('Ctrl Pts',(-5.29976814257746,-1.88802911972918,
-18.3199998273778)) ;
#137700 = CARTESIAN_POINT('Ctrl Pts',(-5.4,-1.88802831720455,-18.320232593543)) ;
#137701 = CARTESIAN_POINT('Ctrl Pts',(-5.4,-1.88791746283071,-18.2200001624624)) ;
#137702 = CARTESIAN_POINT('Ctrl Pts',(-5.31153957531163,-1.92331224822996,
-18.3199864676889)) ;
#137703 = CARTESIAN_POINT('Ctrl Pts',(-5.4,-1.92148676945281,-18.3089778925376)) ;
#137704 = CARTESIAN_POINT('Ctrl Pts',(-5.4,-1.94671708614657,-18.2199317130282)) ;
#137705 = CARTESIAN_POINT('Ctrl Pts',(-5.32318090226694,-1.9581752705225,
-18.3307844972681)) ;
#137706 = CARTESIAN_POINT('Ctrl Pts',(-5.4,-1.96527310172481,-18.3121633837529)) ;
#137707 = CARTESIAN_POINT('Ctrl Pts',(-5.4,-2.00485091174287,-18.2414960748893)) ;
#137708 = CARTESIAN_POINT('Ctrl Pts',(-5.33978950165956,-2.00789652656154,
-18.3678649650196)) ;
#137709 = CARTESIAN_POINT('Ctrl Pts',(-5.4,-2.02908601268745,-18.3513665145317)) ;
#137710 = CARTESIAN_POINT('Ctrl Pts',(-5.4,-2.087770056524,-18.3156612126361)) ;
#137711 = CARTESIAN_POINT('Ctrl Pts',(-5.34461954754097,-2.02234798681676,
-18.3938461447183)) ;
#137712 = CARTESIAN_POINT('Ctrl Pts',(-5.4,-2.04997459329993,-18.38567566484)) ;
#137713 = CARTESIAN_POINT('Ctrl Pts',(-5.4,-2.1118797455067,-18.3676576869739)) ;
#137714 = CARTESIAN_POINT('Ctrl Pts',(-5.34460423617422,-2.02230212313483,
-18.4201247518701)) ;
#137715 = CARTESIAN_POINT('Ctrl Pts',(-5.4,-2.04990938338631,-18.4201637542765)) ;
#137716 = CARTESIAN_POINT('Ctrl Pts',(-5.4,-2.11180321723903,-18.4202496688804)) ;
#137717 = CARTESIAN_POINT('Origin',(-5.29999999999992,-1.88819660112476,-18.4200000000002)) ;
#137718 = CARTESIAN_POINT('Origin',(-5.3,-2.11180339887499,-18.42)) ;
#137719 = CARTESIAN_POINT('Ctrl Pts',(-5.3,3.9369800677651,-22.32)) ;
#137720 = CARTESIAN_POINT('Ctrl Pts',(-5.4,3.9369800677651,-22.32)) ;
#137721 = CARTESIAN_POINT('Ctrl Pts',(-5.4,3.9369800677651,-22.42)) ;
#137722 = CARTESIAN_POINT('Ctrl Pts',(-5.31962206268973,3.99857154231912,
-22.32)) ;
#137723 = CARTESIAN_POINT('Ctrl Pts',(-5.40000000000063,3.993469331275,-22.3379964925736)) ;
#137724 = CARTESIAN_POINT('Ctrl Pts',(-5.4,4.01601337581889,-22.4199999995189)) ;
#137725 = CARTESIAN_POINT('Ctrl Pts',(-5.33901380460613,4.05944006555646,
-22.3092226431215)) ;
#137726 = CARTESIAN_POINT('Ctrl Pts',(-5.40000000000006,4.06625640449647,
-22.3368673633861)) ;
#137727 = CARTESIAN_POINT('Ctrl Pts',(-5.4,4.09411900298413,-22.3984452862429)) ;
#137728 = CARTESIAN_POINT('Ctrl Pts',(-5.36668583490652,4.14629949399955,
-22.2721987131158)) ;
#137729 = CARTESIAN_POINT('Ctrl Pts',(-5.39999999999995,4.16739198385616,
-22.295332164934)) ;
#137730 = CARTESIAN_POINT('Ctrl Pts',(-5.4,4.20557579169423,-22.3243974262317)) ;
#137731 = CARTESIAN_POINT('Ctrl Pts',(-5.37474093064202,4.17158354697228,
-22.246253435939)) ;
#137732 = CARTESIAN_POINT('Ctrl Pts',(-5.4,4.19999999724801,-22.2575185872012)) ;
#137733 = CARTESIAN_POINT('Ctrl Pts',(-5.4,4.23801992976516,-22.2725068719098)) ;
#137734 = CARTESIAN_POINT('Ctrl Pts',(-5.37474093186837,4.17158354835192,
-22.22)) ;
#137735 = CARTESIAN_POINT('Ctrl Pts',(-5.4,4.2,-22.22)) ;
#137736 = CARTESIAN_POINT('Ctrl Pts',(-5.4,4.23801993223491,-22.22)) ;
#137737 = CARTESIAN_POINT('Origin',(-5.3,3.9369800677651,-22.42)) ;
#137738 = CARTESIAN_POINT('Ctrl Pts',(-5.37474093186837,4.17158354835192,
-22.22)) ;
#137739 = CARTESIAN_POINT('Ctrl Pts',(-5.37474093064202,4.17158354697228,
-22.246253435939)) ;
#137740 = CARTESIAN_POINT('Ctrl Pts',(-5.36668583490652,4.14629949399955,
-22.2721987131158)) ;
#137741 = CARTESIAN_POINT('Ctrl Pts',(-5.33901380460613,4.05944006555646,
-22.3092226431215)) ;
#137742 = CARTESIAN_POINT('Ctrl Pts',(-5.31962206268973,3.99857154231912,
-22.32)) ;
#137743 = CARTESIAN_POINT('Ctrl Pts',(-5.3,3.9369800677651,-22.32)) ;
#137744 = CARTESIAN_POINT('Ctrl Pts',(-3.42983432543734,1.98356361611701,
-21.9370629755912)) ;
#137745 = CARTESIAN_POINT('Ctrl Pts',(-3.42093333711585,1.97355000425533,
-22.0195614824061)) ;
#137746 = CARTESIAN_POINT('Ctrl Pts',(-3.48082994825801,1.91712723223402,
-22.0342028762409)) ;
#137747 = CARTESIAN_POINT('Ctrl Pts',(-3.41101314049054,1.96238978305186,
-21.9278615070839)) ;
#137748 = CARTESIAN_POINT('Ctrl Pts',(-3.39538881861725,1.95068928167332,
-22.0133172667734)) ;
#137749 = CARTESIAN_POINT('Ctrl Pts',(-3.44316973238529,1.87475949194142,
-22.0249970456942)) ;
#137750 = CARTESIAN_POINT('Ctrl Pts',(-3.38343213690425,1.95,-21.9143774611971)) ;
#137751 = CARTESIAN_POINT('Ctrl Pts',(-3.36046743872486,1.94345445676967,
-22.0047809294657)) ;
#137752 = CARTESIAN_POINT('Ctrl Pts',(-3.38803897426451,1.85000000162387,
-22.0115206381536)) ;
#137753 = CARTESIAN_POINT('Ctrl Pts',(-3.35509339356897,1.95,-21.9005229644555)) ;
#137754 = CARTESIAN_POINT('Ctrl Pts',(-3.33134808452128,1.95,-21.9976628651052)) ;
#137755 = CARTESIAN_POINT('Ctrl Pts',(-3.33134808452128,1.85,-21.9976628651052)) ;
#137756 = CARTESIAN_POINT('Origin',(-3.50457525730571,1.91712723223402,-21.9370629755912)) ;
#137757 = CARTESIAN_POINT('Origin',(-4.66204490261456,1.95,-18.42)) ;
#137758 = CARTESIAN_POINT('Origin',(-4.66204490261456,-1.5692190524323,-18.42)) ;
#137759 = CARTESIAN_POINT('Origin',(-3.84472135955,-1.16055728090002,-18.42)) ;
#137760 = CARTESIAN_POINT('Origin',(-4.66204490261456,-1.5692190524323,-18.42)) ;
#137761 = CARTESIAN_POINT('Origin',(-5.3,-2.11180339887499,-17.78)) ;
#137762 = CARTESIAN_POINT('Origin',(-5.3,-2.11180339887499,-22.22)) ;
#137763 = CARTESIAN_POINT('Origin',(-5.3,1.95,-22.42)) ;
#137764 = CARTESIAN_POINT('Origin',(-5.3,-1.88819660112501,-22.42)) ;
#137765 = CARTESIAN_POINT('Origin',(-4.0264650697994,2.50425327128942,-22.22)) ;
#137766 = CARTESIAN_POINT('Origin',(-4.66204490261456,3.21928058320648,-22.22)) ;
#137767 = CARTESIAN_POINT('Origin',(-3.02790825149799,1.38087685070033,-21.8205443741715)) ;
#137768 = CARTESIAN_POINT('Origin',(-4.66204490261456,3.21928058320648,-22.22)) ;
#137769 = CARTESIAN_POINT('Origin',(-4.66204490261456,-1.5692190524323,-18.42)) ;
#137770 = CARTESIAN_POINT('Origin',(-4.66204490261456,-1.5692190524323,-18.42)) ;
#137771 = CARTESIAN_POINT('Ctrl Pts',(-5.34460423617422,-2.02230212313483,
-22.2198752481299)) ;
#137772 = CARTESIAN_POINT('Ctrl Pts',(-5.4,-2.0499093833863,-22.2198362457235)) ;
#137773 = CARTESIAN_POINT('Ctrl Pts',(-5.4,-2.11180321723903,-22.2197503311196)) ;
#137774 = CARTESIAN_POINT('Ctrl Pts',(-5.34461954754096,-2.02234798681675,
-22.2461538552817)) ;
#137775 = CARTESIAN_POINT('Ctrl Pts',(-5.4,-2.04997459329993,-22.25432433516)) ;
#137776 = CARTESIAN_POINT('Ctrl Pts',(-5.4,-2.11187974550671,-22.2723423130261)) ;
#137777 = CARTESIAN_POINT('Ctrl Pts',(-5.33978950165955,-2.00789652656154,
-22.2721350349804)) ;
#137778 = CARTESIAN_POINT('Ctrl Pts',(-5.4,-2.02908601268745,-22.2886334854683)) ;
#137779 = CARTESIAN_POINT('Ctrl Pts',(-5.4,-2.087770056524,-22.3243387873639)) ;
#137780 = CARTESIAN_POINT('Ctrl Pts',(-5.32318090226694,-1.9581752705225,
-22.3092155027319)) ;
#137781 = CARTESIAN_POINT('Ctrl Pts',(-5.4,-1.96527310172481,-22.3278366162471)) ;
#137782 = CARTESIAN_POINT('Ctrl Pts',(-5.4,-2.00485091174287,-22.3985039251107)) ;
#137783 = CARTESIAN_POINT('Ctrl Pts',(-5.31153957531164,-1.92331224822995,
-22.3200135323111)) ;
#137784 = CARTESIAN_POINT('Ctrl Pts',(-5.39999999999961,-1.9214867694528,
-22.3310221074624)) ;
#137785 = CARTESIAN_POINT('Ctrl Pts',(-5.4,-1.94671708614656,-22.4200682869718)) ;
#137786 = CARTESIAN_POINT('Ctrl Pts',(-5.29976814257746,-1.88802911972917,
-22.3200001726222)) ;
#137787 = CARTESIAN_POINT('Ctrl Pts',(-5.4,-1.88802831720455,-22.319767406457)) ;
#137788 = CARTESIAN_POINT('Ctrl Pts',(-5.4,-1.8879174628307,-22.4199998375376)) ;
#137789 = CARTESIAN_POINT('Origin',(-5.30000000000006,-1.88819660112518,-22.2200000000001)) ;
#137790 = CARTESIAN_POINT('Origin',(-4.66204490261456,3.21928058320648,-22.22)) ;
#137791 = CARTESIAN_POINT('Origin',(-4.66204490261456,3.21928058320648,-22.22)) ;
#137792 = CARTESIAN_POINT('Origin',(0.175392621986784,-0.95,-19.6024847282359)) ;
#137793 = CARTESIAN_POINT('Origin',(-3.37639320225,-0.95,-18.7342704156447)) ;
#137794 = CARTESIAN_POINT('Origin',(-3.32804538583365,-0.902219294041845,
-18.7460887707687)) ;
#137795 = CARTESIAN_POINT('Origin',(-3.46583592134999,-0.971114561800017,
-18.7124066398647)) ;
#137796 = CARTESIAN_POINT('Origin',(-3.24472135955,-0.860557280900019,-22.22)) ;
#137797 = CARTESIAN_POINT('Origin',(-4.66204490261456,-1.5692190524323,-22.22)) ;
#137798 = CARTESIAN_POINT('Origin',(-4.66204490261456,1.95,-22.22)) ;
#137799 = CARTESIAN_POINT('Origin',(-4.66204490261456,-1.5692190524323,-22.22)) ;
#137800 = CARTESIAN_POINT('Ctrl Pts',(-3.4211145618,-1.06055728090001,-18.7124066398647)) ;
#137801 = CARTESIAN_POINT('Ctrl Pts',(-3.40394191641935,-1.05197095820969,
-18.6245919759864)) ;
#137802 = CARTESIAN_POINT('Ctrl Pts',(-3.44209061230229,-0.971114561800017,
-18.615266739215)) ;
#137803 = CARTESIAN_POINT('Ctrl Pts',(-3.40727897628737,-1.05363948814369,
-18.7191707039916)) ;
#137804 = CARTESIAN_POINT('Ctrl Pts',(-3.38665319245551,-1.04670310838585,
-18.628818108511)) ;
#137805 = CARTESIAN_POINT('Ctrl Pts',(-3.4144159452097,-0.957277229261615,
-18.6220316578376)) ;
#137806 = CARTESIAN_POINT('Ctrl Pts',(-3.39186274464434,-1.05,-18.726707528252)) ;
#137807 = CARTESIAN_POINT('Ctrl Pts',(-3.36870744055528,-1.04639008266723,
-18.6332048478644)) ;
#137808 = CARTESIAN_POINT('Ctrl Pts',(-3.38358960366097,-0.950000000886305,
-18.6295669857718)) ;
#137809 = CARTESIAN_POINT('Ctrl Pts',(-3.37639320225,-1.05,-18.7342704156447)) ;
#137810 = CARTESIAN_POINT('Ctrl Pts',(-3.3526478932023,-1.05,-18.637130514995)) ;
#137811 = CARTESIAN_POINT('Ctrl Pts',(-3.3526478932023,-0.95,-18.637130514995)) ;
#137812 = CARTESIAN_POINT('Origin',(-3.37639320224972,-1.15000000000083,-18.7342704156448)) ;
#137813 = CARTESIAN_POINT('Origin',(-4.66204490261456,-1.5692190524323,-22.22)) ;
#137814 = CARTESIAN_POINT('Origin',(-4.66204490261456,-1.5692190524323,-22.22)) ;
#137815 = CARTESIAN_POINT('Origin',(-3.37639320225,-1.15,-20.32)) ;
#137816 = CARTESIAN_POINT('Origin',(-3.37639320224994,-1.14999999999955,-21.9057295843552)) ;
#137817 = CARTESIAN_POINT('Origin',(-1.50751564693271,0.00804557540861825,
-21.4488928486111)) ;
#137818 = CARTESIAN_POINT('Origin',(-3.46583592134999,-0.971114561800017,
-21.9275933601353)) ;
#137819 = CARTESIAN_POINT('Ctrl Pts',(-3.37639320225,-1.05,-21.9057295843553)) ;
#137820 = CARTESIAN_POINT('Ctrl Pts',(-3.3526478932023,-1.05,-22.002869485005)) ;
#137821 = CARTESIAN_POINT('Ctrl Pts',(-3.3526478932023,-0.95,-22.002869485005)) ;
#137822 = CARTESIAN_POINT('Ctrl Pts',(-3.39186274464434,-1.05,-21.913292471748)) ;
#137823 = CARTESIAN_POINT('Ctrl Pts',(-3.36870744055537,-1.04639008266721,
-22.0067951521356)) ;
#137824 = CARTESIAN_POINT('Ctrl Pts',(-3.38358960366096,-0.950000000886305,
-22.0104330142282)) ;
#137825 = CARTESIAN_POINT('Ctrl Pts',(-3.40727897628737,-1.0536394881437,
-21.9208292960084)) ;
#137826 = CARTESIAN_POINT('Ctrl Pts',(-3.3866531924554,-1.04670310838598,
-22.011181891489)) ;
#137827 = CARTESIAN_POINT('Ctrl Pts',(-3.41441594520971,-0.95727722926162,
-22.0179683421624)) ;
#137828 = CARTESIAN_POINT('Ctrl Pts',(-3.4211145618,-1.06055728090001,-21.9275933601353)) ;
#137829 = CARTESIAN_POINT('Ctrl Pts',(-3.40394191641936,-1.05197095820968,
-22.0154080240136)) ;
#137830 = CARTESIAN_POINT('Ctrl Pts',(-3.44209061230229,-0.971114561800017,
-22.024733260785)) ;
#137831 = CARTESIAN_POINT('Origin',(-3.37639320225,-0.95,-21.9057295843553)) ;
#137832 = CARTESIAN_POINT('Origin',(0.175392621986784,-0.95,-21.0375152717641)) ;
#137833 = CARTESIAN_POINT('Origin',(12.7,2.65,-17.78)) ;
#137834 = CARTESIAN_POINT('Origin',(12.8,2.65,-21.8130460421716)) ;
#137835 = CARTESIAN_POINT('',(4.57524318173533,2.73534903669982,-21.7609351802097)) ;
#137836 = CARTESIAN_POINT('Origin',(4.65232986201019,2.66527023614907,-21.8087542111864)) ;
#137837 = CARTESIAN_POINT('Ctrl Pts',(4.57524318173533,2.73534903669982,-21.7609351802097)) ;
#137838 = CARTESIAN_POINT('Ctrl Pts',(4.5761458558036,2.73452842391049,-21.7595911511832)) ;
#137839 = CARTESIAN_POINT('Ctrl Pts',(4.57705238626145,2.73367683201793,-21.7582681293393)) ;
#137840 = CARTESIAN_POINT('Ctrl Pts',(4.5779495181309,2.73280244902548,-21.7569768488888)) ;
#137841 = CARTESIAN_POINT('Ctrl Pts',(4.58144263576929,2.72939790755547,-21.7519490545686)) ;
#137842 = CARTESIAN_POINT('Ctrl Pts',(4.58496694799971,2.72549786515197,-21.7471699445181)) ;
#137843 = CARTESIAN_POINT('Ctrl Pts',(4.58815670056887,2.72107165565075,-21.742698193853)) ;
#137844 = CARTESIAN_POINT('Ctrl Pts',(4.59069123847463,2.71755464437276,-21.7391449961299)) ;
#137845 = CARTESIAN_POINT('Ctrl Pts',(4.59301454561849,2.71370459823918,-21.7357863127243)) ;
#137846 = CARTESIAN_POINT('Ctrl Pts',(4.5949431309995,2.70950205848694,-21.7326749961674)) ;
#137847 = CARTESIAN_POINT('Ctrl Pts',(4.59651854606295,2.70606910472943,-21.7301334364214)) ;
#137848 = CARTESIAN_POINT('Ctrl Pts',(4.59783685868322,2.70233705077422,-21.7277160861571)) ;
#137849 = CARTESIAN_POINT('Ctrl Pts',(4.59873118971424,2.69838744819993,-21.7255323012123)) ;
#137850 = CARTESIAN_POINT('Ctrl Pts',(4.59916508318198,2.69647125978905,-21.7244728165364)) ;
#137851 = CARTESIAN_POINT('Ctrl Pts',(4.59949917984823,2.69450444432188,-21.723467798882)) ;
#137852 = CARTESIAN_POINT('Ctrl Pts',(4.5997144226265,2.692499226592,-21.7225263440994)) ;
#137853 = CARTESIAN_POINT('Ctrl Pts',(4.59990113259977,2.69075982259552,-21.7217096895352)) ;
#137854 = CARTESIAN_POINT('Ctrl Pts',(4.6,2.68896788689974,-21.7209303122145)) ;
#137855 = CARTESIAN_POINT('Ctrl Pts',(4.6,2.68715716172261,-21.7202056127633)) ;
#137856 = CARTESIAN_POINT('Origin',(4.5,2.1,-21.7019539578284)) ;
#137857 = CARTESIAN_POINT('Origin',(4.6,2.1,-21.7019539578284)) ;
#137858 = CARTESIAN_POINT('Origin',(12.7,2.1,-21.7019539578284)) ;
#137859 = CARTESIAN_POINT('Origin',(12.7,2.76643989873054,-21.7936393923832)) ;
#137860 = CARTESIAN_POINT('Origin',(12.7,2.13287979746107,-21.8992327425948)) ;
#137861 = CARTESIAN_POINT('Origin',(4.4,2.72431432344521,-20.32)) ;
#137862 = CARTESIAN_POINT('Ctrl Pts',(4.48762159086959,2.77250619842349,-18.9311756817495)) ;
#137863 = CARTESIAN_POINT('Ctrl Pts',(4.48806820038223,2.77169418112776,-18.9338355670898)) ;
#137864 = CARTESIAN_POINT('Ctrl Pts',(4.48852084821546,2.77084293101113,-18.9364827150185)) ;
#137865 = CARTESIAN_POINT('Ctrl Pts',(4.49012932137854,2.76769877392856,-18.9457630095207)) ;
#137866 = CARTESIAN_POINT('Ctrl Pts',(4.49131046584974,2.76517764467229,-18.9523441317034)) ;
#137867 = CARTESIAN_POINT('Ctrl Pts',(4.49351977821776,2.75978760391035,-18.964635280162)) ;
#137868 = CARTESIAN_POINT('Ctrl Pts',(4.49455195297826,2.75697653750129,-18.9703677406012)) ;
#137869 = CARTESIAN_POINT('Ctrl Pts',(4.49620670090465,2.75163165728877,-18.9799433216032)) ;
#137870 = CARTESIAN_POINT('Ctrl Pts',(4.49686252944492,2.74924176842725,-18.9838640262033)) ;
#137871 = CARTESIAN_POINT('Ctrl Pts',(4.49822764032847,2.74331716058964,-18.9926446316345)) ;
#137872 = CARTESIAN_POINT('Ctrl Pts',(4.498902033579,2.73961076902736,-18.9974865001601)) ;
#137873 = CARTESIAN_POINT('Ctrl Pts',(4.4997589785602,2.73206576252715,-19.0058277784394)) ;
#137874 = CARTESIAN_POINT('Ctrl Pts',(4.5,2.72833175948635,-19.0094190022917)) ;
#137875 = CARTESIAN_POINT('Ctrl Pts',(4.5,2.72431432344521,-19.012634816645)) ;
#137876 = CARTESIAN_POINT('Ctrl Pts',(4.5,2.72431432344521,-21.627365183355)) ;
#137877 = CARTESIAN_POINT('Ctrl Pts',(4.5,2.72904669151417,-21.6311532753136)) ;
#137878 = CARTESIAN_POINT('Ctrl Pts',(4.49966645684475,2.73338556955535,-21.6354614101758)) ;
#137879 = CARTESIAN_POINT('Ctrl Pts',(4.49869539480396,2.74072289096357,-21.6439802414372)) ;
#137880 = CARTESIAN_POINT('Ctrl Pts',(4.49811062025689,2.74382502998075,-21.6481080596585)) ;
#137881 = CARTESIAN_POINT('Ctrl Pts',(4.49664125196625,2.75020211699685,-21.6575592649405)) ;
#137882 = CARTESIAN_POINT('Ctrl Pts',(4.49570721389712,2.75339870015137,-21.6630103903193)) ;
#137883 = CARTESIAN_POINT('Ctrl Pts',(4.49363760641479,2.75952863263943,-21.6747517051868)) ;
#137884 = CARTESIAN_POINT('Ctrl Pts',(4.49249077386344,2.76240287369067,-21.6810712258307)) ;
#137885 = CARTESIAN_POINT('Ctrl Pts',(4.49055019898874,2.76677757270135,-21.6919141256208)) ;
#137886 = CARTESIAN_POINT('Ctrl Pts',(4.48975662823144,2.76842729450632,-21.6963872919226)) ;
#137887 = CARTESIAN_POINT('Ctrl Pts',(4.4885208482156,2.77084293101086,-21.7035172849807)) ;
#137888 = CARTESIAN_POINT('Ctrl Pts',(4.48806820038251,2.77169418112725,-21.7061644329085)) ;
#137889 = CARTESIAN_POINT('Ctrl Pts',(4.48762159086959,2.77250619842348,-21.7088243182478)) ;
#137890 = CARTESIAN_POINT('Origin',(4.6,2.1,-20.32)) ;
#137891 = CARTESIAN_POINT('Origin',(4.6,2.1,-18.9380460421716)) ;
#137892 = CARTESIAN_POINT('Origin',(4.6,2.1,-21.7019539578284)) ;
#137893 = CARTESIAN_POINT('Origin',(12.7,2.1,-21.7019539578284)) ;
#137894 = CARTESIAN_POINT('Origin',(12.7,1.9,-21.7019539578284)) ;
#137895 = CARTESIAN_POINT('Origin',(12.7,2.65,-17.78)) ;
#137896 = CARTESIAN_POINT('Origin',(4.5,2.65,-18.8269539578284)) ;
#137897 = CARTESIAN_POINT('',(4.6,2.68715716172261,-18.9197943872367)) ;
#137898 = CARTESIAN_POINT('',(4.57524318173443,2.73534903670064,-18.8790648197889)) ;
#137899 = CARTESIAN_POINT('Ctrl Pts',(4.6,2.68715716172262,-18.9197943872367)) ;
#137900 = CARTESIAN_POINT('Ctrl Pts',(4.6,2.6910603667141,-18.9182322227785)) ;
#137901 = CARTESIAN_POINT('Ctrl Pts',(4.59952510519174,2.6948886188898,-18.9164097094748)) ;
#137902 = CARTESIAN_POINT('Ctrl Pts',(4.59869497748257,2.69852743640759,-18.9143901512251)) ;
#137903 = CARTESIAN_POINT('Ctrl Pts',(4.59815316003467,2.70090246232122,-18.9130720023612)) ;
#137904 = CARTESIAN_POINT('Ctrl Pts',(4.5974600110878,2.70319720658043,-18.9116709680453)) ;
#137905 = CARTESIAN_POINT('Ctrl Pts',(4.59664880273703,2.70538659711789,-18.9102145418985)) ;
#137906 = CARTESIAN_POINT('Ctrl Pts',(4.59612777291939,2.70679281754375,-18.9092790960924)) ;
#137907 = CARTESIAN_POINT('Ctrl Pts',(4.59555051815356,2.70817855133089,-18.9083049299072)) ;
#137908 = CARTESIAN_POINT('Ctrl Pts',(4.59494172533681,2.70950512149371,-18.9073227360698)) ;
#137909 = CARTESIAN_POINT('Ctrl Pts',(4.59250947890868,2.71480502887002,-18.9033986794992)) ;
#137910 = CARTESIAN_POINT('Ctrl Pts',(4.58944857813008,2.71954517005227,-18.8990823375811)) ;
#137911 = CARTESIAN_POINT('Ctrl Pts',(4.5861276864684,2.72376361218885,-18.8944738031841)) ;
#137912 = CARTESIAN_POINT('Ctrl Pts',(4.58350334758193,2.72709724148698,-18.8908319029778)) ;
#137913 = CARTESIAN_POINT('Ctrl Pts',(4.58071664514671,2.73010548898765,-18.8870059959317)) ;
#137914 = CARTESIAN_POINT('Ctrl Pts',(4.5779495181309,2.73280244902546,-18.8830231511112)) ;
#137915 = CARTESIAN_POINT('Ctrl Pts',(4.57705238626115,2.7336768320182,-18.8817318706603)) ;
#137916 = CARTESIAN_POINT('Ctrl Pts',(4.57614585580299,2.73452842391107,-18.8804088488159)) ;
#137917 = CARTESIAN_POINT('Ctrl Pts',(4.57524318173444,2.73534903670067,-18.8790648197889)) ;
#137918 = CARTESIAN_POINT('Origin',(4.65232986199444,2.66527023616352,-18.8312457888174)) ;
#137919 = CARTESIAN_POINT('Origin',(4.6,2.65,-18.8269539578284)) ;
#137920 = CARTESIAN_POINT('Origin',(12.7,1.9,-21.82)) ;
#137921 = CARTESIAN_POINT('Origin',(12.7,2.01643989873054,-18.7213606076168)) ;
#137922 = CARTESIAN_POINT('Origin',(-3.65,10.7,-19.57)) ;
#137923 = CARTESIAN_POINT('Origin',(-3.65,10.7,-19.57)) ;
#137924 = CARTESIAN_POINT('Origin',(-3.65,10.7,-19.57)) ;
#137925 = CARTESIAN_POINT('Origin',(0.,10.7,-19.57)) ;
#137926 = CARTESIAN_POINT('Origin',(-2.9,10.7,-19.57)) ;
#137927 = CARTESIAN_POINT('Origin',(-3.65,10.7,-20.32)) ;
#137928 = CARTESIAN_POINT('Origin',(-3.65,10.7,-21.07)) ;
#137929 = CARTESIAN_POINT('Origin',(-2.9,10.7,-19.57)) ;
#137930 = CARTESIAN_POINT('Origin',(-2.9,10.7,-19.57)) ;
#137931 = CARTESIAN_POINT('Origin',(-3.65,10.7,-21.07)) ;
#137932 = CARTESIAN_POINT('Origin',(-3.65,10.7,-21.07)) ;
#137933 = CARTESIAN_POINT('Origin',(-2.9,10.7,-20.32)) ;
#137934 = CARTESIAN_POINT('Origin',(-2.9,10.7,-21.07)) ;
#137935 = CARTESIAN_POINT('Origin',(0.,10.7,-21.07)) ;
#137936 = CARTESIAN_POINT('Origin',(-2.9,10.7,-21.07)) ;
#137937 = CARTESIAN_POINT('Origin',(-2.9,10.7,-21.07)) ;
#137938 = CARTESIAN_POINT('Origin',(-3.05,-3.95,-19.32)) ;
#137939 = CARTESIAN_POINT('Origin',(-3.05,-3.95,-21.22)) ;
#137940 = CARTESIAN_POINT('Origin',(-3.05,-3.95,-19.42)) ;
#137941 = CARTESIAN_POINT('Origin',(-3.25,-3.95,-19.42)) ;
#137942 = CARTESIAN_POINT('Origin',(-3.25,-3.95,-19.22)) ;
#137943 = CARTESIAN_POINT('Origin',(-3.25,-3.95,-19.42)) ;
#137944 = CARTESIAN_POINT('Origin',(-3.25,-3.95,-21.22)) ;
#137945 = CARTESIAN_POINT('Origin',(-3.25,-3.95,-21.22)) ;
#137946 = CARTESIAN_POINT('Origin',(-3.25,-3.95,-21.42)) ;
#137947 = CARTESIAN_POINT('Origin',(-4.4,-3.95,-19.22)) ;
#137948 = CARTESIAN_POINT('Origin',(-4.3,-3.95,-19.22)) ;
#137949 = CARTESIAN_POINT('Origin',(-3.25,-3.9,-19.42)) ;
#137950 = CARTESIAN_POINT('Origin',(-3.25,-3.85,-19.42)) ;
#137951 = CARTESIAN_POINT('Origin',(-3.25,-3.85,-20.32)) ;
#137952 = CARTESIAN_POINT('Origin',(-3.25,-3.85,-21.22)) ;
#137953 = CARTESIAN_POINT('Origin',(-3.25,-3.85,-19.42)) ;
#137954 = CARTESIAN_POINT('Origin',(-3.25,-3.9,-21.22)) ;
#137955 = CARTESIAN_POINT('Origin',(-3.25,-3.85,-21.22)) ;
#137956 = CARTESIAN_POINT('Origin',(-4.4,-3.95,-21.42)) ;
#137957 = CARTESIAN_POINT('Origin',(-4.3,-3.95,-21.42)) ;
#137958 = CARTESIAN_POINT('Origin',(-4.5,-3.95,-19.32)) ;
#137959 = CARTESIAN_POINT('Origin',(-4.5,-3.95,-19.42)) ;
#137960 = CARTESIAN_POINT('Origin',(-4.5,-3.95,-21.22)) ;
#137961 = CARTESIAN_POINT('Origin',(-4.3,-3.95,-19.42)) ;
#137962 = CARTESIAN_POINT('Origin',(-4.3,-3.95,-19.42)) ;
#137963 = CARTESIAN_POINT('Origin',(-3.25,-3.85,-19.42)) ;
#137964 = CARTESIAN_POINT('Origin',(-3.25,-3.85,-19.42)) ;
#137965 = CARTESIAN_POINT('Origin',(-3.25,-3.85,-21.22)) ;
#137966 = CARTESIAN_POINT('Origin',(-3.25,-3.85,-21.22)) ;
#137967 = CARTESIAN_POINT('Origin',(-4.3,-3.95,-21.22)) ;
#137968 = CARTESIAN_POINT('Origin',(-4.3,-3.95,-21.22)) ;
#137969 = CARTESIAN_POINT('Origin',(-4.3,-3.9,-19.42)) ;
#137970 = CARTESIAN_POINT('Origin',(-4.3,-3.85,-19.42)) ;
#137971 = CARTESIAN_POINT('Origin',(-1.56125112837913E-16,-3.85,-19.42)) ;
#137972 = CARTESIAN_POINT('Origin',(-4.3,-3.85,-19.42)) ;
#137973 = CARTESIAN_POINT('Origin',(-1.56125112837913E-16,-3.85,-21.22)) ;
#137974 = CARTESIAN_POINT('Origin',(-4.3,-3.85,-21.22)) ;
#137975 = CARTESIAN_POINT('Origin',(-4.3,-3.9,-21.22)) ;
#137976 = CARTESIAN_POINT('Origin',(-4.3,-3.85,-21.22)) ;
#137977 = CARTESIAN_POINT('Origin',(-4.3,-3.85,-19.42)) ;
#137978 = CARTESIAN_POINT('Origin',(-4.3,-3.85,-19.42)) ;
#137979 = CARTESIAN_POINT('Origin',(-4.3,-3.85,-21.22)) ;
#137980 = CARTESIAN_POINT('Origin',(-4.3,-3.85,-21.22)) ;
#137981 = CARTESIAN_POINT('Origin',(-4.3,-3.85,-20.32)) ;
#137982 = CARTESIAN_POINT('Origin',(-4.,10.85,-21.32)) ;
#137983 = CARTESIAN_POINT('Origin',(-4.,10.85,-21.22)) ;
#137984 = CARTESIAN_POINT('Origin',(-4.,10.85,-19.42)) ;
#137985 = CARTESIAN_POINT('Origin',(-3.8,10.85,-19.42)) ;
#137986 = CARTESIAN_POINT('Origin',(-3.8,10.85,-19.22)) ;
#137987 = CARTESIAN_POINT('Origin',(-3.8,10.85,-19.42)) ;
#137988 = CARTESIAN_POINT('Origin',(-3.8,10.85,-21.22)) ;
#137989 = CARTESIAN_POINT('Origin',(-3.8,10.85,-21.22)) ;
#137990 = CARTESIAN_POINT('Origin',(-3.8,10.85,-21.42)) ;
#137991 = CARTESIAN_POINT('Origin',(-3.9,10.85,-19.22)) ;
#137992 = CARTESIAN_POINT('Origin',(-2.75,10.85,-19.22)) ;
#137993 = CARTESIAN_POINT('Origin',(-3.8,10.8,-19.42)) ;
#137994 = CARTESIAN_POINT('Origin',(-3.8,10.75,-19.42)) ;
#137995 = CARTESIAN_POINT('Origin',(-3.8,10.75,-20.32)) ;
#137996 = CARTESIAN_POINT('Origin',(-3.8,10.75,-21.22)) ;
#137997 = CARTESIAN_POINT('Origin',(-3.8,10.75,-19.42)) ;
#137998 = CARTESIAN_POINT('Origin',(-3.8,10.8,-21.22)) ;
#137999 = CARTESIAN_POINT('Origin',(-3.8,10.75,-21.22)) ;
#138000 = CARTESIAN_POINT('Origin',(-3.9,10.85,-21.42)) ;
#138001 = CARTESIAN_POINT('Origin',(-2.75,10.85,-21.42)) ;
#138002 = CARTESIAN_POINT('Origin',(-2.55,10.85,-21.32)) ;
#138003 = CARTESIAN_POINT('Origin',(-2.55,10.85,-19.42)) ;
#138004 = CARTESIAN_POINT('Origin',(-2.55,10.85,-21.22)) ;
#138005 = CARTESIAN_POINT('Origin',(-2.75,10.85,-19.42)) ;
#138006 = CARTESIAN_POINT('Origin',(-2.75,10.85,-19.42)) ;
#138007 = CARTESIAN_POINT('Origin',(-3.8,10.75,-19.42)) ;
#138008 = CARTESIAN_POINT('Origin',(-3.8,10.75,-19.42)) ;
#138009 = CARTESIAN_POINT('Origin',(-3.8,10.75,-21.22)) ;
#138010 = CARTESIAN_POINT('Origin',(-3.8,10.75,-21.22)) ;
#138011 = CARTESIAN_POINT('Origin',(-2.75,10.85,-21.22)) ;
#138012 = CARTESIAN_POINT('Origin',(-2.75,10.85,-21.22)) ;
#138013 = CARTESIAN_POINT('Origin',(-2.75,10.8,-19.42)) ;
#138014 = CARTESIAN_POINT('Origin',(-2.75,10.75,-19.42)) ;
#138015 = CARTESIAN_POINT('Origin',(1.56125112837912E-16,10.75,-19.42)) ;
#138016 = CARTESIAN_POINT('Origin',(-2.75,10.75,-19.42)) ;
#138017 = CARTESIAN_POINT('Origin',(-1.56125112837913E-16,10.75,-21.22)) ;
#138018 = CARTESIAN_POINT('Origin',(-2.75,10.75,-21.22)) ;
#138019 = CARTESIAN_POINT('Origin',(-2.75,10.8,-21.22)) ;
#138020 = CARTESIAN_POINT('Origin',(-2.75,10.75,-21.22)) ;
#138021 = CARTESIAN_POINT('Origin',(-2.75,10.75,-19.42)) ;
#138022 = CARTESIAN_POINT('Origin',(-2.75,10.75,-19.42)) ;
#138023 = CARTESIAN_POINT('Origin',(-2.75,10.75,-21.22)) ;
#138024 = CARTESIAN_POINT('Origin',(-2.75,10.75,-21.22)) ;
#138025 = CARTESIAN_POINT('Origin',(-2.75,10.75,-20.32)) ;
#138026 = CARTESIAN_POINT('Origin',(4.6,0.,-20.32)) ;
#138027 = CARTESIAN_POINT('Ctrl Pts',(4.5,-2.7,-18.7968453788272)) ;
#138028 = CARTESIAN_POINT('Ctrl Pts',(4.5,-2.71827986285823,-18.8719647391751)) ;
#138029 = CARTESIAN_POINT('Ctrl Pts',(4.50597963419107,-2.73556801027185,
-18.9467398604528)) ;
#138030 = CARTESIAN_POINT('Ctrl Pts',(4.52394923367545,-2.75977758633329,
-19.0584368340216)) ;
#138031 = CARTESIAN_POINT('Ctrl Pts',(4.53141024883993,-2.76757607569523,
-19.0956832823903)) ;
#138032 = CARTESIAN_POINT('Ctrl Pts',(4.54734065524867,-2.77857284247615,
-19.150165689583)) ;
#138033 = CARTESIAN_POINT('Ctrl Pts',(4.55339248498576,-2.78214991573955,
-19.1682382744149)) ;
#138034 = CARTESIAN_POINT('Ctrl Pts',(4.56567492147096,-2.787183259287,-19.1941467218607)) ;
#138035 = CARTESIAN_POINT('Ctrl Pts',(4.5702469143305,-2.78880341224557,-19.2025726050508)) ;
#138036 = CARTESIAN_POINT('Ctrl Pts',(4.58215938980081,-2.79169669265294,
-19.2177434798851)) ;
#138037 = CARTESIAN_POINT('Ctrl Pts',(4.59005470866978,-2.79310344827587,
-19.2252063540423)) ;
#138038 = CARTESIAN_POINT('Ctrl Pts',(4.6,-2.79310344827586,-19.2252063540422)) ;
#138039 = CARTESIAN_POINT('Origin',(4.6,-2.4,-18.3578583129651)) ;
#138040 = CARTESIAN_POINT('Origin',(4.6,-2.4,-17.78)) ;
#138041 = CARTESIAN_POINT('Origin',(4.6,-2.4,-17.2021416870349)) ;
#138042 = CARTESIAN_POINT('Origin',(4.6,-2.4,-18.3578583129651)) ;
#138043 = CARTESIAN_POINT('Origin',(4.6,-2.4,-18.3578583129651)) ;
#138044 = CARTESIAN_POINT('Origin',(4.6,-2.4,-18.3578583129651)) ;
#138045 = CARTESIAN_POINT('Origin',(0.584645609909622,-2.4,-18.3578583129651)) ;
#138046 = CARTESIAN_POINT('Origin',(12.7,-2.4,-18.3578583129651)) ;
#138047 = CARTESIAN_POINT('Origin',(12.7,-2.2,-17.78)) ;
#138048 = CARTESIAN_POINT('Origin',(12.7,-2.2,-17.2021416870349)) ;
#138049 = CARTESIAN_POINT('Origin',(12.7,-2.2,-18.3578583129651)) ;
#138050 = CARTESIAN_POINT('Origin',(12.7,-2.4,-18.3578583129651)) ;
#138051 = CARTESIAN_POINT('Origin',(12.7,-2.24516129032258,-18.4844480992255)) ;
#138052 = CARTESIAN_POINT('Origin',(12.7,0.,-20.32)) ;
#138053 = CARTESIAN_POINT('Origin',(12.7,-2.24516129032258,-22.1555519007745)) ;
#138054 = CARTESIAN_POINT('Origin',(12.7,-2.2,-17.78)) ;
#138055 = CARTESIAN_POINT('Origin',(12.7,-2.2,-22.2821416870349)) ;
#138056 = CARTESIAN_POINT('Origin',(12.7,-2.4,-22.2821416870349)) ;
#138057 = CARTESIAN_POINT('Origin',(12.7,-2.4,-22.2821416870349)) ;
#138058 = CARTESIAN_POINT('Origin',(0.584645609909622,-2.4,-22.2821416870349)) ;
#138059 = CARTESIAN_POINT('Origin',(4.6,-2.4,-22.2821416870349)) ;
#138060 = CARTESIAN_POINT('Origin',(4.6,-2.4,-17.78)) ;
#138061 = CARTESIAN_POINT('Origin',(4.6,-2.4,-22.2821416870349)) ;
#138062 = CARTESIAN_POINT('Origin',(4.6,-2.4,-22.2821416870349)) ;
#138063 = CARTESIAN_POINT('Origin',(4.6,-2.4,-22.2821416870349)) ;
#138064 = CARTESIAN_POINT('Origin',(4.6,0.,-20.32)) ;
#138065 = CARTESIAN_POINT('Ctrl Pts',(4.6,-2.79310344827586,-21.4147936459578)) ;
#138066 = CARTESIAN_POINT('Ctrl Pts',(4.59007568892311,-2.79310344827586,
-21.4147936459578)) ;
#138067 = CARTESIAN_POINT('Ctrl Pts',(4.58219207637239,-2.79170232102183,
-21.422226742276)) ;
#138068 = CARTESIAN_POINT('Ctrl Pts',(4.57028631514659,-2.78881527838255,
-21.43736543899)) ;
#138069 = CARTESIAN_POINT('Ctrl Pts',(4.56571532154372,-2.78719767797524,
-21.4457784885835)) ;
#138070 = CARTESIAN_POINT('Ctrl Pts',(4.55343865632726,-2.78217307830036,
-21.4716436333089)) ;
#138071 = CARTESIAN_POINT('Ctrl Pts',(4.54738888873344,-2.77860151743012,
-21.4896900859661)) ;
#138072 = CARTESIAN_POINT('Ctrl Pts',(4.53146440752602,-2.76762263748299,
-21.5440903156831)) ;
#138073 = CARTESIAN_POINT('Ctrl Pts',(4.52400917967609,-2.75984503873828,
-21.5812455063058)) ;
#138074 = CARTESIAN_POINT('Ctrl Pts',(4.50599905604505,-2.7356206423885,-21.6930301354693)) ;
#138075 = CARTESIAN_POINT('Ctrl Pts',(4.5,-2.71826422026483,-21.7680995425769)) ;
#138076 = CARTESIAN_POINT('Ctrl Pts',(4.5,-2.7,-21.8431546211728)) ;
#138077 = CARTESIAN_POINT('Origin',(3.7,-2.9,-17.78)) ;
#138078 = CARTESIAN_POINT('Origin',(3.7,-2.9,-12.7)) ;
#138079 = CARTESIAN_POINT('Origin',(3.5,-3.95,-17.78)) ;
#138080 = CARTESIAN_POINT('Origin',(3.5,-3.95,-12.7)) ;
#138081 = CARTESIAN_POINT('Origin',(-5.3,-3.95,-17.78)) ;
#138082 = CARTESIAN_POINT('Origin',(-5.3,-3.95,-12.7)) ;
#138083 = CARTESIAN_POINT('Origin',(-5.3,5.19009804864072,-17.78)) ;
#138084 = CARTESIAN_POINT('Origin',(-5.3,5.19009804864072,-12.7)) ;
#138085 = CARTESIAN_POINT('Origin',(-4.8,10.3,-17.78)) ;
#138086 = CARTESIAN_POINT('Origin',(-4.8,10.3,-12.7)) ;
#138087 = CARTESIAN_POINT('Origin',(-4.8,10.85,-17.78)) ;
#138088 = CARTESIAN_POINT('Origin',(-4.8,10.85,-12.7)) ;
#138089 = CARTESIAN_POINT('Origin',(-0.362523114814661,9.05,-20.4890473046963)) ;
#138090 = CARTESIAN_POINT('Origin',(0.36252311481466,9.05,-20.1509526953037)) ;
#138091 = CARTESIAN_POINT('Origin',(-1.31845674202095,9.85,-18.9122813422351)) ;
#138092 = CARTESIAN_POINT('Origin',(-0.230887397576972,9.85,-18.4051394281462)) ;
#138093 = CARTESIAN_POINT('Origin',(3.3,10.85,-17.78)) ;
#138094 = CARTESIAN_POINT('Origin',(3.3,10.85,-12.7)) ;
#138095 = CARTESIAN_POINT('Origin',(3.85,6.92431432344521,-17.78)) ;
#138096 = CARTESIAN_POINT('Origin',(3.85,6.92431432344521,-12.7)) ;
#138097 = CARTESIAN_POINT('Origin',(4.05,3.77568567655479,-17.78)) ;
#138098 = CARTESIAN_POINT('Origin',(4.05,3.77568567655479,-12.7)) ;
#138099 = CARTESIAN_POINT('Origin',(4.6,2.1,-18.9380460421716)) ;
#138100 = CARTESIAN_POINT('Origin',(4.6,2.1,-18.9380460421716)) ;
#138101 = CARTESIAN_POINT('Origin',(4.6,0.280857398566761,-18.6348556085994)) ;
#138102 = CARTESIAN_POINT('Origin',(4.6,2.61712020253893,-19.0242327425948)) ;
#138103 = CARTESIAN_POINT('Origin',(4.6,2.65,-18.8269539578284)) ;
#138104 = CARTESIAN_POINT('Origin',(4.6,2.72431432344521,-19.012634816645)) ;
#138105 = CARTESIAN_POINT('Ctrl Pts',(4.48762159086906,2.77250619842445,-18.9311756817496)) ;
#138106 = CARTESIAN_POINT('Ctrl Pts',(4.51316716229104,2.72605970493114,-18.8942387941972)) ;
#138107 = CARTESIAN_POINT('Ctrl Pts',(4.57527453405851,2.73535372386122,-18.879057153198)) ;
#138108 = CARTESIAN_POINT('Ctrl Pts',(4.49363662433155,2.76156977394747,-18.9669995924716)) ;
#138109 = CARTESIAN_POINT('Ctrl Pts',(4.5146945995807,2.70766535161861,-18.9162008473932)) ;
#138110 = CARTESIAN_POINT('Ctrl Pts',(4.58732693581885,2.72440392220678,-18.8969950412341)) ;
#138111 = CARTESIAN_POINT('Ctrl Pts',(4.5,2.74488438438033,-18.9961692160663)) ;
#138112 = CARTESIAN_POINT('Ctrl Pts',(4.50856472873626,2.69031482079677,-18.9184911137048)) ;
#138113 = CARTESIAN_POINT('Ctrl Pts',(4.60003980620507,2.70775073269831,-18.9115523113747)) ;
#138114 = CARTESIAN_POINT('Ctrl Pts',(4.5,2.72431432344521,-19.012634816645)) ;
#138115 = CARTESIAN_POINT('Ctrl Pts',(4.5,2.68714136424467,-18.9197549158517)) ;
#138116 = CARTESIAN_POINT('Ctrl Pts',(4.60004250625998,2.68715716507935,-18.9197943956238)) ;
#138117 = CARTESIAN_POINT('Origin',(4.57524318173443,2.82069807340128,-18.9311756817495)) ;
#138118 = CARTESIAN_POINT('Ctrl Pts',(4.47150553123747,2.80180812502279,-18.8269539578284)) ;
#138119 = CARTESIAN_POINT('Ctrl Pts',(4.5,2.75,-18.8269539578284)) ;
#138120 = CARTESIAN_POINT('Ctrl Pts',(4.55912712210514,2.75,-18.8269539578284)) ;
#138121 = CARTESIAN_POINT('Ctrl Pts',(4.47150553186688,2.8018081238784,-18.8635744727347)) ;
#138122 = CARTESIAN_POINT('Ctrl Pts',(4.50000000073523,2.74999999866316,-18.8512580842688)) ;
#138123 = CARTESIAN_POINT('Ctrl Pts',(4.5591271227348,2.75,-18.8452720457593)) ;
#138124 = CARTESIAN_POINT('Ctrl Pts',(4.47712448971608,2.79159183687986,-18.8999165373524)) ;
#138125 = CARTESIAN_POINT('Ctrl Pts',(4.50480340096849,2.74126654369362,-18.8755379509981)) ;
#138126 = CARTESIAN_POINT('Ctrl Pts',(4.56473907811156,2.74489822224644,-18.8634248215823)) ;
#138127 = CARTESIAN_POINT('Ctrl Pts',(4.48762159086676,2.77250619842407,-18.9311756817495)) ;
#138128 = CARTESIAN_POINT('Ctrl Pts',(4.51315802400618,2.72607631998876,-18.8942520074343)) ;
#138129 = CARTESIAN_POINT('Ctrl Pts',(4.57524318173443,2.73534903670064,-18.8790648197889)) ;
#138130 = CARTESIAN_POINT('Origin',(4.55912712210513,2.85,-18.8269539578284)) ;
#138131 = CARTESIAN_POINT('Origin',(4.55912712210514,2.85,-17.78)) ;
#138132 = CARTESIAN_POINT('Origin',(4.55912712210514,2.85,-16.7330460421716)) ;
#138133 = CARTESIAN_POINT('Origin',(4.55912712210514,2.85,-17.78)) ;
#138134 = CARTESIAN_POINT('Origin',(4.55912712210514,2.85,-21.8130460421716)) ;
#138135 = CARTESIAN_POINT('Ctrl Pts',(4.48762159086766,2.77250619842243,-21.7088243182478)) ;
#138136 = CARTESIAN_POINT('Ctrl Pts',(4.51315802400691,2.72607631998744,-21.7457479925641)) ;
#138137 = CARTESIAN_POINT('Ctrl Pts',(4.57524318173533,2.73534903669982,-21.7609351802097)) ;
#138138 = CARTESIAN_POINT('Ctrl Pts',(4.47712448971643,2.79159183687922,-21.7400834626457)) ;
#138139 = CARTESIAN_POINT('Ctrl Pts',(4.50480340096883,2.74126654369304,-21.7644620490007)) ;
#138140 = CARTESIAN_POINT('Ctrl Pts',(4.56473907811197,2.74489822224618,-21.7765751784167)) ;
#138141 = CARTESIAN_POINT('Ctrl Pts',(4.47150553186688,2.8018081238784,-21.7764255272642)) ;
#138142 = CARTESIAN_POINT('Ctrl Pts',(4.50000000073523,2.74999999866316,-21.7887419157304)) ;
#138143 = CARTESIAN_POINT('Ctrl Pts',(4.5591271227348,2.75,-21.7947279542402)) ;
#138144 = CARTESIAN_POINT('Ctrl Pts',(4.47150553123747,2.80180812502279,-21.8130460421716)) ;
#138145 = CARTESIAN_POINT('Ctrl Pts',(4.5,2.75,-21.8130460421716)) ;
#138146 = CARTESIAN_POINT('Ctrl Pts',(4.55912712210513,2.75,-21.8130460421716)) ;
#138147 = CARTESIAN_POINT('Origin',(4.57524318173533,2.82069807339964,-21.7088243182478)) ;
#138148 = CARTESIAN_POINT('Ctrl Pts',(4.57527448145479,2.73535371598842,-21.7609428339419)) ;
#138149 = CARTESIAN_POINT('Ctrl Pts',(4.51316714695683,2.7260597328105,-21.7457611836292)) ;
#138150 = CARTESIAN_POINT('Ctrl Pts',(4.48762159086951,2.77250619842363,-21.7088243182477)) ;
#138151 = CARTESIAN_POINT('Ctrl Pts',(4.5873268774263,2.72440390874888,-21.7430049433246)) ;
#138152 = CARTESIAN_POINT('Ctrl Pts',(4.51469458626373,2.70766538570662,-21.7237991204817)) ;
#138153 = CARTESIAN_POINT('Ctrl Pts',(4.49363662433185,2.76156977394669,-21.6730004075269)) ;
#138154 = CARTESIAN_POINT('Ctrl Pts',(4.60003973844309,2.70775071978185,-21.728447683485)) ;
#138155 = CARTESIAN_POINT('Ctrl Pts',(4.50856472285784,2.6903148582481,-21.721508832984)) ;
#138156 = CARTESIAN_POINT('Ctrl Pts',(4.5,2.74488438437978,-21.6438307839333)) ;
#138157 = CARTESIAN_POINT('Ctrl Pts',(4.60004243494351,2.6871571650681,-21.7202056044043)) ;
#138158 = CARTESIAN_POINT('Ctrl Pts',(4.5,2.68714139075511,-21.7202450179097)) ;
#138159 = CARTESIAN_POINT('Ctrl Pts',(4.5,2.72431432344521,-21.627365183355)) ;
#138160 = CARTESIAN_POINT('Origin',(4.6,0.280857398566761,-22.0051443914006)) ;
#138161 = CARTESIAN_POINT('Origin',(4.6,2.1,-21.7019539578284)) ;
#138162 = CARTESIAN_POINT('Origin',(4.6,2.1,-21.7019539578284)) ;
#138163 = CARTESIAN_POINT('Origin',(4.6,0.,-20.32)) ;
#138164 = CARTESIAN_POINT('',(4.5,-2.9,-20.3200000000039)) ;
#138165 = CARTESIAN_POINT('',(4.57439618084313,-2.80937499999937,-21.3627958671254)) ;
#138166 = CARTESIAN_POINT('Ctrl Pts',(4.5,-2.9,-20.3200000000039)) ;
#138167 = CARTESIAN_POINT('Ctrl Pts',(4.5,-2.9000000234111,-20.4961762625703)) ;
#138168 = CARTESIAN_POINT('Ctrl Pts',(4.49893459747296,-2.89187728142186,
-20.6722938225552)) ;
#138169 = CARTESIAN_POINT('Ctrl Pts',(4.50498172725087,-2.86839426105774,
-20.9349432768872)) ;
#138170 = CARTESIAN_POINT('Ctrl Pts',(4.50826226558342,-2.85869729223562,
-21.0222870271135)) ;
#138171 = CARTESIAN_POINT('Ctrl Pts',(4.52028413974051,-2.84160518746962,
-21.1528409654328)) ;
#138172 = CARTESIAN_POINT('Ctrl Pts',(4.52545003690602,-2.8354696349403,-21.196363113622)) ;
#138173 = CARTESIAN_POINT('Ctrl Pts',(4.53741870680499,-2.82581179679252,
-21.2606394550108)) ;
#138174 = CARTESIAN_POINT('Ctrl Pts',(4.54209540184575,-2.82251395224859,
-21.2819200182606)) ;
#138175 = CARTESIAN_POINT('Ctrl Pts',(4.55451190949429,-2.81582803324483,
-21.3238742105328)) ;
#138176 = CARTESIAN_POINT('Ctrl Pts',(4.56139306411848,-2.8124020390272,-21.3447435318249)) ;
#138177 = CARTESIAN_POINT('Ctrl Pts',(4.57439618084313,-2.80937499999937,
-21.3627958671254)) ;
#138178 = CARTESIAN_POINT('Ctrl Pts',(4.57439618084312,-2.80937499999939,
-21.3627958671254)) ;
#138179 = CARTESIAN_POINT('Ctrl Pts',(4.57788811720509,-2.80856205104935,
-21.3676438845913)) ;
#138180 = CARTESIAN_POINT('Ctrl Pts',(4.58132110715661,-2.80743849592504,
-21.3726543114197)) ;
#138181 = CARTESIAN_POINT('Ctrl Pts',(4.58591063786558,-2.80541025280319,
-21.3800683491597)) ;
#138182 = CARTESIAN_POINT('Ctrl Pts',(4.58721694730497,-2.80476695238161,
-21.3822683250837)) ;
#138183 = CARTESIAN_POINT('Ctrl Pts',(4.58874498026859,-2.80393035430395,
-21.3849717146408)) ;
#138184 = CARTESIAN_POINT('Ctrl Pts',(4.58900094431508,-2.80378708879839,
-21.385429423373)) ;
#138185 = CARTESIAN_POINT('Ctrl Pts',(4.58924476828968,-2.80364801935069,
-21.38586949326)) ;
#138186 = CARTESIAN_POINT('Ctrl Pts',(4.58924931741448,-2.80364542371033,
-21.3858777053493)) ;
#138187 = CARTESIAN_POINT('Ctrl Pts',(4.59158188358133,-2.80231401319274,
-21.3900892401221)) ;
#138188 = CARTESIAN_POINT('Ctrl Pts',(4.59377134212491,-2.80081309849101,
-21.3944383923964)) ;
#138189 = CARTESIAN_POINT('Ctrl Pts',(4.59570408210449,-2.79909049146272,
-21.3991378632085)) ;
#138190 = CARTESIAN_POINT('Ctrl Pts',(4.5957084873849,-2.79908656285629,-21.3991485795779)) ;
#138191 = CARTESIAN_POINT('Ctrl Pts',(4.59603576097762,-2.79879453264352,
-21.3999450754362)) ;
#138192 = CARTESIAN_POINT('Ctrl Pts',(4.59633794834607,-2.79851279959495,
-21.4007065253189)) ;
#138193 = CARTESIAN_POINT('Ctrl Pts',(4.59727216584803,-2.79759800070515,
-21.40316063341)) ;
#138194 = CARTESIAN_POINT('Ctrl Pts',(4.59785661125443,-2.79695684051616,
-21.4048529156094)) ;
#138195 = CARTESIAN_POINT('Ctrl Pts',(4.59875882816121,-2.7958009226755,-21.4078683242216)) ;
#138196 = CARTESIAN_POINT('Ctrl Pts',(4.59910960512327,-2.79529211440566,
-21.4091844992176)) ;
#138197 = CARTESIAN_POINT('Ctrl Pts',(4.59950074890552,-2.79458032370895,
-21.4110150784121)) ;
#138198 = CARTESIAN_POINT('Ctrl Pts',(4.59959271145697,-2.79439474074567,
-21.4114948405808)) ;
#138199 = CARTESIAN_POINT('Ctrl Pts',(4.59970479219924,-2.79411978912795,
-21.4122025710462)) ;
#138200 = CARTESIAN_POINT('Ctrl Pts',(4.59973686334512,-2.79403231884248,
-21.4124272684452)) ;
#138201 = CARTESIAN_POINT('Ctrl Pts',(4.59980956306601,-2.7938042827674,-21.4130108264021)) ;
#138202 = CARTESIAN_POINT('Ctrl Pts',(4.59984405921136,-2.79366555090847,
-21.4133689790042)) ;
#138203 = CARTESIAN_POINT('Ctrl Pts',(4.59992170638736,-2.79338632637294,
-21.4140824135446)) ;
#138204 = CARTESIAN_POINT('Ctrl Pts',(4.59995882625634,-2.79324305250058,
-21.4144374792565)) ;
#138205 = CARTESIAN_POINT('Ctrl Pts',(4.59999999999999,-2.79310344827586,
-21.4147936459578)) ;
#138206 = CARTESIAN_POINT('',(4.57439618084271,-2.80937499999947,-19.2772041328751)) ;
#138207 = CARTESIAN_POINT('Ctrl Pts',(4.59999999999999,-2.79310344827586,
-19.2252063540422)) ;
#138208 = CARTESIAN_POINT('Ctrl Pts',(4.59995895305209,-2.79324111387632,
-19.2255620070442)) ;
#138209 = CARTESIAN_POINT('Ctrl Pts',(4.59992125133673,-2.79338175512528,
-19.2259166499952)) ;
#138210 = CARTESIAN_POINT('Ctrl Pts',(4.59984242179761,-2.79365985893298,
-19.2266272182547)) ;
#138211 = CARTESIAN_POINT('Ctrl Pts',(4.5998070294299,-2.79379858543765,-19.226981904003)) ;
#138212 = CARTESIAN_POINT('Ctrl Pts',(4.59973261548695,-2.79401893257626,
-19.2275458212796)) ;
#138213 = CARTESIAN_POINT('Ctrl Pts',(4.59970092564442,-2.7941005010842,-19.2277547044526)) ;
#138214 = CARTESIAN_POINT('Ctrl Pts',(4.59958060815602,-2.79437456977472,
-19.2284570742577)) ;
#138215 = CARTESIAN_POINT('Ctrl Pts',(4.59947821517874,-2.79456857658396,
-19.2289550953807)) ;
#138216 = CARTESIAN_POINT('Ctrl Pts',(4.5990597198479,-2.79527981802027,-19.2307850643885)) ;
#138217 = CARTESIAN_POINT('Ctrl Pts',(4.59869396429225,-2.79579226918927,
-19.2321114012001)) ;
#138218 = CARTESIAN_POINT('Ctrl Pts',(4.59768320083749,-2.79706868650734,
-19.2354440738933)) ;
#138219 = CARTESIAN_POINT('Ctrl Pts',(4.59698254015873,-2.79783590182173,
-19.2374731996627)) ;
#138220 = CARTESIAN_POINT('Ctrl Pts',(4.5959970522588,-2.79876532988113,-19.2399846842385)) ;
#138221 = CARTESIAN_POINT('Ctrl Pts',(4.59580678362761,-2.7989396411024,-19.2404581050039)) ;
#138222 = CARTESIAN_POINT('Ctrl Pts',(4.59367882781298,-2.80083904916685,
-19.2456449119971)) ;
#138223 = CARTESIAN_POINT('Ctrl Pts',(4.59150707087689,-2.80233337893514,
-19.2499793277041)) ;
#138224 = CARTESIAN_POINT('Ctrl Pts',(4.58628071719247,-2.80532570224264,
-19.259451467429)) ;
#138225 = CARTESIAN_POINT('Ctrl Pts',(4.58313959595737,-2.80673110767396,
-19.2645102480653)) ;
#138226 = CARTESIAN_POINT('Ctrl Pts',(4.57802611146366,-2.80844040952806,
-19.2720963574913)) ;
#138227 = CARTESIAN_POINT('Ctrl Pts',(4.57624387811663,-2.80894486836992,
-19.2746389593415)) ;
#138228 = CARTESIAN_POINT('Ctrl Pts',(4.57439618084271,-2.80937499999947,
-19.2772041328751)) ;
#138229 = CARTESIAN_POINT('Ctrl Pts',(4.57439618084271,-2.80937499999947,
-19.2772041328751)) ;
#138230 = CARTESIAN_POINT('Ctrl Pts',(4.56149777794589,-2.81237766235467,
-19.2951110931668)) ;
#138231 = CARTESIAN_POINT('Ctrl Pts',(4.55451596106519,-2.81582788236477,
-19.3161262422968)) ;
#138232 = CARTESIAN_POINT('Ctrl Pts',(4.54213610452188,-2.82249001163036,
-19.3579283596283)) ;
#138233 = CARTESIAN_POINT('Ctrl Pts',(4.53742891479326,-2.82580422498964,
-19.379310967236)) ;
#138234 = CARTESIAN_POINT('Ctrl Pts',(4.525451614243,-2.8354670333868,-19.4436179437949)) ;
#138235 = CARTESIAN_POINT('Ctrl Pts',(4.52032009146395,-2.84156292603926,
-19.4868565734785)) ;
#138236 = CARTESIAN_POINT('Ctrl Pts',(4.50830110904356,-2.85862448221642,
-19.6171164259574)) ;
#138237 = CARTESIAN_POINT('Ctrl Pts',(4.50499166750953,-2.86836219567853,
-19.7047300385823)) ;
#138238 = CARTESIAN_POINT('Ctrl Pts',(4.49892845988062,-2.8918880660271,-19.9677629968379)) ;
#138239 = CARTESIAN_POINT('Ctrl Pts',(4.49999999999474,-2.89999999999869,
-20.1438300901178)) ;
#138240 = CARTESIAN_POINT('Ctrl Pts',(4.5,-2.9,-20.3200000000039)) ;
#138241 = CARTESIAN_POINT('Origin',(4.4,-2.7,-17.78)) ;
#138242 = CARTESIAN_POINT('Origin',(4.4,-2.7,-16.7631546211728)) ;
#138243 = CARTESIAN_POINT('Origin',(4.4,-2.7,-18.7968453788272)) ;
#138244 = CARTESIAN_POINT('Ctrl Pts',(4.40227435089069,-2.79999990867355,
-18.729400692882)) ;
#138245 = CARTESIAN_POINT('Ctrl Pts',(4.51828879250233,-2.80015667527383,
-18.7387855667922)) ;
#138246 = CARTESIAN_POINT('Ctrl Pts',(4.50118227077258,-2.68533700727761,
-18.7379711074493)) ;
#138247 = CARTESIAN_POINT('Ctrl Pts',(4.39419482113923,-2.79999992837382,
-18.8436876996692)) ;
#138248 = CARTESIAN_POINT('Ctrl Pts',(4.48571792501716,-2.80010751836587,
-18.822671366751)) ;
#138249 = CARTESIAN_POINT('Ctrl Pts',(4.49717570077253,-2.71006921719264,
-18.8370318982147)) ;
#138250 = CARTESIAN_POINT('Ctrl Pts',(4.40636790575266,-2.79999994706265,
-18.9549089073543)) ;
#138251 = CARTESIAN_POINT('Ctrl Pts',(4.47481046024546,-2.80007242131916,
-18.9333224277989)) ;
#138252 = CARTESIAN_POINT('Ctrl Pts',(4.50328131876399,-2.73353293829091,
-18.9370258748099)) ;
#138253 = CARTESIAN_POINT('Ctrl Pts',(4.45479736994228,-2.79999997092221,
-19.1050736654711)) ;
#138254 = CARTESIAN_POINT('Ctrl Pts',(4.49869786247045,-2.80003603117403,
-19.0862792434959)) ;
#138255 = CARTESIAN_POINT('Ctrl Pts',(4.52748687875414,-2.7634897604751,-19.0762891728588)) ;
#138256 = CARTESIAN_POINT('Ctrl Pts',(4.47221929614095,-2.79999997745988,
-19.1473040602233)) ;
#138257 = CARTESIAN_POINT('Ctrl Pts',(4.50880556767619,-2.8000272573648,-19.1282748482859)) ;
#138258 = CARTESIAN_POINT('Ctrl Pts',(4.53619137795526,-2.77169834185703,
-19.1159836823675)) ;
#138259 = CARTESIAN_POINT('Ctrl Pts',(4.50882352800135,-2.7999999860536,-19.2042843496091)) ;
#138260 = CARTESIAN_POINT('Ctrl Pts',(4.53367802911268,-2.80001636071785,
-19.1853587024204)) ;
#138261 = CARTESIAN_POINT('Ctrl Pts',(4.55447319025663,-2.78248861123827,
-19.1700956814255)) ;
#138262 = CARTESIAN_POINT('Ctrl Pts',(4.52308919141483,-2.79999998878206,
-19.2226625616911)) ;
#138263 = CARTESIAN_POINT('Ctrl Pts',(4.54363962638622,-2.80001303821803,
-19.2037261501717)) ;
#138264 = CARTESIAN_POINT('Ctrl Pts',(4.56159739427507,-2.78591449131415,
-19.1876542708947)) ;
#138265 = CARTESIAN_POINT('Ctrl Pts',(4.57467506176493,-2.79999999510246,
-19.2656965083993)) ;
#138266 = CARTESIAN_POINT('Ctrl Pts',(4.58062405303288,-2.80000557393877,
-19.2463341632777)) ;
#138267 = CARTESIAN_POINT('Ctrl Pts',(4.58735613403293,-2.79385049254301,
-19.2289198149932)) ;
#138268 = CARTESIAN_POINT('Ctrl Pts',(4.62437069655637,-2.79999999703807,
-19.2795313430603)) ;
#138269 = CARTESIAN_POINT('Ctrl Pts',(4.61827372661892,-2.80000334969055,
-19.2609340454874)) ;
#138270 = CARTESIAN_POINT('Ctrl Pts',(4.61212682540742,-2.79628090446614,
-19.242402814218)) ;
#138271 = CARTESIAN_POINT('Ctrl Pts',(4.67161368302032,-2.7999999886062,-19.2207898267647)) ;
#138272 = CARTESIAN_POINT('Ctrl Pts',(4.65407010102633,-2.80001325705931,
-19.2004637395898)) ;
#138273 = CARTESIAN_POINT('Ctrl Pts',(4.63587130780619,-2.78569367459218,
-19.1856281295949)) ;
#138274 = CARTESIAN_POINT('Ctrl Pts',(4.54879236204369,-2.8,-19.2435655563675)) ;
#138275 = CARTESIAN_POINT('Ctrl Pts',(4.55448837802399,-2.7999999999815,-19.2411788209136)) ;
#138276 = CARTESIAN_POINT('Ctrl Pts',(4.56021842726626,-2.79959150783238,
-19.2388395427341)) ;
#138277 = CARTESIAN_POINT('Ctrl Pts',(4.56730671985007,-2.79865167182172,
-19.2359788838635)) ;
#138278 = CARTESIAN_POINT('Ctrl Pts',(4.56847770958281,-2.79848295770256,
-19.2355073268347)) ;
#138279 = CARTESIAN_POINT('Ctrl Pts',(4.5710752309902,-2.79808046368154,-19.234462962897)) ;
#138280 = CARTESIAN_POINT('Ctrl Pts',(4.5725009361248,-2.79784058543152,-19.233889643028)) ;
#138281 = CARTESIAN_POINT('Ctrl Pts',(4.5764383594612,-2.79713266293194,-19.2323136864649)) ;
#138282 = CARTESIAN_POINT('Ctrl Pts',(4.57879956048961,-2.79666132938901,
-19.2313758003969)) ;
#138283 = CARTESIAN_POINT('Ctrl Pts',(4.58293855712953,-2.79579586318667,
-19.2297608159296)) ;
#138284 = CARTESIAN_POINT('Ctrl Pts',(4.58471363403687,-2.79540911153441,
-19.2290746171912)) ;
#138285 = CARTESIAN_POINT('Ctrl Pts',(4.58699082729421,-2.7949269768198,-19.228244529262)) ;
#138286 = CARTESIAN_POINT('Ctrl Pts',(4.58739952300692,-2.79484234870239,
-19.2281019268464)) ;
#138287 = CARTESIAN_POINT('Ctrl Pts',(4.58871515235485,-2.79457617288695,
-19.2276611291009)) ;
#138288 = CARTESIAN_POINT('Ctrl Pts',(4.5896169059614,-2.7944024780556,-19.2273849869995)) ;
#138289 = CARTESIAN_POINT('Ctrl Pts',(4.59105375065865,-2.79414748185765,
-19.2269829818179)) ;
#138290 = CARTESIAN_POINT('Ctrl Pts',(4.59155303909546,-2.79406229662442,
-19.2268492435071)) ;
#138291 = CARTESIAN_POINT('Ctrl Pts',(4.59245965385668,-2.79391282221553,
-19.2266125941149)) ;
#138292 = CARTESIAN_POINT('Ctrl Pts',(4.59286388425103,-2.79384761399903,
-19.2265084217845)) ;
#138293 = CARTESIAN_POINT('Ctrl Pts',(4.59368973959979,-2.79370598615371,
-19.2262676726516)) ;
#138294 = CARTESIAN_POINT('Ctrl Pts',(4.59407665941121,-2.79363973714592,
-19.2261515212332)) ;
#138295 = CARTESIAN_POINT('Ctrl Pts',(4.5944437128773,-2.79357284110655,-19.2260267927279)) ;
#138296 = CARTESIAN_POINT('Ctrl Pts',(4.59448890259158,-2.79356452972317,
-19.2260111581995)) ;
#138297 = CARTESIAN_POINT('Ctrl Pts',(4.5947084233491,-2.79352377141065,-19.2259338254522)) ;
#138298 = CARTESIAN_POINT('Ctrl Pts',(4.59483598733268,-2.79349361011836,
-19.2258723314841)) ;
#138299 = CARTESIAN_POINT('Ctrl Pts',(4.59514620525222,-2.7934297131363,-19.2257459400492)) ;
#138300 = CARTESIAN_POINT('Ctrl Pts',(4.595333342751,-2.79339696908416,-19.2256838378534)) ;
#138301 = CARTESIAN_POINT('Ctrl Pts',(4.59563785533346,-2.79335634095568,
-19.2256129903403)) ;
#138302 = CARTESIAN_POINT('Ctrl Pts',(4.59571710962761,-2.79334654412182,
-19.2255963912876)) ;
#138303 = CARTESIAN_POINT('Ctrl Pts',(4.59594411915586,-2.79332043135007,
-19.2255533496182)) ;
#138304 = CARTESIAN_POINT('Ctrl Pts',(4.59600288191152,-2.79330503361987,
-19.2255339512408)) ;
#138305 = CARTESIAN_POINT('Ctrl Pts',(4.59613307952173,-2.79327450473787,
-19.2254992805194)) ;
#138306 = CARTESIAN_POINT('Ctrl Pts',(4.59620389659311,-2.7932597078882,-19.2254850060586)) ;
#138307 = CARTESIAN_POINT('Ctrl Pts',(4.5965119298477,-2.79322709231927,-19.2254502778629)) ;
#138308 = CARTESIAN_POINT('Ctrl Pts',(4.59679543741294,-2.79320989448355,
-19.2254293441824)) ;
#138309 = CARTESIAN_POINT('Ctrl Pts',(4.59784475938521,-2.793166495242,-19.2253578835066)) ;
#138310 = CARTESIAN_POINT('Ctrl Pts',(4.59874915064778,-2.79313948637392,
-19.2252992643107)) ;
#138311 = CARTESIAN_POINT('Ctrl Pts',(4.59999999999999,-2.79310344827586,
-19.2252063540422)) ;
#138312 = CARTESIAN_POINT('Origin',(4.4,-2.7,-17.78)) ;
#138313 = CARTESIAN_POINT('Origin',(4.4,-2.7,-21.8431546211728)) ;
#138314 = CARTESIAN_POINT('Ctrl Pts',(4.5011795914298,-2.68531903459919,-21.9020290201724)) ;
#138315 = CARTESIAN_POINT('Ctrl Pts',(4.5182867035893,-2.8,-21.9012138251407)) ;
#138316 = CARTESIAN_POINT('Ctrl Pts',(4.40240952225579,-2.8,-21.9105883721108)) ;
#138317 = CARTESIAN_POINT('Ctrl Pts',(4.49717774927195,-2.71005310920086,
-21.8029655323624)) ;
#138318 = CARTESIAN_POINT('Ctrl Pts',(4.48574628541093,-2.8,-21.81731485204)) ;
#138319 = CARTESIAN_POINT('Ctrl Pts',(4.39431668173579,-2.8,-21.7963402695081)) ;
#138320 = CARTESIAN_POINT('Ctrl Pts',(4.50328690685189,-2.7335198760256,-21.7029733978621)) ;
#138321 = CARTESIAN_POINT('Ctrl Pts',(4.47485145549547,-2.8,-21.7066766957415)) ;
#138322 = CARTESIAN_POINT('Ctrl Pts',(4.40646789472125,-2.8,-21.6851226186384)) ;
#138323 = CARTESIAN_POINT('Ctrl Pts',(4.52749311797091,-2.76348183928883,
-21.5637129921594)) ;
#138324 = CARTESIAN_POINT('Ctrl Pts',(4.49873206155793,-2.8,-21.5537330953069)) ;
#138325 = CARTESIAN_POINT('Ctrl Pts',(4.4548681704377,-2.8,-21.5349566433661)) ;
#138326 = CARTESIAN_POINT('Ctrl Pts',(4.53619745972496,-2.77169205010104,
-21.5240190471853)) ;
#138327 = CARTESIAN_POINT('Ctrl Pts',(4.50883664816672,-2.79999999999998,
-21.5117394381722)) ;
#138328 = CARTESIAN_POINT('Ctrl Pts',(4.47227975612143,-2.8,-21.4927273846038)) ;
#138329 = CARTESIAN_POINT('Ctrl Pts',(4.5544779509001,-2.78248459830341,-21.4699078127333)) ;
#138330 = CARTESIAN_POINT('Ctrl Pts',(4.53370055749883,-2.80000000000001,
-21.4546579183699)) ;
#138331 = CARTESIAN_POINT('Ctrl Pts',(4.50886586566856,-2.8,-21.4357478882722)) ;
#138332 = CARTESIAN_POINT('Ctrl Pts',(4.56160154376425,-2.78591123334062,
-21.4523494428157)) ;
#138333 = CARTESIAN_POINT('Ctrl Pts',(4.54365878772218,-2.8,-21.4362910664543)) ;
#138334 = CARTESIAN_POINT('Ctrl Pts',(4.52312452397685,-2.8,-21.4173699954867)) ;
#138335 = CARTESIAN_POINT('Ctrl Pts',(4.58735772267362,-2.79384903998488,
-21.4110842943985)) ;
#138336 = CARTESIAN_POINT('Ctrl Pts',(4.58063087367386,-2.8,-21.3936839633808)) ;
#138337 = CARTESIAN_POINT('Ctrl Pts',(4.5746855076719,-2.8,-21.3743374866056)) ;
#138338 = CARTESIAN_POINT('Ctrl Pts',(4.61212536563479,-2.79628002040276,
-21.3976015865954)) ;
#138339 = CARTESIAN_POINT('Ctrl Pts',(4.61826745782993,-2.80000000000002,
-21.3790848793757)) ;
#138340 = CARTESIAN_POINT('Ctrl Pts',(4.62435992349572,-2.8,-21.3605015173211)) ;
#138341 = CARTESIAN_POINT('Ctrl Pts',(4.63586710715927,-2.78569036914666,
-21.4543752946752)) ;
#138342 = CARTESIAN_POINT('Ctrl Pts',(4.6540510694572,-2.79999999999994,-21.4395525238841)) ;
#138343 = CARTESIAN_POINT('Ctrl Pts',(4.67158355065736,-2.8,-21.4192450797819)) ;
#138344 = CARTESIAN_POINT('Ctrl Pts',(4.59999999999999,-2.79310344827586,
-21.4147936459578)) ;
#138345 = CARTESIAN_POINT('Ctrl Pts',(4.59840954578207,-2.79314968944989,
-21.4146756726912)) ;
#138346 = CARTESIAN_POINT('Ctrl Pts',(4.59737383489079,-2.79318159606221,
-21.4146133239717)) ;
#138347 = CARTESIAN_POINT('Ctrl Pts',(4.59650507521642,-2.79322931786013,
-21.41455037726)) ;
#138348 = CARTESIAN_POINT('Ctrl Pts',(4.59632758424299,-2.79324472590582,
-21.4145345791767)) ;
#138349 = CARTESIAN_POINT('Ctrl Pts',(4.59611847210843,-2.79327477162037,
-21.4145047565772)) ;
#138350 = CARTESIAN_POINT('Ctrl Pts',(4.59606489504924,-2.79328892979787,
-21.4144910265853)) ;
#138351 = CARTESIAN_POINT('Ctrl Pts',(4.59594601677692,-2.79331605564258,
-21.414459114495)) ;
#138352 = CARTESIAN_POINT('Ctrl Pts',(4.59588597444856,-2.7933285533825,-21.4144426561835)) ;
#138353 = CARTESIAN_POINT('Ctrl Pts',(4.59549967474362,-2.79337285752324,
-21.4143702787605)) ;
#138354 = CARTESIAN_POINT('Ctrl Pts',(4.59527331486236,-2.79340622385959,
-21.4143100807083)) ;
#138355 = CARTESIAN_POINT('Ctrl Pts',(4.59493201239528,-2.79346950514991,
-21.4141870402937)) ;
#138356 = CARTESIAN_POINT('Ctrl Pts',(4.59480393230127,-2.79349821606423,
-21.414128474279)) ;
#138357 = CARTESIAN_POINT('Ctrl Pts',(4.59460326813593,-2.79353924388982,
-21.4140476351491)) ;
#138358 = CARTESIAN_POINT('Ctrl Pts',(4.59455075953095,-2.79354963432651,
-21.4140274276715)) ;
#138359 = CARTESIAN_POINT('Ctrl Pts',(4.59417008680874,-2.79361944405452,
-21.4138955937176)) ;
#138360 = CARTESIAN_POINT('Ctrl Pts',(4.59377742096551,-2.79368602572532,
-21.4137773461555)) ;
#138361 = CARTESIAN_POINT('Ctrl Pts',(4.59289939109635,-2.7938335466559,-21.4135254190241)) ;
#138362 = CARTESIAN_POINT('Ctrl Pts',(4.59245006584786,-2.79390305456781,
-21.413416036199)) ;
#138363 = CARTESIAN_POINT('Ctrl Pts',(4.59099552519241,-2.79413629528604,
-21.4130568524093)) ;
#138364 = CARTESIAN_POINT('Ctrl Pts',(4.59002197881585,-2.79430302757315,
-21.412806370176)) ;
#138365 = CARTESIAN_POINT('Ctrl Pts',(4.58861122644683,-2.794567934557,-21.4123921365669)) ;
#138366 = CARTESIAN_POINT('Ctrl Pts',(4.58817904894403,-2.79465210327453,
-21.4122585234306)) ;
#138367 = CARTESIAN_POINT('Ctrl Pts',(4.58736872283365,-2.79481449815582,
-21.4119941835896)) ;
#138368 = CARTESIAN_POINT('Ctrl Pts',(4.58699491219416,-2.79489135860974,
-21.4118665823581)) ;
#138369 = CARTESIAN_POINT('Ctrl Pts',(4.58468897497188,-2.79537899446709,
-21.4110351906196)) ;
#138370 = CARTESIAN_POINT('Ctrl Pts',(4.58290717718701,-2.79577019617637,
-21.4103420642284)) ;
#138371 = CARTESIAN_POINT('Ctrl Pts',(4.57867627871776,-2.79666451416567,
-21.4086707882875)) ;
#138372 = CARTESIAN_POINT('Ctrl Pts',(4.57626321554131,-2.79715040843617,
-21.4076877651429)) ;
#138373 = CARTESIAN_POINT('Ctrl Pts',(4.57243386308706,-2.79784156172336,
-21.4061367865103)) ;
#138374 = CARTESIAN_POINT('Ctrl Pts',(4.57107519984217,-2.79807176647234,
-21.405584021445)) ;
#138375 = CARTESIAN_POINT('Ctrl Pts',(4.56513452430471,-2.79900074294391,
-21.4031693903581)) ;
#138376 = CARTESIAN_POINT('Ctrl Pts',(4.56062162665738,-2.7995126701138,-21.4013309293494)) ;
#138377 = CARTESIAN_POINT('Ctrl Pts',(4.55365420596628,-2.79992470862867,
-21.3984610302783)) ;
#138378 = CARTESIAN_POINT('Ctrl Pts',(4.55124660967264,-2.79999983267432,
-21.3974632392507)) ;
#138379 = CARTESIAN_POINT('Ctrl Pts',(4.54880051362942,-2.79999999972164,
-21.3964378607329)) ;
#138380 = CARTESIAN_POINT('Ctrl Pts',(4.54879236166274,-2.8,-19.2435655565152)) ;
#138381 = CARTESIAN_POINT('Ctrl Pts',(4.5622387183224,-2.79999999999679,-19.2612315262749)) ;
#138382 = CARTESIAN_POINT('Ctrl Pts',(4.57442182196495,-2.80939476060287,
-19.2772378204668)) ;
#138383 = CARTESIAN_POINT('Ctrl Pts',(4.55556842517593,-2.79999999999889,
-19.2407250640489)) ;
#138384 = CARTESIAN_POINT('Ctrl Pts',(4.56783337210914,-2.80040661803737,
-19.2561863015519)) ;
#138385 = CARTESIAN_POINT('Ctrl Pts',(4.57961823522371,-2.80818164104597,
-19.2700183413272)) ;
#138386 = CARTESIAN_POINT('Ctrl Pts',(4.56238982831618,-2.7994260255176,-19.2379528515171)) ;
#138387 = CARTESIAN_POINT('Ctrl Pts',(4.57357810388182,-2.80014618986473,
-19.2509310721412)) ;
#138388 = CARTESIAN_POINT('Ctrl Pts',(4.58462643299473,-2.80630261261112,
-19.2625232711649)) ;
#138389 = CARTESIAN_POINT('Ctrl Pts',(4.57328757735258,-2.7977370397245,-19.2335699979501)) ;
#138390 = CARTESIAN_POINT('Ctrl Pts',(4.58237922839514,-2.79856394574987,
-19.2422664089313)) ;
#138391 = CARTESIAN_POINT('Ctrl Pts',(4.59151541127592,-2.80237286596198,
-19.2500830028806)) ;
#138392 = CARTESIAN_POINT('Ctrl Pts',(4.57700059755675,-2.7970371466716,-19.232076076342)) ;
#138393 = CARTESIAN_POINT('Ctrl Pts',(4.58532305318677,-2.79784352093717,
-19.2392625430045)) ;
#138394 = CARTESIAN_POINT('Ctrl Pts',(4.59370961102545,-2.80088045369937,
-19.2457455141894)) ;
#138395 = CARTESIAN_POINT('Ctrl Pts',(4.58319893207066,-2.79574016930783,
-19.2296546705211)) ;
#138396 = CARTESIAN_POINT('Ctrl Pts',(4.58990416109239,-2.79637293360539,
-19.2343303545622)) ;
#138397 = CARTESIAN_POINT('Ctrl Pts',(4.59665800356694,-2.79825577077759,
-19.2385819448697)) ;
#138398 = CARTESIAN_POINT('Ctrl Pts',(4.58534994317985,-2.79526732601294,
-19.2288188618872)) ;
#138399 = CARTESIAN_POINT('Ctrl Pts',(4.59144552977844,-2.79581844972913,
-19.2326200366107)) ;
#138400 = CARTESIAN_POINT('Ctrl Pts',(4.59758018705035,-2.79731769672697,
-19.2360885803939)) ;
#138401 = CARTESIAN_POINT('Ctrl Pts',(4.58899927751306,-2.79450268149332,
-19.2275173012671)) ;
#138402 = CARTESIAN_POINT('Ctrl Pts',(4.59386223202754,-2.79488630507105,
-19.2299495170303)) ;
#138403 = CARTESIAN_POINT('Ctrl Pts',(4.59874684688641,-2.79582009356911,
-19.2321813652447)) ;
#138404 = CARTESIAN_POINT('Ctrl Pts',(4.5902675569287,-2.79423885380164,-19.22707439958)) ;
#138405 = CARTESIAN_POINT('Ctrl Pts',(4.59467706068311,-2.79455862385203,
-19.2290405433361)) ;
#138406 = CARTESIAN_POINT('Ctrl Pts',(4.59910266898802,-2.79530499526365,
-19.2308486399022)) ;
#138407 = CARTESIAN_POINT('Ctrl Pts',(4.59257623319511,-2.79382131826659,
-19.22638413145)) ;
#138408 = CARTESIAN_POINT('Ctrl Pts',(4.59605751036344,-2.79403163929514,
-19.2276227610336)) ;
#138409 = CARTESIAN_POINT('Ctrl Pts',(4.59954701072604,-2.79449510806573,
-19.228765766817)) ;
#138410 = CARTESIAN_POINT('Ctrl Pts',(4.59342976933296,-2.79367543507711,
-19.2261445374534)) ;
#138411 = CARTESIAN_POINT('Ctrl Pts',(4.59655016100493,-2.79384713427255,
-19.2271348895303)) ;
#138412 = CARTESIAN_POINT('Ctrl Pts',(4.59967640178298,-2.79421605292372,
-19.228050213937)) ;
#138413 = CARTESIAN_POINT('Ctrl Pts',(4.59428414179642,-2.79346156087783,
-19.2257069361853)) ;
#138414 = CARTESIAN_POINT('Ctrl Pts',(4.59704519451433,-2.79355469746529,
-19.226373635748)) ;
#138415 = CARTESIAN_POINT('Ctrl Pts',(4.5998104157401,-2.79379877456676,-19.2269823712707)) ;
#138416 = CARTESIAN_POINT('Ctrl Pts',(4.59432658472651,-2.7933916625364,-19.2255338181495)) ;
#138417 = CARTESIAN_POINT('Ctrl Pts',(4.59708408719787,-2.79345234504014,
-19.2261090766463)) ;
#138418 = CARTESIAN_POINT('Ctrl Pts',(4.59984563524626,-2.79366003518351,
-19.2266276543527)) ;
#138419 = CARTESIAN_POINT('Ctrl Pts',(4.59537197237732,-2.79324260992761,
-19.2252872615938)) ;
#138420 = CARTESIAN_POINT('Ctrl Pts',(4.59764722167538,-2.79326383513929,
-19.225620961855)) ;
#138421 = CARTESIAN_POINT('Ctrl Pts',(4.59992475053754,-2.79338190759658,
-19.2259170306476)) ;
#138422 = CARTESIAN_POINT('Ctrl Pts',(4.5936418339237,-2.79313407032025,-19.2252844788451)) ;
#138423 = CARTESIAN_POINT('Ctrl Pts',(4.59684754854888,-2.79327107597598,
-19.2256389310452)) ;
#138424 = CARTESIAN_POINT('Ctrl Pts',(4.59996664298755,-2.79324102308607,
-19.2255617736815)) ;
#138425 = CARTESIAN_POINT('Ctrl Pts',(4.59999999999999,-2.79310344827586,
-19.2252063540422)) ;
#138426 = CARTESIAN_POINT('Ctrl Pts',(4.59999999999999,-2.79310344827586,
-19.2252063540422)) ;
#138427 = CARTESIAN_POINT('Ctrl Pts',(4.59999999999999,-2.79310344827586,
-19.2252063540422)) ;
#138428 = CARTESIAN_POINT('Origin',(4.54879236168542,-2.9,-19.2435655565161)) ;
#138429 = CARTESIAN_POINT('Ctrl Pts',(4.39959973407451,-2.8,-20.4305922428025)) ;
#138430 = CARTESIAN_POINT('Ctrl Pts',(4.49922290141883,-2.8,-20.4301052483314)) ;
#138431 = CARTESIAN_POINT('Ctrl Pts',(4.49980764094185,-2.89969504276379,
-20.430608045895)) ;
#138432 = CARTESIAN_POINT('Ctrl Pts',(4.40142712570759,-2.8,-20.2095338960077)) ;
#138433 = CARTESIAN_POINT('Ctrl Pts',(4.50593622119657,-2.8,-20.2060480134683)) ;
#138434 = CARTESIAN_POINT('Ctrl Pts',(4.50067611734352,-2.90411960318544,
-20.2096502871254)) ;
#138435 = CARTESIAN_POINT('Ctrl Pts',(4.39573539165433,-2.8,-19.9876225417885)) ;
#138436 = CARTESIAN_POINT('Ctrl Pts',(4.49039105203437,-2.8,-20.0064448660088)) ;
#138437 = CARTESIAN_POINT('Ctrl Pts',(4.49793210898571,-2.89506044297342,
-19.9865928350696)) ;
#138438 = CARTESIAN_POINT('Ctrl Pts',(4.41164816536272,-2.8,-19.6744921486565)) ;
#138439 = CARTESIAN_POINT('Ctrl Pts',(4.48203507549541,-2.8,-19.6830075383891)) ;
#138440 = CARTESIAN_POINT('Ctrl Pts',(4.50604587949365,-2.86657833599735,
-19.6817916334551)) ;
#138441 = CARTESIAN_POINT('Ctrl Pts',(4.41940490599905,-2.8,-19.5821571319988)) ;
#138442 = CARTESIAN_POINT('Ctrl Pts',(4.48133975791573,-2.8,-19.5933274637386)) ;
#138443 = CARTESIAN_POINT('Ctrl Pts',(4.50997623336227,-2.85625883833135,
-19.593064643239)) ;
#138444 = CARTESIAN_POINT('Ctrl Pts',(4.44577434373644,-2.8,-19.4470206588259)) ;
#138445 = CARTESIAN_POINT('Ctrl Pts',(4.49360122670477,-2.8,-19.4593305876678)) ;
#138446 = CARTESIAN_POINT('Ctrl Pts',(4.52318558604184,-2.83896465559566,
-19.4654850424376)) ;
#138447 = CARTESIAN_POINT('Ctrl Pts',(4.45692583760033,-2.8,-19.4024768930528)) ;
#138448 = CARTESIAN_POINT('Ctrl Pts',(4.49949391572662,-2.8,-19.4160543026461)) ;
#138449 = CARTESIAN_POINT('Ctrl Pts',(4.52876348458384,-2.83289258157629,
-19.4238029886043)) ;
#138450 = CARTESIAN_POINT('Ctrl Pts',(4.50378503771657,-2.8,-19.2810759162582)) ;
#138451 = CARTESIAN_POINT('Ctrl Pts',(4.52873519606818,-2.8,-19.2999253422748)) ;
#138452 = CARTESIAN_POINT('Ctrl Pts',(4.55214466721903,-2.81552005845344,
-19.3112248698016)) ;
#138453 = CARTESIAN_POINT('Ctrl Pts',(4.54714423790153,-2.8,-19.202268495047)) ;
#138454 = CARTESIAN_POINT('Ctrl Pts',(4.55761617337286,-2.8,-19.2232065641883)) ;
#138455 = CARTESIAN_POINT('Ctrl Pts',(4.57259584813385,-2.80338245043788,
-19.2412385951886)) ;
#138456 = CARTESIAN_POINT('Ctrl Pts',(4.67762904165671,-2.8,-19.2114950447958)) ;
#138457 = CARTESIAN_POINT('Ctrl Pts',(4.6609348472501,-2.8,-19.227067065838)) ;
#138458 = CARTESIAN_POINT('Ctrl Pts',(4.64133868807456,-2.80368623369359,
-19.244688006387)) ;
#138459 = CARTESIAN_POINT('Origin',(4.4,-2.9,-20.3200000000039)) ;
#138460 = CARTESIAN_POINT('Ctrl Pts',(4.72172783566993,-2.8000000024879,-21.4203629549132)) ;
#138461 = CARTESIAN_POINT('Ctrl Pts',(4.69645430308119,-2.79999660525783,
-21.4070700473094)) ;
#138462 = CARTESIAN_POINT('Ctrl Pts',(4.66463283184998,-2.80454824226955,
-21.3894903682926)) ;
#138463 = CARTESIAN_POINT('Ctrl Pts',(4.55709227475146,-2.80000000030524,
-21.45599643631)) ;
#138464 = CARTESIAN_POINT('Ctrl Pts',(4.56399237478645,-2.79999958643658,
-21.4339593792008)) ;
#138465 = CARTESIAN_POINT('Ctrl Pts',(4.5772937099949,-2.80055804294512,-21.4151759050809)) ;
#138466 = CARTESIAN_POINT('Ctrl Pts',(4.50667826286324,-2.80000000784871,
-21.3666146479982)) ;
#138467 = CARTESIAN_POINT('Ctrl Pts',(4.53037382014976,-2.79998899178916,
-21.3470846001168)) ;
#138468 = CARTESIAN_POINT('Ctrl Pts',(4.55348183854635,-2.81434699509192,
-21.3359466041139)) ;
#138469 = CARTESIAN_POINT('Ctrl Pts',(4.4569228015872,-2.80000001789831,-21.2376422182876)) ;
#138470 = CARTESIAN_POINT('Ctrl Pts',(4.49938029267362,-2.79997354447564,
-21.2240998880093)) ;
#138471 = CARTESIAN_POINT('Ctrl Pts',(4.52864149761198,-2.83271033979002,
-21.21632906208)) ;
#138472 = CARTESIAN_POINT('Ctrl Pts',(4.44554661086163,-2.80000002126189,
-21.1923774400141)) ;
#138473 = CARTESIAN_POINT('Ctrl Pts',(4.4933366515485,-2.7999679796365,-21.1800969398739)) ;
#138474 = CARTESIAN_POINT('Ctrl Pts',(4.52295544156354,-2.83885474437117,
-21.1739678582281)) ;
#138475 = CARTESIAN_POINT('Ctrl Pts',(4.4190332210433,-2.8000000307772,-21.0558947975771)) ;
#138476 = CARTESIAN_POINT('Ctrl Pts',(4.48100616080231,-2.79995095769178,
-21.0447300040204)) ;
#138477 = CARTESIAN_POINT('Ctrl Pts',(4.50969337368895,-2.8562317909387,-21.0450696236088)) ;
#138478 = CARTESIAN_POINT('Ctrl Pts',(4.41147189908671,-2.8000000363501,-20.9642415900435)) ;
#138479 = CARTESIAN_POINT('Ctrl Pts',(4.48178828424047,-2.79993989905026,
-20.9557891492056)) ;
#138480 = CARTESIAN_POINT('Ctrl Pts',(4.50589025525737,-2.86640526991132,
-20.9569681512011)) ;
#138481 = CARTESIAN_POINT('Ctrl Pts',(4.39523119070906,-2.80000005228416,
-20.6431795198329)) ;
#138482 = CARTESIAN_POINT('Ctrl Pts',(4.49033836345893,-2.799902616883,-20.6230741316605)) ;
#138483 = CARTESIAN_POINT('Ctrl Pts',(4.49769757367177,-2.89547737952995,
-20.6443332157617)) ;
#138484 = CARTESIAN_POINT('Ctrl Pts',(4.40178225889352,-2.80000005718968,
-20.4126239782851)) ;
#138485 = CARTESIAN_POINT('Ctrl Pts',(4.5068134101818,-2.79988784121837,-20.4170581988245)) ;
#138486 = CARTESIAN_POINT('Ctrl Pts',(4.50092255053476,-2.90441958896086,
-20.4124406960391)) ;
#138487 = CARTESIAN_POINT('Ctrl Pts',(4.39924589760301,-2.80000005405718,
-20.1830311688801)) ;
#138488 = CARTESIAN_POINT('Ctrl Pts',(4.49795607191397,-2.79989746608212,
-20.183922937496)) ;
#138489 = CARTESIAN_POINT('Ctrl Pts',(4.49968270404899,-2.89870974459557,
-20.1830284945916)) ;
#138490 = CARTESIAN_POINT('Origin',(4.54879236168626,-2.9,-21.3964344434846)) ;
#138491 = CARTESIAN_POINT('Ctrl Pts',(4.57442492185552,-2.80939715119899,
-21.3627581068621)) ;
#138492 = CARTESIAN_POINT('Ctrl Pts',(4.56210583156797,-2.7998961275033,-21.3789430617887)) ;
#138493 = CARTESIAN_POINT('Ctrl Pts',(4.54850917782858,-2.80000109307748,
-21.396806493488)) ;
#138494 = CARTESIAN_POINT('Ctrl Pts',(4.57959763980855,-2.80818914940071,
-21.3699453004955)) ;
#138495 = CARTESIAN_POINT('Ctrl Pts',(4.56768008075466,-2.80031924975226,
-21.3839410457291)) ;
#138496 = CARTESIAN_POINT('Ctrl Pts',(4.55527876038347,-2.79999229227378,
-21.3995899763868)) ;
#138497 = CARTESIAN_POINT('Ctrl Pts',(4.58464248447265,-2.80630474344638,
-21.3774843126383)) ;
#138498 = CARTESIAN_POINT('Ctrl Pts',(4.57346944634373,-2.80008318972135,
-21.3892012910521)) ;
#138499 = CARTESIAN_POINT('Ctrl Pts',(4.56216307187796,-2.79941338753917,
-21.4023280915335)) ;
#138500 = CARTESIAN_POINT('Ctrl Pts',(4.59159231899494,-2.80232720646228,
-21.3900563692959)) ;
#138501 = CARTESIAN_POINT('Ctrl Pts',(4.58237910662986,-2.79850221241048,
-21.3979149362578)) ;
#138502 = CARTESIAN_POINT('Ctrl Pts',(4.57321634584969,-2.79769868647539,
-21.4066644864947)) ;
#138503 = CARTESIAN_POINT('Ctrl Pts',(4.59378564167737,-2.8008235544484,-21.3944145837655)) ;
#138504 = CARTESIAN_POINT('Ctrl Pts',(4.58533966160573,-2.79778056279966,
-21.4009180694478)) ;
#138505 = CARTESIAN_POINT('Ctrl Pts',(4.5769613009382,-2.79699227428058,-21.4081320740362)) ;
#138506 = CARTESIAN_POINT('Ctrl Pts',(4.59669734138576,-2.79821861236081,
-21.4015174469091)) ;
#138507 = CARTESIAN_POINT('Ctrl Pts',(4.58989502505308,-2.79633072300511,
-21.405783702985)) ;
#138508 = CARTESIAN_POINT('Ctrl Pts',(4.58314295739388,-2.79570785369251,
-21.4104789031814)) ;
#138509 = CARTESIAN_POINT('Ctrl Pts',(4.59760632414569,-2.79728965034655,
-21.4039852466291)) ;
#138510 = CARTESIAN_POINT('Ctrl Pts',(4.59142619397024,-2.79578507327359,
-21.4074678937229)) ;
#138511 = CARTESIAN_POINT('Ctrl Pts',(4.58528630332435,-2.79524119148169,
-21.411287378375)) ;
#138512 = CARTESIAN_POINT('Ctrl Pts',(4.59875741430932,-2.79580683383092,
-21.407853004496)) ;
#138513 = CARTESIAN_POINT('Ctrl Pts',(4.59383193680336,-2.79486773439435,
-21.4100980055339)) ;
#138514 = CARTESIAN_POINT('Ctrl Pts',(4.58892874314202,-2.79448758877844,
-21.4125464730129)) ;
#138515 = CARTESIAN_POINT('Ctrl Pts',(4.59910834609946,-2.79529718130591,
-21.4091714993015)) ;
#138516 = CARTESIAN_POINT('Ctrl Pts',(4.59464343907619,-2.79454543406795,
-21.4109926958501)) ;
#138517 = CARTESIAN_POINT('Ctrl Pts',(4.59019511689892,-2.79422790851556,
-21.4129746712091)) ;
#138518 = CARTESIAN_POINT('Ctrl Pts',(4.59954688679867,-2.79449699552073,
-21.4112293846587)) ;
#138519 = CARTESIAN_POINT('Ctrl Pts',(4.59601732089137,-2.79402779797775,
-21.4123863363518)) ;
#138520 = CARTESIAN_POINT('Ctrl Pts',(4.59249627585273,-2.79381771894921,
-21.4136411141675)) ;
#138521 = CARTESIAN_POINT('Ctrl Pts',(4.59967529310588,-2.79422450025963,
-21.4119354645612)) ;
#138522 = CARTESIAN_POINT('Ctrl Pts',(4.59651100242294,-2.79384821317134,
-21.4128644108735)) ;
#138523 = CARTESIAN_POINT('Ctrl Pts',(4.593352874124,-2.79367727499394,-21.4138714476574)) ;
#138524 = CARTESIAN_POINT('Ctrl Pts',(4.59980981518572,-2.79380630943631,
-21.4130056452101)) ;
#138525 = CARTESIAN_POINT('Ctrl Pts',(4.59701056623719,-2.79355888022806,
-21.4136249350365)) ;
#138526 = CARTESIAN_POINT('Ctrl Pts',(4.59421559911326,-2.79346462438277,
-21.4143030289899)) ;
#138527 = CARTESIAN_POINT('Ctrl Pts',(4.59984534134842,-2.79366726490194,
-21.4133646067489)) ;
#138528 = CARTESIAN_POINT('Ctrl Pts',(4.59705039509825,-2.79345667046144,
-21.4138917393962)) ;
#138529 = CARTESIAN_POINT('Ctrl Pts',(4.59425962044002,-2.79339574833516,
-21.4144765637042)) ;
#138530 = CARTESIAN_POINT('Ctrl Pts',(4.59992484646001,-2.7933873519883,-21.41407980384)) ;
#138531 = CARTESIAN_POINT('Ctrl Pts',(4.59761652863209,-2.79326682373741,
-21.414380589531)) ;
#138532 = CARTESIAN_POINT('Ctrl Pts',(4.59531061070857,-2.79324678512396,
-21.4147204137335)) ;
#138533 = CARTESIAN_POINT('Ctrl Pts',(4.59996721368508,-2.79324340897637,
-21.414436569794)) ;
#138534 = CARTESIAN_POINT('Ctrl Pts',(4.59680854952869,-2.79327323421043,
-21.4143604778616)) ;
#138535 = CARTESIAN_POINT('Ctrl Pts',(4.59356174266139,-2.79313094944462,
-21.4147234833207)) ;
#138536 = CARTESIAN_POINT('Ctrl Pts',(4.59999999999999,-2.79310344827586,
-21.4147936459578)) ;
#138537 = CARTESIAN_POINT('Ctrl Pts',(4.59999999999999,-2.79310344827586,
-21.4147936459578)) ;
#138538 = CARTESIAN_POINT('Ctrl Pts',(4.59999999999999,-2.79310344827586,
-21.4147936459578)) ;
#138539 = CARTESIAN_POINT('Origin',(0.,0.,-22.36)) ;
#138540 = CARTESIAN_POINT('Origin',(7.26810489940853,5.50476046277485,-18.945)) ;
#138541 = CARTESIAN_POINT('',(4.03523814377473,5.98727788898885,-18.845)) ;
#138542 = CARTESIAN_POINT('',(4.03523814377473,5.98727788898885,-17.545)) ;
#138543 = CARTESIAN_POINT('',(4.03523814377473,5.98727788898885,-18.945)) ;
#138544 = CARTESIAN_POINT('',(7.26810489940853,5.50476046277485,-17.545)) ;
#138545 = CARTESIAN_POINT('',(7.26810489940853,5.50476046277485,-17.545)) ;
#138546 = CARTESIAN_POINT('',(7.26810489940853,5.50476046277485,-18.845)) ;
#138547 = CARTESIAN_POINT('',(7.26810489940853,5.50476046277485,-18.945)) ;
#138548 = CARTESIAN_POINT('',(3.95,6.,-18.845)) ;
#138549 = CARTESIAN_POINT('Origin',(7.25334304318326,5.40585602606554,-18.945)) ;
#138550 = CARTESIAN_POINT('',(7.32310496992715,5.47750289324744,-17.545)) ;
#138551 = CARTESIAN_POINT('Origin',(7.25334304318326,5.40585602606554,-17.545)) ;
#138552 = CARTESIAN_POINT('',(7.32310496992715,5.47750289324744,-18.845)) ;
#138553 = CARTESIAN_POINT('',(7.32310496992715,5.47750289324744,-18.945)) ;
#138554 = CARTESIAN_POINT('Origin',(7.25334304318326,5.40585602606554,-18.845)) ;
#138555 = CARTESIAN_POINT('Origin',(8.66976192674389,4.16627481495487,-18.945)) ;
#138556 = CARTESIAN_POINT('',(8.66976192674389,4.16627481495487,-17.545)) ;
#138557 = CARTESIAN_POINT('',(8.66976192674389,4.16627481495487,-17.545)) ;
#138558 = CARTESIAN_POINT('',(8.66976192674389,4.16627481495487,-18.845)) ;
#138559 = CARTESIAN_POINT('',(8.66976192674389,4.16627481495487,-18.945)) ;
#138560 = CARTESIAN_POINT('',(7.32310496992715,5.47750289324744,-18.845)) ;
#138561 = CARTESIAN_POINT('Origin',(8.6,4.09462794777298,-18.945)) ;
#138562 = CARTESIAN_POINT('',(8.7,4.09462794777298,-17.545)) ;
#138563 = CARTESIAN_POINT('Origin',(8.6,4.09462794777298,-17.545)) ;
#138564 = CARTESIAN_POINT('',(8.7,4.09462794777298,-18.845)) ;
#138565 = CARTESIAN_POINT('',(8.7,4.09462794777298,-18.945)) ;
#138566 = CARTESIAN_POINT('Origin',(8.6,4.09462794777298,-18.845)) ;
#138567 = CARTESIAN_POINT('Origin',(8.7,3.95,-18.945)) ;
#138568 = CARTESIAN_POINT('',(8.7,3.95,-17.545)) ;
#138569 = CARTESIAN_POINT('',(8.7,3.95,-17.545)) ;
#138570 = CARTESIAN_POINT('',(8.7,3.95,-18.845)) ;
#138571 = CARTESIAN_POINT('',(8.7,3.95,-18.945)) ;
#138572 = CARTESIAN_POINT('',(8.7,4.09462794777298,-18.845)) ;
#138573 = CARTESIAN_POINT('Origin',(8.6,3.95,-18.945)) ;
#138574 = CARTESIAN_POINT('',(8.55460943381591,3.86089502538305,-17.545)) ;
#138575 = CARTESIAN_POINT('Origin',(8.6,3.95,-17.545)) ;
#138576 = CARTESIAN_POINT('',(8.55460943381591,3.86089502538305,-18.845)) ;
#138577 = CARTESIAN_POINT('',(8.55460943381591,3.86089502538305,-18.945)) ;
#138578 = CARTESIAN_POINT('Origin',(8.6,3.95,-18.845)) ;
#138579 = CARTESIAN_POINT('Origin',(7.3213877252879,4.48910497461695,-18.945)) ;
#138580 = CARTESIAN_POINT('',(7.3213877252879,4.48910497461695,-17.545)) ;
#138581 = CARTESIAN_POINT('',(7.3213877252879,4.48910497461695,-17.545)) ;
#138582 = CARTESIAN_POINT('',(7.3213877252879,4.48910497461695,-18.845)) ;
#138583 = CARTESIAN_POINT('',(7.3213877252879,4.48910497461695,-18.945)) ;
#138584 = CARTESIAN_POINT('',(8.55460943381591,3.86089502538305,-18.845)) ;
#138585 = CARTESIAN_POINT('Origin',(7.27599715910381,4.4,-18.945)) ;
#138586 = CARTESIAN_POINT('',(7.27599715910381,4.5,-17.545)) ;
#138587 = CARTESIAN_POINT('Origin',(7.27599715910381,4.4,-17.545)) ;
#138588 = CARTESIAN_POINT('',(7.27599715910381,4.5,-18.845)) ;
#138589 = CARTESIAN_POINT('',(7.27599715910381,4.5,-18.945)) ;
#138590 = CARTESIAN_POINT('Origin',(7.27599715910381,4.4,-18.845)) ;
#138591 = CARTESIAN_POINT('Origin',(3.95,4.5,-18.945)) ;
#138592 = CARTESIAN_POINT('',(4.05,4.5,-17.545)) ;
#138593 = CARTESIAN_POINT('',(3.95,4.5,-17.545)) ;
#138594 = CARTESIAN_POINT('',(4.05,4.5,-18.845)) ;
#138595 = CARTESIAN_POINT('',(4.05,4.5,-18.945)) ;
#138596 = CARTESIAN_POINT('',(7.27599715910381,4.5,-18.845)) ;
#138597 = CARTESIAN_POINT('Origin',(7.25334304318326,5.40585602606554,-18.945)) ;
#138598 = CARTESIAN_POINT('',(7.36677829147199,4.5782099492339,-18.945)) ;
#138599 = CARTESIAN_POINT('',(7.27599715910381,4.6,-18.945)) ;
#138600 = CARTESIAN_POINT('Origin',(7.27599715910381,4.4,-18.945)) ;
#138601 = CARTESIAN_POINT('',(4.05,4.6,-18.945)) ;
#138602 = CARTESIAN_POINT('',(3.95,4.6,-18.945)) ;
#138603 = CARTESIAN_POINT('',(4.05,5.88396692803319,-18.945)) ;
#138604 = CARTESIAN_POINT('',(4.05,6.,-18.945)) ;
#138605 = CARTESIAN_POINT('',(7.25334304318326,5.40585602606554,-18.945)) ;
#138606 = CARTESIAN_POINT('',(7.25334304318326,5.40585602606554,-18.945)) ;
#138607 = CARTESIAN_POINT('',(8.6,4.09462794777298,-18.945)) ;
#138608 = CARTESIAN_POINT('',(8.6,4.09462794777298,-18.945)) ;
#138609 = CARTESIAN_POINT('',(8.6,3.95,-18.945)) ;
#138610 = CARTESIAN_POINT('',(8.6,3.95,-18.945)) ;
#138611 = CARTESIAN_POINT('',(7.36677829147199,4.5782099492339,-18.945)) ;
#138612 = CARTESIAN_POINT('Origin',(7.25334304318326,5.40585602606554,-17.445)) ;
#138613 = CARTESIAN_POINT('',(8.6,4.09462794777298,-17.445)) ;
#138614 = CARTESIAN_POINT('',(7.25334304318326,5.40585602606554,-17.445)) ;
#138615 = CARTESIAN_POINT('',(7.25334304318326,5.40585602606554,-17.445)) ;
#138616 = CARTESIAN_POINT('',(4.05,5.88396692803319,-17.445)) ;
#138617 = CARTESIAN_POINT('',(7.25334304318326,5.40585602606554,-17.445)) ;
#138618 = CARTESIAN_POINT('',(4.05,4.6,-17.445)) ;
#138619 = CARTESIAN_POINT('',(4.05,5.40585602606554,-17.445)) ;
#138620 = CARTESIAN_POINT('',(7.27599715910381,4.6,-17.445)) ;
#138621 = CARTESIAN_POINT('',(7.25334304318326,4.6,-17.445)) ;
#138622 = CARTESIAN_POINT('',(7.36677829147199,4.5782099492339,-17.445)) ;
#138623 = CARTESIAN_POINT('Origin',(7.27599715910381,4.4,-17.445)) ;
#138624 = CARTESIAN_POINT('',(8.6,3.95,-17.445)) ;
#138625 = CARTESIAN_POINT('',(6.94197060168454,4.79460933256464,-17.445)) ;
#138626 = CARTESIAN_POINT('',(8.6,5.40585602606554,-17.445)) ;
#138627 = CARTESIAN_POINT('Origin',(4.5,-2.3,-12.7)) ;
#138628 = CARTESIAN_POINT('',(4.6,-2.3,-12.7)) ;
#138629 = CARTESIAN_POINT('',(12.7,-2.3,-12.7)) ;
#138630 = CARTESIAN_POINT('',(4.5,-2.3,-12.7)) ;
#138631 = CARTESIAN_POINT('',(4.6,-2.3,-13.2778583129651)) ;
#138632 = CARTESIAN_POINT('',(4.6,-2.3,-13.3138639715742)) ;
#138633 = CARTESIAN_POINT('',(12.7,-2.3,-13.2778583129651)) ;
#138634 = CARTESIAN_POINT('',(4.5,-2.3,-13.2778583129651)) ;
#138635 = CARTESIAN_POINT('',(12.7,-2.3,-12.7)) ;
#138636 = CARTESIAN_POINT('Origin',(0.,9.95,-15.24)) ;
#138637 = CARTESIAN_POINT('',(0.230887397576971,9.95,-17.1548605718538)) ;
#138638 = CARTESIAN_POINT('Origin',(12.8,2.75,-12.7)) ;
#138639 = CARTESIAN_POINT('',(4.55912712210513,2.75,-13.7469539578284)) ;
#138640 = CARTESIAN_POINT('',(12.8,2.75,-13.7469539578284)) ;
#138641 = CARTESIAN_POINT('',(4.55912712210514,2.75,-12.7)) ;
#138642 = CARTESIAN_POINT('',(4.55912712210514,2.75,-12.7)) ;
#138643 = CARTESIAN_POINT('',(12.7,2.75,-12.7)) ;
#138644 = CARTESIAN_POINT('',(12.8,2.75,-12.7)) ;
#138645 = CARTESIAN_POINT('',(12.7,2.75,-12.7)) ;
#138646 = CARTESIAN_POINT('Origin',(4.5,-2.8,-12.7)) ;
#138647 = CARTESIAN_POINT('',(4.5,-2.7,-12.7)) ;
#138648 = CARTESIAN_POINT('',(4.5,-2.4,-12.7)) ;
#138649 = CARTESIAN_POINT('',(4.5,-2.8,-12.7)) ;
#138650 = CARTESIAN_POINT('',(4.5,-2.7,-13.7168453788272)) ;
#138651 = CARTESIAN_POINT('',(4.5,-2.7,-12.7)) ;
#138652 = CARTESIAN_POINT('',(4.5,-2.4,-13.2778583129651)) ;
#138653 = CARTESIAN_POINT('Origin',(4.5,0.,-15.24)) ;
#138654 = CARTESIAN_POINT('',(4.5,-2.4,-12.7)) ;
#138655 = CARTESIAN_POINT('Origin',(0.,0.,-12.7)) ;
#138656 = CARTESIAN_POINT('Origin',(4.4,-2.7,-12.7)) ;
#138657 = CARTESIAN_POINT('Origin',(4.6,-2.4,-12.7)) ;
#138658 = CARTESIAN_POINT('Origin',(12.7,-2.2,-12.7)) ;
#138659 = CARTESIAN_POINT('Origin',(12.7,2.65,-12.7)) ;
#138660 = CARTESIAN_POINT('Origin',(4.55912712210514,2.85,-12.7)) ;
#138661 = CARTESIAN_POINT('Origin',(-4.65,1.95,-17.24)) ;
#138662 = CARTESIAN_POINT('',(-4.66204490261456,3.21928058320648,-17.24)) ;
#138663 = CARTESIAN_POINT('',(-5.3,3.9369800677651,-17.24)) ;
#138664 = CARTESIAN_POINT('',(-5.47474093186837,4.13356361611701,-17.24)) ;
#138665 = CARTESIAN_POINT('',(-5.3,-1.88819660112501,-17.24)) ;
#138666 = CARTESIAN_POINT('',(-5.3,-2.05,-17.24)) ;
#138667 = CARTESIAN_POINT('',(-4.66204490261456,-1.5692190524323,-17.24)) ;
#138668 = CARTESIAN_POINT('',(-4.69472135955,-1.58555728090001,-17.24)) ;
#138669 = CARTESIAN_POINT('',(-4.66204490261456,3.35625,-17.24)) ;
#138670 = CARTESIAN_POINT('Origin',(-5.4,1.95,-13.24)) ;
#138671 = CARTESIAN_POINT('',(-4.66204490261456,-1.5692190524323,-13.24)) ;
#138672 = CARTESIAN_POINT('',(-5.3,-1.88819660112502,-13.24)) ;
#138673 = CARTESIAN_POINT('',(-5.44472135955,-1.96055728090001,-13.24)) ;
#138674 = CARTESIAN_POINT('',(-5.3,3.9369800677651,-13.24)) ;
#138675 = CARTESIAN_POINT('',(-5.3,4.20000000000001,-13.24)) ;
#138676 = CARTESIAN_POINT('',(-4.66204490261456,3.21928058320648,-13.24)) ;
#138677 = CARTESIAN_POINT('',(-4.72474093186837,3.28981361611701,-13.24)) ;
#138678 = CARTESIAN_POINT('',(-4.66204490261456,-1.67500000000001,-13.24)) ;
#138679 = CARTESIAN_POINT('Origin',(-4.65,1.95,-13.24)) ;
#138680 = CARTESIAN_POINT('',(-3.33134808452128,1.85,-13.5623371348948)) ;
#138681 = CARTESIAN_POINT('',(-3.48082994825801,1.91712723223402,-13.5257971237592)) ;
#138682 = CARTESIAN_POINT('Origin',(-3.34328863644877,2.0234124498231,-13.5594183333125)) ;
#138683 = CARTESIAN_POINT('',(-2.4,1.85,-13.79)) ;
#138684 = CARTESIAN_POINT('',(-4.65,1.85,-13.24)) ;
#138685 = CARTESIAN_POINT('',(-2.4,-0.95,-13.79)) ;
#138686 = CARTESIAN_POINT('',(-2.4,1.95,-13.79)) ;
#138687 = CARTESIAN_POINT('',(-3.3526478932023,-0.95,-13.557130514995)) ;
#138688 = CARTESIAN_POINT('',(-3.39999999999998,-0.95,-13.5455555555556)) ;
#138689 = CARTESIAN_POINT('',(-3.44209061230229,-0.971114561800017,-13.535266739215)) ;
#138690 = CARTESIAN_POINT('Origin',(-3.36201220558139,-1.11033257691422,-13.554841460858)) ;
#138691 = CARTESIAN_POINT('',(-4.63829959356686,-1.5692190524323,-13.2428600993503)) ;
#138692 = CARTESIAN_POINT('',(-4.68814869588294,-1.59414360359034,-13.2306747632286)) ;
#138693 = CARTESIAN_POINT('',(-4.63829959356686,3.21928058320648,-13.2428600993503)) ;
#138694 = CARTESIAN_POINT('',(-4.63829959356686,3.35625,-13.2428600993503)) ;
#138695 = CARTESIAN_POINT('',(-3.45989661114215,1.89357722797868,-13.5309141617208)) ;
#138696 = CARTESIAN_POINT('Origin',(-2.4,1.95,-13.79)) ;
#138697 = CARTESIAN_POINT('',(-2.4,1.85,-16.69)) ;
#138698 = CARTESIAN_POINT('',(-2.4,-0.95,-16.69)) ;
#138699 = CARTESIAN_POINT('',(-2.4,1.95,-16.69)) ;
#138700 = CARTESIAN_POINT('',(-2.4,-1.05,-16.587055690472)) ;
#138701 = CARTESIAN_POINT('Origin',(-2.4,-0.949999999999943,-16.5870556904719)) ;
#138702 = CARTESIAN_POINT('',(-2.4,-1.05,-13.892944309528)) ;
#138703 = CARTESIAN_POINT('',(-2.4,-1.05,-13.79)) ;
#138704 = CARTESIAN_POINT('Origin',(-2.4,-0.949999999999926,-13.8929443095281)) ;
#138705 = CARTESIAN_POINT('',(-2.4,1.95,-13.892944309528)) ;
#138706 = CARTESIAN_POINT('Origin',(-2.4,1.85000000000001,-13.892944309528)) ;
#138707 = CARTESIAN_POINT('',(-2.4,1.95,-16.587055690472)) ;
#138708 = CARTESIAN_POINT('',(-2.4,1.95,-13.79)) ;
#138709 = CARTESIAN_POINT('Origin',(-2.4,1.85000000000016,-16.5870556904722)) ;
#138710 = CARTESIAN_POINT('Origin',(-2.4,1.95,-16.69)) ;
#138711 = CARTESIAN_POINT('',(-3.3526478932023,-0.95,-16.922869485005)) ;
#138712 = CARTESIAN_POINT('',(-3.44209061230229,-0.971114561800017,-16.944733260785)) ;
#138713 = CARTESIAN_POINT('Origin',(-3.36201220558205,-1.1103325769103,-16.9251585391424)) ;
#138714 = CARTESIAN_POINT('',(-2.4,-0.95,-16.69)) ;
#138715 = CARTESIAN_POINT('',(-3.33134808452128,1.85,-16.9176628651052)) ;
#138716 = CARTESIAN_POINT('',(-2.4,1.85,-16.69)) ;
#138717 = CARTESIAN_POINT('',(-3.48082994825801,1.91712723223402,-16.9542028762408)) ;
#138718 = CARTESIAN_POINT('Origin',(-3.3432886364489,2.02341244982209,-16.9205816666875)) ;
#138719 = CARTESIAN_POINT('',(-4.63829959356686,3.21928058320648,-17.2371399006497)) ;
#138720 = CARTESIAN_POINT('',(-4.70989661114216,3.29982722797869,-17.2546413938348)) ;
#138721 = CARTESIAN_POINT('',(-4.63829959356686,-1.5692190524323,-17.2371399006497)) ;
#138722 = CARTESIAN_POINT('',(-4.63829959356686,-1.67500000000001,-17.2371399006497)) ;
#138723 = CARTESIAN_POINT('',(-3.43814869588292,-0.969143603590331,-16.9437696812158)) ;
#138724 = CARTESIAN_POINT('Origin',(0.,1.95,-15.24)) ;
#138725 = CARTESIAN_POINT('',(-3.35509339356897,1.95,-13.6594770355445)) ;
#138726 = CARTESIAN_POINT('',(0.175392621986784,1.95,-14.5224847282359)) ;
#138727 = CARTESIAN_POINT('',(-3.35509339356897,1.95,-16.8205229644555)) ;
#138728 = CARTESIAN_POINT('',(-3.35509339356897,1.95,-16.9344444444444)) ;
#138729 = CARTESIAN_POINT('',(0.175392621986784,1.95,-15.9575152717641)) ;
#138730 = CARTESIAN_POINT('Origin',(0.,-1.05,-15.24)) ;
#138731 = CARTESIAN_POINT('',(-3.37639320225,-1.05,-16.8257295843553)) ;
#138732 = CARTESIAN_POINT('',(-3.42374530904768,-1.05,-16.8373045437948)) ;
#138733 = CARTESIAN_POINT('',(-3.37639320225,-1.05,-13.6542704156447)) ;
#138734 = CARTESIAN_POINT('',(-3.37639320225,-1.05,-15.24)) ;
#138735 = CARTESIAN_POINT('',(-2.4237453090477,-1.05,-13.8871399006497)) ;
#138736 = CARTESIAN_POINT('Origin',(-3.39999999999998,-1.05,-15.24)) ;
#138737 = CARTESIAN_POINT('',(-3.4211145618,-1.06055728090001,-13.6324066398647)) ;
#138738 = CARTESIAN_POINT('',(-3.4211145618,-1.06055728090001,-16.8475933601353)) ;
#138739 = CARTESIAN_POINT('',(-3.4211145618,-1.06055728090001,-15.24)) ;
#138740 = CARTESIAN_POINT('',(-4.61732354306457,-1.65866177153229,-17.14)) ;
#138741 = CARTESIAN_POINT('',(-4.66717264538064,-1.68358632269033,-17.1521853361217)) ;
#138742 = CARTESIAN_POINT('',(-5.34472135954999,-2.022360679775,-17.14)) ;
#138743 = CARTESIAN_POINT('',(-5.4,-2.05,-17.14)) ;
#138744 = CARTESIAN_POINT('',(-5.34472135954999,-2.022360679775,-13.34)) ;
#138745 = CARTESIAN_POINT('',(-5.34472135954999,-2.022360679775,-13.24)) ;
#138746 = CARTESIAN_POINT('',(-4.61732354306457,-1.65866177153229,-13.34)) ;
#138747 = CARTESIAN_POINT('',(-4.65,-1.67500000000001,-13.34)) ;
#138748 = CARTESIAN_POINT('',(-3.41717264538063,-1.05858632269032,-13.6333702194339)) ;
#138749 = CARTESIAN_POINT('Origin',(-5.4,4.20000000000001,-12.7)) ;
#138750 = CARTESIAN_POINT('',(-5.37474093186837,4.17158354835192,-13.34)) ;
#138751 = CARTESIAN_POINT('',(-5.37474093186837,4.17158354835192,-17.14)) ;
#138752 = CARTESIAN_POINT('',(-5.37474093186837,4.17158354835192,-17.24)) ;
#138753 = CARTESIAN_POINT('',(-4.58730397074619,3.28571696708947,-17.14)) ;
#138754 = CARTESIAN_POINT('',(-4.65,3.35625,-17.14)) ;
#138755 = CARTESIAN_POINT('',(-3.42983432543734,1.98356361611701,-16.8570629755912)) ;
#138756 = CARTESIAN_POINT('',(-3.40890098832149,1.96001361186167,-16.8519459376295)) ;
#138757 = CARTESIAN_POINT('',(-3.42983432543734,1.98356361611701,-13.6229370244088)) ;
#138758 = CARTESIAN_POINT('',(-3.42983432543734,1.98356361611701,-13.5455555555556)) ;
#138759 = CARTESIAN_POINT('',(-4.58730397074619,3.28571696708947,-13.34)) ;
#138760 = CARTESIAN_POINT('',(-4.65890098832149,3.36626361186168,-13.3224985068149)) ;
#138761 = CARTESIAN_POINT('',(-5.4,4.20000000000001,-13.34)) ;
#138762 = CARTESIAN_POINT('Origin',(-3.15,-3.9,-14.24)) ;
#138763 = CARTESIAN_POINT('',(-3.15,-3.95,-14.34)) ;
#138764 = CARTESIAN_POINT('',(-3.15,-3.85,-14.34)) ;
#138765 = CARTESIAN_POINT('',(-3.15,-3.75,-14.34)) ;
#138766 = CARTESIAN_POINT('',(-3.15,-3.85,-16.14)) ;
#138767 = CARTESIAN_POINT('',(-3.15,-3.85,-14.24)) ;
#138768 = CARTESIAN_POINT('',(-3.15,-3.95,-16.14)) ;
#138769 = CARTESIAN_POINT('',(-3.15,-4.05,-16.14)) ;
#138770 = CARTESIAN_POINT('',(-3.15,-3.95,-14.24)) ;
#138771 = CARTESIAN_POINT('Origin',(-4.4,-3.9,-16.24)) ;
#138772 = CARTESIAN_POINT('',(-3.25,-3.85,-16.24)) ;
#138773 = CARTESIAN_POINT('',(-4.3,-3.85,-16.24)) ;
#138774 = CARTESIAN_POINT('',(-4.4,-3.85,-16.24)) ;
#138775 = CARTESIAN_POINT('',(-4.3,-3.95,-16.24)) ;
#138776 = CARTESIAN_POINT('',(-4.3,-4.05,-16.24)) ;
#138777 = CARTESIAN_POINT('',(-3.25,-3.95,-16.24)) ;
#138778 = CARTESIAN_POINT('',(-4.4,-3.95,-16.24)) ;
#138779 = CARTESIAN_POINT('',(-3.25,-3.75,-16.24)) ;
#138780 = CARTESIAN_POINT('Origin',(-4.4,-3.9,-14.24)) ;
#138781 = CARTESIAN_POINT('',(-4.4,-3.85,-16.14)) ;
#138782 = CARTESIAN_POINT('',(-4.4,-3.85,-14.34)) ;
#138783 = CARTESIAN_POINT('',(-4.4,-3.85,-14.24)) ;
#138784 = CARTESIAN_POINT('',(-4.4,-3.95,-14.34)) ;
#138785 = CARTESIAN_POINT('',(-4.4,-4.05,-14.34)) ;
#138786 = CARTESIAN_POINT('',(-4.4,-3.95,-16.14)) ;
#138787 = CARTESIAN_POINT('',(-4.4,-3.95,-14.24)) ;
#138788 = CARTESIAN_POINT('',(-4.4,-3.75,-16.14)) ;
#138789 = CARTESIAN_POINT('Origin',(-4.4,-3.9,-14.24)) ;
#138790 = CARTESIAN_POINT('',(-4.3,-3.95,-14.24)) ;
#138791 = CARTESIAN_POINT('',(-4.3,-3.85,-14.24)) ;
#138792 = CARTESIAN_POINT('',(-4.3,-3.75,-14.24)) ;
#138793 = CARTESIAN_POINT('',(-3.25,-3.85,-14.24)) ;
#138794 = CARTESIAN_POINT('',(-4.4,-3.85,-14.24)) ;
#138795 = CARTESIAN_POINT('',(-3.25,-3.95,-14.24)) ;
#138796 = CARTESIAN_POINT('',(-3.25,-4.05,-14.24)) ;
#138797 = CARTESIAN_POINT('',(-4.4,-3.95,-14.24)) ;
#138798 = CARTESIAN_POINT('Origin',(0.,-3.75,-15.24)) ;
#138799 = CARTESIAN_POINT('',(-3.25,-3.75,-14.34)) ;
#138800 = CARTESIAN_POINT('',(-4.3,-3.75,-14.34)) ;
#138801 = CARTESIAN_POINT('',(-1.56125112837913E-16,-3.75,-14.34)) ;
#138802 = CARTESIAN_POINT('',(-4.3,-3.75,-16.14)) ;
#138803 = CARTESIAN_POINT('',(-4.3,-3.75,-15.24)) ;
#138804 = CARTESIAN_POINT('',(-3.25,-3.75,-16.14)) ;
#138805 = CARTESIAN_POINT('',(-1.56125112837913E-16,-3.75,-16.14)) ;
#138806 = CARTESIAN_POINT('',(-3.25,-3.75,-15.24)) ;
#138807 = CARTESIAN_POINT('',(-4.15,-3.75,-16.09)) ;
#138808 = CARTESIAN_POINT('',(-3.4,-3.75,-16.09)) ;
#138809 = CARTESIAN_POINT('',(-4.15,-3.75,-16.09)) ;
#138810 = CARTESIAN_POINT('',(-4.25,-3.75,-15.99)) ;
#138811 = CARTESIAN_POINT('Origin',(-4.15,-3.75,-15.99)) ;
#138812 = CARTESIAN_POINT('',(-4.25,-3.75,-14.49)) ;
#138813 = CARTESIAN_POINT('',(-4.25,-3.75,-14.49)) ;
#138814 = CARTESIAN_POINT('',(-4.15,-3.75,-14.39)) ;
#138815 = CARTESIAN_POINT('Origin',(-4.15,-3.75,-14.49)) ;
#138816 = CARTESIAN_POINT('',(-3.4,-3.75,-14.39)) ;
#138817 = CARTESIAN_POINT('',(-3.4,-3.75,-14.39)) ;
#138818 = CARTESIAN_POINT('',(-3.3,-3.75,-14.49)) ;
#138819 = CARTESIAN_POINT('Origin',(-3.4,-3.75,-14.49)) ;
#138820 = CARTESIAN_POINT('',(-3.3,-3.75,-15.99)) ;
#138821 = CARTESIAN_POINT('',(-3.3,-3.75,-15.99)) ;
#138822 = CARTESIAN_POINT('Origin',(-3.4,-3.75,-15.99)) ;
#138823 = CARTESIAN_POINT('Origin',(-3.4,-3.75,-15.99)) ;
#138824 = CARTESIAN_POINT('',(-3.4,-3.9,-16.09)) ;
#138825 = CARTESIAN_POINT('',(-3.3,-3.9,-15.99)) ;
#138826 = CARTESIAN_POINT('Origin',(-3.4,-3.9,-15.99)) ;
#138827 = CARTESIAN_POINT('',(-3.4,-3.75,-16.09)) ;
#138828 = CARTESIAN_POINT('',(-3.3,-3.75,-15.99)) ;
#138829 = CARTESIAN_POINT('Origin',(-4.15,-3.75,-16.09)) ;
#138830 = CARTESIAN_POINT('',(-4.15,-3.9,-16.09)) ;
#138831 = CARTESIAN_POINT('',(-4.15,-3.9,-16.09)) ;
#138832 = CARTESIAN_POINT('',(-4.15,-3.75,-16.09)) ;
#138833 = CARTESIAN_POINT('Origin',(-4.15,-3.75,-15.99)) ;
#138834 = CARTESIAN_POINT('',(-4.25,-3.9,-15.99)) ;
#138835 = CARTESIAN_POINT('Origin',(-4.15,-3.9,-15.99)) ;
#138836 = CARTESIAN_POINT('',(-4.25,-3.75,-15.99)) ;
#138837 = CARTESIAN_POINT('Origin',(-4.25,-3.75,-14.49)) ;
#138838 = CARTESIAN_POINT('',(-4.25,-3.9,-14.49)) ;
#138839 = CARTESIAN_POINT('',(-4.25,-3.9,-14.49)) ;
#138840 = CARTESIAN_POINT('',(-4.25,-3.75,-14.49)) ;
#138841 = CARTESIAN_POINT('Origin',(-4.15,-3.75,-14.49)) ;
#138842 = CARTESIAN_POINT('',(-4.15,-3.9,-14.39)) ;
#138843 = CARTESIAN_POINT('Origin',(-4.15,-3.9,-14.49)) ;
#138844 = CARTESIAN_POINT('',(-4.15,-3.75,-14.39)) ;
#138845 = CARTESIAN_POINT('Origin',(-3.4,-3.75,-14.39)) ;
#138846 = CARTESIAN_POINT('',(-3.4,-3.9,-14.39)) ;
#138847 = CARTESIAN_POINT('',(-3.4,-3.9,-14.39)) ;
#138848 = CARTESIAN_POINT('',(-3.4,-3.75,-14.39)) ;
#138849 = CARTESIAN_POINT('Origin',(-3.4,-3.75,-14.49)) ;
#138850 = CARTESIAN_POINT('',(-3.3,-3.9,-14.49)) ;
#138851 = CARTESIAN_POINT('Origin',(-3.4,-3.9,-14.49)) ;
#138852 = CARTESIAN_POINT('',(-3.3,-3.75,-14.49)) ;
#138853 = CARTESIAN_POINT('Origin',(-3.3,-3.75,-15.99)) ;
#138854 = CARTESIAN_POINT('',(-3.3,-3.9,-15.99)) ;
#138855 = CARTESIAN_POINT('Origin',(0.,-3.9,-15.24)) ;
#138856 = CARTESIAN_POINT('Origin',(0.,9.95,-15.24)) ;
#138857 = CARTESIAN_POINT('',(-0.230887397576972,9.95,-13.3251394281462)) ;
#138858 = CARTESIAN_POINT('Origin',(-0.321518176280637,8.95,-13.3674012543203)) ;
#138859 = CARTESIAN_POINT('',(-0.321518176280637,9.05,-13.3674012543203)) ;
#138860 = CARTESIAN_POINT('',(1.22782596331729,9.85,-16.689980483939)) ;
#138861 = CARTESIAN_POINT('Origin',(-1.22782596331729,8.95,-13.790019516061)) ;
#138862 = CARTESIAN_POINT('',(-1.22782596331729,9.05,-13.790019516061)) ;
#138863 = CARTESIAN_POINT('',(-1.22782596331729,9.85,-13.790019516061)) ;
#138864 = CARTESIAN_POINT('Origin',(0.,8.95,-15.24)) ;
#138865 = CARTESIAN_POINT('',(-0.362523114814661,8.95,-15.4090473046963)) ;
#138866 = CARTESIAN_POINT('',(0.36252311481466,8.95,-15.0709526953037)) ;
#138867 = CARTESIAN_POINT('Origin',(-2.65,10.8,-16.24)) ;
#138868 = CARTESIAN_POINT('',(-2.65,10.75,-16.14)) ;
#138869 = CARTESIAN_POINT('',(-2.65,10.75,-14.34)) ;
#138870 = CARTESIAN_POINT('',(-2.65,10.75,-16.24)) ;
#138871 = CARTESIAN_POINT('',(-2.65,10.85,-14.34)) ;
#138872 = CARTESIAN_POINT('',(-2.65,10.95,-14.34)) ;
#138873 = CARTESIAN_POINT('',(-2.65,10.85,-16.14)) ;
#138874 = CARTESIAN_POINT('',(-2.65,10.85,-16.24)) ;
#138875 = CARTESIAN_POINT('',(-2.65,10.65,-16.14)) ;
#138876 = CARTESIAN_POINT('Origin',(-3.9,10.8,-14.24)) ;
#138877 = CARTESIAN_POINT('',(-2.75,10.85,-14.24)) ;
#138878 = CARTESIAN_POINT('',(-2.75,10.75,-14.24)) ;
#138879 = CARTESIAN_POINT('',(-2.75,10.65,-14.24)) ;
#138880 = CARTESIAN_POINT('',(-3.8,10.75,-14.24)) ;
#138881 = CARTESIAN_POINT('',(-3.9,10.75,-14.24)) ;
#138882 = CARTESIAN_POINT('',(-3.8,10.85,-14.24)) ;
#138883 = CARTESIAN_POINT('',(-3.8,10.95,-14.24)) ;
#138884 = CARTESIAN_POINT('',(-3.9,10.85,-14.24)) ;
#138885 = CARTESIAN_POINT('Origin',(-3.9,10.8,-16.24)) ;
#138886 = CARTESIAN_POINT('',(-3.9,10.85,-14.34)) ;
#138887 = CARTESIAN_POINT('',(-3.9,10.75,-14.34)) ;
#138888 = CARTESIAN_POINT('',(-3.9,10.65,-14.34)) ;
#138889 = CARTESIAN_POINT('',(-3.9,10.75,-16.14)) ;
#138890 = CARTESIAN_POINT('',(-3.9,10.75,-16.24)) ;
#138891 = CARTESIAN_POINT('',(-3.9,10.85,-16.14)) ;
#138892 = CARTESIAN_POINT('',(-3.9,10.95,-16.14)) ;
#138893 = CARTESIAN_POINT('',(-3.9,10.85,-16.24)) ;
#138894 = CARTESIAN_POINT('Origin',(-3.9,10.8,-16.24)) ;
#138895 = CARTESIAN_POINT('',(-3.8,10.75,-16.24)) ;
#138896 = CARTESIAN_POINT('',(-2.75,10.75,-16.24)) ;
#138897 = CARTESIAN_POINT('',(-3.9,10.75,-16.24)) ;
#138898 = CARTESIAN_POINT('',(-2.75,10.85,-16.24)) ;
#138899 = CARTESIAN_POINT('',(-2.75,10.95,-16.24)) ;
#138900 = CARTESIAN_POINT('',(-3.8,10.85,-16.24)) ;
#138901 = CARTESIAN_POINT('',(-3.9,10.85,-16.24)) ;
#138902 = CARTESIAN_POINT('',(-3.8,10.65,-16.24)) ;
#138903 = CARTESIAN_POINT('Origin',(0.,10.65,-15.24)) ;
#138904 = CARTESIAN_POINT('',(-3.8,10.65,-14.34)) ;
#138905 = CARTESIAN_POINT('',(-2.75,10.65,-14.34)) ;
#138906 = CARTESIAN_POINT('',(1.56125112837912E-16,10.65,-14.34)) ;
#138907 = CARTESIAN_POINT('',(-2.75,10.65,-16.14)) ;
#138908 = CARTESIAN_POINT('',(-2.75,10.65,-15.24)) ;
#138909 = CARTESIAN_POINT('',(-3.8,10.65,-16.14)) ;
#138910 = CARTESIAN_POINT('',(-1.56125112837913E-16,10.65,-16.14)) ;
#138911 = CARTESIAN_POINT('',(-3.8,10.65,-15.24)) ;
#138912 = CARTESIAN_POINT('',(-3.65,10.65,-14.39)) ;
#138913 = CARTESIAN_POINT('',(-2.9,10.65,-14.39)) ;
#138914 = CARTESIAN_POINT('',(-3.65,10.65,-14.39)) ;
#138915 = CARTESIAN_POINT('',(-3.75,10.65,-14.49)) ;
#138916 = CARTESIAN_POINT('Origin',(-3.65,10.65,-14.49)) ;
#138917 = CARTESIAN_POINT('',(-3.75,10.65,-15.99)) ;
#138918 = CARTESIAN_POINT('',(-3.75,10.65,-15.99)) ;
#138919 = CARTESIAN_POINT('',(-3.65,10.65,-16.09)) ;
#138920 = CARTESIAN_POINT('Origin',(-3.65,10.65,-15.99)) ;
#138921 = CARTESIAN_POINT('',(-2.9,10.65,-16.09)) ;
#138922 = CARTESIAN_POINT('',(-2.9,10.65,-16.09)) ;
#138923 = CARTESIAN_POINT('',(-2.8,10.65,-15.99)) ;
#138924 = CARTESIAN_POINT('Origin',(-2.9,10.65,-15.99)) ;
#138925 = CARTESIAN_POINT('',(-2.8,10.65,-14.49)) ;
#138926 = CARTESIAN_POINT('',(-2.8,10.65,-14.49)) ;
#138927 = CARTESIAN_POINT('Origin',(-2.9,10.65,-14.49)) ;
#138928 = CARTESIAN_POINT('Origin',(-2.9,10.65,-14.49)) ;
#138929 = CARTESIAN_POINT('',(-2.8,10.7,-14.49)) ;
#138930 = CARTESIAN_POINT('',(-2.8,10.65,-14.49)) ;
#138931 = CARTESIAN_POINT('',(-2.9,10.7,-14.39)) ;
#138932 = CARTESIAN_POINT('Origin',(-2.9,10.7,-14.49)) ;
#138933 = CARTESIAN_POINT('',(-2.9,10.65,-14.39)) ;
#138934 = CARTESIAN_POINT('Origin',(-3.65,10.65,-14.39)) ;
#138935 = CARTESIAN_POINT('',(-3.65,10.7,-14.39)) ;
#138936 = CARTESIAN_POINT('',(-3.65,10.7,-14.39)) ;
#138937 = CARTESIAN_POINT('',(-3.65,10.65,-14.39)) ;
#138938 = CARTESIAN_POINT('Origin',(-3.65,10.65,-14.49)) ;
#138939 = CARTESIAN_POINT('',(-3.75,10.7,-14.49)) ;
#138940 = CARTESIAN_POINT('Origin',(-3.65,10.7,-14.49)) ;
#138941 = CARTESIAN_POINT('',(-3.75,10.65,-14.49)) ;
#138942 = CARTESIAN_POINT('Origin',(-3.75,10.65,-15.99)) ;
#138943 = CARTESIAN_POINT('',(-3.75,10.7,-15.99)) ;
#138944 = CARTESIAN_POINT('',(-3.75,10.7,-15.99)) ;
#138945 = CARTESIAN_POINT('',(-3.75,10.65,-15.99)) ;
#138946 = CARTESIAN_POINT('Origin',(-3.65,10.65,-15.99)) ;
#138947 = CARTESIAN_POINT('',(-3.65,10.7,-16.09)) ;
#138948 = CARTESIAN_POINT('Origin',(-3.65,10.7,-15.99)) ;
#138949 = CARTESIAN_POINT('',(-3.65,10.65,-16.09)) ;
#138950 = CARTESIAN_POINT('Origin',(-2.9,10.65,-16.09)) ;
#138951 = CARTESIAN_POINT('',(-2.9,10.7,-16.09)) ;
#138952 = CARTESIAN_POINT('',(-2.9,10.7,-16.09)) ;
#138953 = CARTESIAN_POINT('',(-2.9,10.65,-16.09)) ;
#138954 = CARTESIAN_POINT('Origin',(-2.9,10.65,-15.99)) ;
#138955 = CARTESIAN_POINT('',(-2.8,10.7,-15.99)) ;
#138956 = CARTESIAN_POINT('Origin',(-2.9,10.7,-15.99)) ;
#138957 = CARTESIAN_POINT('',(-2.8,10.65,-15.99)) ;
#138958 = CARTESIAN_POINT('Origin',(-2.8,10.65,-14.49)) ;
#138959 = CARTESIAN_POINT('',(-2.8,10.7,-14.49)) ;
#138960 = CARTESIAN_POINT('Origin',(0.,10.8,-15.24)) ;
#138961 = CARTESIAN_POINT('',(-3.65,10.8,-14.49)) ;
#138962 = CARTESIAN_POINT('',(-2.9,10.8,-14.49)) ;
#138963 = CARTESIAN_POINT('',(0.,10.8,-14.49)) ;
#138964 = CARTESIAN_POINT('',(-2.9,10.8,-15.99)) ;
#138965 = CARTESIAN_POINT('',(-2.9,10.8,-15.24)) ;
#138966 = CARTESIAN_POINT('',(-3.65,10.8,-15.99)) ;
#138967 = CARTESIAN_POINT('',(0.,10.8,-15.99)) ;
#138968 = CARTESIAN_POINT('',(-3.65,10.8,-15.24)) ;
#138969 = CARTESIAN_POINT('Origin',(4.5,2.75,-16.615)) ;
#138970 = CARTESIAN_POINT('',(4.5,2.63356010126946,-16.6344066497884)) ;
#138971 = CARTESIAN_POINT('',(4.6,2.11643989873054,-16.7205933502116)) ;
#138972 = CARTESIAN_POINT('',(4.6,2.11643989873054,-16.7205933502116)) ;
#138973 = CARTESIAN_POINT('',(12.7,2.11643989873054,-16.7205933502116)) ;
#138974 = CARTESIAN_POINT('',(12.8,2.11643989873054,-16.7205933502116)) ;
#138975 = CARTESIAN_POINT('',(12.7,2.75,-16.615)) ;
#138976 = CARTESIAN_POINT('Origin',(4.5,2.,-16.74)) ;
#138977 = CARTESIAN_POINT('',(4.6,2.,-16.6219539578284)) ;
#138978 = CARTESIAN_POINT('',(4.6,2.,-13.74)) ;
#138979 = CARTESIAN_POINT('',(12.7,2.,-16.6219539578284)) ;
#138980 = CARTESIAN_POINT('',(12.7,2.,-16.74)) ;
#138981 = CARTESIAN_POINT('',(4.5,2.,-16.6219539578284)) ;
#138982 = CARTESIAN_POINT('Origin',(4.5,2.,-13.74)) ;
#138983 = CARTESIAN_POINT('',(4.6,2.63356010126946,-13.8455933502116)) ;
#138984 = CARTESIAN_POINT('',(4.6,2.63356010126947,-13.8455933502116)) ;
#138985 = CARTESIAN_POINT('',(4.5,2.63356010126946,-13.8455933502116)) ;
#138986 = CARTESIAN_POINT('',(12.7,2.,-13.74)) ;
#138987 = CARTESIAN_POINT('Origin',(4.5,0.,-15.24)) ;
#138988 = CARTESIAN_POINT('',(4.5,2.72431432344521,-13.932634816645)) ;
#138989 = CARTESIAN_POINT('',(4.5,2.72431432344521,-15.24)) ;
#138990 = CARTESIAN_POINT('',(4.5,2.61712020253893,-13.9442327425948)) ;
#138991 = CARTESIAN_POINT('Origin',(4.5,2.65,-13.7469539578284)) ;
#138992 = CARTESIAN_POINT('',(4.5,2.1,-13.8580460421716)) ;
#138993 = CARTESIAN_POINT('',(4.5,2.1,-13.8580460421716)) ;
#138994 = CARTESIAN_POINT('',(4.5,2.1,-16.6219539578284)) ;
#138995 = CARTESIAN_POINT('',(4.5,2.1,-16.74)) ;
#138996 = CARTESIAN_POINT('',(4.5,2.61712020253893,-16.5357672574052)) ;
#138997 = CARTESIAN_POINT('Origin',(10.3,0.,-15.24)) ;
#138998 = CARTESIAN_POINT('Origin',(0.584645609909621,0.,-15.24)) ;
#138999 = CARTESIAN_POINT('',(4.6,-2.32258064516129,-13.3411532060953)) ;
#139000 = CARTESIAN_POINT('',(4.6,-2.79310344827574,-14.1452063540419)) ;
#139001 = CARTESIAN_POINT('Origin',(4.6,0.,-15.24)) ;
#139002 = CARTESIAN_POINT('',(4.6,-2.79310344827574,-16.3347936459581)) ;
#139003 = CARTESIAN_POINT('Origin',(4.6,0.,-15.24)) ;
#139004 = CARTESIAN_POINT('',(4.6,-2.32258064516129,-17.1388467939047)) ;
#139005 = CARTESIAN_POINT('Origin',(4.6,0.,-15.24)) ;
#139006 = CARTESIAN_POINT('',(12.7,-2.32258064516129,-17.1388467939047)) ;
#139007 = CARTESIAN_POINT('',(0.584645609909621,-2.32258064516129,-17.1388467939047)) ;
#139008 = CARTESIAN_POINT('',(12.7,-2.32258064516129,-13.3411532060953)) ;
#139009 = CARTESIAN_POINT('Origin',(12.7,0.,-15.24)) ;
#139010 = CARTESIAN_POINT('',(0.584645609909621,-2.32258064516129,-13.3411532060953)) ;
#139011 = CARTESIAN_POINT('Ctrl Pts',(-5.37474093186837,4.17158354835192,
-13.34)) ;
#139012 = CARTESIAN_POINT('Ctrl Pts',(-5.4,4.2,-13.34)) ;
#139013 = CARTESIAN_POINT('Ctrl Pts',(-5.4,4.23801993223491,-13.34)) ;
#139014 = CARTESIAN_POINT('Ctrl Pts',(-5.37474093064202,4.17158354697228,
-13.313746564061)) ;
#139015 = CARTESIAN_POINT('Ctrl Pts',(-5.4,4.19999999724801,-13.302481412799)) ;
#139016 = CARTESIAN_POINT('Ctrl Pts',(-5.4,4.23801992976516,-13.2874931280902)) ;
#139017 = CARTESIAN_POINT('Ctrl Pts',(-5.36668583490655,4.14629949399955,
-13.2878012868841)) ;
#139018 = CARTESIAN_POINT('Ctrl Pts',(-5.40000000000003,4.16739198385627,
-13.2646678350658)) ;
#139019 = CARTESIAN_POINT('Ctrl Pts',(-5.4,4.20557579169425,-13.2356025737683)) ;
#139020 = CARTESIAN_POINT('Ctrl Pts',(-5.3390138046061,4.05944006555646,-13.2507773568786)) ;
#139021 = CARTESIAN_POINT('Ctrl Pts',(-5.39999999999997,4.06625640449636,
-13.2231326366142)) ;
#139022 = CARTESIAN_POINT('Ctrl Pts',(-5.4,4.09411900298411,-13.1615547137571)) ;
#139023 = CARTESIAN_POINT('Ctrl Pts',(-5.31962206268973,3.99857154231912,
-13.24)) ;
#139024 = CARTESIAN_POINT('Ctrl Pts',(-5.4,3.99346933127521,-13.2220035074266)) ;
#139025 = CARTESIAN_POINT('Ctrl Pts',(-5.4,4.0160133758189,-13.1400000004813)) ;
#139026 = CARTESIAN_POINT('Ctrl Pts',(-5.3,3.9369800677651,-13.24)) ;
#139027 = CARTESIAN_POINT('Ctrl Pts',(-5.4,3.9369800677651,-13.24)) ;
#139028 = CARTESIAN_POINT('Ctrl Pts',(-5.4,3.9369800677651,-13.14)) ;
#139029 = CARTESIAN_POINT('Origin',(-5.3,4.23801993223491,-13.34)) ;
#139030 = CARTESIAN_POINT('Ctrl Pts',(-5.3,3.9369800677651,-13.24)) ;
#139031 = CARTESIAN_POINT('Ctrl Pts',(-5.31962206268973,3.99857154231912,
-13.24)) ;
#139032 = CARTESIAN_POINT('Ctrl Pts',(-5.3390138046061,4.05944006555646,-13.2507773568786)) ;
#139033 = CARTESIAN_POINT('Ctrl Pts',(-5.36668583490655,4.14629949399955,
-13.2878012868841)) ;
#139034 = CARTESIAN_POINT('Ctrl Pts',(-5.37474093064202,4.17158354697228,
-13.313746564061)) ;
#139035 = CARTESIAN_POINT('Ctrl Pts',(-5.37474093186837,4.17158354835192,
-13.34)) ;
#139036 = CARTESIAN_POINT('Origin',(-5.3,3.9369800677651,-13.14)) ;
#139037 = CARTESIAN_POINT('Origin',(-4.6737453090477,1.85,-13.3371399006497)) ;
#139038 = CARTESIAN_POINT('Origin',(-3.35509339356897,1.85,-13.6594770355445)) ;
#139039 = CARTESIAN_POINT('Ctrl Pts',(-3.35509339356897,1.95,-13.6594770355445)) ;
#139040 = CARTESIAN_POINT('Ctrl Pts',(-3.33134808452127,1.95,-13.5623371348948)) ;
#139041 = CARTESIAN_POINT('Ctrl Pts',(-3.33134808452128,1.85,-13.5623371348948)) ;
#139042 = CARTESIAN_POINT('Ctrl Pts',(-3.38343213690417,1.95,-13.6456225388028)) ;
#139043 = CARTESIAN_POINT('Ctrl Pts',(-3.36046743872478,1.94345445676983,
-13.5552190705338)) ;
#139044 = CARTESIAN_POINT('Ctrl Pts',(-3.38803897426454,1.85000000162387,
-13.5484793618464)) ;
#139045 = CARTESIAN_POINT('Ctrl Pts',(-3.41101314049054,1.96238978305186,
-13.6321384929162)) ;
#139046 = CARTESIAN_POINT('Ctrl Pts',(-3.39538881861726,1.95068928167318,
-13.5466827332267)) ;
#139047 = CARTESIAN_POINT('Ctrl Pts',(-3.44316973238525,1.87475949194144,
-13.5350029543058)) ;
#139048 = CARTESIAN_POINT('Ctrl Pts',(-3.42983432543734,1.98356361611701,
-13.6229370244088)) ;
#139049 = CARTESIAN_POINT('Ctrl Pts',(-3.42093333711585,1.97355000425533,
-13.5404385175939)) ;
#139050 = CARTESIAN_POINT('Ctrl Pts',(-3.48082994825801,1.91712723223402,
-13.5257971237592)) ;
#139051 = CARTESIAN_POINT('Origin',(-3.50457525730571,1.91712723223402,-13.6229370244088)) ;
#139052 = CARTESIAN_POINT('Origin',(-3.36128627567781,2.036213614357,-13.6564494043351)) ;
#139053 = CARTESIAN_POINT('Origin',(-4.05330900605469,2.53445269957662,-13.488802108048)) ;
#139054 = CARTESIAN_POINT('Origin',(-4.66204490261456,3.21928058320648,-13.34)) ;
#139055 = CARTESIAN_POINT('Origin',(-4.35749955255802,2.87666706439287,-13.34)) ;
#139056 = CARTESIAN_POINT('Origin',(-4.66204490261456,3.21928058320648,-13.34)) ;
#139057 = CARTESIAN_POINT('Origin',(-5.3,5.2,-13.14)) ;
#139058 = CARTESIAN_POINT('Origin',(-5.3,-1.88819660112502,-13.14)) ;
#139059 = CARTESIAN_POINT('Origin',(-5.3,4.23801993223491,-12.7)) ;
#139060 = CARTESIAN_POINT('Origin',(-5.3,4.23801993223491,-17.14)) ;
#139061 = CARTESIAN_POINT('Origin',(-3.35509339356897,2.05,-15.24)) ;
#139062 = CARTESIAN_POINT('Origin',(-3.36128627567723,2.03621361435801,-16.8235505956649)) ;
#139063 = CARTESIAN_POINT('Origin',(-2.4237453090477,1.85,-16.5928600993503)) ;
#139064 = CARTESIAN_POINT('Origin',(-3.35509339356897,1.85,-16.8205229644555)) ;
#139065 = CARTESIAN_POINT('Origin',(-4.66204490261456,3.21928058320648,-13.34)) ;
#139066 = CARTESIAN_POINT('Origin',(-4.66204490261456,3.21928058320648,-13.34)) ;
#139067 = CARTESIAN_POINT('Ctrl Pts',(-5.29976814257747,-1.88802911972919,
-13.2399998273778)) ;
#139068 = CARTESIAN_POINT('Ctrl Pts',(-5.4,-1.88802831720456,-13.240232593543)) ;
#139069 = CARTESIAN_POINT('Ctrl Pts',(-5.4,-1.88791746283072,-13.1400001624624)) ;
#139070 = CARTESIAN_POINT('Ctrl Pts',(-5.31153957531165,-1.92331224822998,
-13.2399864676889)) ;
#139071 = CARTESIAN_POINT('Ctrl Pts',(-5.39999999999995,-1.92148676945297,
-13.2289778925381)) ;
#139072 = CARTESIAN_POINT('Ctrl Pts',(-5.4,-1.94671708614657,-13.1399317130284)) ;
#139073 = CARTESIAN_POINT('Ctrl Pts',(-5.32318090226696,-1.95817527052249,
-13.2507844972681)) ;
#139074 = CARTESIAN_POINT('Ctrl Pts',(-5.4,-1.96527310172483,-13.2321633837528)) ;
#139075 = CARTESIAN_POINT('Ctrl Pts',(-5.4,-2.00485091174287,-13.1614960748893)) ;
#139076 = CARTESIAN_POINT('Ctrl Pts',(-5.33978950165955,-2.00789652656156,
-13.2878649650197)) ;
#139077 = CARTESIAN_POINT('Ctrl Pts',(-5.4,-2.02908601268744,-13.2713665145317)) ;
#139078 = CARTESIAN_POINT('Ctrl Pts',(-5.4,-2.08777005652399,-13.235661212636)) ;
#139079 = CARTESIAN_POINT('Ctrl Pts',(-5.34461954754097,-2.02234798681676,
-13.3138461447183)) ;
#139080 = CARTESIAN_POINT('Ctrl Pts',(-5.4,-2.04997459329993,-13.30567566484)) ;
#139081 = CARTESIAN_POINT('Ctrl Pts',(-5.4,-2.1118797455067,-13.2876576869739)) ;
#139082 = CARTESIAN_POINT('Ctrl Pts',(-5.34460423617423,-2.02230212313483,
-13.3401247518701)) ;
#139083 = CARTESIAN_POINT('Ctrl Pts',(-5.4,-2.04990938338631,-13.3401637542765)) ;
#139084 = CARTESIAN_POINT('Ctrl Pts',(-5.4,-2.11180321723903,-13.3402496688804)) ;
#139085 = CARTESIAN_POINT('Origin',(-5.30000000000002,-1.88819660112506,-13.34)) ;
#139086 = CARTESIAN_POINT('Origin',(-5.3,-2.11180339887499,-13.34)) ;
#139087 = CARTESIAN_POINT('Ctrl Pts',(-5.3,3.9369800677651,-17.24)) ;
#139088 = CARTESIAN_POINT('Ctrl Pts',(-5.4,3.9369800677651,-17.24)) ;
#139089 = CARTESIAN_POINT('Ctrl Pts',(-5.4,3.9369800677651,-17.34)) ;
#139090 = CARTESIAN_POINT('Ctrl Pts',(-5.31962206268973,3.99857154231911,
-17.24)) ;
#139091 = CARTESIAN_POINT('Ctrl Pts',(-5.4,3.99346933127509,-17.2579964925735)) ;
#139092 = CARTESIAN_POINT('Ctrl Pts',(-5.4,4.01601337581888,-17.3399999995189)) ;
#139093 = CARTESIAN_POINT('Ctrl Pts',(-5.33901380460613,4.05944006555646,
-17.2292226431215)) ;
#139094 = CARTESIAN_POINT('Ctrl Pts',(-5.4,4.06625640449645,-17.2568673633859)) ;
#139095 = CARTESIAN_POINT('Ctrl Pts',(-5.4,4.09411900298413,-17.3184452862429)) ;
#139096 = CARTESIAN_POINT('Ctrl Pts',(-5.36668583490652,4.14629949399955,
-17.1921987131158)) ;
#139097 = CARTESIAN_POINT('Ctrl Pts',(-5.4,4.1673919838562,-17.2153321649341)) ;
#139098 = CARTESIAN_POINT('Ctrl Pts',(-5.4,4.20557579169423,-17.2443974262317)) ;
#139099 = CARTESIAN_POINT('Ctrl Pts',(-5.37474093064202,4.17158354697228,
-17.166253435939)) ;
#139100 = CARTESIAN_POINT('Ctrl Pts',(-5.4,4.19999999724801,-17.1775185872011)) ;
#139101 = CARTESIAN_POINT('Ctrl Pts',(-5.4,4.23801992976516,-17.1925068719098)) ;
#139102 = CARTESIAN_POINT('Ctrl Pts',(-5.37474093186837,4.17158354835192,
-17.14)) ;
#139103 = CARTESIAN_POINT('Ctrl Pts',(-5.4,4.2,-17.14)) ;
#139104 = CARTESIAN_POINT('Ctrl Pts',(-5.4,4.23801993223491,-17.14)) ;
#139105 = CARTESIAN_POINT('Origin',(-5.3,3.9369800677651,-17.34)) ;
#139106 = CARTESIAN_POINT('Ctrl Pts',(-5.37474093186837,4.17158354835192,
-17.14)) ;
#139107 = CARTESIAN_POINT('Ctrl Pts',(-5.37474093064202,4.17158354697228,
-17.166253435939)) ;
#139108 = CARTESIAN_POINT('Ctrl Pts',(-5.36668583490652,4.14629949399955,
-17.1921987131158)) ;
#139109 = CARTESIAN_POINT('Ctrl Pts',(-5.33901380460613,4.05944006555646,
-17.2292226431215)) ;
#139110 = CARTESIAN_POINT('Ctrl Pts',(-5.31962206268973,3.99857154231911,
-17.24)) ;
#139111 = CARTESIAN_POINT('Ctrl Pts',(-5.3,3.9369800677651,-17.24)) ;
#139112 = CARTESIAN_POINT('Ctrl Pts',(-3.42983432543734,1.98356361611701,
-16.8570629755912)) ;
#139113 = CARTESIAN_POINT('Ctrl Pts',(-3.42093333711585,1.97355000425533,
-16.9395614824061)) ;
#139114 = CARTESIAN_POINT('Ctrl Pts',(-3.48082994825801,1.91712723223402,
-16.9542028762408)) ;
#139115 = CARTESIAN_POINT('Ctrl Pts',(-3.41101314049054,1.96238978305186,
-16.8478615070839)) ;
#139116 = CARTESIAN_POINT('Ctrl Pts',(-3.39538881861725,1.95068928167332,
-16.9333172667734)) ;
#139117 = CARTESIAN_POINT('Ctrl Pts',(-3.44316973238528,1.87475949194142,
-16.9449970456942)) ;
#139118 = CARTESIAN_POINT('Ctrl Pts',(-3.38343213690423,1.95,-16.8343774611971)) ;
#139119 = CARTESIAN_POINT('Ctrl Pts',(-3.36046743872485,1.94345445676967,
-16.9247809294657)) ;
#139120 = CARTESIAN_POINT('Ctrl Pts',(-3.38803897426452,1.85000000162387,
-16.9315206381536)) ;
#139121 = CARTESIAN_POINT('Ctrl Pts',(-3.35509339356897,1.95,-16.8205229644555)) ;
#139122 = CARTESIAN_POINT('Ctrl Pts',(-3.33134808452128,1.95,-16.9176628651052)) ;
#139123 = CARTESIAN_POINT('Ctrl Pts',(-3.33134808452128,1.85,-16.9176628651052)) ;
#139124 = CARTESIAN_POINT('Origin',(-3.50457525730571,1.91712723223402,-16.8570629755912)) ;
#139125 = CARTESIAN_POINT('Origin',(-4.66204490261456,1.95,-13.34)) ;
#139126 = CARTESIAN_POINT('Origin',(-4.66204490261456,-1.5692190524323,-13.34)) ;
#139127 = CARTESIAN_POINT('Origin',(-3.84472135955,-1.16055728090002,-13.34)) ;
#139128 = CARTESIAN_POINT('Origin',(-4.66204490261456,-1.5692190524323,-13.34)) ;
#139129 = CARTESIAN_POINT('Origin',(-5.3,-2.11180339887499,-12.7)) ;
#139130 = CARTESIAN_POINT('Origin',(-5.3,-2.11180339887499,-17.14)) ;
#139131 = CARTESIAN_POINT('Origin',(-5.3,1.95,-17.34)) ;
#139132 = CARTESIAN_POINT('Origin',(-5.3,-1.88819660112501,-17.34)) ;
#139133 = CARTESIAN_POINT('Origin',(-4.0264650697994,2.50425327128942,-17.14)) ;
#139134 = CARTESIAN_POINT('Origin',(-4.66204490261456,3.21928058320648,-17.14)) ;
#139135 = CARTESIAN_POINT('Origin',(-3.02790825149799,1.38087685070033,-16.7405443741715)) ;
#139136 = CARTESIAN_POINT('Origin',(-4.66204490261456,3.21928058320648,-17.14)) ;
#139137 = CARTESIAN_POINT('Origin',(-4.66204490261456,-1.5692190524323,-13.34)) ;
#139138 = CARTESIAN_POINT('Origin',(-4.66204490261456,-1.5692190524323,-13.34)) ;
#139139 = CARTESIAN_POINT('Ctrl Pts',(-5.34460423617422,-2.02230212313483,
-17.1398752481299)) ;
#139140 = CARTESIAN_POINT('Ctrl Pts',(-5.4,-2.04990938338631,-17.1398362457235)) ;
#139141 = CARTESIAN_POINT('Ctrl Pts',(-5.4,-2.11180321723903,-17.1397503311196)) ;
#139142 = CARTESIAN_POINT('Ctrl Pts',(-5.34461954754097,-2.02234798681675,
-17.1661538552817)) ;
#139143 = CARTESIAN_POINT('Ctrl Pts',(-5.4,-2.04997459329993,-17.17432433516)) ;
#139144 = CARTESIAN_POINT('Ctrl Pts',(-5.4,-2.1118797455067,-17.1923423130261)) ;
#139145 = CARTESIAN_POINT('Ctrl Pts',(-5.33978950165956,-2.00789652656154,
-17.1921350349804)) ;
#139146 = CARTESIAN_POINT('Ctrl Pts',(-5.4,-2.02908601268745,-17.2086334854683)) ;
#139147 = CARTESIAN_POINT('Ctrl Pts',(-5.4,-2.087770056524,-17.244338787364)) ;
#139148 = CARTESIAN_POINT('Ctrl Pts',(-5.32318090226695,-1.95817527052251,
-17.2292155027319)) ;
#139149 = CARTESIAN_POINT('Ctrl Pts',(-5.4,-1.96527310172481,-17.2478366162471)) ;
#139150 = CARTESIAN_POINT('Ctrl Pts',(-5.4,-2.00485091174287,-17.3185039251107)) ;
#139151 = CARTESIAN_POINT('Ctrl Pts',(-5.31153957531164,-1.92331224822996,
-17.2400135323111)) ;
#139152 = CARTESIAN_POINT('Ctrl Pts',(-5.4,-1.9214867694528,-17.2510221074624)) ;
#139153 = CARTESIAN_POINT('Ctrl Pts',(-5.4,-1.94671708614657,-17.3400682869718)) ;
#139154 = CARTESIAN_POINT('Ctrl Pts',(-5.29976814257746,-1.88802911972918,
-17.2400001726222)) ;
#139155 = CARTESIAN_POINT('Ctrl Pts',(-5.4,-1.88802831720455,-17.239767406457)) ;
#139156 = CARTESIAN_POINT('Ctrl Pts',(-5.4,-1.88791746283071,-17.3399998375376)) ;
#139157 = CARTESIAN_POINT('Origin',(-5.30000000000006,-1.8881966011252,-17.1400000000001)) ;
#139158 = CARTESIAN_POINT('Origin',(-4.66204490261456,3.21928058320648,-17.14)) ;
#139159 = CARTESIAN_POINT('Origin',(-4.66204490261456,3.21928058320648,-17.14)) ;
#139160 = CARTESIAN_POINT('Origin',(0.175392621986784,-0.95,-14.5224847282359)) ;
#139161 = CARTESIAN_POINT('Origin',(-3.37639320225,-0.95,-13.6542704156447)) ;
#139162 = CARTESIAN_POINT('Origin',(-3.32804538583365,-0.902219294041845,
-13.6660887707687)) ;
#139163 = CARTESIAN_POINT('Origin',(-3.46583592134999,-0.971114561800017,
-13.6324066398647)) ;
#139164 = CARTESIAN_POINT('Origin',(-3.24472135955,-0.860557280900019,-17.14)) ;
#139165 = CARTESIAN_POINT('Origin',(-4.66204490261456,-1.5692190524323,-17.14)) ;
#139166 = CARTESIAN_POINT('Origin',(-4.66204490261456,1.95,-17.14)) ;
#139167 = CARTESIAN_POINT('Origin',(-4.66204490261456,-1.5692190524323,-17.14)) ;
#139168 = CARTESIAN_POINT('Ctrl Pts',(-3.4211145618,-1.06055728090001,-13.6324066398647)) ;
#139169 = CARTESIAN_POINT('Ctrl Pts',(-3.40394191641935,-1.05197095820969,
-13.5445919759864)) ;
#139170 = CARTESIAN_POINT('Ctrl Pts',(-3.44209061230229,-0.971114561800017,
-13.535266739215)) ;
#139171 = CARTESIAN_POINT('Ctrl Pts',(-3.40727897628737,-1.05363948814369,
-13.6391707039916)) ;
#139172 = CARTESIAN_POINT('Ctrl Pts',(-3.38665319245543,-1.04670310838585,
-13.5488181085109)) ;
#139173 = CARTESIAN_POINT('Ctrl Pts',(-3.4144159452097,-0.957277229261619,
-13.5420316578376)) ;
#139174 = CARTESIAN_POINT('Ctrl Pts',(-3.39186274464429,-1.05,-13.6467075282519)) ;
#139175 = CARTESIAN_POINT('Ctrl Pts',(-3.36870744055528,-1.04639008266731,
-13.5532048478642)) ;
#139176 = CARTESIAN_POINT('Ctrl Pts',(-3.38358960366098,-0.950000000886305,
-13.5495669857718)) ;
#139177 = CARTESIAN_POINT('Ctrl Pts',(-3.37639320225,-1.05,-13.6542704156447)) ;
#139178 = CARTESIAN_POINT('Ctrl Pts',(-3.3526478932023,-1.05,-13.557130514995)) ;
#139179 = CARTESIAN_POINT('Ctrl Pts',(-3.3526478932023,-0.95,-13.557130514995)) ;
#139180 = CARTESIAN_POINT('Origin',(-3.37639320224937,-1.1500000000029,-13.654270415645)) ;
#139181 = CARTESIAN_POINT('Origin',(-4.66204490261456,-1.5692190524323,-17.14)) ;
#139182 = CARTESIAN_POINT('Origin',(-4.66204490261456,-1.5692190524323,-17.14)) ;
#139183 = CARTESIAN_POINT('Origin',(-3.37639320225,-1.15,-15.24)) ;
#139184 = CARTESIAN_POINT('Origin',(-3.37639320225038,-1.14999999999817,-16.8257295843555)) ;
#139185 = CARTESIAN_POINT('Origin',(-1.50751564693271,0.00804557540861825,
-16.3688928486111)) ;
#139186 = CARTESIAN_POINT('Origin',(-3.46583592134999,-0.971114561800017,
-16.8475933601353)) ;
#139187 = CARTESIAN_POINT('Ctrl Pts',(-3.37639320225,-1.05,-16.8257295843553)) ;
#139188 = CARTESIAN_POINT('Ctrl Pts',(-3.3526478932023,-1.05,-16.922869485005)) ;
#139189 = CARTESIAN_POINT('Ctrl Pts',(-3.3526478932023,-0.95,-16.922869485005)) ;
#139190 = CARTESIAN_POINT('Ctrl Pts',(-3.39186274464434,-1.05,-16.833292471748)) ;
#139191 = CARTESIAN_POINT('Ctrl Pts',(-3.36870744055529,-1.04639008266723,
-16.9267951521356)) ;
#139192 = CARTESIAN_POINT('Ctrl Pts',(-3.38358960366097,-0.950000000886305,
-16.9304330142282)) ;
#139193 = CARTESIAN_POINT('Ctrl Pts',(-3.40727897628736,-1.05363948814369,
-16.8408292960084)) ;
#139194 = CARTESIAN_POINT('Ctrl Pts',(-3.3866531924555,-1.04670310838586,
-16.931181891489)) ;
#139195 = CARTESIAN_POINT('Ctrl Pts',(-3.4144159452097,-0.957277229261615,
-16.9379683421624)) ;
#139196 = CARTESIAN_POINT('Ctrl Pts',(-3.4211145618,-1.06055728090001,-16.8475933601353)) ;
#139197 = CARTESIAN_POINT('Ctrl Pts',(-3.40394191641935,-1.05197095820969,
-16.9354080240136)) ;
#139198 = CARTESIAN_POINT('Ctrl Pts',(-3.44209061230229,-0.971114561800017,
-16.944733260785)) ;
#139199 = CARTESIAN_POINT('Origin',(-3.37639320225,-0.95,-16.8257295843553)) ;
#139200 = CARTESIAN_POINT('Origin',(0.175392621986784,-0.95,-15.9575152717641)) ;
#139201 = CARTESIAN_POINT('Origin',(12.8,2.65,-16.7330460421716)) ;
#139202 = CARTESIAN_POINT('',(4.57524318173533,2.73534903669982,-16.6809351802097)) ;
#139203 = CARTESIAN_POINT('Origin',(4.65232986200977,2.66527023614941,-16.7287542111863)) ;
#139204 = CARTESIAN_POINT('Ctrl Pts',(4.57524318173533,2.73534903669982,-16.6809351802097)) ;
#139205 = CARTESIAN_POINT('Ctrl Pts',(4.5761458558036,2.73452842391049,-16.6795911511832)) ;
#139206 = CARTESIAN_POINT('Ctrl Pts',(4.57705238626145,2.73367683201793,-16.6782681293393)) ;
#139207 = CARTESIAN_POINT('Ctrl Pts',(4.5779495181309,2.73280244902548,-16.6769768488888)) ;
#139208 = CARTESIAN_POINT('Ctrl Pts',(4.58144263576934,2.7293979075554,-16.6719490545685)) ;
#139209 = CARTESIAN_POINT('Ctrl Pts',(4.58496694799982,2.72549786515183,-16.6671699445179)) ;
#139210 = CARTESIAN_POINT('Ctrl Pts',(4.58815670056902,2.72107165565054,-16.6626981938528)) ;
#139211 = CARTESIAN_POINT('Ctrl Pts',(4.59069123847472,2.71755464437262,-16.6591449961298)) ;
#139212 = CARTESIAN_POINT('Ctrl Pts',(4.59301454561853,2.71370459823908,-16.6557863127242)) ;
#139213 = CARTESIAN_POINT('Ctrl Pts',(4.5949431309995,2.70950205848695,-16.6526749961674)) ;
#139214 = CARTESIAN_POINT('Ctrl Pts',(4.59651854606294,2.7060691047295,-16.6501334364215)) ;
#139215 = CARTESIAN_POINT('Ctrl Pts',(4.59783685868319,2.70233705077427,-16.6477160861571)) ;
#139216 = CARTESIAN_POINT('Ctrl Pts',(4.59873118971422,2.69838744820002,-16.6455323012123)) ;
#139217 = CARTESIAN_POINT('Ctrl Pts',(4.59916508318197,2.6964712597891,-16.6444728165364)) ;
#139218 = CARTESIAN_POINT('Ctrl Pts',(4.59949917984822,2.6945044443219,-16.643467798882)) ;
#139219 = CARTESIAN_POINT('Ctrl Pts',(4.5997144226265,2.692499226592,-16.6425263440994)) ;
#139220 = CARTESIAN_POINT('Ctrl Pts',(4.59990113259977,2.69075982259552,-16.6417096895352)) ;
#139221 = CARTESIAN_POINT('Ctrl Pts',(4.6,2.68896788689974,-16.6409303122145)) ;
#139222 = CARTESIAN_POINT('Ctrl Pts',(4.6,2.68715716172261,-16.6402056127633)) ;
#139223 = CARTESIAN_POINT('Origin',(4.5,2.1,-16.6219539578284)) ;
#139224 = CARTESIAN_POINT('Origin',(4.6,2.1,-16.6219539578284)) ;
#139225 = CARTESIAN_POINT('Origin',(12.7,2.1,-16.6219539578284)) ;
#139226 = CARTESIAN_POINT('Origin',(12.7,2.76643989873054,-16.7136393923832)) ;
#139227 = CARTESIAN_POINT('Origin',(12.7,2.13287979746107,-16.8192327425948)) ;
#139228 = CARTESIAN_POINT('Origin',(4.4,2.72431432344521,-15.24)) ;
#139229 = CARTESIAN_POINT('Ctrl Pts',(4.48762159086959,2.77250619842349,-13.8511756817495)) ;
#139230 = CARTESIAN_POINT('Ctrl Pts',(4.48806820038223,2.77169418112776,-13.8538355670898)) ;
#139231 = CARTESIAN_POINT('Ctrl Pts',(4.48852084821546,2.77084293101113,-13.8564827150185)) ;
#139232 = CARTESIAN_POINT('Ctrl Pts',(4.49012932137854,2.76769877392856,-13.8657630095207)) ;
#139233 = CARTESIAN_POINT('Ctrl Pts',(4.49131046584974,2.76517764467229,-13.8723441317034)) ;
#139234 = CARTESIAN_POINT('Ctrl Pts',(4.49351977821776,2.75978760391033,-13.884635280162)) ;
#139235 = CARTESIAN_POINT('Ctrl Pts',(4.49455195297827,2.75697653750127,-13.8903677406013)) ;
#139236 = CARTESIAN_POINT('Ctrl Pts',(4.49620670090465,2.75163165728875,-13.8999433216032)) ;
#139237 = CARTESIAN_POINT('Ctrl Pts',(4.49686252944492,2.74924176842724,-13.9038640262033)) ;
#139238 = CARTESIAN_POINT('Ctrl Pts',(4.49822764032848,2.74331716058958,-13.9126446316346)) ;
#139239 = CARTESIAN_POINT('Ctrl Pts',(4.49890203357901,2.73961076902724,-13.9174865001603)) ;
#139240 = CARTESIAN_POINT('Ctrl Pts',(4.49975897856021,2.73206576252701,-13.9258277784396)) ;
#139241 = CARTESIAN_POINT('Ctrl Pts',(4.5,2.72833175948628,-13.9294190022917)) ;
#139242 = CARTESIAN_POINT('Ctrl Pts',(4.5,2.72431432344521,-13.932634816645)) ;
#139243 = CARTESIAN_POINT('Ctrl Pts',(4.5,2.72431432344521,-16.547365183355)) ;
#139244 = CARTESIAN_POINT('Ctrl Pts',(4.5,2.72904669151416,-16.5511532753135)) ;
#139245 = CARTESIAN_POINT('Ctrl Pts',(4.49966645684475,2.73338556955534,-16.5554614101758)) ;
#139246 = CARTESIAN_POINT('Ctrl Pts',(4.49869539480397,2.74072289096356,-16.5639802414372)) ;
#139247 = CARTESIAN_POINT('Ctrl Pts',(4.49811062025689,2.74382502998075,-16.5681080596585)) ;
#139248 = CARTESIAN_POINT('Ctrl Pts',(4.49664125196625,2.75020211699685,-16.5775592649405)) ;
#139249 = CARTESIAN_POINT('Ctrl Pts',(4.49570721389712,2.75339870015137,-16.5830103903193)) ;
#139250 = CARTESIAN_POINT('Ctrl Pts',(4.49363760641479,2.75952863263942,-16.5947517051868)) ;
#139251 = CARTESIAN_POINT('Ctrl Pts',(4.49249077386345,2.76240287369066,-16.6010712258307)) ;
#139252 = CARTESIAN_POINT('Ctrl Pts',(4.49055019898874,2.76677757270134,-16.6119141256208)) ;
#139253 = CARTESIAN_POINT('Ctrl Pts',(4.48975662823144,2.76842729450632,-16.6163872919226)) ;
#139254 = CARTESIAN_POINT('Ctrl Pts',(4.4885208482156,2.77084293101086,-16.6235172849807)) ;
#139255 = CARTESIAN_POINT('Ctrl Pts',(4.48806820038251,2.77169418112725,-16.6261644329085)) ;
#139256 = CARTESIAN_POINT('Ctrl Pts',(4.48762159086959,2.77250619842348,-16.6288243182478)) ;
#139257 = CARTESIAN_POINT('Origin',(4.6,2.1,-15.24)) ;
#139258 = CARTESIAN_POINT('Origin',(4.6,2.1,-13.8580460421716)) ;
#139259 = CARTESIAN_POINT('Origin',(4.6,2.1,-16.6219539578284)) ;
#139260 = CARTESIAN_POINT('Origin',(12.7,2.1,-16.6219539578284)) ;
#139261 = CARTESIAN_POINT('Origin',(12.7,1.9,-16.6219539578284)) ;
#139262 = CARTESIAN_POINT('Origin',(12.7,2.65,-12.7)) ;
#139263 = CARTESIAN_POINT('Origin',(4.5,2.65,-13.7469539578284)) ;
#139264 = CARTESIAN_POINT('',(4.6,2.68715716172261,-13.8397943872367)) ;
#139265 = CARTESIAN_POINT('',(4.57524318173443,2.73534903670064,-13.7990648197889)) ;
#139266 = CARTESIAN_POINT('Ctrl Pts',(4.6,2.68715716172261,-13.8397943872367)) ;
#139267 = CARTESIAN_POINT('Ctrl Pts',(4.6,2.69106036671411,-13.8382322227785)) ;
#139268 = CARTESIAN_POINT('Ctrl Pts',(4.59952510519174,2.69488861888981,-13.8364097094748)) ;
#139269 = CARTESIAN_POINT('Ctrl Pts',(4.59869497748257,2.6985274364076,-13.8343901512251)) ;
#139270 = CARTESIAN_POINT('Ctrl Pts',(4.59815316003466,2.70090246232122,-13.8330720023612)) ;
#139271 = CARTESIAN_POINT('Ctrl Pts',(4.5974600110878,2.70319720658043,-13.8316709680453)) ;
#139272 = CARTESIAN_POINT('Ctrl Pts',(4.59664880273703,2.70538659711789,-13.8302145418985)) ;
#139273 = CARTESIAN_POINT('Ctrl Pts',(4.59612777291939,2.70679281754375,-13.8292790960924)) ;
#139274 = CARTESIAN_POINT('Ctrl Pts',(4.59555051815356,2.70817855133088,-13.8283049299072)) ;
#139275 = CARTESIAN_POINT('Ctrl Pts',(4.59494172533681,2.7095051214937,-13.8273227360698)) ;
#139276 = CARTESIAN_POINT('Ctrl Pts',(4.59250947890868,2.71480502887001,-13.8233986794992)) ;
#139277 = CARTESIAN_POINT('Ctrl Pts',(4.58944857813008,2.71954517005227,-13.8190823375811)) ;
#139278 = CARTESIAN_POINT('Ctrl Pts',(4.5861276864684,2.72376361218884,-13.8144738031841)) ;
#139279 = CARTESIAN_POINT('Ctrl Pts',(4.58350334758194,2.72709724148698,-13.8108319029778)) ;
#139280 = CARTESIAN_POINT('Ctrl Pts',(4.58071664514672,2.73010548898765,-13.8070059959317)) ;
#139281 = CARTESIAN_POINT('Ctrl Pts',(4.5779495181309,2.73280244902546,-13.8030231511112)) ;
#139282 = CARTESIAN_POINT('Ctrl Pts',(4.57705238626115,2.7336768320182,-13.8017318706603)) ;
#139283 = CARTESIAN_POINT('Ctrl Pts',(4.576145855803,2.73452842391107,-13.8004088488159)) ;
#139284 = CARTESIAN_POINT('Ctrl Pts',(4.57524318173444,2.73534903670067,-13.7990648197889)) ;
#139285 = CARTESIAN_POINT('Origin',(4.65232986201396,2.66527023614562,-13.7512457888124)) ;
#139286 = CARTESIAN_POINT('Origin',(4.6,2.65,-13.7469539578284)) ;
#139287 = CARTESIAN_POINT('Origin',(12.7,1.9,-16.74)) ;
#139288 = CARTESIAN_POINT('Origin',(12.7,2.01643989873054,-13.6413606076168)) ;
#139289 = CARTESIAN_POINT('Origin',(-3.65,10.7,-14.49)) ;
#139290 = CARTESIAN_POINT('Origin',(-3.65,10.7,-14.49)) ;
#139291 = CARTESIAN_POINT('Origin',(-3.65,10.7,-14.49)) ;
#139292 = CARTESIAN_POINT('Origin',(0.,10.7,-14.49)) ;
#139293 = CARTESIAN_POINT('Origin',(-2.9,10.7,-14.49)) ;
#139294 = CARTESIAN_POINT('Origin',(-3.65,10.7,-15.24)) ;
#139295 = CARTESIAN_POINT('Origin',(-3.65,10.7,-15.99)) ;
#139296 = CARTESIAN_POINT('Origin',(-2.9,10.7,-14.49)) ;
#139297 = CARTESIAN_POINT('Origin',(-2.9,10.7,-14.49)) ;
#139298 = CARTESIAN_POINT('Origin',(-3.65,10.7,-15.99)) ;
#139299 = CARTESIAN_POINT('Origin',(-3.65,10.7,-15.99)) ;
#139300 = CARTESIAN_POINT('Origin',(-2.9,10.7,-15.24)) ;
#139301 = CARTESIAN_POINT('Origin',(-2.9,10.7,-15.99)) ;
#139302 = CARTESIAN_POINT('Origin',(0.,10.7,-15.99)) ;
#139303 = CARTESIAN_POINT('Origin',(-2.9,10.7,-15.99)) ;
#139304 = CARTESIAN_POINT('Origin',(-2.9,10.7,-15.99)) ;
#139305 = CARTESIAN_POINT('Origin',(-3.05,-3.95,-14.24)) ;
#139306 = CARTESIAN_POINT('Origin',(-3.05,-3.95,-16.14)) ;
#139307 = CARTESIAN_POINT('Origin',(-3.05,-3.95,-14.34)) ;
#139308 = CARTESIAN_POINT('Origin',(-3.25,-3.95,-14.34)) ;
#139309 = CARTESIAN_POINT('Origin',(-3.25,-3.95,-14.14)) ;
#139310 = CARTESIAN_POINT('Origin',(-3.25,-3.95,-14.34)) ;
#139311 = CARTESIAN_POINT('Origin',(-3.25,-3.95,-16.14)) ;
#139312 = CARTESIAN_POINT('Origin',(-3.25,-3.95,-16.14)) ;
#139313 = CARTESIAN_POINT('Origin',(-3.25,-3.95,-16.34)) ;
#139314 = CARTESIAN_POINT('Origin',(-4.4,-3.95,-14.14)) ;
#139315 = CARTESIAN_POINT('Origin',(-4.3,-3.95,-14.14)) ;
#139316 = CARTESIAN_POINT('Origin',(-3.25,-3.9,-14.34)) ;
#139317 = CARTESIAN_POINT('Origin',(-3.25,-3.85,-14.34)) ;
#139318 = CARTESIAN_POINT('Origin',(-3.25,-3.85,-15.24)) ;
#139319 = CARTESIAN_POINT('Origin',(-3.25,-3.85,-16.14)) ;
#139320 = CARTESIAN_POINT('Origin',(-3.25,-3.85,-14.34)) ;
#139321 = CARTESIAN_POINT('Origin',(-3.25,-3.9,-16.14)) ;
#139322 = CARTESIAN_POINT('Origin',(-3.25,-3.85,-16.14)) ;
#139323 = CARTESIAN_POINT('Origin',(-4.4,-3.95,-16.34)) ;
#139324 = CARTESIAN_POINT('Origin',(-4.3,-3.95,-16.34)) ;
#139325 = CARTESIAN_POINT('Origin',(-4.5,-3.95,-14.24)) ;
#139326 = CARTESIAN_POINT('Origin',(-4.5,-3.95,-14.34)) ;
#139327 = CARTESIAN_POINT('Origin',(-4.5,-3.95,-16.14)) ;
#139328 = CARTESIAN_POINT('Origin',(-4.3,-3.95,-14.34)) ;
#139329 = CARTESIAN_POINT('Origin',(-4.3,-3.95,-14.34)) ;
#139330 = CARTESIAN_POINT('Origin',(-3.25,-3.85,-14.34)) ;
#139331 = CARTESIAN_POINT('Origin',(-3.25,-3.85,-14.34)) ;
#139332 = CARTESIAN_POINT('Origin',(-3.25,-3.85,-16.14)) ;
#139333 = CARTESIAN_POINT('Origin',(-3.25,-3.85,-16.14)) ;
#139334 = CARTESIAN_POINT('Origin',(-4.3,-3.95,-16.14)) ;
#139335 = CARTESIAN_POINT('Origin',(-4.3,-3.95,-16.14)) ;
#139336 = CARTESIAN_POINT('Origin',(-4.3,-3.9,-14.34)) ;
#139337 = CARTESIAN_POINT('Origin',(-4.3,-3.85,-14.34)) ;
#139338 = CARTESIAN_POINT('Origin',(-1.56125112837913E-16,-3.85,-14.34)) ;
#139339 = CARTESIAN_POINT('Origin',(-4.3,-3.85,-14.34)) ;
#139340 = CARTESIAN_POINT('Origin',(-1.56125112837913E-16,-3.85,-16.14)) ;
#139341 = CARTESIAN_POINT('Origin',(-4.3,-3.85,-16.14)) ;
#139342 = CARTESIAN_POINT('Origin',(-4.3,-3.9,-16.14)) ;
#139343 = CARTESIAN_POINT('Origin',(-4.3,-3.85,-16.14)) ;
#139344 = CARTESIAN_POINT('Origin',(-4.3,-3.85,-14.34)) ;
#139345 = CARTESIAN_POINT('Origin',(-4.3,-3.85,-14.34)) ;
#139346 = CARTESIAN_POINT('Origin',(-4.3,-3.85,-16.14)) ;
#139347 = CARTESIAN_POINT('Origin',(-4.3,-3.85,-16.14)) ;
#139348 = CARTESIAN_POINT('Origin',(-4.3,-3.85,-15.24)) ;
#139349 = CARTESIAN_POINT('Origin',(-4.,10.85,-16.24)) ;
#139350 = CARTESIAN_POINT('Origin',(-4.,10.85,-16.14)) ;
#139351 = CARTESIAN_POINT('Origin',(-4.,10.85,-14.34)) ;
#139352 = CARTESIAN_POINT('Origin',(-3.8,10.85,-14.34)) ;
#139353 = CARTESIAN_POINT('Origin',(-3.8,10.85,-14.14)) ;
#139354 = CARTESIAN_POINT('Origin',(-3.8,10.85,-14.34)) ;
#139355 = CARTESIAN_POINT('Origin',(-3.8,10.85,-16.14)) ;
#139356 = CARTESIAN_POINT('Origin',(-3.8,10.85,-16.14)) ;
#139357 = CARTESIAN_POINT('Origin',(-3.8,10.85,-16.34)) ;
#139358 = CARTESIAN_POINT('Origin',(-3.9,10.85,-14.14)) ;
#139359 = CARTESIAN_POINT('Origin',(-2.75,10.85,-14.14)) ;
#139360 = CARTESIAN_POINT('Origin',(-3.8,10.8,-14.34)) ;
#139361 = CARTESIAN_POINT('Origin',(-3.8,10.75,-14.34)) ;
#139362 = CARTESIAN_POINT('Origin',(-3.8,10.75,-15.24)) ;
#139363 = CARTESIAN_POINT('Origin',(-3.8,10.75,-16.14)) ;
#139364 = CARTESIAN_POINT('Origin',(-3.8,10.75,-14.34)) ;
#139365 = CARTESIAN_POINT('Origin',(-3.8,10.8,-16.14)) ;
#139366 = CARTESIAN_POINT('Origin',(-3.8,10.75,-16.14)) ;
#139367 = CARTESIAN_POINT('Origin',(-3.9,10.85,-16.34)) ;
#139368 = CARTESIAN_POINT('Origin',(-2.75,10.85,-16.34)) ;
#139369 = CARTESIAN_POINT('Origin',(-2.55,10.85,-16.24)) ;
#139370 = CARTESIAN_POINT('Origin',(-2.55,10.85,-14.34)) ;
#139371 = CARTESIAN_POINT('Origin',(-2.55,10.85,-16.14)) ;
#139372 = CARTESIAN_POINT('Origin',(-2.75,10.85,-14.34)) ;
#139373 = CARTESIAN_POINT('Origin',(-2.75,10.85,-14.34)) ;
#139374 = CARTESIAN_POINT('Origin',(-3.8,10.75,-14.34)) ;
#139375 = CARTESIAN_POINT('Origin',(-3.8,10.75,-14.34)) ;
#139376 = CARTESIAN_POINT('Origin',(-3.8,10.75,-16.14)) ;
#139377 = CARTESIAN_POINT('Origin',(-3.8,10.75,-16.14)) ;
#139378 = CARTESIAN_POINT('Origin',(-2.75,10.85,-16.14)) ;
#139379 = CARTESIAN_POINT('Origin',(-2.75,10.85,-16.14)) ;
#139380 = CARTESIAN_POINT('Origin',(-2.75,10.8,-14.34)) ;
#139381 = CARTESIAN_POINT('Origin',(-2.75,10.75,-14.34)) ;
#139382 = CARTESIAN_POINT('Origin',(1.56125112837912E-16,10.75,-14.34)) ;
#139383 = CARTESIAN_POINT('Origin',(-2.75,10.75,-14.34)) ;
#139384 = CARTESIAN_POINT('Origin',(-1.56125112837913E-16,10.75,-16.14)) ;
#139385 = CARTESIAN_POINT('Origin',(-2.75,10.75,-16.14)) ;
#139386 = CARTESIAN_POINT('Origin',(-2.75,10.8,-16.14)) ;
#139387 = CARTESIAN_POINT('Origin',(-2.75,10.75,-16.14)) ;
#139388 = CARTESIAN_POINT('Origin',(-2.75,10.75,-14.34)) ;
#139389 = CARTESIAN_POINT('Origin',(-2.75,10.75,-14.34)) ;
#139390 = CARTESIAN_POINT('Origin',(-2.75,10.75,-16.14)) ;
#139391 = CARTESIAN_POINT('Origin',(-2.75,10.75,-16.14)) ;
#139392 = CARTESIAN_POINT('Origin',(-2.75,10.75,-15.24)) ;
#139393 = CARTESIAN_POINT('Origin',(4.6,0.,-15.24)) ;
#139394 = CARTESIAN_POINT('Ctrl Pts',(4.5,-2.7,-13.7168453788272)) ;
#139395 = CARTESIAN_POINT('Ctrl Pts',(4.5,-2.71827986285823,-13.7919647391751)) ;
#139396 = CARTESIAN_POINT('Ctrl Pts',(4.50597963419107,-2.73556801027185,
-13.8667398604528)) ;
#139397 = CARTESIAN_POINT('Ctrl Pts',(4.52394923367545,-2.75977758633329,
-13.9784368340216)) ;
#139398 = CARTESIAN_POINT('Ctrl Pts',(4.53141024883993,-2.76757607569523,
-14.0156832823903)) ;
#139399 = CARTESIAN_POINT('Ctrl Pts',(4.54734065524867,-2.77857284247615,
-14.070165689583)) ;
#139400 = CARTESIAN_POINT('Ctrl Pts',(4.55339248498575,-2.78214991573955,
-14.0882382744149)) ;
#139401 = CARTESIAN_POINT('Ctrl Pts',(4.56567492147096,-2.787183259287,-14.1141467218607)) ;
#139402 = CARTESIAN_POINT('Ctrl Pts',(4.5702469143305,-2.78880341224556,-14.1225726050508)) ;
#139403 = CARTESIAN_POINT('Ctrl Pts',(4.58215938980081,-2.79169669265294,
-14.1377434798851)) ;
#139404 = CARTESIAN_POINT('Ctrl Pts',(4.59005470866978,-2.79310344827587,
-14.1452063540423)) ;
#139405 = CARTESIAN_POINT('Ctrl Pts',(4.6,-2.79310344827586,-14.1452063540422)) ;
#139406 = CARTESIAN_POINT('Origin',(4.6,-2.4,-13.2778583129651)) ;
#139407 = CARTESIAN_POINT('Origin',(4.6,-2.4,-12.7)) ;
#139408 = CARTESIAN_POINT('Origin',(4.6,-2.4,-13.2778583129651)) ;
#139409 = CARTESIAN_POINT('Origin',(4.6,-2.4,-13.2778583129651)) ;
#139410 = CARTESIAN_POINT('Origin',(4.6,-2.4,-13.2778583129651)) ;
#139411 = CARTESIAN_POINT('Origin',(0.584645609909622,-2.4,-13.2778583129651)) ;
#139412 = CARTESIAN_POINT('Origin',(12.7,-2.4,-13.2778583129651)) ;
#139413 = CARTESIAN_POINT('Origin',(12.7,-2.2,-12.7)) ;
#139414 = CARTESIAN_POINT('Origin',(12.7,-2.2,-13.2778583129651)) ;
#139415 = CARTESIAN_POINT('Origin',(12.7,-2.4,-13.2778583129651)) ;
#139416 = CARTESIAN_POINT('Origin',(12.7,-2.24516129032258,-13.4044480992255)) ;
#139417 = CARTESIAN_POINT('Origin',(12.7,0.,-15.24)) ;
#139418 = CARTESIAN_POINT('Origin',(12.7,-2.24516129032258,-17.0755519007745)) ;
#139419 = CARTESIAN_POINT('Origin',(12.7,-2.4,-17.2021416870349)) ;
#139420 = CARTESIAN_POINT('Origin',(12.7,-2.4,-17.2021416870349)) ;
#139421 = CARTESIAN_POINT('Origin',(0.584645609909622,-2.4,-17.2021416870349)) ;
#139422 = CARTESIAN_POINT('Origin',(4.6,-2.4,-17.2021416870349)) ;
#139423 = CARTESIAN_POINT('Origin',(4.6,-2.4,-17.2021416870349)) ;
#139424 = CARTESIAN_POINT('Origin',(4.6,-2.4,-17.2021416870349)) ;
#139425 = CARTESIAN_POINT('Origin',(4.6,0.,-15.24)) ;
#139426 = CARTESIAN_POINT('Ctrl Pts',(4.6,-2.79310344827586,-16.3347936459578)) ;
#139427 = CARTESIAN_POINT('Ctrl Pts',(4.59007568892311,-2.79310344827586,
-16.3347936459578)) ;
#139428 = CARTESIAN_POINT('Ctrl Pts',(4.58219207637239,-2.79170232102183,
-16.342226742276)) ;
#139429 = CARTESIAN_POINT('Ctrl Pts',(4.57028631514659,-2.78881527838255,
-16.35736543899)) ;
#139430 = CARTESIAN_POINT('Ctrl Pts',(4.56571532154372,-2.78719767797524,
-16.3657784885835)) ;
#139431 = CARTESIAN_POINT('Ctrl Pts',(4.55343865632726,-2.78217307830036,
-16.3916436333089)) ;
#139432 = CARTESIAN_POINT('Ctrl Pts',(4.54738888873344,-2.77860151743012,
-16.4096900859661)) ;
#139433 = CARTESIAN_POINT('Ctrl Pts',(4.53146440752602,-2.76762263748299,
-16.4640903156831)) ;
#139434 = CARTESIAN_POINT('Ctrl Pts',(4.52400917967609,-2.75984503873828,
-16.5012455063058)) ;
#139435 = CARTESIAN_POINT('Ctrl Pts',(4.50599905604505,-2.7356206423885,-16.6130301354693)) ;
#139436 = CARTESIAN_POINT('Ctrl Pts',(4.5,-2.71826422026483,-16.6880995425769)) ;
#139437 = CARTESIAN_POINT('Ctrl Pts',(4.5,-2.7,-16.7631546211728)) ;
#139438 = CARTESIAN_POINT('Origin',(-0.362523114814661,9.05,-15.4090473046963)) ;
#139439 = CARTESIAN_POINT('Origin',(0.36252311481466,9.05,-15.0709526953037)) ;
#139440 = CARTESIAN_POINT('Origin',(-1.31845674202095,9.85,-13.8322813422351)) ;
#139441 = CARTESIAN_POINT('Origin',(-0.230887397576972,9.85,-13.3251394281462)) ;
#139442 = CARTESIAN_POINT('Origin',(4.6,2.1,-13.8580460421716)) ;
#139443 = CARTESIAN_POINT('Origin',(4.6,2.1,-13.8580460421716)) ;
#139444 = CARTESIAN_POINT('Origin',(4.6,0.280857398566761,-13.5548556085994)) ;
#139445 = CARTESIAN_POINT('Origin',(4.6,2.61712020253893,-13.9442327425948)) ;
#139446 = CARTESIAN_POINT('Origin',(4.6,2.65,-13.7469539578284)) ;
#139447 = CARTESIAN_POINT('Origin',(4.6,2.72431432344521,-13.932634816645)) ;
#139448 = CARTESIAN_POINT('Ctrl Pts',(4.48762159086906,2.77250619842445,-13.8511756817496)) ;
#139449 = CARTESIAN_POINT('Ctrl Pts',(4.51316716229104,2.72605970493114,-13.8142387941972)) ;
#139450 = CARTESIAN_POINT('Ctrl Pts',(4.57527453405851,2.73535372386122,-13.799057153198)) ;
#139451 = CARTESIAN_POINT('Ctrl Pts',(4.49363662433154,2.76156977394749,-13.8869995924717)) ;
#139452 = CARTESIAN_POINT('Ctrl Pts',(4.5146945995807,2.70766535161857,-13.8362008473933)) ;
#139453 = CARTESIAN_POINT('Ctrl Pts',(4.58732693581886,2.72440392220679,-13.816995041234)) ;
#139454 = CARTESIAN_POINT('Ctrl Pts',(4.5,2.74488438438029,-13.9161692160662)) ;
#139455 = CARTESIAN_POINT('Ctrl Pts',(4.50856472873622,2.69031482079682,-13.8384911137046)) ;
#139456 = CARTESIAN_POINT('Ctrl Pts',(4.60003980620506,2.7077507326983,-13.8315523113747)) ;
#139457 = CARTESIAN_POINT('Ctrl Pts',(4.5,2.72431432344521,-13.932634816645)) ;
#139458 = CARTESIAN_POINT('Ctrl Pts',(4.5,2.68714136424468,-13.8397549158517)) ;
#139459 = CARTESIAN_POINT('Ctrl Pts',(4.60004250625997,2.68715716507935,-13.8397943956238)) ;
#139460 = CARTESIAN_POINT('Origin',(4.57524318173443,2.82069807340128,-13.8511756817495)) ;
#139461 = CARTESIAN_POINT('Ctrl Pts',(4.47150553123747,2.80180812502279,-13.7469539578284)) ;
#139462 = CARTESIAN_POINT('Ctrl Pts',(4.5,2.75,-13.7469539578284)) ;
#139463 = CARTESIAN_POINT('Ctrl Pts',(4.55912712210514,2.75,-13.7469539578284)) ;
#139464 = CARTESIAN_POINT('Ctrl Pts',(4.47150553186688,2.8018081238784,-13.7835744727347)) ;
#139465 = CARTESIAN_POINT('Ctrl Pts',(4.50000000073523,2.74999999866316,-13.7712580842688)) ;
#139466 = CARTESIAN_POINT('Ctrl Pts',(4.5591271227348,2.75,-13.7652720457593)) ;
#139467 = CARTESIAN_POINT('Ctrl Pts',(4.4771244897161,2.79159183687982,-13.8199165373523)) ;
#139468 = CARTESIAN_POINT('Ctrl Pts',(4.50480340096853,2.74126654369358,-13.795537950998)) ;
#139469 = CARTESIAN_POINT('Ctrl Pts',(4.56473907811163,2.74489822224648,-13.7834248215822)) ;
#139470 = CARTESIAN_POINT('Ctrl Pts',(4.48762159086676,2.77250619842407,-13.8511756817495)) ;
#139471 = CARTESIAN_POINT('Ctrl Pts',(4.51315802400618,2.72607631998876,-13.8142520074343)) ;
#139472 = CARTESIAN_POINT('Ctrl Pts',(4.57524318173443,2.73534903670064,-13.7990648197889)) ;
#139473 = CARTESIAN_POINT('Origin',(4.55912712210513,2.85,-13.7469539578284)) ;
#139474 = CARTESIAN_POINT('Origin',(4.55912712210514,2.85,-12.7)) ;
#139475 = CARTESIAN_POINT('Ctrl Pts',(4.48762159086766,2.77250619842243,-16.6288243182478)) ;
#139476 = CARTESIAN_POINT('Ctrl Pts',(4.51315802400691,2.72607631998744,-16.6657479925641)) ;
#139477 = CARTESIAN_POINT('Ctrl Pts',(4.57524318173533,2.73534903669982,-16.6809351802097)) ;
#139478 = CARTESIAN_POINT('Ctrl Pts',(4.47712448971643,2.79159183687922,-16.6600834626457)) ;
#139479 = CARTESIAN_POINT('Ctrl Pts',(4.50480340096884,2.74126654369303,-16.6844620490007)) ;
#139480 = CARTESIAN_POINT('Ctrl Pts',(4.56473907811196,2.74489822224618,-16.6965751784167)) ;
#139481 = CARTESIAN_POINT('Ctrl Pts',(4.47150553186688,2.8018081238784,-16.6964255272642)) ;
#139482 = CARTESIAN_POINT('Ctrl Pts',(4.50000000073523,2.74999999866316,-16.7087419157305)) ;
#139483 = CARTESIAN_POINT('Ctrl Pts',(4.5591271227348,2.75,-16.7147279542401)) ;
#139484 = CARTESIAN_POINT('Ctrl Pts',(4.47150553123747,2.80180812502279,-16.7330460421716)) ;
#139485 = CARTESIAN_POINT('Ctrl Pts',(4.5,2.75,-16.7330460421716)) ;
#139486 = CARTESIAN_POINT('Ctrl Pts',(4.55912712210513,2.75,-16.7330460421716)) ;
#139487 = CARTESIAN_POINT('Origin',(4.57524318173533,2.82069807339964,-16.6288243182478)) ;
#139488 = CARTESIAN_POINT('Ctrl Pts',(4.57527448145479,2.73535371598842,-16.6809428339419)) ;
#139489 = CARTESIAN_POINT('Ctrl Pts',(4.51316714695683,2.7260597328105,-16.6657611836292)) ;
#139490 = CARTESIAN_POINT('Ctrl Pts',(4.48762159086951,2.77250619842363,-16.6288243182477)) ;
#139491 = CARTESIAN_POINT('Ctrl Pts',(4.5873268774263,2.72440390874888,-16.6630049433246)) ;
#139492 = CARTESIAN_POINT('Ctrl Pts',(4.5146945862635,2.7076653857066,-16.6437991204817)) ;
#139493 = CARTESIAN_POINT('Ctrl Pts',(4.49363662433185,2.76156977394669,-16.5930004075269)) ;
#139494 = CARTESIAN_POINT('Ctrl Pts',(4.60003973844309,2.70775071978185,-16.648447683485)) ;
#139495 = CARTESIAN_POINT('Ctrl Pts',(4.50856472285798,2.69031485824816,-16.6415088329841)) ;
#139496 = CARTESIAN_POINT('Ctrl Pts',(4.5,2.74488438437978,-16.5638307839333)) ;
#139497 = CARTESIAN_POINT('Ctrl Pts',(4.60004243494351,2.6871571650681,-16.6402056044043)) ;
#139498 = CARTESIAN_POINT('Ctrl Pts',(4.5,2.68714139075511,-16.6402450179097)) ;
#139499 = CARTESIAN_POINT('Ctrl Pts',(4.5,2.72431432344521,-16.547365183355)) ;
#139500 = CARTESIAN_POINT('Origin',(4.6,0.280857398566761,-16.9251443914006)) ;
#139501 = CARTESIAN_POINT('Origin',(4.6,2.1,-16.6219539578284)) ;
#139502 = CARTESIAN_POINT('Origin',(4.6,2.1,-16.6219539578284)) ;
#139503 = CARTESIAN_POINT('Origin',(4.6,0.,-15.24)) ;
#139504 = CARTESIAN_POINT('',(4.5,-2.9,-15.2400000000038)) ;
#139505 = CARTESIAN_POINT('',(4.57439618084313,-2.80937499999937,-16.2827958671254)) ;
#139506 = CARTESIAN_POINT('Ctrl Pts',(4.5,-2.9,-15.2400000000038)) ;
#139507 = CARTESIAN_POINT('Ctrl Pts',(4.5,-2.9000000234111,-15.4161762625703)) ;
#139508 = CARTESIAN_POINT('Ctrl Pts',(4.49893459747296,-2.89187728142186,
-15.5922938225552)) ;
#139509 = CARTESIAN_POINT('Ctrl Pts',(4.50498172725087,-2.86839426105774,
-15.8549432768872)) ;
#139510 = CARTESIAN_POINT('Ctrl Pts',(4.50826226558342,-2.85869729223562,
-15.9422870271135)) ;
#139511 = CARTESIAN_POINT('Ctrl Pts',(4.52028413974051,-2.84160518746962,
-16.0728409654328)) ;
#139512 = CARTESIAN_POINT('Ctrl Pts',(4.52545003690602,-2.8354696349403,-16.116363113622)) ;
#139513 = CARTESIAN_POINT('Ctrl Pts',(4.53741870680498,-2.82581179679252,
-16.1806394550107)) ;
#139514 = CARTESIAN_POINT('Ctrl Pts',(4.54209540184575,-2.82251395224859,
-16.2019200182606)) ;
#139515 = CARTESIAN_POINT('Ctrl Pts',(4.55451190949429,-2.81582803324483,
-16.2438742105328)) ;
#139516 = CARTESIAN_POINT('Ctrl Pts',(4.56139306411848,-2.8124020390272,-16.2647435318249)) ;
#139517 = CARTESIAN_POINT('Ctrl Pts',(4.57439618084313,-2.80937499999937,
-16.2827958671254)) ;
#139518 = CARTESIAN_POINT('Ctrl Pts',(4.57439618084313,-2.80937499999939,
-16.2827958671254)) ;
#139519 = CARTESIAN_POINT('Ctrl Pts',(4.5778881172051,-2.80856205104936,-16.2876438845913)) ;
#139520 = CARTESIAN_POINT('Ctrl Pts',(4.58132110715662,-2.80743849592505,
-16.2926543114197)) ;
#139521 = CARTESIAN_POINT('Ctrl Pts',(4.58591063786559,-2.80541025280315,
-16.3000683491598)) ;
#139522 = CARTESIAN_POINT('Ctrl Pts',(4.58721694730497,-2.80476695238161,
-16.3022683250837)) ;
#139523 = CARTESIAN_POINT('Ctrl Pts',(4.5887449802686,-2.80393035430392,-16.3049717146409)) ;
#139524 = CARTESIAN_POINT('Ctrl Pts',(4.58900094431508,-2.80378708879839,
-16.305429423373)) ;
#139525 = CARTESIAN_POINT('Ctrl Pts',(4.58924476828968,-2.80364801935069,
-16.30586949326)) ;
#139526 = CARTESIAN_POINT('Ctrl Pts',(4.58924931741448,-2.80364542371033,
-16.3058777053493)) ;
#139527 = CARTESIAN_POINT('Ctrl Pts',(4.59158188358133,-2.80231401319274,
-16.3100892401221)) ;
#139528 = CARTESIAN_POINT('Ctrl Pts',(4.59377134212491,-2.80081309849101,
-16.3144383923964)) ;
#139529 = CARTESIAN_POINT('Ctrl Pts',(4.59570408210449,-2.79909049146272,
-16.3191378632085)) ;
#139530 = CARTESIAN_POINT('Ctrl Pts',(4.5957084873849,-2.79908656285629,-16.3191485795779)) ;
#139531 = CARTESIAN_POINT('Ctrl Pts',(4.59603576097762,-2.79879453264352,
-16.3199450754362)) ;
#139532 = CARTESIAN_POINT('Ctrl Pts',(4.59633794834607,-2.79851279959495,
-16.3207065253189)) ;
#139533 = CARTESIAN_POINT('Ctrl Pts',(4.59727216584803,-2.79759800070515,
-16.32316063341)) ;
#139534 = CARTESIAN_POINT('Ctrl Pts',(4.59785661125443,-2.79695684051616,
-16.3248529156094)) ;
#139535 = CARTESIAN_POINT('Ctrl Pts',(4.59875882816121,-2.7958009226755,-16.3278683242216)) ;
#139536 = CARTESIAN_POINT('Ctrl Pts',(4.59910960512327,-2.79529211440566,
-16.3291844992176)) ;
#139537 = CARTESIAN_POINT('Ctrl Pts',(4.59950074890552,-2.79458032370895,
-16.3310150784121)) ;
#139538 = CARTESIAN_POINT('Ctrl Pts',(4.59959271145697,-2.79439474074567,
-16.3314948405808)) ;
#139539 = CARTESIAN_POINT('Ctrl Pts',(4.59970479219924,-2.79411978912795,
-16.3322025710462)) ;
#139540 = CARTESIAN_POINT('Ctrl Pts',(4.59973686334512,-2.79403231884248,
-16.3324272684452)) ;
#139541 = CARTESIAN_POINT('Ctrl Pts',(4.59980956306601,-2.7938042827674,-16.3330108264021)) ;
#139542 = CARTESIAN_POINT('Ctrl Pts',(4.59984405921136,-2.79366555090847,
-16.3333689790042)) ;
#139543 = CARTESIAN_POINT('Ctrl Pts',(4.59992170638736,-2.79338632637294,
-16.3340824135446)) ;
#139544 = CARTESIAN_POINT('Ctrl Pts',(4.59995882625634,-2.79324305250058,
-16.3344374792565)) ;
#139545 = CARTESIAN_POINT('Ctrl Pts',(4.59999999999999,-2.79310344827586,
-16.3347936459578)) ;
#139546 = CARTESIAN_POINT('',(4.57439618084271,-2.80937499999947,-14.1972041328751)) ;
#139547 = CARTESIAN_POINT('Ctrl Pts',(4.59999999999999,-2.79310344827586,
-14.1452063540422)) ;
#139548 = CARTESIAN_POINT('Ctrl Pts',(4.59995895305209,-2.79324111387631,
-14.1455620070442)) ;
#139549 = CARTESIAN_POINT('Ctrl Pts',(4.59992125133673,-2.79338175512528,
-14.1459166499952)) ;
#139550 = CARTESIAN_POINT('Ctrl Pts',(4.59984242179761,-2.79365985893298,
-14.1466272182547)) ;
#139551 = CARTESIAN_POINT('Ctrl Pts',(4.5998070294299,-2.79379858543765,-14.146981904003)) ;
#139552 = CARTESIAN_POINT('Ctrl Pts',(4.59973261548695,-2.79401893257626,
-14.1475458212796)) ;
#139553 = CARTESIAN_POINT('Ctrl Pts',(4.59970092564442,-2.7941005010842,-14.1477547044526)) ;
#139554 = CARTESIAN_POINT('Ctrl Pts',(4.59958060815602,-2.79437456977472,
-14.1484570742577)) ;
#139555 = CARTESIAN_POINT('Ctrl Pts',(4.59947821517875,-2.79456857658396,
-14.1489550953807)) ;
#139556 = CARTESIAN_POINT('Ctrl Pts',(4.5990597198479,-2.79527981802028,-14.1507850643885)) ;
#139557 = CARTESIAN_POINT('Ctrl Pts',(4.59869396429225,-2.79579226918928,
-14.1521114012001)) ;
#139558 = CARTESIAN_POINT('Ctrl Pts',(4.59768320083749,-2.79706868650734,
-14.1554440738933)) ;
#139559 = CARTESIAN_POINT('Ctrl Pts',(4.59698254015873,-2.79783590182173,
-14.1574731996627)) ;
#139560 = CARTESIAN_POINT('Ctrl Pts',(4.59599705225881,-2.79876532988112,
-14.1599846842385)) ;
#139561 = CARTESIAN_POINT('Ctrl Pts',(4.59580678362762,-2.7989396411024,-14.1604581050039)) ;
#139562 = CARTESIAN_POINT('Ctrl Pts',(4.59367882781299,-2.80083904916685,
-14.1656449119971)) ;
#139563 = CARTESIAN_POINT('Ctrl Pts',(4.59150707087691,-2.80233337893514,
-14.1699793277041)) ;
#139564 = CARTESIAN_POINT('Ctrl Pts',(4.58628071719236,-2.80532570224271,
-14.1794514674292)) ;
#139565 = CARTESIAN_POINT('Ctrl Pts',(4.58313959595708,-2.8067311076741,-14.1845102480658)) ;
#139566 = CARTESIAN_POINT('Ctrl Pts',(4.57802611146331,-2.80844040952816,
-14.1920963574918)) ;
#139567 = CARTESIAN_POINT('Ctrl Pts',(4.57624387811645,-2.80894486836997,
-14.1946389593417)) ;
#139568 = CARTESIAN_POINT('Ctrl Pts',(4.57439618084271,-2.80937499999947,
-14.1972041328751)) ;
#139569 = CARTESIAN_POINT('Ctrl Pts',(4.57439618084271,-2.80937499999947,
-14.1972041328751)) ;
#139570 = CARTESIAN_POINT('Ctrl Pts',(4.56149777794589,-2.81237766235467,
-14.2151110931668)) ;
#139571 = CARTESIAN_POINT('Ctrl Pts',(4.55451596106519,-2.81582788236477,
-14.2361262422968)) ;
#139572 = CARTESIAN_POINT('Ctrl Pts',(4.54213610452188,-2.82249001163036,
-14.2779283596283)) ;
#139573 = CARTESIAN_POINT('Ctrl Pts',(4.53742891479326,-2.82580422498964,
-14.299310967236)) ;
#139574 = CARTESIAN_POINT('Ctrl Pts',(4.525451614243,-2.8354670333868,-14.3636179437949)) ;
#139575 = CARTESIAN_POINT('Ctrl Pts',(4.52032009146395,-2.84156292603926,
-14.4068565734785)) ;
#139576 = CARTESIAN_POINT('Ctrl Pts',(4.50830110904356,-2.85862448221642,
-14.5371164259574)) ;
#139577 = CARTESIAN_POINT('Ctrl Pts',(4.50499166750953,-2.86836219567853,
-14.6247300385823)) ;
#139578 = CARTESIAN_POINT('Ctrl Pts',(4.49892845988062,-2.8918880660271,-14.8877629968379)) ;
#139579 = CARTESIAN_POINT('Ctrl Pts',(4.49999999999475,-2.89999999999869,
-15.0638300901178)) ;
#139580 = CARTESIAN_POINT('Ctrl Pts',(4.5,-2.9,-15.2400000000038)) ;
#139581 = CARTESIAN_POINT('Origin',(4.4,-2.7,-12.7)) ;
#139582 = CARTESIAN_POINT('Origin',(4.4,-2.7,-13.7168453788272)) ;
#139583 = CARTESIAN_POINT('Ctrl Pts',(4.40227435089074,-2.79999990867355,
-13.6494006928819)) ;
#139584 = CARTESIAN_POINT('Ctrl Pts',(4.51828879250226,-2.80015667527379,
-13.6587855667925)) ;
#139585 = CARTESIAN_POINT('Ctrl Pts',(4.50118227077259,-2.68533700727772,
-13.6579711074494)) ;
#139586 = CARTESIAN_POINT('Ctrl Pts',(4.39419482113926,-2.79999992837382,
-13.7636876996691)) ;
#139587 = CARTESIAN_POINT('Ctrl Pts',(4.48571792501723,-2.80010751836584,
-13.7426713667506)) ;
#139588 = CARTESIAN_POINT('Ctrl Pts',(4.49717570077252,-2.71006921719248,
-13.7570318982145)) ;
#139589 = CARTESIAN_POINT('Ctrl Pts',(4.40636790575269,-2.79999994706265,
-13.8749089073543)) ;
#139590 = CARTESIAN_POINT('Ctrl Pts',(4.47481046024546,-2.80007242131914,
-13.8533224277991)) ;
#139591 = CARTESIAN_POINT('Ctrl Pts',(4.503281318764,-2.73353293829095,-13.85702587481)) ;
#139592 = CARTESIAN_POINT('Ctrl Pts',(4.4547973699423,-2.79999997092221,-14.0250736654711)) ;
#139593 = CARTESIAN_POINT('Ctrl Pts',(4.49869786247046,-2.80003603117402,
-14.0062792434958)) ;
#139594 = CARTESIAN_POINT('Ctrl Pts',(4.52748687875414,-2.76348976047509,
-13.9962891728587)) ;
#139595 = CARTESIAN_POINT('Ctrl Pts',(4.47221929614096,-2.79999997745988,
-14.0673040602233)) ;
#139596 = CARTESIAN_POINT('Ctrl Pts',(4.50880556767621,-2.80002725736477,
-14.0482748482858)) ;
#139597 = CARTESIAN_POINT('Ctrl Pts',(4.53619137795527,-2.77169834185704,
-14.0359836823676)) ;
#139598 = CARTESIAN_POINT('Ctrl Pts',(4.50882352800136,-2.79999998605361,
-14.1242843496091)) ;
#139599 = CARTESIAN_POINT('Ctrl Pts',(4.53367802911268,-2.80001636071785,
-14.1053587024204)) ;
#139600 = CARTESIAN_POINT('Ctrl Pts',(4.55447319025662,-2.78248861123826,
-14.0900956814255)) ;
#139601 = CARTESIAN_POINT('Ctrl Pts',(4.52308919141484,-2.79999998878206,
-14.1426625616911)) ;
#139602 = CARTESIAN_POINT('Ctrl Pts',(4.54363962638622,-2.80001303821803,
-14.1237261501717)) ;
#139603 = CARTESIAN_POINT('Ctrl Pts',(4.56159739427507,-2.78591449131413,
-14.1076542708947)) ;
#139604 = CARTESIAN_POINT('Ctrl Pts',(4.57467506176495,-2.79999999510246,
-14.1856965083993)) ;
#139605 = CARTESIAN_POINT('Ctrl Pts',(4.5806240530329,-2.80000557393877,-14.1663341632778)) ;
#139606 = CARTESIAN_POINT('Ctrl Pts',(4.58735613403293,-2.79385049254303,
-14.1489198149933)) ;
#139607 = CARTESIAN_POINT('Ctrl Pts',(4.62437069655636,-2.79999999703807,
-14.1995313430601)) ;
#139608 = CARTESIAN_POINT('Ctrl Pts',(4.61827372661888,-2.80000334969057,
-14.1809340454876)) ;
#139609 = CARTESIAN_POINT('Ctrl Pts',(4.61212682540743,-2.79628090446622,
-14.1624028142182)) ;
#139610 = CARTESIAN_POINT('Ctrl Pts',(4.67161368302037,-2.79999998860619,
-14.1407898267653)) ;
#139611 = CARTESIAN_POINT('Ctrl Pts',(4.6540701010264,-2.80001325705921,-14.1204637395888)) ;
#139612 = CARTESIAN_POINT('Ctrl Pts',(4.63587130780614,-2.78569367459188,
-14.1056281295941)) ;
#139613 = CARTESIAN_POINT('Ctrl Pts',(4.54879236204369,-2.8,-14.1635655563675)) ;
#139614 = CARTESIAN_POINT('Ctrl Pts',(4.55448837802385,-2.7999999999815,-14.1611788209137)) ;
#139615 = CARTESIAN_POINT('Ctrl Pts',(4.56021842726587,-2.79959150783241,
-14.1588395427342)) ;
#139616 = CARTESIAN_POINT('Ctrl Pts',(4.56730671984965,-2.79865167182178,
-14.1559788838636)) ;
#139617 = CARTESIAN_POINT('Ctrl Pts',(4.5684777095826,-2.79848295770259,-14.1555073268348)) ;
#139618 = CARTESIAN_POINT('Ctrl Pts',(4.57107523099021,-2.79808046368154,
-14.154462962897)) ;
#139619 = CARTESIAN_POINT('Ctrl Pts',(4.5725009361248,-2.79784058543152,-14.153889643028)) ;
#139620 = CARTESIAN_POINT('Ctrl Pts',(4.5764383594612,-2.79713266293194,-14.1523136864649)) ;
#139621 = CARTESIAN_POINT('Ctrl Pts',(4.57879956048961,-2.79666132938901,
-14.1513758003969)) ;
#139622 = CARTESIAN_POINT('Ctrl Pts',(4.58293855712952,-2.79579586318667,
-14.1497608159296)) ;
#139623 = CARTESIAN_POINT('Ctrl Pts',(4.58471363403686,-2.79540911153441,
-14.1490746171912)) ;
#139624 = CARTESIAN_POINT('Ctrl Pts',(4.58699082729421,-2.7949269768198,-14.148244529262)) ;
#139625 = CARTESIAN_POINT('Ctrl Pts',(4.58739952300692,-2.79484234870239,
-14.1481019268464)) ;
#139626 = CARTESIAN_POINT('Ctrl Pts',(4.58871515235475,-2.79457617288697,
-14.1476611291009)) ;
#139627 = CARTESIAN_POINT('Ctrl Pts',(4.58961690596118,-2.79440247805564,
-14.1473849869996)) ;
#139628 = CARTESIAN_POINT('Ctrl Pts',(4.5910537506584,-2.79414748185769,-14.146982981818)) ;
#139629 = CARTESIAN_POINT('Ctrl Pts',(4.59155303909532,-2.79406229662444,
-14.1468492435071)) ;
#139630 = CARTESIAN_POINT('Ctrl Pts',(4.59245965385665,-2.79391282221553,
-14.1466125941148)) ;
#139631 = CARTESIAN_POINT('Ctrl Pts',(4.59286388425101,-2.79384761399903,
-14.1465084217845)) ;
#139632 = CARTESIAN_POINT('Ctrl Pts',(4.59368973959976,-2.79370598615372,
-14.1462676726517)) ;
#139633 = CARTESIAN_POINT('Ctrl Pts',(4.59407665941116,-2.79363973714593,
-14.1461515212332)) ;
#139634 = CARTESIAN_POINT('Ctrl Pts',(4.59444371287726,-2.79357284110656,
-14.1460267927279)) ;
#139635 = CARTESIAN_POINT('Ctrl Pts',(4.59448890259156,-2.79356452972317,
-14.1460111581995)) ;
#139636 = CARTESIAN_POINT('Ctrl Pts',(4.5947084233491,-2.79352377141065,-14.1459338254522)) ;
#139637 = CARTESIAN_POINT('Ctrl Pts',(4.59483598733268,-2.79349361011835,
-14.1458723314841)) ;
#139638 = CARTESIAN_POINT('Ctrl Pts',(4.59514620525223,-2.79342971313629,
-14.1457459400492)) ;
#139639 = CARTESIAN_POINT('Ctrl Pts',(4.59533334275102,-2.79339696908415,
-14.1456838378534)) ;
#139640 = CARTESIAN_POINT('Ctrl Pts',(4.59563785533348,-2.79335634095568,
-14.1456129903403)) ;
#139641 = CARTESIAN_POINT('Ctrl Pts',(4.59571710962763,-2.79334654412181,
-14.1455963912877)) ;
#139642 = CARTESIAN_POINT('Ctrl Pts',(4.59594411915585,-2.79332043135007,
-14.1455533496182)) ;
#139643 = CARTESIAN_POINT('Ctrl Pts',(4.59600288191152,-2.79330503361987,
-14.1455339512408)) ;
#139644 = CARTESIAN_POINT('Ctrl Pts',(4.59613307952173,-2.79327450473786,
-14.1454992805194)) ;
#139645 = CARTESIAN_POINT('Ctrl Pts',(4.59620389659311,-2.79325970788819,
-14.1454850060586)) ;
#139646 = CARTESIAN_POINT('Ctrl Pts',(4.59651192984771,-2.79322709231927,
-14.1454502778629)) ;
#139647 = CARTESIAN_POINT('Ctrl Pts',(4.59679543741296,-2.79320989448354,
-14.1454293441824)) ;
#139648 = CARTESIAN_POINT('Ctrl Pts',(4.59784475938524,-2.793166495242,-14.1453578835066)) ;
#139649 = CARTESIAN_POINT('Ctrl Pts',(4.5987491506478,-2.79313948637392,-14.1452992643108)) ;
#139650 = CARTESIAN_POINT('Ctrl Pts',(4.59999999999999,-2.79310344827586,
-14.1452063540422)) ;
#139651 = CARTESIAN_POINT('Ctrl Pts',(4.5011795914298,-2.68531903459914,-16.8220290201724)) ;
#139652 = CARTESIAN_POINT('Ctrl Pts',(4.51828670358959,-2.8,-16.8212138251408)) ;
#139653 = CARTESIAN_POINT('Ctrl Pts',(4.4024095222558,-2.8,-16.8305883721109)) ;
#139654 = CARTESIAN_POINT('Ctrl Pts',(4.49717774927194,-2.71005310920082,
-16.7229655323624)) ;
#139655 = CARTESIAN_POINT('Ctrl Pts',(4.4857462854107,-2.8,-16.7373148520403)) ;
#139656 = CARTESIAN_POINT('Ctrl Pts',(4.39431668173578,-2.8,-16.7163402695083)) ;
#139657 = CARTESIAN_POINT('Ctrl Pts',(4.5032869068519,-2.73351987602557,-16.6229733978621)) ;
#139658 = CARTESIAN_POINT('Ctrl Pts',(4.47485145549547,-2.8,-16.6266766957416)) ;
#139659 = CARTESIAN_POINT('Ctrl Pts',(4.40646789472124,-2.8,-16.6051226186384)) ;
#139660 = CARTESIAN_POINT('Ctrl Pts',(4.52749311797092,-2.76348183928883,
-16.4837129921594)) ;
#139661 = CARTESIAN_POINT('Ctrl Pts',(4.49873206155793,-2.8,-16.4737330953069)) ;
#139662 = CARTESIAN_POINT('Ctrl Pts',(4.4548681704377,-2.8,-16.4549566433661)) ;
#139663 = CARTESIAN_POINT('Ctrl Pts',(4.53619745972496,-2.77169205010104,
-16.4440190471853)) ;
#139664 = CARTESIAN_POINT('Ctrl Pts',(4.50883664816671,-2.8,-16.4317394381723)) ;
#139665 = CARTESIAN_POINT('Ctrl Pts',(4.47227975612143,-2.8,-16.4127273846038)) ;
#139666 = CARTESIAN_POINT('Ctrl Pts',(4.55447795090011,-2.78248459830341,
-16.3899078127333)) ;
#139667 = CARTESIAN_POINT('Ctrl Pts',(4.53370055749884,-2.8,-16.3746579183699)) ;
#139668 = CARTESIAN_POINT('Ctrl Pts',(4.50886586566856,-2.8,-16.3557478882722)) ;
#139669 = CARTESIAN_POINT('Ctrl Pts',(4.56160154376425,-2.78591123334062,
-16.3723494428157)) ;
#139670 = CARTESIAN_POINT('Ctrl Pts',(4.54365878772218,-2.8,-16.3562910664543)) ;
#139671 = CARTESIAN_POINT('Ctrl Pts',(4.52312452397685,-2.8,-16.3373699954867)) ;
#139672 = CARTESIAN_POINT('Ctrl Pts',(4.58735772267362,-2.79384903998488,
-16.3310842943985)) ;
#139673 = CARTESIAN_POINT('Ctrl Pts',(4.58063087367386,-2.8,-16.3136839633808)) ;
#139674 = CARTESIAN_POINT('Ctrl Pts',(4.57468550767191,-2.8,-16.2943374866056)) ;
#139675 = CARTESIAN_POINT('Ctrl Pts',(4.61212536563479,-2.79628002040276,
-16.3176015865955)) ;
#139676 = CARTESIAN_POINT('Ctrl Pts',(4.61826745782994,-2.80000000000002,
-16.2990848793757)) ;
#139677 = CARTESIAN_POINT('Ctrl Pts',(4.62435992349573,-2.8,-16.2805015173211)) ;
#139678 = CARTESIAN_POINT('Ctrl Pts',(4.63586710715927,-2.78569036914665,
-16.3743752946751)) ;
#139679 = CARTESIAN_POINT('Ctrl Pts',(4.6540510694572,-2.79999999999994,-16.3595525238841)) ;
#139680 = CARTESIAN_POINT('Ctrl Pts',(4.67158355065736,-2.8,-16.3392450797819)) ;
#139681 = CARTESIAN_POINT('Ctrl Pts',(4.59999999999999,-2.79310344827586,
-16.3347936459578)) ;
#139682 = CARTESIAN_POINT('Ctrl Pts',(4.59840954578222,-2.79314968944988,
-16.3346756726912)) ;
#139683 = CARTESIAN_POINT('Ctrl Pts',(4.59737383489099,-2.7931815960622,-16.3346133239717)) ;
#139684 = CARTESIAN_POINT('Ctrl Pts',(4.59650507521656,-2.79322931786012,
-16.33455037726)) ;
#139685 = CARTESIAN_POINT('Ctrl Pts',(4.59632758424309,-2.79324472590582,
-16.3345345791767)) ;
#139686 = CARTESIAN_POINT('Ctrl Pts',(4.5961184721085,-2.79327477162036,-16.3345047565773)) ;
#139687 = CARTESIAN_POINT('Ctrl Pts',(4.5960648950493,-2.79328892979786,-16.3344910265853)) ;
#139688 = CARTESIAN_POINT('Ctrl Pts',(4.59594601677698,-2.79331605564258,
-16.334459114495)) ;
#139689 = CARTESIAN_POINT('Ctrl Pts',(4.59588597444861,-2.7933285533825,-16.3344426561835)) ;
#139690 = CARTESIAN_POINT('Ctrl Pts',(4.59549967474365,-2.79337285752324,
-16.3343702787606)) ;
#139691 = CARTESIAN_POINT('Ctrl Pts',(4.59527331486238,-2.7934062238596,-16.3343100807083)) ;
#139692 = CARTESIAN_POINT('Ctrl Pts',(4.5949320123953,-2.79346950514991,-16.3341870402937)) ;
#139693 = CARTESIAN_POINT('Ctrl Pts',(4.59480393230128,-2.79349821606423,
-16.334128474279)) ;
#139694 = CARTESIAN_POINT('Ctrl Pts',(4.59460326813595,-2.79353924388982,
-16.3340476351491)) ;
#139695 = CARTESIAN_POINT('Ctrl Pts',(4.59455075953096,-2.79354963432651,
-16.3340274276715)) ;
#139696 = CARTESIAN_POINT('Ctrl Pts',(4.59417008680875,-2.79361944405452,
-16.3338955937176)) ;
#139697 = CARTESIAN_POINT('Ctrl Pts',(4.59377742096551,-2.79368602572532,
-16.3337773461555)) ;
#139698 = CARTESIAN_POINT('Ctrl Pts',(4.59289939109635,-2.7938335466559,-16.3335254190241)) ;
#139699 = CARTESIAN_POINT('Ctrl Pts',(4.59245006584786,-2.79390305456781,
-16.333416036199)) ;
#139700 = CARTESIAN_POINT('Ctrl Pts',(4.59099552519247,-2.79413629528603,
-16.3330568524094)) ;
#139701 = CARTESIAN_POINT('Ctrl Pts',(4.59002197881598,-2.79430302757313,
-16.332806370176)) ;
#139702 = CARTESIAN_POINT('Ctrl Pts',(4.58861122644696,-2.79456793455697,
-16.3323921365669)) ;
#139703 = CARTESIAN_POINT('Ctrl Pts',(4.58817904894409,-2.79465210327451,
-16.3322585234305)) ;
#139704 = CARTESIAN_POINT('Ctrl Pts',(4.58736872283366,-2.79481449815582,
-16.3319941835896)) ;
#139705 = CARTESIAN_POINT('Ctrl Pts',(4.58699491219416,-2.79489135860974,
-16.3318665823581)) ;
#139706 = CARTESIAN_POINT('Ctrl Pts',(4.58468897497187,-2.79537899446708,
-16.3310351906196)) ;
#139707 = CARTESIAN_POINT('Ctrl Pts',(4.58290717718701,-2.79577019617636,
-16.3303420642284)) ;
#139708 = CARTESIAN_POINT('Ctrl Pts',(4.57867627871774,-2.79666451416567,
-16.3286707882875)) ;
#139709 = CARTESIAN_POINT('Ctrl Pts',(4.5762632155413,-2.79715040843617,-16.3276877651429)) ;
#139710 = CARTESIAN_POINT('Ctrl Pts',(4.57243386308705,-2.79784156172336,
-16.3261367865103)) ;
#139711 = CARTESIAN_POINT('Ctrl Pts',(4.57107519984216,-2.79807176647234,
-16.325584021445)) ;
#139712 = CARTESIAN_POINT('Ctrl Pts',(4.56513452430521,-2.79900074294384,
-16.3231693903582)) ;
#139713 = CARTESIAN_POINT('Ctrl Pts',(4.56062162665837,-2.79951267011368,
-16.3213309293498)) ;
#139714 = CARTESIAN_POINT('Ctrl Pts',(4.5536542059673,-2.79992470862864,-16.3184610302787)) ;
#139715 = CARTESIAN_POINT('Ctrl Pts',(4.55124660967315,-2.79999983267432,
-16.3174632392509)) ;
#139716 = CARTESIAN_POINT('Ctrl Pts',(4.54880051362942,-2.79999999972164,
-16.3164378607329)) ;
#139717 = CARTESIAN_POINT('Ctrl Pts',(4.54879236166274,-2.8,-14.1635655565152)) ;
#139718 = CARTESIAN_POINT('Ctrl Pts',(4.5622387183224,-2.79999999999679,-14.1812315262749)) ;
#139719 = CARTESIAN_POINT('Ctrl Pts',(4.57442182196495,-2.80939476060286,
-14.1972378204668)) ;
#139720 = CARTESIAN_POINT('Ctrl Pts',(4.555568425176,-2.79999999999889,-14.1607250640488)) ;
#139721 = CARTESIAN_POINT('Ctrl Pts',(4.56783337210912,-2.80040661803736,
-14.1761863015518)) ;
#139722 = CARTESIAN_POINT('Ctrl Pts',(4.57961823522365,-2.80818164104597,
-14.1900183413273)) ;
#139723 = CARTESIAN_POINT('Ctrl Pts',(4.56238982831618,-2.7994260255176,-14.1579528515171)) ;
#139724 = CARTESIAN_POINT('Ctrl Pts',(4.5735781038818,-2.80014618986471,-14.1709310721412)) ;
#139725 = CARTESIAN_POINT('Ctrl Pts',(4.58462643299473,-2.80630261261111,
-14.1825232711649)) ;
#139726 = CARTESIAN_POINT('Ctrl Pts',(4.57328757735258,-2.7977370397245,-14.1535699979501)) ;
#139727 = CARTESIAN_POINT('Ctrl Pts',(4.58237922839515,-2.79856394574987,
-14.1622664089314)) ;
#139728 = CARTESIAN_POINT('Ctrl Pts',(4.59151541127591,-2.80237286596199,
-14.1700830028806)) ;
#139729 = CARTESIAN_POINT('Ctrl Pts',(4.57700059755674,-2.7970371466716,-14.152076076342)) ;
#139730 = CARTESIAN_POINT('Ctrl Pts',(4.58532305318674,-2.79784352093717,
-14.1592625430044)) ;
#139731 = CARTESIAN_POINT('Ctrl Pts',(4.59370961102545,-2.80088045369937,
-14.1657455141894)) ;
#139732 = CARTESIAN_POINT('Ctrl Pts',(4.58319893207066,-2.79574016930783,
-14.1496546705211)) ;
#139733 = CARTESIAN_POINT('Ctrl Pts',(4.5899041610924,-2.79637293360539,-14.1543303545622)) ;
#139734 = CARTESIAN_POINT('Ctrl Pts',(4.59665800356694,-2.79825577077759,
-14.1585819448697)) ;
#139735 = CARTESIAN_POINT('Ctrl Pts',(4.58534994317985,-2.79526732601294,
-14.1488188618872)) ;
#139736 = CARTESIAN_POINT('Ctrl Pts',(4.59144552977843,-2.79581844972913,
-14.1526200366107)) ;
#139737 = CARTESIAN_POINT('Ctrl Pts',(4.59758018705035,-2.79731769672696,
-14.1560885803939)) ;
#139738 = CARTESIAN_POINT('Ctrl Pts',(4.58899927751307,-2.79450268149332,
-14.1475173012671)) ;
#139739 = CARTESIAN_POINT('Ctrl Pts',(4.59386223202755,-2.79488630507105,
-14.1499495170303)) ;
#139740 = CARTESIAN_POINT('Ctrl Pts',(4.59874684688641,-2.79582009356912,
-14.1521813652447)) ;
#139741 = CARTESIAN_POINT('Ctrl Pts',(4.59026755692867,-2.79423885380164,
-14.14707439958)) ;
#139742 = CARTESIAN_POINT('Ctrl Pts',(4.5946770606831,-2.79455862385202,-14.149040543336)) ;
#139743 = CARTESIAN_POINT('Ctrl Pts',(4.59910266898802,-2.79530499526365,
-14.1508486399022)) ;
#139744 = CARTESIAN_POINT('Ctrl Pts',(4.59257623319511,-2.79382131826659,
-14.14638413145)) ;
#139745 = CARTESIAN_POINT('Ctrl Pts',(4.59605751036343,-2.79403163929513,
-14.1476227610336)) ;
#139746 = CARTESIAN_POINT('Ctrl Pts',(4.59954701072604,-2.79449510806573,
-14.148765766817)) ;
#139747 = CARTESIAN_POINT('Ctrl Pts',(4.593429769333,-2.79367543507711,-14.1461445374534)) ;
#139748 = CARTESIAN_POINT('Ctrl Pts',(4.59655016100495,-2.79384713427256,
-14.1471348895303)) ;
#139749 = CARTESIAN_POINT('Ctrl Pts',(4.59967640178298,-2.79421605292373,
-14.148050213937)) ;
#139750 = CARTESIAN_POINT('Ctrl Pts',(4.59428414179641,-2.79346156087783,
-14.1457069361853)) ;
#139751 = CARTESIAN_POINT('Ctrl Pts',(4.59704519451433,-2.79355469746529,
-14.146373635748)) ;
#139752 = CARTESIAN_POINT('Ctrl Pts',(4.5998104157401,-2.79379877456676,-14.1469823712707)) ;
#139753 = CARTESIAN_POINT('Ctrl Pts',(4.59432658472652,-2.7933916625364,-14.1455338181495)) ;
#139754 = CARTESIAN_POINT('Ctrl Pts',(4.59708408719785,-2.79345234504014,
-14.1461090766463)) ;
#139755 = CARTESIAN_POINT('Ctrl Pts',(4.59984563524625,-2.79366003518351,
-14.1466276543527)) ;
#139756 = CARTESIAN_POINT('Ctrl Pts',(4.59537197237732,-2.79324260992761,
-14.1452872615939)) ;
#139757 = CARTESIAN_POINT('Ctrl Pts',(4.59764722167536,-2.79326383513928,
-14.145620961855)) ;
#139758 = CARTESIAN_POINT('Ctrl Pts',(4.59992475053754,-2.79338190759658,
-14.1459170306476)) ;
#139759 = CARTESIAN_POINT('Ctrl Pts',(4.59364183392371,-2.79313407032025,
-14.1452844788451)) ;
#139760 = CARTESIAN_POINT('Ctrl Pts',(4.59684754854894,-2.79327107597598,
-14.1456389310452)) ;
#139761 = CARTESIAN_POINT('Ctrl Pts',(4.59996664298755,-2.79324102308607,
-14.1455617736815)) ;
#139762 = CARTESIAN_POINT('Ctrl Pts',(4.59999999999999,-2.79310344827586,
-14.1452063540422)) ;
#139763 = CARTESIAN_POINT('Ctrl Pts',(4.59999999999999,-2.79310344827586,
-14.1452063540422)) ;
#139764 = CARTESIAN_POINT('Ctrl Pts',(4.59999999999999,-2.79310344827586,
-14.1452063540422)) ;
#139765 = CARTESIAN_POINT('Origin',(4.54879236168542,-2.9,-14.1635655565161)) ;
#139766 = CARTESIAN_POINT('Ctrl Pts',(4.39959973407451,-2.8,-15.3505922428027)) ;
#139767 = CARTESIAN_POINT('Ctrl Pts',(4.49922290141874,-2.8,-15.3501052483316)) ;
#139768 = CARTESIAN_POINT('Ctrl Pts',(4.49980764094185,-2.8996950427637,-15.3506080458952)) ;
#139769 = CARTESIAN_POINT('Ctrl Pts',(4.40142712570759,-2.8,-15.1295338960075)) ;
#139770 = CARTESIAN_POINT('Ctrl Pts',(4.50593622119642,-2.8,-15.126048013468)) ;
#139771 = CARTESIAN_POINT('Ctrl Pts',(4.50067611734352,-2.90411960318532,
-15.1296502871252)) ;
#139772 = CARTESIAN_POINT('Ctrl Pts',(4.39573539165433,-2.8,-14.9076225417887)) ;
#139773 = CARTESIAN_POINT('Ctrl Pts',(4.49039105203438,-2.8,-14.926444866009)) ;
#139774 = CARTESIAN_POINT('Ctrl Pts',(4.4979321089857,-2.89506044297337,-14.9065928350698)) ;
#139775 = CARTESIAN_POINT('Ctrl Pts',(4.41164816536272,-2.8,-14.5944921486564)) ;
#139776 = CARTESIAN_POINT('Ctrl Pts',(4.48203507549531,-2.8,-14.6030075383891)) ;
#139777 = CARTESIAN_POINT('Ctrl Pts',(4.50604587949362,-2.86657833599726,
-14.601791633455)) ;
#139778 = CARTESIAN_POINT('Ctrl Pts',(4.41940490599909,-2.8,-14.5021571319988)) ;
#139779 = CARTESIAN_POINT('Ctrl Pts',(4.48133975791563,-2.8,-14.5133274637387)) ;
#139780 = CARTESIAN_POINT('Ctrl Pts',(4.50997623336223,-2.85625883833129,
-14.5130646432391)) ;
#139781 = CARTESIAN_POINT('Ctrl Pts',(4.44577434373642,-2.8,-14.3670206588259)) ;
#139782 = CARTESIAN_POINT('Ctrl Pts',(4.49360122670476,-2.8,-14.3793305876678)) ;
#139783 = CARTESIAN_POINT('Ctrl Pts',(4.52318558604181,-2.8389646555956,-14.3854850424376)) ;
#139784 = CARTESIAN_POINT('Ctrl Pts',(4.45692583760033,-2.8,-14.3224768930528)) ;
#139785 = CARTESIAN_POINT('Ctrl Pts',(4.49949391572662,-2.8,-14.3360543026461)) ;
#139786 = CARTESIAN_POINT('Ctrl Pts',(4.5287634845838,-2.83289258157625,-14.3438029886043)) ;
#139787 = CARTESIAN_POINT('Ctrl Pts',(4.50378503771657,-2.8,-14.2010759162583)) ;
#139788 = CARTESIAN_POINT('Ctrl Pts',(4.52873519606809,-2.8,-14.2199253422749)) ;
#139789 = CARTESIAN_POINT('Ctrl Pts',(4.55214466721901,-2.81552005845342,
-14.2312248698016)) ;
#139790 = CARTESIAN_POINT('Ctrl Pts',(4.54714423790168,-2.8,-14.1222684950466)) ;
#139791 = CARTESIAN_POINT('Ctrl Pts',(4.55761617337351,-2.80000000000013,
-14.1432065641883)) ;
#139792 = CARTESIAN_POINT('Ctrl Pts',(4.57259584813406,-2.80338245043801,
-14.1612385951887)) ;
#139793 = CARTESIAN_POINT('Ctrl Pts',(4.67762904165635,-2.8,-14.1314950447963)) ;
#139794 = CARTESIAN_POINT('Ctrl Pts',(4.66093484724865,-2.79999999999969,
-14.1470670658377)) ;
#139795 = CARTESIAN_POINT('Ctrl Pts',(4.64133868807401,-2.80368623369325,
-14.1646880063865)) ;
#139796 = CARTESIAN_POINT('Origin',(4.4,-2.9,-15.2400000000038)) ;
#139797 = CARTESIAN_POINT('Ctrl Pts',(4.72172783566991,-2.8000000024879,-16.3403629549132)) ;
#139798 = CARTESIAN_POINT('Ctrl Pts',(4.69645430308101,-2.79999660525791,
-16.3270700473085)) ;
#139799 = CARTESIAN_POINT('Ctrl Pts',(4.66463283185001,-2.80454824226955,
-16.3094903682925)) ;
#139800 = CARTESIAN_POINT('Ctrl Pts',(4.55709227475149,-2.80000000030524,
-16.3759964363101)) ;
#139801 = CARTESIAN_POINT('Ctrl Pts',(4.5639923747865,-2.79999958643654,-16.3539593792013)) ;
#139802 = CARTESIAN_POINT('Ctrl Pts',(4.57729370999489,-2.80055804294511,
-16.335175905081)) ;
#139803 = CARTESIAN_POINT('Ctrl Pts',(4.50667826286324,-2.80000000784871,
-16.2866146479982)) ;
#139804 = CARTESIAN_POINT('Ctrl Pts',(4.5303738201498,-2.79998899178919,-16.2670846001166)) ;
#139805 = CARTESIAN_POINT('Ctrl Pts',(4.55348183854634,-2.81434699509191,
-16.2559466041139)) ;
#139806 = CARTESIAN_POINT('Ctrl Pts',(4.4569228015872,-2.80000001789831,-16.1576422182876)) ;
#139807 = CARTESIAN_POINT('Ctrl Pts',(4.4993802926736,-2.79997354447563,-16.1440998880094)) ;
#139808 = CARTESIAN_POINT('Ctrl Pts',(4.52864149761197,-2.83271033979001,
-16.13632906208)) ;
#139809 = CARTESIAN_POINT('Ctrl Pts',(4.44554661086163,-2.80000002126189,
-16.1123774400141)) ;
#139810 = CARTESIAN_POINT('Ctrl Pts',(4.49333665154847,-2.79996797963649,
-16.100096939874)) ;
#139811 = CARTESIAN_POINT('Ctrl Pts',(4.52295544156353,-2.83885474437116,
-16.0939678582281)) ;
#139812 = CARTESIAN_POINT('Ctrl Pts',(4.41903322104331,-2.8000000307772,-15.9758947975771)) ;
#139813 = CARTESIAN_POINT('Ctrl Pts',(4.48100616080234,-2.7999509576918,-15.9647300040203)) ;
#139814 = CARTESIAN_POINT('Ctrl Pts',(4.50969337368894,-2.85623179093868,
-15.9650696236088)) ;
#139815 = CARTESIAN_POINT('Ctrl Pts',(4.41147189908668,-2.8000000363501,-15.8842415900433)) ;
#139816 = CARTESIAN_POINT('Ctrl Pts',(4.48178828424042,-2.79993989905027,
-15.8757891492055)) ;
#139817 = CARTESIAN_POINT('Ctrl Pts',(4.50589025525736,-2.86640526991131,
-15.8769681512009)) ;
#139818 = CARTESIAN_POINT('Ctrl Pts',(4.39523119070916,-2.80000005228414,
-15.5631795198334)) ;
#139819 = CARTESIAN_POINT('Ctrl Pts',(4.49033836345901,-2.799902616883,-15.5430741316609)) ;
#139820 = CARTESIAN_POINT('Ctrl Pts',(4.49769757367179,-2.89547737952989,
-15.5643332157621)) ;
#139821 = CARTESIAN_POINT('Ctrl Pts',(4.40178225889348,-2.80000005718968,
-15.3326239782844)) ;
#139822 = CARTESIAN_POINT('Ctrl Pts',(4.50681341018172,-2.79988784121838,
-15.3370581988237)) ;
#139823 = CARTESIAN_POINT('Ctrl Pts',(4.50092255053475,-2.90441958896084,
-15.3324406960384)) ;
#139824 = CARTESIAN_POINT('Ctrl Pts',(4.39924589760303,-2.80000005405718,
-15.1030311688804)) ;
#139825 = CARTESIAN_POINT('Ctrl Pts',(4.49795607191395,-2.79989746608213,
-15.1039229374963)) ;
#139826 = CARTESIAN_POINT('Ctrl Pts',(4.49968270404899,-2.89870974459554,
-15.1030284945919)) ;
#139827 = CARTESIAN_POINT('Origin',(4.54879236168626,-2.9,-16.3164344434846)) ;
#139828 = CARTESIAN_POINT('Ctrl Pts',(4.57442492185553,-2.80939715119899,
-16.2827581068621)) ;
#139829 = CARTESIAN_POINT('Ctrl Pts',(4.56210583156797,-2.7998961275033,-16.2989430617887)) ;
#139830 = CARTESIAN_POINT('Ctrl Pts',(4.54850917782859,-2.80000109307748,
-16.316806493488)) ;
#139831 = CARTESIAN_POINT('Ctrl Pts',(4.57959763980855,-2.80818914940071,
-16.2899453004955)) ;
#139832 = CARTESIAN_POINT('Ctrl Pts',(4.56768008075466,-2.80031924975227,
-16.3039410457291)) ;
#139833 = CARTESIAN_POINT('Ctrl Pts',(4.55527876038348,-2.79999229227378,
-16.3195899763868)) ;
#139834 = CARTESIAN_POINT('Ctrl Pts',(4.58464248447265,-2.80630474344638,
-16.2974843126383)) ;
#139835 = CARTESIAN_POINT('Ctrl Pts',(4.57346944634374,-2.80008318972136,
-16.3092012910521)) ;
#139836 = CARTESIAN_POINT('Ctrl Pts',(4.56216307187797,-2.79941338753917,
-16.3223280915334)) ;
#139837 = CARTESIAN_POINT('Ctrl Pts',(4.59159231899494,-2.80232720646228,
-16.3100563692959)) ;
#139838 = CARTESIAN_POINT('Ctrl Pts',(4.58237910662986,-2.79850221241048,
-16.3179149362578)) ;
#139839 = CARTESIAN_POINT('Ctrl Pts',(4.57321634584969,-2.79769868647539,
-16.3266644864947)) ;
#139840 = CARTESIAN_POINT('Ctrl Pts',(4.59378564167737,-2.8008235544484,-16.3144145837655)) ;
#139841 = CARTESIAN_POINT('Ctrl Pts',(4.58533966160573,-2.79778056279966,
-16.3209180694478)) ;
#139842 = CARTESIAN_POINT('Ctrl Pts',(4.57696130093821,-2.79699227428058,
-16.3281320740362)) ;
#139843 = CARTESIAN_POINT('Ctrl Pts',(4.59669734138576,-2.79821861236081,
-16.3215174469091)) ;
#139844 = CARTESIAN_POINT('Ctrl Pts',(4.58989502505308,-2.79633072300511,
-16.325783702985)) ;
#139845 = CARTESIAN_POINT('Ctrl Pts',(4.58314295739389,-2.79570785369251,
-16.3304789031814)) ;
#139846 = CARTESIAN_POINT('Ctrl Pts',(4.59760632414569,-2.79728965034655,
-16.3239852466291)) ;
#139847 = CARTESIAN_POINT('Ctrl Pts',(4.59142619397024,-2.79578507327359,
-16.3274678937229)) ;
#139848 = CARTESIAN_POINT('Ctrl Pts',(4.58528630332435,-2.79524119148169,
-16.3312873783749)) ;
#139849 = CARTESIAN_POINT('Ctrl Pts',(4.59875741430933,-2.79580683383092,
-16.327853004496)) ;
#139850 = CARTESIAN_POINT('Ctrl Pts',(4.59383193680336,-2.79486773439435,
-16.3300980055339)) ;
#139851 = CARTESIAN_POINT('Ctrl Pts',(4.58892874314203,-2.79448758877844,
-16.3325464730129)) ;
#139852 = CARTESIAN_POINT('Ctrl Pts',(4.59910834609946,-2.79529718130591,
-16.3291714993015)) ;
#139853 = CARTESIAN_POINT('Ctrl Pts',(4.59464343907619,-2.79454543406795,
-16.3309926958501)) ;
#139854 = CARTESIAN_POINT('Ctrl Pts',(4.59019511689892,-2.79422790851556,
-16.3329746712091)) ;
#139855 = CARTESIAN_POINT('Ctrl Pts',(4.59954688679868,-2.79449699552073,
-16.3312293846587)) ;
#139856 = CARTESIAN_POINT('Ctrl Pts',(4.59601732089137,-2.79402779797775,
-16.3323863363518)) ;
#139857 = CARTESIAN_POINT('Ctrl Pts',(4.59249627585273,-2.79381771894921,
-16.3336411141675)) ;
#139858 = CARTESIAN_POINT('Ctrl Pts',(4.59967529310588,-2.79422450025963,
-16.3319354645612)) ;
#139859 = CARTESIAN_POINT('Ctrl Pts',(4.59651100242294,-2.79384821317135,
-16.3328644108735)) ;
#139860 = CARTESIAN_POINT('Ctrl Pts',(4.593352874124,-2.79367727499394,-16.3338714476574)) ;
#139861 = CARTESIAN_POINT('Ctrl Pts',(4.59980981518572,-2.79380630943631,
-16.3330056452101)) ;
#139862 = CARTESIAN_POINT('Ctrl Pts',(4.59701056623718,-2.79355888022806,
-16.3336249350365)) ;
#139863 = CARTESIAN_POINT('Ctrl Pts',(4.59421559911326,-2.79346462438277,
-16.3343030289899)) ;
#139864 = CARTESIAN_POINT('Ctrl Pts',(4.59984534134842,-2.79366726490194,
-16.3333646067489)) ;
#139865 = CARTESIAN_POINT('Ctrl Pts',(4.59705039509825,-2.79345667046144,
-16.3338917393962)) ;
#139866 = CARTESIAN_POINT('Ctrl Pts',(4.59425962044002,-2.79339574833516,
-16.3344765637043)) ;
#139867 = CARTESIAN_POINT('Ctrl Pts',(4.59992484646001,-2.7933873519883,-16.33407980384)) ;
#139868 = CARTESIAN_POINT('Ctrl Pts',(4.59761652863209,-2.79326682373741,
-16.334380589531)) ;
#139869 = CARTESIAN_POINT('Ctrl Pts',(4.59531061070857,-2.79324678512396,
-16.3347204137335)) ;
#139870 = CARTESIAN_POINT('Ctrl Pts',(4.59996721368508,-2.79324340897637,
-16.334436569794)) ;
#139871 = CARTESIAN_POINT('Ctrl Pts',(4.59680854952869,-2.79327323421043,
-16.3343604778616)) ;
#139872 = CARTESIAN_POINT('Ctrl Pts',(4.59356174266139,-2.79313094944461,
-16.3347234833207)) ;
#139873 = CARTESIAN_POINT('Ctrl Pts',(4.59999999999999,-2.79310344827586,
-16.3347936459578)) ;
#139874 = CARTESIAN_POINT('Ctrl Pts',(4.59999999999999,-2.79310344827586,
-16.3347936459578)) ;
#139875 = CARTESIAN_POINT('Ctrl Pts',(4.59999999999999,-2.79310344827586,
-16.3347936459578)) ;
#139876 = CARTESIAN_POINT('Origin',(8.6,4.09462794777298,-18.845)) ;
#139877 = CARTESIAN_POINT('Origin',(8.6,4.09462794777298,-18.845)) ;
#139878 = CARTESIAN_POINT('Origin',(8.6,4.09462794777298,-18.845)) ;
#139879 = CARTESIAN_POINT('Origin',(8.6,4.09462794777298,-17.545)) ;
#139880 = CARTESIAN_POINT('Origin',(8.6,4.09462794777298,-17.545)) ;
#139881 = CARTESIAN_POINT('Origin',(8.6,4.09462794777298,-17.545)) ;
#139882 = CARTESIAN_POINT('Origin',(8.6,3.95,-18.845)) ;
#139883 = CARTESIAN_POINT('Origin',(8.6,3.95,-18.845)) ;
#139884 = CARTESIAN_POINT('Origin',(8.6,4.09462794777298,-18.845)) ;
#139885 = CARTESIAN_POINT('Origin',(7.25334304318326,5.40585602606554,-18.845)) ;
#139886 = CARTESIAN_POINT('Origin',(7.25334304318326,5.40585602606554,-17.545)) ;
#139887 = CARTESIAN_POINT('Origin',(7.25334304318326,5.40585602606554,-17.545)) ;
#139888 = CARTESIAN_POINT('Origin',(8.6,5.40585602606554,-17.545)) ;
#139889 = CARTESIAN_POINT('Origin',(8.6,3.95,-17.545)) ;
#139890 = CARTESIAN_POINT('Origin',(8.6,3.95,-18.845)) ;
#139891 = CARTESIAN_POINT('Origin',(8.6,3.95,-18.845)) ;
#139892 = CARTESIAN_POINT('Origin',(7.25334304318326,5.40585602606554,-18.845)) ;
#139893 = CARTESIAN_POINT('Origin',(7.25334304318326,5.40585602606554,-18.845)) ;
#139894 = CARTESIAN_POINT('Origin',(7.25334304318326,5.40585602606554,-17.545)) ;
#139895 = CARTESIAN_POINT('Origin',(7.25334304318326,5.40585602606554,-17.545)) ;
#139896 = CARTESIAN_POINT('Origin',(8.6,3.95,-17.545)) ;
#139897 = CARTESIAN_POINT('Origin',(8.6,3.95,-17.545)) ;
#139898 = CARTESIAN_POINT('Origin',(7.36677829147199,4.5782099492339,-18.845)) ;
#139899 = CARTESIAN_POINT('Origin',(7.36677829147199,4.5782099492339,-18.845)) ;
#139900 = CARTESIAN_POINT('Origin',(7.25334304318326,5.40585602606554,-18.845)) ;
#139901 = CARTESIAN_POINT('Ctrl Pts',(4.03523814377473,5.98727788898885,-18.845)) ;
#139902 = CARTESIAN_POINT('Ctrl Pts',(4.03523814427722,5.98727788891385,-18.8994712801668)) ;
#139903 = CARTESIAN_POINT('Ctrl Pts',(4.04195902792202,5.94024173112809,-18.945)) ;
#139904 = CARTESIAN_POINT('Ctrl Pts',(4.05,5.88396692803319,-18.945)) ;
#139905 = CARTESIAN_POINT('Origin',(4.05,6.08618232569815,-18.945)) ;
#139906 = CARTESIAN_POINT('Origin',(4.05,6.08618232569815,-17.545)) ;
#139907 = CARTESIAN_POINT('Origin',(4.05,6.08618232569815,-18.845)) ;
#139908 = CARTESIAN_POINT('Origin',(7.25334304318326,5.40585602606554,-17.545)) ;
#139909 = CARTESIAN_POINT('Ctrl Pts',(4.05,5.88396692803319,-17.445)) ;
#139910 = CARTESIAN_POINT('Ctrl Pts',(4.04195902792202,5.94024173112809,-17.445)) ;
#139911 = CARTESIAN_POINT('Ctrl Pts',(4.03523814427722,5.98727788891385,-17.4905287198332)) ;
#139912 = CARTESIAN_POINT('Ctrl Pts',(4.03523814377473,5.98727788898885,-17.545)) ;
#139913 = CARTESIAN_POINT('Origin',(6.94197060168454,4.79460933256464,-17.545)) ;
#139914 = CARTESIAN_POINT('Origin',(7.36677829147199,4.5782099492339,-17.545)) ;
#139915 = CARTESIAN_POINT('Origin',(7.27599715910381,4.4,-18.845)) ;
#139916 = CARTESIAN_POINT('Origin',(7.27599715910381,4.6,-18.845)) ;
#139917 = CARTESIAN_POINT('Ctrl Pts',(3.95,6.08618232569815,-18.845)) ;
#139918 = CARTESIAN_POINT('Ctrl Pts',(3.95,6.,-18.845)) ;
#139919 = CARTESIAN_POINT('Ctrl Pts',(4.03523814377473,5.98727788898885,-18.845)) ;
#139920 = CARTESIAN_POINT('Ctrl Pts',(3.95,6.08618232225605,-18.9539425627718)) ;
#139921 = CARTESIAN_POINT('Ctrl Pts',(3.95,5.99999999675454,-18.9083359403855)) ;
#139922 = CARTESIAN_POINT('Ctrl Pts',(4.03523814427722,5.98727788891385,-18.8994712801668)) ;
#139923 = CARTESIAN_POINT('Ctrl Pts',(3.95,5.9941162463882,-19.0449999967068)) ;
#139924 = CARTESIAN_POINT('Ctrl Pts',(3.95,5.93865134487238,-18.9528138978372)) ;
#139925 = CARTESIAN_POINT('Ctrl Pts',(4.04195902792202,5.94024173112809,-18.945)) ;
#139926 = CARTESIAN_POINT('Ctrl Pts',(3.95,5.88396692803319,-19.045)) ;
#139927 = CARTESIAN_POINT('Ctrl Pts',(3.95,5.8839669280332,-18.945)) ;
#139928 = CARTESIAN_POINT('Ctrl Pts',(4.05,5.88396692803319,-18.945)) ;
#139929 = CARTESIAN_POINT('Origin',(4.05,5.88396692803319,-19.045)) ;
#139930 = CARTESIAN_POINT('Ctrl Pts',(3.95,5.88396692803319,-17.345)) ;
#139931 = CARTESIAN_POINT('Ctrl Pts',(3.95,5.8839669280332,-17.445)) ;
#139932 = CARTESIAN_POINT('Ctrl Pts',(4.05,5.88396692803319,-17.445)) ;
#139933 = CARTESIAN_POINT('Ctrl Pts',(3.95,5.9941162463882,-17.3450000032932)) ;
#139934 = CARTESIAN_POINT('Ctrl Pts',(3.95,5.93865134487238,-17.4371861021628)) ;
#139935 = CARTESIAN_POINT('Ctrl Pts',(4.04195902792202,5.94024173112809,-17.445)) ;
#139936 = CARTESIAN_POINT('Ctrl Pts',(3.95,6.08618232225605,-17.4360574372282)) ;
#139937 = CARTESIAN_POINT('Ctrl Pts',(3.95,5.99999999675454,-17.4816640596145)) ;
#139938 = CARTESIAN_POINT('Ctrl Pts',(4.03523814427722,5.98727788891385,-17.4905287198332)) ;
#139939 = CARTESIAN_POINT('Ctrl Pts',(3.95,6.08618232569815,-17.545)) ;
#139940 = CARTESIAN_POINT('Ctrl Pts',(3.95,6.,-17.545)) ;
#139941 = CARTESIAN_POINT('Ctrl Pts',(4.03523814377473,5.98727788898885,-17.545)) ;
#139942 = CARTESIAN_POINT('Origin',(4.05,5.88396692803319,-17.345)) ;
#139943 = CARTESIAN_POINT('Origin',(7.27599715910381,4.4,-17.545)) ;
#139944 = CARTESIAN_POINT('Origin',(7.27599715910381,4.6,-17.545)) ;
#139945 = CARTESIAN_POINT('Origin',(3.95,4.6,-18.845)) ;
#139946 = CARTESIAN_POINT('Origin',(4.05,4.6,-18.845)) ;
#139947 = CARTESIAN_POINT('Origin',(4.05,3.75,-19.045)) ;
#139948 = CARTESIAN_POINT('Origin',(4.05,4.6,-19.045)) ;
#139949 = CARTESIAN_POINT('Origin',(4.05,5.40585602606554,-17.345)) ;
#139950 = CARTESIAN_POINT('Origin',(4.05,4.6,-17.345)) ;
#139951 = CARTESIAN_POINT('Origin',(7.25334304318326,4.6,-17.545)) ;
#139952 = CARTESIAN_POINT('Origin',(4.05,4.6,-17.545)) ;
#139953 = CARTESIAN_POINT('Origin',(4.05,4.6,-18.845)) ;
#139954 = CARTESIAN_POINT('Origin',(4.05,4.4,-18.845)) ;
#139955 = CARTESIAN_POINT('Origin',(4.05,4.6,-17.545)) ;
#139956 = CARTESIAN_POINT('Origin',(4.05,4.4,-17.545)) ;
#139957 = CARTESIAN_POINT('Origin',(4.05,4.4,-17.78)) ;
#139958 = CARTESIAN_POINT('Origin',(4.6,2.65,-11.6530460421716)) ;
#139959 = CARTESIAN_POINT('',(4.5,2.61712020253893,-11.4557672574052)) ;
#139960 = CARTESIAN_POINT('',(4.5,2.72431432344521,-11.467365183355)) ;
#139961 = CARTESIAN_POINT('Origin',(4.5,2.65,-11.6530460421716)) ;
#139962 = CARTESIAN_POINT('',(4.6,2.63356010126946,-11.5544066497884)) ;
#139963 = CARTESIAN_POINT('Origin',(4.6,2.61712020253893,-11.4557672574052)) ;
#139964 = CARTESIAN_POINT('',(4.6,2.68715716172261,-11.5602056127633)) ;
#139965 = CARTESIAN_POINT('Origin',(4.6,2.65,-11.6530460421716)) ;
#139966 = CARTESIAN_POINT('Origin',(4.6,2.72431432344521,-11.467365183355)) ;
#139967 = CARTESIAN_POINT('Origin',(-4.52198039027186,10.1,-7.62)) ;
#139968 = CARTESIAN_POINT('',(-4.42392232270277,10.0803883864862,-12.7)) ;
#139969 = CARTESIAN_POINT('',(-4.52198039027186,10.2,-12.7)) ;
#139970 = CARTESIAN_POINT('Origin',(-4.52198039027186,10.1,-12.7)) ;
#139971 = CARTESIAN_POINT('',(-4.42392232270277,10.0803883864862,-7.62)) ;
#139972 = CARTESIAN_POINT('',(-4.42392232270277,10.0803883864862,-12.7)) ;
#139973 = CARTESIAN_POINT('',(-4.52198039027186,10.2,-7.62)) ;
#139974 = CARTESIAN_POINT('Origin',(-4.52198039027186,10.1,-7.62)) ;
#139975 = CARTESIAN_POINT('',(-4.52198039027186,10.2,-7.62)) ;
#139976 = CARTESIAN_POINT('Origin',(0.,10.85,-10.16)) ;
#139977 = CARTESIAN_POINT('',(-2.44929359829471E-16,10.95,-8.16)) ;
#139978 = CARTESIAN_POINT('Origin',(0.,10.95,-10.16)) ;
#139979 = CARTESIAN_POINT('',(-2.32682891837997E-16,10.85,-8.26)) ;
#139980 = CARTESIAN_POINT('Origin',(-2.44929359829471E-16,10.85,-8.16)) ;
#139981 = CARTESIAN_POINT('',(2.32682891837997E-16,10.85,-12.06)) ;
#139982 = CARTESIAN_POINT('Origin',(0.,10.85,-10.16)) ;
#139983 = CARTESIAN_POINT('Origin',(0.,10.85,-10.16)) ;
#139984 = CARTESIAN_POINT('Origin',(11.0914213562373,0.,-10.16)) ;
#139985 = CARTESIAN_POINT('',(11.0207106781187,-1.80110112442984E-16,-8.68928932188135)) ;
#139986 = CARTESIAN_POINT('Origin',(11.0207106781187,0.,-10.16)) ;
#139987 = CARTESIAN_POINT('',(11.0914213562373,-1.83697019872103E-16,-8.66)) ;
#139988 = CARTESIAN_POINT('Origin',(11.0914213562373,-1.71450551880629E-16,
-8.76)) ;
#139989 = CARTESIAN_POINT('Origin',(11.0914213562373,0.,-10.16)) ;
#139990 = CARTESIAN_POINT('Origin',(12.7,0.,-10.16)) ;
#139991 = CARTESIAN_POINT('',(12.8,-1.95943487863577E-16,-11.76)) ;
#139992 = CARTESIAN_POINT('Origin',(12.8,0.,-10.16)) ;
#139993 = CARTESIAN_POINT('',(12.7,-1.83697019872103E-16,-11.66)) ;
#139994 = CARTESIAN_POINT('Origin',(12.7,-1.95943487863577E-16,-11.76)) ;
#139995 = CARTESIAN_POINT('',(12.7,1.83697019872103E-16,-8.66)) ;
#139996 = CARTESIAN_POINT('Origin',(12.7,0.,-10.16)) ;
#139997 = CARTESIAN_POINT('Origin',(12.7,0.,-10.16)) ;
#139998 = CARTESIAN_POINT('Origin',(12.7,2.1,-8.77804604217164)) ;
#139999 = CARTESIAN_POINT('',(12.7,2.,-8.77804604217164)) ;
#140000 = CARTESIAN_POINT('',(12.7,2.11643989873054,-8.67940664978842)) ;
#140001 = CARTESIAN_POINT('Origin',(12.7,2.1,-8.77804604217164)) ;
#140002 = CARTESIAN_POINT('',(12.8,2.13287979746107,-8.58076725740521)) ;
#140003 = CARTESIAN_POINT('Origin',(12.7,2.13287979746107,-8.58076725740521)) ;
#140004 = CARTESIAN_POINT('',(12.8,1.9,-8.77804604217164)) ;
#140005 = CARTESIAN_POINT('Origin',(12.8,2.1,-8.77804604217164)) ;
#140006 = CARTESIAN_POINT('Origin',(12.7,1.9,-8.77804604217164)) ;
#140007 = CARTESIAN_POINT('Origin',(12.7,2.65,-8.66695395782836)) ;
#140008 = CARTESIAN_POINT('',(12.7,2.63356010126947,-8.76559335021158)) ;
#140009 = CARTESIAN_POINT('',(12.7,2.75,-8.66695395782836)) ;
#140010 = CARTESIAN_POINT('Origin',(12.7,2.65,-8.66695395782836)) ;
#140011 = CARTESIAN_POINT('',(12.8,2.65,-8.66695395782836)) ;
#140012 = CARTESIAN_POINT('Origin',(12.7,2.65,-8.66695395782836)) ;
#140013 = CARTESIAN_POINT('Origin',(12.7,2.65,-8.66695395782836)) ;
#140014 = CARTESIAN_POINT('Origin',(4.5,2.1,-8.77804604217164)) ;
#140015 = CARTESIAN_POINT('',(4.6,2.,-8.77804604217164)) ;
#140016 = CARTESIAN_POINT('',(12.8,2.,-8.77804604217164)) ;
#140017 = CARTESIAN_POINT('',(4.6,2.11643989873054,-8.67940664978842)) ;
#140018 = CARTESIAN_POINT('Origin',(4.6,2.1,-8.77804604217164)) ;
#140019 = CARTESIAN_POINT('',(4.5,2.11643989873054,-8.67940664978842)) ;
#140020 = CARTESIAN_POINT('Origin',(12.7,2.65,-11.6530460421716)) ;
#140021 = CARTESIAN_POINT('',(12.8,2.65,-11.6530460421716)) ;
#140022 = CARTESIAN_POINT('',(12.7,2.63356010126947,-11.5544066497884)) ;
#140023 = CARTESIAN_POINT('Origin',(12.7,2.65,-11.6530460421716)) ;
#140024 = CARTESIAN_POINT('',(12.7,2.75,-11.6530460421716)) ;
#140025 = CARTESIAN_POINT('Origin',(12.7,2.65,-11.6530460421716)) ;
#140026 = CARTESIAN_POINT('Origin',(12.7,2.65,-11.6530460421716)) ;
#140027 = CARTESIAN_POINT('Origin',(11.05,0.,-10.16)) ;
#140028 = CARTESIAN_POINT('',(10.3,-9.1848509936051E-17,-9.41000000000001)) ;
#140029 = CARTESIAN_POINT('Origin',(10.3,0.,-10.16)) ;
#140030 = CARTESIAN_POINT('',(11.05,-1.83697019872103E-16,-8.66)) ;
#140031 = CARTESIAN_POINT('Origin',(11.05,0.,-10.16)) ;
#140032 = CARTESIAN_POINT('',(11.05,-1.83697019872103E-16,-8.66)) ;
#140033 = CARTESIAN_POINT('Origin',(0.,9.95,-10.16)) ;
#140034 = CARTESIAN_POINT('',(0.218101234104781,9.95,-12.0474405558009)) ;
#140035 = CARTESIAN_POINT('',(-2.32682891837997E-16,9.95,-12.06)) ;
#140036 = CARTESIAN_POINT('Origin',(0.,9.95,-10.16)) ;
#140037 = CARTESIAN_POINT('',(0.321518176280636,9.85,-12.0325987456797)) ;
#140038 = CARTESIAN_POINT('Ctrl Pts',(0.218101234104783,9.95,-12.0474405558009)) ;
#140039 = CARTESIAN_POINT('Ctrl Pts',(0.231193919344581,9.95,-12.0459276441493)) ;
#140040 = CARTESIAN_POINT('Ctrl Pts',(0.245192892440024,9.94751445938575,
-12.0441565825739)) ;
#140041 = CARTESIAN_POINT('Ctrl Pts',(0.270990685773162,9.93716996065971,
-12.0406215789467)) ;
#140042 = CARTESIAN_POINT('Ctrl Pts',(0.282791986325044,9.92931613918426,
-12.0388607093668)) ;
#140043 = CARTESIAN_POINT('Ctrl Pts',(0.300953024019397,9.91135900604096,
-12.0360350266619)) ;
#140044 = CARTESIAN_POINT('Ctrl Pts',(0.308688523153916,9.90025653083842,
-12.034762561801)) ;
#140045 = CARTESIAN_POINT('Ctrl Pts',(0.318969164829205,9.87583423571802,
-12.0330429866749)) ;
#140046 = CARTESIAN_POINT('Ctrl Pts',(0.321518176280638,9.86251584266313,
-12.0325987456797)) ;
#140047 = CARTESIAN_POINT('Ctrl Pts',(0.321518176280638,9.85,-12.0325987456797)) ;
#140048 = CARTESIAN_POINT('',(0.321518176280636,9.05,-12.0325987456797)) ;
#140049 = CARTESIAN_POINT('',(0.321518176280636,8.95,-12.0325987456797)) ;
#140050 = CARTESIAN_POINT('',(0.422455466606969,8.95,-12.0124393050068)) ;
#140051 = CARTESIAN_POINT('Ctrl Pts',(0.321518176280627,9.05,-12.0325987456797)) ;
#140052 = CARTESIAN_POINT('Ctrl Pts',(0.321518176280627,9.03744936090869,
-12.0325987456797)) ;
#140053 = CARTESIAN_POINT('Ctrl Pts',(0.324085473150902,9.02409774280079,
-12.0321645622427)) ;
#140054 = CARTESIAN_POINT('Ctrl Pts',(0.334387313650431,8.99960748025859,
-12.0303498579077)) ;
#140055 = CARTESIAN_POINT('Ctrl Pts',(0.34212249945656,8.98846937989492,-12.0289656420615)) ;
#140056 = CARTESIAN_POINT('Ctrl Pts',(0.360004521225388,8.97064401154629,
-12.0256049780795)) ;
#140057 = CARTESIAN_POINT('Ctrl Pts',(0.371447108749463,8.96285745107738,
-12.0233820840476)) ;
#140058 = CARTESIAN_POINT('Ctrl Pts',(0.39637397952969,8.95253508546271,-12.0182373032789)) ;
#140059 = CARTESIAN_POINT('Ctrl Pts',(0.409857901997321,8.95,-12.0153122250646)) ;
#140060 = CARTESIAN_POINT('Ctrl Pts',(0.422455466606959,8.95,-12.0124393050068)) ;
#140061 = CARTESIAN_POINT('',(1.14750169623629,8.95,-11.6743446956142)) ;
#140062 = CARTESIAN_POINT('Origin',(0.,8.95,-10.16)) ;
#140063 = CARTESIAN_POINT('',(1.22782596331729,9.05,-11.609980483939)) ;
#140064 = CARTESIAN_POINT('Ctrl Pts',(1.14750169623629,8.95,-11.6743446956142)) ;
#140065 = CARTESIAN_POINT('Ctrl Pts',(1.15780003912542,8.95,-11.6665410786649)) ;
#140066 = CARTESIAN_POINT('Ctrl Pts',(1.16870807732935,8.95253508546271,-11.6580919988207)) ;
#140067 = CARTESIAN_POINT('Ctrl Pts',(1.18867189173408,8.96285745107738,-11.6423039093078)) ;
#140068 = CARTESIAN_POINT('Ctrl Pts',(1.19772988083811,8.97064401154629,-11.6349672274615)) ;
#140069 = CARTESIAN_POINT('Ctrl Pts',(1.21179864083581,8.98846937989492,-11.6234289972217)) ;
#140070 = CARTESIAN_POINT('Ctrl Pts',(1.21783109328768,8.99960748025859,-11.6183932579134)) ;
#140071 = CARTESIAN_POINT('Ctrl Pts',(1.22584313288946,9.02409774280079,-11.6116680597067)) ;
#140072 = CARTESIAN_POINT('Ctrl Pts',(1.22782596331729,9.03744936090869,-11.609980483939)) ;
#140073 = CARTESIAN_POINT('Ctrl Pts',(1.22782596331729,9.05,-11.609980483939)) ;
#140074 = CARTESIAN_POINT('',(1.22782596331729,9.85,-11.609980483939)) ;
#140075 = CARTESIAN_POINT('',(1.22782596331729,8.95,-11.609980483939)) ;
#140076 = CARTESIAN_POINT('',(1.30567057854876,9.95,-11.5402986417121)) ;
#140077 = CARTESIAN_POINT('Ctrl Pts',(1.22782596331729,9.85,-11.609980483939)) ;
#140078 = CARTESIAN_POINT('Ctrl Pts',(1.22782596331729,9.85579162428539,-11.609980483939)) ;
#140079 = CARTESIAN_POINT('Ctrl Pts',(1.22822745887818,9.86162764920014,-11.6096405714653)) ;
#140080 = CARTESIAN_POINT('Ctrl Pts',(1.22902753823171,9.86736607146313,-11.6089619546779)) ;
#140081 = CARTESIAN_POINT('Ctrl Pts',(1.22973095933685,9.87241123018668,-11.6083653221458)) ;
#140082 = CARTESIAN_POINT('Ctrl Pts',(1.2307416875192,9.87738020477702,-11.6075074302535)) ;
#140083 = CARTESIAN_POINT('Ctrl Pts',(1.23203099150182,9.88218322835582,-11.6064092214793)) ;
#140084 = CARTESIAN_POINT('Ctrl Pts',(1.23351897101725,9.88772637473068,-11.6051417840233)) ;
#140085 = CARTESIAN_POINT('Ctrl Pts',(1.23540145579029,9.89313280655105,-11.6035343365783)) ;
#140086 = CARTESIAN_POINT('Ctrl Pts',(1.23763252770621,9.89827011881555,-11.6016189827484)) ;
#140087 = CARTESIAN_POINT('Ctrl Pts',(1.23953000874362,9.90263929783465,-11.5999900134865)) ;
#140088 = CARTESIAN_POINT('Ctrl Pts',(1.24167862345461,9.90681364346946,-11.5981390311988)) ;
#140089 = CARTESIAN_POINT('Ctrl Pts',(1.24403025306866,9.91072825704926,-11.5961019216791)) ;
#140090 = CARTESIAN_POINT('Ctrl Pts',(1.24687926059922,9.91547082513966,-11.5936339563467)) ;
#140091 = CARTESIAN_POINT('Ctrl Pts',(1.25006974298105,9.91990270163235,-11.5908551265321)) ;
#140092 = CARTESIAN_POINT('Ctrl Pts',(1.25351940932648,9.92391762881322,-11.5878266146309)) ;
#140093 = CARTESIAN_POINT('Ctrl Pts',(1.2563462050552,9.92720762206752,-11.5853449298389)) ;
#140094 = CARTESIAN_POINT('Ctrl Pts',(1.25934609941472,9.93021806933732,-11.5826963101588)) ;
#140095 = CARTESIAN_POINT('Ctrl Pts',(1.26246241000316,9.93291206679729,-11.5799255837293)) ;
#140096 = CARTESIAN_POINT('Ctrl Pts',(1.26649145911189,9.93639511117203,-11.5763433371803)) ;
#140097 = CARTESIAN_POINT('Ctrl Pts',(1.27077652588473,9.93940081548805,-11.5725022625241)) ;
#140098 = CARTESIAN_POINT('Ctrl Pts',(1.27520851369615,9.94185862744775,-11.5684896739102)) ;
#140099 = CARTESIAN_POINT('Ctrl Pts',(1.27864718185096,9.94376558208659,-11.5653764070711)) ;
#140100 = CARTESIAN_POINT('Ctrl Pts',(1.28217366418729,9.94534362661778,-11.5621604997622)) ;
#140101 = CARTESIAN_POINT('Ctrl Pts',(1.28573335778226,9.94658081625577,-11.5588887492202)) ;
#140102 = CARTESIAN_POINT('Ctrl Pts',(1.29026904082681,9.94815721599754,-11.5547199568612)) ;
#140103 = CARTESIAN_POINT('Ctrl Pts',(1.29492021413415,9.9491996901822,-11.5504036518226)) ;
#140104 = CARTESIAN_POINT('Ctrl Pts',(1.29957290046263,9.9496832238817,-11.5460412243876)) ;
#140105 = CARTESIAN_POINT('Ctrl Pts',(1.30160833994475,9.94989475836165,-11.5441327662599)) ;
#140106 = CARTESIAN_POINT('Ctrl Pts',(1.30364403319562,9.95,-11.5422156186355)) ;
#140107 = CARTESIAN_POINT('Ctrl Pts',(1.30567057854874,9.95,-11.5402986417121)) ;
#140108 = CARTESIAN_POINT('',(-0.218101234104782,9.95,-8.27255944419911)) ;
#140109 = CARTESIAN_POINT('Origin',(0.,9.95,-10.16)) ;
#140110 = CARTESIAN_POINT('',(-0.321518176280637,9.85,-8.2874012543203)) ;
#140111 = CARTESIAN_POINT('Ctrl Pts',(-0.218101234104781,9.95,-8.27255944419911)) ;
#140112 = CARTESIAN_POINT('Ctrl Pts',(-0.231193919344579,9.95,-8.2740723558507)) ;
#140113 = CARTESIAN_POINT('Ctrl Pts',(-0.245192892440022,9.94751445938575,
-8.27584341742608)) ;
#140114 = CARTESIAN_POINT('Ctrl Pts',(-0.270990685773159,9.93716996065971,
-8.27937842105327)) ;
#140115 = CARTESIAN_POINT('Ctrl Pts',(-0.282791986325042,9.92931613918426,
-8.28113929063325)) ;
#140116 = CARTESIAN_POINT('Ctrl Pts',(-0.300953024019395,9.91135900604096,
-8.28396497333807)) ;
#140117 = CARTESIAN_POINT('Ctrl Pts',(-0.308688523153914,9.90025653083842,
-8.28523743819905)) ;
#140118 = CARTESIAN_POINT('Ctrl Pts',(-0.318969164829202,9.87583423571802,
-8.28695701332505)) ;
#140119 = CARTESIAN_POINT('Ctrl Pts',(-0.321518176280635,9.86251584266313,
-8.2874012543203)) ;
#140120 = CARTESIAN_POINT('Ctrl Pts',(-0.321518176280635,9.85,-8.2874012543203)) ;
#140121 = CARTESIAN_POINT('',(-0.321518176280637,9.05,-8.2874012543203)) ;
#140122 = CARTESIAN_POINT('',(-0.321518176280637,8.95,-8.2874012543203)) ;
#140123 = CARTESIAN_POINT('',(-0.422455466606969,8.95,-8.30756069499325)) ;
#140124 = CARTESIAN_POINT('Ctrl Pts',(-0.321518176280636,9.05,-8.2874012543203)) ;
#140125 = CARTESIAN_POINT('Ctrl Pts',(-0.321518176280636,9.03744936090869,
-8.2874012543203)) ;
#140126 = CARTESIAN_POINT('Ctrl Pts',(-0.324085473150912,9.02409774280079,
-8.28783543775733)) ;
#140127 = CARTESIAN_POINT('Ctrl Pts',(-0.334387313650441,8.99960748025859,
-8.28965014209231)) ;
#140128 = CARTESIAN_POINT('Ctrl Pts',(-0.342122499456568,8.98846937989492,
-8.29103435793852)) ;
#140129 = CARTESIAN_POINT('Ctrl Pts',(-0.360004521225397,8.97064401154629,
-8.29439502192046)) ;
#140130 = CARTESIAN_POINT('Ctrl Pts',(-0.371447108749471,8.96285745107738,
-8.29661791595238)) ;
#140131 = CARTESIAN_POINT('Ctrl Pts',(-0.396373979529699,8.95253508546271,
-8.30176269672111)) ;
#140132 = CARTESIAN_POINT('Ctrl Pts',(-0.409857901997331,8.95,-8.30468777493541)) ;
#140133 = CARTESIAN_POINT('Ctrl Pts',(-0.422455466606968,8.95,-8.30756069499325)) ;
#140134 = CARTESIAN_POINT('',(-1.14750169623629,8.95,-8.64565530438581)) ;
#140135 = CARTESIAN_POINT('Origin',(0.,8.95,-10.16)) ;
#140136 = CARTESIAN_POINT('',(-1.22782596331729,9.05,-8.710019516061)) ;
#140137 = CARTESIAN_POINT('Ctrl Pts',(-1.1475016962363,8.95,-8.64565530438581)) ;
#140138 = CARTESIAN_POINT('Ctrl Pts',(-1.15780003912543,8.95,-8.65345892133506)) ;
#140139 = CARTESIAN_POINT('Ctrl Pts',(-1.16870807732935,8.95253508546271,
-8.66190800117932)) ;
#140140 = CARTESIAN_POINT('Ctrl Pts',(-1.18867189173409,8.96285745107738,
-8.67769609069216)) ;
#140141 = CARTESIAN_POINT('Ctrl Pts',(-1.19772988083812,8.97064401154629,
-8.68503277253852)) ;
#140142 = CARTESIAN_POINT('Ctrl Pts',(-1.21179864083582,8.98846937989492,
-8.69657100277835)) ;
#140143 = CARTESIAN_POINT('Ctrl Pts',(-1.21783109328768,8.99960748025859,
-8.70160674208656)) ;
#140144 = CARTESIAN_POINT('Ctrl Pts',(-1.22584313288947,9.02409774280079,
-8.70833194029334)) ;
#140145 = CARTESIAN_POINT('Ctrl Pts',(-1.22782596331729,9.03744936090869,
-8.71001951606101)) ;
#140146 = CARTESIAN_POINT('Ctrl Pts',(-1.22782596331729,9.05,-8.71001951606101)) ;
#140147 = CARTESIAN_POINT('',(-1.22782596331729,9.85,-8.710019516061)) ;
#140148 = CARTESIAN_POINT('',(-1.22782596331729,8.95,-8.710019516061)) ;
#140149 = CARTESIAN_POINT('',(-1.30567057854876,9.95,-8.77970135828795)) ;
#140150 = CARTESIAN_POINT('Ctrl Pts',(-1.22782596331729,9.85,-8.710019516061)) ;
#140151 = CARTESIAN_POINT('Ctrl Pts',(-1.22782596331729,9.8557916242854,-8.710019516061)) ;
#140152 = CARTESIAN_POINT('Ctrl Pts',(-1.22822745887816,9.86162764920014,
-8.71035942853478)) ;
#140153 = CARTESIAN_POINT('Ctrl Pts',(-1.22902753823169,9.86736607146313,
-8.71103804532216)) ;
#140154 = CARTESIAN_POINT('Ctrl Pts',(-1.22973095933683,9.87241123018669,
-8.71163467785421)) ;
#140155 = CARTESIAN_POINT('Ctrl Pts',(-1.23074168751919,9.87738020477703,
-8.71249256974653)) ;
#140156 = CARTESIAN_POINT('Ctrl Pts',(-1.23203099150182,9.88218322835582,
-8.71359077852072)) ;
#140157 = CARTESIAN_POINT('Ctrl Pts',(-1.23351897101725,9.88772637473068,
-8.71485821597665)) ;
#140158 = CARTESIAN_POINT('Ctrl Pts',(-1.2354014557903,9.89313280655103,-8.71646566342165)) ;
#140159 = CARTESIAN_POINT('Ctrl Pts',(-1.23763252770622,9.89827011881554,
-8.71838101725154)) ;
#140160 = CARTESIAN_POINT('Ctrl Pts',(-1.23953000874363,9.90263929783464,
-8.72000998651346)) ;
#140161 = CARTESIAN_POINT('Ctrl Pts',(-1.24167862345459,9.90681364346946,
-8.72186096880123)) ;
#140162 = CARTESIAN_POINT('Ctrl Pts',(-1.24403025306866,9.91072825704926,
-8.72389807832091)) ;
#140163 = CARTESIAN_POINT('Ctrl Pts',(-1.24687926059923,9.91547082513966,
-8.72636604365333)) ;
#140164 = CARTESIAN_POINT('Ctrl Pts',(-1.25006974298105,9.91990270163234,
-8.72914487346783)) ;
#140165 = CARTESIAN_POINT('Ctrl Pts',(-1.25351940932649,9.92391762881322,
-8.73217338536911)) ;
#140166 = CARTESIAN_POINT('Ctrl Pts',(-1.25634620505522,9.92720762206752,
-8.7346550701611)) ;
#140167 = CARTESIAN_POINT('Ctrl Pts',(-1.25934609941473,9.93021806933732,
-8.73730368984121)) ;
#140168 = CARTESIAN_POINT('Ctrl Pts',(-1.26246241000317,9.93291206679729,
-8.74007441627068)) ;
#140169 = CARTESIAN_POINT('Ctrl Pts',(-1.26649145911191,9.93639511117205,
-8.74365666281975)) ;
#140170 = CARTESIAN_POINT('Ctrl Pts',(-1.27077652588473,9.93940081548806,
-8.74749773747593)) ;
#140171 = CARTESIAN_POINT('Ctrl Pts',(-1.27520851369618,9.94185862744776,
-8.7515103260898)) ;
#140172 = CARTESIAN_POINT('Ctrl Pts',(-1.27864718185098,9.9437655820866,-8.75462359292894)) ;
#140173 = CARTESIAN_POINT('Ctrl Pts',(-1.2821736641873,9.94534362661778,-8.75783950023776)) ;
#140174 = CARTESIAN_POINT('Ctrl Pts',(-1.28573335778226,9.94658081625577,
-8.76111125077976)) ;
#140175 = CARTESIAN_POINT('Ctrl Pts',(-1.29026904082682,9.94815721599755,
-8.76528004313887)) ;
#140176 = CARTESIAN_POINT('Ctrl Pts',(-1.29492021413418,9.94919969018221,
-8.7695963481774)) ;
#140177 = CARTESIAN_POINT('Ctrl Pts',(-1.2995729004627,9.94968322388171,-8.77395877561253)) ;
#140178 = CARTESIAN_POINT('Ctrl Pts',(-1.30160833994481,9.94989475836166,
-8.77586723374024)) ;
#140179 = CARTESIAN_POINT('Ctrl Pts',(-1.30364403319567,9.95,-8.7777843813645)) ;
#140180 = CARTESIAN_POINT('Ctrl Pts',(-1.30567057854876,9.95,-8.77970135828795)) ;
#140181 = CARTESIAN_POINT('Origin',(0.,9.95,-10.16)) ;
#140182 = CARTESIAN_POINT('',(-2.32682891837997E-16,9.95,-12.06)) ;
#140183 = CARTESIAN_POINT('Origin',(4.5,-2.8,-7.62)) ;
#140184 = CARTESIAN_POINT('',(4.5,-2.4,-12.1221416870349)) ;
#140185 = CARTESIAN_POINT('',(4.5,-2.7,-11.6831546211728)) ;
#140186 = CARTESIAN_POINT('Origin',(4.5,0.,-10.16)) ;
#140187 = CARTESIAN_POINT('',(4.5,-2.7,-12.7)) ;
#140188 = CARTESIAN_POINT('',(4.5,-2.7,-7.62)) ;
#140189 = CARTESIAN_POINT('',(4.5,-2.4,-12.7)) ;
#140190 = CARTESIAN_POINT('',(4.5,-2.8,-12.7)) ;
#140191 = CARTESIAN_POINT('',(4.5,-2.4,-12.0861360284258)) ;
#140192 = CARTESIAN_POINT('Origin',(4.5,-2.3,-7.62)) ;
#140193 = CARTESIAN_POINT('',(4.6,-2.3,-7.62)) ;
#140194 = CARTESIAN_POINT('',(12.7,-2.3,-7.62)) ;
#140195 = CARTESIAN_POINT('',(4.5,-2.3,-7.62)) ;
#140196 = CARTESIAN_POINT('',(4.6,-2.3,-8.19785831296514)) ;
#140197 = CARTESIAN_POINT('',(4.6,-2.3,-8.23386397157418)) ;
#140198 = CARTESIAN_POINT('',(12.7,-2.3,-8.19785831296514)) ;
#140199 = CARTESIAN_POINT('',(4.5,-2.3,-8.19785831296514)) ;
#140200 = CARTESIAN_POINT('',(12.7,-2.3,-7.62)) ;
#140201 = CARTESIAN_POINT('Origin',(12.8,2.75,-7.62)) ;
#140202 = CARTESIAN_POINT('',(12.7,2.75,-12.7)) ;
#140203 = CARTESIAN_POINT('',(4.55912712210514,2.75,-12.7)) ;
#140204 = CARTESIAN_POINT('',(12.8,2.75,-12.7)) ;
#140205 = CARTESIAN_POINT('',(4.55912712210513,2.75,-11.6530460421716)) ;
#140206 = CARTESIAN_POINT('',(4.55912712210514,2.75,-11.6530460421716)) ;
#140207 = CARTESIAN_POINT('',(12.8,2.75,-11.6530460421716)) ;
#140208 = CARTESIAN_POINT('',(12.7,2.75,-7.62)) ;
#140209 = CARTESIAN_POINT('Origin',(0.,9.95,-10.16)) ;
#140210 = CARTESIAN_POINT('',(0.230887397576971,9.95,-12.0748605718538)) ;
#140211 = CARTESIAN_POINT('Origin',(12.8,-2.3,-7.62)) ;
#140212 = CARTESIAN_POINT('',(12.8,-2.3359925337019,-7.83595520221138)) ;
#140213 = CARTESIAN_POINT('',(12.8,2.65,-7.62)) ;
#140214 = CARTESIAN_POINT('',(12.8,2.65,-7.62)) ;
#140215 = CARTESIAN_POINT('',(12.8,-2.2,-7.62)) ;
#140216 = CARTESIAN_POINT('',(12.8,-2.3,-7.62)) ;
#140217 = CARTESIAN_POINT('',(12.8,-2.2,-8.19785831296514)) ;
#140218 = CARTESIAN_POINT('',(12.8,-2.2,-7.62)) ;
#140219 = CARTESIAN_POINT('',(12.8,-2.24516129032258,-8.32444809922546)) ;
#140220 = CARTESIAN_POINT('Origin',(12.8,-2.4,-8.19785831296514)) ;
#140221 = CARTESIAN_POINT('',(12.8,-2.24516129032258,-11.9955519007745)) ;
#140222 = CARTESIAN_POINT('Origin',(12.8,0.,-10.16)) ;
#140223 = CARTESIAN_POINT('',(12.8,-2.2,-12.1221416870349)) ;
#140224 = CARTESIAN_POINT('Origin',(12.8,-2.4,-12.1221416870349)) ;
#140225 = CARTESIAN_POINT('',(12.8,-2.2,-12.7)) ;
#140226 = CARTESIAN_POINT('',(12.8,-2.2,-7.62)) ;
#140227 = CARTESIAN_POINT('',(12.8,2.65,-12.7)) ;
#140228 = CARTESIAN_POINT('',(12.8,-2.3,-12.7)) ;
#140229 = CARTESIAN_POINT('',(12.8,2.65,-7.62)) ;
#140230 = CARTESIAN_POINT('',(12.8,2.13287979746107,-11.7392327425948)) ;
#140231 = CARTESIAN_POINT('',(12.8,-1.51220874991811,-12.3467475004913)) ;
#140232 = CARTESIAN_POINT('',(12.8,1.9,-11.5419539578284)) ;
#140233 = CARTESIAN_POINT('Origin',(12.8,2.1,-11.5419539578284)) ;
#140234 = CARTESIAN_POINT('',(12.8,1.9,-7.62)) ;
#140235 = CARTESIAN_POINT('Origin',(12.8,2.75,-7.62)) ;
#140236 = CARTESIAN_POINT('',(4.55912712210513,2.75,-8.66695395782836)) ;
#140237 = CARTESIAN_POINT('',(12.8,2.75,-8.66695395782836)) ;
#140238 = CARTESIAN_POINT('',(4.55912712210514,2.75,-7.62)) ;
#140239 = CARTESIAN_POINT('',(4.55912712210514,2.75,-7.62)) ;
#140240 = CARTESIAN_POINT('',(12.7,2.75,-7.62)) ;
#140241 = CARTESIAN_POINT('',(12.8,2.75,-7.62)) ;
#140242 = CARTESIAN_POINT('',(12.7,2.75,-7.62)) ;
#140243 = CARTESIAN_POINT('Origin',(4.5,2.75,-7.62)) ;
#140244 = CARTESIAN_POINT('',(4.47150553123747,2.80180812502278,-7.62)) ;
#140245 = CARTESIAN_POINT('',(3.96237840913234,3.72749380157757,-7.62)) ;
#140246 = CARTESIAN_POINT('',(4.5,2.75,-7.62)) ;
#140247 = CARTESIAN_POINT('',(4.47150553123747,2.80180812502279,-8.66695395782836)) ;
#140248 = CARTESIAN_POINT('',(4.47150553123747,2.80180812502278,-8.66695395782836)) ;
#140249 = CARTESIAN_POINT('',(4.48762159086767,2.77250619842243,-8.77117568174948)) ;
#140250 = CARTESIAN_POINT('Origin',(4.56263299594785,2.6361218255494,-8.67660029409629)) ;
#140251 = CARTESIAN_POINT('',(4.48762159086767,2.77250619842243,-11.5488243182478)) ;
#140252 = CARTESIAN_POINT('',(4.48762159086767,2.77250619842243,-7.62)) ;
#140253 = CARTESIAN_POINT('',(4.47150553123747,2.80180812502279,-11.6530460421716)) ;
#140254 = CARTESIAN_POINT('Origin',(4.56263299596657,2.63612182551533,-11.6433997058941)) ;
#140255 = CARTESIAN_POINT('',(4.47150553123747,2.80180812502278,-12.7)) ;
#140256 = CARTESIAN_POINT('',(4.47150553123747,2.80180812502278,-12.7)) ;
#140257 = CARTESIAN_POINT('',(3.96237840913234,3.72749380157757,-12.7)) ;
#140258 = CARTESIAN_POINT('',(4.5,2.75,-12.7)) ;
#140259 = CARTESIAN_POINT('',(3.96237840913234,3.72749380157757,-7.62)) ;
#140260 = CARTESIAN_POINT('Origin',(3.95,3.75,-7.62)) ;
#140261 = CARTESIAN_POINT('',(3.95,3.77568567655479,-12.7)) ;
#140262 = CARTESIAN_POINT('',(3.95,6.92431432344521,-12.7)) ;
#140263 = CARTESIAN_POINT('',(3.95,3.75,-12.7)) ;
#140264 = CARTESIAN_POINT('',(3.95,6.92431432344521,-7.62)) ;
#140265 = CARTESIAN_POINT('',(3.95,6.92431432344521,-7.62)) ;
#140266 = CARTESIAN_POINT('',(3.95,3.77568567655479,-7.62)) ;
#140267 = CARTESIAN_POINT('',(3.95,3.75,-7.62)) ;
#140268 = CARTESIAN_POINT('',(3.95,3.77568567655479,-12.7)) ;
#140269 = CARTESIAN_POINT('Origin',(3.95,6.95,-7.62)) ;
#140270 = CARTESIAN_POINT('',(3.93762159086767,6.97250619842243,-12.7)) ;
#140271 = CARTESIAN_POINT('',(3.42849446876253,7.89819187497721,-12.7)) ;
#140272 = CARTESIAN_POINT('',(3.95,6.95,-12.7)) ;
#140273 = CARTESIAN_POINT('',(3.42849446876253,7.89819187497721,-7.62)) ;
#140274 = CARTESIAN_POINT('',(3.42849446876253,7.89819187497721,-7.62)) ;
#140275 = CARTESIAN_POINT('',(3.93762159086767,6.97250619842243,-7.62)) ;
#140276 = CARTESIAN_POINT('',(3.95,6.95,-7.62)) ;
#140277 = CARTESIAN_POINT('',(3.93762159086767,6.97250619842243,-7.62)) ;
#140278 = CARTESIAN_POINT('Origin',(3.4,7.95,-7.62)) ;
#140279 = CARTESIAN_POINT('',(3.34087287789487,7.95,-12.7)) ;
#140280 = CARTESIAN_POINT('',(3.,7.95,-12.7)) ;
#140281 = CARTESIAN_POINT('',(3.4,7.95,-12.7)) ;
#140282 = CARTESIAN_POINT('',(3.,7.95,-7.62)) ;
#140283 = CARTESIAN_POINT('',(3.,7.95,-7.62)) ;
#140284 = CARTESIAN_POINT('',(3.34087287789487,7.95,-7.62)) ;
#140285 = CARTESIAN_POINT('',(3.4,7.95,-7.62)) ;
#140286 = CARTESIAN_POINT('',(3.34087287789487,7.95,-7.62)) ;
#140287 = CARTESIAN_POINT('Origin',(2.9,7.95,-7.62)) ;
#140288 = CARTESIAN_POINT('',(2.9,8.05,-12.7)) ;
#140289 = CARTESIAN_POINT('',(2.9,9.85,-12.7)) ;
#140290 = CARTESIAN_POINT('',(2.9,7.95,-12.7)) ;
#140291 = CARTESIAN_POINT('',(2.9,9.85,-7.62)) ;
#140292 = CARTESIAN_POINT('',(2.9,9.85,-7.62)) ;
#140293 = CARTESIAN_POINT('',(2.9,8.05,-7.62)) ;
#140294 = CARTESIAN_POINT('',(2.9,7.95,-7.62)) ;
#140295 = CARTESIAN_POINT('',(2.9,8.05,-12.7)) ;
#140296 = CARTESIAN_POINT('Origin',(2.9,9.95,-7.62)) ;
#140297 = CARTESIAN_POINT('',(3.,9.95,-12.7)) ;
#140298 = CARTESIAN_POINT('',(3.3,9.95,-12.7)) ;
#140299 = CARTESIAN_POINT('',(2.9,9.95,-12.7)) ;
#140300 = CARTESIAN_POINT('',(3.3,9.95,-7.62)) ;
#140301 = CARTESIAN_POINT('',(3.3,9.95,-7.62)) ;
#140302 = CARTESIAN_POINT('',(3.,9.95,-7.62)) ;
#140303 = CARTESIAN_POINT('',(2.9,9.95,-7.62)) ;
#140304 = CARTESIAN_POINT('',(3.,9.95,-12.7)) ;
#140305 = CARTESIAN_POINT('Origin',(3.4,9.95,-7.62)) ;
#140306 = CARTESIAN_POINT('',(3.4,10.05,-12.7)) ;
#140307 = CARTESIAN_POINT('',(3.4,10.85,-12.7)) ;
#140308 = CARTESIAN_POINT('',(3.4,9.95,-12.7)) ;
#140309 = CARTESIAN_POINT('',(3.4,10.85,-7.62)) ;
#140310 = CARTESIAN_POINT('',(3.4,10.85,-7.62)) ;
#140311 = CARTESIAN_POINT('',(3.4,10.05,-7.62)) ;
#140312 = CARTESIAN_POINT('',(3.4,9.95,-7.62)) ;
#140313 = CARTESIAN_POINT('',(3.4,10.05,-7.62)) ;
#140314 = CARTESIAN_POINT('Origin',(3.4,10.95,-7.62)) ;
#140315 = CARTESIAN_POINT('',(3.3,10.95,-12.7)) ;
#140316 = CARTESIAN_POINT('',(-4.8,10.95,-12.7)) ;
#140317 = CARTESIAN_POINT('',(3.4,10.95,-12.7)) ;
#140318 = CARTESIAN_POINT('',(-4.8,10.95,-7.62)) ;
#140319 = CARTESIAN_POINT('',(-4.8,10.95,-7.62)) ;
#140320 = CARTESIAN_POINT('',(3.3,10.95,-7.62)) ;
#140321 = CARTESIAN_POINT('',(3.4,10.95,-7.62)) ;
#140322 = CARTESIAN_POINT('',(3.3,10.95,-7.62)) ;
#140323 = CARTESIAN_POINT('',(-2.55,10.95,-11.06)) ;
#140324 = CARTESIAN_POINT('',(-2.75,10.95,-11.26)) ;
#140325 = CARTESIAN_POINT('Origin',(-2.75,10.95,-11.06)) ;
#140326 = CARTESIAN_POINT('',(-2.55,10.95,-9.26)) ;
#140327 = CARTESIAN_POINT('',(-2.55,10.95,-7.62)) ;
#140328 = CARTESIAN_POINT('',(-2.75,10.95,-9.06)) ;
#140329 = CARTESIAN_POINT('Origin',(-2.75,10.95,-9.26)) ;
#140330 = CARTESIAN_POINT('',(-3.8,10.95,-9.06)) ;
#140331 = CARTESIAN_POINT('',(3.4,10.95,-9.06)) ;
#140332 = CARTESIAN_POINT('',(-4.,10.95,-9.26)) ;
#140333 = CARTESIAN_POINT('Origin',(-3.8,10.95,-9.26)) ;
#140334 = CARTESIAN_POINT('',(-4.,10.95,-11.06)) ;
#140335 = CARTESIAN_POINT('',(-4.,10.95,-7.62)) ;
#140336 = CARTESIAN_POINT('',(-3.8,10.95,-11.26)) ;
#140337 = CARTESIAN_POINT('Origin',(-3.8,10.95,-11.06)) ;
#140338 = CARTESIAN_POINT('',(3.4,10.95,-11.26)) ;
#140339 = CARTESIAN_POINT('Origin',(-4.9,10.95,-7.62)) ;
#140340 = CARTESIAN_POINT('',(-4.9,10.85,-12.7)) ;
#140341 = CARTESIAN_POINT('',(-4.9,10.3,-12.7)) ;
#140342 = CARTESIAN_POINT('',(-4.9,10.95,-12.7)) ;
#140343 = CARTESIAN_POINT('',(-4.9,10.3,-7.62)) ;
#140344 = CARTESIAN_POINT('',(-4.9,10.3,-7.62)) ;
#140345 = CARTESIAN_POINT('',(-4.9,10.85,-7.62)) ;
#140346 = CARTESIAN_POINT('',(-4.9,10.95,-7.62)) ;
#140347 = CARTESIAN_POINT('',(-4.9,10.85,-7.62)) ;
#140348 = CARTESIAN_POINT('Origin',(-4.9,10.2,-7.62)) ;
#140349 = CARTESIAN_POINT('',(-4.8,10.2,-12.7)) ;
#140350 = CARTESIAN_POINT('',(-4.9,10.2,-12.7)) ;
#140351 = CARTESIAN_POINT('',(-4.8,10.2,-7.62)) ;
#140352 = CARTESIAN_POINT('',(-4.9,10.2,-7.62)) ;
#140353 = CARTESIAN_POINT('',(-4.8,10.2,-7.62)) ;
#140354 = CARTESIAN_POINT('Origin',(-4.4,10.2,-7.62)) ;
#140355 = CARTESIAN_POINT('',(-5.39805806756909,5.20970966215454,-12.7)) ;
#140356 = CARTESIAN_POINT('',(-4.4,10.2,-12.7)) ;
#140357 = CARTESIAN_POINT('',(-5.39805806756909,5.20970966215454,-7.62)) ;
#140358 = CARTESIAN_POINT('',(-5.39805806756909,5.20970966215454,-7.62)) ;
#140359 = CARTESIAN_POINT('',(-4.4,10.2,-7.62)) ;
#140360 = CARTESIAN_POINT('Origin',(-5.4,5.2,-7.62)) ;
#140361 = CARTESIAN_POINT('',(-5.4,5.19009804864072,-12.7)) ;
#140362 = CARTESIAN_POINT('',(-5.4,-3.95,-12.7)) ;
#140363 = CARTESIAN_POINT('',(-5.4,5.2,-12.7)) ;
#140364 = CARTESIAN_POINT('',(-5.4,-3.95,-7.62)) ;
#140365 = CARTESIAN_POINT('',(-5.4,-3.95,-7.62)) ;
#140366 = CARTESIAN_POINT('',(-5.4,5.19009804864072,-7.62)) ;
#140367 = CARTESIAN_POINT('',(-5.4,5.2,-7.62)) ;
#140368 = CARTESIAN_POINT('',(-5.4,5.19009804864072,-7.62)) ;
#140369 = CARTESIAN_POINT('',(-5.4,4.23801993223491,-12.06)) ;
#140370 = CARTESIAN_POINT('',(-5.4,4.23801993223491,-8.26)) ;
#140371 = CARTESIAN_POINT('',(-5.4,4.23801993223491,-8.16)) ;
#140372 = CARTESIAN_POINT('',(-5.4,3.9369800677651,-8.06)) ;
#140373 = CARTESIAN_POINT('Ctrl Pts',(-5.4,4.23801993223491,-8.26)) ;
#140374 = CARTESIAN_POINT('Ctrl Pts',(-5.4,4.23801992976516,-8.20749312809024)) ;
#140375 = CARTESIAN_POINT('Ctrl Pts',(-5.4,4.20557579169425,-8.15560257376828)) ;
#140376 = CARTESIAN_POINT('Ctrl Pts',(-5.4,4.09411900298411,-8.0815547137571)) ;
#140377 = CARTESIAN_POINT('Ctrl Pts',(-5.4,4.0160133758189,-8.06000000048129)) ;
#140378 = CARTESIAN_POINT('Ctrl Pts',(-5.4,3.9369800677651,-8.06)) ;
#140379 = CARTESIAN_POINT('',(-5.4,-1.88819660112502,-8.06)) ;
#140380 = CARTESIAN_POINT('',(-5.4,-2.05,-8.06)) ;
#140381 = CARTESIAN_POINT('',(-5.4,-2.11180339887499,-8.26)) ;
#140382 = CARTESIAN_POINT('Ctrl Pts',(-5.4,-2.11180339887499,-8.26)) ;
#140383 = CARTESIAN_POINT('Ctrl Pts',(-5.4,-2.11180339704051,-8.20749316010866)) ;
#140384 = CARTESIAN_POINT('Ctrl Pts',(-5.4,-2.0877044485962,-8.15560253112148)) ;
#140385 = CARTESIAN_POINT('Ctrl Pts',(-5.4,-2.00491651967066,-8.0815547564039)) ;
#140386 = CARTESIAN_POINT('Ctrl Pts',(-5.4,-1.946901032774,-8.06000000117406)) ;
#140387 = CARTESIAN_POINT('Ctrl Pts',(-5.4,-1.88819660112502,-8.06)) ;
#140388 = CARTESIAN_POINT('',(-5.4,-2.11180339887499,-12.06)) ;
#140389 = CARTESIAN_POINT('',(-5.4,-2.11180339887499,-12.16)) ;
#140390 = CARTESIAN_POINT('',(-5.4,-1.88819660112501,-12.26)) ;
#140391 = CARTESIAN_POINT('Ctrl Pts',(-5.4,-1.88819660112501,-12.26)) ;
#140392 = CARTESIAN_POINT('Ctrl Pts',(-5.4,-1.946901032774,-12.2599999988259)) ;
#140393 = CARTESIAN_POINT('Ctrl Pts',(-5.4,-2.00491651967066,-12.2384452435961)) ;
#140394 = CARTESIAN_POINT('Ctrl Pts',(-5.4,-2.0877044485962,-12.1643974688785)) ;
#140395 = CARTESIAN_POINT('Ctrl Pts',(-5.4,-2.11180339704051,-12.1125068398913)) ;
#140396 = CARTESIAN_POINT('Ctrl Pts',(-5.4,-2.11180339887499,-12.06)) ;
#140397 = CARTESIAN_POINT('',(-5.4,3.9369800677651,-12.26)) ;
#140398 = CARTESIAN_POINT('',(-5.4,4.20000000000001,-12.26)) ;
#140399 = CARTESIAN_POINT('Ctrl Pts',(-5.4,3.9369800677651,-12.26)) ;
#140400 = CARTESIAN_POINT('Ctrl Pts',(-5.4,4.01601337581888,-12.2599999995187)) ;
#140401 = CARTESIAN_POINT('Ctrl Pts',(-5.4,4.09411900298413,-12.2384452862428)) ;
#140402 = CARTESIAN_POINT('Ctrl Pts',(-5.4,4.20557579169423,-12.1643974262318)) ;
#140403 = CARTESIAN_POINT('Ctrl Pts',(-5.4,4.23801992976516,-12.1125068719097)) ;
#140404 = CARTESIAN_POINT('Ctrl Pts',(-5.4,4.23801993223491,-12.06)) ;
#140405 = CARTESIAN_POINT('Origin',(-5.4,-4.05,-7.62)) ;
#140406 = CARTESIAN_POINT('',(-5.3,-4.05,-12.7)) ;
#140407 = CARTESIAN_POINT('',(3.5,-4.05,-12.7)) ;
#140408 = CARTESIAN_POINT('',(-5.4,-4.05,-12.7)) ;
#140409 = CARTESIAN_POINT('',(3.5,-4.05,-7.62)) ;
#140410 = CARTESIAN_POINT('',(3.5,-4.05,-7.62)) ;
#140411 = CARTESIAN_POINT('',(-5.3,-4.05,-7.62)) ;
#140412 = CARTESIAN_POINT('',(-5.4,-4.05,-7.62)) ;
#140413 = CARTESIAN_POINT('',(-5.3,-4.05,-7.62)) ;
#140414 = CARTESIAN_POINT('',(-4.5,-4.05,-11.06)) ;
#140415 = CARTESIAN_POINT('',(-4.3,-4.05,-11.26)) ;
#140416 = CARTESIAN_POINT('Origin',(-4.3,-4.05,-11.06)) ;
#140417 = CARTESIAN_POINT('',(-4.5,-4.05,-9.26)) ;
#140418 = CARTESIAN_POINT('',(-4.5,-4.05,-7.62)) ;
#140419 = CARTESIAN_POINT('',(-4.3,-4.05,-9.06)) ;
#140420 = CARTESIAN_POINT('Origin',(-4.3,-4.05,-9.26)) ;
#140421 = CARTESIAN_POINT('',(-3.25,-4.05,-9.06)) ;
#140422 = CARTESIAN_POINT('',(-5.4,-4.05,-9.06)) ;
#140423 = CARTESIAN_POINT('',(-3.05,-4.05,-9.26)) ;
#140424 = CARTESIAN_POINT('Origin',(-3.25,-4.05,-9.26)) ;
#140425 = CARTESIAN_POINT('',(-3.05,-4.05,-11.06)) ;
#140426 = CARTESIAN_POINT('',(-3.05,-4.05,-7.62)) ;
#140427 = CARTESIAN_POINT('',(-3.25,-4.05,-11.26)) ;
#140428 = CARTESIAN_POINT('Origin',(-3.25,-4.05,-11.06)) ;
#140429 = CARTESIAN_POINT('',(-5.4,-4.05,-11.26)) ;
#140430 = CARTESIAN_POINT('Origin',(3.6,-4.05,-7.62)) ;
#140431 = CARTESIAN_POINT('',(3.6,-3.95,-12.7)) ;
#140432 = CARTESIAN_POINT('',(3.6,-2.9,-12.7)) ;
#140433 = CARTESIAN_POINT('',(3.6,-4.05,-12.7)) ;
#140434 = CARTESIAN_POINT('',(3.6,-2.9,-7.62)) ;
#140435 = CARTESIAN_POINT('',(3.6,-2.9,-7.62)) ;
#140436 = CARTESIAN_POINT('',(3.6,-3.95,-7.62)) ;
#140437 = CARTESIAN_POINT('',(3.6,-4.05,-7.62)) ;
#140438 = CARTESIAN_POINT('',(3.6,-3.95,-7.62)) ;
#140439 = CARTESIAN_POINT('Origin',(3.6,-2.8,-7.62)) ;
#140440 = CARTESIAN_POINT('',(4.4,-2.8,-11.6831546211728)) ;
#140441 = CARTESIAN_POINT('',(4.54880051362942,-2.79999999972164,-11.2364378607329)) ;
#140442 = CARTESIAN_POINT('Ctrl Pts',(4.4,-2.8,-11.6831546211728)) ;
#140443 = CARTESIAN_POINT('Ctrl Pts',(4.40001102013632,-2.8,-11.6464400198561)) ;
#140444 = CARTESIAN_POINT('Ctrl Pts',(4.40220140384574,-2.79999999812164,
-11.6100681661137)) ;
#140445 = CARTESIAN_POINT('Ctrl Pts',(4.4066417499344,-2.79999999722267,-11.5740727380185)) ;
#140446 = CARTESIAN_POINT('Ctrl Pts',(4.41108209602305,-2.79999999632371,
-11.5380773099234)) ;
#140447 = CARTESIAN_POINT('Ctrl Pts',(4.41777240449119,-2.79999999692353,
-11.5024583074757)) ;
#140448 = CARTESIAN_POINT('Ctrl Pts',(4.42678327414413,-2.79999999844302,
-11.4672494087483)) ;
#140449 = CARTESIAN_POINT('Ctrl Pts',(4.42864654534549,-2.79999999875722,
-11.4599688987024)) ;
#140450 = CARTESIAN_POINT('Ctrl Pts',(4.43060908635821,-2.79999999907333,
-11.4527059171227)) ;
#140451 = CARTESIAN_POINT('Ctrl Pts',(4.43267155768736,-2.79999999933982,
-11.4454607590652)) ;
#140452 = CARTESIAN_POINT('Ctrl Pts',(4.43529000378769,-2.79999999967816,
-11.4362625435099)) ;
#140453 = CARTESIAN_POINT('Ctrl Pts',(4.4380733085653,-2.79999999966609,-11.4270911025424)) ;
#140454 = CARTESIAN_POINT('Ctrl Pts',(4.44102157277562,-2.79999999954234,
-11.4179480782015)) ;
#140455 = CARTESIAN_POINT('Ctrl Pts',(4.4504649956914,-2.79999999914597,-11.388662559869)) ;
#140456 = CARTESIAN_POINT('Ctrl Pts',(4.46157908226633,-2.79999999505379,
-11.3597202134932)) ;
#140457 = CARTESIAN_POINT('Ctrl Pts',(4.47540732315415,-2.79999999166095,
-11.3322492625065)) ;
#140458 = CARTESIAN_POINT('Ctrl Pts',(4.47702479055525,-2.79999999126409,
-11.3290360289464)) ;
#140459 = CARTESIAN_POINT('Ctrl Pts',(4.47867903313992,-2.79999999107055,
-11.3258427221255)) ;
#140460 = CARTESIAN_POINT('Ctrl Pts',(4.48037187481471,-2.79999999105954,
-11.322671097194)) ;
#140461 = CARTESIAN_POINT('Ctrl Pts',(4.48545039983908,-2.79999999102651,
-11.3131562223995)) ;
#140462 = CARTESIAN_POINT('Ctrl Pts',(4.49087631667453,-2.79999999265304,
-11.3038364846096)) ;
#140463 = CARTESIAN_POINT('Ctrl Pts',(4.49669887079745,-2.79999999431461,
-11.2947592728789)) ;
#140464 = CARTESIAN_POINT('Ctrl Pts',(4.5088870500619,-2.79999999779274,-11.2757582157036)) ;
#140465 = CARTESIAN_POINT('Ctrl Pts',(4.52313265843748,-2.79999999982394,
-11.25737449918)) ;
#140466 = CARTESIAN_POINT('Ctrl Pts',(4.54066913339539,-2.79999999997241,
-11.2427304219711)) ;
#140467 = CARTESIAN_POINT('Ctrl Pts',(4.54329026609835,-2.79999999999461,
-11.240541608668)) ;
#140468 = CARTESIAN_POINT('Ctrl Pts',(4.5460045281952,-2.8,-11.2384393445787)) ;
#140469 = CARTESIAN_POINT('Ctrl Pts',(4.54880363749517,-2.8,-11.236450206041)) ;
#140470 = CARTESIAN_POINT('',(4.4,-2.8,-10.1600000000039)) ;
#140471 = CARTESIAN_POINT('Ctrl Pts',(4.54879236168152,-2.8,-11.23643444348)) ;
#140472 = CARTESIAN_POINT('Ctrl Pts',(4.51096310105345,-2.8,-11.2076409078196)) ;
#140473 = CARTESIAN_POINT('Ctrl Pts',(4.49022331291407,-2.8,-11.1638291192761)) ;
#140474 = CARTESIAN_POINT('Ctrl Pts',(4.45698031182017,-2.8,-11.0776238713958)) ;
#140475 = CARTESIAN_POINT('Ctrl Pts',(4.44561000227039,-2.8,-11.0323611449586)) ;
#140476 = CARTESIAN_POINT('Ctrl Pts',(4.41911102299977,-2.8,-10.8958807916569)) ;
#140477 = CARTESIAN_POINT('Ctrl Pts',(4.41155688769424,-2.8,-10.804231375192)) ;
#140478 = CARTESIAN_POINT('Ctrl Pts',(4.39763503647248,-2.8,-10.528710456933)) ;
#140479 = CARTESIAN_POINT('Ctrl Pts',(4.4,-2.8,-10.3442606621178)) ;
#140480 = CARTESIAN_POINT('Ctrl Pts',(4.4,-2.8,-10.1600000000039)) ;
#140481 = CARTESIAN_POINT('',(4.54879236179094,-2.79999999953044,-9.08356555650414)) ;
#140482 = CARTESIAN_POINT('Ctrl Pts',(4.4,-2.8,-10.1600000000039)) ;
#140483 = CARTESIAN_POINT('Ctrl Pts',(4.4,-2.8,-9.9754847183429)) ;
#140484 = CARTESIAN_POINT('Ctrl Pts',(4.39760751905643,-2.8,-9.79078367328513)) ;
#140485 = CARTESIAN_POINT('Ctrl Pts',(4.40696794948104,-2.8,-9.60658932370333)) ;
#140486 = CARTESIAN_POINT('Ctrl Pts',(4.41164816469334,-2.8,-9.51449214891243)) ;
#140487 = CARTESIAN_POINT('Ctrl Pts',(4.41940496802384,-2.80000000000001,
-9.42215714350079)) ;
#140488 = CARTESIAN_POINT('Ctrl Pts',(4.43698455094238,-2.8,-9.3320661537484)) ;
#140489 = CARTESIAN_POINT('Ctrl Pts',(4.44577434240166,-2.8,-9.2870206588722)) ;
#140490 = CARTESIAN_POINT('Ctrl Pts',(4.456925956929,-2.80000000000001,-9.24247691748965)) ;
#140491 = CARTESIAN_POINT('Ctrl Pts',(4.47366127850409,-2.8,-9.19911940609041)) ;
#140492 = CARTESIAN_POINT('Ctrl Pts',(4.47575319370098,-2.8,-9.19369971716552)) ;
#140493 = CARTESIAN_POINT('Ctrl Pts',(4.47791173590511,-2.79999999997843,
-9.18827415478058)) ;
#140494 = CARTESIAN_POINT('Ctrl Pts',(4.48016062485992,-2.80000000010461,
-9.18287328752205)) ;
#140495 = CARTESIAN_POINT('Ctrl Pts',(4.48803173620173,-2.80000000054624,
-9.1639702521172)) ;
#140496 = CARTESIAN_POINT('Ctrl Pts',(4.49700942865457,-2.80000000534986,
-9.14536966581437)) ;
#140497 = CARTESIAN_POINT('Ctrl Pts',(4.50810946414921,-2.80000000469598,
-9.12838166513933)) ;
#140498 = CARTESIAN_POINT('Ctrl Pts',(4.51435323411495,-2.80000000432818,
-9.11882591475961)) ;
#140499 = CARTESIAN_POINT('Ctrl Pts',(4.52126852668377,-2.80000000204489,
-9.10978039655139)) ;
#140500 = CARTESIAN_POINT('Ctrl Pts',(4.5290361256546,-2.80000000089509,-9.10147828666764)) ;
#140501 = CARTESIAN_POINT('Ctrl Pts',(4.5320568585877,-2.80000000044794,-9.09824968837951)) ;
#140502 = CARTESIAN_POINT('Ctrl Pts',(4.53520648971123,-2.80000000018876,
-9.09513351912811)) ;
#140503 = CARTESIAN_POINT('Ctrl Pts',(4.53849565154303,-2.80000000008376,
-9.09214349280593)) ;
#140504 = CARTESIAN_POINT('Ctrl Pts',(4.54178481337482,-2.79999999997876,
-9.08915346648376)) ;
#140505 = CARTESIAN_POINT('Ctrl Pts',(4.54521363891047,-2.8,-9.08628975782186)) ;
#140506 = CARTESIAN_POINT('Ctrl Pts',(4.54879236168087,-2.8,-9.08356555651953)) ;
#140507 = CARTESIAN_POINT('',(4.4,-2.8,-8.63684537882721)) ;
#140508 = CARTESIAN_POINT('Ctrl Pts',(4.54879236168109,-2.79999999812176,
-9.08356555651923)) ;
#140509 = CARTESIAN_POINT('Ctrl Pts',(4.54599316991904,-2.79999999835896,
-9.08157561433548)) ;
#140510 = CARTESIAN_POINT('Ctrl Pts',(4.54327885465675,-2.7999999985882,-9.07947265683989)) ;
#140511 = CARTESIAN_POINT('Ctrl Pts',(4.52311604063301,-2.80000000023132,
-9.06263105969308)) ;
#140512 = CARTESIAN_POINT('Ctrl Pts',(4.50886780632329,-2.80000000100534,
-9.04424219964313)) ;
#140513 = CARTESIAN_POINT('Ctrl Pts',(4.48892103801305,-2.79999999510253,
-9.01312902183043)) ;
#140514 = CARTESIAN_POINT('Ctrl Pts',(4.4818652331329,-2.79999999099551,-9.00058320502371)) ;
#140515 = CARTESIAN_POINT('Ctrl Pts',(4.46162186753408,-2.79999997126272,
-8.96025671394186)) ;
#140516 = CARTESIAN_POINT('Ctrl Pts',(4.45052849087262,-2.7999999685384,-8.93131896170922)) ;
#140517 = CARTESIAN_POINT('Ctrl Pts',(4.43813540717735,-2.79999997674815,
-8.8929060591291)) ;
#140518 = CARTESIAN_POINT('Ctrl Pts',(4.43535270120344,-2.79999997903695,
-8.88375026405077)) ;
#140519 = CARTESIAN_POINT('Ctrl Pts',(4.41677772587857,-2.79999999273252,
-8.81866880149579)) ;
#140520 = CARTESIAN_POINT('Ctrl Pts',(4.40678488791117,-2.79999999887621,
-8.76171951851187)) ;
#140521 = CARTESIAN_POINT('Ctrl Pts',(4.40081887576568,-2.80000000006435,
-8.68161989678019)) ;
#140522 = CARTESIAN_POINT('Ctrl Pts',(4.4,-2.8,-8.65930189818788)) ;
#140523 = CARTESIAN_POINT('Ctrl Pts',(4.4,-2.8,-8.63684537882721)) ;
#140524 = CARTESIAN_POINT('',(4.4,-2.8,-7.62)) ;
#140525 = CARTESIAN_POINT('',(4.4,-2.8,-7.62)) ;
#140526 = CARTESIAN_POINT('',(3.7,-2.8,-7.62)) ;
#140527 = CARTESIAN_POINT('',(3.6,-2.8,-7.62)) ;
#140528 = CARTESIAN_POINT('',(3.7,-2.8,-12.7)) ;
#140529 = CARTESIAN_POINT('',(3.7,-2.8,-12.7)) ;
#140530 = CARTESIAN_POINT('',(4.4,-2.8,-12.7)) ;
#140531 = CARTESIAN_POINT('',(3.6,-2.8,-12.7)) ;
#140532 = CARTESIAN_POINT('',(4.4,-2.8,-7.62)) ;
#140533 = CARTESIAN_POINT('Origin',(4.5,-2.8,-7.62)) ;
#140534 = CARTESIAN_POINT('',(4.5,-2.7,-7.62)) ;
#140535 = CARTESIAN_POINT('',(4.5,-2.4,-7.62)) ;
#140536 = CARTESIAN_POINT('',(4.5,-2.8,-7.62)) ;
#140537 = CARTESIAN_POINT('',(4.5,-2.7,-8.63684537882721)) ;
#140538 = CARTESIAN_POINT('',(4.5,-2.7,-7.62)) ;
#140539 = CARTESIAN_POINT('',(4.5,-2.4,-8.19785831296514)) ;
#140540 = CARTESIAN_POINT('Origin',(4.5,0.,-10.16)) ;
#140541 = CARTESIAN_POINT('',(4.5,-2.4,-7.62)) ;
#140542 = CARTESIAN_POINT('Origin',(4.5,-2.3,-7.62)) ;
#140543 = CARTESIAN_POINT('',(12.7,-2.3,-12.1221416870349)) ;
#140544 = CARTESIAN_POINT('',(4.6,-2.3,-12.1221416870349)) ;
#140545 = CARTESIAN_POINT('',(4.5,-2.3,-12.1221416870349)) ;
#140546 = CARTESIAN_POINT('',(4.6,-2.3,-12.7)) ;
#140547 = CARTESIAN_POINT('',(4.6,-2.3,-12.7)) ;
#140548 = CARTESIAN_POINT('',(12.7,-2.3,-12.7)) ;
#140549 = CARTESIAN_POINT('',(4.5,-2.3,-12.7)) ;
#140550 = CARTESIAN_POINT('',(12.7,-2.3,-7.62)) ;
#140551 = CARTESIAN_POINT('Origin',(0.,0.,-7.62)) ;
#140552 = CARTESIAN_POINT('Origin',(4.4,-2.7,-7.62)) ;
#140553 = CARTESIAN_POINT('Origin',(4.6,-2.4,-7.62)) ;
#140554 = CARTESIAN_POINT('Origin',(12.7,-2.2,-7.62)) ;
#140555 = CARTESIAN_POINT('Origin',(12.7,2.65,-7.62)) ;
#140556 = CARTESIAN_POINT('Origin',(4.55912712210514,2.85,-7.62)) ;
#140557 = CARTESIAN_POINT('Origin',(4.05,3.77568567655479,-7.62)) ;
#140558 = CARTESIAN_POINT('Origin',(3.85,6.92431432344521,-7.62)) ;
#140559 = CARTESIAN_POINT('Origin',(3.34087287789487,7.85,-7.62)) ;
#140560 = CARTESIAN_POINT('Origin',(3.,8.05,-7.62)) ;
#140561 = CARTESIAN_POINT('Origin',(3.,9.85,-7.62)) ;
#140562 = CARTESIAN_POINT('Origin',(3.3,10.05,-7.62)) ;
#140563 = CARTESIAN_POINT('Origin',(3.3,10.85,-7.62)) ;
#140564 = CARTESIAN_POINT('Origin',(-4.8,10.85,-7.62)) ;
#140565 = CARTESIAN_POINT('Origin',(-4.8,10.3,-7.62)) ;
#140566 = CARTESIAN_POINT('Origin',(-5.3,5.19009804864072,-7.62)) ;
#140567 = CARTESIAN_POINT('Origin',(-5.3,-3.95,-7.62)) ;
#140568 = CARTESIAN_POINT('Origin',(3.5,-3.95,-7.62)) ;
#140569 = CARTESIAN_POINT('Origin',(3.7,-2.9,-7.62)) ;
#140570 = CARTESIAN_POINT('Origin',(0.,0.,-12.7)) ;
#140571 = CARTESIAN_POINT('Origin',(4.4,-2.7,-12.7)) ;
#140572 = CARTESIAN_POINT('Origin',(3.7,-2.9,-12.7)) ;
#140573 = CARTESIAN_POINT('Origin',(3.5,-3.95,-12.7)) ;
#140574 = CARTESIAN_POINT('Origin',(-5.3,-3.95,-12.7)) ;
#140575 = CARTESIAN_POINT('Origin',(-5.3,5.19009804864072,-12.7)) ;
#140576 = CARTESIAN_POINT('Origin',(-4.8,10.3,-12.7)) ;
#140577 = CARTESIAN_POINT('Origin',(-4.8,10.85,-12.7)) ;
#140578 = CARTESIAN_POINT('Origin',(3.3,10.85,-12.7)) ;
#140579 = CARTESIAN_POINT('Origin',(3.3,10.05,-12.7)) ;
#140580 = CARTESIAN_POINT('Origin',(3.,9.85,-12.7)) ;
#140581 = CARTESIAN_POINT('Origin',(3.,8.05,-12.7)) ;
#140582 = CARTESIAN_POINT('Origin',(3.34087287789487,7.85,-12.7)) ;
#140583 = CARTESIAN_POINT('Origin',(3.85,6.92431432344521,-12.7)) ;
#140584 = CARTESIAN_POINT('Origin',(4.05,3.77568567655479,-12.7)) ;
#140585 = CARTESIAN_POINT('Origin',(4.55912712210514,2.85,-12.7)) ;
#140586 = CARTESIAN_POINT('Origin',(12.7,2.65,-12.7)) ;
#140587 = CARTESIAN_POINT('Origin',(12.7,-2.2,-12.7)) ;
#140588 = CARTESIAN_POINT('Origin',(4.6,-2.4,-12.7)) ;
#140589 = CARTESIAN_POINT('Origin',(-4.65,1.95,-12.16)) ;
#140590 = CARTESIAN_POINT('',(-4.66204490261456,3.21928058320648,-12.16)) ;
#140591 = CARTESIAN_POINT('',(-5.3,3.9369800677651,-12.16)) ;
#140592 = CARTESIAN_POINT('',(-5.47474093186837,4.13356361611701,-12.16)) ;
#140593 = CARTESIAN_POINT('',(-5.3,-1.88819660112501,-12.16)) ;
#140594 = CARTESIAN_POINT('',(-5.3,-2.05,-12.16)) ;
#140595 = CARTESIAN_POINT('',(-4.66204490261456,-1.5692190524323,-12.16)) ;
#140596 = CARTESIAN_POINT('',(-4.69472135955,-1.58555728090001,-12.16)) ;
#140597 = CARTESIAN_POINT('',(-4.66204490261456,3.35625,-12.16)) ;
#140598 = CARTESIAN_POINT('Origin',(-5.4,1.95,-8.16)) ;
#140599 = CARTESIAN_POINT('',(-4.66204490261456,-1.5692190524323,-8.16)) ;
#140600 = CARTESIAN_POINT('',(-5.3,-1.88819660112502,-8.16)) ;
#140601 = CARTESIAN_POINT('',(-5.44472135955,-1.96055728090001,-8.16)) ;
#140602 = CARTESIAN_POINT('',(-5.3,3.9369800677651,-8.16)) ;
#140603 = CARTESIAN_POINT('',(-5.3,4.20000000000001,-8.16)) ;
#140604 = CARTESIAN_POINT('',(-4.66204490261456,3.21928058320648,-8.16)) ;
#140605 = CARTESIAN_POINT('',(-4.72474093186837,3.28981361611701,-8.16)) ;
#140606 = CARTESIAN_POINT('',(-4.66204490261456,-1.67500000000001,-8.16)) ;
#140607 = CARTESIAN_POINT('Origin',(-4.65,1.95,-8.16)) ;
#140608 = CARTESIAN_POINT('',(-3.33134808452128,1.85,-8.4823371348948)) ;
#140609 = CARTESIAN_POINT('',(-3.48082994825801,1.91712723223402,-8.44579712375915)) ;
#140610 = CARTESIAN_POINT('Origin',(-3.34328863644876,2.02341244982311,-8.47941833331253)) ;
#140611 = CARTESIAN_POINT('',(-2.4,1.85,-8.71)) ;
#140612 = CARTESIAN_POINT('',(-4.65,1.85,-8.16)) ;
#140613 = CARTESIAN_POINT('',(-2.4,-0.95,-8.71)) ;
#140614 = CARTESIAN_POINT('',(-2.4,1.95,-8.71)) ;
#140615 = CARTESIAN_POINT('',(-3.3526478932023,-0.95,-8.47713051499499)) ;
#140616 = CARTESIAN_POINT('',(-3.39999999999998,-0.95,-8.46555555555556)) ;
#140617 = CARTESIAN_POINT('',(-3.44209061230229,-0.971114561800017,-8.455266739215)) ;
#140618 = CARTESIAN_POINT('Origin',(-3.36201220558124,-1.11033257691482,-8.47484146085793)) ;
#140619 = CARTESIAN_POINT('',(-4.63829959356686,-1.5692190524323,-8.16286009935032)) ;
#140620 = CARTESIAN_POINT('',(-4.68814869588294,-1.59414360359034,-8.15067476322861)) ;
#140621 = CARTESIAN_POINT('',(-4.63829959356686,3.21928058320648,-8.16286009935032)) ;
#140622 = CARTESIAN_POINT('',(-4.63829959356686,3.35625,-8.16286009935032)) ;
#140623 = CARTESIAN_POINT('',(-3.45989661114215,1.89357722797868,-8.45091416172081)) ;
#140624 = CARTESIAN_POINT('Origin',(-2.4,1.95,-8.71)) ;
#140625 = CARTESIAN_POINT('',(-2.4,1.85,-11.61)) ;
#140626 = CARTESIAN_POINT('',(-2.4,-0.95,-11.61)) ;
#140627 = CARTESIAN_POINT('',(-2.4,1.95,-11.61)) ;
#140628 = CARTESIAN_POINT('',(-2.4,-1.05,-11.507055690472)) ;
#140629 = CARTESIAN_POINT('Origin',(-2.4,-0.949999999999936,-11.5070556904719)) ;
#140630 = CARTESIAN_POINT('',(-2.4,-1.05,-8.81294430952801)) ;
#140631 = CARTESIAN_POINT('',(-2.4,-1.05,-8.71)) ;
#140632 = CARTESIAN_POINT('Origin',(-2.4,-0.9499999999999,-8.8129443095281)) ;
#140633 = CARTESIAN_POINT('',(-2.4,1.95,-8.81294430952801)) ;
#140634 = CARTESIAN_POINT('Origin',(-2.4,1.84999999999991,-8.81294430952809)) ;
#140635 = CARTESIAN_POINT('',(-2.4,1.95,-11.507055690472)) ;
#140636 = CARTESIAN_POINT('',(-2.4,1.95,-8.71)) ;
#140637 = CARTESIAN_POINT('Origin',(-2.4,1.85000000000013,-11.5070556904721)) ;
#140638 = CARTESIAN_POINT('Origin',(-2.4,1.95,-11.61)) ;
#140639 = CARTESIAN_POINT('',(-3.3526478932023,-0.95,-11.842869485005)) ;
#140640 = CARTESIAN_POINT('',(-3.44209061230229,-0.971114561800017,-11.864733260785)) ;
#140641 = CARTESIAN_POINT('Origin',(-3.36201220558131,-1.11033257691521,-11.8451585391422)) ;
#140642 = CARTESIAN_POINT('',(-2.4,-0.95,-11.61)) ;
#140643 = CARTESIAN_POINT('',(-3.33134808452128,1.85,-11.8376628651052)) ;
#140644 = CARTESIAN_POINT('',(-2.4,1.85,-11.61)) ;
#140645 = CARTESIAN_POINT('',(-3.48082994825801,1.91712723223402,-11.8742028762408)) ;
#140646 = CARTESIAN_POINT('Origin',(-3.34328863644893,2.02341244982219,-11.8405816666875)) ;
#140647 = CARTESIAN_POINT('',(-4.63829959356686,3.21928058320648,-12.1571399006497)) ;
#140648 = CARTESIAN_POINT('',(-4.70989661114216,3.29982722797869,-12.1746413938348)) ;
#140649 = CARTESIAN_POINT('',(-4.63829959356686,-1.5692190524323,-12.1571399006497)) ;
#140650 = CARTESIAN_POINT('',(-4.63829959356686,-1.67500000000001,-12.1571399006497)) ;
#140651 = CARTESIAN_POINT('',(-3.43814869588292,-0.969143603590331,-11.8637696812158)) ;
#140652 = CARTESIAN_POINT('Origin',(0.,1.95,-10.16)) ;
#140653 = CARTESIAN_POINT('',(-3.35509339356897,1.95,-8.57947703554448)) ;
#140654 = CARTESIAN_POINT('',(0.175392621986784,1.95,-9.44248472823589)) ;
#140655 = CARTESIAN_POINT('',(-3.35509339356897,1.95,-11.7405229644555)) ;
#140656 = CARTESIAN_POINT('',(-3.35509339356897,1.95,-11.8544444444444)) ;
#140657 = CARTESIAN_POINT('',(0.175392621986784,1.95,-10.8775152717641)) ;
#140658 = CARTESIAN_POINT('Origin',(0.,-1.05,-10.16)) ;
#140659 = CARTESIAN_POINT('',(-3.37639320225,-1.05,-11.7457295843553)) ;
#140660 = CARTESIAN_POINT('',(-3.42374530904768,-1.05,-11.7573045437948)) ;
#140661 = CARTESIAN_POINT('',(-3.37639320225,-1.05,-8.57427041564467)) ;
#140662 = CARTESIAN_POINT('',(-3.37639320225,-1.05,-10.16)) ;
#140663 = CARTESIAN_POINT('',(-2.4237453090477,-1.05,-8.80713990064968)) ;
#140664 = CARTESIAN_POINT('Origin',(-3.39999999999998,-1.05,-10.16)) ;
#140665 = CARTESIAN_POINT('',(-3.4211145618,-1.06055728090001,-8.55240663986467)) ;
#140666 = CARTESIAN_POINT('',(-3.4211145618,-1.06055728090001,-11.7675933601353)) ;
#140667 = CARTESIAN_POINT('',(-3.4211145618,-1.06055728090001,-10.16)) ;
#140668 = CARTESIAN_POINT('',(-4.61732354306457,-1.65866177153229,-12.06)) ;
#140669 = CARTESIAN_POINT('',(-4.66717264538064,-1.68358632269033,-12.0721853361217)) ;
#140670 = CARTESIAN_POINT('',(-5.34472135954999,-2.022360679775,-12.06)) ;
#140671 = CARTESIAN_POINT('',(-5.4,-2.05,-12.06)) ;
#140672 = CARTESIAN_POINT('',(-5.34472135954999,-2.022360679775,-8.26)) ;
#140673 = CARTESIAN_POINT('',(-5.34472135954999,-2.022360679775,-8.16)) ;
#140674 = CARTESIAN_POINT('',(-4.61732354306457,-1.65866177153229,-8.26)) ;
#140675 = CARTESIAN_POINT('',(-4.65,-1.67500000000001,-8.26)) ;
#140676 = CARTESIAN_POINT('',(-3.41717264538063,-1.05858632269032,-8.55337021943385)) ;
#140677 = CARTESIAN_POINT('Origin',(-5.4,4.20000000000001,-7.62)) ;
#140678 = CARTESIAN_POINT('',(-5.37474093186837,4.17158354835192,-8.26)) ;
#140679 = CARTESIAN_POINT('',(-5.37474093186837,4.17158354835192,-12.06)) ;
#140680 = CARTESIAN_POINT('',(-5.37474093186837,4.17158354835192,-12.16)) ;
#140681 = CARTESIAN_POINT('',(-4.58730397074619,3.28571696708947,-12.06)) ;
#140682 = CARTESIAN_POINT('',(-4.65,3.35625,-12.06)) ;
#140683 = CARTESIAN_POINT('',(-3.42983432543734,1.98356361611701,-11.7770629755912)) ;
#140684 = CARTESIAN_POINT('',(-3.40890098832149,1.96001361186167,-11.7719459376295)) ;
#140685 = CARTESIAN_POINT('',(-3.42983432543734,1.98356361611701,-8.54293702440883)) ;
#140686 = CARTESIAN_POINT('',(-3.42983432543734,1.98356361611701,-8.46555555555556)) ;
#140687 = CARTESIAN_POINT('',(-4.58730397074619,3.28571696708947,-8.26)) ;
#140688 = CARTESIAN_POINT('',(-4.65890098832149,3.36626361186168,-8.24249850681493)) ;
#140689 = CARTESIAN_POINT('',(-5.4,4.20000000000001,-8.26)) ;
#140690 = CARTESIAN_POINT('Origin',(-3.15,-3.9,-9.16)) ;
#140691 = CARTESIAN_POINT('',(-3.15,-3.95,-9.26)) ;
#140692 = CARTESIAN_POINT('',(-3.15,-3.85,-9.26)) ;
#140693 = CARTESIAN_POINT('',(-3.15,-3.75,-9.26)) ;
#140694 = CARTESIAN_POINT('',(-3.15,-3.85,-11.06)) ;
#140695 = CARTESIAN_POINT('',(-3.15,-3.85,-9.16)) ;
#140696 = CARTESIAN_POINT('',(-3.15,-3.95,-11.06)) ;
#140697 = CARTESIAN_POINT('',(-3.15,-4.05,-11.06)) ;
#140698 = CARTESIAN_POINT('',(-3.15,-3.95,-9.16)) ;
#140699 = CARTESIAN_POINT('Origin',(-4.4,-3.9,-11.16)) ;
#140700 = CARTESIAN_POINT('',(-3.25,-3.85,-11.16)) ;
#140701 = CARTESIAN_POINT('',(-4.3,-3.85,-11.16)) ;
#140702 = CARTESIAN_POINT('',(-4.4,-3.85,-11.16)) ;
#140703 = CARTESIAN_POINT('',(-4.3,-3.95,-11.16)) ;
#140704 = CARTESIAN_POINT('',(-4.3,-4.05,-11.16)) ;
#140705 = CARTESIAN_POINT('',(-3.25,-3.95,-11.16)) ;
#140706 = CARTESIAN_POINT('',(-4.4,-3.95,-11.16)) ;
#140707 = CARTESIAN_POINT('',(-3.25,-3.75,-11.16)) ;
#140708 = CARTESIAN_POINT('Origin',(-4.4,-3.9,-9.16)) ;
#140709 = CARTESIAN_POINT('',(-4.4,-3.85,-11.06)) ;
#140710 = CARTESIAN_POINT('',(-4.4,-3.85,-9.26)) ;
#140711 = CARTESIAN_POINT('',(-4.4,-3.85,-9.16)) ;
#140712 = CARTESIAN_POINT('',(-4.4,-3.95,-9.26)) ;
#140713 = CARTESIAN_POINT('',(-4.4,-4.05,-9.26)) ;
#140714 = CARTESIAN_POINT('',(-4.4,-3.95,-11.06)) ;
#140715 = CARTESIAN_POINT('',(-4.4,-3.95,-9.16)) ;
#140716 = CARTESIAN_POINT('',(-4.4,-3.75,-11.06)) ;
#140717 = CARTESIAN_POINT('Origin',(-4.4,-3.9,-9.16)) ;
#140718 = CARTESIAN_POINT('',(-4.3,-3.95,-9.16)) ;
#140719 = CARTESIAN_POINT('',(-4.3,-3.85,-9.16)) ;
#140720 = CARTESIAN_POINT('',(-4.3,-3.75,-9.16)) ;
#140721 = CARTESIAN_POINT('',(-3.25,-3.85,-9.16)) ;
#140722 = CARTESIAN_POINT('',(-4.4,-3.85,-9.16)) ;
#140723 = CARTESIAN_POINT('',(-3.25,-3.95,-9.16)) ;
#140724 = CARTESIAN_POINT('',(-3.25,-4.05,-9.16)) ;
#140725 = CARTESIAN_POINT('',(-4.4,-3.95,-9.16)) ;
#140726 = CARTESIAN_POINT('Origin',(0.,-3.75,-10.16)) ;
#140727 = CARTESIAN_POINT('',(-3.25,-3.75,-9.26)) ;
#140728 = CARTESIAN_POINT('',(-4.3,-3.75,-9.26)) ;
#140729 = CARTESIAN_POINT('',(-1.56125112837913E-16,-3.75,-9.26)) ;
#140730 = CARTESIAN_POINT('',(-4.3,-3.75,-11.06)) ;
#140731 = CARTESIAN_POINT('',(-4.3,-3.75,-10.16)) ;
#140732 = CARTESIAN_POINT('',(-3.25,-3.75,-11.06)) ;
#140733 = CARTESIAN_POINT('',(-1.56125112837913E-16,-3.75,-11.06)) ;
#140734 = CARTESIAN_POINT('',(-3.25,-3.75,-10.16)) ;
#140735 = CARTESIAN_POINT('',(-4.15,-3.75,-11.01)) ;
#140736 = CARTESIAN_POINT('',(-3.4,-3.75,-11.01)) ;
#140737 = CARTESIAN_POINT('',(-4.15,-3.75,-11.01)) ;
#140738 = CARTESIAN_POINT('',(-4.25,-3.75,-10.91)) ;
#140739 = CARTESIAN_POINT('Origin',(-4.15,-3.75,-10.91)) ;
#140740 = CARTESIAN_POINT('',(-4.25,-3.75,-9.41)) ;
#140741 = CARTESIAN_POINT('',(-4.25,-3.75,-9.41)) ;
#140742 = CARTESIAN_POINT('',(-4.15,-3.75,-9.31)) ;
#140743 = CARTESIAN_POINT('Origin',(-4.15,-3.75,-9.41)) ;
#140744 = CARTESIAN_POINT('',(-3.4,-3.75,-9.31)) ;
#140745 = CARTESIAN_POINT('',(-3.4,-3.75,-9.31)) ;
#140746 = CARTESIAN_POINT('',(-3.3,-3.75,-9.41)) ;
#140747 = CARTESIAN_POINT('Origin',(-3.4,-3.75,-9.41)) ;
#140748 = CARTESIAN_POINT('',(-3.3,-3.75,-10.91)) ;
#140749 = CARTESIAN_POINT('',(-3.3,-3.75,-10.91)) ;
#140750 = CARTESIAN_POINT('Origin',(-3.4,-3.75,-10.91)) ;
#140751 = CARTESIAN_POINT('Origin',(-3.4,-3.75,-10.91)) ;
#140752 = CARTESIAN_POINT('',(-3.4,-3.9,-11.01)) ;
#140753 = CARTESIAN_POINT('',(-3.3,-3.9,-10.91)) ;
#140754 = CARTESIAN_POINT('Origin',(-3.4,-3.9,-10.91)) ;
#140755 = CARTESIAN_POINT('',(-3.4,-3.75,-11.01)) ;
#140756 = CARTESIAN_POINT('',(-3.3,-3.75,-10.91)) ;
#140757 = CARTESIAN_POINT('Origin',(-4.15,-3.75,-11.01)) ;
#140758 = CARTESIAN_POINT('',(-4.15,-3.9,-11.01)) ;
#140759 = CARTESIAN_POINT('',(-4.15,-3.9,-11.01)) ;
#140760 = CARTESIAN_POINT('',(-4.15,-3.75,-11.01)) ;
#140761 = CARTESIAN_POINT('Origin',(-4.15,-3.75,-10.91)) ;
#140762 = CARTESIAN_POINT('',(-4.25,-3.9,-10.91)) ;
#140763 = CARTESIAN_POINT('Origin',(-4.15,-3.9,-10.91)) ;
#140764 = CARTESIAN_POINT('',(-4.25,-3.75,-10.91)) ;
#140765 = CARTESIAN_POINT('Origin',(-4.25,-3.75,-9.41)) ;
#140766 = CARTESIAN_POINT('',(-4.25,-3.9,-9.41)) ;
#140767 = CARTESIAN_POINT('',(-4.25,-3.9,-9.41)) ;
#140768 = CARTESIAN_POINT('',(-4.25,-3.75,-9.41)) ;
#140769 = CARTESIAN_POINT('Origin',(-4.15,-3.75,-9.41)) ;
#140770 = CARTESIAN_POINT('',(-4.15,-3.9,-9.31)) ;
#140771 = CARTESIAN_POINT('Origin',(-4.15,-3.9,-9.41)) ;
#140772 = CARTESIAN_POINT('',(-4.15,-3.75,-9.31)) ;
#140773 = CARTESIAN_POINT('Origin',(-3.4,-3.75,-9.31)) ;
#140774 = CARTESIAN_POINT('',(-3.4,-3.9,-9.31)) ;
#140775 = CARTESIAN_POINT('',(-3.4,-3.9,-9.31)) ;
#140776 = CARTESIAN_POINT('',(-3.4,-3.75,-9.31)) ;
#140777 = CARTESIAN_POINT('Origin',(-3.4,-3.75,-9.41)) ;
#140778 = CARTESIAN_POINT('',(-3.3,-3.9,-9.41)) ;
#140779 = CARTESIAN_POINT('Origin',(-3.4,-3.9,-9.41)) ;
#140780 = CARTESIAN_POINT('',(-3.3,-3.75,-9.41)) ;
#140781 = CARTESIAN_POINT('Origin',(-3.3,-3.75,-10.91)) ;
#140782 = CARTESIAN_POINT('',(-3.3,-3.9,-10.91)) ;
#140783 = CARTESIAN_POINT('Origin',(0.,-3.9,-10.16)) ;
#140784 = CARTESIAN_POINT('Origin',(0.,9.95,-10.16)) ;
#140785 = CARTESIAN_POINT('',(-0.230887397576972,9.95,-8.24513942814623)) ;
#140786 = CARTESIAN_POINT('Origin',(-0.321518176280637,8.95,-8.2874012543203)) ;
#140787 = CARTESIAN_POINT('',(-0.321518176280637,9.05,-8.2874012543203)) ;
#140788 = CARTESIAN_POINT('',(1.22782596331729,9.85,-11.609980483939)) ;
#140789 = CARTESIAN_POINT('Origin',(-1.22782596331729,8.95,-8.710019516061)) ;
#140790 = CARTESIAN_POINT('',(-1.22782596331729,9.05,-8.710019516061)) ;
#140791 = CARTESIAN_POINT('',(-1.22782596331729,9.85,-8.710019516061)) ;
#140792 = CARTESIAN_POINT('Origin',(0.,8.95,-10.16)) ;
#140793 = CARTESIAN_POINT('',(-0.362523114814661,8.95,-10.3290473046963)) ;
#140794 = CARTESIAN_POINT('',(0.36252311481466,8.95,-9.99095269530372)) ;
#140795 = CARTESIAN_POINT('Origin',(-2.65,10.8,-11.16)) ;
#140796 = CARTESIAN_POINT('',(-2.65,10.75,-11.06)) ;
#140797 = CARTESIAN_POINT('',(-2.65,10.75,-9.26)) ;
#140798 = CARTESIAN_POINT('',(-2.65,10.75,-11.16)) ;
#140799 = CARTESIAN_POINT('',(-2.65,10.85,-9.26)) ;
#140800 = CARTESIAN_POINT('',(-2.65,10.95,-9.26)) ;
#140801 = CARTESIAN_POINT('',(-2.65,10.85,-11.06)) ;
#140802 = CARTESIAN_POINT('',(-2.65,10.85,-11.16)) ;
#140803 = CARTESIAN_POINT('',(-2.65,10.65,-11.06)) ;
#140804 = CARTESIAN_POINT('Origin',(-3.9,10.8,-9.16)) ;
#140805 = CARTESIAN_POINT('',(-2.75,10.85,-9.16)) ;
#140806 = CARTESIAN_POINT('',(-2.75,10.75,-9.16)) ;
#140807 = CARTESIAN_POINT('',(-2.75,10.65,-9.16)) ;
#140808 = CARTESIAN_POINT('',(-3.8,10.75,-9.16)) ;
#140809 = CARTESIAN_POINT('',(-3.9,10.75,-9.16)) ;
#140810 = CARTESIAN_POINT('',(-3.8,10.85,-9.16)) ;
#140811 = CARTESIAN_POINT('',(-3.8,10.95,-9.16)) ;
#140812 = CARTESIAN_POINT('',(-3.9,10.85,-9.16)) ;
#140813 = CARTESIAN_POINT('Origin',(-3.9,10.8,-11.16)) ;
#140814 = CARTESIAN_POINT('',(-3.9,10.85,-9.26)) ;
#140815 = CARTESIAN_POINT('',(-3.9,10.75,-9.26)) ;
#140816 = CARTESIAN_POINT('',(-3.9,10.65,-9.26)) ;
#140817 = CARTESIAN_POINT('',(-3.9,10.75,-11.06)) ;
#140818 = CARTESIAN_POINT('',(-3.9,10.75,-11.16)) ;
#140819 = CARTESIAN_POINT('',(-3.9,10.85,-11.06)) ;
#140820 = CARTESIAN_POINT('',(-3.9,10.95,-11.06)) ;
#140821 = CARTESIAN_POINT('',(-3.9,10.85,-11.16)) ;
#140822 = CARTESIAN_POINT('Origin',(-3.9,10.8,-11.16)) ;
#140823 = CARTESIAN_POINT('',(-3.8,10.75,-11.16)) ;
#140824 = CARTESIAN_POINT('',(-2.75,10.75,-11.16)) ;
#140825 = CARTESIAN_POINT('',(-3.9,10.75,-11.16)) ;
#140826 = CARTESIAN_POINT('',(-2.75,10.85,-11.16)) ;
#140827 = CARTESIAN_POINT('',(-2.75,10.95,-11.16)) ;
#140828 = CARTESIAN_POINT('',(-3.8,10.85,-11.16)) ;
#140829 = CARTESIAN_POINT('',(-3.9,10.85,-11.16)) ;
#140830 = CARTESIAN_POINT('',(-3.8,10.65,-11.16)) ;
#140831 = CARTESIAN_POINT('Origin',(0.,10.65,-10.16)) ;
#140832 = CARTESIAN_POINT('',(-3.8,10.65,-9.26)) ;
#140833 = CARTESIAN_POINT('',(-2.75,10.65,-9.26)) ;
#140834 = CARTESIAN_POINT('',(1.56125112837912E-16,10.65,-9.26)) ;
#140835 = CARTESIAN_POINT('',(-2.75,10.65,-11.06)) ;
#140836 = CARTESIAN_POINT('',(-2.75,10.65,-10.16)) ;
#140837 = CARTESIAN_POINT('',(-3.8,10.65,-11.06)) ;
#140838 = CARTESIAN_POINT('',(-1.56125112837913E-16,10.65,-11.06)) ;
#140839 = CARTESIAN_POINT('',(-3.8,10.65,-10.16)) ;
#140840 = CARTESIAN_POINT('',(-3.65,10.65,-9.31)) ;
#140841 = CARTESIAN_POINT('',(-2.9,10.65,-9.31)) ;
#140842 = CARTESIAN_POINT('',(-3.65,10.65,-9.31)) ;
#140843 = CARTESIAN_POINT('',(-3.75,10.65,-9.41)) ;
#140844 = CARTESIAN_POINT('Origin',(-3.65,10.65,-9.41)) ;
#140845 = CARTESIAN_POINT('',(-3.75,10.65,-10.91)) ;
#140846 = CARTESIAN_POINT('',(-3.75,10.65,-10.91)) ;
#140847 = CARTESIAN_POINT('',(-3.65,10.65,-11.01)) ;
#140848 = CARTESIAN_POINT('Origin',(-3.65,10.65,-10.91)) ;
#140849 = CARTESIAN_POINT('',(-2.9,10.65,-11.01)) ;
#140850 = CARTESIAN_POINT('',(-2.9,10.65,-11.01)) ;
#140851 = CARTESIAN_POINT('',(-2.8,10.65,-10.91)) ;
#140852 = CARTESIAN_POINT('Origin',(-2.9,10.65,-10.91)) ;
#140853 = CARTESIAN_POINT('',(-2.8,10.65,-9.41)) ;
#140854 = CARTESIAN_POINT('',(-2.8,10.65,-9.41)) ;
#140855 = CARTESIAN_POINT('Origin',(-2.9,10.65,-9.41)) ;
#140856 = CARTESIAN_POINT('Origin',(-2.9,10.65,-9.41)) ;
#140857 = CARTESIAN_POINT('',(-2.8,10.7,-9.41)) ;
#140858 = CARTESIAN_POINT('',(-2.8,10.65,-9.41)) ;
#140859 = CARTESIAN_POINT('',(-2.9,10.7,-9.31)) ;
#140860 = CARTESIAN_POINT('Origin',(-2.9,10.7,-9.41)) ;
#140861 = CARTESIAN_POINT('',(-2.9,10.65,-9.31)) ;
#140862 = CARTESIAN_POINT('Origin',(-3.65,10.65,-9.31)) ;
#140863 = CARTESIAN_POINT('',(-3.65,10.7,-9.31)) ;
#140864 = CARTESIAN_POINT('',(-3.65,10.7,-9.31)) ;
#140865 = CARTESIAN_POINT('',(-3.65,10.65,-9.31)) ;
#140866 = CARTESIAN_POINT('Origin',(-3.65,10.65,-9.41)) ;
#140867 = CARTESIAN_POINT('',(-3.75,10.7,-9.41)) ;
#140868 = CARTESIAN_POINT('Origin',(-3.65,10.7,-9.41)) ;
#140869 = CARTESIAN_POINT('',(-3.75,10.65,-9.41)) ;
#140870 = CARTESIAN_POINT('Origin',(-3.75,10.65,-10.91)) ;
#140871 = CARTESIAN_POINT('',(-3.75,10.7,-10.91)) ;
#140872 = CARTESIAN_POINT('',(-3.75,10.7,-10.91)) ;
#140873 = CARTESIAN_POINT('',(-3.75,10.65,-10.91)) ;
#140874 = CARTESIAN_POINT('Origin',(-3.65,10.65,-10.91)) ;
#140875 = CARTESIAN_POINT('',(-3.65,10.7,-11.01)) ;
#140876 = CARTESIAN_POINT('Origin',(-3.65,10.7,-10.91)) ;
#140877 = CARTESIAN_POINT('',(-3.65,10.65,-11.01)) ;
#140878 = CARTESIAN_POINT('Origin',(-2.9,10.65,-11.01)) ;
#140879 = CARTESIAN_POINT('',(-2.9,10.7,-11.01)) ;
#140880 = CARTESIAN_POINT('',(-2.9,10.7,-11.01)) ;
#140881 = CARTESIAN_POINT('',(-2.9,10.65,-11.01)) ;
#140882 = CARTESIAN_POINT('Origin',(-2.9,10.65,-10.91)) ;
#140883 = CARTESIAN_POINT('',(-2.8,10.7,-10.91)) ;
#140884 = CARTESIAN_POINT('Origin',(-2.9,10.7,-10.91)) ;
#140885 = CARTESIAN_POINT('',(-2.8,10.65,-10.91)) ;
#140886 = CARTESIAN_POINT('Origin',(-2.8,10.65,-9.41)) ;
#140887 = CARTESIAN_POINT('',(-2.8,10.7,-9.41)) ;
#140888 = CARTESIAN_POINT('Origin',(0.,10.8,-10.16)) ;
#140889 = CARTESIAN_POINT('',(-3.65,10.8,-9.41)) ;
#140890 = CARTESIAN_POINT('',(-2.9,10.8,-9.41)) ;
#140891 = CARTESIAN_POINT('',(0.,10.8,-9.41)) ;
#140892 = CARTESIAN_POINT('',(-2.9,10.8,-10.91)) ;
#140893 = CARTESIAN_POINT('',(-2.9,10.8,-10.16)) ;
#140894 = CARTESIAN_POINT('',(-3.65,10.8,-10.91)) ;
#140895 = CARTESIAN_POINT('',(0.,10.8,-10.91)) ;
#140896 = CARTESIAN_POINT('',(-3.65,10.8,-10.16)) ;
#140897 = CARTESIAN_POINT('Origin',(4.5,2.75,-11.535)) ;
#140898 = CARTESIAN_POINT('',(4.5,2.63356010126946,-11.5544066497884)) ;
#140899 = CARTESIAN_POINT('',(4.6,2.11643989873054,-11.6405933502116)) ;
#140900 = CARTESIAN_POINT('',(4.6,2.11643989873054,-11.6405933502116)) ;
#140901 = CARTESIAN_POINT('',(12.7,2.11643989873054,-11.6405933502116)) ;
#140902 = CARTESIAN_POINT('',(12.8,2.11643989873054,-11.6405933502116)) ;
#140903 = CARTESIAN_POINT('',(12.7,2.75,-11.535)) ;
#140904 = CARTESIAN_POINT('Origin',(4.5,2.,-11.66)) ;
#140905 = CARTESIAN_POINT('',(4.6,2.,-11.5419539578284)) ;
#140906 = CARTESIAN_POINT('',(4.6,2.,-8.66)) ;
#140907 = CARTESIAN_POINT('',(12.7,2.,-11.5419539578284)) ;
#140908 = CARTESIAN_POINT('',(12.7,2.,-11.66)) ;
#140909 = CARTESIAN_POINT('',(4.5,2.,-11.5419539578284)) ;
#140910 = CARTESIAN_POINT('Origin',(4.5,2.,-8.66)) ;
#140911 = CARTESIAN_POINT('',(4.6,2.63356010126946,-8.76559335021158)) ;
#140912 = CARTESIAN_POINT('',(4.6,2.63356010126947,-8.76559335021158)) ;
#140913 = CARTESIAN_POINT('',(4.5,2.63356010126946,-8.76559335021158)) ;
#140914 = CARTESIAN_POINT('',(12.7,2.,-8.66)) ;
#140915 = CARTESIAN_POINT('Origin',(4.5,0.,-10.16)) ;
#140916 = CARTESIAN_POINT('',(4.5,2.72431432344521,-8.85263481664499)) ;
#140917 = CARTESIAN_POINT('',(4.5,2.72431432344521,-10.16)) ;
#140918 = CARTESIAN_POINT('',(4.5,2.61712020253893,-8.86423274259479)) ;
#140919 = CARTESIAN_POINT('Origin',(4.5,2.65,-8.66695395782836)) ;
#140920 = CARTESIAN_POINT('',(4.5,2.1,-8.77804604217164)) ;
#140921 = CARTESIAN_POINT('',(4.5,2.1,-8.77804604217164)) ;
#140922 = CARTESIAN_POINT('',(4.5,2.1,-11.5419539578284)) ;
#140923 = CARTESIAN_POINT('',(4.5,2.1,-11.66)) ;
#140924 = CARTESIAN_POINT('',(4.5,2.61712020253893,-11.4557672574052)) ;
#140925 = CARTESIAN_POINT('Origin',(10.3,0.,-10.16)) ;
#140926 = CARTESIAN_POINT('Origin',(0.584645609909621,0.,-10.16)) ;
#140927 = CARTESIAN_POINT('',(4.6,-2.32258064516129,-8.2611532060953)) ;
#140928 = CARTESIAN_POINT('',(4.6,-2.79310344827574,-9.06520635404194)) ;
#140929 = CARTESIAN_POINT('Origin',(4.6,0.,-10.16)) ;
#140930 = CARTESIAN_POINT('',(4.6,-2.79310344827574,-11.2547936459581)) ;
#140931 = CARTESIAN_POINT('Origin',(4.6,0.,-10.16)) ;
#140932 = CARTESIAN_POINT('',(4.6,-2.32258064516129,-12.0588467939047)) ;
#140933 = CARTESIAN_POINT('Origin',(4.6,0.,-10.16)) ;
#140934 = CARTESIAN_POINT('',(12.7,-2.32258064516129,-12.0588467939047)) ;
#140935 = CARTESIAN_POINT('',(0.584645609909621,-2.32258064516129,-12.0588467939047)) ;
#140936 = CARTESIAN_POINT('',(12.7,-2.32258064516129,-8.2611532060953)) ;
#140937 = CARTESIAN_POINT('Origin',(12.7,0.,-10.16)) ;
#140938 = CARTESIAN_POINT('',(0.584645609909621,-2.32258064516129,-8.2611532060953)) ;
#140939 = CARTESIAN_POINT('Ctrl Pts',(-5.37474093186837,4.17158354835192,
-8.26)) ;
#140940 = CARTESIAN_POINT('Ctrl Pts',(-5.4,4.2,-8.26)) ;
#140941 = CARTESIAN_POINT('Ctrl Pts',(-5.4,4.23801993223491,-8.26)) ;
#140942 = CARTESIAN_POINT('Ctrl Pts',(-5.37474093064202,4.17158354697228,
-8.23374656406105)) ;
#140943 = CARTESIAN_POINT('Ctrl Pts',(-5.4,4.19999999724801,-8.22248141279891)) ;
#140944 = CARTESIAN_POINT('Ctrl Pts',(-5.4,4.23801992976516,-8.20749312809024)) ;
#140945 = CARTESIAN_POINT('Ctrl Pts',(-5.36668583490655,4.14629949399955,
-8.20780128688413)) ;
#140946 = CARTESIAN_POINT('Ctrl Pts',(-5.4,4.16739198385624,-8.18466783506585)) ;
#140947 = CARTESIAN_POINT('Ctrl Pts',(-5.4,4.20557579169425,-8.15560257376828)) ;
#140948 = CARTESIAN_POINT('Ctrl Pts',(-5.3390138046061,4.05944006555646,-8.17077735687856)) ;
#140949 = CARTESIAN_POINT('Ctrl Pts',(-5.4,4.06625640449639,-8.14313263661412)) ;
#140950 = CARTESIAN_POINT('Ctrl Pts',(-5.4,4.09411900298411,-8.0815547137571)) ;
#140951 = CARTESIAN_POINT('Ctrl Pts',(-5.31962206268973,3.99857154231912,
-8.16)) ;
#140952 = CARTESIAN_POINT('Ctrl Pts',(-5.4,3.99346933127518,-8.14200350742663)) ;
#140953 = CARTESIAN_POINT('Ctrl Pts',(-5.4,4.0160133758189,-8.06000000048129)) ;
#140954 = CARTESIAN_POINT('Ctrl Pts',(-5.3,3.9369800677651,-8.16)) ;
#140955 = CARTESIAN_POINT('Ctrl Pts',(-5.4,3.9369800677651,-8.16)) ;
#140956 = CARTESIAN_POINT('Ctrl Pts',(-5.4,3.9369800677651,-8.06)) ;
#140957 = CARTESIAN_POINT('Origin',(-5.3,4.23801993223491,-8.26)) ;
#140958 = CARTESIAN_POINT('Ctrl Pts',(-5.3,3.9369800677651,-8.16)) ;
#140959 = CARTESIAN_POINT('Ctrl Pts',(-5.31962206268973,3.99857154231912,
-8.16)) ;
#140960 = CARTESIAN_POINT('Ctrl Pts',(-5.3390138046061,4.05944006555646,-8.17077735687856)) ;
#140961 = CARTESIAN_POINT('Ctrl Pts',(-5.36668583490655,4.14629949399955,
-8.20780128688413)) ;
#140962 = CARTESIAN_POINT('Ctrl Pts',(-5.37474093064202,4.17158354697228,
-8.23374656406105)) ;
#140963 = CARTESIAN_POINT('Ctrl Pts',(-5.37474093186837,4.17158354835192,
-8.26)) ;
#140964 = CARTESIAN_POINT('Origin',(-5.3,3.9369800677651,-8.06)) ;
#140965 = CARTESIAN_POINT('Origin',(-4.6737453090477,1.85,-8.25713990064968)) ;
#140966 = CARTESIAN_POINT('Origin',(-3.35509339356897,1.85,-8.57947703554448)) ;
#140967 = CARTESIAN_POINT('Ctrl Pts',(-3.35509339356897,1.95,-8.57947703554448)) ;
#140968 = CARTESIAN_POINT('Ctrl Pts',(-3.33134808452128,1.95,-8.4823371348948)) ;
#140969 = CARTESIAN_POINT('Ctrl Pts',(-3.33134808452128,1.85,-8.4823371348948)) ;
#140970 = CARTESIAN_POINT('Ctrl Pts',(-3.38343213690417,1.95,-8.56562253880276)) ;
#140971 = CARTESIAN_POINT('Ctrl Pts',(-3.36046743872483,1.94345445676969,
-8.47521907053384)) ;
#140972 = CARTESIAN_POINT('Ctrl Pts',(-3.38803897426454,1.85000000162387,
-8.46847936184645)) ;
#140973 = CARTESIAN_POINT('Ctrl Pts',(-3.41101314049054,1.96238978305186,
-8.55213849291617)) ;
#140974 = CARTESIAN_POINT('Ctrl Pts',(-3.39538881861723,1.95068928167334,
-8.46668273322692)) ;
#140975 = CARTESIAN_POINT('Ctrl Pts',(-3.44316973238525,1.87475949194143,
-8.45500295430583)) ;
#140976 = CARTESIAN_POINT('Ctrl Pts',(-3.42983432543734,1.98356361611701,
-8.54293702440883)) ;
#140977 = CARTESIAN_POINT('Ctrl Pts',(-3.42093333711585,1.97355000425533,
-8.4604385175939)) ;
#140978 = CARTESIAN_POINT('Ctrl Pts',(-3.48082994825801,1.91712723223402,
-8.44579712375915)) ;
#140979 = CARTESIAN_POINT('Origin',(-3.50457525730571,1.91712723223402,-8.54293702440883)) ;
#140980 = CARTESIAN_POINT('Origin',(-3.36128627567764,2.03621361435732,-8.57644940433519)) ;
#140981 = CARTESIAN_POINT('Origin',(-4.05330900605469,2.53445269957662,-8.40880210804797)) ;
#140982 = CARTESIAN_POINT('Origin',(-4.66204490261456,3.21928058320648,-8.26)) ;
#140983 = CARTESIAN_POINT('Origin',(-4.35749955255802,2.87666706439287,-8.26)) ;
#140984 = CARTESIAN_POINT('Origin',(-4.66204490261456,3.21928058320648,-8.26)) ;
#140985 = CARTESIAN_POINT('Origin',(-5.3,5.2,-8.06)) ;
#140986 = CARTESIAN_POINT('Origin',(-5.3,-1.88819660112502,-8.06)) ;
#140987 = CARTESIAN_POINT('Origin',(-5.3,4.23801993223491,-7.62)) ;
#140988 = CARTESIAN_POINT('Origin',(-5.3,4.23801993223491,-12.06)) ;
#140989 = CARTESIAN_POINT('Origin',(-3.35509339356897,2.05,-10.16)) ;
#140990 = CARTESIAN_POINT('Origin',(-3.36128627567776,2.03621361435703,-11.7435505956648)) ;
#140991 = CARTESIAN_POINT('Origin',(-2.4237453090477,1.85,-11.5128600993503)) ;
#140992 = CARTESIAN_POINT('Origin',(-3.35509339356897,1.85,-11.7405229644555)) ;
#140993 = CARTESIAN_POINT('Origin',(-4.66204490261456,3.21928058320648,-8.26)) ;
#140994 = CARTESIAN_POINT('Origin',(-4.66204490261456,3.21928058320648,-8.26)) ;
#140995 = CARTESIAN_POINT('Ctrl Pts',(-5.29976814257748,-1.88802911972919,
-8.15999982737782)) ;
#140996 = CARTESIAN_POINT('Ctrl Pts',(-5.4,-1.88802831720456,-8.16023259354297)) ;
#140997 = CARTESIAN_POINT('Ctrl Pts',(-5.4,-1.88791746283072,-8.06000016246237)) ;
#140998 = CARTESIAN_POINT('Ctrl Pts',(-5.31153957531165,-1.92331224822998,
-8.15998646768893)) ;
#140999 = CARTESIAN_POINT('Ctrl Pts',(-5.4,-1.92148676945297,-8.14897789253814)) ;
#141000 = CARTESIAN_POINT('Ctrl Pts',(-5.4,-1.94671708614658,-8.05993171302843)) ;
#141001 = CARTESIAN_POINT('Ctrl Pts',(-5.32318090226696,-1.95817527052249,
-8.17078449726811)) ;
#141002 = CARTESIAN_POINT('Ctrl Pts',(-5.4,-1.96527310172483,-8.15216338375281)) ;
#141003 = CARTESIAN_POINT('Ctrl Pts',(-5.4,-2.00485091174287,-8.08149607488934)) ;
#141004 = CARTESIAN_POINT('Ctrl Pts',(-5.33978950165955,-2.00789652656156,
-8.20786496501965)) ;
#141005 = CARTESIAN_POINT('Ctrl Pts',(-5.4,-2.02908601268744,-8.1913665145317)) ;
#141006 = CARTESIAN_POINT('Ctrl Pts',(-5.4,-2.08777005652399,-8.15566121263604)) ;
#141007 = CARTESIAN_POINT('Ctrl Pts',(-5.34461954754097,-2.02234798681676,
-8.2338461447183)) ;
#141008 = CARTESIAN_POINT('Ctrl Pts',(-5.4,-2.04997459329993,-8.22567566483998)) ;
#141009 = CARTESIAN_POINT('Ctrl Pts',(-5.4,-2.1118797455067,-8.20765768697394)) ;
#141010 = CARTESIAN_POINT('Ctrl Pts',(-5.34460423617423,-2.02230212313483,
-8.26012475187013)) ;
#141011 = CARTESIAN_POINT('Ctrl Pts',(-5.4,-2.04990938338631,-8.26016375427653)) ;
#141012 = CARTESIAN_POINT('Ctrl Pts',(-5.4,-2.11180321723903,-8.26024966888043)) ;
#141013 = CARTESIAN_POINT('Origin',(-5.29999999999998,-1.88819660112496,-8.26000000000004)) ;
#141014 = CARTESIAN_POINT('Origin',(-5.3,-2.11180339887499,-8.26)) ;
#141015 = CARTESIAN_POINT('Ctrl Pts',(-5.3,3.9369800677651,-12.16)) ;
#141016 = CARTESIAN_POINT('Ctrl Pts',(-5.4,3.9369800677651,-12.16)) ;
#141017 = CARTESIAN_POINT('Ctrl Pts',(-5.4,3.9369800677651,-12.26)) ;
#141018 = CARTESIAN_POINT('Ctrl Pts',(-5.31962206268973,3.9985715423191,-12.16)) ;
#141019 = CARTESIAN_POINT('Ctrl Pts',(-5.40000000000019,3.99346933127519,
-12.1779964925734)) ;
#141020 = CARTESIAN_POINT('Ctrl Pts',(-5.4,4.01601337581888,-12.2599999995187)) ;
#141021 = CARTESIAN_POINT('Ctrl Pts',(-5.33901380460608,4.05944006555649,
-12.1492226431214)) ;
#141022 = CARTESIAN_POINT('Ctrl Pts',(-5.39999999999997,4.06625640449642,
-12.1768673633858)) ;
#141023 = CARTESIAN_POINT('Ctrl Pts',(-5.4,4.09411900298413,-12.2384452862428)) ;
#141024 = CARTESIAN_POINT('Ctrl Pts',(-5.36668583490657,4.14629949399951,
-12.1121987131159)) ;
#141025 = CARTESIAN_POINT('Ctrl Pts',(-5.40000000000003,4.16739198385622,
-12.1353321649343)) ;
#141026 = CARTESIAN_POINT('Ctrl Pts',(-5.4,4.20557579169423,-12.1643974262318)) ;
#141027 = CARTESIAN_POINT('Ctrl Pts',(-5.37474093064202,4.17158354697228,
-12.0862534359389)) ;
#141028 = CARTESIAN_POINT('Ctrl Pts',(-5.4,4.19999999724801,-12.097518587201)) ;
#141029 = CARTESIAN_POINT('Ctrl Pts',(-5.4,4.23801992976516,-12.1125068719097)) ;
#141030 = CARTESIAN_POINT('Ctrl Pts',(-5.37474093186837,4.17158354835192,
-12.06)) ;
#141031 = CARTESIAN_POINT('Ctrl Pts',(-5.4,4.2,-12.06)) ;
#141032 = CARTESIAN_POINT('Ctrl Pts',(-5.4,4.23801993223491,-12.06)) ;
#141033 = CARTESIAN_POINT('Origin',(-5.3,3.9369800677651,-12.26)) ;
#141034 = CARTESIAN_POINT('Ctrl Pts',(-5.37474093186837,4.17158354835192,
-12.06)) ;
#141035 = CARTESIAN_POINT('Ctrl Pts',(-5.37474093064202,4.17158354697228,
-12.0862534359389)) ;
#141036 = CARTESIAN_POINT('Ctrl Pts',(-5.36668583490657,4.14629949399951,
-12.1121987131159)) ;
#141037 = CARTESIAN_POINT('Ctrl Pts',(-5.33901380460608,4.05944006555649,
-12.1492226431214)) ;
#141038 = CARTESIAN_POINT('Ctrl Pts',(-5.31962206268973,3.9985715423191,-12.16)) ;
#141039 = CARTESIAN_POINT('Ctrl Pts',(-5.3,3.9369800677651,-12.16)) ;
#141040 = CARTESIAN_POINT('Ctrl Pts',(-3.42983432543734,1.98356361611701,
-11.7770629755912)) ;
#141041 = CARTESIAN_POINT('Ctrl Pts',(-3.42093333711585,1.97355000425533,
-11.8595614824061)) ;
#141042 = CARTESIAN_POINT('Ctrl Pts',(-3.48082994825801,1.91712723223402,
-11.8742028762408)) ;
#141043 = CARTESIAN_POINT('Ctrl Pts',(-3.41101314049054,1.96238978305186,
-11.7678615070838)) ;
#141044 = CARTESIAN_POINT('Ctrl Pts',(-3.39538881861728,1.95068928167332,
-11.8533172667731)) ;
#141045 = CARTESIAN_POINT('Ctrl Pts',(-3.44316973238528,1.87475949194142,
-11.8649970456942)) ;
#141046 = CARTESIAN_POINT('Ctrl Pts',(-3.38343213690417,1.95,-11.7543774611972)) ;
#141047 = CARTESIAN_POINT('Ctrl Pts',(-3.36046743872479,1.94345445676969,
-11.8447809294662)) ;
#141048 = CARTESIAN_POINT('Ctrl Pts',(-3.38803897426452,1.85000000162387,
-11.8515206381536)) ;
#141049 = CARTESIAN_POINT('Ctrl Pts',(-3.35509339356897,1.95,-11.7405229644555)) ;
#141050 = CARTESIAN_POINT('Ctrl Pts',(-3.33134808452128,1.95,-11.8376628651052)) ;
#141051 = CARTESIAN_POINT('Ctrl Pts',(-3.33134808452128,1.85,-11.8376628651052)) ;
#141052 = CARTESIAN_POINT('Origin',(-3.50457525730571,1.91712723223402,-11.7770629755912)) ;
#141053 = CARTESIAN_POINT('Origin',(-4.66204490261456,1.95,-8.26)) ;
#141054 = CARTESIAN_POINT('Origin',(-4.66204490261456,-1.5692190524323,-8.26)) ;
#141055 = CARTESIAN_POINT('Origin',(-3.84472135955,-1.16055728090002,-8.26)) ;
#141056 = CARTESIAN_POINT('Origin',(-4.66204490261456,-1.5692190524323,-8.26)) ;
#141057 = CARTESIAN_POINT('Origin',(-5.3,-2.11180339887499,-7.62)) ;
#141058 = CARTESIAN_POINT('Origin',(-5.3,-2.11180339887499,-12.06)) ;
#141059 = CARTESIAN_POINT('Origin',(-5.3,1.95,-12.26)) ;
#141060 = CARTESIAN_POINT('Origin',(-5.3,-1.88819660112501,-12.26)) ;
#141061 = CARTESIAN_POINT('Origin',(-4.0264650697994,2.50425327128942,-12.06)) ;
#141062 = CARTESIAN_POINT('Origin',(-4.66204490261456,3.21928058320648,-12.06)) ;
#141063 = CARTESIAN_POINT('Origin',(-3.02790825149799,1.38087685070033,-11.6605443741715)) ;
#141064 = CARTESIAN_POINT('Origin',(-4.66204490261456,3.21928058320648,-12.06)) ;
#141065 = CARTESIAN_POINT('Origin',(-4.66204490261456,-1.5692190524323,-8.26)) ;
#141066 = CARTESIAN_POINT('Origin',(-4.66204490261456,-1.5692190524323,-8.26)) ;
#141067 = CARTESIAN_POINT('Ctrl Pts',(-5.34460423617423,-2.02230212313483,
-12.0598752481299)) ;
#141068 = CARTESIAN_POINT('Ctrl Pts',(-5.4,-2.04990938338631,-12.0598362457235)) ;
#141069 = CARTESIAN_POINT('Ctrl Pts',(-5.4,-2.11180321723903,-12.0597503311196)) ;
#141070 = CARTESIAN_POINT('Ctrl Pts',(-5.34461954754098,-2.02234798681676,
-12.0861538552817)) ;
#141071 = CARTESIAN_POINT('Ctrl Pts',(-5.4,-2.04997459329993,-12.09432433516)) ;
#141072 = CARTESIAN_POINT('Ctrl Pts',(-5.4,-2.1118797455067,-12.1123423130261)) ;
#141073 = CARTESIAN_POINT('Ctrl Pts',(-5.33978950165958,-2.00789652656157,
-12.1121350349804)) ;
#141074 = CARTESIAN_POINT('Ctrl Pts',(-5.4,-2.02908601268744,-12.1286334854683)) ;
#141075 = CARTESIAN_POINT('Ctrl Pts',(-5.4,-2.08777005652399,-12.164338787364)) ;
#141076 = CARTESIAN_POINT('Ctrl Pts',(-5.32318090226695,-1.95817527052248,
-12.1492155027319)) ;
#141077 = CARTESIAN_POINT('Ctrl Pts',(-5.4,-1.96527310172483,-12.1678366162472)) ;
#141078 = CARTESIAN_POINT('Ctrl Pts',(-5.4,-2.00485091174288,-12.2385039251107)) ;
#141079 = CARTESIAN_POINT('Ctrl Pts',(-5.31153957531166,-1.92331224822999,
-12.1600135323111)) ;
#141080 = CARTESIAN_POINT('Ctrl Pts',(-5.40000000000019,-1.92148676945297,
-12.1710221074619)) ;
#141081 = CARTESIAN_POINT('Ctrl Pts',(-5.4,-1.94671708614658,-12.2600682869716)) ;
#141082 = CARTESIAN_POINT('Ctrl Pts',(-5.29976814257748,-1.88802911972919,
-12.1600001726222)) ;
#141083 = CARTESIAN_POINT('Ctrl Pts',(-5.4,-1.88802831720457,-12.159767406457)) ;
#141084 = CARTESIAN_POINT('Ctrl Pts',(-5.4,-1.88791746283074,-12.2599998375376)) ;
#141085 = CARTESIAN_POINT('Origin',(-5.30000000000005,-1.88819660112517,-12.0600000000001)) ;
#141086 = CARTESIAN_POINT('Origin',(-4.66204490261456,3.21928058320648,-12.06)) ;
#141087 = CARTESIAN_POINT('Origin',(-4.66204490261456,3.21928058320648,-12.06)) ;
#141088 = CARTESIAN_POINT('Origin',(0.175392621986784,-0.95,-9.44248472823589)) ;
#141089 = CARTESIAN_POINT('Origin',(-3.37639320225,-0.95,-8.57427041564467)) ;
#141090 = CARTESIAN_POINT('Origin',(-3.32804538583365,-0.902219294041845,
-8.58608877076867)) ;
#141091 = CARTESIAN_POINT('Origin',(-3.46583592134999,-0.971114561800017,
-8.55240663986467)) ;
#141092 = CARTESIAN_POINT('Origin',(-3.24472135955,-0.860557280900019,-12.06)) ;
#141093 = CARTESIAN_POINT('Origin',(-4.66204490261456,-1.5692190524323,-12.06)) ;
#141094 = CARTESIAN_POINT('Origin',(-4.66204490261456,1.95,-12.06)) ;
#141095 = CARTESIAN_POINT('Origin',(-4.66204490261456,-1.5692190524323,-12.06)) ;
#141096 = CARTESIAN_POINT('Ctrl Pts',(-3.4211145618,-1.06055728090001,-8.55240663986467)) ;
#141097 = CARTESIAN_POINT('Ctrl Pts',(-3.40394191641935,-1.05197095820969,
-8.46459197598638)) ;
#141098 = CARTESIAN_POINT('Ctrl Pts',(-3.44209061230229,-0.971114561800017,
-8.455266739215)) ;
#141099 = CARTESIAN_POINT('Ctrl Pts',(-3.40727897628737,-1.05363948814369,
-8.55917070399163)) ;
#141100 = CARTESIAN_POINT('Ctrl Pts',(-3.38665319245547,-1.04670310838587,
-8.46881810851093)) ;
#141101 = CARTESIAN_POINT('Ctrl Pts',(-3.4144159452097,-0.957277229261619,
-8.46203165783763)) ;
#141102 = CARTESIAN_POINT('Ctrl Pts',(-3.39186274464429,-1.05,-8.56670752825188)) ;
#141103 = CARTESIAN_POINT('Ctrl Pts',(-3.36870744055524,-1.04639008266724,
-8.47320484786421)) ;
#141104 = CARTESIAN_POINT('Ctrl Pts',(-3.38358960366098,-0.950000000886305,
-8.46956698577176)) ;
#141105 = CARTESIAN_POINT('Ctrl Pts',(-3.37639320225,-1.05,-8.57427041564467)) ;
#141106 = CARTESIAN_POINT('Ctrl Pts',(-3.3526478932023,-1.05,-8.47713051499499)) ;
#141107 = CARTESIAN_POINT('Ctrl Pts',(-3.3526478932023,-0.95,-8.47713051499499)) ;
#141108 = CARTESIAN_POINT('Origin',(-3.37639320224955,-1.15000000000196,-8.57427041564492)) ;
#141109 = CARTESIAN_POINT('Origin',(-4.66204490261456,-1.5692190524323,-12.06)) ;
#141110 = CARTESIAN_POINT('Origin',(-4.66204490261456,-1.5692190524323,-12.06)) ;
#141111 = CARTESIAN_POINT('Origin',(-3.37639320225,-1.15,-10.16)) ;
#141112 = CARTESIAN_POINT('Origin',(-3.37639320224944,-1.15000000000305,-11.745729584355)) ;
#141113 = CARTESIAN_POINT('Origin',(-1.50751564693271,0.00804557540861825,
-11.2888928486111)) ;
#141114 = CARTESIAN_POINT('Origin',(-3.46583592134999,-0.971114561800017,
-11.7675933601353)) ;
#141115 = CARTESIAN_POINT('Ctrl Pts',(-3.37639320225,-1.05,-11.7457295843553)) ;
#141116 = CARTESIAN_POINT('Ctrl Pts',(-3.3526478932023,-1.05,-11.842869485005)) ;
#141117 = CARTESIAN_POINT('Ctrl Pts',(-3.3526478932023,-0.95,-11.842869485005)) ;
#141118 = CARTESIAN_POINT('Ctrl Pts',(-3.3918627446443,-1.05,-11.7532924717481)) ;
#141119 = CARTESIAN_POINT('Ctrl Pts',(-3.36870744055522,-1.04639008266722,
-11.8467951521358)) ;
#141120 = CARTESIAN_POINT('Ctrl Pts',(-3.38358960366098,-0.950000000886305,
-11.8504330142282)) ;
#141121 = CARTESIAN_POINT('Ctrl Pts',(-3.40727897628736,-1.05363948814369,
-11.7608292960084)) ;
#141122 = CARTESIAN_POINT('Ctrl Pts',(-3.38665319245549,-1.04670310838587,
-11.8511818914891)) ;
#141123 = CARTESIAN_POINT('Ctrl Pts',(-3.41441594520969,-0.957277229261623,
-11.8579683421624)) ;
#141124 = CARTESIAN_POINT('Ctrl Pts',(-3.4211145618,-1.06055728090001,-11.7675933601353)) ;
#141125 = CARTESIAN_POINT('Ctrl Pts',(-3.40394191641935,-1.05197095820969,
-11.8554080240136)) ;
#141126 = CARTESIAN_POINT('Ctrl Pts',(-3.44209061230229,-0.971114561800017,
-11.864733260785)) ;
#141127 = CARTESIAN_POINT('Origin',(-3.37639320225,-0.95,-11.7457295843553)) ;
#141128 = CARTESIAN_POINT('Origin',(0.175392621986784,-0.95,-10.8775152717641)) ;
#141129 = CARTESIAN_POINT('Origin',(12.7,2.65,-7.62)) ;
#141130 = CARTESIAN_POINT('Origin',(12.8,2.65,-11.6530460421716)) ;
#141131 = CARTESIAN_POINT('',(4.57524318173533,2.73534903669982,-11.6009351802097)) ;
#141132 = CARTESIAN_POINT('Origin',(4.65232986199875,2.66527023615951,-11.6487542111836)) ;
#141133 = CARTESIAN_POINT('Ctrl Pts',(4.57524318173533,2.73534903669982,-11.6009351802097)) ;
#141134 = CARTESIAN_POINT('Ctrl Pts',(4.5761458558036,2.73452842391049,-11.5995911511832)) ;
#141135 = CARTESIAN_POINT('Ctrl Pts',(4.57705238626145,2.73367683201793,-11.5982681293393)) ;
#141136 = CARTESIAN_POINT('Ctrl Pts',(4.5779495181309,2.73280244902548,-11.5969768488888)) ;
#141137 = CARTESIAN_POINT('Ctrl Pts',(4.58144263576927,2.72939790755547,-11.5919490545686)) ;
#141138 = CARTESIAN_POINT('Ctrl Pts',(4.58496694799967,2.72549786515199,-11.5871699445181)) ;
#141139 = CARTESIAN_POINT('Ctrl Pts',(4.58815670056882,2.72107165565079,-11.582698193853)) ;
#141140 = CARTESIAN_POINT('Ctrl Pts',(4.5906912384746,2.71755464437279,-11.5791449961299)) ;
#141141 = CARTESIAN_POINT('Ctrl Pts',(4.59301454561848,2.7137045982392,-11.5757863127243)) ;
#141142 = CARTESIAN_POINT('Ctrl Pts',(4.5949431309995,2.70950205848694,-11.5726749961674)) ;
#141143 = CARTESIAN_POINT('Ctrl Pts',(4.59651854606295,2.70606910472943,-11.5701334364214)) ;
#141144 = CARTESIAN_POINT('Ctrl Pts',(4.59783685868322,2.70233705077422,-11.5677160861571)) ;
#141145 = CARTESIAN_POINT('Ctrl Pts',(4.59873118971425,2.69838744819993,-11.5655323012123)) ;
#141146 = CARTESIAN_POINT('Ctrl Pts',(4.59916508318199,2.69647125978905,-11.5644728165364)) ;
#141147 = CARTESIAN_POINT('Ctrl Pts',(4.59949917984823,2.69450444432188,-11.563467798882)) ;
#141148 = CARTESIAN_POINT('Ctrl Pts',(4.5997144226265,2.692499226592,-11.5625263440994)) ;
#141149 = CARTESIAN_POINT('Ctrl Pts',(4.59990113259977,2.69075982259552,-11.5617096895352)) ;
#141150 = CARTESIAN_POINT('Ctrl Pts',(4.6,2.68896788689974,-11.5609303122145)) ;
#141151 = CARTESIAN_POINT('Ctrl Pts',(4.6,2.68715716172261,-11.5602056127633)) ;
#141152 = CARTESIAN_POINT('Origin',(4.5,2.1,-11.5419539578284)) ;
#141153 = CARTESIAN_POINT('Origin',(4.6,2.1,-11.5419539578284)) ;
#141154 = CARTESIAN_POINT('Origin',(12.7,2.1,-11.5419539578284)) ;
#141155 = CARTESIAN_POINT('Origin',(12.7,2.76643989873054,-11.6336393923832)) ;
#141156 = CARTESIAN_POINT('Origin',(12.7,2.13287979746107,-11.7392327425948)) ;
#141157 = CARTESIAN_POINT('Origin',(4.4,2.72431432344521,-10.16)) ;
#141158 = CARTESIAN_POINT('Ctrl Pts',(4.48762159086959,2.77250619842348,-8.77117568174948)) ;
#141159 = CARTESIAN_POINT('Ctrl Pts',(4.48806820038223,2.77169418112776,-8.77383556708983)) ;
#141160 = CARTESIAN_POINT('Ctrl Pts',(4.48852084821546,2.77084293101113,-8.77648271501847)) ;
#141161 = CARTESIAN_POINT('Ctrl Pts',(4.49012932137854,2.76769877392855,-8.78576300952073)) ;
#141162 = CARTESIAN_POINT('Ctrl Pts',(4.49131046584974,2.76517764467229,-8.79234413170344)) ;
#141163 = CARTESIAN_POINT('Ctrl Pts',(4.49351977821776,2.75978760391033,-8.80463528016206)) ;
#141164 = CARTESIAN_POINT('Ctrl Pts',(4.49455195297827,2.75697653750126,-8.8103677406013)) ;
#141165 = CARTESIAN_POINT('Ctrl Pts',(4.49620670090465,2.75163165728875,-8.81994332160325)) ;
#141166 = CARTESIAN_POINT('Ctrl Pts',(4.49686252944492,2.74924176842724,-8.82386402620333)) ;
#141167 = CARTESIAN_POINT('Ctrl Pts',(4.49822764032849,2.74331716058958,-8.83264463163462)) ;
#141168 = CARTESIAN_POINT('Ctrl Pts',(4.49890203357902,2.73961076902722,-8.8374865001603)) ;
#141169 = CARTESIAN_POINT('Ctrl Pts',(4.49975897856021,2.73206576252699,-8.84582777843958)) ;
#141170 = CARTESIAN_POINT('Ctrl Pts',(4.5,2.72833175948626,-8.84941900229172)) ;
#141171 = CARTESIAN_POINT('Ctrl Pts',(4.5,2.72431432344521,-8.85263481664499)) ;
#141172 = CARTESIAN_POINT('Ctrl Pts',(4.5,2.72431432344521,-11.467365183355)) ;
#141173 = CARTESIAN_POINT('Ctrl Pts',(4.5,2.72904669151454,-11.4711532753139)) ;
#141174 = CARTESIAN_POINT('Ctrl Pts',(4.4996664568447,2.73338556955604,-11.4754614101765)) ;
#141175 = CARTESIAN_POINT('Ctrl Pts',(4.49869539480385,2.74072289096416,-11.483980241438)) ;
#141176 = CARTESIAN_POINT('Ctrl Pts',(4.49811062025683,2.74382502998103,-11.4881080596589)) ;
#141177 = CARTESIAN_POINT('Ctrl Pts',(4.49664125196624,2.7502021169969,-11.4975592649406)) ;
#141178 = CARTESIAN_POINT('Ctrl Pts',(4.49570721389709,2.75339870015146,-11.5030103903194)) ;
#141179 = CARTESIAN_POINT('Ctrl Pts',(4.49363760641474,2.75952863263957,-11.5147517051871)) ;
#141180 = CARTESIAN_POINT('Ctrl Pts',(4.49249077386338,2.76240287369082,-11.521071225831)) ;
#141181 = CARTESIAN_POINT('Ctrl Pts',(4.49055019898869,2.76677757270145,-11.531914125621)) ;
#141182 = CARTESIAN_POINT('Ctrl Pts',(4.48975662823142,2.76842729450637,-11.5363872919227)) ;
#141183 = CARTESIAN_POINT('Ctrl Pts',(4.4885208482156,2.77084293101086,-11.5435172849807)) ;
#141184 = CARTESIAN_POINT('Ctrl Pts',(4.48806820038252,2.77169418112725,-11.5461644329085)) ;
#141185 = CARTESIAN_POINT('Ctrl Pts',(4.48762159086959,2.77250619842348,-11.5488243182478)) ;
#141186 = CARTESIAN_POINT('Origin',(4.6,2.1,-10.16)) ;
#141187 = CARTESIAN_POINT('Origin',(4.6,2.1,-8.77804604217164)) ;
#141188 = CARTESIAN_POINT('Origin',(4.6,2.1,-11.5419539578284)) ;
#141189 = CARTESIAN_POINT('Origin',(12.7,2.1,-11.5419539578284)) ;
#141190 = CARTESIAN_POINT('Origin',(12.7,1.9,-11.5419539578284)) ;
#141191 = CARTESIAN_POINT('Origin',(12.7,2.65,-7.62)) ;
#141192 = CARTESIAN_POINT('Origin',(4.5,2.65,-8.66695395782836)) ;
#141193 = CARTESIAN_POINT('',(4.6,2.68715716172261,-8.75979438723668)) ;
#141194 = CARTESIAN_POINT('',(4.57524318173443,2.73534903670064,-8.71906481978892)) ;
#141195 = CARTESIAN_POINT('Ctrl Pts',(4.6,2.68715716172261,-8.75979438723667)) ;
#141196 = CARTESIAN_POINT('Ctrl Pts',(4.6,2.6910603667141,-8.75823222277848)) ;
#141197 = CARTESIAN_POINT('Ctrl Pts',(4.59952510519174,2.69488861888984,-8.75640970947472)) ;
#141198 = CARTESIAN_POINT('Ctrl Pts',(4.59869497748256,2.69852743640765,-8.75439015122504)) ;
#141199 = CARTESIAN_POINT('Ctrl Pts',(4.59815316003465,2.70090246232124,-8.75307200236116)) ;
#141200 = CARTESIAN_POINT('Ctrl Pts',(4.59746001108779,2.70319720658045,-8.75167096804522)) ;
#141201 = CARTESIAN_POINT('Ctrl Pts',(4.59664880273703,2.70538659711789,-8.7502145418985)) ;
#141202 = CARTESIAN_POINT('Ctrl Pts',(4.59612777291939,2.70679281754376,-8.74927909609234)) ;
#141203 = CARTESIAN_POINT('Ctrl Pts',(4.59555051815356,2.70817855133085,-8.74830492990722)) ;
#141204 = CARTESIAN_POINT('Ctrl Pts',(4.59494172533681,2.70950512149367,-8.74732273606981)) ;
#141205 = CARTESIAN_POINT('Ctrl Pts',(4.59250947890864,2.7148050288701,-8.74339867949909)) ;
#141206 = CARTESIAN_POINT('Ctrl Pts',(4.58944857812998,2.71954517005242,-8.73908233758092)) ;
#141207 = CARTESIAN_POINT('Ctrl Pts',(4.58612768646824,2.72376361218905,-8.73447380318381)) ;
#141208 = CARTESIAN_POINT('Ctrl Pts',(4.58350334758182,2.72709724148711,-8.73083190297759)) ;
#141209 = CARTESIAN_POINT('Ctrl Pts',(4.58071664514666,2.73010548898771,-8.72700599593156)) ;
#141210 = CARTESIAN_POINT('Ctrl Pts',(4.5779495181309,2.73280244902547,-8.72302315111116)) ;
#141211 = CARTESIAN_POINT('Ctrl Pts',(4.57705238626115,2.73367683201821,-8.72173187066024)) ;
#141212 = CARTESIAN_POINT('Ctrl Pts',(4.576145855803,2.73452842391106,-8.72040884881589)) ;
#141213 = CARTESIAN_POINT('Ctrl Pts',(4.57524318173443,2.73534903670064,-8.71906481978892)) ;
#141214 = CARTESIAN_POINT('Origin',(4.65232986200533,2.66527023615349,-8.67124578881467)) ;
#141215 = CARTESIAN_POINT('Origin',(4.6,2.65,-8.66695395782836)) ;
#141216 = CARTESIAN_POINT('Origin',(12.7,1.9,-11.66)) ;
#141217 = CARTESIAN_POINT('Origin',(12.7,2.01643989873054,-8.56136060761679)) ;
#141218 = CARTESIAN_POINT('Origin',(-3.65,10.7,-9.41)) ;
#141219 = CARTESIAN_POINT('Origin',(-3.65,10.7,-9.41)) ;
#141220 = CARTESIAN_POINT('Origin',(-3.65,10.7,-9.41)) ;
#141221 = CARTESIAN_POINT('Origin',(0.,10.7,-9.41)) ;
#141222 = CARTESIAN_POINT('Origin',(-2.9,10.7,-9.41)) ;
#141223 = CARTESIAN_POINT('Origin',(-3.65,10.7,-10.16)) ;
#141224 = CARTESIAN_POINT('Origin',(-3.65,10.7,-10.91)) ;
#141225 = CARTESIAN_POINT('Origin',(-2.9,10.7,-9.41)) ;
#141226 = CARTESIAN_POINT('Origin',(-2.9,10.7,-9.41)) ;
#141227 = CARTESIAN_POINT('Origin',(-3.65,10.7,-10.91)) ;
#141228 = CARTESIAN_POINT('Origin',(-3.65,10.7,-10.91)) ;
#141229 = CARTESIAN_POINT('Origin',(-2.9,10.7,-10.16)) ;
#141230 = CARTESIAN_POINT('Origin',(-2.9,10.7,-10.91)) ;
#141231 = CARTESIAN_POINT('Origin',(0.,10.7,-10.91)) ;
#141232 = CARTESIAN_POINT('Origin',(-2.9,10.7,-10.91)) ;
#141233 = CARTESIAN_POINT('Origin',(-2.9,10.7,-10.91)) ;
#141234 = CARTESIAN_POINT('Origin',(-3.05,-3.95,-9.16)) ;
#141235 = CARTESIAN_POINT('Origin',(-3.05,-3.95,-11.06)) ;
#141236 = CARTESIAN_POINT('Origin',(-3.05,-3.95,-9.26)) ;
#141237 = CARTESIAN_POINT('Origin',(-3.25,-3.95,-9.26)) ;
#141238 = CARTESIAN_POINT('Origin',(-3.25,-3.95,-9.06)) ;
#141239 = CARTESIAN_POINT('Origin',(-3.25,-3.95,-9.26)) ;
#141240 = CARTESIAN_POINT('Origin',(-3.25,-3.95,-11.06)) ;
#141241 = CARTESIAN_POINT('Origin',(-3.25,-3.95,-11.06)) ;
#141242 = CARTESIAN_POINT('Origin',(-3.25,-3.95,-11.26)) ;
#141243 = CARTESIAN_POINT('Origin',(-4.4,-3.95,-9.06)) ;
#141244 = CARTESIAN_POINT('Origin',(-4.3,-3.95,-9.06)) ;
#141245 = CARTESIAN_POINT('Origin',(-3.25,-3.9,-9.26)) ;
#141246 = CARTESIAN_POINT('Origin',(-3.25,-3.85,-9.26)) ;
#141247 = CARTESIAN_POINT('Origin',(-3.25,-3.85,-10.16)) ;
#141248 = CARTESIAN_POINT('Origin',(-3.25,-3.85,-11.06)) ;
#141249 = CARTESIAN_POINT('Origin',(-3.25,-3.85,-9.26)) ;
#141250 = CARTESIAN_POINT('Origin',(-3.25,-3.9,-11.06)) ;
#141251 = CARTESIAN_POINT('Origin',(-3.25,-3.85,-11.06)) ;
#141252 = CARTESIAN_POINT('Origin',(-4.4,-3.95,-11.26)) ;
#141253 = CARTESIAN_POINT('Origin',(-4.3,-3.95,-11.26)) ;
#141254 = CARTESIAN_POINT('Origin',(-4.5,-3.95,-9.16)) ;
#141255 = CARTESIAN_POINT('Origin',(-4.5,-3.95,-9.26)) ;
#141256 = CARTESIAN_POINT('Origin',(-4.5,-3.95,-11.06)) ;
#141257 = CARTESIAN_POINT('Origin',(-4.3,-3.95,-9.26)) ;
#141258 = CARTESIAN_POINT('Origin',(-4.3,-3.95,-9.26)) ;
#141259 = CARTESIAN_POINT('Origin',(-3.25,-3.85,-9.26)) ;
#141260 = CARTESIAN_POINT('Origin',(-3.25,-3.85,-9.26)) ;
#141261 = CARTESIAN_POINT('Origin',(-3.25,-3.85,-11.06)) ;
#141262 = CARTESIAN_POINT('Origin',(-3.25,-3.85,-11.06)) ;
#141263 = CARTESIAN_POINT('Origin',(-4.3,-3.95,-11.06)) ;
#141264 = CARTESIAN_POINT('Origin',(-4.3,-3.95,-11.06)) ;
#141265 = CARTESIAN_POINT('Origin',(-4.3,-3.9,-9.26)) ;
#141266 = CARTESIAN_POINT('Origin',(-4.3,-3.85,-9.26)) ;
#141267 = CARTESIAN_POINT('Origin',(-1.56125112837913E-16,-3.85,-9.26)) ;
#141268 = CARTESIAN_POINT('Origin',(-4.3,-3.85,-9.26)) ;
#141269 = CARTESIAN_POINT('Origin',(-1.56125112837913E-16,-3.85,-11.06)) ;
#141270 = CARTESIAN_POINT('Origin',(-4.3,-3.85,-11.06)) ;
#141271 = CARTESIAN_POINT('Origin',(-4.3,-3.9,-11.06)) ;
#141272 = CARTESIAN_POINT('Origin',(-4.3,-3.85,-11.06)) ;
#141273 = CARTESIAN_POINT('Origin',(-4.3,-3.85,-9.26)) ;
#141274 = CARTESIAN_POINT('Origin',(-4.3,-3.85,-9.26)) ;
#141275 = CARTESIAN_POINT('Origin',(-4.3,-3.85,-11.06)) ;
#141276 = CARTESIAN_POINT('Origin',(-4.3,-3.85,-11.06)) ;
#141277 = CARTESIAN_POINT('Origin',(-4.3,-3.85,-10.16)) ;
#141278 = CARTESIAN_POINT('Origin',(-4.,10.85,-11.16)) ;
#141279 = CARTESIAN_POINT('Origin',(-4.,10.85,-11.06)) ;
#141280 = CARTESIAN_POINT('Origin',(-4.,10.85,-9.26)) ;
#141281 = CARTESIAN_POINT('Origin',(-3.8,10.85,-9.26)) ;
#141282 = CARTESIAN_POINT('Origin',(-3.8,10.85,-9.06)) ;
#141283 = CARTESIAN_POINT('Origin',(-3.8,10.85,-9.26)) ;
#141284 = CARTESIAN_POINT('Origin',(-3.8,10.85,-11.06)) ;
#141285 = CARTESIAN_POINT('Origin',(-3.8,10.85,-11.06)) ;
#141286 = CARTESIAN_POINT('Origin',(-3.8,10.85,-11.26)) ;
#141287 = CARTESIAN_POINT('Origin',(-3.9,10.85,-9.06)) ;
#141288 = CARTESIAN_POINT('Origin',(-2.75,10.85,-9.06)) ;
#141289 = CARTESIAN_POINT('Origin',(-3.8,10.8,-9.26)) ;
#141290 = CARTESIAN_POINT('Origin',(-3.8,10.75,-9.26)) ;
#141291 = CARTESIAN_POINT('Origin',(-3.8,10.75,-10.16)) ;
#141292 = CARTESIAN_POINT('Origin',(-3.8,10.75,-11.06)) ;
#141293 = CARTESIAN_POINT('Origin',(-3.8,10.75,-9.26)) ;
#141294 = CARTESIAN_POINT('Origin',(-3.8,10.8,-11.06)) ;
#141295 = CARTESIAN_POINT('Origin',(-3.8,10.75,-11.06)) ;
#141296 = CARTESIAN_POINT('Origin',(-3.9,10.85,-11.26)) ;
#141297 = CARTESIAN_POINT('Origin',(-2.75,10.85,-11.26)) ;
#141298 = CARTESIAN_POINT('Origin',(-2.55,10.85,-11.16)) ;
#141299 = CARTESIAN_POINT('Origin',(-2.55,10.85,-9.26)) ;
#141300 = CARTESIAN_POINT('Origin',(-2.55,10.85,-11.06)) ;
#141301 = CARTESIAN_POINT('Origin',(-2.75,10.85,-9.26)) ;
#141302 = CARTESIAN_POINT('Origin',(-2.75,10.85,-9.26)) ;
#141303 = CARTESIAN_POINT('Origin',(-3.8,10.75,-9.26)) ;
#141304 = CARTESIAN_POINT('Origin',(-3.8,10.75,-9.26)) ;
#141305 = CARTESIAN_POINT('Origin',(-3.8,10.75,-11.06)) ;
#141306 = CARTESIAN_POINT('Origin',(-3.8,10.75,-11.06)) ;
#141307 = CARTESIAN_POINT('Origin',(-2.75,10.85,-11.06)) ;
#141308 = CARTESIAN_POINT('Origin',(-2.75,10.85,-11.06)) ;
#141309 = CARTESIAN_POINT('Origin',(-2.75,10.8,-9.26)) ;
#141310 = CARTESIAN_POINT('Origin',(-2.75,10.75,-9.26)) ;
#141311 = CARTESIAN_POINT('Origin',(1.56125112837912E-16,10.75,-9.26)) ;
#141312 = CARTESIAN_POINT('Origin',(-2.75,10.75,-9.26)) ;
#141313 = CARTESIAN_POINT('Origin',(-1.56125112837913E-16,10.75,-11.06)) ;
#141314 = CARTESIAN_POINT('Origin',(-2.75,10.75,-11.06)) ;
#141315 = CARTESIAN_POINT('Origin',(-2.75,10.8,-11.06)) ;
#141316 = CARTESIAN_POINT('Origin',(-2.75,10.75,-11.06)) ;
#141317 = CARTESIAN_POINT('Origin',(-2.75,10.75,-9.26)) ;
#141318 = CARTESIAN_POINT('Origin',(-2.75,10.75,-9.26)) ;
#141319 = CARTESIAN_POINT('Origin',(-2.75,10.75,-11.06)) ;
#141320 = CARTESIAN_POINT('Origin',(-2.75,10.75,-11.06)) ;
#141321 = CARTESIAN_POINT('Origin',(-2.75,10.75,-10.16)) ;
#141322 = CARTESIAN_POINT('Origin',(4.6,0.,-10.16)) ;
#141323 = CARTESIAN_POINT('Ctrl Pts',(4.5,-2.7,-8.63684537882721)) ;
#141324 = CARTESIAN_POINT('Ctrl Pts',(4.5,-2.71827986285823,-8.71196473917507)) ;
#141325 = CARTESIAN_POINT('Ctrl Pts',(4.50597963419107,-2.73556801027185,
-8.78673986045281)) ;
#141326 = CARTESIAN_POINT('Ctrl Pts',(4.52394923367545,-2.75977758633329,
-8.89843683402156)) ;
#141327 = CARTESIAN_POINT('Ctrl Pts',(4.53141024883993,-2.76757607569523,
-8.93568328239029)) ;
#141328 = CARTESIAN_POINT('Ctrl Pts',(4.54734065524867,-2.77857284247615,
-8.99016568958296)) ;
#141329 = CARTESIAN_POINT('Ctrl Pts',(4.55339248498575,-2.78214991573955,
-9.00823827441494)) ;
#141330 = CARTESIAN_POINT('Ctrl Pts',(4.56567492147096,-2.787183259287,-9.03414672186072)) ;
#141331 = CARTESIAN_POINT('Ctrl Pts',(4.5702469143305,-2.78880341224557,-9.04257260505081)) ;
#141332 = CARTESIAN_POINT('Ctrl Pts',(4.58215938980081,-2.79169669265294,
-9.0577434798851)) ;
#141333 = CARTESIAN_POINT('Ctrl Pts',(4.59005470866978,-2.79310344827587,
-9.06520635404226)) ;
#141334 = CARTESIAN_POINT('Ctrl Pts',(4.6,-2.79310344827586,-9.06520635404224)) ;
#141335 = CARTESIAN_POINT('Origin',(4.6,-2.4,-8.19785831296514)) ;
#141336 = CARTESIAN_POINT('Origin',(4.6,-2.4,-7.62)) ;
#141337 = CARTESIAN_POINT('Origin',(4.6,-2.4,-8.19785831296514)) ;
#141338 = CARTESIAN_POINT('Origin',(4.6,-2.4,-8.19785831296514)) ;
#141339 = CARTESIAN_POINT('Origin',(4.6,-2.4,-8.19785831296514)) ;
#141340 = CARTESIAN_POINT('Origin',(0.584645609909622,-2.4,-8.19785831296514)) ;
#141341 = CARTESIAN_POINT('Origin',(12.7,-2.4,-8.19785831296514)) ;
#141342 = CARTESIAN_POINT('Origin',(12.7,-2.2,-7.62)) ;
#141343 = CARTESIAN_POINT('Origin',(12.7,-2.2,-8.19785831296514)) ;
#141344 = CARTESIAN_POINT('Origin',(12.7,-2.4,-8.19785831296514)) ;
#141345 = CARTESIAN_POINT('Origin',(12.7,-2.24516129032258,-8.32444809922546)) ;
#141346 = CARTESIAN_POINT('Origin',(12.7,0.,-10.16)) ;
#141347 = CARTESIAN_POINT('Origin',(12.7,-2.24516129032258,-11.9955519007745)) ;
#141348 = CARTESIAN_POINT('Origin',(12.7,-2.2,-7.62)) ;
#141349 = CARTESIAN_POINT('Origin',(12.7,-2.2,-12.1221416870349)) ;
#141350 = CARTESIAN_POINT('Origin',(12.7,-2.4,-12.1221416870349)) ;
#141351 = CARTESIAN_POINT('Origin',(12.7,-2.4,-12.1221416870349)) ;
#141352 = CARTESIAN_POINT('Origin',(0.584645609909622,-2.4,-12.1221416870349)) ;
#141353 = CARTESIAN_POINT('Origin',(4.6,-2.4,-12.1221416870349)) ;
#141354 = CARTESIAN_POINT('Origin',(4.6,-2.4,-7.62)) ;
#141355 = CARTESIAN_POINT('Origin',(4.6,-2.4,-12.1221416870349)) ;
#141356 = CARTESIAN_POINT('Origin',(4.6,-2.4,-12.1221416870349)) ;
#141357 = CARTESIAN_POINT('Origin',(4.6,-2.4,-12.1221416870349)) ;
#141358 = CARTESIAN_POINT('Origin',(4.6,0.,-10.16)) ;
#141359 = CARTESIAN_POINT('Ctrl Pts',(4.6,-2.79310344827586,-11.2547936459578)) ;
#141360 = CARTESIAN_POINT('Ctrl Pts',(4.59007568892311,-2.79310344827586,
-11.2547936459578)) ;
#141361 = CARTESIAN_POINT('Ctrl Pts',(4.58219207637239,-2.79170232102182,
-11.262226742276)) ;
#141362 = CARTESIAN_POINT('Ctrl Pts',(4.57028631514659,-2.78881527838255,
-11.27736543899)) ;
#141363 = CARTESIAN_POINT('Ctrl Pts',(4.56571532154372,-2.78719767797524,
-11.2857784885835)) ;
#141364 = CARTESIAN_POINT('Ctrl Pts',(4.55343865632726,-2.78217307830036,
-11.3116436333089)) ;
#141365 = CARTESIAN_POINT('Ctrl Pts',(4.54738888873343,-2.77860151743012,
-11.3296900859661)) ;
#141366 = CARTESIAN_POINT('Ctrl Pts',(4.53146440752601,-2.76762263748299,
-11.3840903156831)) ;
#141367 = CARTESIAN_POINT('Ctrl Pts',(4.52400917967609,-2.75984503873828,
-11.4212455063058)) ;
#141368 = CARTESIAN_POINT('Ctrl Pts',(4.50599905604505,-2.7356206423885,-11.5330301354693)) ;
#141369 = CARTESIAN_POINT('Ctrl Pts',(4.5,-2.71826422026483,-11.6080995425769)) ;
#141370 = CARTESIAN_POINT('Ctrl Pts',(4.5,-2.7,-11.6831546211728)) ;
#141371 = CARTESIAN_POINT('Origin',(3.7,-2.9,-7.62)) ;
#141372 = CARTESIAN_POINT('Origin',(3.5,-3.95,-7.62)) ;
#141373 = CARTESIAN_POINT('Origin',(-5.3,-3.95,-7.62)) ;
#141374 = CARTESIAN_POINT('Origin',(-5.3,5.19009804864072,-7.62)) ;
#141375 = CARTESIAN_POINT('Origin',(-4.8,10.3,-7.62)) ;
#141376 = CARTESIAN_POINT('Origin',(-4.8,10.85,-7.62)) ;
#141377 = CARTESIAN_POINT('Origin',(-0.362523114814661,9.05,-10.3290473046963)) ;
#141378 = CARTESIAN_POINT('Origin',(0.36252311481466,9.05,-9.99095269530372)) ;
#141379 = CARTESIAN_POINT('Origin',(-1.31845674202095,9.85,-8.75228134223507)) ;
#141380 = CARTESIAN_POINT('Origin',(-0.230887397576972,9.85,-8.24513942814623)) ;
#141381 = CARTESIAN_POINT('Origin',(3.3,10.85,-7.62)) ;
#141382 = CARTESIAN_POINT('Origin',(3.3,10.05,-7.62)) ;
#141383 = CARTESIAN_POINT('Origin',(3.,9.85,-7.62)) ;
#141384 = CARTESIAN_POINT('Origin',(3.,8.05,-7.62)) ;
#141385 = CARTESIAN_POINT('Origin',(3.34087287789487,7.85,-7.62)) ;
#141386 = CARTESIAN_POINT('Origin',(3.85,6.92431432344521,-7.62)) ;
#141387 = CARTESIAN_POINT('Origin',(4.05,3.77568567655479,-7.62)) ;
#141388 = CARTESIAN_POINT('Origin',(4.6,2.1,-8.77804604217164)) ;
#141389 = CARTESIAN_POINT('Origin',(4.6,2.1,-8.77804604217164)) ;
#141390 = CARTESIAN_POINT('Origin',(4.6,0.280857398566761,-8.47485560859943)) ;
#141391 = CARTESIAN_POINT('Origin',(4.6,2.61712020253893,-8.86423274259479)) ;
#141392 = CARTESIAN_POINT('Origin',(4.6,2.65,-8.66695395782836)) ;
#141393 = CARTESIAN_POINT('Origin',(4.6,2.72431432344521,-8.85263481664499)) ;
#141394 = CARTESIAN_POINT('Ctrl Pts',(4.48762159086906,2.77250619842445,-8.77117568174961)) ;
#141395 = CARTESIAN_POINT('Ctrl Pts',(4.51316716229104,2.72605970493114,-8.73423879419717)) ;
#141396 = CARTESIAN_POINT('Ctrl Pts',(4.5752745340585,2.73535372386122,-8.71905715319801)) ;
#141397 = CARTESIAN_POINT('Ctrl Pts',(4.49363662433154,2.76156977394749,-8.80699959247167)) ;
#141398 = CARTESIAN_POINT('Ctrl Pts',(4.5146945995807,2.70766535161862,-8.75620084739328)) ;
#141399 = CARTESIAN_POINT('Ctrl Pts',(4.58732693581886,2.72440392220679,-8.73699504123404)) ;
#141400 = CARTESIAN_POINT('Ctrl Pts',(4.5,2.7448843843803,-8.8361692160662)) ;
#141401 = CARTESIAN_POINT('Ctrl Pts',(4.50856472873623,2.69031482079683,-8.75849111370477)) ;
#141402 = CARTESIAN_POINT('Ctrl Pts',(4.60003980620505,2.7077507326983,-8.75155231137473)) ;
#141403 = CARTESIAN_POINT('Ctrl Pts',(4.5,2.72431432344521,-8.85263481664499)) ;
#141404 = CARTESIAN_POINT('Ctrl Pts',(4.5,2.68714136424468,-8.75975491585172)) ;
#141405 = CARTESIAN_POINT('Ctrl Pts',(4.60004250625996,2.68715716507935,-8.7597943956238)) ;
#141406 = CARTESIAN_POINT('Origin',(4.57524318173443,2.82069807340128,-8.77117568174948)) ;
#141407 = CARTESIAN_POINT('Ctrl Pts',(4.47150553123747,2.80180812502279,-8.66695395782836)) ;
#141408 = CARTESIAN_POINT('Ctrl Pts',(4.5,2.75,-8.66695395782836)) ;
#141409 = CARTESIAN_POINT('Ctrl Pts',(4.55912712210514,2.75,-8.66695395782836)) ;
#141410 = CARTESIAN_POINT('Ctrl Pts',(4.47150553186688,2.8018081238784,-8.7035744727347)) ;
#141411 = CARTESIAN_POINT('Ctrl Pts',(4.50000000073523,2.74999999866316,-8.69125808426882)) ;
#141412 = CARTESIAN_POINT('Ctrl Pts',(4.5591271227348,2.75,-8.68527204575931)) ;
#141413 = CARTESIAN_POINT('Ctrl Pts',(4.4771244897161,2.79159183687982,-8.73991653735229)) ;
#141414 = CARTESIAN_POINT('Ctrl Pts',(4.50480340096853,2.74126654369358,-8.71553795099799)) ;
#141415 = CARTESIAN_POINT('Ctrl Pts',(4.56473907811163,2.74489822224647,-8.70342482158223)) ;
#141416 = CARTESIAN_POINT('Ctrl Pts',(4.48762159086676,2.77250619842407,-8.77117568174948)) ;
#141417 = CARTESIAN_POINT('Ctrl Pts',(4.51315802400618,2.72607631998876,-8.7342520074343)) ;
#141418 = CARTESIAN_POINT('Ctrl Pts',(4.57524318173443,2.73534903670064,-8.71906481978892)) ;
#141419 = CARTESIAN_POINT('Origin',(4.55912712210513,2.85,-8.66695395782836)) ;
#141420 = CARTESIAN_POINT('Origin',(4.55912712210514,2.85,-7.62)) ;
#141421 = CARTESIAN_POINT('Origin',(4.55912712210514,2.85,-7.62)) ;
#141422 = CARTESIAN_POINT('Origin',(4.55912712210514,2.85,-11.6530460421716)) ;
#141423 = CARTESIAN_POINT('Ctrl Pts',(4.48762159086767,2.77250619842243,-11.5488243182478)) ;
#141424 = CARTESIAN_POINT('Ctrl Pts',(4.51315802400691,2.72607631998743,-11.5857479925641)) ;
#141425 = CARTESIAN_POINT('Ctrl Pts',(4.57524318173533,2.73534903669982,-11.6009351802097)) ;
#141426 = CARTESIAN_POINT('Ctrl Pts',(4.47712448971642,2.79159183687924,-11.5800834626456)) ;
#141427 = CARTESIAN_POINT('Ctrl Pts',(4.50480340096883,2.7412665436931,-11.6044620490005)) ;
#141428 = CARTESIAN_POINT('Ctrl Pts',(4.56473907811193,2.74489822224616,-11.6165751784167)) ;
#141429 = CARTESIAN_POINT('Ctrl Pts',(4.47150553186688,2.8018081238784,-11.6164255272643)) ;
#141430 = CARTESIAN_POINT('Ctrl Pts',(4.50000000073523,2.74999999866316,-11.6287419157305)) ;
#141431 = CARTESIAN_POINT('Ctrl Pts',(4.5591271227348,2.75,-11.6347279542402)) ;
#141432 = CARTESIAN_POINT('Ctrl Pts',(4.47150553123747,2.80180812502279,-11.6530460421716)) ;
#141433 = CARTESIAN_POINT('Ctrl Pts',(4.5,2.75,-11.6530460421716)) ;
#141434 = CARTESIAN_POINT('Ctrl Pts',(4.55912712210513,2.75,-11.6530460421716)) ;
#141435 = CARTESIAN_POINT('Origin',(4.57524318173533,2.82069807339964,-11.5488243182478)) ;
#141436 = CARTESIAN_POINT('Ctrl Pts',(4.57527448145475,2.73535371598842,-11.6009428339419)) ;
#141437 = CARTESIAN_POINT('Ctrl Pts',(4.51316714695681,2.72605973281053,-11.5857611836291)) ;
#141438 = CARTESIAN_POINT('Ctrl Pts',(4.48762159086951,2.77250619842363,-11.5488243182477)) ;
#141439 = CARTESIAN_POINT('Ctrl Pts',(4.58732687742636,2.72440390874893,-11.5830049433246)) ;
#141440 = CARTESIAN_POINT('Ctrl Pts',(4.51469458626359,2.70766538570633,-11.5637991204816)) ;
#141441 = CARTESIAN_POINT('Ctrl Pts',(4.49363662433188,2.76156977394663,-11.5130004075268)) ;
#141442 = CARTESIAN_POINT('Ctrl Pts',(4.60003973844303,2.70775071978178,-11.568447683485)) ;
#141443 = CARTESIAN_POINT('Ctrl Pts',(4.50856472285792,2.69031485824814,-11.5615088329844)) ;
#141444 = CARTESIAN_POINT('Ctrl Pts',(4.5,2.74488438437974,-11.4838307839335)) ;
#141445 = CARTESIAN_POINT('Ctrl Pts',(4.60004243494346,2.6871571650681,-11.5602056044043)) ;
#141446 = CARTESIAN_POINT('Ctrl Pts',(4.5,2.68714139075513,-11.5602450179096)) ;
#141447 = CARTESIAN_POINT('Ctrl Pts',(4.5,2.72431432344521,-11.467365183355)) ;
#141448 = CARTESIAN_POINT('Origin',(4.6,0.280857398566761,-11.8451443914006)) ;
#141449 = CARTESIAN_POINT('Origin',(4.6,2.1,-11.5419539578284)) ;
#141450 = CARTESIAN_POINT('Origin',(4.6,2.1,-11.5419539578284)) ;
#141451 = CARTESIAN_POINT('Origin',(4.6,0.,-10.16)) ;
#141452 = CARTESIAN_POINT('',(4.5,-2.9,-10.1600000000039)) ;
#141453 = CARTESIAN_POINT('',(4.57439618084313,-2.80937499999937,-11.2027958671254)) ;
#141454 = CARTESIAN_POINT('Ctrl Pts',(4.5,-2.9,-10.1600000000039)) ;
#141455 = CARTESIAN_POINT('Ctrl Pts',(4.5,-2.9000000234111,-10.3361762625703)) ;
#141456 = CARTESIAN_POINT('Ctrl Pts',(4.49893459747296,-2.89187728142186,
-10.5122938225552)) ;
#141457 = CARTESIAN_POINT('Ctrl Pts',(4.50498172725087,-2.86839426105774,
-10.7749432768872)) ;
#141458 = CARTESIAN_POINT('Ctrl Pts',(4.50826226558342,-2.85869729223562,
-10.8622870271135)) ;
#141459 = CARTESIAN_POINT('Ctrl Pts',(4.52028413974051,-2.84160518746962,
-10.9928409654328)) ;
#141460 = CARTESIAN_POINT('Ctrl Pts',(4.52545003690602,-2.8354696349403,-11.036363113622)) ;
#141461 = CARTESIAN_POINT('Ctrl Pts',(4.53741870680498,-2.82581179679252,
-11.1006394550108)) ;
#141462 = CARTESIAN_POINT('Ctrl Pts',(4.54209540184575,-2.82251395224859,
-11.1219200182606)) ;
#141463 = CARTESIAN_POINT('Ctrl Pts',(4.55451190949429,-2.81582803324483,
-11.1638742105328)) ;
#141464 = CARTESIAN_POINT('Ctrl Pts',(4.56139306411848,-2.8124020390272,-11.1847435318249)) ;
#141465 = CARTESIAN_POINT('Ctrl Pts',(4.57439618084313,-2.80937499999937,
-11.2027958671254)) ;
#141466 = CARTESIAN_POINT('Ctrl Pts',(4.57439618084312,-2.80937499999939,
-11.2027958671254)) ;
#141467 = CARTESIAN_POINT('Ctrl Pts',(4.57788811720513,-2.80856205104937,
-11.2076438845913)) ;
#141468 = CARTESIAN_POINT('Ctrl Pts',(4.58132110715668,-2.80743849592502,
-11.2126543114198)) ;
#141469 = CARTESIAN_POINT('Ctrl Pts',(4.58591063786564,-2.80541025280312,
-11.2200683491599)) ;
#141470 = CARTESIAN_POINT('Ctrl Pts',(4.58721694730502,-2.80476695238159,
-11.2222683250838)) ;
#141471 = CARTESIAN_POINT('Ctrl Pts',(4.5887449802686,-2.80393035430396,-11.2249717146408)) ;
#141472 = CARTESIAN_POINT('Ctrl Pts',(4.58900094431508,-2.80378708879839,
-11.225429423373)) ;
#141473 = CARTESIAN_POINT('Ctrl Pts',(4.58924476828968,-2.80364801935069,
-11.22586949326)) ;
#141474 = CARTESIAN_POINT('Ctrl Pts',(4.58924931741448,-2.80364542371033,
-11.2258777053493)) ;
#141475 = CARTESIAN_POINT('Ctrl Pts',(4.59158188358133,-2.80231401319274,
-11.2300892401221)) ;
#141476 = CARTESIAN_POINT('Ctrl Pts',(4.59377134212491,-2.800813098491,-11.2344383923963)) ;
#141477 = CARTESIAN_POINT('Ctrl Pts',(4.59570408210449,-2.79909049146272,
-11.2391378632085)) ;
#141478 = CARTESIAN_POINT('Ctrl Pts',(4.5957084873849,-2.79908656285628,-11.2391485795778)) ;
#141479 = CARTESIAN_POINT('Ctrl Pts',(4.59603576097762,-2.79879453264352,
-11.2399450754361)) ;
#141480 = CARTESIAN_POINT('Ctrl Pts',(4.59633794834607,-2.79851279959495,
-11.2407065253189)) ;
#141481 = CARTESIAN_POINT('Ctrl Pts',(4.59727216584803,-2.79759800070515,
-11.24316063341)) ;
#141482 = CARTESIAN_POINT('Ctrl Pts',(4.59785661125443,-2.79695684051616,
-11.2448529156094)) ;
#141483 = CARTESIAN_POINT('Ctrl Pts',(4.59875882816121,-2.79580092267551,
-11.2478683242216)) ;
#141484 = CARTESIAN_POINT('Ctrl Pts',(4.59910960512328,-2.79529211440566,
-11.2491844992175)) ;
#141485 = CARTESIAN_POINT('Ctrl Pts',(4.59950074890552,-2.79458032370894,
-11.2510150784121)) ;
#141486 = CARTESIAN_POINT('Ctrl Pts',(4.59959271145697,-2.79439474074567,
-11.2514948405808)) ;
#141487 = CARTESIAN_POINT('Ctrl Pts',(4.59970479219924,-2.79411978912794,
-11.2522025710462)) ;
#141488 = CARTESIAN_POINT('Ctrl Pts',(4.59973686334512,-2.79403231884248,
-11.2524272684452)) ;
#141489 = CARTESIAN_POINT('Ctrl Pts',(4.59980956306602,-2.7938042827674,-11.2530108264021)) ;
#141490 = CARTESIAN_POINT('Ctrl Pts',(4.59984405921136,-2.79366555090847,
-11.2533689790042)) ;
#141491 = CARTESIAN_POINT('Ctrl Pts',(4.59992170638737,-2.79338632637294,
-11.2540824135446)) ;
#141492 = CARTESIAN_POINT('Ctrl Pts',(4.59995882625635,-2.79324305250058,
-11.2544374792565)) ;
#141493 = CARTESIAN_POINT('Ctrl Pts',(4.59999999999999,-2.79310344827586,
-11.2547936459578)) ;
#141494 = CARTESIAN_POINT('',(4.57439618084271,-2.80937499999947,-9.11720413287514)) ;
#141495 = CARTESIAN_POINT('Ctrl Pts',(4.59999999999999,-2.79310344827586,
-9.06520635404223)) ;
#141496 = CARTESIAN_POINT('Ctrl Pts',(4.59995895305209,-2.79324111387631,
-9.06556200704419)) ;
#141497 = CARTESIAN_POINT('Ctrl Pts',(4.59992125133673,-2.79338175512528,
-9.06591664999517)) ;
#141498 = CARTESIAN_POINT('Ctrl Pts',(4.59984242179761,-2.79365985893298,
-9.06662721825472)) ;
#141499 = CARTESIAN_POINT('Ctrl Pts',(4.5998070294299,-2.79379858543765,-9.06698190400296)) ;
#141500 = CARTESIAN_POINT('Ctrl Pts',(4.59973261548694,-2.79401893257626,
-9.06754582127962)) ;
#141501 = CARTESIAN_POINT('Ctrl Pts',(4.59970092564442,-2.79410050108421,
-9.06775470445263)) ;
#141502 = CARTESIAN_POINT('Ctrl Pts',(4.59958060815602,-2.79437456977472,
-9.06845707425772)) ;
#141503 = CARTESIAN_POINT('Ctrl Pts',(4.59947821517875,-2.79456857658396,
-9.06895509538074)) ;
#141504 = CARTESIAN_POINT('Ctrl Pts',(4.59905971984789,-2.79527981802027,
-9.07078506438848)) ;
#141505 = CARTESIAN_POINT('Ctrl Pts',(4.59869396429224,-2.79579226918927,
-9.07211140120008)) ;
#141506 = CARTESIAN_POINT('Ctrl Pts',(4.59768320083748,-2.79706868650734,
-9.07544407389332)) ;
#141507 = CARTESIAN_POINT('Ctrl Pts',(4.59698254015872,-2.79783590182172,
-9.07747319966266)) ;
#141508 = CARTESIAN_POINT('Ctrl Pts',(4.5959970522588,-2.79876532988112,-9.07998468423845)) ;
#141509 = CARTESIAN_POINT('Ctrl Pts',(4.59580678362761,-2.79893964110239,
-9.08045810500392)) ;
#141510 = CARTESIAN_POINT('Ctrl Pts',(4.59367882781298,-2.80083904916685,
-9.0856449119971)) ;
#141511 = CARTESIAN_POINT('Ctrl Pts',(4.5915070708769,-2.80233337893514,-9.08997932770411)) ;
#141512 = CARTESIAN_POINT('Ctrl Pts',(4.58628071719239,-2.80532570224269,
-9.09945146742918)) ;
#141513 = CARTESIAN_POINT('Ctrl Pts',(4.58313959595716,-2.80673110767406,
-9.10451024806567)) ;
#141514 = CARTESIAN_POINT('Ctrl Pts',(4.5780261114634,-2.80844040952813,-9.11209635749167)) ;
#141515 = CARTESIAN_POINT('Ctrl Pts',(4.57624387811649,-2.80894486836995,
-9.11463895934166)) ;
#141516 = CARTESIAN_POINT('Ctrl Pts',(4.57439618084271,-2.80937499999947,
-9.11720413287514)) ;
#141517 = CARTESIAN_POINT('Ctrl Pts',(4.57439618084271,-2.80937499999947,
-9.11720413287514)) ;
#141518 = CARTESIAN_POINT('Ctrl Pts',(4.56149777794589,-2.81237766235468,
-9.1351110931668)) ;
#141519 = CARTESIAN_POINT('Ctrl Pts',(4.55451596106519,-2.81582788236477,
-9.15612624229681)) ;
#141520 = CARTESIAN_POINT('Ctrl Pts',(4.54213610452188,-2.82249001163036,
-9.19792835962828)) ;
#141521 = CARTESIAN_POINT('Ctrl Pts',(4.53742891479326,-2.82580422498964,
-9.219310967236)) ;
#141522 = CARTESIAN_POINT('Ctrl Pts',(4.525451614243,-2.8354670333868,-9.28361794379489)) ;
#141523 = CARTESIAN_POINT('Ctrl Pts',(4.52032009146395,-2.84156292603926,
-9.32685657347848)) ;
#141524 = CARTESIAN_POINT('Ctrl Pts',(4.50830110904356,-2.85862448221642,
-9.45711642595738)) ;
#141525 = CARTESIAN_POINT('Ctrl Pts',(4.50499166750953,-2.86836219567853,
-9.5447300385823)) ;
#141526 = CARTESIAN_POINT('Ctrl Pts',(4.49892845988062,-2.8918880660271,-9.80776299683786)) ;
#141527 = CARTESIAN_POINT('Ctrl Pts',(4.49999999999474,-2.89999999999869,
-9.98383009011777)) ;
#141528 = CARTESIAN_POINT('Ctrl Pts',(4.5,-2.9,-10.1600000000039)) ;
#141529 = CARTESIAN_POINT('Origin',(4.4,-2.7,-7.62)) ;
#141530 = CARTESIAN_POINT('Origin',(4.4,-2.7,-8.63684537882721)) ;
#141531 = CARTESIAN_POINT('Ctrl Pts',(4.40227435089074,-2.79999990867355,
-8.56940069288188)) ;
#141532 = CARTESIAN_POINT('Ctrl Pts',(4.51828879250235,-2.80015667527379,
-8.57878556679247)) ;
#141533 = CARTESIAN_POINT('Ctrl Pts',(4.50118227077259,-2.68533700727769,
-8.57797110744942)) ;
#141534 = CARTESIAN_POINT('Ctrl Pts',(4.39419482113926,-2.79999992837382,
-8.68368769966915)) ;
#141535 = CARTESIAN_POINT('Ctrl Pts',(4.4857179250172,-2.80010751836584,-8.66267136675065)) ;
#141536 = CARTESIAN_POINT('Ctrl Pts',(4.49717570077253,-2.71006921719245,
-8.67703189821457)) ;
#141537 = CARTESIAN_POINT('Ctrl Pts',(4.40636790575269,-2.79999994706265,
-8.79490890735427)) ;
#141538 = CARTESIAN_POINT('Ctrl Pts',(4.47481046024548,-2.80007242131914,
-8.77332242779906)) ;
#141539 = CARTESIAN_POINT('Ctrl Pts',(4.50328131876401,-2.73353293829092,
-8.77702587481)) ;
#141540 = CARTESIAN_POINT('Ctrl Pts',(4.4547973699423,-2.79999997092221,-8.94507366547111)) ;
#141541 = CARTESIAN_POINT('Ctrl Pts',(4.49869786247047,-2.80003603117402,
-8.92627924349578)) ;
#141542 = CARTESIAN_POINT('Ctrl Pts',(4.52748687875415,-2.76348976047508,
-8.91628917285872)) ;
#141543 = CARTESIAN_POINT('Ctrl Pts',(4.47221929614096,-2.79999997745988,
-8.98730406022326)) ;
#141544 = CARTESIAN_POINT('Ctrl Pts',(4.5088055676762,-2.80002725736479,-8.9682748482859)) ;
#141545 = CARTESIAN_POINT('Ctrl Pts',(4.53619137795529,-2.77169834185702,
-8.95598368236755)) ;
#141546 = CARTESIAN_POINT('Ctrl Pts',(4.50882352800136,-2.79999998605361,
-9.04428434960906)) ;
#141547 = CARTESIAN_POINT('Ctrl Pts',(4.5336780291127,-2.80001636071784,-9.02535870242034)) ;
#141548 = CARTESIAN_POINT('Ctrl Pts',(4.55447319025663,-2.78248861123826,
-9.01009568142552)) ;
#141549 = CARTESIAN_POINT('Ctrl Pts',(4.52308919141484,-2.79999998878206,
-9.06266256169107)) ;
#141550 = CARTESIAN_POINT('Ctrl Pts',(4.54363962638622,-2.80001303821803,
-9.04372615017166)) ;
#141551 = CARTESIAN_POINT('Ctrl Pts',(4.56159739427507,-2.78591449131413,
-9.0276542708947)) ;
#141552 = CARTESIAN_POINT('Ctrl Pts',(4.57467506176493,-2.79999999510246,
-9.10569650839936)) ;
#141553 = CARTESIAN_POINT('Ctrl Pts',(4.5806240530329,-2.80000557393877,-9.08633416327778)) ;
#141554 = CARTESIAN_POINT('Ctrl Pts',(4.58735613403293,-2.79385049254303,
-9.06891981499325)) ;
#141555 = CARTESIAN_POINT('Ctrl Pts',(4.62437069655637,-2.79999999703807,
-9.11953134306007)) ;
#141556 = CARTESIAN_POINT('Ctrl Pts',(4.61827372661886,-2.80000334969057,
-9.10093404548759)) ;
#141557 = CARTESIAN_POINT('Ctrl Pts',(4.61212682540743,-2.79628090446621,
-9.08240281421819)) ;
#141558 = CARTESIAN_POINT('Ctrl Pts',(4.67161368302031,-2.79999998860619,
-9.06078982676527)) ;
#141559 = CARTESIAN_POINT('Ctrl Pts',(4.65407010102641,-2.80001325705921,
-9.04046373958886)) ;
#141560 = CARTESIAN_POINT('Ctrl Pts',(4.63587130780614,-2.78569367459188,
-9.02562812959412)) ;
#141561 = CARTESIAN_POINT('Ctrl Pts',(4.54879236204369,-2.8,-9.0835655563675)) ;
#141562 = CARTESIAN_POINT('Ctrl Pts',(4.55448837802391,-2.7999999999815,-9.08117882091364)) ;
#141563 = CARTESIAN_POINT('Ctrl Pts',(4.56021842726602,-2.7995915078324,-9.07883954273416)) ;
#141564 = CARTESIAN_POINT('Ctrl Pts',(4.5673067198498,-2.79865167182176,-9.07597888386358)) ;
#141565 = CARTESIAN_POINT('Ctrl Pts',(4.56847770958267,-2.79848295770258,
-9.07550732683475)) ;
#141566 = CARTESIAN_POINT('Ctrl Pts',(4.5710752309902,-2.79808046368153,-9.07446296289698)) ;
#141567 = CARTESIAN_POINT('Ctrl Pts',(4.57250093612479,-2.79784058543152,
-9.07388964302801)) ;
#141568 = CARTESIAN_POINT('Ctrl Pts',(4.5764383594612,-2.79713266293194,-9.07231368646489)) ;
#141569 = CARTESIAN_POINT('Ctrl Pts',(4.57879956048961,-2.79666132938902,
-9.07137580039694)) ;
#141570 = CARTESIAN_POINT('Ctrl Pts',(4.58293855712952,-2.79579586318667,
-9.06976081592962)) ;
#141571 = CARTESIAN_POINT('Ctrl Pts',(4.58471363403686,-2.79540911153441,
-9.06907461719118)) ;
#141572 = CARTESIAN_POINT('Ctrl Pts',(4.58699082729421,-2.7949269768198,-9.06824452926202)) ;
#141573 = CARTESIAN_POINT('Ctrl Pts',(4.58739952300691,-2.79484234870239,
-9.0681019268464)) ;
#141574 = CARTESIAN_POINT('Ctrl Pts',(4.58871515235473,-2.79457617288697,
-9.06766112910089)) ;
#141575 = CARTESIAN_POINT('Ctrl Pts',(4.58961690596117,-2.79440247805564,
-9.06738498699956)) ;
#141576 = CARTESIAN_POINT('Ctrl Pts',(4.59105375065842,-2.79414748185769,
-9.06698298181798)) ;
#141577 = CARTESIAN_POINT('Ctrl Pts',(4.59155303909535,-2.79406229662444,
-9.06684924350716)) ;
#141578 = CARTESIAN_POINT('Ctrl Pts',(4.59245965385672,-2.79391282221553,
-9.06661259411486)) ;
#141579 = CARTESIAN_POINT('Ctrl Pts',(4.59286388425107,-2.79384761399903,
-9.06650842178453)) ;
#141580 = CARTESIAN_POINT('Ctrl Pts',(4.59368973959986,-2.7937059861537,-9.06626767265164)) ;
#141581 = CARTESIAN_POINT('Ctrl Pts',(4.59407665941131,-2.7936397371459,-9.06615152123315)) ;
#141582 = CARTESIAN_POINT('Ctrl Pts',(4.59444371287738,-2.79357284110654,
-9.06602679272787)) ;
#141583 = CARTESIAN_POINT('Ctrl Pts',(4.59448890259162,-2.79356452972316,
-9.0660111581995)) ;
#141584 = CARTESIAN_POINT('Ctrl Pts',(4.59470842334911,-2.79352377141065,
-9.06593382545217)) ;
#141585 = CARTESIAN_POINT('Ctrl Pts',(4.5948359873327,-2.79349361011836,-9.0658723314841)) ;
#141586 = CARTESIAN_POINT('Ctrl Pts',(4.59514620525224,-2.7934297131363,-9.0657459400492)) ;
#141587 = CARTESIAN_POINT('Ctrl Pts',(4.59533334275102,-2.79339696908416,
-9.06568383785339)) ;
#141588 = CARTESIAN_POINT('Ctrl Pts',(4.59563785533348,-2.79335634095568,
-9.06561299034027)) ;
#141589 = CARTESIAN_POINT('Ctrl Pts',(4.59571710962763,-2.79334654412181,
-9.06559639128765)) ;
#141590 = CARTESIAN_POINT('Ctrl Pts',(4.59594411915586,-2.79332043135007,
-9.0655533496182)) ;
#141591 = CARTESIAN_POINT('Ctrl Pts',(4.59600288191152,-2.79330503361987,
-9.06553395124079)) ;
#141592 = CARTESIAN_POINT('Ctrl Pts',(4.59613307952173,-2.79327450473786,
-9.06549928051942)) ;
#141593 = CARTESIAN_POINT('Ctrl Pts',(4.59620389659311,-2.79325970788819,
-9.06548500605856)) ;
#141594 = CARTESIAN_POINT('Ctrl Pts',(4.5965119298477,-2.79322709231927,-9.06545027786287)) ;
#141595 = CARTESIAN_POINT('Ctrl Pts',(4.59679543741295,-2.79320989448354,
-9.06542934418242)) ;
#141596 = CARTESIAN_POINT('Ctrl Pts',(4.59784475938522,-2.793166495242,-9.0653578835066)) ;
#141597 = CARTESIAN_POINT('Ctrl Pts',(4.59874915064779,-2.79313948637392,
-9.06529926431075)) ;
#141598 = CARTESIAN_POINT('Ctrl Pts',(4.59999999999999,-2.79310344827586,
-9.06520635404224)) ;
#141599 = CARTESIAN_POINT('Origin',(4.4,-2.7,-7.62)) ;
#141600 = CARTESIAN_POINT('Origin',(4.4,-2.7,-11.6831546211728)) ;
#141601 = CARTESIAN_POINT('Ctrl Pts',(4.5011795914298,-2.68531903459926,-11.7420290201723)) ;
#141602 = CARTESIAN_POINT('Ctrl Pts',(4.51828670358939,-2.8,-11.7412138251405)) ;
#141603 = CARTESIAN_POINT('Ctrl Pts',(4.40240952225579,-2.8,-11.7505883721107)) ;
#141604 = CARTESIAN_POINT('Ctrl Pts',(4.49717774927193,-2.71005310920069,
-11.6429655323627)) ;
#141605 = CARTESIAN_POINT('Ctrl Pts',(4.48574628541092,-2.8,-11.6573148520406)) ;
#141606 = CARTESIAN_POINT('Ctrl Pts',(4.39431668173581,-2.8,-11.6363402695085)) ;
#141607 = CARTESIAN_POINT('Ctrl Pts',(4.50328690685192,-2.73351987602563,
-11.5429733978619)) ;
#141608 = CARTESIAN_POINT('Ctrl Pts',(4.47485145549543,-2.8,-11.5466766957412)) ;
#141609 = CARTESIAN_POINT('Ctrl Pts',(4.40646789472119,-2.8,-11.5251226186383)) ;
#141610 = CARTESIAN_POINT('Ctrl Pts',(4.52749311797091,-2.76348183928881,
-11.4037129921595)) ;
#141611 = CARTESIAN_POINT('Ctrl Pts',(4.49873206155795,-2.8,-11.3937330953071)) ;
#141612 = CARTESIAN_POINT('Ctrl Pts',(4.45486817043772,-2.8,-11.3749566433661)) ;
#141613 = CARTESIAN_POINT('Ctrl Pts',(4.53619745972499,-2.77169205010106,
-11.3640190471852)) ;
#141614 = CARTESIAN_POINT('Ctrl Pts',(4.50883664816671,-2.8,-11.3517394381721)) ;
#141615 = CARTESIAN_POINT('Ctrl Pts',(4.47227975612147,-2.8,-11.3327273846037)) ;
#141616 = CARTESIAN_POINT('Ctrl Pts',(4.55447795090009,-2.78248459830339,
-11.3099078127334)) ;
#141617 = CARTESIAN_POINT('Ctrl Pts',(4.53370055749885,-2.8,-11.2946579183699)) ;
#141618 = CARTESIAN_POINT('Ctrl Pts',(4.50886586566854,-2.8,-11.2757478882722)) ;
#141619 = CARTESIAN_POINT('Ctrl Pts',(4.56160154376425,-2.78591123334062,
-11.2923494428157)) ;
#141620 = CARTESIAN_POINT('Ctrl Pts',(4.54365878772218,-2.8,-11.2762910664542)) ;
#141621 = CARTESIAN_POINT('Ctrl Pts',(4.52312452397684,-2.8,-11.2573699954867)) ;
#141622 = CARTESIAN_POINT('Ctrl Pts',(4.58735772267363,-2.79384903998488,
-11.2510842943985)) ;
#141623 = CARTESIAN_POINT('Ctrl Pts',(4.58063087367387,-2.79999999999999,
-11.2336839633809)) ;
#141624 = CARTESIAN_POINT('Ctrl Pts',(4.57468550767192,-2.8,-11.2143374866056)) ;
#141625 = CARTESIAN_POINT('Ctrl Pts',(4.61212536563478,-2.79628002040289,
-11.2376015865952)) ;
#141626 = CARTESIAN_POINT('Ctrl Pts',(4.61826745782989,-2.79999999999994,
-11.2190848793758)) ;
#141627 = CARTESIAN_POINT('Ctrl Pts',(4.62435992349563,-2.8,-11.2005015173212)) ;
#141628 = CARTESIAN_POINT('Ctrl Pts',(4.63586710715927,-2.78569036914628,
-11.2943752946759)) ;
#141629 = CARTESIAN_POINT('Ctrl Pts',(4.65405106945726,-2.80000000000018,
-11.2795525238836)) ;
#141630 = CARTESIAN_POINT('Ctrl Pts',(4.67158355065755,-2.8,-11.2592450797815)) ;
#141631 = CARTESIAN_POINT('Ctrl Pts',(4.59999999999999,-2.79310344827586,
-11.2547936459578)) ;
#141632 = CARTESIAN_POINT('Ctrl Pts',(4.59840954578226,-2.79314968944988,
-11.2546756726912)) ;
#141633 = CARTESIAN_POINT('Ctrl Pts',(4.59737383489105,-2.7931815960622,-11.2546133239717)) ;
#141634 = CARTESIAN_POINT('Ctrl Pts',(4.59650507521659,-2.79322931786012,
-11.25455037726)) ;
#141635 = CARTESIAN_POINT('Ctrl Pts',(4.59632758424311,-2.79324472590582,
-11.2545345791767)) ;
#141636 = CARTESIAN_POINT('Ctrl Pts',(4.5961184721085,-2.79327477162036,-11.2545047565773)) ;
#141637 = CARTESIAN_POINT('Ctrl Pts',(4.59606489504931,-2.79328892979786,
-11.2544910265853)) ;
#141638 = CARTESIAN_POINT('Ctrl Pts',(4.59594601677698,-2.79331605564258,
-11.254459114495)) ;
#141639 = CARTESIAN_POINT('Ctrl Pts',(4.59588597444861,-2.7933285533825,-11.2544426561835)) ;
#141640 = CARTESIAN_POINT('Ctrl Pts',(4.59549967474365,-2.79337285752324,
-11.2543702787606)) ;
#141641 = CARTESIAN_POINT('Ctrl Pts',(4.59527331486238,-2.7934062238596,-11.2543100807084)) ;
#141642 = CARTESIAN_POINT('Ctrl Pts',(4.5949320123953,-2.79346950514992,-11.2541870402937)) ;
#141643 = CARTESIAN_POINT('Ctrl Pts',(4.59480393230128,-2.79349821606423,
-11.254128474279)) ;
#141644 = CARTESIAN_POINT('Ctrl Pts',(4.59460326813595,-2.79353924388983,
-11.2540476351491)) ;
#141645 = CARTESIAN_POINT('Ctrl Pts',(4.59455075953096,-2.79354963432651,
-11.2540274276715)) ;
#141646 = CARTESIAN_POINT('Ctrl Pts',(4.59417008680875,-2.79361944405452,
-11.2538955937176)) ;
#141647 = CARTESIAN_POINT('Ctrl Pts',(4.59377742096549,-2.79368602572532,
-11.2537773461555)) ;
#141648 = CARTESIAN_POINT('Ctrl Pts',(4.59289939109632,-2.7938335466559,-11.2535254190241)) ;
#141649 = CARTESIAN_POINT('Ctrl Pts',(4.59245006584783,-2.79390305456781,
-11.253416036199)) ;
#141650 = CARTESIAN_POINT('Ctrl Pts',(4.59099552519185,-2.79413629528614,
-11.2530568524092)) ;
#141651 = CARTESIAN_POINT('Ctrl Pts',(4.5900219788147,-2.79430302757336,-11.2528063701757)) ;
#141652 = CARTESIAN_POINT('Ctrl Pts',(4.58861122644562,-2.79456793455724,
-11.2523921365665)) ;
#141653 = CARTESIAN_POINT('Ctrl Pts',(4.5881790489434,-2.79465210327465,-11.2522585234303)) ;
#141654 = CARTESIAN_POINT('Ctrl Pts',(4.58736872283365,-2.79481449815582,
-11.2519941835896)) ;
#141655 = CARTESIAN_POINT('Ctrl Pts',(4.58699491219415,-2.79489135860975,
-11.2518665823581)) ;
#141656 = CARTESIAN_POINT('Ctrl Pts',(4.58468897497187,-2.79537899446709,
-11.2510351906196)) ;
#141657 = CARTESIAN_POINT('Ctrl Pts',(4.582907177187,-2.79577019617637,-11.2503420642284)) ;
#141658 = CARTESIAN_POINT('Ctrl Pts',(4.57867627871776,-2.79666451416568,
-11.2486707882875)) ;
#141659 = CARTESIAN_POINT('Ctrl Pts',(4.57626321554131,-2.79715040843618,
-11.2476877651429)) ;
#141660 = CARTESIAN_POINT('Ctrl Pts',(4.57243386308706,-2.79784156172336,
-11.2461367865103)) ;
#141661 = CARTESIAN_POINT('Ctrl Pts',(4.57107519984216,-2.79807176647234,
-11.245584021445)) ;
#141662 = CARTESIAN_POINT('Ctrl Pts',(4.56513452430478,-2.7990007429439,-11.2431693903581)) ;
#141663 = CARTESIAN_POINT('Ctrl Pts',(4.56062162665752,-2.79951267011378,
-11.2413309293495)) ;
#141664 = CARTESIAN_POINT('Ctrl Pts',(4.55365420596644,-2.79992470862867,
-11.2384610302784)) ;
#141665 = CARTESIAN_POINT('Ctrl Pts',(4.55124660967272,-2.79999983267432,
-11.2374632392507)) ;
#141666 = CARTESIAN_POINT('Ctrl Pts',(4.54880051362942,-2.79999999972164,
-11.2364378607329)) ;
#141667 = CARTESIAN_POINT('Ctrl Pts',(4.54879236166274,-2.8,-9.08356555651516)) ;
#141668 = CARTESIAN_POINT('Ctrl Pts',(4.5622387183224,-2.79999999999679,-9.10123152627487)) ;
#141669 = CARTESIAN_POINT('Ctrl Pts',(4.57442182196495,-2.80939476060287,
-9.11723782046681)) ;
#141670 = CARTESIAN_POINT('Ctrl Pts',(4.55556842517599,-2.79999999999889,
-9.0807250640488)) ;
#141671 = CARTESIAN_POINT('Ctrl Pts',(4.56783337210914,-2.80040661803736,
-9.09618630155187)) ;
#141672 = CARTESIAN_POINT('Ctrl Pts',(4.57961823522365,-2.80818164104597,
-9.11001834132729)) ;
#141673 = CARTESIAN_POINT('Ctrl Pts',(4.56238982831619,-2.79942602551759,
-9.07795285151706)) ;
#141674 = CARTESIAN_POINT('Ctrl Pts',(4.57357810388182,-2.80014618986472,
-9.09093107214123)) ;
#141675 = CARTESIAN_POINT('Ctrl Pts',(4.58462643299474,-2.80630261261112,
-9.10252327116488)) ;
#141676 = CARTESIAN_POINT('Ctrl Pts',(4.57328757735258,-2.7977370397245,-9.07356999795014)) ;
#141677 = CARTESIAN_POINT('Ctrl Pts',(4.58237922839514,-2.79856394574987,
-9.08226640893135)) ;
#141678 = CARTESIAN_POINT('Ctrl Pts',(4.59151541127592,-2.80237286596198,
-9.09008300288059)) ;
#141679 = CARTESIAN_POINT('Ctrl Pts',(4.57700059755676,-2.79703714667161,
-9.07207607634204)) ;
#141680 = CARTESIAN_POINT('Ctrl Pts',(4.58532305318675,-2.79784352093717,
-9.07926254300446)) ;
#141681 = CARTESIAN_POINT('Ctrl Pts',(4.59370961102546,-2.80088045369937,
-9.08574551418945)) ;
#141682 = CARTESIAN_POINT('Ctrl Pts',(4.58319893207065,-2.79574016930783,
-9.06965467052113)) ;
#141683 = CARTESIAN_POINT('Ctrl Pts',(4.5899041610924,-2.79637293360539,-9.07433035456224)) ;
#141684 = CARTESIAN_POINT('Ctrl Pts',(4.59665800356694,-2.79825577077759,
-9.07858194486972)) ;
#141685 = CARTESIAN_POINT('Ctrl Pts',(4.58534994317986,-2.79526732601294,
-9.06881886188718)) ;
#141686 = CARTESIAN_POINT('Ctrl Pts',(4.59144552977844,-2.79581844972913,
-9.07262003661071)) ;
#141687 = CARTESIAN_POINT('Ctrl Pts',(4.59758018705035,-2.79731769672697,
-9.07608858039388)) ;
#141688 = CARTESIAN_POINT('Ctrl Pts',(4.58899927751306,-2.79450268149332,
-9.06751730126711)) ;
#141689 = CARTESIAN_POINT('Ctrl Pts',(4.59386223202755,-2.79488630507105,
-9.06994951703029)) ;
#141690 = CARTESIAN_POINT('Ctrl Pts',(4.59874684688641,-2.79582009356912,
-9.07218136524475)) ;
#141691 = CARTESIAN_POINT('Ctrl Pts',(4.59026755692868,-2.79423885380164,
-9.06707439958003)) ;
#141692 = CARTESIAN_POINT('Ctrl Pts',(4.59467706068311,-2.79455862385203,
-9.06904054333605)) ;
#141693 = CARTESIAN_POINT('Ctrl Pts',(4.59910266898802,-2.79530499526365,
-9.07084863990216)) ;
#141694 = CARTESIAN_POINT('Ctrl Pts',(4.59257623319517,-2.79382131826659,
-9.06638413145)) ;
#141695 = CARTESIAN_POINT('Ctrl Pts',(4.59605751036346,-2.79403163929513,
-9.06762276103362)) ;
#141696 = CARTESIAN_POINT('Ctrl Pts',(4.59954701072604,-2.79449510806573,
-9.06876576681698)) ;
#141697 = CARTESIAN_POINT('Ctrl Pts',(4.59342976933296,-2.79367543507711,
-9.06614453745337)) ;
#141698 = CARTESIAN_POINT('Ctrl Pts',(4.59655016100493,-2.79384713427256,
-9.06713488953029)) ;
#141699 = CARTESIAN_POINT('Ctrl Pts',(4.59967640178298,-2.79421605292373,
-9.06805021393703)) ;
#141700 = CARTESIAN_POINT('Ctrl Pts',(4.59428414179641,-2.79346156087783,
-9.06570693618526)) ;
#141701 = CARTESIAN_POINT('Ctrl Pts',(4.59704519451433,-2.7935546974653,-9.06637363574795)) ;
#141702 = CARTESIAN_POINT('Ctrl Pts',(4.5998104157401,-2.79379877456676,-9.06698237127069)) ;
#141703 = CARTESIAN_POINT('Ctrl Pts',(4.59432658472653,-2.7933916625364,-9.06553381814949)) ;
#141704 = CARTESIAN_POINT('Ctrl Pts',(4.59708408719786,-2.79345234504014,
-9.06610907664629)) ;
#141705 = CARTESIAN_POINT('Ctrl Pts',(4.59984563524626,-2.79366003518351,
-9.06662765435266)) ;
#141706 = CARTESIAN_POINT('Ctrl Pts',(4.59537197237733,-2.79324260992761,
-9.06528726159385)) ;
#141707 = CARTESIAN_POINT('Ctrl Pts',(4.59764722167537,-2.79326383513928,
-9.065620961855)) ;
#141708 = CARTESIAN_POINT('Ctrl Pts',(4.59992475053754,-2.79338190759658,
-9.06591703064758)) ;
#141709 = CARTESIAN_POINT('Ctrl Pts',(4.59364183392371,-2.79313407032025,
-9.06528447884512)) ;
#141710 = CARTESIAN_POINT('Ctrl Pts',(4.59684754854893,-2.79327107597598,
-9.06563893104521)) ;
#141711 = CARTESIAN_POINT('Ctrl Pts',(4.59996664298755,-2.79324102308608,
-9.06556177368153)) ;
#141712 = CARTESIAN_POINT('Ctrl Pts',(4.59999999999999,-2.79310344827586,
-9.06520635404224)) ;
#141713 = CARTESIAN_POINT('Ctrl Pts',(4.59999999999999,-2.79310344827586,
-9.06520635404224)) ;
#141714 = CARTESIAN_POINT('Ctrl Pts',(4.59999999999999,-2.79310344827586,
-9.06520635404224)) ;
#141715 = CARTESIAN_POINT('Origin',(4.54879236168542,-2.9,-9.08356555651607)) ;
#141716 = CARTESIAN_POINT('Ctrl Pts',(4.39959973407451,-2.8,-10.2705922428027)) ;
#141717 = CARTESIAN_POINT('Ctrl Pts',(4.49922290141875,-2.8,-10.2701052483316)) ;
#141718 = CARTESIAN_POINT('Ctrl Pts',(4.49980764094185,-2.8996950427637,-10.2706080458952)) ;
#141719 = CARTESIAN_POINT('Ctrl Pts',(4.40142712570759,-2.8,-10.0495338960075)) ;
#141720 = CARTESIAN_POINT('Ctrl Pts',(4.50593622119643,-2.8,-10.046048013468)) ;
#141721 = CARTESIAN_POINT('Ctrl Pts',(4.50067611734352,-2.90411960318532,
-10.0496502871252)) ;
#141722 = CARTESIAN_POINT('Ctrl Pts',(4.39573539165433,-2.8,-9.82762254178866)) ;
#141723 = CARTESIAN_POINT('Ctrl Pts',(4.49039105203439,-2.8,-9.84644486600902)) ;
#141724 = CARTESIAN_POINT('Ctrl Pts',(4.4979321089857,-2.89506044297338,-9.82659283506982)) ;
#141725 = CARTESIAN_POINT('Ctrl Pts',(4.41164816536272,-2.8,-9.51449214865639)) ;
#141726 = CARTESIAN_POINT('Ctrl Pts',(4.48203507549531,-2.8,-9.52300753838907)) ;
#141727 = CARTESIAN_POINT('Ctrl Pts',(4.50604587949362,-2.86657833599726,
-9.52179163345499)) ;
#141728 = CARTESIAN_POINT('Ctrl Pts',(4.41940490599909,-2.8,-9.42215713199873)) ;
#141729 = CARTESIAN_POINT('Ctrl Pts',(4.48133975791564,-2.8,-9.43332746373862)) ;
#141730 = CARTESIAN_POINT('Ctrl Pts',(4.50997623336224,-2.85625883833129,
-9.43306464323899)) ;
#141731 = CARTESIAN_POINT('Ctrl Pts',(4.44577434373642,-2.8,-9.28702065882596)) ;
#141732 = CARTESIAN_POINT('Ctrl Pts',(4.49360122670476,-2.8,-9.29933058766784)) ;
#141733 = CARTESIAN_POINT('Ctrl Pts',(4.5231855860418,-2.83896465559561,-9.3054850424376)) ;
#141734 = CARTESIAN_POINT('Ctrl Pts',(4.45692583760033,-2.8,-9.2424768930528)) ;
#141735 = CARTESIAN_POINT('Ctrl Pts',(4.49949391572663,-2.8,-9.25605430264614)) ;
#141736 = CARTESIAN_POINT('Ctrl Pts',(4.52876348458379,-2.83289258157626,
-9.26380298860431)) ;
#141737 = CARTESIAN_POINT('Ctrl Pts',(4.50378503771657,-2.8,-9.12107591625827)) ;
#141738 = CARTESIAN_POINT('Ctrl Pts',(4.5287351960681,-2.8,-9.13992534227475)) ;
#141739 = CARTESIAN_POINT('Ctrl Pts',(4.55214466721902,-2.81552005845341,
-9.15122486980152)) ;
#141740 = CARTESIAN_POINT('Ctrl Pts',(4.54714423790162,-2.8,-9.0422684950468)) ;
#141741 = CARTESIAN_POINT('Ctrl Pts',(4.55761617337313,-2.8,-9.06320656418836)) ;
#141742 = CARTESIAN_POINT('Ctrl Pts',(4.572595848134,-2.80338245043804,-9.08123859518892)) ;
#141743 = CARTESIAN_POINT('Ctrl Pts',(4.67762904165649,-2.8,-9.05149504479602)) ;
#141744 = CARTESIAN_POINT('Ctrl Pts',(4.66093484724955,-2.8,-9.06706706583778)) ;
#141745 = CARTESIAN_POINT('Ctrl Pts',(4.64133868807413,-2.80368623369319,
-9.08468800638624)) ;
#141746 = CARTESIAN_POINT('Origin',(4.4,-2.9,-10.1600000000039)) ;
#141747 = CARTESIAN_POINT('Ctrl Pts',(4.7217278356698,-2.8000000024879,-11.2603629549123)) ;
#141748 = CARTESIAN_POINT('Ctrl Pts',(4.69645430307825,-2.79999660525747,
-11.247070047311)) ;
#141749 = CARTESIAN_POINT('Ctrl Pts',(4.66463283185016,-2.80454824226955,
-11.2294903682927)) ;
#141750 = CARTESIAN_POINT('Ctrl Pts',(4.55709227475155,-2.80000000030524,
-11.2959964363105)) ;
#141751 = CARTESIAN_POINT('Ctrl Pts',(4.56399237478739,-2.79999958643667,
-11.2739593792004)) ;
#141752 = CARTESIAN_POINT('Ctrl Pts',(4.57729370999484,-2.80055804294512,
-11.2551759050809)) ;
#141753 = CARTESIAN_POINT('Ctrl Pts',(4.50667826286321,-2.80000000784871,
-11.2066146479981)) ;
#141754 = CARTESIAN_POINT('Ctrl Pts',(4.53037382014981,-2.79998899178922,
-11.1870846001166)) ;
#141755 = CARTESIAN_POINT('Ctrl Pts',(4.55348183854634,-2.81434699509191,
-11.1759466041139)) ;
#141756 = CARTESIAN_POINT('Ctrl Pts',(4.45692280158725,-2.80000001789831,
-11.0776422182876)) ;
#141757 = CARTESIAN_POINT('Ctrl Pts',(4.4993802926736,-2.79997354447563,-11.0640998880094)) ;
#141758 = CARTESIAN_POINT('Ctrl Pts',(4.52864149761196,-2.83271033979,-11.05632906208)) ;
#141759 = CARTESIAN_POINT('Ctrl Pts',(4.44554661086166,-2.80000002126189,
-11.032377440014)) ;
#141760 = CARTESIAN_POINT('Ctrl Pts',(4.49333665154849,-2.7999679796365,-11.0200969398739)) ;
#141761 = CARTESIAN_POINT('Ctrl Pts',(4.52295544156351,-2.83885474437117,
-11.013967858228)) ;
#141762 = CARTESIAN_POINT('Ctrl Pts',(4.41903322104334,-2.8000000307772,-10.8958947975772)) ;
#141763 = CARTESIAN_POINT('Ctrl Pts',(4.4810061608023,-2.79995095769182,-10.8847300040205)) ;
#141764 = CARTESIAN_POINT('Ctrl Pts',(4.50969337368895,-2.85623179093863,
-10.885069623609)) ;
#141765 = CARTESIAN_POINT('Ctrl Pts',(4.41147189908675,-2.8000000363501,-10.8042415900435)) ;
#141766 = CARTESIAN_POINT('Ctrl Pts',(4.48178828424046,-2.79993989905029,
-10.7957891492056)) ;
#141767 = CARTESIAN_POINT('Ctrl Pts',(4.50589025525737,-2.86640526991131,
-10.7969681512011)) ;
#141768 = CARTESIAN_POINT('Ctrl Pts',(4.39523119070911,-2.80000005228415,
-10.4831795198329)) ;
#141769 = CARTESIAN_POINT('Ctrl Pts',(4.4903383634589,-2.79990261688304,-10.4630741316606)) ;
#141770 = CARTESIAN_POINT('Ctrl Pts',(4.49769757367176,-2.89547737952985,
-10.4843332157617)) ;
#141771 = CARTESIAN_POINT('Ctrl Pts',(4.40178225889357,-2.80000005718968,
-10.2526239782851)) ;
#141772 = CARTESIAN_POINT('Ctrl Pts',(4.50681341018175,-2.79988784121843,
-10.2570581988245)) ;
#141773 = CARTESIAN_POINT('Ctrl Pts',(4.50092255053476,-2.90441958896084,
-10.2524406960391)) ;
#141774 = CARTESIAN_POINT('Ctrl Pts',(4.39924589760307,-2.80000005405717,
-10.0230311688801)) ;
#141775 = CARTESIAN_POINT('Ctrl Pts',(4.49795607191393,-2.79989746608217,
-10.023922937496)) ;
#141776 = CARTESIAN_POINT('Ctrl Pts',(4.49968270404898,-2.89870974459553,
-10.0230284945916)) ;
#141777 = CARTESIAN_POINT('Origin',(4.54879236168626,-2.9,-11.2364344434846)) ;
#141778 = CARTESIAN_POINT('Ctrl Pts',(4.57442492185553,-2.809397151199,-11.2027581068621)) ;
#141779 = CARTESIAN_POINT('Ctrl Pts',(4.56210583156796,-2.7998961275033,-11.2189430617887)) ;
#141780 = CARTESIAN_POINT('Ctrl Pts',(4.54850917782857,-2.80000109307748,
-11.2368064934881)) ;
#141781 = CARTESIAN_POINT('Ctrl Pts',(4.57959763980856,-2.80818914940072,
-11.2099453004955)) ;
#141782 = CARTESIAN_POINT('Ctrl Pts',(4.56768008075465,-2.80031924975225,
-11.2239410457291)) ;
#141783 = CARTESIAN_POINT('Ctrl Pts',(4.55527876038347,-2.79999229227378,
-11.2395899763868)) ;
#141784 = CARTESIAN_POINT('Ctrl Pts',(4.58464248447265,-2.80630474344638,
-11.2174843126383)) ;
#141785 = CARTESIAN_POINT('Ctrl Pts',(4.57346944634371,-2.80008318972135,
-11.2292012910522)) ;
#141786 = CARTESIAN_POINT('Ctrl Pts',(4.56216307187795,-2.79941338753917,
-11.2423280915335)) ;
#141787 = CARTESIAN_POINT('Ctrl Pts',(4.59159231899494,-2.80232720646228,
-11.2300563692959)) ;
#141788 = CARTESIAN_POINT('Ctrl Pts',(4.58237910662986,-2.79850221241048,
-11.2379149362578)) ;
#141789 = CARTESIAN_POINT('Ctrl Pts',(4.57321634584968,-2.79769868647539,
-11.2466644864947)) ;
#141790 = CARTESIAN_POINT('Ctrl Pts',(4.59378564167737,-2.8008235544484,-11.2344145837654)) ;
#141791 = CARTESIAN_POINT('Ctrl Pts',(4.58533966160572,-2.79778056279966,
-11.2409180694478)) ;
#141792 = CARTESIAN_POINT('Ctrl Pts',(4.5769613009382,-2.79699227428059,-11.2481320740362)) ;
#141793 = CARTESIAN_POINT('Ctrl Pts',(4.59669734138576,-2.79821861236081,
-11.2415174469091)) ;
#141794 = CARTESIAN_POINT('Ctrl Pts',(4.58989502505307,-2.79633072300511,
-11.245783702985)) ;
#141795 = CARTESIAN_POINT('Ctrl Pts',(4.58314295739386,-2.79570785369251,
-11.2504789031814)) ;
#141796 = CARTESIAN_POINT('Ctrl Pts',(4.59760632414569,-2.79728965034655,
-11.2439852466291)) ;
#141797 = CARTESIAN_POINT('Ctrl Pts',(4.59142619397023,-2.79578507327358,
-11.2474678937229)) ;
#141798 = CARTESIAN_POINT('Ctrl Pts',(4.58528630332434,-2.79524119148169,
-11.251287378375)) ;
#141799 = CARTESIAN_POINT('Ctrl Pts',(4.59875741430933,-2.79580683383093,
-11.247853004496)) ;
#141800 = CARTESIAN_POINT('Ctrl Pts',(4.59383193680337,-2.79486773439436,
-11.2500980055339)) ;
#141801 = CARTESIAN_POINT('Ctrl Pts',(4.58892874314202,-2.79448758877844,
-11.2525464730129)) ;
#141802 = CARTESIAN_POINT('Ctrl Pts',(4.59910834609947,-2.79529718130591,
-11.2491714993014)) ;
#141803 = CARTESIAN_POINT('Ctrl Pts',(4.59464343907624,-2.79454543406795,
-11.2509926958501)) ;
#141804 = CARTESIAN_POINT('Ctrl Pts',(4.59019511689903,-2.79422790851556,
-11.2529746712091)) ;
#141805 = CARTESIAN_POINT('Ctrl Pts',(4.59954688679867,-2.79449699552072,
-11.2512293846587)) ;
#141806 = CARTESIAN_POINT('Ctrl Pts',(4.59601732089133,-2.79402779797774,
-11.2523863363518)) ;
#141807 = CARTESIAN_POINT('Ctrl Pts',(4.59249627585267,-2.79381771894921,
-11.2536411141675)) ;
#141808 = CARTESIAN_POINT('Ctrl Pts',(4.59967529310588,-2.79422450025963,
-11.2519354645612)) ;
#141809 = CARTESIAN_POINT('Ctrl Pts',(4.59651100242295,-2.79384821317135,
-11.2528644108735)) ;
#141810 = CARTESIAN_POINT('Ctrl Pts',(4.593352874124,-2.79367727499394,-11.2538714476574)) ;
#141811 = CARTESIAN_POINT('Ctrl Pts',(4.59980981518572,-2.79380630943631,
-11.2530056452101)) ;
#141812 = CARTESIAN_POINT('Ctrl Pts',(4.59701056623719,-2.79355888022806,
-11.2536249350365)) ;
#141813 = CARTESIAN_POINT('Ctrl Pts',(4.59421559911326,-2.79346462438277,
-11.2543030289899)) ;
#141814 = CARTESIAN_POINT('Ctrl Pts',(4.59984534134842,-2.79366726490194,
-11.2533646067489)) ;
#141815 = CARTESIAN_POINT('Ctrl Pts',(4.59705039509825,-2.79345667046145,
-11.2538917393962)) ;
#141816 = CARTESIAN_POINT('Ctrl Pts',(4.59425962044003,-2.79339574833516,
-11.2544765637043)) ;
#141817 = CARTESIAN_POINT('Ctrl Pts',(4.59992484646001,-2.7933873519883,-11.25407980384)) ;
#141818 = CARTESIAN_POINT('Ctrl Pts',(4.59761652863209,-2.79326682373741,
-11.254380589531)) ;
#141819 = CARTESIAN_POINT('Ctrl Pts',(4.59531061070857,-2.79324678512396,
-11.2547204137335)) ;
#141820 = CARTESIAN_POINT('Ctrl Pts',(4.59996721368508,-2.79324340897637,
-11.254436569794)) ;
#141821 = CARTESIAN_POINT('Ctrl Pts',(4.59680854952869,-2.79327323421043,
-11.2543604778616)) ;
#141822 = CARTESIAN_POINT('Ctrl Pts',(4.59356174266138,-2.79313094944462,
-11.2547234833207)) ;
#141823 = CARTESIAN_POINT('Ctrl Pts',(4.59999999999999,-2.79310344827586,
-11.2547936459578)) ;
#141824 = CARTESIAN_POINT('Ctrl Pts',(4.59999999999999,-2.79310344827586,
-11.2547936459578)) ;
#141825 = CARTESIAN_POINT('Ctrl Pts',(4.59999999999999,-2.79310344827586,
-11.2547936459578)) ;
#141826 = CARTESIAN_POINT('',(0.,0.,0.)) ;
#141827 = CARTESIAN_POINT('Origin',(2.3,0.,-34.29)) ;
#141828 = CARTESIAN_POINT('',(2.4,-1.10218211923262E-16,-33.39)) ;
#141829 = CARTESIAN_POINT('Origin',(2.4,0.,-34.29)) ;
#141830 = CARTESIAN_POINT('',(2.3,-1.22464679914735E-16,-33.29)) ;
#141831 = CARTESIAN_POINT('Origin',(2.3,-1.10218211923262E-16,-33.39)) ;
#141832 = CARTESIAN_POINT('',(2.3,1.22464679914735E-16,-35.29)) ;
#141833 = CARTESIAN_POINT('Origin',(2.3,0.,-34.29)) ;
#141834 = CARTESIAN_POINT('Origin',(2.3,0.,-34.29)) ;
#141835 = CARTESIAN_POINT('Origin',(1.5,0.,-34.29)) ;
#141836 = CARTESIAN_POINT('',(1.4,-1.34711147906208E-16,-35.39)) ;
#141837 = CARTESIAN_POINT('Origin',(1.4,0.,-34.29)) ;
#141838 = CARTESIAN_POINT('',(1.5,-1.22464679914735E-16,-35.29)) ;
#141839 = CARTESIAN_POINT('Origin',(1.5,-1.34711147906209E-16,-35.39)) ;
#141840 = CARTESIAN_POINT('Origin',(1.5,0.,-34.29)) ;
#141841 = CARTESIAN_POINT('Origin',(1.5,3.15,-33.0314213562373)) ;
#141842 = CARTESIAN_POINT('',(1.5,3.07928932188135,-32.9607106781187)) ;
#141843 = CARTESIAN_POINT('',(1.5,3.25,-33.0314213562373)) ;
#141844 = CARTESIAN_POINT('Origin',(1.5,3.15,-33.0314213562373)) ;
#141845 = CARTESIAN_POINT('',(1.4,3.15,-33.0314213562373)) ;
#141846 = CARTESIAN_POINT('Origin',(1.5,3.15,-33.0314213562373)) ;
#141847 = CARTESIAN_POINT('Origin',(1.5,3.15,-33.0314213562373)) ;
#141848 = CARTESIAN_POINT('Origin',(0.500000000000001,-4.56640444411537E-17,
-34.69)) ;
#141849 = CARTESIAN_POINT('',(0.600000000000001,0.4,-34.69)) ;
#141850 = CARTESIAN_POINT('',(0.59561299721608,0.370705721320401,-34.6607057213204)) ;
#141851 = CARTESIAN_POINT('Origin',(0.500000000014529,0.399999999998192,-34.6899999999979)) ;
#141852 = CARTESIAN_POINT('',(0.500000000000001,0.4,-34.79)) ;
#141853 = CARTESIAN_POINT('Origin',(0.500000000000001,0.4,-34.69)) ;
#141854 = CARTESIAN_POINT('',(0.500000000000001,-1.9,-34.79)) ;
#141855 = CARTESIAN_POINT('',(0.500000000000001,0.5,-34.79)) ;
#141856 = CARTESIAN_POINT('',(0.600000000000001,-1.9,-34.69)) ;
#141857 = CARTESIAN_POINT('Origin',(0.500000000000001,-1.9,-34.69)) ;
#141858 = CARTESIAN_POINT('',(0.600000000000001,-0.3,-34.69)) ;
#141859 = CARTESIAN_POINT('',(0.600000000000001,-2.39800009914437E-17,-34.69)) ;
#141860 = CARTESIAN_POINT('',(0.600000000000001,0.299999999999999,-34.69)) ;
#141861 = CARTESIAN_POINT('',(0.600000000000001,-2.39800009914437E-17,-34.69)) ;
#141862 = CARTESIAN_POINT('Ctrl Pts',(0.600000000000001,0.300000000000003,
-34.69)) ;
#141863 = CARTESIAN_POINT('Ctrl Pts',(0.600000000000001,0.312243016306297,
-34.69)) ;
#141864 = CARTESIAN_POINT('Ctrl Pts',(0.60006974742297,0.324350425899703,
-34.6877515285214)) ;
#141865 = CARTESIAN_POINT('Ctrl Pts',(0.599517124288205,0.34619696929781,
-34.6793954490601)) ;
#141866 = CARTESIAN_POINT('Ctrl Pts',(0.598927484301131,0.355857825373572,
-34.6736750447227)) ;
#141867 = CARTESIAN_POINT('Ctrl Pts',(0.596766673872563,0.366539012308038,
-34.6647023851096)) ;
#141868 = CARTESIAN_POINT('Ctrl Pts',(0.59623562910414,0.368676603883175,
-34.6627379168092)) ;
#141869 = CARTESIAN_POINT('Ctrl Pts',(0.59561299721608,0.370705721320409,
-34.6607057213204)) ;
#141870 = CARTESIAN_POINT('Origin',(2.3,0.,-30.48)) ;
#141871 = CARTESIAN_POINT('',(2.4,-1.10218211923262E-16,-29.58)) ;
#141872 = CARTESIAN_POINT('Origin',(2.4,0.,-30.48)) ;
#141873 = CARTESIAN_POINT('',(2.3,-1.22464679914735E-16,-29.48)) ;
#141874 = CARTESIAN_POINT('Origin',(2.3,-1.10218211923262E-16,-29.58)) ;
#141875 = CARTESIAN_POINT('',(2.3,1.22464679914735E-16,-31.48)) ;
#141876 = CARTESIAN_POINT('Origin',(2.3,0.,-30.48)) ;
#141877 = CARTESIAN_POINT('Origin',(2.3,0.,-30.48)) ;
#141878 = CARTESIAN_POINT('Origin',(1.5,0.,-30.48)) ;
#141879 = CARTESIAN_POINT('',(1.4,-1.34711147906209E-16,-31.58)) ;
#141880 = CARTESIAN_POINT('Origin',(1.4,0.,-30.48)) ;
#141881 = CARTESIAN_POINT('',(1.5,-1.22464679914735E-16,-31.48)) ;
#141882 = CARTESIAN_POINT('Origin',(1.5,-1.34711147906209E-16,-31.58)) ;
#141883 = CARTESIAN_POINT('Origin',(1.5,0.,-30.48)) ;
#141884 = CARTESIAN_POINT('Origin',(1.5,3.15,-29.2214213562373)) ;
#141885 = CARTESIAN_POINT('',(1.5,3.07928932188135,-29.1507106781187)) ;
#141886 = CARTESIAN_POINT('',(1.5,3.25,-29.2214213562373)) ;
#141887 = CARTESIAN_POINT('Origin',(1.5,3.15,-29.2214213562373)) ;
#141888 = CARTESIAN_POINT('',(1.4,3.15,-29.2214213562373)) ;
#141889 = CARTESIAN_POINT('Origin',(1.5,3.15,-29.2214213562373)) ;
#141890 = CARTESIAN_POINT('Origin',(1.5,3.15,-29.2214213562373)) ;
#141891 = CARTESIAN_POINT('Origin',(0.500000000000001,-4.56640444411542E-17,
-30.88)) ;
#141892 = CARTESIAN_POINT('',(0.600000000000001,0.4,-30.88)) ;
#141893 = CARTESIAN_POINT('',(0.595612997216081,0.370705721320403,-30.8507057213204)) ;
#141894 = CARTESIAN_POINT('Origin',(0.500000000043895,0.399999999994469,-30.8799999999944)) ;
#141895 = CARTESIAN_POINT('',(0.500000000000001,0.4,-30.98)) ;
#141896 = CARTESIAN_POINT('Origin',(0.500000000000001,0.4,-30.88)) ;
#141897 = CARTESIAN_POINT('',(0.500000000000001,-1.9,-30.98)) ;
#141898 = CARTESIAN_POINT('',(0.500000000000001,0.5,-30.98)) ;
#141899 = CARTESIAN_POINT('',(0.600000000000001,-1.9,-30.88)) ;
#141900 = CARTESIAN_POINT('Origin',(0.500000000000001,-1.9,-30.88)) ;
#141901 = CARTESIAN_POINT('',(0.600000000000001,-0.3,-30.88)) ;
#141902 = CARTESIAN_POINT('',(0.600000000000001,-2.39800009914441E-17,-30.88)) ;
#141903 = CARTESIAN_POINT('',(0.600000000000001,0.299999999999999,-30.88)) ;
#141904 = CARTESIAN_POINT('',(0.600000000000001,-2.39800009914441E-17,-30.88)) ;
#141905 = CARTESIAN_POINT('Ctrl Pts',(0.600000000000001,0.300000000000003,
-30.88)) ;
#141906 = CARTESIAN_POINT('Ctrl Pts',(0.600000000000001,0.312243016306059,
-30.88)) ;
#141907 = CARTESIAN_POINT('Ctrl Pts',(0.600069747422976,0.324350425899479,
-30.8777515285215)) ;
#141908 = CARTESIAN_POINT('Ctrl Pts',(0.59951712428821,0.346196969297596,
-30.8693954490601)) ;
#141909 = CARTESIAN_POINT('Ctrl Pts',(0.598927484301166,0.355857825373397,
-30.8636750447228)) ;
#141910 = CARTESIAN_POINT('Ctrl Pts',(0.596766673872565,0.36653901230802,
-30.8547023851096)) ;
#141911 = CARTESIAN_POINT('Ctrl Pts',(0.596235629104145,0.368676603883157,
-30.8527379168092)) ;
#141912 = CARTESIAN_POINT('Ctrl Pts',(0.595612997216081,0.370705721320405,
-30.8507057213204)) ;
#141913 = CARTESIAN_POINT('Origin',(2.3,0.,-26.67)) ;
#141914 = CARTESIAN_POINT('',(2.4,-1.10218211923262E-16,-25.77)) ;
#141915 = CARTESIAN_POINT('Origin',(2.4,0.,-26.67)) ;
#141916 = CARTESIAN_POINT('',(2.3,-1.22464679914735E-16,-25.67)) ;
#141917 = CARTESIAN_POINT('Origin',(2.3,-1.10218211923262E-16,-25.77)) ;
#141918 = CARTESIAN_POINT('',(2.3,1.22464679914735E-16,-27.67)) ;
#141919 = CARTESIAN_POINT('Origin',(2.3,0.,-26.67)) ;
#141920 = CARTESIAN_POINT('Origin',(2.3,0.,-26.67)) ;
#141921 = CARTESIAN_POINT('Origin',(1.5,0.,-26.67)) ;
#141922 = CARTESIAN_POINT('',(1.4,-1.34711147906209E-16,-27.77)) ;
#141923 = CARTESIAN_POINT('Origin',(1.4,0.,-26.67)) ;
#141924 = CARTESIAN_POINT('',(1.5,-1.22464679914735E-16,-27.67)) ;
#141925 = CARTESIAN_POINT('Origin',(1.5,-1.34711147906209E-16,-27.77)) ;
#141926 = CARTESIAN_POINT('Origin',(1.5,0.,-26.67)) ;
#141927 = CARTESIAN_POINT('Origin',(1.5,3.15,-25.4114213562373)) ;
#141928 = CARTESIAN_POINT('',(1.5,3.07928932188135,-25.3407106781187)) ;
#141929 = CARTESIAN_POINT('',(1.5,3.25,-25.4114213562373)) ;
#141930 = CARTESIAN_POINT('Origin',(1.5,3.15,-25.4114213562373)) ;
#141931 = CARTESIAN_POINT('',(1.4,3.15,-25.4114213562373)) ;
#141932 = CARTESIAN_POINT('Origin',(1.5,3.15,-25.4114213562373)) ;
#141933 = CARTESIAN_POINT('Origin',(1.5,3.15,-25.4114213562373)) ;
#141934 = CARTESIAN_POINT('Origin',(0.500000000000001,-4.56640444411542E-17,
-27.07)) ;
#141935 = CARTESIAN_POINT('',(0.600000000000001,0.4,-27.07)) ;
#141936 = CARTESIAN_POINT('',(0.595612997216081,0.370705721320403,-27.0407057213204)) ;
#141937 = CARTESIAN_POINT('Origin',(0.500000000043127,0.39999999999434,-27.0699999999943)) ;
#141938 = CARTESIAN_POINT('',(0.500000000000001,0.4,-27.17)) ;
#141939 = CARTESIAN_POINT('Origin',(0.500000000000001,0.4,-27.07)) ;
#141940 = CARTESIAN_POINT('',(0.500000000000001,-1.9,-27.17)) ;
#141941 = CARTESIAN_POINT('',(0.500000000000001,0.5,-27.17)) ;
#141942 = CARTESIAN_POINT('',(0.600000000000001,-1.9,-27.07)) ;
#141943 = CARTESIAN_POINT('Origin',(0.500000000000001,-1.9,-27.07)) ;
#141944 = CARTESIAN_POINT('',(0.600000000000001,-0.3,-27.07)) ;
#141945 = CARTESIAN_POINT('',(0.600000000000001,-2.39800009914441E-17,-27.07)) ;
#141946 = CARTESIAN_POINT('',(0.600000000000001,0.299999999999999,-27.07)) ;
#141947 = CARTESIAN_POINT('',(0.600000000000001,-2.39800009914441E-17,-27.07)) ;
#141948 = CARTESIAN_POINT('Ctrl Pts',(0.600000000000001,0.300000000000003,
-27.07)) ;
#141949 = CARTESIAN_POINT('Ctrl Pts',(0.600000000000001,0.312243016306037,
-27.07)) ;
#141950 = CARTESIAN_POINT('Ctrl Pts',(0.600069747422976,0.324350425899459,
-27.0677515285215)) ;
#141951 = CARTESIAN_POINT('Ctrl Pts',(0.59951712428821,0.346196969297585,
-27.0593954490602)) ;
#141952 = CARTESIAN_POINT('Ctrl Pts',(0.598927484301167,0.355857825373385,
-27.0536750447229)) ;
#141953 = CARTESIAN_POINT('Ctrl Pts',(0.596766673872565,0.366539012308015,
-27.0447023851096)) ;
#141954 = CARTESIAN_POINT('Ctrl Pts',(0.596235629104144,0.368676603883154,
-27.0427379168092)) ;
#141955 = CARTESIAN_POINT('Ctrl Pts',(0.59561299721608,0.370705721320403,
-27.0407057213204)) ;
#141956 = CARTESIAN_POINT('Origin',(2.3,0.,-22.86)) ;
#141957 = CARTESIAN_POINT('',(2.4,-1.10218211923262E-16,-21.96)) ;
#141958 = CARTESIAN_POINT('Origin',(2.4,0.,-22.86)) ;
#141959 = CARTESIAN_POINT('',(2.3,-1.22464679914735E-16,-21.86)) ;
#141960 = CARTESIAN_POINT('Origin',(2.3,-1.10218211923262E-16,-21.96)) ;
#141961 = CARTESIAN_POINT('',(2.3,1.22464679914735E-16,-23.86)) ;
#141962 = CARTESIAN_POINT('Origin',(2.3,0.,-22.86)) ;
#141963 = CARTESIAN_POINT('Origin',(2.3,0.,-22.86)) ;
#141964 = CARTESIAN_POINT('Origin',(1.5,0.,-22.86)) ;
#141965 = CARTESIAN_POINT('',(1.4,-1.34711147906209E-16,-23.96)) ;
#141966 = CARTESIAN_POINT('Origin',(1.4,0.,-22.86)) ;
#141967 = CARTESIAN_POINT('',(1.5,-1.22464679914735E-16,-23.86)) ;
#141968 = CARTESIAN_POINT('Origin',(1.5,-1.34711147906209E-16,-23.96)) ;
#141969 = CARTESIAN_POINT('Origin',(1.5,0.,-22.86)) ;
#141970 = CARTESIAN_POINT('Origin',(1.5,3.15,-21.6014213562373)) ;
#141971 = CARTESIAN_POINT('',(1.5,3.07928932188135,-21.5307106781187)) ;
#141972 = CARTESIAN_POINT('',(1.5,3.25,-21.6014213562373)) ;
#141973 = CARTESIAN_POINT('Origin',(1.5,3.15,-21.6014213562373)) ;
#141974 = CARTESIAN_POINT('',(1.4,3.15,-21.6014213562373)) ;
#141975 = CARTESIAN_POINT('Origin',(1.5,3.15,-21.6014213562373)) ;
#141976 = CARTESIAN_POINT('Origin',(1.5,3.15,-21.6014213562373)) ;
#141977 = CARTESIAN_POINT('Origin',(0.500000000000001,-4.56640444411542E-17,
-23.26)) ;
#141978 = CARTESIAN_POINT('',(0.600000000000001,0.4,-23.26)) ;
#141979 = CARTESIAN_POINT('',(0.595612997216081,0.370705721320403,-23.2307057213204)) ;
#141980 = CARTESIAN_POINT('Origin',(0.50000000005309,0.399999999992667,-23.2599999999926)) ;
#141981 = CARTESIAN_POINT('',(0.500000000000001,0.4,-23.36)) ;
#141982 = CARTESIAN_POINT('Origin',(0.500000000000001,0.4,-23.26)) ;
#141983 = CARTESIAN_POINT('',(0.500000000000001,-1.9,-23.36)) ;
#141984 = CARTESIAN_POINT('',(0.500000000000001,0.5,-23.36)) ;
#141985 = CARTESIAN_POINT('',(0.600000000000001,-1.9,-23.26)) ;
#141986 = CARTESIAN_POINT('Origin',(0.500000000000001,-1.9,-23.26)) ;
#141987 = CARTESIAN_POINT('',(0.600000000000001,-0.3,-23.26)) ;
#141988 = CARTESIAN_POINT('',(0.600000000000001,-2.39800009914441E-17,-23.26)) ;
#141989 = CARTESIAN_POINT('',(0.600000000000001,0.299999999999999,-23.26)) ;
#141990 = CARTESIAN_POINT('',(0.600000000000001,-2.39800009914441E-17,-23.26)) ;
#141991 = CARTESIAN_POINT('Ctrl Pts',(0.600000000000001,0.300000000000003,
-23.26)) ;
#141992 = CARTESIAN_POINT('Ctrl Pts',(0.600000000000001,0.312243016306061,
-23.26)) ;
#141993 = CARTESIAN_POINT('Ctrl Pts',(0.600069747422976,0.324350425899477,
-23.2577515285215)) ;
#141994 = CARTESIAN_POINT('Ctrl Pts',(0.599517124288211,0.346196969297576,
-23.2493954490602)) ;
#141995 = CARTESIAN_POINT('Ctrl Pts',(0.598927484301166,0.35585782537339,
-23.2436750447229)) ;
#141996 = CARTESIAN_POINT('Ctrl Pts',(0.596766673872565,0.36653901230802,
-23.2347023851096)) ;
#141997 = CARTESIAN_POINT('Ctrl Pts',(0.596235629104145,0.368676603883157,
-23.2327379168092)) ;
#141998 = CARTESIAN_POINT('Ctrl Pts',(0.595612997216081,0.370705721320404,
-23.2307057213204)) ;
#141999 = CARTESIAN_POINT('Origin',(2.3,0.,-19.05)) ;
#142000 = CARTESIAN_POINT('',(2.4,-1.10218211923262E-16,-18.15)) ;
#142001 = CARTESIAN_POINT('Origin',(2.4,0.,-19.05)) ;
#142002 = CARTESIAN_POINT('',(2.3,-1.22464679914735E-16,-18.05)) ;
#142003 = CARTESIAN_POINT('Origin',(2.3,-1.10218211923262E-16,-18.15)) ;
#142004 = CARTESIAN_POINT('',(2.3,1.22464679914735E-16,-20.05)) ;
#142005 = CARTESIAN_POINT('Origin',(2.3,0.,-19.05)) ;
#142006 = CARTESIAN_POINT('Origin',(2.3,0.,-19.05)) ;
#142007 = CARTESIAN_POINT('Origin',(1.5,0.,-19.05)) ;
#142008 = CARTESIAN_POINT('',(1.4,-1.34711147906209E-16,-20.15)) ;
#142009 = CARTESIAN_POINT('Origin',(1.4,0.,-19.05)) ;
#142010 = CARTESIAN_POINT('',(1.5,-1.22464679914735E-16,-20.05)) ;
#142011 = CARTESIAN_POINT('Origin',(1.5,-1.34711147906209E-16,-20.15)) ;
#142012 = CARTESIAN_POINT('Origin',(1.5,0.,-19.05)) ;
#142013 = CARTESIAN_POINT('Origin',(1.5,3.15,-17.7914213562373)) ;
#142014 = CARTESIAN_POINT('',(1.5,3.07928932188135,-17.7207106781187)) ;
#142015 = CARTESIAN_POINT('',(1.5,3.25,-17.7914213562373)) ;
#142016 = CARTESIAN_POINT('Origin',(1.5,3.15,-17.7914213562373)) ;
#142017 = CARTESIAN_POINT('',(1.4,3.15,-17.7914213562373)) ;
#142018 = CARTESIAN_POINT('Origin',(1.5,3.15,-17.7914213562373)) ;
#142019 = CARTESIAN_POINT('Origin',(1.5,3.15,-17.7914213562373)) ;
#142020 = CARTESIAN_POINT('Origin',(0.500000000000001,-4.56640444411542E-17,
-19.45)) ;
#142021 = CARTESIAN_POINT('',(0.600000000000001,0.4,-19.45)) ;
#142022 = CARTESIAN_POINT('',(0.595612997216081,0.370705721320403,-19.4207057213204)) ;
#142023 = CARTESIAN_POINT('Origin',(0.500000000041676,0.399999999994165,-19.4499999999941)) ;
#142024 = CARTESIAN_POINT('',(0.500000000000001,0.4,-19.55)) ;
#142025 = CARTESIAN_POINT('Origin',(0.500000000000001,0.4,-19.45)) ;
#142026 = CARTESIAN_POINT('',(0.500000000000001,-1.9,-19.55)) ;
#142027 = CARTESIAN_POINT('',(0.500000000000001,0.5,-19.55)) ;
#142028 = CARTESIAN_POINT('',(0.600000000000001,-1.9,-19.45)) ;
#142029 = CARTESIAN_POINT('Origin',(0.500000000000001,-1.9,-19.45)) ;
#142030 = CARTESIAN_POINT('',(0.600000000000001,-0.3,-19.45)) ;
#142031 = CARTESIAN_POINT('',(0.600000000000001,-2.39800009914441E-17,-19.45)) ;
#142032 = CARTESIAN_POINT('',(0.600000000000001,0.299999999999999,-19.45)) ;
#142033 = CARTESIAN_POINT('',(0.600000000000001,-2.39800009914441E-17,-19.45)) ;
#142034 = CARTESIAN_POINT('Ctrl Pts',(0.600000000000001,0.300000000000003,
-19.45)) ;
#142035 = CARTESIAN_POINT('Ctrl Pts',(0.600000000000001,0.312243016306433,
-19.45)) ;
#142036 = CARTESIAN_POINT('Ctrl Pts',(0.600069747422966,0.324350425899823,
-19.4477515285214)) ;
#142037 = CARTESIAN_POINT('Ctrl Pts',(0.599517124288202,0.346196969297921,
-19.43939544906)) ;
#142038 = CARTESIAN_POINT('Ctrl Pts',(0.598927484301112,0.355857825373661,
-19.4336750447226)) ;
#142039 = CARTESIAN_POINT('Ctrl Pts',(0.596766673872561,0.366539012308041,
-19.4247023851096)) ;
#142040 = CARTESIAN_POINT('Ctrl Pts',(0.596235629104139,0.368676603883175,
-19.4227379168092)) ;
#142041 = CARTESIAN_POINT('Ctrl Pts',(0.595612997216081,0.370705721320404,
-19.4207057213204)) ;
#142042 = CARTESIAN_POINT('Origin',(2.3,0.,-15.24)) ;
#142043 = CARTESIAN_POINT('',(2.4,-1.10218211923262E-16,-14.34)) ;
#142044 = CARTESIAN_POINT('Origin',(2.4,0.,-15.24)) ;
#142045 = CARTESIAN_POINT('',(2.3,-1.22464679914735E-16,-14.24)) ;
#142046 = CARTESIAN_POINT('Origin',(2.3,-1.10218211923262E-16,-14.34)) ;
#142047 = CARTESIAN_POINT('',(2.3,1.22464679914735E-16,-16.24)) ;
#142048 = CARTESIAN_POINT('Origin',(2.3,0.,-15.24)) ;
#142049 = CARTESIAN_POINT('Origin',(2.3,0.,-15.24)) ;
#142050 = CARTESIAN_POINT('Origin',(1.5,0.,-15.24)) ;
#142051 = CARTESIAN_POINT('',(1.4,-1.34711147906209E-16,-16.34)) ;
#142052 = CARTESIAN_POINT('Origin',(1.4,0.,-15.24)) ;
#142053 = CARTESIAN_POINT('',(1.5,-1.22464679914735E-16,-16.24)) ;
#142054 = CARTESIAN_POINT('Origin',(1.5,-1.34711147906209E-16,-16.34)) ;
#142055 = CARTESIAN_POINT('Origin',(1.5,0.,-15.24)) ;
#142056 = CARTESIAN_POINT('Origin',(1.5,3.15,-13.9814213562373)) ;
#142057 = CARTESIAN_POINT('',(1.5,3.07928932188135,-13.9107106781187)) ;
#142058 = CARTESIAN_POINT('',(1.5,3.25,-13.9814213562373)) ;
#142059 = CARTESIAN_POINT('Origin',(1.5,3.15,-13.9814213562373)) ;
#142060 = CARTESIAN_POINT('',(1.4,3.15,-13.9814213562373)) ;
#142061 = CARTESIAN_POINT('Origin',(1.5,3.15,-13.9814213562373)) ;
#142062 = CARTESIAN_POINT('Origin',(1.5,3.15,-13.9814213562373)) ;
#142063 = CARTESIAN_POINT('Origin',(0.500000000000001,-4.56640444411542E-17,
-15.64)) ;
#142064 = CARTESIAN_POINT('',(0.600000000000001,0.4,-15.64)) ;
#142065 = CARTESIAN_POINT('',(0.595612997216081,0.370705721320403,-15.6107057213204)) ;
#142066 = CARTESIAN_POINT('Origin',(0.499999999962138,0.400000000005185,-15.6400000000051)) ;
#142067 = CARTESIAN_POINT('',(0.500000000000001,0.4,-15.74)) ;
#142068 = CARTESIAN_POINT('Origin',(0.500000000000001,0.4,-15.64)) ;
#142069 = CARTESIAN_POINT('',(0.500000000000001,-1.9,-15.74)) ;
#142070 = CARTESIAN_POINT('',(0.500000000000001,0.5,-15.74)) ;
#142071 = CARTESIAN_POINT('',(0.600000000000001,-1.9,-15.64)) ;
#142072 = CARTESIAN_POINT('Origin',(0.500000000000001,-1.9,-15.64)) ;
#142073 = CARTESIAN_POINT('',(0.600000000000001,-0.3,-15.64)) ;
#142074 = CARTESIAN_POINT('',(0.600000000000001,-2.39800009914441E-17,-15.64)) ;
#142075 = CARTESIAN_POINT('',(0.600000000000001,0.299999999999999,-15.64)) ;
#142076 = CARTESIAN_POINT('',(0.600000000000001,-2.39800009914441E-17,-15.64)) ;
#142077 = CARTESIAN_POINT('Ctrl Pts',(0.600000000000001,0.300000000000003,
-15.64)) ;
#142078 = CARTESIAN_POINT('Ctrl Pts',(0.600000000000001,0.312243016306305,
-15.64)) ;
#142079 = CARTESIAN_POINT('Ctrl Pts',(0.60006974742297,0.324350425899701,
-15.6377515285214)) ;
#142080 = CARTESIAN_POINT('Ctrl Pts',(0.599517124288205,0.346196969297796,
-15.6293954490601)) ;
#142081 = CARTESIAN_POINT('Ctrl Pts',(0.59892748430113,0.355857825373563,
-15.6236750447227)) ;
#142082 = CARTESIAN_POINT('Ctrl Pts',(0.596766673872562,0.366539012308031,
-15.6147023851096)) ;
#142083 = CARTESIAN_POINT('Ctrl Pts',(0.596235629104141,0.368676603883168,
-15.6127379168092)) ;
#142084 = CARTESIAN_POINT('Ctrl Pts',(0.59561299721608,0.370705721320404,
-15.6107057213204)) ;
#142085 = CARTESIAN_POINT('Origin',(2.3,0.,-11.43)) ;
#142086 = CARTESIAN_POINT('',(2.4,-1.10218211923262E-16,-10.53)) ;
#142087 = CARTESIAN_POINT('Origin',(2.4,0.,-11.43)) ;
#142088 = CARTESIAN_POINT('',(2.3,-1.22464679914735E-16,-10.43)) ;
#142089 = CARTESIAN_POINT('Origin',(2.3,-1.10218211923262E-16,-10.53)) ;
#142090 = CARTESIAN_POINT('',(2.3,1.22464679914735E-16,-12.43)) ;
#142091 = CARTESIAN_POINT('Origin',(2.3,0.,-11.43)) ;
#142092 = CARTESIAN_POINT('Origin',(2.3,0.,-11.43)) ;
#142093 = CARTESIAN_POINT('Origin',(1.5,0.,-11.43)) ;
#142094 = CARTESIAN_POINT('',(1.4,-1.34711147906209E-16,-12.53)) ;
#142095 = CARTESIAN_POINT('Origin',(1.4,0.,-11.43)) ;
#142096 = CARTESIAN_POINT('',(1.5,-1.22464679914735E-16,-12.43)) ;
#142097 = CARTESIAN_POINT('Origin',(1.5,-1.34711147906209E-16,-12.53)) ;
#142098 = CARTESIAN_POINT('Origin',(1.5,0.,-11.43)) ;
#142099 = CARTESIAN_POINT('Origin',(1.5,3.15,-10.1714213562373)) ;
#142100 = CARTESIAN_POINT('',(1.5,3.07928932188135,-10.1007106781187)) ;
#142101 = CARTESIAN_POINT('',(1.5,3.25,-10.1714213562373)) ;
#142102 = CARTESIAN_POINT('Origin',(1.5,3.15,-10.1714213562373)) ;
#142103 = CARTESIAN_POINT('',(1.4,3.15,-10.1714213562373)) ;
#142104 = CARTESIAN_POINT('Origin',(1.5,3.15,-10.1714213562373)) ;
#142105 = CARTESIAN_POINT('Origin',(1.5,3.15,-10.1714213562373)) ;
#142106 = CARTESIAN_POINT('Origin',(0.500000000000001,-4.56640444411542E-17,
-11.83)) ;
#142107 = CARTESIAN_POINT('',(0.600000000000001,0.4,-11.83)) ;
#142108 = CARTESIAN_POINT('',(0.59561299721608,0.370705721320402,-11.8007057213204)) ;
#142109 = CARTESIAN_POINT('Origin',(0.500000000002749,0.399999999999878,-11.8299999999996)) ;
#142110 = CARTESIAN_POINT('',(0.500000000000001,0.4,-11.93)) ;
#142111 = CARTESIAN_POINT('Origin',(0.500000000000001,0.4,-11.83)) ;
#142112 = CARTESIAN_POINT('',(0.500000000000001,-1.9,-11.93)) ;
#142113 = CARTESIAN_POINT('',(0.500000000000001,0.5,-11.93)) ;
#142114 = CARTESIAN_POINT('',(0.600000000000001,-1.9,-11.83)) ;
#142115 = CARTESIAN_POINT('Origin',(0.500000000000001,-1.9,-11.83)) ;
#142116 = CARTESIAN_POINT('',(0.600000000000001,-0.3,-11.83)) ;
#142117 = CARTESIAN_POINT('',(0.600000000000001,-2.39800009914441E-17,-11.83)) ;
#142118 = CARTESIAN_POINT('',(0.600000000000001,0.299999999999999,-11.83)) ;
#142119 = CARTESIAN_POINT('',(0.600000000000001,-2.39800009914441E-17,-11.83)) ;
#142120 = CARTESIAN_POINT('Ctrl Pts',(0.600000000000001,0.300000000000003,
-11.83)) ;
#142121 = CARTESIAN_POINT('Ctrl Pts',(0.600000000000001,0.312243016306181,
-11.83)) ;
#142122 = CARTESIAN_POINT('Ctrl Pts',(0.600069747422973,0.324350425899585,
-11.8277515285214)) ;
#142123 = CARTESIAN_POINT('Ctrl Pts',(0.599517124288208,0.346196969297684,
-11.8193954490601)) ;
#142124 = CARTESIAN_POINT('Ctrl Pts',(0.598927484301148,0.355857825373472,
-11.8136750447228)) ;
#142125 = CARTESIAN_POINT('Ctrl Pts',(0.596766673872564,0.366539012308024,
-11.8047023851096)) ;
#142126 = CARTESIAN_POINT('Ctrl Pts',(0.596235629104143,0.368676603883159,
-11.8027379168092)) ;
#142127 = CARTESIAN_POINT('Ctrl Pts',(0.595612997216081,0.370705721320402,
-11.8007057213204)) ;
#142128 = CARTESIAN_POINT('Origin',(2.3,0.,-7.62)) ;
#142129 = CARTESIAN_POINT('',(2.4,-1.10218211923262E-16,-6.72)) ;
#142130 = CARTESIAN_POINT('Origin',(2.4,0.,-7.62)) ;
#142131 = CARTESIAN_POINT('',(2.3,-1.22464679914735E-16,-6.62)) ;
#142132 = CARTESIAN_POINT('Origin',(2.3,-1.10218211923262E-16,-6.72)) ;
#142133 = CARTESIAN_POINT('',(2.3,1.22464679914735E-16,-8.62)) ;
#142134 = CARTESIAN_POINT('Origin',(2.3,0.,-7.62)) ;
#142135 = CARTESIAN_POINT('Origin',(2.3,0.,-7.62)) ;
#142136 = CARTESIAN_POINT('Origin',(1.5,0.,-7.62)) ;
#142137 = CARTESIAN_POINT('',(1.4,-1.34711147906209E-16,-8.72)) ;
#142138 = CARTESIAN_POINT('Origin',(1.4,0.,-7.62)) ;
#142139 = CARTESIAN_POINT('',(1.5,-1.22464679914735E-16,-8.62)) ;
#142140 = CARTESIAN_POINT('Origin',(1.5,-1.34711147906209E-16,-8.72)) ;
#142141 = CARTESIAN_POINT('Origin',(1.5,0.,-7.62)) ;
#142142 = CARTESIAN_POINT('Origin',(1.5,3.15,-6.36142135623731)) ;
#142143 = CARTESIAN_POINT('',(1.5,3.07928932188135,-6.29071067811866)) ;
#142144 = CARTESIAN_POINT('',(1.5,3.25,-6.36142135623731)) ;
#142145 = CARTESIAN_POINT('Origin',(1.5,3.15,-6.36142135623731)) ;
#142146 = CARTESIAN_POINT('',(1.4,3.15,-6.36142135623731)) ;
#142147 = CARTESIAN_POINT('Origin',(1.5,3.15,-6.36142135623731)) ;
#142148 = CARTESIAN_POINT('Origin',(1.5,3.15,-6.36142135623731)) ;
#142149 = CARTESIAN_POINT('Origin',(0.500000000000001,-4.56640444411542E-17,
-8.02)) ;
#142150 = CARTESIAN_POINT('',(0.600000000000001,0.4,-8.02)) ;
#142151 = CARTESIAN_POINT('',(0.59561299721608,0.370705721320402,-7.9907057213204)) ;
#142152 = CARTESIAN_POINT('Origin',(0.499999999996157,0.400000000000788,-8.02000000000056)) ;
#142153 = CARTESIAN_POINT('',(0.500000000000001,0.4,-8.12)) ;
#142154 = CARTESIAN_POINT('Origin',(0.500000000000001,0.4,-8.02)) ;
#142155 = CARTESIAN_POINT('',(0.500000000000001,-1.9,-8.12)) ;
#142156 = CARTESIAN_POINT('',(0.500000000000001,0.5,-8.12)) ;
#142157 = CARTESIAN_POINT('',(0.600000000000001,-1.9,-8.02)) ;
#142158 = CARTESIAN_POINT('Origin',(0.500000000000001,-1.9,-8.02)) ;
#142159 = CARTESIAN_POINT('',(0.600000000000001,-0.3,-8.02)) ;
#142160 = CARTESIAN_POINT('',(0.600000000000001,-2.39800009914441E-17,-8.02)) ;
#142161 = CARTESIAN_POINT('',(0.600000000000001,0.299999999999999,-8.02)) ;
#142162 = CARTESIAN_POINT('',(0.600000000000001,-2.39800009914441E-17,-8.02)) ;
#142163 = CARTESIAN_POINT('Ctrl Pts',(0.600000000000001,0.300000000000003,
-8.02)) ;
#142164 = CARTESIAN_POINT('Ctrl Pts',(0.600000000000001,0.312243016306057,
-8.02)) ;
#142165 = CARTESIAN_POINT('Ctrl Pts',(0.600069747422976,0.32435042589947,
-8.01775152852148)) ;
#142166 = CARTESIAN_POINT('Ctrl Pts',(0.599517124288211,0.346196969297575,
-8.00939544906016)) ;
#142167 = CARTESIAN_POINT('Ctrl Pts',(0.598927484301167,0.355857825373384,
-8.00367504472285)) ;
#142168 = CARTESIAN_POINT('Ctrl Pts',(0.596766673872565,0.366539012308017,
-7.99470238510958)) ;
#142169 = CARTESIAN_POINT('Ctrl Pts',(0.596235629104145,0.368676603883154,
-7.9927379168092)) ;
#142170 = CARTESIAN_POINT('Ctrl Pts',(0.59561299721608,0.370705721320404,
-7.9907057213204)) ;
#142171 = CARTESIAN_POINT('Origin',(2.3,0.,-3.81)) ;
#142172 = CARTESIAN_POINT('',(2.4,-1.10218211923262E-16,-2.91)) ;
#142173 = CARTESIAN_POINT('Origin',(2.4,0.,-3.81)) ;
#142174 = CARTESIAN_POINT('',(2.3,-1.22464679914735E-16,-2.81)) ;
#142175 = CARTESIAN_POINT('Origin',(2.3,-1.10218211923262E-16,-2.91)) ;
#142176 = CARTESIAN_POINT('',(2.3,1.22464679914735E-16,-4.81)) ;
#142177 = CARTESIAN_POINT('Origin',(2.3,0.,-3.81)) ;
#142178 = CARTESIAN_POINT('Origin',(2.3,0.,-3.81)) ;
#142179 = CARTESIAN_POINT('Origin',(7.9,3.15,-5.06857864376269)) ;
#142180 = CARTESIAN_POINT('',(8.,3.35,-5.06857864376269)) ;
#142181 = CARTESIAN_POINT('',(8.,3.00857864376269,-5.21)) ;
#142182 = CARTESIAN_POINT('Origin',(8.,3.15,-5.06857864376269)) ;
#142183 = CARTESIAN_POINT('',(7.9,3.25,-5.06857864376269)) ;
#142184 = CARTESIAN_POINT('Origin',(7.9,3.35,-5.06857864376269)) ;
#142185 = CARTESIAN_POINT('',(7.9,3.07928932188135,-5.13928932188135)) ;
#142186 = CARTESIAN_POINT('Origin',(7.9,3.15,-5.06857864376269)) ;
#142187 = CARTESIAN_POINT('Origin',(7.9,3.00857864376269,-5.21)) ;
#142188 = CARTESIAN_POINT('Origin',(7.9,3.15,-8.87857864376269)) ;
#142189 = CARTESIAN_POINT('',(8.,3.35,-8.87857864376269)) ;
#142190 = CARTESIAN_POINT('',(8.,3.00857864376269,-9.02)) ;
#142191 = CARTESIAN_POINT('Origin',(8.,3.15,-8.87857864376269)) ;
#142192 = CARTESIAN_POINT('',(7.9,3.25,-8.87857864376269)) ;
#142193 = CARTESIAN_POINT('Origin',(7.9,3.35,-8.87857864376269)) ;
#142194 = CARTESIAN_POINT('',(7.9,3.07928932188135,-8.94928932188134)) ;
#142195 = CARTESIAN_POINT('Origin',(7.9,3.15,-8.87857864376269)) ;
#142196 = CARTESIAN_POINT('Origin',(7.9,3.00857864376269,-9.02)) ;
#142197 = CARTESIAN_POINT('Origin',(7.9,3.15,-12.6885786437627)) ;
#142198 = CARTESIAN_POINT('',(8.,3.35,-12.6885786437627)) ;
#142199 = CARTESIAN_POINT('',(8.,3.00857864376269,-12.83)) ;
#142200 = CARTESIAN_POINT('Origin',(8.,3.15,-12.6885786437627)) ;
#142201 = CARTESIAN_POINT('',(7.9,3.25,-12.6885786437627)) ;
#142202 = CARTESIAN_POINT('Origin',(7.9,3.35,-12.6885786437627)) ;
#142203 = CARTESIAN_POINT('',(7.9,3.07928932188135,-12.7592893218813)) ;
#142204 = CARTESIAN_POINT('Origin',(7.9,3.15,-12.6885786437627)) ;
#142205 = CARTESIAN_POINT('Origin',(7.9,3.00857864376269,-12.83)) ;
#142206 = CARTESIAN_POINT('Origin',(7.9,3.15,-16.4985786437627)) ;
#142207 = CARTESIAN_POINT('',(8.,3.35,-16.4985786437627)) ;
#142208 = CARTESIAN_POINT('',(8.,3.00857864376269,-16.64)) ;
#142209 = CARTESIAN_POINT('Origin',(8.,3.15,-16.4985786437627)) ;
#142210 = CARTESIAN_POINT('',(7.9,3.25,-16.4985786437627)) ;
#142211 = CARTESIAN_POINT('Origin',(7.9,3.35,-16.4985786437627)) ;
#142212 = CARTESIAN_POINT('',(7.9,3.07928932188135,-16.5692893218813)) ;
#142213 = CARTESIAN_POINT('Origin',(7.9,3.15,-16.4985786437627)) ;
#142214 = CARTESIAN_POINT('Origin',(7.9,3.00857864376269,-16.64)) ;
#142215 = CARTESIAN_POINT('Origin',(7.9,3.15,-20.3085786437627)) ;
#142216 = CARTESIAN_POINT('',(8.,3.35,-20.3085786437627)) ;
#142217 = CARTESIAN_POINT('',(8.,3.00857864376269,-20.45)) ;
#142218 = CARTESIAN_POINT('Origin',(8.,3.15,-20.3085786437627)) ;
#142219 = CARTESIAN_POINT('',(7.9,3.25,-20.3085786437627)) ;
#142220 = CARTESIAN_POINT('Origin',(7.9,3.35,-20.3085786437627)) ;
#142221 = CARTESIAN_POINT('',(7.9,3.07928932188135,-20.3792893218813)) ;
#142222 = CARTESIAN_POINT('Origin',(7.9,3.15,-20.3085786437627)) ;
#142223 = CARTESIAN_POINT('Origin',(7.9,3.00857864376269,-20.45)) ;
#142224 = CARTESIAN_POINT('Origin',(7.9,3.15,-24.1185786437627)) ;
#142225 = CARTESIAN_POINT('',(8.,3.35,-24.1185786437627)) ;
#142226 = CARTESIAN_POINT('',(8.,3.00857864376269,-24.26)) ;
#142227 = CARTESIAN_POINT('Origin',(8.,3.15,-24.1185786437627)) ;
#142228 = CARTESIAN_POINT('',(7.9,3.25,-24.1185786437627)) ;
#142229 = CARTESIAN_POINT('Origin',(7.9,3.35,-24.1185786437627)) ;
#142230 = CARTESIAN_POINT('',(7.9,3.07928932188135,-24.1892893218813)) ;
#142231 = CARTESIAN_POINT('Origin',(7.9,3.15,-24.1185786437627)) ;
#142232 = CARTESIAN_POINT('Origin',(7.9,3.00857864376269,-24.26)) ;
#142233 = CARTESIAN_POINT('Origin',(7.9,3.15,-27.9285786437627)) ;
#142234 = CARTESIAN_POINT('',(8.,3.35,-27.9285786437627)) ;
#142235 = CARTESIAN_POINT('',(8.,3.00857864376269,-28.07)) ;
#142236 = CARTESIAN_POINT('Origin',(8.,3.15,-27.9285786437627)) ;
#142237 = CARTESIAN_POINT('',(7.9,3.25,-27.9285786437627)) ;
#142238 = CARTESIAN_POINT('Origin',(7.9,3.35,-27.9285786437627)) ;
#142239 = CARTESIAN_POINT('',(7.9,3.07928932188135,-27.9992893218813)) ;
#142240 = CARTESIAN_POINT('Origin',(7.9,3.15,-27.9285786437627)) ;
#142241 = CARTESIAN_POINT('Origin',(7.9,3.00857864376269,-28.07)) ;
#142242 = CARTESIAN_POINT('Origin',(7.9,3.15,-31.7385786437627)) ;
#142243 = CARTESIAN_POINT('',(8.,3.35,-31.7385786437627)) ;
#142244 = CARTESIAN_POINT('',(8.,3.00857864376269,-31.88)) ;
#142245 = CARTESIAN_POINT('Origin',(8.,3.15,-31.7385786437627)) ;
#142246 = CARTESIAN_POINT('',(7.9,3.25,-31.7385786437627)) ;
#142247 = CARTESIAN_POINT('Origin',(7.9,3.35,-31.7385786437627)) ;
#142248 = CARTESIAN_POINT('',(7.9,3.07928932188135,-31.8092893218813)) ;
#142249 = CARTESIAN_POINT('Origin',(7.9,3.15,-31.7385786437627)) ;
#142250 = CARTESIAN_POINT('Origin',(7.9,3.00857864376269,-31.88)) ;
#142251 = CARTESIAN_POINT('Origin',(7.9,3.15,-35.5485786437627)) ;
#142252 = CARTESIAN_POINT('',(8.,3.35,-35.5485786437627)) ;
#142253 = CARTESIAN_POINT('',(8.,3.00857864376269,-35.69)) ;
#142254 = CARTESIAN_POINT('Origin',(8.,3.15,-35.5485786437627)) ;
#142255 = CARTESIAN_POINT('',(7.9,3.25,-35.5485786437627)) ;
#142256 = CARTESIAN_POINT('Origin',(7.9,3.35,-35.5485786437627)) ;
#142257 = CARTESIAN_POINT('',(7.9,3.07928932188135,-35.6192893218813)) ;
#142258 = CARTESIAN_POINT('Origin',(7.9,3.15,-35.5485786437627)) ;
#142259 = CARTESIAN_POINT('Origin',(7.9,3.00857864376269,-35.69)) ;
#142260 = CARTESIAN_POINT('Origin',(1.5,0.,-3.81)) ;
#142261 = CARTESIAN_POINT('',(1.4,-1.34711147906209E-16,-4.91)) ;
#142262 = CARTESIAN_POINT('Origin',(1.4,0.,-3.81)) ;
#142263 = CARTESIAN_POINT('',(1.5,-1.22464679914735E-16,-4.81)) ;
#142264 = CARTESIAN_POINT('Origin',(1.5,-1.34711147906209E-16,-4.91)) ;
#142265 = CARTESIAN_POINT('Origin',(1.5,0.,-3.81)) ;
#142266 = CARTESIAN_POINT('Origin',(1.5,3.15,-2.55142135623731)) ;
#142267 = CARTESIAN_POINT('',(1.5,3.07928932188135,-2.48071067811865)) ;
#142268 = CARTESIAN_POINT('',(1.5,3.25,-2.55142135623731)) ;
#142269 = CARTESIAN_POINT('Origin',(1.5,3.15,-2.55142135623731)) ;
#142270 = CARTESIAN_POINT('',(1.4,3.15,-2.55142135623731)) ;
#142271 = CARTESIAN_POINT('Origin',(1.5,3.15,-2.55142135623731)) ;
#142272 = CARTESIAN_POINT('Origin',(1.5,3.15,-2.55142135623731)) ;
#142273 = CARTESIAN_POINT('Origin',(0.500000000000001,-4.56640444411539E-17,
-4.21)) ;
#142274 = CARTESIAN_POINT('',(0.600000000000001,0.4,-4.21)) ;
#142275 = CARTESIAN_POINT('',(0.595612997216081,0.370705721320403,-4.1807057213204)) ;
#142276 = CARTESIAN_POINT('Origin',(0.499999999992608,0.400000000001211,-4.21000000000122)) ;
#142277 = CARTESIAN_POINT('',(0.500000000000001,0.4,-4.31)) ;
#142278 = CARTESIAN_POINT('Origin',(0.500000000000001,0.4,-4.21)) ;
#142279 = CARTESIAN_POINT('',(0.500000000000001,-1.9,-4.31)) ;
#142280 = CARTESIAN_POINT('',(0.500000000000001,0.5,-4.31)) ;
#142281 = CARTESIAN_POINT('',(0.600000000000001,-1.9,-4.21)) ;
#142282 = CARTESIAN_POINT('Origin',(0.500000000000001,-1.9,-4.21)) ;
#142283 = CARTESIAN_POINT('',(0.600000000000001,-0.3,-4.21)) ;
#142284 = CARTESIAN_POINT('',(0.600000000000001,-2.39800009914439E-17,-4.21)) ;
#142285 = CARTESIAN_POINT('',(0.600000000000001,0.299999999999999,-4.21)) ;
#142286 = CARTESIAN_POINT('',(0.600000000000001,-2.39800009914439E-17,-4.21)) ;
#142287 = CARTESIAN_POINT('Ctrl Pts',(0.600000000000001,0.300000000000003,
-4.21)) ;
#142288 = CARTESIAN_POINT('Ctrl Pts',(0.600000000000001,0.312243016306119,
-4.21)) ;
#142289 = CARTESIAN_POINT('Ctrl Pts',(0.600069747422974,0.324350425899533,
-4.20775152852146)) ;
#142290 = CARTESIAN_POINT('Ctrl Pts',(0.599517124288209,0.346196969297642,
-4.19939544906013)) ;
#142291 = CARTESIAN_POINT('Ctrl Pts',(0.598927484301157,0.355857825373437,
-4.19367504472281)) ;
#142292 = CARTESIAN_POINT('Ctrl Pts',(0.596766673872564,0.366539012308024,
-4.18470238510957)) ;
#142293 = CARTESIAN_POINT('Ctrl Pts',(0.596235629104143,0.36867660388316,
-4.18273791680919)) ;
#142294 = CARTESIAN_POINT('Ctrl Pts',(0.595612997216081,0.370705721320404,
-4.1807057213204)) ;
#142295 = CARTESIAN_POINT('Origin',(2.4,0.,-34.29)) ;
#142296 = CARTESIAN_POINT('',(2.4,-1.22464679914735E-16,-35.29)) ;
#142297 = CARTESIAN_POINT('Origin',(2.4,0.,-30.48)) ;
#142298 = CARTESIAN_POINT('',(2.4,-1.22464679914735E-16,-31.48)) ;
#142299 = CARTESIAN_POINT('Origin',(2.4,0.,-26.67)) ;
#142300 = CARTESIAN_POINT('',(2.4,-1.22464679914735E-16,-27.67)) ;
#142301 = CARTESIAN_POINT('Origin',(2.4,0.,-22.86)) ;
#142302 = CARTESIAN_POINT('',(2.4,-1.22464679914735E-16,-23.86)) ;
#142303 = CARTESIAN_POINT('Origin',(2.4,0.,-19.05)) ;
#142304 = CARTESIAN_POINT('',(2.4,-1.22464679914735E-16,-20.05)) ;
#142305 = CARTESIAN_POINT('Origin',(2.4,0.,-15.24)) ;
#142306 = CARTESIAN_POINT('',(2.4,-1.22464679914735E-16,-16.24)) ;
#142307 = CARTESIAN_POINT('Origin',(2.4,0.,-11.43)) ;
#142308 = CARTESIAN_POINT('',(2.4,-1.22464679914735E-16,-12.43)) ;
#142309 = CARTESIAN_POINT('Origin',(2.4,0.,-7.62)) ;
#142310 = CARTESIAN_POINT('',(2.4,-1.22464679914735E-16,-8.62)) ;
#142311 = CARTESIAN_POINT('Origin',(2.4,0.,-3.81)) ;
#142312 = CARTESIAN_POINT('',(2.4,-1.22464679914735E-16,-4.81)) ;
#142313 = CARTESIAN_POINT('Origin',(1.4,3.15,-5.06857864376269)) ;
#142314 = CARTESIAN_POINT('',(1.5,3.25,-5.06857864376269)) ;
#142315 = CARTESIAN_POINT('',(1.5,3.07928932188135,-5.13928932188135)) ;
#142316 = CARTESIAN_POINT('Origin',(1.5,3.15,-5.06857864376269)) ;
#142317 = CARTESIAN_POINT('',(1.4,3.07928932188135,-5.13928932188135)) ;
#142318 = CARTESIAN_POINT('',(1.4,3.25,-5.06857864376269)) ;
#142319 = CARTESIAN_POINT('Origin',(1.4,3.15,-8.87857864376269)) ;
#142320 = CARTESIAN_POINT('',(1.5,3.25,-8.87857864376269)) ;
#142321 = CARTESIAN_POINT('',(1.5,3.07928932188135,-8.94928932188134)) ;
#142322 = CARTESIAN_POINT('Origin',(1.5,3.15,-8.87857864376269)) ;
#142323 = CARTESIAN_POINT('',(1.4,3.07928932188135,-8.94928932188134)) ;
#142324 = CARTESIAN_POINT('',(1.4,3.25,-8.87857864376269)) ;
#142325 = CARTESIAN_POINT('Origin',(1.4,3.15,-12.6885786437627)) ;
#142326 = CARTESIAN_POINT('',(1.5,3.25,-12.6885786437627)) ;
#142327 = CARTESIAN_POINT('',(1.5,3.07928932188135,-12.7592893218813)) ;
#142328 = CARTESIAN_POINT('Origin',(1.5,3.15,-12.6885786437627)) ;
#142329 = CARTESIAN_POINT('',(1.4,3.07928932188135,-12.7592893218813)) ;
#142330 = CARTESIAN_POINT('',(1.4,3.25,-12.6885786437627)) ;
#142331 = CARTESIAN_POINT('Origin',(1.4,3.15,-16.4985786437627)) ;
#142332 = CARTESIAN_POINT('',(1.5,3.25,-16.4985786437627)) ;
#142333 = CARTESIAN_POINT('',(1.5,3.07928932188135,-16.5692893218813)) ;
#142334 = CARTESIAN_POINT('Origin',(1.5,3.15,-16.4985786437627)) ;
#142335 = CARTESIAN_POINT('',(1.4,3.07928932188135,-16.5692893218813)) ;
#142336 = CARTESIAN_POINT('',(1.4,3.25,-16.4985786437627)) ;
#142337 = CARTESIAN_POINT('Origin',(1.4,3.15,-20.3085786437627)) ;
#142338 = CARTESIAN_POINT('',(1.5,3.25,-20.3085786437627)) ;
#142339 = CARTESIAN_POINT('',(1.5,3.07928932188135,-20.3792893218813)) ;
#142340 = CARTESIAN_POINT('Origin',(1.5,3.15,-20.3085786437627)) ;
#142341 = CARTESIAN_POINT('',(1.4,3.07928932188135,-20.3792893218813)) ;
#142342 = CARTESIAN_POINT('',(1.4,3.25,-20.3085786437627)) ;
#142343 = CARTESIAN_POINT('Origin',(1.4,3.15,-24.1185786437627)) ;
#142344 = CARTESIAN_POINT('',(1.5,3.25,-24.1185786437627)) ;
#142345 = CARTESIAN_POINT('',(1.5,3.07928932188135,-24.1892893218813)) ;
#142346 = CARTESIAN_POINT('Origin',(1.5,3.15,-24.1185786437627)) ;
#142347 = CARTESIAN_POINT('',(1.4,3.07928932188135,-24.1892893218813)) ;
#142348 = CARTESIAN_POINT('',(1.4,3.25,-24.1185786437627)) ;
#142349 = CARTESIAN_POINT('Origin',(1.4,3.15,-27.9285786437627)) ;
#142350 = CARTESIAN_POINT('',(1.5,3.25,-27.9285786437627)) ;
#142351 = CARTESIAN_POINT('',(1.5,3.07928932188135,-27.9992893218813)) ;
#142352 = CARTESIAN_POINT('Origin',(1.5,3.15,-27.9285786437627)) ;
#142353 = CARTESIAN_POINT('',(1.4,3.07928932188135,-27.9992893218813)) ;
#142354 = CARTESIAN_POINT('',(1.4,3.25,-27.9285786437627)) ;
#142355 = CARTESIAN_POINT('Origin',(1.4,3.15,-31.7385786437627)) ;
#142356 = CARTESIAN_POINT('',(1.5,3.25,-31.7385786437627)) ;
#142357 = CARTESIAN_POINT('',(1.5,3.07928932188135,-31.8092893218813)) ;
#142358 = CARTESIAN_POINT('Origin',(1.5,3.15,-31.7385786437627)) ;
#142359 = CARTESIAN_POINT('',(1.4,3.07928932188135,-31.8092893218813)) ;
#142360 = CARTESIAN_POINT('',(1.4,3.25,-31.7385786437627)) ;
#142361 = CARTESIAN_POINT('Origin',(1.4,3.15,-35.5485786437627)) ;
#142362 = CARTESIAN_POINT('',(1.5,3.25,-35.5485786437627)) ;
#142363 = CARTESIAN_POINT('',(1.5,3.07928932188135,-35.6192893218813)) ;
#142364 = CARTESIAN_POINT('Origin',(1.5,3.15,-35.5485786437627)) ;
#142365 = CARTESIAN_POINT('',(1.4,3.07928932188135,-35.6192893218813)) ;
#142366 = CARTESIAN_POINT('',(1.4,3.25,-35.5485786437627)) ;
#142367 = CARTESIAN_POINT('Origin',(2.3,0.,0.)) ;
#142368 = CARTESIAN_POINT('',(2.4,-1.10218211923262E-16,0.9)) ;
#142369 = CARTESIAN_POINT('Origin',(2.4,0.,0.)) ;
#142370 = CARTESIAN_POINT('',(2.3,-1.22464679914735E-16,1.)) ;
#142371 = CARTESIAN_POINT('Origin',(2.3,-1.10218211923262E-16,0.9)) ;
#142372 = CARTESIAN_POINT('',(2.3,1.22464679914735E-16,-1.)) ;
#142373 = CARTESIAN_POINT('Origin',(2.3,0.,0.)) ;
#142374 = CARTESIAN_POINT('Origin',(2.3,0.,0.)) ;
#142375 = CARTESIAN_POINT('Origin',(7.9,3.15,-1.25857864376269)) ;
#142376 = CARTESIAN_POINT('',(8.,3.35,-1.25857864376269)) ;
#142377 = CARTESIAN_POINT('',(8.,3.00857864376269,-1.4)) ;
#142378 = CARTESIAN_POINT('Origin',(8.,3.15,-1.25857864376269)) ;
#142379 = CARTESIAN_POINT('',(7.9,3.25,-1.25857864376269)) ;
#142380 = CARTESIAN_POINT('Origin',(7.9,3.35,-1.25857864376269)) ;
#142381 = CARTESIAN_POINT('',(7.9,3.07928932188135,-1.32928932188135)) ;
#142382 = CARTESIAN_POINT('Origin',(7.9,3.15,-1.25857864376269)) ;
#142383 = CARTESIAN_POINT('Origin',(7.9,3.00857864376269,-1.4)) ;
#142384 = CARTESIAN_POINT('Origin',(1.5,0.,0.)) ;
#142385 = CARTESIAN_POINT('',(1.4,-1.34711147906209E-16,-1.1)) ;
#142386 = CARTESIAN_POINT('Origin',(1.4,0.,0.)) ;
#142387 = CARTESIAN_POINT('',(1.5,-1.22464679914735E-16,-1.)) ;
#142388 = CARTESIAN_POINT('Origin',(1.5,-1.34711147906209E-16,-1.1)) ;
#142389 = CARTESIAN_POINT('Origin',(1.5,0.,0.)) ;
#142390 = CARTESIAN_POINT('Origin',(1.5,3.15,1.25857864376269)) ;
#142391 = CARTESIAN_POINT('',(1.5,3.07928932188135,1.32928932188135)) ;
#142392 = CARTESIAN_POINT('',(1.5,3.25,1.25857864376269)) ;
#142393 = CARTESIAN_POINT('Origin',(1.5,3.15,1.25857864376269)) ;
#142394 = CARTESIAN_POINT('',(1.4,3.15,1.25857864376269)) ;
#142395 = CARTESIAN_POINT('Origin',(1.5,3.15,1.25857864376269)) ;
#142396 = CARTESIAN_POINT('Origin',(1.5,3.15,1.25857864376269)) ;
#142397 = CARTESIAN_POINT('Origin',(0.500000000000001,-4.5664044441154E-17,
-0.4)) ;
#142398 = CARTESIAN_POINT('',(0.600000000000001,0.4,-0.4)) ;
#142399 = CARTESIAN_POINT('',(0.595612997216081,0.370705721320403,-0.370705721320403)) ;
#142400 = CARTESIAN_POINT('Origin',(0.499999999989667,0.400000000001553,-0.400000000001553)) ;
#142401 = CARTESIAN_POINT('',(0.500000000000001,0.4,-0.5)) ;
#142402 = CARTESIAN_POINT('Origin',(0.500000000000001,0.4,-0.4)) ;
#142403 = CARTESIAN_POINT('',(0.500000000000001,-1.9,-0.5)) ;
#142404 = CARTESIAN_POINT('',(0.500000000000001,0.5,-0.5)) ;
#142405 = CARTESIAN_POINT('',(0.600000000000001,-1.9,-0.4)) ;
#142406 = CARTESIAN_POINT('Origin',(0.500000000000001,-1.9,-0.4)) ;
#142407 = CARTESIAN_POINT('',(0.600000000000001,-0.3,-0.4)) ;
#142408 = CARTESIAN_POINT('',(0.600000000000001,-2.3980000991444E-17,-0.4)) ;
#142409 = CARTESIAN_POINT('',(0.600000000000001,0.299999999999999,-0.4)) ;
#142410 = CARTESIAN_POINT('',(0.600000000000001,-2.3980000991444E-17,-0.4)) ;
#142411 = CARTESIAN_POINT('Ctrl Pts',(0.600000000000001,0.300000000000003,
-0.4)) ;
#142412 = CARTESIAN_POINT('Ctrl Pts',(0.600000000000001,0.312243016306053,
-0.4)) ;
#142413 = CARTESIAN_POINT('Ctrl Pts',(0.600069747422976,0.324350425899471,
-0.397751528521482)) ;
#142414 = CARTESIAN_POINT('Ctrl Pts',(0.599517124288211,0.34619696929758,
-0.389395449060154)) ;
#142415 = CARTESIAN_POINT('Ctrl Pts',(0.598927484301167,0.355857825373388,
-0.383675044722851)) ;
#142416 = CARTESIAN_POINT('Ctrl Pts',(0.596766673872565,0.36653901230802,
-0.374702385109574)) ;
#142417 = CARTESIAN_POINT('Ctrl Pts',(0.596235629104145,0.368676603883155,
-0.372737916809195)) ;
#142418 = CARTESIAN_POINT('Ctrl Pts',(0.595612997216081,0.370705721320403,
-0.370705721320403)) ;
#142419 = CARTESIAN_POINT('Origin',(2.4,0.,0.)) ;
#142420 = CARTESIAN_POINT('',(2.4,-1.22464679914735E-16,-1.)) ;
#142421 = CARTESIAN_POINT('Origin',(1.4,3.15,-1.25857864376269)) ;
#142422 = CARTESIAN_POINT('',(1.5,3.25,-1.25857864376269)) ;
#142423 = CARTESIAN_POINT('',(1.5,3.07928932188135,-1.32928932188135)) ;
#142424 = CARTESIAN_POINT('Origin',(1.5,3.15,-1.25857864376269)) ;
#142425 = CARTESIAN_POINT('',(1.4,3.07928932188135,-1.32928932188135)) ;
#142426 = CARTESIAN_POINT('',(1.4,3.25,-1.25857864376269)) ;
#142427 = CARTESIAN_POINT('Origin',(0.600000000000001,2.80617032878603E-17,
-34.29)) ;
#142428 = CARTESIAN_POINT('',(0.600000000000001,-1.9,-33.89)) ;
#142429 = CARTESIAN_POINT('',(0.600000000000001,-0.3,-33.89)) ;
#142430 = CARTESIAN_POINT('',(0.600000000000001,-2.39800009914436E-17,-33.89)) ;
#142431 = CARTESIAN_POINT('',(0.6,-0.4,-33.99)) ;
#142432 = CARTESIAN_POINT('Origin',(0.6,-0.3,-33.99)) ;
#142433 = CARTESIAN_POINT('',(0.6,-0.4,-34.59)) ;
#142434 = CARTESIAN_POINT('',(0.6,-0.4,-33.89)) ;
#142435 = CARTESIAN_POINT('Origin',(0.6,-0.3,-34.59)) ;
#142436 = CARTESIAN_POINT('',(0.600000000000001,-2.1,-34.89)) ;
#142437 = CARTESIAN_POINT('Origin',(0.600000000000001,-1.9,-34.89)) ;
#142438 = CARTESIAN_POINT('',(0.600000000000001,-2.1,-35.565)) ;
#142439 = CARTESIAN_POINT('',(0.600000000000001,-2.1,-34.29)) ;
#142440 = CARTESIAN_POINT('',(0.600000000000001,-2.9,-35.565)) ;
#142441 = CARTESIAN_POINT('',(0.600000000000001,-3.69904270612699E-17,-35.565)) ;
#142442 = CARTESIAN_POINT('',(0.600000000000001,-2.9,-33.015)) ;
#142443 = CARTESIAN_POINT('',(0.600000000000001,-2.9,-34.29)) ;
#142444 = CARTESIAN_POINT('',(0.600000000000001,-2.1,-33.015)) ;
#142445 = CARTESIAN_POINT('',(0.600000000000001,1.58165963986121E-16,-33.015)) ;
#142446 = CARTESIAN_POINT('',(0.600000000000001,-2.1,-33.69)) ;
#142447 = CARTESIAN_POINT('',(0.600000000000001,-2.1,-34.29)) ;
#142448 = CARTESIAN_POINT('Origin',(0.600000000000001,-1.9,-33.69)) ;
#142449 = CARTESIAN_POINT('Origin',(0.600000000000001,2.80617032878603E-17,
-30.48)) ;
#142450 = CARTESIAN_POINT('',(0.600000000000001,-1.9,-30.08)) ;
#142451 = CARTESIAN_POINT('',(0.600000000000001,-0.3,-30.08)) ;
#142452 = CARTESIAN_POINT('',(0.600000000000001,-2.39800009914441E-17,-30.08)) ;
#142453 = CARTESIAN_POINT('',(0.6,-0.4,-30.18)) ;
#142454 = CARTESIAN_POINT('Origin',(0.6,-0.3,-30.18)) ;
#142455 = CARTESIAN_POINT('',(0.6,-0.4,-30.78)) ;
#142456 = CARTESIAN_POINT('',(0.6,-0.4,-30.08)) ;
#142457 = CARTESIAN_POINT('Origin',(0.6,-0.3,-30.78)) ;
#142458 = CARTESIAN_POINT('',(0.600000000000001,-2.1,-31.08)) ;
#142459 = CARTESIAN_POINT('Origin',(0.600000000000001,-1.9,-31.08)) ;
#142460 = CARTESIAN_POINT('',(0.600000000000001,-2.1,-31.755)) ;
#142461 = CARTESIAN_POINT('',(0.600000000000001,-2.1,-30.48)) ;
#142462 = CARTESIAN_POINT('',(0.600000000000001,-2.9,-31.755)) ;
#142463 = CARTESIAN_POINT('',(0.600000000000001,-3.69904270612699E-17,-31.755)) ;
#142464 = CARTESIAN_POINT('',(0.600000000000001,-2.9,-29.205)) ;
#142465 = CARTESIAN_POINT('',(0.600000000000001,-2.9,-30.48)) ;
#142466 = CARTESIAN_POINT('',(0.600000000000001,-2.1,-29.205)) ;
#142467 = CARTESIAN_POINT('',(0.600000000000001,1.58165963986121E-16,-29.205)) ;
#142468 = CARTESIAN_POINT('',(0.600000000000001,-2.1,-29.88)) ;
#142469 = CARTESIAN_POINT('',(0.600000000000001,-2.1,-30.48)) ;
#142470 = CARTESIAN_POINT('Origin',(0.600000000000001,-1.9,-29.88)) ;
#142471 = CARTESIAN_POINT('Origin',(0.600000000000001,2.80617032878603E-17,
-26.67)) ;
#142472 = CARTESIAN_POINT('',(0.600000000000001,-1.9,-26.27)) ;
#142473 = CARTESIAN_POINT('',(0.600000000000001,-0.3,-26.27)) ;
#142474 = CARTESIAN_POINT('',(0.600000000000001,-2.39800009914441E-17,-26.27)) ;
#142475 = CARTESIAN_POINT('',(0.6,-0.4,-26.37)) ;
#142476 = CARTESIAN_POINT('Origin',(0.6,-0.3,-26.37)) ;
#142477 = CARTESIAN_POINT('',(0.6,-0.4,-26.97)) ;
#142478 = CARTESIAN_POINT('',(0.6,-0.4,-26.27)) ;
#142479 = CARTESIAN_POINT('Origin',(0.6,-0.3,-26.97)) ;
#142480 = CARTESIAN_POINT('',(0.600000000000001,-2.1,-27.27)) ;
#142481 = CARTESIAN_POINT('Origin',(0.600000000000001,-1.9,-27.27)) ;
#142482 = CARTESIAN_POINT('',(0.600000000000001,-2.1,-27.945)) ;
#142483 = CARTESIAN_POINT('',(0.600000000000001,-2.1,-26.67)) ;
#142484 = CARTESIAN_POINT('',(0.600000000000001,-2.9,-27.945)) ;
#142485 = CARTESIAN_POINT('',(0.600000000000001,-3.69904270612701E-17,-27.945)) ;
#142486 = CARTESIAN_POINT('',(0.600000000000001,-2.9,-25.395)) ;
#142487 = CARTESIAN_POINT('',(0.600000000000001,-2.9,-26.67)) ;
#142488 = CARTESIAN_POINT('',(0.600000000000001,-2.1,-25.395)) ;
#142489 = CARTESIAN_POINT('',(0.600000000000001,1.58165963986121E-16,-25.395)) ;
#142490 = CARTESIAN_POINT('',(0.600000000000001,-2.1,-26.07)) ;
#142491 = CARTESIAN_POINT('',(0.600000000000001,-2.1,-26.67)) ;
#142492 = CARTESIAN_POINT('Origin',(0.600000000000001,-1.9,-26.07)) ;
#142493 = CARTESIAN_POINT('Origin',(0.600000000000001,2.80617032878603E-17,
-22.86)) ;
#142494 = CARTESIAN_POINT('',(0.600000000000001,-1.9,-22.46)) ;
#142495 = CARTESIAN_POINT('',(0.600000000000001,-0.3,-22.46)) ;
#142496 = CARTESIAN_POINT('',(0.600000000000001,-2.39800009914441E-17,-22.46)) ;
#142497 = CARTESIAN_POINT('',(0.6,-0.4,-22.56)) ;
#142498 = CARTESIAN_POINT('Origin',(0.6,-0.3,-22.56)) ;
#142499 = CARTESIAN_POINT('',(0.6,-0.4,-23.16)) ;
#142500 = CARTESIAN_POINT('',(0.6,-0.4,-22.46)) ;
#142501 = CARTESIAN_POINT('Origin',(0.6,-0.3,-23.16)) ;
#142502 = CARTESIAN_POINT('',(0.600000000000001,-2.1,-23.46)) ;
#142503 = CARTESIAN_POINT('Origin',(0.600000000000001,-1.9,-23.46)) ;
#142504 = CARTESIAN_POINT('',(0.600000000000001,-2.1,-24.135)) ;
#142505 = CARTESIAN_POINT('',(0.600000000000001,-2.1,-22.86)) ;
#142506 = CARTESIAN_POINT('',(0.600000000000001,-2.9,-24.135)) ;
#142507 = CARTESIAN_POINT('',(0.600000000000001,-3.69904270612701E-17,-24.135)) ;
#142508 = CARTESIAN_POINT('',(0.600000000000001,-2.9,-21.585)) ;
#142509 = CARTESIAN_POINT('',(0.600000000000001,-2.9,-22.86)) ;
#142510 = CARTESIAN_POINT('',(0.600000000000001,-2.1,-21.585)) ;
#142511 = CARTESIAN_POINT('',(0.600000000000001,1.58165963986121E-16,-21.585)) ;
#142512 = CARTESIAN_POINT('',(0.600000000000001,-2.1,-22.26)) ;
#142513 = CARTESIAN_POINT('',(0.600000000000001,-2.1,-22.86)) ;
#142514 = CARTESIAN_POINT('Origin',(0.600000000000001,-1.9,-22.26)) ;
#142515 = CARTESIAN_POINT('Origin',(0.600000000000001,2.80617032878603E-17,
-19.05)) ;
#142516 = CARTESIAN_POINT('',(0.600000000000001,-1.9,-18.65)) ;
#142517 = CARTESIAN_POINT('',(0.600000000000001,-0.3,-18.65)) ;
#142518 = CARTESIAN_POINT('',(0.600000000000001,-2.39800009914441E-17,-18.65)) ;
#142519 = CARTESIAN_POINT('',(0.6,-0.4,-18.75)) ;
#142520 = CARTESIAN_POINT('Origin',(0.6,-0.3,-18.75)) ;
#142521 = CARTESIAN_POINT('',(0.6,-0.4,-19.35)) ;
#142522 = CARTESIAN_POINT('',(0.6,-0.4,-18.65)) ;
#142523 = CARTESIAN_POINT('Origin',(0.6,-0.3,-19.35)) ;
#142524 = CARTESIAN_POINT('',(0.600000000000001,-2.1,-19.65)) ;
#142525 = CARTESIAN_POINT('Origin',(0.600000000000001,-1.9,-19.65)) ;
#142526 = CARTESIAN_POINT('',(0.600000000000001,-2.1,-20.325)) ;
#142527 = CARTESIAN_POINT('',(0.600000000000001,-2.1,-19.05)) ;
#142528 = CARTESIAN_POINT('',(0.600000000000001,-2.9,-20.325)) ;
#142529 = CARTESIAN_POINT('',(0.600000000000001,-3.69904270612701E-17,-20.325)) ;
#142530 = CARTESIAN_POINT('',(0.600000000000001,-2.9,-17.775)) ;
#142531 = CARTESIAN_POINT('',(0.600000000000001,-2.9,-19.05)) ;
#142532 = CARTESIAN_POINT('',(0.600000000000001,-2.1,-17.775)) ;
#142533 = CARTESIAN_POINT('',(0.600000000000001,1.58165963986121E-16,-17.775)) ;
#142534 = CARTESIAN_POINT('',(0.600000000000001,-2.1,-18.45)) ;
#142535 = CARTESIAN_POINT('',(0.600000000000001,-2.1,-19.05)) ;
#142536 = CARTESIAN_POINT('Origin',(0.600000000000001,-1.9,-18.45)) ;
#142537 = CARTESIAN_POINT('Origin',(0.600000000000001,2.80617032878603E-17,
-15.24)) ;
#142538 = CARTESIAN_POINT('',(0.600000000000001,-1.9,-14.84)) ;
#142539 = CARTESIAN_POINT('',(0.600000000000001,-0.3,-14.84)) ;
#142540 = CARTESIAN_POINT('',(0.600000000000001,-2.39800009914441E-17,-14.84)) ;
#142541 = CARTESIAN_POINT('',(0.6,-0.4,-14.94)) ;
#142542 = CARTESIAN_POINT('Origin',(0.6,-0.3,-14.94)) ;
#142543 = CARTESIAN_POINT('',(0.6,-0.4,-15.54)) ;
#142544 = CARTESIAN_POINT('',(0.6,-0.4,-14.84)) ;
#142545 = CARTESIAN_POINT('Origin',(0.6,-0.3,-15.54)) ;
#142546 = CARTESIAN_POINT('',(0.600000000000001,-2.1,-15.84)) ;
#142547 = CARTESIAN_POINT('Origin',(0.600000000000001,-1.9,-15.84)) ;
#142548 = CARTESIAN_POINT('',(0.600000000000001,-2.1,-16.515)) ;
#142549 = CARTESIAN_POINT('',(0.600000000000001,-2.1,-15.24)) ;
#142550 = CARTESIAN_POINT('',(0.600000000000001,-2.9,-16.515)) ;
#142551 = CARTESIAN_POINT('',(0.600000000000001,-3.69904270612701E-17,-16.515)) ;
#142552 = CARTESIAN_POINT('',(0.600000000000001,-2.9,-13.965)) ;
#142553 = CARTESIAN_POINT('',(0.600000000000001,-2.9,-15.24)) ;
#142554 = CARTESIAN_POINT('',(0.600000000000001,-2.1,-13.965)) ;
#142555 = CARTESIAN_POINT('',(0.600000000000001,1.58165963986121E-16,-13.965)) ;
#142556 = CARTESIAN_POINT('',(0.600000000000001,-2.1,-14.64)) ;
#142557 = CARTESIAN_POINT('',(0.600000000000001,-2.1,-15.24)) ;
#142558 = CARTESIAN_POINT('Origin',(0.600000000000001,-1.9,-14.64)) ;
#142559 = CARTESIAN_POINT('Origin',(0.600000000000001,2.80617032878603E-17,
-11.43)) ;
#142560 = CARTESIAN_POINT('',(0.600000000000001,-1.9,-11.03)) ;
#142561 = CARTESIAN_POINT('',(0.600000000000001,-0.3,-11.03)) ;
#142562 = CARTESIAN_POINT('',(0.600000000000001,-2.39800009914441E-17,-11.03)) ;
#142563 = CARTESIAN_POINT('',(0.6,-0.4,-11.13)) ;
#142564 = CARTESIAN_POINT('Origin',(0.6,-0.3,-11.13)) ;
#142565 = CARTESIAN_POINT('',(0.6,-0.4,-11.73)) ;
#142566 = CARTESIAN_POINT('',(0.6,-0.4,-11.03)) ;
#142567 = CARTESIAN_POINT('Origin',(0.6,-0.3,-11.73)) ;
#142568 = CARTESIAN_POINT('',(0.600000000000001,-2.1,-12.03)) ;
#142569 = CARTESIAN_POINT('Origin',(0.600000000000001,-1.9,-12.03)) ;
#142570 = CARTESIAN_POINT('',(0.600000000000001,-2.1,-12.705)) ;
#142571 = CARTESIAN_POINT('',(0.600000000000001,-2.1,-11.43)) ;
#142572 = CARTESIAN_POINT('',(0.600000000000001,-2.9,-12.705)) ;
#142573 = CARTESIAN_POINT('',(0.600000000000001,-3.69904270612701E-17,-12.705)) ;
#142574 = CARTESIAN_POINT('',(0.600000000000001,-2.9,-10.155)) ;
#142575 = CARTESIAN_POINT('',(0.600000000000001,-2.9,-11.43)) ;
#142576 = CARTESIAN_POINT('',(0.600000000000001,-2.1,-10.155)) ;
#142577 = CARTESIAN_POINT('',(0.600000000000001,1.58165963986121E-16,-10.155)) ;
#142578 = CARTESIAN_POINT('',(0.600000000000001,-2.1,-10.83)) ;
#142579 = CARTESIAN_POINT('',(0.600000000000001,-2.1,-11.43)) ;
#142580 = CARTESIAN_POINT('Origin',(0.600000000000001,-1.9,-10.83)) ;
#142581 = CARTESIAN_POINT('Origin',(0.600000000000001,2.80617032878603E-17,
-7.62)) ;
#142582 = CARTESIAN_POINT('',(0.600000000000001,-1.9,-7.22)) ;
#142583 = CARTESIAN_POINT('',(0.600000000000001,-0.3,-7.22)) ;
#142584 = CARTESIAN_POINT('',(0.600000000000001,-2.39800009914439E-17,-7.22)) ;
#142585 = CARTESIAN_POINT('',(0.6,-0.4,-7.32)) ;
#142586 = CARTESIAN_POINT('Origin',(0.6,-0.3,-7.32)) ;
#142587 = CARTESIAN_POINT('',(0.6,-0.4,-7.92)) ;
#142588 = CARTESIAN_POINT('',(0.6,-0.4,-7.22)) ;
#142589 = CARTESIAN_POINT('Origin',(0.6,-0.3,-7.92)) ;
#142590 = CARTESIAN_POINT('',(0.600000000000001,-2.1,-8.22)) ;
#142591 = CARTESIAN_POINT('Origin',(0.600000000000001,-1.9,-8.22)) ;
#142592 = CARTESIAN_POINT('',(0.600000000000001,-2.1,-8.895)) ;
#142593 = CARTESIAN_POINT('',(0.600000000000001,-2.1,-7.62)) ;
#142594 = CARTESIAN_POINT('',(0.600000000000001,-2.9,-8.895)) ;
#142595 = CARTESIAN_POINT('',(0.600000000000001,-3.69904270612701E-17,-8.895)) ;
#142596 = CARTESIAN_POINT('',(0.600000000000001,-2.9,-6.345)) ;
#142597 = CARTESIAN_POINT('',(0.600000000000001,-2.9,-7.62)) ;
#142598 = CARTESIAN_POINT('',(0.600000000000001,-2.1,-6.345)) ;
#142599 = CARTESIAN_POINT('',(0.600000000000001,1.58165963986121E-16,-6.345)) ;
#142600 = CARTESIAN_POINT('',(0.600000000000001,-2.1,-7.02)) ;
#142601 = CARTESIAN_POINT('',(0.600000000000001,-2.1,-7.62)) ;
#142602 = CARTESIAN_POINT('Origin',(0.600000000000001,-1.9,-7.02)) ;
#142603 = CARTESIAN_POINT('Origin',(0.600000000000001,2.80617032878603E-17,
-3.81)) ;
#142604 = CARTESIAN_POINT('',(0.600000000000001,-1.9,-3.41)) ;
#142605 = CARTESIAN_POINT('',(0.600000000000001,-0.3,-3.41)) ;
#142606 = CARTESIAN_POINT('',(0.600000000000001,-2.3980000991444E-17,-3.41)) ;
#142607 = CARTESIAN_POINT('',(0.6,-0.4,-3.51)) ;
#142608 = CARTESIAN_POINT('Origin',(0.6,-0.3,-3.51)) ;
#142609 = CARTESIAN_POINT('',(0.6,-0.4,-4.11)) ;
#142610 = CARTESIAN_POINT('',(0.6,-0.4,-3.41)) ;
#142611 = CARTESIAN_POINT('Origin',(0.6,-0.3,-4.11)) ;
#142612 = CARTESIAN_POINT('',(0.600000000000001,-2.1,-4.41)) ;
#142613 = CARTESIAN_POINT('Origin',(0.600000000000001,-1.9,-4.41)) ;
#142614 = CARTESIAN_POINT('',(0.600000000000001,-2.1,-5.085)) ;
#142615 = CARTESIAN_POINT('',(0.600000000000001,-2.1,-3.81)) ;
#142616 = CARTESIAN_POINT('',(0.600000000000001,-2.9,-5.085)) ;
#142617 = CARTESIAN_POINT('',(0.600000000000001,-3.699042706127E-17,-5.085)) ;
#142618 = CARTESIAN_POINT('',(0.600000000000001,-2.9,-2.535)) ;
#142619 = CARTESIAN_POINT('',(0.600000000000001,-2.9,-3.81)) ;
#142620 = CARTESIAN_POINT('',(0.600000000000001,-2.1,-2.535)) ;
#142621 = CARTESIAN_POINT('',(0.600000000000001,1.58165963986121E-16,-2.535)) ;
#142622 = CARTESIAN_POINT('',(0.600000000000001,-2.1,-3.21)) ;
#142623 = CARTESIAN_POINT('',(0.600000000000001,-2.1,-3.81)) ;
#142624 = CARTESIAN_POINT('Origin',(0.600000000000001,-1.9,-3.21)) ;
#142625 = CARTESIAN_POINT('Origin',(-0.999999999999999,1.25,-35.665)) ;
#142626 = CARTESIAN_POINT('',(-1.1,-1.9,-35.665)) ;
#142627 = CARTESIAN_POINT('',(-0.899999999999999,-2.1,-35.665)) ;
#142628 = CARTESIAN_POINT('Origin',(-0.899999999999999,-1.9,-35.665)) ;
#142629 = CARTESIAN_POINT('',(-1.1,-2.9,-35.665)) ;
#142630 = CARTESIAN_POINT('',(-1.1,-2.9,-35.665)) ;
#142631 = CARTESIAN_POINT('',(0.500000000000001,-2.9,-35.665)) ;
#142632 = CARTESIAN_POINT('',(0.600000000000001,-2.9,-35.665)) ;
#142633 = CARTESIAN_POINT('',(0.500000000000001,-2.1,-35.665)) ;
#142634 = CARTESIAN_POINT('',(0.5,1.25,-35.665)) ;
#142635 = CARTESIAN_POINT('',(-0.999999999999999,-2.1,-35.665)) ;
#142636 = CARTESIAN_POINT('Origin',(-0.999999999999999,1.25,-32.915)) ;
#142637 = CARTESIAN_POINT('',(-0.899999999999999,-2.1,-32.915)) ;
#142638 = CARTESIAN_POINT('',(-1.1,-1.9,-32.915)) ;
#142639 = CARTESIAN_POINT('Origin',(-0.899999999999999,-1.9,-32.915)) ;
#142640 = CARTESIAN_POINT('',(0.500000000000001,-2.1,-32.915)) ;
#142641 = CARTESIAN_POINT('',(0.600000000000001,-2.1,-32.915)) ;
#142642 = CARTESIAN_POINT('',(0.500000000000001,-2.9,-32.915)) ;
#142643 = CARTESIAN_POINT('',(0.5,1.25,-32.915)) ;
#142644 = CARTESIAN_POINT('',(-1.1,-2.9,-32.915)) ;
#142645 = CARTESIAN_POINT('',(-1.1,-2.9,-32.915)) ;
#142646 = CARTESIAN_POINT('',(-1.1,1.25,-32.915)) ;
#142647 = CARTESIAN_POINT('Origin',(-0.999999999999999,1.25,-31.855)) ;
#142648 = CARTESIAN_POINT('',(-1.1,-1.9,-31.855)) ;
#142649 = CARTESIAN_POINT('',(-0.899999999999999,-2.1,-31.855)) ;
#142650 = CARTESIAN_POINT('Origin',(-0.899999999999999,-1.9,-31.855)) ;
#142651 = CARTESIAN_POINT('',(-1.1,-2.9,-31.855)) ;
#142652 = CARTESIAN_POINT('',(-1.1,-2.9,-31.855)) ;
#142653 = CARTESIAN_POINT('',(0.500000000000001,-2.9,-31.855)) ;
#142654 = CARTESIAN_POINT('',(0.600000000000001,-2.9,-31.855)) ;
#142655 = CARTESIAN_POINT('',(0.500000000000001,-2.1,-31.855)) ;
#142656 = CARTESIAN_POINT('',(0.5,1.25,-31.855)) ;
#142657 = CARTESIAN_POINT('',(-0.999999999999999,-2.1,-31.855)) ;
#142658 = CARTESIAN_POINT('Origin',(-0.999999999999999,1.25,-29.105)) ;
#142659 = CARTESIAN_POINT('',(-0.899999999999999,-2.1,-29.105)) ;
#142660 = CARTESIAN_POINT('',(-1.1,-1.9,-29.105)) ;
#142661 = CARTESIAN_POINT('Origin',(-0.899999999999999,-1.9,-29.105)) ;
#142662 = CARTESIAN_POINT('',(0.500000000000001,-2.1,-29.105)) ;
#142663 = CARTESIAN_POINT('',(0.600000000000001,-2.1,-29.105)) ;
#142664 = CARTESIAN_POINT('',(0.500000000000001,-2.9,-29.105)) ;
#142665 = CARTESIAN_POINT('',(0.5,1.25,-29.105)) ;
#142666 = CARTESIAN_POINT('',(-1.1,-2.9,-29.105)) ;
#142667 = CARTESIAN_POINT('',(-1.1,-2.9,-29.105)) ;
#142668 = CARTESIAN_POINT('',(-1.1,1.25,-29.105)) ;
#142669 = CARTESIAN_POINT('Origin',(-0.999999999999999,1.25,-28.045)) ;
#142670 = CARTESIAN_POINT('',(-1.1,-1.9,-28.045)) ;
#142671 = CARTESIAN_POINT('',(-0.899999999999999,-2.1,-28.045)) ;
#142672 = CARTESIAN_POINT('Origin',(-0.899999999999999,-1.9,-28.045)) ;
#142673 = CARTESIAN_POINT('',(-1.1,-2.9,-28.045)) ;
#142674 = CARTESIAN_POINT('',(-1.1,-2.9,-28.045)) ;
#142675 = CARTESIAN_POINT('',(0.500000000000001,-2.9,-28.045)) ;
#142676 = CARTESIAN_POINT('',(0.600000000000001,-2.9,-28.045)) ;
#142677 = CARTESIAN_POINT('',(0.500000000000001,-2.1,-28.045)) ;
#142678 = CARTESIAN_POINT('',(0.5,1.25,-28.045)) ;
#142679 = CARTESIAN_POINT('',(-0.999999999999999,-2.1,-28.045)) ;
#142680 = CARTESIAN_POINT('Origin',(-0.999999999999999,1.25,-25.295)) ;
#142681 = CARTESIAN_POINT('',(-0.899999999999999,-2.1,-25.295)) ;
#142682 = CARTESIAN_POINT('',(-1.1,-1.9,-25.295)) ;
#142683 = CARTESIAN_POINT('Origin',(-0.899999999999999,-1.9,-25.295)) ;
#142684 = CARTESIAN_POINT('',(0.500000000000001,-2.1,-25.295)) ;
#142685 = CARTESIAN_POINT('',(0.600000000000001,-2.1,-25.295)) ;
#142686 = CARTESIAN_POINT('',(0.500000000000001,-2.9,-25.295)) ;
#142687 = CARTESIAN_POINT('',(0.5,1.25,-25.295)) ;
#142688 = CARTESIAN_POINT('',(-1.1,-2.9,-25.295)) ;
#142689 = CARTESIAN_POINT('',(-1.1,-2.9,-25.295)) ;
#142690 = CARTESIAN_POINT('',(-1.1,1.25,-25.295)) ;
#142691 = CARTESIAN_POINT('Origin',(-0.999999999999999,1.25,-24.235)) ;
#142692 = CARTESIAN_POINT('',(-1.1,-1.9,-24.235)) ;
#142693 = CARTESIAN_POINT('',(-0.899999999999999,-2.1,-24.235)) ;
#142694 = CARTESIAN_POINT('Origin',(-0.899999999999999,-1.9,-24.235)) ;
#142695 = CARTESIAN_POINT('',(-1.1,-2.9,-24.235)) ;
#142696 = CARTESIAN_POINT('',(-1.1,-2.9,-24.235)) ;
#142697 = CARTESIAN_POINT('',(0.500000000000001,-2.9,-24.235)) ;
#142698 = CARTESIAN_POINT('',(0.600000000000001,-2.9,-24.235)) ;
#142699 = CARTESIAN_POINT('',(0.500000000000001,-2.1,-24.235)) ;
#142700 = CARTESIAN_POINT('',(0.5,1.25,-24.235)) ;
#142701 = CARTESIAN_POINT('',(-0.999999999999999,-2.1,-24.235)) ;
#142702 = CARTESIAN_POINT('Origin',(-0.999999999999999,1.25,-21.485)) ;
#142703 = CARTESIAN_POINT('',(-0.899999999999999,-2.1,-21.485)) ;
#142704 = CARTESIAN_POINT('',(-1.1,-1.9,-21.485)) ;
#142705 = CARTESIAN_POINT('Origin',(-0.899999999999999,-1.9,-21.485)) ;
#142706 = CARTESIAN_POINT('',(0.500000000000001,-2.1,-21.485)) ;
#142707 = CARTESIAN_POINT('',(0.600000000000001,-2.1,-21.485)) ;
#142708 = CARTESIAN_POINT('',(0.500000000000001,-2.9,-21.485)) ;
#142709 = CARTESIAN_POINT('',(0.5,1.25,-21.485)) ;
#142710 = CARTESIAN_POINT('',(-1.1,-2.9,-21.485)) ;
#142711 = CARTESIAN_POINT('',(-1.1,-2.9,-21.485)) ;
#142712 = CARTESIAN_POINT('',(-1.1,1.25,-21.485)) ;
#142713 = CARTESIAN_POINT('Origin',(-0.999999999999999,1.25,-20.425)) ;
#142714 = CARTESIAN_POINT('',(-1.1,-1.9,-20.425)) ;
#142715 = CARTESIAN_POINT('',(-0.899999999999999,-2.1,-20.425)) ;
#142716 = CARTESIAN_POINT('Origin',(-0.899999999999999,-1.9,-20.425)) ;
#142717 = CARTESIAN_POINT('',(-1.1,-2.9,-20.425)) ;
#142718 = CARTESIAN_POINT('',(-1.1,-2.9,-20.425)) ;
#142719 = CARTESIAN_POINT('',(0.500000000000001,-2.9,-20.425)) ;
#142720 = CARTESIAN_POINT('',(0.600000000000001,-2.9,-20.425)) ;
#142721 = CARTESIAN_POINT('',(0.500000000000001,-2.1,-20.425)) ;
#142722 = CARTESIAN_POINT('',(0.5,1.25,-20.425)) ;
#142723 = CARTESIAN_POINT('',(-0.999999999999999,-2.1,-20.425)) ;
#142724 = CARTESIAN_POINT('Origin',(-0.999999999999999,1.25,-17.675)) ;
#142725 = CARTESIAN_POINT('',(-0.899999999999999,-2.1,-17.675)) ;
#142726 = CARTESIAN_POINT('',(-1.1,-1.9,-17.675)) ;
#142727 = CARTESIAN_POINT('Origin',(-0.899999999999999,-1.9,-17.675)) ;
#142728 = CARTESIAN_POINT('',(0.500000000000001,-2.1,-17.675)) ;
#142729 = CARTESIAN_POINT('',(0.600000000000001,-2.1,-17.675)) ;
#142730 = CARTESIAN_POINT('',(0.500000000000001,-2.9,-17.675)) ;
#142731 = CARTESIAN_POINT('',(0.5,1.25,-17.675)) ;
#142732 = CARTESIAN_POINT('',(-1.1,-2.9,-17.675)) ;
#142733 = CARTESIAN_POINT('',(-1.1,-2.9,-17.675)) ;
#142734 = CARTESIAN_POINT('',(-1.1,1.25,-17.675)) ;
#142735 = CARTESIAN_POINT('Origin',(-0.999999999999999,1.25,-16.615)) ;
#142736 = CARTESIAN_POINT('',(-1.1,-1.9,-16.615)) ;
#142737 = CARTESIAN_POINT('',(-0.899999999999999,-2.1,-16.615)) ;
#142738 = CARTESIAN_POINT('Origin',(-0.899999999999999,-1.9,-16.615)) ;
#142739 = CARTESIAN_POINT('',(-1.1,-2.9,-16.615)) ;
#142740 = CARTESIAN_POINT('',(-1.1,-2.9,-16.615)) ;
#142741 = CARTESIAN_POINT('',(0.500000000000001,-2.9,-16.615)) ;
#142742 = CARTESIAN_POINT('',(0.600000000000001,-2.9,-16.615)) ;
#142743 = CARTESIAN_POINT('',(0.500000000000001,-2.1,-16.615)) ;
#142744 = CARTESIAN_POINT('',(0.5,1.25,-16.615)) ;
#142745 = CARTESIAN_POINT('',(-0.999999999999999,-2.1,-16.615)) ;
#142746 = CARTESIAN_POINT('Origin',(-0.999999999999999,1.25,-13.865)) ;
#142747 = CARTESIAN_POINT('',(-0.899999999999999,-2.1,-13.865)) ;
#142748 = CARTESIAN_POINT('',(-1.1,-1.9,-13.865)) ;
#142749 = CARTESIAN_POINT('Origin',(-0.899999999999999,-1.9,-13.865)) ;
#142750 = CARTESIAN_POINT('',(0.500000000000001,-2.1,-13.865)) ;
#142751 = CARTESIAN_POINT('',(0.600000000000001,-2.1,-13.865)) ;
#142752 = CARTESIAN_POINT('',(0.500000000000001,-2.9,-13.865)) ;
#142753 = CARTESIAN_POINT('',(0.5,1.25,-13.865)) ;
#142754 = CARTESIAN_POINT('',(-1.1,-2.9,-13.865)) ;
#142755 = CARTESIAN_POINT('',(-1.1,-2.9,-13.865)) ;
#142756 = CARTESIAN_POINT('',(-1.1,1.25,-13.865)) ;
#142757 = CARTESIAN_POINT('Origin',(-0.999999999999999,1.25,-12.805)) ;
#142758 = CARTESIAN_POINT('',(-1.1,-1.9,-12.805)) ;
#142759 = CARTESIAN_POINT('',(-0.899999999999999,-2.1,-12.805)) ;
#142760 = CARTESIAN_POINT('Origin',(-0.899999999999999,-1.9,-12.805)) ;
#142761 = CARTESIAN_POINT('',(-1.1,-2.9,-12.805)) ;
#142762 = CARTESIAN_POINT('',(-1.1,-2.9,-12.805)) ;
#142763 = CARTESIAN_POINT('',(0.500000000000001,-2.9,-12.805)) ;
#142764 = CARTESIAN_POINT('',(0.600000000000001,-2.9,-12.805)) ;
#142765 = CARTESIAN_POINT('',(0.500000000000001,-2.1,-12.805)) ;
#142766 = CARTESIAN_POINT('',(0.5,1.25,-12.805)) ;
#142767 = CARTESIAN_POINT('',(-0.999999999999999,-2.1,-12.805)) ;
#142768 = CARTESIAN_POINT('Origin',(-0.999999999999999,1.25,-10.055)) ;
#142769 = CARTESIAN_POINT('',(-0.899999999999999,-2.1,-10.055)) ;
#142770 = CARTESIAN_POINT('',(-1.1,-1.9,-10.055)) ;
#142771 = CARTESIAN_POINT('Origin',(-0.899999999999999,-1.9,-10.055)) ;
#142772 = CARTESIAN_POINT('',(0.500000000000001,-2.1,-10.055)) ;
#142773 = CARTESIAN_POINT('',(0.600000000000001,-2.1,-10.055)) ;
#142774 = CARTESIAN_POINT('',(0.500000000000001,-2.9,-10.055)) ;
#142775 = CARTESIAN_POINT('',(0.5,1.25,-10.055)) ;
#142776 = CARTESIAN_POINT('',(-1.1,-2.9,-10.055)) ;
#142777 = CARTESIAN_POINT('',(-1.1,-2.9,-10.055)) ;
#142778 = CARTESIAN_POINT('',(-1.1,1.25,-10.055)) ;
#142779 = CARTESIAN_POINT('Origin',(-0.999999999999999,1.25,-8.995)) ;
#142780 = CARTESIAN_POINT('',(-1.1,-1.9,-8.995)) ;
#142781 = CARTESIAN_POINT('',(-0.899999999999999,-2.1,-8.995)) ;
#142782 = CARTESIAN_POINT('Origin',(-0.899999999999999,-1.9,-8.995)) ;
#142783 = CARTESIAN_POINT('',(-1.1,-2.9,-8.995)) ;
#142784 = CARTESIAN_POINT('',(-1.1,-2.9,-8.995)) ;
#142785 = CARTESIAN_POINT('',(0.500000000000001,-2.9,-8.995)) ;
#142786 = CARTESIAN_POINT('',(0.600000000000001,-2.9,-8.995)) ;
#142787 = CARTESIAN_POINT('',(0.500000000000001,-2.1,-8.995)) ;
#142788 = CARTESIAN_POINT('',(0.5,1.25,-8.995)) ;
#142789 = CARTESIAN_POINT('',(-0.999999999999999,-2.1,-8.995)) ;
#142790 = CARTESIAN_POINT('Origin',(-0.999999999999999,1.25,-6.245)) ;
#142791 = CARTESIAN_POINT('',(-0.899999999999999,-2.1,-6.245)) ;
#142792 = CARTESIAN_POINT('',(-1.1,-1.9,-6.245)) ;
#142793 = CARTESIAN_POINT('Origin',(-0.899999999999999,-1.9,-6.245)) ;
#142794 = CARTESIAN_POINT('',(0.500000000000001,-2.1,-6.245)) ;
#142795 = CARTESIAN_POINT('',(0.600000000000001,-2.1,-6.245)) ;
#142796 = CARTESIAN_POINT('',(0.500000000000001,-2.9,-6.245)) ;
#142797 = CARTESIAN_POINT('',(0.5,1.25,-6.245)) ;
#142798 = CARTESIAN_POINT('',(-1.1,-2.9,-6.245)) ;
#142799 = CARTESIAN_POINT('',(-1.1,-2.9,-6.245)) ;
#142800 = CARTESIAN_POINT('',(-1.1,1.25,-6.245)) ;
#142801 = CARTESIAN_POINT('Origin',(-0.999999999999999,1.25,-5.185)) ;
#142802 = CARTESIAN_POINT('',(-1.1,-1.9,-5.185)) ;
#142803 = CARTESIAN_POINT('',(-0.899999999999999,-2.1,-5.185)) ;
#142804 = CARTESIAN_POINT('Origin',(-0.899999999999999,-1.9,-5.185)) ;
#142805 = CARTESIAN_POINT('',(-1.1,-2.9,-5.185)) ;
#142806 = CARTESIAN_POINT('',(-1.1,-2.9,-5.185)) ;
#142807 = CARTESIAN_POINT('',(0.500000000000001,-2.9,-5.185)) ;
#142808 = CARTESIAN_POINT('',(0.600000000000001,-2.9,-5.185)) ;
#142809 = CARTESIAN_POINT('',(0.500000000000001,-2.1,-5.185)) ;
#142810 = CARTESIAN_POINT('',(0.5,1.25,-5.185)) ;
#142811 = CARTESIAN_POINT('',(-0.999999999999999,-2.1,-5.185)) ;
#142812 = CARTESIAN_POINT('Origin',(-0.999999999999999,1.25,-2.435)) ;
#142813 = CARTESIAN_POINT('',(-0.899999999999999,-2.1,-2.435)) ;
#142814 = CARTESIAN_POINT('',(-1.1,-1.9,-2.435)) ;
#142815 = CARTESIAN_POINT('Origin',(-0.899999999999999,-1.9,-2.435)) ;
#142816 = CARTESIAN_POINT('',(0.500000000000001,-2.1,-2.435)) ;
#142817 = CARTESIAN_POINT('',(0.600000000000001,-2.1,-2.435)) ;
#142818 = CARTESIAN_POINT('',(0.500000000000001,-2.9,-2.435)) ;
#142819 = CARTESIAN_POINT('',(0.5,1.25,-2.435)) ;
#142820 = CARTESIAN_POINT('',(-1.1,-2.9,-2.435)) ;
#142821 = CARTESIAN_POINT('',(-1.1,-2.9,-2.435)) ;
#142822 = CARTESIAN_POINT('',(-1.1,1.25,-2.435)) ;
#142823 = CARTESIAN_POINT('Origin',(-1.1,-2.9,-36.89)) ;
#142824 = CARTESIAN_POINT('',(-1.2,-2.9,-2.335)) ;
#142825 = CARTESIAN_POINT('',(-1.2,-2.9,-1.475)) ;
#142826 = CARTESIAN_POINT('',(-1.2,-2.9,-36.89)) ;
#142827 = CARTESIAN_POINT('',(-1.1,-3.,-2.335)) ;
#142828 = CARTESIAN_POINT('Origin',(-1.1,-2.9,-2.335)) ;
#142829 = CARTESIAN_POINT('',(-1.1,-3.,-1.475)) ;
#142830 = CARTESIAN_POINT('',(-1.1,-3.,-36.89)) ;
#142831 = CARTESIAN_POINT('Origin',(-1.1,-2.9,-1.475)) ;
#142832 = CARTESIAN_POINT('Origin',(-1.1,-2.9,-36.89)) ;
#142833 = CARTESIAN_POINT('',(-1.2,-2.9,-6.145)) ;
#142834 = CARTESIAN_POINT('',(-1.2,-2.9,-5.285)) ;
#142835 = CARTESIAN_POINT('',(-1.2,-2.9,-36.89)) ;
#142836 = CARTESIAN_POINT('',(-1.1,-3.,-6.145)) ;
#142837 = CARTESIAN_POINT('Origin',(-1.1,-2.9,-6.145)) ;
#142838 = CARTESIAN_POINT('',(-1.1,-3.,-5.285)) ;
#142839 = CARTESIAN_POINT('',(-1.1,-3.,-36.89)) ;
#142840 = CARTESIAN_POINT('Origin',(-1.1,-2.9,-5.285)) ;
#142841 = CARTESIAN_POINT('Origin',(-1.1,-2.9,-36.89)) ;
#142842 = CARTESIAN_POINT('',(-1.2,-2.9,-9.955)) ;
#142843 = CARTESIAN_POINT('',(-1.2,-2.9,-9.095)) ;
#142844 = CARTESIAN_POINT('',(-1.2,-2.9,-36.89)) ;
#142845 = CARTESIAN_POINT('',(-1.1,-3.,-9.955)) ;
#142846 = CARTESIAN_POINT('Origin',(-1.1,-2.9,-9.955)) ;
#142847 = CARTESIAN_POINT('',(-1.1,-3.,-9.095)) ;
#142848 = CARTESIAN_POINT('',(-1.1,-3.,-36.89)) ;
#142849 = CARTESIAN_POINT('Origin',(-1.1,-2.9,-9.095)) ;
#142850 = CARTESIAN_POINT('Origin',(-1.1,-2.9,-36.89)) ;
#142851 = CARTESIAN_POINT('',(-1.2,-2.9,-13.765)) ;
#142852 = CARTESIAN_POINT('',(-1.2,-2.9,-12.905)) ;
#142853 = CARTESIAN_POINT('',(-1.2,-2.9,-36.89)) ;
#142854 = CARTESIAN_POINT('',(-1.1,-3.,-13.765)) ;
#142855 = CARTESIAN_POINT('Origin',(-1.1,-2.9,-13.765)) ;
#142856 = CARTESIAN_POINT('',(-1.1,-3.,-12.905)) ;
#142857 = CARTESIAN_POINT('',(-1.1,-3.,-36.89)) ;
#142858 = CARTESIAN_POINT('Origin',(-1.1,-2.9,-12.905)) ;
#142859 = CARTESIAN_POINT('Origin',(-1.1,-2.9,-36.89)) ;
#142860 = CARTESIAN_POINT('',(-1.2,-2.9,-17.575)) ;
#142861 = CARTESIAN_POINT('',(-1.2,-2.9,-16.715)) ;
#142862 = CARTESIAN_POINT('',(-1.2,-2.9,-36.89)) ;
#142863 = CARTESIAN_POINT('',(-1.1,-3.,-17.575)) ;
#142864 = CARTESIAN_POINT('Origin',(-1.1,-2.9,-17.575)) ;
#142865 = CARTESIAN_POINT('',(-1.1,-3.,-16.715)) ;
#142866 = CARTESIAN_POINT('',(-1.1,-3.,-36.89)) ;
#142867 = CARTESIAN_POINT('Origin',(-1.1,-2.9,-16.715)) ;
#142868 = CARTESIAN_POINT('Origin',(-1.1,-2.9,-36.89)) ;
#142869 = CARTESIAN_POINT('',(-1.2,-2.9,-21.385)) ;
#142870 = CARTESIAN_POINT('',(-1.2,-2.9,-20.525)) ;
#142871 = CARTESIAN_POINT('',(-1.2,-2.9,-36.89)) ;
#142872 = CARTESIAN_POINT('',(-1.1,-3.,-21.385)) ;
#142873 = CARTESIAN_POINT('Origin',(-1.1,-2.9,-21.385)) ;
#142874 = CARTESIAN_POINT('',(-1.1,-3.,-20.525)) ;
#142875 = CARTESIAN_POINT('',(-1.1,-3.,-36.89)) ;
#142876 = CARTESIAN_POINT('Origin',(-1.1,-2.9,-20.525)) ;
#142877 = CARTESIAN_POINT('Origin',(-1.1,-2.9,-36.89)) ;
#142878 = CARTESIAN_POINT('',(-1.2,-2.9,-25.195)) ;
#142879 = CARTESIAN_POINT('',(-1.2,-2.9,-24.335)) ;
#142880 = CARTESIAN_POINT('',(-1.2,-2.9,-36.89)) ;
#142881 = CARTESIAN_POINT('',(-1.1,-3.,-25.195)) ;
#142882 = CARTESIAN_POINT('Origin',(-1.1,-2.9,-25.195)) ;
#142883 = CARTESIAN_POINT('',(-1.1,-3.,-24.335)) ;
#142884 = CARTESIAN_POINT('',(-1.1,-3.,-36.89)) ;
#142885 = CARTESIAN_POINT('Origin',(-1.1,-2.9,-24.335)) ;
#142886 = CARTESIAN_POINT('Origin',(-1.1,-2.9,-36.89)) ;
#142887 = CARTESIAN_POINT('',(-1.2,-2.9,-29.005)) ;
#142888 = CARTESIAN_POINT('',(-1.2,-2.9,-28.145)) ;
#142889 = CARTESIAN_POINT('',(-1.2,-2.9,-36.89)) ;
#142890 = CARTESIAN_POINT('',(-1.1,-3.,-29.005)) ;
#142891 = CARTESIAN_POINT('Origin',(-1.1,-2.9,-29.005)) ;
#142892 = CARTESIAN_POINT('',(-1.1,-3.,-28.145)) ;
#142893 = CARTESIAN_POINT('',(-1.1,-3.,-36.89)) ;
#142894 = CARTESIAN_POINT('Origin',(-1.1,-2.9,-28.145)) ;
#142895 = CARTESIAN_POINT('Origin',(-1.1,-2.9,-36.89)) ;
#142896 = CARTESIAN_POINT('',(-1.2,-2.9,-32.815)) ;
#142897 = CARTESIAN_POINT('',(-1.2,-2.9,-31.955)) ;
#142898 = CARTESIAN_POINT('',(-1.2,-2.9,-36.89)) ;
#142899 = CARTESIAN_POINT('',(-1.1,-3.,-32.815)) ;
#142900 = CARTESIAN_POINT('Origin',(-1.1,-2.9,-32.815)) ;
#142901 = CARTESIAN_POINT('',(-1.1,-3.,-31.955)) ;
#142902 = CARTESIAN_POINT('',(-1.1,-3.,-36.89)) ;
#142903 = CARTESIAN_POINT('Origin',(-1.1,-2.9,-31.955)) ;
#142904 = CARTESIAN_POINT('Origin',(0.600000000000001,2.80617032878603E-17,
0.)) ;
#142905 = CARTESIAN_POINT('',(0.600000000000001,-1.9,0.4)) ;
#142906 = CARTESIAN_POINT('',(0.600000000000001,-0.3,0.4)) ;
#142907 = CARTESIAN_POINT('',(0.600000000000001,-2.3980000991444E-17,0.4)) ;
#142908 = CARTESIAN_POINT('',(0.6,-0.4,0.3)) ;
#142909 = CARTESIAN_POINT('Origin',(0.6,-0.3,0.3)) ;
#142910 = CARTESIAN_POINT('',(0.6,-0.4,-0.3)) ;
#142911 = CARTESIAN_POINT('',(0.6,-0.4,0.4)) ;
#142912 = CARTESIAN_POINT('Origin',(0.6,-0.3,-0.3)) ;
#142913 = CARTESIAN_POINT('',(0.600000000000001,-2.1,-0.6)) ;
#142914 = CARTESIAN_POINT('Origin',(0.600000000000001,-1.9,-0.6)) ;
#142915 = CARTESIAN_POINT('',(0.600000000000001,-2.1,-1.275)) ;
#142916 = CARTESIAN_POINT('',(0.600000000000001,-2.1,0.)) ;
#142917 = CARTESIAN_POINT('',(0.600000000000001,-2.9,-1.275)) ;
#142918 = CARTESIAN_POINT('',(0.600000000000001,-3.699042706127E-17,-1.275)) ;
#142919 = CARTESIAN_POINT('',(0.600000000000001,-2.9,1.275)) ;
#142920 = CARTESIAN_POINT('',(0.600000000000001,-2.9,0.)) ;
#142921 = CARTESIAN_POINT('',(0.600000000000001,-2.1,1.275)) ;
#142922 = CARTESIAN_POINT('',(0.600000000000001,1.58165963986121E-16,1.275)) ;
#142923 = CARTESIAN_POINT('',(0.600000000000001,-2.1,0.6)) ;
#142924 = CARTESIAN_POINT('',(0.600000000000001,-2.1,0.)) ;
#142925 = CARTESIAN_POINT('Origin',(0.600000000000001,-1.9,0.6)) ;
#142926 = CARTESIAN_POINT('Origin',(-0.999999999999999,1.25,-1.375)) ;
#142927 = CARTESIAN_POINT('',(-1.1,-1.9,-1.375)) ;
#142928 = CARTESIAN_POINT('',(-0.899999999999999,-2.1,-1.375)) ;
#142929 = CARTESIAN_POINT('Origin',(-0.899999999999999,-1.9,-1.375)) ;
#142930 = CARTESIAN_POINT('',(-1.1,-2.9,-1.375)) ;
#142931 = CARTESIAN_POINT('',(-1.1,-2.9,-1.375)) ;
#142932 = CARTESIAN_POINT('',(0.500000000000001,-2.9,-1.375)) ;
#142933 = CARTESIAN_POINT('',(0.600000000000001,-2.9,-1.375)) ;
#142934 = CARTESIAN_POINT('',(0.500000000000001,-2.1,-1.375)) ;
#142935 = CARTESIAN_POINT('',(0.5,1.25,-1.375)) ;
#142936 = CARTESIAN_POINT('',(-0.999999999999999,-2.1,-1.375)) ;
#142937 = CARTESIAN_POINT('Origin',(-0.999999999999999,1.25,1.375)) ;
#142938 = CARTESIAN_POINT('',(-0.899999999999999,-2.1,1.375)) ;
#142939 = CARTESIAN_POINT('',(-1.1,-1.9,1.375)) ;
#142940 = CARTESIAN_POINT('Origin',(-0.899999999999999,-1.9,1.375)) ;
#142941 = CARTESIAN_POINT('',(0.500000000000001,-2.1,1.375)) ;
#142942 = CARTESIAN_POINT('',(0.600000000000001,-2.1,1.375)) ;
#142943 = CARTESIAN_POINT('',(0.500000000000001,-2.9,1.375)) ;
#142944 = CARTESIAN_POINT('',(0.5,1.25,1.375)) ;
#142945 = CARTESIAN_POINT('',(-1.1,-2.9,1.375)) ;
#142946 = CARTESIAN_POINT('',(-1.1,-2.9,1.375)) ;
#142947 = CARTESIAN_POINT('',(-1.1,1.25,1.375)) ;
#142948 = CARTESIAN_POINT('Origin',(-1.1,-2.9,-36.89)) ;
#142949 = CARTESIAN_POINT('',(-1.2,-2.9,1.475)) ;
#142950 = CARTESIAN_POINT('',(-1.2,-2.9,2.5)) ;
#142951 = CARTESIAN_POINT('',(-1.2,-2.9,-36.89)) ;
#142952 = CARTESIAN_POINT('',(-1.1,-3.,1.475)) ;
#142953 = CARTESIAN_POINT('Origin',(-1.1,-2.9,1.475)) ;
#142954 = CARTESIAN_POINT('',(-1.1,-3.,2.5)) ;
#142955 = CARTESIAN_POINT('',(-1.1,-3.,-36.89)) ;
#142956 = CARTESIAN_POINT('Origin',(-1.1,-2.9,2.5)) ;
#142957 = CARTESIAN_POINT('Origin',(7.9,-2.9,-36.89)) ;
#142958 = CARTESIAN_POINT('',(7.9,-3.,-36.79)) ;
#142959 = CARTESIAN_POINT('',(7.9,-3.,2.5)) ;
#142960 = CARTESIAN_POINT('',(7.9,-3.,-36.89)) ;
#142961 = CARTESIAN_POINT('',(8.,-2.9,-36.79)) ;
#142962 = CARTESIAN_POINT('Origin',(7.9,-2.9,-36.79)) ;
#142963 = CARTESIAN_POINT('',(8.,-2.9,2.5)) ;
#142964 = CARTESIAN_POINT('',(8.,-2.9,-36.89)) ;
#142965 = CARTESIAN_POINT('Origin',(7.9,-2.9,2.5)) ;
#142966 = CARTESIAN_POINT('Origin',(-1.1,-3.,-36.89)) ;
#142967 = CARTESIAN_POINT('',(0.500000000000001,-3.,-35.765)) ;
#142968 = CARTESIAN_POINT('',(0.700000000000002,-3.,-35.565)) ;
#142969 = CARTESIAN_POINT('Origin',(0.500000000000001,-3.,-35.565)) ;
#142970 = CARTESIAN_POINT('',(-1.1,-3.,-35.765)) ;
#142971 = CARTESIAN_POINT('',(-1.1,-3.,-35.765)) ;
#142972 = CARTESIAN_POINT('',(-1.1,-3.,-36.79)) ;
#142973 = CARTESIAN_POINT('',(-1.1,-3.,-36.89)) ;
#142974 = CARTESIAN_POINT('',(7.9,-3.,-36.79)) ;
#142975 = CARTESIAN_POINT('',(-1.1,-3.,2.5)) ;
#142976 = CARTESIAN_POINT('',(0.500000000000001,-3.,1.475)) ;
#142977 = CARTESIAN_POINT('',(0.600000000000001,-3.,1.475)) ;
#142978 = CARTESIAN_POINT('',(0.700000000000002,-3.,1.275)) ;
#142979 = CARTESIAN_POINT('Origin',(0.500000000000001,-3.,1.275)) ;
#142980 = CARTESIAN_POINT('',(0.700000000000002,-3.,-1.275)) ;
#142981 = CARTESIAN_POINT('',(0.700000000000002,-3.,-36.89)) ;
#142982 = CARTESIAN_POINT('',(0.500000000000001,-3.,-1.475)) ;
#142983 = CARTESIAN_POINT('Origin',(0.500000000000001,-3.,-1.275)) ;
#142984 = CARTESIAN_POINT('',(-1.1,-3.,-1.475)) ;
#142985 = CARTESIAN_POINT('',(0.500000000000001,-3.,-2.335)) ;
#142986 = CARTESIAN_POINT('',(0.600000000000001,-3.,-2.335)) ;
#142987 = CARTESIAN_POINT('',(0.700000000000002,-3.,-2.535)) ;
#142988 = CARTESIAN_POINT('Origin',(0.500000000000001,-3.,-2.535)) ;
#142989 = CARTESIAN_POINT('',(0.700000000000002,-3.,-5.085)) ;
#142990 = CARTESIAN_POINT('',(0.700000000000002,-3.,-36.89)) ;
#142991 = CARTESIAN_POINT('',(0.500000000000001,-3.,-5.285)) ;
#142992 = CARTESIAN_POINT('Origin',(0.500000000000001,-3.,-5.085)) ;
#142993 = CARTESIAN_POINT('',(-1.1,-3.,-5.285)) ;
#142994 = CARTESIAN_POINT('',(0.500000000000001,-3.,-6.145)) ;
#142995 = CARTESIAN_POINT('',(0.600000000000001,-3.,-6.145)) ;
#142996 = CARTESIAN_POINT('',(0.700000000000002,-3.,-6.345)) ;
#142997 = CARTESIAN_POINT('Origin',(0.500000000000001,-3.,-6.345)) ;
#142998 = CARTESIAN_POINT('',(0.700000000000002,-3.,-8.895)) ;
#142999 = CARTESIAN_POINT('',(0.700000000000002,-3.,-36.89)) ;
#143000 = CARTESIAN_POINT('',(0.500000000000001,-3.,-9.095)) ;
#143001 = CARTESIAN_POINT('Origin',(0.500000000000001,-3.,-8.895)) ;
#143002 = CARTESIAN_POINT('',(-1.1,-3.,-9.095)) ;
#143003 = CARTESIAN_POINT('',(0.500000000000001,-3.,-9.955)) ;
#143004 = CARTESIAN_POINT('',(0.600000000000001,-3.,-9.955)) ;
#143005 = CARTESIAN_POINT('',(0.700000000000002,-3.,-10.155)) ;
#143006 = CARTESIAN_POINT('Origin',(0.500000000000001,-3.,-10.155)) ;
#143007 = CARTESIAN_POINT('',(0.700000000000002,-3.,-12.705)) ;
#143008 = CARTESIAN_POINT('',(0.700000000000002,-3.,-36.89)) ;
#143009 = CARTESIAN_POINT('',(0.500000000000001,-3.,-12.905)) ;
#143010 = CARTESIAN_POINT('Origin',(0.500000000000001,-3.,-12.705)) ;
#143011 = CARTESIAN_POINT('',(-1.1,-3.,-12.905)) ;
#143012 = CARTESIAN_POINT('',(0.500000000000001,-3.,-13.765)) ;
#143013 = CARTESIAN_POINT('',(0.600000000000001,-3.,-13.765)) ;
#143014 = CARTESIAN_POINT('',(0.700000000000002,-3.,-13.965)) ;
#143015 = CARTESIAN_POINT('Origin',(0.500000000000001,-3.,-13.965)) ;
#143016 = CARTESIAN_POINT('',(0.700000000000002,-3.,-16.515)) ;
#143017 = CARTESIAN_POINT('',(0.700000000000002,-3.,-36.89)) ;
#143018 = CARTESIAN_POINT('',(0.500000000000001,-3.,-16.715)) ;
#143019 = CARTESIAN_POINT('Origin',(0.500000000000001,-3.,-16.515)) ;
#143020 = CARTESIAN_POINT('',(-1.1,-3.,-16.715)) ;
#143021 = CARTESIAN_POINT('',(0.500000000000001,-3.,-17.575)) ;
#143022 = CARTESIAN_POINT('',(0.600000000000001,-3.,-17.575)) ;
#143023 = CARTESIAN_POINT('',(0.700000000000002,-3.,-17.775)) ;
#143024 = CARTESIAN_POINT('Origin',(0.500000000000001,-3.,-17.775)) ;
#143025 = CARTESIAN_POINT('',(0.700000000000002,-3.,-20.325)) ;
#143026 = CARTESIAN_POINT('',(0.700000000000002,-3.,-36.89)) ;
#143027 = CARTESIAN_POINT('',(0.500000000000001,-3.,-20.525)) ;
#143028 = CARTESIAN_POINT('Origin',(0.500000000000001,-3.,-20.325)) ;
#143029 = CARTESIAN_POINT('',(-1.1,-3.,-20.525)) ;
#143030 = CARTESIAN_POINT('',(0.500000000000001,-3.,-21.385)) ;
#143031 = CARTESIAN_POINT('',(0.600000000000001,-3.,-21.385)) ;
#143032 = CARTESIAN_POINT('',(0.700000000000002,-3.,-21.585)) ;
#143033 = CARTESIAN_POINT('Origin',(0.500000000000001,-3.,-21.585)) ;
#143034 = CARTESIAN_POINT('',(0.700000000000002,-3.,-24.135)) ;
#143035 = CARTESIAN_POINT('',(0.700000000000002,-3.,-36.89)) ;
#143036 = CARTESIAN_POINT('',(0.500000000000001,-3.,-24.335)) ;
#143037 = CARTESIAN_POINT('Origin',(0.500000000000001,-3.,-24.135)) ;
#143038 = CARTESIAN_POINT('',(-1.1,-3.,-24.335)) ;
#143039 = CARTESIAN_POINT('',(0.500000000000001,-3.,-25.195)) ;
#143040 = CARTESIAN_POINT('',(0.600000000000001,-3.,-25.195)) ;
#143041 = CARTESIAN_POINT('',(0.700000000000002,-3.,-25.395)) ;
#143042 = CARTESIAN_POINT('Origin',(0.500000000000001,-3.,-25.395)) ;
#143043 = CARTESIAN_POINT('',(0.700000000000002,-3.,-27.945)) ;
#143044 = CARTESIAN_POINT('',(0.700000000000002,-3.,-36.89)) ;
#143045 = CARTESIAN_POINT('',(0.500000000000001,-3.,-28.145)) ;
#143046 = CARTESIAN_POINT('Origin',(0.500000000000001,-3.,-27.945)) ;
#143047 = CARTESIAN_POINT('',(-1.1,-3.,-28.145)) ;
#143048 = CARTESIAN_POINT('',(0.500000000000001,-3.,-29.005)) ;
#143049 = CARTESIAN_POINT('',(0.600000000000001,-3.,-29.005)) ;
#143050 = CARTESIAN_POINT('',(0.700000000000002,-3.,-29.205)) ;
#143051 = CARTESIAN_POINT('Origin',(0.500000000000001,-3.,-29.205)) ;
#143052 = CARTESIAN_POINT('',(0.700000000000002,-3.,-31.755)) ;
#143053 = CARTESIAN_POINT('',(0.700000000000002,-3.,-36.89)) ;
#143054 = CARTESIAN_POINT('',(0.500000000000001,-3.,-31.955)) ;
#143055 = CARTESIAN_POINT('Origin',(0.500000000000001,-3.,-31.755)) ;
#143056 = CARTESIAN_POINT('',(-1.1,-3.,-31.955)) ;
#143057 = CARTESIAN_POINT('',(0.500000000000001,-3.,-32.815)) ;
#143058 = CARTESIAN_POINT('',(0.600000000000001,-3.,-32.815)) ;
#143059 = CARTESIAN_POINT('',(0.700000000000002,-3.,-33.015)) ;
#143060 = CARTESIAN_POINT('Origin',(0.500000000000001,-3.,-33.015)) ;
#143061 = CARTESIAN_POINT('',(0.700000000000002,-3.,-36.89)) ;
#143062 = CARTESIAN_POINT('Origin',(-1.1,-2.9,-36.89)) ;
#143063 = CARTESIAN_POINT('',(-1.2,-2.9,-35.765)) ;
#143064 = CARTESIAN_POINT('Origin',(-1.1,-2.9,-35.765)) ;
#143065 = CARTESIAN_POINT('',(-1.2,-2.9,-36.79)) ;
#143066 = CARTESIAN_POINT('',(-1.2,-2.9,-36.89)) ;
#143067 = CARTESIAN_POINT('Origin',(-1.1,-2.9,-36.79)) ;
#143068 = CARTESIAN_POINT('Origin',(-1.2,4.15,-36.89)) ;
#143069 = CARTESIAN_POINT('',(-1.2,1.15,-32.815)) ;
#143070 = CARTESIAN_POINT('',(-1.2,1.35,-33.015)) ;
#143071 = CARTESIAN_POINT('Origin',(-1.2,1.15,-33.015)) ;
#143072 = CARTESIAN_POINT('',(-1.2,-2.9,-32.815)) ;
#143073 = CARTESIAN_POINT('',(-1.2,1.15,-31.955)) ;
#143074 = CARTESIAN_POINT('',(-1.2,1.25,-31.955)) ;
#143075 = CARTESIAN_POINT('',(-1.2,1.35,-31.755)) ;
#143076 = CARTESIAN_POINT('Origin',(-1.2,1.15,-31.755)) ;
#143077 = CARTESIAN_POINT('',(-1.2,1.35,-29.205)) ;
#143078 = CARTESIAN_POINT('',(-1.2,1.35,-29.105)) ;
#143079 = CARTESIAN_POINT('',(-1.2,1.15,-29.005)) ;
#143080 = CARTESIAN_POINT('Origin',(-1.2,1.15,-29.205)) ;
#143081 = CARTESIAN_POINT('',(-1.2,-2.9,-29.005)) ;
#143082 = CARTESIAN_POINT('',(-1.2,1.15,-28.145)) ;
#143083 = CARTESIAN_POINT('',(-1.2,1.25,-28.145)) ;
#143084 = CARTESIAN_POINT('',(-1.2,1.35,-27.945)) ;
#143085 = CARTESIAN_POINT('Origin',(-1.2,1.15,-27.945)) ;
#143086 = CARTESIAN_POINT('',(-1.2,1.35,-25.395)) ;
#143087 = CARTESIAN_POINT('',(-1.2,1.35,-25.295)) ;
#143088 = CARTESIAN_POINT('',(-1.2,1.15,-25.195)) ;
#143089 = CARTESIAN_POINT('Origin',(-1.2,1.15,-25.395)) ;
#143090 = CARTESIAN_POINT('',(-1.2,-2.9,-25.195)) ;
#143091 = CARTESIAN_POINT('',(-1.2,1.15,-24.335)) ;
#143092 = CARTESIAN_POINT('',(-1.2,1.25,-24.335)) ;
#143093 = CARTESIAN_POINT('',(-1.2,1.35,-24.135)) ;
#143094 = CARTESIAN_POINT('Origin',(-1.2,1.15,-24.135)) ;
#143095 = CARTESIAN_POINT('',(-1.2,1.35,-21.585)) ;
#143096 = CARTESIAN_POINT('',(-1.2,1.35,-21.485)) ;
#143097 = CARTESIAN_POINT('',(-1.2,1.15,-21.385)) ;
#143098 = CARTESIAN_POINT('Origin',(-1.2,1.15,-21.585)) ;
#143099 = CARTESIAN_POINT('',(-1.2,-2.9,-21.385)) ;
#143100 = CARTESIAN_POINT('',(-1.2,1.15,-20.525)) ;
#143101 = CARTESIAN_POINT('',(-1.2,1.25,-20.525)) ;
#143102 = CARTESIAN_POINT('',(-1.2,1.35,-20.325)) ;
#143103 = CARTESIAN_POINT('Origin',(-1.2,1.15,-20.325)) ;
#143104 = CARTESIAN_POINT('',(-1.2,1.35,-17.775)) ;
#143105 = CARTESIAN_POINT('',(-1.2,1.35,-17.675)) ;
#143106 = CARTESIAN_POINT('',(-1.2,1.15,-17.575)) ;
#143107 = CARTESIAN_POINT('Origin',(-1.2,1.15,-17.775)) ;
#143108 = CARTESIAN_POINT('',(-1.2,-2.9,-17.575)) ;
#143109 = CARTESIAN_POINT('',(-1.2,1.15,-16.715)) ;
#143110 = CARTESIAN_POINT('',(-1.2,1.25,-16.715)) ;
#143111 = CARTESIAN_POINT('',(-1.2,1.35,-16.515)) ;
#143112 = CARTESIAN_POINT('Origin',(-1.2,1.15,-16.515)) ;
#143113 = CARTESIAN_POINT('',(-1.2,1.35,-13.965)) ;
#143114 = CARTESIAN_POINT('',(-1.2,1.35,-13.865)) ;
#143115 = CARTESIAN_POINT('',(-1.2,1.15,-13.765)) ;
#143116 = CARTESIAN_POINT('Origin',(-1.2,1.15,-13.965)) ;
#143117 = CARTESIAN_POINT('',(-1.2,-2.9,-13.765)) ;
#143118 = CARTESIAN_POINT('',(-1.2,1.15,-12.905)) ;
#143119 = CARTESIAN_POINT('',(-1.2,1.25,-12.905)) ;
#143120 = CARTESIAN_POINT('',(-1.2,1.35,-12.705)) ;
#143121 = CARTESIAN_POINT('Origin',(-1.2,1.15,-12.705)) ;
#143122 = CARTESIAN_POINT('',(-1.2,1.35,-10.155)) ;
#143123 = CARTESIAN_POINT('',(-1.2,1.35,-10.055)) ;
#143124 = CARTESIAN_POINT('',(-1.2,1.15,-9.955)) ;
#143125 = CARTESIAN_POINT('Origin',(-1.2,1.15,-10.155)) ;
#143126 = CARTESIAN_POINT('',(-1.2,-2.9,-9.955)) ;
#143127 = CARTESIAN_POINT('',(-1.2,1.15,-9.095)) ;
#143128 = CARTESIAN_POINT('',(-1.2,1.25,-9.095)) ;
#143129 = CARTESIAN_POINT('',(-1.2,1.35,-8.895)) ;
#143130 = CARTESIAN_POINT('Origin',(-1.2,1.15,-8.895)) ;
#143131 = CARTESIAN_POINT('',(-1.2,1.35,-6.345)) ;
#143132 = CARTESIAN_POINT('',(-1.2,1.35,-6.245)) ;
#143133 = CARTESIAN_POINT('',(-1.2,1.15,-6.145)) ;
#143134 = CARTESIAN_POINT('Origin',(-1.2,1.15,-6.345)) ;
#143135 = CARTESIAN_POINT('',(-1.2,-2.9,-6.145)) ;
#143136 = CARTESIAN_POINT('',(-1.2,1.15,-5.285)) ;
#143137 = CARTESIAN_POINT('',(-1.2,1.25,-5.285)) ;
#143138 = CARTESIAN_POINT('',(-1.2,1.35,-5.085)) ;
#143139 = CARTESIAN_POINT('Origin',(-1.2,1.15,-5.085)) ;
#143140 = CARTESIAN_POINT('',(-1.2,1.35,-2.535)) ;
#143141 = CARTESIAN_POINT('',(-1.2,1.35,-2.435)) ;
#143142 = CARTESIAN_POINT('',(-1.2,1.15,-2.335)) ;
#143143 = CARTESIAN_POINT('Origin',(-1.2,1.15,-2.535)) ;
#143144 = CARTESIAN_POINT('',(-1.2,-2.9,-2.335)) ;
#143145 = CARTESIAN_POINT('',(-1.2,1.15,-1.475)) ;
#143146 = CARTESIAN_POINT('',(-1.2,1.25,-1.475)) ;
#143147 = CARTESIAN_POINT('',(-1.2,1.35,-1.275)) ;
#143148 = CARTESIAN_POINT('Origin',(-1.2,1.15,-1.275)) ;
#143149 = CARTESIAN_POINT('',(-1.2,1.35,1.275)) ;
#143150 = CARTESIAN_POINT('',(-1.2,1.35,1.37499999999999)) ;
#143151 = CARTESIAN_POINT('',(-1.2,1.15,1.475)) ;
#143152 = CARTESIAN_POINT('Origin',(-1.2,1.15,1.275)) ;
#143153 = CARTESIAN_POINT('',(-1.2,-2.9,1.475)) ;
#143154 = CARTESIAN_POINT('',(-1.2,4.15,2.5)) ;
#143155 = CARTESIAN_POINT('',(-1.2,4.15,2.5)) ;
#143156 = CARTESIAN_POINT('',(-1.2,4.15,-36.79)) ;
#143157 = CARTESIAN_POINT('',(-1.2,4.15,-36.89)) ;
#143158 = CARTESIAN_POINT('',(-1.2,-2.9,-36.79)) ;
#143159 = CARTESIAN_POINT('',(-1.2,1.15,-35.765)) ;
#143160 = CARTESIAN_POINT('',(-1.2,1.25,-35.765)) ;
#143161 = CARTESIAN_POINT('',(-1.2,1.35,-35.565)) ;
#143162 = CARTESIAN_POINT('Origin',(-1.2,1.15,-35.565)) ;
#143163 = CARTESIAN_POINT('',(-1.2,1.35,-32.915)) ;
#143164 = CARTESIAN_POINT('Origin',(-1.1,4.15,-36.89)) ;
#143165 = CARTESIAN_POINT('',(-1.1,4.25,-36.79)) ;
#143166 = CARTESIAN_POINT('',(-1.1,4.25,2.5)) ;
#143167 = CARTESIAN_POINT('',(-1.1,4.25,-36.89)) ;
#143168 = CARTESIAN_POINT('Origin',(-1.1,4.15,-36.79)) ;
#143169 = CARTESIAN_POINT('Origin',(-1.1,4.15,2.5)) ;
#143170 = CARTESIAN_POINT('Origin',(-1.1,4.25,-36.89)) ;
#143171 = CARTESIAN_POINT('',(4.35,4.25,-36.79)) ;
#143172 = CARTESIAN_POINT('',(4.35,4.25,2.5)) ;
#143173 = CARTESIAN_POINT('',(4.35,4.25,-36.89)) ;
#143174 = CARTESIAN_POINT('',(-1.1,4.25,-36.79)) ;
#143175 = CARTESIAN_POINT('',(-1.1,4.25,2.5)) ;
#143176 = CARTESIAN_POINT('Origin',(4.35,4.35,-36.89)) ;
#143177 = CARTESIAN_POINT('',(4.45,4.35,-36.79)) ;
#143178 = CARTESIAN_POINT('',(4.45,4.35,2.5)) ;
#143179 = CARTESIAN_POINT('',(4.45,4.35,-36.89)) ;
#143180 = CARTESIAN_POINT('Origin',(4.35,4.35,-36.79)) ;
#143181 = CARTESIAN_POINT('Origin',(4.35,4.35,2.5)) ;
#143182 = CARTESIAN_POINT('Origin',(4.45,4.55,-36.89)) ;
#143183 = CARTESIAN_POINT('',(4.45,4.55,-36.79)) ;
#143184 = CARTESIAN_POINT('',(4.45,4.55,2.5)) ;
#143185 = CARTESIAN_POINT('',(4.45,4.55,-36.89)) ;
#143186 = CARTESIAN_POINT('',(4.45,4.35,-36.79)) ;
#143187 = CARTESIAN_POINT('',(4.45,4.55,2.5)) ;
#143188 = CARTESIAN_POINT('Origin',(4.55,4.55,-36.89)) ;
#143189 = CARTESIAN_POINT('',(4.55,4.65,-36.79)) ;
#143190 = CARTESIAN_POINT('',(4.55,4.65,2.5)) ;
#143191 = CARTESIAN_POINT('',(4.55,4.65,-36.89)) ;
#143192 = CARTESIAN_POINT('Origin',(4.55,4.55,-36.79)) ;
#143193 = CARTESIAN_POINT('Origin',(4.55,4.55,2.5)) ;
#143194 = CARTESIAN_POINT('Origin',(4.75,4.65,-36.89)) ;
#143195 = CARTESIAN_POINT('',(4.75,4.65,-36.79)) ;
#143196 = CARTESIAN_POINT('',(4.75,4.65,2.5)) ;
#143197 = CARTESIAN_POINT('',(4.75,4.65,-36.89)) ;
#143198 = CARTESIAN_POINT('',(4.55,4.65,-36.79)) ;
#143199 = CARTESIAN_POINT('',(4.75,4.65,2.5)) ;
#143200 = CARTESIAN_POINT('Origin',(4.75,4.55,-36.89)) ;
#143201 = CARTESIAN_POINT('',(4.85,4.55,-36.79)) ;
#143202 = CARTESIAN_POINT('',(4.85,4.55,2.5)) ;
#143203 = CARTESIAN_POINT('',(4.85,4.55,-36.89)) ;
#143204 = CARTESIAN_POINT('Origin',(4.75,4.55,-36.79)) ;
#143205 = CARTESIAN_POINT('Origin',(4.75,4.55,2.5)) ;
#143206 = CARTESIAN_POINT('Origin',(4.85,4.35,-36.89)) ;
#143207 = CARTESIAN_POINT('',(4.85,4.35,-36.79)) ;
#143208 = CARTESIAN_POINT('',(4.85,4.35,2.5)) ;
#143209 = CARTESIAN_POINT('',(4.85,4.35,-36.89)) ;
#143210 = CARTESIAN_POINT('',(4.85,4.55,-36.79)) ;
#143211 = CARTESIAN_POINT('',(4.85,4.35,2.5)) ;
#143212 = CARTESIAN_POINT('Origin',(4.95,4.35,-36.89)) ;
#143213 = CARTESIAN_POINT('',(4.95,4.25,-36.79)) ;
#143214 = CARTESIAN_POINT('',(4.95,4.25,2.5)) ;
#143215 = CARTESIAN_POINT('',(4.95,4.25,-36.89)) ;
#143216 = CARTESIAN_POINT('Origin',(4.95,4.35,-36.79)) ;
#143217 = CARTESIAN_POINT('Origin',(4.95,4.35,2.5)) ;
#143218 = CARTESIAN_POINT('Origin',(4.95,4.25,-36.89)) ;
#143219 = CARTESIAN_POINT('',(7.9,4.25,-36.79)) ;
#143220 = CARTESIAN_POINT('',(7.9,4.25,2.5)) ;
#143221 = CARTESIAN_POINT('',(7.9,4.25,-36.89)) ;
#143222 = CARTESIAN_POINT('',(4.95,4.25,-36.79)) ;
#143223 = CARTESIAN_POINT('',(4.95,4.25,2.5)) ;
#143224 = CARTESIAN_POINT('Origin',(7.9,4.15,-36.89)) ;
#143225 = CARTESIAN_POINT('',(8.,4.15,-36.79)) ;
#143226 = CARTESIAN_POINT('',(8.,4.15,2.5)) ;
#143227 = CARTESIAN_POINT('',(8.,4.15,-36.89)) ;
#143228 = CARTESIAN_POINT('Origin',(7.9,4.15,-36.79)) ;
#143229 = CARTESIAN_POINT('Origin',(7.9,4.15,2.5)) ;
#143230 = CARTESIAN_POINT('Origin',(8.,4.15,-36.89)) ;
#143231 = CARTESIAN_POINT('',(8.,4.15,-36.79)) ;
#143232 = CARTESIAN_POINT('',(8.,4.15,2.5)) ;
#143233 = CARTESIAN_POINT('',(8.,1.9,-32.54)) ;
#143234 = CARTESIAN_POINT('',(8.,2.1,-32.74)) ;
#143235 = CARTESIAN_POINT('Origin',(8.,1.9,-32.74)) ;
#143236 = CARTESIAN_POINT('',(8.,2.1,-33.69)) ;
#143237 = CARTESIAN_POINT('',(8.,2.1,-33.69)) ;
#143238 = CARTESIAN_POINT('',(8.,2.4,-33.69)) ;
#143239 = CARTESIAN_POINT('',(8.,2.4,-33.69)) ;
#143240 = CARTESIAN_POINT('',(8.,2.4,-33.5814213562373)) ;
#143241 = CARTESIAN_POINT('',(8.,2.4,-33.5814213562373)) ;
#143242 = CARTESIAN_POINT('',(8.,2.45857864376269,-33.44)) ;
#143243 = CARTESIAN_POINT('Origin',(8.,2.6,-33.5814213562373)) ;
#143244 = CARTESIAN_POINT('',(8.,3.00857864376269,-32.89)) ;
#143245 = CARTESIAN_POINT('',(8.,3.00857864376269,-32.89)) ;
#143246 = CARTESIAN_POINT('',(8.,3.35,-33.0314213562373)) ;
#143247 = CARTESIAN_POINT('Origin',(8.,3.15,-33.0314213562373)) ;
#143248 = CARTESIAN_POINT('',(8.,3.35,-35.5485786437627)) ;
#143249 = CARTESIAN_POINT('',(8.,2.45857864376269,-35.14)) ;
#143250 = CARTESIAN_POINT('',(8.,2.45857864376269,-35.14)) ;
#143251 = CARTESIAN_POINT('',(8.,2.4,-34.9985786437627)) ;
#143252 = CARTESIAN_POINT('Origin',(8.,2.6,-34.9985786437627)) ;
#143253 = CARTESIAN_POINT('',(8.,2.4,-34.89)) ;
#143254 = CARTESIAN_POINT('',(8.,2.4,-34.89)) ;
#143255 = CARTESIAN_POINT('',(8.,2.1,-34.89)) ;
#143256 = CARTESIAN_POINT('',(8.,2.1,-34.89)) ;
#143257 = CARTESIAN_POINT('',(8.,2.1,-35.84)) ;
#143258 = CARTESIAN_POINT('',(8.,2.1,-35.84)) ;
#143259 = CARTESIAN_POINT('',(8.,1.9,-36.04)) ;
#143260 = CARTESIAN_POINT('Origin',(8.,1.9,-35.84)) ;
#143261 = CARTESIAN_POINT('',(8.,-2.15,-36.04)) ;
#143262 = CARTESIAN_POINT('',(8.,-2.15,-36.04)) ;
#143263 = CARTESIAN_POINT('',(8.,-2.35,-35.84)) ;
#143264 = CARTESIAN_POINT('Origin',(8.,-2.15,-35.84)) ;
#143265 = CARTESIAN_POINT('',(8.,-2.35,-35.1931195934094)) ;
#143266 = CARTESIAN_POINT('',(8.,-2.35,-35.1931195934094)) ;
#143267 = CARTESIAN_POINT('',(8.,-2.32153024911032,-35.0902732340176)) ;
#143268 = CARTESIAN_POINT('Origin',(8.,-2.15,-35.1931195934094)) ;
#143269 = CARTESIAN_POINT('',(8.,-2.32153024911033,-33.4897267659824)) ;
#143270 = CARTESIAN_POINT('Origin',(8.,-3.65625,-34.29)) ;
#143271 = CARTESIAN_POINT('',(8.,-2.35,-33.3868804065906)) ;
#143272 = CARTESIAN_POINT('Origin',(8.,-2.15,-33.3868804065906)) ;
#143273 = CARTESIAN_POINT('',(8.,-2.35,-32.74)) ;
#143274 = CARTESIAN_POINT('',(8.,-2.35,-32.74)) ;
#143275 = CARTESIAN_POINT('',(8.,-2.15,-32.54)) ;
#143276 = CARTESIAN_POINT('Origin',(8.,-2.15,-32.74)) ;
#143277 = CARTESIAN_POINT('',(8.,1.9,-32.54)) ;
#143278 = CARTESIAN_POINT('',(8.,1.9,-28.73)) ;
#143279 = CARTESIAN_POINT('',(8.,2.1,-28.93)) ;
#143280 = CARTESIAN_POINT('Origin',(8.,1.9,-28.93)) ;
#143281 = CARTESIAN_POINT('',(8.,2.1,-29.88)) ;
#143282 = CARTESIAN_POINT('',(8.,2.1,-29.88)) ;
#143283 = CARTESIAN_POINT('',(8.,2.4,-29.88)) ;
#143284 = CARTESIAN_POINT('',(8.,2.4,-29.88)) ;
#143285 = CARTESIAN_POINT('',(8.,2.4,-29.7714213562373)) ;
#143286 = CARTESIAN_POINT('',(8.,2.4,-29.7714213562373)) ;
#143287 = CARTESIAN_POINT('',(8.,2.45857864376269,-29.63)) ;
#143288 = CARTESIAN_POINT('Origin',(8.,2.6,-29.7714213562373)) ;
#143289 = CARTESIAN_POINT('',(8.,3.00857864376269,-29.08)) ;
#143290 = CARTESIAN_POINT('',(8.,3.00857864376269,-29.08)) ;
#143291 = CARTESIAN_POINT('',(8.,3.35,-29.2214213562373)) ;
#143292 = CARTESIAN_POINT('Origin',(8.,3.15,-29.2214213562373)) ;
#143293 = CARTESIAN_POINT('',(8.,3.35,-31.7385786437627)) ;
#143294 = CARTESIAN_POINT('',(8.,2.45857864376269,-31.33)) ;
#143295 = CARTESIAN_POINT('',(8.,2.45857864376269,-31.33)) ;
#143296 = CARTESIAN_POINT('',(8.,2.4,-31.1885786437627)) ;
#143297 = CARTESIAN_POINT('Origin',(8.,2.6,-31.1885786437627)) ;
#143298 = CARTESIAN_POINT('',(8.,2.4,-31.08)) ;
#143299 = CARTESIAN_POINT('',(8.,2.4,-31.08)) ;
#143300 = CARTESIAN_POINT('',(8.,2.1,-31.08)) ;
#143301 = CARTESIAN_POINT('',(8.,2.1,-31.08)) ;
#143302 = CARTESIAN_POINT('',(8.,2.1,-32.03)) ;
#143303 = CARTESIAN_POINT('',(8.,2.1,-32.03)) ;
#143304 = CARTESIAN_POINT('',(8.,1.9,-32.23)) ;
#143305 = CARTESIAN_POINT('Origin',(8.,1.9,-32.03)) ;
#143306 = CARTESIAN_POINT('',(8.,-2.15,-32.23)) ;
#143307 = CARTESIAN_POINT('',(8.,-2.15,-32.23)) ;
#143308 = CARTESIAN_POINT('',(8.,-2.35,-32.03)) ;
#143309 = CARTESIAN_POINT('Origin',(8.,-2.15,-32.03)) ;
#143310 = CARTESIAN_POINT('',(8.,-2.35,-31.3831195934094)) ;
#143311 = CARTESIAN_POINT('',(8.,-2.35,-31.3831195934094)) ;
#143312 = CARTESIAN_POINT('',(8.,-2.32153024911032,-31.2802732340176)) ;
#143313 = CARTESIAN_POINT('Origin',(8.,-2.15,-31.3831195934094)) ;
#143314 = CARTESIAN_POINT('',(8.,-2.32153024911032,-29.6797267659824)) ;
#143315 = CARTESIAN_POINT('Origin',(8.,-3.65625,-30.48)) ;
#143316 = CARTESIAN_POINT('',(8.,-2.35,-29.5768804065906)) ;
#143317 = CARTESIAN_POINT('Origin',(8.,-2.15,-29.5768804065906)) ;
#143318 = CARTESIAN_POINT('',(8.,-2.35,-28.93)) ;
#143319 = CARTESIAN_POINT('',(8.,-2.35,-28.93)) ;
#143320 = CARTESIAN_POINT('',(8.,-2.15,-28.73)) ;
#143321 = CARTESIAN_POINT('Origin',(8.,-2.15,-28.93)) ;
#143322 = CARTESIAN_POINT('',(8.,1.9,-28.73)) ;
#143323 = CARTESIAN_POINT('',(8.,1.9,-24.92)) ;
#143324 = CARTESIAN_POINT('',(8.,2.1,-25.12)) ;
#143325 = CARTESIAN_POINT('Origin',(8.,1.9,-25.12)) ;
#143326 = CARTESIAN_POINT('',(8.,2.1,-26.07)) ;
#143327 = CARTESIAN_POINT('',(8.,2.1,-26.07)) ;
#143328 = CARTESIAN_POINT('',(8.,2.4,-26.07)) ;
#143329 = CARTESIAN_POINT('',(8.,2.4,-26.07)) ;
#143330 = CARTESIAN_POINT('',(8.,2.4,-25.9614213562373)) ;
#143331 = CARTESIAN_POINT('',(8.,2.4,-25.9614213562373)) ;
#143332 = CARTESIAN_POINT('',(8.,2.45857864376269,-25.82)) ;
#143333 = CARTESIAN_POINT('Origin',(8.,2.6,-25.9614213562373)) ;
#143334 = CARTESIAN_POINT('',(8.,3.00857864376269,-25.27)) ;
#143335 = CARTESIAN_POINT('',(8.,3.00857864376269,-25.27)) ;
#143336 = CARTESIAN_POINT('',(8.,3.35,-25.4114213562373)) ;
#143337 = CARTESIAN_POINT('Origin',(8.,3.15,-25.4114213562373)) ;
#143338 = CARTESIAN_POINT('',(8.,3.35,-27.9285786437627)) ;
#143339 = CARTESIAN_POINT('',(8.,2.45857864376269,-27.52)) ;
#143340 = CARTESIAN_POINT('',(8.,2.45857864376269,-27.52)) ;
#143341 = CARTESIAN_POINT('',(8.,2.4,-27.3785786437627)) ;
#143342 = CARTESIAN_POINT('Origin',(8.,2.6,-27.3785786437627)) ;
#143343 = CARTESIAN_POINT('',(8.,2.4,-27.27)) ;
#143344 = CARTESIAN_POINT('',(8.,2.4,-27.27)) ;
#143345 = CARTESIAN_POINT('',(8.,2.1,-27.27)) ;
#143346 = CARTESIAN_POINT('',(8.,2.1,-27.27)) ;
#143347 = CARTESIAN_POINT('',(8.,2.1,-28.22)) ;
#143348 = CARTESIAN_POINT('',(8.,2.1,-28.22)) ;
#143349 = CARTESIAN_POINT('',(8.,1.9,-28.42)) ;
#143350 = CARTESIAN_POINT('Origin',(8.,1.9,-28.22)) ;
#143351 = CARTESIAN_POINT('',(8.,-2.15,-28.42)) ;
#143352 = CARTESIAN_POINT('',(8.,-2.15,-28.42)) ;
#143353 = CARTESIAN_POINT('',(8.,-2.35,-28.22)) ;
#143354 = CARTESIAN_POINT('Origin',(8.,-2.15,-28.22)) ;
#143355 = CARTESIAN_POINT('',(8.,-2.35,-27.5731195934094)) ;
#143356 = CARTESIAN_POINT('',(8.,-2.35,-27.5731195934094)) ;
#143357 = CARTESIAN_POINT('',(8.,-2.32153024911032,-27.4702732340176)) ;
#143358 = CARTESIAN_POINT('Origin',(8.,-2.15,-27.5731195934094)) ;
#143359 = CARTESIAN_POINT('',(8.,-2.32153024911032,-25.8697267659824)) ;
#143360 = CARTESIAN_POINT('Origin',(8.,-3.65625,-26.67)) ;
#143361 = CARTESIAN_POINT('',(8.,-2.35,-25.7668804065906)) ;
#143362 = CARTESIAN_POINT('Origin',(8.,-2.15,-25.7668804065906)) ;
#143363 = CARTESIAN_POINT('',(8.,-2.35,-25.12)) ;
#143364 = CARTESIAN_POINT('',(8.,-2.35,-25.12)) ;
#143365 = CARTESIAN_POINT('',(8.,-2.15,-24.92)) ;
#143366 = CARTESIAN_POINT('Origin',(8.,-2.15,-25.12)) ;
#143367 = CARTESIAN_POINT('',(8.,1.9,-24.92)) ;
#143368 = CARTESIAN_POINT('',(8.,1.9,-21.11)) ;
#143369 = CARTESIAN_POINT('',(8.,2.1,-21.31)) ;
#143370 = CARTESIAN_POINT('Origin',(8.,1.9,-21.31)) ;
#143371 = CARTESIAN_POINT('',(8.,2.1,-22.26)) ;
#143372 = CARTESIAN_POINT('',(8.,2.1,-22.26)) ;
#143373 = CARTESIAN_POINT('',(8.,2.4,-22.26)) ;
#143374 = CARTESIAN_POINT('',(8.,2.4,-22.26)) ;
#143375 = CARTESIAN_POINT('',(8.,2.4,-22.1514213562373)) ;
#143376 = CARTESIAN_POINT('',(8.,2.4,-22.1514213562373)) ;
#143377 = CARTESIAN_POINT('',(8.,2.45857864376269,-22.01)) ;
#143378 = CARTESIAN_POINT('Origin',(8.,2.6,-22.1514213562373)) ;
#143379 = CARTESIAN_POINT('',(8.,3.00857864376269,-21.46)) ;
#143380 = CARTESIAN_POINT('',(8.,3.00857864376269,-21.46)) ;
#143381 = CARTESIAN_POINT('',(8.,3.35,-21.6014213562373)) ;
#143382 = CARTESIAN_POINT('Origin',(8.,3.15,-21.6014213562373)) ;
#143383 = CARTESIAN_POINT('',(8.,3.35,-24.1185786437627)) ;
#143384 = CARTESIAN_POINT('',(8.,2.45857864376269,-23.71)) ;
#143385 = CARTESIAN_POINT('',(8.,2.45857864376269,-23.71)) ;
#143386 = CARTESIAN_POINT('',(8.,2.4,-23.5685786437627)) ;
#143387 = CARTESIAN_POINT('Origin',(8.,2.6,-23.5685786437627)) ;
#143388 = CARTESIAN_POINT('',(8.,2.4,-23.46)) ;
#143389 = CARTESIAN_POINT('',(8.,2.4,-23.46)) ;
#143390 = CARTESIAN_POINT('',(8.,2.1,-23.46)) ;
#143391 = CARTESIAN_POINT('',(8.,2.1,-23.46)) ;
#143392 = CARTESIAN_POINT('',(8.,2.1,-24.41)) ;
#143393 = CARTESIAN_POINT('',(8.,2.1,-24.41)) ;
#143394 = CARTESIAN_POINT('',(8.,1.9,-24.61)) ;
#143395 = CARTESIAN_POINT('Origin',(8.,1.9,-24.41)) ;
#143396 = CARTESIAN_POINT('',(8.,-2.15,-24.61)) ;
#143397 = CARTESIAN_POINT('',(8.,-2.15,-24.61)) ;
#143398 = CARTESIAN_POINT('',(8.,-2.35,-24.41)) ;
#143399 = CARTESIAN_POINT('Origin',(8.,-2.15,-24.41)) ;
#143400 = CARTESIAN_POINT('',(8.,-2.35,-23.7631195934094)) ;
#143401 = CARTESIAN_POINT('',(8.,-2.35,-23.7631195934094)) ;
#143402 = CARTESIAN_POINT('',(8.,-2.32153024911032,-23.6602732340176)) ;
#143403 = CARTESIAN_POINT('Origin',(8.,-2.15,-23.7631195934094)) ;
#143404 = CARTESIAN_POINT('',(8.,-2.32153024911032,-22.0597267659824)) ;
#143405 = CARTESIAN_POINT('Origin',(8.,-3.65625,-22.86)) ;
#143406 = CARTESIAN_POINT('',(8.,-2.35,-21.9568804065906)) ;
#143407 = CARTESIAN_POINT('Origin',(8.,-2.15,-21.9568804065906)) ;
#143408 = CARTESIAN_POINT('',(8.,-2.35,-21.31)) ;
#143409 = CARTESIAN_POINT('',(8.,-2.35,-21.31)) ;
#143410 = CARTESIAN_POINT('',(8.,-2.15,-21.11)) ;
#143411 = CARTESIAN_POINT('Origin',(8.,-2.15,-21.31)) ;
#143412 = CARTESIAN_POINT('',(8.,1.9,-21.11)) ;
#143413 = CARTESIAN_POINT('',(8.,1.9,-17.3)) ;
#143414 = CARTESIAN_POINT('',(8.,2.1,-17.5)) ;
#143415 = CARTESIAN_POINT('Origin',(8.,1.9,-17.5)) ;
#143416 = CARTESIAN_POINT('',(8.,2.1,-18.45)) ;
#143417 = CARTESIAN_POINT('',(8.,2.1,-18.45)) ;
#143418 = CARTESIAN_POINT('',(8.,2.4,-18.45)) ;
#143419 = CARTESIAN_POINT('',(8.,2.4,-18.45)) ;
#143420 = CARTESIAN_POINT('',(8.,2.4,-18.3414213562373)) ;
#143421 = CARTESIAN_POINT('',(8.,2.4,-18.3414213562373)) ;
#143422 = CARTESIAN_POINT('',(8.,2.45857864376269,-18.2)) ;
#143423 = CARTESIAN_POINT('Origin',(8.,2.6,-18.3414213562373)) ;
#143424 = CARTESIAN_POINT('',(8.,3.00857864376269,-17.65)) ;
#143425 = CARTESIAN_POINT('',(8.,3.00857864376269,-17.65)) ;
#143426 = CARTESIAN_POINT('',(8.,3.35,-17.7914213562373)) ;
#143427 = CARTESIAN_POINT('Origin',(8.,3.15,-17.7914213562373)) ;
#143428 = CARTESIAN_POINT('',(8.,3.35,-20.3085786437627)) ;
#143429 = CARTESIAN_POINT('',(8.,2.45857864376269,-19.9)) ;
#143430 = CARTESIAN_POINT('',(8.,2.45857864376269,-19.9)) ;
#143431 = CARTESIAN_POINT('',(8.,2.4,-19.7585786437627)) ;
#143432 = CARTESIAN_POINT('Origin',(8.,2.6,-19.7585786437627)) ;
#143433 = CARTESIAN_POINT('',(8.,2.4,-19.65)) ;
#143434 = CARTESIAN_POINT('',(8.,2.4,-19.65)) ;
#143435 = CARTESIAN_POINT('',(8.,2.1,-19.65)) ;
#143436 = CARTESIAN_POINT('',(8.,2.1,-19.65)) ;
#143437 = CARTESIAN_POINT('',(8.,2.1,-20.6)) ;
#143438 = CARTESIAN_POINT('',(8.,2.1,-20.6)) ;
#143439 = CARTESIAN_POINT('',(8.,1.9,-20.8)) ;
#143440 = CARTESIAN_POINT('Origin',(8.,1.9,-20.6)) ;
#143441 = CARTESIAN_POINT('',(8.,-2.15,-20.8)) ;
#143442 = CARTESIAN_POINT('',(8.,-2.15,-20.8)) ;
#143443 = CARTESIAN_POINT('',(8.,-2.35,-20.6)) ;
#143444 = CARTESIAN_POINT('Origin',(8.,-2.15,-20.6)) ;
#143445 = CARTESIAN_POINT('',(8.,-2.35,-19.9531195934094)) ;
#143446 = CARTESIAN_POINT('',(8.,-2.35,-19.9531195934094)) ;
#143447 = CARTESIAN_POINT('',(8.,-2.32153024911032,-19.8502732340176)) ;
#143448 = CARTESIAN_POINT('Origin',(8.,-2.15,-19.9531195934094)) ;
#143449 = CARTESIAN_POINT('',(8.,-2.32153024911032,-18.2497267659824)) ;
#143450 = CARTESIAN_POINT('Origin',(8.,-3.65625,-19.05)) ;
#143451 = CARTESIAN_POINT('',(8.,-2.35,-18.1468804065906)) ;
#143452 = CARTESIAN_POINT('Origin',(8.,-2.15,-18.1468804065906)) ;
#143453 = CARTESIAN_POINT('',(8.,-2.35,-17.5)) ;
#143454 = CARTESIAN_POINT('',(8.,-2.35,-17.5)) ;
#143455 = CARTESIAN_POINT('',(8.,-2.15,-17.3)) ;
#143456 = CARTESIAN_POINT('Origin',(8.,-2.15,-17.5)) ;
#143457 = CARTESIAN_POINT('',(8.,1.9,-17.3)) ;
#143458 = CARTESIAN_POINT('',(8.,1.9,-13.49)) ;
#143459 = CARTESIAN_POINT('',(8.,2.1,-13.69)) ;
#143460 = CARTESIAN_POINT('Origin',(8.,1.9,-13.69)) ;
#143461 = CARTESIAN_POINT('',(8.,2.1,-14.64)) ;
#143462 = CARTESIAN_POINT('',(8.,2.1,-14.64)) ;
#143463 = CARTESIAN_POINT('',(8.,2.4,-14.64)) ;
#143464 = CARTESIAN_POINT('',(8.,2.4,-14.64)) ;
#143465 = CARTESIAN_POINT('',(8.,2.4,-14.5314213562373)) ;
#143466 = CARTESIAN_POINT('',(8.,2.4,-14.5314213562373)) ;
#143467 = CARTESIAN_POINT('',(8.,2.45857864376269,-14.39)) ;
#143468 = CARTESIAN_POINT('Origin',(8.,2.6,-14.5314213562373)) ;
#143469 = CARTESIAN_POINT('',(8.,3.00857864376269,-13.84)) ;
#143470 = CARTESIAN_POINT('',(8.,3.00857864376269,-13.84)) ;
#143471 = CARTESIAN_POINT('',(8.,3.35,-13.9814213562373)) ;
#143472 = CARTESIAN_POINT('Origin',(8.,3.15,-13.9814213562373)) ;
#143473 = CARTESIAN_POINT('',(8.,3.35,-16.4985786437627)) ;
#143474 = CARTESIAN_POINT('',(8.,2.45857864376269,-16.09)) ;
#143475 = CARTESIAN_POINT('',(8.,2.45857864376269,-16.09)) ;
#143476 = CARTESIAN_POINT('',(8.,2.4,-15.9485786437627)) ;
#143477 = CARTESIAN_POINT('Origin',(8.,2.6,-15.9485786437627)) ;
#143478 = CARTESIAN_POINT('',(8.,2.4,-15.84)) ;
#143479 = CARTESIAN_POINT('',(8.,2.4,-15.84)) ;
#143480 = CARTESIAN_POINT('',(8.,2.1,-15.84)) ;
#143481 = CARTESIAN_POINT('',(8.,2.1,-15.84)) ;
#143482 = CARTESIAN_POINT('',(8.,2.1,-16.79)) ;
#143483 = CARTESIAN_POINT('',(8.,2.1,-16.79)) ;
#143484 = CARTESIAN_POINT('',(8.,1.9,-16.99)) ;
#143485 = CARTESIAN_POINT('Origin',(8.,1.9,-16.79)) ;
#143486 = CARTESIAN_POINT('',(8.,-2.15,-16.99)) ;
#143487 = CARTESIAN_POINT('',(8.,-2.15,-16.99)) ;
#143488 = CARTESIAN_POINT('',(8.,-2.35,-16.79)) ;
#143489 = CARTESIAN_POINT('Origin',(8.,-2.15,-16.79)) ;
#143490 = CARTESIAN_POINT('',(8.,-2.35,-16.1431195934094)) ;
#143491 = CARTESIAN_POINT('',(8.,-2.35,-16.1431195934094)) ;
#143492 = CARTESIAN_POINT('',(8.,-2.32153024911032,-16.0402732340176)) ;
#143493 = CARTESIAN_POINT('Origin',(8.,-2.15,-16.1431195934094)) ;
#143494 = CARTESIAN_POINT('',(8.,-2.32153024911032,-14.4397267659824)) ;
#143495 = CARTESIAN_POINT('Origin',(8.,-3.65625,-15.24)) ;
#143496 = CARTESIAN_POINT('',(8.,-2.35,-14.3368804065906)) ;
#143497 = CARTESIAN_POINT('Origin',(8.,-2.15,-14.3368804065906)) ;
#143498 = CARTESIAN_POINT('',(8.,-2.35,-13.69)) ;
#143499 = CARTESIAN_POINT('',(8.,-2.35,-13.69)) ;
#143500 = CARTESIAN_POINT('',(8.,-2.15,-13.49)) ;
#143501 = CARTESIAN_POINT('Origin',(8.,-2.15,-13.69)) ;
#143502 = CARTESIAN_POINT('',(8.,1.9,-13.49)) ;
#143503 = CARTESIAN_POINT('',(8.,1.9,-9.68)) ;
#143504 = CARTESIAN_POINT('',(8.,2.1,-9.88)) ;
#143505 = CARTESIAN_POINT('Origin',(8.,1.9,-9.88)) ;
#143506 = CARTESIAN_POINT('',(8.,2.1,-10.83)) ;
#143507 = CARTESIAN_POINT('',(8.,2.1,-10.83)) ;
#143508 = CARTESIAN_POINT('',(8.,2.4,-10.83)) ;
#143509 = CARTESIAN_POINT('',(8.,2.4,-10.83)) ;
#143510 = CARTESIAN_POINT('',(8.,2.4,-10.7214213562373)) ;
#143511 = CARTESIAN_POINT('',(8.,2.4,-10.7214213562373)) ;
#143512 = CARTESIAN_POINT('',(8.,2.45857864376269,-10.58)) ;
#143513 = CARTESIAN_POINT('Origin',(8.,2.6,-10.7214213562373)) ;
#143514 = CARTESIAN_POINT('',(8.,3.00857864376269,-10.03)) ;
#143515 = CARTESIAN_POINT('',(8.,3.00857864376269,-10.03)) ;
#143516 = CARTESIAN_POINT('',(8.,3.35,-10.1714213562373)) ;
#143517 = CARTESIAN_POINT('Origin',(8.,3.15,-10.1714213562373)) ;
#143518 = CARTESIAN_POINT('',(8.,3.35,-12.6885786437627)) ;
#143519 = CARTESIAN_POINT('',(8.,2.45857864376269,-12.28)) ;
#143520 = CARTESIAN_POINT('',(8.,2.45857864376269,-12.28)) ;
#143521 = CARTESIAN_POINT('',(8.,2.4,-12.1385786437627)) ;
#143522 = CARTESIAN_POINT('Origin',(8.,2.6,-12.1385786437627)) ;
#143523 = CARTESIAN_POINT('',(8.,2.4,-12.03)) ;
#143524 = CARTESIAN_POINT('',(8.,2.4,-12.03)) ;
#143525 = CARTESIAN_POINT('',(8.,2.1,-12.03)) ;
#143526 = CARTESIAN_POINT('',(8.,2.1,-12.03)) ;
#143527 = CARTESIAN_POINT('',(8.,2.1,-12.98)) ;
#143528 = CARTESIAN_POINT('',(8.,2.1,-12.98)) ;
#143529 = CARTESIAN_POINT('',(8.,1.9,-13.18)) ;
#143530 = CARTESIAN_POINT('Origin',(8.,1.9,-12.98)) ;
#143531 = CARTESIAN_POINT('',(8.,-2.15,-13.18)) ;
#143532 = CARTESIAN_POINT('',(8.,-2.15,-13.18)) ;
#143533 = CARTESIAN_POINT('',(8.,-2.35,-12.98)) ;
#143534 = CARTESIAN_POINT('Origin',(8.,-2.15,-12.98)) ;
#143535 = CARTESIAN_POINT('',(8.,-2.35,-12.3331195934094)) ;
#143536 = CARTESIAN_POINT('',(8.,-2.35,-12.3331195934094)) ;
#143537 = CARTESIAN_POINT('',(8.,-2.32153024911032,-12.2302732340176)) ;
#143538 = CARTESIAN_POINT('Origin',(8.,-2.15,-12.3331195934094)) ;
#143539 = CARTESIAN_POINT('',(8.,-2.32153024911032,-10.6297267659824)) ;
#143540 = CARTESIAN_POINT('Origin',(8.,-3.65625,-11.43)) ;
#143541 = CARTESIAN_POINT('',(8.,-2.35,-10.5268804065906)) ;
#143542 = CARTESIAN_POINT('Origin',(8.,-2.15,-10.5268804065906)) ;
#143543 = CARTESIAN_POINT('',(8.,-2.35,-9.88)) ;
#143544 = CARTESIAN_POINT('',(8.,-2.35,-9.88)) ;
#143545 = CARTESIAN_POINT('',(8.,-2.15,-9.68)) ;
#143546 = CARTESIAN_POINT('Origin',(8.,-2.15,-9.88)) ;
#143547 = CARTESIAN_POINT('',(8.,1.9,-9.68)) ;
#143548 = CARTESIAN_POINT('',(8.,1.9,-5.87)) ;
#143549 = CARTESIAN_POINT('',(8.,2.1,-6.07)) ;
#143550 = CARTESIAN_POINT('Origin',(8.,1.9,-6.07)) ;
#143551 = CARTESIAN_POINT('',(8.,2.1,-7.02)) ;
#143552 = CARTESIAN_POINT('',(8.,2.1,-7.02)) ;
#143553 = CARTESIAN_POINT('',(8.,2.4,-7.02)) ;
#143554 = CARTESIAN_POINT('',(8.,2.4,-7.02)) ;
#143555 = CARTESIAN_POINT('',(8.,2.4,-6.91142135623731)) ;
#143556 = CARTESIAN_POINT('',(8.,2.4,-6.91142135623731)) ;
#143557 = CARTESIAN_POINT('',(8.,2.45857864376269,-6.77)) ;
#143558 = CARTESIAN_POINT('Origin',(8.,2.6,-6.91142135623731)) ;
#143559 = CARTESIAN_POINT('',(8.,3.00857864376269,-6.22)) ;
#143560 = CARTESIAN_POINT('',(8.,3.00857864376269,-6.22)) ;
#143561 = CARTESIAN_POINT('',(8.,3.35,-6.36142135623731)) ;
#143562 = CARTESIAN_POINT('Origin',(8.,3.15,-6.36142135623731)) ;
#143563 = CARTESIAN_POINT('',(8.,3.35,-8.87857864376269)) ;
#143564 = CARTESIAN_POINT('',(8.,2.45857864376269,-8.47)) ;
#143565 = CARTESIAN_POINT('',(8.,2.45857864376269,-8.47)) ;
#143566 = CARTESIAN_POINT('',(8.,2.4,-8.32857864376269)) ;
#143567 = CARTESIAN_POINT('Origin',(8.,2.6,-8.32857864376269)) ;
#143568 = CARTESIAN_POINT('',(8.,2.4,-8.22)) ;
#143569 = CARTESIAN_POINT('',(8.,2.4,-8.22)) ;
#143570 = CARTESIAN_POINT('',(8.,2.1,-8.22)) ;
#143571 = CARTESIAN_POINT('',(8.,2.1,-8.22)) ;
#143572 = CARTESIAN_POINT('',(8.,2.1,-9.17)) ;
#143573 = CARTESIAN_POINT('',(8.,2.1,-9.17)) ;
#143574 = CARTESIAN_POINT('',(8.,1.9,-9.37)) ;
#143575 = CARTESIAN_POINT('Origin',(8.,1.9,-9.17)) ;
#143576 = CARTESIAN_POINT('',(8.,-2.15,-9.37)) ;
#143577 = CARTESIAN_POINT('',(8.,-2.15,-9.37)) ;
#143578 = CARTESIAN_POINT('',(8.,-2.35,-9.17)) ;
#143579 = CARTESIAN_POINT('Origin',(8.,-2.15,-9.17)) ;
#143580 = CARTESIAN_POINT('',(8.,-2.35,-8.52311959340942)) ;
#143581 = CARTESIAN_POINT('',(8.,-2.35,-8.52311959340942)) ;
#143582 = CARTESIAN_POINT('',(8.,-2.32153024911032,-8.4202732340176)) ;
#143583 = CARTESIAN_POINT('Origin',(8.,-2.15,-8.52311959340942)) ;
#143584 = CARTESIAN_POINT('',(8.,-2.32153024911032,-6.8197267659824)) ;
#143585 = CARTESIAN_POINT('Origin',(8.,-3.65625,-7.62)) ;
#143586 = CARTESIAN_POINT('',(8.,-2.35,-6.71688040659058)) ;
#143587 = CARTESIAN_POINT('Origin',(8.,-2.15,-6.71688040659058)) ;
#143588 = CARTESIAN_POINT('',(8.,-2.35,-6.07)) ;
#143589 = CARTESIAN_POINT('',(8.,-2.35,-6.07)) ;
#143590 = CARTESIAN_POINT('',(8.,-2.15,-5.87)) ;
#143591 = CARTESIAN_POINT('Origin',(8.,-2.15,-6.07)) ;
#143592 = CARTESIAN_POINT('',(8.,1.9,-5.87)) ;
#143593 = CARTESIAN_POINT('',(8.,1.9,-2.06)) ;
#143594 = CARTESIAN_POINT('',(8.,2.1,-2.26)) ;
#143595 = CARTESIAN_POINT('Origin',(8.,1.9,-2.26)) ;
#143596 = CARTESIAN_POINT('',(8.,2.1,-3.21)) ;
#143597 = CARTESIAN_POINT('',(8.,2.1,-3.21)) ;
#143598 = CARTESIAN_POINT('',(8.,2.4,-3.21)) ;
#143599 = CARTESIAN_POINT('',(8.,2.4,-3.21)) ;
#143600 = CARTESIAN_POINT('',(8.,2.4,-3.10142135623731)) ;
#143601 = CARTESIAN_POINT('',(8.,2.4,-3.10142135623731)) ;
#143602 = CARTESIAN_POINT('',(8.,2.45857864376269,-2.96)) ;
#143603 = CARTESIAN_POINT('Origin',(8.,2.6,-3.10142135623731)) ;
#143604 = CARTESIAN_POINT('',(8.,3.00857864376269,-2.41)) ;
#143605 = CARTESIAN_POINT('',(8.,3.00857864376269,-2.41)) ;
#143606 = CARTESIAN_POINT('',(8.,3.35,-2.55142135623731)) ;
#143607 = CARTESIAN_POINT('Origin',(8.,3.15,-2.55142135623731)) ;
#143608 = CARTESIAN_POINT('',(8.,3.35,-5.06857864376269)) ;
#143609 = CARTESIAN_POINT('',(8.,2.45857864376269,-4.66)) ;
#143610 = CARTESIAN_POINT('',(8.,2.45857864376269,-4.66)) ;
#143611 = CARTESIAN_POINT('',(8.,2.4,-4.51857864376269)) ;
#143612 = CARTESIAN_POINT('Origin',(8.,2.6,-4.51857864376269)) ;
#143613 = CARTESIAN_POINT('',(8.,2.4,-4.41)) ;
#143614 = CARTESIAN_POINT('',(8.,2.4,-4.41)) ;
#143615 = CARTESIAN_POINT('',(8.,2.1,-4.41)) ;
#143616 = CARTESIAN_POINT('',(8.,2.1,-4.41)) ;
#143617 = CARTESIAN_POINT('',(8.,2.1,-5.36)) ;
#143618 = CARTESIAN_POINT('',(8.,2.1,-5.36)) ;
#143619 = CARTESIAN_POINT('',(8.,1.9,-5.56)) ;
#143620 = CARTESIAN_POINT('Origin',(8.,1.9,-5.36)) ;
#143621 = CARTESIAN_POINT('',(8.,-2.15,-5.56)) ;
#143622 = CARTESIAN_POINT('',(8.,-2.15,-5.56)) ;
#143623 = CARTESIAN_POINT('',(8.,-2.35,-5.36)) ;
#143624 = CARTESIAN_POINT('Origin',(8.,-2.15,-5.36)) ;
#143625 = CARTESIAN_POINT('',(8.,-2.35,-4.71311959340942)) ;
#143626 = CARTESIAN_POINT('',(8.,-2.35,-4.71311959340942)) ;
#143627 = CARTESIAN_POINT('',(8.,-2.32153024911032,-4.6102732340176)) ;
#143628 = CARTESIAN_POINT('Origin',(8.,-2.15,-4.71311959340942)) ;
#143629 = CARTESIAN_POINT('',(8.,-2.32153024911032,-3.0097267659824)) ;
#143630 = CARTESIAN_POINT('Origin',(8.,-3.65625,-3.81)) ;
#143631 = CARTESIAN_POINT('',(8.,-2.35,-2.90688040659058)) ;
#143632 = CARTESIAN_POINT('Origin',(8.,-2.15,-2.90688040659058)) ;
#143633 = CARTESIAN_POINT('',(8.,-2.35,-2.26)) ;
#143634 = CARTESIAN_POINT('',(8.,-2.35,-2.26)) ;
#143635 = CARTESIAN_POINT('',(8.,-2.15,-2.06)) ;
#143636 = CARTESIAN_POINT('Origin',(8.,-2.15,-2.26)) ;
#143637 = CARTESIAN_POINT('',(8.,1.9,-2.06)) ;
#143638 = CARTESIAN_POINT('',(8.,1.9,1.75)) ;
#143639 = CARTESIAN_POINT('',(8.,2.1,1.55)) ;
#143640 = CARTESIAN_POINT('Origin',(8.,1.9,1.55)) ;
#143641 = CARTESIAN_POINT('',(8.,2.1,0.6)) ;
#143642 = CARTESIAN_POINT('',(8.,2.1,0.600000000000003)) ;
#143643 = CARTESIAN_POINT('',(8.,2.4,0.6)) ;
#143644 = CARTESIAN_POINT('',(8.,2.4,0.6)) ;
#143645 = CARTESIAN_POINT('',(8.,2.4,0.70857864376269)) ;
#143646 = CARTESIAN_POINT('',(8.,2.4,0.70857864376269)) ;
#143647 = CARTESIAN_POINT('',(8.,2.45857864376269,0.849999999999999)) ;
#143648 = CARTESIAN_POINT('Origin',(8.,2.6,0.70857864376269)) ;
#143649 = CARTESIAN_POINT('',(8.,3.00857864376269,1.4)) ;
#143650 = CARTESIAN_POINT('',(8.,3.00857864376269,1.4)) ;
#143651 = CARTESIAN_POINT('',(8.,3.35,1.25857864376269)) ;
#143652 = CARTESIAN_POINT('Origin',(8.,3.15,1.25857864376269)) ;
#143653 = CARTESIAN_POINT('',(8.,3.35,-1.25857864376269)) ;
#143654 = CARTESIAN_POINT('',(8.,2.45857864376269,-0.850000000000001)) ;
#143655 = CARTESIAN_POINT('',(8.,2.45857864376269,-0.85)) ;
#143656 = CARTESIAN_POINT('',(8.,2.4,-0.70857864376269)) ;
#143657 = CARTESIAN_POINT('Origin',(8.,2.6,-0.70857864376269)) ;
#143658 = CARTESIAN_POINT('',(8.,2.4,-0.6)) ;
#143659 = CARTESIAN_POINT('',(8.,2.4,-0.6)) ;
#143660 = CARTESIAN_POINT('',(8.,2.1,-0.6)) ;
#143661 = CARTESIAN_POINT('',(8.,2.1,-0.6)) ;
#143662 = CARTESIAN_POINT('',(8.,2.1,-1.55)) ;
#143663 = CARTESIAN_POINT('',(8.,2.1,-1.55)) ;
#143664 = CARTESIAN_POINT('',(8.,1.9,-1.75)) ;
#143665 = CARTESIAN_POINT('Origin',(8.,1.9,-1.55)) ;
#143666 = CARTESIAN_POINT('',(8.,-2.15,-1.75)) ;
#143667 = CARTESIAN_POINT('',(8.,-2.15,-1.75)) ;
#143668 = CARTESIAN_POINT('',(8.,-2.35,-1.55)) ;
#143669 = CARTESIAN_POINT('Origin',(8.,-2.15,-1.55)) ;
#143670 = CARTESIAN_POINT('',(8.,-2.35,-0.903119593409422)) ;
#143671 = CARTESIAN_POINT('',(8.,-2.35,-0.903119593409422)) ;
#143672 = CARTESIAN_POINT('',(8.,-2.32153024911032,-0.800273234017602)) ;
#143673 = CARTESIAN_POINT('Origin',(8.,-2.15,-0.903119593409422)) ;
#143674 = CARTESIAN_POINT('',(8.,-2.32153024911032,0.800273234017602)) ;
#143675 = CARTESIAN_POINT('Origin',(8.,-3.65625,0.)) ;
#143676 = CARTESIAN_POINT('',(8.,-2.35,0.903119593409422)) ;
#143677 = CARTESIAN_POINT('Origin',(8.,-2.15,0.903119593409422)) ;
#143678 = CARTESIAN_POINT('',(8.,-2.35,1.55)) ;
#143679 = CARTESIAN_POINT('',(8.,-2.35,1.55)) ;
#143680 = CARTESIAN_POINT('',(8.,-2.15,1.75)) ;
#143681 = CARTESIAN_POINT('Origin',(8.,-2.15,1.55)) ;
#143682 = CARTESIAN_POINT('',(8.,1.9,1.75)) ;
#143683 = CARTESIAN_POINT('Origin',(7.9,-2.9,-36.89)) ;
#143684 = CARTESIAN_POINT('',(7.9,4.15,-36.89)) ;
#143685 = CARTESIAN_POINT('',(7.9,-2.9,-36.89)) ;
#143686 = CARTESIAN_POINT('',(7.9,-2.9,-36.89)) ;
#143687 = CARTESIAN_POINT('',(-1.1,-2.9,-36.89)) ;
#143688 = CARTESIAN_POINT('',(-1.1,-2.9,-36.89)) ;
#143689 = CARTESIAN_POINT('',(-1.1,4.15,-36.89)) ;
#143690 = CARTESIAN_POINT('',(-1.1,4.15,-36.89)) ;
#143691 = CARTESIAN_POINT('',(4.35,4.15,-36.89)) ;
#143692 = CARTESIAN_POINT('',(4.35,4.15,-36.89)) ;
#143693 = CARTESIAN_POINT('',(4.55,4.35,-36.89)) ;
#143694 = CARTESIAN_POINT('Origin',(4.35,4.35,-36.89)) ;
#143695 = CARTESIAN_POINT('',(4.55,4.55,-36.89)) ;
#143696 = CARTESIAN_POINT('',(4.55,4.55,-36.89)) ;
#143697 = CARTESIAN_POINT('',(4.75,4.55,-36.89)) ;
#143698 = CARTESIAN_POINT('',(4.75,4.55,-36.89)) ;
#143699 = CARTESIAN_POINT('',(4.75,4.35,-36.89)) ;
#143700 = CARTESIAN_POINT('',(4.75,4.35,-36.89)) ;
#143701 = CARTESIAN_POINT('',(4.95,4.15,-36.89)) ;
#143702 = CARTESIAN_POINT('Origin',(4.95,4.35,-36.89)) ;
#143703 = CARTESIAN_POINT('',(7.9,4.15,-36.89)) ;
#143704 = CARTESIAN_POINT('Origin',(7.9,-2.9,2.6)) ;
#143705 = CARTESIAN_POINT('',(-1.1,4.15,2.6)) ;
#143706 = CARTESIAN_POINT('',(-1.1,-2.9,2.6)) ;
#143707 = CARTESIAN_POINT('',(-1.1,-2.9,2.6)) ;
#143708 = CARTESIAN_POINT('',(7.9,-2.9,2.6)) ;
#143709 = CARTESIAN_POINT('',(7.9,-2.9,2.6)) ;
#143710 = CARTESIAN_POINT('',(7.9,4.15,2.6)) ;
#143711 = CARTESIAN_POINT('',(7.9,-2.9,2.6)) ;
#143712 = CARTESIAN_POINT('',(4.95,4.15,2.6)) ;
#143713 = CARTESIAN_POINT('',(7.9,4.15,2.6)) ;
#143714 = CARTESIAN_POINT('',(4.75,4.35,2.6)) ;
#143715 = CARTESIAN_POINT('Origin',(4.95,4.35,2.6)) ;
#143716 = CARTESIAN_POINT('',(4.75,4.55,2.6)) ;
#143717 = CARTESIAN_POINT('',(4.74999999999997,-2.89999999999999,2.6)) ;
#143718 = CARTESIAN_POINT('',(4.55,4.55,2.6)) ;
#143719 = CARTESIAN_POINT('',(7.9,4.55,2.6)) ;
#143720 = CARTESIAN_POINT('',(4.55,4.35,2.6)) ;
#143721 = CARTESIAN_POINT('',(4.55,-2.9,2.6)) ;
#143722 = CARTESIAN_POINT('',(4.35,4.15,2.6)) ;
#143723 = CARTESIAN_POINT('Origin',(4.35,4.35,2.6)) ;
#143724 = CARTESIAN_POINT('',(7.9,4.15,2.6)) ;
#143725 = CARTESIAN_POINT('Origin',(-0.999999999999999,-1.59070596587277E-16,
0.)) ;
#143726 = CARTESIAN_POINT('',(-0.999999999999999,-1.9,0.6)) ;
#143727 = CARTESIAN_POINT('',(-0.999999999999999,-1.9,1.275)) ;
#143728 = CARTESIAN_POINT('',(-0.999999999999999,-1.9,1.375)) ;
#143729 = CARTESIAN_POINT('',(-0.999999999999999,1.15,1.275)) ;
#143730 = CARTESIAN_POINT('',(-0.999999999999999,-2.89663358890161E-17,1.275)) ;
#143731 = CARTESIAN_POINT('',(-0.999999999999999,1.15,-1.275)) ;
#143732 = CARTESIAN_POINT('',(-0.999999999999999,1.15,0.)) ;
#143733 = CARTESIAN_POINT('',(-0.999999999999999,-1.9,-1.275)) ;
#143734 = CARTESIAN_POINT('',(-0.999999999999999,-2.24122726936407E-16,-1.275)) ;
#143735 = CARTESIAN_POINT('',(-0.999999999999999,-1.9,-0.6)) ;
#143736 = CARTESIAN_POINT('',(-0.999999999999999,-1.9,-0.5)) ;
#143737 = CARTESIAN_POINT('',(-0.999999999999999,0.4,-0.6)) ;
#143738 = CARTESIAN_POINT('',(-0.999999999999999,0.5,-0.6)) ;
#143739 = CARTESIAN_POINT('',(-0.999999999999999,0.6,-0.4)) ;
#143740 = CARTESIAN_POINT('Origin',(-0.999999999999999,0.4,-0.4)) ;
#143741 = CARTESIAN_POINT('',(-0.999999999999999,0.6,0.4)) ;
#143742 = CARTESIAN_POINT('',(-0.999999999999999,0.6,0.5)) ;
#143743 = CARTESIAN_POINT('',(-0.999999999999999,0.4,0.6)) ;
#143744 = CARTESIAN_POINT('Origin',(-0.999999999999999,0.4,0.4)) ;
#143745 = CARTESIAN_POINT('',(-0.999999999999999,-2.,0.6)) ;
#143746 = CARTESIAN_POINT('Origin',(0.600000000000001,-2.,-0.5)) ;
#143747 = CARTESIAN_POINT('',(0.500000000000001,-2.,-0.6)) ;
#143748 = CARTESIAN_POINT('',(-0.899999999999999,-2.,-0.6)) ;
#143749 = CARTESIAN_POINT('',(0.600000000000001,-2.,-0.6)) ;
#143750 = CARTESIAN_POINT('',(-0.899999999999999,-2.,-1.275)) ;
#143751 = CARTESIAN_POINT('',(-0.899999999999999,-2.,-1.375)) ;
#143752 = CARTESIAN_POINT('',(0.500000000000001,-2.,-1.275)) ;
#143753 = CARTESIAN_POINT('',(0.600000000000001,-2.,-1.275)) ;
#143754 = CARTESIAN_POINT('',(0.500000000000001,-2.,-0.5)) ;
#143755 = CARTESIAN_POINT('Origin',(0.600000000000001,0.5,-0.5)) ;
#143756 = CARTESIAN_POINT('',(-0.899999999999999,0.4,-0.5)) ;
#143757 = CARTESIAN_POINT('',(-0.999999999999999,0.4,-0.5)) ;
#143758 = CARTESIAN_POINT('',(-0.899999999999999,-1.9,-0.5)) ;
#143759 = CARTESIAN_POINT('',(-0.899999999999999,-2.,-0.5)) ;
#143760 = CARTESIAN_POINT('',(0.600000000000001,-1.9,-0.5)) ;
#143761 = CARTESIAN_POINT('Origin',(0.600000000000001,0.5,0.5)) ;
#143762 = CARTESIAN_POINT('',(0.500000000000001,0.5,0.4)) ;
#143763 = CARTESIAN_POINT('',(-0.899999999999999,0.5,0.4)) ;
#143764 = CARTESIAN_POINT('',(-0.999999999999999,0.5,0.4)) ;
#143765 = CARTESIAN_POINT('',(-0.899999999999999,0.5,-0.4)) ;
#143766 = CARTESIAN_POINT('',(-0.899999999999999,0.5,-0.5)) ;
#143767 = CARTESIAN_POINT('',(0.500000000000001,0.5,-0.4)) ;
#143768 = CARTESIAN_POINT('',(0.600000000000001,0.5,-0.4)) ;
#143769 = CARTESIAN_POINT('',(0.500000000000001,0.5,0.5)) ;
#143770 = CARTESIAN_POINT('Origin',(0.600000000000001,-2.,0.5)) ;
#143771 = CARTESIAN_POINT('',(0.500000000000001,-1.9,0.5)) ;
#143772 = CARTESIAN_POINT('',(-0.899999999999999,-1.9,0.5)) ;
#143773 = CARTESIAN_POINT('',(0.600000000000001,-1.9,0.5)) ;
#143774 = CARTESIAN_POINT('',(-0.899999999999999,0.4,0.5)) ;
#143775 = CARTESIAN_POINT('',(-0.899999999999999,0.5,0.5)) ;
#143776 = CARTESIAN_POINT('',(0.500000000000001,0.4,0.5)) ;
#143777 = CARTESIAN_POINT('',(0.600000000000001,0.4,0.5)) ;
#143778 = CARTESIAN_POINT('',(0.500000000000001,-2.,0.5)) ;
#143779 = CARTESIAN_POINT('Origin',(0.600000000000001,-2.,1.375)) ;
#143780 = CARTESIAN_POINT('',(0.500000000000001,-2.,1.275)) ;
#143781 = CARTESIAN_POINT('',(-0.899999999999999,-2.,1.275)) ;
#143782 = CARTESIAN_POINT('',(-0.999999999999999,-2.,1.275)) ;
#143783 = CARTESIAN_POINT('',(-0.899999999999999,-2.,0.6)) ;
#143784 = CARTESIAN_POINT('',(-0.899999999999999,-2.,0.5)) ;
#143785 = CARTESIAN_POINT('',(0.500000000000001,-2.,0.6)) ;
#143786 = CARTESIAN_POINT('',(0.600000000000001,-2.,0.6)) ;
#143787 = CARTESIAN_POINT('',(0.500000000000001,-2.,1.375)) ;
#143788 = CARTESIAN_POINT('Origin',(1.4,2.1,0.6)) ;
#143789 = CARTESIAN_POINT('',(1.5,2.,0.6)) ;
#143790 = CARTESIAN_POINT('',(7.9,2.,0.6)) ;
#143791 = CARTESIAN_POINT('',(1.4,2.,0.6)) ;
#143792 = CARTESIAN_POINT('',(1.5,2.1,0.5)) ;
#143793 = CARTESIAN_POINT('Origin',(1.5,2.1,0.6)) ;
#143794 = CARTESIAN_POINT('',(7.9,2.1,0.5)) ;
#143795 = CARTESIAN_POINT('',(1.4,2.1,0.5)) ;
#143796 = CARTESIAN_POINT('Origin',(7.9,2.1,0.6)) ;
#143797 = CARTESIAN_POINT('Origin',(1.4,2.4,0.5)) ;
#143798 = CARTESIAN_POINT('',(1.5,2.4,0.5)) ;
#143799 = CARTESIAN_POINT('',(1.5,2.4,0.5)) ;
#143800 = CARTESIAN_POINT('',(7.9,2.4,0.5)) ;
#143801 = CARTESIAN_POINT('',(1.4,2.4,0.5)) ;
#143802 = CARTESIAN_POINT('',(7.9,2.1,0.5)) ;
#143803 = CARTESIAN_POINT('Origin',(1.4,2.4,0.6)) ;
#143804 = CARTESIAN_POINT('',(1.5,2.5,0.6)) ;
#143805 = CARTESIAN_POINT('Origin',(1.5,2.4,0.6)) ;
#143806 = CARTESIAN_POINT('',(7.9,2.5,0.6)) ;
#143807 = CARTESIAN_POINT('',(1.4,2.5,0.6)) ;
#143808 = CARTESIAN_POINT('Origin',(7.9,2.4,0.6)) ;
#143809 = CARTESIAN_POINT('Origin',(1.4,2.5,0.70857864376269)) ;
#143810 = CARTESIAN_POINT('',(1.5,2.5,0.70857864376269)) ;
#143811 = CARTESIAN_POINT('',(1.5,2.5,0.70857864376269)) ;
#143812 = CARTESIAN_POINT('',(7.9,2.5,0.70857864376269)) ;
#143813 = CARTESIAN_POINT('',(1.4,2.5,0.70857864376269)) ;
#143814 = CARTESIAN_POINT('',(7.9,2.5,0.6)) ;
#143815 = CARTESIAN_POINT('Origin',(1.4,2.6,0.70857864376269)) ;
#143816 = CARTESIAN_POINT('',(1.5,2.52928932188135,0.779289321881344)) ;
#143817 = CARTESIAN_POINT('Origin',(1.5,2.6,0.70857864376269)) ;
#143818 = CARTESIAN_POINT('',(7.9,2.52928932188135,0.779289321881344)) ;
#143819 = CARTESIAN_POINT('',(1.4,2.52928932188135,0.779289321881344)) ;
#143820 = CARTESIAN_POINT('Origin',(7.9,2.6,0.70857864376269)) ;
#143821 = CARTESIAN_POINT('Origin',(1.4,3.07928932188135,1.32928932188135)) ;
#143822 = CARTESIAN_POINT('',(1.5,3.07928932188135,1.32928932188134)) ;
#143823 = CARTESIAN_POINT('',(7.9,3.07928932188135,1.32928932188135)) ;
#143824 = CARTESIAN_POINT('',(1.4,3.07928932188135,1.32928932188135)) ;
#143825 = CARTESIAN_POINT('',(7.9,2.52928932188135,0.779289321881344)) ;
#143826 = CARTESIAN_POINT('Origin',(1.4,3.15,1.25857864376269)) ;
#143827 = CARTESIAN_POINT('',(7.9,3.25,1.25857864376269)) ;
#143828 = CARTESIAN_POINT('',(1.4,3.25,1.25857864376269)) ;
#143829 = CARTESIAN_POINT('Origin',(7.9,3.15,1.25857864376269)) ;
#143830 = CARTESIAN_POINT('Origin',(1.4,3.25,-1.25857864376269)) ;
#143831 = CARTESIAN_POINT('',(1.5,3.25,-1.25857864376269)) ;
#143832 = CARTESIAN_POINT('',(7.9,3.25,1.25857864376269)) ;
#143833 = CARTESIAN_POINT('Origin',(1.4,2.52928932188134,-0.779289321881346)) ;
#143834 = CARTESIAN_POINT('',(1.5,2.52928932188134,-0.779289321881346)) ;
#143835 = CARTESIAN_POINT('',(1.5,2.52928932188134,-0.779289321881346)) ;
#143836 = CARTESIAN_POINT('',(7.9,2.52928932188134,-0.779289321881346)) ;
#143837 = CARTESIAN_POINT('',(1.4,2.52928932188134,-0.779289321881346)) ;
#143838 = CARTESIAN_POINT('',(7.9,3.07928932188135,-1.32928932188135)) ;
#143839 = CARTESIAN_POINT('Origin',(1.4,2.6,-0.70857864376269)) ;
#143840 = CARTESIAN_POINT('',(1.5,2.5,-0.70857864376269)) ;
#143841 = CARTESIAN_POINT('Origin',(1.5,2.6,-0.70857864376269)) ;
#143842 = CARTESIAN_POINT('',(7.9,2.5,-0.70857864376269)) ;
#143843 = CARTESIAN_POINT('',(1.4,2.5,-0.70857864376269)) ;
#143844 = CARTESIAN_POINT('Origin',(7.9,2.6,-0.70857864376269)) ;
#143845 = CARTESIAN_POINT('Origin',(1.4,2.5,-0.6)) ;
#143846 = CARTESIAN_POINT('',(1.5,2.5,-0.6)) ;
#143847 = CARTESIAN_POINT('',(1.5,2.5,-0.6)) ;
#143848 = CARTESIAN_POINT('',(7.9,2.5,-0.6)) ;
#143849 = CARTESIAN_POINT('',(1.4,2.5,-0.6)) ;
#143850 = CARTESIAN_POINT('',(7.9,2.5,-0.70857864376269)) ;
#143851 = CARTESIAN_POINT('Origin',(1.4,2.4,-0.6)) ;
#143852 = CARTESIAN_POINT('',(1.5,2.4,-0.5)) ;
#143853 = CARTESIAN_POINT('Origin',(1.5,2.4,-0.6)) ;
#143854 = CARTESIAN_POINT('',(7.9,2.4,-0.5)) ;
#143855 = CARTESIAN_POINT('',(1.4,2.4,-0.5)) ;
#143856 = CARTESIAN_POINT('Origin',(7.9,2.4,-0.6)) ;
#143857 = CARTESIAN_POINT('Origin',(1.4,2.1,-0.5)) ;
#143858 = CARTESIAN_POINT('',(1.5,2.1,-0.5)) ;
#143859 = CARTESIAN_POINT('',(1.5,2.1,-0.5)) ;
#143860 = CARTESIAN_POINT('',(7.9,2.1,-0.5)) ;
#143861 = CARTESIAN_POINT('',(1.4,2.1,-0.5)) ;
#143862 = CARTESIAN_POINT('',(7.9,2.4,-0.5)) ;
#143863 = CARTESIAN_POINT('Origin',(1.4,2.1,-0.6)) ;
#143864 = CARTESIAN_POINT('',(1.5,2.,-0.6)) ;
#143865 = CARTESIAN_POINT('Origin',(1.5,2.1,-0.6)) ;
#143866 = CARTESIAN_POINT('',(7.9,2.,-0.6)) ;
#143867 = CARTESIAN_POINT('',(1.4,2.,-0.6)) ;
#143868 = CARTESIAN_POINT('Origin',(7.9,2.1,-0.6)) ;
#143869 = CARTESIAN_POINT('Origin',(1.4,2.,-0.6)) ;
#143870 = CARTESIAN_POINT('',(1.5,2.,-1.55)) ;
#143871 = CARTESIAN_POINT('',(1.5,2.,-1.55)) ;
#143872 = CARTESIAN_POINT('',(7.9,2.,-1.55)) ;
#143873 = CARTESIAN_POINT('',(1.4,2.,-1.55)) ;
#143874 = CARTESIAN_POINT('',(7.9,2.,-0.6)) ;
#143875 = CARTESIAN_POINT('Origin',(1.4,1.9,-1.55)) ;
#143876 = CARTESIAN_POINT('',(1.5,1.9,-1.65)) ;
#143877 = CARTESIAN_POINT('Origin',(1.5,1.9,-1.55)) ;
#143878 = CARTESIAN_POINT('',(7.9,1.9,-1.65)) ;
#143879 = CARTESIAN_POINT('',(1.4,1.9,-1.65)) ;
#143880 = CARTESIAN_POINT('Origin',(7.9,1.9,-1.55)) ;
#143881 = CARTESIAN_POINT('Origin',(1.4,1.9,-1.65)) ;
#143882 = CARTESIAN_POINT('',(1.5,-2.15,-1.65)) ;
#143883 = CARTESIAN_POINT('',(1.5,-2.15,-1.65)) ;
#143884 = CARTESIAN_POINT('',(7.9,-2.15,-1.65)) ;
#143885 = CARTESIAN_POINT('',(1.4,-2.15,-1.65)) ;
#143886 = CARTESIAN_POINT('',(7.9,1.9,-1.65)) ;
#143887 = CARTESIAN_POINT('Origin',(1.4,-2.15,-1.55)) ;
#143888 = CARTESIAN_POINT('',(1.5,-2.25,-1.55)) ;
#143889 = CARTESIAN_POINT('Origin',(1.5,-2.15,-1.55)) ;
#143890 = CARTESIAN_POINT('',(7.9,-2.25,-1.55)) ;
#143891 = CARTESIAN_POINT('',(1.4,-2.25,-1.55)) ;
#143892 = CARTESIAN_POINT('Origin',(7.9,-2.15,-1.55)) ;
#143893 = CARTESIAN_POINT('Origin',(1.4,-2.25,-0.903119593409422)) ;
#143894 = CARTESIAN_POINT('',(1.5,-2.25,-0.903119593409422)) ;
#143895 = CARTESIAN_POINT('',(1.5,-2.25,-0.903119593409423)) ;
#143896 = CARTESIAN_POINT('',(7.9,-2.25,-0.903119593409422)) ;
#143897 = CARTESIAN_POINT('',(1.4,-2.25,-0.903119593409422)) ;
#143898 = CARTESIAN_POINT('',(7.9,-2.25,-1.55)) ;
#143899 = CARTESIAN_POINT('Origin',(1.4,-2.15,-0.903119593409422)) ;
#143900 = CARTESIAN_POINT('',(1.5,-2.23576512455516,-0.851696413713512)) ;
#143901 = CARTESIAN_POINT('Origin',(1.5,-2.15,-0.903119593409422)) ;
#143902 = CARTESIAN_POINT('',(7.9,-2.23576512455516,-0.851696413713512)) ;
#143903 = CARTESIAN_POINT('',(1.4,-2.23576512455516,-0.851696413713512)) ;
#143904 = CARTESIAN_POINT('Origin',(7.9,-2.15,-0.903119593409422)) ;
#143905 = CARTESIAN_POINT('Origin',(1.4,-3.65625,0.)) ;
#143906 = CARTESIAN_POINT('',(1.5,-2.23576512455516,0.851696413713512)) ;
#143907 = CARTESIAN_POINT('Origin',(1.5,-3.65625,0.)) ;
#143908 = CARTESIAN_POINT('',(7.9,-2.23576512455516,0.851696413713512)) ;
#143909 = CARTESIAN_POINT('',(1.4,-2.23576512455516,0.851696413713512)) ;
#143910 = CARTESIAN_POINT('Origin',(7.9,-3.65625,0.)) ;
#143911 = CARTESIAN_POINT('Origin',(1.4,-2.15,0.903119593409422)) ;
#143912 = CARTESIAN_POINT('',(1.5,-2.25,0.903119593409422)) ;
#143913 = CARTESIAN_POINT('Origin',(1.5,-2.15,0.903119593409422)) ;
#143914 = CARTESIAN_POINT('',(7.9,-2.25,0.903119593409422)) ;
#143915 = CARTESIAN_POINT('',(1.4,-2.25,0.903119593409422)) ;
#143916 = CARTESIAN_POINT('Origin',(7.9,-2.15,0.903119593409422)) ;
#143917 = CARTESIAN_POINT('Origin',(1.4,-2.25,1.55)) ;
#143918 = CARTESIAN_POINT('',(1.5,-2.25,1.55)) ;
#143919 = CARTESIAN_POINT('',(1.5,-2.25,1.55)) ;
#143920 = CARTESIAN_POINT('',(7.9,-2.25,1.55)) ;
#143921 = CARTESIAN_POINT('',(1.4,-2.25,1.55)) ;
#143922 = CARTESIAN_POINT('',(7.9,-2.25,0.903119593409422)) ;
#143923 = CARTESIAN_POINT('Origin',(1.4,-2.15,1.55)) ;
#143924 = CARTESIAN_POINT('',(1.5,-2.15,1.65)) ;
#143925 = CARTESIAN_POINT('Origin',(1.5,-2.15,1.55)) ;
#143926 = CARTESIAN_POINT('',(7.9,-2.15,1.65)) ;
#143927 = CARTESIAN_POINT('',(1.4,-2.15,1.65)) ;
#143928 = CARTESIAN_POINT('Origin',(7.9,-2.15,1.55)) ;
#143929 = CARTESIAN_POINT('Origin',(1.4,1.9,1.65)) ;
#143930 = CARTESIAN_POINT('',(1.5,1.9,1.65)) ;
#143931 = CARTESIAN_POINT('',(1.5,1.9,1.65)) ;
#143932 = CARTESIAN_POINT('',(7.9,1.9,1.65)) ;
#143933 = CARTESIAN_POINT('',(1.4,1.9,1.65)) ;
#143934 = CARTESIAN_POINT('',(7.9,-2.15,1.65)) ;
#143935 = CARTESIAN_POINT('Origin',(1.4,1.9,1.55)) ;
#143936 = CARTESIAN_POINT('',(1.5,2.,1.55)) ;
#143937 = CARTESIAN_POINT('Origin',(1.5,1.9,1.55)) ;
#143938 = CARTESIAN_POINT('',(7.9,2.,1.55)) ;
#143939 = CARTESIAN_POINT('',(1.4,2.,1.55)) ;
#143940 = CARTESIAN_POINT('Origin',(7.9,1.9,1.55)) ;
#143941 = CARTESIAN_POINT('Origin',(1.4,2.,1.55)) ;
#143942 = CARTESIAN_POINT('',(1.5,2.,0.6)) ;
#143943 = CARTESIAN_POINT('',(7.9,2.,1.55)) ;
#143944 = CARTESIAN_POINT('Origin',(1.4,2.1,0.6)) ;
#143945 = CARTESIAN_POINT('',(1.4,2.6,0.6)) ;
#143946 = CARTESIAN_POINT('',(1.4,2.4,0.4)) ;
#143947 = CARTESIAN_POINT('Origin',(1.4,2.4,0.6)) ;
#143948 = CARTESIAN_POINT('',(1.4,2.1,0.4)) ;
#143949 = CARTESIAN_POINT('',(1.4,2.1,0.4)) ;
#143950 = CARTESIAN_POINT('',(1.4,1.9,0.6)) ;
#143951 = CARTESIAN_POINT('Origin',(1.4,2.1,0.6)) ;
#143952 = CARTESIAN_POINT('',(1.4,1.9,1.55)) ;
#143953 = CARTESIAN_POINT('',(1.4,1.9,1.55)) ;
#143954 = CARTESIAN_POINT('',(1.4,-2.15,1.55)) ;
#143955 = CARTESIAN_POINT('',(1.4,-2.15,1.55)) ;
#143956 = CARTESIAN_POINT('',(1.4,-2.15,0.903119593409422)) ;
#143957 = CARTESIAN_POINT('',(1.4,-2.15,0.903119593409422)) ;
#143958 = CARTESIAN_POINT('',(1.4,-2.15,-0.903119593409422)) ;
#143959 = CARTESIAN_POINT('Origin',(1.4,-3.65625,0.)) ;
#143960 = CARTESIAN_POINT('',(1.4,-2.15,-1.55)) ;
#143961 = CARTESIAN_POINT('',(1.4,-2.15,-1.55)) ;
#143962 = CARTESIAN_POINT('',(1.4,1.9,-1.55)) ;
#143963 = CARTESIAN_POINT('',(1.4,1.9,-1.55)) ;
#143964 = CARTESIAN_POINT('',(1.4,1.9,-0.6)) ;
#143965 = CARTESIAN_POINT('',(1.4,1.9,-0.6)) ;
#143966 = CARTESIAN_POINT('',(1.4,2.1,-0.4)) ;
#143967 = CARTESIAN_POINT('Origin',(1.4,2.1,-0.6)) ;
#143968 = CARTESIAN_POINT('',(1.4,2.4,-0.4)) ;
#143969 = CARTESIAN_POINT('',(1.4,2.4,-0.4)) ;
#143970 = CARTESIAN_POINT('',(1.4,2.6,-0.6)) ;
#143971 = CARTESIAN_POINT('Origin',(1.4,2.4,-0.6)) ;
#143972 = CARTESIAN_POINT('',(1.4,2.6,-0.70857864376269)) ;
#143973 = CARTESIAN_POINT('',(1.4,2.6,-0.70857864376269)) ;
#143974 = CARTESIAN_POINT('',(1.4,3.15,-1.25857864376269)) ;
#143975 = CARTESIAN_POINT('',(1.4,3.15,-1.25857864376269)) ;
#143976 = CARTESIAN_POINT('',(1.4,3.15,1.25857864376269)) ;
#143977 = CARTESIAN_POINT('',(1.4,2.6,0.708578643762689)) ;
#143978 = CARTESIAN_POINT('',(1.4,2.6,0.708578643762689)) ;
#143979 = CARTESIAN_POINT('',(1.4,2.6,0.6)) ;
#143980 = CARTESIAN_POINT('Origin',(2.4,0.,0.)) ;
#143981 = CARTESIAN_POINT('',(2.4,0.3,0.4)) ;
#143982 = CARTESIAN_POINT('',(2.4,-0.3,0.4)) ;
#143983 = CARTESIAN_POINT('',(2.4,0.,0.4)) ;
#143984 = CARTESIAN_POINT('',(2.4,0.4,0.3)) ;
#143985 = CARTESIAN_POINT('Origin',(2.4,0.3,0.3)) ;
#143986 = CARTESIAN_POINT('',(2.4,0.4,-0.3)) ;
#143987 = CARTESIAN_POINT('',(2.4,0.4,0.)) ;
#143988 = CARTESIAN_POINT('',(2.4,0.3,-0.4)) ;
#143989 = CARTESIAN_POINT('Origin',(2.4,0.3,-0.3)) ;
#143990 = CARTESIAN_POINT('',(2.4,-0.3,-0.4)) ;
#143991 = CARTESIAN_POINT('',(2.4,0.,-0.4)) ;
#143992 = CARTESIAN_POINT('',(2.4,-0.4,-0.3)) ;
#143993 = CARTESIAN_POINT('Origin',(2.4,-0.3,-0.3)) ;
#143994 = CARTESIAN_POINT('',(2.4,-0.4,0.3)) ;
#143995 = CARTESIAN_POINT('',(2.4,-0.4,0.)) ;
#143996 = CARTESIAN_POINT('Origin',(2.4,-0.3,0.3)) ;
#143997 = CARTESIAN_POINT('Origin',(-0.899999999999999,-2.,0.6)) ;
#143998 = CARTESIAN_POINT('Origin',(-0.899999999999999,0.4,0.6)) ;
#143999 = CARTESIAN_POINT('Origin',(-0.899999999999999,-1.9,0.6)) ;
#144000 = CARTESIAN_POINT('Origin',(0.600000000000001,0.4,0.4)) ;
#144001 = CARTESIAN_POINT('Origin',(0.500000000000001,0.4,0.4)) ;
#144002 = CARTESIAN_POINT('Origin',(-0.899999999999999,0.4,0.4)) ;
#144003 = CARTESIAN_POINT('Origin',(0.500000000000001,0.4,0.4)) ;
#144004 = CARTESIAN_POINT('',(0.600000000000001,0.4,0.4)) ;
#144005 = CARTESIAN_POINT('Origin',(0.500000000000001,0.4,0.4)) ;
#144006 = CARTESIAN_POINT('Origin',(0.500000000000001,0.4,0.4)) ;
#144007 = CARTESIAN_POINT('Origin',(-0.899999999999999,-1.9,0.6)) ;
#144008 = CARTESIAN_POINT('Origin',(-0.899999999999999,-1.9,0.6)) ;
#144009 = CARTESIAN_POINT('Origin',(-0.899999999999999,-1.9,0.6)) ;
#144010 = CARTESIAN_POINT('Origin',(-0.899999999999999,0.4,0.4)) ;
#144011 = CARTESIAN_POINT('Origin',(-0.899999999999999,0.6,0.4)) ;
#144012 = CARTESIAN_POINT('Origin',(0.500000000000001,0.4,0.)) ;
#144013 = CARTESIAN_POINT('Origin',(0.500000000000001,0.4,-0.4)) ;
#144014 = CARTESIAN_POINT('',(0.600000000000001,0.4,-0.3)) ;
#144015 = CARTESIAN_POINT('Ctrl Pts',(0.595612997216081,0.370705721320403,
-0.370705721320403)) ;
#144016 = CARTESIAN_POINT('Ctrl Pts',(0.596180587760892,0.372558268494357,
-0.368855498832167)) ;
#144017 = CARTESIAN_POINT('Ctrl Pts',(0.596672461925686,0.374355839771985,
-0.36691417986631)) ;
#144018 = CARTESIAN_POINT('Ctrl Pts',(0.599015141889212,0.383869350930065,
-0.355764993656267)) ;
#144019 = CARTESIAN_POINT('Ctrl Pts',(0.599609996542525,0.390224332900451,
-0.34497260265412)) ;
#144020 = CARTESIAN_POINT('Ctrl Pts',(0.600050586298726,0.398117439141561,
-0.32233105320467)) ;
#144021 = CARTESIAN_POINT('Ctrl Pts',(0.600000000000001,0.399999999999999,
-0.311201250633524)) ;
#144022 = CARTESIAN_POINT('Ctrl Pts',(0.600000000000001,0.399999999999999,
-0.3)) ;
#144023 = CARTESIAN_POINT('',(0.600000000000001,0.4,0.)) ;
#144024 = CARTESIAN_POINT('Origin',(0.500000000000001,-4.5664044441154E-17,
0.4)) ;
#144025 = CARTESIAN_POINT('',(0.500000000000001,0.394987437106619,0.3)) ;
#144026 = CARTESIAN_POINT('Ctrl Pts',(0.500000000000001,0.394987437106619,
0.3)) ;
#144027 = CARTESIAN_POINT('Ctrl Pts',(0.505940567948951,0.3955844866499,0.3)) ;
#144028 = CARTESIAN_POINT('Ctrl Pts',(0.511931971019139,0.396132036079018,
0.300533699672039)) ;
#144029 = CARTESIAN_POINT('Ctrl Pts',(0.517829015308548,0.396618246075354,
0.301602204226276)) ;
#144030 = CARTESIAN_POINT('Ctrl Pts',(0.522982218721202,0.397043126556053,
0.30253592984289)) ;
#144031 = CARTESIAN_POINT('Ctrl Pts',(0.528062648970231,0.397421319341388,
0.303877173202936)) ;
#144032 = CARTESIAN_POINT('Ctrl Pts',(0.532978106724001,0.397751505046071,
0.305594256123367)) ;
#144033 = CARTESIAN_POINT('Ctrl Pts',(0.538583536338965,0.398128038182999,
0.307552362150451)) ;
#144034 = CARTESIAN_POINT('Ctrl Pts',(0.544059405914892,0.398447721828296,
0.310029991688954)) ;
#144035 = CARTESIAN_POINT('Ctrl Pts',(0.549268572255782,0.398712331108984,
0.312979268057107)) ;
#144036 = CARTESIAN_POINT('Ctrl Pts',(0.553856850427146,0.398945401221756,
0.315577015853159)) ;
#144037 = CARTESIAN_POINT('Ctrl Pts',(0.558237825069326,0.399135987683843,
0.318539615020013)) ;
#144038 = CARTESIAN_POINT('Ctrl Pts',(0.562333836086213,0.399290378266507,
0.32180477713583)) ;
#144039 = CARTESIAN_POINT('Ctrl Pts',(0.566990328957893,0.399465895042381,
0.325516731047696)) ;
#144040 = CARTESIAN_POINT('Ctrl Pts',(0.571349096493423,0.399597278936107,
0.329677193515201)) ;
#144041 = CARTESIAN_POINT('Ctrl Pts',(0.575296920056712,0.399694832180837,
0.334194424020656)) ;
#144042 = CARTESIAN_POINT('Ctrl Pts',(0.578744263667908,0.399780018245913,
0.338138988784921)) ;
#144043 = CARTESIAN_POINT('Ctrl Pts',(0.58187831456043,0.399839626289636,
0.342354478157894)) ;
#144044 = CARTESIAN_POINT('Ctrl Pts',(0.584648147334856,0.399882153365958,
0.346758182292707)) ;
#144045 = CARTESIAN_POINT('Ctrl Pts',(0.587839270208173,0.399931148788079,
0.351831687495501)) ;
#144046 = CARTESIAN_POINT('Ctrl Pts',(0.590595054415093,0.399958289583404,
0.357233363755549)) ;
#144047 = CARTESIAN_POINT('Ctrl Pts',(0.592838618943104,0.399974357003159,
0.362838314990607)) ;
#144048 = CARTESIAN_POINT('Ctrl Pts',(0.594777336851655,0.399988241245861,
0.367681687757603)) ;
#144049 = CARTESIAN_POINT('Ctrl Pts',(0.596334051506189,0.399993946552814,
0.372675833772872)) ;
#144050 = CARTESIAN_POINT('Ctrl Pts',(0.597488309822308,0.39999684570125,
0.377728281431604)) ;
#144051 = CARTESIAN_POINT('Ctrl Pts',(0.598804024094401,0.400000150378306,
0.383487458039442)) ;
#144052 = CARTESIAN_POINT('Ctrl Pts',(0.599612685195431,0.399999963509465,
0.389397156109403)) ;
#144053 = CARTESIAN_POINT('Ctrl Pts',(0.599890230999721,0.399999993975383,
0.395315797738928)) ;
#144054 = CARTESIAN_POINT('Ctrl Pts',(0.5999634645494,0.400000002014155,0.396877497210183)) ;
#144055 = CARTESIAN_POINT('Ctrl Pts',(0.600000000000001,0.399999999999999,
0.398439778490821)) ;
#144056 = CARTESIAN_POINT('Ctrl Pts',(0.600000000000001,0.399999999999999,
0.4)) ;
#144057 = CARTESIAN_POINT('',(0.600000000000001,0.299999999999999,0.4)) ;
#144058 = CARTESIAN_POINT('Ctrl Pts',(0.500000000000001,0.394987437106619,
0.3)) ;
#144059 = CARTESIAN_POINT('Ctrl Pts',(0.500454935589698,0.395033159853734,
0.3)) ;
#144060 = CARTESIAN_POINT('Ctrl Pts',(0.500909898680399,0.395078570329052,
0.300003104508874)) ;
#144061 = CARTESIAN_POINT('Ctrl Pts',(0.502892456245148,0.395275075889088,
0.300030166058056)) ;
#144062 = CARTESIAN_POINT('Ctrl Pts',(0.504418747482362,0.395422812032197,
0.300086014579005)) ;
#144063 = CARTESIAN_POINT('Ctrl Pts',(0.508462199543372,0.395804395682036,
0.300326718943359)) ;
#144064 = CARTESIAN_POINT('Ctrl Pts',(0.510974953343318,0.396031485023319,
0.300572060854946)) ;
#144065 = CARTESIAN_POINT('Ctrl Pts',(0.521160739721334,0.396903453186241,
0.301957205508451)) ;
#144066 = CARTESIAN_POINT('Ctrl Pts',(0.528708678528457,0.397444933153163,
0.303895782295333)) ;
#144067 = CARTESIAN_POINT('Ctrl Pts',(0.54594320635814,0.398105551684111,
0.310535360548881)) ;
#144068 = CARTESIAN_POINT('Ctrl Pts',(0.555229535466871,0.397987646678423,
0.315964641164077)) ;
#144069 = CARTESIAN_POINT('Ctrl Pts',(0.571394604995807,0.395490482808029,
0.329224486636193)) ;
#144070 = CARTESIAN_POINT('Ctrl Pts',(0.578055313702881,0.393198948698321,
0.336759254368297)) ;
#144071 = CARTESIAN_POINT('Ctrl Pts',(0.58855913220255,0.385442756729278,
0.352607766016028)) ;
#144072 = CARTESIAN_POINT('Ctrl Pts',(0.592167355639995,0.380240075126846,
0.360451734393248)) ;
#144073 = CARTESIAN_POINT('Ctrl Pts',(0.597496615531129,0.365892753466911,
0.376074478204782)) ;
#144074 = CARTESIAN_POINT('Ctrl Pts',(0.598734255154207,0.356660564300593,
0.38322725827313)) ;
#144075 = CARTESIAN_POINT('Ctrl Pts',(0.600012754681692,0.335223914398488,
0.394417694134416)) ;
#144076 = CARTESIAN_POINT('Ctrl Pts',(0.59999390055981,0.32265503709182,0.398338480634425)) ;
#144077 = CARTESIAN_POINT('Ctrl Pts',(0.600000296204999,0.306106913582345,
0.399860373652956)) ;
#144078 = CARTESIAN_POINT('Ctrl Pts',(0.600000000000001,0.303050992413431,
0.4)) ;
#144079 = CARTESIAN_POINT('Ctrl Pts',(0.600000000000001,0.299999999999999,
0.4)) ;
#144080 = CARTESIAN_POINT('',(0.600000000000001,-2.3980000991444E-17,0.4)) ;
#144081 = CARTESIAN_POINT('Origin',(0.500000000000001,-1.9,0.4)) ;
#144082 = CARTESIAN_POINT('Origin',(0.600000000000001,-1.9,0.6)) ;
#144083 = CARTESIAN_POINT('Origin',(0.500000000000001,-1.9,0.6)) ;
#144084 = CARTESIAN_POINT('Origin',(-0.899999999999999,-1.9,1.375)) ;
#144085 = CARTESIAN_POINT('Origin',(-0.899999999999999,-1.9,1.275)) ;
#144086 = CARTESIAN_POINT('Origin',(-0.899999999999999,0.6,0.5)) ;
#144087 = CARTESIAN_POINT('Origin',(-0.899999999999999,0.6,-0.4)) ;
#144088 = CARTESIAN_POINT('Origin',(0.600000000000001,0.4,-0.4)) ;
#144089 = CARTESIAN_POINT('Origin',(0.500000000000001,0.4,-0.4)) ;
#144090 = CARTESIAN_POINT('Origin',(-0.899999999999999,0.4,-0.4)) ;
#144091 = CARTESIAN_POINT('Origin',(0.500000000000001,0.4,-0.4)) ;
#144092 = CARTESIAN_POINT('Origin',(0.500000000000001,-1.9,0.6)) ;
#144093 = CARTESIAN_POINT('Origin',(0.500000000000001,-2.1,0.6)) ;
#144094 = CARTESIAN_POINT('Origin',(-0.899999999999999,-1.9,1.275)) ;
#144095 = CARTESIAN_POINT('Origin',(-1.1,-1.9,1.275)) ;
#144096 = CARTESIAN_POINT('Origin',(-0.899999999999999,-2.1,1.275)) ;
#144097 = CARTESIAN_POINT('Origin',(-0.899999999999999,0.4,-0.4)) ;
#144098 = CARTESIAN_POINT('Origin',(-0.899999999999999,0.4,-0.6)) ;
#144099 = CARTESIAN_POINT('Origin',(0.500000000000001,-2.1,0.)) ;
#144100 = CARTESIAN_POINT('Origin',(0.500000000000001,-2.1,1.275)) ;
#144101 = CARTESIAN_POINT('Origin',(0.600000000000001,-2.1,1.275)) ;
#144102 = CARTESIAN_POINT('Origin',(0.500000000000001,-2.1,1.275)) ;
#144103 = CARTESIAN_POINT('Origin',(-1.1,-4.42727195005762E-17,1.275)) ;
#144104 = CARTESIAN_POINT('',(-1.1,1.15,1.375)) ;
#144105 = CARTESIAN_POINT('',(-1.1,1.25,1.375)) ;
#144106 = CARTESIAN_POINT('Origin',(-1.1,1.15,1.275)) ;
#144107 = CARTESIAN_POINT('Origin',(-0.899999999999999,0.5,-0.6)) ;
#144108 = CARTESIAN_POINT('Origin',(-0.899999999999999,-1.9,-0.6)) ;
#144109 = CARTESIAN_POINT('Origin',(0.600000000000001,-1.9,-0.6)) ;
#144110 = CARTESIAN_POINT('Origin',(0.500000000000001,-1.9,-0.6)) ;
#144111 = CARTESIAN_POINT('Origin',(-0.899999999999999,-1.9,-0.6)) ;
#144112 = CARTESIAN_POINT('Origin',(0.500000000000001,-1.9,-0.6)) ;
#144113 = CARTESIAN_POINT('Origin',(0.500000000000001,-2.1,-0.6)) ;
#144114 = CARTESIAN_POINT('Origin',(0.500000000000001,-2.1,1.275)) ;
#144115 = CARTESIAN_POINT('Origin',(0.500000000000001,-2.1,1.275)) ;
#144116 = CARTESIAN_POINT('Origin',(-1.1,-2.9,1.475)) ;
#144117 = CARTESIAN_POINT('Origin',(-1.1,-2.9,1.475)) ;
#144118 = CARTESIAN_POINT('Origin',(-1.1,-2.9,1.475)) ;
#144119 = CARTESIAN_POINT('Origin',(-1.1,1.25,1.475)) ;
#144120 = CARTESIAN_POINT('Origin',(-1.1,1.15,1.475)) ;
#144121 = CARTESIAN_POINT('Origin',(-1.1,1.15,1.275)) ;
#144122 = CARTESIAN_POINT('',(-1.1,1.25,1.275)) ;
#144123 = CARTESIAN_POINT('Origin',(-1.1,1.15,1.275)) ;
#144124 = CARTESIAN_POINT('Origin',(-1.1,1.15,1.275)) ;
#144125 = CARTESIAN_POINT('Origin',(-0.899999999999999,-1.9,-0.6)) ;
#144126 = CARTESIAN_POINT('Origin',(-0.899999999999999,-1.9,-0.6)) ;
#144127 = CARTESIAN_POINT('Origin',(0.500000000000001,-2.1,0.)) ;
#144128 = CARTESIAN_POINT('Origin',(0.500000000000001,-2.1,-1.275)) ;
#144129 = CARTESIAN_POINT('Origin',(0.500000000000001,1.36481920536411E-16,
1.275)) ;
#144130 = CARTESIAN_POINT('Origin',(0.500000000000001,-2.9,1.275)) ;
#144131 = CARTESIAN_POINT('Origin',(-0.999999999999999,-2.9,1.475)) ;
#144132 = CARTESIAN_POINT('Origin',(0.500000000000001,-2.9,1.475)) ;
#144133 = CARTESIAN_POINT('Origin',(-1.1,1.15,1.275)) ;
#144134 = CARTESIAN_POINT('Origin',(-1.1,1.35,1.275)) ;
#144135 = CARTESIAN_POINT('Origin',(-1.1,1.15,0.)) ;
#144136 = CARTESIAN_POINT('',(-1.1,1.25,-1.275)) ;
#144137 = CARTESIAN_POINT('',(-1.1,1.25,-1.375)) ;
#144138 = CARTESIAN_POINT('Origin',(-1.1,1.15,-1.275)) ;
#144139 = CARTESIAN_POINT('Origin',(-0.899999999999999,-1.9,-0.5)) ;
#144140 = CARTESIAN_POINT('Origin',(-0.899999999999999,-1.9,-1.275)) ;
#144141 = CARTESIAN_POINT('Origin',(-0.999999999999999,-2.1,-1.275)) ;
#144142 = CARTESIAN_POINT('Origin',(0.500000000000001,-2.1,-1.275)) ;
#144143 = CARTESIAN_POINT('Origin',(-0.899999999999999,-2.1,-1.275)) ;
#144144 = CARTESIAN_POINT('Origin',(0.500000000000001,-2.1,-1.275)) ;
#144145 = CARTESIAN_POINT('Origin',(0.500000000000001,-2.1,-1.275)) ;
#144146 = CARTESIAN_POINT('Origin',(0.500000000000001,-2.9,1.275)) ;
#144147 = CARTESIAN_POINT('Origin',(0.700000000000002,-2.9,1.275)) ;
#144148 = CARTESIAN_POINT('Origin',(-1.1,1.35,-1.375)) ;
#144149 = CARTESIAN_POINT('Origin',(-1.1,1.35,-1.275)) ;
#144150 = CARTESIAN_POINT('Origin',(-1.1,1.15,-1.275)) ;
#144151 = CARTESIAN_POINT('',(-1.1,1.15,-1.375)) ;
#144152 = CARTESIAN_POINT('Origin',(-1.1,1.15,-1.275)) ;
#144153 = CARTESIAN_POINT('Origin',(-1.1,1.15,-1.275)) ;
#144154 = CARTESIAN_POINT('Origin',(-0.899999999999999,-1.9,-1.275)) ;
#144155 = CARTESIAN_POINT('Origin',(-1.1,-1.9,-1.275)) ;
#144156 = CARTESIAN_POINT('Origin',(0.500000000000001,-5.86744705109801E-17,
-1.275)) ;
#144157 = CARTESIAN_POINT('Origin',(0.500000000000001,-2.9,-1.275)) ;
#144158 = CARTESIAN_POINT('Origin',(0.700000000000002,-2.9,0.)) ;
#144159 = CARTESIAN_POINT('Origin',(0.700000000000002,-2.9,-1.275)) ;
#144160 = CARTESIAN_POINT('Origin',(-1.1,1.15,-1.275)) ;
#144161 = CARTESIAN_POINT('Origin',(-1.1,1.15,-1.475)) ;
#144162 = CARTESIAN_POINT('Origin',(-1.1,-2.39429110547967E-16,-1.275)) ;
#144163 = CARTESIAN_POINT('',(-1.1,1.25,-1.375)) ;
#144164 = CARTESIAN_POINT('Origin',(0.500000000000001,-2.9,-1.275)) ;
#144165 = CARTESIAN_POINT('Origin',(0.500000000000001,-2.9,-1.475)) ;
#144166 = CARTESIAN_POINT('Origin',(-1.1,1.25,-1.475)) ;
#144167 = CARTESIAN_POINT('Origin',(-1.1,-2.9,-1.475)) ;
#144168 = CARTESIAN_POINT('Origin',(-1.1,-2.9,-1.475)) ;
#144169 = CARTESIAN_POINT('Origin',(-1.1,-2.9,-1.475)) ;
#144170 = CARTESIAN_POINT('Origin',(-1.1,-2.9,-1.475)) ;
#144171 = CARTESIAN_POINT('Origin',(4.55,4.55,-36.79)) ;
#144172 = CARTESIAN_POINT('Origin',(4.55,4.55,-36.79)) ;
#144173 = CARTESIAN_POINT('Origin',(4.55,4.55,-36.79)) ;
#144174 = CARTESIAN_POINT('Origin',(4.55,4.55,-36.79)) ;
#144175 = CARTESIAN_POINT('Origin',(4.55,4.35,-36.79)) ;
#144176 = CARTESIAN_POINT('Origin',(4.75,4.55,-36.79)) ;
#144177 = CARTESIAN_POINT('Origin',(4.75,4.55,-36.79)) ;
#144178 = CARTESIAN_POINT('Origin',(4.35,4.35,-36.79)) ;
#144179 = CARTESIAN_POINT('Origin',(4.35,4.15,-36.79)) ;
#144180 = CARTESIAN_POINT('Origin',(4.75,4.55,-36.79)) ;
#144181 = CARTESIAN_POINT('Origin',(4.75,4.55,-36.79)) ;
#144182 = CARTESIAN_POINT('Origin',(-1.1,4.15,-36.79)) ;
#144183 = CARTESIAN_POINT('Origin',(-1.1,4.15,-36.79)) ;
#144184 = CARTESIAN_POINT('Origin',(4.75,4.35,-36.79)) ;
#144185 = CARTESIAN_POINT('Origin',(4.75,4.35,-36.79)) ;
#144186 = CARTESIAN_POINT('Origin',(-1.1,4.15,-36.79)) ;
#144187 = CARTESIAN_POINT('Origin',(-1.1,4.15,-36.79)) ;
#144188 = CARTESIAN_POINT('Origin',(4.95,4.35,-36.79)) ;
#144189 = CARTESIAN_POINT('Origin',(4.95,4.15,-36.79)) ;
#144190 = CARTESIAN_POINT('Origin',(-1.1,4.15,-36.79)) ;
#144191 = CARTESIAN_POINT('Origin',(-1.1,-2.9,-36.79)) ;
#144192 = CARTESIAN_POINT('Origin',(4.95,4.15,-36.79)) ;
#144193 = CARTESIAN_POINT('Origin',(7.9,4.15,-36.79)) ;
#144194 = CARTESIAN_POINT('Origin',(-1.1,-2.9,-36.79)) ;
#144195 = CARTESIAN_POINT('Origin',(-1.1,-2.9,-36.79)) ;
#144196 = CARTESIAN_POINT('Origin',(7.9,4.15,-36.79)) ;
#144197 = CARTESIAN_POINT('Origin',(7.9,4.15,-36.79)) ;
#144198 = CARTESIAN_POINT('Origin',(-1.1,-2.9,-36.79)) ;
#144199 = CARTESIAN_POINT('Origin',(7.9,-2.9,-36.79)) ;
#144200 = CARTESIAN_POINT('Origin',(7.9,4.15,-36.79)) ;
#144201 = CARTESIAN_POINT('Origin',(7.9,-2.9,-36.79)) ;
#144202 = CARTESIAN_POINT('Origin',(7.9,-2.9,-36.79)) ;
#144203 = CARTESIAN_POINT('Origin',(4.55,4.55,2.5)) ;
#144204 = CARTESIAN_POINT('Origin',(4.55,4.55,2.5)) ;
#144205 = CARTESIAN_POINT('Origin',(4.55,4.55,2.5)) ;
#144206 = CARTESIAN_POINT('Origin',(4.55,-2.9,2.5)) ;
#144207 = CARTESIAN_POINT('Origin',(4.55,4.35,2.5)) ;
#144208 = CARTESIAN_POINT('Origin',(7.9,4.55,2.5)) ;
#144209 = CARTESIAN_POINT('Origin',(4.75,4.55,2.5)) ;
#144210 = CARTESIAN_POINT('Origin',(4.35,4.35,2.5)) ;
#144211 = CARTESIAN_POINT('Origin',(4.35,4.15,2.5)) ;
#144212 = CARTESIAN_POINT('Origin',(4.75,4.55,2.5)) ;
#144213 = CARTESIAN_POINT('Origin',(4.75,4.55,2.5)) ;
#144214 = CARTESIAN_POINT('Origin',(7.9,4.15,2.5)) ;
#144215 = CARTESIAN_POINT('Origin',(-1.1,4.15,2.5)) ;
#144216 = CARTESIAN_POINT('Origin',(4.74999999999997,-2.89999999999999,2.5)) ;
#144217 = CARTESIAN_POINT('Origin',(4.75,4.35,2.5)) ;
#144218 = CARTESIAN_POINT('Origin',(-1.1,4.15,2.5)) ;
#144219 = CARTESIAN_POINT('Origin',(-1.1,4.15,2.5)) ;
#144220 = CARTESIAN_POINT('Origin',(4.95,4.35,2.5)) ;
#144221 = CARTESIAN_POINT('Origin',(4.95,4.15,2.5)) ;
#144222 = CARTESIAN_POINT('Origin',(-1.1,-2.9,2.5)) ;
#144223 = CARTESIAN_POINT('Origin',(-1.1,-2.9,2.5)) ;
#144224 = CARTESIAN_POINT('Origin',(7.9,4.15,2.5)) ;
#144225 = CARTESIAN_POINT('Origin',(7.9,4.15,2.5)) ;
#144226 = CARTESIAN_POINT('Origin',(-1.1,-2.9,2.5)) ;
#144227 = CARTESIAN_POINT('Origin',(-1.1,-2.9,2.5)) ;
#144228 = CARTESIAN_POINT('Origin',(7.9,4.15,2.5)) ;
#144229 = CARTESIAN_POINT('Origin',(7.9,4.15,2.5)) ;
#144230 = CARTESIAN_POINT('Origin',(7.9,-2.9,2.5)) ;
#144231 = CARTESIAN_POINT('Origin',(7.9,-2.9,2.5)) ;
#144232 = CARTESIAN_POINT('Origin',(7.9,-2.9,2.5)) ;
#144233 = CARTESIAN_POINT('Origin',(7.9,-2.9,2.5)) ;
#144234 = CARTESIAN_POINT('Origin',(7.9,-2.9,2.5)) ;
#144235 = CARTESIAN_POINT('Origin',(1.5,1.9,0.6)) ;
#144236 = CARTESIAN_POINT('Origin',(1.5,1.9,-1.55)) ;
#144237 = CARTESIAN_POINT('Origin',(1.5,1.9,-0.6)) ;
#144238 = CARTESIAN_POINT('Origin',(1.5,2.1,-0.6)) ;
#144239 = CARTESIAN_POINT('Origin',(1.5,2.1,-0.4)) ;
#144240 = CARTESIAN_POINT('Origin',(1.5,1.9,-1.55)) ;
#144241 = CARTESIAN_POINT('Origin',(1.5,1.9,-1.55)) ;
#144242 = CARTESIAN_POINT('Origin',(1.5,2.1,-0.4)) ;
#144243 = CARTESIAN_POINT('Origin',(1.5,2.4,-0.4)) ;
#144244 = CARTESIAN_POINT('Origin',(1.5,2.1,-1.55)) ;
#144245 = CARTESIAN_POINT('Origin',(1.5,-2.15,-1.55)) ;
#144246 = CARTESIAN_POINT('Origin',(1.5,2.4,-0.6)) ;
#144247 = CARTESIAN_POINT('Origin',(1.5,2.6,-0.6)) ;
#144248 = CARTESIAN_POINT('Origin',(1.5,-2.15,-1.55)) ;
#144249 = CARTESIAN_POINT('Origin',(1.5,-2.15,-1.55)) ;
#144250 = CARTESIAN_POINT('Origin',(1.5,2.6,0.6)) ;
#144251 = CARTESIAN_POINT('Origin',(1.5,2.6,-0.70857864376269)) ;
#144252 = CARTESIAN_POINT('Origin',(1.5,-2.15,0.6)) ;
#144253 = CARTESIAN_POINT('Origin',(1.5,-2.15,-0.903119593409422)) ;
#144254 = CARTESIAN_POINT('Origin',(1.5,2.6,-0.70857864376269)) ;
#144255 = CARTESIAN_POINT('Origin',(1.5,2.6,-0.70857864376269)) ;
#144256 = CARTESIAN_POINT('Origin',(1.5,-2.15,-0.903119593409422)) ;
#144257 = CARTESIAN_POINT('Origin',(1.5,-2.15,-0.903119593409422)) ;
#144258 = CARTESIAN_POINT('Origin',(1.5,1.69571067811865,0.195710678118654)) ;
#144259 = CARTESIAN_POINT('Origin',(1.5,3.15,-1.25857864376269)) ;
#144260 = CARTESIAN_POINT('Origin',(1.5,-3.65625,0.)) ;
#144261 = CARTESIAN_POINT('Origin',(1.5,-2.15,0.903119593409423)) ;
#144262 = CARTESIAN_POINT('Origin',(1.5,3.15,-1.25857864376269)) ;
#144263 = CARTESIAN_POINT('Origin',(1.5,3.15,-1.25857864376269)) ;
#144264 = CARTESIAN_POINT('Origin',(1.5,-2.15,0.903119593409422)) ;
#144265 = CARTESIAN_POINT('Origin',(1.5,-2.15,0.903119593409422)) ;
#144266 = CARTESIAN_POINT('Origin',(1.5,3.15,0.6)) ;
#144267 = CARTESIAN_POINT('Origin',(1.5,-2.15,0.6)) ;
#144268 = CARTESIAN_POINT('Origin',(1.5,-2.15,1.55)) ;
#144269 = CARTESIAN_POINT('Origin',(1.5,-2.15,1.55)) ;
#144270 = CARTESIAN_POINT('Origin',(1.5,-2.15,1.55)) ;
#144271 = CARTESIAN_POINT('Origin',(1.5,2.29571067811866,0.404289321881344)) ;
#144272 = CARTESIAN_POINT('Origin',(1.5,2.6,0.708578643762689)) ;
#144273 = CARTESIAN_POINT('Origin',(1.5,2.1,1.55)) ;
#144274 = CARTESIAN_POINT('Origin',(1.5,1.9,1.55)) ;
#144275 = CARTESIAN_POINT('Origin',(1.5,2.6,0.70857864376269)) ;
#144276 = CARTESIAN_POINT('Origin',(1.5,2.6,0.70857864376269)) ;
#144277 = CARTESIAN_POINT('Origin',(1.5,1.9,1.55)) ;
#144278 = CARTESIAN_POINT('Origin',(1.5,1.9,1.55)) ;
#144279 = CARTESIAN_POINT('Origin',(1.5,2.6,0.599999999999998)) ;
#144280 = CARTESIAN_POINT('Origin',(1.5,2.6,0.6)) ;
#144281 = CARTESIAN_POINT('Origin',(1.5,1.9,0.6)) ;
#144282 = CARTESIAN_POINT('Origin',(1.5,1.9,0.6)) ;
#144283 = CARTESIAN_POINT('Origin',(1.5,2.4,0.6)) ;
#144284 = CARTESIAN_POINT('Origin',(1.5,2.4,0.4)) ;
#144285 = CARTESIAN_POINT('Origin',(1.5,2.1,0.6)) ;
#144286 = CARTESIAN_POINT('Origin',(1.5,2.1,0.4)) ;
#144287 = CARTESIAN_POINT('Origin',(1.5,2.1,0.4)) ;
#144288 = CARTESIAN_POINT('Origin',(7.9,2.1,-0.6)) ;
#144289 = CARTESIAN_POINT('Origin',(7.9,2.4,-0.6)) ;
#144290 = CARTESIAN_POINT('Origin',(7.9,2.1,-0.6)) ;
#144291 = CARTESIAN_POINT('Origin',(7.9,2.4,-0.6)) ;
#144292 = CARTESIAN_POINT('Origin',(7.9,2.4,-0.6)) ;
#144293 = CARTESIAN_POINT('Origin',(7.9,2.1,-0.6)) ;
#144294 = CARTESIAN_POINT('Origin',(7.9,2.1,-0.6)) ;
#144295 = CARTESIAN_POINT('Origin',(7.9,2.4,-0.6)) ;
#144296 = CARTESIAN_POINT('Origin',(7.9,2.4,-0.70857864376269)) ;
#144297 = CARTESIAN_POINT('Origin',(7.9,2.1,-0.6)) ;
#144298 = CARTESIAN_POINT('Origin',(7.9,2.1,-1.55)) ;
#144299 = CARTESIAN_POINT('Origin',(7.9,2.6,-0.70857864376269)) ;
#144300 = CARTESIAN_POINT('Origin',(7.9,2.45857864376269,-0.85)) ;
#144301 = CARTESIAN_POINT('Origin',(7.9,1.9,-1.55)) ;
#144302 = CARTESIAN_POINT('Origin',(7.9,1.9,-1.75)) ;
#144303 = CARTESIAN_POINT('Origin',(7.9,2.45857864376269,-0.85)) ;
#144304 = CARTESIAN_POINT('Origin',(7.9,1.9,-1.75)) ;
#144305 = CARTESIAN_POINT('Origin',(7.9,-2.15,-1.75)) ;
#144306 = CARTESIAN_POINT('Origin',(7.9,-2.15,-1.55)) ;
#144307 = CARTESIAN_POINT('Origin',(7.9,-2.35,-1.55)) ;
#144308 = CARTESIAN_POINT('Origin',(7.9,3.35,-1.25857864376269)) ;
#144309 = CARTESIAN_POINT('Origin',(7.9,3.35,1.25857864376269)) ;
#144310 = CARTESIAN_POINT('Origin',(7.9,-2.35,-0.903119593409422)) ;
#144311 = CARTESIAN_POINT('Origin',(7.9,-2.35,-0.903119593409422)) ;
#144312 = CARTESIAN_POINT('Origin',(7.9,3.15,1.25857864376269)) ;
#144313 = CARTESIAN_POINT('Origin',(7.9,3.00857864376269,1.4)) ;
#144314 = CARTESIAN_POINT('Origin',(7.9,-2.15,-0.903119593409422)) ;
#144315 = CARTESIAN_POINT('Origin',(7.9,-2.32153024911032,-0.800273234017602)) ;
#144316 = CARTESIAN_POINT('Origin',(7.9,3.00857864376269,1.4)) ;
#144317 = CARTESIAN_POINT('Origin',(7.9,2.45857864376269,0.849999999999999)) ;
#144318 = CARTESIAN_POINT('Origin',(7.9,-3.65625,0.)) ;
#144319 = CARTESIAN_POINT('Origin',(7.9,-2.32153024911032,0.800273234017602)) ;
#144320 = CARTESIAN_POINT('Origin',(7.9,2.6,0.70857864376269)) ;
#144321 = CARTESIAN_POINT('Origin',(7.9,2.4,0.70857864376269)) ;
#144322 = CARTESIAN_POINT('Origin',(7.9,-2.15,0.903119593409422)) ;
#144323 = CARTESIAN_POINT('Origin',(7.9,-2.35,0.903119593409422)) ;
#144324 = CARTESIAN_POINT('Origin',(7.9,2.4,0.70857864376269)) ;
#144325 = CARTESIAN_POINT('Origin',(7.9,2.4,0.600000000000001)) ;
#144326 = CARTESIAN_POINT('Origin',(7.9,-2.35,1.55)) ;
#144327 = CARTESIAN_POINT('Origin',(7.9,-2.35,1.55)) ;
#144328 = CARTESIAN_POINT('Origin',(7.9,2.4,0.6)) ;
#144329 = CARTESIAN_POINT('Origin',(7.9,2.4,0.6)) ;
#144330 = CARTESIAN_POINT('Origin',(7.9,-2.15,1.55)) ;
#144331 = CARTESIAN_POINT('Origin',(7.9,-2.15,1.75)) ;
#144332 = CARTESIAN_POINT('Origin',(7.9,2.4,0.6)) ;
#144333 = CARTESIAN_POINT('Origin',(7.9,2.1,0.6)) ;
#144334 = CARTESIAN_POINT('Origin',(7.9,1.9,1.75)) ;
#144335 = CARTESIAN_POINT('Origin',(7.9,1.9,1.75)) ;
#144336 = CARTESIAN_POINT('Origin',(7.9,2.1,0.6)) ;
#144337 = CARTESIAN_POINT('Origin',(7.9,2.1,0.6)) ;
#144338 = CARTESIAN_POINT('Origin',(7.9,1.9,1.55)) ;
#144339 = CARTESIAN_POINT('Origin',(7.9,2.1,1.55)) ;
#144340 = CARTESIAN_POINT('Origin',(7.9,2.1,1.55)) ;
#144341 = CARTESIAN_POINT('Origin',(-0.4,-0.600000000000001,0.4)) ;
#144342 = CARTESIAN_POINT('',(-0.4,-0.600000000000001,0.3)) ;
#144343 = CARTESIAN_POINT('',(-0.4,-0.600000000000001,-0.3)) ;
#144344 = CARTESIAN_POINT('',(-0.4,-0.600000000000001,0.4)) ;
#144345 = CARTESIAN_POINT('',(-0.4,-6.05857864376269,-0.3)) ;
#144346 = CARTESIAN_POINT('',(-0.4,-0.600000000000001,-0.3)) ;
#144347 = CARTESIAN_POINT('',(-0.4,-6.05857864376269,0.3)) ;
#144348 = CARTESIAN_POINT('',(-0.4,-6.05857864376269,0.4)) ;
#144349 = CARTESIAN_POINT('',(-0.4,-0.600000000000001,0.3)) ;
#144350 = CARTESIAN_POINT('Origin',(-0.4,-6.1,0.4)) ;
#144351 = CARTESIAN_POINT('',(-0.129289321881346,-6.37071067811866,-0.0585786437626899)) ;
#144352 = CARTESIAN_POINT('',(-0.129289321881346,-6.37071067811866,0.0585786437626899)) ;
#144353 = CARTESIAN_POINT('',(-0.129289321881346,-6.37071067811866,0.4)) ;
#144354 = CARTESIAN_POINT('',(-0.370710678118655,-6.12928932188134,0.3)) ;
#144355 = CARTESIAN_POINT('',(-0.423570226039552,-6.07642977396045,0.352859547920897)) ;
#144356 = CARTESIAN_POINT('',(-0.370710678118655,-6.12928932188134,-0.3)) ;
#144357 = CARTESIAN_POINT('',(-0.370710678118655,-6.12928932188134,0.4)) ;
#144358 = CARTESIAN_POINT('',(-0.156903559372884,-6.34309644062712,-0.0861928812542289)) ;
#144359 = CARTESIAN_POINT('Origin',(-0.1,-6.4,0.4)) ;
#144360 = CARTESIAN_POINT('',(0.0585786437626908,-6.4,-0.0585786437626897)) ;
#144361 = CARTESIAN_POINT('',(0.0585786437626908,-6.4,0.0585786437626898)) ;
#144362 = CARTESIAN_POINT('',(0.0585786437626908,-6.4,0.4)) ;
#144363 = CARTESIAN_POINT('',(-0.0585786437626908,-6.4,0.0585786437626898)) ;
#144364 = CARTESIAN_POINT('',(-0.1,-6.4,0.0585786437626898)) ;
#144365 = CARTESIAN_POINT('',(-0.0585786437626908,-6.4,-0.0585786437626897)) ;
#144366 = CARTESIAN_POINT('',(-0.0585786437626908,-6.4,0.4)) ;
#144367 = CARTESIAN_POINT('',(-0.1,-6.4,-0.0585786437626898)) ;
#144368 = CARTESIAN_POINT('Origin',(0.1,-6.4,0.4)) ;
#144369 = CARTESIAN_POINT('',(0.370710678118655,-6.12928932188134,-0.3)) ;
#144370 = CARTESIAN_POINT('',(0.370710678118655,-6.12928932188134,0.299999999999999)) ;
#144371 = CARTESIAN_POINT('',(0.370710678118655,-6.12928932188134,0.4)) ;
#144372 = CARTESIAN_POINT('',(0.129289321881346,-6.37071067811866,0.0585786437626892)) ;
#144373 = CARTESIAN_POINT('',(0.223570226039552,-6.27642977396045,0.152859547920897)) ;
#144374 = CARTESIAN_POINT('',(0.129289321881346,-6.37071067811866,-0.05857864376269)) ;
#144375 = CARTESIAN_POINT('',(0.129289321881346,-6.37071067811866,0.4)) ;
#144376 = CARTESIAN_POINT('',(-0.0430964406271149,-6.54309644062712,0.113807118745771)) ;
#144377 = CARTESIAN_POINT('Origin',(0.4,-6.1,0.4)) ;
#144378 = CARTESIAN_POINT('',(0.4,-6.05857864376269,0.3)) ;
#144379 = CARTESIAN_POINT('',(0.4,-6.05857864376269,-0.3)) ;
#144380 = CARTESIAN_POINT('',(0.4,-6.05857864376269,0.4)) ;
#144381 = CARTESIAN_POINT('',(0.4,-0.6,-0.3)) ;
#144382 = CARTESIAN_POINT('',(0.4,-6.1,-0.3)) ;
#144383 = CARTESIAN_POINT('',(0.4,-0.6,0.3)) ;
#144384 = CARTESIAN_POINT('',(0.4,-0.6,0.4)) ;
#144385 = CARTESIAN_POINT('',(0.4,-6.05857864376269,0.3)) ;
#144386 = CARTESIAN_POINT('Origin',(0.6,-0.600000000000001,0.4)) ;
#144387 = CARTESIAN_POINT('',(0.3,-6.05857864376269,0.4)) ;
#144388 = CARTESIAN_POINT('',(0.3,-0.6,0.4)) ;
#144389 = CARTESIAN_POINT('',(0.3,-0.6,0.4)) ;
#144390 = CARTESIAN_POINT('Origin',(0.6,-0.6,0.4)) ;
#144391 = CARTESIAN_POINT('',(-0.3,-0.600000000000001,0.4)) ;
#144392 = CARTESIAN_POINT('Origin',(0.6,-0.600000000000001,0.4)) ;
#144393 = CARTESIAN_POINT('',(-0.3,-6.05857864376269,0.4)) ;
#144394 = CARTESIAN_POINT('',(-0.3,-0.600000000000001,0.4)) ;
#144395 = CARTESIAN_POINT('',(0.4,-6.05857864376269,0.4)) ;
#144396 = CARTESIAN_POINT('Origin',(0.6,-0.600000000000001,-0.4)) ;
#144397 = CARTESIAN_POINT('',(-0.3,-6.05857864376269,-0.4)) ;
#144398 = CARTESIAN_POINT('',(-0.3,-0.600000000000001,-0.4)) ;
#144399 = CARTESIAN_POINT('',(-0.3,-0.600000000000001,-0.4)) ;
#144400 = CARTESIAN_POINT('Origin',(0.6,-0.600000000000001,-0.4)) ;
#144401 = CARTESIAN_POINT('',(0.3,-0.6,-0.4)) ;
#144402 = CARTESIAN_POINT('Origin',(0.6,-0.6,-0.4)) ;
#144403 = CARTESIAN_POINT('',(0.3,-6.05857864376269,-0.4)) ;
#144404 = CARTESIAN_POINT('',(0.3,-0.600000000000001,-0.4)) ;
#144405 = CARTESIAN_POINT('',(0.6,-6.05857864376269,-0.4)) ;
#144406 = CARTESIAN_POINT('Origin',(0.6,-0.600000000000001,0.4)) ;
#144407 = CARTESIAN_POINT('Origin',(0.6,-0.600000000000001,-0.3)) ;
#144408 = CARTESIAN_POINT('Origin',(0.6,-0.600000000000001,0.3)) ;
#144409 = CARTESIAN_POINT('Origin',(0.6,-0.6,0.4)) ;
#144410 = CARTESIAN_POINT('Origin',(0.6,-0.6,-0.3)) ;
#144411 = CARTESIAN_POINT('Origin',(0.6,-0.6,0.3)) ;
#144412 = CARTESIAN_POINT('Origin',(7.,0.1,0.4)) ;
#144413 = CARTESIAN_POINT('',(6.72928932188135,0.370710678118655,-0.3)) ;
#144414 = CARTESIAN_POINT('',(6.72928932188135,0.370710678118655,0.3)) ;
#144415 = CARTESIAN_POINT('',(6.72928932188135,0.370710678118655,0.4)) ;
#144416 = CARTESIAN_POINT('',(6.97071067811866,0.129289321881346,0.0585786437626902)) ;
#144417 = CARTESIAN_POINT('',(6.87642977396045,0.223570226039552,0.152859547920897)) ;
#144418 = CARTESIAN_POINT('',(6.97071067811866,0.129289321881346,-0.0585786437626903)) ;
#144419 = CARTESIAN_POINT('',(6.97071067811866,0.129289321881346,0.4)) ;
#144420 = CARTESIAN_POINT('',(7.14309644062712,-0.043096440627115,0.11380711874577)) ;
#144421 = CARTESIAN_POINT('Origin',(6.7,0.400000000000001,0.4)) ;
#144422 = CARTESIAN_POINT('',(6.65857864376269,0.400000000000001,0.3)) ;
#144423 = CARTESIAN_POINT('',(6.65857864376269,0.400000000000001,-0.3)) ;
#144424 = CARTESIAN_POINT('',(6.65857864376269,0.400000000000001,0.4)) ;
#144425 = CARTESIAN_POINT('',(6.7,0.400000000000001,-0.3)) ;
#144426 = CARTESIAN_POINT('',(6.65857864376269,0.400000000000001,0.3)) ;
#144427 = CARTESIAN_POINT('Origin',(0.6,-0.4,0.4)) ;
#144428 = CARTESIAN_POINT('',(6.65857864376269,-0.400000000000001,-0.3)) ;
#144429 = CARTESIAN_POINT('',(0.6,-0.4,-0.3)) ;
#144430 = CARTESIAN_POINT('',(6.65857864376269,-0.400000000000001,0.3)) ;
#144431 = CARTESIAN_POINT('',(6.65857864376269,-0.400000000000001,0.4)) ;
#144432 = CARTESIAN_POINT('',(2.4,-0.4,0.3)) ;
#144433 = CARTESIAN_POINT('Origin',(6.7,-0.400000000000001,0.4)) ;
#144434 = CARTESIAN_POINT('',(6.97071067811866,-0.129289321881346,-0.0585786437626903)) ;
#144435 = CARTESIAN_POINT('',(6.97071067811866,-0.129289321881346,0.0585786437626901)) ;
#144436 = CARTESIAN_POINT('',(6.97071067811866,-0.129289321881346,0.4)) ;
#144437 = CARTESIAN_POINT('',(6.72928932188135,-0.370710678118655,0.3)) ;
#144438 = CARTESIAN_POINT('',(6.67642977396045,-0.423570226039552,0.352859547920897)) ;
#144439 = CARTESIAN_POINT('',(6.72928932188135,-0.370710678118655,-0.3)) ;
#144440 = CARTESIAN_POINT('',(6.72928932188135,-0.370710678118655,0.4)) ;
#144441 = CARTESIAN_POINT('',(6.94309644062712,-0.156903559372885,-0.0861928812542298)) ;
#144442 = CARTESIAN_POINT('Origin',(7.,-0.1,0.4)) ;
#144443 = CARTESIAN_POINT('',(7.,-0.0585786437626909,0.0585786437626901)) ;
#144444 = CARTESIAN_POINT('',(7.,-0.0585786437626909,-0.05857864376269)) ;
#144445 = CARTESIAN_POINT('',(7.,-0.0585786437626909,0.4)) ;
#144446 = CARTESIAN_POINT('',(7.,0.0585786437626909,-0.05857864376269)) ;
#144447 = CARTESIAN_POINT('',(7.,-0.1,-0.05857864376269)) ;
#144448 = CARTESIAN_POINT('',(7.,0.0585786437626909,0.05857864376269)) ;
#144449 = CARTESIAN_POINT('',(7.,0.0585786437626909,0.4)) ;
#144450 = CARTESIAN_POINT('',(7.,-0.1,0.0585786437626901)) ;
#144451 = CARTESIAN_POINT('Origin',(0.6,-0.600000000000001,0.4)) ;
#144452 = CARTESIAN_POINT('',(6.65857864376269,-0.300000000000001,0.4)) ;
#144453 = CARTESIAN_POINT('',(6.65857864376269,0.300000000000001,0.4)) ;
#144454 = CARTESIAN_POINT('',(6.65857864376269,-0.399999999999999,0.4)) ;
#144455 = CARTESIAN_POINT('',(2.4,0.3,0.4)) ;
#144456 = CARTESIAN_POINT('',(6.65857864376269,-0.300000000000001,0.4)) ;
#144457 = CARTESIAN_POINT('Origin',(0.6,-0.600000000000001,-0.4)) ;
#144458 = CARTESIAN_POINT('',(6.65857864376269,0.300000000000001,-0.4)) ;
#144459 = CARTESIAN_POINT('',(0.6,0.299999999999999,-0.4)) ;
#144460 = CARTESIAN_POINT('',(6.65857864376269,-0.300000000000001,-0.4)) ;
#144461 = CARTESIAN_POINT('',(6.65857864376269,-0.6,-0.4)) ;
#144462 = CARTESIAN_POINT('',(0.6,-0.3,-0.4)) ;
#144463 = CARTESIAN_POINT('Origin',(0.4,-6.4,-0.0999999999999988)) ;
#144464 = CARTESIAN_POINT('',(-0.0585786437626909,-6.37071067811866,-0.129289321881344)) ;
#144465 = CARTESIAN_POINT('',(-0.3,-6.12928932188134,-0.370710678118655)) ;
#144466 = CARTESIAN_POINT('',(0.113807118745769,-6.54309644062712,0.0430964406271166)) ;
#144467 = CARTESIAN_POINT('',(0.3,-6.12928932188134,-0.370710678118655)) ;
#144468 = CARTESIAN_POINT('',(0.4,-6.12928932188134,-0.370710678118654)) ;
#144469 = CARTESIAN_POINT('',(0.058578643762691,-6.37071067811866,-0.129289321881344)) ;
#144470 = CARTESIAN_POINT('',(0.152859547920897,-6.27642977396045,-0.22357022603955)) ;
#144471 = CARTESIAN_POINT('',(0.4,-6.37071067811866,-0.129289321881344)) ;
#144472 = CARTESIAN_POINT('Origin',(0.4,-6.1,0.4)) ;
#144473 = CARTESIAN_POINT('',(0.0585786437626902,-6.37071067811866,0.129289321881344)) ;
#144474 = CARTESIAN_POINT('',(0.299999999999999,-6.12928932188134,0.370710678118655)) ;
#144475 = CARTESIAN_POINT('',(0.352859547920896,-6.07642977396045,0.423570226039552)) ;
#144476 = CARTESIAN_POINT('',(-0.3,-6.12928932188134,0.370710678118655)) ;
#144477 = CARTESIAN_POINT('',(0.4,-6.12928932188134,0.370710678118654)) ;
#144478 = CARTESIAN_POINT('',(-0.058578643762691,-6.37071067811866,0.129289321881344)) ;
#144479 = CARTESIAN_POINT('',(-0.086192881254231,-6.34309644062712,0.156903559372885)) ;
#144480 = CARTESIAN_POINT('',(0.4,-6.37071067811866,0.129289321881344)) ;
#144481 = CARTESIAN_POINT('Origin',(6.7,-0.399999999999999,-0.4)) ;
#144482 = CARTESIAN_POINT('',(6.97071067811866,-0.0585786437626912,-0.129289321881345)) ;
#144483 = CARTESIAN_POINT('',(6.72928932188135,-0.300000000000001,-0.370710678118655)) ;
#144484 = CARTESIAN_POINT('',(6.67642977396045,-0.352859547920897,-0.423570226039551)) ;
#144485 = CARTESIAN_POINT('',(6.72928932188135,0.300000000000001,-0.370710678118655)) ;
#144486 = CARTESIAN_POINT('',(6.72928932188135,-0.399999999999999,-0.370710678118655)) ;
#144487 = CARTESIAN_POINT('',(6.97071067811866,0.0585786437626912,-0.129289321881345)) ;
#144488 = CARTESIAN_POINT('',(6.94309644062712,0.0861928812542309,-0.156903559372884)) ;
#144489 = CARTESIAN_POINT('',(6.97071067811866,-0.4,-0.129289321881345)) ;
#144490 = CARTESIAN_POINT('Origin',(7.,-0.399999999999999,0.0999999999999993)) ;
#144491 = CARTESIAN_POINT('',(6.97071067811866,0.0585786437626911,0.129289321881345)) ;
#144492 = CARTESIAN_POINT('',(6.72928932188135,0.300000000000001,0.370710678118655)) ;
#144493 = CARTESIAN_POINT('',(7.14309644062712,-0.113807118745769,-0.043096440627116)) ;
#144494 = CARTESIAN_POINT('',(6.72928932188135,-0.300000000000001,0.370710678118655)) ;
#144495 = CARTESIAN_POINT('',(6.72928932188135,-0.399999999999999,0.370710678118655)) ;
#144496 = CARTESIAN_POINT('',(6.97071067811866,-0.0585786437626911,0.129289321881345)) ;
#144497 = CARTESIAN_POINT('',(6.87642977396045,-0.152859547920897,0.223570226039551)) ;
#144498 = CARTESIAN_POINT('',(6.97071067811866,-0.399999999999999,0.129289321881345)) ;
#144499 = CARTESIAN_POINT('Origin',(-0.11380711874577,-6.47238576250846,0.113807118745771)) ;
#144500 = CARTESIAN_POINT('Origin',(0.3,-6.05857864376269,-0.3)) ;
#144501 = CARTESIAN_POINT('Origin',(0.058578643762691,-6.3,-0.0585786437626897)) ;
#144502 = CARTESIAN_POINT('Origin',(0.3,-6.05857864376269,0.4)) ;
#144503 = CARTESIAN_POINT('Origin',(0.3,-6.05857864376269,-0.3)) ;
#144504 = CARTESIAN_POINT('Origin',(0.3,-6.05857864376269,0.3)) ;
#144505 = CARTESIAN_POINT('Origin',(0.0585786437626908,-6.3,-0.0585786437626897)) ;
#144506 = CARTESIAN_POINT('Origin',(0.0585786437626908,-6.3,-0.0585786437626897)) ;
#144507 = CARTESIAN_POINT('Origin',(0.0585786437626908,-6.3,-0.05857864376269)) ;
#144508 = CARTESIAN_POINT('Origin',(0.152859547920897,-6.20571909584179,0.152859547920897)) ;
#144509 = CARTESIAN_POINT('Origin',(0.3,-6.05857864376269,0.3)) ;
#144510 = CARTESIAN_POINT('Origin',(0.0585786437626908,-6.3,0.0585786437626892)) ;
#144511 = CARTESIAN_POINT('Origin',(0.0585786437626908,-6.3,0.4)) ;
#144512 = CARTESIAN_POINT('Origin',(0.0585786437626908,-6.3,0.0585786437626898)) ;
#144513 = CARTESIAN_POINT('Origin',(0.4,-6.3,-0.0585786437626897)) ;
#144514 = CARTESIAN_POINT('Origin',(-0.0585786437626909,-6.3,-0.0585786437626897)) ;
#144515 = CARTESIAN_POINT('Origin',(0.0585786437626908,-6.3,0.0585786437626898)) ;
#144516 = CARTESIAN_POINT('Origin',(0.0585786437626902,-6.3,0.0585786437626897)) ;
#144517 = CARTESIAN_POINT('Origin',(-0.0585786437626908,-6.3,-0.0585786437626897)) ;
#144518 = CARTESIAN_POINT('Origin',(-0.0585786437626908,-6.3,-0.0585786437626899)) ;
#144519 = CARTESIAN_POINT('Origin',(-0.0585786437626908,-6.3,-0.0585786437626897)) ;
#144520 = CARTESIAN_POINT('Origin',(-0.1,-6.3,0.0585786437626898)) ;
#144521 = CARTESIAN_POINT('Origin',(-0.0585786437626908,-6.3,0.0585786437626898)) ;
#144522 = CARTESIAN_POINT('Origin',(-0.0585786437626908,-6.3,0.4)) ;
#144523 = CARTESIAN_POINT('Origin',(-0.0585786437626908,-6.3,0.0585786437626899)) ;
#144524 = CARTESIAN_POINT('Origin',(-0.0861928812542298,-6.27238576250846,
-0.0861928812542288)) ;
#144525 = CARTESIAN_POINT('Origin',(-0.3,-6.05857864376269,-0.3)) ;
#144526 = CARTESIAN_POINT('Origin',(-0.0585786437626909,-6.3,0.0585786437626898)) ;
#144527 = CARTESIAN_POINT('Origin',(-0.058578643762691,-6.3,0.0585786437626897)) ;
#144528 = CARTESIAN_POINT('Origin',(-0.3,-6.05857864376269,0.4)) ;
#144529 = CARTESIAN_POINT('Origin',(-0.3,-6.05857864376269,-0.3)) ;
#144530 = CARTESIAN_POINT('Origin',(-0.3,-6.05857864376269,0.3)) ;
#144531 = CARTESIAN_POINT('Origin',(-0.352859547920897,-6.00571909584179,
0.352859547920897)) ;
#144532 = CARTESIAN_POINT('Origin',(-0.3,-6.05857864376269,0.3)) ;
#144533 = CARTESIAN_POINT('Origin',(7.07238576250846,-0.11380711874577,0.113807118745771)) ;
#144534 = CARTESIAN_POINT('Origin',(6.65857864376269,0.300000000000001,-0.3)) ;
#144535 = CARTESIAN_POINT('Origin',(6.9,0.0585786437626912,-0.05857864376269)) ;
#144536 = CARTESIAN_POINT('Origin',(6.65857864376269,0.300000000000001,0.4)) ;
#144537 = CARTESIAN_POINT('Origin',(6.65857864376269,0.300000000000001,-0.3)) ;
#144538 = CARTESIAN_POINT('Origin',(6.65857864376269,0.300000000000001,0.3)) ;
#144539 = CARTESIAN_POINT('Origin',(6.9,0.0585786437626909,-0.05857864376269)) ;
#144540 = CARTESIAN_POINT('Origin',(6.9,0.0585786437626909,-0.05857864376269)) ;
#144541 = CARTESIAN_POINT('Origin',(6.9,0.0585786437626909,-0.0585786437626903)) ;
#144542 = CARTESIAN_POINT('Origin',(6.80571909584179,0.152859547920897,0.152859547920897)) ;
#144543 = CARTESIAN_POINT('Origin',(6.65857864376269,0.300000000000001,0.3)) ;
#144544 = CARTESIAN_POINT('Origin',(6.9,0.0585786437626909,0.0585786437626902)) ;
#144545 = CARTESIAN_POINT('Origin',(6.9,0.0585786437626909,0.4)) ;
#144546 = CARTESIAN_POINT('Origin',(6.9,0.0585786437626909,0.05857864376269)) ;
#144547 = CARTESIAN_POINT('Origin',(6.9,-0.1,-0.05857864376269)) ;
#144548 = CARTESIAN_POINT('Origin',(6.9,-0.0585786437626912,-0.05857864376269)) ;
#144549 = CARTESIAN_POINT('Origin',(6.9,0.0585786437626909,0.05857864376269)) ;
#144550 = CARTESIAN_POINT('Origin',(6.9,0.0585786437626911,0.05857864376269)) ;
#144551 = CARTESIAN_POINT('Origin',(6.9,-0.058578643762691,-0.0585786437626901)) ;
#144552 = CARTESIAN_POINT('Origin',(6.9,-0.0585786437626909,-0.0585786437626903)) ;
#144553 = CARTESIAN_POINT('Origin',(6.9,-0.0585786437626909,-0.05857864376269)) ;
#144554 = CARTESIAN_POINT('Origin',(6.9,-0.399999999999999,0.0585786437626901)) ;
#144555 = CARTESIAN_POINT('Origin',(6.9,-0.0585786437626909,0.0585786437626901)) ;
#144556 = CARTESIAN_POINT('Origin',(6.9,-0.0585786437626909,0.4)) ;
#144557 = CARTESIAN_POINT('Origin',(6.9,-0.0585786437626909,0.0585786437626901)) ;
#144558 = CARTESIAN_POINT('Origin',(6.87238576250846,-0.0861928812542305,
-0.0861928812542296)) ;
#144559 = CARTESIAN_POINT('Origin',(6.65857864376269,-0.300000000000001,-0.3)) ;
#144560 = CARTESIAN_POINT('Origin',(6.9,-0.058578643762691,0.0585786437626901)) ;
#144561 = CARTESIAN_POINT('Origin',(6.9,-0.0585786437626911,0.05857864376269)) ;
#144562 = CARTESIAN_POINT('Origin',(6.65857864376269,-0.300000000000001,0.4)) ;
#144563 = CARTESIAN_POINT('Origin',(6.65857864376269,-0.300000000000001,-0.3)) ;
#144564 = CARTESIAN_POINT('Origin',(6.65857864376269,-0.300000000000001,0.3)) ;
#144565 = CARTESIAN_POINT('Origin',(6.60571909584179,-0.352859547920898,0.352859547920897)) ;
#144566 = CARTESIAN_POINT('Origin',(6.65857864376269,-0.300000000000001,0.3)) ;
#144567 = CARTESIAN_POINT('Origin',(0.6,-0.6,-0.3)) ;
#144568 = CARTESIAN_POINT('Origin',(0.3,-0.6,-0.3)) ;
#144569 = CARTESIAN_POINT('Origin',(0.3,-6.1,-0.3)) ;
#144570 = CARTESIAN_POINT('Origin',(0.3,-6.05857864376269,-0.3)) ;
#144571 = CARTESIAN_POINT('Origin',(0.3,-6.05857864376269,-0.3)) ;
#144572 = CARTESIAN_POINT('Origin',(0.3,-6.05857864376269,-0.3)) ;
#144573 = CARTESIAN_POINT('Origin',(0.4,-6.05857864376269,-0.3)) ;
#144574 = CARTESIAN_POINT('Origin',(-0.3,-6.05857864376269,-0.3)) ;
#144575 = CARTESIAN_POINT('Origin',(-0.3,-6.05857864376269,-0.3)) ;
#144576 = CARTESIAN_POINT('Origin',(-0.3,-6.05857864376269,-0.3)) ;
#144577 = CARTESIAN_POINT('Origin',(-0.3,-0.600000000000001,-0.3)) ;
#144578 = CARTESIAN_POINT('Origin',(-0.3,-0.600000000000001,-0.3)) ;
#144579 = CARTESIAN_POINT('Origin',(0.6,-0.600000000000001,-0.3)) ;
#144580 = CARTESIAN_POINT('Origin',(0.6,-0.600000000000001,0.3)) ;
#144581 = CARTESIAN_POINT('Origin',(-0.3,-0.600000000000001,0.3)) ;
#144582 = CARTESIAN_POINT('Origin',(-0.3,-0.600000000000001,0.3)) ;
#144583 = CARTESIAN_POINT('Origin',(-0.3,-6.05857864376269,0.3)) ;
#144584 = CARTESIAN_POINT('Origin',(-0.3,-6.05857864376269,0.3)) ;
#144585 = CARTESIAN_POINT('Origin',(-0.3,-6.05857864376269,0.3)) ;
#144586 = CARTESIAN_POINT('Origin',(0.4,-6.05857864376269,0.3)) ;
#144587 = CARTESIAN_POINT('Origin',(0.299999999999999,-6.05857864376269,0.3)) ;
#144588 = CARTESIAN_POINT('Origin',(0.3,-6.05857864376269,0.3)) ;
#144589 = CARTESIAN_POINT('Origin',(0.3,-6.05857864376269,0.3)) ;
#144590 = CARTESIAN_POINT('Origin',(0.3,-0.600000000000001,0.3)) ;
#144591 = CARTESIAN_POINT('Origin',(0.3,-0.6,0.3)) ;
#144592 = CARTESIAN_POINT('Origin',(0.6,-0.6,0.3)) ;
#144593 = CARTESIAN_POINT('Origin',(6.7,0.300000000000001,-0.3)) ;
#144594 = CARTESIAN_POINT('Origin',(6.65857864376269,0.300000000000001,-0.3)) ;
#144595 = CARTESIAN_POINT('Origin',(6.65857864376269,0.300000000000001,-0.3)) ;
#144596 = CARTESIAN_POINT('Origin',(6.65857864376269,0.300000000000001,-0.3)) ;
#144597 = CARTESIAN_POINT('Origin',(6.65857864376269,-0.399999999999999,-0.3)) ;
#144598 = CARTESIAN_POINT('Origin',(6.65857864376269,-0.300000000000001,-0.3)) ;
#144599 = CARTESIAN_POINT('Origin',(6.65857864376269,-0.300000000000001,-0.3)) ;
#144600 = CARTESIAN_POINT('Origin',(6.65857864376269,-0.300000000000001,-0.3)) ;
#144601 = CARTESIAN_POINT('Origin',(0.6,-0.3,-0.3)) ;
#144602 = CARTESIAN_POINT('Origin',(0.6,0.299999999999999,0.3)) ;
#144603 = CARTESIAN_POINT('Origin',(6.65857864376269,0.300000000000001,0.3)) ;
#144604 = CARTESIAN_POINT('Origin',(6.65857864376269,0.300000000000001,0.3)) ;
#144605 = CARTESIAN_POINT('Origin',(6.65857864376269,0.300000000000001,0.3)) ;
#144606 = CARTESIAN_POINT('Origin',(6.65857864376269,-0.399999999999999,0.3)) ;
#144607 = CARTESIAN_POINT('Origin',(6.65857864376269,-0.300000000000001,0.3)) ;
#144608 = CARTESIAN_POINT('Origin',(0.6,-0.3,0.3)) ;
#144609 = CARTESIAN_POINT('Origin',(6.65857864376269,-0.300000000000001,0.3)) ;
#144610 = CARTESIAN_POINT('Origin',(6.65857864376269,-0.300000000000001,0.3)) ;
#144611 = CARTESIAN_POINT('Origin',(-0.999999999999999,-1.59070596587277E-16,
-34.29)) ;
#144612 = CARTESIAN_POINT('',(-0.999999999999999,-1.9,-33.69)) ;
#144613 = CARTESIAN_POINT('',(-0.999999999999999,-1.9,-33.015)) ;
#144614 = CARTESIAN_POINT('',(-0.999999999999999,-1.9,-32.915)) ;
#144615 = CARTESIAN_POINT('',(-0.999999999999999,1.15,-33.015)) ;
#144616 = CARTESIAN_POINT('',(-0.999999999999999,-2.89663358890162E-17,-33.015)) ;
#144617 = CARTESIAN_POINT('',(-0.999999999999999,1.15,-35.565)) ;
#144618 = CARTESIAN_POINT('',(-0.999999999999999,1.15,-34.29)) ;
#144619 = CARTESIAN_POINT('',(-0.999999999999999,-1.9,-35.565)) ;
#144620 = CARTESIAN_POINT('',(-0.999999999999999,-2.24122726936407E-16,-35.565)) ;
#144621 = CARTESIAN_POINT('',(-0.999999999999999,-1.9,-34.89)) ;
#144622 = CARTESIAN_POINT('',(-0.999999999999999,-1.9,-34.79)) ;
#144623 = CARTESIAN_POINT('',(-0.999999999999999,0.4,-34.89)) ;
#144624 = CARTESIAN_POINT('',(-0.999999999999999,0.5,-34.89)) ;
#144625 = CARTESIAN_POINT('',(-0.999999999999999,0.6,-34.69)) ;
#144626 = CARTESIAN_POINT('Origin',(-0.999999999999999,0.4,-34.69)) ;
#144627 = CARTESIAN_POINT('',(-0.999999999999999,0.6,-33.89)) ;
#144628 = CARTESIAN_POINT('',(-0.999999999999999,0.6,-33.79)) ;
#144629 = CARTESIAN_POINT('',(-0.999999999999999,0.4,-33.69)) ;
#144630 = CARTESIAN_POINT('Origin',(-0.999999999999999,0.4,-33.89)) ;
#144631 = CARTESIAN_POINT('',(-0.999999999999999,-2.,-33.69)) ;
#144632 = CARTESIAN_POINT('Origin',(-0.999999999999999,-1.59070596587277E-16,
-30.48)) ;
#144633 = CARTESIAN_POINT('',(-0.999999999999999,-1.9,-29.88)) ;
#144634 = CARTESIAN_POINT('',(-0.999999999999999,-1.9,-29.205)) ;
#144635 = CARTESIAN_POINT('',(-0.999999999999999,-1.9,-29.105)) ;
#144636 = CARTESIAN_POINT('',(-0.999999999999999,1.15,-29.205)) ;
#144637 = CARTESIAN_POINT('',(-0.999999999999999,-2.89663358890162E-17,-29.205)) ;
#144638 = CARTESIAN_POINT('',(-0.999999999999999,1.15,-31.755)) ;
#144639 = CARTESIAN_POINT('',(-0.999999999999999,1.15,-30.48)) ;
#144640 = CARTESIAN_POINT('',(-0.999999999999999,-1.9,-31.755)) ;
#144641 = CARTESIAN_POINT('',(-0.999999999999999,-2.24122726936407E-16,-31.755)) ;
#144642 = CARTESIAN_POINT('',(-0.999999999999999,-1.9,-31.08)) ;
#144643 = CARTESIAN_POINT('',(-0.999999999999999,-1.9,-30.98)) ;
#144644 = CARTESIAN_POINT('',(-0.999999999999999,0.4,-31.08)) ;
#144645 = CARTESIAN_POINT('',(-0.999999999999999,0.5,-31.08)) ;
#144646 = CARTESIAN_POINT('',(-0.999999999999999,0.6,-30.88)) ;
#144647 = CARTESIAN_POINT('Origin',(-0.999999999999999,0.4,-30.88)) ;
#144648 = CARTESIAN_POINT('',(-0.999999999999999,0.6,-30.08)) ;
#144649 = CARTESIAN_POINT('',(-0.999999999999999,0.6,-29.98)) ;
#144650 = CARTESIAN_POINT('',(-0.999999999999999,0.4,-29.88)) ;
#144651 = CARTESIAN_POINT('Origin',(-0.999999999999999,0.4,-30.08)) ;
#144652 = CARTESIAN_POINT('',(-0.999999999999999,-2.,-29.88)) ;
#144653 = CARTESIAN_POINT('Origin',(-0.999999999999999,-1.59070596587277E-16,
-26.67)) ;
#144654 = CARTESIAN_POINT('',(-0.999999999999999,-1.9,-26.07)) ;
#144655 = CARTESIAN_POINT('',(-0.999999999999999,-1.9,-25.395)) ;
#144656 = CARTESIAN_POINT('',(-0.999999999999999,-1.9,-25.295)) ;
#144657 = CARTESIAN_POINT('',(-0.999999999999999,1.15,-25.395)) ;
#144658 = CARTESIAN_POINT('',(-0.999999999999999,-2.89663358890162E-17,-25.395)) ;
#144659 = CARTESIAN_POINT('',(-0.999999999999999,1.15,-27.945)) ;
#144660 = CARTESIAN_POINT('',(-0.999999999999999,1.15,-26.67)) ;
#144661 = CARTESIAN_POINT('',(-0.999999999999999,-1.9,-27.945)) ;
#144662 = CARTESIAN_POINT('',(-0.999999999999999,-2.24122726936407E-16,-27.945)) ;
#144663 = CARTESIAN_POINT('',(-0.999999999999999,-1.9,-27.27)) ;
#144664 = CARTESIAN_POINT('',(-0.999999999999999,-1.9,-27.17)) ;
#144665 = CARTESIAN_POINT('',(-0.999999999999999,0.4,-27.27)) ;
#144666 = CARTESIAN_POINT('',(-0.999999999999999,0.5,-27.27)) ;
#144667 = CARTESIAN_POINT('',(-0.999999999999999,0.6,-27.07)) ;
#144668 = CARTESIAN_POINT('Origin',(-0.999999999999999,0.4,-27.07)) ;
#144669 = CARTESIAN_POINT('',(-0.999999999999999,0.6,-26.27)) ;
#144670 = CARTESIAN_POINT('',(-0.999999999999999,0.6,-26.17)) ;
#144671 = CARTESIAN_POINT('',(-0.999999999999999,0.4,-26.07)) ;
#144672 = CARTESIAN_POINT('Origin',(-0.999999999999999,0.4,-26.27)) ;
#144673 = CARTESIAN_POINT('',(-0.999999999999999,-2.,-26.07)) ;
#144674 = CARTESIAN_POINT('Origin',(-0.999999999999999,-1.59070596587277E-16,
-22.86)) ;
#144675 = CARTESIAN_POINT('',(-0.999999999999999,-1.9,-22.26)) ;
#144676 = CARTESIAN_POINT('',(-0.999999999999999,-1.9,-21.585)) ;
#144677 = CARTESIAN_POINT('',(-0.999999999999999,-1.9,-21.485)) ;
#144678 = CARTESIAN_POINT('',(-0.999999999999999,1.15,-21.585)) ;
#144679 = CARTESIAN_POINT('',(-0.999999999999999,-2.89663358890162E-17,-21.585)) ;
#144680 = CARTESIAN_POINT('',(-0.999999999999999,1.15,-24.135)) ;
#144681 = CARTESIAN_POINT('',(-0.999999999999999,1.15,-22.86)) ;
#144682 = CARTESIAN_POINT('',(-0.999999999999999,-1.9,-24.135)) ;
#144683 = CARTESIAN_POINT('',(-0.999999999999999,-2.24122726936407E-16,-24.135)) ;
#144684 = CARTESIAN_POINT('',(-0.999999999999999,-1.9,-23.46)) ;
#144685 = CARTESIAN_POINT('',(-0.999999999999999,-1.9,-23.36)) ;
#144686 = CARTESIAN_POINT('',(-0.999999999999999,0.4,-23.46)) ;
#144687 = CARTESIAN_POINT('',(-0.999999999999999,0.5,-23.46)) ;
#144688 = CARTESIAN_POINT('',(-0.999999999999999,0.6,-23.26)) ;
#144689 = CARTESIAN_POINT('Origin',(-0.999999999999999,0.4,-23.26)) ;
#144690 = CARTESIAN_POINT('',(-0.999999999999999,0.6,-22.46)) ;
#144691 = CARTESIAN_POINT('',(-0.999999999999999,0.6,-22.36)) ;
#144692 = CARTESIAN_POINT('',(-0.999999999999999,0.4,-22.26)) ;
#144693 = CARTESIAN_POINT('Origin',(-0.999999999999999,0.4,-22.46)) ;
#144694 = CARTESIAN_POINT('',(-0.999999999999999,-2.,-22.26)) ;
#144695 = CARTESIAN_POINT('Origin',(-0.999999999999999,-1.59070596587277E-16,
-19.05)) ;
#144696 = CARTESIAN_POINT('',(-0.999999999999999,-1.9,-18.45)) ;
#144697 = CARTESIAN_POINT('',(-0.999999999999999,-1.9,-17.775)) ;
#144698 = CARTESIAN_POINT('',(-0.999999999999999,-1.9,-17.675)) ;
#144699 = CARTESIAN_POINT('',(-0.999999999999999,1.15,-17.775)) ;
#144700 = CARTESIAN_POINT('',(-0.999999999999999,-2.89663358890162E-17,-17.775)) ;
#144701 = CARTESIAN_POINT('',(-0.999999999999999,1.15,-20.325)) ;
#144702 = CARTESIAN_POINT('',(-0.999999999999999,1.15,-19.05)) ;
#144703 = CARTESIAN_POINT('',(-0.999999999999999,-1.9,-20.325)) ;
#144704 = CARTESIAN_POINT('',(-0.999999999999999,-2.24122726936407E-16,-20.325)) ;
#144705 = CARTESIAN_POINT('',(-0.999999999999999,-1.9,-19.65)) ;
#144706 = CARTESIAN_POINT('',(-0.999999999999999,-1.9,-19.55)) ;
#144707 = CARTESIAN_POINT('',(-0.999999999999999,0.4,-19.65)) ;
#144708 = CARTESIAN_POINT('',(-0.999999999999999,0.5,-19.65)) ;
#144709 = CARTESIAN_POINT('',(-0.999999999999999,0.6,-19.45)) ;
#144710 = CARTESIAN_POINT('Origin',(-0.999999999999999,0.4,-19.45)) ;
#144711 = CARTESIAN_POINT('',(-0.999999999999999,0.6,-18.65)) ;
#144712 = CARTESIAN_POINT('',(-0.999999999999999,0.6,-18.55)) ;
#144713 = CARTESIAN_POINT('',(-0.999999999999999,0.4,-18.45)) ;
#144714 = CARTESIAN_POINT('Origin',(-0.999999999999999,0.4,-18.65)) ;
#144715 = CARTESIAN_POINT('',(-0.999999999999999,-2.,-18.45)) ;
#144716 = CARTESIAN_POINT('Origin',(-0.999999999999999,-1.59070596587277E-16,
-15.24)) ;
#144717 = CARTESIAN_POINT('',(-0.999999999999999,-1.9,-14.64)) ;
#144718 = CARTESIAN_POINT('',(-0.999999999999999,-1.9,-13.965)) ;
#144719 = CARTESIAN_POINT('',(-0.999999999999999,-1.9,-13.865)) ;
#144720 = CARTESIAN_POINT('',(-0.999999999999999,1.15,-13.965)) ;
#144721 = CARTESIAN_POINT('',(-0.999999999999999,-2.8966335889016E-17,-13.965)) ;
#144722 = CARTESIAN_POINT('',(-0.999999999999999,1.15,-16.515)) ;
#144723 = CARTESIAN_POINT('',(-0.999999999999999,1.15,-15.24)) ;
#144724 = CARTESIAN_POINT('',(-0.999999999999999,-1.9,-16.515)) ;
#144725 = CARTESIAN_POINT('',(-0.999999999999999,-2.24122726936407E-16,-16.515)) ;
#144726 = CARTESIAN_POINT('',(-0.999999999999999,-1.9,-15.84)) ;
#144727 = CARTESIAN_POINT('',(-0.999999999999999,-1.9,-15.74)) ;
#144728 = CARTESIAN_POINT('',(-0.999999999999999,0.4,-15.84)) ;
#144729 = CARTESIAN_POINT('',(-0.999999999999999,0.5,-15.84)) ;
#144730 = CARTESIAN_POINT('',(-0.999999999999999,0.6,-15.64)) ;
#144731 = CARTESIAN_POINT('Origin',(-0.999999999999999,0.4,-15.64)) ;
#144732 = CARTESIAN_POINT('',(-0.999999999999999,0.6,-14.84)) ;
#144733 = CARTESIAN_POINT('',(-0.999999999999999,0.6,-14.74)) ;
#144734 = CARTESIAN_POINT('',(-0.999999999999999,0.4,-14.64)) ;
#144735 = CARTESIAN_POINT('Origin',(-0.999999999999999,0.4,-14.84)) ;
#144736 = CARTESIAN_POINT('',(-0.999999999999999,-2.,-14.64)) ;
#144737 = CARTESIAN_POINT('Origin',(-0.999999999999999,-1.59070596587277E-16,
-11.43)) ;
#144738 = CARTESIAN_POINT('',(-0.999999999999999,-1.9,-10.83)) ;
#144739 = CARTESIAN_POINT('',(-0.999999999999999,-1.9,-10.155)) ;
#144740 = CARTESIAN_POINT('',(-0.999999999999999,-1.9,-10.055)) ;
#144741 = CARTESIAN_POINT('',(-0.999999999999999,1.15,-10.155)) ;
#144742 = CARTESIAN_POINT('',(-0.999999999999999,-2.8966335889016E-17,-10.155)) ;
#144743 = CARTESIAN_POINT('',(-0.999999999999999,1.15,-12.705)) ;
#144744 = CARTESIAN_POINT('',(-0.999999999999999,1.15,-11.43)) ;
#144745 = CARTESIAN_POINT('',(-0.999999999999999,-1.9,-12.705)) ;
#144746 = CARTESIAN_POINT('',(-0.999999999999999,-2.24122726936407E-16,-12.705)) ;
#144747 = CARTESIAN_POINT('',(-0.999999999999999,-1.9,-12.03)) ;
#144748 = CARTESIAN_POINT('',(-0.999999999999999,-1.9,-11.93)) ;
#144749 = CARTESIAN_POINT('',(-0.999999999999999,0.4,-12.03)) ;
#144750 = CARTESIAN_POINT('',(-0.999999999999999,0.5,-12.03)) ;
#144751 = CARTESIAN_POINT('',(-0.999999999999999,0.6,-11.83)) ;
#144752 = CARTESIAN_POINT('Origin',(-0.999999999999999,0.4,-11.83)) ;
#144753 = CARTESIAN_POINT('',(-0.999999999999999,0.6,-11.03)) ;
#144754 = CARTESIAN_POINT('',(-0.999999999999999,0.6,-10.93)) ;
#144755 = CARTESIAN_POINT('',(-0.999999999999999,0.4,-10.83)) ;
#144756 = CARTESIAN_POINT('Origin',(-0.999999999999999,0.4,-11.03)) ;
#144757 = CARTESIAN_POINT('',(-0.999999999999999,-2.,-10.83)) ;
#144758 = CARTESIAN_POINT('Origin',(-0.999999999999999,-1.59070596587277E-16,
-7.62)) ;
#144759 = CARTESIAN_POINT('',(-0.999999999999999,-1.9,-7.02)) ;
#144760 = CARTESIAN_POINT('',(-0.999999999999999,-1.9,-6.345)) ;
#144761 = CARTESIAN_POINT('',(-0.999999999999999,-1.9,-6.245)) ;
#144762 = CARTESIAN_POINT('',(-0.999999999999999,1.15,-6.345)) ;
#144763 = CARTESIAN_POINT('',(-0.999999999999999,-2.89663358890161E-17,-6.345)) ;
#144764 = CARTESIAN_POINT('',(-0.999999999999999,1.15,-8.895)) ;
#144765 = CARTESIAN_POINT('',(-0.999999999999999,1.15,-7.62)) ;
#144766 = CARTESIAN_POINT('',(-0.999999999999999,-1.9,-8.895)) ;
#144767 = CARTESIAN_POINT('',(-0.999999999999999,-2.24122726936407E-16,-8.895)) ;
#144768 = CARTESIAN_POINT('',(-0.999999999999999,-1.9,-8.22)) ;
#144769 = CARTESIAN_POINT('',(-0.999999999999999,-1.9,-8.12)) ;
#144770 = CARTESIAN_POINT('',(-0.999999999999999,0.4,-8.22)) ;
#144771 = CARTESIAN_POINT('',(-0.999999999999999,0.5,-8.22)) ;
#144772 = CARTESIAN_POINT('',(-0.999999999999999,0.6,-8.02)) ;
#144773 = CARTESIAN_POINT('Origin',(-0.999999999999999,0.4,-8.02)) ;
#144774 = CARTESIAN_POINT('',(-0.999999999999999,0.6,-7.22)) ;
#144775 = CARTESIAN_POINT('',(-0.999999999999999,0.6,-7.12)) ;
#144776 = CARTESIAN_POINT('',(-0.999999999999999,0.4,-7.02)) ;
#144777 = CARTESIAN_POINT('Origin',(-0.999999999999999,0.4,-7.22)) ;
#144778 = CARTESIAN_POINT('',(-0.999999999999999,-2.,-7.02)) ;
#144779 = CARTESIAN_POINT('Origin',(-0.999999999999999,-1.59070596587277E-16,
-3.81)) ;
#144780 = CARTESIAN_POINT('',(-0.999999999999999,-1.9,-3.21)) ;
#144781 = CARTESIAN_POINT('',(-0.999999999999999,-1.9,-2.535)) ;
#144782 = CARTESIAN_POINT('',(-0.999999999999999,-1.9,-2.435)) ;
#144783 = CARTESIAN_POINT('',(-0.999999999999999,1.15,-2.535)) ;
#144784 = CARTESIAN_POINT('',(-0.999999999999999,-2.89663358890161E-17,-2.535)) ;
#144785 = CARTESIAN_POINT('',(-0.999999999999999,1.15,-5.085)) ;
#144786 = CARTESIAN_POINT('',(-0.999999999999999,1.15,-3.81)) ;
#144787 = CARTESIAN_POINT('',(-0.999999999999999,-1.9,-5.085)) ;
#144788 = CARTESIAN_POINT('',(-0.999999999999999,-2.24122726936407E-16,-5.085)) ;
#144789 = CARTESIAN_POINT('',(-0.999999999999999,-1.9,-4.41)) ;
#144790 = CARTESIAN_POINT('',(-0.999999999999999,-1.9,-4.31)) ;
#144791 = CARTESIAN_POINT('',(-0.999999999999999,0.4,-4.41)) ;
#144792 = CARTESIAN_POINT('',(-0.999999999999999,0.5,-4.41)) ;
#144793 = CARTESIAN_POINT('',(-0.999999999999999,0.6,-4.21)) ;
#144794 = CARTESIAN_POINT('Origin',(-0.999999999999999,0.4,-4.21)) ;
#144795 = CARTESIAN_POINT('',(-0.999999999999999,0.6,-3.41)) ;
#144796 = CARTESIAN_POINT('',(-0.999999999999999,0.6,-3.31)) ;
#144797 = CARTESIAN_POINT('',(-0.999999999999999,0.4,-3.21)) ;
#144798 = CARTESIAN_POINT('Origin',(-0.999999999999999,0.4,-3.41)) ;
#144799 = CARTESIAN_POINT('',(-0.999999999999999,-2.,-3.21)) ;
#144800 = CARTESIAN_POINT('Origin',(0.600000000000001,-2.,-4.31)) ;
#144801 = CARTESIAN_POINT('',(0.500000000000001,-2.,-4.41)) ;
#144802 = CARTESIAN_POINT('',(-0.899999999999999,-2.,-4.41)) ;
#144803 = CARTESIAN_POINT('',(0.600000000000001,-2.,-4.41)) ;
#144804 = CARTESIAN_POINT('',(-0.899999999999999,-2.,-5.085)) ;
#144805 = CARTESIAN_POINT('',(-0.899999999999999,-2.,-5.185)) ;
#144806 = CARTESIAN_POINT('',(0.500000000000001,-2.,-5.085)) ;
#144807 = CARTESIAN_POINT('',(0.600000000000001,-2.,-5.085)) ;
#144808 = CARTESIAN_POINT('',(0.500000000000001,-2.,-4.31)) ;
#144809 = CARTESIAN_POINT('Origin',(0.600000000000001,0.5,-4.31)) ;
#144810 = CARTESIAN_POINT('',(-0.899999999999999,0.4,-4.31)) ;
#144811 = CARTESIAN_POINT('',(-0.999999999999999,0.4,-4.31)) ;
#144812 = CARTESIAN_POINT('',(-0.899999999999999,-1.9,-4.31)) ;
#144813 = CARTESIAN_POINT('',(-0.899999999999999,-2.,-4.31)) ;
#144814 = CARTESIAN_POINT('',(0.600000000000001,-1.9,-4.31)) ;
#144815 = CARTESIAN_POINT('Origin',(0.600000000000001,0.5,-3.31)) ;
#144816 = CARTESIAN_POINT('',(0.500000000000001,0.5,-3.41)) ;
#144817 = CARTESIAN_POINT('',(-0.899999999999999,0.5,-3.41)) ;
#144818 = CARTESIAN_POINT('',(-0.999999999999999,0.5,-3.41)) ;
#144819 = CARTESIAN_POINT('',(-0.899999999999999,0.5,-4.21)) ;
#144820 = CARTESIAN_POINT('',(-0.899999999999999,0.5,-4.31)) ;
#144821 = CARTESIAN_POINT('',(0.500000000000001,0.5,-4.21)) ;
#144822 = CARTESIAN_POINT('',(0.600000000000001,0.5,-4.21)) ;
#144823 = CARTESIAN_POINT('',(0.500000000000001,0.5,-3.31)) ;
#144824 = CARTESIAN_POINT('Origin',(0.600000000000001,-2.,-3.31)) ;
#144825 = CARTESIAN_POINT('',(0.500000000000001,-1.9,-3.31)) ;
#144826 = CARTESIAN_POINT('',(-0.899999999999999,-1.9,-3.31)) ;
#144827 = CARTESIAN_POINT('',(0.600000000000001,-1.9,-3.31)) ;
#144828 = CARTESIAN_POINT('',(-0.899999999999999,0.4,-3.31)) ;
#144829 = CARTESIAN_POINT('',(-0.899999999999999,0.5,-3.31)) ;
#144830 = CARTESIAN_POINT('',(0.500000000000001,0.4,-3.31)) ;
#144831 = CARTESIAN_POINT('',(0.600000000000001,0.4,-3.31)) ;
#144832 = CARTESIAN_POINT('',(0.500000000000001,-2.,-3.31)) ;
#144833 = CARTESIAN_POINT('Origin',(0.600000000000001,-2.,-2.435)) ;
#144834 = CARTESIAN_POINT('',(0.500000000000001,-2.,-2.535)) ;
#144835 = CARTESIAN_POINT('',(-0.899999999999999,-2.,-2.535)) ;
#144836 = CARTESIAN_POINT('',(-0.999999999999999,-2.,-2.535)) ;
#144837 = CARTESIAN_POINT('',(-0.899999999999999,-2.,-3.21)) ;
#144838 = CARTESIAN_POINT('',(-0.899999999999999,-2.,-3.31)) ;
#144839 = CARTESIAN_POINT('',(0.500000000000001,-2.,-3.21)) ;
#144840 = CARTESIAN_POINT('',(0.600000000000001,-2.,-3.21)) ;
#144841 = CARTESIAN_POINT('',(0.500000000000001,-2.,-2.435)) ;
#144842 = CARTESIAN_POINT('Origin',(0.600000000000001,-2.,-8.12)) ;
#144843 = CARTESIAN_POINT('',(0.500000000000001,-2.,-8.22)) ;
#144844 = CARTESIAN_POINT('',(-0.899999999999999,-2.,-8.22)) ;
#144845 = CARTESIAN_POINT('',(0.600000000000001,-2.,-8.22)) ;
#144846 = CARTESIAN_POINT('',(-0.899999999999999,-2.,-8.895)) ;
#144847 = CARTESIAN_POINT('',(-0.899999999999999,-2.,-8.995)) ;
#144848 = CARTESIAN_POINT('',(0.500000000000001,-2.,-8.895)) ;
#144849 = CARTESIAN_POINT('',(0.600000000000001,-2.,-8.895)) ;
#144850 = CARTESIAN_POINT('',(0.500000000000001,-2.,-8.12)) ;
#144851 = CARTESIAN_POINT('Origin',(0.600000000000001,0.5,-8.12)) ;
#144852 = CARTESIAN_POINT('',(-0.899999999999999,0.4,-8.12)) ;
#144853 = CARTESIAN_POINT('',(-0.999999999999999,0.4,-8.12)) ;
#144854 = CARTESIAN_POINT('',(-0.899999999999999,-1.9,-8.12)) ;
#144855 = CARTESIAN_POINT('',(-0.899999999999999,-2.,-8.12)) ;
#144856 = CARTESIAN_POINT('',(0.600000000000001,-1.9,-8.12)) ;
#144857 = CARTESIAN_POINT('Origin',(0.600000000000001,0.5,-7.12)) ;
#144858 = CARTESIAN_POINT('',(0.500000000000001,0.5,-7.22)) ;
#144859 = CARTESIAN_POINT('',(-0.899999999999999,0.5,-7.22)) ;
#144860 = CARTESIAN_POINT('',(-0.999999999999999,0.5,-7.22)) ;
#144861 = CARTESIAN_POINT('',(-0.899999999999999,0.5,-8.02)) ;
#144862 = CARTESIAN_POINT('',(-0.899999999999999,0.5,-8.12)) ;
#144863 = CARTESIAN_POINT('',(0.500000000000001,0.5,-8.02)) ;
#144864 = CARTESIAN_POINT('',(0.600000000000001,0.5,-8.02)) ;
#144865 = CARTESIAN_POINT('',(0.500000000000001,0.5,-7.12)) ;
#144866 = CARTESIAN_POINT('Origin',(0.600000000000001,-2.,-7.12)) ;
#144867 = CARTESIAN_POINT('',(0.500000000000001,-1.9,-7.12)) ;
#144868 = CARTESIAN_POINT('',(-0.899999999999999,-1.9,-7.12)) ;
#144869 = CARTESIAN_POINT('',(0.600000000000001,-1.9,-7.12)) ;
#144870 = CARTESIAN_POINT('',(-0.899999999999999,0.4,-7.12)) ;
#144871 = CARTESIAN_POINT('',(-0.899999999999999,0.5,-7.12)) ;
#144872 = CARTESIAN_POINT('',(0.500000000000001,0.4,-7.12)) ;
#144873 = CARTESIAN_POINT('',(0.600000000000001,0.4,-7.12)) ;
#144874 = CARTESIAN_POINT('',(0.500000000000001,-2.,-7.12)) ;
#144875 = CARTESIAN_POINT('Origin',(0.600000000000001,-2.,-6.245)) ;
#144876 = CARTESIAN_POINT('',(0.500000000000001,-2.,-6.345)) ;
#144877 = CARTESIAN_POINT('',(-0.899999999999999,-2.,-6.345)) ;
#144878 = CARTESIAN_POINT('',(-0.999999999999999,-2.,-6.345)) ;
#144879 = CARTESIAN_POINT('',(-0.899999999999999,-2.,-7.02)) ;
#144880 = CARTESIAN_POINT('',(-0.899999999999999,-2.,-7.12)) ;
#144881 = CARTESIAN_POINT('',(0.500000000000001,-2.,-7.02)) ;
#144882 = CARTESIAN_POINT('',(0.600000000000001,-2.,-7.02)) ;
#144883 = CARTESIAN_POINT('',(0.500000000000001,-2.,-6.245)) ;
#144884 = CARTESIAN_POINT('Origin',(0.600000000000001,-2.,-11.93)) ;
#144885 = CARTESIAN_POINT('',(0.500000000000001,-2.,-12.03)) ;
#144886 = CARTESIAN_POINT('',(-0.899999999999999,-2.,-12.03)) ;
#144887 = CARTESIAN_POINT('',(0.600000000000001,-2.,-12.03)) ;
#144888 = CARTESIAN_POINT('',(-0.899999999999999,-2.,-12.705)) ;
#144889 = CARTESIAN_POINT('',(-0.899999999999999,-2.,-12.805)) ;
#144890 = CARTESIAN_POINT('',(0.500000000000001,-2.,-12.705)) ;
#144891 = CARTESIAN_POINT('',(0.600000000000001,-2.,-12.705)) ;
#144892 = CARTESIAN_POINT('',(0.500000000000001,-2.,-11.93)) ;
#144893 = CARTESIAN_POINT('Origin',(0.600000000000001,0.5,-11.93)) ;
#144894 = CARTESIAN_POINT('',(-0.899999999999999,0.4,-11.93)) ;
#144895 = CARTESIAN_POINT('',(-0.999999999999999,0.4,-11.93)) ;
#144896 = CARTESIAN_POINT('',(-0.899999999999999,-1.9,-11.93)) ;
#144897 = CARTESIAN_POINT('',(-0.899999999999999,-2.,-11.93)) ;
#144898 = CARTESIAN_POINT('',(0.600000000000001,-1.9,-11.93)) ;
#144899 = CARTESIAN_POINT('Origin',(0.600000000000001,0.5,-10.93)) ;
#144900 = CARTESIAN_POINT('',(0.500000000000001,0.5,-11.03)) ;
#144901 = CARTESIAN_POINT('',(-0.899999999999999,0.5,-11.03)) ;
#144902 = CARTESIAN_POINT('',(-0.999999999999999,0.5,-11.03)) ;
#144903 = CARTESIAN_POINT('',(-0.899999999999999,0.5,-11.83)) ;
#144904 = CARTESIAN_POINT('',(-0.899999999999999,0.5,-11.93)) ;
#144905 = CARTESIAN_POINT('',(0.500000000000001,0.5,-11.83)) ;
#144906 = CARTESIAN_POINT('',(0.600000000000001,0.5,-11.83)) ;
#144907 = CARTESIAN_POINT('',(0.500000000000001,0.5,-10.93)) ;
#144908 = CARTESIAN_POINT('Origin',(0.600000000000001,-2.,-10.93)) ;
#144909 = CARTESIAN_POINT('',(0.500000000000001,-1.9,-10.93)) ;
#144910 = CARTESIAN_POINT('',(-0.899999999999999,-1.9,-10.93)) ;
#144911 = CARTESIAN_POINT('',(0.600000000000001,-1.9,-10.93)) ;
#144912 = CARTESIAN_POINT('',(-0.899999999999999,0.4,-10.93)) ;
#144913 = CARTESIAN_POINT('',(-0.899999999999999,0.5,-10.93)) ;
#144914 = CARTESIAN_POINT('',(0.500000000000001,0.4,-10.93)) ;
#144915 = CARTESIAN_POINT('',(0.600000000000001,0.4,-10.93)) ;
#144916 = CARTESIAN_POINT('',(0.500000000000001,-2.,-10.93)) ;
#144917 = CARTESIAN_POINT('Origin',(0.600000000000001,-2.,-10.055)) ;
#144918 = CARTESIAN_POINT('',(0.500000000000001,-2.,-10.155)) ;
#144919 = CARTESIAN_POINT('',(-0.899999999999999,-2.,-10.155)) ;
#144920 = CARTESIAN_POINT('',(-0.999999999999999,-2.,-10.155)) ;
#144921 = CARTESIAN_POINT('',(-0.899999999999999,-2.,-10.83)) ;
#144922 = CARTESIAN_POINT('',(-0.899999999999999,-2.,-10.93)) ;
#144923 = CARTESIAN_POINT('',(0.500000000000001,-2.,-10.83)) ;
#144924 = CARTESIAN_POINT('',(0.600000000000001,-2.,-10.83)) ;
#144925 = CARTESIAN_POINT('',(0.500000000000001,-2.,-10.055)) ;
#144926 = CARTESIAN_POINT('Origin',(0.600000000000001,-2.,-15.74)) ;
#144927 = CARTESIAN_POINT('',(0.500000000000001,-2.,-15.84)) ;
#144928 = CARTESIAN_POINT('',(-0.899999999999999,-2.,-15.84)) ;
#144929 = CARTESIAN_POINT('',(0.600000000000001,-2.,-15.84)) ;
#144930 = CARTESIAN_POINT('',(-0.899999999999999,-2.,-16.515)) ;
#144931 = CARTESIAN_POINT('',(-0.899999999999999,-2.,-16.615)) ;
#144932 = CARTESIAN_POINT('',(0.500000000000001,-2.,-16.515)) ;
#144933 = CARTESIAN_POINT('',(0.600000000000001,-2.,-16.515)) ;
#144934 = CARTESIAN_POINT('',(0.500000000000001,-2.,-15.74)) ;
#144935 = CARTESIAN_POINT('Origin',(0.600000000000001,0.5,-15.74)) ;
#144936 = CARTESIAN_POINT('',(-0.899999999999999,0.4,-15.74)) ;
#144937 = CARTESIAN_POINT('',(-0.999999999999999,0.4,-15.74)) ;
#144938 = CARTESIAN_POINT('',(-0.899999999999999,-1.9,-15.74)) ;
#144939 = CARTESIAN_POINT('',(-0.899999999999999,-2.,-15.74)) ;
#144940 = CARTESIAN_POINT('',(0.600000000000001,-1.9,-15.74)) ;
#144941 = CARTESIAN_POINT('Origin',(0.600000000000001,0.5,-14.74)) ;
#144942 = CARTESIAN_POINT('',(0.500000000000001,0.5,-14.84)) ;
#144943 = CARTESIAN_POINT('',(-0.899999999999999,0.5,-14.84)) ;
#144944 = CARTESIAN_POINT('',(-0.999999999999999,0.5,-14.84)) ;
#144945 = CARTESIAN_POINT('',(-0.899999999999999,0.5,-15.64)) ;
#144946 = CARTESIAN_POINT('',(-0.899999999999999,0.5,-15.74)) ;
#144947 = CARTESIAN_POINT('',(0.500000000000001,0.5,-15.64)) ;
#144948 = CARTESIAN_POINT('',(0.600000000000001,0.5,-15.64)) ;
#144949 = CARTESIAN_POINT('',(0.500000000000001,0.5,-14.74)) ;
#144950 = CARTESIAN_POINT('Origin',(0.600000000000001,-2.,-14.74)) ;
#144951 = CARTESIAN_POINT('',(0.500000000000001,-1.9,-14.74)) ;
#144952 = CARTESIAN_POINT('',(-0.899999999999999,-1.9,-14.74)) ;
#144953 = CARTESIAN_POINT('',(0.600000000000001,-1.9,-14.74)) ;
#144954 = CARTESIAN_POINT('',(-0.899999999999999,0.4,-14.74)) ;
#144955 = CARTESIAN_POINT('',(-0.899999999999999,0.5,-14.74)) ;
#144956 = CARTESIAN_POINT('',(0.500000000000001,0.4,-14.74)) ;
#144957 = CARTESIAN_POINT('',(0.600000000000001,0.4,-14.74)) ;
#144958 = CARTESIAN_POINT('',(0.500000000000001,-2.,-14.74)) ;
#144959 = CARTESIAN_POINT('Origin',(0.600000000000001,-2.,-13.865)) ;
#144960 = CARTESIAN_POINT('',(0.500000000000001,-2.,-13.965)) ;
#144961 = CARTESIAN_POINT('',(-0.899999999999999,-2.,-13.965)) ;
#144962 = CARTESIAN_POINT('',(-0.999999999999999,-2.,-13.965)) ;
#144963 = CARTESIAN_POINT('',(-0.899999999999999,-2.,-14.64)) ;
#144964 = CARTESIAN_POINT('',(-0.899999999999999,-2.,-14.74)) ;
#144965 = CARTESIAN_POINT('',(0.500000000000001,-2.,-14.64)) ;
#144966 = CARTESIAN_POINT('',(0.600000000000001,-2.,-14.64)) ;
#144967 = CARTESIAN_POINT('',(0.500000000000001,-2.,-13.865)) ;
#144968 = CARTESIAN_POINT('Origin',(0.600000000000001,-2.,-19.55)) ;
#144969 = CARTESIAN_POINT('',(0.500000000000001,-2.,-19.65)) ;
#144970 = CARTESIAN_POINT('',(-0.899999999999999,-2.,-19.65)) ;
#144971 = CARTESIAN_POINT('',(0.600000000000001,-2.,-19.65)) ;
#144972 = CARTESIAN_POINT('',(-0.899999999999999,-2.,-20.325)) ;
#144973 = CARTESIAN_POINT('',(-0.899999999999999,-2.,-20.425)) ;
#144974 = CARTESIAN_POINT('',(0.500000000000001,-2.,-20.325)) ;
#144975 = CARTESIAN_POINT('',(0.600000000000001,-2.,-20.325)) ;
#144976 = CARTESIAN_POINT('',(0.500000000000001,-2.,-19.55)) ;
#144977 = CARTESIAN_POINT('Origin',(0.600000000000001,0.5,-19.55)) ;
#144978 = CARTESIAN_POINT('',(-0.899999999999999,0.4,-19.55)) ;
#144979 = CARTESIAN_POINT('',(-0.999999999999999,0.4,-19.55)) ;
#144980 = CARTESIAN_POINT('',(-0.899999999999999,-1.9,-19.55)) ;
#144981 = CARTESIAN_POINT('',(-0.899999999999999,-2.,-19.55)) ;
#144982 = CARTESIAN_POINT('',(0.600000000000001,-1.9,-19.55)) ;
#144983 = CARTESIAN_POINT('Origin',(0.600000000000001,0.5,-18.55)) ;
#144984 = CARTESIAN_POINT('',(0.500000000000001,0.5,-18.65)) ;
#144985 = CARTESIAN_POINT('',(-0.899999999999999,0.5,-18.65)) ;
#144986 = CARTESIAN_POINT('',(-0.999999999999999,0.5,-18.65)) ;
#144987 = CARTESIAN_POINT('',(-0.899999999999999,0.5,-19.45)) ;
#144988 = CARTESIAN_POINT('',(-0.899999999999999,0.5,-19.55)) ;
#144989 = CARTESIAN_POINT('',(0.500000000000001,0.5,-19.45)) ;
#144990 = CARTESIAN_POINT('',(0.600000000000001,0.5,-19.45)) ;
#144991 = CARTESIAN_POINT('',(0.500000000000001,0.5,-18.55)) ;
#144992 = CARTESIAN_POINT('Origin',(0.600000000000001,-2.,-18.55)) ;
#144993 = CARTESIAN_POINT('',(0.500000000000001,-1.9,-18.55)) ;
#144994 = CARTESIAN_POINT('',(-0.899999999999999,-1.9,-18.55)) ;
#144995 = CARTESIAN_POINT('',(0.600000000000001,-1.9,-18.55)) ;
#144996 = CARTESIAN_POINT('',(-0.899999999999999,0.4,-18.55)) ;
#144997 = CARTESIAN_POINT('',(-0.899999999999999,0.5,-18.55)) ;
#144998 = CARTESIAN_POINT('',(0.500000000000001,0.4,-18.55)) ;
#144999 = CARTESIAN_POINT('',(0.600000000000001,0.4,-18.55)) ;
#145000 = CARTESIAN_POINT('',(0.500000000000001,-2.,-18.55)) ;
#145001 = CARTESIAN_POINT('Origin',(0.600000000000001,-2.,-17.675)) ;
#145002 = CARTESIAN_POINT('',(0.500000000000001,-2.,-17.775)) ;
#145003 = CARTESIAN_POINT('',(-0.899999999999999,-2.,-17.775)) ;
#145004 = CARTESIAN_POINT('',(-0.999999999999999,-2.,-17.775)) ;
#145005 = CARTESIAN_POINT('',(-0.899999999999999,-2.,-18.45)) ;
#145006 = CARTESIAN_POINT('',(-0.899999999999999,-2.,-18.55)) ;
#145007 = CARTESIAN_POINT('',(0.500000000000001,-2.,-18.45)) ;
#145008 = CARTESIAN_POINT('',(0.600000000000001,-2.,-18.45)) ;
#145009 = CARTESIAN_POINT('',(0.500000000000001,-2.,-17.675)) ;
#145010 = CARTESIAN_POINT('Origin',(0.600000000000001,-2.,-23.36)) ;
#145011 = CARTESIAN_POINT('',(0.500000000000001,-2.,-23.46)) ;
#145012 = CARTESIAN_POINT('',(-0.899999999999999,-2.,-23.46)) ;
#145013 = CARTESIAN_POINT('',(0.600000000000001,-2.,-23.46)) ;
#145014 = CARTESIAN_POINT('',(-0.899999999999999,-2.,-24.135)) ;
#145015 = CARTESIAN_POINT('',(-0.899999999999999,-2.,-24.235)) ;
#145016 = CARTESIAN_POINT('',(0.500000000000001,-2.,-24.135)) ;
#145017 = CARTESIAN_POINT('',(0.600000000000001,-2.,-24.135)) ;
#145018 = CARTESIAN_POINT('',(0.500000000000001,-2.,-23.36)) ;
#145019 = CARTESIAN_POINT('Origin',(0.600000000000001,0.5,-23.36)) ;
#145020 = CARTESIAN_POINT('',(-0.899999999999999,0.4,-23.36)) ;
#145021 = CARTESIAN_POINT('',(-0.999999999999999,0.4,-23.36)) ;
#145022 = CARTESIAN_POINT('',(-0.899999999999999,-1.9,-23.36)) ;
#145023 = CARTESIAN_POINT('',(-0.899999999999999,-2.,-23.36)) ;
#145024 = CARTESIAN_POINT('',(0.600000000000001,-1.9,-23.36)) ;
#145025 = CARTESIAN_POINT('Origin',(0.600000000000001,0.5,-22.36)) ;
#145026 = CARTESIAN_POINT('',(0.500000000000001,0.5,-22.46)) ;
#145027 = CARTESIAN_POINT('',(-0.899999999999999,0.5,-22.46)) ;
#145028 = CARTESIAN_POINT('',(-0.999999999999999,0.5,-22.46)) ;
#145029 = CARTESIAN_POINT('',(-0.899999999999999,0.5,-23.26)) ;
#145030 = CARTESIAN_POINT('',(-0.899999999999999,0.5,-23.36)) ;
#145031 = CARTESIAN_POINT('',(0.500000000000001,0.5,-23.26)) ;
#145032 = CARTESIAN_POINT('',(0.600000000000001,0.5,-23.26)) ;
#145033 = CARTESIAN_POINT('',(0.500000000000001,0.5,-22.36)) ;
#145034 = CARTESIAN_POINT('Origin',(0.600000000000001,-2.,-22.36)) ;
#145035 = CARTESIAN_POINT('',(0.500000000000001,-1.9,-22.36)) ;
#145036 = CARTESIAN_POINT('',(-0.899999999999999,-1.9,-22.36)) ;
#145037 = CARTESIAN_POINT('',(0.600000000000001,-1.9,-22.36)) ;
#145038 = CARTESIAN_POINT('',(-0.899999999999999,0.4,-22.36)) ;
#145039 = CARTESIAN_POINT('',(-0.899999999999999,0.5,-22.36)) ;
#145040 = CARTESIAN_POINT('',(0.500000000000001,0.4,-22.36)) ;
#145041 = CARTESIAN_POINT('',(0.600000000000001,0.4,-22.36)) ;
#145042 = CARTESIAN_POINT('',(0.500000000000001,-2.,-22.36)) ;
#145043 = CARTESIAN_POINT('Origin',(0.600000000000001,-2.,-21.485)) ;
#145044 = CARTESIAN_POINT('',(0.500000000000001,-2.,-21.585)) ;
#145045 = CARTESIAN_POINT('',(-0.899999999999999,-2.,-21.585)) ;
#145046 = CARTESIAN_POINT('',(-0.999999999999999,-2.,-21.585)) ;
#145047 = CARTESIAN_POINT('',(-0.899999999999999,-2.,-22.26)) ;
#145048 = CARTESIAN_POINT('',(-0.899999999999999,-2.,-22.36)) ;
#145049 = CARTESIAN_POINT('',(0.500000000000001,-2.,-22.26)) ;
#145050 = CARTESIAN_POINT('',(0.600000000000001,-2.,-22.26)) ;
#145051 = CARTESIAN_POINT('',(0.500000000000001,-2.,-21.485)) ;
#145052 = CARTESIAN_POINT('Origin',(0.600000000000001,-2.,-27.17)) ;
#145053 = CARTESIAN_POINT('',(0.500000000000001,-2.,-27.27)) ;
#145054 = CARTESIAN_POINT('',(-0.899999999999999,-2.,-27.27)) ;
#145055 = CARTESIAN_POINT('',(0.600000000000001,-2.,-27.27)) ;
#145056 = CARTESIAN_POINT('',(-0.899999999999999,-2.,-27.945)) ;
#145057 = CARTESIAN_POINT('',(-0.899999999999999,-2.,-28.045)) ;
#145058 = CARTESIAN_POINT('',(0.500000000000001,-2.,-27.945)) ;
#145059 = CARTESIAN_POINT('',(0.600000000000001,-2.,-27.945)) ;
#145060 = CARTESIAN_POINT('',(0.500000000000001,-2.,-27.17)) ;
#145061 = CARTESIAN_POINT('Origin',(0.600000000000001,0.5,-27.17)) ;
#145062 = CARTESIAN_POINT('',(-0.899999999999999,0.4,-27.17)) ;
#145063 = CARTESIAN_POINT('',(-0.999999999999999,0.4,-27.17)) ;
#145064 = CARTESIAN_POINT('',(-0.899999999999999,-1.9,-27.17)) ;
#145065 = CARTESIAN_POINT('',(-0.899999999999999,-2.,-27.17)) ;
#145066 = CARTESIAN_POINT('',(0.600000000000001,-1.9,-27.17)) ;
#145067 = CARTESIAN_POINT('Origin',(0.600000000000001,0.5,-26.17)) ;
#145068 = CARTESIAN_POINT('',(0.500000000000001,0.5,-26.27)) ;
#145069 = CARTESIAN_POINT('',(-0.899999999999999,0.5,-26.27)) ;
#145070 = CARTESIAN_POINT('',(-0.999999999999999,0.5,-26.27)) ;
#145071 = CARTESIAN_POINT('',(-0.899999999999999,0.5,-27.07)) ;
#145072 = CARTESIAN_POINT('',(-0.899999999999999,0.5,-27.17)) ;
#145073 = CARTESIAN_POINT('',(0.500000000000001,0.5,-27.07)) ;
#145074 = CARTESIAN_POINT('',(0.600000000000001,0.5,-27.07)) ;
#145075 = CARTESIAN_POINT('',(0.500000000000001,0.5,-26.17)) ;
#145076 = CARTESIAN_POINT('Origin',(0.600000000000001,-2.,-26.17)) ;
#145077 = CARTESIAN_POINT('',(0.500000000000001,-1.9,-26.17)) ;
#145078 = CARTESIAN_POINT('',(-0.899999999999999,-1.9,-26.17)) ;
#145079 = CARTESIAN_POINT('',(0.600000000000001,-1.9,-26.17)) ;
#145080 = CARTESIAN_POINT('',(-0.899999999999999,0.4,-26.17)) ;
#145081 = CARTESIAN_POINT('',(-0.899999999999999,0.5,-26.17)) ;
#145082 = CARTESIAN_POINT('',(0.500000000000001,0.4,-26.17)) ;
#145083 = CARTESIAN_POINT('',(0.600000000000001,0.4,-26.17)) ;
#145084 = CARTESIAN_POINT('',(0.500000000000001,-2.,-26.17)) ;
#145085 = CARTESIAN_POINT('Origin',(0.600000000000001,-2.,-25.295)) ;
#145086 = CARTESIAN_POINT('',(0.500000000000001,-2.,-25.395)) ;
#145087 = CARTESIAN_POINT('',(-0.899999999999999,-2.,-25.395)) ;
#145088 = CARTESIAN_POINT('',(-0.999999999999999,-2.,-25.395)) ;
#145089 = CARTESIAN_POINT('',(-0.899999999999999,-2.,-26.07)) ;
#145090 = CARTESIAN_POINT('',(-0.899999999999999,-2.,-26.17)) ;
#145091 = CARTESIAN_POINT('',(0.500000000000001,-2.,-26.07)) ;
#145092 = CARTESIAN_POINT('',(0.600000000000001,-2.,-26.07)) ;
#145093 = CARTESIAN_POINT('',(0.500000000000001,-2.,-25.295)) ;
#145094 = CARTESIAN_POINT('Origin',(0.600000000000001,-2.,-30.98)) ;
#145095 = CARTESIAN_POINT('',(0.500000000000001,-2.,-31.08)) ;
#145096 = CARTESIAN_POINT('',(-0.899999999999999,-2.,-31.08)) ;
#145097 = CARTESIAN_POINT('',(0.600000000000001,-2.,-31.08)) ;
#145098 = CARTESIAN_POINT('',(-0.899999999999999,-2.,-31.755)) ;
#145099 = CARTESIAN_POINT('',(-0.899999999999999,-2.,-31.855)) ;
#145100 = CARTESIAN_POINT('',(0.500000000000001,-2.,-31.755)) ;
#145101 = CARTESIAN_POINT('',(0.600000000000001,-2.,-31.755)) ;
#145102 = CARTESIAN_POINT('',(0.500000000000001,-2.,-30.98)) ;
#145103 = CARTESIAN_POINT('Origin',(0.600000000000001,0.5,-30.98)) ;
#145104 = CARTESIAN_POINT('',(-0.899999999999999,0.4,-30.98)) ;
#145105 = CARTESIAN_POINT('',(-0.999999999999999,0.4,-30.98)) ;
#145106 = CARTESIAN_POINT('',(-0.899999999999999,-1.9,-30.98)) ;
#145107 = CARTESIAN_POINT('',(-0.899999999999999,-2.,-30.98)) ;
#145108 = CARTESIAN_POINT('',(0.600000000000001,-1.9,-30.98)) ;
#145109 = CARTESIAN_POINT('Origin',(0.600000000000001,0.5,-29.98)) ;
#145110 = CARTESIAN_POINT('',(0.500000000000001,0.5,-30.08)) ;
#145111 = CARTESIAN_POINT('',(-0.899999999999999,0.5,-30.08)) ;
#145112 = CARTESIAN_POINT('',(-0.999999999999999,0.5,-30.08)) ;
#145113 = CARTESIAN_POINT('',(-0.899999999999999,0.5,-30.88)) ;
#145114 = CARTESIAN_POINT('',(-0.899999999999999,0.5,-30.98)) ;
#145115 = CARTESIAN_POINT('',(0.500000000000001,0.5,-30.88)) ;
#145116 = CARTESIAN_POINT('',(0.600000000000001,0.5,-30.88)) ;
#145117 = CARTESIAN_POINT('',(0.500000000000001,0.5,-29.98)) ;
#145118 = CARTESIAN_POINT('Origin',(0.600000000000001,-2.,-29.98)) ;
#145119 = CARTESIAN_POINT('',(0.500000000000001,-1.9,-29.98)) ;
#145120 = CARTESIAN_POINT('',(-0.899999999999999,-1.9,-29.98)) ;
#145121 = CARTESIAN_POINT('',(0.600000000000001,-1.9,-29.98)) ;
#145122 = CARTESIAN_POINT('',(-0.899999999999999,0.4,-29.98)) ;
#145123 = CARTESIAN_POINT('',(-0.899999999999999,0.5,-29.98)) ;
#145124 = CARTESIAN_POINT('',(0.500000000000001,0.4,-29.98)) ;
#145125 = CARTESIAN_POINT('',(0.600000000000001,0.4,-29.98)) ;
#145126 = CARTESIAN_POINT('',(0.500000000000001,-2.,-29.98)) ;
#145127 = CARTESIAN_POINT('Origin',(0.600000000000001,-2.,-29.105)) ;
#145128 = CARTESIAN_POINT('',(0.500000000000001,-2.,-29.205)) ;
#145129 = CARTESIAN_POINT('',(-0.899999999999999,-2.,-29.205)) ;
#145130 = CARTESIAN_POINT('',(-0.999999999999999,-2.,-29.205)) ;
#145131 = CARTESIAN_POINT('',(-0.899999999999999,-2.,-29.88)) ;
#145132 = CARTESIAN_POINT('',(-0.899999999999999,-2.,-29.98)) ;
#145133 = CARTESIAN_POINT('',(0.500000000000001,-2.,-29.88)) ;
#145134 = CARTESIAN_POINT('',(0.600000000000001,-2.,-29.88)) ;
#145135 = CARTESIAN_POINT('',(0.500000000000001,-2.,-29.105)) ;
#145136 = CARTESIAN_POINT('Origin',(0.600000000000001,-2.,-34.79)) ;
#145137 = CARTESIAN_POINT('',(0.500000000000001,-2.,-34.89)) ;
#145138 = CARTESIAN_POINT('',(-0.899999999999999,-2.,-34.89)) ;
#145139 = CARTESIAN_POINT('',(0.600000000000001,-2.,-34.89)) ;
#145140 = CARTESIAN_POINT('',(-0.899999999999999,-2.,-35.565)) ;
#145141 = CARTESIAN_POINT('',(-0.899999999999999,-2.,-35.665)) ;
#145142 = CARTESIAN_POINT('',(0.500000000000001,-2.,-35.565)) ;
#145143 = CARTESIAN_POINT('',(0.600000000000001,-2.,-35.565)) ;
#145144 = CARTESIAN_POINT('',(0.500000000000001,-2.,-34.79)) ;
#145145 = CARTESIAN_POINT('Origin',(0.600000000000001,0.5,-34.79)) ;
#145146 = CARTESIAN_POINT('',(-0.899999999999999,0.4,-34.79)) ;
#145147 = CARTESIAN_POINT('',(-0.999999999999999,0.4,-34.79)) ;
#145148 = CARTESIAN_POINT('',(-0.899999999999999,-1.9,-34.79)) ;
#145149 = CARTESIAN_POINT('',(-0.899999999999999,-2.,-34.79)) ;
#145150 = CARTESIAN_POINT('',(0.600000000000001,-1.9,-34.79)) ;
#145151 = CARTESIAN_POINT('Origin',(0.600000000000001,0.5,-33.79)) ;
#145152 = CARTESIAN_POINT('',(0.500000000000001,0.5,-33.89)) ;
#145153 = CARTESIAN_POINT('',(-0.899999999999999,0.5,-33.89)) ;
#145154 = CARTESIAN_POINT('',(-0.999999999999999,0.5,-33.89)) ;
#145155 = CARTESIAN_POINT('',(-0.899999999999999,0.5,-34.69)) ;
#145156 = CARTESIAN_POINT('',(-0.899999999999999,0.5,-34.79)) ;
#145157 = CARTESIAN_POINT('',(0.500000000000001,0.5,-34.69)) ;
#145158 = CARTESIAN_POINT('',(0.600000000000001,0.5,-34.69)) ;
#145159 = CARTESIAN_POINT('',(0.500000000000001,0.5,-33.79)) ;
#145160 = CARTESIAN_POINT('Origin',(0.600000000000001,-2.,-33.79)) ;
#145161 = CARTESIAN_POINT('',(0.500000000000001,-1.9,-33.79)) ;
#145162 = CARTESIAN_POINT('',(-0.899999999999999,-1.9,-33.79)) ;
#145163 = CARTESIAN_POINT('',(0.600000000000001,-1.9,-33.79)) ;
#145164 = CARTESIAN_POINT('',(-0.899999999999999,0.4,-33.79)) ;
#145165 = CARTESIAN_POINT('',(-0.899999999999999,0.5,-33.79)) ;
#145166 = CARTESIAN_POINT('',(0.500000000000001,0.4,-33.79)) ;
#145167 = CARTESIAN_POINT('',(0.600000000000001,0.4,-33.79)) ;
#145168 = CARTESIAN_POINT('',(0.500000000000001,-2.,-33.79)) ;
#145169 = CARTESIAN_POINT('Origin',(0.600000000000001,-2.,-32.915)) ;
#145170 = CARTESIAN_POINT('',(0.500000000000001,-2.,-33.015)) ;
#145171 = CARTESIAN_POINT('',(-0.899999999999999,-2.,-33.015)) ;
#145172 = CARTESIAN_POINT('',(-0.999999999999999,-2.,-33.015)) ;
#145173 = CARTESIAN_POINT('',(-0.899999999999999,-2.,-33.69)) ;
#145174 = CARTESIAN_POINT('',(-0.899999999999999,-2.,-33.79)) ;
#145175 = CARTESIAN_POINT('',(0.500000000000001,-2.,-33.69)) ;
#145176 = CARTESIAN_POINT('',(0.600000000000001,-2.,-33.69)) ;
#145177 = CARTESIAN_POINT('',(0.500000000000001,-2.,-32.915)) ;
#145178 = CARTESIAN_POINT('Origin',(1.4,2.1,-33.69)) ;
#145179 = CARTESIAN_POINT('',(1.5,2.,-33.69)) ;
#145180 = CARTESIAN_POINT('',(7.9,2.,-33.69)) ;
#145181 = CARTESIAN_POINT('',(1.4,2.,-33.69)) ;
#145182 = CARTESIAN_POINT('',(1.5,2.1,-33.79)) ;
#145183 = CARTESIAN_POINT('Origin',(1.5,2.1,-33.69)) ;
#145184 = CARTESIAN_POINT('',(7.9,2.1,-33.79)) ;
#145185 = CARTESIAN_POINT('',(1.4,2.1,-33.79)) ;
#145186 = CARTESIAN_POINT('Origin',(7.9,2.1,-33.69)) ;
#145187 = CARTESIAN_POINT('Origin',(1.4,2.4,-33.79)) ;
#145188 = CARTESIAN_POINT('',(1.5,2.4,-33.79)) ;
#145189 = CARTESIAN_POINT('',(1.5,2.4,-33.79)) ;
#145190 = CARTESIAN_POINT('',(7.9,2.4,-33.79)) ;
#145191 = CARTESIAN_POINT('',(1.4,2.4,-33.79)) ;
#145192 = CARTESIAN_POINT('',(7.9,2.1,-33.79)) ;
#145193 = CARTESIAN_POINT('Origin',(1.4,2.4,-33.69)) ;
#145194 = CARTESIAN_POINT('',(1.5,2.5,-33.69)) ;
#145195 = CARTESIAN_POINT('Origin',(1.5,2.4,-33.69)) ;
#145196 = CARTESIAN_POINT('',(7.9,2.5,-33.69)) ;
#145197 = CARTESIAN_POINT('',(1.4,2.5,-33.69)) ;
#145198 = CARTESIAN_POINT('Origin',(7.9,2.4,-33.69)) ;
#145199 = CARTESIAN_POINT('Origin',(1.4,2.5,-33.5814213562373)) ;
#145200 = CARTESIAN_POINT('',(1.5,2.5,-33.5814213562373)) ;
#145201 = CARTESIAN_POINT('',(1.5,2.5,-33.5814213562373)) ;
#145202 = CARTESIAN_POINT('',(7.9,2.5,-33.5814213562373)) ;
#145203 = CARTESIAN_POINT('',(1.4,2.5,-33.5814213562373)) ;
#145204 = CARTESIAN_POINT('',(7.9,2.5,-33.69)) ;
#145205 = CARTESIAN_POINT('Origin',(1.4,2.6,-33.5814213562373)) ;
#145206 = CARTESIAN_POINT('',(1.5,2.52928932188135,-33.5107106781187)) ;
#145207 = CARTESIAN_POINT('Origin',(1.5,2.6,-33.5814213562373)) ;
#145208 = CARTESIAN_POINT('',(7.9,2.52928932188135,-33.5107106781187)) ;
#145209 = CARTESIAN_POINT('',(1.4,2.52928932188135,-33.5107106781187)) ;
#145210 = CARTESIAN_POINT('Origin',(7.9,2.6,-33.5814213562373)) ;
#145211 = CARTESIAN_POINT('Origin',(1.4,3.07928932188135,-32.9607106781187)) ;
#145212 = CARTESIAN_POINT('',(1.5,3.07928932188135,-32.9607106781187)) ;
#145213 = CARTESIAN_POINT('',(7.9,3.07928932188135,-32.9607106781187)) ;
#145214 = CARTESIAN_POINT('',(1.4,3.07928932188135,-32.9607106781187)) ;
#145215 = CARTESIAN_POINT('',(7.9,2.52928932188135,-33.5107106781187)) ;
#145216 = CARTESIAN_POINT('Origin',(1.4,3.15,-33.0314213562373)) ;
#145217 = CARTESIAN_POINT('',(7.9,3.25,-33.0314213562373)) ;
#145218 = CARTESIAN_POINT('',(1.4,3.25,-33.0314213562373)) ;
#145219 = CARTESIAN_POINT('Origin',(7.9,3.15,-33.0314213562373)) ;
#145220 = CARTESIAN_POINT('Origin',(1.4,3.25,-35.5485786437627)) ;
#145221 = CARTESIAN_POINT('',(1.5,3.25,-35.5485786437627)) ;
#145222 = CARTESIAN_POINT('',(7.9,3.25,-33.0314213562373)) ;
#145223 = CARTESIAN_POINT('Origin',(1.4,2.52928932188134,-35.0692893218813)) ;
#145224 = CARTESIAN_POINT('',(1.5,2.52928932188134,-35.0692893218813)) ;
#145225 = CARTESIAN_POINT('',(1.5,2.52928932188134,-35.0692893218813)) ;
#145226 = CARTESIAN_POINT('',(7.9,2.52928932188134,-35.0692893218813)) ;
#145227 = CARTESIAN_POINT('',(1.4,2.52928932188134,-35.0692893218813)) ;
#145228 = CARTESIAN_POINT('',(7.9,3.07928932188135,-35.6192893218813)) ;
#145229 = CARTESIAN_POINT('Origin',(1.4,2.6,-34.9985786437627)) ;
#145230 = CARTESIAN_POINT('',(1.5,2.5,-34.9985786437627)) ;
#145231 = CARTESIAN_POINT('Origin',(1.5,2.6,-34.9985786437627)) ;
#145232 = CARTESIAN_POINT('',(7.9,2.5,-34.9985786437627)) ;
#145233 = CARTESIAN_POINT('',(1.4,2.5,-34.9985786437627)) ;
#145234 = CARTESIAN_POINT('Origin',(7.9,2.6,-34.9985786437627)) ;
#145235 = CARTESIAN_POINT('Origin',(1.4,2.5,-34.89)) ;
#145236 = CARTESIAN_POINT('',(1.5,2.5,-34.89)) ;
#145237 = CARTESIAN_POINT('',(1.5,2.5,-34.89)) ;
#145238 = CARTESIAN_POINT('',(7.9,2.5,-34.89)) ;
#145239 = CARTESIAN_POINT('',(1.4,2.5,-34.89)) ;
#145240 = CARTESIAN_POINT('',(7.9,2.5,-34.9985786437627)) ;
#145241 = CARTESIAN_POINT('Origin',(1.4,2.4,-34.89)) ;
#145242 = CARTESIAN_POINT('',(1.5,2.4,-34.79)) ;
#145243 = CARTESIAN_POINT('Origin',(1.5,2.4,-34.89)) ;
#145244 = CARTESIAN_POINT('',(7.9,2.4,-34.79)) ;
#145245 = CARTESIAN_POINT('',(1.4,2.4,-34.79)) ;
#145246 = CARTESIAN_POINT('Origin',(7.9,2.4,-34.89)) ;
#145247 = CARTESIAN_POINT('Origin',(1.4,2.1,-34.79)) ;
#145248 = CARTESIAN_POINT('',(1.5,2.1,-34.79)) ;
#145249 = CARTESIAN_POINT('',(1.5,2.1,-34.79)) ;
#145250 = CARTESIAN_POINT('',(7.9,2.1,-34.79)) ;
#145251 = CARTESIAN_POINT('',(1.4,2.1,-34.79)) ;
#145252 = CARTESIAN_POINT('',(7.9,2.4,-34.79)) ;
#145253 = CARTESIAN_POINT('Origin',(1.4,2.1,-34.89)) ;
#145254 = CARTESIAN_POINT('',(1.5,2.,-34.89)) ;
#145255 = CARTESIAN_POINT('Origin',(1.5,2.1,-34.89)) ;
#145256 = CARTESIAN_POINT('',(7.9,2.,-34.89)) ;
#145257 = CARTESIAN_POINT('',(1.4,2.,-34.89)) ;
#145258 = CARTESIAN_POINT('Origin',(7.9,2.1,-34.89)) ;
#145259 = CARTESIAN_POINT('Origin',(1.4,2.,-34.89)) ;
#145260 = CARTESIAN_POINT('',(1.5,2.,-35.84)) ;
#145261 = CARTESIAN_POINT('',(1.5,2.,-35.84)) ;
#145262 = CARTESIAN_POINT('',(7.9,2.,-35.84)) ;
#145263 = CARTESIAN_POINT('',(1.4,2.,-35.84)) ;
#145264 = CARTESIAN_POINT('',(7.9,2.,-34.89)) ;
#145265 = CARTESIAN_POINT('Origin',(1.4,1.9,-35.84)) ;
#145266 = CARTESIAN_POINT('',(1.5,1.9,-35.94)) ;
#145267 = CARTESIAN_POINT('Origin',(1.5,1.9,-35.84)) ;
#145268 = CARTESIAN_POINT('',(7.9,1.9,-35.94)) ;
#145269 = CARTESIAN_POINT('',(1.4,1.9,-35.94)) ;
#145270 = CARTESIAN_POINT('Origin',(7.9,1.9,-35.84)) ;
#145271 = CARTESIAN_POINT('Origin',(1.4,1.9,-35.94)) ;
#145272 = CARTESIAN_POINT('',(1.5,-2.15,-35.94)) ;
#145273 = CARTESIAN_POINT('',(1.5,-2.15,-35.94)) ;
#145274 = CARTESIAN_POINT('',(7.9,-2.15,-35.94)) ;
#145275 = CARTESIAN_POINT('',(1.4,-2.15,-35.94)) ;
#145276 = CARTESIAN_POINT('',(7.9,1.9,-35.94)) ;
#145277 = CARTESIAN_POINT('Origin',(1.4,-2.15,-35.84)) ;
#145278 = CARTESIAN_POINT('',(1.5,-2.25,-35.84)) ;
#145279 = CARTESIAN_POINT('Origin',(1.5,-2.15,-35.84)) ;
#145280 = CARTESIAN_POINT('',(7.9,-2.25,-35.84)) ;
#145281 = CARTESIAN_POINT('',(1.4,-2.25,-35.84)) ;
#145282 = CARTESIAN_POINT('Origin',(7.9,-2.15,-35.84)) ;
#145283 = CARTESIAN_POINT('Origin',(1.4,-2.25,-35.1931195934094)) ;
#145284 = CARTESIAN_POINT('',(1.5,-2.25,-35.1931195934094)) ;
#145285 = CARTESIAN_POINT('',(1.5,-2.25,-35.1931195934094)) ;
#145286 = CARTESIAN_POINT('',(7.9,-2.25,-35.1931195934094)) ;
#145287 = CARTESIAN_POINT('',(1.4,-2.25,-35.1931195934094)) ;
#145288 = CARTESIAN_POINT('',(7.9,-2.25,-35.84)) ;
#145289 = CARTESIAN_POINT('Origin',(1.4,-2.15,-35.1931195934094)) ;
#145290 = CARTESIAN_POINT('',(1.5,-2.23576512455516,-35.1416964137135)) ;
#145291 = CARTESIAN_POINT('Origin',(1.5,-2.15,-35.1931195934094)) ;
#145292 = CARTESIAN_POINT('',(7.9,-2.23576512455516,-35.1416964137135)) ;
#145293 = CARTESIAN_POINT('',(1.4,-2.23576512455516,-35.1416964137135)) ;
#145294 = CARTESIAN_POINT('Origin',(7.9,-2.15,-35.1931195934094)) ;
#145295 = CARTESIAN_POINT('Origin',(1.4,-3.65625,-34.29)) ;
#145296 = CARTESIAN_POINT('',(1.5,-2.23576512455516,-33.4383035862865)) ;
#145297 = CARTESIAN_POINT('Origin',(1.5,-3.65625,-34.29)) ;
#145298 = CARTESIAN_POINT('',(7.9,-2.23576512455516,-33.4383035862865)) ;
#145299 = CARTESIAN_POINT('',(1.4,-2.23576512455516,-33.4383035862865)) ;
#145300 = CARTESIAN_POINT('Origin',(7.9,-3.65625,-34.29)) ;
#145301 = CARTESIAN_POINT('Origin',(1.4,-2.15,-33.3868804065906)) ;
#145302 = CARTESIAN_POINT('',(1.5,-2.25,-33.3868804065906)) ;
#145303 = CARTESIAN_POINT('Origin',(1.5,-2.15,-33.3868804065906)) ;
#145304 = CARTESIAN_POINT('',(7.9,-2.25,-33.3868804065906)) ;
#145305 = CARTESIAN_POINT('',(1.4,-2.25,-33.3868804065906)) ;
#145306 = CARTESIAN_POINT('Origin',(7.9,-2.15,-33.3868804065906)) ;
#145307 = CARTESIAN_POINT('Origin',(1.4,-2.25,-32.74)) ;
#145308 = CARTESIAN_POINT('',(1.5,-2.25,-32.74)) ;
#145309 = CARTESIAN_POINT('',(1.5,-2.25,-32.74)) ;
#145310 = CARTESIAN_POINT('',(7.9,-2.25,-32.74)) ;
#145311 = CARTESIAN_POINT('',(1.4,-2.25,-32.74)) ;
#145312 = CARTESIAN_POINT('',(7.9,-2.25,-33.3868804065906)) ;
#145313 = CARTESIAN_POINT('Origin',(1.4,-2.15,-32.74)) ;
#145314 = CARTESIAN_POINT('',(1.5,-2.15,-32.64)) ;
#145315 = CARTESIAN_POINT('Origin',(1.5,-2.15,-32.74)) ;
#145316 = CARTESIAN_POINT('',(7.9,-2.15,-32.64)) ;
#145317 = CARTESIAN_POINT('',(1.4,-2.15,-32.64)) ;
#145318 = CARTESIAN_POINT('Origin',(7.9,-2.15,-32.74)) ;
#145319 = CARTESIAN_POINT('Origin',(1.4,1.9,-32.64)) ;
#145320 = CARTESIAN_POINT('',(1.5,1.9,-32.64)) ;
#145321 = CARTESIAN_POINT('',(1.5,1.9,-32.64)) ;
#145322 = CARTESIAN_POINT('',(7.9,1.9,-32.64)) ;
#145323 = CARTESIAN_POINT('',(1.4,1.9,-32.64)) ;
#145324 = CARTESIAN_POINT('',(7.9,-2.15,-32.64)) ;
#145325 = CARTESIAN_POINT('Origin',(1.4,1.9,-32.74)) ;
#145326 = CARTESIAN_POINT('',(1.5,2.,-32.74)) ;
#145327 = CARTESIAN_POINT('Origin',(1.5,1.9,-32.74)) ;
#145328 = CARTESIAN_POINT('',(7.9,2.,-32.74)) ;
#145329 = CARTESIAN_POINT('',(1.4,2.,-32.74)) ;
#145330 = CARTESIAN_POINT('Origin',(7.9,1.9,-32.74)) ;
#145331 = CARTESIAN_POINT('Origin',(1.4,2.,-32.74)) ;
#145332 = CARTESIAN_POINT('',(1.5,2.,-33.69)) ;
#145333 = CARTESIAN_POINT('',(7.9,2.,-32.74)) ;
#145334 = CARTESIAN_POINT('Origin',(1.4,2.1,-33.69)) ;
#145335 = CARTESIAN_POINT('',(1.4,2.6,-33.69)) ;
#145336 = CARTESIAN_POINT('',(1.4,2.4,-33.89)) ;
#145337 = CARTESIAN_POINT('Origin',(1.4,2.4,-33.69)) ;
#145338 = CARTESIAN_POINT('',(1.4,2.1,-33.89)) ;
#145339 = CARTESIAN_POINT('',(1.4,2.1,-33.89)) ;
#145340 = CARTESIAN_POINT('',(1.4,1.9,-33.69)) ;
#145341 = CARTESIAN_POINT('Origin',(1.4,2.1,-33.69)) ;
#145342 = CARTESIAN_POINT('',(1.4,1.9,-32.74)) ;
#145343 = CARTESIAN_POINT('',(1.4,1.9,-32.74)) ;
#145344 = CARTESIAN_POINT('',(1.4,-2.15,-32.74)) ;
#145345 = CARTESIAN_POINT('',(1.4,-2.15,-32.74)) ;
#145346 = CARTESIAN_POINT('',(1.4,-2.15,-33.3868804065906)) ;
#145347 = CARTESIAN_POINT('',(1.4,-2.15,-33.3868804065906)) ;
#145348 = CARTESIAN_POINT('',(1.4,-2.15,-35.1931195934094)) ;
#145349 = CARTESIAN_POINT('Origin',(1.4,-3.65625,-34.29)) ;
#145350 = CARTESIAN_POINT('',(1.4,-2.15,-35.84)) ;
#145351 = CARTESIAN_POINT('',(1.4,-2.15,-35.84)) ;
#145352 = CARTESIAN_POINT('',(1.4,1.9,-35.84)) ;
#145353 = CARTESIAN_POINT('',(1.4,1.9,-35.84)) ;
#145354 = CARTESIAN_POINT('',(1.4,1.9,-34.89)) ;
#145355 = CARTESIAN_POINT('',(1.4,1.9,-34.89)) ;
#145356 = CARTESIAN_POINT('',(1.4,2.1,-34.69)) ;
#145357 = CARTESIAN_POINT('Origin',(1.4,2.1,-34.89)) ;
#145358 = CARTESIAN_POINT('',(1.4,2.4,-34.69)) ;
#145359 = CARTESIAN_POINT('',(1.4,2.4,-34.69)) ;
#145360 = CARTESIAN_POINT('',(1.4,2.6,-34.89)) ;
#145361 = CARTESIAN_POINT('Origin',(1.4,2.4,-34.89)) ;
#145362 = CARTESIAN_POINT('',(1.4,2.6,-34.9985786437627)) ;
#145363 = CARTESIAN_POINT('',(1.4,2.6,-34.9985786437627)) ;
#145364 = CARTESIAN_POINT('',(1.4,3.15,-35.5485786437627)) ;
#145365 = CARTESIAN_POINT('',(1.4,3.15,-35.5485786437627)) ;
#145366 = CARTESIAN_POINT('',(1.4,3.15,-33.0314213562373)) ;
#145367 = CARTESIAN_POINT('',(1.4,2.6,-33.5814213562373)) ;
#145368 = CARTESIAN_POINT('',(1.4,2.6,-33.5814213562373)) ;
#145369 = CARTESIAN_POINT('',(1.4,2.6,-33.69)) ;
#145370 = CARTESIAN_POINT('Origin',(1.4,2.1,-29.88)) ;
#145371 = CARTESIAN_POINT('',(1.5,2.,-29.88)) ;
#145372 = CARTESIAN_POINT('',(7.9,2.,-29.88)) ;
#145373 = CARTESIAN_POINT('',(1.4,2.,-29.88)) ;
#145374 = CARTESIAN_POINT('',(1.5,2.1,-29.98)) ;
#145375 = CARTESIAN_POINT('Origin',(1.5,2.1,-29.88)) ;
#145376 = CARTESIAN_POINT('',(7.9,2.1,-29.98)) ;
#145377 = CARTESIAN_POINT('',(1.4,2.1,-29.98)) ;
#145378 = CARTESIAN_POINT('Origin',(7.9,2.1,-29.88)) ;
#145379 = CARTESIAN_POINT('Origin',(1.4,2.4,-29.98)) ;
#145380 = CARTESIAN_POINT('',(1.5,2.4,-29.98)) ;
#145381 = CARTESIAN_POINT('',(1.5,2.4,-29.98)) ;
#145382 = CARTESIAN_POINT('',(7.9,2.4,-29.98)) ;
#145383 = CARTESIAN_POINT('',(1.4,2.4,-29.98)) ;
#145384 = CARTESIAN_POINT('',(7.9,2.1,-29.98)) ;
#145385 = CARTESIAN_POINT('Origin',(1.4,2.4,-29.88)) ;
#145386 = CARTESIAN_POINT('',(1.5,2.5,-29.88)) ;
#145387 = CARTESIAN_POINT('Origin',(1.5,2.4,-29.88)) ;
#145388 = CARTESIAN_POINT('',(7.9,2.5,-29.88)) ;
#145389 = CARTESIAN_POINT('',(1.4,2.5,-29.88)) ;
#145390 = CARTESIAN_POINT('Origin',(7.9,2.4,-29.88)) ;
#145391 = CARTESIAN_POINT('Origin',(1.4,2.5,-29.7714213562373)) ;
#145392 = CARTESIAN_POINT('',(1.5,2.5,-29.7714213562373)) ;
#145393 = CARTESIAN_POINT('',(1.5,2.5,-29.7714213562373)) ;
#145394 = CARTESIAN_POINT('',(7.9,2.5,-29.7714213562373)) ;
#145395 = CARTESIAN_POINT('',(1.4,2.5,-29.7714213562373)) ;
#145396 = CARTESIAN_POINT('',(7.9,2.5,-29.88)) ;
#145397 = CARTESIAN_POINT('Origin',(1.4,2.6,-29.7714213562373)) ;
#145398 = CARTESIAN_POINT('',(1.5,2.52928932188135,-29.7007106781187)) ;
#145399 = CARTESIAN_POINT('Origin',(1.5,2.6,-29.7714213562373)) ;
#145400 = CARTESIAN_POINT('',(7.9,2.52928932188135,-29.7007106781187)) ;
#145401 = CARTESIAN_POINT('',(1.4,2.52928932188135,-29.7007106781187)) ;
#145402 = CARTESIAN_POINT('Origin',(7.9,2.6,-29.7714213562373)) ;
#145403 = CARTESIAN_POINT('Origin',(1.4,3.07928932188135,-29.1507106781187)) ;
#145404 = CARTESIAN_POINT('',(1.5,3.07928932188135,-29.1507106781187)) ;
#145405 = CARTESIAN_POINT('',(7.9,3.07928932188135,-29.1507106781187)) ;
#145406 = CARTESIAN_POINT('',(1.4,3.07928932188135,-29.1507106781187)) ;
#145407 = CARTESIAN_POINT('',(7.9,2.52928932188135,-29.7007106781187)) ;
#145408 = CARTESIAN_POINT('Origin',(1.4,3.15,-29.2214213562373)) ;
#145409 = CARTESIAN_POINT('',(7.9,3.25,-29.2214213562373)) ;
#145410 = CARTESIAN_POINT('',(1.4,3.25,-29.2214213562373)) ;
#145411 = CARTESIAN_POINT('Origin',(7.9,3.15,-29.2214213562373)) ;
#145412 = CARTESIAN_POINT('Origin',(1.4,3.25,-31.7385786437627)) ;
#145413 = CARTESIAN_POINT('',(1.5,3.25,-31.7385786437627)) ;
#145414 = CARTESIAN_POINT('',(7.9,3.25,-29.2214213562373)) ;
#145415 = CARTESIAN_POINT('Origin',(1.4,2.52928932188134,-31.2592893218813)) ;
#145416 = CARTESIAN_POINT('',(1.5,2.52928932188134,-31.2592893218813)) ;
#145417 = CARTESIAN_POINT('',(1.5,2.52928932188135,-31.2592893218813)) ;
#145418 = CARTESIAN_POINT('',(7.9,2.52928932188134,-31.2592893218813)) ;
#145419 = CARTESIAN_POINT('',(1.4,2.52928932188134,-31.2592893218813)) ;
#145420 = CARTESIAN_POINT('',(7.9,3.07928932188135,-31.8092893218813)) ;
#145421 = CARTESIAN_POINT('Origin',(1.4,2.6,-31.1885786437627)) ;
#145422 = CARTESIAN_POINT('',(1.5,2.5,-31.1885786437627)) ;
#145423 = CARTESIAN_POINT('Origin',(1.5,2.6,-31.1885786437627)) ;
#145424 = CARTESIAN_POINT('',(7.9,2.5,-31.1885786437627)) ;
#145425 = CARTESIAN_POINT('',(1.4,2.5,-31.1885786437627)) ;
#145426 = CARTESIAN_POINT('Origin',(7.9,2.6,-31.1885786437627)) ;
#145427 = CARTESIAN_POINT('Origin',(1.4,2.5,-31.08)) ;
#145428 = CARTESIAN_POINT('',(1.5,2.5,-31.08)) ;
#145429 = CARTESIAN_POINT('',(1.5,2.5,-31.08)) ;
#145430 = CARTESIAN_POINT('',(7.9,2.5,-31.08)) ;
#145431 = CARTESIAN_POINT('',(1.4,2.5,-31.08)) ;
#145432 = CARTESIAN_POINT('',(7.9,2.5,-31.1885786437627)) ;
#145433 = CARTESIAN_POINT('Origin',(1.4,2.4,-31.08)) ;
#145434 = CARTESIAN_POINT('',(1.5,2.4,-30.98)) ;
#145435 = CARTESIAN_POINT('Origin',(1.5,2.4,-31.08)) ;
#145436 = CARTESIAN_POINT('',(7.9,2.4,-30.98)) ;
#145437 = CARTESIAN_POINT('',(1.4,2.4,-30.98)) ;
#145438 = CARTESIAN_POINT('Origin',(7.9,2.4,-31.08)) ;
#145439 = CARTESIAN_POINT('Origin',(1.4,2.1,-30.98)) ;
#145440 = CARTESIAN_POINT('',(1.5,2.1,-30.98)) ;
#145441 = CARTESIAN_POINT('',(1.5,2.1,-30.98)) ;
#145442 = CARTESIAN_POINT('',(7.9,2.1,-30.98)) ;
#145443 = CARTESIAN_POINT('',(1.4,2.1,-30.98)) ;
#145444 = CARTESIAN_POINT('',(7.9,2.4,-30.98)) ;
#145445 = CARTESIAN_POINT('Origin',(1.4,2.1,-31.08)) ;
#145446 = CARTESIAN_POINT('',(1.5,2.,-31.08)) ;
#145447 = CARTESIAN_POINT('Origin',(1.5,2.1,-31.08)) ;
#145448 = CARTESIAN_POINT('',(7.9,2.,-31.08)) ;
#145449 = CARTESIAN_POINT('',(1.4,2.,-31.08)) ;
#145450 = CARTESIAN_POINT('Origin',(7.9,2.1,-31.08)) ;
#145451 = CARTESIAN_POINT('Origin',(1.4,2.,-31.08)) ;
#145452 = CARTESIAN_POINT('',(1.5,2.,-32.03)) ;
#145453 = CARTESIAN_POINT('',(1.5,2.,-32.03)) ;
#145454 = CARTESIAN_POINT('',(7.9,2.,-32.03)) ;
#145455 = CARTESIAN_POINT('',(1.4,2.,-32.03)) ;
#145456 = CARTESIAN_POINT('',(7.9,2.,-31.08)) ;
#145457 = CARTESIAN_POINT('Origin',(1.4,1.9,-32.03)) ;
#145458 = CARTESIAN_POINT('',(1.5,1.9,-32.13)) ;
#145459 = CARTESIAN_POINT('Origin',(1.5,1.9,-32.03)) ;
#145460 = CARTESIAN_POINT('',(7.9,1.9,-32.13)) ;
#145461 = CARTESIAN_POINT('',(1.4,1.9,-32.13)) ;
#145462 = CARTESIAN_POINT('Origin',(7.9,1.9,-32.03)) ;
#145463 = CARTESIAN_POINT('Origin',(1.4,1.9,-32.13)) ;
#145464 = CARTESIAN_POINT('',(1.5,-2.15,-32.13)) ;
#145465 = CARTESIAN_POINT('',(1.5,-2.15,-32.13)) ;
#145466 = CARTESIAN_POINT('',(7.9,-2.15,-32.13)) ;
#145467 = CARTESIAN_POINT('',(1.4,-2.15,-32.13)) ;
#145468 = CARTESIAN_POINT('',(7.9,1.9,-32.13)) ;
#145469 = CARTESIAN_POINT('Origin',(1.4,-2.15,-32.03)) ;
#145470 = CARTESIAN_POINT('',(1.5,-2.25,-32.03)) ;
#145471 = CARTESIAN_POINT('Origin',(1.5,-2.15,-32.03)) ;
#145472 = CARTESIAN_POINT('',(7.9,-2.25,-32.03)) ;
#145473 = CARTESIAN_POINT('',(1.4,-2.25,-32.03)) ;
#145474 = CARTESIAN_POINT('Origin',(7.9,-2.15,-32.03)) ;
#145475 = CARTESIAN_POINT('Origin',(1.4,-2.25,-31.3831195934094)) ;
#145476 = CARTESIAN_POINT('',(1.5,-2.25,-31.3831195934094)) ;
#145477 = CARTESIAN_POINT('',(1.5,-2.25,-31.3831195934094)) ;
#145478 = CARTESIAN_POINT('',(7.9,-2.25,-31.3831195934094)) ;
#145479 = CARTESIAN_POINT('',(1.4,-2.25,-31.3831195934094)) ;
#145480 = CARTESIAN_POINT('',(7.9,-2.25,-32.03)) ;
#145481 = CARTESIAN_POINT('Origin',(1.4,-2.15,-31.3831195934094)) ;
#145482 = CARTESIAN_POINT('',(1.5,-2.23576512455516,-31.3316964137135)) ;
#145483 = CARTESIAN_POINT('Origin',(1.5,-2.15,-31.3831195934094)) ;
#145484 = CARTESIAN_POINT('',(7.9,-2.23576512455516,-31.3316964137135)) ;
#145485 = CARTESIAN_POINT('',(1.4,-2.23576512455516,-31.3316964137135)) ;
#145486 = CARTESIAN_POINT('Origin',(7.9,-2.15,-31.3831195934094)) ;
#145487 = CARTESIAN_POINT('Origin',(1.4,-3.65625,-30.48)) ;
#145488 = CARTESIAN_POINT('',(1.5,-2.23576512455516,-29.6283035862865)) ;
#145489 = CARTESIAN_POINT('Origin',(1.5,-3.65625,-30.48)) ;
#145490 = CARTESIAN_POINT('',(7.9,-2.23576512455516,-29.6283035862865)) ;
#145491 = CARTESIAN_POINT('',(1.4,-2.23576512455516,-29.6283035862865)) ;
#145492 = CARTESIAN_POINT('Origin',(7.9,-3.65625,-30.48)) ;
#145493 = CARTESIAN_POINT('Origin',(1.4,-2.15,-29.5768804065906)) ;
#145494 = CARTESIAN_POINT('',(1.5,-2.25,-29.5768804065906)) ;
#145495 = CARTESIAN_POINT('Origin',(1.5,-2.15,-29.5768804065906)) ;
#145496 = CARTESIAN_POINT('',(7.9,-2.25,-29.5768804065906)) ;
#145497 = CARTESIAN_POINT('',(1.4,-2.25,-29.5768804065906)) ;
#145498 = CARTESIAN_POINT('Origin',(7.9,-2.15,-29.5768804065906)) ;
#145499 = CARTESIAN_POINT('Origin',(1.4,-2.25,-28.93)) ;
#145500 = CARTESIAN_POINT('',(1.5,-2.25,-28.93)) ;
#145501 = CARTESIAN_POINT('',(1.5,-2.25,-28.93)) ;
#145502 = CARTESIAN_POINT('',(7.9,-2.25,-28.93)) ;
#145503 = CARTESIAN_POINT('',(1.4,-2.25,-28.93)) ;
#145504 = CARTESIAN_POINT('',(7.9,-2.25,-29.5768804065906)) ;
#145505 = CARTESIAN_POINT('Origin',(1.4,-2.15,-28.93)) ;
#145506 = CARTESIAN_POINT('',(1.5,-2.15,-28.83)) ;
#145507 = CARTESIAN_POINT('Origin',(1.5,-2.15,-28.93)) ;
#145508 = CARTESIAN_POINT('',(7.9,-2.15,-28.83)) ;
#145509 = CARTESIAN_POINT('',(1.4,-2.15,-28.83)) ;
#145510 = CARTESIAN_POINT('Origin',(7.9,-2.15,-28.93)) ;
#145511 = CARTESIAN_POINT('Origin',(1.4,1.9,-28.83)) ;
#145512 = CARTESIAN_POINT('',(1.5,1.9,-28.83)) ;
#145513 = CARTESIAN_POINT('',(1.5,1.9,-28.83)) ;
#145514 = CARTESIAN_POINT('',(7.9,1.9,-28.83)) ;
#145515 = CARTESIAN_POINT('',(1.4,1.9,-28.83)) ;
#145516 = CARTESIAN_POINT('',(7.9,-2.15,-28.83)) ;
#145517 = CARTESIAN_POINT('Origin',(1.4,1.9,-28.93)) ;
#145518 = CARTESIAN_POINT('',(1.5,2.,-28.93)) ;
#145519 = CARTESIAN_POINT('Origin',(1.5,1.9,-28.93)) ;
#145520 = CARTESIAN_POINT('',(7.9,2.,-28.93)) ;
#145521 = CARTESIAN_POINT('',(1.4,2.,-28.93)) ;
#145522 = CARTESIAN_POINT('Origin',(7.9,1.9,-28.93)) ;
#145523 = CARTESIAN_POINT('Origin',(1.4,2.,-28.93)) ;
#145524 = CARTESIAN_POINT('',(1.5,2.,-29.88)) ;
#145525 = CARTESIAN_POINT('',(7.9,2.,-28.93)) ;
#145526 = CARTESIAN_POINT('Origin',(1.4,2.1,-29.88)) ;
#145527 = CARTESIAN_POINT('',(1.4,2.6,-29.88)) ;
#145528 = CARTESIAN_POINT('',(1.4,2.4,-30.08)) ;
#145529 = CARTESIAN_POINT('Origin',(1.4,2.4,-29.88)) ;
#145530 = CARTESIAN_POINT('',(1.4,2.1,-30.08)) ;
#145531 = CARTESIAN_POINT('',(1.4,2.1,-30.08)) ;
#145532 = CARTESIAN_POINT('',(1.4,1.9,-29.88)) ;
#145533 = CARTESIAN_POINT('Origin',(1.4,2.1,-29.88)) ;
#145534 = CARTESIAN_POINT('',(1.4,1.9,-28.93)) ;
#145535 = CARTESIAN_POINT('',(1.4,1.9,-28.93)) ;
#145536 = CARTESIAN_POINT('',(1.4,-2.15,-28.93)) ;
#145537 = CARTESIAN_POINT('',(1.4,-2.15,-28.93)) ;
#145538 = CARTESIAN_POINT('',(1.4,-2.15,-29.5768804065906)) ;
#145539 = CARTESIAN_POINT('',(1.4,-2.15,-29.5768804065906)) ;
#145540 = CARTESIAN_POINT('',(1.4,-2.15,-31.3831195934094)) ;
#145541 = CARTESIAN_POINT('Origin',(1.4,-3.65625,-30.48)) ;
#145542 = CARTESIAN_POINT('',(1.4,-2.15,-32.03)) ;
#145543 = CARTESIAN_POINT('',(1.4,-2.15,-32.03)) ;
#145544 = CARTESIAN_POINT('',(1.4,1.9,-32.03)) ;
#145545 = CARTESIAN_POINT('',(1.4,1.9,-32.03)) ;
#145546 = CARTESIAN_POINT('',(1.4,1.9,-31.08)) ;
#145547 = CARTESIAN_POINT('',(1.4,1.9,-31.08)) ;
#145548 = CARTESIAN_POINT('',(1.4,2.1,-30.88)) ;
#145549 = CARTESIAN_POINT('Origin',(1.4,2.1,-31.08)) ;
#145550 = CARTESIAN_POINT('',(1.4,2.4,-30.88)) ;
#145551 = CARTESIAN_POINT('',(1.4,2.4,-30.88)) ;
#145552 = CARTESIAN_POINT('',(1.4,2.6,-31.08)) ;
#145553 = CARTESIAN_POINT('Origin',(1.4,2.4,-31.08)) ;
#145554 = CARTESIAN_POINT('',(1.4,2.6,-31.1885786437627)) ;
#145555 = CARTESIAN_POINT('',(1.4,2.6,-31.1885786437627)) ;
#145556 = CARTESIAN_POINT('',(1.4,3.15,-31.7385786437627)) ;
#145557 = CARTESIAN_POINT('',(1.4,3.15,-31.7385786437627)) ;
#145558 = CARTESIAN_POINT('',(1.4,3.15,-29.2214213562373)) ;
#145559 = CARTESIAN_POINT('',(1.4,2.6,-29.7714213562373)) ;
#145560 = CARTESIAN_POINT('',(1.4,2.6,-29.7714213562373)) ;
#145561 = CARTESIAN_POINT('',(1.4,2.6,-29.88)) ;
#145562 = CARTESIAN_POINT('Origin',(1.4,2.1,-26.07)) ;
#145563 = CARTESIAN_POINT('',(1.5,2.,-26.07)) ;
#145564 = CARTESIAN_POINT('',(7.9,2.,-26.07)) ;
#145565 = CARTESIAN_POINT('',(1.4,2.,-26.07)) ;
#145566 = CARTESIAN_POINT('',(1.5,2.1,-26.17)) ;
#145567 = CARTESIAN_POINT('Origin',(1.5,2.1,-26.07)) ;
#145568 = CARTESIAN_POINT('',(7.9,2.1,-26.17)) ;
#145569 = CARTESIAN_POINT('',(1.4,2.1,-26.17)) ;
#145570 = CARTESIAN_POINT('Origin',(7.9,2.1,-26.07)) ;
#145571 = CARTESIAN_POINT('Origin',(1.4,2.4,-26.17)) ;
#145572 = CARTESIAN_POINT('',(1.5,2.4,-26.17)) ;
#145573 = CARTESIAN_POINT('',(1.5,2.4,-26.17)) ;
#145574 = CARTESIAN_POINT('',(7.9,2.4,-26.17)) ;
#145575 = CARTESIAN_POINT('',(1.4,2.4,-26.17)) ;
#145576 = CARTESIAN_POINT('',(7.9,2.1,-26.17)) ;
#145577 = CARTESIAN_POINT('Origin',(1.4,2.4,-26.07)) ;
#145578 = CARTESIAN_POINT('',(1.5,2.5,-26.07)) ;
#145579 = CARTESIAN_POINT('Origin',(1.5,2.4,-26.07)) ;
#145580 = CARTESIAN_POINT('',(7.9,2.5,-26.07)) ;
#145581 = CARTESIAN_POINT('',(1.4,2.5,-26.07)) ;
#145582 = CARTESIAN_POINT('Origin',(7.9,2.4,-26.07)) ;
#145583 = CARTESIAN_POINT('Origin',(1.4,2.5,-25.9614213562373)) ;
#145584 = CARTESIAN_POINT('',(1.5,2.5,-25.9614213562373)) ;
#145585 = CARTESIAN_POINT('',(1.5,2.5,-25.9614213562373)) ;
#145586 = CARTESIAN_POINT('',(7.9,2.5,-25.9614213562373)) ;
#145587 = CARTESIAN_POINT('',(1.4,2.5,-25.9614213562373)) ;
#145588 = CARTESIAN_POINT('',(7.9,2.5,-26.07)) ;
#145589 = CARTESIAN_POINT('Origin',(1.4,2.6,-25.9614213562373)) ;
#145590 = CARTESIAN_POINT('',(1.5,2.52928932188135,-25.8907106781187)) ;
#145591 = CARTESIAN_POINT('Origin',(1.5,2.6,-25.9614213562373)) ;
#145592 = CARTESIAN_POINT('',(7.9,2.52928932188135,-25.8907106781187)) ;
#145593 = CARTESIAN_POINT('',(1.4,2.52928932188135,-25.8907106781187)) ;
#145594 = CARTESIAN_POINT('Origin',(7.9,2.6,-25.9614213562373)) ;
#145595 = CARTESIAN_POINT('Origin',(1.4,3.07928932188135,-25.3407106781187)) ;
#145596 = CARTESIAN_POINT('',(1.5,3.07928932188135,-25.3407106781187)) ;
#145597 = CARTESIAN_POINT('',(7.9,3.07928932188135,-25.3407106781187)) ;
#145598 = CARTESIAN_POINT('',(1.4,3.07928932188135,-25.3407106781187)) ;
#145599 = CARTESIAN_POINT('',(7.9,2.52928932188135,-25.8907106781187)) ;
#145600 = CARTESIAN_POINT('Origin',(1.4,3.15,-25.4114213562373)) ;
#145601 = CARTESIAN_POINT('',(7.9,3.25,-25.4114213562373)) ;
#145602 = CARTESIAN_POINT('',(1.4,3.25,-25.4114213562373)) ;
#145603 = CARTESIAN_POINT('Origin',(7.9,3.15,-25.4114213562373)) ;
#145604 = CARTESIAN_POINT('Origin',(1.4,3.25,-27.9285786437627)) ;
#145605 = CARTESIAN_POINT('',(1.5,3.25,-27.9285786437627)) ;
#145606 = CARTESIAN_POINT('',(7.9,3.25,-25.4114213562373)) ;
#145607 = CARTESIAN_POINT('Origin',(1.4,2.52928932188134,-27.4492893218813)) ;
#145608 = CARTESIAN_POINT('',(1.5,2.52928932188134,-27.4492893218813)) ;
#145609 = CARTESIAN_POINT('',(1.5,2.52928932188135,-27.4492893218813)) ;
#145610 = CARTESIAN_POINT('',(7.9,2.52928932188134,-27.4492893218813)) ;
#145611 = CARTESIAN_POINT('',(1.4,2.52928932188134,-27.4492893218813)) ;
#145612 = CARTESIAN_POINT('',(7.9,3.07928932188134,-27.9992893218813)) ;
#145613 = CARTESIAN_POINT('Origin',(1.4,2.6,-27.3785786437627)) ;
#145614 = CARTESIAN_POINT('',(1.5,2.5,-27.3785786437627)) ;
#145615 = CARTESIAN_POINT('Origin',(1.5,2.6,-27.3785786437627)) ;
#145616 = CARTESIAN_POINT('',(7.9,2.5,-27.3785786437627)) ;
#145617 = CARTESIAN_POINT('',(1.4,2.5,-27.3785786437627)) ;
#145618 = CARTESIAN_POINT('Origin',(7.9,2.6,-27.3785786437627)) ;
#145619 = CARTESIAN_POINT('Origin',(1.4,2.5,-27.27)) ;
#145620 = CARTESIAN_POINT('',(1.5,2.5,-27.27)) ;
#145621 = CARTESIAN_POINT('',(1.5,2.5,-27.27)) ;
#145622 = CARTESIAN_POINT('',(7.9,2.5,-27.27)) ;
#145623 = CARTESIAN_POINT('',(1.4,2.5,-27.27)) ;
#145624 = CARTESIAN_POINT('',(7.9,2.5,-27.3785786437627)) ;
#145625 = CARTESIAN_POINT('Origin',(1.4,2.4,-27.27)) ;
#145626 = CARTESIAN_POINT('',(1.5,2.4,-27.17)) ;
#145627 = CARTESIAN_POINT('Origin',(1.5,2.4,-27.27)) ;
#145628 = CARTESIAN_POINT('',(7.9,2.4,-27.17)) ;
#145629 = CARTESIAN_POINT('',(1.4,2.4,-27.17)) ;
#145630 = CARTESIAN_POINT('Origin',(7.9,2.4,-27.27)) ;
#145631 = CARTESIAN_POINT('Origin',(1.4,2.1,-27.17)) ;
#145632 = CARTESIAN_POINT('',(1.5,2.1,-27.17)) ;
#145633 = CARTESIAN_POINT('',(1.5,2.1,-27.17)) ;
#145634 = CARTESIAN_POINT('',(7.9,2.1,-27.17)) ;
#145635 = CARTESIAN_POINT('',(1.4,2.1,-27.17)) ;
#145636 = CARTESIAN_POINT('',(7.9,2.4,-27.17)) ;
#145637 = CARTESIAN_POINT('Origin',(1.4,2.1,-27.27)) ;
#145638 = CARTESIAN_POINT('',(1.5,2.,-27.27)) ;
#145639 = CARTESIAN_POINT('Origin',(1.5,2.1,-27.27)) ;
#145640 = CARTESIAN_POINT('',(7.9,2.,-27.27)) ;
#145641 = CARTESIAN_POINT('',(1.4,2.,-27.27)) ;
#145642 = CARTESIAN_POINT('Origin',(7.9,2.1,-27.27)) ;
#145643 = CARTESIAN_POINT('Origin',(1.4,2.,-27.27)) ;
#145644 = CARTESIAN_POINT('',(1.5,2.,-28.22)) ;
#145645 = CARTESIAN_POINT('',(1.5,2.,-28.22)) ;
#145646 = CARTESIAN_POINT('',(7.9,2.,-28.22)) ;
#145647 = CARTESIAN_POINT('',(1.4,2.,-28.22)) ;
#145648 = CARTESIAN_POINT('',(7.9,2.,-27.27)) ;
#145649 = CARTESIAN_POINT('Origin',(1.4,1.9,-28.22)) ;
#145650 = CARTESIAN_POINT('',(1.5,1.9,-28.32)) ;
#145651 = CARTESIAN_POINT('Origin',(1.5,1.9,-28.22)) ;
#145652 = CARTESIAN_POINT('',(7.9,1.9,-28.32)) ;
#145653 = CARTESIAN_POINT('',(1.4,1.9,-28.32)) ;
#145654 = CARTESIAN_POINT('Origin',(7.9,1.9,-28.22)) ;
#145655 = CARTESIAN_POINT('Origin',(1.4,1.9,-28.32)) ;
#145656 = CARTESIAN_POINT('',(1.5,-2.15,-28.32)) ;
#145657 = CARTESIAN_POINT('',(1.5,-2.15,-28.32)) ;
#145658 = CARTESIAN_POINT('',(7.9,-2.15,-28.32)) ;
#145659 = CARTESIAN_POINT('',(1.4,-2.15,-28.32)) ;
#145660 = CARTESIAN_POINT('',(7.9,1.9,-28.32)) ;
#145661 = CARTESIAN_POINT('Origin',(1.4,-2.15,-28.22)) ;
#145662 = CARTESIAN_POINT('',(1.5,-2.25,-28.22)) ;
#145663 = CARTESIAN_POINT('Origin',(1.5,-2.15,-28.22)) ;
#145664 = CARTESIAN_POINT('',(7.9,-2.25,-28.22)) ;
#145665 = CARTESIAN_POINT('',(1.4,-2.25,-28.22)) ;
#145666 = CARTESIAN_POINT('Origin',(7.9,-2.15,-28.22)) ;
#145667 = CARTESIAN_POINT('Origin',(1.4,-2.25,-27.5731195934094)) ;
#145668 = CARTESIAN_POINT('',(1.5,-2.25,-27.5731195934094)) ;
#145669 = CARTESIAN_POINT('',(1.5,-2.25,-27.5731195934094)) ;
#145670 = CARTESIAN_POINT('',(7.9,-2.25,-27.5731195934094)) ;
#145671 = CARTESIAN_POINT('',(1.4,-2.25,-27.5731195934094)) ;
#145672 = CARTESIAN_POINT('',(7.9,-2.25,-28.22)) ;
#145673 = CARTESIAN_POINT('Origin',(1.4,-2.15,-27.5731195934094)) ;
#145674 = CARTESIAN_POINT('',(1.5,-2.23576512455516,-27.5216964137135)) ;
#145675 = CARTESIAN_POINT('Origin',(1.5,-2.15,-27.5731195934094)) ;
#145676 = CARTESIAN_POINT('',(7.9,-2.23576512455516,-27.5216964137135)) ;
#145677 = CARTESIAN_POINT('',(1.4,-2.23576512455516,-27.5216964137135)) ;
#145678 = CARTESIAN_POINT('Origin',(7.9,-2.15,-27.5731195934094)) ;
#145679 = CARTESIAN_POINT('Origin',(1.4,-3.65625,-26.67)) ;
#145680 = CARTESIAN_POINT('',(1.5,-2.23576512455516,-25.8183035862865)) ;
#145681 = CARTESIAN_POINT('Origin',(1.5,-3.65625,-26.67)) ;
#145682 = CARTESIAN_POINT('',(7.9,-2.23576512455516,-25.8183035862865)) ;
#145683 = CARTESIAN_POINT('',(1.4,-2.23576512455516,-25.8183035862865)) ;
#145684 = CARTESIAN_POINT('Origin',(7.9,-3.65625,-26.67)) ;
#145685 = CARTESIAN_POINT('Origin',(1.4,-2.15,-25.7668804065906)) ;
#145686 = CARTESIAN_POINT('',(1.5,-2.25,-25.7668804065906)) ;
#145687 = CARTESIAN_POINT('Origin',(1.5,-2.15,-25.7668804065906)) ;
#145688 = CARTESIAN_POINT('',(7.9,-2.25,-25.7668804065906)) ;
#145689 = CARTESIAN_POINT('',(1.4,-2.25,-25.7668804065906)) ;
#145690 = CARTESIAN_POINT('Origin',(7.9,-2.15,-25.7668804065906)) ;
#145691 = CARTESIAN_POINT('Origin',(1.4,-2.25,-25.12)) ;
#145692 = CARTESIAN_POINT('',(1.5,-2.25,-25.12)) ;
#145693 = CARTESIAN_POINT('',(1.5,-2.25,-25.12)) ;
#145694 = CARTESIAN_POINT('',(7.9,-2.25,-25.12)) ;
#145695 = CARTESIAN_POINT('',(1.4,-2.25,-25.12)) ;
#145696 = CARTESIAN_POINT('',(7.9,-2.25,-25.7668804065906)) ;
#145697 = CARTESIAN_POINT('Origin',(1.4,-2.15,-25.12)) ;
#145698 = CARTESIAN_POINT('',(1.5,-2.15,-25.02)) ;
#145699 = CARTESIAN_POINT('Origin',(1.5,-2.15,-25.12)) ;
#145700 = CARTESIAN_POINT('',(7.9,-2.15,-25.02)) ;
#145701 = CARTESIAN_POINT('',(1.4,-2.15,-25.02)) ;
#145702 = CARTESIAN_POINT('Origin',(7.9,-2.15,-25.12)) ;
#145703 = CARTESIAN_POINT('Origin',(1.4,1.9,-25.02)) ;
#145704 = CARTESIAN_POINT('',(1.5,1.9,-25.02)) ;
#145705 = CARTESIAN_POINT('',(1.5,1.9,-25.02)) ;
#145706 = CARTESIAN_POINT('',(7.9,1.9,-25.02)) ;
#145707 = CARTESIAN_POINT('',(1.4,1.9,-25.02)) ;
#145708 = CARTESIAN_POINT('',(7.9,-2.15,-25.02)) ;
#145709 = CARTESIAN_POINT('Origin',(1.4,1.9,-25.12)) ;
#145710 = CARTESIAN_POINT('',(1.5,2.,-25.12)) ;
#145711 = CARTESIAN_POINT('Origin',(1.5,1.9,-25.12)) ;
#145712 = CARTESIAN_POINT('',(7.9,2.,-25.12)) ;
#145713 = CARTESIAN_POINT('',(1.4,2.,-25.12)) ;
#145714 = CARTESIAN_POINT('Origin',(7.9,1.9,-25.12)) ;
#145715 = CARTESIAN_POINT('Origin',(1.4,2.,-25.12)) ;
#145716 = CARTESIAN_POINT('',(1.5,2.,-26.07)) ;
#145717 = CARTESIAN_POINT('',(7.9,2.,-25.12)) ;
#145718 = CARTESIAN_POINT('Origin',(1.4,2.1,-26.07)) ;
#145719 = CARTESIAN_POINT('',(1.4,2.6,-26.07)) ;
#145720 = CARTESIAN_POINT('',(1.4,2.4,-26.27)) ;
#145721 = CARTESIAN_POINT('Origin',(1.4,2.4,-26.07)) ;
#145722 = CARTESIAN_POINT('',(1.4,2.1,-26.27)) ;
#145723 = CARTESIAN_POINT('',(1.4,2.1,-26.27)) ;
#145724 = CARTESIAN_POINT('',(1.4,1.9,-26.07)) ;
#145725 = CARTESIAN_POINT('Origin',(1.4,2.1,-26.07)) ;
#145726 = CARTESIAN_POINT('',(1.4,1.9,-25.12)) ;
#145727 = CARTESIAN_POINT('',(1.4,1.9,-25.12)) ;
#145728 = CARTESIAN_POINT('',(1.4,-2.15,-25.12)) ;
#145729 = CARTESIAN_POINT('',(1.4,-2.15,-25.12)) ;
#145730 = CARTESIAN_POINT('',(1.4,-2.15,-25.7668804065906)) ;
#145731 = CARTESIAN_POINT('',(1.4,-2.15,-25.7668804065906)) ;
#145732 = CARTESIAN_POINT('',(1.4,-2.15,-27.5731195934094)) ;
#145733 = CARTESIAN_POINT('Origin',(1.4,-3.65625,-26.67)) ;
#145734 = CARTESIAN_POINT('',(1.4,-2.15,-28.22)) ;
#145735 = CARTESIAN_POINT('',(1.4,-2.15,-28.22)) ;
#145736 = CARTESIAN_POINT('',(1.4,1.9,-28.22)) ;
#145737 = CARTESIAN_POINT('',(1.4,1.9,-28.22)) ;
#145738 = CARTESIAN_POINT('',(1.4,1.9,-27.27)) ;
#145739 = CARTESIAN_POINT('',(1.4,1.9,-27.27)) ;
#145740 = CARTESIAN_POINT('',(1.4,2.1,-27.07)) ;
#145741 = CARTESIAN_POINT('Origin',(1.4,2.1,-27.27)) ;
#145742 = CARTESIAN_POINT('',(1.4,2.4,-27.07)) ;
#145743 = CARTESIAN_POINT('',(1.4,2.4,-27.07)) ;
#145744 = CARTESIAN_POINT('',(1.4,2.6,-27.27)) ;
#145745 = CARTESIAN_POINT('Origin',(1.4,2.4,-27.27)) ;
#145746 = CARTESIAN_POINT('',(1.4,2.6,-27.3785786437627)) ;
#145747 = CARTESIAN_POINT('',(1.4,2.6,-27.3785786437627)) ;
#145748 = CARTESIAN_POINT('',(1.4,3.15,-27.9285786437627)) ;
#145749 = CARTESIAN_POINT('',(1.4,3.15,-27.9285786437627)) ;
#145750 = CARTESIAN_POINT('',(1.4,3.15,-25.4114213562373)) ;
#145751 = CARTESIAN_POINT('',(1.4,2.6,-25.9614213562373)) ;
#145752 = CARTESIAN_POINT('',(1.4,2.6,-25.9614213562373)) ;
#145753 = CARTESIAN_POINT('',(1.4,2.6,-26.07)) ;
#145754 = CARTESIAN_POINT('Origin',(1.4,2.1,-22.26)) ;
#145755 = CARTESIAN_POINT('',(1.5,2.,-22.26)) ;
#145756 = CARTESIAN_POINT('',(7.9,2.,-22.26)) ;
#145757 = CARTESIAN_POINT('',(1.4,2.,-22.26)) ;
#145758 = CARTESIAN_POINT('',(1.5,2.1,-22.36)) ;
#145759 = CARTESIAN_POINT('Origin',(1.5,2.1,-22.26)) ;
#145760 = CARTESIAN_POINT('',(7.9,2.1,-22.36)) ;
#145761 = CARTESIAN_POINT('',(1.4,2.1,-22.36)) ;
#145762 = CARTESIAN_POINT('Origin',(7.9,2.1,-22.26)) ;
#145763 = CARTESIAN_POINT('Origin',(1.4,2.4,-22.36)) ;
#145764 = CARTESIAN_POINT('',(1.5,2.4,-22.36)) ;
#145765 = CARTESIAN_POINT('',(1.5,2.4,-22.36)) ;
#145766 = CARTESIAN_POINT('',(7.9,2.4,-22.36)) ;
#145767 = CARTESIAN_POINT('',(1.4,2.4,-22.36)) ;
#145768 = CARTESIAN_POINT('',(7.9,2.1,-22.36)) ;
#145769 = CARTESIAN_POINT('Origin',(1.4,2.4,-22.26)) ;
#145770 = CARTESIAN_POINT('',(1.5,2.5,-22.26)) ;
#145771 = CARTESIAN_POINT('Origin',(1.5,2.4,-22.26)) ;
#145772 = CARTESIAN_POINT('',(7.9,2.5,-22.26)) ;
#145773 = CARTESIAN_POINT('',(1.4,2.5,-22.26)) ;
#145774 = CARTESIAN_POINT('Origin',(7.9,2.4,-22.26)) ;
#145775 = CARTESIAN_POINT('Origin',(1.4,2.5,-22.1514213562373)) ;
#145776 = CARTESIAN_POINT('',(1.5,2.5,-22.1514213562373)) ;
#145777 = CARTESIAN_POINT('',(1.5,2.5,-22.1514213562373)) ;
#145778 = CARTESIAN_POINT('',(7.9,2.5,-22.1514213562373)) ;
#145779 = CARTESIAN_POINT('',(1.4,2.5,-22.1514213562373)) ;
#145780 = CARTESIAN_POINT('',(7.9,2.5,-22.26)) ;
#145781 = CARTESIAN_POINT('Origin',(1.4,2.6,-22.1514213562373)) ;
#145782 = CARTESIAN_POINT('',(1.5,2.52928932188135,-22.0807106781187)) ;
#145783 = CARTESIAN_POINT('Origin',(1.5,2.6,-22.1514213562373)) ;
#145784 = CARTESIAN_POINT('',(7.9,2.52928932188135,-22.0807106781187)) ;
#145785 = CARTESIAN_POINT('',(1.4,2.52928932188135,-22.0807106781187)) ;
#145786 = CARTESIAN_POINT('Origin',(7.9,2.6,-22.1514213562373)) ;
#145787 = CARTESIAN_POINT('Origin',(1.4,3.07928932188135,-21.5307106781187)) ;
#145788 = CARTESIAN_POINT('',(1.5,3.07928932188135,-21.5307106781187)) ;
#145789 = CARTESIAN_POINT('',(7.9,3.07928932188135,-21.5307106781187)) ;
#145790 = CARTESIAN_POINT('',(1.4,3.07928932188135,-21.5307106781187)) ;
#145791 = CARTESIAN_POINT('',(7.9,2.52928932188135,-22.0807106781187)) ;
#145792 = CARTESIAN_POINT('Origin',(1.4,3.15,-21.6014213562373)) ;
#145793 = CARTESIAN_POINT('',(7.9,3.25,-21.6014213562373)) ;
#145794 = CARTESIAN_POINT('',(1.4,3.25,-21.6014213562373)) ;
#145795 = CARTESIAN_POINT('Origin',(7.9,3.15,-21.6014213562373)) ;
#145796 = CARTESIAN_POINT('Origin',(1.4,3.25,-24.1185786437627)) ;
#145797 = CARTESIAN_POINT('',(1.5,3.25,-24.1185786437627)) ;
#145798 = CARTESIAN_POINT('',(7.9,3.25,-21.6014213562373)) ;
#145799 = CARTESIAN_POINT('Origin',(1.4,2.52928932188134,-23.6392893218813)) ;
#145800 = CARTESIAN_POINT('',(1.5,2.52928932188134,-23.6392893218813)) ;
#145801 = CARTESIAN_POINT('',(1.5,2.52928932188135,-23.6392893218813)) ;
#145802 = CARTESIAN_POINT('',(7.9,2.52928932188134,-23.6392893218813)) ;
#145803 = CARTESIAN_POINT('',(1.4,2.52928932188134,-23.6392893218813)) ;
#145804 = CARTESIAN_POINT('',(7.9,3.07928932188134,-24.1892893218813)) ;
#145805 = CARTESIAN_POINT('Origin',(1.4,2.6,-23.5685786437627)) ;
#145806 = CARTESIAN_POINT('',(1.5,2.5,-23.5685786437627)) ;
#145807 = CARTESIAN_POINT('Origin',(1.5,2.6,-23.5685786437627)) ;
#145808 = CARTESIAN_POINT('',(7.9,2.5,-23.5685786437627)) ;
#145809 = CARTESIAN_POINT('',(1.4,2.5,-23.5685786437627)) ;
#145810 = CARTESIAN_POINT('Origin',(7.9,2.6,-23.5685786437627)) ;
#145811 = CARTESIAN_POINT('Origin',(1.4,2.5,-23.46)) ;
#145812 = CARTESIAN_POINT('',(1.5,2.5,-23.46)) ;
#145813 = CARTESIAN_POINT('',(1.5,2.5,-23.46)) ;
#145814 = CARTESIAN_POINT('',(7.9,2.5,-23.46)) ;
#145815 = CARTESIAN_POINT('',(1.4,2.5,-23.46)) ;
#145816 = CARTESIAN_POINT('',(7.9,2.5,-23.5685786437627)) ;
#145817 = CARTESIAN_POINT('Origin',(1.4,2.4,-23.46)) ;
#145818 = CARTESIAN_POINT('',(1.5,2.4,-23.36)) ;
#145819 = CARTESIAN_POINT('Origin',(1.5,2.4,-23.46)) ;
#145820 = CARTESIAN_POINT('',(7.9,2.4,-23.36)) ;
#145821 = CARTESIAN_POINT('',(1.4,2.4,-23.36)) ;
#145822 = CARTESIAN_POINT('Origin',(7.9,2.4,-23.46)) ;
#145823 = CARTESIAN_POINT('Origin',(1.4,2.1,-23.36)) ;
#145824 = CARTESIAN_POINT('',(1.5,2.1,-23.36)) ;
#145825 = CARTESIAN_POINT('',(1.5,2.1,-23.36)) ;
#145826 = CARTESIAN_POINT('',(7.9,2.1,-23.36)) ;
#145827 = CARTESIAN_POINT('',(1.4,2.1,-23.36)) ;
#145828 = CARTESIAN_POINT('',(7.9,2.4,-23.36)) ;
#145829 = CARTESIAN_POINT('Origin',(1.4,2.1,-23.46)) ;
#145830 = CARTESIAN_POINT('',(1.5,2.,-23.46)) ;
#145831 = CARTESIAN_POINT('Origin',(1.5,2.1,-23.46)) ;
#145832 = CARTESIAN_POINT('',(7.9,2.,-23.46)) ;
#145833 = CARTESIAN_POINT('',(1.4,2.,-23.46)) ;
#145834 = CARTESIAN_POINT('Origin',(7.9,2.1,-23.46)) ;
#145835 = CARTESIAN_POINT('Origin',(1.4,2.,-23.46)) ;
#145836 = CARTESIAN_POINT('',(1.5,2.,-24.41)) ;
#145837 = CARTESIAN_POINT('',(1.5,2.,-24.41)) ;
#145838 = CARTESIAN_POINT('',(7.9,2.,-24.41)) ;
#145839 = CARTESIAN_POINT('',(1.4,2.,-24.41)) ;
#145840 = CARTESIAN_POINT('',(7.9,2.,-23.46)) ;
#145841 = CARTESIAN_POINT('Origin',(1.4,1.9,-24.41)) ;
#145842 = CARTESIAN_POINT('',(1.5,1.9,-24.51)) ;
#145843 = CARTESIAN_POINT('Origin',(1.5,1.9,-24.41)) ;
#145844 = CARTESIAN_POINT('',(7.9,1.9,-24.51)) ;
#145845 = CARTESIAN_POINT('',(1.4,1.9,-24.51)) ;
#145846 = CARTESIAN_POINT('Origin',(7.9,1.9,-24.41)) ;
#145847 = CARTESIAN_POINT('Origin',(1.4,1.9,-24.51)) ;
#145848 = CARTESIAN_POINT('',(1.5,-2.15,-24.51)) ;
#145849 = CARTESIAN_POINT('',(1.5,-2.15,-24.51)) ;
#145850 = CARTESIAN_POINT('',(7.9,-2.15,-24.51)) ;
#145851 = CARTESIAN_POINT('',(1.4,-2.15,-24.51)) ;
#145852 = CARTESIAN_POINT('',(7.9,1.9,-24.51)) ;
#145853 = CARTESIAN_POINT('Origin',(1.4,-2.15,-24.41)) ;
#145854 = CARTESIAN_POINT('',(1.5,-2.25,-24.41)) ;
#145855 = CARTESIAN_POINT('Origin',(1.5,-2.15,-24.41)) ;
#145856 = CARTESIAN_POINT('',(7.9,-2.25,-24.41)) ;
#145857 = CARTESIAN_POINT('',(1.4,-2.25,-24.41)) ;
#145858 = CARTESIAN_POINT('Origin',(7.9,-2.15,-24.41)) ;
#145859 = CARTESIAN_POINT('Origin',(1.4,-2.25,-23.7631195934094)) ;
#145860 = CARTESIAN_POINT('',(1.5,-2.25,-23.7631195934094)) ;
#145861 = CARTESIAN_POINT('',(1.5,-2.25,-23.7631195934094)) ;
#145862 = CARTESIAN_POINT('',(7.9,-2.25,-23.7631195934094)) ;
#145863 = CARTESIAN_POINT('',(1.4,-2.25,-23.7631195934094)) ;
#145864 = CARTESIAN_POINT('',(7.9,-2.25,-24.41)) ;
#145865 = CARTESIAN_POINT('Origin',(1.4,-2.15,-23.7631195934094)) ;
#145866 = CARTESIAN_POINT('',(1.5,-2.23576512455516,-23.7116964137135)) ;
#145867 = CARTESIAN_POINT('Origin',(1.5,-2.15,-23.7631195934094)) ;
#145868 = CARTESIAN_POINT('',(7.9,-2.23576512455516,-23.7116964137135)) ;
#145869 = CARTESIAN_POINT('',(1.4,-2.23576512455516,-23.7116964137135)) ;
#145870 = CARTESIAN_POINT('Origin',(7.9,-2.15,-23.7631195934094)) ;
#145871 = CARTESIAN_POINT('Origin',(1.4,-3.65625,-22.86)) ;
#145872 = CARTESIAN_POINT('',(1.5,-2.23576512455516,-22.0083035862865)) ;
#145873 = CARTESIAN_POINT('Origin',(1.5,-3.65625,-22.86)) ;
#145874 = CARTESIAN_POINT('',(7.9,-2.23576512455516,-22.0083035862865)) ;
#145875 = CARTESIAN_POINT('',(1.4,-2.23576512455516,-22.0083035862865)) ;
#145876 = CARTESIAN_POINT('Origin',(7.9,-3.65625,-22.86)) ;
#145877 = CARTESIAN_POINT('Origin',(1.4,-2.15,-21.9568804065906)) ;
#145878 = CARTESIAN_POINT('',(1.5,-2.25,-21.9568804065906)) ;
#145879 = CARTESIAN_POINT('Origin',(1.5,-2.15,-21.9568804065906)) ;
#145880 = CARTESIAN_POINT('',(7.9,-2.25,-21.9568804065906)) ;
#145881 = CARTESIAN_POINT('',(1.4,-2.25,-21.9568804065906)) ;
#145882 = CARTESIAN_POINT('Origin',(7.9,-2.15,-21.9568804065906)) ;
#145883 = CARTESIAN_POINT('Origin',(1.4,-2.25,-21.31)) ;
#145884 = CARTESIAN_POINT('',(1.5,-2.25,-21.31)) ;
#145885 = CARTESIAN_POINT('',(1.5,-2.25,-21.31)) ;
#145886 = CARTESIAN_POINT('',(7.9,-2.25,-21.31)) ;
#145887 = CARTESIAN_POINT('',(1.4,-2.25,-21.31)) ;
#145888 = CARTESIAN_POINT('',(7.9,-2.25,-21.9568804065906)) ;
#145889 = CARTESIAN_POINT('Origin',(1.4,-2.15,-21.31)) ;
#145890 = CARTESIAN_POINT('',(1.5,-2.15,-21.21)) ;
#145891 = CARTESIAN_POINT('Origin',(1.5,-2.15,-21.31)) ;
#145892 = CARTESIAN_POINT('',(7.9,-2.15,-21.21)) ;
#145893 = CARTESIAN_POINT('',(1.4,-2.15,-21.21)) ;
#145894 = CARTESIAN_POINT('Origin',(7.9,-2.15,-21.31)) ;
#145895 = CARTESIAN_POINT('Origin',(1.4,1.9,-21.21)) ;
#145896 = CARTESIAN_POINT('',(1.5,1.9,-21.21)) ;
#145897 = CARTESIAN_POINT('',(1.5,1.9,-21.21)) ;
#145898 = CARTESIAN_POINT('',(7.9,1.9,-21.21)) ;
#145899 = CARTESIAN_POINT('',(1.4,1.9,-21.21)) ;
#145900 = CARTESIAN_POINT('',(7.9,-2.15,-21.21)) ;
#145901 = CARTESIAN_POINT('Origin',(1.4,1.9,-21.31)) ;
#145902 = CARTESIAN_POINT('',(1.5,2.,-21.31)) ;
#145903 = CARTESIAN_POINT('Origin',(1.5,1.9,-21.31)) ;
#145904 = CARTESIAN_POINT('',(7.9,2.,-21.31)) ;
#145905 = CARTESIAN_POINT('',(1.4,2.,-21.31)) ;
#145906 = CARTESIAN_POINT('Origin',(7.9,1.9,-21.31)) ;
#145907 = CARTESIAN_POINT('Origin',(1.4,2.,-21.31)) ;
#145908 = CARTESIAN_POINT('',(1.5,2.,-22.26)) ;
#145909 = CARTESIAN_POINT('',(7.9,2.,-21.31)) ;
#145910 = CARTESIAN_POINT('Origin',(1.4,2.1,-22.26)) ;
#145911 = CARTESIAN_POINT('',(1.4,2.6,-22.26)) ;
#145912 = CARTESIAN_POINT('',(1.4,2.4,-22.46)) ;
#145913 = CARTESIAN_POINT('Origin',(1.4,2.4,-22.26)) ;
#145914 = CARTESIAN_POINT('',(1.4,2.1,-22.46)) ;
#145915 = CARTESIAN_POINT('',(1.4,2.1,-22.46)) ;
#145916 = CARTESIAN_POINT('',(1.4,1.9,-22.26)) ;
#145917 = CARTESIAN_POINT('Origin',(1.4,2.1,-22.26)) ;
#145918 = CARTESIAN_POINT('',(1.4,1.9,-21.31)) ;
#145919 = CARTESIAN_POINT('',(1.4,1.9,-21.31)) ;
#145920 = CARTESIAN_POINT('',(1.4,-2.15,-21.31)) ;
#145921 = CARTESIAN_POINT('',(1.4,-2.15,-21.31)) ;
#145922 = CARTESIAN_POINT('',(1.4,-2.15,-21.9568804065906)) ;
#145923 = CARTESIAN_POINT('',(1.4,-2.15,-21.9568804065906)) ;
#145924 = CARTESIAN_POINT('',(1.4,-2.15,-23.7631195934094)) ;
#145925 = CARTESIAN_POINT('Origin',(1.4,-3.65625,-22.86)) ;
#145926 = CARTESIAN_POINT('',(1.4,-2.15,-24.41)) ;
#145927 = CARTESIAN_POINT('',(1.4,-2.15,-24.41)) ;
#145928 = CARTESIAN_POINT('',(1.4,1.9,-24.41)) ;
#145929 = CARTESIAN_POINT('',(1.4,1.9,-24.41)) ;
#145930 = CARTESIAN_POINT('',(1.4,1.9,-23.46)) ;
#145931 = CARTESIAN_POINT('',(1.4,1.9,-23.46)) ;
#145932 = CARTESIAN_POINT('',(1.4,2.1,-23.26)) ;
#145933 = CARTESIAN_POINT('Origin',(1.4,2.1,-23.46)) ;
#145934 = CARTESIAN_POINT('',(1.4,2.4,-23.26)) ;
#145935 = CARTESIAN_POINT('',(1.4,2.4,-23.26)) ;
#145936 = CARTESIAN_POINT('',(1.4,2.6,-23.46)) ;
#145937 = CARTESIAN_POINT('Origin',(1.4,2.4,-23.46)) ;
#145938 = CARTESIAN_POINT('',(1.4,2.6,-23.5685786437627)) ;
#145939 = CARTESIAN_POINT('',(1.4,2.6,-23.5685786437627)) ;
#145940 = CARTESIAN_POINT('',(1.4,3.15,-24.1185786437627)) ;
#145941 = CARTESIAN_POINT('',(1.4,3.15,-24.1185786437627)) ;
#145942 = CARTESIAN_POINT('',(1.4,3.15,-21.6014213562373)) ;
#145943 = CARTESIAN_POINT('',(1.4,2.6,-22.1514213562373)) ;
#145944 = CARTESIAN_POINT('',(1.4,2.6,-22.1514213562373)) ;
#145945 = CARTESIAN_POINT('',(1.4,2.6,-22.26)) ;
#145946 = CARTESIAN_POINT('Origin',(1.4,2.1,-18.45)) ;
#145947 = CARTESIAN_POINT('',(1.5,2.,-18.45)) ;
#145948 = CARTESIAN_POINT('',(7.9,2.,-18.45)) ;
#145949 = CARTESIAN_POINT('',(1.4,2.,-18.45)) ;
#145950 = CARTESIAN_POINT('',(1.5,2.1,-18.55)) ;
#145951 = CARTESIAN_POINT('Origin',(1.5,2.1,-18.45)) ;
#145952 = CARTESIAN_POINT('',(7.9,2.1,-18.55)) ;
#145953 = CARTESIAN_POINT('',(1.4,2.1,-18.55)) ;
#145954 = CARTESIAN_POINT('Origin',(7.9,2.1,-18.45)) ;
#145955 = CARTESIAN_POINT('Origin',(1.4,2.4,-18.55)) ;
#145956 = CARTESIAN_POINT('',(1.5,2.4,-18.55)) ;
#145957 = CARTESIAN_POINT('',(1.5,2.4,-18.55)) ;
#145958 = CARTESIAN_POINT('',(7.9,2.4,-18.55)) ;
#145959 = CARTESIAN_POINT('',(1.4,2.4,-18.55)) ;
#145960 = CARTESIAN_POINT('',(7.9,2.1,-18.55)) ;
#145961 = CARTESIAN_POINT('Origin',(1.4,2.4,-18.45)) ;
#145962 = CARTESIAN_POINT('',(1.5,2.5,-18.45)) ;
#145963 = CARTESIAN_POINT('Origin',(1.5,2.4,-18.45)) ;
#145964 = CARTESIAN_POINT('',(7.9,2.5,-18.45)) ;
#145965 = CARTESIAN_POINT('',(1.4,2.5,-18.45)) ;
#145966 = CARTESIAN_POINT('Origin',(7.9,2.4,-18.45)) ;
#145967 = CARTESIAN_POINT('Origin',(1.4,2.5,-18.3414213562373)) ;
#145968 = CARTESIAN_POINT('',(1.5,2.5,-18.3414213562373)) ;
#145969 = CARTESIAN_POINT('',(1.5,2.5,-18.3414213562373)) ;
#145970 = CARTESIAN_POINT('',(7.9,2.5,-18.3414213562373)) ;
#145971 = CARTESIAN_POINT('',(1.4,2.5,-18.3414213562373)) ;
#145972 = CARTESIAN_POINT('',(7.9,2.5,-18.45)) ;
#145973 = CARTESIAN_POINT('Origin',(1.4,2.6,-18.3414213562373)) ;
#145974 = CARTESIAN_POINT('',(1.5,2.52928932188135,-18.2707106781187)) ;
#145975 = CARTESIAN_POINT('Origin',(1.5,2.6,-18.3414213562373)) ;
#145976 = CARTESIAN_POINT('',(7.9,2.52928932188135,-18.2707106781187)) ;
#145977 = CARTESIAN_POINT('',(1.4,2.52928932188135,-18.2707106781187)) ;
#145978 = CARTESIAN_POINT('Origin',(7.9,2.6,-18.3414213562373)) ;
#145979 = CARTESIAN_POINT('Origin',(1.4,3.07928932188135,-17.7207106781187)) ;
#145980 = CARTESIAN_POINT('',(1.5,3.07928932188135,-17.7207106781187)) ;
#145981 = CARTESIAN_POINT('',(7.9,3.07928932188135,-17.7207106781187)) ;
#145982 = CARTESIAN_POINT('',(1.4,3.07928932188135,-17.7207106781187)) ;
#145983 = CARTESIAN_POINT('',(7.9,2.52928932188135,-18.2707106781187)) ;
#145984 = CARTESIAN_POINT('Origin',(1.4,3.15,-17.7914213562373)) ;
#145985 = CARTESIAN_POINT('',(7.9,3.25,-17.7914213562373)) ;
#145986 = CARTESIAN_POINT('',(1.4,3.25,-17.7914213562373)) ;
#145987 = CARTESIAN_POINT('Origin',(7.9,3.15,-17.7914213562373)) ;
#145988 = CARTESIAN_POINT('Origin',(1.4,3.25,-20.3085786437627)) ;
#145989 = CARTESIAN_POINT('',(1.5,3.25,-20.3085786437627)) ;
#145990 = CARTESIAN_POINT('',(7.9,3.25,-17.7914213562373)) ;
#145991 = CARTESIAN_POINT('Origin',(1.4,2.52928932188134,-19.8292893218813)) ;
#145992 = CARTESIAN_POINT('',(1.5,2.52928932188134,-19.8292893218813)) ;
#145993 = CARTESIAN_POINT('',(1.5,2.52928932188135,-19.8292893218813)) ;
#145994 = CARTESIAN_POINT('',(7.9,2.52928932188134,-19.8292893218813)) ;
#145995 = CARTESIAN_POINT('',(1.4,2.52928932188134,-19.8292893218813)) ;
#145996 = CARTESIAN_POINT('',(7.9,3.07928932188134,-20.3792893218813)) ;
#145997 = CARTESIAN_POINT('Origin',(1.4,2.6,-19.7585786437627)) ;
#145998 = CARTESIAN_POINT('',(1.5,2.5,-19.7585786437627)) ;
#145999 = CARTESIAN_POINT('Origin',(1.5,2.6,-19.7585786437627)) ;
#146000 = CARTESIAN_POINT('',(7.9,2.5,-19.7585786437627)) ;
#146001 = CARTESIAN_POINT('',(1.4,2.5,-19.7585786437627)) ;
#146002 = CARTESIAN_POINT('Origin',(7.9,2.6,-19.7585786437627)) ;
#146003 = CARTESIAN_POINT('Origin',(1.4,2.5,-19.65)) ;
#146004 = CARTESIAN_POINT('',(1.5,2.5,-19.65)) ;
#146005 = CARTESIAN_POINT('',(1.5,2.5,-19.65)) ;
#146006 = CARTESIAN_POINT('',(7.9,2.5,-19.65)) ;
#146007 = CARTESIAN_POINT('',(1.4,2.5,-19.65)) ;
#146008 = CARTESIAN_POINT('',(7.9,2.5,-19.7585786437627)) ;
#146009 = CARTESIAN_POINT('Origin',(1.4,2.4,-19.65)) ;
#146010 = CARTESIAN_POINT('',(1.5,2.4,-19.55)) ;
#146011 = CARTESIAN_POINT('Origin',(1.5,2.4,-19.65)) ;
#146012 = CARTESIAN_POINT('',(7.9,2.4,-19.55)) ;
#146013 = CARTESIAN_POINT('',(1.4,2.4,-19.55)) ;
#146014 = CARTESIAN_POINT('Origin',(7.9,2.4,-19.65)) ;
#146015 = CARTESIAN_POINT('Origin',(1.4,2.1,-19.55)) ;
#146016 = CARTESIAN_POINT('',(1.5,2.1,-19.55)) ;
#146017 = CARTESIAN_POINT('',(1.5,2.1,-19.55)) ;
#146018 = CARTESIAN_POINT('',(7.9,2.1,-19.55)) ;
#146019 = CARTESIAN_POINT('',(1.4,2.1,-19.55)) ;
#146020 = CARTESIAN_POINT('',(7.9,2.4,-19.55)) ;
#146021 = CARTESIAN_POINT('Origin',(1.4,2.1,-19.65)) ;
#146022 = CARTESIAN_POINT('',(1.5,2.,-19.65)) ;
#146023 = CARTESIAN_POINT('Origin',(1.5,2.1,-19.65)) ;
#146024 = CARTESIAN_POINT('',(7.9,2.,-19.65)) ;
#146025 = CARTESIAN_POINT('',(1.4,2.,-19.65)) ;
#146026 = CARTESIAN_POINT('Origin',(7.9,2.1,-19.65)) ;
#146027 = CARTESIAN_POINT('Origin',(1.4,2.,-19.65)) ;
#146028 = CARTESIAN_POINT('',(1.5,2.,-20.6)) ;
#146029 = CARTESIAN_POINT('',(1.5,2.,-20.6)) ;
#146030 = CARTESIAN_POINT('',(7.9,2.,-20.6)) ;
#146031 = CARTESIAN_POINT('',(1.4,2.,-20.6)) ;
#146032 = CARTESIAN_POINT('',(7.9,2.,-19.65)) ;
#146033 = CARTESIAN_POINT('Origin',(1.4,1.9,-20.6)) ;
#146034 = CARTESIAN_POINT('',(1.5,1.9,-20.7)) ;
#146035 = CARTESIAN_POINT('Origin',(1.5,1.9,-20.6)) ;
#146036 = CARTESIAN_POINT('',(7.9,1.9,-20.7)) ;
#146037 = CARTESIAN_POINT('',(1.4,1.9,-20.7)) ;
#146038 = CARTESIAN_POINT('Origin',(7.9,1.9,-20.6)) ;
#146039 = CARTESIAN_POINT('Origin',(1.4,1.9,-20.7)) ;
#146040 = CARTESIAN_POINT('',(1.5,-2.15,-20.7)) ;
#146041 = CARTESIAN_POINT('',(1.5,-2.15,-20.7)) ;
#146042 = CARTESIAN_POINT('',(7.9,-2.15,-20.7)) ;
#146043 = CARTESIAN_POINT('',(1.4,-2.15,-20.7)) ;
#146044 = CARTESIAN_POINT('',(7.9,1.9,-20.7)) ;
#146045 = CARTESIAN_POINT('Origin',(1.4,-2.15,-20.6)) ;
#146046 = CARTESIAN_POINT('',(1.5,-2.25,-20.6)) ;
#146047 = CARTESIAN_POINT('Origin',(1.5,-2.15,-20.6)) ;
#146048 = CARTESIAN_POINT('',(7.9,-2.25,-20.6)) ;
#146049 = CARTESIAN_POINT('',(1.4,-2.25,-20.6)) ;
#146050 = CARTESIAN_POINT('Origin',(7.9,-2.15,-20.6)) ;
#146051 = CARTESIAN_POINT('Origin',(1.4,-2.25,-19.9531195934094)) ;
#146052 = CARTESIAN_POINT('',(1.5,-2.25,-19.9531195934094)) ;
#146053 = CARTESIAN_POINT('',(1.5,-2.25,-19.9531195934094)) ;
#146054 = CARTESIAN_POINT('',(7.9,-2.25,-19.9531195934094)) ;
#146055 = CARTESIAN_POINT('',(1.4,-2.25,-19.9531195934094)) ;
#146056 = CARTESIAN_POINT('',(7.9,-2.25,-20.6)) ;
#146057 = CARTESIAN_POINT('Origin',(1.4,-2.15,-19.9531195934094)) ;
#146058 = CARTESIAN_POINT('',(1.5,-2.23576512455516,-19.9016964137135)) ;
#146059 = CARTESIAN_POINT('Origin',(1.5,-2.15,-19.9531195934094)) ;
#146060 = CARTESIAN_POINT('',(7.9,-2.23576512455516,-19.9016964137135)) ;
#146061 = CARTESIAN_POINT('',(1.4,-2.23576512455516,-19.9016964137135)) ;
#146062 = CARTESIAN_POINT('Origin',(7.9,-2.15,-19.9531195934094)) ;
#146063 = CARTESIAN_POINT('Origin',(1.4,-3.65625,-19.05)) ;
#146064 = CARTESIAN_POINT('',(1.5,-2.23576512455516,-18.1983035862865)) ;
#146065 = CARTESIAN_POINT('Origin',(1.5,-3.65625,-19.05)) ;
#146066 = CARTESIAN_POINT('',(7.9,-2.23576512455516,-18.1983035862865)) ;
#146067 = CARTESIAN_POINT('',(1.4,-2.23576512455516,-18.1983035862865)) ;
#146068 = CARTESIAN_POINT('Origin',(7.9,-3.65625,-19.05)) ;
#146069 = CARTESIAN_POINT('Origin',(1.4,-2.15,-18.1468804065906)) ;
#146070 = CARTESIAN_POINT('',(1.5,-2.25,-18.1468804065906)) ;
#146071 = CARTESIAN_POINT('Origin',(1.5,-2.15,-18.1468804065906)) ;
#146072 = CARTESIAN_POINT('',(7.9,-2.25,-18.1468804065906)) ;
#146073 = CARTESIAN_POINT('',(1.4,-2.25,-18.1468804065906)) ;
#146074 = CARTESIAN_POINT('Origin',(7.9,-2.15,-18.1468804065906)) ;
#146075 = CARTESIAN_POINT('Origin',(1.4,-2.25,-17.5)) ;
#146076 = CARTESIAN_POINT('',(1.5,-2.25,-17.5)) ;
#146077 = CARTESIAN_POINT('',(1.5,-2.25,-17.5)) ;
#146078 = CARTESIAN_POINT('',(7.9,-2.25,-17.5)) ;
#146079 = CARTESIAN_POINT('',(1.4,-2.25,-17.5)) ;
#146080 = CARTESIAN_POINT('',(7.9,-2.25,-18.1468804065906)) ;
#146081 = CARTESIAN_POINT('Origin',(1.4,-2.15,-17.5)) ;
#146082 = CARTESIAN_POINT('',(1.5,-2.15,-17.4)) ;
#146083 = CARTESIAN_POINT('Origin',(1.5,-2.15,-17.5)) ;
#146084 = CARTESIAN_POINT('',(7.9,-2.15,-17.4)) ;
#146085 = CARTESIAN_POINT('',(1.4,-2.15,-17.4)) ;
#146086 = CARTESIAN_POINT('Origin',(7.9,-2.15,-17.5)) ;
#146087 = CARTESIAN_POINT('Origin',(1.4,1.9,-17.4)) ;
#146088 = CARTESIAN_POINT('',(1.5,1.9,-17.4)) ;
#146089 = CARTESIAN_POINT('',(1.5,1.9,-17.4)) ;
#146090 = CARTESIAN_POINT('',(7.9,1.9,-17.4)) ;
#146091 = CARTESIAN_POINT('',(1.4,1.9,-17.4)) ;
#146092 = CARTESIAN_POINT('',(7.9,-2.15,-17.4)) ;
#146093 = CARTESIAN_POINT('Origin',(1.4,1.9,-17.5)) ;
#146094 = CARTESIAN_POINT('',(1.5,2.,-17.5)) ;
#146095 = CARTESIAN_POINT('Origin',(1.5,1.9,-17.5)) ;
#146096 = CARTESIAN_POINT('',(7.9,2.,-17.5)) ;
#146097 = CARTESIAN_POINT('',(1.4,2.,-17.5)) ;
#146098 = CARTESIAN_POINT('Origin',(7.9,1.9,-17.5)) ;
#146099 = CARTESIAN_POINT('Origin',(1.4,2.,-17.5)) ;
#146100 = CARTESIAN_POINT('',(1.5,2.,-18.45)) ;
#146101 = CARTESIAN_POINT('',(7.9,2.,-17.5)) ;
#146102 = CARTESIAN_POINT('Origin',(1.4,2.1,-18.45)) ;
#146103 = CARTESIAN_POINT('',(1.4,2.6,-18.45)) ;
#146104 = CARTESIAN_POINT('',(1.4,2.4,-18.65)) ;
#146105 = CARTESIAN_POINT('Origin',(1.4,2.4,-18.45)) ;
#146106 = CARTESIAN_POINT('',(1.4,2.1,-18.65)) ;
#146107 = CARTESIAN_POINT('',(1.4,2.1,-18.65)) ;
#146108 = CARTESIAN_POINT('',(1.4,1.9,-18.45)) ;
#146109 = CARTESIAN_POINT('Origin',(1.4,2.1,-18.45)) ;
#146110 = CARTESIAN_POINT('',(1.4,1.9,-17.5)) ;
#146111 = CARTESIAN_POINT('',(1.4,1.9,-17.5)) ;
#146112 = CARTESIAN_POINT('',(1.4,-2.15,-17.5)) ;
#146113 = CARTESIAN_POINT('',(1.4,-2.15,-17.5)) ;
#146114 = CARTESIAN_POINT('',(1.4,-2.15,-18.1468804065906)) ;
#146115 = CARTESIAN_POINT('',(1.4,-2.15,-18.1468804065906)) ;
#146116 = CARTESIAN_POINT('',(1.4,-2.15,-19.9531195934094)) ;
#146117 = CARTESIAN_POINT('Origin',(1.4,-3.65625,-19.05)) ;
#146118 = CARTESIAN_POINT('',(1.4,-2.15,-20.6)) ;
#146119 = CARTESIAN_POINT('',(1.4,-2.15,-20.6)) ;
#146120 = CARTESIAN_POINT('',(1.4,1.9,-20.6)) ;
#146121 = CARTESIAN_POINT('',(1.4,1.9,-20.6)) ;
#146122 = CARTESIAN_POINT('',(1.4,1.9,-19.65)) ;
#146123 = CARTESIAN_POINT('',(1.4,1.9,-19.65)) ;
#146124 = CARTESIAN_POINT('',(1.4,2.1,-19.45)) ;
#146125 = CARTESIAN_POINT('Origin',(1.4,2.1,-19.65)) ;
#146126 = CARTESIAN_POINT('',(1.4,2.4,-19.45)) ;
#146127 = CARTESIAN_POINT('',(1.4,2.4,-19.45)) ;
#146128 = CARTESIAN_POINT('',(1.4,2.6,-19.65)) ;
#146129 = CARTESIAN_POINT('Origin',(1.4,2.4,-19.65)) ;
#146130 = CARTESIAN_POINT('',(1.4,2.6,-19.7585786437627)) ;
#146131 = CARTESIAN_POINT('',(1.4,2.6,-19.7585786437627)) ;
#146132 = CARTESIAN_POINT('',(1.4,3.15,-20.3085786437627)) ;
#146133 = CARTESIAN_POINT('',(1.4,3.15,-20.3085786437627)) ;
#146134 = CARTESIAN_POINT('',(1.4,3.15,-17.7914213562373)) ;
#146135 = CARTESIAN_POINT('',(1.4,2.6,-18.3414213562373)) ;
#146136 = CARTESIAN_POINT('',(1.4,2.6,-18.3414213562373)) ;
#146137 = CARTESIAN_POINT('',(1.4,2.6,-18.45)) ;
#146138 = CARTESIAN_POINT('Origin',(1.4,2.1,-14.64)) ;
#146139 = CARTESIAN_POINT('',(1.5,2.,-14.64)) ;
#146140 = CARTESIAN_POINT('',(7.9,2.,-14.64)) ;
#146141 = CARTESIAN_POINT('',(1.4,2.,-14.64)) ;
#146142 = CARTESIAN_POINT('',(1.5,2.1,-14.74)) ;
#146143 = CARTESIAN_POINT('Origin',(1.5,2.1,-14.64)) ;
#146144 = CARTESIAN_POINT('',(7.9,2.1,-14.74)) ;
#146145 = CARTESIAN_POINT('',(1.4,2.1,-14.74)) ;
#146146 = CARTESIAN_POINT('Origin',(7.9,2.1,-14.64)) ;
#146147 = CARTESIAN_POINT('Origin',(1.4,2.4,-14.74)) ;
#146148 = CARTESIAN_POINT('',(1.5,2.4,-14.74)) ;
#146149 = CARTESIAN_POINT('',(1.5,2.4,-14.74)) ;
#146150 = CARTESIAN_POINT('',(7.9,2.4,-14.74)) ;
#146151 = CARTESIAN_POINT('',(1.4,2.4,-14.74)) ;
#146152 = CARTESIAN_POINT('',(7.9,2.1,-14.74)) ;
#146153 = CARTESIAN_POINT('Origin',(1.4,2.4,-14.64)) ;
#146154 = CARTESIAN_POINT('',(1.5,2.5,-14.64)) ;
#146155 = CARTESIAN_POINT('Origin',(1.5,2.4,-14.64)) ;
#146156 = CARTESIAN_POINT('',(7.9,2.5,-14.64)) ;
#146157 = CARTESIAN_POINT('',(1.4,2.5,-14.64)) ;
#146158 = CARTESIAN_POINT('Origin',(7.9,2.4,-14.64)) ;
#146159 = CARTESIAN_POINT('Origin',(1.4,2.5,-14.5314213562373)) ;
#146160 = CARTESIAN_POINT('',(1.5,2.5,-14.5314213562373)) ;
#146161 = CARTESIAN_POINT('',(1.5,2.5,-14.5314213562373)) ;
#146162 = CARTESIAN_POINT('',(7.9,2.5,-14.5314213562373)) ;
#146163 = CARTESIAN_POINT('',(1.4,2.5,-14.5314213562373)) ;
#146164 = CARTESIAN_POINT('',(7.9,2.5,-14.64)) ;
#146165 = CARTESIAN_POINT('Origin',(1.4,2.6,-14.5314213562373)) ;
#146166 = CARTESIAN_POINT('',(1.5,2.52928932188135,-14.4607106781187)) ;
#146167 = CARTESIAN_POINT('Origin',(1.5,2.6,-14.5314213562373)) ;
#146168 = CARTESIAN_POINT('',(7.9,2.52928932188135,-14.4607106781187)) ;
#146169 = CARTESIAN_POINT('',(1.4,2.52928932188135,-14.4607106781187)) ;
#146170 = CARTESIAN_POINT('Origin',(7.9,2.6,-14.5314213562373)) ;
#146171 = CARTESIAN_POINT('Origin',(1.4,3.07928932188135,-13.9107106781187)) ;
#146172 = CARTESIAN_POINT('',(1.5,3.07928932188135,-13.9107106781187)) ;
#146173 = CARTESIAN_POINT('',(7.9,3.07928932188135,-13.9107106781187)) ;
#146174 = CARTESIAN_POINT('',(1.4,3.07928932188135,-13.9107106781187)) ;
#146175 = CARTESIAN_POINT('',(7.9,2.52928932188135,-14.4607106781187)) ;
#146176 = CARTESIAN_POINT('Origin',(1.4,3.15,-13.9814213562373)) ;
#146177 = CARTESIAN_POINT('',(7.9,3.25,-13.9814213562373)) ;
#146178 = CARTESIAN_POINT('',(1.4,3.25,-13.9814213562373)) ;
#146179 = CARTESIAN_POINT('Origin',(7.9,3.15,-13.9814213562373)) ;
#146180 = CARTESIAN_POINT('Origin',(1.4,3.25,-16.4985786437627)) ;
#146181 = CARTESIAN_POINT('',(1.5,3.25,-16.4985786437627)) ;
#146182 = CARTESIAN_POINT('',(7.9,3.25,-13.9814213562373)) ;
#146183 = CARTESIAN_POINT('Origin',(1.4,2.52928932188134,-16.0192893218813)) ;
#146184 = CARTESIAN_POINT('',(1.5,2.52928932188134,-16.0192893218813)) ;
#146185 = CARTESIAN_POINT('',(1.5,2.52928932188135,-16.0192893218813)) ;
#146186 = CARTESIAN_POINT('',(7.9,2.52928932188134,-16.0192893218813)) ;
#146187 = CARTESIAN_POINT('',(1.4,2.52928932188134,-16.0192893218813)) ;
#146188 = CARTESIAN_POINT('',(7.9,3.07928932188134,-16.5692893218813)) ;
#146189 = CARTESIAN_POINT('Origin',(1.4,2.6,-15.9485786437627)) ;
#146190 = CARTESIAN_POINT('',(1.5,2.5,-15.9485786437627)) ;
#146191 = CARTESIAN_POINT('Origin',(1.5,2.6,-15.9485786437627)) ;
#146192 = CARTESIAN_POINT('',(7.9,2.5,-15.9485786437627)) ;
#146193 = CARTESIAN_POINT('',(1.4,2.5,-15.9485786437627)) ;
#146194 = CARTESIAN_POINT('Origin',(7.9,2.6,-15.9485786437627)) ;
#146195 = CARTESIAN_POINT('Origin',(1.4,2.5,-15.84)) ;
#146196 = CARTESIAN_POINT('',(1.5,2.5,-15.84)) ;
#146197 = CARTESIAN_POINT('',(1.5,2.5,-15.84)) ;
#146198 = CARTESIAN_POINT('',(7.9,2.5,-15.84)) ;
#146199 = CARTESIAN_POINT('',(1.4,2.5,-15.84)) ;
#146200 = CARTESIAN_POINT('',(7.9,2.5,-15.9485786437627)) ;
#146201 = CARTESIAN_POINT('Origin',(1.4,2.4,-15.84)) ;
#146202 = CARTESIAN_POINT('',(1.5,2.4,-15.74)) ;
#146203 = CARTESIAN_POINT('Origin',(1.5,2.4,-15.84)) ;
#146204 = CARTESIAN_POINT('',(7.9,2.4,-15.74)) ;
#146205 = CARTESIAN_POINT('',(1.4,2.4,-15.74)) ;
#146206 = CARTESIAN_POINT('Origin',(7.9,2.4,-15.84)) ;
#146207 = CARTESIAN_POINT('Origin',(1.4,2.1,-15.74)) ;
#146208 = CARTESIAN_POINT('',(1.5,2.1,-15.74)) ;
#146209 = CARTESIAN_POINT('',(1.5,2.1,-15.74)) ;
#146210 = CARTESIAN_POINT('',(7.9,2.1,-15.74)) ;
#146211 = CARTESIAN_POINT('',(1.4,2.1,-15.74)) ;
#146212 = CARTESIAN_POINT('',(7.9,2.4,-15.74)) ;
#146213 = CARTESIAN_POINT('Origin',(1.4,2.1,-15.84)) ;
#146214 = CARTESIAN_POINT('',(1.5,2.,-15.84)) ;
#146215 = CARTESIAN_POINT('Origin',(1.5,2.1,-15.84)) ;
#146216 = CARTESIAN_POINT('',(7.9,2.,-15.84)) ;
#146217 = CARTESIAN_POINT('',(1.4,2.,-15.84)) ;
#146218 = CARTESIAN_POINT('Origin',(7.9,2.1,-15.84)) ;
#146219 = CARTESIAN_POINT('Origin',(1.4,2.,-15.84)) ;
#146220 = CARTESIAN_POINT('',(1.5,2.,-16.79)) ;
#146221 = CARTESIAN_POINT('',(1.5,2.,-16.79)) ;
#146222 = CARTESIAN_POINT('',(7.9,2.,-16.79)) ;
#146223 = CARTESIAN_POINT('',(1.4,2.,-16.79)) ;
#146224 = CARTESIAN_POINT('',(7.9,2.,-15.84)) ;
#146225 = CARTESIAN_POINT('Origin',(1.4,1.9,-16.79)) ;
#146226 = CARTESIAN_POINT('',(1.5,1.9,-16.89)) ;
#146227 = CARTESIAN_POINT('Origin',(1.5,1.9,-16.79)) ;
#146228 = CARTESIAN_POINT('',(7.9,1.9,-16.89)) ;
#146229 = CARTESIAN_POINT('',(1.4,1.9,-16.89)) ;
#146230 = CARTESIAN_POINT('Origin',(7.9,1.9,-16.79)) ;
#146231 = CARTESIAN_POINT('Origin',(1.4,1.9,-16.89)) ;
#146232 = CARTESIAN_POINT('',(1.5,-2.15,-16.89)) ;
#146233 = CARTESIAN_POINT('',(1.5,-2.15,-16.89)) ;
#146234 = CARTESIAN_POINT('',(7.9,-2.15,-16.89)) ;
#146235 = CARTESIAN_POINT('',(1.4,-2.15,-16.89)) ;
#146236 = CARTESIAN_POINT('',(7.9,1.9,-16.89)) ;
#146237 = CARTESIAN_POINT('Origin',(1.4,-2.15,-16.79)) ;
#146238 = CARTESIAN_POINT('',(1.5,-2.25,-16.79)) ;
#146239 = CARTESIAN_POINT('Origin',(1.5,-2.15,-16.79)) ;
#146240 = CARTESIAN_POINT('',(7.9,-2.25,-16.79)) ;
#146241 = CARTESIAN_POINT('',(1.4,-2.25,-16.79)) ;
#146242 = CARTESIAN_POINT('Origin',(7.9,-2.15,-16.79)) ;
#146243 = CARTESIAN_POINT('Origin',(1.4,-2.25,-16.1431195934094)) ;
#146244 = CARTESIAN_POINT('',(1.5,-2.25,-16.1431195934094)) ;
#146245 = CARTESIAN_POINT('',(1.5,-2.25,-16.1431195934094)) ;
#146246 = CARTESIAN_POINT('',(7.9,-2.25,-16.1431195934094)) ;
#146247 = CARTESIAN_POINT('',(1.4,-2.25,-16.1431195934094)) ;
#146248 = CARTESIAN_POINT('',(7.9,-2.25,-16.79)) ;
#146249 = CARTESIAN_POINT('Origin',(1.4,-2.15,-16.1431195934094)) ;
#146250 = CARTESIAN_POINT('',(1.5,-2.23576512455516,-16.0916964137135)) ;
#146251 = CARTESIAN_POINT('Origin',(1.5,-2.15,-16.1431195934094)) ;
#146252 = CARTESIAN_POINT('',(7.9,-2.23576512455516,-16.0916964137135)) ;
#146253 = CARTESIAN_POINT('',(1.4,-2.23576512455516,-16.0916964137135)) ;
#146254 = CARTESIAN_POINT('Origin',(7.9,-2.15,-16.1431195934094)) ;
#146255 = CARTESIAN_POINT('Origin',(1.4,-3.65625,-15.24)) ;
#146256 = CARTESIAN_POINT('',(1.5,-2.23576512455516,-14.3883035862865)) ;
#146257 = CARTESIAN_POINT('Origin',(1.5,-3.65625,-15.24)) ;
#146258 = CARTESIAN_POINT('',(7.9,-2.23576512455516,-14.3883035862865)) ;
#146259 = CARTESIAN_POINT('',(1.4,-2.23576512455516,-14.3883035862865)) ;
#146260 = CARTESIAN_POINT('Origin',(7.9,-3.65625,-15.24)) ;
#146261 = CARTESIAN_POINT('Origin',(1.4,-2.15,-14.3368804065906)) ;
#146262 = CARTESIAN_POINT('',(1.5,-2.25,-14.3368804065906)) ;
#146263 = CARTESIAN_POINT('Origin',(1.5,-2.15,-14.3368804065906)) ;
#146264 = CARTESIAN_POINT('',(7.9,-2.25,-14.3368804065906)) ;
#146265 = CARTESIAN_POINT('',(1.4,-2.25,-14.3368804065906)) ;
#146266 = CARTESIAN_POINT('Origin',(7.9,-2.15,-14.3368804065906)) ;
#146267 = CARTESIAN_POINT('Origin',(1.4,-2.25,-13.69)) ;
#146268 = CARTESIAN_POINT('',(1.5,-2.25,-13.69)) ;
#146269 = CARTESIAN_POINT('',(1.5,-2.25,-13.69)) ;
#146270 = CARTESIAN_POINT('',(7.9,-2.25,-13.69)) ;
#146271 = CARTESIAN_POINT('',(1.4,-2.25,-13.69)) ;
#146272 = CARTESIAN_POINT('',(7.9,-2.25,-14.3368804065906)) ;
#146273 = CARTESIAN_POINT('Origin',(1.4,-2.15,-13.69)) ;
#146274 = CARTESIAN_POINT('',(1.5,-2.15,-13.59)) ;
#146275 = CARTESIAN_POINT('Origin',(1.5,-2.15,-13.69)) ;
#146276 = CARTESIAN_POINT('',(7.9,-2.15,-13.59)) ;
#146277 = CARTESIAN_POINT('',(1.4,-2.15,-13.59)) ;
#146278 = CARTESIAN_POINT('Origin',(7.9,-2.15,-13.69)) ;
#146279 = CARTESIAN_POINT('Origin',(1.4,1.9,-13.59)) ;
#146280 = CARTESIAN_POINT('',(1.5,1.9,-13.59)) ;
#146281 = CARTESIAN_POINT('',(1.5,1.9,-13.59)) ;
#146282 = CARTESIAN_POINT('',(7.9,1.9,-13.59)) ;
#146283 = CARTESIAN_POINT('',(1.4,1.9,-13.59)) ;
#146284 = CARTESIAN_POINT('',(7.9,-2.15,-13.59)) ;
#146285 = CARTESIAN_POINT('Origin',(1.4,1.9,-13.69)) ;
#146286 = CARTESIAN_POINT('',(1.5,2.,-13.69)) ;
#146287 = CARTESIAN_POINT('Origin',(1.5,1.9,-13.69)) ;
#146288 = CARTESIAN_POINT('',(7.9,2.,-13.69)) ;
#146289 = CARTESIAN_POINT('',(1.4,2.,-13.69)) ;
#146290 = CARTESIAN_POINT('Origin',(7.9,1.9,-13.69)) ;
#146291 = CARTESIAN_POINT('Origin',(1.4,2.,-13.69)) ;
#146292 = CARTESIAN_POINT('',(1.5,2.,-14.64)) ;
#146293 = CARTESIAN_POINT('',(7.9,2.,-13.69)) ;
#146294 = CARTESIAN_POINT('Origin',(1.4,2.1,-14.64)) ;
#146295 = CARTESIAN_POINT('',(1.4,2.6,-14.64)) ;
#146296 = CARTESIAN_POINT('',(1.4,2.4,-14.84)) ;
#146297 = CARTESIAN_POINT('Origin',(1.4,2.4,-14.64)) ;
#146298 = CARTESIAN_POINT('',(1.4,2.1,-14.84)) ;
#146299 = CARTESIAN_POINT('',(1.4,2.1,-14.84)) ;
#146300 = CARTESIAN_POINT('',(1.4,1.9,-14.64)) ;
#146301 = CARTESIAN_POINT('Origin',(1.4,2.1,-14.64)) ;
#146302 = CARTESIAN_POINT('',(1.4,1.9,-13.69)) ;
#146303 = CARTESIAN_POINT('',(1.4,1.9,-13.69)) ;
#146304 = CARTESIAN_POINT('',(1.4,-2.15,-13.69)) ;
#146305 = CARTESIAN_POINT('',(1.4,-2.15,-13.69)) ;
#146306 = CARTESIAN_POINT('',(1.4,-2.15,-14.3368804065906)) ;
#146307 = CARTESIAN_POINT('',(1.4,-2.15,-14.3368804065906)) ;
#146308 = CARTESIAN_POINT('',(1.4,-2.15,-16.1431195934094)) ;
#146309 = CARTESIAN_POINT('Origin',(1.4,-3.65625,-15.24)) ;
#146310 = CARTESIAN_POINT('',(1.4,-2.15,-16.79)) ;
#146311 = CARTESIAN_POINT('',(1.4,-2.15,-16.79)) ;
#146312 = CARTESIAN_POINT('',(1.4,1.9,-16.79)) ;
#146313 = CARTESIAN_POINT('',(1.4,1.9,-16.79)) ;
#146314 = CARTESIAN_POINT('',(1.4,1.9,-15.84)) ;
#146315 = CARTESIAN_POINT('',(1.4,1.9,-15.84)) ;
#146316 = CARTESIAN_POINT('',(1.4,2.1,-15.64)) ;
#146317 = CARTESIAN_POINT('Origin',(1.4,2.1,-15.84)) ;
#146318 = CARTESIAN_POINT('',(1.4,2.4,-15.64)) ;
#146319 = CARTESIAN_POINT('',(1.4,2.4,-15.64)) ;
#146320 = CARTESIAN_POINT('',(1.4,2.6,-15.84)) ;
#146321 = CARTESIAN_POINT('Origin',(1.4,2.4,-15.84)) ;
#146322 = CARTESIAN_POINT('',(1.4,2.6,-15.9485786437627)) ;
#146323 = CARTESIAN_POINT('',(1.4,2.6,-15.9485786437627)) ;
#146324 = CARTESIAN_POINT('',(1.4,3.15,-16.4985786437627)) ;
#146325 = CARTESIAN_POINT('',(1.4,3.15,-16.4985786437627)) ;
#146326 = CARTESIAN_POINT('',(1.4,3.15,-13.9814213562373)) ;
#146327 = CARTESIAN_POINT('',(1.4,2.6,-14.5314213562373)) ;
#146328 = CARTESIAN_POINT('',(1.4,2.6,-14.5314213562373)) ;
#146329 = CARTESIAN_POINT('',(1.4,2.6,-14.64)) ;
#146330 = CARTESIAN_POINT('Origin',(1.4,2.1,-10.83)) ;
#146331 = CARTESIAN_POINT('',(1.5,2.,-10.83)) ;
#146332 = CARTESIAN_POINT('',(7.9,2.,-10.83)) ;
#146333 = CARTESIAN_POINT('',(1.4,2.,-10.83)) ;
#146334 = CARTESIAN_POINT('',(1.5,2.1,-10.93)) ;
#146335 = CARTESIAN_POINT('Origin',(1.5,2.1,-10.83)) ;
#146336 = CARTESIAN_POINT('',(7.9,2.1,-10.93)) ;
#146337 = CARTESIAN_POINT('',(1.4,2.1,-10.93)) ;
#146338 = CARTESIAN_POINT('Origin',(7.9,2.1,-10.83)) ;
#146339 = CARTESIAN_POINT('Origin',(1.4,2.4,-10.93)) ;
#146340 = CARTESIAN_POINT('',(1.5,2.4,-10.93)) ;
#146341 = CARTESIAN_POINT('',(1.5,2.4,-10.93)) ;
#146342 = CARTESIAN_POINT('',(7.9,2.4,-10.93)) ;
#146343 = CARTESIAN_POINT('',(1.4,2.4,-10.93)) ;
#146344 = CARTESIAN_POINT('',(7.9,2.1,-10.93)) ;
#146345 = CARTESIAN_POINT('Origin',(1.4,2.4,-10.83)) ;
#146346 = CARTESIAN_POINT('',(1.5,2.5,-10.83)) ;
#146347 = CARTESIAN_POINT('Origin',(1.5,2.4,-10.83)) ;
#146348 = CARTESIAN_POINT('',(7.9,2.5,-10.83)) ;
#146349 = CARTESIAN_POINT('',(1.4,2.5,-10.83)) ;
#146350 = CARTESIAN_POINT('Origin',(7.9,2.4,-10.83)) ;
#146351 = CARTESIAN_POINT('Origin',(1.4,2.5,-10.7214213562373)) ;
#146352 = CARTESIAN_POINT('',(1.5,2.5,-10.7214213562373)) ;
#146353 = CARTESIAN_POINT('',(1.5,2.5,-10.7214213562373)) ;
#146354 = CARTESIAN_POINT('',(7.9,2.5,-10.7214213562373)) ;
#146355 = CARTESIAN_POINT('',(1.4,2.5,-10.7214213562373)) ;
#146356 = CARTESIAN_POINT('',(7.9,2.5,-10.83)) ;
#146357 = CARTESIAN_POINT('Origin',(1.4,2.6,-10.7214213562373)) ;
#146358 = CARTESIAN_POINT('',(1.5,2.52928932188135,-10.6507106781187)) ;
#146359 = CARTESIAN_POINT('Origin',(1.5,2.6,-10.7214213562373)) ;
#146360 = CARTESIAN_POINT('',(7.9,2.52928932188135,-10.6507106781187)) ;
#146361 = CARTESIAN_POINT('',(1.4,2.52928932188135,-10.6507106781187)) ;
#146362 = CARTESIAN_POINT('Origin',(7.9,2.6,-10.7214213562373)) ;
#146363 = CARTESIAN_POINT('Origin',(1.4,3.07928932188135,-10.1007106781187)) ;
#146364 = CARTESIAN_POINT('',(1.5,3.07928932188135,-10.1007106781187)) ;
#146365 = CARTESIAN_POINT('',(7.9,3.07928932188135,-10.1007106781187)) ;
#146366 = CARTESIAN_POINT('',(1.4,3.07928932188135,-10.1007106781187)) ;
#146367 = CARTESIAN_POINT('',(7.9,2.52928932188135,-10.6507106781187)) ;
#146368 = CARTESIAN_POINT('Origin',(1.4,3.15,-10.1714213562373)) ;
#146369 = CARTESIAN_POINT('',(7.9,3.25,-10.1714213562373)) ;
#146370 = CARTESIAN_POINT('',(1.4,3.25,-10.1714213562373)) ;
#146371 = CARTESIAN_POINT('Origin',(7.9,3.15,-10.1714213562373)) ;
#146372 = CARTESIAN_POINT('Origin',(1.4,3.25,-12.6885786437627)) ;
#146373 = CARTESIAN_POINT('',(1.5,3.25,-12.6885786437627)) ;
#146374 = CARTESIAN_POINT('',(7.9,3.25,-10.1714213562373)) ;
#146375 = CARTESIAN_POINT('Origin',(1.4,2.52928932188134,-12.2092893218813)) ;
#146376 = CARTESIAN_POINT('',(1.5,2.52928932188134,-12.2092893218813)) ;
#146377 = CARTESIAN_POINT('',(1.5,2.52928932188134,-12.2092893218813)) ;
#146378 = CARTESIAN_POINT('',(7.9,2.52928932188134,-12.2092893218813)) ;
#146379 = CARTESIAN_POINT('',(1.4,2.52928932188134,-12.2092893218813)) ;
#146380 = CARTESIAN_POINT('',(7.9,3.07928932188135,-12.7592893218813)) ;
#146381 = CARTESIAN_POINT('Origin',(1.4,2.6,-12.1385786437627)) ;
#146382 = CARTESIAN_POINT('',(1.5,2.5,-12.1385786437627)) ;
#146383 = CARTESIAN_POINT('Origin',(1.5,2.6,-12.1385786437627)) ;
#146384 = CARTESIAN_POINT('',(7.9,2.5,-12.1385786437627)) ;
#146385 = CARTESIAN_POINT('',(1.4,2.5,-12.1385786437627)) ;
#146386 = CARTESIAN_POINT('Origin',(7.9,2.6,-12.1385786437627)) ;
#146387 = CARTESIAN_POINT('Origin',(1.4,2.5,-12.03)) ;
#146388 = CARTESIAN_POINT('',(1.5,2.5,-12.03)) ;
#146389 = CARTESIAN_POINT('',(1.5,2.5,-12.03)) ;
#146390 = CARTESIAN_POINT('',(7.9,2.5,-12.03)) ;
#146391 = CARTESIAN_POINT('',(1.4,2.5,-12.03)) ;
#146392 = CARTESIAN_POINT('',(7.9,2.5,-12.1385786437627)) ;
#146393 = CARTESIAN_POINT('Origin',(1.4,2.4,-12.03)) ;
#146394 = CARTESIAN_POINT('',(1.5,2.4,-11.93)) ;
#146395 = CARTESIAN_POINT('Origin',(1.5,2.4,-12.03)) ;
#146396 = CARTESIAN_POINT('',(7.9,2.4,-11.93)) ;
#146397 = CARTESIAN_POINT('',(1.4,2.4,-11.93)) ;
#146398 = CARTESIAN_POINT('Origin',(7.9,2.4,-12.03)) ;
#146399 = CARTESIAN_POINT('Origin',(1.4,2.1,-11.93)) ;
#146400 = CARTESIAN_POINT('',(1.5,2.1,-11.93)) ;
#146401 = CARTESIAN_POINT('',(1.5,2.1,-11.93)) ;
#146402 = CARTESIAN_POINT('',(7.9,2.1,-11.93)) ;
#146403 = CARTESIAN_POINT('',(1.4,2.1,-11.93)) ;
#146404 = CARTESIAN_POINT('',(7.9,2.4,-11.93)) ;
#146405 = CARTESIAN_POINT('Origin',(1.4,2.1,-12.03)) ;
#146406 = CARTESIAN_POINT('',(1.5,2.,-12.03)) ;
#146407 = CARTESIAN_POINT('Origin',(1.5,2.1,-12.03)) ;
#146408 = CARTESIAN_POINT('',(7.9,2.,-12.03)) ;
#146409 = CARTESIAN_POINT('',(1.4,2.,-12.03)) ;
#146410 = CARTESIAN_POINT('Origin',(7.9,2.1,-12.03)) ;
#146411 = CARTESIAN_POINT('Origin',(1.4,2.,-12.03)) ;
#146412 = CARTESIAN_POINT('',(1.5,2.,-12.98)) ;
#146413 = CARTESIAN_POINT('',(1.5,2.,-12.98)) ;
#146414 = CARTESIAN_POINT('',(7.9,2.,-12.98)) ;
#146415 = CARTESIAN_POINT('',(1.4,2.,-12.98)) ;
#146416 = CARTESIAN_POINT('',(7.9,2.,-12.03)) ;
#146417 = CARTESIAN_POINT('Origin',(1.4,1.9,-12.98)) ;
#146418 = CARTESIAN_POINT('',(1.5,1.9,-13.08)) ;
#146419 = CARTESIAN_POINT('Origin',(1.5,1.9,-12.98)) ;
#146420 = CARTESIAN_POINT('',(7.9,1.9,-13.08)) ;
#146421 = CARTESIAN_POINT('',(1.4,1.9,-13.08)) ;
#146422 = CARTESIAN_POINT('Origin',(7.9,1.9,-12.98)) ;
#146423 = CARTESIAN_POINT('Origin',(1.4,1.9,-13.08)) ;
#146424 = CARTESIAN_POINT('',(1.5,-2.15,-13.08)) ;
#146425 = CARTESIAN_POINT('',(1.5,-2.15,-13.08)) ;
#146426 = CARTESIAN_POINT('',(7.9,-2.15,-13.08)) ;
#146427 = CARTESIAN_POINT('',(1.4,-2.15,-13.08)) ;
#146428 = CARTESIAN_POINT('',(7.9,1.9,-13.08)) ;
#146429 = CARTESIAN_POINT('Origin',(1.4,-2.15,-12.98)) ;
#146430 = CARTESIAN_POINT('',(1.5,-2.25,-12.98)) ;
#146431 = CARTESIAN_POINT('Origin',(1.5,-2.15,-12.98)) ;
#146432 = CARTESIAN_POINT('',(7.9,-2.25,-12.98)) ;
#146433 = CARTESIAN_POINT('',(1.4,-2.25,-12.98)) ;
#146434 = CARTESIAN_POINT('Origin',(7.9,-2.15,-12.98)) ;
#146435 = CARTESIAN_POINT('Origin',(1.4,-2.25,-12.3331195934094)) ;
#146436 = CARTESIAN_POINT('',(1.5,-2.25,-12.3331195934094)) ;
#146437 = CARTESIAN_POINT('',(1.5,-2.25,-12.3331195934094)) ;
#146438 = CARTESIAN_POINT('',(7.9,-2.25,-12.3331195934094)) ;
#146439 = CARTESIAN_POINT('',(1.4,-2.25,-12.3331195934094)) ;
#146440 = CARTESIAN_POINT('',(7.9,-2.25,-12.98)) ;
#146441 = CARTESIAN_POINT('Origin',(1.4,-2.15,-12.3331195934094)) ;
#146442 = CARTESIAN_POINT('',(1.5,-2.23576512455516,-12.2816964137135)) ;
#146443 = CARTESIAN_POINT('Origin',(1.5,-2.15,-12.3331195934094)) ;
#146444 = CARTESIAN_POINT('',(7.9,-2.23576512455516,-12.2816964137135)) ;
#146445 = CARTESIAN_POINT('',(1.4,-2.23576512455516,-12.2816964137135)) ;
#146446 = CARTESIAN_POINT('Origin',(7.9,-2.15,-12.3331195934094)) ;
#146447 = CARTESIAN_POINT('Origin',(1.4,-3.65625,-11.43)) ;
#146448 = CARTESIAN_POINT('',(1.5,-2.23576512455516,-10.5783035862865)) ;
#146449 = CARTESIAN_POINT('Origin',(1.5,-3.65625,-11.43)) ;
#146450 = CARTESIAN_POINT('',(7.9,-2.23576512455516,-10.5783035862865)) ;
#146451 = CARTESIAN_POINT('',(1.4,-2.23576512455516,-10.5783035862865)) ;
#146452 = CARTESIAN_POINT('Origin',(7.9,-3.65625,-11.43)) ;
#146453 = CARTESIAN_POINT('Origin',(1.4,-2.15,-10.5268804065906)) ;
#146454 = CARTESIAN_POINT('',(1.5,-2.25,-10.5268804065906)) ;
#146455 = CARTESIAN_POINT('Origin',(1.5,-2.15,-10.5268804065906)) ;
#146456 = CARTESIAN_POINT('',(7.9,-2.25,-10.5268804065906)) ;
#146457 = CARTESIAN_POINT('',(1.4,-2.25,-10.5268804065906)) ;
#146458 = CARTESIAN_POINT('Origin',(7.9,-2.15,-10.5268804065906)) ;
#146459 = CARTESIAN_POINT('Origin',(1.4,-2.25,-9.88)) ;
#146460 = CARTESIAN_POINT('',(1.5,-2.25,-9.88)) ;
#146461 = CARTESIAN_POINT('',(1.5,-2.25,-9.88)) ;
#146462 = CARTESIAN_POINT('',(7.9,-2.25,-9.88)) ;
#146463 = CARTESIAN_POINT('',(1.4,-2.25,-9.88)) ;
#146464 = CARTESIAN_POINT('',(7.9,-2.25,-10.5268804065906)) ;
#146465 = CARTESIAN_POINT('Origin',(1.4,-2.15,-9.88)) ;
#146466 = CARTESIAN_POINT('',(1.5,-2.15,-9.78)) ;
#146467 = CARTESIAN_POINT('Origin',(1.5,-2.15,-9.88)) ;
#146468 = CARTESIAN_POINT('',(7.9,-2.15,-9.78)) ;
#146469 = CARTESIAN_POINT('',(1.4,-2.15,-9.78)) ;
#146470 = CARTESIAN_POINT('Origin',(7.9,-2.15,-9.88)) ;
#146471 = CARTESIAN_POINT('Origin',(1.4,1.9,-9.78)) ;
#146472 = CARTESIAN_POINT('',(1.5,1.9,-9.78)) ;
#146473 = CARTESIAN_POINT('',(1.5,1.9,-9.78)) ;
#146474 = CARTESIAN_POINT('',(7.9,1.9,-9.78)) ;
#146475 = CARTESIAN_POINT('',(1.4,1.9,-9.78)) ;
#146476 = CARTESIAN_POINT('',(7.9,-2.15,-9.78)) ;
#146477 = CARTESIAN_POINT('Origin',(1.4,1.9,-9.88)) ;
#146478 = CARTESIAN_POINT('',(1.5,2.,-9.88)) ;
#146479 = CARTESIAN_POINT('Origin',(1.5,1.9,-9.88)) ;
#146480 = CARTESIAN_POINT('',(7.9,2.,-9.88)) ;
#146481 = CARTESIAN_POINT('',(1.4,2.,-9.88)) ;
#146482 = CARTESIAN_POINT('Origin',(7.9,1.9,-9.88)) ;
#146483 = CARTESIAN_POINT('Origin',(1.4,2.,-9.88)) ;
#146484 = CARTESIAN_POINT('',(1.5,2.,-10.83)) ;
#146485 = CARTESIAN_POINT('',(7.9,2.,-9.88)) ;
#146486 = CARTESIAN_POINT('Origin',(1.4,2.1,-10.83)) ;
#146487 = CARTESIAN_POINT('',(1.4,2.6,-10.83)) ;
#146488 = CARTESIAN_POINT('',(1.4,2.4,-11.03)) ;
#146489 = CARTESIAN_POINT('Origin',(1.4,2.4,-10.83)) ;
#146490 = CARTESIAN_POINT('',(1.4,2.1,-11.03)) ;
#146491 = CARTESIAN_POINT('',(1.4,2.1,-11.03)) ;
#146492 = CARTESIAN_POINT('',(1.4,1.9,-10.83)) ;
#146493 = CARTESIAN_POINT('Origin',(1.4,2.1,-10.83)) ;
#146494 = CARTESIAN_POINT('',(1.4,1.9,-9.88)) ;
#146495 = CARTESIAN_POINT('',(1.4,1.9,-9.88)) ;
#146496 = CARTESIAN_POINT('',(1.4,-2.15,-9.88)) ;
#146497 = CARTESIAN_POINT('',(1.4,-2.15,-9.88)) ;
#146498 = CARTESIAN_POINT('',(1.4,-2.15,-10.5268804065906)) ;
#146499 = CARTESIAN_POINT('',(1.4,-2.15,-10.5268804065906)) ;
#146500 = CARTESIAN_POINT('',(1.4,-2.15,-12.3331195934094)) ;
#146501 = CARTESIAN_POINT('Origin',(1.4,-3.65625,-11.43)) ;
#146502 = CARTESIAN_POINT('',(1.4,-2.15,-12.98)) ;
#146503 = CARTESIAN_POINT('',(1.4,-2.15,-12.98)) ;
#146504 = CARTESIAN_POINT('',(1.4,1.9,-12.98)) ;
#146505 = CARTESIAN_POINT('',(1.4,1.9,-12.98)) ;
#146506 = CARTESIAN_POINT('',(1.4,1.9,-12.03)) ;
#146507 = CARTESIAN_POINT('',(1.4,1.9,-12.03)) ;
#146508 = CARTESIAN_POINT('',(1.4,2.1,-11.83)) ;
#146509 = CARTESIAN_POINT('Origin',(1.4,2.1,-12.03)) ;
#146510 = CARTESIAN_POINT('',(1.4,2.4,-11.83)) ;
#146511 = CARTESIAN_POINT('',(1.4,2.4,-11.83)) ;
#146512 = CARTESIAN_POINT('',(1.4,2.6,-12.03)) ;
#146513 = CARTESIAN_POINT('Origin',(1.4,2.4,-12.03)) ;
#146514 = CARTESIAN_POINT('',(1.4,2.6,-12.1385786437627)) ;
#146515 = CARTESIAN_POINT('',(1.4,2.6,-12.1385786437627)) ;
#146516 = CARTESIAN_POINT('',(1.4,3.15,-12.6885786437627)) ;
#146517 = CARTESIAN_POINT('',(1.4,3.15,-12.6885786437627)) ;
#146518 = CARTESIAN_POINT('',(1.4,3.15,-10.1714213562373)) ;
#146519 = CARTESIAN_POINT('',(1.4,2.6,-10.7214213562373)) ;
#146520 = CARTESIAN_POINT('',(1.4,2.6,-10.7214213562373)) ;
#146521 = CARTESIAN_POINT('',(1.4,2.6,-10.83)) ;
#146522 = CARTESIAN_POINT('Origin',(1.4,2.1,-7.02)) ;
#146523 = CARTESIAN_POINT('',(1.5,2.,-7.02)) ;
#146524 = CARTESIAN_POINT('',(7.9,2.,-7.02)) ;
#146525 = CARTESIAN_POINT('',(1.4,2.,-7.02)) ;
#146526 = CARTESIAN_POINT('',(1.5,2.1,-7.12)) ;
#146527 = CARTESIAN_POINT('Origin',(1.5,2.1,-7.02)) ;
#146528 = CARTESIAN_POINT('',(7.9,2.1,-7.12)) ;
#146529 = CARTESIAN_POINT('',(1.4,2.1,-7.12)) ;
#146530 = CARTESIAN_POINT('Origin',(7.9,2.1,-7.02)) ;
#146531 = CARTESIAN_POINT('Origin',(1.4,2.4,-7.12)) ;
#146532 = CARTESIAN_POINT('',(1.5,2.4,-7.12)) ;
#146533 = CARTESIAN_POINT('',(1.5,2.4,-7.12)) ;
#146534 = CARTESIAN_POINT('',(7.9,2.4,-7.12)) ;
#146535 = CARTESIAN_POINT('',(1.4,2.4,-7.12)) ;
#146536 = CARTESIAN_POINT('',(7.9,2.1,-7.12)) ;
#146537 = CARTESIAN_POINT('Origin',(1.4,2.4,-7.02)) ;
#146538 = CARTESIAN_POINT('',(1.5,2.5,-7.02)) ;
#146539 = CARTESIAN_POINT('Origin',(1.5,2.4,-7.02)) ;
#146540 = CARTESIAN_POINT('',(7.9,2.5,-7.02)) ;
#146541 = CARTESIAN_POINT('',(1.4,2.5,-7.02)) ;
#146542 = CARTESIAN_POINT('Origin',(7.9,2.4,-7.02)) ;
#146543 = CARTESIAN_POINT('Origin',(1.4,2.5,-6.91142135623731)) ;
#146544 = CARTESIAN_POINT('',(1.5,2.5,-6.91142135623731)) ;
#146545 = CARTESIAN_POINT('',(1.5,2.5,-6.91142135623731)) ;
#146546 = CARTESIAN_POINT('',(7.9,2.5,-6.91142135623731)) ;
#146547 = CARTESIAN_POINT('',(1.4,2.5,-6.91142135623731)) ;
#146548 = CARTESIAN_POINT('',(7.9,2.5,-7.02)) ;
#146549 = CARTESIAN_POINT('Origin',(1.4,2.6,-6.91142135623731)) ;
#146550 = CARTESIAN_POINT('',(1.5,2.52928932188135,-6.84071067811866)) ;
#146551 = CARTESIAN_POINT('Origin',(1.5,2.6,-6.91142135623731)) ;
#146552 = CARTESIAN_POINT('',(7.9,2.52928932188135,-6.84071067811866)) ;
#146553 = CARTESIAN_POINT('',(1.4,2.52928932188135,-6.84071067811866)) ;
#146554 = CARTESIAN_POINT('Origin',(7.9,2.6,-6.91142135623731)) ;
#146555 = CARTESIAN_POINT('Origin',(1.4,3.07928932188135,-6.29071067811866)) ;
#146556 = CARTESIAN_POINT('',(1.5,3.07928932188135,-6.29071067811866)) ;
#146557 = CARTESIAN_POINT('',(7.9,3.07928932188135,-6.29071067811866)) ;
#146558 = CARTESIAN_POINT('',(1.4,3.07928932188135,-6.29071067811866)) ;
#146559 = CARTESIAN_POINT('',(7.9,2.52928932188135,-6.84071067811866)) ;
#146560 = CARTESIAN_POINT('Origin',(1.4,3.15,-6.36142135623731)) ;
#146561 = CARTESIAN_POINT('',(7.9,3.25,-6.36142135623731)) ;
#146562 = CARTESIAN_POINT('',(1.4,3.25,-6.36142135623731)) ;
#146563 = CARTESIAN_POINT('Origin',(7.9,3.15,-6.36142135623731)) ;
#146564 = CARTESIAN_POINT('Origin',(1.4,3.25,-8.87857864376269)) ;
#146565 = CARTESIAN_POINT('',(1.5,3.25,-8.87857864376269)) ;
#146566 = CARTESIAN_POINT('',(7.9,3.25,-6.36142135623731)) ;
#146567 = CARTESIAN_POINT('Origin',(1.4,2.52928932188134,-8.39928932188135)) ;
#146568 = CARTESIAN_POINT('',(1.5,2.52928932188134,-8.39928932188135)) ;
#146569 = CARTESIAN_POINT('',(1.5,2.52928932188134,-8.39928932188135)) ;
#146570 = CARTESIAN_POINT('',(7.9,2.52928932188134,-8.39928932188135)) ;
#146571 = CARTESIAN_POINT('',(1.4,2.52928932188134,-8.39928932188135)) ;
#146572 = CARTESIAN_POINT('',(7.9,3.07928932188135,-8.94928932188134)) ;
#146573 = CARTESIAN_POINT('Origin',(1.4,2.6,-8.32857864376269)) ;
#146574 = CARTESIAN_POINT('',(1.5,2.5,-8.32857864376269)) ;
#146575 = CARTESIAN_POINT('Origin',(1.5,2.6,-8.32857864376269)) ;
#146576 = CARTESIAN_POINT('',(7.9,2.5,-8.32857864376269)) ;
#146577 = CARTESIAN_POINT('',(1.4,2.5,-8.32857864376269)) ;
#146578 = CARTESIAN_POINT('Origin',(7.9,2.6,-8.32857864376269)) ;
#146579 = CARTESIAN_POINT('Origin',(1.4,2.5,-8.22)) ;
#146580 = CARTESIAN_POINT('',(1.5,2.5,-8.22)) ;
#146581 = CARTESIAN_POINT('',(1.5,2.5,-8.22)) ;
#146582 = CARTESIAN_POINT('',(7.9,2.5,-8.22)) ;
#146583 = CARTESIAN_POINT('',(1.4,2.5,-8.22)) ;
#146584 = CARTESIAN_POINT('',(7.9,2.5,-8.32857864376269)) ;
#146585 = CARTESIAN_POINT('Origin',(1.4,2.4,-8.22)) ;
#146586 = CARTESIAN_POINT('',(1.5,2.4,-8.12)) ;
#146587 = CARTESIAN_POINT('Origin',(1.5,2.4,-8.22)) ;
#146588 = CARTESIAN_POINT('',(7.9,2.4,-8.12)) ;
#146589 = CARTESIAN_POINT('',(1.4,2.4,-8.12)) ;
#146590 = CARTESIAN_POINT('Origin',(7.9,2.4,-8.22)) ;
#146591 = CARTESIAN_POINT('Origin',(1.4,2.1,-8.12)) ;
#146592 = CARTESIAN_POINT('',(1.5,2.1,-8.12)) ;
#146593 = CARTESIAN_POINT('',(1.5,2.1,-8.12)) ;
#146594 = CARTESIAN_POINT('',(7.9,2.1,-8.12)) ;
#146595 = CARTESIAN_POINT('',(1.4,2.1,-8.12)) ;
#146596 = CARTESIAN_POINT('',(7.9,2.4,-8.12)) ;
#146597 = CARTESIAN_POINT('Origin',(1.4,2.1,-8.22)) ;
#146598 = CARTESIAN_POINT('',(1.5,2.,-8.22)) ;
#146599 = CARTESIAN_POINT('Origin',(1.5,2.1,-8.22)) ;
#146600 = CARTESIAN_POINT('',(7.9,2.,-8.22)) ;
#146601 = CARTESIAN_POINT('',(1.4,2.,-8.22)) ;
#146602 = CARTESIAN_POINT('Origin',(7.9,2.1,-8.22)) ;
#146603 = CARTESIAN_POINT('Origin',(1.4,2.,-8.22)) ;
#146604 = CARTESIAN_POINT('',(1.5,2.,-9.17)) ;
#146605 = CARTESIAN_POINT('',(1.5,2.,-9.17)) ;
#146606 = CARTESIAN_POINT('',(7.9,2.,-9.17)) ;
#146607 = CARTESIAN_POINT('',(1.4,2.,-9.17)) ;
#146608 = CARTESIAN_POINT('',(7.9,2.,-8.22)) ;
#146609 = CARTESIAN_POINT('Origin',(1.4,1.9,-9.17)) ;
#146610 = CARTESIAN_POINT('',(1.5,1.9,-9.27)) ;
#146611 = CARTESIAN_POINT('Origin',(1.5,1.9,-9.17)) ;
#146612 = CARTESIAN_POINT('',(7.9,1.9,-9.27)) ;
#146613 = CARTESIAN_POINT('',(1.4,1.9,-9.27)) ;
#146614 = CARTESIAN_POINT('Origin',(7.9,1.9,-9.17)) ;
#146615 = CARTESIAN_POINT('Origin',(1.4,1.9,-9.27)) ;
#146616 = CARTESIAN_POINT('',(1.5,-2.15,-9.27)) ;
#146617 = CARTESIAN_POINT('',(1.5,-2.15,-9.27)) ;
#146618 = CARTESIAN_POINT('',(7.9,-2.15,-9.27)) ;
#146619 = CARTESIAN_POINT('',(1.4,-2.15,-9.27)) ;
#146620 = CARTESIAN_POINT('',(7.9,1.9,-9.27)) ;
#146621 = CARTESIAN_POINT('Origin',(1.4,-2.15,-9.17)) ;
#146622 = CARTESIAN_POINT('',(1.5,-2.25,-9.17)) ;
#146623 = CARTESIAN_POINT('Origin',(1.5,-2.15,-9.17)) ;
#146624 = CARTESIAN_POINT('',(7.9,-2.25,-9.17)) ;
#146625 = CARTESIAN_POINT('',(1.4,-2.25,-9.17)) ;
#146626 = CARTESIAN_POINT('Origin',(7.9,-2.15,-9.17)) ;
#146627 = CARTESIAN_POINT('Origin',(1.4,-2.25,-8.52311959340942)) ;
#146628 = CARTESIAN_POINT('',(1.5,-2.25,-8.52311959340942)) ;
#146629 = CARTESIAN_POINT('',(1.5,-2.25,-8.52311959340942)) ;
#146630 = CARTESIAN_POINT('',(7.9,-2.25,-8.52311959340942)) ;
#146631 = CARTESIAN_POINT('',(1.4,-2.25,-8.52311959340942)) ;
#146632 = CARTESIAN_POINT('',(7.9,-2.25,-9.17)) ;
#146633 = CARTESIAN_POINT('Origin',(1.4,-2.15,-8.52311959340942)) ;
#146634 = CARTESIAN_POINT('',(1.5,-2.23576512455516,-8.47169641371351)) ;
#146635 = CARTESIAN_POINT('Origin',(1.5,-2.15,-8.52311959340942)) ;
#146636 = CARTESIAN_POINT('',(7.9,-2.23576512455516,-8.47169641371351)) ;
#146637 = CARTESIAN_POINT('',(1.4,-2.23576512455516,-8.47169641371351)) ;
#146638 = CARTESIAN_POINT('Origin',(7.9,-2.15,-8.52311959340942)) ;
#146639 = CARTESIAN_POINT('Origin',(1.4,-3.65625,-7.62)) ;
#146640 = CARTESIAN_POINT('',(1.5,-2.23576512455516,-6.76830358628649)) ;
#146641 = CARTESIAN_POINT('Origin',(1.5,-3.65625,-7.62)) ;
#146642 = CARTESIAN_POINT('',(7.9,-2.23576512455516,-6.76830358628649)) ;
#146643 = CARTESIAN_POINT('',(1.4,-2.23576512455516,-6.76830358628649)) ;
#146644 = CARTESIAN_POINT('Origin',(7.9,-3.65625,-7.62)) ;
#146645 = CARTESIAN_POINT('Origin',(1.4,-2.15,-6.71688040659058)) ;
#146646 = CARTESIAN_POINT('',(1.5,-2.25,-6.71688040659058)) ;
#146647 = CARTESIAN_POINT('Origin',(1.5,-2.15,-6.71688040659058)) ;
#146648 = CARTESIAN_POINT('',(7.9,-2.25,-6.71688040659058)) ;
#146649 = CARTESIAN_POINT('',(1.4,-2.25,-6.71688040659058)) ;
#146650 = CARTESIAN_POINT('Origin',(7.9,-2.15,-6.71688040659058)) ;
#146651 = CARTESIAN_POINT('Origin',(1.4,-2.25,-6.07)) ;
#146652 = CARTESIAN_POINT('',(1.5,-2.25,-6.07)) ;
#146653 = CARTESIAN_POINT('',(1.5,-2.25,-6.07)) ;
#146654 = CARTESIAN_POINT('',(7.9,-2.25,-6.07)) ;
#146655 = CARTESIAN_POINT('',(1.4,-2.25,-6.07)) ;
#146656 = CARTESIAN_POINT('',(7.9,-2.25,-6.71688040659058)) ;
#146657 = CARTESIAN_POINT('Origin',(1.4,-2.15,-6.07)) ;
#146658 = CARTESIAN_POINT('',(1.5,-2.15,-5.97)) ;
#146659 = CARTESIAN_POINT('Origin',(1.5,-2.15,-6.07)) ;
#146660 = CARTESIAN_POINT('',(7.9,-2.15,-5.97)) ;
#146661 = CARTESIAN_POINT('',(1.4,-2.15,-5.97)) ;
#146662 = CARTESIAN_POINT('Origin',(7.9,-2.15,-6.07)) ;
#146663 = CARTESIAN_POINT('Origin',(1.4,1.9,-5.97)) ;
#146664 = CARTESIAN_POINT('',(1.5,1.9,-5.97)) ;
#146665 = CARTESIAN_POINT('',(1.5,1.9,-5.97)) ;
#146666 = CARTESIAN_POINT('',(7.9,1.9,-5.97)) ;
#146667 = CARTESIAN_POINT('',(1.4,1.9,-5.97)) ;
#146668 = CARTESIAN_POINT('',(7.9,-2.15,-5.97)) ;
#146669 = CARTESIAN_POINT('Origin',(1.4,1.9,-6.07)) ;
#146670 = CARTESIAN_POINT('',(1.5,2.,-6.07)) ;
#146671 = CARTESIAN_POINT('Origin',(1.5,1.9,-6.07)) ;
#146672 = CARTESIAN_POINT('',(7.9,2.,-6.07)) ;
#146673 = CARTESIAN_POINT('',(1.4,2.,-6.07)) ;
#146674 = CARTESIAN_POINT('Origin',(7.9,1.9,-6.07)) ;
#146675 = CARTESIAN_POINT('Origin',(1.4,2.,-6.07)) ;
#146676 = CARTESIAN_POINT('',(1.5,2.,-7.02)) ;
#146677 = CARTESIAN_POINT('',(7.9,2.,-6.07)) ;
#146678 = CARTESIAN_POINT('Origin',(1.4,2.1,-7.02)) ;
#146679 = CARTESIAN_POINT('',(1.4,2.6,-7.02)) ;
#146680 = CARTESIAN_POINT('',(1.4,2.4,-7.22)) ;
#146681 = CARTESIAN_POINT('Origin',(1.4,2.4,-7.02)) ;
#146682 = CARTESIAN_POINT('',(1.4,2.1,-7.22)) ;
#146683 = CARTESIAN_POINT('',(1.4,2.1,-7.22)) ;
#146684 = CARTESIAN_POINT('',(1.4,1.9,-7.02)) ;
#146685 = CARTESIAN_POINT('Origin',(1.4,2.1,-7.02)) ;
#146686 = CARTESIAN_POINT('',(1.4,1.9,-6.07)) ;
#146687 = CARTESIAN_POINT('',(1.4,1.9,-6.07)) ;
#146688 = CARTESIAN_POINT('',(1.4,-2.15,-6.07)) ;
#146689 = CARTESIAN_POINT('',(1.4,-2.15,-6.07)) ;
#146690 = CARTESIAN_POINT('',(1.4,-2.15,-6.71688040659058)) ;
#146691 = CARTESIAN_POINT('',(1.4,-2.15,-6.71688040659058)) ;
#146692 = CARTESIAN_POINT('',(1.4,-2.15,-8.52311959340942)) ;
#146693 = CARTESIAN_POINT('Origin',(1.4,-3.65625,-7.62)) ;
#146694 = CARTESIAN_POINT('',(1.4,-2.15,-9.17)) ;
#146695 = CARTESIAN_POINT('',(1.4,-2.15,-9.17)) ;
#146696 = CARTESIAN_POINT('',(1.4,1.9,-9.17)) ;
#146697 = CARTESIAN_POINT('',(1.4,1.9,-9.17)) ;
#146698 = CARTESIAN_POINT('',(1.4,1.9,-8.22)) ;
#146699 = CARTESIAN_POINT('',(1.4,1.9,-8.22)) ;
#146700 = CARTESIAN_POINT('',(1.4,2.1,-8.02)) ;
#146701 = CARTESIAN_POINT('Origin',(1.4,2.1,-8.22)) ;
#146702 = CARTESIAN_POINT('',(1.4,2.4,-8.02)) ;
#146703 = CARTESIAN_POINT('',(1.4,2.4,-8.02)) ;
#146704 = CARTESIAN_POINT('',(1.4,2.6,-8.22)) ;
#146705 = CARTESIAN_POINT('Origin',(1.4,2.4,-8.22)) ;
#146706 = CARTESIAN_POINT('',(1.4,2.6,-8.32857864376269)) ;
#146707 = CARTESIAN_POINT('',(1.4,2.6,-8.32857864376269)) ;
#146708 = CARTESIAN_POINT('',(1.4,3.15,-8.87857864376269)) ;
#146709 = CARTESIAN_POINT('',(1.4,3.15,-8.87857864376269)) ;
#146710 = CARTESIAN_POINT('',(1.4,3.15,-6.36142135623731)) ;
#146711 = CARTESIAN_POINT('',(1.4,2.6,-6.91142135623731)) ;
#146712 = CARTESIAN_POINT('',(1.4,2.6,-6.91142135623731)) ;
#146713 = CARTESIAN_POINT('',(1.4,2.6,-7.02)) ;
#146714 = CARTESIAN_POINT('Origin',(1.4,2.1,-3.21)) ;
#146715 = CARTESIAN_POINT('',(1.5,2.,-3.21)) ;
#146716 = CARTESIAN_POINT('',(7.9,2.,-3.21)) ;
#146717 = CARTESIAN_POINT('',(1.4,2.,-3.21)) ;
#146718 = CARTESIAN_POINT('',(1.5,2.1,-3.31)) ;
#146719 = CARTESIAN_POINT('Origin',(1.5,2.1,-3.21)) ;
#146720 = CARTESIAN_POINT('',(7.9,2.1,-3.31)) ;
#146721 = CARTESIAN_POINT('',(1.4,2.1,-3.31)) ;
#146722 = CARTESIAN_POINT('Origin',(7.9,2.1,-3.21)) ;
#146723 = CARTESIAN_POINT('Origin',(1.4,2.4,-3.31)) ;
#146724 = CARTESIAN_POINT('',(1.5,2.4,-3.31)) ;
#146725 = CARTESIAN_POINT('',(1.5,2.4,-3.31)) ;
#146726 = CARTESIAN_POINT('',(7.9,2.4,-3.31)) ;
#146727 = CARTESIAN_POINT('',(1.4,2.4,-3.31)) ;
#146728 = CARTESIAN_POINT('',(7.9,2.1,-3.31)) ;
#146729 = CARTESIAN_POINT('Origin',(1.4,2.4,-3.21)) ;
#146730 = CARTESIAN_POINT('',(1.5,2.5,-3.21)) ;
#146731 = CARTESIAN_POINT('Origin',(1.5,2.4,-3.21)) ;
#146732 = CARTESIAN_POINT('',(7.9,2.5,-3.21)) ;
#146733 = CARTESIAN_POINT('',(1.4,2.5,-3.21)) ;
#146734 = CARTESIAN_POINT('Origin',(7.9,2.4,-3.21)) ;
#146735 = CARTESIAN_POINT('Origin',(1.4,2.5,-3.10142135623731)) ;
#146736 = CARTESIAN_POINT('',(1.5,2.5,-3.10142135623731)) ;
#146737 = CARTESIAN_POINT('',(1.5,2.5,-3.10142135623731)) ;
#146738 = CARTESIAN_POINT('',(7.9,2.5,-3.10142135623731)) ;
#146739 = CARTESIAN_POINT('',(1.4,2.5,-3.10142135623731)) ;
#146740 = CARTESIAN_POINT('',(7.9,2.5,-3.21)) ;
#146741 = CARTESIAN_POINT('Origin',(1.4,2.6,-3.10142135623731)) ;
#146742 = CARTESIAN_POINT('',(1.5,2.52928932188135,-3.03071067811866)) ;
#146743 = CARTESIAN_POINT('Origin',(1.5,2.6,-3.10142135623731)) ;
#146744 = CARTESIAN_POINT('',(7.9,2.52928932188135,-3.03071067811866)) ;
#146745 = CARTESIAN_POINT('',(1.4,2.52928932188135,-3.03071067811866)) ;
#146746 = CARTESIAN_POINT('Origin',(7.9,2.6,-3.10142135623731)) ;
#146747 = CARTESIAN_POINT('Origin',(1.4,3.07928932188135,-2.48071067811865)) ;
#146748 = CARTESIAN_POINT('',(1.5,3.07928932188135,-2.48071067811865)) ;
#146749 = CARTESIAN_POINT('',(7.9,3.07928932188135,-2.48071067811865)) ;
#146750 = CARTESIAN_POINT('',(1.4,3.07928932188135,-2.48071067811865)) ;
#146751 = CARTESIAN_POINT('',(7.9,2.52928932188135,-3.03071067811866)) ;
#146752 = CARTESIAN_POINT('Origin',(1.4,3.15,-2.55142135623731)) ;
#146753 = CARTESIAN_POINT('',(7.9,3.25,-2.55142135623731)) ;
#146754 = CARTESIAN_POINT('',(1.4,3.25,-2.55142135623731)) ;
#146755 = CARTESIAN_POINT('Origin',(7.9,3.15,-2.55142135623731)) ;
#146756 = CARTESIAN_POINT('Origin',(1.4,3.25,-5.06857864376269)) ;
#146757 = CARTESIAN_POINT('',(1.5,3.25,-5.06857864376269)) ;
#146758 = CARTESIAN_POINT('',(7.9,3.25,-2.55142135623731)) ;
#146759 = CARTESIAN_POINT('Origin',(1.4,2.52928932188134,-4.58928932188135)) ;
#146760 = CARTESIAN_POINT('',(1.5,2.52928932188134,-4.58928932188135)) ;
#146761 = CARTESIAN_POINT('',(1.5,2.52928932188134,-4.58928932188135)) ;
#146762 = CARTESIAN_POINT('',(7.9,2.52928932188134,-4.58928932188135)) ;
#146763 = CARTESIAN_POINT('',(1.4,2.52928932188134,-4.58928932188135)) ;
#146764 = CARTESIAN_POINT('',(7.9,3.07928932188135,-5.13928932188135)) ;
#146765 = CARTESIAN_POINT('Origin',(1.4,2.6,-4.51857864376269)) ;
#146766 = CARTESIAN_POINT('',(1.5,2.5,-4.51857864376269)) ;
#146767 = CARTESIAN_POINT('Origin',(1.5,2.6,-4.51857864376269)) ;
#146768 = CARTESIAN_POINT('',(7.9,2.5,-4.51857864376269)) ;
#146769 = CARTESIAN_POINT('',(1.4,2.5,-4.51857864376269)) ;
#146770 = CARTESIAN_POINT('Origin',(7.9,2.6,-4.51857864376269)) ;
#146771 = CARTESIAN_POINT('Origin',(1.4,2.5,-4.41)) ;
#146772 = CARTESIAN_POINT('',(1.5,2.5,-4.41)) ;
#146773 = CARTESIAN_POINT('',(1.5,2.5,-4.41)) ;
#146774 = CARTESIAN_POINT('',(7.9,2.5,-4.41)) ;
#146775 = CARTESIAN_POINT('',(1.4,2.5,-4.41)) ;
#146776 = CARTESIAN_POINT('',(7.9,2.5,-4.51857864376269)) ;
#146777 = CARTESIAN_POINT('Origin',(1.4,2.4,-4.41)) ;
#146778 = CARTESIAN_POINT('',(1.5,2.4,-4.31)) ;
#146779 = CARTESIAN_POINT('Origin',(1.5,2.4,-4.41)) ;
#146780 = CARTESIAN_POINT('',(7.9,2.4,-4.31)) ;
#146781 = CARTESIAN_POINT('',(1.4,2.4,-4.31)) ;
#146782 = CARTESIAN_POINT('Origin',(7.9,2.4,-4.41)) ;
#146783 = CARTESIAN_POINT('Origin',(1.4,2.1,-4.31)) ;
#146784 = CARTESIAN_POINT('',(1.5,2.1,-4.31)) ;
#146785 = CARTESIAN_POINT('',(1.5,2.1,-4.31)) ;
#146786 = CARTESIAN_POINT('',(7.9,2.1,-4.31)) ;
#146787 = CARTESIAN_POINT('',(1.4,2.1,-4.31)) ;
#146788 = CARTESIAN_POINT('',(7.9,2.4,-4.31)) ;
#146789 = CARTESIAN_POINT('Origin',(1.4,2.1,-4.41)) ;
#146790 = CARTESIAN_POINT('',(1.5,2.,-4.41)) ;
#146791 = CARTESIAN_POINT('Origin',(1.5,2.1,-4.41)) ;
#146792 = CARTESIAN_POINT('',(7.9,2.,-4.41)) ;
#146793 = CARTESIAN_POINT('',(1.4,2.,-4.41)) ;
#146794 = CARTESIAN_POINT('Origin',(7.9,2.1,-4.41)) ;
#146795 = CARTESIAN_POINT('Origin',(1.4,2.,-4.41)) ;
#146796 = CARTESIAN_POINT('',(1.5,2.,-5.36)) ;
#146797 = CARTESIAN_POINT('',(1.5,2.,-5.36)) ;
#146798 = CARTESIAN_POINT('',(7.9,2.,-5.36)) ;
#146799 = CARTESIAN_POINT('',(1.4,2.,-5.36)) ;
#146800 = CARTESIAN_POINT('',(7.9,2.,-4.41)) ;
#146801 = CARTESIAN_POINT('Origin',(1.4,1.9,-5.36)) ;
#146802 = CARTESIAN_POINT('',(1.5,1.9,-5.46)) ;
#146803 = CARTESIAN_POINT('Origin',(1.5,1.9,-5.36)) ;
#146804 = CARTESIAN_POINT('',(7.9,1.9,-5.46)) ;
#146805 = CARTESIAN_POINT('',(1.4,1.9,-5.46)) ;
#146806 = CARTESIAN_POINT('Origin',(7.9,1.9,-5.36)) ;
#146807 = CARTESIAN_POINT('Origin',(1.4,1.9,-5.46)) ;
#146808 = CARTESIAN_POINT('',(1.5,-2.15,-5.46)) ;
#146809 = CARTESIAN_POINT('',(1.5,-2.15,-5.46)) ;
#146810 = CARTESIAN_POINT('',(7.9,-2.15,-5.46)) ;
#146811 = CARTESIAN_POINT('',(1.4,-2.15,-5.46)) ;
#146812 = CARTESIAN_POINT('',(7.9,1.9,-5.46)) ;
#146813 = CARTESIAN_POINT('Origin',(1.4,-2.15,-5.36)) ;
#146814 = CARTESIAN_POINT('',(1.5,-2.25,-5.36)) ;
#146815 = CARTESIAN_POINT('Origin',(1.5,-2.15,-5.36)) ;
#146816 = CARTESIAN_POINT('',(7.9,-2.25,-5.36)) ;
#146817 = CARTESIAN_POINT('',(1.4,-2.25,-5.36)) ;
#146818 = CARTESIAN_POINT('Origin',(7.9,-2.15,-5.36)) ;
#146819 = CARTESIAN_POINT('Origin',(1.4,-2.25,-4.71311959340942)) ;
#146820 = CARTESIAN_POINT('',(1.5,-2.25,-4.71311959340942)) ;
#146821 = CARTESIAN_POINT('',(1.5,-2.25,-4.71311959340942)) ;
#146822 = CARTESIAN_POINT('',(7.9,-2.25,-4.71311959340942)) ;
#146823 = CARTESIAN_POINT('',(1.4,-2.25,-4.71311959340942)) ;
#146824 = CARTESIAN_POINT('',(7.9,-2.25,-5.36)) ;
#146825 = CARTESIAN_POINT('Origin',(1.4,-2.15,-4.71311959340942)) ;
#146826 = CARTESIAN_POINT('',(1.5,-2.23576512455516,-4.66169641371351)) ;
#146827 = CARTESIAN_POINT('Origin',(1.5,-2.15,-4.71311959340942)) ;
#146828 = CARTESIAN_POINT('',(7.9,-2.23576512455516,-4.66169641371351)) ;
#146829 = CARTESIAN_POINT('',(1.4,-2.23576512455516,-4.66169641371351)) ;
#146830 = CARTESIAN_POINT('Origin',(7.9,-2.15,-4.71311959340942)) ;
#146831 = CARTESIAN_POINT('Origin',(1.4,-3.65625,-3.81)) ;
#146832 = CARTESIAN_POINT('',(1.5,-2.23576512455516,-2.95830358628649)) ;
#146833 = CARTESIAN_POINT('Origin',(1.5,-3.65625,-3.81)) ;
#146834 = CARTESIAN_POINT('',(7.9,-2.23576512455516,-2.95830358628649)) ;
#146835 = CARTESIAN_POINT('',(1.4,-2.23576512455516,-2.95830358628649)) ;
#146836 = CARTESIAN_POINT('Origin',(7.9,-3.65625,-3.81)) ;
#146837 = CARTESIAN_POINT('Origin',(1.4,-2.15,-2.90688040659058)) ;
#146838 = CARTESIAN_POINT('',(1.5,-2.25,-2.90688040659058)) ;
#146839 = CARTESIAN_POINT('Origin',(1.5,-2.15,-2.90688040659058)) ;
#146840 = CARTESIAN_POINT('',(7.9,-2.25,-2.90688040659058)) ;
#146841 = CARTESIAN_POINT('',(1.4,-2.25,-2.90688040659058)) ;
#146842 = CARTESIAN_POINT('Origin',(7.9,-2.15,-2.90688040659058)) ;
#146843 = CARTESIAN_POINT('Origin',(1.4,-2.25,-2.26)) ;
#146844 = CARTESIAN_POINT('',(1.5,-2.25,-2.26)) ;
#146845 = CARTESIAN_POINT('',(1.5,-2.25,-2.26)) ;
#146846 = CARTESIAN_POINT('',(7.9,-2.25,-2.26)) ;
#146847 = CARTESIAN_POINT('',(1.4,-2.25,-2.26)) ;
#146848 = CARTESIAN_POINT('',(7.9,-2.25,-2.90688040659058)) ;
#146849 = CARTESIAN_POINT('Origin',(1.4,-2.15,-2.26)) ;
#146850 = CARTESIAN_POINT('',(1.5,-2.15,-2.16)) ;
#146851 = CARTESIAN_POINT('Origin',(1.5,-2.15,-2.26)) ;
#146852 = CARTESIAN_POINT('',(7.9,-2.15,-2.16)) ;
#146853 = CARTESIAN_POINT('',(1.4,-2.15,-2.16)) ;
#146854 = CARTESIAN_POINT('Origin',(7.9,-2.15,-2.26)) ;
#146855 = CARTESIAN_POINT('Origin',(1.4,1.9,-2.16)) ;
#146856 = CARTESIAN_POINT('',(1.5,1.9,-2.16)) ;
#146857 = CARTESIAN_POINT('',(1.5,1.9,-2.16)) ;
#146858 = CARTESIAN_POINT('',(7.9,1.9,-2.16)) ;
#146859 = CARTESIAN_POINT('',(1.4,1.9,-2.16)) ;
#146860 = CARTESIAN_POINT('',(7.9,-2.15,-2.16)) ;
#146861 = CARTESIAN_POINT('Origin',(1.4,1.9,-2.26)) ;
#146862 = CARTESIAN_POINT('',(1.5,2.,-2.26)) ;
#146863 = CARTESIAN_POINT('Origin',(1.5,1.9,-2.26)) ;
#146864 = CARTESIAN_POINT('',(7.9,2.,-2.26)) ;
#146865 = CARTESIAN_POINT('',(1.4,2.,-2.26)) ;
#146866 = CARTESIAN_POINT('Origin',(7.9,1.9,-2.26)) ;
#146867 = CARTESIAN_POINT('Origin',(1.4,2.,-2.26)) ;
#146868 = CARTESIAN_POINT('',(1.5,2.,-3.21)) ;
#146869 = CARTESIAN_POINT('',(7.9,2.,-2.26)) ;
#146870 = CARTESIAN_POINT('Origin',(1.4,2.1,-3.21)) ;
#146871 = CARTESIAN_POINT('',(1.4,2.6,-3.21)) ;
#146872 = CARTESIAN_POINT('',(1.4,2.4,-3.41)) ;
#146873 = CARTESIAN_POINT('Origin',(1.4,2.4,-3.21)) ;
#146874 = CARTESIAN_POINT('',(1.4,2.1,-3.41)) ;
#146875 = CARTESIAN_POINT('',(1.4,2.1,-3.41)) ;
#146876 = CARTESIAN_POINT('',(1.4,1.9,-3.21)) ;
#146877 = CARTESIAN_POINT('Origin',(1.4,2.1,-3.21)) ;
#146878 = CARTESIAN_POINT('',(1.4,1.9,-2.26)) ;
#146879 = CARTESIAN_POINT('',(1.4,1.9,-2.26)) ;
#146880 = CARTESIAN_POINT('',(1.4,-2.15,-2.26)) ;
#146881 = CARTESIAN_POINT('',(1.4,-2.15,-2.26)) ;
#146882 = CARTESIAN_POINT('',(1.4,-2.15,-2.90688040659058)) ;
#146883 = CARTESIAN_POINT('',(1.4,-2.15,-2.90688040659058)) ;
#146884 = CARTESIAN_POINT('',(1.4,-2.15,-4.71311959340942)) ;
#146885 = CARTESIAN_POINT('Origin',(1.4,-3.65625,-3.81)) ;
#146886 = CARTESIAN_POINT('',(1.4,-2.15,-5.36)) ;
#146887 = CARTESIAN_POINT('',(1.4,-2.15,-5.36)) ;
#146888 = CARTESIAN_POINT('',(1.4,1.9,-5.36)) ;
#146889 = CARTESIAN_POINT('',(1.4,1.9,-5.36)) ;
#146890 = CARTESIAN_POINT('',(1.4,1.9,-4.41)) ;
#146891 = CARTESIAN_POINT('',(1.4,1.9,-4.41)) ;
#146892 = CARTESIAN_POINT('',(1.4,2.1,-4.21)) ;
#146893 = CARTESIAN_POINT('Origin',(1.4,2.1,-4.41)) ;
#146894 = CARTESIAN_POINT('',(1.4,2.4,-4.21)) ;
#146895 = CARTESIAN_POINT('',(1.4,2.4,-4.21)) ;
#146896 = CARTESIAN_POINT('',(1.4,2.6,-4.41)) ;
#146897 = CARTESIAN_POINT('Origin',(1.4,2.4,-4.41)) ;
#146898 = CARTESIAN_POINT('',(1.4,2.6,-4.51857864376269)) ;
#146899 = CARTESIAN_POINT('',(1.4,2.6,-4.51857864376269)) ;
#146900 = CARTESIAN_POINT('',(1.4,3.15,-5.06857864376269)) ;
#146901 = CARTESIAN_POINT('',(1.4,3.15,-5.06857864376269)) ;
#146902 = CARTESIAN_POINT('',(1.4,3.15,-2.55142135623731)) ;
#146903 = CARTESIAN_POINT('',(1.4,2.6,-3.10142135623731)) ;
#146904 = CARTESIAN_POINT('',(1.4,2.6,-3.10142135623731)) ;
#146905 = CARTESIAN_POINT('',(1.4,2.6,-3.21)) ;
#146906 = CARTESIAN_POINT('Origin',(2.4,0.,-3.81)) ;
#146907 = CARTESIAN_POINT('',(2.4,0.3,-3.41)) ;
#146908 = CARTESIAN_POINT('',(2.4,-0.3,-3.41)) ;
#146909 = CARTESIAN_POINT('',(2.4,0.,-3.41)) ;
#146910 = CARTESIAN_POINT('',(2.4,0.4,-3.51)) ;
#146911 = CARTESIAN_POINT('Origin',(2.4,0.3,-3.51)) ;
#146912 = CARTESIAN_POINT('',(2.4,0.4,-4.11)) ;
#146913 = CARTESIAN_POINT('',(2.4,0.4,-3.81)) ;
#146914 = CARTESIAN_POINT('',(2.4,0.3,-4.21)) ;
#146915 = CARTESIAN_POINT('Origin',(2.4,0.3,-4.11)) ;
#146916 = CARTESIAN_POINT('',(2.4,-0.3,-4.21)) ;
#146917 = CARTESIAN_POINT('',(2.4,0.,-4.21)) ;
#146918 = CARTESIAN_POINT('',(2.4,-0.4,-4.11)) ;
#146919 = CARTESIAN_POINT('Origin',(2.4,-0.3,-4.11)) ;
#146920 = CARTESIAN_POINT('',(2.4,-0.4,-3.51)) ;
#146921 = CARTESIAN_POINT('',(2.4,-0.4,-3.81)) ;
#146922 = CARTESIAN_POINT('Origin',(2.4,-0.3,-3.51)) ;
#146923 = CARTESIAN_POINT('Origin',(2.4,0.,-7.62)) ;
#146924 = CARTESIAN_POINT('',(2.4,0.3,-7.22)) ;
#146925 = CARTESIAN_POINT('',(2.4,-0.3,-7.22)) ;
#146926 = CARTESIAN_POINT('',(2.4,0.,-7.22)) ;
#146927 = CARTESIAN_POINT('',(2.4,0.4,-7.32)) ;
#146928 = CARTESIAN_POINT('Origin',(2.4,0.3,-7.32)) ;
#146929 = CARTESIAN_POINT('',(2.4,0.4,-7.92)) ;
#146930 = CARTESIAN_POINT('',(2.4,0.4,-7.62)) ;
#146931 = CARTESIAN_POINT('',(2.4,0.3,-8.02)) ;
#146932 = CARTESIAN_POINT('Origin',(2.4,0.3,-7.92)) ;
#146933 = CARTESIAN_POINT('',(2.4,-0.3,-8.02)) ;
#146934 = CARTESIAN_POINT('',(2.4,0.,-8.02)) ;
#146935 = CARTESIAN_POINT('',(2.4,-0.4,-7.92)) ;
#146936 = CARTESIAN_POINT('Origin',(2.4,-0.3,-7.92)) ;
#146937 = CARTESIAN_POINT('',(2.4,-0.4,-7.32)) ;
#146938 = CARTESIAN_POINT('',(2.4,-0.4,-7.62)) ;
#146939 = CARTESIAN_POINT('Origin',(2.4,-0.3,-7.32)) ;
#146940 = CARTESIAN_POINT('Origin',(2.4,0.,-11.43)) ;
#146941 = CARTESIAN_POINT('',(2.4,0.3,-11.03)) ;
#146942 = CARTESIAN_POINT('',(2.4,-0.3,-11.03)) ;
#146943 = CARTESIAN_POINT('',(2.4,0.,-11.03)) ;
#146944 = CARTESIAN_POINT('',(2.4,0.4,-11.13)) ;
#146945 = CARTESIAN_POINT('Origin',(2.4,0.3,-11.13)) ;
#146946 = CARTESIAN_POINT('',(2.4,0.4,-11.73)) ;
#146947 = CARTESIAN_POINT('',(2.4,0.4,-11.43)) ;
#146948 = CARTESIAN_POINT('',(2.4,0.3,-11.83)) ;
#146949 = CARTESIAN_POINT('Origin',(2.4,0.3,-11.73)) ;
#146950 = CARTESIAN_POINT('',(2.4,-0.3,-11.83)) ;
#146951 = CARTESIAN_POINT('',(2.4,0.,-11.83)) ;
#146952 = CARTESIAN_POINT('',(2.4,-0.4,-11.73)) ;
#146953 = CARTESIAN_POINT('Origin',(2.4,-0.3,-11.73)) ;
#146954 = CARTESIAN_POINT('',(2.4,-0.4,-11.13)) ;
#146955 = CARTESIAN_POINT('',(2.4,-0.4,-11.43)) ;
#146956 = CARTESIAN_POINT('Origin',(2.4,-0.3,-11.13)) ;
#146957 = CARTESIAN_POINT('Origin',(2.4,0.,-15.24)) ;
#146958 = CARTESIAN_POINT('',(2.4,0.3,-14.84)) ;
#146959 = CARTESIAN_POINT('',(2.4,-0.3,-14.84)) ;
#146960 = CARTESIAN_POINT('',(2.4,0.,-14.84)) ;
#146961 = CARTESIAN_POINT('',(2.4,0.4,-14.94)) ;
#146962 = CARTESIAN_POINT('Origin',(2.4,0.3,-14.94)) ;
#146963 = CARTESIAN_POINT('',(2.4,0.4,-15.54)) ;
#146964 = CARTESIAN_POINT('',(2.4,0.4,-15.24)) ;
#146965 = CARTESIAN_POINT('',(2.4,0.3,-15.64)) ;
#146966 = CARTESIAN_POINT('Origin',(2.4,0.3,-15.54)) ;
#146967 = CARTESIAN_POINT('',(2.4,-0.3,-15.64)) ;
#146968 = CARTESIAN_POINT('',(2.4,0.,-15.64)) ;
#146969 = CARTESIAN_POINT('',(2.4,-0.4,-15.54)) ;
#146970 = CARTESIAN_POINT('Origin',(2.4,-0.3,-15.54)) ;
#146971 = CARTESIAN_POINT('',(2.4,-0.4,-14.94)) ;
#146972 = CARTESIAN_POINT('',(2.4,-0.4,-15.24)) ;
#146973 = CARTESIAN_POINT('Origin',(2.4,-0.3,-14.94)) ;
#146974 = CARTESIAN_POINT('Origin',(2.4,0.,-19.05)) ;
#146975 = CARTESIAN_POINT('',(2.4,0.3,-18.65)) ;
#146976 = CARTESIAN_POINT('',(2.4,-0.3,-18.65)) ;
#146977 = CARTESIAN_POINT('',(2.4,0.,-18.65)) ;
#146978 = CARTESIAN_POINT('',(2.4,0.4,-18.75)) ;
#146979 = CARTESIAN_POINT('Origin',(2.4,0.3,-18.75)) ;
#146980 = CARTESIAN_POINT('',(2.4,0.4,-19.35)) ;
#146981 = CARTESIAN_POINT('',(2.4,0.4,-19.05)) ;
#146982 = CARTESIAN_POINT('',(2.4,0.3,-19.45)) ;
#146983 = CARTESIAN_POINT('Origin',(2.4,0.3,-19.35)) ;
#146984 = CARTESIAN_POINT('',(2.4,-0.3,-19.45)) ;
#146985 = CARTESIAN_POINT('',(2.4,0.,-19.45)) ;
#146986 = CARTESIAN_POINT('',(2.4,-0.4,-19.35)) ;
#146987 = CARTESIAN_POINT('Origin',(2.4,-0.3,-19.35)) ;
#146988 = CARTESIAN_POINT('',(2.4,-0.4,-18.75)) ;
#146989 = CARTESIAN_POINT('',(2.4,-0.4,-19.05)) ;
#146990 = CARTESIAN_POINT('Origin',(2.4,-0.3,-18.75)) ;
#146991 = CARTESIAN_POINT('Origin',(2.4,0.,-22.86)) ;
#146992 = CARTESIAN_POINT('',(2.4,0.3,-22.46)) ;
#146993 = CARTESIAN_POINT('',(2.4,-0.3,-22.46)) ;
#146994 = CARTESIAN_POINT('',(2.4,0.,-22.46)) ;
#146995 = CARTESIAN_POINT('',(2.4,0.4,-22.56)) ;
#146996 = CARTESIAN_POINT('Origin',(2.4,0.3,-22.56)) ;
#146997 = CARTESIAN_POINT('',(2.4,0.4,-23.16)) ;
#146998 = CARTESIAN_POINT('',(2.4,0.4,-22.86)) ;
#146999 = CARTESIAN_POINT('',(2.4,0.3,-23.26)) ;
#147000 = CARTESIAN_POINT('Origin',(2.4,0.3,-23.16)) ;
#147001 = CARTESIAN_POINT('',(2.4,-0.3,-23.26)) ;
#147002 = CARTESIAN_POINT('',(2.4,0.,-23.26)) ;
#147003 = CARTESIAN_POINT('',(2.4,-0.4,-23.16)) ;
#147004 = CARTESIAN_POINT('Origin',(2.4,-0.3,-23.16)) ;
#147005 = CARTESIAN_POINT('',(2.4,-0.4,-22.56)) ;
#147006 = CARTESIAN_POINT('',(2.4,-0.4,-22.86)) ;
#147007 = CARTESIAN_POINT('Origin',(2.4,-0.3,-22.56)) ;
#147008 = CARTESIAN_POINT('Origin',(2.4,0.,-26.67)) ;
#147009 = CARTESIAN_POINT('',(2.4,0.3,-26.27)) ;
#147010 = CARTESIAN_POINT('',(2.4,-0.3,-26.27)) ;
#147011 = CARTESIAN_POINT('',(2.4,0.,-26.27)) ;
#147012 = CARTESIAN_POINT('',(2.4,0.4,-26.37)) ;
#147013 = CARTESIAN_POINT('Origin',(2.4,0.3,-26.37)) ;
#147014 = CARTESIAN_POINT('',(2.4,0.4,-26.97)) ;
#147015 = CARTESIAN_POINT('',(2.4,0.4,-26.67)) ;
#147016 = CARTESIAN_POINT('',(2.4,0.3,-27.07)) ;
#147017 = CARTESIAN_POINT('Origin',(2.4,0.3,-26.97)) ;
#147018 = CARTESIAN_POINT('',(2.4,-0.3,-27.07)) ;
#147019 = CARTESIAN_POINT('',(2.4,0.,-27.07)) ;
#147020 = CARTESIAN_POINT('',(2.4,-0.4,-26.97)) ;
#147021 = CARTESIAN_POINT('Origin',(2.4,-0.3,-26.97)) ;
#147022 = CARTESIAN_POINT('',(2.4,-0.4,-26.37)) ;
#147023 = CARTESIAN_POINT('',(2.4,-0.4,-26.67)) ;
#147024 = CARTESIAN_POINT('Origin',(2.4,-0.3,-26.37)) ;
#147025 = CARTESIAN_POINT('Origin',(2.4,0.,-30.48)) ;
#147026 = CARTESIAN_POINT('',(2.4,0.3,-30.08)) ;
#147027 = CARTESIAN_POINT('',(2.4,-0.3,-30.08)) ;
#147028 = CARTESIAN_POINT('',(2.4,0.,-30.08)) ;
#147029 = CARTESIAN_POINT('',(2.4,0.4,-30.18)) ;
#147030 = CARTESIAN_POINT('Origin',(2.4,0.3,-30.18)) ;
#147031 = CARTESIAN_POINT('',(2.4,0.4,-30.78)) ;
#147032 = CARTESIAN_POINT('',(2.4,0.4,-30.48)) ;
#147033 = CARTESIAN_POINT('',(2.4,0.3,-30.88)) ;
#147034 = CARTESIAN_POINT('Origin',(2.4,0.3,-30.78)) ;
#147035 = CARTESIAN_POINT('',(2.4,-0.3,-30.88)) ;
#147036 = CARTESIAN_POINT('',(2.4,0.,-30.88)) ;
#147037 = CARTESIAN_POINT('',(2.4,-0.4,-30.78)) ;
#147038 = CARTESIAN_POINT('Origin',(2.4,-0.3,-30.78)) ;
#147039 = CARTESIAN_POINT('',(2.4,-0.4,-30.18)) ;
#147040 = CARTESIAN_POINT('',(2.4,-0.4,-30.48)) ;
#147041 = CARTESIAN_POINT('Origin',(2.4,-0.3,-30.18)) ;
#147042 = CARTESIAN_POINT('Origin',(2.4,0.,-34.29)) ;
#147043 = CARTESIAN_POINT('',(2.4,0.3,-33.89)) ;
#147044 = CARTESIAN_POINT('',(2.4,-0.3,-33.89)) ;
#147045 = CARTESIAN_POINT('',(2.4,0.,-33.89)) ;
#147046 = CARTESIAN_POINT('',(2.4,0.4,-33.99)) ;
#147047 = CARTESIAN_POINT('Origin',(2.4,0.3,-33.99)) ;
#147048 = CARTESIAN_POINT('',(2.4,0.4,-34.59)) ;
#147049 = CARTESIAN_POINT('',(2.4,0.4,-34.29)) ;
#147050 = CARTESIAN_POINT('',(2.4,0.3,-34.69)) ;
#147051 = CARTESIAN_POINT('Origin',(2.4,0.3,-34.59)) ;
#147052 = CARTESIAN_POINT('',(2.4,-0.3,-34.69)) ;
#147053 = CARTESIAN_POINT('',(2.4,0.,-34.69)) ;
#147054 = CARTESIAN_POINT('',(2.4,-0.4,-34.59)) ;
#147055 = CARTESIAN_POINT('Origin',(2.4,-0.3,-34.59)) ;
#147056 = CARTESIAN_POINT('',(2.4,-0.4,-33.99)) ;
#147057 = CARTESIAN_POINT('',(2.4,-0.4,-34.29)) ;
#147058 = CARTESIAN_POINT('Origin',(2.4,-0.3,-33.99)) ;
#147059 = CARTESIAN_POINT('Origin',(-0.899999999999999,-2.,-3.21)) ;
#147060 = CARTESIAN_POINT('Origin',(-0.899999999999999,0.4,-3.21)) ;
#147061 = CARTESIAN_POINT('Origin',(-0.899999999999999,-1.9,-3.21)) ;
#147062 = CARTESIAN_POINT('Origin',(0.600000000000001,0.4,-3.41)) ;
#147063 = CARTESIAN_POINT('Origin',(0.500000000000001,0.4,-3.41)) ;
#147064 = CARTESIAN_POINT('Origin',(-0.899999999999999,0.4,-3.41)) ;
#147065 = CARTESIAN_POINT('Origin',(0.500000000000001,0.4,-3.41)) ;
#147066 = CARTESIAN_POINT('',(0.600000000000001,0.4,-3.41)) ;
#147067 = CARTESIAN_POINT('Origin',(0.500000000000001,0.4,-3.41)) ;
#147068 = CARTESIAN_POINT('Origin',(0.500000000000001,0.4,-3.41)) ;
#147069 = CARTESIAN_POINT('Origin',(-0.899999999999999,-1.9,-3.21)) ;
#147070 = CARTESIAN_POINT('Origin',(-0.899999999999999,-1.9,-3.21)) ;
#147071 = CARTESIAN_POINT('Origin',(-0.899999999999999,-1.9,-3.21)) ;
#147072 = CARTESIAN_POINT('Origin',(-0.899999999999999,0.4,-3.41)) ;
#147073 = CARTESIAN_POINT('Origin',(-0.899999999999999,0.6,-3.41)) ;
#147074 = CARTESIAN_POINT('Origin',(0.500000000000001,0.4,-3.81)) ;
#147075 = CARTESIAN_POINT('Origin',(0.500000000000001,0.4,-4.21)) ;
#147076 = CARTESIAN_POINT('',(0.600000000000001,0.4,-4.11)) ;
#147077 = CARTESIAN_POINT('Ctrl Pts',(0.595612997216081,0.370705721320404,
-4.1807057213204)) ;
#147078 = CARTESIAN_POINT('Ctrl Pts',(0.596180587760892,0.372558268494358,
-4.17885549883217)) ;
#147079 = CARTESIAN_POINT('Ctrl Pts',(0.596672461925686,0.374355839771985,
-4.17691417986631)) ;
#147080 = CARTESIAN_POINT('Ctrl Pts',(0.599015141889212,0.383869350930066,
-4.16576499365627)) ;
#147081 = CARTESIAN_POINT('Ctrl Pts',(0.599609996542525,0.390224332900452,
-4.15497260265412)) ;
#147082 = CARTESIAN_POINT('Ctrl Pts',(0.600050586298726,0.398117439141561,
-4.13233105320467)) ;
#147083 = CARTESIAN_POINT('Ctrl Pts',(0.600000000000001,0.399999999999999,
-4.12120125063352)) ;
#147084 = CARTESIAN_POINT('Ctrl Pts',(0.600000000000001,0.399999999999999,
-4.11)) ;
#147085 = CARTESIAN_POINT('',(0.600000000000001,0.4,-3.81)) ;
#147086 = CARTESIAN_POINT('Origin',(0.500000000000001,-4.56640444411541E-17,
-3.41)) ;
#147087 = CARTESIAN_POINT('',(0.500000000000001,0.394987437106619,-3.51)) ;
#147088 = CARTESIAN_POINT('Ctrl Pts',(0.500000000000001,0.394987437106619,
-3.51)) ;
#147089 = CARTESIAN_POINT('Ctrl Pts',(0.505940567948953,0.3955844866499,-3.51)) ;
#147090 = CARTESIAN_POINT('Ctrl Pts',(0.511931971019142,0.396132036079018,
-3.50946630032796)) ;
#147091 = CARTESIAN_POINT('Ctrl Pts',(0.517829015308552,0.396618246075354,
-3.50839779577372)) ;
#147092 = CARTESIAN_POINT('Ctrl Pts',(0.522982218721203,0.397043126556053,
-3.50746407015711)) ;
#147093 = CARTESIAN_POINT('Ctrl Pts',(0.528062648970231,0.397421319341388,
-3.50612282679706)) ;
#147094 = CARTESIAN_POINT('Ctrl Pts',(0.532978106724,0.397751505046071,-3.50440574387663)) ;
#147095 = CARTESIAN_POINT('Ctrl Pts',(0.538583536338964,0.398128038182999,
-3.50244763784955)) ;
#147096 = CARTESIAN_POINT('Ctrl Pts',(0.544059405914891,0.398447721828295,
-3.49997000831105)) ;
#147097 = CARTESIAN_POINT('Ctrl Pts',(0.549268572255782,0.398712331108983,
-3.49702073194289)) ;
#147098 = CARTESIAN_POINT('Ctrl Pts',(0.553856850427147,0.398945401221756,
-3.49442298414684)) ;
#147099 = CARTESIAN_POINT('Ctrl Pts',(0.558237825069328,0.399135987683843,
-3.49146038497999)) ;
#147100 = CARTESIAN_POINT('Ctrl Pts',(0.562333836086213,0.399290378266507,
-3.48819522286417)) ;
#147101 = CARTESIAN_POINT('Ctrl Pts',(0.56699032895789,0.399465895042381,
-3.48448326895231)) ;
#147102 = CARTESIAN_POINT('Ctrl Pts',(0.571349096493424,0.399597278936107,
-3.4803228064848)) ;
#147103 = CARTESIAN_POINT('Ctrl Pts',(0.57529692005671,0.399694832180837,
-3.47580557597935)) ;
#147104 = CARTESIAN_POINT('Ctrl Pts',(0.578744263667905,0.399780018245913,
-3.47186101121508)) ;
#147105 = CARTESIAN_POINT('Ctrl Pts',(0.581878314560428,0.399839626289636,
-3.46764552184211)) ;
#147106 = CARTESIAN_POINT('Ctrl Pts',(0.584648147334855,0.399882153365958,
-3.4632418177073)) ;
#147107 = CARTESIAN_POINT('Ctrl Pts',(0.587839270208174,0.399931148788079,
-3.4581683125045)) ;
#147108 = CARTESIAN_POINT('Ctrl Pts',(0.590595054415095,0.399958289583404,
-3.45276663624445)) ;
#147109 = CARTESIAN_POINT('Ctrl Pts',(0.592838618943107,0.399974357003159,
-3.44716168500939)) ;
#147110 = CARTESIAN_POINT('Ctrl Pts',(0.594777336851657,0.399988241245861,
-3.44231831224239)) ;
#147111 = CARTESIAN_POINT('Ctrl Pts',(0.59633405150619,0.399993946552814,
-3.43732416622712)) ;
#147112 = CARTESIAN_POINT('Ctrl Pts',(0.597488309822309,0.39999684570125,
-3.43227171856839)) ;
#147113 = CARTESIAN_POINT('Ctrl Pts',(0.598804024094397,0.400000150378306,
-3.42651254196058)) ;
#147114 = CARTESIAN_POINT('Ctrl Pts',(0.599612685195426,0.399999963509465,
-3.42060284389063)) ;
#147115 = CARTESIAN_POINT('Ctrl Pts',(0.599890230999718,0.399999993975383,
-3.41468420226113)) ;
#147116 = CARTESIAN_POINT('Ctrl Pts',(0.599963464549399,0.400000002014155,
-3.41312250278986)) ;
#147117 = CARTESIAN_POINT('Ctrl Pts',(0.600000000000001,0.399999999999999,
-3.4115602215092)) ;
#147118 = CARTESIAN_POINT('Ctrl Pts',(0.600000000000001,0.399999999999999,
-3.41)) ;
#147119 = CARTESIAN_POINT('',(0.600000000000001,0.299999999999999,-3.41)) ;
#147120 = CARTESIAN_POINT('Ctrl Pts',(0.500000000000001,0.394987437106619,
-3.51)) ;
#147121 = CARTESIAN_POINT('Ctrl Pts',(0.500454935589683,0.395033159853733,
-3.51)) ;
#147122 = CARTESIAN_POINT('Ctrl Pts',(0.500909898680391,0.395078570329052,
-3.50999689549113)) ;
#147123 = CARTESIAN_POINT('Ctrl Pts',(0.502892456245154,0.395275075889088,
-3.50996983394194)) ;
#147124 = CARTESIAN_POINT('Ctrl Pts',(0.504418747482365,0.395422812032198,
-3.50991398542099)) ;
#147125 = CARTESIAN_POINT('Ctrl Pts',(0.508462199543374,0.395804395682036,
-3.50967328105664)) ;
#147126 = CARTESIAN_POINT('Ctrl Pts',(0.51097495334332,0.396031485023319,
-3.50942793914505)) ;
#147127 = CARTESIAN_POINT('Ctrl Pts',(0.521160739721337,0.396903453186241,
-3.50804279449155)) ;
#147128 = CARTESIAN_POINT('Ctrl Pts',(0.528708678528462,0.397444933153163,
-3.50610421770467)) ;
#147129 = CARTESIAN_POINT('Ctrl Pts',(0.545943206358151,0.398105551684111,
-3.49946463945111)) ;
#147130 = CARTESIAN_POINT('Ctrl Pts',(0.555229535466881,0.397987646678422,
-3.49403535883592)) ;
#147131 = CARTESIAN_POINT('Ctrl Pts',(0.571394604995817,0.395490482808027,
-3.4807755133638)) ;
#147132 = CARTESIAN_POINT('Ctrl Pts',(0.578055313702888,0.393198948698317,
-3.47324074563169)) ;
#147133 = CARTESIAN_POINT('Ctrl Pts',(0.588559132202554,0.385442756729274,
-3.45739223398396)) ;
#147134 = CARTESIAN_POINT('Ctrl Pts',(0.592167355639999,0.380240075126842,
-3.44954826560675)) ;
#147135 = CARTESIAN_POINT('Ctrl Pts',(0.597496615531132,0.365892753466902,
-3.43392552179521)) ;
#147136 = CARTESIAN_POINT('Ctrl Pts',(0.598734255154207,0.35666056430058,
-3.42677274172686)) ;
#147137 = CARTESIAN_POINT('Ctrl Pts',(0.600012754681691,0.335223914398476,
-3.41558230586558)) ;
#147138 = CARTESIAN_POINT('Ctrl Pts',(0.59999390055981,0.322655037091807,
-3.41166151936557)) ;
#147139 = CARTESIAN_POINT('Ctrl Pts',(0.600000296204999,0.306106913582338,
-3.41013962634704)) ;
#147140 = CARTESIAN_POINT('Ctrl Pts',(0.600000000000001,0.303050992413427,
-3.41)) ;
#147141 = CARTESIAN_POINT('Ctrl Pts',(0.600000000000001,0.299999999999999,
-3.41)) ;
#147142 = CARTESIAN_POINT('',(0.600000000000001,-2.3980000991444E-17,-3.41)) ;
#147143 = CARTESIAN_POINT('Origin',(0.500000000000001,-1.9,-3.41)) ;
#147144 = CARTESIAN_POINT('Origin',(0.600000000000001,-1.9,-3.21)) ;
#147145 = CARTESIAN_POINT('Origin',(0.500000000000001,-1.9,-3.21)) ;
#147146 = CARTESIAN_POINT('Origin',(-0.899999999999999,-1.9,-2.435)) ;
#147147 = CARTESIAN_POINT('Origin',(-0.899999999999999,-1.9,-2.535)) ;
#147148 = CARTESIAN_POINT('Origin',(-0.899999999999999,0.6,-3.31)) ;
#147149 = CARTESIAN_POINT('Origin',(-0.899999999999999,0.6,-4.21)) ;
#147150 = CARTESIAN_POINT('Origin',(0.600000000000001,0.4,-4.21)) ;
#147151 = CARTESIAN_POINT('Origin',(0.500000000000001,0.4,-4.21)) ;
#147152 = CARTESIAN_POINT('Origin',(-0.899999999999999,0.4,-4.21)) ;
#147153 = CARTESIAN_POINT('Origin',(0.500000000000001,0.4,-4.21)) ;
#147154 = CARTESIAN_POINT('Origin',(0.500000000000001,-1.9,-3.21)) ;
#147155 = CARTESIAN_POINT('Origin',(0.500000000000001,-2.1,-3.21)) ;
#147156 = CARTESIAN_POINT('Origin',(-0.899999999999999,-1.9,-2.535)) ;
#147157 = CARTESIAN_POINT('Origin',(-1.1,-1.9,-2.535)) ;
#147158 = CARTESIAN_POINT('Origin',(-0.899999999999999,-2.1,-2.535)) ;
#147159 = CARTESIAN_POINT('Origin',(-0.899999999999999,0.4,-4.21)) ;
#147160 = CARTESIAN_POINT('Origin',(-0.899999999999999,0.4,-4.41)) ;
#147161 = CARTESIAN_POINT('Origin',(0.500000000000001,-2.1,-3.81)) ;
#147162 = CARTESIAN_POINT('Origin',(0.500000000000001,-2.1,-2.535)) ;
#147163 = CARTESIAN_POINT('Origin',(0.600000000000001,-2.1,-2.535)) ;
#147164 = CARTESIAN_POINT('Origin',(0.500000000000001,-2.1,-2.535)) ;
#147165 = CARTESIAN_POINT('Origin',(-1.1,-4.42727195005761E-17,-2.535)) ;
#147166 = CARTESIAN_POINT('',(-1.1,1.15,-2.435)) ;
#147167 = CARTESIAN_POINT('',(-1.1,1.25,-2.435)) ;
#147168 = CARTESIAN_POINT('Origin',(-1.1,1.15,-2.535)) ;
#147169 = CARTESIAN_POINT('Origin',(-0.899999999999999,0.5,-4.41)) ;
#147170 = CARTESIAN_POINT('Origin',(-0.899999999999999,-1.9,-4.41)) ;
#147171 = CARTESIAN_POINT('Origin',(0.600000000000001,-1.9,-4.41)) ;
#147172 = CARTESIAN_POINT('Origin',(0.500000000000001,-1.9,-4.41)) ;
#147173 = CARTESIAN_POINT('Origin',(-0.899999999999999,-1.9,-4.41)) ;
#147174 = CARTESIAN_POINT('Origin',(0.500000000000001,-1.9,-4.41)) ;
#147175 = CARTESIAN_POINT('Origin',(0.500000000000001,-2.1,-4.41)) ;
#147176 = CARTESIAN_POINT('Origin',(0.500000000000001,-2.1,-2.535)) ;
#147177 = CARTESIAN_POINT('Origin',(0.500000000000001,-2.1,-2.535)) ;
#147178 = CARTESIAN_POINT('Origin',(-1.1,-2.9,-2.335)) ;
#147179 = CARTESIAN_POINT('Origin',(-1.1,-2.9,-2.335)) ;
#147180 = CARTESIAN_POINT('Origin',(-1.1,-2.9,-2.335)) ;
#147181 = CARTESIAN_POINT('Origin',(-1.1,1.25,-2.335)) ;
#147182 = CARTESIAN_POINT('Origin',(-1.1,1.15,-2.335)) ;
#147183 = CARTESIAN_POINT('Origin',(-1.1,1.15,-2.535)) ;
#147184 = CARTESIAN_POINT('',(-1.1,1.25,-2.535)) ;
#147185 = CARTESIAN_POINT('Origin',(-1.1,1.15,-2.535)) ;
#147186 = CARTESIAN_POINT('Origin',(-1.1,1.15,-2.535)) ;
#147187 = CARTESIAN_POINT('Origin',(-0.899999999999999,-1.9,-4.41)) ;
#147188 = CARTESIAN_POINT('Origin',(-0.899999999999999,-1.9,-4.41)) ;
#147189 = CARTESIAN_POINT('Origin',(0.500000000000001,-2.1,-3.81)) ;
#147190 = CARTESIAN_POINT('Origin',(0.500000000000001,-2.1,-5.085)) ;
#147191 = CARTESIAN_POINT('Origin',(0.500000000000001,1.36481920536411E-16,
-2.535)) ;
#147192 = CARTESIAN_POINT('Origin',(0.500000000000001,-2.9,-2.535)) ;
#147193 = CARTESIAN_POINT('Origin',(-0.999999999999999,-2.9,-2.335)) ;
#147194 = CARTESIAN_POINT('Origin',(0.500000000000001,-2.9,-2.335)) ;
#147195 = CARTESIAN_POINT('Origin',(-1.1,1.15,-2.535)) ;
#147196 = CARTESIAN_POINT('Origin',(-1.1,1.35,-2.535)) ;
#147197 = CARTESIAN_POINT('Origin',(-1.1,1.15,-3.81)) ;
#147198 = CARTESIAN_POINT('',(-1.1,1.25,-5.085)) ;
#147199 = CARTESIAN_POINT('',(-1.1,1.25,-5.185)) ;
#147200 = CARTESIAN_POINT('Origin',(-1.1,1.15,-5.085)) ;
#147201 = CARTESIAN_POINT('Origin',(-0.899999999999999,-1.9,-4.31)) ;
#147202 = CARTESIAN_POINT('Origin',(-0.899999999999999,-1.9,-5.085)) ;
#147203 = CARTESIAN_POINT('Origin',(-0.999999999999999,-2.1,-5.085)) ;
#147204 = CARTESIAN_POINT('Origin',(0.500000000000001,-2.1,-5.085)) ;
#147205 = CARTESIAN_POINT('Origin',(-0.899999999999999,-2.1,-5.085)) ;
#147206 = CARTESIAN_POINT('Origin',(0.500000000000001,-2.1,-5.085)) ;
#147207 = CARTESIAN_POINT('Origin',(0.500000000000001,-2.1,-5.085)) ;
#147208 = CARTESIAN_POINT('Origin',(0.500000000000001,-2.9,-2.535)) ;
#147209 = CARTESIAN_POINT('Origin',(0.700000000000002,-2.9,-2.535)) ;
#147210 = CARTESIAN_POINT('Origin',(-1.1,1.35,-5.185)) ;
#147211 = CARTESIAN_POINT('Origin',(-1.1,1.35,-5.085)) ;
#147212 = CARTESIAN_POINT('Origin',(-1.1,1.15,-5.085)) ;
#147213 = CARTESIAN_POINT('',(-1.1,1.15,-5.185)) ;
#147214 = CARTESIAN_POINT('Origin',(-1.1,1.15,-5.085)) ;
#147215 = CARTESIAN_POINT('Origin',(-1.1,1.15,-5.085)) ;
#147216 = CARTESIAN_POINT('Origin',(-0.899999999999999,-1.9,-5.085)) ;
#147217 = CARTESIAN_POINT('Origin',(-1.1,-1.9,-5.085)) ;
#147218 = CARTESIAN_POINT('Origin',(0.500000000000001,-5.86744705109801E-17,
-5.085)) ;
#147219 = CARTESIAN_POINT('Origin',(0.500000000000001,-2.9,-5.085)) ;
#147220 = CARTESIAN_POINT('Origin',(0.700000000000002,-2.9,-3.81)) ;
#147221 = CARTESIAN_POINT('Origin',(0.700000000000002,-2.9,-5.085)) ;
#147222 = CARTESIAN_POINT('Origin',(-1.1,1.15,-5.085)) ;
#147223 = CARTESIAN_POINT('Origin',(-1.1,1.15,-5.285)) ;
#147224 = CARTESIAN_POINT('Origin',(-1.1,-2.39429110547967E-16,-5.085)) ;
#147225 = CARTESIAN_POINT('',(-1.1,1.25,-5.185)) ;
#147226 = CARTESIAN_POINT('Origin',(0.500000000000001,-2.9,-5.085)) ;
#147227 = CARTESIAN_POINT('Origin',(0.500000000000001,-2.9,-5.285)) ;
#147228 = CARTESIAN_POINT('Origin',(-1.1,1.25,-5.285)) ;
#147229 = CARTESIAN_POINT('Origin',(-1.1,-2.9,-5.285)) ;
#147230 = CARTESIAN_POINT('Origin',(-1.1,-2.9,-5.285)) ;
#147231 = CARTESIAN_POINT('Origin',(-1.1,-2.9,-5.285)) ;
#147232 = CARTESIAN_POINT('Origin',(-1.1,-2.9,-5.285)) ;
#147233 = CARTESIAN_POINT('Origin',(1.5,1.9,-3.21)) ;
#147234 = CARTESIAN_POINT('Origin',(1.5,1.9,-5.36)) ;
#147235 = CARTESIAN_POINT('Origin',(1.5,1.9,-4.41)) ;
#147236 = CARTESIAN_POINT('Origin',(1.5,2.1,-4.41)) ;
#147237 = CARTESIAN_POINT('Origin',(1.5,2.1,-4.21)) ;
#147238 = CARTESIAN_POINT('Origin',(1.5,1.9,-5.36)) ;
#147239 = CARTESIAN_POINT('Origin',(1.5,1.9,-5.36)) ;
#147240 = CARTESIAN_POINT('Origin',(1.5,2.1,-4.21)) ;
#147241 = CARTESIAN_POINT('Origin',(1.5,2.4,-4.21)) ;
#147242 = CARTESIAN_POINT('Origin',(1.5,2.1,-5.36)) ;
#147243 = CARTESIAN_POINT('Origin',(1.5,-2.15,-5.36)) ;
#147244 = CARTESIAN_POINT('Origin',(1.5,2.4,-4.41)) ;
#147245 = CARTESIAN_POINT('Origin',(1.5,2.6,-4.41)) ;
#147246 = CARTESIAN_POINT('Origin',(1.5,-2.15,-5.36)) ;
#147247 = CARTESIAN_POINT('Origin',(1.5,-2.15,-5.36)) ;
#147248 = CARTESIAN_POINT('Origin',(1.5,2.6,-3.21)) ;
#147249 = CARTESIAN_POINT('Origin',(1.5,2.6,-4.51857864376269)) ;
#147250 = CARTESIAN_POINT('Origin',(1.5,-2.15,-3.21)) ;
#147251 = CARTESIAN_POINT('Origin',(1.5,-2.15,-4.71311959340942)) ;
#147252 = CARTESIAN_POINT('Origin',(1.5,2.6,-4.51857864376269)) ;
#147253 = CARTESIAN_POINT('Origin',(1.5,2.6,-4.51857864376269)) ;
#147254 = CARTESIAN_POINT('Origin',(1.5,-2.15,-4.71311959340942)) ;
#147255 = CARTESIAN_POINT('Origin',(1.5,-2.15,-4.71311959340942)) ;
#147256 = CARTESIAN_POINT('Origin',(1.5,1.69571067811865,-3.61428932188135)) ;
#147257 = CARTESIAN_POINT('Origin',(1.5,3.15,-5.06857864376269)) ;
#147258 = CARTESIAN_POINT('Origin',(1.5,-3.65625,-3.81)) ;
#147259 = CARTESIAN_POINT('Origin',(1.5,-2.15,-2.90688040659058)) ;
#147260 = CARTESIAN_POINT('Origin',(1.5,3.15,-5.06857864376269)) ;
#147261 = CARTESIAN_POINT('Origin',(1.5,3.15,-5.06857864376269)) ;
#147262 = CARTESIAN_POINT('Origin',(1.5,-2.15,-2.90688040659058)) ;
#147263 = CARTESIAN_POINT('Origin',(1.5,-2.15,-2.90688040659058)) ;
#147264 = CARTESIAN_POINT('Origin',(1.5,3.15,-3.21)) ;
#147265 = CARTESIAN_POINT('Origin',(1.5,-2.15,-3.21)) ;
#147266 = CARTESIAN_POINT('Origin',(1.5,-2.15,-2.26)) ;
#147267 = CARTESIAN_POINT('Origin',(1.5,-2.15,-2.26)) ;
#147268 = CARTESIAN_POINT('Origin',(1.5,-2.15,-2.26)) ;
#147269 = CARTESIAN_POINT('Origin',(1.5,2.29571067811866,-3.40571067811866)) ;
#147270 = CARTESIAN_POINT('Origin',(1.5,2.6,-3.10142135623731)) ;
#147271 = CARTESIAN_POINT('Origin',(1.5,2.1,-2.26)) ;
#147272 = CARTESIAN_POINT('Origin',(1.5,1.9,-2.26)) ;
#147273 = CARTESIAN_POINT('Origin',(1.5,2.6,-3.10142135623731)) ;
#147274 = CARTESIAN_POINT('Origin',(1.5,2.6,-3.10142135623731)) ;
#147275 = CARTESIAN_POINT('Origin',(1.5,1.9,-2.26)) ;
#147276 = CARTESIAN_POINT('Origin',(1.5,1.9,-2.26)) ;
#147277 = CARTESIAN_POINT('Origin',(1.5,2.6,-3.21)) ;
#147278 = CARTESIAN_POINT('Origin',(1.5,2.6,-3.21)) ;
#147279 = CARTESIAN_POINT('Origin',(1.5,1.9,-3.21)) ;
#147280 = CARTESIAN_POINT('Origin',(1.5,1.9,-3.21)) ;
#147281 = CARTESIAN_POINT('Origin',(1.5,2.4,-3.21)) ;
#147282 = CARTESIAN_POINT('Origin',(1.5,2.4,-3.41)) ;
#147283 = CARTESIAN_POINT('Origin',(1.5,2.1,-3.21)) ;
#147284 = CARTESIAN_POINT('Origin',(1.5,2.1,-3.41)) ;
#147285 = CARTESIAN_POINT('Origin',(1.5,2.1,-3.41)) ;
#147286 = CARTESIAN_POINT('Origin',(7.9,2.1,-34.89)) ;
#147287 = CARTESIAN_POINT('Origin',(7.9,2.4,-34.89)) ;
#147288 = CARTESIAN_POINT('Origin',(7.9,2.1,-34.89)) ;
#147289 = CARTESIAN_POINT('Origin',(7.9,2.4,-34.89)) ;
#147290 = CARTESIAN_POINT('Origin',(7.9,2.4,-34.89)) ;
#147291 = CARTESIAN_POINT('Origin',(7.9,2.1,-34.89)) ;
#147292 = CARTESIAN_POINT('Origin',(7.9,2.1,-34.89)) ;
#147293 = CARTESIAN_POINT('Origin',(7.9,2.4,-34.89)) ;
#147294 = CARTESIAN_POINT('Origin',(7.9,2.4,-34.9985786437627)) ;
#147295 = CARTESIAN_POINT('Origin',(7.9,2.1,-34.89)) ;
#147296 = CARTESIAN_POINT('Origin',(7.9,2.1,-35.84)) ;
#147297 = CARTESIAN_POINT('Origin',(7.9,2.6,-34.9985786437627)) ;
#147298 = CARTESIAN_POINT('Origin',(7.9,2.45857864376269,-35.14)) ;
#147299 = CARTESIAN_POINT('Origin',(7.9,1.9,-35.84)) ;
#147300 = CARTESIAN_POINT('Origin',(7.9,1.9,-36.04)) ;
#147301 = CARTESIAN_POINT('Origin',(7.9,2.45857864376269,-35.14)) ;
#147302 = CARTESIAN_POINT('Origin',(7.9,1.9,-36.04)) ;
#147303 = CARTESIAN_POINT('Origin',(7.9,-2.15,-36.04)) ;
#147304 = CARTESIAN_POINT('Origin',(7.9,-2.15,-35.84)) ;
#147305 = CARTESIAN_POINT('Origin',(7.9,-2.35,-35.84)) ;
#147306 = CARTESIAN_POINT('Origin',(7.9,3.35,-35.5485786437627)) ;
#147307 = CARTESIAN_POINT('Origin',(7.9,3.35,-33.0314213562373)) ;
#147308 = CARTESIAN_POINT('Origin',(7.9,-2.35,-35.1931195934094)) ;
#147309 = CARTESIAN_POINT('Origin',(7.9,-2.35,-35.1931195934094)) ;
#147310 = CARTESIAN_POINT('Origin',(7.9,3.15,-33.0314213562373)) ;
#147311 = CARTESIAN_POINT('Origin',(7.9,3.00857864376269,-32.89)) ;
#147312 = CARTESIAN_POINT('Origin',(7.9,-2.15,-35.1931195934094)) ;
#147313 = CARTESIAN_POINT('Origin',(7.9,-2.32153024911032,-35.0902732340176)) ;
#147314 = CARTESIAN_POINT('Origin',(7.9,3.00857864376269,-32.89)) ;
#147315 = CARTESIAN_POINT('Origin',(7.9,2.45857864376269,-33.44)) ;
#147316 = CARTESIAN_POINT('Origin',(7.9,-3.65625,-34.29)) ;
#147317 = CARTESIAN_POINT('Origin',(7.9,-2.32153024911033,-33.4897267659824)) ;
#147318 = CARTESIAN_POINT('Origin',(7.9,2.6,-33.5814213562373)) ;
#147319 = CARTESIAN_POINT('Origin',(7.9,2.4,-33.5814213562373)) ;
#147320 = CARTESIAN_POINT('Origin',(7.9,-2.15,-33.3868804065906)) ;
#147321 = CARTESIAN_POINT('Origin',(7.9,-2.35,-33.3868804065906)) ;
#147322 = CARTESIAN_POINT('Origin',(7.9,2.4,-33.5814213562373)) ;
#147323 = CARTESIAN_POINT('Origin',(7.9,2.4,-33.69)) ;
#147324 = CARTESIAN_POINT('Origin',(7.9,-2.35,-32.74)) ;
#147325 = CARTESIAN_POINT('Origin',(7.9,-2.35,-32.74)) ;
#147326 = CARTESIAN_POINT('Origin',(7.9,2.4,-33.69)) ;
#147327 = CARTESIAN_POINT('Origin',(7.9,2.4,-33.69)) ;
#147328 = CARTESIAN_POINT('Origin',(7.9,-2.15,-32.74)) ;
#147329 = CARTESIAN_POINT('Origin',(7.9,-2.15,-32.54)) ;
#147330 = CARTESIAN_POINT('Origin',(7.9,2.4,-33.69)) ;
#147331 = CARTESIAN_POINT('Origin',(7.9,2.1,-33.69)) ;
#147332 = CARTESIAN_POINT('Origin',(7.9,1.9,-32.54)) ;
#147333 = CARTESIAN_POINT('Origin',(7.9,1.9,-32.54)) ;
#147334 = CARTESIAN_POINT('Origin',(7.9,2.1,-33.69)) ;
#147335 = CARTESIAN_POINT('Origin',(7.9,2.1,-33.69)) ;
#147336 = CARTESIAN_POINT('Origin',(7.9,1.9,-32.74)) ;
#147337 = CARTESIAN_POINT('Origin',(7.9,2.1,-32.74)) ;
#147338 = CARTESIAN_POINT('Origin',(7.9,2.1,-32.74)) ;
#147339 = CARTESIAN_POINT('Origin',(7.9,2.1,-31.08)) ;
#147340 = CARTESIAN_POINT('Origin',(7.9,2.4,-31.08)) ;
#147341 = CARTESIAN_POINT('Origin',(7.9,2.1,-31.08)) ;
#147342 = CARTESIAN_POINT('Origin',(7.9,2.4,-31.08)) ;
#147343 = CARTESIAN_POINT('Origin',(7.9,2.4,-31.08)) ;
#147344 = CARTESIAN_POINT('Origin',(7.9,2.1,-31.08)) ;
#147345 = CARTESIAN_POINT('Origin',(7.9,2.1,-31.08)) ;
#147346 = CARTESIAN_POINT('Origin',(7.9,2.4,-31.08)) ;
#147347 = CARTESIAN_POINT('Origin',(7.9,2.4,-31.1885786437627)) ;
#147348 = CARTESIAN_POINT('Origin',(7.9,2.1,-31.08)) ;
#147349 = CARTESIAN_POINT('Origin',(7.9,2.1,-32.03)) ;
#147350 = CARTESIAN_POINT('Origin',(7.9,2.6,-31.1885786437627)) ;
#147351 = CARTESIAN_POINT('Origin',(7.9,2.45857864376269,-31.33)) ;
#147352 = CARTESIAN_POINT('Origin',(7.9,1.9,-32.03)) ;
#147353 = CARTESIAN_POINT('Origin',(7.9,1.9,-32.23)) ;
#147354 = CARTESIAN_POINT('Origin',(7.9,2.45857864376269,-31.33)) ;
#147355 = CARTESIAN_POINT('Origin',(7.9,1.9,-32.23)) ;
#147356 = CARTESIAN_POINT('Origin',(7.9,-2.15,-32.23)) ;
#147357 = CARTESIAN_POINT('Origin',(7.9,-2.15,-32.03)) ;
#147358 = CARTESIAN_POINT('Origin',(7.9,-2.35,-32.03)) ;
#147359 = CARTESIAN_POINT('Origin',(7.9,3.35,-31.7385786437627)) ;
#147360 = CARTESIAN_POINT('Origin',(7.9,3.35,-29.2214213562373)) ;
#147361 = CARTESIAN_POINT('Origin',(7.9,-2.35,-31.3831195934094)) ;
#147362 = CARTESIAN_POINT('Origin',(7.9,-2.35,-31.3831195934094)) ;
#147363 = CARTESIAN_POINT('Origin',(7.9,3.15,-29.2214213562373)) ;
#147364 = CARTESIAN_POINT('Origin',(7.9,3.00857864376269,-29.08)) ;
#147365 = CARTESIAN_POINT('Origin',(7.9,-2.15,-31.3831195934094)) ;
#147366 = CARTESIAN_POINT('Origin',(7.9,-2.32153024911032,-31.2802732340176)) ;
#147367 = CARTESIAN_POINT('Origin',(7.9,3.00857864376269,-29.08)) ;
#147368 = CARTESIAN_POINT('Origin',(7.9,2.45857864376269,-29.63)) ;
#147369 = CARTESIAN_POINT('Origin',(7.9,-3.65625,-30.48)) ;
#147370 = CARTESIAN_POINT('Origin',(7.9,-2.32153024911032,-29.6797267659824)) ;
#147371 = CARTESIAN_POINT('Origin',(7.9,2.6,-29.7714213562373)) ;
#147372 = CARTESIAN_POINT('Origin',(7.9,2.4,-29.7714213562373)) ;
#147373 = CARTESIAN_POINT('Origin',(7.9,-2.15,-29.5768804065906)) ;
#147374 = CARTESIAN_POINT('Origin',(7.9,-2.35,-29.5768804065906)) ;
#147375 = CARTESIAN_POINT('Origin',(7.9,2.4,-29.7714213562373)) ;
#147376 = CARTESIAN_POINT('Origin',(7.9,2.4,-29.88)) ;
#147377 = CARTESIAN_POINT('Origin',(7.9,-2.35,-28.93)) ;
#147378 = CARTESIAN_POINT('Origin',(7.9,-2.35,-28.93)) ;
#147379 = CARTESIAN_POINT('Origin',(7.9,2.4,-29.88)) ;
#147380 = CARTESIAN_POINT('Origin',(7.9,2.4,-29.88)) ;
#147381 = CARTESIAN_POINT('Origin',(7.9,-2.15,-28.93)) ;
#147382 = CARTESIAN_POINT('Origin',(7.9,-2.15,-28.73)) ;
#147383 = CARTESIAN_POINT('Origin',(7.9,2.4,-29.88)) ;
#147384 = CARTESIAN_POINT('Origin',(7.9,2.1,-29.88)) ;
#147385 = CARTESIAN_POINT('Origin',(7.9,1.9,-28.73)) ;
#147386 = CARTESIAN_POINT('Origin',(7.9,1.9,-28.73)) ;
#147387 = CARTESIAN_POINT('Origin',(7.9,2.1,-29.88)) ;
#147388 = CARTESIAN_POINT('Origin',(7.9,2.1,-29.88)) ;
#147389 = CARTESIAN_POINT('Origin',(7.9,1.9,-28.93)) ;
#147390 = CARTESIAN_POINT('Origin',(7.9,2.1,-28.93)) ;
#147391 = CARTESIAN_POINT('Origin',(7.9,2.1,-28.93)) ;
#147392 = CARTESIAN_POINT('Origin',(7.9,2.1,-27.27)) ;
#147393 = CARTESIAN_POINT('Origin',(7.9,2.4,-27.27)) ;
#147394 = CARTESIAN_POINT('Origin',(7.9,2.1,-27.27)) ;
#147395 = CARTESIAN_POINT('Origin',(7.9,2.4,-27.27)) ;
#147396 = CARTESIAN_POINT('Origin',(7.9,2.4,-27.27)) ;
#147397 = CARTESIAN_POINT('Origin',(7.9,2.1,-27.27)) ;
#147398 = CARTESIAN_POINT('Origin',(7.9,2.1,-27.27)) ;
#147399 = CARTESIAN_POINT('Origin',(7.9,2.4,-27.27)) ;
#147400 = CARTESIAN_POINT('Origin',(7.9,2.4,-27.3785786437627)) ;
#147401 = CARTESIAN_POINT('Origin',(7.9,2.1,-27.27)) ;
#147402 = CARTESIAN_POINT('Origin',(7.9,2.1,-28.22)) ;
#147403 = CARTESIAN_POINT('Origin',(7.9,2.6,-27.3785786437627)) ;
#147404 = CARTESIAN_POINT('Origin',(7.9,2.45857864376269,-27.52)) ;
#147405 = CARTESIAN_POINT('Origin',(7.9,1.9,-28.22)) ;
#147406 = CARTESIAN_POINT('Origin',(7.9,1.9,-28.42)) ;
#147407 = CARTESIAN_POINT('Origin',(7.9,2.45857864376269,-27.52)) ;
#147408 = CARTESIAN_POINT('Origin',(7.9,1.9,-28.42)) ;
#147409 = CARTESIAN_POINT('Origin',(7.9,-2.15,-28.42)) ;
#147410 = CARTESIAN_POINT('Origin',(7.9,-2.15,-28.22)) ;
#147411 = CARTESIAN_POINT('Origin',(7.9,-2.35,-28.22)) ;
#147412 = CARTESIAN_POINT('Origin',(7.9,3.35,-27.9285786437627)) ;
#147413 = CARTESIAN_POINT('Origin',(7.9,3.35,-25.4114213562373)) ;
#147414 = CARTESIAN_POINT('Origin',(7.9,-2.35,-27.5731195934094)) ;
#147415 = CARTESIAN_POINT('Origin',(7.9,-2.35,-27.5731195934094)) ;
#147416 = CARTESIAN_POINT('Origin',(7.9,3.15,-25.4114213562373)) ;
#147417 = CARTESIAN_POINT('Origin',(7.9,3.00857864376269,-25.27)) ;
#147418 = CARTESIAN_POINT('Origin',(7.9,-2.15,-27.5731195934094)) ;
#147419 = CARTESIAN_POINT('Origin',(7.9,-2.32153024911032,-27.4702732340176)) ;
#147420 = CARTESIAN_POINT('Origin',(7.9,3.00857864376269,-25.27)) ;
#147421 = CARTESIAN_POINT('Origin',(7.9,2.45857864376269,-25.82)) ;
#147422 = CARTESIAN_POINT('Origin',(7.9,-3.65625,-26.67)) ;
#147423 = CARTESIAN_POINT('Origin',(7.9,-2.32153024911032,-25.8697267659824)) ;
#147424 = CARTESIAN_POINT('Origin',(7.9,2.6,-25.9614213562373)) ;
#147425 = CARTESIAN_POINT('Origin',(7.9,2.4,-25.9614213562373)) ;
#147426 = CARTESIAN_POINT('Origin',(7.9,-2.15,-25.7668804065906)) ;
#147427 = CARTESIAN_POINT('Origin',(7.9,-2.35,-25.7668804065906)) ;
#147428 = CARTESIAN_POINT('Origin',(7.9,2.4,-25.9614213562373)) ;
#147429 = CARTESIAN_POINT('Origin',(7.9,2.4,-26.07)) ;
#147430 = CARTESIAN_POINT('Origin',(7.9,-2.35,-25.12)) ;
#147431 = CARTESIAN_POINT('Origin',(7.9,-2.35,-25.12)) ;
#147432 = CARTESIAN_POINT('Origin',(7.9,2.4,-26.07)) ;
#147433 = CARTESIAN_POINT('Origin',(7.9,2.4,-26.07)) ;
#147434 = CARTESIAN_POINT('Origin',(7.9,-2.15,-25.12)) ;
#147435 = CARTESIAN_POINT('Origin',(7.9,-2.15,-24.92)) ;
#147436 = CARTESIAN_POINT('Origin',(7.9,2.4,-26.07)) ;
#147437 = CARTESIAN_POINT('Origin',(7.9,2.1,-26.07)) ;
#147438 = CARTESIAN_POINT('Origin',(7.9,1.9,-24.92)) ;
#147439 = CARTESIAN_POINT('Origin',(7.9,1.9,-24.92)) ;
#147440 = CARTESIAN_POINT('Origin',(7.9,2.1,-26.07)) ;
#147441 = CARTESIAN_POINT('Origin',(7.9,2.1,-26.07)) ;
#147442 = CARTESIAN_POINT('Origin',(7.9,1.9,-25.12)) ;
#147443 = CARTESIAN_POINT('Origin',(7.9,2.1,-25.12)) ;
#147444 = CARTESIAN_POINT('Origin',(7.9,2.1,-25.12)) ;
#147445 = CARTESIAN_POINT('Origin',(7.9,2.1,-23.46)) ;
#147446 = CARTESIAN_POINT('Origin',(7.9,2.4,-23.46)) ;
#147447 = CARTESIAN_POINT('Origin',(7.9,2.1,-23.46)) ;
#147448 = CARTESIAN_POINT('Origin',(7.9,2.4,-23.46)) ;
#147449 = CARTESIAN_POINT('Origin',(7.9,2.4,-23.46)) ;
#147450 = CARTESIAN_POINT('Origin',(7.9,2.1,-23.46)) ;
#147451 = CARTESIAN_POINT('Origin',(7.9,2.1,-23.46)) ;
#147452 = CARTESIAN_POINT('Origin',(7.9,2.4,-23.46)) ;
#147453 = CARTESIAN_POINT('Origin',(7.9,2.4,-23.5685786437627)) ;
#147454 = CARTESIAN_POINT('Origin',(7.9,2.1,-23.46)) ;
#147455 = CARTESIAN_POINT('Origin',(7.9,2.1,-24.41)) ;
#147456 = CARTESIAN_POINT('Origin',(7.9,2.6,-23.5685786437627)) ;
#147457 = CARTESIAN_POINT('Origin',(7.9,2.45857864376269,-23.71)) ;
#147458 = CARTESIAN_POINT('Origin',(7.9,1.9,-24.41)) ;
#147459 = CARTESIAN_POINT('Origin',(7.9,1.9,-24.61)) ;
#147460 = CARTESIAN_POINT('Origin',(7.9,2.45857864376269,-23.71)) ;
#147461 = CARTESIAN_POINT('Origin',(7.9,1.9,-24.61)) ;
#147462 = CARTESIAN_POINT('Origin',(7.9,-2.15,-24.61)) ;
#147463 = CARTESIAN_POINT('Origin',(7.9,-2.15,-24.41)) ;
#147464 = CARTESIAN_POINT('Origin',(7.9,-2.35,-24.41)) ;
#147465 = CARTESIAN_POINT('Origin',(7.9,3.35,-24.1185786437627)) ;
#147466 = CARTESIAN_POINT('Origin',(7.9,3.35,-21.6014213562373)) ;
#147467 = CARTESIAN_POINT('Origin',(7.9,-2.35,-23.7631195934094)) ;
#147468 = CARTESIAN_POINT('Origin',(7.9,-2.35,-23.7631195934094)) ;
#147469 = CARTESIAN_POINT('Origin',(7.9,3.15,-21.6014213562373)) ;
#147470 = CARTESIAN_POINT('Origin',(7.9,3.00857864376269,-21.46)) ;
#147471 = CARTESIAN_POINT('Origin',(7.9,-2.15,-23.7631195934094)) ;
#147472 = CARTESIAN_POINT('Origin',(7.9,-2.32153024911032,-23.6602732340176)) ;
#147473 = CARTESIAN_POINT('Origin',(7.9,3.00857864376269,-21.46)) ;
#147474 = CARTESIAN_POINT('Origin',(7.9,2.45857864376269,-22.01)) ;
#147475 = CARTESIAN_POINT('Origin',(7.9,-3.65625,-22.86)) ;
#147476 = CARTESIAN_POINT('Origin',(7.9,-2.32153024911032,-22.0597267659824)) ;
#147477 = CARTESIAN_POINT('Origin',(7.9,2.6,-22.1514213562373)) ;
#147478 = CARTESIAN_POINT('Origin',(7.9,2.4,-22.1514213562373)) ;
#147479 = CARTESIAN_POINT('Origin',(7.9,-2.15,-21.9568804065906)) ;
#147480 = CARTESIAN_POINT('Origin',(7.9,-2.35,-21.9568804065906)) ;
#147481 = CARTESIAN_POINT('Origin',(7.9,2.4,-22.1514213562373)) ;
#147482 = CARTESIAN_POINT('Origin',(7.9,2.4,-22.26)) ;
#147483 = CARTESIAN_POINT('Origin',(7.9,-2.35,-21.31)) ;
#147484 = CARTESIAN_POINT('Origin',(7.9,-2.35,-21.31)) ;
#147485 = CARTESIAN_POINT('Origin',(7.9,2.4,-22.26)) ;
#147486 = CARTESIAN_POINT('Origin',(7.9,2.4,-22.26)) ;
#147487 = CARTESIAN_POINT('Origin',(7.9,-2.15,-21.31)) ;
#147488 = CARTESIAN_POINT('Origin',(7.9,-2.15,-21.11)) ;
#147489 = CARTESIAN_POINT('Origin',(7.9,2.4,-22.26)) ;
#147490 = CARTESIAN_POINT('Origin',(7.9,2.1,-22.26)) ;
#147491 = CARTESIAN_POINT('Origin',(7.9,1.9,-21.11)) ;
#147492 = CARTESIAN_POINT('Origin',(7.9,1.9,-21.11)) ;
#147493 = CARTESIAN_POINT('Origin',(7.9,2.1,-22.26)) ;
#147494 = CARTESIAN_POINT('Origin',(7.9,2.1,-22.26)) ;
#147495 = CARTESIAN_POINT('Origin',(7.9,1.9,-21.31)) ;
#147496 = CARTESIAN_POINT('Origin',(7.9,2.1,-21.31)) ;
#147497 = CARTESIAN_POINT('Origin',(7.9,2.1,-21.31)) ;
#147498 = CARTESIAN_POINT('Origin',(7.9,2.1,-19.65)) ;
#147499 = CARTESIAN_POINT('Origin',(7.9,2.4,-19.65)) ;
#147500 = CARTESIAN_POINT('Origin',(7.9,2.1,-19.65)) ;
#147501 = CARTESIAN_POINT('Origin',(7.9,2.4,-19.65)) ;
#147502 = CARTESIAN_POINT('Origin',(7.9,2.4,-19.65)) ;
#147503 = CARTESIAN_POINT('Origin',(7.9,2.1,-19.65)) ;
#147504 = CARTESIAN_POINT('Origin',(7.9,2.1,-19.65)) ;
#147505 = CARTESIAN_POINT('Origin',(7.9,2.4,-19.65)) ;
#147506 = CARTESIAN_POINT('Origin',(7.9,2.4,-19.7585786437627)) ;
#147507 = CARTESIAN_POINT('Origin',(7.9,2.1,-19.65)) ;
#147508 = CARTESIAN_POINT('Origin',(7.9,2.1,-20.6)) ;
#147509 = CARTESIAN_POINT('Origin',(7.9,2.6,-19.7585786437627)) ;
#147510 = CARTESIAN_POINT('Origin',(7.9,2.45857864376269,-19.9)) ;
#147511 = CARTESIAN_POINT('Origin',(7.9,1.9,-20.6)) ;
#147512 = CARTESIAN_POINT('Origin',(7.9,1.9,-20.8)) ;
#147513 = CARTESIAN_POINT('Origin',(7.9,2.45857864376269,-19.9)) ;
#147514 = CARTESIAN_POINT('Origin',(7.9,1.9,-20.8)) ;
#147515 = CARTESIAN_POINT('Origin',(7.9,-2.15,-20.8)) ;
#147516 = CARTESIAN_POINT('Origin',(7.9,-2.15,-20.6)) ;
#147517 = CARTESIAN_POINT('Origin',(7.9,-2.35,-20.6)) ;
#147518 = CARTESIAN_POINT('Origin',(7.9,3.35,-20.3085786437627)) ;
#147519 = CARTESIAN_POINT('Origin',(7.9,3.35,-17.7914213562373)) ;
#147520 = CARTESIAN_POINT('Origin',(7.9,-2.35,-19.9531195934094)) ;
#147521 = CARTESIAN_POINT('Origin',(7.9,-2.35,-19.9531195934094)) ;
#147522 = CARTESIAN_POINT('Origin',(7.9,3.15,-17.7914213562373)) ;
#147523 = CARTESIAN_POINT('Origin',(7.9,3.00857864376269,-17.65)) ;
#147524 = CARTESIAN_POINT('Origin',(7.9,-2.15,-19.9531195934094)) ;
#147525 = CARTESIAN_POINT('Origin',(7.9,-2.32153024911032,-19.8502732340176)) ;
#147526 = CARTESIAN_POINT('Origin',(7.9,3.00857864376269,-17.65)) ;
#147527 = CARTESIAN_POINT('Origin',(7.9,2.45857864376269,-18.2)) ;
#147528 = CARTESIAN_POINT('Origin',(7.9,-3.65625,-19.05)) ;
#147529 = CARTESIAN_POINT('Origin',(7.9,-2.32153024911032,-18.2497267659824)) ;
#147530 = CARTESIAN_POINT('Origin',(7.9,2.6,-18.3414213562373)) ;
#147531 = CARTESIAN_POINT('Origin',(7.9,2.4,-18.3414213562373)) ;
#147532 = CARTESIAN_POINT('Origin',(7.9,-2.15,-18.1468804065906)) ;
#147533 = CARTESIAN_POINT('Origin',(7.9,-2.35,-18.1468804065906)) ;
#147534 = CARTESIAN_POINT('Origin',(7.9,2.4,-18.3414213562373)) ;
#147535 = CARTESIAN_POINT('Origin',(7.9,2.4,-18.45)) ;
#147536 = CARTESIAN_POINT('Origin',(7.9,-2.35,-17.5)) ;
#147537 = CARTESIAN_POINT('Origin',(7.9,-2.35,-17.5)) ;
#147538 = CARTESIAN_POINT('Origin',(7.9,2.4,-18.45)) ;
#147539 = CARTESIAN_POINT('Origin',(7.9,2.4,-18.45)) ;
#147540 = CARTESIAN_POINT('Origin',(7.9,-2.15,-17.5)) ;
#147541 = CARTESIAN_POINT('Origin',(7.9,-2.15,-17.3)) ;
#147542 = CARTESIAN_POINT('Origin',(7.9,2.4,-18.45)) ;
#147543 = CARTESIAN_POINT('Origin',(7.9,2.1,-18.45)) ;
#147544 = CARTESIAN_POINT('Origin',(7.9,1.9,-17.3)) ;
#147545 = CARTESIAN_POINT('Origin',(7.9,1.9,-17.3)) ;
#147546 = CARTESIAN_POINT('Origin',(7.9,2.1,-18.45)) ;
#147547 = CARTESIAN_POINT('Origin',(7.9,2.1,-18.45)) ;
#147548 = CARTESIAN_POINT('Origin',(7.9,1.9,-17.5)) ;
#147549 = CARTESIAN_POINT('Origin',(7.9,2.1,-17.5)) ;
#147550 = CARTESIAN_POINT('Origin',(7.9,2.1,-17.5)) ;
#147551 = CARTESIAN_POINT('Origin',(7.9,2.1,-15.84)) ;
#147552 = CARTESIAN_POINT('Origin',(7.9,2.4,-15.84)) ;
#147553 = CARTESIAN_POINT('Origin',(7.9,2.1,-15.84)) ;
#147554 = CARTESIAN_POINT('Origin',(7.9,2.4,-15.84)) ;
#147555 = CARTESIAN_POINT('Origin',(7.9,2.4,-15.84)) ;
#147556 = CARTESIAN_POINT('Origin',(7.9,2.1,-15.84)) ;
#147557 = CARTESIAN_POINT('Origin',(7.9,2.1,-15.84)) ;
#147558 = CARTESIAN_POINT('Origin',(7.9,2.4,-15.84)) ;
#147559 = CARTESIAN_POINT('Origin',(7.9,2.4,-15.9485786437627)) ;
#147560 = CARTESIAN_POINT('Origin',(7.9,2.1,-15.84)) ;
#147561 = CARTESIAN_POINT('Origin',(7.9,2.1,-16.79)) ;
#147562 = CARTESIAN_POINT('Origin',(7.9,2.6,-15.9485786437627)) ;
#147563 = CARTESIAN_POINT('Origin',(7.9,2.45857864376269,-16.09)) ;
#147564 = CARTESIAN_POINT('Origin',(7.9,1.9,-16.79)) ;
#147565 = CARTESIAN_POINT('Origin',(7.9,1.9,-16.99)) ;
#147566 = CARTESIAN_POINT('Origin',(7.9,2.45857864376269,-16.09)) ;
#147567 = CARTESIAN_POINT('Origin',(7.9,1.9,-16.99)) ;
#147568 = CARTESIAN_POINT('Origin',(7.9,-2.15,-16.99)) ;
#147569 = CARTESIAN_POINT('Origin',(7.9,-2.15,-16.79)) ;
#147570 = CARTESIAN_POINT('Origin',(7.9,-2.35,-16.79)) ;
#147571 = CARTESIAN_POINT('Origin',(7.9,3.35,-16.4985786437627)) ;
#147572 = CARTESIAN_POINT('Origin',(7.9,3.35,-13.9814213562373)) ;
#147573 = CARTESIAN_POINT('Origin',(7.9,-2.35,-16.1431195934094)) ;
#147574 = CARTESIAN_POINT('Origin',(7.9,-2.35,-16.1431195934094)) ;
#147575 = CARTESIAN_POINT('Origin',(7.9,3.15,-13.9814213562373)) ;
#147576 = CARTESIAN_POINT('Origin',(7.9,3.00857864376269,-13.84)) ;
#147577 = CARTESIAN_POINT('Origin',(7.9,-2.15,-16.1431195934094)) ;
#147578 = CARTESIAN_POINT('Origin',(7.9,-2.32153024911032,-16.0402732340176)) ;
#147579 = CARTESIAN_POINT('Origin',(7.9,3.00857864376269,-13.84)) ;
#147580 = CARTESIAN_POINT('Origin',(7.9,2.45857864376269,-14.39)) ;
#147581 = CARTESIAN_POINT('Origin',(7.9,-3.65625,-15.24)) ;
#147582 = CARTESIAN_POINT('Origin',(7.9,-2.32153024911032,-14.4397267659824)) ;
#147583 = CARTESIAN_POINT('Origin',(7.9,2.6,-14.5314213562373)) ;
#147584 = CARTESIAN_POINT('Origin',(7.9,2.4,-14.5314213562373)) ;
#147585 = CARTESIAN_POINT('Origin',(7.9,-2.15,-14.3368804065906)) ;
#147586 = CARTESIAN_POINT('Origin',(7.9,-2.35,-14.3368804065906)) ;
#147587 = CARTESIAN_POINT('Origin',(7.9,2.4,-14.5314213562373)) ;
#147588 = CARTESIAN_POINT('Origin',(7.9,2.4,-14.64)) ;
#147589 = CARTESIAN_POINT('Origin',(7.9,-2.35,-13.69)) ;
#147590 = CARTESIAN_POINT('Origin',(7.9,-2.35,-13.69)) ;
#147591 = CARTESIAN_POINT('Origin',(7.9,2.4,-14.64)) ;
#147592 = CARTESIAN_POINT('Origin',(7.9,2.4,-14.64)) ;
#147593 = CARTESIAN_POINT('Origin',(7.9,-2.15,-13.69)) ;
#147594 = CARTESIAN_POINT('Origin',(7.9,-2.15,-13.49)) ;
#147595 = CARTESIAN_POINT('Origin',(7.9,2.4,-14.64)) ;
#147596 = CARTESIAN_POINT('Origin',(7.9,2.1,-14.64)) ;
#147597 = CARTESIAN_POINT('Origin',(7.9,1.9,-13.49)) ;
#147598 = CARTESIAN_POINT('Origin',(7.9,1.9,-13.49)) ;
#147599 = CARTESIAN_POINT('Origin',(7.9,2.1,-14.64)) ;
#147600 = CARTESIAN_POINT('Origin',(7.9,2.1,-14.64)) ;
#147601 = CARTESIAN_POINT('Origin',(7.9,1.9,-13.69)) ;
#147602 = CARTESIAN_POINT('Origin',(7.9,2.1,-13.69)) ;
#147603 = CARTESIAN_POINT('Origin',(7.9,2.1,-13.69)) ;
#147604 = CARTESIAN_POINT('Origin',(7.9,2.1,-12.03)) ;
#147605 = CARTESIAN_POINT('Origin',(7.9,2.4,-12.03)) ;
#147606 = CARTESIAN_POINT('Origin',(7.9,2.1,-12.03)) ;
#147607 = CARTESIAN_POINT('Origin',(7.9,2.4,-12.03)) ;
#147608 = CARTESIAN_POINT('Origin',(7.9,2.4,-12.03)) ;
#147609 = CARTESIAN_POINT('Origin',(7.9,2.1,-12.03)) ;
#147610 = CARTESIAN_POINT('Origin',(7.9,2.1,-12.03)) ;
#147611 = CARTESIAN_POINT('Origin',(7.9,2.4,-12.03)) ;
#147612 = CARTESIAN_POINT('Origin',(7.9,2.4,-12.1385786437627)) ;
#147613 = CARTESIAN_POINT('Origin',(7.9,2.1,-12.03)) ;
#147614 = CARTESIAN_POINT('Origin',(7.9,2.1,-12.98)) ;
#147615 = CARTESIAN_POINT('Origin',(7.9,2.6,-12.1385786437627)) ;
#147616 = CARTESIAN_POINT('Origin',(7.9,2.45857864376269,-12.28)) ;
#147617 = CARTESIAN_POINT('Origin',(7.9,1.9,-12.98)) ;
#147618 = CARTESIAN_POINT('Origin',(7.9,1.9,-13.18)) ;
#147619 = CARTESIAN_POINT('Origin',(7.9,2.45857864376269,-12.28)) ;
#147620 = CARTESIAN_POINT('Origin',(7.9,1.9,-13.18)) ;
#147621 = CARTESIAN_POINT('Origin',(7.9,-2.15,-13.18)) ;
#147622 = CARTESIAN_POINT('Origin',(7.9,-2.15,-12.98)) ;
#147623 = CARTESIAN_POINT('Origin',(7.9,-2.35,-12.98)) ;
#147624 = CARTESIAN_POINT('Origin',(7.9,3.35,-12.6885786437627)) ;
#147625 = CARTESIAN_POINT('Origin',(7.9,3.35,-10.1714213562373)) ;
#147626 = CARTESIAN_POINT('Origin',(7.9,-2.35,-12.3331195934094)) ;
#147627 = CARTESIAN_POINT('Origin',(7.9,-2.35,-12.3331195934094)) ;
#147628 = CARTESIAN_POINT('Origin',(7.9,3.15,-10.1714213562373)) ;
#147629 = CARTESIAN_POINT('Origin',(7.9,3.00857864376269,-10.03)) ;
#147630 = CARTESIAN_POINT('Origin',(7.9,-2.15,-12.3331195934094)) ;
#147631 = CARTESIAN_POINT('Origin',(7.9,-2.32153024911032,-12.2302732340176)) ;
#147632 = CARTESIAN_POINT('Origin',(7.9,3.00857864376269,-10.03)) ;
#147633 = CARTESIAN_POINT('Origin',(7.9,2.45857864376269,-10.58)) ;
#147634 = CARTESIAN_POINT('Origin',(7.9,-3.65625,-11.43)) ;
#147635 = CARTESIAN_POINT('Origin',(7.9,-2.32153024911032,-10.6297267659824)) ;
#147636 = CARTESIAN_POINT('Origin',(7.9,2.6,-10.7214213562373)) ;
#147637 = CARTESIAN_POINT('Origin',(7.9,2.4,-10.7214213562373)) ;
#147638 = CARTESIAN_POINT('Origin',(7.9,-2.15,-10.5268804065906)) ;
#147639 = CARTESIAN_POINT('Origin',(7.9,-2.35,-10.5268804065906)) ;
#147640 = CARTESIAN_POINT('Origin',(7.9,2.4,-10.7214213562373)) ;
#147641 = CARTESIAN_POINT('Origin',(7.9,2.4,-10.83)) ;
#147642 = CARTESIAN_POINT('Origin',(7.9,-2.35,-9.88)) ;
#147643 = CARTESIAN_POINT('Origin',(7.9,-2.35,-9.88)) ;
#147644 = CARTESIAN_POINT('Origin',(7.9,2.4,-10.83)) ;
#147645 = CARTESIAN_POINT('Origin',(7.9,2.4,-10.83)) ;
#147646 = CARTESIAN_POINT('Origin',(7.9,-2.15,-9.88)) ;
#147647 = CARTESIAN_POINT('Origin',(7.9,-2.15,-9.68)) ;
#147648 = CARTESIAN_POINT('Origin',(7.9,2.4,-10.83)) ;
#147649 = CARTESIAN_POINT('Origin',(7.9,2.1,-10.83)) ;
#147650 = CARTESIAN_POINT('Origin',(7.9,1.9,-9.68)) ;
#147651 = CARTESIAN_POINT('Origin',(7.9,1.9,-9.68)) ;
#147652 = CARTESIAN_POINT('Origin',(7.9,2.1,-10.83)) ;
#147653 = CARTESIAN_POINT('Origin',(7.9,2.1,-10.83)) ;
#147654 = CARTESIAN_POINT('Origin',(7.9,1.9,-9.88)) ;
#147655 = CARTESIAN_POINT('Origin',(7.9,2.1,-9.88)) ;
#147656 = CARTESIAN_POINT('Origin',(7.9,2.1,-9.88)) ;
#147657 = CARTESIAN_POINT('Origin',(7.9,2.1,-8.22)) ;
#147658 = CARTESIAN_POINT('Origin',(7.9,2.4,-8.22)) ;
#147659 = CARTESIAN_POINT('Origin',(7.9,2.1,-8.22)) ;
#147660 = CARTESIAN_POINT('Origin',(7.9,2.4,-8.22)) ;
#147661 = CARTESIAN_POINT('Origin',(7.9,2.4,-8.22)) ;
#147662 = CARTESIAN_POINT('Origin',(7.9,2.1,-8.22)) ;
#147663 = CARTESIAN_POINT('Origin',(7.9,2.1,-8.22)) ;
#147664 = CARTESIAN_POINT('Origin',(7.9,2.4,-8.22)) ;
#147665 = CARTESIAN_POINT('Origin',(7.9,2.4,-8.32857864376269)) ;
#147666 = CARTESIAN_POINT('Origin',(7.9,2.1,-8.22)) ;
#147667 = CARTESIAN_POINT('Origin',(7.9,2.1,-9.17)) ;
#147668 = CARTESIAN_POINT('Origin',(7.9,2.6,-8.32857864376269)) ;
#147669 = CARTESIAN_POINT('Origin',(7.9,2.45857864376269,-8.47)) ;
#147670 = CARTESIAN_POINT('Origin',(7.9,1.9,-9.17)) ;
#147671 = CARTESIAN_POINT('Origin',(7.9,1.9,-9.37)) ;
#147672 = CARTESIAN_POINT('Origin',(7.9,2.45857864376269,-8.47)) ;
#147673 = CARTESIAN_POINT('Origin',(7.9,1.9,-9.37)) ;
#147674 = CARTESIAN_POINT('Origin',(7.9,-2.15,-9.37)) ;
#147675 = CARTESIAN_POINT('Origin',(7.9,-2.15,-9.17)) ;
#147676 = CARTESIAN_POINT('Origin',(7.9,-2.35,-9.17)) ;
#147677 = CARTESIAN_POINT('Origin',(7.9,3.35,-8.87857864376269)) ;
#147678 = CARTESIAN_POINT('Origin',(7.9,3.35,-6.36142135623731)) ;
#147679 = CARTESIAN_POINT('Origin',(7.9,-2.35,-8.52311959340942)) ;
#147680 = CARTESIAN_POINT('Origin',(7.9,-2.35,-8.52311959340942)) ;
#147681 = CARTESIAN_POINT('Origin',(7.9,3.15,-6.36142135623731)) ;
#147682 = CARTESIAN_POINT('Origin',(7.9,3.00857864376269,-6.22)) ;
#147683 = CARTESIAN_POINT('Origin',(7.9,-2.15,-8.52311959340942)) ;
#147684 = CARTESIAN_POINT('Origin',(7.9,-2.32153024911032,-8.4202732340176)) ;
#147685 = CARTESIAN_POINT('Origin',(7.9,3.00857864376269,-6.22)) ;
#147686 = CARTESIAN_POINT('Origin',(7.9,2.45857864376269,-6.77)) ;
#147687 = CARTESIAN_POINT('Origin',(7.9,-3.65625,-7.62)) ;
#147688 = CARTESIAN_POINT('Origin',(7.9,-2.32153024911032,-6.8197267659824)) ;
#147689 = CARTESIAN_POINT('Origin',(7.9,2.6,-6.91142135623731)) ;
#147690 = CARTESIAN_POINT('Origin',(7.9,2.4,-6.91142135623731)) ;
#147691 = CARTESIAN_POINT('Origin',(7.9,-2.15,-6.71688040659058)) ;
#147692 = CARTESIAN_POINT('Origin',(7.9,-2.35,-6.71688040659058)) ;
#147693 = CARTESIAN_POINT('Origin',(7.9,2.4,-6.91142135623731)) ;
#147694 = CARTESIAN_POINT('Origin',(7.9,2.4,-7.02)) ;
#147695 = CARTESIAN_POINT('Origin',(7.9,-2.35,-6.07)) ;
#147696 = CARTESIAN_POINT('Origin',(7.9,-2.35,-6.07)) ;
#147697 = CARTESIAN_POINT('Origin',(7.9,2.4,-7.02)) ;
#147698 = CARTESIAN_POINT('Origin',(7.9,2.4,-7.02)) ;
#147699 = CARTESIAN_POINT('Origin',(7.9,-2.15,-6.07)) ;
#147700 = CARTESIAN_POINT('Origin',(7.9,-2.15,-5.87)) ;
#147701 = CARTESIAN_POINT('Origin',(7.9,2.4,-7.02)) ;
#147702 = CARTESIAN_POINT('Origin',(7.9,2.1,-7.02)) ;
#147703 = CARTESIAN_POINT('Origin',(7.9,1.9,-5.87)) ;
#147704 = CARTESIAN_POINT('Origin',(7.9,1.9,-5.87)) ;
#147705 = CARTESIAN_POINT('Origin',(7.9,2.1,-7.02)) ;
#147706 = CARTESIAN_POINT('Origin',(7.9,2.1,-7.02)) ;
#147707 = CARTESIAN_POINT('Origin',(7.9,1.9,-6.07)) ;
#147708 = CARTESIAN_POINT('Origin',(7.9,2.1,-6.07)) ;
#147709 = CARTESIAN_POINT('Origin',(7.9,2.1,-6.07)) ;
#147710 = CARTESIAN_POINT('Origin',(7.9,2.1,-4.41)) ;
#147711 = CARTESIAN_POINT('Origin',(7.9,2.4,-4.41)) ;
#147712 = CARTESIAN_POINT('Origin',(7.9,2.1,-4.41)) ;
#147713 = CARTESIAN_POINT('Origin',(7.9,2.4,-4.41)) ;
#147714 = CARTESIAN_POINT('Origin',(7.9,2.4,-4.41)) ;
#147715 = CARTESIAN_POINT('Origin',(7.9,2.1,-4.41)) ;
#147716 = CARTESIAN_POINT('Origin',(7.9,2.1,-4.41)) ;
#147717 = CARTESIAN_POINT('Origin',(7.9,2.4,-4.41)) ;
#147718 = CARTESIAN_POINT('Origin',(7.9,2.4,-4.51857864376269)) ;
#147719 = CARTESIAN_POINT('Origin',(7.9,2.1,-4.41)) ;
#147720 = CARTESIAN_POINT('Origin',(7.9,2.1,-5.36)) ;
#147721 = CARTESIAN_POINT('Origin',(7.9,2.6,-4.51857864376269)) ;
#147722 = CARTESIAN_POINT('Origin',(7.9,2.45857864376269,-4.66)) ;
#147723 = CARTESIAN_POINT('Origin',(7.9,1.9,-5.36)) ;
#147724 = CARTESIAN_POINT('Origin',(7.9,1.9,-5.56)) ;
#147725 = CARTESIAN_POINT('Origin',(7.9,2.45857864376269,-4.66)) ;
#147726 = CARTESIAN_POINT('Origin',(7.9,1.9,-5.56)) ;
#147727 = CARTESIAN_POINT('Origin',(7.9,-2.15,-5.56)) ;
#147728 = CARTESIAN_POINT('Origin',(7.9,-2.15,-5.36)) ;
#147729 = CARTESIAN_POINT('Origin',(7.9,-2.35,-5.36)) ;
#147730 = CARTESIAN_POINT('Origin',(7.9,3.35,-5.06857864376269)) ;
#147731 = CARTESIAN_POINT('Origin',(7.9,3.35,-2.55142135623731)) ;
#147732 = CARTESIAN_POINT('Origin',(7.9,-2.35,-4.71311959340942)) ;
#147733 = CARTESIAN_POINT('Origin',(7.9,-2.35,-4.71311959340942)) ;
#147734 = CARTESIAN_POINT('Origin',(7.9,3.15,-2.55142135623731)) ;
#147735 = CARTESIAN_POINT('Origin',(7.9,3.00857864376269,-2.41)) ;
#147736 = CARTESIAN_POINT('Origin',(7.9,-2.15,-4.71311959340942)) ;
#147737 = CARTESIAN_POINT('Origin',(7.9,-2.32153024911032,-4.6102732340176)) ;
#147738 = CARTESIAN_POINT('Origin',(7.9,3.00857864376269,-2.41)) ;
#147739 = CARTESIAN_POINT('Origin',(7.9,2.45857864376269,-2.96)) ;
#147740 = CARTESIAN_POINT('Origin',(7.9,-3.65625,-3.81)) ;
#147741 = CARTESIAN_POINT('Origin',(7.9,-2.32153024911032,-3.0097267659824)) ;
#147742 = CARTESIAN_POINT('Origin',(7.9,2.6,-3.10142135623731)) ;
#147743 = CARTESIAN_POINT('Origin',(7.9,2.4,-3.10142135623731)) ;
#147744 = CARTESIAN_POINT('Origin',(7.9,-2.15,-2.90688040659058)) ;
#147745 = CARTESIAN_POINT('Origin',(7.9,-2.35,-2.90688040659058)) ;
#147746 = CARTESIAN_POINT('Origin',(7.9,2.4,-3.10142135623731)) ;
#147747 = CARTESIAN_POINT('Origin',(7.9,2.4,-3.21)) ;
#147748 = CARTESIAN_POINT('Origin',(7.9,-2.35,-2.26)) ;
#147749 = CARTESIAN_POINT('Origin',(7.9,-2.35,-2.26)) ;
#147750 = CARTESIAN_POINT('Origin',(7.9,2.4,-3.21)) ;
#147751 = CARTESIAN_POINT('Origin',(7.9,2.4,-3.21)) ;
#147752 = CARTESIAN_POINT('Origin',(7.9,-2.15,-2.26)) ;
#147753 = CARTESIAN_POINT('Origin',(7.9,-2.15,-2.06)) ;
#147754 = CARTESIAN_POINT('Origin',(7.9,2.4,-3.21)) ;
#147755 = CARTESIAN_POINT('Origin',(7.9,2.1,-3.21)) ;
#147756 = CARTESIAN_POINT('Origin',(7.9,1.9,-2.06)) ;
#147757 = CARTESIAN_POINT('Origin',(7.9,1.9,-2.06)) ;
#147758 = CARTESIAN_POINT('Origin',(7.9,2.1,-3.21)) ;
#147759 = CARTESIAN_POINT('Origin',(7.9,2.1,-3.21)) ;
#147760 = CARTESIAN_POINT('Origin',(7.9,1.9,-2.26)) ;
#147761 = CARTESIAN_POINT('Origin',(7.9,2.1,-2.26)) ;
#147762 = CARTESIAN_POINT('Origin',(7.9,2.1,-2.26)) ;
#147763 = CARTESIAN_POINT('Origin',(-0.899999999999999,-2.,-7.02)) ;
#147764 = CARTESIAN_POINT('Origin',(-0.899999999999999,0.4,-7.02)) ;
#147765 = CARTESIAN_POINT('Origin',(-0.899999999999999,-1.9,-7.02)) ;
#147766 = CARTESIAN_POINT('Origin',(0.600000000000001,0.4,-7.22)) ;
#147767 = CARTESIAN_POINT('Origin',(0.500000000000001,0.4,-7.22)) ;
#147768 = CARTESIAN_POINT('Origin',(-0.899999999999999,0.4,-7.22)) ;
#147769 = CARTESIAN_POINT('Origin',(0.500000000000001,0.4,-7.22)) ;
#147770 = CARTESIAN_POINT('',(0.600000000000001,0.4,-7.22)) ;
#147771 = CARTESIAN_POINT('Origin',(0.500000000000001,0.4,-7.22)) ;
#147772 = CARTESIAN_POINT('Origin',(0.500000000000001,0.4,-7.22)) ;
#147773 = CARTESIAN_POINT('Origin',(-0.899999999999999,-1.9,-7.02)) ;
#147774 = CARTESIAN_POINT('Origin',(-0.899999999999999,-1.9,-7.02)) ;
#147775 = CARTESIAN_POINT('Origin',(-0.899999999999999,-1.9,-7.02)) ;
#147776 = CARTESIAN_POINT('Origin',(-0.899999999999999,0.4,-7.22)) ;
#147777 = CARTESIAN_POINT('Origin',(-0.899999999999999,0.6,-7.22)) ;
#147778 = CARTESIAN_POINT('Origin',(0.500000000000001,0.4,-7.62)) ;
#147779 = CARTESIAN_POINT('Origin',(0.500000000000001,0.4,-8.02)) ;
#147780 = CARTESIAN_POINT('',(0.600000000000001,0.4,-7.92)) ;
#147781 = CARTESIAN_POINT('Ctrl Pts',(0.595612997216081,0.370705721320404,
-7.9907057213204)) ;
#147782 = CARTESIAN_POINT('Ctrl Pts',(0.596180587760891,0.372558268494353,
-7.98885549883217)) ;
#147783 = CARTESIAN_POINT('Ctrl Pts',(0.596672461925684,0.374355839771976,
-7.98691417986632)) ;
#147784 = CARTESIAN_POINT('Ctrl Pts',(0.599015141889213,0.383869350930064,
-7.97576499365627)) ;
#147785 = CARTESIAN_POINT('Ctrl Pts',(0.599609996542524,0.390224332900447,
-7.96497260265412)) ;
#147786 = CARTESIAN_POINT('Ctrl Pts',(0.600050586298725,0.398117439141558,
-7.94233105320469)) ;
#147787 = CARTESIAN_POINT('Ctrl Pts',(0.600000000000001,0.399999999999999,
-7.93120125063353)) ;
#147788 = CARTESIAN_POINT('Ctrl Pts',(0.600000000000001,0.399999999999999,
-7.92)) ;
#147789 = CARTESIAN_POINT('',(0.600000000000001,0.4,-7.62)) ;
#147790 = CARTESIAN_POINT('Origin',(0.500000000000001,-4.5664044441154E-17,
-7.22)) ;
#147791 = CARTESIAN_POINT('',(0.500000000000001,0.394987437106619,-7.32)) ;
#147792 = CARTESIAN_POINT('Ctrl Pts',(0.500000000000001,0.394987437106619,
-7.32)) ;
#147793 = CARTESIAN_POINT('Ctrl Pts',(0.505940567948952,0.3955844866499,-7.32)) ;
#147794 = CARTESIAN_POINT('Ctrl Pts',(0.51193197101914,0.396132036079018,
-7.31946630032796)) ;
#147795 = CARTESIAN_POINT('Ctrl Pts',(0.517829015308548,0.396618246075354,
-7.31839779577372)) ;
#147796 = CARTESIAN_POINT('Ctrl Pts',(0.522982218721201,0.397043126556053,
-7.31746407015711)) ;
#147797 = CARTESIAN_POINT('Ctrl Pts',(0.52806264897023,0.397421319341388,
-7.31612282679706)) ;
#147798 = CARTESIAN_POINT('Ctrl Pts',(0.532978106724,0.397751505046071,-7.31440574387663)) ;
#147799 = CARTESIAN_POINT('Ctrl Pts',(0.538583536338966,0.398128038182999,
-7.31244763784955)) ;
#147800 = CARTESIAN_POINT('Ctrl Pts',(0.544059405914893,0.398447721828296,
-7.30997000831105)) ;
#147801 = CARTESIAN_POINT('Ctrl Pts',(0.549268572255785,0.398712331108984,
-7.30702073194289)) ;
#147802 = CARTESIAN_POINT('Ctrl Pts',(0.553856850427149,0.398945401221756,
-7.30442298414684)) ;
#147803 = CARTESIAN_POINT('Ctrl Pts',(0.558237825069329,0.399135987683843,
-7.30146038497999)) ;
#147804 = CARTESIAN_POINT('Ctrl Pts',(0.562333836086214,0.399290378266507,
-7.29819522286417)) ;
#147805 = CARTESIAN_POINT('Ctrl Pts',(0.566990328957901,0.399465895042381,
-7.2944832689523)) ;
#147806 = CARTESIAN_POINT('Ctrl Pts',(0.571349096493437,0.399597278936107,
-7.29032280648479)) ;
#147807 = CARTESIAN_POINT('Ctrl Pts',(0.57529692005673,0.399694832180838,
-7.28580557597932)) ;
#147808 = CARTESIAN_POINT('Ctrl Pts',(0.578744263667919,0.399780018245914,
-7.28186101121506)) ;
#147809 = CARTESIAN_POINT('Ctrl Pts',(0.581878314560434,0.399839626289636,
-7.2776455218421)) ;
#147810 = CARTESIAN_POINT('Ctrl Pts',(0.584648147334856,0.399882153365958,
-7.27324181770729)) ;
#147811 = CARTESIAN_POINT('Ctrl Pts',(0.587839270208173,0.399931148788079,
-7.2681683125045)) ;
#147812 = CARTESIAN_POINT('Ctrl Pts',(0.590595054415089,0.399958289583404,
-7.26276663624446)) ;
#147813 = CARTESIAN_POINT('Ctrl Pts',(0.5928386189431,0.399974357003159,-7.2571616850094)) ;
#147814 = CARTESIAN_POINT('Ctrl Pts',(0.594777336851653,0.399988241245861,
-7.2523183122424)) ;
#147815 = CARTESIAN_POINT('Ctrl Pts',(0.596334051506188,0.399993946552814,
-7.24732416622713)) ;
#147816 = CARTESIAN_POINT('Ctrl Pts',(0.597488309822308,0.39999684570125,
-7.24227171856839)) ;
#147817 = CARTESIAN_POINT('Ctrl Pts',(0.598804024094406,0.400000150378306,
-7.23651254196053)) ;
#147818 = CARTESIAN_POINT('Ctrl Pts',(0.599612685195437,0.399999963509465,
-7.23060284389055)) ;
#147819 = CARTESIAN_POINT('Ctrl Pts',(0.599890230999724,0.399999993975383,
-7.224684202261)) ;
#147820 = CARTESIAN_POINT('Ctrl Pts',(0.599963464549401,0.400000002014155,
-7.22312250278977)) ;
#147821 = CARTESIAN_POINT('Ctrl Pts',(0.600000000000001,0.399999999999999,
-7.22156022150916)) ;
#147822 = CARTESIAN_POINT('Ctrl Pts',(0.600000000000001,0.399999999999999,
-7.22)) ;
#147823 = CARTESIAN_POINT('',(0.600000000000001,0.299999999999999,-7.22)) ;
#147824 = CARTESIAN_POINT('Ctrl Pts',(0.500000000000001,0.394987437106619,
-7.32)) ;
#147825 = CARTESIAN_POINT('Ctrl Pts',(0.500454935589846,0.395033159853749,
-7.32)) ;
#147826 = CARTESIAN_POINT('Ctrl Pts',(0.500909898680472,0.39507857032906,
-7.31999689549112)) ;
#147827 = CARTESIAN_POINT('Ctrl Pts',(0.502892456245169,0.39527507588909,
-7.31996983394194)) ;
#147828 = CARTESIAN_POINT('Ctrl Pts',(0.504418747482366,0.395422812032198,
-7.31991398542099)) ;
#147829 = CARTESIAN_POINT('Ctrl Pts',(0.508462199543345,0.395804395682033,
-7.31967328105664)) ;
#147830 = CARTESIAN_POINT('Ctrl Pts',(0.510974953343295,0.396031485023317,
-7.31942793914506)) ;
#147831 = CARTESIAN_POINT('Ctrl Pts',(0.521160739721272,0.396903453186235,
-7.31804279449156)) ;
#147832 = CARTESIAN_POINT('Ctrl Pts',(0.528708678528402,0.397444933153161,
-7.31610421770469)) ;
#147833 = CARTESIAN_POINT('Ctrl Pts',(0.545943206358073,0.398105551684108,
-7.30946463945115)) ;
#147834 = CARTESIAN_POINT('Ctrl Pts',(0.555229535466813,0.397987646678431,
-7.30403535883597)) ;
#147835 = CARTESIAN_POINT('Ctrl Pts',(0.571394604995744,0.395490482808038,
-7.29077551336386)) ;
#147836 = CARTESIAN_POINT('Ctrl Pts',(0.578055313702842,0.39319894869835,
-7.28324074563176)) ;
#147837 = CARTESIAN_POINT('Ctrl Pts',(0.588559132202514,0.385442756729305,
-7.26739223398403)) ;
#147838 = CARTESIAN_POINT('Ctrl Pts',(0.592167355639978,0.380240075126892,
-7.2595482656068)) ;
#147839 = CARTESIAN_POINT('Ctrl Pts',(0.597496615531108,0.365892753466966,
-7.24392552179528)) ;
#147840 = CARTESIAN_POINT('Ctrl Pts',(0.598734255154202,0.356660564300668,
-7.23677274172691)) ;
#147841 = CARTESIAN_POINT('Ctrl Pts',(0.600012754681688,0.335223914398549,
-7.22558230586562)) ;
#147842 = CARTESIAN_POINT('Ctrl Pts',(0.59999390055981,0.322655037091896,
-7.22166151936558)) ;
#147843 = CARTESIAN_POINT('Ctrl Pts',(0.600000296204999,0.30610691358235,
-7.22013962634704)) ;
#147844 = CARTESIAN_POINT('Ctrl Pts',(0.600000000000001,0.303050992413436,
-7.22)) ;
#147845 = CARTESIAN_POINT('Ctrl Pts',(0.600000000000001,0.299999999999999,
-7.22)) ;
#147846 = CARTESIAN_POINT('',(0.600000000000001,-2.39800009914439E-17,-7.22)) ;
#147847 = CARTESIAN_POINT('Origin',(0.500000000000001,-1.9,-7.22)) ;
#147848 = CARTESIAN_POINT('Origin',(0.600000000000001,-1.9,-7.02)) ;
#147849 = CARTESIAN_POINT('Origin',(0.500000000000001,-1.9,-7.02)) ;
#147850 = CARTESIAN_POINT('Origin',(-0.899999999999999,-1.9,-6.245)) ;
#147851 = CARTESIAN_POINT('Origin',(-0.899999999999999,-1.9,-6.345)) ;
#147852 = CARTESIAN_POINT('Origin',(-0.899999999999999,0.6,-7.12)) ;
#147853 = CARTESIAN_POINT('Origin',(-0.899999999999999,0.6,-8.02)) ;
#147854 = CARTESIAN_POINT('Origin',(0.600000000000001,0.4,-8.02)) ;
#147855 = CARTESIAN_POINT('Origin',(0.500000000000001,0.4,-8.02)) ;
#147856 = CARTESIAN_POINT('Origin',(-0.899999999999999,0.4,-8.02)) ;
#147857 = CARTESIAN_POINT('Origin',(0.500000000000001,0.4,-8.02)) ;
#147858 = CARTESIAN_POINT('Origin',(0.500000000000001,-1.9,-7.02)) ;
#147859 = CARTESIAN_POINT('Origin',(0.500000000000001,-2.1,-7.02)) ;
#147860 = CARTESIAN_POINT('Origin',(-0.899999999999999,-1.9,-6.345)) ;
#147861 = CARTESIAN_POINT('Origin',(-1.1,-1.9,-6.345)) ;
#147862 = CARTESIAN_POINT('Origin',(-0.899999999999999,-2.1,-6.345)) ;
#147863 = CARTESIAN_POINT('Origin',(-0.899999999999999,0.4,-8.02)) ;
#147864 = CARTESIAN_POINT('Origin',(-0.899999999999999,0.4,-8.22)) ;
#147865 = CARTESIAN_POINT('Origin',(0.500000000000001,-2.1,-7.62)) ;
#147866 = CARTESIAN_POINT('Origin',(0.500000000000001,-2.1,-6.345)) ;
#147867 = CARTESIAN_POINT('Origin',(0.600000000000001,-2.1,-6.345)) ;
#147868 = CARTESIAN_POINT('Origin',(0.500000000000001,-2.1,-6.345)) ;
#147869 = CARTESIAN_POINT('Origin',(-1.1,-4.42727195005761E-17,-6.345)) ;
#147870 = CARTESIAN_POINT('',(-1.1,1.15,-6.245)) ;
#147871 = CARTESIAN_POINT('',(-1.1,1.25,-6.245)) ;
#147872 = CARTESIAN_POINT('Origin',(-1.1,1.15,-6.345)) ;
#147873 = CARTESIAN_POINT('Origin',(-0.899999999999999,0.5,-8.22)) ;
#147874 = CARTESIAN_POINT('Origin',(-0.899999999999999,-1.9,-8.22)) ;
#147875 = CARTESIAN_POINT('Origin',(0.600000000000001,-1.9,-8.22)) ;
#147876 = CARTESIAN_POINT('Origin',(0.500000000000001,-1.9,-8.22)) ;
#147877 = CARTESIAN_POINT('Origin',(-0.899999999999999,-1.9,-8.22)) ;
#147878 = CARTESIAN_POINT('Origin',(0.500000000000001,-1.9,-8.22)) ;
#147879 = CARTESIAN_POINT('Origin',(0.500000000000001,-2.1,-8.22)) ;
#147880 = CARTESIAN_POINT('Origin',(0.500000000000001,-2.1,-6.345)) ;
#147881 = CARTESIAN_POINT('Origin',(0.500000000000001,-2.1,-6.345)) ;
#147882 = CARTESIAN_POINT('Origin',(-1.1,-2.9,-6.145)) ;
#147883 = CARTESIAN_POINT('Origin',(-1.1,-2.9,-6.145)) ;
#147884 = CARTESIAN_POINT('Origin',(-1.1,-2.9,-6.145)) ;
#147885 = CARTESIAN_POINT('Origin',(-1.1,1.25,-6.145)) ;
#147886 = CARTESIAN_POINT('Origin',(-1.1,1.15,-6.145)) ;
#147887 = CARTESIAN_POINT('Origin',(-1.1,1.15,-6.345)) ;
#147888 = CARTESIAN_POINT('',(-1.1,1.25,-6.345)) ;
#147889 = CARTESIAN_POINT('Origin',(-1.1,1.15,-6.345)) ;
#147890 = CARTESIAN_POINT('Origin',(-1.1,1.15,-6.345)) ;
#147891 = CARTESIAN_POINT('Origin',(-0.899999999999999,-1.9,-8.22)) ;
#147892 = CARTESIAN_POINT('Origin',(-0.899999999999999,-1.9,-8.22)) ;
#147893 = CARTESIAN_POINT('Origin',(0.500000000000001,-2.1,-7.62)) ;
#147894 = CARTESIAN_POINT('Origin',(0.500000000000001,-2.1,-8.895)) ;
#147895 = CARTESIAN_POINT('Origin',(0.500000000000001,1.36481920536411E-16,
-6.345)) ;
#147896 = CARTESIAN_POINT('Origin',(0.500000000000001,-2.9,-6.345)) ;
#147897 = CARTESIAN_POINT('Origin',(-0.999999999999999,-2.9,-6.145)) ;
#147898 = CARTESIAN_POINT('Origin',(0.500000000000001,-2.9,-6.145)) ;
#147899 = CARTESIAN_POINT('Origin',(-1.1,1.15,-6.345)) ;
#147900 = CARTESIAN_POINT('Origin',(-1.1,1.35,-6.345)) ;
#147901 = CARTESIAN_POINT('Origin',(-1.1,1.15,-7.62)) ;
#147902 = CARTESIAN_POINT('',(-1.1,1.25,-8.895)) ;
#147903 = CARTESIAN_POINT('',(-1.1,1.25,-8.995)) ;
#147904 = CARTESIAN_POINT('Origin',(-1.1,1.15,-8.895)) ;
#147905 = CARTESIAN_POINT('Origin',(-0.899999999999999,-1.9,-8.12)) ;
#147906 = CARTESIAN_POINT('Origin',(-0.899999999999999,-1.9,-8.895)) ;
#147907 = CARTESIAN_POINT('Origin',(-0.999999999999999,-2.1,-8.895)) ;
#147908 = CARTESIAN_POINT('Origin',(0.500000000000001,-2.1,-8.895)) ;
#147909 = CARTESIAN_POINT('Origin',(-0.899999999999999,-2.1,-8.895)) ;
#147910 = CARTESIAN_POINT('Origin',(0.500000000000001,-2.1,-8.895)) ;
#147911 = CARTESIAN_POINT('Origin',(0.500000000000001,-2.1,-8.895)) ;
#147912 = CARTESIAN_POINT('Origin',(0.500000000000001,-2.9,-6.345)) ;
#147913 = CARTESIAN_POINT('Origin',(0.700000000000002,-2.9,-6.345)) ;
#147914 = CARTESIAN_POINT('Origin',(-1.1,1.35,-8.995)) ;
#147915 = CARTESIAN_POINT('Origin',(-1.1,1.35,-8.895)) ;
#147916 = CARTESIAN_POINT('Origin',(-1.1,1.15,-8.895)) ;
#147917 = CARTESIAN_POINT('',(-1.1,1.15,-8.995)) ;
#147918 = CARTESIAN_POINT('Origin',(-1.1,1.15,-8.895)) ;
#147919 = CARTESIAN_POINT('Origin',(-1.1,1.15,-8.895)) ;
#147920 = CARTESIAN_POINT('Origin',(-0.899999999999999,-1.9,-8.895)) ;
#147921 = CARTESIAN_POINT('Origin',(-1.1,-1.9,-8.895)) ;
#147922 = CARTESIAN_POINT('Origin',(0.500000000000001,-5.86744705109802E-17,
-8.895)) ;
#147923 = CARTESIAN_POINT('Origin',(0.500000000000001,-2.9,-8.895)) ;
#147924 = CARTESIAN_POINT('Origin',(0.700000000000002,-2.9,-7.62)) ;
#147925 = CARTESIAN_POINT('Origin',(0.700000000000002,-2.9,-8.895)) ;
#147926 = CARTESIAN_POINT('Origin',(-1.1,1.15,-8.895)) ;
#147927 = CARTESIAN_POINT('Origin',(-1.1,1.15,-9.095)) ;
#147928 = CARTESIAN_POINT('Origin',(-1.1,-2.39429110547967E-16,-8.895)) ;
#147929 = CARTESIAN_POINT('',(-1.1,1.25,-8.995)) ;
#147930 = CARTESIAN_POINT('Origin',(0.500000000000001,-2.9,-8.895)) ;
#147931 = CARTESIAN_POINT('Origin',(0.500000000000001,-2.9,-9.095)) ;
#147932 = CARTESIAN_POINT('Origin',(-1.1,1.25,-9.095)) ;
#147933 = CARTESIAN_POINT('Origin',(-1.1,-2.9,-9.095)) ;
#147934 = CARTESIAN_POINT('Origin',(-1.1,-2.9,-9.095)) ;
#147935 = CARTESIAN_POINT('Origin',(-1.1,-2.9,-9.095)) ;
#147936 = CARTESIAN_POINT('Origin',(-1.1,-2.9,-9.095)) ;
#147937 = CARTESIAN_POINT('Origin',(1.5,1.9,-7.02)) ;
#147938 = CARTESIAN_POINT('Origin',(1.5,1.9,-9.17)) ;
#147939 = CARTESIAN_POINT('Origin',(1.5,1.9,-8.22)) ;
#147940 = CARTESIAN_POINT('Origin',(1.5,2.1,-8.22)) ;
#147941 = CARTESIAN_POINT('Origin',(1.5,2.1,-8.02)) ;
#147942 = CARTESIAN_POINT('Origin',(1.5,1.9,-9.17)) ;
#147943 = CARTESIAN_POINT('Origin',(1.5,1.9,-9.17)) ;
#147944 = CARTESIAN_POINT('Origin',(1.5,2.1,-8.02)) ;
#147945 = CARTESIAN_POINT('Origin',(1.5,2.4,-8.02)) ;
#147946 = CARTESIAN_POINT('Origin',(1.5,2.1,-9.17)) ;
#147947 = CARTESIAN_POINT('Origin',(1.5,-2.15,-9.17)) ;
#147948 = CARTESIAN_POINT('Origin',(1.5,2.4,-8.22)) ;
#147949 = CARTESIAN_POINT('Origin',(1.5,2.6,-8.22)) ;
#147950 = CARTESIAN_POINT('Origin',(1.5,-2.15,-9.17)) ;
#147951 = CARTESIAN_POINT('Origin',(1.5,-2.15,-9.17)) ;
#147952 = CARTESIAN_POINT('Origin',(1.5,2.6,-7.02)) ;
#147953 = CARTESIAN_POINT('Origin',(1.5,2.6,-8.32857864376269)) ;
#147954 = CARTESIAN_POINT('Origin',(1.5,-2.15,-7.02)) ;
#147955 = CARTESIAN_POINT('Origin',(1.5,-2.15,-8.52311959340942)) ;
#147956 = CARTESIAN_POINT('Origin',(1.5,2.6,-8.32857864376269)) ;
#147957 = CARTESIAN_POINT('Origin',(1.5,2.6,-8.32857864376269)) ;
#147958 = CARTESIAN_POINT('Origin',(1.5,-2.15,-8.52311959340942)) ;
#147959 = CARTESIAN_POINT('Origin',(1.5,-2.15,-8.52311959340942)) ;
#147960 = CARTESIAN_POINT('Origin',(1.5,1.69571067811865,-7.42428932188135)) ;
#147961 = CARTESIAN_POINT('Origin',(1.5,3.15,-8.87857864376269)) ;
#147962 = CARTESIAN_POINT('Origin',(1.5,-3.65625,-7.62)) ;
#147963 = CARTESIAN_POINT('Origin',(1.5,-2.15,-6.71688040659058)) ;
#147964 = CARTESIAN_POINT('Origin',(1.5,3.15,-8.87857864376269)) ;
#147965 = CARTESIAN_POINT('Origin',(1.5,3.15,-8.87857864376269)) ;
#147966 = CARTESIAN_POINT('Origin',(1.5,-2.15,-6.71688040659058)) ;
#147967 = CARTESIAN_POINT('Origin',(1.5,-2.15,-6.71688040659058)) ;
#147968 = CARTESIAN_POINT('Origin',(1.5,3.15,-7.02)) ;
#147969 = CARTESIAN_POINT('Origin',(1.5,-2.15,-7.02)) ;
#147970 = CARTESIAN_POINT('Origin',(1.5,-2.15,-6.07)) ;
#147971 = CARTESIAN_POINT('Origin',(1.5,-2.15,-6.07)) ;
#147972 = CARTESIAN_POINT('Origin',(1.5,-2.15,-6.07)) ;
#147973 = CARTESIAN_POINT('Origin',(1.5,2.29571067811866,-7.21571067811866)) ;
#147974 = CARTESIAN_POINT('Origin',(1.5,2.6,-6.91142135623731)) ;
#147975 = CARTESIAN_POINT('Origin',(1.5,2.1,-6.07)) ;
#147976 = CARTESIAN_POINT('Origin',(1.5,1.9,-6.07)) ;
#147977 = CARTESIAN_POINT('Origin',(1.5,2.6,-6.91142135623731)) ;
#147978 = CARTESIAN_POINT('Origin',(1.5,2.6,-6.91142135623731)) ;
#147979 = CARTESIAN_POINT('Origin',(1.5,1.9,-6.07)) ;
#147980 = CARTESIAN_POINT('Origin',(1.5,1.9,-6.07)) ;
#147981 = CARTESIAN_POINT('Origin',(1.5,2.6,-7.02)) ;
#147982 = CARTESIAN_POINT('Origin',(1.5,2.6,-7.02)) ;
#147983 = CARTESIAN_POINT('Origin',(1.5,1.9,-7.02)) ;
#147984 = CARTESIAN_POINT('Origin',(1.5,1.9,-7.02)) ;
#147985 = CARTESIAN_POINT('Origin',(1.5,2.4,-7.02)) ;
#147986 = CARTESIAN_POINT('Origin',(1.5,2.4,-7.22)) ;
#147987 = CARTESIAN_POINT('Origin',(1.5,2.1,-7.02)) ;
#147988 = CARTESIAN_POINT('Origin',(1.5,2.1,-7.22)) ;
#147989 = CARTESIAN_POINT('Origin',(1.5,2.1,-7.22)) ;
#147990 = CARTESIAN_POINT('Origin',(-0.899999999999999,-2.,-10.83)) ;
#147991 = CARTESIAN_POINT('Origin',(-0.899999999999999,0.4,-10.83)) ;
#147992 = CARTESIAN_POINT('Origin',(-0.899999999999999,-1.9,-10.83)) ;
#147993 = CARTESIAN_POINT('Origin',(0.600000000000001,0.4,-11.03)) ;
#147994 = CARTESIAN_POINT('Origin',(0.500000000000001,0.4,-11.03)) ;
#147995 = CARTESIAN_POINT('Origin',(-0.899999999999999,0.4,-11.03)) ;
#147996 = CARTESIAN_POINT('Origin',(0.500000000000001,0.4,-11.03)) ;
#147997 = CARTESIAN_POINT('',(0.600000000000001,0.4,-11.03)) ;
#147998 = CARTESIAN_POINT('Origin',(0.500000000000001,0.4,-11.03)) ;
#147999 = CARTESIAN_POINT('Origin',(0.500000000000001,0.4,-11.03)) ;
#148000 = CARTESIAN_POINT('Origin',(-0.899999999999999,-1.9,-10.83)) ;
#148001 = CARTESIAN_POINT('Origin',(-0.899999999999999,-1.9,-10.83)) ;
#148002 = CARTESIAN_POINT('Origin',(-0.899999999999999,-1.9,-10.83)) ;
#148003 = CARTESIAN_POINT('Origin',(-0.899999999999999,0.4,-11.03)) ;
#148004 = CARTESIAN_POINT('Origin',(-0.899999999999999,0.6,-11.03)) ;
#148005 = CARTESIAN_POINT('Origin',(0.500000000000001,0.4,-11.43)) ;
#148006 = CARTESIAN_POINT('Origin',(0.500000000000001,0.4,-11.83)) ;
#148007 = CARTESIAN_POINT('',(0.600000000000001,0.4,-11.73)) ;
#148008 = CARTESIAN_POINT('Ctrl Pts',(0.595612997216082,0.370705721320405,
-11.8007057213204)) ;
#148009 = CARTESIAN_POINT('Ctrl Pts',(0.596180587760892,0.372558268494355,
-11.7988554988322)) ;
#148010 = CARTESIAN_POINT('Ctrl Pts',(0.596672461925685,0.374355839771978,
-11.7969141798663)) ;
#148011 = CARTESIAN_POINT('Ctrl Pts',(0.599015141889211,0.383869350930053,
-11.7857649936563)) ;
#148012 = CARTESIAN_POINT('Ctrl Pts',(0.599609996542523,0.390224332900442,
-11.7749726026541)) ;
#148013 = CARTESIAN_POINT('Ctrl Pts',(0.600050586298725,0.398117439141559,
-11.7523310532047)) ;
#148014 = CARTESIAN_POINT('Ctrl Pts',(0.600000000000001,0.399999999999999,
-11.7412012506335)) ;
#148015 = CARTESIAN_POINT('Ctrl Pts',(0.600000000000001,0.399999999999999,
-11.73)) ;
#148016 = CARTESIAN_POINT('',(0.600000000000001,0.4,-11.43)) ;
#148017 = CARTESIAN_POINT('Origin',(0.500000000000001,-4.56640444411542E-17,
-11.03)) ;
#148018 = CARTESIAN_POINT('',(0.500000000000001,0.394987437106619,-11.13)) ;
#148019 = CARTESIAN_POINT('Ctrl Pts',(0.500000000000001,0.394987437106619,
-11.13)) ;
#148020 = CARTESIAN_POINT('Ctrl Pts',(0.505940567948954,0.395584486649901,
-11.13)) ;
#148021 = CARTESIAN_POINT('Ctrl Pts',(0.511931971019137,0.396132036079018,
-11.129466300328)) ;
#148022 = CARTESIAN_POINT('Ctrl Pts',(0.51782901530855,0.396618246075355,
-11.1283977957737)) ;
#148023 = CARTESIAN_POINT('Ctrl Pts',(0.522982218721202,0.397043126556054,
-11.1274640701571)) ;
#148024 = CARTESIAN_POINT('Ctrl Pts',(0.528062648970239,0.397421319341388,
-11.1261228267971)) ;
#148025 = CARTESIAN_POINT('Ctrl Pts',(0.532978106724003,0.397751505046071,
-11.1244057438766)) ;
#148026 = CARTESIAN_POINT('Ctrl Pts',(0.538583536338951,0.398128038182998,
-11.1224476378496)) ;
#148027 = CARTESIAN_POINT('Ctrl Pts',(0.544059405914855,0.398447721828294,
-11.1199700083111)) ;
#148028 = CARTESIAN_POINT('Ctrl Pts',(0.549268572255748,0.398712331108982,
-11.1170207319429)) ;
#148029 = CARTESIAN_POINT('Ctrl Pts',(0.553856850427136,0.398945401221755,
-11.1144229841468)) ;
#148030 = CARTESIAN_POINT('Ctrl Pts',(0.558237825069313,0.399135987683842,
-11.11146038498)) ;
#148031 = CARTESIAN_POINT('Ctrl Pts',(0.562333836086205,0.399290378266507,
-11.1081952228642)) ;
#148032 = CARTESIAN_POINT('Ctrl Pts',(0.566990328957881,0.399465895042381,
-11.1044832689523)) ;
#148033 = CARTESIAN_POINT('Ctrl Pts',(0.571349096493411,0.399597278936107,
-11.1003228064848)) ;
#148034 = CARTESIAN_POINT('Ctrl Pts',(0.575296920056702,0.399694832180837,
-11.0958055759794)) ;
#148035 = CARTESIAN_POINT('Ctrl Pts',(0.578744263667896,0.399780018245913,
-11.0918610112151)) ;
#148036 = CARTESIAN_POINT('Ctrl Pts',(0.581878314560452,0.399839626289636,
-11.0876455218421)) ;
#148037 = CARTESIAN_POINT('Ctrl Pts',(0.584648147334861,0.399882153365958,
-11.0832418177073)) ;
#148038 = CARTESIAN_POINT('Ctrl Pts',(0.587839270208171,0.399931148788079,
-11.0781683125045)) ;
#148039 = CARTESIAN_POINT('Ctrl Pts',(0.590595054415094,0.399958289583404,
-11.0727666362445)) ;
#148040 = CARTESIAN_POINT('Ctrl Pts',(0.59283861894311,0.399974357003159,
-11.0671616850094)) ;
#148041 = CARTESIAN_POINT('Ctrl Pts',(0.594777336851653,0.399988241245861,
-11.0623183122424)) ;
#148042 = CARTESIAN_POINT('Ctrl Pts',(0.596334051506183,0.399993946552814,
-11.0573241662271)) ;
#148043 = CARTESIAN_POINT('Ctrl Pts',(0.597488309822303,0.39999684570125,
-11.0522717185684)) ;
#148044 = CARTESIAN_POINT('Ctrl Pts',(0.598804024094406,0.400000150378306,
-11.0465125419605)) ;
#148045 = CARTESIAN_POINT('Ctrl Pts',(0.599612685195435,0.399999963509465,
-11.0406028438906)) ;
#148046 = CARTESIAN_POINT('Ctrl Pts',(0.599890230999722,0.399999993975383,
-11.034684202261)) ;
#148047 = CARTESIAN_POINT('Ctrl Pts',(0.5999634645494,0.400000002014155,-11.0331225027898)) ;
#148048 = CARTESIAN_POINT('Ctrl Pts',(0.600000000000001,0.399999999999999,
-11.0315602215092)) ;
#148049 = CARTESIAN_POINT('Ctrl Pts',(0.600000000000001,0.399999999999999,
-11.03)) ;
#148050 = CARTESIAN_POINT('',(0.600000000000001,0.299999999999999,-11.03)) ;
#148051 = CARTESIAN_POINT('Ctrl Pts',(0.500000000000001,0.394987437106619,
-11.13)) ;
#148052 = CARTESIAN_POINT('Ctrl Pts',(0.50045493559049,0.395033159853814,
-11.13)) ;
#148053 = CARTESIAN_POINT('Ctrl Pts',(0.500909898680794,0.395078570329092,
-11.1299968954911)) ;
#148054 = CARTESIAN_POINT('Ctrl Pts',(0.502892456245032,0.395275075889076,
-11.1299698339419)) ;
#148055 = CARTESIAN_POINT('Ctrl Pts',(0.504418747482277,0.395422812032189,
-11.129913985421)) ;
#148056 = CARTESIAN_POINT('Ctrl Pts',(0.508462199543281,0.395804395682027,
-11.1296732810566)) ;
#148057 = CARTESIAN_POINT('Ctrl Pts',(0.510974953343229,0.396031485023311,
-11.1294279391451)) ;
#148058 = CARTESIAN_POINT('Ctrl Pts',(0.521160739721084,0.396903453186219,
-11.1280427944916)) ;
#148059 = CARTESIAN_POINT('Ctrl Pts',(0.528708678528227,0.397444933153154,
-11.1261042177048)) ;
#148060 = CARTESIAN_POINT('Ctrl Pts',(0.545943206357832,0.398105551684098,
-11.1194646394512)) ;
#148061 = CARTESIAN_POINT('Ctrl Pts',(0.555229535466621,0.397987646678464,
-11.1140353588361)) ;
#148062 = CARTESIAN_POINT('Ctrl Pts',(0.571394604995555,0.395490482808064,
-11.100775513364)) ;
#148063 = CARTESIAN_POINT('Ctrl Pts',(0.57805531370272,0.393198948698444,
-11.093240745632)) ;
#148064 = CARTESIAN_POINT('Ctrl Pts',(0.588559132202387,0.385442756729392,
-11.0773922339842)) ;
#148065 = CARTESIAN_POINT('Ctrl Pts',(0.592167355639922,0.380240075127053,
-11.069548265607)) ;
#148066 = CARTESIAN_POINT('Ctrl Pts',(0.597496615531038,0.36589275346714,
-11.0539255217955)) ;
#148067 = CARTESIAN_POINT('Ctrl Pts',(0.598734255154188,0.356660564300906,
-11.046772741727)) ;
#148068 = CARTESIAN_POINT('Ctrl Pts',(0.60001275468167,0.335223914398785,
-11.0355823058657)) ;
#148069 = CARTESIAN_POINT('Ctrl Pts',(0.59999390055981,0.322655037092193,
-11.0316615193656)) ;
#148070 = CARTESIAN_POINT('Ctrl Pts',(0.600000296204999,0.30610691358234,
-11.030139626347)) ;
#148071 = CARTESIAN_POINT('Ctrl Pts',(0.600000000000001,0.303050992413441,
-11.03)) ;
#148072 = CARTESIAN_POINT('Ctrl Pts',(0.600000000000001,0.299999999999999,
-11.03)) ;
#148073 = CARTESIAN_POINT('',(0.600000000000001,-2.39800009914441E-17,-11.03)) ;
#148074 = CARTESIAN_POINT('Origin',(0.500000000000001,-1.9,-11.03)) ;
#148075 = CARTESIAN_POINT('Origin',(0.600000000000001,-1.9,-10.83)) ;
#148076 = CARTESIAN_POINT('Origin',(0.500000000000001,-1.9,-10.83)) ;
#148077 = CARTESIAN_POINT('Origin',(-0.899999999999999,-1.9,-10.055)) ;
#148078 = CARTESIAN_POINT('Origin',(-0.899999999999999,-1.9,-10.155)) ;
#148079 = CARTESIAN_POINT('Origin',(-0.899999999999999,0.6,-10.93)) ;
#148080 = CARTESIAN_POINT('Origin',(-0.899999999999999,0.6,-11.83)) ;
#148081 = CARTESIAN_POINT('Origin',(0.600000000000001,0.4,-11.83)) ;
#148082 = CARTESIAN_POINT('Origin',(0.500000000000001,0.4,-11.83)) ;
#148083 = CARTESIAN_POINT('Origin',(-0.899999999999999,0.4,-11.83)) ;
#148084 = CARTESIAN_POINT('Origin',(0.500000000000001,0.4,-11.83)) ;
#148085 = CARTESIAN_POINT('Origin',(0.500000000000001,-1.9,-10.83)) ;
#148086 = CARTESIAN_POINT('Origin',(0.500000000000001,-2.1,-10.83)) ;
#148087 = CARTESIAN_POINT('Origin',(-0.899999999999999,-1.9,-10.155)) ;
#148088 = CARTESIAN_POINT('Origin',(-1.1,-1.9,-10.155)) ;
#148089 = CARTESIAN_POINT('Origin',(-0.899999999999999,-2.1,-10.155)) ;
#148090 = CARTESIAN_POINT('Origin',(-0.899999999999999,0.4,-11.83)) ;
#148091 = CARTESIAN_POINT('Origin',(-0.899999999999999,0.4,-12.03)) ;
#148092 = CARTESIAN_POINT('Origin',(0.500000000000001,-2.1,-11.43)) ;
#148093 = CARTESIAN_POINT('Origin',(0.500000000000001,-2.1,-10.155)) ;
#148094 = CARTESIAN_POINT('Origin',(0.600000000000001,-2.1,-10.155)) ;
#148095 = CARTESIAN_POINT('Origin',(0.500000000000001,-2.1,-10.155)) ;
#148096 = CARTESIAN_POINT('Origin',(-1.1,-4.4272719500576E-17,-10.155)) ;
#148097 = CARTESIAN_POINT('',(-1.1,1.15,-10.055)) ;
#148098 = CARTESIAN_POINT('',(-1.1,1.25,-10.055)) ;
#148099 = CARTESIAN_POINT('Origin',(-1.1,1.15,-10.155)) ;
#148100 = CARTESIAN_POINT('Origin',(-0.899999999999999,0.5,-12.03)) ;
#148101 = CARTESIAN_POINT('Origin',(-0.899999999999999,-1.9,-12.03)) ;
#148102 = CARTESIAN_POINT('Origin',(0.600000000000001,-1.9,-12.03)) ;
#148103 = CARTESIAN_POINT('Origin',(0.500000000000001,-1.9,-12.03)) ;
#148104 = CARTESIAN_POINT('Origin',(-0.899999999999999,-1.9,-12.03)) ;
#148105 = CARTESIAN_POINT('Origin',(0.500000000000001,-1.9,-12.03)) ;
#148106 = CARTESIAN_POINT('Origin',(0.500000000000001,-2.1,-12.03)) ;
#148107 = CARTESIAN_POINT('Origin',(0.500000000000001,-2.1,-10.155)) ;
#148108 = CARTESIAN_POINT('Origin',(0.500000000000001,-2.1,-10.155)) ;
#148109 = CARTESIAN_POINT('Origin',(-1.1,-2.9,-9.955)) ;
#148110 = CARTESIAN_POINT('Origin',(-1.1,-2.9,-9.955)) ;
#148111 = CARTESIAN_POINT('Origin',(-1.1,-2.9,-9.955)) ;
#148112 = CARTESIAN_POINT('Origin',(-1.1,1.25,-9.955)) ;
#148113 = CARTESIAN_POINT('Origin',(-1.1,1.15,-9.955)) ;
#148114 = CARTESIAN_POINT('Origin',(-1.1,1.15,-10.155)) ;
#148115 = CARTESIAN_POINT('',(-1.1,1.25,-10.155)) ;
#148116 = CARTESIAN_POINT('Origin',(-1.1,1.15,-10.155)) ;
#148117 = CARTESIAN_POINT('Origin',(-1.1,1.15,-10.155)) ;
#148118 = CARTESIAN_POINT('Origin',(-0.899999999999999,-1.9,-12.03)) ;
#148119 = CARTESIAN_POINT('Origin',(-0.899999999999999,-1.9,-12.03)) ;
#148120 = CARTESIAN_POINT('Origin',(0.500000000000001,-2.1,-11.43)) ;
#148121 = CARTESIAN_POINT('Origin',(0.500000000000001,-2.1,-12.705)) ;
#148122 = CARTESIAN_POINT('Origin',(0.500000000000001,1.36481920536411E-16,
-10.155)) ;
#148123 = CARTESIAN_POINT('Origin',(0.500000000000001,-2.9,-10.155)) ;
#148124 = CARTESIAN_POINT('Origin',(-0.999999999999999,-2.9,-9.955)) ;
#148125 = CARTESIAN_POINT('Origin',(0.500000000000001,-2.9,-9.955)) ;
#148126 = CARTESIAN_POINT('Origin',(-1.1,1.15,-10.155)) ;
#148127 = CARTESIAN_POINT('Origin',(-1.1,1.35,-10.155)) ;
#148128 = CARTESIAN_POINT('Origin',(-1.1,1.15,-11.43)) ;
#148129 = CARTESIAN_POINT('',(-1.1,1.25,-12.705)) ;
#148130 = CARTESIAN_POINT('',(-1.1,1.25,-12.805)) ;
#148131 = CARTESIAN_POINT('Origin',(-1.1,1.15,-12.705)) ;
#148132 = CARTESIAN_POINT('Origin',(-0.899999999999999,-1.9,-11.93)) ;
#148133 = CARTESIAN_POINT('Origin',(-0.899999999999999,-1.9,-12.705)) ;
#148134 = CARTESIAN_POINT('Origin',(-0.999999999999999,-2.1,-12.705)) ;
#148135 = CARTESIAN_POINT('Origin',(0.500000000000001,-2.1,-12.705)) ;
#148136 = CARTESIAN_POINT('Origin',(-0.899999999999999,-2.1,-12.705)) ;
#148137 = CARTESIAN_POINT('Origin',(0.500000000000001,-2.1,-12.705)) ;
#148138 = CARTESIAN_POINT('Origin',(0.500000000000001,-2.1,-12.705)) ;
#148139 = CARTESIAN_POINT('Origin',(0.500000000000001,-2.9,-10.155)) ;
#148140 = CARTESIAN_POINT('Origin',(0.700000000000002,-2.9,-10.155)) ;
#148141 = CARTESIAN_POINT('Origin',(-1.1,1.35,-12.805)) ;
#148142 = CARTESIAN_POINT('Origin',(-1.1,1.35,-12.705)) ;
#148143 = CARTESIAN_POINT('Origin',(-1.1,1.15,-12.705)) ;
#148144 = CARTESIAN_POINT('',(-1.1,1.15,-12.805)) ;
#148145 = CARTESIAN_POINT('Origin',(-1.1,1.15,-12.705)) ;
#148146 = CARTESIAN_POINT('Origin',(-1.1,1.15,-12.705)) ;
#148147 = CARTESIAN_POINT('Origin',(-0.899999999999999,-1.9,-12.705)) ;
#148148 = CARTESIAN_POINT('Origin',(-1.1,-1.9,-12.705)) ;
#148149 = CARTESIAN_POINT('Origin',(0.500000000000001,-5.86744705109802E-17,
-12.705)) ;
#148150 = CARTESIAN_POINT('Origin',(0.500000000000001,-2.9,-12.705)) ;
#148151 = CARTESIAN_POINT('Origin',(0.700000000000002,-2.9,-11.43)) ;
#148152 = CARTESIAN_POINT('Origin',(0.700000000000002,-2.9,-12.705)) ;
#148153 = CARTESIAN_POINT('Origin',(-1.1,1.15,-12.705)) ;
#148154 = CARTESIAN_POINT('Origin',(-1.1,1.15,-12.905)) ;
#148155 = CARTESIAN_POINT('Origin',(-1.1,-2.39429110547967E-16,-12.705)) ;
#148156 = CARTESIAN_POINT('',(-1.1,1.25,-12.805)) ;
#148157 = CARTESIAN_POINT('Origin',(0.500000000000001,-2.9,-12.705)) ;
#148158 = CARTESIAN_POINT('Origin',(0.500000000000001,-2.9,-12.905)) ;
#148159 = CARTESIAN_POINT('Origin',(-1.1,1.25,-12.905)) ;
#148160 = CARTESIAN_POINT('Origin',(-1.1,-2.9,-12.905)) ;
#148161 = CARTESIAN_POINT('Origin',(-1.1,-2.9,-12.905)) ;
#148162 = CARTESIAN_POINT('Origin',(-1.1,-2.9,-12.905)) ;
#148163 = CARTESIAN_POINT('Origin',(-1.1,-2.9,-12.905)) ;
#148164 = CARTESIAN_POINT('Origin',(1.5,1.9,-10.83)) ;
#148165 = CARTESIAN_POINT('Origin',(1.5,1.9,-12.98)) ;
#148166 = CARTESIAN_POINT('Origin',(1.5,1.9,-12.03)) ;
#148167 = CARTESIAN_POINT('Origin',(1.5,2.1,-12.03)) ;
#148168 = CARTESIAN_POINT('Origin',(1.5,2.1,-11.83)) ;
#148169 = CARTESIAN_POINT('Origin',(1.5,1.9,-12.98)) ;
#148170 = CARTESIAN_POINT('Origin',(1.5,1.9,-12.98)) ;
#148171 = CARTESIAN_POINT('Origin',(1.5,2.1,-11.83)) ;
#148172 = CARTESIAN_POINT('Origin',(1.5,2.4,-11.83)) ;
#148173 = CARTESIAN_POINT('Origin',(1.5,2.1,-12.98)) ;
#148174 = CARTESIAN_POINT('Origin',(1.5,-2.15,-12.98)) ;
#148175 = CARTESIAN_POINT('Origin',(1.5,2.4,-12.03)) ;
#148176 = CARTESIAN_POINT('Origin',(1.5,2.6,-12.03)) ;
#148177 = CARTESIAN_POINT('Origin',(1.5,-2.15,-12.98)) ;
#148178 = CARTESIAN_POINT('Origin',(1.5,-2.15,-12.98)) ;
#148179 = CARTESIAN_POINT('Origin',(1.5,2.6,-10.83)) ;
#148180 = CARTESIAN_POINT('Origin',(1.5,2.6,-12.1385786437627)) ;
#148181 = CARTESIAN_POINT('Origin',(1.5,-2.15,-10.83)) ;
#148182 = CARTESIAN_POINT('Origin',(1.5,-2.15,-12.3331195934094)) ;
#148183 = CARTESIAN_POINT('Origin',(1.5,2.6,-12.1385786437627)) ;
#148184 = CARTESIAN_POINT('Origin',(1.5,2.6,-12.1385786437627)) ;
#148185 = CARTESIAN_POINT('Origin',(1.5,-2.15,-12.3331195934094)) ;
#148186 = CARTESIAN_POINT('Origin',(1.5,-2.15,-12.3331195934094)) ;
#148187 = CARTESIAN_POINT('Origin',(1.5,1.69571067811865,-11.2342893218813)) ;
#148188 = CARTESIAN_POINT('Origin',(1.5,3.15,-12.6885786437627)) ;
#148189 = CARTESIAN_POINT('Origin',(1.5,-3.65625,-11.43)) ;
#148190 = CARTESIAN_POINT('Origin',(1.5,-2.15,-10.5268804065906)) ;
#148191 = CARTESIAN_POINT('Origin',(1.5,3.15,-12.6885786437627)) ;
#148192 = CARTESIAN_POINT('Origin',(1.5,3.15,-12.6885786437627)) ;
#148193 = CARTESIAN_POINT('Origin',(1.5,-2.15,-10.5268804065906)) ;
#148194 = CARTESIAN_POINT('Origin',(1.5,-2.15,-10.5268804065906)) ;
#148195 = CARTESIAN_POINT('Origin',(1.5,3.15,-10.83)) ;
#148196 = CARTESIAN_POINT('Origin',(1.5,-2.15,-10.83)) ;
#148197 = CARTESIAN_POINT('Origin',(1.5,-2.15,-9.88)) ;
#148198 = CARTESIAN_POINT('Origin',(1.5,-2.15,-9.88)) ;
#148199 = CARTESIAN_POINT('Origin',(1.5,-2.15,-9.88)) ;
#148200 = CARTESIAN_POINT('Origin',(1.5,2.29571067811866,-11.0257106781187)) ;
#148201 = CARTESIAN_POINT('Origin',(1.5,2.6,-10.7214213562373)) ;
#148202 = CARTESIAN_POINT('Origin',(1.5,2.1,-9.88)) ;
#148203 = CARTESIAN_POINT('Origin',(1.5,1.9,-9.88)) ;
#148204 = CARTESIAN_POINT('Origin',(1.5,2.6,-10.7214213562373)) ;
#148205 = CARTESIAN_POINT('Origin',(1.5,2.6,-10.7214213562373)) ;
#148206 = CARTESIAN_POINT('Origin',(1.5,1.9,-9.88)) ;
#148207 = CARTESIAN_POINT('Origin',(1.5,1.9,-9.88)) ;
#148208 = CARTESIAN_POINT('Origin',(1.5,2.6,-10.83)) ;
#148209 = CARTESIAN_POINT('Origin',(1.5,2.6,-10.83)) ;
#148210 = CARTESIAN_POINT('Origin',(1.5,1.9,-10.83)) ;
#148211 = CARTESIAN_POINT('Origin',(1.5,1.9,-10.83)) ;
#148212 = CARTESIAN_POINT('Origin',(1.5,2.4,-10.83)) ;
#148213 = CARTESIAN_POINT('Origin',(1.5,2.4,-11.03)) ;
#148214 = CARTESIAN_POINT('Origin',(1.5,2.1,-10.83)) ;
#148215 = CARTESIAN_POINT('Origin',(1.5,2.1,-11.03)) ;
#148216 = CARTESIAN_POINT('Origin',(1.5,2.1,-11.03)) ;
#148217 = CARTESIAN_POINT('Origin',(-0.899999999999999,-2.,-14.64)) ;
#148218 = CARTESIAN_POINT('Origin',(-0.899999999999999,0.4,-14.64)) ;
#148219 = CARTESIAN_POINT('Origin',(-0.899999999999999,-1.9,-14.64)) ;
#148220 = CARTESIAN_POINT('Origin',(0.600000000000001,0.4,-14.84)) ;
#148221 = CARTESIAN_POINT('Origin',(0.500000000000001,0.4,-14.84)) ;
#148222 = CARTESIAN_POINT('Origin',(-0.899999999999999,0.4,-14.84)) ;
#148223 = CARTESIAN_POINT('Origin',(0.500000000000001,0.4,-14.84)) ;
#148224 = CARTESIAN_POINT('',(0.600000000000001,0.4,-14.84)) ;
#148225 = CARTESIAN_POINT('Origin',(0.500000000000001,0.4,-14.84)) ;
#148226 = CARTESIAN_POINT('Origin',(0.500000000000001,0.4,-14.84)) ;
#148227 = CARTESIAN_POINT('Origin',(-0.899999999999999,-1.9,-14.64)) ;
#148228 = CARTESIAN_POINT('Origin',(-0.899999999999999,-1.9,-14.64)) ;
#148229 = CARTESIAN_POINT('Origin',(-0.899999999999999,-1.9,-14.64)) ;
#148230 = CARTESIAN_POINT('Origin',(-0.899999999999999,0.4,-14.84)) ;
#148231 = CARTESIAN_POINT('Origin',(-0.899999999999999,0.6,-14.84)) ;
#148232 = CARTESIAN_POINT('Origin',(0.500000000000001,0.4,-15.24)) ;
#148233 = CARTESIAN_POINT('Origin',(0.500000000000001,0.4,-15.64)) ;
#148234 = CARTESIAN_POINT('',(0.600000000000001,0.4,-15.54)) ;
#148235 = CARTESIAN_POINT('Ctrl Pts',(0.595612997216082,0.370705721320405,
-15.6107057213204)) ;
#148236 = CARTESIAN_POINT('Ctrl Pts',(0.596180587760893,0.372558268494361,
-15.6088554988322)) ;
#148237 = CARTESIAN_POINT('Ctrl Pts',(0.596672461925687,0.374355839771988,
-15.6069141798663)) ;
#148238 = CARTESIAN_POINT('Ctrl Pts',(0.599015141889213,0.383869350930072,
-15.5957649936563)) ;
#148239 = CARTESIAN_POINT('Ctrl Pts',(0.599609996542525,0.390224332900456,
-15.5849726026541)) ;
#148240 = CARTESIAN_POINT('Ctrl Pts',(0.600050586298725,0.398117439141561,
-15.5623310532047)) ;
#148241 = CARTESIAN_POINT('Ctrl Pts',(0.600000000000001,0.4,-15.5512012506335)) ;
#148242 = CARTESIAN_POINT('Ctrl Pts',(0.600000000000001,0.399999999999999,
-15.54)) ;
#148243 = CARTESIAN_POINT('',(0.600000000000001,0.4,-15.24)) ;
#148244 = CARTESIAN_POINT('Origin',(0.500000000000001,-4.56640444411542E-17,
-14.84)) ;
#148245 = CARTESIAN_POINT('',(0.500000000000001,0.394987437106619,-14.94)) ;
#148246 = CARTESIAN_POINT('Ctrl Pts',(0.500000000000001,0.394987437106619,
-14.94)) ;
#148247 = CARTESIAN_POINT('Ctrl Pts',(0.505940567948958,0.395584486649901,
-14.94)) ;
#148248 = CARTESIAN_POINT('Ctrl Pts',(0.511931971019147,0.396132036079019,
-14.939466300328)) ;
#148249 = CARTESIAN_POINT('Ctrl Pts',(0.517829015308562,0.396618246075356,
-14.9383977957737)) ;
#148250 = CARTESIAN_POINT('Ctrl Pts',(0.522982218721209,0.397043126556054,
-14.9374640701571)) ;
#148251 = CARTESIAN_POINT('Ctrl Pts',(0.528062648970245,0.397421319341388,
-14.9361228267971)) ;
#148252 = CARTESIAN_POINT('Ctrl Pts',(0.532978106724004,0.397751505046071,
-14.9344057438766)) ;
#148253 = CARTESIAN_POINT('Ctrl Pts',(0.538583536338963,0.398128038182999,
-14.9324476378495)) ;
#148254 = CARTESIAN_POINT('Ctrl Pts',(0.544059405914874,0.398447721828296,
-14.9299700083111)) ;
#148255 = CARTESIAN_POINT('Ctrl Pts',(0.549268572255776,0.398712331108984,
-14.9270207319429)) ;
#148256 = CARTESIAN_POINT('Ctrl Pts',(0.553856850427151,0.398945401221756,
-14.9244229841468)) ;
#148257 = CARTESIAN_POINT('Ctrl Pts',(0.558237825069319,0.399135987683843,
-14.92146038498)) ;
#148258 = CARTESIAN_POINT('Ctrl Pts',(0.562333836086205,0.399290378266507,
-14.9181952228642)) ;
#148259 = CARTESIAN_POINT('Ctrl Pts',(0.56699032895788,0.399465895042381,
-14.9144832689523)) ;
#148260 = CARTESIAN_POINT('Ctrl Pts',(0.571349096493406,0.399597278936107,
-14.9103228064848)) ;
#148261 = CARTESIAN_POINT('Ctrl Pts',(0.575296920056693,0.399694832180837,
-14.9058055759794)) ;
#148262 = CARTESIAN_POINT('Ctrl Pts',(0.578744263667893,0.399780018245913,
-14.9018610112151)) ;
#148263 = CARTESIAN_POINT('Ctrl Pts',(0.581878314560404,0.399839626289636,
-14.8976455218421)) ;
#148264 = CARTESIAN_POINT('Ctrl Pts',(0.584648147334845,0.399882153365958,
-14.8932418177073)) ;
#148265 = CARTESIAN_POINT('Ctrl Pts',(0.587839270208164,0.399931148788079,
-14.8881683125045)) ;
#148266 = CARTESIAN_POINT('Ctrl Pts',(0.590595054415084,0.399958289583404,
-14.8827666362445)) ;
#148267 = CARTESIAN_POINT('Ctrl Pts',(0.592838618943089,0.399974357003159,
-14.8771616850094)) ;
#148268 = CARTESIAN_POINT('Ctrl Pts',(0.594777336851653,0.399988241245861,
-14.8723183122424)) ;
#148269 = CARTESIAN_POINT('Ctrl Pts',(0.596334051506184,0.399993946552814,
-14.8673241662272)) ;
#148270 = CARTESIAN_POINT('Ctrl Pts',(0.597488309822312,0.39999684570125,
-14.8622717185684)) ;
#148271 = CARTESIAN_POINT('Ctrl Pts',(0.598804024094403,0.400000150378306,
-14.8565125419605)) ;
#148272 = CARTESIAN_POINT('Ctrl Pts',(0.599612685195422,0.399999963509465,
-14.8506028438907)) ;
#148273 = CARTESIAN_POINT('Ctrl Pts',(0.599890230999715,0.399999993975383,
-14.8446842022612)) ;
#148274 = CARTESIAN_POINT('Ctrl Pts',(0.599963464549397,0.400000002014155,
-14.8431225027899)) ;
#148275 = CARTESIAN_POINT('Ctrl Pts',(0.600000000000001,0.399999999999999,
-14.8415602215092)) ;
#148276 = CARTESIAN_POINT('Ctrl Pts',(0.600000000000001,0.399999999999999,
-14.84)) ;
#148277 = CARTESIAN_POINT('',(0.600000000000001,0.299999999999999,-14.84)) ;
#148278 = CARTESIAN_POINT('Ctrl Pts',(0.500000000000001,0.394987437106619,
-14.94)) ;
#148279 = CARTESIAN_POINT('Ctrl Pts',(0.500454935590171,0.395033159853782,
-14.94)) ;
#148280 = CARTESIAN_POINT('Ctrl Pts',(0.500909898680634,0.395078570329076,
-14.9399968954911)) ;
#148281 = CARTESIAN_POINT('Ctrl Pts',(0.502892456245054,0.395275075889078,
-14.9399698339419)) ;
#148282 = CARTESIAN_POINT('Ctrl Pts',(0.504418747482298,0.395422812032191,
-14.939913985421)) ;
#148283 = CARTESIAN_POINT('Ctrl Pts',(0.508462199543321,0.395804395682031,
-14.9396732810566)) ;
#148284 = CARTESIAN_POINT('Ctrl Pts',(0.510974953343265,0.396031485023314,
-14.9394279391451)) ;
#148285 = CARTESIAN_POINT('Ctrl Pts',(0.521160739721169,0.396903453186227,
-14.9380427944916)) ;
#148286 = CARTESIAN_POINT('Ctrl Pts',(0.528708678528302,0.397444933153157,
-14.9361042177047)) ;
#148287 = CARTESIAN_POINT('Ctrl Pts',(0.54594320635793,0.398105551684103,
-14.9294646394512)) ;
#148288 = CARTESIAN_POINT('Ctrl Pts',(0.555229535466698,0.397987646678449,
-14.9240353588361)) ;
#148289 = CARTESIAN_POINT('Ctrl Pts',(0.571394604995641,0.395490482808055,
-14.9107755133639)) ;
#148290 = CARTESIAN_POINT('Ctrl Pts',(0.578055313702769,0.393198948698403,
-14.9032407456319)) ;
#148291 = CARTESIAN_POINT('Ctrl Pts',(0.58855913220244,0.385442756729361,
-14.8873922339841)) ;
#148292 = CARTESIAN_POINT('Ctrl Pts',(0.592167355639942,0.380240075126989,
-14.8795482656069)) ;
#148293 = CARTESIAN_POINT('Ctrl Pts',(0.59749661553107,0.365892753467073,
-14.8639255217954)) ;
#148294 = CARTESIAN_POINT('Ctrl Pts',(0.598734255154193,0.356660564300806,
-14.856772741727)) ;
#148295 = CARTESIAN_POINT('Ctrl Pts',(0.600012754681677,0.335223914398739,
-14.8455823058657)) ;
#148296 = CARTESIAN_POINT('Ctrl Pts',(0.59999390055981,0.322655037092125,
-14.8416615193656)) ;
#148297 = CARTESIAN_POINT('Ctrl Pts',(0.600000296204999,0.306106913582367,
-14.840139626347)) ;
#148298 = CARTESIAN_POINT('Ctrl Pts',(0.600000000000001,0.303050992413449,
-14.84)) ;
#148299 = CARTESIAN_POINT('Ctrl Pts',(0.600000000000001,0.299999999999999,
-14.84)) ;
#148300 = CARTESIAN_POINT('',(0.600000000000001,-2.39800009914441E-17,-14.84)) ;
#148301 = CARTESIAN_POINT('Origin',(0.500000000000001,-1.9,-14.84)) ;
#148302 = CARTESIAN_POINT('Origin',(0.600000000000001,-1.9,-14.64)) ;
#148303 = CARTESIAN_POINT('Origin',(0.500000000000001,-1.9,-14.64)) ;
#148304 = CARTESIAN_POINT('Origin',(-0.899999999999999,-1.9,-13.865)) ;
#148305 = CARTESIAN_POINT('Origin',(-0.899999999999999,-1.9,-13.965)) ;
#148306 = CARTESIAN_POINT('Origin',(-0.899999999999999,0.6,-14.74)) ;
#148307 = CARTESIAN_POINT('Origin',(-0.899999999999999,0.6,-15.64)) ;
#148308 = CARTESIAN_POINT('Origin',(0.600000000000001,0.4,-15.64)) ;
#148309 = CARTESIAN_POINT('Origin',(0.500000000000001,0.4,-15.64)) ;
#148310 = CARTESIAN_POINT('Origin',(-0.899999999999999,0.4,-15.64)) ;
#148311 = CARTESIAN_POINT('Origin',(0.500000000000001,0.4,-15.64)) ;
#148312 = CARTESIAN_POINT('Origin',(0.500000000000001,-1.9,-14.64)) ;
#148313 = CARTESIAN_POINT('Origin',(0.500000000000001,-2.1,-14.64)) ;
#148314 = CARTESIAN_POINT('Origin',(-0.899999999999999,-1.9,-13.965)) ;
#148315 = CARTESIAN_POINT('Origin',(-1.1,-1.9,-13.965)) ;
#148316 = CARTESIAN_POINT('Origin',(-0.899999999999999,-2.1,-13.965)) ;
#148317 = CARTESIAN_POINT('Origin',(-0.899999999999999,0.4,-15.64)) ;
#148318 = CARTESIAN_POINT('Origin',(-0.899999999999999,0.4,-15.84)) ;
#148319 = CARTESIAN_POINT('Origin',(0.500000000000001,-2.1,-15.24)) ;
#148320 = CARTESIAN_POINT('Origin',(0.500000000000001,-2.1,-13.965)) ;
#148321 = CARTESIAN_POINT('Origin',(0.600000000000001,-2.1,-13.965)) ;
#148322 = CARTESIAN_POINT('Origin',(0.500000000000001,-2.1,-13.965)) ;
#148323 = CARTESIAN_POINT('Origin',(-1.1,-4.4272719500576E-17,-13.965)) ;
#148324 = CARTESIAN_POINT('',(-1.1,1.15,-13.865)) ;
#148325 = CARTESIAN_POINT('',(-1.1,1.25,-13.865)) ;
#148326 = CARTESIAN_POINT('Origin',(-1.1,1.15,-13.965)) ;
#148327 = CARTESIAN_POINT('Origin',(-0.899999999999999,0.5,-15.84)) ;
#148328 = CARTESIAN_POINT('Origin',(-0.899999999999999,-1.9,-15.84)) ;
#148329 = CARTESIAN_POINT('Origin',(0.600000000000001,-1.9,-15.84)) ;
#148330 = CARTESIAN_POINT('Origin',(0.500000000000001,-1.9,-15.84)) ;
#148331 = CARTESIAN_POINT('Origin',(-0.899999999999999,-1.9,-15.84)) ;
#148332 = CARTESIAN_POINT('Origin',(0.500000000000001,-1.9,-15.84)) ;
#148333 = CARTESIAN_POINT('Origin',(0.500000000000001,-2.1,-15.84)) ;
#148334 = CARTESIAN_POINT('Origin',(0.500000000000001,-2.1,-13.965)) ;
#148335 = CARTESIAN_POINT('Origin',(0.500000000000001,-2.1,-13.965)) ;
#148336 = CARTESIAN_POINT('Origin',(-1.1,-2.9,-13.765)) ;
#148337 = CARTESIAN_POINT('Origin',(-1.1,-2.9,-13.765)) ;
#148338 = CARTESIAN_POINT('Origin',(-1.1,-2.9,-13.765)) ;
#148339 = CARTESIAN_POINT('Origin',(-1.1,1.25,-13.765)) ;
#148340 = CARTESIAN_POINT('Origin',(-1.1,1.15,-13.765)) ;
#148341 = CARTESIAN_POINT('Origin',(-1.1,1.15,-13.965)) ;
#148342 = CARTESIAN_POINT('',(-1.1,1.25,-13.965)) ;
#148343 = CARTESIAN_POINT('Origin',(-1.1,1.15,-13.965)) ;
#148344 = CARTESIAN_POINT('Origin',(-1.1,1.15,-13.965)) ;
#148345 = CARTESIAN_POINT('Origin',(-0.899999999999999,-1.9,-15.84)) ;
#148346 = CARTESIAN_POINT('Origin',(-0.899999999999999,-1.9,-15.84)) ;
#148347 = CARTESIAN_POINT('Origin',(0.500000000000001,-2.1,-15.24)) ;
#148348 = CARTESIAN_POINT('Origin',(0.500000000000001,-2.1,-16.515)) ;
#148349 = CARTESIAN_POINT('Origin',(0.500000000000001,1.36481920536411E-16,
-13.965)) ;
#148350 = CARTESIAN_POINT('Origin',(0.500000000000001,-2.9,-13.965)) ;
#148351 = CARTESIAN_POINT('Origin',(-0.999999999999999,-2.9,-13.765)) ;
#148352 = CARTESIAN_POINT('Origin',(0.500000000000001,-2.9,-13.765)) ;
#148353 = CARTESIAN_POINT('Origin',(-1.1,1.15,-13.965)) ;
#148354 = CARTESIAN_POINT('Origin',(-1.1,1.35,-13.965)) ;
#148355 = CARTESIAN_POINT('Origin',(-1.1,1.15,-15.24)) ;
#148356 = CARTESIAN_POINT('',(-1.1,1.25,-16.515)) ;
#148357 = CARTESIAN_POINT('',(-1.1,1.25,-16.615)) ;
#148358 = CARTESIAN_POINT('Origin',(-1.1,1.15,-16.515)) ;
#148359 = CARTESIAN_POINT('Origin',(-0.899999999999999,-1.9,-15.74)) ;
#148360 = CARTESIAN_POINT('Origin',(-0.899999999999999,-1.9,-16.515)) ;
#148361 = CARTESIAN_POINT('Origin',(-0.999999999999999,-2.1,-16.515)) ;
#148362 = CARTESIAN_POINT('Origin',(0.500000000000001,-2.1,-16.515)) ;
#148363 = CARTESIAN_POINT('Origin',(-0.899999999999999,-2.1,-16.515)) ;
#148364 = CARTESIAN_POINT('Origin',(0.500000000000001,-2.1,-16.515)) ;
#148365 = CARTESIAN_POINT('Origin',(0.500000000000001,-2.1,-16.515)) ;
#148366 = CARTESIAN_POINT('Origin',(0.500000000000001,-2.9,-13.965)) ;
#148367 = CARTESIAN_POINT('Origin',(0.700000000000002,-2.9,-13.965)) ;
#148368 = CARTESIAN_POINT('Origin',(-1.1,1.35,-16.615)) ;
#148369 = CARTESIAN_POINT('Origin',(-1.1,1.35,-16.515)) ;
#148370 = CARTESIAN_POINT('Origin',(-1.1,1.15,-16.515)) ;
#148371 = CARTESIAN_POINT('',(-1.1,1.15,-16.615)) ;
#148372 = CARTESIAN_POINT('Origin',(-1.1,1.15,-16.515)) ;
#148373 = CARTESIAN_POINT('Origin',(-1.1,1.15,-16.515)) ;
#148374 = CARTESIAN_POINT('Origin',(-0.899999999999999,-1.9,-16.515)) ;
#148375 = CARTESIAN_POINT('Origin',(-1.1,-1.9,-16.515)) ;
#148376 = CARTESIAN_POINT('Origin',(0.500000000000001,-5.86744705109802E-17,
-16.515)) ;
#148377 = CARTESIAN_POINT('Origin',(0.500000000000001,-2.9,-16.515)) ;
#148378 = CARTESIAN_POINT('Origin',(0.700000000000002,-2.9,-15.24)) ;
#148379 = CARTESIAN_POINT('Origin',(0.700000000000002,-2.9,-16.515)) ;
#148380 = CARTESIAN_POINT('Origin',(-1.1,1.15,-16.515)) ;
#148381 = CARTESIAN_POINT('Origin',(-1.1,1.15,-16.715)) ;
#148382 = CARTESIAN_POINT('Origin',(-1.1,-2.39429110547967E-16,-16.515)) ;
#148383 = CARTESIAN_POINT('',(-1.1,1.25,-16.615)) ;
#148384 = CARTESIAN_POINT('Origin',(0.500000000000001,-2.9,-16.515)) ;
#148385 = CARTESIAN_POINT('Origin',(0.500000000000001,-2.9,-16.715)) ;
#148386 = CARTESIAN_POINT('Origin',(-1.1,1.25,-16.715)) ;
#148387 = CARTESIAN_POINT('Origin',(-1.1,-2.9,-16.715)) ;
#148388 = CARTESIAN_POINT('Origin',(-1.1,-2.9,-16.715)) ;
#148389 = CARTESIAN_POINT('Origin',(-1.1,-2.9,-16.715)) ;
#148390 = CARTESIAN_POINT('Origin',(-1.1,-2.9,-16.715)) ;
#148391 = CARTESIAN_POINT('Origin',(1.5,1.9,-14.64)) ;
#148392 = CARTESIAN_POINT('Origin',(1.5,1.9,-16.79)) ;
#148393 = CARTESIAN_POINT('Origin',(1.5,1.9,-15.84)) ;
#148394 = CARTESIAN_POINT('Origin',(1.5,2.1,-15.84)) ;
#148395 = CARTESIAN_POINT('Origin',(1.5,2.1,-15.64)) ;
#148396 = CARTESIAN_POINT('Origin',(1.5,1.9,-16.79)) ;
#148397 = CARTESIAN_POINT('Origin',(1.5,1.9,-16.79)) ;
#148398 = CARTESIAN_POINT('Origin',(1.5,2.1,-15.64)) ;
#148399 = CARTESIAN_POINT('Origin',(1.5,2.4,-15.64)) ;
#148400 = CARTESIAN_POINT('Origin',(1.5,2.1,-16.79)) ;
#148401 = CARTESIAN_POINT('Origin',(1.5,-2.15,-16.79)) ;
#148402 = CARTESIAN_POINT('Origin',(1.5,2.4,-15.84)) ;
#148403 = CARTESIAN_POINT('Origin',(1.5,2.6,-15.84)) ;
#148404 = CARTESIAN_POINT('Origin',(1.5,-2.15,-16.79)) ;
#148405 = CARTESIAN_POINT('Origin',(1.5,-2.15,-16.79)) ;
#148406 = CARTESIAN_POINT('Origin',(1.5,2.6,-14.64)) ;
#148407 = CARTESIAN_POINT('Origin',(1.5,2.6,-15.9485786437627)) ;
#148408 = CARTESIAN_POINT('Origin',(1.5,-2.15,-14.64)) ;
#148409 = CARTESIAN_POINT('Origin',(1.5,-2.15,-16.1431195934094)) ;
#148410 = CARTESIAN_POINT('Origin',(1.5,2.6,-15.9485786437627)) ;
#148411 = CARTESIAN_POINT('Origin',(1.5,2.6,-15.9485786437627)) ;
#148412 = CARTESIAN_POINT('Origin',(1.5,-2.15,-16.1431195934094)) ;
#148413 = CARTESIAN_POINT('Origin',(1.5,-2.15,-16.1431195934094)) ;
#148414 = CARTESIAN_POINT('Origin',(1.5,1.69571067811865,-15.0442893218814)) ;
#148415 = CARTESIAN_POINT('Origin',(1.5,3.15,-16.4985786437627)) ;
#148416 = CARTESIAN_POINT('Origin',(1.5,-3.65625,-15.24)) ;
#148417 = CARTESIAN_POINT('Origin',(1.5,-2.15,-14.3368804065906)) ;
#148418 = CARTESIAN_POINT('Origin',(1.5,3.15,-16.4985786437627)) ;
#148419 = CARTESIAN_POINT('Origin',(1.5,3.15,-16.4985786437627)) ;
#148420 = CARTESIAN_POINT('Origin',(1.5,-2.15,-14.3368804065906)) ;
#148421 = CARTESIAN_POINT('Origin',(1.5,-2.15,-14.3368804065906)) ;
#148422 = CARTESIAN_POINT('Origin',(1.5,3.15,-14.64)) ;
#148423 = CARTESIAN_POINT('Origin',(1.5,-2.15,-14.64)) ;
#148424 = CARTESIAN_POINT('Origin',(1.5,-2.15,-13.69)) ;
#148425 = CARTESIAN_POINT('Origin',(1.5,-2.15,-13.69)) ;
#148426 = CARTESIAN_POINT('Origin',(1.5,-2.15,-13.69)) ;
#148427 = CARTESIAN_POINT('Origin',(1.5,2.29571067811866,-14.8357106781187)) ;
#148428 = CARTESIAN_POINT('Origin',(1.5,2.6,-14.5314213562373)) ;
#148429 = CARTESIAN_POINT('Origin',(1.5,2.1,-13.69)) ;
#148430 = CARTESIAN_POINT('Origin',(1.5,1.9,-13.69)) ;
#148431 = CARTESIAN_POINT('Origin',(1.5,2.6,-14.5314213562373)) ;
#148432 = CARTESIAN_POINT('Origin',(1.5,2.6,-14.5314213562373)) ;
#148433 = CARTESIAN_POINT('Origin',(1.5,1.9,-13.69)) ;
#148434 = CARTESIAN_POINT('Origin',(1.5,1.9,-13.69)) ;
#148435 = CARTESIAN_POINT('Origin',(1.5,2.6,-14.64)) ;
#148436 = CARTESIAN_POINT('Origin',(1.5,2.6,-14.64)) ;
#148437 = CARTESIAN_POINT('Origin',(1.5,1.9,-14.64)) ;
#148438 = CARTESIAN_POINT('Origin',(1.5,1.9,-14.64)) ;
#148439 = CARTESIAN_POINT('Origin',(1.5,2.4,-14.64)) ;
#148440 = CARTESIAN_POINT('Origin',(1.5,2.4,-14.84)) ;
#148441 = CARTESIAN_POINT('Origin',(1.5,2.1,-14.64)) ;
#148442 = CARTESIAN_POINT('Origin',(1.5,2.1,-14.84)) ;
#148443 = CARTESIAN_POINT('Origin',(1.5,2.1,-14.84)) ;
#148444 = CARTESIAN_POINT('Origin',(-0.899999999999999,-2.,-18.45)) ;
#148445 = CARTESIAN_POINT('Origin',(-0.899999999999999,0.4,-18.45)) ;
#148446 = CARTESIAN_POINT('Origin',(-0.899999999999999,-1.9,-18.45)) ;
#148447 = CARTESIAN_POINT('Origin',(0.600000000000001,0.4,-18.65)) ;
#148448 = CARTESIAN_POINT('Origin',(0.500000000000001,0.4,-18.65)) ;
#148449 = CARTESIAN_POINT('Origin',(-0.899999999999999,0.4,-18.65)) ;
#148450 = CARTESIAN_POINT('Origin',(0.500000000000001,0.4,-18.65)) ;
#148451 = CARTESIAN_POINT('',(0.600000000000001,0.4,-18.65)) ;
#148452 = CARTESIAN_POINT('Origin',(0.500000000000001,0.4,-18.65)) ;
#148453 = CARTESIAN_POINT('Origin',(0.500000000000001,0.4,-18.65)) ;
#148454 = CARTESIAN_POINT('Origin',(-0.899999999999999,-1.9,-18.45)) ;
#148455 = CARTESIAN_POINT('Origin',(-0.899999999999999,-1.9,-18.45)) ;
#148456 = CARTESIAN_POINT('Origin',(-0.899999999999999,-1.9,-18.45)) ;
#148457 = CARTESIAN_POINT('Origin',(-0.899999999999999,0.4,-18.65)) ;
#148458 = CARTESIAN_POINT('Origin',(-0.899999999999999,0.6,-18.65)) ;
#148459 = CARTESIAN_POINT('Origin',(0.500000000000001,0.4,-19.05)) ;
#148460 = CARTESIAN_POINT('Origin',(0.500000000000001,0.4,-19.45)) ;
#148461 = CARTESIAN_POINT('',(0.600000000000001,0.4,-19.35)) ;
#148462 = CARTESIAN_POINT('Ctrl Pts',(0.595612997216082,0.370705721320406,
-19.4207057213204)) ;
#148463 = CARTESIAN_POINT('Ctrl Pts',(0.596180587760892,0.372558268494356,
-19.4188554988322)) ;
#148464 = CARTESIAN_POINT('Ctrl Pts',(0.596672461925685,0.374355839771979,
-19.4169141798663)) ;
#148465 = CARTESIAN_POINT('Ctrl Pts',(0.599015141889215,0.38386935093007,
-19.4057649936563)) ;
#148466 = CARTESIAN_POINT('Ctrl Pts',(0.599609996542524,0.390224332900451,
-19.3949726026541)) ;
#148467 = CARTESIAN_POINT('Ctrl Pts',(0.600050586298725,0.398117439141558,
-19.3723310532047)) ;
#148468 = CARTESIAN_POINT('Ctrl Pts',(0.600000000000001,0.399999999999999,
-19.3612012506335)) ;
#148469 = CARTESIAN_POINT('Ctrl Pts',(0.600000000000001,0.399999999999999,
-19.35)) ;
#148470 = CARTESIAN_POINT('',(0.600000000000001,0.4,-19.05)) ;
#148471 = CARTESIAN_POINT('Origin',(0.500000000000001,-4.56640444411542E-17,
-18.65)) ;
#148472 = CARTESIAN_POINT('',(0.500000000000001,0.394987437106619,-18.75)) ;
#148473 = CARTESIAN_POINT('Ctrl Pts',(0.500000000000001,0.394987437106619,
-18.75)) ;
#148474 = CARTESIAN_POINT('Ctrl Pts',(0.505940567948962,0.395584486649901,
-18.75)) ;
#148475 = CARTESIAN_POINT('Ctrl Pts',(0.511931971019156,0.39613203607902,
-18.749466300328)) ;
#148476 = CARTESIAN_POINT('Ctrl Pts',(0.517829015308575,0.396618246075357,
-18.7483977957737)) ;
#148477 = CARTESIAN_POINT('Ctrl Pts',(0.522982218721217,0.397043126556055,
-18.7474640701571)) ;
#148478 = CARTESIAN_POINT('Ctrl Pts',(0.528062648970247,0.397421319341388,
-18.7461228267971)) ;
#148479 = CARTESIAN_POINT('Ctrl Pts',(0.532978106724002,0.39775150504607,
-18.7444057438766)) ;
#148480 = CARTESIAN_POINT('Ctrl Pts',(0.538583536338963,0.398128038182999,
-18.7424476378495)) ;
#148481 = CARTESIAN_POINT('Ctrl Pts',(0.544059405914878,0.398447721828296,
-18.7399700083111)) ;
#148482 = CARTESIAN_POINT('Ctrl Pts',(0.549268572255783,0.398712331108984,
-18.7370207319429)) ;
#148483 = CARTESIAN_POINT('Ctrl Pts',(0.553856850427154,0.398945401221756,
-18.7344229841468)) ;
#148484 = CARTESIAN_POINT('Ctrl Pts',(0.558237825069319,0.399135987683843,
-18.73146038498)) ;
#148485 = CARTESIAN_POINT('Ctrl Pts',(0.5623338360862,0.399290378266507,-18.7281952228642)) ;
#148486 = CARTESIAN_POINT('Ctrl Pts',(0.566990328957884,0.399465895042381,
-18.7244832689523)) ;
#148487 = CARTESIAN_POINT('Ctrl Pts',(0.571349096493418,0.399597278936107,
-18.7203228064848)) ;
#148488 = CARTESIAN_POINT('Ctrl Pts',(0.575296920056713,0.399694832180838,
-18.7158055759793)) ;
#148489 = CARTESIAN_POINT('Ctrl Pts',(0.5787442636679,0.399780018245914,-18.7118610112151)) ;
#148490 = CARTESIAN_POINT('Ctrl Pts',(0.581878314560451,0.399839626289636,
-18.7076455218421)) ;
#148491 = CARTESIAN_POINT('Ctrl Pts',(0.584648147334859,0.399882153365958,
-18.7032418177073)) ;
#148492 = CARTESIAN_POINT('Ctrl Pts',(0.587839270208173,0.399931148788079,
-18.6981683125045)) ;
#148493 = CARTESIAN_POINT('Ctrl Pts',(0.590595054415093,0.399958289583404,
-18.6927666362444)) ;
#148494 = CARTESIAN_POINT('Ctrl Pts',(0.59283861894311,0.399974357003159,
-18.6871616850094)) ;
#148495 = CARTESIAN_POINT('Ctrl Pts',(0.594777336851653,0.399988241245861,
-18.6823183122424)) ;
#148496 = CARTESIAN_POINT('Ctrl Pts',(0.596334051506184,0.399993946552814,
-18.6773241662271)) ;
#148497 = CARTESIAN_POINT('Ctrl Pts',(0.597488309822305,0.39999684570125,
-18.6722717185684)) ;
#148498 = CARTESIAN_POINT('Ctrl Pts',(0.598804024094405,0.400000150378306,
-18.6665125419605)) ;
#148499 = CARTESIAN_POINT('Ctrl Pts',(0.599612685195428,0.399999963509465,
-18.6606028438907)) ;
#148500 = CARTESIAN_POINT('Ctrl Pts',(0.59989023099972,0.399999993975383,
-18.6546842022611)) ;
#148501 = CARTESIAN_POINT('Ctrl Pts',(0.5999634645494,0.400000002014155,-18.6531225027898)) ;
#148502 = CARTESIAN_POINT('Ctrl Pts',(0.600000000000001,0.399999999999999,
-18.6515602215092)) ;
#148503 = CARTESIAN_POINT('Ctrl Pts',(0.600000000000001,0.399999999999999,
-18.65)) ;
#148504 = CARTESIAN_POINT('',(0.600000000000001,0.299999999999999,-18.65)) ;
#148505 = CARTESIAN_POINT('Ctrl Pts',(0.500000000000001,0.394987437106619,
-18.75)) ;
#148506 = CARTESIAN_POINT('Ctrl Pts',(0.500454935590171,0.395033159853782,
-18.75)) ;
#148507 = CARTESIAN_POINT('Ctrl Pts',(0.500909898680634,0.395078570329076,
-18.7499968954911)) ;
#148508 = CARTESIAN_POINT('Ctrl Pts',(0.502892456245054,0.395275075889078,
-18.7499698339419)) ;
#148509 = CARTESIAN_POINT('Ctrl Pts',(0.504418747482298,0.395422812032191,
-18.749913985421)) ;
#148510 = CARTESIAN_POINT('Ctrl Pts',(0.508462199543321,0.395804395682031,
-18.7496732810566)) ;
#148511 = CARTESIAN_POINT('Ctrl Pts',(0.510974953343265,0.396031485023314,
-18.7494279391451)) ;
#148512 = CARTESIAN_POINT('Ctrl Pts',(0.521160739721169,0.396903453186227,
-18.7480427944916)) ;
#148513 = CARTESIAN_POINT('Ctrl Pts',(0.528708678528302,0.397444933153157,
-18.7461042177047)) ;
#148514 = CARTESIAN_POINT('Ctrl Pts',(0.54594320635793,0.398105551684103,
-18.7394646394512)) ;
#148515 = CARTESIAN_POINT('Ctrl Pts',(0.555229535466698,0.397987646678449,
-18.7340353588361)) ;
#148516 = CARTESIAN_POINT('Ctrl Pts',(0.571394604995641,0.395490482808055,
-18.7207755133639)) ;
#148517 = CARTESIAN_POINT('Ctrl Pts',(0.578055313702769,0.393198948698403,
-18.7132407456319)) ;
#148518 = CARTESIAN_POINT('Ctrl Pts',(0.58855913220244,0.385442756729361,
-18.6973922339841)) ;
#148519 = CARTESIAN_POINT('Ctrl Pts',(0.592167355639942,0.380240075126989,
-18.6895482656069)) ;
#148520 = CARTESIAN_POINT('Ctrl Pts',(0.59749661553107,0.365892753467073,
-18.6739255217954)) ;
#148521 = CARTESIAN_POINT('Ctrl Pts',(0.598734255154193,0.356660564300806,
-18.666772741727)) ;
#148522 = CARTESIAN_POINT('Ctrl Pts',(0.600012754681677,0.335223914398739,
-18.6555823058657)) ;
#148523 = CARTESIAN_POINT('Ctrl Pts',(0.59999390055981,0.322655037092125,
-18.6516615193656)) ;
#148524 = CARTESIAN_POINT('Ctrl Pts',(0.600000296204999,0.306106913582367,
-18.650139626347)) ;
#148525 = CARTESIAN_POINT('Ctrl Pts',(0.600000000000001,0.303050992413449,
-18.65)) ;
#148526 = CARTESIAN_POINT('Ctrl Pts',(0.600000000000001,0.299999999999999,
-18.65)) ;
#148527 = CARTESIAN_POINT('',(0.600000000000001,-2.39800009914441E-17,-18.65)) ;
#148528 = CARTESIAN_POINT('Origin',(0.500000000000001,-1.9,-18.65)) ;
#148529 = CARTESIAN_POINT('Origin',(0.600000000000001,-1.9,-18.45)) ;
#148530 = CARTESIAN_POINT('Origin',(0.500000000000001,-1.9,-18.45)) ;
#148531 = CARTESIAN_POINT('Origin',(-0.899999999999999,-1.9,-17.675)) ;
#148532 = CARTESIAN_POINT('Origin',(-0.899999999999999,-1.9,-17.775)) ;
#148533 = CARTESIAN_POINT('Origin',(-0.899999999999999,0.6,-18.55)) ;
#148534 = CARTESIAN_POINT('Origin',(-0.899999999999999,0.6,-19.45)) ;
#148535 = CARTESIAN_POINT('Origin',(0.600000000000001,0.4,-19.45)) ;
#148536 = CARTESIAN_POINT('Origin',(0.500000000000001,0.4,-19.45)) ;
#148537 = CARTESIAN_POINT('Origin',(-0.899999999999999,0.4,-19.45)) ;
#148538 = CARTESIAN_POINT('Origin',(0.500000000000001,0.4,-19.45)) ;
#148539 = CARTESIAN_POINT('Origin',(0.500000000000001,-1.9,-18.45)) ;
#148540 = CARTESIAN_POINT('Origin',(0.500000000000001,-2.1,-18.45)) ;
#148541 = CARTESIAN_POINT('Origin',(-0.899999999999999,-1.9,-17.775)) ;
#148542 = CARTESIAN_POINT('Origin',(-1.1,-1.9,-17.775)) ;
#148543 = CARTESIAN_POINT('Origin',(-0.899999999999999,-2.1,-17.775)) ;
#148544 = CARTESIAN_POINT('Origin',(-0.899999999999999,0.4,-19.45)) ;
#148545 = CARTESIAN_POINT('Origin',(-0.899999999999999,0.4,-19.65)) ;
#148546 = CARTESIAN_POINT('Origin',(0.500000000000001,-2.1,-19.05)) ;
#148547 = CARTESIAN_POINT('Origin',(0.500000000000001,-2.1,-17.775)) ;
#148548 = CARTESIAN_POINT('Origin',(0.600000000000001,-2.1,-17.775)) ;
#148549 = CARTESIAN_POINT('Origin',(0.500000000000001,-2.1,-17.775)) ;
#148550 = CARTESIAN_POINT('Origin',(-1.1,-4.42727195005762E-17,-17.775)) ;
#148551 = CARTESIAN_POINT('',(-1.1,1.15,-17.675)) ;
#148552 = CARTESIAN_POINT('',(-1.1,1.25,-17.675)) ;
#148553 = CARTESIAN_POINT('Origin',(-1.1,1.15,-17.775)) ;
#148554 = CARTESIAN_POINT('Origin',(-0.899999999999999,0.5,-19.65)) ;
#148555 = CARTESIAN_POINT('Origin',(-0.899999999999999,-1.9,-19.65)) ;
#148556 = CARTESIAN_POINT('Origin',(0.600000000000001,-1.9,-19.65)) ;
#148557 = CARTESIAN_POINT('Origin',(0.500000000000001,-1.9,-19.65)) ;
#148558 = CARTESIAN_POINT('Origin',(-0.899999999999999,-1.9,-19.65)) ;
#148559 = CARTESIAN_POINT('Origin',(0.500000000000001,-1.9,-19.65)) ;
#148560 = CARTESIAN_POINT('Origin',(0.500000000000001,-2.1,-19.65)) ;
#148561 = CARTESIAN_POINT('Origin',(0.500000000000001,-2.1,-17.775)) ;
#148562 = CARTESIAN_POINT('Origin',(0.500000000000001,-2.1,-17.775)) ;
#148563 = CARTESIAN_POINT('Origin',(-1.1,-2.9,-17.575)) ;
#148564 = CARTESIAN_POINT('Origin',(-1.1,-2.9,-17.575)) ;
#148565 = CARTESIAN_POINT('Origin',(-1.1,-2.9,-17.575)) ;
#148566 = CARTESIAN_POINT('Origin',(-1.1,1.25,-17.575)) ;
#148567 = CARTESIAN_POINT('Origin',(-1.1,1.15,-17.575)) ;
#148568 = CARTESIAN_POINT('Origin',(-1.1,1.15,-17.775)) ;
#148569 = CARTESIAN_POINT('',(-1.1,1.25,-17.775)) ;
#148570 = CARTESIAN_POINT('Origin',(-1.1,1.15,-17.775)) ;
#148571 = CARTESIAN_POINT('Origin',(-1.1,1.15,-17.775)) ;
#148572 = CARTESIAN_POINT('Origin',(-0.899999999999999,-1.9,-19.65)) ;
#148573 = CARTESIAN_POINT('Origin',(-0.899999999999999,-1.9,-19.65)) ;
#148574 = CARTESIAN_POINT('Origin',(0.500000000000001,-2.1,-19.05)) ;
#148575 = CARTESIAN_POINT('Origin',(0.500000000000001,-2.1,-20.325)) ;
#148576 = CARTESIAN_POINT('Origin',(0.500000000000001,1.36481920536411E-16,
-17.775)) ;
#148577 = CARTESIAN_POINT('Origin',(0.500000000000001,-2.9,-17.775)) ;
#148578 = CARTESIAN_POINT('Origin',(-0.999999999999999,-2.9,-17.575)) ;
#148579 = CARTESIAN_POINT('Origin',(0.500000000000001,-2.9,-17.575)) ;
#148580 = CARTESIAN_POINT('Origin',(-1.1,1.15,-17.775)) ;
#148581 = CARTESIAN_POINT('Origin',(-1.1,1.35,-17.775)) ;
#148582 = CARTESIAN_POINT('Origin',(-1.1,1.15,-19.05)) ;
#148583 = CARTESIAN_POINT('',(-1.1,1.25,-20.325)) ;
#148584 = CARTESIAN_POINT('',(-1.1,1.25,-20.425)) ;
#148585 = CARTESIAN_POINT('Origin',(-1.1,1.15,-20.325)) ;
#148586 = CARTESIAN_POINT('Origin',(-0.899999999999999,-1.9,-19.55)) ;
#148587 = CARTESIAN_POINT('Origin',(-0.899999999999999,-1.9,-20.325)) ;
#148588 = CARTESIAN_POINT('Origin',(-0.999999999999999,-2.1,-20.325)) ;
#148589 = CARTESIAN_POINT('Origin',(0.500000000000001,-2.1,-20.325)) ;
#148590 = CARTESIAN_POINT('Origin',(-0.899999999999999,-2.1,-20.325)) ;
#148591 = CARTESIAN_POINT('Origin',(0.500000000000001,-2.1,-20.325)) ;
#148592 = CARTESIAN_POINT('Origin',(0.500000000000001,-2.1,-20.325)) ;
#148593 = CARTESIAN_POINT('Origin',(0.500000000000001,-2.9,-17.775)) ;
#148594 = CARTESIAN_POINT('Origin',(0.700000000000002,-2.9,-17.775)) ;
#148595 = CARTESIAN_POINT('Origin',(-1.1,1.35,-20.425)) ;
#148596 = CARTESIAN_POINT('Origin',(-1.1,1.35,-20.325)) ;
#148597 = CARTESIAN_POINT('Origin',(-1.1,1.15,-20.325)) ;
#148598 = CARTESIAN_POINT('',(-1.1,1.15,-20.425)) ;
#148599 = CARTESIAN_POINT('Origin',(-1.1,1.15,-20.325)) ;
#148600 = CARTESIAN_POINT('Origin',(-1.1,1.15,-20.325)) ;
#148601 = CARTESIAN_POINT('Origin',(-0.899999999999999,-1.9,-20.325)) ;
#148602 = CARTESIAN_POINT('Origin',(-1.1,-1.9,-20.325)) ;
#148603 = CARTESIAN_POINT('Origin',(0.500000000000001,-5.86744705109802E-17,
-20.325)) ;
#148604 = CARTESIAN_POINT('Origin',(0.500000000000001,-2.9,-20.325)) ;
#148605 = CARTESIAN_POINT('Origin',(0.700000000000002,-2.9,-19.05)) ;
#148606 = CARTESIAN_POINT('Origin',(0.700000000000002,-2.9,-20.325)) ;
#148607 = CARTESIAN_POINT('Origin',(-1.1,1.15,-20.325)) ;
#148608 = CARTESIAN_POINT('Origin',(-1.1,1.15,-20.525)) ;
#148609 = CARTESIAN_POINT('Origin',(-1.1,-2.39429110547967E-16,-20.325)) ;
#148610 = CARTESIAN_POINT('',(-1.1,1.25,-20.425)) ;
#148611 = CARTESIAN_POINT('Origin',(0.500000000000001,-2.9,-20.325)) ;
#148612 = CARTESIAN_POINT('Origin',(0.500000000000001,-2.9,-20.525)) ;
#148613 = CARTESIAN_POINT('Origin',(-1.1,1.25,-20.525)) ;
#148614 = CARTESIAN_POINT('Origin',(-1.1,-2.9,-20.525)) ;
#148615 = CARTESIAN_POINT('Origin',(-1.1,-2.9,-20.525)) ;
#148616 = CARTESIAN_POINT('Origin',(-1.1,-2.9,-20.525)) ;
#148617 = CARTESIAN_POINT('Origin',(-1.1,-2.9,-20.525)) ;
#148618 = CARTESIAN_POINT('Origin',(1.5,1.9,-18.45)) ;
#148619 = CARTESIAN_POINT('Origin',(1.5,1.9,-20.6)) ;
#148620 = CARTESIAN_POINT('Origin',(1.5,1.9,-19.65)) ;
#148621 = CARTESIAN_POINT('Origin',(1.5,2.1,-19.65)) ;
#148622 = CARTESIAN_POINT('Origin',(1.5,2.1,-19.45)) ;
#148623 = CARTESIAN_POINT('Origin',(1.5,1.9,-20.6)) ;
#148624 = CARTESIAN_POINT('Origin',(1.5,1.9,-20.6)) ;
#148625 = CARTESIAN_POINT('Origin',(1.5,2.1,-19.45)) ;
#148626 = CARTESIAN_POINT('Origin',(1.5,2.4,-19.45)) ;
#148627 = CARTESIAN_POINT('Origin',(1.5,2.1,-20.6)) ;
#148628 = CARTESIAN_POINT('Origin',(1.5,-2.15,-20.6)) ;
#148629 = CARTESIAN_POINT('Origin',(1.5,2.4,-19.65)) ;
#148630 = CARTESIAN_POINT('Origin',(1.5,2.6,-19.65)) ;
#148631 = CARTESIAN_POINT('Origin',(1.5,-2.15,-20.6)) ;
#148632 = CARTESIAN_POINT('Origin',(1.5,-2.15,-20.6)) ;
#148633 = CARTESIAN_POINT('Origin',(1.5,2.6,-18.45)) ;
#148634 = CARTESIAN_POINT('Origin',(1.5,2.6,-19.7585786437627)) ;
#148635 = CARTESIAN_POINT('Origin',(1.5,-2.15,-18.45)) ;
#148636 = CARTESIAN_POINT('Origin',(1.5,-2.15,-19.9531195934094)) ;
#148637 = CARTESIAN_POINT('Origin',(1.5,2.6,-19.7585786437627)) ;
#148638 = CARTESIAN_POINT('Origin',(1.5,2.6,-19.7585786437627)) ;
#148639 = CARTESIAN_POINT('Origin',(1.5,-2.15,-19.9531195934094)) ;
#148640 = CARTESIAN_POINT('Origin',(1.5,-2.15,-19.9531195934094)) ;
#148641 = CARTESIAN_POINT('Origin',(1.5,1.69571067811865,-18.8542893218813)) ;
#148642 = CARTESIAN_POINT('Origin',(1.5,3.15,-20.3085786437627)) ;
#148643 = CARTESIAN_POINT('Origin',(1.5,-3.65625,-19.05)) ;
#148644 = CARTESIAN_POINT('Origin',(1.5,-2.15,-18.1468804065906)) ;
#148645 = CARTESIAN_POINT('Origin',(1.5,3.15,-20.3085786437627)) ;
#148646 = CARTESIAN_POINT('Origin',(1.5,3.15,-20.3085786437627)) ;
#148647 = CARTESIAN_POINT('Origin',(1.5,-2.15,-18.1468804065906)) ;
#148648 = CARTESIAN_POINT('Origin',(1.5,-2.15,-18.1468804065906)) ;
#148649 = CARTESIAN_POINT('Origin',(1.5,3.15,-18.45)) ;
#148650 = CARTESIAN_POINT('Origin',(1.5,-2.15,-18.45)) ;
#148651 = CARTESIAN_POINT('Origin',(1.5,-2.15,-17.5)) ;
#148652 = CARTESIAN_POINT('Origin',(1.5,-2.15,-17.5)) ;
#148653 = CARTESIAN_POINT('Origin',(1.5,-2.15,-17.5)) ;
#148654 = CARTESIAN_POINT('Origin',(1.5,2.29571067811866,-18.6457106781187)) ;
#148655 = CARTESIAN_POINT('Origin',(1.5,2.6,-18.3414213562373)) ;
#148656 = CARTESIAN_POINT('Origin',(1.5,2.1,-17.5)) ;
#148657 = CARTESIAN_POINT('Origin',(1.5,1.9,-17.5)) ;
#148658 = CARTESIAN_POINT('Origin',(1.5,2.6,-18.3414213562373)) ;
#148659 = CARTESIAN_POINT('Origin',(1.5,2.6,-18.3414213562373)) ;
#148660 = CARTESIAN_POINT('Origin',(1.5,1.9,-17.5)) ;
#148661 = CARTESIAN_POINT('Origin',(1.5,1.9,-17.5)) ;
#148662 = CARTESIAN_POINT('Origin',(1.5,2.6,-18.45)) ;
#148663 = CARTESIAN_POINT('Origin',(1.5,2.6,-18.45)) ;
#148664 = CARTESIAN_POINT('Origin',(1.5,1.9,-18.45)) ;
#148665 = CARTESIAN_POINT('Origin',(1.5,1.9,-18.45)) ;
#148666 = CARTESIAN_POINT('Origin',(1.5,2.4,-18.45)) ;
#148667 = CARTESIAN_POINT('Origin',(1.5,2.4,-18.65)) ;
#148668 = CARTESIAN_POINT('Origin',(1.5,2.1,-18.45)) ;
#148669 = CARTESIAN_POINT('Origin',(1.5,2.1,-18.65)) ;
#148670 = CARTESIAN_POINT('Origin',(1.5,2.1,-18.65)) ;
#148671 = CARTESIAN_POINT('Origin',(-0.899999999999999,-2.,-22.26)) ;
#148672 = CARTESIAN_POINT('Origin',(-0.899999999999999,0.4,-22.26)) ;
#148673 = CARTESIAN_POINT('Origin',(-0.899999999999999,-1.9,-22.26)) ;
#148674 = CARTESIAN_POINT('Origin',(0.600000000000001,0.4,-22.46)) ;
#148675 = CARTESIAN_POINT('Origin',(0.500000000000001,0.4,-22.46)) ;
#148676 = CARTESIAN_POINT('Origin',(-0.899999999999999,0.4,-22.46)) ;
#148677 = CARTESIAN_POINT('Origin',(0.500000000000001,0.4,-22.46)) ;
#148678 = CARTESIAN_POINT('',(0.600000000000001,0.4,-22.46)) ;
#148679 = CARTESIAN_POINT('Origin',(0.500000000000001,0.4,-22.46)) ;
#148680 = CARTESIAN_POINT('Origin',(0.500000000000001,0.4,-22.46)) ;
#148681 = CARTESIAN_POINT('Origin',(-0.899999999999999,-1.9,-22.26)) ;
#148682 = CARTESIAN_POINT('Origin',(-0.899999999999999,-1.9,-22.26)) ;
#148683 = CARTESIAN_POINT('Origin',(-0.899999999999999,-1.9,-22.26)) ;
#148684 = CARTESIAN_POINT('Origin',(-0.899999999999999,0.4,-22.46)) ;
#148685 = CARTESIAN_POINT('Origin',(-0.899999999999999,0.6,-22.46)) ;
#148686 = CARTESIAN_POINT('Origin',(0.500000000000001,0.4,-22.86)) ;
#148687 = CARTESIAN_POINT('Origin',(0.500000000000001,0.4,-23.26)) ;
#148688 = CARTESIAN_POINT('',(0.600000000000001,0.4,-23.16)) ;
#148689 = CARTESIAN_POINT('Ctrl Pts',(0.595612997216081,0.370705721320404,
-23.2307057213204)) ;
#148690 = CARTESIAN_POINT('Ctrl Pts',(0.596180587760893,0.372558268494359,
-23.2288554988322)) ;
#148691 = CARTESIAN_POINT('Ctrl Pts',(0.596672461925686,0.374355839771986,
-23.2269141798663)) ;
#148692 = CARTESIAN_POINT('Ctrl Pts',(0.599015141889206,0.38386935093004,
-23.2157649936563)) ;
#148693 = CARTESIAN_POINT('Ctrl Pts',(0.599609996542524,0.390224332900438,
-23.2049726026542)) ;
#148694 = CARTESIAN_POINT('Ctrl Pts',(0.600050586298726,0.398117439141562,
-23.1823310532047)) ;
#148695 = CARTESIAN_POINT('Ctrl Pts',(0.600000000000001,0.4,-23.1712012506335)) ;
#148696 = CARTESIAN_POINT('Ctrl Pts',(0.600000000000001,0.399999999999999,
-23.16)) ;
#148697 = CARTESIAN_POINT('',(0.600000000000001,0.4,-22.86)) ;
#148698 = CARTESIAN_POINT('Origin',(0.500000000000001,-4.56640444411542E-17,
-22.46)) ;
#148699 = CARTESIAN_POINT('',(0.500000000000001,0.394987437106619,-22.56)) ;
#148700 = CARTESIAN_POINT('Ctrl Pts',(0.500000000000001,0.394987437106619,
-22.56)) ;
#148701 = CARTESIAN_POINT('Ctrl Pts',(0.50594056794894,0.395584486649899,
-22.56)) ;
#148702 = CARTESIAN_POINT('Ctrl Pts',(0.511931971019111,0.396132036079016,
-22.559466300328)) ;
#148703 = CARTESIAN_POINT('Ctrl Pts',(0.517829015308511,0.396618246075352,
-22.5583977957737)) ;
#148704 = CARTESIAN_POINT('Ctrl Pts',(0.522982218721178,0.397043126556052,
-22.5574640701571)) ;
#148705 = CARTESIAN_POINT('Ctrl Pts',(0.528062648970232,0.397421319341387,
-22.5561228267971)) ;
#148706 = CARTESIAN_POINT('Ctrl Pts',(0.532978106724004,0.397751505046071,
-22.5544057438766)) ;
#148707 = CARTESIAN_POINT('Ctrl Pts',(0.538583536338997,0.398128038183002,
-22.5524476378495)) ;
#148708 = CARTESIAN_POINT('Ctrl Pts',(0.544059405914977,0.3984477218283,-22.549970008311)) ;
#148709 = CARTESIAN_POINT('Ctrl Pts',(0.549268572255885,0.398712331108989,
-22.5470207319428)) ;
#148710 = CARTESIAN_POINT('Ctrl Pts',(0.553856850427199,0.398945401221759,
-22.5444229841468)) ;
#148711 = CARTESIAN_POINT('Ctrl Pts',(0.558237825069336,0.399135987683844,
-22.54146038498)) ;
#148712 = CARTESIAN_POINT('Ctrl Pts',(0.562333836086193,0.399290378266507,
-22.5381952228642)) ;
#148713 = CARTESIAN_POINT('Ctrl Pts',(0.56699032895789,0.399465895042382,
-22.5344832689523)) ;
#148714 = CARTESIAN_POINT('Ctrl Pts',(0.571349096493477,0.399597278936108,
-22.5303228064847)) ;
#148715 = CARTESIAN_POINT('Ctrl Pts',(0.575296920056774,0.399694832180838,
-22.5258055759793)) ;
#148716 = CARTESIAN_POINT('Ctrl Pts',(0.578744263667953,0.399780018245914,
-22.521861011215)) ;
#148717 = CARTESIAN_POINT('Ctrl Pts',(0.581878314560456,0.399839626289636,
-22.5176455218421)) ;
#148718 = CARTESIAN_POINT('Ctrl Pts',(0.584648147334871,0.399882153365958,
-22.5132418177073)) ;
#148719 = CARTESIAN_POINT('Ctrl Pts',(0.587839270208222,0.39993114878808,
-22.5081683125044)) ;
#148720 = CARTESIAN_POINT('Ctrl Pts',(0.590595054415142,0.399958289583405,
-22.5027666362444)) ;
#148721 = CARTESIAN_POINT('Ctrl Pts',(0.592838618943166,0.39997435700316,
-22.4971616850092)) ;
#148722 = CARTESIAN_POINT('Ctrl Pts',(0.594777336851685,0.399988241245861,
-22.4923183122423)) ;
#148723 = CARTESIAN_POINT('Ctrl Pts',(0.596334051506206,0.399993946552814,
-22.4873241662271)) ;
#148724 = CARTESIAN_POINT('Ctrl Pts',(0.59748830982231,0.39999684570125,-22.4822717185684)) ;
#148725 = CARTESIAN_POINT('Ctrl Pts',(0.598804024094403,0.400000150378306,
-22.4765125419605)) ;
#148726 = CARTESIAN_POINT('Ctrl Pts',(0.599612685195435,0.399999963509465,
-22.4706028438905)) ;
#148727 = CARTESIAN_POINT('Ctrl Pts',(0.599890230999722,0.399999993975383,
-22.4646842022611)) ;
#148728 = CARTESIAN_POINT('Ctrl Pts',(0.5999634645494,0.400000002014155,-22.4631225027898)) ;
#148729 = CARTESIAN_POINT('Ctrl Pts',(0.600000000000001,0.399999999999999,
-22.4615602215092)) ;
#148730 = CARTESIAN_POINT('Ctrl Pts',(0.600000000000001,0.399999999999999,
-22.46)) ;
#148731 = CARTESIAN_POINT('',(0.600000000000001,0.299999999999999,-22.46)) ;
#148732 = CARTESIAN_POINT('Ctrl Pts',(0.500000000000001,0.394987437106619,
-22.56)) ;
#148733 = CARTESIAN_POINT('Ctrl Pts',(0.50045493558952,0.395033159853717,
-22.56)) ;
#148734 = CARTESIAN_POINT('Ctrl Pts',(0.50090989868031,0.395078570329044,
-22.5599968954911)) ;
#148735 = CARTESIAN_POINT('Ctrl Pts',(0.502892456245184,0.395275075889091,
-22.5599698339419)) ;
#148736 = CARTESIAN_POINT('Ctrl Pts',(0.504418747482384,0.395422812032199,
-22.559913985421)) ;
#148737 = CARTESIAN_POINT('Ctrl Pts',(0.508462199543371,0.395804395682036,
-22.5596732810566)) ;
#148738 = CARTESIAN_POINT('Ctrl Pts',(0.510974953343326,0.396031485023319,
-22.5594279391451)) ;
#148739 = CARTESIAN_POINT('Ctrl Pts',(0.521160739721382,0.396903453186245,
-22.5580427944915)) ;
#148740 = CARTESIAN_POINT('Ctrl Pts',(0.528708678528517,0.397444933153166,
-22.5561042177046)) ;
#148741 = CARTESIAN_POINT('Ctrl Pts',(0.545943206358243,0.398105551684114,
-22.5494646394511)) ;
#148742 = CARTESIAN_POINT('Ctrl Pts',(0.555229535466965,0.397987646678414,
-22.5440353588359)) ;
#148743 = CARTESIAN_POINT('Ctrl Pts',(0.57139460499589,0.395490482808011,
-22.5307755133637)) ;
#148744 = CARTESIAN_POINT('Ctrl Pts',(0.578055313702948,0.393198948698283,
-22.5232407456316)) ;
#148745 = CARTESIAN_POINT('Ctrl Pts',(0.588559132202604,0.385442756729229,
-22.5073922339839)) ;
#148746 = CARTESIAN_POINT('Ctrl Pts',(0.592167355640029,0.380240075126779,
-22.4995482656067)) ;
#148747 = CARTESIAN_POINT('Ctrl Pts',(0.597496615531157,0.365892753466814,
-22.4839255217951)) ;
#148748 = CARTESIAN_POINT('Ctrl Pts',(0.598734255154217,0.35666056430046,
-22.4767727417268)) ;
#148749 = CARTESIAN_POINT('Ctrl Pts',(0.600012754681695,0.335223914398355,
-22.4655823058655)) ;
#148750 = CARTESIAN_POINT('Ctrl Pts',(0.59999390055981,0.322655037091671,
-22.4616615193655)) ;
#148751 = CARTESIAN_POINT('Ctrl Pts',(0.600000296204999,0.306106913582289,
-22.460139626347)) ;
#148752 = CARTESIAN_POINT('Ctrl Pts',(0.600000000000001,0.303050992413402,
-22.46)) ;
#148753 = CARTESIAN_POINT('Ctrl Pts',(0.600000000000001,0.299999999999999,
-22.46)) ;
#148754 = CARTESIAN_POINT('',(0.600000000000001,-2.39800009914441E-17,-22.46)) ;
#148755 = CARTESIAN_POINT('Origin',(0.500000000000001,-1.9,-22.46)) ;
#148756 = CARTESIAN_POINT('Origin',(0.600000000000001,-1.9,-22.26)) ;
#148757 = CARTESIAN_POINT('Origin',(0.500000000000001,-1.9,-22.26)) ;
#148758 = CARTESIAN_POINT('Origin',(-0.899999999999999,-1.9,-21.485)) ;
#148759 = CARTESIAN_POINT('Origin',(-0.899999999999999,-1.9,-21.585)) ;
#148760 = CARTESIAN_POINT('Origin',(-0.899999999999999,0.6,-22.36)) ;
#148761 = CARTESIAN_POINT('Origin',(-0.899999999999999,0.6,-23.26)) ;
#148762 = CARTESIAN_POINT('Origin',(0.600000000000001,0.4,-23.26)) ;
#148763 = CARTESIAN_POINT('Origin',(0.500000000000001,0.4,-23.26)) ;
#148764 = CARTESIAN_POINT('Origin',(-0.899999999999999,0.4,-23.26)) ;
#148765 = CARTESIAN_POINT('Origin',(0.500000000000001,0.4,-23.26)) ;
#148766 = CARTESIAN_POINT('Origin',(0.500000000000001,-1.9,-22.26)) ;
#148767 = CARTESIAN_POINT('Origin',(0.500000000000001,-2.1,-22.26)) ;
#148768 = CARTESIAN_POINT('Origin',(-0.899999999999999,-1.9,-21.585)) ;
#148769 = CARTESIAN_POINT('Origin',(-1.1,-1.9,-21.585)) ;
#148770 = CARTESIAN_POINT('Origin',(-0.899999999999999,-2.1,-21.585)) ;
#148771 = CARTESIAN_POINT('Origin',(-0.899999999999999,0.4,-23.26)) ;
#148772 = CARTESIAN_POINT('Origin',(-0.899999999999999,0.4,-23.46)) ;
#148773 = CARTESIAN_POINT('Origin',(0.500000000000001,-2.1,-22.86)) ;
#148774 = CARTESIAN_POINT('Origin',(0.500000000000001,-2.1,-21.585)) ;
#148775 = CARTESIAN_POINT('Origin',(0.600000000000001,-2.1,-21.585)) ;
#148776 = CARTESIAN_POINT('Origin',(0.500000000000001,-2.1,-21.585)) ;
#148777 = CARTESIAN_POINT('Origin',(-1.1,-4.42727195005762E-17,-21.585)) ;
#148778 = CARTESIAN_POINT('',(-1.1,1.15,-21.485)) ;
#148779 = CARTESIAN_POINT('',(-1.1,1.25,-21.485)) ;
#148780 = CARTESIAN_POINT('Origin',(-1.1,1.15,-21.585)) ;
#148781 = CARTESIAN_POINT('Origin',(-0.899999999999999,0.5,-23.46)) ;
#148782 = CARTESIAN_POINT('Origin',(-0.899999999999999,-1.9,-23.46)) ;
#148783 = CARTESIAN_POINT('Origin',(0.600000000000001,-1.9,-23.46)) ;
#148784 = CARTESIAN_POINT('Origin',(0.500000000000001,-1.9,-23.46)) ;
#148785 = CARTESIAN_POINT('Origin',(-0.899999999999999,-1.9,-23.46)) ;
#148786 = CARTESIAN_POINT('Origin',(0.500000000000001,-1.9,-23.46)) ;
#148787 = CARTESIAN_POINT('Origin',(0.500000000000001,-2.1,-23.46)) ;
#148788 = CARTESIAN_POINT('Origin',(0.500000000000001,-2.1,-21.585)) ;
#148789 = CARTESIAN_POINT('Origin',(0.500000000000001,-2.1,-21.585)) ;
#148790 = CARTESIAN_POINT('Origin',(-1.1,-2.9,-21.385)) ;
#148791 = CARTESIAN_POINT('Origin',(-1.1,-2.9,-21.385)) ;
#148792 = CARTESIAN_POINT('Origin',(-1.1,-2.9,-21.385)) ;
#148793 = CARTESIAN_POINT('Origin',(-1.1,1.25,-21.385)) ;
#148794 = CARTESIAN_POINT('Origin',(-1.1,1.15,-21.385)) ;
#148795 = CARTESIAN_POINT('Origin',(-1.1,1.15,-21.585)) ;
#148796 = CARTESIAN_POINT('',(-1.1,1.25,-21.585)) ;
#148797 = CARTESIAN_POINT('Origin',(-1.1,1.15,-21.585)) ;
#148798 = CARTESIAN_POINT('Origin',(-1.1,1.15,-21.585)) ;
#148799 = CARTESIAN_POINT('Origin',(-0.899999999999999,-1.9,-23.46)) ;
#148800 = CARTESIAN_POINT('Origin',(-0.899999999999999,-1.9,-23.46)) ;
#148801 = CARTESIAN_POINT('Origin',(0.500000000000001,-2.1,-22.86)) ;
#148802 = CARTESIAN_POINT('Origin',(0.500000000000001,-2.1,-24.135)) ;
#148803 = CARTESIAN_POINT('Origin',(0.500000000000001,1.36481920536411E-16,
-21.585)) ;
#148804 = CARTESIAN_POINT('Origin',(0.500000000000001,-2.9,-21.585)) ;
#148805 = CARTESIAN_POINT('Origin',(-0.999999999999999,-2.9,-21.385)) ;
#148806 = CARTESIAN_POINT('Origin',(0.500000000000001,-2.9,-21.385)) ;
#148807 = CARTESIAN_POINT('Origin',(-1.1,1.15,-21.585)) ;
#148808 = CARTESIAN_POINT('Origin',(-1.1,1.35,-21.585)) ;
#148809 = CARTESIAN_POINT('Origin',(-1.1,1.15,-22.86)) ;
#148810 = CARTESIAN_POINT('',(-1.1,1.25,-24.135)) ;
#148811 = CARTESIAN_POINT('',(-1.1,1.25,-24.235)) ;
#148812 = CARTESIAN_POINT('Origin',(-1.1,1.15,-24.135)) ;
#148813 = CARTESIAN_POINT('Origin',(-0.899999999999999,-1.9,-23.36)) ;
#148814 = CARTESIAN_POINT('Origin',(-0.899999999999999,-1.9,-24.135)) ;
#148815 = CARTESIAN_POINT('Origin',(-0.999999999999999,-2.1,-24.135)) ;
#148816 = CARTESIAN_POINT('Origin',(0.500000000000001,-2.1,-24.135)) ;
#148817 = CARTESIAN_POINT('Origin',(-0.899999999999999,-2.1,-24.135)) ;
#148818 = CARTESIAN_POINT('Origin',(0.500000000000001,-2.1,-24.135)) ;
#148819 = CARTESIAN_POINT('Origin',(0.500000000000001,-2.1,-24.135)) ;
#148820 = CARTESIAN_POINT('Origin',(0.500000000000001,-2.9,-21.585)) ;
#148821 = CARTESIAN_POINT('Origin',(0.700000000000002,-2.9,-21.585)) ;
#148822 = CARTESIAN_POINT('Origin',(-1.1,1.35,-24.235)) ;
#148823 = CARTESIAN_POINT('Origin',(-1.1,1.35,-24.135)) ;
#148824 = CARTESIAN_POINT('Origin',(-1.1,1.15,-24.135)) ;
#148825 = CARTESIAN_POINT('',(-1.1,1.15,-24.235)) ;
#148826 = CARTESIAN_POINT('Origin',(-1.1,1.15,-24.135)) ;
#148827 = CARTESIAN_POINT('Origin',(-1.1,1.15,-24.135)) ;
#148828 = CARTESIAN_POINT('Origin',(-0.899999999999999,-1.9,-24.135)) ;
#148829 = CARTESIAN_POINT('Origin',(-1.1,-1.9,-24.135)) ;
#148830 = CARTESIAN_POINT('Origin',(0.500000000000001,-5.86744705109802E-17,
-24.135)) ;
#148831 = CARTESIAN_POINT('Origin',(0.500000000000001,-2.9,-24.135)) ;
#148832 = CARTESIAN_POINT('Origin',(0.700000000000002,-2.9,-22.86)) ;
#148833 = CARTESIAN_POINT('Origin',(0.700000000000002,-2.9,-24.135)) ;
#148834 = CARTESIAN_POINT('Origin',(-1.1,1.15,-24.135)) ;
#148835 = CARTESIAN_POINT('Origin',(-1.1,1.15,-24.335)) ;
#148836 = CARTESIAN_POINT('Origin',(-1.1,-2.39429110547967E-16,-24.135)) ;
#148837 = CARTESIAN_POINT('',(-1.1,1.25,-24.235)) ;
#148838 = CARTESIAN_POINT('Origin',(0.500000000000001,-2.9,-24.135)) ;
#148839 = CARTESIAN_POINT('Origin',(0.500000000000001,-2.9,-24.335)) ;
#148840 = CARTESIAN_POINT('Origin',(-1.1,1.25,-24.335)) ;
#148841 = CARTESIAN_POINT('Origin',(-1.1,-2.9,-24.335)) ;
#148842 = CARTESIAN_POINT('Origin',(-1.1,-2.9,-24.335)) ;
#148843 = CARTESIAN_POINT('Origin',(-1.1,-2.9,-24.335)) ;
#148844 = CARTESIAN_POINT('Origin',(-1.1,-2.9,-24.335)) ;
#148845 = CARTESIAN_POINT('Origin',(1.5,1.9,-22.26)) ;
#148846 = CARTESIAN_POINT('Origin',(1.5,1.9,-24.41)) ;
#148847 = CARTESIAN_POINT('Origin',(1.5,1.9,-23.46)) ;
#148848 = CARTESIAN_POINT('Origin',(1.5,2.1,-23.46)) ;
#148849 = CARTESIAN_POINT('Origin',(1.5,2.1,-23.26)) ;
#148850 = CARTESIAN_POINT('Origin',(1.5,1.9,-24.41)) ;
#148851 = CARTESIAN_POINT('Origin',(1.5,1.9,-24.41)) ;
#148852 = CARTESIAN_POINT('Origin',(1.5,2.1,-23.26)) ;
#148853 = CARTESIAN_POINT('Origin',(1.5,2.4,-23.26)) ;
#148854 = CARTESIAN_POINT('Origin',(1.5,2.1,-24.41)) ;
#148855 = CARTESIAN_POINT('Origin',(1.5,-2.15,-24.41)) ;
#148856 = CARTESIAN_POINT('Origin',(1.5,2.4,-23.46)) ;
#148857 = CARTESIAN_POINT('Origin',(1.5,2.6,-23.46)) ;
#148858 = CARTESIAN_POINT('Origin',(1.5,-2.15,-24.41)) ;
#148859 = CARTESIAN_POINT('Origin',(1.5,-2.15,-24.41)) ;
#148860 = CARTESIAN_POINT('Origin',(1.5,2.6,-22.26)) ;
#148861 = CARTESIAN_POINT('Origin',(1.5,2.6,-23.5685786437627)) ;
#148862 = CARTESIAN_POINT('Origin',(1.5,-2.15,-22.26)) ;
#148863 = CARTESIAN_POINT('Origin',(1.5,-2.15,-23.7631195934094)) ;
#148864 = CARTESIAN_POINT('Origin',(1.5,2.6,-23.5685786437627)) ;
#148865 = CARTESIAN_POINT('Origin',(1.5,2.6,-23.5685786437627)) ;
#148866 = CARTESIAN_POINT('Origin',(1.5,-2.15,-23.7631195934094)) ;
#148867 = CARTESIAN_POINT('Origin',(1.5,-2.15,-23.7631195934094)) ;
#148868 = CARTESIAN_POINT('Origin',(1.5,1.69571067811865,-22.6642893218813)) ;
#148869 = CARTESIAN_POINT('Origin',(1.5,3.15,-24.1185786437627)) ;
#148870 = CARTESIAN_POINT('Origin',(1.5,-3.65625,-22.86)) ;
#148871 = CARTESIAN_POINT('Origin',(1.5,-2.15,-21.9568804065906)) ;
#148872 = CARTESIAN_POINT('Origin',(1.5,3.15,-24.1185786437627)) ;
#148873 = CARTESIAN_POINT('Origin',(1.5,3.15,-24.1185786437627)) ;
#148874 = CARTESIAN_POINT('Origin',(1.5,-2.15,-21.9568804065906)) ;
#148875 = CARTESIAN_POINT('Origin',(1.5,-2.15,-21.9568804065906)) ;
#148876 = CARTESIAN_POINT('Origin',(1.5,3.15,-22.26)) ;
#148877 = CARTESIAN_POINT('Origin',(1.5,-2.15,-22.26)) ;
#148878 = CARTESIAN_POINT('Origin',(1.5,-2.15,-21.31)) ;
#148879 = CARTESIAN_POINT('Origin',(1.5,-2.15,-21.31)) ;
#148880 = CARTESIAN_POINT('Origin',(1.5,-2.15,-21.31)) ;
#148881 = CARTESIAN_POINT('Origin',(1.5,2.29571067811866,-22.4557106781187)) ;
#148882 = CARTESIAN_POINT('Origin',(1.5,2.6,-22.1514213562373)) ;
#148883 = CARTESIAN_POINT('Origin',(1.5,2.1,-21.31)) ;
#148884 = CARTESIAN_POINT('Origin',(1.5,1.9,-21.31)) ;
#148885 = CARTESIAN_POINT('Origin',(1.5,2.6,-22.1514213562373)) ;
#148886 = CARTESIAN_POINT('Origin',(1.5,2.6,-22.1514213562373)) ;
#148887 = CARTESIAN_POINT('Origin',(1.5,1.9,-21.31)) ;
#148888 = CARTESIAN_POINT('Origin',(1.5,1.9,-21.31)) ;
#148889 = CARTESIAN_POINT('Origin',(1.5,2.6,-22.26)) ;
#148890 = CARTESIAN_POINT('Origin',(1.5,2.6,-22.26)) ;
#148891 = CARTESIAN_POINT('Origin',(1.5,1.9,-22.26)) ;
#148892 = CARTESIAN_POINT('Origin',(1.5,1.9,-22.26)) ;
#148893 = CARTESIAN_POINT('Origin',(1.5,2.4,-22.26)) ;
#148894 = CARTESIAN_POINT('Origin',(1.5,2.4,-22.46)) ;
#148895 = CARTESIAN_POINT('Origin',(1.5,2.1,-22.26)) ;
#148896 = CARTESIAN_POINT('Origin',(1.5,2.1,-22.46)) ;
#148897 = CARTESIAN_POINT('Origin',(1.5,2.1,-22.46)) ;
#148898 = CARTESIAN_POINT('Origin',(-0.899999999999999,-2.,-26.07)) ;
#148899 = CARTESIAN_POINT('Origin',(-0.899999999999999,0.4,-26.07)) ;
#148900 = CARTESIAN_POINT('Origin',(-0.899999999999999,-1.9,-26.07)) ;
#148901 = CARTESIAN_POINT('Origin',(0.600000000000001,0.4,-26.27)) ;
#148902 = CARTESIAN_POINT('Origin',(0.500000000000001,0.4,-26.27)) ;
#148903 = CARTESIAN_POINT('Origin',(-0.899999999999999,0.4,-26.27)) ;
#148904 = CARTESIAN_POINT('Origin',(0.500000000000001,0.4,-26.27)) ;
#148905 = CARTESIAN_POINT('',(0.600000000000001,0.4,-26.27)) ;
#148906 = CARTESIAN_POINT('Origin',(0.500000000000001,0.4,-26.27)) ;
#148907 = CARTESIAN_POINT('Origin',(0.500000000000001,0.4,-26.27)) ;
#148908 = CARTESIAN_POINT('Origin',(-0.899999999999999,-1.9,-26.07)) ;
#148909 = CARTESIAN_POINT('Origin',(-0.899999999999999,-1.9,-26.07)) ;
#148910 = CARTESIAN_POINT('Origin',(-0.899999999999999,-1.9,-26.07)) ;
#148911 = CARTESIAN_POINT('Origin',(-0.899999999999999,0.4,-26.27)) ;
#148912 = CARTESIAN_POINT('Origin',(-0.899999999999999,0.6,-26.27)) ;
#148913 = CARTESIAN_POINT('Origin',(0.500000000000001,0.4,-26.67)) ;
#148914 = CARTESIAN_POINT('Origin',(0.500000000000001,0.4,-27.07)) ;
#148915 = CARTESIAN_POINT('',(0.600000000000001,0.4,-26.97)) ;
#148916 = CARTESIAN_POINT('Ctrl Pts',(0.595612997216081,0.370705721320404,
-27.0407057213204)) ;
#148917 = CARTESIAN_POINT('Ctrl Pts',(0.596180587760891,0.372558268494353,
-27.0388554988322)) ;
#148918 = CARTESIAN_POINT('Ctrl Pts',(0.596672461925684,0.374355839771976,
-27.0369141798663)) ;
#148919 = CARTESIAN_POINT('Ctrl Pts',(0.599015141889213,0.383869350930061,
-27.0257649936563)) ;
#148920 = CARTESIAN_POINT('Ctrl Pts',(0.599609996542524,0.390224332900445,
-27.0149726026541)) ;
#148921 = CARTESIAN_POINT('Ctrl Pts',(0.600050586298725,0.398117439141558,
-26.9923310532047)) ;
#148922 = CARTESIAN_POINT('Ctrl Pts',(0.600000000000001,0.4,-26.9812012506335)) ;
#148923 = CARTESIAN_POINT('Ctrl Pts',(0.600000000000001,0.399999999999999,
-26.97)) ;
#148924 = CARTESIAN_POINT('',(0.600000000000001,0.4,-26.67)) ;
#148925 = CARTESIAN_POINT('Origin',(0.500000000000001,-4.56640444411542E-17,
-26.27)) ;
#148926 = CARTESIAN_POINT('',(0.500000000000001,0.394987437106619,-26.37)) ;
#148927 = CARTESIAN_POINT('Ctrl Pts',(0.500000000000001,0.394987437106619,
-26.37)) ;
#148928 = CARTESIAN_POINT('Ctrl Pts',(0.505940567948943,0.395584486649899,
-26.37)) ;
#148929 = CARTESIAN_POINT('Ctrl Pts',(0.511931971019117,0.396132036079017,
-26.369466300328)) ;
#148930 = CARTESIAN_POINT('Ctrl Pts',(0.517829015308519,0.396618246075352,
-26.3683977957737)) ;
#148931 = CARTESIAN_POINT('Ctrl Pts',(0.522982218721183,0.397043126556052,
-26.3674640701571)) ;
#148932 = CARTESIAN_POINT('Ctrl Pts',(0.528062648970233,0.397421319341387,
-26.3661228267971)) ;
#148933 = CARTESIAN_POINT('Ctrl Pts',(0.532978106724005,0.397751505046071,
-26.3644057438766)) ;
#148934 = CARTESIAN_POINT('Ctrl Pts',(0.538583536338987,0.398128038183001,
-26.3624476378495)) ;
#148935 = CARTESIAN_POINT('Ctrl Pts',(0.544059405914956,0.398447721828298,
-26.359970008311)) ;
#148936 = CARTESIAN_POINT('Ctrl Pts',(0.549268572255855,0.398712331108987,
-26.3570207319429)) ;
#148937 = CARTESIAN_POINT('Ctrl Pts',(0.553856850427182,0.398945401221758,
-26.3544229841468)) ;
#148938 = CARTESIAN_POINT('Ctrl Pts',(0.558237825069334,0.399135987683844,
-26.35146038498)) ;
#148939 = CARTESIAN_POINT('Ctrl Pts',(0.562333836086203,0.399290378266507,
-26.3481952228642)) ;
#148940 = CARTESIAN_POINT('Ctrl Pts',(0.566990328957878,0.399465895042381,
-26.3444832689523)) ;
#148941 = CARTESIAN_POINT('Ctrl Pts',(0.571349096493401,0.399597278936106,
-26.3403228064848)) ;
#148942 = CARTESIAN_POINT('Ctrl Pts',(0.575296920056684,0.399694832180836,
-26.3358055759794)) ;
#148943 = CARTESIAN_POINT('Ctrl Pts',(0.57874426366789,0.399780018245913,
-26.3318610112151)) ;
#148944 = CARTESIAN_POINT('Ctrl Pts',(0.581878314560405,0.399839626289636,
-26.3276455218421)) ;
#148945 = CARTESIAN_POINT('Ctrl Pts',(0.584648147334854,0.399882153365959,
-26.3232418177073)) ;
#148946 = CARTESIAN_POINT('Ctrl Pts',(0.587839270208225,0.39993114878808,
-26.3181683125044)) ;
#148947 = CARTESIAN_POINT('Ctrl Pts',(0.590595054415145,0.399958289583405,
-26.3127666362444)) ;
#148948 = CARTESIAN_POINT('Ctrl Pts',(0.592838618943168,0.39997435700316,
-26.3071616850092)) ;
#148949 = CARTESIAN_POINT('Ctrl Pts',(0.594777336851685,0.399988241245861,
-26.3023183122423)) ;
#148950 = CARTESIAN_POINT('Ctrl Pts',(0.596334051506207,0.399993946552814,
-26.2973241662271)) ;
#148951 = CARTESIAN_POINT('Ctrl Pts',(0.597488309822313,0.39999684570125,
-26.2922717185684)) ;
#148952 = CARTESIAN_POINT('Ctrl Pts',(0.598804024094449,0.400000150378306,
-26.2865125419603)) ;
#148953 = CARTESIAN_POINT('Ctrl Pts',(0.599612685195482,0.399999963509465,
-26.2806028438903)) ;
#148954 = CARTESIAN_POINT('Ctrl Pts',(0.599890230999748,0.399999993975383,
-26.2746842022605)) ;
#148955 = CARTESIAN_POINT('Ctrl Pts',(0.59996346454941,0.400000002014155,
-26.2731225027894)) ;
#148956 = CARTESIAN_POINT('Ctrl Pts',(0.600000000000001,0.399999999999999,
-26.271560221509)) ;
#148957 = CARTESIAN_POINT('Ctrl Pts',(0.600000000000001,0.399999999999999,
-26.27)) ;
#148958 = CARTESIAN_POINT('',(0.600000000000001,0.299999999999999,-26.27)) ;
#148959 = CARTESIAN_POINT('Ctrl Pts',(0.500000000000001,0.394987437106619,
-26.37)) ;
#148960 = CARTESIAN_POINT('Ctrl Pts',(0.500454935590171,0.395033159853782,
-26.37)) ;
#148961 = CARTESIAN_POINT('Ctrl Pts',(0.500909898680634,0.395078570329076,
-26.3699968954911)) ;
#148962 = CARTESIAN_POINT('Ctrl Pts',(0.502892456244958,0.395275075889069,
-26.3699698339419)) ;
#148963 = CARTESIAN_POINT('Ctrl Pts',(0.50441874748225,0.395422812032187,
-26.369913985421)) ;
#148964 = CARTESIAN_POINT('Ctrl Pts',(0.508462199543321,0.395804395682031,
-26.3696732810567)) ;
#148965 = CARTESIAN_POINT('Ctrl Pts',(0.510974953343264,0.396031485023314,
-26.3694279391451)) ;
#148966 = CARTESIAN_POINT('Ctrl Pts',(0.521160739721166,0.396903453186226,
-26.3680427944916)) ;
#148967 = CARTESIAN_POINT('Ctrl Pts',(0.528708678528252,0.397444933153152,
-26.3661042177047)) ;
#148968 = CARTESIAN_POINT('Ctrl Pts',(0.545943206357825,0.398105551684101,
-26.3594646394513)) ;
#148969 = CARTESIAN_POINT('Ctrl Pts',(0.555229535466584,0.397987646678453,
-26.3540353588361)) ;
#148970 = CARTESIAN_POINT('Ctrl Pts',(0.571394604995541,0.395490482808082,
-26.3407755133641)) ;
#148971 = CARTESIAN_POINT('Ctrl Pts',(0.578055313702682,0.393198948698442,
-26.333240745632)) ;
#148972 = CARTESIAN_POINT('Ctrl Pts',(0.588559132202378,0.385442756729426,
-26.3173922339843)) ;
#148973 = CARTESIAN_POINT('Ctrl Pts',(0.592167355639896,0.380240075127069,
-26.309548265607)) ;
#148974 = CARTESIAN_POINT('Ctrl Pts',(0.597496615531045,0.365892753467188,
-26.2939255217955)) ;
#148975 = CARTESIAN_POINT('Ctrl Pts',(0.598734255154177,0.356660564300953,
-26.2867727417271)) ;
#148976 = CARTESIAN_POINT('Ctrl Pts',(0.60001275468168,0.335223914398804,
-26.2755823058657)) ;
#148977 = CARTESIAN_POINT('Ctrl Pts',(0.599993900559809,0.322655037092181,
-26.2716615193656)) ;
#148978 = CARTESIAN_POINT('Ctrl Pts',(0.600000296204999,0.30610691358248,
-26.2701396263471)) ;
#148979 = CARTESIAN_POINT('Ctrl Pts',(0.600000000000001,0.303050992413506,
-26.27)) ;
#148980 = CARTESIAN_POINT('Ctrl Pts',(0.600000000000001,0.299999999999999,
-26.27)) ;
#148981 = CARTESIAN_POINT('',(0.600000000000001,-2.39800009914441E-17,-26.27)) ;
#148982 = CARTESIAN_POINT('Origin',(0.500000000000001,-1.9,-26.27)) ;
#148983 = CARTESIAN_POINT('Origin',(0.600000000000001,-1.9,-26.07)) ;
#148984 = CARTESIAN_POINT('Origin',(0.500000000000001,-1.9,-26.07)) ;
#148985 = CARTESIAN_POINT('Origin',(-0.899999999999999,-1.9,-25.295)) ;
#148986 = CARTESIAN_POINT('Origin',(-0.899999999999999,-1.9,-25.395)) ;
#148987 = CARTESIAN_POINT('Origin',(-0.899999999999999,0.6,-26.17)) ;
#148988 = CARTESIAN_POINT('Origin',(-0.899999999999999,0.6,-27.07)) ;
#148989 = CARTESIAN_POINT('Origin',(0.600000000000001,0.4,-27.07)) ;
#148990 = CARTESIAN_POINT('Origin',(0.500000000000001,0.4,-27.07)) ;
#148991 = CARTESIAN_POINT('Origin',(-0.899999999999999,0.4,-27.07)) ;
#148992 = CARTESIAN_POINT('Origin',(0.500000000000001,0.4,-27.07)) ;
#148993 = CARTESIAN_POINT('Origin',(0.500000000000001,-1.9,-26.07)) ;
#148994 = CARTESIAN_POINT('Origin',(0.500000000000001,-2.1,-26.07)) ;
#148995 = CARTESIAN_POINT('Origin',(-0.899999999999999,-1.9,-25.395)) ;
#148996 = CARTESIAN_POINT('Origin',(-1.1,-1.9,-25.395)) ;
#148997 = CARTESIAN_POINT('Origin',(-0.899999999999999,-2.1,-25.395)) ;
#148998 = CARTESIAN_POINT('Origin',(-0.899999999999999,0.4,-27.07)) ;
#148999 = CARTESIAN_POINT('Origin',(-0.899999999999999,0.4,-27.27)) ;
#149000 = CARTESIAN_POINT('Origin',(0.500000000000001,-2.1,-26.67)) ;
#149001 = CARTESIAN_POINT('Origin',(0.500000000000001,-2.1,-25.395)) ;
#149002 = CARTESIAN_POINT('Origin',(0.600000000000001,-2.1,-25.395)) ;
#149003 = CARTESIAN_POINT('Origin',(0.500000000000001,-2.1,-25.395)) ;
#149004 = CARTESIAN_POINT('Origin',(-1.1,-4.42727195005762E-17,-25.395)) ;
#149005 = CARTESIAN_POINT('',(-1.1,1.15,-25.295)) ;
#149006 = CARTESIAN_POINT('',(-1.1,1.25,-25.295)) ;
#149007 = CARTESIAN_POINT('Origin',(-1.1,1.15,-25.395)) ;
#149008 = CARTESIAN_POINT('Origin',(-0.899999999999999,0.5,-27.27)) ;
#149009 = CARTESIAN_POINT('Origin',(-0.899999999999999,-1.9,-27.27)) ;
#149010 = CARTESIAN_POINT('Origin',(0.600000000000001,-1.9,-27.27)) ;
#149011 = CARTESIAN_POINT('Origin',(0.500000000000001,-1.9,-27.27)) ;
#149012 = CARTESIAN_POINT('Origin',(-0.899999999999999,-1.9,-27.27)) ;
#149013 = CARTESIAN_POINT('Origin',(0.500000000000001,-1.9,-27.27)) ;
#149014 = CARTESIAN_POINT('Origin',(0.500000000000001,-2.1,-27.27)) ;
#149015 = CARTESIAN_POINT('Origin',(0.500000000000001,-2.1,-25.395)) ;
#149016 = CARTESIAN_POINT('Origin',(0.500000000000001,-2.1,-25.395)) ;
#149017 = CARTESIAN_POINT('Origin',(-1.1,-2.9,-25.195)) ;
#149018 = CARTESIAN_POINT('Origin',(-1.1,-2.9,-25.195)) ;
#149019 = CARTESIAN_POINT('Origin',(-1.1,-2.9,-25.195)) ;
#149020 = CARTESIAN_POINT('Origin',(-1.1,1.25,-25.195)) ;
#149021 = CARTESIAN_POINT('Origin',(-1.1,1.15,-25.195)) ;
#149022 = CARTESIAN_POINT('Origin',(-1.1,1.15,-25.395)) ;
#149023 = CARTESIAN_POINT('',(-1.1,1.25,-25.395)) ;
#149024 = CARTESIAN_POINT('Origin',(-1.1,1.15,-25.395)) ;
#149025 = CARTESIAN_POINT('Origin',(-1.1,1.15,-25.395)) ;
#149026 = CARTESIAN_POINT('Origin',(-0.899999999999999,-1.9,-27.27)) ;
#149027 = CARTESIAN_POINT('Origin',(-0.899999999999999,-1.9,-27.27)) ;
#149028 = CARTESIAN_POINT('Origin',(0.500000000000001,-2.1,-26.67)) ;
#149029 = CARTESIAN_POINT('Origin',(0.500000000000001,-2.1,-27.945)) ;
#149030 = CARTESIAN_POINT('Origin',(0.500000000000001,1.36481920536411E-16,
-25.395)) ;
#149031 = CARTESIAN_POINT('Origin',(0.500000000000001,-2.9,-25.395)) ;
#149032 = CARTESIAN_POINT('Origin',(-0.999999999999999,-2.9,-25.195)) ;
#149033 = CARTESIAN_POINT('Origin',(0.500000000000001,-2.9,-25.195)) ;
#149034 = CARTESIAN_POINT('Origin',(-1.1,1.15,-25.395)) ;
#149035 = CARTESIAN_POINT('Origin',(-1.1,1.35,-25.395)) ;
#149036 = CARTESIAN_POINT('Origin',(-1.1,1.15,-26.67)) ;
#149037 = CARTESIAN_POINT('',(-1.1,1.25,-27.945)) ;
#149038 = CARTESIAN_POINT('',(-1.1,1.25,-28.045)) ;
#149039 = CARTESIAN_POINT('Origin',(-1.1,1.15,-27.945)) ;
#149040 = CARTESIAN_POINT('Origin',(-0.899999999999999,-1.9,-27.17)) ;
#149041 = CARTESIAN_POINT('Origin',(-0.899999999999999,-1.9,-27.945)) ;
#149042 = CARTESIAN_POINT('Origin',(-0.999999999999999,-2.1,-27.945)) ;
#149043 = CARTESIAN_POINT('Origin',(0.500000000000001,-2.1,-27.945)) ;
#149044 = CARTESIAN_POINT('Origin',(-0.899999999999999,-2.1,-27.945)) ;
#149045 = CARTESIAN_POINT('Origin',(0.500000000000001,-2.1,-27.945)) ;
#149046 = CARTESIAN_POINT('Origin',(0.500000000000001,-2.1,-27.945)) ;
#149047 = CARTESIAN_POINT('Origin',(0.500000000000001,-2.9,-25.395)) ;
#149048 = CARTESIAN_POINT('Origin',(0.700000000000002,-2.9,-25.395)) ;
#149049 = CARTESIAN_POINT('Origin',(-1.1,1.35,-28.045)) ;
#149050 = CARTESIAN_POINT('Origin',(-1.1,1.35,-27.945)) ;
#149051 = CARTESIAN_POINT('Origin',(-1.1,1.15,-27.945)) ;
#149052 = CARTESIAN_POINT('',(-1.1,1.15,-28.045)) ;
#149053 = CARTESIAN_POINT('Origin',(-1.1,1.15,-27.945)) ;
#149054 = CARTESIAN_POINT('Origin',(-1.1,1.15,-27.945)) ;
#149055 = CARTESIAN_POINT('Origin',(-0.899999999999999,-1.9,-27.945)) ;
#149056 = CARTESIAN_POINT('Origin',(-1.1,-1.9,-27.945)) ;
#149057 = CARTESIAN_POINT('Origin',(0.500000000000001,-5.86744705109802E-17,
-27.945)) ;
#149058 = CARTESIAN_POINT('Origin',(0.500000000000001,-2.9,-27.945)) ;
#149059 = CARTESIAN_POINT('Origin',(0.700000000000002,-2.9,-26.67)) ;
#149060 = CARTESIAN_POINT('Origin',(0.700000000000002,-2.9,-27.945)) ;
#149061 = CARTESIAN_POINT('Origin',(-1.1,1.15,-27.945)) ;
#149062 = CARTESIAN_POINT('Origin',(-1.1,1.15,-28.145)) ;
#149063 = CARTESIAN_POINT('Origin',(-1.1,-2.39429110547967E-16,-27.945)) ;
#149064 = CARTESIAN_POINT('',(-1.1,1.25,-28.045)) ;
#149065 = CARTESIAN_POINT('Origin',(0.500000000000001,-2.9,-27.945)) ;
#149066 = CARTESIAN_POINT('Origin',(0.500000000000001,-2.9,-28.145)) ;
#149067 = CARTESIAN_POINT('Origin',(-1.1,1.25,-28.145)) ;
#149068 = CARTESIAN_POINT('Origin',(-1.1,-2.9,-28.145)) ;
#149069 = CARTESIAN_POINT('Origin',(-1.1,-2.9,-28.145)) ;
#149070 = CARTESIAN_POINT('Origin',(-1.1,-2.9,-28.145)) ;
#149071 = CARTESIAN_POINT('Origin',(-1.1,-2.9,-28.145)) ;
#149072 = CARTESIAN_POINT('Origin',(1.5,1.9,-26.07)) ;
#149073 = CARTESIAN_POINT('Origin',(1.5,1.9,-28.22)) ;
#149074 = CARTESIAN_POINT('Origin',(1.5,1.9,-27.27)) ;
#149075 = CARTESIAN_POINT('Origin',(1.5,2.1,-27.27)) ;
#149076 = CARTESIAN_POINT('Origin',(1.5,2.1,-27.07)) ;
#149077 = CARTESIAN_POINT('Origin',(1.5,1.9,-28.22)) ;
#149078 = CARTESIAN_POINT('Origin',(1.5,1.9,-28.22)) ;
#149079 = CARTESIAN_POINT('Origin',(1.5,2.1,-27.07)) ;
#149080 = CARTESIAN_POINT('Origin',(1.5,2.4,-27.07)) ;
#149081 = CARTESIAN_POINT('Origin',(1.5,2.1,-28.22)) ;
#149082 = CARTESIAN_POINT('Origin',(1.5,-2.15,-28.22)) ;
#149083 = CARTESIAN_POINT('Origin',(1.5,2.4,-27.27)) ;
#149084 = CARTESIAN_POINT('Origin',(1.5,2.6,-27.27)) ;
#149085 = CARTESIAN_POINT('Origin',(1.5,-2.15,-28.22)) ;
#149086 = CARTESIAN_POINT('Origin',(1.5,-2.15,-28.22)) ;
#149087 = CARTESIAN_POINT('Origin',(1.5,2.6,-26.07)) ;
#149088 = CARTESIAN_POINT('Origin',(1.5,2.6,-27.3785786437627)) ;
#149089 = CARTESIAN_POINT('Origin',(1.5,-2.15,-26.07)) ;
#149090 = CARTESIAN_POINT('Origin',(1.5,-2.15,-27.5731195934094)) ;
#149091 = CARTESIAN_POINT('Origin',(1.5,2.6,-27.3785786437627)) ;
#149092 = CARTESIAN_POINT('Origin',(1.5,2.6,-27.3785786437627)) ;
#149093 = CARTESIAN_POINT('Origin',(1.5,-2.15,-27.5731195934094)) ;
#149094 = CARTESIAN_POINT('Origin',(1.5,-2.15,-27.5731195934094)) ;
#149095 = CARTESIAN_POINT('Origin',(1.5,1.69571067811865,-26.4742893218813)) ;
#149096 = CARTESIAN_POINT('Origin',(1.5,3.15,-27.9285786437627)) ;
#149097 = CARTESIAN_POINT('Origin',(1.5,-3.65625,-26.67)) ;
#149098 = CARTESIAN_POINT('Origin',(1.5,-2.15,-25.7668804065906)) ;
#149099 = CARTESIAN_POINT('Origin',(1.5,3.15,-27.9285786437627)) ;
#149100 = CARTESIAN_POINT('Origin',(1.5,3.15,-27.9285786437627)) ;
#149101 = CARTESIAN_POINT('Origin',(1.5,-2.15,-25.7668804065906)) ;
#149102 = CARTESIAN_POINT('Origin',(1.5,-2.15,-25.7668804065906)) ;
#149103 = CARTESIAN_POINT('Origin',(1.5,3.15,-26.07)) ;
#149104 = CARTESIAN_POINT('Origin',(1.5,-2.15,-26.07)) ;
#149105 = CARTESIAN_POINT('Origin',(1.5,-2.15,-25.12)) ;
#149106 = CARTESIAN_POINT('Origin',(1.5,-2.15,-25.12)) ;
#149107 = CARTESIAN_POINT('Origin',(1.5,-2.15,-25.12)) ;
#149108 = CARTESIAN_POINT('Origin',(1.5,2.29571067811866,-26.2657106781187)) ;
#149109 = CARTESIAN_POINT('Origin',(1.5,2.6,-25.9614213562373)) ;
#149110 = CARTESIAN_POINT('Origin',(1.5,2.1,-25.12)) ;
#149111 = CARTESIAN_POINT('Origin',(1.5,1.9,-25.12)) ;
#149112 = CARTESIAN_POINT('Origin',(1.5,2.6,-25.9614213562373)) ;
#149113 = CARTESIAN_POINT('Origin',(1.5,2.6,-25.9614213562373)) ;
#149114 = CARTESIAN_POINT('Origin',(1.5,1.9,-25.12)) ;
#149115 = CARTESIAN_POINT('Origin',(1.5,1.9,-25.12)) ;
#149116 = CARTESIAN_POINT('Origin',(1.5,2.6,-26.07)) ;
#149117 = CARTESIAN_POINT('Origin',(1.5,2.6,-26.07)) ;
#149118 = CARTESIAN_POINT('Origin',(1.5,1.9,-26.07)) ;
#149119 = CARTESIAN_POINT('Origin',(1.5,1.9,-26.07)) ;
#149120 = CARTESIAN_POINT('Origin',(1.5,2.4,-26.07)) ;
#149121 = CARTESIAN_POINT('Origin',(1.5,2.4,-26.27)) ;
#149122 = CARTESIAN_POINT('Origin',(1.5,2.1,-26.07)) ;
#149123 = CARTESIAN_POINT('Origin',(1.5,2.1,-26.27)) ;
#149124 = CARTESIAN_POINT('Origin',(1.5,2.1,-26.27)) ;
#149125 = CARTESIAN_POINT('Origin',(-0.899999999999999,-2.,-29.88)) ;
#149126 = CARTESIAN_POINT('Origin',(-0.899999999999999,0.4,-29.88)) ;
#149127 = CARTESIAN_POINT('Origin',(-0.899999999999999,-1.9,-29.88)) ;
#149128 = CARTESIAN_POINT('Origin',(0.600000000000001,0.4,-30.08)) ;
#149129 = CARTESIAN_POINT('Origin',(0.500000000000001,0.4,-30.08)) ;
#149130 = CARTESIAN_POINT('Origin',(-0.899999999999999,0.4,-30.08)) ;
#149131 = CARTESIAN_POINT('Origin',(0.500000000000001,0.4,-30.08)) ;
#149132 = CARTESIAN_POINT('',(0.600000000000001,0.4,-30.08)) ;
#149133 = CARTESIAN_POINT('Origin',(0.500000000000001,0.4,-30.08)) ;
#149134 = CARTESIAN_POINT('Origin',(0.500000000000001,0.4,-30.08)) ;
#149135 = CARTESIAN_POINT('Origin',(-0.899999999999999,-1.9,-29.88)) ;
#149136 = CARTESIAN_POINT('Origin',(-0.899999999999999,-1.9,-29.88)) ;
#149137 = CARTESIAN_POINT('Origin',(-0.899999999999999,-1.9,-29.88)) ;
#149138 = CARTESIAN_POINT('Origin',(-0.899999999999999,0.4,-30.08)) ;
#149139 = CARTESIAN_POINT('Origin',(-0.899999999999999,0.6,-30.08)) ;
#149140 = CARTESIAN_POINT('Origin',(0.500000000000001,0.4,-30.48)) ;
#149141 = CARTESIAN_POINT('Origin',(0.500000000000001,0.4,-30.88)) ;
#149142 = CARTESIAN_POINT('',(0.600000000000001,0.4,-30.78)) ;
#149143 = CARTESIAN_POINT('Ctrl Pts',(0.595612997216081,0.370705721320405,
-30.8507057213204)) ;
#149144 = CARTESIAN_POINT('Ctrl Pts',(0.596180587760891,0.372558268494354,
-30.8488554988322)) ;
#149145 = CARTESIAN_POINT('Ctrl Pts',(0.596672461925684,0.374355839771976,
-30.8469141798663)) ;
#149146 = CARTESIAN_POINT('Ctrl Pts',(0.599015141889203,0.383869350930023,
-30.8357649936563)) ;
#149147 = CARTESIAN_POINT('Ctrl Pts',(0.599609996542522,0.390224332900425,
-30.8249726026542)) ;
#149148 = CARTESIAN_POINT('Ctrl Pts',(0.600050586298725,0.398117439141557,
-30.8023310532047)) ;
#149149 = CARTESIAN_POINT('Ctrl Pts',(0.600000000000001,0.399999999999999,
-30.7912012506335)) ;
#149150 = CARTESIAN_POINT('Ctrl Pts',(0.600000000000001,0.399999999999999,
-30.78)) ;
#149151 = CARTESIAN_POINT('',(0.600000000000001,0.4,-30.48)) ;
#149152 = CARTESIAN_POINT('Origin',(0.500000000000001,-4.56640444411542E-17,
-30.08)) ;
#149153 = CARTESIAN_POINT('',(0.500000000000001,0.394987437106619,-30.18)) ;
#149154 = CARTESIAN_POINT('Ctrl Pts',(0.500000000000001,0.394987437106619,
-30.18)) ;
#149155 = CARTESIAN_POINT('Ctrl Pts',(0.505940567948935,0.395584486649899,
-30.18)) ;
#149156 = CARTESIAN_POINT('Ctrl Pts',(0.511931971019101,0.396132036079015,
-30.179466300328)) ;
#149157 = CARTESIAN_POINT('Ctrl Pts',(0.517829015308496,0.39661824607535,
-30.1783977957737)) ;
#149158 = CARTESIAN_POINT('Ctrl Pts',(0.522982218721168,0.397043126556051,
-30.1774640701571)) ;
#149159 = CARTESIAN_POINT('Ctrl Pts',(0.528062648970226,0.397421319341387,
-30.1761228267971)) ;
#149160 = CARTESIAN_POINT('Ctrl Pts',(0.532978106724004,0.397751505046071,
-30.1744057438766)) ;
#149161 = CARTESIAN_POINT('Ctrl Pts',(0.538583536338982,0.398128038183001,
-30.1724476378495)) ;
#149162 = CARTESIAN_POINT('Ctrl Pts',(0.544059405914951,0.398447721828298,
-30.169970008311)) ;
#149163 = CARTESIAN_POINT('Ctrl Pts',(0.549268572255847,0.398712331108986,
-30.1670207319429)) ;
#149164 = CARTESIAN_POINT('Ctrl Pts',(0.553856850427178,0.398945401221757,
-30.1644229841468)) ;
#149165 = CARTESIAN_POINT('Ctrl Pts',(0.558237825069329,0.399135987683843,
-30.16146038498)) ;
#149166 = CARTESIAN_POINT('Ctrl Pts',(0.562333836086197,0.399290378266506,
-30.1581952228642)) ;
#149167 = CARTESIAN_POINT('Ctrl Pts',(0.566990328957886,0.399465895042381,
-30.1544832689523)) ;
#149168 = CARTESIAN_POINT('Ctrl Pts',(0.57134909649342,0.399597278936108,
-30.1503228064848)) ;
#149169 = CARTESIAN_POINT('Ctrl Pts',(0.575296920056715,0.399694832180838,
-30.1458055759793)) ;
#149170 = CARTESIAN_POINT('Ctrl Pts',(0.5787442636679,0.399780018245914,-30.1418610112151)) ;
#149171 = CARTESIAN_POINT('Ctrl Pts',(0.581878314560451,0.399839626289636,
-30.1376455218421)) ;
#149172 = CARTESIAN_POINT('Ctrl Pts',(0.584648147334861,0.399882153365958,
-30.1332418177073)) ;
#149173 = CARTESIAN_POINT('Ctrl Pts',(0.587839270208171,0.399931148788079,
-30.1281683125045)) ;
#149174 = CARTESIAN_POINT('Ctrl Pts',(0.590595054415091,0.399958289583404,
-30.1227666362445)) ;
#149175 = CARTESIAN_POINT('Ctrl Pts',(0.592838618943106,0.399974357003159,
-30.1171616850094)) ;
#149176 = CARTESIAN_POINT('Ctrl Pts',(0.594777336851655,0.399988241245861,
-30.1123183122424)) ;
#149177 = CARTESIAN_POINT('Ctrl Pts',(0.596334051506183,0.399993946552814,
-30.1073241662271)) ;
#149178 = CARTESIAN_POINT('Ctrl Pts',(0.597488309822302,0.39999684570125,
-30.1022717185684)) ;
#149179 = CARTESIAN_POINT('Ctrl Pts',(0.598804024094428,0.400000150378306,
-30.0965125419604)) ;
#149180 = CARTESIAN_POINT('Ctrl Pts',(0.599612685195468,0.399999963509465,
-30.0906028438904)) ;
#149181 = CARTESIAN_POINT('Ctrl Pts',(0.599890230999741,0.399999993975383,
-30.0846842022606)) ;
#149182 = CARTESIAN_POINT('Ctrl Pts',(0.599963464549407,0.400000002014155,
-30.0831225027895)) ;
#149183 = CARTESIAN_POINT('Ctrl Pts',(0.600000000000001,0.399999999999999,
-30.081560221509)) ;
#149184 = CARTESIAN_POINT('Ctrl Pts',(0.600000000000001,0.399999999999999,
-30.08)) ;
#149185 = CARTESIAN_POINT('',(0.600000000000001,0.299999999999999,-30.08)) ;
#149186 = CARTESIAN_POINT('Ctrl Pts',(0.500000000000001,0.394987437106619,
-30.18)) ;
#149187 = CARTESIAN_POINT('Ctrl Pts',(0.500454935590171,0.395033159853782,
-30.18)) ;
#149188 = CARTESIAN_POINT('Ctrl Pts',(0.500909898680634,0.395078570329076,
-30.1799968954911)) ;
#149189 = CARTESIAN_POINT('Ctrl Pts',(0.502892456244958,0.395275075889069,
-30.1799698339419)) ;
#149190 = CARTESIAN_POINT('Ctrl Pts',(0.50441874748225,0.395422812032187,
-30.179913985421)) ;
#149191 = CARTESIAN_POINT('Ctrl Pts',(0.508462199543321,0.395804395682031,
-30.1796732810567)) ;
#149192 = CARTESIAN_POINT('Ctrl Pts',(0.510974953343264,0.396031485023314,
-30.1794279391451)) ;
#149193 = CARTESIAN_POINT('Ctrl Pts',(0.521160739721166,0.396903453186226,
-30.1780427944916)) ;
#149194 = CARTESIAN_POINT('Ctrl Pts',(0.528708678528252,0.397444933153152,
-30.1761042177047)) ;
#149195 = CARTESIAN_POINT('Ctrl Pts',(0.545943206357825,0.398105551684101,
-30.1694646394513)) ;
#149196 = CARTESIAN_POINT('Ctrl Pts',(0.555229535466584,0.397987646678453,
-30.1640353588361)) ;
#149197 = CARTESIAN_POINT('Ctrl Pts',(0.571394604995541,0.395490482808082,
-30.150775513364)) ;
#149198 = CARTESIAN_POINT('Ctrl Pts',(0.578055313702682,0.393198948698442,
-30.143240745632)) ;
#149199 = CARTESIAN_POINT('Ctrl Pts',(0.588559132202378,0.385442756729426,
-30.1273922339842)) ;
#149200 = CARTESIAN_POINT('Ctrl Pts',(0.592167355639896,0.380240075127069,
-30.119548265607)) ;
#149201 = CARTESIAN_POINT('Ctrl Pts',(0.597496615531045,0.365892753467188,
-30.1039255217955)) ;
#149202 = CARTESIAN_POINT('Ctrl Pts',(0.598734255154177,0.356660564300953,
-30.0967727417271)) ;
#149203 = CARTESIAN_POINT('Ctrl Pts',(0.60001275468168,0.335223914398804,
-30.0855823058657)) ;
#149204 = CARTESIAN_POINT('Ctrl Pts',(0.599993900559809,0.322655037092181,
-30.0816615193656)) ;
#149205 = CARTESIAN_POINT('Ctrl Pts',(0.600000296204999,0.30610691358248,
-30.0801396263471)) ;
#149206 = CARTESIAN_POINT('Ctrl Pts',(0.600000000000001,0.303050992413506,
-30.08)) ;
#149207 = CARTESIAN_POINT('Ctrl Pts',(0.600000000000001,0.299999999999999,
-30.08)) ;
#149208 = CARTESIAN_POINT('',(0.600000000000001,-2.39800009914441E-17,-30.08)) ;
#149209 = CARTESIAN_POINT('Origin',(0.500000000000001,-1.9,-30.08)) ;
#149210 = CARTESIAN_POINT('Origin',(0.600000000000001,-1.9,-29.88)) ;
#149211 = CARTESIAN_POINT('Origin',(0.500000000000001,-1.9,-29.88)) ;
#149212 = CARTESIAN_POINT('Origin',(-0.899999999999999,-1.9,-29.105)) ;
#149213 = CARTESIAN_POINT('Origin',(-0.899999999999999,-1.9,-29.205)) ;
#149214 = CARTESIAN_POINT('Origin',(-0.899999999999999,0.6,-29.98)) ;
#149215 = CARTESIAN_POINT('Origin',(-0.899999999999999,0.6,-30.88)) ;
#149216 = CARTESIAN_POINT('Origin',(0.600000000000001,0.4,-30.88)) ;
#149217 = CARTESIAN_POINT('Origin',(0.500000000000001,0.4,-30.88)) ;
#149218 = CARTESIAN_POINT('Origin',(-0.899999999999999,0.4,-30.88)) ;
#149219 = CARTESIAN_POINT('Origin',(0.500000000000001,0.4,-30.88)) ;
#149220 = CARTESIAN_POINT('Origin',(0.500000000000001,-1.9,-29.88)) ;
#149221 = CARTESIAN_POINT('Origin',(0.500000000000001,-2.1,-29.88)) ;
#149222 = CARTESIAN_POINT('Origin',(-0.899999999999999,-1.9,-29.205)) ;
#149223 = CARTESIAN_POINT('Origin',(-1.1,-1.9,-29.205)) ;
#149224 = CARTESIAN_POINT('Origin',(-0.899999999999999,-2.1,-29.205)) ;
#149225 = CARTESIAN_POINT('Origin',(-0.899999999999999,0.4,-30.88)) ;
#149226 = CARTESIAN_POINT('Origin',(-0.899999999999999,0.4,-31.08)) ;
#149227 = CARTESIAN_POINT('Origin',(0.500000000000001,-2.1,-30.48)) ;
#149228 = CARTESIAN_POINT('Origin',(0.500000000000001,-2.1,-29.205)) ;
#149229 = CARTESIAN_POINT('Origin',(0.600000000000001,-2.1,-29.205)) ;
#149230 = CARTESIAN_POINT('Origin',(0.500000000000001,-2.1,-29.205)) ;
#149231 = CARTESIAN_POINT('Origin',(-1.1,-4.42727195005762E-17,-29.205)) ;
#149232 = CARTESIAN_POINT('',(-1.1,1.15,-29.105)) ;
#149233 = CARTESIAN_POINT('',(-1.1,1.25,-29.105)) ;
#149234 = CARTESIAN_POINT('Origin',(-1.1,1.15,-29.205)) ;
#149235 = CARTESIAN_POINT('Origin',(-0.899999999999999,0.5,-31.08)) ;
#149236 = CARTESIAN_POINT('Origin',(-0.899999999999999,-1.9,-31.08)) ;
#149237 = CARTESIAN_POINT('Origin',(0.600000000000001,-1.9,-31.08)) ;
#149238 = CARTESIAN_POINT('Origin',(0.500000000000001,-1.9,-31.08)) ;
#149239 = CARTESIAN_POINT('Origin',(-0.899999999999999,-1.9,-31.08)) ;
#149240 = CARTESIAN_POINT('Origin',(0.500000000000001,-1.9,-31.08)) ;
#149241 = CARTESIAN_POINT('Origin',(0.500000000000001,-2.1,-31.08)) ;
#149242 = CARTESIAN_POINT('Origin',(0.500000000000001,-2.1,-29.205)) ;
#149243 = CARTESIAN_POINT('Origin',(0.500000000000001,-2.1,-29.205)) ;
#149244 = CARTESIAN_POINT('Origin',(-1.1,-2.9,-29.005)) ;
#149245 = CARTESIAN_POINT('Origin',(-1.1,-2.9,-29.005)) ;
#149246 = CARTESIAN_POINT('Origin',(-1.1,-2.9,-29.005)) ;
#149247 = CARTESIAN_POINT('Origin',(-1.1,1.25,-29.005)) ;
#149248 = CARTESIAN_POINT('Origin',(-1.1,1.15,-29.005)) ;
#149249 = CARTESIAN_POINT('Origin',(-1.1,1.15,-29.205)) ;
#149250 = CARTESIAN_POINT('',(-1.1,1.25,-29.205)) ;
#149251 = CARTESIAN_POINT('Origin',(-1.1,1.15,-29.205)) ;
#149252 = CARTESIAN_POINT('Origin',(-1.1,1.15,-29.205)) ;
#149253 = CARTESIAN_POINT('Origin',(-0.899999999999999,-1.9,-31.08)) ;
#149254 = CARTESIAN_POINT('Origin',(-0.899999999999999,-1.9,-31.08)) ;
#149255 = CARTESIAN_POINT('Origin',(0.500000000000001,-2.1,-30.48)) ;
#149256 = CARTESIAN_POINT('Origin',(0.500000000000001,-2.1,-31.755)) ;
#149257 = CARTESIAN_POINT('Origin',(0.500000000000001,1.36481920536411E-16,
-29.205)) ;
#149258 = CARTESIAN_POINT('Origin',(0.500000000000001,-2.9,-29.205)) ;
#149259 = CARTESIAN_POINT('Origin',(-0.999999999999999,-2.9,-29.005)) ;
#149260 = CARTESIAN_POINT('Origin',(0.500000000000001,-2.9,-29.005)) ;
#149261 = CARTESIAN_POINT('Origin',(-1.1,1.15,-29.205)) ;
#149262 = CARTESIAN_POINT('Origin',(-1.1,1.35,-29.205)) ;
#149263 = CARTESIAN_POINT('Origin',(-1.1,1.15,-30.48)) ;
#149264 = CARTESIAN_POINT('',(-1.1,1.25,-31.755)) ;
#149265 = CARTESIAN_POINT('',(-1.1,1.25,-31.855)) ;
#149266 = CARTESIAN_POINT('Origin',(-1.1,1.15,-31.755)) ;
#149267 = CARTESIAN_POINT('Origin',(-0.899999999999999,-1.9,-30.98)) ;
#149268 = CARTESIAN_POINT('Origin',(-0.899999999999999,-1.9,-31.755)) ;
#149269 = CARTESIAN_POINT('Origin',(-0.999999999999999,-2.1,-31.755)) ;
#149270 = CARTESIAN_POINT('Origin',(0.500000000000001,-2.1,-31.755)) ;
#149271 = CARTESIAN_POINT('Origin',(-0.899999999999999,-2.1,-31.755)) ;
#149272 = CARTESIAN_POINT('Origin',(0.500000000000001,-2.1,-31.755)) ;
#149273 = CARTESIAN_POINT('Origin',(0.500000000000001,-2.1,-31.755)) ;
#149274 = CARTESIAN_POINT('Origin',(0.500000000000001,-2.9,-29.205)) ;
#149275 = CARTESIAN_POINT('Origin',(0.700000000000002,-2.9,-29.205)) ;
#149276 = CARTESIAN_POINT('Origin',(-1.1,1.35,-31.855)) ;
#149277 = CARTESIAN_POINT('Origin',(-1.1,1.35,-31.755)) ;
#149278 = CARTESIAN_POINT('Origin',(-1.1,1.15,-31.755)) ;
#149279 = CARTESIAN_POINT('',(-1.1,1.15,-31.855)) ;
#149280 = CARTESIAN_POINT('Origin',(-1.1,1.15,-31.755)) ;
#149281 = CARTESIAN_POINT('Origin',(-1.1,1.15,-31.755)) ;
#149282 = CARTESIAN_POINT('Origin',(-0.899999999999999,-1.9,-31.755)) ;
#149283 = CARTESIAN_POINT('Origin',(-1.1,-1.9,-31.755)) ;
#149284 = CARTESIAN_POINT('Origin',(0.500000000000001,-5.867447051098E-17,
-31.755)) ;
#149285 = CARTESIAN_POINT('Origin',(0.500000000000001,-2.9,-31.755)) ;
#149286 = CARTESIAN_POINT('Origin',(0.700000000000002,-2.9,-30.48)) ;
#149287 = CARTESIAN_POINT('Origin',(0.700000000000002,-2.9,-31.755)) ;
#149288 = CARTESIAN_POINT('Origin',(-1.1,1.15,-31.755)) ;
#149289 = CARTESIAN_POINT('Origin',(-1.1,1.15,-31.955)) ;
#149290 = CARTESIAN_POINT('Origin',(-1.1,-2.39429110547967E-16,-31.755)) ;
#149291 = CARTESIAN_POINT('',(-1.1,1.25,-31.855)) ;
#149292 = CARTESIAN_POINT('Origin',(0.500000000000001,-2.9,-31.755)) ;
#149293 = CARTESIAN_POINT('Origin',(0.500000000000001,-2.9,-31.955)) ;
#149294 = CARTESIAN_POINT('Origin',(-1.1,1.25,-31.955)) ;
#149295 = CARTESIAN_POINT('Origin',(-1.1,-2.9,-31.955)) ;
#149296 = CARTESIAN_POINT('Origin',(-1.1,-2.9,-31.955)) ;
#149297 = CARTESIAN_POINT('Origin',(-1.1,-2.9,-31.955)) ;
#149298 = CARTESIAN_POINT('Origin',(-1.1,-2.9,-31.955)) ;
#149299 = CARTESIAN_POINT('Origin',(1.5,1.9,-29.88)) ;
#149300 = CARTESIAN_POINT('Origin',(1.5,1.9,-32.03)) ;
#149301 = CARTESIAN_POINT('Origin',(1.5,1.9,-31.08)) ;
#149302 = CARTESIAN_POINT('Origin',(1.5,2.1,-31.08)) ;
#149303 = CARTESIAN_POINT('Origin',(1.5,2.1,-30.88)) ;
#149304 = CARTESIAN_POINT('Origin',(1.5,1.9,-32.03)) ;
#149305 = CARTESIAN_POINT('Origin',(1.5,1.9,-32.03)) ;
#149306 = CARTESIAN_POINT('Origin',(1.5,2.1,-30.88)) ;
#149307 = CARTESIAN_POINT('Origin',(1.5,2.4,-30.88)) ;
#149308 = CARTESIAN_POINT('Origin',(1.5,2.1,-32.03)) ;
#149309 = CARTESIAN_POINT('Origin',(1.5,-2.15,-32.03)) ;
#149310 = CARTESIAN_POINT('Origin',(1.5,2.4,-31.08)) ;
#149311 = CARTESIAN_POINT('Origin',(1.5,2.6,-31.08)) ;
#149312 = CARTESIAN_POINT('Origin',(1.5,-2.15,-32.03)) ;
#149313 = CARTESIAN_POINT('Origin',(1.5,-2.15,-32.03)) ;
#149314 = CARTESIAN_POINT('Origin',(1.5,2.6,-29.88)) ;
#149315 = CARTESIAN_POINT('Origin',(1.5,2.6,-31.1885786437627)) ;
#149316 = CARTESIAN_POINT('Origin',(1.5,-2.15,-29.88)) ;
#149317 = CARTESIAN_POINT('Origin',(1.5,-2.15,-31.3831195934094)) ;
#149318 = CARTESIAN_POINT('Origin',(1.5,2.6,-31.1885786437627)) ;
#149319 = CARTESIAN_POINT('Origin',(1.5,2.6,-31.1885786437627)) ;
#149320 = CARTESIAN_POINT('Origin',(1.5,-2.15,-31.3831195934094)) ;
#149321 = CARTESIAN_POINT('Origin',(1.5,-2.15,-31.3831195934094)) ;
#149322 = CARTESIAN_POINT('Origin',(1.5,1.69571067811865,-30.2842893218813)) ;
#149323 = CARTESIAN_POINT('Origin',(1.5,3.15,-31.7385786437627)) ;
#149324 = CARTESIAN_POINT('Origin',(1.5,-3.65625,-30.48)) ;
#149325 = CARTESIAN_POINT('Origin',(1.5,-2.15,-29.5768804065906)) ;
#149326 = CARTESIAN_POINT('Origin',(1.5,3.15,-31.7385786437627)) ;
#149327 = CARTESIAN_POINT('Origin',(1.5,3.15,-31.7385786437627)) ;
#149328 = CARTESIAN_POINT('Origin',(1.5,-2.15,-29.5768804065906)) ;
#149329 = CARTESIAN_POINT('Origin',(1.5,-2.15,-29.5768804065906)) ;
#149330 = CARTESIAN_POINT('Origin',(1.5,3.15,-29.88)) ;
#149331 = CARTESIAN_POINT('Origin',(1.5,-2.15,-29.88)) ;
#149332 = CARTESIAN_POINT('Origin',(1.5,-2.15,-28.93)) ;
#149333 = CARTESIAN_POINT('Origin',(1.5,-2.15,-28.93)) ;
#149334 = CARTESIAN_POINT('Origin',(1.5,-2.15,-28.93)) ;
#149335 = CARTESIAN_POINT('Origin',(1.5,2.29571067811866,-30.0757106781187)) ;
#149336 = CARTESIAN_POINT('Origin',(1.5,2.6,-29.7714213562373)) ;
#149337 = CARTESIAN_POINT('Origin',(1.5,2.1,-28.93)) ;
#149338 = CARTESIAN_POINT('Origin',(1.5,1.9,-28.93)) ;
#149339 = CARTESIAN_POINT('Origin',(1.5,2.6,-29.7714213562373)) ;
#149340 = CARTESIAN_POINT('Origin',(1.5,2.6,-29.7714213562373)) ;
#149341 = CARTESIAN_POINT('Origin',(1.5,1.9,-28.93)) ;
#149342 = CARTESIAN_POINT('Origin',(1.5,1.9,-28.93)) ;
#149343 = CARTESIAN_POINT('Origin',(1.5,2.6,-29.88)) ;
#149344 = CARTESIAN_POINT('Origin',(1.5,2.6,-29.88)) ;
#149345 = CARTESIAN_POINT('Origin',(1.5,1.9,-29.88)) ;
#149346 = CARTESIAN_POINT('Origin',(1.5,1.9,-29.88)) ;
#149347 = CARTESIAN_POINT('Origin',(1.5,2.4,-29.88)) ;
#149348 = CARTESIAN_POINT('Origin',(1.5,2.4,-30.08)) ;
#149349 = CARTESIAN_POINT('Origin',(1.5,2.1,-29.88)) ;
#149350 = CARTESIAN_POINT('Origin',(1.5,2.1,-30.08)) ;
#149351 = CARTESIAN_POINT('Origin',(1.5,2.1,-30.08)) ;
#149352 = CARTESIAN_POINT('Origin',(-0.899999999999999,-2.,-33.69)) ;
#149353 = CARTESIAN_POINT('Origin',(-0.899999999999999,0.4,-33.69)) ;
#149354 = CARTESIAN_POINT('Origin',(-0.899999999999999,-1.9,-33.69)) ;
#149355 = CARTESIAN_POINT('Origin',(0.600000000000001,0.4,-33.89)) ;
#149356 = CARTESIAN_POINT('Origin',(0.500000000000001,0.4,-33.89)) ;
#149357 = CARTESIAN_POINT('Origin',(-0.899999999999999,0.4,-33.89)) ;
#149358 = CARTESIAN_POINT('Origin',(0.500000000000001,0.4,-33.89)) ;
#149359 = CARTESIAN_POINT('',(0.600000000000001,0.4,-33.89)) ;
#149360 = CARTESIAN_POINT('Origin',(0.500000000000001,0.4,-33.89)) ;
#149361 = CARTESIAN_POINT('Origin',(0.500000000000001,0.4,-33.89)) ;
#149362 = CARTESIAN_POINT('Origin',(-0.899999999999999,-1.9,-33.69)) ;
#149363 = CARTESIAN_POINT('Origin',(-0.899999999999999,-1.9,-33.69)) ;
#149364 = CARTESIAN_POINT('Origin',(-0.899999999999999,-1.9,-33.69)) ;
#149365 = CARTESIAN_POINT('Origin',(-0.899999999999999,0.4,-33.89)) ;
#149366 = CARTESIAN_POINT('Origin',(-0.899999999999999,0.6,-33.89)) ;
#149367 = CARTESIAN_POINT('Origin',(0.500000000000001,0.4,-34.29)) ;
#149368 = CARTESIAN_POINT('Origin',(0.500000000000001,0.4,-34.69)) ;
#149369 = CARTESIAN_POINT('',(0.600000000000001,0.4,-34.59)) ;
#149370 = CARTESIAN_POINT('Ctrl Pts',(0.595612997216083,0.370705721320409,
-34.6607057213204)) ;
#149371 = CARTESIAN_POINT('Ctrl Pts',(0.596180587760894,0.372558268494363,
-34.6588554988322)) ;
#149372 = CARTESIAN_POINT('Ctrl Pts',(0.596672461925687,0.374355839771987,
-34.6569141798663)) ;
#149373 = CARTESIAN_POINT('Ctrl Pts',(0.599015141889206,0.383869350930039,
-34.6457649936563)) ;
#149374 = CARTESIAN_POINT('Ctrl Pts',(0.599609996542524,0.390224332900438,
-34.6349726026542)) ;
#149375 = CARTESIAN_POINT('Ctrl Pts',(0.600050586298726,0.39811743914156,
-34.6123310532047)) ;
#149376 = CARTESIAN_POINT('Ctrl Pts',(0.600000000000001,0.4,-34.6012012506335)) ;
#149377 = CARTESIAN_POINT('Ctrl Pts',(0.600000000000001,0.399999999999999,
-34.59)) ;
#149378 = CARTESIAN_POINT('',(0.600000000000001,0.4,-34.29)) ;
#149379 = CARTESIAN_POINT('Origin',(0.500000000000001,-4.56640444411538E-17,
-33.89)) ;
#149380 = CARTESIAN_POINT('',(0.500000000000001,0.394987437106619,-33.99)) ;
#149381 = CARTESIAN_POINT('Ctrl Pts',(0.500000000000001,0.394987437106619,
-33.99)) ;
#149382 = CARTESIAN_POINT('Ctrl Pts',(0.505940567948938,0.395584486649899,
-33.99)) ;
#149383 = CARTESIAN_POINT('Ctrl Pts',(0.511931971019108,0.396132036079016,
-33.989466300328)) ;
#149384 = CARTESIAN_POINT('Ctrl Pts',(0.517829015308506,0.396618246075351,
-33.9883977957737)) ;
#149385 = CARTESIAN_POINT('Ctrl Pts',(0.522982218721175,0.397043126556051,
-33.9874640701571)) ;
#149386 = CARTESIAN_POINT('Ctrl Pts',(0.52806264897023,0.397421319341387,
-33.9861228267971)) ;
#149387 = CARTESIAN_POINT('Ctrl Pts',(0.532978106724009,0.397751505046071,
-33.9844057438766)) ;
#149388 = CARTESIAN_POINT('Ctrl Pts',(0.538583536338943,0.398128038182998,
-33.9824476378496)) ;
#149389 = CARTESIAN_POINT('Ctrl Pts',(0.544059405914837,0.398447721828293,
-33.9799700083111)) ;
#149390 = CARTESIAN_POINT('Ctrl Pts',(0.549268572255721,0.39871233110898,
-33.9770207319429)) ;
#149391 = CARTESIAN_POINT('Ctrl Pts',(0.553856850427124,0.398945401221754,
-33.9744229841469)) ;
#149392 = CARTESIAN_POINT('Ctrl Pts',(0.55823782506931,0.399135987683842,
-33.97146038498)) ;
#149393 = CARTESIAN_POINT('Ctrl Pts',(0.56233383608621,0.399290378266507,
-33.9681952228642)) ;
#149394 = CARTESIAN_POINT('Ctrl Pts',(0.566990328957886,0.399465895042381,
-33.9644832689523)) ;
#149395 = CARTESIAN_POINT('Ctrl Pts',(0.571349096493416,0.399597278936107,
-33.9603228064848)) ;
#149396 = CARTESIAN_POINT('Ctrl Pts',(0.575296920056707,0.399694832180838,
-33.9558055759793)) ;
#149397 = CARTESIAN_POINT('Ctrl Pts',(0.578744263667898,0.399780018245914,
-33.9518610112151)) ;
#149398 = CARTESIAN_POINT('Ctrl Pts',(0.581878314560451,0.399839626289636,
-33.9476455218421)) ;
#149399 = CARTESIAN_POINT('Ctrl Pts',(0.584648147334857,0.399882153365958,
-33.9432418177073)) ;
#149400 = CARTESIAN_POINT('Ctrl Pts',(0.587839270208177,0.399931148788079,
-33.9381683125045)) ;
#149401 = CARTESIAN_POINT('Ctrl Pts',(0.590595054415139,0.399958289583405,
-33.9327666362444)) ;
#149402 = CARTESIAN_POINT('Ctrl Pts',(0.592838618943155,0.39997435700316,
-33.9271616850093)) ;
#149403 = CARTESIAN_POINT('Ctrl Pts',(0.594777336851684,0.399988241245861,
-33.9223183122423)) ;
#149404 = CARTESIAN_POINT('Ctrl Pts',(0.596334051506209,0.399993946552814,
-33.917324166227)) ;
#149405 = CARTESIAN_POINT('Ctrl Pts',(0.597488309822315,0.39999684570125,
-33.9122717185684)) ;
#149406 = CARTESIAN_POINT('Ctrl Pts',(0.598804024094335,0.400000150378306,
-33.9065125419608)) ;
#149407 = CARTESIAN_POINT('Ctrl Pts',(0.599612685195353,0.399999963509465,
-33.9006028438911)) ;
#149408 = CARTESIAN_POINT('Ctrl Pts',(0.599890230999679,0.399999993975383,
-33.894684202262)) ;
#149409 = CARTESIAN_POINT('Ctrl Pts',(0.599963464549386,0.400000002014155,
-33.8931225027904)) ;
#149410 = CARTESIAN_POINT('Ctrl Pts',(0.600000000000001,0.399999999999999,
-33.8915602215095)) ;
#149411 = CARTESIAN_POINT('Ctrl Pts',(0.600000000000001,0.399999999999999,
-33.89)) ;
#149412 = CARTESIAN_POINT('',(0.600000000000001,0.299999999999999,-33.89)) ;
#149413 = CARTESIAN_POINT('Ctrl Pts',(0.500000000000001,0.394987437106619,
-33.99)) ;
#149414 = CARTESIAN_POINT('Ctrl Pts',(0.500454935590171,0.395033159853782,
-33.99)) ;
#149415 = CARTESIAN_POINT('Ctrl Pts',(0.500909898680634,0.395078570329076,
-33.9899968954911)) ;
#149416 = CARTESIAN_POINT('Ctrl Pts',(0.502892456244958,0.395275075889069,
-33.9899698339419)) ;
#149417 = CARTESIAN_POINT('Ctrl Pts',(0.50441874748225,0.395422812032187,
-33.989913985421)) ;
#149418 = CARTESIAN_POINT('Ctrl Pts',(0.508462199543321,0.395804395682031,
-33.9896732810567)) ;
#149419 = CARTESIAN_POINT('Ctrl Pts',(0.510974953343264,0.396031485023314,
-33.9894279391451)) ;
#149420 = CARTESIAN_POINT('Ctrl Pts',(0.521160739721166,0.396903453186226,
-33.9880427944916)) ;
#149421 = CARTESIAN_POINT('Ctrl Pts',(0.528708678528252,0.397444933153152,
-33.9861042177047)) ;
#149422 = CARTESIAN_POINT('Ctrl Pts',(0.545943206357825,0.398105551684101,
-33.9794646394513)) ;
#149423 = CARTESIAN_POINT('Ctrl Pts',(0.555229535466584,0.397987646678453,
-33.9740353588361)) ;
#149424 = CARTESIAN_POINT('Ctrl Pts',(0.571394604995541,0.395490482808082,
-33.960775513364)) ;
#149425 = CARTESIAN_POINT('Ctrl Pts',(0.578055313702682,0.393198948698442,
-33.953240745632)) ;
#149426 = CARTESIAN_POINT('Ctrl Pts',(0.588559132202378,0.385442756729426,
-33.9373922339843)) ;
#149427 = CARTESIAN_POINT('Ctrl Pts',(0.592167355639896,0.380240075127069,
-33.929548265607)) ;
#149428 = CARTESIAN_POINT('Ctrl Pts',(0.597496615531045,0.365892753467188,
-33.9139255217955)) ;
#149429 = CARTESIAN_POINT('Ctrl Pts',(0.598734255154177,0.356660564300953,
-33.9067727417271)) ;
#149430 = CARTESIAN_POINT('Ctrl Pts',(0.60001275468168,0.335223914398804,
-33.8955823058657)) ;
#149431 = CARTESIAN_POINT('Ctrl Pts',(0.599993900559809,0.322655037092181,
-33.8916615193656)) ;
#149432 = CARTESIAN_POINT('Ctrl Pts',(0.600000296204999,0.30610691358248,
-33.8901396263471)) ;
#149433 = CARTESIAN_POINT('Ctrl Pts',(0.600000000000001,0.303050992413506,
-33.89)) ;
#149434 = CARTESIAN_POINT('Ctrl Pts',(0.600000000000001,0.299999999999999,
-33.89)) ;
#149435 = CARTESIAN_POINT('',(0.600000000000001,-2.39800009914436E-17,-33.89)) ;
#149436 = CARTESIAN_POINT('Origin',(0.500000000000001,-1.9,-33.89)) ;
#149437 = CARTESIAN_POINT('Origin',(0.600000000000001,-1.9,-33.69)) ;
#149438 = CARTESIAN_POINT('Origin',(0.500000000000001,-1.9,-33.69)) ;
#149439 = CARTESIAN_POINT('Origin',(-0.899999999999999,-1.9,-32.915)) ;
#149440 = CARTESIAN_POINT('Origin',(-0.899999999999999,-1.9,-33.015)) ;
#149441 = CARTESIAN_POINT('Origin',(-0.899999999999999,0.6,-33.79)) ;
#149442 = CARTESIAN_POINT('Origin',(-0.899999999999999,0.6,-34.69)) ;
#149443 = CARTESIAN_POINT('Origin',(0.600000000000001,0.4,-34.69)) ;
#149444 = CARTESIAN_POINT('Origin',(0.500000000000001,0.4,-34.69)) ;
#149445 = CARTESIAN_POINT('Origin',(-0.899999999999999,0.4,-34.69)) ;
#149446 = CARTESIAN_POINT('Origin',(0.500000000000001,0.4,-34.69)) ;
#149447 = CARTESIAN_POINT('Origin',(0.500000000000001,-1.9,-33.69)) ;
#149448 = CARTESIAN_POINT('Origin',(0.500000000000001,-2.1,-33.69)) ;
#149449 = CARTESIAN_POINT('Origin',(-0.899999999999999,-1.9,-33.015)) ;
#149450 = CARTESIAN_POINT('Origin',(-1.1,-1.9,-33.015)) ;
#149451 = CARTESIAN_POINT('Origin',(-0.899999999999999,-2.1,-33.015)) ;
#149452 = CARTESIAN_POINT('Origin',(-0.899999999999999,0.4,-34.69)) ;
#149453 = CARTESIAN_POINT('Origin',(-0.899999999999999,0.4,-34.89)) ;
#149454 = CARTESIAN_POINT('Origin',(0.500000000000001,-2.1,-34.29)) ;
#149455 = CARTESIAN_POINT('Origin',(0.500000000000001,-2.1,-33.015)) ;
#149456 = CARTESIAN_POINT('Origin',(0.600000000000001,-2.1,-33.015)) ;
#149457 = CARTESIAN_POINT('Origin',(0.500000000000001,-2.1,-33.015)) ;
#149458 = CARTESIAN_POINT('Origin',(-1.1,-4.42727195005762E-17,-33.015)) ;
#149459 = CARTESIAN_POINT('',(-1.1,1.15,-32.915)) ;
#149460 = CARTESIAN_POINT('',(-1.1,1.25,-32.915)) ;
#149461 = CARTESIAN_POINT('Origin',(-1.1,1.15,-33.015)) ;
#149462 = CARTESIAN_POINT('Origin',(-0.899999999999999,0.5,-34.89)) ;
#149463 = CARTESIAN_POINT('Origin',(-0.899999999999999,-1.9,-34.89)) ;
#149464 = CARTESIAN_POINT('Origin',(0.600000000000001,-1.9,-34.89)) ;
#149465 = CARTESIAN_POINT('Origin',(0.500000000000001,-1.9,-34.89)) ;
#149466 = CARTESIAN_POINT('Origin',(-0.899999999999999,-1.9,-34.89)) ;
#149467 = CARTESIAN_POINT('Origin',(0.500000000000001,-1.9,-34.89)) ;
#149468 = CARTESIAN_POINT('Origin',(0.500000000000001,-2.1,-34.89)) ;
#149469 = CARTESIAN_POINT('Origin',(0.500000000000001,-2.1,-33.015)) ;
#149470 = CARTESIAN_POINT('Origin',(0.500000000000001,-2.1,-33.015)) ;
#149471 = CARTESIAN_POINT('Origin',(-1.1,-2.9,-32.815)) ;
#149472 = CARTESIAN_POINT('Origin',(-1.1,-2.9,-32.815)) ;
#149473 = CARTESIAN_POINT('Origin',(-1.1,-2.9,-32.815)) ;
#149474 = CARTESIAN_POINT('Origin',(-1.1,1.25,-32.815)) ;
#149475 = CARTESIAN_POINT('Origin',(-1.1,1.15,-32.815)) ;
#149476 = CARTESIAN_POINT('Origin',(-1.1,1.15,-33.015)) ;
#149477 = CARTESIAN_POINT('',(-1.1,1.25,-33.015)) ;
#149478 = CARTESIAN_POINT('Origin',(-1.1,1.15,-33.015)) ;
#149479 = CARTESIAN_POINT('Origin',(-1.1,1.15,-33.015)) ;
#149480 = CARTESIAN_POINT('Origin',(-0.899999999999999,-1.9,-34.89)) ;
#149481 = CARTESIAN_POINT('Origin',(-0.899999999999999,-1.9,-34.89)) ;
#149482 = CARTESIAN_POINT('Origin',(0.500000000000001,-2.1,-34.29)) ;
#149483 = CARTESIAN_POINT('Origin',(0.500000000000001,-2.1,-35.565)) ;
#149484 = CARTESIAN_POINT('Origin',(0.500000000000001,1.36481920536411E-16,
-33.015)) ;
#149485 = CARTESIAN_POINT('Origin',(0.500000000000001,-2.9,-33.015)) ;
#149486 = CARTESIAN_POINT('Origin',(-0.999999999999999,-2.9,-32.815)) ;
#149487 = CARTESIAN_POINT('Origin',(0.500000000000001,-2.9,-32.815)) ;
#149488 = CARTESIAN_POINT('Origin',(-1.1,1.15,-33.015)) ;
#149489 = CARTESIAN_POINT('Origin',(-1.1,1.35,-33.015)) ;
#149490 = CARTESIAN_POINT('Origin',(-1.1,1.15,-34.29)) ;
#149491 = CARTESIAN_POINT('',(-1.1,1.25,-35.565)) ;
#149492 = CARTESIAN_POINT('',(-1.1,1.25,-35.665)) ;
#149493 = CARTESIAN_POINT('Origin',(-1.1,1.15,-35.565)) ;
#149494 = CARTESIAN_POINT('Origin',(-0.899999999999999,-1.9,-34.79)) ;
#149495 = CARTESIAN_POINT('Origin',(-0.899999999999999,-1.9,-35.565)) ;
#149496 = CARTESIAN_POINT('Origin',(-0.999999999999999,-2.1,-35.565)) ;
#149497 = CARTESIAN_POINT('Origin',(0.500000000000001,-2.1,-35.565)) ;
#149498 = CARTESIAN_POINT('Origin',(-0.899999999999999,-2.1,-35.565)) ;
#149499 = CARTESIAN_POINT('Origin',(0.500000000000001,-2.1,-35.565)) ;
#149500 = CARTESIAN_POINT('Origin',(0.500000000000001,-2.1,-35.565)) ;
#149501 = CARTESIAN_POINT('Origin',(0.500000000000001,-2.9,-33.015)) ;
#149502 = CARTESIAN_POINT('Origin',(0.700000000000002,-2.9,-33.015)) ;
#149503 = CARTESIAN_POINT('Origin',(-1.1,1.35,-35.665)) ;
#149504 = CARTESIAN_POINT('Origin',(-1.1,1.35,-35.565)) ;
#149505 = CARTESIAN_POINT('Origin',(-1.1,1.15,-35.565)) ;
#149506 = CARTESIAN_POINT('',(-1.1,1.15,-35.665)) ;
#149507 = CARTESIAN_POINT('Origin',(-1.1,1.15,-35.565)) ;
#149508 = CARTESIAN_POINT('Origin',(-1.1,1.15,-35.565)) ;
#149509 = CARTESIAN_POINT('Origin',(-0.899999999999999,-1.9,-35.565)) ;
#149510 = CARTESIAN_POINT('Origin',(-1.1,-1.9,-35.565)) ;
#149511 = CARTESIAN_POINT('Origin',(0.500000000000001,-5.867447051098E-17,
-35.565)) ;
#149512 = CARTESIAN_POINT('Origin',(0.500000000000001,-2.9,-35.565)) ;
#149513 = CARTESIAN_POINT('Origin',(0.700000000000002,-2.9,-34.29)) ;
#149514 = CARTESIAN_POINT('Origin',(0.700000000000002,-2.9,-35.565)) ;
#149515 = CARTESIAN_POINT('Origin',(-1.1,1.15,-35.565)) ;
#149516 = CARTESIAN_POINT('Origin',(-1.1,1.15,-35.765)) ;
#149517 = CARTESIAN_POINT('Origin',(-1.1,-2.39429110547967E-16,-35.565)) ;
#149518 = CARTESIAN_POINT('',(-1.1,1.25,-35.665)) ;
#149519 = CARTESIAN_POINT('Origin',(0.500000000000001,-2.9,-35.565)) ;
#149520 = CARTESIAN_POINT('Origin',(0.500000000000001,-2.9,-35.765)) ;
#149521 = CARTESIAN_POINT('Origin',(-1.1,1.25,-35.765)) ;
#149522 = CARTESIAN_POINT('Origin',(-1.1,-2.9,-35.765)) ;
#149523 = CARTESIAN_POINT('Origin',(-1.1,-2.9,-35.765)) ;
#149524 = CARTESIAN_POINT('Origin',(-1.1,-2.9,-35.765)) ;
#149525 = CARTESIAN_POINT('Origin',(-1.1,-2.9,-35.765)) ;
#149526 = CARTESIAN_POINT('Origin',(1.5,1.9,-33.69)) ;
#149527 = CARTESIAN_POINT('Origin',(1.5,1.9,-35.84)) ;
#149528 = CARTESIAN_POINT('Origin',(1.5,1.9,-34.89)) ;
#149529 = CARTESIAN_POINT('Origin',(1.5,2.1,-34.89)) ;
#149530 = CARTESIAN_POINT('Origin',(1.5,2.1,-34.69)) ;
#149531 = CARTESIAN_POINT('Origin',(1.5,1.9,-35.84)) ;
#149532 = CARTESIAN_POINT('Origin',(1.5,1.9,-35.84)) ;
#149533 = CARTESIAN_POINT('Origin',(1.5,2.1,-34.69)) ;
#149534 = CARTESIAN_POINT('Origin',(1.5,2.4,-34.69)) ;
#149535 = CARTESIAN_POINT('Origin',(1.5,2.1,-35.84)) ;
#149536 = CARTESIAN_POINT('Origin',(1.5,-2.15,-35.84)) ;
#149537 = CARTESIAN_POINT('Origin',(1.5,2.4,-34.89)) ;
#149538 = CARTESIAN_POINT('Origin',(1.5,2.6,-34.89)) ;
#149539 = CARTESIAN_POINT('Origin',(1.5,-2.15,-35.84)) ;
#149540 = CARTESIAN_POINT('Origin',(1.5,-2.15,-35.84)) ;
#149541 = CARTESIAN_POINT('Origin',(1.5,2.6,-33.69)) ;
#149542 = CARTESIAN_POINT('Origin',(1.5,2.6,-34.9985786437627)) ;
#149543 = CARTESIAN_POINT('Origin',(1.5,-2.15,-33.69)) ;
#149544 = CARTESIAN_POINT('Origin',(1.5,-2.15,-35.1931195934094)) ;
#149545 = CARTESIAN_POINT('Origin',(1.5,2.6,-34.9985786437627)) ;
#149546 = CARTESIAN_POINT('Origin',(1.5,2.6,-34.9985786437627)) ;
#149547 = CARTESIAN_POINT('Origin',(1.5,-2.15,-35.1931195934094)) ;
#149548 = CARTESIAN_POINT('Origin',(1.5,-2.15,-35.1931195934094)) ;
#149549 = CARTESIAN_POINT('Origin',(1.5,1.69571067811865,-34.0942893218813)) ;
#149550 = CARTESIAN_POINT('Origin',(1.5,3.15,-35.5485786437627)) ;
#149551 = CARTESIAN_POINT('Origin',(1.5,-3.65625,-34.29)) ;
#149552 = CARTESIAN_POINT('Origin',(1.5,-2.15,-33.3868804065906)) ;
#149553 = CARTESIAN_POINT('Origin',(1.5,3.15,-35.5485786437627)) ;
#149554 = CARTESIAN_POINT('Origin',(1.5,3.15,-35.5485786437627)) ;
#149555 = CARTESIAN_POINT('Origin',(1.5,-2.15,-33.3868804065906)) ;
#149556 = CARTESIAN_POINT('Origin',(1.5,-2.15,-33.3868804065906)) ;
#149557 = CARTESIAN_POINT('Origin',(1.5,3.15,-33.69)) ;
#149558 = CARTESIAN_POINT('Origin',(1.5,-2.15,-33.69)) ;
#149559 = CARTESIAN_POINT('Origin',(1.5,-2.15,-32.74)) ;
#149560 = CARTESIAN_POINT('Origin',(1.5,-2.15,-32.74)) ;
#149561 = CARTESIAN_POINT('Origin',(1.5,-2.15,-32.74)) ;
#149562 = CARTESIAN_POINT('Origin',(1.5,2.29571067811866,-33.8857106781187)) ;
#149563 = CARTESIAN_POINT('Origin',(1.5,2.6,-33.5814213562373)) ;
#149564 = CARTESIAN_POINT('Origin',(1.5,2.1,-32.74)) ;
#149565 = CARTESIAN_POINT('Origin',(1.5,1.9,-32.74)) ;
#149566 = CARTESIAN_POINT('Origin',(1.5,2.6,-33.5814213562373)) ;
#149567 = CARTESIAN_POINT('Origin',(1.5,2.6,-33.5814213562373)) ;
#149568 = CARTESIAN_POINT('Origin',(1.5,1.9,-32.74)) ;
#149569 = CARTESIAN_POINT('Origin',(1.5,1.9,-32.74)) ;
#149570 = CARTESIAN_POINT('Origin',(1.5,2.6,-33.69)) ;
#149571 = CARTESIAN_POINT('Origin',(1.5,2.6,-33.69)) ;
#149572 = CARTESIAN_POINT('Origin',(1.5,1.9,-33.69)) ;
#149573 = CARTESIAN_POINT('Origin',(1.5,1.9,-33.69)) ;
#149574 = CARTESIAN_POINT('Origin',(1.5,2.4,-33.69)) ;
#149575 = CARTESIAN_POINT('Origin',(1.5,2.4,-33.89)) ;
#149576 = CARTESIAN_POINT('Origin',(1.5,2.1,-33.69)) ;
#149577 = CARTESIAN_POINT('Origin',(1.5,2.1,-33.89)) ;
#149578 = CARTESIAN_POINT('Origin',(1.5,2.1,-33.89)) ;
#149579 = CARTESIAN_POINT('Origin',(-0.4,-0.600000000000001,-3.41)) ;
#149580 = CARTESIAN_POINT('',(-0.4,-0.600000000000001,-3.51)) ;
#149581 = CARTESIAN_POINT('',(-0.4,-0.600000000000001,-4.11)) ;
#149582 = CARTESIAN_POINT('',(-0.4,-0.600000000000001,-3.41)) ;
#149583 = CARTESIAN_POINT('',(-0.4,-6.05857864376269,-4.11)) ;
#149584 = CARTESIAN_POINT('',(-0.4,-0.600000000000001,-4.11)) ;
#149585 = CARTESIAN_POINT('',(-0.4,-6.05857864376269,-3.51)) ;
#149586 = CARTESIAN_POINT('',(-0.4,-6.05857864376269,-3.41)) ;
#149587 = CARTESIAN_POINT('',(-0.4,-0.600000000000001,-3.51)) ;
#149588 = CARTESIAN_POINT('Origin',(-0.4,-6.1,-3.41)) ;
#149589 = CARTESIAN_POINT('',(-0.129289321881346,-6.37071067811866,-3.86857864376269)) ;
#149590 = CARTESIAN_POINT('',(-0.129289321881346,-6.37071067811866,-3.75142135623731)) ;
#149591 = CARTESIAN_POINT('',(-0.129289321881346,-6.37071067811866,-3.41)) ;
#149592 = CARTESIAN_POINT('',(-0.370710678118655,-6.12928932188134,-3.51)) ;
#149593 = CARTESIAN_POINT('',(-0.423570226039552,-6.07642977396045,-3.4571404520791)) ;
#149594 = CARTESIAN_POINT('',(-0.370710678118655,-6.12928932188134,-4.11)) ;
#149595 = CARTESIAN_POINT('',(-0.370710678118655,-6.12928932188134,-3.41)) ;
#149596 = CARTESIAN_POINT('',(-0.156903559372885,-6.34309644062712,-3.89619288125423)) ;
#149597 = CARTESIAN_POINT('Origin',(-0.1,-6.4,-3.41)) ;
#149598 = CARTESIAN_POINT('',(0.0585786437626908,-6.4,-3.86857864376269)) ;
#149599 = CARTESIAN_POINT('',(0.0585786437626908,-6.4,-3.75142135623731)) ;
#149600 = CARTESIAN_POINT('',(0.0585786437626908,-6.4,-3.41)) ;
#149601 = CARTESIAN_POINT('',(-0.0585786437626908,-6.4,-3.75142135623731)) ;
#149602 = CARTESIAN_POINT('',(-0.1,-6.4,-3.75142135623731)) ;
#149603 = CARTESIAN_POINT('',(-0.0585786437626908,-6.4,-3.86857864376269)) ;
#149604 = CARTESIAN_POINT('',(-0.0585786437626908,-6.4,-3.41)) ;
#149605 = CARTESIAN_POINT('',(-0.1,-6.4,-3.86857864376269)) ;
#149606 = CARTESIAN_POINT('Origin',(0.1,-6.4,-3.41)) ;
#149607 = CARTESIAN_POINT('',(0.370710678118655,-6.12928932188134,-4.11)) ;
#149608 = CARTESIAN_POINT('',(0.370710678118655,-6.12928932188134,-3.51)) ;
#149609 = CARTESIAN_POINT('',(0.370710678118655,-6.12928932188134,-3.41)) ;
#149610 = CARTESIAN_POINT('',(0.129289321881346,-6.37071067811866,-3.75142135623731)) ;
#149611 = CARTESIAN_POINT('',(0.223570226039552,-6.27642977396045,-3.6571404520791)) ;
#149612 = CARTESIAN_POINT('',(0.129289321881346,-6.37071067811866,-3.86857864376269)) ;
#149613 = CARTESIAN_POINT('',(0.129289321881346,-6.37071067811866,-3.41)) ;
#149614 = CARTESIAN_POINT('',(-0.0430964406271149,-6.54309644062712,-3.69619288125423)) ;
#149615 = CARTESIAN_POINT('Origin',(0.4,-6.1,-3.41)) ;
#149616 = CARTESIAN_POINT('',(0.4,-6.05857864376269,-3.51)) ;
#149617 = CARTESIAN_POINT('',(0.4,-6.05857864376269,-4.11)) ;
#149618 = CARTESIAN_POINT('',(0.4,-6.05857864376269,-3.41)) ;
#149619 = CARTESIAN_POINT('',(0.4,-0.6,-4.11)) ;
#149620 = CARTESIAN_POINT('',(0.4,-6.1,-4.11)) ;
#149621 = CARTESIAN_POINT('',(0.4,-0.6,-3.51)) ;
#149622 = CARTESIAN_POINT('',(0.4,-0.6,-3.41)) ;
#149623 = CARTESIAN_POINT('',(0.4,-6.05857864376269,-3.51)) ;
#149624 = CARTESIAN_POINT('Origin',(0.6,-0.600000000000001,-3.41)) ;
#149625 = CARTESIAN_POINT('',(0.3,-6.05857864376269,-3.41)) ;
#149626 = CARTESIAN_POINT('',(0.3,-0.6,-3.41)) ;
#149627 = CARTESIAN_POINT('',(0.3,-0.6,-3.41)) ;
#149628 = CARTESIAN_POINT('Origin',(0.6,-0.6,-3.41)) ;
#149629 = CARTESIAN_POINT('',(-0.3,-0.600000000000001,-3.41)) ;
#149630 = CARTESIAN_POINT('Origin',(0.6,-0.600000000000001,-3.41)) ;
#149631 = CARTESIAN_POINT('',(-0.299999999999999,-6.05857864376269,-3.41)) ;
#149632 = CARTESIAN_POINT('',(-0.3,-0.600000000000001,-3.41)) ;
#149633 = CARTESIAN_POINT('',(0.4,-6.05857864376269,-3.41)) ;
#149634 = CARTESIAN_POINT('Origin',(0.6,-0.600000000000001,-4.21)) ;
#149635 = CARTESIAN_POINT('',(-0.300000000000001,-6.05857864376269,-4.21)) ;
#149636 = CARTESIAN_POINT('',(-0.3,-0.600000000000001,-4.21)) ;
#149637 = CARTESIAN_POINT('',(-0.3,-0.600000000000001,-4.21)) ;
#149638 = CARTESIAN_POINT('Origin',(0.6,-0.600000000000001,-4.21)) ;
#149639 = CARTESIAN_POINT('',(0.3,-0.6,-4.21)) ;
#149640 = CARTESIAN_POINT('Origin',(0.6,-0.6,-4.21)) ;
#149641 = CARTESIAN_POINT('',(0.3,-6.05857864376269,-4.21)) ;
#149642 = CARTESIAN_POINT('',(0.3,-0.600000000000001,-4.21)) ;
#149643 = CARTESIAN_POINT('',(0.6,-6.05857864376269,-4.21)) ;
#149644 = CARTESIAN_POINT('Origin',(0.6,-0.600000000000001,-3.41)) ;
#149645 = CARTESIAN_POINT('Origin',(0.6,-0.600000000000001,-4.11)) ;
#149646 = CARTESIAN_POINT('Origin',(0.6,-0.600000000000001,-3.51)) ;
#149647 = CARTESIAN_POINT('Origin',(0.6,-0.6,-3.41)) ;
#149648 = CARTESIAN_POINT('Origin',(0.6,-0.6,-4.11)) ;
#149649 = CARTESIAN_POINT('Origin',(0.6,-0.6,-3.51)) ;
#149650 = CARTESIAN_POINT('Origin',(7.,0.1,-3.41)) ;
#149651 = CARTESIAN_POINT('',(6.72928932188135,0.370710678118655,-4.11)) ;
#149652 = CARTESIAN_POINT('',(6.72928932188135,0.370710678118655,-3.51)) ;
#149653 = CARTESIAN_POINT('',(6.72928932188135,0.370710678118655,-3.41)) ;
#149654 = CARTESIAN_POINT('',(6.97071067811866,0.129289321881346,-3.75142135623731)) ;
#149655 = CARTESIAN_POINT('',(6.87642977396045,0.223570226039552,-3.6571404520791)) ;
#149656 = CARTESIAN_POINT('',(6.97071067811866,0.129289321881346,-3.86857864376269)) ;
#149657 = CARTESIAN_POINT('',(6.97071067811866,0.129289321881346,-3.41)) ;
#149658 = CARTESIAN_POINT('',(7.14309644062712,-0.0430964406271146,-3.69619288125423)) ;
#149659 = CARTESIAN_POINT('Origin',(6.7,0.400000000000001,-3.41)) ;
#149660 = CARTESIAN_POINT('',(6.65857864376269,0.400000000000001,-3.51)) ;
#149661 = CARTESIAN_POINT('',(6.65857864376269,0.400000000000001,-4.11)) ;
#149662 = CARTESIAN_POINT('',(6.65857864376269,0.400000000000001,-3.41)) ;
#149663 = CARTESIAN_POINT('',(6.7,0.400000000000001,-4.11)) ;
#149664 = CARTESIAN_POINT('',(6.65857864376269,0.400000000000001,-3.51)) ;
#149665 = CARTESIAN_POINT('Origin',(0.6,-0.4,-3.41)) ;
#149666 = CARTESIAN_POINT('',(6.65857864376269,-0.400000000000001,-4.11)) ;
#149667 = CARTESIAN_POINT('',(0.6,-0.4,-4.11)) ;
#149668 = CARTESIAN_POINT('',(6.65857864376269,-0.400000000000001,-3.51)) ;
#149669 = CARTESIAN_POINT('',(6.65857864376269,-0.400000000000001,-3.41)) ;
#149670 = CARTESIAN_POINT('',(2.4,-0.4,-3.51)) ;
#149671 = CARTESIAN_POINT('Origin',(6.7,-0.400000000000001,-3.41)) ;
#149672 = CARTESIAN_POINT('',(6.97071067811866,-0.129289321881346,-3.86857864376269)) ;
#149673 = CARTESIAN_POINT('',(6.97071067811866,-0.129289321881346,-3.75142135623731)) ;
#149674 = CARTESIAN_POINT('',(6.97071067811866,-0.129289321881346,-3.41)) ;
#149675 = CARTESIAN_POINT('',(6.72928932188135,-0.370710678118655,-3.51)) ;
#149676 = CARTESIAN_POINT('',(6.67642977396045,-0.423570226039552,-3.4571404520791)) ;
#149677 = CARTESIAN_POINT('',(6.72928932188135,-0.370710678118655,-4.11)) ;
#149678 = CARTESIAN_POINT('',(6.72928932188135,-0.370710678118655,-3.41)) ;
#149679 = CARTESIAN_POINT('',(6.94309644062712,-0.156903559372885,-3.89619288125423)) ;
#149680 = CARTESIAN_POINT('Origin',(7.,-0.1,-3.41)) ;
#149681 = CARTESIAN_POINT('',(7.,-0.0585786437626909,-3.75142135623731)) ;
#149682 = CARTESIAN_POINT('',(7.,-0.0585786437626909,-3.86857864376269)) ;
#149683 = CARTESIAN_POINT('',(7.,-0.0585786437626909,-3.41)) ;
#149684 = CARTESIAN_POINT('',(7.,0.0585786437626909,-3.86857864376269)) ;
#149685 = CARTESIAN_POINT('',(7.,-0.1,-3.86857864376269)) ;
#149686 = CARTESIAN_POINT('',(7.,0.0585786437626909,-3.75142135623731)) ;
#149687 = CARTESIAN_POINT('',(7.,0.0585786437626909,-3.41)) ;
#149688 = CARTESIAN_POINT('',(7.,-0.1,-3.75142135623731)) ;
#149689 = CARTESIAN_POINT('Origin',(0.6,-0.600000000000001,-3.41)) ;
#149690 = CARTESIAN_POINT('',(6.65857864376269,-0.300000000000001,-3.41)) ;
#149691 = CARTESIAN_POINT('',(6.65857864376269,0.3,-3.41)) ;
#149692 = CARTESIAN_POINT('',(6.65857864376269,-0.399999999999999,-3.41)) ;
#149693 = CARTESIAN_POINT('',(2.4,0.3,-3.41)) ;
#149694 = CARTESIAN_POINT('',(6.65857864376269,-0.300000000000001,-3.41)) ;
#149695 = CARTESIAN_POINT('Origin',(0.6,-0.600000000000001,-4.21)) ;
#149696 = CARTESIAN_POINT('',(6.65857864376269,0.300000000000001,-4.21)) ;
#149697 = CARTESIAN_POINT('',(0.6,0.299999999999999,-4.21)) ;
#149698 = CARTESIAN_POINT('',(6.65857864376269,-0.300000000000001,-4.21)) ;
#149699 = CARTESIAN_POINT('',(6.65857864376269,-0.6,-4.21)) ;
#149700 = CARTESIAN_POINT('',(0.6,-0.3,-4.21)) ;
#149701 = CARTESIAN_POINT('Origin',(-0.4,-0.600000000000001,-7.22)) ;
#149702 = CARTESIAN_POINT('',(-0.4,-0.600000000000001,-7.32)) ;
#149703 = CARTESIAN_POINT('',(-0.4,-0.600000000000001,-7.92)) ;
#149704 = CARTESIAN_POINT('',(-0.4,-0.600000000000001,-7.22)) ;
#149705 = CARTESIAN_POINT('',(-0.4,-6.05857864376269,-7.92)) ;
#149706 = CARTESIAN_POINT('',(-0.4,-0.600000000000001,-7.92)) ;
#149707 = CARTESIAN_POINT('',(-0.4,-6.05857864376269,-7.32)) ;
#149708 = CARTESIAN_POINT('',(-0.4,-6.05857864376269,-7.22)) ;
#149709 = CARTESIAN_POINT('',(-0.4,-0.600000000000001,-7.32)) ;
#149710 = CARTESIAN_POINT('Origin',(-0.4,-6.1,-7.22)) ;
#149711 = CARTESIAN_POINT('',(-0.129289321881345,-6.37071067811866,-7.67857864376269)) ;
#149712 = CARTESIAN_POINT('',(-0.129289321881346,-6.37071067811866,-7.56142135623731)) ;
#149713 = CARTESIAN_POINT('',(-0.129289321881346,-6.37071067811866,-7.22)) ;
#149714 = CARTESIAN_POINT('',(-0.370710678118655,-6.12928932188134,-7.32)) ;
#149715 = CARTESIAN_POINT('',(-0.423570226039552,-6.07642977396045,-7.2671404520791)) ;
#149716 = CARTESIAN_POINT('',(-0.370710678118655,-6.12928932188134,-7.92)) ;
#149717 = CARTESIAN_POINT('',(-0.370710678118655,-6.12928932188134,-7.22)) ;
#149718 = CARTESIAN_POINT('',(-0.156903559372885,-6.34309644062712,-7.70619288125423)) ;
#149719 = CARTESIAN_POINT('Origin',(-0.1,-6.4,-7.22)) ;
#149720 = CARTESIAN_POINT('',(0.0585786437626908,-6.4,-7.67857864376269)) ;
#149721 = CARTESIAN_POINT('',(0.0585786437626908,-6.4,-7.56142135623731)) ;
#149722 = CARTESIAN_POINT('',(0.0585786437626908,-6.4,-7.22)) ;
#149723 = CARTESIAN_POINT('',(-0.0585786437626908,-6.4,-7.56142135623731)) ;
#149724 = CARTESIAN_POINT('',(-0.1,-6.4,-7.56142135623731)) ;
#149725 = CARTESIAN_POINT('',(-0.0585786437626908,-6.4,-7.67857864376269)) ;
#149726 = CARTESIAN_POINT('',(-0.0585786437626908,-6.4,-7.22)) ;
#149727 = CARTESIAN_POINT('',(-0.1,-6.4,-7.67857864376269)) ;
#149728 = CARTESIAN_POINT('Origin',(0.1,-6.4,-7.22)) ;
#149729 = CARTESIAN_POINT('',(0.370710678118655,-6.12928932188134,-7.92)) ;
#149730 = CARTESIAN_POINT('',(0.370710678118655,-6.12928932188134,-7.32)) ;
#149731 = CARTESIAN_POINT('',(0.370710678118655,-6.12928932188134,-7.22)) ;
#149732 = CARTESIAN_POINT('',(0.129289321881346,-6.37071067811866,-7.56142135623731)) ;
#149733 = CARTESIAN_POINT('',(0.223570226039553,-6.27642977396045,-7.4671404520791)) ;
#149734 = CARTESIAN_POINT('',(0.129289321881346,-6.37071067811866,-7.67857864376269)) ;
#149735 = CARTESIAN_POINT('',(0.129289321881346,-6.37071067811866,-7.22)) ;
#149736 = CARTESIAN_POINT('',(-0.0430964406271151,-6.54309644062712,-7.50619288125423)) ;
#149737 = CARTESIAN_POINT('Origin',(0.4,-6.1,-7.22)) ;
#149738 = CARTESIAN_POINT('',(0.4,-6.05857864376269,-7.32)) ;
#149739 = CARTESIAN_POINT('',(0.4,-6.05857864376269,-7.92)) ;
#149740 = CARTESIAN_POINT('',(0.4,-6.05857864376269,-7.22)) ;
#149741 = CARTESIAN_POINT('',(0.4,-0.6,-7.92)) ;
#149742 = CARTESIAN_POINT('',(0.4,-6.1,-7.92)) ;
#149743 = CARTESIAN_POINT('',(0.4,-0.6,-7.32)) ;
#149744 = CARTESIAN_POINT('',(0.4,-0.6,-7.22)) ;
#149745 = CARTESIAN_POINT('',(0.4,-6.05857864376269,-7.32)) ;
#149746 = CARTESIAN_POINT('Origin',(0.6,-0.600000000000001,-7.22)) ;
#149747 = CARTESIAN_POINT('',(0.3,-6.05857864376269,-7.22)) ;
#149748 = CARTESIAN_POINT('',(0.3,-0.6,-7.22)) ;
#149749 = CARTESIAN_POINT('',(0.3,-0.6,-7.22)) ;
#149750 = CARTESIAN_POINT('Origin',(0.6,-0.6,-7.22)) ;
#149751 = CARTESIAN_POINT('',(-0.3,-0.600000000000001,-7.22)) ;
#149752 = CARTESIAN_POINT('Origin',(0.6,-0.600000000000001,-7.22)) ;
#149753 = CARTESIAN_POINT('',(-0.300000000000001,-6.05857864376269,-7.22)) ;
#149754 = CARTESIAN_POINT('',(-0.3,-0.600000000000001,-7.22)) ;
#149755 = CARTESIAN_POINT('',(0.4,-6.05857864376269,-7.22)) ;
#149756 = CARTESIAN_POINT('Origin',(0.6,-0.600000000000001,-8.02)) ;
#149757 = CARTESIAN_POINT('',(-0.299999999999999,-6.05857864376269,-8.02)) ;
#149758 = CARTESIAN_POINT('',(-0.3,-0.600000000000001,-8.02)) ;
#149759 = CARTESIAN_POINT('',(-0.3,-0.600000000000001,-8.02)) ;
#149760 = CARTESIAN_POINT('Origin',(0.6,-0.600000000000001,-8.02)) ;
#149761 = CARTESIAN_POINT('',(0.3,-0.6,-8.02)) ;
#149762 = CARTESIAN_POINT('Origin',(0.6,-0.6,-8.02)) ;
#149763 = CARTESIAN_POINT('',(0.3,-6.05857864376269,-8.02)) ;
#149764 = CARTESIAN_POINT('',(0.3,-0.600000000000001,-8.02)) ;
#149765 = CARTESIAN_POINT('',(0.6,-6.05857864376269,-8.02)) ;
#149766 = CARTESIAN_POINT('Origin',(0.6,-0.600000000000001,-7.22)) ;
#149767 = CARTESIAN_POINT('Origin',(0.6,-0.600000000000001,-7.92)) ;
#149768 = CARTESIAN_POINT('Origin',(0.6,-0.600000000000001,-7.32)) ;
#149769 = CARTESIAN_POINT('Origin',(0.6,-0.6,-7.22)) ;
#149770 = CARTESIAN_POINT('Origin',(0.6,-0.6,-7.92)) ;
#149771 = CARTESIAN_POINT('Origin',(0.6,-0.6,-7.32)) ;
#149772 = CARTESIAN_POINT('Origin',(7.,0.1,-7.22)) ;
#149773 = CARTESIAN_POINT('',(6.72928932188135,0.370710678118655,-7.92)) ;
#149774 = CARTESIAN_POINT('',(6.72928932188135,0.370710678118655,-7.32)) ;
#149775 = CARTESIAN_POINT('',(6.72928932188135,0.370710678118655,-7.22)) ;
#149776 = CARTESIAN_POINT('',(6.97071067811866,0.129289321881346,-7.56142135623731)) ;
#149777 = CARTESIAN_POINT('',(6.87642977396045,0.223570226039553,-7.4671404520791)) ;
#149778 = CARTESIAN_POINT('',(6.97071067811866,0.129289321881346,-7.67857864376269)) ;
#149779 = CARTESIAN_POINT('',(6.97071067811866,0.129289321881346,-7.22)) ;
#149780 = CARTESIAN_POINT('',(7.14309644062712,-0.0430964406271152,-7.50619288125423)) ;
#149781 = CARTESIAN_POINT('Origin',(6.7,0.400000000000001,-7.22)) ;
#149782 = CARTESIAN_POINT('',(6.65857864376269,0.400000000000001,-7.32)) ;
#149783 = CARTESIAN_POINT('',(6.65857864376269,0.400000000000001,-7.92)) ;
#149784 = CARTESIAN_POINT('',(6.65857864376269,0.400000000000001,-7.22)) ;
#149785 = CARTESIAN_POINT('',(6.7,0.400000000000001,-7.92)) ;
#149786 = CARTESIAN_POINT('',(6.65857864376269,0.400000000000001,-7.32)) ;
#149787 = CARTESIAN_POINT('Origin',(0.6,-0.4,-7.22)) ;
#149788 = CARTESIAN_POINT('',(6.65857864376269,-0.400000000000001,-7.92)) ;
#149789 = CARTESIAN_POINT('',(0.6,-0.4,-7.92)) ;
#149790 = CARTESIAN_POINT('',(6.65857864376269,-0.400000000000001,-7.32)) ;
#149791 = CARTESIAN_POINT('',(6.65857864376269,-0.400000000000001,-7.22)) ;
#149792 = CARTESIAN_POINT('',(2.4,-0.4,-7.32)) ;
#149793 = CARTESIAN_POINT('Origin',(6.7,-0.400000000000001,-7.22)) ;
#149794 = CARTESIAN_POINT('',(6.97071067811866,-0.129289321881346,-7.67857864376269)) ;
#149795 = CARTESIAN_POINT('',(6.97071067811866,-0.129289321881346,-7.56142135623731)) ;
#149796 = CARTESIAN_POINT('',(6.97071067811866,-0.129289321881346,-7.22)) ;
#149797 = CARTESIAN_POINT('',(6.72928932188135,-0.370710678118655,-7.32)) ;
#149798 = CARTESIAN_POINT('',(6.67642977396045,-0.423570226039553,-7.2671404520791)) ;
#149799 = CARTESIAN_POINT('',(6.72928932188135,-0.370710678118655,-7.92)) ;
#149800 = CARTESIAN_POINT('',(6.72928932188135,-0.370710678118655,-7.22)) ;
#149801 = CARTESIAN_POINT('',(6.94309644062712,-0.156903559372885,-7.70619288125423)) ;
#149802 = CARTESIAN_POINT('Origin',(7.,-0.1,-7.22)) ;
#149803 = CARTESIAN_POINT('',(7.,-0.0585786437626909,-7.56142135623731)) ;
#149804 = CARTESIAN_POINT('',(7.,-0.0585786437626909,-7.67857864376269)) ;
#149805 = CARTESIAN_POINT('',(7.,-0.0585786437626909,-7.22)) ;
#149806 = CARTESIAN_POINT('',(7.,0.0585786437626909,-7.67857864376269)) ;
#149807 = CARTESIAN_POINT('',(7.,-0.1,-7.67857864376269)) ;
#149808 = CARTESIAN_POINT('',(7.,0.0585786437626909,-7.56142135623731)) ;
#149809 = CARTESIAN_POINT('',(7.,0.0585786437626909,-7.22)) ;
#149810 = CARTESIAN_POINT('',(7.,-0.1,-7.56142135623731)) ;
#149811 = CARTESIAN_POINT('Origin',(0.6,-0.600000000000001,-7.22)) ;
#149812 = CARTESIAN_POINT('',(6.65857864376269,-0.300000000000001,-7.22)) ;
#149813 = CARTESIAN_POINT('',(6.65857864376269,0.300000000000002,-7.22)) ;
#149814 = CARTESIAN_POINT('',(6.65857864376269,-0.399999999999999,-7.22)) ;
#149815 = CARTESIAN_POINT('',(2.4,0.3,-7.22)) ;
#149816 = CARTESIAN_POINT('',(6.65857864376269,-0.300000000000001,-7.22)) ;
#149817 = CARTESIAN_POINT('Origin',(0.6,-0.600000000000001,-8.02)) ;
#149818 = CARTESIAN_POINT('',(6.65857864376269,0.300000000000002,-8.02)) ;
#149819 = CARTESIAN_POINT('',(0.6,0.299999999999999,-8.02)) ;
#149820 = CARTESIAN_POINT('',(6.65857864376269,-0.300000000000001,-8.02)) ;
#149821 = CARTESIAN_POINT('',(6.65857864376269,-0.6,-8.02)) ;
#149822 = CARTESIAN_POINT('',(0.6,-0.3,-8.02)) ;
#149823 = CARTESIAN_POINT('Origin',(-0.4,-0.600000000000001,-11.03)) ;
#149824 = CARTESIAN_POINT('',(-0.4,-0.600000000000001,-11.13)) ;
#149825 = CARTESIAN_POINT('',(-0.4,-0.600000000000001,-11.73)) ;
#149826 = CARTESIAN_POINT('',(-0.4,-0.600000000000001,-11.03)) ;
#149827 = CARTESIAN_POINT('',(-0.4,-6.05857864376269,-11.73)) ;
#149828 = CARTESIAN_POINT('',(-0.4,-0.600000000000001,-11.73)) ;
#149829 = CARTESIAN_POINT('',(-0.4,-6.05857864376269,-11.13)) ;
#149830 = CARTESIAN_POINT('',(-0.4,-6.05857864376269,-11.03)) ;
#149831 = CARTESIAN_POINT('',(-0.4,-0.600000000000001,-11.13)) ;
#149832 = CARTESIAN_POINT('Origin',(-0.4,-6.1,-11.03)) ;
#149833 = CARTESIAN_POINT('',(-0.129289321881346,-6.37071067811866,-11.4885786437627)) ;
#149834 = CARTESIAN_POINT('',(-0.129289321881346,-6.37071067811866,-11.3714213562373)) ;
#149835 = CARTESIAN_POINT('',(-0.129289321881346,-6.37071067811866,-11.03)) ;
#149836 = CARTESIAN_POINT('',(-0.370710678118655,-6.12928932188134,-11.13)) ;
#149837 = CARTESIAN_POINT('',(-0.423570226039552,-6.07642977396045,-11.0771404520791)) ;
#149838 = CARTESIAN_POINT('',(-0.370710678118655,-6.12928932188134,-11.73)) ;
#149839 = CARTESIAN_POINT('',(-0.370710678118655,-6.12928932188134,-11.03)) ;
#149840 = CARTESIAN_POINT('',(-0.156903559372884,-6.34309644062712,-11.5161928812542)) ;
#149841 = CARTESIAN_POINT('Origin',(-0.1,-6.4,-11.03)) ;
#149842 = CARTESIAN_POINT('',(0.0585786437626908,-6.4,-11.4885786437627)) ;
#149843 = CARTESIAN_POINT('',(0.0585786437626908,-6.4,-11.3714213562373)) ;
#149844 = CARTESIAN_POINT('',(0.0585786437626908,-6.4,-11.03)) ;
#149845 = CARTESIAN_POINT('',(-0.0585786437626908,-6.4,-11.3714213562373)) ;
#149846 = CARTESIAN_POINT('',(-0.1,-6.4,-11.3714213562373)) ;
#149847 = CARTESIAN_POINT('',(-0.0585786437626908,-6.4,-11.4885786437627)) ;
#149848 = CARTESIAN_POINT('',(-0.0585786437626908,-6.4,-11.03)) ;
#149849 = CARTESIAN_POINT('',(-0.1,-6.4,-11.4885786437627)) ;
#149850 = CARTESIAN_POINT('Origin',(0.1,-6.4,-11.03)) ;
#149851 = CARTESIAN_POINT('',(0.370710678118655,-6.12928932188134,-11.73)) ;
#149852 = CARTESIAN_POINT('',(0.370710678118655,-6.12928932188134,-11.13)) ;
#149853 = CARTESIAN_POINT('',(0.370710678118655,-6.12928932188134,-11.03)) ;
#149854 = CARTESIAN_POINT('',(0.129289321881346,-6.37071067811866,-11.3714213562373)) ;
#149855 = CARTESIAN_POINT('',(0.223570226039553,-6.27642977396045,-11.2771404520791)) ;
#149856 = CARTESIAN_POINT('',(0.129289321881346,-6.37071067811866,-11.4885786437627)) ;
#149857 = CARTESIAN_POINT('',(0.129289321881346,-6.37071067811866,-11.03)) ;
#149858 = CARTESIAN_POINT('',(-0.0430964406271157,-6.54309644062712,-11.3161928812542)) ;
#149859 = CARTESIAN_POINT('Origin',(0.4,-6.1,-11.03)) ;
#149860 = CARTESIAN_POINT('',(0.4,-6.05857864376269,-11.13)) ;
#149861 = CARTESIAN_POINT('',(0.4,-6.05857864376269,-11.73)) ;
#149862 = CARTESIAN_POINT('',(0.4,-6.05857864376269,-11.03)) ;
#149863 = CARTESIAN_POINT('',(0.4,-0.6,-11.73)) ;
#149864 = CARTESIAN_POINT('',(0.4,-6.1,-11.73)) ;
#149865 = CARTESIAN_POINT('',(0.4,-0.6,-11.13)) ;
#149866 = CARTESIAN_POINT('',(0.4,-0.6,-11.03)) ;
#149867 = CARTESIAN_POINT('',(0.4,-6.05857864376269,-11.13)) ;
#149868 = CARTESIAN_POINT('Origin',(0.6,-0.600000000000001,-11.03)) ;
#149869 = CARTESIAN_POINT('',(0.3,-6.05857864376269,-11.03)) ;
#149870 = CARTESIAN_POINT('',(0.3,-0.6,-11.03)) ;
#149871 = CARTESIAN_POINT('',(0.3,-0.6,-11.03)) ;
#149872 = CARTESIAN_POINT('Origin',(0.6,-0.6,-11.03)) ;
#149873 = CARTESIAN_POINT('',(-0.3,-0.600000000000001,-11.03)) ;
#149874 = CARTESIAN_POINT('Origin',(0.6,-0.600000000000001,-11.03)) ;
#149875 = CARTESIAN_POINT('',(-0.300000000000003,-6.05857864376269,-11.03)) ;
#149876 = CARTESIAN_POINT('',(-0.3,-0.600000000000001,-11.03)) ;
#149877 = CARTESIAN_POINT('',(0.4,-6.05857864376269,-11.03)) ;
#149878 = CARTESIAN_POINT('Origin',(0.6,-0.600000000000001,-11.83)) ;
#149879 = CARTESIAN_POINT('',(-0.299999999999999,-6.05857864376269,-11.83)) ;
#149880 = CARTESIAN_POINT('',(-0.3,-0.600000000000001,-11.83)) ;
#149881 = CARTESIAN_POINT('',(-0.3,-0.600000000000001,-11.83)) ;
#149882 = CARTESIAN_POINT('Origin',(0.6,-0.600000000000001,-11.83)) ;
#149883 = CARTESIAN_POINT('',(0.3,-0.6,-11.83)) ;
#149884 = CARTESIAN_POINT('Origin',(0.6,-0.6,-11.83)) ;
#149885 = CARTESIAN_POINT('',(0.3,-6.05857864376269,-11.83)) ;
#149886 = CARTESIAN_POINT('',(0.3,-0.600000000000001,-11.83)) ;
#149887 = CARTESIAN_POINT('',(0.6,-6.05857864376269,-11.83)) ;
#149888 = CARTESIAN_POINT('Origin',(0.6,-0.600000000000001,-11.03)) ;
#149889 = CARTESIAN_POINT('Origin',(0.6,-0.600000000000001,-11.73)) ;
#149890 = CARTESIAN_POINT('Origin',(0.6,-0.600000000000001,-11.13)) ;
#149891 = CARTESIAN_POINT('Origin',(0.6,-0.6,-11.03)) ;
#149892 = CARTESIAN_POINT('Origin',(0.6,-0.6,-11.73)) ;
#149893 = CARTESIAN_POINT('Origin',(0.6,-0.6,-11.13)) ;
#149894 = CARTESIAN_POINT('Origin',(7.,0.1,-11.03)) ;
#149895 = CARTESIAN_POINT('',(6.72928932188135,0.370710678118655,-11.73)) ;
#149896 = CARTESIAN_POINT('',(6.72928932188135,0.370710678118655,-11.13)) ;
#149897 = CARTESIAN_POINT('',(6.72928932188135,0.370710678118655,-11.03)) ;
#149898 = CARTESIAN_POINT('',(6.97071067811866,0.129289321881346,-11.3714213562373)) ;
#149899 = CARTESIAN_POINT('',(6.87642977396045,0.223570226039553,-11.2771404520791)) ;
#149900 = CARTESIAN_POINT('',(6.97071067811866,0.129289321881346,-11.4885786437627)) ;
#149901 = CARTESIAN_POINT('',(6.97071067811866,0.129289321881346,-11.03)) ;
#149902 = CARTESIAN_POINT('',(7.14309644062712,-0.0430964406271147,-11.3161928812542)) ;
#149903 = CARTESIAN_POINT('Origin',(6.7,0.400000000000001,-11.03)) ;
#149904 = CARTESIAN_POINT('',(6.65857864376269,0.400000000000001,-11.13)) ;
#149905 = CARTESIAN_POINT('',(6.65857864376269,0.400000000000001,-11.73)) ;
#149906 = CARTESIAN_POINT('',(6.65857864376269,0.400000000000001,-11.03)) ;
#149907 = CARTESIAN_POINT('',(6.7,0.400000000000001,-11.73)) ;
#149908 = CARTESIAN_POINT('',(6.65857864376269,0.400000000000001,-11.13)) ;
#149909 = CARTESIAN_POINT('Origin',(0.6,-0.4,-11.03)) ;
#149910 = CARTESIAN_POINT('',(6.65857864376269,-0.400000000000001,-11.73)) ;
#149911 = CARTESIAN_POINT('',(0.6,-0.4,-11.73)) ;
#149912 = CARTESIAN_POINT('',(6.65857864376269,-0.400000000000001,-11.13)) ;
#149913 = CARTESIAN_POINT('',(6.65857864376269,-0.400000000000001,-11.03)) ;
#149914 = CARTESIAN_POINT('',(2.4,-0.4,-11.13)) ;
#149915 = CARTESIAN_POINT('Origin',(6.7,-0.400000000000001,-11.03)) ;
#149916 = CARTESIAN_POINT('',(6.97071067811866,-0.129289321881346,-11.4885786437627)) ;
#149917 = CARTESIAN_POINT('',(6.97071067811866,-0.129289321881346,-11.3714213562373)) ;
#149918 = CARTESIAN_POINT('',(6.97071067811866,-0.129289321881346,-11.03)) ;
#149919 = CARTESIAN_POINT('',(6.72928932188135,-0.370710678118655,-11.13)) ;
#149920 = CARTESIAN_POINT('',(6.67642977396045,-0.423570226039553,-11.0771404520791)) ;
#149921 = CARTESIAN_POINT('',(6.72928932188135,-0.370710678118655,-11.73)) ;
#149922 = CARTESIAN_POINT('',(6.72928932188135,-0.370710678118655,-11.03)) ;
#149923 = CARTESIAN_POINT('',(6.94309644062712,-0.156903559372885,-11.5161928812542)) ;
#149924 = CARTESIAN_POINT('Origin',(7.,-0.1,-11.03)) ;
#149925 = CARTESIAN_POINT('',(7.,-0.0585786437626909,-11.3714213562373)) ;
#149926 = CARTESIAN_POINT('',(7.,-0.0585786437626909,-11.4885786437627)) ;
#149927 = CARTESIAN_POINT('',(7.,-0.0585786437626909,-11.03)) ;
#149928 = CARTESIAN_POINT('',(7.,0.0585786437626909,-11.4885786437627)) ;
#149929 = CARTESIAN_POINT('',(7.,-0.1,-11.4885786437627)) ;
#149930 = CARTESIAN_POINT('',(7.,0.0585786437626909,-11.3714213562373)) ;
#149931 = CARTESIAN_POINT('',(7.,0.0585786437626909,-11.03)) ;
#149932 = CARTESIAN_POINT('',(7.,-0.1,-11.3714213562373)) ;
#149933 = CARTESIAN_POINT('Origin',(0.6,-0.600000000000001,-11.03)) ;
#149934 = CARTESIAN_POINT('',(6.65857864376269,-0.300000000000001,-11.03)) ;
#149935 = CARTESIAN_POINT('',(6.65857864376269,0.300000000000002,-11.03)) ;
#149936 = CARTESIAN_POINT('',(6.65857864376269,-0.399999999999999,-11.03)) ;
#149937 = CARTESIAN_POINT('',(2.4,0.3,-11.03)) ;
#149938 = CARTESIAN_POINT('',(6.65857864376269,-0.300000000000001,-11.03)) ;
#149939 = CARTESIAN_POINT('Origin',(0.6,-0.600000000000001,-11.83)) ;
#149940 = CARTESIAN_POINT('',(6.65857864376269,0.300000000000002,-11.83)) ;
#149941 = CARTESIAN_POINT('',(0.6,0.299999999999999,-11.83)) ;
#149942 = CARTESIAN_POINT('',(6.65857864376269,-0.300000000000001,-11.83)) ;
#149943 = CARTESIAN_POINT('',(6.65857864376269,-0.6,-11.83)) ;
#149944 = CARTESIAN_POINT('',(0.6,-0.3,-11.83)) ;
#149945 = CARTESIAN_POINT('Origin',(-0.4,-0.600000000000001,-14.84)) ;
#149946 = CARTESIAN_POINT('',(-0.4,-0.600000000000001,-14.94)) ;
#149947 = CARTESIAN_POINT('',(-0.4,-0.600000000000001,-15.54)) ;
#149948 = CARTESIAN_POINT('',(-0.4,-0.600000000000001,-14.84)) ;
#149949 = CARTESIAN_POINT('',(-0.4,-6.05857864376269,-15.54)) ;
#149950 = CARTESIAN_POINT('',(-0.4,-0.600000000000001,-15.54)) ;
#149951 = CARTESIAN_POINT('',(-0.4,-6.05857864376269,-14.94)) ;
#149952 = CARTESIAN_POINT('',(-0.4,-6.05857864376269,-14.84)) ;
#149953 = CARTESIAN_POINT('',(-0.4,-0.600000000000001,-14.94)) ;
#149954 = CARTESIAN_POINT('Origin',(-0.4,-6.1,-14.84)) ;
#149955 = CARTESIAN_POINT('',(-0.129289321881346,-6.37071067811866,-15.2985786437627)) ;
#149956 = CARTESIAN_POINT('',(-0.129289321881346,-6.37071067811866,-15.1814213562373)) ;
#149957 = CARTESIAN_POINT('',(-0.129289321881346,-6.37071067811866,-14.84)) ;
#149958 = CARTESIAN_POINT('',(-0.370710678118655,-6.12928932188134,-14.94)) ;
#149959 = CARTESIAN_POINT('',(-0.423570226039552,-6.07642977396045,-14.8871404520791)) ;
#149960 = CARTESIAN_POINT('',(-0.370710678118655,-6.12928932188134,-15.54)) ;
#149961 = CARTESIAN_POINT('',(-0.370710678118655,-6.12928932188134,-14.84)) ;
#149962 = CARTESIAN_POINT('',(-0.156903559372884,-6.34309644062712,-15.3261928812542)) ;
#149963 = CARTESIAN_POINT('Origin',(-0.1,-6.4,-14.84)) ;
#149964 = CARTESIAN_POINT('',(0.0585786437626908,-6.4,-15.2985786437627)) ;
#149965 = CARTESIAN_POINT('',(0.0585786437626908,-6.4,-15.1814213562373)) ;
#149966 = CARTESIAN_POINT('',(0.0585786437626908,-6.4,-14.84)) ;
#149967 = CARTESIAN_POINT('',(-0.0585786437626908,-6.4,-15.1814213562373)) ;
#149968 = CARTESIAN_POINT('',(-0.1,-6.4,-15.1814213562373)) ;
#149969 = CARTESIAN_POINT('',(-0.0585786437626908,-6.4,-15.2985786437627)) ;
#149970 = CARTESIAN_POINT('',(-0.0585786437626908,-6.4,-14.84)) ;
#149971 = CARTESIAN_POINT('',(-0.1,-6.4,-15.2985786437627)) ;
#149972 = CARTESIAN_POINT('Origin',(0.1,-6.4,-14.84)) ;
#149973 = CARTESIAN_POINT('',(0.370710678118655,-6.12928932188134,-15.54)) ;
#149974 = CARTESIAN_POINT('',(0.370710678118655,-6.12928932188134,-14.94)) ;
#149975 = CARTESIAN_POINT('',(0.370710678118655,-6.12928932188134,-14.84)) ;
#149976 = CARTESIAN_POINT('',(0.129289321881346,-6.37071067811866,-15.1814213562373)) ;
#149977 = CARTESIAN_POINT('',(0.223570226039553,-6.27642977396045,-15.0871404520791)) ;
#149978 = CARTESIAN_POINT('',(0.129289321881346,-6.37071067811866,-15.2985786437627)) ;
#149979 = CARTESIAN_POINT('',(0.129289321881346,-6.37071067811866,-14.84)) ;
#149980 = CARTESIAN_POINT('',(-0.0430964406271151,-6.54309644062712,-15.1261928812542)) ;
#149981 = CARTESIAN_POINT('Origin',(0.4,-6.1,-14.84)) ;
#149982 = CARTESIAN_POINT('',(0.4,-6.05857864376269,-14.94)) ;
#149983 = CARTESIAN_POINT('',(0.4,-6.05857864376269,-15.54)) ;
#149984 = CARTESIAN_POINT('',(0.4,-6.05857864376269,-14.84)) ;
#149985 = CARTESIAN_POINT('',(0.4,-0.6,-15.54)) ;
#149986 = CARTESIAN_POINT('',(0.4,-6.1,-15.54)) ;
#149987 = CARTESIAN_POINT('',(0.4,-0.6,-14.94)) ;
#149988 = CARTESIAN_POINT('',(0.4,-0.6,-14.84)) ;
#149989 = CARTESIAN_POINT('',(0.4,-6.05857864376269,-14.94)) ;
#149990 = CARTESIAN_POINT('Origin',(0.6,-0.600000000000001,-14.84)) ;
#149991 = CARTESIAN_POINT('',(0.3,-6.05857864376269,-14.84)) ;
#149992 = CARTESIAN_POINT('',(0.3,-0.6,-14.84)) ;
#149993 = CARTESIAN_POINT('',(0.3,-0.6,-14.84)) ;
#149994 = CARTESIAN_POINT('Origin',(0.6,-0.6,-14.84)) ;
#149995 = CARTESIAN_POINT('',(-0.3,-0.600000000000001,-14.84)) ;
#149996 = CARTESIAN_POINT('Origin',(0.6,-0.600000000000001,-14.84)) ;
#149997 = CARTESIAN_POINT('',(-0.300000000000001,-6.05857864376269,-14.84)) ;
#149998 = CARTESIAN_POINT('',(-0.3,-0.600000000000001,-14.84)) ;
#149999 = CARTESIAN_POINT('',(0.4,-6.05857864376269,-14.84)) ;
#150000 = CARTESIAN_POINT('Origin',(0.6,-0.600000000000001,-15.64)) ;
#150001 = CARTESIAN_POINT('',(-0.299999999999999,-6.05857864376269,-15.64)) ;
#150002 = CARTESIAN_POINT('',(-0.3,-0.600000000000001,-15.64)) ;
#150003 = CARTESIAN_POINT('',(-0.3,-0.600000000000001,-15.64)) ;
#150004 = CARTESIAN_POINT('Origin',(0.6,-0.600000000000001,-15.64)) ;
#150005 = CARTESIAN_POINT('',(0.3,-0.6,-15.64)) ;
#150006 = CARTESIAN_POINT('Origin',(0.6,-0.6,-15.64)) ;
#150007 = CARTESIAN_POINT('',(0.3,-6.05857864376269,-15.64)) ;
#150008 = CARTESIAN_POINT('',(0.3,-0.600000000000001,-15.64)) ;
#150009 = CARTESIAN_POINT('',(0.6,-6.05857864376269,-15.64)) ;
#150010 = CARTESIAN_POINT('Origin',(0.6,-0.600000000000001,-14.84)) ;
#150011 = CARTESIAN_POINT('Origin',(0.6,-0.600000000000001,-15.54)) ;
#150012 = CARTESIAN_POINT('Origin',(0.6,-0.600000000000001,-14.94)) ;
#150013 = CARTESIAN_POINT('Origin',(0.6,-0.6,-14.84)) ;
#150014 = CARTESIAN_POINT('Origin',(0.6,-0.6,-15.54)) ;
#150015 = CARTESIAN_POINT('Origin',(0.6,-0.6,-14.94)) ;
#150016 = CARTESIAN_POINT('Origin',(7.,0.1,-14.84)) ;
#150017 = CARTESIAN_POINT('',(6.72928932188135,0.370710678118655,-15.54)) ;
#150018 = CARTESIAN_POINT('',(6.72928932188135,0.370710678118655,-14.94)) ;
#150019 = CARTESIAN_POINT('',(6.72928932188135,0.370710678118655,-14.84)) ;
#150020 = CARTESIAN_POINT('',(6.97071067811866,0.129289321881346,-15.1814213562373)) ;
#150021 = CARTESIAN_POINT('',(6.87642977396045,0.223570226039552,-15.0871404520791)) ;
#150022 = CARTESIAN_POINT('',(6.97071067811866,0.129289321881346,-15.2985786437627)) ;
#150023 = CARTESIAN_POINT('',(6.97071067811866,0.129289321881346,-14.84)) ;
#150024 = CARTESIAN_POINT('',(7.14309644062712,-0.0430964406271147,-15.1261928812542)) ;
#150025 = CARTESIAN_POINT('Origin',(6.7,0.400000000000001,-14.84)) ;
#150026 = CARTESIAN_POINT('',(6.65857864376269,0.400000000000001,-14.94)) ;
#150027 = CARTESIAN_POINT('',(6.65857864376269,0.400000000000001,-15.54)) ;
#150028 = CARTESIAN_POINT('',(6.65857864376269,0.400000000000001,-14.84)) ;
#150029 = CARTESIAN_POINT('',(6.7,0.400000000000001,-15.54)) ;
#150030 = CARTESIAN_POINT('',(6.65857864376269,0.400000000000001,-14.94)) ;
#150031 = CARTESIAN_POINT('Origin',(0.6,-0.4,-14.84)) ;
#150032 = CARTESIAN_POINT('',(6.65857864376269,-0.400000000000001,-15.54)) ;
#150033 = CARTESIAN_POINT('',(0.6,-0.4,-15.54)) ;
#150034 = CARTESIAN_POINT('',(6.65857864376269,-0.400000000000001,-14.94)) ;
#150035 = CARTESIAN_POINT('',(6.65857864376269,-0.400000000000001,-14.84)) ;
#150036 = CARTESIAN_POINT('',(2.4,-0.4,-14.94)) ;
#150037 = CARTESIAN_POINT('Origin',(6.7,-0.400000000000001,-14.84)) ;
#150038 = CARTESIAN_POINT('',(6.97071067811866,-0.129289321881346,-15.2985786437627)) ;
#150039 = CARTESIAN_POINT('',(6.97071067811866,-0.129289321881346,-15.1814213562373)) ;
#150040 = CARTESIAN_POINT('',(6.97071067811866,-0.129289321881346,-14.84)) ;
#150041 = CARTESIAN_POINT('',(6.72928932188135,-0.370710678118655,-14.94)) ;
#150042 = CARTESIAN_POINT('',(6.67642977396045,-0.423570226039552,-14.8871404520791)) ;
#150043 = CARTESIAN_POINT('',(6.72928932188135,-0.370710678118655,-15.54)) ;
#150044 = CARTESIAN_POINT('',(6.72928932188135,-0.370710678118655,-14.84)) ;
#150045 = CARTESIAN_POINT('',(6.94309644062712,-0.156903559372885,-15.3261928812542)) ;
#150046 = CARTESIAN_POINT('Origin',(7.,-0.1,-14.84)) ;
#150047 = CARTESIAN_POINT('',(7.,-0.0585786437626909,-15.1814213562373)) ;
#150048 = CARTESIAN_POINT('',(7.,-0.0585786437626909,-15.2985786437627)) ;
#150049 = CARTESIAN_POINT('',(7.,-0.0585786437626909,-14.84)) ;
#150050 = CARTESIAN_POINT('',(7.,0.0585786437626909,-15.2985786437627)) ;
#150051 = CARTESIAN_POINT('',(7.,-0.1,-15.2985786437627)) ;
#150052 = CARTESIAN_POINT('',(7.,0.0585786437626909,-15.1814213562373)) ;
#150053 = CARTESIAN_POINT('',(7.,0.0585786437626909,-14.84)) ;
#150054 = CARTESIAN_POINT('',(7.,-0.1,-15.1814213562373)) ;
#150055 = CARTESIAN_POINT('Origin',(0.6,-0.600000000000001,-14.84)) ;
#150056 = CARTESIAN_POINT('',(6.65857864376269,-0.300000000000001,-14.84)) ;
#150057 = CARTESIAN_POINT('',(6.65857864376269,0.3,-14.84)) ;
#150058 = CARTESIAN_POINT('',(6.65857864376269,-0.399999999999999,-14.84)) ;
#150059 = CARTESIAN_POINT('',(2.4,0.3,-14.84)) ;
#150060 = CARTESIAN_POINT('',(6.65857864376269,-0.300000000000001,-14.84)) ;
#150061 = CARTESIAN_POINT('Origin',(0.6,-0.600000000000001,-15.64)) ;
#150062 = CARTESIAN_POINT('',(6.65857864376269,0.300000000000003,-15.64)) ;
#150063 = CARTESIAN_POINT('',(0.6,0.299999999999999,-15.64)) ;
#150064 = CARTESIAN_POINT('',(6.65857864376269,-0.300000000000001,-15.64)) ;
#150065 = CARTESIAN_POINT('',(6.65857864376269,-0.6,-15.64)) ;
#150066 = CARTESIAN_POINT('',(0.6,-0.3,-15.64)) ;
#150067 = CARTESIAN_POINT('Origin',(-0.4,-0.600000000000001,-18.65)) ;
#150068 = CARTESIAN_POINT('',(-0.4,-0.600000000000001,-18.75)) ;
#150069 = CARTESIAN_POINT('',(-0.4,-0.600000000000001,-19.35)) ;
#150070 = CARTESIAN_POINT('',(-0.4,-0.600000000000001,-18.65)) ;
#150071 = CARTESIAN_POINT('',(-0.4,-6.05857864376269,-19.35)) ;
#150072 = CARTESIAN_POINT('',(-0.4,-0.600000000000001,-19.35)) ;
#150073 = CARTESIAN_POINT('',(-0.4,-6.05857864376269,-18.75)) ;
#150074 = CARTESIAN_POINT('',(-0.4,-6.05857864376269,-18.65)) ;
#150075 = CARTESIAN_POINT('',(-0.4,-0.600000000000001,-18.75)) ;
#150076 = CARTESIAN_POINT('Origin',(-0.4,-6.1,-18.65)) ;
#150077 = CARTESIAN_POINT('',(-0.129289321881345,-6.37071067811866,-19.1085786437627)) ;
#150078 = CARTESIAN_POINT('',(-0.129289321881346,-6.37071067811866,-18.9914213562373)) ;
#150079 = CARTESIAN_POINT('',(-0.129289321881346,-6.37071067811866,-18.65)) ;
#150080 = CARTESIAN_POINT('',(-0.370710678118655,-6.12928932188134,-18.75)) ;
#150081 = CARTESIAN_POINT('',(-0.423570226039551,-6.07642977396045,-18.6971404520791)) ;
#150082 = CARTESIAN_POINT('',(-0.370710678118655,-6.12928932188134,-19.35)) ;
#150083 = CARTESIAN_POINT('',(-0.370710678118655,-6.12928932188134,-18.65)) ;
#150084 = CARTESIAN_POINT('',(-0.156903559372884,-6.34309644062712,-19.1361928812542)) ;
#150085 = CARTESIAN_POINT('Origin',(-0.1,-6.4,-18.65)) ;
#150086 = CARTESIAN_POINT('',(0.0585786437626908,-6.4,-19.1085786437627)) ;
#150087 = CARTESIAN_POINT('',(0.0585786437626908,-6.4,-18.9914213562373)) ;
#150088 = CARTESIAN_POINT('',(0.0585786437626908,-6.4,-18.65)) ;
#150089 = CARTESIAN_POINT('',(-0.0585786437626908,-6.4,-18.9914213562373)) ;
#150090 = CARTESIAN_POINT('',(-0.1,-6.4,-18.9914213562373)) ;
#150091 = CARTESIAN_POINT('',(-0.0585786437626908,-6.4,-19.1085786437627)) ;
#150092 = CARTESIAN_POINT('',(-0.0585786437626908,-6.4,-18.65)) ;
#150093 = CARTESIAN_POINT('',(-0.1,-6.4,-19.1085786437627)) ;
#150094 = CARTESIAN_POINT('Origin',(0.1,-6.4,-18.65)) ;
#150095 = CARTESIAN_POINT('',(0.370710678118654,-6.12928932188135,-19.35)) ;
#150096 = CARTESIAN_POINT('',(0.370710678118655,-6.12928932188134,-18.75)) ;
#150097 = CARTESIAN_POINT('',(0.370710678118655,-6.12928932188134,-18.65)) ;
#150098 = CARTESIAN_POINT('',(0.129289321881346,-6.37071067811866,-18.9914213562373)) ;
#150099 = CARTESIAN_POINT('',(0.223570226039551,-6.27642977396045,-18.8971404520791)) ;
#150100 = CARTESIAN_POINT('',(0.129289321881346,-6.37071067811866,-19.1085786437627)) ;
#150101 = CARTESIAN_POINT('',(0.129289321881346,-6.37071067811866,-18.65)) ;
#150102 = CARTESIAN_POINT('',(-0.0430964406271139,-6.54309644062711,-18.9361928812542)) ;
#150103 = CARTESIAN_POINT('Origin',(0.4,-6.1,-18.65)) ;
#150104 = CARTESIAN_POINT('',(0.4,-6.05857864376269,-18.75)) ;
#150105 = CARTESIAN_POINT('',(0.4,-6.05857864376269,-19.35)) ;
#150106 = CARTESIAN_POINT('',(0.4,-6.05857864376269,-18.65)) ;
#150107 = CARTESIAN_POINT('',(0.4,-0.6,-19.35)) ;
#150108 = CARTESIAN_POINT('',(0.4,-6.1,-19.35)) ;
#150109 = CARTESIAN_POINT('',(0.4,-0.6,-18.75)) ;
#150110 = CARTESIAN_POINT('',(0.4,-0.6,-18.65)) ;
#150111 = CARTESIAN_POINT('',(0.4,-6.05857864376269,-18.75)) ;
#150112 = CARTESIAN_POINT('Origin',(0.6,-0.600000000000001,-18.65)) ;
#150113 = CARTESIAN_POINT('',(0.3,-6.05857864376269,-18.65)) ;
#150114 = CARTESIAN_POINT('',(0.3,-0.6,-18.65)) ;
#150115 = CARTESIAN_POINT('',(0.3,-0.6,-18.65)) ;
#150116 = CARTESIAN_POINT('Origin',(0.6,-0.6,-18.65)) ;
#150117 = CARTESIAN_POINT('',(-0.3,-0.600000000000001,-18.65)) ;
#150118 = CARTESIAN_POINT('Origin',(0.6,-0.600000000000001,-18.65)) ;
#150119 = CARTESIAN_POINT('',(-0.299999999999994,-6.0585786437627,-18.65)) ;
#150120 = CARTESIAN_POINT('',(-0.3,-0.600000000000001,-18.65)) ;
#150121 = CARTESIAN_POINT('',(0.4,-6.0585786437627,-18.65)) ;
#150122 = CARTESIAN_POINT('Origin',(0.6,-0.600000000000001,-19.45)) ;
#150123 = CARTESIAN_POINT('',(-0.299999999999994,-6.0585786437627,-19.45)) ;
#150124 = CARTESIAN_POINT('',(-0.3,-0.600000000000001,-19.45)) ;
#150125 = CARTESIAN_POINT('',(-0.3,-0.600000000000001,-19.45)) ;
#150126 = CARTESIAN_POINT('Origin',(0.6,-0.600000000000001,-19.45)) ;
#150127 = CARTESIAN_POINT('',(0.3,-0.6,-19.45)) ;
#150128 = CARTESIAN_POINT('Origin',(0.6,-0.6,-19.45)) ;
#150129 = CARTESIAN_POINT('',(0.3,-6.05857864376269,-19.45)) ;
#150130 = CARTESIAN_POINT('',(0.3,-0.600000000000001,-19.45)) ;
#150131 = CARTESIAN_POINT('',(0.6,-6.05857864376269,-19.45)) ;
#150132 = CARTESIAN_POINT('Origin',(0.6,-0.600000000000001,-18.65)) ;
#150133 = CARTESIAN_POINT('Origin',(0.6,-0.600000000000001,-19.35)) ;
#150134 = CARTESIAN_POINT('Origin',(0.6,-0.600000000000001,-18.75)) ;
#150135 = CARTESIAN_POINT('Origin',(0.6,-0.6,-18.65)) ;
#150136 = CARTESIAN_POINT('Origin',(0.6,-0.6,-19.35)) ;
#150137 = CARTESIAN_POINT('Origin',(0.6,-0.6,-18.75)) ;
#150138 = CARTESIAN_POINT('Origin',(7.,0.1,-18.65)) ;
#150139 = CARTESIAN_POINT('',(6.72928932188135,0.370710678118656,-19.35)) ;
#150140 = CARTESIAN_POINT('',(6.72928932188135,0.370710678118655,-18.75)) ;
#150141 = CARTESIAN_POINT('',(6.72928932188135,0.370710678118655,-18.65)) ;
#150142 = CARTESIAN_POINT('',(6.97071067811866,0.129289321881346,-18.9914213562373)) ;
#150143 = CARTESIAN_POINT('',(6.87642977396045,0.22357022603955,-18.8971404520791)) ;
#150144 = CARTESIAN_POINT('',(6.97071067811866,0.129289321881346,-19.1085786437627)) ;
#150145 = CARTESIAN_POINT('',(6.97071067811866,0.129289321881346,-18.65)) ;
#150146 = CARTESIAN_POINT('',(7.14309644062712,-0.0430964406271155,-18.9361928812542)) ;
#150147 = CARTESIAN_POINT('Origin',(6.7,0.400000000000001,-18.65)) ;
#150148 = CARTESIAN_POINT('',(6.65857864376269,0.400000000000001,-18.75)) ;
#150149 = CARTESIAN_POINT('',(6.65857864376269,0.400000000000001,-19.35)) ;
#150150 = CARTESIAN_POINT('',(6.65857864376269,0.400000000000001,-18.65)) ;
#150151 = CARTESIAN_POINT('',(6.7,0.400000000000001,-19.35)) ;
#150152 = CARTESIAN_POINT('',(6.65857864376269,0.400000000000001,-18.75)) ;
#150153 = CARTESIAN_POINT('Origin',(0.6,-0.4,-18.65)) ;
#150154 = CARTESIAN_POINT('',(6.65857864376269,-0.400000000000001,-19.35)) ;
#150155 = CARTESIAN_POINT('',(0.6,-0.4,-19.35)) ;
#150156 = CARTESIAN_POINT('',(6.65857864376269,-0.400000000000001,-18.75)) ;
#150157 = CARTESIAN_POINT('',(6.65857864376269,-0.400000000000001,-18.65)) ;
#150158 = CARTESIAN_POINT('',(2.4,-0.4,-18.75)) ;
#150159 = CARTESIAN_POINT('Origin',(6.7,-0.400000000000001,-18.65)) ;
#150160 = CARTESIAN_POINT('',(6.97071067811866,-0.129289321881345,-19.1085786437627)) ;
#150161 = CARTESIAN_POINT('',(6.97071067811866,-0.129289321881346,-18.9914213562373)) ;
#150162 = CARTESIAN_POINT('',(6.97071067811866,-0.129289321881346,-18.65)) ;
#150163 = CARTESIAN_POINT('',(6.72928932188135,-0.370710678118655,-18.75)) ;
#150164 = CARTESIAN_POINT('',(6.67642977396045,-0.423570226039551,-18.6971404520791)) ;
#150165 = CARTESIAN_POINT('',(6.72928932188135,-0.370710678118655,-19.35)) ;
#150166 = CARTESIAN_POINT('',(6.72928932188135,-0.370710678118655,-18.65)) ;
#150167 = CARTESIAN_POINT('',(6.94309644062712,-0.156903559372885,-19.1361928812542)) ;
#150168 = CARTESIAN_POINT('Origin',(7.,-0.1,-18.65)) ;
#150169 = CARTESIAN_POINT('',(7.,-0.0585786437626909,-18.9914213562373)) ;
#150170 = CARTESIAN_POINT('',(7.,-0.0585786437626909,-19.1085786437627)) ;
#150171 = CARTESIAN_POINT('',(7.,-0.0585786437626909,-18.65)) ;
#150172 = CARTESIAN_POINT('',(7.,0.0585786437626909,-19.1085786437627)) ;
#150173 = CARTESIAN_POINT('',(7.,-0.1,-19.1085786437627)) ;
#150174 = CARTESIAN_POINT('',(7.,0.0585786437626909,-18.9914213562373)) ;
#150175 = CARTESIAN_POINT('',(7.,0.0585786437626909,-18.65)) ;
#150176 = CARTESIAN_POINT('',(7.,-0.1,-18.9914213562373)) ;
#150177 = CARTESIAN_POINT('Origin',(0.6,-0.600000000000001,-18.65)) ;
#150178 = CARTESIAN_POINT('',(6.65857864376269,-0.300000000000001,-18.65)) ;
#150179 = CARTESIAN_POINT('',(6.6585786437627,0.299999999999992,-18.65)) ;
#150180 = CARTESIAN_POINT('',(6.6585786437627,-0.399999999999999,-18.65)) ;
#150181 = CARTESIAN_POINT('',(2.4,0.3,-18.65)) ;
#150182 = CARTESIAN_POINT('',(6.65857864376269,-0.300000000000001,-18.65)) ;
#150183 = CARTESIAN_POINT('Origin',(0.6,-0.600000000000001,-19.45)) ;
#150184 = CARTESIAN_POINT('',(6.65857864376269,0.299999999999998,-19.45)) ;
#150185 = CARTESIAN_POINT('',(0.6,0.299999999999999,-19.45)) ;
#150186 = CARTESIAN_POINT('',(6.65857864376269,-0.300000000000001,-19.45)) ;
#150187 = CARTESIAN_POINT('',(6.65857864376269,-0.6,-19.45)) ;
#150188 = CARTESIAN_POINT('',(0.6,-0.3,-19.45)) ;
#150189 = CARTESIAN_POINT('Origin',(-0.4,-0.600000000000001,-22.46)) ;
#150190 = CARTESIAN_POINT('',(-0.4,-0.600000000000001,-22.56)) ;
#150191 = CARTESIAN_POINT('',(-0.4,-0.600000000000001,-23.16)) ;
#150192 = CARTESIAN_POINT('',(-0.4,-0.600000000000001,-22.46)) ;
#150193 = CARTESIAN_POINT('',(-0.4,-6.05857864376269,-23.16)) ;
#150194 = CARTESIAN_POINT('',(-0.4,-0.600000000000001,-23.16)) ;
#150195 = CARTESIAN_POINT('',(-0.4,-6.05857864376269,-22.56)) ;
#150196 = CARTESIAN_POINT('',(-0.4,-6.05857864376269,-22.46)) ;
#150197 = CARTESIAN_POINT('',(-0.4,-0.600000000000001,-22.56)) ;
#150198 = CARTESIAN_POINT('Origin',(-0.4,-6.1,-22.46)) ;
#150199 = CARTESIAN_POINT('',(-0.129289321881345,-6.37071067811866,-22.9185786437627)) ;
#150200 = CARTESIAN_POINT('',(-0.129289321881346,-6.37071067811866,-22.8014213562373)) ;
#150201 = CARTESIAN_POINT('',(-0.129289321881346,-6.37071067811866,-22.46)) ;
#150202 = CARTESIAN_POINT('',(-0.370710678118655,-6.12928932188134,-22.56)) ;
#150203 = CARTESIAN_POINT('',(-0.423570226039551,-6.07642977396045,-22.5071404520791)) ;
#150204 = CARTESIAN_POINT('',(-0.370710678118655,-6.12928932188134,-23.16)) ;
#150205 = CARTESIAN_POINT('',(-0.370710678118655,-6.12928932188134,-22.46)) ;
#150206 = CARTESIAN_POINT('',(-0.156903559372884,-6.34309644062712,-22.9461928812542)) ;
#150207 = CARTESIAN_POINT('Origin',(-0.1,-6.4,-22.46)) ;
#150208 = CARTESIAN_POINT('',(0.0585786437626908,-6.4,-22.9185786437627)) ;
#150209 = CARTESIAN_POINT('',(0.0585786437626908,-6.4,-22.8014213562373)) ;
#150210 = CARTESIAN_POINT('',(0.0585786437626908,-6.4,-22.46)) ;
#150211 = CARTESIAN_POINT('',(-0.0585786437626908,-6.4,-22.8014213562373)) ;
#150212 = CARTESIAN_POINT('',(-0.1,-6.4,-22.8014213562373)) ;
#150213 = CARTESIAN_POINT('',(-0.0585786437626908,-6.4,-22.9185786437627)) ;
#150214 = CARTESIAN_POINT('',(-0.0585786437626908,-6.4,-22.46)) ;
#150215 = CARTESIAN_POINT('',(-0.1,-6.4,-22.9185786437627)) ;
#150216 = CARTESIAN_POINT('Origin',(0.1,-6.4,-22.46)) ;
#150217 = CARTESIAN_POINT('',(0.370710678118654,-6.12928932188135,-23.16)) ;
#150218 = CARTESIAN_POINT('',(0.370710678118655,-6.12928932188134,-22.56)) ;
#150219 = CARTESIAN_POINT('',(0.370710678118655,-6.12928932188134,-22.46)) ;
#150220 = CARTESIAN_POINT('',(0.129289321881346,-6.37071067811866,-22.8014213562373)) ;
#150221 = CARTESIAN_POINT('',(0.223570226039551,-6.27642977396045,-22.7071404520791)) ;
#150222 = CARTESIAN_POINT('',(0.129289321881346,-6.37071067811866,-22.9185786437627)) ;
#150223 = CARTESIAN_POINT('',(0.129289321881346,-6.37071067811866,-22.46)) ;
#150224 = CARTESIAN_POINT('',(-0.0430964406271139,-6.54309644062711,-22.7461928812542)) ;
#150225 = CARTESIAN_POINT('Origin',(0.4,-6.1,-22.46)) ;
#150226 = CARTESIAN_POINT('',(0.4,-6.05857864376269,-22.56)) ;
#150227 = CARTESIAN_POINT('',(0.4,-6.05857864376269,-23.16)) ;
#150228 = CARTESIAN_POINT('',(0.4,-6.05857864376269,-22.46)) ;
#150229 = CARTESIAN_POINT('',(0.4,-0.6,-23.16)) ;
#150230 = CARTESIAN_POINT('',(0.4,-6.1,-23.16)) ;
#150231 = CARTESIAN_POINT('',(0.4,-0.6,-22.56)) ;
#150232 = CARTESIAN_POINT('',(0.4,-0.6,-22.46)) ;
#150233 = CARTESIAN_POINT('',(0.4,-6.05857864376269,-22.56)) ;
#150234 = CARTESIAN_POINT('Origin',(0.6,-0.600000000000001,-22.46)) ;
#150235 = CARTESIAN_POINT('',(0.3,-6.05857864376269,-22.46)) ;
#150236 = CARTESIAN_POINT('',(0.3,-0.6,-22.46)) ;
#150237 = CARTESIAN_POINT('',(0.3,-0.6,-22.46)) ;
#150238 = CARTESIAN_POINT('Origin',(0.6,-0.6,-22.46)) ;
#150239 = CARTESIAN_POINT('',(-0.3,-0.600000000000001,-22.46)) ;
#150240 = CARTESIAN_POINT('Origin',(0.6,-0.600000000000001,-22.46)) ;
#150241 = CARTESIAN_POINT('',(-0.299999999999994,-6.0585786437627,-22.46)) ;
#150242 = CARTESIAN_POINT('',(-0.3,-0.600000000000001,-22.46)) ;
#150243 = CARTESIAN_POINT('',(0.4,-6.0585786437627,-22.46)) ;
#150244 = CARTESIAN_POINT('Origin',(0.6,-0.600000000000001,-23.26)) ;
#150245 = CARTESIAN_POINT('',(-0.299999999999994,-6.0585786437627,-23.26)) ;
#150246 = CARTESIAN_POINT('',(-0.3,-0.600000000000001,-23.26)) ;
#150247 = CARTESIAN_POINT('',(-0.3,-0.600000000000001,-23.26)) ;
#150248 = CARTESIAN_POINT('Origin',(0.6,-0.600000000000001,-23.26)) ;
#150249 = CARTESIAN_POINT('',(0.3,-0.6,-23.26)) ;
#150250 = CARTESIAN_POINT('Origin',(0.6,-0.6,-23.26)) ;
#150251 = CARTESIAN_POINT('',(0.3,-6.05857864376269,-23.26)) ;
#150252 = CARTESIAN_POINT('',(0.3,-0.600000000000001,-23.26)) ;
#150253 = CARTESIAN_POINT('',(0.6,-6.05857864376269,-23.26)) ;
#150254 = CARTESIAN_POINT('Origin',(0.6,-0.600000000000001,-22.46)) ;
#150255 = CARTESIAN_POINT('Origin',(0.6,-0.600000000000001,-23.16)) ;
#150256 = CARTESIAN_POINT('Origin',(0.6,-0.600000000000001,-22.56)) ;
#150257 = CARTESIAN_POINT('Origin',(0.6,-0.6,-22.46)) ;
#150258 = CARTESIAN_POINT('Origin',(0.6,-0.6,-23.16)) ;
#150259 = CARTESIAN_POINT('Origin',(0.6,-0.6,-22.56)) ;
#150260 = CARTESIAN_POINT('Origin',(7.,0.1,-22.46)) ;
#150261 = CARTESIAN_POINT('',(6.72928932188135,0.370710678118656,-23.16)) ;
#150262 = CARTESIAN_POINT('',(6.72928932188135,0.370710678118655,-22.56)) ;
#150263 = CARTESIAN_POINT('',(6.72928932188135,0.370710678118655,-22.46)) ;
#150264 = CARTESIAN_POINT('',(6.97071067811866,0.129289321881346,-22.8014213562373)) ;
#150265 = CARTESIAN_POINT('',(6.87642977396045,0.22357022603955,-22.7071404520791)) ;
#150266 = CARTESIAN_POINT('',(6.97071067811866,0.129289321881346,-22.9185786437627)) ;
#150267 = CARTESIAN_POINT('',(6.97071067811866,0.129289321881346,-22.46)) ;
#150268 = CARTESIAN_POINT('',(7.14309644062712,-0.0430964406271155,-22.7461928812542)) ;
#150269 = CARTESIAN_POINT('Origin',(6.7,0.400000000000001,-22.46)) ;
#150270 = CARTESIAN_POINT('',(6.65857864376269,0.400000000000001,-22.56)) ;
#150271 = CARTESIAN_POINT('',(6.65857864376269,0.400000000000001,-23.16)) ;
#150272 = CARTESIAN_POINT('',(6.65857864376269,0.400000000000001,-22.46)) ;
#150273 = CARTESIAN_POINT('',(6.7,0.400000000000001,-23.16)) ;
#150274 = CARTESIAN_POINT('',(6.65857864376269,0.400000000000001,-22.56)) ;
#150275 = CARTESIAN_POINT('Origin',(0.6,-0.4,-22.46)) ;
#150276 = CARTESIAN_POINT('',(6.65857864376269,-0.400000000000001,-23.16)) ;
#150277 = CARTESIAN_POINT('',(0.6,-0.4,-23.16)) ;
#150278 = CARTESIAN_POINT('',(6.65857864376269,-0.400000000000001,-22.56)) ;
#150279 = CARTESIAN_POINT('',(6.65857864376269,-0.400000000000001,-22.46)) ;
#150280 = CARTESIAN_POINT('',(2.4,-0.4,-22.56)) ;
#150281 = CARTESIAN_POINT('Origin',(6.7,-0.400000000000001,-22.46)) ;
#150282 = CARTESIAN_POINT('',(6.97071067811866,-0.129289321881345,-22.9185786437627)) ;
#150283 = CARTESIAN_POINT('',(6.97071067811866,-0.129289321881346,-22.8014213562373)) ;
#150284 = CARTESIAN_POINT('',(6.97071067811866,-0.129289321881346,-22.46)) ;
#150285 = CARTESIAN_POINT('',(6.72928932188135,-0.370710678118655,-22.56)) ;
#150286 = CARTESIAN_POINT('',(6.67642977396045,-0.423570226039551,-22.5071404520791)) ;
#150287 = CARTESIAN_POINT('',(6.72928932188135,-0.370710678118655,-23.16)) ;
#150288 = CARTESIAN_POINT('',(6.72928932188135,-0.370710678118655,-22.46)) ;
#150289 = CARTESIAN_POINT('',(6.94309644062712,-0.156903559372885,-22.9461928812542)) ;
#150290 = CARTESIAN_POINT('Origin',(7.,-0.1,-22.46)) ;
#150291 = CARTESIAN_POINT('',(7.,-0.0585786437626909,-22.8014213562373)) ;
#150292 = CARTESIAN_POINT('',(7.,-0.0585786437626909,-22.9185786437627)) ;
#150293 = CARTESIAN_POINT('',(7.,-0.0585786437626909,-22.46)) ;
#150294 = CARTESIAN_POINT('',(7.,0.0585786437626909,-22.9185786437627)) ;
#150295 = CARTESIAN_POINT('',(7.,-0.1,-22.9185786437627)) ;
#150296 = CARTESIAN_POINT('',(7.,0.0585786437626909,-22.8014213562373)) ;
#150297 = CARTESIAN_POINT('',(7.,0.0585786437626909,-22.46)) ;
#150298 = CARTESIAN_POINT('',(7.,-0.1,-22.8014213562373)) ;
#150299 = CARTESIAN_POINT('Origin',(0.6,-0.600000000000001,-22.46)) ;
#150300 = CARTESIAN_POINT('',(6.65857864376269,-0.300000000000001,-22.46)) ;
#150301 = CARTESIAN_POINT('',(6.6585786437627,0.299999999999994,-22.46)) ;
#150302 = CARTESIAN_POINT('',(6.6585786437627,-0.399999999999999,-22.46)) ;
#150303 = CARTESIAN_POINT('',(2.4,0.3,-22.46)) ;
#150304 = CARTESIAN_POINT('',(6.65857864376269,-0.300000000000001,-22.46)) ;
#150305 = CARTESIAN_POINT('Origin',(0.6,-0.600000000000001,-23.26)) ;
#150306 = CARTESIAN_POINT('',(6.65857864376269,0.299999999999998,-23.26)) ;
#150307 = CARTESIAN_POINT('',(0.6,0.299999999999999,-23.26)) ;
#150308 = CARTESIAN_POINT('',(6.65857864376269,-0.300000000000001,-23.26)) ;
#150309 = CARTESIAN_POINT('',(6.65857864376269,-0.6,-23.26)) ;
#150310 = CARTESIAN_POINT('',(0.6,-0.3,-23.26)) ;
#150311 = CARTESIAN_POINT('Origin',(-0.4,-0.600000000000001,-26.27)) ;
#150312 = CARTESIAN_POINT('',(-0.4,-0.600000000000001,-26.37)) ;
#150313 = CARTESIAN_POINT('',(-0.4,-0.600000000000001,-26.97)) ;
#150314 = CARTESIAN_POINT('',(-0.4,-0.600000000000001,-26.27)) ;
#150315 = CARTESIAN_POINT('',(-0.4,-6.05857864376269,-26.97)) ;
#150316 = CARTESIAN_POINT('',(-0.4,-0.600000000000001,-26.97)) ;
#150317 = CARTESIAN_POINT('',(-0.4,-6.05857864376269,-26.37)) ;
#150318 = CARTESIAN_POINT('',(-0.4,-6.05857864376269,-26.27)) ;
#150319 = CARTESIAN_POINT('',(-0.4,-0.600000000000001,-26.37)) ;
#150320 = CARTESIAN_POINT('Origin',(-0.4,-6.1,-26.27)) ;
#150321 = CARTESIAN_POINT('',(-0.129289321881345,-6.37071067811866,-26.7285786437627)) ;
#150322 = CARTESIAN_POINT('',(-0.129289321881346,-6.37071067811866,-26.6114213562373)) ;
#150323 = CARTESIAN_POINT('',(-0.129289321881346,-6.37071067811866,-26.27)) ;
#150324 = CARTESIAN_POINT('',(-0.370710678118655,-6.12928932188134,-26.37)) ;
#150325 = CARTESIAN_POINT('',(-0.423570226039551,-6.07642977396045,-26.3171404520791)) ;
#150326 = CARTESIAN_POINT('',(-0.370710678118655,-6.12928932188134,-26.97)) ;
#150327 = CARTESIAN_POINT('',(-0.370710678118655,-6.12928932188134,-26.27)) ;
#150328 = CARTESIAN_POINT('',(-0.156903559372884,-6.34309644062712,-26.7561928812542)) ;
#150329 = CARTESIAN_POINT('Origin',(-0.1,-6.4,-26.27)) ;
#150330 = CARTESIAN_POINT('',(0.0585786437626908,-6.4,-26.7285786437627)) ;
#150331 = CARTESIAN_POINT('',(0.0585786437626908,-6.4,-26.6114213562373)) ;
#150332 = CARTESIAN_POINT('',(0.0585786437626908,-6.4,-26.27)) ;
#150333 = CARTESIAN_POINT('',(-0.0585786437626908,-6.4,-26.6114213562373)) ;
#150334 = CARTESIAN_POINT('',(-0.1,-6.4,-26.6114213562373)) ;
#150335 = CARTESIAN_POINT('',(-0.0585786437626908,-6.4,-26.7285786437627)) ;
#150336 = CARTESIAN_POINT('',(-0.0585786437626908,-6.4,-26.27)) ;
#150337 = CARTESIAN_POINT('',(-0.1,-6.4,-26.7285786437627)) ;
#150338 = CARTESIAN_POINT('Origin',(0.1,-6.4,-26.27)) ;
#150339 = CARTESIAN_POINT('',(0.370710678118654,-6.12928932188135,-26.97)) ;
#150340 = CARTESIAN_POINT('',(0.370710678118655,-6.12928932188134,-26.37)) ;
#150341 = CARTESIAN_POINT('',(0.370710678118655,-6.12928932188134,-26.27)) ;
#150342 = CARTESIAN_POINT('',(0.129289321881346,-6.37071067811866,-26.6114213562373)) ;
#150343 = CARTESIAN_POINT('',(0.223570226039551,-6.27642977396045,-26.5171404520791)) ;
#150344 = CARTESIAN_POINT('',(0.129289321881346,-6.37071067811866,-26.7285786437627)) ;
#150345 = CARTESIAN_POINT('',(0.129289321881346,-6.37071067811866,-26.27)) ;
#150346 = CARTESIAN_POINT('',(-0.0430964406271139,-6.54309644062711,-26.5561928812542)) ;
#150347 = CARTESIAN_POINT('Origin',(0.4,-6.1,-26.27)) ;
#150348 = CARTESIAN_POINT('',(0.4,-6.05857864376269,-26.37)) ;
#150349 = CARTESIAN_POINT('',(0.4,-6.05857864376269,-26.97)) ;
#150350 = CARTESIAN_POINT('',(0.4,-6.05857864376269,-26.27)) ;
#150351 = CARTESIAN_POINT('',(0.4,-0.6,-26.97)) ;
#150352 = CARTESIAN_POINT('',(0.4,-6.1,-26.97)) ;
#150353 = CARTESIAN_POINT('',(0.4,-0.6,-26.37)) ;
#150354 = CARTESIAN_POINT('',(0.4,-0.6,-26.27)) ;
#150355 = CARTESIAN_POINT('',(0.4,-6.05857864376269,-26.37)) ;
#150356 = CARTESIAN_POINT('Origin',(0.6,-0.600000000000001,-26.27)) ;
#150357 = CARTESIAN_POINT('',(0.3,-6.05857864376269,-26.27)) ;
#150358 = CARTESIAN_POINT('',(0.3,-0.6,-26.27)) ;
#150359 = CARTESIAN_POINT('',(0.3,-0.6,-26.27)) ;
#150360 = CARTESIAN_POINT('Origin',(0.6,-0.6,-26.27)) ;
#150361 = CARTESIAN_POINT('',(-0.3,-0.600000000000001,-26.27)) ;
#150362 = CARTESIAN_POINT('Origin',(0.6,-0.600000000000001,-26.27)) ;
#150363 = CARTESIAN_POINT('',(-0.299999999999994,-6.0585786437627,-26.27)) ;
#150364 = CARTESIAN_POINT('',(-0.3,-0.600000000000001,-26.27)) ;
#150365 = CARTESIAN_POINT('',(0.4,-6.0585786437627,-26.27)) ;
#150366 = CARTESIAN_POINT('Origin',(0.6,-0.600000000000001,-27.07)) ;
#150367 = CARTESIAN_POINT('',(-0.299999999999994,-6.0585786437627,-27.07)) ;
#150368 = CARTESIAN_POINT('',(-0.3,-0.600000000000001,-27.07)) ;
#150369 = CARTESIAN_POINT('',(-0.3,-0.600000000000001,-27.07)) ;
#150370 = CARTESIAN_POINT('Origin',(0.6,-0.600000000000001,-27.07)) ;
#150371 = CARTESIAN_POINT('',(0.3,-0.6,-27.07)) ;
#150372 = CARTESIAN_POINT('Origin',(0.6,-0.6,-27.07)) ;
#150373 = CARTESIAN_POINT('',(0.3,-6.05857864376269,-27.07)) ;
#150374 = CARTESIAN_POINT('',(0.3,-0.600000000000001,-27.07)) ;
#150375 = CARTESIAN_POINT('',(0.6,-6.05857864376269,-27.07)) ;
#150376 = CARTESIAN_POINT('Origin',(0.6,-0.600000000000001,-26.27)) ;
#150377 = CARTESIAN_POINT('Origin',(0.6,-0.600000000000001,-26.97)) ;
#150378 = CARTESIAN_POINT('Origin',(0.6,-0.600000000000001,-26.37)) ;
#150379 = CARTESIAN_POINT('Origin',(0.6,-0.6,-26.27)) ;
#150380 = CARTESIAN_POINT('Origin',(0.6,-0.6,-26.97)) ;
#150381 = CARTESIAN_POINT('Origin',(0.6,-0.6,-26.37)) ;
#150382 = CARTESIAN_POINT('Origin',(7.,0.1,-26.27)) ;
#150383 = CARTESIAN_POINT('',(6.72928932188135,0.370710678118656,-26.97)) ;
#150384 = CARTESIAN_POINT('',(6.72928932188135,0.370710678118655,-26.37)) ;
#150385 = CARTESIAN_POINT('',(6.72928932188135,0.370710678118655,-26.27)) ;
#150386 = CARTESIAN_POINT('',(6.97071067811866,0.129289321881346,-26.6114213562373)) ;
#150387 = CARTESIAN_POINT('',(6.87642977396045,0.22357022603955,-26.5171404520791)) ;
#150388 = CARTESIAN_POINT('',(6.97071067811866,0.129289321881346,-26.7285786437627)) ;
#150389 = CARTESIAN_POINT('',(6.97071067811866,0.129289321881346,-26.27)) ;
#150390 = CARTESIAN_POINT('',(7.14309644062712,-0.0430964406271155,-26.5561928812542)) ;
#150391 = CARTESIAN_POINT('Origin',(6.7,0.400000000000001,-26.27)) ;
#150392 = CARTESIAN_POINT('',(6.65857864376269,0.400000000000001,-26.37)) ;
#150393 = CARTESIAN_POINT('',(6.65857864376269,0.400000000000001,-26.97)) ;
#150394 = CARTESIAN_POINT('',(6.65857864376269,0.400000000000001,-26.27)) ;
#150395 = CARTESIAN_POINT('',(6.7,0.400000000000001,-26.97)) ;
#150396 = CARTESIAN_POINT('',(6.65857864376269,0.400000000000001,-26.37)) ;
#150397 = CARTESIAN_POINT('Origin',(0.6,-0.4,-26.27)) ;
#150398 = CARTESIAN_POINT('',(6.65857864376269,-0.400000000000001,-26.97)) ;
#150399 = CARTESIAN_POINT('',(0.6,-0.4,-26.97)) ;
#150400 = CARTESIAN_POINT('',(6.65857864376269,-0.400000000000001,-26.37)) ;
#150401 = CARTESIAN_POINT('',(6.65857864376269,-0.400000000000001,-26.27)) ;
#150402 = CARTESIAN_POINT('',(2.4,-0.4,-26.37)) ;
#150403 = CARTESIAN_POINT('Origin',(6.7,-0.400000000000001,-26.27)) ;
#150404 = CARTESIAN_POINT('',(6.97071067811866,-0.129289321881345,-26.7285786437627)) ;
#150405 = CARTESIAN_POINT('',(6.97071067811866,-0.129289321881346,-26.6114213562373)) ;
#150406 = CARTESIAN_POINT('',(6.97071067811866,-0.129289321881346,-26.27)) ;
#150407 = CARTESIAN_POINT('',(6.72928932188135,-0.370710678118655,-26.37)) ;
#150408 = CARTESIAN_POINT('',(6.67642977396045,-0.423570226039551,-26.3171404520791)) ;
#150409 = CARTESIAN_POINT('',(6.72928932188135,-0.370710678118655,-26.97)) ;
#150410 = CARTESIAN_POINT('',(6.72928932188135,-0.370710678118655,-26.27)) ;
#150411 = CARTESIAN_POINT('',(6.94309644062712,-0.156903559372885,-26.7561928812542)) ;
#150412 = CARTESIAN_POINT('Origin',(7.,-0.1,-26.27)) ;
#150413 = CARTESIAN_POINT('',(7.,-0.0585786437626909,-26.6114213562373)) ;
#150414 = CARTESIAN_POINT('',(7.,-0.0585786437626909,-26.7285786437627)) ;
#150415 = CARTESIAN_POINT('',(7.,-0.0585786437626909,-26.27)) ;
#150416 = CARTESIAN_POINT('',(7.,0.0585786437626909,-26.7285786437627)) ;
#150417 = CARTESIAN_POINT('',(7.,-0.1,-26.7285786437627)) ;
#150418 = CARTESIAN_POINT('',(7.,0.0585786437626909,-26.6114213562373)) ;
#150419 = CARTESIAN_POINT('',(7.,0.0585786437626909,-26.27)) ;
#150420 = CARTESIAN_POINT('',(7.,-0.1,-26.6114213562373)) ;
#150421 = CARTESIAN_POINT('Origin',(0.6,-0.600000000000001,-26.27)) ;
#150422 = CARTESIAN_POINT('',(6.65857864376269,-0.300000000000001,-26.27)) ;
#150423 = CARTESIAN_POINT('',(6.6585786437627,0.299999999999994,-26.27)) ;
#150424 = CARTESIAN_POINT('',(6.6585786437627,-0.399999999999999,-26.27)) ;
#150425 = CARTESIAN_POINT('',(2.4,0.3,-26.27)) ;
#150426 = CARTESIAN_POINT('',(6.65857864376269,-0.300000000000001,-26.27)) ;
#150427 = CARTESIAN_POINT('Origin',(0.6,-0.600000000000001,-27.07)) ;
#150428 = CARTESIAN_POINT('',(6.65857864376269,0.299999999999998,-27.07)) ;
#150429 = CARTESIAN_POINT('',(0.6,0.299999999999999,-27.07)) ;
#150430 = CARTESIAN_POINT('',(6.65857864376269,-0.300000000000001,-27.07)) ;
#150431 = CARTESIAN_POINT('',(6.65857864376269,-0.6,-27.07)) ;
#150432 = CARTESIAN_POINT('',(0.6,-0.3,-27.07)) ;
#150433 = CARTESIAN_POINT('Origin',(-0.4,-0.600000000000001,-30.08)) ;
#150434 = CARTESIAN_POINT('',(-0.4,-0.600000000000001,-30.18)) ;
#150435 = CARTESIAN_POINT('',(-0.4,-0.600000000000001,-30.78)) ;
#150436 = CARTESIAN_POINT('',(-0.4,-0.600000000000001,-30.08)) ;
#150437 = CARTESIAN_POINT('',(-0.4,-6.05857864376269,-30.78)) ;
#150438 = CARTESIAN_POINT('',(-0.4,-0.600000000000001,-30.78)) ;
#150439 = CARTESIAN_POINT('',(-0.4,-6.05857864376269,-30.18)) ;
#150440 = CARTESIAN_POINT('',(-0.4,-6.05857864376269,-30.08)) ;
#150441 = CARTESIAN_POINT('',(-0.4,-0.600000000000001,-30.18)) ;
#150442 = CARTESIAN_POINT('Origin',(-0.4,-6.1,-30.08)) ;
#150443 = CARTESIAN_POINT('',(-0.129289321881345,-6.37071067811866,-30.5385786437627)) ;
#150444 = CARTESIAN_POINT('',(-0.129289321881346,-6.37071067811866,-30.4214213562373)) ;
#150445 = CARTESIAN_POINT('',(-0.129289321881346,-6.37071067811866,-30.08)) ;
#150446 = CARTESIAN_POINT('',(-0.370710678118655,-6.12928932188134,-30.18)) ;
#150447 = CARTESIAN_POINT('',(-0.423570226039551,-6.07642977396045,-30.1271404520791)) ;
#150448 = CARTESIAN_POINT('',(-0.370710678118655,-6.12928932188134,-30.78)) ;
#150449 = CARTESIAN_POINT('',(-0.370710678118655,-6.12928932188134,-30.08)) ;
#150450 = CARTESIAN_POINT('',(-0.156903559372884,-6.34309644062712,-30.5661928812542)) ;
#150451 = CARTESIAN_POINT('Origin',(-0.1,-6.4,-30.08)) ;
#150452 = CARTESIAN_POINT('',(0.0585786437626908,-6.4,-30.5385786437627)) ;
#150453 = CARTESIAN_POINT('',(0.0585786437626908,-6.4,-30.4214213562373)) ;
#150454 = CARTESIAN_POINT('',(0.0585786437626908,-6.4,-30.08)) ;
#150455 = CARTESIAN_POINT('',(-0.0585786437626908,-6.4,-30.4214213562373)) ;
#150456 = CARTESIAN_POINT('',(-0.1,-6.4,-30.4214213562373)) ;
#150457 = CARTESIAN_POINT('',(-0.0585786437626908,-6.4,-30.5385786437627)) ;
#150458 = CARTESIAN_POINT('',(-0.0585786437626908,-6.4,-30.08)) ;
#150459 = CARTESIAN_POINT('',(-0.1,-6.4,-30.5385786437627)) ;
#150460 = CARTESIAN_POINT('Origin',(0.1,-6.4,-30.08)) ;
#150461 = CARTESIAN_POINT('',(0.370710678118654,-6.12928932188135,-30.78)) ;
#150462 = CARTESIAN_POINT('',(0.370710678118655,-6.12928932188134,-30.18)) ;
#150463 = CARTESIAN_POINT('',(0.370710678118655,-6.12928932188134,-30.08)) ;
#150464 = CARTESIAN_POINT('',(0.129289321881346,-6.37071067811866,-30.4214213562373)) ;
#150465 = CARTESIAN_POINT('',(0.223570226039551,-6.27642977396045,-30.3271404520791)) ;
#150466 = CARTESIAN_POINT('',(0.129289321881346,-6.37071067811866,-30.5385786437627)) ;
#150467 = CARTESIAN_POINT('',(0.129289321881346,-6.37071067811866,-30.08)) ;
#150468 = CARTESIAN_POINT('',(-0.0430964406271139,-6.54309644062711,-30.3661928812542)) ;
#150469 = CARTESIAN_POINT('Origin',(0.4,-6.1,-30.08)) ;
#150470 = CARTESIAN_POINT('',(0.4,-6.05857864376269,-30.18)) ;
#150471 = CARTESIAN_POINT('',(0.4,-6.05857864376269,-30.78)) ;
#150472 = CARTESIAN_POINT('',(0.4,-6.05857864376269,-30.08)) ;
#150473 = CARTESIAN_POINT('',(0.4,-0.6,-30.78)) ;
#150474 = CARTESIAN_POINT('',(0.4,-6.1,-30.78)) ;
#150475 = CARTESIAN_POINT('',(0.4,-0.6,-30.18)) ;
#150476 = CARTESIAN_POINT('',(0.4,-0.6,-30.08)) ;
#150477 = CARTESIAN_POINT('',(0.4,-6.05857864376269,-30.18)) ;
#150478 = CARTESIAN_POINT('Origin',(0.6,-0.600000000000001,-30.08)) ;
#150479 = CARTESIAN_POINT('',(0.3,-6.05857864376269,-30.08)) ;
#150480 = CARTESIAN_POINT('',(0.3,-0.6,-30.08)) ;
#150481 = CARTESIAN_POINT('',(0.3,-0.6,-30.08)) ;
#150482 = CARTESIAN_POINT('Origin',(0.6,-0.6,-30.08)) ;
#150483 = CARTESIAN_POINT('',(-0.3,-0.600000000000001,-30.08)) ;
#150484 = CARTESIAN_POINT('Origin',(0.6,-0.600000000000001,-30.08)) ;
#150485 = CARTESIAN_POINT('',(-0.299999999999994,-6.0585786437627,-30.08)) ;
#150486 = CARTESIAN_POINT('',(-0.3,-0.600000000000001,-30.08)) ;
#150487 = CARTESIAN_POINT('',(0.4,-6.0585786437627,-30.08)) ;
#150488 = CARTESIAN_POINT('Origin',(0.6,-0.600000000000001,-30.88)) ;
#150489 = CARTESIAN_POINT('',(-0.299999999999994,-6.0585786437627,-30.88)) ;
#150490 = CARTESIAN_POINT('',(-0.3,-0.600000000000001,-30.88)) ;
#150491 = CARTESIAN_POINT('',(-0.3,-0.600000000000001,-30.88)) ;
#150492 = CARTESIAN_POINT('Origin',(0.6,-0.600000000000001,-30.88)) ;
#150493 = CARTESIAN_POINT('',(0.3,-0.6,-30.88)) ;
#150494 = CARTESIAN_POINT('Origin',(0.6,-0.6,-30.88)) ;
#150495 = CARTESIAN_POINT('',(0.3,-6.05857864376269,-30.88)) ;
#150496 = CARTESIAN_POINT('',(0.3,-0.600000000000001,-30.88)) ;
#150497 = CARTESIAN_POINT('',(0.6,-6.05857864376269,-30.88)) ;
#150498 = CARTESIAN_POINT('Origin',(0.6,-0.600000000000001,-30.08)) ;
#150499 = CARTESIAN_POINT('Origin',(0.6,-0.600000000000001,-30.78)) ;
#150500 = CARTESIAN_POINT('Origin',(0.6,-0.600000000000001,-30.18)) ;
#150501 = CARTESIAN_POINT('Origin',(0.6,-0.6,-30.08)) ;
#150502 = CARTESIAN_POINT('Origin',(0.6,-0.6,-30.78)) ;
#150503 = CARTESIAN_POINT('Origin',(0.6,-0.6,-30.18)) ;
#150504 = CARTESIAN_POINT('Origin',(7.,0.1,-30.08)) ;
#150505 = CARTESIAN_POINT('',(6.72928932188135,0.370710678118656,-30.78)) ;
#150506 = CARTESIAN_POINT('',(6.72928932188135,0.370710678118655,-30.18)) ;
#150507 = CARTESIAN_POINT('',(6.72928932188135,0.370710678118655,-30.08)) ;
#150508 = CARTESIAN_POINT('',(6.97071067811866,0.129289321881346,-30.4214213562373)) ;
#150509 = CARTESIAN_POINT('',(6.87642977396045,0.22357022603955,-30.3271404520791)) ;
#150510 = CARTESIAN_POINT('',(6.97071067811866,0.129289321881346,-30.5385786437627)) ;
#150511 = CARTESIAN_POINT('',(6.97071067811866,0.129289321881346,-30.08)) ;
#150512 = CARTESIAN_POINT('',(7.14309644062712,-0.0430964406271155,-30.3661928812542)) ;
#150513 = CARTESIAN_POINT('Origin',(6.7,0.400000000000001,-30.08)) ;
#150514 = CARTESIAN_POINT('',(6.65857864376269,0.400000000000001,-30.18)) ;
#150515 = CARTESIAN_POINT('',(6.65857864376269,0.400000000000001,-30.78)) ;
#150516 = CARTESIAN_POINT('',(6.65857864376269,0.400000000000001,-30.08)) ;
#150517 = CARTESIAN_POINT('',(6.7,0.400000000000001,-30.78)) ;
#150518 = CARTESIAN_POINT('',(6.65857864376269,0.400000000000001,-30.18)) ;
#150519 = CARTESIAN_POINT('Origin',(0.6,-0.4,-30.08)) ;
#150520 = CARTESIAN_POINT('',(6.65857864376269,-0.400000000000001,-30.78)) ;
#150521 = CARTESIAN_POINT('',(0.6,-0.4,-30.78)) ;
#150522 = CARTESIAN_POINT('',(6.65857864376269,-0.400000000000001,-30.18)) ;
#150523 = CARTESIAN_POINT('',(6.65857864376269,-0.400000000000001,-30.08)) ;
#150524 = CARTESIAN_POINT('',(2.4,-0.4,-30.18)) ;
#150525 = CARTESIAN_POINT('Origin',(6.7,-0.400000000000001,-30.08)) ;
#150526 = CARTESIAN_POINT('',(6.97071067811866,-0.129289321881345,-30.5385786437627)) ;
#150527 = CARTESIAN_POINT('',(6.97071067811866,-0.129289321881346,-30.4214213562373)) ;
#150528 = CARTESIAN_POINT('',(6.97071067811866,-0.129289321881346,-30.08)) ;
#150529 = CARTESIAN_POINT('',(6.72928932188135,-0.370710678118655,-30.18)) ;
#150530 = CARTESIAN_POINT('',(6.67642977396045,-0.423570226039551,-30.1271404520791)) ;
#150531 = CARTESIAN_POINT('',(6.72928932188135,-0.370710678118655,-30.78)) ;
#150532 = CARTESIAN_POINT('',(6.72928932188135,-0.370710678118655,-30.08)) ;
#150533 = CARTESIAN_POINT('',(6.94309644062712,-0.156903559372885,-30.5661928812542)) ;
#150534 = CARTESIAN_POINT('Origin',(7.,-0.1,-30.08)) ;
#150535 = CARTESIAN_POINT('',(7.,-0.0585786437626909,-30.4214213562373)) ;
#150536 = CARTESIAN_POINT('',(7.,-0.0585786437626909,-30.5385786437627)) ;
#150537 = CARTESIAN_POINT('',(7.,-0.0585786437626909,-30.08)) ;
#150538 = CARTESIAN_POINT('',(7.,0.0585786437626909,-30.5385786437627)) ;
#150539 = CARTESIAN_POINT('',(7.,-0.1,-30.5385786437627)) ;
#150540 = CARTESIAN_POINT('',(7.,0.0585786437626909,-30.4214213562373)) ;
#150541 = CARTESIAN_POINT('',(7.,0.0585786437626909,-30.08)) ;
#150542 = CARTESIAN_POINT('',(7.,-0.1,-30.4214213562373)) ;
#150543 = CARTESIAN_POINT('Origin',(0.6,-0.600000000000001,-30.08)) ;
#150544 = CARTESIAN_POINT('',(6.65857864376269,-0.300000000000001,-30.08)) ;
#150545 = CARTESIAN_POINT('',(6.6585786437627,0.299999999999994,-30.08)) ;
#150546 = CARTESIAN_POINT('',(6.6585786437627,-0.399999999999999,-30.08)) ;
#150547 = CARTESIAN_POINT('',(2.4,0.3,-30.08)) ;
#150548 = CARTESIAN_POINT('',(6.65857864376269,-0.300000000000001,-30.08)) ;
#150549 = CARTESIAN_POINT('Origin',(0.6,-0.600000000000001,-30.88)) ;
#150550 = CARTESIAN_POINT('',(6.65857864376269,0.299999999999998,-30.88)) ;
#150551 = CARTESIAN_POINT('',(0.6,0.299999999999999,-30.88)) ;
#150552 = CARTESIAN_POINT('',(6.65857864376269,-0.300000000000001,-30.88)) ;
#150553 = CARTESIAN_POINT('',(6.65857864376269,-0.6,-30.88)) ;
#150554 = CARTESIAN_POINT('',(0.6,-0.3,-30.88)) ;
#150555 = CARTESIAN_POINT('Origin',(-0.4,-0.600000000000001,-33.89)) ;
#150556 = CARTESIAN_POINT('',(-0.4,-0.600000000000001,-33.99)) ;
#150557 = CARTESIAN_POINT('',(-0.4,-0.600000000000001,-34.59)) ;
#150558 = CARTESIAN_POINT('',(-0.4,-0.600000000000001,-33.89)) ;
#150559 = CARTESIAN_POINT('',(-0.4,-6.05857864376269,-34.59)) ;
#150560 = CARTESIAN_POINT('',(-0.4,-0.600000000000001,-34.59)) ;
#150561 = CARTESIAN_POINT('',(-0.4,-6.05857864376269,-33.99)) ;
#150562 = CARTESIAN_POINT('',(-0.4,-6.05857864376269,-33.89)) ;
#150563 = CARTESIAN_POINT('',(-0.4,-0.600000000000001,-33.99)) ;
#150564 = CARTESIAN_POINT('Origin',(-0.4,-6.1,-33.89)) ;
#150565 = CARTESIAN_POINT('',(-0.129289321881345,-6.37071067811866,-34.3485786437627)) ;
#150566 = CARTESIAN_POINT('',(-0.129289321881346,-6.37071067811866,-34.2314213562373)) ;
#150567 = CARTESIAN_POINT('',(-0.129289321881346,-6.37071067811866,-33.89)) ;
#150568 = CARTESIAN_POINT('',(-0.370710678118655,-6.12928932188134,-33.99)) ;
#150569 = CARTESIAN_POINT('',(-0.423570226039552,-6.07642977396045,-33.9371404520791)) ;
#150570 = CARTESIAN_POINT('',(-0.370710678118655,-6.12928932188134,-34.59)) ;
#150571 = CARTESIAN_POINT('',(-0.370710678118655,-6.12928932188134,-33.89)) ;
#150572 = CARTESIAN_POINT('',(-0.156903559372882,-6.34309644062712,-34.3761928812542)) ;
#150573 = CARTESIAN_POINT('Origin',(-0.1,-6.4,-33.89)) ;
#150574 = CARTESIAN_POINT('',(0.0585786437626908,-6.4,-34.3485786437627)) ;
#150575 = CARTESIAN_POINT('',(0.0585786437626908,-6.4,-34.2314213562373)) ;
#150576 = CARTESIAN_POINT('',(0.0585786437626908,-6.4,-33.89)) ;
#150577 = CARTESIAN_POINT('',(-0.0585786437626908,-6.4,-34.2314213562373)) ;
#150578 = CARTESIAN_POINT('',(-0.1,-6.4,-34.2314213562373)) ;
#150579 = CARTESIAN_POINT('',(-0.0585786437626908,-6.4,-34.3485786437627)) ;
#150580 = CARTESIAN_POINT('',(-0.0585786437626908,-6.4,-33.89)) ;
#150581 = CARTESIAN_POINT('',(-0.1,-6.4,-34.3485786437627)) ;
#150582 = CARTESIAN_POINT('Origin',(0.1,-6.4,-33.89)) ;
#150583 = CARTESIAN_POINT('',(0.370710678118654,-6.12928932188135,-34.59)) ;
#150584 = CARTESIAN_POINT('',(0.370710678118655,-6.12928932188134,-33.99)) ;
#150585 = CARTESIAN_POINT('',(0.370710678118655,-6.12928932188134,-33.89)) ;
#150586 = CARTESIAN_POINT('',(0.129289321881346,-6.37071067811866,-34.2314213562373)) ;
#150587 = CARTESIAN_POINT('',(0.223570226039555,-6.27642977396044,-34.1371404520791)) ;
#150588 = CARTESIAN_POINT('',(0.129289321881346,-6.37071067811866,-34.3485786437627)) ;
#150589 = CARTESIAN_POINT('',(0.129289321881346,-6.37071067811866,-33.89)) ;
#150590 = CARTESIAN_POINT('',(-0.0430964406271177,-6.54309644062712,-34.1761928812542)) ;
#150591 = CARTESIAN_POINT('Origin',(0.4,-6.1,-33.89)) ;
#150592 = CARTESIAN_POINT('',(0.4,-6.05857864376269,-33.99)) ;
#150593 = CARTESIAN_POINT('',(0.4,-6.05857864376269,-34.59)) ;
#150594 = CARTESIAN_POINT('',(0.4,-6.05857864376269,-33.89)) ;
#150595 = CARTESIAN_POINT('',(0.4,-0.6,-34.59)) ;
#150596 = CARTESIAN_POINT('',(0.4,-6.1,-34.59)) ;
#150597 = CARTESIAN_POINT('',(0.4,-0.6,-33.99)) ;
#150598 = CARTESIAN_POINT('',(0.4,-0.6,-33.89)) ;
#150599 = CARTESIAN_POINT('',(0.4,-6.05857864376269,-33.99)) ;
#150600 = CARTESIAN_POINT('Origin',(0.6,-0.600000000000001,-33.89)) ;
#150601 = CARTESIAN_POINT('',(0.3,-6.05857864376269,-33.89)) ;
#150602 = CARTESIAN_POINT('',(0.3,-0.6,-33.89)) ;
#150603 = CARTESIAN_POINT('',(0.3,-0.6,-33.89)) ;
#150604 = CARTESIAN_POINT('Origin',(0.6,-0.6,-33.89)) ;
#150605 = CARTESIAN_POINT('',(-0.3,-0.600000000000001,-33.89)) ;
#150606 = CARTESIAN_POINT('Origin',(0.6,-0.600000000000001,-33.89)) ;
#150607 = CARTESIAN_POINT('',(-0.300000000000006,-6.05857864376268,-33.89)) ;
#150608 = CARTESIAN_POINT('',(-0.3,-0.600000000000001,-33.89)) ;
#150609 = CARTESIAN_POINT('',(0.4,-6.05857864376269,-33.89)) ;
#150610 = CARTESIAN_POINT('Origin',(0.6,-0.600000000000001,-34.69)) ;
#150611 = CARTESIAN_POINT('',(-0.299999999999998,-6.05857864376269,-34.69)) ;
#150612 = CARTESIAN_POINT('',(-0.3,-0.600000000000001,-34.69)) ;
#150613 = CARTESIAN_POINT('',(-0.3,-0.600000000000001,-34.69)) ;
#150614 = CARTESIAN_POINT('Origin',(0.6,-0.600000000000001,-34.69)) ;
#150615 = CARTESIAN_POINT('',(0.3,-0.6,-34.69)) ;
#150616 = CARTESIAN_POINT('Origin',(0.6,-0.6,-34.69)) ;
#150617 = CARTESIAN_POINT('',(0.3,-6.05857864376269,-34.69)) ;
#150618 = CARTESIAN_POINT('',(0.3,-0.600000000000001,-34.69)) ;
#150619 = CARTESIAN_POINT('',(0.6,-6.05857864376269,-34.69)) ;
#150620 = CARTESIAN_POINT('Origin',(0.6,-0.600000000000001,-33.89)) ;
#150621 = CARTESIAN_POINT('Origin',(0.6,-0.600000000000001,-34.59)) ;
#150622 = CARTESIAN_POINT('Origin',(0.6,-0.600000000000001,-33.99)) ;
#150623 = CARTESIAN_POINT('Origin',(0.6,-0.6,-33.89)) ;
#150624 = CARTESIAN_POINT('Origin',(0.6,-0.6,-34.59)) ;
#150625 = CARTESIAN_POINT('Origin',(0.6,-0.6,-33.99)) ;
#150626 = CARTESIAN_POINT('Origin',(7.,0.1,-33.89)) ;
#150627 = CARTESIAN_POINT('',(6.72928932188135,0.370710678118655,-34.59)) ;
#150628 = CARTESIAN_POINT('',(6.72928932188135,0.370710678118655,-33.99)) ;
#150629 = CARTESIAN_POINT('',(6.72928932188135,0.370710678118655,-33.89)) ;
#150630 = CARTESIAN_POINT('',(6.97071067811866,0.129289321881346,-34.2314213562373)) ;
#150631 = CARTESIAN_POINT('',(6.87642977396044,0.223570226039555,-34.1371404520791)) ;
#150632 = CARTESIAN_POINT('',(6.97071067811866,0.129289321881346,-34.3485786437627)) ;
#150633 = CARTESIAN_POINT('',(6.97071067811866,0.129289321881346,-33.89)) ;
#150634 = CARTESIAN_POINT('',(7.14309644062712,-0.0430964406271179,-34.1761928812542)) ;
#150635 = CARTESIAN_POINT('Origin',(6.7,0.400000000000001,-33.89)) ;
#150636 = CARTESIAN_POINT('',(6.65857864376269,0.400000000000001,-33.99)) ;
#150637 = CARTESIAN_POINT('',(6.65857864376269,0.400000000000001,-34.59)) ;
#150638 = CARTESIAN_POINT('',(6.65857864376269,0.400000000000001,-33.89)) ;
#150639 = CARTESIAN_POINT('',(6.7,0.400000000000001,-34.59)) ;
#150640 = CARTESIAN_POINT('',(6.65857864376269,0.400000000000001,-33.99)) ;
#150641 = CARTESIAN_POINT('Origin',(0.6,-0.4,-33.89)) ;
#150642 = CARTESIAN_POINT('',(6.65857864376269,-0.400000000000001,-34.59)) ;
#150643 = CARTESIAN_POINT('',(0.6,-0.4,-34.59)) ;
#150644 = CARTESIAN_POINT('',(6.65857864376269,-0.400000000000001,-33.99)) ;
#150645 = CARTESIAN_POINT('',(6.65857864376269,-0.400000000000001,-33.89)) ;
#150646 = CARTESIAN_POINT('',(2.4,-0.4,-33.99)) ;
#150647 = CARTESIAN_POINT('Origin',(6.7,-0.400000000000001,-33.89)) ;
#150648 = CARTESIAN_POINT('',(6.97071067811866,-0.129289321881345,-34.3485786437627)) ;
#150649 = CARTESIAN_POINT('',(6.97071067811866,-0.129289321881346,-34.2314213562373)) ;
#150650 = CARTESIAN_POINT('',(6.97071067811866,-0.129289321881346,-33.89)) ;
#150651 = CARTESIAN_POINT('',(6.72928932188135,-0.370710678118655,-33.99)) ;
#150652 = CARTESIAN_POINT('',(6.67642977396045,-0.423570226039555,-33.9371404520791)) ;
#150653 = CARTESIAN_POINT('',(6.72928932188135,-0.370710678118655,-34.59)) ;
#150654 = CARTESIAN_POINT('',(6.72928932188135,-0.370710678118655,-33.89)) ;
#150655 = CARTESIAN_POINT('',(6.94309644062712,-0.156903559372885,-34.3761928812542)) ;
#150656 = CARTESIAN_POINT('Origin',(7.,-0.1,-33.89)) ;
#150657 = CARTESIAN_POINT('',(7.,-0.0585786437626909,-34.2314213562373)) ;
#150658 = CARTESIAN_POINT('',(7.,-0.0585786437626909,-34.3485786437627)) ;
#150659 = CARTESIAN_POINT('',(7.,-0.0585786437626909,-33.89)) ;
#150660 = CARTESIAN_POINT('',(7.,0.0585786437626909,-34.3485786437627)) ;
#150661 = CARTESIAN_POINT('',(7.,-0.1,-34.3485786437627)) ;
#150662 = CARTESIAN_POINT('',(7.,0.0585786437626909,-34.2314213562373)) ;
#150663 = CARTESIAN_POINT('',(7.,0.0585786437626909,-33.89)) ;
#150664 = CARTESIAN_POINT('',(7.,-0.1,-34.2314213562373)) ;
#150665 = CARTESIAN_POINT('Origin',(0.6,-0.600000000000001,-33.89)) ;
#150666 = CARTESIAN_POINT('',(6.65857864376269,-0.300000000000001,-33.89)) ;
#150667 = CARTESIAN_POINT('',(6.65857864376269,0.300000000000007,-33.89)) ;
#150668 = CARTESIAN_POINT('',(6.65857864376269,-0.399999999999999,-33.89)) ;
#150669 = CARTESIAN_POINT('',(2.4,0.3,-33.89)) ;
#150670 = CARTESIAN_POINT('',(6.65857864376269,-0.300000000000001,-33.89)) ;
#150671 = CARTESIAN_POINT('Origin',(0.6,-0.600000000000001,-34.69)) ;
#150672 = CARTESIAN_POINT('',(6.65857864376269,0.3,-34.69)) ;
#150673 = CARTESIAN_POINT('',(0.6,0.299999999999999,-34.69)) ;
#150674 = CARTESIAN_POINT('',(6.65857864376269,-0.300000000000001,-34.69)) ;
#150675 = CARTESIAN_POINT('',(6.6585786437627,-0.6,-34.69)) ;
#150676 = CARTESIAN_POINT('',(0.6,-0.3,-34.69)) ;
#150677 = CARTESIAN_POINT('Origin',(0.4,-6.4,-34.39)) ;
#150678 = CARTESIAN_POINT('',(-0.0585786437626895,-6.37071067811866,-34.4192893218813)) ;
#150679 = CARTESIAN_POINT('',(-0.299999999999997,-6.12928932188135,-34.6607106781186)) ;
#150680 = CARTESIAN_POINT('',(0.113807118745769,-6.54309644062712,-34.2469035593729)) ;
#150681 = CARTESIAN_POINT('',(0.299999999999999,-6.12928932188134,-34.6607106781187)) ;
#150682 = CARTESIAN_POINT('',(0.4,-6.12928932188135,-34.6607106781186)) ;
#150683 = CARTESIAN_POINT('',(0.0585786437626844,-6.37071067811866,-34.4192893218813)) ;
#150684 = CARTESIAN_POINT('',(0.152859547920894,-6.27642977396045,-34.5135702260395)) ;
#150685 = CARTESIAN_POINT('',(0.4,-6.37071067811866,-34.4192893218813)) ;
#150686 = CARTESIAN_POINT('Origin',(0.4,-6.1,-33.89)) ;
#150687 = CARTESIAN_POINT('',(0.058578643762689,-6.37071067811866,-34.1607106781187)) ;
#150688 = CARTESIAN_POINT('',(0.300000000000011,-6.12928932188133,-33.9192893218813)) ;
#150689 = CARTESIAN_POINT('',(0.352859547920897,-6.07642977396045,-33.8664297739605)) ;
#150690 = CARTESIAN_POINT('',(-0.300000000000007,-6.12928932188133,-33.9192893218813)) ;
#150691 = CARTESIAN_POINT('',(0.4,-6.12928932188134,-33.9192893218814)) ;
#150692 = CARTESIAN_POINT('',(-0.0585786437626846,-6.37071067811866,-34.1607106781187)) ;
#150693 = CARTESIAN_POINT('',(-0.0861928812542284,-6.34309644062711,-34.1330964406271)) ;
#150694 = CARTESIAN_POINT('',(0.4,-6.37071067811866,-34.1607106781187)) ;
#150695 = CARTESIAN_POINT('Origin',(0.4,-6.4,-30.58)) ;
#150696 = CARTESIAN_POINT('',(-0.0585786437626899,-6.37071067811865,-30.6092893218813)) ;
#150697 = CARTESIAN_POINT('',(-0.299999999999994,-6.12928932188135,-30.8507106781187)) ;
#150698 = CARTESIAN_POINT('',(0.11380711874577,-6.54309644062711,-30.4369035593729)) ;
#150699 = CARTESIAN_POINT('',(0.299999999999999,-6.12928932188135,-30.8507106781187)) ;
#150700 = CARTESIAN_POINT('',(0.4,-6.12928932188134,-30.8507106781187)) ;
#150701 = CARTESIAN_POINT('',(0.058578643762692,-6.37071067811865,-30.6092893218813)) ;
#150702 = CARTESIAN_POINT('',(0.152859547920897,-6.27642977396045,-30.7035702260396)) ;
#150703 = CARTESIAN_POINT('',(0.4,-6.37071067811865,-30.6092893218813)) ;
#150704 = CARTESIAN_POINT('Origin',(0.4,-6.1,-30.08)) ;
#150705 = CARTESIAN_POINT('',(0.0585786437626916,-6.37071067811865,-30.3507106781187)) ;
#150706 = CARTESIAN_POINT('',(0.299999999999992,-6.12928932188135,-30.1092893218814)) ;
#150707 = CARTESIAN_POINT('',(0.352859547920897,-6.07642977396045,-30.0564297739604)) ;
#150708 = CARTESIAN_POINT('',(-0.299999999999994,-6.12928932188135,-30.1092893218814)) ;
#150709 = CARTESIAN_POINT('',(0.4,-6.12928932188135,-30.1092893218813)) ;
#150710 = CARTESIAN_POINT('',(-0.0585786437626909,-6.37071067811865,-30.3507106781187)) ;
#150711 = CARTESIAN_POINT('',(-0.0861928812542305,-6.34309644062712,-30.3230964406271)) ;
#150712 = CARTESIAN_POINT('',(0.4,-6.37071067811865,-30.3507106781187)) ;
#150713 = CARTESIAN_POINT('Origin',(0.4,-6.4,-26.77)) ;
#150714 = CARTESIAN_POINT('',(-0.0585786437626899,-6.37071067811865,-26.7992893218813)) ;
#150715 = CARTESIAN_POINT('',(-0.299999999999994,-6.12928932188135,-27.0407106781187)) ;
#150716 = CARTESIAN_POINT('',(0.11380711874577,-6.54309644062711,-26.6269035593729)) ;
#150717 = CARTESIAN_POINT('',(0.299999999999999,-6.12928932188135,-27.0407106781187)) ;
#150718 = CARTESIAN_POINT('',(0.4,-6.12928932188134,-27.0407106781187)) ;
#150719 = CARTESIAN_POINT('',(0.058578643762692,-6.37071067811865,-26.7992893218813)) ;
#150720 = CARTESIAN_POINT('',(0.152859547920897,-6.27642977396045,-26.8935702260396)) ;
#150721 = CARTESIAN_POINT('',(0.4,-6.37071067811865,-26.7992893218813)) ;
#150722 = CARTESIAN_POINT('Origin',(0.4,-6.1,-26.27)) ;
#150723 = CARTESIAN_POINT('',(0.0585786437626916,-6.37071067811865,-26.5407106781187)) ;
#150724 = CARTESIAN_POINT('',(0.299999999999992,-6.12928932188135,-26.2992893218814)) ;
#150725 = CARTESIAN_POINT('',(0.352859547920897,-6.07642977396045,-26.2464297739604)) ;
#150726 = CARTESIAN_POINT('',(-0.299999999999994,-6.12928932188135,-26.2992893218814)) ;
#150727 = CARTESIAN_POINT('',(0.4,-6.12928932188135,-26.2992893218813)) ;
#150728 = CARTESIAN_POINT('',(-0.0585786437626909,-6.37071067811865,-26.5407106781187)) ;
#150729 = CARTESIAN_POINT('',(-0.0861928812542305,-6.34309644062712,-26.5130964406271)) ;
#150730 = CARTESIAN_POINT('',(0.4,-6.37071067811865,-26.5407106781187)) ;
#150731 = CARTESIAN_POINT('Origin',(0.4,-6.4,-22.96)) ;
#150732 = CARTESIAN_POINT('',(-0.0585786437626899,-6.37071067811865,-22.9892893218813)) ;
#150733 = CARTESIAN_POINT('',(-0.299999999999994,-6.12928932188135,-23.2307106781187)) ;
#150734 = CARTESIAN_POINT('',(0.11380711874577,-6.54309644062711,-22.8169035593729)) ;
#150735 = CARTESIAN_POINT('',(0.299999999999999,-6.12928932188135,-23.2307106781187)) ;
#150736 = CARTESIAN_POINT('',(0.4,-6.12928932188134,-23.2307106781187)) ;
#150737 = CARTESIAN_POINT('',(0.058578643762692,-6.37071067811865,-22.9892893218813)) ;
#150738 = CARTESIAN_POINT('',(0.152859547920897,-6.27642977396045,-23.0835702260395)) ;
#150739 = CARTESIAN_POINT('',(0.4,-6.37071067811865,-22.9892893218813)) ;
#150740 = CARTESIAN_POINT('Origin',(0.4,-6.1,-22.46)) ;
#150741 = CARTESIAN_POINT('',(0.0585786437626916,-6.37071067811865,-22.7307106781187)) ;
#150742 = CARTESIAN_POINT('',(0.299999999999992,-6.12928932188135,-22.4892893218814)) ;
#150743 = CARTESIAN_POINT('',(0.352859547920897,-6.07642977396045,-22.4364297739604)) ;
#150744 = CARTESIAN_POINT('',(-0.299999999999994,-6.12928932188135,-22.4892893218814)) ;
#150745 = CARTESIAN_POINT('',(0.4,-6.12928932188135,-22.4892893218814)) ;
#150746 = CARTESIAN_POINT('',(-0.0585786437626909,-6.37071067811865,-22.7307106781187)) ;
#150747 = CARTESIAN_POINT('',(-0.0861928812542305,-6.34309644062712,-22.7030964406271)) ;
#150748 = CARTESIAN_POINT('',(0.4,-6.37071067811865,-22.7307106781187)) ;
#150749 = CARTESIAN_POINT('Origin',(0.4,-6.4,-19.15)) ;
#150750 = CARTESIAN_POINT('',(-0.0585786437626899,-6.37071067811865,-19.1792893218813)) ;
#150751 = CARTESIAN_POINT('',(-0.299999999999994,-6.12928932188135,-19.4207106781187)) ;
#150752 = CARTESIAN_POINT('',(0.11380711874577,-6.54309644062711,-19.0069035593729)) ;
#150753 = CARTESIAN_POINT('',(0.299999999999999,-6.12928932188135,-19.4207106781187)) ;
#150754 = CARTESIAN_POINT('',(0.4,-6.12928932188134,-19.4207106781187)) ;
#150755 = CARTESIAN_POINT('',(0.058578643762692,-6.37071067811865,-19.1792893218813)) ;
#150756 = CARTESIAN_POINT('',(0.152859547920897,-6.27642977396045,-19.2735702260396)) ;
#150757 = CARTESIAN_POINT('',(0.4,-6.37071067811865,-19.1792893218813)) ;
#150758 = CARTESIAN_POINT('Origin',(0.4,-6.1,-18.65)) ;
#150759 = CARTESIAN_POINT('',(0.0585786437626916,-6.37071067811865,-18.9207106781187)) ;
#150760 = CARTESIAN_POINT('',(0.299999999999992,-6.12928932188135,-18.6792893218814)) ;
#150761 = CARTESIAN_POINT('',(0.352859547920897,-6.07642977396045,-18.6264297739605)) ;
#150762 = CARTESIAN_POINT('',(-0.299999999999994,-6.12928932188135,-18.6792893218814)) ;
#150763 = CARTESIAN_POINT('',(0.4,-6.12928932188135,-18.6792893218813)) ;
#150764 = CARTESIAN_POINT('',(-0.0585786437626909,-6.37071067811865,-18.9207106781187)) ;
#150765 = CARTESIAN_POINT('',(-0.0861928812542305,-6.34309644062712,-18.8930964406271)) ;
#150766 = CARTESIAN_POINT('',(0.4,-6.37071067811865,-18.9207106781187)) ;
#150767 = CARTESIAN_POINT('Origin',(0.4,-6.4,-15.34)) ;
#150768 = CARTESIAN_POINT('',(-0.0585786437626904,-6.37071067811866,-15.3692893218813)) ;
#150769 = CARTESIAN_POINT('',(-0.299999999999999,-6.12928932188134,-15.6107106781187)) ;
#150770 = CARTESIAN_POINT('',(0.11380711874577,-6.54309644062711,-15.1969035593729)) ;
#150771 = CARTESIAN_POINT('',(0.3,-6.12928932188134,-15.6107106781187)) ;
#150772 = CARTESIAN_POINT('',(0.4,-6.12928932188134,-15.6107106781187)) ;
#150773 = CARTESIAN_POINT('',(0.0585786437626911,-6.37071067811866,-15.3692893218813)) ;
#150774 = CARTESIAN_POINT('',(0.152859547920897,-6.27642977396045,-15.4635702260396)) ;
#150775 = CARTESIAN_POINT('',(0.4,-6.37071067811866,-15.3692893218813)) ;
#150776 = CARTESIAN_POINT('Origin',(0.4,-6.1,-14.84)) ;
#150777 = CARTESIAN_POINT('',(0.0585786437626904,-6.37071067811866,-15.1107106781187)) ;
#150778 = CARTESIAN_POINT('',(0.299999999999999,-6.12928932188135,-14.8692893218813)) ;
#150779 = CARTESIAN_POINT('',(0.352859547920896,-6.07642977396045,-14.8164297739604)) ;
#150780 = CARTESIAN_POINT('',(-0.300000000000001,-6.12928932188134,-14.8692893218813)) ;
#150781 = CARTESIAN_POINT('',(0.4,-6.12928932188134,-14.8692893218813)) ;
#150782 = CARTESIAN_POINT('',(-0.0585786437626914,-6.37071067811866,-15.1107106781187)) ;
#150783 = CARTESIAN_POINT('',(-0.0861928812542312,-6.34309644062712,-15.0830964406271)) ;
#150784 = CARTESIAN_POINT('',(0.4,-6.37071067811866,-15.1107106781187)) ;
#150785 = CARTESIAN_POINT('Origin',(0.4,-6.4,-11.53)) ;
#150786 = CARTESIAN_POINT('',(-0.0585786437626916,-6.37071067811866,-11.5592893218813)) ;
#150787 = CARTESIAN_POINT('',(-0.3,-6.12928932188135,-11.8007106781187)) ;
#150788 = CARTESIAN_POINT('',(0.113807118745769,-6.54309644062712,-11.3869035593729)) ;
#150789 = CARTESIAN_POINT('',(0.299999999999998,-6.12928932188135,-11.8007106781187)) ;
#150790 = CARTESIAN_POINT('',(0.4,-6.12928932188134,-11.8007106781187)) ;
#150791 = CARTESIAN_POINT('',(0.0585786437626907,-6.37071067811866,-11.5592893218813)) ;
#150792 = CARTESIAN_POINT('',(0.152859547920896,-6.27642977396045,-11.6535702260396)) ;
#150793 = CARTESIAN_POINT('',(0.4,-6.37071067811866,-11.5592893218813)) ;
#150794 = CARTESIAN_POINT('Origin',(0.4,-6.1,-11.03)) ;
#150795 = CARTESIAN_POINT('',(0.0585786437626913,-6.37071067811866,-11.3007106781187)) ;
#150796 = CARTESIAN_POINT('',(0.300000000000001,-6.12928932188134,-11.0592893218813)) ;
#150797 = CARTESIAN_POINT('',(0.352859547920897,-6.07642977396045,-11.0064297739604)) ;
#150798 = CARTESIAN_POINT('',(-0.300000000000003,-6.12928932188134,-11.0592893218813)) ;
#150799 = CARTESIAN_POINT('',(0.4,-6.12928932188134,-11.0592893218813)) ;
#150800 = CARTESIAN_POINT('',(-0.0585786437626915,-6.37071067811866,-11.3007106781187)) ;
#150801 = CARTESIAN_POINT('',(-0.0861928812542312,-6.34309644062712,-11.2730964406271)) ;
#150802 = CARTESIAN_POINT('',(0.4,-6.37071067811866,-11.3007106781187)) ;
#150803 = CARTESIAN_POINT('Origin',(0.4,-6.4,-7.72)) ;
#150804 = CARTESIAN_POINT('',(-0.0585786437626906,-6.37071067811866,-7.74928932188134)) ;
#150805 = CARTESIAN_POINT('',(-0.299999999999999,-6.12928932188134,-7.99071067811865)) ;
#150806 = CARTESIAN_POINT('',(0.113807118745769,-6.54309644062711,-7.57690355937288)) ;
#150807 = CARTESIAN_POINT('',(0.3,-6.12928932188134,-7.99071067811865)) ;
#150808 = CARTESIAN_POINT('',(0.4,-6.12928932188134,-7.99071067811866)) ;
#150809 = CARTESIAN_POINT('',(0.0585786437626912,-6.37071067811866,-7.74928932188134)) ;
#150810 = CARTESIAN_POINT('',(0.152859547920897,-6.27642977396045,-7.84357022603955)) ;
#150811 = CARTESIAN_POINT('',(0.4,-6.37071067811866,-7.74928932188134)) ;
#150812 = CARTESIAN_POINT('Origin',(0.4,-6.1,-7.22)) ;
#150813 = CARTESIAN_POINT('',(0.0585786437626908,-6.37071067811866,-7.49071067811866)) ;
#150814 = CARTESIAN_POINT('',(0.300000000000002,-6.12928932188134,-7.24928932188134)) ;
#150815 = CARTESIAN_POINT('',(0.352859547920897,-6.07642977396045,-7.19642977396045)) ;
#150816 = CARTESIAN_POINT('',(-0.300000000000001,-6.12928932188134,-7.24928932188134)) ;
#150817 = CARTESIAN_POINT('',(0.4,-6.12928932188134,-7.24928932188134)) ;
#150818 = CARTESIAN_POINT('',(-0.0585786437626907,-6.37071067811866,-7.49071067811866)) ;
#150819 = CARTESIAN_POINT('',(-0.0861928812542307,-6.34309644062712,-7.46309644062712)) ;
#150820 = CARTESIAN_POINT('',(0.4,-6.37071067811866,-7.49071067811866)) ;
#150821 = CARTESIAN_POINT('Origin',(0.4,-6.4,-3.91)) ;
#150822 = CARTESIAN_POINT('',(-0.0585786437626904,-6.37071067811866,-3.93928932188134)) ;
#150823 = CARTESIAN_POINT('',(-0.300000000000001,-6.12928932188134,-4.18071067811866)) ;
#150824 = CARTESIAN_POINT('',(0.11380711874577,-6.54309644062711,-3.76690355937288)) ;
#150825 = CARTESIAN_POINT('',(0.300000000000001,-6.12928932188134,-4.18071067811866)) ;
#150826 = CARTESIAN_POINT('',(0.4,-6.12928932188134,-4.18071067811865)) ;
#150827 = CARTESIAN_POINT('',(0.0585786437626911,-6.37071067811866,-3.93928932188134)) ;
#150828 = CARTESIAN_POINT('',(0.152859547920897,-6.27642977396045,-4.03357022603955)) ;
#150829 = CARTESIAN_POINT('',(0.4,-6.37071067811866,-3.93928932188134)) ;
#150830 = CARTESIAN_POINT('Origin',(0.4,-6.1,-3.41)) ;
#150831 = CARTESIAN_POINT('',(0.0585786437626907,-6.37071067811866,-3.68071067811866)) ;
#150832 = CARTESIAN_POINT('',(0.299999999999999,-6.12928932188135,-3.43928932188135)) ;
#150833 = CARTESIAN_POINT('',(0.352859547920897,-6.07642977396045,-3.38642977396045)) ;
#150834 = CARTESIAN_POINT('',(-0.299999999999999,-6.12928932188135,-3.43928932188135)) ;
#150835 = CARTESIAN_POINT('',(0.4,-6.12928932188134,-3.43928932188135)) ;
#150836 = CARTESIAN_POINT('',(-0.0585786437626909,-6.37071067811866,-3.68071067811866)) ;
#150837 = CARTESIAN_POINT('',(-0.086192881254231,-6.34309644062712,-3.65309644062712)) ;
#150838 = CARTESIAN_POINT('',(0.4,-6.37071067811866,-3.68071067811866)) ;
#150839 = CARTESIAN_POINT('Origin',(6.7,-0.399999999999999,-34.69)) ;
#150840 = CARTESIAN_POINT('',(6.97071067811865,-0.0585786437626952,-34.4192893218813)) ;
#150841 = CARTESIAN_POINT('',(6.72928932188135,-0.300000000000001,-34.6607106781186)) ;
#150842 = CARTESIAN_POINT('',(6.67642977396045,-0.352859547920898,-34.7135702260396)) ;
#150843 = CARTESIAN_POINT('',(6.72928932188134,0.3,-34.6607106781187)) ;
#150844 = CARTESIAN_POINT('',(6.72928932188135,-0.399999999999999,-34.6607106781186)) ;
#150845 = CARTESIAN_POINT('',(6.97071067811865,0.0585786437626901,-34.4192893218813)) ;
#150846 = CARTESIAN_POINT('',(6.94309644062711,0.0861928812542281,-34.4469035593729)) ;
#150847 = CARTESIAN_POINT('',(6.97071067811865,-0.4,-34.4192893218813)) ;
#150848 = CARTESIAN_POINT('Origin',(7.,-0.399999999999999,-34.19)) ;
#150849 = CARTESIAN_POINT('',(6.97071067811866,0.0585786437626919,-34.1607106781187)) ;
#150850 = CARTESIAN_POINT('',(6.72928932188134,0.300000000000006,-33.9192893218814)) ;
#150851 = CARTESIAN_POINT('',(7.14309644062712,-0.113807118745768,-34.3330964406271)) ;
#150852 = CARTESIAN_POINT('',(6.72928932188134,-0.300000000000007,-33.9192893218813)) ;
#150853 = CARTESIAN_POINT('',(6.72928932188134,-0.399999999999999,-33.9192893218814)) ;
#150854 = CARTESIAN_POINT('',(6.97071067811866,-0.058578643762684,-34.1607106781187)) ;
#150855 = CARTESIAN_POINT('',(6.87642977396045,-0.152859547920894,-34.0664297739605)) ;
#150856 = CARTESIAN_POINT('',(6.97071067811866,-0.399999999999999,-34.1607106781187)) ;
#150857 = CARTESIAN_POINT('Origin',(6.7,-0.399999999999999,-30.88)) ;
#150858 = CARTESIAN_POINT('',(6.97071067811866,-0.0585786437626901,-30.6092893218813)) ;
#150859 = CARTESIAN_POINT('',(6.72928932188135,-0.299999999999997,-30.8507106781187)) ;
#150860 = CARTESIAN_POINT('',(6.67642977396045,-0.352859547920897,-30.9035702260396)) ;
#150861 = CARTESIAN_POINT('',(6.72928932188135,0.299999999999998,-30.8507106781187)) ;
#150862 = CARTESIAN_POINT('',(6.72928932188135,-0.399999999999999,-30.8507106781187)) ;
#150863 = CARTESIAN_POINT('',(6.97071067811866,0.0585786437626903,-30.6092893218813)) ;
#150864 = CARTESIAN_POINT('',(6.94309644062712,0.0861928812542301,-30.6369035593729)) ;
#150865 = CARTESIAN_POINT('',(6.97071067811866,-0.4,-30.6092893218813)) ;
#150866 = CARTESIAN_POINT('Origin',(7.,-0.399999999999999,-30.38)) ;
#150867 = CARTESIAN_POINT('',(6.97071067811865,0.058578643762691,-30.3507106781187)) ;
#150868 = CARTESIAN_POINT('',(6.72928932188135,0.299999999999994,-30.1092893218813)) ;
#150869 = CARTESIAN_POINT('',(7.14309644062712,-0.11380711874577,-30.5230964406271)) ;
#150870 = CARTESIAN_POINT('',(6.72928932188135,-0.299999999999999,-30.1092893218813)) ;
#150871 = CARTESIAN_POINT('',(6.72928932188135,-0.399999999999999,-30.1092893218813)) ;
#150872 = CARTESIAN_POINT('',(6.97071067811865,-0.0585786437626907,-30.3507106781187)) ;
#150873 = CARTESIAN_POINT('',(6.87642977396045,-0.152859547920896,-30.2564297739604)) ;
#150874 = CARTESIAN_POINT('',(6.97071067811865,-0.399999999999999,-30.3507106781187)) ;
#150875 = CARTESIAN_POINT('Origin',(6.7,-0.399999999999999,-27.07)) ;
#150876 = CARTESIAN_POINT('',(6.97071067811866,-0.0585786437626901,-26.7992893218813)) ;
#150877 = CARTESIAN_POINT('',(6.72928932188135,-0.299999999999997,-27.0407106781187)) ;
#150878 = CARTESIAN_POINT('',(6.67642977396045,-0.352859547920897,-27.0935702260396)) ;
#150879 = CARTESIAN_POINT('',(6.72928932188135,0.299999999999998,-27.0407106781187)) ;
#150880 = CARTESIAN_POINT('',(6.72928932188135,-0.399999999999999,-27.0407106781187)) ;
#150881 = CARTESIAN_POINT('',(6.97071067811866,0.0585786437626903,-26.7992893218813)) ;
#150882 = CARTESIAN_POINT('',(6.94309644062712,0.0861928812542301,-26.8269035593729)) ;
#150883 = CARTESIAN_POINT('',(6.97071067811866,-0.4,-26.7992893218813)) ;
#150884 = CARTESIAN_POINT('Origin',(7.,-0.399999999999999,-26.57)) ;
#150885 = CARTESIAN_POINT('',(6.97071067811865,0.058578643762691,-26.5407106781187)) ;
#150886 = CARTESIAN_POINT('',(6.72928932188135,0.299999999999994,-26.2992893218813)) ;
#150887 = CARTESIAN_POINT('',(7.14309644062712,-0.11380711874577,-26.7130964406271)) ;
#150888 = CARTESIAN_POINT('',(6.72928932188135,-0.299999999999999,-26.2992893218813)) ;
#150889 = CARTESIAN_POINT('',(6.72928932188135,-0.399999999999999,-26.2992893218813)) ;
#150890 = CARTESIAN_POINT('',(6.97071067811865,-0.0585786437626907,-26.5407106781187)) ;
#150891 = CARTESIAN_POINT('',(6.87642977396045,-0.152859547920896,-26.4464297739605)) ;
#150892 = CARTESIAN_POINT('',(6.97071067811865,-0.399999999999999,-26.5407106781187)) ;
#150893 = CARTESIAN_POINT('Origin',(6.7,-0.399999999999999,-23.26)) ;
#150894 = CARTESIAN_POINT('',(6.97071067811866,-0.0585786437626901,-22.9892893218813)) ;
#150895 = CARTESIAN_POINT('',(6.72928932188135,-0.299999999999997,-23.2307106781187)) ;
#150896 = CARTESIAN_POINT('',(6.67642977396045,-0.352859547920897,-23.2835702260396)) ;
#150897 = CARTESIAN_POINT('',(6.72928932188135,0.299999999999998,-23.2307106781187)) ;
#150898 = CARTESIAN_POINT('',(6.72928932188135,-0.399999999999999,-23.2307106781187)) ;
#150899 = CARTESIAN_POINT('',(6.97071067811866,0.0585786437626903,-22.9892893218813)) ;
#150900 = CARTESIAN_POINT('',(6.94309644062712,0.0861928812542301,-23.0169035593729)) ;
#150901 = CARTESIAN_POINT('',(6.97071067811866,-0.4,-22.9892893218813)) ;
#150902 = CARTESIAN_POINT('Origin',(7.,-0.399999999999999,-22.76)) ;
#150903 = CARTESIAN_POINT('',(6.97071067811865,0.058578643762691,-22.7307106781187)) ;
#150904 = CARTESIAN_POINT('',(6.72928932188135,0.299999999999994,-22.4892893218814)) ;
#150905 = CARTESIAN_POINT('',(7.14309644062712,-0.11380711874577,-22.9030964406271)) ;
#150906 = CARTESIAN_POINT('',(6.72928932188135,-0.299999999999999,-22.4892893218813)) ;
#150907 = CARTESIAN_POINT('',(6.72928932188135,-0.399999999999999,-22.4892893218814)) ;
#150908 = CARTESIAN_POINT('',(6.97071067811865,-0.0585786437626907,-22.7307106781187)) ;
#150909 = CARTESIAN_POINT('',(6.87642977396045,-0.152859547920896,-22.6364297739605)) ;
#150910 = CARTESIAN_POINT('',(6.97071067811865,-0.399999999999999,-22.7307106781187)) ;
#150911 = CARTESIAN_POINT('Origin',(6.7,-0.399999999999999,-19.45)) ;
#150912 = CARTESIAN_POINT('',(6.97071067811866,-0.0585786437626901,-19.1792893218813)) ;
#150913 = CARTESIAN_POINT('',(6.72928932188135,-0.299999999999997,-19.4207106781187)) ;
#150914 = CARTESIAN_POINT('',(6.67642977396045,-0.352859547920897,-19.4735702260396)) ;
#150915 = CARTESIAN_POINT('',(6.72928932188135,0.299999999999998,-19.4207106781187)) ;
#150916 = CARTESIAN_POINT('',(6.72928932188135,-0.399999999999999,-19.4207106781187)) ;
#150917 = CARTESIAN_POINT('',(6.97071067811866,0.0585786437626903,-19.1792893218813)) ;
#150918 = CARTESIAN_POINT('',(6.94309644062712,0.0861928812542301,-19.2069035593729)) ;
#150919 = CARTESIAN_POINT('',(6.97071067811866,-0.4,-19.1792893218813)) ;
#150920 = CARTESIAN_POINT('Origin',(7.,-0.399999999999999,-18.95)) ;
#150921 = CARTESIAN_POINT('',(6.97071067811865,0.058578643762691,-18.9207106781187)) ;
#150922 = CARTESIAN_POINT('',(6.72928932188135,0.299999999999992,-18.6792893218814)) ;
#150923 = CARTESIAN_POINT('',(7.14309644062712,-0.11380711874577,-19.0930964406271)) ;
#150924 = CARTESIAN_POINT('',(6.72928932188135,-0.299999999999999,-18.6792893218813)) ;
#150925 = CARTESIAN_POINT('',(6.72928932188135,-0.399999999999999,-18.6792893218813)) ;
#150926 = CARTESIAN_POINT('',(6.97071067811865,-0.0585786437626907,-18.9207106781187)) ;
#150927 = CARTESIAN_POINT('',(6.87642977396045,-0.152859547920896,-18.8264297739604)) ;
#150928 = CARTESIAN_POINT('',(6.97071067811865,-0.399999999999999,-18.9207106781187)) ;
#150929 = CARTESIAN_POINT('Origin',(6.7,-0.399999999999999,-15.64)) ;
#150930 = CARTESIAN_POINT('',(6.97071067811866,-0.058578643762691,-15.3692893218813)) ;
#150931 = CARTESIAN_POINT('',(6.72928932188135,-0.299999999999999,-15.6107106781187)) ;
#150932 = CARTESIAN_POINT('',(6.67642977396045,-0.352859547920897,-15.6635702260396)) ;
#150933 = CARTESIAN_POINT('',(6.72928932188134,0.300000000000003,-15.6107106781187)) ;
#150934 = CARTESIAN_POINT('',(6.72928932188135,-0.399999999999999,-15.6107106781187)) ;
#150935 = CARTESIAN_POINT('',(6.97071067811866,0.0585786437626913,-15.3692893218813)) ;
#150936 = CARTESIAN_POINT('',(6.94309644062712,0.086192881254231,-15.3969035593729)) ;
#150937 = CARTESIAN_POINT('',(6.97071067811866,-0.4,-15.3692893218813)) ;
#150938 = CARTESIAN_POINT('Origin',(7.,-0.399999999999999,-15.14)) ;
#150939 = CARTESIAN_POINT('',(6.97071067811865,0.0585786437626917,-15.1107106781187)) ;
#150940 = CARTESIAN_POINT('',(6.72928932188135,0.3,-14.8692893218813)) ;
#150941 = CARTESIAN_POINT('',(7.14309644062712,-0.11380711874577,-15.2830964406271)) ;
#150942 = CARTESIAN_POINT('',(6.72928932188135,-0.299999999999999,-14.8692893218813)) ;
#150943 = CARTESIAN_POINT('',(6.72928932188135,-0.399999999999999,-14.8692893218813)) ;
#150944 = CARTESIAN_POINT('',(6.97071067811865,-0.0585786437626915,-15.1107106781187)) ;
#150945 = CARTESIAN_POINT('',(6.87642977396045,-0.152859547920897,-15.0164297739605)) ;
#150946 = CARTESIAN_POINT('',(6.97071067811865,-0.399999999999999,-15.1107106781187)) ;
#150947 = CARTESIAN_POINT('Origin',(6.7,-0.399999999999999,-11.83)) ;
#150948 = CARTESIAN_POINT('',(6.97071067811866,-0.058578643762691,-11.5592893218813)) ;
#150949 = CARTESIAN_POINT('',(6.72928932188134,-0.300000000000002,-11.8007106781187)) ;
#150950 = CARTESIAN_POINT('',(6.67642977396045,-0.352859547920897,-11.8535702260395)) ;
#150951 = CARTESIAN_POINT('',(6.72928932188135,0.300000000000002,-11.8007106781187)) ;
#150952 = CARTESIAN_POINT('',(6.72928932188135,-0.399999999999999,-11.8007106781187)) ;
#150953 = CARTESIAN_POINT('',(6.97071067811866,0.0585786437626919,-11.5592893218813)) ;
#150954 = CARTESIAN_POINT('',(6.94309644062712,0.0861928812542313,-11.5869035593729)) ;
#150955 = CARTESIAN_POINT('',(6.97071067811866,-0.4,-11.5592893218813)) ;
#150956 = CARTESIAN_POINT('Origin',(7.,-0.399999999999999,-11.33)) ;
#150957 = CARTESIAN_POINT('',(6.97071067811865,0.0585786437626923,-11.3007106781187)) ;
#150958 = CARTESIAN_POINT('',(6.72928932188135,0.300000000000001,-11.0592893218813)) ;
#150959 = CARTESIAN_POINT('',(7.14309644062712,-0.113807118745769,-11.4730964406271)) ;
#150960 = CARTESIAN_POINT('',(6.72928932188135,-0.300000000000002,-11.0592893218813)) ;
#150961 = CARTESIAN_POINT('',(6.72928932188134,-0.399999999999999,-11.0592893218813)) ;
#150962 = CARTESIAN_POINT('',(6.97071067811865,-0.0585786437626925,-11.3007106781187)) ;
#150963 = CARTESIAN_POINT('',(6.87642977396045,-0.152859547920897,-11.2064297739604)) ;
#150964 = CARTESIAN_POINT('',(6.97071067811865,-0.399999999999999,-11.3007106781187)) ;
#150965 = CARTESIAN_POINT('Origin',(6.7,-0.399999999999999,-8.02)) ;
#150966 = CARTESIAN_POINT('',(6.97071067811866,-0.0585786437626908,-7.74928932188134)) ;
#150967 = CARTESIAN_POINT('',(6.72928932188134,-0.300000000000002,-7.99071067811866)) ;
#150968 = CARTESIAN_POINT('',(6.67642977396045,-0.352859547920897,-8.04357022603955)) ;
#150969 = CARTESIAN_POINT('',(6.72928932188135,0.300000000000002,-7.99071067811866)) ;
#150970 = CARTESIAN_POINT('',(6.72928932188135,-0.399999999999999,-7.99071067811866)) ;
#150971 = CARTESIAN_POINT('',(6.97071067811866,0.0585786437626916,-7.74928932188134)) ;
#150972 = CARTESIAN_POINT('',(6.94309644062712,0.0861928812542312,-7.77690355937288)) ;
#150973 = CARTESIAN_POINT('',(6.97071067811866,-0.4,-7.74928932188134)) ;
#150974 = CARTESIAN_POINT('Origin',(7.,-0.399999999999999,-7.52)) ;
#150975 = CARTESIAN_POINT('',(6.97071067811866,0.0585786437626905,-7.49071067811866)) ;
#150976 = CARTESIAN_POINT('',(6.72928932188134,0.300000000000002,-7.24928932188134)) ;
#150977 = CARTESIAN_POINT('',(7.14309644062712,-0.11380711874577,-7.66309644062712)) ;
#150978 = CARTESIAN_POINT('',(6.72928932188135,-0.300000000000002,-7.24928932188134)) ;
#150979 = CARTESIAN_POINT('',(6.72928932188135,-0.399999999999999,-7.24928932188134)) ;
#150980 = CARTESIAN_POINT('',(6.97071067811866,-0.058578643762691,-7.49071067811866)) ;
#150981 = CARTESIAN_POINT('',(6.87642977396045,-0.152859547920897,-7.39642977396045)) ;
#150982 = CARTESIAN_POINT('',(6.97071067811866,-0.399999999999999,-7.49071067811866)) ;
#150983 = CARTESIAN_POINT('Origin',(6.7,-0.399999999999999,-4.21)) ;
#150984 = CARTESIAN_POINT('',(6.97071067811866,-0.058578643762691,-3.93928932188135)) ;
#150985 = CARTESIAN_POINT('',(6.72928932188135,-0.300000000000001,-4.18071067811866)) ;
#150986 = CARTESIAN_POINT('',(6.67642977396045,-0.352859547920897,-4.23357022603955)) ;
#150987 = CARTESIAN_POINT('',(6.72928932188135,0.300000000000001,-4.18071067811866)) ;
#150988 = CARTESIAN_POINT('',(6.72928932188135,-0.399999999999999,-4.18071067811866)) ;
#150989 = CARTESIAN_POINT('',(6.97071067811866,0.0585786437626911,-3.93928932188135)) ;
#150990 = CARTESIAN_POINT('',(6.94309644062712,0.0861928812542308,-3.96690355937289)) ;
#150991 = CARTESIAN_POINT('',(6.97071067811866,-0.4,-3.93928932188135)) ;
#150992 = CARTESIAN_POINT('Origin',(7.,-0.399999999999999,-3.71)) ;
#150993 = CARTESIAN_POINT('',(6.97071067811866,0.058578643762691,-3.68071067811866)) ;
#150994 = CARTESIAN_POINT('',(6.72928932188135,0.3,-3.43928932188135)) ;
#150995 = CARTESIAN_POINT('',(7.14309644062712,-0.11380711874577,-3.85309644062712)) ;
#150996 = CARTESIAN_POINT('',(6.72928932188135,-0.3,-3.43928932188135)) ;
#150997 = CARTESIAN_POINT('',(6.72928932188135,-0.399999999999999,-3.43928932188135)) ;
#150998 = CARTESIAN_POINT('',(6.97071067811866,-0.0585786437626913,-3.68071067811866)) ;
#150999 = CARTESIAN_POINT('',(6.87642977396045,-0.152859547920897,-3.58642977396045)) ;
#151000 = CARTESIAN_POINT('',(6.97071067811866,-0.399999999999999,-3.68071067811866)) ;
#151001 = CARTESIAN_POINT('Origin',(-0.113807118745769,-6.47238576250846,
-3.69619288125423)) ;
#151002 = CARTESIAN_POINT('Origin',(0.3,-6.05857864376269,-4.11)) ;
#151003 = CARTESIAN_POINT('Origin',(0.0585786437626911,-6.3,-3.86857864376269)) ;
#151004 = CARTESIAN_POINT('Origin',(0.3,-6.05857864376269,-3.41)) ;
#151005 = CARTESIAN_POINT('Origin',(0.3,-6.05857864376269,-4.11)) ;
#151006 = CARTESIAN_POINT('Origin',(0.3,-6.05857864376269,-3.51)) ;
#151007 = CARTESIAN_POINT('Origin',(0.0585786437626908,-6.3,-3.86857864376269)) ;
#151008 = CARTESIAN_POINT('Origin',(0.0585786437626908,-6.3,-3.86857864376269)) ;
#151009 = CARTESIAN_POINT('Origin',(0.0585786437626908,-6.3,-3.86857864376269)) ;
#151010 = CARTESIAN_POINT('Origin',(0.152859547920897,-6.20571909584179,-3.6571404520791)) ;
#151011 = CARTESIAN_POINT('Origin',(0.3,-6.05857864376269,-3.51)) ;
#151012 = CARTESIAN_POINT('Origin',(0.0585786437626908,-6.3,-3.75142135623731)) ;
#151013 = CARTESIAN_POINT('Origin',(0.0585786437626908,-6.3,-3.41)) ;
#151014 = CARTESIAN_POINT('Origin',(0.0585786437626908,-6.3,-3.75142135623731)) ;
#151015 = CARTESIAN_POINT('Origin',(0.4,-6.3,-3.86857864376269)) ;
#151016 = CARTESIAN_POINT('Origin',(-0.0585786437626904,-6.3,-3.86857864376269)) ;
#151017 = CARTESIAN_POINT('Origin',(0.0585786437626908,-6.3,-3.75142135623731)) ;
#151018 = CARTESIAN_POINT('Origin',(0.0585786437626907,-6.3,-3.75142135623731)) ;
#151019 = CARTESIAN_POINT('Origin',(-0.0585786437626908,-6.3,-3.86857864376269)) ;
#151020 = CARTESIAN_POINT('Origin',(-0.0585786437626908,-6.3,-3.86857864376269)) ;
#151021 = CARTESIAN_POINT('Origin',(-0.0585786437626908,-6.3,-3.86857864376269)) ;
#151022 = CARTESIAN_POINT('Origin',(-0.1,-6.3,-3.75142135623731)) ;
#151023 = CARTESIAN_POINT('Origin',(-0.0585786437626908,-6.3,-3.75142135623731)) ;
#151024 = CARTESIAN_POINT('Origin',(-0.0585786437626908,-6.3,-3.41)) ;
#151025 = CARTESIAN_POINT('Origin',(-0.0585786437626908,-6.3,-3.75142135623731)) ;
#151026 = CARTESIAN_POINT('Origin',(-0.0861928812542299,-6.27238576250846,
-3.89619288125423)) ;
#151027 = CARTESIAN_POINT('Origin',(-0.3,-6.05857864376269,-4.11)) ;
#151028 = CARTESIAN_POINT('Origin',(-0.0585786437626908,-6.3,-3.75142135623731)) ;
#151029 = CARTESIAN_POINT('Origin',(-0.0585786437626909,-6.3,-3.75142135623731)) ;
#151030 = CARTESIAN_POINT('Origin',(-0.3,-6.05857864376269,-3.41)) ;
#151031 = CARTESIAN_POINT('Origin',(-0.3,-6.05857864376269,-4.11)) ;
#151032 = CARTESIAN_POINT('Origin',(-0.3,-6.05857864376269,-3.51)) ;
#151033 = CARTESIAN_POINT('Origin',(-0.352859547920897,-6.00571909584179,
-3.4571404520791)) ;
#151034 = CARTESIAN_POINT('Origin',(-0.3,-6.05857864376269,-3.51)) ;
#151035 = CARTESIAN_POINT('Origin',(7.07238576250846,-0.11380711874577,-3.69619288125423)) ;
#151036 = CARTESIAN_POINT('Origin',(6.65857864376269,0.300000000000001,-4.11)) ;
#151037 = CARTESIAN_POINT('Origin',(6.9,0.0585786437626911,-3.86857864376269)) ;
#151038 = CARTESIAN_POINT('Origin',(6.65857864376269,0.300000000000001,-3.41)) ;
#151039 = CARTESIAN_POINT('Origin',(6.65857864376269,0.300000000000001,-4.11)) ;
#151040 = CARTESIAN_POINT('Origin',(6.65857864376269,0.300000000000001,-3.51)) ;
#151041 = CARTESIAN_POINT('Origin',(6.9,0.0585786437626909,-3.86857864376269)) ;
#151042 = CARTESIAN_POINT('Origin',(6.9,0.0585786437626909,-3.86857864376269)) ;
#151043 = CARTESIAN_POINT('Origin',(6.9,0.0585786437626909,-3.86857864376269)) ;
#151044 = CARTESIAN_POINT('Origin',(6.80571909584179,0.152859547920897,-3.6571404520791)) ;
#151045 = CARTESIAN_POINT('Origin',(6.65857864376269,0.300000000000001,-3.51)) ;
#151046 = CARTESIAN_POINT('Origin',(6.9,0.0585786437626909,-3.75142135623731)) ;
#151047 = CARTESIAN_POINT('Origin',(6.9,0.0585786437626909,-3.41)) ;
#151048 = CARTESIAN_POINT('Origin',(6.9,0.0585786437626909,-3.75142135623731)) ;
#151049 = CARTESIAN_POINT('Origin',(6.9,-0.1,-3.86857864376269)) ;
#151050 = CARTESIAN_POINT('Origin',(6.9,-0.058578643762691,-3.86857864376269)) ;
#151051 = CARTESIAN_POINT('Origin',(6.9,0.0585786437626909,-3.75142135623731)) ;
#151052 = CARTESIAN_POINT('Origin',(6.9,0.058578643762691,-3.75142135623731)) ;
#151053 = CARTESIAN_POINT('Origin',(6.9,-0.0585786437626909,-3.86857864376269)) ;
#151054 = CARTESIAN_POINT('Origin',(6.9,-0.0585786437626909,-3.86857864376269)) ;
#151055 = CARTESIAN_POINT('Origin',(6.9,-0.0585786437626909,-3.86857864376269)) ;
#151056 = CARTESIAN_POINT('Origin',(6.9,-0.399999999999999,-3.75142135623731)) ;
#151057 = CARTESIAN_POINT('Origin',(6.9,-0.0585786437626909,-3.75142135623731)) ;
#151058 = CARTESIAN_POINT('Origin',(6.9,-0.0585786437626909,-3.41)) ;
#151059 = CARTESIAN_POINT('Origin',(6.9,-0.0585786437626909,-3.75142135623731)) ;
#151060 = CARTESIAN_POINT('Origin',(6.87238576250846,-0.0861928812542305,
-3.89619288125423)) ;
#151061 = CARTESIAN_POINT('Origin',(6.65857864376269,-0.3,-4.11)) ;
#151062 = CARTESIAN_POINT('Origin',(6.9,-0.0585786437626909,-3.75142135623731)) ;
#151063 = CARTESIAN_POINT('Origin',(6.9,-0.0585786437626913,-3.75142135623731)) ;
#151064 = CARTESIAN_POINT('Origin',(6.65857864376269,-0.300000000000001,-3.41)) ;
#151065 = CARTESIAN_POINT('Origin',(6.65857864376269,-0.300000000000001,-4.11)) ;
#151066 = CARTESIAN_POINT('Origin',(6.65857864376269,-0.300000000000001,-3.51)) ;
#151067 = CARTESIAN_POINT('Origin',(6.60571909584179,-0.352859547920897,-3.4571404520791)) ;
#151068 = CARTESIAN_POINT('Origin',(6.65857864376269,-0.300000000000001,-3.51)) ;
#151069 = CARTESIAN_POINT('Origin',(-0.11380711874577,-6.47238576250846,-7.50619288125423)) ;
#151070 = CARTESIAN_POINT('Origin',(0.300000000000001,-6.05857864376269,-7.92)) ;
#151071 = CARTESIAN_POINT('Origin',(0.0585786437626912,-6.3,-7.67857864376269)) ;
#151072 = CARTESIAN_POINT('Origin',(0.3,-6.05857864376269,-7.22)) ;
#151073 = CARTESIAN_POINT('Origin',(0.3,-6.05857864376269,-7.92)) ;
#151074 = CARTESIAN_POINT('Origin',(0.3,-6.05857864376269,-7.32)) ;
#151075 = CARTESIAN_POINT('Origin',(0.0585786437626908,-6.3,-7.67857864376269)) ;
#151076 = CARTESIAN_POINT('Origin',(0.0585786437626908,-6.3,-7.67857864376269)) ;
#151077 = CARTESIAN_POINT('Origin',(0.0585786437626908,-6.3,-7.67857864376269)) ;
#151078 = CARTESIAN_POINT('Origin',(0.152859547920898,-6.20571909584179,-7.4671404520791)) ;
#151079 = CARTESIAN_POINT('Origin',(0.300000000000001,-6.05857864376269,-7.32)) ;
#151080 = CARTESIAN_POINT('Origin',(0.0585786437626908,-6.3,-7.56142135623731)) ;
#151081 = CARTESIAN_POINT('Origin',(0.0585786437626908,-6.3,-7.22)) ;
#151082 = CARTESIAN_POINT('Origin',(0.0585786437626908,-6.3,-7.56142135623731)) ;
#151083 = CARTESIAN_POINT('Origin',(0.4,-6.3,-7.67857864376269)) ;
#151084 = CARTESIAN_POINT('Origin',(-0.0585786437626906,-6.3,-7.67857864376269)) ;
#151085 = CARTESIAN_POINT('Origin',(0.0585786437626908,-6.3,-7.56142135623731)) ;
#151086 = CARTESIAN_POINT('Origin',(0.0585786437626908,-6.3,-7.56142135623731)) ;
#151087 = CARTESIAN_POINT('Origin',(-0.0585786437626908,-6.3,-7.67857864376269)) ;
#151088 = CARTESIAN_POINT('Origin',(-0.0585786437626907,-6.3,-7.67857864376269)) ;
#151089 = CARTESIAN_POINT('Origin',(-0.0585786437626908,-6.3,-7.67857864376269)) ;
#151090 = CARTESIAN_POINT('Origin',(-0.1,-6.3,-7.56142135623731)) ;
#151091 = CARTESIAN_POINT('Origin',(-0.0585786437626908,-6.3,-7.56142135623731)) ;
#151092 = CARTESIAN_POINT('Origin',(-0.0585786437626908,-6.3,-7.22)) ;
#151093 = CARTESIAN_POINT('Origin',(-0.0585786437626908,-6.3,-7.56142135623731)) ;
#151094 = CARTESIAN_POINT('Origin',(-0.0861928812542296,-6.27238576250846,
-7.70619288125423)) ;
#151095 = CARTESIAN_POINT('Origin',(-0.3,-6.05857864376269,-7.92)) ;
#151096 = CARTESIAN_POINT('Origin',(-0.0585786437626908,-6.3,-7.56142135623731)) ;
#151097 = CARTESIAN_POINT('Origin',(-0.0585786437626907,-6.3,-7.56142135623731)) ;
#151098 = CARTESIAN_POINT('Origin',(-0.3,-6.05857864376269,-7.22)) ;
#151099 = CARTESIAN_POINT('Origin',(-0.3,-6.05857864376269,-7.92)) ;
#151100 = CARTESIAN_POINT('Origin',(-0.3,-6.05857864376269,-7.32)) ;
#151101 = CARTESIAN_POINT('Origin',(-0.352859547920897,-6.00571909584179,
-7.2671404520791)) ;
#151102 = CARTESIAN_POINT('Origin',(-0.300000000000001,-6.05857864376269,
-7.32)) ;
#151103 = CARTESIAN_POINT('Origin',(7.07238576250846,-0.11380711874577,-7.50619288125423)) ;
#151104 = CARTESIAN_POINT('Origin',(6.65857864376269,0.300000000000002,-7.92)) ;
#151105 = CARTESIAN_POINT('Origin',(6.9,0.0585786437626916,-7.67857864376269)) ;
#151106 = CARTESIAN_POINT('Origin',(6.65857864376269,0.300000000000001,-7.22)) ;
#151107 = CARTESIAN_POINT('Origin',(6.65857864376269,0.300000000000001,-7.92)) ;
#151108 = CARTESIAN_POINT('Origin',(6.65857864376269,0.300000000000001,-7.32)) ;
#151109 = CARTESIAN_POINT('Origin',(6.9,0.0585786437626909,-7.67857864376269)) ;
#151110 = CARTESIAN_POINT('Origin',(6.9,0.0585786437626909,-7.67857864376269)) ;
#151111 = CARTESIAN_POINT('Origin',(6.9,0.0585786437626909,-7.67857864376269)) ;
#151112 = CARTESIAN_POINT('Origin',(6.80571909584179,0.152859547920898,-7.4671404520791)) ;
#151113 = CARTESIAN_POINT('Origin',(6.65857864376269,0.300000000000002,-7.32)) ;
#151114 = CARTESIAN_POINT('Origin',(6.9,0.0585786437626908,-7.56142135623731)) ;
#151115 = CARTESIAN_POINT('Origin',(6.9,0.0585786437626909,-7.22)) ;
#151116 = CARTESIAN_POINT('Origin',(6.9,0.0585786437626909,-7.56142135623731)) ;
#151117 = CARTESIAN_POINT('Origin',(6.9,-0.1,-7.67857864376269)) ;
#151118 = CARTESIAN_POINT('Origin',(6.9,-0.0585786437626908,-7.67857864376269)) ;
#151119 = CARTESIAN_POINT('Origin',(6.9,0.0585786437626909,-7.56142135623731)) ;
#151120 = CARTESIAN_POINT('Origin',(6.9,0.0585786437626905,-7.56142135623731)) ;
#151121 = CARTESIAN_POINT('Origin',(6.9,-0.058578643762691,-7.67857864376269)) ;
#151122 = CARTESIAN_POINT('Origin',(6.9,-0.058578643762691,-7.67857864376269)) ;
#151123 = CARTESIAN_POINT('Origin',(6.9,-0.0585786437626909,-7.67857864376269)) ;
#151124 = CARTESIAN_POINT('Origin',(6.9,-0.399999999999999,-7.56142135623731)) ;
#151125 = CARTESIAN_POINT('Origin',(6.9,-0.0585786437626909,-7.56142135623731)) ;
#151126 = CARTESIAN_POINT('Origin',(6.9,-0.0585786437626909,-7.22)) ;
#151127 = CARTESIAN_POINT('Origin',(6.9,-0.0585786437626909,-7.56142135623731)) ;
#151128 = CARTESIAN_POINT('Origin',(6.87238576250846,-0.0861928812542304,
-7.70619288125423)) ;
#151129 = CARTESIAN_POINT('Origin',(6.65857864376269,-0.300000000000001,-7.92)) ;
#151130 = CARTESIAN_POINT('Origin',(6.9,-0.058578643762691,-7.56142135623731)) ;
#151131 = CARTESIAN_POINT('Origin',(6.9,-0.058578643762691,-7.56142135623731)) ;
#151132 = CARTESIAN_POINT('Origin',(6.65857864376269,-0.300000000000001,-7.22)) ;
#151133 = CARTESIAN_POINT('Origin',(6.65857864376269,-0.300000000000001,-7.92)) ;
#151134 = CARTESIAN_POINT('Origin',(6.65857864376269,-0.300000000000001,-7.32)) ;
#151135 = CARTESIAN_POINT('Origin',(6.60571909584179,-0.352859547920898,-7.2671404520791)) ;
#151136 = CARTESIAN_POINT('Origin',(6.65857864376269,-0.300000000000001,-7.32)) ;
#151137 = CARTESIAN_POINT('Origin',(-0.11380711874577,-6.47238576250846,-11.3161928812542)) ;
#151138 = CARTESIAN_POINT('Origin',(0.299999999999999,-6.05857864376269,-11.73)) ;
#151139 = CARTESIAN_POINT('Origin',(0.0585786437626907,-6.3,-11.4885786437627)) ;
#151140 = CARTESIAN_POINT('Origin',(0.3,-6.05857864376269,-11.03)) ;
#151141 = CARTESIAN_POINT('Origin',(0.3,-6.05857864376269,-11.73)) ;
#151142 = CARTESIAN_POINT('Origin',(0.3,-6.05857864376269,-11.13)) ;
#151143 = CARTESIAN_POINT('Origin',(0.0585786437626908,-6.3,-11.4885786437627)) ;
#151144 = CARTESIAN_POINT('Origin',(0.0585786437626908,-6.3,-11.4885786437627)) ;
#151145 = CARTESIAN_POINT('Origin',(0.0585786437626908,-6.3,-11.4885786437627)) ;
#151146 = CARTESIAN_POINT('Origin',(0.152859547920898,-6.20571909584179,-11.2771404520791)) ;
#151147 = CARTESIAN_POINT('Origin',(0.300000000000003,-6.05857864376269,-11.13)) ;
#151148 = CARTESIAN_POINT('Origin',(0.0585786437626905,-6.3,-11.3714213562373)) ;
#151149 = CARTESIAN_POINT('Origin',(0.0585786437626908,-6.3,-11.03)) ;
#151150 = CARTESIAN_POINT('Origin',(0.0585786437626908,-6.3,-11.3714213562373)) ;
#151151 = CARTESIAN_POINT('Origin',(0.4,-6.3,-11.4885786437627)) ;
#151152 = CARTESIAN_POINT('Origin',(-0.0585786437626916,-6.3,-11.4885786437627)) ;
#151153 = CARTESIAN_POINT('Origin',(0.0585786437626908,-6.3,-11.3714213562373)) ;
#151154 = CARTESIAN_POINT('Origin',(0.0585786437626913,-6.3,-11.3714213562373)) ;
#151155 = CARTESIAN_POINT('Origin',(-0.0585786437626908,-6.3,-11.4885786437627)) ;
#151156 = CARTESIAN_POINT('Origin',(-0.0585786437626908,-6.3,-11.4885786437627)) ;
#151157 = CARTESIAN_POINT('Origin',(-0.0585786437626908,-6.3,-11.4885786437627)) ;
#151158 = CARTESIAN_POINT('Origin',(-0.1,-6.3,-11.3714213562373)) ;
#151159 = CARTESIAN_POINT('Origin',(-0.0585786437626908,-6.3,-11.3714213562373)) ;
#151160 = CARTESIAN_POINT('Origin',(-0.0585786437626908,-6.3,-11.03)) ;
#151161 = CARTESIAN_POINT('Origin',(-0.0585786437626908,-6.3,-11.3714213562373)) ;
#151162 = CARTESIAN_POINT('Origin',(-0.0861928812542293,-6.27238576250846,
-11.5161928812542)) ;
#151163 = CARTESIAN_POINT('Origin',(-0.3,-6.05857864376269,-11.73)) ;
#151164 = CARTESIAN_POINT('Origin',(-0.0585786437626908,-6.3,-11.3714213562373)) ;
#151165 = CARTESIAN_POINT('Origin',(-0.0585786437626915,-6.3,-11.3714213562373)) ;
#151166 = CARTESIAN_POINT('Origin',(-0.3,-6.05857864376269,-11.03)) ;
#151167 = CARTESIAN_POINT('Origin',(-0.3,-6.05857864376269,-11.73)) ;
#151168 = CARTESIAN_POINT('Origin',(-0.3,-6.05857864376269,-11.13)) ;
#151169 = CARTESIAN_POINT('Origin',(-0.352859547920898,-6.00571909584179,
-11.0771404520791)) ;
#151170 = CARTESIAN_POINT('Origin',(-0.300000000000003,-6.05857864376269,
-11.13)) ;
#151171 = CARTESIAN_POINT('Origin',(7.07238576250846,-0.11380711874577,-11.3161928812542)) ;
#151172 = CARTESIAN_POINT('Origin',(6.65857864376269,0.300000000000003,-11.73)) ;
#151173 = CARTESIAN_POINT('Origin',(6.9,0.0585786437626919,-11.4885786437627)) ;
#151174 = CARTESIAN_POINT('Origin',(6.65857864376269,0.300000000000001,-11.03)) ;
#151175 = CARTESIAN_POINT('Origin',(6.65857864376269,0.300000000000001,-11.73)) ;
#151176 = CARTESIAN_POINT('Origin',(6.65857864376269,0.300000000000001,-11.13)) ;
#151177 = CARTESIAN_POINT('Origin',(6.9,0.0585786437626909,-11.4885786437627)) ;
#151178 = CARTESIAN_POINT('Origin',(6.9,0.0585786437626909,-11.4885786437627)) ;
#151179 = CARTESIAN_POINT('Origin',(6.9,0.0585786437626909,-11.4885786437627)) ;
#151180 = CARTESIAN_POINT('Origin',(6.80571909584179,0.152859547920898,-11.2771404520791)) ;
#151181 = CARTESIAN_POINT('Origin',(6.65857864376269,0.300000000000003,-11.13)) ;
#151182 = CARTESIAN_POINT('Origin',(6.9,0.0585786437626911,-11.3714213562373)) ;
#151183 = CARTESIAN_POINT('Origin',(6.9,0.0585786437626909,-11.03)) ;
#151184 = CARTESIAN_POINT('Origin',(6.9,0.0585786437626909,-11.3714213562373)) ;
#151185 = CARTESIAN_POINT('Origin',(6.9,-0.1,-11.4885786437627)) ;
#151186 = CARTESIAN_POINT('Origin',(6.9,-0.058578643762691,-11.4885786437627)) ;
#151187 = CARTESIAN_POINT('Origin',(6.9,0.0585786437626909,-11.3714213562373)) ;
#151188 = CARTESIAN_POINT('Origin',(6.9,0.0585786437626923,-11.3714213562373)) ;
#151189 = CARTESIAN_POINT('Origin',(6.9,-0.058578643762691,-11.4885786437627)) ;
#151190 = CARTESIAN_POINT('Origin',(6.9,-0.0585786437626912,-11.4885786437627)) ;
#151191 = CARTESIAN_POINT('Origin',(6.9,-0.0585786437626909,-11.4885786437627)) ;
#151192 = CARTESIAN_POINT('Origin',(6.9,-0.399999999999999,-11.3714213562373)) ;
#151193 = CARTESIAN_POINT('Origin',(6.9,-0.0585786437626909,-11.3714213562373)) ;
#151194 = CARTESIAN_POINT('Origin',(6.9,-0.0585786437626909,-11.03)) ;
#151195 = CARTESIAN_POINT('Origin',(6.9,-0.0585786437626909,-11.3714213562373)) ;
#151196 = CARTESIAN_POINT('Origin',(6.87238576250846,-0.0861928812542304,
-11.5161928812542)) ;
#151197 = CARTESIAN_POINT('Origin',(6.65857864376269,-0.300000000000002,-11.73)) ;
#151198 = CARTESIAN_POINT('Origin',(6.9,-0.058578643762691,-11.3714213562373)) ;
#151199 = CARTESIAN_POINT('Origin',(6.9,-0.0585786437626925,-11.3714213562373)) ;
#151200 = CARTESIAN_POINT('Origin',(6.65857864376269,-0.300000000000001,-11.03)) ;
#151201 = CARTESIAN_POINT('Origin',(6.65857864376269,-0.300000000000001,-11.73)) ;
#151202 = CARTESIAN_POINT('Origin',(6.65857864376269,-0.300000000000001,-11.13)) ;
#151203 = CARTESIAN_POINT('Origin',(6.60571909584179,-0.352859547920898,-11.0771404520791)) ;
#151204 = CARTESIAN_POINT('Origin',(6.65857864376269,-0.300000000000003,-11.13)) ;
#151205 = CARTESIAN_POINT('Origin',(-0.113807118745769,-6.47238576250846,
-15.1261928812542)) ;
#151206 = CARTESIAN_POINT('Origin',(0.300000000000001,-6.05857864376269,-15.54)) ;
#151207 = CARTESIAN_POINT('Origin',(0.0585786437626911,-6.3,-15.2985786437627)) ;
#151208 = CARTESIAN_POINT('Origin',(0.3,-6.05857864376269,-14.84)) ;
#151209 = CARTESIAN_POINT('Origin',(0.3,-6.05857864376269,-15.54)) ;
#151210 = CARTESIAN_POINT('Origin',(0.3,-6.05857864376269,-14.94)) ;
#151211 = CARTESIAN_POINT('Origin',(0.0585786437626908,-6.3,-15.2985786437627)) ;
#151212 = CARTESIAN_POINT('Origin',(0.0585786437626908,-6.3,-15.2985786437627)) ;
#151213 = CARTESIAN_POINT('Origin',(0.0585786437626908,-6.3,-15.2985786437627)) ;
#151214 = CARTESIAN_POINT('Origin',(0.152859547920898,-6.20571909584179,-15.0871404520791)) ;
#151215 = CARTESIAN_POINT('Origin',(0.300000000000001,-6.05857864376269,-14.94)) ;
#151216 = CARTESIAN_POINT('Origin',(0.0585786437626911,-6.3,-15.1814213562373)) ;
#151217 = CARTESIAN_POINT('Origin',(0.0585786437626908,-6.3,-14.84)) ;
#151218 = CARTESIAN_POINT('Origin',(0.0585786437626908,-6.3,-15.1814213562373)) ;
#151219 = CARTESIAN_POINT('Origin',(0.4,-6.3,-15.2985786437627)) ;
#151220 = CARTESIAN_POINT('Origin',(-0.0585786437626904,-6.3,-15.2985786437627)) ;
#151221 = CARTESIAN_POINT('Origin',(0.0585786437626908,-6.3,-15.1814213562373)) ;
#151222 = CARTESIAN_POINT('Origin',(0.0585786437626904,-6.3,-15.1814213562373)) ;
#151223 = CARTESIAN_POINT('Origin',(-0.0585786437626908,-6.3,-15.2985786437627)) ;
#151224 = CARTESIAN_POINT('Origin',(-0.0585786437626908,-6.3,-15.2985786437627)) ;
#151225 = CARTESIAN_POINT('Origin',(-0.0585786437626908,-6.3,-15.2985786437627)) ;
#151226 = CARTESIAN_POINT('Origin',(-0.1,-6.3,-15.1814213562373)) ;
#151227 = CARTESIAN_POINT('Origin',(-0.0585786437626908,-6.3,-15.1814213562373)) ;
#151228 = CARTESIAN_POINT('Origin',(-0.0585786437626908,-6.3,-14.84)) ;
#151229 = CARTESIAN_POINT('Origin',(-0.0585786437626908,-6.3,-15.1814213562373)) ;
#151230 = CARTESIAN_POINT('Origin',(-0.0861928812542299,-6.27238576250846,
-15.3261928812542)) ;
#151231 = CARTESIAN_POINT('Origin',(-0.300000000000001,-6.05857864376269,
-15.54)) ;
#151232 = CARTESIAN_POINT('Origin',(-0.0585786437626908,-6.3,-15.1814213562373)) ;
#151233 = CARTESIAN_POINT('Origin',(-0.0585786437626914,-6.3,-15.1814213562373)) ;
#151234 = CARTESIAN_POINT('Origin',(-0.3,-6.05857864376269,-14.84)) ;
#151235 = CARTESIAN_POINT('Origin',(-0.3,-6.05857864376269,-15.54)) ;
#151236 = CARTESIAN_POINT('Origin',(-0.3,-6.05857864376269,-14.94)) ;
#151237 = CARTESIAN_POINT('Origin',(-0.352859547920897,-6.00571909584179,
-14.8871404520791)) ;
#151238 = CARTESIAN_POINT('Origin',(-0.3,-6.05857864376269,-14.94)) ;
#151239 = CARTESIAN_POINT('Origin',(7.07238576250846,-0.11380711874577,-15.1261928812542)) ;
#151240 = CARTESIAN_POINT('Origin',(6.65857864376269,0.300000000000003,-15.54)) ;
#151241 = CARTESIAN_POINT('Origin',(6.9,0.0585786437626913,-15.2985786437627)) ;
#151242 = CARTESIAN_POINT('Origin',(6.65857864376269,0.300000000000001,-14.84)) ;
#151243 = CARTESIAN_POINT('Origin',(6.65857864376269,0.300000000000001,-15.54)) ;
#151244 = CARTESIAN_POINT('Origin',(6.65857864376269,0.300000000000001,-14.94)) ;
#151245 = CARTESIAN_POINT('Origin',(6.9,0.0585786437626909,-15.2985786437627)) ;
#151246 = CARTESIAN_POINT('Origin',(6.9,0.0585786437626909,-15.2985786437627)) ;
#151247 = CARTESIAN_POINT('Origin',(6.9,0.0585786437626909,-15.2985786437627)) ;
#151248 = CARTESIAN_POINT('Origin',(6.80571909584179,0.152859547920897,-15.0871404520791)) ;
#151249 = CARTESIAN_POINT('Origin',(6.65857864376269,0.300000000000001,-14.94)) ;
#151250 = CARTESIAN_POINT('Origin',(6.9,0.0585786437626909,-15.1814213562373)) ;
#151251 = CARTESIAN_POINT('Origin',(6.9,0.0585786437626909,-14.84)) ;
#151252 = CARTESIAN_POINT('Origin',(6.9,0.0585786437626909,-15.1814213562373)) ;
#151253 = CARTESIAN_POINT('Origin',(6.9,-0.1,-15.2985786437627)) ;
#151254 = CARTESIAN_POINT('Origin',(6.9,-0.058578643762691,-15.2985786437627)) ;
#151255 = CARTESIAN_POINT('Origin',(6.9,0.0585786437626909,-15.1814213562373)) ;
#151256 = CARTESIAN_POINT('Origin',(6.9,0.0585786437626917,-15.1814213562373)) ;
#151257 = CARTESIAN_POINT('Origin',(6.9,-0.0585786437626909,-15.2985786437627)) ;
#151258 = CARTESIAN_POINT('Origin',(6.9,-0.058578643762691,-15.2985786437627)) ;
#151259 = CARTESIAN_POINT('Origin',(6.9,-0.0585786437626909,-15.2985786437627)) ;
#151260 = CARTESIAN_POINT('Origin',(6.9,-0.399999999999999,-15.1814213562373)) ;
#151261 = CARTESIAN_POINT('Origin',(6.9,-0.0585786437626909,-15.1814213562373)) ;
#151262 = CARTESIAN_POINT('Origin',(6.9,-0.0585786437626909,-14.84)) ;
#151263 = CARTESIAN_POINT('Origin',(6.9,-0.0585786437626909,-15.1814213562373)) ;
#151264 = CARTESIAN_POINT('Origin',(6.87238576250846,-0.0861928812542304,
-15.3261928812542)) ;
#151265 = CARTESIAN_POINT('Origin',(6.65857864376269,-0.300000000000002,-15.54)) ;
#151266 = CARTESIAN_POINT('Origin',(6.9,-0.058578643762691,-15.1814213562373)) ;
#151267 = CARTESIAN_POINT('Origin',(6.9,-0.0585786437626915,-15.1814213562373)) ;
#151268 = CARTESIAN_POINT('Origin',(6.65857864376269,-0.300000000000001,-14.84)) ;
#151269 = CARTESIAN_POINT('Origin',(6.65857864376269,-0.300000000000001,-15.54)) ;
#151270 = CARTESIAN_POINT('Origin',(6.65857864376269,-0.300000000000001,-14.94)) ;
#151271 = CARTESIAN_POINT('Origin',(6.60571909584179,-0.352859547920897,-14.8871404520791)) ;
#151272 = CARTESIAN_POINT('Origin',(6.65857864376269,-0.300000000000001,-14.94)) ;
#151273 = CARTESIAN_POINT('Origin',(-0.113807118745769,-6.47238576250846,
-18.9361928812542)) ;
#151274 = CARTESIAN_POINT('Origin',(0.300000000000001,-6.05857864376269,-19.35)) ;
#151275 = CARTESIAN_POINT('Origin',(0.058578643762692,-6.3,-19.1085786437627)) ;
#151276 = CARTESIAN_POINT('Origin',(0.3,-6.05857864376269,-18.65)) ;
#151277 = CARTESIAN_POINT('Origin',(0.3,-6.05857864376269,-19.35)) ;
#151278 = CARTESIAN_POINT('Origin',(0.3,-6.05857864376269,-18.75)) ;
#151279 = CARTESIAN_POINT('Origin',(0.0585786437626908,-6.3,-19.1085786437627)) ;
#151280 = CARTESIAN_POINT('Origin',(0.0585786437626908,-6.3,-19.1085786437627)) ;
#151281 = CARTESIAN_POINT('Origin',(0.0585786437626908,-6.3,-19.1085786437627)) ;
#151282 = CARTESIAN_POINT('Origin',(0.152859547920896,-6.2057190958418,-18.8971404520791)) ;
#151283 = CARTESIAN_POINT('Origin',(0.299999999999995,-6.0585786437627,-18.75)) ;
#151284 = CARTESIAN_POINT('Origin',(0.0585786437626908,-6.3,-18.9914213562373)) ;
#151285 = CARTESIAN_POINT('Origin',(0.0585786437626908,-6.3,-18.65)) ;
#151286 = CARTESIAN_POINT('Origin',(0.0585786437626908,-6.3,-18.9914213562373)) ;
#151287 = CARTESIAN_POINT('Origin',(0.4,-6.3,-19.1085786437627)) ;
#151288 = CARTESIAN_POINT('Origin',(-0.0585786437626899,-6.3,-19.1085786437627)) ;
#151289 = CARTESIAN_POINT('Origin',(0.0585786437626908,-6.3,-18.9914213562373)) ;
#151290 = CARTESIAN_POINT('Origin',(0.0585786437626916,-6.3,-18.9914213562373)) ;
#151291 = CARTESIAN_POINT('Origin',(-0.0585786437626908,-6.3,-19.1085786437627)) ;
#151292 = CARTESIAN_POINT('Origin',(-0.0585786437626905,-6.3,-19.1085786437627)) ;
#151293 = CARTESIAN_POINT('Origin',(-0.0585786437626908,-6.3,-19.1085786437627)) ;
#151294 = CARTESIAN_POINT('Origin',(-0.1,-6.3,-18.9914213562373)) ;
#151295 = CARTESIAN_POINT('Origin',(-0.0585786437626908,-6.3,-18.9914213562373)) ;
#151296 = CARTESIAN_POINT('Origin',(-0.0585786437626908,-6.3,-18.65)) ;
#151297 = CARTESIAN_POINT('Origin',(-0.0585786437626908,-6.3,-18.9914213562373)) ;
#151298 = CARTESIAN_POINT('Origin',(-0.0861928812542299,-6.27238576250846,
-19.1361928812542)) ;
#151299 = CARTESIAN_POINT('Origin',(-0.299999999999999,-6.05857864376269,
-19.35)) ;
#151300 = CARTESIAN_POINT('Origin',(-0.0585786437626908,-6.3,-18.9914213562373)) ;
#151301 = CARTESIAN_POINT('Origin',(-0.0585786437626909,-6.3,-18.9914213562373)) ;
#151302 = CARTESIAN_POINT('Origin',(-0.3,-6.05857864376269,-18.65)) ;
#151303 = CARTESIAN_POINT('Origin',(-0.3,-6.05857864376269,-19.35)) ;
#151304 = CARTESIAN_POINT('Origin',(-0.3,-6.05857864376269,-18.75)) ;
#151305 = CARTESIAN_POINT('Origin',(-0.352859547920895,-6.00571909584179,
-18.6971404520791)) ;
#151306 = CARTESIAN_POINT('Origin',(-0.299999999999997,-6.05857864376269,
-18.75)) ;
#151307 = CARTESIAN_POINT('Origin',(7.07238576250846,-0.11380711874577,-18.9361928812542)) ;
#151308 = CARTESIAN_POINT('Origin',(6.65857864376269,0.299999999999999,-19.35)) ;
#151309 = CARTESIAN_POINT('Origin',(6.9,0.0585786437626903,-19.1085786437627)) ;
#151310 = CARTESIAN_POINT('Origin',(6.65857864376269,0.300000000000001,-18.65)) ;
#151311 = CARTESIAN_POINT('Origin',(6.65857864376269,0.300000000000001,-19.35)) ;
#151312 = CARTESIAN_POINT('Origin',(6.65857864376269,0.300000000000001,-18.75)) ;
#151313 = CARTESIAN_POINT('Origin',(6.9,0.0585786437626909,-19.1085786437627)) ;
#151314 = CARTESIAN_POINT('Origin',(6.9,0.0585786437626909,-19.1085786437627)) ;
#151315 = CARTESIAN_POINT('Origin',(6.9,0.0585786437626909,-19.1085786437627)) ;
#151316 = CARTESIAN_POINT('Origin',(6.8057190958418,0.152859547920896,-18.8971404520791)) ;
#151317 = CARTESIAN_POINT('Origin',(6.6585786437627,0.299999999999996,-18.75)) ;
#151318 = CARTESIAN_POINT('Origin',(6.9,0.0585786437626908,-18.9914213562373)) ;
#151319 = CARTESIAN_POINT('Origin',(6.9,0.0585786437626909,-18.65)) ;
#151320 = CARTESIAN_POINT('Origin',(6.9,0.0585786437626909,-18.9914213562373)) ;
#151321 = CARTESIAN_POINT('Origin',(6.9,-0.1,-19.1085786437627)) ;
#151322 = CARTESIAN_POINT('Origin',(6.9,-0.0585786437626902,-19.1085786437627)) ;
#151323 = CARTESIAN_POINT('Origin',(6.9,0.0585786437626909,-18.9914213562373)) ;
#151324 = CARTESIAN_POINT('Origin',(6.9,0.058578643762691,-18.9914213562373)) ;
#151325 = CARTESIAN_POINT('Origin',(6.9,-0.0585786437626909,-19.1085786437627)) ;
#151326 = CARTESIAN_POINT('Origin',(6.9,-0.0585786437626907,-19.1085786437627)) ;
#151327 = CARTESIAN_POINT('Origin',(6.9,-0.0585786437626909,-19.1085786437627)) ;
#151328 = CARTESIAN_POINT('Origin',(6.9,-0.399999999999999,-18.9914213562373)) ;
#151329 = CARTESIAN_POINT('Origin',(6.9,-0.0585786437626909,-18.9914213562373)) ;
#151330 = CARTESIAN_POINT('Origin',(6.9,-0.0585786437626909,-18.65)) ;
#151331 = CARTESIAN_POINT('Origin',(6.9,-0.058578643762691,-18.9914213562373)) ;
#151332 = CARTESIAN_POINT('Origin',(6.87238576250846,-0.0861928812542304,
-19.1361928812542)) ;
#151333 = CARTESIAN_POINT('Origin',(6.65857864376269,-0.3,-19.35)) ;
#151334 = CARTESIAN_POINT('Origin',(6.9,-0.0585786437626909,-18.9914213562373)) ;
#151335 = CARTESIAN_POINT('Origin',(6.9,-0.0585786437626907,-18.9914213562373)) ;
#151336 = CARTESIAN_POINT('Origin',(6.65857864376269,-0.300000000000001,-18.65)) ;
#151337 = CARTESIAN_POINT('Origin',(6.65857864376269,-0.300000000000001,-19.35)) ;
#151338 = CARTESIAN_POINT('Origin',(6.65857864376269,-0.300000000000001,-18.75)) ;
#151339 = CARTESIAN_POINT('Origin',(6.6057190958418,-0.352859547920896,-18.6971404520791)) ;
#151340 = CARTESIAN_POINT('Origin',(6.65857864376269,-0.299999999999998,-18.75)) ;
#151341 = CARTESIAN_POINT('Origin',(-0.113807118745769,-6.47238576250846,
-22.7461928812542)) ;
#151342 = CARTESIAN_POINT('Origin',(0.300000000000001,-6.05857864376269,-23.16)) ;
#151343 = CARTESIAN_POINT('Origin',(0.058578643762692,-6.3,-22.9185786437627)) ;
#151344 = CARTESIAN_POINT('Origin',(0.3,-6.05857864376269,-22.46)) ;
#151345 = CARTESIAN_POINT('Origin',(0.3,-6.05857864376269,-23.16)) ;
#151346 = CARTESIAN_POINT('Origin',(0.3,-6.05857864376269,-22.56)) ;
#151347 = CARTESIAN_POINT('Origin',(0.0585786437626908,-6.3,-22.9185786437627)) ;
#151348 = CARTESIAN_POINT('Origin',(0.0585786437626908,-6.3,-22.9185786437627)) ;
#151349 = CARTESIAN_POINT('Origin',(0.0585786437626908,-6.3,-22.9185786437627)) ;
#151350 = CARTESIAN_POINT('Origin',(0.152859547920896,-6.2057190958418,-22.7071404520791)) ;
#151351 = CARTESIAN_POINT('Origin',(0.299999999999995,-6.0585786437627,-22.56)) ;
#151352 = CARTESIAN_POINT('Origin',(0.0585786437626908,-6.3,-22.8014213562373)) ;
#151353 = CARTESIAN_POINT('Origin',(0.0585786437626908,-6.3,-22.46)) ;
#151354 = CARTESIAN_POINT('Origin',(0.0585786437626908,-6.3,-22.8014213562373)) ;
#151355 = CARTESIAN_POINT('Origin',(0.4,-6.3,-22.9185786437627)) ;
#151356 = CARTESIAN_POINT('Origin',(-0.0585786437626899,-6.3,-22.9185786437627)) ;
#151357 = CARTESIAN_POINT('Origin',(0.0585786437626908,-6.3,-22.8014213562373)) ;
#151358 = CARTESIAN_POINT('Origin',(0.0585786437626916,-6.3,-22.8014213562373)) ;
#151359 = CARTESIAN_POINT('Origin',(-0.0585786437626908,-6.3,-22.9185786437627)) ;
#151360 = CARTESIAN_POINT('Origin',(-0.0585786437626905,-6.3,-22.9185786437627)) ;
#151361 = CARTESIAN_POINT('Origin',(-0.0585786437626908,-6.3,-22.9185786437627)) ;
#151362 = CARTESIAN_POINT('Origin',(-0.1,-6.3,-22.8014213562373)) ;
#151363 = CARTESIAN_POINT('Origin',(-0.0585786437626908,-6.3,-22.8014213562373)) ;
#151364 = CARTESIAN_POINT('Origin',(-0.0585786437626908,-6.3,-22.46)) ;
#151365 = CARTESIAN_POINT('Origin',(-0.0585786437626908,-6.3,-22.8014213562373)) ;
#151366 = CARTESIAN_POINT('Origin',(-0.0861928812542299,-6.27238576250846,
-22.9461928812542)) ;
#151367 = CARTESIAN_POINT('Origin',(-0.299999999999999,-6.05857864376269,
-23.16)) ;
#151368 = CARTESIAN_POINT('Origin',(-0.0585786437626908,-6.3,-22.8014213562373)) ;
#151369 = CARTESIAN_POINT('Origin',(-0.0585786437626909,-6.3,-22.8014213562373)) ;
#151370 = CARTESIAN_POINT('Origin',(-0.3,-6.05857864376269,-22.46)) ;
#151371 = CARTESIAN_POINT('Origin',(-0.3,-6.05857864376269,-23.16)) ;
#151372 = CARTESIAN_POINT('Origin',(-0.3,-6.05857864376269,-22.56)) ;
#151373 = CARTESIAN_POINT('Origin',(-0.352859547920895,-6.00571909584179,
-22.5071404520791)) ;
#151374 = CARTESIAN_POINT('Origin',(-0.299999999999997,-6.05857864376269,
-22.56)) ;
#151375 = CARTESIAN_POINT('Origin',(7.07238576250846,-0.11380711874577,-22.7461928812542)) ;
#151376 = CARTESIAN_POINT('Origin',(6.65857864376269,0.299999999999999,-23.16)) ;
#151377 = CARTESIAN_POINT('Origin',(6.9,0.0585786437626903,-22.9185786437627)) ;
#151378 = CARTESIAN_POINT('Origin',(6.65857864376269,0.300000000000001,-22.46)) ;
#151379 = CARTESIAN_POINT('Origin',(6.65857864376269,0.300000000000001,-23.16)) ;
#151380 = CARTESIAN_POINT('Origin',(6.65857864376269,0.300000000000001,-22.56)) ;
#151381 = CARTESIAN_POINT('Origin',(6.9,0.0585786437626909,-22.9185786437627)) ;
#151382 = CARTESIAN_POINT('Origin',(6.9,0.0585786437626909,-22.9185786437627)) ;
#151383 = CARTESIAN_POINT('Origin',(6.9,0.0585786437626909,-22.9185786437627)) ;
#151384 = CARTESIAN_POINT('Origin',(6.8057190958418,0.152859547920896,-22.7071404520791)) ;
#151385 = CARTESIAN_POINT('Origin',(6.6585786437627,0.299999999999996,-22.56)) ;
#151386 = CARTESIAN_POINT('Origin',(6.9,0.0585786437626908,-22.8014213562373)) ;
#151387 = CARTESIAN_POINT('Origin',(6.9,0.0585786437626909,-22.46)) ;
#151388 = CARTESIAN_POINT('Origin',(6.9,0.0585786437626909,-22.8014213562373)) ;
#151389 = CARTESIAN_POINT('Origin',(6.9,-0.1,-22.9185786437627)) ;
#151390 = CARTESIAN_POINT('Origin',(6.9,-0.0585786437626902,-22.9185786437627)) ;
#151391 = CARTESIAN_POINT('Origin',(6.9,0.0585786437626909,-22.8014213562373)) ;
#151392 = CARTESIAN_POINT('Origin',(6.9,0.058578643762691,-22.8014213562373)) ;
#151393 = CARTESIAN_POINT('Origin',(6.9,-0.0585786437626909,-22.9185786437627)) ;
#151394 = CARTESIAN_POINT('Origin',(6.9,-0.0585786437626907,-22.9185786437627)) ;
#151395 = CARTESIAN_POINT('Origin',(6.9,-0.0585786437626909,-22.9185786437627)) ;
#151396 = CARTESIAN_POINT('Origin',(6.9,-0.399999999999999,-22.8014213562373)) ;
#151397 = CARTESIAN_POINT('Origin',(6.9,-0.0585786437626909,-22.8014213562373)) ;
#151398 = CARTESIAN_POINT('Origin',(6.9,-0.0585786437626909,-22.46)) ;
#151399 = CARTESIAN_POINT('Origin',(6.9,-0.058578643762691,-22.8014213562373)) ;
#151400 = CARTESIAN_POINT('Origin',(6.87238576250846,-0.0861928812542304,
-22.9461928812542)) ;
#151401 = CARTESIAN_POINT('Origin',(6.65857864376269,-0.3,-23.16)) ;
#151402 = CARTESIAN_POINT('Origin',(6.9,-0.0585786437626909,-22.8014213562373)) ;
#151403 = CARTESIAN_POINT('Origin',(6.9,-0.0585786437626907,-22.8014213562373)) ;
#151404 = CARTESIAN_POINT('Origin',(6.65857864376269,-0.300000000000001,-22.46)) ;
#151405 = CARTESIAN_POINT('Origin',(6.65857864376269,-0.300000000000001,-23.16)) ;
#151406 = CARTESIAN_POINT('Origin',(6.65857864376269,-0.300000000000001,-22.56)) ;
#151407 = CARTESIAN_POINT('Origin',(6.6057190958418,-0.352859547920896,-22.5071404520791)) ;
#151408 = CARTESIAN_POINT('Origin',(6.65857864376269,-0.299999999999998,-22.56)) ;
#151409 = CARTESIAN_POINT('Origin',(-0.113807118745769,-6.47238576250846,
-26.5561928812542)) ;
#151410 = CARTESIAN_POINT('Origin',(0.300000000000001,-6.05857864376269,-26.97)) ;
#151411 = CARTESIAN_POINT('Origin',(0.058578643762692,-6.3,-26.7285786437627)) ;
#151412 = CARTESIAN_POINT('Origin',(0.3,-6.05857864376269,-26.27)) ;
#151413 = CARTESIAN_POINT('Origin',(0.3,-6.05857864376269,-26.97)) ;
#151414 = CARTESIAN_POINT('Origin',(0.3,-6.05857864376269,-26.37)) ;
#151415 = CARTESIAN_POINT('Origin',(0.0585786437626908,-6.3,-26.7285786437627)) ;
#151416 = CARTESIAN_POINT('Origin',(0.0585786437626908,-6.3,-26.7285786437627)) ;
#151417 = CARTESIAN_POINT('Origin',(0.0585786437626908,-6.3,-26.7285786437627)) ;
#151418 = CARTESIAN_POINT('Origin',(0.152859547920896,-6.2057190958418,-26.5171404520791)) ;
#151419 = CARTESIAN_POINT('Origin',(0.299999999999995,-6.0585786437627,-26.37)) ;
#151420 = CARTESIAN_POINT('Origin',(0.0585786437626908,-6.3,-26.6114213562373)) ;
#151421 = CARTESIAN_POINT('Origin',(0.0585786437626908,-6.3,-26.27)) ;
#151422 = CARTESIAN_POINT('Origin',(0.0585786437626908,-6.3,-26.6114213562373)) ;
#151423 = CARTESIAN_POINT('Origin',(0.4,-6.3,-26.7285786437627)) ;
#151424 = CARTESIAN_POINT('Origin',(-0.0585786437626899,-6.3,-26.7285786437627)) ;
#151425 = CARTESIAN_POINT('Origin',(0.0585786437626908,-6.3,-26.6114213562373)) ;
#151426 = CARTESIAN_POINT('Origin',(0.0585786437626916,-6.3,-26.6114213562373)) ;
#151427 = CARTESIAN_POINT('Origin',(-0.0585786437626908,-6.3,-26.7285786437627)) ;
#151428 = CARTESIAN_POINT('Origin',(-0.0585786437626905,-6.3,-26.7285786437627)) ;
#151429 = CARTESIAN_POINT('Origin',(-0.0585786437626908,-6.3,-26.7285786437627)) ;
#151430 = CARTESIAN_POINT('Origin',(-0.1,-6.3,-26.6114213562373)) ;
#151431 = CARTESIAN_POINT('Origin',(-0.0585786437626908,-6.3,-26.6114213562373)) ;
#151432 = CARTESIAN_POINT('Origin',(-0.0585786437626908,-6.3,-26.27)) ;
#151433 = CARTESIAN_POINT('Origin',(-0.0585786437626908,-6.3,-26.6114213562373)) ;
#151434 = CARTESIAN_POINT('Origin',(-0.0861928812542299,-6.27238576250846,
-26.7561928812542)) ;
#151435 = CARTESIAN_POINT('Origin',(-0.299999999999999,-6.05857864376269,
-26.97)) ;
#151436 = CARTESIAN_POINT('Origin',(-0.0585786437626908,-6.3,-26.6114213562373)) ;
#151437 = CARTESIAN_POINT('Origin',(-0.0585786437626909,-6.3,-26.6114213562373)) ;
#151438 = CARTESIAN_POINT('Origin',(-0.3,-6.05857864376269,-26.27)) ;
#151439 = CARTESIAN_POINT('Origin',(-0.3,-6.05857864376269,-26.97)) ;
#151440 = CARTESIAN_POINT('Origin',(-0.3,-6.05857864376269,-26.37)) ;
#151441 = CARTESIAN_POINT('Origin',(-0.352859547920895,-6.00571909584179,
-26.3171404520791)) ;
#151442 = CARTESIAN_POINT('Origin',(-0.299999999999997,-6.05857864376269,
-26.37)) ;
#151443 = CARTESIAN_POINT('Origin',(7.07238576250846,-0.11380711874577,-26.5561928812542)) ;
#151444 = CARTESIAN_POINT('Origin',(6.65857864376269,0.299999999999999,-26.97)) ;
#151445 = CARTESIAN_POINT('Origin',(6.9,0.0585786437626903,-26.7285786437627)) ;
#151446 = CARTESIAN_POINT('Origin',(6.65857864376269,0.300000000000001,-26.27)) ;
#151447 = CARTESIAN_POINT('Origin',(6.65857864376269,0.300000000000001,-26.97)) ;
#151448 = CARTESIAN_POINT('Origin',(6.65857864376269,0.300000000000001,-26.37)) ;
#151449 = CARTESIAN_POINT('Origin',(6.9,0.0585786437626909,-26.7285786437627)) ;
#151450 = CARTESIAN_POINT('Origin',(6.9,0.0585786437626909,-26.7285786437627)) ;
#151451 = CARTESIAN_POINT('Origin',(6.9,0.0585786437626909,-26.7285786437627)) ;
#151452 = CARTESIAN_POINT('Origin',(6.8057190958418,0.152859547920896,-26.5171404520791)) ;
#151453 = CARTESIAN_POINT('Origin',(6.6585786437627,0.299999999999996,-26.37)) ;
#151454 = CARTESIAN_POINT('Origin',(6.9,0.0585786437626908,-26.6114213562373)) ;
#151455 = CARTESIAN_POINT('Origin',(6.9,0.0585786437626909,-26.27)) ;
#151456 = CARTESIAN_POINT('Origin',(6.9,0.0585786437626909,-26.6114213562373)) ;
#151457 = CARTESIAN_POINT('Origin',(6.9,-0.1,-26.7285786437627)) ;
#151458 = CARTESIAN_POINT('Origin',(6.9,-0.0585786437626902,-26.7285786437627)) ;
#151459 = CARTESIAN_POINT('Origin',(6.9,0.0585786437626909,-26.6114213562373)) ;
#151460 = CARTESIAN_POINT('Origin',(6.9,0.058578643762691,-26.6114213562373)) ;
#151461 = CARTESIAN_POINT('Origin',(6.9,-0.0585786437626909,-26.7285786437627)) ;
#151462 = CARTESIAN_POINT('Origin',(6.9,-0.0585786437626907,-26.7285786437627)) ;
#151463 = CARTESIAN_POINT('Origin',(6.9,-0.0585786437626909,-26.7285786437627)) ;
#151464 = CARTESIAN_POINT('Origin',(6.9,-0.399999999999999,-26.6114213562373)) ;
#151465 = CARTESIAN_POINT('Origin',(6.9,-0.0585786437626909,-26.6114213562373)) ;
#151466 = CARTESIAN_POINT('Origin',(6.9,-0.0585786437626909,-26.27)) ;
#151467 = CARTESIAN_POINT('Origin',(6.9,-0.058578643762691,-26.6114213562373)) ;
#151468 = CARTESIAN_POINT('Origin',(6.87238576250846,-0.0861928812542304,
-26.7561928812542)) ;
#151469 = CARTESIAN_POINT('Origin',(6.65857864376269,-0.3,-26.97)) ;
#151470 = CARTESIAN_POINT('Origin',(6.9,-0.0585786437626909,-26.6114213562373)) ;
#151471 = CARTESIAN_POINT('Origin',(6.9,-0.0585786437626907,-26.6114213562373)) ;
#151472 = CARTESIAN_POINT('Origin',(6.65857864376269,-0.300000000000001,-26.27)) ;
#151473 = CARTESIAN_POINT('Origin',(6.65857864376269,-0.300000000000001,-26.97)) ;
#151474 = CARTESIAN_POINT('Origin',(6.65857864376269,-0.300000000000001,-26.37)) ;
#151475 = CARTESIAN_POINT('Origin',(6.6057190958418,-0.352859547920896,-26.3171404520791)) ;
#151476 = CARTESIAN_POINT('Origin',(6.65857864376269,-0.299999999999998,-26.37)) ;
#151477 = CARTESIAN_POINT('Origin',(-0.113807118745769,-6.47238576250846,
-30.3661928812542)) ;
#151478 = CARTESIAN_POINT('Origin',(0.300000000000001,-6.05857864376269,-30.78)) ;
#151479 = CARTESIAN_POINT('Origin',(0.058578643762692,-6.3,-30.5385786437627)) ;
#151480 = CARTESIAN_POINT('Origin',(0.3,-6.05857864376269,-30.08)) ;
#151481 = CARTESIAN_POINT('Origin',(0.3,-6.05857864376269,-30.78)) ;
#151482 = CARTESIAN_POINT('Origin',(0.3,-6.05857864376269,-30.18)) ;
#151483 = CARTESIAN_POINT('Origin',(0.0585786437626908,-6.3,-30.5385786437627)) ;
#151484 = CARTESIAN_POINT('Origin',(0.0585786437626908,-6.3,-30.5385786437627)) ;
#151485 = CARTESIAN_POINT('Origin',(0.0585786437626908,-6.3,-30.5385786437627)) ;
#151486 = CARTESIAN_POINT('Origin',(0.152859547920896,-6.2057190958418,-30.3271404520791)) ;
#151487 = CARTESIAN_POINT('Origin',(0.299999999999995,-6.0585786437627,-30.18)) ;
#151488 = CARTESIAN_POINT('Origin',(0.0585786437626908,-6.3,-30.4214213562373)) ;
#151489 = CARTESIAN_POINT('Origin',(0.0585786437626908,-6.3,-30.08)) ;
#151490 = CARTESIAN_POINT('Origin',(0.0585786437626908,-6.3,-30.4214213562373)) ;
#151491 = CARTESIAN_POINT('Origin',(0.4,-6.3,-30.5385786437627)) ;
#151492 = CARTESIAN_POINT('Origin',(-0.0585786437626899,-6.3,-30.5385786437627)) ;
#151493 = CARTESIAN_POINT('Origin',(0.0585786437626908,-6.3,-30.4214213562373)) ;
#151494 = CARTESIAN_POINT('Origin',(0.0585786437626916,-6.3,-30.4214213562373)) ;
#151495 = CARTESIAN_POINT('Origin',(-0.0585786437626908,-6.3,-30.5385786437627)) ;
#151496 = CARTESIAN_POINT('Origin',(-0.0585786437626905,-6.3,-30.5385786437627)) ;
#151497 = CARTESIAN_POINT('Origin',(-0.0585786437626908,-6.3,-30.5385786437627)) ;
#151498 = CARTESIAN_POINT('Origin',(-0.1,-6.3,-30.4214213562373)) ;
#151499 = CARTESIAN_POINT('Origin',(-0.0585786437626908,-6.3,-30.4214213562373)) ;
#151500 = CARTESIAN_POINT('Origin',(-0.0585786437626908,-6.3,-30.08)) ;
#151501 = CARTESIAN_POINT('Origin',(-0.0585786437626908,-6.3,-30.4214213562373)) ;
#151502 = CARTESIAN_POINT('Origin',(-0.0861928812542299,-6.27238576250846,
-30.5661928812542)) ;
#151503 = CARTESIAN_POINT('Origin',(-0.299999999999999,-6.05857864376269,
-30.78)) ;
#151504 = CARTESIAN_POINT('Origin',(-0.0585786437626908,-6.3,-30.4214213562373)) ;
#151505 = CARTESIAN_POINT('Origin',(-0.0585786437626909,-6.3,-30.4214213562373)) ;
#151506 = CARTESIAN_POINT('Origin',(-0.3,-6.05857864376269,-30.08)) ;
#151507 = CARTESIAN_POINT('Origin',(-0.3,-6.05857864376269,-30.78)) ;
#151508 = CARTESIAN_POINT('Origin',(-0.3,-6.05857864376269,-30.18)) ;
#151509 = CARTESIAN_POINT('Origin',(-0.352859547920895,-6.00571909584179,
-30.1271404520791)) ;
#151510 = CARTESIAN_POINT('Origin',(-0.299999999999997,-6.05857864376269,
-30.18)) ;
#151511 = CARTESIAN_POINT('Origin',(7.07238576250846,-0.11380711874577,-30.3661928812542)) ;
#151512 = CARTESIAN_POINT('Origin',(6.65857864376269,0.299999999999999,-30.78)) ;
#151513 = CARTESIAN_POINT('Origin',(6.9,0.0585786437626903,-30.5385786437627)) ;
#151514 = CARTESIAN_POINT('Origin',(6.65857864376269,0.300000000000001,-30.08)) ;
#151515 = CARTESIAN_POINT('Origin',(6.65857864376269,0.300000000000001,-30.78)) ;
#151516 = CARTESIAN_POINT('Origin',(6.65857864376269,0.300000000000001,-30.18)) ;
#151517 = CARTESIAN_POINT('Origin',(6.9,0.0585786437626909,-30.5385786437627)) ;
#151518 = CARTESIAN_POINT('Origin',(6.9,0.0585786437626909,-30.5385786437627)) ;
#151519 = CARTESIAN_POINT('Origin',(6.9,0.0585786437626909,-30.5385786437627)) ;
#151520 = CARTESIAN_POINT('Origin',(6.8057190958418,0.152859547920896,-30.3271404520791)) ;
#151521 = CARTESIAN_POINT('Origin',(6.6585786437627,0.299999999999996,-30.18)) ;
#151522 = CARTESIAN_POINT('Origin',(6.9,0.0585786437626908,-30.4214213562373)) ;
#151523 = CARTESIAN_POINT('Origin',(6.9,0.0585786437626909,-30.08)) ;
#151524 = CARTESIAN_POINT('Origin',(6.9,0.0585786437626909,-30.4214213562373)) ;
#151525 = CARTESIAN_POINT('Origin',(6.9,-0.1,-30.5385786437627)) ;
#151526 = CARTESIAN_POINT('Origin',(6.9,-0.0585786437626902,-30.5385786437627)) ;
#151527 = CARTESIAN_POINT('Origin',(6.9,0.0585786437626909,-30.4214213562373)) ;
#151528 = CARTESIAN_POINT('Origin',(6.9,0.058578643762691,-30.4214213562373)) ;
#151529 = CARTESIAN_POINT('Origin',(6.9,-0.0585786437626909,-30.5385786437627)) ;
#151530 = CARTESIAN_POINT('Origin',(6.9,-0.0585786437626907,-30.5385786437627)) ;
#151531 = CARTESIAN_POINT('Origin',(6.9,-0.0585786437626909,-30.5385786437627)) ;
#151532 = CARTESIAN_POINT('Origin',(6.9,-0.399999999999999,-30.4214213562373)) ;
#151533 = CARTESIAN_POINT('Origin',(6.9,-0.0585786437626909,-30.4214213562373)) ;
#151534 = CARTESIAN_POINT('Origin',(6.9,-0.0585786437626909,-30.08)) ;
#151535 = CARTESIAN_POINT('Origin',(6.9,-0.058578643762691,-30.4214213562373)) ;
#151536 = CARTESIAN_POINT('Origin',(6.87238576250846,-0.0861928812542304,
-30.5661928812542)) ;
#151537 = CARTESIAN_POINT('Origin',(6.65857864376269,-0.3,-30.78)) ;
#151538 = CARTESIAN_POINT('Origin',(6.9,-0.0585786437626909,-30.4214213562373)) ;
#151539 = CARTESIAN_POINT('Origin',(6.9,-0.0585786437626907,-30.4214213562373)) ;
#151540 = CARTESIAN_POINT('Origin',(6.65857864376269,-0.300000000000001,-30.08)) ;
#151541 = CARTESIAN_POINT('Origin',(6.65857864376269,-0.300000000000001,-30.78)) ;
#151542 = CARTESIAN_POINT('Origin',(6.65857864376269,-0.300000000000001,-30.18)) ;
#151543 = CARTESIAN_POINT('Origin',(6.6057190958418,-0.352859547920896,-30.1271404520791)) ;
#151544 = CARTESIAN_POINT('Origin',(6.65857864376269,-0.299999999999998,-30.18)) ;
#151545 = CARTESIAN_POINT('Origin',(-0.113807118745771,-6.47238576250846,
-34.1761928812542)) ;
#151546 = CARTESIAN_POINT('Origin',(0.299999999999993,-6.0585786437627,-34.59)) ;
#151547 = CARTESIAN_POINT('Origin',(0.0585786437626844,-6.3,-34.3485786437627)) ;
#151548 = CARTESIAN_POINT('Origin',(0.3,-6.05857864376269,-33.89)) ;
#151549 = CARTESIAN_POINT('Origin',(0.3,-6.05857864376269,-34.59)) ;
#151550 = CARTESIAN_POINT('Origin',(0.3,-6.05857864376269,-33.99)) ;
#151551 = CARTESIAN_POINT('Origin',(0.0585786437626887,-6.3,-34.3485786437627)) ;
#151552 = CARTESIAN_POINT('Origin',(0.0585786437626908,-6.3,-34.3485786437627)) ;
#151553 = CARTESIAN_POINT('Origin',(0.0585786437626908,-6.3,-34.3485786437627)) ;
#151554 = CARTESIAN_POINT('Origin',(0.152859547920899,-6.20571909584179,-34.1371404520791)) ;
#151555 = CARTESIAN_POINT('Origin',(0.300000000000006,-6.05857864376268,-33.99)) ;
#151556 = CARTESIAN_POINT('Origin',(0.0585786437626911,-6.3,-34.2314213562373)) ;
#151557 = CARTESIAN_POINT('Origin',(0.0585786437626908,-6.3,-33.89)) ;
#151558 = CARTESIAN_POINT('Origin',(0.0585786437626908,-6.3,-34.2314213562373)) ;
#151559 = CARTESIAN_POINT('Origin',(0.4,-6.3,-34.3485786437627)) ;
#151560 = CARTESIAN_POINT('Origin',(-0.0585786437626895,-6.3,-34.3485786437627)) ;
#151561 = CARTESIAN_POINT('Origin',(0.0585786437626903,-6.3,-34.2314213562373)) ;
#151562 = CARTESIAN_POINT('Origin',(0.058578643762689,-6.3,-34.2314213562373)) ;
#151563 = CARTESIAN_POINT('Origin',(-0.0585786437626902,-6.3,-34.3485786437627)) ;
#151564 = CARTESIAN_POINT('Origin',(-0.0585786437626905,-6.3,-34.3485786437627)) ;
#151565 = CARTESIAN_POINT('Origin',(-0.0585786437626908,-6.3,-34.3485786437627)) ;
#151566 = CARTESIAN_POINT('Origin',(-0.1,-6.3,-34.2314213562373)) ;
#151567 = CARTESIAN_POINT('Origin',(-0.0585786437626908,-6.3,-34.2314213562373)) ;
#151568 = CARTESIAN_POINT('Origin',(-0.0585786437626908,-6.3,-33.89)) ;
#151569 = CARTESIAN_POINT('Origin',(-0.0585786437626908,-6.3,-34.2314213562373)) ;
#151570 = CARTESIAN_POINT('Origin',(-0.0861928812542287,-6.27238576250846,
-34.3761928812542)) ;
#151571 = CARTESIAN_POINT('Origin',(-0.299999999999994,-6.0585786437627,-34.59)) ;
#151572 = CARTESIAN_POINT('Origin',(-0.0585786437626908,-6.3,-34.2314213562373)) ;
#151573 = CARTESIAN_POINT('Origin',(-0.0585786437626846,-6.3,-34.2314213562373)) ;
#151574 = CARTESIAN_POINT('Origin',(-0.3,-6.05857864376269,-33.89)) ;
#151575 = CARTESIAN_POINT('Origin',(-0.3,-6.05857864376269,-34.59)) ;
#151576 = CARTESIAN_POINT('Origin',(-0.3,-6.05857864376269,-33.99)) ;
#151577 = CARTESIAN_POINT('Origin',(-0.352859547920899,-6.00571909584179,
-33.9371404520791)) ;
#151578 = CARTESIAN_POINT('Origin',(-0.3,-6.05857864376269,-33.99)) ;
#151579 = CARTESIAN_POINT('Origin',(7.07238576250846,-0.113807118745771,-34.1761928812542)) ;
#151580 = CARTESIAN_POINT('Origin',(6.6585786437627,0.299999999999994,-34.59)) ;
#151581 = CARTESIAN_POINT('Origin',(6.9,0.0585786437626901,-34.3485786437627)) ;
#151582 = CARTESIAN_POINT('Origin',(6.65857864376269,0.300000000000001,-33.89)) ;
#151583 = CARTESIAN_POINT('Origin',(6.65857864376269,0.300000000000001,-34.59)) ;
#151584 = CARTESIAN_POINT('Origin',(6.65857864376269,0.300000000000001,-33.99)) ;
#151585 = CARTESIAN_POINT('Origin',(6.9,0.0585786437626906,-34.3485786437627)) ;
#151586 = CARTESIAN_POINT('Origin',(6.9,0.0585786437626909,-34.3485786437627)) ;
#151587 = CARTESIAN_POINT('Origin',(6.9,0.0585786437626909,-34.3485786437627)) ;
#151588 = CARTESIAN_POINT('Origin',(6.80571909584179,0.1528595479209,-34.1371404520791)) ;
#151589 = CARTESIAN_POINT('Origin',(6.65857864376268,0.300000000000007,-33.99)) ;
#151590 = CARTESIAN_POINT('Origin',(6.9,0.0585786437626911,-34.2314213562373)) ;
#151591 = CARTESIAN_POINT('Origin',(6.9,0.0585786437626909,-33.89)) ;
#151592 = CARTESIAN_POINT('Origin',(6.9,0.0585786437626909,-34.2314213562373)) ;
#151593 = CARTESIAN_POINT('Origin',(6.9,-0.1,-34.3485786437627)) ;
#151594 = CARTESIAN_POINT('Origin',(6.9,-0.0585786437626952,-34.3485786437627)) ;
#151595 = CARTESIAN_POINT('Origin',(6.9,0.0585786437626913,-34.2314213562373)) ;
#151596 = CARTESIAN_POINT('Origin',(6.9,0.0585786437626919,-34.2314213562373)) ;
#151597 = CARTESIAN_POINT('Origin',(6.9,-0.0585786437626923,-34.3485786437627)) ;
#151598 = CARTESIAN_POINT('Origin',(6.9,-0.0585786437626907,-34.3485786437627)) ;
#151599 = CARTESIAN_POINT('Origin',(6.9,-0.0585786437626909,-34.3485786437627)) ;
#151600 = CARTESIAN_POINT('Origin',(6.9,-0.399999999999999,-34.2314213562373)) ;
#151601 = CARTESIAN_POINT('Origin',(6.9,-0.0585786437626909,-34.2314213562373)) ;
#151602 = CARTESIAN_POINT('Origin',(6.9,-0.0585786437626909,-33.89)) ;
#151603 = CARTESIAN_POINT('Origin',(6.9,-0.058578643762691,-34.2314213562373)) ;
#151604 = CARTESIAN_POINT('Origin',(6.87238576250846,-0.0861928812542292,
-34.3761928812542)) ;
#151605 = CARTESIAN_POINT('Origin',(6.6585786437627,-0.299999999999995,-34.59)) ;
#151606 = CARTESIAN_POINT('Origin',(6.9,-0.0585786437626886,-34.2314213562373)) ;
#151607 = CARTESIAN_POINT('Origin',(6.9,-0.058578643762684,-34.2314213562373)) ;
#151608 = CARTESIAN_POINT('Origin',(6.65857864376269,-0.300000000000001,-33.89)) ;
#151609 = CARTESIAN_POINT('Origin',(6.65857864376269,-0.300000000000001,-34.59)) ;
#151610 = CARTESIAN_POINT('Origin',(6.65857864376269,-0.300000000000001,-33.99)) ;
#151611 = CARTESIAN_POINT('Origin',(6.60571909584179,-0.3528595479209,-33.9371404520791)) ;
#151612 = CARTESIAN_POINT('Origin',(6.65857864376269,-0.300000000000001,-33.99)) ;
#151613 = CARTESIAN_POINT('Origin',(0.6,-0.6,-4.11)) ;
#151614 = CARTESIAN_POINT('Origin',(0.3,-0.6,-4.11)) ;
#151615 = CARTESIAN_POINT('Origin',(0.3,-6.1,-4.11)) ;
#151616 = CARTESIAN_POINT('Origin',(0.3,-6.05857864376269,-4.11)) ;
#151617 = CARTESIAN_POINT('Origin',(0.3,-6.05857864376269,-4.11)) ;
#151618 = CARTESIAN_POINT('Origin',(0.3,-6.05857864376269,-4.11)) ;
#151619 = CARTESIAN_POINT('Origin',(0.4,-6.05857864376269,-4.11)) ;
#151620 = CARTESIAN_POINT('Origin',(-0.300000000000001,-6.05857864376269,
-4.11)) ;
#151621 = CARTESIAN_POINT('Origin',(-0.3,-6.05857864376269,-4.11)) ;
#151622 = CARTESIAN_POINT('Origin',(-0.3,-6.05857864376269,-4.11)) ;
#151623 = CARTESIAN_POINT('Origin',(-0.3,-0.600000000000001,-4.11)) ;
#151624 = CARTESIAN_POINT('Origin',(-0.3,-0.600000000000001,-4.11)) ;
#151625 = CARTESIAN_POINT('Origin',(0.6,-0.600000000000001,-4.11)) ;
#151626 = CARTESIAN_POINT('Origin',(0.6,-0.600000000000001,-3.51)) ;
#151627 = CARTESIAN_POINT('Origin',(-0.3,-0.600000000000001,-3.51)) ;
#151628 = CARTESIAN_POINT('Origin',(-0.3,-0.600000000000001,-3.51)) ;
#151629 = CARTESIAN_POINT('Origin',(-0.3,-6.05857864376269,-3.51)) ;
#151630 = CARTESIAN_POINT('Origin',(-0.3,-6.05857864376269,-3.51)) ;
#151631 = CARTESIAN_POINT('Origin',(-0.299999999999999,-6.05857864376269,
-3.51)) ;
#151632 = CARTESIAN_POINT('Origin',(0.4,-6.05857864376269,-3.51)) ;
#151633 = CARTESIAN_POINT('Origin',(0.299999999999999,-6.05857864376269,-3.51)) ;
#151634 = CARTESIAN_POINT('Origin',(0.3,-6.05857864376269,-3.51)) ;
#151635 = CARTESIAN_POINT('Origin',(0.3,-6.05857864376269,-3.51)) ;
#151636 = CARTESIAN_POINT('Origin',(0.3,-0.600000000000001,-3.51)) ;
#151637 = CARTESIAN_POINT('Origin',(0.3,-0.6,-3.51)) ;
#151638 = CARTESIAN_POINT('Origin',(0.6,-0.6,-3.51)) ;
#151639 = CARTESIAN_POINT('Origin',(6.7,0.300000000000001,-4.11)) ;
#151640 = CARTESIAN_POINT('Origin',(6.65857864376269,0.300000000000001,-4.11)) ;
#151641 = CARTESIAN_POINT('Origin',(6.65857864376269,0.300000000000001,-4.11)) ;
#151642 = CARTESIAN_POINT('Origin',(6.65857864376269,0.300000000000001,-4.11)) ;
#151643 = CARTESIAN_POINT('Origin',(6.65857864376269,-0.399999999999999,-4.11)) ;
#151644 = CARTESIAN_POINT('Origin',(6.65857864376269,-0.300000000000001,-4.11)) ;
#151645 = CARTESIAN_POINT('Origin',(6.65857864376269,-0.3,-4.11)) ;
#151646 = CARTESIAN_POINT('Origin',(6.65857864376269,-0.300000000000001,-4.11)) ;
#151647 = CARTESIAN_POINT('Origin',(0.6,-0.3,-4.11)) ;
#151648 = CARTESIAN_POINT('Origin',(0.6,0.299999999999999,-3.51)) ;
#151649 = CARTESIAN_POINT('Origin',(6.65857864376269,0.300000000000001,-3.51)) ;
#151650 = CARTESIAN_POINT('Origin',(6.65857864376269,0.300000000000001,-3.51)) ;
#151651 = CARTESIAN_POINT('Origin',(6.65857864376269,0.3,-3.51)) ;
#151652 = CARTESIAN_POINT('Origin',(6.65857864376269,-0.399999999999999,-3.51)) ;
#151653 = CARTESIAN_POINT('Origin',(6.65857864376269,-0.3,-3.51)) ;
#151654 = CARTESIAN_POINT('Origin',(0.6,-0.3,-3.51)) ;
#151655 = CARTESIAN_POINT('Origin',(6.65857864376269,-0.300000000000001,-3.51)) ;
#151656 = CARTESIAN_POINT('Origin',(6.65857864376269,-0.300000000000001,-3.51)) ;
#151657 = CARTESIAN_POINT('Origin',(0.6,-0.6,-7.92)) ;
#151658 = CARTESIAN_POINT('Origin',(0.3,-0.6,-7.92)) ;
#151659 = CARTESIAN_POINT('Origin',(0.3,-6.1,-7.92)) ;
#151660 = CARTESIAN_POINT('Origin',(0.3,-6.05857864376269,-7.92)) ;
#151661 = CARTESIAN_POINT('Origin',(0.3,-6.05857864376269,-7.92)) ;
#151662 = CARTESIAN_POINT('Origin',(0.3,-6.05857864376269,-7.92)) ;
#151663 = CARTESIAN_POINT('Origin',(0.4,-6.05857864376269,-7.92)) ;
#151664 = CARTESIAN_POINT('Origin',(-0.299999999999999,-6.05857864376269,
-7.92)) ;
#151665 = CARTESIAN_POINT('Origin',(-0.3,-6.05857864376269,-7.92)) ;
#151666 = CARTESIAN_POINT('Origin',(-0.3,-6.05857864376269,-7.92)) ;
#151667 = CARTESIAN_POINT('Origin',(-0.3,-0.600000000000001,-7.92)) ;
#151668 = CARTESIAN_POINT('Origin',(-0.3,-0.600000000000001,-7.92)) ;
#151669 = CARTESIAN_POINT('Origin',(0.6,-0.600000000000001,-7.92)) ;
#151670 = CARTESIAN_POINT('Origin',(0.6,-0.600000000000001,-7.32)) ;
#151671 = CARTESIAN_POINT('Origin',(-0.3,-0.600000000000001,-7.32)) ;
#151672 = CARTESIAN_POINT('Origin',(-0.3,-0.600000000000001,-7.32)) ;
#151673 = CARTESIAN_POINT('Origin',(-0.3,-6.05857864376269,-7.32)) ;
#151674 = CARTESIAN_POINT('Origin',(-0.3,-6.05857864376269,-7.32)) ;
#151675 = CARTESIAN_POINT('Origin',(-0.300000000000001,-6.05857864376269,
-7.32)) ;
#151676 = CARTESIAN_POINT('Origin',(0.4,-6.05857864376269,-7.32)) ;
#151677 = CARTESIAN_POINT('Origin',(0.300000000000002,-6.05857864376269,-7.32)) ;
#151678 = CARTESIAN_POINT('Origin',(0.300000000000001,-6.05857864376269,-7.32)) ;
#151679 = CARTESIAN_POINT('Origin',(0.3,-6.05857864376269,-7.32)) ;
#151680 = CARTESIAN_POINT('Origin',(0.3,-0.600000000000001,-7.32)) ;
#151681 = CARTESIAN_POINT('Origin',(0.3,-0.6,-7.32)) ;
#151682 = CARTESIAN_POINT('Origin',(0.6,-0.6,-7.32)) ;
#151683 = CARTESIAN_POINT('Origin',(6.7,0.300000000000001,-7.92)) ;
#151684 = CARTESIAN_POINT('Origin',(6.65857864376269,0.300000000000001,-7.92)) ;
#151685 = CARTESIAN_POINT('Origin',(6.65857864376269,0.300000000000001,-7.92)) ;
#151686 = CARTESIAN_POINT('Origin',(6.65857864376269,0.300000000000002,-7.92)) ;
#151687 = CARTESIAN_POINT('Origin',(6.65857864376269,-0.399999999999999,-7.92)) ;
#151688 = CARTESIAN_POINT('Origin',(6.65857864376269,-0.300000000000002,-7.92)) ;
#151689 = CARTESIAN_POINT('Origin',(6.65857864376269,-0.300000000000001,-7.92)) ;
#151690 = CARTESIAN_POINT('Origin',(6.65857864376269,-0.300000000000001,-7.92)) ;
#151691 = CARTESIAN_POINT('Origin',(0.6,-0.3,-7.92)) ;
#151692 = CARTESIAN_POINT('Origin',(0.6,0.299999999999999,-7.32)) ;
#151693 = CARTESIAN_POINT('Origin',(6.65857864376269,0.300000000000001,-7.32)) ;
#151694 = CARTESIAN_POINT('Origin',(6.65857864376269,0.300000000000001,-7.32)) ;
#151695 = CARTESIAN_POINT('Origin',(6.65857864376269,0.300000000000002,-7.32)) ;
#151696 = CARTESIAN_POINT('Origin',(6.65857864376269,-0.399999999999999,-7.32)) ;
#151697 = CARTESIAN_POINT('Origin',(6.65857864376269,-0.300000000000002,-7.32)) ;
#151698 = CARTESIAN_POINT('Origin',(0.6,-0.3,-7.32)) ;
#151699 = CARTESIAN_POINT('Origin',(6.65857864376269,-0.300000000000001,-7.32)) ;
#151700 = CARTESIAN_POINT('Origin',(6.65857864376269,-0.300000000000001,-7.32)) ;
#151701 = CARTESIAN_POINT('Origin',(0.6,-0.6,-11.73)) ;
#151702 = CARTESIAN_POINT('Origin',(0.3,-0.6,-11.73)) ;
#151703 = CARTESIAN_POINT('Origin',(0.3,-6.1,-11.73)) ;
#151704 = CARTESIAN_POINT('Origin',(0.3,-6.05857864376269,-11.73)) ;
#151705 = CARTESIAN_POINT('Origin',(0.3,-6.05857864376269,-11.73)) ;
#151706 = CARTESIAN_POINT('Origin',(0.299999999999998,-6.05857864376269,-11.73)) ;
#151707 = CARTESIAN_POINT('Origin',(0.4,-6.05857864376269,-11.73)) ;
#151708 = CARTESIAN_POINT('Origin',(-0.299999999999999,-6.05857864376269,
-11.73)) ;
#151709 = CARTESIAN_POINT('Origin',(-0.3,-6.05857864376269,-11.73)) ;
#151710 = CARTESIAN_POINT('Origin',(-0.3,-6.05857864376269,-11.73)) ;
#151711 = CARTESIAN_POINT('Origin',(-0.3,-0.600000000000001,-11.73)) ;
#151712 = CARTESIAN_POINT('Origin',(-0.3,-0.600000000000001,-11.73)) ;
#151713 = CARTESIAN_POINT('Origin',(0.6,-0.600000000000001,-11.73)) ;
#151714 = CARTESIAN_POINT('Origin',(0.6,-0.600000000000001,-11.13)) ;
#151715 = CARTESIAN_POINT('Origin',(-0.3,-0.600000000000001,-11.13)) ;
#151716 = CARTESIAN_POINT('Origin',(-0.3,-0.600000000000001,-11.13)) ;
#151717 = CARTESIAN_POINT('Origin',(-0.3,-6.05857864376269,-11.13)) ;
#151718 = CARTESIAN_POINT('Origin',(-0.3,-6.05857864376269,-11.13)) ;
#151719 = CARTESIAN_POINT('Origin',(-0.300000000000002,-6.05857864376269,
-11.13)) ;
#151720 = CARTESIAN_POINT('Origin',(0.4,-6.05857864376269,-11.13)) ;
#151721 = CARTESIAN_POINT('Origin',(0.300000000000001,-6.05857864376269,-11.13)) ;
#151722 = CARTESIAN_POINT('Origin',(0.300000000000003,-6.05857864376269,-11.13)) ;
#151723 = CARTESIAN_POINT('Origin',(0.3,-6.05857864376269,-11.13)) ;
#151724 = CARTESIAN_POINT('Origin',(0.3,-0.600000000000001,-11.13)) ;
#151725 = CARTESIAN_POINT('Origin',(0.3,-0.6,-11.13)) ;
#151726 = CARTESIAN_POINT('Origin',(0.6,-0.6,-11.13)) ;
#151727 = CARTESIAN_POINT('Origin',(6.7,0.300000000000001,-11.73)) ;
#151728 = CARTESIAN_POINT('Origin',(6.65857864376269,0.300000000000001,-11.73)) ;
#151729 = CARTESIAN_POINT('Origin',(6.65857864376269,0.300000000000001,-11.73)) ;
#151730 = CARTESIAN_POINT('Origin',(6.65857864376269,0.300000000000001,-11.73)) ;
#151731 = CARTESIAN_POINT('Origin',(6.65857864376269,-0.399999999999999,-11.73)) ;
#151732 = CARTESIAN_POINT('Origin',(6.65857864376269,-0.300000000000002,-11.73)) ;
#151733 = CARTESIAN_POINT('Origin',(6.65857864376269,-0.300000000000002,-11.73)) ;
#151734 = CARTESIAN_POINT('Origin',(6.65857864376269,-0.300000000000001,-11.73)) ;
#151735 = CARTESIAN_POINT('Origin',(0.6,-0.3,-11.73)) ;
#151736 = CARTESIAN_POINT('Origin',(0.6,0.299999999999999,-11.13)) ;
#151737 = CARTESIAN_POINT('Origin',(6.65857864376269,0.300000000000001,-11.13)) ;
#151738 = CARTESIAN_POINT('Origin',(6.65857864376269,0.300000000000001,-11.13)) ;
#151739 = CARTESIAN_POINT('Origin',(6.65857864376269,0.300000000000001,-11.13)) ;
#151740 = CARTESIAN_POINT('Origin',(6.65857864376269,-0.399999999999999,-11.13)) ;
#151741 = CARTESIAN_POINT('Origin',(6.65857864376269,-0.300000000000002,-11.13)) ;
#151742 = CARTESIAN_POINT('Origin',(0.6,-0.3,-11.13)) ;
#151743 = CARTESIAN_POINT('Origin',(6.65857864376269,-0.300000000000001,-11.13)) ;
#151744 = CARTESIAN_POINT('Origin',(6.65857864376269,-0.300000000000003,-11.13)) ;
#151745 = CARTESIAN_POINT('Origin',(0.6,-0.6,-15.54)) ;
#151746 = CARTESIAN_POINT('Origin',(0.3,-0.6,-15.54)) ;
#151747 = CARTESIAN_POINT('Origin',(0.3,-6.1,-15.54)) ;
#151748 = CARTESIAN_POINT('Origin',(0.3,-6.05857864376269,-15.54)) ;
#151749 = CARTESIAN_POINT('Origin',(0.3,-6.05857864376269,-15.54)) ;
#151750 = CARTESIAN_POINT('Origin',(0.3,-6.05857864376269,-15.54)) ;
#151751 = CARTESIAN_POINT('Origin',(0.4,-6.05857864376269,-15.54)) ;
#151752 = CARTESIAN_POINT('Origin',(-0.299999999999999,-6.05857864376269,
-15.54)) ;
#151753 = CARTESIAN_POINT('Origin',(-0.300000000000001,-6.05857864376269,
-15.54)) ;
#151754 = CARTESIAN_POINT('Origin',(-0.3,-6.05857864376269,-15.54)) ;
#151755 = CARTESIAN_POINT('Origin',(-0.3,-0.600000000000001,-15.54)) ;
#151756 = CARTESIAN_POINT('Origin',(-0.3,-0.600000000000001,-15.54)) ;
#151757 = CARTESIAN_POINT('Origin',(0.6,-0.600000000000001,-15.54)) ;
#151758 = CARTESIAN_POINT('Origin',(0.6,-0.600000000000001,-14.94)) ;
#151759 = CARTESIAN_POINT('Origin',(-0.3,-0.600000000000001,-14.94)) ;
#151760 = CARTESIAN_POINT('Origin',(-0.3,-0.600000000000001,-14.94)) ;
#151761 = CARTESIAN_POINT('Origin',(-0.3,-6.05857864376269,-14.94)) ;
#151762 = CARTESIAN_POINT('Origin',(-0.3,-6.05857864376269,-14.94)) ;
#151763 = CARTESIAN_POINT('Origin',(-0.3,-6.05857864376269,-14.94)) ;
#151764 = CARTESIAN_POINT('Origin',(0.4,-6.05857864376269,-14.94)) ;
#151765 = CARTESIAN_POINT('Origin',(0.299999999999999,-6.05857864376269,-14.94)) ;
#151766 = CARTESIAN_POINT('Origin',(0.300000000000001,-6.05857864376269,-14.94)) ;
#151767 = CARTESIAN_POINT('Origin',(0.3,-6.05857864376269,-14.94)) ;
#151768 = CARTESIAN_POINT('Origin',(0.3,-0.600000000000001,-14.94)) ;
#151769 = CARTESIAN_POINT('Origin',(0.3,-0.6,-14.94)) ;
#151770 = CARTESIAN_POINT('Origin',(0.6,-0.6,-14.94)) ;
#151771 = CARTESIAN_POINT('Origin',(6.7,0.300000000000001,-15.54)) ;
#151772 = CARTESIAN_POINT('Origin',(6.65857864376269,0.300000000000001,-15.54)) ;
#151773 = CARTESIAN_POINT('Origin',(6.65857864376269,0.300000000000001,-15.54)) ;
#151774 = CARTESIAN_POINT('Origin',(6.65857864376269,0.300000000000003,-15.54)) ;
#151775 = CARTESIAN_POINT('Origin',(6.65857864376269,-0.399999999999999,-15.54)) ;
#151776 = CARTESIAN_POINT('Origin',(6.65857864376269,-0.3,-15.54)) ;
#151777 = CARTESIAN_POINT('Origin',(6.65857864376269,-0.300000000000002,-15.54)) ;
#151778 = CARTESIAN_POINT('Origin',(6.65857864376269,-0.300000000000001,-15.54)) ;
#151779 = CARTESIAN_POINT('Origin',(0.6,-0.3,-15.54)) ;
#151780 = CARTESIAN_POINT('Origin',(0.6,0.299999999999999,-14.94)) ;
#151781 = CARTESIAN_POINT('Origin',(6.65857864376269,0.300000000000001,-14.94)) ;
#151782 = CARTESIAN_POINT('Origin',(6.65857864376269,0.300000000000001,-14.94)) ;
#151783 = CARTESIAN_POINT('Origin',(6.65857864376269,0.3,-14.94)) ;
#151784 = CARTESIAN_POINT('Origin',(6.65857864376269,-0.399999999999999,-14.94)) ;
#151785 = CARTESIAN_POINT('Origin',(6.65857864376269,-0.299999999999999,-14.94)) ;
#151786 = CARTESIAN_POINT('Origin',(0.6,-0.3,-14.94)) ;
#151787 = CARTESIAN_POINT('Origin',(6.65857864376269,-0.300000000000001,-14.94)) ;
#151788 = CARTESIAN_POINT('Origin',(6.65857864376269,-0.300000000000001,-14.94)) ;
#151789 = CARTESIAN_POINT('Origin',(0.6,-0.6,-19.35)) ;
#151790 = CARTESIAN_POINT('Origin',(0.3,-0.6,-19.35)) ;
#151791 = CARTESIAN_POINT('Origin',(0.3,-6.1,-19.35)) ;
#151792 = CARTESIAN_POINT('Origin',(0.3,-6.05857864376269,-19.35)) ;
#151793 = CARTESIAN_POINT('Origin',(0.3,-6.05857864376269,-19.35)) ;
#151794 = CARTESIAN_POINT('Origin',(0.299999999999999,-6.05857864376269,-19.35)) ;
#151795 = CARTESIAN_POINT('Origin',(0.4,-6.05857864376269,-19.35)) ;
#151796 = CARTESIAN_POINT('Origin',(-0.299999999999994,-6.0585786437627,-19.35)) ;
#151797 = CARTESIAN_POINT('Origin',(-0.299999999999999,-6.05857864376269,
-19.35)) ;
#151798 = CARTESIAN_POINT('Origin',(-0.3,-6.05857864376269,-19.35)) ;
#151799 = CARTESIAN_POINT('Origin',(-0.3,-0.600000000000001,-19.35)) ;
#151800 = CARTESIAN_POINT('Origin',(-0.3,-0.600000000000001,-19.35)) ;
#151801 = CARTESIAN_POINT('Origin',(0.6,-0.600000000000001,-19.35)) ;
#151802 = CARTESIAN_POINT('Origin',(0.6,-0.600000000000001,-18.75)) ;
#151803 = CARTESIAN_POINT('Origin',(-0.3,-0.600000000000001,-18.75)) ;
#151804 = CARTESIAN_POINT('Origin',(-0.3,-0.600000000000001,-18.75)) ;
#151805 = CARTESIAN_POINT('Origin',(-0.3,-6.05857864376269,-18.75)) ;
#151806 = CARTESIAN_POINT('Origin',(-0.3,-6.05857864376269,-18.75)) ;
#151807 = CARTESIAN_POINT('Origin',(-0.299999999999994,-6.0585786437627,-18.75)) ;
#151808 = CARTESIAN_POINT('Origin',(0.4,-6.0585786437627,-18.75)) ;
#151809 = CARTESIAN_POINT('Origin',(0.299999999999993,-6.0585786437627,-18.75)) ;
#151810 = CARTESIAN_POINT('Origin',(0.299999999999996,-6.0585786437627,-18.75)) ;
#151811 = CARTESIAN_POINT('Origin',(0.3,-6.05857864376269,-18.75)) ;
#151812 = CARTESIAN_POINT('Origin',(0.3,-0.600000000000001,-18.75)) ;
#151813 = CARTESIAN_POINT('Origin',(0.3,-0.6,-18.75)) ;
#151814 = CARTESIAN_POINT('Origin',(0.6,-0.6,-18.75)) ;
#151815 = CARTESIAN_POINT('Origin',(6.7,0.300000000000001,-19.35)) ;
#151816 = CARTESIAN_POINT('Origin',(6.65857864376269,0.300000000000001,-19.35)) ;
#151817 = CARTESIAN_POINT('Origin',(6.65857864376269,0.300000000000001,-19.35)) ;
#151818 = CARTESIAN_POINT('Origin',(6.65857864376269,0.299999999999997,-19.35)) ;
#151819 = CARTESIAN_POINT('Origin',(6.65857864376269,-0.399999999999999,-19.35)) ;
#151820 = CARTESIAN_POINT('Origin',(6.65857864376269,-0.299999999999997,-19.35)) ;
#151821 = CARTESIAN_POINT('Origin',(6.65857864376269,-0.3,-19.35)) ;
#151822 = CARTESIAN_POINT('Origin',(6.65857864376269,-0.300000000000001,-19.35)) ;
#151823 = CARTESIAN_POINT('Origin',(0.6,-0.3,-19.35)) ;
#151824 = CARTESIAN_POINT('Origin',(0.6,0.299999999999999,-18.75)) ;
#151825 = CARTESIAN_POINT('Origin',(6.65857864376269,0.300000000000001,-18.75)) ;
#151826 = CARTESIAN_POINT('Origin',(6.65857864376269,0.300000000000001,-18.75)) ;
#151827 = CARTESIAN_POINT('Origin',(6.6585786437627,0.299999999999995,-18.75)) ;
#151828 = CARTESIAN_POINT('Origin',(6.6585786437627,-0.399999999999999,-18.75)) ;
#151829 = CARTESIAN_POINT('Origin',(6.6585786437627,-0.299999999999994,-18.75)) ;
#151830 = CARTESIAN_POINT('Origin',(0.6,-0.3,-18.75)) ;
#151831 = CARTESIAN_POINT('Origin',(6.65857864376269,-0.300000000000001,-18.75)) ;
#151832 = CARTESIAN_POINT('Origin',(6.65857864376269,-0.299999999999998,-18.75)) ;
#151833 = CARTESIAN_POINT('Origin',(0.6,-0.6,-23.16)) ;
#151834 = CARTESIAN_POINT('Origin',(0.3,-0.6,-23.16)) ;
#151835 = CARTESIAN_POINT('Origin',(0.3,-6.1,-23.16)) ;
#151836 = CARTESIAN_POINT('Origin',(0.3,-6.05857864376269,-23.16)) ;
#151837 = CARTESIAN_POINT('Origin',(0.3,-6.05857864376269,-23.16)) ;
#151838 = CARTESIAN_POINT('Origin',(0.299999999999999,-6.05857864376269,-23.16)) ;
#151839 = CARTESIAN_POINT('Origin',(0.4,-6.05857864376269,-23.16)) ;
#151840 = CARTESIAN_POINT('Origin',(-0.299999999999994,-6.0585786437627,-23.16)) ;
#151841 = CARTESIAN_POINT('Origin',(-0.299999999999999,-6.05857864376269,
-23.16)) ;
#151842 = CARTESIAN_POINT('Origin',(-0.3,-6.05857864376269,-23.16)) ;
#151843 = CARTESIAN_POINT('Origin',(-0.3,-0.600000000000001,-23.16)) ;
#151844 = CARTESIAN_POINT('Origin',(-0.3,-0.600000000000001,-23.16)) ;
#151845 = CARTESIAN_POINT('Origin',(0.6,-0.600000000000001,-23.16)) ;
#151846 = CARTESIAN_POINT('Origin',(0.6,-0.600000000000001,-22.56)) ;
#151847 = CARTESIAN_POINT('Origin',(-0.3,-0.600000000000001,-22.56)) ;
#151848 = CARTESIAN_POINT('Origin',(-0.3,-0.600000000000001,-22.56)) ;
#151849 = CARTESIAN_POINT('Origin',(-0.3,-6.05857864376269,-22.56)) ;
#151850 = CARTESIAN_POINT('Origin',(-0.3,-6.05857864376269,-22.56)) ;
#151851 = CARTESIAN_POINT('Origin',(-0.299999999999994,-6.0585786437627,-22.56)) ;
#151852 = CARTESIAN_POINT('Origin',(0.4,-6.0585786437627,-22.56)) ;
#151853 = CARTESIAN_POINT('Origin',(0.299999999999993,-6.0585786437627,-22.56)) ;
#151854 = CARTESIAN_POINT('Origin',(0.299999999999996,-6.0585786437627,-22.56)) ;
#151855 = CARTESIAN_POINT('Origin',(0.3,-6.05857864376269,-22.56)) ;
#151856 = CARTESIAN_POINT('Origin',(0.3,-0.600000000000001,-22.56)) ;
#151857 = CARTESIAN_POINT('Origin',(0.3,-0.6,-22.56)) ;
#151858 = CARTESIAN_POINT('Origin',(0.6,-0.6,-22.56)) ;
#151859 = CARTESIAN_POINT('Origin',(6.7,0.300000000000001,-23.16)) ;
#151860 = CARTESIAN_POINT('Origin',(6.65857864376269,0.300000000000001,-23.16)) ;
#151861 = CARTESIAN_POINT('Origin',(6.65857864376269,0.300000000000001,-23.16)) ;
#151862 = CARTESIAN_POINT('Origin',(6.65857864376269,0.299999999999997,-23.16)) ;
#151863 = CARTESIAN_POINT('Origin',(6.65857864376269,-0.399999999999999,-23.16)) ;
#151864 = CARTESIAN_POINT('Origin',(6.65857864376269,-0.299999999999997,-23.16)) ;
#151865 = CARTESIAN_POINT('Origin',(6.65857864376269,-0.3,-23.16)) ;
#151866 = CARTESIAN_POINT('Origin',(6.65857864376269,-0.300000000000001,-23.16)) ;
#151867 = CARTESIAN_POINT('Origin',(0.6,-0.3,-23.16)) ;
#151868 = CARTESIAN_POINT('Origin',(0.6,0.299999999999999,-22.56)) ;
#151869 = CARTESIAN_POINT('Origin',(6.65857864376269,0.300000000000001,-22.56)) ;
#151870 = CARTESIAN_POINT('Origin',(6.65857864376269,0.300000000000001,-22.56)) ;
#151871 = CARTESIAN_POINT('Origin',(6.6585786437627,0.299999999999995,-22.56)) ;
#151872 = CARTESIAN_POINT('Origin',(6.6585786437627,-0.399999999999999,-22.56)) ;
#151873 = CARTESIAN_POINT('Origin',(6.6585786437627,-0.299999999999994,-22.56)) ;
#151874 = CARTESIAN_POINT('Origin',(0.6,-0.3,-22.56)) ;
#151875 = CARTESIAN_POINT('Origin',(6.65857864376269,-0.300000000000001,-22.56)) ;
#151876 = CARTESIAN_POINT('Origin',(6.65857864376269,-0.299999999999998,-22.56)) ;
#151877 = CARTESIAN_POINT('Origin',(0.6,-0.6,-26.97)) ;
#151878 = CARTESIAN_POINT('Origin',(0.3,-0.6,-26.97)) ;
#151879 = CARTESIAN_POINT('Origin',(0.3,-6.1,-26.97)) ;
#151880 = CARTESIAN_POINT('Origin',(0.3,-6.05857864376269,-26.97)) ;
#151881 = CARTESIAN_POINT('Origin',(0.3,-6.05857864376269,-26.97)) ;
#151882 = CARTESIAN_POINT('Origin',(0.299999999999999,-6.05857864376269,-26.97)) ;
#151883 = CARTESIAN_POINT('Origin',(0.4,-6.05857864376269,-26.97)) ;
#151884 = CARTESIAN_POINT('Origin',(-0.299999999999994,-6.0585786437627,-26.97)) ;
#151885 = CARTESIAN_POINT('Origin',(-0.299999999999999,-6.05857864376269,
-26.97)) ;
#151886 = CARTESIAN_POINT('Origin',(-0.3,-6.05857864376269,-26.97)) ;
#151887 = CARTESIAN_POINT('Origin',(-0.3,-0.600000000000001,-26.97)) ;
#151888 = CARTESIAN_POINT('Origin',(-0.3,-0.600000000000001,-26.97)) ;
#151889 = CARTESIAN_POINT('Origin',(0.6,-0.600000000000001,-26.97)) ;
#151890 = CARTESIAN_POINT('Origin',(0.6,-0.600000000000001,-26.37)) ;
#151891 = CARTESIAN_POINT('Origin',(-0.3,-0.600000000000001,-26.37)) ;
#151892 = CARTESIAN_POINT('Origin',(-0.3,-0.600000000000001,-26.37)) ;
#151893 = CARTESIAN_POINT('Origin',(-0.3,-6.05857864376269,-26.37)) ;
#151894 = CARTESIAN_POINT('Origin',(-0.3,-6.05857864376269,-26.37)) ;
#151895 = CARTESIAN_POINT('Origin',(-0.299999999999994,-6.0585786437627,-26.37)) ;
#151896 = CARTESIAN_POINT('Origin',(0.4,-6.0585786437627,-26.37)) ;
#151897 = CARTESIAN_POINT('Origin',(0.299999999999993,-6.0585786437627,-26.37)) ;
#151898 = CARTESIAN_POINT('Origin',(0.299999999999996,-6.0585786437627,-26.37)) ;
#151899 = CARTESIAN_POINT('Origin',(0.3,-6.05857864376269,-26.37)) ;
#151900 = CARTESIAN_POINT('Origin',(0.3,-0.600000000000001,-26.37)) ;
#151901 = CARTESIAN_POINT('Origin',(0.3,-0.6,-26.37)) ;
#151902 = CARTESIAN_POINT('Origin',(0.6,-0.6,-26.37)) ;
#151903 = CARTESIAN_POINT('Origin',(6.7,0.300000000000001,-26.97)) ;
#151904 = CARTESIAN_POINT('Origin',(6.65857864376269,0.300000000000001,-26.97)) ;
#151905 = CARTESIAN_POINT('Origin',(6.65857864376269,0.300000000000001,-26.97)) ;
#151906 = CARTESIAN_POINT('Origin',(6.65857864376269,0.299999999999997,-26.97)) ;
#151907 = CARTESIAN_POINT('Origin',(6.65857864376269,-0.399999999999999,-26.97)) ;
#151908 = CARTESIAN_POINT('Origin',(6.65857864376269,-0.299999999999997,-26.97)) ;
#151909 = CARTESIAN_POINT('Origin',(6.65857864376269,-0.3,-26.97)) ;
#151910 = CARTESIAN_POINT('Origin',(6.65857864376269,-0.300000000000001,-26.97)) ;
#151911 = CARTESIAN_POINT('Origin',(0.6,-0.3,-26.97)) ;
#151912 = CARTESIAN_POINT('Origin',(0.6,0.299999999999999,-26.37)) ;
#151913 = CARTESIAN_POINT('Origin',(6.65857864376269,0.300000000000001,-26.37)) ;
#151914 = CARTESIAN_POINT('Origin',(6.65857864376269,0.300000000000001,-26.37)) ;
#151915 = CARTESIAN_POINT('Origin',(6.6585786437627,0.299999999999995,-26.37)) ;
#151916 = CARTESIAN_POINT('Origin',(6.6585786437627,-0.399999999999999,-26.37)) ;
#151917 = CARTESIAN_POINT('Origin',(6.6585786437627,-0.299999999999994,-26.37)) ;
#151918 = CARTESIAN_POINT('Origin',(0.6,-0.3,-26.37)) ;
#151919 = CARTESIAN_POINT('Origin',(6.65857864376269,-0.300000000000001,-26.37)) ;
#151920 = CARTESIAN_POINT('Origin',(6.65857864376269,-0.299999999999998,-26.37)) ;
#151921 = CARTESIAN_POINT('Origin',(0.6,-0.6,-30.78)) ;
#151922 = CARTESIAN_POINT('Origin',(0.3,-0.6,-30.78)) ;
#151923 = CARTESIAN_POINT('Origin',(0.3,-6.1,-30.78)) ;
#151924 = CARTESIAN_POINT('Origin',(0.3,-6.05857864376269,-30.78)) ;
#151925 = CARTESIAN_POINT('Origin',(0.3,-6.05857864376269,-30.78)) ;
#151926 = CARTESIAN_POINT('Origin',(0.299999999999999,-6.05857864376269,-30.78)) ;
#151927 = CARTESIAN_POINT('Origin',(0.4,-6.05857864376269,-30.78)) ;
#151928 = CARTESIAN_POINT('Origin',(-0.299999999999994,-6.0585786437627,-30.78)) ;
#151929 = CARTESIAN_POINT('Origin',(-0.299999999999999,-6.05857864376269,
-30.78)) ;
#151930 = CARTESIAN_POINT('Origin',(-0.3,-6.05857864376269,-30.78)) ;
#151931 = CARTESIAN_POINT('Origin',(-0.3,-0.600000000000001,-30.78)) ;
#151932 = CARTESIAN_POINT('Origin',(-0.3,-0.600000000000001,-30.78)) ;
#151933 = CARTESIAN_POINT('Origin',(0.6,-0.600000000000001,-30.78)) ;
#151934 = CARTESIAN_POINT('Origin',(0.6,-0.600000000000001,-30.18)) ;
#151935 = CARTESIAN_POINT('Origin',(-0.3,-0.600000000000001,-30.18)) ;
#151936 = CARTESIAN_POINT('Origin',(-0.3,-0.600000000000001,-30.18)) ;
#151937 = CARTESIAN_POINT('Origin',(-0.3,-6.05857864376269,-30.18)) ;
#151938 = CARTESIAN_POINT('Origin',(-0.3,-6.05857864376269,-30.18)) ;
#151939 = CARTESIAN_POINT('Origin',(-0.299999999999994,-6.0585786437627,-30.18)) ;
#151940 = CARTESIAN_POINT('Origin',(0.4,-6.0585786437627,-30.18)) ;
#151941 = CARTESIAN_POINT('Origin',(0.299999999999993,-6.0585786437627,-30.18)) ;
#151942 = CARTESIAN_POINT('Origin',(0.299999999999996,-6.0585786437627,-30.18)) ;
#151943 = CARTESIAN_POINT('Origin',(0.3,-6.05857864376269,-30.18)) ;
#151944 = CARTESIAN_POINT('Origin',(0.3,-0.600000000000001,-30.18)) ;
#151945 = CARTESIAN_POINT('Origin',(0.3,-0.6,-30.18)) ;
#151946 = CARTESIAN_POINT('Origin',(0.6,-0.6,-30.18)) ;
#151947 = CARTESIAN_POINT('Origin',(6.7,0.300000000000001,-30.78)) ;
#151948 = CARTESIAN_POINT('Origin',(6.65857864376269,0.300000000000001,-30.78)) ;
#151949 = CARTESIAN_POINT('Origin',(6.65857864376269,0.300000000000001,-30.78)) ;
#151950 = CARTESIAN_POINT('Origin',(6.65857864376269,0.299999999999997,-30.78)) ;
#151951 = CARTESIAN_POINT('Origin',(6.65857864376269,-0.399999999999999,-30.78)) ;
#151952 = CARTESIAN_POINT('Origin',(6.65857864376269,-0.299999999999997,-30.78)) ;
#151953 = CARTESIAN_POINT('Origin',(6.65857864376269,-0.3,-30.78)) ;
#151954 = CARTESIAN_POINT('Origin',(6.65857864376269,-0.300000000000001,-30.78)) ;
#151955 = CARTESIAN_POINT('Origin',(0.6,-0.3,-30.78)) ;
#151956 = CARTESIAN_POINT('Origin',(0.6,0.299999999999999,-30.18)) ;
#151957 = CARTESIAN_POINT('Origin',(6.65857864376269,0.300000000000001,-30.18)) ;
#151958 = CARTESIAN_POINT('Origin',(6.65857864376269,0.300000000000001,-30.18)) ;
#151959 = CARTESIAN_POINT('Origin',(6.6585786437627,0.299999999999995,-30.18)) ;
#151960 = CARTESIAN_POINT('Origin',(6.6585786437627,-0.399999999999999,-30.18)) ;
#151961 = CARTESIAN_POINT('Origin',(6.6585786437627,-0.299999999999994,-30.18)) ;
#151962 = CARTESIAN_POINT('Origin',(0.6,-0.3,-30.18)) ;
#151963 = CARTESIAN_POINT('Origin',(6.65857864376269,-0.300000000000001,-30.18)) ;
#151964 = CARTESIAN_POINT('Origin',(6.65857864376269,-0.299999999999998,-30.18)) ;
#151965 = CARTESIAN_POINT('Origin',(0.6,-0.6,-34.59)) ;
#151966 = CARTESIAN_POINT('Origin',(0.3,-0.6,-34.59)) ;
#151967 = CARTESIAN_POINT('Origin',(0.3,-6.1,-34.59)) ;
#151968 = CARTESIAN_POINT('Origin',(0.3,-6.05857864376269,-34.59)) ;
#151969 = CARTESIAN_POINT('Origin',(0.3,-6.05857864376269,-34.59)) ;
#151970 = CARTESIAN_POINT('Origin',(0.3,-6.05857864376269,-34.59)) ;
#151971 = CARTESIAN_POINT('Origin',(0.4,-6.05857864376269,-34.59)) ;
#151972 = CARTESIAN_POINT('Origin',(-0.299999999999998,-6.05857864376269,
-34.59)) ;
#151973 = CARTESIAN_POINT('Origin',(-0.299999999999994,-6.0585786437627,-34.59)) ;
#151974 = CARTESIAN_POINT('Origin',(-0.3,-6.05857864376269,-34.59)) ;
#151975 = CARTESIAN_POINT('Origin',(-0.3,-0.600000000000001,-34.59)) ;
#151976 = CARTESIAN_POINT('Origin',(-0.3,-0.600000000000001,-34.59)) ;
#151977 = CARTESIAN_POINT('Origin',(0.6,-0.600000000000001,-34.59)) ;
#151978 = CARTESIAN_POINT('Origin',(0.6,-0.600000000000001,-33.99)) ;
#151979 = CARTESIAN_POINT('Origin',(-0.3,-0.600000000000001,-33.99)) ;
#151980 = CARTESIAN_POINT('Origin',(-0.3,-0.600000000000001,-33.99)) ;
#151981 = CARTESIAN_POINT('Origin',(-0.3,-6.05857864376269,-33.99)) ;
#151982 = CARTESIAN_POINT('Origin',(-0.3,-6.05857864376269,-33.99)) ;
#151983 = CARTESIAN_POINT('Origin',(-0.300000000000007,-6.05857864376268,
-33.99)) ;
#151984 = CARTESIAN_POINT('Origin',(0.4,-6.05857864376269,-33.99)) ;
#151985 = CARTESIAN_POINT('Origin',(0.30000000000001,-6.05857864376268,-33.99)) ;
#151986 = CARTESIAN_POINT('Origin',(0.300000000000006,-6.05857864376268,-33.99)) ;
#151987 = CARTESIAN_POINT('Origin',(0.3,-6.05857864376269,-33.99)) ;
#151988 = CARTESIAN_POINT('Origin',(0.3,-0.600000000000001,-33.99)) ;
#151989 = CARTESIAN_POINT('Origin',(0.3,-0.6,-33.99)) ;
#151990 = CARTESIAN_POINT('Origin',(0.6,-0.6,-33.99)) ;
#151991 = CARTESIAN_POINT('Origin',(6.7,0.300000000000001,-34.59)) ;
#151992 = CARTESIAN_POINT('Origin',(6.65857864376269,0.300000000000001,-34.59)) ;
#151993 = CARTESIAN_POINT('Origin',(6.65857864376269,0.300000000000001,-34.59)) ;
#151994 = CARTESIAN_POINT('Origin',(6.65857864376269,0.300000000000001,-34.59)) ;
#151995 = CARTESIAN_POINT('Origin',(6.6585786437627,-0.399999999999999,-34.59)) ;
#151996 = CARTESIAN_POINT('Origin',(6.65857864376269,-0.300000000000002,-34.59)) ;
#151997 = CARTESIAN_POINT('Origin',(6.6585786437627,-0.299999999999996,-34.59)) ;
#151998 = CARTESIAN_POINT('Origin',(6.65857864376269,-0.300000000000001,-34.59)) ;
#151999 = CARTESIAN_POINT('Origin',(0.6,-0.3,-34.59)) ;
#152000 = CARTESIAN_POINT('Origin',(0.6,0.299999999999999,-33.99)) ;
#152001 = CARTESIAN_POINT('Origin',(6.65857864376269,0.300000000000001,-33.99)) ;
#152002 = CARTESIAN_POINT('Origin',(6.65857864376269,0.300000000000001,-33.99)) ;
#152003 = CARTESIAN_POINT('Origin',(6.65857864376269,0.300000000000005,-33.99)) ;
#152004 = CARTESIAN_POINT('Origin',(6.65857864376269,-0.399999999999999,-33.99)) ;
#152005 = CARTESIAN_POINT('Origin',(6.65857864376268,-0.300000000000006,-33.99)) ;
#152006 = CARTESIAN_POINT('Origin',(0.6,-0.3,-33.99)) ;
#152007 = CARTESIAN_POINT('Origin',(6.65857864376269,-0.300000000000001,-33.99)) ;
#152008 = CARTESIAN_POINT('Origin',(6.65857864376269,-0.300000000000001,-33.99)) ;
#152009 = CARTESIAN_POINT('',(0.,0.,0.)) ;
#152010 = CARTESIAN_POINT('Origin',(-3.91058726874632,3.70028042224035,-36.59)) ;
#152011 = CARTESIAN_POINT('',(-3.8208783653803,3.65609543998544,-36.49)) ;
#152012 = CARTESIAN_POINT('',(-3.90529363437316,3.80014021112017,-36.49)) ;
#152013 = CARTESIAN_POINT('Origin',(-3.91058726874632,3.70028042224035,-36.49)) ;
#152014 = CARTESIAN_POINT('',(-3.8208783653803,3.65609543998544,2.2)) ;
#152015 = CARTESIAN_POINT('',(-3.8208783653803,3.65609543998544,-36.49)) ;
#152016 = CARTESIAN_POINT('',(-3.90529363437316,3.80014021112017,2.2)) ;
#152017 = CARTESIAN_POINT('Origin',(-3.91058726874632,3.70028042224035,2.2)) ;
#152018 = CARTESIAN_POINT('',(-3.90529363437316,3.80014021112017,-36.59)) ;
#152019 = CARTESIAN_POINT('Origin',(1.77490703981927,4.45,1.4854875)) ;
#152020 = CARTESIAN_POINT('',(1.77490703981927,4.55,1.65)) ;
#152021 = CARTESIAN_POINT('',(1.6487489852016,4.55,1.37990100507126)) ;
#152022 = CARTESIAN_POINT('Origin',(1.77490703981927,4.55,1.4854875)) ;
#152023 = CARTESIAN_POINT('',(1.77490703981927,4.45,1.55)) ;
#152024 = CARTESIAN_POINT('Origin',(1.77490703981927,4.45,1.65)) ;
#152025 = CARTESIAN_POINT('',(1.72543498451331,4.45,1.4440824471676)) ;
#152026 = CARTESIAN_POINT('Origin',(1.77490703981927,4.45,1.4854875)) ;
#152027 = CARTESIAN_POINT('Origin',(1.6487489852016,4.45,1.37990100507126)) ;
#152028 = CARTESIAN_POINT('Origin',(1.3145125,4.45,-1.905)) ;
#152029 = CARTESIAN_POINT('',(1.22107868287598,4.55,-1.76959510912125)) ;
#152030 = CARTESIAN_POINT('',(1.22107868287598,4.55,-2.04040489087875)) ;
#152031 = CARTESIAN_POINT('Origin',(1.3145125,4.55,-1.905)) ;
#152032 = CARTESIAN_POINT('',(1.27787304021905,4.45,-1.85190185838271)) ;
#152033 = CARTESIAN_POINT('Origin',(1.22107868287598,4.45,-1.76959510912125)) ;
#152034 = CARTESIAN_POINT('',(1.27787304021905,4.45,-1.9580981416173)) ;
#152035 = CARTESIAN_POINT('Origin',(1.3145125,4.45,-1.905)) ;
#152036 = CARTESIAN_POINT('Origin',(1.22107868287598,4.45,-2.04040489087875)) ;
#152037 = CARTESIAN_POINT('Origin',(-8.21365282185989E-16,2.85,0.)) ;
#152038 = CARTESIAN_POINT('',(1.37603597336697,2.75,-1.905)) ;
#152039 = CARTESIAN_POINT('',(1.84932420089069,2.75,1.45)) ;
#152040 = CARTESIAN_POINT('Origin',(-8.13551212474381E-16,2.75,0.)) ;
#152041 = CARTESIAN_POINT('',(1.27787304021905,2.85,-1.85190185838271)) ;
#152042 = CARTESIAN_POINT('Ctrl Pts',(1.37603597336697,2.75,-1.905)) ;
#152043 = CARTESIAN_POINT('Ctrl Pts',(1.37543428354306,2.75,-1.90468005811351)) ;
#152044 = CARTESIAN_POINT('Ctrl Pts',(1.37483253111456,2.75000531372589,-1.90436018434118)) ;
#152045 = CARTESIAN_POINT('Ctrl Pts',(1.37388722675069,2.75002207412045,-1.903857355793)) ;
#152046 = CARTESIAN_POINT('Ctrl Pts',(1.37354350385561,2.75002991650282,-1.90367448583784)) ;
#152047 = CARTESIAN_POINT('Ctrl Pts',(1.37285611423782,2.75004911307826,-1.9033087011159)) ;
#152048 = CARTESIAN_POINT('Ctrl Pts',(1.37251244753524,2.75006046723047,-1.90312578638849)) ;
#152049 = CARTESIAN_POINT('Ctrl Pts',(1.3714815944481,2.75009981984526,-1.90257700530504)) ;
#152050 = CARTESIAN_POINT('Ctrl Pts',(1.37079455494331,2.75013310886333,-1.90221110179681)) ;
#152051 = CARTESIAN_POINT('Ctrl Pts',(1.36873453110893,2.75025430438115,-1.90111349441338)) ;
#152052 = CARTESIAN_POINT('Ctrl Pts',(1.36736263966052,2.75036354665963,-1.90038189075796)) ;
#152053 = CARTESIAN_POINT('Ctrl Pts',(1.36413470836879,2.75068903914081,-1.8986589310622)) ;
#152054 = CARTESIAN_POINT('Ctrl Pts',(1.36227932197148,2.75092980851021,-1.89766736227896)) ;
#152055 = CARTESIAN_POINT('Ctrl Pts',(1.35746012444743,2.75169859670379,-1.89508881807843)) ;
#152056 = CARTESIAN_POINT('Ctrl Pts',(1.35450425835489,2.7523133271765,-1.89350423745892)) ;
#152057 = CARTESIAN_POINT('Ctrl Pts',(1.34886973918565,2.75377034241463,-1.89047916949336)) ;
#152058 = CARTESIAN_POINT('Ctrl Pts',(1.34617831568151,2.75459534478003,-1.88903214074158)) ;
#152059 = CARTESIAN_POINT('Ctrl Pts',(1.34314242260183,2.75567798707048,-1.88739846987703)) ;
#152060 = CARTESIAN_POINT('Ctrl Pts',(1.34256163823226,2.75588931242806,-1.887085898215)) ;
#152061 = CARTESIAN_POINT('Ctrl Pts',(1.34198261999809,2.75610647364238,-1.8867742184185)) ;
#152062 = CARTESIAN_POINT('Ctrl Pts',(1.3413216052292,2.75635697290856,-1.88641837801666)) ;
#152063 = CARTESIAN_POINT('Ctrl Pts',(1.3408629143507,2.75653491456656,-1.88617141746806)) ;
#152064 = CARTESIAN_POINT('Ctrl Pts',(1.33918548989956,2.7572007950357,-1.88526816249943)) ;
#152065 = CARTESIAN_POINT('Ctrl Pts',(1.33797416370948,2.75771112313095,-1.88461565173485)) ;
#152066 = CARTESIAN_POINT('Ctrl Pts',(1.33648532079705,2.75837521508442,-1.88381336705108)) ;
#152067 = CARTESIAN_POINT('Ctrl Pts',(1.33619776328718,2.75850521488808,-1.88365840269789)) ;
#152068 = CARTESIAN_POINT('Ctrl Pts',(1.33107968015626,2.76084915994917,-1.88089996028831)) ;
#152069 = CARTESIAN_POINT('Ctrl Pts',(1.32635908659477,2.7635069333901,-1.8783519804515)) ;
#152070 = CARTESIAN_POINT('Ctrl Pts',(1.32109760626031,2.76707470328413,-1.87550528308814)) ;
#152071 = CARTESIAN_POINT('Ctrl Pts',(1.32035743991824,2.76759128788297,-1.87510464755506)) ;
#152072 = CARTESIAN_POINT('Ctrl Pts',(1.3182480554607,2.7691058422748,-1.87396233738911)) ;
#152073 = CARTESIAN_POINT('Ctrl Pts',(1.31689309423376,2.77013099976528,-1.87322773664117)) ;
#152074 = CARTESIAN_POINT('Ctrl Pts',(1.31545882361435,2.77127278201747,-1.87244887805927)) ;
#152075 = CARTESIAN_POINT('Ctrl Pts',(1.31535582310958,2.77135510350022,-1.87239293834655)) ;
#152076 = CARTESIAN_POINT('Ctrl Pts',(1.3150485309221,2.77160168095797,-1.87222602655303)) ;
#152077 = CARTESIAN_POINT('Ctrl Pts',(1.31461168315426,2.77195498754742,-1.87198869314584)) ;
#152078 = CARTESIAN_POINT('Ctrl Pts',(1.31417742224138,2.77231219724368,-1.87175266294293)) ;
#152079 = CARTESIAN_POINT('Ctrl Pts',(1.31333096026315,2.77301480846571,-1.87129249386306)) ;
#152080 = CARTESIAN_POINT('Ctrl Pts',(1.31272070342856,2.77353368974768,-1.87096054315942)) ;
#152081 = CARTESIAN_POINT('Ctrl Pts',(1.30969774837134,2.77616736630455,-1.86931544276183)) ;
#152082 = CARTESIAN_POINT('Ctrl Pts',(1.30737022788701,2.77840054644572,-1.86804652010492)) ;
#152083 = CARTESIAN_POINT('Ctrl Pts',(1.30464757270885,2.78128817542222,-1.86656129665113)) ;
#152084 = CARTESIAN_POINT('Ctrl Pts',(1.3041484598108,2.78182967606622,-1.86628898736925)) ;
#152085 = CARTESIAN_POINT('Ctrl Pts',(1.30260826844056,2.78353926416388,-1.86544857136307)) ;
#152086 = CARTESIAN_POINT('Ctrl Pts',(1.30158324720849,2.78473373830865,-1.86488876707862)) ;
#152087 = CARTESIAN_POINT('Ctrl Pts',(1.30024935135332,2.78636738852738,-1.86416018728324)) ;
#152088 = CARTESIAN_POINT('Ctrl Pts',(1.29991860867237,2.78677921519271,-1.86397952491896)) ;
#152089 = CARTESIAN_POINT('Ctrl Pts',(1.29915346420735,2.78774794465154,-1.8635615807717)) ;
#152090 = CARTESIAN_POINT('Ctrl Pts',(1.29872125904468,2.78830744810472,-1.86332550011269)) ;
#152091 = CARTESIAN_POINT('Ctrl Pts',(1.29658637826222,2.79113377451591,-1.8621594679259)) ;
#152092 = CARTESIAN_POINT('Ctrl Pts',(1.29496240940488,2.79348720429746,-1.86127301363021)) ;
#152093 = CARTESIAN_POINT('Ctrl Pts',(1.29231665668156,2.79769679694546,-1.85982835199505)) ;
#152094 = CARTESIAN_POINT('Ctrl Pts',(1.29125115601061,2.79951540543443,-1.8592459513193)) ;
#152095 = CARTESIAN_POINT('Ctrl Pts',(1.28927619853496,2.80313430045115,-1.85816512101871)) ;
#152096 = CARTESIAN_POINT('Ctrl Pts',(1.2883624199782,2.80493500363977,-1.85766462065405)) ;
#152097 = CARTESIAN_POINT('Ctrl Pts',(1.28732027925586,2.80715235940913,-1.8570931587537)) ;
#152098 = CARTESIAN_POINT('Ctrl Pts',(1.28695835013166,2.80793550920675,-1.85689461743542)) ;
#152099 = CARTESIAN_POINT('Ctrl Pts',(1.28660568774191,2.80872522382218,-1.85670104370722)) ;
#152100 = CARTESIAN_POINT('Ctrl Pts',(1.28608376699196,2.80991454434775,-1.85641450210149)) ;
#152101 = CARTESIAN_POINT('Ctrl Pts',(1.28574525149601,2.81071375754612,-1.85622856810943)) ;
#152102 = CARTESIAN_POINT('Ctrl Pts',(1.28475894023896,2.81312894312824,-1.85568673335099)) ;
#152103 = CARTESIAN_POINT('Ctrl Pts',(1.28414040309303,2.81476247656143,-1.85534683370203)) ;
#152104 = CARTESIAN_POINT('Ctrl Pts',(1.28339818260913,2.8168875602015,-1.854939111358)) ;
#152105 = CARTESIAN_POINT('Ctrl Pts',(1.28323661013043,2.81736137575529,-1.85485036282194)) ;
#152106 = CARTESIAN_POINT('Ctrl Pts',(1.2826566889388,2.81910411140435,-1.85453185264633)) ;
#152107 = CARTESIAN_POINT('Ctrl Pts',(1.28225920250333,2.82038205281187,-1.85431360767476)) ;
#152108 = CARTESIAN_POINT('Ctrl Pts',(1.28170385606936,2.82230051526768,-1.85400866501641)) ;
#152109 = CARTESIAN_POINT('Ctrl Pts',(1.28152700208472,2.82293438010912,-1.85391155822972)) ;
#152110 = CARTESIAN_POINT('Ctrl Pts',(1.28107448868731,2.82461913389174,-1.85366309085072)) ;
#152111 = CARTESIAN_POINT('Ctrl Pts',(1.28081016954773,2.82567198476339,-1.85351801104593)) ;
#152112 = CARTESIAN_POINT('Ctrl Pts',(1.28009910353321,2.82871092361135,-1.85312783198231)) ;
#152113 = CARTESIAN_POINT('Ctrl Pts',(1.27969380338795,2.83071459002995,-1.85290512911995)) ;
#152114 = CARTESIAN_POINT('Ctrl Pts',(1.27923282767964,2.83340629334539,-1.85265154626654)) ;
#152115 = CARTESIAN_POINT('Ctrl Pts',(1.27912420342282,2.83408089926113,-1.85259176478417)) ;
#152116 = CARTESIAN_POINT('Ctrl Pts',(1.27861441353188,2.83746106027949,-1.85231109118167)) ;
#152117 = CARTESIAN_POINT('Ctrl Pts',(1.2783132428757,2.84018799487022,-1.85214490175664)) ;
#152118 = CARTESIAN_POINT('Ctrl Pts',(1.27795656969993,2.84527977141542,-1.85194801334391)) ;
#152119 = CARTESIAN_POINT('Ctrl Pts',(1.27787304021905,2.8476428621108,-1.8519018583827)) ;
#152120 = CARTESIAN_POINT('Ctrl Pts',(1.27787304021905,2.85,-1.8519018583827)) ;
#152121 = CARTESIAN_POINT('',(1.72543498451331,2.85,1.4440824471676)) ;
#152122 = CARTESIAN_POINT('Origin',(-8.21365282185989E-16,2.85,0.)) ;
#152123 = CARTESIAN_POINT('Ctrl Pts',(1.84932420089069,2.75,1.45)) ;
#152124 = CARTESIAN_POINT('Ctrl Pts',(1.84863058979364,2.75,1.44997563735877)) ;
#152125 = CARTESIAN_POINT('Ctrl Pts',(1.84793752344315,2.75000415508919,1.44995131206652)) ;
#152126 = CARTESIAN_POINT('Ctrl Pts',(1.8466682790665,2.75001949937859,1.44990654329321)) ;
#152127 = CARTESIAN_POINT('Ctrl Pts',(1.84609162157503,2.75002939777795,1.44988606034608)) ;
#152128 = CARTESIAN_POINT('Ctrl Pts',(1.84477120566863,2.75005887738453,1.44983884278185)) ;
#152129 = CARTESIAN_POINT('Ctrl Pts',(1.84402746838178,2.7500804333137,1.44981204894611)) ;
#152130 = CARTESIAN_POINT('Ctrl Pts',(1.84209973630459,2.75014939605369,1.44974205847089)) ;
#152131 = CARTESIAN_POINT('Ctrl Pts',(1.84091590068203,2.75020455995514,1.44969854506027)) ;
#152132 = CARTESIAN_POINT('Ctrl Pts',(1.83783446245764,2.75038253459787,1.44958383066685)) ;
#152133 = CARTESIAN_POINT('Ctrl Pts',(1.83593755875625,2.75052613609568,1.4495117702051)) ;
#152134 = CARTESIAN_POINT('Ctrl Pts',(1.8309456297289,2.75099782379543,1.44931834596177)) ;
#152135 = CARTESIAN_POINT('Ctrl Pts',(1.82785402838571,2.7513859024504,1.44919458503464)) ;
#152136 = CARTESIAN_POINT('Ctrl Pts',(1.81948035994712,2.7527115862255,1.4488527720359)) ;
#152137 = CARTESIAN_POINT('Ctrl Pts',(1.81421215989036,2.75385085634789,1.44862821117908)) ;
#152138 = CARTESIAN_POINT('Ctrl Pts',(1.8031061499061,2.75695526843004,1.44814117174278)) ;
#152139 = CARTESIAN_POINT('Ctrl Pts',(1.79730846849538,2.75900870786305,1.44788414257244)) ;
#152140 = CARTESIAN_POINT('Ctrl Pts',(1.78961597328954,2.76232847656554,1.44753373419531)) ;
#152141 = CARTESIAN_POINT('Ctrl Pts',(1.7875531568042,2.76328057020225,1.44743866638175)) ;
#152142 = CARTESIAN_POINT('Ctrl Pts',(1.78290815273718,2.76556355836601,1.44722066393822)) ;
#152143 = CARTESIAN_POINT('Ctrl Pts',(1.78033073359788,2.76693246555895,1.44709649577908)) ;
#152144 = CARTESIAN_POINT('Ctrl Pts',(1.77699233515397,2.76883988197513,1.44693042742489)) ;
#152145 = CARTESIAN_POINT('Ctrl Pts',(1.77620130341379,2.76930169056972,1.4468906872056)) ;
#152146 = CARTESIAN_POINT('Ctrl Pts',(1.7700212686611,2.77299328866811,1.44657696433726)) ;
#152147 = CARTESIAN_POINT('Ctrl Pts',(1.76495428804002,2.77651771769392,1.44630647059977)) ;
#152148 = CARTESIAN_POINT('Ctrl Pts',(1.75938438664977,2.78118533571325,1.4460042033466)) ;
#152149 = CARTESIAN_POINT('Ctrl Pts',(1.75866155314252,2.78180749701142,1.44596487872825)) ;
#152150 = CARTESIAN_POINT('Ctrl Pts',(1.75440101126574,2.7855766156533,1.44573272620675)) ;
#152151 = CARTESIAN_POINT('Ctrl Pts',(1.75110534239503,2.78891118859354,1.44556220259829)) ;
#152152 = CARTESIAN_POINT('Ctrl Pts',(1.74704475763671,2.79358254909136,1.44534353205998)) ;
#152153 = CARTESIAN_POINT('Ctrl Pts',(1.74604050383924,2.79479094319554,1.44528857933487)) ;
#152154 = CARTESIAN_POINT('Ctrl Pts',(1.74487333929765,2.79625803001555,1.44522266035845)) ;
#152155 = CARTESIAN_POINT('Ctrl Pts',(1.74467927949937,2.79650417922903,1.44521163325506)) ;
#152156 = CARTESIAN_POINT('Ctrl Pts',(1.74115657836476,2.80101412428662,1.44501009724943)) ;
#152157 = CARTESIAN_POINT('Ctrl Pts',(1.73808736282551,2.80561663574426,1.44483055636364)) ;
#152158 = CARTESIAN_POINT('Ctrl Pts',(1.73411503311364,2.81315073291951,1.44459732117177)) ;
#152159 = CARTESIAN_POINT('Ctrl Pts',(1.73300100590538,2.81551882664672,1.444535439772)) ;
#152160 = CARTESIAN_POINT('Ctrl Pts',(1.73189652742022,2.8181493620667,1.44447069895227)) ;
#152161 = CARTESIAN_POINT('Ctrl Pts',(1.73180208385959,2.81837683840677,1.44446516169542)) ;
#152162 = CARTESIAN_POINT('Ctrl Pts',(1.73016675860464,2.82236036724297,1.44436925395154)) ;
#152163 = CARTESIAN_POINT('Ctrl Pts',(1.72888947962583,2.82624394235942,1.44429466669055)) ;
#152164 = CARTESIAN_POINT('Ctrl Pts',(1.72770663337626,2.83096681005806,1.4442247776102)) ;
#152165 = CARTESIAN_POINT('Ctrl Pts',(1.72752382530083,2.83174344980706,1.44421394009748)) ;
#152166 = CARTESIAN_POINT('Ctrl Pts',(1.7271933356899,2.83324353771473,1.44419425207312)) ;
#152167 = CARTESIAN_POINT('Ctrl Pts',(1.72704413780188,2.83396640281164,1.44418527971536)) ;
#152168 = CARTESIAN_POINT('Ctrl Pts',(1.7260250143745,2.83926193720951,1.44412308045111)) ;
#152169 = CARTESIAN_POINT('Ctrl Pts',(1.72552996843222,2.84393088107443,1.44408905620284)) ;
#152170 = CARTESIAN_POINT('Ctrl Pts',(1.72543914472539,2.84906100604569,1.44408273999325)) ;
#152171 = CARTESIAN_POINT('Ctrl Pts',(1.72543498451331,2.84953057829521,1.4440824471676)) ;
#152172 = CARTESIAN_POINT('Ctrl Pts',(1.72543498451331,2.85,1.4440824471676)) ;
#152173 = CARTESIAN_POINT('Origin',(1.3145125,4.45,-5.715)) ;
#152174 = CARTESIAN_POINT('',(1.22107868287598,4.55,-5.57959510912125)) ;
#152175 = CARTESIAN_POINT('',(1.22107868287598,4.55,-5.85040489087875)) ;
#152176 = CARTESIAN_POINT('Origin',(1.3145125,4.55,-5.715)) ;
#152177 = CARTESIAN_POINT('',(1.27787304021905,4.45,-5.66190185838271)) ;
#152178 = CARTESIAN_POINT('Origin',(1.22107868287598,4.45,-5.57959510912125)) ;
#152179 = CARTESIAN_POINT('',(1.27787304021905,4.45,-5.76809814161729)) ;
#152180 = CARTESIAN_POINT('Origin',(1.3145125,4.45,-5.715)) ;
#152181 = CARTESIAN_POINT('Origin',(1.22107868287598,4.45,-5.85040489087875)) ;
#152182 = CARTESIAN_POINT('Origin',(-8.21365282185989E-16,2.85,-3.81)) ;
#152183 = CARTESIAN_POINT('',(1.37603597336697,2.75,-5.715)) ;
#152184 = CARTESIAN_POINT('Origin',(-8.13551212474381E-16,2.75,-3.81)) ;
#152185 = CARTESIAN_POINT('',(1.27787304021905,2.85,-5.66190185838271)) ;
#152186 = CARTESIAN_POINT('Ctrl Pts',(1.37603597336697,2.75,-5.715)) ;
#152187 = CARTESIAN_POINT('Ctrl Pts',(1.37543428354307,2.75,-5.71468005811352)) ;
#152188 = CARTESIAN_POINT('Ctrl Pts',(1.37483253111456,2.7500053137259,-5.71436018434118)) ;
#152189 = CARTESIAN_POINT('Ctrl Pts',(1.37388722675069,2.75002207412044,-5.713857355793)) ;
#152190 = CARTESIAN_POINT('Ctrl Pts',(1.37354350385561,2.75002991650282,-5.71367448583784)) ;
#152191 = CARTESIAN_POINT('Ctrl Pts',(1.37285611423782,2.75004911307826,-5.71330870111591)) ;
#152192 = CARTESIAN_POINT('Ctrl Pts',(1.37251244753524,2.75006046723047,-5.71312578638849)) ;
#152193 = CARTESIAN_POINT('Ctrl Pts',(1.3714815944481,2.75009981984526,-5.71257700530505)) ;
#152194 = CARTESIAN_POINT('Ctrl Pts',(1.37079455494331,2.75013310886333,-5.71221110179682)) ;
#152195 = CARTESIAN_POINT('Ctrl Pts',(1.36873453110892,2.75025430438116,-5.71111349441339)) ;
#152196 = CARTESIAN_POINT('Ctrl Pts',(1.36736263966051,2.75036354665963,-5.71038189075797)) ;
#152197 = CARTESIAN_POINT('Ctrl Pts',(1.36413470836879,2.75068903914081,-5.7086589310622)) ;
#152198 = CARTESIAN_POINT('Ctrl Pts',(1.36227932197148,2.75092980851022,-5.70766736227896)) ;
#152199 = CARTESIAN_POINT('Ctrl Pts',(1.35746012444743,2.7516985967038,-5.70508881807843)) ;
#152200 = CARTESIAN_POINT('Ctrl Pts',(1.35450425835489,2.75231332717651,-5.70350423745893)) ;
#152201 = CARTESIAN_POINT('Ctrl Pts',(1.34886973918565,2.75377034241464,-5.70047916949337)) ;
#152202 = CARTESIAN_POINT('Ctrl Pts',(1.34617831568151,2.75459534478003,-5.69903214074159)) ;
#152203 = CARTESIAN_POINT('Ctrl Pts',(1.34314242260183,2.75567798707049,-5.69739846987704)) ;
#152204 = CARTESIAN_POINT('Ctrl Pts',(1.34256163823226,2.75588931242806,-5.697085898215)) ;
#152205 = CARTESIAN_POINT('Ctrl Pts',(1.34198261999809,2.75610647364238,-5.69677421841851)) ;
#152206 = CARTESIAN_POINT('Ctrl Pts',(1.3413216052292,2.75635697290857,-5.69641837801666)) ;
#152207 = CARTESIAN_POINT('Ctrl Pts',(1.3408629143507,2.75653491456656,-5.69617141746806)) ;
#152208 = CARTESIAN_POINT('Ctrl Pts',(1.33918548989956,2.7572007950357,-5.69526816249943)) ;
#152209 = CARTESIAN_POINT('Ctrl Pts',(1.33797416370948,2.75771112313095,-5.69461565173486)) ;
#152210 = CARTESIAN_POINT('Ctrl Pts',(1.33648532079705,2.75837521508442,-5.69381336705109)) ;
#152211 = CARTESIAN_POINT('Ctrl Pts',(1.33619776328718,2.75850521488809,-5.69365840269788)) ;
#152212 = CARTESIAN_POINT('Ctrl Pts',(1.33107968015654,2.76084915994904,-5.69089996028846)) ;
#152213 = CARTESIAN_POINT('Ctrl Pts',(1.32635908659532,2.76350693338979,-5.68835198045179)) ;
#152214 = CARTESIAN_POINT('Ctrl Pts',(1.32109760626083,2.76707470328377,-5.68550528308842)) ;
#152215 = CARTESIAN_POINT('Ctrl Pts',(1.32035743991849,2.76759128788279,-5.68510464755519)) ;
#152216 = CARTESIAN_POINT('Ctrl Pts',(1.31824805546069,2.7691058422748,-5.6839623373891)) ;
#152217 = CARTESIAN_POINT('Ctrl Pts',(1.31689309423376,2.77013099976529,-5.68322773664116)) ;
#152218 = CARTESIAN_POINT('Ctrl Pts',(1.31545882361434,2.77127278201747,-5.68244887805927)) ;
#152219 = CARTESIAN_POINT('Ctrl Pts',(1.31535582310956,2.77135510350023,-5.68239293834654)) ;
#152220 = CARTESIAN_POINT('Ctrl Pts',(1.31504853092208,2.77160168095798,-5.68222602655302)) ;
#152221 = CARTESIAN_POINT('Ctrl Pts',(1.31461168315424,2.77195498754745,-5.68198869314584)) ;
#152222 = CARTESIAN_POINT('Ctrl Pts',(1.31417742224136,2.77231219724369,-5.68175266294292)) ;
#152223 = CARTESIAN_POINT('Ctrl Pts',(1.31333096026313,2.77301480846573,-5.68129249386305)) ;
#152224 = CARTESIAN_POINT('Ctrl Pts',(1.31272070342853,2.7735336897477,-5.68096054315941)) ;
#152225 = CARTESIAN_POINT('Ctrl Pts',(1.30969774837131,2.77616736630457,-5.67931544276182)) ;
#152226 = CARTESIAN_POINT('Ctrl Pts',(1.30737022788698,2.77840054644575,-5.67804652010491)) ;
#152227 = CARTESIAN_POINT('Ctrl Pts',(1.30464757270883,2.78128817542224,-5.67656129665112)) ;
#152228 = CARTESIAN_POINT('Ctrl Pts',(1.30414845981079,2.78182967606623,-5.67628898736924)) ;
#152229 = CARTESIAN_POINT('Ctrl Pts',(1.30260826844056,2.78353926416388,-5.67544857136307)) ;
#152230 = CARTESIAN_POINT('Ctrl Pts',(1.30158324720849,2.78473373830865,-5.67488876707862)) ;
#152231 = CARTESIAN_POINT('Ctrl Pts',(1.30024935135332,2.78636738852738,-5.67416018728324)) ;
#152232 = CARTESIAN_POINT('Ctrl Pts',(1.29991860867237,2.78677921519272,-5.67397952491896)) ;
#152233 = CARTESIAN_POINT('Ctrl Pts',(1.29915346420734,2.78774794465155,-5.67356158077169)) ;
#152234 = CARTESIAN_POINT('Ctrl Pts',(1.29872125904468,2.78830744810472,-5.67332550011269)) ;
#152235 = CARTESIAN_POINT('Ctrl Pts',(1.29658637826221,2.79113377451592,-5.6721594679259)) ;
#152236 = CARTESIAN_POINT('Ctrl Pts',(1.29496240940487,2.79348720429747,-5.67127301363021)) ;
#152237 = CARTESIAN_POINT('Ctrl Pts',(1.29231665668155,2.79769679694548,-5.66982835199504)) ;
#152238 = CARTESIAN_POINT('Ctrl Pts',(1.29125115601061,2.79951540543445,-5.6692459513193)) ;
#152239 = CARTESIAN_POINT('Ctrl Pts',(1.28927619853496,2.80313430045116,-5.66816512101871)) ;
#152240 = CARTESIAN_POINT('Ctrl Pts',(1.2883624199782,2.80493500363978,-5.66766462065405)) ;
#152241 = CARTESIAN_POINT('Ctrl Pts',(1.28732027925586,2.80715235940914,-5.6670931587537)) ;
#152242 = CARTESIAN_POINT('Ctrl Pts',(1.28695835013166,2.80793550920674,-5.66689461743542)) ;
#152243 = CARTESIAN_POINT('Ctrl Pts',(1.28660568774191,2.80872522382218,-5.66670104370723)) ;
#152244 = CARTESIAN_POINT('Ctrl Pts',(1.28608376699196,2.80991454434776,-5.6664145021015)) ;
#152245 = CARTESIAN_POINT('Ctrl Pts',(1.28574525149601,2.81071375754612,-5.66622856810943)) ;
#152246 = CARTESIAN_POINT('Ctrl Pts',(1.28475894023895,2.81312894312825,-5.66568673335099)) ;
#152247 = CARTESIAN_POINT('Ctrl Pts',(1.28414040309303,2.81476247656144,-5.66534683370204)) ;
#152248 = CARTESIAN_POINT('Ctrl Pts',(1.28339818260912,2.81688756020151,-5.664939111358)) ;
#152249 = CARTESIAN_POINT('Ctrl Pts',(1.28323661013043,2.8173613757553,-5.66485036282194)) ;
#152250 = CARTESIAN_POINT('Ctrl Pts',(1.28265668893879,2.81910411140437,-5.66453185264632)) ;
#152251 = CARTESIAN_POINT('Ctrl Pts',(1.28225920250332,2.82038205281189,-5.66431360767476)) ;
#152252 = CARTESIAN_POINT('Ctrl Pts',(1.28170385606936,2.8223005152677,-5.66400866501641)) ;
#152253 = CARTESIAN_POINT('Ctrl Pts',(1.28152700208472,2.82293438010912,-5.66391155822972)) ;
#152254 = CARTESIAN_POINT('Ctrl Pts',(1.28107448868731,2.82461913389174,-5.66366309085072)) ;
#152255 = CARTESIAN_POINT('Ctrl Pts',(1.28081016954773,2.82567198476339,-5.66351801104592)) ;
#152256 = CARTESIAN_POINT('Ctrl Pts',(1.28009910353321,2.82871092361135,-5.6631278319823)) ;
#152257 = CARTESIAN_POINT('Ctrl Pts',(1.27969380338794,2.83071459002995,-5.66290512911995)) ;
#152258 = CARTESIAN_POINT('Ctrl Pts',(1.27923282767964,2.83340629334539,-5.66265154626654)) ;
#152259 = CARTESIAN_POINT('Ctrl Pts',(1.27912420342282,2.83408089926113,-5.66259176478417)) ;
#152260 = CARTESIAN_POINT('Ctrl Pts',(1.27861441353188,2.8374610602795,-5.66231109118167)) ;
#152261 = CARTESIAN_POINT('Ctrl Pts',(1.2783132428757,2.84018799487024,-5.66214490175664)) ;
#152262 = CARTESIAN_POINT('Ctrl Pts',(1.27795656969993,2.84527977141544,-5.66194801334391)) ;
#152263 = CARTESIAN_POINT('Ctrl Pts',(1.27787304021905,2.8476428621108,-5.6619018583827)) ;
#152264 = CARTESIAN_POINT('Ctrl Pts',(1.27787304021905,2.85,-5.6619018583827)) ;
#152265 = CARTESIAN_POINT('',(1.27787304021905,2.85,-1.9580981416173)) ;
#152266 = CARTESIAN_POINT('Origin',(-8.21365282185989E-16,2.85,-3.81)) ;
#152267 = CARTESIAN_POINT('Ctrl Pts',(1.37603597336697,2.75,-1.905)) ;
#152268 = CARTESIAN_POINT('Ctrl Pts',(1.37573512845501,2.75,-1.90515997094324)) ;
#152269 = CARTESIAN_POINT('Ctrl Pts',(1.37543426791745,2.75000132857104,-1.90531992480456)) ;
#152270 = CARTESIAN_POINT('Ctrl Pts',(1.37483257571475,2.75000665190009,-1.90563984485733)) ;
#152271 = CARTESIAN_POINT('Ctrl Pts',(1.37453174406034,2.75001064672751,-1.90579981102493)) ;
#152272 = CARTESIAN_POINT('Ctrl Pts',(1.37388722675069,2.75002207412045,-1.90614264420702)) ;
#152273 = CARTESIAN_POINT('Ctrl Pts',(1.37354350385561,2.75002991650282,-1.90632551416212)) ;
#152274 = CARTESIAN_POINT('Ctrl Pts',(1.37285611423782,2.75004911307826,-1.9066912988841)) ;
#152275 = CARTESIAN_POINT('Ctrl Pts',(1.37251244753524,2.75006046723047,-1.90687421361152)) ;
#152276 = CARTESIAN_POINT('Ctrl Pts',(1.3714815944481,2.75009981984526,-1.90742299469496)) ;
#152277 = CARTESIAN_POINT('Ctrl Pts',(1.37079455494331,2.75013310886333,-1.90778889820319)) ;
#152278 = CARTESIAN_POINT('Ctrl Pts',(1.36873453110892,2.75025430438115,-1.90888650558662)) ;
#152279 = CARTESIAN_POINT('Ctrl Pts',(1.36736263966051,2.75036354665963,-1.90961810924204)) ;
#152280 = CARTESIAN_POINT('Ctrl Pts',(1.36413470836879,2.75068903914081,-1.91134106893781)) ;
#152281 = CARTESIAN_POINT('Ctrl Pts',(1.36227932197148,2.75092980851022,-1.91233263772104)) ;
#152282 = CARTESIAN_POINT('Ctrl Pts',(1.35746012444743,2.7516985967038,-1.91491118192158)) ;
#152283 = CARTESIAN_POINT('Ctrl Pts',(1.35450425835489,2.75231332717651,-1.91649576254108)) ;
#152284 = CARTESIAN_POINT('Ctrl Pts',(1.34886973918565,2.75377034241464,-1.91952083050664)) ;
#152285 = CARTESIAN_POINT('Ctrl Pts',(1.34617831568151,2.75459534478003,-1.92096785925842)) ;
#152286 = CARTESIAN_POINT('Ctrl Pts',(1.34314242260183,2.75567798707048,-1.92260153012297)) ;
#152287 = CARTESIAN_POINT('Ctrl Pts',(1.34256163823226,2.75588931242806,-1.922914101785)) ;
#152288 = CARTESIAN_POINT('Ctrl Pts',(1.34198261999809,2.75610647364238,-1.9232257815815)) ;
#152289 = CARTESIAN_POINT('Ctrl Pts',(1.3413216052292,2.75635697290856,-1.92358162198335)) ;
#152290 = CARTESIAN_POINT('Ctrl Pts',(1.3408629143507,2.75653491456656,-1.92382858253194)) ;
#152291 = CARTESIAN_POINT('Ctrl Pts',(1.33918548989955,2.7572007950357,-1.92473183750057)) ;
#152292 = CARTESIAN_POINT('Ctrl Pts',(1.33797416370948,2.75771112313095,-1.92538434826515)) ;
#152293 = CARTESIAN_POINT('Ctrl Pts',(1.33648532079705,2.75837521508442,-1.92618663294892)) ;
#152294 = CARTESIAN_POINT('Ctrl Pts',(1.33619776328718,2.75850521488809,-1.92634159730212)) ;
#152295 = CARTESIAN_POINT('Ctrl Pts',(1.3310796801563,2.76084915994915,-1.92910003971167)) ;
#152296 = CARTESIAN_POINT('Ctrl Pts',(1.32635908659486,2.76350693339004,-1.93164801954846)) ;
#152297 = CARTESIAN_POINT('Ctrl Pts',(1.32109760626039,2.76707470328407,-1.93449471691182)) ;
#152298 = CARTESIAN_POINT('Ctrl Pts',(1.32035743991827,2.76759128788294,-1.93489535244492)) ;
#152299 = CARTESIAN_POINT('Ctrl Pts',(1.3182480554607,2.76910584227479,-1.93603766261089)) ;
#152300 = CARTESIAN_POINT('Ctrl Pts',(1.31689309423376,2.77013099976528,-1.93677226335883)) ;
#152301 = CARTESIAN_POINT('Ctrl Pts',(1.31545882361434,2.77127278201747,-1.93755112194073)) ;
#152302 = CARTESIAN_POINT('Ctrl Pts',(1.31535582310957,2.77135510350021,-1.93760706165345)) ;
#152303 = CARTESIAN_POINT('Ctrl Pts',(1.31504853092209,2.77160168095797,-1.93777397344698)) ;
#152304 = CARTESIAN_POINT('Ctrl Pts',(1.31461168315425,2.77195498754744,-1.93801130685414)) ;
#152305 = CARTESIAN_POINT('Ctrl Pts',(1.31417742224137,2.77231219724368,-1.93824733705707)) ;
#152306 = CARTESIAN_POINT('Ctrl Pts',(1.31333096026314,2.77301480846571,-1.93870750613694)) ;
#152307 = CARTESIAN_POINT('Ctrl Pts',(1.31272070342855,2.77353368974768,-1.93903945684058)) ;
#152308 = CARTESIAN_POINT('Ctrl Pts',(1.30969774837133,2.77616736630456,-1.94068455723817)) ;
#152309 = CARTESIAN_POINT('Ctrl Pts',(1.307370227887,2.77840054644573,-1.94195347989508)) ;
#152310 = CARTESIAN_POINT('Ctrl Pts',(1.30464757270885,2.78128817542222,-1.94343870334887)) ;
#152311 = CARTESIAN_POINT('Ctrl Pts',(1.30414845981079,2.78182967606621,-1.94371101263075)) ;
#152312 = CARTESIAN_POINT('Ctrl Pts',(1.30260826844056,2.78353926416388,-1.94455142863693)) ;
#152313 = CARTESIAN_POINT('Ctrl Pts',(1.30158324720849,2.78473373830865,-1.94511123292138)) ;
#152314 = CARTESIAN_POINT('Ctrl Pts',(1.30024935135332,2.78636738852738,-1.94583981271676)) ;
#152315 = CARTESIAN_POINT('Ctrl Pts',(1.29991860867237,2.78677921519272,-1.94602047508104)) ;
#152316 = CARTESIAN_POINT('Ctrl Pts',(1.29915346420735,2.78774794465154,-1.94643841922831)) ;
#152317 = CARTESIAN_POINT('Ctrl Pts',(1.29872125904468,2.78830744810472,-1.94667449988731)) ;
#152318 = CARTESIAN_POINT('Ctrl Pts',(1.29658637826222,2.79113377451592,-1.9478405320741)) ;
#152319 = CARTESIAN_POINT('Ctrl Pts',(1.29496240940488,2.79348720429747,-1.94872698636979)) ;
#152320 = CARTESIAN_POINT('Ctrl Pts',(1.29231665668155,2.79769679694547,-1.95017164800495)) ;
#152321 = CARTESIAN_POINT('Ctrl Pts',(1.29125115601061,2.79951540543444,-1.95075404868069)) ;
#152322 = CARTESIAN_POINT('Ctrl Pts',(1.28927619853496,2.80313430045115,-1.95183487898129)) ;
#152323 = CARTESIAN_POINT('Ctrl Pts',(1.2883624199782,2.80493500363977,-1.95233537934595)) ;
#152324 = CARTESIAN_POINT('Ctrl Pts',(1.28732027925586,2.80715235940913,-1.9529068412463)) ;
#152325 = CARTESIAN_POINT('Ctrl Pts',(1.28695835013166,2.80793550920675,-1.95310538256458)) ;
#152326 = CARTESIAN_POINT('Ctrl Pts',(1.28660568774191,2.80872522382218,-1.95329895629277)) ;
#152327 = CARTESIAN_POINT('Ctrl Pts',(1.28608376699196,2.80991454434775,-1.95358549789851)) ;
#152328 = CARTESIAN_POINT('Ctrl Pts',(1.28574525149601,2.81071375754612,-1.95377143189057)) ;
#152329 = CARTESIAN_POINT('Ctrl Pts',(1.28475894023896,2.81312894312824,-1.95431326664901)) ;
#152330 = CARTESIAN_POINT('Ctrl Pts',(1.28414040309303,2.81476247656143,-1.95465316629796)) ;
#152331 = CARTESIAN_POINT('Ctrl Pts',(1.28339818260913,2.8168875602015,-1.955060888642)) ;
#152332 = CARTESIAN_POINT('Ctrl Pts',(1.28323661013043,2.81736137575529,-1.95514963717806)) ;
#152333 = CARTESIAN_POINT('Ctrl Pts',(1.2826566889388,2.81910411140435,-1.95546814735368)) ;
#152334 = CARTESIAN_POINT('Ctrl Pts',(1.28225920250333,2.82038205281187,-1.95568639232524)) ;
#152335 = CARTESIAN_POINT('Ctrl Pts',(1.28170385606936,2.82230051526768,-1.95599133498359)) ;
#152336 = CARTESIAN_POINT('Ctrl Pts',(1.28152700208472,2.82293438010912,-1.95608844177028)) ;
#152337 = CARTESIAN_POINT('Ctrl Pts',(1.28107448868731,2.82461913389174,-1.95633690914928)) ;
#152338 = CARTESIAN_POINT('Ctrl Pts',(1.28081016954773,2.82567198476339,-1.95648198895408)) ;
#152339 = CARTESIAN_POINT('Ctrl Pts',(1.28009910353321,2.82871092361134,-1.95687216801769)) ;
#152340 = CARTESIAN_POINT('Ctrl Pts',(1.27969380338795,2.83071459002995,-1.95709487088005)) ;
#152341 = CARTESIAN_POINT('Ctrl Pts',(1.27923282767965,2.83340629334537,-1.95734845373346)) ;
#152342 = CARTESIAN_POINT('Ctrl Pts',(1.27912420342282,2.83408089926112,-1.95740823521583)) ;
#152343 = CARTESIAN_POINT('Ctrl Pts',(1.27861441353188,2.83746106027947,-1.95768890881833)) ;
#152344 = CARTESIAN_POINT('Ctrl Pts',(1.2783132428757,2.8401879948702,-1.95785509824336)) ;
#152345 = CARTESIAN_POINT('Ctrl Pts',(1.27795656969993,2.8452797714154,-1.95805198665609)) ;
#152346 = CARTESIAN_POINT('Ctrl Pts',(1.27787304021905,2.84764286211078,-1.9580981416173)) ;
#152347 = CARTESIAN_POINT('Ctrl Pts',(1.27787304021905,2.85,-1.9580981416173)) ;
#152348 = CARTESIAN_POINT('Origin',(1.3145125,4.45,-9.525)) ;
#152349 = CARTESIAN_POINT('',(1.22107868287598,4.55,-9.38959510912125)) ;
#152350 = CARTESIAN_POINT('',(1.22107868287598,4.55,-9.66040489087875)) ;
#152351 = CARTESIAN_POINT('Origin',(1.3145125,4.55,-9.525)) ;
#152352 = CARTESIAN_POINT('',(1.27787304021905,4.45,-9.4719018583827)) ;
#152353 = CARTESIAN_POINT('Origin',(1.22107868287598,4.45,-9.38959510912125)) ;
#152354 = CARTESIAN_POINT('',(1.27787304021905,4.45,-9.57809814161729)) ;
#152355 = CARTESIAN_POINT('Origin',(1.3145125,4.45,-9.525)) ;
#152356 = CARTESIAN_POINT('Origin',(1.22107868287598,4.45,-9.66040489087875)) ;
#152357 = CARTESIAN_POINT('Origin',(-8.21365282185989E-16,2.85,-7.62)) ;
#152358 = CARTESIAN_POINT('',(1.37603597336697,2.75,-9.525)) ;
#152359 = CARTESIAN_POINT('Origin',(-8.13551212474381E-16,2.75,-7.62)) ;
#152360 = CARTESIAN_POINT('',(1.27787304021905,2.85,-9.4719018583827)) ;
#152361 = CARTESIAN_POINT('Ctrl Pts',(1.37603597336697,2.75,-9.525)) ;
#152362 = CARTESIAN_POINT('Ctrl Pts',(1.37599182636237,2.75000002234121,-9.52497652572716)) ;
#152363 = CARTESIAN_POINT('Ctrl Pts',(1.37594767935777,2.75000004468243,-9.52495305145431)) ;
#152364 = CARTESIAN_POINT('Ctrl Pts',(1.3756975209442,2.75000017127862,-9.52482003479991)) ;
#152365 = CARTESIAN_POINT('Ctrl Pts',(1.37511460540165,2.75000290680017,-9.52451012344317)) ;
#152366 = CARTESIAN_POINT('Ctrl Pts',(1.37453174406036,2.75001064672751,-9.52420018897501)) ;
#152367 = CARTESIAN_POINT('Ctrl Pts',(1.3738872267507,2.75002207412045,-9.52385735579295)) ;
#152368 = CARTESIAN_POINT('Ctrl Pts',(1.37354350385558,2.75002991650282,-9.52367448583783)) ;
#152369 = CARTESIAN_POINT('Ctrl Pts',(1.37285611423782,2.75004911307825,-9.52330870111588)) ;
#152370 = CARTESIAN_POINT('Ctrl Pts',(1.37251244753524,2.75006046723047,-9.52312578638847)) ;
#152371 = CARTESIAN_POINT('Ctrl Pts',(1.37148159444809,2.75009981984525,-9.52257700530504)) ;
#152372 = CARTESIAN_POINT('Ctrl Pts',(1.37079455494331,2.75013310886332,-9.52221110179681)) ;
#152373 = CARTESIAN_POINT('Ctrl Pts',(1.36873453110892,2.75025430438115,-9.52111349441339)) ;
#152374 = CARTESIAN_POINT('Ctrl Pts',(1.36736263966052,2.75036354665962,-9.52038189075796)) ;
#152375 = CARTESIAN_POINT('Ctrl Pts',(1.36413470836879,2.7506890391408,-9.51865893106218)) ;
#152376 = CARTESIAN_POINT('Ctrl Pts',(1.36227932197148,2.7509298085102,-9.51766736227895)) ;
#152377 = CARTESIAN_POINT('Ctrl Pts',(1.35746012444742,2.75169859670377,-9.51508881807842)) ;
#152378 = CARTESIAN_POINT('Ctrl Pts',(1.35450425835489,2.75231332717647,-9.51350423745891)) ;
#152379 = CARTESIAN_POINT('Ctrl Pts',(1.34886973918564,2.7537703424146,-9.51047916949335)) ;
#152380 = CARTESIAN_POINT('Ctrl Pts',(1.3461783156815,2.75459534477999,-9.50903214074156)) ;
#152381 = CARTESIAN_POINT('Ctrl Pts',(1.34314242260182,2.75567798707045,-9.50739846987701)) ;
#152382 = CARTESIAN_POINT('Ctrl Pts',(1.34256163823225,2.75588931242802,-9.50708589821498)) ;
#152383 = CARTESIAN_POINT('Ctrl Pts',(1.34198261999809,2.75610647364234,-9.50677421841848)) ;
#152384 = CARTESIAN_POINT('Ctrl Pts',(1.34132160522919,2.75635697290853,-9.50641837801664)) ;
#152385 = CARTESIAN_POINT('Ctrl Pts',(1.34086291435069,2.75653491456652,-9.50617141746804)) ;
#152386 = CARTESIAN_POINT('Ctrl Pts',(1.33918548989955,2.75720079503567,-9.50526816249941)) ;
#152387 = CARTESIAN_POINT('Ctrl Pts',(1.33797416370947,2.75771112313092,-9.50461565173483)) ;
#152388 = CARTESIAN_POINT('Ctrl Pts',(1.33648532079704,2.75837521508439,-9.50381336705106)) ;
#152389 = CARTESIAN_POINT('Ctrl Pts',(1.33619776328717,2.75850521488806,-9.50365840269787)) ;
#152390 = CARTESIAN_POINT('Ctrl Pts',(1.33107968015649,2.76084915994903,-9.50089996028843)) ;
#152391 = CARTESIAN_POINT('Ctrl Pts',(1.32635908659524,2.76350693338982,-9.49835198045175)) ;
#152392 = CARTESIAN_POINT('Ctrl Pts',(1.32109760626075,2.76707470328381,-9.49550528308838)) ;
#152393 = CARTESIAN_POINT('Ctrl Pts',(1.32035743991845,2.76759128788282,-9.49510464755518)) ;
#152394 = CARTESIAN_POINT('Ctrl Pts',(1.31824805546069,2.7691058422748,-9.49396233738911)) ;
#152395 = CARTESIAN_POINT('Ctrl Pts',(1.31689309423376,2.77013099976528,-9.49322773664117)) ;
#152396 = CARTESIAN_POINT('Ctrl Pts',(1.31545882361434,2.77127278201747,-9.49244887805927)) ;
#152397 = CARTESIAN_POINT('Ctrl Pts',(1.31535582310956,2.77135510350022,-9.49239293834655)) ;
#152398 = CARTESIAN_POINT('Ctrl Pts',(1.31504853092208,2.77160168095798,-9.49222602655302)) ;
#152399 = CARTESIAN_POINT('Ctrl Pts',(1.31461168315426,2.77195498754743,-9.49198869314583)) ;
#152400 = CARTESIAN_POINT('Ctrl Pts',(1.31417742224137,2.77231219724369,-9.49175266294293)) ;
#152401 = CARTESIAN_POINT('Ctrl Pts',(1.31333096026314,2.77301480846572,-9.49129249386305)) ;
#152402 = CARTESIAN_POINT('Ctrl Pts',(1.31272070342854,2.77353368974769,-9.49096054315942)) ;
#152403 = CARTESIAN_POINT('Ctrl Pts',(1.30969774837133,2.77616736630456,-9.48931544276183)) ;
#152404 = CARTESIAN_POINT('Ctrl Pts',(1.307370227887,2.77840054644573,-9.48804652010492)) ;
#152405 = CARTESIAN_POINT('Ctrl Pts',(1.30464757270884,2.78128817542223,-9.48656129665113)) ;
#152406 = CARTESIAN_POINT('Ctrl Pts',(1.30414845981079,2.78182967606623,-9.48628898736924)) ;
#152407 = CARTESIAN_POINT('Ctrl Pts',(1.30260826844056,2.78353926416389,-9.48544857136307)) ;
#152408 = CARTESIAN_POINT('Ctrl Pts',(1.30158324720849,2.78473373830866,-9.48488876707862)) ;
#152409 = CARTESIAN_POINT('Ctrl Pts',(1.30024935135332,2.78636738852739,-9.48416018728324)) ;
#152410 = CARTESIAN_POINT('Ctrl Pts',(1.29991860867237,2.78677921519272,-9.48397952491896)) ;
#152411 = CARTESIAN_POINT('Ctrl Pts',(1.29915346420735,2.78774794465155,-9.48356158077169)) ;
#152412 = CARTESIAN_POINT('Ctrl Pts',(1.29872125904468,2.78830744810473,-9.48332550011269)) ;
#152413 = CARTESIAN_POINT('Ctrl Pts',(1.29658637826222,2.79113377451592,-9.4821594679259)) ;
#152414 = CARTESIAN_POINT('Ctrl Pts',(1.29496240940488,2.79348720429747,-9.48127301363021)) ;
#152415 = CARTESIAN_POINT('Ctrl Pts',(1.29231665668155,2.79769679694548,-9.47982835199505)) ;
#152416 = CARTESIAN_POINT('Ctrl Pts',(1.29125115601061,2.79951540543445,-9.4792459513193)) ;
#152417 = CARTESIAN_POINT('Ctrl Pts',(1.28927619853496,2.80313430045116,-9.47816512101871)) ;
#152418 = CARTESIAN_POINT('Ctrl Pts',(1.2883624199782,2.80493500363978,-9.47766462065405)) ;
#152419 = CARTESIAN_POINT('Ctrl Pts',(1.28732027925585,2.80715235940914,-9.4770931587537)) ;
#152420 = CARTESIAN_POINT('Ctrl Pts',(1.28695835013167,2.80793550920674,-9.47689461743542)) ;
#152421 = CARTESIAN_POINT('Ctrl Pts',(1.28660568774191,2.80872522382218,-9.47670104370723)) ;
#152422 = CARTESIAN_POINT('Ctrl Pts',(1.28608376699196,2.80991454434776,-9.47641450210149)) ;
#152423 = CARTESIAN_POINT('Ctrl Pts',(1.28574525149601,2.81071375754613,-9.47622856810943)) ;
#152424 = CARTESIAN_POINT('Ctrl Pts',(1.28475894023896,2.81312894312825,-9.47568673335099)) ;
#152425 = CARTESIAN_POINT('Ctrl Pts',(1.28414040309303,2.81476247656144,-9.47534683370204)) ;
#152426 = CARTESIAN_POINT('Ctrl Pts',(1.28339818260913,2.81688756020151,-9.474939111358)) ;
#152427 = CARTESIAN_POINT('Ctrl Pts',(1.28323661013043,2.8173613757553,-9.47485036282194)) ;
#152428 = CARTESIAN_POINT('Ctrl Pts',(1.28265668893879,2.81910411140437,-9.47453185264632)) ;
#152429 = CARTESIAN_POINT('Ctrl Pts',(1.28225920250332,2.82038205281189,-9.47431360767476)) ;
#152430 = CARTESIAN_POINT('Ctrl Pts',(1.28170385606936,2.8223005152677,-9.47400866501641)) ;
#152431 = CARTESIAN_POINT('Ctrl Pts',(1.28152700208472,2.82293438010913,-9.47391155822972)) ;
#152432 = CARTESIAN_POINT('Ctrl Pts',(1.28107448868731,2.82461913389175,-9.47366309085072)) ;
#152433 = CARTESIAN_POINT('Ctrl Pts',(1.28081016954773,2.82567198476339,-9.47351801104593)) ;
#152434 = CARTESIAN_POINT('Ctrl Pts',(1.28009910353322,2.82871092361134,-9.47312783198231)) ;
#152435 = CARTESIAN_POINT('Ctrl Pts',(1.27969380338795,2.83071459002995,-9.47290512911995)) ;
#152436 = CARTESIAN_POINT('Ctrl Pts',(1.27923282767965,2.83340629334537,-9.47265154626654)) ;
#152437 = CARTESIAN_POINT('Ctrl Pts',(1.27912420342282,2.83408089926112,-9.47259176478417)) ;
#152438 = CARTESIAN_POINT('Ctrl Pts',(1.27861441353188,2.83746106027947,-9.47231109118166)) ;
#152439 = CARTESIAN_POINT('Ctrl Pts',(1.2783132428757,2.8401879948702,-9.47214490175664)) ;
#152440 = CARTESIAN_POINT('Ctrl Pts',(1.27795656969993,2.8452797714154,-9.4719480133439)) ;
#152441 = CARTESIAN_POINT('Ctrl Pts',(1.27787304021905,2.84764286211078,-9.4719018583827)) ;
#152442 = CARTESIAN_POINT('Ctrl Pts',(1.27787304021905,2.85,-9.4719018583827)) ;
#152443 = CARTESIAN_POINT('',(1.27787304021905,2.85,-5.76809814161729)) ;
#152444 = CARTESIAN_POINT('Origin',(-8.21365282185989E-16,2.85,-7.62)) ;
#152445 = CARTESIAN_POINT('Ctrl Pts',(1.37603597336697,2.75,-5.715)) ;
#152446 = CARTESIAN_POINT('Ctrl Pts',(1.37543428354306,2.75,-5.71531994188649)) ;
#152447 = CARTESIAN_POINT('Ctrl Pts',(1.37483253111456,2.7500053137259,-5.71563981565882)) ;
#152448 = CARTESIAN_POINT('Ctrl Pts',(1.37388722675069,2.75002207412044,-5.71614264420701)) ;
#152449 = CARTESIAN_POINT('Ctrl Pts',(1.37354350385561,2.75002991650282,-5.71632551416217)) ;
#152450 = CARTESIAN_POINT('Ctrl Pts',(1.37285611423782,2.75004911307826,-5.7166912988841)) ;
#152451 = CARTESIAN_POINT('Ctrl Pts',(1.37251244753524,2.75006046723047,-5.71687421361152)) ;
#152452 = CARTESIAN_POINT('Ctrl Pts',(1.3714815944481,2.75009981984526,-5.71742299469496)) ;
#152453 = CARTESIAN_POINT('Ctrl Pts',(1.37079455494331,2.75013310886333,-5.71778889820319)) ;
#152454 = CARTESIAN_POINT('Ctrl Pts',(1.36873453110892,2.75025430438115,-5.71888650558662)) ;
#152455 = CARTESIAN_POINT('Ctrl Pts',(1.36736263966051,2.75036354665963,-5.71961810924204)) ;
#152456 = CARTESIAN_POINT('Ctrl Pts',(1.36413470836879,2.75068903914081,-5.72134106893781)) ;
#152457 = CARTESIAN_POINT('Ctrl Pts',(1.36227932197148,2.75092980851021,-5.72233263772104)) ;
#152458 = CARTESIAN_POINT('Ctrl Pts',(1.35746012444743,2.7516985967038,-5.72491118192158)) ;
#152459 = CARTESIAN_POINT('Ctrl Pts',(1.35450425835489,2.7523133271765,-5.72649576254108)) ;
#152460 = CARTESIAN_POINT('Ctrl Pts',(1.34886973918565,2.75377034241463,-5.72952083050664)) ;
#152461 = CARTESIAN_POINT('Ctrl Pts',(1.3461783156815,2.75459534478002,-5.73096785925842)) ;
#152462 = CARTESIAN_POINT('Ctrl Pts',(1.34314242260183,2.75567798707048,-5.73260153012297)) ;
#152463 = CARTESIAN_POINT('Ctrl Pts',(1.34256163823226,2.75588931242805,-5.73291410178501)) ;
#152464 = CARTESIAN_POINT('Ctrl Pts',(1.34198261999809,2.75610647364238,-5.7332257815815)) ;
#152465 = CARTESIAN_POINT('Ctrl Pts',(1.3413216052292,2.75635697290856,-5.73358162198335)) ;
#152466 = CARTESIAN_POINT('Ctrl Pts',(1.3408629143507,2.75653491456656,-5.73382858253195)) ;
#152467 = CARTESIAN_POINT('Ctrl Pts',(1.33918548989955,2.7572007950357,-5.73473183750058)) ;
#152468 = CARTESIAN_POINT('Ctrl Pts',(1.33797416370948,2.75771112313095,-5.73538434826515)) ;
#152469 = CARTESIAN_POINT('Ctrl Pts',(1.33648532079705,2.75837521508442,-5.73618663294892)) ;
#152470 = CARTESIAN_POINT('Ctrl Pts',(1.33619776328717,2.75850521488808,-5.73634159730212)) ;
#152471 = CARTESIAN_POINT('Ctrl Pts',(1.33107968015659,2.76084915994901,-5.73910003971151)) ;
#152472 = CARTESIAN_POINT('Ctrl Pts',(1.32635908659541,2.76350693338973,-5.74164801954816)) ;
#152473 = CARTESIAN_POINT('Ctrl Pts',(1.3210976062609,2.76707470328371,-5.74449471691154)) ;
#152474 = CARTESIAN_POINT('Ctrl Pts',(1.32035743991852,2.76759128788277,-5.74489535244479)) ;
#152475 = CARTESIAN_POINT('Ctrl Pts',(1.31824805546068,2.76910584227481,-5.7460376626109)) ;
#152476 = CARTESIAN_POINT('Ctrl Pts',(1.31689309423375,2.77013099976529,-5.74677226335884)) ;
#152477 = CARTESIAN_POINT('Ctrl Pts',(1.31545882361434,2.77127278201747,-5.74755112194074)) ;
#152478 = CARTESIAN_POINT('Ctrl Pts',(1.31535582310955,2.77135510350023,-5.74760706165346)) ;
#152479 = CARTESIAN_POINT('Ctrl Pts',(1.31504853092206,2.77160168095799,-5.74777397344699)) ;
#152480 = CARTESIAN_POINT('Ctrl Pts',(1.31461168315424,2.77195498754746,-5.74801130685418)) ;
#152481 = CARTESIAN_POINT('Ctrl Pts',(1.31417742224134,2.77231219724371,-5.74824733705709)) ;
#152482 = CARTESIAN_POINT('Ctrl Pts',(1.31333096026311,2.77301480846574,-5.74870750613696)) ;
#152483 = CARTESIAN_POINT('Ctrl Pts',(1.31272070342852,2.77353368974771,-5.7490394568406)) ;
#152484 = CARTESIAN_POINT('Ctrl Pts',(1.3096977483713,2.77616736630459,-5.75068455723819)) ;
#152485 = CARTESIAN_POINT('Ctrl Pts',(1.30737022788696,2.77840054644576,-5.7519534798951)) ;
#152486 = CARTESIAN_POINT('Ctrl Pts',(1.30464757270882,2.78128817542225,-5.75343870334889)) ;
#152487 = CARTESIAN_POINT('Ctrl Pts',(1.30414845981078,2.78182967606623,-5.75371101263076)) ;
#152488 = CARTESIAN_POINT('Ctrl Pts',(1.30260826844056,2.78353926416388,-5.75455142863693)) ;
#152489 = CARTESIAN_POINT('Ctrl Pts',(1.30158324720849,2.78473373830865,-5.75511123292138)) ;
#152490 = CARTESIAN_POINT('Ctrl Pts',(1.30024935135332,2.78636738852737,-5.75583981271676)) ;
#152491 = CARTESIAN_POINT('Ctrl Pts',(1.29991860867237,2.78677921519271,-5.75602047508104)) ;
#152492 = CARTESIAN_POINT('Ctrl Pts',(1.29915346420734,2.78774794465154,-5.75643841922831)) ;
#152493 = CARTESIAN_POINT('Ctrl Pts',(1.29872125904468,2.78830744810472,-5.75667449988731)) ;
#152494 = CARTESIAN_POINT('Ctrl Pts',(1.29658637826222,2.79113377451591,-5.7578405320741)) ;
#152495 = CARTESIAN_POINT('Ctrl Pts',(1.29496240940487,2.79348720429746,-5.75872698636979)) ;
#152496 = CARTESIAN_POINT('Ctrl Pts',(1.29231665668155,2.79769679694547,-5.76017164800495)) ;
#152497 = CARTESIAN_POINT('Ctrl Pts',(1.29125115601061,2.79951540543444,-5.7607540486807)) ;
#152498 = CARTESIAN_POINT('Ctrl Pts',(1.28927619853496,2.80313430045115,-5.76183487898129)) ;
#152499 = CARTESIAN_POINT('Ctrl Pts',(1.2883624199782,2.80493500363977,-5.76233537934595)) ;
#152500 = CARTESIAN_POINT('Ctrl Pts',(1.28732027925585,2.80715235940913,-5.7629068412463)) ;
#152501 = CARTESIAN_POINT('Ctrl Pts',(1.28695835013167,2.80793550920675,-5.76310538256458)) ;
#152502 = CARTESIAN_POINT('Ctrl Pts',(1.28660568774191,2.80872522382218,-5.76329895629278)) ;
#152503 = CARTESIAN_POINT('Ctrl Pts',(1.28608376699196,2.80991454434776,-5.76358549789851)) ;
#152504 = CARTESIAN_POINT('Ctrl Pts',(1.28574525149601,2.81071375754613,-5.76377143189058)) ;
#152505 = CARTESIAN_POINT('Ctrl Pts',(1.28475894023895,2.81312894312825,-5.76431326664902)) ;
#152506 = CARTESIAN_POINT('Ctrl Pts',(1.28414040309303,2.81476247656144,-5.76465316629797)) ;
#152507 = CARTESIAN_POINT('Ctrl Pts',(1.28339818260913,2.81688756020152,-5.765060888642)) ;
#152508 = CARTESIAN_POINT('Ctrl Pts',(1.28323661013043,2.81736137575531,-5.76514963717807)) ;
#152509 = CARTESIAN_POINT('Ctrl Pts',(1.28265668893879,2.81910411140438,-5.76546814735368)) ;
#152510 = CARTESIAN_POINT('Ctrl Pts',(1.28225920250332,2.8203820528119,-5.76568639232524)) ;
#152511 = CARTESIAN_POINT('Ctrl Pts',(1.28170385606936,2.8223005152677,-5.76599133498359)) ;
#152512 = CARTESIAN_POINT('Ctrl Pts',(1.28152700208472,2.82293438010913,-5.76608844177028)) ;
#152513 = CARTESIAN_POINT('Ctrl Pts',(1.28107448868731,2.82461913389174,-5.76633690914928)) ;
#152514 = CARTESIAN_POINT('Ctrl Pts',(1.28081016954773,2.82567198476339,-5.76648198895407)) ;
#152515 = CARTESIAN_POINT('Ctrl Pts',(1.28009910353322,2.82871092361134,-5.76687216801769)) ;
#152516 = CARTESIAN_POINT('Ctrl Pts',(1.27969380338795,2.83071459002994,-5.76709487088005)) ;
#152517 = CARTESIAN_POINT('Ctrl Pts',(1.27923282767965,2.83340629334537,-5.76734845373346)) ;
#152518 = CARTESIAN_POINT('Ctrl Pts',(1.27912420342282,2.83408089926112,-5.76740823521583)) ;
#152519 = CARTESIAN_POINT('Ctrl Pts',(1.27861441353188,2.83746106027947,-5.76768890881833)) ;
#152520 = CARTESIAN_POINT('Ctrl Pts',(1.2783132428757,2.8401879948702,-5.76785509824336)) ;
#152521 = CARTESIAN_POINT('Ctrl Pts',(1.27795656969993,2.8452797714154,-5.76805198665609)) ;
#152522 = CARTESIAN_POINT('Ctrl Pts',(1.27787304021905,2.84764286211079,-5.7680981416173)) ;
#152523 = CARTESIAN_POINT('Ctrl Pts',(1.27787304021905,2.85,-5.7680981416173)) ;
#152524 = CARTESIAN_POINT('Origin',(1.3145125,4.45,-13.335)) ;
#152525 = CARTESIAN_POINT('',(1.22107868287598,4.55,-13.1995951091212)) ;
#152526 = CARTESIAN_POINT('',(1.22107868287598,4.55,-13.4704048908787)) ;
#152527 = CARTESIAN_POINT('Origin',(1.3145125,4.55,-13.335)) ;
#152528 = CARTESIAN_POINT('',(1.27787304021905,4.45,-13.2819018583827)) ;
#152529 = CARTESIAN_POINT('Origin',(1.22107868287598,4.45,-13.1995951091212)) ;
#152530 = CARTESIAN_POINT('',(1.27787304021905,4.45,-13.3880981416173)) ;
#152531 = CARTESIAN_POINT('Origin',(1.3145125,4.45,-13.335)) ;
#152532 = CARTESIAN_POINT('Origin',(1.22107868287598,4.45,-13.4704048908787)) ;
#152533 = CARTESIAN_POINT('Origin',(-8.21365282185989E-16,2.85,-11.43)) ;
#152534 = CARTESIAN_POINT('',(1.37603597336697,2.75,-13.335)) ;
#152535 = CARTESIAN_POINT('Origin',(-8.13551212474381E-16,2.75,-11.43)) ;
#152536 = CARTESIAN_POINT('',(1.27787304021905,2.85,-13.2819018583827)) ;
#152537 = CARTESIAN_POINT('Ctrl Pts',(1.37603597336697,2.75,-13.335)) ;
#152538 = CARTESIAN_POINT('Ctrl Pts',(1.37573512845501,2.75,-13.3348400290568)) ;
#152539 = CARTESIAN_POINT('Ctrl Pts',(1.37513340737757,2.7500026571284,-13.3345201213288)) ;
#152540 = CARTESIAN_POINT('Ctrl Pts',(1.37453174406033,2.75001064672752,-13.3342001889751)) ;
#152541 = CARTESIAN_POINT('Ctrl Pts',(1.37388722675068,2.75002207412044,-13.333857355793)) ;
#152542 = CARTESIAN_POINT('Ctrl Pts',(1.3735435038556,2.75002991650282,-13.3336744858378)) ;
#152543 = CARTESIAN_POINT('Ctrl Pts',(1.37285611423781,2.75004911307826,-13.3333087011159)) ;
#152544 = CARTESIAN_POINT('Ctrl Pts',(1.37251244753524,2.75006046723047,-13.3331257863885)) ;
#152545 = CARTESIAN_POINT('Ctrl Pts',(1.3714815944481,2.75009981984526,-13.332577005305)) ;
#152546 = CARTESIAN_POINT('Ctrl Pts',(1.37079455494331,2.75013310886333,-13.3322111017968)) ;
#152547 = CARTESIAN_POINT('Ctrl Pts',(1.36873453110892,2.75025430438116,-13.3311134944134)) ;
#152548 = CARTESIAN_POINT('Ctrl Pts',(1.36736263966051,2.75036354665964,-13.3303818907579)) ;
#152549 = CARTESIAN_POINT('Ctrl Pts',(1.36413470836878,2.75068903914083,-13.3286589310622)) ;
#152550 = CARTESIAN_POINT('Ctrl Pts',(1.36227932197147,2.75092980851023,-13.327667362279)) ;
#152551 = CARTESIAN_POINT('Ctrl Pts',(1.35746012444742,2.75169859670383,-13.3250888180784)) ;
#152552 = CARTESIAN_POINT('Ctrl Pts',(1.3545042583549,2.75231332717655,-13.3235042374589)) ;
#152553 = CARTESIAN_POINT('Ctrl Pts',(1.34886973918565,2.75377034241467,-13.3204791694934)) ;
#152554 = CARTESIAN_POINT('Ctrl Pts',(1.34617831568151,2.75459534478006,-13.3190321407416)) ;
#152555 = CARTESIAN_POINT('Ctrl Pts',(1.34314242260183,2.75567798707052,-13.3173984698771)) ;
#152556 = CARTESIAN_POINT('Ctrl Pts',(1.34256163823227,2.75588931242809,-13.317085898215)) ;
#152557 = CARTESIAN_POINT('Ctrl Pts',(1.3419826199981,2.75610647364241,-13.3167742184185)) ;
#152558 = CARTESIAN_POINT('Ctrl Pts',(1.34132160522921,2.7563569729086,-13.3164183780167)) ;
#152559 = CARTESIAN_POINT('Ctrl Pts',(1.34086291435071,2.75653491456659,-13.3161714174681)) ;
#152560 = CARTESIAN_POINT('Ctrl Pts',(1.33918548989956,2.75720079503573,-13.3152681624994)) ;
#152561 = CARTESIAN_POINT('Ctrl Pts',(1.33797416370949,2.75771112313098,-13.3146156517349)) ;
#152562 = CARTESIAN_POINT('Ctrl Pts',(1.33648532079706,2.75837521508446,-13.3138133670511)) ;
#152563 = CARTESIAN_POINT('Ctrl Pts',(1.33619776328718,2.75850521488813,-13.3136584026979)) ;
#152564 = CARTESIAN_POINT('Ctrl Pts',(1.33107968015567,2.76084915994947,-13.310899960288)) ;
#152565 = CARTESIAN_POINT('Ctrl Pts',(1.32635908659362,2.76350693339075,-13.3083519804509)) ;
#152566 = CARTESIAN_POINT('Ctrl Pts',(1.32109760625921,2.76707470328488,-13.3055052830876)) ;
#152567 = CARTESIAN_POINT('Ctrl Pts',(1.32035743991769,2.76759128788335,-13.3051046475548)) ;
#152568 = CARTESIAN_POINT('Ctrl Pts',(1.31824805546069,2.76910584227479,-13.3039623373891)) ;
#152569 = CARTESIAN_POINT('Ctrl Pts',(1.31689309423375,2.77013099976527,-13.3032277366412)) ;
#152570 = CARTESIAN_POINT('Ctrl Pts',(1.31545882361434,2.77127278201746,-13.3024488780593)) ;
#152571 = CARTESIAN_POINT('Ctrl Pts',(1.31535582310956,2.77135510350021,-13.3023929383466)) ;
#152572 = CARTESIAN_POINT('Ctrl Pts',(1.31504853092208,2.77160168095796,-13.302226026553)) ;
#152573 = CARTESIAN_POINT('Ctrl Pts',(1.31461168315426,2.77195498754743,-13.3019886931459)) ;
#152574 = CARTESIAN_POINT('Ctrl Pts',(1.31417742224136,2.77231219724367,-13.3017526629429)) ;
#152575 = CARTESIAN_POINT('Ctrl Pts',(1.31333096026314,2.77301480846571,-13.3012924938631)) ;
#152576 = CARTESIAN_POINT('Ctrl Pts',(1.31272070342854,2.77353368974768,-13.3009605431594)) ;
#152577 = CARTESIAN_POINT('Ctrl Pts',(1.30969774837133,2.77616736630456,-13.2993154427618)) ;
#152578 = CARTESIAN_POINT('Ctrl Pts',(1.30737022788699,2.77840054644573,-13.2980465201049)) ;
#152579 = CARTESIAN_POINT('Ctrl Pts',(1.30464757270884,2.78128817542222,-13.2965612966511)) ;
#152580 = CARTESIAN_POINT('Ctrl Pts',(1.30414845981078,2.7818296760662,-13.2962889873693)) ;
#152581 = CARTESIAN_POINT('Ctrl Pts',(1.30260826844055,2.78353926416386,-13.2954485713631)) ;
#152582 = CARTESIAN_POINT('Ctrl Pts',(1.30158324720848,2.78473373830863,-13.2948887670786)) ;
#152583 = CARTESIAN_POINT('Ctrl Pts',(1.30024935135331,2.78636738852735,-13.2941601872833)) ;
#152584 = CARTESIAN_POINT('Ctrl Pts',(1.29991860867236,2.78677921519269,-13.293979524919)) ;
#152585 = CARTESIAN_POINT('Ctrl Pts',(1.29915346420733,2.78774794465152,-13.2935615807717)) ;
#152586 = CARTESIAN_POINT('Ctrl Pts',(1.29872125904467,2.78830744810469,-13.2933255001127)) ;
#152587 = CARTESIAN_POINT('Ctrl Pts',(1.29658637826221,2.79113377451589,-13.2921594679259)) ;
#152588 = CARTESIAN_POINT('Ctrl Pts',(1.29496240940488,2.79348720429744,-13.2912730136302)) ;
#152589 = CARTESIAN_POINT('Ctrl Pts',(1.29231665668155,2.79769679694545,-13.2898283519951)) ;
#152590 = CARTESIAN_POINT('Ctrl Pts',(1.29125115601061,2.79951540543443,-13.2892459513193)) ;
#152591 = CARTESIAN_POINT('Ctrl Pts',(1.28927619853495,2.80313430045115,-13.2881651210187)) ;
#152592 = CARTESIAN_POINT('Ctrl Pts',(1.28836241997819,2.80493500363977,-13.2876646206541)) ;
#152593 = CARTESIAN_POINT('Ctrl Pts',(1.28732027925585,2.80715235940913,-13.2870931587537)) ;
#152594 = CARTESIAN_POINT('Ctrl Pts',(1.28695835013165,2.80793550920675,-13.2868946174355)) ;
#152595 = CARTESIAN_POINT('Ctrl Pts',(1.2866056877419,2.80872522382218,-13.2867010437072)) ;
#152596 = CARTESIAN_POINT('Ctrl Pts',(1.28608376699196,2.80991454434775,-13.2864145021015)) ;
#152597 = CARTESIAN_POINT('Ctrl Pts',(1.285745251496,2.81071375754612,-13.2862285681094)) ;
#152598 = CARTESIAN_POINT('Ctrl Pts',(1.28475894023895,2.81312894312824,-13.285686733351)) ;
#152599 = CARTESIAN_POINT('Ctrl Pts',(1.28414040309303,2.81476247656143,-13.285346833702)) ;
#152600 = CARTESIAN_POINT('Ctrl Pts',(1.28339818260913,2.8168875602015,-13.284939111358)) ;
#152601 = CARTESIAN_POINT('Ctrl Pts',(1.28323661013044,2.81736137575529,-13.2848503628219)) ;
#152602 = CARTESIAN_POINT('Ctrl Pts',(1.2826566889388,2.81910411140436,-13.2845318526463)) ;
#152603 = CARTESIAN_POINT('Ctrl Pts',(1.28225920250333,2.82038205281188,-13.2843136076747)) ;
#152604 = CARTESIAN_POINT('Ctrl Pts',(1.28170385606937,2.82230051526769,-13.2840086650164)) ;
#152605 = CARTESIAN_POINT('Ctrl Pts',(1.28152700208473,2.82293438010912,-13.2839115582297)) ;
#152606 = CARTESIAN_POINT('Ctrl Pts',(1.28107448868732,2.82461913389175,-13.2836630908507)) ;
#152607 = CARTESIAN_POINT('Ctrl Pts',(1.28081016954773,2.82567198476339,-13.2835180110459)) ;
#152608 = CARTESIAN_POINT('Ctrl Pts',(1.28009910353321,2.82871092361135,-13.2831278319823)) ;
#152609 = CARTESIAN_POINT('Ctrl Pts',(1.27969380338794,2.83071459002995,-13.28290512912)) ;
#152610 = CARTESIAN_POINT('Ctrl Pts',(1.27923282767964,2.83340629334539,-13.2826515462665)) ;
#152611 = CARTESIAN_POINT('Ctrl Pts',(1.27912420342281,2.83408089926113,-13.2825917647842)) ;
#152612 = CARTESIAN_POINT('Ctrl Pts',(1.27861441353187,2.83746106027949,-13.2823110911817)) ;
#152613 = CARTESIAN_POINT('Ctrl Pts',(1.2783132428757,2.84018799487023,-13.2821449017566)) ;
#152614 = CARTESIAN_POINT('Ctrl Pts',(1.27795656969994,2.84527977141544,-13.2819480133439)) ;
#152615 = CARTESIAN_POINT('Ctrl Pts',(1.27787304021904,2.8476428621108,-13.2819018583827)) ;
#152616 = CARTESIAN_POINT('Ctrl Pts',(1.27787304021905,2.85,-13.2819018583827)) ;
#152617 = CARTESIAN_POINT('',(1.27787304021905,2.85,-9.57809814161729)) ;
#152618 = CARTESIAN_POINT('Origin',(-8.21365282185989E-16,2.85,-11.43)) ;
#152619 = CARTESIAN_POINT('Ctrl Pts',(1.37603597327321,2.75,-9.52500000004986)) ;
#152620 = CARTESIAN_POINT('Ctrl Pts',(1.37573512836126,2.75000000000028,-9.52515997099309)) ;
#152621 = CARTESIAN_POINT('Ctrl Pts',(1.37543426791168,2.7500013285371,-9.52531992481688)) ;
#152622 = CARTESIAN_POINT('Ctrl Pts',(1.37483257571475,2.75000665190009,-9.5256398448573)) ;
#152623 = CARTESIAN_POINT('Ctrl Pts',(1.37453174406034,2.75001064672751,-9.5257998110249)) ;
#152624 = CARTESIAN_POINT('Ctrl Pts',(1.37388722675069,2.75002207412045,-9.52614264420698)) ;
#152625 = CARTESIAN_POINT('Ctrl Pts',(1.37354350385557,2.75002991650282,-9.52632551416214)) ;
#152626 = CARTESIAN_POINT('Ctrl Pts',(1.37285611423782,2.75004911307826,-9.52669129888408)) ;
#152627 = CARTESIAN_POINT('Ctrl Pts',(1.37251244753524,2.75006046723047,-9.5268742136115)) ;
#152628 = CARTESIAN_POINT('Ctrl Pts',(1.3714815944481,2.75009981984526,-9.52742299469495)) ;
#152629 = CARTESIAN_POINT('Ctrl Pts',(1.37079455494331,2.75013310886333,-9.52778889820318)) ;
#152630 = CARTESIAN_POINT('Ctrl Pts',(1.36873453110892,2.75025430438116,-9.52888650558661)) ;
#152631 = CARTESIAN_POINT('Ctrl Pts',(1.36736263966051,2.75036354665964,-9.52961810924203)) ;
#152632 = CARTESIAN_POINT('Ctrl Pts',(1.36413470836879,2.75068903914083,-9.5313410689378)) ;
#152633 = CARTESIAN_POINT('Ctrl Pts',(1.36227932197147,2.75092980851024,-9.53233263772104)) ;
#152634 = CARTESIAN_POINT('Ctrl Pts',(1.35746012444742,2.75169859670383,-9.53491118192157)) ;
#152635 = CARTESIAN_POINT('Ctrl Pts',(1.35450425835489,2.75231332717654,-9.53649576254107)) ;
#152636 = CARTESIAN_POINT('Ctrl Pts',(1.34886973918565,2.75377034241467,-9.53952083050663)) ;
#152637 = CARTESIAN_POINT('Ctrl Pts',(1.34617831568151,2.75459534478006,-9.54096785925841)) ;
#152638 = CARTESIAN_POINT('Ctrl Pts',(1.34314242260183,2.75567798707052,-9.54260153012296)) ;
#152639 = CARTESIAN_POINT('Ctrl Pts',(1.34256163823227,2.75588931242809,-9.54291410178499)) ;
#152640 = CARTESIAN_POINT('Ctrl Pts',(1.3419826199981,2.75610647364241,-9.54322578158149)) ;
#152641 = CARTESIAN_POINT('Ctrl Pts',(1.34132160522921,2.7563569729086,-9.54358162198333)) ;
#152642 = CARTESIAN_POINT('Ctrl Pts',(1.34086291435071,2.75653491456659,-9.54382858253193)) ;
#152643 = CARTESIAN_POINT('Ctrl Pts',(1.33918548989956,2.75720079503573,-9.54473183750056)) ;
#152644 = CARTESIAN_POINT('Ctrl Pts',(1.33797416370949,2.75771112313098,-9.54538434826513)) ;
#152645 = CARTESIAN_POINT('Ctrl Pts',(1.33648532079706,2.75837521508445,-9.5461866329489)) ;
#152646 = CARTESIAN_POINT('Ctrl Pts',(1.33619776328718,2.75850521488811,-9.5463415973021)) ;
#152647 = CARTESIAN_POINT('Ctrl Pts',(1.33107968015623,2.7608491599492,-9.54910003971169)) ;
#152648 = CARTESIAN_POINT('Ctrl Pts',(1.32635908659471,2.76350693339014,-9.55164801954852)) ;
#152649 = CARTESIAN_POINT('Ctrl Pts',(1.32109760626024,2.76707470328417,-9.55449471691189)) ;
#152650 = CARTESIAN_POINT('Ctrl Pts',(1.3203574399182,2.767591287883,-9.55489535244495)) ;
#152651 = CARTESIAN_POINT('Ctrl Pts',(1.31824805546069,2.7691058422748,-9.55603766261088)) ;
#152652 = CARTESIAN_POINT('Ctrl Pts',(1.31689309423376,2.77013099976528,-9.55677226335883)) ;
#152653 = CARTESIAN_POINT('Ctrl Pts',(1.31545882361435,2.77127278201747,-9.55755112194072)) ;
#152654 = CARTESIAN_POINT('Ctrl Pts',(1.31535582310957,2.77135510350022,-9.55760706165345)) ;
#152655 = CARTESIAN_POINT('Ctrl Pts',(1.31504853092209,2.77160168095797,-9.55777397344697)) ;
#152656 = CARTESIAN_POINT('Ctrl Pts',(1.31461168315425,2.77195498754744,-9.55801130685416)) ;
#152657 = CARTESIAN_POINT('Ctrl Pts',(1.31417742224137,2.77231219724368,-9.55824733705706)) ;
#152658 = CARTESIAN_POINT('Ctrl Pts',(1.31333096026314,2.77301480846571,-9.55870750613694)) ;
#152659 = CARTESIAN_POINT('Ctrl Pts',(1.31272070342855,2.77353368974768,-9.55903945684058)) ;
#152660 = CARTESIAN_POINT('Ctrl Pts',(1.30969774837134,2.77616736630456,-9.56068455723817)) ;
#152661 = CARTESIAN_POINT('Ctrl Pts',(1.30737022788701,2.77840054644572,-9.56195347989507)) ;
#152662 = CARTESIAN_POINT('Ctrl Pts',(1.30464757270885,2.78128817542222,-9.56343870334886)) ;
#152663 = CARTESIAN_POINT('Ctrl Pts',(1.3041484598108,2.78182967606622,-9.56371101263075)) ;
#152664 = CARTESIAN_POINT('Ctrl Pts',(1.30260826844056,2.78353926416388,-9.56455142863692)) ;
#152665 = CARTESIAN_POINT('Ctrl Pts',(1.30158324720849,2.78473373830865,-9.56511123292138)) ;
#152666 = CARTESIAN_POINT('Ctrl Pts',(1.30024935135332,2.78636738852738,-9.56583981271676)) ;
#152667 = CARTESIAN_POINT('Ctrl Pts',(1.29991860867237,2.78677921519272,-9.56602047508104)) ;
#152668 = CARTESIAN_POINT('Ctrl Pts',(1.29915346420735,2.78774794465155,-9.5664384192283)) ;
#152669 = CARTESIAN_POINT('Ctrl Pts',(1.29872125904468,2.78830744810473,-9.56667449988731)) ;
#152670 = CARTESIAN_POINT('Ctrl Pts',(1.29658637826222,2.79113377451592,-9.5678405320741)) ;
#152671 = CARTESIAN_POINT('Ctrl Pts',(1.29496240940488,2.79348720429747,-9.56872698636979)) ;
#152672 = CARTESIAN_POINT('Ctrl Pts',(1.29231665668155,2.79769679694547,-9.57017164800495)) ;
#152673 = CARTESIAN_POINT('Ctrl Pts',(1.29125115601061,2.79951540543444,-9.5707540486807)) ;
#152674 = CARTESIAN_POINT('Ctrl Pts',(1.28927619853496,2.80313430045115,-9.57183487898129)) ;
#152675 = CARTESIAN_POINT('Ctrl Pts',(1.2883624199782,2.80493500363977,-9.57233537934596)) ;
#152676 = CARTESIAN_POINT('Ctrl Pts',(1.28732027925585,2.80715235940913,-9.5729068412463)) ;
#152677 = CARTESIAN_POINT('Ctrl Pts',(1.28695835013167,2.80793550920673,-9.57310538256458)) ;
#152678 = CARTESIAN_POINT('Ctrl Pts',(1.28660568774191,2.80872522382218,-9.57329895629278)) ;
#152679 = CARTESIAN_POINT('Ctrl Pts',(1.28608376699196,2.80991454434775,-9.57358549789851)) ;
#152680 = CARTESIAN_POINT('Ctrl Pts',(1.28574525149602,2.81071375754612,-9.57377143189058)) ;
#152681 = CARTESIAN_POINT('Ctrl Pts',(1.28475894023896,2.81312894312824,-9.57431326664902)) ;
#152682 = CARTESIAN_POINT('Ctrl Pts',(1.28414040309303,2.81476247656142,-9.57465316629797)) ;
#152683 = CARTESIAN_POINT('Ctrl Pts',(1.28339818260913,2.8168875602015,-9.575060888642)) ;
#152684 = CARTESIAN_POINT('Ctrl Pts',(1.28323661013044,2.81736137575528,-9.57514963717806)) ;
#152685 = CARTESIAN_POINT('Ctrl Pts',(1.2826566889388,2.81910411140435,-9.57546814735368)) ;
#152686 = CARTESIAN_POINT('Ctrl Pts',(1.28225920250333,2.82038205281187,-9.57568639232524)) ;
#152687 = CARTESIAN_POINT('Ctrl Pts',(1.28170385606936,2.82230051526768,-9.57599133498359)) ;
#152688 = CARTESIAN_POINT('Ctrl Pts',(1.28152700208472,2.82293438010912,-9.57608844177028)) ;
#152689 = CARTESIAN_POINT('Ctrl Pts',(1.28107448868731,2.82461913389174,-9.57633690914928)) ;
#152690 = CARTESIAN_POINT('Ctrl Pts',(1.28081016954773,2.82567198476339,-9.57648198895408)) ;
#152691 = CARTESIAN_POINT('Ctrl Pts',(1.28009910353322,2.82871092361134,-9.57687216801769)) ;
#152692 = CARTESIAN_POINT('Ctrl Pts',(1.27969380338795,2.83071459002995,-9.57709487088005)) ;
#152693 = CARTESIAN_POINT('Ctrl Pts',(1.27923282767965,2.83340629334538,-9.57734845373346)) ;
#152694 = CARTESIAN_POINT('Ctrl Pts',(1.27912420342282,2.83408089926112,-9.57740823521583)) ;
#152695 = CARTESIAN_POINT('Ctrl Pts',(1.27861441353188,2.83746106027948,-9.57768890881833)) ;
#152696 = CARTESIAN_POINT('Ctrl Pts',(1.2783132428757,2.84018799487021,-9.57785509824336)) ;
#152697 = CARTESIAN_POINT('Ctrl Pts',(1.27795656969993,2.84527977141542,-9.57805198665609)) ;
#152698 = CARTESIAN_POINT('Ctrl Pts',(1.27787304021905,2.84764286211079,-9.57809814161729)) ;
#152699 = CARTESIAN_POINT('Ctrl Pts',(1.27787304021905,2.85,-9.57809814161729)) ;
#152700 = CARTESIAN_POINT('Origin',(1.3145125,4.45,-17.145)) ;
#152701 = CARTESIAN_POINT('',(1.22107868287598,4.55,-17.0095951091213)) ;
#152702 = CARTESIAN_POINT('',(1.22107868287598,4.55,-17.2804048908787)) ;
#152703 = CARTESIAN_POINT('Origin',(1.3145125,4.55,-17.145)) ;
#152704 = CARTESIAN_POINT('',(1.27787304021905,4.45,-17.0919018583827)) ;
#152705 = CARTESIAN_POINT('Origin',(1.22107868287598,4.45,-17.0095951091213)) ;
#152706 = CARTESIAN_POINT('',(1.27787304021905,4.45,-17.1980981416173)) ;
#152707 = CARTESIAN_POINT('Origin',(1.3145125,4.45,-17.145)) ;
#152708 = CARTESIAN_POINT('Origin',(1.22107868287598,4.45,-17.2804048908787)) ;
#152709 = CARTESIAN_POINT('Origin',(-8.21365282185989E-16,2.85,-15.24)) ;
#152710 = CARTESIAN_POINT('',(1.37603597336697,2.75,-17.145)) ;
#152711 = CARTESIAN_POINT('Origin',(-8.13551212474381E-16,2.75,-15.24)) ;
#152712 = CARTESIAN_POINT('',(1.27787304021905,2.85,-17.0919018583827)) ;
#152713 = CARTESIAN_POINT('Ctrl Pts',(1.37603597336697,2.75,-17.145)) ;
#152714 = CARTESIAN_POINT('Ctrl Pts',(1.37543428354306,2.75,-17.1446800581135)) ;
#152715 = CARTESIAN_POINT('Ctrl Pts',(1.37483253111456,2.75000531372589,-17.1443601843412)) ;
#152716 = CARTESIAN_POINT('Ctrl Pts',(1.37388722675069,2.75002207412045,-17.143857355793)) ;
#152717 = CARTESIAN_POINT('Ctrl Pts',(1.37354350385561,2.75002991650282,-17.1436744858378)) ;
#152718 = CARTESIAN_POINT('Ctrl Pts',(1.37285611423782,2.75004911307826,-17.1433087011159)) ;
#152719 = CARTESIAN_POINT('Ctrl Pts',(1.37251244753524,2.75006046723047,-17.1431257863885)) ;
#152720 = CARTESIAN_POINT('Ctrl Pts',(1.3714815944481,2.75009981984526,-17.142577005305)) ;
#152721 = CARTESIAN_POINT('Ctrl Pts',(1.37079455494331,2.75013310886333,-17.1422111017968)) ;
#152722 = CARTESIAN_POINT('Ctrl Pts',(1.36873453110892,2.75025430438115,-17.1411134944134)) ;
#152723 = CARTESIAN_POINT('Ctrl Pts',(1.36736263966051,2.75036354665963,-17.1403818907579)) ;
#152724 = CARTESIAN_POINT('Ctrl Pts',(1.36413470836879,2.75068903914081,-17.1386589310622)) ;
#152725 = CARTESIAN_POINT('Ctrl Pts',(1.36227932197147,2.75092980851021,-17.137667362279)) ;
#152726 = CARTESIAN_POINT('Ctrl Pts',(1.35746012444742,2.7516985967038,-17.1350888180784)) ;
#152727 = CARTESIAN_POINT('Ctrl Pts',(1.35450425835489,2.75231332717651,-17.1335042374589)) ;
#152728 = CARTESIAN_POINT('Ctrl Pts',(1.34886973918565,2.75377034241464,-17.1304791694934)) ;
#152729 = CARTESIAN_POINT('Ctrl Pts',(1.3461783156815,2.75459534478002,-17.1290321407416)) ;
#152730 = CARTESIAN_POINT('Ctrl Pts',(1.34314242260183,2.75567798707048,-17.1273984698771)) ;
#152731 = CARTESIAN_POINT('Ctrl Pts',(1.34256163823226,2.75588931242806,-17.127085898215)) ;
#152732 = CARTESIAN_POINT('Ctrl Pts',(1.34198261999809,2.75610647364238,-17.1267742184185)) ;
#152733 = CARTESIAN_POINT('Ctrl Pts',(1.3413216052292,2.75635697290856,-17.1264183780167)) ;
#152734 = CARTESIAN_POINT('Ctrl Pts',(1.3408629143507,2.75653491456656,-17.1261714174681)) ;
#152735 = CARTESIAN_POINT('Ctrl Pts',(1.33918548989955,2.7572007950357,-17.1252681624994)) ;
#152736 = CARTESIAN_POINT('Ctrl Pts',(1.33797416370948,2.75771112313095,-17.1246156517348)) ;
#152737 = CARTESIAN_POINT('Ctrl Pts',(1.33648532079705,2.75837521508443,-17.1238133670511)) ;
#152738 = CARTESIAN_POINT('Ctrl Pts',(1.33619776328717,2.7585052148881,-17.1236584026979)) ;
#152739 = CARTESIAN_POINT('Ctrl Pts',(1.33107968015588,2.76084915994935,-17.1208999602881)) ;
#152740 = CARTESIAN_POINT('Ctrl Pts',(1.32635908659402,2.76350693339051,-17.1183519804511)) ;
#152741 = CARTESIAN_POINT('Ctrl Pts',(1.32109760625958,2.76707470328462,-17.1155052830878)) ;
#152742 = CARTESIAN_POINT('Ctrl Pts',(1.32035743991785,2.76759128788324,-17.1151046475549)) ;
#152743 = CARTESIAN_POINT('Ctrl Pts',(1.31824805546066,2.76910584227481,-17.1139623373891)) ;
#152744 = CARTESIAN_POINT('Ctrl Pts',(1.31689309423374,2.77013099976528,-17.1132277366412)) ;
#152745 = CARTESIAN_POINT('Ctrl Pts',(1.31545882361432,2.77127278201747,-17.1124488780593)) ;
#152746 = CARTESIAN_POINT('Ctrl Pts',(1.31535582310953,2.77135510350024,-17.1123929383466)) ;
#152747 = CARTESIAN_POINT('Ctrl Pts',(1.31504853092203,2.771601680958,-17.112226026553)) ;
#152748 = CARTESIAN_POINT('Ctrl Pts',(1.31461168315421,2.77195498754747,-17.1119886931459)) ;
#152749 = CARTESIAN_POINT('Ctrl Pts',(1.31417742224132,2.77231219724372,-17.1117526629429)) ;
#152750 = CARTESIAN_POINT('Ctrl Pts',(1.31333096026309,2.77301480846575,-17.1112924938631)) ;
#152751 = CARTESIAN_POINT('Ctrl Pts',(1.31272070342849,2.77353368974772,-17.1109605431594)) ;
#152752 = CARTESIAN_POINT('Ctrl Pts',(1.30969774837127,2.77616736630461,-17.1093154427618)) ;
#152753 = CARTESIAN_POINT('Ctrl Pts',(1.30737022788694,2.77840054644579,-17.1080465201049)) ;
#152754 = CARTESIAN_POINT('Ctrl Pts',(1.3046475727088,2.78128817542226,-17.1065612966511)) ;
#152755 = CARTESIAN_POINT('Ctrl Pts',(1.30414845981076,2.78182967606623,-17.1062889873693)) ;
#152756 = CARTESIAN_POINT('Ctrl Pts',(1.30260826844056,2.78353926416388,-17.1054485713631)) ;
#152757 = CARTESIAN_POINT('Ctrl Pts',(1.30158324720849,2.78473373830866,-17.1048887670786)) ;
#152758 = CARTESIAN_POINT('Ctrl Pts',(1.30024935135332,2.78636738852739,-17.1041601872832)) ;
#152759 = CARTESIAN_POINT('Ctrl Pts',(1.29991860867237,2.78677921519272,-17.103979524919)) ;
#152760 = CARTESIAN_POINT('Ctrl Pts',(1.29915346420734,2.78774794465155,-17.1035615807717)) ;
#152761 = CARTESIAN_POINT('Ctrl Pts',(1.29872125904467,2.78830744810473,-17.1033255001127)) ;
#152762 = CARTESIAN_POINT('Ctrl Pts',(1.2965863782622,2.79113377451592,-17.1021594679259)) ;
#152763 = CARTESIAN_POINT('Ctrl Pts',(1.29496240940485,2.79348720429746,-17.1012730136302)) ;
#152764 = CARTESIAN_POINT('Ctrl Pts',(1.29231665668153,2.79769679694546,-17.099828351995)) ;
#152765 = CARTESIAN_POINT('Ctrl Pts',(1.29125115601059,2.79951540543443,-17.0992459513193)) ;
#152766 = CARTESIAN_POINT('Ctrl Pts',(1.28927619853494,2.80313430045113,-17.0981651210187)) ;
#152767 = CARTESIAN_POINT('Ctrl Pts',(1.28836241997818,2.80493500363976,-17.097664620654)) ;
#152768 = CARTESIAN_POINT('Ctrl Pts',(1.28732027925584,2.80715235940912,-17.0970931587537)) ;
#152769 = CARTESIAN_POINT('Ctrl Pts',(1.28695835013164,2.80793550920672,-17.0968946174353)) ;
#152770 = CARTESIAN_POINT('Ctrl Pts',(1.28660568774189,2.80872522382217,-17.0967010437072)) ;
#152771 = CARTESIAN_POINT('Ctrl Pts',(1.28608376699194,2.80991454434775,-17.0964145021015)) ;
#152772 = CARTESIAN_POINT('Ctrl Pts',(1.28574525149599,2.81071375754612,-17.0962285681094)) ;
#152773 = CARTESIAN_POINT('Ctrl Pts',(1.28475894023894,2.81312894312825,-17.095686733351)) ;
#152774 = CARTESIAN_POINT('Ctrl Pts',(1.28414040309302,2.81476247656145,-17.095346833702)) ;
#152775 = CARTESIAN_POINT('Ctrl Pts',(1.28339818260912,2.81688756020153,-17.094939111358)) ;
#152776 = CARTESIAN_POINT('Ctrl Pts',(1.28323661013042,2.81736137575532,-17.0948503628219)) ;
#152777 = CARTESIAN_POINT('Ctrl Pts',(1.28265668893879,2.8191041114044,-17.0945318526463)) ;
#152778 = CARTESIAN_POINT('Ctrl Pts',(1.28225920250332,2.82038205281193,-17.0943136076747)) ;
#152779 = CARTESIAN_POINT('Ctrl Pts',(1.28170385606936,2.82230051526773,-17.0940086650164)) ;
#152780 = CARTESIAN_POINT('Ctrl Pts',(1.28152700208472,2.82293438010914,-17.0939115582297)) ;
#152781 = CARTESIAN_POINT('Ctrl Pts',(1.28107448868731,2.82461913389175,-17.0936630908507)) ;
#152782 = CARTESIAN_POINT('Ctrl Pts',(1.28081016954772,2.82567198476339,-17.0935180110459)) ;
#152783 = CARTESIAN_POINT('Ctrl Pts',(1.2800991035332,2.82871092361134,-17.0931278319823)) ;
#152784 = CARTESIAN_POINT('Ctrl Pts',(1.27969380338793,2.83071459002993,-17.0929051291199)) ;
#152785 = CARTESIAN_POINT('Ctrl Pts',(1.27923282767964,2.83340629334536,-17.0926515462665)) ;
#152786 = CARTESIAN_POINT('Ctrl Pts',(1.27912420342281,2.8340808992611,-17.0925917647842)) ;
#152787 = CARTESIAN_POINT('Ctrl Pts',(1.27861441353188,2.83746106027945,-17.0923110911817)) ;
#152788 = CARTESIAN_POINT('Ctrl Pts',(1.27831324287571,2.84018799487017,-17.0921449017566)) ;
#152789 = CARTESIAN_POINT('Ctrl Pts',(1.27795656969996,2.84527977141539,-17.0919480133439)) ;
#152790 = CARTESIAN_POINT('Ctrl Pts',(1.27787304021907,2.84764286211077,-17.0919018583827)) ;
#152791 = CARTESIAN_POINT('Ctrl Pts',(1.27787304021907,2.85,-17.0919018583827)) ;
#152792 = CARTESIAN_POINT('',(1.27787304021905,2.85,-13.3880981416173)) ;
#152793 = CARTESIAN_POINT('Origin',(-8.21365282185989E-16,2.85,-15.24)) ;
#152794 = CARTESIAN_POINT('Ctrl Pts',(1.37603597336697,2.75,-13.335)) ;
#152795 = CARTESIAN_POINT('Ctrl Pts',(1.37573512845505,2.75,-13.3351599709432)) ;
#152796 = CARTESIAN_POINT('Ctrl Pts',(1.37543426791753,2.75000132857281,-13.3353199248048)) ;
#152797 = CARTESIAN_POINT('Ctrl Pts',(1.37483257571477,2.75000665190009,-13.3356398448574)) ;
#152798 = CARTESIAN_POINT('Ctrl Pts',(1.37453174406036,2.75001064672752,-13.335799811025)) ;
#152799 = CARTESIAN_POINT('Ctrl Pts',(1.3738872267507,2.75002207412044,-13.3361426442071)) ;
#152800 = CARTESIAN_POINT('Ctrl Pts',(1.37354350385558,2.75002991650282,-13.3363255141619)) ;
#152801 = CARTESIAN_POINT('Ctrl Pts',(1.37285611423782,2.75004911307826,-13.3366912988841)) ;
#152802 = CARTESIAN_POINT('Ctrl Pts',(1.37251244753524,2.75006046723047,-13.3368742136115)) ;
#152803 = CARTESIAN_POINT('Ctrl Pts',(1.37148159444809,2.75009981984526,-13.337422994695)) ;
#152804 = CARTESIAN_POINT('Ctrl Pts',(1.37079455494331,2.75013310886333,-13.3377888982032)) ;
#152805 = CARTESIAN_POINT('Ctrl Pts',(1.36873453110893,2.75025430438115,-13.3388865055866)) ;
#152806 = CARTESIAN_POINT('Ctrl Pts',(1.36736263966052,2.75036354665962,-13.3396181092421)) ;
#152807 = CARTESIAN_POINT('Ctrl Pts',(1.36413470836879,2.7506890391408,-13.3413410689378)) ;
#152808 = CARTESIAN_POINT('Ctrl Pts',(1.36227932197148,2.7509298085102,-13.342332637721)) ;
#152809 = CARTESIAN_POINT('Ctrl Pts',(1.35746012444742,2.75169859670378,-13.3449111819216)) ;
#152810 = CARTESIAN_POINT('Ctrl Pts',(1.35450425835489,2.75231332717648,-13.3464957625411)) ;
#152811 = CARTESIAN_POINT('Ctrl Pts',(1.34886973918563,2.7537703424146,-13.3495208305066)) ;
#152812 = CARTESIAN_POINT('Ctrl Pts',(1.34617831568149,2.75459534477999,-13.3509678592584)) ;
#152813 = CARTESIAN_POINT('Ctrl Pts',(1.34314242260182,2.75567798707045,-13.352601530123)) ;
#152814 = CARTESIAN_POINT('Ctrl Pts',(1.34256163823225,2.75588931242803,-13.352914101785)) ;
#152815 = CARTESIAN_POINT('Ctrl Pts',(1.34198261999808,2.75610647364235,-13.3532257815815)) ;
#152816 = CARTESIAN_POINT('Ctrl Pts',(1.34132160522919,2.75635697290854,-13.3535816219834)) ;
#152817 = CARTESIAN_POINT('Ctrl Pts',(1.34086291435069,2.75653491456653,-13.3538285825319)) ;
#152818 = CARTESIAN_POINT('Ctrl Pts',(1.33918548989955,2.75720079503567,-13.3547318375006)) ;
#152819 = CARTESIAN_POINT('Ctrl Pts',(1.33797416370947,2.75771112313093,-13.3553843482652)) ;
#152820 = CARTESIAN_POINT('Ctrl Pts',(1.33648532079705,2.75837521508441,-13.3561866329489)) ;
#152821 = CARTESIAN_POINT('Ctrl Pts',(1.33619776328717,2.75850521488808,-13.3563415973022)) ;
#152822 = CARTESIAN_POINT('Ctrl Pts',(1.33107968015608,2.76084915994924,-13.3591000397118)) ;
#152823 = CARTESIAN_POINT('Ctrl Pts',(1.32635908659443,2.76350693339028,-13.3616480195487)) ;
#152824 = CARTESIAN_POINT('Ctrl Pts',(1.32109760625997,2.76707470328435,-13.364494716912)) ;
#152825 = CARTESIAN_POINT('Ctrl Pts',(1.32035743991805,2.7675912878831,-13.364895352445)) ;
#152826 = CARTESIAN_POINT('Ctrl Pts',(1.31824805546067,2.76910584227481,-13.3660376626109)) ;
#152827 = CARTESIAN_POINT('Ctrl Pts',(1.31689309423375,2.77013099976529,-13.3667722633588)) ;
#152828 = CARTESIAN_POINT('Ctrl Pts',(1.31545882361433,2.77127278201748,-13.3675511219407)) ;
#152829 = CARTESIAN_POINT('Ctrl Pts',(1.31535582310954,2.77135510350024,-13.3676070616534)) ;
#152830 = CARTESIAN_POINT('Ctrl Pts',(1.31504853092205,2.77160168095801,-13.367773973447)) ;
#152831 = CARTESIAN_POINT('Ctrl Pts',(1.31461168315421,2.77195498754746,-13.3680113068541)) ;
#152832 = CARTESIAN_POINT('Ctrl Pts',(1.31417742224133,2.77231219724372,-13.3682473370571)) ;
#152833 = CARTESIAN_POINT('Ctrl Pts',(1.3133309602631,2.77301480846575,-13.3687075061369)) ;
#152834 = CARTESIAN_POINT('Ctrl Pts',(1.31272070342851,2.77353368974773,-13.3690394568406)) ;
#152835 = CARTESIAN_POINT('Ctrl Pts',(1.30969774837129,2.77616736630461,-13.3706845572382)) ;
#152836 = CARTESIAN_POINT('Ctrl Pts',(1.30737022788695,2.77840054644579,-13.3719534798951)) ;
#152837 = CARTESIAN_POINT('Ctrl Pts',(1.30464757270881,2.78128817542227,-13.3734387033489)) ;
#152838 = CARTESIAN_POINT('Ctrl Pts',(1.30414845981078,2.78182967606624,-13.3737110126307)) ;
#152839 = CARTESIAN_POINT('Ctrl Pts',(1.30260826844057,2.78353926416389,-13.3745514286369)) ;
#152840 = CARTESIAN_POINT('Ctrl Pts',(1.30158324720849,2.78473373830867,-13.3751112329214)) ;
#152841 = CARTESIAN_POINT('Ctrl Pts',(1.30024935135332,2.7863673885274,-13.3758398127168)) ;
#152842 = CARTESIAN_POINT('Ctrl Pts',(1.29991860867237,2.78677921519273,-13.376020475081)) ;
#152843 = CARTESIAN_POINT('Ctrl Pts',(1.29915346420734,2.78774794465156,-13.3764384192283)) ;
#152844 = CARTESIAN_POINT('Ctrl Pts',(1.29872125904468,2.78830744810474,-13.3766744998873)) ;
#152845 = CARTESIAN_POINT('Ctrl Pts',(1.29658637826221,2.79113377451593,-13.3778405320741)) ;
#152846 = CARTESIAN_POINT('Ctrl Pts',(1.29496240940486,2.79348720429747,-13.3787269863698)) ;
#152847 = CARTESIAN_POINT('Ctrl Pts',(1.29231665668153,2.79769679694547,-13.3801716480049)) ;
#152848 = CARTESIAN_POINT('Ctrl Pts',(1.29125115601059,2.79951540543443,-13.3807540486807)) ;
#152849 = CARTESIAN_POINT('Ctrl Pts',(1.28927619853494,2.80313430045114,-13.3818348789813)) ;
#152850 = CARTESIAN_POINT('Ctrl Pts',(1.28836241997818,2.80493500363976,-13.382335379346)) ;
#152851 = CARTESIAN_POINT('Ctrl Pts',(1.28732027925584,2.80715235940912,-13.3829068412463)) ;
#152852 = CARTESIAN_POINT('Ctrl Pts',(1.28695835013164,2.80793550920674,-13.3831053825645)) ;
#152853 = CARTESIAN_POINT('Ctrl Pts',(1.28660568774189,2.80872522382217,-13.3832989562928)) ;
#152854 = CARTESIAN_POINT('Ctrl Pts',(1.28608376699195,2.80991454434774,-13.3835854978985)) ;
#152855 = CARTESIAN_POINT('Ctrl Pts',(1.285745251496,2.81071375754611,-13.3837714318906)) ;
#152856 = CARTESIAN_POINT('Ctrl Pts',(1.28475894023895,2.81312894312824,-13.384313266649)) ;
#152857 = CARTESIAN_POINT('Ctrl Pts',(1.28414040309303,2.81476247656143,-13.384653166298)) ;
#152858 = CARTESIAN_POINT('Ctrl Pts',(1.28339818260913,2.81688756020151,-13.385060888642)) ;
#152859 = CARTESIAN_POINT('Ctrl Pts',(1.28323661013044,2.8173613757553,-13.3851496371781)) ;
#152860 = CARTESIAN_POINT('Ctrl Pts',(1.28265668893881,2.81910411140437,-13.3854681473537)) ;
#152861 = CARTESIAN_POINT('Ctrl Pts',(1.28225920250334,2.82038205281189,-13.3856863923252)) ;
#152862 = CARTESIAN_POINT('Ctrl Pts',(1.28170385606938,2.8223005152677,-13.3859913349836)) ;
#152863 = CARTESIAN_POINT('Ctrl Pts',(1.28152700208474,2.82293438010913,-13.3860884417703)) ;
#152864 = CARTESIAN_POINT('Ctrl Pts',(1.28107448868732,2.82461913389175,-13.3863369091493)) ;
#152865 = CARTESIAN_POINT('Ctrl Pts',(1.28081016954773,2.8256719847634,-13.3864819889541)) ;
#152866 = CARTESIAN_POINT('Ctrl Pts',(1.28009910353321,2.82871092361134,-13.3868721680177)) ;
#152867 = CARTESIAN_POINT('Ctrl Pts',(1.27969380338794,2.83071459002995,-13.38709487088)) ;
#152868 = CARTESIAN_POINT('Ctrl Pts',(1.27923282767964,2.83340629334538,-13.3873484537334)) ;
#152869 = CARTESIAN_POINT('Ctrl Pts',(1.27912420342282,2.83408089926112,-13.3874082352158)) ;
#152870 = CARTESIAN_POINT('Ctrl Pts',(1.27861441353188,2.83746106027948,-13.3876889088183)) ;
#152871 = CARTESIAN_POINT('Ctrl Pts',(1.2783132428757,2.84018799487021,-13.3878550982434)) ;
#152872 = CARTESIAN_POINT('Ctrl Pts',(1.27795656969994,2.84527977141541,-13.3880519866561)) ;
#152873 = CARTESIAN_POINT('Ctrl Pts',(1.27787304021904,2.84764286211079,-13.3880981416173)) ;
#152874 = CARTESIAN_POINT('Ctrl Pts',(1.27787304021904,2.85,-13.3880981416173)) ;
#152875 = CARTESIAN_POINT('Origin',(1.3145125,4.45,-20.955)) ;
#152876 = CARTESIAN_POINT('',(1.22107868287598,4.55,-20.8195951091213)) ;
#152877 = CARTESIAN_POINT('',(1.22107868287598,4.55,-21.0904048908787)) ;
#152878 = CARTESIAN_POINT('Origin',(1.3145125,4.55,-20.955)) ;
#152879 = CARTESIAN_POINT('',(1.27787304021905,4.45,-20.9019018583827)) ;
#152880 = CARTESIAN_POINT('Origin',(1.22107868287598,4.45,-20.8195951091213)) ;
#152881 = CARTESIAN_POINT('',(1.27787304021905,4.45,-21.0080981416173)) ;
#152882 = CARTESIAN_POINT('Origin',(1.3145125,4.45,-20.955)) ;
#152883 = CARTESIAN_POINT('Origin',(1.22107868287598,4.45,-21.0904048908787)) ;
#152884 = CARTESIAN_POINT('Origin',(-8.21365282185989E-16,2.85,-19.05)) ;
#152885 = CARTESIAN_POINT('',(1.37603597336697,2.75,-20.955)) ;
#152886 = CARTESIAN_POINT('Origin',(-8.13551212474381E-16,2.75,-19.05)) ;
#152887 = CARTESIAN_POINT('',(1.27787304021905,2.85,-20.9019018583827)) ;
#152888 = CARTESIAN_POINT('Ctrl Pts',(1.37603597336697,2.75,-20.955)) ;
#152889 = CARTESIAN_POINT('Ctrl Pts',(1.37543428354306,2.75,-20.9546800581135)) ;
#152890 = CARTESIAN_POINT('Ctrl Pts',(1.37483253111456,2.7500053137259,-20.9543601843411)) ;
#152891 = CARTESIAN_POINT('Ctrl Pts',(1.37388722675069,2.75002207412044,-20.9538573557929)) ;
#152892 = CARTESIAN_POINT('Ctrl Pts',(1.37354350385561,2.75002991650282,-20.9536744858381)) ;
#152893 = CARTESIAN_POINT('Ctrl Pts',(1.37285611423782,2.75004911307826,-20.9533087011159)) ;
#152894 = CARTESIAN_POINT('Ctrl Pts',(1.37251244753524,2.75006046723047,-20.9531257863885)) ;
#152895 = CARTESIAN_POINT('Ctrl Pts',(1.3714815944481,2.75009981984526,-20.952577005305)) ;
#152896 = CARTESIAN_POINT('Ctrl Pts',(1.37079455494331,2.75013310886333,-20.9522111017968)) ;
#152897 = CARTESIAN_POINT('Ctrl Pts',(1.36873453110892,2.75025430438116,-20.9511134944134)) ;
#152898 = CARTESIAN_POINT('Ctrl Pts',(1.36736263966051,2.75036354665963,-20.9503818907579)) ;
#152899 = CARTESIAN_POINT('Ctrl Pts',(1.36413470836879,2.75068903914081,-20.9486589310622)) ;
#152900 = CARTESIAN_POINT('Ctrl Pts',(1.36227932197147,2.75092980851022,-20.947667362279)) ;
#152901 = CARTESIAN_POINT('Ctrl Pts',(1.35746012444742,2.7516985967038,-20.9450888180784)) ;
#152902 = CARTESIAN_POINT('Ctrl Pts',(1.35450425835489,2.7523133271765,-20.943504237459)) ;
#152903 = CARTESIAN_POINT('Ctrl Pts',(1.34886973918564,2.75377034241463,-20.9404791694934)) ;
#152904 = CARTESIAN_POINT('Ctrl Pts',(1.3461783156815,2.75459534478002,-20.9390321407416)) ;
#152905 = CARTESIAN_POINT('Ctrl Pts',(1.34314242260183,2.75567798707048,-20.9373984698771)) ;
#152906 = CARTESIAN_POINT('Ctrl Pts',(1.34256163823226,2.75588931242806,-20.937085898215)) ;
#152907 = CARTESIAN_POINT('Ctrl Pts',(1.34198261999809,2.75610647364238,-20.9367742184185)) ;
#152908 = CARTESIAN_POINT('Ctrl Pts',(1.3413216052292,2.75635697290857,-20.9364183780167)) ;
#152909 = CARTESIAN_POINT('Ctrl Pts',(1.3408629143507,2.75653491456656,-20.9361714174681)) ;
#152910 = CARTESIAN_POINT('Ctrl Pts',(1.33918548989955,2.7572007950357,-20.9352681624994)) ;
#152911 = CARTESIAN_POINT('Ctrl Pts',(1.33797416370948,2.75771112313095,-20.9346156517349)) ;
#152912 = CARTESIAN_POINT('Ctrl Pts',(1.33648532079705,2.75837521508443,-20.9338133670511)) ;
#152913 = CARTESIAN_POINT('Ctrl Pts',(1.33619776328717,2.7585052148881,-20.9336584026979)) ;
#152914 = CARTESIAN_POINT('Ctrl Pts',(1.33107968015532,2.76084915994961,-20.9308999602878)) ;
#152915 = CARTESIAN_POINT('Ctrl Pts',(1.32635908659293,2.76350693339113,-20.9283519804505)) ;
#152916 = CARTESIAN_POINT('Ctrl Pts',(1.32109760625854,2.76707470328536,-20.9255052830872)) ;
#152917 = CARTESIAN_POINT('Ctrl Pts',(1.32035743991734,2.76759128788362,-20.9251046475546)) ;
#152918 = CARTESIAN_POINT('Ctrl Pts',(1.31824805546067,2.76910584227483,-20.9239623373891)) ;
#152919 = CARTESIAN_POINT('Ctrl Pts',(1.31689309423375,2.77013099976531,-20.9232277366411)) ;
#152920 = CARTESIAN_POINT('Ctrl Pts',(1.31545882361433,2.7712727820175,-20.9224488780592)) ;
#152921 = CARTESIAN_POINT('Ctrl Pts',(1.31535582310954,2.77135510350026,-20.9223929383465)) ;
#152922 = CARTESIAN_POINT('Ctrl Pts',(1.31504853092203,2.77160168095803,-20.922226026553)) ;
#152923 = CARTESIAN_POINT('Ctrl Pts',(1.31461168315421,2.7719549875475,-20.9219886931459)) ;
#152924 = CARTESIAN_POINT('Ctrl Pts',(1.31417742224132,2.77231219724374,-20.9217526629429)) ;
#152925 = CARTESIAN_POINT('Ctrl Pts',(1.31333096026308,2.77301480846578,-20.921292493863)) ;
#152926 = CARTESIAN_POINT('Ctrl Pts',(1.31272070342849,2.77353368974775,-20.9209605431594)) ;
#152927 = CARTESIAN_POINT('Ctrl Pts',(1.30969774837126,2.77616736630462,-20.9193154427618)) ;
#152928 = CARTESIAN_POINT('Ctrl Pts',(1.30737022788692,2.7784005464458,-20.9180465201049)) ;
#152929 = CARTESIAN_POINT('Ctrl Pts',(1.30464757270879,2.78128817542227,-20.9165612966511)) ;
#152930 = CARTESIAN_POINT('Ctrl Pts',(1.30414845981076,2.78182967606623,-20.9162889873692)) ;
#152931 = CARTESIAN_POINT('Ctrl Pts',(1.30260826844055,2.78353926416386,-20.9154485713631)) ;
#152932 = CARTESIAN_POINT('Ctrl Pts',(1.30158324720848,2.78473373830863,-20.9148887670786)) ;
#152933 = CARTESIAN_POINT('Ctrl Pts',(1.30024935135331,2.78636738852735,-20.9141601872833)) ;
#152934 = CARTESIAN_POINT('Ctrl Pts',(1.29991860867236,2.78677921519269,-20.913979524919)) ;
#152935 = CARTESIAN_POINT('Ctrl Pts',(1.29915346420734,2.78774794465152,-20.9135615807717)) ;
#152936 = CARTESIAN_POINT('Ctrl Pts',(1.29872125904468,2.78830744810469,-20.9133255001127)) ;
#152937 = CARTESIAN_POINT('Ctrl Pts',(1.29658637826222,2.79113377451588,-20.9121594679259)) ;
#152938 = CARTESIAN_POINT('Ctrl Pts',(1.29496240940488,2.79348720429743,-20.9112730136302)) ;
#152939 = CARTESIAN_POINT('Ctrl Pts',(1.29231665668155,2.79769679694544,-20.909828351995)) ;
#152940 = CARTESIAN_POINT('Ctrl Pts',(1.2912511560106,2.79951540543442,-20.9092459513193)) ;
#152941 = CARTESIAN_POINT('Ctrl Pts',(1.28927619853494,2.80313430045114,-20.9081651210187)) ;
#152942 = CARTESIAN_POINT('Ctrl Pts',(1.28836241997818,2.80493500363976,-20.907664620654)) ;
#152943 = CARTESIAN_POINT('Ctrl Pts',(1.28732027925583,2.80715235940912,-20.9070931587537)) ;
#152944 = CARTESIAN_POINT('Ctrl Pts',(1.28695835013165,2.80793550920672,-20.9068946174353)) ;
#152945 = CARTESIAN_POINT('Ctrl Pts',(1.28660568774189,2.80872522382216,-20.9067010437072)) ;
#152946 = CARTESIAN_POINT('Ctrl Pts',(1.28608376699195,2.80991454434774,-20.9064145021015)) ;
#152947 = CARTESIAN_POINT('Ctrl Pts',(1.285745251496,2.8107137575461,-20.9062285681094)) ;
#152948 = CARTESIAN_POINT('Ctrl Pts',(1.28475894023895,2.81312894312822,-20.905686733351)) ;
#152949 = CARTESIAN_POINT('Ctrl Pts',(1.28414040309303,2.81476247656142,-20.905346833702)) ;
#152950 = CARTESIAN_POINT('Ctrl Pts',(1.28339818260913,2.81688756020149,-20.904939111358)) ;
#152951 = CARTESIAN_POINT('Ctrl Pts',(1.28323661013043,2.81736137575528,-20.9048503628219)) ;
#152952 = CARTESIAN_POINT('Ctrl Pts',(1.2826566889388,2.81910411140435,-20.9045318526463)) ;
#152953 = CARTESIAN_POINT('Ctrl Pts',(1.28225920250334,2.82038205281187,-20.9043136076747)) ;
#152954 = CARTESIAN_POINT('Ctrl Pts',(1.28170385606937,2.82230051526769,-20.9040086650164)) ;
#152955 = CARTESIAN_POINT('Ctrl Pts',(1.28152700208473,2.82293438010912,-20.9039115582297)) ;
#152956 = CARTESIAN_POINT('Ctrl Pts',(1.28107448868731,2.82461913389174,-20.9036630908507)) ;
#152957 = CARTESIAN_POINT('Ctrl Pts',(1.28081016954772,2.82567198476339,-20.9035180110459)) ;
#152958 = CARTESIAN_POINT('Ctrl Pts',(1.2800991035332,2.82871092361133,-20.9031278319823)) ;
#152959 = CARTESIAN_POINT('Ctrl Pts',(1.27969380338793,2.83071459002993,-20.9029051291199)) ;
#152960 = CARTESIAN_POINT('Ctrl Pts',(1.27923282767964,2.83340629334536,-20.9026515462665)) ;
#152961 = CARTESIAN_POINT('Ctrl Pts',(1.27912420342282,2.8340808992611,-20.9025917647842)) ;
#152962 = CARTESIAN_POINT('Ctrl Pts',(1.27861441353189,2.83746106027945,-20.9023110911817)) ;
#152963 = CARTESIAN_POINT('Ctrl Pts',(1.27831324287571,2.84018799487017,-20.9021449017566)) ;
#152964 = CARTESIAN_POINT('Ctrl Pts',(1.27795656969996,2.84527977141539,-20.9019480133439)) ;
#152965 = CARTESIAN_POINT('Ctrl Pts',(1.27787304021906,2.84764286211077,-20.9019018583827)) ;
#152966 = CARTESIAN_POINT('Ctrl Pts',(1.27787304021907,2.85,-20.9019018583827)) ;
#152967 = CARTESIAN_POINT('',(1.27787304021905,2.85,-17.1980981416173)) ;
#152968 = CARTESIAN_POINT('Origin',(-8.21365282185989E-16,2.85,-19.05)) ;
#152969 = CARTESIAN_POINT('Ctrl Pts',(1.37603597336697,2.75,-17.145)) ;
#152970 = CARTESIAN_POINT('Ctrl Pts',(1.37573512845497,2.75,-17.1451599709439)) ;
#152971 = CARTESIAN_POINT('Ctrl Pts',(1.37543426791699,2.75000132857849,-17.1453199247894)) ;
#152972 = CARTESIAN_POINT('Ctrl Pts',(1.37483257571475,2.75000665190009,-17.1456398448574)) ;
#152973 = CARTESIAN_POINT('Ctrl Pts',(1.37453174406034,2.75001064672751,-17.145799811025)) ;
#152974 = CARTESIAN_POINT('Ctrl Pts',(1.37388722675069,2.75002207412045,-17.1461426442071)) ;
#152975 = CARTESIAN_POINT('Ctrl Pts',(1.37354350385561,2.75002991650282,-17.1463255141619)) ;
#152976 = CARTESIAN_POINT('Ctrl Pts',(1.37285611423782,2.75004911307826,-17.1466912988841)) ;
#152977 = CARTESIAN_POINT('Ctrl Pts',(1.37251244753524,2.75006046723047,-17.1468742136116)) ;
#152978 = CARTESIAN_POINT('Ctrl Pts',(1.3714815944481,2.75009981984526,-17.147422994695)) ;
#152979 = CARTESIAN_POINT('Ctrl Pts',(1.37079455494331,2.75013310886333,-17.1477888982032)) ;
#152980 = CARTESIAN_POINT('Ctrl Pts',(1.36873453110892,2.75025430438115,-17.1488865055866)) ;
#152981 = CARTESIAN_POINT('Ctrl Pts',(1.36736263966051,2.75036354665963,-17.1496181092421)) ;
#152982 = CARTESIAN_POINT('Ctrl Pts',(1.36413470836879,2.75068903914081,-17.1513410689378)) ;
#152983 = CARTESIAN_POINT('Ctrl Pts',(1.36227932197147,2.75092980851021,-17.152332637721)) ;
#152984 = CARTESIAN_POINT('Ctrl Pts',(1.35746012444742,2.7516985967038,-17.1549111819216)) ;
#152985 = CARTESIAN_POINT('Ctrl Pts',(1.35450425835489,2.75231332717652,-17.1564957625411)) ;
#152986 = CARTESIAN_POINT('Ctrl Pts',(1.34886973918565,2.75377034241464,-17.1595208305066)) ;
#152987 = CARTESIAN_POINT('Ctrl Pts',(1.3461783156815,2.75459534478002,-17.1609678592584)) ;
#152988 = CARTESIAN_POINT('Ctrl Pts',(1.34314242260183,2.75567798707048,-17.1626015301229)) ;
#152989 = CARTESIAN_POINT('Ctrl Pts',(1.34256163823226,2.75588931242806,-17.162914101785)) ;
#152990 = CARTESIAN_POINT('Ctrl Pts',(1.34198261999809,2.75610647364238,-17.1632257815815)) ;
#152991 = CARTESIAN_POINT('Ctrl Pts',(1.3413216052292,2.75635697290857,-17.1635816219833)) ;
#152992 = CARTESIAN_POINT('Ctrl Pts',(1.3408629143507,2.75653491456656,-17.1638285825319)) ;
#152993 = CARTESIAN_POINT('Ctrl Pts',(1.33918548989955,2.7572007950357,-17.1647318375006)) ;
#152994 = CARTESIAN_POINT('Ctrl Pts',(1.33797416370948,2.75771112313095,-17.1653843482652)) ;
#152995 = CARTESIAN_POINT('Ctrl Pts',(1.33648532079705,2.75837521508443,-17.1661866329489)) ;
#152996 = CARTESIAN_POINT('Ctrl Pts',(1.33619776328717,2.7585052148881,-17.1663415973021)) ;
#152997 = CARTESIAN_POINT('Ctrl Pts',(1.33107968015773,2.7608491599485,-17.1691000397109)) ;
#152998 = CARTESIAN_POINT('Ctrl Pts',(1.32635908659765,2.76350693338849,-17.171648019547)) ;
#152999 = CARTESIAN_POINT('Ctrl Pts',(1.32109760626303,2.76707470328226,-17.1744947169104)) ;
#153000 = CARTESIAN_POINT('Ctrl Pts',(1.32035743991956,2.76759128788205,-17.1748953524443)) ;
#153001 = CARTESIAN_POINT('Ctrl Pts',(1.31824805546067,2.76910584227484,-17.1760376626109)) ;
#153002 = CARTESIAN_POINT('Ctrl Pts',(1.31689309423375,2.77013099976532,-17.1767722633589)) ;
#153003 = CARTESIAN_POINT('Ctrl Pts',(1.31545882361434,2.77127278201751,-17.1775511219408)) ;
#153004 = CARTESIAN_POINT('Ctrl Pts',(1.31535582310954,2.77135510350027,-17.1776070616535)) ;
#153005 = CARTESIAN_POINT('Ctrl Pts',(1.31504853092204,2.77160168095804,-17.177773973447)) ;
#153006 = CARTESIAN_POINT('Ctrl Pts',(1.3146116831542,2.77195498754749,-17.1780113068541)) ;
#153007 = CARTESIAN_POINT('Ctrl Pts',(1.31417742224132,2.77231219724375,-17.1782473370571)) ;
#153008 = CARTESIAN_POINT('Ctrl Pts',(1.31333096026309,2.77301480846578,-17.178707506137)) ;
#153009 = CARTESIAN_POINT('Ctrl Pts',(1.31272070342849,2.77353368974775,-17.1790394568406)) ;
#153010 = CARTESIAN_POINT('Ctrl Pts',(1.30969774837126,2.77616736630463,-17.1806845572382)) ;
#153011 = CARTESIAN_POINT('Ctrl Pts',(1.30737022788692,2.7784005464458,-17.1819534798951)) ;
#153012 = CARTESIAN_POINT('Ctrl Pts',(1.30464757270879,2.78128817542227,-17.1834387033489)) ;
#153013 = CARTESIAN_POINT('Ctrl Pts',(1.30414845981076,2.78182967606624,-17.1837110126307)) ;
#153014 = CARTESIAN_POINT('Ctrl Pts',(1.30260826844056,2.78353926416388,-17.1845514286369)) ;
#153015 = CARTESIAN_POINT('Ctrl Pts',(1.30158324720849,2.78473373830866,-17.1851112329214)) ;
#153016 = CARTESIAN_POINT('Ctrl Pts',(1.30024935135332,2.78636738852739,-17.1858398127168)) ;
#153017 = CARTESIAN_POINT('Ctrl Pts',(1.29991860867237,2.78677921519272,-17.186020475081)) ;
#153018 = CARTESIAN_POINT('Ctrl Pts',(1.29915346420734,2.78774794465155,-17.1864384192283)) ;
#153019 = CARTESIAN_POINT('Ctrl Pts',(1.29872125904467,2.78830744810473,-17.1866744998873)) ;
#153020 = CARTESIAN_POINT('Ctrl Pts',(1.2965863782622,2.79113377451592,-17.1878405320741)) ;
#153021 = CARTESIAN_POINT('Ctrl Pts',(1.29496240940485,2.79348720429746,-17.1887269863698)) ;
#153022 = CARTESIAN_POINT('Ctrl Pts',(1.29231665668153,2.79769679694546,-17.190171648005)) ;
#153023 = CARTESIAN_POINT('Ctrl Pts',(1.29125115601059,2.79951540543443,-17.1907540486807)) ;
#153024 = CARTESIAN_POINT('Ctrl Pts',(1.28927619853494,2.80313430045113,-17.1918348789813)) ;
#153025 = CARTESIAN_POINT('Ctrl Pts',(1.28836241997818,2.80493500363976,-17.192335379346)) ;
#153026 = CARTESIAN_POINT('Ctrl Pts',(1.28732027925583,2.80715235940912,-17.1929068412463)) ;
#153027 = CARTESIAN_POINT('Ctrl Pts',(1.28695835013165,2.80793550920674,-17.1931053825647)) ;
#153028 = CARTESIAN_POINT('Ctrl Pts',(1.28660568774189,2.80872522382217,-17.1932989562928)) ;
#153029 = CARTESIAN_POINT('Ctrl Pts',(1.28608376699194,2.80991454434774,-17.1935854978985)) ;
#153030 = CARTESIAN_POINT('Ctrl Pts',(1.28574525149599,2.81071375754611,-17.1937714318906)) ;
#153031 = CARTESIAN_POINT('Ctrl Pts',(1.28475894023894,2.81312894312823,-17.194313266649)) ;
#153032 = CARTESIAN_POINT('Ctrl Pts',(1.28414040309303,2.81476247656143,-17.194653166298)) ;
#153033 = CARTESIAN_POINT('Ctrl Pts',(1.28339818260913,2.81688756020151,-17.195060888642)) ;
#153034 = CARTESIAN_POINT('Ctrl Pts',(1.28323661013044,2.81736137575529,-17.1951496371781)) ;
#153035 = CARTESIAN_POINT('Ctrl Pts',(1.2826566889388,2.81910411140436,-17.1954681473537)) ;
#153036 = CARTESIAN_POINT('Ctrl Pts',(1.28225920250334,2.82038205281189,-17.1956863923252)) ;
#153037 = CARTESIAN_POINT('Ctrl Pts',(1.28170385606938,2.8223005152677,-17.1959913349836)) ;
#153038 = CARTESIAN_POINT('Ctrl Pts',(1.28152700208473,2.82293438010913,-17.1960884417703)) ;
#153039 = CARTESIAN_POINT('Ctrl Pts',(1.28107448868731,2.82461913389174,-17.1963369091493)) ;
#153040 = CARTESIAN_POINT('Ctrl Pts',(1.28081016954773,2.82567198476338,-17.1964819889541)) ;
#153041 = CARTESIAN_POINT('Ctrl Pts',(1.2800991035332,2.82871092361133,-17.1968721680177)) ;
#153042 = CARTESIAN_POINT('Ctrl Pts',(1.27969380338793,2.83071459002993,-17.1970948708801)) ;
#153043 = CARTESIAN_POINT('Ctrl Pts',(1.27923282767964,2.83340629334536,-17.1973484537335)) ;
#153044 = CARTESIAN_POINT('Ctrl Pts',(1.27912420342282,2.83408089926111,-17.1974082352158)) ;
#153045 = CARTESIAN_POINT('Ctrl Pts',(1.27861441353188,2.83746106027946,-17.1976889088183)) ;
#153046 = CARTESIAN_POINT('Ctrl Pts',(1.27831324287571,2.84018799487019,-17.1978550982434)) ;
#153047 = CARTESIAN_POINT('Ctrl Pts',(1.27795656969996,2.8452797714154,-17.1980519866561)) ;
#153048 = CARTESIAN_POINT('Ctrl Pts',(1.27787304021907,2.84764286211078,-17.1980981416173)) ;
#153049 = CARTESIAN_POINT('Ctrl Pts',(1.27787304021907,2.85,-17.1980981416173)) ;
#153050 = CARTESIAN_POINT('Origin',(1.3145125,4.45,-24.765)) ;
#153051 = CARTESIAN_POINT('',(1.22107868287598,4.55,-24.6295951091213)) ;
#153052 = CARTESIAN_POINT('',(1.22107868287598,4.55,-24.9004048908787)) ;
#153053 = CARTESIAN_POINT('Origin',(1.3145125,4.55,-24.765)) ;
#153054 = CARTESIAN_POINT('',(1.27787304021905,4.45,-24.7119018583827)) ;
#153055 = CARTESIAN_POINT('Origin',(1.22107868287598,4.45,-24.6295951091213)) ;
#153056 = CARTESIAN_POINT('',(1.27787304021905,4.45,-24.8180981416173)) ;
#153057 = CARTESIAN_POINT('Origin',(1.3145125,4.45,-24.765)) ;
#153058 = CARTESIAN_POINT('Origin',(1.22107868287598,4.45,-24.9004048908787)) ;
#153059 = CARTESIAN_POINT('Origin',(-8.21365282185989E-16,2.85,-22.86)) ;
#153060 = CARTESIAN_POINT('',(1.37603597336697,2.75,-24.765)) ;
#153061 = CARTESIAN_POINT('Origin',(-8.13551212474381E-16,2.75,-22.86)) ;
#153062 = CARTESIAN_POINT('',(1.27787304021905,2.85,-24.7119018583827)) ;
#153063 = CARTESIAN_POINT('Ctrl Pts',(1.37603597336697,2.75,-24.765)) ;
#153064 = CARTESIAN_POINT('Ctrl Pts',(1.37543428354307,2.75,-24.7646800581135)) ;
#153065 = CARTESIAN_POINT('Ctrl Pts',(1.37483253111456,2.7500053137259,-24.7643601843412)) ;
#153066 = CARTESIAN_POINT('Ctrl Pts',(1.37388722675069,2.75002207412044,-24.763857355793)) ;
#153067 = CARTESIAN_POINT('Ctrl Pts',(1.37354350385561,2.75002991650282,-24.7636744858378)) ;
#153068 = CARTESIAN_POINT('Ctrl Pts',(1.37285611423782,2.75004911307826,-24.7633087011159)) ;
#153069 = CARTESIAN_POINT('Ctrl Pts',(1.37251244753524,2.75006046723047,-24.7631257863885)) ;
#153070 = CARTESIAN_POINT('Ctrl Pts',(1.3714815944481,2.75009981984526,-24.7625770053051)) ;
#153071 = CARTESIAN_POINT('Ctrl Pts',(1.37079455494331,2.75013310886333,-24.7622111017968)) ;
#153072 = CARTESIAN_POINT('Ctrl Pts',(1.36873453110893,2.75025430438115,-24.7611134944134)) ;
#153073 = CARTESIAN_POINT('Ctrl Pts',(1.36736263966052,2.75036354665963,-24.760381890758)) ;
#153074 = CARTESIAN_POINT('Ctrl Pts',(1.36413470836879,2.75068903914081,-24.7586589310622)) ;
#153075 = CARTESIAN_POINT('Ctrl Pts',(1.36227932197148,2.75092980851021,-24.757667362279)) ;
#153076 = CARTESIAN_POINT('Ctrl Pts',(1.35746012444743,2.7516985967038,-24.7550888180784)) ;
#153077 = CARTESIAN_POINT('Ctrl Pts',(1.35450425835489,2.75231332717649,-24.753504237459)) ;
#153078 = CARTESIAN_POINT('Ctrl Pts',(1.34886973918564,2.75377034241463,-24.7504791694934)) ;
#153079 = CARTESIAN_POINT('Ctrl Pts',(1.34617831568151,2.75459534478002,-24.7490321407416)) ;
#153080 = CARTESIAN_POINT('Ctrl Pts',(1.34314242260183,2.75567798707047,-24.7473984698771)) ;
#153081 = CARTESIAN_POINT('Ctrl Pts',(1.34256163823227,2.75588931242805,-24.747085898215)) ;
#153082 = CARTESIAN_POINT('Ctrl Pts',(1.3419826199981,2.75610647364237,-24.7467742184185)) ;
#153083 = CARTESIAN_POINT('Ctrl Pts',(1.3413216052292,2.75635697290856,-24.7464183780167)) ;
#153084 = CARTESIAN_POINT('Ctrl Pts',(1.34086291435071,2.75653491456655,-24.7461714174681)) ;
#153085 = CARTESIAN_POINT('Ctrl Pts',(1.33918548989956,2.7572007950357,-24.7452681624994)) ;
#153086 = CARTESIAN_POINT('Ctrl Pts',(1.33797416370948,2.75771112313095,-24.7446156517348)) ;
#153087 = CARTESIAN_POINT('Ctrl Pts',(1.33648532079705,2.75837521508443,-24.7438133670511)) ;
#153088 = CARTESIAN_POINT('Ctrl Pts',(1.33619776328718,2.7585052148881,-24.7436584026979)) ;
#153089 = CARTESIAN_POINT('Ctrl Pts',(1.33107968015587,2.76084915994935,-24.7408999602881)) ;
#153090 = CARTESIAN_POINT('Ctrl Pts',(1.326359086594,2.76350693339053,-24.7383519804511)) ;
#153091 = CARTESIAN_POINT('Ctrl Pts',(1.32109760625957,2.76707470328464,-24.7355052830878)) ;
#153092 = CARTESIAN_POINT('Ctrl Pts',(1.32035743991787,2.76759128788323,-24.7351046475549)) ;
#153093 = CARTESIAN_POINT('Ctrl Pts',(1.31824805546069,2.76910584227479,-24.7339623373891)) ;
#153094 = CARTESIAN_POINT('Ctrl Pts',(1.31689309423376,2.77013099976528,-24.7332277366412)) ;
#153095 = CARTESIAN_POINT('Ctrl Pts',(1.31545882361435,2.77127278201747,-24.7324488780593)) ;
#153096 = CARTESIAN_POINT('Ctrl Pts',(1.31535582310957,2.77135510350022,-24.7323929383466)) ;
#153097 = CARTESIAN_POINT('Ctrl Pts',(1.31504853092209,2.77160168095797,-24.732226026553)) ;
#153098 = CARTESIAN_POINT('Ctrl Pts',(1.31461168315425,2.77195498754744,-24.7319886931459)) ;
#153099 = CARTESIAN_POINT('Ctrl Pts',(1.31417742224137,2.77231219724369,-24.7317526629429)) ;
#153100 = CARTESIAN_POINT('Ctrl Pts',(1.31333096026314,2.77301480846572,-24.7312924938631)) ;
#153101 = CARTESIAN_POINT('Ctrl Pts',(1.31272070342855,2.77353368974769,-24.7309605431594)) ;
#153102 = CARTESIAN_POINT('Ctrl Pts',(1.30969774837133,2.77616736630457,-24.7293154427618)) ;
#153103 = CARTESIAN_POINT('Ctrl Pts',(1.307370227887,2.77840054644575,-24.7280465201049)) ;
#153104 = CARTESIAN_POINT('Ctrl Pts',(1.30464757270885,2.78128817542223,-24.7265612966511)) ;
#153105 = CARTESIAN_POINT('Ctrl Pts',(1.30414845981079,2.78182967606622,-24.7262889873693)) ;
#153106 = CARTESIAN_POINT('Ctrl Pts',(1.30260826844056,2.78353926416387,-24.7254485713631)) ;
#153107 = CARTESIAN_POINT('Ctrl Pts',(1.30158324720849,2.78473373830863,-24.7248887670787)) ;
#153108 = CARTESIAN_POINT('Ctrl Pts',(1.30024935135333,2.78636738852735,-24.7241601872833)) ;
#153109 = CARTESIAN_POINT('Ctrl Pts',(1.29991860867238,2.78677921519269,-24.723979524919)) ;
#153110 = CARTESIAN_POINT('Ctrl Pts',(1.29915346420736,2.78774794465151,-24.7235615807717)) ;
#153111 = CARTESIAN_POINT('Ctrl Pts',(1.2987212590447,2.78830744810469,-24.7233255001127)) ;
#153112 = CARTESIAN_POINT('Ctrl Pts',(1.29658637826224,2.79113377451587,-24.7221594679259)) ;
#153113 = CARTESIAN_POINT('Ctrl Pts',(1.29496240940491,2.79348720429741,-24.7212730136302)) ;
#153114 = CARTESIAN_POINT('Ctrl Pts',(1.29231665668157,2.79769679694542,-24.7198283519951)) ;
#153115 = CARTESIAN_POINT('Ctrl Pts',(1.29125115601062,2.79951540543441,-24.7192459513193)) ;
#153116 = CARTESIAN_POINT('Ctrl Pts',(1.28927619853494,2.80313430045114,-24.7181651210187)) ;
#153117 = CARTESIAN_POINT('Ctrl Pts',(1.28836241997818,2.80493500363977,-24.7176646206541)) ;
#153118 = CARTESIAN_POINT('Ctrl Pts',(1.28732027925584,2.80715235940912,-24.7170931587537)) ;
#153119 = CARTESIAN_POINT('Ctrl Pts',(1.28695835013164,2.80793550920674,-24.7168946174355)) ;
#153120 = CARTESIAN_POINT('Ctrl Pts',(1.2866056877419,2.80872522382218,-24.7167010437072)) ;
#153121 = CARTESIAN_POINT('Ctrl Pts',(1.28608376699195,2.80991454434775,-24.7164145021015)) ;
#153122 = CARTESIAN_POINT('Ctrl Pts',(1.285745251496,2.81071375754612,-24.7162285681094)) ;
#153123 = CARTESIAN_POINT('Ctrl Pts',(1.28475894023895,2.81312894312825,-24.715686733351)) ;
#153124 = CARTESIAN_POINT('Ctrl Pts',(1.28414040309302,2.81476247656145,-24.715346833702)) ;
#153125 = CARTESIAN_POINT('Ctrl Pts',(1.28339818260913,2.81688756020153,-24.714939111358)) ;
#153126 = CARTESIAN_POINT('Ctrl Pts',(1.28323661013044,2.81736137575531,-24.7148503628219)) ;
#153127 = CARTESIAN_POINT('Ctrl Pts',(1.2826566889388,2.81910411140439,-24.7145318526463)) ;
#153128 = CARTESIAN_POINT('Ctrl Pts',(1.28225920250333,2.82038205281191,-24.7143136076748)) ;
#153129 = CARTESIAN_POINT('Ctrl Pts',(1.28170385606937,2.82230051526772,-24.7140086650164)) ;
#153130 = CARTESIAN_POINT('Ctrl Pts',(1.28152700208474,2.82293438010913,-24.7139115582297)) ;
#153131 = CARTESIAN_POINT('Ctrl Pts',(1.28107448868732,2.82461913389174,-24.7136630908507)) ;
#153132 = CARTESIAN_POINT('Ctrl Pts',(1.28081016954773,2.82567198476338,-24.7135180110459)) ;
#153133 = CARTESIAN_POINT('Ctrl Pts',(1.28009910353321,2.82871092361133,-24.7131278319823)) ;
#153134 = CARTESIAN_POINT('Ctrl Pts',(1.27969380338794,2.83071459002993,-24.71290512912)) ;
#153135 = CARTESIAN_POINT('Ctrl Pts',(1.27923282767965,2.83340629334535,-24.7126515462666)) ;
#153136 = CARTESIAN_POINT('Ctrl Pts',(1.27912420342283,2.83408089926109,-24.7125917647842)) ;
#153137 = CARTESIAN_POINT('Ctrl Pts',(1.27861441353189,2.83746106027943,-24.7123110911817)) ;
#153138 = CARTESIAN_POINT('Ctrl Pts',(1.27831324287572,2.84018799487015,-24.7121449017567)) ;
#153139 = CARTESIAN_POINT('Ctrl Pts',(1.27795656969997,2.84527977141537,-24.7119480133439)) ;
#153140 = CARTESIAN_POINT('Ctrl Pts',(1.27787304021907,2.84764286211077,-24.7119018583827)) ;
#153141 = CARTESIAN_POINT('Ctrl Pts',(1.27787304021907,2.85,-24.7119018583827)) ;
#153142 = CARTESIAN_POINT('',(1.27787304021905,2.85,-21.0080981416173)) ;
#153143 = CARTESIAN_POINT('Origin',(-8.21365282185989E-16,2.85,-22.86)) ;
#153144 = CARTESIAN_POINT('Ctrl Pts',(1.37603597336697,2.75,-20.955)) ;
#153145 = CARTESIAN_POINT('Ctrl Pts',(1.37573512845497,2.75,-20.9551599709441)) ;
#153146 = CARTESIAN_POINT('Ctrl Pts',(1.37543426791699,2.75000132857849,-20.9553199247806)) ;
#153147 = CARTESIAN_POINT('Ctrl Pts',(1.37483257571475,2.75000665190009,-20.9556398448574)) ;
#153148 = CARTESIAN_POINT('Ctrl Pts',(1.37453174406034,2.75001064672752,-20.955799811025)) ;
#153149 = CARTESIAN_POINT('Ctrl Pts',(1.37388722675069,2.75002207412044,-20.9561426442071)) ;
#153150 = CARTESIAN_POINT('Ctrl Pts',(1.37354350385561,2.75002991650282,-20.9563255141619)) ;
#153151 = CARTESIAN_POINT('Ctrl Pts',(1.37285611423782,2.75004911307826,-20.9566912988841)) ;
#153152 = CARTESIAN_POINT('Ctrl Pts',(1.37251244753524,2.75006046723047,-20.9568742136115)) ;
#153153 = CARTESIAN_POINT('Ctrl Pts',(1.3714815944481,2.75009981984526,-20.957422994695)) ;
#153154 = CARTESIAN_POINT('Ctrl Pts',(1.37079455494331,2.75013310886333,-20.9577888982032)) ;
#153155 = CARTESIAN_POINT('Ctrl Pts',(1.36873453110892,2.75025430438116,-20.9588865055866)) ;
#153156 = CARTESIAN_POINT('Ctrl Pts',(1.36736263966051,2.75036354665963,-20.9596181092421)) ;
#153157 = CARTESIAN_POINT('Ctrl Pts',(1.36413470836879,2.75068903914081,-20.9613410689378)) ;
#153158 = CARTESIAN_POINT('Ctrl Pts',(1.36227932197147,2.75092980851022,-20.962332637721)) ;
#153159 = CARTESIAN_POINT('Ctrl Pts',(1.35746012444742,2.7516985967038,-20.9649111819216)) ;
#153160 = CARTESIAN_POINT('Ctrl Pts',(1.35450425835489,2.75231332717652,-20.9664957625411)) ;
#153161 = CARTESIAN_POINT('Ctrl Pts',(1.34886973918565,2.75377034241464,-20.9695208305066)) ;
#153162 = CARTESIAN_POINT('Ctrl Pts',(1.3461783156815,2.75459534478003,-20.9709678592584)) ;
#153163 = CARTESIAN_POINT('Ctrl Pts',(1.34314242260183,2.75567798707048,-20.9726015301229)) ;
#153164 = CARTESIAN_POINT('Ctrl Pts',(1.34256163823226,2.75588931242806,-20.972914101785)) ;
#153165 = CARTESIAN_POINT('Ctrl Pts',(1.34198261999809,2.75610647364238,-20.9732257815815)) ;
#153166 = CARTESIAN_POINT('Ctrl Pts',(1.3413216052292,2.75635697290857,-20.9735816219833)) ;
#153167 = CARTESIAN_POINT('Ctrl Pts',(1.3408629143507,2.75653491456656,-20.9738285825319)) ;
#153168 = CARTESIAN_POINT('Ctrl Pts',(1.33918548989956,2.7572007950357,-20.9747318375006)) ;
#153169 = CARTESIAN_POINT('Ctrl Pts',(1.33797416370948,2.75771112313096,-20.9753843482651)) ;
#153170 = CARTESIAN_POINT('Ctrl Pts',(1.33648532079705,2.75837521508444,-20.9761866329489)) ;
#153171 = CARTESIAN_POINT('Ctrl Pts',(1.33619776328717,2.7585052148881,-20.9763415973021)) ;
#153172 = CARTESIAN_POINT('Ctrl Pts',(1.33107968015759,2.76084915994857,-20.979100039711)) ;
#153173 = CARTESIAN_POINT('Ctrl Pts',(1.32635908659737,2.76350693338865,-20.9816480195471)) ;
#153174 = CARTESIAN_POINT('Ctrl Pts',(1.32109760626276,2.76707470328244,-20.9844947169106)) ;
#153175 = CARTESIAN_POINT('Ctrl Pts',(1.32035743991943,2.76759128788214,-20.9848953524443)) ;
#153176 = CARTESIAN_POINT('Ctrl Pts',(1.31824805546067,2.76910584227485,-20.9860376626109)) ;
#153177 = CARTESIAN_POINT('Ctrl Pts',(1.31689309423375,2.77013099976532,-20.9867722633589)) ;
#153178 = CARTESIAN_POINT('Ctrl Pts',(1.31545882361433,2.77127278201751,-20.9875511219408)) ;
#153179 = CARTESIAN_POINT('Ctrl Pts',(1.31535582310953,2.77135510350028,-20.9876070616535)) ;
#153180 = CARTESIAN_POINT('Ctrl Pts',(1.31504853092203,2.77160168095805,-20.987773973447)) ;
#153181 = CARTESIAN_POINT('Ctrl Pts',(1.31461168315419,2.7719549875475,-20.9880113068541)) ;
#153182 = CARTESIAN_POINT('Ctrl Pts',(1.31417742224131,2.77231219724376,-20.9882473370571)) ;
#153183 = CARTESIAN_POINT('Ctrl Pts',(1.31333096026308,2.77301480846579,-20.988707506137)) ;
#153184 = CARTESIAN_POINT('Ctrl Pts',(1.31272070342848,2.77353368974776,-20.9890394568406)) ;
#153185 = CARTESIAN_POINT('Ctrl Pts',(1.30969774837125,2.77616736630464,-20.9906845572382)) ;
#153186 = CARTESIAN_POINT('Ctrl Pts',(1.30737022788691,2.77840054644581,-20.9919534798951)) ;
#153187 = CARTESIAN_POINT('Ctrl Pts',(1.30464757270878,2.78128817542228,-20.9934387033489)) ;
#153188 = CARTESIAN_POINT('Ctrl Pts',(1.30414845981075,2.78182967606624,-20.9937110126307)) ;
#153189 = CARTESIAN_POINT('Ctrl Pts',(1.30260826844056,2.78353926416389,-20.9945514286369)) ;
#153190 = CARTESIAN_POINT('Ctrl Pts',(1.30158324720848,2.78473373830866,-20.9951112329214)) ;
#153191 = CARTESIAN_POINT('Ctrl Pts',(1.30024935135331,2.7863673885274,-20.9958398127168)) ;
#153192 = CARTESIAN_POINT('Ctrl Pts',(1.29991860867236,2.78677921519273,-20.996020475081)) ;
#153193 = CARTESIAN_POINT('Ctrl Pts',(1.29915346420733,2.78774794465156,-20.9964384192283)) ;
#153194 = CARTESIAN_POINT('Ctrl Pts',(1.29872125904466,2.78830744810474,-20.9966744998873)) ;
#153195 = CARTESIAN_POINT('Ctrl Pts',(1.29658637826218,2.79113377451594,-20.9978405320741)) ;
#153196 = CARTESIAN_POINT('Ctrl Pts',(1.29496240940483,2.79348720429749,-20.9987269863698)) ;
#153197 = CARTESIAN_POINT('Ctrl Pts',(1.29231665668151,2.79769679694549,-21.000171648005)) ;
#153198 = CARTESIAN_POINT('Ctrl Pts',(1.29125115601058,2.79951540543444,-21.0007540486807)) ;
#153199 = CARTESIAN_POINT('Ctrl Pts',(1.28927619853494,2.80313430045113,-21.0018348789813)) ;
#153200 = CARTESIAN_POINT('Ctrl Pts',(1.28836241997818,2.80493500363975,-21.002335379346)) ;
#153201 = CARTESIAN_POINT('Ctrl Pts',(1.28732027925583,2.80715235940912,-21.0029068412463)) ;
#153202 = CARTESIAN_POINT('Ctrl Pts',(1.28695835013163,2.80793550920672,-21.0031053825645)) ;
#153203 = CARTESIAN_POINT('Ctrl Pts',(1.28660568774189,2.80872522382217,-21.0032989562928)) ;
#153204 = CARTESIAN_POINT('Ctrl Pts',(1.28608376699194,2.80991454434776,-21.0035854978985)) ;
#153205 = CARTESIAN_POINT('Ctrl Pts',(1.28574525149598,2.81071375754613,-21.0037714318906)) ;
#153206 = CARTESIAN_POINT('Ctrl Pts',(1.28475894023893,2.81312894312826,-21.004313266649)) ;
#153207 = CARTESIAN_POINT('Ctrl Pts',(1.284140403093,2.81476247656146,-21.004653166298)) ;
#153208 = CARTESIAN_POINT('Ctrl Pts',(1.2833981826091,2.81688756020155,-21.005060888642)) ;
#153209 = CARTESIAN_POINT('Ctrl Pts',(1.28323661013042,2.81736137575535,-21.0051496371781)) ;
#153210 = CARTESIAN_POINT('Ctrl Pts',(1.28265668893878,2.81910411140443,-21.0054681473537)) ;
#153211 = CARTESIAN_POINT('Ctrl Pts',(1.28225920250331,2.82038205281195,-21.0056863923253)) ;
#153212 = CARTESIAN_POINT('Ctrl Pts',(1.28170385606935,2.82230051526775,-21.0059913349836)) ;
#153213 = CARTESIAN_POINT('Ctrl Pts',(1.28152700208472,2.82293438010915,-21.0060884417703)) ;
#153214 = CARTESIAN_POINT('Ctrl Pts',(1.28107448868731,2.82461913389174,-21.0063369091493)) ;
#153215 = CARTESIAN_POINT('Ctrl Pts',(1.28081016954772,2.82567198476338,-21.0064819889541)) ;
#153216 = CARTESIAN_POINT('Ctrl Pts',(1.2800991035332,2.82871092361133,-21.0068721680177)) ;
#153217 = CARTESIAN_POINT('Ctrl Pts',(1.27969380338793,2.83071459002992,-21.00709487088)) ;
#153218 = CARTESIAN_POINT('Ctrl Pts',(1.27923282767964,2.83340629334535,-21.0073484537334)) ;
#153219 = CARTESIAN_POINT('Ctrl Pts',(1.27912420342281,2.83408089926109,-21.0074082352158)) ;
#153220 = CARTESIAN_POINT('Ctrl Pts',(1.27861441353188,2.83746106027943,-21.0076889088183)) ;
#153221 = CARTESIAN_POINT('Ctrl Pts',(1.27831324287571,2.84018799487015,-21.0078550982434)) ;
#153222 = CARTESIAN_POINT('Ctrl Pts',(1.27795656969996,2.84527977141538,-21.0080519866561)) ;
#153223 = CARTESIAN_POINT('Ctrl Pts',(1.27787304021907,2.84764286211077,-21.0080981416173)) ;
#153224 = CARTESIAN_POINT('Ctrl Pts',(1.27787304021907,2.85,-21.0080981416173)) ;
#153225 = CARTESIAN_POINT('Origin',(1.3145125,4.45,-28.575)) ;
#153226 = CARTESIAN_POINT('',(1.22107868287598,4.55,-28.4395951091213)) ;
#153227 = CARTESIAN_POINT('',(1.22107868287598,4.55,-28.7104048908787)) ;
#153228 = CARTESIAN_POINT('Origin',(1.3145125,4.55,-28.575)) ;
#153229 = CARTESIAN_POINT('',(1.27787304021905,4.45,-28.5219018583827)) ;
#153230 = CARTESIAN_POINT('Origin',(1.22107868287598,4.45,-28.4395951091213)) ;
#153231 = CARTESIAN_POINT('',(1.27787304021905,4.45,-28.6280981416173)) ;
#153232 = CARTESIAN_POINT('Origin',(1.3145125,4.45,-28.575)) ;
#153233 = CARTESIAN_POINT('Origin',(1.22107868287598,4.45,-28.7104048908787)) ;
#153234 = CARTESIAN_POINT('Origin',(-8.21365282185989E-16,2.85,-26.67)) ;
#153235 = CARTESIAN_POINT('',(1.37603597336697,2.75,-28.575)) ;
#153236 = CARTESIAN_POINT('Origin',(-8.13551212474381E-16,2.75,-26.67)) ;
#153237 = CARTESIAN_POINT('',(1.27787304021905,2.85,-28.5219018583827)) ;
#153238 = CARTESIAN_POINT('Ctrl Pts',(1.37603597336697,2.75,-28.575)) ;
#153239 = CARTESIAN_POINT('Ctrl Pts',(1.37573512845497,2.75,-28.5748400290576)) ;
#153240 = CARTESIAN_POINT('Ctrl Pts',(1.37543426791934,2.75000132857352,-28.5746800751649)) ;
#153241 = CARTESIAN_POINT('Ctrl Pts',(1.37483257571476,2.75000665190009,-28.5743601551427)) ;
#153242 = CARTESIAN_POINT('Ctrl Pts',(1.37453174406035,2.75001064672751,-28.5742001889751)) ;
#153243 = CARTESIAN_POINT('Ctrl Pts',(1.37388722675069,2.75002207412045,-28.573857355793)) ;
#153244 = CARTESIAN_POINT('Ctrl Pts',(1.37354350385561,2.75002991650282,-28.5736744858378)) ;
#153245 = CARTESIAN_POINT('Ctrl Pts',(1.37285611423782,2.75004911307826,-28.5733087011159)) ;
#153246 = CARTESIAN_POINT('Ctrl Pts',(1.37251244753524,2.75006046723047,-28.5731257863885)) ;
#153247 = CARTESIAN_POINT('Ctrl Pts',(1.3714815944481,2.75009981984526,-28.572577005305)) ;
#153248 = CARTESIAN_POINT('Ctrl Pts',(1.37079455494331,2.75013310886333,-28.5722111017968)) ;
#153249 = CARTESIAN_POINT('Ctrl Pts',(1.36873453110893,2.75025430438115,-28.5711134944134)) ;
#153250 = CARTESIAN_POINT('Ctrl Pts',(1.36736263966052,2.75036354665963,-28.5703818907579)) ;
#153251 = CARTESIAN_POINT('Ctrl Pts',(1.36413470836879,2.75068903914081,-28.5686589310622)) ;
#153252 = CARTESIAN_POINT('Ctrl Pts',(1.36227932197148,2.75092980851021,-28.567667362279)) ;
#153253 = CARTESIAN_POINT('Ctrl Pts',(1.35746012444743,2.7516985967038,-28.5650888180784)) ;
#153254 = CARTESIAN_POINT('Ctrl Pts',(1.35450425835489,2.75231332717651,-28.5635042374589)) ;
#153255 = CARTESIAN_POINT('Ctrl Pts',(1.34886973918565,2.75377034241464,-28.5604791694934)) ;
#153256 = CARTESIAN_POINT('Ctrl Pts',(1.34617831568151,2.75459534478003,-28.5590321407416)) ;
#153257 = CARTESIAN_POINT('Ctrl Pts',(1.34314242260183,2.75567798707048,-28.5573984698771)) ;
#153258 = CARTESIAN_POINT('Ctrl Pts',(1.34256163823226,2.75588931242806,-28.557085898215)) ;
#153259 = CARTESIAN_POINT('Ctrl Pts',(1.34198261999809,2.75610647364238,-28.5567742184185)) ;
#153260 = CARTESIAN_POINT('Ctrl Pts',(1.3413216052292,2.75635697290856,-28.5564183780167)) ;
#153261 = CARTESIAN_POINT('Ctrl Pts',(1.3408629143507,2.75653491456656,-28.5561714174681)) ;
#153262 = CARTESIAN_POINT('Ctrl Pts',(1.33918548989956,2.7572007950357,-28.5552681624994)) ;
#153263 = CARTESIAN_POINT('Ctrl Pts',(1.33797416370948,2.75771112313095,-28.5546156517349)) ;
#153264 = CARTESIAN_POINT('Ctrl Pts',(1.33648532079705,2.75837521508443,-28.5538133670511)) ;
#153265 = CARTESIAN_POINT('Ctrl Pts',(1.33619776328718,2.7585052148881,-28.5536584026979)) ;
#153266 = CARTESIAN_POINT('Ctrl Pts',(1.33107968015599,2.7608491599493,-28.5508999602882)) ;
#153267 = CARTESIAN_POINT('Ctrl Pts',(1.32635908659425,2.76350693339039,-28.5483519804512)) ;
#153268 = CARTESIAN_POINT('Ctrl Pts',(1.32109760625981,2.76707470328447,-28.5455052830879)) ;
#153269 = CARTESIAN_POINT('Ctrl Pts',(1.32035743991799,2.76759128788314,-28.545104647555)) ;
#153270 = CARTESIAN_POINT('Ctrl Pts',(1.3182480554607,2.76910584227479,-28.5439623373891)) ;
#153271 = CARTESIAN_POINT('Ctrl Pts',(1.31689309423377,2.77013099976528,-28.5432277366412)) ;
#153272 = CARTESIAN_POINT('Ctrl Pts',(1.31545882361435,2.77127278201747,-28.5424488780593)) ;
#153273 = CARTESIAN_POINT('Ctrl Pts',(1.31535582310958,2.77135510350021,-28.5423929383466)) ;
#153274 = CARTESIAN_POINT('Ctrl Pts',(1.31504853092211,2.77160168095796,-28.542226026553)) ;
#153275 = CARTESIAN_POINT('Ctrl Pts',(1.31461168315429,2.77195498754743,-28.5419886931459)) ;
#153276 = CARTESIAN_POINT('Ctrl Pts',(1.31417742224139,2.77231219724367,-28.5417526629429)) ;
#153277 = CARTESIAN_POINT('Ctrl Pts',(1.31333096026317,2.77301480846571,-28.5412924938631)) ;
#153278 = CARTESIAN_POINT('Ctrl Pts',(1.31272070342857,2.77353368974768,-28.5409605431594)) ;
#153279 = CARTESIAN_POINT('Ctrl Pts',(1.30969774837136,2.77616736630455,-28.5393154427618)) ;
#153280 = CARTESIAN_POINT('Ctrl Pts',(1.30737022788703,2.77840054644572,-28.5380465201049)) ;
#153281 = CARTESIAN_POINT('Ctrl Pts',(1.30464757270886,2.78128817542221,-28.5365612966511)) ;
#153282 = CARTESIAN_POINT('Ctrl Pts',(1.3041484598108,2.78182967606621,-28.5362889873693)) ;
#153283 = CARTESIAN_POINT('Ctrl Pts',(1.30260826844056,2.78353926416386,-28.5354485713631)) ;
#153284 = CARTESIAN_POINT('Ctrl Pts',(1.30158324720849,2.78473373830863,-28.5348887670786)) ;
#153285 = CARTESIAN_POINT('Ctrl Pts',(1.30024935135332,2.78636738852735,-28.5341601872833)) ;
#153286 = CARTESIAN_POINT('Ctrl Pts',(1.29991860867238,2.78677921519269,-28.533979524919)) ;
#153287 = CARTESIAN_POINT('Ctrl Pts',(1.29915346420735,2.78774794465151,-28.5335615807717)) ;
#153288 = CARTESIAN_POINT('Ctrl Pts',(1.29872125904469,2.78830744810468,-28.5333255001127)) ;
#153289 = CARTESIAN_POINT('Ctrl Pts',(1.29658637826223,2.79113377451586,-28.5321594679259)) ;
#153290 = CARTESIAN_POINT('Ctrl Pts',(1.29496240940489,2.79348720429741,-28.5312730136302)) ;
#153291 = CARTESIAN_POINT('Ctrl Pts',(1.29231665668156,2.79769679694542,-28.5298283519951)) ;
#153292 = CARTESIAN_POINT('Ctrl Pts',(1.2912511560106,2.79951540543441,-28.5292459513193)) ;
#153293 = CARTESIAN_POINT('Ctrl Pts',(1.28927619853494,2.80313430045114,-28.5281651210187)) ;
#153294 = CARTESIAN_POINT('Ctrl Pts',(1.28836241997818,2.80493500363976,-28.527664620654)) ;
#153295 = CARTESIAN_POINT('Ctrl Pts',(1.28732027925583,2.80715235940912,-28.5270931587537)) ;
#153296 = CARTESIAN_POINT('Ctrl Pts',(1.28695835013163,2.80793550920674,-28.5268946174353)) ;
#153297 = CARTESIAN_POINT('Ctrl Pts',(1.28660568774188,2.80872522382217,-28.5267010437072)) ;
#153298 = CARTESIAN_POINT('Ctrl Pts',(1.28608376699193,2.80991454434775,-28.5264145021015)) ;
#153299 = CARTESIAN_POINT('Ctrl Pts',(1.28574525149598,2.81071375754612,-28.5262285681094)) ;
#153300 = CARTESIAN_POINT('Ctrl Pts',(1.28475894023892,2.81312894312826,-28.525686733351)) ;
#153301 = CARTESIAN_POINT('Ctrl Pts',(1.284140403093,2.81476247656147,-28.525346833702)) ;
#153302 = CARTESIAN_POINT('Ctrl Pts',(1.2833981826091,2.81688756020156,-28.524939111358)) ;
#153303 = CARTESIAN_POINT('Ctrl Pts',(1.28323661013041,2.81736137575535,-28.5248503628219)) ;
#153304 = CARTESIAN_POINT('Ctrl Pts',(1.28265668893878,2.81910411140443,-28.5245318526463)) ;
#153305 = CARTESIAN_POINT('Ctrl Pts',(1.2822592025033,2.82038205281196,-28.5243136076747)) ;
#153306 = CARTESIAN_POINT('Ctrl Pts',(1.28170385606935,2.82230051526775,-28.5240086650164)) ;
#153307 = CARTESIAN_POINT('Ctrl Pts',(1.28152700208472,2.82293438010915,-28.5239115582297)) ;
#153308 = CARTESIAN_POINT('Ctrl Pts',(1.2810744886873,2.82461913389174,-28.5236630908507)) ;
#153309 = CARTESIAN_POINT('Ctrl Pts',(1.28081016954772,2.82567198476338,-28.5235180110459)) ;
#153310 = CARTESIAN_POINT('Ctrl Pts',(1.2800991035332,2.82871092361133,-28.5231278319823)) ;
#153311 = CARTESIAN_POINT('Ctrl Pts',(1.27969380338793,2.83071459002993,-28.52290512912)) ;
#153312 = CARTESIAN_POINT('Ctrl Pts',(1.27923282767963,2.83340629334536,-28.5226515462665)) ;
#153313 = CARTESIAN_POINT('Ctrl Pts',(1.27912420342281,2.8340808992611,-28.5225917647842)) ;
#153314 = CARTESIAN_POINT('Ctrl Pts',(1.27861441353188,2.83746106027946,-28.5223110911817)) ;
#153315 = CARTESIAN_POINT('Ctrl Pts',(1.2783132428757,2.84018799487019,-28.5221449017566)) ;
#153316 = CARTESIAN_POINT('Ctrl Pts',(1.27795656969995,2.8452797714154,-28.5219480133439)) ;
#153317 = CARTESIAN_POINT('Ctrl Pts',(1.27787304021906,2.84764286211078,-28.5219018583827)) ;
#153318 = CARTESIAN_POINT('Ctrl Pts',(1.27787304021907,2.85,-28.5219018583827)) ;
#153319 = CARTESIAN_POINT('',(1.27787304021905,2.85,-24.8180981416173)) ;
#153320 = CARTESIAN_POINT('Origin',(-8.21365282185989E-16,2.85,-26.67)) ;
#153321 = CARTESIAN_POINT('Ctrl Pts',(1.37603597336697,2.75,-24.765)) ;
#153322 = CARTESIAN_POINT('Ctrl Pts',(1.37573512845502,2.75,-24.7651599709433)) ;
#153323 = CARTESIAN_POINT('Ctrl Pts',(1.37513340736836,2.75000265707422,-24.7654798786905)) ;
#153324 = CARTESIAN_POINT('Ctrl Pts',(1.37453174406034,2.75001064672752,-24.7657998110249)) ;
#153325 = CARTESIAN_POINT('Ctrl Pts',(1.37388722675069,2.75002207412044,-24.766142644207)) ;
#153326 = CARTESIAN_POINT('Ctrl Pts',(1.37354350385561,2.75002991650282,-24.7663255141622)) ;
#153327 = CARTESIAN_POINT('Ctrl Pts',(1.37285611423782,2.75004911307826,-24.7666912988841)) ;
#153328 = CARTESIAN_POINT('Ctrl Pts',(1.37251244753524,2.75006046723047,-24.7668742136115)) ;
#153329 = CARTESIAN_POINT('Ctrl Pts',(1.3714815944481,2.75009981984526,-24.767422994695)) ;
#153330 = CARTESIAN_POINT('Ctrl Pts',(1.37079455494331,2.75013310886333,-24.7677888982032)) ;
#153331 = CARTESIAN_POINT('Ctrl Pts',(1.36873453110893,2.75025430438116,-24.7688865055866)) ;
#153332 = CARTESIAN_POINT('Ctrl Pts',(1.36736263966052,2.75036354665963,-24.7696181092421)) ;
#153333 = CARTESIAN_POINT('Ctrl Pts',(1.36413470836879,2.75068903914081,-24.7713410689378)) ;
#153334 = CARTESIAN_POINT('Ctrl Pts',(1.36227932197148,2.75092980851021,-24.772332637721)) ;
#153335 = CARTESIAN_POINT('Ctrl Pts',(1.35746012444743,2.7516985967038,-24.7749111819216)) ;
#153336 = CARTESIAN_POINT('Ctrl Pts',(1.35450425835489,2.75231332717651,-24.7764957625411)) ;
#153337 = CARTESIAN_POINT('Ctrl Pts',(1.34886973918564,2.75377034241463,-24.7795208305066)) ;
#153338 = CARTESIAN_POINT('Ctrl Pts',(1.3461783156815,2.75459534478002,-24.7809678592584)) ;
#153339 = CARTESIAN_POINT('Ctrl Pts',(1.34314242260182,2.75567798707047,-24.7826015301229)) ;
#153340 = CARTESIAN_POINT('Ctrl Pts',(1.34256163823226,2.75588931242805,-24.782914101785)) ;
#153341 = CARTESIAN_POINT('Ctrl Pts',(1.34198261999809,2.75610647364237,-24.7832257815815)) ;
#153342 = CARTESIAN_POINT('Ctrl Pts',(1.3413216052292,2.75635697290856,-24.7835816219833)) ;
#153343 = CARTESIAN_POINT('Ctrl Pts',(1.3408629143507,2.75653491456655,-24.7838285825319)) ;
#153344 = CARTESIAN_POINT('Ctrl Pts',(1.33918548989955,2.75720079503569,-24.7847318375006)) ;
#153345 = CARTESIAN_POINT('Ctrl Pts',(1.33797416370948,2.75771112313095,-24.7853843482652)) ;
#153346 = CARTESIAN_POINT('Ctrl Pts',(1.33648532079705,2.75837521508443,-24.7861866329489)) ;
#153347 = CARTESIAN_POINT('Ctrl Pts',(1.33619776328718,2.75850521488809,-24.7863415973021)) ;
#153348 = CARTESIAN_POINT('Ctrl Pts',(1.33107968015567,2.76084915994944,-24.789100039712)) ;
#153349 = CARTESIAN_POINT('Ctrl Pts',(1.32635908659363,2.76350693339074,-24.7916480195491)) ;
#153350 = CARTESIAN_POINT('Ctrl Pts',(1.32109760625924,2.76707470328487,-24.7944947169124)) ;
#153351 = CARTESIAN_POINT('Ctrl Pts',(1.32035743991773,2.76759128788333,-24.7948953524452)) ;
#153352 = CARTESIAN_POINT('Ctrl Pts',(1.31824805546073,2.76910584227477,-24.7960376626109)) ;
#153353 = CARTESIAN_POINT('Ctrl Pts',(1.31689309423378,2.77013099976526,-24.7967722633588)) ;
#153354 = CARTESIAN_POINT('Ctrl Pts',(1.31545882361437,2.77127278201745,-24.7975511219407)) ;
#153355 = CARTESIAN_POINT('Ctrl Pts',(1.31535582310962,2.77135510350017,-24.7976070616534)) ;
#153356 = CARTESIAN_POINT('Ctrl Pts',(1.31504853092216,2.77160168095791,-24.7977739734469)) ;
#153357 = CARTESIAN_POINT('Ctrl Pts',(1.31461168315434,2.77195498754736,-24.7980113068543)) ;
#153358 = CARTESIAN_POINT('Ctrl Pts',(1.31417742224145,2.77231219724361,-24.798247337057)) ;
#153359 = CARTESIAN_POINT('Ctrl Pts',(1.31333096026322,2.77301480846564,-24.7987075061369)) ;
#153360 = CARTESIAN_POINT('Ctrl Pts',(1.31272070342863,2.77353368974761,-24.7990394568406)) ;
#153361 = CARTESIAN_POINT('Ctrl Pts',(1.30969774837141,2.77616736630447,-24.8006845572381)) ;
#153362 = CARTESIAN_POINT('Ctrl Pts',(1.30737022788708,2.77840054644563,-24.801953479895)) ;
#153363 = CARTESIAN_POINT('Ctrl Pts',(1.30464757270891,2.78128817542216,-24.8034387033489)) ;
#153364 = CARTESIAN_POINT('Ctrl Pts',(1.30414845981082,2.78182967606617,-24.8037110126308)) ;
#153365 = CARTESIAN_POINT('Ctrl Pts',(1.30260826844055,2.78353926416387,-24.804551428637)) ;
#153366 = CARTESIAN_POINT('Ctrl Pts',(1.30158324720848,2.78473373830866,-24.8051112329214)) ;
#153367 = CARTESIAN_POINT('Ctrl Pts',(1.3002493513533,2.78636738852739,-24.8058398127168)) ;
#153368 = CARTESIAN_POINT('Ctrl Pts',(1.29991860867235,2.78677921519272,-24.8060204750811)) ;
#153369 = CARTESIAN_POINT('Ctrl Pts',(1.29915346420732,2.78774794465155,-24.8064384192283)) ;
#153370 = CARTESIAN_POINT('Ctrl Pts',(1.29872125904465,2.78830744810474,-24.8066744998873)) ;
#153371 = CARTESIAN_POINT('Ctrl Pts',(1.29658637826217,2.79113377451593,-24.8078405320741)) ;
#153372 = CARTESIAN_POINT('Ctrl Pts',(1.29496240940481,2.79348720429748,-24.8087269863698)) ;
#153373 = CARTESIAN_POINT('Ctrl Pts',(1.2923166566815,2.79769679694548,-24.810171648005)) ;
#153374 = CARTESIAN_POINT('Ctrl Pts',(1.29125115601058,2.79951540543444,-24.8107540486807)) ;
#153375 = CARTESIAN_POINT('Ctrl Pts',(1.28927619853494,2.80313430045114,-24.8118348789813)) ;
#153376 = CARTESIAN_POINT('Ctrl Pts',(1.28836241997819,2.80493500363977,-24.8123353793459)) ;
#153377 = CARTESIAN_POINT('Ctrl Pts',(1.28732027925585,2.80715235940913,-24.8129068412463)) ;
#153378 = CARTESIAN_POINT('Ctrl Pts',(1.28695835013167,2.80793550920673,-24.8131053825645)) ;
#153379 = CARTESIAN_POINT('Ctrl Pts',(1.28660568774192,2.80872522382217,-24.8132989562928)) ;
#153380 = CARTESIAN_POINT('Ctrl Pts',(1.28608376699197,2.80991454434774,-24.8135854978985)) ;
#153381 = CARTESIAN_POINT('Ctrl Pts',(1.28574525149603,2.8107137575461,-24.8137714318906)) ;
#153382 = CARTESIAN_POINT('Ctrl Pts',(1.28475894023898,2.81312894312821,-24.814313266649)) ;
#153383 = CARTESIAN_POINT('Ctrl Pts',(1.28414040309306,2.81476247656139,-24.8146531662979)) ;
#153384 = CARTESIAN_POINT('Ctrl Pts',(1.28339818260916,2.81688756020145,-24.815060888642)) ;
#153385 = CARTESIAN_POINT('Ctrl Pts',(1.28323661013047,2.81736137575524,-24.815149637178)) ;
#153386 = CARTESIAN_POINT('Ctrl Pts',(1.28265668893884,2.81910411140429,-24.8154681473537)) ;
#153387 = CARTESIAN_POINT('Ctrl Pts',(1.28225920250336,2.8203820528118,-24.8156863923252)) ;
#153388 = CARTESIAN_POINT('Ctrl Pts',(1.28170385606938,2.82230051526763,-24.8159913349835)) ;
#153389 = CARTESIAN_POINT('Ctrl Pts',(1.28152700208473,2.82293438010909,-24.8160884417702)) ;
#153390 = CARTESIAN_POINT('Ctrl Pts',(1.28107448868731,2.82461913389175,-24.8163369091493)) ;
#153391 = CARTESIAN_POINT('Ctrl Pts',(1.28081016954774,2.8256719847634,-24.8164819889541)) ;
#153392 = CARTESIAN_POINT('Ctrl Pts',(1.28009910353322,2.82871092361135,-24.8168721680177)) ;
#153393 = CARTESIAN_POINT('Ctrl Pts',(1.27969380338795,2.83071459002995,-24.81709487088)) ;
#153394 = CARTESIAN_POINT('Ctrl Pts',(1.27923282767965,2.83340629334538,-24.8173484537334)) ;
#153395 = CARTESIAN_POINT('Ctrl Pts',(1.27912420342283,2.83408089926112,-24.8174082352158)) ;
#153396 = CARTESIAN_POINT('Ctrl Pts',(1.27861441353189,2.83746106027947,-24.8176889088183)) ;
#153397 = CARTESIAN_POINT('Ctrl Pts',(1.27831324287571,2.8401879948702,-24.8178550982434)) ;
#153398 = CARTESIAN_POINT('Ctrl Pts',(1.27795656969995,2.84527977141541,-24.8180519866561)) ;
#153399 = CARTESIAN_POINT('Ctrl Pts',(1.27787304021905,2.84764286211078,-24.8180981416173)) ;
#153400 = CARTESIAN_POINT('Ctrl Pts',(1.27787304021904,2.85,-24.8180981416173)) ;
#153401 = CARTESIAN_POINT('Origin',(1.31451250000001,4.45,-32.385)) ;
#153402 = CARTESIAN_POINT('',(1.22107868287598,4.55,-32.2495951091213)) ;
#153403 = CARTESIAN_POINT('',(1.22107868287599,4.55,-32.5204048908788)) ;
#153404 = CARTESIAN_POINT('Origin',(1.31451250000001,4.55,-32.385)) ;
#153405 = CARTESIAN_POINT('',(1.27787304021906,4.45,-32.3319018583827)) ;
#153406 = CARTESIAN_POINT('Origin',(1.22107868287598,4.45,-32.2495951091213)) ;
#153407 = CARTESIAN_POINT('',(1.27787304021906,4.45,-32.4380981416173)) ;
#153408 = CARTESIAN_POINT('Origin',(1.31451250000001,4.45,-32.385)) ;
#153409 = CARTESIAN_POINT('Origin',(1.22107868287599,4.45,-32.5204048908788)) ;
#153410 = CARTESIAN_POINT('Origin',(-3.7454256867681E-16,2.85,-30.48)) ;
#153411 = CARTESIAN_POINT('',(1.37603597336698,2.75,-32.385)) ;
#153412 = CARTESIAN_POINT('Origin',(-3.66728498965203E-16,2.75,-30.48)) ;
#153413 = CARTESIAN_POINT('',(1.27787304021906,2.85,-32.3319018583827)) ;
#153414 = CARTESIAN_POINT('Ctrl Pts',(1.37603597336698,2.75,-32.385)) ;
#153415 = CARTESIAN_POINT('Ctrl Pts',(1.37573512845502,2.75,-32.3848400290568)) ;
#153416 = CARTESIAN_POINT('Ctrl Pts',(1.37513340736834,2.75000265707422,-32.3845201213094)) ;
#153417 = CARTESIAN_POINT('Ctrl Pts',(1.37453174406034,2.75001064672751,-32.3842001889751)) ;
#153418 = CARTESIAN_POINT('Ctrl Pts',(1.37388722675068,2.75002207412045,-32.383857355793)) ;
#153419 = CARTESIAN_POINT('Ctrl Pts',(1.3735435038556,2.75002991650282,-32.3836744858382)) ;
#153420 = CARTESIAN_POINT('Ctrl Pts',(1.37285611423781,2.75004911307826,-32.3833087011159)) ;
#153421 = CARTESIAN_POINT('Ctrl Pts',(1.37251244753524,2.75006046723047,-32.3831257863885)) ;
#153422 = CARTESIAN_POINT('Ctrl Pts',(1.3714815944481,2.75009981984526,-32.382577005305)) ;
#153423 = CARTESIAN_POINT('Ctrl Pts',(1.37079455494331,2.75013310886333,-32.3822111017968)) ;
#153424 = CARTESIAN_POINT('Ctrl Pts',(1.36873453110892,2.75025430438116,-32.3811134944134)) ;
#153425 = CARTESIAN_POINT('Ctrl Pts',(1.36736263966051,2.75036354665963,-32.380381890758)) ;
#153426 = CARTESIAN_POINT('Ctrl Pts',(1.36413470836879,2.75068903914081,-32.3786589310622)) ;
#153427 = CARTESIAN_POINT('Ctrl Pts',(1.36227932197147,2.75092980851022,-32.377667362279)) ;
#153428 = CARTESIAN_POINT('Ctrl Pts',(1.35746012444743,2.75169859670379,-32.3750888180785)) ;
#153429 = CARTESIAN_POINT('Ctrl Pts',(1.35450425835489,2.75231332717652,-32.3735042374589)) ;
#153430 = CARTESIAN_POINT('Ctrl Pts',(1.34886973918565,2.75377034241464,-32.3704791694934)) ;
#153431 = CARTESIAN_POINT('Ctrl Pts',(1.34617831568151,2.75459534478003,-32.3690321407416)) ;
#153432 = CARTESIAN_POINT('Ctrl Pts',(1.34314242260183,2.75567798707049,-32.3673984698771)) ;
#153433 = CARTESIAN_POINT('Ctrl Pts',(1.34256163823227,2.75588931242806,-32.367085898215)) ;
#153434 = CARTESIAN_POINT('Ctrl Pts',(1.3419826199981,2.75610647364238,-32.3667742184185)) ;
#153435 = CARTESIAN_POINT('Ctrl Pts',(1.34132160522921,2.75635697290857,-32.3664183780167)) ;
#153436 = CARTESIAN_POINT('Ctrl Pts',(1.34086291435071,2.75653491456656,-32.3661714174681)) ;
#153437 = CARTESIAN_POINT('Ctrl Pts',(1.33918548989957,2.7572007950357,-32.3652681624994)) ;
#153438 = CARTESIAN_POINT('Ctrl Pts',(1.33797416370949,2.75771112313095,-32.3646156517349)) ;
#153439 = CARTESIAN_POINT('Ctrl Pts',(1.33648532079706,2.75837521508443,-32.3638133670511)) ;
#153440 = CARTESIAN_POINT('Ctrl Pts',(1.33619776328718,2.7585052148881,-32.3636584026979)) ;
#153441 = CARTESIAN_POINT('Ctrl Pts',(1.33107968015827,2.76084915994826,-32.3608999602894)) ;
#153442 = CARTESIAN_POINT('Ctrl Pts',(1.3263590865987,2.76350693338791,-32.3583519804536)) ;
#153443 = CARTESIAN_POINT('Ctrl Pts',(1.32109760626403,2.76707470328156,-32.3555052830901)) ;
#153444 = CARTESIAN_POINT('Ctrl Pts',(1.32035743992007,2.76759128788168,-32.355104647556)) ;
#153445 = CARTESIAN_POINT('Ctrl Pts',(1.31824805546069,2.76910584227482,-32.3539623373891)) ;
#153446 = CARTESIAN_POINT('Ctrl Pts',(1.31689309423376,2.7701309997653,-32.3532277366412)) ;
#153447 = CARTESIAN_POINT('Ctrl Pts',(1.31545882361434,2.77127278201748,-32.3524488780593)) ;
#153448 = CARTESIAN_POINT('Ctrl Pts',(1.31535582310956,2.77135510350024,-32.3523929383466)) ;
#153449 = CARTESIAN_POINT('Ctrl Pts',(1.31504853092207,2.771601680958,-32.352226026553)) ;
#153450 = CARTESIAN_POINT('Ctrl Pts',(1.31461168315425,2.77195498754747,-32.3519886931459)) ;
#153451 = CARTESIAN_POINT('Ctrl Pts',(1.31417742224135,2.77231219724371,-32.3517526629429)) ;
#153452 = CARTESIAN_POINT('Ctrl Pts',(1.31333096026312,2.77301480846575,-32.351292493863)) ;
#153453 = CARTESIAN_POINT('Ctrl Pts',(1.31272070342853,2.77353368974772,-32.3509605431594)) ;
#153454 = CARTESIAN_POINT('Ctrl Pts',(1.30969774837131,2.7761673663046,-32.3493154427618)) ;
#153455 = CARTESIAN_POINT('Ctrl Pts',(1.30737022788697,2.77840054644578,-32.3480465201049)) ;
#153456 = CARTESIAN_POINT('Ctrl Pts',(1.30464757270883,2.78128817542226,-32.3465612966511)) ;
#153457 = CARTESIAN_POINT('Ctrl Pts',(1.30414845981079,2.78182967606624,-32.3462889873692)) ;
#153458 = CARTESIAN_POINT('Ctrl Pts',(1.30260826844057,2.78353926416389,-32.3454485713631)) ;
#153459 = CARTESIAN_POINT('Ctrl Pts',(1.3015832472085,2.78473373830867,-32.3448887670786)) ;
#153460 = CARTESIAN_POINT('Ctrl Pts',(1.30024935135333,2.78636738852739,-32.3441601872832)) ;
#153461 = CARTESIAN_POINT('Ctrl Pts',(1.29991860867238,2.78677921519273,-32.343979524919)) ;
#153462 = CARTESIAN_POINT('Ctrl Pts',(1.29915346420735,2.78774794465156,-32.3435615807717)) ;
#153463 = CARTESIAN_POINT('Ctrl Pts',(1.29872125904468,2.78830744810473,-32.3433255001127)) ;
#153464 = CARTESIAN_POINT('Ctrl Pts',(1.29658637826221,2.79113377451592,-32.3421594679259)) ;
#153465 = CARTESIAN_POINT('Ctrl Pts',(1.29496240940486,2.79348720429747,-32.3412730136302)) ;
#153466 = CARTESIAN_POINT('Ctrl Pts',(1.29231665668154,2.79769679694547,-32.339828351995)) ;
#153467 = CARTESIAN_POINT('Ctrl Pts',(1.2912511560106,2.79951540543444,-32.3392459513193)) ;
#153468 = CARTESIAN_POINT('Ctrl Pts',(1.28927619853495,2.80313430045114,-32.3381651210187)) ;
#153469 = CARTESIAN_POINT('Ctrl Pts',(1.28836241997819,2.80493500363976,-32.337664620654)) ;
#153470 = CARTESIAN_POINT('Ctrl Pts',(1.28732027925585,2.80715235940912,-32.3370931587537)) ;
#153471 = CARTESIAN_POINT('Ctrl Pts',(1.28695835013165,2.80793550920672,-32.3368946174355)) ;
#153472 = CARTESIAN_POINT('Ctrl Pts',(1.2866056877419,2.80872522382217,-32.3367010437072)) ;
#153473 = CARTESIAN_POINT('Ctrl Pts',(1.28608376699195,2.80991454434775,-32.3364145021015)) ;
#153474 = CARTESIAN_POINT('Ctrl Pts',(1.28574525149599,2.81071375754612,-32.3362285681094)) ;
#153475 = CARTESIAN_POINT('Ctrl Pts',(1.28475894023894,2.81312894312826,-32.335686733351)) ;
#153476 = CARTESIAN_POINT('Ctrl Pts',(1.28414040309302,2.81476247656146,-32.335346833702)) ;
#153477 = CARTESIAN_POINT('Ctrl Pts',(1.28339818260913,2.81688756020155,-32.334939111358)) ;
#153478 = CARTESIAN_POINT('Ctrl Pts',(1.28323661013043,2.81736137575533,-32.3348503628219)) ;
#153479 = CARTESIAN_POINT('Ctrl Pts',(1.2826566889388,2.81910411140441,-32.3345318526463)) ;
#153480 = CARTESIAN_POINT('Ctrl Pts',(1.28225920250332,2.82038205281194,-32.3343136076747)) ;
#153481 = CARTESIAN_POINT('Ctrl Pts',(1.28170385606937,2.82230051526773,-32.3340086650164)) ;
#153482 = CARTESIAN_POINT('Ctrl Pts',(1.28152700208473,2.82293438010914,-32.3339115582297)) ;
#153483 = CARTESIAN_POINT('Ctrl Pts',(1.28107448868731,2.82461913389174,-32.3336630908507)) ;
#153484 = CARTESIAN_POINT('Ctrl Pts',(1.28081016954773,2.82567198476338,-32.3335180110459)) ;
#153485 = CARTESIAN_POINT('Ctrl Pts',(1.28009910353321,2.82871092361133,-32.3331278319823)) ;
#153486 = CARTESIAN_POINT('Ctrl Pts',(1.27969380338794,2.83071459002993,-32.33290512912)) ;
#153487 = CARTESIAN_POINT('Ctrl Pts',(1.27923282767964,2.83340629334536,-32.3326515462665)) ;
#153488 = CARTESIAN_POINT('Ctrl Pts',(1.27912420342282,2.83408089926111,-32.3325917647842)) ;
#153489 = CARTESIAN_POINT('Ctrl Pts',(1.27861441353189,2.83746106027946,-32.3323110911817)) ;
#153490 = CARTESIAN_POINT('Ctrl Pts',(1.27831324287571,2.84018799487018,-32.3321449017566)) ;
#153491 = CARTESIAN_POINT('Ctrl Pts',(1.27795656969997,2.8452797714154,-32.3319480133439)) ;
#153492 = CARTESIAN_POINT('Ctrl Pts',(1.27787304021907,2.84764286211078,-32.3319018583827)) ;
#153493 = CARTESIAN_POINT('Ctrl Pts',(1.27787304021907,2.85,-32.3319018583827)) ;
#153494 = CARTESIAN_POINT('',(1.27787304021905,2.85,-28.6280981416173)) ;
#153495 = CARTESIAN_POINT('Origin',(-3.7454256867681E-16,2.85,-30.48)) ;
#153496 = CARTESIAN_POINT('Ctrl Pts',(1.37603597336697,2.75,-28.575)) ;
#153497 = CARTESIAN_POINT('Ctrl Pts',(1.37543428354306,2.75,-28.5753199418865)) ;
#153498 = CARTESIAN_POINT('Ctrl Pts',(1.37483253111456,2.7500053137259,-28.5756398156588)) ;
#153499 = CARTESIAN_POINT('Ctrl Pts',(1.37388722675069,2.75002207412044,-28.576142644207)) ;
#153500 = CARTESIAN_POINT('Ctrl Pts',(1.37354350385561,2.75002991650282,-28.5763255141622)) ;
#153501 = CARTESIAN_POINT('Ctrl Pts',(1.37285611423782,2.75004911307826,-28.5766912988841)) ;
#153502 = CARTESIAN_POINT('Ctrl Pts',(1.37251244753524,2.75006046723047,-28.5768742136115)) ;
#153503 = CARTESIAN_POINT('Ctrl Pts',(1.3714815944481,2.75009981984526,-28.577422994695)) ;
#153504 = CARTESIAN_POINT('Ctrl Pts',(1.37079455494331,2.75013310886333,-28.5777888982032)) ;
#153505 = CARTESIAN_POINT('Ctrl Pts',(1.36873453110892,2.75025430438116,-28.5788865055866)) ;
#153506 = CARTESIAN_POINT('Ctrl Pts',(1.36736263966051,2.75036354665963,-28.5796181092421)) ;
#153507 = CARTESIAN_POINT('Ctrl Pts',(1.36413470836879,2.75068903914081,-28.5813410689378)) ;
#153508 = CARTESIAN_POINT('Ctrl Pts',(1.36227932197147,2.75092980851022,-28.582332637721)) ;
#153509 = CARTESIAN_POINT('Ctrl Pts',(1.35746012444742,2.75169859670381,-28.5849111819216)) ;
#153510 = CARTESIAN_POINT('Ctrl Pts',(1.35450425835489,2.75231332717652,-28.5864957625411)) ;
#153511 = CARTESIAN_POINT('Ctrl Pts',(1.34886973918565,2.75377034241464,-28.5895208305066)) ;
#153512 = CARTESIAN_POINT('Ctrl Pts',(1.3461783156815,2.75459534478003,-28.5909678592584)) ;
#153513 = CARTESIAN_POINT('Ctrl Pts',(1.34314242260182,2.75567798707048,-28.5926015301229)) ;
#153514 = CARTESIAN_POINT('Ctrl Pts',(1.34256163823226,2.75588931242806,-28.592914101785)) ;
#153515 = CARTESIAN_POINT('Ctrl Pts',(1.34198261999809,2.75610647364238,-28.5932257815815)) ;
#153516 = CARTESIAN_POINT('Ctrl Pts',(1.3413216052292,2.75635697290856,-28.5935816219833)) ;
#153517 = CARTESIAN_POINT('Ctrl Pts',(1.3408629143507,2.75653491456656,-28.5938285825319)) ;
#153518 = CARTESIAN_POINT('Ctrl Pts',(1.33918548989955,2.7572007950357,-28.5947318375006)) ;
#153519 = CARTESIAN_POINT('Ctrl Pts',(1.33797416370948,2.75771112313095,-28.5953843482651)) ;
#153520 = CARTESIAN_POINT('Ctrl Pts',(1.33648532079705,2.75837521508443,-28.5961866329489)) ;
#153521 = CARTESIAN_POINT('Ctrl Pts',(1.33619776328718,2.7585052148881,-28.5963415973021)) ;
#153522 = CARTESIAN_POINT('Ctrl Pts',(1.33107968015592,2.76084915994933,-28.5991000397119)) ;
#153523 = CARTESIAN_POINT('Ctrl Pts',(1.32635908659411,2.76350693339047,-28.6016480195489)) ;
#153524 = CARTESIAN_POINT('Ctrl Pts',(1.32109760625968,2.76707470328456,-28.6044947169122)) ;
#153525 = CARTESIAN_POINT('Ctrl Pts',(1.32035743991793,2.76759128788319,-28.6048953524451)) ;
#153526 = CARTESIAN_POINT('Ctrl Pts',(1.31824805546071,2.76910584227479,-28.6060376626109)) ;
#153527 = CARTESIAN_POINT('Ctrl Pts',(1.31689309423377,2.77013099976528,-28.6067722633588)) ;
#153528 = CARTESIAN_POINT('Ctrl Pts',(1.31545882361436,2.77127278201746,-28.6075511219407)) ;
#153529 = CARTESIAN_POINT('Ctrl Pts',(1.31535582310959,2.77135510350021,-28.6076070616534)) ;
#153530 = CARTESIAN_POINT('Ctrl Pts',(1.31504853092212,2.77160168095795,-28.607773973447)) ;
#153531 = CARTESIAN_POINT('Ctrl Pts',(1.31461168315428,2.77195498754742,-28.6080113068541)) ;
#153532 = CARTESIAN_POINT('Ctrl Pts',(1.3141774222414,2.77231219724366,-28.6082473370571)) ;
#153533 = CARTESIAN_POINT('Ctrl Pts',(1.31333096026317,2.77301480846569,-28.6087075061369)) ;
#153534 = CARTESIAN_POINT('Ctrl Pts',(1.31272070342858,2.77353368974767,-28.6090394568406)) ;
#153535 = CARTESIAN_POINT('Ctrl Pts',(1.30969774837137,2.77616736630455,-28.6106845572382)) ;
#153536 = CARTESIAN_POINT('Ctrl Pts',(1.30737022788704,2.77840054644571,-28.6119534798951)) ;
#153537 = CARTESIAN_POINT('Ctrl Pts',(1.30464757270887,2.7812881754222,-28.6134387033489)) ;
#153538 = CARTESIAN_POINT('Ctrl Pts',(1.3041484598108,2.7818296760662,-28.6137110126307)) ;
#153539 = CARTESIAN_POINT('Ctrl Pts',(1.30260826844057,2.78353926416388,-28.6145514286369)) ;
#153540 = CARTESIAN_POINT('Ctrl Pts',(1.3015832472085,2.78473373830865,-28.6151112329214)) ;
#153541 = CARTESIAN_POINT('Ctrl Pts',(1.30024935135333,2.78636738852737,-28.6158398127168)) ;
#153542 = CARTESIAN_POINT('Ctrl Pts',(1.29991860867239,2.78677921519271,-28.616020475081)) ;
#153543 = CARTESIAN_POINT('Ctrl Pts',(1.29915346420736,2.78774794465154,-28.6164384192283)) ;
#153544 = CARTESIAN_POINT('Ctrl Pts',(1.29872125904469,2.78830744810471,-28.6166744998873)) ;
#153545 = CARTESIAN_POINT('Ctrl Pts',(1.29658637826223,2.79113377451589,-28.6178405320741)) ;
#153546 = CARTESIAN_POINT('Ctrl Pts',(1.29496240940489,2.79348720429744,-28.6187269863698)) ;
#153547 = CARTESIAN_POINT('Ctrl Pts',(1.29231665668157,2.79769679694545,-28.6201716480049)) ;
#153548 = CARTESIAN_POINT('Ctrl Pts',(1.29125115601062,2.79951540543443,-28.6207540486807)) ;
#153549 = CARTESIAN_POINT('Ctrl Pts',(1.28927619853496,2.80313430045116,-28.6218348789813)) ;
#153550 = CARTESIAN_POINT('Ctrl Pts',(1.2883624199782,2.80493500363978,-28.6223353793459)) ;
#153551 = CARTESIAN_POINT('Ctrl Pts',(1.28732027925586,2.80715235940914,-28.6229068412463)) ;
#153552 = CARTESIAN_POINT('Ctrl Pts',(1.28695835013168,2.80793550920674,-28.6231053825645)) ;
#153553 = CARTESIAN_POINT('Ctrl Pts',(1.28660568774192,2.80872522382218,-28.6232989562928)) ;
#153554 = CARTESIAN_POINT('Ctrl Pts',(1.28608376699197,2.80991454434775,-28.6235854978985)) ;
#153555 = CARTESIAN_POINT('Ctrl Pts',(1.28574525149602,2.81071375754612,-28.6237714318906)) ;
#153556 = CARTESIAN_POINT('Ctrl Pts',(1.28475894023896,2.81312894312823,-28.624313266649)) ;
#153557 = CARTESIAN_POINT('Ctrl Pts',(1.28414040309304,2.81476247656142,-28.624653166298)) ;
#153558 = CARTESIAN_POINT('Ctrl Pts',(1.28339818260914,2.81688756020149,-28.625060888642)) ;
#153559 = CARTESIAN_POINT('Ctrl Pts',(1.28323661013045,2.81736137575528,-28.6251496371781)) ;
#153560 = CARTESIAN_POINT('Ctrl Pts',(1.28265668893881,2.81910411140434,-28.6254681473537)) ;
#153561 = CARTESIAN_POINT('Ctrl Pts',(1.28225920250334,2.82038205281186,-28.6256863923253)) ;
#153562 = CARTESIAN_POINT('Ctrl Pts',(1.28170385606937,2.82230051526767,-28.6259913349836)) ;
#153563 = CARTESIAN_POINT('Ctrl Pts',(1.28152700208473,2.82293438010911,-28.6260884417703)) ;
#153564 = CARTESIAN_POINT('Ctrl Pts',(1.2810744886873,2.82461913389174,-28.6263369091493)) ;
#153565 = CARTESIAN_POINT('Ctrl Pts',(1.28081016954771,2.82567198476339,-28.6264819889541)) ;
#153566 = CARTESIAN_POINT('Ctrl Pts',(1.28009910353319,2.82871092361134,-28.6268721680177)) ;
#153567 = CARTESIAN_POINT('Ctrl Pts',(1.27969380338793,2.83071459002994,-28.6270948708801)) ;
#153568 = CARTESIAN_POINT('Ctrl Pts',(1.27923282767963,2.83340629334537,-28.6273484537335)) ;
#153569 = CARTESIAN_POINT('Ctrl Pts',(1.27912420342281,2.83408089926111,-28.6274082352158)) ;
#153570 = CARTESIAN_POINT('Ctrl Pts',(1.27861441353187,2.83746106027946,-28.6276889088183)) ;
#153571 = CARTESIAN_POINT('Ctrl Pts',(1.27831324287571,2.8401879948702,-28.6278550982434)) ;
#153572 = CARTESIAN_POINT('Ctrl Pts',(1.27795656969996,2.84527977141541,-28.6280519866561)) ;
#153573 = CARTESIAN_POINT('Ctrl Pts',(1.27787304021906,2.84764286211078,-28.6280981416173)) ;
#153574 = CARTESIAN_POINT('Ctrl Pts',(1.27787304021907,2.85,-28.6280981416173)) ;
#153575 = CARTESIAN_POINT('Origin',(1.77490703981929,4.45,-35.7754875)) ;
#153576 = CARTESIAN_POINT('',(1.64874898520161,4.55,-35.6699010050713)) ;
#153577 = CARTESIAN_POINT('',(1.77490703981929,4.55,-35.94)) ;
#153578 = CARTESIAN_POINT('Origin',(1.77490703981929,4.55,-35.7754875)) ;
#153579 = CARTESIAN_POINT('',(1.72543498451332,4.45,-35.7340824471676)) ;
#153580 = CARTESIAN_POINT('Origin',(1.64874898520161,4.45,-35.6699010050713)) ;
#153581 = CARTESIAN_POINT('',(1.77490703981929,4.45,-35.84)) ;
#153582 = CARTESIAN_POINT('Origin',(1.77490703981929,4.45,-35.7754875)) ;
#153583 = CARTESIAN_POINT('Origin',(1.77490703981929,4.45,-35.94)) ;
#153584 = CARTESIAN_POINT('Origin',(-3.7454256867681E-16,2.85,-34.29)) ;
#153585 = CARTESIAN_POINT('',(1.8493242008907,2.75,-35.74)) ;
#153586 = CARTESIAN_POINT('Origin',(-3.66728498965203E-16,2.75,-34.29)) ;
#153587 = CARTESIAN_POINT('',(1.72543498451332,2.85,-35.7340824471676)) ;
#153588 = CARTESIAN_POINT('Ctrl Pts',(1.8493242008907,2.75,-35.74)) ;
#153589 = CARTESIAN_POINT('Ctrl Pts',(1.84863058979382,2.75,-35.7399756373587)) ;
#153590 = CARTESIAN_POINT('Ctrl Pts',(1.84793752344333,2.75000415508911,-35.7399513120665)) ;
#153591 = CARTESIAN_POINT('Ctrl Pts',(1.84666827906651,2.75001949937824,-35.7399065432933)) ;
#153592 = CARTESIAN_POINT('Ctrl Pts',(1.84609162157503,2.75002939777743,-35.7398860603461)) ;
#153593 = CARTESIAN_POINT('Ctrl Pts',(1.84477120566862,2.75005887738352,-35.7398388427818)) ;
#153594 = CARTESIAN_POINT('Ctrl Pts',(1.84402746838176,2.75008043331235,-35.7398120489461)) ;
#153595 = CARTESIAN_POINT('Ctrl Pts',(1.84209973630451,2.75014939605133,-35.7397420584709)) ;
#153596 = CARTESIAN_POINT('Ctrl Pts',(1.84091590068189,2.75020455995203,-35.7396985450601)) ;
#153597 = CARTESIAN_POINT('Ctrl Pts',(1.83783446245732,2.75038253459259,-35.7395838306667)) ;
#153598 = CARTESIAN_POINT('Ctrl Pts',(1.83593755875577,2.75052613608887,-35.7395117702048)) ;
#153599 = CARTESIAN_POINT('Ctrl Pts',(1.83094562972781,2.75099782378457,-35.7393183459611)) ;
#153600 = CARTESIAN_POINT('Ctrl Pts',(1.82785402838397,2.75138590243717,-35.7391945850334)) ;
#153601 = CARTESIAN_POINT('Ctrl Pts',(1.8194803599521,2.75271158620497,-35.7388527720391)) ;
#153602 = CARTESIAN_POINT('Ctrl Pts',(1.81421216401677,2.75385084739026,-35.7386282240443)) ;
#153603 = CARTESIAN_POINT('Ctrl Pts',(1.80309951666291,2.7569571777553,-35.7381406444328)) ;
#153604 = CARTESIAN_POINT('Ctrl Pts',(1.79729559107017,2.75901332923639,-35.7378834222529)) ;
#153605 = CARTESIAN_POINT('Ctrl Pts',(1.78960373217334,2.76233413717723,-35.7375331406995)) ;
#153606 = CARTESIAN_POINT('Ctrl Pts',(1.78754713318247,2.76328353076603,-35.7374383836782)) ;
#153607 = CARTESIAN_POINT('Ctrl Pts',(1.7829081527366,2.76556355836307,-35.7372206639426)) ;
#153608 = CARTESIAN_POINT('Ctrl Pts',(1.78033073359812,2.76693246555665,-35.7370964957842)) ;
#153609 = CARTESIAN_POINT('Ctrl Pts',(1.7769923351545,2.76883988197349,-35.7369304274279)) ;
#153610 = CARTESIAN_POINT('Ctrl Pts',(1.77620130341387,2.7693016905685,-35.7368906872082)) ;
#153611 = CARTESIAN_POINT('Ctrl Pts',(1.7700212686897,2.77299328865073,-35.7365769643392)) ;
#153612 = CARTESIAN_POINT('Ctrl Pts',(1.76495428809394,2.77651771765647,-35.7363064706027)) ;
#153613 = CARTESIAN_POINT('Ctrl Pts',(1.75938438670095,2.78118533566922,-35.7360042033494)) ;
#153614 = CARTESIAN_POINT('Ctrl Pts',(1.75866155316797,2.78180749698893,-35.7359648787297)) ;
#153615 = CARTESIAN_POINT('Ctrl Pts',(1.75440101126575,2.78557661565333,-35.7357327262068)) ;
#153616 = CARTESIAN_POINT('Ctrl Pts',(1.75110534239499,2.7889111885936,-35.7355622025983)) ;
#153617 = CARTESIAN_POINT('Ctrl Pts',(1.74704475763666,2.79358254909143,-35.73534353206)) ;
#153618 = CARTESIAN_POINT('Ctrl Pts',(1.74604050383922,2.79479094319558,-35.7352885793349)) ;
#153619 = CARTESIAN_POINT('Ctrl Pts',(1.74487333929766,2.79625803001554,-35.7352226603584)) ;
#153620 = CARTESIAN_POINT('Ctrl Pts',(1.74467927949938,2.79650417922903,-35.7352116332551)) ;
#153621 = CARTESIAN_POINT('Ctrl Pts',(1.74115657836479,2.8010141242866,-35.7350100972494)) ;
#153622 = CARTESIAN_POINT('Ctrl Pts',(1.73808736282556,2.80561663574421,-35.7348305563636)) ;
#153623 = CARTESIAN_POINT('Ctrl Pts',(1.73411503311369,2.81315073291946,-35.7345973211718)) ;
#153624 = CARTESIAN_POINT('Ctrl Pts',(1.73300100590541,2.81551882664669,-35.734535439772)) ;
#153625 = CARTESIAN_POINT('Ctrl Pts',(1.73189652742024,2.8181493620667,-35.7344706989523)) ;
#153626 = CARTESIAN_POINT('Ctrl Pts',(1.73180208385961,2.81837683840677,-35.7344651616954)) ;
#153627 = CARTESIAN_POINT('Ctrl Pts',(1.73016675860412,2.82236036724429,-35.7343692539515)) ;
#153628 = CARTESIAN_POINT('Ctrl Pts',(1.72888947962493,2.82624394236213,-35.7342946666905)) ;
#153629 = CARTESIAN_POINT('Ctrl Pts',(1.7277066333756,2.83096681006087,-35.7342247776101)) ;
#153630 = CARTESIAN_POINT('Ctrl Pts',(1.72752382530051,2.83174344980853,-35.7342139400975)) ;
#153631 = CARTESIAN_POINT('Ctrl Pts',(1.72719333568989,2.83324353771481,-35.7341942520731)) ;
#153632 = CARTESIAN_POINT('Ctrl Pts',(1.72704413780186,2.83396640281167,-35.7341852797154)) ;
#153633 = CARTESIAN_POINT('Ctrl Pts',(1.72602501437422,2.83926193721102,-35.7341230804511)) ;
#153634 = CARTESIAN_POINT('Ctrl Pts',(1.7255299684319,2.84393088107749,-35.7340890562028)) ;
#153635 = CARTESIAN_POINT('Ctrl Pts',(1.72543914472536,2.84906100604876,-35.7340827399932)) ;
#153636 = CARTESIAN_POINT('Ctrl Pts',(1.72543498451331,2.84953057829675,-35.7340824471676)) ;
#153637 = CARTESIAN_POINT('Ctrl Pts',(1.72543498451331,2.85,-35.7340824471676)) ;
#153638 = CARTESIAN_POINT('',(1.27787304021906,2.85,-32.4380981416173)) ;
#153639 = CARTESIAN_POINT('Origin',(-3.7454256867681E-16,2.85,-34.29)) ;
#153640 = CARTESIAN_POINT('Ctrl Pts',(1.37603597336698,2.75,-32.385)) ;
#153641 = CARTESIAN_POINT('Ctrl Pts',(1.37543428354307,2.75,-32.3853199418865)) ;
#153642 = CARTESIAN_POINT('Ctrl Pts',(1.37483253111457,2.7500053137259,-32.3856398156589)) ;
#153643 = CARTESIAN_POINT('Ctrl Pts',(1.3738872267507,2.75002207412044,-32.3861426442071)) ;
#153644 = CARTESIAN_POINT('Ctrl Pts',(1.37354350385558,2.75002991650282,-32.3863255141623)) ;
#153645 = CARTESIAN_POINT('Ctrl Pts',(1.37285611423782,2.75004911307826,-32.3866912988841)) ;
#153646 = CARTESIAN_POINT('Ctrl Pts',(1.37251244753525,2.75006046723047,-32.3868742136115)) ;
#153647 = CARTESIAN_POINT('Ctrl Pts',(1.3714815944481,2.75009981984526,-32.387422994695)) ;
#153648 = CARTESIAN_POINT('Ctrl Pts',(1.37079455494331,2.75013310886333,-32.3877888982032)) ;
#153649 = CARTESIAN_POINT('Ctrl Pts',(1.36873453110893,2.75025430438115,-32.3888865055866)) ;
#153650 = CARTESIAN_POINT('Ctrl Pts',(1.36736263966052,2.75036354665963,-32.3896181092421)) ;
#153651 = CARTESIAN_POINT('Ctrl Pts',(1.36413470836879,2.75068903914081,-32.3913410689378)) ;
#153652 = CARTESIAN_POINT('Ctrl Pts',(1.36227932197148,2.75092980851021,-32.392332637721)) ;
#153653 = CARTESIAN_POINT('Ctrl Pts',(1.35746012444743,2.7516985967038,-32.3949111819216)) ;
#153654 = CARTESIAN_POINT('Ctrl Pts',(1.35450425835489,2.75231332717651,-32.3964957625411)) ;
#153655 = CARTESIAN_POINT('Ctrl Pts',(1.34886973918565,2.75377034241463,-32.3995208305066)) ;
#153656 = CARTESIAN_POINT('Ctrl Pts',(1.34617831568151,2.75459534478001,-32.4009678592584)) ;
#153657 = CARTESIAN_POINT('Ctrl Pts',(1.34314242260183,2.75567798707047,-32.4026015301229)) ;
#153658 = CARTESIAN_POINT('Ctrl Pts',(1.34256163823227,2.75588931242805,-32.402914101785)) ;
#153659 = CARTESIAN_POINT('Ctrl Pts',(1.3419826199981,2.75610647364237,-32.4032257815815)) ;
#153660 = CARTESIAN_POINT('Ctrl Pts',(1.34132160522921,2.75635697290855,-32.4035816219833)) ;
#153661 = CARTESIAN_POINT('Ctrl Pts',(1.34086291435071,2.75653491456655,-32.4038285825319)) ;
#153662 = CARTESIAN_POINT('Ctrl Pts',(1.33918548989956,2.75720079503569,-32.4047318375006)) ;
#153663 = CARTESIAN_POINT('Ctrl Pts',(1.33797416370949,2.75771112313094,-32.4053843482652)) ;
#153664 = CARTESIAN_POINT('Ctrl Pts',(1.33648532079706,2.75837521508442,-32.4061866329489)) ;
#153665 = CARTESIAN_POINT('Ctrl Pts',(1.33619776328718,2.75850521488809,-32.4063415973022)) ;
#153666 = CARTESIAN_POINT('Ctrl Pts',(1.33107968015782,2.76084915994844,-32.4091000397109)) ;
#153667 = CARTESIAN_POINT('Ctrl Pts',(1.32635908659783,2.76350693338837,-32.4116480195469)) ;
#153668 = CARTESIAN_POINT('Ctrl Pts',(1.32109760626318,2.76707470328213,-32.4144947169103)) ;
#153669 = CARTESIAN_POINT('Ctrl Pts',(1.32035743991961,2.76759128788199,-32.4148953524442)) ;
#153670 = CARTESIAN_POINT('Ctrl Pts',(1.31824805546064,2.76910584227485,-32.4160376626109)) ;
#153671 = CARTESIAN_POINT('Ctrl Pts',(1.31689309423374,2.77013099976531,-32.4167722633589)) ;
#153672 = CARTESIAN_POINT('Ctrl Pts',(1.31545882361431,2.77127278201751,-32.4175511219408)) ;
#153673 = CARTESIAN_POINT('Ctrl Pts',(1.31535582310949,2.77135510350029,-32.4176070616535)) ;
#153674 = CARTESIAN_POINT('Ctrl Pts',(1.31504853092197,2.77160168095808,-32.4177739734471)) ;
#153675 = CARTESIAN_POINT('Ctrl Pts',(1.31461168315413,2.77195498754755,-32.4180113068542)) ;
#153676 = CARTESIAN_POINT('Ctrl Pts',(1.31417742224124,2.77231219724379,-32.4182473370572)) ;
#153677 = CARTESIAN_POINT('Ctrl Pts',(1.31333096026301,2.77301480846583,-32.418707506137)) ;
#153678 = CARTESIAN_POINT('Ctrl Pts',(1.31272070342842,2.77353368974781,-32.4190394568407)) ;
#153679 = CARTESIAN_POINT('Ctrl Pts',(1.30969774837119,2.77616736630471,-32.4206845572383)) ;
#153680 = CARTESIAN_POINT('Ctrl Pts',(1.30737022788685,2.7784005464459,-32.4219534798952)) ;
#153681 = CARTESIAN_POINT('Ctrl Pts',(1.30464757270875,2.78128817542236,-32.423438703349)) ;
#153682 = CARTESIAN_POINT('Ctrl Pts',(1.30414845981073,2.78182967606625,-32.4237110126308)) ;
#153683 = CARTESIAN_POINT('Ctrl Pts',(1.30260826844057,2.78353926416386,-32.4245514286369)) ;
#153684 = CARTESIAN_POINT('Ctrl Pts',(1.30158324720851,2.78473373830864,-32.4251112329214)) ;
#153685 = CARTESIAN_POINT('Ctrl Pts',(1.30024935135334,2.78636738852736,-32.4258398127168)) ;
#153686 = CARTESIAN_POINT('Ctrl Pts',(1.29991860867239,2.7867792151927,-32.4260204750811)) ;
#153687 = CARTESIAN_POINT('Ctrl Pts',(1.29915346420736,2.78774794465152,-32.4264384192283)) ;
#153688 = CARTESIAN_POINT('Ctrl Pts',(1.2987212590447,2.7883074481047,-32.4266744998873)) ;
#153689 = CARTESIAN_POINT('Ctrl Pts',(1.29658637826224,2.79113377451588,-32.4278405320741)) ;
#153690 = CARTESIAN_POINT('Ctrl Pts',(1.29496240940489,2.79348720429742,-32.4287269863698)) ;
#153691 = CARTESIAN_POINT('Ctrl Pts',(1.29231665668157,2.79769679694543,-32.430171648005)) ;
#153692 = CARTESIAN_POINT('Ctrl Pts',(1.29125115601062,2.79951540543442,-32.4307540486807)) ;
#153693 = CARTESIAN_POINT('Ctrl Pts',(1.28927619853496,2.80313430045114,-32.4318348789813)) ;
#153694 = CARTESIAN_POINT('Ctrl Pts',(1.2883624199782,2.80493500363976,-32.4323353793459)) ;
#153695 = CARTESIAN_POINT('Ctrl Pts',(1.28732027925586,2.80715235940912,-32.4329068412463)) ;
#153696 = CARTESIAN_POINT('Ctrl Pts',(1.28695835013166,2.80793550920672,-32.4331053825645)) ;
#153697 = CARTESIAN_POINT('Ctrl Pts',(1.28660568774192,2.80872522382215,-32.4332989562928)) ;
#153698 = CARTESIAN_POINT('Ctrl Pts',(1.28608376699198,2.80991454434771,-32.4335854978985)) ;
#153699 = CARTESIAN_POINT('Ctrl Pts',(1.28574525149603,2.81071375754607,-32.4337714318906)) ;
#153700 = CARTESIAN_POINT('Ctrl Pts',(1.28475894023899,2.81312894312816,-32.434313266649)) ;
#153701 = CARTESIAN_POINT('Ctrl Pts',(1.28414040309307,2.81476247656134,-32.434653166298)) ;
#153702 = CARTESIAN_POINT('Ctrl Pts',(1.28339818260918,2.81688756020139,-32.435060888642)) ;
#153703 = CARTESIAN_POINT('Ctrl Pts',(1.28323661013049,2.81736137575517,-32.4351496371781)) ;
#153704 = CARTESIAN_POINT('Ctrl Pts',(1.28265668893886,2.81910411140422,-32.4354681473537)) ;
#153705 = CARTESIAN_POINT('Ctrl Pts',(1.2822592025034,2.82038205281173,-32.4356863923252)) ;
#153706 = CARTESIAN_POINT('Ctrl Pts',(1.28170385606942,2.82230051526758,-32.4359913349836)) ;
#153707 = CARTESIAN_POINT('Ctrl Pts',(1.28152700208476,2.82293438010907,-32.4360884417703)) ;
#153708 = CARTESIAN_POINT('Ctrl Pts',(1.28107448868733,2.82461913389174,-32.4363369091493)) ;
#153709 = CARTESIAN_POINT('Ctrl Pts',(1.28081016954774,2.82567198476339,-32.4364819889541)) ;
#153710 = CARTESIAN_POINT('Ctrl Pts',(1.28009910353322,2.82871092361133,-32.4368721680177)) ;
#153711 = CARTESIAN_POINT('Ctrl Pts',(1.27969380338795,2.83071459002993,-32.43709487088)) ;
#153712 = CARTESIAN_POINT('Ctrl Pts',(1.27923282767965,2.83340629334535,-32.4373484537334)) ;
#153713 = CARTESIAN_POINT('Ctrl Pts',(1.27912420342283,2.83408089926109,-32.4374082352158)) ;
#153714 = CARTESIAN_POINT('Ctrl Pts',(1.27861441353189,2.83746106027944,-32.4376889088183)) ;
#153715 = CARTESIAN_POINT('Ctrl Pts',(1.27831324287571,2.84018799487016,-32.4378550982434)) ;
#153716 = CARTESIAN_POINT('Ctrl Pts',(1.27795656969996,2.84527977141538,-32.4380519866561)) ;
#153717 = CARTESIAN_POINT('Ctrl Pts',(1.27787304021906,2.84764286211077,-32.4380981416173)) ;
#153718 = CARTESIAN_POINT('Ctrl Pts',(1.27787304021907,2.85,-32.4380981416173)) ;
#153719 = CARTESIAN_POINT('Origin',(1.3145125,-1.51907484122731,-28.575)) ;
#153720 = CARTESIAN_POINT('Origin',(1.3145125,2.85,-28.575)) ;
#153721 = CARTESIAN_POINT('',(1.27787304021905,-1.51907484122731,-28.6280981416173)) ;
#153722 = CARTESIAN_POINT('',(1.27787304021905,-1.51907484122731,-28.5219018583827)) ;
#153723 = CARTESIAN_POINT('Origin',(1.3145125,-1.51907484122731,-24.765)) ;
#153724 = CARTESIAN_POINT('Origin',(1.3145125,2.85,-24.765)) ;
#153725 = CARTESIAN_POINT('',(1.27787304021905,-1.51907484122731,-24.8180981416173)) ;
#153726 = CARTESIAN_POINT('',(1.27787304021905,-1.51907484122731,-24.7119018583827)) ;
#153727 = CARTESIAN_POINT('Origin',(1.3145125,-1.51907484122731,-20.955)) ;
#153728 = CARTESIAN_POINT('Origin',(1.3145125,2.85,-20.955)) ;
#153729 = CARTESIAN_POINT('',(1.27787304021905,-1.51907484122731,-21.0080981416173)) ;
#153730 = CARTESIAN_POINT('',(1.27787304021905,-1.51907484122731,-20.9019018583827)) ;
#153731 = CARTESIAN_POINT('Origin',(1.3145125,-1.51907484122731,-17.145)) ;
#153732 = CARTESIAN_POINT('Origin',(1.3145125,2.85,-17.145)) ;
#153733 = CARTESIAN_POINT('',(1.27787304021905,-1.51907484122731,-17.1980981416173)) ;
#153734 = CARTESIAN_POINT('',(1.27787304021905,-1.51907484122731,-17.0919018583827)) ;
#153735 = CARTESIAN_POINT('Origin',(1.3145125,-1.51907484122731,-13.335)) ;
#153736 = CARTESIAN_POINT('Origin',(1.3145125,2.85,-13.335)) ;
#153737 = CARTESIAN_POINT('',(1.27787304021905,-1.51907484122731,-13.3880981416173)) ;
#153738 = CARTESIAN_POINT('',(1.27787304021905,-1.51907484122731,-13.2819018583827)) ;
#153739 = CARTESIAN_POINT('Origin',(1.3145125,-1.51907484122731,-9.525)) ;
#153740 = CARTESIAN_POINT('Origin',(1.3145125,2.85,-9.525)) ;
#153741 = CARTESIAN_POINT('',(1.27787304021905,-1.51907484122731,-9.57809814161729)) ;
#153742 = CARTESIAN_POINT('',(1.27787304021905,-1.51907484122731,-9.4719018583827)) ;
#153743 = CARTESIAN_POINT('Origin',(1.3145125,-1.51907484122731,-5.715)) ;
#153744 = CARTESIAN_POINT('Origin',(1.3145125,2.85,-5.715)) ;
#153745 = CARTESIAN_POINT('',(1.27787304021905,-1.51907484122731,-5.76809814161729)) ;
#153746 = CARTESIAN_POINT('',(1.27787304021905,-1.51907484122731,-5.66190185838271)) ;
#153747 = CARTESIAN_POINT('Origin',(9.24142135623731,0.,-34.29)) ;
#153748 = CARTESIAN_POINT('',(9.17071067811866,-1.18877772485616E-16,-33.3192893218813)) ;
#153749 = CARTESIAN_POINT('Origin',(9.17071067811866,0.,-34.29)) ;
#153750 = CARTESIAN_POINT('',(9.24142135623731,-1.22464679914736E-16,-33.29)) ;
#153751 = CARTESIAN_POINT('Origin',(9.24142135623731,-1.10218211923262E-16,
-33.39)) ;
#153752 = CARTESIAN_POINT('Origin',(9.24142135623731,0.,-34.29)) ;
#153753 = CARTESIAN_POINT('Origin',(-6.11095769946375E-16,4.45,-34.29)) ;
#153754 = CARTESIAN_POINT('',(1.5,4.45,-34.29)) ;
#153755 = CARTESIAN_POINT('Origin',(-6.11095769946375E-16,4.45,-34.29)) ;
#153756 = CARTESIAN_POINT('',(1.6,4.55,-34.29)) ;
#153757 = CARTESIAN_POINT('Origin',(1.6,4.45,-34.29)) ;
#153758 = CARTESIAN_POINT('Origin',(-6.24237614461351E-16,4.55,-34.29)) ;
#153759 = CARTESIAN_POINT('Origin',(10.1,0.,-34.29)) ;
#153760 = CARTESIAN_POINT('',(10.1,-1.22464679914735E-16,-33.29)) ;
#153761 = CARTESIAN_POINT('Origin',(10.1,0.,-34.29)) ;
#153762 = CARTESIAN_POINT('',(10.2,-1.34711147906209E-16,-33.19)) ;
#153763 = CARTESIAN_POINT('Origin',(10.1,-1.34711147906209E-16,-33.19)) ;
#153764 = CARTESIAN_POINT('Origin',(10.2,0.,-34.29)) ;
#153765 = CARTESIAN_POINT('Origin',(9.24142135623731,0.,-30.48)) ;
#153766 = CARTESIAN_POINT('',(9.17071067811866,-1.18877772485617E-16,-29.5092893218813)) ;
#153767 = CARTESIAN_POINT('Origin',(9.17071067811866,0.,-30.48)) ;
#153768 = CARTESIAN_POINT('',(9.24142135623731,-1.22464679914735E-16,-29.48)) ;
#153769 = CARTESIAN_POINT('Origin',(9.24142135623731,-1.10218211923262E-16,
-29.58)) ;
#153770 = CARTESIAN_POINT('Origin',(9.24142135623731,0.,-30.48)) ;
#153771 = CARTESIAN_POINT('Origin',(-6.11095769946375E-16,4.45,-30.48)) ;
#153772 = CARTESIAN_POINT('',(1.5,4.45,-30.48)) ;
#153773 = CARTESIAN_POINT('Origin',(-6.11095769946375E-16,4.45,-30.48)) ;
#153774 = CARTESIAN_POINT('',(1.6,4.55,-30.48)) ;
#153775 = CARTESIAN_POINT('Origin',(1.6,4.45,-30.48)) ;
#153776 = CARTESIAN_POINT('Origin',(-6.24237614461351E-16,4.55,-30.48)) ;
#153777 = CARTESIAN_POINT('Origin',(10.1,0.,-30.48)) ;
#153778 = CARTESIAN_POINT('',(10.1,-1.22464679914735E-16,-29.48)) ;
#153779 = CARTESIAN_POINT('Origin',(10.1,0.,-30.48)) ;
#153780 = CARTESIAN_POINT('',(10.2,-1.34711147906209E-16,-29.38)) ;
#153781 = CARTESIAN_POINT('Origin',(10.1,-1.34711147906209E-16,-29.38)) ;
#153782 = CARTESIAN_POINT('Origin',(10.2,0.,-30.48)) ;
#153783 = CARTESIAN_POINT('Origin',(9.24142135623731,0.,-26.67)) ;
#153784 = CARTESIAN_POINT('',(9.17071067811866,-1.18877772485617E-16,-25.6992893218813)) ;
#153785 = CARTESIAN_POINT('Origin',(9.17071067811866,0.,-26.67)) ;
#153786 = CARTESIAN_POINT('',(9.24142135623731,-1.22464679914735E-16,-25.67)) ;
#153787 = CARTESIAN_POINT('Origin',(9.24142135623731,-1.10218211923262E-16,
-25.77)) ;
#153788 = CARTESIAN_POINT('Origin',(9.24142135623731,0.,-26.67)) ;
#153789 = CARTESIAN_POINT('Origin',(-6.11095769946375E-16,4.45,-26.67)) ;
#153790 = CARTESIAN_POINT('',(1.5,4.45,-26.67)) ;
#153791 = CARTESIAN_POINT('Origin',(-6.11095769946375E-16,4.45,-26.67)) ;
#153792 = CARTESIAN_POINT('',(1.6,4.55,-26.67)) ;
#153793 = CARTESIAN_POINT('Origin',(1.6,4.45,-26.67)) ;
#153794 = CARTESIAN_POINT('Origin',(-6.24237614461351E-16,4.55,-26.67)) ;
#153795 = CARTESIAN_POINT('Origin',(10.1,0.,-26.67)) ;
#153796 = CARTESIAN_POINT('',(10.1,-1.22464679914735E-16,-25.67)) ;
#153797 = CARTESIAN_POINT('Origin',(10.1,0.,-26.67)) ;
#153798 = CARTESIAN_POINT('',(10.2,-1.34711147906209E-16,-25.57)) ;
#153799 = CARTESIAN_POINT('Origin',(10.1,-1.34711147906209E-16,-25.57)) ;
#153800 = CARTESIAN_POINT('Origin',(10.2,0.,-26.67)) ;
#153801 = CARTESIAN_POINT('Origin',(9.24142135623731,0.,-22.86)) ;
#153802 = CARTESIAN_POINT('',(9.17071067811866,-1.18877772485617E-16,-21.8892893218813)) ;
#153803 = CARTESIAN_POINT('Origin',(9.17071067811866,0.,-22.86)) ;
#153804 = CARTESIAN_POINT('',(9.24142135623731,-1.22464679914735E-16,-21.86)) ;
#153805 = CARTESIAN_POINT('Origin',(9.24142135623731,-1.10218211923262E-16,
-21.96)) ;
#153806 = CARTESIAN_POINT('Origin',(9.24142135623731,0.,-22.86)) ;
#153807 = CARTESIAN_POINT('Origin',(-6.11095769946375E-16,4.45,-22.86)) ;
#153808 = CARTESIAN_POINT('',(1.5,4.45,-22.86)) ;
#153809 = CARTESIAN_POINT('Origin',(-6.11095769946375E-16,4.45,-22.86)) ;
#153810 = CARTESIAN_POINT('',(1.6,4.55,-22.86)) ;
#153811 = CARTESIAN_POINT('Origin',(1.6,4.45,-22.86)) ;
#153812 = CARTESIAN_POINT('Origin',(-6.24237614461351E-16,4.55,-22.86)) ;
#153813 = CARTESIAN_POINT('Origin',(10.1,0.,-22.86)) ;
#153814 = CARTESIAN_POINT('',(10.1,-1.22464679914735E-16,-21.86)) ;
#153815 = CARTESIAN_POINT('Origin',(10.1,0.,-22.86)) ;
#153816 = CARTESIAN_POINT('',(10.2,-1.34711147906209E-16,-21.76)) ;
#153817 = CARTESIAN_POINT('Origin',(10.1,-1.34711147906209E-16,-21.76)) ;
#153818 = CARTESIAN_POINT('Origin',(10.2,0.,-22.86)) ;
#153819 = CARTESIAN_POINT('Origin',(9.24142135623731,0.,-19.05)) ;
#153820 = CARTESIAN_POINT('',(9.17071067811866,-1.18877772485617E-16,-18.0792893218813)) ;
#153821 = CARTESIAN_POINT('Origin',(9.17071067811866,0.,-19.05)) ;
#153822 = CARTESIAN_POINT('',(9.24142135623731,-1.22464679914736E-16,-18.05)) ;
#153823 = CARTESIAN_POINT('Origin',(9.24142135623731,-1.10218211923262E-16,
-18.15)) ;
#153824 = CARTESIAN_POINT('Origin',(9.24142135623731,0.,-19.05)) ;
#153825 = CARTESIAN_POINT('Origin',(-6.11095769946375E-16,4.45,-19.05)) ;
#153826 = CARTESIAN_POINT('',(1.5,4.45,-19.05)) ;
#153827 = CARTESIAN_POINT('Origin',(-6.11095769946375E-16,4.45,-19.05)) ;
#153828 = CARTESIAN_POINT('',(1.6,4.55,-19.05)) ;
#153829 = CARTESIAN_POINT('Origin',(1.6,4.45,-19.05)) ;
#153830 = CARTESIAN_POINT('Origin',(-6.24237614461351E-16,4.55,-19.05)) ;
#153831 = CARTESIAN_POINT('Origin',(10.1,0.,-19.05)) ;
#153832 = CARTESIAN_POINT('',(10.1,-1.22464679914735E-16,-18.05)) ;
#153833 = CARTESIAN_POINT('Origin',(10.1,0.,-19.05)) ;
#153834 = CARTESIAN_POINT('',(10.2,-1.34711147906209E-16,-17.95)) ;
#153835 = CARTESIAN_POINT('Origin',(10.1,-1.34711147906209E-16,-17.95)) ;
#153836 = CARTESIAN_POINT('Origin',(10.2,0.,-19.05)) ;
#153837 = CARTESIAN_POINT('Origin',(9.24142135623732,0.,-15.24)) ;
#153838 = CARTESIAN_POINT('',(9.17071067811866,-1.18877772485617E-16,-14.2692893218813)) ;
#153839 = CARTESIAN_POINT('Origin',(9.17071067811866,0.,-15.24)) ;
#153840 = CARTESIAN_POINT('',(9.24142135623732,-1.22464679914736E-16,-14.24)) ;
#153841 = CARTESIAN_POINT('Origin',(9.24142135623732,-1.10218211923262E-16,
-14.34)) ;
#153842 = CARTESIAN_POINT('Origin',(9.24142135623732,0.,-15.24)) ;
#153843 = CARTESIAN_POINT('Origin',(-6.11095769946375E-16,4.45,-15.24)) ;
#153844 = CARTESIAN_POINT('',(1.5,4.45,-15.24)) ;
#153845 = CARTESIAN_POINT('Origin',(-6.11095769946375E-16,4.45,-15.24)) ;
#153846 = CARTESIAN_POINT('',(1.6,4.55,-15.24)) ;
#153847 = CARTESIAN_POINT('Origin',(1.6,4.45,-15.24)) ;
#153848 = CARTESIAN_POINT('Origin',(-6.24237614461351E-16,4.55,-15.24)) ;
#153849 = CARTESIAN_POINT('Origin',(10.1,0.,-15.24)) ;
#153850 = CARTESIAN_POINT('',(10.1,-1.22464679914735E-16,-14.24)) ;
#153851 = CARTESIAN_POINT('Origin',(10.1,0.,-15.24)) ;
#153852 = CARTESIAN_POINT('',(10.2,-1.34711147906209E-16,-14.14)) ;
#153853 = CARTESIAN_POINT('Origin',(10.1,-1.34711147906209E-16,-14.14)) ;
#153854 = CARTESIAN_POINT('Origin',(10.2,0.,-15.24)) ;
#153855 = CARTESIAN_POINT('Origin',(9.24142135623732,0.,-11.43)) ;
#153856 = CARTESIAN_POINT('',(9.17071067811866,-1.18877772485617E-16,-10.4592893218813)) ;
#153857 = CARTESIAN_POINT('Origin',(9.17071067811866,0.,-11.43)) ;
#153858 = CARTESIAN_POINT('',(9.24142135623732,-1.22464679914736E-16,-10.43)) ;
#153859 = CARTESIAN_POINT('Origin',(9.24142135623732,-1.10218211923262E-16,
-10.53)) ;
#153860 = CARTESIAN_POINT('Origin',(9.24142135623732,0.,-11.43)) ;
#153861 = CARTESIAN_POINT('Origin',(-6.11095769946375E-16,4.45,-11.43)) ;
#153862 = CARTESIAN_POINT('',(1.5,4.45,-11.43)) ;
#153863 = CARTESIAN_POINT('Origin',(-6.11095769946375E-16,4.45,-11.43)) ;
#153864 = CARTESIAN_POINT('',(1.6,4.55,-11.43)) ;
#153865 = CARTESIAN_POINT('Origin',(1.6,4.45,-11.43)) ;
#153866 = CARTESIAN_POINT('Origin',(-6.24237614461351E-16,4.55,-11.43)) ;
#153867 = CARTESIAN_POINT('Origin',(10.1,0.,-11.43)) ;
#153868 = CARTESIAN_POINT('',(10.1,-1.22464679914735E-16,-10.43)) ;
#153869 = CARTESIAN_POINT('Origin',(10.1,0.,-11.43)) ;
#153870 = CARTESIAN_POINT('',(10.2,-1.34711147906209E-16,-10.33)) ;
#153871 = CARTESIAN_POINT('Origin',(10.1,-1.34711147906209E-16,-10.33)) ;
#153872 = CARTESIAN_POINT('Origin',(10.2,0.,-11.43)) ;
#153873 = CARTESIAN_POINT('Origin',(9.24142135623731,0.,-7.62)) ;
#153874 = CARTESIAN_POINT('',(9.17071067811866,-1.18877772485617E-16,-6.64928932188134)) ;
#153875 = CARTESIAN_POINT('Origin',(9.17071067811866,0.,-7.62)) ;
#153876 = CARTESIAN_POINT('',(9.24142135623731,-1.22464679914735E-16,-6.62)) ;
#153877 = CARTESIAN_POINT('Origin',(9.24142135623731,-1.10218211923262E-16,
-6.72)) ;
#153878 = CARTESIAN_POINT('Origin',(9.24142135623731,0.,-7.62)) ;
#153879 = CARTESIAN_POINT('Origin',(-6.11095769946375E-16,4.45,-7.62)) ;
#153880 = CARTESIAN_POINT('',(1.5,4.45,-7.62)) ;
#153881 = CARTESIAN_POINT('Origin',(-6.11095769946375E-16,4.45,-7.62)) ;
#153882 = CARTESIAN_POINT('',(1.6,4.55,-7.62)) ;
#153883 = CARTESIAN_POINT('Origin',(1.6,4.45,-7.62)) ;
#153884 = CARTESIAN_POINT('Origin',(-6.24237614461351E-16,4.55,-7.62)) ;
#153885 = CARTESIAN_POINT('Origin',(10.1,0.,-7.62)) ;
#153886 = CARTESIAN_POINT('',(10.1,-1.22464679914735E-16,-6.62)) ;
#153887 = CARTESIAN_POINT('Origin',(10.1,0.,-7.62)) ;
#153888 = CARTESIAN_POINT('',(10.2,-1.34711147906209E-16,-6.52)) ;
#153889 = CARTESIAN_POINT('Origin',(10.1,-1.34711147906209E-16,-6.52)) ;
#153890 = CARTESIAN_POINT('Origin',(10.2,0.,-7.62)) ;
#153891 = CARTESIAN_POINT('Origin',(9.24142135623731,0.,-3.81)) ;
#153892 = CARTESIAN_POINT('',(9.17071067811866,-1.18877772485617E-16,-2.83928932188134)) ;
#153893 = CARTESIAN_POINT('Origin',(9.17071067811866,0.,-3.81)) ;
#153894 = CARTESIAN_POINT('',(9.24142135623731,-1.22464679914735E-16,-2.81)) ;
#153895 = CARTESIAN_POINT('Origin',(9.24142135623731,-1.10218211923262E-16,
-2.91)) ;
#153896 = CARTESIAN_POINT('Origin',(9.24142135623731,0.,-3.81)) ;
#153897 = CARTESIAN_POINT('Origin',(-6.11095769946375E-16,4.45,-3.81)) ;
#153898 = CARTESIAN_POINT('',(1.5,4.45,-3.81)) ;
#153899 = CARTESIAN_POINT('Origin',(-6.11095769946375E-16,4.45,-3.81)) ;
#153900 = CARTESIAN_POINT('',(1.6,4.55,-3.81)) ;
#153901 = CARTESIAN_POINT('Origin',(1.6,4.45,-3.81)) ;
#153902 = CARTESIAN_POINT('Origin',(-6.24237614461351E-16,4.55,-3.81)) ;
#153903 = CARTESIAN_POINT('Origin',(10.1,0.,-3.81)) ;
#153904 = CARTESIAN_POINT('',(10.1,-1.22464679914735E-16,-2.81)) ;
#153905 = CARTESIAN_POINT('Origin',(10.1,0.,-3.81)) ;
#153906 = CARTESIAN_POINT('',(10.2,-1.34711147906209E-16,-2.71)) ;
#153907 = CARTESIAN_POINT('Origin',(10.1,-1.34711147906209E-16,-2.71)) ;
#153908 = CARTESIAN_POINT('Origin',(10.2,0.,-3.81)) ;
#153909 = CARTESIAN_POINT('Origin',(-7.29372370581158E-16,3.55,-3.81)) ;
#153910 = CARTESIAN_POINT('',(-0.17080731546663,3.55,-2.31975677791071)) ;
#153911 = CARTESIAN_POINT('',(1.5,3.55,-3.81)) ;
#153912 = CARTESIAN_POINT('Origin',(-7.29372370581158E-16,3.55,-3.81)) ;
#153913 = CARTESIAN_POINT('',(-0.273932138433073,3.45,-2.3352250396981)) ;
#153914 = CARTESIAN_POINT('Ctrl Pts',(-0.170807315466632,3.55,-2.31975677791071)) ;
#153915 = CARTESIAN_POINT('Ctrl Pts',(-0.18388243342709,3.55,-2.32125540965426)) ;
#153916 = CARTESIAN_POINT('Ctrl Pts',(-0.197859036177013,3.54752250383109,
-2.32305117609769)) ;
#153917 = CARTESIAN_POINT('Ctrl Pts',(-0.223597793566256,3.53719045839678,
-2.32670064673137)) ;
#153918 = CARTESIAN_POINT('Ctrl Pts',(-0.235362682979178,3.52934133421403,
-2.32855041868906)) ;
#153919 = CARTESIAN_POINT('Ctrl Pts',(-0.253465441530115,3.51138121637726,
-2.33154294802378)) ;
#153920 = CARTESIAN_POINT('Ctrl Pts',(-0.261168570620306,3.50026979217228,
-2.3329034821853)) ;
#153921 = CARTESIAN_POINT('Ctrl Pts',(-0.271399896344097,3.47583586070553,
-2.33474636459954)) ;
#153922 = CARTESIAN_POINT('Ctrl Pts',(-0.273932138433075,3.46251477070021,
-2.3352250396981)) ;
#153923 = CARTESIAN_POINT('Ctrl Pts',(-0.273932138433075,3.45,-2.3352250396981)) ;
#153924 = CARTESIAN_POINT('',(-0.273932138433073,3.15,-2.3352250396981)) ;
#153925 = CARTESIAN_POINT('',(-0.273932138433073,3.05,-2.3352250396981)) ;
#153926 = CARTESIAN_POINT('',(-0.373948193368569,3.05,-2.35736007604211)) ;
#153927 = CARTESIAN_POINT('Ctrl Pts',(-0.273932138433074,3.15,-2.33522503969809)) ;
#153928 = CARTESIAN_POINT('Ctrl Pts',(-0.273932138433074,3.13744372549049,
-2.33522503969809)) ;
#153929 = CARTESIAN_POINT('Ctrl Pts',(-0.276486468486165,3.12408297110069,
-2.33569113023559)) ;
#153930 = CARTESIAN_POINT('Ctrl Pts',(-0.28674027764043,3.0995678553947,-2.33765377899357)) ;
#153931 = CARTESIAN_POINT('Ctrl Pts',(-0.294439768310518,3.08841385970397,
-2.33915484113775)) ;
#153932 = CARTESIAN_POINT('Ctrl Pts',(-0.312194128344973,3.07061084469361,
-2.34281939995099)) ;
#153933 = CARTESIAN_POINT('Ctrl Pts',(-0.323517908844218,3.0628422827531,
-2.3452474862748)) ;
#153934 = CARTESIAN_POINT('Ctrl Pts',(-0.348172117123306,3.05253676672645,
-2.35091383875347)) ;
#153935 = CARTESIAN_POINT('Ctrl Pts',(-0.361501722536398,3.05,-2.35415602305916)) ;
#153936 = CARTESIAN_POINT('Ctrl Pts',(-0.37394819336857,3.05,-2.35736007604211)) ;
#153937 = CARTESIAN_POINT('',(-0.872417476238727,3.05,-2.58980011999949)) ;
#153938 = CARTESIAN_POINT('Origin',(-7.95081593156037E-16,3.05,-3.81)) ;
#153939 = CARTESIAN_POINT('',(-0.953662978710562,3.15,-2.65218873600362)) ;
#153940 = CARTESIAN_POINT('Ctrl Pts',(-0.872417476238727,3.05,-2.58980011999949)) ;
#153941 = CARTESIAN_POINT('Ctrl Pts',(-0.882808783297377,3.05,-2.59722968791498)) ;
#153942 = CARTESIAN_POINT('Ctrl Pts',(-0.893798224191975,3.05250629897269,
-2.60530936231458)) ;
#153943 = CARTESIAN_POINT('Ctrl Pts',(-0.913892243159219,3.06269675232156,
-2.62047776912462)) ;
#153944 = CARTESIAN_POINT('Ctrl Pts',(-0.922999225059833,3.07038074042647,
-2.62756342856912)) ;
#153945 = CARTESIAN_POINT('Ctrl Pts',(-0.937285134131706,3.08810056349785,
-2.63885587110341)) ;
#153946 = CARTESIAN_POINT('Ctrl Pts',(-0.943452174397235,3.09929464195085,
-2.64384309680397)) ;
#153947 = CARTESIAN_POINT('Ctrl Pts',(-0.951639309815362,3.12392729225934,
-2.65051099979639)) ;
#153948 = CARTESIAN_POINT('Ctrl Pts',(-0.953662978710562,3.13736547222678,
-2.65218873600362)) ;
#153949 = CARTESIAN_POINT('Ctrl Pts',(-0.953662978710562,3.15,-2.65218873600362)) ;
#153950 = CARTESIAN_POINT('',(-0.953662978710562,3.45,-2.65218873600362)) ;
#153951 = CARTESIAN_POINT('',(-0.953662978710562,3.05,-2.65218873600362)) ;
#153952 = CARTESIAN_POINT('',(-1.03179971315145,3.55,-2.72124412656437)) ;
#153953 = CARTESIAN_POINT('Ctrl Pts',(-0.953662978710565,3.45,-2.65218873600362)) ;
#153954 = CARTESIAN_POINT('Ctrl Pts',(-0.953662978710565,3.45580715149871,
-2.65218873600362)) ;
#153955 = CARTESIAN_POINT('Ctrl Pts',(-0.954069792639904,3.46165880969181,
-2.65252363156927)) ;
#153956 = CARTESIAN_POINT('Ctrl Pts',(-0.954880405808389,3.46741264967889,
-2.65319273207538)) ;
#153957 = CARTESIAN_POINT('Ctrl Pts',(-0.955592557016219,3.47246759358526,
-2.65378055960165)) ;
#153958 = CARTESIAN_POINT('Ctrl Pts',(-0.956615573654934,3.47744631522377,
-2.65462581144883)) ;
#153959 = CARTESIAN_POINT('Ctrl Pts',(-0.957920385817347,3.48225893605767,
-2.65570864404338)) ;
#153960 = CARTESIAN_POINT('Ctrl Pts',(-0.959423079246192,3.48780141482277,
-2.65695569359675)) ;
#153961 = CARTESIAN_POINT('Ctrl Pts',(-0.961323201468143,3.49320783601914,
-2.65853745938163)) ;
#153962 = CARTESIAN_POINT('Ctrl Pts',(-0.963574238618811,3.49834560049868,
-2.66042425789638)) ;
#153963 = CARTESIAN_POINT('Ctrl Pts',(-0.965499706648001,3.50274028640776,
-2.66203816738543)) ;
#153964 = CARTESIAN_POINT('Ctrl Pts',(-0.967680912999541,3.5069382066956,
-2.66387459445843)) ;
#153965 = CARTESIAN_POINT('Ctrl Pts',(-0.970068248378239,3.51087311165944,
-2.66589878354725)) ;
#153966 = CARTESIAN_POINT('Ctrl Pts',(-0.972933246979055,3.51559532091263,
-2.66832797676366)) ;
#153967 = CARTESIAN_POINT('Ctrl Pts',(-0.976138831290358,3.52000896466723,
-2.67106468556238)) ;
#153968 = CARTESIAN_POINT('Ctrl Pts',(-0.979601776802477,3.52400782220665,
-2.67405098434758)) ;
#153969 = CARTESIAN_POINT('Ctrl Pts',(-0.982467725203494,3.52731729367563,
-2.67652245789472)) ;
#153970 = CARTESIAN_POINT('Ctrl Pts',(-0.985508986896834,3.53034305696182,
-2.67916417360478)) ;
#153971 = CARTESIAN_POINT('Ctrl Pts',(-0.988666612105885,3.53304718478134,
-2.68193159333883)) ;
#153972 = CARTESIAN_POINT('Ctrl Pts',(-0.992701606803651,3.53650267449006,
-2.68546796108803)) ;
#153973 = CARTESIAN_POINT('Ctrl Pts',(-0.996988044734313,3.53948417067186,
-2.68926358811777)) ;
#153974 = CARTESIAN_POINT('Ctrl Pts',(-1.00141585135915,3.54192188246042,
-2.69323403520351)) ;
#153975 = CARTESIAN_POINT('Ctrl Pts',(-1.00487400994927,3.54382575827888,
-2.69633499169497)) ;
#153976 = CARTESIAN_POINT('Ctrl Pts',(-1.00841776012225,3.54539884758397,
-2.69954196087253)) ;
#153977 = CARTESIAN_POINT('Ctrl Pts',(-1.01199129263161,3.54662946216441,
-2.70280822634667)) ;
#153978 = CARTESIAN_POINT('Ctrl Pts',(-1.016523626954,3.54819025857131,-2.70695085190716)) ;
#153979 = CARTESIAN_POINT('Ctrl Pts',(-1.02116533136121,3.54921942038456,
-2.71124536311626)) ;
#153980 = CARTESIAN_POINT('Ctrl Pts',(-1.02580209629924,3.54969340754028,
-2.71559145717195)) ;
#153981 = CARTESIAN_POINT('Ctrl Pts',(-1.02780524115376,3.54989817637043,
-2.71746902829346)) ;
#153982 = CARTESIAN_POINT('Ctrl Pts',(-1.02980744674852,3.55,-2.71935608172969)) ;
#153983 = CARTESIAN_POINT('Ctrl Pts',(-1.03179971315145,3.55,-2.72124412656437)) ;
#153984 = CARTESIAN_POINT('',(0.170807315466631,3.55,-5.30024322208929)) ;
#153985 = CARTESIAN_POINT('Origin',(-7.29372370581158E-16,3.55,-3.81)) ;
#153986 = CARTESIAN_POINT('',(0.273932138433074,3.45,-5.2847749603019)) ;
#153987 = CARTESIAN_POINT('Ctrl Pts',(0.170807315466627,3.55,-5.30024322208929)) ;
#153988 = CARTESIAN_POINT('Ctrl Pts',(0.183882433427085,3.55,-5.29874459034574)) ;
#153989 = CARTESIAN_POINT('Ctrl Pts',(0.197859036177008,3.54752250383109,
-5.29694882390231)) ;
#153990 = CARTESIAN_POINT('Ctrl Pts',(0.223597793566251,3.53719045839678,
-5.29329935326863)) ;
#153991 = CARTESIAN_POINT('Ctrl Pts',(0.235362682979173,3.52934133421403,
-5.29144958131094)) ;
#153992 = CARTESIAN_POINT('Ctrl Pts',(0.25346544153011,3.51138121637726,-5.28845705197622)) ;
#153993 = CARTESIAN_POINT('Ctrl Pts',(0.261168570620301,3.50026979217228,
-5.2870965178147)) ;
#153994 = CARTESIAN_POINT('Ctrl Pts',(0.271399896344092,3.47583586070552,
-5.28525363540046)) ;
#153995 = CARTESIAN_POINT('Ctrl Pts',(0.27393213843307,3.46251477070021,-5.28477496030191)) ;
#153996 = CARTESIAN_POINT('Ctrl Pts',(0.27393213843307,3.45,-5.28477496030191)) ;
#153997 = CARTESIAN_POINT('',(0.273932138433074,3.15,-5.2847749603019)) ;
#153998 = CARTESIAN_POINT('',(0.273932138433074,3.05,-5.2847749603019)) ;
#153999 = CARTESIAN_POINT('',(0.37394819336857,3.05,-5.26263992395789)) ;
#154000 = CARTESIAN_POINT('Ctrl Pts',(0.273932138433074,3.15,-5.2847749603019)) ;
#154001 = CARTESIAN_POINT('Ctrl Pts',(0.273932138433074,3.13736547222678,
-5.2847749603019)) ;
#154002 = CARTESIAN_POINT('Ctrl Pts',(0.276518148223581,3.12392729225934,
-5.28430316803635)) ;
#154003 = CARTESIAN_POINT('Ctrl Pts',(0.28688864746378,3.09929464195085,-5.28231750387035)) ;
#154004 = CARTESIAN_POINT('Ctrl Pts',(0.294673181069391,3.08810056349785,
-5.28079900383148)) ;
#154005 = CARTESIAN_POINT('Ctrl Pts',(0.312506499266534,3.07038074042647,
-5.27711400471621)) ;
#154006 = CARTESIAN_POINT('Ctrl Pts',(0.323788284437181,3.06269675232156,
-5.27469222593504)) ;
#154007 = CARTESIAN_POINT('Ctrl Pts',(0.348324144605931,3.05250629897269,
-5.26904937832144)) ;
#154008 = CARTESIAN_POINT('Ctrl Pts',(0.36157741072639,3.05,-5.26582449278551)) ;
#154009 = CARTESIAN_POINT('Ctrl Pts',(0.37394819336857,3.05,-5.26263992395789)) ;
#154010 = CARTESIAN_POINT('',(0.872417476238728,3.05,-5.03019988000051)) ;
#154011 = CARTESIAN_POINT('Origin',(-7.95081593156037E-16,3.05,-3.81)) ;
#154012 = CARTESIAN_POINT('',(0.953662978710562,3.15,-4.96781126399638)) ;
#154013 = CARTESIAN_POINT('Ctrl Pts',(0.872417476238727,3.05,-5.03019988000051)) ;
#154014 = CARTESIAN_POINT('Ctrl Pts',(0.882872360457018,3.05,-5.0227248557413)) ;
#154015 = CARTESIAN_POINT('Ctrl Pts',(0.893924122929505,3.05253676672645,
-5.01459782148564)) ;
#154016 = CARTESIAN_POINT('Ctrl Pts',(0.914112220366976,3.0628422827531,-4.99935386339936)) ;
#154017 = CARTESIAN_POINT('Ctrl Pts',(0.923251028202469,3.07061084469361,
-4.99224008807701)) ;
#154018 = CARTESIAN_POINT('Ctrl Pts',(0.937470525765898,3.08841385970397,
-4.9809949922316)) ;
#154019 = CARTESIAN_POINT('Ctrl Pts',(0.943569543283849,3.0995678553947,-4.97606170433658)) ;
#154020 = CARTESIAN_POINT('Ctrl Pts',(0.951664040935142,3.12408297110069,
-4.96946839711695)) ;
#154021 = CARTESIAN_POINT('Ctrl Pts',(0.953662978710561,3.13744372549049,
-4.96781126399638)) ;
#154022 = CARTESIAN_POINT('Ctrl Pts',(0.953662978710561,3.15,-4.96781126399638)) ;
#154023 = CARTESIAN_POINT('',(0.953662978710562,3.45,-4.96781126399638)) ;
#154024 = CARTESIAN_POINT('',(0.953662978710562,3.05,-4.96781126399638)) ;
#154025 = CARTESIAN_POINT('',(1.03179971315145,3.55,-4.89875587343563)) ;
#154026 = CARTESIAN_POINT('Ctrl Pts',(0.95366297871056,3.45,-4.96781126399638)) ;
#154027 = CARTESIAN_POINT('Ctrl Pts',(0.95366297871056,3.45580715149871,-4.96781126399638)) ;
#154028 = CARTESIAN_POINT('Ctrl Pts',(0.9540697926399,3.46165880969182,-4.96747636843074)) ;
#154029 = CARTESIAN_POINT('Ctrl Pts',(0.954880405808386,3.46741264967889,
-4.96680726792462)) ;
#154030 = CARTESIAN_POINT('Ctrl Pts',(0.955592557016217,3.47246759358527,
-4.96621944039835)) ;
#154031 = CARTESIAN_POINT('Ctrl Pts',(0.95661557365493,3.47744631522378,-4.96537418855118)) ;
#154032 = CARTESIAN_POINT('Ctrl Pts',(0.957920385817345,3.48225893605768,
-4.96429135595663)) ;
#154033 = CARTESIAN_POINT('Ctrl Pts',(0.959423079246193,3.48780141482279,
-4.96304430640326)) ;
#154034 = CARTESIAN_POINT('Ctrl Pts',(0.961323201468142,3.49320783601915,
-4.96146254061837)) ;
#154035 = CARTESIAN_POINT('Ctrl Pts',(0.963574238618813,3.49834560049869,
-4.95957574210361)) ;
#154036 = CARTESIAN_POINT('Ctrl Pts',(0.965499706648002,3.50274028640777,
-4.95796183261456)) ;
#154037 = CARTESIAN_POINT('Ctrl Pts',(0.967680912999539,3.5069382066956,-4.95612540554157)) ;
#154038 = CARTESIAN_POINT('Ctrl Pts',(0.970068248378239,3.51087311165944,
-4.95410121645275)) ;
#154039 = CARTESIAN_POINT('Ctrl Pts',(0.972933246979058,3.51559532091264,
-4.95167202323633)) ;
#154040 = CARTESIAN_POINT('Ctrl Pts',(0.976138831290365,3.52000896466724,
-4.94893531443762)) ;
#154041 = CARTESIAN_POINT('Ctrl Pts',(0.979601776802482,3.52400782220666,
-4.94594901565242)) ;
#154042 = CARTESIAN_POINT('Ctrl Pts',(0.982467725203495,3.52731729367563,
-4.94347754210529)) ;
#154043 = CARTESIAN_POINT('Ctrl Pts',(0.985508986896837,3.53034305696182,
-4.94083582639522)) ;
#154044 = CARTESIAN_POINT('Ctrl Pts',(0.988666612105885,3.53304718478134,
-4.93806840666118)) ;
#154045 = CARTESIAN_POINT('Ctrl Pts',(0.992701606803651,3.53650267449006,
-4.93453203891197)) ;
#154046 = CARTESIAN_POINT('Ctrl Pts',(0.996988044734314,3.53948417067186,
-4.93073641188224)) ;
#154047 = CARTESIAN_POINT('Ctrl Pts',(1.00141585135915,3.54192188246042,-4.92676596479649)) ;
#154048 = CARTESIAN_POINT('Ctrl Pts',(1.00487400994927,3.54382575827888,-4.92366500830503)) ;
#154049 = CARTESIAN_POINT('Ctrl Pts',(1.00841776012226,3.54539884758397,-4.92045803912747)) ;
#154050 = CARTESIAN_POINT('Ctrl Pts',(1.01199129263161,3.54662946216441,-4.91719177365334)) ;
#154051 = CARTESIAN_POINT('Ctrl Pts',(1.016523626954,3.54819025857131,-4.91304914809286)) ;
#154052 = CARTESIAN_POINT('Ctrl Pts',(1.02116533136121,3.54921942038456,-4.90875463688374)) ;
#154053 = CARTESIAN_POINT('Ctrl Pts',(1.02580209629923,3.54969340754028,-4.90440854282806)) ;
#154054 = CARTESIAN_POINT('Ctrl Pts',(1.02780524115375,3.54989817637043,-4.90253097170654)) ;
#154055 = CARTESIAN_POINT('Ctrl Pts',(1.02980744674851,3.55,-4.90064391827031)) ;
#154056 = CARTESIAN_POINT('Ctrl Pts',(1.03179971315145,3.55,-4.89875587343563)) ;
#154057 = CARTESIAN_POINT('Origin',(-7.29372370581158E-16,3.55,-3.81)) ;
#154058 = CARTESIAN_POINT('',(1.5,3.55,-3.81)) ;
#154059 = CARTESIAN_POINT('Origin',(-7.29372370581158E-16,3.55,-7.62)) ;
#154060 = CARTESIAN_POINT('',(-0.170807315466631,3.55,-6.12975677791071)) ;
#154061 = CARTESIAN_POINT('',(1.5,3.55,-7.62)) ;
#154062 = CARTESIAN_POINT('Origin',(-7.29372370581158E-16,3.55,-7.62)) ;
#154063 = CARTESIAN_POINT('',(-0.273932138433073,3.45,-6.1452250396981)) ;
#154064 = CARTESIAN_POINT('Ctrl Pts',(-0.170807315466633,3.55,-6.1297567779107)) ;
#154065 = CARTESIAN_POINT('Ctrl Pts',(-0.18388243342709,3.55,-6.13125540965426)) ;
#154066 = CARTESIAN_POINT('Ctrl Pts',(-0.197859036177013,3.54752250383109,
-6.13305117609769)) ;
#154067 = CARTESIAN_POINT('Ctrl Pts',(-0.223597793566256,3.53719045839678,
-6.13670064673137)) ;
#154068 = CARTESIAN_POINT('Ctrl Pts',(-0.235362682979179,3.52934133421403,
-6.13855041868906)) ;
#154069 = CARTESIAN_POINT('Ctrl Pts',(-0.253465441530116,3.51138121637726,
-6.14154294802378)) ;
#154070 = CARTESIAN_POINT('Ctrl Pts',(-0.261168570620306,3.50026979217228,
-6.1429034821853)) ;
#154071 = CARTESIAN_POINT('Ctrl Pts',(-0.271399896344097,3.47583586070553,
-6.14474636459954)) ;
#154072 = CARTESIAN_POINT('Ctrl Pts',(-0.273932138433075,3.46251477070021,
-6.1452250396981)) ;
#154073 = CARTESIAN_POINT('Ctrl Pts',(-0.273932138433075,3.45,-6.1452250396981)) ;
#154074 = CARTESIAN_POINT('',(-0.273932138433073,3.15,-6.1452250396981)) ;
#154075 = CARTESIAN_POINT('',(-0.273932138433073,3.05,-6.1452250396981)) ;
#154076 = CARTESIAN_POINT('',(-0.373948193368569,3.05,-6.16736007604211)) ;
#154077 = CARTESIAN_POINT('Ctrl Pts',(-0.273932138433075,3.15,-6.14522503969809)) ;
#154078 = CARTESIAN_POINT('Ctrl Pts',(-0.273932138433075,3.13744372549049,
-6.14522503969809)) ;
#154079 = CARTESIAN_POINT('Ctrl Pts',(-0.276486468486165,3.12408297110069,
-6.1456911302356)) ;
#154080 = CARTESIAN_POINT('Ctrl Pts',(-0.28674027764043,3.0995678553947,-6.14765377899357)) ;
#154081 = CARTESIAN_POINT('Ctrl Pts',(-0.294439768310518,3.08841385970397,
-6.14915484113775)) ;
#154082 = CARTESIAN_POINT('Ctrl Pts',(-0.312194128344973,3.07061084469361,
-6.15281939995099)) ;
#154083 = CARTESIAN_POINT('Ctrl Pts',(-0.323517908844218,3.0628422827531,
-6.1552474862748)) ;
#154084 = CARTESIAN_POINT('Ctrl Pts',(-0.348172117123305,3.05253676672645,
-6.16091383875347)) ;
#154085 = CARTESIAN_POINT('Ctrl Pts',(-0.361501722536398,3.05,-6.16415602305916)) ;
#154086 = CARTESIAN_POINT('Ctrl Pts',(-0.37394819336857,3.05,-6.16736007604211)) ;
#154087 = CARTESIAN_POINT('',(-0.872417476238727,3.05,-6.39980011999949)) ;
#154088 = CARTESIAN_POINT('Origin',(-7.95081593156037E-16,3.05,-7.62)) ;
#154089 = CARTESIAN_POINT('',(-0.953662978710562,3.15,-6.46218873600362)) ;
#154090 = CARTESIAN_POINT('Ctrl Pts',(-0.872417476238727,3.05,-6.39980011999949)) ;
#154091 = CARTESIAN_POINT('Ctrl Pts',(-0.882808783297377,3.05,-6.40722968791498)) ;
#154092 = CARTESIAN_POINT('Ctrl Pts',(-0.893798224191975,3.05250629897269,
-6.41530936231458)) ;
#154093 = CARTESIAN_POINT('Ctrl Pts',(-0.913892243159219,3.06269675232156,
-6.43047776912462)) ;
#154094 = CARTESIAN_POINT('Ctrl Pts',(-0.922999225059833,3.07038074042647,
-6.43756342856912)) ;
#154095 = CARTESIAN_POINT('Ctrl Pts',(-0.937285134131705,3.08810056349785,
-6.44885587110341)) ;
#154096 = CARTESIAN_POINT('Ctrl Pts',(-0.943452174397235,3.09929464195085,
-6.45384309680397)) ;
#154097 = CARTESIAN_POINT('Ctrl Pts',(-0.951639309815362,3.12392729225934,
-6.46051099979639)) ;
#154098 = CARTESIAN_POINT('Ctrl Pts',(-0.953662978710561,3.13736547222678,
-6.46218873600362)) ;
#154099 = CARTESIAN_POINT('Ctrl Pts',(-0.953662978710561,3.15,-6.46218873600362)) ;
#154100 = CARTESIAN_POINT('',(-0.953662978710562,3.45,-6.46218873600362)) ;
#154101 = CARTESIAN_POINT('',(-0.953662978710562,3.05,-6.46218873600362)) ;
#154102 = CARTESIAN_POINT('',(-1.03179971315145,3.55,-6.53124412656437)) ;
#154103 = CARTESIAN_POINT('Ctrl Pts',(-0.953662978710565,3.45,-6.46218873600362)) ;
#154104 = CARTESIAN_POINT('Ctrl Pts',(-0.953662978710565,3.45580715149871,
-6.46218873600362)) ;
#154105 = CARTESIAN_POINT('Ctrl Pts',(-0.954069792639906,3.46165880969183,
-6.46252363156927)) ;
#154106 = CARTESIAN_POINT('Ctrl Pts',(-0.954880405808391,3.4674126496789,
-6.46319273207538)) ;
#154107 = CARTESIAN_POINT('Ctrl Pts',(-0.955592557016221,3.47246759358527,
-6.46378055960165)) ;
#154108 = CARTESIAN_POINT('Ctrl Pts',(-0.956615573654934,3.47744631522377,
-6.46462581144883)) ;
#154109 = CARTESIAN_POINT('Ctrl Pts',(-0.957920385817348,3.48225893605767,
-6.46570864404338)) ;
#154110 = CARTESIAN_POINT('Ctrl Pts',(-0.959423079246195,3.48780141482278,
-6.46695569359675)) ;
#154111 = CARTESIAN_POINT('Ctrl Pts',(-0.961323201468146,3.49320783601915,
-6.46853745938164)) ;
#154112 = CARTESIAN_POINT('Ctrl Pts',(-0.963574238618818,3.49834560049869,
-6.47042425789639)) ;
#154113 = CARTESIAN_POINT('Ctrl Pts',(-0.965499706648006,3.50274028640777,
-6.47203816738544)) ;
#154114 = CARTESIAN_POINT('Ctrl Pts',(-0.967680912999541,3.5069382066956,
-6.47387459445843)) ;
#154115 = CARTESIAN_POINT('Ctrl Pts',(-0.97006824837824,3.51087311165944,
-6.47589878354725)) ;
#154116 = CARTESIAN_POINT('Ctrl Pts',(-0.97293324697906,3.51559532091263,
-6.47832797676366)) ;
#154117 = CARTESIAN_POINT('Ctrl Pts',(-0.976138831290367,3.52000896466724,
-6.48106468556238)) ;
#154118 = CARTESIAN_POINT('Ctrl Pts',(-0.979601776802484,3.52400782220665,
-6.48405098434758)) ;
#154119 = CARTESIAN_POINT('Ctrl Pts',(-0.982467725203496,3.52731729367563,
-6.48652245789472)) ;
#154120 = CARTESIAN_POINT('Ctrl Pts',(-0.985508986896839,3.53034305696182,
-6.48916417360478)) ;
#154121 = CARTESIAN_POINT('Ctrl Pts',(-0.988666612105887,3.53304718478134,
-6.49193159333883)) ;
#154122 = CARTESIAN_POINT('Ctrl Pts',(-0.992701606803653,3.53650267449006,
-6.49546796108803)) ;
#154123 = CARTESIAN_POINT('Ctrl Pts',(-0.996988044734315,3.53948417067186,
-6.49926358811777)) ;
#154124 = CARTESIAN_POINT('Ctrl Pts',(-1.00141585135916,3.54192188246042,
-6.50323403520352)) ;
#154125 = CARTESIAN_POINT('Ctrl Pts',(-1.00487400994927,3.54382575827888,
-6.50633499169497)) ;
#154126 = CARTESIAN_POINT('Ctrl Pts',(-1.00841776012226,3.54539884758397,
-6.50954196087253)) ;
#154127 = CARTESIAN_POINT('Ctrl Pts',(-1.01199129263161,3.54662946216441,
-6.51280822634666)) ;
#154128 = CARTESIAN_POINT('Ctrl Pts',(-1.016523626954,3.54819025857131,-6.51695085190715)) ;
#154129 = CARTESIAN_POINT('Ctrl Pts',(-1.0211653313612,3.54921942038456,-6.52124536311625)) ;
#154130 = CARTESIAN_POINT('Ctrl Pts',(-1.02580209629923,3.54969340754027,
-6.52559145717194)) ;
#154131 = CARTESIAN_POINT('Ctrl Pts',(-1.02780524115375,3.54989817637043,
-6.52746902829346)) ;
#154132 = CARTESIAN_POINT('Ctrl Pts',(-1.02980744674852,3.55,-6.52935608172969)) ;
#154133 = CARTESIAN_POINT('Ctrl Pts',(-1.03179971315145,3.55,-6.53124412656437)) ;
#154134 = CARTESIAN_POINT('',(0.170807315466631,3.55,-9.11024322208929)) ;
#154135 = CARTESIAN_POINT('Origin',(-7.29372370581158E-16,3.55,-7.62)) ;
#154136 = CARTESIAN_POINT('',(0.273932138433074,3.45,-9.0947749603019)) ;
#154137 = CARTESIAN_POINT('Ctrl Pts',(0.170807315466626,3.55,-9.1102432220893)) ;
#154138 = CARTESIAN_POINT('Ctrl Pts',(0.183882433427084,3.55,-9.10874459034575)) ;
#154139 = CARTESIAN_POINT('Ctrl Pts',(0.197859036177007,3.54752250383109,
-9.10694882390231)) ;
#154140 = CARTESIAN_POINT('Ctrl Pts',(0.223597793566251,3.53719045839678,
-9.10329935326863)) ;
#154141 = CARTESIAN_POINT('Ctrl Pts',(0.235362682979173,3.52934133421403,
-9.10144958131094)) ;
#154142 = CARTESIAN_POINT('Ctrl Pts',(0.25346544153011,3.51138121637726,-9.09845705197622)) ;
#154143 = CARTESIAN_POINT('Ctrl Pts',(0.2611685706203,3.50026979217228,-9.0970965178147)) ;
#154144 = CARTESIAN_POINT('Ctrl Pts',(0.271399896344091,3.47583586070553,
-9.09525363540046)) ;
#154145 = CARTESIAN_POINT('Ctrl Pts',(0.273932138433069,3.46251477070021,
-9.0947749603019)) ;
#154146 = CARTESIAN_POINT('Ctrl Pts',(0.273932138433069,3.45,-9.0947749603019)) ;
#154147 = CARTESIAN_POINT('',(0.273932138433074,3.15,-9.0947749603019)) ;
#154148 = CARTESIAN_POINT('',(0.273932138433074,3.05,-9.0947749603019)) ;
#154149 = CARTESIAN_POINT('',(0.37394819336857,3.05,-9.07263992395789)) ;
#154150 = CARTESIAN_POINT('Ctrl Pts',(0.273932138433074,3.15,-9.0947749603019)) ;
#154151 = CARTESIAN_POINT('Ctrl Pts',(0.273932138433074,3.13736547222678,
-9.0947749603019)) ;
#154152 = CARTESIAN_POINT('Ctrl Pts',(0.276518148223582,3.12392729225934,
-9.09430316803635)) ;
#154153 = CARTESIAN_POINT('Ctrl Pts',(0.28688864746378,3.09929464195085,-9.09231750387035)) ;
#154154 = CARTESIAN_POINT('Ctrl Pts',(0.294673181069391,3.08810056349785,
-9.09079900383148)) ;
#154155 = CARTESIAN_POINT('Ctrl Pts',(0.312506499266534,3.07038074042647,
-9.08711400471621)) ;
#154156 = CARTESIAN_POINT('Ctrl Pts',(0.323788284437181,3.06269675232156,
-9.08469222593504)) ;
#154157 = CARTESIAN_POINT('Ctrl Pts',(0.348324144605931,3.05250629897269,
-9.07904937832144)) ;
#154158 = CARTESIAN_POINT('Ctrl Pts',(0.36157741072639,3.05,-9.07582449278551)) ;
#154159 = CARTESIAN_POINT('Ctrl Pts',(0.37394819336857,3.05,-9.07263992395789)) ;
#154160 = CARTESIAN_POINT('',(0.872417476238728,3.05,-8.84019988000051)) ;
#154161 = CARTESIAN_POINT('Origin',(-7.95081593156037E-16,3.05,-7.62)) ;
#154162 = CARTESIAN_POINT('',(0.953662978710562,3.15,-8.77781126399638)) ;
#154163 = CARTESIAN_POINT('Ctrl Pts',(0.872417476238727,3.05,-8.84019988000051)) ;
#154164 = CARTESIAN_POINT('Ctrl Pts',(0.882872360457018,3.05,-8.8327248557413)) ;
#154165 = CARTESIAN_POINT('Ctrl Pts',(0.893924122929505,3.05253676672645,
-8.82459782148564)) ;
#154166 = CARTESIAN_POINT('Ctrl Pts',(0.914112220366976,3.0628422827531,-8.80935386339936)) ;
#154167 = CARTESIAN_POINT('Ctrl Pts',(0.923251028202469,3.07061084469361,
-8.80224008807701)) ;
#154168 = CARTESIAN_POINT('Ctrl Pts',(0.937470525765898,3.08841385970397,
-8.7909949922316)) ;
#154169 = CARTESIAN_POINT('Ctrl Pts',(0.943569543283849,3.0995678553947,-8.78606170433658)) ;
#154170 = CARTESIAN_POINT('Ctrl Pts',(0.951664040935142,3.12408297110069,
-8.77946839711695)) ;
#154171 = CARTESIAN_POINT('Ctrl Pts',(0.953662978710561,3.13744372549049,
-8.77781126399638)) ;
#154172 = CARTESIAN_POINT('Ctrl Pts',(0.953662978710561,3.15,-8.77781126399638)) ;
#154173 = CARTESIAN_POINT('',(0.953662978710562,3.45,-8.77781126399638)) ;
#154174 = CARTESIAN_POINT('',(0.953662978710562,3.05,-8.77781126399638)) ;
#154175 = CARTESIAN_POINT('',(1.03179971315145,3.55,-8.70875587343563)) ;
#154176 = CARTESIAN_POINT('Ctrl Pts',(0.95366297871056,3.45,-8.77781126399638)) ;
#154177 = CARTESIAN_POINT('Ctrl Pts',(0.95366297871056,3.45580715149871,-8.77781126399638)) ;
#154178 = CARTESIAN_POINT('Ctrl Pts',(0.9540697926399,3.46165880969182,-8.77747636843074)) ;
#154179 = CARTESIAN_POINT('Ctrl Pts',(0.954880405808385,3.46741264967889,
-8.77680726792462)) ;
#154180 = CARTESIAN_POINT('Ctrl Pts',(0.955592557016215,3.47246759358526,
-8.77621944039836)) ;
#154181 = CARTESIAN_POINT('Ctrl Pts',(0.956615573654929,3.47744631522378,
-8.77537418855117)) ;
#154182 = CARTESIAN_POINT('Ctrl Pts',(0.957920385817344,3.48225893605768,
-8.77429135595662)) ;
#154183 = CARTESIAN_POINT('Ctrl Pts',(0.959423079246191,3.48780141482278,
-8.77304430640325)) ;
#154184 = CARTESIAN_POINT('Ctrl Pts',(0.961323201468144,3.49320783601915,
-8.77146254061837)) ;
#154185 = CARTESIAN_POINT('Ctrl Pts',(0.963574238618813,3.49834560049869,
-8.76957574210362)) ;
#154186 = CARTESIAN_POINT('Ctrl Pts',(0.965499706648001,3.50274028640777,
-8.76796183261456)) ;
#154187 = CARTESIAN_POINT('Ctrl Pts',(0.967680912999538,3.5069382066956,-8.76612540554157)) ;
#154188 = CARTESIAN_POINT('Ctrl Pts',(0.970068248378235,3.51087311165944,
-8.76410121645275)) ;
#154189 = CARTESIAN_POINT('Ctrl Pts',(0.972933246979052,3.51559532091263,
-8.76167202323634)) ;
#154190 = CARTESIAN_POINT('Ctrl Pts',(0.976138831290364,3.52000896466724,
-8.75893531443762)) ;
#154191 = CARTESIAN_POINT('Ctrl Pts',(0.97960177680248,3.52400782220665,-8.75594901565243)) ;
#154192 = CARTESIAN_POINT('Ctrl Pts',(0.982467725203493,3.52731729367563,
-8.75347754210529)) ;
#154193 = CARTESIAN_POINT('Ctrl Pts',(0.985508986896836,3.53034305696182,
-8.75083582639522)) ;
#154194 = CARTESIAN_POINT('Ctrl Pts',(0.988666612105887,3.53304718478134,
-8.74806840666118)) ;
#154195 = CARTESIAN_POINT('Ctrl Pts',(0.99270160680366,3.53650267449007,-8.74453203891197)) ;
#154196 = CARTESIAN_POINT('Ctrl Pts',(0.996988044734325,3.53948417067186,
-8.74073641188223)) ;
#154197 = CARTESIAN_POINT('Ctrl Pts',(1.00141585135916,3.54192188246042,-8.73676596479647)) ;
#154198 = CARTESIAN_POINT('Ctrl Pts',(1.00487400994927,3.54382575827888,-8.73366500830502)) ;
#154199 = CARTESIAN_POINT('Ctrl Pts',(1.00841776012226,3.54539884758398,-8.73045803912746)) ;
#154200 = CARTESIAN_POINT('Ctrl Pts',(1.01199129263161,3.54662946216441,-8.72719177365333)) ;
#154201 = CARTESIAN_POINT('Ctrl Pts',(1.016523626954,3.54819025857131,-8.72304914809285)) ;
#154202 = CARTESIAN_POINT('Ctrl Pts',(1.02116533136121,3.54921942038456,-8.71875463688375)) ;
#154203 = CARTESIAN_POINT('Ctrl Pts',(1.02580209629923,3.54969340754028,-8.71440854282806)) ;
#154204 = CARTESIAN_POINT('Ctrl Pts',(1.02780524115375,3.54989817637043,-8.71253097170654)) ;
#154205 = CARTESIAN_POINT('Ctrl Pts',(1.02980744674851,3.55,-8.71064391827031)) ;
#154206 = CARTESIAN_POINT('Ctrl Pts',(1.03179971315145,3.55,-8.70875587343563)) ;
#154207 = CARTESIAN_POINT('Origin',(-7.29372370581158E-16,3.55,-7.62)) ;
#154208 = CARTESIAN_POINT('',(1.5,3.55,-7.62)) ;
#154209 = CARTESIAN_POINT('Origin',(-7.29372370581158E-16,3.55,-11.43)) ;
#154210 = CARTESIAN_POINT('',(-0.17080731546663,3.55,-9.9397567779107)) ;
#154211 = CARTESIAN_POINT('',(1.5,3.55,-11.43)) ;
#154212 = CARTESIAN_POINT('Origin',(-7.29372370581158E-16,3.55,-11.43)) ;
#154213 = CARTESIAN_POINT('',(-0.273932138433073,3.45,-9.9552250396981)) ;
#154214 = CARTESIAN_POINT('Ctrl Pts',(-0.170807315466628,3.55,-9.9397567779107)) ;
#154215 = CARTESIAN_POINT('Ctrl Pts',(-0.183882433427086,3.55,-9.94125540965426)) ;
#154216 = CARTESIAN_POINT('Ctrl Pts',(-0.197859036177008,3.54752250383109,
-9.94305117609769)) ;
#154217 = CARTESIAN_POINT('Ctrl Pts',(-0.223597793566252,3.53719045839678,
-9.94670064673137)) ;
#154218 = CARTESIAN_POINT('Ctrl Pts',(-0.235362682979173,3.52934133421403,
-9.94855041868906)) ;
#154219 = CARTESIAN_POINT('Ctrl Pts',(-0.25346544153011,3.51138121637726,
-9.95154294802378)) ;
#154220 = CARTESIAN_POINT('Ctrl Pts',(-0.261168570620301,3.50026979217228,
-9.9529034821853)) ;
#154221 = CARTESIAN_POINT('Ctrl Pts',(-0.271399896344092,3.47583586070553,
-9.95474636459954)) ;
#154222 = CARTESIAN_POINT('Ctrl Pts',(-0.27393213843307,3.46251477070021,
-9.95522503969809)) ;
#154223 = CARTESIAN_POINT('Ctrl Pts',(-0.27393213843307,3.45,-9.95522503969809)) ;
#154224 = CARTESIAN_POINT('',(-0.273932138433073,3.15,-9.9552250396981)) ;
#154225 = CARTESIAN_POINT('',(-0.273932138433073,3.05,-9.9552250396981)) ;
#154226 = CARTESIAN_POINT('',(-0.373948193368569,3.05,-9.97736007604211)) ;
#154227 = CARTESIAN_POINT('Ctrl Pts',(-0.27393213843307,3.15,-9.95522503969809)) ;
#154228 = CARTESIAN_POINT('Ctrl Pts',(-0.27393213843307,3.13744372549049,
-9.95522503969809)) ;
#154229 = CARTESIAN_POINT('Ctrl Pts',(-0.276486468486161,3.12408297110069,
-9.9556911302356)) ;
#154230 = CARTESIAN_POINT('Ctrl Pts',(-0.286740277640426,3.0995678553947,
-9.95765377899357)) ;
#154231 = CARTESIAN_POINT('Ctrl Pts',(-0.294439768310514,3.08841385970397,
-9.95915484113775)) ;
#154232 = CARTESIAN_POINT('Ctrl Pts',(-0.312194128344968,3.07061084469361,
-9.96281939995099)) ;
#154233 = CARTESIAN_POINT('Ctrl Pts',(-0.323517908844214,3.0628422827531,
-9.9652474862748)) ;
#154234 = CARTESIAN_POINT('Ctrl Pts',(-0.348172117123301,3.05253676672645,
-9.97091383875347)) ;
#154235 = CARTESIAN_POINT('Ctrl Pts',(-0.361501722536394,3.05,-9.97415602305916)) ;
#154236 = CARTESIAN_POINT('Ctrl Pts',(-0.373948193368566,3.05,-9.97736007604211)) ;
#154237 = CARTESIAN_POINT('',(-0.872417476238727,3.05,-10.2098001199995)) ;
#154238 = CARTESIAN_POINT('Origin',(-7.95081593156037E-16,3.05,-11.43)) ;
#154239 = CARTESIAN_POINT('',(-0.953662978710562,3.15,-10.2721887360036)) ;
#154240 = CARTESIAN_POINT('Ctrl Pts',(-0.872417476238731,3.05,-10.2098001199995)) ;
#154241 = CARTESIAN_POINT('Ctrl Pts',(-0.882808783297381,3.05,-10.217229687915)) ;
#154242 = CARTESIAN_POINT('Ctrl Pts',(-0.893798224191977,3.05250629897269,
-10.2253093623146)) ;
#154243 = CARTESIAN_POINT('Ctrl Pts',(-0.913892243159222,3.06269675232156,
-10.2404777691246)) ;
#154244 = CARTESIAN_POINT('Ctrl Pts',(-0.922999225059836,3.07038074042647,
-10.2475634285691)) ;
#154245 = CARTESIAN_POINT('Ctrl Pts',(-0.937285134131709,3.08810056349785,
-10.2588558711034)) ;
#154246 = CARTESIAN_POINT('Ctrl Pts',(-0.943452174397238,3.09929464195085,
-10.263843096804)) ;
#154247 = CARTESIAN_POINT('Ctrl Pts',(-0.951639309815365,3.12392729225934,
-10.2705109997964)) ;
#154248 = CARTESIAN_POINT('Ctrl Pts',(-0.953662978710564,3.13736547222678,
-10.2721887360036)) ;
#154249 = CARTESIAN_POINT('Ctrl Pts',(-0.953662978710564,3.15,-10.2721887360036)) ;
#154250 = CARTESIAN_POINT('',(-0.953662978710562,3.45,-10.2721887360036)) ;
#154251 = CARTESIAN_POINT('',(-0.953662978710562,3.05,-10.2721887360036)) ;
#154252 = CARTESIAN_POINT('',(-1.03179971315145,3.55,-10.3412441265644)) ;
#154253 = CARTESIAN_POINT('Ctrl Pts',(-0.953662978710575,3.45,-10.2721887360036)) ;
#154254 = CARTESIAN_POINT('Ctrl Pts',(-0.953662978710575,3.45580715149871,
-10.2721887360036)) ;
#154255 = CARTESIAN_POINT('Ctrl Pts',(-0.954069792639919,3.46165880969182,
-10.2725236315692)) ;
#154256 = CARTESIAN_POINT('Ctrl Pts',(-0.95488040580839,3.4674126496789,-10.2731927320754)) ;
#154257 = CARTESIAN_POINT('Ctrl Pts',(-0.955592557016208,3.47246759358527,
-10.2737805596017)) ;
#154258 = CARTESIAN_POINT('Ctrl Pts',(-0.956615573654938,3.47744631522378,
-10.2746258114488)) ;
#154259 = CARTESIAN_POINT('Ctrl Pts',(-0.957920385817356,3.48225893605768,
-10.2757086440434)) ;
#154260 = CARTESIAN_POINT('Ctrl Pts',(-0.959423079246207,3.48780141482279,
-10.2769556935967)) ;
#154261 = CARTESIAN_POINT('Ctrl Pts',(-0.961323201468137,3.49320783601914,
-10.2785374593817)) ;
#154262 = CARTESIAN_POINT('Ctrl Pts',(-0.963574238618807,3.49834560049868,
-10.2804242578964)) ;
#154263 = CARTESIAN_POINT('Ctrl Pts',(-0.965499706647995,3.50274028640776,
-10.2820381673855)) ;
#154264 = CARTESIAN_POINT('Ctrl Pts',(-0.96768091299954,3.50693820669559,
-10.2838745944584)) ;
#154265 = CARTESIAN_POINT('Ctrl Pts',(-0.970068248378245,3.51087311165943,
-10.2858987835472)) ;
#154266 = CARTESIAN_POINT('Ctrl Pts',(-0.972933246979072,3.51559532091262,
-10.2883279767636)) ;
#154267 = CARTESIAN_POINT('Ctrl Pts',(-0.97613883129036,3.52000896466724,
-10.2910646855624)) ;
#154268 = CARTESIAN_POINT('Ctrl Pts',(-0.979601776802481,3.52400782220665,
-10.2940509843476)) ;
#154269 = CARTESIAN_POINT('Ctrl Pts',(-0.982467725203496,3.52731729367563,
-10.2965224578947)) ;
#154270 = CARTESIAN_POINT('Ctrl Pts',(-0.985508986896836,3.5303430569618,
-10.2991641736047)) ;
#154271 = CARTESIAN_POINT('Ctrl Pts',(-0.988666612105891,3.53304718478134,
-10.3019315933388)) ;
#154272 = CARTESIAN_POINT('Ctrl Pts',(-0.992701606803668,3.53650267449007,
-10.3054679610881)) ;
#154273 = CARTESIAN_POINT('Ctrl Pts',(-0.996988044734306,3.53948417067184,
-10.3092635881177)) ;
#154274 = CARTESIAN_POINT('Ctrl Pts',(-1.00141585135915,3.54192188246041,
-10.3132340352035)) ;
#154275 = CARTESIAN_POINT('Ctrl Pts',(-1.00487400994927,3.54382575827887,
-10.3163349916949)) ;
#154276 = CARTESIAN_POINT('Ctrl Pts',(-1.00841776012226,3.54539884758398,
-10.3195419608726)) ;
#154277 = CARTESIAN_POINT('Ctrl Pts',(-1.01199129263162,3.54662946216441,
-10.3228082263467)) ;
#154278 = CARTESIAN_POINT('Ctrl Pts',(-1.01652362695402,3.54819025857132,
-10.3269508519072)) ;
#154279 = CARTESIAN_POINT('Ctrl Pts',(-1.0211653313612,3.54921942038456,-10.3312453631162)) ;
#154280 = CARTESIAN_POINT('Ctrl Pts',(-1.02580209629924,3.54969340754028,
-10.3355914571719)) ;
#154281 = CARTESIAN_POINT('Ctrl Pts',(-1.02780524115376,3.54989817637043,
-10.3374690282934)) ;
#154282 = CARTESIAN_POINT('Ctrl Pts',(-1.02980744674853,3.55,-10.3393560817297)) ;
#154283 = CARTESIAN_POINT('Ctrl Pts',(-1.03179971315146,3.55,-10.3412441265644)) ;
#154284 = CARTESIAN_POINT('',(0.170807315466631,3.55,-12.9202432220893)) ;
#154285 = CARTESIAN_POINT('Origin',(-7.29372370581158E-16,3.55,-11.43)) ;
#154286 = CARTESIAN_POINT('',(0.273932138433074,3.45,-12.9047749603019)) ;
#154287 = CARTESIAN_POINT('Ctrl Pts',(0.170807315466622,3.55,-12.9202432220893)) ;
#154288 = CARTESIAN_POINT('Ctrl Pts',(0.18388243342708,3.55,-12.9187445903457)) ;
#154289 = CARTESIAN_POINT('Ctrl Pts',(0.197859036177003,3.54752250383109,
-12.9169488239023)) ;
#154290 = CARTESIAN_POINT('Ctrl Pts',(0.223597793566246,3.53719045839678,
-12.9132993532686)) ;
#154291 = CARTESIAN_POINT('Ctrl Pts',(0.235362682979168,3.52934133421403,
-12.9114495813109)) ;
#154292 = CARTESIAN_POINT('Ctrl Pts',(0.253465441530105,3.51138121637726,
-12.9084570519762)) ;
#154293 = CARTESIAN_POINT('Ctrl Pts',(0.261168570620296,3.50026979217228,
-12.9070965178147)) ;
#154294 = CARTESIAN_POINT('Ctrl Pts',(0.271399896344087,3.47583586070553,
-12.9052536354005)) ;
#154295 = CARTESIAN_POINT('Ctrl Pts',(0.273932138433065,3.46251477070021,
-12.9047749603019)) ;
#154296 = CARTESIAN_POINT('Ctrl Pts',(0.273932138433065,3.45,-12.9047749603019)) ;
#154297 = CARTESIAN_POINT('',(0.273932138433074,3.15,-12.9047749603019)) ;
#154298 = CARTESIAN_POINT('',(0.273932138433074,3.05,-12.9047749603019)) ;
#154299 = CARTESIAN_POINT('',(0.37394819336857,3.05,-12.8826399239579)) ;
#154300 = CARTESIAN_POINT('Ctrl Pts',(0.27393213843307,3.15,-12.9047749603019)) ;
#154301 = CARTESIAN_POINT('Ctrl Pts',(0.27393213843307,3.13736547222678,-12.9047749603019)) ;
#154302 = CARTESIAN_POINT('Ctrl Pts',(0.276518148223577,3.12392729225934,
-12.9043031680364)) ;
#154303 = CARTESIAN_POINT('Ctrl Pts',(0.286888647463776,3.09929464195085,
-12.9023175038704)) ;
#154304 = CARTESIAN_POINT('Ctrl Pts',(0.294673181069387,3.08810056349785,
-12.9007990038315)) ;
#154305 = CARTESIAN_POINT('Ctrl Pts',(0.31250649926653,3.07038074042647,-12.8971140047162)) ;
#154306 = CARTESIAN_POINT('Ctrl Pts',(0.323788284437177,3.06269675232156,
-12.894692225935)) ;
#154307 = CARTESIAN_POINT('Ctrl Pts',(0.348324144605927,3.05250629897269,
-12.8890493783214)) ;
#154308 = CARTESIAN_POINT('Ctrl Pts',(0.361577410726386,3.05,-12.8858244927855)) ;
#154309 = CARTESIAN_POINT('Ctrl Pts',(0.373948193368566,3.05,-12.8826399239579)) ;
#154310 = CARTESIAN_POINT('',(0.872417476238727,3.05,-12.6501998800005)) ;
#154311 = CARTESIAN_POINT('Origin',(-7.95081593156037E-16,3.05,-11.43)) ;
#154312 = CARTESIAN_POINT('',(0.953662978710562,3.15,-12.5878112639964)) ;
#154313 = CARTESIAN_POINT('Ctrl Pts',(0.87241747623873,3.05,-12.6501998800005)) ;
#154314 = CARTESIAN_POINT('Ctrl Pts',(0.882872360457021,3.05,-12.6427248557413)) ;
#154315 = CARTESIAN_POINT('Ctrl Pts',(0.893924122929508,3.05253676672645,
-12.6345978214856)) ;
#154316 = CARTESIAN_POINT('Ctrl Pts',(0.914112220366979,3.0628422827531,-12.6193538633994)) ;
#154317 = CARTESIAN_POINT('Ctrl Pts',(0.923251028202472,3.07061084469361,
-12.612240088077)) ;
#154318 = CARTESIAN_POINT('Ctrl Pts',(0.937470525765901,3.08841385970397,
-12.6009949922316)) ;
#154319 = CARTESIAN_POINT('Ctrl Pts',(0.943569543283853,3.0995678553947,-12.5960617043366)) ;
#154320 = CARTESIAN_POINT('Ctrl Pts',(0.951664040935146,3.12408297110069,
-12.5894683971169)) ;
#154321 = CARTESIAN_POINT('Ctrl Pts',(0.953662978710565,3.13744372549049,
-12.5878112639964)) ;
#154322 = CARTESIAN_POINT('Ctrl Pts',(0.953662978710565,3.15,-12.5878112639964)) ;
#154323 = CARTESIAN_POINT('',(0.953662978710562,3.45,-12.5878112639964)) ;
#154324 = CARTESIAN_POINT('',(0.953662978710562,3.05,-12.5878112639964)) ;
#154325 = CARTESIAN_POINT('',(1.03179971315145,3.55,-12.5187558734356)) ;
#154326 = CARTESIAN_POINT('Ctrl Pts',(0.95366297871057,3.45,-12.5878112639964)) ;
#154327 = CARTESIAN_POINT('Ctrl Pts',(0.95366297871057,3.45580715149871,-12.5878112639964)) ;
#154328 = CARTESIAN_POINT('Ctrl Pts',(0.954069792639914,3.46165880969181,
-12.5874763684308)) ;
#154329 = CARTESIAN_POINT('Ctrl Pts',(0.954880405808384,3.46741264967889,
-12.5868072679246)) ;
#154330 = CARTESIAN_POINT('Ctrl Pts',(0.955592557016202,3.47246759358526,
-12.5862194403983)) ;
#154331 = CARTESIAN_POINT('Ctrl Pts',(0.956615573654934,3.47744631522378,
-12.5853741885512)) ;
#154332 = CARTESIAN_POINT('Ctrl Pts',(0.957920385817353,3.48225893605768,
-12.5842913559566)) ;
#154333 = CARTESIAN_POINT('Ctrl Pts',(0.959423079246204,3.48780141482279,
-12.5830443064033)) ;
#154334 = CARTESIAN_POINT('Ctrl Pts',(0.961323201468133,3.49320783601914,
-12.5814625406183)) ;
#154335 = CARTESIAN_POINT('Ctrl Pts',(0.963574238618804,3.49834560049868,
-12.5795757421036)) ;
#154336 = CARTESIAN_POINT('Ctrl Pts',(0.965499706647994,3.50274028640776,
-12.5779618326145)) ;
#154337 = CARTESIAN_POINT('Ctrl Pts',(0.967680912999537,3.5069382066956,-12.5761254055416)) ;
#154338 = CARTESIAN_POINT('Ctrl Pts',(0.970068248378243,3.51087311165944,
-12.5741012164528)) ;
#154339 = CARTESIAN_POINT('Ctrl Pts',(0.972933246979071,3.51559532091263,
-12.5716720232364)) ;
#154340 = CARTESIAN_POINT('Ctrl Pts',(0.97613883129036,3.52000896466724,-12.5689353144376)) ;
#154341 = CARTESIAN_POINT('Ctrl Pts',(0.979601776802481,3.52400782220666,
-12.5659490156524)) ;
#154342 = CARTESIAN_POINT('Ctrl Pts',(0.982467725203496,3.52731729367563,
-12.5634775421053)) ;
#154343 = CARTESIAN_POINT('Ctrl Pts',(0.985508986896835,3.5303430569618,-12.5608358263953)) ;
#154344 = CARTESIAN_POINT('Ctrl Pts',(0.988666612105891,3.53304718478134,
-12.5580684066612)) ;
#154345 = CARTESIAN_POINT('Ctrl Pts',(0.992701606803667,3.53650267449007,
-12.554532038912)) ;
#154346 = CARTESIAN_POINT('Ctrl Pts',(0.996988044734304,3.53948417067185,
-12.5507364118823)) ;
#154347 = CARTESIAN_POINT('Ctrl Pts',(1.00141585135915,3.54192188246041,-12.5467659647965)) ;
#154348 = CARTESIAN_POINT('Ctrl Pts',(1.00487400994927,3.54382575827887,-12.5436650083051)) ;
#154349 = CARTESIAN_POINT('Ctrl Pts',(1.00841776012225,3.54539884758398,-12.5404580391274)) ;
#154350 = CARTESIAN_POINT('Ctrl Pts',(1.01199129263162,3.54662946216441,-12.5371917736533)) ;
#154351 = CARTESIAN_POINT('Ctrl Pts',(1.01652362695402,3.54819025857132,-12.5330491480928)) ;
#154352 = CARTESIAN_POINT('Ctrl Pts',(1.02116533136119,3.54921942038456,-12.5287546368838)) ;
#154353 = CARTESIAN_POINT('Ctrl Pts',(1.02580209629923,3.54969340754027,-12.5244085428281)) ;
#154354 = CARTESIAN_POINT('Ctrl Pts',(1.02780524115376,3.54989817637043,-12.5225309717066)) ;
#154355 = CARTESIAN_POINT('Ctrl Pts',(1.02980744674852,3.55,-12.5206439182703)) ;
#154356 = CARTESIAN_POINT('Ctrl Pts',(1.03179971315146,3.55,-12.5187558734356)) ;
#154357 = CARTESIAN_POINT('Origin',(-7.29372370581158E-16,3.55,-11.43)) ;
#154358 = CARTESIAN_POINT('',(1.5,3.55,-11.43)) ;
#154359 = CARTESIAN_POINT('Origin',(-7.29372370581158E-16,3.55,-15.24)) ;
#154360 = CARTESIAN_POINT('',(-0.17080731546663,3.55,-13.7497567779107)) ;
#154361 = CARTESIAN_POINT('',(1.5,3.55,-15.24)) ;
#154362 = CARTESIAN_POINT('Origin',(-7.29372370581158E-16,3.55,-15.24)) ;
#154363 = CARTESIAN_POINT('',(-0.273932138433073,3.45,-13.7652250396981)) ;
#154364 = CARTESIAN_POINT('Ctrl Pts',(-0.17080731546662,3.55,-13.7497567779107)) ;
#154365 = CARTESIAN_POINT('Ctrl Pts',(-0.183882433427078,3.55,-13.7512554096543)) ;
#154366 = CARTESIAN_POINT('Ctrl Pts',(-0.197859036177,3.54752250383109,-13.7530511760977)) ;
#154367 = CARTESIAN_POINT('Ctrl Pts',(-0.223597793566244,3.53719045839678,
-13.7567006467314)) ;
#154368 = CARTESIAN_POINT('Ctrl Pts',(-0.235362682979166,3.52934133421403,
-13.7585504186891)) ;
#154369 = CARTESIAN_POINT('Ctrl Pts',(-0.253465441530103,3.51138121637726,
-13.7615429480238)) ;
#154370 = CARTESIAN_POINT('Ctrl Pts',(-0.261168570620294,3.50026979217228,
-13.7629034821853)) ;
#154371 = CARTESIAN_POINT('Ctrl Pts',(-0.271399896344085,3.47583586070553,
-13.7647463645995)) ;
#154372 = CARTESIAN_POINT('Ctrl Pts',(-0.273932138433063,3.46251477070021,
-13.7652250396981)) ;
#154373 = CARTESIAN_POINT('Ctrl Pts',(-0.273932138433063,3.45,-13.7652250396981)) ;
#154374 = CARTESIAN_POINT('',(-0.273932138433073,3.15,-13.7652250396981)) ;
#154375 = CARTESIAN_POINT('',(-0.273932138433073,3.05,-13.7652250396981)) ;
#154376 = CARTESIAN_POINT('',(-0.373948193368569,3.05,-13.7873600760421)) ;
#154377 = CARTESIAN_POINT('Ctrl Pts',(-0.27393213843307,3.15,-13.7652250396981)) ;
#154378 = CARTESIAN_POINT('Ctrl Pts',(-0.27393213843307,3.13744372549049,
-13.7652250396981)) ;
#154379 = CARTESIAN_POINT('Ctrl Pts',(-0.276486468486161,3.12408297110069,
-13.7656911302356)) ;
#154380 = CARTESIAN_POINT('Ctrl Pts',(-0.286740277640426,3.0995678553947,
-13.7676537789936)) ;
#154381 = CARTESIAN_POINT('Ctrl Pts',(-0.294439768310514,3.08841385970397,
-13.7691548411377)) ;
#154382 = CARTESIAN_POINT('Ctrl Pts',(-0.312194128344968,3.07061084469361,
-13.772819399951)) ;
#154383 = CARTESIAN_POINT('Ctrl Pts',(-0.323517908844214,3.0628422827531,
-13.7752474862748)) ;
#154384 = CARTESIAN_POINT('Ctrl Pts',(-0.348172117123302,3.05253676672645,
-13.7809138387535)) ;
#154385 = CARTESIAN_POINT('Ctrl Pts',(-0.361501722536394,3.05,-13.7841560230592)) ;
#154386 = CARTESIAN_POINT('Ctrl Pts',(-0.373948193368566,3.05,-13.7873600760421)) ;
#154387 = CARTESIAN_POINT('',(-0.872417476238727,3.05,-14.0198001199995)) ;
#154388 = CARTESIAN_POINT('Origin',(-7.95081593156037E-16,3.05,-15.24)) ;
#154389 = CARTESIAN_POINT('',(-0.953662978710562,3.15,-14.0821887360036)) ;
#154390 = CARTESIAN_POINT('Ctrl Pts',(-0.872417476238731,3.05,-14.0198001199995)) ;
#154391 = CARTESIAN_POINT('Ctrl Pts',(-0.882808783297382,3.05,-14.027229687915)) ;
#154392 = CARTESIAN_POINT('Ctrl Pts',(-0.893798224191979,3.05250629897269,
-14.0353093623146)) ;
#154393 = CARTESIAN_POINT('Ctrl Pts',(-0.913892243159222,3.06269675232156,
-14.0504777691246)) ;
#154394 = CARTESIAN_POINT('Ctrl Pts',(-0.922999225059838,3.07038074042647,
-14.0575634285691)) ;
#154395 = CARTESIAN_POINT('Ctrl Pts',(-0.93728513413171,3.08810056349785,
-14.0688558711034)) ;
#154396 = CARTESIAN_POINT('Ctrl Pts',(-0.943452174397239,3.09929464195085,
-14.073843096804)) ;
#154397 = CARTESIAN_POINT('Ctrl Pts',(-0.951639309815366,3.12392729225934,
-14.0805109997964)) ;
#154398 = CARTESIAN_POINT('Ctrl Pts',(-0.953662978710566,3.13736547222678,
-14.0821887360036)) ;
#154399 = CARTESIAN_POINT('Ctrl Pts',(-0.953662978710566,3.15,-14.0821887360036)) ;
#154400 = CARTESIAN_POINT('',(-0.953662978710562,3.45,-14.0821887360036)) ;
#154401 = CARTESIAN_POINT('',(-0.953662978710562,3.05,-14.0821887360036)) ;
#154402 = CARTESIAN_POINT('',(-1.03179971315145,3.55,-14.1512441265644)) ;
#154403 = CARTESIAN_POINT('Ctrl Pts',(-0.953662978710574,3.45,-14.0821887360036)) ;
#154404 = CARTESIAN_POINT('Ctrl Pts',(-0.953662978710574,3.45580715149871,
-14.0821887360036)) ;
#154405 = CARTESIAN_POINT('Ctrl Pts',(-0.954069792639917,3.46165880969181,
-14.0825236315692)) ;
#154406 = CARTESIAN_POINT('Ctrl Pts',(-0.954880405808387,3.46741264967889,
-14.0831927320754)) ;
#154407 = CARTESIAN_POINT('Ctrl Pts',(-0.955592557016205,3.47246759358526,
-14.0837805596017)) ;
#154408 = CARTESIAN_POINT('Ctrl Pts',(-0.956615573654938,3.47744631522378,
-14.0846258114488)) ;
#154409 = CARTESIAN_POINT('Ctrl Pts',(-0.957920385817356,3.48225893605768,
-14.0857086440434)) ;
#154410 = CARTESIAN_POINT('Ctrl Pts',(-0.959423079246208,3.48780141482279,
-14.0869556935967)) ;
#154411 = CARTESIAN_POINT('Ctrl Pts',(-0.961323201468142,3.49320783601915,
-14.0885374593817)) ;
#154412 = CARTESIAN_POINT('Ctrl Pts',(-0.963574238618814,3.4983456004987,
-14.0904242578964)) ;
#154413 = CARTESIAN_POINT('Ctrl Pts',(-0.965499706648002,3.50274028640777,
-14.0920381673855)) ;
#154414 = CARTESIAN_POINT('Ctrl Pts',(-0.967680912999544,3.5069382066956,
-14.0938745944584)) ;
#154415 = CARTESIAN_POINT('Ctrl Pts',(-0.970068248378245,3.51087311165944,
-14.0958987835472)) ;
#154416 = CARTESIAN_POINT('Ctrl Pts',(-0.97293324697907,3.51559532091262,
-14.0983279767636)) ;
#154417 = CARTESIAN_POINT('Ctrl Pts',(-0.976138831290361,3.52000896466724,
-14.1010646855624)) ;
#154418 = CARTESIAN_POINT('Ctrl Pts',(-0.979601776802482,3.52400782220665,
-14.1040509843476)) ;
#154419 = CARTESIAN_POINT('Ctrl Pts',(-0.982467725203497,3.52731729367563,
-14.1065224578947)) ;
#154420 = CARTESIAN_POINT('Ctrl Pts',(-0.985508986896835,3.5303430569618,
-14.1091641736047)) ;
#154421 = CARTESIAN_POINT('Ctrl Pts',(-0.988666612105892,3.53304718478134,
-14.1119315933388)) ;
#154422 = CARTESIAN_POINT('Ctrl Pts',(-0.99270160680367,3.53650267449007,
-14.1154679610881)) ;
#154423 = CARTESIAN_POINT('Ctrl Pts',(-0.996988044734306,3.53948417067184,
-14.1192635881177)) ;
#154424 = CARTESIAN_POINT('Ctrl Pts',(-1.00141585135915,3.54192188246041,
-14.1232340352035)) ;
#154425 = CARTESIAN_POINT('Ctrl Pts',(-1.00487400994927,3.54382575827887,
-14.1263349916949)) ;
#154426 = CARTESIAN_POINT('Ctrl Pts',(-1.00841776012226,3.54539884758398,
-14.1295419608726)) ;
#154427 = CARTESIAN_POINT('Ctrl Pts',(-1.01199129263162,3.54662946216441,
-14.1328082263467)) ;
#154428 = CARTESIAN_POINT('Ctrl Pts',(-1.01652362695401,3.54819025857132,
-14.1369508519072)) ;
#154429 = CARTESIAN_POINT('Ctrl Pts',(-1.02116533136119,3.54921942038456,
-14.1412453631162)) ;
#154430 = CARTESIAN_POINT('Ctrl Pts',(-1.02580209629922,3.54969340754027,
-14.1455914571719)) ;
#154431 = CARTESIAN_POINT('Ctrl Pts',(-1.02780524115375,3.54989817637043,
-14.1474690282934)) ;
#154432 = CARTESIAN_POINT('Ctrl Pts',(-1.02980744674853,3.55,-14.1493560817297)) ;
#154433 = CARTESIAN_POINT('Ctrl Pts',(-1.03179971315146,3.55,-14.1512441265644)) ;
#154434 = CARTESIAN_POINT('',(0.170807315466632,3.55,-16.7302432220893)) ;
#154435 = CARTESIAN_POINT('Origin',(-7.29372370581158E-16,3.55,-15.24)) ;
#154436 = CARTESIAN_POINT('',(0.273932138433074,3.45,-16.7147749603019)) ;
#154437 = CARTESIAN_POINT('Ctrl Pts',(0.170807315466623,3.55,-16.7302432220893)) ;
#154438 = CARTESIAN_POINT('Ctrl Pts',(0.183882433427081,3.55,-16.7287445903457)) ;
#154439 = CARTESIAN_POINT('Ctrl Pts',(0.197859036177004,3.54752250383109,
-16.7269488239023)) ;
#154440 = CARTESIAN_POINT('Ctrl Pts',(0.223597793566247,3.53719045839678,
-16.7232993532686)) ;
#154441 = CARTESIAN_POINT('Ctrl Pts',(0.235362682979168,3.52934133421403,
-16.7214495813109)) ;
#154442 = CARTESIAN_POINT('Ctrl Pts',(0.253465441530106,3.51138121637726,
-16.7184570519762)) ;
#154443 = CARTESIAN_POINT('Ctrl Pts',(0.261168570620297,3.50026979217228,
-16.7170965178147)) ;
#154444 = CARTESIAN_POINT('Ctrl Pts',(0.271399896344088,3.47583586070553,
-16.7152536354005)) ;
#154445 = CARTESIAN_POINT('Ctrl Pts',(0.273932138433066,3.46251477070021,
-16.7147749603019)) ;
#154446 = CARTESIAN_POINT('Ctrl Pts',(0.273932138433066,3.45,-16.7147749603019)) ;
#154447 = CARTESIAN_POINT('',(0.273932138433074,3.15,-16.7147749603019)) ;
#154448 = CARTESIAN_POINT('',(0.273932138433074,3.05,-16.7147749603019)) ;
#154449 = CARTESIAN_POINT('',(0.37394819336857,3.05,-16.6926399239579)) ;
#154450 = CARTESIAN_POINT('Ctrl Pts',(0.273932138433069,3.15,-16.7147749603019)) ;
#154451 = CARTESIAN_POINT('Ctrl Pts',(0.273932138433069,3.13736547222678,
-16.7147749603019)) ;
#154452 = CARTESIAN_POINT('Ctrl Pts',(0.276518148223576,3.12392729225934,
-16.7143031680364)) ;
#154453 = CARTESIAN_POINT('Ctrl Pts',(0.286888647463775,3.09929464195085,
-16.7123175038704)) ;
#154454 = CARTESIAN_POINT('Ctrl Pts',(0.294673181069385,3.08810056349785,
-16.7107990038315)) ;
#154455 = CARTESIAN_POINT('Ctrl Pts',(0.312506499266529,3.07038074042647,
-16.7071140047162)) ;
#154456 = CARTESIAN_POINT('Ctrl Pts',(0.323788284437176,3.06269675232156,
-16.704692225935)) ;
#154457 = CARTESIAN_POINT('Ctrl Pts',(0.348324144605926,3.05250629897269,
-16.6990493783214)) ;
#154458 = CARTESIAN_POINT('Ctrl Pts',(0.361577410726385,3.05,-16.6958244927855)) ;
#154459 = CARTESIAN_POINT('Ctrl Pts',(0.373948193368565,3.05,-16.6926399239579)) ;
#154460 = CARTESIAN_POINT('',(0.872417476238728,3.05,-16.4601998800005)) ;
#154461 = CARTESIAN_POINT('Origin',(-7.95081593156037E-16,3.05,-15.24)) ;
#154462 = CARTESIAN_POINT('',(0.953662978710562,3.15,-16.3978112639964)) ;
#154463 = CARTESIAN_POINT('Ctrl Pts',(0.87241747623873,3.05,-16.4601998800005)) ;
#154464 = CARTESIAN_POINT('Ctrl Pts',(0.882872360457022,3.05,-16.4527248557413)) ;
#154465 = CARTESIAN_POINT('Ctrl Pts',(0.893924122929508,3.05253676672645,
-16.4445978214856)) ;
#154466 = CARTESIAN_POINT('Ctrl Pts',(0.914112220366979,3.0628422827531,-16.4293538633994)) ;
#154467 = CARTESIAN_POINT('Ctrl Pts',(0.923251028202472,3.07061084469361,
-16.422240088077)) ;
#154468 = CARTESIAN_POINT('Ctrl Pts',(0.937470525765901,3.08841385970397,
-16.4109949922316)) ;
#154469 = CARTESIAN_POINT('Ctrl Pts',(0.943569543283853,3.0995678553947,-16.4060617043366)) ;
#154470 = CARTESIAN_POINT('Ctrl Pts',(0.951664040935145,3.12408297110069,
-16.3994683971169)) ;
#154471 = CARTESIAN_POINT('Ctrl Pts',(0.953662978710565,3.13744372549049,
-16.3978112639964)) ;
#154472 = CARTESIAN_POINT('Ctrl Pts',(0.953662978710565,3.15,-16.3978112639964)) ;
#154473 = CARTESIAN_POINT('',(0.953662978710562,3.45,-16.3978112639964)) ;
#154474 = CARTESIAN_POINT('',(0.953662978710562,3.05,-16.3978112639964)) ;
#154475 = CARTESIAN_POINT('',(1.03179971315145,3.55,-16.3287558734356)) ;
#154476 = CARTESIAN_POINT('Ctrl Pts',(0.953662978710576,3.45,-16.3978112639964)) ;
#154477 = CARTESIAN_POINT('Ctrl Pts',(0.953662978710576,3.45580715149871,
-16.3978112639964)) ;
#154478 = CARTESIAN_POINT('Ctrl Pts',(0.95406979263992,3.46165880969181,-16.3974763684308)) ;
#154479 = CARTESIAN_POINT('Ctrl Pts',(0.95488040580839,3.46741264967889,-16.3968072679246)) ;
#154480 = CARTESIAN_POINT('Ctrl Pts',(0.955592557016207,3.47246759358526,
-16.3962194403983)) ;
#154481 = CARTESIAN_POINT('Ctrl Pts',(0.95661557365494,3.47744631522378,-16.3953741885512)) ;
#154482 = CARTESIAN_POINT('Ctrl Pts',(0.957920385817358,3.48225893605768,
-16.3942913559566)) ;
#154483 = CARTESIAN_POINT('Ctrl Pts',(0.959423079246208,3.48780141482278,
-16.3930443064033)) ;
#154484 = CARTESIAN_POINT('Ctrl Pts',(0.961323201468132,3.49320783601912,
-16.3914625406183)) ;
#154485 = CARTESIAN_POINT('Ctrl Pts',(0.963574238618799,3.49834560049866,
-16.3895757421036)) ;
#154486 = CARTESIAN_POINT('Ctrl Pts',(0.965499706647992,3.50274028640775,
-16.3879618326145)) ;
#154487 = CARTESIAN_POINT('Ctrl Pts',(0.967680912999541,3.50693820669559,
-16.3861254055416)) ;
#154488 = CARTESIAN_POINT('Ctrl Pts',(0.970068248378248,3.51087311165943,
-16.3841012164528)) ;
#154489 = CARTESIAN_POINT('Ctrl Pts',(0.972933246979074,3.51559532091262,
-16.3816720232364)) ;
#154490 = CARTESIAN_POINT('Ctrl Pts',(0.976138831290367,3.52000896466725,
-16.3789353144376)) ;
#154491 = CARTESIAN_POINT('Ctrl Pts',(0.979601776802491,3.52400782220666,
-16.3759490156524)) ;
#154492 = CARTESIAN_POINT('Ctrl Pts',(0.982467725203503,3.52731729367563,
-16.3734775421053)) ;
#154493 = CARTESIAN_POINT('Ctrl Pts',(0.985508986896837,3.5303430569618,-16.3708358263953)) ;
#154494 = CARTESIAN_POINT('Ctrl Pts',(0.988666612105889,3.53304718478133,
-16.3680684066612)) ;
#154495 = CARTESIAN_POINT('Ctrl Pts',(0.992701606803676,3.53650267449008,
-16.3645320389119)) ;
#154496 = CARTESIAN_POINT('Ctrl Pts',(0.996988044734359,3.53948417067189,
-16.3607364118822)) ;
#154497 = CARTESIAN_POINT('Ctrl Pts',(1.0014158513592,3.54192188246044,-16.3567659647965)) ;
#154498 = CARTESIAN_POINT('Ctrl Pts',(1.0048740099493,3.54382575827887,-16.3536650083051)) ;
#154499 = CARTESIAN_POINT('Ctrl Pts',(1.00841776012226,3.54539884758398,-16.3504580391274)) ;
#154500 = CARTESIAN_POINT('Ctrl Pts',(1.01199129263161,3.54662946216441,-16.3471917736533)) ;
#154501 = CARTESIAN_POINT('Ctrl Pts',(1.01652362695402,3.54819025857132,-16.3430491480928)) ;
#154502 = CARTESIAN_POINT('Ctrl Pts',(1.0211653313612,3.54921942038456,-16.3387546368838)) ;
#154503 = CARTESIAN_POINT('Ctrl Pts',(1.02580209629924,3.54969340754027,-16.3344085428281)) ;
#154504 = CARTESIAN_POINT('Ctrl Pts',(1.02780524115376,3.54989817637043,-16.3325309717066)) ;
#154505 = CARTESIAN_POINT('Ctrl Pts',(1.02980744674853,3.55,-16.3306439182703)) ;
#154506 = CARTESIAN_POINT('Ctrl Pts',(1.03179971315146,3.55,-16.3287558734356)) ;
#154507 = CARTESIAN_POINT('Origin',(-7.29372370581158E-16,3.55,-15.24)) ;
#154508 = CARTESIAN_POINT('',(1.5,3.55,-15.24)) ;
#154509 = CARTESIAN_POINT('Origin',(-7.29372370581158E-16,3.55,-19.05)) ;
#154510 = CARTESIAN_POINT('',(-0.170807315466631,3.55,-17.5597567779107)) ;
#154511 = CARTESIAN_POINT('',(1.5,3.55,-19.05)) ;
#154512 = CARTESIAN_POINT('Origin',(-7.29372370581158E-16,3.55,-19.05)) ;
#154513 = CARTESIAN_POINT('',(-0.273932138433073,3.45,-17.5752250396981)) ;
#154514 = CARTESIAN_POINT('Ctrl Pts',(-0.170807315466618,3.55,-17.5597567779107)) ;
#154515 = CARTESIAN_POINT('Ctrl Pts',(-0.183882433427076,3.55,-17.5612554096543)) ;
#154516 = CARTESIAN_POINT('Ctrl Pts',(-0.197859036176998,3.54752250383109,
-17.5630511760977)) ;
#154517 = CARTESIAN_POINT('Ctrl Pts',(-0.223597793566241,3.53719045839678,
-17.5667006467314)) ;
#154518 = CARTESIAN_POINT('Ctrl Pts',(-0.235362682979163,3.52934133421403,
-17.5685504186891)) ;
#154519 = CARTESIAN_POINT('Ctrl Pts',(-0.2534654415301,3.51138121637726,-17.5715429480238)) ;
#154520 = CARTESIAN_POINT('Ctrl Pts',(-0.261168570620293,3.50026979217228,
-17.5729034821853)) ;
#154521 = CARTESIAN_POINT('Ctrl Pts',(-0.271399896344084,3.47583586070553,
-17.5747463645995)) ;
#154522 = CARTESIAN_POINT('Ctrl Pts',(-0.273932138433061,3.46251477070021,
-17.5752250396981)) ;
#154523 = CARTESIAN_POINT('Ctrl Pts',(-0.273932138433061,3.45,-17.5752250396981)) ;
#154524 = CARTESIAN_POINT('',(-0.273932138433073,3.15,-17.5752250396981)) ;
#154525 = CARTESIAN_POINT('',(-0.273932138433073,3.05,-17.5752250396981)) ;
#154526 = CARTESIAN_POINT('',(-0.373948193368567,3.05,-17.5973600760421)) ;
#154527 = CARTESIAN_POINT('Ctrl Pts',(-0.273932138433067,3.15,-17.5752250396981)) ;
#154528 = CARTESIAN_POINT('Ctrl Pts',(-0.273932138433067,3.13744372549049,
-17.5752250396981)) ;
#154529 = CARTESIAN_POINT('Ctrl Pts',(-0.276486468486159,3.12408297110069,
-17.5756911302356)) ;
#154530 = CARTESIAN_POINT('Ctrl Pts',(-0.286740277640424,3.0995678553947,
-17.5776537789936)) ;
#154531 = CARTESIAN_POINT('Ctrl Pts',(-0.294439768310511,3.08841385970397,
-17.5791548411377)) ;
#154532 = CARTESIAN_POINT('Ctrl Pts',(-0.312194128344966,3.07061084469361,
-17.582819399951)) ;
#154533 = CARTESIAN_POINT('Ctrl Pts',(-0.323517908844211,3.0628422827531,
-17.5852474862748)) ;
#154534 = CARTESIAN_POINT('Ctrl Pts',(-0.348172117123299,3.05253676672645,
-17.5909138387535)) ;
#154535 = CARTESIAN_POINT('Ctrl Pts',(-0.361501722536391,3.05,-17.5941560230592)) ;
#154536 = CARTESIAN_POINT('Ctrl Pts',(-0.373948193368564,3.05,-17.5973600760421)) ;
#154537 = CARTESIAN_POINT('',(-0.872417476238727,3.05,-17.8298001199995)) ;
#154538 = CARTESIAN_POINT('Origin',(-7.95081593156037E-16,3.05,-19.05)) ;
#154539 = CARTESIAN_POINT('',(-0.953662978710562,3.15,-17.8921887360036)) ;
#154540 = CARTESIAN_POINT('Ctrl Pts',(-0.87241747623873,3.05,-17.8298001199995)) ;
#154541 = CARTESIAN_POINT('Ctrl Pts',(-0.88280878329738,3.05,-17.837229687915)) ;
#154542 = CARTESIAN_POINT('Ctrl Pts',(-0.893798224191977,3.05250629897269,
-17.8453093623146)) ;
#154543 = CARTESIAN_POINT('Ctrl Pts',(-0.913892243159221,3.06269675232156,
-17.8604777691246)) ;
#154544 = CARTESIAN_POINT('Ctrl Pts',(-0.922999225059836,3.07038074042647,
-17.8675634285691)) ;
#154545 = CARTESIAN_POINT('Ctrl Pts',(-0.937285134131708,3.08810056349785,
-17.8788558711034)) ;
#154546 = CARTESIAN_POINT('Ctrl Pts',(-0.943452174397237,3.09929464195085,
-17.883843096804)) ;
#154547 = CARTESIAN_POINT('Ctrl Pts',(-0.951639309815365,3.12392729225934,
-17.8905109997964)) ;
#154548 = CARTESIAN_POINT('Ctrl Pts',(-0.953662978710563,3.13736547222678,
-17.8921887360036)) ;
#154549 = CARTESIAN_POINT('Ctrl Pts',(-0.953662978710563,3.15,-17.8921887360036)) ;
#154550 = CARTESIAN_POINT('',(-0.953662978710562,3.45,-17.8921887360036)) ;
#154551 = CARTESIAN_POINT('',(-0.953662978710562,3.05,-17.8921887360036)) ;
#154552 = CARTESIAN_POINT('',(-1.03179971315145,3.55,-17.9612441265644)) ;
#154553 = CARTESIAN_POINT('Ctrl Pts',(-0.953662978710576,3.45,-17.8921887360036)) ;
#154554 = CARTESIAN_POINT('Ctrl Pts',(-0.953662978710576,3.45580715149871,
-17.8921887360036)) ;
#154555 = CARTESIAN_POINT('Ctrl Pts',(-0.954069792639918,3.4616588096918,
-17.8925236315692)) ;
#154556 = CARTESIAN_POINT('Ctrl Pts',(-0.954880405808387,3.46741264967887,
-17.8931927320754)) ;
#154557 = CARTESIAN_POINT('Ctrl Pts',(-0.955592557016204,3.47246759358525,
-17.8937805596017)) ;
#154558 = CARTESIAN_POINT('Ctrl Pts',(-0.956615573654935,3.47744631522377,
-17.8946258114488)) ;
#154559 = CARTESIAN_POINT('Ctrl Pts',(-0.957920385817355,3.48225893605768,
-17.8957086440434)) ;
#154560 = CARTESIAN_POINT('Ctrl Pts',(-0.959423079246204,3.48780141482278,
-17.8969556935967)) ;
#154561 = CARTESIAN_POINT('Ctrl Pts',(-0.96132320146813,3.49320783601912,
-17.8985374593817)) ;
#154562 = CARTESIAN_POINT('Ctrl Pts',(-0.963574238618794,3.49834560049866,
-17.9004242578964)) ;
#154563 = CARTESIAN_POINT('Ctrl Pts',(-0.965499706647985,3.50274028640774,
-17.9020381673855)) ;
#154564 = CARTESIAN_POINT('Ctrl Pts',(-0.967680912999533,3.50693820669558,
-17.9038745944584)) ;
#154565 = CARTESIAN_POINT('Ctrl Pts',(-0.970068248378242,3.51087311165943,
-17.9058987835472)) ;
#154566 = CARTESIAN_POINT('Ctrl Pts',(-0.972933246979071,3.51559532091262,
-17.9083279767636)) ;
#154567 = CARTESIAN_POINT('Ctrl Pts',(-0.976138831290368,3.52000896466725,
-17.9110646855624)) ;
#154568 = CARTESIAN_POINT('Ctrl Pts',(-0.979601776802492,3.52400782220666,
-17.9140509843476)) ;
#154569 = CARTESIAN_POINT('Ctrl Pts',(-0.982467725203504,3.52731729367563,
-17.9165224578947)) ;
#154570 = CARTESIAN_POINT('Ctrl Pts',(-0.985508986896838,3.5303430569618,
-17.9191641736047)) ;
#154571 = CARTESIAN_POINT('Ctrl Pts',(-0.988666612105874,3.53304718478133,
-17.9219315933388)) ;
#154572 = CARTESIAN_POINT('Ctrl Pts',(-0.992701606803626,3.53650267449005,
-17.9254679610881)) ;
#154573 = CARTESIAN_POINT('Ctrl Pts',(-0.996988044734298,3.53948417067184,
-17.9292635881177)) ;
#154574 = CARTESIAN_POINT('Ctrl Pts',(-1.00141585135914,3.5419218824604,-17.9332340352035)) ;
#154575 = CARTESIAN_POINT('Ctrl Pts',(-1.00487400994926,3.54382575827887,
-17.9363349916949)) ;
#154576 = CARTESIAN_POINT('Ctrl Pts',(-1.00841776012225,3.54539884758397,
-17.9395419608726)) ;
#154577 = CARTESIAN_POINT('Ctrl Pts',(-1.01199129263161,3.54662946216441,
-17.9428082263467)) ;
#154578 = CARTESIAN_POINT('Ctrl Pts',(-1.01652362695402,3.54819025857132,
-17.9469508519072)) ;
#154579 = CARTESIAN_POINT('Ctrl Pts',(-1.02116533136121,3.54921942038456,
-17.9512453631162)) ;
#154580 = CARTESIAN_POINT('Ctrl Pts',(-1.02580209629926,3.54969340754028,
-17.9555914571719)) ;
#154581 = CARTESIAN_POINT('Ctrl Pts',(-1.02780524115377,3.54989817637043,
-17.9574690282934)) ;
#154582 = CARTESIAN_POINT('Ctrl Pts',(-1.02980744674854,3.55,-17.9593560817297)) ;
#154583 = CARTESIAN_POINT('Ctrl Pts',(-1.03179971315146,3.55,-17.9612441265644)) ;
#154584 = CARTESIAN_POINT('',(0.170807315466633,3.55,-20.5402432220893)) ;
#154585 = CARTESIAN_POINT('Origin',(-7.29372370581158E-16,3.55,-19.05)) ;
#154586 = CARTESIAN_POINT('',(0.273932138433074,3.45,-20.5247749603019)) ;
#154587 = CARTESIAN_POINT('Ctrl Pts',(0.170807315466623,3.55,-20.5402432220893)) ;
#154588 = CARTESIAN_POINT('Ctrl Pts',(0.18388243342708,3.55,-20.5387445903457)) ;
#154589 = CARTESIAN_POINT('Ctrl Pts',(0.197859036177002,3.54752250383109,
-20.5369488239023)) ;
#154590 = CARTESIAN_POINT('Ctrl Pts',(0.223597793566245,3.53719045839678,
-20.5332993532686)) ;
#154591 = CARTESIAN_POINT('Ctrl Pts',(0.235362682979168,3.52934133421403,
-20.531449581311)) ;
#154592 = CARTESIAN_POINT('Ctrl Pts',(0.253465441530105,3.51138121637726,
-20.5284570519762)) ;
#154593 = CARTESIAN_POINT('Ctrl Pts',(0.261168570620294,3.50026979217228,
-20.5270965178147)) ;
#154594 = CARTESIAN_POINT('Ctrl Pts',(0.271399896344085,3.47583586070553,
-20.5252536354005)) ;
#154595 = CARTESIAN_POINT('Ctrl Pts',(0.273932138433065,3.46251477070021,
-20.5247749603019)) ;
#154596 = CARTESIAN_POINT('Ctrl Pts',(0.273932138433065,3.45,-20.5247749603019)) ;
#154597 = CARTESIAN_POINT('',(0.273932138433074,3.15,-20.5247749603019)) ;
#154598 = CARTESIAN_POINT('',(0.273932138433074,3.05,-20.5247749603019)) ;
#154599 = CARTESIAN_POINT('',(0.373948193368569,3.05,-20.5026399239579)) ;
#154600 = CARTESIAN_POINT('Ctrl Pts',(0.273932138433072,3.15,-20.5247749603019)) ;
#154601 = CARTESIAN_POINT('Ctrl Pts',(0.273932138433072,3.13736547222678,
-20.5247749603019)) ;
#154602 = CARTESIAN_POINT('Ctrl Pts',(0.276518148223578,3.12392729225934,
-20.5243031680364)) ;
#154603 = CARTESIAN_POINT('Ctrl Pts',(0.286888647463776,3.09929464195085,
-20.5223175038704)) ;
#154604 = CARTESIAN_POINT('Ctrl Pts',(0.294673181069388,3.08810056349785,
-20.5207990038315)) ;
#154605 = CARTESIAN_POINT('Ctrl Pts',(0.312506499266531,3.07038074042647,
-20.5171140047162)) ;
#154606 = CARTESIAN_POINT('Ctrl Pts',(0.323788284437176,3.06269675232156,
-20.514692225935)) ;
#154607 = CARTESIAN_POINT('Ctrl Pts',(0.348324144605927,3.05250629897269,
-20.5090493783214)) ;
#154608 = CARTESIAN_POINT('Ctrl Pts',(0.361577410726387,3.05,-20.5058244927855)) ;
#154609 = CARTESIAN_POINT('Ctrl Pts',(0.373948193368567,3.05,-20.5026399239579)) ;
#154610 = CARTESIAN_POINT('',(0.872417476238729,3.05,-20.2701998800005)) ;
#154611 = CARTESIAN_POINT('Origin',(-7.95081593156037E-16,3.05,-19.05)) ;
#154612 = CARTESIAN_POINT('',(0.953662978710562,3.15,-20.2078112639964)) ;
#154613 = CARTESIAN_POINT('Ctrl Pts',(0.872417476238732,3.05,-20.2701998800005)) ;
#154614 = CARTESIAN_POINT('Ctrl Pts',(0.88287236045702,3.05,-20.2627248557413)) ;
#154615 = CARTESIAN_POINT('Ctrl Pts',(0.893924122929511,3.05253676672645,
-20.2545978214856)) ;
#154616 = CARTESIAN_POINT('Ctrl Pts',(0.914112220366982,3.0628422827531,-20.2393538633994)) ;
#154617 = CARTESIAN_POINT('Ctrl Pts',(0.923251028202474,3.07061084469361,
-20.232240088077)) ;
#154618 = CARTESIAN_POINT('Ctrl Pts',(0.937470525765903,3.08841385970397,
-20.2209949922316)) ;
#154619 = CARTESIAN_POINT('Ctrl Pts',(0.943569543283854,3.0995678553947,-20.2160617043366)) ;
#154620 = CARTESIAN_POINT('Ctrl Pts',(0.951664040935147,3.12408297110069,
-20.2094683971169)) ;
#154621 = CARTESIAN_POINT('Ctrl Pts',(0.953662978710566,3.13744372549049,
-20.2078112639964)) ;
#154622 = CARTESIAN_POINT('Ctrl Pts',(0.953662978710566,3.15,-20.2078112639964)) ;
#154623 = CARTESIAN_POINT('',(0.953662978710562,3.45,-20.2078112639964)) ;
#154624 = CARTESIAN_POINT('',(0.953662978710562,3.05,-20.2078112639964)) ;
#154625 = CARTESIAN_POINT('',(1.03179971315145,3.55,-20.1387558734356)) ;
#154626 = CARTESIAN_POINT('Ctrl Pts',(0.953662978710579,3.45,-20.2078112639964)) ;
#154627 = CARTESIAN_POINT('Ctrl Pts',(0.953662978710579,3.45580715149871,
-20.2078112639964)) ;
#154628 = CARTESIAN_POINT('Ctrl Pts',(0.954069792639924,3.46165880969181,
-20.2074763684308)) ;
#154629 = CARTESIAN_POINT('Ctrl Pts',(0.954880405808395,3.46741264967889,
-20.2068072679246)) ;
#154630 = CARTESIAN_POINT('Ctrl Pts',(0.955592557016213,3.47246759358527,
-20.2062194403983)) ;
#154631 = CARTESIAN_POINT('Ctrl Pts',(0.956615573654944,3.47744631522378,
-20.2053741885512)) ;
#154632 = CARTESIAN_POINT('Ctrl Pts',(0.957920385817361,3.48225893605768,
-20.2042913559566)) ;
#154633 = CARTESIAN_POINT('Ctrl Pts',(0.959423079246211,3.48780141482278,
-20.2030443064033)) ;
#154634 = CARTESIAN_POINT('Ctrl Pts',(0.961323201468137,3.49320783601913,
-20.2014625406183)) ;
#154635 = CARTESIAN_POINT('Ctrl Pts',(0.963574238618808,3.49834560049867,
-20.1995757421036)) ;
#154636 = CARTESIAN_POINT('Ctrl Pts',(0.965499706647999,3.50274028640776,
-20.1979618326145)) ;
#154637 = CARTESIAN_POINT('Ctrl Pts',(0.967680912999541,3.50693820669559,
-20.1961254055416)) ;
#154638 = CARTESIAN_POINT('Ctrl Pts',(0.970068248378246,3.51087311165943,
-20.1941012164528)) ;
#154639 = CARTESIAN_POINT('Ctrl Pts',(0.972933246979075,3.51559532091262,
-20.1916720232364)) ;
#154640 = CARTESIAN_POINT('Ctrl Pts',(0.97613883129037,3.52000896466725,-20.1889353144376)) ;
#154641 = CARTESIAN_POINT('Ctrl Pts',(0.979601776802495,3.52400782220666,
-20.1859490156524)) ;
#154642 = CARTESIAN_POINT('Ctrl Pts',(0.982467725203507,3.52731729367563,
-20.1834775421053)) ;
#154643 = CARTESIAN_POINT('Ctrl Pts',(0.98550898689684,3.5303430569618,-20.1808358263953)) ;
#154644 = CARTESIAN_POINT('Ctrl Pts',(0.988666612105893,3.53304718478133,
-20.1780684066612)) ;
#154645 = CARTESIAN_POINT('Ctrl Pts',(0.992701606803678,3.53650267449007,
-20.1745320389119)) ;
#154646 = CARTESIAN_POINT('Ctrl Pts',(0.996988044734317,3.53948417067185,
-20.1707364118823)) ;
#154647 = CARTESIAN_POINT('Ctrl Pts',(1.00141585135917,3.54192188246042,-20.1667659647965)) ;
#154648 = CARTESIAN_POINT('Ctrl Pts',(1.00487400994928,3.54382575827887,-20.1636650083051)) ;
#154649 = CARTESIAN_POINT('Ctrl Pts',(1.00841776012227,3.54539884758398,-20.1604580391274)) ;
#154650 = CARTESIAN_POINT('Ctrl Pts',(1.01199129263161,3.54662946216441,-20.1571917736533)) ;
#154651 = CARTESIAN_POINT('Ctrl Pts',(1.01652362695402,3.54819025857132,-20.1530491480928)) ;
#154652 = CARTESIAN_POINT('Ctrl Pts',(1.02116533136121,3.54921942038456,-20.1487546368838)) ;
#154653 = CARTESIAN_POINT('Ctrl Pts',(1.02580209629926,3.54969340754028,-20.1444085428281)) ;
#154654 = CARTESIAN_POINT('Ctrl Pts',(1.02780524115377,3.54989817637043,-20.1425309717066)) ;
#154655 = CARTESIAN_POINT('Ctrl Pts',(1.02980744674853,3.55,-20.1406439182703)) ;
#154656 = CARTESIAN_POINT('Ctrl Pts',(1.03179971315146,3.55,-20.1387558734356)) ;
#154657 = CARTESIAN_POINT('Origin',(-7.29372370581158E-16,3.55,-19.05)) ;
#154658 = CARTESIAN_POINT('',(1.5,3.55,-19.05)) ;
#154659 = CARTESIAN_POINT('Origin',(-7.29372370581158E-16,3.55,-22.86)) ;
#154660 = CARTESIAN_POINT('',(-0.170807315466631,3.55,-21.3697567779107)) ;
#154661 = CARTESIAN_POINT('',(1.5,3.55,-22.86)) ;
#154662 = CARTESIAN_POINT('Origin',(-7.29372370581158E-16,3.55,-22.86)) ;
#154663 = CARTESIAN_POINT('',(-0.273932138433073,3.45,-21.3852250396981)) ;
#154664 = CARTESIAN_POINT('Ctrl Pts',(-0.17080731546662,3.55,-21.3697567779107)) ;
#154665 = CARTESIAN_POINT('Ctrl Pts',(-0.183882433427077,3.55,-21.3712554096543)) ;
#154666 = CARTESIAN_POINT('Ctrl Pts',(-0.197859036177001,3.54752250383109,
-21.3730511760977)) ;
#154667 = CARTESIAN_POINT('Ctrl Pts',(-0.223597793566244,3.53719045839678,
-21.3767006467314)) ;
#154668 = CARTESIAN_POINT('Ctrl Pts',(-0.235362682979166,3.52934133421403,
-21.3785504186891)) ;
#154669 = CARTESIAN_POINT('Ctrl Pts',(-0.253465441530103,3.51138121637726,
-21.3815429480238)) ;
#154670 = CARTESIAN_POINT('Ctrl Pts',(-0.261168570620293,3.50026979217228,
-21.3829034821853)) ;
#154671 = CARTESIAN_POINT('Ctrl Pts',(-0.271399896344084,3.47583586070552,
-21.3847463645995)) ;
#154672 = CARTESIAN_POINT('Ctrl Pts',(-0.273932138433062,3.46251477070021,
-21.3852250396981)) ;
#154673 = CARTESIAN_POINT('Ctrl Pts',(-0.273932138433062,3.45,-21.3852250396981)) ;
#154674 = CARTESIAN_POINT('',(-0.273932138433073,3.15,-21.3852250396981)) ;
#154675 = CARTESIAN_POINT('',(-0.273932138433073,3.05,-21.3852250396981)) ;
#154676 = CARTESIAN_POINT('',(-0.373948193368567,3.05,-21.4073600760421)) ;
#154677 = CARTESIAN_POINT('Ctrl Pts',(-0.27393213843307,3.15,-21.3852250396981)) ;
#154678 = CARTESIAN_POINT('Ctrl Pts',(-0.27393213843307,3.13744372549049,
-21.3852250396981)) ;
#154679 = CARTESIAN_POINT('Ctrl Pts',(-0.276486468486162,3.12408297110069,
-21.3856911302356)) ;
#154680 = CARTESIAN_POINT('Ctrl Pts',(-0.286740277640426,3.0995678553947,
-21.3876537789936)) ;
#154681 = CARTESIAN_POINT('Ctrl Pts',(-0.294439768310513,3.08841385970397,
-21.3891548411377)) ;
#154682 = CARTESIAN_POINT('Ctrl Pts',(-0.312194128344967,3.07061084469361,
-21.392819399951)) ;
#154683 = CARTESIAN_POINT('Ctrl Pts',(-0.323517908844212,3.0628422827531,
-21.3952474862748)) ;
#154684 = CARTESIAN_POINT('Ctrl Pts',(-0.3481721171233,3.05253676672645,-21.4009138387535)) ;
#154685 = CARTESIAN_POINT('Ctrl Pts',(-0.361501722536393,3.05,-21.4041560230592)) ;
#154686 = CARTESIAN_POINT('Ctrl Pts',(-0.373948193368565,3.05,-21.4073600760421)) ;
#154687 = CARTESIAN_POINT('',(-0.872417476238727,3.05,-21.6398001199995)) ;
#154688 = CARTESIAN_POINT('Origin',(-7.95081593156037E-16,3.05,-22.86)) ;
#154689 = CARTESIAN_POINT('',(-0.953662978710562,3.15,-21.7021887360036)) ;
#154690 = CARTESIAN_POINT('Ctrl Pts',(-0.872417476238732,3.05,-21.6398001199995)) ;
#154691 = CARTESIAN_POINT('Ctrl Pts',(-0.882808783297382,3.05,-21.647229687915)) ;
#154692 = CARTESIAN_POINT('Ctrl Pts',(-0.893798224191979,3.05250629897269,
-21.6553093623146)) ;
#154693 = CARTESIAN_POINT('Ctrl Pts',(-0.913892243159223,3.06269675232156,
-21.6704777691246)) ;
#154694 = CARTESIAN_POINT('Ctrl Pts',(-0.922999225059838,3.07038074042647,
-21.6775634285691)) ;
#154695 = CARTESIAN_POINT('Ctrl Pts',(-0.93728513413171,3.08810056349785,
-21.6888558711034)) ;
#154696 = CARTESIAN_POINT('Ctrl Pts',(-0.94345217439724,3.09929464195085,
-21.693843096804)) ;
#154697 = CARTESIAN_POINT('Ctrl Pts',(-0.951639309815367,3.12392729225934,
-21.7005109997964)) ;
#154698 = CARTESIAN_POINT('Ctrl Pts',(-0.953662978710565,3.13736547222678,
-21.7021887360036)) ;
#154699 = CARTESIAN_POINT('Ctrl Pts',(-0.953662978710565,3.15,-21.7021887360036)) ;
#154700 = CARTESIAN_POINT('',(-0.953662978710562,3.45,-21.7021887360036)) ;
#154701 = CARTESIAN_POINT('',(-0.953662978710562,3.05,-21.7021887360036)) ;
#154702 = CARTESIAN_POINT('',(-1.03179971315145,3.55,-21.7712441265644)) ;
#154703 = CARTESIAN_POINT('Ctrl Pts',(-0.953662978710576,3.45,-21.7021887360036)) ;
#154704 = CARTESIAN_POINT('Ctrl Pts',(-0.953662978710576,3.4558071514987,
-21.7021887360036)) ;
#154705 = CARTESIAN_POINT('Ctrl Pts',(-0.954069792639918,3.4616588096918,
-21.7025236315692)) ;
#154706 = CARTESIAN_POINT('Ctrl Pts',(-0.954880405808386,3.46741264967887,
-21.7031927320754)) ;
#154707 = CARTESIAN_POINT('Ctrl Pts',(-0.955592557016204,3.47246759358525,
-21.7037805596017)) ;
#154708 = CARTESIAN_POINT('Ctrl Pts',(-0.956615573654935,3.47744631522377,
-21.7046258114488)) ;
#154709 = CARTESIAN_POINT('Ctrl Pts',(-0.957920385817355,3.48225893605768,
-21.7057086440434)) ;
#154710 = CARTESIAN_POINT('Ctrl Pts',(-0.959423079246203,3.48780141482278,
-21.7069556935967)) ;
#154711 = CARTESIAN_POINT('Ctrl Pts',(-0.961323201468129,3.49320783601912,
-21.7085374593817)) ;
#154712 = CARTESIAN_POINT('Ctrl Pts',(-0.963574238618792,3.49834560049865,
-21.7104242578964)) ;
#154713 = CARTESIAN_POINT('Ctrl Pts',(-0.965499706647984,3.50274028640774,
-21.7120381673855)) ;
#154714 = CARTESIAN_POINT('Ctrl Pts',(-0.967680912999533,3.50693820669559,
-21.7138745944584)) ;
#154715 = CARTESIAN_POINT('Ctrl Pts',(-0.970068248378244,3.51087311165943,
-21.7158987835472)) ;
#154716 = CARTESIAN_POINT('Ctrl Pts',(-0.972933246979067,3.51559532091262,
-21.7183279767636)) ;
#154717 = CARTESIAN_POINT('Ctrl Pts',(-0.976138831290349,3.52000896466723,
-21.7210646855624)) ;
#154718 = CARTESIAN_POINT('Ctrl Pts',(-0.979601776802468,3.52400782220664,
-21.7240509843476)) ;
#154719 = CARTESIAN_POINT('Ctrl Pts',(-0.982467725203489,3.52731729367562,
-21.7265224578947)) ;
#154720 = CARTESIAN_POINT('Ctrl Pts',(-0.98550898689683,3.5303430569618,-21.7291641736047)) ;
#154721 = CARTESIAN_POINT('Ctrl Pts',(-0.988666612105892,3.53304718478134,
-21.7319315933388)) ;
#154722 = CARTESIAN_POINT('Ctrl Pts',(-0.992701606803676,3.53650267449008,
-21.7354679610881)) ;
#154723 = CARTESIAN_POINT('Ctrl Pts',(-0.996988044734315,3.53948417067185,
-21.7392635881177)) ;
#154724 = CARTESIAN_POINT('Ctrl Pts',(-1.00141585135917,3.54192188246042,
-21.7432340352035)) ;
#154725 = CARTESIAN_POINT('Ctrl Pts',(-1.00487400994928,3.54382575827887,
-21.7463349916949)) ;
#154726 = CARTESIAN_POINT('Ctrl Pts',(-1.00841776012226,3.54539884758398,
-21.7495419608726)) ;
#154727 = CARTESIAN_POINT('Ctrl Pts',(-1.01199129263161,3.54662946216441,
-21.7528082263467)) ;
#154728 = CARTESIAN_POINT('Ctrl Pts',(-1.01652362695403,3.54819025857132,
-21.7569508519072)) ;
#154729 = CARTESIAN_POINT('Ctrl Pts',(-1.02116533136127,3.54921942038457,
-21.7612453631163)) ;
#154730 = CARTESIAN_POINT('Ctrl Pts',(-1.0258020962993,3.54969340754028,-21.765591457172)) ;
#154731 = CARTESIAN_POINT('Ctrl Pts',(-1.02780524115378,3.54989817637043,
-21.7674690282935)) ;
#154732 = CARTESIAN_POINT('Ctrl Pts',(-1.02980744674854,3.55,-21.7693560817297)) ;
#154733 = CARTESIAN_POINT('Ctrl Pts',(-1.03179971315146,3.55,-21.7712441265644)) ;
#154734 = CARTESIAN_POINT('',(0.170807315466633,3.55,-24.3502432220893)) ;
#154735 = CARTESIAN_POINT('Origin',(-7.29372370581158E-16,3.55,-22.86)) ;
#154736 = CARTESIAN_POINT('',(0.273932138433074,3.45,-24.3347749603019)) ;
#154737 = CARTESIAN_POINT('Ctrl Pts',(0.170807315466623,3.55,-24.3502432220893)) ;
#154738 = CARTESIAN_POINT('Ctrl Pts',(0.18388243342708,3.55,-24.3487445903457)) ;
#154739 = CARTESIAN_POINT('Ctrl Pts',(0.197859036177004,3.54752250383109,
-24.3469488239023)) ;
#154740 = CARTESIAN_POINT('Ctrl Pts',(0.223597793566247,3.53719045839678,
-24.3432993532686)) ;
#154741 = CARTESIAN_POINT('Ctrl Pts',(0.235362682979169,3.52934133421403,
-24.3414495813109)) ;
#154742 = CARTESIAN_POINT('Ctrl Pts',(0.253465441530107,3.51138121637726,
-24.3384570519762)) ;
#154743 = CARTESIAN_POINT('Ctrl Pts',(0.261168570620295,3.50026979217228,
-24.3370965178147)) ;
#154744 = CARTESIAN_POINT('Ctrl Pts',(0.271399896344086,3.47583586070552,
-24.3352536354005)) ;
#154745 = CARTESIAN_POINT('Ctrl Pts',(0.273932138433066,3.46251477070021,
-24.3347749603019)) ;
#154746 = CARTESIAN_POINT('Ctrl Pts',(0.273932138433066,3.45,-24.3347749603019)) ;
#154747 = CARTESIAN_POINT('',(0.273932138433074,3.15,-24.3347749603019)) ;
#154748 = CARTESIAN_POINT('',(0.273932138433074,3.05,-24.3347749603019)) ;
#154749 = CARTESIAN_POINT('',(0.373948193368569,3.05,-24.3126399239579)) ;
#154750 = CARTESIAN_POINT('Ctrl Pts',(0.273932138433069,3.15,-24.3347749603019)) ;
#154751 = CARTESIAN_POINT('Ctrl Pts',(0.273932138433069,3.13736547222678,
-24.3347749603019)) ;
#154752 = CARTESIAN_POINT('Ctrl Pts',(0.276518148223577,3.12392729225934,
-24.3343031680364)) ;
#154753 = CARTESIAN_POINT('Ctrl Pts',(0.286888647463776,3.09929464195085,
-24.3323175038704)) ;
#154754 = CARTESIAN_POINT('Ctrl Pts',(0.294673181069385,3.08810056349785,
-24.3307990038315)) ;
#154755 = CARTESIAN_POINT('Ctrl Pts',(0.312506499266529,3.07038074042647,
-24.3271140047162)) ;
#154756 = CARTESIAN_POINT('Ctrl Pts',(0.323788284437175,3.06269675232156,
-24.324692225935)) ;
#154757 = CARTESIAN_POINT('Ctrl Pts',(0.348324144605926,3.05250629897269,
-24.3190493783214)) ;
#154758 = CARTESIAN_POINT('Ctrl Pts',(0.361577410726384,3.05,-24.3158244927855)) ;
#154759 = CARTESIAN_POINT('Ctrl Pts',(0.373948193368564,3.05,-24.3126399239579)) ;
#154760 = CARTESIAN_POINT('',(0.872417476238729,3.05,-24.0801998800005)) ;
#154761 = CARTESIAN_POINT('Origin',(-7.95081593156037E-16,3.05,-22.86)) ;
#154762 = CARTESIAN_POINT('',(0.953662978710562,3.15,-24.0178112639964)) ;
#154763 = CARTESIAN_POINT('Ctrl Pts',(0.872417476238731,3.05,-24.0801998800005)) ;
#154764 = CARTESIAN_POINT('Ctrl Pts',(0.882872360457021,3.05,-24.0727248557413)) ;
#154765 = CARTESIAN_POINT('Ctrl Pts',(0.893924122929508,3.05253676672645,
-24.0645978214856)) ;
#154766 = CARTESIAN_POINT('Ctrl Pts',(0.914112220366979,3.0628422827531,-24.0493538633994)) ;
#154767 = CARTESIAN_POINT('Ctrl Pts',(0.923251028202473,3.07061084469361,
-24.042240088077)) ;
#154768 = CARTESIAN_POINT('Ctrl Pts',(0.937470525765902,3.08841385970397,
-24.0309949922316)) ;
#154769 = CARTESIAN_POINT('Ctrl Pts',(0.943569543283853,3.0995678553947,-24.0260617043366)) ;
#154770 = CARTESIAN_POINT('Ctrl Pts',(0.951664040935146,3.12408297110069,
-24.0194683971169)) ;
#154771 = CARTESIAN_POINT('Ctrl Pts',(0.953662978710564,3.13744372549049,
-24.0178112639964)) ;
#154772 = CARTESIAN_POINT('Ctrl Pts',(0.953662978710564,3.15,-24.0178112639964)) ;
#154773 = CARTESIAN_POINT('',(0.953662978710562,3.45,-24.0178112639964)) ;
#154774 = CARTESIAN_POINT('',(0.953662978710562,3.05,-24.0178112639964)) ;
#154775 = CARTESIAN_POINT('',(1.03179971315145,3.55,-23.9487558734356)) ;
#154776 = CARTESIAN_POINT('Ctrl Pts',(0.953662978710579,3.45,-24.0178112639964)) ;
#154777 = CARTESIAN_POINT('Ctrl Pts',(0.953662978710579,3.4558071514987,-24.0178112639964)) ;
#154778 = CARTESIAN_POINT('Ctrl Pts',(0.954069792639922,3.4616588096918,-24.0174763684308)) ;
#154779 = CARTESIAN_POINT('Ctrl Pts',(0.954880405808391,3.46741264967887,
-24.0168072679246)) ;
#154780 = CARTESIAN_POINT('Ctrl Pts',(0.955592557016209,3.47246759358525,
-24.0162194403983)) ;
#154781 = CARTESIAN_POINT('Ctrl Pts',(0.956615573654939,3.47744631522377,
-24.0153741885512)) ;
#154782 = CARTESIAN_POINT('Ctrl Pts',(0.957920385817358,3.48225893605767,
-24.0142913559566)) ;
#154783 = CARTESIAN_POINT('Ctrl Pts',(0.959423079246211,3.48780141482279,
-24.0130443064033)) ;
#154784 = CARTESIAN_POINT('Ctrl Pts',(0.96132320146814,3.49320783601914,-24.0114625406183)) ;
#154785 = CARTESIAN_POINT('Ctrl Pts',(0.963574238618814,3.49834560049869,
-24.0095757421036)) ;
#154786 = CARTESIAN_POINT('Ctrl Pts',(0.965499706648003,3.50274028640777,
-24.0079618326145)) ;
#154787 = CARTESIAN_POINT('Ctrl Pts',(0.967680912999543,3.50693820669559,
-24.0061254055416)) ;
#154788 = CARTESIAN_POINT('Ctrl Pts',(0.970068248378244,3.51087311165943,
-24.0041012164528)) ;
#154789 = CARTESIAN_POINT('Ctrl Pts',(0.972933246979073,3.51559532091262,
-24.0016720232364)) ;
#154790 = CARTESIAN_POINT('Ctrl Pts',(0.976138831290369,3.52000896466725,
-23.9989353144376)) ;
#154791 = CARTESIAN_POINT('Ctrl Pts',(0.979601776802496,3.52400782220667,
-23.9959490156524)) ;
#154792 = CARTESIAN_POINT('Ctrl Pts',(0.982467725203506,3.52731729367563,
-23.9934775421053)) ;
#154793 = CARTESIAN_POINT('Ctrl Pts',(0.985508986896841,3.5303430569618,-23.9908358263953)) ;
#154794 = CARTESIAN_POINT('Ctrl Pts',(0.988666612105891,3.53304718478133,
-23.9880684066612)) ;
#154795 = CARTESIAN_POINT('Ctrl Pts',(0.992701606803682,3.53650267449008,
-23.984532038912)) ;
#154796 = CARTESIAN_POINT('Ctrl Pts',(0.996988044734363,3.53948417067189,
-23.9807364118822)) ;
#154797 = CARTESIAN_POINT('Ctrl Pts',(1.0014158513592,3.54192188246045,-23.9767659647964)) ;
#154798 = CARTESIAN_POINT('Ctrl Pts',(1.00487400994929,3.54382575827889,-23.973665008305)) ;
#154799 = CARTESIAN_POINT('Ctrl Pts',(1.00841776012227,3.54539884758398,-23.9704580391274)) ;
#154800 = CARTESIAN_POINT('Ctrl Pts',(1.01199129263161,3.54662946216441,-23.9671917736533)) ;
#154801 = CARTESIAN_POINT('Ctrl Pts',(1.01652362695402,3.54819025857132,-23.9630491480928)) ;
#154802 = CARTESIAN_POINT('Ctrl Pts',(1.0211653313612,3.54921942038456,-23.9587546368838)) ;
#154803 = CARTESIAN_POINT('Ctrl Pts',(1.02580209629924,3.54969340754027,-23.9544085428281)) ;
#154804 = CARTESIAN_POINT('Ctrl Pts',(1.02780524115376,3.54989817637043,-23.9525309717066)) ;
#154805 = CARTESIAN_POINT('Ctrl Pts',(1.02980744674854,3.55,-23.9506439182703)) ;
#154806 = CARTESIAN_POINT('Ctrl Pts',(1.03179971315146,3.55,-23.9487558734356)) ;
#154807 = CARTESIAN_POINT('Origin',(-7.29372370581158E-16,3.55,-22.86)) ;
#154808 = CARTESIAN_POINT('',(1.5,3.55,-22.86)) ;
#154809 = CARTESIAN_POINT('Origin',(-7.29372370581158E-16,3.55,-26.67)) ;
#154810 = CARTESIAN_POINT('',(-0.170807315466631,3.55,-25.1797567779107)) ;
#154811 = CARTESIAN_POINT('',(1.5,3.55,-26.67)) ;
#154812 = CARTESIAN_POINT('Origin',(-7.29372370581158E-16,3.55,-26.67)) ;
#154813 = CARTESIAN_POINT('',(-0.273932138433073,3.45,-25.1952250396981)) ;
#154814 = CARTESIAN_POINT('Ctrl Pts',(-0.170807315466618,3.55,-25.1797567779107)) ;
#154815 = CARTESIAN_POINT('Ctrl Pts',(-0.183882433427076,3.55,-25.1812554096543)) ;
#154816 = CARTESIAN_POINT('Ctrl Pts',(-0.197859036176999,3.54752250383109,
-25.1830511760977)) ;
#154817 = CARTESIAN_POINT('Ctrl Pts',(-0.223597793566242,3.53719045839678,
-25.1867006467314)) ;
#154818 = CARTESIAN_POINT('Ctrl Pts',(-0.235362682979164,3.52934133421403,
-25.1885504186891)) ;
#154819 = CARTESIAN_POINT('Ctrl Pts',(-0.253465441530101,3.51138121637726,
-25.1915429480238)) ;
#154820 = CARTESIAN_POINT('Ctrl Pts',(-0.261168570620291,3.50026979217228,
-25.1929034821853)) ;
#154821 = CARTESIAN_POINT('Ctrl Pts',(-0.271399896344082,3.47583586070552,
-25.1947463645995)) ;
#154822 = CARTESIAN_POINT('Ctrl Pts',(-0.27393213843306,3.46251477070021,
-25.1952250396981)) ;
#154823 = CARTESIAN_POINT('Ctrl Pts',(-0.27393213843306,3.45,-25.1952250396981)) ;
#154824 = CARTESIAN_POINT('',(-0.273932138433073,3.15,-25.1952250396981)) ;
#154825 = CARTESIAN_POINT('',(-0.273932138433073,3.05,-25.1952250396981)) ;
#154826 = CARTESIAN_POINT('',(-0.373948193368567,3.05,-25.2173600760421)) ;
#154827 = CARTESIAN_POINT('Ctrl Pts',(-0.27393213843307,3.15,-25.1952250396981)) ;
#154828 = CARTESIAN_POINT('Ctrl Pts',(-0.27393213843307,3.13744372549049,
-25.1952250396981)) ;
#154829 = CARTESIAN_POINT('Ctrl Pts',(-0.276486468486162,3.12408297110069,
-25.1956911302356)) ;
#154830 = CARTESIAN_POINT('Ctrl Pts',(-0.286740277640426,3.0995678553947,
-25.1976537789936)) ;
#154831 = CARTESIAN_POINT('Ctrl Pts',(-0.294439768310513,3.08841385970397,
-25.1991548411377)) ;
#154832 = CARTESIAN_POINT('Ctrl Pts',(-0.312194128344967,3.07061084469361,
-25.202819399951)) ;
#154833 = CARTESIAN_POINT('Ctrl Pts',(-0.323517908844212,3.0628422827531,
-25.2052474862748)) ;
#154834 = CARTESIAN_POINT('Ctrl Pts',(-0.3481721171233,3.05253676672645,-25.2109138387535)) ;
#154835 = CARTESIAN_POINT('Ctrl Pts',(-0.361501722536393,3.05,-25.2141560230592)) ;
#154836 = CARTESIAN_POINT('Ctrl Pts',(-0.373948193368565,3.05,-25.2173600760421)) ;
#154837 = CARTESIAN_POINT('',(-0.872417476238727,3.05,-25.4498001199995)) ;
#154838 = CARTESIAN_POINT('Origin',(-7.95081593156037E-16,3.05,-26.67)) ;
#154839 = CARTESIAN_POINT('',(-0.953662978710562,3.15,-25.5121887360036)) ;
#154840 = CARTESIAN_POINT('Ctrl Pts',(-0.872417476238731,3.05,-25.4498001199995)) ;
#154841 = CARTESIAN_POINT('Ctrl Pts',(-0.882808783297381,3.05,-25.457229687915)) ;
#154842 = CARTESIAN_POINT('Ctrl Pts',(-0.893798224191978,3.05250629897269,
-25.4653093623146)) ;
#154843 = CARTESIAN_POINT('Ctrl Pts',(-0.913892243159222,3.06269675232156,
-25.4804777691246)) ;
#154844 = CARTESIAN_POINT('Ctrl Pts',(-0.922999225059836,3.07038074042647,
-25.4875634285691)) ;
#154845 = CARTESIAN_POINT('Ctrl Pts',(-0.937285134131708,3.08810056349785,
-25.4988558711034)) ;
#154846 = CARTESIAN_POINT('Ctrl Pts',(-0.943452174397238,3.09929464195085,
-25.503843096804)) ;
#154847 = CARTESIAN_POINT('Ctrl Pts',(-0.951639309815365,3.12392729225934,
-25.5105109997964)) ;
#154848 = CARTESIAN_POINT('Ctrl Pts',(-0.953662978710564,3.13736547222678,
-25.5121887360036)) ;
#154849 = CARTESIAN_POINT('Ctrl Pts',(-0.953662978710564,3.15,-25.5121887360036)) ;
#154850 = CARTESIAN_POINT('',(-0.953662978710562,3.45,-25.5121887360036)) ;
#154851 = CARTESIAN_POINT('',(-0.953662978710562,3.05,-25.5121887360036)) ;
#154852 = CARTESIAN_POINT('',(-1.03179971315145,3.55,-25.5812441265644)) ;
#154853 = CARTESIAN_POINT('Ctrl Pts',(-0.953662978710574,3.45,-25.5121887360036)) ;
#154854 = CARTESIAN_POINT('Ctrl Pts',(-0.953662978710574,3.45580715149871,
-25.5121887360036)) ;
#154855 = CARTESIAN_POINT('Ctrl Pts',(-0.954069792639918,3.4616588096918,
-25.5125236315693)) ;
#154856 = CARTESIAN_POINT('Ctrl Pts',(-0.954880405808386,3.46741264967887,
-25.5131927320754)) ;
#154857 = CARTESIAN_POINT('Ctrl Pts',(-0.955592557016204,3.47246759358525,
-25.5137805596017)) ;
#154858 = CARTESIAN_POINT('Ctrl Pts',(-0.956615573654937,3.47744631522377,
-25.5146258114488)) ;
#154859 = CARTESIAN_POINT('Ctrl Pts',(-0.957920385817356,3.48225893605768,
-25.5157086440434)) ;
#154860 = CARTESIAN_POINT('Ctrl Pts',(-0.959423079246205,3.48780141482278,
-25.5169556935967)) ;
#154861 = CARTESIAN_POINT('Ctrl Pts',(-0.96132320146813,3.49320783601912,
-25.5185374593817)) ;
#154862 = CARTESIAN_POINT('Ctrl Pts',(-0.963574238618798,3.49834560049866,
-25.5204242578964)) ;
#154863 = CARTESIAN_POINT('Ctrl Pts',(-0.96549970664799,3.50274028640775,
-25.5220381673855)) ;
#154864 = CARTESIAN_POINT('Ctrl Pts',(-0.967680912999533,3.50693820669559,
-25.5238745944585)) ;
#154865 = CARTESIAN_POINT('Ctrl Pts',(-0.970068248378241,3.51087311165943,
-25.5258987835472)) ;
#154866 = CARTESIAN_POINT('Ctrl Pts',(-0.972933246979067,3.51559532091262,
-25.5283279767636)) ;
#154867 = CARTESIAN_POINT('Ctrl Pts',(-0.976138831290359,3.52000896466724,
-25.5310646855624)) ;
#154868 = CARTESIAN_POINT('Ctrl Pts',(-0.97960177680248,3.52400782220665,
-25.5340509843476)) ;
#154869 = CARTESIAN_POINT('Ctrl Pts',(-0.982467725203495,3.52731729367562,
-25.5365224578947)) ;
#154870 = CARTESIAN_POINT('Ctrl Pts',(-0.985508986896829,3.5303430569618,
-25.5391641736047)) ;
#154871 = CARTESIAN_POINT('Ctrl Pts',(-0.988666612105887,3.53304718478133,
-25.5419315933388)) ;
#154872 = CARTESIAN_POINT('Ctrl Pts',(-0.992701606803673,3.53650267449007,
-25.5454679610881)) ;
#154873 = CARTESIAN_POINT('Ctrl Pts',(-0.996988044734313,3.53948417067185,
-25.5492635881177)) ;
#154874 = CARTESIAN_POINT('Ctrl Pts',(-1.00141585135917,3.54192188246042,
-25.5532340352035)) ;
#154875 = CARTESIAN_POINT('Ctrl Pts',(-1.00487400994928,3.54382575827887,
-25.5563349916949)) ;
#154876 = CARTESIAN_POINT('Ctrl Pts',(-1.00841776012226,3.54539884758398,
-25.5595419608726)) ;
#154877 = CARTESIAN_POINT('Ctrl Pts',(-1.01199129263161,3.54662946216441,
-25.5628082263467)) ;
#154878 = CARTESIAN_POINT('Ctrl Pts',(-1.016523626954,3.54819025857132,-25.5669508519072)) ;
#154879 = CARTESIAN_POINT('Ctrl Pts',(-1.0211653313612,3.54921942038456,-25.5712453631162)) ;
#154880 = CARTESIAN_POINT('Ctrl Pts',(-1.02580209629924,3.54969340754027,
-25.5755914571719)) ;
#154881 = CARTESIAN_POINT('Ctrl Pts',(-1.02780524115376,3.54989817637043,
-25.5774690282934)) ;
#154882 = CARTESIAN_POINT('Ctrl Pts',(-1.02980744674854,3.55,-25.5793560817297)) ;
#154883 = CARTESIAN_POINT('Ctrl Pts',(-1.03179971315146,3.55,-25.5812441265644)) ;
#154884 = CARTESIAN_POINT('',(0.170807315466633,3.55,-28.1602432220893)) ;
#154885 = CARTESIAN_POINT('Origin',(-7.29372370581158E-16,3.55,-26.67)) ;
#154886 = CARTESIAN_POINT('',(0.273932138433074,3.45,-28.1447749603019)) ;
#154887 = CARTESIAN_POINT('Ctrl Pts',(0.170807315466623,3.55,-28.1602432220893)) ;
#154888 = CARTESIAN_POINT('Ctrl Pts',(0.18388243342708,3.55,-28.1587445903457)) ;
#154889 = CARTESIAN_POINT('Ctrl Pts',(0.197859036177004,3.54752250383109,
-28.1569488239023)) ;
#154890 = CARTESIAN_POINT('Ctrl Pts',(0.223597793566247,3.53719045839678,
-28.1532993532686)) ;
#154891 = CARTESIAN_POINT('Ctrl Pts',(0.235362682979169,3.52934133421403,
-28.1514495813109)) ;
#154892 = CARTESIAN_POINT('Ctrl Pts',(0.253465441530107,3.51138121637726,
-28.1484570519762)) ;
#154893 = CARTESIAN_POINT('Ctrl Pts',(0.261168570620295,3.50026979217228,
-28.1470965178147)) ;
#154894 = CARTESIAN_POINT('Ctrl Pts',(0.271399896344086,3.47583586070552,
-28.1452536354005)) ;
#154895 = CARTESIAN_POINT('Ctrl Pts',(0.273932138433066,3.46251477070021,
-28.1447749603019)) ;
#154896 = CARTESIAN_POINT('Ctrl Pts',(0.273932138433066,3.45,-28.1447749603019)) ;
#154897 = CARTESIAN_POINT('',(0.273932138433074,3.15,-28.1447749603019)) ;
#154898 = CARTESIAN_POINT('',(0.273932138433074,3.05,-28.1447749603019)) ;
#154899 = CARTESIAN_POINT('',(0.373948193368569,3.05,-28.1226399239579)) ;
#154900 = CARTESIAN_POINT('Ctrl Pts',(0.273932138433071,3.15,-28.1447749603019)) ;
#154901 = CARTESIAN_POINT('Ctrl Pts',(0.273932138433071,3.13736547222678,
-28.1447749603019)) ;
#154902 = CARTESIAN_POINT('Ctrl Pts',(0.276518148223579,3.12392729225934,
-28.1443031680364)) ;
#154903 = CARTESIAN_POINT('Ctrl Pts',(0.286888647463777,3.09929464195085,
-28.1423175038704)) ;
#154904 = CARTESIAN_POINT('Ctrl Pts',(0.294673181069387,3.08810056349785,
-28.1407990038315)) ;
#154905 = CARTESIAN_POINT('Ctrl Pts',(0.31250649926653,3.07038074042647,-28.1371140047162)) ;
#154906 = CARTESIAN_POINT('Ctrl Pts',(0.323788284437176,3.06269675232156,
-28.134692225935)) ;
#154907 = CARTESIAN_POINT('Ctrl Pts',(0.348324144605927,3.05250629897269,
-28.1290493783214)) ;
#154908 = CARTESIAN_POINT('Ctrl Pts',(0.361577410726386,3.05,-28.1258244927855)) ;
#154909 = CARTESIAN_POINT('Ctrl Pts',(0.373948193368566,3.05,-28.1226399239579)) ;
#154910 = CARTESIAN_POINT('',(0.872417476238729,3.05,-27.8901998800005)) ;
#154911 = CARTESIAN_POINT('Origin',(-7.95081593156037E-16,3.05,-26.67)) ;
#154912 = CARTESIAN_POINT('',(0.953662978710562,3.15,-27.8278112639964)) ;
#154913 = CARTESIAN_POINT('Ctrl Pts',(0.872417476238731,3.05,-27.8901998800005)) ;
#154914 = CARTESIAN_POINT('Ctrl Pts',(0.882872360457021,3.05,-27.8827248557413)) ;
#154915 = CARTESIAN_POINT('Ctrl Pts',(0.893924122929508,3.05253676672645,
-27.8745978214856)) ;
#154916 = CARTESIAN_POINT('Ctrl Pts',(0.914112220366979,3.0628422827531,-27.8593538633994)) ;
#154917 = CARTESIAN_POINT('Ctrl Pts',(0.923251028202473,3.07061084469361,
-27.852240088077)) ;
#154918 = CARTESIAN_POINT('Ctrl Pts',(0.937470525765902,3.08841385970397,
-27.8409949922316)) ;
#154919 = CARTESIAN_POINT('Ctrl Pts',(0.943569543283853,3.0995678553947,-27.8360617043366)) ;
#154920 = CARTESIAN_POINT('Ctrl Pts',(0.951664040935146,3.12408297110069,
-27.8294683971169)) ;
#154921 = CARTESIAN_POINT('Ctrl Pts',(0.953662978710564,3.13744372549049,
-27.8278112639964)) ;
#154922 = CARTESIAN_POINT('Ctrl Pts',(0.953662978710564,3.15,-27.8278112639964)) ;
#154923 = CARTESIAN_POINT('',(0.953662978710562,3.45,-27.8278112639964)) ;
#154924 = CARTESIAN_POINT('',(0.953662978710562,3.05,-27.8278112639964)) ;
#154925 = CARTESIAN_POINT('',(1.03179971315145,3.55,-27.7587558734356)) ;
#154926 = CARTESIAN_POINT('Ctrl Pts',(0.953662978710579,3.45,-27.8278112639964)) ;
#154927 = CARTESIAN_POINT('Ctrl Pts',(0.953662978710579,3.45580715149871,
-27.8278112639964)) ;
#154928 = CARTESIAN_POINT('Ctrl Pts',(0.954069792639921,3.4616588096918,-27.8274763684308)) ;
#154929 = CARTESIAN_POINT('Ctrl Pts',(0.954880405808391,3.46741264967888,
-27.8268072679246)) ;
#154930 = CARTESIAN_POINT('Ctrl Pts',(0.95559255701621,3.47246759358526,-27.8262194403983)) ;
#154931 = CARTESIAN_POINT('Ctrl Pts',(0.956615573654943,3.47744631522378,
-27.8253741885512)) ;
#154932 = CARTESIAN_POINT('Ctrl Pts',(0.957920385817362,3.48225893605768,
-27.8242913559566)) ;
#154933 = CARTESIAN_POINT('Ctrl Pts',(0.959423079246214,3.48780141482278,
-27.8230443064033)) ;
#154934 = CARTESIAN_POINT('Ctrl Pts',(0.961323201468142,3.49320783601914,
-27.8214625406183)) ;
#154935 = CARTESIAN_POINT('Ctrl Pts',(0.963574238618811,3.49834560049868,
-27.8195757421036)) ;
#154936 = CARTESIAN_POINT('Ctrl Pts',(0.965499706647999,3.50274028640776,
-27.8179618326145)) ;
#154937 = CARTESIAN_POINT('Ctrl Pts',(0.967680912999544,3.50693820669559,
-27.8161254055416)) ;
#154938 = CARTESIAN_POINT('Ctrl Pts',(0.970068248378247,3.51087311165943,
-27.8141012164528)) ;
#154939 = CARTESIAN_POINT('Ctrl Pts',(0.972933246979075,3.51559532091262,
-27.8116720232364)) ;
#154940 = CARTESIAN_POINT('Ctrl Pts',(0.976138831290371,3.52000896466725,
-27.8089353144376)) ;
#154941 = CARTESIAN_POINT('Ctrl Pts',(0.979601776802497,3.52400782220666,
-27.8059490156524)) ;
#154942 = CARTESIAN_POINT('Ctrl Pts',(0.982467725203508,3.52731729367563,
-27.8034775421053)) ;
#154943 = CARTESIAN_POINT('Ctrl Pts',(0.985508986896839,3.5303430569618,-27.8008358263953)) ;
#154944 = CARTESIAN_POINT('Ctrl Pts',(0.98866661210589,3.53304718478133,-27.7980684066612)) ;
#154945 = CARTESIAN_POINT('Ctrl Pts',(0.99270160680368,3.53650267449008,-27.7945320389119)) ;
#154946 = CARTESIAN_POINT('Ctrl Pts',(0.996988044734364,3.53948417067189,
-27.7907364118822)) ;
#154947 = CARTESIAN_POINT('Ctrl Pts',(1.0014158513592,3.54192188246044,-27.7867659647965)) ;
#154948 = CARTESIAN_POINT('Ctrl Pts',(1.0048740099493,3.54382575827887,-27.7836650083051)) ;
#154949 = CARTESIAN_POINT('Ctrl Pts',(1.00841776012228,3.54539884758398,-27.7804580391274)) ;
#154950 = CARTESIAN_POINT('Ctrl Pts',(1.0119912926316,3.5466294621644,-27.7771917736534)) ;
#154951 = CARTESIAN_POINT('Ctrl Pts',(1.01652362695395,3.54819025857129,-27.7730491480929)) ;
#154952 = CARTESIAN_POINT('Ctrl Pts',(1.02116533136117,3.54921942038455,-27.7687546368838)) ;
#154953 = CARTESIAN_POINT('Ctrl Pts',(1.02580209629915,3.54969340754027,-27.7644085428281)) ;
#154954 = CARTESIAN_POINT('Ctrl Pts',(1.02780524115368,3.54989817637043,-27.7625309717066)) ;
#154955 = CARTESIAN_POINT('Ctrl Pts',(1.02980744674847,3.55,-27.7606439182704)) ;
#154956 = CARTESIAN_POINT('Ctrl Pts',(1.03179971315146,3.55,-27.7587558734356)) ;
#154957 = CARTESIAN_POINT('Origin',(-7.29372370581158E-16,3.55,-26.67)) ;
#154958 = CARTESIAN_POINT('',(1.5,3.55,-26.67)) ;
#154959 = CARTESIAN_POINT('Origin',(-7.29372370581158E-16,3.55,-30.48)) ;
#154960 = CARTESIAN_POINT('',(-0.170807315466631,3.55,-28.9897567779107)) ;
#154961 = CARTESIAN_POINT('',(1.5,3.55,-30.48)) ;
#154962 = CARTESIAN_POINT('Origin',(-7.29372370581158E-16,3.55,-30.48)) ;
#154963 = CARTESIAN_POINT('',(-0.273932138433073,3.45,-29.0052250396981)) ;
#154964 = CARTESIAN_POINT('Ctrl Pts',(-0.17080731546662,3.55,-28.9897567779107)) ;
#154965 = CARTESIAN_POINT('Ctrl Pts',(-0.183882433427078,3.55,-28.9912554096543)) ;
#154966 = CARTESIAN_POINT('Ctrl Pts',(-0.197859036177001,3.54752250383109,
-28.9930511760977)) ;
#154967 = CARTESIAN_POINT('Ctrl Pts',(-0.223597793566244,3.53719045839678,
-28.9967006467314)) ;
#154968 = CARTESIAN_POINT('Ctrl Pts',(-0.235362682979166,3.52934133421403,
-28.9985504186891)) ;
#154969 = CARTESIAN_POINT('Ctrl Pts',(-0.253465441530102,3.51138121637726,
-29.0015429480238)) ;
#154970 = CARTESIAN_POINT('Ctrl Pts',(-0.261168570620293,3.50026979217228,
-29.0029034821853)) ;
#154971 = CARTESIAN_POINT('Ctrl Pts',(-0.271399896344084,3.47583586070553,
-29.0047463645995)) ;
#154972 = CARTESIAN_POINT('Ctrl Pts',(-0.273932138433062,3.46251477070021,
-29.0052250396981)) ;
#154973 = CARTESIAN_POINT('Ctrl Pts',(-0.273932138433062,3.45,-29.0052250396981)) ;
#154974 = CARTESIAN_POINT('',(-0.273932138433073,3.15,-29.0052250396981)) ;
#154975 = CARTESIAN_POINT('',(-0.273932138433073,3.05,-29.0052250396981)) ;
#154976 = CARTESIAN_POINT('',(-0.373948193368567,3.05,-29.0273600760421)) ;
#154977 = CARTESIAN_POINT('Ctrl Pts',(-0.27393213843307,3.15,-29.0052250396981)) ;
#154978 = CARTESIAN_POINT('Ctrl Pts',(-0.27393213843307,3.13744372549049,
-29.0052250396981)) ;
#154979 = CARTESIAN_POINT('Ctrl Pts',(-0.276486468486161,3.12408297110069,
-29.0056911302356)) ;
#154980 = CARTESIAN_POINT('Ctrl Pts',(-0.286740277640426,3.0995678553947,
-29.0076537789936)) ;
#154981 = CARTESIAN_POINT('Ctrl Pts',(-0.294439768310513,3.08841385970397,
-29.0091548411377)) ;
#154982 = CARTESIAN_POINT('Ctrl Pts',(-0.312194128344968,3.07061084469361,
-29.012819399951)) ;
#154983 = CARTESIAN_POINT('Ctrl Pts',(-0.323517908844213,3.0628422827531,
-29.0152474862748)) ;
#154984 = CARTESIAN_POINT('Ctrl Pts',(-0.348172117123301,3.05253676672645,
-29.0209138387535)) ;
#154985 = CARTESIAN_POINT('Ctrl Pts',(-0.361501722536393,3.05,-29.0241560230592)) ;
#154986 = CARTESIAN_POINT('Ctrl Pts',(-0.373948193368565,3.05,-29.0273600760421)) ;
#154987 = CARTESIAN_POINT('',(-0.872417476238727,3.05,-29.2598001199995)) ;
#154988 = CARTESIAN_POINT('Origin',(-7.95081593156037E-16,3.05,-30.48)) ;
#154989 = CARTESIAN_POINT('',(-0.953662978710562,3.15,-29.3221887360036)) ;
#154990 = CARTESIAN_POINT('Ctrl Pts',(-0.87241747623873,3.05,-29.2598001199995)) ;
#154991 = CARTESIAN_POINT('Ctrl Pts',(-0.882808783297378,3.05,-29.267229687915)) ;
#154992 = CARTESIAN_POINT('Ctrl Pts',(-0.893798224191981,3.05250629897269,
-29.2753093623146)) ;
#154993 = CARTESIAN_POINT('Ctrl Pts',(-0.913892243159222,3.06269675232156,
-29.2904777691246)) ;
#154994 = CARTESIAN_POINT('Ctrl Pts',(-0.922999225059836,3.07038074042647,
-29.2975634285691)) ;
#154995 = CARTESIAN_POINT('Ctrl Pts',(-0.937285134131708,3.08810056349785,
-29.3088558711034)) ;
#154996 = CARTESIAN_POINT('Ctrl Pts',(-0.943452174397237,3.09929464195085,
-29.313843096804)) ;
#154997 = CARTESIAN_POINT('Ctrl Pts',(-0.951639309815364,3.12392729225934,
-29.3205109997964)) ;
#154998 = CARTESIAN_POINT('Ctrl Pts',(-0.953662978710564,3.13736547222678,
-29.3221887360036)) ;
#154999 = CARTESIAN_POINT('Ctrl Pts',(-0.953662978710564,3.15,-29.3221887360036)) ;
#155000 = CARTESIAN_POINT('',(-0.953662978710562,3.45,-29.3221887360036)) ;
#155001 = CARTESIAN_POINT('',(-0.953662978710562,3.05,-29.3221887360036)) ;
#155002 = CARTESIAN_POINT('',(-1.03179971315145,3.55,-29.3912441265644)) ;
#155003 = CARTESIAN_POINT('Ctrl Pts',(-0.953662978710576,3.45,-29.3221887360036)) ;
#155004 = CARTESIAN_POINT('Ctrl Pts',(-0.953662978710576,3.4558071514987,
-29.3221887360036)) ;
#155005 = CARTESIAN_POINT('Ctrl Pts',(-0.954069792639918,3.4616588096918,
-29.3225236315693)) ;
#155006 = CARTESIAN_POINT('Ctrl Pts',(-0.954880405808387,3.46741264967887,
-29.3231927320754)) ;
#155007 = CARTESIAN_POINT('Ctrl Pts',(-0.955592557016205,3.47246759358525,
-29.3237805596017)) ;
#155008 = CARTESIAN_POINT('Ctrl Pts',(-0.956615573654937,3.47744631522377,
-29.3246258114488)) ;
#155009 = CARTESIAN_POINT('Ctrl Pts',(-0.957920385817357,3.48225893605768,
-29.3257086440434)) ;
#155010 = CARTESIAN_POINT('Ctrl Pts',(-0.959423079246206,3.48780141482278,
-29.3269556935967)) ;
#155011 = CARTESIAN_POINT('Ctrl Pts',(-0.961323201468129,3.49320783601912,
-29.3285374593817)) ;
#155012 = CARTESIAN_POINT('Ctrl Pts',(-0.963574238618794,3.49834560049866,
-29.3304242578964)) ;
#155013 = CARTESIAN_POINT('Ctrl Pts',(-0.965499706647985,3.50274028640774,
-29.3320381673855)) ;
#155014 = CARTESIAN_POINT('Ctrl Pts',(-0.967680912999537,3.50693820669559,
-29.3338745944584)) ;
#155015 = CARTESIAN_POINT('Ctrl Pts',(-0.970068248378244,3.51087311165943,
-29.3358987835472)) ;
#155016 = CARTESIAN_POINT('Ctrl Pts',(-0.972933246979068,3.51559532091262,
-29.3383279767636)) ;
#155017 = CARTESIAN_POINT('Ctrl Pts',(-0.976138831290358,3.52000896466724,
-29.3410646855624)) ;
#155018 = CARTESIAN_POINT('Ctrl Pts',(-0.979601776802481,3.52400782220665,
-29.3440509843476)) ;
#155019 = CARTESIAN_POINT('Ctrl Pts',(-0.982467725203497,3.52731729367563,
-29.3465224578947)) ;
#155020 = CARTESIAN_POINT('Ctrl Pts',(-0.985508986896832,3.5303430569618,
-29.3491641736047)) ;
#155021 = CARTESIAN_POINT('Ctrl Pts',(-0.988666612105887,3.53304718478133,
-29.3519315933388)) ;
#155022 = CARTESIAN_POINT('Ctrl Pts',(-0.992701606803678,3.53650267449008,
-29.3554679610881)) ;
#155023 = CARTESIAN_POINT('Ctrl Pts',(-0.996988044734361,3.53948417067189,
-29.3592635881178)) ;
#155024 = CARTESIAN_POINT('Ctrl Pts',(-1.0014158513592,3.54192188246045,-29.3632340352036)) ;
#155025 = CARTESIAN_POINT('Ctrl Pts',(-1.00487400994929,3.54382575827889,
-29.366334991695)) ;
#155026 = CARTESIAN_POINT('Ctrl Pts',(-1.00841776012226,3.54539884758397,
-29.3695419608726)) ;
#155027 = CARTESIAN_POINT('Ctrl Pts',(-1.01199129263159,3.5466294621644,-29.3728082263467)) ;
#155028 = CARTESIAN_POINT('Ctrl Pts',(-1.01652362695395,3.54819025857129,
-29.3769508519071)) ;
#155029 = CARTESIAN_POINT('Ctrl Pts',(-1.02116533136117,3.54921942038455,
-29.3812453631162)) ;
#155030 = CARTESIAN_POINT('Ctrl Pts',(-1.02580209629915,3.54969340754027,
-29.3855914571719)) ;
#155031 = CARTESIAN_POINT('Ctrl Pts',(-1.02780524115368,3.54989817637043,
-29.3874690282934)) ;
#155032 = CARTESIAN_POINT('Ctrl Pts',(-1.02980744674846,3.55,-29.3893560817296)) ;
#155033 = CARTESIAN_POINT('Ctrl Pts',(-1.03179971315146,3.55,-29.3912441265644)) ;
#155034 = CARTESIAN_POINT('',(0.170807315466633,3.55,-31.9702432220893)) ;
#155035 = CARTESIAN_POINT('Origin',(-7.29372370581158E-16,3.55,-30.48)) ;
#155036 = CARTESIAN_POINT('',(0.273932138433074,3.45,-31.9547749603019)) ;
#155037 = CARTESIAN_POINT('Ctrl Pts',(0.17080731546662,3.55,-31.9702432220893)) ;
#155038 = CARTESIAN_POINT('Ctrl Pts',(0.183882433427078,3.55,-31.9687445903457)) ;
#155039 = CARTESIAN_POINT('Ctrl Pts',(0.197859036177002,3.54752250383109,
-31.9669488239023)) ;
#155040 = CARTESIAN_POINT('Ctrl Pts',(0.223597793566245,3.53719045839678,
-31.9632993532686)) ;
#155041 = CARTESIAN_POINT('Ctrl Pts',(0.235362682979166,3.52934133421403,
-31.9614495813109)) ;
#155042 = CARTESIAN_POINT('Ctrl Pts',(0.253465441530103,3.51138121637726,
-31.9584570519762)) ;
#155043 = CARTESIAN_POINT('Ctrl Pts',(0.261168570620294,3.50026979217228,
-31.9570965178147)) ;
#155044 = CARTESIAN_POINT('Ctrl Pts',(0.271399896344085,3.47583586070553,
-31.9552536354005)) ;
#155045 = CARTESIAN_POINT('Ctrl Pts',(0.273932138433063,3.46251477070021,
-31.9547749603019)) ;
#155046 = CARTESIAN_POINT('Ctrl Pts',(0.273932138433063,3.45,-31.9547749603019)) ;
#155047 = CARTESIAN_POINT('',(0.273932138433074,3.15,-31.9547749603019)) ;
#155048 = CARTESIAN_POINT('',(0.273932138433074,3.05,-31.9547749603019)) ;
#155049 = CARTESIAN_POINT('',(0.373948193368569,3.05,-31.9326399239579)) ;
#155050 = CARTESIAN_POINT('Ctrl Pts',(0.273932138433071,3.15,-31.9547749603019)) ;
#155051 = CARTESIAN_POINT('Ctrl Pts',(0.273932138433071,3.13736547222678,
-31.9547749603019)) ;
#155052 = CARTESIAN_POINT('Ctrl Pts',(0.276518148223577,3.12392729225934,
-31.9543031680363)) ;
#155053 = CARTESIAN_POINT('Ctrl Pts',(0.286888647463776,3.09929464195085,
-31.9523175038703)) ;
#155054 = CARTESIAN_POINT('Ctrl Pts',(0.294673181069387,3.08810056349785,
-31.9507990038315)) ;
#155055 = CARTESIAN_POINT('Ctrl Pts',(0.31250649926653,3.07038074042647,-31.9471140047162)) ;
#155056 = CARTESIAN_POINT('Ctrl Pts',(0.323788284437177,3.06269675232156,
-31.944692225935)) ;
#155057 = CARTESIAN_POINT('Ctrl Pts',(0.348324144605927,3.05250629897269,
-31.9390493783214)) ;
#155058 = CARTESIAN_POINT('Ctrl Pts',(0.361577410726386,3.05,-31.9358244927855)) ;
#155059 = CARTESIAN_POINT('Ctrl Pts',(0.373948193368566,3.05,-31.9326399239579)) ;
#155060 = CARTESIAN_POINT('',(0.87241747623873,3.05,-31.7001998800005)) ;
#155061 = CARTESIAN_POINT('Origin',(-7.95081593156037E-16,3.05,-30.48)) ;
#155062 = CARTESIAN_POINT('',(0.953662978710562,3.15,-31.6378112639964)) ;
#155063 = CARTESIAN_POINT('Ctrl Pts',(0.872417476238731,3.05,-31.7001998800005)) ;
#155064 = CARTESIAN_POINT('Ctrl Pts',(0.882872360457021,3.05,-31.6927248557413)) ;
#155065 = CARTESIAN_POINT('Ctrl Pts',(0.893924122929511,3.05253676672645,
-31.6845978214856)) ;
#155066 = CARTESIAN_POINT('Ctrl Pts',(0.914112220366982,3.0628422827531,-31.6693538633994)) ;
#155067 = CARTESIAN_POINT('Ctrl Pts',(0.923251028202473,3.07061084469361,
-31.662240088077)) ;
#155068 = CARTESIAN_POINT('Ctrl Pts',(0.937470525765902,3.08841385970397,
-31.6509949922316)) ;
#155069 = CARTESIAN_POINT('Ctrl Pts',(0.943569543283852,3.0995678553947,-31.6460617043366)) ;
#155070 = CARTESIAN_POINT('Ctrl Pts',(0.951664040935145,3.12408297110069,
-31.6394683971169)) ;
#155071 = CARTESIAN_POINT('Ctrl Pts',(0.953662978710564,3.13744372549049,
-31.6378112639964)) ;
#155072 = CARTESIAN_POINT('Ctrl Pts',(0.953662978710564,3.15,-31.6378112639964)) ;
#155073 = CARTESIAN_POINT('',(0.953662978710562,3.45,-31.6378112639964)) ;
#155074 = CARTESIAN_POINT('',(0.953662978710562,3.05,-31.6378112639964)) ;
#155075 = CARTESIAN_POINT('',(1.03179971315145,3.55,-31.5687558734356)) ;
#155076 = CARTESIAN_POINT('Ctrl Pts',(0.953662978710579,3.45,-31.6378112639964)) ;
#155077 = CARTESIAN_POINT('Ctrl Pts',(0.953662978710579,3.4558071514987,-31.6378112639964)) ;
#155078 = CARTESIAN_POINT('Ctrl Pts',(0.954069792639918,3.46165880969179,
-31.6374763684308)) ;
#155079 = CARTESIAN_POINT('Ctrl Pts',(0.954880405808387,3.46741264967886,
-31.6368072679246)) ;
#155080 = CARTESIAN_POINT('Ctrl Pts',(0.955592557016206,3.47246759358525,
-31.6362194403983)) ;
#155081 = CARTESIAN_POINT('Ctrl Pts',(0.956615573654938,3.47744631522377,
-31.6353741885512)) ;
#155082 = CARTESIAN_POINT('Ctrl Pts',(0.957920385817359,3.48225893605768,
-31.6342913559566)) ;
#155083 = CARTESIAN_POINT('Ctrl Pts',(0.959423079246214,3.48780141482279,
-31.6330443064033)) ;
#155084 = CARTESIAN_POINT('Ctrl Pts',(0.96132320146816,3.49320783601916,-31.6314625406184)) ;
#155085 = CARTESIAN_POINT('Ctrl Pts',(0.963574238618836,3.49834560049872,
-31.6295757421036)) ;
#155086 = CARTESIAN_POINT('Ctrl Pts',(0.965499706648023,3.50274028640779,
-31.6279618326145)) ;
#155087 = CARTESIAN_POINT('Ctrl Pts',(0.967680912999547,3.5069382066956,-31.6261254055416)) ;
#155088 = CARTESIAN_POINT('Ctrl Pts',(0.970068248378247,3.51087311165943,
-31.6241012164528)) ;
#155089 = CARTESIAN_POINT('Ctrl Pts',(0.972933246979074,3.51559532091262,
-31.6216720232364)) ;
#155090 = CARTESIAN_POINT('Ctrl Pts',(0.976138831290361,3.52000896466724,
-31.6189353144376)) ;
#155091 = CARTESIAN_POINT('Ctrl Pts',(0.979601776802483,3.52400782220665,
-31.6159490156524)) ;
#155092 = CARTESIAN_POINT('Ctrl Pts',(0.982467725203497,3.52731729367562,
-31.6134775421053)) ;
#155093 = CARTESIAN_POINT('Ctrl Pts',(0.985508986896839,3.5303430569618,-31.6108358263953)) ;
#155094 = CARTESIAN_POINT('Ctrl Pts',(0.988666612105884,3.53304718478132,
-31.6080684066612)) ;
#155095 = CARTESIAN_POINT('Ctrl Pts',(0.992701606803627,3.53650267449002,
-31.604532038912)) ;
#155096 = CARTESIAN_POINT('Ctrl Pts',(0.996988044734275,3.53948417067183,
-31.6007364118823)) ;
#155097 = CARTESIAN_POINT('Ctrl Pts',(1.0014158513591,3.54192188246038,-31.5967659647965)) ;
#155098 = CARTESIAN_POINT('Ctrl Pts',(1.00487400994924,3.54382575827886,-31.5936650083051)) ;
#155099 = CARTESIAN_POINT('Ctrl Pts',(1.00841776012224,3.54539884758397,-31.5904580391274)) ;
#155100 = CARTESIAN_POINT('Ctrl Pts',(1.01199129263162,3.54662946216441,-31.5871917736533)) ;
#155101 = CARTESIAN_POINT('Ctrl Pts',(1.01652362695402,3.54819025857132,-31.5830491480928)) ;
#155102 = CARTESIAN_POINT('Ctrl Pts',(1.02116533136121,3.54921942038456,-31.5787546368838)) ;
#155103 = CARTESIAN_POINT('Ctrl Pts',(1.02580209629926,3.54969340754028,-31.5744085428281)) ;
#155104 = CARTESIAN_POINT('Ctrl Pts',(1.02780524115377,3.54989817637043,-31.5725309717066)) ;
#155105 = CARTESIAN_POINT('Ctrl Pts',(1.02980744674854,3.55,-31.5706439182703)) ;
#155106 = CARTESIAN_POINT('Ctrl Pts',(1.03179971315146,3.55,-31.5687558734356)) ;
#155107 = CARTESIAN_POINT('Origin',(-7.29372370581158E-16,3.55,-30.48)) ;
#155108 = CARTESIAN_POINT('',(1.5,3.55,-30.48)) ;
#155109 = CARTESIAN_POINT('Origin',(-7.29372370581158E-16,3.55,-34.29)) ;
#155110 = CARTESIAN_POINT('',(-0.170807315466631,3.55,-32.7997567779107)) ;
#155111 = CARTESIAN_POINT('',(1.5,3.55,-34.29)) ;
#155112 = CARTESIAN_POINT('Origin',(-7.29372370581158E-16,3.55,-34.29)) ;
#155113 = CARTESIAN_POINT('',(-0.273932138433073,3.45,-32.8152250396981)) ;
#155114 = CARTESIAN_POINT('Ctrl Pts',(-0.17080731546662,3.55,-32.7997567779107)) ;
#155115 = CARTESIAN_POINT('Ctrl Pts',(-0.183882433427078,3.55,-32.8012554096543)) ;
#155116 = CARTESIAN_POINT('Ctrl Pts',(-0.197859036177001,3.54752250383109,
-32.8030511760977)) ;
#155117 = CARTESIAN_POINT('Ctrl Pts',(-0.223597793566244,3.53719045839678,
-32.8067006467314)) ;
#155118 = CARTESIAN_POINT('Ctrl Pts',(-0.235362682979166,3.52934133421403,
-32.8085504186891)) ;
#155119 = CARTESIAN_POINT('Ctrl Pts',(-0.253465441530102,3.51138121637726,
-32.8115429480238)) ;
#155120 = CARTESIAN_POINT('Ctrl Pts',(-0.261168570620293,3.50026979217228,
-32.8129034821853)) ;
#155121 = CARTESIAN_POINT('Ctrl Pts',(-0.271399896344084,3.47583586070553,
-32.8147463645995)) ;
#155122 = CARTESIAN_POINT('Ctrl Pts',(-0.273932138433062,3.46251477070021,
-32.8152250396981)) ;
#155123 = CARTESIAN_POINT('Ctrl Pts',(-0.273932138433062,3.45,-32.8152250396981)) ;
#155124 = CARTESIAN_POINT('',(-0.273932138433073,3.15,-32.8152250396981)) ;
#155125 = CARTESIAN_POINT('',(-0.273932138433073,3.05,-32.8152250396981)) ;
#155126 = CARTESIAN_POINT('',(-0.373948193368568,3.05,-32.8373600760421)) ;
#155127 = CARTESIAN_POINT('Ctrl Pts',(-0.27393213843307,3.15,-32.8152250396981)) ;
#155128 = CARTESIAN_POINT('Ctrl Pts',(-0.27393213843307,3.13744372549049,
-32.8152250396981)) ;
#155129 = CARTESIAN_POINT('Ctrl Pts',(-0.276486468486161,3.12408297110069,
-32.8156911302356)) ;
#155130 = CARTESIAN_POINT('Ctrl Pts',(-0.286740277640426,3.0995678553947,
-32.8176537789936)) ;
#155131 = CARTESIAN_POINT('Ctrl Pts',(-0.294439768310513,3.08841385970397,
-32.8191548411377)) ;
#155132 = CARTESIAN_POINT('Ctrl Pts',(-0.312194128344968,3.07061084469361,
-32.822819399951)) ;
#155133 = CARTESIAN_POINT('Ctrl Pts',(-0.323517908844213,3.0628422827531,
-32.8252474862748)) ;
#155134 = CARTESIAN_POINT('Ctrl Pts',(-0.348172117123301,3.05253676672645,
-32.8309138387535)) ;
#155135 = CARTESIAN_POINT('Ctrl Pts',(-0.361501722536393,3.05,-32.8341560230592)) ;
#155136 = CARTESIAN_POINT('Ctrl Pts',(-0.373948193368565,3.05,-32.8373600760421)) ;
#155137 = CARTESIAN_POINT('',(-0.872417476238727,3.05,-33.0698001199995)) ;
#155138 = CARTESIAN_POINT('Origin',(-7.95081593156037E-16,3.05,-34.29)) ;
#155139 = CARTESIAN_POINT('',(-0.953662978710562,3.15,-33.1321887360036)) ;
#155140 = CARTESIAN_POINT('Ctrl Pts',(-0.872417476238729,3.05,-33.0698001199995)) ;
#155141 = CARTESIAN_POINT('Ctrl Pts',(-0.882808783297379,3.05,-33.077229687915)) ;
#155142 = CARTESIAN_POINT('Ctrl Pts',(-0.893798224191978,3.05250629897269,
-33.0853093623146)) ;
#155143 = CARTESIAN_POINT('Ctrl Pts',(-0.913892243159221,3.06269675232156,
-33.1004777691246)) ;
#155144 = CARTESIAN_POINT('Ctrl Pts',(-0.922999225059835,3.07038074042647,
-33.1075634285691)) ;
#155145 = CARTESIAN_POINT('Ctrl Pts',(-0.937285134131707,3.08810056349785,
-33.1188558711034)) ;
#155146 = CARTESIAN_POINT('Ctrl Pts',(-0.943452174397235,3.09929464195085,
-33.123843096804)) ;
#155147 = CARTESIAN_POINT('Ctrl Pts',(-0.951639309815362,3.12392729225934,
-33.1305109997964)) ;
#155148 = CARTESIAN_POINT('Ctrl Pts',(-0.953662978710562,3.13736547222678,
-33.1321887360036)) ;
#155149 = CARTESIAN_POINT('Ctrl Pts',(-0.953662978710562,3.15,-33.1321887360036)) ;
#155150 = CARTESIAN_POINT('',(-0.953662978710562,3.45,-33.1321887360036)) ;
#155151 = CARTESIAN_POINT('',(-0.953662978710562,3.05,-33.1321887360036)) ;
#155152 = CARTESIAN_POINT('',(-1.03179971315145,3.55,-33.2012441265644)) ;
#155153 = CARTESIAN_POINT('Ctrl Pts',(-0.953662978710574,3.45,-33.1321887360036)) ;
#155154 = CARTESIAN_POINT('Ctrl Pts',(-0.953662978710574,3.45580715149871,
-33.1321887360036)) ;
#155155 = CARTESIAN_POINT('Ctrl Pts',(-0.954069792639916,3.46165880969181,
-33.1325236315692)) ;
#155156 = CARTESIAN_POINT('Ctrl Pts',(-0.954880405808388,3.46741264967889,
-33.1331927320754)) ;
#155157 = CARTESIAN_POINT('Ctrl Pts',(-0.955592557016207,3.47246759358527,
-33.1337805596017)) ;
#155158 = CARTESIAN_POINT('Ctrl Pts',(-0.956615573654936,3.47744631522378,
-33.1346258114488)) ;
#155159 = CARTESIAN_POINT('Ctrl Pts',(-0.957920385817355,3.48225893605768,
-33.1357086440434)) ;
#155160 = CARTESIAN_POINT('Ctrl Pts',(-0.959423079246211,3.4878014148228,
-33.1369556935967)) ;
#155161 = CARTESIAN_POINT('Ctrl Pts',(-0.96132320146816,3.49320783601917,
-33.1385374593816)) ;
#155162 = CARTESIAN_POINT('Ctrl Pts',(-0.96357423861884,3.49834560049873,
-33.1404242578964)) ;
#155163 = CARTESIAN_POINT('Ctrl Pts',(-0.965499706648026,3.5027402864078,
-33.1420381673855)) ;
#155164 = CARTESIAN_POINT('Ctrl Pts',(-0.967680912999544,3.5069382066956,
-33.1438745944585)) ;
#155165 = CARTESIAN_POINT('Ctrl Pts',(-0.970068248378232,3.51087311165944,
-33.1458987835473)) ;
#155166 = CARTESIAN_POINT('Ctrl Pts',(-0.972933246979047,3.51559532091265,
-33.1483279767637)) ;
#155167 = CARTESIAN_POINT('Ctrl Pts',(-0.976138831290362,3.52000896466724,
-33.1510646855624)) ;
#155168 = CARTESIAN_POINT('Ctrl Pts',(-0.979601776802488,3.52400782220666,
-33.1540509843476)) ;
#155169 = CARTESIAN_POINT('Ctrl Pts',(-0.982467725203504,3.52731729367563,
-33.1565224578947)) ;
#155170 = CARTESIAN_POINT('Ctrl Pts',(-0.985508986896833,3.5303430569618,
-33.1591641736047)) ;
#155171 = CARTESIAN_POINT('Ctrl Pts',(-0.988666612105891,3.53304718478134,
-33.1619315933388)) ;
#155172 = CARTESIAN_POINT('Ctrl Pts',(-0.992701606803667,3.53650267449007,
-33.1654679610881)) ;
#155173 = CARTESIAN_POINT('Ctrl Pts',(-0.996988044734294,3.53948417067184,
-33.1692635881177)) ;
#155174 = CARTESIAN_POINT('Ctrl Pts',(-1.00141585135913,3.5419218824604,-33.1732340352035)) ;
#155175 = CARTESIAN_POINT('Ctrl Pts',(-1.00487400994926,3.54382575827887,
-33.1763349916949)) ;
#155176 = CARTESIAN_POINT('Ctrl Pts',(-1.00841776012225,3.54539884758397,
-33.1795419608726)) ;
#155177 = CARTESIAN_POINT('Ctrl Pts',(-1.0119912926316,3.54662946216441,-33.1828082263467)) ;
#155178 = CARTESIAN_POINT('Ctrl Pts',(-1.01652362695394,3.54819025857129,
-33.1869508519071)) ;
#155179 = CARTESIAN_POINT('Ctrl Pts',(-1.0211653313611,3.54921942038454,-33.1912453631161)) ;
#155180 = CARTESIAN_POINT('Ctrl Pts',(-1.02580209629909,3.54969340754026,
-33.1955914571718)) ;
#155181 = CARTESIAN_POINT('Ctrl Pts',(-1.02780524115366,3.54989817637043,
-33.1974690282933)) ;
#155182 = CARTESIAN_POINT('Ctrl Pts',(-1.02980744674846,3.55,-33.1993560817296)) ;
#155183 = CARTESIAN_POINT('Ctrl Pts',(-1.03179971315146,3.55,-33.2012441265644)) ;
#155184 = CARTESIAN_POINT('',(0.170807315466633,3.55,-35.7802432220893)) ;
#155185 = CARTESIAN_POINT('Origin',(-7.29372370581158E-16,3.55,-34.29)) ;
#155186 = CARTESIAN_POINT('',(0.273932138433074,3.45,-35.7647749603019)) ;
#155187 = CARTESIAN_POINT('Ctrl Pts',(0.170807315466624,3.55,-35.7802432220893)) ;
#155188 = CARTESIAN_POINT('Ctrl Pts',(0.183882433427082,3.55,-35.7787445903457)) ;
#155189 = CARTESIAN_POINT('Ctrl Pts',(0.197859036177005,3.54752250383108,
-35.7769488239023)) ;
#155190 = CARTESIAN_POINT('Ctrl Pts',(0.223597793566249,3.53719045839678,
-35.7732993532686)) ;
#155191 = CARTESIAN_POINT('Ctrl Pts',(0.235362682979172,3.52934133421403,
-35.7714495813109)) ;
#155192 = CARTESIAN_POINT('Ctrl Pts',(0.253465441530109,3.51138121637726,
-35.7684570519762)) ;
#155193 = CARTESIAN_POINT('Ctrl Pts',(0.261168570620297,3.50026979217228,
-35.7670965178147)) ;
#155194 = CARTESIAN_POINT('Ctrl Pts',(0.271399896344088,3.47583586070552,
-35.7652536354005)) ;
#155195 = CARTESIAN_POINT('Ctrl Pts',(0.273932138433068,3.46251477070021,
-35.7647749603019)) ;
#155196 = CARTESIAN_POINT('Ctrl Pts',(0.273932138433068,3.45,-35.7647749603019)) ;
#155197 = CARTESIAN_POINT('',(0.273932138433074,3.15,-35.7647749603019)) ;
#155198 = CARTESIAN_POINT('',(0.273932138433074,3.05,-35.7647749603019)) ;
#155199 = CARTESIAN_POINT('',(0.373948193368569,3.05,-35.7426399239579)) ;
#155200 = CARTESIAN_POINT('Ctrl Pts',(0.273932138433073,3.15,-35.7647749603019)) ;
#155201 = CARTESIAN_POINT('Ctrl Pts',(0.273932138433073,3.13736547222678,
-35.7647749603019)) ;
#155202 = CARTESIAN_POINT('Ctrl Pts',(0.276518148223579,3.12392729225934,
-35.7643031680363)) ;
#155203 = CARTESIAN_POINT('Ctrl Pts',(0.286888647463778,3.09929464195085,
-35.7623175038703)) ;
#155204 = CARTESIAN_POINT('Ctrl Pts',(0.294673181069389,3.08810056349785,
-35.7607990038315)) ;
#155205 = CARTESIAN_POINT('Ctrl Pts',(0.312506499266532,3.07038074042647,
-35.7571140047162)) ;
#155206 = CARTESIAN_POINT('Ctrl Pts',(0.323788284437179,3.06269675232156,
-35.754692225935)) ;
#155207 = CARTESIAN_POINT('Ctrl Pts',(0.348324144605929,3.05250629897269,
-35.7490493783214)) ;
#155208 = CARTESIAN_POINT('Ctrl Pts',(0.361577410726388,3.05,-35.7458244927855)) ;
#155209 = CARTESIAN_POINT('Ctrl Pts',(0.373948193368567,3.05,-35.7426399239579)) ;
#155210 = CARTESIAN_POINT('',(0.872417476238728,3.05,-35.5101998800005)) ;
#155211 = CARTESIAN_POINT('Origin',(-7.95081593156037E-16,3.05,-34.29)) ;
#155212 = CARTESIAN_POINT('',(0.953662978710562,3.15,-35.4478112639964)) ;
#155213 = CARTESIAN_POINT('Ctrl Pts',(0.872417476238731,3.05,-35.5101998800005)) ;
#155214 = CARTESIAN_POINT('Ctrl Pts',(0.882872360457019,3.05,-35.5027248557413)) ;
#155215 = CARTESIAN_POINT('Ctrl Pts',(0.893924122929511,3.05253676672645,
-35.4945978214856)) ;
#155216 = CARTESIAN_POINT('Ctrl Pts',(0.914112220366982,3.0628422827531,-35.4793538633994)) ;
#155217 = CARTESIAN_POINT('Ctrl Pts',(0.923251028202473,3.07061084469361,
-35.472240088077)) ;
#155218 = CARTESIAN_POINT('Ctrl Pts',(0.937470525765902,3.08841385970397,
-35.4609949922316)) ;
#155219 = CARTESIAN_POINT('Ctrl Pts',(0.943569543283852,3.0995678553947,-35.4560617043366)) ;
#155220 = CARTESIAN_POINT('Ctrl Pts',(0.951664040935145,3.12408297110069,
-35.4494683971169)) ;
#155221 = CARTESIAN_POINT('Ctrl Pts',(0.953662978710564,3.13744372549049,
-35.4478112639964)) ;
#155222 = CARTESIAN_POINT('Ctrl Pts',(0.953662978710564,3.15,-35.4478112639964)) ;
#155223 = CARTESIAN_POINT('',(0.953662978710562,3.45,-35.4478112639964)) ;
#155224 = CARTESIAN_POINT('',(0.953662978710562,3.05,-35.4478112639964)) ;
#155225 = CARTESIAN_POINT('',(1.03179971315145,3.55,-35.3787558734356)) ;
#155226 = CARTESIAN_POINT('Ctrl Pts',(0.953662978710577,3.45,-35.4478112639964)) ;
#155227 = CARTESIAN_POINT('Ctrl Pts',(0.953662978710577,3.4558071514987,-35.4478112639964)) ;
#155228 = CARTESIAN_POINT('Ctrl Pts',(0.95406979263992,3.4616588096918,-35.4474763684308)) ;
#155229 = CARTESIAN_POINT('Ctrl Pts',(0.954880405808407,3.46741264967886,
-35.4468072679247)) ;
#155230 = CARTESIAN_POINT('Ctrl Pts',(0.955592557016242,3.47246759358524,
-35.4462194403984)) ;
#155231 = CARTESIAN_POINT('Ctrl Pts',(0.956615573654938,3.47744631522377,
-35.4453741885512)) ;
#155232 = CARTESIAN_POINT('Ctrl Pts',(0.957920385817358,3.48225893605768,
-35.4442913559566)) ;
#155233 = CARTESIAN_POINT('Ctrl Pts',(0.95942307924621,3.48780141482279,-35.4430443064033)) ;
#155234 = CARTESIAN_POINT('Ctrl Pts',(0.961323201468138,3.49320783601914,
-35.4414625406184)) ;
#155235 = CARTESIAN_POINT('Ctrl Pts',(0.96357423861882,3.49834560049869,-35.4395757421036)) ;
#155236 = CARTESIAN_POINT('Ctrl Pts',(0.965499706648018,3.50274028640778,
-35.4379618326146)) ;
#155237 = CARTESIAN_POINT('Ctrl Pts',(0.96768091299954,3.50693820669559,-35.4361254055416)) ;
#155238 = CARTESIAN_POINT('Ctrl Pts',(0.970068248378245,3.51087311165943,
-35.4341012164528)) ;
#155239 = CARTESIAN_POINT('Ctrl Pts',(0.972933246979074,3.51559532091262,
-35.4316720232364)) ;
#155240 = CARTESIAN_POINT('Ctrl Pts',(0.976138831290363,3.52000896466724,
-35.4289353144376)) ;
#155241 = CARTESIAN_POINT('Ctrl Pts',(0.979601776802487,3.52400782220666,
-35.4259490156524)) ;
#155242 = CARTESIAN_POINT('Ctrl Pts',(0.982467725203501,3.52731729367563,
-35.4234775421053)) ;
#155243 = CARTESIAN_POINT('Ctrl Pts',(0.985508986896839,3.5303430569618,-35.4208358263953)) ;
#155244 = CARTESIAN_POINT('Ctrl Pts',(0.988666612105879,3.53304718478133,
-35.4180684066612)) ;
#155245 = CARTESIAN_POINT('Ctrl Pts',(0.992701606803641,3.53650267449006,
-35.414532038912)) ;
#155246 = CARTESIAN_POINT('Ctrl Pts',(0.996988044734314,3.53948417067185,
-35.4107364118823)) ;
#155247 = CARTESIAN_POINT('Ctrl Pts',(1.00141585135917,3.54192188246041,-35.4067659647965)) ;
#155248 = CARTESIAN_POINT('Ctrl Pts',(1.00487400994928,3.54382575827887,-35.4036650083051)) ;
#155249 = CARTESIAN_POINT('Ctrl Pts',(1.00841776012226,3.54539884758398,-35.4004580391274)) ;
#155250 = CARTESIAN_POINT('Ctrl Pts',(1.01199129263161,3.54662946216441,-35.3971917736533)) ;
#155251 = CARTESIAN_POINT('Ctrl Pts',(1.01652362695402,3.54819025857132,-35.3930491480928)) ;
#155252 = CARTESIAN_POINT('Ctrl Pts',(1.02116533136126,3.54921942038457,-35.3887546368837)) ;
#155253 = CARTESIAN_POINT('Ctrl Pts',(1.02580209629929,3.54969340754028,-35.384408542828)) ;
#155254 = CARTESIAN_POINT('Ctrl Pts',(1.02780524115378,3.54989817637043,-35.3825309717066)) ;
#155255 = CARTESIAN_POINT('Ctrl Pts',(1.02980744674854,3.55,-35.3806439182703)) ;
#155256 = CARTESIAN_POINT('Ctrl Pts',(1.03179971315146,3.55,-35.3787558734356)) ;
#155257 = CARTESIAN_POINT('Origin',(-7.29372370581158E-16,3.55,-34.29)) ;
#155258 = CARTESIAN_POINT('',(1.5,3.55,-34.29)) ;
#155259 = CARTESIAN_POINT('Origin',(9.2,0.,-34.29)) ;
#155260 = CARTESIAN_POINT('',(8.7,-6.12323399573675E-17,-33.79)) ;
#155261 = CARTESIAN_POINT('Origin',(8.7,0.,-34.29)) ;
#155262 = CARTESIAN_POINT('',(9.2,-1.22464679914735E-16,-33.29)) ;
#155263 = CARTESIAN_POINT('Origin',(9.2,0.,-30.48)) ;
#155264 = CARTESIAN_POINT('',(8.7,-6.12323399573674E-17,-29.98)) ;
#155265 = CARTESIAN_POINT('Origin',(8.7,0.,-30.48)) ;
#155266 = CARTESIAN_POINT('',(9.2,-1.22464679914735E-16,-29.48)) ;
#155267 = CARTESIAN_POINT('Origin',(9.2,0.,-26.67)) ;
#155268 = CARTESIAN_POINT('',(8.7,-6.12323399573674E-17,-26.17)) ;
#155269 = CARTESIAN_POINT('Origin',(8.7,0.,-26.67)) ;
#155270 = CARTESIAN_POINT('',(9.2,-1.22464679914735E-16,-25.67)) ;
#155271 = CARTESIAN_POINT('Origin',(9.2,0.,-22.86)) ;
#155272 = CARTESIAN_POINT('',(8.7,-6.12323399573674E-17,-22.36)) ;
#155273 = CARTESIAN_POINT('Origin',(8.7,0.,-22.86)) ;
#155274 = CARTESIAN_POINT('',(9.2,-1.22464679914735E-16,-21.86)) ;
#155275 = CARTESIAN_POINT('Origin',(9.2,0.,-19.05)) ;
#155276 = CARTESIAN_POINT('',(8.7,-6.12323399573673E-17,-18.55)) ;
#155277 = CARTESIAN_POINT('Origin',(8.7,0.,-19.05)) ;
#155278 = CARTESIAN_POINT('',(9.2,-1.22464679914735E-16,-18.05)) ;
#155279 = CARTESIAN_POINT('Origin',(9.2,0.,-15.24)) ;
#155280 = CARTESIAN_POINT('',(8.7,-6.12323399573673E-17,-14.74)) ;
#155281 = CARTESIAN_POINT('Origin',(8.7,0.,-15.24)) ;
#155282 = CARTESIAN_POINT('',(9.2,-1.22464679914735E-16,-14.24)) ;
#155283 = CARTESIAN_POINT('Origin',(9.2,0.,-11.43)) ;
#155284 = CARTESIAN_POINT('',(8.7,-6.12323399573673E-17,-10.93)) ;
#155285 = CARTESIAN_POINT('Origin',(8.7,0.,-11.43)) ;
#155286 = CARTESIAN_POINT('',(9.2,-1.22464679914735E-16,-10.43)) ;
#155287 = CARTESIAN_POINT('Origin',(9.2,0.,-7.62)) ;
#155288 = CARTESIAN_POINT('',(8.7,-6.12323399573673E-17,-7.12)) ;
#155289 = CARTESIAN_POINT('Origin',(8.7,0.,-7.62)) ;
#155290 = CARTESIAN_POINT('',(9.2,-1.22464679914735E-16,-6.62)) ;
#155291 = CARTESIAN_POINT('Origin',(9.2,0.,-3.81)) ;
#155292 = CARTESIAN_POINT('',(8.7,-6.12323399573674E-17,-3.31)) ;
#155293 = CARTESIAN_POINT('Origin',(8.7,0.,-3.81)) ;
#155294 = CARTESIAN_POINT('',(9.2,-1.22464679914735E-16,-2.81)) ;
#155295 = CARTESIAN_POINT('Origin',(9.2,0.,-3.81)) ;
#155296 = CARTESIAN_POINT('',(9.2,-1.22464679914735E-16,-2.81)) ;
#155297 = CARTESIAN_POINT('Origin',(9.2,0.,-7.62)) ;
#155298 = CARTESIAN_POINT('',(9.2,-1.22464679914735E-16,-6.62)) ;
#155299 = CARTESIAN_POINT('Origin',(9.2,0.,-11.43)) ;
#155300 = CARTESIAN_POINT('',(9.2,-1.22464679914735E-16,-10.43)) ;
#155301 = CARTESIAN_POINT('Origin',(9.2,0.,-15.24)) ;
#155302 = CARTESIAN_POINT('',(9.2,-1.22464679914735E-16,-14.24)) ;
#155303 = CARTESIAN_POINT('Origin',(9.2,0.,-19.05)) ;
#155304 = CARTESIAN_POINT('',(9.2,-1.22464679914735E-16,-18.05)) ;
#155305 = CARTESIAN_POINT('Origin',(9.2,0.,-22.86)) ;
#155306 = CARTESIAN_POINT('',(9.2,-1.22464679914735E-16,-21.86)) ;
#155307 = CARTESIAN_POINT('Origin',(9.2,0.,-26.67)) ;
#155308 = CARTESIAN_POINT('',(9.2,-1.22464679914735E-16,-25.67)) ;
#155309 = CARTESIAN_POINT('Origin',(9.2,0.,-30.48)) ;
#155310 = CARTESIAN_POINT('',(9.2,-1.22464679914735E-16,-29.48)) ;
#155311 = CARTESIAN_POINT('Origin',(9.2,0.,-34.29)) ;
#155312 = CARTESIAN_POINT('',(9.2,-1.22464679914735E-16,-33.29)) ;
#155313 = CARTESIAN_POINT('Origin',(9.24142135623731,0.,0.)) ;
#155314 = CARTESIAN_POINT('',(9.17071067811866,-1.18877772485617E-16,0.970710678118656)) ;
#155315 = CARTESIAN_POINT('Origin',(9.17071067811866,0.,0.)) ;
#155316 = CARTESIAN_POINT('',(9.24142135623731,-1.22464679914735E-16,1.)) ;
#155317 = CARTESIAN_POINT('Origin',(9.24142135623731,-1.10218211923262E-16,
0.9)) ;
#155318 = CARTESIAN_POINT('Origin',(9.24142135623731,0.,0.)) ;
#155319 = CARTESIAN_POINT('Origin',(-6.11095769946375E-16,4.45,0.)) ;
#155320 = CARTESIAN_POINT('',(1.5,4.45,-1.83697019872103E-16)) ;
#155321 = CARTESIAN_POINT('Origin',(-6.11095769946375E-16,4.45,0.)) ;
#155322 = CARTESIAN_POINT('',(1.6,4.55,-1.95943487863577E-16)) ;
#155323 = CARTESIAN_POINT('Origin',(1.6,4.45,-1.95943487863577E-16)) ;
#155324 = CARTESIAN_POINT('Origin',(-6.24237614461351E-16,4.55,0.)) ;
#155325 = CARTESIAN_POINT('Origin',(10.1,0.,0.)) ;
#155326 = CARTESIAN_POINT('',(10.1,-1.22464679914735E-16,1.)) ;
#155327 = CARTESIAN_POINT('Origin',(10.1,0.,0.)) ;
#155328 = CARTESIAN_POINT('',(10.2,-1.34711147906209E-16,1.1)) ;
#155329 = CARTESIAN_POINT('Origin',(10.1,-1.34711147906209E-16,1.1)) ;
#155330 = CARTESIAN_POINT('Origin',(10.2,0.,0.)) ;
#155331 = CARTESIAN_POINT('Origin',(1.31451250000001,-1.51907484122731,-32.385)) ;
#155332 = CARTESIAN_POINT('Origin',(1.31451250000001,2.85,-32.385)) ;
#155333 = CARTESIAN_POINT('',(1.27787304021906,-1.51907484122731,-32.4380981416173)) ;
#155334 = CARTESIAN_POINT('',(1.27787304021906,-1.51907484122731,-32.3319018583827)) ;
#155335 = CARTESIAN_POINT('Origin',(1.77490703981929,-1.51907484122731,-35.7754875)) ;
#155336 = CARTESIAN_POINT('',(1.77490703981929,2.85,-35.84)) ;
#155337 = CARTESIAN_POINT('Origin',(1.77490703981929,2.85,-35.7754875)) ;
#155338 = CARTESIAN_POINT('',(1.77490703981929,-1.51907484122731,-35.84)) ;
#155339 = CARTESIAN_POINT('',(1.72543498451332,-1.51907484122731,-35.7340824471676)) ;
#155340 = CARTESIAN_POINT('Origin',(1.77490703981927,-1.51907484122731,1.4854875)) ;
#155341 = CARTESIAN_POINT('',(1.77490703981927,2.85,1.55)) ;
#155342 = CARTESIAN_POINT('Origin',(1.77490703981927,2.85,1.4854875)) ;
#155343 = CARTESIAN_POINT('',(1.72543498451331,-1.51907484122731,1.4440824471676)) ;
#155344 = CARTESIAN_POINT('',(1.77490703981927,-1.51907484122731,1.55)) ;
#155345 = CARTESIAN_POINT('Origin',(1.3145125,-1.51907484122731,-1.905)) ;
#155346 = CARTESIAN_POINT('Origin',(1.3145125,2.85,-1.905)) ;
#155347 = CARTESIAN_POINT('',(1.27787304021905,-1.51907484122731,-1.9580981416173)) ;
#155348 = CARTESIAN_POINT('',(1.27787304021905,-1.51907484122731,-1.85190185838271)) ;
#155349 = CARTESIAN_POINT('Origin',(-7.29372370581158E-16,3.55,0.)) ;
#155350 = CARTESIAN_POINT('',(-0.17080731546663,3.55,1.49024322208929)) ;
#155351 = CARTESIAN_POINT('',(1.5,3.55,-1.83697019872103E-16)) ;
#155352 = CARTESIAN_POINT('Origin',(-7.29372370581158E-16,3.55,0.)) ;
#155353 = CARTESIAN_POINT('',(-0.273932138433073,3.45,1.4747749603019)) ;
#155354 = CARTESIAN_POINT('Ctrl Pts',(-0.170807315466632,3.55,1.49024322208929)) ;
#155355 = CARTESIAN_POINT('Ctrl Pts',(-0.18388243342709,3.55,1.48874459034574)) ;
#155356 = CARTESIAN_POINT('Ctrl Pts',(-0.197859036177013,3.54752250383109,
1.48694882390231)) ;
#155357 = CARTESIAN_POINT('Ctrl Pts',(-0.223597793566256,3.53719045839678,
1.48329935326863)) ;
#155358 = CARTESIAN_POINT('Ctrl Pts',(-0.235362682979178,3.52934133421403,
1.48144958131094)) ;
#155359 = CARTESIAN_POINT('Ctrl Pts',(-0.253465441530115,3.51138121637726,
1.47845705197622)) ;
#155360 = CARTESIAN_POINT('Ctrl Pts',(-0.261168570620306,3.50026979217228,
1.4770965178147)) ;
#155361 = CARTESIAN_POINT('Ctrl Pts',(-0.271399896344097,3.47583586070553,
1.47525363540046)) ;
#155362 = CARTESIAN_POINT('Ctrl Pts',(-0.273932138433075,3.46251477070021,
1.4747749603019)) ;
#155363 = CARTESIAN_POINT('Ctrl Pts',(-0.273932138433075,3.45,1.4747749603019)) ;
#155364 = CARTESIAN_POINT('',(-0.273932138433073,3.15,1.4747749603019)) ;
#155365 = CARTESIAN_POINT('',(-0.273932138433073,3.05,1.4747749603019)) ;
#155366 = CARTESIAN_POINT('',(-0.373948193368569,3.05,1.45263992395789)) ;
#155367 = CARTESIAN_POINT('Ctrl Pts',(-0.273932138433073,3.15,1.4747749603019)) ;
#155368 = CARTESIAN_POINT('Ctrl Pts',(-0.273932138433073,3.13744372549049,
1.4747749603019)) ;
#155369 = CARTESIAN_POINT('Ctrl Pts',(-0.276486468486165,3.12408297110069,
1.47430886976441)) ;
#155370 = CARTESIAN_POINT('Ctrl Pts',(-0.28674027764043,3.0995678553947,1.47234622100643)) ;
#155371 = CARTESIAN_POINT('Ctrl Pts',(-0.294439768310517,3.08841385970397,
1.47084515886225)) ;
#155372 = CARTESIAN_POINT('Ctrl Pts',(-0.312194128344972,3.07061084469361,
1.46718060004901)) ;
#155373 = CARTESIAN_POINT('Ctrl Pts',(-0.323517908844217,3.0628422827531,
1.4647525137252)) ;
#155374 = CARTESIAN_POINT('Ctrl Pts',(-0.348172117123305,3.05253676672645,
1.45908616124653)) ;
#155375 = CARTESIAN_POINT('Ctrl Pts',(-0.361501722536397,3.05,1.45584397694084)) ;
#155376 = CARTESIAN_POINT('Ctrl Pts',(-0.37394819336857,3.05,1.45263992395789)) ;
#155377 = CARTESIAN_POINT('',(-0.872417476238727,3.05,1.22019988000051)) ;
#155378 = CARTESIAN_POINT('Origin',(-7.95081593156037E-16,3.05,0.)) ;
#155379 = CARTESIAN_POINT('',(-0.953662978710562,3.15,1.15781126399638)) ;
#155380 = CARTESIAN_POINT('Ctrl Pts',(-0.872417476238727,3.05,1.22019988000051)) ;
#155381 = CARTESIAN_POINT('Ctrl Pts',(-0.882808783297377,3.05,1.21277031208502)) ;
#155382 = CARTESIAN_POINT('Ctrl Pts',(-0.893798224191975,3.05250629897269,
1.20469063768542)) ;
#155383 = CARTESIAN_POINT('Ctrl Pts',(-0.913892243159219,3.06269675232156,
1.18952223087538)) ;
#155384 = CARTESIAN_POINT('Ctrl Pts',(-0.922999225059834,3.07038074042647,
1.18243657143088)) ;
#155385 = CARTESIAN_POINT('Ctrl Pts',(-0.937285134131706,3.08810056349785,
1.17114412889658)) ;
#155386 = CARTESIAN_POINT('Ctrl Pts',(-0.943452174397235,3.09929464195085,
1.16615690319603)) ;
#155387 = CARTESIAN_POINT('Ctrl Pts',(-0.951639309815362,3.12392729225934,
1.15948900020361)) ;
#155388 = CARTESIAN_POINT('Ctrl Pts',(-0.953662978710562,3.13736547222678,
1.15781126399638)) ;
#155389 = CARTESIAN_POINT('Ctrl Pts',(-0.953662978710562,3.15,1.15781126399638)) ;
#155390 = CARTESIAN_POINT('',(-0.953662978710562,3.45,1.15781126399638)) ;
#155391 = CARTESIAN_POINT('',(-0.953662978710562,3.05,1.15781126399638)) ;
#155392 = CARTESIAN_POINT('',(-1.03179971315145,3.55,1.08875587343563)) ;
#155393 = CARTESIAN_POINT('Ctrl Pts',(-0.953662978710565,3.45,1.15781126399638)) ;
#155394 = CARTESIAN_POINT('Ctrl Pts',(-0.953662978710565,3.45580715149871,
1.15781126399638)) ;
#155395 = CARTESIAN_POINT('Ctrl Pts',(-0.954069792639904,3.46165880969181,
1.15747636843074)) ;
#155396 = CARTESIAN_POINT('Ctrl Pts',(-0.95488040580839,3.46741264967889,
1.15680726792462)) ;
#155397 = CARTESIAN_POINT('Ctrl Pts',(-0.955592557016221,3.47246759358527,
1.15621944039835)) ;
#155398 = CARTESIAN_POINT('Ctrl Pts',(-0.956615573654933,3.47744631522377,
1.15537418855117)) ;
#155399 = CARTESIAN_POINT('Ctrl Pts',(-0.957920385817348,3.48225893605768,
1.15429135595662)) ;
#155400 = CARTESIAN_POINT('Ctrl Pts',(-0.959423079246195,3.48780141482278,
1.15304430640325)) ;
#155401 = CARTESIAN_POINT('Ctrl Pts',(-0.961323201468143,3.49320783601914,
1.15146254061837)) ;
#155402 = CARTESIAN_POINT('Ctrl Pts',(-0.963574238618815,3.49834560049868,
1.14957574210362)) ;
#155403 = CARTESIAN_POINT('Ctrl Pts',(-0.965499706648006,3.50274028640777,
1.14796183261456)) ;
#155404 = CARTESIAN_POINT('Ctrl Pts',(-0.967680912999541,3.5069382066956,
1.14612540554157)) ;
#155405 = CARTESIAN_POINT('Ctrl Pts',(-0.970068248378241,3.51087311165944,
1.14410121645275)) ;
#155406 = CARTESIAN_POINT('Ctrl Pts',(-0.97293324697906,3.51559532091263,
1.14167202323634)) ;
#155407 = CARTESIAN_POINT('Ctrl Pts',(-0.976138831290367,3.52000896466724,
1.13893531443762)) ;
#155408 = CARTESIAN_POINT('Ctrl Pts',(-0.979601776802485,3.52400782220665,
1.13594901565242)) ;
#155409 = CARTESIAN_POINT('Ctrl Pts',(-0.982467725203496,3.52731729367563,
1.13347754210528)) ;
#155410 = CARTESIAN_POINT('Ctrl Pts',(-0.985508986896839,3.53034305696182,
1.13083582639522)) ;
#155411 = CARTESIAN_POINT('Ctrl Pts',(-0.988666612105887,3.53304718478134,
1.12806840666118)) ;
#155412 = CARTESIAN_POINT('Ctrl Pts',(-0.992701606803652,3.53650267449006,
1.12453203891198)) ;
#155413 = CARTESIAN_POINT('Ctrl Pts',(-0.996988044734313,3.53948417067186,
1.12073641188223)) ;
#155414 = CARTESIAN_POINT('Ctrl Pts',(-1.00141585135915,3.54192188246042,
1.11676596479649)) ;
#155415 = CARTESIAN_POINT('Ctrl Pts',(-1.00487400994927,3.54382575827888,
1.11366500830503)) ;
#155416 = CARTESIAN_POINT('Ctrl Pts',(-1.00841776012225,3.54539884758397,
1.11045803912747)) ;
#155417 = CARTESIAN_POINT('Ctrl Pts',(-1.0119912926316,3.54662946216441,1.10719177365334)) ;
#155418 = CARTESIAN_POINT('Ctrl Pts',(-1.01652362695399,3.54819025857131,
1.10304914809285)) ;
#155419 = CARTESIAN_POINT('Ctrl Pts',(-1.0211653313612,3.54921942038456,1.09875463688375)) ;
#155420 = CARTESIAN_POINT('Ctrl Pts',(-1.02580209629923,3.54969340754027,
1.09440854282807)) ;
#155421 = CARTESIAN_POINT('Ctrl Pts',(-1.02780524115375,3.54989817637043,
1.09253097170655)) ;
#155422 = CARTESIAN_POINT('Ctrl Pts',(-1.02980744674852,3.55,1.09064391827031)) ;
#155423 = CARTESIAN_POINT('Ctrl Pts',(-1.03179971315145,3.55,1.08875587343563)) ;
#155424 = CARTESIAN_POINT('',(0.170807315466631,3.55,-1.49024322208929)) ;
#155425 = CARTESIAN_POINT('Origin',(-7.29372370581158E-16,3.55,0.)) ;
#155426 = CARTESIAN_POINT('',(0.273932138433074,3.45,-1.4747749603019)) ;
#155427 = CARTESIAN_POINT('Ctrl Pts',(0.170807315466627,3.55,-1.4902432220893)) ;
#155428 = CARTESIAN_POINT('Ctrl Pts',(0.183882433427085,3.55,-1.48874459034574)) ;
#155429 = CARTESIAN_POINT('Ctrl Pts',(0.197859036177008,3.54752250383109,
-1.48694882390231)) ;
#155430 = CARTESIAN_POINT('Ctrl Pts',(0.223597793566251,3.53719045839678,
-1.48329935326863)) ;
#155431 = CARTESIAN_POINT('Ctrl Pts',(0.235362682979173,3.52934133421403,
-1.48144958131094)) ;
#155432 = CARTESIAN_POINT('Ctrl Pts',(0.25346544153011,3.51138121637726,-1.47845705197622)) ;
#155433 = CARTESIAN_POINT('Ctrl Pts',(0.261168570620301,3.50026979217228,
-1.4770965178147)) ;
#155434 = CARTESIAN_POINT('Ctrl Pts',(0.271399896344092,3.47583586070553,
-1.47525363540046)) ;
#155435 = CARTESIAN_POINT('Ctrl Pts',(0.27393213843307,3.46251477070021,-1.47477496030191)) ;
#155436 = CARTESIAN_POINT('Ctrl Pts',(0.27393213843307,3.45,-1.47477496030191)) ;
#155437 = CARTESIAN_POINT('',(0.273932138433074,3.15,-1.4747749603019)) ;
#155438 = CARTESIAN_POINT('',(0.273932138433074,3.05,-1.4747749603019)) ;
#155439 = CARTESIAN_POINT('',(0.37394819336857,3.05,-1.45263992395789)) ;
#155440 = CARTESIAN_POINT('Ctrl Pts',(0.273932138433074,3.15,-1.4747749603019)) ;
#155441 = CARTESIAN_POINT('Ctrl Pts',(0.273932138433074,3.13736547222678,
-1.4747749603019)) ;
#155442 = CARTESIAN_POINT('Ctrl Pts',(0.276518148223581,3.12392729225934,
-1.47430316803635)) ;
#155443 = CARTESIAN_POINT('Ctrl Pts',(0.28688864746378,3.09929464195085,-1.47231750387035)) ;
#155444 = CARTESIAN_POINT('Ctrl Pts',(0.294673181069391,3.08810056349785,
-1.47079900383148)) ;
#155445 = CARTESIAN_POINT('Ctrl Pts',(0.312506499266534,3.07038074042647,
-1.46711400471621)) ;
#155446 = CARTESIAN_POINT('Ctrl Pts',(0.32378828443718,3.06269675232156,-1.46469222593504)) ;
#155447 = CARTESIAN_POINT('Ctrl Pts',(0.348324144605931,3.05250629897269,
-1.45904937832144)) ;
#155448 = CARTESIAN_POINT('Ctrl Pts',(0.36157741072639,3.05,-1.45582449278551)) ;
#155449 = CARTESIAN_POINT('Ctrl Pts',(0.37394819336857,3.05,-1.45263992395789)) ;
#155450 = CARTESIAN_POINT('',(0.872417476238728,3.05,-1.22019988000051)) ;
#155451 = CARTESIAN_POINT('Origin',(-7.95081593156037E-16,3.05,0.)) ;
#155452 = CARTESIAN_POINT('',(0.953662978710562,3.15,-1.15781126399638)) ;
#155453 = CARTESIAN_POINT('Ctrl Pts',(0.872417476238728,3.05,-1.22019988000051)) ;
#155454 = CARTESIAN_POINT('Ctrl Pts',(0.882872360457018,3.05,-1.2127248557413)) ;
#155455 = CARTESIAN_POINT('Ctrl Pts',(0.893924122929505,3.05253676672645,
-1.20459782148564)) ;
#155456 = CARTESIAN_POINT('Ctrl Pts',(0.914112220366976,3.0628422827531,-1.18935386339936)) ;
#155457 = CARTESIAN_POINT('Ctrl Pts',(0.923251028202469,3.07061084469361,
-1.18224008807701)) ;
#155458 = CARTESIAN_POINT('Ctrl Pts',(0.937470525765899,3.08841385970397,
-1.1709949922316)) ;
#155459 = CARTESIAN_POINT('Ctrl Pts',(0.94356954328385,3.0995678553947,-1.16606170433658)) ;
#155460 = CARTESIAN_POINT('Ctrl Pts',(0.951664040935143,3.12408297110069,
-1.15946839711695)) ;
#155461 = CARTESIAN_POINT('Ctrl Pts',(0.953662978710562,3.13744372549049,
-1.15781126399638)) ;
#155462 = CARTESIAN_POINT('Ctrl Pts',(0.953662978710562,3.15,-1.15781126399638)) ;
#155463 = CARTESIAN_POINT('',(0.953662978710562,3.45,-1.15781126399638)) ;
#155464 = CARTESIAN_POINT('',(0.953662978710562,3.05,-1.15781126399638)) ;
#155465 = CARTESIAN_POINT('',(1.03179971315145,3.55,-1.08875587343563)) ;
#155466 = CARTESIAN_POINT('Ctrl Pts',(0.95366297871056,3.45,-1.15781126399638)) ;
#155467 = CARTESIAN_POINT('Ctrl Pts',(0.95366297871056,3.45580715149871,-1.15781126399638)) ;
#155468 = CARTESIAN_POINT('Ctrl Pts',(0.954069792639901,3.46165880969183,
-1.15747636843074)) ;
#155469 = CARTESIAN_POINT('Ctrl Pts',(0.954880405808387,3.4674126496789,-1.15680726792462)) ;
#155470 = CARTESIAN_POINT('Ctrl Pts',(0.955592557016217,3.47246759358527,
-1.15621944039835)) ;
#155471 = CARTESIAN_POINT('Ctrl Pts',(0.95661557365493,3.47744631522378,-1.15537418855117)) ;
#155472 = CARTESIAN_POINT('Ctrl Pts',(0.957920385817344,3.48225893605768,
-1.15429135595663)) ;
#155473 = CARTESIAN_POINT('Ctrl Pts',(0.959423079246193,3.48780141482279,
-1.15304430640326)) ;
#155474 = CARTESIAN_POINT('Ctrl Pts',(0.961323201468142,3.49320783601915,
-1.15146254061836)) ;
#155475 = CARTESIAN_POINT('Ctrl Pts',(0.963574238618814,3.49834560049869,
-1.14957574210361)) ;
#155476 = CARTESIAN_POINT('Ctrl Pts',(0.965499706648003,3.50274028640777,
-1.14796183261456)) ;
#155477 = CARTESIAN_POINT('Ctrl Pts',(0.967680912999538,3.5069382066956,-1.14612540554157)) ;
#155478 = CARTESIAN_POINT('Ctrl Pts',(0.970068248378237,3.51087311165944,
-1.14410121645275)) ;
#155479 = CARTESIAN_POINT('Ctrl Pts',(0.972933246979058,3.51559532091264,
-1.14167202323633)) ;
#155480 = CARTESIAN_POINT('Ctrl Pts',(0.976138831290364,3.52000896466724,
-1.13893531443762)) ;
#155481 = CARTESIAN_POINT('Ctrl Pts',(0.979601776802484,3.52400782220666,
-1.13594901565242)) ;
#155482 = CARTESIAN_POINT('Ctrl Pts',(0.982467725203496,3.52731729367563,
-1.13347754210528)) ;
#155483 = CARTESIAN_POINT('Ctrl Pts',(0.985508986896838,3.53034305696182,
-1.13083582639522)) ;
#155484 = CARTESIAN_POINT('Ctrl Pts',(0.988666612105885,3.53304718478134,
-1.12806840666118)) ;
#155485 = CARTESIAN_POINT('Ctrl Pts',(0.992701606803651,3.53650267449006,
-1.12453203891197)) ;
#155486 = CARTESIAN_POINT('Ctrl Pts',(0.996988044734313,3.53948417067186,
-1.12073641188223)) ;
#155487 = CARTESIAN_POINT('Ctrl Pts',(1.00141585135915,3.54192188246042,-1.11676596479648)) ;
#155488 = CARTESIAN_POINT('Ctrl Pts',(1.00487400994927,3.54382575827888,-1.11366500830503)) ;
#155489 = CARTESIAN_POINT('Ctrl Pts',(1.00841776012226,3.54539884758397,-1.11045803912747)) ;
#155490 = CARTESIAN_POINT('Ctrl Pts',(1.01199129263161,3.54662946216441,-1.10719177365333)) ;
#155491 = CARTESIAN_POINT('Ctrl Pts',(1.016523626954,3.54819025857131,-1.10304914809285)) ;
#155492 = CARTESIAN_POINT('Ctrl Pts',(1.02116533136121,3.54921942038456,-1.09875463688374)) ;
#155493 = CARTESIAN_POINT('Ctrl Pts',(1.02580209629923,3.54969340754028,-1.09440854282805)) ;
#155494 = CARTESIAN_POINT('Ctrl Pts',(1.02780524115375,3.54989817637043,-1.09253097170654)) ;
#155495 = CARTESIAN_POINT('Ctrl Pts',(1.02980744674852,3.55,-1.09064391827031)) ;
#155496 = CARTESIAN_POINT('Ctrl Pts',(1.03179971315145,3.55,-1.08875587343563)) ;
#155497 = CARTESIAN_POINT('Origin',(-7.29372370581158E-16,3.55,0.)) ;
#155498 = CARTESIAN_POINT('',(1.5,3.55,-1.83697019872103E-16)) ;
#155499 = CARTESIAN_POINT('Origin',(9.2,0.,0.)) ;
#155500 = CARTESIAN_POINT('',(8.7,-6.12323399573674E-17,0.499999999999998)) ;
#155501 = CARTESIAN_POINT('Origin',(8.7,0.,0.)) ;
#155502 = CARTESIAN_POINT('',(9.2,-1.22464679914735E-16,1.)) ;
#155503 = CARTESIAN_POINT('Origin',(9.2,0.,0.)) ;
#155504 = CARTESIAN_POINT('',(9.2,-1.22464679914735E-16,1.)) ;
#155505 = CARTESIAN_POINT('Origin',(-4.,4.55,-36.59)) ;
#155506 = CARTESIAN_POINT('',(-3.9,4.55,-36.49)) ;
#155507 = CARTESIAN_POINT('',(-3.9,4.55,2.2)) ;
#155508 = CARTESIAN_POINT('',(-3.9,4.55,-36.59)) ;
#155509 = CARTESIAN_POINT('',(2.5,4.55,2.2)) ;
#155510 = CARTESIAN_POINT('',(2.6,4.55,2.2)) ;
#155511 = CARTESIAN_POINT('',(2.5,4.55,1.65)) ;
#155512 = CARTESIAN_POINT('',(2.5,4.55,-36.59)) ;
#155513 = CARTESIAN_POINT('',(1.77490703981927,4.55,1.65)) ;
#155514 = CARTESIAN_POINT('Origin',(-6.24237614461351E-16,4.55,0.)) ;
#155515 = CARTESIAN_POINT('Origin',(-6.24237614461351E-16,4.55,-3.81)) ;
#155516 = CARTESIAN_POINT('Origin',(-6.24237614461351E-16,4.55,-7.62)) ;
#155517 = CARTESIAN_POINT('Origin',(-6.24237614461351E-16,4.55,-11.43)) ;
#155518 = CARTESIAN_POINT('Origin',(-6.24237614461351E-16,4.55,-15.24)) ;
#155519 = CARTESIAN_POINT('Origin',(-6.24237614461351E-16,4.55,-19.05)) ;
#155520 = CARTESIAN_POINT('Origin',(-6.24237614461351E-16,4.55,-22.86)) ;
#155521 = CARTESIAN_POINT('Origin',(-6.24237614461351E-16,4.55,-26.67)) ;
#155522 = CARTESIAN_POINT('Origin',(-5.97953925431399E-16,4.55,-30.48)) ;
#155523 = CARTESIAN_POINT('Origin',(-5.97953925431399E-16,4.55,-34.29)) ;
#155524 = CARTESIAN_POINT('',(2.5,4.55,-35.94)) ;
#155525 = CARTESIAN_POINT('',(2.6,4.55,-35.94)) ;
#155526 = CARTESIAN_POINT('',(2.5,4.55,-36.49)) ;
#155527 = CARTESIAN_POINT('',(2.5,4.55,-36.59)) ;
#155528 = CARTESIAN_POINT('',(-4.,4.55,-36.49)) ;
#155529 = CARTESIAN_POINT('',(-2.1,4.55,-29.38)) ;
#155530 = CARTESIAN_POINT('',(-1.9,4.55,-29.58)) ;
#155531 = CARTESIAN_POINT('Origin',(-2.1,4.55,-29.58)) ;
#155532 = CARTESIAN_POINT('',(-2.9,4.55,-29.38)) ;
#155533 = CARTESIAN_POINT('',(-3.,4.55,-29.38)) ;
#155534 = CARTESIAN_POINT('',(-3.1,4.55,-29.58)) ;
#155535 = CARTESIAN_POINT('Origin',(-2.9,4.55,-29.58)) ;
#155536 = CARTESIAN_POINT('',(-3.1,4.55,-31.38)) ;
#155537 = CARTESIAN_POINT('',(-3.1,4.55,-31.48)) ;
#155538 = CARTESIAN_POINT('',(-2.9,4.55,-31.58)) ;
#155539 = CARTESIAN_POINT('Origin',(-2.9,4.55,-31.38)) ;
#155540 = CARTESIAN_POINT('',(-2.1,4.55,-31.58)) ;
#155541 = CARTESIAN_POINT('',(-2.,4.55,-31.58)) ;
#155542 = CARTESIAN_POINT('',(-1.9,4.55,-31.38)) ;
#155543 = CARTESIAN_POINT('Origin',(-2.1,4.55,-31.38)) ;
#155544 = CARTESIAN_POINT('',(-1.9,4.55,-29.48)) ;
#155545 = CARTESIAN_POINT('',(-2.1,4.55,-21.76)) ;
#155546 = CARTESIAN_POINT('',(-1.9,4.55,-21.96)) ;
#155547 = CARTESIAN_POINT('Origin',(-2.1,4.55,-21.96)) ;
#155548 = CARTESIAN_POINT('',(-2.9,4.55,-21.76)) ;
#155549 = CARTESIAN_POINT('',(-3.,4.55,-21.76)) ;
#155550 = CARTESIAN_POINT('',(-3.1,4.55,-21.96)) ;
#155551 = CARTESIAN_POINT('Origin',(-2.9,4.55,-21.96)) ;
#155552 = CARTESIAN_POINT('',(-3.1,4.55,-23.76)) ;
#155553 = CARTESIAN_POINT('',(-3.1,4.55,-23.86)) ;
#155554 = CARTESIAN_POINT('',(-2.9,4.55,-23.96)) ;
#155555 = CARTESIAN_POINT('Origin',(-2.9,4.55,-23.76)) ;
#155556 = CARTESIAN_POINT('',(-2.1,4.55,-23.96)) ;
#155557 = CARTESIAN_POINT('',(-2.,4.55,-23.96)) ;
#155558 = CARTESIAN_POINT('',(-1.9,4.55,-23.76)) ;
#155559 = CARTESIAN_POINT('Origin',(-2.1,4.55,-23.76)) ;
#155560 = CARTESIAN_POINT('',(-1.9,4.55,-21.86)) ;
#155561 = CARTESIAN_POINT('',(-2.1,4.55,-14.14)) ;
#155562 = CARTESIAN_POINT('',(-1.9,4.55,-14.34)) ;
#155563 = CARTESIAN_POINT('Origin',(-2.1,4.55,-14.34)) ;
#155564 = CARTESIAN_POINT('',(-2.9,4.55,-14.14)) ;
#155565 = CARTESIAN_POINT('',(-3.,4.55,-14.14)) ;
#155566 = CARTESIAN_POINT('',(-3.1,4.55,-14.34)) ;
#155567 = CARTESIAN_POINT('Origin',(-2.9,4.55,-14.34)) ;
#155568 = CARTESIAN_POINT('',(-3.1,4.55,-16.14)) ;
#155569 = CARTESIAN_POINT('',(-3.1,4.55,-16.24)) ;
#155570 = CARTESIAN_POINT('',(-2.9,4.55,-16.34)) ;
#155571 = CARTESIAN_POINT('Origin',(-2.9,4.55,-16.14)) ;
#155572 = CARTESIAN_POINT('',(-2.1,4.55,-16.34)) ;
#155573 = CARTESIAN_POINT('',(-2.,4.55,-16.34)) ;
#155574 = CARTESIAN_POINT('',(-1.9,4.55,-16.14)) ;
#155575 = CARTESIAN_POINT('Origin',(-2.1,4.55,-16.14)) ;
#155576 = CARTESIAN_POINT('',(-1.9,4.55,-14.24)) ;
#155577 = CARTESIAN_POINT('',(-2.1,4.55,-6.52)) ;
#155578 = CARTESIAN_POINT('',(-1.9,4.55,-6.72)) ;
#155579 = CARTESIAN_POINT('Origin',(-2.1,4.55,-6.72)) ;
#155580 = CARTESIAN_POINT('',(-2.9,4.55,-6.52)) ;
#155581 = CARTESIAN_POINT('',(-3.,4.55,-6.52)) ;
#155582 = CARTESIAN_POINT('',(-3.1,4.55,-6.72)) ;
#155583 = CARTESIAN_POINT('Origin',(-2.9,4.55,-6.72)) ;
#155584 = CARTESIAN_POINT('',(-3.1,4.55,-8.52)) ;
#155585 = CARTESIAN_POINT('',(-3.1,4.55,-8.62)) ;
#155586 = CARTESIAN_POINT('',(-2.9,4.55,-8.72)) ;
#155587 = CARTESIAN_POINT('Origin',(-2.9,4.55,-8.52)) ;
#155588 = CARTESIAN_POINT('',(-2.1,4.55,-8.72)) ;
#155589 = CARTESIAN_POINT('',(-2.,4.55,-8.72)) ;
#155590 = CARTESIAN_POINT('',(-1.9,4.55,-8.52)) ;
#155591 = CARTESIAN_POINT('Origin',(-2.1,4.55,-8.52)) ;
#155592 = CARTESIAN_POINT('',(-1.9,4.55,-6.62)) ;
#155593 = CARTESIAN_POINT('',(-2.1,4.55,1.1)) ;
#155594 = CARTESIAN_POINT('',(-1.9,4.55,0.900000000000001)) ;
#155595 = CARTESIAN_POINT('Origin',(-2.1,4.55,0.900000000000001)) ;
#155596 = CARTESIAN_POINT('',(-2.9,4.55,1.1)) ;
#155597 = CARTESIAN_POINT('',(-3.,4.55,1.1)) ;
#155598 = CARTESIAN_POINT('',(-3.1,4.55,0.900000000000001)) ;
#155599 = CARTESIAN_POINT('Origin',(-2.9,4.55,0.900000000000001)) ;
#155600 = CARTESIAN_POINT('',(-3.1,4.55,-0.899999999999999)) ;
#155601 = CARTESIAN_POINT('',(-3.1,4.55,-0.999999999999999)) ;
#155602 = CARTESIAN_POINT('',(-2.9,4.55,-1.1)) ;
#155603 = CARTESIAN_POINT('Origin',(-2.9,4.55,-0.899999999999999)) ;
#155604 = CARTESIAN_POINT('',(-2.1,4.55,-1.1)) ;
#155605 = CARTESIAN_POINT('',(-2.,4.55,-1.1)) ;
#155606 = CARTESIAN_POINT('',(-1.9,4.55,-0.9)) ;
#155607 = CARTESIAN_POINT('Origin',(-2.1,4.55,-0.9)) ;
#155608 = CARTESIAN_POINT('',(-1.9,4.55,1.)) ;
#155609 = CARTESIAN_POINT('',(-2.1,4.55,-2.71)) ;
#155610 = CARTESIAN_POINT('',(-1.9,4.55,-2.91)) ;
#155611 = CARTESIAN_POINT('Origin',(-2.1,4.55,-2.91)) ;
#155612 = CARTESIAN_POINT('',(-2.9,4.55,-2.71)) ;
#155613 = CARTESIAN_POINT('',(-3.,4.55,-2.71)) ;
#155614 = CARTESIAN_POINT('',(-3.1,4.55,-2.91)) ;
#155615 = CARTESIAN_POINT('Origin',(-2.9,4.55,-2.91)) ;
#155616 = CARTESIAN_POINT('',(-3.1,4.55,-4.71)) ;
#155617 = CARTESIAN_POINT('',(-3.1,4.55,-4.81)) ;
#155618 = CARTESIAN_POINT('',(-2.9,4.55,-4.91)) ;
#155619 = CARTESIAN_POINT('Origin',(-2.9,4.55,-4.71)) ;
#155620 = CARTESIAN_POINT('',(-2.1,4.55,-4.91)) ;
#155621 = CARTESIAN_POINT('',(-2.,4.55,-4.91)) ;
#155622 = CARTESIAN_POINT('',(-1.9,4.55,-4.71)) ;
#155623 = CARTESIAN_POINT('Origin',(-2.1,4.55,-4.71)) ;
#155624 = CARTESIAN_POINT('',(-1.9,4.55,-2.81)) ;
#155625 = CARTESIAN_POINT('',(-2.1,4.55,-10.33)) ;
#155626 = CARTESIAN_POINT('',(-1.9,4.55,-10.53)) ;
#155627 = CARTESIAN_POINT('Origin',(-2.1,4.55,-10.53)) ;
#155628 = CARTESIAN_POINT('',(-2.9,4.55,-10.33)) ;
#155629 = CARTESIAN_POINT('',(-3.,4.55,-10.33)) ;
#155630 = CARTESIAN_POINT('',(-3.1,4.55,-10.53)) ;
#155631 = CARTESIAN_POINT('Origin',(-2.9,4.55,-10.53)) ;
#155632 = CARTESIAN_POINT('',(-3.1,4.55,-12.33)) ;
#155633 = CARTESIAN_POINT('',(-3.1,4.55,-12.43)) ;
#155634 = CARTESIAN_POINT('',(-2.9,4.55,-12.53)) ;
#155635 = CARTESIAN_POINT('Origin',(-2.9,4.55,-12.33)) ;
#155636 = CARTESIAN_POINT('',(-2.1,4.55,-12.53)) ;
#155637 = CARTESIAN_POINT('',(-2.,4.55,-12.53)) ;
#155638 = CARTESIAN_POINT('',(-1.9,4.55,-12.33)) ;
#155639 = CARTESIAN_POINT('Origin',(-2.1,4.55,-12.33)) ;
#155640 = CARTESIAN_POINT('',(-1.9,4.55,-10.43)) ;
#155641 = CARTESIAN_POINT('',(-2.1,4.55,-17.95)) ;
#155642 = CARTESIAN_POINT('',(-1.9,4.55,-18.15)) ;
#155643 = CARTESIAN_POINT('Origin',(-2.1,4.55,-18.15)) ;
#155644 = CARTESIAN_POINT('',(-2.9,4.55,-17.95)) ;
#155645 = CARTESIAN_POINT('',(-3.,4.55,-17.95)) ;
#155646 = CARTESIAN_POINT('',(-3.1,4.55,-18.15)) ;
#155647 = CARTESIAN_POINT('Origin',(-2.9,4.55,-18.15)) ;
#155648 = CARTESIAN_POINT('',(-3.1,4.55,-19.95)) ;
#155649 = CARTESIAN_POINT('',(-3.1,4.55,-20.05)) ;
#155650 = CARTESIAN_POINT('',(-2.9,4.55,-20.15)) ;
#155651 = CARTESIAN_POINT('Origin',(-2.9,4.55,-19.95)) ;
#155652 = CARTESIAN_POINT('',(-2.1,4.55,-20.15)) ;
#155653 = CARTESIAN_POINT('',(-2.,4.55,-20.15)) ;
#155654 = CARTESIAN_POINT('',(-1.9,4.55,-19.95)) ;
#155655 = CARTESIAN_POINT('Origin',(-2.1,4.55,-19.95)) ;
#155656 = CARTESIAN_POINT('',(-1.9,4.55,-18.05)) ;
#155657 = CARTESIAN_POINT('',(-2.1,4.55,-25.57)) ;
#155658 = CARTESIAN_POINT('',(-1.9,4.55,-25.77)) ;
#155659 = CARTESIAN_POINT('Origin',(-2.1,4.55,-25.77)) ;
#155660 = CARTESIAN_POINT('',(-2.9,4.55,-25.57)) ;
#155661 = CARTESIAN_POINT('',(-3.,4.55,-25.57)) ;
#155662 = CARTESIAN_POINT('',(-3.1,4.55,-25.77)) ;
#155663 = CARTESIAN_POINT('Origin',(-2.9,4.55,-25.77)) ;
#155664 = CARTESIAN_POINT('',(-3.1,4.55,-27.57)) ;
#155665 = CARTESIAN_POINT('',(-3.1,4.55,-27.67)) ;
#155666 = CARTESIAN_POINT('',(-2.9,4.55,-27.77)) ;
#155667 = CARTESIAN_POINT('Origin',(-2.9,4.55,-27.57)) ;
#155668 = CARTESIAN_POINT('',(-2.1,4.55,-27.77)) ;
#155669 = CARTESIAN_POINT('',(-2.,4.55,-27.77)) ;
#155670 = CARTESIAN_POINT('',(-1.9,4.55,-27.57)) ;
#155671 = CARTESIAN_POINT('Origin',(-2.1,4.55,-27.57)) ;
#155672 = CARTESIAN_POINT('',(-1.9,4.55,-25.67)) ;
#155673 = CARTESIAN_POINT('',(-2.1,4.55,-33.19)) ;
#155674 = CARTESIAN_POINT('',(-1.9,4.55,-33.39)) ;
#155675 = CARTESIAN_POINT('Origin',(-2.1,4.55,-33.39)) ;
#155676 = CARTESIAN_POINT('',(-2.9,4.55,-33.19)) ;
#155677 = CARTESIAN_POINT('',(-3.,4.55,-33.19)) ;
#155678 = CARTESIAN_POINT('',(-3.1,4.55,-33.39)) ;
#155679 = CARTESIAN_POINT('Origin',(-2.9,4.55,-33.39)) ;
#155680 = CARTESIAN_POINT('',(-3.1,4.55,-35.19)) ;
#155681 = CARTESIAN_POINT('',(-3.1,4.55,-35.29)) ;
#155682 = CARTESIAN_POINT('',(-2.9,4.55,-35.39)) ;
#155683 = CARTESIAN_POINT('Origin',(-2.9,4.55,-35.19)) ;
#155684 = CARTESIAN_POINT('',(-2.1,4.55,-35.39)) ;
#155685 = CARTESIAN_POINT('',(-2.,4.55,-35.39)) ;
#155686 = CARTESIAN_POINT('',(-1.9,4.55,-35.19)) ;
#155687 = CARTESIAN_POINT('Origin',(-2.1,4.55,-35.19)) ;
#155688 = CARTESIAN_POINT('',(-1.9,4.55,-33.29)) ;
#155689 = CARTESIAN_POINT('Origin',(10.2,2.,-32.885)) ;
#155690 = CARTESIAN_POINT('',(10.1,2.,-32.985)) ;
#155691 = CARTESIAN_POINT('',(10.1,2.,-35.595)) ;
#155692 = CARTESIAN_POINT('',(10.1,2.,-35.695)) ;
#155693 = CARTESIAN_POINT('',(3.7,2.,-35.595)) ;
#155694 = CARTESIAN_POINT('',(10.2,2.,-35.595)) ;
#155695 = CARTESIAN_POINT('',(3.7,2.,-32.985)) ;
#155696 = CARTESIAN_POINT('',(3.7,2.,-32.885)) ;
#155697 = CARTESIAN_POINT('',(10.2,2.,-32.985)) ;
#155698 = CARTESIAN_POINT('',(9.8,2.,-34.69)) ;
#155699 = CARTESIAN_POINT('',(9.8,2.,-33.89)) ;
#155700 = CARTESIAN_POINT('',(9.8,2.,-33.89)) ;
#155701 = CARTESIAN_POINT('',(9.6,2.,-33.69)) ;
#155702 = CARTESIAN_POINT('Origin',(9.6,2.,-33.89)) ;
#155703 = CARTESIAN_POINT('',(7.8,2.,-33.69)) ;
#155704 = CARTESIAN_POINT('',(7.8,2.,-33.69)) ;
#155705 = CARTESIAN_POINT('',(7.6,2.,-33.89)) ;
#155706 = CARTESIAN_POINT('Origin',(7.8,2.,-33.89)) ;
#155707 = CARTESIAN_POINT('',(7.6,2.,-34.69)) ;
#155708 = CARTESIAN_POINT('',(7.6,2.,-34.69)) ;
#155709 = CARTESIAN_POINT('',(7.8,2.,-34.89)) ;
#155710 = CARTESIAN_POINT('Origin',(7.8,2.,-34.69)) ;
#155711 = CARTESIAN_POINT('',(9.6,2.,-34.89)) ;
#155712 = CARTESIAN_POINT('',(9.6,2.,-34.89)) ;
#155713 = CARTESIAN_POINT('Origin',(9.6,2.,-34.69)) ;
#155714 = CARTESIAN_POINT('Origin',(10.2,2.,-29.075)) ;
#155715 = CARTESIAN_POINT('',(10.1,2.,-29.175)) ;
#155716 = CARTESIAN_POINT('',(10.1,2.,-31.785)) ;
#155717 = CARTESIAN_POINT('',(10.1,2.,-31.885)) ;
#155718 = CARTESIAN_POINT('',(3.7,2.,-31.785)) ;
#155719 = CARTESIAN_POINT('',(10.2,2.,-31.785)) ;
#155720 = CARTESIAN_POINT('',(3.7,2.,-29.175)) ;
#155721 = CARTESIAN_POINT('',(3.7,2.,-29.075)) ;
#155722 = CARTESIAN_POINT('',(10.2,2.,-29.175)) ;
#155723 = CARTESIAN_POINT('',(9.8,2.,-30.88)) ;
#155724 = CARTESIAN_POINT('',(9.8,2.,-30.08)) ;
#155725 = CARTESIAN_POINT('',(9.8,2.,-30.08)) ;
#155726 = CARTESIAN_POINT('',(9.6,2.,-29.88)) ;
#155727 = CARTESIAN_POINT('Origin',(9.6,2.,-30.08)) ;
#155728 = CARTESIAN_POINT('',(7.8,2.,-29.88)) ;
#155729 = CARTESIAN_POINT('',(7.8,2.,-29.88)) ;
#155730 = CARTESIAN_POINT('',(7.6,2.,-30.08)) ;
#155731 = CARTESIAN_POINT('Origin',(7.8,2.,-30.08)) ;
#155732 = CARTESIAN_POINT('',(7.6,2.,-30.88)) ;
#155733 = CARTESIAN_POINT('',(7.6,2.,-30.88)) ;
#155734 = CARTESIAN_POINT('',(7.8,2.,-31.08)) ;
#155735 = CARTESIAN_POINT('Origin',(7.8,2.,-30.88)) ;
#155736 = CARTESIAN_POINT('',(9.6,2.,-31.08)) ;
#155737 = CARTESIAN_POINT('',(9.6,2.,-31.08)) ;
#155738 = CARTESIAN_POINT('Origin',(9.6,2.,-30.88)) ;
#155739 = CARTESIAN_POINT('Origin',(10.2,2.,-25.265)) ;
#155740 = CARTESIAN_POINT('',(10.1,2.,-25.365)) ;
#155741 = CARTESIAN_POINT('',(10.1,2.,-27.975)) ;
#155742 = CARTESIAN_POINT('',(10.1,2.,-28.075)) ;
#155743 = CARTESIAN_POINT('',(3.7,2.,-27.975)) ;
#155744 = CARTESIAN_POINT('',(10.2,2.,-27.975)) ;
#155745 = CARTESIAN_POINT('',(3.7,2.,-25.365)) ;
#155746 = CARTESIAN_POINT('',(3.7,2.,-25.265)) ;
#155747 = CARTESIAN_POINT('',(10.2,2.,-25.365)) ;
#155748 = CARTESIAN_POINT('',(9.8,2.,-27.07)) ;
#155749 = CARTESIAN_POINT('',(9.8,2.,-26.27)) ;
#155750 = CARTESIAN_POINT('',(9.8,2.,-26.27)) ;
#155751 = CARTESIAN_POINT('',(9.6,2.,-26.07)) ;
#155752 = CARTESIAN_POINT('Origin',(9.6,2.,-26.27)) ;
#155753 = CARTESIAN_POINT('',(7.8,2.,-26.07)) ;
#155754 = CARTESIAN_POINT('',(7.8,2.,-26.07)) ;
#155755 = CARTESIAN_POINT('',(7.6,2.,-26.27)) ;
#155756 = CARTESIAN_POINT('Origin',(7.8,2.,-26.27)) ;
#155757 = CARTESIAN_POINT('',(7.6,2.,-27.07)) ;
#155758 = CARTESIAN_POINT('',(7.6,2.,-27.07)) ;
#155759 = CARTESIAN_POINT('',(7.8,2.,-27.27)) ;
#155760 = CARTESIAN_POINT('Origin',(7.8,2.,-27.07)) ;
#155761 = CARTESIAN_POINT('',(9.6,2.,-27.27)) ;
#155762 = CARTESIAN_POINT('',(9.6,2.,-27.27)) ;
#155763 = CARTESIAN_POINT('Origin',(9.6,2.,-27.07)) ;
#155764 = CARTESIAN_POINT('Origin',(10.2,2.,-21.455)) ;
#155765 = CARTESIAN_POINT('',(10.1,2.,-21.555)) ;
#155766 = CARTESIAN_POINT('',(10.1,2.,-24.165)) ;
#155767 = CARTESIAN_POINT('',(10.1,2.,-24.265)) ;
#155768 = CARTESIAN_POINT('',(3.7,2.,-24.165)) ;
#155769 = CARTESIAN_POINT('',(10.2,2.,-24.165)) ;
#155770 = CARTESIAN_POINT('',(3.7,2.,-21.555)) ;
#155771 = CARTESIAN_POINT('',(3.7,2.,-21.455)) ;
#155772 = CARTESIAN_POINT('',(10.2,2.,-21.555)) ;
#155773 = CARTESIAN_POINT('',(9.8,2.,-23.26)) ;
#155774 = CARTESIAN_POINT('',(9.8,2.,-22.46)) ;
#155775 = CARTESIAN_POINT('',(9.8,2.,-22.46)) ;
#155776 = CARTESIAN_POINT('',(9.6,2.,-22.26)) ;
#155777 = CARTESIAN_POINT('Origin',(9.6,2.,-22.46)) ;
#155778 = CARTESIAN_POINT('',(7.8,2.,-22.26)) ;
#155779 = CARTESIAN_POINT('',(7.8,2.,-22.26)) ;
#155780 = CARTESIAN_POINT('',(7.6,2.,-22.46)) ;
#155781 = CARTESIAN_POINT('Origin',(7.8,2.,-22.46)) ;
#155782 = CARTESIAN_POINT('',(7.6,2.,-23.26)) ;
#155783 = CARTESIAN_POINT('',(7.6,2.,-23.26)) ;
#155784 = CARTESIAN_POINT('',(7.8,2.,-23.46)) ;
#155785 = CARTESIAN_POINT('Origin',(7.8,2.,-23.26)) ;
#155786 = CARTESIAN_POINT('',(9.6,2.,-23.46)) ;
#155787 = CARTESIAN_POINT('',(9.6,2.,-23.46)) ;
#155788 = CARTESIAN_POINT('Origin',(9.6,2.,-23.26)) ;
#155789 = CARTESIAN_POINT('Origin',(10.2,2.,-17.645)) ;
#155790 = CARTESIAN_POINT('',(10.1,2.,-17.745)) ;
#155791 = CARTESIAN_POINT('',(10.1,2.,-20.355)) ;
#155792 = CARTESIAN_POINT('',(10.1,2.,-20.455)) ;
#155793 = CARTESIAN_POINT('',(3.7,2.,-20.355)) ;
#155794 = CARTESIAN_POINT('',(10.2,2.,-20.355)) ;
#155795 = CARTESIAN_POINT('',(3.7,2.,-17.745)) ;
#155796 = CARTESIAN_POINT('',(3.7,2.,-17.645)) ;
#155797 = CARTESIAN_POINT('',(10.2,2.,-17.745)) ;
#155798 = CARTESIAN_POINT('',(9.8,2.,-19.45)) ;
#155799 = CARTESIAN_POINT('',(9.8,2.,-18.65)) ;
#155800 = CARTESIAN_POINT('',(9.8,2.,-18.65)) ;
#155801 = CARTESIAN_POINT('',(9.6,2.,-18.45)) ;
#155802 = CARTESIAN_POINT('Origin',(9.6,2.,-18.65)) ;
#155803 = CARTESIAN_POINT('',(7.8,2.,-18.45)) ;
#155804 = CARTESIAN_POINT('',(7.8,2.,-18.45)) ;
#155805 = CARTESIAN_POINT('',(7.6,2.,-18.65)) ;
#155806 = CARTESIAN_POINT('Origin',(7.8,2.,-18.65)) ;
#155807 = CARTESIAN_POINT('',(7.6,2.,-19.45)) ;
#155808 = CARTESIAN_POINT('',(7.6,2.,-19.45)) ;
#155809 = CARTESIAN_POINT('',(7.8,2.,-19.65)) ;
#155810 = CARTESIAN_POINT('Origin',(7.8,2.,-19.45)) ;
#155811 = CARTESIAN_POINT('',(9.6,2.,-19.65)) ;
#155812 = CARTESIAN_POINT('',(9.6,2.,-19.65)) ;
#155813 = CARTESIAN_POINT('Origin',(9.6,2.,-19.45)) ;
#155814 = CARTESIAN_POINT('Origin',(10.2,2.,-13.835)) ;
#155815 = CARTESIAN_POINT('',(10.1,2.,-13.935)) ;
#155816 = CARTESIAN_POINT('',(10.1,2.,-16.545)) ;
#155817 = CARTESIAN_POINT('',(10.1,2.,-16.645)) ;
#155818 = CARTESIAN_POINT('',(3.7,2.,-16.545)) ;
#155819 = CARTESIAN_POINT('',(10.2,2.,-16.545)) ;
#155820 = CARTESIAN_POINT('',(3.7,2.,-13.935)) ;
#155821 = CARTESIAN_POINT('',(3.7,2.,-13.835)) ;
#155822 = CARTESIAN_POINT('',(10.2,2.,-13.935)) ;
#155823 = CARTESIAN_POINT('',(9.8,2.,-15.64)) ;
#155824 = CARTESIAN_POINT('',(9.8,2.,-14.84)) ;
#155825 = CARTESIAN_POINT('',(9.8,2.,-14.84)) ;
#155826 = CARTESIAN_POINT('',(9.6,2.,-14.64)) ;
#155827 = CARTESIAN_POINT('Origin',(9.6,2.,-14.84)) ;
#155828 = CARTESIAN_POINT('',(7.8,2.,-14.64)) ;
#155829 = CARTESIAN_POINT('',(7.8,2.,-14.64)) ;
#155830 = CARTESIAN_POINT('',(7.6,2.,-14.84)) ;
#155831 = CARTESIAN_POINT('Origin',(7.8,2.,-14.84)) ;
#155832 = CARTESIAN_POINT('',(7.6,2.,-15.64)) ;
#155833 = CARTESIAN_POINT('',(7.6,2.,-15.64)) ;
#155834 = CARTESIAN_POINT('',(7.8,2.,-15.84)) ;
#155835 = CARTESIAN_POINT('Origin',(7.8,2.,-15.64)) ;
#155836 = CARTESIAN_POINT('',(9.6,2.,-15.84)) ;
#155837 = CARTESIAN_POINT('',(9.6,2.,-15.84)) ;
#155838 = CARTESIAN_POINT('Origin',(9.6,2.,-15.64)) ;
#155839 = CARTESIAN_POINT('Origin',(10.2,2.,-10.025)) ;
#155840 = CARTESIAN_POINT('',(10.1,2.,-10.125)) ;
#155841 = CARTESIAN_POINT('',(10.1,2.,-12.735)) ;
#155842 = CARTESIAN_POINT('',(10.1,2.,-12.835)) ;
#155843 = CARTESIAN_POINT('',(3.7,2.,-12.735)) ;
#155844 = CARTESIAN_POINT('',(10.2,2.,-12.735)) ;
#155845 = CARTESIAN_POINT('',(3.7,2.,-10.125)) ;
#155846 = CARTESIAN_POINT('',(3.7,2.,-10.025)) ;
#155847 = CARTESIAN_POINT('',(10.2,2.,-10.125)) ;
#155848 = CARTESIAN_POINT('',(9.8,2.,-11.83)) ;
#155849 = CARTESIAN_POINT('',(9.8,2.,-11.03)) ;
#155850 = CARTESIAN_POINT('',(9.8,2.,-11.03)) ;
#155851 = CARTESIAN_POINT('',(9.6,2.,-10.83)) ;
#155852 = CARTESIAN_POINT('Origin',(9.6,2.,-11.03)) ;
#155853 = CARTESIAN_POINT('',(7.8,2.,-10.83)) ;
#155854 = CARTESIAN_POINT('',(7.8,2.,-10.83)) ;
#155855 = CARTESIAN_POINT('',(7.6,2.,-11.03)) ;
#155856 = CARTESIAN_POINT('Origin',(7.8,2.,-11.03)) ;
#155857 = CARTESIAN_POINT('',(7.6,2.,-11.83)) ;
#155858 = CARTESIAN_POINT('',(7.6,2.,-11.83)) ;
#155859 = CARTESIAN_POINT('',(7.8,2.,-12.03)) ;
#155860 = CARTESIAN_POINT('Origin',(7.8,2.,-11.83)) ;
#155861 = CARTESIAN_POINT('',(9.6,2.,-12.03)) ;
#155862 = CARTESIAN_POINT('',(9.6,2.,-12.03)) ;
#155863 = CARTESIAN_POINT('Origin',(9.6,2.,-11.83)) ;
#155864 = CARTESIAN_POINT('Origin',(10.2,2.,-6.215)) ;
#155865 = CARTESIAN_POINT('',(10.1,2.,-6.315)) ;
#155866 = CARTESIAN_POINT('',(10.1,2.,-8.925)) ;
#155867 = CARTESIAN_POINT('',(10.1,2.,-9.025)) ;
#155868 = CARTESIAN_POINT('',(3.7,2.,-8.925)) ;
#155869 = CARTESIAN_POINT('',(10.2,2.,-8.925)) ;
#155870 = CARTESIAN_POINT('',(3.7,2.,-6.315)) ;
#155871 = CARTESIAN_POINT('',(3.7,2.,-6.215)) ;
#155872 = CARTESIAN_POINT('',(10.2,2.,-6.315)) ;
#155873 = CARTESIAN_POINT('',(9.8,2.,-8.02)) ;
#155874 = CARTESIAN_POINT('',(9.8,2.,-7.22)) ;
#155875 = CARTESIAN_POINT('',(9.8,2.,-7.22)) ;
#155876 = CARTESIAN_POINT('',(9.6,2.,-7.02)) ;
#155877 = CARTESIAN_POINT('Origin',(9.6,2.,-7.22)) ;
#155878 = CARTESIAN_POINT('',(7.8,2.,-7.02)) ;
#155879 = CARTESIAN_POINT('',(7.8,2.,-7.02)) ;
#155880 = CARTESIAN_POINT('',(7.6,2.,-7.22)) ;
#155881 = CARTESIAN_POINT('Origin',(7.8,2.,-7.22)) ;
#155882 = CARTESIAN_POINT('',(7.6,2.,-8.02)) ;
#155883 = CARTESIAN_POINT('',(7.6,2.,-8.02)) ;
#155884 = CARTESIAN_POINT('',(7.8,2.,-8.22)) ;
#155885 = CARTESIAN_POINT('Origin',(7.8,2.,-8.02)) ;
#155886 = CARTESIAN_POINT('',(9.6,2.,-8.22)) ;
#155887 = CARTESIAN_POINT('',(9.6,2.,-8.22)) ;
#155888 = CARTESIAN_POINT('Origin',(9.6,2.,-8.02)) ;
#155889 = CARTESIAN_POINT('Origin',(10.2,2.,-2.405)) ;
#155890 = CARTESIAN_POINT('',(10.1,2.,-2.505)) ;
#155891 = CARTESIAN_POINT('',(10.1,2.,-5.115)) ;
#155892 = CARTESIAN_POINT('',(10.1,2.,-5.215)) ;
#155893 = CARTESIAN_POINT('',(3.7,2.,-5.115)) ;
#155894 = CARTESIAN_POINT('',(10.2,2.,-5.115)) ;
#155895 = CARTESIAN_POINT('',(3.7,2.,-2.505)) ;
#155896 = CARTESIAN_POINT('',(3.7,2.,-2.405)) ;
#155897 = CARTESIAN_POINT('',(10.2,2.,-2.505)) ;
#155898 = CARTESIAN_POINT('',(9.8,2.,-4.21)) ;
#155899 = CARTESIAN_POINT('',(9.8,2.,-3.41)) ;
#155900 = CARTESIAN_POINT('',(9.8,2.,-3.41)) ;
#155901 = CARTESIAN_POINT('',(9.6,2.,-3.21)) ;
#155902 = CARTESIAN_POINT('Origin',(9.6,2.,-3.41)) ;
#155903 = CARTESIAN_POINT('',(7.8,2.,-3.21)) ;
#155904 = CARTESIAN_POINT('',(7.8,2.,-3.21)) ;
#155905 = CARTESIAN_POINT('',(7.6,2.,-3.41)) ;
#155906 = CARTESIAN_POINT('Origin',(7.8,2.,-3.41)) ;
#155907 = CARTESIAN_POINT('',(7.6,2.,-4.21)) ;
#155908 = CARTESIAN_POINT('',(7.6,2.,-4.21)) ;
#155909 = CARTESIAN_POINT('',(7.8,2.,-4.41)) ;
#155910 = CARTESIAN_POINT('Origin',(7.8,2.,-4.21)) ;
#155911 = CARTESIAN_POINT('',(9.6,2.,-4.41)) ;
#155912 = CARTESIAN_POINT('',(9.6,2.,-4.41)) ;
#155913 = CARTESIAN_POINT('Origin',(9.6,2.,-4.21)) ;
#155914 = CARTESIAN_POINT('Origin',(-7.29372370581158E-16,3.55,-34.29)) ;
#155915 = CARTESIAN_POINT('',(0.18330135972941,3.55,-35.807036786476)) ;
#155916 = CARTESIAN_POINT('Origin',(-7.29372370581158E-16,3.55,-30.48)) ;
#155917 = CARTESIAN_POINT('',(0.18330135972941,3.55,-31.997036786476)) ;
#155918 = CARTESIAN_POINT('Origin',(-7.29372370581158E-16,3.55,-26.67)) ;
#155919 = CARTESIAN_POINT('',(0.18330135972941,3.55,-28.187036786476)) ;
#155920 = CARTESIAN_POINT('Origin',(-7.29372370581158E-16,3.55,-22.86)) ;
#155921 = CARTESIAN_POINT('',(0.18330135972941,3.55,-24.377036786476)) ;
#155922 = CARTESIAN_POINT('Origin',(-7.29372370581158E-16,3.55,-19.05)) ;
#155923 = CARTESIAN_POINT('',(0.18330135972941,3.55,-20.567036786476)) ;
#155924 = CARTESIAN_POINT('Origin',(-7.29372370581158E-16,3.55,-15.24)) ;
#155925 = CARTESIAN_POINT('',(0.183301359729409,3.55,-16.757036786476)) ;
#155926 = CARTESIAN_POINT('Origin',(-7.29372370581158E-16,3.55,-11.43)) ;
#155927 = CARTESIAN_POINT('',(0.183301359729409,3.55,-12.947036786476)) ;
#155928 = CARTESIAN_POINT('Origin',(-7.29372370581158E-16,3.55,-7.62)) ;
#155929 = CARTESIAN_POINT('',(0.183301359729409,3.55,-9.13703678647597)) ;
#155930 = CARTESIAN_POINT('Origin',(-7.29372370581158E-16,3.55,-3.81)) ;
#155931 = CARTESIAN_POINT('',(0.183301359729409,3.55,-5.32703678647597)) ;
#155932 = CARTESIAN_POINT('Origin',(3.6,7.81406971160724E-17,0.)) ;
#155933 = CARTESIAN_POINT('',(3.6,2.1,-35.795)) ;
#155934 = CARTESIAN_POINT('',(3.6,2.1,-36.49)) ;
#155935 = CARTESIAN_POINT('',(3.6,2.1,-36.59)) ;
#155936 = CARTESIAN_POINT('',(3.6,2.65,-36.49)) ;
#155937 = CARTESIAN_POINT('',(3.6,7.81406971160724E-17,-36.49)) ;
#155938 = CARTESIAN_POINT('',(3.6,2.65,2.2)) ;
#155939 = CARTESIAN_POINT('',(3.6,2.65,-1.51)) ;
#155940 = CARTESIAN_POINT('',(3.6,2.1,2.2)) ;
#155941 = CARTESIAN_POINT('',(3.6,2.1,2.2)) ;
#155942 = CARTESIAN_POINT('',(3.6,2.1,1.505)) ;
#155943 = CARTESIAN_POINT('',(3.6,2.1,1.505)) ;
#155944 = CARTESIAN_POINT('',(3.6,2.07320508075689,1.405)) ;
#155945 = CARTESIAN_POINT('Origin',(3.6,1.9,1.505)) ;
#155946 = CARTESIAN_POINT('',(3.6,2.1,1.305)) ;
#155947 = CARTESIAN_POINT('Origin',(3.6,1.9,1.305)) ;
#155948 = CARTESIAN_POINT('',(3.6,2.1,-1.305)) ;
#155949 = CARTESIAN_POINT('',(3.6,2.1,0.)) ;
#155950 = CARTESIAN_POINT('',(3.6,2.07320508075689,-1.405)) ;
#155951 = CARTESIAN_POINT('Origin',(3.6,1.9,-1.305)) ;
#155952 = CARTESIAN_POINT('',(3.6,2.1,-1.505)) ;
#155953 = CARTESIAN_POINT('Origin',(3.6,1.9,-1.505)) ;
#155954 = CARTESIAN_POINT('',(3.6,2.1,-2.305)) ;
#155955 = CARTESIAN_POINT('',(3.6,2.1,-2.3)) ;
#155956 = CARTESIAN_POINT('',(3.6,2.07320508075689,-2.405)) ;
#155957 = CARTESIAN_POINT('Origin',(3.6,1.9,-2.305)) ;
#155958 = CARTESIAN_POINT('',(3.6,2.1,-2.505)) ;
#155959 = CARTESIAN_POINT('Origin',(3.6,1.9,-2.505)) ;
#155960 = CARTESIAN_POINT('',(3.6,2.1,-5.115)) ;
#155961 = CARTESIAN_POINT('',(3.6,2.1,0.)) ;
#155962 = CARTESIAN_POINT('',(3.6,2.07320508075689,-5.215)) ;
#155963 = CARTESIAN_POINT('Origin',(3.6,1.9,-5.115)) ;
#155964 = CARTESIAN_POINT('',(3.6,2.1,-5.315)) ;
#155965 = CARTESIAN_POINT('Origin',(3.6,1.9,-5.315)) ;
#155966 = CARTESIAN_POINT('',(3.6,2.1,-6.115)) ;
#155967 = CARTESIAN_POINT('',(3.6,2.1,-6.115)) ;
#155968 = CARTESIAN_POINT('',(3.6,2.07320508075689,-6.215)) ;
#155969 = CARTESIAN_POINT('Origin',(3.6,1.9,-6.115)) ;
#155970 = CARTESIAN_POINT('',(3.6,2.1,-6.315)) ;
#155971 = CARTESIAN_POINT('Origin',(3.6,1.9,-6.315)) ;
#155972 = CARTESIAN_POINT('',(3.6,2.1,-8.925)) ;
#155973 = CARTESIAN_POINT('',(3.6,2.1,0.)) ;
#155974 = CARTESIAN_POINT('',(3.6,2.07320508075689,-9.025)) ;
#155975 = CARTESIAN_POINT('Origin',(3.6,1.9,-8.925)) ;
#155976 = CARTESIAN_POINT('',(3.6,2.1,-9.125)) ;
#155977 = CARTESIAN_POINT('Origin',(3.6,1.9,-9.125)) ;
#155978 = CARTESIAN_POINT('',(3.6,2.1,-9.925)) ;
#155979 = CARTESIAN_POINT('',(3.6,2.1,-9.925)) ;
#155980 = CARTESIAN_POINT('',(3.6,2.07320508075689,-10.025)) ;
#155981 = CARTESIAN_POINT('Origin',(3.6,1.9,-9.925)) ;
#155982 = CARTESIAN_POINT('',(3.6,2.1,-10.125)) ;
#155983 = CARTESIAN_POINT('Origin',(3.6,1.9,-10.125)) ;
#155984 = CARTESIAN_POINT('',(3.6,2.1,-12.735)) ;
#155985 = CARTESIAN_POINT('',(3.6,2.1,0.)) ;
#155986 = CARTESIAN_POINT('',(3.6,2.07320508075689,-12.835)) ;
#155987 = CARTESIAN_POINT('Origin',(3.6,1.9,-12.735)) ;
#155988 = CARTESIAN_POINT('',(3.6,2.1,-12.935)) ;
#155989 = CARTESIAN_POINT('Origin',(3.6,1.9,-12.935)) ;
#155990 = CARTESIAN_POINT('',(3.6,2.1,-13.735)) ;
#155991 = CARTESIAN_POINT('',(3.6,2.1,-13.735)) ;
#155992 = CARTESIAN_POINT('',(3.6,2.07320508075689,-13.835)) ;
#155993 = CARTESIAN_POINT('Origin',(3.6,1.9,-13.735)) ;
#155994 = CARTESIAN_POINT('',(3.6,2.1,-13.935)) ;
#155995 = CARTESIAN_POINT('Origin',(3.6,1.9,-13.935)) ;
#155996 = CARTESIAN_POINT('',(3.6,2.1,-16.545)) ;
#155997 = CARTESIAN_POINT('',(3.6,2.1,0.)) ;
#155998 = CARTESIAN_POINT('',(3.6,2.07320508075689,-16.645)) ;
#155999 = CARTESIAN_POINT('Origin',(3.6,1.9,-16.545)) ;
#156000 = CARTESIAN_POINT('',(3.6,2.1,-16.745)) ;
#156001 = CARTESIAN_POINT('Origin',(3.6,1.9,-16.745)) ;
#156002 = CARTESIAN_POINT('',(3.6,2.1,-17.545)) ;
#156003 = CARTESIAN_POINT('',(3.6,2.1,-17.545)) ;
#156004 = CARTESIAN_POINT('',(3.6,2.07320508075689,-17.645)) ;
#156005 = CARTESIAN_POINT('Origin',(3.6,1.9,-17.545)) ;
#156006 = CARTESIAN_POINT('',(3.6,2.1,-17.745)) ;
#156007 = CARTESIAN_POINT('Origin',(3.6,1.9,-17.745)) ;
#156008 = CARTESIAN_POINT('',(3.6,2.1,-20.355)) ;
#156009 = CARTESIAN_POINT('',(3.6,2.1,0.)) ;
#156010 = CARTESIAN_POINT('',(3.6,2.07320508075689,-20.455)) ;
#156011 = CARTESIAN_POINT('Origin',(3.6,1.9,-20.355)) ;
#156012 = CARTESIAN_POINT('',(3.6,2.1,-20.555)) ;
#156013 = CARTESIAN_POINT('Origin',(3.6,1.9,-20.555)) ;
#156014 = CARTESIAN_POINT('',(3.6,2.1,-21.355)) ;
#156015 = CARTESIAN_POINT('',(3.6,2.1,-21.355)) ;
#156016 = CARTESIAN_POINT('',(3.6,2.07320508075689,-21.455)) ;
#156017 = CARTESIAN_POINT('Origin',(3.6,1.9,-21.355)) ;
#156018 = CARTESIAN_POINT('',(3.6,2.1,-21.555)) ;
#156019 = CARTESIAN_POINT('Origin',(3.6,1.9,-21.555)) ;
#156020 = CARTESIAN_POINT('',(3.6,2.1,-24.165)) ;
#156021 = CARTESIAN_POINT('',(3.6,2.1,0.)) ;
#156022 = CARTESIAN_POINT('',(3.6,2.07320508075689,-24.265)) ;
#156023 = CARTESIAN_POINT('Origin',(3.6,1.9,-24.165)) ;
#156024 = CARTESIAN_POINT('',(3.6,2.1,-24.365)) ;
#156025 = CARTESIAN_POINT('Origin',(3.6,1.9,-24.365)) ;
#156026 = CARTESIAN_POINT('',(3.6,2.1,-25.165)) ;
#156027 = CARTESIAN_POINT('',(3.6,2.1,-25.165)) ;
#156028 = CARTESIAN_POINT('',(3.6,2.07320508075689,-25.265)) ;
#156029 = CARTESIAN_POINT('Origin',(3.6,1.9,-25.165)) ;
#156030 = CARTESIAN_POINT('',(3.6,2.1,-25.365)) ;
#156031 = CARTESIAN_POINT('Origin',(3.6,1.9,-25.365)) ;
#156032 = CARTESIAN_POINT('',(3.6,2.1,-27.975)) ;
#156033 = CARTESIAN_POINT('',(3.6,2.1,0.)) ;
#156034 = CARTESIAN_POINT('',(3.6,2.07320508075689,-28.075)) ;
#156035 = CARTESIAN_POINT('Origin',(3.6,1.9,-27.975)) ;
#156036 = CARTESIAN_POINT('',(3.6,2.1,-28.175)) ;
#156037 = CARTESIAN_POINT('Origin',(3.6,1.9,-28.175)) ;
#156038 = CARTESIAN_POINT('',(3.6,2.1,-28.975)) ;
#156039 = CARTESIAN_POINT('',(3.6,2.1,-28.975)) ;
#156040 = CARTESIAN_POINT('',(3.6,2.07320508075689,-29.075)) ;
#156041 = CARTESIAN_POINT('Origin',(3.6,1.9,-28.975)) ;
#156042 = CARTESIAN_POINT('',(3.6,2.1,-29.175)) ;
#156043 = CARTESIAN_POINT('Origin',(3.6,1.9,-29.175)) ;
#156044 = CARTESIAN_POINT('',(3.6,2.1,-31.785)) ;
#156045 = CARTESIAN_POINT('',(3.6,2.1,0.)) ;
#156046 = CARTESIAN_POINT('',(3.6,2.07320508075689,-31.885)) ;
#156047 = CARTESIAN_POINT('Origin',(3.6,1.9,-31.785)) ;
#156048 = CARTESIAN_POINT('',(3.6,2.1,-31.985)) ;
#156049 = CARTESIAN_POINT('Origin',(3.6,1.9,-31.985)) ;
#156050 = CARTESIAN_POINT('',(3.6,2.1,-32.785)) ;
#156051 = CARTESIAN_POINT('',(3.6,2.1,-32.785)) ;
#156052 = CARTESIAN_POINT('',(3.6,2.07320508075689,-32.885)) ;
#156053 = CARTESIAN_POINT('Origin',(3.6,1.9,-32.785)) ;
#156054 = CARTESIAN_POINT('',(3.6,2.1,-32.985)) ;
#156055 = CARTESIAN_POINT('Origin',(3.6,1.9,-32.985)) ;
#156056 = CARTESIAN_POINT('',(3.6,2.1,-35.595)) ;
#156057 = CARTESIAN_POINT('',(3.6,2.1,0.)) ;
#156058 = CARTESIAN_POINT('',(3.6,2.07320508075689,-35.695)) ;
#156059 = CARTESIAN_POINT('Origin',(3.6,1.9,-35.595)) ;
#156060 = CARTESIAN_POINT('Origin',(3.6,1.9,-35.795)) ;
#156061 = CARTESIAN_POINT('Origin',(3.6,7.81406971160724E-17,0.)) ;
#156062 = CARTESIAN_POINT('',(3.6,-2.35,-33.3868804065906)) ;
#156063 = CARTESIAN_POINT('',(3.6,-2.32153024911032,-33.4897267659824)) ;
#156064 = CARTESIAN_POINT('Origin',(3.6,-2.15,-33.3868804065906)) ;
#156065 = CARTESIAN_POINT('',(3.6,-2.35,-32.985)) ;
#156066 = CARTESIAN_POINT('',(3.6,-2.35,0.)) ;
#156067 = CARTESIAN_POINT('',(3.6,-5.15,-32.985)) ;
#156068 = CARTESIAN_POINT('',(3.6,-5.25,-32.985)) ;
#156069 = CARTESIAN_POINT('',(3.6,-5.15,-35.595)) ;
#156070 = CARTESIAN_POINT('',(3.6,-5.15,-35.695)) ;
#156071 = CARTESIAN_POINT('',(3.6,-2.35,-35.595)) ;
#156072 = CARTESIAN_POINT('',(3.6,-2.25,-35.595)) ;
#156073 = CARTESIAN_POINT('',(3.6,-2.35,-35.1931195934094)) ;
#156074 = CARTESIAN_POINT('',(3.6,-2.35,0.)) ;
#156075 = CARTESIAN_POINT('',(3.6,-2.32153024911032,-35.0902732340176)) ;
#156076 = CARTESIAN_POINT('Origin',(3.6,-2.15,-35.1931195934094)) ;
#156077 = CARTESIAN_POINT('Origin',(3.6,-3.65625,-34.29)) ;
#156078 = CARTESIAN_POINT('Origin',(3.6,7.81406971160724E-17,0.)) ;
#156079 = CARTESIAN_POINT('',(3.6,-2.35,-29.5768804065906)) ;
#156080 = CARTESIAN_POINT('',(3.6,-2.32153024911032,-29.6797267659824)) ;
#156081 = CARTESIAN_POINT('Origin',(3.6,-2.15,-29.5768804065906)) ;
#156082 = CARTESIAN_POINT('',(3.6,-2.35,-29.175)) ;
#156083 = CARTESIAN_POINT('',(3.6,-2.35,0.)) ;
#156084 = CARTESIAN_POINT('',(3.6,-5.15,-29.175)) ;
#156085 = CARTESIAN_POINT('',(3.6,-5.25,-29.175)) ;
#156086 = CARTESIAN_POINT('',(3.6,-5.15,-31.785)) ;
#156087 = CARTESIAN_POINT('',(3.6,-5.15,-31.885)) ;
#156088 = CARTESIAN_POINT('',(3.6,-2.35,-31.785)) ;
#156089 = CARTESIAN_POINT('',(3.6,-2.25,-31.785)) ;
#156090 = CARTESIAN_POINT('',(3.6,-2.35,-31.3831195934094)) ;
#156091 = CARTESIAN_POINT('',(3.6,-2.35,0.)) ;
#156092 = CARTESIAN_POINT('',(3.6,-2.32153024911032,-31.2802732340176)) ;
#156093 = CARTESIAN_POINT('Origin',(3.6,-2.15,-31.3831195934094)) ;
#156094 = CARTESIAN_POINT('Origin',(3.6,-3.65625,-30.48)) ;
#156095 = CARTESIAN_POINT('Origin',(3.6,7.81406971160724E-17,0.)) ;
#156096 = CARTESIAN_POINT('',(3.6,-2.35,-25.7668804065906)) ;
#156097 = CARTESIAN_POINT('',(3.6,-2.32153024911032,-25.8697267659824)) ;
#156098 = CARTESIAN_POINT('Origin',(3.6,-2.15,-25.7668804065906)) ;
#156099 = CARTESIAN_POINT('',(3.6,-2.35,-25.365)) ;
#156100 = CARTESIAN_POINT('',(3.6,-2.35,0.)) ;
#156101 = CARTESIAN_POINT('',(3.6,-5.15,-25.365)) ;
#156102 = CARTESIAN_POINT('',(3.6,-5.25,-25.365)) ;
#156103 = CARTESIAN_POINT('',(3.6,-5.15,-27.975)) ;
#156104 = CARTESIAN_POINT('',(3.6,-5.15,-28.075)) ;
#156105 = CARTESIAN_POINT('',(3.6,-2.35,-27.975)) ;
#156106 = CARTESIAN_POINT('',(3.6,-2.25,-27.975)) ;
#156107 = CARTESIAN_POINT('',(3.6,-2.35,-27.5731195934094)) ;
#156108 = CARTESIAN_POINT('',(3.6,-2.35,0.)) ;
#156109 = CARTESIAN_POINT('',(3.6,-2.32153024911032,-27.4702732340176)) ;
#156110 = CARTESIAN_POINT('Origin',(3.6,-2.15,-27.5731195934094)) ;
#156111 = CARTESIAN_POINT('Origin',(3.6,-3.65625,-26.67)) ;
#156112 = CARTESIAN_POINT('Origin',(3.6,7.81406971160724E-17,0.)) ;
#156113 = CARTESIAN_POINT('',(3.6,-2.35,-21.9568804065906)) ;
#156114 = CARTESIAN_POINT('',(3.6,-2.32153024911032,-22.0597267659824)) ;
#156115 = CARTESIAN_POINT('Origin',(3.6,-2.15,-21.9568804065906)) ;
#156116 = CARTESIAN_POINT('',(3.6,-2.35,-21.555)) ;
#156117 = CARTESIAN_POINT('',(3.6,-2.35,0.)) ;
#156118 = CARTESIAN_POINT('',(3.6,-5.15,-21.555)) ;
#156119 = CARTESIAN_POINT('',(3.6,-5.25,-21.555)) ;
#156120 = CARTESIAN_POINT('',(3.6,-5.15,-24.165)) ;
#156121 = CARTESIAN_POINT('',(3.6,-5.15,-24.265)) ;
#156122 = CARTESIAN_POINT('',(3.6,-2.35,-24.165)) ;
#156123 = CARTESIAN_POINT('',(3.6,-2.25,-24.165)) ;
#156124 = CARTESIAN_POINT('',(3.6,-2.35,-23.7631195934094)) ;
#156125 = CARTESIAN_POINT('',(3.6,-2.35,0.)) ;
#156126 = CARTESIAN_POINT('',(3.6,-2.32153024911032,-23.6602732340176)) ;
#156127 = CARTESIAN_POINT('Origin',(3.6,-2.15,-23.7631195934094)) ;
#156128 = CARTESIAN_POINT('Origin',(3.6,-3.65625,-22.86)) ;
#156129 = CARTESIAN_POINT('Origin',(3.6,7.81406971160724E-17,0.)) ;
#156130 = CARTESIAN_POINT('',(3.6,-2.35,-18.1468804065906)) ;
#156131 = CARTESIAN_POINT('',(3.6,-2.32153024911032,-18.2497267659824)) ;
#156132 = CARTESIAN_POINT('Origin',(3.6,-2.15,-18.1468804065906)) ;
#156133 = CARTESIAN_POINT('',(3.6,-2.35,-17.745)) ;
#156134 = CARTESIAN_POINT('',(3.6,-2.35,0.)) ;
#156135 = CARTESIAN_POINT('',(3.6,-5.15,-17.745)) ;
#156136 = CARTESIAN_POINT('',(3.6,-5.25,-17.745)) ;
#156137 = CARTESIAN_POINT('',(3.6,-5.15,-20.355)) ;
#156138 = CARTESIAN_POINT('',(3.6,-5.15,-20.455)) ;
#156139 = CARTESIAN_POINT('',(3.6,-2.35,-20.355)) ;
#156140 = CARTESIAN_POINT('',(3.6,-2.25,-20.355)) ;
#156141 = CARTESIAN_POINT('',(3.6,-2.35,-19.9531195934094)) ;
#156142 = CARTESIAN_POINT('',(3.6,-2.35,0.)) ;
#156143 = CARTESIAN_POINT('',(3.6,-2.32153024911032,-19.8502732340176)) ;
#156144 = CARTESIAN_POINT('Origin',(3.6,-2.15,-19.9531195934094)) ;
#156145 = CARTESIAN_POINT('Origin',(3.6,-3.65625,-19.05)) ;
#156146 = CARTESIAN_POINT('Origin',(3.6,7.81406971160724E-17,0.)) ;
#156147 = CARTESIAN_POINT('',(3.6,-2.35,-14.3368804065906)) ;
#156148 = CARTESIAN_POINT('',(3.6,-2.32153024911032,-14.4397267659824)) ;
#156149 = CARTESIAN_POINT('Origin',(3.6,-2.15,-14.3368804065906)) ;
#156150 = CARTESIAN_POINT('',(3.6,-2.35,-13.935)) ;
#156151 = CARTESIAN_POINT('',(3.6,-2.35,0.)) ;
#156152 = CARTESIAN_POINT('',(3.6,-5.15,-13.935)) ;
#156153 = CARTESIAN_POINT('',(3.6,-5.25,-13.935)) ;
#156154 = CARTESIAN_POINT('',(3.6,-5.15,-16.545)) ;
#156155 = CARTESIAN_POINT('',(3.6,-5.15,-16.645)) ;
#156156 = CARTESIAN_POINT('',(3.6,-2.35,-16.545)) ;
#156157 = CARTESIAN_POINT('',(3.6,-2.25,-16.545)) ;
#156158 = CARTESIAN_POINT('',(3.6,-2.35,-16.1431195934094)) ;
#156159 = CARTESIAN_POINT('',(3.6,-2.35,0.)) ;
#156160 = CARTESIAN_POINT('',(3.6,-2.32153024911032,-16.0402732340176)) ;
#156161 = CARTESIAN_POINT('Origin',(3.6,-2.15,-16.1431195934094)) ;
#156162 = CARTESIAN_POINT('Origin',(3.6,-3.65625,-15.24)) ;
#156163 = CARTESIAN_POINT('Origin',(3.6,7.81406971160724E-17,0.)) ;
#156164 = CARTESIAN_POINT('',(3.6,-2.35,-10.5268804065906)) ;
#156165 = CARTESIAN_POINT('',(3.6,-2.32153024911032,-10.6297267659824)) ;
#156166 = CARTESIAN_POINT('Origin',(3.6,-2.15,-10.5268804065906)) ;
#156167 = CARTESIAN_POINT('',(3.6,-2.35,-10.125)) ;
#156168 = CARTESIAN_POINT('',(3.6,-2.35,0.)) ;
#156169 = CARTESIAN_POINT('',(3.6,-5.15,-10.125)) ;
#156170 = CARTESIAN_POINT('',(3.6,-5.25,-10.125)) ;
#156171 = CARTESIAN_POINT('',(3.6,-5.15,-12.735)) ;
#156172 = CARTESIAN_POINT('',(3.6,-5.15,-12.835)) ;
#156173 = CARTESIAN_POINT('',(3.6,-2.35,-12.735)) ;
#156174 = CARTESIAN_POINT('',(3.6,-2.25,-12.735)) ;
#156175 = CARTESIAN_POINT('',(3.6,-2.35,-12.3331195934094)) ;
#156176 = CARTESIAN_POINT('',(3.6,-2.35,0.)) ;
#156177 = CARTESIAN_POINT('',(3.6,-2.32153024911032,-12.2302732340176)) ;
#156178 = CARTESIAN_POINT('Origin',(3.6,-2.15,-12.3331195934094)) ;
#156179 = CARTESIAN_POINT('Origin',(3.6,-3.65625,-11.43)) ;
#156180 = CARTESIAN_POINT('Origin',(3.6,7.81406971160724E-17,0.)) ;
#156181 = CARTESIAN_POINT('',(3.6,-2.35,-6.71688040659058)) ;
#156182 = CARTESIAN_POINT('',(3.6,-2.32153024911032,-6.8197267659824)) ;
#156183 = CARTESIAN_POINT('Origin',(3.6,-2.15,-6.71688040659058)) ;
#156184 = CARTESIAN_POINT('',(3.6,-2.35,-6.315)) ;
#156185 = CARTESIAN_POINT('',(3.6,-2.35,0.)) ;
#156186 = CARTESIAN_POINT('',(3.6,-5.15,-6.315)) ;
#156187 = CARTESIAN_POINT('',(3.6,-5.25,-6.315)) ;
#156188 = CARTESIAN_POINT('',(3.6,-5.15,-8.925)) ;
#156189 = CARTESIAN_POINT('',(3.6,-5.15,-9.025)) ;
#156190 = CARTESIAN_POINT('',(3.6,-2.35,-8.925)) ;
#156191 = CARTESIAN_POINT('',(3.6,-2.25,-8.925)) ;
#156192 = CARTESIAN_POINT('',(3.6,-2.35,-8.52311959340942)) ;
#156193 = CARTESIAN_POINT('',(3.6,-2.35,0.)) ;
#156194 = CARTESIAN_POINT('',(3.6,-2.32153024911032,-8.4202732340176)) ;
#156195 = CARTESIAN_POINT('Origin',(3.6,-2.15,-8.52311959340942)) ;
#156196 = CARTESIAN_POINT('Origin',(3.6,-3.65625,-7.62)) ;
#156197 = CARTESIAN_POINT('Origin',(3.6,7.81406971160724E-17,0.)) ;
#156198 = CARTESIAN_POINT('',(3.6,-2.35,-2.90688040659058)) ;
#156199 = CARTESIAN_POINT('',(3.6,-2.32153024911032,-3.0097267659824)) ;
#156200 = CARTESIAN_POINT('Origin',(3.6,-2.15,-2.90688040659058)) ;
#156201 = CARTESIAN_POINT('',(3.6,-2.35,-2.505)) ;
#156202 = CARTESIAN_POINT('',(3.6,-2.35,0.)) ;
#156203 = CARTESIAN_POINT('',(3.6,-5.15,-2.505)) ;
#156204 = CARTESIAN_POINT('',(3.6,-5.25,-2.505)) ;
#156205 = CARTESIAN_POINT('',(3.6,-5.15,-5.115)) ;
#156206 = CARTESIAN_POINT('',(3.6,-5.15,-5.215)) ;
#156207 = CARTESIAN_POINT('',(3.6,-2.35,-5.115)) ;
#156208 = CARTESIAN_POINT('',(3.6,-2.25,-5.115)) ;
#156209 = CARTESIAN_POINT('',(3.6,-2.35,-4.71311959340942)) ;
#156210 = CARTESIAN_POINT('',(3.6,-2.35,0.)) ;
#156211 = CARTESIAN_POINT('',(3.6,-2.32153024911032,-4.6102732340176)) ;
#156212 = CARTESIAN_POINT('Origin',(3.6,-2.15,-4.71311959340942)) ;
#156213 = CARTESIAN_POINT('Origin',(3.6,-3.65625,-3.81)) ;
#156214 = CARTESIAN_POINT('Origin',(2.6,4.55,-36.59)) ;
#156215 = CARTESIAN_POINT('',(2.6,2.85,-36.49)) ;
#156216 = CARTESIAN_POINT('',(2.6,4.45,-36.49)) ;
#156217 = CARTESIAN_POINT('',(2.6,4.55,-36.49)) ;
#156218 = CARTESIAN_POINT('',(2.6,4.45,-35.94)) ;
#156219 = CARTESIAN_POINT('',(2.6,4.45,-36.59)) ;
#156220 = CARTESIAN_POINT('',(2.6,2.85,-35.94)) ;
#156221 = CARTESIAN_POINT('',(2.6,2.75,-35.94)) ;
#156222 = CARTESIAN_POINT('',(2.6,2.85,-36.59)) ;
#156223 = CARTESIAN_POINT('Origin',(2.6,4.55,-36.59)) ;
#156224 = CARTESIAN_POINT('',(2.6,-6.45,2.2)) ;
#156225 = CARTESIAN_POINT('',(2.6,-6.45,-36.49)) ;
#156226 = CARTESIAN_POINT('',(2.6,-6.45,-36.59)) ;
#156227 = CARTESIAN_POINT('',(2.6,1.9,-36.49)) ;
#156228 = CARTESIAN_POINT('',(2.6,4.55,-36.49)) ;
#156229 = CARTESIAN_POINT('',(2.6,1.9,-35.795)) ;
#156230 = CARTESIAN_POINT('',(2.6,1.9,-36.59)) ;
#156231 = CARTESIAN_POINT('',(2.6,-5.15,-35.795)) ;
#156232 = CARTESIAN_POINT('',(2.6,4.55,-35.795)) ;
#156233 = CARTESIAN_POINT('',(2.6,-5.35,-35.595)) ;
#156234 = CARTESIAN_POINT('Origin',(2.6,-5.15,-35.595)) ;
#156235 = CARTESIAN_POINT('',(2.6,-5.35,-32.985)) ;
#156236 = CARTESIAN_POINT('',(2.6,-5.35,-36.59)) ;
#156237 = CARTESIAN_POINT('',(2.6,-5.15,-32.785)) ;
#156238 = CARTESIAN_POINT('Origin',(2.6,-5.15,-32.985)) ;
#156239 = CARTESIAN_POINT('',(2.6,1.9,-32.785)) ;
#156240 = CARTESIAN_POINT('',(2.6,4.55,-32.785)) ;
#156241 = CARTESIAN_POINT('',(2.6,1.9,-31.985)) ;
#156242 = CARTESIAN_POINT('',(2.6,1.9,-36.59)) ;
#156243 = CARTESIAN_POINT('',(2.6,-5.15,-31.985)) ;
#156244 = CARTESIAN_POINT('',(2.6,4.55,-31.985)) ;
#156245 = CARTESIAN_POINT('',(2.6,-5.35,-31.785)) ;
#156246 = CARTESIAN_POINT('Origin',(2.6,-5.15,-31.785)) ;
#156247 = CARTESIAN_POINT('',(2.6,-5.35,-29.175)) ;
#156248 = CARTESIAN_POINT('',(2.6,-5.35,-36.59)) ;
#156249 = CARTESIAN_POINT('',(2.6,-5.15,-28.975)) ;
#156250 = CARTESIAN_POINT('Origin',(2.6,-5.15,-29.175)) ;
#156251 = CARTESIAN_POINT('',(2.6,1.9,-28.975)) ;
#156252 = CARTESIAN_POINT('',(2.6,4.55,-28.975)) ;
#156253 = CARTESIAN_POINT('',(2.6,1.9,-28.175)) ;
#156254 = CARTESIAN_POINT('',(2.6,1.9,-36.59)) ;
#156255 = CARTESIAN_POINT('',(2.6,-5.15,-28.175)) ;
#156256 = CARTESIAN_POINT('',(2.6,4.55,-28.175)) ;
#156257 = CARTESIAN_POINT('',(2.6,-5.35,-27.975)) ;
#156258 = CARTESIAN_POINT('Origin',(2.6,-5.15,-27.975)) ;
#156259 = CARTESIAN_POINT('',(2.6,-5.35,-25.365)) ;
#156260 = CARTESIAN_POINT('',(2.6,-5.35,-36.59)) ;
#156261 = CARTESIAN_POINT('',(2.6,-5.15,-25.165)) ;
#156262 = CARTESIAN_POINT('Origin',(2.6,-5.15,-25.365)) ;
#156263 = CARTESIAN_POINT('',(2.6,1.9,-25.165)) ;
#156264 = CARTESIAN_POINT('',(2.6,4.55,-25.165)) ;
#156265 = CARTESIAN_POINT('',(2.6,1.9,-24.365)) ;
#156266 = CARTESIAN_POINT('',(2.6,1.89999999999999,-36.59)) ;
#156267 = CARTESIAN_POINT('',(2.6,-5.15,-24.365)) ;
#156268 = CARTESIAN_POINT('',(2.6,4.55,-24.365)) ;
#156269 = CARTESIAN_POINT('',(2.6,-5.35,-24.165)) ;
#156270 = CARTESIAN_POINT('Origin',(2.6,-5.15,-24.165)) ;
#156271 = CARTESIAN_POINT('',(2.6,-5.35,-21.555)) ;
#156272 = CARTESIAN_POINT('',(2.6,-5.35,-36.59)) ;
#156273 = CARTESIAN_POINT('',(2.6,-5.15,-21.355)) ;
#156274 = CARTESIAN_POINT('Origin',(2.6,-5.15,-21.555)) ;
#156275 = CARTESIAN_POINT('',(2.6,1.9,-21.355)) ;
#156276 = CARTESIAN_POINT('',(2.6,4.55,-21.355)) ;
#156277 = CARTESIAN_POINT('',(2.6,1.9,-20.555)) ;
#156278 = CARTESIAN_POINT('',(2.6,1.89999999999999,-36.59)) ;
#156279 = CARTESIAN_POINT('',(2.6,-5.15,-20.555)) ;
#156280 = CARTESIAN_POINT('',(2.6,4.55,-20.555)) ;
#156281 = CARTESIAN_POINT('',(2.6,-5.35,-20.355)) ;
#156282 = CARTESIAN_POINT('Origin',(2.6,-5.15,-20.355)) ;
#156283 = CARTESIAN_POINT('',(2.6,-5.35,-17.745)) ;
#156284 = CARTESIAN_POINT('',(2.6,-5.35,-36.59)) ;
#156285 = CARTESIAN_POINT('',(2.6,-5.15,-17.545)) ;
#156286 = CARTESIAN_POINT('Origin',(2.6,-5.15,-17.745)) ;
#156287 = CARTESIAN_POINT('',(2.6,1.9,-17.545)) ;
#156288 = CARTESIAN_POINT('',(2.6,4.55,-17.545)) ;
#156289 = CARTESIAN_POINT('',(2.6,1.9,-16.745)) ;
#156290 = CARTESIAN_POINT('',(2.6,1.89999999999999,-36.59)) ;
#156291 = CARTESIAN_POINT('',(2.6,-5.15,-16.745)) ;
#156292 = CARTESIAN_POINT('',(2.6,4.55,-16.745)) ;
#156293 = CARTESIAN_POINT('',(2.6,-5.35,-16.545)) ;
#156294 = CARTESIAN_POINT('Origin',(2.6,-5.15,-16.545)) ;
#156295 = CARTESIAN_POINT('',(2.6,-5.35,-13.935)) ;
#156296 = CARTESIAN_POINT('',(2.6,-5.35,-36.59)) ;
#156297 = CARTESIAN_POINT('',(2.6,-5.15,-13.735)) ;
#156298 = CARTESIAN_POINT('Origin',(2.6,-5.15,-13.935)) ;
#156299 = CARTESIAN_POINT('',(2.6,1.9,-13.735)) ;
#156300 = CARTESIAN_POINT('',(2.6,4.55,-13.735)) ;
#156301 = CARTESIAN_POINT('',(2.6,1.9,-12.935)) ;
#156302 = CARTESIAN_POINT('',(2.6,1.89999999999999,-36.59)) ;
#156303 = CARTESIAN_POINT('',(2.6,-5.15,-12.935)) ;
#156304 = CARTESIAN_POINT('',(2.6,4.55,-12.935)) ;
#156305 = CARTESIAN_POINT('',(2.6,-5.35,-12.735)) ;
#156306 = CARTESIAN_POINT('Origin',(2.6,-5.15,-12.735)) ;
#156307 = CARTESIAN_POINT('',(2.6,-5.35,-10.125)) ;
#156308 = CARTESIAN_POINT('',(2.6,-5.35,-36.59)) ;
#156309 = CARTESIAN_POINT('',(2.6,-5.15,-9.925)) ;
#156310 = CARTESIAN_POINT('Origin',(2.6,-5.15,-10.125)) ;
#156311 = CARTESIAN_POINT('',(2.6,1.9,-9.925)) ;
#156312 = CARTESIAN_POINT('',(2.6,4.55,-9.925)) ;
#156313 = CARTESIAN_POINT('',(2.6,1.9,-9.125)) ;
#156314 = CARTESIAN_POINT('',(2.6,1.89999999999999,-36.59)) ;
#156315 = CARTESIAN_POINT('',(2.6,-5.15,-9.125)) ;
#156316 = CARTESIAN_POINT('',(2.6,4.55,-9.125)) ;
#156317 = CARTESIAN_POINT('',(2.6,-5.35,-8.925)) ;
#156318 = CARTESIAN_POINT('Origin',(2.6,-5.15,-8.925)) ;
#156319 = CARTESIAN_POINT('',(2.6,-5.35,-6.315)) ;
#156320 = CARTESIAN_POINT('',(2.6,-5.35,-36.59)) ;
#156321 = CARTESIAN_POINT('',(2.6,-5.15,-6.115)) ;
#156322 = CARTESIAN_POINT('Origin',(2.6,-5.15,-6.315)) ;
#156323 = CARTESIAN_POINT('',(2.6,1.9,-6.115)) ;
#156324 = CARTESIAN_POINT('',(2.6,4.55,-6.115)) ;
#156325 = CARTESIAN_POINT('',(2.6,1.9,-5.315)) ;
#156326 = CARTESIAN_POINT('',(2.6,1.89999999999999,-36.59)) ;
#156327 = CARTESIAN_POINT('',(2.6,-5.15,-5.315)) ;
#156328 = CARTESIAN_POINT('',(2.6,4.55,-5.315)) ;
#156329 = CARTESIAN_POINT('',(2.6,-5.35,-5.115)) ;
#156330 = CARTESIAN_POINT('Origin',(2.6,-5.15,-5.115)) ;
#156331 = CARTESIAN_POINT('',(2.6,-5.35,-2.505)) ;
#156332 = CARTESIAN_POINT('',(2.6,-5.35,-36.59)) ;
#156333 = CARTESIAN_POINT('',(2.6,-5.15,-2.305)) ;
#156334 = CARTESIAN_POINT('Origin',(2.6,-5.15,-2.505)) ;
#156335 = CARTESIAN_POINT('',(2.6,1.9,-2.305)) ;
#156336 = CARTESIAN_POINT('',(2.6,4.55,-2.305)) ;
#156337 = CARTESIAN_POINT('',(2.6,1.9,-1.505)) ;
#156338 = CARTESIAN_POINT('',(2.6,1.89999999999998,-36.59)) ;
#156339 = CARTESIAN_POINT('',(2.6,-5.15,-1.505)) ;
#156340 = CARTESIAN_POINT('',(2.6,4.55,-1.505)) ;
#156341 = CARTESIAN_POINT('',(2.6,-5.35,-1.305)) ;
#156342 = CARTESIAN_POINT('Origin',(2.6,-5.15,-1.305)) ;
#156343 = CARTESIAN_POINT('',(2.6,-5.35,1.305)) ;
#156344 = CARTESIAN_POINT('',(2.6,-5.35,-36.59)) ;
#156345 = CARTESIAN_POINT('',(2.6,-5.15,1.505)) ;
#156346 = CARTESIAN_POINT('Origin',(2.6,-5.15,1.305)) ;
#156347 = CARTESIAN_POINT('',(2.6,1.9,1.505)) ;
#156348 = CARTESIAN_POINT('',(2.6,4.55,1.505)) ;
#156349 = CARTESIAN_POINT('',(2.6,1.9,2.2)) ;
#156350 = CARTESIAN_POINT('',(2.6,1.90000000000002,-36.59)) ;
#156351 = CARTESIAN_POINT('',(2.6,-6.45,2.2)) ;
#156352 = CARTESIAN_POINT('Origin',(3.5,2.65,0.)) ;
#156353 = CARTESIAN_POINT('',(3.5,2.75,2.2)) ;
#156354 = CARTESIAN_POINT('',(3.5,2.75,-36.49)) ;
#156355 = CARTESIAN_POINT('',(3.5,2.75,-2.3)) ;
#156356 = CARTESIAN_POINT('Origin',(3.5,2.65,2.2)) ;
#156357 = CARTESIAN_POINT('Origin',(3.5,2.65,-36.49)) ;
#156358 = CARTESIAN_POINT('Origin',(3.5,2.1,-1.01757522333835E-15)) ;
#156359 = CARTESIAN_POINT('',(3.5,2.,-2.305)) ;
#156360 = CARTESIAN_POINT('',(3.5,2.,-1.505)) ;
#156361 = CARTESIAN_POINT('',(3.5,2.,-1.505)) ;
#156362 = CARTESIAN_POINT('',(3.55,2.01339745962156,-2.305)) ;
#156363 = CARTESIAN_POINT('Origin',(3.5,2.1,-2.305)) ;
#156364 = CARTESIAN_POINT('Origin',(3.5,2.1,-2.305)) ;
#156365 = CARTESIAN_POINT('',(3.55,2.01339745962156,-1.505)) ;
#156366 = CARTESIAN_POINT('Origin',(3.5,2.1,-1.505)) ;
#156367 = CARTESIAN_POINT('Origin',(3.5,2.1,-1.505)) ;
#156368 = CARTESIAN_POINT('Origin',(-5.9,-6.55,-36.59)) ;
#156369 = CARTESIAN_POINT('',(-5.9,0.35,-36.49)) ;
#156370 = CARTESIAN_POINT('',(-5.9,-6.45,-36.49)) ;
#156371 = CARTESIAN_POINT('',(-5.9,-6.55,-36.49)) ;
#156372 = CARTESIAN_POINT('',(-5.9,-6.45,2.2)) ;
#156373 = CARTESIAN_POINT('',(-5.9,-6.45,-36.59)) ;
#156374 = CARTESIAN_POINT('',(-5.9,0.35,2.2)) ;
#156375 = CARTESIAN_POINT('',(-5.9,0.45,2.2)) ;
#156376 = CARTESIAN_POINT('',(-5.9,0.35,-36.59)) ;
#156377 = CARTESIAN_POINT('',(-5.9,-5.62807764064044,-2.31)) ;
#156378 = CARTESIAN_POINT('',(-5.9,-5.42192235935956,-2.11)) ;
#156379 = CARTESIAN_POINT('Ctrl Pts',(-5.9,-5.62807764064044,-2.31)) ;
#156380 = CARTESIAN_POINT('Ctrl Pts',(-5.9,-5.6280776389491,-2.25749316946912)) ;
#156381 = CARTESIAN_POINT('Ctrl Pts',(-5.9,-5.60585949344389,-2.20560251865551)) ;
#156382 = CARTESIAN_POINT('Ctrl Pts',(-5.9,-5.5295328200175,-2.13155476886987)) ;
#156383 = CARTESIAN_POINT('Ctrl Pts',(-5.9,-5.47604516144825,-2.11000000149821)) ;
#156384 = CARTESIAN_POINT('Ctrl Pts',(-5.9,-5.42192235935956,-2.11)) ;
#156385 = CARTESIAN_POINT('',(-5.9,-5.62807764064044,-5.31)) ;
#156386 = CARTESIAN_POINT('',(-5.9,-5.62807764064044,-36.59)) ;
#156387 = CARTESIAN_POINT('',(-5.9,-5.42192235935956,-5.51)) ;
#156388 = CARTESIAN_POINT('Ctrl Pts',(-5.9,-5.42192235935956,-5.51)) ;
#156389 = CARTESIAN_POINT('Ctrl Pts',(-5.9,-5.47604516144824,-5.50999999850184)) ;
#156390 = CARTESIAN_POINT('Ctrl Pts',(-5.9,-5.52953282001752,-5.48844523113013)) ;
#156391 = CARTESIAN_POINT('Ctrl Pts',(-5.9,-5.60585949344386,-5.41439748134449)) ;
#156392 = CARTESIAN_POINT('Ctrl Pts',(-5.9,-5.6280776389491,-5.36250683053088)) ;
#156393 = CARTESIAN_POINT('Ctrl Pts',(-5.9,-5.62807764064044,-5.31)) ;
#156394 = CARTESIAN_POINT('',(-5.9,-1.2914213562373,-5.51)) ;
#156395 = CARTESIAN_POINT('',(-5.9,-1.04999999999999,-5.51)) ;
#156396 = CARTESIAN_POINT('',(-5.9,-1.00857864376269,-5.31)) ;
#156397 = CARTESIAN_POINT('Ctrl Pts',(-5.9,-1.00857864376269,-5.31)) ;
#156398 = CARTESIAN_POINT('Ctrl Pts',(-5.9,-1.00857864608315,-5.36250686562998)) ;
#156399 = CARTESIAN_POINT('Ctrl Pts',(-5.9,-1.03906162412146,-5.41439743459706)) ;
#156400 = CARTESIAN_POINT('Ctrl Pts',(-5.9,-1.14378108835315,-5.48844527787756)) ;
#156401 = CARTESIAN_POINT('Ctrl Pts',(-5.9,-1.21716543471637,-5.50999999941992)) ;
#156402 = CARTESIAN_POINT('Ctrl Pts',(-5.9,-1.2914213562373,-5.51)) ;
#156403 = CARTESIAN_POINT('',(-5.9,-1.00857864376269,-2.31)) ;
#156404 = CARTESIAN_POINT('',(-5.9,-1.00857864376269,-36.59)) ;
#156405 = CARTESIAN_POINT('',(-5.9,-1.29142135623731,-2.11)) ;
#156406 = CARTESIAN_POINT('Ctrl Pts',(-5.9,-1.29142135623731,-2.11)) ;
#156407 = CARTESIAN_POINT('Ctrl Pts',(-5.9,-1.21716543471638,-2.11000000058011)) ;
#156408 = CARTESIAN_POINT('Ctrl Pts',(-5.9,-1.14378108835315,-2.13155472212247)) ;
#156409 = CARTESIAN_POINT('Ctrl Pts',(-5.9,-1.03906162412146,-2.20560256540291)) ;
#156410 = CARTESIAN_POINT('Ctrl Pts',(-5.9,-1.00857864608315,-2.25749313437004)) ;
#156411 = CARTESIAN_POINT('Ctrl Pts',(-5.9,-1.00857864376269,-2.31)) ;
#156412 = CARTESIAN_POINT('',(-5.9,-5.55,-2.11)) ;
#156413 = CARTESIAN_POINT('',(-5.9,-5.62807764064044,-5.92)) ;
#156414 = CARTESIAN_POINT('',(-5.9,-5.62807764064044,-9.32)) ;
#156415 = CARTESIAN_POINT('',(-5.9,-5.62807764064044,-36.59)) ;
#156416 = CARTESIAN_POINT('',(-5.9,-1.00857864376269,-9.32)) ;
#156417 = CARTESIAN_POINT('',(-5.9,-1.04999999999999,-9.32)) ;
#156418 = CARTESIAN_POINT('',(-5.9,-1.00857864376269,-5.92)) ;
#156419 = CARTESIAN_POINT('',(-5.9,-1.00857864376269,-36.59)) ;
#156420 = CARTESIAN_POINT('',(-5.9,-5.55,-5.92)) ;
#156421 = CARTESIAN_POINT('',(-5.9,-5.62807764064044,-9.73)) ;
#156422 = CARTESIAN_POINT('',(-5.9,-5.62807764064044,-13.13)) ;
#156423 = CARTESIAN_POINT('',(-5.9,-5.62807764064044,-36.59)) ;
#156424 = CARTESIAN_POINT('',(-5.9,-1.00857864376269,-13.13)) ;
#156425 = CARTESIAN_POINT('',(-5.9,-1.04999999999999,-13.13)) ;
#156426 = CARTESIAN_POINT('',(-5.9,-1.00857864376269,-9.73)) ;
#156427 = CARTESIAN_POINT('',(-5.9,-1.00857864376269,-36.59)) ;
#156428 = CARTESIAN_POINT('',(-5.9,-5.55,-9.73)) ;
#156429 = CARTESIAN_POINT('',(-5.9,-5.62807764064044,-13.54)) ;
#156430 = CARTESIAN_POINT('',(-5.9,-5.62807764064044,-16.94)) ;
#156431 = CARTESIAN_POINT('',(-5.9,-5.62807764064044,-36.59)) ;
#156432 = CARTESIAN_POINT('',(-5.9,-1.00857864376269,-16.94)) ;
#156433 = CARTESIAN_POINT('',(-5.9,-1.04999999999999,-16.94)) ;
#156434 = CARTESIAN_POINT('',(-5.9,-1.00857864376269,-13.54)) ;
#156435 = CARTESIAN_POINT('',(-5.9,-1.00857864376269,-36.59)) ;
#156436 = CARTESIAN_POINT('',(-5.9,-5.55,-13.54)) ;
#156437 = CARTESIAN_POINT('',(-5.9,-5.62807764064044,-17.35)) ;
#156438 = CARTESIAN_POINT('',(-5.9,-5.62807764064044,-20.75)) ;
#156439 = CARTESIAN_POINT('',(-5.9,-5.62807764064044,-36.59)) ;
#156440 = CARTESIAN_POINT('',(-5.9,-1.00857864376269,-20.75)) ;
#156441 = CARTESIAN_POINT('',(-5.9,-1.04999999999999,-20.75)) ;
#156442 = CARTESIAN_POINT('',(-5.9,-1.00857864376269,-17.35)) ;
#156443 = CARTESIAN_POINT('',(-5.9,-1.00857864376269,-36.59)) ;
#156444 = CARTESIAN_POINT('',(-5.9,-5.55,-17.35)) ;
#156445 = CARTESIAN_POINT('',(-5.9,-5.62807764064044,-21.16)) ;
#156446 = CARTESIAN_POINT('',(-5.9,-5.62807764064044,-24.56)) ;
#156447 = CARTESIAN_POINT('',(-5.9,-5.62807764064044,-36.59)) ;
#156448 = CARTESIAN_POINT('',(-5.9,-1.00857864376269,-24.56)) ;
#156449 = CARTESIAN_POINT('',(-5.9,-1.04999999999999,-24.56)) ;
#156450 = CARTESIAN_POINT('',(-5.9,-1.00857864376269,-21.16)) ;
#156451 = CARTESIAN_POINT('',(-5.9,-1.00857864376269,-36.59)) ;
#156452 = CARTESIAN_POINT('',(-5.9,-5.55,-21.16)) ;
#156453 = CARTESIAN_POINT('',(-5.9,-5.62807764064044,-24.97)) ;
#156454 = CARTESIAN_POINT('',(-5.9,-5.62807764064044,-28.37)) ;
#156455 = CARTESIAN_POINT('',(-5.9,-5.62807764064044,-36.59)) ;
#156456 = CARTESIAN_POINT('',(-5.9,-1.00857864376269,-28.37)) ;
#156457 = CARTESIAN_POINT('',(-5.9,-1.04999999999999,-28.37)) ;
#156458 = CARTESIAN_POINT('',(-5.9,-1.00857864376269,-24.97)) ;
#156459 = CARTESIAN_POINT('',(-5.9,-1.00857864376269,-36.59)) ;
#156460 = CARTESIAN_POINT('',(-5.9,-5.55,-24.97)) ;
#156461 = CARTESIAN_POINT('',(-5.9,-5.62807764064044,-28.78)) ;
#156462 = CARTESIAN_POINT('',(-5.9,-5.62807764064044,-32.18)) ;
#156463 = CARTESIAN_POINT('',(-5.9,-5.62807764064044,-36.59)) ;
#156464 = CARTESIAN_POINT('',(-5.9,-1.00857864376269,-32.18)) ;
#156465 = CARTESIAN_POINT('',(-5.9,-1.04999999999999,-32.18)) ;
#156466 = CARTESIAN_POINT('',(-5.9,-1.00857864376269,-28.78)) ;
#156467 = CARTESIAN_POINT('',(-5.9,-1.00857864376269,-36.59)) ;
#156468 = CARTESIAN_POINT('',(-5.9,-5.55,-28.78)) ;
#156469 = CARTESIAN_POINT('',(-5.9,-5.62807764064044,-32.59)) ;
#156470 = CARTESIAN_POINT('',(-5.9,-5.62807764064044,-35.99)) ;
#156471 = CARTESIAN_POINT('',(-5.9,-5.62807764064044,-36.59)) ;
#156472 = CARTESIAN_POINT('',(-5.9,-1.00857864376269,-35.99)) ;
#156473 = CARTESIAN_POINT('',(-5.9,-1.04999999999999,-35.99)) ;
#156474 = CARTESIAN_POINT('',(-5.9,-1.00857864376269,-32.59)) ;
#156475 = CARTESIAN_POINT('',(-5.9,-1.00857864376269,-36.59)) ;
#156476 = CARTESIAN_POINT('',(-5.9,-5.55,-32.59)) ;
#156477 = CARTESIAN_POINT('',(-5.9,-5.62807764064044,1.5)) ;
#156478 = CARTESIAN_POINT('',(-5.9,-5.42192235935956,1.7)) ;
#156479 = CARTESIAN_POINT('Ctrl Pts',(-5.9,-5.62807764064044,1.5)) ;
#156480 = CARTESIAN_POINT('Ctrl Pts',(-5.9,-5.6280776389491,1.55250683053087)) ;
#156481 = CARTESIAN_POINT('Ctrl Pts',(-5.9,-5.60585949344389,1.6043974813445)) ;
#156482 = CARTESIAN_POINT('Ctrl Pts',(-5.9,-5.5295328200175,1.67844523113012)) ;
#156483 = CARTESIAN_POINT('Ctrl Pts',(-5.9,-5.47604516144825,1.69999999850179)) ;
#156484 = CARTESIAN_POINT('Ctrl Pts',(-5.9,-5.42192235935956,1.7)) ;
#156485 = CARTESIAN_POINT('',(-5.9,-5.62807764064044,-1.5)) ;
#156486 = CARTESIAN_POINT('',(-5.9,-5.62807764064044,-36.59)) ;
#156487 = CARTESIAN_POINT('',(-5.9,-5.42192235935956,-1.7)) ;
#156488 = CARTESIAN_POINT('Ctrl Pts',(-5.9,-5.42192235935956,-1.7)) ;
#156489 = CARTESIAN_POINT('Ctrl Pts',(-5.9,-5.47604516144823,-1.69999999850179)) ;
#156490 = CARTESIAN_POINT('Ctrl Pts',(-5.9,-5.52953282001752,-1.67844523113013)) ;
#156491 = CARTESIAN_POINT('Ctrl Pts',(-5.9,-5.60585949344386,-1.60439748134449)) ;
#156492 = CARTESIAN_POINT('Ctrl Pts',(-5.9,-5.6280776389491,-1.55250683053088)) ;
#156493 = CARTESIAN_POINT('Ctrl Pts',(-5.9,-5.62807764064044,-1.5)) ;
#156494 = CARTESIAN_POINT('',(-5.9,-1.2914213562373,-1.7)) ;
#156495 = CARTESIAN_POINT('',(-5.9,-1.04999999999999,-1.7)) ;
#156496 = CARTESIAN_POINT('',(-5.9,-1.00857864376268,-1.5)) ;
#156497 = CARTESIAN_POINT('Ctrl Pts',(-5.9,-1.00857864376268,-1.5)) ;
#156498 = CARTESIAN_POINT('Ctrl Pts',(-5.9,-1.00857864608314,-1.55250686562996)) ;
#156499 = CARTESIAN_POINT('Ctrl Pts',(-5.9,-1.03906162412144,-1.60439743459708)) ;
#156500 = CARTESIAN_POINT('Ctrl Pts',(-5.9,-1.14378108835315,-1.67844527787754)) ;
#156501 = CARTESIAN_POINT('Ctrl Pts',(-5.9,-1.21716543471636,-1.69999999941986)) ;
#156502 = CARTESIAN_POINT('Ctrl Pts',(-5.9,-1.2914213562373,-1.7)) ;
#156503 = CARTESIAN_POINT('',(-5.9,-1.00857864376268,1.5)) ;
#156504 = CARTESIAN_POINT('',(-5.9,-1.00857864376268,-36.59)) ;
#156505 = CARTESIAN_POINT('',(-5.9,-1.2914213562373,1.7)) ;
#156506 = CARTESIAN_POINT('Ctrl Pts',(-5.9,-1.2914213562373,1.7)) ;
#156507 = CARTESIAN_POINT('Ctrl Pts',(-5.9,-1.21716543471637,1.69999999941986)) ;
#156508 = CARTESIAN_POINT('Ctrl Pts',(-5.9,-1.14378108835315,1.67844527787754)) ;
#156509 = CARTESIAN_POINT('Ctrl Pts',(-5.9,-1.03906162412145,1.60439743459708)) ;
#156510 = CARTESIAN_POINT('Ctrl Pts',(-5.9,-1.00857864608316,1.55250686562996)) ;
#156511 = CARTESIAN_POINT('Ctrl Pts',(-5.9,-1.00857864376268,1.5)) ;
#156512 = CARTESIAN_POINT('',(-5.9,-5.55,1.7)) ;
#156513 = CARTESIAN_POINT('Origin',(10.2,2.,1.405)) ;
#156514 = CARTESIAN_POINT('',(10.1,2.,1.305)) ;
#156515 = CARTESIAN_POINT('',(10.1,2.,-1.305)) ;
#156516 = CARTESIAN_POINT('',(10.1,2.,-1.405)) ;
#156517 = CARTESIAN_POINT('',(3.7,2.,-1.305)) ;
#156518 = CARTESIAN_POINT('',(10.2,2.,-1.305)) ;
#156519 = CARTESIAN_POINT('',(3.7,2.,1.305)) ;
#156520 = CARTESIAN_POINT('',(3.7,2.,1.405)) ;
#156521 = CARTESIAN_POINT('',(10.2,2.,1.305)) ;
#156522 = CARTESIAN_POINT('',(9.8,2.,-0.399999999999999)) ;
#156523 = CARTESIAN_POINT('',(9.8,2.,0.399999999999999)) ;
#156524 = CARTESIAN_POINT('',(9.8,2.,0.399999999999999)) ;
#156525 = CARTESIAN_POINT('',(9.6,2.,0.6)) ;
#156526 = CARTESIAN_POINT('Origin',(9.6,2.,0.4)) ;
#156527 = CARTESIAN_POINT('',(7.8,2.,0.6)) ;
#156528 = CARTESIAN_POINT('',(7.8,2.,0.6)) ;
#156529 = CARTESIAN_POINT('',(7.6,2.,0.399999999999999)) ;
#156530 = CARTESIAN_POINT('Origin',(7.8,2.,0.4)) ;
#156531 = CARTESIAN_POINT('',(7.6,2.,-0.399999999999999)) ;
#156532 = CARTESIAN_POINT('',(7.6,2.,-0.399999999999999)) ;
#156533 = CARTESIAN_POINT('',(7.8,2.,-0.6)) ;
#156534 = CARTESIAN_POINT('Origin',(7.8,2.,-0.4)) ;
#156535 = CARTESIAN_POINT('',(9.6,2.,-0.6)) ;
#156536 = CARTESIAN_POINT('',(9.6,2.,-0.6)) ;
#156537 = CARTESIAN_POINT('Origin',(9.6,2.,-0.4)) ;
#156538 = CARTESIAN_POINT('Origin',(2.6,4.55,-36.59)) ;
#156539 = CARTESIAN_POINT('',(2.6,2.85,1.65)) ;
#156540 = CARTESIAN_POINT('',(2.6,4.45,1.65)) ;
#156541 = CARTESIAN_POINT('',(2.6,4.55,1.65)) ;
#156542 = CARTESIAN_POINT('',(2.6,4.45,2.2)) ;
#156543 = CARTESIAN_POINT('',(2.6,4.45,-36.59)) ;
#156544 = CARTESIAN_POINT('',(2.6,2.85,2.2)) ;
#156545 = CARTESIAN_POINT('',(2.6,2.75,2.2)) ;
#156546 = CARTESIAN_POINT('',(2.6,2.85,-36.59)) ;
#156547 = CARTESIAN_POINT('Origin',(-7.29372370581158E-16,3.55,0.)) ;
#156548 = CARTESIAN_POINT('',(0.183301359729409,3.55,-1.51703678647597)) ;
#156549 = CARTESIAN_POINT('Origin',(3.6,7.81406971160724E-17,0.)) ;
#156550 = CARTESIAN_POINT('',(3.6,-2.35,1.305)) ;
#156551 = CARTESIAN_POINT('',(3.6,-5.15,1.305)) ;
#156552 = CARTESIAN_POINT('',(3.6,-5.25,1.305)) ;
#156553 = CARTESIAN_POINT('',(3.6,-5.15,-1.305)) ;
#156554 = CARTESIAN_POINT('',(3.6,-5.15,-1.405)) ;
#156555 = CARTESIAN_POINT('',(3.6,-2.35,-1.305)) ;
#156556 = CARTESIAN_POINT('',(3.6,-2.25,-1.305)) ;
#156557 = CARTESIAN_POINT('',(3.6,-2.35,-0.903119593409422)) ;
#156558 = CARTESIAN_POINT('',(3.6,-2.35,0.)) ;
#156559 = CARTESIAN_POINT('',(3.6,-2.32153024911032,-0.800273234017602)) ;
#156560 = CARTESIAN_POINT('Origin',(3.6,-2.15,-0.903119593409422)) ;
#156561 = CARTESIAN_POINT('',(3.6,-2.32153024911032,0.800273234017602)) ;
#156562 = CARTESIAN_POINT('Origin',(3.6,-3.65625,3.25260651745651E-16)) ;
#156563 = CARTESIAN_POINT('',(3.6,-2.35,0.903119593409423)) ;
#156564 = CARTESIAN_POINT('Origin',(3.6,-2.15,0.903119593409423)) ;
#156565 = CARTESIAN_POINT('',(3.6,-2.35,0.)) ;
#156566 = CARTESIAN_POINT('Origin',(-5.9,0.45,-36.59)) ;
#156567 = CARTESIAN_POINT('',(-5.46221792447664,0.45,2.2)) ;
#156568 = CARTESIAN_POINT('',(-5.46221792447664,0.45,-36.49)) ;
#156569 = CARTESIAN_POINT('',(-5.46221792447664,0.45,-36.59)) ;
#156570 = CARTESIAN_POINT('',(-5.8,0.45,-36.49)) ;
#156571 = CARTESIAN_POINT('',(-5.9,0.45,-36.49)) ;
#156572 = CARTESIAN_POINT('',(-5.8,0.45,2.2)) ;
#156573 = CARTESIAN_POINT('',(-5.8,0.45,-36.59)) ;
#156574 = CARTESIAN_POINT('',(-5.4,0.45,2.2)) ;
#156575 = CARTESIAN_POINT('Origin',(-5.4,0.45,-36.59)) ;
#156576 = CARTESIAN_POINT('',(-5.37250902111062,0.505815017745095,2.2)) ;
#156577 = CARTESIAN_POINT('',(-3.75,3.8,2.2)) ;
#156578 = CARTESIAN_POINT('',(-5.37250902111062,0.505815017745095,-36.49)) ;
#156579 = CARTESIAN_POINT('',(-5.4,0.45,-36.49)) ;
#156580 = CARTESIAN_POINT('',(-5.37250902111062,0.505815017745095,2.29999999999998)) ;
#156581 = CARTESIAN_POINT('Origin',(-4.,3.8,-36.59)) ;
#156582 = CARTESIAN_POINT('',(-4.,4.45,-36.49)) ;
#156583 = CARTESIAN_POINT('',(-4.,3.9,-36.49)) ;
#156584 = CARTESIAN_POINT('',(-4.,3.8,-36.49)) ;
#156585 = CARTESIAN_POINT('',(-4.,3.9,2.2)) ;
#156586 = CARTESIAN_POINT('',(-4.,3.9,-36.59)) ;
#156587 = CARTESIAN_POINT('',(-4.,4.45,2.2)) ;
#156588 = CARTESIAN_POINT('',(-4.,4.55,2.2)) ;
#156589 = CARTESIAN_POINT('',(-4.,4.45,-36.59)) ;
#156590 = CARTESIAN_POINT('Origin',(2.6,-6.55,-36.59)) ;
#156591 = CARTESIAN_POINT('',(-5.8,-6.55,-36.49)) ;
#156592 = CARTESIAN_POINT('',(2.5,-6.55,-36.49)) ;
#156593 = CARTESIAN_POINT('',(2.6,-6.55,-36.49)) ;
#156594 = CARTESIAN_POINT('',(2.5,-6.55,2.2)) ;
#156595 = CARTESIAN_POINT('',(2.5,-6.55,-36.59)) ;
#156596 = CARTESIAN_POINT('',(-5.8,-6.55,2.2)) ;
#156597 = CARTESIAN_POINT('',(-5.9,-6.55,2.2)) ;
#156598 = CARTESIAN_POINT('',(-5.8,-6.55,-36.59)) ;
#156599 = CARTESIAN_POINT('',(-5.,-6.55,-35.39)) ;
#156600 = CARTESIAN_POINT('',(-5.,-6.55,-33.19)) ;
#156601 = CARTESIAN_POINT('',(-5.,-6.55,-33.29)) ;
#156602 = CARTESIAN_POINT('',(-3.8,-6.55,-33.19)) ;
#156603 = CARTESIAN_POINT('',(-3.9,-6.55,-33.19)) ;
#156604 = CARTESIAN_POINT('',(-3.8,-6.55,-35.39)) ;
#156605 = CARTESIAN_POINT('',(-3.8,-6.55,-35.29)) ;
#156606 = CARTESIAN_POINT('',(-4.9,-6.55,-35.39)) ;
#156607 = CARTESIAN_POINT('',(-5.,-6.55,-31.58)) ;
#156608 = CARTESIAN_POINT('',(-5.,-6.55,-29.38)) ;
#156609 = CARTESIAN_POINT('',(-5.,-6.55,-29.48)) ;
#156610 = CARTESIAN_POINT('',(-3.8,-6.55,-29.38)) ;
#156611 = CARTESIAN_POINT('',(-3.9,-6.55,-29.38)) ;
#156612 = CARTESIAN_POINT('',(-3.8,-6.55,-31.58)) ;
#156613 = CARTESIAN_POINT('',(-3.8,-6.55,-31.48)) ;
#156614 = CARTESIAN_POINT('',(-4.9,-6.55,-31.58)) ;
#156615 = CARTESIAN_POINT('',(-5.,-6.55,-27.77)) ;
#156616 = CARTESIAN_POINT('',(-5.,-6.55,-25.57)) ;
#156617 = CARTESIAN_POINT('',(-5.,-6.55,-25.67)) ;
#156618 = CARTESIAN_POINT('',(-3.8,-6.55,-25.57)) ;
#156619 = CARTESIAN_POINT('',(-3.9,-6.55,-25.57)) ;
#156620 = CARTESIAN_POINT('',(-3.8,-6.55,-27.77)) ;
#156621 = CARTESIAN_POINT('',(-3.8,-6.55,-27.67)) ;
#156622 = CARTESIAN_POINT('',(-4.9,-6.55,-27.77)) ;
#156623 = CARTESIAN_POINT('',(-5.,-6.55,-23.96)) ;
#156624 = CARTESIAN_POINT('',(-5.,-6.55,-21.76)) ;
#156625 = CARTESIAN_POINT('',(-5.,-6.55,-21.86)) ;
#156626 = CARTESIAN_POINT('',(-3.8,-6.55,-21.76)) ;
#156627 = CARTESIAN_POINT('',(-3.9,-6.55,-21.76)) ;
#156628 = CARTESIAN_POINT('',(-3.8,-6.55,-23.96)) ;
#156629 = CARTESIAN_POINT('',(-3.8,-6.55,-23.86)) ;
#156630 = CARTESIAN_POINT('',(-4.9,-6.55,-23.96)) ;
#156631 = CARTESIAN_POINT('',(-5.,-6.55,-20.15)) ;
#156632 = CARTESIAN_POINT('',(-5.,-6.55,-17.95)) ;
#156633 = CARTESIAN_POINT('',(-5.,-6.55,-18.05)) ;
#156634 = CARTESIAN_POINT('',(-3.8,-6.55,-17.95)) ;
#156635 = CARTESIAN_POINT('',(-3.9,-6.55,-17.95)) ;
#156636 = CARTESIAN_POINT('',(-3.8,-6.55,-20.15)) ;
#156637 = CARTESIAN_POINT('',(-3.8,-6.55,-20.05)) ;
#156638 = CARTESIAN_POINT('',(-4.9,-6.55,-20.15)) ;
#156639 = CARTESIAN_POINT('',(-5.,-6.55,-16.34)) ;
#156640 = CARTESIAN_POINT('',(-5.,-6.55,-14.14)) ;
#156641 = CARTESIAN_POINT('',(-5.,-6.55,-14.24)) ;
#156642 = CARTESIAN_POINT('',(-3.8,-6.55,-14.14)) ;
#156643 = CARTESIAN_POINT('',(-3.9,-6.55,-14.14)) ;
#156644 = CARTESIAN_POINT('',(-3.8,-6.55,-16.34)) ;
#156645 = CARTESIAN_POINT('',(-3.8,-6.55,-16.24)) ;
#156646 = CARTESIAN_POINT('',(-4.9,-6.55,-16.34)) ;
#156647 = CARTESIAN_POINT('',(-5.,-6.55,-12.53)) ;
#156648 = CARTESIAN_POINT('',(-5.,-6.55,-10.33)) ;
#156649 = CARTESIAN_POINT('',(-5.,-6.55,-10.43)) ;
#156650 = CARTESIAN_POINT('',(-3.8,-6.55,-10.33)) ;
#156651 = CARTESIAN_POINT('',(-3.9,-6.55,-10.33)) ;
#156652 = CARTESIAN_POINT('',(-3.8,-6.55,-12.53)) ;
#156653 = CARTESIAN_POINT('',(-3.8,-6.55,-12.43)) ;
#156654 = CARTESIAN_POINT('',(-4.9,-6.55,-12.53)) ;
#156655 = CARTESIAN_POINT('',(-5.,-6.55,-8.72)) ;
#156656 = CARTESIAN_POINT('',(-5.,-6.55,-6.52)) ;
#156657 = CARTESIAN_POINT('',(-5.,-6.55,-6.62)) ;
#156658 = CARTESIAN_POINT('',(-3.8,-6.55,-6.52)) ;
#156659 = CARTESIAN_POINT('',(-3.9,-6.55,-6.52)) ;
#156660 = CARTESIAN_POINT('',(-3.8,-6.55,-8.72)) ;
#156661 = CARTESIAN_POINT('',(-3.8,-6.55,-8.62)) ;
#156662 = CARTESIAN_POINT('',(-4.9,-6.55,-8.72)) ;
#156663 = CARTESIAN_POINT('',(-4.,-6.55,-4.91)) ;
#156664 = CARTESIAN_POINT('',(-3.8,-6.55,-4.71)) ;
#156665 = CARTESIAN_POINT('Origin',(-4.,-6.55,-4.71)) ;
#156666 = CARTESIAN_POINT('',(-4.8,-6.55,-4.91)) ;
#156667 = CARTESIAN_POINT('',(-4.9,-6.55,-4.91)) ;
#156668 = CARTESIAN_POINT('',(-5.,-6.55,-4.71)) ;
#156669 = CARTESIAN_POINT('Origin',(-4.8,-6.55,-4.71)) ;
#156670 = CARTESIAN_POINT('',(-5.,-6.55,-2.91)) ;
#156671 = CARTESIAN_POINT('',(-5.,-6.55,-2.81)) ;
#156672 = CARTESIAN_POINT('',(-4.8,-6.55,-2.71)) ;
#156673 = CARTESIAN_POINT('Origin',(-4.8,-6.55,-2.91)) ;
#156674 = CARTESIAN_POINT('',(-4.,-6.55,-2.71)) ;
#156675 = CARTESIAN_POINT('',(-3.9,-6.55,-2.71)) ;
#156676 = CARTESIAN_POINT('',(-3.8,-6.55,-2.91)) ;
#156677 = CARTESIAN_POINT('Origin',(-4.,-6.55,-2.91)) ;
#156678 = CARTESIAN_POINT('',(-3.8,-6.55,-4.81)) ;
#156679 = CARTESIAN_POINT('',(-4.,-6.55,-1.1)) ;
#156680 = CARTESIAN_POINT('',(-3.8,-6.55,-0.900000000000002)) ;
#156681 = CARTESIAN_POINT('Origin',(-4.,-6.55,-0.900000000000002)) ;
#156682 = CARTESIAN_POINT('',(-4.8,-6.55,-1.1)) ;
#156683 = CARTESIAN_POINT('',(-4.9,-6.55,-1.1)) ;
#156684 = CARTESIAN_POINT('',(-5.,-6.55,-0.900000000000002)) ;
#156685 = CARTESIAN_POINT('Origin',(-4.8,-6.55,-0.900000000000002)) ;
#156686 = CARTESIAN_POINT('',(-5.,-6.55,0.899999999999998)) ;
#156687 = CARTESIAN_POINT('',(-5.,-6.55,0.999999999999998)) ;
#156688 = CARTESIAN_POINT('',(-4.8,-6.55,1.1)) ;
#156689 = CARTESIAN_POINT('Origin',(-4.8,-6.55,0.899999999999998)) ;
#156690 = CARTESIAN_POINT('',(-4.,-6.55,1.1)) ;
#156691 = CARTESIAN_POINT('',(-3.9,-6.55,1.1)) ;
#156692 = CARTESIAN_POINT('',(-3.8,-6.55,0.899999999999998)) ;
#156693 = CARTESIAN_POINT('Origin',(-4.,-6.55,0.899999999999998)) ;
#156694 = CARTESIAN_POINT('',(-3.8,-6.55,-1.)) ;
#156695 = CARTESIAN_POINT('Origin',(0.,0.,-36.59)) ;
#156696 = CARTESIAN_POINT('',(-3.9,3.9,-36.59)) ;
#156697 = CARTESIAN_POINT('',(-3.9,4.45,-36.59)) ;
#156698 = CARTESIAN_POINT('',(-3.9,0.,-36.59)) ;
#156699 = CARTESIAN_POINT('',(2.5,4.45,-36.59)) ;
#156700 = CARTESIAN_POINT('',(-5.84812080916424E-16,4.45,-36.59)) ;
#156701 = CARTESIAN_POINT('',(2.5,2.85,-36.59)) ;
#156702 = CARTESIAN_POINT('',(2.5,1.95351742790181E-16,-36.59)) ;
#156703 = CARTESIAN_POINT('',(2.7,2.65,-36.59)) ;
#156704 = CARTESIAN_POINT('Origin',(2.7,2.85,-36.59)) ;
#156705 = CARTESIAN_POINT('',(3.5,2.65,-36.59)) ;
#156706 = CARTESIAN_POINT('',(3.5,2.65,-36.59)) ;
#156707 = CARTESIAN_POINT('',(3.5,2.1,-36.59)) ;
#156708 = CARTESIAN_POINT('',(3.5,0.,-36.59)) ;
#156709 = CARTESIAN_POINT('',(2.7,2.1,-36.59)) ;
#156710 = CARTESIAN_POINT('',(2.7,2.1,-36.59)) ;
#156711 = CARTESIAN_POINT('',(2.5,1.9,-36.59)) ;
#156712 = CARTESIAN_POINT('Origin',(2.7,1.9,-36.59)) ;
#156713 = CARTESIAN_POINT('',(2.5,-6.45,-36.59)) ;
#156714 = CARTESIAN_POINT('',(2.5,1.95351742790181E-16,-36.59)) ;
#156715 = CARTESIAN_POINT('',(-5.8,-6.45,-36.59)) ;
#156716 = CARTESIAN_POINT('',(0.,-6.45,-36.59)) ;
#156717 = CARTESIAN_POINT('',(-5.8,0.35,-36.59)) ;
#156718 = CARTESIAN_POINT('',(-5.8,-1.4373423086665E-15,-36.59)) ;
#156719 = CARTESIAN_POINT('',(-5.46221792447664,0.35,-36.59)) ;
#156720 = CARTESIAN_POINT('',(0.,0.35,-36.59)) ;
#156721 = CARTESIAN_POINT('',(-5.28280011774461,0.46163003549019,-36.59)) ;
#156722 = CARTESIAN_POINT('Origin',(-5.46221792447664,0.55,-36.59)) ;
#156723 = CARTESIAN_POINT('',(-3.58927461283679,3.9,-36.59)) ;
#156724 = CARTESIAN_POINT('',(-4.43441264557625,2.18411369110472,-36.59)) ;
#156725 = CARTESIAN_POINT('',(0.,3.9,-36.59)) ;
#156726 = CARTESIAN_POINT('Origin',(0.,0.,2.3)) ;
#156727 = CARTESIAN_POINT('',(2.5,2.85,2.3)) ;
#156728 = CARTESIAN_POINT('',(2.5,4.45,2.3)) ;
#156729 = CARTESIAN_POINT('',(2.5,4.55,2.3)) ;
#156730 = CARTESIAN_POINT('',(-3.9,4.45,2.3)) ;
#156731 = CARTESIAN_POINT('',(-3.9,4.45,2.3)) ;
#156732 = CARTESIAN_POINT('',(-3.9,3.9,2.3)) ;
#156733 = CARTESIAN_POINT('',(-3.9,3.8,2.3)) ;
#156734 = CARTESIAN_POINT('',(-3.58927461283679,3.9,2.3)) ;
#156735 = CARTESIAN_POINT('',(-3.75,3.9,2.3)) ;
#156736 = CARTESIAN_POINT('',(-5.28280011774461,0.461630035490191,2.3)) ;
#156737 = CARTESIAN_POINT('',(-5.31029109663398,0.405815017745095,2.3)) ;
#156738 = CARTESIAN_POINT('',(-5.46221792447664,0.35,2.3)) ;
#156739 = CARTESIAN_POINT('Origin',(-5.46221792447664,0.55,2.3)) ;
#156740 = CARTESIAN_POINT('',(-5.8,0.35,2.3)) ;
#156741 = CARTESIAN_POINT('',(-5.9,0.35,2.3)) ;
#156742 = CARTESIAN_POINT('',(-5.8,-6.45,2.3)) ;
#156743 = CARTESIAN_POINT('',(-5.8,-6.55,2.3)) ;
#156744 = CARTESIAN_POINT('',(2.5,-6.45,2.3)) ;
#156745 = CARTESIAN_POINT('',(2.6,-6.45,2.3)) ;
#156746 = CARTESIAN_POINT('',(2.5,1.9,2.3)) ;
#156747 = CARTESIAN_POINT('',(2.5,1.9,2.3)) ;
#156748 = CARTESIAN_POINT('',(2.7,2.1,2.3)) ;
#156749 = CARTESIAN_POINT('Origin',(2.7,1.9,2.3)) ;
#156750 = CARTESIAN_POINT('',(3.5,2.1,2.3)) ;
#156751 = CARTESIAN_POINT('',(-1.64095463943752E-16,2.1,2.3)) ;
#156752 = CARTESIAN_POINT('',(3.5,2.65,2.3)) ;
#156753 = CARTESIAN_POINT('',(3.5,2.65,2.3)) ;
#156754 = CARTESIAN_POINT('',(2.7,2.65,2.3)) ;
#156755 = CARTESIAN_POINT('',(-2.07072847357592E-16,2.65,2.3)) ;
#156756 = CARTESIAN_POINT('Origin',(2.7,2.85,2.3)) ;
#156757 = CARTESIAN_POINT('Origin',(-5.15,-5.05,-1.6)) ;
#156758 = CARTESIAN_POINT('',(-5.8,-5.42192235935956,-1.6)) ;
#156759 = CARTESIAN_POINT('',(-5.17275707706437,-5.26511162862565,-1.6)) ;
#156760 = CARTESIAN_POINT('',(-5.10072415073893,-5.24710339704429,-1.6)) ;
#156761 = CARTESIAN_POINT('',(-5.17275707706437,-1.91866427917293,-1.6)) ;
#156762 = CARTESIAN_POINT('',(-5.17275707706437,-1.79999999999999,-1.6)) ;
#156763 = CARTESIAN_POINT('',(-5.8,-1.2914213562373,-1.6)) ;
#156764 = CARTESIAN_POINT('',(-3.59571067811865,-3.49571067811865,-1.6)) ;
#156765 = CARTESIAN_POINT('',(-5.8,-5.55,-1.6)) ;
#156766 = CARTESIAN_POINT('Origin',(-3.9,-5.05,-1.)) ;
#156767 = CARTESIAN_POINT('',(-5.12948397030589,-1.91866427917293,-1.59015230574683)) ;
#156768 = CARTESIAN_POINT('',(-5.12948397030589,-5.26511162862565,-1.59015230574683)) ;
#156769 = CARTESIAN_POINT('',(-5.12948397030589,-5.3625,-1.59015230574683)) ;
#156770 = CARTESIAN_POINT('',(-3.9,-4.95774063604919,-1.)) ;
#156771 = CARTESIAN_POINT('',(-3.91783961713025,-4.96220054033175,-1.00856301622252)) ;
#156772 = CARTESIAN_POINT('',(-3.9,-3.14814824947882,-1.)) ;
#156773 = CARTESIAN_POINT('',(-3.9,-5.05,-1.)) ;
#156774 = CARTESIAN_POINT('',(-3.04730463122257,-4.00084361825625,-0.590706222986834)) ;
#156775 = CARTESIAN_POINT('Origin',(-3.9,-5.05,1.)) ;
#156776 = CARTESIAN_POINT('',(-3.9,-5.05,0.900718313010847)) ;
#156777 = CARTESIAN_POINT('',(-3.9,-5.05,-0.900718313010846)) ;
#156778 = CARTESIAN_POINT('',(-3.9,-5.05,1.)) ;
#156779 = CARTESIAN_POINT('',(-3.9,-4.95774063604919,1.)) ;
#156780 = CARTESIAN_POINT('Origin',(-3.9,-4.94692235935957,0.889076603009118)) ;
#156781 = CARTESIAN_POINT('',(-3.9,-3.14814824947882,1.)) ;
#156782 = CARTESIAN_POINT('',(-3.9,-5.05,1.)) ;
#156783 = CARTESIAN_POINT('',(-3.9,-3.05,0.923017728506055)) ;
#156784 = CARTESIAN_POINT('Origin',(-3.9,-3.19142135623718,0.889076603009217)) ;
#156785 = CARTESIAN_POINT('',(-3.9,-3.05,-0.923017728506055)) ;
#156786 = CARTESIAN_POINT('',(-3.9,-3.05,1.)) ;
#156787 = CARTESIAN_POINT('Origin',(-3.89999999999999,-3.19142135623722,-0.889076603009188)) ;
#156788 = CARTESIAN_POINT('Origin',(-3.9,-4.94692235935963,-0.889076603009194)) ;
#156789 = CARTESIAN_POINT('Origin',(-5.15,-5.05,1.6)) ;
#156790 = CARTESIAN_POINT('',(-5.12948397030589,-5.26511162862565,1.59015230574683)) ;
#156791 = CARTESIAN_POINT('',(-5.10741344341225,-5.25959399690224,1.57955845283788)) ;
#156792 = CARTESIAN_POINT('',(-5.12948397030589,-1.91866427917293,1.59015230574683)) ;
#156793 = CARTESIAN_POINT('',(-5.12948397030589,-1.79999999999999,1.59015230574683)) ;
#156794 = CARTESIAN_POINT('',(-3.73686704155255,-3.31128120792626,0.921696179945227)) ;
#156795 = CARTESIAN_POINT('Origin',(-5.9,-5.05,1.6)) ;
#156796 = CARTESIAN_POINT('',(-5.17275707706436,-1.91866427917293,1.6)) ;
#156797 = CARTESIAN_POINT('',(-5.17275707706436,-5.26511162862565,1.6)) ;
#156798 = CARTESIAN_POINT('',(-5.17275707706436,-5.3625,1.6)) ;
#156799 = CARTESIAN_POINT('',(-5.8,-5.42192235935956,1.6)) ;
#156800 = CARTESIAN_POINT('',(-5.8066065036801,-5.42357398527959,1.6)) ;
#156801 = CARTESIAN_POINT('',(-5.8,-1.2914213562373,1.6)) ;
#156802 = CARTESIAN_POINT('',(-5.8,-1.04999999999999,1.6)) ;
#156803 = CARTESIAN_POINT('',(-3.97071067811865,-3.12071067811865,1.6)) ;
#156804 = CARTESIAN_POINT('Origin',(-3.89999999999997,-5.05,0.)) ;
#156805 = CARTESIAN_POINT('',(-5.82425356250363,-5.53106339062591,1.5)) ;
#156806 = CARTESIAN_POINT('',(-5.14850351456073,-5.36212587864019,1.5)) ;
#156807 = CARTESIAN_POINT('',(-3.89999999999997,-5.05,1.5)) ;
#156808 = CARTESIAN_POINT('',(-3.56560075006169,-4.96640018751543,0.74020667304046)) ;
#156809 = CARTESIAN_POINT('',(-5.14850351456073,-5.36212587864019,-1.5)) ;
#156810 = CARTESIAN_POINT('',(-3.56560075006169,-4.96640018751543,-0.740206673040459)) ;
#156811 = CARTESIAN_POINT('',(-5.82425356250363,-5.53106339062591,-1.5)) ;
#156812 = CARTESIAN_POINT('',(-3.89999999999997,-5.05,-1.5)) ;
#156813 = CARTESIAN_POINT('',(-5.82425356250363,-5.53106339062591,0.)) ;
#156814 = CARTESIAN_POINT('Origin',(-5.9,-1.04999999999999,-36.59)) ;
#156815 = CARTESIAN_POINT('',(-5.87071067811865,-1.07928932188133,-1.5)) ;
#156816 = CARTESIAN_POINT('',(-5.10204639894571,-1.84795360105428,-1.5)) ;
#156817 = CARTESIAN_POINT('',(-5.9,-1.04999999999999,-1.5)) ;
#156818 = CARTESIAN_POINT('',(-13.3692214357591,6.41922143575911,-5.46824401767042)) ;
#156819 = CARTESIAN_POINT('',(-5.10204639894571,-1.84795360105428,1.5)) ;
#156820 = CARTESIAN_POINT('',(2.37970252406874,-9.32970252406872,-2.09123948304694)) ;
#156821 = CARTESIAN_POINT('',(-5.87071067811865,-1.07928932188133,1.5)) ;
#156822 = CARTESIAN_POINT('',(-5.9,-1.04999999999999,1.5)) ;
#156823 = CARTESIAN_POINT('',(-5.87071067811865,-1.07928932188133,-36.59)) ;
#156824 = CARTESIAN_POINT('Origin',(-3.9,-6.4,0.999999999999998)) ;
#156825 = CARTESIAN_POINT('',(-3.9,-6.35,0.899999999999998)) ;
#156826 = CARTESIAN_POINT('',(-3.9,-6.35,-0.900000000000002)) ;
#156827 = CARTESIAN_POINT('',(-3.9,-6.35,0.999999999999998)) ;
#156828 = CARTESIAN_POINT('',(-3.9,-6.45,-0.900000000000002)) ;
#156829 = CARTESIAN_POINT('',(-3.9,-6.55,-0.900000000000002)) ;
#156830 = CARTESIAN_POINT('',(-3.9,-6.45,0.899999999999998)) ;
#156831 = CARTESIAN_POINT('',(-3.9,-6.45,1.)) ;
#156832 = CARTESIAN_POINT('',(-3.9,-6.25,0.899999999999998)) ;
#156833 = CARTESIAN_POINT('Origin',(-4.9,-6.4,-1.)) ;
#156834 = CARTESIAN_POINT('',(-4.,-6.35,-1.)) ;
#156835 = CARTESIAN_POINT('',(-4.8,-6.35,-1.)) ;
#156836 = CARTESIAN_POINT('',(-4.9,-6.35,-1.)) ;
#156837 = CARTESIAN_POINT('',(-4.8,-6.45,-1.)) ;
#156838 = CARTESIAN_POINT('',(-4.8,-6.55,-1.)) ;
#156839 = CARTESIAN_POINT('',(-4.,-6.45,-1.)) ;
#156840 = CARTESIAN_POINT('',(-3.9,-6.45,-1.)) ;
#156841 = CARTESIAN_POINT('',(-4.,-6.25,-1.)) ;
#156842 = CARTESIAN_POINT('Origin',(-4.9,-6.4,0.999999999999998)) ;
#156843 = CARTESIAN_POINT('',(-4.9,-6.45,-0.900000000000002)) ;
#156844 = CARTESIAN_POINT('',(-4.9,-6.35,-0.900000000000002)) ;
#156845 = CARTESIAN_POINT('',(-4.9,-6.25,-0.900000000000002)) ;
#156846 = CARTESIAN_POINT('',(-4.9,-6.35,0.899999999999998)) ;
#156847 = CARTESIAN_POINT('',(-4.9,-6.35,0.999999999999998)) ;
#156848 = CARTESIAN_POINT('',(-4.9,-6.45,0.899999999999998)) ;
#156849 = CARTESIAN_POINT('',(-4.9,-6.55,0.899999999999998)) ;
#156850 = CARTESIAN_POINT('',(-4.9,-6.45,-1.)) ;
#156851 = CARTESIAN_POINT('Origin',(-4.9,-6.4,0.999999999999998)) ;
#156852 = CARTESIAN_POINT('',(-4.8,-6.45,0.999999999999998)) ;
#156853 = CARTESIAN_POINT('',(-4.8,-6.35,0.999999999999998)) ;
#156854 = CARTESIAN_POINT('',(-4.8,-6.25,0.999999999999998)) ;
#156855 = CARTESIAN_POINT('',(-4.,-6.35,0.999999999999998)) ;
#156856 = CARTESIAN_POINT('',(-4.9,-6.35,0.999999999999998)) ;
#156857 = CARTESIAN_POINT('',(-4.,-6.45,0.999999999999998)) ;
#156858 = CARTESIAN_POINT('',(-4.,-6.55,0.999999999999998)) ;
#156859 = CARTESIAN_POINT('',(-4.9,-6.45,0.999999999999998)) ;
#156860 = CARTESIAN_POINT('Origin',(0.,-6.25,0.)) ;
#156861 = CARTESIAN_POINT('',(-4.8,-6.25,0.899999999999998)) ;
#156862 = CARTESIAN_POINT('',(-4.8,-6.25,-0.900000000000002)) ;
#156863 = CARTESIAN_POINT('',(-4.8,-6.25,0.)) ;
#156864 = CARTESIAN_POINT('',(-4.,-6.25,-0.900000000000002)) ;
#156865 = CARTESIAN_POINT('',(1.95156391047391E-16,-6.25,-0.900000000000001)) ;
#156866 = CARTESIAN_POINT('',(-4.,-6.25,0.899999999999998)) ;
#156867 = CARTESIAN_POINT('',(-4.,-6.25,-8.67361737988403E-16)) ;
#156868 = CARTESIAN_POINT('',(1.9515639104739E-16,-6.25,0.899999999999997)) ;
#156869 = CARTESIAN_POINT('',(-4.65,-6.25,-0.850000000000002)) ;
#156870 = CARTESIAN_POINT('',(-4.15,-6.25,-0.850000000000002)) ;
#156871 = CARTESIAN_POINT('',(-4.75,-6.25,-0.850000000000002)) ;
#156872 = CARTESIAN_POINT('',(-4.75,-6.25,-0.750000000000002)) ;
#156873 = CARTESIAN_POINT('Origin',(-4.65,-6.25,-0.750000000000002)) ;
#156874 = CARTESIAN_POINT('',(-4.75,-6.25,0.749999999999998)) ;
#156875 = CARTESIAN_POINT('',(-4.75,-6.25,0.849999999999998)) ;
#156876 = CARTESIAN_POINT('',(-4.65,-6.25,0.849999999999998)) ;
#156877 = CARTESIAN_POINT('Origin',(-4.65,-6.25,0.749999999999998)) ;
#156878 = CARTESIAN_POINT('',(-4.15,-6.25,0.849999999999998)) ;
#156879 = CARTESIAN_POINT('',(-4.05,-6.25,0.849999999999998)) ;
#156880 = CARTESIAN_POINT('',(-4.05,-6.25,0.749999999999998)) ;
#156881 = CARTESIAN_POINT('Origin',(-4.15,-6.25,0.749999999999998)) ;
#156882 = CARTESIAN_POINT('',(-4.05,-6.25,-0.750000000000002)) ;
#156883 = CARTESIAN_POINT('',(-4.05,-6.25,-0.850000000000002)) ;
#156884 = CARTESIAN_POINT('Origin',(-4.15,-6.25,-0.750000000000002)) ;
#156885 = CARTESIAN_POINT('Origin',(-4.05,-6.25,-0.850000000000002)) ;
#156886 = CARTESIAN_POINT('',(-4.05,-6.3,0.749999999999998)) ;
#156887 = CARTESIAN_POINT('',(-4.05,-6.25,0.749999999999998)) ;
#156888 = CARTESIAN_POINT('',(-4.05,-6.3,-0.750000000000002)) ;
#156889 = CARTESIAN_POINT('',(-4.05,-6.3,-0.850000000000002)) ;
#156890 = CARTESIAN_POINT('',(-4.05,-6.25,-0.750000000000002)) ;
#156891 = CARTESIAN_POINT('Origin',(-4.75,-6.25,-0.850000000000002)) ;
#156892 = CARTESIAN_POINT('',(-4.15,-6.3,-0.850000000000002)) ;
#156893 = CARTESIAN_POINT('',(-4.15,-6.25,-0.850000000000002)) ;
#156894 = CARTESIAN_POINT('',(-4.65,-6.3,-0.850000000000002)) ;
#156895 = CARTESIAN_POINT('',(-4.75,-6.3,-0.850000000000002)) ;
#156896 = CARTESIAN_POINT('',(-4.65,-6.25,-0.850000000000002)) ;
#156897 = CARTESIAN_POINT('Origin',(-4.75,-6.25,0.849999999999998)) ;
#156898 = CARTESIAN_POINT('',(-4.75,-6.3,-0.750000000000002)) ;
#156899 = CARTESIAN_POINT('',(-4.75,-6.3,0.749999999999998)) ;
#156900 = CARTESIAN_POINT('',(-4.75,-6.3,0.849999999999998)) ;
#156901 = CARTESIAN_POINT('',(-4.75,-6.25,0.749999999999998)) ;
#156902 = CARTESIAN_POINT('',(-4.75,-6.25,-0.750000000000002)) ;
#156903 = CARTESIAN_POINT('Origin',(-4.05,-6.25,0.849999999999998)) ;
#156904 = CARTESIAN_POINT('',(-4.65,-6.3,0.849999999999998)) ;
#156905 = CARTESIAN_POINT('',(-4.65,-6.25,0.849999999999998)) ;
#156906 = CARTESIAN_POINT('',(-4.15,-6.3,0.849999999999998)) ;
#156907 = CARTESIAN_POINT('',(-4.05,-6.3,0.849999999999998)) ;
#156908 = CARTESIAN_POINT('',(-4.15,-6.25,0.849999999999998)) ;
#156909 = CARTESIAN_POINT('Origin',(0.,-6.4,0.)) ;
#156910 = CARTESIAN_POINT('',(-4.15,-6.4,0.749999999999998)) ;
#156911 = CARTESIAN_POINT('',(-4.65,-6.4,0.749999999999998)) ;
#156912 = CARTESIAN_POINT('',(0.,-6.4,0.749999999999998)) ;
#156913 = CARTESIAN_POINT('',(-4.65,-6.4,-0.750000000000002)) ;
#156914 = CARTESIAN_POINT('',(-4.65,-6.4,0.)) ;
#156915 = CARTESIAN_POINT('',(-4.15,-6.4,-0.750000000000002)) ;
#156916 = CARTESIAN_POINT('',(0.,-6.4,-0.750000000000002)) ;
#156917 = CARTESIAN_POINT('',(-4.15,-6.4,0.)) ;
#156918 = CARTESIAN_POINT('Origin',(3.6,2.75,-2.3)) ;
#156919 = CARTESIAN_POINT('',(2.7,2.75,-36.49)) ;
#156920 = CARTESIAN_POINT('',(2.6,2.75,-36.49)) ;
#156921 = CARTESIAN_POINT('',(2.7,2.75,-35.94)) ;
#156922 = CARTESIAN_POINT('',(2.7,2.75,-2.3)) ;
#156923 = CARTESIAN_POINT('',(2.5,2.75,-35.74)) ;
#156924 = CARTESIAN_POINT('Origin',(2.5,2.75,-35.94)) ;
#156925 = CARTESIAN_POINT('',(1.77490703981929,2.75,-35.74)) ;
#156926 = CARTESIAN_POINT('',(2.5,2.75,1.45)) ;
#156927 = CARTESIAN_POINT('',(2.6,2.75,1.45)) ;
#156928 = CARTESIAN_POINT('',(2.7,2.75,1.65)) ;
#156929 = CARTESIAN_POINT('Origin',(2.5,2.75,1.65)) ;
#156930 = CARTESIAN_POINT('',(2.7,2.75,2.2)) ;
#156931 = CARTESIAN_POINT('',(2.7,2.75,-2.3)) ;
#156932 = CARTESIAN_POINT('',(3.6,2.75,2.2)) ;
#156933 = CARTESIAN_POINT('Origin',(3.6,2.,2.3)) ;
#156934 = CARTESIAN_POINT('',(3.5,2.,1.505)) ;
#156935 = CARTESIAN_POINT('',(3.5,2.,2.2)) ;
#156936 = CARTESIAN_POINT('',(3.5,2.,2.3)) ;
#156937 = CARTESIAN_POINT('',(2.7,2.,2.2)) ;
#156938 = CARTESIAN_POINT('',(3.6,2.,2.2)) ;
#156939 = CARTESIAN_POINT('',(2.7,2.,1.505)) ;
#156940 = CARTESIAN_POINT('',(2.7,2.,2.3)) ;
#156941 = CARTESIAN_POINT('',(3.6,2.,1.505)) ;
#156942 = CARTESIAN_POINT('Origin',(3.6,2.,1.405)) ;
#156943 = CARTESIAN_POINT('',(3.7,1.9,1.405)) ;
#156944 = CARTESIAN_POINT('',(3.6,1.92679491924311,1.405)) ;
#156945 = CARTESIAN_POINT('Origin',(3.7,2.1,1.405)) ;
#156946 = CARTESIAN_POINT('',(3.5,1.9,1.405)) ;
#156947 = CARTESIAN_POINT('Origin',(3.5,2.1,1.405)) ;
#156948 = CARTESIAN_POINT('',(2.7,1.9,1.405)) ;
#156949 = CARTESIAN_POINT('',(2.6,1.9,1.405)) ;
#156950 = CARTESIAN_POINT('',(2.7,-5.15,1.405)) ;
#156951 = CARTESIAN_POINT('',(2.7,2.,1.405)) ;
#156952 = CARTESIAN_POINT('',(3.5,-5.15,1.405)) ;
#156953 = CARTESIAN_POINT('',(3.6,-5.15,1.405)) ;
#156954 = CARTESIAN_POINT('',(3.5,-2.35,1.405)) ;
#156955 = CARTESIAN_POINT('',(3.5,-2.25,1.405)) ;
#156956 = CARTESIAN_POINT('',(3.7,-2.15,1.405)) ;
#156957 = CARTESIAN_POINT('Origin',(3.7,-2.35,1.405)) ;
#156958 = CARTESIAN_POINT('',(10.1,-2.15,1.405)) ;
#156959 = CARTESIAN_POINT('',(3.6,-2.15,1.405)) ;
#156960 = CARTESIAN_POINT('',(10.1,1.9,1.405)) ;
#156961 = CARTESIAN_POINT('',(10.1,2.,1.405)) ;
#156962 = CARTESIAN_POINT('',(3.6,1.9,1.405)) ;
#156963 = CARTESIAN_POINT('Origin',(3.6,-5.25,1.405)) ;
#156964 = CARTESIAN_POINT('',(3.5,-5.25,1.305)) ;
#156965 = CARTESIAN_POINT('',(2.7,-5.25,1.305)) ;
#156966 = CARTESIAN_POINT('',(3.6,-5.25,1.305)) ;
#156967 = CARTESIAN_POINT('',(2.7,-5.25,-1.305)) ;
#156968 = CARTESIAN_POINT('',(2.7,-5.25,1.405)) ;
#156969 = CARTESIAN_POINT('',(3.5,-5.25,-1.305)) ;
#156970 = CARTESIAN_POINT('',(3.6,-5.25,-1.305)) ;
#156971 = CARTESIAN_POINT('',(3.5,-5.25,1.405)) ;
#156972 = CARTESIAN_POINT('Origin',(3.6,-5.25,-1.405)) ;
#156973 = CARTESIAN_POINT('',(2.7,1.9,-1.405)) ;
#156974 = CARTESIAN_POINT('',(3.5,1.9,-1.405)) ;
#156975 = CARTESIAN_POINT('',(3.6,1.9,-1.405)) ;
#156976 = CARTESIAN_POINT('',(3.6,1.92679491924311,-1.405)) ;
#156977 = CARTESIAN_POINT('Origin',(3.5,2.1,-1.405)) ;
#156978 = CARTESIAN_POINT('',(3.7,1.9,-1.405)) ;
#156979 = CARTESIAN_POINT('Origin',(3.7,2.1,-1.405)) ;
#156980 = CARTESIAN_POINT('',(10.1,1.9,-1.405)) ;
#156981 = CARTESIAN_POINT('',(3.6,1.9,-1.405)) ;
#156982 = CARTESIAN_POINT('',(10.1,-2.15,-1.405)) ;
#156983 = CARTESIAN_POINT('',(10.1,-2.25,-1.405)) ;
#156984 = CARTESIAN_POINT('',(3.7,-2.15,-1.405)) ;
#156985 = CARTESIAN_POINT('',(3.6,-2.15,-1.405)) ;
#156986 = CARTESIAN_POINT('',(3.5,-2.35,-1.405)) ;
#156987 = CARTESIAN_POINT('Origin',(3.7,-2.35,-1.405)) ;
#156988 = CARTESIAN_POINT('',(3.5,-5.15,-1.405)) ;
#156989 = CARTESIAN_POINT('',(3.5,-5.25,-1.405)) ;
#156990 = CARTESIAN_POINT('',(2.7,-5.15,-1.405)) ;
#156991 = CARTESIAN_POINT('',(3.6,-5.15,-1.405)) ;
#156992 = CARTESIAN_POINT('',(2.7,-5.25,-1.405)) ;
#156993 = CARTESIAN_POINT('Origin',(3.6,2.,-1.405)) ;
#156994 = CARTESIAN_POINT('',(2.7,2.,-2.305)) ;
#156995 = CARTESIAN_POINT('',(3.6,2.,-2.305)) ;
#156996 = CARTESIAN_POINT('',(2.7,2.,-1.505)) ;
#156997 = CARTESIAN_POINT('',(2.6,2.,-1.505)) ;
#156998 = CARTESIAN_POINT('',(2.7,2.,-1.405)) ;
#156999 = CARTESIAN_POINT('Origin',(10.2,-2.25,-0.875)) ;
#157000 = CARTESIAN_POINT('',(10.1,-2.25,-0.903119593409422)) ;
#157001 = CARTESIAN_POINT('',(3.7,-2.25,-0.903119593409422)) ;
#157002 = CARTESIAN_POINT('',(10.2,-2.25,-0.903119593409422)) ;
#157003 = CARTESIAN_POINT('',(3.7,-2.25,-1.305)) ;
#157004 = CARTESIAN_POINT('',(3.7,-2.25,-0.875)) ;
#157005 = CARTESIAN_POINT('',(10.1,-2.25,-1.305)) ;
#157006 = CARTESIAN_POINT('',(10.2,-2.25,-1.305)) ;
#157007 = CARTESIAN_POINT('',(10.1,-2.25,-0.875)) ;
#157008 = CARTESIAN_POINT('Origin',(10.2,-2.25,1.405)) ;
#157009 = CARTESIAN_POINT('',(10.1,-2.25,1.305)) ;
#157010 = CARTESIAN_POINT('',(3.7,-2.25,1.305)) ;
#157011 = CARTESIAN_POINT('',(10.2,-2.25,1.305)) ;
#157012 = CARTESIAN_POINT('',(3.7,-2.25,0.903119593409423)) ;
#157013 = CARTESIAN_POINT('',(3.7,-2.25,1.405)) ;
#157014 = CARTESIAN_POINT('',(10.1,-2.25,0.903119593409423)) ;
#157015 = CARTESIAN_POINT('',(10.2,-2.25,0.903119593409423)) ;
#157016 = CARTESIAN_POINT('',(10.1,-2.25,1.405)) ;
#157017 = CARTESIAN_POINT('Origin',(10.2,-3.65625,3.25260651745651E-16)) ;
#157018 = CARTESIAN_POINT('',(10.1,-2.23576512455516,0.851696413713513)) ;
#157019 = CARTESIAN_POINT('',(3.7,-2.23576512455516,0.851696413713513)) ;
#157020 = CARTESIAN_POINT('',(10.2,-2.23576512455516,0.851696413713513)) ;
#157021 = CARTESIAN_POINT('',(3.7,-2.23576512455516,-0.851696413713512)) ;
#157022 = CARTESIAN_POINT('Origin',(3.7,-3.65625,3.25260651745651E-16)) ;
#157023 = CARTESIAN_POINT('',(10.1,-2.23576512455516,-0.851696413713512)) ;
#157024 = CARTESIAN_POINT('',(10.2,-2.23576512455516,-0.851696413713512)) ;
#157025 = CARTESIAN_POINT('Origin',(10.1,-3.65625,3.25260651745651E-16)) ;
#157026 = CARTESIAN_POINT('Origin',(10.2,-3.65625,3.25260651745651E-16)) ;
#157027 = CARTESIAN_POINT('',(10.2,-2.15,1.305)) ;
#157028 = CARTESIAN_POINT('',(10.2,-2.15,0.903119593409424)) ;
#157029 = CARTESIAN_POINT('',(10.2,-2.15,0.875)) ;
#157030 = CARTESIAN_POINT('',(10.2,-2.15,-0.903119593409424)) ;
#157031 = CARTESIAN_POINT('Origin',(10.2,-3.65625,3.25260651745651E-16)) ;
#157032 = CARTESIAN_POINT('',(10.2,-2.15,-1.305)) ;
#157033 = CARTESIAN_POINT('',(10.2,-2.15,-1.405)) ;
#157034 = CARTESIAN_POINT('',(10.2,1.9,-1.305)) ;
#157035 = CARTESIAN_POINT('',(10.2,2.,-1.305)) ;
#157036 = CARTESIAN_POINT('',(10.2,1.9,1.305)) ;
#157037 = CARTESIAN_POINT('',(10.2,1.9,1.405)) ;
#157038 = CARTESIAN_POINT('',(10.2,-2.25,1.305)) ;
#157039 = CARTESIAN_POINT('Origin',(8.7,0.,0.)) ;
#157040 = CARTESIAN_POINT('Origin',(-2.,4.4,-1.)) ;
#157041 = CARTESIAN_POINT('',(-2.,4.35,-0.9)) ;
#157042 = CARTESIAN_POINT('',(-2.,4.35,0.900000000000001)) ;
#157043 = CARTESIAN_POINT('',(-2.,4.35,-1.)) ;
#157044 = CARTESIAN_POINT('',(-2.,4.45,0.900000000000001)) ;
#157045 = CARTESIAN_POINT('',(-2.,4.55,0.900000000000001)) ;
#157046 = CARTESIAN_POINT('',(-2.,4.45,-0.9)) ;
#157047 = CARTESIAN_POINT('',(-2.,4.45,-1.)) ;
#157048 = CARTESIAN_POINT('',(-2.,4.25,-0.9)) ;
#157049 = CARTESIAN_POINT('Origin',(-3.,4.4,1.)) ;
#157050 = CARTESIAN_POINT('',(-2.9,4.45,1.)) ;
#157051 = CARTESIAN_POINT('',(-2.1,4.45,1.)) ;
#157052 = CARTESIAN_POINT('',(-2.,4.45,1.)) ;
#157053 = CARTESIAN_POINT('',(-2.1,4.35,1.)) ;
#157054 = CARTESIAN_POINT('',(-2.1,4.25,1.)) ;
#157055 = CARTESIAN_POINT('',(-2.9,4.35,1.)) ;
#157056 = CARTESIAN_POINT('',(-3.,4.35,1.)) ;
#157057 = CARTESIAN_POINT('',(-2.9,4.55,1.)) ;
#157058 = CARTESIAN_POINT('Origin',(-3.,4.4,-0.999999999999999)) ;
#157059 = CARTESIAN_POINT('',(-3.,4.45,0.900000000000001)) ;
#157060 = CARTESIAN_POINT('',(-3.,4.35,0.900000000000001)) ;
#157061 = CARTESIAN_POINT('',(-3.,4.25,0.900000000000001)) ;
#157062 = CARTESIAN_POINT('',(-3.,4.35,-0.899999999999999)) ;
#157063 = CARTESIAN_POINT('',(-3.,4.35,-0.999999999999999)) ;
#157064 = CARTESIAN_POINT('',(-3.,4.45,-0.899999999999999)) ;
#157065 = CARTESIAN_POINT('',(-3.,4.55,-0.899999999999999)) ;
#157066 = CARTESIAN_POINT('',(-3.,4.45,1.)) ;
#157067 = CARTESIAN_POINT('Origin',(-3.,4.4,-0.999999999999999)) ;
#157068 = CARTESIAN_POINT('',(-2.9,4.35,-0.999999999999999)) ;
#157069 = CARTESIAN_POINT('',(-2.1,4.35,-1.)) ;
#157070 = CARTESIAN_POINT('',(-3.,4.35,-0.999999999999999)) ;
#157071 = CARTESIAN_POINT('',(-2.1,4.45,-1.)) ;
#157072 = CARTESIAN_POINT('',(-2.1,4.55,-1.)) ;
#157073 = CARTESIAN_POINT('',(-2.9,4.45,-0.999999999999999)) ;
#157074 = CARTESIAN_POINT('',(-3.,4.45,-0.999999999999999)) ;
#157075 = CARTESIAN_POINT('',(-2.9,4.25,-0.999999999999999)) ;
#157076 = CARTESIAN_POINT('Origin',(0.,4.25,0.)) ;
#157077 = CARTESIAN_POINT('',(-2.9,4.25,-0.899999999999999)) ;
#157078 = CARTESIAN_POINT('',(-2.9,4.25,0.900000000000001)) ;
#157079 = CARTESIAN_POINT('',(-2.9,4.25,1.25767452008319E-15)) ;
#157080 = CARTESIAN_POINT('',(-2.1,4.25,0.900000000000001)) ;
#157081 = CARTESIAN_POINT('',(-1.95156391047391E-16,4.25,0.900000000000001)) ;
#157082 = CARTESIAN_POINT('',(-2.1,4.25,-0.9)) ;
#157083 = CARTESIAN_POINT('',(-2.1,4.25,4.55364912443912E-16)) ;
#157084 = CARTESIAN_POINT('',(-1.95156391047391E-16,4.25,-0.9)) ;
#157085 = CARTESIAN_POINT('',(-2.75,4.25,0.850000000000001)) ;
#157086 = CARTESIAN_POINT('',(-2.25,4.25,0.850000000000001)) ;
#157087 = CARTESIAN_POINT('',(-2.85,4.25,0.850000000000001)) ;
#157088 = CARTESIAN_POINT('',(-2.85,4.25,0.750000000000001)) ;
#157089 = CARTESIAN_POINT('Origin',(-2.75,4.25,0.750000000000001)) ;
#157090 = CARTESIAN_POINT('',(-2.85,4.25,-0.75)) ;
#157091 = CARTESIAN_POINT('',(-2.85,4.25,-0.85)) ;
#157092 = CARTESIAN_POINT('',(-2.75,4.25,-0.85)) ;
#157093 = CARTESIAN_POINT('Origin',(-2.75,4.25,-0.75)) ;
#157094 = CARTESIAN_POINT('',(-2.25,4.25,-0.85)) ;
#157095 = CARTESIAN_POINT('',(-2.15,4.25,-0.85)) ;
#157096 = CARTESIAN_POINT('',(-2.15,4.25,-0.75)) ;
#157097 = CARTESIAN_POINT('Origin',(-2.25,4.25,-0.75)) ;
#157098 = CARTESIAN_POINT('',(-2.15,4.25,0.750000000000001)) ;
#157099 = CARTESIAN_POINT('',(-2.15,4.25,0.850000000000001)) ;
#157100 = CARTESIAN_POINT('Origin',(-2.25,4.25,0.750000000000001)) ;
#157101 = CARTESIAN_POINT('Origin',(-2.15,4.25,0.850000000000001)) ;
#157102 = CARTESIAN_POINT('',(-2.15,4.3,-0.75)) ;
#157103 = CARTESIAN_POINT('',(-2.15,4.3,0.750000000000001)) ;
#157104 = CARTESIAN_POINT('',(-2.15,4.3,0.850000000000001)) ;
#157105 = CARTESIAN_POINT('',(-2.15,4.25,0.750000000000001)) ;
#157106 = CARTESIAN_POINT('',(-2.15,4.25,-0.75)) ;
#157107 = CARTESIAN_POINT('Origin',(-2.85,4.25,0.850000000000001)) ;
#157108 = CARTESIAN_POINT('',(-2.25,4.3,0.850000000000001)) ;
#157109 = CARTESIAN_POINT('',(-2.75,4.3,0.850000000000001)) ;
#157110 = CARTESIAN_POINT('',(-2.85,4.3,0.850000000000001)) ;
#157111 = CARTESIAN_POINT('',(-2.75,4.25,0.850000000000001)) ;
#157112 = CARTESIAN_POINT('',(-2.25,4.25,0.850000000000001)) ;
#157113 = CARTESIAN_POINT('Origin',(-2.85,4.25,-0.85)) ;
#157114 = CARTESIAN_POINT('',(-2.85,4.3,0.750000000000001)) ;
#157115 = CARTESIAN_POINT('',(-2.85,4.25,0.750000000000001)) ;
#157116 = CARTESIAN_POINT('',(-2.85,4.3,-0.75)) ;
#157117 = CARTESIAN_POINT('',(-2.85,4.3,-0.85)) ;
#157118 = CARTESIAN_POINT('',(-2.85,4.25,-0.75)) ;
#157119 = CARTESIAN_POINT('Origin',(-2.15,4.25,-0.85)) ;
#157120 = CARTESIAN_POINT('',(-2.75,4.3,-0.85)) ;
#157121 = CARTESIAN_POINT('',(-2.25,4.3,-0.85)) ;
#157122 = CARTESIAN_POINT('',(-2.15,4.3,-0.85)) ;
#157123 = CARTESIAN_POINT('',(-2.25,4.25,-0.85)) ;
#157124 = CARTESIAN_POINT('',(-2.75,4.25,-0.85)) ;
#157125 = CARTESIAN_POINT('Origin',(-1.97127667724637E-17,4.4,0.)) ;
#157126 = CARTESIAN_POINT('',(-2.25,4.4,-0.75)) ;
#157127 = CARTESIAN_POINT('',(-2.75,4.4,-0.75)) ;
#157128 = CARTESIAN_POINT('',(-1.97127667724637E-17,4.4,-0.75)) ;
#157129 = CARTESIAN_POINT('',(-2.75,4.4,0.750000000000001)) ;
#157130 = CARTESIAN_POINT('',(-2.75,4.4,0.)) ;
#157131 = CARTESIAN_POINT('',(-2.25,4.4,0.750000000000001)) ;
#157132 = CARTESIAN_POINT('',(-1.97127667724637E-17,4.4,0.750000000000001)) ;
#157133 = CARTESIAN_POINT('',(-2.25,4.4,0.)) ;
#157134 = CARTESIAN_POINT('Origin',(-7.29372370581158E-16,3.55,0.)) ;
#157135 = CARTESIAN_POINT('',(-0.183301359729408,3.55,1.51703678647597)) ;
#157136 = CARTESIAN_POINT('Origin',(-0.273932138433073,3.05,1.4747749603019)) ;
#157137 = CARTESIAN_POINT('',(0.953662978710562,3.45,-1.15781126399638)) ;
#157138 = CARTESIAN_POINT('',(-0.273932138433073,3.15,1.4747749603019)) ;
#157139 = CARTESIAN_POINT('Origin',(-0.953662978710561,3.05,1.15781126399638)) ;
#157140 = CARTESIAN_POINT('',(-0.953662978710561,3.15,1.15781126399638)) ;
#157141 = CARTESIAN_POINT('',(-0.953662978710562,3.45,1.15781126399638)) ;
#157142 = CARTESIAN_POINT('Origin',(-7.95081593156037E-16,3.05,0.)) ;
#157143 = CARTESIAN_POINT('',(0.249234641435079,3.05,0.116220021978692)) ;
#157144 = CARTESIAN_POINT('',(-0.249234641435079,3.05,-0.116220021978691)) ;
#157145 = CARTESIAN_POINT('Origin',(-1.39554230456301E-15,-1.51907484122731,
-3.81)) ;
#157146 = CARTESIAN_POINT('Origin',(-6.11095769946375E-16,4.45,-3.81)) ;
#157147 = CARTESIAN_POINT('Origin',(-1.39554230456301E-15,-1.51907484122731,
0.)) ;
#157148 = CARTESIAN_POINT('Origin',(-6.11095769946375E-16,4.45,0.)) ;
#157149 = CARTESIAN_POINT('Origin',(2.6,-1.51907484122731,1.55)) ;
#157150 = CARTESIAN_POINT('',(2.5,4.45,1.55)) ;
#157151 = CARTESIAN_POINT('',(2.6,4.45,1.55)) ;
#157152 = CARTESIAN_POINT('',(2.5,2.85,1.55)) ;
#157153 = CARTESIAN_POINT('',(2.5,2.75,1.55)) ;
#157154 = CARTESIAN_POINT('',(1.77490703981927,2.85,1.55)) ;
#157155 = CARTESIAN_POINT('Origin',(2.6,-1.51907484122731,-35.84)) ;
#157156 = CARTESIAN_POINT('',(2.5,2.85,-35.84)) ;
#157157 = CARTESIAN_POINT('',(2.5,4.45,-35.84)) ;
#157158 = CARTESIAN_POINT('',(2.5,4.55,-35.84)) ;
#157159 = CARTESIAN_POINT('',(1.77490703981929,4.45,-35.84)) ;
#157160 = CARTESIAN_POINT('',(2.6,2.85,-35.84)) ;
#157161 = CARTESIAN_POINT('Origin',(1.99634453700209E-16,-1.51907484122731,
-34.29)) ;
#157162 = CARTESIAN_POINT('Origin',(-5.84812080916424E-16,4.45,-34.29)) ;
#157163 = CARTESIAN_POINT('Origin',(1.99634453700209E-16,-1.51907484122731,
-30.48)) ;
#157164 = CARTESIAN_POINT('Origin',(-5.84812080916424E-16,4.45,-30.48)) ;
#157165 = CARTESIAN_POINT('Origin',(9.6,3.,-0.4)) ;
#157166 = CARTESIAN_POINT('',(9.7,2.9,-0.399999999999999)) ;
#157167 = CARTESIAN_POINT('',(9.7,2.1,-0.399999999999999)) ;
#157168 = CARTESIAN_POINT('',(9.7,3.,-0.399999999999999)) ;
#157169 = CARTESIAN_POINT('',(9.6,2.1,-0.5)) ;
#157170 = CARTESIAN_POINT('Origin',(9.6,2.1,-0.4)) ;
#157171 = CARTESIAN_POINT('',(9.6,2.9,-0.5)) ;
#157172 = CARTESIAN_POINT('',(9.6,3.,-0.5)) ;
#157173 = CARTESIAN_POINT('Origin',(9.6,2.9,-0.4)) ;
#157174 = CARTESIAN_POINT('Origin',(7.8,3.,-0.5)) ;
#157175 = CARTESIAN_POINT('',(7.8,2.1,-0.5)) ;
#157176 = CARTESIAN_POINT('',(7.8,2.1,-0.5)) ;
#157177 = CARTESIAN_POINT('',(7.8,2.9,-0.5)) ;
#157178 = CARTESIAN_POINT('',(7.8,3.,-0.5)) ;
#157179 = CARTESIAN_POINT('',(7.8,2.9,-0.5)) ;
#157180 = CARTESIAN_POINT('Origin',(7.8,3.,-0.4)) ;
#157181 = CARTESIAN_POINT('',(7.7,2.1,-0.399999999999999)) ;
#157182 = CARTESIAN_POINT('Origin',(7.8,2.1,-0.4)) ;
#157183 = CARTESIAN_POINT('',(7.7,2.9,-0.399999999999999)) ;
#157184 = CARTESIAN_POINT('',(7.7,3.,-0.399999999999999)) ;
#157185 = CARTESIAN_POINT('Origin',(7.8,2.9,-0.4)) ;
#157186 = CARTESIAN_POINT('Origin',(7.7,3.,-0.399999999999999)) ;
#157187 = CARTESIAN_POINT('',(7.7,2.1,0.399999999999999)) ;
#157188 = CARTESIAN_POINT('',(7.7,2.1,0.399999999999999)) ;
#157189 = CARTESIAN_POINT('',(7.7,2.9,0.399999999999999)) ;
#157190 = CARTESIAN_POINT('',(7.7,3.,0.399999999999999)) ;
#157191 = CARTESIAN_POINT('',(7.7,2.9,-0.399999999999999)) ;
#157192 = CARTESIAN_POINT('Origin',(7.8,3.,0.4)) ;
#157193 = CARTESIAN_POINT('',(7.8,2.1,0.5)) ;
#157194 = CARTESIAN_POINT('Origin',(7.8,2.1,0.4)) ;
#157195 = CARTESIAN_POINT('',(7.8,2.9,0.5)) ;
#157196 = CARTESIAN_POINT('',(7.8,3.,0.5)) ;
#157197 = CARTESIAN_POINT('Origin',(7.8,2.9,0.4)) ;
#157198 = CARTESIAN_POINT('Origin',(7.8,3.,0.5)) ;
#157199 = CARTESIAN_POINT('',(9.6,2.1,0.5)) ;
#157200 = CARTESIAN_POINT('',(9.6,2.1,0.5)) ;
#157201 = CARTESIAN_POINT('',(9.6,2.9,0.5)) ;
#157202 = CARTESIAN_POINT('',(9.6,3.,0.5)) ;
#157203 = CARTESIAN_POINT('',(7.8,2.9,0.5)) ;
#157204 = CARTESIAN_POINT('Origin',(9.6,3.,0.4)) ;
#157205 = CARTESIAN_POINT('',(9.7,2.1,0.399999999999999)) ;
#157206 = CARTESIAN_POINT('Origin',(9.6,2.1,0.4)) ;
#157207 = CARTESIAN_POINT('',(9.7,2.9,0.399999999999999)) ;
#157208 = CARTESIAN_POINT('',(9.7,3.,0.399999999999999)) ;
#157209 = CARTESIAN_POINT('Origin',(9.6,2.9,0.4)) ;
#157210 = CARTESIAN_POINT('Origin',(9.7,3.,-0.399999999999999)) ;
#157211 = CARTESIAN_POINT('',(9.7,2.9,-0.399999999999999)) ;
#157212 = CARTESIAN_POINT('',(9.7,2.1,-0.399999999999999)) ;
#157213 = CARTESIAN_POINT('Origin',(9.6,3.,-0.4)) ;
#157214 = CARTESIAN_POINT('',(7.8,3.,0.4)) ;
#157215 = CARTESIAN_POINT('',(9.6,3.,0.4)) ;
#157216 = CARTESIAN_POINT('',(9.6,3.,0.4)) ;
#157217 = CARTESIAN_POINT('',(9.6,3.,-0.4)) ;
#157218 = CARTESIAN_POINT('',(9.6,3.,-0.4)) ;
#157219 = CARTESIAN_POINT('',(7.8,3.,-0.4)) ;
#157220 = CARTESIAN_POINT('',(9.6,3.,-0.4)) ;
#157221 = CARTESIAN_POINT('',(7.8,3.,-0.4)) ;
#157222 = CARTESIAN_POINT('Origin',(0.,-6.45,2.2)) ;
#157223 = CARTESIAN_POINT('Origin',(2.5,-6.45,2.2)) ;
#157224 = CARTESIAN_POINT('Origin',(-5.8,-6.45,2.2)) ;
#157225 = CARTESIAN_POINT('Origin',(-5.8,-6.45,2.2)) ;
#157226 = CARTESIAN_POINT('Origin',(-5.8,-6.45,2.2)) ;
#157227 = CARTESIAN_POINT('Origin',(-5.8,-6.45,2.2)) ;
#157228 = CARTESIAN_POINT('Origin',(2.5,-6.45,-36.59)) ;
#157229 = CARTESIAN_POINT('Origin',(2.5,-6.45,-36.49)) ;
#157230 = CARTESIAN_POINT('Origin',(2.5,-6.45,2.2)) ;
#157231 = CARTESIAN_POINT('Origin',(-5.8,-1.4373423086665E-15,2.2)) ;
#157232 = CARTESIAN_POINT('Origin',(-5.8,0.35,2.2)) ;
#157233 = CARTESIAN_POINT('Origin',(-5.8,-6.45,-36.59)) ;
#157234 = CARTESIAN_POINT('Origin',(-5.8,-6.45,-36.49)) ;
#157235 = CARTESIAN_POINT('Origin',(2.6,-6.45,-36.49)) ;
#157236 = CARTESIAN_POINT('Origin',(2.5,-6.45,-36.49)) ;
#157237 = CARTESIAN_POINT('Origin',(-5.8,-6.45,-36.49)) ;
#157238 = CARTESIAN_POINT('Origin',(-3.9,0.,2.2)) ;
#157239 = CARTESIAN_POINT('Origin',(-3.9,4.45,2.2)) ;
#157240 = CARTESIAN_POINT('Origin',(-3.9,3.9,2.2)) ;
#157241 = CARTESIAN_POINT('Origin',(0.,3.9,2.2)) ;
#157242 = CARTESIAN_POINT('',(-3.9,3.80333655664151,2.22561598559651)) ;
#157243 = CARTESIAN_POINT('Origin',(-3.9,3.9,2.2)) ;
#157244 = CARTESIAN_POINT('',(-3.78531217125694,3.83901474997814,2.27925149386461)) ;
#157245 = CARTESIAN_POINT('Origin',(-3.55328808497345,3.91119503536387,2.19250366916966)) ;
#157246 = CARTESIAN_POINT('Origin',(-3.61336525333204,3.89250565174523,2.22200921288124)) ;
#157247 = CARTESIAN_POINT('Origin',(-5.8,0.35,2.2)) ;
#157248 = CARTESIAN_POINT('Origin',(-5.8,0.35,2.2)) ;
#157249 = CARTESIAN_POINT('Origin',(-5.8,0.35,2.2)) ;
#157250 = CARTESIAN_POINT('Origin',(-5.8,-6.45,-36.49)) ;
#157251 = CARTESIAN_POINT('Origin',(-5.8,-6.45,-36.49)) ;
#157252 = CARTESIAN_POINT('Origin',(-3.9,4.45,-36.59)) ;
#157253 = CARTESIAN_POINT('Origin',(-3.9,4.45,2.2)) ;
#157254 = CARTESIAN_POINT('Origin',(-3.9,4.45,-36.49)) ;
#157255 = CARTESIAN_POINT('Origin',(-3.9,3.9,2.2)) ;
#157256 = CARTESIAN_POINT('Origin',(-3.9,3.9,2.2)) ;
#157257 = CARTESIAN_POINT('Origin',(-3.85599010415589,3.83075002080759,2.20432033664006)) ;
#157258 = CARTESIAN_POINT('Origin',(-4.43441264557625,2.18411369110472,2.2)) ;
#157259 = CARTESIAN_POINT('',(-3.73060297224731,3.75108317805602,2.27925149386461)) ;
#157260 = CARTESIAN_POINT('Origin',(-3.59033063456527,3.89854842868432,2.20056508349004)) ;
#157261 = CARTESIAN_POINT('',(-3.81328428501115,3.6639623879874,2.22561598559544)) ;
#157262 = CARTESIAN_POINT('Origin',(-3.57343778044602,3.91668601355327,2.19535546435355)) ;
#157263 = CARTESIAN_POINT('Origin',(-3.74596198594684,3.73501205571306,2.20243127556096)) ;
#157264 = CARTESIAN_POINT('Origin',(-5.28280011774461,0.461630035490191,2.2)) ;
#157265 = CARTESIAN_POINT('Origin',(0.,0.35,2.2)) ;
#157266 = CARTESIAN_POINT('Origin',(-5.46221792447664,0.35,2.2)) ;
#157267 = CARTESIAN_POINT('Origin',(-5.8,0.35,-36.59)) ;
#157268 = CARTESIAN_POINT('Origin',(-5.8,0.35,-36.49)) ;
#157269 = CARTESIAN_POINT('Origin',(-5.8,-6.55,-36.49)) ;
#157270 = CARTESIAN_POINT('Origin',(-5.8,0.35,-36.49)) ;
#157271 = CARTESIAN_POINT('Origin',(-3.9,3.8,-36.49)) ;
#157272 = CARTESIAN_POINT('Origin',(-3.9,4.45,-36.49)) ;
#157273 = CARTESIAN_POINT('Origin',(-3.9,3.9,-36.49)) ;
#157274 = CARTESIAN_POINT('Origin',(-3.9,3.9,-36.59)) ;
#157275 = CARTESIAN_POINT('Origin',(-3.9,3.9,-36.49)) ;
#157276 = CARTESIAN_POINT('Origin',(-5.46221792447664,0.55,2.2)) ;
#157277 = CARTESIAN_POINT('Origin',(-5.46221792447664,0.55,2.19999999999999)) ;
#157278 = CARTESIAN_POINT('Origin',(-5.8,0.35,-36.49)) ;
#157279 = CARTESIAN_POINT('Origin',(-5.8,0.35,-36.49)) ;
#157280 = CARTESIAN_POINT('Origin',(-3.9,3.9,-36.49)) ;
#157281 = CARTESIAN_POINT('',(-3.9,3.8033365566425,-36.5156159856002)) ;
#157282 = CARTESIAN_POINT('Origin',(-3.9,3.9,-36.49)) ;
#157283 = CARTESIAN_POINT('Origin',(-3.85250686906682,3.83291544204029,-36.4938003888854)) ;
#157284 = CARTESIAN_POINT('Origin',(-5.46221792447664,0.55,-36.59)) ;
#157285 = CARTESIAN_POINT('Origin',(-5.46221792447664,0.55,-36.49)) ;
#157286 = CARTESIAN_POINT('Origin',(-5.9,0.35,-36.49)) ;
#157287 = CARTESIAN_POINT('Origin',(-5.46221792447664,0.35,-36.49)) ;
#157288 = CARTESIAN_POINT('Origin',(-3.75,3.9,-36.49)) ;
#157289 = CARTESIAN_POINT('',(-3.7853121712506,3.83901474998012,-36.5692514938661)) ;
#157290 = CARTESIAN_POINT('Origin',(-3.59104340457654,3.89969403101197,-36.4905650835037)) ;
#157291 = CARTESIAN_POINT('Origin',(-3.56730827154468,3.90683433651809,-36.4853554643623)) ;
#157292 = CARTESIAN_POINT('Origin',(-5.46221792447664,0.55,-36.49)) ;
#157293 = CARTESIAN_POINT('Origin',(-5.28280011774461,0.46163003549019,-36.49)) ;
#157294 = CARTESIAN_POINT('Origin',(-5.31029109663398,0.405815017745095,-36.49)) ;
#157295 = CARTESIAN_POINT('',(-3.8132842850082,3.66396238799052,-36.5156159856002)) ;
#157296 = CARTESIAN_POINT('Origin',(-3.77273229582307,3.7066162135026,-36.4964228703932)) ;
#157297 = CARTESIAN_POINT('',(-3.73060297224274,3.75108317806084,-36.5692514938661)) ;
#157298 = CARTESIAN_POINT('Origin',(-3.57344958540767,3.91667389310731,-36.4853617599003)) ;
#157299 = CARTESIAN_POINT('Origin',(-3.59031431317769,3.89856609733425,-36.4905391368281)) ;
#157300 = CARTESIAN_POINT('Origin',(10.1,-2.15,-0.903119593409422)) ;
#157301 = CARTESIAN_POINT('Origin',(10.1,-2.15,-0.903119593409422)) ;
#157302 = CARTESIAN_POINT('Origin',(10.1,-2.15,-0.903119593409424)) ;
#157303 = CARTESIAN_POINT('Origin',(10.1,-2.15,-0.903119593409422)) ;
#157304 = CARTESIAN_POINT('Origin',(10.1,-3.65625,3.25260651745651E-16)) ;
#157305 = CARTESIAN_POINT('Origin',(10.1,-2.15,0.903119593409423)) ;
#157306 = CARTESIAN_POINT('Origin',(10.2,-2.15,-0.903119593409422)) ;
#157307 = CARTESIAN_POINT('Origin',(3.7,-2.15,-0.903119593409422)) ;
#157308 = CARTESIAN_POINT('Origin',(10.1,-2.15,3.25260651745651E-16)) ;
#157309 = CARTESIAN_POINT('Origin',(10.1,-2.15,-1.305)) ;
#157310 = CARTESIAN_POINT('Origin',(10.1,-3.65625,-1.305)) ;
#157311 = CARTESIAN_POINT('Origin',(10.1,1.9,-1.305)) ;
#157312 = CARTESIAN_POINT('Origin',(10.1,-2.15,-1.305)) ;
#157313 = CARTESIAN_POINT('Origin',(10.1,1.9,3.25260651745651E-16)) ;
#157314 = CARTESIAN_POINT('Origin',(10.1,1.9,-1.305)) ;
#157315 = CARTESIAN_POINT('Origin',(10.1,1.9,1.305)) ;
#157316 = CARTESIAN_POINT('Origin',(10.1,-2.15,0.903119593409423)) ;
#157317 = CARTESIAN_POINT('Origin',(10.1,-2.15,0.903119593409423)) ;
#157318 = CARTESIAN_POINT('Origin',(10.1,-2.15,0.903119593409424)) ;
#157319 = CARTESIAN_POINT('Origin',(3.7,-2.15,-0.903119593409422)) ;
#157320 = CARTESIAN_POINT('Origin',(3.7,-2.35,-0.903119593409422)) ;
#157321 = CARTESIAN_POINT('Origin',(3.7,-2.32153024911032,-0.800273234017602)) ;
#157322 = CARTESIAN_POINT('Origin',(10.1,-2.15,-1.305)) ;
#157323 = CARTESIAN_POINT('Origin',(10.1,-2.15,-1.305)) ;
#157324 = CARTESIAN_POINT('Origin',(10.1,-3.65625,1.305)) ;
#157325 = CARTESIAN_POINT('Origin',(10.1,1.9,1.305)) ;
#157326 = CARTESIAN_POINT('Origin',(10.1,-2.15,1.305)) ;
#157327 = CARTESIAN_POINT('Origin',(10.1,-2.15,3.25260651745651E-16)) ;
#157328 = CARTESIAN_POINT('Origin',(10.1,-2.15,1.305)) ;
#157329 = CARTESIAN_POINT('Origin',(10.2,-2.15,0.903119593409423)) ;
#157330 = CARTESIAN_POINT('Origin',(3.7,-2.15,0.903119593409423)) ;
#157331 = CARTESIAN_POINT('Origin',(3.7,-3.65625,3.25260651745651E-16)) ;
#157332 = CARTESIAN_POINT('Origin',(3.7,-2.32153024911032,0.800273234017602)) ;
#157333 = CARTESIAN_POINT('Origin',(3.7,-2.35,-0.875)) ;
#157334 = CARTESIAN_POINT('Origin',(3.7,-2.35,-1.305)) ;
#157335 = CARTESIAN_POINT('Origin',(3.6,-2.15,-1.305)) ;
#157336 = CARTESIAN_POINT('Origin',(3.7,-2.15,-1.305)) ;
#157337 = CARTESIAN_POINT('Origin',(10.1,-2.15,1.305)) ;
#157338 = CARTESIAN_POINT('Origin',(10.1,-2.15,1.305)) ;
#157339 = CARTESIAN_POINT('Origin',(3.7,-2.15,0.903119593409423)) ;
#157340 = CARTESIAN_POINT('Origin',(3.7,-2.35,0.903119593409423)) ;
#157341 = CARTESIAN_POINT('Origin',(3.7,-2.35,-1.305)) ;
#157342 = CARTESIAN_POINT('Origin',(3.5,-2.35,-1.305)) ;
#157343 = CARTESIAN_POINT('Origin',(10.2,-2.15,1.305)) ;
#157344 = CARTESIAN_POINT('Origin',(3.7,-2.15,1.305)) ;
#157345 = CARTESIAN_POINT('Origin',(3.7,-2.35,1.405)) ;
#157346 = CARTESIAN_POINT('Origin',(3.7,-2.35,1.305)) ;
#157347 = CARTESIAN_POINT('Origin',(3.5,-3.89531375123621E-17,-1.305)) ;
#157348 = CARTESIAN_POINT('Origin',(3.5,-5.15,-1.305)) ;
#157349 = CARTESIAN_POINT('Origin',(3.6,1.9,-1.505)) ;
#157350 = CARTESIAN_POINT('Origin',(3.5,1.9,-1.505)) ;
#157351 = CARTESIAN_POINT('Origin',(2.7,1.9,-1.505)) ;
#157352 = CARTESIAN_POINT('Origin',(2.7,1.9,-1.405)) ;
#157353 = CARTESIAN_POINT('Origin',(2.7,1.9,-1.505)) ;
#157354 = CARTESIAN_POINT('Origin',(2.7,1.9,-2.305)) ;
#157355 = CARTESIAN_POINT('Origin',(3.7,-2.35,1.305)) ;
#157356 = CARTESIAN_POINT('Origin',(3.5,-2.35,1.305)) ;
#157357 = CARTESIAN_POINT('Origin',(3.5,-5.15,-1.305)) ;
#157358 = CARTESIAN_POINT('Origin',(3.5,-5.15,-1.305)) ;
#157359 = CARTESIAN_POINT('Origin',(3.5,-5.15,-1.305)) ;
#157360 = CARTESIAN_POINT('Origin',(2.7,1.9,-1.505)) ;
#157361 = CARTESIAN_POINT('Origin',(2.7,1.9,-1.505)) ;
#157362 = CARTESIAN_POINT('Origin',(3.5,-3.89531375123621E-17,1.305)) ;
#157363 = CARTESIAN_POINT('Origin',(3.5,-5.15,1.305)) ;
#157364 = CARTESIAN_POINT('Origin',(3.5,-5.15,0.)) ;
#157365 = CARTESIAN_POINT('Origin',(3.5,-5.15,1.305)) ;
#157366 = CARTESIAN_POINT('Origin',(3.6,-5.15,-1.305)) ;
#157367 = CARTESIAN_POINT('Origin',(2.7,-5.15,-1.305)) ;
#157368 = CARTESIAN_POINT('Origin',(2.7,-5.25,-1.505)) ;
#157369 = CARTESIAN_POINT('Origin',(2.7,-5.15,-1.505)) ;
#157370 = CARTESIAN_POINT('Origin',(3.5,-5.15,1.305)) ;
#157371 = CARTESIAN_POINT('Origin',(3.5,-5.15,1.305)) ;
#157372 = CARTESIAN_POINT('Origin',(2.7,-5.15,-1.305)) ;
#157373 = CARTESIAN_POINT('Origin',(2.7,-5.35,-1.305)) ;
#157374 = CARTESIAN_POINT('Origin',(2.7,1.9,2.3)) ;
#157375 = CARTESIAN_POINT('Origin',(2.7,1.9,2.2)) ;
#157376 = CARTESIAN_POINT('Origin',(2.7,1.9,1.505)) ;
#157377 = CARTESIAN_POINT('Origin',(3.6,1.9,1.505)) ;
#157378 = CARTESIAN_POINT('Origin',(3.5,1.9,1.505)) ;
#157379 = CARTESIAN_POINT('Origin',(2.7,1.9,1.505)) ;
#157380 = CARTESIAN_POINT('Origin',(3.6,-5.15,1.305)) ;
#157381 = CARTESIAN_POINT('Origin',(2.7,-5.15,1.305)) ;
#157382 = CARTESIAN_POINT('Origin',(2.7,-5.35,1.405)) ;
#157383 = CARTESIAN_POINT('Origin',(2.7,-5.35,1.305)) ;
#157384 = CARTESIAN_POINT('Origin',(2.7,1.9,1.505)) ;
#157385 = CARTESIAN_POINT('Origin',(2.7,1.9,1.505)) ;
#157386 = CARTESIAN_POINT('Origin',(2.7,-5.15,1.305)) ;
#157387 = CARTESIAN_POINT('Origin',(2.7,-5.15,1.505)) ;
#157388 = CARTESIAN_POINT('Origin',(2.7,2.,1.505)) ;
#157389 = CARTESIAN_POINT('Origin',(7.8,2.1,-0.4)) ;
#157390 = CARTESIAN_POINT('Origin',(7.8,2.1,-0.6)) ;
#157391 = CARTESIAN_POINT('Origin',(7.6,2.1,-0.399999999999999)) ;
#157392 = CARTESIAN_POINT('Origin',(7.6,2.1,-0.399999999999999)) ;
#157393 = CARTESIAN_POINT('Origin',(7.6,2.1,0.399999999999999)) ;
#157394 = CARTESIAN_POINT('Origin',(7.8,2.1,-0.6)) ;
#157395 = CARTESIAN_POINT('Origin',(9.6,2.1,-0.6)) ;
#157396 = CARTESIAN_POINT('Origin',(7.8,2.1,0.4)) ;
#157397 = CARTESIAN_POINT('Origin',(7.8,2.1,0.6)) ;
#157398 = CARTESIAN_POINT('Origin',(9.6,2.1,-0.4)) ;
#157399 = CARTESIAN_POINT('Origin',(9.8,2.1,-0.399999999999999)) ;
#157400 = CARTESIAN_POINT('Origin',(7.8,2.1,0.6)) ;
#157401 = CARTESIAN_POINT('Origin',(9.6,2.1,0.6)) ;
#157402 = CARTESIAN_POINT('Origin',(9.8,2.1,-0.399999999999999)) ;
#157403 = CARTESIAN_POINT('Origin',(9.8,2.1,0.399999999999999)) ;
#157404 = CARTESIAN_POINT('Origin',(9.6,2.1,0.4)) ;
#157405 = CARTESIAN_POINT('Origin',(-4.9,-6.45,1.1)) ;
#157406 = CARTESIAN_POINT('Origin',(-4.,-6.45,1.1)) ;
#157407 = CARTESIAN_POINT('Origin',(-4.8,-6.45,1.1)) ;
#157408 = CARTESIAN_POINT('Origin',(-4.8,-6.45,0.899999999999998)) ;
#157409 = CARTESIAN_POINT('Origin',(-5.,-6.45,0.899999999999998)) ;
#157410 = CARTESIAN_POINT('Origin',(-4.8,-6.45,0.899999999999998)) ;
#157411 = CARTESIAN_POINT('Origin',(-4.,-6.45,0.899999999999998)) ;
#157412 = CARTESIAN_POINT('Origin',(-4.,-6.45,0.899999999999998)) ;
#157413 = CARTESIAN_POINT('Origin',(-3.8,-6.45,0.899999999999998)) ;
#157414 = CARTESIAN_POINT('Origin',(-5.,-6.45,0.999999999999998)) ;
#157415 = CARTESIAN_POINT('Origin',(-5.,-6.45,-0.900000000000002)) ;
#157416 = CARTESIAN_POINT('Origin',(-4.8,-6.4,0.899999999999998)) ;
#157417 = CARTESIAN_POINT('Origin',(-4.8,-6.35,0.899999999999998)) ;
#157418 = CARTESIAN_POINT('Origin',(1.9515639104739E-16,-6.35,0.899999999999997)) ;
#157419 = CARTESIAN_POINT('Origin',(-4.,-6.35,0.899999999999998)) ;
#157420 = CARTESIAN_POINT('Origin',(-4.8,-6.35,0.899999999999998)) ;
#157421 = CARTESIAN_POINT('Origin',(-4.,-6.4,0.899999999999998)) ;
#157422 = CARTESIAN_POINT('Origin',(-4.,-6.35,0.899999999999998)) ;
#157423 = CARTESIAN_POINT('Origin',(-3.8,-6.45,0.999999999999998)) ;
#157424 = CARTESIAN_POINT('Origin',(-3.8,-6.45,-0.900000000000002)) ;
#157425 = CARTESIAN_POINT('Origin',(-4.9,-6.45,-1.1)) ;
#157426 = CARTESIAN_POINT('Origin',(-4.8,-6.45,-1.1)) ;
#157427 = CARTESIAN_POINT('Origin',(-4.,-6.45,-1.1)) ;
#157428 = CARTESIAN_POINT('Origin',(-4.8,-6.45,-0.900000000000002)) ;
#157429 = CARTESIAN_POINT('Origin',(-4.8,-6.45,-0.900000000000002)) ;
#157430 = CARTESIAN_POINT('Origin',(-4.8,-6.35,0.899999999999998)) ;
#157431 = CARTESIAN_POINT('Origin',(-4.8,-6.35,0.899999999999998)) ;
#157432 = CARTESIAN_POINT('Origin',(-4.,-6.35,0.899999999999998)) ;
#157433 = CARTESIAN_POINT('Origin',(-4.,-6.35,0.899999999999998)) ;
#157434 = CARTESIAN_POINT('Origin',(-4.,-6.45,-0.900000000000002)) ;
#157435 = CARTESIAN_POINT('Origin',(-4.,-6.45,-0.900000000000002)) ;
#157436 = CARTESIAN_POINT('Origin',(-4.8,-6.4,-0.900000000000002)) ;
#157437 = CARTESIAN_POINT('Origin',(-4.8,-6.35,-0.900000000000002)) ;
#157438 = CARTESIAN_POINT('Origin',(-4.8,-6.35,0.)) ;
#157439 = CARTESIAN_POINT('Origin',(-4.8,-6.35,-0.900000000000002)) ;
#157440 = CARTESIAN_POINT('Origin',(-4.,-6.35,-8.67361737988403E-16)) ;
#157441 = CARTESIAN_POINT('Origin',(-4.,-6.35,-0.900000000000002)) ;
#157442 = CARTESIAN_POINT('Origin',(-4.,-6.4,-0.900000000000002)) ;
#157443 = CARTESIAN_POINT('Origin',(-4.,-6.35,-0.900000000000002)) ;
#157444 = CARTESIAN_POINT('Origin',(-4.8,-6.35,-0.900000000000002)) ;
#157445 = CARTESIAN_POINT('Origin',(-4.8,-6.35,-0.900000000000002)) ;
#157446 = CARTESIAN_POINT('Origin',(-4.,-6.35,-0.900000000000002)) ;
#157447 = CARTESIAN_POINT('Origin',(-4.,-6.35,-0.900000000000002)) ;
#157448 = CARTESIAN_POINT('Origin',(1.95156391047391E-16,-6.35,-0.900000000000001)) ;
#157449 = CARTESIAN_POINT('Origin',(-4.15,-6.25,0.749999999999998)) ;
#157450 = CARTESIAN_POINT('Origin',(-4.15,-6.3,0.749999999999998)) ;
#157451 = CARTESIAN_POINT('Origin',(-4.15,-6.3,0.)) ;
#157452 = CARTESIAN_POINT('Origin',(-4.15,-6.3,-0.750000000000002)) ;
#157453 = CARTESIAN_POINT('Origin',(-4.15,-6.3,0.749999999999998)) ;
#157454 = CARTESIAN_POINT('Origin',(-4.15,-6.25,-0.750000000000002)) ;
#157455 = CARTESIAN_POINT('Origin',(-4.15,-6.3,-0.750000000000002)) ;
#157456 = CARTESIAN_POINT('Origin',(-4.15,-6.3,0.749999999999998)) ;
#157457 = CARTESIAN_POINT('Origin',(-4.15,-6.3,0.749999999999998)) ;
#157458 = CARTESIAN_POINT('Origin',(-4.15,-6.3,-0.750000000000002)) ;
#157459 = CARTESIAN_POINT('Origin',(-4.15,-6.3,-0.750000000000002)) ;
#157460 = CARTESIAN_POINT('Origin',(-4.65,-6.25,0.749999999999998)) ;
#157461 = CARTESIAN_POINT('Origin',(-4.65,-6.3,0.749999999999998)) ;
#157462 = CARTESIAN_POINT('Origin',(0.,-6.3,0.749999999999998)) ;
#157463 = CARTESIAN_POINT('Origin',(-4.65,-6.3,0.749999999999998)) ;
#157464 = CARTESIAN_POINT('Origin',(0.,-6.3,-0.750000000000002)) ;
#157465 = CARTESIAN_POINT('Origin',(-4.65,-6.3,-0.750000000000002)) ;
#157466 = CARTESIAN_POINT('Origin',(-4.65,-6.25,-0.750000000000002)) ;
#157467 = CARTESIAN_POINT('Origin',(-4.65,-6.3,-0.750000000000002)) ;
#157468 = CARTESIAN_POINT('Origin',(-4.65,-6.3,0.749999999999998)) ;
#157469 = CARTESIAN_POINT('Origin',(-4.65,-6.3,0.749999999999998)) ;
#157470 = CARTESIAN_POINT('Origin',(-4.65,-6.3,-0.750000000000002)) ;
#157471 = CARTESIAN_POINT('Origin',(-4.65,-6.3,-0.750000000000002)) ;
#157472 = CARTESIAN_POINT('Origin',(-4.65,-6.3,0.)) ;
#157473 = CARTESIAN_POINT('Origin',(-3.09057773798104,-4.00084361825625,-0.500553917240007)) ;
#157474 = CARTESIAN_POINT('Origin',(-5.17275707706437,-1.91866427917293,-1.5)) ;
#157475 = CARTESIAN_POINT('Origin',(-5.17275707706437,-1.91866427917293,-1.5)) ;
#157476 = CARTESIAN_POINT('Origin',(-5.17275707706437,-1.91866427917293,-1.5)) ;
#157477 = CARTESIAN_POINT('Origin',(-5.17275707706437,-1.91866427917293,-1.5)) ;
#157478 = CARTESIAN_POINT('Origin',(-3.59571067811865,-3.49571067811865,-1.5)) ;
#157479 = CARTESIAN_POINT('Ctrl Pts',(-5.8,-1.2914213562373,-1.6)) ;
#157480 = CARTESIAN_POINT('Ctrl Pts',(-5.81856398038093,-1.23572941509445,
-1.6)) ;
#157481 = CARTESIAN_POINT('Ctrl Pts',(-5.83691006697102,-1.18069115532419,
-1.58922263893877)) ;
#157482 = CARTESIAN_POINT('Ctrl Pts',(-5.86308993302897,-1.1021515571504,
-1.55219871729854)) ;
#157483 = CARTESIAN_POINT('Ctrl Pts',(-5.87071067695841,-1.07928932304158,
-1.5262534328036)) ;
#157484 = CARTESIAN_POINT('Ctrl Pts',(-5.87071067811865,-1.07928932188133,
-1.5)) ;
#157485 = CARTESIAN_POINT('Origin',(-5.17275707706437,-5.05,-1.5)) ;
#157486 = CARTESIAN_POINT('Origin',(-5.17275707706437,-5.26511162862565,-1.5)) ;
#157487 = CARTESIAN_POINT('Origin',(-3.96111272388873,-4.96220054033175,-0.918410710475694)) ;
#157488 = CARTESIAN_POINT('Origin',(-5.17275707706437,-5.26511162862565,-1.5)) ;
#157489 = CARTESIAN_POINT('Ctrl Pts',(-5.9,-1.00857864376268,-1.5)) ;
#157490 = CARTESIAN_POINT('Ctrl Pts',(-5.9,-1.04999999999999,-1.5)) ;
#157491 = CARTESIAN_POINT('Ctrl Pts',(-5.87071067811865,-1.07928932188133,
-1.5)) ;
#157492 = CARTESIAN_POINT('Ctrl Pts',(-5.9,-1.00857864608314,-1.55250686562996)) ;
#157493 = CARTESIAN_POINT('Ctrl Pts',(-5.9,-1.05000000261917,-1.53717194963254)) ;
#157494 = CARTESIAN_POINT('Ctrl Pts',(-5.87071067695841,-1.07928932304158,
-1.5262534328036)) ;
#157495 = CARTESIAN_POINT('Ctrl Pts',(-5.9,-1.03906162412144,-1.60439743459708)) ;
#157496 = CARTESIAN_POINT('Ctrl Pts',(-5.9,-1.08015861705713,-1.57457207120097)) ;
#157497 = CARTESIAN_POINT('Ctrl Pts',(-5.86308993302897,-1.1021515571504,
-1.55219871729854)) ;
#157498 = CARTESIAN_POINT('Ctrl Pts',(-5.9,-1.14378108835315,-1.67844527787754)) ;
#157499 = CARTESIAN_POINT('Ctrl Pts',(-5.9,-1.17342005527962,-1.61578812462635)) ;
#157500 = CARTESIAN_POINT('Ctrl Pts',(-5.83691006697102,-1.18069115532419,
-1.58922263893877)) ;
#157501 = CARTESIAN_POINT('Ctrl Pts',(-5.9,-1.21716543471636,-1.69999999941986)) ;
#157502 = CARTESIAN_POINT('Ctrl Pts',(-5.9,-1.24006789214486,-1.61711774888611)) ;
#157503 = CARTESIAN_POINT('Ctrl Pts',(-5.81856398038093,-1.23572941509445,
-1.6)) ;
#157504 = CARTESIAN_POINT('Ctrl Pts',(-5.9,-1.2914213562373,-1.7)) ;
#157505 = CARTESIAN_POINT('Ctrl Pts',(-5.9,-1.2914213562373,-1.6)) ;
#157506 = CARTESIAN_POINT('Ctrl Pts',(-5.8,-1.2914213562373,-1.6)) ;
#157507 = CARTESIAN_POINT('Origin',(-5.8,-1.2914213562373,-1.7)) ;
#157508 = CARTESIAN_POINT('Origin',(-5.8,-1.00857864376268,-1.5)) ;
#157509 = CARTESIAN_POINT('Origin',(-5.17275707706437,-5.26511162862565,-1.5)) ;
#157510 = CARTESIAN_POINT('Origin',(-5.17275707706437,-5.26511162862565,-1.5)) ;
#157511 = CARTESIAN_POINT('Origin',(-3.78014014831103,-3.31128120792626,0.8315438741984)) ;
#157512 = CARTESIAN_POINT('Origin',(-5.17275707706436,-1.91866427917293,1.5)) ;
#157513 = CARTESIAN_POINT('Origin',(-3.97071067811865,-3.12071067811865,1.5)) ;
#157514 = CARTESIAN_POINT('Ctrl Pts',(-5.87071067811865,-1.07928932188133,
1.5)) ;
#157515 = CARTESIAN_POINT('Ctrl Pts',(-5.8707106769584,-1.07928932304159,
1.52625343280361)) ;
#157516 = CARTESIAN_POINT('Ctrl Pts',(-5.86308993302895,-1.10215155715041,
1.55219871729854)) ;
#157517 = CARTESIAN_POINT('Ctrl Pts',(-5.83691006697104,-1.18069115532418,
1.58922263893878)) ;
#157518 = CARTESIAN_POINT('Ctrl Pts',(-5.81856398038092,-1.23572941509446,
1.6)) ;
#157519 = CARTESIAN_POINT('Ctrl Pts',(-5.8,-1.2914213562373,1.6)) ;
#157520 = CARTESIAN_POINT('Origin',(-5.17275707706436,-1.91866427917293,1.5)) ;
#157521 = CARTESIAN_POINT('Origin',(-5.8,-1.00857864376268,-36.59)) ;
#157522 = CARTESIAN_POINT('Origin',(-5.8,-1.00857864376268,1.5)) ;
#157523 = CARTESIAN_POINT('Origin',(-5.8,-6.55,-1.7)) ;
#157524 = CARTESIAN_POINT('Origin',(-5.8,-5.42192235935956,-1.7)) ;
#157525 = CARTESIAN_POINT('Origin',(-5.10072415073893,-5.24710339704429,-1.5)) ;
#157526 = CARTESIAN_POINT('Origin',(-5.80000000000002,-5.42192235935965,-1.50000000000007)) ;
#157527 = CARTESIAN_POINT('Origin',(-5.17275707706436,-1.91866427917293,1.5)) ;
#157528 = CARTESIAN_POINT('Origin',(-5.17275707706436,-1.91866427917293,1.5)) ;
#157529 = CARTESIAN_POINT('Ctrl Pts',(-5.9,-1.2914213562373,1.7)) ;
#157530 = CARTESIAN_POINT('Ctrl Pts',(-5.9,-1.2914213562373,1.6)) ;
#157531 = CARTESIAN_POINT('Ctrl Pts',(-5.8,-1.2914213562373,1.6)) ;
#157532 = CARTESIAN_POINT('Ctrl Pts',(-5.9,-1.21716543471637,1.69999999941986)) ;
#157533 = CARTESIAN_POINT('Ctrl Pts',(-5.9,-1.24006789214486,1.6171177488861)) ;
#157534 = CARTESIAN_POINT('Ctrl Pts',(-5.81856398038092,-1.23572941509446,
1.6)) ;
#157535 = CARTESIAN_POINT('Ctrl Pts',(-5.9,-1.14378108835315,1.67844527787754)) ;
#157536 = CARTESIAN_POINT('Ctrl Pts',(-5.9,-1.17342005527961,1.61578812462635)) ;
#157537 = CARTESIAN_POINT('Ctrl Pts',(-5.83691006697104,-1.18069115532418,
1.58922263893878)) ;
#157538 = CARTESIAN_POINT('Ctrl Pts',(-5.9,-1.03906162412145,1.60439743459708)) ;
#157539 = CARTESIAN_POINT('Ctrl Pts',(-5.9,-1.08015861705713,1.57457207120097)) ;
#157540 = CARTESIAN_POINT('Ctrl Pts',(-5.86308993302895,-1.10215155715041,
1.55219871729854)) ;
#157541 = CARTESIAN_POINT('Ctrl Pts',(-5.9,-1.00857864608316,1.55250686562996)) ;
#157542 = CARTESIAN_POINT('Ctrl Pts',(-5.9,-1.05000000261919,1.53717194963254)) ;
#157543 = CARTESIAN_POINT('Ctrl Pts',(-5.8707106769584,-1.07928932304159,
1.52625343280361)) ;
#157544 = CARTESIAN_POINT('Ctrl Pts',(-5.9,-1.00857864376268,1.5)) ;
#157545 = CARTESIAN_POINT('Ctrl Pts',(-5.9,-1.04999999999999,1.5)) ;
#157546 = CARTESIAN_POINT('Ctrl Pts',(-5.87071067811865,-1.07928932188133,
1.5)) ;
#157547 = CARTESIAN_POINT('Origin',(-5.8,-1.2914213562373,1.7)) ;
#157548 = CARTESIAN_POINT('Ctrl Pts',(-5.9,-5.42181243301045,-1.69999997036252)) ;
#157549 = CARTESIAN_POINT('Ctrl Pts',(-5.9,-5.42186418462486,-1.5999118155266)) ;
#157550 = CARTESIAN_POINT('Ctrl Pts',(-5.79991187715164,-5.42186416305549,
-1.60000002317701)) ;
#157551 = CARTESIAN_POINT('Ctrl Pts',(-5.9,-5.47597273077135,-1.70002917711601)) ;
#157552 = CARTESIAN_POINT('Ctrl Pts',(-5.9,-5.44963575044052,-1.60611310490823)) ;
#157553 = CARTESIAN_POINT('Ctrl Pts',(-5.80628621775607,-5.45053795385126,
-1.60000983135988)) ;
#157554 = CARTESIAN_POINT('Ctrl Pts',(-5.9,-5.5295069829522,-1.67847029676528)) ;
#157555 = CARTESIAN_POINT('Ctrl Pts',(-5.90000000000002,-5.48352164712825,
-1.60029821762257)) ;
#157556 = CARTESIAN_POINT('Ctrl Pts',(-5.81258729511711,-5.47887520585224,
-1.58922629545968)) ;
#157557 = CARTESIAN_POINT('Ctrl Pts',(-5.9,-5.60588533050918,-1.60437241570934)) ;
#157558 = CARTESIAN_POINT('Ctrl Pts',(-5.89999999999997,-5.53371219741587,
-1.56246819784151)) ;
#157559 = CARTESIAN_POINT('Ctrl Pts',(-5.82157770712951,-5.51930255765375,
-1.55217766736415)) ;
#157560 = CARTESIAN_POINT('Ctrl Pts',(-5.9,-5.62810771557601,-1.55243656245292)) ;
#157561 = CARTESIAN_POINT('Ctrl Pts',(-5.9,-5.54996909580657,-1.5314248414507)) ;
#157562 = CARTESIAN_POINT('Ctrl Pts',(-5.8241936039171,-5.53106345572106,
-1.52621391054005)) ;
#157563 = CARTESIAN_POINT('Ctrl Pts',(-5.9,-5.62807761009112,-1.49989335577685)) ;
#157564 = CARTESIAN_POINT('Ctrl Pts',(-5.9,-5.54994729905278,-1.49993608021398)) ;
#157565 = CARTESIAN_POINT('Ctrl Pts',(-5.82419006898363,-5.53104752404526,
-1.49994668678336)) ;
#157566 = CARTESIAN_POINT('Origin',(-5.8,-5.62807764064044,-1.5)) ;
#157567 = CARTESIAN_POINT('Origin',(-5.15068655017073,-5.25959399690224,1.48940614709106)) ;
#157568 = CARTESIAN_POINT('Origin',(-5.17275707706436,-5.26511162862565,1.5)) ;
#157569 = CARTESIAN_POINT('Origin',(-5.17275707706436,-5.05,1.5)) ;
#157570 = CARTESIAN_POINT('Origin',(-5.17275707706436,-5.26511162862565,1.5)) ;
#157571 = CARTESIAN_POINT('Origin',(-5.8,-5.05,1.7)) ;
#157572 = CARTESIAN_POINT('Origin',(-5.8,-5.42192235935956,1.7)) ;
#157573 = CARTESIAN_POINT('Origin',(-5.8,-5.62807764064044,-36.59)) ;
#157574 = CARTESIAN_POINT('Origin',(-5.8,-5.62807764064044,1.5)) ;
#157575 = CARTESIAN_POINT('Origin',(-5.17275707706436,-5.26511162862565,1.5)) ;
#157576 = CARTESIAN_POINT('Origin',(-5.17275707706436,-5.26511162862565,1.5)) ;
#157577 = CARTESIAN_POINT('Ctrl Pts',(-5.9,-5.62807761009112,1.49989335577687)) ;
#157578 = CARTESIAN_POINT('Ctrl Pts',(-5.9,-5.54994729905279,1.49993608021399)) ;
#157579 = CARTESIAN_POINT('Ctrl Pts',(-5.82419006898364,-5.53104752404526,
1.49994668678337)) ;
#157580 = CARTESIAN_POINT('Ctrl Pts',(-5.9,-5.62810771557601,1.55243656245293)) ;
#157581 = CARTESIAN_POINT('Ctrl Pts',(-5.9,-5.54996909580664,1.5314248414507)) ;
#157582 = CARTESIAN_POINT('Ctrl Pts',(-5.82419360391714,-5.53106345572106,
1.52621391054006)) ;
#157583 = CARTESIAN_POINT('Ctrl Pts',(-5.9,-5.6058853305092,1.60437241570935)) ;
#157584 = CARTESIAN_POINT('Ctrl Pts',(-5.89999999999997,-5.53371219741588,
1.56246819784153)) ;
#157585 = CARTESIAN_POINT('Ctrl Pts',(-5.82157770712952,-5.51930255765375,
1.55217766736414)) ;
#157586 = CARTESIAN_POINT('Ctrl Pts',(-5.9,-5.52950698295218,1.67847029676527)) ;
#157587 = CARTESIAN_POINT('Ctrl Pts',(-5.90000000000002,-5.48352164712826,
1.60029821762257)) ;
#157588 = CARTESIAN_POINT('Ctrl Pts',(-5.81258729511712,-5.47887520585224,
1.58922629545969)) ;
#157589 = CARTESIAN_POINT('Ctrl Pts',(-5.9,-5.47597273077138,1.700029177116)) ;
#157590 = CARTESIAN_POINT('Ctrl Pts',(-5.9,-5.44963575044054,1.60611310490826)) ;
#157591 = CARTESIAN_POINT('Ctrl Pts',(-5.80628621775611,-5.45053795385126,
1.60000983135988)) ;
#157592 = CARTESIAN_POINT('Ctrl Pts',(-5.9,-5.42181243301047,1.69999997036252)) ;
#157593 = CARTESIAN_POINT('Ctrl Pts',(-5.9,-5.42186418462487,1.59991181552662)) ;
#157594 = CARTESIAN_POINT('Ctrl Pts',(-5.79991187715165,-5.4218641630555,
1.60000002317701)) ;
#157595 = CARTESIAN_POINT('Origin',(-5.80000000000001,-5.42192235935961,1.50000000000005)) ;
#157596 = CARTESIAN_POINT('Origin',(-5.8066065036801,-5.42357398527959,1.5)) ;
#157597 = CARTESIAN_POINT('Origin',(-3.,4.45,-1.1)) ;
#157598 = CARTESIAN_POINT('Origin',(-2.1,4.45,-1.1)) ;
#157599 = CARTESIAN_POINT('Origin',(-2.9,4.45,-1.1)) ;
#157600 = CARTESIAN_POINT('Origin',(-2.9,4.45,-0.899999999999999)) ;
#157601 = CARTESIAN_POINT('Origin',(-3.1,4.45,-0.899999999999999)) ;
#157602 = CARTESIAN_POINT('Origin',(-2.9,4.45,-0.899999999999999)) ;
#157603 = CARTESIAN_POINT('Origin',(-2.1,4.45,-0.9)) ;
#157604 = CARTESIAN_POINT('Origin',(-2.1,4.45,-0.9)) ;
#157605 = CARTESIAN_POINT('Origin',(-1.9,4.45,-0.9)) ;
#157606 = CARTESIAN_POINT('Origin',(-3.1,4.45,-0.999999999999999)) ;
#157607 = CARTESIAN_POINT('Origin',(-3.1,4.45,0.900000000000001)) ;
#157608 = CARTESIAN_POINT('Origin',(-2.9,4.4,-0.899999999999999)) ;
#157609 = CARTESIAN_POINT('Origin',(-2.9,4.35,-0.899999999999999)) ;
#157610 = CARTESIAN_POINT('Origin',(-1.95156391047391E-16,4.35,-0.9)) ;
#157611 = CARTESIAN_POINT('Origin',(-2.1,4.35,-0.9)) ;
#157612 = CARTESIAN_POINT('Origin',(-2.9,4.35,-0.899999999999999)) ;
#157613 = CARTESIAN_POINT('Origin',(-2.1,4.4,-0.9)) ;
#157614 = CARTESIAN_POINT('Origin',(-2.1,4.35,-0.9)) ;
#157615 = CARTESIAN_POINT('Origin',(-1.9,4.45,-1.)) ;
#157616 = CARTESIAN_POINT('Origin',(-1.9,4.45,0.900000000000001)) ;
#157617 = CARTESIAN_POINT('Origin',(-3.,4.45,1.1)) ;
#157618 = CARTESIAN_POINT('Origin',(-2.9,4.45,1.1)) ;
#157619 = CARTESIAN_POINT('Origin',(-2.1,4.45,1.1)) ;
#157620 = CARTESIAN_POINT('Origin',(-2.9,4.45,0.900000000000001)) ;
#157621 = CARTESIAN_POINT('Origin',(-2.9,4.45,0.900000000000001)) ;
#157622 = CARTESIAN_POINT('Origin',(-2.9,4.35,-0.899999999999999)) ;
#157623 = CARTESIAN_POINT('Origin',(-2.9,4.35,-0.899999999999999)) ;
#157624 = CARTESIAN_POINT('Origin',(-2.1,4.35,-0.9)) ;
#157625 = CARTESIAN_POINT('Origin',(-2.1,4.35,-0.9)) ;
#157626 = CARTESIAN_POINT('Origin',(-2.1,4.45,0.900000000000001)) ;
#157627 = CARTESIAN_POINT('Origin',(-2.1,4.45,0.900000000000001)) ;
#157628 = CARTESIAN_POINT('Origin',(-2.9,4.4,0.900000000000001)) ;
#157629 = CARTESIAN_POINT('Origin',(-2.9,4.35,0.900000000000001)) ;
#157630 = CARTESIAN_POINT('Origin',(-2.9,4.35,1.25767452008319E-15)) ;
#157631 = CARTESIAN_POINT('Origin',(-2.9,4.35,0.900000000000001)) ;
#157632 = CARTESIAN_POINT('Origin',(-2.1,4.35,4.55364912443912E-16)) ;
#157633 = CARTESIAN_POINT('Origin',(-2.1,4.35,0.900000000000001)) ;
#157634 = CARTESIAN_POINT('Origin',(-2.1,4.4,0.900000000000001)) ;
#157635 = CARTESIAN_POINT('Origin',(-2.1,4.35,0.900000000000001)) ;
#157636 = CARTESIAN_POINT('Origin',(-2.9,4.35,0.900000000000001)) ;
#157637 = CARTESIAN_POINT('Origin',(-2.9,4.35,0.900000000000001)) ;
#157638 = CARTESIAN_POINT('Origin',(-2.1,4.35,0.900000000000001)) ;
#157639 = CARTESIAN_POINT('Origin',(-2.1,4.35,0.900000000000001)) ;
#157640 = CARTESIAN_POINT('Origin',(-1.95156391047391E-16,4.35,0.900000000000001)) ;
#157641 = CARTESIAN_POINT('Origin',(-2.25,4.25,-0.75)) ;
#157642 = CARTESIAN_POINT('Origin',(-2.25,4.3,-0.75)) ;
#157643 = CARTESIAN_POINT('Origin',(-2.25,4.3,0.)) ;
#157644 = CARTESIAN_POINT('Origin',(-2.25,4.3,0.750000000000001)) ;
#157645 = CARTESIAN_POINT('Origin',(-2.25,4.3,-0.75)) ;
#157646 = CARTESIAN_POINT('Origin',(-2.25,4.25,0.750000000000001)) ;
#157647 = CARTESIAN_POINT('Origin',(-2.25,4.3,0.750000000000001)) ;
#157648 = CARTESIAN_POINT('Origin',(-2.25,4.3,-0.75)) ;
#157649 = CARTESIAN_POINT('Origin',(-2.25,4.3,-0.75)) ;
#157650 = CARTESIAN_POINT('Origin',(-2.25,4.3,0.750000000000001)) ;
#157651 = CARTESIAN_POINT('Origin',(-2.25,4.3,0.750000000000001)) ;
#157652 = CARTESIAN_POINT('Origin',(-2.75,4.25,-0.75)) ;
#157653 = CARTESIAN_POINT('Origin',(-2.75,4.3,-0.75)) ;
#157654 = CARTESIAN_POINT('Origin',(-1.97127667724637E-17,4.3,-0.75)) ;
#157655 = CARTESIAN_POINT('Origin',(-2.75,4.3,-0.75)) ;
#157656 = CARTESIAN_POINT('Origin',(-1.97127667724637E-17,4.3,0.750000000000001)) ;
#157657 = CARTESIAN_POINT('Origin',(-2.75,4.3,0.750000000000001)) ;
#157658 = CARTESIAN_POINT('Origin',(-2.75,4.25,0.750000000000001)) ;
#157659 = CARTESIAN_POINT('Origin',(-2.75,4.3,0.750000000000001)) ;
#157660 = CARTESIAN_POINT('Origin',(-2.75,4.3,-0.75)) ;
#157661 = CARTESIAN_POINT('Origin',(-2.75,4.3,-0.75)) ;
#157662 = CARTESIAN_POINT('Origin',(-2.75,4.3,0.750000000000001)) ;
#157663 = CARTESIAN_POINT('Origin',(-2.75,4.3,0.750000000000001)) ;
#157664 = CARTESIAN_POINT('Origin',(-2.75,4.3,0.)) ;
#157665 = CARTESIAN_POINT('Origin',(7.8,2.9,-0.4)) ;
#157666 = CARTESIAN_POINT('Origin',(7.8,2.9,-0.399999999999999)) ;
#157667 = CARTESIAN_POINT('Origin',(7.8,2.9,0.4)) ;
#157668 = CARTESIAN_POINT('Origin',(7.8,2.9,0.4)) ;
#157669 = CARTESIAN_POINT('Origin',(7.8,2.9,0.4)) ;
#157670 = CARTESIAN_POINT('Origin',(7.8,2.9,-0.4)) ;
#157671 = CARTESIAN_POINT('Origin',(7.8,2.9,-0.4)) ;
#157672 = CARTESIAN_POINT('Origin',(9.6,2.9,0.4)) ;
#157673 = CARTESIAN_POINT('Origin',(9.6,2.9,0.4)) ;
#157674 = CARTESIAN_POINT('Origin',(9.6,2.9,-0.4)) ;
#157675 = CARTESIAN_POINT('Origin',(9.6,2.9,-0.4)) ;
#157676 = CARTESIAN_POINT('Origin',(9.6,2.9,0.4)) ;
#157677 = CARTESIAN_POINT('Origin',(9.6,2.9,0.4)) ;
#157678 = CARTESIAN_POINT('Origin',(9.6,2.9,-0.4)) ;
#157679 = CARTESIAN_POINT('Origin',(9.6,2.9,-0.4)) ;
#157680 = CARTESIAN_POINT('Origin',(9.6,2.9,-0.4)) ;
#157681 = CARTESIAN_POINT('Origin',(-0.183301359729408,3.45,1.51703678647597)) ;
#157682 = CARTESIAN_POINT('Origin',(0.249234641435079,3.15,0.116220021978692)) ;
#157683 = CARTESIAN_POINT('Origin',(-0.249234641435079,3.15,-0.116220021978691)) ;
#157684 = CARTESIAN_POINT('Origin',(-1.04429375741423,3.45,1.11554943782231)) ;
#157685 = CARTESIAN_POINT('Origin',(3.7,2.1,1.405)) ;
#157686 = CARTESIAN_POINT('Origin',(3.7,2.1,-1.305)) ;
#157687 = CARTESIAN_POINT('Origin',(3.7,2.1,1.305)) ;
#157688 = CARTESIAN_POINT('Origin',(3.5,1.9,-1.505)) ;
#157689 = CARTESIAN_POINT('Ctrl Pts',(3.6,2.07320508075689,-1.405)) ;
#157690 = CARTESIAN_POINT('Ctrl Pts',(3.6,2.07265589924994,-1.40785357667012)) ;
#157691 = CARTESIAN_POINT('Ctrl Pts',(3.59994554076638,2.07202433860048,-1.41069358004935)) ;
#157692 = CARTESIAN_POINT('Ctrl Pts',(3.59971739924421,2.07059366100574,-1.41637921497761)) ;
#157693 = CARTESIAN_POINT('Ctrl Pts',(3.59954156373429,2.06979274847061,-1.41921873634692)) ;
#157694 = CARTESIAN_POINT('Ctrl Pts',(3.59880783141188,2.06712577191666,-1.42778089072516)) ;
#157695 = CARTESIAN_POINT('Ctrl Pts',(3.59804129495589,2.06501902766395,-1.43341713644376)) ;
#157696 = CARTESIAN_POINT('Ctrl Pts',(3.59624340061598,2.06105248659392,-1.44263353946359)) ;
#157697 = CARTESIAN_POINT('Ctrl Pts',(3.59536494855695,2.05931170891995,-1.44632347138735)) ;
#157698 = CARTESIAN_POINT('Ctrl Pts',(3.5928372720244,2.05479606436795,-1.455199432059)) ;
#157699 = CARTESIAN_POINT('Ctrl Pts',(3.59099650883093,2.05188276467124,-1.46034424200706)) ;
#157700 = CARTESIAN_POINT('Ctrl Pts',(3.58838944624309,2.04823719194674,-1.46622737667939)) ;
#157701 = CARTESIAN_POINT('Ctrl Pts',(3.58794537962076,2.04762948672744,-1.46719091385134)) ;
#157702 = CARTESIAN_POINT('Ctrl Pts',(3.58597371492279,2.04498948329048,-1.47130665172963)) ;
#157703 = CARTESIAN_POINT('Ctrl Pts',(3.58430396743904,2.04289920268562,-1.47439316248021)) ;
#157704 = CARTESIAN_POINT('Ctrl Pts',(3.58008903321357,2.03798436571146,-1.48128092067897)) ;
#157705 = CARTESIAN_POINT('Ctrl Pts',(3.57743593401588,2.03513945367721,-1.48500157292061)) ;
#157706 = CARTESIAN_POINT('Ctrl Pts',(3.57357563759669,2.03136250950851,-1.48958640159683)) ;
#157707 = CARTESIAN_POINT('Ctrl Pts',(3.57257888733677,2.03041544381404,-1.4907065689314)) ;
#157708 = CARTESIAN_POINT('Ctrl Pts',(3.56956839719837,2.02764175140689,-1.49390390778887)) ;
#157709 = CARTESIAN_POINT('Ctrl Pts',(3.56746189551945,2.0258155454478,-1.49598430067905)) ;
#157710 = CARTESIAN_POINT('Ctrl Pts',(3.56503628433181,2.02384076964141,-1.49802226003861)) ;
#157711 = CARTESIAN_POINT('Ctrl Pts',(3.5648141102349,2.02366103014354,-1.49820583968788)) ;
#157712 = CARTESIAN_POINT('Ctrl Pts',(3.56285239425757,2.0220841692406,-1.49979838212051)) ;
#157713 = CARTESIAN_POINT('Ctrl Pts',(3.56093641846876,2.02061618613969,-1.5011871777518)) ;
#157714 = CARTESIAN_POINT('Ctrl Pts',(3.55879736620766,2.01908299720835,-1.50237714025468)) ;
#157715 = CARTESIAN_POINT('Ctrl Pts',(3.55867935922407,2.0189987330146,-1.50244171035243)) ;
#157716 = CARTESIAN_POINT('Ctrl Pts',(3.5578895339955,2.01843691186419,-1.50286648337378)) ;
#157717 = CARTESIAN_POINT('Ctrl Pts',(3.55720723474254,2.01796200020269,-1.503197549106)) ;
#157718 = CARTESIAN_POINT('Ctrl Pts',(3.5550912564315,2.01652382826845,-1.50409794445158)) ;
#157719 = CARTESIAN_POINT('Ctrl Pts',(3.55356547969789,2.01553571874064,-1.50460356135169)) ;
#157720 = CARTESIAN_POINT('Ctrl Pts',(3.55133342567602,2.01417771500981,-1.50494476439962)) ;
#157721 = CARTESIAN_POINT('Ctrl Pts',(3.55066861961528,2.01378348733642,-1.50499963178873)) ;
#157722 = CARTESIAN_POINT('Ctrl Pts',(3.55,2.01339745962156,-1.505)) ;
#157723 = CARTESIAN_POINT('Origin',(3.5,2.1,1.01757522333835E-15)) ;
#157724 = CARTESIAN_POINT('Origin',(3.5,2.1,2.2)) ;
#157725 = CARTESIAN_POINT('',(3.55,2.01339745962156,1.505)) ;
#157726 = CARTESIAN_POINT('Origin',(3.5,2.1,1.505)) ;
#157727 = CARTESIAN_POINT('Origin',(3.5,2.1,1.505)) ;
#157728 = CARTESIAN_POINT('Origin',(3.5,1.9,1.505)) ;
#157729 = CARTESIAN_POINT('Ctrl Pts',(3.55,2.01339745962156,1.505)) ;
#157730 = CARTESIAN_POINT('Ctrl Pts',(3.55164546205118,2.01434746757975,1.505)) ;
#157731 = CARTESIAN_POINT('Ctrl Pts',(3.55326668047441,2.01534654795451,1.50466702196971)) ;
#157732 = CARTESIAN_POINT('Ctrl Pts',(3.55550702654634,2.01680421826673,1.50390173831696)) ;
#157733 = CARTESIAN_POINT('Ctrl Pts',(3.55618577699068,2.01725684095079,1.50362640393618)) ;
#157734 = CARTESIAN_POINT('Ctrl Pts',(3.55727967686454,2.01800266699454,1.5031321699042)) ;
#157735 = CARTESIAN_POINT('Ctrl Pts',(3.55771141786834,2.01830156212325,1.50292168105742)) ;
#157736 = CARTESIAN_POINT('Ctrl Pts',(3.5620282181816,2.02133211263483,1.50082930890279)) ;
#157737 = CARTESIAN_POINT('Ctrl Pts',(3.56570108751482,2.02427663140642,1.4977560683717)) ;
#157738 = CARTESIAN_POINT('Ctrl Pts',(3.56990347726565,2.02797441535149,1.49359799526151)) ;
#157739 = CARTESIAN_POINT('Ctrl Pts',(3.57072473561128,2.02871480216323,1.49275040226905)) ;
#157740 = CARTESIAN_POINT('Ctrl Pts',(3.5738286330762,2.03157464832067,1.48945828106714)) ;
#157741 = CARTESIAN_POINT('Ctrl Pts',(3.5759706937612,2.03369481096682,1.48686226564267)) ;
#157742 = CARTESIAN_POINT('Ctrl Pts',(3.58156103639367,2.03956384830232,1.47924188322025)) ;
#157743 = CARTESIAN_POINT('Ctrl Pts',(3.58475859790494,2.04336775308648,1.47384516147842)) ;
#157744 = CARTESIAN_POINT('Ctrl Pts',(3.58897725231935,2.0490105592432,1.46504516569941)) ;
#157745 = CARTESIAN_POINT('Ctrl Pts',(3.59034871903171,2.05099358132072,1.46177746615682)) ;
#157746 = CARTESIAN_POINT('Ctrl Pts',(3.5936548829273,2.05613355260445,1.45275077139164)) ;
#157747 = CARTESIAN_POINT('Ctrl Pts',(3.59534780095526,2.05919518104046,1.44675628838969)) ;
#157748 = CARTESIAN_POINT('Ctrl Pts',(3.59674625886212,2.06216860863465,1.44003955337032)) ;
#157749 = CARTESIAN_POINT('Ctrl Pts',(3.59685725281059,2.06240883133061,1.43948968489037)) ;
#157750 = CARTESIAN_POINT('Ctrl Pts',(3.59768573690243,2.06423460359408,1.43525346237999)) ;
#157751 = CARTESIAN_POINT('Ctrl Pts',(3.59826864191792,2.06571343564803,1.43147600284345)) ;
#157752 = CARTESIAN_POINT('Ctrl Pts',(3.59959273712775,2.06963221119414,1.42031698563094)) ;
#157753 = CARTESIAN_POINT('Ctrl Pts',(3.6,2.07172309150643,1.4127006420342)) ;
#157754 = CARTESIAN_POINT('Ctrl Pts',(3.6,2.07320508075689,1.405)) ;
#157755 = CARTESIAN_POINT('Origin',(3.7,2.1,-1.305)) ;
#157756 = CARTESIAN_POINT('',(3.7,1.98660254037844,-1.355)) ;
#157757 = CARTESIAN_POINT('Ctrl Pts',(3.60000000000001,1.92679491924311,-1.405)) ;
#157758 = CARTESIAN_POINT('Ctrl Pts',(3.60642117639485,1.92803067521647,-1.405)) ;
#157759 = CARTESIAN_POINT('Ctrl Pts',(3.61278477806503,1.92968896670923,-1.40472281361407)) ;
#157760 = CARTESIAN_POINT('Ctrl Pts',(3.61897283239529,1.93170032347262,-1.40412352491366)) ;
#157761 = CARTESIAN_POINT('Ctrl Pts',(3.62020584678442,1.93210110079269,-1.40400411232427)) ;
#157762 = CARTESIAN_POINT('Ctrl Pts',(3.62143195421093,1.93251577262755,-1.40387200280826)) ;
#157763 = CARTESIAN_POINT('Ctrl Pts',(3.62265032708637,1.93294361409314,-1.40372698243403)) ;
#157764 = CARTESIAN_POINT('Ctrl Pts',(3.62647624625549,1.9342871164786,-1.40327159128008)) ;
#157765 = CARTESIAN_POINT('Ctrl Pts',(3.63025346237246,1.93576539638805,-1.40268573681767)) ;
#157766 = CARTESIAN_POINT('Ctrl Pts',(3.6339385638818,1.93735364065939,-1.40196503626974)) ;
#157767 = CARTESIAN_POINT('Ctrl Pts',(3.63907793749077,1.93956866259897,-1.40095992165713)) ;
#157768 = CARTESIAN_POINT('Ctrl Pts',(3.64410916187591,1.94202076919908,-1.39967872244964)) ;
#157769 = CARTESIAN_POINT('Ctrl Pts',(3.64894317395077,1.94461872744763,-1.39812217773587)) ;
#157770 = CARTESIAN_POINT('Ctrl Pts',(3.64993855309172,1.94515367717668,-1.39780166712976)) ;
#157771 = CARTESIAN_POINT('Ctrl Pts',(3.65092568100083,1.94569474416709,-1.39746960315684)) ;
#157772 = CARTESIAN_POINT('Ctrl Pts',(3.65190395907102,1.94624104404953,-1.3971261809367)) ;
#157773 = CARTESIAN_POINT('Ctrl Pts',(3.65241342868356,1.94652554719634,-1.39694733282514)) ;
#157774 = CARTESIAN_POINT('Ctrl Pts',(3.65292046817501,1.9468114778021,-1.39676540573999)) ;
#157775 = CARTESIAN_POINT('Ctrl Pts',(3.6534249821411,1.94709871486666,-1.39658043363331)) ;
#157776 = CARTESIAN_POINT('Ctrl Pts',(3.65677402871197,1.94900544167845,-1.39535255840841)) ;
#157777 = CARTESIAN_POINT('Ctrl Pts',(3.66003813592315,1.95098496635821,-1.39398063668092)) ;
#157778 = CARTESIAN_POINT('Ctrl Pts',(3.66320312645637,1.95301617633166,-1.39246240139399)) ;
#157779 = CARTESIAN_POINT('Ctrl Pts',(3.66757373088802,1.9558211184692,-1.39036583718514)) ;
#157780 = CARTESIAN_POINT('Ctrl Pts',(3.67181875309355,1.95875330073059,-1.38796612617098)) ;
#157781 = CARTESIAN_POINT('Ctrl Pts',(3.67584388612499,1.96174615985042,-1.38526003578587)) ;
#157782 = CARTESIAN_POINT('Ctrl Pts',(3.67661208162767,1.96231734616851,-1.38474357919985)) ;
#157783 = CARTESIAN_POINT('Ctrl Pts',(3.67737237849352,1.96289065080917,-1.38421601587673)) ;
#157784 = CARTESIAN_POINT('Ctrl Pts',(3.67812428214755,1.96346549105992,-1.38367739883589)) ;
#157785 = CARTESIAN_POINT('Ctrl Pts',(3.6785349394885,1.96377944400799,-1.38338322944251)) ;
#157786 = CARTESIAN_POINT('Ctrl Pts',(3.67894301851534,1.96409388168819,-1.38308575174331)) ;
#157787 = CARTESIAN_POINT('Ctrl Pts',(3.67934840022277,1.96440871854256,-1.38278496939811)) ;
#157788 = CARTESIAN_POINT('Ctrl Pts',(3.68198440184427,1.96645595067818,-1.38082912695353)) ;
#157789 = CARTESIAN_POINT('Ctrl Pts',(3.68449751351864,1.96851545671307,-1.37873828347164)) ;
#157790 = CARTESIAN_POINT('Ctrl Pts',(3.68685379133723,1.97055696562013,-1.37652085039877)) ;
#157791 = CARTESIAN_POINT('Ctrl Pts',(3.68896164651385,1.97238323800784,-1.37453720155032)) ;
#157792 = CARTESIAN_POINT('Ctrl Pts',(3.69104797813205,1.97419718002547,-1.37244243877984)) ;
#157793 = CARTESIAN_POINT('Ctrl Pts',(3.69290978292492,1.97598569412168,-1.37024500103231)) ;
#157794 = CARTESIAN_POINT('Ctrl Pts',(3.69362192319645,1.97666980070416,-1.36940448116677)) ;
#157795 = CARTESIAN_POINT('Ctrl Pts',(3.6943016327186,1.97734979318971,-1.36854897561524)) ;
#157796 = CARTESIAN_POINT('Ctrl Pts',(3.69493905694205,1.97802369895108,-1.36767908836304)) ;
#157797 = CARTESIAN_POINT('Ctrl Pts',(3.69605143900785,1.9791997456958,-1.36616103030527)) ;
#157798 = CARTESIAN_POINT('Ctrl Pts',(3.69703421735413,1.98035885502255,-1.3645986233173)) ;
#157799 = CARTESIAN_POINT('Ctrl Pts',(3.6978475066491,1.98151165953424,-1.36295719153115)) ;
#157800 = CARTESIAN_POINT('Ctrl Pts',(3.69841279947844,1.98231293913809,-1.36181628186433)) ;
#157801 = CARTESIAN_POINT('Ctrl Pts',(3.69890310384956,1.98311438470601,-1.3606332480121)) ;
#157802 = CARTESIAN_POINT('Ctrl Pts',(3.69929098301997,1.9839378326546,-1.35935810707453)) ;
#157803 = CARTESIAN_POINT('Ctrl Pts',(3.69936193271527,1.98408845528532,-1.35912486211608)) ;
#157804 = CARTESIAN_POINT('Ctrl Pts',(3.69942931950318,1.98423979370567,-1.35888851468589)) ;
#157805 = CARTESIAN_POINT('Ctrl Pts',(3.69949277412725,1.98439195189923,-1.35864873028525)) ;
#157806 = CARTESIAN_POINT('Ctrl Pts',(3.69967702385849,1.98483376534754,-1.35795248139834)) ;
#157807 = CARTESIAN_POINT('Ctrl Pts',(3.69981936684304,1.98527475083258,-1.35723933425854)) ;
#157808 = CARTESIAN_POINT('Ctrl Pts',(3.69990669142683,1.98570953653121,-1.35651584102814)) ;
#157809 = CARTESIAN_POINT('Ctrl Pts',(3.69996666908332,1.98600816294479,-1.35601891992581)) ;
#157810 = CARTESIAN_POINT('Ctrl Pts',(3.7,1.98630780592129,-1.35551049505453)) ;
#157811 = CARTESIAN_POINT('Ctrl Pts',(3.7,1.98660254037844,-1.355)) ;
#157812 = CARTESIAN_POINT('Origin',(3.7,1.9,-1.305)) ;
#157813 = CARTESIAN_POINT('Origin',(10.2,1.9,-1.305)) ;
#157814 = CARTESIAN_POINT('Origin',(3.7,1.9,-1.305)) ;
#157815 = CARTESIAN_POINT('Origin',(10.1,1.9,-1.305)) ;
#157816 = CARTESIAN_POINT('Origin',(10.1,1.9,-1.305)) ;
#157817 = CARTESIAN_POINT('Origin',(3.7,2.1,1.305)) ;
#157818 = CARTESIAN_POINT('',(3.7,1.98660254037844,1.355)) ;
#157819 = CARTESIAN_POINT('Origin',(3.7,1.9,1.305)) ;
#157820 = CARTESIAN_POINT('Ctrl Pts',(3.7,1.98660254037844,1.355)) ;
#157821 = CARTESIAN_POINT('Ctrl Pts',(3.69999911718144,1.98567700534182,1.35660307370761)) ;
#157822 = CARTESIAN_POINT('Ctrl Pts',(3.69968163901485,1.984703699336,1.35818199771545)) ;
#157823 = CARTESIAN_POINT('Ctrl Pts',(3.69895427931585,1.98325895404995,1.36040554395919)) ;
#157824 = CARTESIAN_POINT('Ctrl Pts',(3.69867650892745,1.98278649590681,1.36111390157608)) ;
#157825 = CARTESIAN_POINT('Ctrl Pts',(3.69717970712967,1.9804354328423,1.36455908121567)) ;
#157826 = CARTESIAN_POINT('Ctrl Pts',(3.69541014605544,1.97847095301992,1.36717587915573)) ;
#157827 = CARTESIAN_POINT('Ctrl Pts',(3.69146029518774,1.97457001268155,1.37202655649097)) ;
#157828 = CARTESIAN_POINT('Ctrl Pts',(3.68915436790411,1.97254004967205,1.37436779312348)) ;
#157829 = CARTESIAN_POINT('Ctrl Pts',(3.68263623161791,1.96688850447179,1.38050008154324)) ;
#157830 = CARTESIAN_POINT('Ctrl Pts',(3.67796661383157,1.96321337091311,1.38402074771694)) ;
#157831 = CARTESIAN_POINT('Ctrl Pts',(3.67279117399676,1.95950210067475,1.38723765660546)) ;
#157832 = CARTESIAN_POINT('Ctrl Pts',(3.67252519027993,1.95931231248682,1.38740119094185)) ;
#157833 = CARTESIAN_POINT('Ctrl Pts',(3.6693311210617,1.95704457126181,1.38934379569321)) ;
#157834 = CARTESIAN_POINT('Ctrl Pts',(3.66628216680077,1.95498580453519,1.39099038776091)) ;
#157835 = CARTESIAN_POINT('Ctrl Pts',(3.65739884032376,1.94929644648107,1.39524097578772)) ;
#157836 = CARTESIAN_POINT('Ctrl Pts',(3.65126071410426,1.94574201114262,1.39752886673119)) ;
#157837 = CARTESIAN_POINT('Ctrl Pts',(3.64132315686417,1.94068746317945,1.40036203409875)) ;
#157838 = CARTESIAN_POINT('Ctrl Pts',(3.63763353946351,1.93894751340588,1.40124340061523)) ;
#157839 = CARTESIAN_POINT('Ctrl Pts',(3.62813871250318,1.93486114467727,1.40309560864189)) ;
#157840 = CARTESIAN_POINT('Ctrl Pts',(3.62220485293006,1.93266004719379,1.4038846559585)) ;
#157841 = CARTESIAN_POINT('Ctrl Pts',(3.61359543742329,1.93003167234286,1.40457978254887)) ;
#157842 = CARTESIAN_POINT('Ctrl Pts',(3.61101642177011,1.92931331154714,1.40473301744682)) ;
#157843 = CARTESIAN_POINT('Ctrl Pts',(3.60562851963646,1.92796119665945,1.40494674322732)) ;
#157844 = CARTESIAN_POINT('Ctrl Pts',(3.60282089026139,1.92733781012841,1.405)) ;
#157845 = CARTESIAN_POINT('Ctrl Pts',(3.6,1.92679491924311,1.405)) ;
#157846 = CARTESIAN_POINT('Origin',(3.6,1.9,1.305)) ;
#157847 = CARTESIAN_POINT('Origin',(3.7,1.9,1.305)) ;
#157848 = CARTESIAN_POINT('Origin',(10.1,1.9,1.305)) ;
#157849 = CARTESIAN_POINT('Origin',(10.1,1.9,1.305)) ;
#157850 = CARTESIAN_POINT('Origin',(3.7,1.9,-1.305)) ;
#157851 = CARTESIAN_POINT('Origin',(3.7,2.07320508075689,-1.405)) ;
#157852 = CARTESIAN_POINT('Ctrl Pts',(3.60000659411846,1.92678349789492,-1.40500000086965)) ;
#157853 = CARTESIAN_POINT('Ctrl Pts',(3.55,2.01339745962156,-1.40498681089333)) ;
#157854 = CARTESIAN_POINT('Ctrl Pts',(3.55,2.01339745962156,-1.505)) ;
#157855 = CARTESIAN_POINT('Ctrl Pts',(3.61192169694494,1.92907674455598,-1.4050005173338)) ;
#157856 = CARTESIAN_POINT('Ctrl Pts',(3.55199190475227,2.01454315814788,-1.40100027733254)) ;
#157857 = CARTESIAN_POINT('Ctrl Pts',(3.55795064586849,2.01798776715396,-1.5049956215502)) ;
#157858 = CARTESIAN_POINT('Ctrl Pts',(3.62341406508537,1.93280912529606,-1.4040249033077)) ;
#157859 = CARTESIAN_POINT('Ctrl Pts',(3.55602946562208,2.01072041298289,-1.3966898307659)) ;
#157860 = CARTESIAN_POINT('Ctrl Pts',(3.56528619664567,2.02370799306987,-1.49863885617462)) ;
#157861 = CARTESIAN_POINT('Ctrl Pts',(3.64447698054259,1.94188479470202,-1.39990697186185)) ;
#157862 = CARTESIAN_POINT('Ctrl Pts',(3.56481337003729,2.00521659408682,-1.3881887406645)) ;
#157863 = CARTESIAN_POINT('Ctrl Pts',(3.5778513142626,2.03528605841761,-1.48516115437406)) ;
#157864 = CARTESIAN_POINT('Ctrl Pts',(3.6543438360007,1.94732274903781,-1.39671544038559)) ;
#157865 = CARTESIAN_POINT('Ctrl Pts',(3.56964037752545,2.00254785926568,-1.38373800427671)) ;
#157866 = CARTESIAN_POINT('Ctrl Pts',(3.58324299321411,2.04133793352501,-1.4770289695647)) ;
#157867 = CARTESIAN_POINT('Ctrl Pts',(3.67209270719132,1.95869361548257,-1.3882138841634)) ;
#157868 = CARTESIAN_POINT('Ctrl Pts',(3.57877657372944,1.99742369139614,-1.37460192490957)) ;
#157869 = CARTESIAN_POINT('Ctrl Pts',(3.59173571364126,2.05270412132581,-1.4592738450102)) ;
#157870 = CARTESIAN_POINT('Ctrl Pts',(3.68022412057907,1.96474917806412,-1.38281520426601)) ;
#157871 = CARTESIAN_POINT('Ctrl Pts',(3.58322866085249,1.9947527117803,-1.36977362629675)) ;
#157872 = CARTESIAN_POINT('Ctrl Pts',(3.59492343714209,2.05814036366738,-1.449399963424)) ;
#157873 = CARTESIAN_POINT('Ctrl Pts',(3.693683649568,1.97632149420531,-1.37024886281709)) ;
#157874 = CARTESIAN_POINT('Ctrl Pts',(3.59172551342568,1.98925228662578,-1.36099928071625)) ;
#157875 = CARTESIAN_POINT('Ctrl Pts',(3.59903094645825,2.06720241143976,-1.42834396451164)) ;
#157876 = CARTESIAN_POINT('Ctrl Pts',(3.70000914724963,1.98195813651218,-1.36304434431452)) ;
#157877 = CARTESIAN_POINT('Ctrl Pts',(3.59596384548938,1.98543049140365,-1.35700954448628)) ;
#157878 = CARTESIAN_POINT('Ctrl Pts',(3.6,2.07088547209221,-1.41705281147587)) ;
#157879 = CARTESIAN_POINT('Ctrl Pts',(3.70001318823691,1.98660254113158,-1.35500000043482)) ;
#157880 = CARTESIAN_POINT('Ctrl Pts',(3.6,1.98659111827701,-1.35499340544666)) ;
#157881 = CARTESIAN_POINT('Ctrl Pts',(3.6,2.07320508075689,-1.405)) ;
#157882 = CARTESIAN_POINT('Origin',(3.6,1.92679491924311,-1.505)) ;
#157883 = CARTESIAN_POINT('Origin',(3.5,2.1,-1.505)) ;
#157884 = CARTESIAN_POINT('Origin',(3.7,1.9,1.305)) ;
#157885 = CARTESIAN_POINT('Origin',(3.7,2.07320508075689,1.405)) ;
#157886 = CARTESIAN_POINT('Ctrl Pts',(3.70000000000001,1.98660254037844,1.355)) ;
#157887 = CARTESIAN_POINT('Ctrl Pts',(3.59998681089333,1.98660254037844,1.355)) ;
#157888 = CARTESIAN_POINT('Ctrl Pts',(3.60000000086965,2.07321650210508,1.40500659411846)) ;
#157889 = CARTESIAN_POINT('Ctrl Pts',(3.69999562155021,1.98201223284605,1.36295064586848)) ;
#157890 = CARTESIAN_POINT('Ctrl Pts',(3.59600027733256,1.98545684185208,1.35699190475226)) ;
#157891 = CARTESIAN_POINT('Ctrl Pts',(3.60000051733381,2.07092325544402,1.41692169694494)) ;
#157892 = CARTESIAN_POINT('Ctrl Pts',(3.69363885617462,1.97629200693013,1.37028619664567)) ;
#157893 = CARTESIAN_POINT('Ctrl Pts',(3.5916898307659,1.98927958701711,1.36102946562208)) ;
#157894 = CARTESIAN_POINT('Ctrl Pts',(3.59902490330771,2.06719087470394,1.42841406508537)) ;
#157895 = CARTESIAN_POINT('Ctrl Pts',(3.68016115437407,1.9647139415824,1.3828513142626)) ;
#157896 = CARTESIAN_POINT('Ctrl Pts',(3.58318874066451,1.99478340591318,1.36981337003728)) ;
#157897 = CARTESIAN_POINT('Ctrl Pts',(3.59490697186185,2.05811520529798,1.44947698054259)) ;
#157898 = CARTESIAN_POINT('Ctrl Pts',(3.67202896956471,1.95866206647499,1.38824299321411)) ;
#157899 = CARTESIAN_POINT('Ctrl Pts',(3.57873800427672,1.99745214073432,1.37464037752545)) ;
#157900 = CARTESIAN_POINT('Ctrl Pts',(3.59171544038559,2.05267725096219,1.45934383600069)) ;
#157901 = CARTESIAN_POINT('Ctrl Pts',(3.6542738450102,1.94729587867419,1.39673571364126)) ;
#157902 = CARTESIAN_POINT('Ctrl Pts',(3.56960192490957,2.00257630860386,1.38377657372944)) ;
#157903 = CARTESIAN_POINT('Ctrl Pts',(3.5832138841634,2.04130638451743,1.47709270719132)) ;
#157904 = CARTESIAN_POINT('Ctrl Pts',(3.644399963424,1.94185963633262,1.39992343714209)) ;
#157905 = CARTESIAN_POINT('Ctrl Pts',(3.56477362629675,2.0052472882197,1.38822866085248)) ;
#157906 = CARTESIAN_POINT('Ctrl Pts',(3.57781520426602,2.03525082193588,1.48522412057907)) ;
#157907 = CARTESIAN_POINT('Ctrl Pts',(3.62334396451164,1.93279758856024,1.40403094645824)) ;
#157908 = CARTESIAN_POINT('Ctrl Pts',(3.55599928071625,2.01074771337423,1.39672551342568)) ;
#157909 = CARTESIAN_POINT('Ctrl Pts',(3.5652488628171,2.02367850579469,1.498683649568)) ;
#157910 = CARTESIAN_POINT('Ctrl Pts',(3.61205281147587,1.92911452790779,1.405)) ;
#157911 = CARTESIAN_POINT('Ctrl Pts',(3.55200954448627,2.01456950859638,1.40096384548938)) ;
#157912 = CARTESIAN_POINT('Ctrl Pts',(3.55804434431452,2.01804186348783,1.50500914724966)) ;
#157913 = CARTESIAN_POINT('Ctrl Pts',(3.6,1.92679491924311,1.405)) ;
#157914 = CARTESIAN_POINT('Ctrl Pts',(3.54999340544667,2.01340888172299,1.405)) ;
#157915 = CARTESIAN_POINT('Ctrl Pts',(3.55000000043483,2.01339745886842,1.50501318823691)) ;
#157916 = CARTESIAN_POINT('Origin',(3.6,1.92679491924311,1.505)) ;
#157917 = CARTESIAN_POINT('Origin',(3.5,2.1,1.505)) ;
#157918 = CARTESIAN_POINT('Origin',(-5.15,-5.05,-35.89)) ;
#157919 = CARTESIAN_POINT('',(-5.8,-1.29142135623731,-35.89)) ;
#157920 = CARTESIAN_POINT('',(-5.8,-5.42192235935956,-35.89)) ;
#157921 = CARTESIAN_POINT('',(-5.8,-5.55,-35.89)) ;
#157922 = CARTESIAN_POINT('',(-5.17275707706435,-5.26511162862565,-35.89)) ;
#157923 = CARTESIAN_POINT('',(-5.10072415073893,-5.24710339704429,-35.89)) ;
#157924 = CARTESIAN_POINT('',(-5.17275707706435,-1.91866427917295,-35.89)) ;
#157925 = CARTESIAN_POINT('',(-5.17275707706435,-1.8,-35.89)) ;
#157926 = CARTESIAN_POINT('',(-3.59571067811865,-3.49571067811865,-35.89)) ;
#157927 = CARTESIAN_POINT('Origin',(-3.9,-5.05,-35.29)) ;
#157928 = CARTESIAN_POINT('',(-5.12948397030587,-1.91866427917295,-35.8801523057468)) ;
#157929 = CARTESIAN_POINT('',(-5.12948397030587,-5.26511162862565,-35.8801523057468)) ;
#157930 = CARTESIAN_POINT('',(-5.12948397030587,-5.3625,-35.8801523057468)) ;
#157931 = CARTESIAN_POINT('',(-3.9,-4.95774063604919,-35.29)) ;
#157932 = CARTESIAN_POINT('',(-3.91783961713025,-4.96220054033175,-35.2985630162225)) ;
#157933 = CARTESIAN_POINT('',(-3.9,-3.14814824947882,-35.29)) ;
#157934 = CARTESIAN_POINT('',(-3.9,-5.05,-35.29)) ;
#157935 = CARTESIAN_POINT('',(-3.04730463122257,-4.00084361825625,-34.8807062229868)) ;
#157936 = CARTESIAN_POINT('Origin',(-3.9,-5.05,-33.29)) ;
#157937 = CARTESIAN_POINT('',(-3.9,-5.05,-33.3892816869892)) ;
#157938 = CARTESIAN_POINT('',(-3.9,-5.05,-35.1907183130108)) ;
#157939 = CARTESIAN_POINT('',(-3.9,-5.05,-33.29)) ;
#157940 = CARTESIAN_POINT('',(-3.9,-4.95774063604919,-33.29)) ;
#157941 = CARTESIAN_POINT('Origin',(-3.9,-4.94692235935959,-33.4009233969909)) ;
#157942 = CARTESIAN_POINT('',(-3.9,-3.14814824947882,-33.29)) ;
#157943 = CARTESIAN_POINT('',(-3.9,-5.05,-33.29)) ;
#157944 = CARTESIAN_POINT('',(-3.9,-3.05,-33.3669822714939)) ;
#157945 = CARTESIAN_POINT('Origin',(-3.89999999999999,-3.1914213562364,-33.4009233969901)) ;
#157946 = CARTESIAN_POINT('',(-3.9,-3.05,-35.2130177285061)) ;
#157947 = CARTESIAN_POINT('',(-3.9,-3.05,-33.29)) ;
#157948 = CARTESIAN_POINT('Origin',(-3.89999999999999,-3.19142135623724,-35.1790766030092)) ;
#157949 = CARTESIAN_POINT('Origin',(-3.89999999999999,-4.94692235935948,-35.1790766030091)) ;
#157950 = CARTESIAN_POINT('Origin',(-5.15,-5.05,-32.69)) ;
#157951 = CARTESIAN_POINT('',(-5.12948397030588,-5.26511162862565,-32.6998476942532)) ;
#157952 = CARTESIAN_POINT('',(-5.10741344341225,-5.25959399690224,-32.7104415471621)) ;
#157953 = CARTESIAN_POINT('',(-5.12948397030588,-1.91866427917294,-32.6998476942532)) ;
#157954 = CARTESIAN_POINT('',(-5.12948397030588,-1.79999999999999,-32.6998476942532)) ;
#157955 = CARTESIAN_POINT('',(-3.73686704155256,-3.31128120792626,-33.3683038200548)) ;
#157956 = CARTESIAN_POINT('Origin',(-5.9,-5.05,-32.69)) ;
#157957 = CARTESIAN_POINT('',(-5.8,-5.42192235935956,-32.69)) ;
#157958 = CARTESIAN_POINT('',(-5.8,-1.29142135623731,-32.69)) ;
#157959 = CARTESIAN_POINT('',(-5.8,-1.04999999999999,-32.69)) ;
#157960 = CARTESIAN_POINT('',(-5.17275707706436,-1.91866427917294,-32.69)) ;
#157961 = CARTESIAN_POINT('',(-3.97071067811865,-3.12071067811865,-32.69)) ;
#157962 = CARTESIAN_POINT('',(-5.17275707706436,-5.26511162862565,-32.69)) ;
#157963 = CARTESIAN_POINT('',(-5.17275707706436,-5.3625,-32.69)) ;
#157964 = CARTESIAN_POINT('',(-5.8066065036801,-5.42357398527959,-32.69)) ;
#157965 = CARTESIAN_POINT('Origin',(-5.15,-5.05,-32.08)) ;
#157966 = CARTESIAN_POINT('',(-5.8,-1.29142135623731,-32.08)) ;
#157967 = CARTESIAN_POINT('',(-5.8,-5.42192235935956,-32.08)) ;
#157968 = CARTESIAN_POINT('',(-5.8,-5.55,-32.08)) ;
#157969 = CARTESIAN_POINT('',(-5.17275707706435,-5.26511162862565,-32.08)) ;
#157970 = CARTESIAN_POINT('',(-5.10072415073893,-5.24710339704429,-32.08)) ;
#157971 = CARTESIAN_POINT('',(-5.17275707706435,-1.91866427917295,-32.08)) ;
#157972 = CARTESIAN_POINT('',(-5.17275707706435,-1.8,-32.08)) ;
#157973 = CARTESIAN_POINT('',(-3.59571067811865,-3.49571067811865,-32.08)) ;
#157974 = CARTESIAN_POINT('Origin',(-3.9,-5.05,-31.48)) ;
#157975 = CARTESIAN_POINT('',(-5.12948397030587,-1.91866427917295,-32.0701523057468)) ;
#157976 = CARTESIAN_POINT('',(-5.12948397030587,-5.26511162862565,-32.0701523057468)) ;
#157977 = CARTESIAN_POINT('',(-5.12948397030587,-5.3625,-32.0701523057468)) ;
#157978 = CARTESIAN_POINT('',(-3.9,-4.95774063604919,-31.48)) ;
#157979 = CARTESIAN_POINT('',(-3.91783961713025,-4.96220054033175,-31.4885630162225)) ;
#157980 = CARTESIAN_POINT('',(-3.9,-3.14814824947882,-31.48)) ;
#157981 = CARTESIAN_POINT('',(-3.9,-5.05,-31.48)) ;
#157982 = CARTESIAN_POINT('',(-3.04730463122257,-4.00084361825625,-31.0707062229868)) ;
#157983 = CARTESIAN_POINT('Origin',(-3.9,-5.05,-29.48)) ;
#157984 = CARTESIAN_POINT('',(-3.9,-5.05,-29.5792816869892)) ;
#157985 = CARTESIAN_POINT('',(-3.9,-5.05,-31.3807183130108)) ;
#157986 = CARTESIAN_POINT('',(-3.9,-5.05,-29.48)) ;
#157987 = CARTESIAN_POINT('',(-3.9,-4.95774063604918,-29.48)) ;
#157988 = CARTESIAN_POINT('Origin',(-3.9,-4.94692235935937,-29.5909233969911)) ;
#157989 = CARTESIAN_POINT('',(-3.9,-3.14814824947882,-29.48)) ;
#157990 = CARTESIAN_POINT('',(-3.9,-5.05,-29.48)) ;
#157991 = CARTESIAN_POINT('',(-3.9,-3.05,-29.5569822714939)) ;
#157992 = CARTESIAN_POINT('Origin',(-3.9,-3.19142135623589,-29.5909233969898)) ;
#157993 = CARTESIAN_POINT('',(-3.9,-3.05,-31.4030177285061)) ;
#157994 = CARTESIAN_POINT('',(-3.9,-3.05,-29.48)) ;
#157995 = CARTESIAN_POINT('Origin',(-3.89999999999999,-3.19142135623673,-31.3690766030095)) ;
#157996 = CARTESIAN_POINT('Origin',(-3.89999999999999,-4.94692235935935,-31.3690766030089)) ;
#157997 = CARTESIAN_POINT('Origin',(-5.15,-5.05,-28.88)) ;
#157998 = CARTESIAN_POINT('',(-5.12948397030589,-5.26511162862565,-28.8898476942532)) ;
#157999 = CARTESIAN_POINT('',(-5.10741344341225,-5.25959399690224,-28.9004415471621)) ;
#158000 = CARTESIAN_POINT('',(-5.12948397030589,-1.91866427917294,-28.8898476942532)) ;
#158001 = CARTESIAN_POINT('',(-5.12948397030589,-1.79999999999999,-28.8898476942532)) ;
#158002 = CARTESIAN_POINT('',(-3.73686704155256,-3.31128120792626,-29.5583038200548)) ;
#158003 = CARTESIAN_POINT('Origin',(-5.9,-5.05,-28.88)) ;
#158004 = CARTESIAN_POINT('',(-5.8,-5.42192235935956,-28.88)) ;
#158005 = CARTESIAN_POINT('',(-5.8,-1.29142135623731,-28.88)) ;
#158006 = CARTESIAN_POINT('',(-5.8,-1.04999999999999,-28.88)) ;
#158007 = CARTESIAN_POINT('',(-5.17275707706436,-1.91866427917294,-28.88)) ;
#158008 = CARTESIAN_POINT('',(-3.97071067811865,-3.12071067811865,-28.88)) ;
#158009 = CARTESIAN_POINT('',(-5.17275707706436,-5.26511162862565,-28.88)) ;
#158010 = CARTESIAN_POINT('',(-5.17275707706436,-5.3625,-28.88)) ;
#158011 = CARTESIAN_POINT('',(-5.8066065036801,-5.42357398527959,-28.88)) ;
#158012 = CARTESIAN_POINT('Origin',(-5.15,-5.05,-28.27)) ;
#158013 = CARTESIAN_POINT('',(-5.8,-1.29142135623731,-28.27)) ;
#158014 = CARTESIAN_POINT('',(-5.8,-5.42192235935956,-28.27)) ;
#158015 = CARTESIAN_POINT('',(-5.8,-5.55,-28.27)) ;
#158016 = CARTESIAN_POINT('',(-5.17275707706436,-5.26511162862565,-28.27)) ;
#158017 = CARTESIAN_POINT('',(-5.10072415073893,-5.24710339704429,-28.27)) ;
#158018 = CARTESIAN_POINT('',(-5.17275707706436,-1.91866427917293,-28.27)) ;
#158019 = CARTESIAN_POINT('',(-5.17275707706436,-1.79999999999999,-28.27)) ;
#158020 = CARTESIAN_POINT('',(-3.59571067811865,-3.49571067811865,-28.27)) ;
#158021 = CARTESIAN_POINT('Origin',(-3.9,-5.05,-27.67)) ;
#158022 = CARTESIAN_POINT('',(-5.12948397030589,-1.91866427917293,-28.2601523057468)) ;
#158023 = CARTESIAN_POINT('',(-5.12948397030589,-5.26511162862565,-28.2601523057468)) ;
#158024 = CARTESIAN_POINT('',(-5.12948397030589,-5.3625,-28.2601523057468)) ;
#158025 = CARTESIAN_POINT('',(-3.9,-4.95774063604919,-27.67)) ;
#158026 = CARTESIAN_POINT('',(-3.91783961713025,-4.96220054033175,-27.6785630162225)) ;
#158027 = CARTESIAN_POINT('',(-3.9,-3.14814824947882,-27.67)) ;
#158028 = CARTESIAN_POINT('',(-3.9,-5.05,-27.67)) ;
#158029 = CARTESIAN_POINT('',(-3.04730463122257,-4.00084361825625,-27.2607062229868)) ;
#158030 = CARTESIAN_POINT('Origin',(-3.9,-5.05,-25.67)) ;
#158031 = CARTESIAN_POINT('',(-3.9,-5.05,-25.7692816869891)) ;
#158032 = CARTESIAN_POINT('',(-3.9,-5.05,-27.5707183130108)) ;
#158033 = CARTESIAN_POINT('',(-3.9,-5.05,-25.67)) ;
#158034 = CARTESIAN_POINT('',(-3.9,-4.95774063604918,-25.67)) ;
#158035 = CARTESIAN_POINT('Origin',(-3.9,-4.94692235935943,-25.780923396991)) ;
#158036 = CARTESIAN_POINT('',(-3.9,-3.14814824947882,-25.67)) ;
#158037 = CARTESIAN_POINT('',(-3.9,-5.05,-25.67)) ;
#158038 = CARTESIAN_POINT('',(-3.9,-3.05,-25.7469822714939)) ;
#158039 = CARTESIAN_POINT('Origin',(-3.9,-3.1914213562362,-25.7809233969901)) ;
#158040 = CARTESIAN_POINT('',(-3.9,-3.05,-27.5930177285061)) ;
#158041 = CARTESIAN_POINT('',(-3.9,-3.05,-25.67)) ;
#158042 = CARTESIAN_POINT('Origin',(-3.9,-3.19142135623739,-27.559076603009)) ;
#158043 = CARTESIAN_POINT('Origin',(-3.9,-4.94692235935962,-27.5590766030092)) ;
#158044 = CARTESIAN_POINT('Origin',(-5.15,-5.05,-25.07)) ;
#158045 = CARTESIAN_POINT('',(-5.12948397030589,-5.26511162862565,-25.0798476942532)) ;
#158046 = CARTESIAN_POINT('',(-5.10741344341225,-5.25959399690224,-25.0904415471621)) ;
#158047 = CARTESIAN_POINT('',(-5.12948397030589,-1.91866427917294,-25.0798476942532)) ;
#158048 = CARTESIAN_POINT('',(-5.12948397030589,-1.79999999999999,-25.0798476942532)) ;
#158049 = CARTESIAN_POINT('',(-3.73686704155256,-3.31128120792626,-25.7483038200548)) ;
#158050 = CARTESIAN_POINT('Origin',(-5.9,-5.05,-25.07)) ;
#158051 = CARTESIAN_POINT('',(-5.8,-5.42192235935956,-25.07)) ;
#158052 = CARTESIAN_POINT('',(-5.8,-1.29142135623731,-25.07)) ;
#158053 = CARTESIAN_POINT('',(-5.8,-1.04999999999999,-25.07)) ;
#158054 = CARTESIAN_POINT('',(-5.17275707706436,-1.91866427917294,-25.07)) ;
#158055 = CARTESIAN_POINT('',(-3.97071067811865,-3.12071067811865,-25.07)) ;
#158056 = CARTESIAN_POINT('',(-5.17275707706436,-5.26511162862565,-25.07)) ;
#158057 = CARTESIAN_POINT('',(-5.17275707706436,-5.3625,-25.07)) ;
#158058 = CARTESIAN_POINT('',(-5.8066065036801,-5.42357398527959,-25.07)) ;
#158059 = CARTESIAN_POINT('Origin',(-5.15,-5.05,-24.46)) ;
#158060 = CARTESIAN_POINT('',(-5.8,-1.29142135623731,-24.46)) ;
#158061 = CARTESIAN_POINT('',(-5.8,-5.42192235935956,-24.46)) ;
#158062 = CARTESIAN_POINT('',(-5.8,-5.55,-24.46)) ;
#158063 = CARTESIAN_POINT('',(-5.17275707706436,-5.26511162862565,-24.46)) ;
#158064 = CARTESIAN_POINT('',(-5.10072415073893,-5.24710339704429,-24.46)) ;
#158065 = CARTESIAN_POINT('',(-5.17275707706436,-1.91866427917293,-24.46)) ;
#158066 = CARTESIAN_POINT('',(-5.17275707706436,-1.79999999999999,-24.46)) ;
#158067 = CARTESIAN_POINT('',(-3.59571067811865,-3.49571067811865,-24.46)) ;
#158068 = CARTESIAN_POINT('Origin',(-3.9,-5.05,-23.86)) ;
#158069 = CARTESIAN_POINT('',(-5.12948397030589,-1.91866427917293,-24.4501523057468)) ;
#158070 = CARTESIAN_POINT('',(-5.12948397030589,-5.26511162862565,-24.4501523057468)) ;
#158071 = CARTESIAN_POINT('',(-5.12948397030589,-5.3625,-24.4501523057468)) ;
#158072 = CARTESIAN_POINT('',(-3.9,-4.95774063604919,-23.86)) ;
#158073 = CARTESIAN_POINT('',(-3.91783961713025,-4.96220054033175,-23.8685630162225)) ;
#158074 = CARTESIAN_POINT('',(-3.9,-3.14814824947882,-23.86)) ;
#158075 = CARTESIAN_POINT('',(-3.9,-5.05,-23.86)) ;
#158076 = CARTESIAN_POINT('',(-3.04730463122257,-4.00084361825625,-23.4507062229868)) ;
#158077 = CARTESIAN_POINT('Origin',(-3.9,-5.05,-21.86)) ;
#158078 = CARTESIAN_POINT('',(-3.9,-5.05,-21.9592816869892)) ;
#158079 = CARTESIAN_POINT('',(-3.9,-5.05,-23.7607183130108)) ;
#158080 = CARTESIAN_POINT('',(-3.9,-5.05,-21.86)) ;
#158081 = CARTESIAN_POINT('',(-3.9,-4.95774063604918,-21.86)) ;
#158082 = CARTESIAN_POINT('Origin',(-3.9,-4.94692235935955,-21.9709233969909)) ;
#158083 = CARTESIAN_POINT('',(-3.9,-3.14814824947882,-21.86)) ;
#158084 = CARTESIAN_POINT('',(-3.9,-5.05,-21.86)) ;
#158085 = CARTESIAN_POINT('',(-3.9,-3.05,-21.9369822714939)) ;
#158086 = CARTESIAN_POINT('Origin',(-3.9,-3.19142135623605,-21.97092339699)) ;
#158087 = CARTESIAN_POINT('',(-3.9,-3.05,-23.7830177285061)) ;
#158088 = CARTESIAN_POINT('',(-3.9,-3.05,-21.86)) ;
#158089 = CARTESIAN_POINT('Origin',(-3.9,-3.19142135623773,-23.7490766030088)) ;
#158090 = CARTESIAN_POINT('Origin',(-3.9,-4.94692235935942,-23.749076603009)) ;
#158091 = CARTESIAN_POINT('Origin',(-5.15,-5.05,-21.26)) ;
#158092 = CARTESIAN_POINT('',(-5.12948397030589,-5.26511162862565,-21.2698476942532)) ;
#158093 = CARTESIAN_POINT('',(-5.10741344341225,-5.25959399690224,-21.2804415471621)) ;
#158094 = CARTESIAN_POINT('',(-5.12948397030589,-1.91866427917294,-21.2698476942532)) ;
#158095 = CARTESIAN_POINT('',(-5.12948397030589,-1.79999999999999,-21.2698476942532)) ;
#158096 = CARTESIAN_POINT('',(-3.73686704155256,-3.31128120792626,-21.9383038200548)) ;
#158097 = CARTESIAN_POINT('Origin',(-5.9,-5.05,-21.26)) ;
#158098 = CARTESIAN_POINT('',(-5.8,-5.42192235935956,-21.26)) ;
#158099 = CARTESIAN_POINT('',(-5.8,-1.29142135623731,-21.26)) ;
#158100 = CARTESIAN_POINT('',(-5.8,-1.04999999999999,-21.26)) ;
#158101 = CARTESIAN_POINT('',(-5.17275707706436,-1.91866427917294,-21.26)) ;
#158102 = CARTESIAN_POINT('',(-3.97071067811865,-3.12071067811865,-21.26)) ;
#158103 = CARTESIAN_POINT('',(-5.17275707706436,-5.26511162862565,-21.26)) ;
#158104 = CARTESIAN_POINT('',(-5.17275707706436,-5.3625,-21.26)) ;
#158105 = CARTESIAN_POINT('',(-5.8066065036801,-5.42357398527959,-21.26)) ;
#158106 = CARTESIAN_POINT('Origin',(-5.15,-5.05,-20.65)) ;
#158107 = CARTESIAN_POINT('',(-5.8,-1.29142135623731,-20.65)) ;
#158108 = CARTESIAN_POINT('',(-5.8,-5.42192235935956,-20.65)) ;
#158109 = CARTESIAN_POINT('',(-5.8,-5.55,-20.65)) ;
#158110 = CARTESIAN_POINT('',(-5.17275707706436,-5.26511162862565,-20.65)) ;
#158111 = CARTESIAN_POINT('',(-5.10072415073893,-5.24710339704429,-20.65)) ;
#158112 = CARTESIAN_POINT('',(-5.17275707706436,-1.91866427917293,-20.65)) ;
#158113 = CARTESIAN_POINT('',(-5.17275707706436,-1.79999999999999,-20.65)) ;
#158114 = CARTESIAN_POINT('',(-3.59571067811865,-3.49571067811865,-20.65)) ;
#158115 = CARTESIAN_POINT('Origin',(-3.9,-5.05,-20.05)) ;
#158116 = CARTESIAN_POINT('',(-5.12948397030589,-1.91866427917293,-20.6401523057468)) ;
#158117 = CARTESIAN_POINT('',(-5.12948397030589,-5.26511162862565,-20.6401523057468)) ;
#158118 = CARTESIAN_POINT('',(-5.12948397030589,-5.3625,-20.6401523057468)) ;
#158119 = CARTESIAN_POINT('',(-3.9,-4.95774063604919,-20.05)) ;
#158120 = CARTESIAN_POINT('',(-3.91783961713025,-4.96220054033175,-20.0585630162225)) ;
#158121 = CARTESIAN_POINT('',(-3.9,-3.14814824947882,-20.05)) ;
#158122 = CARTESIAN_POINT('',(-3.9,-5.05,-20.05)) ;
#158123 = CARTESIAN_POINT('',(-3.04730463122257,-4.00084361825625,-19.6407062229868)) ;
#158124 = CARTESIAN_POINT('Origin',(-3.9,-5.05,-18.05)) ;
#158125 = CARTESIAN_POINT('',(-3.9,-5.05,-18.1492816869892)) ;
#158126 = CARTESIAN_POINT('',(-3.9,-5.05,-19.9507183130109)) ;
#158127 = CARTESIAN_POINT('',(-3.9,-5.05,-18.05)) ;
#158128 = CARTESIAN_POINT('',(-3.9,-4.95774063604918,-18.05)) ;
#158129 = CARTESIAN_POINT('Origin',(-3.9,-4.94692235935955,-18.1609233969909)) ;
#158130 = CARTESIAN_POINT('',(-3.9,-3.14814824947882,-18.05)) ;
#158131 = CARTESIAN_POINT('',(-3.9,-5.05,-18.05)) ;
#158132 = CARTESIAN_POINT('',(-3.9,-3.05,-18.1269822714939)) ;
#158133 = CARTESIAN_POINT('Origin',(-3.9,-3.19142135623647,-18.1609233969903)) ;
#158134 = CARTESIAN_POINT('',(-3.9,-3.05,-19.9730177285061)) ;
#158135 = CARTESIAN_POINT('',(-3.9,-3.05,-18.05)) ;
#158136 = CARTESIAN_POINT('Origin',(-3.9,-3.19142135623653,-19.9390766030097)) ;
#158137 = CARTESIAN_POINT('Origin',(-3.89999999999999,-4.9469223593596,-19.9390766030092)) ;
#158138 = CARTESIAN_POINT('Origin',(-5.15,-5.05,-17.45)) ;
#158139 = CARTESIAN_POINT('',(-5.12948397030589,-5.26511162862565,-17.4598476942532)) ;
#158140 = CARTESIAN_POINT('',(-5.10741344341225,-5.25959399690224,-17.4704415471621)) ;
#158141 = CARTESIAN_POINT('',(-5.12948397030589,-1.91866427917294,-17.4598476942532)) ;
#158142 = CARTESIAN_POINT('',(-5.12948397030589,-1.79999999999999,-17.4598476942532)) ;
#158143 = CARTESIAN_POINT('',(-3.73686704155256,-3.31128120792626,-18.1283038200548)) ;
#158144 = CARTESIAN_POINT('Origin',(-5.9,-5.05,-17.45)) ;
#158145 = CARTESIAN_POINT('',(-5.8,-5.42192235935956,-17.45)) ;
#158146 = CARTESIAN_POINT('',(-5.8,-1.29142135623731,-17.45)) ;
#158147 = CARTESIAN_POINT('',(-5.8,-1.04999999999999,-17.45)) ;
#158148 = CARTESIAN_POINT('',(-5.17275707706436,-1.91866427917294,-17.45)) ;
#158149 = CARTESIAN_POINT('',(-3.97071067811865,-3.12071067811865,-17.45)) ;
#158150 = CARTESIAN_POINT('',(-5.17275707706436,-5.26511162862565,-17.45)) ;
#158151 = CARTESIAN_POINT('',(-5.17275707706436,-5.3625,-17.45)) ;
#158152 = CARTESIAN_POINT('',(-5.8066065036801,-5.42357398527959,-17.45)) ;
#158153 = CARTESIAN_POINT('Origin',(-5.15,-5.05,-16.84)) ;
#158154 = CARTESIAN_POINT('',(-5.8,-1.29142135623731,-16.84)) ;
#158155 = CARTESIAN_POINT('',(-5.8,-5.42192235935956,-16.84)) ;
#158156 = CARTESIAN_POINT('',(-5.8,-5.55,-16.84)) ;
#158157 = CARTESIAN_POINT('',(-5.17275707706436,-5.26511162862565,-16.84)) ;
#158158 = CARTESIAN_POINT('',(-5.10072415073893,-5.24710339704429,-16.84)) ;
#158159 = CARTESIAN_POINT('',(-5.17275707706436,-1.91866427917293,-16.84)) ;
#158160 = CARTESIAN_POINT('',(-5.17275707706436,-1.79999999999999,-16.84)) ;
#158161 = CARTESIAN_POINT('',(-3.59571067811865,-3.49571067811865,-16.84)) ;
#158162 = CARTESIAN_POINT('Origin',(-3.9,-5.05,-16.24)) ;
#158163 = CARTESIAN_POINT('',(-5.12948397030589,-1.91866427917293,-16.8301523057468)) ;
#158164 = CARTESIAN_POINT('',(-5.12948397030589,-5.26511162862565,-16.8301523057468)) ;
#158165 = CARTESIAN_POINT('',(-5.12948397030589,-5.3625,-16.8301523057468)) ;
#158166 = CARTESIAN_POINT('',(-3.9,-4.95774063604919,-16.24)) ;
#158167 = CARTESIAN_POINT('',(-3.91783961713025,-4.96220054033175,-16.2485630162225)) ;
#158168 = CARTESIAN_POINT('',(-3.9,-3.14814824947882,-16.24)) ;
#158169 = CARTESIAN_POINT('',(-3.9,-5.05,-16.24)) ;
#158170 = CARTESIAN_POINT('',(-3.04730463122257,-4.00084361825625,-15.8307062229868)) ;
#158171 = CARTESIAN_POINT('Origin',(-3.9,-5.05,-14.24)) ;
#158172 = CARTESIAN_POINT('',(-3.9,-5.05,-14.3392816869892)) ;
#158173 = CARTESIAN_POINT('',(-3.9,-5.05,-16.1407183130109)) ;
#158174 = CARTESIAN_POINT('',(-3.9,-5.05,-14.24)) ;
#158175 = CARTESIAN_POINT('',(-3.9,-4.95774063604919,-14.24)) ;
#158176 = CARTESIAN_POINT('Origin',(-3.9,-4.94692235935948,-14.3509233969909)) ;
#158177 = CARTESIAN_POINT('',(-3.9,-3.14814824947882,-14.24)) ;
#158178 = CARTESIAN_POINT('',(-3.9,-5.05,-14.24)) ;
#158179 = CARTESIAN_POINT('',(-3.9,-3.05,-14.3169822714939)) ;
#158180 = CARTESIAN_POINT('Origin',(-3.9,-3.19142135623778,-14.3509233969912)) ;
#158181 = CARTESIAN_POINT('',(-3.9,-3.05,-16.1630177285061)) ;
#158182 = CARTESIAN_POINT('',(-3.9,-3.05,-14.24)) ;
#158183 = CARTESIAN_POINT('Origin',(-3.9,-3.19142135623662,-16.1290766030096)) ;
#158184 = CARTESIAN_POINT('Origin',(-3.89999999999999,-4.9469223593597,-16.1290766030092)) ;
#158185 = CARTESIAN_POINT('Origin',(-5.15,-5.05,-13.64)) ;
#158186 = CARTESIAN_POINT('',(-5.12948397030589,-5.26511162862565,-13.6498476942532)) ;
#158187 = CARTESIAN_POINT('',(-5.10741344341225,-5.25959399690224,-13.6604415471621)) ;
#158188 = CARTESIAN_POINT('',(-5.12948397030589,-1.91866427917294,-13.6498476942532)) ;
#158189 = CARTESIAN_POINT('',(-5.12948397030589,-1.79999999999999,-13.6498476942532)) ;
#158190 = CARTESIAN_POINT('',(-3.73686704155256,-3.31128120792626,-14.3183038200548)) ;
#158191 = CARTESIAN_POINT('Origin',(-5.9,-5.05,-13.64)) ;
#158192 = CARTESIAN_POINT('',(-5.8,-5.42192235935956,-13.64)) ;
#158193 = CARTESIAN_POINT('',(-5.8,-1.29142135623731,-13.64)) ;
#158194 = CARTESIAN_POINT('',(-5.8,-1.04999999999999,-13.64)) ;
#158195 = CARTESIAN_POINT('',(-5.17275707706436,-1.91866427917294,-13.64)) ;
#158196 = CARTESIAN_POINT('',(-3.97071067811865,-3.12071067811865,-13.64)) ;
#158197 = CARTESIAN_POINT('',(-5.17275707706436,-5.26511162862565,-13.64)) ;
#158198 = CARTESIAN_POINT('',(-5.17275707706436,-5.3625,-13.64)) ;
#158199 = CARTESIAN_POINT('',(-5.8066065036801,-5.42357398527959,-13.64)) ;
#158200 = CARTESIAN_POINT('Origin',(-5.15,-5.05,-13.03)) ;
#158201 = CARTESIAN_POINT('',(-5.8,-1.29142135623731,-13.03)) ;
#158202 = CARTESIAN_POINT('',(-5.8,-5.42192235935956,-13.03)) ;
#158203 = CARTESIAN_POINT('',(-5.8,-5.55,-13.03)) ;
#158204 = CARTESIAN_POINT('',(-5.17275707706436,-5.26511162862565,-13.03)) ;
#158205 = CARTESIAN_POINT('',(-5.10072415073893,-5.24710339704429,-13.03)) ;
#158206 = CARTESIAN_POINT('',(-5.17275707706436,-1.91866427917293,-13.03)) ;
#158207 = CARTESIAN_POINT('',(-5.17275707706436,-1.79999999999999,-13.03)) ;
#158208 = CARTESIAN_POINT('',(-3.59571067811865,-3.49571067811865,-13.03)) ;
#158209 = CARTESIAN_POINT('Origin',(-3.9,-5.05,-12.43)) ;
#158210 = CARTESIAN_POINT('',(-5.12948397030589,-1.91866427917294,-13.0201523057468)) ;
#158211 = CARTESIAN_POINT('',(-5.12948397030589,-5.26511162862565,-13.0201523057468)) ;
#158212 = CARTESIAN_POINT('',(-5.12948397030589,-5.3625,-13.0201523057468)) ;
#158213 = CARTESIAN_POINT('',(-3.9,-4.95774063604919,-12.43)) ;
#158214 = CARTESIAN_POINT('',(-3.91783961713025,-4.96220054033175,-12.4385630162225)) ;
#158215 = CARTESIAN_POINT('',(-3.9,-3.14814824947882,-12.43)) ;
#158216 = CARTESIAN_POINT('',(-3.9,-5.05,-12.43)) ;
#158217 = CARTESIAN_POINT('',(-3.04730463122257,-4.00084361825625,-12.0207062229868)) ;
#158218 = CARTESIAN_POINT('Origin',(-3.9,-5.05,-10.43)) ;
#158219 = CARTESIAN_POINT('',(-3.9,-5.05,-10.5292816869892)) ;
#158220 = CARTESIAN_POINT('',(-3.9,-5.05,-12.3307183130108)) ;
#158221 = CARTESIAN_POINT('',(-3.9,-5.05,-10.43)) ;
#158222 = CARTESIAN_POINT('',(-3.9,-4.95774063604919,-10.43)) ;
#158223 = CARTESIAN_POINT('Origin',(-3.9,-4.94692235935962,-10.5409233969908)) ;
#158224 = CARTESIAN_POINT('',(-3.9,-3.14814824947882,-10.43)) ;
#158225 = CARTESIAN_POINT('',(-3.9,-5.05,-10.43)) ;
#158226 = CARTESIAN_POINT('',(-3.9,-3.05,-10.5069822714939)) ;
#158227 = CARTESIAN_POINT('Origin',(-3.9,-3.19142135623743,-10.540923396991)) ;
#158228 = CARTESIAN_POINT('',(-3.9,-3.05,-12.3530177285061)) ;
#158229 = CARTESIAN_POINT('',(-3.9,-3.05,-10.43)) ;
#158230 = CARTESIAN_POINT('Origin',(-3.9,-3.19142135623734,-12.3190766030091)) ;
#158231 = CARTESIAN_POINT('Origin',(-3.89999999999999,-4.94692235935969,-12.3190766030093)) ;
#158232 = CARTESIAN_POINT('Origin',(-5.15,-5.05,-9.83)) ;
#158233 = CARTESIAN_POINT('',(-5.12948397030589,-5.26511162862565,-9.83984769425317)) ;
#158234 = CARTESIAN_POINT('',(-5.10741344341225,-5.25959399690224,-9.85044154716212)) ;
#158235 = CARTESIAN_POINT('',(-5.12948397030589,-1.91866427917294,-9.83984769425317)) ;
#158236 = CARTESIAN_POINT('',(-5.12948397030589,-1.79999999999999,-9.83984769425317)) ;
#158237 = CARTESIAN_POINT('',(-3.73686704155256,-3.31128120792626,-10.5083038200548)) ;
#158238 = CARTESIAN_POINT('Origin',(-5.9,-5.05,-9.83)) ;
#158239 = CARTESIAN_POINT('',(-5.8,-5.42192235935956,-9.83)) ;
#158240 = CARTESIAN_POINT('',(-5.8,-1.29142135623731,-9.83)) ;
#158241 = CARTESIAN_POINT('',(-5.8,-1.04999999999999,-9.83)) ;
#158242 = CARTESIAN_POINT('',(-5.17275707706436,-1.91866427917294,-9.83)) ;
#158243 = CARTESIAN_POINT('',(-3.97071067811865,-3.12071067811865,-9.83)) ;
#158244 = CARTESIAN_POINT('',(-5.17275707706436,-5.26511162862565,-9.83)) ;
#158245 = CARTESIAN_POINT('',(-5.17275707706436,-5.3625,-9.83)) ;
#158246 = CARTESIAN_POINT('',(-5.8066065036801,-5.42357398527959,-9.83)) ;
#158247 = CARTESIAN_POINT('Origin',(-5.15,-5.05,-9.22)) ;
#158248 = CARTESIAN_POINT('',(-5.8,-1.29142135623731,-9.22)) ;
#158249 = CARTESIAN_POINT('',(-5.8,-5.42192235935956,-9.22)) ;
#158250 = CARTESIAN_POINT('',(-5.8,-5.55,-9.22)) ;
#158251 = CARTESIAN_POINT('',(-5.17275707706437,-5.26511162862565,-9.22)) ;
#158252 = CARTESIAN_POINT('',(-5.10072415073893,-5.24710339704429,-9.22)) ;
#158253 = CARTESIAN_POINT('',(-5.17275707706437,-1.91866427917293,-9.22)) ;
#158254 = CARTESIAN_POINT('',(-5.17275707706437,-1.79999999999999,-9.22)) ;
#158255 = CARTESIAN_POINT('',(-3.59571067811865,-3.49571067811865,-9.22)) ;
#158256 = CARTESIAN_POINT('Origin',(-3.9,-5.05,-8.62)) ;
#158257 = CARTESIAN_POINT('',(-5.12948397030589,-1.91866427917293,-9.21015230574683)) ;
#158258 = CARTESIAN_POINT('',(-5.12948397030589,-5.26511162862565,-9.21015230574683)) ;
#158259 = CARTESIAN_POINT('',(-5.12948397030589,-5.3625,-9.21015230574683)) ;
#158260 = CARTESIAN_POINT('',(-3.9,-4.95774063604919,-8.62)) ;
#158261 = CARTESIAN_POINT('',(-3.91783961713025,-4.96220054033175,-8.62856301622252)) ;
#158262 = CARTESIAN_POINT('',(-3.9,-3.14814824947882,-8.62)) ;
#158263 = CARTESIAN_POINT('',(-3.9,-5.05,-8.62)) ;
#158264 = CARTESIAN_POINT('',(-3.04730463122257,-4.00084361825625,-8.21070622298683)) ;
#158265 = CARTESIAN_POINT('Origin',(-3.9,-5.05,-6.62)) ;
#158266 = CARTESIAN_POINT('',(-3.9,-5.05,-6.71928168698915)) ;
#158267 = CARTESIAN_POINT('',(-3.9,-5.05,-8.52071831301085)) ;
#158268 = CARTESIAN_POINT('',(-3.9,-5.05,-6.62)) ;
#158269 = CARTESIAN_POINT('',(-3.9,-4.95774063604918,-6.62)) ;
#158270 = CARTESIAN_POINT('Origin',(-3.9,-4.94692235935954,-6.7309233969909)) ;
#158271 = CARTESIAN_POINT('',(-3.9,-3.14814824947882,-6.62)) ;
#158272 = CARTESIAN_POINT('',(-3.9,-5.05,-6.62)) ;
#158273 = CARTESIAN_POINT('',(-3.9,-3.05,-6.69698227149394)) ;
#158274 = CARTESIAN_POINT('Origin',(-3.9,-3.19142135623718,-6.73092339699078)) ;
#158275 = CARTESIAN_POINT('',(-3.9,-3.05,-8.54301772850605)) ;
#158276 = CARTESIAN_POINT('',(-3.9,-3.05,-6.62)) ;
#158277 = CARTESIAN_POINT('Origin',(-3.9,-3.19142135623772,-8.5090766030088)) ;
#158278 = CARTESIAN_POINT('Origin',(-3.89999999999999,-4.94692235935958,-8.50907660300914)) ;
#158279 = CARTESIAN_POINT('Origin',(-5.15,-5.05,-6.02)) ;
#158280 = CARTESIAN_POINT('',(-5.12948397030589,-5.26511162862565,-6.02984769425317)) ;
#158281 = CARTESIAN_POINT('',(-5.10741344341225,-5.25959399690224,-6.04044154716212)) ;
#158282 = CARTESIAN_POINT('',(-5.12948397030589,-1.91866427917294,-6.02984769425317)) ;
#158283 = CARTESIAN_POINT('',(-5.12948397030589,-1.79999999999999,-6.02984769425317)) ;
#158284 = CARTESIAN_POINT('',(-3.73686704155256,-3.31128120792626,-6.69830382005477)) ;
#158285 = CARTESIAN_POINT('Origin',(-5.9,-5.05,-6.02)) ;
#158286 = CARTESIAN_POINT('',(-5.8,-5.42192235935956,-6.02)) ;
#158287 = CARTESIAN_POINT('',(-5.8,-1.29142135623731,-6.02)) ;
#158288 = CARTESIAN_POINT('',(-5.8,-1.04999999999999,-6.02)) ;
#158289 = CARTESIAN_POINT('',(-5.17275707706436,-1.91866427917294,-6.02)) ;
#158290 = CARTESIAN_POINT('',(-3.97071067811865,-3.12071067811865,-6.02)) ;
#158291 = CARTESIAN_POINT('',(-5.17275707706436,-5.26511162862565,-6.02)) ;
#158292 = CARTESIAN_POINT('',(-5.17275707706436,-5.3625,-6.02)) ;
#158293 = CARTESIAN_POINT('',(-5.8066065036801,-5.42357398527959,-6.02)) ;
#158294 = CARTESIAN_POINT('Origin',(-5.15,-5.05,-5.41)) ;
#158295 = CARTESIAN_POINT('',(-5.8,-5.42192235935956,-5.41)) ;
#158296 = CARTESIAN_POINT('',(-5.17275707706436,-5.26511162862565,-5.41)) ;
#158297 = CARTESIAN_POINT('',(-5.10072415073893,-5.24710339704429,-5.41)) ;
#158298 = CARTESIAN_POINT('',(-5.17275707706436,-1.91866427917294,-5.41)) ;
#158299 = CARTESIAN_POINT('',(-5.17275707706436,-1.79999999999999,-5.41)) ;
#158300 = CARTESIAN_POINT('',(-5.8,-1.2914213562373,-5.41)) ;
#158301 = CARTESIAN_POINT('',(-3.59571067811865,-3.49571067811865,-5.41)) ;
#158302 = CARTESIAN_POINT('',(-5.8,-5.55,-5.41)) ;
#158303 = CARTESIAN_POINT('Origin',(-3.9,-5.05,-4.81)) ;
#158304 = CARTESIAN_POINT('',(-5.12948397030589,-1.91866427917294,-5.40015230574683)) ;
#158305 = CARTESIAN_POINT('',(-5.12948397030589,-5.26511162862565,-5.40015230574683)) ;
#158306 = CARTESIAN_POINT('',(-5.12948397030589,-5.3625,-5.40015230574683)) ;
#158307 = CARTESIAN_POINT('',(-3.9,-4.95774063604919,-4.81)) ;
#158308 = CARTESIAN_POINT('',(-3.91783961713025,-4.96220054033175,-4.81856301622252)) ;
#158309 = CARTESIAN_POINT('',(-3.9,-3.14814824947882,-4.81)) ;
#158310 = CARTESIAN_POINT('',(-3.9,-5.05,-4.81)) ;
#158311 = CARTESIAN_POINT('',(-3.04730463122257,-4.00084361825625,-4.40070622298683)) ;
#158312 = CARTESIAN_POINT('Origin',(-3.9,-5.05,-2.81)) ;
#158313 = CARTESIAN_POINT('',(-3.9,-5.05,-2.90928168698915)) ;
#158314 = CARTESIAN_POINT('',(-3.9,-5.05,-4.71071831301085)) ;
#158315 = CARTESIAN_POINT('',(-3.9,-5.05,-2.81)) ;
#158316 = CARTESIAN_POINT('',(-3.9,-4.95774063604919,-2.81)) ;
#158317 = CARTESIAN_POINT('Origin',(-3.9,-4.94692235935961,-2.92092339699082)) ;
#158318 = CARTESIAN_POINT('',(-3.9,-3.14814824947882,-2.81)) ;
#158319 = CARTESIAN_POINT('',(-3.9,-5.05,-2.81)) ;
#158320 = CARTESIAN_POINT('',(-3.9,-3.05,-2.88698227149394)) ;
#158321 = CARTESIAN_POINT('Origin',(-3.9,-3.19142135623728,-2.92092339699086)) ;
#158322 = CARTESIAN_POINT('',(-3.9,-3.05,-4.73301772850606)) ;
#158323 = CARTESIAN_POINT('',(-3.9,-3.05,-2.81)) ;
#158324 = CARTESIAN_POINT('Origin',(-3.9,-3.19142135623729,-4.69907660300913)) ;
#158325 = CARTESIAN_POINT('Origin',(-3.9,-4.94692235935959,-4.69907660300915)) ;
#158326 = CARTESIAN_POINT('Origin',(-5.15,-5.05,-2.21)) ;
#158327 = CARTESIAN_POINT('',(-5.12948397030589,-5.26511162862565,-2.21984769425317)) ;
#158328 = CARTESIAN_POINT('',(-5.10741344341225,-5.25959399690224,-2.23044154716212)) ;
#158329 = CARTESIAN_POINT('',(-5.12948397030589,-1.91866427917294,-2.21984769425317)) ;
#158330 = CARTESIAN_POINT('',(-5.12948397030589,-1.79999999999999,-2.21984769425317)) ;
#158331 = CARTESIAN_POINT('',(-3.73686704155256,-3.31128120792626,-2.88830382005477)) ;
#158332 = CARTESIAN_POINT('Origin',(-5.9,-5.05,-2.21)) ;
#158333 = CARTESIAN_POINT('',(-5.17275707706436,-1.91866427917294,-2.21)) ;
#158334 = CARTESIAN_POINT('',(-5.17275707706436,-5.26511162862565,-2.21)) ;
#158335 = CARTESIAN_POINT('',(-5.17275707706436,-5.3625,-2.21)) ;
#158336 = CARTESIAN_POINT('',(-5.8,-5.42192235935956,-2.21)) ;
#158337 = CARTESIAN_POINT('',(-5.8066065036801,-5.42357398527959,-2.21)) ;
#158338 = CARTESIAN_POINT('',(-5.8,-1.29142135623731,-2.21)) ;
#158339 = CARTESIAN_POINT('',(-5.8,-1.04999999999999,-2.21)) ;
#158340 = CARTESIAN_POINT('',(-3.97071067811865,-3.12071067811865,-2.21)) ;
#158341 = CARTESIAN_POINT('Origin',(-3.89999999999997,-5.05,-3.81)) ;
#158342 = CARTESIAN_POINT('',(-5.82425356250363,-5.53106339062591,-2.31)) ;
#158343 = CARTESIAN_POINT('',(-5.14850351456073,-5.36212587864019,-2.31)) ;
#158344 = CARTESIAN_POINT('',(-3.89999999999997,-5.05,-2.31)) ;
#158345 = CARTESIAN_POINT('',(-3.56560075006169,-4.96640018751543,-3.06979332695954)) ;
#158346 = CARTESIAN_POINT('',(-5.14850351456073,-5.36212587864019,-5.31)) ;
#158347 = CARTESIAN_POINT('',(-3.56560075006169,-4.96640018751543,-4.55020667304046)) ;
#158348 = CARTESIAN_POINT('',(-5.82425356250363,-5.53106339062591,-5.31)) ;
#158349 = CARTESIAN_POINT('',(-3.89999999999997,-5.05,-5.31)) ;
#158350 = CARTESIAN_POINT('',(-5.82425356250363,-5.53106339062591,-3.81)) ;
#158351 = CARTESIAN_POINT('Origin',(-3.89999999999997,-5.05,-7.62)) ;
#158352 = CARTESIAN_POINT('',(-5.82425356250363,-5.53106339062591,-9.12597149997094)) ;
#158353 = CARTESIAN_POINT('',(-5.82425356250363,-5.53106339062591,-6.11402850002907)) ;
#158354 = CARTESIAN_POINT('',(-5.82425356250363,-5.53106339062591,-7.62)) ;
#158355 = CARTESIAN_POINT('',(-5.77574643749636,-5.51893660937409,-6.12)) ;
#158356 = CARTESIAN_POINT('Origin',(-5.7814888808097,-5.52037222020246,-5.96664642007523)) ;
#158357 = CARTESIAN_POINT('',(-5.14850351456073,-5.36212587864019,-6.12)) ;
#158358 = CARTESIAN_POINT('',(-3.89999999999997,-5.05,-6.12)) ;
#158359 = CARTESIAN_POINT('',(-3.56560075006169,-4.96640018751543,-6.87979332695954)) ;
#158360 = CARTESIAN_POINT('',(-5.14850351456074,-5.36212587864019,-9.12)) ;
#158361 = CARTESIAN_POINT('',(-3.56560075006169,-4.96640018751543,-8.36020667304046)) ;
#158362 = CARTESIAN_POINT('',(-5.77574643749636,-5.51893660937409,-9.12)) ;
#158363 = CARTESIAN_POINT('',(-3.89999999999997,-5.05,-9.12)) ;
#158364 = CARTESIAN_POINT('Origin',(-5.78148888079898,-5.52037222019986,-9.27335357990704)) ;
#158365 = CARTESIAN_POINT('Origin',(-3.89999999999997,-5.05,-11.43)) ;
#158366 = CARTESIAN_POINT('',(-5.82425356250363,-5.53106339062591,-12.9359714999709)) ;
#158367 = CARTESIAN_POINT('',(-5.82425356250363,-5.53106339062591,-9.92402850002907)) ;
#158368 = CARTESIAN_POINT('',(-5.82425356250363,-5.53106339062591,-11.43)) ;
#158369 = CARTESIAN_POINT('',(-5.77574643749636,-5.51893660937409,-9.93)) ;
#158370 = CARTESIAN_POINT('Origin',(-5.78148888078994,-5.52037222019747,-9.77664642000976)) ;
#158371 = CARTESIAN_POINT('',(-5.14850351456073,-5.36212587864019,-9.93)) ;
#158372 = CARTESIAN_POINT('',(-3.89999999999997,-5.05,-9.93)) ;
#158373 = CARTESIAN_POINT('',(-3.56560075006169,-4.96640018751543,-10.6897933269595)) ;
#158374 = CARTESIAN_POINT('',(-5.14850351456073,-5.36212587864019,-12.93)) ;
#158375 = CARTESIAN_POINT('',(-3.56560075006169,-4.96640018751543,-12.1702066730405)) ;
#158376 = CARTESIAN_POINT('',(-5.77574643749636,-5.51893660937409,-12.93)) ;
#158377 = CARTESIAN_POINT('',(-3.89999999999997,-5.05,-12.93)) ;
#158378 = CARTESIAN_POINT('Origin',(-5.78148888076761,-5.52037222019189,-13.0833535801862)) ;
#158379 = CARTESIAN_POINT('Origin',(-3.89999999999997,-5.05,-15.24)) ;
#158380 = CARTESIAN_POINT('',(-5.82425356250363,-5.53106339062591,-16.7459714999709)) ;
#158381 = CARTESIAN_POINT('',(-5.82425356250363,-5.53106339062591,-13.7340285000291)) ;
#158382 = CARTESIAN_POINT('',(-5.82425356250363,-5.53106339062591,-15.24)) ;
#158383 = CARTESIAN_POINT('',(-5.77574643749636,-5.51893660937409,-13.74)) ;
#158384 = CARTESIAN_POINT('Origin',(-5.78148888075282,-5.52037222018823,-13.5866464197048)) ;
#158385 = CARTESIAN_POINT('',(-5.14850351456073,-5.36212587864019,-13.74)) ;
#158386 = CARTESIAN_POINT('',(-3.89999999999997,-5.05,-13.74)) ;
#158387 = CARTESIAN_POINT('',(-3.56560075006169,-4.96640018751543,-14.4997933269595)) ;
#158388 = CARTESIAN_POINT('',(-5.14850351456073,-5.36212587864019,-16.74)) ;
#158389 = CARTESIAN_POINT('',(-3.56560075006169,-4.96640018751543,-15.9802066730405)) ;
#158390 = CARTESIAN_POINT('',(-5.77574643749636,-5.51893660937409,-16.74)) ;
#158391 = CARTESIAN_POINT('',(-3.89999999999997,-5.05,-16.74)) ;
#158392 = CARTESIAN_POINT('Origin',(-5.78148888084216,-5.52037222021054,-16.8933535798564)) ;
#158393 = CARTESIAN_POINT('Origin',(-3.89999999999997,-5.05,-19.05)) ;
#158394 = CARTESIAN_POINT('',(-5.82425356250363,-5.53106339062591,-20.5559714999709)) ;
#158395 = CARTESIAN_POINT('',(-5.82425356250363,-5.53106339062591,-17.5440285000291)) ;
#158396 = CARTESIAN_POINT('',(-5.82425356250363,-5.53106339062591,-19.05)) ;
#158397 = CARTESIAN_POINT('',(-5.77574643749636,-5.51893660937409,-17.55)) ;
#158398 = CARTESIAN_POINT('Origin',(-5.78148888084565,-5.52037222021153,-17.3966464201892)) ;
#158399 = CARTESIAN_POINT('',(-5.14850351456074,-5.36212587864019,-17.55)) ;
#158400 = CARTESIAN_POINT('',(-3.89999999999997,-5.05,-17.55)) ;
#158401 = CARTESIAN_POINT('',(-3.56560075006169,-4.96640018751543,-18.3097933269595)) ;
#158402 = CARTESIAN_POINT('',(-5.14850351456073,-5.36212587864019,-20.55)) ;
#158403 = CARTESIAN_POINT('',(-3.56560075006169,-4.96640018751543,-19.7902066730405)) ;
#158404 = CARTESIAN_POINT('',(-5.77574643749636,-5.51893660937409,-20.55)) ;
#158405 = CARTESIAN_POINT('',(-3.89999999999997,-5.05,-20.55)) ;
#158406 = CARTESIAN_POINT('Origin',(-5.78148888080932,-5.52037222020243,-20.7033535801353)) ;
#158407 = CARTESIAN_POINT('Origin',(-3.89999999999997,-5.05,-22.86)) ;
#158408 = CARTESIAN_POINT('',(-5.82425356250363,-5.53106339062591,-24.3659714999709)) ;
#158409 = CARTESIAN_POINT('',(-5.82425356250363,-5.53106339062591,-21.3540285000291)) ;
#158410 = CARTESIAN_POINT('',(-5.82425356250363,-5.53106339062591,-22.86)) ;
#158411 = CARTESIAN_POINT('',(-5.77574643749636,-5.51893660937409,-21.36)) ;
#158412 = CARTESIAN_POINT('Origin',(-5.7814888808788,-5.52037222021982,-21.2066464204715)) ;
#158413 = CARTESIAN_POINT('',(-5.14850351456074,-5.36212587864019,-21.36)) ;
#158414 = CARTESIAN_POINT('',(-3.89999999999997,-5.05,-21.36)) ;
#158415 = CARTESIAN_POINT('',(-3.56560075006169,-4.96640018751543,-22.1197933269595)) ;
#158416 = CARTESIAN_POINT('',(-5.14850351456073,-5.36212587864019,-24.36)) ;
#158417 = CARTESIAN_POINT('',(-3.56560075006169,-4.96640018751543,-23.6002066730405)) ;
#158418 = CARTESIAN_POINT('',(-5.77574643749636,-5.51893660937409,-24.36)) ;
#158419 = CARTESIAN_POINT('',(-3.89999999999997,-5.05,-24.36)) ;
#158420 = CARTESIAN_POINT('Origin',(-5.7814888808248,-5.5203722202062,-24.513353580007)) ;
#158421 = CARTESIAN_POINT('Origin',(-3.89999999999997,-5.05,-26.67)) ;
#158422 = CARTESIAN_POINT('',(-5.82425356250363,-5.53106339062591,-28.1759714999709)) ;
#158423 = CARTESIAN_POINT('',(-5.82425356250363,-5.53106339062591,-25.1640285000291)) ;
#158424 = CARTESIAN_POINT('',(-5.82425356250363,-5.53106339062591,-26.67)) ;
#158425 = CARTESIAN_POINT('',(-5.77574643749636,-5.51893660937409,-25.17)) ;
#158426 = CARTESIAN_POINT('Origin',(-5.78148888089162,-5.52037222022287,-25.016646420512)) ;
#158427 = CARTESIAN_POINT('',(-5.14850351456074,-5.36212587864019,-25.17)) ;
#158428 = CARTESIAN_POINT('',(-3.89999999999997,-5.05,-25.17)) ;
#158429 = CARTESIAN_POINT('',(-3.56560075006169,-4.96640018751543,-25.9297933269595)) ;
#158430 = CARTESIAN_POINT('',(-5.14850351456073,-5.36212587864019,-28.17)) ;
#158431 = CARTESIAN_POINT('',(-3.56560075006169,-4.96640018751543,-27.4102066730405)) ;
#158432 = CARTESIAN_POINT('',(-5.77574643749636,-5.51893660937409,-28.17)) ;
#158433 = CARTESIAN_POINT('',(-3.89999999999997,-5.05,-28.17)) ;
#158434 = CARTESIAN_POINT('Origin',(-5.78148888087819,-5.52037222021968,-28.3233535795358)) ;
#158435 = CARTESIAN_POINT('Origin',(-3.89999999999997,-5.05,-30.48)) ;
#158436 = CARTESIAN_POINT('',(-5.82425356250363,-5.53106339062591,-31.9859714999709)) ;
#158437 = CARTESIAN_POINT('',(-5.82425356250363,-5.53106339062591,-28.9740285000291)) ;
#158438 = CARTESIAN_POINT('',(-5.82425356250363,-5.53106339062591,-30.48)) ;
#158439 = CARTESIAN_POINT('',(-5.77574643749636,-5.51893660937409,-28.98)) ;
#158440 = CARTESIAN_POINT('Origin',(-5.78148888086266,-5.52037222021575,-28.8266464203985)) ;
#158441 = CARTESIAN_POINT('',(-5.14850351456074,-5.36212587864019,-28.98)) ;
#158442 = CARTESIAN_POINT('',(-3.89999999999997,-5.05,-28.98)) ;
#158443 = CARTESIAN_POINT('',(-3.56560075006169,-4.96640018751543,-29.7397933269595)) ;
#158444 = CARTESIAN_POINT('',(-5.14850351456071,-5.36212587864018,-31.98)) ;
#158445 = CARTESIAN_POINT('',(-3.56560075006169,-4.96640018751543,-31.2202066730405)) ;
#158446 = CARTESIAN_POINT('',(-5.77574643749636,-5.51893660937409,-31.98)) ;
#158447 = CARTESIAN_POINT('',(-3.89999999999997,-5.05,-31.98)) ;
#158448 = CARTESIAN_POINT('Origin',(-5.78148888079375,-5.52037222019844,-32.1333535799531)) ;
#158449 = CARTESIAN_POINT('Origin',(-3.89999999999997,-5.05,-34.29)) ;
#158450 = CARTESIAN_POINT('',(-5.82425356250363,-5.53106339062591,-35.7959714999709)) ;
#158451 = CARTESIAN_POINT('',(-5.82425356250363,-5.53106339062591,-32.7840285000291)) ;
#158452 = CARTESIAN_POINT('',(-5.82425356250363,-5.53106339062591,-34.29)) ;
#158453 = CARTESIAN_POINT('',(-5.77574643749636,-5.51893660937409,-32.79)) ;
#158454 = CARTESIAN_POINT('Origin',(-5.7814888807851,-5.52037222019633,-32.6366464199968)) ;
#158455 = CARTESIAN_POINT('',(-5.14850351456072,-5.36212587864018,-32.79)) ;
#158456 = CARTESIAN_POINT('',(-3.89999999999997,-5.05,-32.79)) ;
#158457 = CARTESIAN_POINT('',(-3.56560075006169,-4.96640018751543,-33.5497933269595)) ;
#158458 = CARTESIAN_POINT('',(-5.14850351456071,-5.36212587864018,-35.79)) ;
#158459 = CARTESIAN_POINT('',(-3.56560075006169,-4.96640018751543,-35.0302066730405)) ;
#158460 = CARTESIAN_POINT('',(-5.77574643749636,-5.51893660937409,-35.79)) ;
#158461 = CARTESIAN_POINT('',(-3.89999999999997,-5.05,-35.79)) ;
#158462 = CARTESIAN_POINT('Origin',(-5.78148888079367,-5.52037222019848,-35.9433535799528)) ;
#158463 = CARTESIAN_POINT('Origin',(-5.9,-1.04999999999999,-36.59)) ;
#158464 = CARTESIAN_POINT('',(-5.87071067811865,-1.07928932188134,-5.31)) ;
#158465 = CARTESIAN_POINT('',(-5.10204639894571,-1.84795360105428,-5.31)) ;
#158466 = CARTESIAN_POINT('',(-5.9,-1.04999999999999,-5.31)) ;
#158467 = CARTESIAN_POINT('',(-12.5492788245683,5.59927882456828,-8.88467156429883)) ;
#158468 = CARTESIAN_POINT('',(-5.10204639894571,-1.84795360105428,-2.31)) ;
#158469 = CARTESIAN_POINT('',(1.55975991287794,-8.50975991287791,-5.50766702967535)) ;
#158470 = CARTESIAN_POINT('',(-5.87071067811865,-1.07928932188134,-2.31)) ;
#158471 = CARTESIAN_POINT('',(-5.9,-1.04999999999999,-2.31)) ;
#158472 = CARTESIAN_POINT('',(-5.87071067811865,-1.07928932188134,-36.59)) ;
#158473 = CARTESIAN_POINT('Origin',(-5.9,-1.04999999999999,-36.59)) ;
#158474 = CARTESIAN_POINT('',(-5.87071067811865,-1.07928932188134,-6.06142135623731)) ;
#158475 = CARTESIAN_POINT('',(-5.87071067811865,-1.07928932188134,-9.17857864376271)) ;
#158476 = CARTESIAN_POINT('',(-5.87071067811865,-1.07928932188134,-36.59)) ;
#158477 = CARTESIAN_POINT('',(-5.72928932188134,-1.22071067811865,-9.12)) ;
#158478 = CARTESIAN_POINT('Origin',(-5.74291017058518,-1.2070898294148,-9.28714114800675)) ;
#158479 = CARTESIAN_POINT('',(-5.10204639894571,-1.84795360105428,-9.12)) ;
#158480 = CARTESIAN_POINT('',(-5.9,-1.04999999999999,-9.12)) ;
#158481 = CARTESIAN_POINT('',(-11.7293362133775,4.77933621337747,-12.3010991109272)) ;
#158482 = CARTESIAN_POINT('',(-5.10204639894571,-1.84795360105428,-6.12)) ;
#158483 = CARTESIAN_POINT('',(0.739817301687122,-7.68981730168709,-8.92409457630375)) ;
#158484 = CARTESIAN_POINT('',(-5.72928932188134,-1.22071067811865,-6.12)) ;
#158485 = CARTESIAN_POINT('',(-5.9,-1.04999999999999,-6.12)) ;
#158486 = CARTESIAN_POINT('Origin',(-5.74291017058796,-1.20708982941201,-5.95285885199633)) ;
#158487 = CARTESIAN_POINT('Origin',(-5.9,-1.04999999999999,-36.59)) ;
#158488 = CARTESIAN_POINT('',(-5.87071067811865,-1.07928932188134,-9.87142135623731)) ;
#158489 = CARTESIAN_POINT('',(-5.87071067811865,-1.07928932188134,-12.9885786437627)) ;
#158490 = CARTESIAN_POINT('',(-5.87071067811865,-1.07928932188134,-36.59)) ;
#158491 = CARTESIAN_POINT('',(-5.72928932188134,-1.22071067811865,-12.93)) ;
#158492 = CARTESIAN_POINT('Origin',(-5.74291017058355,-1.20708982941644,-13.0971411480106)) ;
#158493 = CARTESIAN_POINT('',(-5.10204639894571,-1.84795360105428,-12.93)) ;
#158494 = CARTESIAN_POINT('',(-5.9,-1.04999999999999,-12.93)) ;
#158495 = CARTESIAN_POINT('',(-10.9093936021867,3.95939360218665,-15.7175266575557)) ;
#158496 = CARTESIAN_POINT('',(-5.10204639894571,-1.84795360105428,-9.93)) ;
#158497 = CARTESIAN_POINT('',(-0.0801253095036982,-6.86987469049627,-12.3405221229322)) ;
#158498 = CARTESIAN_POINT('',(-5.72928932188134,-1.22071067811865,-9.93)) ;
#158499 = CARTESIAN_POINT('',(-5.9,-1.04999999999999,-9.93)) ;
#158500 = CARTESIAN_POINT('Origin',(-5.74291017058447,-1.20708982941551,-9.76285885199229)) ;
#158501 = CARTESIAN_POINT('Origin',(-5.9,-1.04999999999999,-36.59)) ;
#158502 = CARTESIAN_POINT('',(-5.87071067811865,-1.07928932188134,-13.6814213562373)) ;
#158503 = CARTESIAN_POINT('',(-5.87071067811865,-1.07928932188134,-16.7985786437627)) ;
#158504 = CARTESIAN_POINT('',(-5.87071067811865,-1.07928932188134,-36.59)) ;
#158505 = CARTESIAN_POINT('',(-5.72928932188134,-1.22071067811865,-16.74)) ;
#158506 = CARTESIAN_POINT('Origin',(-5.74291017058335,-1.20708982941664,-16.9071411480136)) ;
#158507 = CARTESIAN_POINT('',(-5.10204639894571,-1.84795360105428,-16.74)) ;
#158508 = CARTESIAN_POINT('',(-5.9,-1.04999999999999,-16.74)) ;
#158509 = CARTESIAN_POINT('',(-10.0894509909958,3.13945099099583,-19.1339542041841)) ;
#158510 = CARTESIAN_POINT('',(-5.10204639894571,-1.84795360105428,-13.74)) ;
#158511 = CARTESIAN_POINT('',(-0.900067920694518,-6.04993207930546,-15.7569496695606)) ;
#158512 = CARTESIAN_POINT('',(-5.72928932188134,-1.22071067811865,-13.74)) ;
#158513 = CARTESIAN_POINT('',(-5.9,-1.04999999999999,-13.74)) ;
#158514 = CARTESIAN_POINT('Origin',(-5.74291017058507,-1.20708982941492,-13.5728588519939)) ;
#158515 = CARTESIAN_POINT('Origin',(-5.9,-1.04999999999999,-36.59)) ;
#158516 = CARTESIAN_POINT('',(-5.87071067811865,-1.07928932188134,-17.4914213562373)) ;
#158517 = CARTESIAN_POINT('',(-5.87071067811865,-1.07928932188134,-20.6085786437627)) ;
#158518 = CARTESIAN_POINT('',(-5.87071067811865,-1.07928932188134,-36.59)) ;
#158519 = CARTESIAN_POINT('',(-5.72928932188134,-1.22071067811865,-20.55)) ;
#158520 = CARTESIAN_POINT('Origin',(-5.74291017058427,-1.20708982941573,-20.7171411480115)) ;
#158521 = CARTESIAN_POINT('',(-5.10204639894571,-1.84795360105428,-20.55)) ;
#158522 = CARTESIAN_POINT('',(-5.9,-1.04999999999999,-20.55)) ;
#158523 = CARTESIAN_POINT('',(-9.26950837980502,2.31950837980501,-22.5503817508125)) ;
#158524 = CARTESIAN_POINT('',(-5.10204639894571,-1.84795360105428,-17.55)) ;
#158525 = CARTESIAN_POINT('',(-1.72001053188534,-5.22998946811464,-19.173377216189)) ;
#158526 = CARTESIAN_POINT('',(-5.72928932188134,-1.22071067811865,-17.55)) ;
#158527 = CARTESIAN_POINT('',(-5.9,-1.04999999999999,-17.55)) ;
#158528 = CARTESIAN_POINT('Origin',(-5.74291017058526,-1.20708982941474,-17.3828588519974)) ;
#158529 = CARTESIAN_POINT('Origin',(-5.9,-1.04999999999999,-36.59)) ;
#158530 = CARTESIAN_POINT('',(-5.87071067811865,-1.07928932188134,-21.3014213562373)) ;
#158531 = CARTESIAN_POINT('',(-5.87071067811865,-1.07928932188134,-24.4185786437627)) ;
#158532 = CARTESIAN_POINT('',(-5.87071067811865,-1.07928932188134,-36.59)) ;
#158533 = CARTESIAN_POINT('',(-5.72928932188134,-1.22071067811865,-24.36)) ;
#158534 = CARTESIAN_POINT('Origin',(-5.74291017058376,-1.20708982941625,-24.5271411480123)) ;
#158535 = CARTESIAN_POINT('',(-5.10204639894571,-1.84795360105428,-24.36)) ;
#158536 = CARTESIAN_POINT('',(-5.9,-1.04999999999999,-24.36)) ;
#158537 = CARTESIAN_POINT('',(-8.4495657686142,1.49956576861419,-25.9668092974409)) ;
#158538 = CARTESIAN_POINT('',(-5.10204639894571,-1.84795360105428,-21.36)) ;
#158539 = CARTESIAN_POINT('',(-2.53995314307616,-4.41004685692382,-22.5898047628174)) ;
#158540 = CARTESIAN_POINT('',(-5.72928932188134,-1.22071067811865,-21.36)) ;
#158541 = CARTESIAN_POINT('',(-5.9,-1.04999999999999,-21.36)) ;
#158542 = CARTESIAN_POINT('Origin',(-5.74291017058452,-1.20708982941547,-21.1928588519956)) ;
#158543 = CARTESIAN_POINT('Origin',(-5.9,-1.04999999999999,-36.59)) ;
#158544 = CARTESIAN_POINT('',(-5.87071067811865,-1.07928932188134,-25.1114213562373)) ;
#158545 = CARTESIAN_POINT('',(-5.87071067811865,-1.07928932188134,-28.2285786437627)) ;
#158546 = CARTESIAN_POINT('',(-5.87071067811865,-1.07928932188134,-36.59)) ;
#158547 = CARTESIAN_POINT('',(-5.72928932188134,-1.22071067811865,-28.17)) ;
#158548 = CARTESIAN_POINT('Origin',(-5.74291017058572,-1.20708982941426,-28.3371411480073)) ;
#158549 = CARTESIAN_POINT('',(-5.10204639894571,-1.84795360105428,-28.17)) ;
#158550 = CARTESIAN_POINT('',(-5.9,-1.04999999999999,-28.17)) ;
#158551 = CARTESIAN_POINT('',(-7.62962315742338,0.679623157423377,-29.3832368440693)) ;
#158552 = CARTESIAN_POINT('',(-5.10204639894571,-1.84795360105428,-25.17)) ;
#158553 = CARTESIAN_POINT('',(-3.35989575426698,-3.590104245733,-26.0062323094458)) ;
#158554 = CARTESIAN_POINT('',(-5.72928932188134,-1.22071067811865,-25.17)) ;
#158555 = CARTESIAN_POINT('',(-5.9,-1.04999999999999,-25.17)) ;
#158556 = CARTESIAN_POINT('Origin',(-5.7429101705851,-1.20708982941489,-25.0028588519971)) ;
#158557 = CARTESIAN_POINT('Origin',(-5.9,-1.04999999999999,-36.59)) ;
#158558 = CARTESIAN_POINT('',(-5.87071067811865,-1.07928932188134,-28.9214213562373)) ;
#158559 = CARTESIAN_POINT('',(-5.87071067811865,-1.07928932188134,-32.0385786437627)) ;
#158560 = CARTESIAN_POINT('',(-5.87071067811865,-1.07928932188134,-36.59)) ;
#158561 = CARTESIAN_POINT('',(-5.72928932188134,-1.22071067811865,-31.98)) ;
#158562 = CARTESIAN_POINT('Origin',(-5.74291017059717,-1.20708982940281,-32.147141147996)) ;
#158563 = CARTESIAN_POINT('',(-5.1020463989457,-1.84795360105429,-31.98)) ;
#158564 = CARTESIAN_POINT('',(-5.9,-1.04999999999999,-31.98)) ;
#158565 = CARTESIAN_POINT('',(-6.80968054623256,-0.14031945376744,-32.7996643906977)) ;
#158566 = CARTESIAN_POINT('',(-5.10204639894571,-1.84795360105428,-28.98)) ;
#158567 = CARTESIAN_POINT('',(-4.1798383654578,-2.77016163454219,-29.4226598560742)) ;
#158568 = CARTESIAN_POINT('',(-5.72928932188134,-1.22071067811865,-28.98)) ;
#158569 = CARTESIAN_POINT('',(-5.9,-1.04999999999999,-28.98)) ;
#158570 = CARTESIAN_POINT('Origin',(-5.74291017058634,-1.20708982941365,-28.8128588519997)) ;
#158571 = CARTESIAN_POINT('Origin',(-5.9,-1.04999999999999,-36.59)) ;
#158572 = CARTESIAN_POINT('',(-5.87071067811865,-1.07928932188134,-32.7314213562373)) ;
#158573 = CARTESIAN_POINT('',(-5.87071067811865,-1.07928932188134,-35.8485786437627)) ;
#158574 = CARTESIAN_POINT('',(-5.87071067811865,-1.07928932188134,-36.59)) ;
#158575 = CARTESIAN_POINT('',(-5.72928932188134,-1.22071067811865,-35.79)) ;
#158576 = CARTESIAN_POINT('Origin',(-5.74291017059454,-1.20708982940546,-35.9571411480018)) ;
#158577 = CARTESIAN_POINT('',(-5.1020463989457,-1.84795360105429,-35.79)) ;
#158578 = CARTESIAN_POINT('',(-5.9,-1.04999999999999,-35.79)) ;
#158579 = CARTESIAN_POINT('',(-5.98973793504174,-0.960262064958257,-36.2160919373261)) ;
#158580 = CARTESIAN_POINT('',(-5.1020463989457,-1.84795360105429,-32.79)) ;
#158581 = CARTESIAN_POINT('',(-4.99978097664862,-1.95021902335137,-32.8390874027026)) ;
#158582 = CARTESIAN_POINT('',(-5.72928932188134,-1.22071067811865,-32.79)) ;
#158583 = CARTESIAN_POINT('',(-5.9,-1.04999999999999,-32.79)) ;
#158584 = CARTESIAN_POINT('Origin',(-5.74291017059665,-1.20708982940334,-32.622858852003)) ;
#158585 = CARTESIAN_POINT('Origin',(-3.9,-6.4,-33.29)) ;
#158586 = CARTESIAN_POINT('',(-3.9,-6.45,-35.19)) ;
#158587 = CARTESIAN_POINT('',(-3.9,-6.45,-33.39)) ;
#158588 = CARTESIAN_POINT('',(-3.9,-6.45,-33.29)) ;
#158589 = CARTESIAN_POINT('',(-3.9,-6.35,-33.39)) ;
#158590 = CARTESIAN_POINT('',(-3.9,-6.25,-33.39)) ;
#158591 = CARTESIAN_POINT('',(-3.9,-6.35,-35.19)) ;
#158592 = CARTESIAN_POINT('',(-3.9,-6.35,-33.29)) ;
#158593 = CARTESIAN_POINT('',(-3.9,-6.45,-35.19)) ;
#158594 = CARTESIAN_POINT('Origin',(-4.9,-6.4,-35.29)) ;
#158595 = CARTESIAN_POINT('',(-4.,-6.35,-35.29)) ;
#158596 = CARTESIAN_POINT('',(-4.8,-6.35,-35.29)) ;
#158597 = CARTESIAN_POINT('',(-4.9,-6.35,-35.29)) ;
#158598 = CARTESIAN_POINT('',(-4.8,-6.45,-35.29)) ;
#158599 = CARTESIAN_POINT('',(-4.8,-6.45,-35.29)) ;
#158600 = CARTESIAN_POINT('',(-4.,-6.45,-35.29)) ;
#158601 = CARTESIAN_POINT('',(-3.9,-6.45,-35.29)) ;
#158602 = CARTESIAN_POINT('',(-4.,-6.25,-35.29)) ;
#158603 = CARTESIAN_POINT('Origin',(-4.9,-6.4,-33.29)) ;
#158604 = CARTESIAN_POINT('',(-4.9,-6.45,-33.39)) ;
#158605 = CARTESIAN_POINT('',(-4.9,-6.45,-35.19)) ;
#158606 = CARTESIAN_POINT('',(-4.9,-6.45,-35.29)) ;
#158607 = CARTESIAN_POINT('',(-4.9,-6.35,-35.19)) ;
#158608 = CARTESIAN_POINT('',(-4.9,-6.25,-35.19)) ;
#158609 = CARTESIAN_POINT('',(-4.9,-6.35,-33.39)) ;
#158610 = CARTESIAN_POINT('',(-4.9,-6.35,-33.29)) ;
#158611 = CARTESIAN_POINT('',(-4.9,-6.45,-33.39)) ;
#158612 = CARTESIAN_POINT('Origin',(-4.9,-6.4,-33.29)) ;
#158613 = CARTESIAN_POINT('',(-4.,-6.45,-33.29)) ;
#158614 = CARTESIAN_POINT('',(-4.8,-6.45,-33.29)) ;
#158615 = CARTESIAN_POINT('',(-4.9,-6.45,-33.29)) ;
#158616 = CARTESIAN_POINT('',(-4.8,-6.35,-33.29)) ;
#158617 = CARTESIAN_POINT('',(-4.8,-6.25,-33.29)) ;
#158618 = CARTESIAN_POINT('',(-4.,-6.35,-33.29)) ;
#158619 = CARTESIAN_POINT('',(-4.9,-6.35,-33.29)) ;
#158620 = CARTESIAN_POINT('',(-4.,-6.45,-33.29)) ;
#158621 = CARTESIAN_POINT('Origin',(-3.9,-6.4,-29.48)) ;
#158622 = CARTESIAN_POINT('',(-3.9,-6.45,-31.38)) ;
#158623 = CARTESIAN_POINT('',(-3.9,-6.45,-29.58)) ;
#158624 = CARTESIAN_POINT('',(-3.9,-6.45,-29.48)) ;
#158625 = CARTESIAN_POINT('',(-3.9,-6.35,-29.58)) ;
#158626 = CARTESIAN_POINT('',(-3.9,-6.25,-29.58)) ;
#158627 = CARTESIAN_POINT('',(-3.9,-6.35,-31.38)) ;
#158628 = CARTESIAN_POINT('',(-3.9,-6.35,-29.48)) ;
#158629 = CARTESIAN_POINT('',(-3.9,-6.45,-31.38)) ;
#158630 = CARTESIAN_POINT('Origin',(-4.9,-6.4,-31.48)) ;
#158631 = CARTESIAN_POINT('',(-4.,-6.35,-31.48)) ;
#158632 = CARTESIAN_POINT('',(-4.8,-6.35,-31.48)) ;
#158633 = CARTESIAN_POINT('',(-4.9,-6.35,-31.48)) ;
#158634 = CARTESIAN_POINT('',(-4.8,-6.45,-31.48)) ;
#158635 = CARTESIAN_POINT('',(-4.8,-6.45,-31.48)) ;
#158636 = CARTESIAN_POINT('',(-4.,-6.45,-31.48)) ;
#158637 = CARTESIAN_POINT('',(-3.9,-6.45,-31.48)) ;
#158638 = CARTESIAN_POINT('',(-4.,-6.25,-31.48)) ;
#158639 = CARTESIAN_POINT('Origin',(-4.9,-6.4,-29.48)) ;
#158640 = CARTESIAN_POINT('',(-4.9,-6.45,-29.58)) ;
#158641 = CARTESIAN_POINT('',(-4.9,-6.45,-31.38)) ;
#158642 = CARTESIAN_POINT('',(-4.9,-6.45,-31.48)) ;
#158643 = CARTESIAN_POINT('',(-4.9,-6.35,-31.38)) ;
#158644 = CARTESIAN_POINT('',(-4.9,-6.25,-31.38)) ;
#158645 = CARTESIAN_POINT('',(-4.9,-6.35,-29.58)) ;
#158646 = CARTESIAN_POINT('',(-4.9,-6.35,-29.48)) ;
#158647 = CARTESIAN_POINT('',(-4.9,-6.45,-29.58)) ;
#158648 = CARTESIAN_POINT('Origin',(-4.9,-6.4,-29.48)) ;
#158649 = CARTESIAN_POINT('',(-4.,-6.45,-29.48)) ;
#158650 = CARTESIAN_POINT('',(-4.8,-6.45,-29.48)) ;
#158651 = CARTESIAN_POINT('',(-4.9,-6.45,-29.48)) ;
#158652 = CARTESIAN_POINT('',(-4.8,-6.35,-29.48)) ;
#158653 = CARTESIAN_POINT('',(-4.8,-6.25,-29.48)) ;
#158654 = CARTESIAN_POINT('',(-4.,-6.35,-29.48)) ;
#158655 = CARTESIAN_POINT('',(-4.9,-6.35,-29.48)) ;
#158656 = CARTESIAN_POINT('',(-4.,-6.45,-29.48)) ;
#158657 = CARTESIAN_POINT('Origin',(-3.9,-6.4,-25.67)) ;
#158658 = CARTESIAN_POINT('',(-3.9,-6.45,-27.57)) ;
#158659 = CARTESIAN_POINT('',(-3.9,-6.45,-25.77)) ;
#158660 = CARTESIAN_POINT('',(-3.9,-6.45,-25.67)) ;
#158661 = CARTESIAN_POINT('',(-3.9,-6.35,-25.77)) ;
#158662 = CARTESIAN_POINT('',(-3.9,-6.25,-25.77)) ;
#158663 = CARTESIAN_POINT('',(-3.9,-6.35,-27.57)) ;
#158664 = CARTESIAN_POINT('',(-3.9,-6.35,-25.67)) ;
#158665 = CARTESIAN_POINT('',(-3.9,-6.45,-27.57)) ;
#158666 = CARTESIAN_POINT('Origin',(-4.9,-6.4,-27.67)) ;
#158667 = CARTESIAN_POINT('',(-4.,-6.35,-27.67)) ;
#158668 = CARTESIAN_POINT('',(-4.8,-6.35,-27.67)) ;
#158669 = CARTESIAN_POINT('',(-4.9,-6.35,-27.67)) ;
#158670 = CARTESIAN_POINT('',(-4.8,-6.45,-27.67)) ;
#158671 = CARTESIAN_POINT('',(-4.8,-6.45,-27.67)) ;
#158672 = CARTESIAN_POINT('',(-4.,-6.45,-27.67)) ;
#158673 = CARTESIAN_POINT('',(-3.9,-6.45,-27.67)) ;
#158674 = CARTESIAN_POINT('',(-4.,-6.25,-27.67)) ;
#158675 = CARTESIAN_POINT('Origin',(-4.9,-6.4,-25.67)) ;
#158676 = CARTESIAN_POINT('',(-4.9,-6.45,-25.77)) ;
#158677 = CARTESIAN_POINT('',(-4.9,-6.45,-27.57)) ;
#158678 = CARTESIAN_POINT('',(-4.9,-6.45,-27.67)) ;
#158679 = CARTESIAN_POINT('',(-4.9,-6.35,-27.57)) ;
#158680 = CARTESIAN_POINT('',(-4.9,-6.25,-27.57)) ;
#158681 = CARTESIAN_POINT('',(-4.9,-6.35,-25.77)) ;
#158682 = CARTESIAN_POINT('',(-4.9,-6.35,-25.67)) ;
#158683 = CARTESIAN_POINT('',(-4.9,-6.45,-25.77)) ;
#158684 = CARTESIAN_POINT('Origin',(-4.9,-6.4,-25.67)) ;
#158685 = CARTESIAN_POINT('',(-4.,-6.45,-25.67)) ;
#158686 = CARTESIAN_POINT('',(-4.8,-6.45,-25.67)) ;
#158687 = CARTESIAN_POINT('',(-4.9,-6.45,-25.67)) ;
#158688 = CARTESIAN_POINT('',(-4.8,-6.35,-25.67)) ;
#158689 = CARTESIAN_POINT('',(-4.8,-6.25,-25.67)) ;
#158690 = CARTESIAN_POINT('',(-4.,-6.35,-25.67)) ;
#158691 = CARTESIAN_POINT('',(-4.9,-6.35,-25.67)) ;
#158692 = CARTESIAN_POINT('',(-4.,-6.45,-25.67)) ;
#158693 = CARTESIAN_POINT('Origin',(-3.9,-6.4,-21.86)) ;
#158694 = CARTESIAN_POINT('',(-3.9,-6.45,-23.76)) ;
#158695 = CARTESIAN_POINT('',(-3.9,-6.45,-21.96)) ;
#158696 = CARTESIAN_POINT('',(-3.9,-6.45,-21.86)) ;
#158697 = CARTESIAN_POINT('',(-3.9,-6.35,-21.96)) ;
#158698 = CARTESIAN_POINT('',(-3.9,-6.25,-21.96)) ;
#158699 = CARTESIAN_POINT('',(-3.9,-6.35,-23.76)) ;
#158700 = CARTESIAN_POINT('',(-3.9,-6.35,-21.86)) ;
#158701 = CARTESIAN_POINT('',(-3.9,-6.45,-23.76)) ;
#158702 = CARTESIAN_POINT('Origin',(-4.9,-6.4,-23.86)) ;
#158703 = CARTESIAN_POINT('',(-4.,-6.35,-23.86)) ;
#158704 = CARTESIAN_POINT('',(-4.8,-6.35,-23.86)) ;
#158705 = CARTESIAN_POINT('',(-4.9,-6.35,-23.86)) ;
#158706 = CARTESIAN_POINT('',(-4.8,-6.45,-23.86)) ;
#158707 = CARTESIAN_POINT('',(-4.8,-6.45,-23.86)) ;
#158708 = CARTESIAN_POINT('',(-4.,-6.45,-23.86)) ;
#158709 = CARTESIAN_POINT('',(-3.9,-6.45,-23.86)) ;
#158710 = CARTESIAN_POINT('',(-4.,-6.25,-23.86)) ;
#158711 = CARTESIAN_POINT('Origin',(-4.9,-6.4,-21.86)) ;
#158712 = CARTESIAN_POINT('',(-4.9,-6.45,-21.96)) ;
#158713 = CARTESIAN_POINT('',(-4.9,-6.45,-23.76)) ;
#158714 = CARTESIAN_POINT('',(-4.9,-6.45,-23.86)) ;
#158715 = CARTESIAN_POINT('',(-4.9,-6.35,-23.76)) ;
#158716 = CARTESIAN_POINT('',(-4.9,-6.25,-23.76)) ;
#158717 = CARTESIAN_POINT('',(-4.9,-6.35,-21.96)) ;
#158718 = CARTESIAN_POINT('',(-4.9,-6.35,-21.86)) ;
#158719 = CARTESIAN_POINT('',(-4.9,-6.45,-21.96)) ;
#158720 = CARTESIAN_POINT('Origin',(-4.9,-6.4,-21.86)) ;
#158721 = CARTESIAN_POINT('',(-4.,-6.45,-21.86)) ;
#158722 = CARTESIAN_POINT('',(-4.8,-6.45,-21.86)) ;
#158723 = CARTESIAN_POINT('',(-4.9,-6.45,-21.86)) ;
#158724 = CARTESIAN_POINT('',(-4.8,-6.35,-21.86)) ;
#158725 = CARTESIAN_POINT('',(-4.8,-6.25,-21.86)) ;
#158726 = CARTESIAN_POINT('',(-4.,-6.35,-21.86)) ;
#158727 = CARTESIAN_POINT('',(-4.9,-6.35,-21.86)) ;
#158728 = CARTESIAN_POINT('',(-4.,-6.45,-21.86)) ;
#158729 = CARTESIAN_POINT('Origin',(-3.9,-6.4,-18.05)) ;
#158730 = CARTESIAN_POINT('',(-3.9,-6.45,-19.95)) ;
#158731 = CARTESIAN_POINT('',(-3.9,-6.45,-18.15)) ;
#158732 = CARTESIAN_POINT('',(-3.9,-6.45,-18.05)) ;
#158733 = CARTESIAN_POINT('',(-3.9,-6.35,-18.15)) ;
#158734 = CARTESIAN_POINT('',(-3.9,-6.25,-18.15)) ;
#158735 = CARTESIAN_POINT('',(-3.9,-6.35,-19.95)) ;
#158736 = CARTESIAN_POINT('',(-3.9,-6.35,-18.05)) ;
#158737 = CARTESIAN_POINT('',(-3.9,-6.45,-19.95)) ;
#158738 = CARTESIAN_POINT('Origin',(-4.9,-6.4,-20.05)) ;
#158739 = CARTESIAN_POINT('',(-4.,-6.35,-20.05)) ;
#158740 = CARTESIAN_POINT('',(-4.8,-6.35,-20.05)) ;
#158741 = CARTESIAN_POINT('',(-4.9,-6.35,-20.05)) ;
#158742 = CARTESIAN_POINT('',(-4.8,-6.45,-20.05)) ;
#158743 = CARTESIAN_POINT('',(-4.8,-6.45,-20.05)) ;
#158744 = CARTESIAN_POINT('',(-4.,-6.45,-20.05)) ;
#158745 = CARTESIAN_POINT('',(-3.9,-6.45,-20.05)) ;
#158746 = CARTESIAN_POINT('',(-4.,-6.25,-20.05)) ;
#158747 = CARTESIAN_POINT('Origin',(-4.9,-6.4,-18.05)) ;
#158748 = CARTESIAN_POINT('',(-4.9,-6.45,-18.15)) ;
#158749 = CARTESIAN_POINT('',(-4.9,-6.45,-19.95)) ;
#158750 = CARTESIAN_POINT('',(-4.9,-6.45,-20.05)) ;
#158751 = CARTESIAN_POINT('',(-4.9,-6.35,-19.95)) ;
#158752 = CARTESIAN_POINT('',(-4.9,-6.25,-19.95)) ;
#158753 = CARTESIAN_POINT('',(-4.9,-6.35,-18.15)) ;
#158754 = CARTESIAN_POINT('',(-4.9,-6.35,-18.05)) ;
#158755 = CARTESIAN_POINT('',(-4.9,-6.45,-18.15)) ;
#158756 = CARTESIAN_POINT('Origin',(-4.9,-6.4,-18.05)) ;
#158757 = CARTESIAN_POINT('',(-4.,-6.45,-18.05)) ;
#158758 = CARTESIAN_POINT('',(-4.8,-6.45,-18.05)) ;
#158759 = CARTESIAN_POINT('',(-4.9,-6.45,-18.05)) ;
#158760 = CARTESIAN_POINT('',(-4.8,-6.35,-18.05)) ;
#158761 = CARTESIAN_POINT('',(-4.8,-6.25,-18.05)) ;
#158762 = CARTESIAN_POINT('',(-4.,-6.35,-18.05)) ;
#158763 = CARTESIAN_POINT('',(-4.9,-6.35,-18.05)) ;
#158764 = CARTESIAN_POINT('',(-4.,-6.45,-18.05)) ;
#158765 = CARTESIAN_POINT('Origin',(-3.9,-6.4,-14.24)) ;
#158766 = CARTESIAN_POINT('',(-3.9,-6.45,-16.14)) ;
#158767 = CARTESIAN_POINT('',(-3.9,-6.45,-14.34)) ;
#158768 = CARTESIAN_POINT('',(-3.9,-6.45,-14.24)) ;
#158769 = CARTESIAN_POINT('',(-3.9,-6.35,-14.34)) ;
#158770 = CARTESIAN_POINT('',(-3.9,-6.25,-14.34)) ;
#158771 = CARTESIAN_POINT('',(-3.9,-6.35,-16.14)) ;
#158772 = CARTESIAN_POINT('',(-3.9,-6.35,-14.24)) ;
#158773 = CARTESIAN_POINT('',(-3.9,-6.45,-16.14)) ;
#158774 = CARTESIAN_POINT('Origin',(-4.9,-6.4,-16.24)) ;
#158775 = CARTESIAN_POINT('',(-4.,-6.35,-16.24)) ;
#158776 = CARTESIAN_POINT('',(-4.8,-6.35,-16.24)) ;
#158777 = CARTESIAN_POINT('',(-4.9,-6.35,-16.24)) ;
#158778 = CARTESIAN_POINT('',(-4.8,-6.45,-16.24)) ;
#158779 = CARTESIAN_POINT('',(-4.8,-6.45,-16.24)) ;
#158780 = CARTESIAN_POINT('',(-4.,-6.45,-16.24)) ;
#158781 = CARTESIAN_POINT('',(-3.9,-6.45,-16.24)) ;
#158782 = CARTESIAN_POINT('',(-4.,-6.25,-16.24)) ;
#158783 = CARTESIAN_POINT('Origin',(-4.9,-6.4,-14.24)) ;
#158784 = CARTESIAN_POINT('',(-4.9,-6.45,-14.34)) ;
#158785 = CARTESIAN_POINT('',(-4.9,-6.45,-16.14)) ;
#158786 = CARTESIAN_POINT('',(-4.9,-6.45,-16.24)) ;
#158787 = CARTESIAN_POINT('',(-4.9,-6.35,-16.14)) ;
#158788 = CARTESIAN_POINT('',(-4.9,-6.25,-16.14)) ;
#158789 = CARTESIAN_POINT('',(-4.9,-6.35,-14.34)) ;
#158790 = CARTESIAN_POINT('',(-4.9,-6.35,-14.24)) ;
#158791 = CARTESIAN_POINT('',(-4.9,-6.45,-14.34)) ;
#158792 = CARTESIAN_POINT('Origin',(-4.9,-6.4,-14.24)) ;
#158793 = CARTESIAN_POINT('',(-4.,-6.45,-14.24)) ;
#158794 = CARTESIAN_POINT('',(-4.8,-6.45,-14.24)) ;
#158795 = CARTESIAN_POINT('',(-4.9,-6.45,-14.24)) ;
#158796 = CARTESIAN_POINT('',(-4.8,-6.35,-14.24)) ;
#158797 = CARTESIAN_POINT('',(-4.8,-6.25,-14.24)) ;
#158798 = CARTESIAN_POINT('',(-4.,-6.35,-14.24)) ;
#158799 = CARTESIAN_POINT('',(-4.9,-6.35,-14.24)) ;
#158800 = CARTESIAN_POINT('',(-4.,-6.45,-14.24)) ;
#158801 = CARTESIAN_POINT('Origin',(-3.9,-6.4,-10.43)) ;
#158802 = CARTESIAN_POINT('',(-3.9,-6.45,-12.33)) ;
#158803 = CARTESIAN_POINT('',(-3.9,-6.45,-10.53)) ;
#158804 = CARTESIAN_POINT('',(-3.9,-6.45,-10.43)) ;
#158805 = CARTESIAN_POINT('',(-3.9,-6.35,-10.53)) ;
#158806 = CARTESIAN_POINT('',(-3.9,-6.25,-10.53)) ;
#158807 = CARTESIAN_POINT('',(-3.9,-6.35,-12.33)) ;
#158808 = CARTESIAN_POINT('',(-3.9,-6.35,-10.43)) ;
#158809 = CARTESIAN_POINT('',(-3.9,-6.45,-12.33)) ;
#158810 = CARTESIAN_POINT('Origin',(-4.9,-6.4,-12.43)) ;
#158811 = CARTESIAN_POINT('',(-4.,-6.35,-12.43)) ;
#158812 = CARTESIAN_POINT('',(-4.8,-6.35,-12.43)) ;
#158813 = CARTESIAN_POINT('',(-4.9,-6.35,-12.43)) ;
#158814 = CARTESIAN_POINT('',(-4.8,-6.45,-12.43)) ;
#158815 = CARTESIAN_POINT('',(-4.8,-6.45,-12.43)) ;
#158816 = CARTESIAN_POINT('',(-4.,-6.45,-12.43)) ;
#158817 = CARTESIAN_POINT('',(-3.9,-6.45,-12.43)) ;
#158818 = CARTESIAN_POINT('',(-4.,-6.25,-12.43)) ;
#158819 = CARTESIAN_POINT('Origin',(-4.9,-6.4,-10.43)) ;
#158820 = CARTESIAN_POINT('',(-4.9,-6.45,-10.53)) ;
#158821 = CARTESIAN_POINT('',(-4.9,-6.45,-12.33)) ;
#158822 = CARTESIAN_POINT('',(-4.9,-6.45,-12.43)) ;
#158823 = CARTESIAN_POINT('',(-4.9,-6.35,-12.33)) ;
#158824 = CARTESIAN_POINT('',(-4.9,-6.25,-12.33)) ;
#158825 = CARTESIAN_POINT('',(-4.9,-6.35,-10.53)) ;
#158826 = CARTESIAN_POINT('',(-4.9,-6.35,-10.43)) ;
#158827 = CARTESIAN_POINT('',(-4.9,-6.45,-10.53)) ;
#158828 = CARTESIAN_POINT('Origin',(-4.9,-6.4,-10.43)) ;
#158829 = CARTESIAN_POINT('',(-4.,-6.45,-10.43)) ;
#158830 = CARTESIAN_POINT('',(-4.8,-6.45,-10.43)) ;
#158831 = CARTESIAN_POINT('',(-4.9,-6.45,-10.43)) ;
#158832 = CARTESIAN_POINT('',(-4.8,-6.35,-10.43)) ;
#158833 = CARTESIAN_POINT('',(-4.8,-6.25,-10.43)) ;
#158834 = CARTESIAN_POINT('',(-4.,-6.35,-10.43)) ;
#158835 = CARTESIAN_POINT('',(-4.9,-6.35,-10.43)) ;
#158836 = CARTESIAN_POINT('',(-4.,-6.45,-10.43)) ;
#158837 = CARTESIAN_POINT('Origin',(-3.9,-6.4,-6.62)) ;
#158838 = CARTESIAN_POINT('',(-3.9,-6.45,-8.52)) ;
#158839 = CARTESIAN_POINT('',(-3.9,-6.45,-6.72)) ;
#158840 = CARTESIAN_POINT('',(-3.9,-6.45,-6.62)) ;
#158841 = CARTESIAN_POINT('',(-3.9,-6.35,-6.72)) ;
#158842 = CARTESIAN_POINT('',(-3.9,-6.25,-6.72)) ;
#158843 = CARTESIAN_POINT('',(-3.9,-6.35,-8.52)) ;
#158844 = CARTESIAN_POINT('',(-3.9,-6.35,-6.62)) ;
#158845 = CARTESIAN_POINT('',(-3.9,-6.45,-8.52)) ;
#158846 = CARTESIAN_POINT('Origin',(-4.9,-6.4,-8.62)) ;
#158847 = CARTESIAN_POINT('',(-4.,-6.35,-8.62)) ;
#158848 = CARTESIAN_POINT('',(-4.8,-6.35,-8.62)) ;
#158849 = CARTESIAN_POINT('',(-4.9,-6.35,-8.62)) ;
#158850 = CARTESIAN_POINT('',(-4.8,-6.45,-8.62)) ;
#158851 = CARTESIAN_POINT('',(-4.8,-6.45,-8.62)) ;
#158852 = CARTESIAN_POINT('',(-4.,-6.45,-8.62)) ;
#158853 = CARTESIAN_POINT('',(-3.9,-6.45,-8.62)) ;
#158854 = CARTESIAN_POINT('',(-4.,-6.25,-8.62)) ;
#158855 = CARTESIAN_POINT('Origin',(-4.9,-6.4,-6.62)) ;
#158856 = CARTESIAN_POINT('',(-4.9,-6.45,-6.72)) ;
#158857 = CARTESIAN_POINT('',(-4.9,-6.45,-8.52)) ;
#158858 = CARTESIAN_POINT('',(-4.9,-6.45,-8.62)) ;
#158859 = CARTESIAN_POINT('',(-4.9,-6.35,-8.52)) ;
#158860 = CARTESIAN_POINT('',(-4.9,-6.25,-8.52)) ;
#158861 = CARTESIAN_POINT('',(-4.9,-6.35,-6.72)) ;
#158862 = CARTESIAN_POINT('',(-4.9,-6.35,-6.62)) ;
#158863 = CARTESIAN_POINT('',(-4.9,-6.45,-6.72)) ;
#158864 = CARTESIAN_POINT('Origin',(-4.9,-6.4,-6.62)) ;
#158865 = CARTESIAN_POINT('',(-4.,-6.45,-6.62)) ;
#158866 = CARTESIAN_POINT('',(-4.8,-6.45,-6.62)) ;
#158867 = CARTESIAN_POINT('',(-4.9,-6.45,-6.62)) ;
#158868 = CARTESIAN_POINT('',(-4.8,-6.35,-6.62)) ;
#158869 = CARTESIAN_POINT('',(-4.8,-6.25,-6.62)) ;
#158870 = CARTESIAN_POINT('',(-4.,-6.35,-6.62)) ;
#158871 = CARTESIAN_POINT('',(-4.9,-6.35,-6.62)) ;
#158872 = CARTESIAN_POINT('',(-4.,-6.45,-6.62)) ;
#158873 = CARTESIAN_POINT('Origin',(-3.9,-6.4,-2.81)) ;
#158874 = CARTESIAN_POINT('',(-3.9,-6.35,-2.91)) ;
#158875 = CARTESIAN_POINT('',(-3.9,-6.35,-4.71)) ;
#158876 = CARTESIAN_POINT('',(-3.9,-6.35,-2.81)) ;
#158877 = CARTESIAN_POINT('',(-3.9,-6.45,-4.71)) ;
#158878 = CARTESIAN_POINT('',(-3.9,-6.55,-4.71)) ;
#158879 = CARTESIAN_POINT('',(-3.9,-6.45,-2.91)) ;
#158880 = CARTESIAN_POINT('',(-3.9,-6.45,-2.81)) ;
#158881 = CARTESIAN_POINT('',(-3.9,-6.25,-2.91)) ;
#158882 = CARTESIAN_POINT('Origin',(-4.9,-6.4,-4.81)) ;
#158883 = CARTESIAN_POINT('',(-4.,-6.35,-4.81)) ;
#158884 = CARTESIAN_POINT('',(-4.8,-6.35,-4.81)) ;
#158885 = CARTESIAN_POINT('',(-4.9,-6.35,-4.81)) ;
#158886 = CARTESIAN_POINT('',(-4.8,-6.45,-4.81)) ;
#158887 = CARTESIAN_POINT('',(-4.8,-6.55,-4.81)) ;
#158888 = CARTESIAN_POINT('',(-4.,-6.45,-4.81)) ;
#158889 = CARTESIAN_POINT('',(-3.9,-6.45,-4.81)) ;
#158890 = CARTESIAN_POINT('',(-4.,-6.25,-4.81)) ;
#158891 = CARTESIAN_POINT('Origin',(-4.9,-6.4,-2.81)) ;
#158892 = CARTESIAN_POINT('',(-4.9,-6.45,-4.71)) ;
#158893 = CARTESIAN_POINT('',(-4.9,-6.35,-4.71)) ;
#158894 = CARTESIAN_POINT('',(-4.9,-6.25,-4.71)) ;
#158895 = CARTESIAN_POINT('',(-4.9,-6.35,-2.91)) ;
#158896 = CARTESIAN_POINT('',(-4.9,-6.35,-2.81)) ;
#158897 = CARTESIAN_POINT('',(-4.9,-6.45,-2.91)) ;
#158898 = CARTESIAN_POINT('',(-4.9,-6.55,-2.91)) ;
#158899 = CARTESIAN_POINT('',(-4.9,-6.45,-4.81)) ;
#158900 = CARTESIAN_POINT('Origin',(-4.9,-6.4,-2.81)) ;
#158901 = CARTESIAN_POINT('',(-4.8,-6.45,-2.81)) ;
#158902 = CARTESIAN_POINT('',(-4.8,-6.35,-2.81)) ;
#158903 = CARTESIAN_POINT('',(-4.8,-6.25,-2.81)) ;
#158904 = CARTESIAN_POINT('',(-4.,-6.35,-2.81)) ;
#158905 = CARTESIAN_POINT('',(-4.9,-6.35,-2.81)) ;
#158906 = CARTESIAN_POINT('',(-4.,-6.45,-2.81)) ;
#158907 = CARTESIAN_POINT('',(-4.,-6.55,-2.81)) ;
#158908 = CARTESIAN_POINT('',(-4.9,-6.45,-2.81)) ;
#158909 = CARTESIAN_POINT('Origin',(0.,-6.25,-3.81)) ;
#158910 = CARTESIAN_POINT('',(-4.8,-6.25,-2.91)) ;
#158911 = CARTESIAN_POINT('',(-4.8,-6.25,-4.71)) ;
#158912 = CARTESIAN_POINT('',(-4.8,-6.25,-3.81)) ;
#158913 = CARTESIAN_POINT('',(-4.,-6.25,-4.71)) ;
#158914 = CARTESIAN_POINT('',(1.95156391047391E-16,-6.25,-4.71)) ;
#158915 = CARTESIAN_POINT('',(-4.,-6.25,-2.91)) ;
#158916 = CARTESIAN_POINT('',(-4.,-6.25,-3.81)) ;
#158917 = CARTESIAN_POINT('',(1.9515639104739E-16,-6.25,-2.91)) ;
#158918 = CARTESIAN_POINT('',(-4.65,-6.25,-4.66)) ;
#158919 = CARTESIAN_POINT('',(-4.15,-6.25,-4.66)) ;
#158920 = CARTESIAN_POINT('',(-4.75,-6.25,-4.66)) ;
#158921 = CARTESIAN_POINT('',(-4.75,-6.25,-4.56)) ;
#158922 = CARTESIAN_POINT('Origin',(-4.65,-6.25,-4.56)) ;
#158923 = CARTESIAN_POINT('',(-4.75,-6.25,-3.06)) ;
#158924 = CARTESIAN_POINT('',(-4.75,-6.25,-2.96)) ;
#158925 = CARTESIAN_POINT('',(-4.65,-6.25,-2.96)) ;
#158926 = CARTESIAN_POINT('Origin',(-4.65,-6.25,-3.06)) ;
#158927 = CARTESIAN_POINT('',(-4.15,-6.25,-2.96)) ;
#158928 = CARTESIAN_POINT('',(-4.05,-6.25,-2.96)) ;
#158929 = CARTESIAN_POINT('',(-4.05,-6.25,-3.06)) ;
#158930 = CARTESIAN_POINT('Origin',(-4.15,-6.25,-3.06)) ;
#158931 = CARTESIAN_POINT('',(-4.05,-6.25,-4.56)) ;
#158932 = CARTESIAN_POINT('',(-4.05,-6.25,-4.66)) ;
#158933 = CARTESIAN_POINT('Origin',(-4.15,-6.25,-4.56)) ;
#158934 = CARTESIAN_POINT('Origin',(-4.05,-6.25,-4.66)) ;
#158935 = CARTESIAN_POINT('',(-4.05,-6.3,-3.06)) ;
#158936 = CARTESIAN_POINT('',(-4.05,-6.25,-3.06)) ;
#158937 = CARTESIAN_POINT('',(-4.05,-6.3,-4.56)) ;
#158938 = CARTESIAN_POINT('',(-4.05,-6.3,-4.66)) ;
#158939 = CARTESIAN_POINT('',(-4.05,-6.25,-4.56)) ;
#158940 = CARTESIAN_POINT('Origin',(-4.75,-6.25,-4.66)) ;
#158941 = CARTESIAN_POINT('',(-4.15,-6.3,-4.66)) ;
#158942 = CARTESIAN_POINT('',(-4.15,-6.25,-4.66)) ;
#158943 = CARTESIAN_POINT('',(-4.65,-6.3,-4.66)) ;
#158944 = CARTESIAN_POINT('',(-4.75,-6.3,-4.66)) ;
#158945 = CARTESIAN_POINT('',(-4.65,-6.25,-4.66)) ;
#158946 = CARTESIAN_POINT('Origin',(-4.75,-6.25,-2.96)) ;
#158947 = CARTESIAN_POINT('',(-4.75,-6.3,-4.56)) ;
#158948 = CARTESIAN_POINT('',(-4.75,-6.3,-3.06)) ;
#158949 = CARTESIAN_POINT('',(-4.75,-6.3,-2.96)) ;
#158950 = CARTESIAN_POINT('',(-4.75,-6.25,-3.06)) ;
#158951 = CARTESIAN_POINT('',(-4.75,-6.25,-4.56)) ;
#158952 = CARTESIAN_POINT('Origin',(-4.05,-6.25,-2.96)) ;
#158953 = CARTESIAN_POINT('',(-4.65,-6.3,-2.96)) ;
#158954 = CARTESIAN_POINT('',(-4.65,-6.25,-2.96)) ;
#158955 = CARTESIAN_POINT('',(-4.15,-6.3,-2.96)) ;
#158956 = CARTESIAN_POINT('',(-4.05,-6.3,-2.96)) ;
#158957 = CARTESIAN_POINT('',(-4.15,-6.25,-2.96)) ;
#158958 = CARTESIAN_POINT('Origin',(0.,-6.25,-7.62)) ;
#158959 = CARTESIAN_POINT('',(-4.8,-6.25,-6.72)) ;
#158960 = CARTESIAN_POINT('',(-4.8,-6.25,-8.52)) ;
#158961 = CARTESIAN_POINT('',(-4.8,-6.25,-7.62)) ;
#158962 = CARTESIAN_POINT('',(-4.,-6.25,-8.52)) ;
#158963 = CARTESIAN_POINT('',(1.95156391047391E-16,-6.25,-8.52)) ;
#158964 = CARTESIAN_POINT('',(-4.,-6.25,-6.72)) ;
#158965 = CARTESIAN_POINT('',(-4.,-6.25,-7.62)) ;
#158966 = CARTESIAN_POINT('',(1.9515639104739E-16,-6.25,-6.72000000000001)) ;
#158967 = CARTESIAN_POINT('',(-4.65,-6.25,-8.47)) ;
#158968 = CARTESIAN_POINT('',(-4.15,-6.25,-8.47)) ;
#158969 = CARTESIAN_POINT('',(-4.75,-6.25,-8.47)) ;
#158970 = CARTESIAN_POINT('',(-4.75,-6.25,-8.37)) ;
#158971 = CARTESIAN_POINT('Origin',(-4.65,-6.25,-8.37)) ;
#158972 = CARTESIAN_POINT('',(-4.75,-6.25,-6.87)) ;
#158973 = CARTESIAN_POINT('',(-4.75,-6.25,-6.77)) ;
#158974 = CARTESIAN_POINT('',(-4.65,-6.25,-6.77)) ;
#158975 = CARTESIAN_POINT('Origin',(-4.65,-6.25,-6.87)) ;
#158976 = CARTESIAN_POINT('',(-4.15,-6.25,-6.77)) ;
#158977 = CARTESIAN_POINT('',(-4.05,-6.25,-6.77)) ;
#158978 = CARTESIAN_POINT('',(-4.05,-6.25,-6.87)) ;
#158979 = CARTESIAN_POINT('Origin',(-4.15,-6.25,-6.87)) ;
#158980 = CARTESIAN_POINT('',(-4.05,-6.25,-8.37)) ;
#158981 = CARTESIAN_POINT('',(-4.05,-6.25,-8.47)) ;
#158982 = CARTESIAN_POINT('Origin',(-4.15,-6.25,-8.37)) ;
#158983 = CARTESIAN_POINT('Origin',(-4.05,-6.25,-8.47)) ;
#158984 = CARTESIAN_POINT('',(-4.05,-6.3,-6.87)) ;
#158985 = CARTESIAN_POINT('',(-4.05,-6.25,-6.87)) ;
#158986 = CARTESIAN_POINT('',(-4.05,-6.3,-8.37)) ;
#158987 = CARTESIAN_POINT('',(-4.05,-6.3,-8.47)) ;
#158988 = CARTESIAN_POINT('',(-4.05,-6.25,-8.37)) ;
#158989 = CARTESIAN_POINT('Origin',(-4.75,-6.25,-8.47)) ;
#158990 = CARTESIAN_POINT('',(-4.15,-6.3,-8.47)) ;
#158991 = CARTESIAN_POINT('',(-4.15,-6.25,-8.47)) ;
#158992 = CARTESIAN_POINT('',(-4.65,-6.3,-8.47)) ;
#158993 = CARTESIAN_POINT('',(-4.75,-6.3,-8.47)) ;
#158994 = CARTESIAN_POINT('',(-4.65,-6.25,-8.47)) ;
#158995 = CARTESIAN_POINT('Origin',(-4.75,-6.25,-6.77)) ;
#158996 = CARTESIAN_POINT('',(-4.75,-6.3,-8.37)) ;
#158997 = CARTESIAN_POINT('',(-4.75,-6.3,-6.87)) ;
#158998 = CARTESIAN_POINT('',(-4.75,-6.3,-6.77)) ;
#158999 = CARTESIAN_POINT('',(-4.75,-6.25,-6.87)) ;
#159000 = CARTESIAN_POINT('',(-4.75,-6.25,-8.37)) ;
#159001 = CARTESIAN_POINT('Origin',(-4.05,-6.25,-6.77)) ;
#159002 = CARTESIAN_POINT('',(-4.65,-6.3,-6.77)) ;
#159003 = CARTESIAN_POINT('',(-4.65,-6.25,-6.77)) ;
#159004 = CARTESIAN_POINT('',(-4.15,-6.3,-6.77)) ;
#159005 = CARTESIAN_POINT('',(-4.05,-6.3,-6.77)) ;
#159006 = CARTESIAN_POINT('',(-4.15,-6.25,-6.77)) ;
#159007 = CARTESIAN_POINT('Origin',(0.,-6.25,-11.43)) ;
#159008 = CARTESIAN_POINT('',(-4.8,-6.25,-10.53)) ;
#159009 = CARTESIAN_POINT('',(-4.8,-6.25,-12.33)) ;
#159010 = CARTESIAN_POINT('',(-4.8,-6.25,-11.43)) ;
#159011 = CARTESIAN_POINT('',(-4.,-6.25,-12.33)) ;
#159012 = CARTESIAN_POINT('',(1.95156391047391E-16,-6.25,-12.33)) ;
#159013 = CARTESIAN_POINT('',(-4.,-6.25,-10.53)) ;
#159014 = CARTESIAN_POINT('',(-4.,-6.25,-11.43)) ;
#159015 = CARTESIAN_POINT('',(1.9515639104739E-16,-6.25,-10.53)) ;
#159016 = CARTESIAN_POINT('',(-4.65,-6.25,-12.28)) ;
#159017 = CARTESIAN_POINT('',(-4.15,-6.25,-12.28)) ;
#159018 = CARTESIAN_POINT('',(-4.75,-6.25,-12.28)) ;
#159019 = CARTESIAN_POINT('',(-4.75,-6.25,-12.18)) ;
#159020 = CARTESIAN_POINT('Origin',(-4.65,-6.25,-12.18)) ;
#159021 = CARTESIAN_POINT('',(-4.75,-6.25,-10.68)) ;
#159022 = CARTESIAN_POINT('',(-4.75,-6.25,-10.58)) ;
#159023 = CARTESIAN_POINT('',(-4.65,-6.25,-10.58)) ;
#159024 = CARTESIAN_POINT('Origin',(-4.65,-6.25,-10.68)) ;
#159025 = CARTESIAN_POINT('',(-4.15,-6.25,-10.58)) ;
#159026 = CARTESIAN_POINT('',(-4.05,-6.25,-10.58)) ;
#159027 = CARTESIAN_POINT('',(-4.05,-6.25,-10.68)) ;
#159028 = CARTESIAN_POINT('Origin',(-4.15,-6.25,-10.68)) ;
#159029 = CARTESIAN_POINT('',(-4.05,-6.25,-12.18)) ;
#159030 = CARTESIAN_POINT('',(-4.05,-6.25,-12.28)) ;
#159031 = CARTESIAN_POINT('Origin',(-4.15,-6.25,-12.18)) ;
#159032 = CARTESIAN_POINT('Origin',(-4.05,-6.25,-12.28)) ;
#159033 = CARTESIAN_POINT('',(-4.05,-6.3,-10.68)) ;
#159034 = CARTESIAN_POINT('',(-4.05,-6.25,-10.68)) ;
#159035 = CARTESIAN_POINT('',(-4.05,-6.3,-12.18)) ;
#159036 = CARTESIAN_POINT('',(-4.05,-6.3,-12.28)) ;
#159037 = CARTESIAN_POINT('',(-4.05,-6.25,-12.18)) ;
#159038 = CARTESIAN_POINT('Origin',(-4.75,-6.25,-12.28)) ;
#159039 = CARTESIAN_POINT('',(-4.15,-6.3,-12.28)) ;
#159040 = CARTESIAN_POINT('',(-4.15,-6.25,-12.28)) ;
#159041 = CARTESIAN_POINT('',(-4.65,-6.3,-12.28)) ;
#159042 = CARTESIAN_POINT('',(-4.75,-6.3,-12.28)) ;
#159043 = CARTESIAN_POINT('',(-4.65,-6.25,-12.28)) ;
#159044 = CARTESIAN_POINT('Origin',(-4.75,-6.25,-10.58)) ;
#159045 = CARTESIAN_POINT('',(-4.75,-6.3,-12.18)) ;
#159046 = CARTESIAN_POINT('',(-4.75,-6.3,-10.68)) ;
#159047 = CARTESIAN_POINT('',(-4.75,-6.3,-10.58)) ;
#159048 = CARTESIAN_POINT('',(-4.75,-6.25,-10.68)) ;
#159049 = CARTESIAN_POINT('',(-4.75,-6.25,-12.18)) ;
#159050 = CARTESIAN_POINT('Origin',(-4.05,-6.25,-10.58)) ;
#159051 = CARTESIAN_POINT('',(-4.65,-6.3,-10.58)) ;
#159052 = CARTESIAN_POINT('',(-4.65,-6.25,-10.58)) ;
#159053 = CARTESIAN_POINT('',(-4.15,-6.3,-10.58)) ;
#159054 = CARTESIAN_POINT('',(-4.05,-6.3,-10.58)) ;
#159055 = CARTESIAN_POINT('',(-4.15,-6.25,-10.58)) ;
#159056 = CARTESIAN_POINT('Origin',(0.,-6.25,-15.24)) ;
#159057 = CARTESIAN_POINT('',(-4.8,-6.25,-14.34)) ;
#159058 = CARTESIAN_POINT('',(-4.8,-6.25,-16.14)) ;
#159059 = CARTESIAN_POINT('',(-4.8,-6.25,-15.24)) ;
#159060 = CARTESIAN_POINT('',(-4.,-6.25,-16.14)) ;
#159061 = CARTESIAN_POINT('',(1.95156391047391E-16,-6.25,-16.14)) ;
#159062 = CARTESIAN_POINT('',(-4.,-6.25,-14.34)) ;
#159063 = CARTESIAN_POINT('',(-4.,-6.25,-15.24)) ;
#159064 = CARTESIAN_POINT('',(1.9515639104739E-16,-6.25,-14.34)) ;
#159065 = CARTESIAN_POINT('',(-4.65,-6.25,-16.09)) ;
#159066 = CARTESIAN_POINT('',(-4.15,-6.25,-16.09)) ;
#159067 = CARTESIAN_POINT('',(-4.75,-6.25,-16.09)) ;
#159068 = CARTESIAN_POINT('',(-4.75,-6.25,-15.99)) ;
#159069 = CARTESIAN_POINT('Origin',(-4.65,-6.25,-15.99)) ;
#159070 = CARTESIAN_POINT('',(-4.75,-6.25,-14.49)) ;
#159071 = CARTESIAN_POINT('',(-4.75,-6.25,-14.39)) ;
#159072 = CARTESIAN_POINT('',(-4.65,-6.25,-14.39)) ;
#159073 = CARTESIAN_POINT('Origin',(-4.65,-6.25,-14.49)) ;
#159074 = CARTESIAN_POINT('',(-4.15,-6.25,-14.39)) ;
#159075 = CARTESIAN_POINT('',(-4.05,-6.25,-14.39)) ;
#159076 = CARTESIAN_POINT('',(-4.05,-6.25,-14.49)) ;
#159077 = CARTESIAN_POINT('Origin',(-4.15,-6.25,-14.49)) ;
#159078 = CARTESIAN_POINT('',(-4.05,-6.25,-15.99)) ;
#159079 = CARTESIAN_POINT('',(-4.05,-6.25,-16.09)) ;
#159080 = CARTESIAN_POINT('Origin',(-4.15,-6.25,-15.99)) ;
#159081 = CARTESIAN_POINT('Origin',(-4.05,-6.25,-16.09)) ;
#159082 = CARTESIAN_POINT('',(-4.05,-6.3,-14.49)) ;
#159083 = CARTESIAN_POINT('',(-4.05,-6.25,-14.49)) ;
#159084 = CARTESIAN_POINT('',(-4.05,-6.3,-15.99)) ;
#159085 = CARTESIAN_POINT('',(-4.05,-6.3,-16.09)) ;
#159086 = CARTESIAN_POINT('',(-4.05,-6.25,-15.99)) ;
#159087 = CARTESIAN_POINT('Origin',(-4.75,-6.25,-16.09)) ;
#159088 = CARTESIAN_POINT('',(-4.15,-6.3,-16.09)) ;
#159089 = CARTESIAN_POINT('',(-4.15,-6.25,-16.09)) ;
#159090 = CARTESIAN_POINT('',(-4.65,-6.3,-16.09)) ;
#159091 = CARTESIAN_POINT('',(-4.75,-6.3,-16.09)) ;
#159092 = CARTESIAN_POINT('',(-4.65,-6.25,-16.09)) ;
#159093 = CARTESIAN_POINT('Origin',(-4.75,-6.25,-14.39)) ;
#159094 = CARTESIAN_POINT('',(-4.75,-6.3,-15.99)) ;
#159095 = CARTESIAN_POINT('',(-4.75,-6.3,-14.49)) ;
#159096 = CARTESIAN_POINT('',(-4.75,-6.3,-14.39)) ;
#159097 = CARTESIAN_POINT('',(-4.75,-6.25,-14.49)) ;
#159098 = CARTESIAN_POINT('',(-4.75,-6.25,-15.99)) ;
#159099 = CARTESIAN_POINT('Origin',(-4.05,-6.25,-14.39)) ;
#159100 = CARTESIAN_POINT('',(-4.65,-6.3,-14.39)) ;
#159101 = CARTESIAN_POINT('',(-4.65,-6.25,-14.39)) ;
#159102 = CARTESIAN_POINT('',(-4.15,-6.3,-14.39)) ;
#159103 = CARTESIAN_POINT('',(-4.05,-6.3,-14.39)) ;
#159104 = CARTESIAN_POINT('',(-4.15,-6.25,-14.39)) ;
#159105 = CARTESIAN_POINT('Origin',(0.,-6.25,-19.05)) ;
#159106 = CARTESIAN_POINT('',(-4.8,-6.25,-18.15)) ;
#159107 = CARTESIAN_POINT('',(-4.8,-6.25,-19.95)) ;
#159108 = CARTESIAN_POINT('',(-4.8,-6.25,-19.05)) ;
#159109 = CARTESIAN_POINT('',(-4.,-6.25,-19.95)) ;
#159110 = CARTESIAN_POINT('',(1.95156391047391E-16,-6.25,-19.95)) ;
#159111 = CARTESIAN_POINT('',(-4.,-6.25,-18.15)) ;
#159112 = CARTESIAN_POINT('',(-4.,-6.25,-19.05)) ;
#159113 = CARTESIAN_POINT('',(1.9515639104739E-16,-6.25,-18.15)) ;
#159114 = CARTESIAN_POINT('',(-4.65,-6.25,-19.9)) ;
#159115 = CARTESIAN_POINT('',(-4.15,-6.25,-19.9)) ;
#159116 = CARTESIAN_POINT('',(-4.75,-6.25,-19.9)) ;
#159117 = CARTESIAN_POINT('',(-4.75,-6.25,-19.8)) ;
#159118 = CARTESIAN_POINT('Origin',(-4.65,-6.25,-19.8)) ;
#159119 = CARTESIAN_POINT('',(-4.75,-6.25,-18.3)) ;
#159120 = CARTESIAN_POINT('',(-4.75,-6.25,-18.2)) ;
#159121 = CARTESIAN_POINT('',(-4.65,-6.25,-18.2)) ;
#159122 = CARTESIAN_POINT('Origin',(-4.65,-6.25,-18.3)) ;
#159123 = CARTESIAN_POINT('',(-4.15,-6.25,-18.2)) ;
#159124 = CARTESIAN_POINT('',(-4.05,-6.25,-18.2)) ;
#159125 = CARTESIAN_POINT('',(-4.05,-6.25,-18.3)) ;
#159126 = CARTESIAN_POINT('Origin',(-4.15,-6.25,-18.3)) ;
#159127 = CARTESIAN_POINT('',(-4.05,-6.25,-19.8)) ;
#159128 = CARTESIAN_POINT('',(-4.05,-6.25,-19.9)) ;
#159129 = CARTESIAN_POINT('Origin',(-4.15,-6.25,-19.8)) ;
#159130 = CARTESIAN_POINT('Origin',(-4.05,-6.25,-19.9)) ;
#159131 = CARTESIAN_POINT('',(-4.05,-6.3,-18.3)) ;
#159132 = CARTESIAN_POINT('',(-4.05,-6.25,-18.3)) ;
#159133 = CARTESIAN_POINT('',(-4.05,-6.3,-19.8)) ;
#159134 = CARTESIAN_POINT('',(-4.05,-6.3,-19.9)) ;
#159135 = CARTESIAN_POINT('',(-4.05,-6.25,-19.8)) ;
#159136 = CARTESIAN_POINT('Origin',(-4.75,-6.25,-19.9)) ;
#159137 = CARTESIAN_POINT('',(-4.15,-6.3,-19.9)) ;
#159138 = CARTESIAN_POINT('',(-4.15,-6.25,-19.9)) ;
#159139 = CARTESIAN_POINT('',(-4.65,-6.3,-19.9)) ;
#159140 = CARTESIAN_POINT('',(-4.75,-6.3,-19.9)) ;
#159141 = CARTESIAN_POINT('',(-4.65,-6.25,-19.9)) ;
#159142 = CARTESIAN_POINT('Origin',(-4.75,-6.25,-18.2)) ;
#159143 = CARTESIAN_POINT('',(-4.75,-6.3,-19.8)) ;
#159144 = CARTESIAN_POINT('',(-4.75,-6.3,-18.3)) ;
#159145 = CARTESIAN_POINT('',(-4.75,-6.3,-18.2)) ;
#159146 = CARTESIAN_POINT('',(-4.75,-6.25,-18.3)) ;
#159147 = CARTESIAN_POINT('',(-4.75,-6.25,-19.8)) ;
#159148 = CARTESIAN_POINT('Origin',(-4.05,-6.25,-18.2)) ;
#159149 = CARTESIAN_POINT('',(-4.65,-6.3,-18.2)) ;
#159150 = CARTESIAN_POINT('',(-4.65,-6.25,-18.2)) ;
#159151 = CARTESIAN_POINT('',(-4.15,-6.3,-18.2)) ;
#159152 = CARTESIAN_POINT('',(-4.05,-6.3,-18.2)) ;
#159153 = CARTESIAN_POINT('',(-4.15,-6.25,-18.2)) ;
#159154 = CARTESIAN_POINT('Origin',(0.,-6.25,-22.86)) ;
#159155 = CARTESIAN_POINT('',(-4.8,-6.25,-21.96)) ;
#159156 = CARTESIAN_POINT('',(-4.8,-6.25,-23.76)) ;
#159157 = CARTESIAN_POINT('',(-4.8,-6.25,-22.86)) ;
#159158 = CARTESIAN_POINT('',(-4.,-6.25,-23.76)) ;
#159159 = CARTESIAN_POINT('',(1.95156391047391E-16,-6.25,-23.76)) ;
#159160 = CARTESIAN_POINT('',(-4.,-6.25,-21.96)) ;
#159161 = CARTESIAN_POINT('',(-4.,-6.25,-22.86)) ;
#159162 = CARTESIAN_POINT('',(1.9515639104739E-16,-6.25,-21.96)) ;
#159163 = CARTESIAN_POINT('',(-4.65,-6.25,-23.71)) ;
#159164 = CARTESIAN_POINT('',(-4.15,-6.25,-23.71)) ;
#159165 = CARTESIAN_POINT('',(-4.75,-6.25,-23.71)) ;
#159166 = CARTESIAN_POINT('',(-4.75,-6.25,-23.61)) ;
#159167 = CARTESIAN_POINT('Origin',(-4.65,-6.25,-23.61)) ;
#159168 = CARTESIAN_POINT('',(-4.75,-6.25,-22.11)) ;
#159169 = CARTESIAN_POINT('',(-4.75,-6.25,-22.01)) ;
#159170 = CARTESIAN_POINT('',(-4.65,-6.25,-22.01)) ;
#159171 = CARTESIAN_POINT('Origin',(-4.65,-6.25,-22.11)) ;
#159172 = CARTESIAN_POINT('',(-4.15,-6.25,-22.01)) ;
#159173 = CARTESIAN_POINT('',(-4.05,-6.25,-22.01)) ;
#159174 = CARTESIAN_POINT('',(-4.05,-6.25,-22.11)) ;
#159175 = CARTESIAN_POINT('Origin',(-4.15,-6.25,-22.11)) ;
#159176 = CARTESIAN_POINT('',(-4.05,-6.25,-23.61)) ;
#159177 = CARTESIAN_POINT('',(-4.05,-6.25,-23.71)) ;
#159178 = CARTESIAN_POINT('Origin',(-4.15,-6.25,-23.61)) ;
#159179 = CARTESIAN_POINT('Origin',(-4.05,-6.25,-23.71)) ;
#159180 = CARTESIAN_POINT('',(-4.05,-6.3,-22.11)) ;
#159181 = CARTESIAN_POINT('',(-4.05,-6.25,-22.11)) ;
#159182 = CARTESIAN_POINT('',(-4.05,-6.3,-23.61)) ;
#159183 = CARTESIAN_POINT('',(-4.05,-6.3,-23.71)) ;
#159184 = CARTESIAN_POINT('',(-4.05,-6.25,-23.61)) ;
#159185 = CARTESIAN_POINT('Origin',(-4.75,-6.25,-23.71)) ;
#159186 = CARTESIAN_POINT('',(-4.15,-6.3,-23.71)) ;
#159187 = CARTESIAN_POINT('',(-4.15,-6.25,-23.71)) ;
#159188 = CARTESIAN_POINT('',(-4.65,-6.3,-23.71)) ;
#159189 = CARTESIAN_POINT('',(-4.75,-6.3,-23.71)) ;
#159190 = CARTESIAN_POINT('',(-4.65,-6.25,-23.71)) ;
#159191 = CARTESIAN_POINT('Origin',(-4.75,-6.25,-22.01)) ;
#159192 = CARTESIAN_POINT('',(-4.75,-6.3,-23.61)) ;
#159193 = CARTESIAN_POINT('',(-4.75,-6.3,-22.11)) ;
#159194 = CARTESIAN_POINT('',(-4.75,-6.3,-22.01)) ;
#159195 = CARTESIAN_POINT('',(-4.75,-6.25,-22.11)) ;
#159196 = CARTESIAN_POINT('',(-4.75,-6.25,-23.61)) ;
#159197 = CARTESIAN_POINT('Origin',(-4.05,-6.25,-22.01)) ;
#159198 = CARTESIAN_POINT('',(-4.65,-6.3,-22.01)) ;
#159199 = CARTESIAN_POINT('',(-4.65,-6.25,-22.01)) ;
#159200 = CARTESIAN_POINT('',(-4.15,-6.3,-22.01)) ;
#159201 = CARTESIAN_POINT('',(-4.05,-6.3,-22.01)) ;
#159202 = CARTESIAN_POINT('',(-4.15,-6.25,-22.01)) ;
#159203 = CARTESIAN_POINT('Origin',(0.,-6.25,-26.67)) ;
#159204 = CARTESIAN_POINT('',(-4.8,-6.25,-25.77)) ;
#159205 = CARTESIAN_POINT('',(-4.8,-6.25,-27.57)) ;
#159206 = CARTESIAN_POINT('',(-4.8,-6.25,-26.67)) ;
#159207 = CARTESIAN_POINT('',(-4.,-6.25,-27.57)) ;
#159208 = CARTESIAN_POINT('',(1.95156391047391E-16,-6.25,-27.57)) ;
#159209 = CARTESIAN_POINT('',(-4.,-6.25,-25.77)) ;
#159210 = CARTESIAN_POINT('',(-4.,-6.25,-26.67)) ;
#159211 = CARTESIAN_POINT('',(1.9515639104739E-16,-6.25,-25.77)) ;
#159212 = CARTESIAN_POINT('',(-4.65,-6.25,-27.52)) ;
#159213 = CARTESIAN_POINT('',(-4.15,-6.25,-27.52)) ;
#159214 = CARTESIAN_POINT('',(-4.75,-6.25,-27.52)) ;
#159215 = CARTESIAN_POINT('',(-4.75,-6.25,-27.42)) ;
#159216 = CARTESIAN_POINT('Origin',(-4.65,-6.25,-27.42)) ;
#159217 = CARTESIAN_POINT('',(-4.75,-6.25,-25.92)) ;
#159218 = CARTESIAN_POINT('',(-4.75,-6.25,-25.82)) ;
#159219 = CARTESIAN_POINT('',(-4.65,-6.25,-25.82)) ;
#159220 = CARTESIAN_POINT('Origin',(-4.65,-6.25,-25.92)) ;
#159221 = CARTESIAN_POINT('',(-4.15,-6.25,-25.82)) ;
#159222 = CARTESIAN_POINT('',(-4.05,-6.25,-25.82)) ;
#159223 = CARTESIAN_POINT('',(-4.05,-6.25,-25.92)) ;
#159224 = CARTESIAN_POINT('Origin',(-4.15,-6.25,-25.92)) ;
#159225 = CARTESIAN_POINT('',(-4.05,-6.25,-27.42)) ;
#159226 = CARTESIAN_POINT('',(-4.05,-6.25,-27.52)) ;
#159227 = CARTESIAN_POINT('Origin',(-4.15,-6.25,-27.42)) ;
#159228 = CARTESIAN_POINT('Origin',(-4.05,-6.25,-27.52)) ;
#159229 = CARTESIAN_POINT('',(-4.05,-6.3,-25.92)) ;
#159230 = CARTESIAN_POINT('',(-4.05,-6.25,-25.92)) ;
#159231 = CARTESIAN_POINT('',(-4.05,-6.3,-27.42)) ;
#159232 = CARTESIAN_POINT('',(-4.05,-6.3,-27.52)) ;
#159233 = CARTESIAN_POINT('',(-4.05,-6.25,-27.42)) ;
#159234 = CARTESIAN_POINT('Origin',(-4.75,-6.25,-27.52)) ;
#159235 = CARTESIAN_POINT('',(-4.15,-6.3,-27.52)) ;
#159236 = CARTESIAN_POINT('',(-4.15,-6.25,-27.52)) ;
#159237 = CARTESIAN_POINT('',(-4.65,-6.3,-27.52)) ;
#159238 = CARTESIAN_POINT('',(-4.75,-6.3,-27.52)) ;
#159239 = CARTESIAN_POINT('',(-4.65,-6.25,-27.52)) ;
#159240 = CARTESIAN_POINT('Origin',(-4.75,-6.25,-25.82)) ;
#159241 = CARTESIAN_POINT('',(-4.75,-6.3,-27.42)) ;
#159242 = CARTESIAN_POINT('',(-4.75,-6.3,-25.92)) ;
#159243 = CARTESIAN_POINT('',(-4.75,-6.3,-25.82)) ;
#159244 = CARTESIAN_POINT('',(-4.75,-6.25,-25.92)) ;
#159245 = CARTESIAN_POINT('',(-4.75,-6.25,-27.42)) ;
#159246 = CARTESIAN_POINT('Origin',(-4.05,-6.25,-25.82)) ;
#159247 = CARTESIAN_POINT('',(-4.65,-6.3,-25.82)) ;
#159248 = CARTESIAN_POINT('',(-4.65,-6.25,-25.82)) ;
#159249 = CARTESIAN_POINT('',(-4.15,-6.3,-25.82)) ;
#159250 = CARTESIAN_POINT('',(-4.05,-6.3,-25.82)) ;
#159251 = CARTESIAN_POINT('',(-4.15,-6.25,-25.82)) ;
#159252 = CARTESIAN_POINT('Origin',(0.,-6.25,-30.48)) ;
#159253 = CARTESIAN_POINT('',(-4.8,-6.25,-29.58)) ;
#159254 = CARTESIAN_POINT('',(-4.8,-6.25,-31.38)) ;
#159255 = CARTESIAN_POINT('',(-4.8,-6.25,-30.48)) ;
#159256 = CARTESIAN_POINT('',(-4.,-6.25,-31.38)) ;
#159257 = CARTESIAN_POINT('',(1.9515639104739E-16,-6.25,-31.38)) ;
#159258 = CARTESIAN_POINT('',(-4.,-6.25,-29.58)) ;
#159259 = CARTESIAN_POINT('',(-4.,-6.25,-30.48)) ;
#159260 = CARTESIAN_POINT('',(1.9515639104739E-16,-6.25,-29.58)) ;
#159261 = CARTESIAN_POINT('',(-4.65,-6.25,-31.33)) ;
#159262 = CARTESIAN_POINT('',(-4.15,-6.25,-31.33)) ;
#159263 = CARTESIAN_POINT('',(-4.75,-6.25,-31.33)) ;
#159264 = CARTESIAN_POINT('',(-4.75,-6.25,-31.23)) ;
#159265 = CARTESIAN_POINT('Origin',(-4.65,-6.25,-31.23)) ;
#159266 = CARTESIAN_POINT('',(-4.75,-6.25,-29.73)) ;
#159267 = CARTESIAN_POINT('',(-4.75,-6.25,-29.63)) ;
#159268 = CARTESIAN_POINT('',(-4.65,-6.25,-29.63)) ;
#159269 = CARTESIAN_POINT('Origin',(-4.65,-6.25,-29.73)) ;
#159270 = CARTESIAN_POINT('',(-4.15,-6.25,-29.63)) ;
#159271 = CARTESIAN_POINT('',(-4.05,-6.25,-29.63)) ;
#159272 = CARTESIAN_POINT('',(-4.05,-6.25,-29.73)) ;
#159273 = CARTESIAN_POINT('Origin',(-4.15,-6.25,-29.73)) ;
#159274 = CARTESIAN_POINT('',(-4.05,-6.25,-31.23)) ;
#159275 = CARTESIAN_POINT('',(-4.05,-6.25,-31.33)) ;
#159276 = CARTESIAN_POINT('Origin',(-4.15,-6.25,-31.23)) ;
#159277 = CARTESIAN_POINT('Origin',(-4.05,-6.25,-31.33)) ;
#159278 = CARTESIAN_POINT('',(-4.05,-6.3,-29.73)) ;
#159279 = CARTESIAN_POINT('',(-4.05,-6.25,-29.73)) ;
#159280 = CARTESIAN_POINT('',(-4.05,-6.3,-31.23)) ;
#159281 = CARTESIAN_POINT('',(-4.05,-6.3,-31.33)) ;
#159282 = CARTESIAN_POINT('',(-4.05,-6.25,-31.23)) ;
#159283 = CARTESIAN_POINT('Origin',(-4.75,-6.25,-31.33)) ;
#159284 = CARTESIAN_POINT('',(-4.15,-6.3,-31.33)) ;
#159285 = CARTESIAN_POINT('',(-4.15,-6.25,-31.33)) ;
#159286 = CARTESIAN_POINT('',(-4.65,-6.3,-31.33)) ;
#159287 = CARTESIAN_POINT('',(-4.75,-6.3,-31.33)) ;
#159288 = CARTESIAN_POINT('',(-4.65,-6.25,-31.33)) ;
#159289 = CARTESIAN_POINT('Origin',(-4.75,-6.25,-29.63)) ;
#159290 = CARTESIAN_POINT('',(-4.75,-6.3,-31.23)) ;
#159291 = CARTESIAN_POINT('',(-4.75,-6.3,-29.73)) ;
#159292 = CARTESIAN_POINT('',(-4.75,-6.3,-29.63)) ;
#159293 = CARTESIAN_POINT('',(-4.75,-6.25,-29.73)) ;
#159294 = CARTESIAN_POINT('',(-4.75,-6.25,-31.23)) ;
#159295 = CARTESIAN_POINT('Origin',(-4.05,-6.25,-29.63)) ;
#159296 = CARTESIAN_POINT('',(-4.65,-6.3,-29.63)) ;
#159297 = CARTESIAN_POINT('',(-4.65,-6.25,-29.63)) ;
#159298 = CARTESIAN_POINT('',(-4.15,-6.3,-29.63)) ;
#159299 = CARTESIAN_POINT('',(-4.05,-6.3,-29.63)) ;
#159300 = CARTESIAN_POINT('',(-4.15,-6.25,-29.63)) ;
#159301 = CARTESIAN_POINT('Origin',(0.,-6.25,-34.29)) ;
#159302 = CARTESIAN_POINT('',(-4.8,-6.25,-33.39)) ;
#159303 = CARTESIAN_POINT('',(-4.8,-6.25,-35.19)) ;
#159304 = CARTESIAN_POINT('',(-4.8,-6.25,-34.29)) ;
#159305 = CARTESIAN_POINT('',(-4.,-6.25,-35.19)) ;
#159306 = CARTESIAN_POINT('',(1.9515639104739E-16,-6.25,-35.19)) ;
#159307 = CARTESIAN_POINT('',(-4.,-6.25,-33.39)) ;
#159308 = CARTESIAN_POINT('',(-4.,-6.25,-34.29)) ;
#159309 = CARTESIAN_POINT('',(1.9515639104739E-16,-6.25,-33.39)) ;
#159310 = CARTESIAN_POINT('',(-4.65,-6.25,-35.14)) ;
#159311 = CARTESIAN_POINT('',(-4.15,-6.25,-35.14)) ;
#159312 = CARTESIAN_POINT('',(-4.75,-6.25,-35.14)) ;
#159313 = CARTESIAN_POINT('',(-4.75,-6.25,-35.04)) ;
#159314 = CARTESIAN_POINT('Origin',(-4.65,-6.25,-35.04)) ;
#159315 = CARTESIAN_POINT('',(-4.75,-6.25,-33.54)) ;
#159316 = CARTESIAN_POINT('',(-4.75,-6.25,-33.44)) ;
#159317 = CARTESIAN_POINT('',(-4.65,-6.25,-33.44)) ;
#159318 = CARTESIAN_POINT('Origin',(-4.65,-6.25,-33.54)) ;
#159319 = CARTESIAN_POINT('',(-4.15,-6.25,-33.44)) ;
#159320 = CARTESIAN_POINT('',(-4.05,-6.25,-33.44)) ;
#159321 = CARTESIAN_POINT('',(-4.05,-6.25,-33.54)) ;
#159322 = CARTESIAN_POINT('Origin',(-4.15,-6.25,-33.54)) ;
#159323 = CARTESIAN_POINT('',(-4.05,-6.25,-35.04)) ;
#159324 = CARTESIAN_POINT('',(-4.05,-6.25,-35.14)) ;
#159325 = CARTESIAN_POINT('Origin',(-4.15,-6.25,-35.04)) ;
#159326 = CARTESIAN_POINT('Origin',(-4.05,-6.25,-35.14)) ;
#159327 = CARTESIAN_POINT('',(-4.05,-6.3,-33.54)) ;
#159328 = CARTESIAN_POINT('',(-4.05,-6.25,-33.54)) ;
#159329 = CARTESIAN_POINT('',(-4.05,-6.3,-35.04)) ;
#159330 = CARTESIAN_POINT('',(-4.05,-6.3,-35.14)) ;
#159331 = CARTESIAN_POINT('',(-4.05,-6.25,-35.04)) ;
#159332 = CARTESIAN_POINT('Origin',(-4.75,-6.25,-35.14)) ;
#159333 = CARTESIAN_POINT('',(-4.15,-6.3,-35.14)) ;
#159334 = CARTESIAN_POINT('',(-4.15,-6.25,-35.14)) ;
#159335 = CARTESIAN_POINT('',(-4.65,-6.3,-35.14)) ;
#159336 = CARTESIAN_POINT('',(-4.75,-6.3,-35.14)) ;
#159337 = CARTESIAN_POINT('',(-4.65,-6.25,-35.14)) ;
#159338 = CARTESIAN_POINT('Origin',(-4.75,-6.25,-33.44)) ;
#159339 = CARTESIAN_POINT('',(-4.75,-6.3,-35.04)) ;
#159340 = CARTESIAN_POINT('',(-4.75,-6.3,-33.54)) ;
#159341 = CARTESIAN_POINT('',(-4.75,-6.3,-33.44)) ;
#159342 = CARTESIAN_POINT('',(-4.75,-6.25,-33.54)) ;
#159343 = CARTESIAN_POINT('',(-4.75,-6.25,-35.04)) ;
#159344 = CARTESIAN_POINT('Origin',(-4.05,-6.25,-33.44)) ;
#159345 = CARTESIAN_POINT('',(-4.65,-6.3,-33.44)) ;
#159346 = CARTESIAN_POINT('',(-4.65,-6.25,-33.44)) ;
#159347 = CARTESIAN_POINT('',(-4.15,-6.3,-33.44)) ;
#159348 = CARTESIAN_POINT('',(-4.05,-6.3,-33.44)) ;
#159349 = CARTESIAN_POINT('',(-4.15,-6.25,-33.44)) ;
#159350 = CARTESIAN_POINT('Origin',(0.,-6.4,-3.81)) ;
#159351 = CARTESIAN_POINT('',(-4.15,-6.4,-3.06)) ;
#159352 = CARTESIAN_POINT('',(-4.65,-6.4,-3.06)) ;
#159353 = CARTESIAN_POINT('',(0.,-6.4,-3.06)) ;
#159354 = CARTESIAN_POINT('',(-4.65,-6.4,-4.56)) ;
#159355 = CARTESIAN_POINT('',(-4.65,-6.4,-3.81)) ;
#159356 = CARTESIAN_POINT('',(-4.15,-6.4,-4.56)) ;
#159357 = CARTESIAN_POINT('',(0.,-6.4,-4.56)) ;
#159358 = CARTESIAN_POINT('',(-4.15,-6.4,-3.81)) ;
#159359 = CARTESIAN_POINT('Origin',(0.,-6.4,-7.62)) ;
#159360 = CARTESIAN_POINT('',(-4.15,-6.4,-6.87)) ;
#159361 = CARTESIAN_POINT('',(-4.65,-6.4,-6.87)) ;
#159362 = CARTESIAN_POINT('',(0.,-6.4,-6.87)) ;
#159363 = CARTESIAN_POINT('',(-4.65,-6.4,-8.37)) ;
#159364 = CARTESIAN_POINT('',(-4.65,-6.4,-7.62)) ;
#159365 = CARTESIAN_POINT('',(-4.15,-6.4,-8.37)) ;
#159366 = CARTESIAN_POINT('',(0.,-6.4,-8.37)) ;
#159367 = CARTESIAN_POINT('',(-4.15,-6.4,-7.62)) ;
#159368 = CARTESIAN_POINT('Origin',(0.,-6.4,-11.43)) ;
#159369 = CARTESIAN_POINT('',(-4.15,-6.4,-10.68)) ;
#159370 = CARTESIAN_POINT('',(-4.65,-6.4,-10.68)) ;
#159371 = CARTESIAN_POINT('',(0.,-6.4,-10.68)) ;
#159372 = CARTESIAN_POINT('',(-4.65,-6.4,-12.18)) ;
#159373 = CARTESIAN_POINT('',(-4.65,-6.4,-11.43)) ;
#159374 = CARTESIAN_POINT('',(-4.15,-6.4,-12.18)) ;
#159375 = CARTESIAN_POINT('',(0.,-6.4,-12.18)) ;
#159376 = CARTESIAN_POINT('',(-4.15,-6.4,-11.43)) ;
#159377 = CARTESIAN_POINT('Origin',(0.,-6.4,-15.24)) ;
#159378 = CARTESIAN_POINT('',(-4.15,-6.4,-14.49)) ;
#159379 = CARTESIAN_POINT('',(-4.65,-6.4,-14.49)) ;
#159380 = CARTESIAN_POINT('',(0.,-6.4,-14.49)) ;
#159381 = CARTESIAN_POINT('',(-4.65,-6.4,-15.99)) ;
#159382 = CARTESIAN_POINT('',(-4.65,-6.4,-15.24)) ;
#159383 = CARTESIAN_POINT('',(-4.15,-6.4,-15.99)) ;
#159384 = CARTESIAN_POINT('',(0.,-6.4,-15.99)) ;
#159385 = CARTESIAN_POINT('',(-4.15,-6.4,-15.24)) ;
#159386 = CARTESIAN_POINT('Origin',(0.,-6.4,-19.05)) ;
#159387 = CARTESIAN_POINT('',(-4.15,-6.4,-18.3)) ;
#159388 = CARTESIAN_POINT('',(-4.65,-6.4,-18.3)) ;
#159389 = CARTESIAN_POINT('',(0.,-6.4,-18.3)) ;
#159390 = CARTESIAN_POINT('',(-4.65,-6.4,-19.8)) ;
#159391 = CARTESIAN_POINT('',(-4.65,-6.4,-19.05)) ;
#159392 = CARTESIAN_POINT('',(-4.15,-6.4,-19.8)) ;
#159393 = CARTESIAN_POINT('',(0.,-6.4,-19.8)) ;
#159394 = CARTESIAN_POINT('',(-4.15,-6.4,-19.05)) ;
#159395 = CARTESIAN_POINT('Origin',(0.,-6.4,-22.86)) ;
#159396 = CARTESIAN_POINT('',(-4.15,-6.4,-22.11)) ;
#159397 = CARTESIAN_POINT('',(-4.65,-6.4,-22.11)) ;
#159398 = CARTESIAN_POINT('',(0.,-6.4,-22.11)) ;
#159399 = CARTESIAN_POINT('',(-4.65,-6.4,-23.61)) ;
#159400 = CARTESIAN_POINT('',(-4.65,-6.4,-22.86)) ;
#159401 = CARTESIAN_POINT('',(-4.15,-6.4,-23.61)) ;
#159402 = CARTESIAN_POINT('',(0.,-6.4,-23.61)) ;
#159403 = CARTESIAN_POINT('',(-4.15,-6.4,-22.86)) ;
#159404 = CARTESIAN_POINT('Origin',(0.,-6.4,-26.67)) ;
#159405 = CARTESIAN_POINT('',(-4.15,-6.4,-25.92)) ;
#159406 = CARTESIAN_POINT('',(-4.65,-6.4,-25.92)) ;
#159407 = CARTESIAN_POINT('',(0.,-6.4,-25.92)) ;
#159408 = CARTESIAN_POINT('',(-4.65,-6.4,-27.42)) ;
#159409 = CARTESIAN_POINT('',(-4.65,-6.4,-26.67)) ;
#159410 = CARTESIAN_POINT('',(-4.15,-6.4,-27.42)) ;
#159411 = CARTESIAN_POINT('',(0.,-6.4,-27.42)) ;
#159412 = CARTESIAN_POINT('',(-4.15,-6.4,-26.67)) ;
#159413 = CARTESIAN_POINT('Origin',(0.,-6.4,-30.48)) ;
#159414 = CARTESIAN_POINT('',(-4.15,-6.4,-29.73)) ;
#159415 = CARTESIAN_POINT('',(-4.65,-6.4,-29.73)) ;
#159416 = CARTESIAN_POINT('',(0.,-6.4,-29.73)) ;
#159417 = CARTESIAN_POINT('',(-4.65,-6.4,-31.23)) ;
#159418 = CARTESIAN_POINT('',(-4.65,-6.4,-30.48)) ;
#159419 = CARTESIAN_POINT('',(-4.15,-6.4,-31.23)) ;
#159420 = CARTESIAN_POINT('',(0.,-6.4,-31.23)) ;
#159421 = CARTESIAN_POINT('',(-4.15,-6.4,-30.48)) ;
#159422 = CARTESIAN_POINT('Origin',(0.,-6.4,-34.29)) ;
#159423 = CARTESIAN_POINT('',(-4.15,-6.4,-33.54)) ;
#159424 = CARTESIAN_POINT('',(-4.65,-6.4,-33.54)) ;
#159425 = CARTESIAN_POINT('',(0.,-6.4,-33.54)) ;
#159426 = CARTESIAN_POINT('',(-4.65,-6.4,-35.04)) ;
#159427 = CARTESIAN_POINT('',(-4.65,-6.4,-34.29)) ;
#159428 = CARTESIAN_POINT('',(-4.15,-6.4,-35.04)) ;
#159429 = CARTESIAN_POINT('',(0.,-6.4,-35.04)) ;
#159430 = CARTESIAN_POINT('',(-4.15,-6.4,-34.29)) ;
#159431 = CARTESIAN_POINT('Origin',(3.6,2.,-2.405)) ;
#159432 = CARTESIAN_POINT('',(3.7,1.9,-2.405)) ;
#159433 = CARTESIAN_POINT('',(3.6,1.92679491924311,-2.405)) ;
#159434 = CARTESIAN_POINT('Origin',(3.7,2.1,-2.405)) ;
#159435 = CARTESIAN_POINT('',(3.5,1.9,-2.405)) ;
#159436 = CARTESIAN_POINT('Origin',(3.5,2.1,-2.405)) ;
#159437 = CARTESIAN_POINT('',(2.7,1.9,-2.405)) ;
#159438 = CARTESIAN_POINT('',(2.6,1.9,-2.405)) ;
#159439 = CARTESIAN_POINT('',(2.7,-5.15,-2.405)) ;
#159440 = CARTESIAN_POINT('',(2.7,2.,-2.405)) ;
#159441 = CARTESIAN_POINT('',(3.5,-5.15,-2.405)) ;
#159442 = CARTESIAN_POINT('',(3.6,-5.15,-2.405)) ;
#159443 = CARTESIAN_POINT('',(3.5,-2.35,-2.405)) ;
#159444 = CARTESIAN_POINT('',(3.5,-2.25,-2.405)) ;
#159445 = CARTESIAN_POINT('',(3.7,-2.15,-2.405)) ;
#159446 = CARTESIAN_POINT('Origin',(3.7,-2.35,-2.405)) ;
#159447 = CARTESIAN_POINT('',(10.1,-2.15,-2.405)) ;
#159448 = CARTESIAN_POINT('',(3.6,-2.15,-2.405)) ;
#159449 = CARTESIAN_POINT('',(10.1,1.9,-2.405)) ;
#159450 = CARTESIAN_POINT('',(10.1,2.,-2.405)) ;
#159451 = CARTESIAN_POINT('',(3.6,1.9,-2.405)) ;
#159452 = CARTESIAN_POINT('Origin',(3.6,-5.25,-2.405)) ;
#159453 = CARTESIAN_POINT('',(3.5,-5.25,-2.505)) ;
#159454 = CARTESIAN_POINT('',(2.7,-5.25,-2.505)) ;
#159455 = CARTESIAN_POINT('',(3.6,-5.25,-2.505)) ;
#159456 = CARTESIAN_POINT('',(2.7,-5.25,-5.115)) ;
#159457 = CARTESIAN_POINT('',(2.7,-5.25,-2.405)) ;
#159458 = CARTESIAN_POINT('',(3.5,-5.25,-5.115)) ;
#159459 = CARTESIAN_POINT('',(3.6,-5.25,-5.115)) ;
#159460 = CARTESIAN_POINT('',(3.5,-5.25,-2.405)) ;
#159461 = CARTESIAN_POINT('Origin',(3.6,-5.25,-5.215)) ;
#159462 = CARTESIAN_POINT('',(2.7,1.9,-5.215)) ;
#159463 = CARTESIAN_POINT('',(3.5,1.9,-5.215)) ;
#159464 = CARTESIAN_POINT('',(3.6,1.9,-5.215)) ;
#159465 = CARTESIAN_POINT('',(3.6,1.92679491924311,-5.215)) ;
#159466 = CARTESIAN_POINT('Origin',(3.5,2.1,-5.215)) ;
#159467 = CARTESIAN_POINT('',(3.7,1.9,-5.215)) ;
#159468 = CARTESIAN_POINT('Origin',(3.7,2.1,-5.215)) ;
#159469 = CARTESIAN_POINT('',(10.1,1.9,-5.215)) ;
#159470 = CARTESIAN_POINT('',(3.6,1.9,-5.215)) ;
#159471 = CARTESIAN_POINT('',(10.1,-2.15,-5.215)) ;
#159472 = CARTESIAN_POINT('',(10.1,-2.25,-5.215)) ;
#159473 = CARTESIAN_POINT('',(3.7,-2.15,-5.215)) ;
#159474 = CARTESIAN_POINT('',(3.6,-2.15,-5.215)) ;
#159475 = CARTESIAN_POINT('',(3.5,-2.35,-5.215)) ;
#159476 = CARTESIAN_POINT('Origin',(3.7,-2.35,-5.215)) ;
#159477 = CARTESIAN_POINT('',(3.5,-5.15,-5.215)) ;
#159478 = CARTESIAN_POINT('',(3.5,-5.25,-5.215)) ;
#159479 = CARTESIAN_POINT('',(2.7,-5.15,-5.215)) ;
#159480 = CARTESIAN_POINT('',(3.6,-5.15,-5.215)) ;
#159481 = CARTESIAN_POINT('',(2.7,-5.25,-5.215)) ;
#159482 = CARTESIAN_POINT('Origin',(3.6,2.,-5.215)) ;
#159483 = CARTESIAN_POINT('',(2.7,2.,-6.115)) ;
#159484 = CARTESIAN_POINT('',(3.5,2.,-6.115)) ;
#159485 = CARTESIAN_POINT('',(3.6,2.,-6.115)) ;
#159486 = CARTESIAN_POINT('',(3.5,2.,-5.315)) ;
#159487 = CARTESIAN_POINT('',(3.5,2.,-5.315)) ;
#159488 = CARTESIAN_POINT('',(2.7,2.,-5.315)) ;
#159489 = CARTESIAN_POINT('',(2.6,2.,-5.315)) ;
#159490 = CARTESIAN_POINT('',(2.7,2.,-5.215)) ;
#159491 = CARTESIAN_POINT('Origin',(3.6,2.,-6.215)) ;
#159492 = CARTESIAN_POINT('',(3.7,1.9,-6.215)) ;
#159493 = CARTESIAN_POINT('',(3.6,1.92679491924311,-6.215)) ;
#159494 = CARTESIAN_POINT('Origin',(3.7,2.1,-6.215)) ;
#159495 = CARTESIAN_POINT('',(3.5,1.9,-6.215)) ;
#159496 = CARTESIAN_POINT('Origin',(3.5,2.1,-6.215)) ;
#159497 = CARTESIAN_POINT('',(2.7,1.9,-6.215)) ;
#159498 = CARTESIAN_POINT('',(2.7,1.9,-6.215)) ;
#159499 = CARTESIAN_POINT('',(2.7,-5.15,-6.215)) ;
#159500 = CARTESIAN_POINT('',(2.7,2.,-6.215)) ;
#159501 = CARTESIAN_POINT('',(3.5,-5.15,-6.215)) ;
#159502 = CARTESIAN_POINT('',(3.6,-5.15,-6.215)) ;
#159503 = CARTESIAN_POINT('',(3.5,-2.35,-6.215)) ;
#159504 = CARTESIAN_POINT('',(3.5,-2.25,-6.215)) ;
#159505 = CARTESIAN_POINT('',(3.7,-2.15,-6.215)) ;
#159506 = CARTESIAN_POINT('Origin',(3.7,-2.35,-6.215)) ;
#159507 = CARTESIAN_POINT('',(10.1,-2.15,-6.215)) ;
#159508 = CARTESIAN_POINT('',(3.6,-2.15,-6.215)) ;
#159509 = CARTESIAN_POINT('',(10.1,1.9,-6.215)) ;
#159510 = CARTESIAN_POINT('',(10.1,2.,-6.215)) ;
#159511 = CARTESIAN_POINT('',(3.6,1.9,-6.215)) ;
#159512 = CARTESIAN_POINT('Origin',(3.6,-5.25,-6.215)) ;
#159513 = CARTESIAN_POINT('',(3.5,-5.25,-6.315)) ;
#159514 = CARTESIAN_POINT('',(2.7,-5.25,-6.315)) ;
#159515 = CARTESIAN_POINT('',(3.6,-5.25,-6.315)) ;
#159516 = CARTESIAN_POINT('',(2.7,-5.25,-8.925)) ;
#159517 = CARTESIAN_POINT('',(2.7,-5.25,-6.215)) ;
#159518 = CARTESIAN_POINT('',(3.5,-5.25,-8.925)) ;
#159519 = CARTESIAN_POINT('',(3.6,-5.25,-8.925)) ;
#159520 = CARTESIAN_POINT('',(3.5,-5.25,-6.215)) ;
#159521 = CARTESIAN_POINT('Origin',(3.6,-5.25,-9.025)) ;
#159522 = CARTESIAN_POINT('',(2.7,1.9,-9.025)) ;
#159523 = CARTESIAN_POINT('',(3.5,1.9,-9.025)) ;
#159524 = CARTESIAN_POINT('',(3.6,1.9,-9.025)) ;
#159525 = CARTESIAN_POINT('',(3.6,1.92679491924311,-9.025)) ;
#159526 = CARTESIAN_POINT('Origin',(3.5,2.1,-9.025)) ;
#159527 = CARTESIAN_POINT('',(3.7,1.9,-9.025)) ;
#159528 = CARTESIAN_POINT('Origin',(3.7,2.1,-9.025)) ;
#159529 = CARTESIAN_POINT('',(10.1,1.9,-9.025)) ;
#159530 = CARTESIAN_POINT('',(3.6,1.9,-9.025)) ;
#159531 = CARTESIAN_POINT('',(10.1,-2.15,-9.025)) ;
#159532 = CARTESIAN_POINT('',(10.1,-2.25,-9.025)) ;
#159533 = CARTESIAN_POINT('',(3.7,-2.15,-9.025)) ;
#159534 = CARTESIAN_POINT('',(3.6,-2.15,-9.025)) ;
#159535 = CARTESIAN_POINT('',(3.5,-2.35,-9.025)) ;
#159536 = CARTESIAN_POINT('Origin',(3.7,-2.35,-9.025)) ;
#159537 = CARTESIAN_POINT('',(3.5,-5.15,-9.025)) ;
#159538 = CARTESIAN_POINT('',(3.5,-5.25,-9.025)) ;
#159539 = CARTESIAN_POINT('',(2.7,-5.15,-9.025)) ;
#159540 = CARTESIAN_POINT('',(3.6,-5.15,-9.025)) ;
#159541 = CARTESIAN_POINT('',(2.7,-5.25,-9.025)) ;
#159542 = CARTESIAN_POINT('Origin',(3.6,2.,-9.025)) ;
#159543 = CARTESIAN_POINT('',(2.7,2.,-9.925)) ;
#159544 = CARTESIAN_POINT('',(3.5,2.,-9.925)) ;
#159545 = CARTESIAN_POINT('',(3.6,2.,-9.925)) ;
#159546 = CARTESIAN_POINT('',(3.5,2.,-9.125)) ;
#159547 = CARTESIAN_POINT('',(3.5,2.,-9.125)) ;
#159548 = CARTESIAN_POINT('',(2.7,2.,-9.125)) ;
#159549 = CARTESIAN_POINT('',(2.6,2.,-9.125)) ;
#159550 = CARTESIAN_POINT('',(2.7,2.,-9.025)) ;
#159551 = CARTESIAN_POINT('Origin',(3.6,2.,-10.025)) ;
#159552 = CARTESIAN_POINT('',(3.7,1.9,-10.025)) ;
#159553 = CARTESIAN_POINT('',(3.6,1.92679491924311,-10.025)) ;
#159554 = CARTESIAN_POINT('Origin',(3.7,2.1,-10.025)) ;
#159555 = CARTESIAN_POINT('',(3.5,1.9,-10.025)) ;
#159556 = CARTESIAN_POINT('Origin',(3.5,2.1,-10.025)) ;
#159557 = CARTESIAN_POINT('',(2.7,1.9,-10.025)) ;
#159558 = CARTESIAN_POINT('',(2.7,1.9,-10.025)) ;
#159559 = CARTESIAN_POINT('',(2.7,-5.15,-10.025)) ;
#159560 = CARTESIAN_POINT('',(2.7,2.,-10.025)) ;
#159561 = CARTESIAN_POINT('',(3.5,-5.15,-10.025)) ;
#159562 = CARTESIAN_POINT('',(3.6,-5.15,-10.025)) ;
#159563 = CARTESIAN_POINT('',(3.5,-2.35,-10.025)) ;
#159564 = CARTESIAN_POINT('',(3.5,-2.25,-10.025)) ;
#159565 = CARTESIAN_POINT('',(3.7,-2.15,-10.025)) ;
#159566 = CARTESIAN_POINT('Origin',(3.7,-2.35,-10.025)) ;
#159567 = CARTESIAN_POINT('',(10.1,-2.15,-10.025)) ;
#159568 = CARTESIAN_POINT('',(3.6,-2.15,-10.025)) ;
#159569 = CARTESIAN_POINT('',(10.1,1.9,-10.025)) ;
#159570 = CARTESIAN_POINT('',(10.1,2.,-10.025)) ;
#159571 = CARTESIAN_POINT('',(3.6,1.9,-10.025)) ;
#159572 = CARTESIAN_POINT('Origin',(3.6,-5.25,-10.025)) ;
#159573 = CARTESIAN_POINT('',(3.5,-5.25,-10.125)) ;
#159574 = CARTESIAN_POINT('',(2.7,-5.25,-10.125)) ;
#159575 = CARTESIAN_POINT('',(3.6,-5.25,-10.125)) ;
#159576 = CARTESIAN_POINT('',(2.7,-5.25,-12.735)) ;
#159577 = CARTESIAN_POINT('',(2.7,-5.25,-10.025)) ;
#159578 = CARTESIAN_POINT('',(3.5,-5.25,-12.735)) ;
#159579 = CARTESIAN_POINT('',(3.6,-5.25,-12.735)) ;
#159580 = CARTESIAN_POINT('',(3.5,-5.25,-10.025)) ;
#159581 = CARTESIAN_POINT('Origin',(3.6,-5.25,-12.835)) ;
#159582 = CARTESIAN_POINT('',(2.7,1.9,-12.835)) ;
#159583 = CARTESIAN_POINT('',(3.5,1.9,-12.835)) ;
#159584 = CARTESIAN_POINT('',(3.6,1.9,-12.835)) ;
#159585 = CARTESIAN_POINT('',(3.6,1.92679491924311,-12.835)) ;
#159586 = CARTESIAN_POINT('Origin',(3.5,2.1,-12.835)) ;
#159587 = CARTESIAN_POINT('',(3.7,1.9,-12.835)) ;
#159588 = CARTESIAN_POINT('Origin',(3.7,2.1,-12.835)) ;
#159589 = CARTESIAN_POINT('',(10.1,1.9,-12.835)) ;
#159590 = CARTESIAN_POINT('',(3.6,1.9,-12.835)) ;
#159591 = CARTESIAN_POINT('',(10.1,-2.15,-12.835)) ;
#159592 = CARTESIAN_POINT('',(10.1,-2.25,-12.835)) ;
#159593 = CARTESIAN_POINT('',(3.7,-2.15,-12.835)) ;
#159594 = CARTESIAN_POINT('',(3.6,-2.15,-12.835)) ;
#159595 = CARTESIAN_POINT('',(3.5,-2.35,-12.835)) ;
#159596 = CARTESIAN_POINT('Origin',(3.7,-2.35,-12.835)) ;
#159597 = CARTESIAN_POINT('',(3.5,-5.15,-12.835)) ;
#159598 = CARTESIAN_POINT('',(3.5,-5.25,-12.835)) ;
#159599 = CARTESIAN_POINT('',(2.7,-5.15,-12.835)) ;
#159600 = CARTESIAN_POINT('',(3.6,-5.15,-12.835)) ;
#159601 = CARTESIAN_POINT('',(2.7,-5.25,-12.835)) ;
#159602 = CARTESIAN_POINT('Origin',(3.6,2.,-12.835)) ;
#159603 = CARTESIAN_POINT('',(2.7,2.,-13.735)) ;
#159604 = CARTESIAN_POINT('',(3.5,2.,-13.735)) ;
#159605 = CARTESIAN_POINT('',(3.6,2.,-13.735)) ;
#159606 = CARTESIAN_POINT('',(3.5,2.,-12.935)) ;
#159607 = CARTESIAN_POINT('',(3.5,2.,-12.935)) ;
#159608 = CARTESIAN_POINT('',(2.7,2.,-12.935)) ;
#159609 = CARTESIAN_POINT('',(2.6,2.,-12.935)) ;
#159610 = CARTESIAN_POINT('',(2.7,2.,-12.835)) ;
#159611 = CARTESIAN_POINT('Origin',(3.6,2.,-13.835)) ;
#159612 = CARTESIAN_POINT('',(3.7,1.9,-13.835)) ;
#159613 = CARTESIAN_POINT('',(3.6,1.92679491924311,-13.835)) ;
#159614 = CARTESIAN_POINT('Origin',(3.7,2.1,-13.835)) ;
#159615 = CARTESIAN_POINT('',(3.5,1.9,-13.835)) ;
#159616 = CARTESIAN_POINT('Origin',(3.5,2.1,-13.835)) ;
#159617 = CARTESIAN_POINT('',(2.7,1.9,-13.835)) ;
#159618 = CARTESIAN_POINT('',(2.7,1.9,-13.835)) ;
#159619 = CARTESIAN_POINT('',(2.7,-5.15,-13.835)) ;
#159620 = CARTESIAN_POINT('',(2.7,2.,-13.835)) ;
#159621 = CARTESIAN_POINT('',(3.5,-5.15,-13.835)) ;
#159622 = CARTESIAN_POINT('',(3.6,-5.15,-13.835)) ;
#159623 = CARTESIAN_POINT('',(3.5,-2.35,-13.835)) ;
#159624 = CARTESIAN_POINT('',(3.5,-2.25,-13.835)) ;
#159625 = CARTESIAN_POINT('',(3.7,-2.15,-13.835)) ;
#159626 = CARTESIAN_POINT('Origin',(3.7,-2.35,-13.835)) ;
#159627 = CARTESIAN_POINT('',(10.1,-2.15,-13.835)) ;
#159628 = CARTESIAN_POINT('',(3.6,-2.15,-13.835)) ;
#159629 = CARTESIAN_POINT('',(10.1,1.9,-13.835)) ;
#159630 = CARTESIAN_POINT('',(10.1,2.,-13.835)) ;
#159631 = CARTESIAN_POINT('',(3.6,1.9,-13.835)) ;
#159632 = CARTESIAN_POINT('Origin',(3.6,-5.25,-13.835)) ;
#159633 = CARTESIAN_POINT('',(3.5,-5.25,-13.935)) ;
#159634 = CARTESIAN_POINT('',(2.7,-5.25,-13.935)) ;
#159635 = CARTESIAN_POINT('',(3.6,-5.25,-13.935)) ;
#159636 = CARTESIAN_POINT('',(2.7,-5.25,-16.545)) ;
#159637 = CARTESIAN_POINT('',(2.7,-5.25,-13.835)) ;
#159638 = CARTESIAN_POINT('',(3.5,-5.25,-16.545)) ;
#159639 = CARTESIAN_POINT('',(3.6,-5.25,-16.545)) ;
#159640 = CARTESIAN_POINT('',(3.5,-5.25,-13.835)) ;
#159641 = CARTESIAN_POINT('Origin',(3.6,-5.25,-16.645)) ;
#159642 = CARTESIAN_POINT('',(2.7,1.9,-16.645)) ;
#159643 = CARTESIAN_POINT('',(3.5,1.9,-16.645)) ;
#159644 = CARTESIAN_POINT('',(3.6,1.9,-16.645)) ;
#159645 = CARTESIAN_POINT('',(3.6,1.92679491924311,-16.645)) ;
#159646 = CARTESIAN_POINT('Origin',(3.5,2.1,-16.645)) ;
#159647 = CARTESIAN_POINT('',(3.7,1.9,-16.645)) ;
#159648 = CARTESIAN_POINT('Origin',(3.7,2.1,-16.645)) ;
#159649 = CARTESIAN_POINT('',(10.1,1.9,-16.645)) ;
#159650 = CARTESIAN_POINT('',(3.6,1.9,-16.645)) ;
#159651 = CARTESIAN_POINT('',(10.1,-2.15,-16.645)) ;
#159652 = CARTESIAN_POINT('',(10.1,-2.25,-16.645)) ;
#159653 = CARTESIAN_POINT('',(3.7,-2.15,-16.645)) ;
#159654 = CARTESIAN_POINT('',(3.6,-2.15,-16.645)) ;
#159655 = CARTESIAN_POINT('',(3.5,-2.35,-16.645)) ;
#159656 = CARTESIAN_POINT('Origin',(3.7,-2.35,-16.645)) ;
#159657 = CARTESIAN_POINT('',(3.5,-5.15,-16.645)) ;
#159658 = CARTESIAN_POINT('',(3.5,-5.25,-16.645)) ;
#159659 = CARTESIAN_POINT('',(2.7,-5.15,-16.645)) ;
#159660 = CARTESIAN_POINT('',(3.6,-5.15,-16.645)) ;
#159661 = CARTESIAN_POINT('',(2.7,-5.25,-16.645)) ;
#159662 = CARTESIAN_POINT('Origin',(3.6,2.,-16.645)) ;
#159663 = CARTESIAN_POINT('',(2.7,2.,-17.545)) ;
#159664 = CARTESIAN_POINT('',(3.5,2.,-17.545)) ;
#159665 = CARTESIAN_POINT('',(3.6,2.,-17.545)) ;
#159666 = CARTESIAN_POINT('',(3.5,2.,-16.745)) ;
#159667 = CARTESIAN_POINT('',(3.5,2.,-16.745)) ;
#159668 = CARTESIAN_POINT('',(2.7,2.,-16.745)) ;
#159669 = CARTESIAN_POINT('',(2.6,2.,-16.745)) ;
#159670 = CARTESIAN_POINT('',(2.7,2.,-16.645)) ;
#159671 = CARTESIAN_POINT('Origin',(3.6,2.,-17.645)) ;
#159672 = CARTESIAN_POINT('',(3.7,1.9,-17.645)) ;
#159673 = CARTESIAN_POINT('',(3.6,1.92679491924311,-17.645)) ;
#159674 = CARTESIAN_POINT('Origin',(3.7,2.1,-17.645)) ;
#159675 = CARTESIAN_POINT('',(3.5,1.9,-17.645)) ;
#159676 = CARTESIAN_POINT('Origin',(3.5,2.1,-17.645)) ;
#159677 = CARTESIAN_POINT('',(2.7,1.9,-17.645)) ;
#159678 = CARTESIAN_POINT('',(2.7,1.9,-17.645)) ;
#159679 = CARTESIAN_POINT('',(2.7,-5.15,-17.645)) ;
#159680 = CARTESIAN_POINT('',(2.7,2.,-17.645)) ;
#159681 = CARTESIAN_POINT('',(3.5,-5.15,-17.645)) ;
#159682 = CARTESIAN_POINT('',(3.6,-5.15,-17.645)) ;
#159683 = CARTESIAN_POINT('',(3.5,-2.35,-17.645)) ;
#159684 = CARTESIAN_POINT('',(3.5,-2.25,-17.645)) ;
#159685 = CARTESIAN_POINT('',(3.7,-2.15,-17.645)) ;
#159686 = CARTESIAN_POINT('Origin',(3.7,-2.35,-17.645)) ;
#159687 = CARTESIAN_POINT('',(10.1,-2.15,-17.645)) ;
#159688 = CARTESIAN_POINT('',(3.6,-2.15,-17.645)) ;
#159689 = CARTESIAN_POINT('',(10.1,1.9,-17.645)) ;
#159690 = CARTESIAN_POINT('',(10.1,2.,-17.645)) ;
#159691 = CARTESIAN_POINT('',(3.6,1.9,-17.645)) ;
#159692 = CARTESIAN_POINT('Origin',(3.6,-5.25,-17.645)) ;
#159693 = CARTESIAN_POINT('',(3.5,-5.25,-17.745)) ;
#159694 = CARTESIAN_POINT('',(2.7,-5.25,-17.745)) ;
#159695 = CARTESIAN_POINT('',(3.6,-5.25,-17.745)) ;
#159696 = CARTESIAN_POINT('',(2.7,-5.25,-20.355)) ;
#159697 = CARTESIAN_POINT('',(2.7,-5.25,-17.645)) ;
#159698 = CARTESIAN_POINT('',(3.5,-5.25,-20.355)) ;
#159699 = CARTESIAN_POINT('',(3.6,-5.25,-20.355)) ;
#159700 = CARTESIAN_POINT('',(3.5,-5.25,-17.645)) ;
#159701 = CARTESIAN_POINT('Origin',(3.6,-5.25,-20.455)) ;
#159702 = CARTESIAN_POINT('',(2.7,1.9,-20.455)) ;
#159703 = CARTESIAN_POINT('',(3.5,1.9,-20.455)) ;
#159704 = CARTESIAN_POINT('',(3.6,1.9,-20.455)) ;
#159705 = CARTESIAN_POINT('',(3.6,1.92679491924311,-20.455)) ;
#159706 = CARTESIAN_POINT('Origin',(3.5,2.1,-20.455)) ;
#159707 = CARTESIAN_POINT('',(3.7,1.9,-20.455)) ;
#159708 = CARTESIAN_POINT('Origin',(3.7,2.1,-20.455)) ;
#159709 = CARTESIAN_POINT('',(10.1,1.9,-20.455)) ;
#159710 = CARTESIAN_POINT('',(3.6,1.9,-20.455)) ;
#159711 = CARTESIAN_POINT('',(10.1,-2.15,-20.455)) ;
#159712 = CARTESIAN_POINT('',(10.1,-2.25,-20.455)) ;
#159713 = CARTESIAN_POINT('',(3.7,-2.15,-20.455)) ;
#159714 = CARTESIAN_POINT('',(3.6,-2.15,-20.455)) ;
#159715 = CARTESIAN_POINT('',(3.5,-2.35,-20.455)) ;
#159716 = CARTESIAN_POINT('Origin',(3.7,-2.35,-20.455)) ;
#159717 = CARTESIAN_POINT('',(3.5,-5.15,-20.455)) ;
#159718 = CARTESIAN_POINT('',(3.5,-5.25,-20.455)) ;
#159719 = CARTESIAN_POINT('',(2.7,-5.15,-20.455)) ;
#159720 = CARTESIAN_POINT('',(3.6,-5.15,-20.455)) ;
#159721 = CARTESIAN_POINT('',(2.7,-5.25,-20.455)) ;
#159722 = CARTESIAN_POINT('Origin',(3.6,2.,-20.455)) ;
#159723 = CARTESIAN_POINT('',(2.7,2.,-21.355)) ;
#159724 = CARTESIAN_POINT('',(3.5,2.,-21.355)) ;
#159725 = CARTESIAN_POINT('',(3.6,2.,-21.355)) ;
#159726 = CARTESIAN_POINT('',(3.5,2.,-20.555)) ;
#159727 = CARTESIAN_POINT('',(3.5,2.,-20.555)) ;
#159728 = CARTESIAN_POINT('',(2.7,2.,-20.555)) ;
#159729 = CARTESIAN_POINT('',(2.6,2.,-20.555)) ;
#159730 = CARTESIAN_POINT('',(2.7,2.,-20.455)) ;
#159731 = CARTESIAN_POINT('Origin',(3.6,2.,-21.455)) ;
#159732 = CARTESIAN_POINT('',(3.7,1.9,-21.455)) ;
#159733 = CARTESIAN_POINT('',(3.6,1.92679491924311,-21.455)) ;
#159734 = CARTESIAN_POINT('Origin',(3.7,2.1,-21.455)) ;
#159735 = CARTESIAN_POINT('',(3.5,1.9,-21.455)) ;
#159736 = CARTESIAN_POINT('Origin',(3.5,2.1,-21.455)) ;
#159737 = CARTESIAN_POINT('',(2.7,1.9,-21.455)) ;
#159738 = CARTESIAN_POINT('',(2.7,1.9,-21.455)) ;
#159739 = CARTESIAN_POINT('',(2.7,-5.15,-21.455)) ;
#159740 = CARTESIAN_POINT('',(2.7,2.,-21.455)) ;
#159741 = CARTESIAN_POINT('',(3.5,-5.15,-21.455)) ;
#159742 = CARTESIAN_POINT('',(3.6,-5.15,-21.455)) ;
#159743 = CARTESIAN_POINT('',(3.5,-2.35,-21.455)) ;
#159744 = CARTESIAN_POINT('',(3.5,-2.25,-21.455)) ;
#159745 = CARTESIAN_POINT('',(3.7,-2.15,-21.455)) ;
#159746 = CARTESIAN_POINT('Origin',(3.7,-2.35,-21.455)) ;
#159747 = CARTESIAN_POINT('',(10.1,-2.15,-21.455)) ;
#159748 = CARTESIAN_POINT('',(3.6,-2.15,-21.455)) ;
#159749 = CARTESIAN_POINT('',(10.1,1.9,-21.455)) ;
#159750 = CARTESIAN_POINT('',(10.1,2.,-21.455)) ;
#159751 = CARTESIAN_POINT('',(3.6,1.9,-21.455)) ;
#159752 = CARTESIAN_POINT('Origin',(3.6,-5.25,-21.455)) ;
#159753 = CARTESIAN_POINT('',(3.5,-5.25,-21.555)) ;
#159754 = CARTESIAN_POINT('',(2.7,-5.25,-21.555)) ;
#159755 = CARTESIAN_POINT('',(3.6,-5.25,-21.555)) ;
#159756 = CARTESIAN_POINT('',(2.7,-5.25,-24.165)) ;
#159757 = CARTESIAN_POINT('',(2.7,-5.25,-21.455)) ;
#159758 = CARTESIAN_POINT('',(3.5,-5.25,-24.165)) ;
#159759 = CARTESIAN_POINT('',(3.6,-5.25,-24.165)) ;
#159760 = CARTESIAN_POINT('',(3.5,-5.25,-21.455)) ;
#159761 = CARTESIAN_POINT('Origin',(3.6,-5.25,-24.265)) ;
#159762 = CARTESIAN_POINT('',(2.7,1.9,-24.265)) ;
#159763 = CARTESIAN_POINT('',(3.5,1.9,-24.265)) ;
#159764 = CARTESIAN_POINT('',(3.6,1.9,-24.265)) ;
#159765 = CARTESIAN_POINT('',(3.6,1.92679491924311,-24.265)) ;
#159766 = CARTESIAN_POINT('Origin',(3.5,2.1,-24.265)) ;
#159767 = CARTESIAN_POINT('',(3.7,1.9,-24.265)) ;
#159768 = CARTESIAN_POINT('Origin',(3.7,2.1,-24.265)) ;
#159769 = CARTESIAN_POINT('',(10.1,1.9,-24.265)) ;
#159770 = CARTESIAN_POINT('',(3.6,1.9,-24.265)) ;
#159771 = CARTESIAN_POINT('',(10.1,-2.15,-24.265)) ;
#159772 = CARTESIAN_POINT('',(10.1,-2.25,-24.265)) ;
#159773 = CARTESIAN_POINT('',(3.7,-2.15,-24.265)) ;
#159774 = CARTESIAN_POINT('',(3.6,-2.15,-24.265)) ;
#159775 = CARTESIAN_POINT('',(3.5,-2.35,-24.265)) ;
#159776 = CARTESIAN_POINT('Origin',(3.7,-2.35,-24.265)) ;
#159777 = CARTESIAN_POINT('',(3.5,-5.15,-24.265)) ;
#159778 = CARTESIAN_POINT('',(3.5,-5.25,-24.265)) ;
#159779 = CARTESIAN_POINT('',(2.7,-5.15,-24.265)) ;
#159780 = CARTESIAN_POINT('',(3.6,-5.15,-24.265)) ;
#159781 = CARTESIAN_POINT('',(2.7,-5.25,-24.265)) ;
#159782 = CARTESIAN_POINT('Origin',(3.6,2.,-24.265)) ;
#159783 = CARTESIAN_POINT('',(2.7,2.,-25.165)) ;
#159784 = CARTESIAN_POINT('',(3.5,2.,-25.165)) ;
#159785 = CARTESIAN_POINT('',(3.6,2.,-25.165)) ;
#159786 = CARTESIAN_POINT('',(3.5,2.,-24.365)) ;
#159787 = CARTESIAN_POINT('',(3.5,2.,-24.365)) ;
#159788 = CARTESIAN_POINT('',(2.7,2.,-24.365)) ;
#159789 = CARTESIAN_POINT('',(2.6,2.,-24.365)) ;
#159790 = CARTESIAN_POINT('',(2.7,2.,-24.265)) ;
#159791 = CARTESIAN_POINT('Origin',(3.6,2.,-25.265)) ;
#159792 = CARTESIAN_POINT('',(3.7,1.9,-25.265)) ;
#159793 = CARTESIAN_POINT('',(3.6,1.92679491924311,-25.265)) ;
#159794 = CARTESIAN_POINT('Origin',(3.7,2.1,-25.265)) ;
#159795 = CARTESIAN_POINT('',(3.5,1.9,-25.265)) ;
#159796 = CARTESIAN_POINT('Origin',(3.5,2.1,-25.265)) ;
#159797 = CARTESIAN_POINT('',(2.7,1.9,-25.265)) ;
#159798 = CARTESIAN_POINT('',(2.7,1.9,-25.265)) ;
#159799 = CARTESIAN_POINT('',(2.7,-5.15,-25.265)) ;
#159800 = CARTESIAN_POINT('',(2.7,2.,-25.265)) ;
#159801 = CARTESIAN_POINT('',(3.5,-5.15,-25.265)) ;
#159802 = CARTESIAN_POINT('',(3.6,-5.15,-25.265)) ;
#159803 = CARTESIAN_POINT('',(3.5,-2.35,-25.265)) ;
#159804 = CARTESIAN_POINT('',(3.5,-2.25,-25.265)) ;
#159805 = CARTESIAN_POINT('',(3.7,-2.15,-25.265)) ;
#159806 = CARTESIAN_POINT('Origin',(3.7,-2.35,-25.265)) ;
#159807 = CARTESIAN_POINT('',(10.1,-2.15,-25.265)) ;
#159808 = CARTESIAN_POINT('',(3.6,-2.15,-25.265)) ;
#159809 = CARTESIAN_POINT('',(10.1,1.9,-25.265)) ;
#159810 = CARTESIAN_POINT('',(10.1,2.,-25.265)) ;
#159811 = CARTESIAN_POINT('',(3.6,1.9,-25.265)) ;
#159812 = CARTESIAN_POINT('Origin',(3.6,-5.25,-25.265)) ;
#159813 = CARTESIAN_POINT('',(3.5,-5.25,-25.365)) ;
#159814 = CARTESIAN_POINT('',(2.7,-5.25,-25.365)) ;
#159815 = CARTESIAN_POINT('',(3.6,-5.25,-25.365)) ;
#159816 = CARTESIAN_POINT('',(2.7,-5.25,-27.975)) ;
#159817 = CARTESIAN_POINT('',(2.7,-5.25,-25.265)) ;
#159818 = CARTESIAN_POINT('',(3.5,-5.25,-27.975)) ;
#159819 = CARTESIAN_POINT('',(3.6,-5.25,-27.975)) ;
#159820 = CARTESIAN_POINT('',(3.5,-5.25,-25.265)) ;
#159821 = CARTESIAN_POINT('Origin',(3.6,-5.25,-28.075)) ;
#159822 = CARTESIAN_POINT('',(2.7,1.9,-28.075)) ;
#159823 = CARTESIAN_POINT('',(3.5,1.9,-28.075)) ;
#159824 = CARTESIAN_POINT('',(3.6,1.9,-28.075)) ;
#159825 = CARTESIAN_POINT('',(3.6,1.92679491924311,-28.075)) ;
#159826 = CARTESIAN_POINT('Origin',(3.5,2.1,-28.075)) ;
#159827 = CARTESIAN_POINT('',(3.7,1.9,-28.075)) ;
#159828 = CARTESIAN_POINT('Origin',(3.7,2.1,-28.075)) ;
#159829 = CARTESIAN_POINT('',(10.1,1.9,-28.075)) ;
#159830 = CARTESIAN_POINT('',(3.6,1.9,-28.075)) ;
#159831 = CARTESIAN_POINT('',(10.1,-2.15,-28.075)) ;
#159832 = CARTESIAN_POINT('',(10.1,-2.25,-28.075)) ;
#159833 = CARTESIAN_POINT('',(3.7,-2.15,-28.075)) ;
#159834 = CARTESIAN_POINT('',(3.6,-2.15,-28.075)) ;
#159835 = CARTESIAN_POINT('',(3.5,-2.35,-28.075)) ;
#159836 = CARTESIAN_POINT('Origin',(3.7,-2.35,-28.075)) ;
#159837 = CARTESIAN_POINT('',(3.5,-5.15,-28.075)) ;
#159838 = CARTESIAN_POINT('',(3.5,-5.25,-28.075)) ;
#159839 = CARTESIAN_POINT('',(2.7,-5.15,-28.075)) ;
#159840 = CARTESIAN_POINT('',(3.6,-5.15,-28.075)) ;
#159841 = CARTESIAN_POINT('',(2.7,-5.25,-28.075)) ;
#159842 = CARTESIAN_POINT('Origin',(3.6,2.,-28.075)) ;
#159843 = CARTESIAN_POINT('',(2.7,2.,-28.975)) ;
#159844 = CARTESIAN_POINT('',(3.5,2.,-28.975)) ;
#159845 = CARTESIAN_POINT('',(3.6,2.,-28.975)) ;
#159846 = CARTESIAN_POINT('',(3.5,2.,-28.175)) ;
#159847 = CARTESIAN_POINT('',(3.5,2.,-28.175)) ;
#159848 = CARTESIAN_POINT('',(2.7,2.,-28.175)) ;
#159849 = CARTESIAN_POINT('',(2.6,2.,-28.175)) ;
#159850 = CARTESIAN_POINT('',(2.7,2.,-28.075)) ;
#159851 = CARTESIAN_POINT('Origin',(3.6,2.,-29.075)) ;
#159852 = CARTESIAN_POINT('',(3.7,1.9,-29.075)) ;
#159853 = CARTESIAN_POINT('',(3.6,1.92679491924311,-29.075)) ;
#159854 = CARTESIAN_POINT('Origin',(3.7,2.1,-29.075)) ;
#159855 = CARTESIAN_POINT('',(3.5,1.9,-29.075)) ;
#159856 = CARTESIAN_POINT('Origin',(3.5,2.1,-29.075)) ;
#159857 = CARTESIAN_POINT('',(2.7,1.9,-29.075)) ;
#159858 = CARTESIAN_POINT('',(2.7,1.9,-29.075)) ;
#159859 = CARTESIAN_POINT('',(2.7,-5.15,-29.075)) ;
#159860 = CARTESIAN_POINT('',(2.7,2.,-29.075)) ;
#159861 = CARTESIAN_POINT('',(3.5,-5.15,-29.075)) ;
#159862 = CARTESIAN_POINT('',(3.6,-5.15,-29.075)) ;
#159863 = CARTESIAN_POINT('',(3.5,-2.35,-29.075)) ;
#159864 = CARTESIAN_POINT('',(3.5,-2.25,-29.075)) ;
#159865 = CARTESIAN_POINT('',(3.7,-2.15,-29.075)) ;
#159866 = CARTESIAN_POINT('Origin',(3.7,-2.35,-29.075)) ;
#159867 = CARTESIAN_POINT('',(10.1,-2.15,-29.075)) ;
#159868 = CARTESIAN_POINT('',(3.6,-2.15,-29.075)) ;
#159869 = CARTESIAN_POINT('',(10.1,1.9,-29.075)) ;
#159870 = CARTESIAN_POINT('',(10.1,2.,-29.075)) ;
#159871 = CARTESIAN_POINT('',(3.6,1.9,-29.075)) ;
#159872 = CARTESIAN_POINT('Origin',(3.6,-5.25,-29.075)) ;
#159873 = CARTESIAN_POINT('',(3.5,-5.25,-29.175)) ;
#159874 = CARTESIAN_POINT('',(2.7,-5.25,-29.175)) ;
#159875 = CARTESIAN_POINT('',(3.6,-5.25,-29.175)) ;
#159876 = CARTESIAN_POINT('',(2.7,-5.25,-31.785)) ;
#159877 = CARTESIAN_POINT('',(2.7,-5.25,-29.075)) ;
#159878 = CARTESIAN_POINT('',(3.5,-5.25,-31.785)) ;
#159879 = CARTESIAN_POINT('',(3.6,-5.25,-31.785)) ;
#159880 = CARTESIAN_POINT('',(3.5,-5.25,-29.075)) ;
#159881 = CARTESIAN_POINT('Origin',(3.6,-5.25,-31.885)) ;
#159882 = CARTESIAN_POINT('',(2.7,1.9,-31.885)) ;
#159883 = CARTESIAN_POINT('',(3.5,1.9,-31.885)) ;
#159884 = CARTESIAN_POINT('',(3.6,1.9,-31.885)) ;
#159885 = CARTESIAN_POINT('',(3.6,1.92679491924311,-31.885)) ;
#159886 = CARTESIAN_POINT('Origin',(3.5,2.1,-31.885)) ;
#159887 = CARTESIAN_POINT('',(3.7,1.9,-31.885)) ;
#159888 = CARTESIAN_POINT('Origin',(3.7,2.1,-31.885)) ;
#159889 = CARTESIAN_POINT('',(10.1,1.9,-31.885)) ;
#159890 = CARTESIAN_POINT('',(3.6,1.9,-31.885)) ;
#159891 = CARTESIAN_POINT('',(10.1,-2.15,-31.885)) ;
#159892 = CARTESIAN_POINT('',(10.1,-2.25,-31.885)) ;
#159893 = CARTESIAN_POINT('',(3.7,-2.15,-31.885)) ;
#159894 = CARTESIAN_POINT('',(3.6,-2.15,-31.885)) ;
#159895 = CARTESIAN_POINT('',(3.5,-2.35,-31.885)) ;
#159896 = CARTESIAN_POINT('Origin',(3.7,-2.35,-31.885)) ;
#159897 = CARTESIAN_POINT('',(3.5,-5.15,-31.885)) ;
#159898 = CARTESIAN_POINT('',(3.5,-5.25,-31.885)) ;
#159899 = CARTESIAN_POINT('',(2.7,-5.15,-31.885)) ;
#159900 = CARTESIAN_POINT('',(3.6,-5.15,-31.885)) ;
#159901 = CARTESIAN_POINT('',(2.7,-5.25,-31.885)) ;
#159902 = CARTESIAN_POINT('Origin',(3.6,2.,-31.885)) ;
#159903 = CARTESIAN_POINT('',(2.7,2.,-32.785)) ;
#159904 = CARTESIAN_POINT('',(3.5,2.,-32.785)) ;
#159905 = CARTESIAN_POINT('',(3.6,2.,-32.785)) ;
#159906 = CARTESIAN_POINT('',(3.5,2.,-31.985)) ;
#159907 = CARTESIAN_POINT('',(3.5,2.,-31.985)) ;
#159908 = CARTESIAN_POINT('',(2.7,2.,-31.985)) ;
#159909 = CARTESIAN_POINT('',(2.6,2.,-31.985)) ;
#159910 = CARTESIAN_POINT('',(2.7,2.,-31.885)) ;
#159911 = CARTESIAN_POINT('Origin',(3.6,2.,-32.885)) ;
#159912 = CARTESIAN_POINT('',(3.7,1.9,-32.885)) ;
#159913 = CARTESIAN_POINT('',(3.6,1.92679491924311,-32.885)) ;
#159914 = CARTESIAN_POINT('Origin',(3.7,2.1,-32.885)) ;
#159915 = CARTESIAN_POINT('',(3.5,1.9,-32.885)) ;
#159916 = CARTESIAN_POINT('Origin',(3.5,2.1,-32.885)) ;
#159917 = CARTESIAN_POINT('',(2.7,1.9,-32.885)) ;
#159918 = CARTESIAN_POINT('',(2.7,1.9,-32.885)) ;
#159919 = CARTESIAN_POINT('',(2.7,-5.15,-32.885)) ;
#159920 = CARTESIAN_POINT('',(2.7,2.,-32.885)) ;
#159921 = CARTESIAN_POINT('',(3.5,-5.15,-32.885)) ;
#159922 = CARTESIAN_POINT('',(3.6,-5.15,-32.885)) ;
#159923 = CARTESIAN_POINT('',(3.5,-2.35,-32.885)) ;
#159924 = CARTESIAN_POINT('',(3.5,-2.25,-32.885)) ;
#159925 = CARTESIAN_POINT('',(3.7,-2.15,-32.885)) ;
#159926 = CARTESIAN_POINT('Origin',(3.7,-2.35,-32.885)) ;
#159927 = CARTESIAN_POINT('',(10.1,-2.15,-32.885)) ;
#159928 = CARTESIAN_POINT('',(3.6,-2.15,-32.885)) ;
#159929 = CARTESIAN_POINT('',(10.1,1.9,-32.885)) ;
#159930 = CARTESIAN_POINT('',(10.1,2.,-32.885)) ;
#159931 = CARTESIAN_POINT('',(3.6,1.9,-32.885)) ;
#159932 = CARTESIAN_POINT('Origin',(3.6,-5.25,-32.885)) ;
#159933 = CARTESIAN_POINT('',(3.5,-5.25,-32.985)) ;
#159934 = CARTESIAN_POINT('',(2.7,-5.25,-32.985)) ;
#159935 = CARTESIAN_POINT('',(3.6,-5.25,-32.985)) ;
#159936 = CARTESIAN_POINT('',(2.7,-5.25,-35.595)) ;
#159937 = CARTESIAN_POINT('',(2.7,-5.25,-32.885)) ;
#159938 = CARTESIAN_POINT('',(3.5,-5.25,-35.595)) ;
#159939 = CARTESIAN_POINT('',(3.6,-5.25,-35.595)) ;
#159940 = CARTESIAN_POINT('',(3.5,-5.25,-32.885)) ;
#159941 = CARTESIAN_POINT('Origin',(3.6,-5.25,-35.695)) ;
#159942 = CARTESIAN_POINT('',(2.7,1.9,-35.695)) ;
#159943 = CARTESIAN_POINT('',(3.5,1.9,-35.695)) ;
#159944 = CARTESIAN_POINT('',(3.6,1.9,-35.695)) ;
#159945 = CARTESIAN_POINT('',(3.6,1.92679491924311,-35.695)) ;
#159946 = CARTESIAN_POINT('Origin',(3.5,2.1,-35.695)) ;
#159947 = CARTESIAN_POINT('',(3.7,1.9,-35.695)) ;
#159948 = CARTESIAN_POINT('Origin',(3.7,2.1,-35.695)) ;
#159949 = CARTESIAN_POINT('',(10.1,1.9,-35.695)) ;
#159950 = CARTESIAN_POINT('',(3.6,1.9,-35.695)) ;
#159951 = CARTESIAN_POINT('',(10.1,-2.15,-35.695)) ;
#159952 = CARTESIAN_POINT('',(10.1,-2.25,-35.695)) ;
#159953 = CARTESIAN_POINT('',(3.7,-2.15,-35.695)) ;
#159954 = CARTESIAN_POINT('',(3.6,-2.15,-35.695)) ;
#159955 = CARTESIAN_POINT('',(3.5,-2.35,-35.695)) ;
#159956 = CARTESIAN_POINT('Origin',(3.7,-2.35,-35.695)) ;
#159957 = CARTESIAN_POINT('',(3.5,-5.15,-35.695)) ;
#159958 = CARTESIAN_POINT('',(3.5,-5.25,-35.695)) ;
#159959 = CARTESIAN_POINT('',(2.7,-5.15,-35.695)) ;
#159960 = CARTESIAN_POINT('',(3.6,-5.15,-35.695)) ;
#159961 = CARTESIAN_POINT('',(2.7,-5.25,-35.695)) ;
#159962 = CARTESIAN_POINT('Origin',(3.6,2.,-35.695)) ;
#159963 = CARTESIAN_POINT('',(2.7,2.,-35.795)) ;
#159964 = CARTESIAN_POINT('',(2.7,2.,-36.49)) ;
#159965 = CARTESIAN_POINT('',(2.7,2.,-35.695)) ;
#159966 = CARTESIAN_POINT('',(3.5,2.,-36.49)) ;
#159967 = CARTESIAN_POINT('',(3.5,2.,-36.49)) ;
#159968 = CARTESIAN_POINT('',(3.5,2.,-35.795)) ;
#159969 = CARTESIAN_POINT('',(3.5,2.,-35.795)) ;
#159970 = CARTESIAN_POINT('',(2.6,2.,-35.795)) ;
#159971 = CARTESIAN_POINT('Origin',(10.2,-2.25,-4.685)) ;
#159972 = CARTESIAN_POINT('',(10.1,-2.25,-4.71311959340942)) ;
#159973 = CARTESIAN_POINT('',(3.7,-2.25,-4.71311959340942)) ;
#159974 = CARTESIAN_POINT('',(10.2,-2.25,-4.71311959340942)) ;
#159975 = CARTESIAN_POINT('',(3.7,-2.25,-5.115)) ;
#159976 = CARTESIAN_POINT('',(3.7,-2.25,-4.685)) ;
#159977 = CARTESIAN_POINT('',(10.1,-2.25,-5.115)) ;
#159978 = CARTESIAN_POINT('',(10.2,-2.25,-5.115)) ;
#159979 = CARTESIAN_POINT('',(10.1,-2.25,-4.685)) ;
#159980 = CARTESIAN_POINT('Origin',(10.2,-2.25,-2.405)) ;
#159981 = CARTESIAN_POINT('',(10.1,-2.25,-2.505)) ;
#159982 = CARTESIAN_POINT('',(3.7,-2.25,-2.505)) ;
#159983 = CARTESIAN_POINT('',(10.2,-2.25,-2.505)) ;
#159984 = CARTESIAN_POINT('',(3.7,-2.25,-2.90688040659058)) ;
#159985 = CARTESIAN_POINT('',(3.7,-2.25,-2.405)) ;
#159986 = CARTESIAN_POINT('',(10.1,-2.25,-2.90688040659058)) ;
#159987 = CARTESIAN_POINT('',(10.2,-2.25,-2.90688040659058)) ;
#159988 = CARTESIAN_POINT('',(10.1,-2.25,-2.405)) ;
#159989 = CARTESIAN_POINT('Origin',(10.2,-3.65625,-3.81)) ;
#159990 = CARTESIAN_POINT('',(10.1,-2.23576512455516,-2.95830358628649)) ;
#159991 = CARTESIAN_POINT('',(3.7,-2.23576512455516,-2.95830358628649)) ;
#159992 = CARTESIAN_POINT('',(10.2,-2.23576512455516,-2.95830358628649)) ;
#159993 = CARTESIAN_POINT('',(3.7,-2.23576512455516,-4.66169641371351)) ;
#159994 = CARTESIAN_POINT('Origin',(3.7,-3.65625,-3.81)) ;
#159995 = CARTESIAN_POINT('',(10.1,-2.23576512455516,-4.66169641371351)) ;
#159996 = CARTESIAN_POINT('',(10.2,-2.23576512455516,-4.66169641371351)) ;
#159997 = CARTESIAN_POINT('Origin',(10.1,-3.65625,-3.81)) ;
#159998 = CARTESIAN_POINT('Origin',(10.2,-3.65625,-3.81)) ;
#159999 = CARTESIAN_POINT('',(10.2,-2.15,-2.505)) ;
#160000 = CARTESIAN_POINT('',(10.2,-2.15,-2.90688040659058)) ;
#160001 = CARTESIAN_POINT('',(10.2,-2.15,-2.935)) ;
#160002 = CARTESIAN_POINT('',(10.2,-2.15,-4.71311959340942)) ;
#160003 = CARTESIAN_POINT('Origin',(10.2,-3.65625,-3.81)) ;
#160004 = CARTESIAN_POINT('',(10.2,-2.15,-5.115)) ;
#160005 = CARTESIAN_POINT('',(10.2,-2.15,-5.215)) ;
#160006 = CARTESIAN_POINT('',(10.2,1.9,-5.115)) ;
#160007 = CARTESIAN_POINT('',(10.2,2.,-5.115)) ;
#160008 = CARTESIAN_POINT('',(10.2,1.9,-2.505)) ;
#160009 = CARTESIAN_POINT('',(10.2,1.9,-2.405)) ;
#160010 = CARTESIAN_POINT('',(10.2,-2.25,-2.505)) ;
#160011 = CARTESIAN_POINT('Origin',(10.2,-2.25,-8.495)) ;
#160012 = CARTESIAN_POINT('',(10.1,-2.25,-8.52311959340942)) ;
#160013 = CARTESIAN_POINT('',(3.7,-2.25,-8.52311959340942)) ;
#160014 = CARTESIAN_POINT('',(10.2,-2.25,-8.52311959340942)) ;
#160015 = CARTESIAN_POINT('',(3.7,-2.25,-8.925)) ;
#160016 = CARTESIAN_POINT('',(3.7,-2.25,-8.495)) ;
#160017 = CARTESIAN_POINT('',(10.1,-2.25,-8.925)) ;
#160018 = CARTESIAN_POINT('',(10.2,-2.25,-8.925)) ;
#160019 = CARTESIAN_POINT('',(10.1,-2.25,-8.495)) ;
#160020 = CARTESIAN_POINT('Origin',(10.2,-2.25,-6.215)) ;
#160021 = CARTESIAN_POINT('',(10.1,-2.25,-6.315)) ;
#160022 = CARTESIAN_POINT('',(3.7,-2.25,-6.315)) ;
#160023 = CARTESIAN_POINT('',(10.2,-2.25,-6.315)) ;
#160024 = CARTESIAN_POINT('',(3.7,-2.25,-6.71688040659058)) ;
#160025 = CARTESIAN_POINT('',(3.7,-2.25,-6.215)) ;
#160026 = CARTESIAN_POINT('',(10.1,-2.25,-6.71688040659058)) ;
#160027 = CARTESIAN_POINT('',(10.2,-2.25,-6.71688040659058)) ;
#160028 = CARTESIAN_POINT('',(10.1,-2.25,-6.215)) ;
#160029 = CARTESIAN_POINT('Origin',(10.2,-3.65625,-7.62)) ;
#160030 = CARTESIAN_POINT('',(10.1,-2.23576512455516,-6.76830358628649)) ;
#160031 = CARTESIAN_POINT('',(3.7,-2.23576512455516,-6.76830358628649)) ;
#160032 = CARTESIAN_POINT('',(10.2,-2.23576512455516,-6.76830358628649)) ;
#160033 = CARTESIAN_POINT('',(3.7,-2.23576512455516,-8.47169641371351)) ;
#160034 = CARTESIAN_POINT('Origin',(3.7,-3.65625,-7.62)) ;
#160035 = CARTESIAN_POINT('',(10.1,-2.23576512455516,-8.47169641371351)) ;
#160036 = CARTESIAN_POINT('',(10.2,-2.23576512455516,-8.47169641371351)) ;
#160037 = CARTESIAN_POINT('Origin',(10.1,-3.65625,-7.62)) ;
#160038 = CARTESIAN_POINT('Origin',(10.2,-3.65625,-7.62)) ;
#160039 = CARTESIAN_POINT('',(10.2,-2.15,-6.315)) ;
#160040 = CARTESIAN_POINT('',(10.2,-2.15,-6.71688040659058)) ;
#160041 = CARTESIAN_POINT('',(10.2,-2.15,-6.745)) ;
#160042 = CARTESIAN_POINT('',(10.2,-2.15,-8.52311959340943)) ;
#160043 = CARTESIAN_POINT('Origin',(10.2,-3.65625,-7.62)) ;
#160044 = CARTESIAN_POINT('',(10.2,-2.15,-8.925)) ;
#160045 = CARTESIAN_POINT('',(10.2,-2.15,-9.025)) ;
#160046 = CARTESIAN_POINT('',(10.2,1.9,-8.925)) ;
#160047 = CARTESIAN_POINT('',(10.2,2.,-8.925)) ;
#160048 = CARTESIAN_POINT('',(10.2,1.9,-6.315)) ;
#160049 = CARTESIAN_POINT('',(10.2,1.9,-6.215)) ;
#160050 = CARTESIAN_POINT('',(10.2,-2.25,-6.315)) ;
#160051 = CARTESIAN_POINT('Origin',(10.2,-2.25,-12.305)) ;
#160052 = CARTESIAN_POINT('',(10.1,-2.25,-12.3331195934094)) ;
#160053 = CARTESIAN_POINT('',(3.7,-2.25,-12.3331195934094)) ;
#160054 = CARTESIAN_POINT('',(10.2,-2.25,-12.3331195934094)) ;
#160055 = CARTESIAN_POINT('',(3.7,-2.25,-12.735)) ;
#160056 = CARTESIAN_POINT('',(3.7,-2.25,-12.305)) ;
#160057 = CARTESIAN_POINT('',(10.1,-2.25,-12.735)) ;
#160058 = CARTESIAN_POINT('',(10.2,-2.25,-12.735)) ;
#160059 = CARTESIAN_POINT('',(10.1,-2.25,-12.305)) ;
#160060 = CARTESIAN_POINT('Origin',(10.2,-2.25,-10.025)) ;
#160061 = CARTESIAN_POINT('',(10.1,-2.25,-10.125)) ;
#160062 = CARTESIAN_POINT('',(3.7,-2.25,-10.125)) ;
#160063 = CARTESIAN_POINT('',(10.2,-2.25,-10.125)) ;
#160064 = CARTESIAN_POINT('',(3.7,-2.25,-10.5268804065906)) ;
#160065 = CARTESIAN_POINT('',(3.7,-2.25,-10.025)) ;
#160066 = CARTESIAN_POINT('',(10.1,-2.25,-10.5268804065906)) ;
#160067 = CARTESIAN_POINT('',(10.2,-2.25,-10.5268804065906)) ;
#160068 = CARTESIAN_POINT('',(10.1,-2.25,-10.025)) ;
#160069 = CARTESIAN_POINT('Origin',(10.2,-3.65625,-11.43)) ;
#160070 = CARTESIAN_POINT('',(10.1,-2.23576512455516,-10.5783035862865)) ;
#160071 = CARTESIAN_POINT('',(3.7,-2.23576512455516,-10.5783035862865)) ;
#160072 = CARTESIAN_POINT('',(10.2,-2.23576512455516,-10.5783035862865)) ;
#160073 = CARTESIAN_POINT('',(3.7,-2.23576512455516,-12.2816964137135)) ;
#160074 = CARTESIAN_POINT('Origin',(3.7,-3.65625,-11.43)) ;
#160075 = CARTESIAN_POINT('',(10.1,-2.23576512455516,-12.2816964137135)) ;
#160076 = CARTESIAN_POINT('',(10.2,-2.23576512455516,-12.2816964137135)) ;
#160077 = CARTESIAN_POINT('Origin',(10.1,-3.65625,-11.43)) ;
#160078 = CARTESIAN_POINT('Origin',(10.2,-3.65625,-11.43)) ;
#160079 = CARTESIAN_POINT('',(10.2,-2.15,-10.125)) ;
#160080 = CARTESIAN_POINT('',(10.2,-2.15,-10.5268804065906)) ;
#160081 = CARTESIAN_POINT('',(10.2,-2.15,-10.555)) ;
#160082 = CARTESIAN_POINT('',(10.2,-2.15,-12.3331195934094)) ;
#160083 = CARTESIAN_POINT('Origin',(10.2,-3.65625,-11.43)) ;
#160084 = CARTESIAN_POINT('',(10.2,-2.15,-12.735)) ;
#160085 = CARTESIAN_POINT('',(10.2,-2.15,-12.835)) ;
#160086 = CARTESIAN_POINT('',(10.2,1.9,-12.735)) ;
#160087 = CARTESIAN_POINT('',(10.2,2.,-12.735)) ;
#160088 = CARTESIAN_POINT('',(10.2,1.9,-10.125)) ;
#160089 = CARTESIAN_POINT('',(10.2,1.9,-10.025)) ;
#160090 = CARTESIAN_POINT('',(10.2,-2.25,-10.125)) ;
#160091 = CARTESIAN_POINT('Origin',(10.2,-2.25,-16.115)) ;
#160092 = CARTESIAN_POINT('',(10.1,-2.25,-16.1431195934094)) ;
#160093 = CARTESIAN_POINT('',(3.7,-2.25,-16.1431195934094)) ;
#160094 = CARTESIAN_POINT('',(10.2,-2.25,-16.1431195934094)) ;
#160095 = CARTESIAN_POINT('',(3.7,-2.25,-16.545)) ;
#160096 = CARTESIAN_POINT('',(3.7,-2.25,-16.115)) ;
#160097 = CARTESIAN_POINT('',(10.1,-2.25,-16.545)) ;
#160098 = CARTESIAN_POINT('',(10.2,-2.25,-16.545)) ;
#160099 = CARTESIAN_POINT('',(10.1,-2.25,-16.115)) ;
#160100 = CARTESIAN_POINT('Origin',(10.2,-2.25,-13.835)) ;
#160101 = CARTESIAN_POINT('',(10.1,-2.25,-13.935)) ;
#160102 = CARTESIAN_POINT('',(3.7,-2.25,-13.935)) ;
#160103 = CARTESIAN_POINT('',(10.2,-2.25,-13.935)) ;
#160104 = CARTESIAN_POINT('',(3.7,-2.25,-14.3368804065906)) ;
#160105 = CARTESIAN_POINT('',(3.7,-2.25,-13.835)) ;
#160106 = CARTESIAN_POINT('',(10.1,-2.25,-14.3368804065906)) ;
#160107 = CARTESIAN_POINT('',(10.2,-2.25,-14.3368804065906)) ;
#160108 = CARTESIAN_POINT('',(10.1,-2.25,-13.835)) ;
#160109 = CARTESIAN_POINT('Origin',(10.2,-3.65625,-15.24)) ;
#160110 = CARTESIAN_POINT('',(10.1,-2.23576512455516,-14.3883035862865)) ;
#160111 = CARTESIAN_POINT('',(3.7,-2.23576512455516,-14.3883035862865)) ;
#160112 = CARTESIAN_POINT('',(10.2,-2.23576512455516,-14.3883035862865)) ;
#160113 = CARTESIAN_POINT('',(3.7,-2.23576512455516,-16.0916964137135)) ;
#160114 = CARTESIAN_POINT('Origin',(3.7,-3.65625,-15.24)) ;
#160115 = CARTESIAN_POINT('',(10.1,-2.23576512455516,-16.0916964137135)) ;
#160116 = CARTESIAN_POINT('',(10.2,-2.23576512455516,-16.0916964137135)) ;
#160117 = CARTESIAN_POINT('Origin',(10.1,-3.65625,-15.24)) ;
#160118 = CARTESIAN_POINT('Origin',(10.2,-3.65625,-15.24)) ;
#160119 = CARTESIAN_POINT('',(10.2,-2.15,-13.935)) ;
#160120 = CARTESIAN_POINT('',(10.2,-2.15,-14.3368804065906)) ;
#160121 = CARTESIAN_POINT('',(10.2,-2.15,-14.365)) ;
#160122 = CARTESIAN_POINT('',(10.2,-2.15,-16.1431195934094)) ;
#160123 = CARTESIAN_POINT('Origin',(10.2,-3.65625,-15.24)) ;
#160124 = CARTESIAN_POINT('',(10.2,-2.15,-16.545)) ;
#160125 = CARTESIAN_POINT('',(10.2,-2.15,-16.645)) ;
#160126 = CARTESIAN_POINT('',(10.2,1.9,-16.545)) ;
#160127 = CARTESIAN_POINT('',(10.2,2.,-16.545)) ;
#160128 = CARTESIAN_POINT('',(10.2,1.9,-13.935)) ;
#160129 = CARTESIAN_POINT('',(10.2,1.9,-13.835)) ;
#160130 = CARTESIAN_POINT('',(10.2,-2.25,-13.935)) ;
#160131 = CARTESIAN_POINT('Origin',(10.2,-2.25,-19.925)) ;
#160132 = CARTESIAN_POINT('',(10.1,-2.25,-19.9531195934094)) ;
#160133 = CARTESIAN_POINT('',(3.7,-2.25,-19.9531195934094)) ;
#160134 = CARTESIAN_POINT('',(10.2,-2.25,-19.9531195934094)) ;
#160135 = CARTESIAN_POINT('',(3.7,-2.25,-20.355)) ;
#160136 = CARTESIAN_POINT('',(3.7,-2.25,-19.925)) ;
#160137 = CARTESIAN_POINT('',(10.1,-2.25,-20.355)) ;
#160138 = CARTESIAN_POINT('',(10.2,-2.25,-20.355)) ;
#160139 = CARTESIAN_POINT('',(10.1,-2.25,-19.925)) ;
#160140 = CARTESIAN_POINT('Origin',(10.2,-2.25,-17.645)) ;
#160141 = CARTESIAN_POINT('',(10.1,-2.25,-17.745)) ;
#160142 = CARTESIAN_POINT('',(3.7,-2.25,-17.745)) ;
#160143 = CARTESIAN_POINT('',(10.2,-2.25,-17.745)) ;
#160144 = CARTESIAN_POINT('',(3.7,-2.25,-18.1468804065906)) ;
#160145 = CARTESIAN_POINT('',(3.7,-2.25,-17.645)) ;
#160146 = CARTESIAN_POINT('',(10.1,-2.25,-18.1468804065906)) ;
#160147 = CARTESIAN_POINT('',(10.2,-2.25,-18.1468804065906)) ;
#160148 = CARTESIAN_POINT('',(10.1,-2.25,-17.645)) ;
#160149 = CARTESIAN_POINT('Origin',(10.2,-3.65625,-19.05)) ;
#160150 = CARTESIAN_POINT('',(10.1,-2.23576512455516,-18.1983035862865)) ;
#160151 = CARTESIAN_POINT('',(3.7,-2.23576512455516,-18.1983035862865)) ;
#160152 = CARTESIAN_POINT('',(10.2,-2.23576512455516,-18.1983035862865)) ;
#160153 = CARTESIAN_POINT('',(3.7,-2.23576512455516,-19.9016964137135)) ;
#160154 = CARTESIAN_POINT('Origin',(3.7,-3.65625,-19.05)) ;
#160155 = CARTESIAN_POINT('',(10.1,-2.23576512455516,-19.9016964137135)) ;
#160156 = CARTESIAN_POINT('',(10.2,-2.23576512455516,-19.9016964137135)) ;
#160157 = CARTESIAN_POINT('Origin',(10.1,-3.65625,-19.05)) ;
#160158 = CARTESIAN_POINT('Origin',(10.2,-3.65625,-19.05)) ;
#160159 = CARTESIAN_POINT('',(10.2,-2.15,-17.745)) ;
#160160 = CARTESIAN_POINT('',(10.2,-2.15,-18.1468804065906)) ;
#160161 = CARTESIAN_POINT('',(10.2,-2.15,-18.175)) ;
#160162 = CARTESIAN_POINT('',(10.2,-2.15,-19.9531195934094)) ;
#160163 = CARTESIAN_POINT('Origin',(10.2,-3.65625,-19.05)) ;
#160164 = CARTESIAN_POINT('',(10.2,-2.15,-20.355)) ;
#160165 = CARTESIAN_POINT('',(10.2,-2.15,-20.455)) ;
#160166 = CARTESIAN_POINT('',(10.2,1.9,-20.355)) ;
#160167 = CARTESIAN_POINT('',(10.2,2.,-20.355)) ;
#160168 = CARTESIAN_POINT('',(10.2,1.9,-17.745)) ;
#160169 = CARTESIAN_POINT('',(10.2,1.9,-17.645)) ;
#160170 = CARTESIAN_POINT('',(10.2,-2.25,-17.745)) ;
#160171 = CARTESIAN_POINT('Origin',(10.2,-2.25,-23.735)) ;
#160172 = CARTESIAN_POINT('',(10.1,-2.25,-23.7631195934094)) ;
#160173 = CARTESIAN_POINT('',(3.7,-2.25,-23.7631195934094)) ;
#160174 = CARTESIAN_POINT('',(10.2,-2.25,-23.7631195934094)) ;
#160175 = CARTESIAN_POINT('',(3.7,-2.25,-24.165)) ;
#160176 = CARTESIAN_POINT('',(3.7,-2.25,-23.735)) ;
#160177 = CARTESIAN_POINT('',(10.1,-2.25,-24.165)) ;
#160178 = CARTESIAN_POINT('',(10.2,-2.25,-24.165)) ;
#160179 = CARTESIAN_POINT('',(10.1,-2.25,-23.735)) ;
#160180 = CARTESIAN_POINT('Origin',(10.2,-2.25,-21.455)) ;
#160181 = CARTESIAN_POINT('',(10.1,-2.25,-21.555)) ;
#160182 = CARTESIAN_POINT('',(3.7,-2.25,-21.555)) ;
#160183 = CARTESIAN_POINT('',(10.2,-2.25,-21.555)) ;
#160184 = CARTESIAN_POINT('',(3.7,-2.25,-21.9568804065906)) ;
#160185 = CARTESIAN_POINT('',(3.7,-2.25,-21.455)) ;
#160186 = CARTESIAN_POINT('',(10.1,-2.25,-21.9568804065906)) ;
#160187 = CARTESIAN_POINT('',(10.2,-2.25,-21.9568804065906)) ;
#160188 = CARTESIAN_POINT('',(10.1,-2.25,-21.455)) ;
#160189 = CARTESIAN_POINT('Origin',(10.2,-3.65625,-22.86)) ;
#160190 = CARTESIAN_POINT('',(10.1,-2.23576512455516,-22.0083035862865)) ;
#160191 = CARTESIAN_POINT('',(3.7,-2.23576512455516,-22.0083035862865)) ;
#160192 = CARTESIAN_POINT('',(10.2,-2.23576512455516,-22.0083035862865)) ;
#160193 = CARTESIAN_POINT('',(3.7,-2.23576512455516,-23.7116964137135)) ;
#160194 = CARTESIAN_POINT('Origin',(3.7,-3.65625,-22.86)) ;
#160195 = CARTESIAN_POINT('',(10.1,-2.23576512455516,-23.7116964137135)) ;
#160196 = CARTESIAN_POINT('',(10.2,-2.23576512455516,-23.7116964137135)) ;
#160197 = CARTESIAN_POINT('Origin',(10.1,-3.65625,-22.86)) ;
#160198 = CARTESIAN_POINT('Origin',(10.2,-3.65625,-22.86)) ;
#160199 = CARTESIAN_POINT('',(10.2,-2.15,-21.555)) ;
#160200 = CARTESIAN_POINT('',(10.2,-2.15,-21.9568804065906)) ;
#160201 = CARTESIAN_POINT('',(10.2,-2.15,-21.985)) ;
#160202 = CARTESIAN_POINT('',(10.2,-2.15,-23.7631195934094)) ;
#160203 = CARTESIAN_POINT('Origin',(10.2,-3.65625,-22.86)) ;
#160204 = CARTESIAN_POINT('',(10.2,-2.15,-24.165)) ;
#160205 = CARTESIAN_POINT('',(10.2,-2.15,-24.265)) ;
#160206 = CARTESIAN_POINT('',(10.2,1.9,-24.165)) ;
#160207 = CARTESIAN_POINT('',(10.2,2.,-24.165)) ;
#160208 = CARTESIAN_POINT('',(10.2,1.9,-21.555)) ;
#160209 = CARTESIAN_POINT('',(10.2,1.9,-21.455)) ;
#160210 = CARTESIAN_POINT('',(10.2,-2.25,-21.555)) ;
#160211 = CARTESIAN_POINT('Origin',(10.2,-2.25,-27.545)) ;
#160212 = CARTESIAN_POINT('',(10.1,-2.25,-27.5731195934094)) ;
#160213 = CARTESIAN_POINT('',(3.7,-2.25,-27.5731195934094)) ;
#160214 = CARTESIAN_POINT('',(10.2,-2.25,-27.5731195934094)) ;
#160215 = CARTESIAN_POINT('',(3.7,-2.25,-27.975)) ;
#160216 = CARTESIAN_POINT('',(3.7,-2.25,-27.545)) ;
#160217 = CARTESIAN_POINT('',(10.1,-2.25,-27.975)) ;
#160218 = CARTESIAN_POINT('',(10.2,-2.25,-27.975)) ;
#160219 = CARTESIAN_POINT('',(10.1,-2.25,-27.545)) ;
#160220 = CARTESIAN_POINT('Origin',(10.2,-2.25,-25.265)) ;
#160221 = CARTESIAN_POINT('',(10.1,-2.25,-25.365)) ;
#160222 = CARTESIAN_POINT('',(3.7,-2.25,-25.365)) ;
#160223 = CARTESIAN_POINT('',(10.2,-2.25,-25.365)) ;
#160224 = CARTESIAN_POINT('',(3.7,-2.25,-25.7668804065906)) ;
#160225 = CARTESIAN_POINT('',(3.7,-2.25,-25.265)) ;
#160226 = CARTESIAN_POINT('',(10.1,-2.25,-25.7668804065906)) ;
#160227 = CARTESIAN_POINT('',(10.2,-2.25,-25.7668804065906)) ;
#160228 = CARTESIAN_POINT('',(10.1,-2.25,-25.265)) ;
#160229 = CARTESIAN_POINT('Origin',(10.2,-3.65625,-26.67)) ;
#160230 = CARTESIAN_POINT('',(10.1,-2.23576512455516,-25.8183035862865)) ;
#160231 = CARTESIAN_POINT('',(3.7,-2.23576512455516,-25.8183035862865)) ;
#160232 = CARTESIAN_POINT('',(10.2,-2.23576512455516,-25.8183035862865)) ;
#160233 = CARTESIAN_POINT('',(3.7,-2.23576512455516,-27.5216964137135)) ;
#160234 = CARTESIAN_POINT('Origin',(3.7,-3.65625,-26.67)) ;
#160235 = CARTESIAN_POINT('',(10.1,-2.23576512455516,-27.5216964137135)) ;
#160236 = CARTESIAN_POINT('',(10.2,-2.23576512455516,-27.5216964137135)) ;
#160237 = CARTESIAN_POINT('Origin',(10.1,-3.65625,-26.67)) ;
#160238 = CARTESIAN_POINT('Origin',(10.2,-3.65625,-26.67)) ;
#160239 = CARTESIAN_POINT('',(10.2,-2.15,-25.365)) ;
#160240 = CARTESIAN_POINT('',(10.2,-2.15,-25.7668804065906)) ;
#160241 = CARTESIAN_POINT('',(10.2,-2.15,-25.795)) ;
#160242 = CARTESIAN_POINT('',(10.2,-2.15,-27.5731195934094)) ;
#160243 = CARTESIAN_POINT('Origin',(10.2,-3.65625,-26.67)) ;
#160244 = CARTESIAN_POINT('',(10.2,-2.15,-27.975)) ;
#160245 = CARTESIAN_POINT('',(10.2,-2.15,-28.075)) ;
#160246 = CARTESIAN_POINT('',(10.2,1.9,-27.975)) ;
#160247 = CARTESIAN_POINT('',(10.2,2.,-27.975)) ;
#160248 = CARTESIAN_POINT('',(10.2,1.9,-25.365)) ;
#160249 = CARTESIAN_POINT('',(10.2,1.9,-25.265)) ;
#160250 = CARTESIAN_POINT('',(10.2,-2.25,-25.365)) ;
#160251 = CARTESIAN_POINT('Origin',(10.2,-2.25,-31.355)) ;
#160252 = CARTESIAN_POINT('',(10.1,-2.25,-31.3831195934094)) ;
#160253 = CARTESIAN_POINT('',(3.7,-2.25,-31.3831195934094)) ;
#160254 = CARTESIAN_POINT('',(10.2,-2.25,-31.3831195934094)) ;
#160255 = CARTESIAN_POINT('',(3.7,-2.25,-31.785)) ;
#160256 = CARTESIAN_POINT('',(3.7,-2.25,-31.355)) ;
#160257 = CARTESIAN_POINT('',(10.1,-2.25,-31.785)) ;
#160258 = CARTESIAN_POINT('',(10.2,-2.25,-31.785)) ;
#160259 = CARTESIAN_POINT('',(10.1,-2.25,-31.355)) ;
#160260 = CARTESIAN_POINT('Origin',(10.2,-2.25,-29.075)) ;
#160261 = CARTESIAN_POINT('',(10.1,-2.25,-29.175)) ;
#160262 = CARTESIAN_POINT('',(3.7,-2.25,-29.175)) ;
#160263 = CARTESIAN_POINT('',(10.2,-2.25,-29.175)) ;
#160264 = CARTESIAN_POINT('',(3.7,-2.25,-29.5768804065906)) ;
#160265 = CARTESIAN_POINT('',(3.7,-2.25,-29.075)) ;
#160266 = CARTESIAN_POINT('',(10.1,-2.25,-29.5768804065906)) ;
#160267 = CARTESIAN_POINT('',(10.2,-2.25,-29.5768804065906)) ;
#160268 = CARTESIAN_POINT('',(10.1,-2.25,-29.075)) ;
#160269 = CARTESIAN_POINT('Origin',(10.2,-3.65625,-30.48)) ;
#160270 = CARTESIAN_POINT('',(10.1,-2.23576512455516,-29.6283035862865)) ;
#160271 = CARTESIAN_POINT('',(3.7,-2.23576512455516,-29.6283035862865)) ;
#160272 = CARTESIAN_POINT('',(10.2,-2.23576512455516,-29.6283035862865)) ;
#160273 = CARTESIAN_POINT('',(3.7,-2.23576512455516,-31.3316964137135)) ;
#160274 = CARTESIAN_POINT('Origin',(3.7,-3.65625,-30.48)) ;
#160275 = CARTESIAN_POINT('',(10.1,-2.23576512455516,-31.3316964137135)) ;
#160276 = CARTESIAN_POINT('',(10.2,-2.23576512455516,-31.3316964137135)) ;
#160277 = CARTESIAN_POINT('Origin',(10.1,-3.65625,-30.48)) ;
#160278 = CARTESIAN_POINT('Origin',(10.2,-3.65625,-30.48)) ;
#160279 = CARTESIAN_POINT('',(10.2,-2.15,-29.175)) ;
#160280 = CARTESIAN_POINT('',(10.2,-2.15,-29.5768804065906)) ;
#160281 = CARTESIAN_POINT('',(10.2,-2.15,-29.605)) ;
#160282 = CARTESIAN_POINT('',(10.2,-2.15,-31.3831195934094)) ;
#160283 = CARTESIAN_POINT('Origin',(10.2,-3.65625,-30.48)) ;
#160284 = CARTESIAN_POINT('',(10.2,-2.15,-31.785)) ;
#160285 = CARTESIAN_POINT('',(10.2,-2.15,-31.885)) ;
#160286 = CARTESIAN_POINT('',(10.2,1.9,-31.785)) ;
#160287 = CARTESIAN_POINT('',(10.2,2.,-31.785)) ;
#160288 = CARTESIAN_POINT('',(10.2,1.9,-29.175)) ;
#160289 = CARTESIAN_POINT('',(10.2,1.9,-29.075)) ;
#160290 = CARTESIAN_POINT('',(10.2,-2.25,-29.175)) ;
#160291 = CARTESIAN_POINT('Origin',(10.2,-2.25,-35.165)) ;
#160292 = CARTESIAN_POINT('',(10.1,-2.25,-35.1931195934094)) ;
#160293 = CARTESIAN_POINT('',(3.7,-2.25,-35.1931195934094)) ;
#160294 = CARTESIAN_POINT('',(10.2,-2.25,-35.1931195934094)) ;
#160295 = CARTESIAN_POINT('',(3.7,-2.25,-35.595)) ;
#160296 = CARTESIAN_POINT('',(3.7,-2.25,-35.165)) ;
#160297 = CARTESIAN_POINT('',(10.1,-2.25,-35.595)) ;
#160298 = CARTESIAN_POINT('',(10.2,-2.25,-35.595)) ;
#160299 = CARTESIAN_POINT('',(10.1,-2.25,-35.165)) ;
#160300 = CARTESIAN_POINT('Origin',(10.2,-2.25,-32.885)) ;
#160301 = CARTESIAN_POINT('',(10.1,-2.25,-32.985)) ;
#160302 = CARTESIAN_POINT('',(3.7,-2.25,-32.985)) ;
#160303 = CARTESIAN_POINT('',(10.2,-2.25,-32.985)) ;
#160304 = CARTESIAN_POINT('',(3.7,-2.25,-33.3868804065906)) ;
#160305 = CARTESIAN_POINT('',(3.7,-2.25,-32.885)) ;
#160306 = CARTESIAN_POINT('',(10.1,-2.25,-33.3868804065906)) ;
#160307 = CARTESIAN_POINT('',(10.2,-2.25,-33.3868804065906)) ;
#160308 = CARTESIAN_POINT('',(10.1,-2.25,-32.885)) ;
#160309 = CARTESIAN_POINT('Origin',(10.2,-3.65625,-34.29)) ;
#160310 = CARTESIAN_POINT('',(10.1,-2.23576512455516,-33.4383035862865)) ;
#160311 = CARTESIAN_POINT('',(3.7,-2.23576512455516,-33.4383035862865)) ;
#160312 = CARTESIAN_POINT('',(10.2,-2.23576512455516,-33.4383035862865)) ;
#160313 = CARTESIAN_POINT('',(3.7,-2.23576512455516,-35.1416964137135)) ;
#160314 = CARTESIAN_POINT('Origin',(3.7,-3.65625,-34.29)) ;
#160315 = CARTESIAN_POINT('',(10.1,-2.23576512455516,-35.1416964137135)) ;
#160316 = CARTESIAN_POINT('',(10.2,-2.23576512455516,-35.1416964137135)) ;
#160317 = CARTESIAN_POINT('Origin',(10.1,-3.65625,-34.29)) ;
#160318 = CARTESIAN_POINT('Origin',(10.2,-3.65625,-34.29)) ;
#160319 = CARTESIAN_POINT('',(10.2,-2.15,-32.985)) ;
#160320 = CARTESIAN_POINT('',(10.2,-2.15,-33.3868804065906)) ;
#160321 = CARTESIAN_POINT('',(10.2,-2.15,-33.415)) ;
#160322 = CARTESIAN_POINT('',(10.2,-2.15,-35.1931195934094)) ;
#160323 = CARTESIAN_POINT('Origin',(10.2,-3.65625,-34.29)) ;
#160324 = CARTESIAN_POINT('',(10.2,-2.15,-35.595)) ;
#160325 = CARTESIAN_POINT('',(10.2,-2.15,-35.695)) ;
#160326 = CARTESIAN_POINT('',(10.2,1.9,-35.595)) ;
#160327 = CARTESIAN_POINT('',(10.2,2.,-35.595)) ;
#160328 = CARTESIAN_POINT('',(10.2,1.9,-32.985)) ;
#160329 = CARTESIAN_POINT('',(10.2,1.9,-32.885)) ;
#160330 = CARTESIAN_POINT('',(10.2,-2.25,-32.985)) ;
#160331 = CARTESIAN_POINT('Origin',(8.7,0.,-3.81)) ;
#160332 = CARTESIAN_POINT('Origin',(8.7,0.,-7.62)) ;
#160333 = CARTESIAN_POINT('Origin',(8.7,0.,-11.43)) ;
#160334 = CARTESIAN_POINT('Origin',(8.7,0.,-15.24)) ;
#160335 = CARTESIAN_POINT('Origin',(8.7,0.,-19.05)) ;
#160336 = CARTESIAN_POINT('Origin',(8.7,0.,-22.86)) ;
#160337 = CARTESIAN_POINT('Origin',(8.7,0.,-26.67)) ;
#160338 = CARTESIAN_POINT('Origin',(8.7,0.,-30.48)) ;
#160339 = CARTESIAN_POINT('Origin',(8.7,0.,-34.29)) ;
#160340 = CARTESIAN_POINT('Origin',(-2.,4.4,-35.29)) ;
#160341 = CARTESIAN_POINT('',(-2.,4.35,-35.19)) ;
#160342 = CARTESIAN_POINT('',(-2.,4.35,-33.39)) ;
#160343 = CARTESIAN_POINT('',(-2.,4.35,-35.29)) ;
#160344 = CARTESIAN_POINT('',(-2.,4.45,-33.39)) ;
#160345 = CARTESIAN_POINT('',(-2.,4.55,-33.39)) ;
#160346 = CARTESIAN_POINT('',(-2.,4.45,-35.19)) ;
#160347 = CARTESIAN_POINT('',(-2.,4.45,-35.29)) ;
#160348 = CARTESIAN_POINT('',(-2.,4.25,-35.19)) ;
#160349 = CARTESIAN_POINT('Origin',(-3.,4.4,-33.29)) ;
#160350 = CARTESIAN_POINT('',(-2.9,4.45,-33.29)) ;
#160351 = CARTESIAN_POINT('',(-2.1,4.45,-33.29)) ;
#160352 = CARTESIAN_POINT('',(-2.,4.45,-33.29)) ;
#160353 = CARTESIAN_POINT('',(-2.1,4.35,-33.29)) ;
#160354 = CARTESIAN_POINT('',(-2.1,4.25,-33.29)) ;
#160355 = CARTESIAN_POINT('',(-2.9,4.35,-33.29)) ;
#160356 = CARTESIAN_POINT('',(-3.,4.35,-33.29)) ;
#160357 = CARTESIAN_POINT('',(-2.9,4.55,-33.29)) ;
#160358 = CARTESIAN_POINT('Origin',(-3.,4.4,-35.29)) ;
#160359 = CARTESIAN_POINT('',(-3.,4.45,-33.39)) ;
#160360 = CARTESIAN_POINT('',(-3.,4.35,-33.39)) ;
#160361 = CARTESIAN_POINT('',(-3.,4.25,-33.39)) ;
#160362 = CARTESIAN_POINT('',(-3.,4.35,-35.19)) ;
#160363 = CARTESIAN_POINT('',(-3.,4.35,-35.29)) ;
#160364 = CARTESIAN_POINT('',(-3.,4.45,-35.19)) ;
#160365 = CARTESIAN_POINT('',(-3.,4.55,-35.19)) ;
#160366 = CARTESIAN_POINT('',(-3.,4.45,-33.29)) ;
#160367 = CARTESIAN_POINT('Origin',(-3.,4.4,-35.29)) ;
#160368 = CARTESIAN_POINT('',(-2.9,4.35,-35.29)) ;
#160369 = CARTESIAN_POINT('',(-2.1,4.35,-35.29)) ;
#160370 = CARTESIAN_POINT('',(-3.,4.35,-35.29)) ;
#160371 = CARTESIAN_POINT('',(-2.1,4.45,-35.29)) ;
#160372 = CARTESIAN_POINT('',(-2.1,4.55,-35.29)) ;
#160373 = CARTESIAN_POINT('',(-2.9,4.45,-35.29)) ;
#160374 = CARTESIAN_POINT('',(-3.,4.45,-35.29)) ;
#160375 = CARTESIAN_POINT('',(-2.9,4.25,-35.29)) ;
#160376 = CARTESIAN_POINT('Origin',(-2.,4.4,-31.48)) ;
#160377 = CARTESIAN_POINT('',(-2.,4.35,-31.38)) ;
#160378 = CARTESIAN_POINT('',(-2.,4.35,-29.58)) ;
#160379 = CARTESIAN_POINT('',(-2.,4.35,-31.48)) ;
#160380 = CARTESIAN_POINT('',(-2.,4.45,-29.58)) ;
#160381 = CARTESIAN_POINT('',(-2.,4.55,-29.58)) ;
#160382 = CARTESIAN_POINT('',(-2.,4.45,-31.38)) ;
#160383 = CARTESIAN_POINT('',(-2.,4.45,-31.48)) ;
#160384 = CARTESIAN_POINT('',(-2.,4.25,-31.38)) ;
#160385 = CARTESIAN_POINT('Origin',(-3.,4.4,-29.48)) ;
#160386 = CARTESIAN_POINT('',(-2.9,4.45,-29.48)) ;
#160387 = CARTESIAN_POINT('',(-2.1,4.45,-29.48)) ;
#160388 = CARTESIAN_POINT('',(-2.,4.45,-29.48)) ;
#160389 = CARTESIAN_POINT('',(-2.1,4.35,-29.48)) ;
#160390 = CARTESIAN_POINT('',(-2.1,4.25,-29.48)) ;
#160391 = CARTESIAN_POINT('',(-2.9,4.35,-29.48)) ;
#160392 = CARTESIAN_POINT('',(-3.,4.35,-29.48)) ;
#160393 = CARTESIAN_POINT('',(-2.9,4.55,-29.48)) ;
#160394 = CARTESIAN_POINT('Origin',(-3.,4.4,-31.48)) ;
#160395 = CARTESIAN_POINT('',(-3.,4.45,-29.58)) ;
#160396 = CARTESIAN_POINT('',(-3.,4.35,-29.58)) ;
#160397 = CARTESIAN_POINT('',(-3.,4.25,-29.58)) ;
#160398 = CARTESIAN_POINT('',(-3.,4.35,-31.38)) ;
#160399 = CARTESIAN_POINT('',(-3.,4.35,-31.48)) ;
#160400 = CARTESIAN_POINT('',(-3.,4.45,-31.38)) ;
#160401 = CARTESIAN_POINT('',(-3.,4.55,-31.38)) ;
#160402 = CARTESIAN_POINT('',(-3.,4.45,-29.48)) ;
#160403 = CARTESIAN_POINT('Origin',(-3.,4.4,-31.48)) ;
#160404 = CARTESIAN_POINT('',(-2.9,4.35,-31.48)) ;
#160405 = CARTESIAN_POINT('',(-2.1,4.35,-31.48)) ;
#160406 = CARTESIAN_POINT('',(-3.,4.35,-31.48)) ;
#160407 = CARTESIAN_POINT('',(-2.1,4.45,-31.48)) ;
#160408 = CARTESIAN_POINT('',(-2.1,4.55,-31.48)) ;
#160409 = CARTESIAN_POINT('',(-2.9,4.45,-31.48)) ;
#160410 = CARTESIAN_POINT('',(-3.,4.45,-31.48)) ;
#160411 = CARTESIAN_POINT('',(-2.9,4.25,-31.48)) ;
#160412 = CARTESIAN_POINT('Origin',(-2.,4.4,-27.67)) ;
#160413 = CARTESIAN_POINT('',(-2.,4.35,-27.57)) ;
#160414 = CARTESIAN_POINT('',(-2.,4.35,-25.77)) ;
#160415 = CARTESIAN_POINT('',(-2.,4.35,-27.67)) ;
#160416 = CARTESIAN_POINT('',(-2.,4.45,-25.77)) ;
#160417 = CARTESIAN_POINT('',(-2.,4.55,-25.77)) ;
#160418 = CARTESIAN_POINT('',(-2.,4.45,-27.57)) ;
#160419 = CARTESIAN_POINT('',(-2.,4.45,-27.67)) ;
#160420 = CARTESIAN_POINT('',(-2.,4.25,-27.57)) ;
#160421 = CARTESIAN_POINT('Origin',(-3.,4.4,-25.67)) ;
#160422 = CARTESIAN_POINT('',(-2.9,4.45,-25.67)) ;
#160423 = CARTESIAN_POINT('',(-2.1,4.45,-25.67)) ;
#160424 = CARTESIAN_POINT('',(-2.,4.45,-25.67)) ;
#160425 = CARTESIAN_POINT('',(-2.1,4.35,-25.67)) ;
#160426 = CARTESIAN_POINT('',(-2.1,4.25,-25.67)) ;
#160427 = CARTESIAN_POINT('',(-2.9,4.35,-25.67)) ;
#160428 = CARTESIAN_POINT('',(-3.,4.35,-25.67)) ;
#160429 = CARTESIAN_POINT('',(-2.9,4.55,-25.67)) ;
#160430 = CARTESIAN_POINT('Origin',(-3.,4.4,-27.67)) ;
#160431 = CARTESIAN_POINT('',(-3.,4.45,-25.77)) ;
#160432 = CARTESIAN_POINT('',(-3.,4.35,-25.77)) ;
#160433 = CARTESIAN_POINT('',(-3.,4.25,-25.77)) ;
#160434 = CARTESIAN_POINT('',(-3.,4.35,-27.57)) ;
#160435 = CARTESIAN_POINT('',(-3.,4.35,-27.67)) ;
#160436 = CARTESIAN_POINT('',(-3.,4.45,-27.57)) ;
#160437 = CARTESIAN_POINT('',(-3.,4.55,-27.57)) ;
#160438 = CARTESIAN_POINT('',(-3.,4.45,-25.67)) ;
#160439 = CARTESIAN_POINT('Origin',(-3.,4.4,-27.67)) ;
#160440 = CARTESIAN_POINT('',(-2.9,4.35,-27.67)) ;
#160441 = CARTESIAN_POINT('',(-2.1,4.35,-27.67)) ;
#160442 = CARTESIAN_POINT('',(-3.,4.35,-27.67)) ;
#160443 = CARTESIAN_POINT('',(-2.1,4.45,-27.67)) ;
#160444 = CARTESIAN_POINT('',(-2.1,4.55,-27.67)) ;
#160445 = CARTESIAN_POINT('',(-2.9,4.45,-27.67)) ;
#160446 = CARTESIAN_POINT('',(-3.,4.45,-27.67)) ;
#160447 = CARTESIAN_POINT('',(-2.9,4.25,-27.67)) ;
#160448 = CARTESIAN_POINT('Origin',(-2.,4.4,-23.86)) ;
#160449 = CARTESIAN_POINT('',(-2.,4.35,-23.76)) ;
#160450 = CARTESIAN_POINT('',(-2.,4.35,-21.96)) ;
#160451 = CARTESIAN_POINT('',(-2.,4.35,-23.86)) ;
#160452 = CARTESIAN_POINT('',(-2.,4.45,-21.96)) ;
#160453 = CARTESIAN_POINT('',(-2.,4.55,-21.96)) ;
#160454 = CARTESIAN_POINT('',(-2.,4.45,-23.76)) ;
#160455 = CARTESIAN_POINT('',(-2.,4.45,-23.86)) ;
#160456 = CARTESIAN_POINT('',(-2.,4.25,-23.76)) ;
#160457 = CARTESIAN_POINT('Origin',(-3.,4.4,-21.86)) ;
#160458 = CARTESIAN_POINT('',(-2.9,4.45,-21.86)) ;
#160459 = CARTESIAN_POINT('',(-2.1,4.45,-21.86)) ;
#160460 = CARTESIAN_POINT('',(-2.,4.45,-21.86)) ;
#160461 = CARTESIAN_POINT('',(-2.1,4.35,-21.86)) ;
#160462 = CARTESIAN_POINT('',(-2.1,4.25,-21.86)) ;
#160463 = CARTESIAN_POINT('',(-2.9,4.35,-21.86)) ;
#160464 = CARTESIAN_POINT('',(-3.,4.35,-21.86)) ;
#160465 = CARTESIAN_POINT('',(-2.9,4.55,-21.86)) ;
#160466 = CARTESIAN_POINT('Origin',(-3.,4.4,-23.86)) ;
#160467 = CARTESIAN_POINT('',(-3.,4.45,-21.96)) ;
#160468 = CARTESIAN_POINT('',(-3.,4.35,-21.96)) ;
#160469 = CARTESIAN_POINT('',(-3.,4.25,-21.96)) ;
#160470 = CARTESIAN_POINT('',(-3.,4.35,-23.76)) ;
#160471 = CARTESIAN_POINT('',(-3.,4.35,-23.86)) ;
#160472 = CARTESIAN_POINT('',(-3.,4.45,-23.76)) ;
#160473 = CARTESIAN_POINT('',(-3.,4.55,-23.76)) ;
#160474 = CARTESIAN_POINT('',(-3.,4.45,-21.86)) ;
#160475 = CARTESIAN_POINT('Origin',(-3.,4.4,-23.86)) ;
#160476 = CARTESIAN_POINT('',(-2.9,4.35,-23.86)) ;
#160477 = CARTESIAN_POINT('',(-2.1,4.35,-23.86)) ;
#160478 = CARTESIAN_POINT('',(-3.,4.35,-23.86)) ;
#160479 = CARTESIAN_POINT('',(-2.1,4.45,-23.86)) ;
#160480 = CARTESIAN_POINT('',(-2.1,4.55,-23.86)) ;
#160481 = CARTESIAN_POINT('',(-2.9,4.45,-23.86)) ;
#160482 = CARTESIAN_POINT('',(-3.,4.45,-23.86)) ;
#160483 = CARTESIAN_POINT('',(-2.9,4.25,-23.86)) ;
#160484 = CARTESIAN_POINT('Origin',(-2.,4.4,-20.05)) ;
#160485 = CARTESIAN_POINT('',(-2.,4.35,-19.95)) ;
#160486 = CARTESIAN_POINT('',(-2.,4.35,-18.15)) ;
#160487 = CARTESIAN_POINT('',(-2.,4.35,-20.05)) ;
#160488 = CARTESIAN_POINT('',(-2.,4.45,-18.15)) ;
#160489 = CARTESIAN_POINT('',(-2.,4.55,-18.15)) ;
#160490 = CARTESIAN_POINT('',(-2.,4.45,-19.95)) ;
#160491 = CARTESIAN_POINT('',(-2.,4.45,-20.05)) ;
#160492 = CARTESIAN_POINT('',(-2.,4.25,-19.95)) ;
#160493 = CARTESIAN_POINT('Origin',(-3.,4.4,-18.05)) ;
#160494 = CARTESIAN_POINT('',(-2.9,4.45,-18.05)) ;
#160495 = CARTESIAN_POINT('',(-2.1,4.45,-18.05)) ;
#160496 = CARTESIAN_POINT('',(-2.,4.45,-18.05)) ;
#160497 = CARTESIAN_POINT('',(-2.1,4.35,-18.05)) ;
#160498 = CARTESIAN_POINT('',(-2.1,4.25,-18.05)) ;
#160499 = CARTESIAN_POINT('',(-2.9,4.35,-18.05)) ;
#160500 = CARTESIAN_POINT('',(-3.,4.35,-18.05)) ;
#160501 = CARTESIAN_POINT('',(-2.9,4.55,-18.05)) ;
#160502 = CARTESIAN_POINT('Origin',(-3.,4.4,-20.05)) ;
#160503 = CARTESIAN_POINT('',(-3.,4.45,-18.15)) ;
#160504 = CARTESIAN_POINT('',(-3.,4.35,-18.15)) ;
#160505 = CARTESIAN_POINT('',(-3.,4.25,-18.15)) ;
#160506 = CARTESIAN_POINT('',(-3.,4.35,-19.95)) ;
#160507 = CARTESIAN_POINT('',(-3.,4.35,-20.05)) ;
#160508 = CARTESIAN_POINT('',(-3.,4.45,-19.95)) ;
#160509 = CARTESIAN_POINT('',(-3.,4.55,-19.95)) ;
#160510 = CARTESIAN_POINT('',(-3.,4.45,-18.05)) ;
#160511 = CARTESIAN_POINT('Origin',(-3.,4.4,-20.05)) ;
#160512 = CARTESIAN_POINT('',(-2.9,4.35,-20.05)) ;
#160513 = CARTESIAN_POINT('',(-2.1,4.35,-20.05)) ;
#160514 = CARTESIAN_POINT('',(-3.,4.35,-20.05)) ;
#160515 = CARTESIAN_POINT('',(-2.1,4.45,-20.05)) ;
#160516 = CARTESIAN_POINT('',(-2.1,4.55,-20.05)) ;
#160517 = CARTESIAN_POINT('',(-2.9,4.45,-20.05)) ;
#160518 = CARTESIAN_POINT('',(-3.,4.45,-20.05)) ;
#160519 = CARTESIAN_POINT('',(-2.9,4.25,-20.05)) ;
#160520 = CARTESIAN_POINT('Origin',(-2.,4.4,-16.24)) ;
#160521 = CARTESIAN_POINT('',(-2.,4.35,-16.14)) ;
#160522 = CARTESIAN_POINT('',(-2.,4.35,-14.34)) ;
#160523 = CARTESIAN_POINT('',(-2.,4.35,-16.24)) ;
#160524 = CARTESIAN_POINT('',(-2.,4.45,-14.34)) ;
#160525 = CARTESIAN_POINT('',(-2.,4.55,-14.34)) ;
#160526 = CARTESIAN_POINT('',(-2.,4.45,-16.14)) ;
#160527 = CARTESIAN_POINT('',(-2.,4.45,-16.24)) ;
#160528 = CARTESIAN_POINT('',(-2.,4.25,-16.14)) ;
#160529 = CARTESIAN_POINT('Origin',(-3.,4.4,-14.24)) ;
#160530 = CARTESIAN_POINT('',(-2.9,4.45,-14.24)) ;
#160531 = CARTESIAN_POINT('',(-2.1,4.45,-14.24)) ;
#160532 = CARTESIAN_POINT('',(-2.,4.45,-14.24)) ;
#160533 = CARTESIAN_POINT('',(-2.1,4.35,-14.24)) ;
#160534 = CARTESIAN_POINT('',(-2.1,4.25,-14.24)) ;
#160535 = CARTESIAN_POINT('',(-2.9,4.35,-14.24)) ;
#160536 = CARTESIAN_POINT('',(-3.,4.35,-14.24)) ;
#160537 = CARTESIAN_POINT('',(-2.9,4.55,-14.24)) ;
#160538 = CARTESIAN_POINT('Origin',(-3.,4.4,-16.24)) ;
#160539 = CARTESIAN_POINT('',(-3.,4.45,-14.34)) ;
#160540 = CARTESIAN_POINT('',(-3.,4.35,-14.34)) ;
#160541 = CARTESIAN_POINT('',(-3.,4.25,-14.34)) ;
#160542 = CARTESIAN_POINT('',(-3.,4.35,-16.14)) ;
#160543 = CARTESIAN_POINT('',(-3.,4.35,-16.24)) ;
#160544 = CARTESIAN_POINT('',(-3.,4.45,-16.14)) ;
#160545 = CARTESIAN_POINT('',(-3.,4.55,-16.14)) ;
#160546 = CARTESIAN_POINT('',(-3.,4.45,-14.24)) ;
#160547 = CARTESIAN_POINT('Origin',(-3.,4.4,-16.24)) ;
#160548 = CARTESIAN_POINT('',(-2.9,4.35,-16.24)) ;
#160549 = CARTESIAN_POINT('',(-2.1,4.35,-16.24)) ;
#160550 = CARTESIAN_POINT('',(-3.,4.35,-16.24)) ;
#160551 = CARTESIAN_POINT('',(-2.1,4.45,-16.24)) ;
#160552 = CARTESIAN_POINT('',(-2.1,4.55,-16.24)) ;
#160553 = CARTESIAN_POINT('',(-2.9,4.45,-16.24)) ;
#160554 = CARTESIAN_POINT('',(-3.,4.45,-16.24)) ;
#160555 = CARTESIAN_POINT('',(-2.9,4.25,-16.24)) ;
#160556 = CARTESIAN_POINT('Origin',(-2.,4.4,-12.43)) ;
#160557 = CARTESIAN_POINT('',(-2.,4.35,-12.33)) ;
#160558 = CARTESIAN_POINT('',(-2.,4.35,-10.53)) ;
#160559 = CARTESIAN_POINT('',(-2.,4.35,-12.43)) ;
#160560 = CARTESIAN_POINT('',(-2.,4.45,-10.53)) ;
#160561 = CARTESIAN_POINT('',(-2.,4.55,-10.53)) ;
#160562 = CARTESIAN_POINT('',(-2.,4.45,-12.33)) ;
#160563 = CARTESIAN_POINT('',(-2.,4.45,-12.43)) ;
#160564 = CARTESIAN_POINT('',(-2.,4.25,-12.33)) ;
#160565 = CARTESIAN_POINT('Origin',(-3.,4.4,-10.43)) ;
#160566 = CARTESIAN_POINT('',(-2.9,4.45,-10.43)) ;
#160567 = CARTESIAN_POINT('',(-2.1,4.45,-10.43)) ;
#160568 = CARTESIAN_POINT('',(-2.,4.45,-10.43)) ;
#160569 = CARTESIAN_POINT('',(-2.1,4.35,-10.43)) ;
#160570 = CARTESIAN_POINT('',(-2.1,4.25,-10.43)) ;
#160571 = CARTESIAN_POINT('',(-2.9,4.35,-10.43)) ;
#160572 = CARTESIAN_POINT('',(-3.,4.35,-10.43)) ;
#160573 = CARTESIAN_POINT('',(-2.9,4.55,-10.43)) ;
#160574 = CARTESIAN_POINT('Origin',(-3.,4.4,-12.43)) ;
#160575 = CARTESIAN_POINT('',(-3.,4.45,-10.53)) ;
#160576 = CARTESIAN_POINT('',(-3.,4.35,-10.53)) ;
#160577 = CARTESIAN_POINT('',(-3.,4.25,-10.53)) ;
#160578 = CARTESIAN_POINT('',(-3.,4.35,-12.33)) ;
#160579 = CARTESIAN_POINT('',(-3.,4.35,-12.43)) ;
#160580 = CARTESIAN_POINT('',(-3.,4.45,-12.33)) ;
#160581 = CARTESIAN_POINT('',(-3.,4.55,-12.33)) ;
#160582 = CARTESIAN_POINT('',(-3.,4.45,-10.43)) ;
#160583 = CARTESIAN_POINT('Origin',(-3.,4.4,-12.43)) ;
#160584 = CARTESIAN_POINT('',(-2.9,4.35,-12.43)) ;
#160585 = CARTESIAN_POINT('',(-2.1,4.35,-12.43)) ;
#160586 = CARTESIAN_POINT('',(-3.,4.35,-12.43)) ;
#160587 = CARTESIAN_POINT('',(-2.1,4.45,-12.43)) ;
#160588 = CARTESIAN_POINT('',(-2.1,4.55,-12.43)) ;
#160589 = CARTESIAN_POINT('',(-2.9,4.45,-12.43)) ;
#160590 = CARTESIAN_POINT('',(-3.,4.45,-12.43)) ;
#160591 = CARTESIAN_POINT('',(-2.9,4.25,-12.43)) ;
#160592 = CARTESIAN_POINT('Origin',(-2.,4.4,-8.62)) ;
#160593 = CARTESIAN_POINT('',(-2.,4.35,-8.52)) ;
#160594 = CARTESIAN_POINT('',(-2.,4.35,-6.72)) ;
#160595 = CARTESIAN_POINT('',(-2.,4.35,-8.62)) ;
#160596 = CARTESIAN_POINT('',(-2.,4.45,-6.72)) ;
#160597 = CARTESIAN_POINT('',(-2.,4.55,-6.72)) ;
#160598 = CARTESIAN_POINT('',(-2.,4.45,-8.52)) ;
#160599 = CARTESIAN_POINT('',(-2.,4.45,-8.62)) ;
#160600 = CARTESIAN_POINT('',(-2.,4.25,-8.52)) ;
#160601 = CARTESIAN_POINT('Origin',(-3.,4.4,-6.62)) ;
#160602 = CARTESIAN_POINT('',(-2.9,4.45,-6.62)) ;
#160603 = CARTESIAN_POINT('',(-2.1,4.45,-6.62)) ;
#160604 = CARTESIAN_POINT('',(-2.,4.45,-6.62)) ;
#160605 = CARTESIAN_POINT('',(-2.1,4.35,-6.62)) ;
#160606 = CARTESIAN_POINT('',(-2.1,4.25,-6.62)) ;
#160607 = CARTESIAN_POINT('',(-2.9,4.35,-6.62)) ;
#160608 = CARTESIAN_POINT('',(-3.,4.35,-6.62)) ;
#160609 = CARTESIAN_POINT('',(-2.9,4.55,-6.62)) ;
#160610 = CARTESIAN_POINT('Origin',(-3.,4.4,-8.62)) ;
#160611 = CARTESIAN_POINT('',(-3.,4.45,-6.72)) ;
#160612 = CARTESIAN_POINT('',(-3.,4.35,-6.72)) ;
#160613 = CARTESIAN_POINT('',(-3.,4.25,-6.72)) ;
#160614 = CARTESIAN_POINT('',(-3.,4.35,-8.52)) ;
#160615 = CARTESIAN_POINT('',(-3.,4.35,-8.62)) ;
#160616 = CARTESIAN_POINT('',(-3.,4.45,-8.52)) ;
#160617 = CARTESIAN_POINT('',(-3.,4.55,-8.52)) ;
#160618 = CARTESIAN_POINT('',(-3.,4.45,-6.62)) ;
#160619 = CARTESIAN_POINT('Origin',(-3.,4.4,-8.62)) ;
#160620 = CARTESIAN_POINT('',(-2.9,4.35,-8.62)) ;
#160621 = CARTESIAN_POINT('',(-2.1,4.35,-8.62)) ;
#160622 = CARTESIAN_POINT('',(-3.,4.35,-8.62)) ;
#160623 = CARTESIAN_POINT('',(-2.1,4.45,-8.62)) ;
#160624 = CARTESIAN_POINT('',(-2.1,4.55,-8.62)) ;
#160625 = CARTESIAN_POINT('',(-2.9,4.45,-8.62)) ;
#160626 = CARTESIAN_POINT('',(-3.,4.45,-8.62)) ;
#160627 = CARTESIAN_POINT('',(-2.9,4.25,-8.62)) ;
#160628 = CARTESIAN_POINT('Origin',(-2.,4.4,-4.81)) ;
#160629 = CARTESIAN_POINT('',(-2.,4.35,-4.71)) ;
#160630 = CARTESIAN_POINT('',(-2.,4.35,-2.91)) ;
#160631 = CARTESIAN_POINT('',(-2.,4.35,-4.81)) ;
#160632 = CARTESIAN_POINT('',(-2.,4.45,-2.91)) ;
#160633 = CARTESIAN_POINT('',(-2.,4.55,-2.91)) ;
#160634 = CARTESIAN_POINT('',(-2.,4.45,-4.71)) ;
#160635 = CARTESIAN_POINT('',(-2.,4.45,-4.81)) ;
#160636 = CARTESIAN_POINT('',(-2.,4.25,-4.71)) ;
#160637 = CARTESIAN_POINT('Origin',(-3.,4.4,-2.81)) ;
#160638 = CARTESIAN_POINT('',(-2.9,4.45,-2.81)) ;
#160639 = CARTESIAN_POINT('',(-2.1,4.45,-2.81)) ;
#160640 = CARTESIAN_POINT('',(-2.,4.45,-2.81)) ;
#160641 = CARTESIAN_POINT('',(-2.1,4.35,-2.81)) ;
#160642 = CARTESIAN_POINT('',(-2.1,4.25,-2.81)) ;
#160643 = CARTESIAN_POINT('',(-2.9,4.35,-2.81)) ;
#160644 = CARTESIAN_POINT('',(-3.,4.35,-2.81)) ;
#160645 = CARTESIAN_POINT('',(-2.9,4.55,-2.81)) ;
#160646 = CARTESIAN_POINT('Origin',(-3.,4.4,-4.81)) ;
#160647 = CARTESIAN_POINT('',(-3.,4.45,-2.91)) ;
#160648 = CARTESIAN_POINT('',(-3.,4.35,-2.91)) ;
#160649 = CARTESIAN_POINT('',(-3.,4.25,-2.91)) ;
#160650 = CARTESIAN_POINT('',(-3.,4.35,-4.71)) ;
#160651 = CARTESIAN_POINT('',(-3.,4.35,-4.81)) ;
#160652 = CARTESIAN_POINT('',(-3.,4.45,-4.71)) ;
#160653 = CARTESIAN_POINT('',(-3.,4.55,-4.71)) ;
#160654 = CARTESIAN_POINT('',(-3.,4.45,-2.81)) ;
#160655 = CARTESIAN_POINT('Origin',(-3.,4.4,-4.81)) ;
#160656 = CARTESIAN_POINT('',(-2.9,4.35,-4.81)) ;
#160657 = CARTESIAN_POINT('',(-2.1,4.35,-4.81)) ;
#160658 = CARTESIAN_POINT('',(-3.,4.35,-4.81)) ;
#160659 = CARTESIAN_POINT('',(-2.1,4.45,-4.81)) ;
#160660 = CARTESIAN_POINT('',(-2.1,4.55,-4.81)) ;
#160661 = CARTESIAN_POINT('',(-2.9,4.45,-4.81)) ;
#160662 = CARTESIAN_POINT('',(-3.,4.45,-4.81)) ;
#160663 = CARTESIAN_POINT('',(-2.9,4.25,-4.81)) ;
#160664 = CARTESIAN_POINT('Origin',(0.,4.25,-3.81)) ;
#160665 = CARTESIAN_POINT('',(-2.9,4.25,-4.71)) ;
#160666 = CARTESIAN_POINT('',(-2.9,4.25,-2.91)) ;
#160667 = CARTESIAN_POINT('',(-2.9,4.25,-3.81)) ;
#160668 = CARTESIAN_POINT('',(-2.1,4.25,-2.91)) ;
#160669 = CARTESIAN_POINT('',(-1.95156391047391E-16,4.25,-2.91)) ;
#160670 = CARTESIAN_POINT('',(-2.1,4.25,-4.71)) ;
#160671 = CARTESIAN_POINT('',(-2.1,4.25,-3.81)) ;
#160672 = CARTESIAN_POINT('',(-1.95156391047391E-16,4.25,-4.71)) ;
#160673 = CARTESIAN_POINT('',(-2.75,4.25,-2.96)) ;
#160674 = CARTESIAN_POINT('',(-2.25,4.25,-2.96)) ;
#160675 = CARTESIAN_POINT('',(-2.85,4.25,-2.96)) ;
#160676 = CARTESIAN_POINT('',(-2.85,4.25,-3.06)) ;
#160677 = CARTESIAN_POINT('Origin',(-2.75,4.25,-3.06)) ;
#160678 = CARTESIAN_POINT('',(-2.85,4.25,-4.56)) ;
#160679 = CARTESIAN_POINT('',(-2.85,4.25,-4.66)) ;
#160680 = CARTESIAN_POINT('',(-2.75,4.25,-4.66)) ;
#160681 = CARTESIAN_POINT('Origin',(-2.75,4.25,-4.56)) ;
#160682 = CARTESIAN_POINT('',(-2.25,4.25,-4.66)) ;
#160683 = CARTESIAN_POINT('',(-2.15,4.25,-4.66)) ;
#160684 = CARTESIAN_POINT('',(-2.15,4.25,-4.56)) ;
#160685 = CARTESIAN_POINT('Origin',(-2.25,4.25,-4.56)) ;
#160686 = CARTESIAN_POINT('',(-2.15,4.25,-3.06)) ;
#160687 = CARTESIAN_POINT('',(-2.15,4.25,-2.96)) ;
#160688 = CARTESIAN_POINT('Origin',(-2.25,4.25,-3.06)) ;
#160689 = CARTESIAN_POINT('Origin',(-2.15,4.25,-2.96)) ;
#160690 = CARTESIAN_POINT('',(-2.15,4.3,-4.56)) ;
#160691 = CARTESIAN_POINT('',(-2.15,4.3,-3.06)) ;
#160692 = CARTESIAN_POINT('',(-2.15,4.3,-2.96)) ;
#160693 = CARTESIAN_POINT('',(-2.15,4.25,-3.06)) ;
#160694 = CARTESIAN_POINT('',(-2.15,4.25,-4.56)) ;
#160695 = CARTESIAN_POINT('Origin',(-2.85,4.25,-2.96)) ;
#160696 = CARTESIAN_POINT('',(-2.25,4.3,-2.96)) ;
#160697 = CARTESIAN_POINT('',(-2.75,4.3,-2.96)) ;
#160698 = CARTESIAN_POINT('',(-2.85,4.3,-2.96)) ;
#160699 = CARTESIAN_POINT('',(-2.75,4.25,-2.96)) ;
#160700 = CARTESIAN_POINT('',(-2.25,4.25,-2.96)) ;
#160701 = CARTESIAN_POINT('Origin',(-2.85,4.25,-4.66)) ;
#160702 = CARTESIAN_POINT('',(-2.85,4.3,-3.06)) ;
#160703 = CARTESIAN_POINT('',(-2.85,4.25,-3.06)) ;
#160704 = CARTESIAN_POINT('',(-2.85,4.3,-4.56)) ;
#160705 = CARTESIAN_POINT('',(-2.85,4.3,-4.66)) ;
#160706 = CARTESIAN_POINT('',(-2.85,4.25,-4.56)) ;
#160707 = CARTESIAN_POINT('Origin',(-2.15,4.25,-4.66)) ;
#160708 = CARTESIAN_POINT('',(-2.75,4.3,-4.66)) ;
#160709 = CARTESIAN_POINT('',(-2.25,4.3,-4.66)) ;
#160710 = CARTESIAN_POINT('',(-2.15,4.3,-4.66)) ;
#160711 = CARTESIAN_POINT('',(-2.25,4.25,-4.66)) ;
#160712 = CARTESIAN_POINT('',(-2.75,4.25,-4.66)) ;
#160713 = CARTESIAN_POINT('Origin',(0.,4.25,-7.62)) ;
#160714 = CARTESIAN_POINT('',(-2.9,4.25,-8.52)) ;
#160715 = CARTESIAN_POINT('',(-2.9,4.25,-6.72)) ;
#160716 = CARTESIAN_POINT('',(-2.9,4.25,-7.62)) ;
#160717 = CARTESIAN_POINT('',(-2.1,4.25,-6.72)) ;
#160718 = CARTESIAN_POINT('',(-1.95156391047391E-16,4.25,-6.72)) ;
#160719 = CARTESIAN_POINT('',(-2.1,4.25,-8.52)) ;
#160720 = CARTESIAN_POINT('',(-2.1,4.25,-7.62)) ;
#160721 = CARTESIAN_POINT('',(-1.95156391047391E-16,4.25,-8.52)) ;
#160722 = CARTESIAN_POINT('',(-2.75,4.25,-6.77)) ;
#160723 = CARTESIAN_POINT('',(-2.25,4.25,-6.77)) ;
#160724 = CARTESIAN_POINT('',(-2.85,4.25,-6.77)) ;
#160725 = CARTESIAN_POINT('',(-2.85,4.25,-6.87)) ;
#160726 = CARTESIAN_POINT('Origin',(-2.75,4.25,-6.87)) ;
#160727 = CARTESIAN_POINT('',(-2.85,4.25,-8.37)) ;
#160728 = CARTESIAN_POINT('',(-2.85,4.25,-8.47)) ;
#160729 = CARTESIAN_POINT('',(-2.75,4.25,-8.47)) ;
#160730 = CARTESIAN_POINT('Origin',(-2.75,4.25,-8.37)) ;
#160731 = CARTESIAN_POINT('',(-2.25,4.25,-8.47)) ;
#160732 = CARTESIAN_POINT('',(-2.15,4.25,-8.47)) ;
#160733 = CARTESIAN_POINT('',(-2.15,4.25,-8.37)) ;
#160734 = CARTESIAN_POINT('Origin',(-2.25,4.25,-8.37)) ;
#160735 = CARTESIAN_POINT('',(-2.15,4.25,-6.87)) ;
#160736 = CARTESIAN_POINT('',(-2.15,4.25,-6.77)) ;
#160737 = CARTESIAN_POINT('Origin',(-2.25,4.25,-6.87)) ;
#160738 = CARTESIAN_POINT('Origin',(-2.15,4.25,-6.77)) ;
#160739 = CARTESIAN_POINT('',(-2.15,4.3,-8.37)) ;
#160740 = CARTESIAN_POINT('',(-2.15,4.3,-6.87)) ;
#160741 = CARTESIAN_POINT('',(-2.15,4.3,-6.77)) ;
#160742 = CARTESIAN_POINT('',(-2.15,4.25,-6.87)) ;
#160743 = CARTESIAN_POINT('',(-2.15,4.25,-8.37)) ;
#160744 = CARTESIAN_POINT('Origin',(-2.85,4.25,-6.77)) ;
#160745 = CARTESIAN_POINT('',(-2.25,4.3,-6.77)) ;
#160746 = CARTESIAN_POINT('',(-2.75,4.3,-6.77)) ;
#160747 = CARTESIAN_POINT('',(-2.85,4.3,-6.77)) ;
#160748 = CARTESIAN_POINT('',(-2.75,4.25,-6.77)) ;
#160749 = CARTESIAN_POINT('',(-2.25,4.25,-6.77)) ;
#160750 = CARTESIAN_POINT('Origin',(-2.85,4.25,-8.47)) ;
#160751 = CARTESIAN_POINT('',(-2.85,4.3,-6.87)) ;
#160752 = CARTESIAN_POINT('',(-2.85,4.25,-6.87)) ;
#160753 = CARTESIAN_POINT('',(-2.85,4.3,-8.37)) ;
#160754 = CARTESIAN_POINT('',(-2.85,4.3,-8.47)) ;
#160755 = CARTESIAN_POINT('',(-2.85,4.25,-8.37)) ;
#160756 = CARTESIAN_POINT('Origin',(-2.15,4.25,-8.47)) ;
#160757 = CARTESIAN_POINT('',(-2.75,4.3,-8.47)) ;
#160758 = CARTESIAN_POINT('',(-2.25,4.3,-8.47)) ;
#160759 = CARTESIAN_POINT('',(-2.15,4.3,-8.47)) ;
#160760 = CARTESIAN_POINT('',(-2.25,4.25,-8.47)) ;
#160761 = CARTESIAN_POINT('',(-2.75,4.25,-8.47)) ;
#160762 = CARTESIAN_POINT('Origin',(0.,4.25,-11.43)) ;
#160763 = CARTESIAN_POINT('',(-2.9,4.25,-12.33)) ;
#160764 = CARTESIAN_POINT('',(-2.9,4.25,-10.53)) ;
#160765 = CARTESIAN_POINT('',(-2.9,4.25,-11.43)) ;
#160766 = CARTESIAN_POINT('',(-2.1,4.25,-10.53)) ;
#160767 = CARTESIAN_POINT('',(-1.95156391047391E-16,4.25,-10.53)) ;
#160768 = CARTESIAN_POINT('',(-2.1,4.25,-12.33)) ;
#160769 = CARTESIAN_POINT('',(-2.1,4.25,-11.43)) ;
#160770 = CARTESIAN_POINT('',(-1.95156391047391E-16,4.25,-12.33)) ;
#160771 = CARTESIAN_POINT('',(-2.75,4.25,-10.58)) ;
#160772 = CARTESIAN_POINT('',(-2.25,4.25,-10.58)) ;
#160773 = CARTESIAN_POINT('',(-2.85,4.25,-10.58)) ;
#160774 = CARTESIAN_POINT('',(-2.85,4.25,-10.68)) ;
#160775 = CARTESIAN_POINT('Origin',(-2.75,4.25,-10.68)) ;
#160776 = CARTESIAN_POINT('',(-2.85,4.25,-12.18)) ;
#160777 = CARTESIAN_POINT('',(-2.85,4.25,-12.28)) ;
#160778 = CARTESIAN_POINT('',(-2.75,4.25,-12.28)) ;
#160779 = CARTESIAN_POINT('Origin',(-2.75,4.25,-12.18)) ;
#160780 = CARTESIAN_POINT('',(-2.25,4.25,-12.28)) ;
#160781 = CARTESIAN_POINT('',(-2.15,4.25,-12.28)) ;
#160782 = CARTESIAN_POINT('',(-2.15,4.25,-12.18)) ;
#160783 = CARTESIAN_POINT('Origin',(-2.25,4.25,-12.18)) ;
#160784 = CARTESIAN_POINT('',(-2.15,4.25,-10.68)) ;
#160785 = CARTESIAN_POINT('',(-2.15,4.25,-10.58)) ;
#160786 = CARTESIAN_POINT('Origin',(-2.25,4.25,-10.68)) ;
#160787 = CARTESIAN_POINT('Origin',(-2.15,4.25,-10.58)) ;
#160788 = CARTESIAN_POINT('',(-2.15,4.3,-12.18)) ;
#160789 = CARTESIAN_POINT('',(-2.15,4.3,-10.68)) ;
#160790 = CARTESIAN_POINT('',(-2.15,4.3,-10.58)) ;
#160791 = CARTESIAN_POINT('',(-2.15,4.25,-10.68)) ;
#160792 = CARTESIAN_POINT('',(-2.15,4.25,-12.18)) ;
#160793 = CARTESIAN_POINT('Origin',(-2.85,4.25,-10.58)) ;
#160794 = CARTESIAN_POINT('',(-2.25,4.3,-10.58)) ;
#160795 = CARTESIAN_POINT('',(-2.75,4.3,-10.58)) ;
#160796 = CARTESIAN_POINT('',(-2.85,4.3,-10.58)) ;
#160797 = CARTESIAN_POINT('',(-2.75,4.25,-10.58)) ;
#160798 = CARTESIAN_POINT('',(-2.25,4.25,-10.58)) ;
#160799 = CARTESIAN_POINT('Origin',(-2.85,4.25,-12.28)) ;
#160800 = CARTESIAN_POINT('',(-2.85,4.3,-10.68)) ;
#160801 = CARTESIAN_POINT('',(-2.85,4.25,-10.68)) ;
#160802 = CARTESIAN_POINT('',(-2.85,4.3,-12.18)) ;
#160803 = CARTESIAN_POINT('',(-2.85,4.3,-12.28)) ;
#160804 = CARTESIAN_POINT('',(-2.85,4.25,-12.18)) ;
#160805 = CARTESIAN_POINT('Origin',(-2.15,4.25,-12.28)) ;
#160806 = CARTESIAN_POINT('',(-2.75,4.3,-12.28)) ;
#160807 = CARTESIAN_POINT('',(-2.25,4.3,-12.28)) ;
#160808 = CARTESIAN_POINT('',(-2.15,4.3,-12.28)) ;
#160809 = CARTESIAN_POINT('',(-2.25,4.25,-12.28)) ;
#160810 = CARTESIAN_POINT('',(-2.75,4.25,-12.28)) ;
#160811 = CARTESIAN_POINT('Origin',(0.,4.25,-15.24)) ;
#160812 = CARTESIAN_POINT('',(-2.9,4.25,-16.14)) ;
#160813 = CARTESIAN_POINT('',(-2.9,4.25,-14.34)) ;
#160814 = CARTESIAN_POINT('',(-2.9,4.25,-15.24)) ;
#160815 = CARTESIAN_POINT('',(-2.1,4.25,-14.34)) ;
#160816 = CARTESIAN_POINT('',(-1.95156391047391E-16,4.25,-14.34)) ;
#160817 = CARTESIAN_POINT('',(-2.1,4.25,-16.14)) ;
#160818 = CARTESIAN_POINT('',(-2.1,4.25,-15.24)) ;
#160819 = CARTESIAN_POINT('',(-1.95156391047391E-16,4.25,-16.14)) ;
#160820 = CARTESIAN_POINT('',(-2.75,4.25,-14.39)) ;
#160821 = CARTESIAN_POINT('',(-2.25,4.25,-14.39)) ;
#160822 = CARTESIAN_POINT('',(-2.85,4.25,-14.39)) ;
#160823 = CARTESIAN_POINT('',(-2.85,4.25,-14.49)) ;
#160824 = CARTESIAN_POINT('Origin',(-2.75,4.25,-14.49)) ;
#160825 = CARTESIAN_POINT('',(-2.85,4.25,-15.99)) ;
#160826 = CARTESIAN_POINT('',(-2.85,4.25,-16.09)) ;
#160827 = CARTESIAN_POINT('',(-2.75,4.25,-16.09)) ;
#160828 = CARTESIAN_POINT('Origin',(-2.75,4.25,-15.99)) ;
#160829 = CARTESIAN_POINT('',(-2.25,4.25,-16.09)) ;
#160830 = CARTESIAN_POINT('',(-2.15,4.25,-16.09)) ;
#160831 = CARTESIAN_POINT('',(-2.15,4.25,-15.99)) ;
#160832 = CARTESIAN_POINT('Origin',(-2.25,4.25,-15.99)) ;
#160833 = CARTESIAN_POINT('',(-2.15,4.25,-14.49)) ;
#160834 = CARTESIAN_POINT('',(-2.15,4.25,-14.39)) ;
#160835 = CARTESIAN_POINT('Origin',(-2.25,4.25,-14.49)) ;
#160836 = CARTESIAN_POINT('Origin',(-2.15,4.25,-14.39)) ;
#160837 = CARTESIAN_POINT('',(-2.15,4.3,-15.99)) ;
#160838 = CARTESIAN_POINT('',(-2.15,4.3,-14.49)) ;
#160839 = CARTESIAN_POINT('',(-2.15,4.3,-14.39)) ;
#160840 = CARTESIAN_POINT('',(-2.15,4.25,-14.49)) ;
#160841 = CARTESIAN_POINT('',(-2.15,4.25,-15.99)) ;
#160842 = CARTESIAN_POINT('Origin',(-2.85,4.25,-14.39)) ;
#160843 = CARTESIAN_POINT('',(-2.25,4.3,-14.39)) ;
#160844 = CARTESIAN_POINT('',(-2.75,4.3,-14.39)) ;
#160845 = CARTESIAN_POINT('',(-2.85,4.3,-14.39)) ;
#160846 = CARTESIAN_POINT('',(-2.75,4.25,-14.39)) ;
#160847 = CARTESIAN_POINT('',(-2.25,4.25,-14.39)) ;
#160848 = CARTESIAN_POINT('Origin',(-2.85,4.25,-16.09)) ;
#160849 = CARTESIAN_POINT('',(-2.85,4.3,-14.49)) ;
#160850 = CARTESIAN_POINT('',(-2.85,4.25,-14.49)) ;
#160851 = CARTESIAN_POINT('',(-2.85,4.3,-15.99)) ;
#160852 = CARTESIAN_POINT('',(-2.85,4.3,-16.09)) ;
#160853 = CARTESIAN_POINT('',(-2.85,4.25,-15.99)) ;
#160854 = CARTESIAN_POINT('Origin',(-2.15,4.25,-16.09)) ;
#160855 = CARTESIAN_POINT('',(-2.75,4.3,-16.09)) ;
#160856 = CARTESIAN_POINT('',(-2.25,4.3,-16.09)) ;
#160857 = CARTESIAN_POINT('',(-2.15,4.3,-16.09)) ;
#160858 = CARTESIAN_POINT('',(-2.25,4.25,-16.09)) ;
#160859 = CARTESIAN_POINT('',(-2.75,4.25,-16.09)) ;
#160860 = CARTESIAN_POINT('Origin',(0.,4.25,-19.05)) ;
#160861 = CARTESIAN_POINT('',(-2.9,4.25,-19.95)) ;
#160862 = CARTESIAN_POINT('',(-2.9,4.25,-18.15)) ;
#160863 = CARTESIAN_POINT('',(-2.9,4.25,-19.05)) ;
#160864 = CARTESIAN_POINT('',(-2.1,4.25,-18.15)) ;
#160865 = CARTESIAN_POINT('',(-1.95156391047391E-16,4.25,-18.15)) ;
#160866 = CARTESIAN_POINT('',(-2.1,4.25,-19.95)) ;
#160867 = CARTESIAN_POINT('',(-2.1,4.25,-19.05)) ;
#160868 = CARTESIAN_POINT('',(-1.95156391047391E-16,4.25,-19.95)) ;
#160869 = CARTESIAN_POINT('',(-2.75,4.25,-18.2)) ;
#160870 = CARTESIAN_POINT('',(-2.25,4.25,-18.2)) ;
#160871 = CARTESIAN_POINT('',(-2.85,4.25,-18.2)) ;
#160872 = CARTESIAN_POINT('',(-2.85,4.25,-18.3)) ;
#160873 = CARTESIAN_POINT('Origin',(-2.75,4.25,-18.3)) ;
#160874 = CARTESIAN_POINT('',(-2.85,4.25,-19.8)) ;
#160875 = CARTESIAN_POINT('',(-2.85,4.25,-19.9)) ;
#160876 = CARTESIAN_POINT('',(-2.75,4.25,-19.9)) ;
#160877 = CARTESIAN_POINT('Origin',(-2.75,4.25,-19.8)) ;
#160878 = CARTESIAN_POINT('',(-2.25,4.25,-19.9)) ;
#160879 = CARTESIAN_POINT('',(-2.15,4.25,-19.9)) ;
#160880 = CARTESIAN_POINT('',(-2.15,4.25,-19.8)) ;
#160881 = CARTESIAN_POINT('Origin',(-2.25,4.25,-19.8)) ;
#160882 = CARTESIAN_POINT('',(-2.15,4.25,-18.3)) ;
#160883 = CARTESIAN_POINT('',(-2.15,4.25,-18.2)) ;
#160884 = CARTESIAN_POINT('Origin',(-2.25,4.25,-18.3)) ;
#160885 = CARTESIAN_POINT('Origin',(-2.15,4.25,-18.2)) ;
#160886 = CARTESIAN_POINT('',(-2.15,4.3,-19.8)) ;
#160887 = CARTESIAN_POINT('',(-2.15,4.3,-18.3)) ;
#160888 = CARTESIAN_POINT('',(-2.15,4.3,-18.2)) ;
#160889 = CARTESIAN_POINT('',(-2.15,4.25,-18.3)) ;
#160890 = CARTESIAN_POINT('',(-2.15,4.25,-19.8)) ;
#160891 = CARTESIAN_POINT('Origin',(-2.85,4.25,-18.2)) ;
#160892 = CARTESIAN_POINT('',(-2.25,4.3,-18.2)) ;
#160893 = CARTESIAN_POINT('',(-2.75,4.3,-18.2)) ;
#160894 = CARTESIAN_POINT('',(-2.85,4.3,-18.2)) ;
#160895 = CARTESIAN_POINT('',(-2.75,4.25,-18.2)) ;
#160896 = CARTESIAN_POINT('',(-2.25,4.25,-18.2)) ;
#160897 = CARTESIAN_POINT('Origin',(-2.85,4.25,-19.9)) ;
#160898 = CARTESIAN_POINT('',(-2.85,4.3,-18.3)) ;
#160899 = CARTESIAN_POINT('',(-2.85,4.25,-18.3)) ;
#160900 = CARTESIAN_POINT('',(-2.85,4.3,-19.8)) ;
#160901 = CARTESIAN_POINT('',(-2.85,4.3,-19.9)) ;
#160902 = CARTESIAN_POINT('',(-2.85,4.25,-19.8)) ;
#160903 = CARTESIAN_POINT('Origin',(-2.15,4.25,-19.9)) ;
#160904 = CARTESIAN_POINT('',(-2.75,4.3,-19.9)) ;
#160905 = CARTESIAN_POINT('',(-2.25,4.3,-19.9)) ;
#160906 = CARTESIAN_POINT('',(-2.15,4.3,-19.9)) ;
#160907 = CARTESIAN_POINT('',(-2.25,4.25,-19.9)) ;
#160908 = CARTESIAN_POINT('',(-2.75,4.25,-19.9)) ;
#160909 = CARTESIAN_POINT('Origin',(0.,4.25,-22.86)) ;
#160910 = CARTESIAN_POINT('',(-2.9,4.25,-23.76)) ;
#160911 = CARTESIAN_POINT('',(-2.9,4.25,-21.96)) ;
#160912 = CARTESIAN_POINT('',(-2.9,4.25,-22.86)) ;
#160913 = CARTESIAN_POINT('',(-2.1,4.25,-21.96)) ;
#160914 = CARTESIAN_POINT('',(-1.95156391047391E-16,4.25,-21.96)) ;
#160915 = CARTESIAN_POINT('',(-2.1,4.25,-23.76)) ;
#160916 = CARTESIAN_POINT('',(-2.1,4.25,-22.86)) ;
#160917 = CARTESIAN_POINT('',(-1.95156391047391E-16,4.25,-23.76)) ;
#160918 = CARTESIAN_POINT('',(-2.75,4.25,-22.01)) ;
#160919 = CARTESIAN_POINT('',(-2.25,4.25,-22.01)) ;
#160920 = CARTESIAN_POINT('',(-2.85,4.25,-22.01)) ;
#160921 = CARTESIAN_POINT('',(-2.85,4.25,-22.11)) ;
#160922 = CARTESIAN_POINT('Origin',(-2.75,4.25,-22.11)) ;
#160923 = CARTESIAN_POINT('',(-2.85,4.25,-23.61)) ;
#160924 = CARTESIAN_POINT('',(-2.85,4.25,-23.71)) ;
#160925 = CARTESIAN_POINT('',(-2.75,4.25,-23.71)) ;
#160926 = CARTESIAN_POINT('Origin',(-2.75,4.25,-23.61)) ;
#160927 = CARTESIAN_POINT('',(-2.25,4.25,-23.71)) ;
#160928 = CARTESIAN_POINT('',(-2.15,4.25,-23.71)) ;
#160929 = CARTESIAN_POINT('',(-2.15,4.25,-23.61)) ;
#160930 = CARTESIAN_POINT('Origin',(-2.25,4.25,-23.61)) ;
#160931 = CARTESIAN_POINT('',(-2.15,4.25,-22.11)) ;
#160932 = CARTESIAN_POINT('',(-2.15,4.25,-22.01)) ;
#160933 = CARTESIAN_POINT('Origin',(-2.25,4.25,-22.11)) ;
#160934 = CARTESIAN_POINT('Origin',(-2.15,4.25,-22.01)) ;
#160935 = CARTESIAN_POINT('',(-2.15,4.3,-23.61)) ;
#160936 = CARTESIAN_POINT('',(-2.15,4.3,-22.11)) ;
#160937 = CARTESIAN_POINT('',(-2.15,4.3,-22.01)) ;
#160938 = CARTESIAN_POINT('',(-2.15,4.25,-22.11)) ;
#160939 = CARTESIAN_POINT('',(-2.15,4.25,-23.61)) ;
#160940 = CARTESIAN_POINT('Origin',(-2.85,4.25,-22.01)) ;
#160941 = CARTESIAN_POINT('',(-2.25,4.3,-22.01)) ;
#160942 = CARTESIAN_POINT('',(-2.75,4.3,-22.01)) ;
#160943 = CARTESIAN_POINT('',(-2.85,4.3,-22.01)) ;
#160944 = CARTESIAN_POINT('',(-2.75,4.25,-22.01)) ;
#160945 = CARTESIAN_POINT('',(-2.25,4.25,-22.01)) ;
#160946 = CARTESIAN_POINT('Origin',(-2.85,4.25,-23.71)) ;
#160947 = CARTESIAN_POINT('',(-2.85,4.3,-22.11)) ;
#160948 = CARTESIAN_POINT('',(-2.85,4.25,-22.11)) ;
#160949 = CARTESIAN_POINT('',(-2.85,4.3,-23.61)) ;
#160950 = CARTESIAN_POINT('',(-2.85,4.3,-23.71)) ;
#160951 = CARTESIAN_POINT('',(-2.85,4.25,-23.61)) ;
#160952 = CARTESIAN_POINT('Origin',(-2.15,4.25,-23.71)) ;
#160953 = CARTESIAN_POINT('',(-2.75,4.3,-23.71)) ;
#160954 = CARTESIAN_POINT('',(-2.25,4.3,-23.71)) ;
#160955 = CARTESIAN_POINT('',(-2.15,4.3,-23.71)) ;
#160956 = CARTESIAN_POINT('',(-2.25,4.25,-23.71)) ;
#160957 = CARTESIAN_POINT('',(-2.75,4.25,-23.71)) ;
#160958 = CARTESIAN_POINT('Origin',(0.,4.25,-26.67)) ;
#160959 = CARTESIAN_POINT('',(-2.9,4.25,-27.57)) ;
#160960 = CARTESIAN_POINT('',(-2.9,4.25,-25.77)) ;
#160961 = CARTESIAN_POINT('',(-2.9,4.25,-26.67)) ;
#160962 = CARTESIAN_POINT('',(-2.1,4.25,-25.77)) ;
#160963 = CARTESIAN_POINT('',(-1.95156391047391E-16,4.25,-25.77)) ;
#160964 = CARTESIAN_POINT('',(-2.1,4.25,-27.57)) ;
#160965 = CARTESIAN_POINT('',(-2.1,4.25,-26.67)) ;
#160966 = CARTESIAN_POINT('',(-1.95156391047391E-16,4.25,-27.57)) ;
#160967 = CARTESIAN_POINT('',(-2.75,4.25,-25.82)) ;
#160968 = CARTESIAN_POINT('',(-2.25,4.25,-25.82)) ;
#160969 = CARTESIAN_POINT('',(-2.85,4.25,-25.82)) ;
#160970 = CARTESIAN_POINT('',(-2.85,4.25,-25.92)) ;
#160971 = CARTESIAN_POINT('Origin',(-2.75,4.25,-25.92)) ;
#160972 = CARTESIAN_POINT('',(-2.85,4.25,-27.42)) ;
#160973 = CARTESIAN_POINT('',(-2.85,4.25,-27.52)) ;
#160974 = CARTESIAN_POINT('',(-2.75,4.25,-27.52)) ;
#160975 = CARTESIAN_POINT('Origin',(-2.75,4.25,-27.42)) ;
#160976 = CARTESIAN_POINT('',(-2.25,4.25,-27.52)) ;
#160977 = CARTESIAN_POINT('',(-2.15,4.25,-27.52)) ;
#160978 = CARTESIAN_POINT('',(-2.15,4.25,-27.42)) ;
#160979 = CARTESIAN_POINT('Origin',(-2.25,4.25,-27.42)) ;
#160980 = CARTESIAN_POINT('',(-2.15,4.25,-25.92)) ;
#160981 = CARTESIAN_POINT('',(-2.15,4.25,-25.82)) ;
#160982 = CARTESIAN_POINT('Origin',(-2.25,4.25,-25.92)) ;
#160983 = CARTESIAN_POINT('Origin',(-2.15,4.25,-25.82)) ;
#160984 = CARTESIAN_POINT('',(-2.15,4.3,-27.42)) ;
#160985 = CARTESIAN_POINT('',(-2.15,4.3,-25.92)) ;
#160986 = CARTESIAN_POINT('',(-2.15,4.3,-25.82)) ;
#160987 = CARTESIAN_POINT('',(-2.15,4.25,-25.92)) ;
#160988 = CARTESIAN_POINT('',(-2.15,4.25,-27.42)) ;
#160989 = CARTESIAN_POINT('Origin',(-2.85,4.25,-25.82)) ;
#160990 = CARTESIAN_POINT('',(-2.25,4.3,-25.82)) ;
#160991 = CARTESIAN_POINT('',(-2.75,4.3,-25.82)) ;
#160992 = CARTESIAN_POINT('',(-2.85,4.3,-25.82)) ;
#160993 = CARTESIAN_POINT('',(-2.75,4.25,-25.82)) ;
#160994 = CARTESIAN_POINT('',(-2.25,4.25,-25.82)) ;
#160995 = CARTESIAN_POINT('Origin',(-2.85,4.25,-27.52)) ;
#160996 = CARTESIAN_POINT('',(-2.85,4.3,-25.92)) ;
#160997 = CARTESIAN_POINT('',(-2.85,4.25,-25.92)) ;
#160998 = CARTESIAN_POINT('',(-2.85,4.3,-27.42)) ;
#160999 = CARTESIAN_POINT('',(-2.85,4.3,-27.52)) ;
#161000 = CARTESIAN_POINT('',(-2.85,4.25,-27.42)) ;
#161001 = CARTESIAN_POINT('Origin',(-2.15,4.25,-27.52)) ;
#161002 = CARTESIAN_POINT('',(-2.75,4.3,-27.52)) ;
#161003 = CARTESIAN_POINT('',(-2.25,4.3,-27.52)) ;
#161004 = CARTESIAN_POINT('',(-2.15,4.3,-27.52)) ;
#161005 = CARTESIAN_POINT('',(-2.25,4.25,-27.52)) ;
#161006 = CARTESIAN_POINT('',(-2.75,4.25,-27.52)) ;
#161007 = CARTESIAN_POINT('Origin',(0.,4.25,-30.48)) ;
#161008 = CARTESIAN_POINT('',(-2.9,4.25,-31.38)) ;
#161009 = CARTESIAN_POINT('',(-2.9,4.25,-29.58)) ;
#161010 = CARTESIAN_POINT('',(-2.9,4.25,-30.48)) ;
#161011 = CARTESIAN_POINT('',(-2.1,4.25,-29.58)) ;
#161012 = CARTESIAN_POINT('',(-1.95156391047391E-16,4.25,-29.58)) ;
#161013 = CARTESIAN_POINT('',(-2.1,4.25,-31.38)) ;
#161014 = CARTESIAN_POINT('',(-2.1,4.25,-30.48)) ;
#161015 = CARTESIAN_POINT('',(-1.95156391047391E-16,4.25,-31.38)) ;
#161016 = CARTESIAN_POINT('',(-2.75,4.25,-29.63)) ;
#161017 = CARTESIAN_POINT('',(-2.25,4.25,-29.63)) ;
#161018 = CARTESIAN_POINT('',(-2.85,4.25,-29.63)) ;
#161019 = CARTESIAN_POINT('',(-2.85,4.25,-29.73)) ;
#161020 = CARTESIAN_POINT('Origin',(-2.75,4.25,-29.73)) ;
#161021 = CARTESIAN_POINT('',(-2.85,4.25,-31.23)) ;
#161022 = CARTESIAN_POINT('',(-2.85,4.25,-31.33)) ;
#161023 = CARTESIAN_POINT('',(-2.75,4.25,-31.33)) ;
#161024 = CARTESIAN_POINT('Origin',(-2.75,4.25,-31.23)) ;
#161025 = CARTESIAN_POINT('',(-2.25,4.25,-31.33)) ;
#161026 = CARTESIAN_POINT('',(-2.15,4.25,-31.33)) ;
#161027 = CARTESIAN_POINT('',(-2.15,4.25,-31.23)) ;
#161028 = CARTESIAN_POINT('Origin',(-2.25,4.25,-31.23)) ;
#161029 = CARTESIAN_POINT('',(-2.15,4.25,-29.73)) ;
#161030 = CARTESIAN_POINT('',(-2.15,4.25,-29.63)) ;
#161031 = CARTESIAN_POINT('Origin',(-2.25,4.25,-29.73)) ;
#161032 = CARTESIAN_POINT('Origin',(-2.15,4.25,-29.63)) ;
#161033 = CARTESIAN_POINT('',(-2.15,4.3,-31.23)) ;
#161034 = CARTESIAN_POINT('',(-2.15,4.3,-29.73)) ;
#161035 = CARTESIAN_POINT('',(-2.15,4.3,-29.63)) ;
#161036 = CARTESIAN_POINT('',(-2.15,4.25,-29.73)) ;
#161037 = CARTESIAN_POINT('',(-2.15,4.25,-31.23)) ;
#161038 = CARTESIAN_POINT('Origin',(-2.85,4.25,-29.63)) ;
#161039 = CARTESIAN_POINT('',(-2.25,4.3,-29.63)) ;
#161040 = CARTESIAN_POINT('',(-2.75,4.3,-29.63)) ;
#161041 = CARTESIAN_POINT('',(-2.85,4.3,-29.63)) ;
#161042 = CARTESIAN_POINT('',(-2.75,4.25,-29.63)) ;
#161043 = CARTESIAN_POINT('',(-2.25,4.25,-29.63)) ;
#161044 = CARTESIAN_POINT('Origin',(-2.85,4.25,-31.33)) ;
#161045 = CARTESIAN_POINT('',(-2.85,4.3,-29.73)) ;
#161046 = CARTESIAN_POINT('',(-2.85,4.25,-29.73)) ;
#161047 = CARTESIAN_POINT('',(-2.85,4.3,-31.23)) ;
#161048 = CARTESIAN_POINT('',(-2.85,4.3,-31.33)) ;
#161049 = CARTESIAN_POINT('',(-2.85,4.25,-31.23)) ;
#161050 = CARTESIAN_POINT('Origin',(-2.15,4.25,-31.33)) ;
#161051 = CARTESIAN_POINT('',(-2.75,4.3,-31.33)) ;
#161052 = CARTESIAN_POINT('',(-2.25,4.3,-31.33)) ;
#161053 = CARTESIAN_POINT('',(-2.15,4.3,-31.33)) ;
#161054 = CARTESIAN_POINT('',(-2.25,4.25,-31.33)) ;
#161055 = CARTESIAN_POINT('',(-2.75,4.25,-31.33)) ;
#161056 = CARTESIAN_POINT('Origin',(0.,4.25,-34.29)) ;
#161057 = CARTESIAN_POINT('',(-2.9,4.25,-35.19)) ;
#161058 = CARTESIAN_POINT('',(-2.9,4.25,-33.39)) ;
#161059 = CARTESIAN_POINT('',(-2.9,4.25,-34.29)) ;
#161060 = CARTESIAN_POINT('',(-2.1,4.25,-33.39)) ;
#161061 = CARTESIAN_POINT('',(-1.95156391047391E-16,4.25,-33.39)) ;
#161062 = CARTESIAN_POINT('',(-2.1,4.25,-35.19)) ;
#161063 = CARTESIAN_POINT('',(-2.1,4.25,-34.29)) ;
#161064 = CARTESIAN_POINT('',(-1.95156391047391E-16,4.25,-35.19)) ;
#161065 = CARTESIAN_POINT('',(-2.75,4.25,-33.44)) ;
#161066 = CARTESIAN_POINT('',(-2.25,4.25,-33.44)) ;
#161067 = CARTESIAN_POINT('',(-2.85,4.25,-33.44)) ;
#161068 = CARTESIAN_POINT('',(-2.85,4.25,-33.54)) ;
#161069 = CARTESIAN_POINT('Origin',(-2.75,4.25,-33.54)) ;
#161070 = CARTESIAN_POINT('',(-2.85,4.25,-35.04)) ;
#161071 = CARTESIAN_POINT('',(-2.85,4.25,-35.14)) ;
#161072 = CARTESIAN_POINT('',(-2.75,4.25,-35.14)) ;
#161073 = CARTESIAN_POINT('Origin',(-2.75,4.25,-35.04)) ;
#161074 = CARTESIAN_POINT('',(-2.25,4.25,-35.14)) ;
#161075 = CARTESIAN_POINT('',(-2.15,4.25,-35.14)) ;
#161076 = CARTESIAN_POINT('',(-2.15,4.25,-35.04)) ;
#161077 = CARTESIAN_POINT('Origin',(-2.25,4.25,-35.04)) ;
#161078 = CARTESIAN_POINT('',(-2.15,4.25,-33.54)) ;
#161079 = CARTESIAN_POINT('',(-2.15,4.25,-33.44)) ;
#161080 = CARTESIAN_POINT('Origin',(-2.25,4.25,-33.54)) ;
#161081 = CARTESIAN_POINT('Origin',(-2.15,4.25,-33.44)) ;
#161082 = CARTESIAN_POINT('',(-2.15,4.3,-35.04)) ;
#161083 = CARTESIAN_POINT('',(-2.15,4.3,-33.54)) ;
#161084 = CARTESIAN_POINT('',(-2.15,4.3,-33.44)) ;
#161085 = CARTESIAN_POINT('',(-2.15,4.25,-33.54)) ;
#161086 = CARTESIAN_POINT('',(-2.15,4.25,-35.04)) ;
#161087 = CARTESIAN_POINT('Origin',(-2.85,4.25,-33.44)) ;
#161088 = CARTESIAN_POINT('',(-2.25,4.3,-33.44)) ;
#161089 = CARTESIAN_POINT('',(-2.75,4.3,-33.44)) ;
#161090 = CARTESIAN_POINT('',(-2.85,4.3,-33.44)) ;
#161091 = CARTESIAN_POINT('',(-2.75,4.25,-33.44)) ;
#161092 = CARTESIAN_POINT('',(-2.25,4.25,-33.44)) ;
#161093 = CARTESIAN_POINT('Origin',(-2.85,4.25,-35.14)) ;
#161094 = CARTESIAN_POINT('',(-2.85,4.3,-33.54)) ;
#161095 = CARTESIAN_POINT('',(-2.85,4.25,-33.54)) ;
#161096 = CARTESIAN_POINT('',(-2.85,4.3,-35.04)) ;
#161097 = CARTESIAN_POINT('',(-2.85,4.3,-35.14)) ;
#161098 = CARTESIAN_POINT('',(-2.85,4.25,-35.04)) ;
#161099 = CARTESIAN_POINT('Origin',(-2.15,4.25,-35.14)) ;
#161100 = CARTESIAN_POINT('',(-2.75,4.3,-35.14)) ;
#161101 = CARTESIAN_POINT('',(-2.25,4.3,-35.14)) ;
#161102 = CARTESIAN_POINT('',(-2.15,4.3,-35.14)) ;
#161103 = CARTESIAN_POINT('',(-2.25,4.25,-35.14)) ;
#161104 = CARTESIAN_POINT('',(-2.75,4.25,-35.14)) ;
#161105 = CARTESIAN_POINT('Origin',(-1.97127667724637E-17,4.4,-3.81)) ;
#161106 = CARTESIAN_POINT('',(-2.25,4.4,-4.56)) ;
#161107 = CARTESIAN_POINT('',(-2.75,4.4,-4.56)) ;
#161108 = CARTESIAN_POINT('',(-1.97127667724637E-17,4.4,-4.56)) ;
#161109 = CARTESIAN_POINT('',(-2.75,4.4,-3.06)) ;
#161110 = CARTESIAN_POINT('',(-2.75,4.4,-3.81)) ;
#161111 = CARTESIAN_POINT('',(-2.25,4.4,-3.06)) ;
#161112 = CARTESIAN_POINT('',(-1.97127667724637E-17,4.4,-3.06)) ;
#161113 = CARTESIAN_POINT('',(-2.25,4.4,-3.81)) ;
#161114 = CARTESIAN_POINT('Origin',(-1.97127667724637E-17,4.4,-7.62)) ;
#161115 = CARTESIAN_POINT('',(-2.25,4.4,-8.37)) ;
#161116 = CARTESIAN_POINT('',(-2.75,4.4,-8.37)) ;
#161117 = CARTESIAN_POINT('',(-1.97127667724637E-17,4.4,-8.37)) ;
#161118 = CARTESIAN_POINT('',(-2.75,4.4,-6.87)) ;
#161119 = CARTESIAN_POINT('',(-2.75,4.4,-7.62)) ;
#161120 = CARTESIAN_POINT('',(-2.25,4.4,-6.87)) ;
#161121 = CARTESIAN_POINT('',(-1.97127667724637E-17,4.4,-6.87)) ;
#161122 = CARTESIAN_POINT('',(-2.25,4.4,-7.62)) ;
#161123 = CARTESIAN_POINT('Origin',(-1.97127667724637E-17,4.4,-11.43)) ;
#161124 = CARTESIAN_POINT('',(-2.25,4.4,-12.18)) ;
#161125 = CARTESIAN_POINT('',(-2.75,4.4,-12.18)) ;
#161126 = CARTESIAN_POINT('',(-1.97127667724637E-17,4.4,-12.18)) ;
#161127 = CARTESIAN_POINT('',(-2.75,4.4,-10.68)) ;
#161128 = CARTESIAN_POINT('',(-2.75,4.4,-11.43)) ;
#161129 = CARTESIAN_POINT('',(-2.25,4.4,-10.68)) ;
#161130 = CARTESIAN_POINT('',(-1.97127667724637E-17,4.4,-10.68)) ;
#161131 = CARTESIAN_POINT('',(-2.25,4.4,-11.43)) ;
#161132 = CARTESIAN_POINT('Origin',(-1.97127667724637E-17,4.4,-15.24)) ;
#161133 = CARTESIAN_POINT('',(-2.25,4.4,-15.99)) ;
#161134 = CARTESIAN_POINT('',(-2.75,4.4,-15.99)) ;
#161135 = CARTESIAN_POINT('',(-1.97127667724637E-17,4.4,-15.99)) ;
#161136 = CARTESIAN_POINT('',(-2.75,4.4,-14.49)) ;
#161137 = CARTESIAN_POINT('',(-2.75,4.4,-15.24)) ;
#161138 = CARTESIAN_POINT('',(-2.25,4.4,-14.49)) ;
#161139 = CARTESIAN_POINT('',(-1.97127667724637E-17,4.4,-14.49)) ;
#161140 = CARTESIAN_POINT('',(-2.25,4.4,-15.24)) ;
#161141 = CARTESIAN_POINT('Origin',(-1.97127667724637E-17,4.4,-19.05)) ;
#161142 = CARTESIAN_POINT('',(-2.25,4.4,-19.8)) ;
#161143 = CARTESIAN_POINT('',(-2.75,4.4,-19.8)) ;
#161144 = CARTESIAN_POINT('',(-1.97127667724637E-17,4.4,-19.8)) ;
#161145 = CARTESIAN_POINT('',(-2.75,4.4,-18.3)) ;
#161146 = CARTESIAN_POINT('',(-2.75,4.4,-19.05)) ;
#161147 = CARTESIAN_POINT('',(-2.25,4.4,-18.3)) ;
#161148 = CARTESIAN_POINT('',(-1.97127667724637E-17,4.4,-18.3)) ;
#161149 = CARTESIAN_POINT('',(-2.25,4.4,-19.05)) ;
#161150 = CARTESIAN_POINT('Origin',(-1.97127667724637E-17,4.4,-22.86)) ;
#161151 = CARTESIAN_POINT('',(-2.25,4.4,-23.61)) ;
#161152 = CARTESIAN_POINT('',(-2.75,4.4,-23.61)) ;
#161153 = CARTESIAN_POINT('',(-1.97127667724637E-17,4.4,-23.61)) ;
#161154 = CARTESIAN_POINT('',(-2.75,4.4,-22.11)) ;
#161155 = CARTESIAN_POINT('',(-2.75,4.4,-22.86)) ;
#161156 = CARTESIAN_POINT('',(-2.25,4.4,-22.11)) ;
#161157 = CARTESIAN_POINT('',(-1.97127667724637E-17,4.4,-22.11)) ;
#161158 = CARTESIAN_POINT('',(-2.25,4.4,-22.86)) ;
#161159 = CARTESIAN_POINT('Origin',(-1.97127667724637E-17,4.4,-26.67)) ;
#161160 = CARTESIAN_POINT('',(-2.25,4.4,-27.42)) ;
#161161 = CARTESIAN_POINT('',(-2.75,4.4,-27.42)) ;
#161162 = CARTESIAN_POINT('',(-1.97127667724637E-17,4.4,-27.42)) ;
#161163 = CARTESIAN_POINT('',(-2.75,4.4,-25.92)) ;
#161164 = CARTESIAN_POINT('',(-2.75,4.4,-26.67)) ;
#161165 = CARTESIAN_POINT('',(-2.25,4.4,-25.92)) ;
#161166 = CARTESIAN_POINT('',(-1.97127667724637E-17,4.4,-25.92)) ;
#161167 = CARTESIAN_POINT('',(-2.25,4.4,-26.67)) ;
#161168 = CARTESIAN_POINT('Origin',(-1.97127667724637E-17,4.4,-30.48)) ;
#161169 = CARTESIAN_POINT('',(-2.25,4.4,-31.23)) ;
#161170 = CARTESIAN_POINT('',(-2.75,4.4,-31.23)) ;
#161171 = CARTESIAN_POINT('',(-1.97127667724637E-17,4.4,-31.23)) ;
#161172 = CARTESIAN_POINT('',(-2.75,4.4,-29.73)) ;
#161173 = CARTESIAN_POINT('',(-2.75,4.4,-30.48)) ;
#161174 = CARTESIAN_POINT('',(-2.25,4.4,-29.73)) ;
#161175 = CARTESIAN_POINT('',(-1.97127667724637E-17,4.4,-29.73)) ;
#161176 = CARTESIAN_POINT('',(-2.25,4.4,-30.48)) ;
#161177 = CARTESIAN_POINT('Origin',(-1.97127667724637E-17,4.4,-34.29)) ;
#161178 = CARTESIAN_POINT('',(-2.25,4.4,-35.04)) ;
#161179 = CARTESIAN_POINT('',(-2.75,4.4,-35.04)) ;
#161180 = CARTESIAN_POINT('',(-1.97127667724637E-17,4.4,-35.04)) ;
#161181 = CARTESIAN_POINT('',(-2.75,4.4,-33.54)) ;
#161182 = CARTESIAN_POINT('',(-2.75,4.4,-34.29)) ;
#161183 = CARTESIAN_POINT('',(-2.25,4.4,-33.54)) ;
#161184 = CARTESIAN_POINT('',(-1.97127667724637E-17,4.4,-33.54)) ;
#161185 = CARTESIAN_POINT('',(-2.25,4.4,-34.29)) ;
#161186 = CARTESIAN_POINT('Origin',(-7.29372370581158E-16,3.55,-34.29)) ;
#161187 = CARTESIAN_POINT('',(-0.183301359729408,3.55,-32.772963213524)) ;
#161188 = CARTESIAN_POINT('Origin',(-7.29372370581158E-16,3.55,-30.48)) ;
#161189 = CARTESIAN_POINT('',(-0.183301359729408,3.55,-28.962963213524)) ;
#161190 = CARTESIAN_POINT('Origin',(-7.29372370581158E-16,3.55,-26.67)) ;
#161191 = CARTESIAN_POINT('',(-0.183301359729408,3.55,-25.152963213524)) ;
#161192 = CARTESIAN_POINT('Origin',(-7.29372370581158E-16,3.55,-22.86)) ;
#161193 = CARTESIAN_POINT('',(-0.183301359729408,3.55,-21.342963213524)) ;
#161194 = CARTESIAN_POINT('Origin',(-7.29372370581158E-16,3.55,-19.05)) ;
#161195 = CARTESIAN_POINT('',(-0.183301359729408,3.55,-17.532963213524)) ;
#161196 = CARTESIAN_POINT('Origin',(-7.29372370581158E-16,3.55,-15.24)) ;
#161197 = CARTESIAN_POINT('',(-0.183301359729408,3.55,-13.722963213524)) ;
#161198 = CARTESIAN_POINT('Origin',(-7.29372370581158E-16,3.55,-11.43)) ;
#161199 = CARTESIAN_POINT('',(-0.183301359729408,3.55,-9.91296321352402)) ;
#161200 = CARTESIAN_POINT('Origin',(-7.29372370581158E-16,3.55,-7.62)) ;
#161201 = CARTESIAN_POINT('',(-0.183301359729408,3.55,-6.10296321352403)) ;
#161202 = CARTESIAN_POINT('Origin',(-7.29372370581158E-16,3.55,-3.81)) ;
#161203 = CARTESIAN_POINT('',(-0.183301359729408,3.55,-2.29296321352403)) ;
#161204 = CARTESIAN_POINT('Origin',(-0.273932138433073,3.05,-2.3352250396981)) ;
#161205 = CARTESIAN_POINT('',(0.953662978710562,3.45,-4.96781126399638)) ;
#161206 = CARTESIAN_POINT('',(-0.273932138433073,3.15,-2.3352250396981)) ;
#161207 = CARTESIAN_POINT('Origin',(-0.953662978710561,3.05,-2.65218873600362)) ;
#161208 = CARTESIAN_POINT('',(-0.953662978710561,3.15,-2.65218873600362)) ;
#161209 = CARTESIAN_POINT('',(-0.953662978710562,3.45,-2.65218873600362)) ;
#161210 = CARTESIAN_POINT('Origin',(-7.95081593156037E-16,3.05,-3.81)) ;
#161211 = CARTESIAN_POINT('',(0.249234641435079,3.05,-3.69377997802131)) ;
#161212 = CARTESIAN_POINT('',(-0.249234641435079,3.05,-3.92622002197869)) ;
#161213 = CARTESIAN_POINT('Origin',(-0.273932138433073,3.05,-6.1452250396981)) ;
#161214 = CARTESIAN_POINT('',(0.953662978710562,3.45,-8.77781126399638)) ;
#161215 = CARTESIAN_POINT('',(-0.273932138433073,3.15,-6.1452250396981)) ;
#161216 = CARTESIAN_POINT('Origin',(-0.953662978710561,3.05,-6.46218873600362)) ;
#161217 = CARTESIAN_POINT('',(-0.953662978710561,3.15,-6.46218873600362)) ;
#161218 = CARTESIAN_POINT('',(-0.953662978710562,3.45,-6.46218873600362)) ;
#161219 = CARTESIAN_POINT('Origin',(-7.95081593156037E-16,3.05,-7.62)) ;
#161220 = CARTESIAN_POINT('',(0.249234641435079,3.05,-7.50377997802131)) ;
#161221 = CARTESIAN_POINT('',(-0.249234641435079,3.05,-7.73622002197869)) ;
#161222 = CARTESIAN_POINT('Origin',(-0.273932138433073,3.05,-9.9552250396981)) ;
#161223 = CARTESIAN_POINT('',(0.953662978710562,3.45,-12.5878112639964)) ;
#161224 = CARTESIAN_POINT('',(-0.273932138433073,3.15,-9.9552250396981)) ;
#161225 = CARTESIAN_POINT('Origin',(-0.953662978710561,3.05,-10.2721887360036)) ;
#161226 = CARTESIAN_POINT('',(-0.953662978710561,3.15,-10.2721887360036)) ;
#161227 = CARTESIAN_POINT('',(-0.953662978710561,3.45,-10.2721887360036)) ;
#161228 = CARTESIAN_POINT('Origin',(-7.95081593156037E-16,3.05,-11.43)) ;
#161229 = CARTESIAN_POINT('',(0.249234641435079,3.05,-11.3137799780213)) ;
#161230 = CARTESIAN_POINT('',(-0.249234641435079,3.05,-11.5462200219787)) ;
#161231 = CARTESIAN_POINT('Origin',(-0.273932138433073,3.05,-13.7652250396981)) ;
#161232 = CARTESIAN_POINT('',(0.953662978710563,3.45,-16.3978112639964)) ;
#161233 = CARTESIAN_POINT('',(-0.273932138433073,3.15,-13.7652250396981)) ;
#161234 = CARTESIAN_POINT('Origin',(-0.953662978710561,3.05,-14.0821887360036)) ;
#161235 = CARTESIAN_POINT('',(-0.953662978710561,3.15,-14.0821887360036)) ;
#161236 = CARTESIAN_POINT('',(-0.953662978710561,3.45,-14.0821887360036)) ;
#161237 = CARTESIAN_POINT('Origin',(-7.95081593156037E-16,3.05,-15.24)) ;
#161238 = CARTESIAN_POINT('',(0.249234641435079,3.05,-15.1237799780213)) ;
#161239 = CARTESIAN_POINT('',(-0.249234641435079,3.05,-15.3562200219787)) ;
#161240 = CARTESIAN_POINT('Origin',(-0.273932138433073,3.05,-17.5752250396981)) ;
#161241 = CARTESIAN_POINT('',(0.953662978710563,3.45,-20.2078112639964)) ;
#161242 = CARTESIAN_POINT('',(-0.273932138433073,3.15,-17.5752250396981)) ;
#161243 = CARTESIAN_POINT('Origin',(-0.953662978710561,3.05,-17.8921887360036)) ;
#161244 = CARTESIAN_POINT('',(-0.953662978710561,3.15,-17.8921887360036)) ;
#161245 = CARTESIAN_POINT('',(-0.953662978710561,3.45,-17.8921887360036)) ;
#161246 = CARTESIAN_POINT('Origin',(-7.95081593156037E-16,3.05,-19.05)) ;
#161247 = CARTESIAN_POINT('',(0.249234641435081,3.05,-18.9337799780213)) ;
#161248 = CARTESIAN_POINT('',(-0.249234641435079,3.05,-19.1662200219787)) ;
#161249 = CARTESIAN_POINT('Origin',(-0.273932138433073,3.05,-21.3852250396981)) ;
#161250 = CARTESIAN_POINT('',(0.953662978710563,3.45,-24.0178112639964)) ;
#161251 = CARTESIAN_POINT('',(-0.273932138433073,3.15,-21.3852250396981)) ;
#161252 = CARTESIAN_POINT('Origin',(-0.953662978710561,3.05,-21.7021887360036)) ;
#161253 = CARTESIAN_POINT('',(-0.953662978710561,3.15,-21.7021887360036)) ;
#161254 = CARTESIAN_POINT('',(-0.953662978710561,3.45,-21.7021887360036)) ;
#161255 = CARTESIAN_POINT('Origin',(-7.95081593156037E-16,3.05,-22.86)) ;
#161256 = CARTESIAN_POINT('',(0.249234641435081,3.05,-22.7437799780213)) ;
#161257 = CARTESIAN_POINT('',(-0.249234641435079,3.05,-22.9762200219787)) ;
#161258 = CARTESIAN_POINT('Origin',(-0.273932138433073,3.05,-25.1952250396981)) ;
#161259 = CARTESIAN_POINT('',(0.953662978710563,3.45,-27.8278112639964)) ;
#161260 = CARTESIAN_POINT('',(-0.273932138433073,3.15,-25.1952250396981)) ;
#161261 = CARTESIAN_POINT('Origin',(-0.953662978710561,3.05,-25.5121887360036)) ;
#161262 = CARTESIAN_POINT('',(-0.953662978710561,3.15,-25.5121887360036)) ;
#161263 = CARTESIAN_POINT('',(-0.953662978710561,3.45,-25.5121887360036)) ;
#161264 = CARTESIAN_POINT('Origin',(-7.95081593156037E-16,3.05,-26.67)) ;
#161265 = CARTESIAN_POINT('',(0.249234641435081,3.05,-26.5537799780213)) ;
#161266 = CARTESIAN_POINT('',(-0.249234641435079,3.05,-26.7862200219787)) ;
#161267 = CARTESIAN_POINT('Origin',(-0.273932138433073,3.05,-29.0052250396981)) ;
#161268 = CARTESIAN_POINT('',(0.953662978710563,3.45,-31.6378112639964)) ;
#161269 = CARTESIAN_POINT('',(-0.273932138433073,3.15,-29.0052250396981)) ;
#161270 = CARTESIAN_POINT('Origin',(-0.953662978710561,3.05,-29.3221887360036)) ;
#161271 = CARTESIAN_POINT('',(-0.953662978710561,3.15,-29.3221887360036)) ;
#161272 = CARTESIAN_POINT('',(-0.953662978710561,3.45,-29.3221887360036)) ;
#161273 = CARTESIAN_POINT('Origin',(-7.95081593156037E-16,3.05,-30.48)) ;
#161274 = CARTESIAN_POINT('',(0.249234641435081,3.05,-30.3637799780213)) ;
#161275 = CARTESIAN_POINT('',(-0.249234641435079,3.05,-30.5962200219787)) ;
#161276 = CARTESIAN_POINT('Origin',(-0.273932138433073,3.05,-32.8152250396981)) ;
#161277 = CARTESIAN_POINT('',(0.953662978710563,3.45,-35.4478112639964)) ;
#161278 = CARTESIAN_POINT('',(-0.273932138433073,3.15,-32.8152250396981)) ;
#161279 = CARTESIAN_POINT('Origin',(-0.953662978710561,3.05,-33.1321887360036)) ;
#161280 = CARTESIAN_POINT('',(-0.953662978710561,3.15,-33.1321887360036)) ;
#161281 = CARTESIAN_POINT('',(-0.953662978710561,3.45,-33.1321887360036)) ;
#161282 = CARTESIAN_POINT('Origin',(-7.95081593156037E-16,3.05,-34.29)) ;
#161283 = CARTESIAN_POINT('',(0.24923464143508,3.05,-34.1737799780213)) ;
#161284 = CARTESIAN_POINT('',(-0.249234641435079,3.05,-34.4062200219787)) ;
#161285 = CARTESIAN_POINT('Origin',(9.6,3.,-4.21)) ;
#161286 = CARTESIAN_POINT('',(9.7,2.9,-4.21)) ;
#161287 = CARTESIAN_POINT('',(9.7,2.1,-4.21)) ;
#161288 = CARTESIAN_POINT('',(9.7,3.,-4.21)) ;
#161289 = CARTESIAN_POINT('',(9.6,2.1,-4.31)) ;
#161290 = CARTESIAN_POINT('Origin',(9.6,2.1,-4.21)) ;
#161291 = CARTESIAN_POINT('',(9.6,2.9,-4.31)) ;
#161292 = CARTESIAN_POINT('',(9.6,3.,-4.31)) ;
#161293 = CARTESIAN_POINT('Origin',(9.6,2.9,-4.21)) ;
#161294 = CARTESIAN_POINT('Origin',(7.8,3.,-4.31)) ;
#161295 = CARTESIAN_POINT('',(7.8,2.1,-4.31)) ;
#161296 = CARTESIAN_POINT('',(7.8,2.1,-4.31)) ;
#161297 = CARTESIAN_POINT('',(7.8,2.9,-4.31)) ;
#161298 = CARTESIAN_POINT('',(7.8,3.,-4.31)) ;
#161299 = CARTESIAN_POINT('',(7.8,2.9,-4.31)) ;
#161300 = CARTESIAN_POINT('Origin',(7.8,3.,-4.21)) ;
#161301 = CARTESIAN_POINT('',(7.7,2.1,-4.21)) ;
#161302 = CARTESIAN_POINT('Origin',(7.8,2.1,-4.21)) ;
#161303 = CARTESIAN_POINT('',(7.7,2.9,-4.21)) ;
#161304 = CARTESIAN_POINT('',(7.7,3.,-4.21)) ;
#161305 = CARTESIAN_POINT('Origin',(7.8,2.9,-4.21)) ;
#161306 = CARTESIAN_POINT('Origin',(7.7,3.,-4.21)) ;
#161307 = CARTESIAN_POINT('',(7.7,2.1,-3.41)) ;
#161308 = CARTESIAN_POINT('',(7.7,2.1,-3.41)) ;
#161309 = CARTESIAN_POINT('',(7.7,2.9,-3.41)) ;
#161310 = CARTESIAN_POINT('',(7.7,3.,-3.41)) ;
#161311 = CARTESIAN_POINT('',(7.7,2.9,-4.21)) ;
#161312 = CARTESIAN_POINT('Origin',(7.8,3.,-3.41)) ;
#161313 = CARTESIAN_POINT('',(7.8,2.1,-3.31)) ;
#161314 = CARTESIAN_POINT('Origin',(7.8,2.1,-3.41)) ;
#161315 = CARTESIAN_POINT('',(7.8,2.9,-3.31)) ;
#161316 = CARTESIAN_POINT('',(7.8,3.,-3.31)) ;
#161317 = CARTESIAN_POINT('Origin',(7.8,2.9,-3.41)) ;
#161318 = CARTESIAN_POINT('Origin',(7.8,3.,-3.31)) ;
#161319 = CARTESIAN_POINT('',(9.6,2.1,-3.31)) ;
#161320 = CARTESIAN_POINT('',(9.6,2.1,-3.31)) ;
#161321 = CARTESIAN_POINT('',(9.6,2.9,-3.31)) ;
#161322 = CARTESIAN_POINT('',(9.6,3.,-3.31)) ;
#161323 = CARTESIAN_POINT('',(7.8,2.9,-3.31)) ;
#161324 = CARTESIAN_POINT('Origin',(9.6,3.,-3.41)) ;
#161325 = CARTESIAN_POINT('',(9.7,2.1,-3.41)) ;
#161326 = CARTESIAN_POINT('Origin',(9.6,2.1,-3.41)) ;
#161327 = CARTESIAN_POINT('',(9.7,2.9,-3.41)) ;
#161328 = CARTESIAN_POINT('',(9.7,3.,-3.41)) ;
#161329 = CARTESIAN_POINT('Origin',(9.6,2.9,-3.41)) ;
#161330 = CARTESIAN_POINT('Origin',(9.7,3.,-4.21)) ;
#161331 = CARTESIAN_POINT('',(9.7,2.9,-4.21)) ;
#161332 = CARTESIAN_POINT('',(9.7,2.1,-4.21)) ;
#161333 = CARTESIAN_POINT('Origin',(9.6,3.,-4.21)) ;
#161334 = CARTESIAN_POINT('',(7.8,3.,-3.41)) ;
#161335 = CARTESIAN_POINT('',(9.6,3.,-3.41)) ;
#161336 = CARTESIAN_POINT('',(9.6,3.,-3.41)) ;
#161337 = CARTESIAN_POINT('',(9.6,3.,-4.21)) ;
#161338 = CARTESIAN_POINT('',(9.6,3.,-4.21)) ;
#161339 = CARTESIAN_POINT('',(7.8,3.,-4.21)) ;
#161340 = CARTESIAN_POINT('',(9.6,3.,-4.21)) ;
#161341 = CARTESIAN_POINT('',(7.8,3.,-4.21)) ;
#161342 = CARTESIAN_POINT('Origin',(9.6,3.,-8.02)) ;
#161343 = CARTESIAN_POINT('',(9.7,2.9,-8.02)) ;
#161344 = CARTESIAN_POINT('',(9.7,2.1,-8.02)) ;
#161345 = CARTESIAN_POINT('',(9.7,3.,-8.02)) ;
#161346 = CARTESIAN_POINT('',(9.6,2.1,-8.12)) ;
#161347 = CARTESIAN_POINT('Origin',(9.6,2.1,-8.02)) ;
#161348 = CARTESIAN_POINT('',(9.6,2.9,-8.12)) ;
#161349 = CARTESIAN_POINT('',(9.6,3.,-8.12)) ;
#161350 = CARTESIAN_POINT('Origin',(9.6,2.9,-8.02)) ;
#161351 = CARTESIAN_POINT('Origin',(7.8,3.,-8.12)) ;
#161352 = CARTESIAN_POINT('',(7.8,2.1,-8.12)) ;
#161353 = CARTESIAN_POINT('',(7.8,2.1,-8.12)) ;
#161354 = CARTESIAN_POINT('',(7.8,2.9,-8.12)) ;
#161355 = CARTESIAN_POINT('',(7.8,3.,-8.12)) ;
#161356 = CARTESIAN_POINT('',(7.8,2.9,-8.12)) ;
#161357 = CARTESIAN_POINT('Origin',(7.8,3.,-8.02)) ;
#161358 = CARTESIAN_POINT('',(7.7,2.1,-8.02)) ;
#161359 = CARTESIAN_POINT('Origin',(7.8,2.1,-8.02)) ;
#161360 = CARTESIAN_POINT('',(7.7,2.9,-8.02)) ;
#161361 = CARTESIAN_POINT('',(7.7,3.,-8.02)) ;
#161362 = CARTESIAN_POINT('Origin',(7.8,2.9,-8.02)) ;
#161363 = CARTESIAN_POINT('Origin',(7.7,3.,-8.02)) ;
#161364 = CARTESIAN_POINT('',(7.7,2.1,-7.22)) ;
#161365 = CARTESIAN_POINT('',(7.7,2.1,-7.22)) ;
#161366 = CARTESIAN_POINT('',(7.7,2.9,-7.22)) ;
#161367 = CARTESIAN_POINT('',(7.7,3.,-7.22)) ;
#161368 = CARTESIAN_POINT('',(7.7,2.9,-8.02)) ;
#161369 = CARTESIAN_POINT('Origin',(7.8,3.,-7.22)) ;
#161370 = CARTESIAN_POINT('',(7.8,2.1,-7.12)) ;
#161371 = CARTESIAN_POINT('Origin',(7.8,2.1,-7.22)) ;
#161372 = CARTESIAN_POINT('',(7.8,2.9,-7.12)) ;
#161373 = CARTESIAN_POINT('',(7.8,3.,-7.12)) ;
#161374 = CARTESIAN_POINT('Origin',(7.8,2.9,-7.22)) ;
#161375 = CARTESIAN_POINT('Origin',(7.8,3.,-7.12)) ;
#161376 = CARTESIAN_POINT('',(9.6,2.1,-7.12)) ;
#161377 = CARTESIAN_POINT('',(9.6,2.1,-7.12)) ;
#161378 = CARTESIAN_POINT('',(9.6,2.9,-7.12)) ;
#161379 = CARTESIAN_POINT('',(9.6,3.,-7.12)) ;
#161380 = CARTESIAN_POINT('',(7.8,2.9,-7.12)) ;
#161381 = CARTESIAN_POINT('Origin',(9.6,3.,-7.22)) ;
#161382 = CARTESIAN_POINT('',(9.7,2.1,-7.22)) ;
#161383 = CARTESIAN_POINT('Origin',(9.6,2.1,-7.22)) ;
#161384 = CARTESIAN_POINT('',(9.7,2.9,-7.22)) ;
#161385 = CARTESIAN_POINT('',(9.7,3.,-7.22)) ;
#161386 = CARTESIAN_POINT('Origin',(9.6,2.9,-7.22)) ;
#161387 = CARTESIAN_POINT('Origin',(9.7,3.,-8.02)) ;
#161388 = CARTESIAN_POINT('',(9.7,2.9,-8.02)) ;
#161389 = CARTESIAN_POINT('',(9.7,2.1,-8.02)) ;
#161390 = CARTESIAN_POINT('Origin',(9.6,3.,-8.02)) ;
#161391 = CARTESIAN_POINT('',(7.8,3.,-7.22)) ;
#161392 = CARTESIAN_POINT('',(9.6,3.,-7.22)) ;
#161393 = CARTESIAN_POINT('',(9.6,3.,-7.22)) ;
#161394 = CARTESIAN_POINT('',(9.6,3.,-8.02)) ;
#161395 = CARTESIAN_POINT('',(9.6,3.,-8.02)) ;
#161396 = CARTESIAN_POINT('',(7.8,3.,-8.02)) ;
#161397 = CARTESIAN_POINT('',(9.6,3.,-8.02)) ;
#161398 = CARTESIAN_POINT('',(7.8,3.,-8.02)) ;
#161399 = CARTESIAN_POINT('Origin',(9.6,3.,-11.83)) ;
#161400 = CARTESIAN_POINT('',(9.7,2.9,-11.83)) ;
#161401 = CARTESIAN_POINT('',(9.7,2.1,-11.83)) ;
#161402 = CARTESIAN_POINT('',(9.7,3.,-11.83)) ;
#161403 = CARTESIAN_POINT('',(9.6,2.1,-11.93)) ;
#161404 = CARTESIAN_POINT('Origin',(9.6,2.1,-11.83)) ;
#161405 = CARTESIAN_POINT('',(9.6,2.9,-11.93)) ;
#161406 = CARTESIAN_POINT('',(9.6,3.,-11.93)) ;
#161407 = CARTESIAN_POINT('Origin',(9.6,2.9,-11.83)) ;
#161408 = CARTESIAN_POINT('Origin',(7.8,3.,-11.93)) ;
#161409 = CARTESIAN_POINT('',(7.8,2.1,-11.93)) ;
#161410 = CARTESIAN_POINT('',(7.8,2.1,-11.93)) ;
#161411 = CARTESIAN_POINT('',(7.8,2.9,-11.93)) ;
#161412 = CARTESIAN_POINT('',(7.8,3.,-11.93)) ;
#161413 = CARTESIAN_POINT('',(7.8,2.9,-11.93)) ;
#161414 = CARTESIAN_POINT('Origin',(7.8,3.,-11.83)) ;
#161415 = CARTESIAN_POINT('',(7.7,2.1,-11.83)) ;
#161416 = CARTESIAN_POINT('Origin',(7.8,2.1,-11.83)) ;
#161417 = CARTESIAN_POINT('',(7.7,2.9,-11.83)) ;
#161418 = CARTESIAN_POINT('',(7.7,3.,-11.83)) ;
#161419 = CARTESIAN_POINT('Origin',(7.8,2.9,-11.83)) ;
#161420 = CARTESIAN_POINT('Origin',(7.7,3.,-11.83)) ;
#161421 = CARTESIAN_POINT('',(7.7,2.1,-11.03)) ;
#161422 = CARTESIAN_POINT('',(7.7,2.1,-11.03)) ;
#161423 = CARTESIAN_POINT('',(7.7,2.9,-11.03)) ;
#161424 = CARTESIAN_POINT('',(7.7,3.,-11.03)) ;
#161425 = CARTESIAN_POINT('',(7.7,2.9,-11.83)) ;
#161426 = CARTESIAN_POINT('Origin',(7.8,3.,-11.03)) ;
#161427 = CARTESIAN_POINT('',(7.8,2.1,-10.93)) ;
#161428 = CARTESIAN_POINT('Origin',(7.8,2.1,-11.03)) ;
#161429 = CARTESIAN_POINT('',(7.8,2.9,-10.93)) ;
#161430 = CARTESIAN_POINT('',(7.8,3.,-10.93)) ;
#161431 = CARTESIAN_POINT('Origin',(7.8,2.9,-11.03)) ;
#161432 = CARTESIAN_POINT('Origin',(7.8,3.,-10.93)) ;
#161433 = CARTESIAN_POINT('',(9.6,2.1,-10.93)) ;
#161434 = CARTESIAN_POINT('',(9.6,2.1,-10.93)) ;
#161435 = CARTESIAN_POINT('',(9.6,2.9,-10.93)) ;
#161436 = CARTESIAN_POINT('',(9.6,3.,-10.93)) ;
#161437 = CARTESIAN_POINT('',(7.8,2.9,-10.93)) ;
#161438 = CARTESIAN_POINT('Origin',(9.6,3.,-11.03)) ;
#161439 = CARTESIAN_POINT('',(9.7,2.1,-11.03)) ;
#161440 = CARTESIAN_POINT('Origin',(9.6,2.1,-11.03)) ;
#161441 = CARTESIAN_POINT('',(9.7,2.9,-11.03)) ;
#161442 = CARTESIAN_POINT('',(9.7,3.,-11.03)) ;
#161443 = CARTESIAN_POINT('Origin',(9.6,2.9,-11.03)) ;
#161444 = CARTESIAN_POINT('Origin',(9.7,3.,-11.83)) ;
#161445 = CARTESIAN_POINT('',(9.7,2.9,-11.83)) ;
#161446 = CARTESIAN_POINT('',(9.7,2.1,-11.83)) ;
#161447 = CARTESIAN_POINT('Origin',(9.6,3.,-11.83)) ;
#161448 = CARTESIAN_POINT('',(7.8,3.,-11.03)) ;
#161449 = CARTESIAN_POINT('',(9.6,3.,-11.03)) ;
#161450 = CARTESIAN_POINT('',(9.6,3.,-11.03)) ;
#161451 = CARTESIAN_POINT('',(9.6,3.,-11.83)) ;
#161452 = CARTESIAN_POINT('',(9.6,3.,-11.83)) ;
#161453 = CARTESIAN_POINT('',(7.8,3.,-11.83)) ;
#161454 = CARTESIAN_POINT('',(9.6,3.,-11.83)) ;
#161455 = CARTESIAN_POINT('',(7.8,3.,-11.83)) ;
#161456 = CARTESIAN_POINT('Origin',(9.6,3.,-15.64)) ;
#161457 = CARTESIAN_POINT('',(9.7,2.9,-15.64)) ;
#161458 = CARTESIAN_POINT('',(9.7,2.1,-15.64)) ;
#161459 = CARTESIAN_POINT('',(9.7,3.,-15.64)) ;
#161460 = CARTESIAN_POINT('',(9.6,2.1,-15.74)) ;
#161461 = CARTESIAN_POINT('Origin',(9.6,2.1,-15.64)) ;
#161462 = CARTESIAN_POINT('',(9.6,2.9,-15.74)) ;
#161463 = CARTESIAN_POINT('',(9.6,3.,-15.74)) ;
#161464 = CARTESIAN_POINT('Origin',(9.6,2.9,-15.64)) ;
#161465 = CARTESIAN_POINT('Origin',(7.8,3.,-15.74)) ;
#161466 = CARTESIAN_POINT('',(7.8,2.1,-15.74)) ;
#161467 = CARTESIAN_POINT('',(7.8,2.1,-15.74)) ;
#161468 = CARTESIAN_POINT('',(7.8,2.9,-15.74)) ;
#161469 = CARTESIAN_POINT('',(7.8,3.,-15.74)) ;
#161470 = CARTESIAN_POINT('',(7.8,2.9,-15.74)) ;
#161471 = CARTESIAN_POINT('Origin',(7.8,3.,-15.64)) ;
#161472 = CARTESIAN_POINT('',(7.7,2.1,-15.64)) ;
#161473 = CARTESIAN_POINT('Origin',(7.8,2.1,-15.64)) ;
#161474 = CARTESIAN_POINT('',(7.7,2.9,-15.64)) ;
#161475 = CARTESIAN_POINT('',(7.7,3.,-15.64)) ;
#161476 = CARTESIAN_POINT('Origin',(7.8,2.9,-15.64)) ;
#161477 = CARTESIAN_POINT('Origin',(7.7,3.,-15.64)) ;
#161478 = CARTESIAN_POINT('',(7.7,2.1,-14.84)) ;
#161479 = CARTESIAN_POINT('',(7.7,2.1,-14.84)) ;
#161480 = CARTESIAN_POINT('',(7.7,2.9,-14.84)) ;
#161481 = CARTESIAN_POINT('',(7.7,3.,-14.84)) ;
#161482 = CARTESIAN_POINT('',(7.7,2.9,-15.64)) ;
#161483 = CARTESIAN_POINT('Origin',(7.8,3.,-14.84)) ;
#161484 = CARTESIAN_POINT('',(7.8,2.1,-14.74)) ;
#161485 = CARTESIAN_POINT('Origin',(7.8,2.1,-14.84)) ;
#161486 = CARTESIAN_POINT('',(7.8,2.9,-14.74)) ;
#161487 = CARTESIAN_POINT('',(7.8,3.,-14.74)) ;
#161488 = CARTESIAN_POINT('Origin',(7.8,2.9,-14.84)) ;
#161489 = CARTESIAN_POINT('Origin',(7.8,3.,-14.74)) ;
#161490 = CARTESIAN_POINT('',(9.6,2.1,-14.74)) ;
#161491 = CARTESIAN_POINT('',(9.6,2.1,-14.74)) ;
#161492 = CARTESIAN_POINT('',(9.6,2.9,-14.74)) ;
#161493 = CARTESIAN_POINT('',(9.6,3.,-14.74)) ;
#161494 = CARTESIAN_POINT('',(7.8,2.9,-14.74)) ;
#161495 = CARTESIAN_POINT('Origin',(9.6,3.,-14.84)) ;
#161496 = CARTESIAN_POINT('',(9.7,2.1,-14.84)) ;
#161497 = CARTESIAN_POINT('Origin',(9.6,2.1,-14.84)) ;
#161498 = CARTESIAN_POINT('',(9.7,2.9,-14.84)) ;
#161499 = CARTESIAN_POINT('',(9.7,3.,-14.84)) ;
#161500 = CARTESIAN_POINT('Origin',(9.6,2.9,-14.84)) ;
#161501 = CARTESIAN_POINT('Origin',(9.7,3.,-15.64)) ;
#161502 = CARTESIAN_POINT('',(9.7,2.9,-15.64)) ;
#161503 = CARTESIAN_POINT('',(9.7,2.1,-15.64)) ;
#161504 = CARTESIAN_POINT('Origin',(9.6,3.,-15.64)) ;
#161505 = CARTESIAN_POINT('',(7.8,3.,-14.84)) ;
#161506 = CARTESIAN_POINT('',(9.6,3.,-14.84)) ;
#161507 = CARTESIAN_POINT('',(9.6,3.,-14.84)) ;
#161508 = CARTESIAN_POINT('',(9.6,3.,-15.64)) ;
#161509 = CARTESIAN_POINT('',(9.6,3.,-15.64)) ;
#161510 = CARTESIAN_POINT('',(7.8,3.,-15.64)) ;
#161511 = CARTESIAN_POINT('',(9.6,3.,-15.64)) ;
#161512 = CARTESIAN_POINT('',(7.8,3.,-15.64)) ;
#161513 = CARTESIAN_POINT('Origin',(9.6,3.,-19.45)) ;
#161514 = CARTESIAN_POINT('',(9.7,2.9,-19.45)) ;
#161515 = CARTESIAN_POINT('',(9.7,2.1,-19.45)) ;
#161516 = CARTESIAN_POINT('',(9.7,3.,-19.45)) ;
#161517 = CARTESIAN_POINT('',(9.6,2.1,-19.55)) ;
#161518 = CARTESIAN_POINT('Origin',(9.6,2.1,-19.45)) ;
#161519 = CARTESIAN_POINT('',(9.6,2.9,-19.55)) ;
#161520 = CARTESIAN_POINT('',(9.6,3.,-19.55)) ;
#161521 = CARTESIAN_POINT('Origin',(9.6,2.9,-19.45)) ;
#161522 = CARTESIAN_POINT('Origin',(7.8,3.,-19.55)) ;
#161523 = CARTESIAN_POINT('',(7.8,2.1,-19.55)) ;
#161524 = CARTESIAN_POINT('',(7.8,2.1,-19.55)) ;
#161525 = CARTESIAN_POINT('',(7.8,2.9,-19.55)) ;
#161526 = CARTESIAN_POINT('',(7.8,3.,-19.55)) ;
#161527 = CARTESIAN_POINT('',(7.8,2.9,-19.55)) ;
#161528 = CARTESIAN_POINT('Origin',(7.8,3.,-19.45)) ;
#161529 = CARTESIAN_POINT('',(7.7,2.1,-19.45)) ;
#161530 = CARTESIAN_POINT('Origin',(7.8,2.1,-19.45)) ;
#161531 = CARTESIAN_POINT('',(7.7,2.9,-19.45)) ;
#161532 = CARTESIAN_POINT('',(7.7,3.,-19.45)) ;
#161533 = CARTESIAN_POINT('Origin',(7.8,2.9,-19.45)) ;
#161534 = CARTESIAN_POINT('Origin',(7.7,3.,-19.45)) ;
#161535 = CARTESIAN_POINT('',(7.7,2.1,-18.65)) ;
#161536 = CARTESIAN_POINT('',(7.7,2.1,-18.65)) ;
#161537 = CARTESIAN_POINT('',(7.7,2.9,-18.65)) ;
#161538 = CARTESIAN_POINT('',(7.7,3.,-18.65)) ;
#161539 = CARTESIAN_POINT('',(7.7,2.9,-19.45)) ;
#161540 = CARTESIAN_POINT('Origin',(7.8,3.,-18.65)) ;
#161541 = CARTESIAN_POINT('',(7.8,2.1,-18.55)) ;
#161542 = CARTESIAN_POINT('Origin',(7.8,2.1,-18.65)) ;
#161543 = CARTESIAN_POINT('',(7.8,2.9,-18.55)) ;
#161544 = CARTESIAN_POINT('',(7.8,3.,-18.55)) ;
#161545 = CARTESIAN_POINT('Origin',(7.8,2.9,-18.65)) ;
#161546 = CARTESIAN_POINT('Origin',(7.8,3.,-18.55)) ;
#161547 = CARTESIAN_POINT('',(9.6,2.1,-18.55)) ;
#161548 = CARTESIAN_POINT('',(9.6,2.1,-18.55)) ;
#161549 = CARTESIAN_POINT('',(9.6,2.9,-18.55)) ;
#161550 = CARTESIAN_POINT('',(9.6,3.,-18.55)) ;
#161551 = CARTESIAN_POINT('',(7.8,2.9,-18.55)) ;
#161552 = CARTESIAN_POINT('Origin',(9.6,3.,-18.65)) ;
#161553 = CARTESIAN_POINT('',(9.7,2.1,-18.65)) ;
#161554 = CARTESIAN_POINT('Origin',(9.6,2.1,-18.65)) ;
#161555 = CARTESIAN_POINT('',(9.7,2.9,-18.65)) ;
#161556 = CARTESIAN_POINT('',(9.7,3.,-18.65)) ;
#161557 = CARTESIAN_POINT('Origin',(9.6,2.9,-18.65)) ;
#161558 = CARTESIAN_POINT('Origin',(9.7,3.,-19.45)) ;
#161559 = CARTESIAN_POINT('',(9.7,2.9,-19.45)) ;
#161560 = CARTESIAN_POINT('',(9.7,2.1,-19.45)) ;
#161561 = CARTESIAN_POINT('Origin',(9.6,3.,-19.45)) ;
#161562 = CARTESIAN_POINT('',(7.8,3.,-18.65)) ;
#161563 = CARTESIAN_POINT('',(9.6,3.,-18.65)) ;
#161564 = CARTESIAN_POINT('',(9.6,3.,-18.65)) ;
#161565 = CARTESIAN_POINT('',(9.6,3.,-19.45)) ;
#161566 = CARTESIAN_POINT('',(9.6,3.,-19.45)) ;
#161567 = CARTESIAN_POINT('',(7.8,3.,-19.45)) ;
#161568 = CARTESIAN_POINT('',(9.6,3.,-19.45)) ;
#161569 = CARTESIAN_POINT('',(7.8,3.,-19.45)) ;
#161570 = CARTESIAN_POINT('Origin',(9.6,3.,-23.26)) ;
#161571 = CARTESIAN_POINT('',(9.7,2.9,-23.26)) ;
#161572 = CARTESIAN_POINT('',(9.7,2.1,-23.26)) ;
#161573 = CARTESIAN_POINT('',(9.7,3.,-23.26)) ;
#161574 = CARTESIAN_POINT('',(9.6,2.1,-23.36)) ;
#161575 = CARTESIAN_POINT('Origin',(9.6,2.1,-23.26)) ;
#161576 = CARTESIAN_POINT('',(9.6,2.9,-23.36)) ;
#161577 = CARTESIAN_POINT('',(9.6,3.,-23.36)) ;
#161578 = CARTESIAN_POINT('Origin',(9.6,2.9,-23.26)) ;
#161579 = CARTESIAN_POINT('Origin',(7.8,3.,-23.36)) ;
#161580 = CARTESIAN_POINT('',(7.8,2.1,-23.36)) ;
#161581 = CARTESIAN_POINT('',(7.8,2.1,-23.36)) ;
#161582 = CARTESIAN_POINT('',(7.8,2.9,-23.36)) ;
#161583 = CARTESIAN_POINT('',(7.8,3.,-23.36)) ;
#161584 = CARTESIAN_POINT('',(7.8,2.9,-23.36)) ;
#161585 = CARTESIAN_POINT('Origin',(7.8,3.,-23.26)) ;
#161586 = CARTESIAN_POINT('',(7.7,2.1,-23.26)) ;
#161587 = CARTESIAN_POINT('Origin',(7.8,2.1,-23.26)) ;
#161588 = CARTESIAN_POINT('',(7.7,2.9,-23.26)) ;
#161589 = CARTESIAN_POINT('',(7.7,3.,-23.26)) ;
#161590 = CARTESIAN_POINT('Origin',(7.8,2.9,-23.26)) ;
#161591 = CARTESIAN_POINT('Origin',(7.7,3.,-23.26)) ;
#161592 = CARTESIAN_POINT('',(7.7,2.1,-22.46)) ;
#161593 = CARTESIAN_POINT('',(7.7,2.1,-22.46)) ;
#161594 = CARTESIAN_POINT('',(7.7,2.9,-22.46)) ;
#161595 = CARTESIAN_POINT('',(7.7,3.,-22.46)) ;
#161596 = CARTESIAN_POINT('',(7.7,2.9,-23.26)) ;
#161597 = CARTESIAN_POINT('Origin',(7.8,3.,-22.46)) ;
#161598 = CARTESIAN_POINT('',(7.8,2.1,-22.36)) ;
#161599 = CARTESIAN_POINT('Origin',(7.8,2.1,-22.46)) ;
#161600 = CARTESIAN_POINT('',(7.8,2.9,-22.36)) ;
#161601 = CARTESIAN_POINT('',(7.8,3.,-22.36)) ;
#161602 = CARTESIAN_POINT('Origin',(7.8,2.9,-22.46)) ;
#161603 = CARTESIAN_POINT('Origin',(7.8,3.,-22.36)) ;
#161604 = CARTESIAN_POINT('',(9.6,2.1,-22.36)) ;
#161605 = CARTESIAN_POINT('',(9.6,2.1,-22.36)) ;
#161606 = CARTESIAN_POINT('',(9.6,2.9,-22.36)) ;
#161607 = CARTESIAN_POINT('',(9.6,3.,-22.36)) ;
#161608 = CARTESIAN_POINT('',(7.8,2.9,-22.36)) ;
#161609 = CARTESIAN_POINT('Origin',(9.6,3.,-22.46)) ;
#161610 = CARTESIAN_POINT('',(9.7,2.1,-22.46)) ;
#161611 = CARTESIAN_POINT('Origin',(9.6,2.1,-22.46)) ;
#161612 = CARTESIAN_POINT('',(9.7,2.9,-22.46)) ;
#161613 = CARTESIAN_POINT('',(9.7,3.,-22.46)) ;
#161614 = CARTESIAN_POINT('Origin',(9.6,2.9,-22.46)) ;
#161615 = CARTESIAN_POINT('Origin',(9.7,3.,-23.26)) ;
#161616 = CARTESIAN_POINT('',(9.7,2.9,-23.26)) ;
#161617 = CARTESIAN_POINT('',(9.7,2.1,-23.26)) ;
#161618 = CARTESIAN_POINT('Origin',(9.6,3.,-23.26)) ;
#161619 = CARTESIAN_POINT('',(7.8,3.,-22.46)) ;
#161620 = CARTESIAN_POINT('',(9.6,3.,-22.46)) ;
#161621 = CARTESIAN_POINT('',(9.6,3.,-22.46)) ;
#161622 = CARTESIAN_POINT('',(9.6,3.,-23.26)) ;
#161623 = CARTESIAN_POINT('',(9.6,3.,-23.26)) ;
#161624 = CARTESIAN_POINT('',(7.8,3.,-23.26)) ;
#161625 = CARTESIAN_POINT('',(9.6,3.,-23.26)) ;
#161626 = CARTESIAN_POINT('',(7.8,3.,-23.26)) ;
#161627 = CARTESIAN_POINT('Origin',(9.6,3.,-27.07)) ;
#161628 = CARTESIAN_POINT('',(9.7,2.9,-27.07)) ;
#161629 = CARTESIAN_POINT('',(9.7,2.1,-27.07)) ;
#161630 = CARTESIAN_POINT('',(9.7,3.,-27.07)) ;
#161631 = CARTESIAN_POINT('',(9.6,2.1,-27.17)) ;
#161632 = CARTESIAN_POINT('Origin',(9.6,2.1,-27.07)) ;
#161633 = CARTESIAN_POINT('',(9.6,2.9,-27.17)) ;
#161634 = CARTESIAN_POINT('',(9.6,3.,-27.17)) ;
#161635 = CARTESIAN_POINT('Origin',(9.6,2.9,-27.07)) ;
#161636 = CARTESIAN_POINT('Origin',(7.8,3.,-27.17)) ;
#161637 = CARTESIAN_POINT('',(7.8,2.1,-27.17)) ;
#161638 = CARTESIAN_POINT('',(7.8,2.1,-27.17)) ;
#161639 = CARTESIAN_POINT('',(7.8,2.9,-27.17)) ;
#161640 = CARTESIAN_POINT('',(7.8,3.,-27.17)) ;
#161641 = CARTESIAN_POINT('',(7.8,2.9,-27.17)) ;
#161642 = CARTESIAN_POINT('Origin',(7.8,3.,-27.07)) ;
#161643 = CARTESIAN_POINT('',(7.7,2.1,-27.07)) ;
#161644 = CARTESIAN_POINT('Origin',(7.8,2.1,-27.07)) ;
#161645 = CARTESIAN_POINT('',(7.7,2.9,-27.07)) ;
#161646 = CARTESIAN_POINT('',(7.7,3.,-27.07)) ;
#161647 = CARTESIAN_POINT('Origin',(7.8,2.9,-27.07)) ;
#161648 = CARTESIAN_POINT('Origin',(7.7,3.,-27.07)) ;
#161649 = CARTESIAN_POINT('',(7.7,2.1,-26.27)) ;
#161650 = CARTESIAN_POINT('',(7.7,2.1,-26.27)) ;
#161651 = CARTESIAN_POINT('',(7.7,2.9,-26.27)) ;
#161652 = CARTESIAN_POINT('',(7.7,3.,-26.27)) ;
#161653 = CARTESIAN_POINT('',(7.7,2.9,-27.07)) ;
#161654 = CARTESIAN_POINT('Origin',(7.8,3.,-26.27)) ;
#161655 = CARTESIAN_POINT('',(7.8,2.1,-26.17)) ;
#161656 = CARTESIAN_POINT('Origin',(7.8,2.1,-26.27)) ;
#161657 = CARTESIAN_POINT('',(7.8,2.9,-26.17)) ;
#161658 = CARTESIAN_POINT('',(7.8,3.,-26.17)) ;
#161659 = CARTESIAN_POINT('Origin',(7.8,2.9,-26.27)) ;
#161660 = CARTESIAN_POINT('Origin',(7.8,3.,-26.17)) ;
#161661 = CARTESIAN_POINT('',(9.6,2.1,-26.17)) ;
#161662 = CARTESIAN_POINT('',(9.6,2.1,-26.17)) ;
#161663 = CARTESIAN_POINT('',(9.6,2.9,-26.17)) ;
#161664 = CARTESIAN_POINT('',(9.6,3.,-26.17)) ;
#161665 = CARTESIAN_POINT('',(7.8,2.9,-26.17)) ;
#161666 = CARTESIAN_POINT('Origin',(9.6,3.,-26.27)) ;
#161667 = CARTESIAN_POINT('',(9.7,2.1,-26.27)) ;
#161668 = CARTESIAN_POINT('Origin',(9.6,2.1,-26.27)) ;
#161669 = CARTESIAN_POINT('',(9.7,2.9,-26.27)) ;
#161670 = CARTESIAN_POINT('',(9.7,3.,-26.27)) ;
#161671 = CARTESIAN_POINT('Origin',(9.6,2.9,-26.27)) ;
#161672 = CARTESIAN_POINT('Origin',(9.7,3.,-27.07)) ;
#161673 = CARTESIAN_POINT('',(9.7,2.9,-27.07)) ;
#161674 = CARTESIAN_POINT('',(9.7,2.1,-27.07)) ;
#161675 = CARTESIAN_POINT('Origin',(9.6,3.,-27.07)) ;
#161676 = CARTESIAN_POINT('',(7.8,3.,-26.27)) ;
#161677 = CARTESIAN_POINT('',(9.6,3.,-26.27)) ;
#161678 = CARTESIAN_POINT('',(9.6,3.,-26.27)) ;
#161679 = CARTESIAN_POINT('',(9.6,3.,-27.07)) ;
#161680 = CARTESIAN_POINT('',(9.6,3.,-27.07)) ;
#161681 = CARTESIAN_POINT('',(7.8,3.,-27.07)) ;
#161682 = CARTESIAN_POINT('',(9.6,3.,-27.07)) ;
#161683 = CARTESIAN_POINT('',(7.8,3.,-27.07)) ;
#161684 = CARTESIAN_POINT('Origin',(9.6,3.,-30.88)) ;
#161685 = CARTESIAN_POINT('',(9.7,2.9,-30.88)) ;
#161686 = CARTESIAN_POINT('',(9.7,2.1,-30.88)) ;
#161687 = CARTESIAN_POINT('',(9.7,3.,-30.88)) ;
#161688 = CARTESIAN_POINT('',(9.6,2.1,-30.98)) ;
#161689 = CARTESIAN_POINT('Origin',(9.6,2.1,-30.88)) ;
#161690 = CARTESIAN_POINT('',(9.6,2.9,-30.98)) ;
#161691 = CARTESIAN_POINT('',(9.6,3.,-30.98)) ;
#161692 = CARTESIAN_POINT('Origin',(9.6,2.9,-30.88)) ;
#161693 = CARTESIAN_POINT('Origin',(7.8,3.,-30.98)) ;
#161694 = CARTESIAN_POINT('',(7.8,2.1,-30.98)) ;
#161695 = CARTESIAN_POINT('',(7.8,2.1,-30.98)) ;
#161696 = CARTESIAN_POINT('',(7.8,2.9,-30.98)) ;
#161697 = CARTESIAN_POINT('',(7.8,3.,-30.98)) ;
#161698 = CARTESIAN_POINT('',(7.8,2.9,-30.98)) ;
#161699 = CARTESIAN_POINT('Origin',(7.8,3.,-30.88)) ;
#161700 = CARTESIAN_POINT('',(7.7,2.1,-30.88)) ;
#161701 = CARTESIAN_POINT('Origin',(7.8,2.1,-30.88)) ;
#161702 = CARTESIAN_POINT('',(7.7,2.9,-30.88)) ;
#161703 = CARTESIAN_POINT('',(7.7,3.,-30.88)) ;
#161704 = CARTESIAN_POINT('Origin',(7.8,2.9,-30.88)) ;
#161705 = CARTESIAN_POINT('Origin',(7.7,3.,-30.88)) ;
#161706 = CARTESIAN_POINT('',(7.7,2.1,-30.08)) ;
#161707 = CARTESIAN_POINT('',(7.7,2.1,-30.08)) ;
#161708 = CARTESIAN_POINT('',(7.7,2.9,-30.08)) ;
#161709 = CARTESIAN_POINT('',(7.7,3.,-30.08)) ;
#161710 = CARTESIAN_POINT('',(7.7,2.9,-30.88)) ;
#161711 = CARTESIAN_POINT('Origin',(7.8,3.,-30.08)) ;
#161712 = CARTESIAN_POINT('',(7.8,2.1,-29.98)) ;
#161713 = CARTESIAN_POINT('Origin',(7.8,2.1,-30.08)) ;
#161714 = CARTESIAN_POINT('',(7.8,2.9,-29.98)) ;
#161715 = CARTESIAN_POINT('',(7.8,3.,-29.98)) ;
#161716 = CARTESIAN_POINT('Origin',(7.8,2.9,-30.08)) ;
#161717 = CARTESIAN_POINT('Origin',(7.8,3.,-29.98)) ;
#161718 = CARTESIAN_POINT('',(9.6,2.1,-29.98)) ;
#161719 = CARTESIAN_POINT('',(9.6,2.1,-29.98)) ;
#161720 = CARTESIAN_POINT('',(9.6,2.9,-29.98)) ;
#161721 = CARTESIAN_POINT('',(9.6,3.,-29.98)) ;
#161722 = CARTESIAN_POINT('',(7.8,2.9,-29.98)) ;
#161723 = CARTESIAN_POINT('Origin',(9.6,3.,-30.08)) ;
#161724 = CARTESIAN_POINT('',(9.7,2.1,-30.08)) ;
#161725 = CARTESIAN_POINT('Origin',(9.6,2.1,-30.08)) ;
#161726 = CARTESIAN_POINT('',(9.7,2.9,-30.08)) ;
#161727 = CARTESIAN_POINT('',(9.7,3.,-30.08)) ;
#161728 = CARTESIAN_POINT('Origin',(9.6,2.9,-30.08)) ;
#161729 = CARTESIAN_POINT('Origin',(9.7,3.,-30.88)) ;
#161730 = CARTESIAN_POINT('',(9.7,2.9,-30.88)) ;
#161731 = CARTESIAN_POINT('',(9.7,2.1,-30.88)) ;
#161732 = CARTESIAN_POINT('Origin',(9.6,3.,-30.88)) ;
#161733 = CARTESIAN_POINT('',(7.8,3.,-30.08)) ;
#161734 = CARTESIAN_POINT('',(9.6,3.,-30.08)) ;
#161735 = CARTESIAN_POINT('',(9.6,3.,-30.08)) ;
#161736 = CARTESIAN_POINT('',(9.6,3.,-30.88)) ;
#161737 = CARTESIAN_POINT('',(9.6,3.,-30.88)) ;
#161738 = CARTESIAN_POINT('',(7.8,3.,-30.88)) ;
#161739 = CARTESIAN_POINT('',(9.6,3.,-30.88)) ;
#161740 = CARTESIAN_POINT('',(7.8,3.,-30.88)) ;
#161741 = CARTESIAN_POINT('Origin',(9.6,3.,-34.69)) ;
#161742 = CARTESIAN_POINT('',(9.7,2.9,-34.69)) ;
#161743 = CARTESIAN_POINT('',(9.7,2.1,-34.69)) ;
#161744 = CARTESIAN_POINT('',(9.7,3.,-34.69)) ;
#161745 = CARTESIAN_POINT('',(9.6,2.1,-34.79)) ;
#161746 = CARTESIAN_POINT('Origin',(9.6,2.1,-34.69)) ;
#161747 = CARTESIAN_POINT('',(9.6,2.9,-34.79)) ;
#161748 = CARTESIAN_POINT('',(9.6,3.,-34.79)) ;
#161749 = CARTESIAN_POINT('Origin',(9.6,2.9,-34.69)) ;
#161750 = CARTESIAN_POINT('Origin',(7.8,3.,-34.79)) ;
#161751 = CARTESIAN_POINT('',(7.8,2.1,-34.79)) ;
#161752 = CARTESIAN_POINT('',(7.8,2.1,-34.79)) ;
#161753 = CARTESIAN_POINT('',(7.8,2.9,-34.79)) ;
#161754 = CARTESIAN_POINT('',(7.8,3.,-34.79)) ;
#161755 = CARTESIAN_POINT('',(7.8,2.9,-34.79)) ;
#161756 = CARTESIAN_POINT('Origin',(7.8,3.,-34.69)) ;
#161757 = CARTESIAN_POINT('',(7.7,2.1,-34.69)) ;
#161758 = CARTESIAN_POINT('Origin',(7.8,2.1,-34.69)) ;
#161759 = CARTESIAN_POINT('',(7.7,2.9,-34.69)) ;
#161760 = CARTESIAN_POINT('',(7.7,3.,-34.69)) ;
#161761 = CARTESIAN_POINT('Origin',(7.8,2.9,-34.69)) ;
#161762 = CARTESIAN_POINT('Origin',(7.7,3.,-34.69)) ;
#161763 = CARTESIAN_POINT('',(7.7,2.1,-33.89)) ;
#161764 = CARTESIAN_POINT('',(7.7,2.1,-33.89)) ;
#161765 = CARTESIAN_POINT('',(7.7,2.9,-33.89)) ;
#161766 = CARTESIAN_POINT('',(7.7,3.,-33.89)) ;
#161767 = CARTESIAN_POINT('',(7.7,2.9,-34.69)) ;
#161768 = CARTESIAN_POINT('Origin',(7.8,3.,-33.89)) ;
#161769 = CARTESIAN_POINT('',(7.8,2.1,-33.79)) ;
#161770 = CARTESIAN_POINT('Origin',(7.8,2.1,-33.89)) ;
#161771 = CARTESIAN_POINT('',(7.8,2.9,-33.79)) ;
#161772 = CARTESIAN_POINT('',(7.8,3.,-33.79)) ;
#161773 = CARTESIAN_POINT('Origin',(7.8,2.9,-33.89)) ;
#161774 = CARTESIAN_POINT('Origin',(7.8,3.,-33.79)) ;
#161775 = CARTESIAN_POINT('',(9.6,2.1,-33.79)) ;
#161776 = CARTESIAN_POINT('',(9.6,2.1,-33.79)) ;
#161777 = CARTESIAN_POINT('',(9.6,2.9,-33.79)) ;
#161778 = CARTESIAN_POINT('',(9.6,3.,-33.79)) ;
#161779 = CARTESIAN_POINT('',(7.8,2.9,-33.79)) ;
#161780 = CARTESIAN_POINT('Origin',(9.6,3.,-33.89)) ;
#161781 = CARTESIAN_POINT('',(9.7,2.1,-33.89)) ;
#161782 = CARTESIAN_POINT('Origin',(9.6,2.1,-33.89)) ;
#161783 = CARTESIAN_POINT('',(9.7,2.9,-33.89)) ;
#161784 = CARTESIAN_POINT('',(9.7,3.,-33.89)) ;
#161785 = CARTESIAN_POINT('Origin',(9.6,2.9,-33.89)) ;
#161786 = CARTESIAN_POINT('Origin',(9.7,3.,-34.69)) ;
#161787 = CARTESIAN_POINT('',(9.7,2.9,-34.69)) ;
#161788 = CARTESIAN_POINT('',(9.7,2.1,-34.69)) ;
#161789 = CARTESIAN_POINT('Origin',(9.6,3.,-34.69)) ;
#161790 = CARTESIAN_POINT('',(7.8,3.,-33.89)) ;
#161791 = CARTESIAN_POINT('',(9.6,3.,-33.89)) ;
#161792 = CARTESIAN_POINT('',(9.6,3.,-33.89)) ;
#161793 = CARTESIAN_POINT('',(9.6,3.,-34.69)) ;
#161794 = CARTESIAN_POINT('',(9.6,3.,-34.69)) ;
#161795 = CARTESIAN_POINT('',(7.8,3.,-34.69)) ;
#161796 = CARTESIAN_POINT('',(9.6,3.,-34.69)) ;
#161797 = CARTESIAN_POINT('',(7.8,3.,-34.69)) ;
#161798 = CARTESIAN_POINT('Origin',(10.1,-2.15,-4.71311959340942)) ;
#161799 = CARTESIAN_POINT('Origin',(10.1,-2.15,-4.71311959340942)) ;
#161800 = CARTESIAN_POINT('Origin',(10.1,-2.15,-4.71311959340942)) ;
#161801 = CARTESIAN_POINT('Origin',(10.1,-2.15,-4.71311959340942)) ;
#161802 = CARTESIAN_POINT('Origin',(10.1,-3.65625,-3.81)) ;
#161803 = CARTESIAN_POINT('Origin',(10.1,-2.15,-2.90688040659058)) ;
#161804 = CARTESIAN_POINT('Origin',(10.2,-2.15,-4.71311959340942)) ;
#161805 = CARTESIAN_POINT('Origin',(3.7,-2.15,-4.71311959340942)) ;
#161806 = CARTESIAN_POINT('Origin',(10.1,-2.15,-3.81)) ;
#161807 = CARTESIAN_POINT('Origin',(10.1,-2.15,-5.115)) ;
#161808 = CARTESIAN_POINT('Origin',(10.1,-3.65625,-5.115)) ;
#161809 = CARTESIAN_POINT('Origin',(10.1,1.9,-5.115)) ;
#161810 = CARTESIAN_POINT('Origin',(10.1,-2.15,-5.115)) ;
#161811 = CARTESIAN_POINT('Origin',(10.1,1.9,-3.81)) ;
#161812 = CARTESIAN_POINT('Origin',(10.1,1.9,-5.115)) ;
#161813 = CARTESIAN_POINT('Origin',(10.1,1.9,-2.505)) ;
#161814 = CARTESIAN_POINT('Origin',(10.1,-2.15,-2.90688040659058)) ;
#161815 = CARTESIAN_POINT('Origin',(10.1,-2.15,-2.90688040659058)) ;
#161816 = CARTESIAN_POINT('Origin',(10.1,-2.15,-2.90688040659058)) ;
#161817 = CARTESIAN_POINT('Origin',(3.7,-2.15,-4.71311959340942)) ;
#161818 = CARTESIAN_POINT('Origin',(3.7,-2.35,-4.71311959340942)) ;
#161819 = CARTESIAN_POINT('Origin',(3.7,-2.32153024911032,-4.6102732340176)) ;
#161820 = CARTESIAN_POINT('Origin',(10.1,-2.15,-5.115)) ;
#161821 = CARTESIAN_POINT('Origin',(10.1,-2.15,-5.115)) ;
#161822 = CARTESIAN_POINT('Origin',(10.1,-3.65625,-2.505)) ;
#161823 = CARTESIAN_POINT('Origin',(10.1,1.9,-2.505)) ;
#161824 = CARTESIAN_POINT('Origin',(10.1,-2.15,-2.505)) ;
#161825 = CARTESIAN_POINT('Origin',(10.1,-2.15,-3.81)) ;
#161826 = CARTESIAN_POINT('Origin',(10.1,-2.15,-2.505)) ;
#161827 = CARTESIAN_POINT('Origin',(10.2,-2.15,-2.90688040659058)) ;
#161828 = CARTESIAN_POINT('Origin',(3.7,-2.15,-2.90688040659058)) ;
#161829 = CARTESIAN_POINT('Origin',(3.7,-3.65625,-3.81)) ;
#161830 = CARTESIAN_POINT('Origin',(3.7,-2.32153024911032,-3.0097267659824)) ;
#161831 = CARTESIAN_POINT('Origin',(3.7,-2.35,-4.685)) ;
#161832 = CARTESIAN_POINT('Origin',(3.7,-2.35,-5.115)) ;
#161833 = CARTESIAN_POINT('Origin',(3.6,-2.15,-5.115)) ;
#161834 = CARTESIAN_POINT('Origin',(3.7,-2.15,-5.115)) ;
#161835 = CARTESIAN_POINT('Origin',(10.1,-2.15,-2.505)) ;
#161836 = CARTESIAN_POINT('Origin',(10.1,-2.15,-2.505)) ;
#161837 = CARTESIAN_POINT('Origin',(3.7,-2.15,-2.90688040659058)) ;
#161838 = CARTESIAN_POINT('Origin',(3.7,-2.35,-2.90688040659058)) ;
#161839 = CARTESIAN_POINT('Origin',(3.7,-2.35,-5.115)) ;
#161840 = CARTESIAN_POINT('Origin',(3.5,-2.35,-5.115)) ;
#161841 = CARTESIAN_POINT('Origin',(10.2,-2.15,-2.505)) ;
#161842 = CARTESIAN_POINT('Origin',(3.7,-2.15,-2.505)) ;
#161843 = CARTESIAN_POINT('Origin',(3.7,-2.35,-2.405)) ;
#161844 = CARTESIAN_POINT('Origin',(3.7,-2.35,-2.505)) ;
#161845 = CARTESIAN_POINT('Origin',(3.5,-3.80813298381585E-16,-5.115)) ;
#161846 = CARTESIAN_POINT('Origin',(3.5,-5.15,-5.115)) ;
#161847 = CARTESIAN_POINT('Origin',(3.6,1.9,-5.315)) ;
#161848 = CARTESIAN_POINT('Origin',(3.5,1.9,-5.315)) ;
#161849 = CARTESIAN_POINT('Origin',(2.7,1.9,-5.315)) ;
#161850 = CARTESIAN_POINT('Origin',(2.7,1.9,-5.215)) ;
#161851 = CARTESIAN_POINT('Origin',(2.7,1.9,-6.115)) ;
#161852 = CARTESIAN_POINT('Origin',(2.7,1.9,-5.315)) ;
#161853 = CARTESIAN_POINT('Origin',(3.7,-2.35,-2.505)) ;
#161854 = CARTESIAN_POINT('Origin',(3.5,-2.35,-2.505)) ;
#161855 = CARTESIAN_POINT('Origin',(3.5,-5.15,-5.115)) ;
#161856 = CARTESIAN_POINT('Origin',(3.5,-5.15,-5.115)) ;
#161857 = CARTESIAN_POINT('Origin',(3.5,-5.15,-5.115)) ;
#161858 = CARTESIAN_POINT('Origin',(2.7,1.9,-5.315)) ;
#161859 = CARTESIAN_POINT('Origin',(2.7,1.9,-5.315)) ;
#161860 = CARTESIAN_POINT('Origin',(3.5,3.0290702335686E-16,-2.505)) ;
#161861 = CARTESIAN_POINT('Origin',(3.5,-5.15,-2.505)) ;
#161862 = CARTESIAN_POINT('Origin',(3.5,-5.15,0.)) ;
#161863 = CARTESIAN_POINT('Origin',(3.5,-5.15,-2.505)) ;
#161864 = CARTESIAN_POINT('Origin',(3.6,-5.15,-5.115)) ;
#161865 = CARTESIAN_POINT('Origin',(2.7,-5.15,-5.115)) ;
#161866 = CARTESIAN_POINT('Origin',(2.7,-5.25,-5.315)) ;
#161867 = CARTESIAN_POINT('Origin',(2.7,-5.15,-5.315)) ;
#161868 = CARTESIAN_POINT('Origin',(3.5,-5.15,-2.505)) ;
#161869 = CARTESIAN_POINT('Origin',(3.5,-5.15,-2.505)) ;
#161870 = CARTESIAN_POINT('Origin',(2.7,-5.15,-5.115)) ;
#161871 = CARTESIAN_POINT('Origin',(2.7,-5.35,-5.115)) ;
#161872 = CARTESIAN_POINT('Origin',(3.6,1.9,-2.305)) ;
#161873 = CARTESIAN_POINT('Origin',(3.5,1.9,-2.305)) ;
#161874 = CARTESIAN_POINT('Origin',(2.7,1.9,-2.305)) ;
#161875 = CARTESIAN_POINT('Origin',(3.6,-5.15,-2.505)) ;
#161876 = CARTESIAN_POINT('Origin',(2.7,-5.15,-2.505)) ;
#161877 = CARTESIAN_POINT('Origin',(2.7,-5.35,-2.405)) ;
#161878 = CARTESIAN_POINT('Origin',(2.7,-5.35,-2.505)) ;
#161879 = CARTESIAN_POINT('Origin',(2.7,1.9,-2.305)) ;
#161880 = CARTESIAN_POINT('Origin',(2.7,1.9,-2.305)) ;
#161881 = CARTESIAN_POINT('Origin',(2.7,-5.15,-2.505)) ;
#161882 = CARTESIAN_POINT('Origin',(2.7,-5.15,-2.305)) ;
#161883 = CARTESIAN_POINT('Origin',(2.7,2.,-2.305)) ;
#161884 = CARTESIAN_POINT('Origin',(7.8,2.1,-4.21)) ;
#161885 = CARTESIAN_POINT('Origin',(7.8,2.1,-4.41)) ;
#161886 = CARTESIAN_POINT('Origin',(7.6,2.1,-4.21)) ;
#161887 = CARTESIAN_POINT('Origin',(7.6,2.1,-4.21)) ;
#161888 = CARTESIAN_POINT('Origin',(7.6,2.1,-3.41)) ;
#161889 = CARTESIAN_POINT('Origin',(7.8,2.1,-4.41)) ;
#161890 = CARTESIAN_POINT('Origin',(9.6,2.1,-4.41)) ;
#161891 = CARTESIAN_POINT('Origin',(7.8,2.1,-3.41)) ;
#161892 = CARTESIAN_POINT('Origin',(7.8,2.1,-3.21)) ;
#161893 = CARTESIAN_POINT('Origin',(9.6,2.1,-4.21)) ;
#161894 = CARTESIAN_POINT('Origin',(9.8,2.1,-4.21)) ;
#161895 = CARTESIAN_POINT('Origin',(7.8,2.1,-3.21)) ;
#161896 = CARTESIAN_POINT('Origin',(9.6,2.1,-3.21)) ;
#161897 = CARTESIAN_POINT('Origin',(9.8,2.1,-4.21)) ;
#161898 = CARTESIAN_POINT('Origin',(9.8,2.1,-3.41)) ;
#161899 = CARTESIAN_POINT('Origin',(9.6,2.1,-3.41)) ;
#161900 = CARTESIAN_POINT('Origin',(-4.9,-6.45,-35.39)) ;
#161901 = CARTESIAN_POINT('',(-4.85857864376269,-6.52071067811866,-35.3192893218814)) ;
#161902 = CARTESIAN_POINT('Origin',(-5.01417009506433,-6.44703459697317,-35.3970866853867)) ;
#161903 = CARTESIAN_POINT('Ctrl Pts',(-4.85857864376269,-6.52071067811868,
-35.3192893218814)) ;
#161904 = CARTESIAN_POINT('Ctrl Pts',(-4.86759079869274,-6.5252167555837,
-35.3237953993464)) ;
#161905 = CARTESIAN_POINT('Ctrl Pts',(-4.87748625817285,-6.52928079264427,
-35.3287264816717)) ;
#161906 = CARTESIAN_POINT('Ctrl Pts',(-4.89811277057011,-6.53624680748678,
-35.3390208825486)) ;
#161907 = CARTESIAN_POINT('Ctrl Pts',(-4.90880509433771,-6.53918030781879,
-35.3443639841507)) ;
#161908 = CARTESIAN_POINT('Ctrl Pts',(-4.92101859322336,-6.54185985500363,
-35.3504747545345)) ;
#161909 = CARTESIAN_POINT('Ctrl Pts',(-4.92228751722852,-6.54213045061265,
-35.3511097099098)) ;
#161910 = CARTESIAN_POINT('Ctrl Pts',(-4.9350493700286,-6.54477467909837,
-35.3574962891342)) ;
#161911 = CARTESIAN_POINT('Ctrl Pts',(-4.94677936428208,-6.54657370273658,
-35.3633715724064)) ;
#161912 = CARTESIAN_POINT('Ctrl Pts',(-4.96920025888411,-6.5489600764314,
-35.3745957747614)) ;
#161913 = CARTESIAN_POINT('Ctrl Pts',(-4.97990192168179,-6.5496301025519,
-35.3799500759452)) ;
#161914 = CARTESIAN_POINT('Ctrl Pts',(-4.99357116034318,-6.54996164986963,
-35.3867855738171)) ;
#161915 = CARTESIAN_POINT('Ctrl Pts',(-4.99680282631925,-6.55,-35.3884014131596)) ;
#161916 = CARTESIAN_POINT('Ctrl Pts',(-5.,-6.55,-35.39)) ;
#161917 = CARTESIAN_POINT('',(-3.94142135623684,-6.52071067811842,-35.3192893218811)) ;
#161918 = CARTESIAN_POINT('Ctrl Pts',(-3.8,-6.55,-35.39)) ;
#161919 = CARTESIAN_POINT('Ctrl Pts',(-3.81016571653571,-6.55,-35.3849171417321)) ;
#161920 = CARTESIAN_POINT('Ctrl Pts',(-3.82068315091917,-6.54961031187957,
-35.3796576838579)) ;
#161921 = CARTESIAN_POINT('Ctrl Pts',(-3.84304266527945,-6.54783411578236,
-35.3684679497194)) ;
#161922 = CARTESIAN_POINT('Ctrl Pts',(-3.85491327259758,-6.54635217950662,
-35.3625227617952)) ;
#161923 = CARTESIAN_POINT('Ctrl Pts',(-3.87771616261517,-6.54231439116937,
-35.3511067603977)) ;
#161924 = CARTESIAN_POINT('Ctrl Pts',(-3.88866251834261,-6.53982180675303,
-35.345629861311)) ;
#161925 = CARTESIAN_POINT('Ctrl Pts',(-3.90045005710787,-6.53645537933612,
-35.3397406960422)) ;
#161926 = CARTESIAN_POINT('Ctrl Pts',(-3.90170928105007,-6.53608665347898,
-35.3391116827677)) ;
#161927 = CARTESIAN_POINT('Ctrl Pts',(-3.91388077026579,-6.53243308776766,
-35.333032751352)) ;
#161928 = CARTESIAN_POINT('Ctrl Pts',(-3.92429308263634,-6.52859969139749,
-35.3278422384292)) ;
#161929 = CARTESIAN_POINT('Ctrl Pts',(-3.93645488997201,-6.52312881451524,
-35.3217711869642)) ;
#161930 = CARTESIAN_POINT('Ctrl Pts',(-3.93897066587108,-6.52193602330131,
-35.320514667064)) ;
#161931 = CARTESIAN_POINT('Ctrl Pts',(-3.94142135623684,-6.52071067811842,
-35.3192893218811)) ;
#161932 = CARTESIAN_POINT('Origin',(-3.78571994569831,-6.44700925664017,-35.397142104249)) ;
#161933 = CARTESIAN_POINT('Origin',(-3.8,-6.45,-33.29)) ;
#161934 = CARTESIAN_POINT('',(-3.87071067811865,-6.52071067811866,-33.3314213562373)) ;
#161935 = CARTESIAN_POINT('Ctrl Pts',(-3.8,-6.55,-33.19)) ;
#161936 = CARTESIAN_POINT('Ctrl Pts',(-3.80508285826794,-6.55,-33.2001657165359)) ;
#161937 = CARTESIAN_POINT('Ctrl Pts',(-3.81034231614204,-6.54961031187957,
-33.2106831509196)) ;
#161938 = CARTESIAN_POINT('Ctrl Pts',(-3.82153205028074,-6.54783411578234,
-33.2330426652806)) ;
#161939 = CARTESIAN_POINT('Ctrl Pts',(-3.82747723820518,-6.54635217950653,
-33.2449132725992)) ;
#161940 = CARTESIAN_POINT('Ctrl Pts',(-3.83889323960396,-6.54231439116874,
-33.2677161626196)) ;
#161941 = CARTESIAN_POINT('Ctrl Pts',(-3.84437013869177,-6.53982180675175,
-33.2786625183492)) ;
#161942 = CARTESIAN_POINT('Ctrl Pts',(-3.8502593039605,-6.53645537933455,
-33.2904500571143)) ;
#161943 = CARTESIAN_POINT('Ctrl Pts',(-3.85088831723394,-6.53608665347802,
-33.2917092810543)) ;
#161944 = CARTESIAN_POINT('Ctrl Pts',(-3.85696724864837,-6.53243308776737,
-33.3038807702676)) ;
#161945 = CARTESIAN_POINT('Ctrl Pts',(-3.86215776157101,-6.52859969139729,
-33.3142930826378)) ;
#161946 = CARTESIAN_POINT('Ctrl Pts',(-3.86822881303577,-6.52312881451525,
-33.3264548899729)) ;
#161947 = CARTESIAN_POINT('Ctrl Pts',(-3.86948533293589,-6.52193602330142,
-33.3289706658718)) ;
#161948 = CARTESIAN_POINT('Ctrl Pts',(-3.87071067811865,-6.52071067811866,
-33.3314213562373)) ;
#161949 = CARTESIAN_POINT('Origin',(-3.79285789576313,-6.44700925664404,-33.1757199457244)) ;
#161950 = CARTESIAN_POINT('',(-3.87071067811865,-6.52071067811866,-35.2485786437627)) ;
#161951 = CARTESIAN_POINT('Origin',(-3.79291331463517,-6.44703459698217,-35.4041700950208)) ;
#161952 = CARTESIAN_POINT('Ctrl Pts',(-3.87071067811865,-6.52071067811866,
-35.2485786437627)) ;
#161953 = CARTESIAN_POINT('Ctrl Pts',(-3.86620460065363,-6.52521675558368,
-35.2575907986928)) ;
#161954 = CARTESIAN_POINT('Ctrl Pts',(-3.86127351832835,-6.52928079264423,
-35.2674862581729)) ;
#161955 = CARTESIAN_POINT('Ctrl Pts',(-3.85097911745215,-6.5362468074863,
-35.2881127705688)) ;
#161956 = CARTESIAN_POINT('Ctrl Pts',(-3.84563601585079,-6.53918030781798,
-35.2988050943349)) ;
#161957 = CARTESIAN_POINT('Ctrl Pts',(-3.83952524546706,-6.54185985500296,
-35.3110185932205)) ;
#161958 = CARTESIAN_POINT('Ctrl Pts',(-3.83889029009099,-6.5421304506123,
-35.3122875172271)) ;
#161959 = CARTESIAN_POINT('Ctrl Pts',(-3.832503710866,-6.54477467909831,-35.3250493700286)) ;
#161960 = CARTESIAN_POINT('Ctrl Pts',(-3.82662842759374,-6.54657370273655,
-35.336779364282)) ;
#161961 = CARTESIAN_POINT('Ctrl Pts',(-3.81540422523868,-6.54896007643138,
-35.3592002588841)) ;
#161962 = CARTESIAN_POINT('Ctrl Pts',(-3.81004992405483,-6.54963010255189,
-35.3699019216818)) ;
#161963 = CARTESIAN_POINT('Ctrl Pts',(-3.80321442618285,-6.54996164986963,
-35.3835711603432)) ;
#161964 = CARTESIAN_POINT('Ctrl Pts',(-3.80159858684037,-6.55,-35.3868028263193)) ;
#161965 = CARTESIAN_POINT('Ctrl Pts',(-3.8,-6.55,-35.39)) ;
#161966 = CARTESIAN_POINT('Origin',(-5.,-6.45,-33.29)) ;
#161967 = CARTESIAN_POINT('',(-4.92928932188134,-6.52071067811866,-35.2485786437627)) ;
#161968 = CARTESIAN_POINT('Ctrl Pts',(-5.,-6.55,-35.39)) ;
#161969 = CARTESIAN_POINT('Ctrl Pts',(-4.99491714173205,-6.55,-35.3798342834641)) ;
#161970 = CARTESIAN_POINT('Ctrl Pts',(-4.98965768385794,-6.54961031187957,
-35.3693168490804)) ;
#161971 = CARTESIAN_POINT('Ctrl Pts',(-4.97846794971924,-6.54783411578233,
-35.3469573347195)) ;
#161972 = CARTESIAN_POINT('Ctrl Pts',(-4.9725227617948,-6.54635217950652,
-35.3350867274009)) ;
#161973 = CARTESIAN_POINT('Ctrl Pts',(-4.96110676039595,-6.54231439116871,
-35.3122838373804)) ;
#161974 = CARTESIAN_POINT('Ctrl Pts',(-4.95562986130807,-6.53982180675168,
-35.3013374816505)) ;
#161975 = CARTESIAN_POINT('Ctrl Pts',(-4.94974069603936,-6.53645537933446,
-35.2895499428855)) ;
#161976 = CARTESIAN_POINT('Ctrl Pts',(-4.949111682766,-6.53608665347798,-35.2882907189456)) ;
#161977 = CARTESIAN_POINT('Ctrl Pts',(-4.94303275135165,-6.53243308776738,
-35.2761192297325)) ;
#161978 = CARTESIAN_POINT('Ctrl Pts',(-4.93784223842901,-6.52859969139732,
-35.2657069173623)) ;
#161979 = CARTESIAN_POINT('Ctrl Pts',(-4.93177118696425,-6.52312881451527,
-35.2535451100271)) ;
#161980 = CARTESIAN_POINT('Ctrl Pts',(-4.93051466706411,-6.52193602330142,
-35.2510293341283)) ;
#161981 = CARTESIAN_POINT('Ctrl Pts',(-4.92928932188135,-6.52071067811866,
-35.2485786437627)) ;
#161982 = CARTESIAN_POINT('Origin',(-5.007142104231,-6.44700925664598,-35.4042800542639)) ;
#161983 = CARTESIAN_POINT('',(-4.92928932188135,-6.52071067811866,-33.3314213562373)) ;
#161984 = CARTESIAN_POINT('Origin',(-5.00708668535334,-6.44703459698616,-33.1758299050023)) ;
#161985 = CARTESIAN_POINT('Ctrl Pts',(-4.92928932188135,-6.52071067811866,
-33.3314213562373)) ;
#161986 = CARTESIAN_POINT('Ctrl Pts',(-4.93379539934637,-6.52521675558368,
-33.3224092013072)) ;
#161987 = CARTESIAN_POINT('Ctrl Pts',(-4.93872648167165,-6.52928079264423,
-33.3125137418271)) ;
#161988 = CARTESIAN_POINT('Ctrl Pts',(-4.94902088254777,-6.53624680748625,
-33.2918872294312)) ;
#161989 = CARTESIAN_POINT('Ctrl Pts',(-4.95436398414905,-6.53918030781789,
-33.2811949056653)) ;
#161990 = CARTESIAN_POINT('Ctrl Pts',(-4.96047475453277,-6.54185985500289,
-33.2689814067798)) ;
#161991 = CARTESIAN_POINT('Ctrl Pts',(-4.96110970990891,-6.54213045061226,
-33.2677124827731)) ;
#161992 = CARTESIAN_POINT('Ctrl Pts',(-4.96749628913395,-6.5447746790983,
-33.2549506299714)) ;
#161993 = CARTESIAN_POINT('Ctrl Pts',(-4.97337157240622,-6.54657370273654,
-33.2432206357179)) ;
#161994 = CARTESIAN_POINT('Ctrl Pts',(-4.98459577476128,-6.54896007643137,
-33.2207997411159)) ;
#161995 = CARTESIAN_POINT('Ctrl Pts',(-4.98995007594513,-6.54963010255189,
-33.2100980783182)) ;
#161996 = CARTESIAN_POINT('Ctrl Pts',(-4.99678557381713,-6.54996164986963,
-33.1964288396568)) ;
#161997 = CARTESIAN_POINT('Ctrl Pts',(-4.99840141315962,-6.55,-33.1931971736808)) ;
#161998 = CARTESIAN_POINT('Ctrl Pts',(-5.,-6.55,-33.19)) ;
#161999 = CARTESIAN_POINT('Origin',(-4.9,-6.45,-33.19)) ;
#162000 = CARTESIAN_POINT('',(-4.85857864376269,-6.52071067811865,-33.2607106781187)) ;
#162001 = CARTESIAN_POINT('Ctrl Pts',(-5.,-6.55,-33.19)) ;
#162002 = CARTESIAN_POINT('Ctrl Pts',(-4.98983428346409,-6.55,-33.1950828582679)) ;
#162003 = CARTESIAN_POINT('Ctrl Pts',(-4.97931684908043,-6.54961031187958,
-33.200342316142)) ;
#162004 = CARTESIAN_POINT('Ctrl Pts',(-4.95695733471947,-6.54783411578237,
-33.2115320502806)) ;
#162005 = CARTESIAN_POINT('Ctrl Pts',(-4.94508672740085,-6.54635217950657,
-33.217477238205)) ;
#162006 = CARTESIAN_POINT('Ctrl Pts',(-4.92228383738129,-6.54231439116894,
-33.2288932396034)) ;
#162007 = CARTESIAN_POINT('Ctrl Pts',(-4.91133748165239,-6.53982180675217,
-33.2343701386909)) ;
#162008 = CARTESIAN_POINT('Ctrl Pts',(-4.89954994288722,-6.53645537933505,
-33.2402593039596)) ;
#162009 = CARTESIAN_POINT('Ctrl Pts',(-4.8982907189464,-6.5360866534783,-33.2408883172335)) ;
#162010 = CARTESIAN_POINT('Ctrl Pts',(-4.88611922973238,-6.53243308776742,
-33.2469672486483)) ;
#162011 = CARTESIAN_POINT('Ctrl Pts',(-4.87570691736216,-6.52859969139732,
-33.252157761571)) ;
#162012 = CARTESIAN_POINT('Ctrl Pts',(-4.86354511002705,-6.52312881451524,
-33.2582288130358)) ;
#162013 = CARTESIAN_POINT('Ctrl Pts',(-4.86102933412822,-6.52193602330141,
-33.2594853329359)) ;
#162014 = CARTESIAN_POINT('Ctrl Pts',(-4.85857864376269,-6.52071067811863,
-33.2607106781187)) ;
#162015 = CARTESIAN_POINT('Origin',(-5.01428005430853,-6.44700925663641,-33.1828578957469)) ;
#162016 = CARTESIAN_POINT('',(-3.94142135623684,-6.52071067811842,-33.2607106781189)) ;
#162017 = CARTESIAN_POINT('Origin',(-3.7858299049171,-6.44703459697097,-33.1829133146053)) ;
#162018 = CARTESIAN_POINT('Ctrl Pts',(-3.94142135623684,-6.52071067811842,
-33.2607106781189)) ;
#162019 = CARTESIAN_POINT('Ctrl Pts',(-3.93240920130662,-6.52521675558355,
-33.2562046006538)) ;
#162020 = CARTESIAN_POINT('Ctrl Pts',(-3.92251374182629,-6.52928079264416,
-33.2512735183285)) ;
#162021 = CARTESIAN_POINT('Ctrl Pts',(-3.90188722942757,-6.53624680748717,
-33.2409791174509)) ;
#162022 = CARTESIAN_POINT('Ctrl Pts',(-3.89119490565864,-6.53918030781945,
-33.2356360158481)) ;
#162023 = CARTESIAN_POINT('Ctrl Pts',(-3.87898140677303,-6.54185985500413,
-33.2295252454643)) ;
#162024 = CARTESIAN_POINT('Ctrl Pts',(-3.87771248276927,-6.54213045061284,
-33.2288902900897)) ;
#162025 = CARTESIAN_POINT('Ctrl Pts',(-3.86495062997103,-6.54477467909819,
-33.2225037108663)) ;
#162026 = CARTESIAN_POINT('Ctrl Pts',(-3.85322063571802,-6.54657370273639,
-33.2166284275943)) ;
#162027 = CARTESIAN_POINT('Ctrl Pts',(-3.83079974111668,-6.54896007643127,
-33.2054042252394)) ;
#162028 = CARTESIAN_POINT('Ctrl Pts',(-3.82009807831922,-6.54963010255182,
-33.2000499240556)) ;
#162029 = CARTESIAN_POINT('Ctrl Pts',(-3.80642883965762,-6.54996164986962,
-33.1932144261834)) ;
#162030 = CARTESIAN_POINT('Ctrl Pts',(-3.80319717368114,-6.55,-33.1915985868406)) ;
#162031 = CARTESIAN_POINT('Ctrl Pts',(-3.8,-6.55,-33.19)) ;
#162032 = CARTESIAN_POINT('Origin',(-4.9,-6.45,-31.58)) ;
#162033 = CARTESIAN_POINT('',(-4.85857864376269,-6.52071067811866,-31.5092893218814)) ;
#162034 = CARTESIAN_POINT('Origin',(-5.01417009505135,-6.44703459697586,-31.5870866853803)) ;
#162035 = CARTESIAN_POINT('Ctrl Pts',(-4.85857864376269,-6.52071067811868,
-31.5092893218814)) ;
#162036 = CARTESIAN_POINT('Ctrl Pts',(-4.86759079869273,-6.5252167555837,
-31.5137953993464)) ;
#162037 = CARTESIAN_POINT('Ctrl Pts',(-4.87748625817284,-6.52928079264427,
-31.5187264816717)) ;
#162038 = CARTESIAN_POINT('Ctrl Pts',(-4.89811277056898,-6.53624680748639,
-31.529020882548)) ;
#162039 = CARTESIAN_POINT('Ctrl Pts',(-4.90880509433532,-6.53918030781814,
-31.5343639841495)) ;
#162040 = CARTESIAN_POINT('Ctrl Pts',(-4.92101859322092,-6.54185985500311,
-31.5404747545333)) ;
#162041 = CARTESIAN_POINT('Ctrl Pts',(-4.9222875172273,-6.5421304506124,-31.5411097099092)) ;
#162042 = CARTESIAN_POINT('Ctrl Pts',(-4.9350493700286,-6.54477467909837,
-31.5474962891341)) ;
#162043 = CARTESIAN_POINT('Ctrl Pts',(-4.94677936428206,-6.54657370273659,
-31.5533715724064)) ;
#162044 = CARTESIAN_POINT('Ctrl Pts',(-4.96920025888408,-6.5489600764314,
-31.5645957747614)) ;
#162045 = CARTESIAN_POINT('Ctrl Pts',(-4.97990192168176,-6.5496301025519,
-31.5699500759452)) ;
#162046 = CARTESIAN_POINT('Ctrl Pts',(-4.99357116034316,-6.54996164986963,
-31.5767855738171)) ;
#162047 = CARTESIAN_POINT('Ctrl Pts',(-4.99680282631924,-6.55,-31.5784014131596)) ;
#162048 = CARTESIAN_POINT('Ctrl Pts',(-5.,-6.55,-31.58)) ;
#162049 = CARTESIAN_POINT('',(-3.94142135623683,-6.52071067811842,-31.5092893218811)) ;
#162050 = CARTESIAN_POINT('Ctrl Pts',(-3.8,-6.55,-31.58)) ;
#162051 = CARTESIAN_POINT('Ctrl Pts',(-3.81016571653571,-6.55,-31.5749171417321)) ;
#162052 = CARTESIAN_POINT('Ctrl Pts',(-3.82068315091917,-6.54961031187957,
-31.5696576838579)) ;
#162053 = CARTESIAN_POINT('Ctrl Pts',(-3.84304266527945,-6.54783411578236,
-31.5584679497194)) ;
#162054 = CARTESIAN_POINT('Ctrl Pts',(-3.85491327259759,-6.54635217950662,
-31.5525227617952)) ;
#162055 = CARTESIAN_POINT('Ctrl Pts',(-3.87771616261546,-6.54231439116932,
-31.5411067603976)) ;
#162056 = CARTESIAN_POINT('Ctrl Pts',(-3.88866251834317,-6.53982180675291,
-31.5356298613107)) ;
#162057 = CARTESIAN_POINT('Ctrl Pts',(-3.90045005710841,-6.53645537933597,
-31.5297406960419)) ;
#162058 = CARTESIAN_POINT('Ctrl Pts',(-3.90170928105035,-6.5360866534789,
-31.5291116827675)) ;
#162059 = CARTESIAN_POINT('Ctrl Pts',(-3.9138807702658,-6.53243308776766,
-31.523032751352)) ;
#162060 = CARTESIAN_POINT('Ctrl Pts',(-3.92429308263635,-6.5285996913975,
-31.5178422384292)) ;
#162061 = CARTESIAN_POINT('Ctrl Pts',(-3.93645488997202,-6.52312881451524,
-31.5117711869642)) ;
#162062 = CARTESIAN_POINT('Ctrl Pts',(-3.93897066587108,-6.52193602330131,
-31.510514667064)) ;
#162063 = CARTESIAN_POINT('Ctrl Pts',(-3.94142135623683,-6.52071067811842,
-31.5092893218811)) ;
#162064 = CARTESIAN_POINT('Origin',(-3.78571994569106,-6.44700925663902,-31.5871421042526)) ;
#162065 = CARTESIAN_POINT('Origin',(-3.8,-6.45,-29.48)) ;
#162066 = CARTESIAN_POINT('',(-3.87071067811865,-6.52071067811866,-29.5214213562373)) ;
#162067 = CARTESIAN_POINT('Ctrl Pts',(-3.8,-6.55,-29.38)) ;
#162068 = CARTESIAN_POINT('Ctrl Pts',(-3.80508285826792,-6.55,-29.3901657165359)) ;
#162069 = CARTESIAN_POINT('Ctrl Pts',(-3.81034231614199,-6.54961031187958,
-29.4006831509195)) ;
#162070 = CARTESIAN_POINT('Ctrl Pts',(-3.82153205028065,-6.54783411578235,
-29.4230426652804)) ;
#162071 = CARTESIAN_POINT('Ctrl Pts',(-3.82747723820507,-6.54635217950656,
-29.4349132725989)) ;
#162072 = CARTESIAN_POINT('Ctrl Pts',(-3.83889323960381,-6.5423143911688,
-29.4577161626192)) ;
#162073 = CARTESIAN_POINT('Ctrl Pts',(-3.8443701386916,-6.53982180675183,
-29.4686625183489)) ;
#162074 = CARTESIAN_POINT('Ctrl Pts',(-3.85025930396034,-6.53645537933464,
-29.480450057114)) ;
#162075 = CARTESIAN_POINT('Ctrl Pts',(-3.8508883172338,-6.5360866534781,-29.4817092810541)) ;
#162076 = CARTESIAN_POINT('Ctrl Pts',(-3.85696724864826,-6.53243308776744,
-29.4938807702674)) ;
#162077 = CARTESIAN_POINT('Ctrl Pts',(-3.86215776157091,-6.52859969139737,
-29.5042930826376)) ;
#162078 = CARTESIAN_POINT('Ctrl Pts',(-3.86822881303572,-6.5231288145153,
-29.5164548899728)) ;
#162079 = CARTESIAN_POINT('Ctrl Pts',(-3.86948533293586,-6.52193602330145,
-29.5189706658717)) ;
#162080 = CARTESIAN_POINT('Ctrl Pts',(-3.87071067811865,-6.52071067811866,
-29.5214213562373)) ;
#162081 = CARTESIAN_POINT('Origin',(-3.7928578957674,-6.44700925664559,-29.3657199457331)) ;
#162082 = CARTESIAN_POINT('',(-3.87071067811865,-6.52071067811866,-31.4385786437627)) ;
#162083 = CARTESIAN_POINT('Origin',(-3.79291331463673,-6.44703459698258,-31.5941700950176)) ;
#162084 = CARTESIAN_POINT('Ctrl Pts',(-3.87071067811865,-6.52071067811866,
-31.4385786437627)) ;
#162085 = CARTESIAN_POINT('Ctrl Pts',(-3.86620460065363,-6.52521675558368,
-31.4475907986928)) ;
#162086 = CARTESIAN_POINT('Ctrl Pts',(-3.86127351832835,-6.52928079264423,
-31.4574862581729)) ;
#162087 = CARTESIAN_POINT('Ctrl Pts',(-3.85097911745211,-6.53624680748632,
-31.4781127705689)) ;
#162088 = CARTESIAN_POINT('Ctrl Pts',(-3.84563601585071,-6.53918030781802,
-31.4888050943351)) ;
#162089 = CARTESIAN_POINT('Ctrl Pts',(-3.83952524546698,-6.541859855003,-31.5010185932206)) ;
#162090 = CARTESIAN_POINT('Ctrl Pts',(-3.83889029009095,-6.54213045061232,
-31.5022875172272)) ;
#162091 = CARTESIAN_POINT('Ctrl Pts',(-3.832503710866,-6.54477467909831,-31.5150493700286)) ;
#162092 = CARTESIAN_POINT('Ctrl Pts',(-3.82662842759373,-6.54657370273655,
-31.5267793642821)) ;
#162093 = CARTESIAN_POINT('Ctrl Pts',(-3.81540422523867,-6.54896007643138,
-31.5492002588841)) ;
#162094 = CARTESIAN_POINT('Ctrl Pts',(-3.81004992405483,-6.54963010255189,
-31.5599019216818)) ;
#162095 = CARTESIAN_POINT('Ctrl Pts',(-3.80321442618285,-6.54996164986963,
-31.5735711603432)) ;
#162096 = CARTESIAN_POINT('Ctrl Pts',(-3.80159858684036,-6.55,-31.5768028263193)) ;
#162097 = CARTESIAN_POINT('Ctrl Pts',(-3.8,-6.55,-31.58)) ;
#162098 = CARTESIAN_POINT('Origin',(-5.,-6.45,-29.48)) ;
#162099 = CARTESIAN_POINT('',(-4.92928932188134,-6.52071067811866,-31.4385786437627)) ;
#162100 = CARTESIAN_POINT('Ctrl Pts',(-5.,-6.55,-31.58)) ;
#162101 = CARTESIAN_POINT('Ctrl Pts',(-4.99491714173205,-6.55,-31.5698342834641)) ;
#162102 = CARTESIAN_POINT('Ctrl Pts',(-4.98965768385794,-6.54961031187957,
-31.5593168490804)) ;
#162103 = CARTESIAN_POINT('Ctrl Pts',(-4.97846794971924,-6.54783411578233,
-31.5369573347195)) ;
#162104 = CARTESIAN_POINT('Ctrl Pts',(-4.9725227617948,-6.54635217950652,
-31.5250867274009)) ;
#162105 = CARTESIAN_POINT('Ctrl Pts',(-4.96110676039594,-6.54231439116871,
-31.5022838373803)) ;
#162106 = CARTESIAN_POINT('Ctrl Pts',(-4.95562986130805,-6.53982180675167,
-31.4913374816505)) ;
#162107 = CARTESIAN_POINT('Ctrl Pts',(-4.94974069603934,-6.53645537933445,
-31.4795499428854)) ;
#162108 = CARTESIAN_POINT('Ctrl Pts',(-4.94911168276599,-6.53608665347797,
-31.4782907189456)) ;
#162109 = CARTESIAN_POINT('Ctrl Pts',(-4.94303275135165,-6.53243308776738,
-31.4661192297325)) ;
#162110 = CARTESIAN_POINT('Ctrl Pts',(-4.93784223842901,-6.52859969139731,
-31.4557069173623)) ;
#162111 = CARTESIAN_POINT('Ctrl Pts',(-4.93177118696424,-6.52312881451526,
-31.4435451100271)) ;
#162112 = CARTESIAN_POINT('Ctrl Pts',(-4.93051466706411,-6.52193602330142,
-31.4410293341282)) ;
#162113 = CARTESIAN_POINT('Ctrl Pts',(-4.92928932188135,-6.52071067811866,
-31.4385786437627)) ;
#162114 = CARTESIAN_POINT('Origin',(-5.0071421042338,-6.44700925664485,-31.5942800542696)) ;
#162115 = CARTESIAN_POINT('',(-4.92928932188133,-6.52071067811864,-29.5214213562373)) ;
#162116 = CARTESIAN_POINT('Origin',(-5.00708668536686,-6.44703459698117,-29.3658299049752)) ;
#162117 = CARTESIAN_POINT('Ctrl Pts',(-4.92928932188133,-6.52071067811864,
-29.5214213562373)) ;
#162118 = CARTESIAN_POINT('Ctrl Pts',(-4.93379539934636,-6.52521675558367,
-29.5124092013072)) ;
#162119 = CARTESIAN_POINT('Ctrl Pts',(-4.93872648167164,-6.52928079264422,
-29.5025137418271)) ;
#162120 = CARTESIAN_POINT('Ctrl Pts',(-4.94902088254797,-6.53624680748638,
-29.4818872294309)) ;
#162121 = CARTESIAN_POINT('Ctrl Pts',(-4.95436398414947,-6.53918030781812,
-29.4711949056645)) ;
#162122 = CARTESIAN_POINT('Ctrl Pts',(-4.9604747545332,-6.54185985500307,
-29.4589814067789)) ;
#162123 = CARTESIAN_POINT('Ctrl Pts',(-4.96110970990912,-6.54213045061235,
-29.4577124827726)) ;
#162124 = CARTESIAN_POINT('Ctrl Pts',(-4.96749628913392,-6.54477467909829,
-29.4449506299714)) ;
#162125 = CARTESIAN_POINT('Ctrl Pts',(-4.97337157240617,-6.54657370273652,
-29.433220635718)) ;
#162126 = CARTESIAN_POINT('Ctrl Pts',(-4.98459577476118,-6.54896007643136,
-29.4107997411161)) ;
#162127 = CARTESIAN_POINT('Ctrl Pts',(-4.989950075945,-6.54963010255188,-29.4000980783185)) ;
#162128 = CARTESIAN_POINT('Ctrl Pts',(-4.99678557381703,-6.54996164986962,
-29.386428839657)) ;
#162129 = CARTESIAN_POINT('Ctrl Pts',(-4.99840141315957,-6.55,-29.3831971736808)) ;
#162130 = CARTESIAN_POINT('Ctrl Pts',(-5.,-6.55,-29.38)) ;
#162131 = CARTESIAN_POINT('Origin',(-4.9,-6.45,-29.38)) ;
#162132 = CARTESIAN_POINT('',(-4.85857864376276,-6.52071067811862,-29.4507106781187)) ;
#162133 = CARTESIAN_POINT('Ctrl Pts',(-5.,-6.55,-29.38)) ;
#162134 = CARTESIAN_POINT('Ctrl Pts',(-4.98983428346421,-6.55,-29.3850828582679)) ;
#162135 = CARTESIAN_POINT('Ctrl Pts',(-4.97931684908067,-6.54961031187958,
-29.390342316142)) ;
#162136 = CARTESIAN_POINT('Ctrl Pts',(-4.95695733471996,-6.54783411578236,
-29.4015320502806)) ;
#162137 = CARTESIAN_POINT('Ctrl Pts',(-4.94508672740148,-6.54635217950657,
-29.407477238205)) ;
#162138 = CARTESIAN_POINT('Ctrl Pts',(-4.92228383737806,-6.54231439116827,
-29.4188932396053)) ;
#162139 = CARTESIAN_POINT('Ctrl Pts',(-4.91133748164525,-6.53982180675044,
-29.4243701386947)) ;
#162140 = CARTESIAN_POINT('Ctrl Pts',(-4.89954994288043,-6.53645537933293,
-29.4302593039633)) ;
#162141 = CARTESIAN_POINT('Ctrl Pts',(-4.89829071894342,-6.53608665347727,
-29.4308883172352)) ;
#162142 = CARTESIAN_POINT('Ctrl Pts',(-4.88611922973308,-6.53243308776751,
-29.4369672486482)) ;
#162143 = CARTESIAN_POINT('Ctrl Pts',(-4.87570691736278,-6.52859969139747,
-29.4421577615708)) ;
#162144 = CARTESIAN_POINT('Ctrl Pts',(-4.86354511002741,-6.52312881451534,
-29.4482288130357)) ;
#162145 = CARTESIAN_POINT('Ctrl Pts',(-4.86102933412843,-6.52193602330143,
-29.4494853329359)) ;
#162146 = CARTESIAN_POINT('Ctrl Pts',(-4.85857864376276,-6.52071067811861,
-29.4507106781187)) ;
#162147 = CARTESIAN_POINT('Origin',(-5.01428005428586,-6.44700925664139,-29.3728578957581)) ;
#162148 = CARTESIAN_POINT('',(-3.94142135623731,-6.52071067811866,-29.4507106781187)) ;
#162149 = CARTESIAN_POINT('Origin',(-3.78582990494928,-6.44703459697472,-29.3729133146205)) ;
#162150 = CARTESIAN_POINT('Ctrl Pts',(-3.94142135623731,-6.52071067811863,
-29.4507106781187)) ;
#162151 = CARTESIAN_POINT('Ctrl Pts',(-3.93240920130726,-6.52521675558369,
-29.4462046006536)) ;
#162152 = CARTESIAN_POINT('Ctrl Pts',(-3.92251374182714,-6.5292807926442,
-29.4412735183284)) ;
#162153 = CARTESIAN_POINT('Ctrl Pts',(-3.90188722943347,-6.5362468074855,
-29.4309791174533)) ;
#162154 = CARTESIAN_POINT('Ctrl Pts',(-3.89119490566987,-6.53918030781666,
-29.4256360158532)) ;
#162155 = CARTESIAN_POINT('Ctrl Pts',(-3.87898140678443,-6.5418598550019,
-29.4195252454696)) ;
#162156 = CARTESIAN_POINT('Ctrl Pts',(-3.8777124827754,-6.54213045061177,
-29.4188902900923)) ;
#162157 = CARTESIAN_POINT('Ctrl Pts',(-3.86495062997147,-6.54477467909826,
-29.4125037108661)) ;
#162158 = CARTESIAN_POINT('Ctrl Pts',(-3.85322063571804,-6.54657370273652,
-29.4066284275938)) ;
#162159 = CARTESIAN_POINT('Ctrl Pts',(-3.83079974111613,-6.54896007643135,
-29.3954042252389)) ;
#162160 = CARTESIAN_POINT('Ctrl Pts',(-3.82009807831852,-6.54963010255187,
-29.3900499240551)) ;
#162161 = CARTESIAN_POINT('Ctrl Pts',(-3.80642883965707,-6.54996164986962,
-29.383214426183)) ;
#162162 = CARTESIAN_POINT('Ctrl Pts',(-3.80319717368087,-6.55,-29.3815985868404)) ;
#162163 = CARTESIAN_POINT('Ctrl Pts',(-3.8,-6.55,-29.38)) ;
#162164 = CARTESIAN_POINT('Origin',(-4.9,-6.45,-27.77)) ;
#162165 = CARTESIAN_POINT('',(-4.85857864376276,-6.52071067811862,-27.6992893218813)) ;
#162166 = CARTESIAN_POINT('Origin',(-5.01417009503991,-6.4470345969778,-27.7770866853742)) ;
#162167 = CARTESIAN_POINT('Ctrl Pts',(-4.85857864376276,-6.52071067811861,
-27.6992893218813)) ;
#162168 = CARTESIAN_POINT('Ctrl Pts',(-4.86759079869284,-6.52521675558363,
-27.7037953993463)) ;
#162169 = CARTESIAN_POINT('Ctrl Pts',(-4.877486258173,-6.52928079264421,-27.7087264816716)) ;
#162170 = CARTESIAN_POINT('Ctrl Pts',(-4.89811277056682,-6.53624680748554,
-27.7190208825467)) ;
#162171 = CARTESIAN_POINT('Ctrl Pts',(-4.90880509433053,-6.53918030781672,
-27.7243639841469)) ;
#162172 = CARTESIAN_POINT('Ctrl Pts',(-4.92101859321596,-6.54185985500196,
-27.7304747545306)) ;
#162173 = CARTESIAN_POINT('Ctrl Pts',(-4.92228751722488,-6.5421304506118,
-27.7311097099078)) ;
#162174 = CARTESIAN_POINT('Ctrl Pts',(-4.93504937002862,-6.54477467909826,
-27.7374962891339)) ;
#162175 = CARTESIAN_POINT('Ctrl Pts',(-4.94677936428197,-6.5465737027365,
-27.7433715724061)) ;
#162176 = CARTESIAN_POINT('Ctrl Pts',(-4.96920025888377,-6.54896007643133,
-27.754595774761)) ;
#162177 = CARTESIAN_POINT('Ctrl Pts',(-4.97990192168136,-6.54963010255186,
-27.7599500759448)) ;
#162178 = CARTESIAN_POINT('Ctrl Pts',(-4.99357116034283,-6.54996164986962,
-27.766785573817)) ;
#162179 = CARTESIAN_POINT('Ctrl Pts',(-4.99680282631908,-6.55,-27.7684014131595)) ;
#162180 = CARTESIAN_POINT('Ctrl Pts',(-5.,-6.55,-27.77)) ;
#162181 = CARTESIAN_POINT('',(-3.94142135623731,-6.52071067811866,-27.6992893218813)) ;
#162182 = CARTESIAN_POINT('Ctrl Pts',(-3.8,-6.55,-27.77)) ;
#162183 = CARTESIAN_POINT('Ctrl Pts',(-3.81016571653584,-6.55,-27.7649171417321)) ;
#162184 = CARTESIAN_POINT('Ctrl Pts',(-3.82068315091945,-6.54961031187958,
-27.759657683858)) ;
#162185 = CARTESIAN_POINT('Ctrl Pts',(-3.84304266528029,-6.54783411578235,
-27.7484679497193)) ;
#162186 = CARTESIAN_POINT('Ctrl Pts',(-3.85491327259885,-6.54635217950657,
-27.742522761795)) ;
#162187 = CARTESIAN_POINT('Ctrl Pts',(-3.87771616262343,-6.54231439116804,
-27.731106760394)) ;
#162188 = CARTESIAN_POINT('Ctrl Pts',(-3.88866251835728,-6.53982180674991,
-27.7256298613042)) ;
#162189 = CARTESIAN_POINT('Ctrl Pts',(-3.900450057122,-6.53645537933228,-27.7197406960356)) ;
#162190 = CARTESIAN_POINT('Ctrl Pts',(-3.901709281058,-6.5360866534769,-27.7191116827642)) ;
#162191 = CARTESIAN_POINT('Ctrl Pts',(-3.91388077026728,-6.53243308776744,
-27.7130327513517)) ;
#162192 = CARTESIAN_POINT('Ctrl Pts',(-3.92429308263753,-6.5285996913974,
-27.7078422384291)) ;
#162193 = CARTESIAN_POINT('Ctrl Pts',(-3.93645488997278,-6.52312881451533,
-27.7017711869643)) ;
#162194 = CARTESIAN_POINT('Ctrl Pts',(-3.9389706658717,-6.52193602330143,
-27.7005146670641)) ;
#162195 = CARTESIAN_POINT('Ctrl Pts',(-3.94142135623731,-6.52071067811863,
-27.6992893218813)) ;
#162196 = CARTESIAN_POINT('Origin',(-3.78571994570707,-6.44700925663904,-27.7771421042453)) ;
#162197 = CARTESIAN_POINT('Origin',(-3.8,-6.45,-25.67)) ;
#162198 = CARTESIAN_POINT('',(-3.87071067811865,-6.52071067811866,-25.7114213562373)) ;
#162199 = CARTESIAN_POINT('Ctrl Pts',(-3.8,-6.55,-25.57)) ;
#162200 = CARTESIAN_POINT('Ctrl Pts',(-3.80508285826791,-6.55,-25.5801657165359)) ;
#162201 = CARTESIAN_POINT('Ctrl Pts',(-3.81034231614198,-6.54961031187958,
-25.5906831509195)) ;
#162202 = CARTESIAN_POINT('Ctrl Pts',(-3.82153205028064,-6.54783411578236,
-25.6130426652803)) ;
#162203 = CARTESIAN_POINT('Ctrl Pts',(-3.82747723820505,-6.54635217950656,
-25.6249132725989)) ;
#162204 = CARTESIAN_POINT('Ctrl Pts',(-3.83889323960423,-6.54231439116865,
-25.6477161626201)) ;
#162205 = CARTESIAN_POINT('Ctrl Pts',(-3.84437013869244,-6.53982180675145,
-25.6586625183506)) ;
#162206 = CARTESIAN_POINT('Ctrl Pts',(-3.85025930396114,-6.53645537933417,
-25.6704500571156)) ;
#162207 = CARTESIAN_POINT('Ctrl Pts',(-3.8508883172342,-6.53608665347786,
-25.6717092810549)) ;
#162208 = CARTESIAN_POINT('Ctrl Pts',(-3.85696724864826,-6.53243308776744,
-25.6838807702674)) ;
#162209 = CARTESIAN_POINT('Ctrl Pts',(-3.86215776157091,-6.52859969139737,
-25.6942930826377)) ;
#162210 = CARTESIAN_POINT('Ctrl Pts',(-3.86822881303572,-6.5231288145153,
-25.7064548899729)) ;
#162211 = CARTESIAN_POINT('Ctrl Pts',(-3.86948533293586,-6.52193602330144,
-25.7089706658717)) ;
#162212 = CARTESIAN_POINT('Ctrl Pts',(-3.87071067811865,-6.52071067811866,
-25.7114213562373)) ;
#162213 = CARTESIAN_POINT('Origin',(-3.79285789576216,-6.44700925664358,-25.5557199457226)) ;
#162214 = CARTESIAN_POINT('',(-3.87071067811865,-6.52071067811866,-27.6285786437627)) ;
#162215 = CARTESIAN_POINT('Origin',(-3.79291331463346,-6.4470345969815,-27.7841700950241)) ;
#162216 = CARTESIAN_POINT('Ctrl Pts',(-3.87071067811865,-6.52071067811866,
-27.6285786437627)) ;
#162217 = CARTESIAN_POINT('Ctrl Pts',(-3.86620460065363,-6.52521675558368,
-27.6375907986927)) ;
#162218 = CARTESIAN_POINT('Ctrl Pts',(-3.86127351832835,-6.52928079264423,
-27.6474862581729)) ;
#162219 = CARTESIAN_POINT('Ctrl Pts',(-3.85097911745203,-6.53624680748638,
-27.668112770569)) ;
#162220 = CARTESIAN_POINT('Ctrl Pts',(-3.84563601585054,-6.53918030781812,
-27.6788050943354)) ;
#162221 = CARTESIAN_POINT('Ctrl Pts',(-3.8395252454668,-6.54185985500308,
-27.6910185932209)) ;
#162222 = CARTESIAN_POINT('Ctrl Pts',(-3.83889029009086,-6.54213045061235,
-27.6922875172273)) ;
#162223 = CARTESIAN_POINT('Ctrl Pts',(-3.83250371086603,-6.5447746790983,
-27.7050493700285)) ;
#162224 = CARTESIAN_POINT('Ctrl Pts',(-3.82662842759379,-6.54657370273653,
-27.716779364282)) ;
#162225 = CARTESIAN_POINT('Ctrl Pts',(-3.81540422523878,-6.54896007643136,
-27.7392002588839)) ;
#162226 = CARTESIAN_POINT('Ctrl Pts',(-3.81004992405496,-6.54963010255188,
-27.7499019216815)) ;
#162227 = CARTESIAN_POINT('Ctrl Pts',(-3.80321442618296,-6.54996164986962,
-27.763571160343)) ;
#162228 = CARTESIAN_POINT('Ctrl Pts',(-3.80159858684042,-6.55,-27.7668028263191)) ;
#162229 = CARTESIAN_POINT('Ctrl Pts',(-3.8,-6.55,-27.77)) ;
#162230 = CARTESIAN_POINT('Origin',(-5.,-6.45,-25.67)) ;
#162231 = CARTESIAN_POINT('',(-4.92928932188133,-6.52071067811864,-27.6285786437627)) ;
#162232 = CARTESIAN_POINT('Ctrl Pts',(-5.,-6.55,-27.77)) ;
#162233 = CARTESIAN_POINT('Ctrl Pts',(-4.99491714173208,-6.55,-27.7598342834642)) ;
#162234 = CARTESIAN_POINT('Ctrl Pts',(-4.989657683858,-6.54961031187958,-27.7493168490806)) ;
#162235 = CARTESIAN_POINT('Ctrl Pts',(-4.97846794971935,-6.54783411578236,
-27.7269573347198)) ;
#162236 = CARTESIAN_POINT('Ctrl Pts',(-4.97252276179495,-6.54635217950656,
-27.7150867274012)) ;
#162237 = CARTESIAN_POINT('Ctrl Pts',(-4.96110676039612,-6.54231439116878,
-27.6922838373808)) ;
#162238 = CARTESIAN_POINT('Ctrl Pts',(-4.95562986130823,-6.53982180675176,
-27.6813374816509)) ;
#162239 = CARTESIAN_POINT('Ctrl Pts',(-4.94974069603951,-6.53645537933455,
-27.6695499428858)) ;
#162240 = CARTESIAN_POINT('Ctrl Pts',(-4.94911168276615,-6.53608665347807,
-27.6682907189459)) ;
#162241 = CARTESIAN_POINT('Ctrl Pts',(-4.94303275135179,-6.53243308776748,
-27.6561192297328)) ;
#162242 = CARTESIAN_POINT('Ctrl Pts',(-4.93784223842914,-6.52859969139742,
-27.6457069173625)) ;
#162243 = CARTESIAN_POINT('Ctrl Pts',(-4.93177118696431,-6.52312881451532,
-27.6335451100273)) ;
#162244 = CARTESIAN_POINT('Ctrl Pts',(-4.93051466706414,-6.52193602330145,
-27.6310293341283)) ;
#162245 = CARTESIAN_POINT('Ctrl Pts',(-4.92928932188133,-6.52071067811864,
-27.6285786437627)) ;
#162246 = CARTESIAN_POINT('Origin',(-5.00714210424853,-6.44700925663946,-27.7842800542989)) ;
#162247 = CARTESIAN_POINT('',(-4.92928932188133,-6.52071067811864,-25.7114213562373)) ;
#162248 = CARTESIAN_POINT('Origin',(-5.00708668536615,-6.44703459698157,-25.5558299049765)) ;
#162249 = CARTESIAN_POINT('Ctrl Pts',(-4.92928932188133,-6.52071067811864,
-25.7114213562373)) ;
#162250 = CARTESIAN_POINT('Ctrl Pts',(-4.93379539934636,-6.52521675558367,
-25.7024092013072)) ;
#162251 = CARTESIAN_POINT('Ctrl Pts',(-4.93872648167164,-6.52928079264422,
-25.6925137418271)) ;
#162252 = CARTESIAN_POINT('Ctrl Pts',(-4.9490208825476,-6.53624680748613,
-25.6718872294316)) ;
#162253 = CARTESIAN_POINT('Ctrl Pts',(-4.95436398414871,-6.53918030781771,
-25.661194905666)) ;
#162254 = CARTESIAN_POINT('Ctrl Pts',(-4.96047475453242,-6.54185985500274,
-25.6489814067805)) ;
#162255 = CARTESIAN_POINT('Ctrl Pts',(-4.96110970990874,-6.54213045061219,
-25.6477124827734)) ;
#162256 = CARTESIAN_POINT('Ctrl Pts',(-4.96749628913393,-6.54477467909829,
-25.6349506299714)) ;
#162257 = CARTESIAN_POINT('Ctrl Pts',(-4.97337157240618,-6.54657370273652,
-25.623220635718)) ;
#162258 = CARTESIAN_POINT('Ctrl Pts',(-4.98459577476119,-6.54896007643136,
-25.6007997411161)) ;
#162259 = CARTESIAN_POINT('Ctrl Pts',(-4.98995007594501,-6.54963010255188,
-25.5900980783184)) ;
#162260 = CARTESIAN_POINT('Ctrl Pts',(-4.99678557381703,-6.54996164986962,
-25.576428839657)) ;
#162261 = CARTESIAN_POINT('Ctrl Pts',(-4.99840141315958,-6.55,-25.5731971736808)) ;
#162262 = CARTESIAN_POINT('Ctrl Pts',(-5.,-6.55,-25.57)) ;
#162263 = CARTESIAN_POINT('Origin',(-4.9,-6.45,-25.57)) ;
#162264 = CARTESIAN_POINT('',(-4.85857864376276,-6.52071067811862,-25.6407106781187)) ;
#162265 = CARTESIAN_POINT('Ctrl Pts',(-5.,-6.55,-25.57)) ;
#162266 = CARTESIAN_POINT('Ctrl Pts',(-4.9898342834642,-6.55,-25.5750828582679)) ;
#162267 = CARTESIAN_POINT('Ctrl Pts',(-4.97931684908064,-6.54961031187958,
-25.580342316142)) ;
#162268 = CARTESIAN_POINT('Ctrl Pts',(-4.95695733471992,-6.54783411578236,
-25.5915320502806)) ;
#162269 = CARTESIAN_POINT('Ctrl Pts',(-4.94508672740143,-6.54635217950657,
-25.597477238205)) ;
#162270 = CARTESIAN_POINT('Ctrl Pts',(-4.92228383737812,-6.54231439116829,
-25.6088932396053)) ;
#162271 = CARTESIAN_POINT('Ctrl Pts',(-4.91133748164544,-6.5398218067505,
-25.6143701386945)) ;
#162272 = CARTESIAN_POINT('Ctrl Pts',(-4.89954994288061,-6.536455379333,-25.6202593039631)) ;
#162273 = CARTESIAN_POINT('Ctrl Pts',(-4.89829071894348,-6.5360866534773,
-25.6208883172351)) ;
#162274 = CARTESIAN_POINT('Ctrl Pts',(-4.88611922973303,-6.53243308776751,
-25.6269672486482)) ;
#162275 = CARTESIAN_POINT('Ctrl Pts',(-4.87570691736273,-6.52859969139746,
-25.6321577615708)) ;
#162276 = CARTESIAN_POINT('Ctrl Pts',(-4.86354511002739,-6.52312881451533,
-25.6382288130357)) ;
#162277 = CARTESIAN_POINT('Ctrl Pts',(-4.86102933412842,-6.52193602330143,
-25.6394853329359)) ;
#162278 = CARTESIAN_POINT('Ctrl Pts',(-4.85857864376276,-6.52071067811862,
-25.6407106781187)) ;
#162279 = CARTESIAN_POINT('Origin',(-5.01428005427684,-6.44700925664322,-25.5628578957626)) ;
#162280 = CARTESIAN_POINT('',(-3.94142135623731,-6.52071067811866,-25.6407106781187)) ;
#162281 = CARTESIAN_POINT('Origin',(-3.78582990495265,-6.44703459697566,-25.5629133146221)) ;
#162282 = CARTESIAN_POINT('Ctrl Pts',(-3.94142135623731,-6.52071067811864,
-25.6407106781187)) ;
#162283 = CARTESIAN_POINT('Ctrl Pts',(-3.93240920130726,-6.52521675558369,
-25.6362046006536)) ;
#162284 = CARTESIAN_POINT('Ctrl Pts',(-3.92251374182714,-6.52928079264421,
-25.6312735183284)) ;
#162285 = CARTESIAN_POINT('Ctrl Pts',(-3.90188722943356,-6.53624680748547,
-25.6209791174534)) ;
#162286 = CARTESIAN_POINT('Ctrl Pts',(-3.89119490567006,-6.53918030781661,
-25.6156360158533)) ;
#162287 = CARTESIAN_POINT('Ctrl Pts',(-3.87898140678463,-6.54185985500186,
-25.6095252454697)) ;
#162288 = CARTESIAN_POINT('Ctrl Pts',(-3.8777124827755,-6.54213045061175,
-25.6088902900923)) ;
#162289 = CARTESIAN_POINT('Ctrl Pts',(-3.86495062997148,-6.54477467909826,
-25.6025037108661)) ;
#162290 = CARTESIAN_POINT('Ctrl Pts',(-3.85322063571806,-6.54657370273652,
-25.5966284275938)) ;
#162291 = CARTESIAN_POINT('Ctrl Pts',(-3.83079974111614,-6.54896007643135,
-25.5854042252389)) ;
#162292 = CARTESIAN_POINT('Ctrl Pts',(-3.82009807831852,-6.54963010255187,
-25.5800499240551)) ;
#162293 = CARTESIAN_POINT('Ctrl Pts',(-3.80642883965707,-6.54996164986963,
-25.573214426183)) ;
#162294 = CARTESIAN_POINT('Ctrl Pts',(-3.80319717368087,-6.55,-25.5715985868404)) ;
#162295 = CARTESIAN_POINT('Ctrl Pts',(-3.8,-6.55,-25.57)) ;
#162296 = CARTESIAN_POINT('Origin',(-4.9,-6.45,-23.96)) ;
#162297 = CARTESIAN_POINT('',(-4.85857864376276,-6.52071067811862,-23.8892893218813)) ;
#162298 = CARTESIAN_POINT('Origin',(-5.01417009504266,-6.44703459697728,-23.9670866853756)) ;
#162299 = CARTESIAN_POINT('Ctrl Pts',(-4.85857864376276,-6.52071067811861,
-23.8892893218813)) ;
#162300 = CARTESIAN_POINT('Ctrl Pts',(-4.86759079869285,-6.52521675558364,
-23.8937953993463)) ;
#162301 = CARTESIAN_POINT('Ctrl Pts',(-4.87748625817302,-6.52928079264421,
-23.8987264816716)) ;
#162302 = CARTESIAN_POINT('Ctrl Pts',(-4.8981127705669,-6.53624680748557,
-23.9090208825468)) ;
#162303 = CARTESIAN_POINT('Ctrl Pts',(-4.90880509433068,-6.53918030781676,
-23.914363984147)) ;
#162304 = CARTESIAN_POINT('Ctrl Pts',(-4.92101859321611,-6.54185985500198,
-23.9204747545306)) ;
#162305 = CARTESIAN_POINT('Ctrl Pts',(-4.92228751722495,-6.54213045061181,
-23.9211097099078)) ;
#162306 = CARTESIAN_POINT('Ctrl Pts',(-4.93504937002862,-6.54477467909826,
-23.9274962891339)) ;
#162307 = CARTESIAN_POINT('Ctrl Pts',(-4.94677936428196,-6.5465737027365,
-23.9333715724061)) ;
#162308 = CARTESIAN_POINT('Ctrl Pts',(-4.96920025888376,-6.54896007643133,
-23.944595774761)) ;
#162309 = CARTESIAN_POINT('Ctrl Pts',(-4.97990192168134,-6.54963010255186,
-23.9499500759448)) ;
#162310 = CARTESIAN_POINT('Ctrl Pts',(-4.99357116034282,-6.54996164986962,
-23.9567855738169)) ;
#162311 = CARTESIAN_POINT('Ctrl Pts',(-4.99680282631907,-6.55,-23.9584014131595)) ;
#162312 = CARTESIAN_POINT('Ctrl Pts',(-5.,-6.55,-23.96)) ;
#162313 = CARTESIAN_POINT('',(-3.94142135623731,-6.52071067811866,-23.8892893218813)) ;
#162314 = CARTESIAN_POINT('Ctrl Pts',(-3.8,-6.55,-23.96)) ;
#162315 = CARTESIAN_POINT('Ctrl Pts',(-3.81016571653584,-6.55,-23.9549171417321)) ;
#162316 = CARTESIAN_POINT('Ctrl Pts',(-3.82068315091944,-6.54961031187958,
-23.949657683858)) ;
#162317 = CARTESIAN_POINT('Ctrl Pts',(-3.84304266528028,-6.54783411578234,
-23.9384679497193)) ;
#162318 = CARTESIAN_POINT('Ctrl Pts',(-3.85491327259884,-6.54635217950657,
-23.932522761795)) ;
#162319 = CARTESIAN_POINT('Ctrl Pts',(-3.87771616262351,-6.54231439116802,
-23.921106760394)) ;
#162320 = CARTESIAN_POINT('Ctrl Pts',(-3.88866251835745,-6.53982180674987,
-23.9156298613041)) ;
#162321 = CARTESIAN_POINT('Ctrl Pts',(-3.90045005712217,-6.53645537933222,
-23.9097406960355)) ;
#162322 = CARTESIAN_POINT('Ctrl Pts',(-3.90170928105808,-6.53608665347687,
-23.9091116827642)) ;
#162323 = CARTESIAN_POINT('Ctrl Pts',(-3.91388077026727,-6.53243308776744,
-23.9030327513517)) ;
#162324 = CARTESIAN_POINT('Ctrl Pts',(-3.92429308263752,-6.5285996913974,
-23.8978422384291)) ;
#162325 = CARTESIAN_POINT('Ctrl Pts',(-3.93645488997277,-6.52312881451532,
-23.8917711869643)) ;
#162326 = CARTESIAN_POINT('Ctrl Pts',(-3.93897066587169,-6.52193602330143,
-23.8905146670641)) ;
#162327 = CARTESIAN_POINT('Ctrl Pts',(-3.94142135623731,-6.52071067811863,
-23.8892893218813)) ;
#162328 = CARTESIAN_POINT('Origin',(-3.78571994570344,-6.44700925663849,-23.9671421042471)) ;
#162329 = CARTESIAN_POINT('Origin',(-3.8,-6.45,-21.86)) ;
#162330 = CARTESIAN_POINT('',(-3.87071067811865,-6.52071067811866,-21.9014213562373)) ;
#162331 = CARTESIAN_POINT('Ctrl Pts',(-3.8,-6.55,-21.76)) ;
#162332 = CARTESIAN_POINT('Ctrl Pts',(-3.80508285826791,-6.55,-21.7701657165358)) ;
#162333 = CARTESIAN_POINT('Ctrl Pts',(-3.81034231614198,-6.54961031187958,
-21.7806831509195)) ;
#162334 = CARTESIAN_POINT('Ctrl Pts',(-3.82153205028064,-6.54783411578236,
-21.8030426652803)) ;
#162335 = CARTESIAN_POINT('Ctrl Pts',(-3.82747723820505,-6.54635217950656,
-21.8149132725989)) ;
#162336 = CARTESIAN_POINT('Ctrl Pts',(-3.83889323960399,-6.54231439116874,
-21.8377161626196)) ;
#162337 = CARTESIAN_POINT('Ctrl Pts',(-3.84437013869197,-6.53982180675166,
-21.8486625183496)) ;
#162338 = CARTESIAN_POINT('Ctrl Pts',(-3.8502593039607,-6.53645537933443,
-21.8604500571147)) ;
#162339 = CARTESIAN_POINT('Ctrl Pts',(-3.85088831723398,-6.53608665347799,
-21.8617092810544)) ;
#162340 = CARTESIAN_POINT('Ctrl Pts',(-3.85696724864826,-6.53243308776744,
-21.8738807702674)) ;
#162341 = CARTESIAN_POINT('Ctrl Pts',(-3.86215776157091,-6.52859969139738,
-21.8842930826377)) ;
#162342 = CARTESIAN_POINT('Ctrl Pts',(-3.86822881303572,-6.5231288145153,
-21.8964548899729)) ;
#162343 = CARTESIAN_POINT('Ctrl Pts',(-3.86948533293587,-6.52193602330144,
-21.8989706658717)) ;
#162344 = CARTESIAN_POINT('Ctrl Pts',(-3.87071067811865,-6.52071067811866,
-21.9014213562373)) ;
#162345 = CARTESIAN_POINT('Origin',(-3.79285789575771,-6.44700925664161,-21.7457199457137)) ;
#162346 = CARTESIAN_POINT('',(-3.87071067811865,-6.52071067811866,-23.8185786437627)) ;
#162347 = CARTESIAN_POINT('Origin',(-3.79291331460805,-6.44703459697049,-23.9741700950758)) ;
#162348 = CARTESIAN_POINT('Ctrl Pts',(-3.87071067811865,-6.52071067811866,
-23.8185786437627)) ;
#162349 = CARTESIAN_POINT('Ctrl Pts',(-3.86620460065363,-6.52521675558368,
-23.8275907986927)) ;
#162350 = CARTESIAN_POINT('Ctrl Pts',(-3.86127351832836,-6.52928079264422,
-23.8374862581728)) ;
#162351 = CARTESIAN_POINT('Ctrl Pts',(-3.85097911745241,-6.53624680748612,
-23.8581127705683)) ;
#162352 = CARTESIAN_POINT('Ctrl Pts',(-3.84563601585132,-6.53918030781769,
-23.8688050943338)) ;
#162353 = CARTESIAN_POINT('Ctrl Pts',(-3.8395252454676,-6.54185985500273,
-23.8810185932193)) ;
#162354 = CARTESIAN_POINT('Ctrl Pts',(-3.83889029009126,-6.54213045061219,
-23.8822875172265)) ;
#162355 = CARTESIAN_POINT('Ctrl Pts',(-3.83250371086603,-6.5447746790983,
-23.8950493700285)) ;
#162356 = CARTESIAN_POINT('Ctrl Pts',(-3.82662842759379,-6.54657370273653,
-23.906779364282)) ;
#162357 = CARTESIAN_POINT('Ctrl Pts',(-3.81540422523878,-6.54896007643136,
-23.9292002588839)) ;
#162358 = CARTESIAN_POINT('Ctrl Pts',(-3.81004992405496,-6.54963010255188,
-23.9399019216815)) ;
#162359 = CARTESIAN_POINT('Ctrl Pts',(-3.80321442618295,-6.54996164986962,
-23.953571160343)) ;
#162360 = CARTESIAN_POINT('Ctrl Pts',(-3.80159858684042,-6.55,-23.9568028263192)) ;
#162361 = CARTESIAN_POINT('Ctrl Pts',(-3.8,-6.55,-23.96)) ;
#162362 = CARTESIAN_POINT('Origin',(-5.,-6.45,-21.86)) ;
#162363 = CARTESIAN_POINT('',(-4.92928932188133,-6.52071067811864,-23.8185786437627)) ;
#162364 = CARTESIAN_POINT('Ctrl Pts',(-5.,-6.55,-23.96)) ;
#162365 = CARTESIAN_POINT('Ctrl Pts',(-4.99491714173208,-6.55,-23.9498342834642)) ;
#162366 = CARTESIAN_POINT('Ctrl Pts',(-4.989657683858,-6.54961031187958,-23.9393168490806)) ;
#162367 = CARTESIAN_POINT('Ctrl Pts',(-4.97846794971936,-6.54783411578236,
-23.9169573347198)) ;
#162368 = CARTESIAN_POINT('Ctrl Pts',(-4.97252276179495,-6.54635217950656,
-23.9050867274012)) ;
#162369 = CARTESIAN_POINT('Ctrl Pts',(-4.96110676039623,-6.54231439116882,
-23.882283837381)) ;
#162370 = CARTESIAN_POINT('Ctrl Pts',(-4.95562986130845,-6.53982180675186,
-23.8713374816513)) ;
#162371 = CARTESIAN_POINT('Ctrl Pts',(-4.94974069603971,-6.53645537933467,
-23.8595499428862)) ;
#162372 = CARTESIAN_POINT('Ctrl Pts',(-4.94911168276625,-6.53608665347813,
-23.8582907189461)) ;
#162373 = CARTESIAN_POINT('Ctrl Pts',(-4.94303275135179,-6.53243308776748,
-23.8461192297328)) ;
#162374 = CARTESIAN_POINT('Ctrl Pts',(-4.93784223842914,-6.52859969139742,
-23.8357069173625)) ;
#162375 = CARTESIAN_POINT('Ctrl Pts',(-4.93177118696431,-6.52312881451533,
-23.8235451100273)) ;
#162376 = CARTESIAN_POINT('Ctrl Pts',(-4.93051466706414,-6.52193602330145,
-23.8210293341283)) ;
#162377 = CARTESIAN_POINT('Ctrl Pts',(-4.92928932188133,-6.52071067811864,
-23.8185786437627)) ;
#162378 = CARTESIAN_POINT('Origin',(-5.00714210424667,-6.44700925664039,-23.9742800542952)) ;
#162379 = CARTESIAN_POINT('',(-4.92928932188133,-6.52071067811864,-21.9014213562373)) ;
#162380 = CARTESIAN_POINT('Origin',(-5.00708668537149,-6.44703459697967,-21.7458299049658)) ;
#162381 = CARTESIAN_POINT('Ctrl Pts',(-4.92928932188133,-6.52071067811864,
-21.9014213562373)) ;
#162382 = CARTESIAN_POINT('Ctrl Pts',(-4.93379539934636,-6.52521675558367,
-21.8924092013072)) ;
#162383 = CARTESIAN_POINT('Ctrl Pts',(-4.93872648167163,-6.52928079264421,
-21.8825137418271)) ;
#162384 = CARTESIAN_POINT('Ctrl Pts',(-4.94902088254783,-6.53624680748629,
-21.8618872294312)) ;
#162385 = CARTESIAN_POINT('Ctrl Pts',(-4.9543639841492,-6.53918030781798,
-21.851194905665)) ;
#162386 = CARTESIAN_POINT('Ctrl Pts',(-4.96047475453293,-6.54185985500296,
-21.8389814067794)) ;
#162387 = CARTESIAN_POINT('Ctrl Pts',(-4.96110970990898,-6.54213045061229,
-21.8377124827729)) ;
#162388 = CARTESIAN_POINT('Ctrl Pts',(-4.96749628913391,-6.54477467909828,
-21.8249506299714)) ;
#162389 = CARTESIAN_POINT('Ctrl Pts',(-4.97337157240615,-6.54657370273652,
-21.813220635718)) ;
#162390 = CARTESIAN_POINT('Ctrl Pts',(-4.98459577476116,-6.54896007643135,
-21.7907997411161)) ;
#162391 = CARTESIAN_POINT('Ctrl Pts',(-4.98995007594499,-6.54963010255188,
-21.7800980783185)) ;
#162392 = CARTESIAN_POINT('Ctrl Pts',(-4.99678557381703,-6.54996164986962,
-21.766428839657)) ;
#162393 = CARTESIAN_POINT('Ctrl Pts',(-4.99840141315957,-6.55,-21.7631971736809)) ;
#162394 = CARTESIAN_POINT('Ctrl Pts',(-5.,-6.55,-21.76)) ;
#162395 = CARTESIAN_POINT('Origin',(-4.9,-6.45,-21.76)) ;
#162396 = CARTESIAN_POINT('',(-4.85857864376276,-6.52071067811862,-21.8307106781187)) ;
#162397 = CARTESIAN_POINT('Ctrl Pts',(-5.,-6.55,-21.76)) ;
#162398 = CARTESIAN_POINT('Ctrl Pts',(-4.98983428346421,-6.55,-21.7650828582679)) ;
#162399 = CARTESIAN_POINT('Ctrl Pts',(-4.97931684908065,-6.54961031187958,
-21.770342316142)) ;
#162400 = CARTESIAN_POINT('Ctrl Pts',(-4.95695733471994,-6.54783411578236,
-21.7815320502806)) ;
#162401 = CARTESIAN_POINT('Ctrl Pts',(-4.94508672740146,-6.54635217950657,
-21.787477238205)) ;
#162402 = CARTESIAN_POINT('Ctrl Pts',(-4.92228383737779,-6.54231439116823,
-21.7988932396055)) ;
#162403 = CARTESIAN_POINT('Ctrl Pts',(-4.91133748164475,-6.53982180675033,
-21.8043701386949)) ;
#162404 = CARTESIAN_POINT('Ctrl Pts',(-4.89954994287995,-6.5364553793328,
-21.8102593039635)) ;
#162405 = CARTESIAN_POINT('Ctrl Pts',(-4.89829071894318,-6.5360866534772,
-21.8108883172353)) ;
#162406 = CARTESIAN_POINT('Ctrl Pts',(-4.88611922973306,-6.53243308776752,
-21.8169672486482)) ;
#162407 = CARTESIAN_POINT('Ctrl Pts',(-4.87570691736276,-6.52859969139747,
-21.8221577615708)) ;
#162408 = CARTESIAN_POINT('Ctrl Pts',(-4.86354511002741,-6.52312881451533,
-21.8282288130357)) ;
#162409 = CARTESIAN_POINT('Ctrl Pts',(-4.86102933412843,-6.52193602330143,
-21.8294853329359)) ;
#162410 = CARTESIAN_POINT('Ctrl Pts',(-4.85857864376276,-6.52071067811862,
-21.8307106781187)) ;
#162411 = CARTESIAN_POINT('Origin',(-5.01428005428387,-6.44700925664178,-21.7528578957592)) ;
#162412 = CARTESIAN_POINT('',(-3.94142135623731,-6.52071067811866,-21.8307106781187)) ;
#162413 = CARTESIAN_POINT('Origin',(-3.7858299049486,-6.44703459697488,-21.7529133146201)) ;
#162414 = CARTESIAN_POINT('Ctrl Pts',(-3.94142135623731,-6.52071067811864,
-21.8307106781187)) ;
#162415 = CARTESIAN_POINT('Ctrl Pts',(-3.93240920130726,-6.52521675558369,
-21.8262046006536)) ;
#162416 = CARTESIAN_POINT('Ctrl Pts',(-3.92251374182714,-6.52928079264421,
-21.8212735183284)) ;
#162417 = CARTESIAN_POINT('Ctrl Pts',(-3.901887229432,-6.536246807486,-21.8109791174526)) ;
#162418 = CARTESIAN_POINT('Ctrl Pts',(-3.89119490566676,-6.53918030781751,
-21.8056360158517)) ;
#162419 = CARTESIAN_POINT('Ctrl Pts',(-3.87898140678124,-6.54185985500259,
-21.7995252454679)) ;
#162420 = CARTESIAN_POINT('Ctrl Pts',(-3.8777124827738,-6.54213045061211,
-21.7988902900914)) ;
#162421 = CARTESIAN_POINT('Ctrl Pts',(-3.86495062997147,-6.5447746790983,
-21.7925037108661)) ;
#162422 = CARTESIAN_POINT('Ctrl Pts',(-3.85322063571804,-6.54657370273652,
-21.7866284275938)) ;
#162423 = CARTESIAN_POINT('Ctrl Pts',(-3.83079974111613,-6.54896007643135,
-21.7754042252389)) ;
#162424 = CARTESIAN_POINT('Ctrl Pts',(-3.82009807831852,-6.54963010255187,
-21.7700499240551)) ;
#162425 = CARTESIAN_POINT('Ctrl Pts',(-3.80642883965707,-6.54996164986963,
-21.763214426183)) ;
#162426 = CARTESIAN_POINT('Ctrl Pts',(-3.80319717368087,-6.55,-21.7615985868404)) ;
#162427 = CARTESIAN_POINT('Ctrl Pts',(-3.8,-6.55,-21.76)) ;
#162428 = CARTESIAN_POINT('Origin',(-4.9,-6.45,-20.15)) ;
#162429 = CARTESIAN_POINT('',(-4.85857864376276,-6.52071067811862,-20.0792893218813)) ;
#162430 = CARTESIAN_POINT('Origin',(-5.01417009505195,-6.44703459697568,-20.1570866853802)) ;
#162431 = CARTESIAN_POINT('Ctrl Pts',(-4.85857864376276,-6.52071067811862,
-20.0792893218813)) ;
#162432 = CARTESIAN_POINT('Ctrl Pts',(-4.86759079869283,-6.52521675558363,
-20.0837953993463)) ;
#162433 = CARTESIAN_POINT('Ctrl Pts',(-4.87748625817297,-6.5292807926442,
-20.0887264816716)) ;
#162434 = CARTESIAN_POINT('Ctrl Pts',(-4.89811277056717,-6.53624680748567,
-20.0990208825469)) ;
#162435 = CARTESIAN_POINT('Ctrl Pts',(-4.90880509433133,-6.53918030781695,
-20.1043639841473)) ;
#162436 = CARTESIAN_POINT('Ctrl Pts',(-4.92101859321678,-6.54185985500213,
-20.110474754531)) ;
#162437 = CARTESIAN_POINT('Ctrl Pts',(-4.92228751722526,-6.54213045061188,
-20.111109709908)) ;
#162438 = CARTESIAN_POINT('Ctrl Pts',(-4.93504937002857,-6.54477467909826,
-20.1174962891339)) ;
#162439 = CARTESIAN_POINT('Ctrl Pts',(-4.94677936428192,-6.5465737027365,
-20.1233715724061)) ;
#162440 = CARTESIAN_POINT('Ctrl Pts',(-4.96920025888373,-6.54896007643133,
-20.134595774761)) ;
#162441 = CARTESIAN_POINT('Ctrl Pts',(-4.97990192168131,-6.54963010255186,
-20.1399500759448)) ;
#162442 = CARTESIAN_POINT('Ctrl Pts',(-4.9935711603428,-6.54996164986962,
-20.1467855738169)) ;
#162443 = CARTESIAN_POINT('Ctrl Pts',(-4.99680282631906,-6.55,-20.1484014131595)) ;
#162444 = CARTESIAN_POINT('Ctrl Pts',(-5.,-6.55,-20.15)) ;
#162445 = CARTESIAN_POINT('',(-3.94142135623731,-6.52071067811866,-20.0792893218813)) ;
#162446 = CARTESIAN_POINT('Ctrl Pts',(-3.8,-6.55,-20.15)) ;
#162447 = CARTESIAN_POINT('Ctrl Pts',(-3.81016571653584,-6.55,-20.1449171417321)) ;
#162448 = CARTESIAN_POINT('Ctrl Pts',(-3.82068315091945,-6.54961031187958,
-20.139657683858)) ;
#162449 = CARTESIAN_POINT('Ctrl Pts',(-3.84304266528029,-6.54783411578235,
-20.1284679497193)) ;
#162450 = CARTESIAN_POINT('Ctrl Pts',(-3.85491327259885,-6.54635217950657,
-20.122522761795)) ;
#162451 = CARTESIAN_POINT('Ctrl Pts',(-3.87771616262406,-6.54231439116792,
-20.1111067603937)) ;
#162452 = CARTESIAN_POINT('Ctrl Pts',(-3.88866251835853,-6.53982180674963,
-20.1056298613036)) ;
#162453 = CARTESIAN_POINT('Ctrl Pts',(-3.9004500571232,-6.53645537933192,
-20.099740696035)) ;
#162454 = CARTESIAN_POINT('Ctrl Pts',(-3.90170928105859,-6.53608665347672,
-20.0991116827639)) ;
#162455 = CARTESIAN_POINT('Ctrl Pts',(-3.91388077026728,-6.53243308776744,
-20.0930327513517)) ;
#162456 = CARTESIAN_POINT('Ctrl Pts',(-3.92429308263753,-6.5285996913974,
-20.0878422384291)) ;
#162457 = CARTESIAN_POINT('Ctrl Pts',(-3.93645488997278,-6.52312881451532,
-20.0817711869643)) ;
#162458 = CARTESIAN_POINT('Ctrl Pts',(-3.9389706658717,-6.52193602330149,
-20.0805146670642)) ;
#162459 = CARTESIAN_POINT('Ctrl Pts',(-3.94142135623731,-6.52071067811864,
-20.0792893218813)) ;
#162460 = CARTESIAN_POINT('Origin',(-3.78571994570446,-6.44700925663872,-20.1571421042466)) ;
#162461 = CARTESIAN_POINT('Origin',(-3.8,-6.45,-18.05)) ;
#162462 = CARTESIAN_POINT('',(-3.87071067811865,-6.52071067811866,-18.0914213562373)) ;
#162463 = CARTESIAN_POINT('Ctrl Pts',(-3.8,-6.55,-17.95)) ;
#162464 = CARTESIAN_POINT('Ctrl Pts',(-3.80508285826791,-6.55,-17.9601657165359)) ;
#162465 = CARTESIAN_POINT('Ctrl Pts',(-3.81034231614198,-6.54961031187958,
-17.9706831509195)) ;
#162466 = CARTESIAN_POINT('Ctrl Pts',(-3.82153205028063,-6.54783411578236,
-17.9930426652803)) ;
#162467 = CARTESIAN_POINT('Ctrl Pts',(-3.82747723820505,-6.54635217950656,
-18.0049132725989)) ;
#162468 = CARTESIAN_POINT('Ctrl Pts',(-3.83889323960378,-6.54231439116881,
-18.0277161626192)) ;
#162469 = CARTESIAN_POINT('Ctrl Pts',(-3.84437013869156,-6.53982180675185,
-18.0386625183488)) ;
#162470 = CARTESIAN_POINT('Ctrl Pts',(-3.8502593039603,-6.53645537933466,
-18.0504500571139)) ;
#162471 = CARTESIAN_POINT('Ctrl Pts',(-3.85088831723378,-6.53608665347812,
-18.051709281054)) ;
#162472 = CARTESIAN_POINT('Ctrl Pts',(-3.85696724864825,-6.53243308776745,
-18.0638807702674)) ;
#162473 = CARTESIAN_POINT('Ctrl Pts',(-3.86215776157091,-6.52859969139737,
-18.0742930826376)) ;
#162474 = CARTESIAN_POINT('Ctrl Pts',(-3.86822881303572,-6.5231288145153,
-18.0864548899729)) ;
#162475 = CARTESIAN_POINT('Ctrl Pts',(-3.86948533293586,-6.52193602330144,
-18.0889706658717)) ;
#162476 = CARTESIAN_POINT('Ctrl Pts',(-3.87071067811865,-6.52071067811866,
-18.0914213562373)) ;
#162477 = CARTESIAN_POINT('Origin',(-3.79285789576042,-6.44700925664281,-17.9357199457191)) ;
#162478 = CARTESIAN_POINT('',(-3.87071067811865,-6.52071067811866,-20.0085786437627)) ;
#162479 = CARTESIAN_POINT('Origin',(-3.79291331463951,-6.4470345969837,-20.164170095012)) ;
#162480 = CARTESIAN_POINT('Ctrl Pts',(-3.87071067811865,-6.52071067811866,
-20.0085786437627)) ;
#162481 = CARTESIAN_POINT('Ctrl Pts',(-3.86620460065363,-6.52521675558368,
-20.0175907986927)) ;
#162482 = CARTESIAN_POINT('Ctrl Pts',(-3.86127351832835,-6.52928079264423,
-20.0274862581729)) ;
#162483 = CARTESIAN_POINT('Ctrl Pts',(-3.85097911745214,-6.5362468074863,
-20.0481127705688)) ;
#162484 = CARTESIAN_POINT('Ctrl Pts',(-3.84563601585077,-6.53918030781799,
-20.0588050943349)) ;
#162485 = CARTESIAN_POINT('Ctrl Pts',(-3.83952524546704,-6.54185985500297,
-20.0710185932205)) ;
#162486 = CARTESIAN_POINT('Ctrl Pts',(-3.83889029009097,-6.54213045061231,
-20.0722875172271)) ;
#162487 = CARTESIAN_POINT('Ctrl Pts',(-3.83250371086602,-6.5447746790983,
-20.0850493700286)) ;
#162488 = CARTESIAN_POINT('Ctrl Pts',(-3.82662842759378,-6.54657370273654,
-20.096779364282)) ;
#162489 = CARTESIAN_POINT('Ctrl Pts',(-3.81540422523877,-6.54896007643136,
-20.1192002588839)) ;
#162490 = CARTESIAN_POINT('Ctrl Pts',(-3.81004992405495,-6.54963010255188,
-20.1299019216816)) ;
#162491 = CARTESIAN_POINT('Ctrl Pts',(-3.80321442618295,-6.54996164986962,
-20.143571160343)) ;
#162492 = CARTESIAN_POINT('Ctrl Pts',(-3.80159858684041,-6.55,-20.1468028263192)) ;
#162493 = CARTESIAN_POINT('Ctrl Pts',(-3.8,-6.55,-20.15)) ;
#162494 = CARTESIAN_POINT('Origin',(-5.,-6.45,-18.05)) ;
#162495 = CARTESIAN_POINT('',(-4.92928932188133,-6.52071067811864,-20.0085786437627)) ;
#162496 = CARTESIAN_POINT('Ctrl Pts',(-5.,-6.55,-20.15)) ;
#162497 = CARTESIAN_POINT('Ctrl Pts',(-4.99491714173208,-6.55,-20.1398342834642)) ;
#162498 = CARTESIAN_POINT('Ctrl Pts',(-4.98965768385801,-6.54961031187958,
-20.1293168490806)) ;
#162499 = CARTESIAN_POINT('Ctrl Pts',(-4.97846794971936,-6.54783411578236,
-20.1069573347198)) ;
#162500 = CARTESIAN_POINT('Ctrl Pts',(-4.97252276179496,-6.54635217950657,
-20.0950867274012)) ;
#162501 = CARTESIAN_POINT('Ctrl Pts',(-4.9611067603961,-6.54231439116877,
-20.0722838373807)) ;
#162502 = CARTESIAN_POINT('Ctrl Pts',(-4.95562986130818,-6.53982180675173,
-20.0613374816508)) ;
#162503 = CARTESIAN_POINT('Ctrl Pts',(-4.94974069603945,-6.53645537933452,
-20.0495499428857)) ;
#162504 = CARTESIAN_POINT('Ctrl Pts',(-4.94911168276612,-6.53608665347806,
-20.0482907189459)) ;
#162505 = CARTESIAN_POINT('Ctrl Pts',(-4.94303275135179,-6.53243308776748,
-20.0361192297328)) ;
#162506 = CARTESIAN_POINT('Ctrl Pts',(-4.93784223842913,-6.52859969139741,
-20.0257069173625)) ;
#162507 = CARTESIAN_POINT('Ctrl Pts',(-4.9317711869643,-6.52312881451532,
-20.0135451100273)) ;
#162508 = CARTESIAN_POINT('Ctrl Pts',(-4.93051466706414,-6.52193602330145,
-20.0110293341283)) ;
#162509 = CARTESIAN_POINT('Ctrl Pts',(-4.92928932188133,-6.52071067811864,
-20.0085786437627)) ;
#162510 = CARTESIAN_POINT('Origin',(-5.00714210424655,-6.44700925664027,-20.1642800542949)) ;
#162511 = CARTESIAN_POINT('',(-4.92928932188133,-6.52071067811864,-18.0914213562373)) ;
#162512 = CARTESIAN_POINT('Origin',(-5.00708668537412,-6.44703459697887,-17.9358299049606)) ;
#162513 = CARTESIAN_POINT('Ctrl Pts',(-4.92928932188133,-6.52071067811864,
-18.0914213562373)) ;
#162514 = CARTESIAN_POINT('Ctrl Pts',(-4.93379539934636,-6.52521675558368,
-18.0824092013072)) ;
#162515 = CARTESIAN_POINT('Ctrl Pts',(-4.93872648167165,-6.52928079264423,
-18.0725137418271)) ;
#162516 = CARTESIAN_POINT('Ctrl Pts',(-4.94902088254759,-6.53624680748613,
-18.0518872294316)) ;
#162517 = CARTESIAN_POINT('Ctrl Pts',(-4.95436398414867,-6.53918030781768,
-18.0411949056661)) ;
#162518 = CARTESIAN_POINT('Ctrl Pts',(-4.96047475453238,-6.54185985500273,
-18.0289814067806)) ;
#162519 = CARTESIAN_POINT('Ctrl Pts',(-4.96110970990873,-6.54213045061218,
-18.0277124827734)) ;
#162520 = CARTESIAN_POINT('Ctrl Pts',(-4.96749628913394,-6.54477467909829,
-18.0149506299714)) ;
#162521 = CARTESIAN_POINT('Ctrl Pts',(-4.97337157240618,-6.54657370273652,
-18.003220635718)) ;
#162522 = CARTESIAN_POINT('Ctrl Pts',(-4.98459577476118,-6.54896007643136,
-17.9807997411161)) ;
#162523 = CARTESIAN_POINT('Ctrl Pts',(-4.989950075945,-6.54963010255188,-17.9700980783185)) ;
#162524 = CARTESIAN_POINT('Ctrl Pts',(-4.99678557381704,-6.54996164986962,
-17.956428839657)) ;
#162525 = CARTESIAN_POINT('Ctrl Pts',(-4.99840141315957,-6.55,-17.9531971736809)) ;
#162526 = CARTESIAN_POINT('Ctrl Pts',(-5.,-6.55,-17.95)) ;
#162527 = CARTESIAN_POINT('Origin',(-4.9,-6.45,-17.95)) ;
#162528 = CARTESIAN_POINT('',(-4.85857864376276,-6.52071067811862,-18.0207106781187)) ;
#162529 = CARTESIAN_POINT('Ctrl Pts',(-5.,-6.55,-17.95)) ;
#162530 = CARTESIAN_POINT('Ctrl Pts',(-4.98983428346421,-6.55,-17.9550828582679)) ;
#162531 = CARTESIAN_POINT('Ctrl Pts',(-4.97931684908065,-6.54961031187958,
-17.960342316142)) ;
#162532 = CARTESIAN_POINT('Ctrl Pts',(-4.95695733471993,-6.54783411578236,
-17.9715320502806)) ;
#162533 = CARTESIAN_POINT('Ctrl Pts',(-4.94508672740146,-6.54635217950657,
-17.977477238205)) ;
#162534 = CARTESIAN_POINT('Ctrl Pts',(-4.92228383737789,-6.54231439116824,
-17.9888932396054)) ;
#162535 = CARTESIAN_POINT('Ctrl Pts',(-4.91133748164494,-6.53982180675038,
-17.9943701386948)) ;
#162536 = CARTESIAN_POINT('Ctrl Pts',(-4.89954994288014,-6.53645537933285,
-18.0002593039634)) ;
#162537 = CARTESIAN_POINT('Ctrl Pts',(-4.89829071894327,-6.53608665347723,
-18.0008883172352)) ;
#162538 = CARTESIAN_POINT('Ctrl Pts',(-4.88611922973307,-6.53243308776751,
-18.0069672486482)) ;
#162539 = CARTESIAN_POINT('Ctrl Pts',(-4.87570691736276,-6.52859969139747,
-18.0121577615708)) ;
#162540 = CARTESIAN_POINT('Ctrl Pts',(-4.8635451100274,-6.52312881451533,
-18.0182288130357)) ;
#162541 = CARTESIAN_POINT('Ctrl Pts',(-4.86102933412843,-6.52193602330143,
-18.0194853329359)) ;
#162542 = CARTESIAN_POINT('Ctrl Pts',(-4.85857864376276,-6.52071067811861,
-18.0207106781187)) ;
#162543 = CARTESIAN_POINT('Origin',(-5.01428005427931,-6.44700925664276,-17.9428578957614)) ;
#162544 = CARTESIAN_POINT('',(-3.94142135623731,-6.52071067811866,-18.0207106781187)) ;
#162545 = CARTESIAN_POINT('Origin',(-3.78582990494094,-6.44703459697309,-17.9429133146163)) ;
#162546 = CARTESIAN_POINT('Ctrl Pts',(-3.94142135623731,-6.52071067811863,
-18.0207106781187)) ;
#162547 = CARTESIAN_POINT('Ctrl Pts',(-3.93240920130726,-6.52521675558369,
-18.0162046006536)) ;
#162548 = CARTESIAN_POINT('Ctrl Pts',(-3.92251374182714,-6.52928079264421,
-18.0112735183284)) ;
#162549 = CARTESIAN_POINT('Ctrl Pts',(-3.90188722943185,-6.53624680748605,
-18.0009791174525)) ;
#162550 = CARTESIAN_POINT('Ctrl Pts',(-3.89119490566645,-6.53918030781759,
-17.9956360158515)) ;
#162551 = CARTESIAN_POINT('Ctrl Pts',(-3.87898140678092,-6.54185985500266,
-17.9895252454678)) ;
#162552 = CARTESIAN_POINT('Ctrl Pts',(-3.87771248277363,-6.54213045061215,
-17.9888902900914)) ;
#162553 = CARTESIAN_POINT('Ctrl Pts',(-3.86495062997146,-6.5447746790983,
-17.982503710866)) ;
#162554 = CARTESIAN_POINT('Ctrl Pts',(-3.85322063571804,-6.54657370273652,
-17.9766284275938)) ;
#162555 = CARTESIAN_POINT('Ctrl Pts',(-3.83079974111613,-6.54896007643134,
-17.9654042252389)) ;
#162556 = CARTESIAN_POINT('Ctrl Pts',(-3.82009807831851,-6.54963010255187,
-17.9600499240551)) ;
#162557 = CARTESIAN_POINT('Ctrl Pts',(-3.80642883965706,-6.54996164986962,
-17.953214426183)) ;
#162558 = CARTESIAN_POINT('Ctrl Pts',(-3.80319717368087,-6.55,-17.9515985868404)) ;
#162559 = CARTESIAN_POINT('Ctrl Pts',(-3.8,-6.55,-17.95)) ;
#162560 = CARTESIAN_POINT('Origin',(-4.9,-6.45,-16.34)) ;
#162561 = CARTESIAN_POINT('',(-4.85857864376276,-6.52071067811862,-16.2692893218813)) ;
#162562 = CARTESIAN_POINT('Origin',(-5.01417009504985,-6.44703459697582,-16.3470866853791)) ;
#162563 = CARTESIAN_POINT('Ctrl Pts',(-4.85857864376276,-6.52071067811861,
-16.2692893218813)) ;
#162564 = CARTESIAN_POINT('Ctrl Pts',(-4.86759079869283,-6.52521675558363,
-16.2737953993463)) ;
#162565 = CARTESIAN_POINT('Ctrl Pts',(-4.87748625817297,-6.5292807926442,
-16.2787264816716)) ;
#162566 = CARTESIAN_POINT('Ctrl Pts',(-4.89811277056686,-6.53624680748557,
-16.2890208825468)) ;
#162567 = CARTESIAN_POINT('Ctrl Pts',(-4.90880509433066,-6.53918030781677,
-16.294363984147)) ;
#162568 = CARTESIAN_POINT('Ctrl Pts',(-4.92101859321609,-6.54185985500199,
-16.3004747545307)) ;
#162569 = CARTESIAN_POINT('Ctrl Pts',(-4.92228751722491,-6.54213045061181,
-16.3011097099078)) ;
#162570 = CARTESIAN_POINT('Ctrl Pts',(-4.93504937002856,-6.54477467909826,
-16.3074962891339)) ;
#162571 = CARTESIAN_POINT('Ctrl Pts',(-4.94677936428192,-6.5465737027365,
-16.3133715724061)) ;
#162572 = CARTESIAN_POINT('Ctrl Pts',(-4.96920025888373,-6.54896007643133,
-16.324595774761)) ;
#162573 = CARTESIAN_POINT('Ctrl Pts',(-4.97990192168131,-6.54963010255186,
-16.3299500759448)) ;
#162574 = CARTESIAN_POINT('Ctrl Pts',(-4.9935711603428,-6.54996164986962,
-16.3367855738169)) ;
#162575 = CARTESIAN_POINT('Ctrl Pts',(-4.99680282631906,-6.55,-16.3384014131595)) ;
#162576 = CARTESIAN_POINT('Ctrl Pts',(-5.,-6.55,-16.34)) ;
#162577 = CARTESIAN_POINT('',(-3.94142135623731,-6.52071067811866,-16.2692893218813)) ;
#162578 = CARTESIAN_POINT('Ctrl Pts',(-3.8,-6.55,-16.34)) ;
#162579 = CARTESIAN_POINT('Ctrl Pts',(-3.81016571653584,-6.55,-16.3349171417321)) ;
#162580 = CARTESIAN_POINT('Ctrl Pts',(-3.82068315091945,-6.54961031187958,
-16.329657683858)) ;
#162581 = CARTESIAN_POINT('Ctrl Pts',(-3.84304266528029,-6.54783411578235,
-16.3184679497193)) ;
#162582 = CARTESIAN_POINT('Ctrl Pts',(-3.85491327259885,-6.54635217950657,
-16.312522761795)) ;
#162583 = CARTESIAN_POINT('Ctrl Pts',(-3.87771616262369,-6.54231439116799,
-16.3011067603939)) ;
#162584 = CARTESIAN_POINT('Ctrl Pts',(-3.8886625183578,-6.53982180674979,
-16.2956298613039)) ;
#162585 = CARTESIAN_POINT('Ctrl Pts',(-3.9004500571225,-6.53645537933213,
-16.2897406960354)) ;
#162586 = CARTESIAN_POINT('Ctrl Pts',(-3.90170928105824,-6.53608665347683,
-16.2891116827641)) ;
#162587 = CARTESIAN_POINT('Ctrl Pts',(-3.91388077026727,-6.53243308776745,
-16.2830327513517)) ;
#162588 = CARTESIAN_POINT('Ctrl Pts',(-3.92429308263753,-6.5285996913974,
-16.2778422384291)) ;
#162589 = CARTESIAN_POINT('Ctrl Pts',(-3.93645488997277,-6.52312881451532,
-16.2717711869643)) ;
#162590 = CARTESIAN_POINT('Ctrl Pts',(-3.93897066587169,-6.52193602330143,
-16.2705146670641)) ;
#162591 = CARTESIAN_POINT('Ctrl Pts',(-3.94142135623731,-6.52071067811863,
-16.2692893218813)) ;
#162592 = CARTESIAN_POINT('Origin',(-3.78571994570709,-6.44700925663911,-16.3471421042453)) ;
#162593 = CARTESIAN_POINT('Origin',(-3.8,-6.45,-14.24)) ;
#162594 = CARTESIAN_POINT('',(-3.87071067811867,-6.52071067811863,-14.2814213562373)) ;
#162595 = CARTESIAN_POINT('Ctrl Pts',(-3.8,-6.55,-14.14)) ;
#162596 = CARTESIAN_POINT('Ctrl Pts',(-3.80508285826792,-6.55,-14.1501657165358)) ;
#162597 = CARTESIAN_POINT('Ctrl Pts',(-3.810342316142,-6.54961031187958,-14.1606831509194)) ;
#162598 = CARTESIAN_POINT('Ctrl Pts',(-3.82153205028064,-6.54783411578236,
-14.1830426652802)) ;
#162599 = CARTESIAN_POINT('Ctrl Pts',(-3.82747723820505,-6.54635217950656,
-14.1949132725988)) ;
#162600 = CARTESIAN_POINT('Ctrl Pts',(-3.8388932396039,-6.54231439116878,
-14.2177161626193)) ;
#162601 = CARTESIAN_POINT('Ctrl Pts',(-3.84437013869181,-6.53982180675174,
-14.2286625183492)) ;
#162602 = CARTESIAN_POINT('Ctrl Pts',(-3.85025930396054,-6.53645537933452,
-14.2404500571143)) ;
#162603 = CARTESIAN_POINT('Ctrl Pts',(-3.85088831723387,-6.53608665347806,
-14.2417092810541)) ;
#162604 = CARTESIAN_POINT('Ctrl Pts',(-3.85696724864822,-6.53243308776747,
-14.2538807702672)) ;
#162605 = CARTESIAN_POINT('Ctrl Pts',(-3.86215776157089,-6.5285996913974,
-14.2642930826375)) ;
#162606 = CARTESIAN_POINT('Ctrl Pts',(-3.86822881303571,-6.52312881451531,
-14.2764548899728)) ;
#162607 = CARTESIAN_POINT('Ctrl Pts',(-3.86948533293587,-6.52193602330144,
-14.2789706658717)) ;
#162608 = CARTESIAN_POINT('Ctrl Pts',(-3.87071067811867,-6.52071067811864,
-14.2814213562373)) ;
#162609 = CARTESIAN_POINT('Origin',(-3.7928578957324,-6.44700925663102,-14.1257199456631)) ;
#162610 = CARTESIAN_POINT('',(-3.87071067811865,-6.52071067811866,-16.1985786437627)) ;
#162611 = CARTESIAN_POINT('Origin',(-3.79291331463642,-6.44703459698195,-16.3541700950182)) ;
#162612 = CARTESIAN_POINT('Ctrl Pts',(-3.87071067811865,-6.52071067811866,
-16.1985786437627)) ;
#162613 = CARTESIAN_POINT('Ctrl Pts',(-3.86620460065363,-6.52521675558368,
-16.2075907986927)) ;
#162614 = CARTESIAN_POINT('Ctrl Pts',(-3.86127351832835,-6.52928079264423,
-16.2174862581729)) ;
#162615 = CARTESIAN_POINT('Ctrl Pts',(-3.85097911745215,-6.53624680748629,
-16.2381127705688)) ;
#162616 = CARTESIAN_POINT('Ctrl Pts',(-3.8456360158508,-6.53918030781797,
-16.2488050943348)) ;
#162617 = CARTESIAN_POINT('Ctrl Pts',(-3.83952524546706,-6.54185985500296,
-16.2610185932204)) ;
#162618 = CARTESIAN_POINT('Ctrl Pts',(-3.83889029009099,-6.5421304506123,
-16.262287517227)) ;
#162619 = CARTESIAN_POINT('Ctrl Pts',(-3.83250371086603,-6.5447746790983,
-16.2750493700286)) ;
#162620 = CARTESIAN_POINT('Ctrl Pts',(-3.82662842759378,-6.54657370273654,
-16.286779364282)) ;
#162621 = CARTESIAN_POINT('Ctrl Pts',(-3.81540422523877,-6.54896007643136,
-16.3092002588839)) ;
#162622 = CARTESIAN_POINT('Ctrl Pts',(-3.81004992405495,-6.54963010255188,
-16.3199019216816)) ;
#162623 = CARTESIAN_POINT('Ctrl Pts',(-3.80321442618295,-6.54996164986963,
-16.333571160343)) ;
#162624 = CARTESIAN_POINT('Ctrl Pts',(-3.80159858684041,-6.55,-16.3368028263192)) ;
#162625 = CARTESIAN_POINT('Ctrl Pts',(-3.8,-6.55,-16.34)) ;
#162626 = CARTESIAN_POINT('Origin',(-5.,-6.45,-14.24)) ;
#162627 = CARTESIAN_POINT('',(-4.92928932188133,-6.52071067811864,-16.1985786437627)) ;
#162628 = CARTESIAN_POINT('Ctrl Pts',(-5.,-6.55,-16.34)) ;
#162629 = CARTESIAN_POINT('Ctrl Pts',(-4.99491714173208,-6.55,-16.3298342834642)) ;
#162630 = CARTESIAN_POINT('Ctrl Pts',(-4.989657683858,-6.54961031187958,-16.3193168490806)) ;
#162631 = CARTESIAN_POINT('Ctrl Pts',(-4.97846794971935,-6.54783411578236,
-16.2969573347197)) ;
#162632 = CARTESIAN_POINT('Ctrl Pts',(-4.97252276179495,-6.54635217950656,
-16.2850867274012)) ;
#162633 = CARTESIAN_POINT('Ctrl Pts',(-4.96110676039589,-6.5423143911687,
-16.2622838373803)) ;
#162634 = CARTESIAN_POINT('Ctrl Pts',(-4.95562986130779,-6.53982180675155,
-16.25133748165)) ;
#162635 = CARTESIAN_POINT('Ctrl Pts',(-4.94974069603908,-6.5364553793343,
-16.239549942885)) ;
#162636 = CARTESIAN_POINT('Ctrl Pts',(-4.94911168276594,-6.53608665347795,
-16.2382907189455)) ;
#162637 = CARTESIAN_POINT('Ctrl Pts',(-4.94303275135179,-6.53243308776748,
-16.2261192297328)) ;
#162638 = CARTESIAN_POINT('Ctrl Pts',(-4.93784223842914,-6.52859969139742,
-16.2157069173625)) ;
#162639 = CARTESIAN_POINT('Ctrl Pts',(-4.93177118696431,-6.52312881451533,
-16.2035451100273)) ;
#162640 = CARTESIAN_POINT('Ctrl Pts',(-4.93051466706414,-6.52193602330145,
-16.2010293341283)) ;
#162641 = CARTESIAN_POINT('Ctrl Pts',(-4.92928932188133,-6.52071067811864,
-16.1985786437627)) ;
#162642 = CARTESIAN_POINT('Origin',(-5.0071421042461,-6.44700925664031,-16.354280054294)) ;
#162643 = CARTESIAN_POINT('',(-4.9292893218813,-6.52071067811861,-14.2814213562372)) ;
#162644 = CARTESIAN_POINT('Origin',(-5.00708668537856,-6.44703459697599,-14.1258299049512)) ;
#162645 = CARTESIAN_POINT('Ctrl Pts',(-4.9292893218813,-6.52071067811861,
-14.2814213562372)) ;
#162646 = CARTESIAN_POINT('Ctrl Pts',(-4.93379539934635,-6.52521675558366,
-14.2724092013071)) ;
#162647 = CARTESIAN_POINT('Ctrl Pts',(-4.93872648167166,-6.52928079264424,
-14.2625137418269)) ;
#162648 = CARTESIAN_POINT('Ctrl Pts',(-4.94902088254798,-6.53624680748638,
-14.2418872294307)) ;
#162649 = CARTESIAN_POINT('Ctrl Pts',(-4.95436398414945,-6.53918030781811,
-14.2311949056644)) ;
#162650 = CARTESIAN_POINT('Ctrl Pts',(-4.96047475453317,-6.54185985500306,
-14.2189814067788)) ;
#162651 = CARTESIAN_POINT('Ctrl Pts',(-4.96110970990912,-6.54213045061234,
-14.2177124827724)) ;
#162652 = CARTESIAN_POINT('Ctrl Pts',(-4.96749628913392,-6.54477467909828,
-14.2049506299712)) ;
#162653 = CARTESIAN_POINT('Ctrl Pts',(-4.97337157240614,-6.54657370273651,
-14.1932206357179)) ;
#162654 = CARTESIAN_POINT('Ctrl Pts',(-4.98459577476115,-6.54896007643135,
-14.170799741116)) ;
#162655 = CARTESIAN_POINT('Ctrl Pts',(-4.98995007594499,-6.54963010255188,
-14.1600980783184)) ;
#162656 = CARTESIAN_POINT('Ctrl Pts',(-4.99678557381703,-6.54996164986962,
-14.146428839657)) ;
#162657 = CARTESIAN_POINT('Ctrl Pts',(-4.99840141315957,-6.55,-14.1431971736808)) ;
#162658 = CARTESIAN_POINT('Ctrl Pts',(-5.,-6.55,-14.14)) ;
#162659 = CARTESIAN_POINT('Origin',(-4.9,-6.45,-14.14)) ;
#162660 = CARTESIAN_POINT('',(-4.85857864376269,-6.52071067811866,-14.2107106781187)) ;
#162661 = CARTESIAN_POINT('Ctrl Pts',(-5.,-6.55,-14.14)) ;
#162662 = CARTESIAN_POINT('Ctrl Pts',(-4.98983428346412,-6.55,-14.1450828582679)) ;
#162663 = CARTESIAN_POINT('Ctrl Pts',(-4.97931684908049,-6.54961031187958,
-14.150342316142)) ;
#162664 = CARTESIAN_POINT('Ctrl Pts',(-4.95695733471958,-6.54783411578236,
-14.1615320502806)) ;
#162665 = CARTESIAN_POINT('Ctrl Pts',(-4.94508672740099,-6.54635217950657,
-14.167477238205)) ;
#162666 = CARTESIAN_POINT('Ctrl Pts',(-4.92228383738157,-6.54231439116896,
-14.1788932396034)) ;
#162667 = CARTESIAN_POINT('Ctrl Pts',(-4.91133748165278,-6.53982180675222,
-14.1843701386908)) ;
#162668 = CARTESIAN_POINT('Ctrl Pts',(-4.8995499428876,-6.53645537933512,
-14.1902593039595)) ;
#162669 = CARTESIAN_POINT('Ctrl Pts',(-4.89829071894667,-6.53608665347833,
-14.1908883172334)) ;
#162670 = CARTESIAN_POINT('Ctrl Pts',(-4.88611922973252,-6.53243308776743,
-14.1969672486483)) ;
#162671 = CARTESIAN_POINT('Ctrl Pts',(-4.87570691736228,-6.52859969139738,
-14.2021577615709)) ;
#162672 = CARTESIAN_POINT('Ctrl Pts',(-4.86354511002712,-6.5231288145153,
-14.2082288130357)) ;
#162673 = CARTESIAN_POINT('Ctrl Pts',(-4.86102933412825,-6.52193602330142,
-14.2094853329359)) ;
#162674 = CARTESIAN_POINT('Ctrl Pts',(-4.85857864376269,-6.52071067811863,
-14.2107106781187)) ;
#162675 = CARTESIAN_POINT('Origin',(-5.01428005427037,-6.44700925664399,-14.1328578957658)) ;
#162676 = CARTESIAN_POINT('',(-3.94142135623725,-6.52071067811863,-14.2107106781187)) ;
#162677 = CARTESIAN_POINT('Origin',(-3.78582990492081,-6.44703459697004,-14.1329133146062)) ;
#162678 = CARTESIAN_POINT('Ctrl Pts',(-3.94142135623725,-6.52071067811862,
-14.2107106781187)) ;
#162679 = CARTESIAN_POINT('Ctrl Pts',(-3.93240920130718,-6.52521675558364,
-14.2062046006537)) ;
#162680 = CARTESIAN_POINT('Ctrl Pts',(-3.92251374182704,-6.52928079264421,
-14.2012735183284)) ;
#162681 = CARTESIAN_POINT('Ctrl Pts',(-3.90188722943303,-6.53624680748561,
-14.1909791174532)) ;
#162682 = CARTESIAN_POINT('Ctrl Pts',(-3.89119490566909,-6.53918030781684,
-14.1856360158529)) ;
#162683 = CARTESIAN_POINT('Ctrl Pts',(-3.87898140678365,-6.54185985500205,
-14.1795252454692)) ;
#162684 = CARTESIAN_POINT('Ctrl Pts',(-3.87771248277495,-6.54213045061184,
-14.1788902900921)) ;
#162685 = CARTESIAN_POINT('Ctrl Pts',(-3.8649506299714,-6.54477467909827,
-14.1725037108661)) ;
#162686 = CARTESIAN_POINT('Ctrl Pts',(-3.85322063571803,-6.5465737027365,
-14.1666284275939)) ;
#162687 = CARTESIAN_POINT('Ctrl Pts',(-3.83079974111618,-6.54896007643135,
-14.1554042252389)) ;
#162688 = CARTESIAN_POINT('Ctrl Pts',(-3.82009807831857,-6.54963010255187,
-14.1500499240551)) ;
#162689 = CARTESIAN_POINT('Ctrl Pts',(-3.80642883965711,-6.54996164986962,
-14.1432144261831)) ;
#162690 = CARTESIAN_POINT('Ctrl Pts',(-3.80319717368089,-6.55,-14.1415985868405)) ;
#162691 = CARTESIAN_POINT('Ctrl Pts',(-3.8,-6.55,-14.14)) ;
#162692 = CARTESIAN_POINT('Origin',(-4.9,-6.45,-12.53)) ;
#162693 = CARTESIAN_POINT('',(-4.85857864376269,-6.52071067811866,-12.4592893218813)) ;
#162694 = CARTESIAN_POINT('Origin',(-5.01417009504273,-6.44703459697676,-12.5370866853755)) ;
#162695 = CARTESIAN_POINT('Ctrl Pts',(-4.85857864376269,-6.52071067811863,
-12.4592893218813)) ;
#162696 = CARTESIAN_POINT('Ctrl Pts',(-4.86759079869274,-6.5252167555837,
-12.4637953993464)) ;
#162697 = CARTESIAN_POINT('Ctrl Pts',(-4.87748625817285,-6.52928079264422,
-12.4687264816716)) ;
#162698 = CARTESIAN_POINT('Ctrl Pts',(-4.89811277056884,-6.53624680748634,
-12.4790208825479)) ;
#162699 = CARTESIAN_POINT('Ctrl Pts',(-4.90880509433502,-6.53918030781804,
-12.4843639841493)) ;
#162700 = CARTESIAN_POINT('Ctrl Pts',(-4.9210185932206,-6.54185985500302,
-12.4904747545331)) ;
#162701 = CARTESIAN_POINT('Ctrl Pts',(-4.92228751722714,-6.54213045061234,
-12.4911097099091)) ;
#162702 = CARTESIAN_POINT('Ctrl Pts',(-4.93504937002859,-6.54477467909833,
-12.4974962891341)) ;
#162703 = CARTESIAN_POINT('Ctrl Pts',(-4.94677936428205,-6.54657370273655,
-12.5033715724063)) ;
#162704 = CARTESIAN_POINT('Ctrl Pts',(-4.96920025888403,-6.54896007643138,
-12.5145957747613)) ;
#162705 = CARTESIAN_POINT('Ctrl Pts',(-4.97990192168169,-6.54963010255189,
-12.5199500759451)) ;
#162706 = CARTESIAN_POINT('Ctrl Pts',(-4.99357116034309,-6.54996164986963,
-12.5267855738171)) ;
#162707 = CARTESIAN_POINT('Ctrl Pts',(-4.99680282631921,-6.55,-12.5284014131596)) ;
#162708 = CARTESIAN_POINT('Ctrl Pts',(-5.,-6.55,-12.53)) ;
#162709 = CARTESIAN_POINT('',(-3.94142135623725,-6.52071067811863,-12.4592893218813)) ;
#162710 = CARTESIAN_POINT('Ctrl Pts',(-3.8,-6.55,-12.53)) ;
#162711 = CARTESIAN_POINT('Ctrl Pts',(-3.81016571653583,-6.55,-12.5249171417321)) ;
#162712 = CARTESIAN_POINT('Ctrl Pts',(-3.82068315091943,-6.54961031187958,
-12.519657683858)) ;
#162713 = CARTESIAN_POINT('Ctrl Pts',(-3.84304266528023,-6.54783411578235,
-12.5084679497193)) ;
#162714 = CARTESIAN_POINT('Ctrl Pts',(-3.85491327259876,-6.54635217950657,
-12.502522761795)) ;
#162715 = CARTESIAN_POINT('Ctrl Pts',(-3.87771616262383,-6.54231439116795,
-12.4911067603938)) ;
#162716 = CARTESIAN_POINT('Ctrl Pts',(-3.8886625183582,-6.53982180674967,
-12.4856298613037)) ;
#162717 = CARTESIAN_POINT('Ctrl Pts',(-3.90045005712288,-6.53645537933199,
-12.4797406960351)) ;
#162718 = CARTESIAN_POINT('Ctrl Pts',(-3.90170928105837,-6.53608665347676,
-12.479111682764)) ;
#162719 = CARTESIAN_POINT('Ctrl Pts',(-3.91388077026718,-6.53243308776745,
-12.4730327513517)) ;
#162720 = CARTESIAN_POINT('Ctrl Pts',(-3.92429308263747,-6.52859969139739,
-12.4678422384291)) ;
#162721 = CARTESIAN_POINT('Ctrl Pts',(-3.93645488997274,-6.52312881451531,
-12.4617711869643)) ;
#162722 = CARTESIAN_POINT('Ctrl Pts',(-3.93897066587165,-6.52193602330142,
-12.4605146670641)) ;
#162723 = CARTESIAN_POINT('Ctrl Pts',(-3.94142135623725,-6.52071067811862,
-12.4592893218813)) ;
#162724 = CARTESIAN_POINT('Origin',(-3.78571994569861,-6.44700925663807,-12.5371421042496)) ;
#162725 = CARTESIAN_POINT('Origin',(-3.8,-6.45,-10.43)) ;
#162726 = CARTESIAN_POINT('',(-3.87071067811867,-6.52071067811864,-10.4714213562373)) ;
#162727 = CARTESIAN_POINT('Ctrl Pts',(-3.8,-6.55,-10.33)) ;
#162728 = CARTESIAN_POINT('Ctrl Pts',(-3.80508285826792,-6.55,-10.3401657165358)) ;
#162729 = CARTESIAN_POINT('Ctrl Pts',(-3.810342316142,-6.54961031187958,-10.3506831509194)) ;
#162730 = CARTESIAN_POINT('Ctrl Pts',(-3.82153205028064,-6.54783411578236,
-10.3730426652802)) ;
#162731 = CARTESIAN_POINT('Ctrl Pts',(-3.82747723820505,-6.54635217950656,
-10.3849132725988)) ;
#162732 = CARTESIAN_POINT('Ctrl Pts',(-3.83889323960397,-6.54231439116875,
-10.4077161626194)) ;
#162733 = CARTESIAN_POINT('Ctrl Pts',(-3.84437013869195,-6.53982180675168,
-10.4186625183494)) ;
#162734 = CARTESIAN_POINT('Ctrl Pts',(-3.85025930396067,-6.53645537933445,
-10.4304500571145)) ;
#162735 = CARTESIAN_POINT('Ctrl Pts',(-3.85088831723394,-6.53608665347802,
-10.4317092810542)) ;
#162736 = CARTESIAN_POINT('Ctrl Pts',(-3.85696724864823,-6.53243308776747,
-10.4438807702672)) ;
#162737 = CARTESIAN_POINT('Ctrl Pts',(-3.86215776157089,-6.5285996913974,
-10.4542930826375)) ;
#162738 = CARTESIAN_POINT('Ctrl Pts',(-3.86822881303571,-6.5231288145153,
-10.4664548899728)) ;
#162739 = CARTESIAN_POINT('Ctrl Pts',(-3.86948533293587,-6.52193602330144,
-10.4689706658717)) ;
#162740 = CARTESIAN_POINT('Ctrl Pts',(-3.87071067811867,-6.52071067811864,
-10.4714213562373)) ;
#162741 = CARTESIAN_POINT('Origin',(-3.79285789573469,-6.44700925663192,-10.3157199456678)) ;
#162742 = CARTESIAN_POINT('',(-3.87071067811865,-6.52071067811866,-12.3885786437627)) ;
#162743 = CARTESIAN_POINT('Origin',(-3.79291331463695,-6.44703459698198,-12.544170095017)) ;
#162744 = CARTESIAN_POINT('Ctrl Pts',(-3.87071067811865,-6.52071067811866,
-12.3885786437627)) ;
#162745 = CARTESIAN_POINT('Ctrl Pts',(-3.86620460065363,-6.52521675558368,
-12.3975907986927)) ;
#162746 = CARTESIAN_POINT('Ctrl Pts',(-3.86127351832835,-6.52928079264423,
-12.4074862581729)) ;
#162747 = CARTESIAN_POINT('Ctrl Pts',(-3.8509791174523,-6.5362468074862,-12.4281127705685)) ;
#162748 = CARTESIAN_POINT('Ctrl Pts',(-3.84563601585109,-6.53918030781781,
-12.4388050943343)) ;
#162749 = CARTESIAN_POINT('Ctrl Pts',(-3.83952524546737,-6.54185985500283,
-12.4510185932199)) ;
#162750 = CARTESIAN_POINT('Ctrl Pts',(-3.83889029009115,-6.54213045061223,
-12.4522875172268)) ;
#162751 = CARTESIAN_POINT('Ctrl Pts',(-3.83250371086605,-6.54477467909829,
-12.4650493700286)) ;
#162752 = CARTESIAN_POINT('Ctrl Pts',(-3.8266284275938,-6.54657370273653,
-12.476779364282)) ;
#162753 = CARTESIAN_POINT('Ctrl Pts',(-3.81540422523879,-6.54896007643136,
-12.499200258884)) ;
#162754 = CARTESIAN_POINT('Ctrl Pts',(-3.81004992405497,-6.54963010255188,
-12.5099019216816)) ;
#162755 = CARTESIAN_POINT('Ctrl Pts',(-3.80321442618295,-6.54996164986962,
-12.523571160343)) ;
#162756 = CARTESIAN_POINT('Ctrl Pts',(-3.80159858684041,-6.55,-12.5268028263192)) ;
#162757 = CARTESIAN_POINT('Ctrl Pts',(-3.8,-6.55,-12.53)) ;
#162758 = CARTESIAN_POINT('Origin',(-5.,-6.45,-10.43)) ;
#162759 = CARTESIAN_POINT('',(-4.9292893218813,-6.52071067811861,-12.3885786437628)) ;
#162760 = CARTESIAN_POINT('Ctrl Pts',(-5.,-6.55,-12.53)) ;
#162761 = CARTESIAN_POINT('Ctrl Pts',(-4.99491714173206,-6.55,-12.5198342834642)) ;
#162762 = CARTESIAN_POINT('Ctrl Pts',(-4.98965768385797,-6.54961031187957,
-12.5093168490806)) ;
#162763 = CARTESIAN_POINT('Ctrl Pts',(-4.97846794971932,-6.54783411578235,
-12.4869573347198)) ;
#162764 = CARTESIAN_POINT('Ctrl Pts',(-4.97252276179494,-6.54635217950656,
-12.4750867274013)) ;
#162765 = CARTESIAN_POINT('Ctrl Pts',(-4.96110676039596,-6.54231439116872,
-12.4522838373806)) ;
#162766 = CARTESIAN_POINT('Ctrl Pts',(-4.95562986130792,-6.53982180675161,
-12.4413374816505)) ;
#162767 = CARTESIAN_POINT('Ctrl Pts',(-4.94974069603921,-6.53645537933438,
-12.4295499428854)) ;
#162768 = CARTESIAN_POINT('Ctrl Pts',(-4.94911168276601,-6.53608665347799,
-12.4282907189459)) ;
#162769 = CARTESIAN_POINT('Ctrl Pts',(-4.94303275135178,-6.53243308776748,
-12.416119229733)) ;
#162770 = CARTESIAN_POINT('Ctrl Pts',(-4.93784223842911,-6.52859969139739,
-12.4057069173626)) ;
#162771 = CARTESIAN_POINT('Ctrl Pts',(-4.93177118696427,-6.52312881451529,
-12.3935451100273)) ;
#162772 = CARTESIAN_POINT('Ctrl Pts',(-4.9305146670641,-6.52193602330142,
-12.3910293341284)) ;
#162773 = CARTESIAN_POINT('Ctrl Pts',(-4.9292893218813,-6.52071067811861,
-12.3885786437628)) ;
#162774 = CARTESIAN_POINT('Origin',(-5.00714210425336,-6.44700925663617,-12.5442800543089)) ;
#162775 = CARTESIAN_POINT('',(-4.9292893218813,-6.52071067811861,-10.4714213562372)) ;
#162776 = CARTESIAN_POINT('Origin',(-5.00708668538065,-6.44703459697523,-10.3158299049469)) ;
#162777 = CARTESIAN_POINT('Ctrl Pts',(-4.9292893218813,-6.52071067811861,
-10.4714213562372)) ;
#162778 = CARTESIAN_POINT('Ctrl Pts',(-4.93379539934634,-6.52521675558366,
-10.4624092013071)) ;
#162779 = CARTESIAN_POINT('Ctrl Pts',(-4.93872648167164,-6.52928079264423,
-10.4525137418269)) ;
#162780 = CARTESIAN_POINT('Ctrl Pts',(-4.94902088254777,-6.53624680748624,
-10.4318872294311)) ;
#162781 = CARTESIAN_POINT('Ctrl Pts',(-4.95436398414903,-6.53918030781788,
-10.4211949056652)) ;
#162782 = CARTESIAN_POINT('Ctrl Pts',(-4.96047475453275,-6.54185985500288,
-10.4089814067796)) ;
#162783 = CARTESIAN_POINT('Ctrl Pts',(-4.96110970990889,-6.54213045061225,
-10.4077124827729)) ;
#162784 = CARTESIAN_POINT('Ctrl Pts',(-4.9674962891339,-6.54477467909827,
-10.3949506299713)) ;
#162785 = CARTESIAN_POINT('Ctrl Pts',(-4.97337157240611,-6.5465737027365,
-10.3832206357179)) ;
#162786 = CARTESIAN_POINT('Ctrl Pts',(-4.98459577476111,-6.54896007643135,
-10.3607997411161)) ;
#162787 = CARTESIAN_POINT('Ctrl Pts',(-4.98995007594495,-6.54963010255187,
-10.3500980783185)) ;
#162788 = CARTESIAN_POINT('Ctrl Pts',(-4.99678557381701,-6.54996164986962,
-10.3364288396571)) ;
#162789 = CARTESIAN_POINT('Ctrl Pts',(-4.99840141315956,-6.55,-10.3331971736809)) ;
#162790 = CARTESIAN_POINT('Ctrl Pts',(-5.,-6.55,-10.33)) ;
#162791 = CARTESIAN_POINT('Origin',(-4.9,-6.45,-10.33)) ;
#162792 = CARTESIAN_POINT('',(-4.85857864376269,-6.52071067811866,-10.4007106781187)) ;
#162793 = CARTESIAN_POINT('Ctrl Pts',(-5.,-6.55,-10.33)) ;
#162794 = CARTESIAN_POINT('Ctrl Pts',(-4.98983428346413,-6.55,-10.3350828582679)) ;
#162795 = CARTESIAN_POINT('Ctrl Pts',(-4.9793168490805,-6.54961031187958,
-10.340342316142)) ;
#162796 = CARTESIAN_POINT('Ctrl Pts',(-4.9569573347196,-6.54783411578236,
-10.3515320502806)) ;
#162797 = CARTESIAN_POINT('Ctrl Pts',(-4.94508672740101,-6.54635217950657,
-10.357477238205)) ;
#162798 = CARTESIAN_POINT('Ctrl Pts',(-4.9222838373818,-6.542314391169,-10.3688932396033)) ;
#162799 = CARTESIAN_POINT('Ctrl Pts',(-4.91133748165322,-6.53982180675231,
-10.3743701386905)) ;
#162800 = CARTESIAN_POINT('Ctrl Pts',(-4.89954994288802,-6.53645537933523,
-10.3802593039593)) ;
#162801 = CARTESIAN_POINT('Ctrl Pts',(-4.89829071894688,-6.53608665347839,
-10.3808883172333)) ;
#162802 = CARTESIAN_POINT('Ctrl Pts',(-4.88611922973253,-6.53243308776743,
-10.3869672486483)) ;
#162803 = CARTESIAN_POINT('Ctrl Pts',(-4.87570691736229,-6.52859969139738,
-10.3921577615709)) ;
#162804 = CARTESIAN_POINT('Ctrl Pts',(-4.86354511002712,-6.5231288145153,
-10.3982288130357)) ;
#162805 = CARTESIAN_POINT('Ctrl Pts',(-4.86102933412825,-6.52193602330142,
-10.3994853329359)) ;
#162806 = CARTESIAN_POINT('Ctrl Pts',(-4.85857864376269,-6.52071067811863,
-10.4007106781187)) ;
#162807 = CARTESIAN_POINT('Origin',(-5.01428005429581,-6.44700925663878,-10.3228578957533)) ;
#162808 = CARTESIAN_POINT('',(-3.94142135623724,-6.52071067811862,-10.4007106781187)) ;
#162809 = CARTESIAN_POINT('Origin',(-3.78582990492664,-6.44703459697108,-10.3229133146092)) ;
#162810 = CARTESIAN_POINT('Ctrl Pts',(-3.94142135623724,-6.52071067811862,
-10.4007106781187)) ;
#162811 = CARTESIAN_POINT('Ctrl Pts',(-3.93240920130719,-6.52521675558363,
-10.3962046006537)) ;
#162812 = CARTESIAN_POINT('Ctrl Pts',(-3.92251374182705,-6.52928079264421,
-10.3912735183284)) ;
#162813 = CARTESIAN_POINT('Ctrl Pts',(-3.90188722943306,-6.53624680748561,
-10.3809791174532)) ;
#162814 = CARTESIAN_POINT('Ctrl Pts',(-3.89119490566911,-6.53918030781684,
-10.3756360158529)) ;
#162815 = CARTESIAN_POINT('Ctrl Pts',(-3.87898140678367,-6.54185985500205,
-10.3695252454692)) ;
#162816 = CARTESIAN_POINT('Ctrl Pts',(-3.87771248277498,-6.54213045061184,
-10.3688902900921)) ;
#162817 = CARTESIAN_POINT('Ctrl Pts',(-3.86495062997144,-6.54477467909826,
-10.3625037108661)) ;
#162818 = CARTESIAN_POINT('Ctrl Pts',(-3.85322063571806,-6.5465737027365,
-10.3566284275939)) ;
#162819 = CARTESIAN_POINT('Ctrl Pts',(-3.83079974111621,-6.54896007643133,
-10.345404225239)) ;
#162820 = CARTESIAN_POINT('Ctrl Pts',(-3.82009807831861,-6.54963010255187,
-10.3400499240551)) ;
#162821 = CARTESIAN_POINT('Ctrl Pts',(-3.80642883965713,-6.54996164986962,
-10.3332144261831)) ;
#162822 = CARTESIAN_POINT('Ctrl Pts',(-3.8031971736809,-6.55,-10.3315985868405)) ;
#162823 = CARTESIAN_POINT('Ctrl Pts',(-3.8,-6.55,-10.33)) ;
#162824 = CARTESIAN_POINT('Origin',(-4.9,-6.45,-8.72)) ;
#162825 = CARTESIAN_POINT('',(-4.85857864376269,-6.52071067811866,-8.64928932188135)) ;
#162826 = CARTESIAN_POINT('Origin',(-5.0141700950508,-6.44703459697536,-8.72708668537973)) ;
#162827 = CARTESIAN_POINT('Ctrl Pts',(-4.85857864376269,-6.52071067811865,
-8.64928932188135)) ;
#162828 = CARTESIAN_POINT('Ctrl Pts',(-4.86759079869274,-6.52521675558369,
-8.65379539934638)) ;
#162829 = CARTESIAN_POINT('Ctrl Pts',(-4.87748625817286,-6.52928079264424,
-8.65872648167166)) ;
#162830 = CARTESIAN_POINT('Ctrl Pts',(-4.89811277056854,-6.53624680748623,
-8.66902088254776)) ;
#162831 = CARTESIAN_POINT('Ctrl Pts',(-4.90880509433436,-6.53918030781786,
-8.67436398414899)) ;
#162832 = CARTESIAN_POINT('Ctrl Pts',(-4.92101859321993,-6.54185985500287,
-8.68047475453273)) ;
#162833 = CARTESIAN_POINT('Ctrl Pts',(-4.92228751722681,-6.54213045061227,
-8.68110970990893)) ;
#162834 = CARTESIAN_POINT('Ctrl Pts',(-4.93504937002862,-6.54477467909833,
-8.68749628913405)) ;
#162835 = CARTESIAN_POINT('Ctrl Pts',(-4.94677936428208,-6.54657370273656,
-8.69337157240631)) ;
#162836 = CARTESIAN_POINT('Ctrl Pts',(-4.96920025888408,-6.54896007643138,
-8.70459577476134)) ;
#162837 = CARTESIAN_POINT('Ctrl Pts',(-4.97990192168174,-6.54963010255189,
-8.70995007594516)) ;
#162838 = CARTESIAN_POINT('Ctrl Pts',(-4.99357116034313,-6.54996164986963,
-8.71678557381714)) ;
#162839 = CARTESIAN_POINT('Ctrl Pts',(-4.99680282631923,-6.55,-8.71840141315963)) ;
#162840 = CARTESIAN_POINT('Ctrl Pts',(-5.,-6.55,-8.72)) ;
#162841 = CARTESIAN_POINT('',(-3.94142135623725,-6.52071067811863,-8.64928932188132)) ;
#162842 = CARTESIAN_POINT('Ctrl Pts',(-3.8,-6.55,-8.72)) ;
#162843 = CARTESIAN_POINT('Ctrl Pts',(-3.81016571653583,-6.55,-8.71491714173207)) ;
#162844 = CARTESIAN_POINT('Ctrl Pts',(-3.82068315091943,-6.54961031187958,
-8.70965768385799)) ;
#162845 = CARTESIAN_POINT('Ctrl Pts',(-3.84304266528024,-6.54783411578235,
-8.69846794971933)) ;
#162846 = CARTESIAN_POINT('Ctrl Pts',(-3.85491327259876,-6.54635217950656,
-8.69252276179493)) ;
#162847 = CARTESIAN_POINT('Ctrl Pts',(-3.87771616261911,-6.5423143911688,
-8.68110676039617)) ;
#162848 = CARTESIAN_POINT('Ctrl Pts',(-3.88866251834886,-6.5398218067518,
-8.67562986130833)) ;
#162849 = CARTESIAN_POINT('Ctrl Pts',(-3.90045005711395,-6.53645537933461,
-8.66974069603961)) ;
#162850 = CARTESIAN_POINT('Ctrl Pts',(-3.90170928105393,-6.5360866534781,
-8.66911168276619)) ;
#162851 = CARTESIAN_POINT('Ctrl Pts',(-3.91388077026719,-6.53243308776746,
-8.66303275135177)) ;
#162852 = CARTESIAN_POINT('Ctrl Pts',(-3.92429308263748,-6.52859969139739,
-8.6578422384291)) ;
#162853 = CARTESIAN_POINT('Ctrl Pts',(-3.93645488997274,-6.5231288145153,
-8.65177118696428)) ;
#162854 = CARTESIAN_POINT('Ctrl Pts',(-3.93897066587165,-6.52193602330143,
-8.65051466706412)) ;
#162855 = CARTESIAN_POINT('Ctrl Pts',(-3.94142135623725,-6.52071067811863,
-8.64928932188132)) ;
#162856 = CARTESIAN_POINT('Origin',(-3.78571994570435,-6.44700925663925,-8.72714210424676)) ;
#162857 = CARTESIAN_POINT('Origin',(-3.8,-6.45,-6.62)) ;
#162858 = CARTESIAN_POINT('',(-3.87071067811865,-6.52071067811866,-6.66142135623731)) ;
#162859 = CARTESIAN_POINT('Ctrl Pts',(-3.8,-6.55,-6.52)) ;
#162860 = CARTESIAN_POINT('Ctrl Pts',(-3.80508285826792,-6.55,-6.53016571653586)) ;
#162861 = CARTESIAN_POINT('Ctrl Pts',(-3.810342316142,-6.54961031187958,-6.54068315091949)) ;
#162862 = CARTESIAN_POINT('Ctrl Pts',(-3.82153205028068,-6.54783411578235,
-6.56304266528037)) ;
#162863 = CARTESIAN_POINT('Ctrl Pts',(-3.8274772382051,-6.54635217950655,
-6.57491327259895)) ;
#162864 = CARTESIAN_POINT('Ctrl Pts',(-3.83889323960401,-6.54231439116873,
-6.59771616261959)) ;
#162865 = CARTESIAN_POINT('Ctrl Pts',(-3.84437013869196,-6.53982180675167,
-6.6086625183496)) ;
#162866 = CARTESIAN_POINT('Ctrl Pts',(-3.85025930396068,-6.53645537933444,
-6.62045005711466)) ;
#162867 = CARTESIAN_POINT('Ctrl Pts',(-3.85088831723398,-6.53608665347799,
-6.62170928105441)) ;
#162868 = CARTESIAN_POINT('Ctrl Pts',(-3.85696724864827,-6.53243308776743,
-6.6338807702674)) ;
#162869 = CARTESIAN_POINT('Ctrl Pts',(-3.86215776157092,-6.52859969139737,
-6.64429308263765)) ;
#162870 = CARTESIAN_POINT('Ctrl Pts',(-3.86822881303572,-6.5231288145153,
-6.65645488997285)) ;
#162871 = CARTESIAN_POINT('Ctrl Pts',(-3.86948533293586,-6.52193602330144,
-6.65897066587173)) ;
#162872 = CARTESIAN_POINT('Ctrl Pts',(-3.87071067811865,-6.52071067811866,
-6.66142135623731)) ;
#162873 = CARTESIAN_POINT('Origin',(-3.79285789575055,-6.44700925663822,-6.5057199456992)) ;
#162874 = CARTESIAN_POINT('',(-3.87071067811865,-6.52071067811866,-8.57857864376269)) ;
#162875 = CARTESIAN_POINT('Origin',(-3.79291331460542,-6.44703459696871,-8.73417009508047)) ;
#162876 = CARTESIAN_POINT('Ctrl Pts',(-3.87071067811865,-6.52071067811866,
-8.57857864376269)) ;
#162877 = CARTESIAN_POINT('Ctrl Pts',(-3.86620460065363,-6.52521675558368,
-8.58759079869274)) ;
#162878 = CARTESIAN_POINT('Ctrl Pts',(-3.86127351832835,-6.52928079264423,
-8.59748625817286)) ;
#162879 = CARTESIAN_POINT('Ctrl Pts',(-3.85097911745197,-6.53624680748642,
-8.61811277056917)) ;
#162880 = CARTESIAN_POINT('Ctrl Pts',(-3.84563601585041,-6.53918030781819,
-8.62880509433569)) ;
#162881 = CARTESIAN_POINT('Ctrl Pts',(-3.83952524546667,-6.54185985500313,
-8.64101859322128)) ;
#162882 = CARTESIAN_POINT('Ctrl Pts',(-3.8388902900908,-6.54213045061238,
-8.64228751722748)) ;
#162883 = CARTESIAN_POINT('Ctrl Pts',(-3.83250371086605,-6.5447746790983,
-8.65504937002858)) ;
#162884 = CARTESIAN_POINT('Ctrl Pts',(-3.8266284275938,-6.54657370273653,
-8.66677936428201)) ;
#162885 = CARTESIAN_POINT('Ctrl Pts',(-3.8154042252388,-6.54896007643136,
-8.68920025888395)) ;
#162886 = CARTESIAN_POINT('Ctrl Pts',(-3.81004992405497,-6.54963010255188,
-8.69990192168157)) ;
#162887 = CARTESIAN_POINT('Ctrl Pts',(-3.80321442618295,-6.54996164986962,
-8.713571160343)) ;
#162888 = CARTESIAN_POINT('Ctrl Pts',(-3.80159858684042,-6.55,-8.71680282631917)) ;
#162889 = CARTESIAN_POINT('Ctrl Pts',(-3.8,-6.55,-8.72)) ;
#162890 = CARTESIAN_POINT('Origin',(-5.,-6.45,-6.62)) ;
#162891 = CARTESIAN_POINT('',(-4.9292893218813,-6.52071067811861,-8.57857864376279)) ;
#162892 = CARTESIAN_POINT('Ctrl Pts',(-5.,-6.55,-8.72)) ;
#162893 = CARTESIAN_POINT('Ctrl Pts',(-4.99491714173206,-6.55,-8.70983428346417)) ;
#162894 = CARTESIAN_POINT('Ctrl Pts',(-4.98965768385797,-6.54961031187957,
-8.69931684908058)) ;
#162895 = CARTESIAN_POINT('Ctrl Pts',(-4.97846794971931,-6.54783411578235,
-8.67695733471982)) ;
#162896 = CARTESIAN_POINT('Ctrl Pts',(-4.97252276179493,-6.54635217950656,
-8.66508672740134)) ;
#162897 = CARTESIAN_POINT('Ctrl Pts',(-4.96110676039608,-6.54231439116877,
-8.64228383738083)) ;
#162898 = CARTESIAN_POINT('Ctrl Pts',(-4.95562986130815,-6.53982180675172,
-8.63133748165089)) ;
#162899 = CARTESIAN_POINT('Ctrl Pts',(-4.94974069603943,-6.53645537933451,
-8.61954994288583)) ;
#162900 = CARTESIAN_POINT('Ctrl Pts',(-4.94911168276612,-6.53608665347805,
-8.61829071894605)) ;
#162901 = CARTESIAN_POINT('Ctrl Pts',(-4.94303275135178,-6.53243308776748,
-8.60611922973296)) ;
#162902 = CARTESIAN_POINT('Ctrl Pts',(-4.93784223842912,-6.5285996913974,
-8.59570691736265)) ;
#162903 = CARTESIAN_POINT('Ctrl Pts',(-4.93177118696428,-6.5231288145153,
-8.58354511002734)) ;
#162904 = CARTESIAN_POINT('Ctrl Pts',(-4.9305146670641,-6.52193602330142,
-8.58102933412841)) ;
#162905 = CARTESIAN_POINT('Ctrl Pts',(-4.9292893218813,-6.52071067811861,
-8.57857864376279)) ;
#162906 = CARTESIAN_POINT('Origin',(-5.00714210425842,-6.4470092566342,-8.73428005431905)) ;
#162907 = CARTESIAN_POINT('',(-4.92928932188132,-6.52071067811863,-6.66142135623726)) ;
#162908 = CARTESIAN_POINT('Origin',(-5.007086685383,-6.44703459697434,-6.50582990494236)) ;
#162909 = CARTESIAN_POINT('Ctrl Pts',(-4.92928932188132,-6.52071067811863,
-6.66142135623726)) ;
#162910 = CARTESIAN_POINT('Ctrl Pts',(-4.93379539934634,-6.52521675558365,
-6.6524092013072)) ;
#162911 = CARTESIAN_POINT('Ctrl Pts',(-4.93872648167162,-6.5292807926442,
-6.64251374182708)) ;
#162912 = CARTESIAN_POINT('Ctrl Pts',(-4.94902088254778,-6.53624680748625,
-6.62188722943121)) ;
#162913 = CARTESIAN_POINT('Ctrl Pts',(-4.9543639841491,-6.53918030781792,
-6.61119490566518)) ;
#162914 = CARTESIAN_POINT('Ctrl Pts',(-4.96047475453282,-6.54185985500291,
-6.59898140677963)) ;
#162915 = CARTESIAN_POINT('Ctrl Pts',(-4.96110970990891,-6.54213045061226,
-6.59771248277296)) ;
#162916 = CARTESIAN_POINT('Ctrl Pts',(-4.96749628913387,-6.54477467909827,
-6.58495062997146)) ;
#162917 = CARTESIAN_POINT('Ctrl Pts',(-4.9733715724061,-6.5465737027365,-6.57322063571808)) ;
#162918 = CARTESIAN_POINT('Ctrl Pts',(-4.98459577476108,-6.54896007643134,
-6.55079974111622)) ;
#162919 = CARTESIAN_POINT('Ctrl Pts',(-4.98995007594491,-6.54963010255187,
-6.54009807831861)) ;
#162920 = CARTESIAN_POINT('Ctrl Pts',(-4.99678557381697,-6.54996164986962,
-6.52642883965713)) ;
#162921 = CARTESIAN_POINT('Ctrl Pts',(-4.99840141315954,-6.55,-6.5231971736809)) ;
#162922 = CARTESIAN_POINT('Ctrl Pts',(-5.,-6.55,-6.52)) ;
#162923 = CARTESIAN_POINT('Origin',(-4.9,-6.45,-6.52)) ;
#162924 = CARTESIAN_POINT('',(-4.85857864376269,-6.52071067811866,-6.59071067811866)) ;
#162925 = CARTESIAN_POINT('Ctrl Pts',(-5.,-6.55,-6.52)) ;
#162926 = CARTESIAN_POINT('Ctrl Pts',(-4.98983428346415,-6.55,-6.52508285826791)) ;
#162927 = CARTESIAN_POINT('Ctrl Pts',(-4.97931684908054,-6.54961031187958,
-6.53034231614198)) ;
#162928 = CARTESIAN_POINT('Ctrl Pts',(-4.95695733471967,-6.54783411578236,
-6.54153205028064)) ;
#162929 = CARTESIAN_POINT('Ctrl Pts',(-4.9450867274011,-6.54635217950656,
-6.54747723820505)) ;
#162930 = CARTESIAN_POINT('Ctrl Pts',(-4.92228383738093,-6.54231439116883,
-6.55889323960373)) ;
#162931 = CARTESIAN_POINT('Ctrl Pts',(-4.91133748165139,-6.5398218067519,
-6.56437013869147)) ;
#162932 = CARTESIAN_POINT('Ctrl Pts',(-4.89954994288627,-6.53645537933471,
-6.57025930396021)) ;
#162933 = CARTESIAN_POINT('Ctrl Pts',(-4.89829071894607,-6.53608665347814,
-6.57088831723374)) ;
#162934 = CARTESIAN_POINT('Ctrl Pts',(-4.88611922973263,-6.53243308776745,
-6.57696724864825)) ;
#162935 = CARTESIAN_POINT('Ctrl Pts',(-4.87570691736238,-6.52859969139738,
-6.5821577615709)) ;
#162936 = CARTESIAN_POINT('Ctrl Pts',(-4.86354511002717,-6.5231288145153,
-6.58822881303571)) ;
#162937 = CARTESIAN_POINT('Ctrl Pts',(-4.86102933412828,-6.52193602330145,
-6.58948533293586)) ;
#162938 = CARTESIAN_POINT('Ctrl Pts',(-4.85857864376269,-6.52071067811865,
-6.59071067811866)) ;
#162939 = CARTESIAN_POINT('Origin',(-5.0142800542992,-6.44700925663862,-6.51285789575134)) ;
#162940 = CARTESIAN_POINT('',(-3.94142135623721,-6.52071067811861,-6.59071067811871)) ;
#162941 = CARTESIAN_POINT('Origin',(-3.78582990493307,-6.44703459697233,-6.51291331461247)) ;
#162942 = CARTESIAN_POINT('Ctrl Pts',(-3.94142135623721,-6.52071067811861,
-6.5907106781187)) ;
#162943 = CARTESIAN_POINT('Ctrl Pts',(-3.93240920130712,-6.52521675558366,
-6.58620460065366)) ;
#162944 = CARTESIAN_POINT('Ctrl Pts',(-3.92251374182695,-6.52928079264422,
-6.58127351832836)) ;
#162945 = CARTESIAN_POINT('Ctrl Pts',(-3.90188722943119,-6.53624680748622,
-6.57097911745226)) ;
#162946 = CARTESIAN_POINT('Ctrl Pts',(-3.89119490566534,-6.53918030781785,
-6.56563601585102)) ;
#162947 = CARTESIAN_POINT('Ctrl Pts',(-3.8789814067798,-6.54185985500286,
-6.55952524546731)) ;
#162948 = CARTESIAN_POINT('Ctrl Pts',(-3.87771248277297,-6.54213045061224,
-6.55889029009113)) ;
#162949 = CARTESIAN_POINT('Ctrl Pts',(-3.86495062997132,-6.54477467909828,
-6.5525037108661)) ;
#162950 = CARTESIAN_POINT('Ctrl Pts',(-3.85322063571796,-6.54657370273651,
-6.54662842759388)) ;
#162951 = CARTESIAN_POINT('Ctrl Pts',(-3.83079974111614,-6.54896007643134,
-6.5354042252389)) ;
#162952 = CARTESIAN_POINT('Ctrl Pts',(-3.82009807831854,-6.54963010255187,
-6.53004992405507)) ;
#162953 = CARTESIAN_POINT('Ctrl Pts',(-3.80642883965709,-6.54996164986962,
-6.52321442618302)) ;
#162954 = CARTESIAN_POINT('Ctrl Pts',(-3.80319717368088,-6.55,-6.52159858684045)) ;
#162955 = CARTESIAN_POINT('Ctrl Pts',(-3.8,-6.55,-6.52)) ;
#162956 = CARTESIAN_POINT('Origin',(-4.9,-6.45,-2.71)) ;
#162957 = CARTESIAN_POINT('Origin',(-4.,-6.45,-2.71)) ;
#162958 = CARTESIAN_POINT('Origin',(-4.8,-6.45,-2.71)) ;
#162959 = CARTESIAN_POINT('Origin',(-4.8,-6.45,-2.91)) ;
#162960 = CARTESIAN_POINT('Origin',(-5.,-6.45,-2.91)) ;
#162961 = CARTESIAN_POINT('Origin',(-4.8,-6.45,-2.91)) ;
#162962 = CARTESIAN_POINT('Origin',(-4.,-6.45,-2.91)) ;
#162963 = CARTESIAN_POINT('Origin',(-4.,-6.45,-2.91)) ;
#162964 = CARTESIAN_POINT('Origin',(-3.8,-6.45,-2.91)) ;
#162965 = CARTESIAN_POINT('Origin',(-5.,-6.45,-2.81)) ;
#162966 = CARTESIAN_POINT('Origin',(-5.,-6.45,-4.71)) ;
#162967 = CARTESIAN_POINT('Origin',(-4.8,-6.4,-2.91)) ;
#162968 = CARTESIAN_POINT('Origin',(-4.8,-6.35,-2.91)) ;
#162969 = CARTESIAN_POINT('Origin',(1.9515639104739E-16,-6.35,-2.91)) ;
#162970 = CARTESIAN_POINT('Origin',(-4.,-6.35,-2.91)) ;
#162971 = CARTESIAN_POINT('Origin',(-4.8,-6.35,-2.91)) ;
#162972 = CARTESIAN_POINT('Origin',(-4.,-6.4,-2.91)) ;
#162973 = CARTESIAN_POINT('Origin',(-4.,-6.35,-2.91)) ;
#162974 = CARTESIAN_POINT('Origin',(-3.8,-6.45,-2.81)) ;
#162975 = CARTESIAN_POINT('Origin',(-3.8,-6.45,-4.71)) ;
#162976 = CARTESIAN_POINT('Origin',(-4.9,-6.45,-4.91)) ;
#162977 = CARTESIAN_POINT('Origin',(-4.8,-6.45,-4.91)) ;
#162978 = CARTESIAN_POINT('Origin',(-4.,-6.45,-4.91)) ;
#162979 = CARTESIAN_POINT('Origin',(-4.8,-6.45,-4.71)) ;
#162980 = CARTESIAN_POINT('Origin',(-4.8,-6.45,-4.71)) ;
#162981 = CARTESIAN_POINT('Origin',(-4.8,-6.35,-2.91)) ;
#162982 = CARTESIAN_POINT('Origin',(-4.8,-6.35,-2.91)) ;
#162983 = CARTESIAN_POINT('Origin',(-4.,-6.35,-2.91)) ;
#162984 = CARTESIAN_POINT('Origin',(-4.,-6.35,-2.91)) ;
#162985 = CARTESIAN_POINT('Origin',(-4.,-6.45,-4.71)) ;
#162986 = CARTESIAN_POINT('Origin',(-4.,-6.45,-4.71)) ;
#162987 = CARTESIAN_POINT('Origin',(-4.8,-6.4,-4.71)) ;
#162988 = CARTESIAN_POINT('Origin',(-4.8,-6.35,-4.71)) ;
#162989 = CARTESIAN_POINT('Origin',(-4.8,-6.35,-3.81)) ;
#162990 = CARTESIAN_POINT('Origin',(-4.8,-6.35,-4.71)) ;
#162991 = CARTESIAN_POINT('Origin',(-4.,-6.35,-3.81)) ;
#162992 = CARTESIAN_POINT('Origin',(-4.,-6.35,-4.71)) ;
#162993 = CARTESIAN_POINT('Origin',(-4.,-6.4,-4.71)) ;
#162994 = CARTESIAN_POINT('Origin',(-4.,-6.35,-4.71)) ;
#162995 = CARTESIAN_POINT('Origin',(-4.8,-6.35,-4.71)) ;
#162996 = CARTESIAN_POINT('Origin',(-4.8,-6.35,-4.71)) ;
#162997 = CARTESIAN_POINT('Origin',(-4.,-6.35,-4.71)) ;
#162998 = CARTESIAN_POINT('Origin',(-4.,-6.35,-4.71)) ;
#162999 = CARTESIAN_POINT('Origin',(1.95156391047391E-16,-6.35,-4.71)) ;
#163000 = CARTESIAN_POINT('Origin',(-4.15,-6.25,-3.06)) ;
#163001 = CARTESIAN_POINT('Origin',(-4.15,-6.3,-3.06)) ;
#163002 = CARTESIAN_POINT('Origin',(-4.15,-6.3,-3.81)) ;
#163003 = CARTESIAN_POINT('Origin',(-4.15,-6.3,-4.56)) ;
#163004 = CARTESIAN_POINT('Origin',(-4.15,-6.3,-3.06)) ;
#163005 = CARTESIAN_POINT('Origin',(-4.15,-6.25,-4.56)) ;
#163006 = CARTESIAN_POINT('Origin',(-4.15,-6.3,-4.56)) ;
#163007 = CARTESIAN_POINT('Origin',(-4.15,-6.3,-3.06)) ;
#163008 = CARTESIAN_POINT('Origin',(-4.15,-6.3,-3.06)) ;
#163009 = CARTESIAN_POINT('Origin',(-4.15,-6.3,-4.56)) ;
#163010 = CARTESIAN_POINT('Origin',(-4.15,-6.3,-4.56)) ;
#163011 = CARTESIAN_POINT('Origin',(-4.65,-6.25,-3.06)) ;
#163012 = CARTESIAN_POINT('Origin',(-4.65,-6.3,-3.06)) ;
#163013 = CARTESIAN_POINT('Origin',(0.,-6.3,-3.06)) ;
#163014 = CARTESIAN_POINT('Origin',(-4.65,-6.3,-3.06)) ;
#163015 = CARTESIAN_POINT('Origin',(0.,-6.3,-4.56)) ;
#163016 = CARTESIAN_POINT('Origin',(-4.65,-6.3,-4.56)) ;
#163017 = CARTESIAN_POINT('Origin',(-4.65,-6.25,-4.56)) ;
#163018 = CARTESIAN_POINT('Origin',(-4.65,-6.3,-4.56)) ;
#163019 = CARTESIAN_POINT('Origin',(-4.65,-6.3,-3.06)) ;
#163020 = CARTESIAN_POINT('Origin',(-4.65,-6.3,-3.06)) ;
#163021 = CARTESIAN_POINT('Origin',(-4.65,-6.3,-4.56)) ;
#163022 = CARTESIAN_POINT('Origin',(-4.65,-6.3,-4.56)) ;
#163023 = CARTESIAN_POINT('Origin',(-4.65,-6.3,-3.81)) ;
#163024 = CARTESIAN_POINT('Origin',(-3.09057773798104,-4.00084361825625,-4.31055391724001)) ;
#163025 = CARTESIAN_POINT('Origin',(-5.17275707706436,-1.91866427917294,-5.31)) ;
#163026 = CARTESIAN_POINT('Origin',(-5.17275707706436,-1.91866427917294,-5.31)) ;
#163027 = CARTESIAN_POINT('Origin',(-5.17275707706436,-1.91866427917294,-5.31)) ;
#163028 = CARTESIAN_POINT('Origin',(-5.17275707706436,-1.91866427917294,-5.31)) ;
#163029 = CARTESIAN_POINT('Origin',(-3.59571067811865,-3.49571067811865,-5.31)) ;
#163030 = CARTESIAN_POINT('Ctrl Pts',(-5.8,-1.2914213562373,-5.41)) ;
#163031 = CARTESIAN_POINT('Ctrl Pts',(-5.81856398038092,-1.23572941509446,
-5.41)) ;
#163032 = CARTESIAN_POINT('Ctrl Pts',(-5.83691006697105,-1.1806911553242,
-5.39922263893878)) ;
#163033 = CARTESIAN_POINT('Ctrl Pts',(-5.86308993302895,-1.10215155715041,
-5.36219871729853)) ;
#163034 = CARTESIAN_POINT('Ctrl Pts',(-5.8707106769584,-1.0792893230416,-5.33625343280361)) ;
#163035 = CARTESIAN_POINT('Ctrl Pts',(-5.87071067811865,-1.07928932188134,
-5.31)) ;
#163036 = CARTESIAN_POINT('Origin',(-5.17275707706436,-5.05,-5.31)) ;
#163037 = CARTESIAN_POINT('Origin',(-5.17275707706436,-5.26511162862565,-5.31)) ;
#163038 = CARTESIAN_POINT('Origin',(-3.96111272388873,-4.96220054033175,-4.72841071047569)) ;
#163039 = CARTESIAN_POINT('Origin',(-5.17275707706436,-5.26511162862565,-5.31)) ;
#163040 = CARTESIAN_POINT('Ctrl Pts',(-5.9,-1.00857864376269,-5.31)) ;
#163041 = CARTESIAN_POINT('Ctrl Pts',(-5.9,-1.04999999999999,-5.31)) ;
#163042 = CARTESIAN_POINT('Ctrl Pts',(-5.87071067811865,-1.07928932188134,
-5.31)) ;
#163043 = CARTESIAN_POINT('Ctrl Pts',(-5.9,-1.00857864608315,-5.36250686562998)) ;
#163044 = CARTESIAN_POINT('Ctrl Pts',(-5.9,-1.0500000026192,-5.34717194963253)) ;
#163045 = CARTESIAN_POINT('Ctrl Pts',(-5.8707106769584,-1.0792893230416,-5.33625343280361)) ;
#163046 = CARTESIAN_POINT('Ctrl Pts',(-5.9,-1.03906162412146,-5.41439743459706)) ;
#163047 = CARTESIAN_POINT('Ctrl Pts',(-5.9,-1.08015861705713,-5.38457207120098)) ;
#163048 = CARTESIAN_POINT('Ctrl Pts',(-5.86308993302894,-1.10215155715041,
-5.36219871729853)) ;
#163049 = CARTESIAN_POINT('Ctrl Pts',(-5.9,-1.14378108835315,-5.48844527787756)) ;
#163050 = CARTESIAN_POINT('Ctrl Pts',(-5.9,-1.17342005527962,-5.42578812462634)) ;
#163051 = CARTESIAN_POINT('Ctrl Pts',(-5.83691006697105,-1.1806911553242,
-5.39922263893878)) ;
#163052 = CARTESIAN_POINT('Ctrl Pts',(-5.9,-1.21716543471637,-5.50999999941992)) ;
#163053 = CARTESIAN_POINT('Ctrl Pts',(-5.89999999999991,-1.24006789214487,
-5.42711774888614)) ;
#163054 = CARTESIAN_POINT('Ctrl Pts',(-5.81856398038092,-1.23572941509446,
-5.41)) ;
#163055 = CARTESIAN_POINT('Ctrl Pts',(-5.9,-1.2914213562373,-5.51)) ;
#163056 = CARTESIAN_POINT('Ctrl Pts',(-5.9,-1.2914213562373,-5.41)) ;
#163057 = CARTESIAN_POINT('Ctrl Pts',(-5.8,-1.2914213562373,-5.41)) ;
#163058 = CARTESIAN_POINT('Origin',(-5.8,-1.2914213562373,-5.51)) ;
#163059 = CARTESIAN_POINT('Origin',(-5.8,-1.00857864376269,-5.31)) ;
#163060 = CARTESIAN_POINT('Origin',(-5.17275707706436,-5.26511162862565,-5.31)) ;
#163061 = CARTESIAN_POINT('Origin',(-5.17275707706436,-5.26511162862565,-5.31)) ;
#163062 = CARTESIAN_POINT('Origin',(-3.78014014831103,-3.31128120792626,-2.9784561258016)) ;
#163063 = CARTESIAN_POINT('Origin',(-5.17275707706436,-1.91866427917294,-2.31)) ;
#163064 = CARTESIAN_POINT('Origin',(-3.97071067811865,-3.12071067811865,-2.31)) ;
#163065 = CARTESIAN_POINT('Ctrl Pts',(-5.87071067811865,-1.07928932188134,
-2.31)) ;
#163066 = CARTESIAN_POINT('Ctrl Pts',(-5.87071067695842,-1.07928932304157,
-2.28374656719639)) ;
#163067 = CARTESIAN_POINT('Ctrl Pts',(-5.86308993302895,-1.10215155715042,
-2.25780128270147)) ;
#163068 = CARTESIAN_POINT('Ctrl Pts',(-5.83691006697105,-1.18069115532419,
-2.22077736106122)) ;
#163069 = CARTESIAN_POINT('Ctrl Pts',(-5.81856398038092,-1.23572941509447,
-2.21)) ;
#163070 = CARTESIAN_POINT('Ctrl Pts',(-5.8,-1.29142135623731,-2.21)) ;
#163071 = CARTESIAN_POINT('Origin',(-5.17275707706436,-1.91866427917294,-2.31)) ;
#163072 = CARTESIAN_POINT('Origin',(-5.8,-1.00857864376269,-36.59)) ;
#163073 = CARTESIAN_POINT('Origin',(-5.8,-1.00857864376269,-2.31)) ;
#163074 = CARTESIAN_POINT('Origin',(-5.8,-6.55,-5.51)) ;
#163075 = CARTESIAN_POINT('Origin',(-5.8,-5.42192235935956,-5.51)) ;
#163076 = CARTESIAN_POINT('Origin',(-5.10072415073893,-5.24710339704429,-5.31)) ;
#163077 = CARTESIAN_POINT('Origin',(-5.80000000000002,-5.42192235935964,-5.31000000000008)) ;
#163078 = CARTESIAN_POINT('Origin',(-5.17275707706436,-1.91866427917293,-2.31)) ;
#163079 = CARTESIAN_POINT('Origin',(-5.17275707706436,-1.91866427917294,-2.31)) ;
#163080 = CARTESIAN_POINT('Ctrl Pts',(-5.9,-1.29142135623731,-2.11)) ;
#163081 = CARTESIAN_POINT('Ctrl Pts',(-5.9,-1.29142135623731,-2.21)) ;
#163082 = CARTESIAN_POINT('Ctrl Pts',(-5.8,-1.29142135623731,-2.21)) ;
#163083 = CARTESIAN_POINT('Ctrl Pts',(-5.9,-1.21716543471638,-2.11000000058011)) ;
#163084 = CARTESIAN_POINT('Ctrl Pts',(-5.9,-1.24006789214487,-2.19288225111391)) ;
#163085 = CARTESIAN_POINT('Ctrl Pts',(-5.81856398038092,-1.23572941509447,
-2.21)) ;
#163086 = CARTESIAN_POINT('Ctrl Pts',(-5.9,-1.14378108835315,-2.13155472212247)) ;
#163087 = CARTESIAN_POINT('Ctrl Pts',(-5.9,-1.1734200552796,-2.19421187537365)) ;
#163088 = CARTESIAN_POINT('Ctrl Pts',(-5.83691006697105,-1.18069115532419,
-2.22077736106122)) ;
#163089 = CARTESIAN_POINT('Ctrl Pts',(-5.9,-1.03906162412146,-2.20560256540291)) ;
#163090 = CARTESIAN_POINT('Ctrl Pts',(-5.9,-1.08015861705715,-2.23542792879904)) ;
#163091 = CARTESIAN_POINT('Ctrl Pts',(-5.86308993302895,-1.10215155715042,
-2.25780128270147)) ;
#163092 = CARTESIAN_POINT('Ctrl Pts',(-5.9,-1.00857864608315,-2.25749313437004)) ;
#163093 = CARTESIAN_POINT('Ctrl Pts',(-5.9,-1.05000000261917,-2.27282805036745)) ;
#163094 = CARTESIAN_POINT('Ctrl Pts',(-5.87071067695842,-1.07928932304157,
-2.28374656719639)) ;
#163095 = CARTESIAN_POINT('Ctrl Pts',(-5.9,-1.00857864376269,-2.31)) ;
#163096 = CARTESIAN_POINT('Ctrl Pts',(-5.9,-1.05,-2.31)) ;
#163097 = CARTESIAN_POINT('Ctrl Pts',(-5.87071067811865,-1.07928932188134,
-2.31)) ;
#163098 = CARTESIAN_POINT('Origin',(-5.8,-1.29142135623731,-2.11)) ;
#163099 = CARTESIAN_POINT('Ctrl Pts',(-5.9,-5.42181243301045,-5.50999997036252)) ;
#163100 = CARTESIAN_POINT('Ctrl Pts',(-5.9,-5.42186418462486,-5.4099118155266)) ;
#163101 = CARTESIAN_POINT('Ctrl Pts',(-5.79991187715164,-5.42186416305549,
-5.41000002317701)) ;
#163102 = CARTESIAN_POINT('Ctrl Pts',(-5.9,-5.47597273077136,-5.51002917711606)) ;
#163103 = CARTESIAN_POINT('Ctrl Pts',(-5.89999999999995,-5.44963575044053,
-5.41611310490821)) ;
#163104 = CARTESIAN_POINT('Ctrl Pts',(-5.80628621775607,-5.45053795385125,
-5.41000983135988)) ;
#163105 = CARTESIAN_POINT('Ctrl Pts',(-5.9,-5.5295069829522,-5.48847029676528)) ;
#163106 = CARTESIAN_POINT('Ctrl Pts',(-5.90000000000004,-5.48352164712825,
-5.41029821762256)) ;
#163107 = CARTESIAN_POINT('Ctrl Pts',(-5.81258729511711,-5.47887520585225,
-5.39922629545968)) ;
#163108 = CARTESIAN_POINT('Ctrl Pts',(-5.9,-5.60588533050919,-5.41437241570934)) ;
#163109 = CARTESIAN_POINT('Ctrl Pts',(-5.89999999999995,-5.53371219741587,
-5.37246819784151)) ;
#163110 = CARTESIAN_POINT('Ctrl Pts',(-5.82157770712951,-5.51930255765374,
-5.36217766736416)) ;
#163111 = CARTESIAN_POINT('Ctrl Pts',(-5.9,-5.62810771557601,-5.36243656245292)) ;
#163112 = CARTESIAN_POINT('Ctrl Pts',(-5.9,-5.54996909580657,-5.34142484145069)) ;
#163113 = CARTESIAN_POINT('Ctrl Pts',(-5.8241936039171,-5.53106345572106,
-5.33621391054005)) ;
#163114 = CARTESIAN_POINT('Ctrl Pts',(-5.9,-5.62807761009112,-5.30989335577685)) ;
#163115 = CARTESIAN_POINT('Ctrl Pts',(-5.9,-5.54994729905278,-5.30993608021398)) ;
#163116 = CARTESIAN_POINT('Ctrl Pts',(-5.82419006898362,-5.53104752404526,
-5.30994668678336)) ;
#163117 = CARTESIAN_POINT('Origin',(-5.8,-5.62807764064044,-5.31)) ;
#163118 = CARTESIAN_POINT('Origin',(-5.15068655017073,-5.25959399690224,-2.32059385290894)) ;
#163119 = CARTESIAN_POINT('Origin',(-5.17275707706436,-5.26511162862565,-2.31)) ;
#163120 = CARTESIAN_POINT('Origin',(-5.17275707706436,-5.05,-2.31)) ;
#163121 = CARTESIAN_POINT('Origin',(-5.17275707706436,-5.26511162862565,-2.31)) ;
#163122 = CARTESIAN_POINT('Origin',(-5.8,-5.05,-2.11)) ;
#163123 = CARTESIAN_POINT('Origin',(-5.8,-5.42192235935956,-2.11)) ;
#163124 = CARTESIAN_POINT('Origin',(-5.8,-5.62807764064044,-36.59)) ;
#163125 = CARTESIAN_POINT('Origin',(-5.8,-5.62807764064044,-2.31)) ;
#163126 = CARTESIAN_POINT('Origin',(-5.17275707706436,-5.26511162862565,-2.31)) ;
#163127 = CARTESIAN_POINT('Origin',(-5.17275707706436,-5.26511162862565,-2.31)) ;
#163128 = CARTESIAN_POINT('Ctrl Pts',(-5.9,-5.62807761009112,-2.31010664422313)) ;
#163129 = CARTESIAN_POINT('Ctrl Pts',(-5.9,-5.54994729905279,-2.31006391978601)) ;
#163130 = CARTESIAN_POINT('Ctrl Pts',(-5.82419006898363,-5.53104752404526,
-2.31005331321663)) ;
#163131 = CARTESIAN_POINT('Ctrl Pts',(-5.9,-5.628107715576,-2.25756343754707)) ;
#163132 = CARTESIAN_POINT('Ctrl Pts',(-5.9,-5.54996909580664,-2.27857515854929)) ;
#163133 = CARTESIAN_POINT('Ctrl Pts',(-5.82419360391713,-5.53106345572106,
-2.28378608945993)) ;
#163134 = CARTESIAN_POINT('Ctrl Pts',(-5.9,-5.6058853305092,-2.20562758429065)) ;
#163135 = CARTESIAN_POINT('Ctrl Pts',(-5.89999999999998,-5.53371219741588,
-2.24753180215848)) ;
#163136 = CARTESIAN_POINT('Ctrl Pts',(-5.82157770712952,-5.51930255765375,
-2.25782233263586)) ;
#163137 = CARTESIAN_POINT('Ctrl Pts',(-5.9,-5.52950698295218,-2.13152970323473)) ;
#163138 = CARTESIAN_POINT('Ctrl Pts',(-5.90000000000002,-5.48352164712826,
-2.20970178237743)) ;
#163139 = CARTESIAN_POINT('Ctrl Pts',(-5.81258729511713,-5.47887520585223,
-2.22077370454031)) ;
#163140 = CARTESIAN_POINT('Ctrl Pts',(-5.9,-5.47597273077139,-2.109970822884)) ;
#163141 = CARTESIAN_POINT('Ctrl Pts',(-5.9,-5.44963575044054,-2.20388689509175)) ;
#163142 = CARTESIAN_POINT('Ctrl Pts',(-5.80628621775611,-5.45053795385126,
-2.20999016864012)) ;
#163143 = CARTESIAN_POINT('Ctrl Pts',(-5.9,-5.42181243301047,-2.11000002963748)) ;
#163144 = CARTESIAN_POINT('Ctrl Pts',(-5.9,-5.42186418462488,-2.21008818447338)) ;
#163145 = CARTESIAN_POINT('Ctrl Pts',(-5.79991187715166,-5.42186416305551,
-2.20999997682299)) ;
#163146 = CARTESIAN_POINT('Origin',(-5.79999999999999,-5.42192235935953,-2.31000000000002)) ;
#163147 = CARTESIAN_POINT('Origin',(-5.8066065036801,-5.42357398527959,-2.31)) ;
#163148 = CARTESIAN_POINT('Origin',(-5.8,-5.05,-5.92)) ;
#163149 = CARTESIAN_POINT('',(-5.87071067811865,-1.15,-5.99071067811865)) ;
#163150 = CARTESIAN_POINT('Origin',(-5.81947611583159,-1.02473736077622,-5.92807935738799)) ;
#163151 = CARTESIAN_POINT('Origin',(-5.80807935817055,-1.27526264085863,-5.93947611975157)) ;
#163152 = CARTESIAN_POINT('',(-5.82425356250363,-5.43404914061138,-6.01701425001453)) ;
#163153 = CARTESIAN_POINT('Origin',(-5.79999999999984,-5.42192235935956,-5.91999999998403)) ;
#163154 = CARTESIAN_POINT('',(-5.87882054380159,-5.50499519875994,-5.98154122094028)) ;
#163155 = CARTESIAN_POINT('Origin',(-5.79625409004975,-5.63940739348982,-5.91433454802145)) ;
#163156 = CARTESIAN_POINT('Origin',(-5.80048106423751,-5.62703482768928,-5.92027064077534)) ;
#163157 = CARTESIAN_POINT('Origin',(-5.8,-5.62807764064044,-36.59)) ;
#163158 = CARTESIAN_POINT('',(-5.87882054380158,-5.56653641970014,-6.04308244188047)) ;
#163159 = CARTESIAN_POINT('Origin',(-5.80050013342543,-5.62780271840948,-5.92105207279234)) ;
#163160 = CARTESIAN_POINT('Origin',(-5.7962598489436,-5.63373078324888,-5.90869550130923)) ;
#163161 = CARTESIAN_POINT('',(-5.87882054380156,-5.56653641970012,-9.19691755811957)) ;
#163162 = CARTESIAN_POINT('Origin',(-5.79625409005666,-5.6337430926113,-9.33132975283448)) ;
#163163 = CARTESIAN_POINT('Origin',(-5.80048106423679,-5.6278069998655,-9.31895718704807)) ;
#163164 = CARTESIAN_POINT('Origin',(-5.8,-1.00857864376269,-36.59)) ;
#163165 = CARTESIAN_POINT('Origin',(-5.81947611583159,-1.01665800115047,-5.93615871701256)) ;
#163166 = CARTESIAN_POINT('Origin',(-5.81947611583101,-1.0166580011502,-9.30384128298823)) ;
#163167 = CARTESIAN_POINT('Origin',(-5.8,-6.55,-9.32)) ;
#163168 = CARTESIAN_POINT('',(-5.87882054380161,-5.50499519875992,-9.25845877905974)) ;
#163169 = CARTESIAN_POINT('Origin',(-5.80050013341907,-5.62702556785333,-9.31972507777035)) ;
#163170 = CARTESIAN_POINT('',(-5.82425356250363,-5.43404914061138,-9.22298574998547)) ;
#163171 = CARTESIAN_POINT('Origin',(-5.79625984894763,-5.63938213931645,-9.3256531426013)) ;
#163172 = CARTESIAN_POINT('Origin',(-5.79999999997662,-5.42192235934795,-9.32000000018081)) ;
#163173 = CARTESIAN_POINT('',(-5.87071067811866,-1.14999999999999,-9.24928932188135)) ;
#163174 = CARTESIAN_POINT('Origin',(-5.80807935817046,-1.27526264085876,-9.30052388024865)) ;
#163175 = CARTESIAN_POINT('Origin',(-5.81947611583072,-1.02473736077575,-9.3119206426126)) ;
#163176 = CARTESIAN_POINT('Origin',(-5.8,-5.05,-9.73)) ;
#163177 = CARTESIAN_POINT('',(-5.87071067811865,-1.14999999999999,-9.80071067811865)) ;
#163178 = CARTESIAN_POINT('Origin',(-5.81947611583089,-1.02473736077631,-9.73807935738754)) ;
#163179 = CARTESIAN_POINT('Origin',(-5.80807935817105,-1.27526264085796,-9.74947611975234)) ;
#163180 = CARTESIAN_POINT('',(-5.82425356250363,-5.43404914061138,-9.82701425001453)) ;
#163181 = CARTESIAN_POINT('Origin',(-5.80000000000621,-5.42192235936274,-9.73000000003557)) ;
#163182 = CARTESIAN_POINT('',(-5.87882054380157,-5.50499519875999,-9.79154122094031)) ;
#163183 = CARTESIAN_POINT('Origin',(-5.79625409004102,-5.6394073935196,-9.72433454800673)) ;
#163184 = CARTESIAN_POINT('Origin',(-5.80048106424258,-5.62703482768541,-9.73027064077687)) ;
#163185 = CARTESIAN_POINT('Origin',(-5.8,-5.62807764064044,-36.59)) ;
#163186 = CARTESIAN_POINT('',(-5.87882054380156,-5.56653641970012,-9.85308244188044)) ;
#163187 = CARTESIAN_POINT('Origin',(-5.80050013342664,-5.62780271840903,-9.73105207279395)) ;
#163188 = CARTESIAN_POINT('Origin',(-5.79625984896595,-5.63373078321645,-9.71869550137418)) ;
#163189 = CARTESIAN_POINT('',(-5.87882054380156,-5.56653641970012,-13.0069175581196)) ;
#163190 = CARTESIAN_POINT('Origin',(-5.79625409005982,-5.63374309260352,-13.1413297528191)) ;
#163191 = CARTESIAN_POINT('Origin',(-5.80048106424012,-5.62780699986454,-13.1289571870464)) ;
#163192 = CARTESIAN_POINT('Origin',(-5.8,-1.00857864376269,-36.59)) ;
#163193 = CARTESIAN_POINT('Origin',(-5.81947611583026,-1.01665800114985,-9.7461587170121)) ;
#163194 = CARTESIAN_POINT('Origin',(-5.81947611583107,-1.01665800115014,-13.1138412829883)) ;
#163195 = CARTESIAN_POINT('Origin',(-5.8,-6.55,-13.13)) ;
#163196 = CARTESIAN_POINT('',(-5.87882054380161,-5.50499519875992,-13.0684587790597)) ;
#163197 = CARTESIAN_POINT('Origin',(-5.80050013342204,-5.62702556785267,-13.1297250777694)) ;
#163198 = CARTESIAN_POINT('',(-5.82425356250363,-5.43404914061138,-13.0329857499855)) ;
#163199 = CARTESIAN_POINT('Origin',(-5.79625984894408,-5.6393821393244,-13.135653142605)) ;
#163200 = CARTESIAN_POINT('Origin',(-5.79999999997599,-5.42192235934763,-13.1300000002057)) ;
#163201 = CARTESIAN_POINT('',(-5.87071067811866,-1.14999999999999,-13.0592893218813)) ;
#163202 = CARTESIAN_POINT('Origin',(-5.80807935817108,-1.27526264085755,-13.1105238802474)) ;
#163203 = CARTESIAN_POINT('Origin',(-5.81947611582975,-1.02473736077495,-13.121920642613)) ;
#163204 = CARTESIAN_POINT('Origin',(-5.8,-5.05,-13.54)) ;
#163205 = CARTESIAN_POINT('',(-5.87071067811865,-1.14999999999999,-13.6107106781187)) ;
#163206 = CARTESIAN_POINT('Origin',(-5.8194761158307,-1.02473736077617,-13.5480793573875)) ;
#163207 = CARTESIAN_POINT('Origin',(-5.80807935817103,-1.27526264085801,-13.5594761197523)) ;
#163208 = CARTESIAN_POINT('',(-5.82425356250363,-5.43404914061138,-13.6370142500145)) ;
#163209 = CARTESIAN_POINT('Origin',(-5.79999999999483,-5.42192235935705,-13.5399999999823)) ;
#163210 = CARTESIAN_POINT('',(-5.87882054380157,-5.50499519875999,-13.6015412209403)) ;
#163211 = CARTESIAN_POINT('Origin',(-5.79625409003451,-5.63940739354352,-13.5343345479947)) ;
#163212 = CARTESIAN_POINT('Origin',(-5.80048106423289,-5.62703482768967,-13.5402706407743)) ;
#163213 = CARTESIAN_POINT('Origin',(-5.8,-5.62807764064044,-36.59)) ;
#163214 = CARTESIAN_POINT('',(-5.87882054380156,-5.56653641970012,-13.6630824418804)) ;
#163215 = CARTESIAN_POINT('Origin',(-5.80050013342366,-5.62780271841002,-13.5410520727912)) ;
#163216 = CARTESIAN_POINT('Origin',(-5.79625984897398,-5.63373078320201,-13.5286955014033)) ;
#163217 = CARTESIAN_POINT('',(-5.8788205438016,-5.56653641970017,-16.8169175581195)) ;
#163218 = CARTESIAN_POINT('Origin',(-5.79625409000273,-5.63374309268844,-16.9513297529886)) ;
#163219 = CARTESIAN_POINT('Origin',(-5.80048106422758,-5.62780699986791,-16.9389571870545)) ;
#163220 = CARTESIAN_POINT('Origin',(-5.8,-1.00857864376269,-36.59)) ;
#163221 = CARTESIAN_POINT('Origin',(-5.81947611583107,-1.01665800115022,-13.5561587170129)) ;
#163222 = CARTESIAN_POINT('Origin',(-5.81947611583164,-1.01665800115088,-16.9238412829861)) ;
#163223 = CARTESIAN_POINT('Origin',(-5.8,-6.55,-16.94)) ;
#163224 = CARTESIAN_POINT('',(-5.87882054380158,-5.50499519875998,-16.8784587790597)) ;
#163225 = CARTESIAN_POINT('Origin',(-5.800500133426,-5.62702556784527,-16.9397250777684)) ;
#163226 = CARTESIAN_POINT('',(-5.82425356250363,-5.43404914061138,-16.8429857499855)) ;
#163227 = CARTESIAN_POINT('Origin',(-5.79625984893017,-5.63938213937326,-16.9456531426293)) ;
#163228 = CARTESIAN_POINT('Origin',(-5.79999999994122,-5.42192235933025,-16.9400000004754)) ;
#163229 = CARTESIAN_POINT('',(-5.87071067811866,-1.14999999999999,-16.8692893218814)) ;
#163230 = CARTESIAN_POINT('Origin',(-5.80807935817212,-1.27526264085654,-16.9205238802451)) ;
#163231 = CARTESIAN_POINT('Origin',(-5.81947611583181,-1.02473736077525,-16.9319206426127)) ;
#163232 = CARTESIAN_POINT('Origin',(-5.8,-5.05,-17.35)) ;
#163233 = CARTESIAN_POINT('',(-5.87071067811865,-1.14999999999999,-17.4207106781187)) ;
#163234 = CARTESIAN_POINT('Origin',(-5.81947611583148,-1.02473736077474,-17.3580793573875)) ;
#163235 = CARTESIAN_POINT('Origin',(-5.8080793581705,-1.27526264085864,-17.3694761197517)) ;
#163236 = CARTESIAN_POINT('',(-5.82425356250363,-5.43404914061138,-17.4470142500145)) ;
#163237 = CARTESIAN_POINT('Origin',(-5.79999999996682,-5.42192235934304,-17.3499999997148)) ;
#163238 = CARTESIAN_POINT('',(-5.87882054380156,-5.50499519876001,-17.4115412209403)) ;
#163239 = CARTESIAN_POINT('Origin',(-5.79625409003878,-5.63940739353005,-17.3443345480014)) ;
#163240 = CARTESIAN_POINT('Origin',(-5.80048106423185,-5.62703482769178,-17.350270640774)) ;
#163241 = CARTESIAN_POINT('Origin',(-5.8,-5.62807764064044,-36.59)) ;
#163242 = CARTESIAN_POINT('',(-5.8788205438016,-5.56653641970017,-17.4730824418805)) ;
#163243 = CARTESIAN_POINT('Origin',(-5.80050013342676,-5.6278027184087,-17.3510520727938)) ;
#163244 = CARTESIAN_POINT('Origin',(-5.79625984893998,-5.63373078325259,-17.338695501302)) ;
#163245 = CARTESIAN_POINT('',(-5.8788205438016,-5.56653641970017,-20.6269175581195)) ;
#163246 = CARTESIAN_POINT('Origin',(-5.7962540900391,-5.63374309263502,-20.7613297528817)) ;
#163247 = CARTESIAN_POINT('Origin',(-5.80048106423735,-5.62780699986498,-20.7489571870481)) ;
#163248 = CARTESIAN_POINT('Origin',(-5.8,-1.00857864376269,-36.59)) ;
#163249 = CARTESIAN_POINT('Origin',(-5.81947611583098,-1.0166580011507,-17.3661587170137)) ;
#163250 = CARTESIAN_POINT('Origin',(-5.8194761158317,-1.01665800115097,-20.7338412829858)) ;
#163251 = CARTESIAN_POINT('Origin',(-5.8,-6.55,-20.75)) ;
#163252 = CARTESIAN_POINT('',(-5.87882054380158,-5.50499519875998,-20.6884587790597)) ;
#163253 = CARTESIAN_POINT('Origin',(-5.80050013342497,-5.62702556784867,-20.7497250777695)) ;
#163254 = CARTESIAN_POINT('',(-5.82425356250363,-5.43404914061138,-20.6529857499855)) ;
#163255 = CARTESIAN_POINT('Origin',(-5.7962598489347,-5.63938213935898,-20.7556531426222)) ;
#163256 = CARTESIAN_POINT('Origin',(-5.79999999987016,-5.42192235929471,-20.750000001076)) ;
#163257 = CARTESIAN_POINT('',(-5.87071067811866,-1.14999999999999,-20.6792893218814)) ;
#163258 = CARTESIAN_POINT('Origin',(-5.80807935817138,-1.27526264085804,-20.7305238802469)) ;
#163259 = CARTESIAN_POINT('Origin',(-5.81947611583102,-1.02473736077477,-20.741920642613)) ;
#163260 = CARTESIAN_POINT('Origin',(-5.8,-5.05,-21.16)) ;
#163261 = CARTESIAN_POINT('',(-5.87071067811865,-1.14999999999999,-21.2307106781187)) ;
#163262 = CARTESIAN_POINT('Origin',(-5.81947611583222,-1.02473736077531,-21.1680793573878)) ;
#163263 = CARTESIAN_POINT('Origin',(-5.80807935817091,-1.27526264085785,-21.1794761197522)) ;
#163264 = CARTESIAN_POINT('',(-5.82425356250363,-5.43404914061138,-21.2570142500145)) ;
#163265 = CARTESIAN_POINT('Origin',(-5.7999999999067,-5.42192235931299,-21.1599999992661)) ;
#163266 = CARTESIAN_POINT('',(-5.87882054380156,-5.50499519876001,-21.2215412209403)) ;
#163267 = CARTESIAN_POINT('Origin',(-5.7962540900276,-5.63940739356463,-21.1543345479843)) ;
#163268 = CARTESIAN_POINT('Origin',(-5.80048106422407,-5.62703482769801,-21.1602706407706)) ;
#163269 = CARTESIAN_POINT('Origin',(-5.8,-5.62807764064044,-36.59)) ;
#163270 = CARTESIAN_POINT('',(-5.8788205438016,-5.56653641970017,-21.2830824418805)) ;
#163271 = CARTESIAN_POINT('Origin',(-5.80050013342682,-5.62780271840868,-21.1610520727937)) ;
#163272 = CARTESIAN_POINT('Origin',(-5.79625984898204,-5.63373078318931,-21.1486955014297)) ;
#163273 = CARTESIAN_POINT('',(-5.8788205438016,-5.56653641970017,-24.4369175581195)) ;
#163274 = CARTESIAN_POINT('Origin',(-5.79625409005601,-5.63374309260924,-24.5713297528292)) ;
#163275 = CARTESIAN_POINT('Origin',(-5.80048106422965,-5.62780699986711,-24.5589571870534)) ;
#163276 = CARTESIAN_POINT('Origin',(-5.8,-1.00857864376269,-36.59)) ;
#163277 = CARTESIAN_POINT('Origin',(-5.81947611583065,-1.01665800115061,-21.1761587170135)) ;
#163278 = CARTESIAN_POINT('Origin',(-5.81947611583029,-1.01665800115036,-24.5438412829871)) ;
#163279 = CARTESIAN_POINT('Origin',(-5.8,-6.55,-24.56)) ;
#163280 = CARTESIAN_POINT('',(-5.87882054380158,-5.50499519875998,-24.4984587790597)) ;
#163281 = CARTESIAN_POINT('Origin',(-5.80050013343402,-5.62702556784164,-24.5597250777665)) ;
#163282 = CARTESIAN_POINT('',(-5.82425356250363,-5.43404914061138,-24.4629857499855)) ;
#163283 = CARTESIAN_POINT('Origin',(-5.79625984894703,-5.63938213932085,-24.5656531426033)) ;
#163284 = CARTESIAN_POINT('Origin',(-5.79999999991183,-5.42192235931555,-24.5600000007655)) ;
#163285 = CARTESIAN_POINT('',(-5.87071067811866,-1.14999999999999,-24.4892893218814)) ;
#163286 = CARTESIAN_POINT('Origin',(-5.80807935817052,-1.27526264085979,-24.5405238802492)) ;
#163287 = CARTESIAN_POINT('Origin',(-5.81947611583105,-1.02473736077468,-24.551920642613)) ;
#163288 = CARTESIAN_POINT('Origin',(-5.8,-5.05,-24.97)) ;
#163289 = CARTESIAN_POINT('',(-5.87071067811865,-1.14999999999999,-25.0407106781187)) ;
#163290 = CARTESIAN_POINT('Origin',(-5.8194761158313,-1.02473736077457,-24.9780793573874)) ;
#163291 = CARTESIAN_POINT('Origin',(-5.8080793581727,-1.27526264085426,-24.9894761197567)) ;
#163292 = CARTESIAN_POINT('',(-5.82425356250363,-5.43404914061138,-25.0670142500145)) ;
#163293 = CARTESIAN_POINT('Origin',(-5.80000000000354,-5.4219223593614,-24.9699999999744)) ;
#163294 = CARTESIAN_POINT('',(-5.87882054380156,-5.50499519876001,-25.0315412209403)) ;
#163295 = CARTESIAN_POINT('Origin',(-5.79625409003997,-5.63940739352596,-24.9643345480035)) ;
#163296 = CARTESIAN_POINT('Origin',(-5.80048106421586,-5.62703482770278,-24.9702706407684)) ;
#163297 = CARTESIAN_POINT('Origin',(-5.8,-5.62807764064044,-36.59)) ;
#163298 = CARTESIAN_POINT('',(-5.8788205438016,-5.56653641970017,-25.0930824418805)) ;
#163299 = CARTESIAN_POINT('Origin',(-5.80050013342709,-5.62780271840868,-24.971052072793)) ;
#163300 = CARTESIAN_POINT('Origin',(-5.79625984896229,-5.63373078321765,-24.9586955013721)) ;
#163301 = CARTESIAN_POINT('',(-5.8788205438016,-5.56653641970017,-28.2469175581195)) ;
#163302 = CARTESIAN_POINT('Origin',(-5.79625409004022,-5.63374309263231,-28.3813297528758)) ;
#163303 = CARTESIAN_POINT('Origin',(-5.80048106423845,-5.62780699986491,-28.3689571870478)) ;
#163304 = CARTESIAN_POINT('Origin',(-5.8,-1.00857864376269,-36.59)) ;
#163305 = CARTESIAN_POINT('Origin',(-5.81947611583176,-1.01665800115109,-24.9861587170145)) ;
#163306 = CARTESIAN_POINT('Origin',(-5.81947611583163,-1.01665800115093,-28.3538412829859)) ;
#163307 = CARTESIAN_POINT('Origin',(-5.8,-6.55,-28.37)) ;
#163308 = CARTESIAN_POINT('',(-5.87882054380158,-5.50499519875998,-28.3084587790597)) ;
#163309 = CARTESIAN_POINT('Origin',(-5.80050013342543,-5.62702556784578,-28.3697250777687)) ;
#163310 = CARTESIAN_POINT('',(-5.82425356250363,-5.43404914061138,-28.2729857499855)) ;
#163311 = CARTESIAN_POINT('Origin',(-5.79625984893296,-5.63938213936453,-28.375653142625)) ;
#163312 = CARTESIAN_POINT('Origin',(-5.79999999972037,-5.42192235921982,-28.3700000022139)) ;
#163313 = CARTESIAN_POINT('',(-5.87071067811866,-1.14999999999999,-28.2992893218814)) ;
#163314 = CARTESIAN_POINT('Origin',(-5.80807935817205,-1.2752626408567,-28.3505238802449)) ;
#163315 = CARTESIAN_POINT('Origin',(-5.81947611583196,-1.02473736077544,-28.3619206426126)) ;
#163316 = CARTESIAN_POINT('Origin',(-5.8,-5.05,-28.78)) ;
#163317 = CARTESIAN_POINT('',(-5.87071067811865,-1.14999999999999,-28.8507106781187)) ;
#163318 = CARTESIAN_POINT('Origin',(-5.81947611583263,-1.02473736077566,-28.788079357388)) ;
#163319 = CARTESIAN_POINT('Origin',(-5.80807935817064,-1.27526264085834,-28.799476119752)) ;
#163320 = CARTESIAN_POINT('',(-5.82425356250363,-5.43404914061138,-28.8770142500145)) ;
#163321 = CARTESIAN_POINT('Origin',(-5.80000000005041,-5.42192235938484,-28.7800000004842)) ;
#163322 = CARTESIAN_POINT('',(-5.87882054380157,-5.50499519876,-28.8415412209403)) ;
#163323 = CARTESIAN_POINT('Origin',(-5.79625409004087,-5.63940739352319,-28.7743345480048)) ;
#163324 = CARTESIAN_POINT('Origin',(-5.80048106422166,-5.62703482769908,-28.7802706407702)) ;
#163325 = CARTESIAN_POINT('Origin',(-5.8,-5.62807764064044,-36.59)) ;
#163326 = CARTESIAN_POINT('',(-5.8788205438016,-5.56653641970017,-28.9030824418805)) ;
#163327 = CARTESIAN_POINT('Origin',(-5.80050013342867,-5.62780271840836,-28.7810520727939)) ;
#163328 = CARTESIAN_POINT('Origin',(-5.79625984893701,-5.63373078325649,-28.7686955012943)) ;
#163329 = CARTESIAN_POINT('',(-5.87882054380161,-5.56653641970018,-32.0569175581195)) ;
#163330 = CARTESIAN_POINT('Origin',(-5.79625409009991,-5.63374309254529,-32.1913297527016)) ;
#163331 = CARTESIAN_POINT('Origin',(-5.80048106422874,-5.62780699986764,-32.1789571870542)) ;
#163332 = CARTESIAN_POINT('Origin',(-5.8,-1.00857864376269,-36.59)) ;
#163333 = CARTESIAN_POINT('Origin',(-5.8194761158303,-1.01665800115047,-28.7961587170133)) ;
#163334 = CARTESIAN_POINT('Origin',(-5.81947611583233,-1.01665800115071,-32.1638412829882)) ;
#163335 = CARTESIAN_POINT('Origin',(-5.8,-6.55,-32.18)) ;
#163336 = CARTESIAN_POINT('',(-5.87882054380161,-5.50499519875991,-32.1184587790597)) ;
#163337 = CARTESIAN_POINT('Origin',(-5.80050013341193,-5.627025567861,-32.1797250777728)) ;
#163338 = CARTESIAN_POINT('',(-5.82425356250363,-5.43404914061138,-32.0829857499855)) ;
#163339 = CARTESIAN_POINT('Origin',(-5.79625984894212,-5.63938213933443,-32.1856531426101)) ;
#163340 = CARTESIAN_POINT('Origin',(-5.79999999989758,-5.42192235930843,-32.1800000008904)) ;
#163341 = CARTESIAN_POINT('',(-5.87071067811866,-1.14999999999999,-32.1092893218813)) ;
#163342 = CARTESIAN_POINT('Origin',(-5.80807935817142,-1.27526264085807,-32.1605238802468)) ;
#163343 = CARTESIAN_POINT('Origin',(-5.81947611582863,-1.02473736077885,-32.1719206426146)) ;
#163344 = CARTESIAN_POINT('Origin',(-5.8,-5.05,-32.59)) ;
#163345 = CARTESIAN_POINT('',(-5.87071067811865,-1.14999999999999,-32.6607106781187)) ;
#163346 = CARTESIAN_POINT('Origin',(-5.81947611582916,-1.02473736077846,-32.5980793573863)) ;
#163347 = CARTESIAN_POINT('Origin',(-5.80807935817332,-1.27526264085422,-32.6094761197577)) ;
#163348 = CARTESIAN_POINT('',(-5.82425356250363,-5.43404914061138,-32.6870142500145)) ;
#163349 = CARTESIAN_POINT('Origin',(-5.80000000004998,-5.42192235938451,-32.5900000003247)) ;
#163350 = CARTESIAN_POINT('',(-5.87882054380129,-5.50499519876057,-32.6515412209407)) ;
#163351 = CARTESIAN_POINT('Origin',(-5.79625409004923,-5.63940739351318,-32.5843345480113)) ;
#163352 = CARTESIAN_POINT('Origin',(-5.80048106428436,-5.62703482765259,-32.5902706407885)) ;
#163353 = CARTESIAN_POINT('Origin',(-5.8,-5.62807764064044,-36.59)) ;
#163354 = CARTESIAN_POINT('',(-5.87882054380161,-5.56653641970018,-32.7130824418805)) ;
#163355 = CARTESIAN_POINT('Origin',(-5.80050013340937,-5.62780271841368,-32.5910520727818)) ;
#163356 = CARTESIAN_POINT('Origin',(-5.7962598489414,-5.6337307832541,-32.5786955012984)) ;
#163357 = CARTESIAN_POINT('',(-5.87882054380161,-5.56653641970018,-35.8669175581195)) ;
#163358 = CARTESIAN_POINT('Origin',(-5.79625409008121,-5.63374309257359,-36.0013297527579)) ;
#163359 = CARTESIAN_POINT('Origin',(-5.80048106425034,-5.62780699986083,-35.9889571870404)) ;
#163360 = CARTESIAN_POINT('Origin',(-5.8,-1.00857864376269,-36.59)) ;
#163361 = CARTESIAN_POINT('Origin',(-5.81947611583112,-1.01665800115005,-32.60615871701)) ;
#163362 = CARTESIAN_POINT('Origin',(-5.81947611583247,-1.01665800115081,-35.973841282988)) ;
#163363 = CARTESIAN_POINT('Origin',(-5.8,-6.55,-35.99)) ;
#163364 = CARTESIAN_POINT('',(-5.87882054380161,-5.50499519875991,-35.9284587790597)) ;
#163365 = CARTESIAN_POINT('Origin',(-5.80050013341824,-5.62702556785893,-35.9897250777713)) ;
#163366 = CARTESIAN_POINT('',(-5.82425356250363,-5.43404914061138,-35.8929857499855)) ;
#163367 = CARTESIAN_POINT('Origin',(-5.79625984893577,-5.63938213935148,-35.9956531426186)) ;
#163368 = CARTESIAN_POINT('Origin',(-5.80000000007751,-5.42192235939839,-35.9899999994296)) ;
#163369 = CARTESIAN_POINT('',(-5.87071067811866,-1.14999999999999,-35.9192893218814)) ;
#163370 = CARTESIAN_POINT('Origin',(-5.80807935817112,-1.2752626408587,-35.9705238802469)) ;
#163371 = CARTESIAN_POINT('Origin',(-5.81947611582896,-1.02473736077925,-35.9819206426144)) ;
#163372 = CARTESIAN_POINT('Origin',(-3.,4.45,-4.91)) ;
#163373 = CARTESIAN_POINT('Origin',(-2.1,4.45,-4.91)) ;
#163374 = CARTESIAN_POINT('Origin',(-2.9,4.45,-4.91)) ;
#163375 = CARTESIAN_POINT('Origin',(-2.9,4.45,-4.71)) ;
#163376 = CARTESIAN_POINT('Origin',(-3.1,4.45,-4.71)) ;
#163377 = CARTESIAN_POINT('Origin',(-2.9,4.45,-4.71)) ;
#163378 = CARTESIAN_POINT('Origin',(-2.1,4.45,-4.71)) ;
#163379 = CARTESIAN_POINT('Origin',(-2.1,4.45,-4.71)) ;
#163380 = CARTESIAN_POINT('Origin',(-1.9,4.45,-4.71)) ;
#163381 = CARTESIAN_POINT('Origin',(-3.1,4.45,-4.81)) ;
#163382 = CARTESIAN_POINT('Origin',(-3.1,4.45,-2.91)) ;
#163383 = CARTESIAN_POINT('Origin',(-2.9,4.4,-4.71)) ;
#163384 = CARTESIAN_POINT('Origin',(-2.9,4.35,-4.71)) ;
#163385 = CARTESIAN_POINT('Origin',(-1.95156391047391E-16,4.35,-4.71)) ;
#163386 = CARTESIAN_POINT('Origin',(-2.1,4.35,-4.71)) ;
#163387 = CARTESIAN_POINT('Origin',(-2.9,4.35,-4.71)) ;
#163388 = CARTESIAN_POINT('Origin',(-2.1,4.4,-4.71)) ;
#163389 = CARTESIAN_POINT('Origin',(-2.1,4.35,-4.71)) ;
#163390 = CARTESIAN_POINT('Origin',(-1.9,4.45,-4.81)) ;
#163391 = CARTESIAN_POINT('Origin',(-1.9,4.45,-2.91)) ;
#163392 = CARTESIAN_POINT('Origin',(-3.,4.45,-2.71)) ;
#163393 = CARTESIAN_POINT('Origin',(-2.9,4.45,-2.71)) ;
#163394 = CARTESIAN_POINT('Origin',(-2.1,4.45,-2.71)) ;
#163395 = CARTESIAN_POINT('Origin',(-2.9,4.45,-2.91)) ;
#163396 = CARTESIAN_POINT('Origin',(-2.9,4.45,-2.91)) ;
#163397 = CARTESIAN_POINT('Origin',(-2.9,4.35,-4.71)) ;
#163398 = CARTESIAN_POINT('Origin',(-2.9,4.35,-4.71)) ;
#163399 = CARTESIAN_POINT('Origin',(-2.1,4.35,-4.71)) ;
#163400 = CARTESIAN_POINT('Origin',(-2.1,4.35,-4.71)) ;
#163401 = CARTESIAN_POINT('Origin',(-2.1,4.45,-2.91)) ;
#163402 = CARTESIAN_POINT('Origin',(-2.1,4.45,-2.91)) ;
#163403 = CARTESIAN_POINT('Origin',(-2.9,4.4,-2.91)) ;
#163404 = CARTESIAN_POINT('Origin',(-2.9,4.35,-2.91)) ;
#163405 = CARTESIAN_POINT('Origin',(-2.9,4.35,-3.81)) ;
#163406 = CARTESIAN_POINT('Origin',(-2.9,4.35,-2.91)) ;
#163407 = CARTESIAN_POINT('Origin',(-2.1,4.35,-3.81)) ;
#163408 = CARTESIAN_POINT('Origin',(-2.1,4.35,-2.91)) ;
#163409 = CARTESIAN_POINT('Origin',(-2.1,4.4,-2.91)) ;
#163410 = CARTESIAN_POINT('Origin',(-2.1,4.35,-2.91)) ;
#163411 = CARTESIAN_POINT('Origin',(-2.9,4.35,-2.91)) ;
#163412 = CARTESIAN_POINT('Origin',(-2.9,4.35,-2.91)) ;
#163413 = CARTESIAN_POINT('Origin',(-2.1,4.35,-2.91)) ;
#163414 = CARTESIAN_POINT('Origin',(-2.1,4.35,-2.91)) ;
#163415 = CARTESIAN_POINT('Origin',(-1.95156391047391E-16,4.35,-2.91)) ;
#163416 = CARTESIAN_POINT('Origin',(-2.25,4.25,-4.56)) ;
#163417 = CARTESIAN_POINT('Origin',(-2.25,4.3,-4.56)) ;
#163418 = CARTESIAN_POINT('Origin',(-2.25,4.3,-3.81)) ;
#163419 = CARTESIAN_POINT('Origin',(-2.25,4.3,-3.06)) ;
#163420 = CARTESIAN_POINT('Origin',(-2.25,4.3,-4.56)) ;
#163421 = CARTESIAN_POINT('Origin',(-2.25,4.25,-3.06)) ;
#163422 = CARTESIAN_POINT('Origin',(-2.25,4.3,-3.06)) ;
#163423 = CARTESIAN_POINT('Origin',(-2.25,4.3,-4.56)) ;
#163424 = CARTESIAN_POINT('Origin',(-2.25,4.3,-4.56)) ;
#163425 = CARTESIAN_POINT('Origin',(-2.25,4.3,-3.06)) ;
#163426 = CARTESIAN_POINT('Origin',(-2.25,4.3,-3.06)) ;
#163427 = CARTESIAN_POINT('Origin',(-2.75,4.25,-4.56)) ;
#163428 = CARTESIAN_POINT('Origin',(-2.75,4.3,-4.56)) ;
#163429 = CARTESIAN_POINT('Origin',(-1.97127667724637E-17,4.3,-4.56)) ;
#163430 = CARTESIAN_POINT('Origin',(-2.75,4.3,-4.56)) ;
#163431 = CARTESIAN_POINT('Origin',(-1.97127667724637E-17,4.3,-3.06)) ;
#163432 = CARTESIAN_POINT('Origin',(-2.75,4.3,-3.06)) ;
#163433 = CARTESIAN_POINT('Origin',(-2.75,4.25,-3.06)) ;
#163434 = CARTESIAN_POINT('Origin',(-2.75,4.3,-3.06)) ;
#163435 = CARTESIAN_POINT('Origin',(-2.75,4.3,-4.56)) ;
#163436 = CARTESIAN_POINT('Origin',(-2.75,4.3,-4.56)) ;
#163437 = CARTESIAN_POINT('Origin',(-2.75,4.3,-3.06)) ;
#163438 = CARTESIAN_POINT('Origin',(-2.75,4.3,-3.06)) ;
#163439 = CARTESIAN_POINT('Origin',(-2.75,4.3,-3.81)) ;
#163440 = CARTESIAN_POINT('Origin',(7.8,2.9,-4.21)) ;
#163441 = CARTESIAN_POINT('Origin',(7.8,2.9,-4.21)) ;
#163442 = CARTESIAN_POINT('Origin',(7.8,2.9,-3.41)) ;
#163443 = CARTESIAN_POINT('Origin',(7.8,2.9,-3.41)) ;
#163444 = CARTESIAN_POINT('Origin',(7.8,2.9,-3.41)) ;
#163445 = CARTESIAN_POINT('Origin',(7.8,2.9,-4.21)) ;
#163446 = CARTESIAN_POINT('Origin',(7.8,2.9,-4.21)) ;
#163447 = CARTESIAN_POINT('Origin',(9.6,2.9,-3.41)) ;
#163448 = CARTESIAN_POINT('Origin',(9.6,2.9,-3.41)) ;
#163449 = CARTESIAN_POINT('Origin',(9.6,2.9,-4.21)) ;
#163450 = CARTESIAN_POINT('Origin',(9.6,2.9,-4.21)) ;
#163451 = CARTESIAN_POINT('Origin',(9.6,2.9,-3.41)) ;
#163452 = CARTESIAN_POINT('Origin',(9.6,2.9,-3.41)) ;
#163453 = CARTESIAN_POINT('Origin',(9.6,2.9,-4.21)) ;
#163454 = CARTESIAN_POINT('Origin',(9.6,2.9,-4.21)) ;
#163455 = CARTESIAN_POINT('Origin',(9.6,2.9,-4.21)) ;
#163456 = CARTESIAN_POINT('Origin',(-0.183301359729408,3.45,-2.29296321352403)) ;
#163457 = CARTESIAN_POINT('Origin',(0.249234641435079,3.15,-3.69377997802131)) ;
#163458 = CARTESIAN_POINT('Origin',(-0.249234641435079,3.15,-3.92622002197869)) ;
#163459 = CARTESIAN_POINT('Origin',(-1.04429375741423,3.45,-2.69445056217769)) ;
#163460 = CARTESIAN_POINT('Origin',(10.1,-2.15,-6.71688040659058)) ;
#163461 = CARTESIAN_POINT('Origin',(10.1,-2.15,-6.71688040659058)) ;
#163462 = CARTESIAN_POINT('Origin',(10.1,-2.15,-6.71688040659058)) ;
#163463 = CARTESIAN_POINT('Origin',(10.1,-2.15,-6.71688040659058)) ;
#163464 = CARTESIAN_POINT('Origin',(10.1,-2.15,-7.62)) ;
#163465 = CARTESIAN_POINT('Origin',(10.1,-2.15,-6.315)) ;
#163466 = CARTESIAN_POINT('Origin',(10.2,-2.15,-6.71688040659058)) ;
#163467 = CARTESIAN_POINT('Origin',(3.7,-2.15,-6.71688040659058)) ;
#163468 = CARTESIAN_POINT('Origin',(10.1,-3.65625,-7.62)) ;
#163469 = CARTESIAN_POINT('Origin',(10.1,-2.15,-8.52311959340943)) ;
#163470 = CARTESIAN_POINT('Origin',(10.1,-3.65625,-6.315)) ;
#163471 = CARTESIAN_POINT('Origin',(10.1,1.9,-6.315)) ;
#163472 = CARTESIAN_POINT('Origin',(10.1,-2.15,-6.315)) ;
#163473 = CARTESIAN_POINT('Origin',(10.1,-2.15,-6.315)) ;
#163474 = CARTESIAN_POINT('Origin',(10.1,-2.15,-6.315)) ;
#163475 = CARTESIAN_POINT('Origin',(3.7,-2.15,-6.71688040659058)) ;
#163476 = CARTESIAN_POINT('Origin',(3.7,-2.32153024911032,-6.8197267659824)) ;
#163477 = CARTESIAN_POINT('Origin',(3.7,-2.35,-6.71688040659058)) ;
#163478 = CARTESIAN_POINT('Origin',(10.1,-2.15,-8.52311959340942)) ;
#163479 = CARTESIAN_POINT('Origin',(10.1,-2.15,-8.52311959340942)) ;
#163480 = CARTESIAN_POINT('Origin',(10.1,-2.15,-8.52311959340942)) ;
#163481 = CARTESIAN_POINT('Origin',(10.1,1.9,-7.62)) ;
#163482 = CARTESIAN_POINT('Origin',(10.1,1.9,-8.925)) ;
#163483 = CARTESIAN_POINT('Origin',(10.1,1.9,-6.315)) ;
#163484 = CARTESIAN_POINT('Origin',(10.2,-2.15,-6.315)) ;
#163485 = CARTESIAN_POINT('Origin',(3.7,-2.15,-6.315)) ;
#163486 = CARTESIAN_POINT('Origin',(3.7,-2.35,-6.215)) ;
#163487 = CARTESIAN_POINT('Origin',(3.7,-2.35,-6.315)) ;
#163488 = CARTESIAN_POINT('Origin',(3.7,-3.65625,-7.62)) ;
#163489 = CARTESIAN_POINT('Origin',(3.7,-2.32153024911032,-8.4202732340176)) ;
#163490 = CARTESIAN_POINT('Origin',(10.2,-2.15,-8.52311959340942)) ;
#163491 = CARTESIAN_POINT('Origin',(3.7,-2.15,-8.52311959340942)) ;
#163492 = CARTESIAN_POINT('Origin',(10.1,-2.15,-7.62)) ;
#163493 = CARTESIAN_POINT('Origin',(10.1,-2.15,-8.925)) ;
#163494 = CARTESIAN_POINT('Origin',(10.1,-3.65625,-8.925)) ;
#163495 = CARTESIAN_POINT('Origin',(10.1,1.9,-8.925)) ;
#163496 = CARTESIAN_POINT('Origin',(10.1,-2.15,-8.925)) ;
#163497 = CARTESIAN_POINT('Origin',(3.7,-2.35,-6.315)) ;
#163498 = CARTESIAN_POINT('Origin',(3.5,-2.35,-6.315)) ;
#163499 = CARTESIAN_POINT('Origin',(3.7,-2.15,-8.52311959340942)) ;
#163500 = CARTESIAN_POINT('Origin',(3.7,-2.35,-8.52311959340942)) ;
#163501 = CARTESIAN_POINT('Origin',(10.1,-2.15,-8.925)) ;
#163502 = CARTESIAN_POINT('Origin',(10.1,-2.15,-8.925)) ;
#163503 = CARTESIAN_POINT('Origin',(3.6,1.9,-6.115)) ;
#163504 = CARTESIAN_POINT('Origin',(3.5,1.9,-6.115)) ;
#163505 = CARTESIAN_POINT('Origin',(2.7,1.9,-6.115)) ;
#163506 = CARTESIAN_POINT('Origin',(3.5,6.44767184226083E-16,-6.315)) ;
#163507 = CARTESIAN_POINT('Origin',(3.5,-5.15,-6.315)) ;
#163508 = CARTESIAN_POINT('Origin',(3.7,-2.35,-8.495)) ;
#163509 = CARTESIAN_POINT('Origin',(3.7,-2.35,-8.925)) ;
#163510 = CARTESIAN_POINT('Origin',(3.6,-2.15,-8.925)) ;
#163511 = CARTESIAN_POINT('Origin',(3.7,-2.15,-8.925)) ;
#163512 = CARTESIAN_POINT('Origin',(2.7,1.9,-6.115)) ;
#163513 = CARTESIAN_POINT('Origin',(2.7,1.9,-6.115)) ;
#163514 = CARTESIAN_POINT('Origin',(3.5,-5.15,-6.315)) ;
#163515 = CARTESIAN_POINT('Origin',(3.5,-5.15,-6.315)) ;
#163516 = CARTESIAN_POINT('Origin',(3.5,-5.15,-6.315)) ;
#163517 = CARTESIAN_POINT('Origin',(3.7,-2.35,-8.925)) ;
#163518 = CARTESIAN_POINT('Origin',(3.5,-2.35,-8.925)) ;
#163519 = CARTESIAN_POINT('Origin',(2.7,2.,-6.115)) ;
#163520 = CARTESIAN_POINT('Origin',(2.7,-5.15,-6.115)) ;
#163521 = CARTESIAN_POINT('Origin',(3.6,-5.15,-6.315)) ;
#163522 = CARTESIAN_POINT('Origin',(2.7,-5.15,-6.315)) ;
#163523 = CARTESIAN_POINT('Origin',(3.5,-5.15,0.)) ;
#163524 = CARTESIAN_POINT('Origin',(3.5,-5.15,-8.925)) ;
#163525 = CARTESIAN_POINT('Origin',(3.5,-7.22673459250807E-16,-8.925)) ;
#163526 = CARTESIAN_POINT('Origin',(3.5,-5.15,-8.925)) ;
#163527 = CARTESIAN_POINT('Origin',(2.7,-5.15,-6.315)) ;
#163528 = CARTESIAN_POINT('Origin',(2.7,-5.35,-6.315)) ;
#163529 = CARTESIAN_POINT('Origin',(3.5,-5.15,-8.925)) ;
#163530 = CARTESIAN_POINT('Origin',(3.5,-5.15,-8.925)) ;
#163531 = CARTESIAN_POINT('Origin',(2.7,-5.35,-6.215)) ;
#163532 = CARTESIAN_POINT('Origin',(2.7,-5.35,-8.925)) ;
#163533 = CARTESIAN_POINT('Origin',(3.6,-5.15,-8.925)) ;
#163534 = CARTESIAN_POINT('Origin',(2.7,-5.15,-8.925)) ;
#163535 = CARTESIAN_POINT('Origin',(3.6,1.9,-9.125)) ;
#163536 = CARTESIAN_POINT('Origin',(3.5,1.9,-9.125)) ;
#163537 = CARTESIAN_POINT('Origin',(2.7,1.9,-9.125)) ;
#163538 = CARTESIAN_POINT('Origin',(2.7,1.9,-9.025)) ;
#163539 = CARTESIAN_POINT('Origin',(2.7,1.9,-9.925)) ;
#163540 = CARTESIAN_POINT('Origin',(2.7,1.9,-9.125)) ;
#163541 = CARTESIAN_POINT('Origin',(2.7,-5.15,-8.925)) ;
#163542 = CARTESIAN_POINT('Origin',(2.7,-5.15,-9.125)) ;
#163543 = CARTESIAN_POINT('Origin',(2.7,1.9,-9.125)) ;
#163544 = CARTESIAN_POINT('Origin',(2.7,1.9,-9.125)) ;
#163545 = CARTESIAN_POINT('Origin',(2.7,-5.25,-9.125)) ;
#163546 = CARTESIAN_POINT('Ctrl Pts',(-3.8,-6.55,-6.52)) ;
#163547 = CARTESIAN_POINT('Ctrl Pts',(-3.8,-6.55,-6.52)) ;
#163548 = CARTESIAN_POINT('Ctrl Pts',(-3.8,-6.55,-6.52)) ;
#163549 = CARTESIAN_POINT('Ctrl Pts',(-3.82625343282635,-6.55,-6.57250686565274)) ;
#163550 = CARTESIAN_POINT('Ctrl Pts',(-3.83954133268481,-6.55,-6.55954133268496)) ;
#163551 = CARTESIAN_POINT('Ctrl Pts',(-3.85250686565268,-6.55,-6.54625343282645)) ;
#163552 = CARTESIAN_POINT('Ctrl Pts',(-3.85219871729854,-6.53922263893877,
-6.62439743459706)) ;
#163553 = CARTESIAN_POINT('Ctrl Pts',(-3.87914655110981,-6.52362528614068,
-6.59914655110983)) ;
#163554 = CARTESIAN_POINT('Ctrl Pts',(-3.90439743459708,-6.53922263893878,
-6.57219871729853)) ;
#163555 = CARTESIAN_POINT('Ctrl Pts',(-3.87996665852871,-6.5114546977086,
-6.67993331705744)) ;
#163556 = CARTESIAN_POINT('Ctrl Pts',(-3.9028838031416,-6.48208554016478,
-6.6228838031416)) ;
#163557 = CARTESIAN_POINT('Ctrl Pts',(-3.95993331705742,-6.51145469770859,
-6.59996665852872)) ;
#163558 = CARTESIAN_POINT('Ctrl Pts',(-3.88737865704135,-6.5003618540841,
-6.69475731408271)) ;
#163559 = CARTESIAN_POINT('Ctrl Pts',(-3.90501307588292,-6.46792722356047,
-6.62501307588294)) ;
#163560 = CARTESIAN_POINT('Ctrl Pts',(-3.9747573140827,-6.5003618540841,-6.60737865704135)) ;
#163561 = CARTESIAN_POINT('Ctrl Pts',(-3.8973972494609,-6.47617483238892,
-6.71479449892181)) ;
#163562 = CARTESIAN_POINT('Ctrl Pts',(-3.90329674356411,-6.4509405986842,
-6.6232967435641)) ;
#163563 = CARTESIAN_POINT('Ctrl Pts',(-3.99479449892181,-6.47617483238892,
-6.61739724946091)) ;
#163564 = CARTESIAN_POINT('Ctrl Pts',(-3.9,-6.46309229646328,-6.71999999918177)) ;
#163565 = CARTESIAN_POINT('Ctrl Pts',(-3.90000730397382,-6.44945650155155,
-6.62000730395969)) ;
#163566 = CARTESIAN_POINT('Ctrl Pts',(-3.99999999918173,-6.46309229646328,
-6.62)) ;
#163567 = CARTESIAN_POINT('Ctrl Pts',(-3.9,-6.45,-6.72)) ;
#163568 = CARTESIAN_POINT('Ctrl Pts',(-3.9,-6.45,-6.62)) ;
#163569 = CARTESIAN_POINT('Ctrl Pts',(-4.,-6.45,-6.62)) ;
#163570 = CARTESIAN_POINT('Origin',(-4.,-6.45,-6.72)) ;
#163571 = CARTESIAN_POINT('Origin',(-4.,-6.4,-6.72)) ;
#163572 = CARTESIAN_POINT('Origin',(-4.,-6.35,-6.72)) ;
#163573 = CARTESIAN_POINT('Ctrl Pts',(-5.,-6.55,-6.52)) ;
#163574 = CARTESIAN_POINT('Ctrl Pts',(-5.,-6.55,-6.52)) ;
#163575 = CARTESIAN_POINT('Ctrl Pts',(-5.,-6.55,-6.52)) ;
#163576 = CARTESIAN_POINT('Ctrl Pts',(-4.94749313434726,-6.55,-6.54625343282631)) ;
#163577 = CARTESIAN_POINT('Ctrl Pts',(-4.96045866731611,-6.55,-6.55954133268376)) ;
#163578 = CARTESIAN_POINT('Ctrl Pts',(-4.97374656717359,-6.55,-6.57250686565269)) ;
#163579 = CARTESIAN_POINT('Ctrl Pts',(-4.89560256540291,-6.53922263893877,
-6.57219871729855)) ;
#163580 = CARTESIAN_POINT('Ctrl Pts',(-4.9208534488902,-6.52362528614071,
-6.59914655110988)) ;
#163581 = CARTESIAN_POINT('Ctrl Pts',(-4.94780128270146,-6.53922263893877,
-6.62439743459709)) ;
#163582 = CARTESIAN_POINT('Ctrl Pts',(-4.84006668294258,-6.5114546977086,
-6.59996665852871)) ;
#163583 = CARTESIAN_POINT('Ctrl Pts',(-4.89711619685839,-6.48208554016476,
-6.62288380314157)) ;
#163584 = CARTESIAN_POINT('Ctrl Pts',(-4.92003334147129,-6.5114546977086,
-6.67993331705742)) ;
#163585 = CARTESIAN_POINT('Ctrl Pts',(-4.82524268591729,-6.5003618540841,
-6.60737865704136)) ;
#163586 = CARTESIAN_POINT('Ctrl Pts',(-4.89498692411706,-6.46792722356047,
-6.62501307588293)) ;
#163587 = CARTESIAN_POINT('Ctrl Pts',(-4.91262134295865,-6.5003618540841,
-6.6947573140827)) ;
#163588 = CARTESIAN_POINT('Ctrl Pts',(-4.80520550107819,-6.47617483238892,
-6.61739724946091)) ;
#163589 = CARTESIAN_POINT('Ctrl Pts',(-4.8967032564359,-6.4509405986842,-6.62329674356412)) ;
#163590 = CARTESIAN_POINT('Ctrl Pts',(-4.90260275053909,-6.47617483238892,
-6.71479449892182)) ;
#163591 = CARTESIAN_POINT('Ctrl Pts',(-4.80000000081823,-6.46309229646328,
-6.62)) ;
#163592 = CARTESIAN_POINT('Ctrl Pts',(-4.89999269600723,-6.44945650155945,
-6.62000730395977)) ;
#163593 = CARTESIAN_POINT('Ctrl Pts',(-4.9,-6.46309229646328,-6.71999999918177)) ;
#163594 = CARTESIAN_POINT('Ctrl Pts',(-4.8,-6.45,-6.62)) ;
#163595 = CARTESIAN_POINT('Ctrl Pts',(-4.9,-6.45,-6.62)) ;
#163596 = CARTESIAN_POINT('Ctrl Pts',(-4.9,-6.45,-6.72)) ;
#163597 = CARTESIAN_POINT('Origin',(-4.8,-6.45,-6.72)) ;
#163598 = CARTESIAN_POINT('Origin',(-4.,-6.35,-6.72)) ;
#163599 = CARTESIAN_POINT('Origin',(-4.,-6.35,-6.72)) ;
#163600 = CARTESIAN_POINT('Origin',(-4.,-6.35,-6.72)) ;
#163601 = CARTESIAN_POINT('Ctrl Pts',(-3.8,-6.55,-8.72)) ;
#163602 = CARTESIAN_POINT('Ctrl Pts',(-3.8,-6.55,-8.72)) ;
#163603 = CARTESIAN_POINT('Ctrl Pts',(-3.8,-6.55,-8.72)) ;
#163604 = CARTESIAN_POINT('Ctrl Pts',(-3.8525068656527,-6.55,-8.69374656717358)) ;
#163605 = CARTESIAN_POINT('Ctrl Pts',(-3.83954133268498,-6.55,-8.68045866731507)) ;
#163606 = CARTESIAN_POINT('Ctrl Pts',(-3.82625343282636,-6.55,-8.66749313434729)) ;
#163607 = CARTESIAN_POINT('Ctrl Pts',(-3.90439743459706,-6.53922263893877,
-8.66780128270146)) ;
#163608 = CARTESIAN_POINT('Ctrl Pts',(-3.8791465511098,-6.52362528614071,
-8.64085344889018)) ;
#163609 = CARTESIAN_POINT('Ctrl Pts',(-3.85219871729855,-6.53922263893876,
-8.61560256540292)) ;
#163610 = CARTESIAN_POINT('Ctrl Pts',(-3.95993331705743,-6.5114546977086,
-8.64003334147129)) ;
#163611 = CARTESIAN_POINT('Ctrl Pts',(-3.90288380314161,-6.48208554016476,
-8.6171161968584)) ;
#163612 = CARTESIAN_POINT('Ctrl Pts',(-3.8799666585287,-6.5114546977086,-8.56006668294258)) ;
#163613 = CARTESIAN_POINT('Ctrl Pts',(-3.97475731408271,-6.5003618540841,
-8.63262134295865)) ;
#163614 = CARTESIAN_POINT('Ctrl Pts',(-3.90501307588293,-6.46792722356048,
-8.61498692411705)) ;
#163615 = CARTESIAN_POINT('Ctrl Pts',(-3.88737865704135,-6.5003618540841,
-8.54524268591729)) ;
#163616 = CARTESIAN_POINT('Ctrl Pts',(-3.9947944989218,-6.47617483238892,
-8.6226027505391)) ;
#163617 = CARTESIAN_POINT('Ctrl Pts',(-3.9032967435641,-6.45094059868419,
-8.61670325643593)) ;
#163618 = CARTESIAN_POINT('Ctrl Pts',(-3.89739724946091,-6.47617483238892,
-8.5252055010782)) ;
#163619 = CARTESIAN_POINT('Ctrl Pts',(-3.99999999918176,-6.46309229646328,
-8.62)) ;
#163620 = CARTESIAN_POINT('Ctrl Pts',(-3.90000730395526,-6.44945650152442,
-8.61999269608717)) ;
#163621 = CARTESIAN_POINT('Ctrl Pts',(-3.9,-6.46309229646328,-8.52000000081831)) ;
#163622 = CARTESIAN_POINT('Ctrl Pts',(-4.,-6.45,-8.62)) ;
#163623 = CARTESIAN_POINT('Ctrl Pts',(-3.9,-6.45,-8.62)) ;
#163624 = CARTESIAN_POINT('Ctrl Pts',(-3.9,-6.45,-8.52)) ;
#163625 = CARTESIAN_POINT('Origin',(-4.,-6.45,-8.52)) ;
#163626 = CARTESIAN_POINT('Origin',(-4.8,-6.4,-6.72)) ;
#163627 = CARTESIAN_POINT('Origin',(-4.8,-6.35,-6.72)) ;
#163628 = CARTESIAN_POINT('Origin',(1.9515639104739E-16,-6.35,-6.72000000000001)) ;
#163629 = CARTESIAN_POINT('Origin',(-4.8,-6.35,-6.72)) ;
#163630 = CARTESIAN_POINT('Origin',(-4.,-6.35,-7.62)) ;
#163631 = CARTESIAN_POINT('Origin',(-4.,-6.35,-8.52)) ;
#163632 = CARTESIAN_POINT('Origin',(-4.,-6.4,-8.52)) ;
#163633 = CARTESIAN_POINT('Origin',(-4.,-6.35,-8.52)) ;
#163634 = CARTESIAN_POINT('Origin',(-4.8,-6.35,-6.72)) ;
#163635 = CARTESIAN_POINT('Origin',(-4.8,-6.35,-6.72)) ;
#163636 = CARTESIAN_POINT('Origin',(-4.,-6.35,-8.52)) ;
#163637 = CARTESIAN_POINT('Origin',(-4.,-6.35,-8.52)) ;
#163638 = CARTESIAN_POINT('Origin',(-4.8,-6.35,-7.62)) ;
#163639 = CARTESIAN_POINT('Origin',(-4.8,-6.35,-8.52)) ;
#163640 = CARTESIAN_POINT('Origin',(1.95156391047391E-16,-6.35,-8.52)) ;
#163641 = CARTESIAN_POINT('Origin',(-4.8,-6.35,-8.52)) ;
#163642 = CARTESIAN_POINT('Origin',(-4.8,-6.35,-8.52)) ;
#163643 = CARTESIAN_POINT('Origin',(-4.8,-6.35,-8.52)) ;
#163644 = CARTESIAN_POINT('Origin',(-4.8,-6.4,-8.52)) ;
#163645 = CARTESIAN_POINT('Origin',(-4.8,-6.45,-8.52)) ;
#163646 = CARTESIAN_POINT('Ctrl Pts',(-5.,-6.55,-8.72)) ;
#163647 = CARTESIAN_POINT('Ctrl Pts',(-5.,-6.55,-8.72)) ;
#163648 = CARTESIAN_POINT('Ctrl Pts',(-5.,-6.55,-8.72)) ;
#163649 = CARTESIAN_POINT('Ctrl Pts',(-4.97374656717352,-6.55,-8.66749313434731)) ;
#163650 = CARTESIAN_POINT('Ctrl Pts',(-4.96045866731608,-6.55,-8.68045866731609)) ;
#163651 = CARTESIAN_POINT('Ctrl Pts',(-4.94749313434721,-6.55,-8.69374656717377)) ;
#163652 = CARTESIAN_POINT('Ctrl Pts',(-4.94780128270146,-6.53922263893877,
-8.61560256540297)) ;
#163653 = CARTESIAN_POINT('Ctrl Pts',(-4.92085344889017,-6.52362528614071,
-8.64085344889023)) ;
#163654 = CARTESIAN_POINT('Ctrl Pts',(-4.89560256540291,-6.53922263893879,
-8.66780128270149)) ;
#163655 = CARTESIAN_POINT('Ctrl Pts',(-4.92003334147129,-6.5114546977086,
-8.56006668294255)) ;
#163656 = CARTESIAN_POINT('Ctrl Pts',(-4.8971161968584,-6.48208554016476,
-8.61711619685837)) ;
#163657 = CARTESIAN_POINT('Ctrl Pts',(-4.84006668294258,-6.51145469770858,
-8.64003334147128)) ;
#163658 = CARTESIAN_POINT('Ctrl Pts',(-4.91262134295865,-6.5003618540841,
-8.54524268591729)) ;
#163659 = CARTESIAN_POINT('Ctrl Pts',(-4.89498692411706,-6.46792722356048,
-8.61498692411705)) ;
#163660 = CARTESIAN_POINT('Ctrl Pts',(-4.82524268591729,-6.5003618540841,
-8.63262134295865)) ;
#163661 = CARTESIAN_POINT('Ctrl Pts',(-4.90260275053909,-6.47617483238892,
-8.5252055010782)) ;
#163662 = CARTESIAN_POINT('Ctrl Pts',(-4.8967032564359,-6.45094059868419,
-8.61670325643593)) ;
#163663 = CARTESIAN_POINT('Ctrl Pts',(-4.80520550107819,-6.47617483238892,
-8.6226027505391)) ;
#163664 = CARTESIAN_POINT('Ctrl Pts',(-4.9,-6.46309229646328,-8.52000000081831)) ;
#163665 = CARTESIAN_POINT('Ctrl Pts',(-4.89999269604004,-6.44945650152635,
-8.6199926960872)) ;
#163666 = CARTESIAN_POINT('Ctrl Pts',(-4.80000000081823,-6.46309229646328,
-8.62)) ;
#163667 = CARTESIAN_POINT('Ctrl Pts',(-4.9,-6.45,-8.52)) ;
#163668 = CARTESIAN_POINT('Ctrl Pts',(-4.9,-6.45,-8.62)) ;
#163669 = CARTESIAN_POINT('Ctrl Pts',(-4.8,-6.45,-8.62)) ;
#163670 = CARTESIAN_POINT('Ctrl Pts',(-5.82426676739355,-5.43399303700595,
-6.01701096596876)) ;
#163671 = CARTESIAN_POINT('Ctrl Pts',(-5.8026698877831,-5.52572360682934,
-6.02235401735037)) ;
#163672 = CARTESIAN_POINT('Ctrl Pts',(-5.82426676352017,-5.53106667371342,
-6.11408458718272)) ;
#163673 = CARTESIAN_POINT('Ctrl Pts',(-5.83498671931123,-5.43935351191891,
-6.01432945819615)) ;
#163674 = CARTESIAN_POINT('Ctrl Pts',(-5.80595263122263,-5.52411753147702,
-6.02396009354016)) ;
#163675 = CARTESIAN_POINT('Ctrl Pts',(-5.83498671397627,-5.53374818067469,
-6.10872411314632)) ;
#163676 = CARTESIAN_POINT('Ctrl Pts',(-5.8452610584572,-5.44830326289477,
-6.00985284019614)) ;
#163677 = CARTESIAN_POINT('Ctrl Pts',(-5.81370932746129,-5.52260132030851,
-6.02547630599891)) ;
#163678 = CARTESIAN_POINT('Ctrl Pts',(-5.84526105243721,-5.53822479746339,
-6.0997743635698)) ;
#163679 = CARTESIAN_POINT('Ctrl Pts',(-5.86378685403706,-5.47240020430389,
-5.99780325130861)) ;
#163680 = CARTESIAN_POINT('Ctrl Pts',(-5.83531854275282,-5.52733067404477,
-6.02074695511457)) ;
#163681 = CARTESIAN_POINT('Ctrl Pts',(-5.86378684816461,-5.550274384599,-6.07567742500549)) ;
#163682 = CARTESIAN_POINT('Ctrl Pts',(-5.87203852631583,-5.48754495134725,
-5.99023155289433)) ;
#163683 = CARTESIAN_POINT('Ctrl Pts',(-5.84834787930679,-5.53310199490444,
-6.01497563577601)) ;
#163684 = CARTESIAN_POINT('Ctrl Pts',(-5.8720385212304,-5.55784608243457,
-6.06053267951394)) ;
#163685 = CARTESIAN_POINT('Ctrl Pts',(-5.892427473048,-5.53981202333449,-5.96410565113754)) ;
#163686 = CARTESIAN_POINT('Ctrl Pts',(-5.88223383300418,-5.56084219179273,
-5.9872354431742)) ;
#163687 = CARTESIAN_POINT('Ctrl Pts',(-5.89242747063502,-5.58397198402774,
-6.00826561232782)) ;
#163688 = CARTESIAN_POINT('Ctrl Pts',(-5.9,-5.58381083947293,-5.94211940014292)) ;
#163689 = CARTESIAN_POINT('Ctrl Pts',(-5.9,-5.59485304502627,-5.95322459288698)) ;
#163690 = CARTESIAN_POINT('Ctrl Pts',(-5.9,-5.60595823775499,-5.96426679844055)) ;
#163691 = CARTESIAN_POINT('Ctrl Pts',(-5.9,-5.62807764064044,-5.92)) ;
#163692 = CARTESIAN_POINT('Ctrl Pts',(-5.9,-5.62807764064044,-5.92)) ;
#163693 = CARTESIAN_POINT('Ctrl Pts',(-5.9,-5.62807764064044,-5.92)) ;
#163694 = CARTESIAN_POINT('Origin',(-5.84850712500726,-5.43404914061138,-6.11402850002907)) ;
#163695 = CARTESIAN_POINT('Ctrl Pts',(-5.82425356250363,-5.53106339062591,
-6.11402850002907)) ;
#163696 = CARTESIAN_POINT('Ctrl Pts',(-5.80269484027818,-5.52567371006955,
-6.0224039305709)) ;
#163697 = CARTESIAN_POINT('Ctrl Pts',(-5.82425356250363,-5.43404914061138,
-6.01701425001453)) ;
#163698 = CARTESIAN_POINT('Ctrl Pts',(-5.80840777707093,-5.52710194426774,
-6.11798994590434)) ;
#163699 = CARTESIAN_POINT('Ctrl Pts',(-5.79341417645228,-5.52335354411309,
-6.0228358498184)) ;
#163700 = CARTESIAN_POINT('Ctrl Pts',(-5.81633079157288,-5.43008775511759,
-6.01899494274722)) ;
#163701 = CARTESIAN_POINT('Ctrl Pts',(-5.79207992677991,-5.52301998169498,
-6.11999999953396)) ;
#163702 = CARTESIAN_POINT('Ctrl Pts',(-5.78430903206645,-5.52107725801661,
-6.02196139543286)) ;
#163703 = CARTESIAN_POINT('Ctrl Pts',(-5.808166653183,-5.42600568595106,-6.02)) ;
#163704 = CARTESIAN_POINT('Ctrl Pts',(-5.77574643749636,-5.51893660937409,
-6.12)) ;
#163705 = CARTESIAN_POINT('Ctrl Pts',(-5.77574643749636,-5.51893660937409,
-6.02)) ;
#163706 = CARTESIAN_POINT('Ctrl Pts',(-5.8,-5.42192235935956,-6.02)) ;
#163707 = CARTESIAN_POINT('Origin',(-5.8,-5.42192235935956,-6.12)) ;
#163708 = CARTESIAN_POINT('Origin',(-5.8066065036801,-5.42357398527959,-6.12)) ;
#163709 = CARTESIAN_POINT('Origin',(-5.17275707706436,-5.26511162862565,-6.12)) ;
#163710 = CARTESIAN_POINT('Origin',(-5.15068655017073,-5.25959399690224,-6.13059385290895)) ;
#163711 = CARTESIAN_POINT('Origin',(-5.17275707706436,-5.26511162862565,-6.12)) ;
#163712 = CARTESIAN_POINT('Origin',(-5.17275707706436,-5.26511162862565,-6.12)) ;
#163713 = CARTESIAN_POINT('Origin',(-5.17275707706436,-5.26511162862565,-6.12)) ;
#163714 = CARTESIAN_POINT('Origin',(-5.17275707706436,-5.05,-6.12)) ;
#163715 = CARTESIAN_POINT('Origin',(-5.17275707706436,-1.91866427917294,-6.12)) ;
#163716 = CARTESIAN_POINT('Origin',(-3.78014014831103,-3.31128120792626,-6.7884561258016)) ;
#163717 = CARTESIAN_POINT('Origin',(-5.17275707706436,-1.91866427917294,-6.12)) ;
#163718 = CARTESIAN_POINT('Origin',(-5.17275707706436,-1.91866427917293,-6.12)) ;
#163719 = CARTESIAN_POINT('Origin',(-5.17275707706436,-1.91866427917294,-6.12)) ;
#163720 = CARTESIAN_POINT('Origin',(-3.97071067811865,-3.12071067811865,-6.12)) ;
#163721 = CARTESIAN_POINT('Origin',(-5.8,-1.2914213562373,-6.12)) ;
#163722 = CARTESIAN_POINT('Ctrl Pts',(-5.87071067811865,-1.14999999999999,
-5.99071067811865)) ;
#163723 = CARTESIAN_POINT('Ctrl Pts',(-5.8471404520791,-1.10285954792089,
-6.01428090415821)) ;
#163724 = CARTESIAN_POINT('Ctrl Pts',(-5.87071067811865,-1.07928932188134,
-6.06142135623731)) ;
#163725 = CARTESIAN_POINT('Ctrl Pts',(-5.85217562795663,-1.18707010095462,
-6.00924572828067)) ;
#163726 = CARTESIAN_POINT('Ctrl Pts',(-5.81261165662048,-1.13738834337934,
-6.03586147194932)) ;
#163727 = CARTESIAN_POINT('Ctrl Pts',(-5.83353949671043,-1.11646050328957,
-6.09859253638095)) ;
#163728 = CARTESIAN_POINT('Ctrl Pts',(-5.82627077431954,-1.23887980759834,
-6.02)) ;
#163729 = CARTESIAN_POINT('Ctrl Pts',(-5.76566787907959,-1.18433212092047,
-6.037148943713)) ;
#163730 = CARTESIAN_POINT('Ctrl Pts',(-5.78190678732234,-1.16809321267766,
-6.11999999941873)) ;
#163731 = CARTESIAN_POINT('Ctrl Pts',(-5.8,-1.2914213562373,-6.02)) ;
#163732 = CARTESIAN_POINT('Ctrl Pts',(-5.72928932188134,-1.22071067811865,
-6.02)) ;
#163733 = CARTESIAN_POINT('Ctrl Pts',(-5.72928932188134,-1.22071067811865,
-6.12)) ;
#163734 = CARTESIAN_POINT('Origin',(-5.94142135623731,-1.15,-6.06142135623731)) ;
#163735 = CARTESIAN_POINT('Ctrl Pts',(-5.9,-1.00857864376269,-5.92)) ;
#163736 = CARTESIAN_POINT('Ctrl Pts',(-5.9,-1.00857864376269,-5.92)) ;
#163737 = CARTESIAN_POINT('Ctrl Pts',(-5.9,-1.00857864376269,-5.92)) ;
#163738 = CARTESIAN_POINT('Ctrl Pts',(-5.9,-1.0611201924017,-5.94627077431948)) ;
#163739 = CARTESIAN_POINT('Ctrl Pts',(-5.9,-1.04860238143826,-5.9600237376757)) ;
#163740 = CARTESIAN_POINT('Ctrl Pts',(-5.9,-1.03484941808215,-5.97254154863899)) ;
#163741 = CARTESIAN_POINT('Ctrl Pts',(-5.88924572828065,-1.11292989904533,
-5.97217562795666)) ;
#163742 = CARTESIAN_POINT('Ctrl Pts',(-5.8745170062455,-1.08721613124893,
-5.99863748748648)) ;
#163743 = CARTESIAN_POINT('Ctrl Pts',(-5.88924572828069,-1.0607542717193,
-6.02435125528271)) ;
#163744 = CARTESIAN_POINT('Ctrl Pts',(-5.87071067811865,-1.14999999999999,
-5.99071067811865)) ;
#163745 = CARTESIAN_POINT('Ctrl Pts',(-5.8471404520791,-1.10285954792089,
-6.01428090415821)) ;
#163746 = CARTESIAN_POINT('Ctrl Pts',(-5.87071067811865,-1.07928932188134,
-6.06142135623731)) ;
#163747 = CARTESIAN_POINT('Ctrl Pts',(-5.87071067811866,-1.14999999999999,
-9.24928932188135)) ;
#163748 = CARTESIAN_POINT('Ctrl Pts',(-5.84714045207911,-1.10285954792089,
-9.2257190958418)) ;
#163749 = CARTESIAN_POINT('Ctrl Pts',(-5.87071067811866,-1.07928932188134,
-9.1785786437627)) ;
#163750 = CARTESIAN_POINT('Ctrl Pts',(-5.88924572828065,-1.11292989904533,
-9.26782437204335)) ;
#163751 = CARTESIAN_POINT('Ctrl Pts',(-5.87451700627504,-1.08721613123207,
-9.24136251253051)) ;
#163752 = CARTESIAN_POINT('Ctrl Pts',(-5.8892457282807,-1.06075427171929,
-9.21564874471729)) ;
#163753 = CARTESIAN_POINT('Ctrl Pts',(-5.9,-1.06112019240166,-9.29372922568044)) ;
#163754 = CARTESIAN_POINT('Ctrl Pts',(-5.9,-1.04860238145159,-9.27997626231091)) ;
#163755 = CARTESIAN_POINT('Ctrl Pts',(-5.9,-1.03484941808214,-9.26745845136102)) ;
#163756 = CARTESIAN_POINT('Ctrl Pts',(-5.9,-1.00857864376269,-9.32)) ;
#163757 = CARTESIAN_POINT('Ctrl Pts',(-5.9,-1.00857864376269,-9.32)) ;
#163758 = CARTESIAN_POINT('Ctrl Pts',(-5.9,-1.00857864376269,-9.32)) ;
#163759 = CARTESIAN_POINT('Origin',(-5.94142135623734,-1.14999999999996,-9.17857864376272)) ;
#163760 = CARTESIAN_POINT('Ctrl Pts',(-5.8,-1.2914213562373,-9.22)) ;
#163761 = CARTESIAN_POINT('Ctrl Pts',(-5.72928932188134,-1.22071067811865,
-9.22)) ;
#163762 = CARTESIAN_POINT('Ctrl Pts',(-5.72928932188134,-1.22071067811865,
-9.12)) ;
#163763 = CARTESIAN_POINT('Ctrl Pts',(-5.82627077431945,-1.23887980759835,
-9.22)) ;
#163764 = CARTESIAN_POINT('Ctrl Pts',(-5.76566787907942,-1.18433212092059,
-9.2028510562869)) ;
#163765 = CARTESIAN_POINT('Ctrl Pts',(-5.78190678732237,-1.16809321267762,
-9.1200000005814)) ;
#163766 = CARTESIAN_POINT('Ctrl Pts',(-5.85217562795658,-1.18707010095451,
-9.23075427171927)) ;
#163767 = CARTESIAN_POINT('Ctrl Pts',(-5.81261165662068,-1.13738834337918,
-9.20413852805062)) ;
#163768 = CARTESIAN_POINT('Ctrl Pts',(-5.83353949671039,-1.1164605032896,
-9.141407463619)) ;
#163769 = CARTESIAN_POINT('Ctrl Pts',(-5.87071067811866,-1.14999999999999,
-9.24928932188135)) ;
#163770 = CARTESIAN_POINT('Ctrl Pts',(-5.84714045207911,-1.10285954792089,
-9.2257190958418)) ;
#163771 = CARTESIAN_POINT('Ctrl Pts',(-5.87071067811866,-1.07928932188133,
-9.1785786437627)) ;
#163772 = CARTESIAN_POINT('Origin',(-5.8,-1.29142135623731,-9.12)) ;
#163773 = CARTESIAN_POINT('Origin',(-3.59571067811865,-3.49571067811865,-9.12)) ;
#163774 = CARTESIAN_POINT('Origin',(-5.17275707706437,-1.91866427917293,-9.12)) ;
#163775 = CARTESIAN_POINT('Origin',(-3.09057773798104,-4.00084361825625,-8.12055391724001)) ;
#163776 = CARTESIAN_POINT('Origin',(-5.17275707706437,-1.91866427917293,-9.12)) ;
#163777 = CARTESIAN_POINT('Origin',(-5.17275707706437,-1.91866427917293,-9.12)) ;
#163778 = CARTESIAN_POINT('Origin',(-5.17275707706437,-1.91866427917293,-9.12)) ;
#163779 = CARTESIAN_POINT('Origin',(-5.17275707706437,-5.05,-9.12)) ;
#163780 = CARTESIAN_POINT('Origin',(-5.17275707706437,-5.26511162862565,-9.12)) ;
#163781 = CARTESIAN_POINT('Origin',(-3.96111272388873,-4.96220054033175,-8.53841071047569)) ;
#163782 = CARTESIAN_POINT('Origin',(-5.17275707706437,-5.26511162862565,-9.12)) ;
#163783 = CARTESIAN_POINT('Origin',(-5.17275707706437,-5.26511162862565,-9.12)) ;
#163784 = CARTESIAN_POINT('Origin',(-5.17275707706437,-5.26511162862565,-9.12)) ;
#163785 = CARTESIAN_POINT('Origin',(-5.10072415073893,-5.24710339704429,-9.12)) ;
#163786 = CARTESIAN_POINT('Origin',(-5.8,-5.42192235935956,-9.12)) ;
#163787 = CARTESIAN_POINT('Ctrl Pts',(-5.77574643749636,-5.51893660937409,
-9.12)) ;
#163788 = CARTESIAN_POINT('Ctrl Pts',(-5.77574643749636,-5.51893660937409,
-9.22)) ;
#163789 = CARTESIAN_POINT('Ctrl Pts',(-5.8,-5.42192235935956,-9.22)) ;
#163790 = CARTESIAN_POINT('Ctrl Pts',(-5.79207992677989,-5.52301998169497,
-9.12000000046604)) ;
#163791 = CARTESIAN_POINT('Ctrl Pts',(-5.78430903206643,-5.5210772580166,
-9.21803860456717)) ;
#163792 = CARTESIAN_POINT('Ctrl Pts',(-5.808166653183,-5.42600568595104,-9.22)) ;
#163793 = CARTESIAN_POINT('Ctrl Pts',(-5.80840777707096,-5.52710194426774,
-9.12201005409562)) ;
#163794 = CARTESIAN_POINT('Ctrl Pts',(-5.79341417645231,-5.52335354411309,
-9.21716415018153)) ;
#163795 = CARTESIAN_POINT('Ctrl Pts',(-5.81633079157287,-5.4300877551176,
-9.22100505725278)) ;
#163796 = CARTESIAN_POINT('Ctrl Pts',(-5.82425356250363,-5.53106339062591,
-9.12597149997094)) ;
#163797 = CARTESIAN_POINT('Ctrl Pts',(-5.80269484027818,-5.52567371006955,
-9.21759606942911)) ;
#163798 = CARTESIAN_POINT('Ctrl Pts',(-5.82425356250363,-5.43404914061138,
-9.22298574998547)) ;
#163799 = CARTESIAN_POINT('Origin',(-5.84850712500726,-5.43404914061138,-9.12597149997094)) ;
#163800 = CARTESIAN_POINT('Ctrl Pts',(-5.82426676739349,-5.53106667467168,
-9.1259153963657)) ;
#163801 = CARTESIAN_POINT('Ctrl Pts',(-5.80266988778307,-5.52572362328987,
-9.21764596618925)) ;
#163802 = CARTESIAN_POINT('Ctrl Pts',(-5.82426676352025,-5.43399305345737,
-9.222989033073)) ;
#163803 = CARTESIAN_POINT('Ctrl Pts',(-5.83498671931119,-5.53374818244428,
-9.1312758712786)) ;
#163804 = CARTESIAN_POINT('Ctrl Pts',(-5.80595263122257,-5.5241175471001,
-9.21603989083685)) ;
#163805 = CARTESIAN_POINT('Ctrl Pts',(-5.83498671397637,-5.4393535274938,
-9.22567054003428)) ;
#163806 = CARTESIAN_POINT('Ctrl Pts',(-5.84526105845713,-5.53822480044428,
-9.14022562225452)) ;
#163807 = CARTESIAN_POINT('Ctrl Pts',(-5.81370932746126,-5.52260133464133,
-9.21452367966838)) ;
#163808 = CARTESIAN_POINT('Ctrl Pts',(-5.84526105243735,-5.44830327707035,
-9.23014715682302)) ;
#163809 = CARTESIAN_POINT('Ctrl Pts',(-5.86378685403698,-5.55027438933176,
-9.16432256366359)) ;
#163810 = CARTESIAN_POINT('Ctrl Pts',(-5.83531854275277,-5.5273306855257,
-9.21925303340452)) ;
#163811 = CARTESIAN_POINT('Ctrl Pts',(-5.86378684816472,-5.47240021563471,
-9.24219674395865)) ;
#163812 = CARTESIAN_POINT('Ctrl Pts',(-5.87203852631577,-5.55784608774606,
-9.17946731070693)) ;
#163813 = CARTESIAN_POINT('Ctrl Pts',(-5.84834787930678,-5.5331020048643,
-9.22502435426416)) ;
#163814 = CARTESIAN_POINT('Ctrl Pts',(-5.87203852123051,-5.48754496112629,
-9.24976844179423)) ;
#163815 = CARTESIAN_POINT('Ctrl Pts',(-5.89242747304796,-5.58397198950281,
-9.23173438269412)) ;
#163816 = CARTESIAN_POINT('Ctrl Pts',(-5.88223383300416,-5.56084219746612,
-9.25276455115244)) ;
#163817 = CARTESIAN_POINT('Ctrl Pts',(-5.89242747063508,-5.53981202831252,
-9.27589434338744)) ;
#163818 = CARTESIAN_POINT('Ctrl Pts',(-5.9,-5.60595824049742,-9.27573319883257)) ;
#163819 = CARTESIAN_POINT('Ctrl Pts',(-5.9,-5.59485304775401,-9.28677540438623)) ;
#163820 = CARTESIAN_POINT('Ctrl Pts',(-5.9,-5.58381084219975,-9.29788059711478)) ;
#163821 = CARTESIAN_POINT('Ctrl Pts',(-5.9,-5.62807764064044,-9.32)) ;
#163822 = CARTESIAN_POINT('Ctrl Pts',(-5.9,-5.62807764064044,-9.32)) ;
#163823 = CARTESIAN_POINT('Ctrl Pts',(-5.9,-5.62807764064044,-9.32)) ;
#163824 = CARTESIAN_POINT('Origin',(7.8,2.1,-8.02)) ;
#163825 = CARTESIAN_POINT('Origin',(7.8,2.1,-8.22)) ;
#163826 = CARTESIAN_POINT('Origin',(7.6,2.1,-8.02)) ;
#163827 = CARTESIAN_POINT('Origin',(7.6,2.1,-8.02)) ;
#163828 = CARTESIAN_POINT('Origin',(7.6,2.1,-7.22)) ;
#163829 = CARTESIAN_POINT('Origin',(7.8,2.1,-8.22)) ;
#163830 = CARTESIAN_POINT('Origin',(9.6,2.1,-8.22)) ;
#163831 = CARTESIAN_POINT('Origin',(7.8,2.1,-7.22)) ;
#163832 = CARTESIAN_POINT('Origin',(7.8,2.1,-7.02)) ;
#163833 = CARTESIAN_POINT('Origin',(9.6,2.1,-8.02)) ;
#163834 = CARTESIAN_POINT('Origin',(9.8,2.1,-8.02)) ;
#163835 = CARTESIAN_POINT('Origin',(7.8,2.1,-7.02)) ;
#163836 = CARTESIAN_POINT('Origin',(9.6,2.1,-7.02)) ;
#163837 = CARTESIAN_POINT('Origin',(9.8,2.1,-8.02)) ;
#163838 = CARTESIAN_POINT('Origin',(9.8,2.1,-7.22)) ;
#163839 = CARTESIAN_POINT('Origin',(9.6,2.1,-7.22)) ;
#163840 = CARTESIAN_POINT('Origin',(-4.15,-6.25,-6.87)) ;
#163841 = CARTESIAN_POINT('Origin',(-4.15,-6.3,-6.87)) ;
#163842 = CARTESIAN_POINT('Origin',(-4.15,-6.3,-7.62)) ;
#163843 = CARTESIAN_POINT('Origin',(-4.15,-6.3,-8.37)) ;
#163844 = CARTESIAN_POINT('Origin',(-4.15,-6.3,-6.87)) ;
#163845 = CARTESIAN_POINT('Origin',(-4.15,-6.25,-8.37)) ;
#163846 = CARTESIAN_POINT('Origin',(-4.15,-6.3,-8.37)) ;
#163847 = CARTESIAN_POINT('Origin',(-4.15,-6.3,-6.87)) ;
#163848 = CARTESIAN_POINT('Origin',(-4.15,-6.3,-6.87)) ;
#163849 = CARTESIAN_POINT('Origin',(-4.15,-6.3,-8.37)) ;
#163850 = CARTESIAN_POINT('Origin',(-4.15,-6.3,-8.37)) ;
#163851 = CARTESIAN_POINT('Origin',(-4.65,-6.25,-6.87)) ;
#163852 = CARTESIAN_POINT('Origin',(-4.65,-6.3,-6.87)) ;
#163853 = CARTESIAN_POINT('Origin',(0.,-6.3,-6.87)) ;
#163854 = CARTESIAN_POINT('Origin',(-4.65,-6.3,-6.87)) ;
#163855 = CARTESIAN_POINT('Origin',(0.,-6.3,-8.37)) ;
#163856 = CARTESIAN_POINT('Origin',(-4.65,-6.3,-8.37)) ;
#163857 = CARTESIAN_POINT('Origin',(-4.65,-6.25,-8.37)) ;
#163858 = CARTESIAN_POINT('Origin',(-4.65,-6.3,-8.37)) ;
#163859 = CARTESIAN_POINT('Origin',(-4.65,-6.3,-6.87)) ;
#163860 = CARTESIAN_POINT('Origin',(-4.65,-6.3,-6.87)) ;
#163861 = CARTESIAN_POINT('Origin',(-4.65,-6.3,-8.37)) ;
#163862 = CARTESIAN_POINT('Origin',(-4.65,-6.3,-8.37)) ;
#163863 = CARTESIAN_POINT('Origin',(-4.65,-6.3,-7.62)) ;
#163864 = CARTESIAN_POINT('Origin',(-3.,4.45,-8.72)) ;
#163865 = CARTESIAN_POINT('Origin',(-2.1,4.45,-8.72)) ;
#163866 = CARTESIAN_POINT('Origin',(-2.9,4.45,-8.72)) ;
#163867 = CARTESIAN_POINT('Origin',(-2.9,4.45,-8.52)) ;
#163868 = CARTESIAN_POINT('Origin',(-3.1,4.45,-8.52)) ;
#163869 = CARTESIAN_POINT('Origin',(-2.9,4.45,-8.52)) ;
#163870 = CARTESIAN_POINT('Origin',(-2.1,4.45,-8.52)) ;
#163871 = CARTESIAN_POINT('Origin',(-2.1,4.45,-8.52)) ;
#163872 = CARTESIAN_POINT('Origin',(-1.9,4.45,-8.52)) ;
#163873 = CARTESIAN_POINT('Origin',(-3.1,4.45,-8.62)) ;
#163874 = CARTESIAN_POINT('Origin',(-3.1,4.45,-6.72)) ;
#163875 = CARTESIAN_POINT('Origin',(-2.9,4.4,-8.52)) ;
#163876 = CARTESIAN_POINT('Origin',(-2.9,4.35,-8.52)) ;
#163877 = CARTESIAN_POINT('Origin',(-1.95156391047391E-16,4.35,-8.52)) ;
#163878 = CARTESIAN_POINT('Origin',(-2.1,4.35,-8.52)) ;
#163879 = CARTESIAN_POINT('Origin',(-2.9,4.35,-8.52)) ;
#163880 = CARTESIAN_POINT('Origin',(-2.1,4.4,-8.52)) ;
#163881 = CARTESIAN_POINT('Origin',(-2.1,4.35,-8.52)) ;
#163882 = CARTESIAN_POINT('Origin',(-1.9,4.45,-8.62)) ;
#163883 = CARTESIAN_POINT('Origin',(-1.9,4.45,-6.72)) ;
#163884 = CARTESIAN_POINT('Origin',(-3.,4.45,-6.52)) ;
#163885 = CARTESIAN_POINT('Origin',(-2.9,4.45,-6.52)) ;
#163886 = CARTESIAN_POINT('Origin',(-2.1,4.45,-6.52)) ;
#163887 = CARTESIAN_POINT('Origin',(-2.9,4.45,-6.72)) ;
#163888 = CARTESIAN_POINT('Origin',(-2.9,4.45,-6.72)) ;
#163889 = CARTESIAN_POINT('Origin',(-2.9,4.35,-8.52)) ;
#163890 = CARTESIAN_POINT('Origin',(-2.9,4.35,-8.52)) ;
#163891 = CARTESIAN_POINT('Origin',(-2.1,4.35,-8.52)) ;
#163892 = CARTESIAN_POINT('Origin',(-2.1,4.35,-8.52)) ;
#163893 = CARTESIAN_POINT('Origin',(-2.1,4.45,-6.72)) ;
#163894 = CARTESIAN_POINT('Origin',(-2.1,4.45,-6.72)) ;
#163895 = CARTESIAN_POINT('Origin',(-2.9,4.4,-6.72)) ;
#163896 = CARTESIAN_POINT('Origin',(-2.9,4.35,-6.72)) ;
#163897 = CARTESIAN_POINT('Origin',(-2.9,4.35,-7.62)) ;
#163898 = CARTESIAN_POINT('Origin',(-2.9,4.35,-6.72)) ;
#163899 = CARTESIAN_POINT('Origin',(-2.1,4.35,-7.62)) ;
#163900 = CARTESIAN_POINT('Origin',(-2.1,4.35,-6.72)) ;
#163901 = CARTESIAN_POINT('Origin',(-2.1,4.4,-6.72)) ;
#163902 = CARTESIAN_POINT('Origin',(-2.1,4.35,-6.72)) ;
#163903 = CARTESIAN_POINT('Origin',(-2.9,4.35,-6.72)) ;
#163904 = CARTESIAN_POINT('Origin',(-2.9,4.35,-6.72)) ;
#163905 = CARTESIAN_POINT('Origin',(-2.1,4.35,-6.72)) ;
#163906 = CARTESIAN_POINT('Origin',(-2.1,4.35,-6.72)) ;
#163907 = CARTESIAN_POINT('Origin',(-1.95156391047391E-16,4.35,-6.72)) ;
#163908 = CARTESIAN_POINT('Origin',(-2.25,4.25,-8.37)) ;
#163909 = CARTESIAN_POINT('Origin',(-2.25,4.3,-8.37)) ;
#163910 = CARTESIAN_POINT('Origin',(-2.25,4.3,-7.62)) ;
#163911 = CARTESIAN_POINT('Origin',(-2.25,4.3,-6.87)) ;
#163912 = CARTESIAN_POINT('Origin',(-2.25,4.3,-8.37)) ;
#163913 = CARTESIAN_POINT('Origin',(-2.25,4.25,-6.87)) ;
#163914 = CARTESIAN_POINT('Origin',(-2.25,4.3,-6.87)) ;
#163915 = CARTESIAN_POINT('Origin',(-2.25,4.3,-8.37)) ;
#163916 = CARTESIAN_POINT('Origin',(-2.25,4.3,-8.37)) ;
#163917 = CARTESIAN_POINT('Origin',(-2.25,4.3,-6.87)) ;
#163918 = CARTESIAN_POINT('Origin',(-2.25,4.3,-6.87)) ;
#163919 = CARTESIAN_POINT('Origin',(-2.75,4.25,-8.37)) ;
#163920 = CARTESIAN_POINT('Origin',(-2.75,4.3,-8.37)) ;
#163921 = CARTESIAN_POINT('Origin',(-1.97127667724637E-17,4.3,-8.37)) ;
#163922 = CARTESIAN_POINT('Origin',(-2.75,4.3,-8.37)) ;
#163923 = CARTESIAN_POINT('Origin',(-1.97127667724637E-17,4.3,-6.87)) ;
#163924 = CARTESIAN_POINT('Origin',(-2.75,4.3,-6.87)) ;
#163925 = CARTESIAN_POINT('Origin',(-2.75,4.25,-6.87)) ;
#163926 = CARTESIAN_POINT('Origin',(-2.75,4.3,-6.87)) ;
#163927 = CARTESIAN_POINT('Origin',(-2.75,4.3,-8.37)) ;
#163928 = CARTESIAN_POINT('Origin',(-2.75,4.3,-8.37)) ;
#163929 = CARTESIAN_POINT('Origin',(-2.75,4.3,-6.87)) ;
#163930 = CARTESIAN_POINT('Origin',(-2.75,4.3,-6.87)) ;
#163931 = CARTESIAN_POINT('Origin',(-2.75,4.3,-7.62)) ;
#163932 = CARTESIAN_POINT('Origin',(7.8,2.9,-8.02)) ;
#163933 = CARTESIAN_POINT('Origin',(7.8,2.9,-8.02)) ;
#163934 = CARTESIAN_POINT('Origin',(7.8,2.9,-7.22)) ;
#163935 = CARTESIAN_POINT('Origin',(7.8,2.9,-7.22)) ;
#163936 = CARTESIAN_POINT('Origin',(7.8,2.9,-7.22)) ;
#163937 = CARTESIAN_POINT('Origin',(7.8,2.9,-8.02)) ;
#163938 = CARTESIAN_POINT('Origin',(7.8,2.9,-8.02)) ;
#163939 = CARTESIAN_POINT('Origin',(9.6,2.9,-7.22)) ;
#163940 = CARTESIAN_POINT('Origin',(9.6,2.9,-7.22)) ;
#163941 = CARTESIAN_POINT('Origin',(9.6,2.9,-8.02)) ;
#163942 = CARTESIAN_POINT('Origin',(9.6,2.9,-8.02)) ;
#163943 = CARTESIAN_POINT('Origin',(9.6,2.9,-7.22)) ;
#163944 = CARTESIAN_POINT('Origin',(9.6,2.9,-7.22)) ;
#163945 = CARTESIAN_POINT('Origin',(9.6,2.9,-8.02)) ;
#163946 = CARTESIAN_POINT('Origin',(9.6,2.9,-8.02)) ;
#163947 = CARTESIAN_POINT('Origin',(9.6,2.9,-8.02)) ;
#163948 = CARTESIAN_POINT('Origin',(-0.183301359729408,3.45,-6.10296321352403)) ;
#163949 = CARTESIAN_POINT('Origin',(0.249234641435079,3.15,-7.50377997802131)) ;
#163950 = CARTESIAN_POINT('Origin',(-0.249234641435079,3.15,-7.73622002197869)) ;
#163951 = CARTESIAN_POINT('Origin',(-1.04429375741423,3.45,-6.50445056217769)) ;
#163952 = CARTESIAN_POINT('Origin',(10.1,-2.15,-10.5268804065906)) ;
#163953 = CARTESIAN_POINT('Origin',(10.1,-2.15,-10.5268804065906)) ;
#163954 = CARTESIAN_POINT('Origin',(10.1,-2.15,-10.5268804065906)) ;
#163955 = CARTESIAN_POINT('Origin',(10.1,-2.15,-10.5268804065906)) ;
#163956 = CARTESIAN_POINT('Origin',(10.1,-2.15,-11.43)) ;
#163957 = CARTESIAN_POINT('Origin',(10.1,-2.15,-10.125)) ;
#163958 = CARTESIAN_POINT('Origin',(10.2,-2.15,-10.5268804065906)) ;
#163959 = CARTESIAN_POINT('Origin',(3.7,-2.15,-10.5268804065906)) ;
#163960 = CARTESIAN_POINT('Origin',(10.1,-3.65625,-11.43)) ;
#163961 = CARTESIAN_POINT('Origin',(10.1,-2.15,-12.3331195934094)) ;
#163962 = CARTESIAN_POINT('Origin',(10.1,-3.65625,-10.125)) ;
#163963 = CARTESIAN_POINT('Origin',(10.1,1.9,-10.125)) ;
#163964 = CARTESIAN_POINT('Origin',(10.1,-2.15,-10.125)) ;
#163965 = CARTESIAN_POINT('Origin',(10.1,-2.15,-10.125)) ;
#163966 = CARTESIAN_POINT('Origin',(10.1,-2.15,-10.125)) ;
#163967 = CARTESIAN_POINT('Origin',(3.7,-2.15,-10.5268804065906)) ;
#163968 = CARTESIAN_POINT('Origin',(3.7,-2.32153024911032,-10.6297267659824)) ;
#163969 = CARTESIAN_POINT('Origin',(3.7,-2.35,-10.5268804065906)) ;
#163970 = CARTESIAN_POINT('Origin',(10.1,-2.15,-12.3331195934094)) ;
#163971 = CARTESIAN_POINT('Origin',(10.1,-2.15,-12.3331195934094)) ;
#163972 = CARTESIAN_POINT('Origin',(10.1,-2.15,-12.3331195934094)) ;
#163973 = CARTESIAN_POINT('Origin',(10.1,1.9,-11.43)) ;
#163974 = CARTESIAN_POINT('Origin',(10.1,1.9,-12.735)) ;
#163975 = CARTESIAN_POINT('Origin',(10.1,1.9,-10.125)) ;
#163976 = CARTESIAN_POINT('Origin',(10.2,-2.15,-10.125)) ;
#163977 = CARTESIAN_POINT('Origin',(3.7,-2.15,-10.125)) ;
#163978 = CARTESIAN_POINT('Origin',(3.7,-2.35,-10.025)) ;
#163979 = CARTESIAN_POINT('Origin',(3.7,-2.35,-10.125)) ;
#163980 = CARTESIAN_POINT('Origin',(3.7,-3.65625,-11.43)) ;
#163981 = CARTESIAN_POINT('Origin',(3.7,-2.32153024911032,-12.2302732340176)) ;
#163982 = CARTESIAN_POINT('Origin',(10.2,-2.15,-12.3331195934094)) ;
#163983 = CARTESIAN_POINT('Origin',(3.7,-2.15,-12.3331195934094)) ;
#163984 = CARTESIAN_POINT('Origin',(10.1,-2.15,-11.43)) ;
#163985 = CARTESIAN_POINT('Origin',(10.1,-2.15,-12.735)) ;
#163986 = CARTESIAN_POINT('Origin',(10.1,-3.65625,-12.735)) ;
#163987 = CARTESIAN_POINT('Origin',(10.1,1.9,-12.735)) ;
#163988 = CARTESIAN_POINT('Origin',(10.1,-2.15,-12.735)) ;
#163989 = CARTESIAN_POINT('Origin',(3.7,-2.35,-10.125)) ;
#163990 = CARTESIAN_POINT('Origin',(3.5,-2.35,-10.125)) ;
#163991 = CARTESIAN_POINT('Origin',(3.7,-2.15,-12.3331195934094)) ;
#163992 = CARTESIAN_POINT('Origin',(3.7,-2.35,-12.3331195934094)) ;
#163993 = CARTESIAN_POINT('Origin',(10.1,-2.15,-12.735)) ;
#163994 = CARTESIAN_POINT('Origin',(10.1,-2.15,-12.735)) ;
#163995 = CARTESIAN_POINT('Origin',(3.6,1.9,-9.925)) ;
#163996 = CARTESIAN_POINT('Origin',(3.5,1.9,-9.925)) ;
#163997 = CARTESIAN_POINT('Origin',(2.7,1.9,-9.925)) ;
#163998 = CARTESIAN_POINT('Origin',(3.5,9.86627345095305E-16,-10.125)) ;
#163999 = CARTESIAN_POINT('Origin',(3.5,-5.15,-10.125)) ;
#164000 = CARTESIAN_POINT('Origin',(3.7,-2.35,-12.305)) ;
#164001 = CARTESIAN_POINT('Origin',(3.7,-2.35,-12.735)) ;
#164002 = CARTESIAN_POINT('Origin',(3.6,-2.15,-12.735)) ;
#164003 = CARTESIAN_POINT('Origin',(3.7,-2.15,-12.735)) ;
#164004 = CARTESIAN_POINT('Origin',(2.7,1.9,-9.925)) ;
#164005 = CARTESIAN_POINT('Origin',(2.7,1.9,-9.925)) ;
#164006 = CARTESIAN_POINT('Origin',(3.5,-5.15,-10.125)) ;
#164007 = CARTESIAN_POINT('Origin',(3.5,-5.15,-10.125)) ;
#164008 = CARTESIAN_POINT('Origin',(3.5,-5.15,-10.125)) ;
#164009 = CARTESIAN_POINT('Origin',(3.7,-2.35,-12.735)) ;
#164010 = CARTESIAN_POINT('Origin',(3.5,-2.35,-12.735)) ;
#164011 = CARTESIAN_POINT('Origin',(2.7,2.,-9.925)) ;
#164012 = CARTESIAN_POINT('Origin',(2.7,-5.15,-9.925)) ;
#164013 = CARTESIAN_POINT('Origin',(3.6,-5.15,-10.125)) ;
#164014 = CARTESIAN_POINT('Origin',(2.7,-5.15,-10.125)) ;
#164015 = CARTESIAN_POINT('Origin',(3.5,-5.15,0.)) ;
#164016 = CARTESIAN_POINT('Origin',(3.5,-5.15,-12.735)) ;
#164017 = CARTESIAN_POINT('Origin',(3.5,-1.06453362012003E-15,-12.735)) ;
#164018 = CARTESIAN_POINT('Origin',(3.5,-5.15,-12.735)) ;
#164019 = CARTESIAN_POINT('Origin',(2.7,-5.15,-10.125)) ;
#164020 = CARTESIAN_POINT('Origin',(2.7,-5.35,-10.125)) ;
#164021 = CARTESIAN_POINT('Origin',(3.5,-5.15,-12.735)) ;
#164022 = CARTESIAN_POINT('Origin',(3.5,-5.15,-12.735)) ;
#164023 = CARTESIAN_POINT('Origin',(2.7,-5.35,-10.025)) ;
#164024 = CARTESIAN_POINT('Origin',(2.7,-5.35,-12.735)) ;
#164025 = CARTESIAN_POINT('Origin',(3.6,-5.15,-12.735)) ;
#164026 = CARTESIAN_POINT('Origin',(2.7,-5.15,-12.735)) ;
#164027 = CARTESIAN_POINT('Origin',(3.6,1.9,-12.935)) ;
#164028 = CARTESIAN_POINT('Origin',(3.5,1.9,-12.935)) ;
#164029 = CARTESIAN_POINT('Origin',(2.7,1.9,-12.935)) ;
#164030 = CARTESIAN_POINT('Origin',(2.7,1.9,-12.835)) ;
#164031 = CARTESIAN_POINT('Origin',(2.7,1.9,-13.735)) ;
#164032 = CARTESIAN_POINT('Origin',(2.7,1.9,-12.935)) ;
#164033 = CARTESIAN_POINT('Origin',(2.7,-5.15,-12.735)) ;
#164034 = CARTESIAN_POINT('Origin',(2.7,-5.15,-12.935)) ;
#164035 = CARTESIAN_POINT('Origin',(2.7,1.9,-12.935)) ;
#164036 = CARTESIAN_POINT('Origin',(2.7,1.9,-12.935)) ;
#164037 = CARTESIAN_POINT('Origin',(2.7,-5.25,-12.935)) ;
#164038 = CARTESIAN_POINT('Ctrl Pts',(-3.8,-6.55,-10.33)) ;
#164039 = CARTESIAN_POINT('Ctrl Pts',(-3.8,-6.55,-10.33)) ;
#164040 = CARTESIAN_POINT('Ctrl Pts',(-3.8,-6.55,-10.33)) ;
#164041 = CARTESIAN_POINT('Ctrl Pts',(-3.82625343282639,-6.55,-10.3825068656527)) ;
#164042 = CARTESIAN_POINT('Ctrl Pts',(-3.83954133268484,-6.55,-10.3695413326849)) ;
#164043 = CARTESIAN_POINT('Ctrl Pts',(-3.85250686565269,-6.55,-10.3562534328264)) ;
#164044 = CARTESIAN_POINT('Ctrl Pts',(-3.85219871729854,-6.53922263893877,
-10.4343974345971)) ;
#164045 = CARTESIAN_POINT('Ctrl Pts',(-3.87914655110982,-6.52362528614073,
-10.4091465511098)) ;
#164046 = CARTESIAN_POINT('Ctrl Pts',(-3.90439743459708,-6.53922263893877,
-10.3821987172985)) ;
#164047 = CARTESIAN_POINT('Ctrl Pts',(-3.87996665852871,-6.5114546977086,
-10.4899333170574)) ;
#164048 = CARTESIAN_POINT('Ctrl Pts',(-3.9028838031416,-6.48208554016475,
-10.4328838031416)) ;
#164049 = CARTESIAN_POINT('Ctrl Pts',(-3.95993331705742,-6.5114546977086,
-10.4099666585287)) ;
#164050 = CARTESIAN_POINT('Ctrl Pts',(-3.88737865704135,-6.5003618540841,
-10.5047573140827)) ;
#164051 = CARTESIAN_POINT('Ctrl Pts',(-3.9050130758829,-6.46792722356045,
-10.435013075883)) ;
#164052 = CARTESIAN_POINT('Ctrl Pts',(-3.9747573140827,-6.5003618540841,-10.4173786570414)) ;
#164053 = CARTESIAN_POINT('Ctrl Pts',(-3.8973972494609,-6.47617483238892,
-10.5247944989218)) ;
#164054 = CARTESIAN_POINT('Ctrl Pts',(-3.90329674356413,-6.45094059868423,
-10.4332967435641)) ;
#164055 = CARTESIAN_POINT('Ctrl Pts',(-3.99479449892181,-6.47617483238892,
-10.4273972494609)) ;
#164056 = CARTESIAN_POINT('Ctrl Pts',(-3.9,-6.46309229646327,-10.5299999991817)) ;
#164057 = CARTESIAN_POINT('Ctrl Pts',(-3.90000730395039,-6.4494565015223,
-10.4300073039127)) ;
#164058 = CARTESIAN_POINT('Ctrl Pts',(-3.99999999918173,-6.46309229646328,
-10.43)) ;
#164059 = CARTESIAN_POINT('Ctrl Pts',(-3.9,-6.45,-10.53)) ;
#164060 = CARTESIAN_POINT('Ctrl Pts',(-3.9,-6.45,-10.43)) ;
#164061 = CARTESIAN_POINT('Ctrl Pts',(-4.,-6.45,-10.43)) ;
#164062 = CARTESIAN_POINT('Origin',(-4.,-6.45,-10.53)) ;
#164063 = CARTESIAN_POINT('Origin',(-4.,-6.4,-10.53)) ;
#164064 = CARTESIAN_POINT('Origin',(-4.,-6.35,-10.53)) ;
#164065 = CARTESIAN_POINT('Ctrl Pts',(-5.,-6.55,-10.33)) ;
#164066 = CARTESIAN_POINT('Ctrl Pts',(-5.,-6.55,-10.33)) ;
#164067 = CARTESIAN_POINT('Ctrl Pts',(-5.,-6.55,-10.33)) ;
#164068 = CARTESIAN_POINT('Ctrl Pts',(-4.94749313434721,-6.55,-10.3562534328262)) ;
#164069 = CARTESIAN_POINT('Ctrl Pts',(-4.96045866731606,-6.55,-10.3695413326839)) ;
#164070 = CARTESIAN_POINT('Ctrl Pts',(-4.97374656717352,-6.55,-10.3825068656527)) ;
#164071 = CARTESIAN_POINT('Ctrl Pts',(-4.89560256540291,-6.53922263893879,
-10.3821987172985)) ;
#164072 = CARTESIAN_POINT('Ctrl Pts',(-4.92085344889017,-6.52362528614073,
-10.4091465511097)) ;
#164073 = CARTESIAN_POINT('Ctrl Pts',(-4.94780128270146,-6.53922263893877,
-10.434397434597)) ;
#164074 = CARTESIAN_POINT('Ctrl Pts',(-4.84006668294258,-6.51145469770858,
-10.4099666585287)) ;
#164075 = CARTESIAN_POINT('Ctrl Pts',(-4.8971161968584,-6.48208554016475,
-10.4328838031417)) ;
#164076 = CARTESIAN_POINT('Ctrl Pts',(-4.92003334147129,-6.5114546977086,
-10.4899333170575)) ;
#164077 = CARTESIAN_POINT('Ctrl Pts',(-4.82524268591729,-6.5003618540841,
-10.4173786570414)) ;
#164078 = CARTESIAN_POINT('Ctrl Pts',(-4.89498692411708,-6.46792722356046,
-10.435013075883)) ;
#164079 = CARTESIAN_POINT('Ctrl Pts',(-4.91262134295865,-6.5003618540841,
-10.5047573140827)) ;
#164080 = CARTESIAN_POINT('Ctrl Pts',(-4.80520550107819,-6.47617483238892,
-10.4273972494609)) ;
#164081 = CARTESIAN_POINT('Ctrl Pts',(-4.89670325643589,-6.45094059868422,
-10.4332967435641)) ;
#164082 = CARTESIAN_POINT('Ctrl Pts',(-4.90260275053909,-6.47617483238892,
-10.5247944989218)) ;
#164083 = CARTESIAN_POINT('Ctrl Pts',(-4.80000000081823,-6.46309229646328,
-10.43)) ;
#164084 = CARTESIAN_POINT('Ctrl Pts',(-4.89999269603066,-6.4494565015302,
-10.4300073039128)) ;
#164085 = CARTESIAN_POINT('Ctrl Pts',(-4.9,-6.46309229646328,-10.5299999991817)) ;
#164086 = CARTESIAN_POINT('Ctrl Pts',(-4.8,-6.45,-10.43)) ;
#164087 = CARTESIAN_POINT('Ctrl Pts',(-4.9,-6.45,-10.43)) ;
#164088 = CARTESIAN_POINT('Ctrl Pts',(-4.9,-6.45,-10.53)) ;
#164089 = CARTESIAN_POINT('Origin',(-4.8,-6.45,-10.53)) ;
#164090 = CARTESIAN_POINT('Origin',(-4.,-6.35,-10.53)) ;
#164091 = CARTESIAN_POINT('Origin',(-4.,-6.35,-10.53)) ;
#164092 = CARTESIAN_POINT('Origin',(-4.,-6.35,-10.53)) ;
#164093 = CARTESIAN_POINT('Ctrl Pts',(-3.8,-6.55,-12.53)) ;
#164094 = CARTESIAN_POINT('Ctrl Pts',(-3.8,-6.55,-12.53)) ;
#164095 = CARTESIAN_POINT('Ctrl Pts',(-3.8,-6.55,-12.53)) ;
#164096 = CARTESIAN_POINT('Ctrl Pts',(-3.8525068656527,-6.55,-12.5037465671736)) ;
#164097 = CARTESIAN_POINT('Ctrl Pts',(-3.83954133268456,-6.55,-12.4904586673157)) ;
#164098 = CARTESIAN_POINT('Ctrl Pts',(-3.82625343282636,-6.55,-12.4774931343473)) ;
#164099 = CARTESIAN_POINT('Ctrl Pts',(-3.90439743459706,-6.53922263893877,
-12.4778012827015)) ;
#164100 = CARTESIAN_POINT('Ctrl Pts',(-3.87914655110982,-6.52362528614073,
-12.4508534488902)) ;
#164101 = CARTESIAN_POINT('Ctrl Pts',(-3.85219871729855,-6.53922263893876,
-12.4256025654029)) ;
#164102 = CARTESIAN_POINT('Ctrl Pts',(-3.95993331705743,-6.5114546977086,
-12.4500333414713)) ;
#164103 = CARTESIAN_POINT('Ctrl Pts',(-3.9028838031416,-6.48208554016474,
-12.4271161968584)) ;
#164104 = CARTESIAN_POINT('Ctrl Pts',(-3.8799666585287,-6.5114546977086,-12.3700666829426)) ;
#164105 = CARTESIAN_POINT('Ctrl Pts',(-3.97475731408271,-6.5003618540841,
-12.4426213429587)) ;
#164106 = CARTESIAN_POINT('Ctrl Pts',(-3.90501307588293,-6.46792722356048,
-12.424986924117)) ;
#164107 = CARTESIAN_POINT('Ctrl Pts',(-3.88737865704135,-6.5003618540841,
-12.3552426859173)) ;
#164108 = CARTESIAN_POINT('Ctrl Pts',(-3.9947944989218,-6.47617483238892,
-12.4326027505391)) ;
#164109 = CARTESIAN_POINT('Ctrl Pts',(-3.9032967435641,-6.45094059868419,
-12.4267032564359)) ;
#164110 = CARTESIAN_POINT('Ctrl Pts',(-3.89739724946091,-6.47617483238892,
-12.3352055010782)) ;
#164111 = CARTESIAN_POINT('Ctrl Pts',(-3.99999999918176,-6.46309229646328,
-12.43)) ;
#164112 = CARTESIAN_POINT('Ctrl Pts',(-3.90000730395526,-6.44945650152442,
-12.4299926960872)) ;
#164113 = CARTESIAN_POINT('Ctrl Pts',(-3.9,-6.46309229646328,-12.3300000008183)) ;
#164114 = CARTESIAN_POINT('Ctrl Pts',(-4.,-6.45,-12.43)) ;
#164115 = CARTESIAN_POINT('Ctrl Pts',(-3.9,-6.45,-12.43)) ;
#164116 = CARTESIAN_POINT('Ctrl Pts',(-3.9,-6.45,-12.33)) ;
#164117 = CARTESIAN_POINT('Origin',(-4.,-6.45,-12.33)) ;
#164118 = CARTESIAN_POINT('Origin',(-4.8,-6.4,-10.53)) ;
#164119 = CARTESIAN_POINT('Origin',(-4.8,-6.35,-10.53)) ;
#164120 = CARTESIAN_POINT('Origin',(1.9515639104739E-16,-6.35,-10.53)) ;
#164121 = CARTESIAN_POINT('Origin',(-4.8,-6.35,-10.53)) ;
#164122 = CARTESIAN_POINT('Origin',(-4.,-6.35,-11.43)) ;
#164123 = CARTESIAN_POINT('Origin',(-4.,-6.35,-12.33)) ;
#164124 = CARTESIAN_POINT('Origin',(-4.,-6.4,-12.33)) ;
#164125 = CARTESIAN_POINT('Origin',(-4.,-6.35,-12.33)) ;
#164126 = CARTESIAN_POINT('Origin',(-4.8,-6.35,-10.53)) ;
#164127 = CARTESIAN_POINT('Origin',(-4.8,-6.35,-10.53)) ;
#164128 = CARTESIAN_POINT('Origin',(-4.,-6.35,-12.33)) ;
#164129 = CARTESIAN_POINT('Origin',(-4.,-6.35,-12.33)) ;
#164130 = CARTESIAN_POINT('Origin',(-4.8,-6.35,-11.43)) ;
#164131 = CARTESIAN_POINT('Origin',(-4.8,-6.35,-12.33)) ;
#164132 = CARTESIAN_POINT('Origin',(1.95156391047391E-16,-6.35,-12.33)) ;
#164133 = CARTESIAN_POINT('Origin',(-4.8,-6.35,-12.33)) ;
#164134 = CARTESIAN_POINT('Origin',(-4.8,-6.35,-12.33)) ;
#164135 = CARTESIAN_POINT('Origin',(-4.8,-6.35,-12.33)) ;
#164136 = CARTESIAN_POINT('Origin',(-4.8,-6.4,-12.33)) ;
#164137 = CARTESIAN_POINT('Origin',(-4.8,-6.45,-12.33)) ;
#164138 = CARTESIAN_POINT('Ctrl Pts',(-5.,-6.55,-12.53)) ;
#164139 = CARTESIAN_POINT('Ctrl Pts',(-5.,-6.55,-12.53)) ;
#164140 = CARTESIAN_POINT('Ctrl Pts',(-5.,-6.55,-12.53)) ;
#164141 = CARTESIAN_POINT('Ctrl Pts',(-4.97374656717353,-6.55,-12.4774931343473)) ;
#164142 = CARTESIAN_POINT('Ctrl Pts',(-4.96045866731541,-6.55,-12.4904586673157)) ;
#164143 = CARTESIAN_POINT('Ctrl Pts',(-4.94749313434721,-6.55,-12.5037465671738)) ;
#164144 = CARTESIAN_POINT('Ctrl Pts',(-4.94780128270146,-6.53922263893877,
-12.425602565403)) ;
#164145 = CARTESIAN_POINT('Ctrl Pts',(-4.92085344889015,-6.52362528614073,
-12.4508534488903)) ;
#164146 = CARTESIAN_POINT('Ctrl Pts',(-4.89560256540291,-6.53922263893879,
-12.4778012827015)) ;
#164147 = CARTESIAN_POINT('Ctrl Pts',(-4.92003334147129,-6.5114546977086,
-12.3700666829426)) ;
#164148 = CARTESIAN_POINT('Ctrl Pts',(-4.89711619685841,-6.48208554016475,
-12.4271161968583)) ;
#164149 = CARTESIAN_POINT('Ctrl Pts',(-4.84006668294258,-6.51145469770858,
-12.4500333414713)) ;
#164150 = CARTESIAN_POINT('Ctrl Pts',(-4.91262134295865,-6.5003618540841,
-12.3552426859173)) ;
#164151 = CARTESIAN_POINT('Ctrl Pts',(-4.89498692411706,-6.46792722356048,
-12.424986924117)) ;
#164152 = CARTESIAN_POINT('Ctrl Pts',(-4.82524268591729,-6.5003618540841,
-12.4426213429587)) ;
#164153 = CARTESIAN_POINT('Ctrl Pts',(-4.90260275053909,-6.47617483238892,
-12.3352055010782)) ;
#164154 = CARTESIAN_POINT('Ctrl Pts',(-4.8967032564359,-6.45094059868419,
-12.4267032564359)) ;
#164155 = CARTESIAN_POINT('Ctrl Pts',(-4.80520550107819,-6.47617483238892,
-12.4326027505391)) ;
#164156 = CARTESIAN_POINT('Ctrl Pts',(-4.9,-6.46309229646328,-12.3300000008183)) ;
#164157 = CARTESIAN_POINT('Ctrl Pts',(-4.89999269604004,-6.44945650152635,
-12.4299926960872)) ;
#164158 = CARTESIAN_POINT('Ctrl Pts',(-4.80000000081823,-6.46309229646328,
-12.43)) ;
#164159 = CARTESIAN_POINT('Ctrl Pts',(-4.9,-6.45,-12.33)) ;
#164160 = CARTESIAN_POINT('Ctrl Pts',(-4.9,-6.45,-12.43)) ;
#164161 = CARTESIAN_POINT('Ctrl Pts',(-4.8,-6.45,-12.43)) ;
#164162 = CARTESIAN_POINT('Ctrl Pts',(-5.82426676739351,-5.4339930370061,
-9.82701096596875)) ;
#164163 = CARTESIAN_POINT('Ctrl Pts',(-5.80266988778316,-5.52572360682928,
-9.83235401735051)) ;
#164164 = CARTESIAN_POINT('Ctrl Pts',(-5.82426676352015,-5.53106667371341,
-9.92408458718265)) ;
#164165 = CARTESIAN_POINT('Ctrl Pts',(-5.83498671931116,-5.43935351191906,
-9.82432945819617)) ;
#164166 = CARTESIAN_POINT('Ctrl Pts',(-5.80595263122268,-5.52411753147701,
-9.83396009354034)) ;
#164167 = CARTESIAN_POINT('Ctrl Pts',(-5.83498671397627,-5.53374818067468,
-9.9187241131463)) ;
#164168 = CARTESIAN_POINT('Ctrl Pts',(-5.84526105845716,-5.44830326289491,
-9.81985284019616)) ;
#164169 = CARTESIAN_POINT('Ctrl Pts',(-5.81370932746138,-5.52260132030847,
-9.83547630599898)) ;
#164170 = CARTESIAN_POINT('Ctrl Pts',(-5.84526105243718,-5.53822479746337,
-9.90977436356971)) ;
#164171 = CARTESIAN_POINT('Ctrl Pts',(-5.86378685403699,-5.47240020430401,
-9.80780325130868)) ;
#164172 = CARTESIAN_POINT('Ctrl Pts',(-5.83531854275287,-5.52733067404477,
-9.83074695511466)) ;
#164173 = CARTESIAN_POINT('Ctrl Pts',(-5.86378684816458,-5.55027438459897,
-9.88567742500545)) ;
#164174 = CARTESIAN_POINT('Ctrl Pts',(-5.87203852631578,-5.48754495134734,
-9.80023155289438)) ;
#164175 = CARTESIAN_POINT('Ctrl Pts',(-5.84834787930686,-5.53310199490447,
-9.82497563577609)) ;
#164176 = CARTESIAN_POINT('Ctrl Pts',(-5.87203852123038,-5.55784608243454,
-9.8705326795139)) ;
#164177 = CARTESIAN_POINT('Ctrl Pts',(-5.89242747304797,-5.53981202333454,
-9.7741056511376)) ;
#164178 = CARTESIAN_POINT('Ctrl Pts',(-5.88223383300419,-5.56084219179272,
-9.79723544317417)) ;
#164179 = CARTESIAN_POINT('Ctrl Pts',(-5.892427470635,-5.58397198402772,-9.81826561232779)) ;
#164180 = CARTESIAN_POINT('Ctrl Pts',(-5.9,-5.58381083947299,-9.752119400143)) ;
#164181 = CARTESIAN_POINT('Ctrl Pts',(-5.9,-5.59485304502621,-9.76322459288697)) ;
#164182 = CARTESIAN_POINT('Ctrl Pts',(-5.9,-5.60595823775496,-9.77426679844052)) ;
#164183 = CARTESIAN_POINT('Ctrl Pts',(-5.9,-5.62807764064044,-9.73)) ;
#164184 = CARTESIAN_POINT('Ctrl Pts',(-5.9,-5.62807764064044,-9.73)) ;
#164185 = CARTESIAN_POINT('Ctrl Pts',(-5.9,-5.62807764064044,-9.73)) ;
#164186 = CARTESIAN_POINT('Origin',(-5.84850712500726,-5.43404914061138,-9.92402850002907)) ;
#164187 = CARTESIAN_POINT('Ctrl Pts',(-5.82425356250363,-5.53106339062591,
-9.92402850002907)) ;
#164188 = CARTESIAN_POINT('Ctrl Pts',(-5.80269484027818,-5.52567371006955,
-9.83240393057089)) ;
#164189 = CARTESIAN_POINT('Ctrl Pts',(-5.82425356250363,-5.43404914061138,
-9.82701425001453)) ;
#164190 = CARTESIAN_POINT('Ctrl Pts',(-5.80840777707097,-5.52710194426774,
-9.92798994590438)) ;
#164191 = CARTESIAN_POINT('Ctrl Pts',(-5.7934141764523,-5.52335354411309,
-9.83283584981848)) ;
#164192 = CARTESIAN_POINT('Ctrl Pts',(-5.81633079157287,-5.4300877551176,
-9.82899494274722)) ;
#164193 = CARTESIAN_POINT('Ctrl Pts',(-5.79207992677988,-5.52301998169497,
-9.92999999953396)) ;
#164194 = CARTESIAN_POINT('Ctrl Pts',(-5.78430903206643,-5.52107725801661,
-9.83196139543284)) ;
#164195 = CARTESIAN_POINT('Ctrl Pts',(-5.808166653183,-5.42600568595106,-9.83)) ;
#164196 = CARTESIAN_POINT('Ctrl Pts',(-5.77574643749636,-5.51893660937409,
-9.93)) ;
#164197 = CARTESIAN_POINT('Ctrl Pts',(-5.77574643749636,-5.51893660937409,
-9.83)) ;
#164198 = CARTESIAN_POINT('Ctrl Pts',(-5.8,-5.42192235935956,-9.83)) ;
#164199 = CARTESIAN_POINT('Origin',(-5.8,-5.42192235935956,-9.93)) ;
#164200 = CARTESIAN_POINT('Origin',(-5.8066065036801,-5.42357398527959,-9.93)) ;
#164201 = CARTESIAN_POINT('Origin',(-5.17275707706436,-5.26511162862565,-9.93)) ;
#164202 = CARTESIAN_POINT('Origin',(-5.15068655017073,-5.25959399690224,-9.94059385290894)) ;
#164203 = CARTESIAN_POINT('Origin',(-5.17275707706436,-5.26511162862565,-9.93)) ;
#164204 = CARTESIAN_POINT('Origin',(-5.17275707706436,-5.26511162862565,-9.93)) ;
#164205 = CARTESIAN_POINT('Origin',(-5.17275707706436,-5.26511162862565,-9.93)) ;
#164206 = CARTESIAN_POINT('Origin',(-5.17275707706436,-5.05,-9.93)) ;
#164207 = CARTESIAN_POINT('Origin',(-5.17275707706436,-1.91866427917294,-9.93)) ;
#164208 = CARTESIAN_POINT('Origin',(-3.78014014831103,-3.31128120792626,-10.5984561258016)) ;
#164209 = CARTESIAN_POINT('Origin',(-5.17275707706437,-1.91866427917293,-9.93)) ;
#164210 = CARTESIAN_POINT('Origin',(-5.17275707706436,-1.91866427917293,-9.93)) ;
#164211 = CARTESIAN_POINT('Origin',(-5.17275707706436,-1.91866427917294,-9.93)) ;
#164212 = CARTESIAN_POINT('Origin',(-3.97071067811865,-3.12071067811865,-9.93)) ;
#164213 = CARTESIAN_POINT('Origin',(-5.8,-1.2914213562373,-9.93)) ;
#164214 = CARTESIAN_POINT('Ctrl Pts',(-5.87071067811865,-1.14999999999999,
-9.80071067811865)) ;
#164215 = CARTESIAN_POINT('Ctrl Pts',(-5.8471404520791,-1.10285954792089,
-9.8242809041582)) ;
#164216 = CARTESIAN_POINT('Ctrl Pts',(-5.87071067811865,-1.07928932188134,
-9.87142135623731)) ;
#164217 = CARTESIAN_POINT('Ctrl Pts',(-5.85217562795664,-1.18707010095463,
-9.81924572828067)) ;
#164218 = CARTESIAN_POINT('Ctrl Pts',(-5.81261165662074,-1.13738834337929,
-9.84586147194964)) ;
#164219 = CARTESIAN_POINT('Ctrl Pts',(-5.83353949671041,-1.11646050328958,
-9.90859253638103)) ;
#164220 = CARTESIAN_POINT('Ctrl Pts',(-5.82627077431947,-1.23887980759831,
-9.83)) ;
#164221 = CARTESIAN_POINT('Ctrl Pts',(-5.76566787907945,-1.18433212092055,
-9.84714894371283)) ;
#164222 = CARTESIAN_POINT('Ctrl Pts',(-5.78190678732235,-1.16809321267764,
-9.9299999994186)) ;
#164223 = CARTESIAN_POINT('Ctrl Pts',(-5.8,-1.2914213562373,-9.83)) ;
#164224 = CARTESIAN_POINT('Ctrl Pts',(-5.72928932188134,-1.22071067811865,
-9.83)) ;
#164225 = CARTESIAN_POINT('Ctrl Pts',(-5.72928932188134,-1.22071067811865,
-9.93)) ;
#164226 = CARTESIAN_POINT('Origin',(-5.94142135623731,-1.14999999999999,-9.87142135623731)) ;
#164227 = CARTESIAN_POINT('Ctrl Pts',(-5.9,-1.00857864376269,-9.73)) ;
#164228 = CARTESIAN_POINT('Ctrl Pts',(-5.9,-1.00857864376269,-9.73)) ;
#164229 = CARTESIAN_POINT('Ctrl Pts',(-5.9,-1.00857864376269,-9.73)) ;
#164230 = CARTESIAN_POINT('Ctrl Pts',(-5.9,-1.06112019240168,-9.75627077431956)) ;
#164231 = CARTESIAN_POINT('Ctrl Pts',(-5.9,-1.04860238143836,-9.77002373767573)) ;
#164232 = CARTESIAN_POINT('Ctrl Pts',(-5.9,-1.03484941808221,-9.78254154863898)) ;
#164233 = CARTESIAN_POINT('Ctrl Pts',(-5.88924572828063,-1.11292989904529,
-9.78217562795668)) ;
#164234 = CARTESIAN_POINT('Ctrl Pts',(-5.87451700624548,-1.08721613124892,
-9.80863748748634)) ;
#164235 = CARTESIAN_POINT('Ctrl Pts',(-5.88924572828066,-1.06075427171933,
-9.83435125528267)) ;
#164236 = CARTESIAN_POINT('Ctrl Pts',(-5.87071067811865,-1.14999999999999,
-9.80071067811865)) ;
#164237 = CARTESIAN_POINT('Ctrl Pts',(-5.8471404520791,-1.10285954792089,
-9.82428090415821)) ;
#164238 = CARTESIAN_POINT('Ctrl Pts',(-5.87071067811865,-1.07928932188134,
-9.87142135623731)) ;
#164239 = CARTESIAN_POINT('Ctrl Pts',(-5.87071067811866,-1.14999999999999,
-13.0592893218813)) ;
#164240 = CARTESIAN_POINT('Ctrl Pts',(-5.84714045207911,-1.10285954792089,
-13.0357190958418)) ;
#164241 = CARTESIAN_POINT('Ctrl Pts',(-5.87071067811866,-1.07928932188134,
-12.9885786437627)) ;
#164242 = CARTESIAN_POINT('Ctrl Pts',(-5.88924572828065,-1.11292989904533,
-13.0778243720433)) ;
#164243 = CARTESIAN_POINT('Ctrl Pts',(-5.87451700625929,-1.08721613124107,
-13.0513625125215)) ;
#164244 = CARTESIAN_POINT('Ctrl Pts',(-5.8892457282807,-1.06075427171929,
-13.0256487447173)) ;
#164245 = CARTESIAN_POINT('Ctrl Pts',(-5.9,-1.06112019240165,-13.1037292256804)) ;
#164246 = CARTESIAN_POINT('Ctrl Pts',(-5.9,-1.04860238144452,-13.0899762623181)) ;
#164247 = CARTESIAN_POINT('Ctrl Pts',(-5.9,-1.03484941808214,-13.077458451361)) ;
#164248 = CARTESIAN_POINT('Ctrl Pts',(-5.9,-1.00857864376269,-13.13)) ;
#164249 = CARTESIAN_POINT('Ctrl Pts',(-5.9,-1.00857864376269,-13.13)) ;
#164250 = CARTESIAN_POINT('Ctrl Pts',(-5.9,-1.00857864376269,-13.13)) ;
#164251 = CARTESIAN_POINT('Origin',(-5.94142135623734,-1.14999999999996,-12.9885786437627)) ;
#164252 = CARTESIAN_POINT('Ctrl Pts',(-5.8,-1.2914213562373,-13.03)) ;
#164253 = CARTESIAN_POINT('Ctrl Pts',(-5.72928932188134,-1.22071067811865,
-13.03)) ;
#164254 = CARTESIAN_POINT('Ctrl Pts',(-5.72928932188134,-1.22071067811865,
-12.93)) ;
#164255 = CARTESIAN_POINT('Ctrl Pts',(-5.82627077431945,-1.23887980759835,
-13.03)) ;
#164256 = CARTESIAN_POINT('Ctrl Pts',(-5.76566787907943,-1.18433212092059,
-13.0128510562869)) ;
#164257 = CARTESIAN_POINT('Ctrl Pts',(-5.78190678732238,-1.16809321267762,
-12.9300000005814)) ;
#164258 = CARTESIAN_POINT('Ctrl Pts',(-5.85217562795658,-1.18707010095451,
-13.0407542717193)) ;
#164259 = CARTESIAN_POINT('Ctrl Pts',(-5.81261165662068,-1.13738834337918,
-13.0141385280506)) ;
#164260 = CARTESIAN_POINT('Ctrl Pts',(-5.83353949671039,-1.11646050328961,
-12.951407463619)) ;
#164261 = CARTESIAN_POINT('Ctrl Pts',(-5.87071067811866,-1.14999999999999,
-13.0592893218813)) ;
#164262 = CARTESIAN_POINT('Ctrl Pts',(-5.84714045207911,-1.10285954792089,
-13.0357190958418)) ;
#164263 = CARTESIAN_POINT('Ctrl Pts',(-5.87071067811866,-1.07928932188133,
-12.9885786437627)) ;
#164264 = CARTESIAN_POINT('Origin',(-5.8,-1.29142135623731,-12.93)) ;
#164265 = CARTESIAN_POINT('Origin',(-3.59571067811865,-3.49571067811865,-12.93)) ;
#164266 = CARTESIAN_POINT('Origin',(-5.17275707706436,-1.91866427917293,-12.93)) ;
#164267 = CARTESIAN_POINT('Origin',(-3.09057773798104,-4.00084361825625,-11.93055391724)) ;
#164268 = CARTESIAN_POINT('Origin',(-5.17275707706436,-1.91866427917294,-12.93)) ;
#164269 = CARTESIAN_POINT('Origin',(-5.17275707706436,-1.91866427917293,-12.93)) ;
#164270 = CARTESIAN_POINT('Origin',(-5.17275707706436,-1.91866427917293,-12.93)) ;
#164271 = CARTESIAN_POINT('Origin',(-5.17275707706436,-5.05,-12.93)) ;
#164272 = CARTESIAN_POINT('Origin',(-5.17275707706436,-5.26511162862565,-12.93)) ;
#164273 = CARTESIAN_POINT('Origin',(-3.96111272388873,-4.96220054033175,-12.3484107104757)) ;
#164274 = CARTESIAN_POINT('Origin',(-5.17275707706437,-5.26511162862565,-12.93)) ;
#164275 = CARTESIAN_POINT('Origin',(-5.17275707706436,-5.26511162862565,-12.93)) ;
#164276 = CARTESIAN_POINT('Origin',(-5.17275707706436,-5.26511162862565,-12.93)) ;
#164277 = CARTESIAN_POINT('Origin',(-5.10072415073893,-5.24710339704429,-12.93)) ;
#164278 = CARTESIAN_POINT('Origin',(-5.8,-5.42192235935956,-12.93)) ;
#164279 = CARTESIAN_POINT('Ctrl Pts',(-5.77574643749636,-5.51893660937409,
-12.93)) ;
#164280 = CARTESIAN_POINT('Ctrl Pts',(-5.77574643749636,-5.51893660937409,
-13.03)) ;
#164281 = CARTESIAN_POINT('Ctrl Pts',(-5.8,-5.42192235935956,-13.03)) ;
#164282 = CARTESIAN_POINT('Ctrl Pts',(-5.79207992677988,-5.52301998169497,
-12.930000000466)) ;
#164283 = CARTESIAN_POINT('Ctrl Pts',(-5.78430903206646,-5.52107725801655,
-13.0280386045672)) ;
#164284 = CARTESIAN_POINT('Ctrl Pts',(-5.808166653183,-5.42600568595104,-13.03)) ;
#164285 = CARTESIAN_POINT('Ctrl Pts',(-5.80840777707096,-5.52710194426774,
-12.9320100540956)) ;
#164286 = CARTESIAN_POINT('Ctrl Pts',(-5.7934141764523,-5.52335354411304,
-13.0271641501816)) ;
#164287 = CARTESIAN_POINT('Ctrl Pts',(-5.81633079157287,-5.4300877551176,
-13.0310050572528)) ;
#164288 = CARTESIAN_POINT('Ctrl Pts',(-5.82425356250363,-5.53106339062591,
-12.9359714999709)) ;
#164289 = CARTESIAN_POINT('Ctrl Pts',(-5.80269484027818,-5.52567371006955,
-13.0275960694291)) ;
#164290 = CARTESIAN_POINT('Ctrl Pts',(-5.82425356250363,-5.43404914061138,
-13.0329857499855)) ;
#164291 = CARTESIAN_POINT('Origin',(-5.84850712500726,-5.43404914061138,-12.9359714999709)) ;
#164292 = CARTESIAN_POINT('Ctrl Pts',(-5.82426676739353,-5.53106667467168,
-12.9359153963655)) ;
#164293 = CARTESIAN_POINT('Ctrl Pts',(-5.80266988778304,-5.52572362328999,
-13.0276459661892)) ;
#164294 = CARTESIAN_POINT('Ctrl Pts',(-5.82426676352026,-5.43399305345736,
-13.0329890330731)) ;
#164295 = CARTESIAN_POINT('Ctrl Pts',(-5.83498671931122,-5.53374818244429,
-12.9412758712785)) ;
#164296 = CARTESIAN_POINT('Ctrl Pts',(-5.80595263122252,-5.52411754710016,
-13.0260398908369)) ;
#164297 = CARTESIAN_POINT('Ctrl Pts',(-5.83498671397638,-5.4393535274938,
-13.0356705400343)) ;
#164298 = CARTESIAN_POINT('Ctrl Pts',(-5.84526105845717,-5.53822480044429,
-12.9502256222545)) ;
#164299 = CARTESIAN_POINT('Ctrl Pts',(-5.81370932746123,-5.52260133464142,
-13.0245236796683)) ;
#164300 = CARTESIAN_POINT('Ctrl Pts',(-5.84526105243736,-5.44830327707034,
-13.0401471568231)) ;
#164301 = CARTESIAN_POINT('Ctrl Pts',(-5.86378685403702,-5.5502743893318,
-12.9743225636635)) ;
#164302 = CARTESIAN_POINT('Ctrl Pts',(-5.83531854275273,-5.52733068552576,
-13.0292530334046)) ;
#164303 = CARTESIAN_POINT('Ctrl Pts',(-5.86378684816473,-5.47240021563469,
-13.0521967439587)) ;
#164304 = CARTESIAN_POINT('Ctrl Pts',(-5.87203852631581,-5.5578460877461,
-12.9894673107069)) ;
#164305 = CARTESIAN_POINT('Ctrl Pts',(-5.84834787930675,-5.53310200486434,
-13.0350243542641)) ;
#164306 = CARTESIAN_POINT('Ctrl Pts',(-5.87203852123052,-5.48754496112629,
-13.0597684417942)) ;
#164307 = CARTESIAN_POINT('Ctrl Pts',(-5.89242747304798,-5.58397198950286,
-13.0417343826941)) ;
#164308 = CARTESIAN_POINT('Ctrl Pts',(-5.88223383300414,-5.56084219746614,
-13.0627645511524)) ;
#164309 = CARTESIAN_POINT('Ctrl Pts',(-5.89242747063508,-5.53981202831252,
-13.0858943433875)) ;
#164310 = CARTESIAN_POINT('Ctrl Pts',(-5.9,-5.60595824049745,-13.0857331988325)) ;
#164311 = CARTESIAN_POINT('Ctrl Pts',(-5.9,-5.59485304775402,-13.0967754043861)) ;
#164312 = CARTESIAN_POINT('Ctrl Pts',(-5.9,-5.58381084219975,-13.1078805971148)) ;
#164313 = CARTESIAN_POINT('Ctrl Pts',(-5.9,-5.62807764064044,-13.13)) ;
#164314 = CARTESIAN_POINT('Ctrl Pts',(-5.9,-5.62807764064044,-13.13)) ;
#164315 = CARTESIAN_POINT('Ctrl Pts',(-5.9,-5.62807764064044,-13.13)) ;
#164316 = CARTESIAN_POINT('Origin',(7.8,2.1,-11.83)) ;
#164317 = CARTESIAN_POINT('Origin',(7.8,2.1,-12.03)) ;
#164318 = CARTESIAN_POINT('Origin',(7.6,2.1,-11.83)) ;
#164319 = CARTESIAN_POINT('Origin',(7.6,2.1,-11.83)) ;
#164320 = CARTESIAN_POINT('Origin',(7.6,2.1,-11.03)) ;
#164321 = CARTESIAN_POINT('Origin',(7.8,2.1,-12.03)) ;
#164322 = CARTESIAN_POINT('Origin',(9.6,2.1,-12.03)) ;
#164323 = CARTESIAN_POINT('Origin',(7.8,2.1,-11.03)) ;
#164324 = CARTESIAN_POINT('Origin',(7.8,2.1,-10.83)) ;
#164325 = CARTESIAN_POINT('Origin',(9.6,2.1,-11.83)) ;
#164326 = CARTESIAN_POINT('Origin',(9.8,2.1,-11.83)) ;
#164327 = CARTESIAN_POINT('Origin',(7.8,2.1,-10.83)) ;
#164328 = CARTESIAN_POINT('Origin',(9.6,2.1,-10.83)) ;
#164329 = CARTESIAN_POINT('Origin',(9.8,2.1,-11.83)) ;
#164330 = CARTESIAN_POINT('Origin',(9.8,2.1,-11.03)) ;
#164331 = CARTESIAN_POINT('Origin',(9.6,2.1,-11.03)) ;
#164332 = CARTESIAN_POINT('Origin',(-4.15,-6.25,-10.68)) ;
#164333 = CARTESIAN_POINT('Origin',(-4.15,-6.3,-10.68)) ;
#164334 = CARTESIAN_POINT('Origin',(-4.15,-6.3,-11.43)) ;
#164335 = CARTESIAN_POINT('Origin',(-4.15,-6.3,-12.18)) ;
#164336 = CARTESIAN_POINT('Origin',(-4.15,-6.3,-10.68)) ;
#164337 = CARTESIAN_POINT('Origin',(-4.15,-6.25,-12.18)) ;
#164338 = CARTESIAN_POINT('Origin',(-4.15,-6.3,-12.18)) ;
#164339 = CARTESIAN_POINT('Origin',(-4.15,-6.3,-10.68)) ;
#164340 = CARTESIAN_POINT('Origin',(-4.15,-6.3,-10.68)) ;
#164341 = CARTESIAN_POINT('Origin',(-4.15,-6.3,-12.18)) ;
#164342 = CARTESIAN_POINT('Origin',(-4.15,-6.3,-12.18)) ;
#164343 = CARTESIAN_POINT('Origin',(-4.65,-6.25,-10.68)) ;
#164344 = CARTESIAN_POINT('Origin',(-4.65,-6.3,-10.68)) ;
#164345 = CARTESIAN_POINT('Origin',(0.,-6.3,-10.68)) ;
#164346 = CARTESIAN_POINT('Origin',(-4.65,-6.3,-10.68)) ;
#164347 = CARTESIAN_POINT('Origin',(0.,-6.3,-12.18)) ;
#164348 = CARTESIAN_POINT('Origin',(-4.65,-6.3,-12.18)) ;
#164349 = CARTESIAN_POINT('Origin',(-4.65,-6.25,-12.18)) ;
#164350 = CARTESIAN_POINT('Origin',(-4.65,-6.3,-12.18)) ;
#164351 = CARTESIAN_POINT('Origin',(-4.65,-6.3,-10.68)) ;
#164352 = CARTESIAN_POINT('Origin',(-4.65,-6.3,-10.68)) ;
#164353 = CARTESIAN_POINT('Origin',(-4.65,-6.3,-12.18)) ;
#164354 = CARTESIAN_POINT('Origin',(-4.65,-6.3,-12.18)) ;
#164355 = CARTESIAN_POINT('Origin',(-4.65,-6.3,-11.43)) ;
#164356 = CARTESIAN_POINT('Origin',(-3.,4.45,-12.53)) ;
#164357 = CARTESIAN_POINT('Origin',(-2.1,4.45,-12.53)) ;
#164358 = CARTESIAN_POINT('Origin',(-2.9,4.45,-12.53)) ;
#164359 = CARTESIAN_POINT('Origin',(-2.9,4.45,-12.33)) ;
#164360 = CARTESIAN_POINT('Origin',(-3.1,4.45,-12.33)) ;
#164361 = CARTESIAN_POINT('Origin',(-2.9,4.45,-12.33)) ;
#164362 = CARTESIAN_POINT('Origin',(-2.1,4.45,-12.33)) ;
#164363 = CARTESIAN_POINT('Origin',(-2.1,4.45,-12.33)) ;
#164364 = CARTESIAN_POINT('Origin',(-1.9,4.45,-12.33)) ;
#164365 = CARTESIAN_POINT('Origin',(-3.1,4.45,-12.43)) ;
#164366 = CARTESIAN_POINT('Origin',(-3.1,4.45,-10.53)) ;
#164367 = CARTESIAN_POINT('Origin',(-2.9,4.4,-12.33)) ;
#164368 = CARTESIAN_POINT('Origin',(-2.9,4.35,-12.33)) ;
#164369 = CARTESIAN_POINT('Origin',(-1.95156391047391E-16,4.35,-12.33)) ;
#164370 = CARTESIAN_POINT('Origin',(-2.1,4.35,-12.33)) ;
#164371 = CARTESIAN_POINT('Origin',(-2.9,4.35,-12.33)) ;
#164372 = CARTESIAN_POINT('Origin',(-2.1,4.4,-12.33)) ;
#164373 = CARTESIAN_POINT('Origin',(-2.1,4.35,-12.33)) ;
#164374 = CARTESIAN_POINT('Origin',(-1.9,4.45,-12.43)) ;
#164375 = CARTESIAN_POINT('Origin',(-1.9,4.45,-10.53)) ;
#164376 = CARTESIAN_POINT('Origin',(-3.,4.45,-10.33)) ;
#164377 = CARTESIAN_POINT('Origin',(-2.9,4.45,-10.33)) ;
#164378 = CARTESIAN_POINT('Origin',(-2.1,4.45,-10.33)) ;
#164379 = CARTESIAN_POINT('Origin',(-2.9,4.45,-10.53)) ;
#164380 = CARTESIAN_POINT('Origin',(-2.9,4.45,-10.53)) ;
#164381 = CARTESIAN_POINT('Origin',(-2.9,4.35,-12.33)) ;
#164382 = CARTESIAN_POINT('Origin',(-2.9,4.35,-12.33)) ;
#164383 = CARTESIAN_POINT('Origin',(-2.1,4.35,-12.33)) ;
#164384 = CARTESIAN_POINT('Origin',(-2.1,4.35,-12.33)) ;
#164385 = CARTESIAN_POINT('Origin',(-2.1,4.45,-10.53)) ;
#164386 = CARTESIAN_POINT('Origin',(-2.1,4.45,-10.53)) ;
#164387 = CARTESIAN_POINT('Origin',(-2.9,4.4,-10.53)) ;
#164388 = CARTESIAN_POINT('Origin',(-2.9,4.35,-10.53)) ;
#164389 = CARTESIAN_POINT('Origin',(-2.9,4.35,-11.43)) ;
#164390 = CARTESIAN_POINT('Origin',(-2.9,4.35,-10.53)) ;
#164391 = CARTESIAN_POINT('Origin',(-2.1,4.35,-11.43)) ;
#164392 = CARTESIAN_POINT('Origin',(-2.1,4.35,-10.53)) ;
#164393 = CARTESIAN_POINT('Origin',(-2.1,4.4,-10.53)) ;
#164394 = CARTESIAN_POINT('Origin',(-2.1,4.35,-10.53)) ;
#164395 = CARTESIAN_POINT('Origin',(-2.9,4.35,-10.53)) ;
#164396 = CARTESIAN_POINT('Origin',(-2.9,4.35,-10.53)) ;
#164397 = CARTESIAN_POINT('Origin',(-2.1,4.35,-10.53)) ;
#164398 = CARTESIAN_POINT('Origin',(-2.1,4.35,-10.53)) ;
#164399 = CARTESIAN_POINT('Origin',(-1.95156391047391E-16,4.35,-10.53)) ;
#164400 = CARTESIAN_POINT('Origin',(-2.25,4.25,-12.18)) ;
#164401 = CARTESIAN_POINT('Origin',(-2.25,4.3,-12.18)) ;
#164402 = CARTESIAN_POINT('Origin',(-2.25,4.3,-11.43)) ;
#164403 = CARTESIAN_POINT('Origin',(-2.25,4.3,-10.68)) ;
#164404 = CARTESIAN_POINT('Origin',(-2.25,4.3,-12.18)) ;
#164405 = CARTESIAN_POINT('Origin',(-2.25,4.25,-10.68)) ;
#164406 = CARTESIAN_POINT('Origin',(-2.25,4.3,-10.68)) ;
#164407 = CARTESIAN_POINT('Origin',(-2.25,4.3,-12.18)) ;
#164408 = CARTESIAN_POINT('Origin',(-2.25,4.3,-12.18)) ;
#164409 = CARTESIAN_POINT('Origin',(-2.25,4.3,-10.68)) ;
#164410 = CARTESIAN_POINT('Origin',(-2.25,4.3,-10.68)) ;
#164411 = CARTESIAN_POINT('Origin',(-2.75,4.25,-12.18)) ;
#164412 = CARTESIAN_POINT('Origin',(-2.75,4.3,-12.18)) ;
#164413 = CARTESIAN_POINT('Origin',(-1.97127667724637E-17,4.3,-12.18)) ;
#164414 = CARTESIAN_POINT('Origin',(-2.75,4.3,-12.18)) ;
#164415 = CARTESIAN_POINT('Origin',(-1.97127667724637E-17,4.3,-10.68)) ;
#164416 = CARTESIAN_POINT('Origin',(-2.75,4.3,-10.68)) ;
#164417 = CARTESIAN_POINT('Origin',(-2.75,4.25,-10.68)) ;
#164418 = CARTESIAN_POINT('Origin',(-2.75,4.3,-10.68)) ;
#164419 = CARTESIAN_POINT('Origin',(-2.75,4.3,-12.18)) ;
#164420 = CARTESIAN_POINT('Origin',(-2.75,4.3,-12.18)) ;
#164421 = CARTESIAN_POINT('Origin',(-2.75,4.3,-10.68)) ;
#164422 = CARTESIAN_POINT('Origin',(-2.75,4.3,-10.68)) ;
#164423 = CARTESIAN_POINT('Origin',(-2.75,4.3,-11.43)) ;
#164424 = CARTESIAN_POINT('Origin',(7.8,2.9,-11.83)) ;
#164425 = CARTESIAN_POINT('Origin',(7.8,2.9,-11.83)) ;
#164426 = CARTESIAN_POINT('Origin',(7.8,2.9,-11.03)) ;
#164427 = CARTESIAN_POINT('Origin',(7.8,2.9,-11.03)) ;
#164428 = CARTESIAN_POINT('Origin',(7.8,2.9,-11.03)) ;
#164429 = CARTESIAN_POINT('Origin',(7.8,2.9,-11.83)) ;
#164430 = CARTESIAN_POINT('Origin',(7.8,2.9,-11.83)) ;
#164431 = CARTESIAN_POINT('Origin',(9.6,2.9,-11.03)) ;
#164432 = CARTESIAN_POINT('Origin',(9.6,2.9,-11.03)) ;
#164433 = CARTESIAN_POINT('Origin',(9.6,2.9,-11.83)) ;
#164434 = CARTESIAN_POINT('Origin',(9.6,2.9,-11.83)) ;
#164435 = CARTESIAN_POINT('Origin',(9.6,2.9,-11.03)) ;
#164436 = CARTESIAN_POINT('Origin',(9.6,2.9,-11.03)) ;
#164437 = CARTESIAN_POINT('Origin',(9.6,2.9,-11.83)) ;
#164438 = CARTESIAN_POINT('Origin',(9.6,2.9,-11.83)) ;
#164439 = CARTESIAN_POINT('Origin',(9.6,2.9,-11.83)) ;
#164440 = CARTESIAN_POINT('Origin',(-0.183301359729408,3.45,-9.91296321352402)) ;
#164441 = CARTESIAN_POINT('Origin',(0.249234641435079,3.15,-11.3137799780213)) ;
#164442 = CARTESIAN_POINT('Origin',(-0.249234641435079,3.15,-11.5462200219787)) ;
#164443 = CARTESIAN_POINT('Origin',(-1.04429375741423,3.45,-10.3144505621777)) ;
#164444 = CARTESIAN_POINT('Origin',(10.1,-2.15,-14.3368804065906)) ;
#164445 = CARTESIAN_POINT('Origin',(10.1,-2.15,-14.3368804065906)) ;
#164446 = CARTESIAN_POINT('Origin',(10.1,-2.15,-14.3368804065906)) ;
#164447 = CARTESIAN_POINT('Origin',(10.1,-2.15,-14.3368804065906)) ;
#164448 = CARTESIAN_POINT('Origin',(10.1,-2.15,-15.24)) ;
#164449 = CARTESIAN_POINT('Origin',(10.1,-2.15,-13.935)) ;
#164450 = CARTESIAN_POINT('Origin',(10.2,-2.15,-14.3368804065906)) ;
#164451 = CARTESIAN_POINT('Origin',(3.7,-2.15,-14.3368804065906)) ;
#164452 = CARTESIAN_POINT('Origin',(10.1,-3.65625,-15.24)) ;
#164453 = CARTESIAN_POINT('Origin',(10.1,-2.15,-16.1431195934094)) ;
#164454 = CARTESIAN_POINT('Origin',(10.1,-3.65625,-13.935)) ;
#164455 = CARTESIAN_POINT('Origin',(10.1,1.9,-13.935)) ;
#164456 = CARTESIAN_POINT('Origin',(10.1,-2.15,-13.935)) ;
#164457 = CARTESIAN_POINT('Origin',(10.1,-2.15,-13.935)) ;
#164458 = CARTESIAN_POINT('Origin',(10.1,-2.15,-13.935)) ;
#164459 = CARTESIAN_POINT('Origin',(3.7,-2.15,-14.3368804065906)) ;
#164460 = CARTESIAN_POINT('Origin',(3.7,-2.32153024911032,-14.4397267659824)) ;
#164461 = CARTESIAN_POINT('Origin',(3.7,-2.35,-14.3368804065906)) ;
#164462 = CARTESIAN_POINT('Origin',(10.1,-2.15,-16.1431195934094)) ;
#164463 = CARTESIAN_POINT('Origin',(10.1,-2.15,-16.1431195934094)) ;
#164464 = CARTESIAN_POINT('Origin',(10.1,-2.15,-16.1431195934094)) ;
#164465 = CARTESIAN_POINT('Origin',(10.1,1.9,-15.24)) ;
#164466 = CARTESIAN_POINT('Origin',(10.1,1.9,-16.545)) ;
#164467 = CARTESIAN_POINT('Origin',(10.1,1.9,-13.935)) ;
#164468 = CARTESIAN_POINT('Origin',(10.2,-2.15,-13.935)) ;
#164469 = CARTESIAN_POINT('Origin',(3.7,-2.15,-13.935)) ;
#164470 = CARTESIAN_POINT('Origin',(3.7,-2.35,-13.835)) ;
#164471 = CARTESIAN_POINT('Origin',(3.7,-2.35,-13.935)) ;
#164472 = CARTESIAN_POINT('Origin',(3.7,-3.65625,-15.24)) ;
#164473 = CARTESIAN_POINT('Origin',(3.7,-2.32153024911032,-16.0402732340176)) ;
#164474 = CARTESIAN_POINT('Origin',(10.2,-2.15,-16.1431195934094)) ;
#164475 = CARTESIAN_POINT('Origin',(3.7,-2.15,-16.1431195934094)) ;
#164476 = CARTESIAN_POINT('Origin',(10.1,-2.15,-15.24)) ;
#164477 = CARTESIAN_POINT('Origin',(10.1,-2.15,-16.545)) ;
#164478 = CARTESIAN_POINT('Origin',(10.1,-3.65625,-16.545)) ;
#164479 = CARTESIAN_POINT('Origin',(10.1,1.9,-16.545)) ;
#164480 = CARTESIAN_POINT('Origin',(10.1,-2.15,-16.545)) ;
#164481 = CARTESIAN_POINT('Origin',(3.7,-2.35,-13.935)) ;
#164482 = CARTESIAN_POINT('Origin',(3.5,-2.35,-13.935)) ;
#164483 = CARTESIAN_POINT('Origin',(3.7,-2.15,-16.1431195934094)) ;
#164484 = CARTESIAN_POINT('Origin',(3.7,-2.35,-16.1431195934094)) ;
#164485 = CARTESIAN_POINT('Origin',(10.1,-2.15,-16.545)) ;
#164486 = CARTESIAN_POINT('Origin',(10.1,-2.15,-16.545)) ;
#164487 = CARTESIAN_POINT('Origin',(3.6,1.9,-13.735)) ;
#164488 = CARTESIAN_POINT('Origin',(3.5,1.9,-13.735)) ;
#164489 = CARTESIAN_POINT('Origin',(2.7,1.9,-13.735)) ;
#164490 = CARTESIAN_POINT('Origin',(3.5,1.32848750596453E-15,-13.935)) ;
#164491 = CARTESIAN_POINT('Origin',(3.5,-5.15,-13.935)) ;
#164492 = CARTESIAN_POINT('Origin',(3.7,-2.35,-16.115)) ;
#164493 = CARTESIAN_POINT('Origin',(3.7,-2.35,-16.545)) ;
#164494 = CARTESIAN_POINT('Origin',(3.6,-2.15,-16.545)) ;
#164495 = CARTESIAN_POINT('Origin',(3.7,-2.15,-16.545)) ;
#164496 = CARTESIAN_POINT('Origin',(2.7,1.9,-13.735)) ;
#164497 = CARTESIAN_POINT('Origin',(2.7,1.9,-13.735)) ;
#164498 = CARTESIAN_POINT('Origin',(3.5,-5.15,-13.935)) ;
#164499 = CARTESIAN_POINT('Origin',(3.5,-5.15,-13.935)) ;
#164500 = CARTESIAN_POINT('Origin',(3.5,-5.15,-13.935)) ;
#164501 = CARTESIAN_POINT('Origin',(3.7,-2.35,-16.545)) ;
#164502 = CARTESIAN_POINT('Origin',(3.5,-2.35,-16.545)) ;
#164503 = CARTESIAN_POINT('Origin',(2.7,2.,-13.735)) ;
#164504 = CARTESIAN_POINT('Origin',(2.7,-5.15,-13.735)) ;
#164505 = CARTESIAN_POINT('Origin',(3.6,-5.15,-13.935)) ;
#164506 = CARTESIAN_POINT('Origin',(2.7,-5.15,-13.935)) ;
#164507 = CARTESIAN_POINT('Origin',(3.5,-5.15,0.)) ;
#164508 = CARTESIAN_POINT('Origin',(3.5,-5.15,-16.545)) ;
#164509 = CARTESIAN_POINT('Origin',(3.5,-1.40639378098925E-15,-16.545)) ;
#164510 = CARTESIAN_POINT('Origin',(3.5,-5.15,-16.545)) ;
#164511 = CARTESIAN_POINT('Origin',(2.7,-5.15,-13.935)) ;
#164512 = CARTESIAN_POINT('Origin',(2.7,-5.35,-13.935)) ;
#164513 = CARTESIAN_POINT('Origin',(3.5,-5.15,-16.545)) ;
#164514 = CARTESIAN_POINT('Origin',(3.5,-5.15,-16.545)) ;
#164515 = CARTESIAN_POINT('Origin',(2.7,-5.35,-13.835)) ;
#164516 = CARTESIAN_POINT('Origin',(2.7,-5.35,-16.545)) ;
#164517 = CARTESIAN_POINT('Origin',(3.6,-5.15,-16.545)) ;
#164518 = CARTESIAN_POINT('Origin',(2.7,-5.15,-16.545)) ;
#164519 = CARTESIAN_POINT('Origin',(3.6,1.9,-16.745)) ;
#164520 = CARTESIAN_POINT('Origin',(3.5,1.9,-16.745)) ;
#164521 = CARTESIAN_POINT('Origin',(2.7,1.9,-16.745)) ;
#164522 = CARTESIAN_POINT('Origin',(2.7,1.9,-16.645)) ;
#164523 = CARTESIAN_POINT('Origin',(2.7,1.9,-17.545)) ;
#164524 = CARTESIAN_POINT('Origin',(2.7,1.9,-16.745)) ;
#164525 = CARTESIAN_POINT('Origin',(2.7,-5.15,-16.545)) ;
#164526 = CARTESIAN_POINT('Origin',(2.7,-5.15,-16.745)) ;
#164527 = CARTESIAN_POINT('Origin',(2.7,1.9,-16.745)) ;
#164528 = CARTESIAN_POINT('Origin',(2.7,1.9,-16.745)) ;
#164529 = CARTESIAN_POINT('Origin',(2.7,-5.25,-16.745)) ;
#164530 = CARTESIAN_POINT('Ctrl Pts',(-3.8,-6.55,-14.14)) ;
#164531 = CARTESIAN_POINT('Ctrl Pts',(-3.8,-6.55,-14.14)) ;
#164532 = CARTESIAN_POINT('Ctrl Pts',(-3.8,-6.55,-14.14)) ;
#164533 = CARTESIAN_POINT('Ctrl Pts',(-3.8262534328264,-6.55,-14.1925068656527)) ;
#164534 = CARTESIAN_POINT('Ctrl Pts',(-3.83954133268484,-6.55,-14.1795413326849)) ;
#164535 = CARTESIAN_POINT('Ctrl Pts',(-3.85250686565269,-6.55,-14.1662534328264)) ;
#164536 = CARTESIAN_POINT('Ctrl Pts',(-3.85219871729854,-6.53922263893877,
-14.2443974345971)) ;
#164537 = CARTESIAN_POINT('Ctrl Pts',(-3.87914655110982,-6.52362528614073,
-14.2191465511098)) ;
#164538 = CARTESIAN_POINT('Ctrl Pts',(-3.90439743459708,-6.53922263893877,
-14.1921987172985)) ;
#164539 = CARTESIAN_POINT('Ctrl Pts',(-3.87996665852871,-6.5114546977086,
-14.2999333170574)) ;
#164540 = CARTESIAN_POINT('Ctrl Pts',(-3.9028838031416,-6.48208554016475,
-14.2428838031416)) ;
#164541 = CARTESIAN_POINT('Ctrl Pts',(-3.95993331705742,-6.5114546977086,
-14.2199666585287)) ;
#164542 = CARTESIAN_POINT('Ctrl Pts',(-3.88737865704135,-6.5003618540841,
-14.3147573140827)) ;
#164543 = CARTESIAN_POINT('Ctrl Pts',(-3.90501307588294,-6.46792722356047,
-14.2450130758829)) ;
#164544 = CARTESIAN_POINT('Ctrl Pts',(-3.9747573140827,-6.5003618540841,-14.2273786570414)) ;
#164545 = CARTESIAN_POINT('Ctrl Pts',(-3.8973972494609,-6.47617483238892,
-14.3347944989218)) ;
#164546 = CARTESIAN_POINT('Ctrl Pts',(-3.90329674356409,-6.4509405986842,
-14.2432967435641)) ;
#164547 = CARTESIAN_POINT('Ctrl Pts',(-3.99479449892181,-6.47617483238892,
-14.2373972494609)) ;
#164548 = CARTESIAN_POINT('Ctrl Pts',(-3.9,-6.46309229646327,-14.3399999991817)) ;
#164549 = CARTESIAN_POINT('Ctrl Pts',(-3.90000730393163,-6.44945650151458,
-14.2400073039128)) ;
#164550 = CARTESIAN_POINT('Ctrl Pts',(-3.99999999918173,-6.46309229646328,
-14.24)) ;
#164551 = CARTESIAN_POINT('Ctrl Pts',(-3.9,-6.45,-14.34)) ;
#164552 = CARTESIAN_POINT('Ctrl Pts',(-3.9,-6.45,-14.24)) ;
#164553 = CARTESIAN_POINT('Ctrl Pts',(-4.,-6.45,-14.24)) ;
#164554 = CARTESIAN_POINT('Origin',(-4.,-6.45,-14.34)) ;
#164555 = CARTESIAN_POINT('Origin',(-4.,-6.4,-14.34)) ;
#164556 = CARTESIAN_POINT('Origin',(-4.,-6.35,-14.34)) ;
#164557 = CARTESIAN_POINT('Ctrl Pts',(-5.,-6.55,-14.14)) ;
#164558 = CARTESIAN_POINT('Ctrl Pts',(-5.,-6.55,-14.14)) ;
#164559 = CARTESIAN_POINT('Ctrl Pts',(-5.,-6.55,-14.14)) ;
#164560 = CARTESIAN_POINT('Ctrl Pts',(-4.94749313434721,-6.55,-14.1662534328262)) ;
#164561 = CARTESIAN_POINT('Ctrl Pts',(-4.96045866731609,-6.55,-14.1795413326839)) ;
#164562 = CARTESIAN_POINT('Ctrl Pts',(-4.97374656717352,-6.55,-14.1925068656527)) ;
#164563 = CARTESIAN_POINT('Ctrl Pts',(-4.89560256540291,-6.53922263893879,
-14.1921987172985)) ;
#164564 = CARTESIAN_POINT('Ctrl Pts',(-4.9208534488902,-6.52362528614071,
-14.2191465511098)) ;
#164565 = CARTESIAN_POINT('Ctrl Pts',(-4.94780128270146,-6.53922263893877,
-14.244397434597)) ;
#164566 = CARTESIAN_POINT('Ctrl Pts',(-4.84006668294258,-6.51145469770858,
-14.2199666585287)) ;
#164567 = CARTESIAN_POINT('Ctrl Pts',(-4.89711619685838,-6.48208554016476,
-14.2428838031416)) ;
#164568 = CARTESIAN_POINT('Ctrl Pts',(-4.92003334147129,-6.5114546977086,
-14.2999333170575)) ;
#164569 = CARTESIAN_POINT('Ctrl Pts',(-4.82524268591729,-6.5003618540841,
-14.2273786570414)) ;
#164570 = CARTESIAN_POINT('Ctrl Pts',(-4.89498692411705,-6.46792722356049,
-14.2450130758829)) ;
#164571 = CARTESIAN_POINT('Ctrl Pts',(-4.91262134295865,-6.5003618540841,
-14.3147573140827)) ;
#164572 = CARTESIAN_POINT('Ctrl Pts',(-4.80520550107819,-6.47617483238892,
-14.2373972494609)) ;
#164573 = CARTESIAN_POINT('Ctrl Pts',(-4.89670325643591,-6.45094059868419,
-14.2432967435641)) ;
#164574 = CARTESIAN_POINT('Ctrl Pts',(-4.90260275053909,-6.47617483238892,
-14.3347944989218)) ;
#164575 = CARTESIAN_POINT('Ctrl Pts',(-4.80000000081823,-6.46309229646328,
-14.24)) ;
#164576 = CARTESIAN_POINT('Ctrl Pts',(-4.89999269604942,-6.44945650152248,
-14.2400073039129)) ;
#164577 = CARTESIAN_POINT('Ctrl Pts',(-4.9,-6.46309229646328,-14.3399999991817)) ;
#164578 = CARTESIAN_POINT('Ctrl Pts',(-4.8,-6.45,-14.24)) ;
#164579 = CARTESIAN_POINT('Ctrl Pts',(-4.9,-6.45,-14.24)) ;
#164580 = CARTESIAN_POINT('Ctrl Pts',(-4.9,-6.45,-14.34)) ;
#164581 = CARTESIAN_POINT('Origin',(-4.8,-6.45,-14.34)) ;
#164582 = CARTESIAN_POINT('Origin',(-4.,-6.35,-14.34)) ;
#164583 = CARTESIAN_POINT('Origin',(-4.,-6.35,-14.34)) ;
#164584 = CARTESIAN_POINT('Origin',(-4.,-6.35,-14.34)) ;
#164585 = CARTESIAN_POINT('Ctrl Pts',(-3.8,-6.55,-16.34)) ;
#164586 = CARTESIAN_POINT('Ctrl Pts',(-3.8,-6.55,-16.34)) ;
#164587 = CARTESIAN_POINT('Ctrl Pts',(-3.8,-6.55,-16.34)) ;
#164588 = CARTESIAN_POINT('Ctrl Pts',(-3.85250686565272,-6.55,-16.3137465671736)) ;
#164589 = CARTESIAN_POINT('Ctrl Pts',(-3.83954133268385,-6.55,-16.3004586673161)) ;
#164590 = CARTESIAN_POINT('Ctrl Pts',(-3.82625343282628,-6.55,-16.2874931343472)) ;
#164591 = CARTESIAN_POINT('Ctrl Pts',(-3.90439743459706,-6.53922263893874,
-16.2878012827014)) ;
#164592 = CARTESIAN_POINT('Ctrl Pts',(-3.87914655110978,-6.52362528614071,
-16.2608534488901)) ;
#164593 = CARTESIAN_POINT('Ctrl Pts',(-3.85219871729855,-6.53922263893876,
-16.2356025654029)) ;
#164594 = CARTESIAN_POINT('Ctrl Pts',(-3.95993331705743,-6.51145469770861,
-16.2600333414713)) ;
#164595 = CARTESIAN_POINT('Ctrl Pts',(-3.90288380314162,-6.48208554016476,
-16.2371161968584)) ;
#164596 = CARTESIAN_POINT('Ctrl Pts',(-3.8799666585287,-6.5114546977086,-16.1800666829426)) ;
#164597 = CARTESIAN_POINT('Ctrl Pts',(-3.97475731408271,-6.5003618540841,
-16.2526213429587)) ;
#164598 = CARTESIAN_POINT('Ctrl Pts',(-3.90501307588293,-6.46792722356047,
-16.2349869241171)) ;
#164599 = CARTESIAN_POINT('Ctrl Pts',(-3.88737865704135,-6.5003618540841,
-16.1652426859173)) ;
#164600 = CARTESIAN_POINT('Ctrl Pts',(-3.9947944989218,-6.47617483238891,
-16.2426027505391)) ;
#164601 = CARTESIAN_POINT('Ctrl Pts',(-3.9032967435641,-6.4509405986842,-16.2367032564358)) ;
#164602 = CARTESIAN_POINT('Ctrl Pts',(-3.89739724946091,-6.47617483238892,
-16.1452055010782)) ;
#164603 = CARTESIAN_POINT('Ctrl Pts',(-3.99999999918176,-6.46309229646328,
-16.24)) ;
#164604 = CARTESIAN_POINT('Ctrl Pts',(-3.90000730395532,-6.44945650152054,
-16.2399926960966)) ;
#164605 = CARTESIAN_POINT('Ctrl Pts',(-3.9,-6.46309229646328,-16.1400000008182)) ;
#164606 = CARTESIAN_POINT('Ctrl Pts',(-4.,-6.45,-16.24)) ;
#164607 = CARTESIAN_POINT('Ctrl Pts',(-3.9,-6.45,-16.24)) ;
#164608 = CARTESIAN_POINT('Ctrl Pts',(-3.9,-6.45,-16.14)) ;
#164609 = CARTESIAN_POINT('Origin',(-4.,-6.45,-16.14)) ;
#164610 = CARTESIAN_POINT('Origin',(-4.8,-6.4,-14.34)) ;
#164611 = CARTESIAN_POINT('Origin',(-4.8,-6.35,-14.34)) ;
#164612 = CARTESIAN_POINT('Origin',(1.9515639104739E-16,-6.35,-14.34)) ;
#164613 = CARTESIAN_POINT('Origin',(-4.8,-6.35,-14.34)) ;
#164614 = CARTESIAN_POINT('Origin',(-4.,-6.35,-15.24)) ;
#164615 = CARTESIAN_POINT('Origin',(-4.,-6.35,-16.14)) ;
#164616 = CARTESIAN_POINT('Origin',(-4.,-6.4,-16.14)) ;
#164617 = CARTESIAN_POINT('Origin',(-4.,-6.35,-16.14)) ;
#164618 = CARTESIAN_POINT('Origin',(-4.8,-6.35,-14.34)) ;
#164619 = CARTESIAN_POINT('Origin',(-4.8,-6.35,-14.34)) ;
#164620 = CARTESIAN_POINT('Origin',(-4.,-6.35,-16.14)) ;
#164621 = CARTESIAN_POINT('Origin',(-4.,-6.35,-16.14)) ;
#164622 = CARTESIAN_POINT('Origin',(-4.8,-6.35,-15.24)) ;
#164623 = CARTESIAN_POINT('Origin',(-4.8,-6.35,-16.14)) ;
#164624 = CARTESIAN_POINT('Origin',(1.95156391047391E-16,-6.35,-16.14)) ;
#164625 = CARTESIAN_POINT('Origin',(-4.8,-6.35,-16.14)) ;
#164626 = CARTESIAN_POINT('Origin',(-4.8,-6.35,-16.14)) ;
#164627 = CARTESIAN_POINT('Origin',(-4.8,-6.35,-16.14)) ;
#164628 = CARTESIAN_POINT('Origin',(-4.8,-6.4,-16.14)) ;
#164629 = CARTESIAN_POINT('Origin',(-4.8,-6.45,-16.14)) ;
#164630 = CARTESIAN_POINT('Ctrl Pts',(-5.,-6.55,-16.34)) ;
#164631 = CARTESIAN_POINT('Ctrl Pts',(-5.,-6.55,-16.34)) ;
#164632 = CARTESIAN_POINT('Ctrl Pts',(-5.,-6.55,-16.34)) ;
#164633 = CARTESIAN_POINT('Ctrl Pts',(-4.97374656717361,-6.55,-16.2874931343473)) ;
#164634 = CARTESIAN_POINT('Ctrl Pts',(-4.96045866731621,-6.55,-16.300458667316)) ;
#164635 = CARTESIAN_POINT('Ctrl Pts',(-4.94749313434733,-6.55,-16.3137465671736)) ;
#164636 = CARTESIAN_POINT('Ctrl Pts',(-4.94780128270146,-6.53922263893877,
-16.2356025654029)) ;
#164637 = CARTESIAN_POINT('Ctrl Pts',(-4.92085344889017,-6.52362528614074,
-16.2608534488901)) ;
#164638 = CARTESIAN_POINT('Ctrl Pts',(-4.89560256540291,-6.53922263893874,
-16.2878012827014)) ;
#164639 = CARTESIAN_POINT('Ctrl Pts',(-4.92003334147129,-6.5114546977086,
-16.1800666829426)) ;
#164640 = CARTESIAN_POINT('Ctrl Pts',(-4.8971161968584,-6.48208554016475,
-16.2371161968584)) ;
#164641 = CARTESIAN_POINT('Ctrl Pts',(-4.84006668294258,-6.51145469770861,
-16.2600333414713)) ;
#164642 = CARTESIAN_POINT('Ctrl Pts',(-4.91262134295865,-6.5003618540841,
-16.1652426859173)) ;
#164643 = CARTESIAN_POINT('Ctrl Pts',(-4.89498692411706,-6.46792722356047,
-16.2349869241171)) ;
#164644 = CARTESIAN_POINT('Ctrl Pts',(-4.82524268591729,-6.5003618540841,
-16.2526213429587)) ;
#164645 = CARTESIAN_POINT('Ctrl Pts',(-4.90260275053909,-6.47617483238892,
-16.1452055010782)) ;
#164646 = CARTESIAN_POINT('Ctrl Pts',(-4.8967032564359,-6.4509405986842,-16.2367032564358)) ;
#164647 = CARTESIAN_POINT('Ctrl Pts',(-4.80520550107819,-6.47617483238891,
-16.2426027505391)) ;
#164648 = CARTESIAN_POINT('Ctrl Pts',(-4.9,-6.46309229646328,-16.1400000008182)) ;
#164649 = CARTESIAN_POINT('Ctrl Pts',(-4.89999269603999,-6.44945650152247,
-16.2399926960966)) ;
#164650 = CARTESIAN_POINT('Ctrl Pts',(-4.80000000081823,-6.46309229646328,
-16.24)) ;
#164651 = CARTESIAN_POINT('Ctrl Pts',(-4.9,-6.45,-16.14)) ;
#164652 = CARTESIAN_POINT('Ctrl Pts',(-4.9,-6.45,-16.24)) ;
#164653 = CARTESIAN_POINT('Ctrl Pts',(-4.8,-6.45,-16.24)) ;
#164654 = CARTESIAN_POINT('Ctrl Pts',(-5.8242667673935,-5.43399303700614,
-13.6370109659688)) ;
#164655 = CARTESIAN_POINT('Ctrl Pts',(-5.80266988778317,-5.52572360682923,
-13.6423540173506)) ;
#164656 = CARTESIAN_POINT('Ctrl Pts',(-5.82426676352013,-5.53106667371341,
-13.7340845871826)) ;
#164657 = CARTESIAN_POINT('Ctrl Pts',(-5.83498671931115,-5.4393535119191,
-13.6343294581962)) ;
#164658 = CARTESIAN_POINT('Ctrl Pts',(-5.8059526312227,-5.52411753147693,
-13.6439600935404)) ;
#164659 = CARTESIAN_POINT('Ctrl Pts',(-5.83498671397625,-5.53374818067468,
-13.7287241131462)) ;
#164660 = CARTESIAN_POINT('Ctrl Pts',(-5.84526105845714,-5.44830326289495,
-13.6298528401961)) ;
#164661 = CARTESIAN_POINT('Ctrl Pts',(-5.81370932746142,-5.52260132030844,
-13.6454763059991)) ;
#164662 = CARTESIAN_POINT('Ctrl Pts',(-5.84526105243717,-5.53822479746337,
-13.7197743635697)) ;
#164663 = CARTESIAN_POINT('Ctrl Pts',(-5.86378685403697,-5.47240020430403,
-13.6178032513087)) ;
#164664 = CARTESIAN_POINT('Ctrl Pts',(-5.83531854275289,-5.52733067404475,
-13.6407469551147)) ;
#164665 = CARTESIAN_POINT('Ctrl Pts',(-5.86378684816457,-5.55027438459895,
-13.6956774250055)) ;
#164666 = CARTESIAN_POINT('Ctrl Pts',(-5.87203852631577,-5.48754495134736,
-13.6102315528944)) ;
#164667 = CARTESIAN_POINT('Ctrl Pts',(-5.84834787930687,-5.53310199490446,
-13.6349756357761)) ;
#164668 = CARTESIAN_POINT('Ctrl Pts',(-5.87203852123036,-5.55784608243453,
-13.6805326795138)) ;
#164669 = CARTESIAN_POINT('Ctrl Pts',(-5.89242747304797,-5.53981202333455,
-13.5841056511376)) ;
#164670 = CARTESIAN_POINT('Ctrl Pts',(-5.88223383300419,-5.56084219179272,
-13.6072354431742)) ;
#164671 = CARTESIAN_POINT('Ctrl Pts',(-5.89242747063499,-5.5839719840277,
-13.6282656123278)) ;
#164672 = CARTESIAN_POINT('Ctrl Pts',(-5.9,-5.58381083947298,-13.562119400143)) ;
#164673 = CARTESIAN_POINT('Ctrl Pts',(-5.9,-5.5948530450262,-13.5732245928869)) ;
#164674 = CARTESIAN_POINT('Ctrl Pts',(-5.9,-5.60595823775494,-13.5842667984405)) ;
#164675 = CARTESIAN_POINT('Ctrl Pts',(-5.9,-5.62807764064044,-13.54)) ;
#164676 = CARTESIAN_POINT('Ctrl Pts',(-5.9,-5.62807764064044,-13.54)) ;
#164677 = CARTESIAN_POINT('Ctrl Pts',(-5.9,-5.62807764064044,-13.54)) ;
#164678 = CARTESIAN_POINT('Origin',(-5.84850712500726,-5.43404914061138,-13.7340285000291)) ;
#164679 = CARTESIAN_POINT('Ctrl Pts',(-5.82425356250363,-5.53106339062591,
-13.7340285000291)) ;
#164680 = CARTESIAN_POINT('Ctrl Pts',(-5.80269484027818,-5.52567371006955,
-13.6424039305709)) ;
#164681 = CARTESIAN_POINT('Ctrl Pts',(-5.82425356250363,-5.43404914061138,
-13.6370142500145)) ;
#164682 = CARTESIAN_POINT('Ctrl Pts',(-5.80840777707097,-5.52710194426774,
-13.7379899459044)) ;
#164683 = CARTESIAN_POINT('Ctrl Pts',(-5.79341417645231,-5.52335354411303,
-13.6428358498184)) ;
#164684 = CARTESIAN_POINT('Ctrl Pts',(-5.81633079157288,-5.4300877551176,
-13.6389949427472)) ;
#164685 = CARTESIAN_POINT('Ctrl Pts',(-5.79207992677989,-5.52301998169497,
-13.739999999534)) ;
#164686 = CARTESIAN_POINT('Ctrl Pts',(-5.78430903206645,-5.52107725801655,
-13.6419613954328)) ;
#164687 = CARTESIAN_POINT('Ctrl Pts',(-5.80816665318298,-5.42600568595105,
-13.64)) ;
#164688 = CARTESIAN_POINT('Ctrl Pts',(-5.77574643749636,-5.51893660937409,
-13.74)) ;
#164689 = CARTESIAN_POINT('Ctrl Pts',(-5.77574643749636,-5.51893660937409,
-13.64)) ;
#164690 = CARTESIAN_POINT('Ctrl Pts',(-5.8,-5.42192235935956,-13.64)) ;
#164691 = CARTESIAN_POINT('Origin',(-5.8,-5.42192235935956,-13.74)) ;
#164692 = CARTESIAN_POINT('Origin',(-5.8066065036801,-5.42357398527959,-13.74)) ;
#164693 = CARTESIAN_POINT('Origin',(-5.17275707706436,-5.26511162862565,-13.74)) ;
#164694 = CARTESIAN_POINT('Origin',(-5.15068655017073,-5.25959399690224,-13.7505938529089)) ;
#164695 = CARTESIAN_POINT('Origin',(-5.17275707706436,-5.26511162862565,-13.74)) ;
#164696 = CARTESIAN_POINT('Origin',(-5.17275707706436,-5.26511162862565,-13.74)) ;
#164697 = CARTESIAN_POINT('Origin',(-5.17275707706436,-5.26511162862565,-13.74)) ;
#164698 = CARTESIAN_POINT('Origin',(-5.17275707706436,-5.05,-13.74)) ;
#164699 = CARTESIAN_POINT('Origin',(-5.17275707706436,-1.91866427917294,-13.74)) ;
#164700 = CARTESIAN_POINT('Origin',(-3.78014014831103,-3.31128120792626,-14.4084561258016)) ;
#164701 = CARTESIAN_POINT('Origin',(-5.17275707706437,-1.91866427917293,-13.74)) ;
#164702 = CARTESIAN_POINT('Origin',(-5.17275707706436,-1.91866427917293,-13.74)) ;
#164703 = CARTESIAN_POINT('Origin',(-5.17275707706436,-1.91866427917294,-13.74)) ;
#164704 = CARTESIAN_POINT('Origin',(-3.97071067811865,-3.12071067811865,-13.74)) ;
#164705 = CARTESIAN_POINT('Origin',(-5.8,-1.2914213562373,-13.74)) ;
#164706 = CARTESIAN_POINT('Ctrl Pts',(-5.87071067811865,-1.14999999999999,
-13.6107106781187)) ;
#164707 = CARTESIAN_POINT('Ctrl Pts',(-5.8471404520791,-1.10285954792089,
-13.6342809041582)) ;
#164708 = CARTESIAN_POINT('Ctrl Pts',(-5.87071067811865,-1.07928932188134,
-13.6814213562373)) ;
#164709 = CARTESIAN_POINT('Ctrl Pts',(-5.85217562795664,-1.18707010095462,
-13.6292457282807)) ;
#164710 = CARTESIAN_POINT('Ctrl Pts',(-5.81261165662076,-1.13738834337924,
-13.6558614719497)) ;
#164711 = CARTESIAN_POINT('Ctrl Pts',(-5.83353949671041,-1.11646050328959,
-13.718592536381)) ;
#164712 = CARTESIAN_POINT('Ctrl Pts',(-5.82627077431947,-1.23887980759831,
-13.64)) ;
#164713 = CARTESIAN_POINT('Ctrl Pts',(-5.76566787907943,-1.18433212092057,
-13.6571489437128)) ;
#164714 = CARTESIAN_POINT('Ctrl Pts',(-5.78190678732235,-1.16809321267764,
-13.7399999994186)) ;
#164715 = CARTESIAN_POINT('Ctrl Pts',(-5.8,-1.2914213562373,-13.64)) ;
#164716 = CARTESIAN_POINT('Ctrl Pts',(-5.72928932188134,-1.22071067811865,
-13.64)) ;
#164717 = CARTESIAN_POINT('Ctrl Pts',(-5.72928932188134,-1.22071067811865,
-13.74)) ;
#164718 = CARTESIAN_POINT('Origin',(-5.94142135623731,-1.14999999999999,-13.6814213562373)) ;
#164719 = CARTESIAN_POINT('Ctrl Pts',(-5.9,-1.00857864376269,-13.54)) ;
#164720 = CARTESIAN_POINT('Ctrl Pts',(-5.9,-1.00857864376269,-13.54)) ;
#164721 = CARTESIAN_POINT('Ctrl Pts',(-5.9,-1.00857864376269,-13.54)) ;
#164722 = CARTESIAN_POINT('Ctrl Pts',(-5.9,-1.06112019240168,-13.5662707743196)) ;
#164723 = CARTESIAN_POINT('Ctrl Pts',(-5.9,-1.04860238143836,-13.5800237376757)) ;
#164724 = CARTESIAN_POINT('Ctrl Pts',(-5.9,-1.03484941808221,-13.592541548639)) ;
#164725 = CARTESIAN_POINT('Ctrl Pts',(-5.88924572828063,-1.11292989904529,
-13.5921756279567)) ;
#164726 = CARTESIAN_POINT('Ctrl Pts',(-5.87451700624548,-1.08721613124892,
-13.6186374874863)) ;
#164727 = CARTESIAN_POINT('Ctrl Pts',(-5.88924572828066,-1.06075427171933,
-13.6443512552827)) ;
#164728 = CARTESIAN_POINT('Ctrl Pts',(-5.87071067811865,-1.14999999999999,
-13.6107106781187)) ;
#164729 = CARTESIAN_POINT('Ctrl Pts',(-5.8471404520791,-1.10285954792089,
-13.6342809041582)) ;
#164730 = CARTESIAN_POINT('Ctrl Pts',(-5.87071067811865,-1.07928932188134,
-13.6814213562373)) ;
#164731 = CARTESIAN_POINT('Ctrl Pts',(-5.87071067811866,-1.14999999999999,
-16.8692893218813)) ;
#164732 = CARTESIAN_POINT('Ctrl Pts',(-5.84714045207911,-1.10285954792089,
-16.8457190958418)) ;
#164733 = CARTESIAN_POINT('Ctrl Pts',(-5.87071067811866,-1.07928932188134,
-16.7985786437627)) ;
#164734 = CARTESIAN_POINT('Ctrl Pts',(-5.88924572828071,-1.11292989904541,
-16.8878243720434)) ;
#164735 = CARTESIAN_POINT('Ctrl Pts',(-5.87451700627498,-1.08721613123208,
-16.8613625125308)) ;
#164736 = CARTESIAN_POINT('Ctrl Pts',(-5.88924572828061,-1.06075427171938,
-16.8356487447174)) ;
#164737 = CARTESIAN_POINT('Ctrl Pts',(-5.9,-1.06112019240159,-16.9137292256804)) ;
#164738 = CARTESIAN_POINT('Ctrl Pts',(-5.9,-1.04860238145164,-16.8999762623108)) ;
#164739 = CARTESIAN_POINT('Ctrl Pts',(-5.9,-1.03484941808214,-16.887458451361)) ;
#164740 = CARTESIAN_POINT('Ctrl Pts',(-5.9,-1.00857864376269,-16.94)) ;
#164741 = CARTESIAN_POINT('Ctrl Pts',(-5.9,-1.00857864376269,-16.94)) ;
#164742 = CARTESIAN_POINT('Ctrl Pts',(-5.9,-1.00857864376269,-16.94)) ;
#164743 = CARTESIAN_POINT('Origin',(-5.94142135623734,-1.14999999999996,-16.7985786437627)) ;
#164744 = CARTESIAN_POINT('Ctrl Pts',(-5.8,-1.2914213562373,-16.84)) ;
#164745 = CARTESIAN_POINT('Ctrl Pts',(-5.72928932188134,-1.22071067811865,
-16.84)) ;
#164746 = CARTESIAN_POINT('Ctrl Pts',(-5.72928932188134,-1.22071067811865,
-16.74)) ;
#164747 = CARTESIAN_POINT('Ctrl Pts',(-5.82627077431952,-1.23887980759821,
-16.84)) ;
#164748 = CARTESIAN_POINT('Ctrl Pts',(-5.76566787907979,-1.18433212092022,
-16.8228510562871)) ;
#164749 = CARTESIAN_POINT('Ctrl Pts',(-5.78190678732242,-1.16809321267757,
-16.7400000005814)) ;
#164750 = CARTESIAN_POINT('Ctrl Pts',(-5.85217562795678,-1.18707010095484,
-16.8507542717195)) ;
#164751 = CARTESIAN_POINT('Ctrl Pts',(-5.81261165662032,-1.13738834337968,
-16.8241385280508)) ;
#164752 = CARTESIAN_POINT('Ctrl Pts',(-5.83353949671032,-1.11646050328967,
-16.7614074636191)) ;
#164753 = CARTESIAN_POINT('Ctrl Pts',(-5.87071067811866,-1.14999999999999,
-16.8692893218813)) ;
#164754 = CARTESIAN_POINT('Ctrl Pts',(-5.84714045207911,-1.10285954792088,
-16.8457190958418)) ;
#164755 = CARTESIAN_POINT('Ctrl Pts',(-5.87071067811866,-1.07928932188133,
-16.7985786437627)) ;
#164756 = CARTESIAN_POINT('Origin',(-5.8,-1.29142135623731,-16.74)) ;
#164757 = CARTESIAN_POINT('Origin',(-3.59571067811865,-3.49571067811865,-16.74)) ;
#164758 = CARTESIAN_POINT('Origin',(-5.17275707706437,-1.91866427917293,-16.74)) ;
#164759 = CARTESIAN_POINT('Origin',(-3.09057773798104,-4.00084361825625,-15.74055391724)) ;
#164760 = CARTESIAN_POINT('Origin',(-5.17275707706436,-1.91866427917293,-16.74)) ;
#164761 = CARTESIAN_POINT('Origin',(-5.17275707706436,-1.91866427917293,-16.74)) ;
#164762 = CARTESIAN_POINT('Origin',(-5.17275707706436,-1.91866427917293,-16.74)) ;
#164763 = CARTESIAN_POINT('Origin',(-5.17275707706436,-5.05,-16.74)) ;
#164764 = CARTESIAN_POINT('Origin',(-5.17275707706436,-5.26511162862565,-16.74)) ;
#164765 = CARTESIAN_POINT('Origin',(-3.96111272388873,-4.96220054033175,-16.1584107104757)) ;
#164766 = CARTESIAN_POINT('Origin',(-5.17275707706436,-5.26511162862565,-16.74)) ;
#164767 = CARTESIAN_POINT('Origin',(-5.17275707706436,-5.26511162862565,-16.74)) ;
#164768 = CARTESIAN_POINT('Origin',(-5.17275707706436,-5.26511162862565,-16.74)) ;
#164769 = CARTESIAN_POINT('Origin',(-5.10072415073893,-5.24710339704429,-16.74)) ;
#164770 = CARTESIAN_POINT('Origin',(-5.8,-5.42192235935956,-16.74)) ;
#164771 = CARTESIAN_POINT('Ctrl Pts',(-5.77574643749636,-5.51893660937409,
-16.74)) ;
#164772 = CARTESIAN_POINT('Ctrl Pts',(-5.77574643749636,-5.51893660937409,
-16.84)) ;
#164773 = CARTESIAN_POINT('Ctrl Pts',(-5.8,-5.42192235935956,-16.84)) ;
#164774 = CARTESIAN_POINT('Ctrl Pts',(-5.7920799267799,-5.52301998169498,
-16.740000000466)) ;
#164775 = CARTESIAN_POINT('Ctrl Pts',(-5.78430903206643,-5.5210772580166,
-16.8380386045671)) ;
#164776 = CARTESIAN_POINT('Ctrl Pts',(-5.808166653183,-5.42600568595105,-16.84)) ;
#164777 = CARTESIAN_POINT('Ctrl Pts',(-5.80840777707094,-5.52710194426774,
-16.7420100540957)) ;
#164778 = CARTESIAN_POINT('Ctrl Pts',(-5.7934141764523,-5.52335354411309,
-16.8371641501816)) ;
#164779 = CARTESIAN_POINT('Ctrl Pts',(-5.81633079157288,-5.43008775511759,
-16.8410050572528)) ;
#164780 = CARTESIAN_POINT('Ctrl Pts',(-5.82425356250363,-5.53106339062591,
-16.7459714999709)) ;
#164781 = CARTESIAN_POINT('Ctrl Pts',(-5.80269484027818,-5.52567371006955,
-16.8375960694291)) ;
#164782 = CARTESIAN_POINT('Ctrl Pts',(-5.82425356250363,-5.43404914061138,
-16.8429857499855)) ;
#164783 = CARTESIAN_POINT('Origin',(-5.84850712500726,-5.43404914061138,-16.7459714999709)) ;
#164784 = CARTESIAN_POINT('Ctrl Pts',(-5.82426676739356,-5.5310666746717,
-16.7459153963654)) ;
#164785 = CARTESIAN_POINT('Ctrl Pts',(-5.80266988778307,-5.52572362329014,
-16.8376459661889)) ;
#164786 = CARTESIAN_POINT('Ctrl Pts',(-5.82426676352019,-5.43399305345765,
-16.842989033073)) ;
#164787 = CARTESIAN_POINT('Ctrl Pts',(-5.83498671931125,-5.53374818244431,
-16.7512758712784)) ;
#164788 = CARTESIAN_POINT('Ctrl Pts',(-5.80595263122257,-5.52411754710035,
-16.8360398908367)) ;
#164789 = CARTESIAN_POINT('Ctrl Pts',(-5.8349867139763,-5.43935352749406,
-16.8456705400343)) ;
#164790 = CARTESIAN_POINT('Ctrl Pts',(-5.84526105845723,-5.53822480044432,
-16.7602256222542)) ;
#164791 = CARTESIAN_POINT('Ctrl Pts',(-5.81370932746128,-5.52260133464156,
-16.8345236796681)) ;
#164792 = CARTESIAN_POINT('Ctrl Pts',(-5.84526105243723,-5.44830327707059,
-16.850147156823)) ;
#164793 = CARTESIAN_POINT('Ctrl Pts',(-5.86378685403707,-5.55027438933184,
-16.7843225636634)) ;
#164794 = CARTESIAN_POINT('Ctrl Pts',(-5.83531854275277,-5.52733068552589,
-16.8392530334044)) ;
#164795 = CARTESIAN_POINT('Ctrl Pts',(-5.86378684816465,-5.4724002156349,
-16.8621967439586)) ;
#164796 = CARTESIAN_POINT('Ctrl Pts',(-5.87203852631585,-5.55784608774615,
-16.7994673107067)) ;
#164797 = CARTESIAN_POINT('Ctrl Pts',(-5.84834787930678,-5.53310200486445,
-16.845024354264)) ;
#164798 = CARTESIAN_POINT('Ctrl Pts',(-5.87203852123043,-5.48754496112646,
-16.8697684417941)) ;
#164799 = CARTESIAN_POINT('Ctrl Pts',(-5.892427473048,-5.58397198950291,-16.851734382694)) ;
#164800 = CARTESIAN_POINT('Ctrl Pts',(-5.88223383300415,-5.56084219746622,
-16.8727645511521)) ;
#164801 = CARTESIAN_POINT('Ctrl Pts',(-5.89242747063501,-5.5398120283126,
-16.8958943433873)) ;
#164802 = CARTESIAN_POINT('Ctrl Pts',(-5.9,-5.60595824049753,-16.8957331988325)) ;
#164803 = CARTESIAN_POINT('Ctrl Pts',(-5.9,-5.59485304775418,-16.9067754043861)) ;
#164804 = CARTESIAN_POINT('Ctrl Pts',(-5.9,-5.58381084219989,-16.9178805971146)) ;
#164805 = CARTESIAN_POINT('Ctrl Pts',(-5.9,-5.62807764064044,-16.94)) ;
#164806 = CARTESIAN_POINT('Ctrl Pts',(-5.9,-5.62807764064044,-16.94)) ;
#164807 = CARTESIAN_POINT('Ctrl Pts',(-5.9,-5.62807764064044,-16.94)) ;
#164808 = CARTESIAN_POINT('Origin',(7.8,2.1,-15.64)) ;
#164809 = CARTESIAN_POINT('Origin',(7.8,2.1,-15.84)) ;
#164810 = CARTESIAN_POINT('Origin',(7.6,2.1,-15.64)) ;
#164811 = CARTESIAN_POINT('Origin',(7.6,2.1,-15.64)) ;
#164812 = CARTESIAN_POINT('Origin',(7.6,2.1,-14.84)) ;
#164813 = CARTESIAN_POINT('Origin',(7.8,2.1,-15.84)) ;
#164814 = CARTESIAN_POINT('Origin',(9.6,2.1,-15.84)) ;
#164815 = CARTESIAN_POINT('Origin',(7.8,2.1,-14.84)) ;
#164816 = CARTESIAN_POINT('Origin',(7.8,2.1,-14.64)) ;
#164817 = CARTESIAN_POINT('Origin',(9.6,2.1,-15.64)) ;
#164818 = CARTESIAN_POINT('Origin',(9.8,2.1,-15.64)) ;
#164819 = CARTESIAN_POINT('Origin',(7.8,2.1,-14.64)) ;
#164820 = CARTESIAN_POINT('Origin',(9.6,2.1,-14.64)) ;
#164821 = CARTESIAN_POINT('Origin',(9.8,2.1,-15.64)) ;
#164822 = CARTESIAN_POINT('Origin',(9.8,2.1,-14.84)) ;
#164823 = CARTESIAN_POINT('Origin',(9.6,2.1,-14.84)) ;
#164824 = CARTESIAN_POINT('Origin',(-4.15,-6.25,-14.49)) ;
#164825 = CARTESIAN_POINT('Origin',(-4.15,-6.3,-14.49)) ;
#164826 = CARTESIAN_POINT('Origin',(-4.15,-6.3,-15.24)) ;
#164827 = CARTESIAN_POINT('Origin',(-4.15,-6.3,-15.99)) ;
#164828 = CARTESIAN_POINT('Origin',(-4.15,-6.3,-14.49)) ;
#164829 = CARTESIAN_POINT('Origin',(-4.15,-6.25,-15.99)) ;
#164830 = CARTESIAN_POINT('Origin',(-4.15,-6.3,-15.99)) ;
#164831 = CARTESIAN_POINT('Origin',(-4.15,-6.3,-14.49)) ;
#164832 = CARTESIAN_POINT('Origin',(-4.15,-6.3,-14.49)) ;
#164833 = CARTESIAN_POINT('Origin',(-4.15,-6.3,-15.99)) ;
#164834 = CARTESIAN_POINT('Origin',(-4.15,-6.3,-15.99)) ;
#164835 = CARTESIAN_POINT('Origin',(-4.65,-6.25,-14.49)) ;
#164836 = CARTESIAN_POINT('Origin',(-4.65,-6.3,-14.49)) ;
#164837 = CARTESIAN_POINT('Origin',(0.,-6.3,-14.49)) ;
#164838 = CARTESIAN_POINT('Origin',(-4.65,-6.3,-14.49)) ;
#164839 = CARTESIAN_POINT('Origin',(0.,-6.3,-15.99)) ;
#164840 = CARTESIAN_POINT('Origin',(-4.65,-6.3,-15.99)) ;
#164841 = CARTESIAN_POINT('Origin',(-4.65,-6.25,-15.99)) ;
#164842 = CARTESIAN_POINT('Origin',(-4.65,-6.3,-15.99)) ;
#164843 = CARTESIAN_POINT('Origin',(-4.65,-6.3,-14.49)) ;
#164844 = CARTESIAN_POINT('Origin',(-4.65,-6.3,-14.49)) ;
#164845 = CARTESIAN_POINT('Origin',(-4.65,-6.3,-15.99)) ;
#164846 = CARTESIAN_POINT('Origin',(-4.65,-6.3,-15.99)) ;
#164847 = CARTESIAN_POINT('Origin',(-4.65,-6.3,-15.24)) ;
#164848 = CARTESIAN_POINT('Origin',(-3.,4.45,-16.34)) ;
#164849 = CARTESIAN_POINT('Origin',(-2.1,4.45,-16.34)) ;
#164850 = CARTESIAN_POINT('Origin',(-2.9,4.45,-16.34)) ;
#164851 = CARTESIAN_POINT('Origin',(-2.9,4.45,-16.14)) ;
#164852 = CARTESIAN_POINT('Origin',(-3.1,4.45,-16.14)) ;
#164853 = CARTESIAN_POINT('Origin',(-2.9,4.45,-16.14)) ;
#164854 = CARTESIAN_POINT('Origin',(-2.1,4.45,-16.14)) ;
#164855 = CARTESIAN_POINT('Origin',(-2.1,4.45,-16.14)) ;
#164856 = CARTESIAN_POINT('Origin',(-1.9,4.45,-16.14)) ;
#164857 = CARTESIAN_POINT('Origin',(-3.1,4.45,-16.24)) ;
#164858 = CARTESIAN_POINT('Origin',(-3.1,4.45,-14.34)) ;
#164859 = CARTESIAN_POINT('Origin',(-2.9,4.4,-16.14)) ;
#164860 = CARTESIAN_POINT('Origin',(-2.9,4.35,-16.14)) ;
#164861 = CARTESIAN_POINT('Origin',(-1.95156391047391E-16,4.35,-16.14)) ;
#164862 = CARTESIAN_POINT('Origin',(-2.1,4.35,-16.14)) ;
#164863 = CARTESIAN_POINT('Origin',(-2.9,4.35,-16.14)) ;
#164864 = CARTESIAN_POINT('Origin',(-2.1,4.4,-16.14)) ;
#164865 = CARTESIAN_POINT('Origin',(-2.1,4.35,-16.14)) ;
#164866 = CARTESIAN_POINT('Origin',(-1.9,4.45,-16.24)) ;
#164867 = CARTESIAN_POINT('Origin',(-1.9,4.45,-14.34)) ;
#164868 = CARTESIAN_POINT('Origin',(-3.,4.45,-14.14)) ;
#164869 = CARTESIAN_POINT('Origin',(-2.9,4.45,-14.14)) ;
#164870 = CARTESIAN_POINT('Origin',(-2.1,4.45,-14.14)) ;
#164871 = CARTESIAN_POINT('Origin',(-2.9,4.45,-14.34)) ;
#164872 = CARTESIAN_POINT('Origin',(-2.9,4.45,-14.34)) ;
#164873 = CARTESIAN_POINT('Origin',(-2.9,4.35,-16.14)) ;
#164874 = CARTESIAN_POINT('Origin',(-2.9,4.35,-16.14)) ;
#164875 = CARTESIAN_POINT('Origin',(-2.1,4.35,-16.14)) ;
#164876 = CARTESIAN_POINT('Origin',(-2.1,4.35,-16.14)) ;
#164877 = CARTESIAN_POINT('Origin',(-2.1,4.45,-14.34)) ;
#164878 = CARTESIAN_POINT('Origin',(-2.1,4.45,-14.34)) ;
#164879 = CARTESIAN_POINT('Origin',(-2.9,4.4,-14.34)) ;
#164880 = CARTESIAN_POINT('Origin',(-2.9,4.35,-14.34)) ;
#164881 = CARTESIAN_POINT('Origin',(-2.9,4.35,-15.24)) ;
#164882 = CARTESIAN_POINT('Origin',(-2.9,4.35,-14.34)) ;
#164883 = CARTESIAN_POINT('Origin',(-2.1,4.35,-15.24)) ;
#164884 = CARTESIAN_POINT('Origin',(-2.1,4.35,-14.34)) ;
#164885 = CARTESIAN_POINT('Origin',(-2.1,4.4,-14.34)) ;
#164886 = CARTESIAN_POINT('Origin',(-2.1,4.35,-14.34)) ;
#164887 = CARTESIAN_POINT('Origin',(-2.9,4.35,-14.34)) ;
#164888 = CARTESIAN_POINT('Origin',(-2.9,4.35,-14.34)) ;
#164889 = CARTESIAN_POINT('Origin',(-2.1,4.35,-14.34)) ;
#164890 = CARTESIAN_POINT('Origin',(-2.1,4.35,-14.34)) ;
#164891 = CARTESIAN_POINT('Origin',(-1.95156391047391E-16,4.35,-14.34)) ;
#164892 = CARTESIAN_POINT('Origin',(-2.25,4.25,-15.99)) ;
#164893 = CARTESIAN_POINT('Origin',(-2.25,4.3,-15.99)) ;
#164894 = CARTESIAN_POINT('Origin',(-2.25,4.3,-15.24)) ;
#164895 = CARTESIAN_POINT('Origin',(-2.25,4.3,-14.49)) ;
#164896 = CARTESIAN_POINT('Origin',(-2.25,4.3,-15.99)) ;
#164897 = CARTESIAN_POINT('Origin',(-2.25,4.25,-14.49)) ;
#164898 = CARTESIAN_POINT('Origin',(-2.25,4.3,-14.49)) ;
#164899 = CARTESIAN_POINT('Origin',(-2.25,4.3,-15.99)) ;
#164900 = CARTESIAN_POINT('Origin',(-2.25,4.3,-15.99)) ;
#164901 = CARTESIAN_POINT('Origin',(-2.25,4.3,-14.49)) ;
#164902 = CARTESIAN_POINT('Origin',(-2.25,4.3,-14.49)) ;
#164903 = CARTESIAN_POINT('Origin',(-2.75,4.25,-15.99)) ;
#164904 = CARTESIAN_POINT('Origin',(-2.75,4.3,-15.99)) ;
#164905 = CARTESIAN_POINT('Origin',(-1.97127667724637E-17,4.3,-15.99)) ;
#164906 = CARTESIAN_POINT('Origin',(-2.75,4.3,-15.99)) ;
#164907 = CARTESIAN_POINT('Origin',(-1.97127667724637E-17,4.3,-14.49)) ;
#164908 = CARTESIAN_POINT('Origin',(-2.75,4.3,-14.49)) ;
#164909 = CARTESIAN_POINT('Origin',(-2.75,4.25,-14.49)) ;
#164910 = CARTESIAN_POINT('Origin',(-2.75,4.3,-14.49)) ;
#164911 = CARTESIAN_POINT('Origin',(-2.75,4.3,-15.99)) ;
#164912 = CARTESIAN_POINT('Origin',(-2.75,4.3,-15.99)) ;
#164913 = CARTESIAN_POINT('Origin',(-2.75,4.3,-14.49)) ;
#164914 = CARTESIAN_POINT('Origin',(-2.75,4.3,-14.49)) ;
#164915 = CARTESIAN_POINT('Origin',(-2.75,4.3,-15.24)) ;
#164916 = CARTESIAN_POINT('Origin',(7.8,2.9,-15.64)) ;
#164917 = CARTESIAN_POINT('Origin',(7.8,2.9,-15.64)) ;
#164918 = CARTESIAN_POINT('Origin',(7.8,2.9,-14.84)) ;
#164919 = CARTESIAN_POINT('Origin',(7.8,2.9,-14.84)) ;
#164920 = CARTESIAN_POINT('Origin',(7.8,2.9,-14.84)) ;
#164921 = CARTESIAN_POINT('Origin',(7.8,2.9,-15.64)) ;
#164922 = CARTESIAN_POINT('Origin',(7.8,2.9,-15.64)) ;
#164923 = CARTESIAN_POINT('Origin',(9.6,2.9,-14.84)) ;
#164924 = CARTESIAN_POINT('Origin',(9.6,2.9,-14.84)) ;
#164925 = CARTESIAN_POINT('Origin',(9.6,2.9,-15.64)) ;
#164926 = CARTESIAN_POINT('Origin',(9.6,2.9,-15.64)) ;
#164927 = CARTESIAN_POINT('Origin',(9.6,2.9,-14.84)) ;
#164928 = CARTESIAN_POINT('Origin',(9.6,2.9,-14.84)) ;
#164929 = CARTESIAN_POINT('Origin',(9.6,2.9,-15.64)) ;
#164930 = CARTESIAN_POINT('Origin',(9.6,2.9,-15.64)) ;
#164931 = CARTESIAN_POINT('Origin',(9.6,2.9,-15.64)) ;
#164932 = CARTESIAN_POINT('Origin',(-0.183301359729408,3.45,-13.722963213524)) ;
#164933 = CARTESIAN_POINT('Origin',(0.249234641435079,3.15,-15.1237799780213)) ;
#164934 = CARTESIAN_POINT('Origin',(-0.249234641435079,3.15,-15.3562200219787)) ;
#164935 = CARTESIAN_POINT('Origin',(-1.04429375741423,3.45,-14.1244505621777)) ;
#164936 = CARTESIAN_POINT('Origin',(10.1,-2.15,-18.1468804065906)) ;
#164937 = CARTESIAN_POINT('Origin',(10.1,-2.15,-18.1468804065906)) ;
#164938 = CARTESIAN_POINT('Origin',(10.1,-2.15,-18.1468804065906)) ;
#164939 = CARTESIAN_POINT('Origin',(10.1,-2.15,-18.1468804065906)) ;
#164940 = CARTESIAN_POINT('Origin',(10.1,-2.15,-19.05)) ;
#164941 = CARTESIAN_POINT('Origin',(10.1,-2.15,-17.745)) ;
#164942 = CARTESIAN_POINT('Origin',(10.2,-2.15,-18.1468804065906)) ;
#164943 = CARTESIAN_POINT('Origin',(3.7,-2.15,-18.1468804065906)) ;
#164944 = CARTESIAN_POINT('Origin',(10.1,-3.65625,-19.05)) ;
#164945 = CARTESIAN_POINT('Origin',(10.1,-2.15,-19.9531195934094)) ;
#164946 = CARTESIAN_POINT('Origin',(10.1,-3.65625,-17.745)) ;
#164947 = CARTESIAN_POINT('Origin',(10.1,1.9,-17.745)) ;
#164948 = CARTESIAN_POINT('Origin',(10.1,-2.15,-17.745)) ;
#164949 = CARTESIAN_POINT('Origin',(10.1,-2.15,-17.745)) ;
#164950 = CARTESIAN_POINT('Origin',(10.1,-2.15,-17.745)) ;
#164951 = CARTESIAN_POINT('Origin',(3.7,-2.15,-18.1468804065906)) ;
#164952 = CARTESIAN_POINT('Origin',(3.7,-2.32153024911032,-18.2497267659824)) ;
#164953 = CARTESIAN_POINT('Origin',(3.7,-2.35,-18.1468804065906)) ;
#164954 = CARTESIAN_POINT('Origin',(10.1,-2.15,-19.9531195934094)) ;
#164955 = CARTESIAN_POINT('Origin',(10.1,-2.15,-19.9531195934094)) ;
#164956 = CARTESIAN_POINT('Origin',(10.1,-2.15,-19.9531195934094)) ;
#164957 = CARTESIAN_POINT('Origin',(10.1,1.9,-19.05)) ;
#164958 = CARTESIAN_POINT('Origin',(10.1,1.9,-20.355)) ;
#164959 = CARTESIAN_POINT('Origin',(10.1,1.9,-17.745)) ;
#164960 = CARTESIAN_POINT('Origin',(10.2,-2.15,-17.745)) ;
#164961 = CARTESIAN_POINT('Origin',(3.7,-2.15,-17.745)) ;
#164962 = CARTESIAN_POINT('Origin',(3.7,-2.35,-17.645)) ;
#164963 = CARTESIAN_POINT('Origin',(3.7,-2.35,-17.745)) ;
#164964 = CARTESIAN_POINT('Origin',(3.7,-3.65625,-19.05)) ;
#164965 = CARTESIAN_POINT('Origin',(3.7,-2.32153024911032,-19.8502732340176)) ;
#164966 = CARTESIAN_POINT('Origin',(10.2,-2.15,-19.9531195934094)) ;
#164967 = CARTESIAN_POINT('Origin',(3.7,-2.15,-19.9531195934094)) ;
#164968 = CARTESIAN_POINT('Origin',(10.1,-2.15,-19.05)) ;
#164969 = CARTESIAN_POINT('Origin',(10.1,-2.15,-20.355)) ;
#164970 = CARTESIAN_POINT('Origin',(10.1,-3.65625,-20.355)) ;
#164971 = CARTESIAN_POINT('Origin',(10.1,1.9,-20.355)) ;
#164972 = CARTESIAN_POINT('Origin',(10.1,-2.15,-20.355)) ;
#164973 = CARTESIAN_POINT('Origin',(3.7,-2.35,-17.745)) ;
#164974 = CARTESIAN_POINT('Origin',(3.5,-2.35,-17.745)) ;
#164975 = CARTESIAN_POINT('Origin',(3.7,-2.15,-19.9531195934094)) ;
#164976 = CARTESIAN_POINT('Origin',(3.7,-2.35,-19.9531195934094)) ;
#164977 = CARTESIAN_POINT('Origin',(10.1,-2.15,-20.355)) ;
#164978 = CARTESIAN_POINT('Origin',(10.1,-2.15,-20.355)) ;
#164979 = CARTESIAN_POINT('Origin',(3.6,1.9,-17.545)) ;
#164980 = CARTESIAN_POINT('Origin',(3.5,1.9,-17.545)) ;
#164981 = CARTESIAN_POINT('Origin',(2.7,1.9,-17.545)) ;
#164982 = CARTESIAN_POINT('Origin',(3.5,1.67034766683375E-15,-17.745)) ;
#164983 = CARTESIAN_POINT('Origin',(3.5,-5.15,-17.745)) ;
#164984 = CARTESIAN_POINT('Origin',(3.7,-2.35,-19.925)) ;
#164985 = CARTESIAN_POINT('Origin',(3.7,-2.35,-20.355)) ;
#164986 = CARTESIAN_POINT('Origin',(3.6,-2.15,-20.355)) ;
#164987 = CARTESIAN_POINT('Origin',(3.7,-2.15,-20.355)) ;
#164988 = CARTESIAN_POINT('Origin',(2.7,1.9,-17.545)) ;
#164989 = CARTESIAN_POINT('Origin',(2.7,1.9,-17.545)) ;
#164990 = CARTESIAN_POINT('Origin',(3.5,-5.15,-17.745)) ;
#164991 = CARTESIAN_POINT('Origin',(3.5,-5.15,-17.745)) ;
#164992 = CARTESIAN_POINT('Origin',(3.5,-5.15,-17.745)) ;
#164993 = CARTESIAN_POINT('Origin',(3.7,-2.35,-20.355)) ;
#164994 = CARTESIAN_POINT('Origin',(3.5,-2.35,-20.355)) ;
#164995 = CARTESIAN_POINT('Origin',(2.7,2.,-17.545)) ;
#164996 = CARTESIAN_POINT('Origin',(2.7,-5.15,-17.545)) ;
#164997 = CARTESIAN_POINT('Origin',(3.6,-5.15,-17.745)) ;
#164998 = CARTESIAN_POINT('Origin',(2.7,-5.15,-17.745)) ;
#164999 = CARTESIAN_POINT('Origin',(3.5,-5.15,0.)) ;
#165000 = CARTESIAN_POINT('Origin',(3.5,-5.15,-20.355)) ;
#165001 = CARTESIAN_POINT('Origin',(3.5,-1.74825394185847E-15,-20.355)) ;
#165002 = CARTESIAN_POINT('Origin',(3.5,-5.15,-20.355)) ;
#165003 = CARTESIAN_POINT('Origin',(2.7,-5.15,-17.745)) ;
#165004 = CARTESIAN_POINT('Origin',(2.7,-5.35,-17.745)) ;
#165005 = CARTESIAN_POINT('Origin',(3.5,-5.15,-20.355)) ;
#165006 = CARTESIAN_POINT('Origin',(3.5,-5.15,-20.355)) ;
#165007 = CARTESIAN_POINT('Origin',(2.7,-5.35,-17.645)) ;
#165008 = CARTESIAN_POINT('Origin',(2.7,-5.35,-20.355)) ;
#165009 = CARTESIAN_POINT('Origin',(3.6,-5.15,-20.355)) ;
#165010 = CARTESIAN_POINT('Origin',(2.7,-5.15,-20.355)) ;
#165011 = CARTESIAN_POINT('Origin',(3.6,1.9,-20.555)) ;
#165012 = CARTESIAN_POINT('Origin',(3.5,1.9,-20.555)) ;
#165013 = CARTESIAN_POINT('Origin',(2.7,1.9,-20.555)) ;
#165014 = CARTESIAN_POINT('Origin',(2.7,1.9,-20.455)) ;
#165015 = CARTESIAN_POINT('Origin',(2.7,1.9,-21.355)) ;
#165016 = CARTESIAN_POINT('Origin',(2.7,1.9,-20.555)) ;
#165017 = CARTESIAN_POINT('Origin',(2.7,-5.15,-20.355)) ;
#165018 = CARTESIAN_POINT('Origin',(2.7,-5.15,-20.555)) ;
#165019 = CARTESIAN_POINT('Origin',(2.7,1.9,-20.555)) ;
#165020 = CARTESIAN_POINT('Origin',(2.7,1.9,-20.555)) ;
#165021 = CARTESIAN_POINT('Origin',(2.7,-5.25,-20.555)) ;
#165022 = CARTESIAN_POINT('Ctrl Pts',(-3.8,-6.55,-17.95)) ;
#165023 = CARTESIAN_POINT('Ctrl Pts',(-3.8,-6.55,-17.95)) ;
#165024 = CARTESIAN_POINT('Ctrl Pts',(-3.8,-6.55,-17.95)) ;
#165025 = CARTESIAN_POINT('Ctrl Pts',(-3.82625343282631,-6.55,-18.0025068656527)) ;
#165026 = CARTESIAN_POINT('Ctrl Pts',(-3.83954133268377,-6.55,-17.9895413326839)) ;
#165027 = CARTESIAN_POINT('Ctrl Pts',(-3.8525068656527,-6.55,-17.9762534328264)) ;
#165028 = CARTESIAN_POINT('Ctrl Pts',(-3.85219871729854,-6.53922263893877,
-18.0543974345971)) ;
#165029 = CARTESIAN_POINT('Ctrl Pts',(-3.87914655110981,-6.52362528614074,
-18.0291465511099)) ;
#165030 = CARTESIAN_POINT('Ctrl Pts',(-3.90439743459708,-6.53922263893874,
-18.0021987172986)) ;
#165031 = CARTESIAN_POINT('Ctrl Pts',(-3.87996665852871,-6.5114546977086,
-18.1099333170574)) ;
#165032 = CARTESIAN_POINT('Ctrl Pts',(-3.90288380314161,-6.48208554016475,
-18.0528838031416)) ;
#165033 = CARTESIAN_POINT('Ctrl Pts',(-3.95993331705742,-6.51145469770861,
-18.0299666585287)) ;
#165034 = CARTESIAN_POINT('Ctrl Pts',(-3.88737865704135,-6.5003618540841,
-18.1247573140827)) ;
#165035 = CARTESIAN_POINT('Ctrl Pts',(-3.90501307588293,-6.46792722356046,
-18.0550130758829)) ;
#165036 = CARTESIAN_POINT('Ctrl Pts',(-3.9747573140827,-6.5003618540841,-18.0373786570414)) ;
#165037 = CARTESIAN_POINT('Ctrl Pts',(-3.8973972494609,-6.47617483238892,
-18.1447944989218)) ;
#165038 = CARTESIAN_POINT('Ctrl Pts',(-3.9032967435641,-6.45094059868421,
-18.0532967435641)) ;
#165039 = CARTESIAN_POINT('Ctrl Pts',(-3.99479449892181,-6.47617483238891,
-18.0473972494609)) ;
#165040 = CARTESIAN_POINT('Ctrl Pts',(-3.9,-6.46309229646327,-18.1499999991818)) ;
#165041 = CARTESIAN_POINT('Ctrl Pts',(-3.90000730394106,-6.44945650151457,
-18.0500073039033)) ;
#165042 = CARTESIAN_POINT('Ctrl Pts',(-3.99999999918173,-6.46309229646329,
-18.05)) ;
#165043 = CARTESIAN_POINT('Ctrl Pts',(-3.9,-6.45,-18.15)) ;
#165044 = CARTESIAN_POINT('Ctrl Pts',(-3.9,-6.45,-18.05)) ;
#165045 = CARTESIAN_POINT('Ctrl Pts',(-4.,-6.45,-18.05)) ;
#165046 = CARTESIAN_POINT('Origin',(-4.,-6.45,-18.15)) ;
#165047 = CARTESIAN_POINT('Origin',(-4.,-6.4,-18.15)) ;
#165048 = CARTESIAN_POINT('Origin',(-4.,-6.35,-18.15)) ;
#165049 = CARTESIAN_POINT('Ctrl Pts',(-5.,-6.55,-17.95)) ;
#165050 = CARTESIAN_POINT('Ctrl Pts',(-5.,-6.55,-17.95)) ;
#165051 = CARTESIAN_POINT('Ctrl Pts',(-5.,-6.55,-17.95)) ;
#165052 = CARTESIAN_POINT('Ctrl Pts',(-4.94749313434733,-6.55,-17.9762534328264)) ;
#165053 = CARTESIAN_POINT('Ctrl Pts',(-4.96045866731622,-6.55,-17.989541332684)) ;
#165054 = CARTESIAN_POINT('Ctrl Pts',(-4.97374656717362,-6.55,-18.0025068656527)) ;
#165055 = CARTESIAN_POINT('Ctrl Pts',(-4.89560256540291,-6.53922263893874,
-18.0021987172986)) ;
#165056 = CARTESIAN_POINT('Ctrl Pts',(-4.92085344889017,-6.52362528614074,
-18.0291465511099)) ;
#165057 = CARTESIAN_POINT('Ctrl Pts',(-4.94780128270146,-6.53922263893877,
-18.0543974345971)) ;
#165058 = CARTESIAN_POINT('Ctrl Pts',(-4.84006668294258,-6.51145469770861,
-18.0299666585287)) ;
#165059 = CARTESIAN_POINT('Ctrl Pts',(-4.8971161968584,-6.48208554016475,
-18.0528838031416)) ;
#165060 = CARTESIAN_POINT('Ctrl Pts',(-4.92003334147129,-6.5114546977086,
-18.1099333170574)) ;
#165061 = CARTESIAN_POINT('Ctrl Pts',(-4.82524268591729,-6.5003618540841,
-18.0373786570414)) ;
#165062 = CARTESIAN_POINT('Ctrl Pts',(-4.89498692411706,-6.46792722356047,
-18.0550130758829)) ;
#165063 = CARTESIAN_POINT('Ctrl Pts',(-4.91262134295865,-6.5003618540841,
-18.1247573140827)) ;
#165064 = CARTESIAN_POINT('Ctrl Pts',(-4.80520550107819,-6.47617483238891,
-18.0473972494609)) ;
#165065 = CARTESIAN_POINT('Ctrl Pts',(-4.8967032564359,-6.4509405986842,-18.0532967435642)) ;
#165066 = CARTESIAN_POINT('Ctrl Pts',(-4.90260275053909,-6.47617483238892,
-18.1447944989218)) ;
#165067 = CARTESIAN_POINT('Ctrl Pts',(-4.80000000081823,-6.46309229646328,
-18.05)) ;
#165068 = CARTESIAN_POINT('Ctrl Pts',(-4.89999269603999,-6.44945650152247,
-18.0500073039034)) ;
#165069 = CARTESIAN_POINT('Ctrl Pts',(-4.9,-6.46309229646329,-18.1499999991818)) ;
#165070 = CARTESIAN_POINT('Ctrl Pts',(-4.8,-6.45,-18.05)) ;
#165071 = CARTESIAN_POINT('Ctrl Pts',(-4.9,-6.45,-18.05)) ;
#165072 = CARTESIAN_POINT('Ctrl Pts',(-4.9,-6.45,-18.15)) ;
#165073 = CARTESIAN_POINT('Origin',(-4.8,-6.45,-18.15)) ;
#165074 = CARTESIAN_POINT('Origin',(-4.,-6.35,-18.15)) ;
#165075 = CARTESIAN_POINT('Origin',(-4.,-6.35,-18.15)) ;
#165076 = CARTESIAN_POINT('Origin',(-4.,-6.35,-18.15)) ;
#165077 = CARTESIAN_POINT('Ctrl Pts',(-3.8,-6.55,-20.15)) ;
#165078 = CARTESIAN_POINT('Ctrl Pts',(-3.8,-6.55,-20.15)) ;
#165079 = CARTESIAN_POINT('Ctrl Pts',(-3.8,-6.55,-20.15)) ;
#165080 = CARTESIAN_POINT('Ctrl Pts',(-3.85250686565272,-6.55,-20.1237465671736)) ;
#165081 = CARTESIAN_POINT('Ctrl Pts',(-3.83954133268385,-6.55,-20.1104586673161)) ;
#165082 = CARTESIAN_POINT('Ctrl Pts',(-3.82625343282627,-6.55,-20.0974931343473)) ;
#165083 = CARTESIAN_POINT('Ctrl Pts',(-3.90439743459706,-6.53922263893874,
-20.0978012827014)) ;
#165084 = CARTESIAN_POINT('Ctrl Pts',(-3.87914655110978,-6.52362528614071,
-20.0708534488901)) ;
#165085 = CARTESIAN_POINT('Ctrl Pts',(-3.85219871729855,-6.53922263893876,
-20.0456025654029)) ;
#165086 = CARTESIAN_POINT('Ctrl Pts',(-3.95993331705743,-6.51145469770861,
-20.0700333414713)) ;
#165087 = CARTESIAN_POINT('Ctrl Pts',(-3.90288380314162,-6.48208554016476,
-20.0471161968584)) ;
#165088 = CARTESIAN_POINT('Ctrl Pts',(-3.8799666585287,-6.5114546977086,-19.9900666829426)) ;
#165089 = CARTESIAN_POINT('Ctrl Pts',(-3.97475731408271,-6.5003618540841,
-20.0626213429587)) ;
#165090 = CARTESIAN_POINT('Ctrl Pts',(-3.90501307588293,-6.46792722356047,
-20.0449869241171)) ;
#165091 = CARTESIAN_POINT('Ctrl Pts',(-3.88737865704135,-6.5003618540841,
-19.9752426859173)) ;
#165092 = CARTESIAN_POINT('Ctrl Pts',(-3.9947944989218,-6.47617483238891,
-20.0526027505391)) ;
#165093 = CARTESIAN_POINT('Ctrl Pts',(-3.9032967435641,-6.4509405986842,-20.0467032564358)) ;
#165094 = CARTESIAN_POINT('Ctrl Pts',(-3.89739724946091,-6.47617483238892,
-19.9552055010782)) ;
#165095 = CARTESIAN_POINT('Ctrl Pts',(-3.99999999918176,-6.46309229646328,
-20.05)) ;
#165096 = CARTESIAN_POINT('Ctrl Pts',(-3.90000730395532,-6.44945650152054,
-20.0499926960966)) ;
#165097 = CARTESIAN_POINT('Ctrl Pts',(-3.9,-6.46309229646328,-19.9500000008182)) ;
#165098 = CARTESIAN_POINT('Ctrl Pts',(-4.,-6.45,-20.05)) ;
#165099 = CARTESIAN_POINT('Ctrl Pts',(-3.9,-6.45,-20.05)) ;
#165100 = CARTESIAN_POINT('Ctrl Pts',(-3.9,-6.45,-19.95)) ;
#165101 = CARTESIAN_POINT('Origin',(-4.,-6.45,-19.95)) ;
#165102 = CARTESIAN_POINT('Origin',(-4.8,-6.4,-18.15)) ;
#165103 = CARTESIAN_POINT('Origin',(-4.8,-6.35,-18.15)) ;
#165104 = CARTESIAN_POINT('Origin',(1.9515639104739E-16,-6.35,-18.15)) ;
#165105 = CARTESIAN_POINT('Origin',(-4.8,-6.35,-18.15)) ;
#165106 = CARTESIAN_POINT('Origin',(-4.,-6.35,-19.05)) ;
#165107 = CARTESIAN_POINT('Origin',(-4.,-6.35,-19.95)) ;
#165108 = CARTESIAN_POINT('Origin',(-4.,-6.4,-19.95)) ;
#165109 = CARTESIAN_POINT('Origin',(-4.,-6.35,-19.95)) ;
#165110 = CARTESIAN_POINT('Origin',(-4.8,-6.35,-18.15)) ;
#165111 = CARTESIAN_POINT('Origin',(-4.8,-6.35,-18.15)) ;
#165112 = CARTESIAN_POINT('Origin',(-4.,-6.35,-19.95)) ;
#165113 = CARTESIAN_POINT('Origin',(-4.,-6.35,-19.95)) ;
#165114 = CARTESIAN_POINT('Origin',(-4.8,-6.35,-19.05)) ;
#165115 = CARTESIAN_POINT('Origin',(-4.8,-6.35,-19.95)) ;
#165116 = CARTESIAN_POINT('Origin',(1.95156391047391E-16,-6.35,-19.95)) ;
#165117 = CARTESIAN_POINT('Origin',(-4.8,-6.35,-19.95)) ;
#165118 = CARTESIAN_POINT('Origin',(-4.8,-6.35,-19.95)) ;
#165119 = CARTESIAN_POINT('Origin',(-4.8,-6.35,-19.95)) ;
#165120 = CARTESIAN_POINT('Origin',(-4.8,-6.4,-19.95)) ;
#165121 = CARTESIAN_POINT('Origin',(-4.8,-6.45,-19.95)) ;
#165122 = CARTESIAN_POINT('Ctrl Pts',(-5.,-6.55,-20.15)) ;
#165123 = CARTESIAN_POINT('Ctrl Pts',(-5.,-6.55,-20.15)) ;
#165124 = CARTESIAN_POINT('Ctrl Pts',(-5.,-6.55,-20.15)) ;
#165125 = CARTESIAN_POINT('Ctrl Pts',(-4.97374656717362,-6.55,-20.0974931343473)) ;
#165126 = CARTESIAN_POINT('Ctrl Pts',(-4.96045866731623,-6.55,-20.110458667316)) ;
#165127 = CARTESIAN_POINT('Ctrl Pts',(-4.94749313434733,-6.55,-20.1237465671736)) ;
#165128 = CARTESIAN_POINT('Ctrl Pts',(-4.94780128270146,-6.53922263893877,
-20.0456025654029)) ;
#165129 = CARTESIAN_POINT('Ctrl Pts',(-4.92085344889017,-6.52362528614074,
-20.0708534488901)) ;
#165130 = CARTESIAN_POINT('Ctrl Pts',(-4.89560256540291,-6.53922263893874,
-20.0978012827014)) ;
#165131 = CARTESIAN_POINT('Ctrl Pts',(-4.92003334147129,-6.5114546977086,
-19.9900666829426)) ;
#165132 = CARTESIAN_POINT('Ctrl Pts',(-4.8971161968584,-6.48208554016475,
-20.0471161968584)) ;
#165133 = CARTESIAN_POINT('Ctrl Pts',(-4.84006668294258,-6.51145469770861,
-20.0700333414713)) ;
#165134 = CARTESIAN_POINT('Ctrl Pts',(-4.91262134295865,-6.5003618540841,
-19.9752426859173)) ;
#165135 = CARTESIAN_POINT('Ctrl Pts',(-4.89498692411706,-6.46792722356047,
-20.0449869241171)) ;
#165136 = CARTESIAN_POINT('Ctrl Pts',(-4.82524268591729,-6.5003618540841,
-20.0626213429587)) ;
#165137 = CARTESIAN_POINT('Ctrl Pts',(-4.90260275053909,-6.47617483238892,
-19.9552055010782)) ;
#165138 = CARTESIAN_POINT('Ctrl Pts',(-4.8967032564359,-6.4509405986842,-20.0467032564358)) ;
#165139 = CARTESIAN_POINT('Ctrl Pts',(-4.80520550107819,-6.47617483238891,
-20.0526027505391)) ;
#165140 = CARTESIAN_POINT('Ctrl Pts',(-4.9,-6.46309229646328,-19.9500000008182)) ;
#165141 = CARTESIAN_POINT('Ctrl Pts',(-4.89999269603999,-6.44945650152247,
-20.0499926960966)) ;
#165142 = CARTESIAN_POINT('Ctrl Pts',(-4.80000000081823,-6.46309229646328,
-20.05)) ;
#165143 = CARTESIAN_POINT('Ctrl Pts',(-4.9,-6.45,-19.95)) ;
#165144 = CARTESIAN_POINT('Ctrl Pts',(-4.9,-6.45,-20.05)) ;
#165145 = CARTESIAN_POINT('Ctrl Pts',(-4.8,-6.45,-20.05)) ;
#165146 = CARTESIAN_POINT('Ctrl Pts',(-5.82426676739348,-5.43399303700626,
-17.4470109659688)) ;
#165147 = CARTESIAN_POINT('Ctrl Pts',(-5.80266988778314,-5.52572360682945,
-17.4523540173507)) ;
#165148 = CARTESIAN_POINT('Ctrl Pts',(-5.82426676352019,-5.53106667371342,
-17.5440845871829)) ;
#165149 = CARTESIAN_POINT('Ctrl Pts',(-5.83498671931113,-5.43935351191921,
-17.4443294581962)) ;
#165150 = CARTESIAN_POINT('Ctrl Pts',(-5.80595263122268,-5.52411753147717,
-17.4539600935404)) ;
#165151 = CARTESIAN_POINT('Ctrl Pts',(-5.8349867139763,-5.5337481806747,-17.5387241131464)) ;
#165152 = CARTESIAN_POINT('Ctrl Pts',(-5.84526105845708,-5.44830326289504,
-17.4398528401961)) ;
#165153 = CARTESIAN_POINT('Ctrl Pts',(-5.8137093274614,-5.52260132030862,
-17.4554763059992)) ;
#165154 = CARTESIAN_POINT('Ctrl Pts',(-5.84526105243725,-5.53822479746341,
-17.5297743635699)) ;
#165155 = CARTESIAN_POINT('Ctrl Pts',(-5.86378685403694,-5.47240020430411,
-17.4278032513088)) ;
#165156 = CARTESIAN_POINT('Ctrl Pts',(-5.83531854275286,-5.52733067404489,
-17.4507469551147)) ;
#165157 = CARTESIAN_POINT('Ctrl Pts',(-5.86378684816464,-5.55027438459902,
-17.5056774250056)) ;
#165158 = CARTESIAN_POINT('Ctrl Pts',(-5.87203852631572,-5.48754495134743,
-17.4202315528944)) ;
#165159 = CARTESIAN_POINT('Ctrl Pts',(-5.84834787930686,-5.53310199490459,
-17.4449756357761)) ;
#165160 = CARTESIAN_POINT('Ctrl Pts',(-5.87203852123043,-5.5578460824346,
-17.490532679514)) ;
#165161 = CARTESIAN_POINT('Ctrl Pts',(-5.89242747304799,-5.53981202333459,
-17.3941056511376)) ;
#165162 = CARTESIAN_POINT('Ctrl Pts',(-5.88223383300419,-5.56084219179275,
-17.4172354431742)) ;
#165163 = CARTESIAN_POINT('Ctrl Pts',(-5.89242747063503,-5.58397198402777,
-17.4382656123278)) ;
#165164 = CARTESIAN_POINT('Ctrl Pts',(-5.9,-5.58381083947301,-17.3721194001431)) ;
#165165 = CARTESIAN_POINT('Ctrl Pts',(-5.9,-5.59485304502678,-17.3832245928864)) ;
#165166 = CARTESIAN_POINT('Ctrl Pts',(-5.9,-5.60595823775504,-17.3942667984405)) ;
#165167 = CARTESIAN_POINT('Ctrl Pts',(-5.9,-5.62807764064044,-17.35)) ;
#165168 = CARTESIAN_POINT('Ctrl Pts',(-5.9,-5.62807764064044,-17.35)) ;
#165169 = CARTESIAN_POINT('Ctrl Pts',(-5.9,-5.62807764064044,-17.35)) ;
#165170 = CARTESIAN_POINT('Origin',(-5.84850712500726,-5.43404914061138,-17.5440285000291)) ;
#165171 = CARTESIAN_POINT('Ctrl Pts',(-5.82425356250363,-5.53106339062591,
-17.5440285000291)) ;
#165172 = CARTESIAN_POINT('Ctrl Pts',(-5.80269484027818,-5.52567371006955,
-17.4524039305709)) ;
#165173 = CARTESIAN_POINT('Ctrl Pts',(-5.82425356250363,-5.43404914061138,
-17.4470142500145)) ;
#165174 = CARTESIAN_POINT('Ctrl Pts',(-5.80840777707096,-5.52710194426774,
-17.5479899459043)) ;
#165175 = CARTESIAN_POINT('Ctrl Pts',(-5.7934141764523,-5.52335354411309,
-17.4528358498184)) ;
#165176 = CARTESIAN_POINT('Ctrl Pts',(-5.81633079157288,-5.43008775511759,
-17.4489949427472)) ;
#165177 = CARTESIAN_POINT('Ctrl Pts',(-5.79207992677989,-5.52301998169497,
-17.549999999534)) ;
#165178 = CARTESIAN_POINT('Ctrl Pts',(-5.78430903206643,-5.52107725801661,
-17.4519613954329)) ;
#165179 = CARTESIAN_POINT('Ctrl Pts',(-5.80816665318299,-5.42600568595106,
-17.45)) ;
#165180 = CARTESIAN_POINT('Ctrl Pts',(-5.77574643749636,-5.51893660937409,
-17.55)) ;
#165181 = CARTESIAN_POINT('Ctrl Pts',(-5.77574643749636,-5.51893660937409,
-17.45)) ;
#165182 = CARTESIAN_POINT('Ctrl Pts',(-5.8,-5.42192235935956,-17.45)) ;
#165183 = CARTESIAN_POINT('Origin',(-5.8,-5.42192235935956,-17.55)) ;
#165184 = CARTESIAN_POINT('Origin',(-5.8066065036801,-5.42357398527959,-17.55)) ;
#165185 = CARTESIAN_POINT('Origin',(-5.17275707706437,-5.26511162862565,-17.55)) ;
#165186 = CARTESIAN_POINT('Origin',(-5.15068655017073,-5.25959399690224,-17.5605938529089)) ;
#165187 = CARTESIAN_POINT('Origin',(-5.17275707706436,-5.26511162862565,-17.55)) ;
#165188 = CARTESIAN_POINT('Origin',(-5.17275707706436,-5.26511162862565,-17.55)) ;
#165189 = CARTESIAN_POINT('Origin',(-5.17275707706436,-5.26511162862565,-17.55)) ;
#165190 = CARTESIAN_POINT('Origin',(-5.17275707706436,-5.05,-17.55)) ;
#165191 = CARTESIAN_POINT('Origin',(-5.17275707706436,-1.91866427917294,-17.55)) ;
#165192 = CARTESIAN_POINT('Origin',(-3.78014014831103,-3.31128120792626,-18.2184561258016)) ;
#165193 = CARTESIAN_POINT('Origin',(-5.17275707706436,-1.91866427917294,-17.55)) ;
#165194 = CARTESIAN_POINT('Origin',(-5.17275707706436,-1.91866427917293,-17.55)) ;
#165195 = CARTESIAN_POINT('Origin',(-5.17275707706436,-1.91866427917294,-17.55)) ;
#165196 = CARTESIAN_POINT('Origin',(-3.97071067811865,-3.12071067811865,-17.55)) ;
#165197 = CARTESIAN_POINT('Origin',(-5.8,-1.2914213562373,-17.55)) ;
#165198 = CARTESIAN_POINT('Ctrl Pts',(-5.87071067811865,-1.14999999999999,
-17.4207106781187)) ;
#165199 = CARTESIAN_POINT('Ctrl Pts',(-5.8471404520791,-1.10285954792089,
-17.4442809041582)) ;
#165200 = CARTESIAN_POINT('Ctrl Pts',(-5.87071067811865,-1.07928932188134,
-17.4914213562373)) ;
#165201 = CARTESIAN_POINT('Ctrl Pts',(-5.85217562795657,-1.18707010095452,
-17.4392457282807)) ;
#165202 = CARTESIAN_POINT('Ctrl Pts',(-5.81261165662082,-1.1373883433793,
-17.4658614719499)) ;
#165203 = CARTESIAN_POINT('Ctrl Pts',(-5.8335394967105,-1.1164605032895,-17.5285925363811)) ;
#165204 = CARTESIAN_POINT('Ctrl Pts',(-5.82627077431945,-1.23887980759835,
-17.45)) ;
#165205 = CARTESIAN_POINT('Ctrl Pts',(-5.76566787907942,-1.18433212092055,
-17.4671489437127)) ;
#165206 = CARTESIAN_POINT('Ctrl Pts',(-5.78190678732229,-1.16809321267771,
-17.5499999994186)) ;
#165207 = CARTESIAN_POINT('Ctrl Pts',(-5.8,-1.2914213562373,-17.45)) ;
#165208 = CARTESIAN_POINT('Ctrl Pts',(-5.72928932188134,-1.22071067811865,
-17.45)) ;
#165209 = CARTESIAN_POINT('Ctrl Pts',(-5.72928932188134,-1.22071067811865,
-17.55)) ;
#165210 = CARTESIAN_POINT('Origin',(-5.94142135623731,-1.15,-17.4914213562373)) ;
#165211 = CARTESIAN_POINT('Ctrl Pts',(-5.9,-1.00857864376269,-17.35)) ;
#165212 = CARTESIAN_POINT('Ctrl Pts',(-5.9,-1.00857864376269,-17.35)) ;
#165213 = CARTESIAN_POINT('Ctrl Pts',(-5.9,-1.00857864376269,-17.35)) ;
#165214 = CARTESIAN_POINT('Ctrl Pts',(-5.9,-1.06112019240164,-17.3762707743195)) ;
#165215 = CARTESIAN_POINT('Ctrl Pts',(-5.9,-1.04860238145267,-17.3900237376901)) ;
#165216 = CARTESIAN_POINT('Ctrl Pts',(-5.9,-1.03484941808214,-17.402541548639)) ;
#165217 = CARTESIAN_POINT('Ctrl Pts',(-5.88924572828071,-1.11292989904543,
-17.4021756279566)) ;
#165218 = CARTESIAN_POINT('Ctrl Pts',(-5.87451700627693,-1.08721613123091,
-17.4286374874681)) ;
#165219 = CARTESIAN_POINT('Ctrl Pts',(-5.88924572828062,-1.06075427171938,
-17.4543512552826)) ;
#165220 = CARTESIAN_POINT('Ctrl Pts',(-5.87071067811865,-1.14999999999999,
-17.4207106781187)) ;
#165221 = CARTESIAN_POINT('Ctrl Pts',(-5.8471404520791,-1.10285954792089,
-17.4442809041582)) ;
#165222 = CARTESIAN_POINT('Ctrl Pts',(-5.87071067811865,-1.07928932188134,
-17.4914213562373)) ;
#165223 = CARTESIAN_POINT('Ctrl Pts',(-5.87071067811866,-1.14999999999999,
-20.6792893218813)) ;
#165224 = CARTESIAN_POINT('Ctrl Pts',(-5.84714045207911,-1.10285954792089,
-20.6557190958418)) ;
#165225 = CARTESIAN_POINT('Ctrl Pts',(-5.87071067811866,-1.07928932188134,
-20.6085786437627)) ;
#165226 = CARTESIAN_POINT('Ctrl Pts',(-5.8892457282807,-1.11292989904542,
-20.6978243720434)) ;
#165227 = CARTESIAN_POINT('Ctrl Pts',(-5.87451700627498,-1.08721613123207,
-20.6713625125308)) ;
#165228 = CARTESIAN_POINT('Ctrl Pts',(-5.88924572828062,-1.06075427171937,
-20.6456487447174)) ;
#165229 = CARTESIAN_POINT('Ctrl Pts',(-5.9,-1.06112019240159,-20.7237292256804)) ;
#165230 = CARTESIAN_POINT('Ctrl Pts',(-5.9,-1.04860238145164,-20.7099762623107)) ;
#165231 = CARTESIAN_POINT('Ctrl Pts',(-5.9,-1.03484941808214,-20.697458451361)) ;
#165232 = CARTESIAN_POINT('Ctrl Pts',(-5.9,-1.00857864376269,-20.75)) ;
#165233 = CARTESIAN_POINT('Ctrl Pts',(-5.9,-1.00857864376269,-20.75)) ;
#165234 = CARTESIAN_POINT('Ctrl Pts',(-5.9,-1.00857864376269,-20.75)) ;
#165235 = CARTESIAN_POINT('Origin',(-5.94142135623734,-1.14999999999996,-20.6085786437627)) ;
#165236 = CARTESIAN_POINT('Ctrl Pts',(-5.8,-1.2914213562373,-20.65)) ;
#165237 = CARTESIAN_POINT('Ctrl Pts',(-5.72928932188134,-1.22071067811865,
-20.65)) ;
#165238 = CARTESIAN_POINT('Ctrl Pts',(-5.72928932188134,-1.22071067811865,
-20.55)) ;
#165239 = CARTESIAN_POINT('Ctrl Pts',(-5.82627077431951,-1.23887980759822,
-20.65)) ;
#165240 = CARTESIAN_POINT('Ctrl Pts',(-5.76566787907979,-1.18433212092022,
-20.6328510562872)) ;
#165241 = CARTESIAN_POINT('Ctrl Pts',(-5.78190678732243,-1.16809321267756,
-20.5500000005814)) ;
#165242 = CARTESIAN_POINT('Ctrl Pts',(-5.85217562795678,-1.18707010095483,
-20.6607542717195)) ;
#165243 = CARTESIAN_POINT('Ctrl Pts',(-5.81261165662032,-1.13738834337969,
-20.6341385280508)) ;
#165244 = CARTESIAN_POINT('Ctrl Pts',(-5.83353949671031,-1.11646050328968,
-20.571407463619)) ;
#165245 = CARTESIAN_POINT('Ctrl Pts',(-5.87071067811866,-1.14999999999999,
-20.6792893218813)) ;
#165246 = CARTESIAN_POINT('Ctrl Pts',(-5.84714045207911,-1.10285954792088,
-20.6557190958418)) ;
#165247 = CARTESIAN_POINT('Ctrl Pts',(-5.87071067811866,-1.07928932188133,
-20.6085786437627)) ;
#165248 = CARTESIAN_POINT('Origin',(-5.8,-1.29142135623731,-20.55)) ;
#165249 = CARTESIAN_POINT('Origin',(-3.59571067811865,-3.49571067811865,-20.55)) ;
#165250 = CARTESIAN_POINT('Origin',(-5.17275707706437,-1.91866427917293,-20.55)) ;
#165251 = CARTESIAN_POINT('Origin',(-3.09057773798104,-4.00084361825625,-19.55055391724)) ;
#165252 = CARTESIAN_POINT('Origin',(-5.17275707706436,-1.91866427917293,-20.55)) ;
#165253 = CARTESIAN_POINT('Origin',(-5.17275707706436,-1.91866427917293,-20.55)) ;
#165254 = CARTESIAN_POINT('Origin',(-5.17275707706436,-1.91866427917293,-20.55)) ;
#165255 = CARTESIAN_POINT('Origin',(-5.17275707706436,-5.05,-20.55)) ;
#165256 = CARTESIAN_POINT('Origin',(-5.17275707706436,-5.26511162862565,-20.55)) ;
#165257 = CARTESIAN_POINT('Origin',(-3.96111272388873,-4.96220054033175,-19.9684107104757)) ;
#165258 = CARTESIAN_POINT('Origin',(-5.17275707706436,-5.26511162862565,-20.55)) ;
#165259 = CARTESIAN_POINT('Origin',(-5.17275707706436,-5.26511162862565,-20.55)) ;
#165260 = CARTESIAN_POINT('Origin',(-5.17275707706436,-5.26511162862565,-20.55)) ;
#165261 = CARTESIAN_POINT('Origin',(-5.10072415073893,-5.24710339704429,-20.55)) ;
#165262 = CARTESIAN_POINT('Origin',(-5.8,-5.42192235935956,-20.55)) ;
#165263 = CARTESIAN_POINT('Ctrl Pts',(-5.77574643749636,-5.51893660937409,
-20.55)) ;
#165264 = CARTESIAN_POINT('Ctrl Pts',(-5.77574643749636,-5.51893660937409,
-20.65)) ;
#165265 = CARTESIAN_POINT('Ctrl Pts',(-5.8,-5.42192235935956,-20.65)) ;
#165266 = CARTESIAN_POINT('Ctrl Pts',(-5.79207992677989,-5.52301998169497,
-20.550000000466)) ;
#165267 = CARTESIAN_POINT('Ctrl Pts',(-5.78430903206644,-5.5210772580166,
-20.6480386045671)) ;
#165268 = CARTESIAN_POINT('Ctrl Pts',(-5.80816665318301,-5.42600568595105,
-20.65)) ;
#165269 = CARTESIAN_POINT('Ctrl Pts',(-5.80840777707096,-5.52710194426774,
-20.5520100540957)) ;
#165270 = CARTESIAN_POINT('Ctrl Pts',(-5.7934141764523,-5.52335354411309,
-20.6471641501816)) ;
#165271 = CARTESIAN_POINT('Ctrl Pts',(-5.81633079157287,-5.43008775511759,
-20.6510050572528)) ;
#165272 = CARTESIAN_POINT('Ctrl Pts',(-5.82425356250363,-5.53106339062591,
-20.5559714999709)) ;
#165273 = CARTESIAN_POINT('Ctrl Pts',(-5.80269484027818,-5.52567371006955,
-20.6475960694291)) ;
#165274 = CARTESIAN_POINT('Ctrl Pts',(-5.82425356250363,-5.43404914061138,
-20.6529857499855)) ;
#165275 = CARTESIAN_POINT('Origin',(-5.84850712500726,-5.43404914061138,-20.5559714999709)) ;
#165276 = CARTESIAN_POINT('Ctrl Pts',(-5.82426676739356,-5.5310666746717,
-20.5559153963654)) ;
#165277 = CARTESIAN_POINT('Ctrl Pts',(-5.80266988778305,-5.52572362329012,
-20.647645966189)) ;
#165278 = CARTESIAN_POINT('Ctrl Pts',(-5.82426676352021,-5.43399305345753,
-20.652989033073)) ;
#165279 = CARTESIAN_POINT('Ctrl Pts',(-5.83498671931124,-5.53374818244431,
-20.5612758712785)) ;
#165280 = CARTESIAN_POINT('Ctrl Pts',(-5.80595263122255,-5.52411754710033,
-20.6460398908368)) ;
#165281 = CARTESIAN_POINT('Ctrl Pts',(-5.83498671397632,-5.43935352749395,
-20.6556705400343)) ;
#165282 = CARTESIAN_POINT('Ctrl Pts',(-5.84526105845722,-5.53822480044432,
-20.5702256222543)) ;
#165283 = CARTESIAN_POINT('Ctrl Pts',(-5.81370932746126,-5.52260133464154,
-20.6445236796681)) ;
#165284 = CARTESIAN_POINT('Ctrl Pts',(-5.84526105243727,-5.4483032770705,
-20.660147156823)) ;
#165285 = CARTESIAN_POINT('Ctrl Pts',(-5.86378685403706,-5.55027438933182,
-20.5943225636634)) ;
#165286 = CARTESIAN_POINT('Ctrl Pts',(-5.83531854275274,-5.52733068552585,
-20.6492530334044)) ;
#165287 = CARTESIAN_POINT('Ctrl Pts',(-5.86378684816468,-5.47240021563482,
-20.6721967439586)) ;
#165288 = CARTESIAN_POINT('Ctrl Pts',(-5.87203852631585,-5.55784608774614,
-20.6094673107067)) ;
#165289 = CARTESIAN_POINT('Ctrl Pts',(-5.84834787930676,-5.53310200486442,
-20.6550243542642)) ;
#165290 = CARTESIAN_POINT('Ctrl Pts',(-5.87203852123047,-5.4875449611264,
-20.6797684417942)) ;
#165291 = CARTESIAN_POINT('Ctrl Pts',(-5.892427473048,-5.5839719895029,-20.661734382694)) ;
#165292 = CARTESIAN_POINT('Ctrl Pts',(-5.88223383300415,-5.56084219746619,
-20.6827645511522)) ;
#165293 = CARTESIAN_POINT('Ctrl Pts',(-5.89242747063503,-5.53981202831257,
-20.7058943433874)) ;
#165294 = CARTESIAN_POINT('Ctrl Pts',(-5.9,-5.60595824049752,-20.7057331988325)) ;
#165295 = CARTESIAN_POINT('Ctrl Pts',(-5.9,-5.59485304775417,-20.7167754043861)) ;
#165296 = CARTESIAN_POINT('Ctrl Pts',(-5.9,-5.58381084219988,-20.7278805971145)) ;
#165297 = CARTESIAN_POINT('Ctrl Pts',(-5.9,-5.62807764064044,-20.75)) ;
#165298 = CARTESIAN_POINT('Ctrl Pts',(-5.9,-5.62807764064044,-20.75)) ;
#165299 = CARTESIAN_POINT('Ctrl Pts',(-5.9,-5.62807764064044,-20.75)) ;
#165300 = CARTESIAN_POINT('Origin',(7.8,2.1,-19.45)) ;
#165301 = CARTESIAN_POINT('Origin',(7.8,2.1,-19.65)) ;
#165302 = CARTESIAN_POINT('Origin',(7.6,2.1,-19.45)) ;
#165303 = CARTESIAN_POINT('Origin',(7.6,2.1,-19.45)) ;
#165304 = CARTESIAN_POINT('Origin',(7.6,2.1,-18.65)) ;
#165305 = CARTESIAN_POINT('Origin',(7.8,2.1,-19.65)) ;
#165306 = CARTESIAN_POINT('Origin',(9.6,2.1,-19.65)) ;
#165307 = CARTESIAN_POINT('Origin',(7.8,2.1,-18.65)) ;
#165308 = CARTESIAN_POINT('Origin',(7.8,2.1,-18.45)) ;
#165309 = CARTESIAN_POINT('Origin',(9.6,2.1,-19.45)) ;
#165310 = CARTESIAN_POINT('Origin',(9.8,2.1,-19.45)) ;
#165311 = CARTESIAN_POINT('Origin',(7.8,2.1,-18.45)) ;
#165312 = CARTESIAN_POINT('Origin',(9.6,2.1,-18.45)) ;
#165313 = CARTESIAN_POINT('Origin',(9.8,2.1,-19.45)) ;
#165314 = CARTESIAN_POINT('Origin',(9.8,2.1,-18.65)) ;
#165315 = CARTESIAN_POINT('Origin',(9.6,2.1,-18.65)) ;
#165316 = CARTESIAN_POINT('Origin',(-4.15,-6.25,-18.3)) ;
#165317 = CARTESIAN_POINT('Origin',(-4.15,-6.3,-18.3)) ;
#165318 = CARTESIAN_POINT('Origin',(-4.15,-6.3,-19.05)) ;
#165319 = CARTESIAN_POINT('Origin',(-4.15,-6.3,-19.8)) ;
#165320 = CARTESIAN_POINT('Origin',(-4.15,-6.3,-18.3)) ;
#165321 = CARTESIAN_POINT('Origin',(-4.15,-6.25,-19.8)) ;
#165322 = CARTESIAN_POINT('Origin',(-4.15,-6.3,-19.8)) ;
#165323 = CARTESIAN_POINT('Origin',(-4.15,-6.3,-18.3)) ;
#165324 = CARTESIAN_POINT('Origin',(-4.15,-6.3,-18.3)) ;
#165325 = CARTESIAN_POINT('Origin',(-4.15,-6.3,-19.8)) ;
#165326 = CARTESIAN_POINT('Origin',(-4.15,-6.3,-19.8)) ;
#165327 = CARTESIAN_POINT('Origin',(-4.65,-6.25,-18.3)) ;
#165328 = CARTESIAN_POINT('Origin',(-4.65,-6.3,-18.3)) ;
#165329 = CARTESIAN_POINT('Origin',(0.,-6.3,-18.3)) ;
#165330 = CARTESIAN_POINT('Origin',(-4.65,-6.3,-18.3)) ;
#165331 = CARTESIAN_POINT('Origin',(0.,-6.3,-19.8)) ;
#165332 = CARTESIAN_POINT('Origin',(-4.65,-6.3,-19.8)) ;
#165333 = CARTESIAN_POINT('Origin',(-4.65,-6.25,-19.8)) ;
#165334 = CARTESIAN_POINT('Origin',(-4.65,-6.3,-19.8)) ;
#165335 = CARTESIAN_POINT('Origin',(-4.65,-6.3,-18.3)) ;
#165336 = CARTESIAN_POINT('Origin',(-4.65,-6.3,-18.3)) ;
#165337 = CARTESIAN_POINT('Origin',(-4.65,-6.3,-19.8)) ;
#165338 = CARTESIAN_POINT('Origin',(-4.65,-6.3,-19.8)) ;
#165339 = CARTESIAN_POINT('Origin',(-4.65,-6.3,-19.05)) ;
#165340 = CARTESIAN_POINT('Origin',(-3.,4.45,-20.15)) ;
#165341 = CARTESIAN_POINT('Origin',(-2.1,4.45,-20.15)) ;
#165342 = CARTESIAN_POINT('Origin',(-2.9,4.45,-20.15)) ;
#165343 = CARTESIAN_POINT('Origin',(-2.9,4.45,-19.95)) ;
#165344 = CARTESIAN_POINT('Origin',(-3.1,4.45,-19.95)) ;
#165345 = CARTESIAN_POINT('Origin',(-2.9,4.45,-19.95)) ;
#165346 = CARTESIAN_POINT('Origin',(-2.1,4.45,-19.95)) ;
#165347 = CARTESIAN_POINT('Origin',(-2.1,4.45,-19.95)) ;
#165348 = CARTESIAN_POINT('Origin',(-1.9,4.45,-19.95)) ;
#165349 = CARTESIAN_POINT('Origin',(-3.1,4.45,-20.05)) ;
#165350 = CARTESIAN_POINT('Origin',(-3.1,4.45,-18.15)) ;
#165351 = CARTESIAN_POINT('Origin',(-2.9,4.4,-19.95)) ;
#165352 = CARTESIAN_POINT('Origin',(-2.9,4.35,-19.95)) ;
#165353 = CARTESIAN_POINT('Origin',(-1.95156391047391E-16,4.35,-19.95)) ;
#165354 = CARTESIAN_POINT('Origin',(-2.1,4.35,-19.95)) ;
#165355 = CARTESIAN_POINT('Origin',(-2.9,4.35,-19.95)) ;
#165356 = CARTESIAN_POINT('Origin',(-2.1,4.4,-19.95)) ;
#165357 = CARTESIAN_POINT('Origin',(-2.1,4.35,-19.95)) ;
#165358 = CARTESIAN_POINT('Origin',(-1.9,4.45,-20.05)) ;
#165359 = CARTESIAN_POINT('Origin',(-1.9,4.45,-18.15)) ;
#165360 = CARTESIAN_POINT('Origin',(-3.,4.45,-17.95)) ;
#165361 = CARTESIAN_POINT('Origin',(-2.9,4.45,-17.95)) ;
#165362 = CARTESIAN_POINT('Origin',(-2.1,4.45,-17.95)) ;
#165363 = CARTESIAN_POINT('Origin',(-2.9,4.45,-18.15)) ;
#165364 = CARTESIAN_POINT('Origin',(-2.9,4.45,-18.15)) ;
#165365 = CARTESIAN_POINT('Origin',(-2.9,4.35,-19.95)) ;
#165366 = CARTESIAN_POINT('Origin',(-2.9,4.35,-19.95)) ;
#165367 = CARTESIAN_POINT('Origin',(-2.1,4.35,-19.95)) ;
#165368 = CARTESIAN_POINT('Origin',(-2.1,4.35,-19.95)) ;
#165369 = CARTESIAN_POINT('Origin',(-2.1,4.45,-18.15)) ;
#165370 = CARTESIAN_POINT('Origin',(-2.1,4.45,-18.15)) ;
#165371 = CARTESIAN_POINT('Origin',(-2.9,4.4,-18.15)) ;
#165372 = CARTESIAN_POINT('Origin',(-2.9,4.35,-18.15)) ;
#165373 = CARTESIAN_POINT('Origin',(-2.9,4.35,-19.05)) ;
#165374 = CARTESIAN_POINT('Origin',(-2.9,4.35,-18.15)) ;
#165375 = CARTESIAN_POINT('Origin',(-2.1,4.35,-19.05)) ;
#165376 = CARTESIAN_POINT('Origin',(-2.1,4.35,-18.15)) ;
#165377 = CARTESIAN_POINT('Origin',(-2.1,4.4,-18.15)) ;
#165378 = CARTESIAN_POINT('Origin',(-2.1,4.35,-18.15)) ;
#165379 = CARTESIAN_POINT('Origin',(-2.9,4.35,-18.15)) ;
#165380 = CARTESIAN_POINT('Origin',(-2.9,4.35,-18.15)) ;
#165381 = CARTESIAN_POINT('Origin',(-2.1,4.35,-18.15)) ;
#165382 = CARTESIAN_POINT('Origin',(-2.1,4.35,-18.15)) ;
#165383 = CARTESIAN_POINT('Origin',(-1.95156391047391E-16,4.35,-18.15)) ;
#165384 = CARTESIAN_POINT('Origin',(-2.25,4.25,-19.8)) ;
#165385 = CARTESIAN_POINT('Origin',(-2.25,4.3,-19.8)) ;
#165386 = CARTESIAN_POINT('Origin',(-2.25,4.3,-19.05)) ;
#165387 = CARTESIAN_POINT('Origin',(-2.25,4.3,-18.3)) ;
#165388 = CARTESIAN_POINT('Origin',(-2.25,4.3,-19.8)) ;
#165389 = CARTESIAN_POINT('Origin',(-2.25,4.25,-18.3)) ;
#165390 = CARTESIAN_POINT('Origin',(-2.25,4.3,-18.3)) ;
#165391 = CARTESIAN_POINT('Origin',(-2.25,4.3,-19.8)) ;
#165392 = CARTESIAN_POINT('Origin',(-2.25,4.3,-19.8)) ;
#165393 = CARTESIAN_POINT('Origin',(-2.25,4.3,-18.3)) ;
#165394 = CARTESIAN_POINT('Origin',(-2.25,4.3,-18.3)) ;
#165395 = CARTESIAN_POINT('Origin',(-2.75,4.25,-19.8)) ;
#165396 = CARTESIAN_POINT('Origin',(-2.75,4.3,-19.8)) ;
#165397 = CARTESIAN_POINT('Origin',(-1.97127667724637E-17,4.3,-19.8)) ;
#165398 = CARTESIAN_POINT('Origin',(-2.75,4.3,-19.8)) ;
#165399 = CARTESIAN_POINT('Origin',(-1.97127667724637E-17,4.3,-18.3)) ;
#165400 = CARTESIAN_POINT('Origin',(-2.75,4.3,-18.3)) ;
#165401 = CARTESIAN_POINT('Origin',(-2.75,4.25,-18.3)) ;
#165402 = CARTESIAN_POINT('Origin',(-2.75,4.3,-18.3)) ;
#165403 = CARTESIAN_POINT('Origin',(-2.75,4.3,-19.8)) ;
#165404 = CARTESIAN_POINT('Origin',(-2.75,4.3,-19.8)) ;
#165405 = CARTESIAN_POINT('Origin',(-2.75,4.3,-18.3)) ;
#165406 = CARTESIAN_POINT('Origin',(-2.75,4.3,-18.3)) ;
#165407 = CARTESIAN_POINT('Origin',(-2.75,4.3,-19.05)) ;
#165408 = CARTESIAN_POINT('Origin',(7.8,2.9,-19.45)) ;
#165409 = CARTESIAN_POINT('Origin',(7.8,2.9,-19.45)) ;
#165410 = CARTESIAN_POINT('Origin',(7.8,2.9,-18.65)) ;
#165411 = CARTESIAN_POINT('Origin',(7.8,2.9,-18.65)) ;
#165412 = CARTESIAN_POINT('Origin',(7.8,2.9,-18.65)) ;
#165413 = CARTESIAN_POINT('Origin',(7.8,2.9,-19.45)) ;
#165414 = CARTESIAN_POINT('Origin',(7.8,2.9,-19.45)) ;
#165415 = CARTESIAN_POINT('Origin',(9.6,2.9,-18.65)) ;
#165416 = CARTESIAN_POINT('Origin',(9.6,2.9,-18.65)) ;
#165417 = CARTESIAN_POINT('Origin',(9.6,2.9,-19.45)) ;
#165418 = CARTESIAN_POINT('Origin',(9.6,2.9,-19.45)) ;
#165419 = CARTESIAN_POINT('Origin',(9.6,2.9,-18.65)) ;
#165420 = CARTESIAN_POINT('Origin',(9.6,2.9,-18.65)) ;
#165421 = CARTESIAN_POINT('Origin',(9.6,2.9,-19.45)) ;
#165422 = CARTESIAN_POINT('Origin',(9.6,2.9,-19.45)) ;
#165423 = CARTESIAN_POINT('Origin',(9.6,2.9,-19.45)) ;
#165424 = CARTESIAN_POINT('Origin',(-0.183301359729408,3.45,-17.532963213524)) ;
#165425 = CARTESIAN_POINT('Origin',(0.24923464143508,3.15,-18.9337799780213)) ;
#165426 = CARTESIAN_POINT('Origin',(-0.249234641435079,3.15,-19.1662200219787)) ;
#165427 = CARTESIAN_POINT('Origin',(-1.04429375741423,3.45,-17.9344505621777)) ;
#165428 = CARTESIAN_POINT('Origin',(10.1,-2.15,-21.9568804065906)) ;
#165429 = CARTESIAN_POINT('Origin',(10.1,-2.15,-21.9568804065906)) ;
#165430 = CARTESIAN_POINT('Origin',(10.1,-2.15,-21.9568804065906)) ;
#165431 = CARTESIAN_POINT('Origin',(10.1,-2.15,-21.9568804065906)) ;
#165432 = CARTESIAN_POINT('Origin',(10.1,-2.15,-22.86)) ;
#165433 = CARTESIAN_POINT('Origin',(10.1,-2.15,-21.555)) ;
#165434 = CARTESIAN_POINT('Origin',(10.2,-2.15,-21.9568804065906)) ;
#165435 = CARTESIAN_POINT('Origin',(3.7,-2.15,-21.9568804065906)) ;
#165436 = CARTESIAN_POINT('Origin',(10.1,-3.65625,-22.86)) ;
#165437 = CARTESIAN_POINT('Origin',(10.1,-2.15,-23.7631195934094)) ;
#165438 = CARTESIAN_POINT('Origin',(10.1,-3.65625,-21.555)) ;
#165439 = CARTESIAN_POINT('Origin',(10.1,1.9,-21.555)) ;
#165440 = CARTESIAN_POINT('Origin',(10.1,-2.15,-21.555)) ;
#165441 = CARTESIAN_POINT('Origin',(10.1,-2.15,-21.555)) ;
#165442 = CARTESIAN_POINT('Origin',(10.1,-2.15,-21.555)) ;
#165443 = CARTESIAN_POINT('Origin',(3.7,-2.15,-21.9568804065906)) ;
#165444 = CARTESIAN_POINT('Origin',(3.7,-2.32153024911032,-22.0597267659824)) ;
#165445 = CARTESIAN_POINT('Origin',(3.7,-2.35,-21.9568804065906)) ;
#165446 = CARTESIAN_POINT('Origin',(10.1,-2.15,-23.7631195934094)) ;
#165447 = CARTESIAN_POINT('Origin',(10.1,-2.15,-23.7631195934094)) ;
#165448 = CARTESIAN_POINT('Origin',(10.1,-2.15,-23.7631195934094)) ;
#165449 = CARTESIAN_POINT('Origin',(10.1,1.9,-22.86)) ;
#165450 = CARTESIAN_POINT('Origin',(10.1,1.9,-24.165)) ;
#165451 = CARTESIAN_POINT('Origin',(10.1,1.9,-21.555)) ;
#165452 = CARTESIAN_POINT('Origin',(10.2,-2.15,-21.555)) ;
#165453 = CARTESIAN_POINT('Origin',(3.7,-2.15,-21.555)) ;
#165454 = CARTESIAN_POINT('Origin',(3.7,-2.35,-21.455)) ;
#165455 = CARTESIAN_POINT('Origin',(3.7,-2.35,-21.555)) ;
#165456 = CARTESIAN_POINT('Origin',(3.7,-3.65625,-22.86)) ;
#165457 = CARTESIAN_POINT('Origin',(3.7,-2.32153024911032,-23.6602732340176)) ;
#165458 = CARTESIAN_POINT('Origin',(10.2,-2.15,-23.7631195934094)) ;
#165459 = CARTESIAN_POINT('Origin',(3.7,-2.15,-23.7631195934094)) ;
#165460 = CARTESIAN_POINT('Origin',(10.1,-2.15,-22.86)) ;
#165461 = CARTESIAN_POINT('Origin',(10.1,-2.15,-24.165)) ;
#165462 = CARTESIAN_POINT('Origin',(10.1,-3.65625,-24.165)) ;
#165463 = CARTESIAN_POINT('Origin',(10.1,1.9,-24.165)) ;
#165464 = CARTESIAN_POINT('Origin',(10.1,-2.15,-24.165)) ;
#165465 = CARTESIAN_POINT('Origin',(3.7,-2.35,-21.555)) ;
#165466 = CARTESIAN_POINT('Origin',(3.5,-2.35,-21.555)) ;
#165467 = CARTESIAN_POINT('Origin',(3.7,-2.15,-23.7631195934094)) ;
#165468 = CARTESIAN_POINT('Origin',(3.7,-2.35,-23.7631195934094)) ;
#165469 = CARTESIAN_POINT('Origin',(10.1,-2.15,-24.165)) ;
#165470 = CARTESIAN_POINT('Origin',(10.1,-2.15,-24.165)) ;
#165471 = CARTESIAN_POINT('Origin',(3.6,1.9,-21.355)) ;
#165472 = CARTESIAN_POINT('Origin',(3.5,1.9,-21.355)) ;
#165473 = CARTESIAN_POINT('Origin',(2.7,1.9,-21.355)) ;
#165474 = CARTESIAN_POINT('Origin',(3.5,2.01220782770297E-15,-21.555)) ;
#165475 = CARTESIAN_POINT('Origin',(3.5,-5.15,-21.555)) ;
#165476 = CARTESIAN_POINT('Origin',(3.7,-2.35,-23.735)) ;
#165477 = CARTESIAN_POINT('Origin',(3.7,-2.35,-24.165)) ;
#165478 = CARTESIAN_POINT('Origin',(3.6,-2.15,-24.165)) ;
#165479 = CARTESIAN_POINT('Origin',(3.7,-2.15,-24.165)) ;
#165480 = CARTESIAN_POINT('Origin',(2.7,1.9,-21.355)) ;
#165481 = CARTESIAN_POINT('Origin',(2.7,1.9,-21.355)) ;
#165482 = CARTESIAN_POINT('Origin',(3.5,-5.15,-21.555)) ;
#165483 = CARTESIAN_POINT('Origin',(3.5,-5.15,-21.555)) ;
#165484 = CARTESIAN_POINT('Origin',(3.5,-5.15,-21.555)) ;
#165485 = CARTESIAN_POINT('Origin',(3.7,-2.35,-24.165)) ;
#165486 = CARTESIAN_POINT('Origin',(3.5,-2.35,-24.165)) ;
#165487 = CARTESIAN_POINT('Origin',(2.7,2.,-21.355)) ;
#165488 = CARTESIAN_POINT('Origin',(2.7,-5.15,-21.355)) ;
#165489 = CARTESIAN_POINT('Origin',(3.6,-5.15,-21.555)) ;
#165490 = CARTESIAN_POINT('Origin',(2.7,-5.15,-21.555)) ;
#165491 = CARTESIAN_POINT('Origin',(3.5,-5.15,0.)) ;
#165492 = CARTESIAN_POINT('Origin',(3.5,-5.15,-24.165)) ;
#165493 = CARTESIAN_POINT('Origin',(3.5,-2.0901141027277E-15,-24.165)) ;
#165494 = CARTESIAN_POINT('Origin',(3.5,-5.15,-24.165)) ;
#165495 = CARTESIAN_POINT('Origin',(2.7,-5.15,-21.555)) ;
#165496 = CARTESIAN_POINT('Origin',(2.7,-5.35,-21.555)) ;
#165497 = CARTESIAN_POINT('Origin',(3.5,-5.15,-24.165)) ;
#165498 = CARTESIAN_POINT('Origin',(3.5,-5.15,-24.165)) ;
#165499 = CARTESIAN_POINT('Origin',(2.7,-5.35,-21.455)) ;
#165500 = CARTESIAN_POINT('Origin',(2.7,-5.35,-24.165)) ;
#165501 = CARTESIAN_POINT('Origin',(3.6,-5.15,-24.165)) ;
#165502 = CARTESIAN_POINT('Origin',(2.7,-5.15,-24.165)) ;
#165503 = CARTESIAN_POINT('Origin',(3.6,1.9,-24.365)) ;
#165504 = CARTESIAN_POINT('Origin',(3.5,1.9,-24.365)) ;
#165505 = CARTESIAN_POINT('Origin',(2.7,1.9,-24.365)) ;
#165506 = CARTESIAN_POINT('Origin',(2.7,1.9,-24.265)) ;
#165507 = CARTESIAN_POINT('Origin',(2.7,1.9,-25.165)) ;
#165508 = CARTESIAN_POINT('Origin',(2.7,1.9,-24.365)) ;
#165509 = CARTESIAN_POINT('Origin',(2.7,-5.15,-24.165)) ;
#165510 = CARTESIAN_POINT('Origin',(2.7,-5.15,-24.365)) ;
#165511 = CARTESIAN_POINT('Origin',(2.7,1.9,-24.365)) ;
#165512 = CARTESIAN_POINT('Origin',(2.7,1.9,-24.365)) ;
#165513 = CARTESIAN_POINT('Origin',(2.7,-5.25,-24.365)) ;
#165514 = CARTESIAN_POINT('Ctrl Pts',(-3.8,-6.55,-21.76)) ;
#165515 = CARTESIAN_POINT('Ctrl Pts',(-3.8,-6.55,-21.76)) ;
#165516 = CARTESIAN_POINT('Ctrl Pts',(-3.8,-6.55,-21.76)) ;
#165517 = CARTESIAN_POINT('Ctrl Pts',(-3.82625343282631,-6.55,-21.8125068656527)) ;
#165518 = CARTESIAN_POINT('Ctrl Pts',(-3.83954133268389,-6.55,-21.7995413326847)) ;
#165519 = CARTESIAN_POINT('Ctrl Pts',(-3.8525068656527,-6.55,-21.7862534328264)) ;
#165520 = CARTESIAN_POINT('Ctrl Pts',(-3.85219871729854,-6.53922263893877,
-21.8643974345971)) ;
#165521 = CARTESIAN_POINT('Ctrl Pts',(-3.87914655110976,-6.52362528614071,
-21.83914655111)) ;
#165522 = CARTESIAN_POINT('Ctrl Pts',(-3.90439743459708,-6.53922263893874,
-21.8121987172986)) ;
#165523 = CARTESIAN_POINT('Ctrl Pts',(-3.87996665852871,-6.5114546977086,
-21.9199333170574)) ;
#165524 = CARTESIAN_POINT('Ctrl Pts',(-3.90288380314163,-6.48208554016476,
-21.8628838031415)) ;
#165525 = CARTESIAN_POINT('Ctrl Pts',(-3.95993331705742,-6.51145469770861,
-21.8399666585287)) ;
#165526 = CARTESIAN_POINT('Ctrl Pts',(-3.88737865704135,-6.5003618540841,
-21.9347573140827)) ;
#165527 = CARTESIAN_POINT('Ctrl Pts',(-3.90501307588293,-6.46792722356046,
-21.8650130758829)) ;
#165528 = CARTESIAN_POINT('Ctrl Pts',(-3.9747573140827,-6.5003618540841,-21.8473786570414)) ;
#165529 = CARTESIAN_POINT('Ctrl Pts',(-3.8973972494609,-6.47617483238892,
-21.9547944989218)) ;
#165530 = CARTESIAN_POINT('Ctrl Pts',(-3.9032967435641,-6.45094059868421,
-21.8632967435641)) ;
#165531 = CARTESIAN_POINT('Ctrl Pts',(-3.99479449892181,-6.47617483238891,
-21.8573972494609)) ;
#165532 = CARTESIAN_POINT('Ctrl Pts',(-3.9,-6.46309229646327,-21.9599999991818)) ;
#165533 = CARTESIAN_POINT('Ctrl Pts',(-3.90000730399733,-6.44945650153778,
-21.860007303903)) ;
#165534 = CARTESIAN_POINT('Ctrl Pts',(-3.99999999918173,-6.46309229646329,
-21.86)) ;
#165535 = CARTESIAN_POINT('Ctrl Pts',(-3.9,-6.45,-21.96)) ;
#165536 = CARTESIAN_POINT('Ctrl Pts',(-3.89999999999999,-6.45,-21.86)) ;
#165537 = CARTESIAN_POINT('Ctrl Pts',(-4.,-6.45,-21.86)) ;
#165538 = CARTESIAN_POINT('Origin',(-4.,-6.45,-21.96)) ;
#165539 = CARTESIAN_POINT('Origin',(-4.,-6.4,-21.96)) ;
#165540 = CARTESIAN_POINT('Origin',(-4.,-6.35,-21.96)) ;
#165541 = CARTESIAN_POINT('Ctrl Pts',(-5.,-6.55,-21.76)) ;
#165542 = CARTESIAN_POINT('Ctrl Pts',(-5.,-6.55,-21.76)) ;
#165543 = CARTESIAN_POINT('Ctrl Pts',(-5.,-6.55,-21.76)) ;
#165544 = CARTESIAN_POINT('Ctrl Pts',(-4.94749313434733,-6.55,-21.7862534328264)) ;
#165545 = CARTESIAN_POINT('Ctrl Pts',(-4.9604586673161,-6.55,-21.7995413326849)) ;
#165546 = CARTESIAN_POINT('Ctrl Pts',(-4.97374656717362,-6.55,-21.8125068656527)) ;
#165547 = CARTESIAN_POINT('Ctrl Pts',(-4.89560256540291,-6.53922263893874,
-21.8121987172986)) ;
#165548 = CARTESIAN_POINT('Ctrl Pts',(-4.92085344889023,-6.52362528614071,
-21.83914655111)) ;
#165549 = CARTESIAN_POINT('Ctrl Pts',(-4.94780128270146,-6.53922263893877,
-21.8643974345971)) ;
#165550 = CARTESIAN_POINT('Ctrl Pts',(-4.84006668294258,-6.51145469770861,
-21.8399666585287)) ;
#165551 = CARTESIAN_POINT('Ctrl Pts',(-4.89711619685837,-6.48208554016477,
-21.8628838031415)) ;
#165552 = CARTESIAN_POINT('Ctrl Pts',(-4.92003334147129,-6.5114546977086,
-21.9199333170574)) ;
#165553 = CARTESIAN_POINT('Ctrl Pts',(-4.82524268591729,-6.5003618540841,
-21.8473786570414)) ;
#165554 = CARTESIAN_POINT('Ctrl Pts',(-4.89498692411706,-6.46792722356047,
-21.8650130758829)) ;
#165555 = CARTESIAN_POINT('Ctrl Pts',(-4.91262134295865,-6.5003618540841,
-21.9347573140827)) ;
#165556 = CARTESIAN_POINT('Ctrl Pts',(-4.80520550107819,-6.47617483238891,
-21.8573972494609)) ;
#165557 = CARTESIAN_POINT('Ctrl Pts',(-4.8967032564359,-6.4509405986842,-21.8632967435642)) ;
#165558 = CARTESIAN_POINT('Ctrl Pts',(-4.90260275053909,-6.47617483238892,
-21.9547944989218)) ;
#165559 = CARTESIAN_POINT('Ctrl Pts',(-4.80000000081823,-6.46309229646328,
-21.86)) ;
#165560 = CARTESIAN_POINT('Ctrl Pts',(-4.89999269598372,-6.4494565015457,
-21.8600073039031)) ;
#165561 = CARTESIAN_POINT('Ctrl Pts',(-4.9,-6.46309229646328,-21.9599999991818)) ;
#165562 = CARTESIAN_POINT('Ctrl Pts',(-4.8,-6.45,-21.86)) ;
#165563 = CARTESIAN_POINT('Ctrl Pts',(-4.9,-6.45,-21.86)) ;
#165564 = CARTESIAN_POINT('Ctrl Pts',(-4.9,-6.45,-21.96)) ;
#165565 = CARTESIAN_POINT('Origin',(-4.8,-6.45,-21.96)) ;
#165566 = CARTESIAN_POINT('Origin',(-4.,-6.35,-21.96)) ;
#165567 = CARTESIAN_POINT('Origin',(-4.,-6.35,-21.96)) ;
#165568 = CARTESIAN_POINT('Origin',(-4.,-6.35,-21.96)) ;
#165569 = CARTESIAN_POINT('Ctrl Pts',(-3.8,-6.55,-23.96)) ;
#165570 = CARTESIAN_POINT('Ctrl Pts',(-3.8,-6.55,-23.96)) ;
#165571 = CARTESIAN_POINT('Ctrl Pts',(-3.8,-6.55,-23.96)) ;
#165572 = CARTESIAN_POINT('Ctrl Pts',(-3.85250686565272,-6.55,-23.9337465671736)) ;
#165573 = CARTESIAN_POINT('Ctrl Pts',(-3.83954133268377,-6.55,-23.9204586673159)) ;
#165574 = CARTESIAN_POINT('Ctrl Pts',(-3.82625343282628,-6.55,-23.9074931343472)) ;
#165575 = CARTESIAN_POINT('Ctrl Pts',(-3.90439743459706,-6.53922263893874,
-23.9078012827014)) ;
#165576 = CARTESIAN_POINT('Ctrl Pts',(-3.87914655110984,-6.52362528614073,
-23.8808534488902)) ;
#165577 = CARTESIAN_POINT('Ctrl Pts',(-3.85219871729855,-6.53922263893876,
-23.8556025654029)) ;
#165578 = CARTESIAN_POINT('Ctrl Pts',(-3.95993331705743,-6.51145469770861,
-23.8800333414713)) ;
#165579 = CARTESIAN_POINT('Ctrl Pts',(-3.90288380314159,-6.48208554016475,
-23.8571161968584)) ;
#165580 = CARTESIAN_POINT('Ctrl Pts',(-3.8799666585287,-6.5114546977086,-23.8000666829426)) ;
#165581 = CARTESIAN_POINT('Ctrl Pts',(-3.97475731408271,-6.5003618540841,
-23.8726213429587)) ;
#165582 = CARTESIAN_POINT('Ctrl Pts',(-3.90501307588293,-6.46792722356048,
-23.8549869241171)) ;
#165583 = CARTESIAN_POINT('Ctrl Pts',(-3.88737865704135,-6.5003618540841,
-23.7852426859173)) ;
#165584 = CARTESIAN_POINT('Ctrl Pts',(-3.9947944989218,-6.47617483238891,
-23.8626027505391)) ;
#165585 = CARTESIAN_POINT('Ctrl Pts',(-3.9032967435641,-6.4509405986842,-23.8567032564358)) ;
#165586 = CARTESIAN_POINT('Ctrl Pts',(-3.89739724946091,-6.47617483238892,
-23.7652055010782)) ;
#165587 = CARTESIAN_POINT('Ctrl Pts',(-3.99999999918176,-6.46309229646328,
-23.86)) ;
#165588 = CARTESIAN_POINT('Ctrl Pts',(-3.90000730403035,-6.4494565015515,
-23.859992696097)) ;
#165589 = CARTESIAN_POINT('Ctrl Pts',(-3.9,-6.46309229646329,-23.7600000008182)) ;
#165590 = CARTESIAN_POINT('Ctrl Pts',(-4.,-6.45,-23.86)) ;
#165591 = CARTESIAN_POINT('Ctrl Pts',(-3.9,-6.45,-23.86)) ;
#165592 = CARTESIAN_POINT('Ctrl Pts',(-3.9,-6.45,-23.76)) ;
#165593 = CARTESIAN_POINT('Origin',(-4.,-6.45,-23.76)) ;
#165594 = CARTESIAN_POINT('Origin',(-4.8,-6.4,-21.96)) ;
#165595 = CARTESIAN_POINT('Origin',(-4.8,-6.35,-21.96)) ;
#165596 = CARTESIAN_POINT('Origin',(1.9515639104739E-16,-6.35,-21.96)) ;
#165597 = CARTESIAN_POINT('Origin',(-4.8,-6.35,-21.96)) ;
#165598 = CARTESIAN_POINT('Origin',(-4.,-6.35,-22.86)) ;
#165599 = CARTESIAN_POINT('Origin',(-4.,-6.35,-23.76)) ;
#165600 = CARTESIAN_POINT('Origin',(-4.,-6.4,-23.76)) ;
#165601 = CARTESIAN_POINT('Origin',(-4.,-6.35,-23.76)) ;
#165602 = CARTESIAN_POINT('Origin',(-4.8,-6.35,-21.96)) ;
#165603 = CARTESIAN_POINT('Origin',(-4.8,-6.35,-21.96)) ;
#165604 = CARTESIAN_POINT('Origin',(-4.,-6.35,-23.76)) ;
#165605 = CARTESIAN_POINT('Origin',(-4.,-6.35,-23.76)) ;
#165606 = CARTESIAN_POINT('Origin',(-4.8,-6.35,-22.86)) ;
#165607 = CARTESIAN_POINT('Origin',(-4.8,-6.35,-23.76)) ;
#165608 = CARTESIAN_POINT('Origin',(1.95156391047391E-16,-6.35,-23.76)) ;
#165609 = CARTESIAN_POINT('Origin',(-4.8,-6.35,-23.76)) ;
#165610 = CARTESIAN_POINT('Origin',(-4.8,-6.35,-23.76)) ;
#165611 = CARTESIAN_POINT('Origin',(-4.8,-6.35,-23.76)) ;
#165612 = CARTESIAN_POINT('Origin',(-4.8,-6.4,-23.76)) ;
#165613 = CARTESIAN_POINT('Origin',(-4.8,-6.45,-23.76)) ;
#165614 = CARTESIAN_POINT('Ctrl Pts',(-5.,-6.55,-23.96)) ;
#165615 = CARTESIAN_POINT('Ctrl Pts',(-5.,-6.55,-23.96)) ;
#165616 = CARTESIAN_POINT('Ctrl Pts',(-5.,-6.55,-23.96)) ;
#165617 = CARTESIAN_POINT('Ctrl Pts',(-4.97374656717362,-6.55,-23.9074931343473)) ;
#165618 = CARTESIAN_POINT('Ctrl Pts',(-4.96045866731629,-6.55,-23.9204586673159)) ;
#165619 = CARTESIAN_POINT('Ctrl Pts',(-4.94749313434732,-6.55,-23.9337465671736)) ;
#165620 = CARTESIAN_POINT('Ctrl Pts',(-4.94780128270146,-6.53922263893877,
-23.8556025654029)) ;
#165621 = CARTESIAN_POINT('Ctrl Pts',(-4.92085344889012,-6.52362528614073,
-23.8808534488902)) ;
#165622 = CARTESIAN_POINT('Ctrl Pts',(-4.89560256540291,-6.53922263893874,
-23.9078012827014)) ;
#165623 = CARTESIAN_POINT('Ctrl Pts',(-4.92003334147129,-6.5114546977086,
-23.8000666829426)) ;
#165624 = CARTESIAN_POINT('Ctrl Pts',(-4.89711619685843,-6.48208554016475,
-23.8571161968584)) ;
#165625 = CARTESIAN_POINT('Ctrl Pts',(-4.84006668294258,-6.51145469770861,
-23.8800333414713)) ;
#165626 = CARTESIAN_POINT('Ctrl Pts',(-4.91262134295865,-6.5003618540841,
-23.7852426859173)) ;
#165627 = CARTESIAN_POINT('Ctrl Pts',(-4.89498692411706,-6.46792722356048,
-23.8549869241171)) ;
#165628 = CARTESIAN_POINT('Ctrl Pts',(-4.82524268591729,-6.5003618540841,
-23.8726213429587)) ;
#165629 = CARTESIAN_POINT('Ctrl Pts',(-4.90260275053909,-6.47617483238892,
-23.7652055010782)) ;
#165630 = CARTESIAN_POINT('Ctrl Pts',(-4.8967032564359,-6.4509405986842,-23.8567032564358)) ;
#165631 = CARTESIAN_POINT('Ctrl Pts',(-4.80520550107819,-6.47617483238891,
-23.8626027505391)) ;
#165632 = CARTESIAN_POINT('Ctrl Pts',(-4.9,-6.46309229646329,-23.7600000008182)) ;
#165633 = CARTESIAN_POINT('Ctrl Pts',(-4.89999269596496,-6.44945650155343,
-23.859992696097)) ;
#165634 = CARTESIAN_POINT('Ctrl Pts',(-4.80000000081823,-6.46309229646328,
-23.86)) ;
#165635 = CARTESIAN_POINT('Ctrl Pts',(-4.9,-6.45,-23.76)) ;
#165636 = CARTESIAN_POINT('Ctrl Pts',(-4.9,-6.45,-23.86)) ;
#165637 = CARTESIAN_POINT('Ctrl Pts',(-4.8,-6.45,-23.86)) ;
#165638 = CARTESIAN_POINT('Ctrl Pts',(-5.82426676739348,-5.43399303700622,
-21.2570109659688)) ;
#165639 = CARTESIAN_POINT('Ctrl Pts',(-5.80266988778317,-5.52572360682937,
-21.2623540173507)) ;
#165640 = CARTESIAN_POINT('Ctrl Pts',(-5.82426676352017,-5.53106667371342,
-21.3540845871828)) ;
#165641 = CARTESIAN_POINT('Ctrl Pts',(-5.83498671931114,-5.43935351191918,
-21.2543294581962)) ;
#165642 = CARTESIAN_POINT('Ctrl Pts',(-5.80595263122269,-5.52411753147702,
-21.2639600935403)) ;
#165643 = CARTESIAN_POINT('Ctrl Pts',(-5.83498671397627,-5.53374818067469,
-21.3487241131463)) ;
#165644 = CARTESIAN_POINT('Ctrl Pts',(-5.84526105845709,-5.44830326289501,
-21.2498528401961)) ;
#165645 = CARTESIAN_POINT('Ctrl Pts',(-5.81370932746141,-5.52260132030856,
-21.2654763059991)) ;
#165646 = CARTESIAN_POINT('Ctrl Pts',(-5.84526105243722,-5.5382247974634,
-21.3397743635698)) ;
#165647 = CARTESIAN_POINT('Ctrl Pts',(-5.86378685403696,-5.47240020430408,
-21.2378032513087)) ;
#165648 = CARTESIAN_POINT('Ctrl Pts',(-5.83531854275287,-5.52733067404484,
-21.2607469551147)) ;
#165649 = CARTESIAN_POINT('Ctrl Pts',(-5.86378684816461,-5.550274384599,-21.3156774250055)) ;
#165650 = CARTESIAN_POINT('Ctrl Pts',(-5.87203852631573,-5.48754495134741,
-21.2302315528944)) ;
#165651 = CARTESIAN_POINT('Ctrl Pts',(-5.84834787930687,-5.53310199490454,
-21.2549756357761)) ;
#165652 = CARTESIAN_POINT('Ctrl Pts',(-5.87203852123041,-5.55784608243458,
-21.300532679514)) ;
#165653 = CARTESIAN_POINT('Ctrl Pts',(-5.89242747304799,-5.53981202333458,
-21.2041056511376)) ;
#165654 = CARTESIAN_POINT('Ctrl Pts',(-5.88223383300419,-5.56084219179274,
-21.2272354431742)) ;
#165655 = CARTESIAN_POINT('Ctrl Pts',(-5.89242747063502,-5.58397198402775,
-21.2482656123278)) ;
#165656 = CARTESIAN_POINT('Ctrl Pts',(-5.9,-5.58381083947299,-21.182119400143)) ;
#165657 = CARTESIAN_POINT('Ctrl Pts',(-5.9,-5.59485304502619,-21.1932245928863)) ;
#165658 = CARTESIAN_POINT('Ctrl Pts',(-5.9,-5.60595823775503,-21.2042667984405)) ;
#165659 = CARTESIAN_POINT('Ctrl Pts',(-5.9,-5.62807764064044,-21.16)) ;
#165660 = CARTESIAN_POINT('Ctrl Pts',(-5.9,-5.62807764064044,-21.16)) ;
#165661 = CARTESIAN_POINT('Ctrl Pts',(-5.9,-5.62807764064044,-21.16)) ;
#165662 = CARTESIAN_POINT('Origin',(-5.84850712500726,-5.43404914061138,-21.3540285000291)) ;
#165663 = CARTESIAN_POINT('Ctrl Pts',(-5.82425356250363,-5.53106339062591,
-21.3540285000291)) ;
#165664 = CARTESIAN_POINT('Ctrl Pts',(-5.80269484027818,-5.52567371006955,
-21.2624039305709)) ;
#165665 = CARTESIAN_POINT('Ctrl Pts',(-5.82425356250363,-5.43404914061138,
-21.2570142500145)) ;
#165666 = CARTESIAN_POINT('Ctrl Pts',(-5.80840777707096,-5.52710194426774,
-21.3579899459043)) ;
#165667 = CARTESIAN_POINT('Ctrl Pts',(-5.79341417645232,-5.52335354411302,
-21.2628358498184)) ;
#165668 = CARTESIAN_POINT('Ctrl Pts',(-5.81633079157288,-5.43008775511759,
-21.2589949427472)) ;
#165669 = CARTESIAN_POINT('Ctrl Pts',(-5.79207992677988,-5.52301998169497,
-21.359999999534)) ;
#165670 = CARTESIAN_POINT('Ctrl Pts',(-5.78430903206641,-5.52107725801669,
-21.2619613954329)) ;
#165671 = CARTESIAN_POINT('Ctrl Pts',(-5.808166653183,-5.42600568595106,-21.26)) ;
#165672 = CARTESIAN_POINT('Ctrl Pts',(-5.77574643749636,-5.51893660937409,
-21.36)) ;
#165673 = CARTESIAN_POINT('Ctrl Pts',(-5.77574643749636,-5.51893660937409,
-21.26)) ;
#165674 = CARTESIAN_POINT('Ctrl Pts',(-5.8,-5.42192235935956,-21.26)) ;
#165675 = CARTESIAN_POINT('Origin',(-5.8,-5.42192235935956,-21.36)) ;
#165676 = CARTESIAN_POINT('Origin',(-5.8066065036801,-5.42357398527959,-21.36)) ;
#165677 = CARTESIAN_POINT('Origin',(-5.17275707706437,-5.26511162862565,-21.36)) ;
#165678 = CARTESIAN_POINT('Origin',(-5.15068655017073,-5.25959399690224,-21.3705938529089)) ;
#165679 = CARTESIAN_POINT('Origin',(-5.17275707706436,-5.26511162862565,-21.36)) ;
#165680 = CARTESIAN_POINT('Origin',(-5.17275707706436,-5.26511162862565,-21.36)) ;
#165681 = CARTESIAN_POINT('Origin',(-5.17275707706436,-5.26511162862565,-21.36)) ;
#165682 = CARTESIAN_POINT('Origin',(-5.17275707706436,-5.05,-21.36)) ;
#165683 = CARTESIAN_POINT('Origin',(-5.17275707706436,-1.91866427917294,-21.36)) ;
#165684 = CARTESIAN_POINT('Origin',(-3.78014014831103,-3.31128120792626,-22.0284561258016)) ;
#165685 = CARTESIAN_POINT('Origin',(-5.17275707706436,-1.91866427917294,-21.36)) ;
#165686 = CARTESIAN_POINT('Origin',(-5.17275707706436,-1.91866427917293,-21.36)) ;
#165687 = CARTESIAN_POINT('Origin',(-5.17275707706436,-1.91866427917294,-21.36)) ;
#165688 = CARTESIAN_POINT('Origin',(-3.97071067811865,-3.12071067811865,-21.36)) ;
#165689 = CARTESIAN_POINT('Origin',(-5.8,-1.2914213562373,-21.36)) ;
#165690 = CARTESIAN_POINT('Ctrl Pts',(-5.87071067811865,-1.14999999999999,
-21.2307106781187)) ;
#165691 = CARTESIAN_POINT('Ctrl Pts',(-5.8471404520791,-1.10285954792089,
-21.2542809041582)) ;
#165692 = CARTESIAN_POINT('Ctrl Pts',(-5.87071067811865,-1.07928932188134,
-21.3014213562373)) ;
#165693 = CARTESIAN_POINT('Ctrl Pts',(-5.85217562795657,-1.18707010095452,
-21.2492457282807)) ;
#165694 = CARTESIAN_POINT('Ctrl Pts',(-5.81261165662081,-1.13738834337931,
-21.2758614719499)) ;
#165695 = CARTESIAN_POINT('Ctrl Pts',(-5.83353949671049,-1.1164605032895,
-21.3385925363811)) ;
#165696 = CARTESIAN_POINT('Ctrl Pts',(-5.82627077431945,-1.23887980759835,
-21.26)) ;
#165697 = CARTESIAN_POINT('Ctrl Pts',(-5.7656678790793,-1.18433212092041,
-21.2771489437127)) ;
#165698 = CARTESIAN_POINT('Ctrl Pts',(-5.78190678732229,-1.1680932126777,
-21.3599999994186)) ;
#165699 = CARTESIAN_POINT('Ctrl Pts',(-5.8,-1.2914213562373,-21.26)) ;
#165700 = CARTESIAN_POINT('Ctrl Pts',(-5.72928932188135,-1.22071067811865,
-21.26)) ;
#165701 = CARTESIAN_POINT('Ctrl Pts',(-5.72928932188134,-1.22071067811865,
-21.36)) ;
#165702 = CARTESIAN_POINT('Origin',(-5.94142135623731,-1.15,-21.3014213562373)) ;
#165703 = CARTESIAN_POINT('Ctrl Pts',(-5.9,-1.00857864376269,-21.16)) ;
#165704 = CARTESIAN_POINT('Ctrl Pts',(-5.9,-1.00857864376269,-21.16)) ;
#165705 = CARTESIAN_POINT('Ctrl Pts',(-5.9,-1.00857864376269,-21.16)) ;
#165706 = CARTESIAN_POINT('Ctrl Pts',(-5.9,-1.06112019240165,-21.1862707743195)) ;
#165707 = CARTESIAN_POINT('Ctrl Pts',(-5.9,-1.04860238144602,-21.2000237376826)) ;
#165708 = CARTESIAN_POINT('Ctrl Pts',(-5.9,-1.03484941808214,-21.212541548639)) ;
#165709 = CARTESIAN_POINT('Ctrl Pts',(-5.88924572828071,-1.11292989904543,
-21.2121756279566)) ;
#165710 = CARTESIAN_POINT('Ctrl Pts',(-5.87451700626115,-1.08721613124018,
-21.2386374874767)) ;
#165711 = CARTESIAN_POINT('Ctrl Pts',(-5.88924572828062,-1.06075427171937,
-21.2643512552826)) ;
#165712 = CARTESIAN_POINT('Ctrl Pts',(-5.87071067811865,-1.14999999999999,
-21.2307106781187)) ;
#165713 = CARTESIAN_POINT('Ctrl Pts',(-5.8471404520791,-1.10285954792089,
-21.2542809041582)) ;
#165714 = CARTESIAN_POINT('Ctrl Pts',(-5.87071067811865,-1.07928932188134,
-21.3014213562373)) ;
#165715 = CARTESIAN_POINT('Ctrl Pts',(-5.87071067811866,-1.14999999999999,
-24.4892893218813)) ;
#165716 = CARTESIAN_POINT('Ctrl Pts',(-5.84714045207911,-1.10285954792089,
-24.4657190958418)) ;
#165717 = CARTESIAN_POINT('Ctrl Pts',(-5.87071067811866,-1.07928932188134,
-24.4185786437627)) ;
#165718 = CARTESIAN_POINT('Ctrl Pts',(-5.8892457282807,-1.11292989904542,
-24.5078243720434)) ;
#165719 = CARTESIAN_POINT('Ctrl Pts',(-5.87451700625923,-1.08721613124108,
-24.4813625125218)) ;
#165720 = CARTESIAN_POINT('Ctrl Pts',(-5.88924572828062,-1.06075427171937,
-24.4556487447174)) ;
#165721 = CARTESIAN_POINT('Ctrl Pts',(-5.9,-1.06112019240159,-24.5337292256804)) ;
#165722 = CARTESIAN_POINT('Ctrl Pts',(-5.9,-1.04860238144416,-24.5199762623175)) ;
#165723 = CARTESIAN_POINT('Ctrl Pts',(-5.9,-1.03484941808214,-24.507458451361)) ;
#165724 = CARTESIAN_POINT('Ctrl Pts',(-5.9,-1.00857864376269,-24.56)) ;
#165725 = CARTESIAN_POINT('Ctrl Pts',(-5.9,-1.00857864376269,-24.56)) ;
#165726 = CARTESIAN_POINT('Ctrl Pts',(-5.9,-1.00857864376269,-24.56)) ;
#165727 = CARTESIAN_POINT('Origin',(-5.94142135623734,-1.14999999999996,-24.4185786437627)) ;
#165728 = CARTESIAN_POINT('Ctrl Pts',(-5.8,-1.2914213562373,-24.46)) ;
#165729 = CARTESIAN_POINT('Ctrl Pts',(-5.72928932188134,-1.22071067811865,
-24.46)) ;
#165730 = CARTESIAN_POINT('Ctrl Pts',(-5.72928932188134,-1.22071067811865,
-24.36)) ;
#165731 = CARTESIAN_POINT('Ctrl Pts',(-5.82627077431951,-1.23887980759822,
-24.46)) ;
#165732 = CARTESIAN_POINT('Ctrl Pts',(-5.76566787908001,-1.18433212092034,
-24.4428510562871)) ;
#165733 = CARTESIAN_POINT('Ctrl Pts',(-5.78190678732243,-1.16809321267757,
-24.3600000005814)) ;
#165734 = CARTESIAN_POINT('Ctrl Pts',(-5.85217562795678,-1.18707010095483,
-24.4707542717195)) ;
#165735 = CARTESIAN_POINT('Ctrl Pts',(-5.81261165662028,-1.13738834337977,
-24.4441385280509)) ;
#165736 = CARTESIAN_POINT('Ctrl Pts',(-5.83353949671032,-1.11646050328967,
-24.3814074636191)) ;
#165737 = CARTESIAN_POINT('Ctrl Pts',(-5.87071067811866,-1.14999999999999,
-24.4892893218813)) ;
#165738 = CARTESIAN_POINT('Ctrl Pts',(-5.84714045207911,-1.10285954792088,
-24.4657190958418)) ;
#165739 = CARTESIAN_POINT('Ctrl Pts',(-5.87071067811866,-1.07928932188133,
-24.4185786437627)) ;
#165740 = CARTESIAN_POINT('Origin',(-5.8,-1.29142135623731,-24.36)) ;
#165741 = CARTESIAN_POINT('Origin',(-3.59571067811865,-3.49571067811865,-24.36)) ;
#165742 = CARTESIAN_POINT('Origin',(-5.17275707706437,-1.91866427917293,-24.36)) ;
#165743 = CARTESIAN_POINT('Origin',(-3.09057773798104,-4.00084361825625,-23.36055391724)) ;
#165744 = CARTESIAN_POINT('Origin',(-5.17275707706436,-1.91866427917293,-24.36)) ;
#165745 = CARTESIAN_POINT('Origin',(-5.17275707706436,-1.91866427917293,-24.36)) ;
#165746 = CARTESIAN_POINT('Origin',(-5.17275707706436,-1.91866427917293,-24.36)) ;
#165747 = CARTESIAN_POINT('Origin',(-5.17275707706436,-5.05,-24.36)) ;
#165748 = CARTESIAN_POINT('Origin',(-5.17275707706436,-5.26511162862565,-24.36)) ;
#165749 = CARTESIAN_POINT('Origin',(-3.96111272388873,-4.96220054033175,-23.7784107104757)) ;
#165750 = CARTESIAN_POINT('Origin',(-5.17275707706436,-5.26511162862565,-24.36)) ;
#165751 = CARTESIAN_POINT('Origin',(-5.17275707706436,-5.26511162862565,-24.36)) ;
#165752 = CARTESIAN_POINT('Origin',(-5.17275707706436,-5.26511162862565,-24.36)) ;
#165753 = CARTESIAN_POINT('Origin',(-5.10072415073893,-5.24710339704429,-24.36)) ;
#165754 = CARTESIAN_POINT('Origin',(-5.8,-5.42192235935956,-24.36)) ;
#165755 = CARTESIAN_POINT('Ctrl Pts',(-5.77574643749636,-5.51893660937409,
-24.36)) ;
#165756 = CARTESIAN_POINT('Ctrl Pts',(-5.77574643749636,-5.5189366093741,
-24.46)) ;
#165757 = CARTESIAN_POINT('Ctrl Pts',(-5.8,-5.42192235935956,-24.46)) ;
#165758 = CARTESIAN_POINT('Ctrl Pts',(-5.7920799267799,-5.52301998169498,
-24.360000000466)) ;
#165759 = CARTESIAN_POINT('Ctrl Pts',(-5.78430903206646,-5.52107725801652,
-24.4580386045671)) ;
#165760 = CARTESIAN_POINT('Ctrl Pts',(-5.80816665318299,-5.42600568595104,
-24.46)) ;
#165761 = CARTESIAN_POINT('Ctrl Pts',(-5.80840777707095,-5.52710194426774,
-24.3620100540957)) ;
#165762 = CARTESIAN_POINT('Ctrl Pts',(-5.79341417645228,-5.52335354411315,
-24.4571641501816)) ;
#165763 = CARTESIAN_POINT('Ctrl Pts',(-5.81633079157289,-5.4300877551176,
-24.4610050572528)) ;
#165764 = CARTESIAN_POINT('Ctrl Pts',(-5.82425356250363,-5.53106339062591,
-24.3659714999709)) ;
#165765 = CARTESIAN_POINT('Ctrl Pts',(-5.80269484027818,-5.52567371006954,
-24.4575960694291)) ;
#165766 = CARTESIAN_POINT('Ctrl Pts',(-5.82425356250363,-5.43404914061138,
-24.4629857499855)) ;
#165767 = CARTESIAN_POINT('Origin',(-5.84850712500726,-5.43404914061138,-24.3659714999709)) ;
#165768 = CARTESIAN_POINT('Ctrl Pts',(-5.82426676739355,-5.53106667467169,
-24.3659153963654)) ;
#165769 = CARTESIAN_POINT('Ctrl Pts',(-5.80266988778311,-5.52572362329009,
-24.4576459661888)) ;
#165770 = CARTESIAN_POINT('Ctrl Pts',(-5.82426676352016,-5.43399305345777,
-24.462989033073)) ;
#165771 = CARTESIAN_POINT('Ctrl Pts',(-5.83498671931122,-5.5337481824443,
-24.3712758712785)) ;
#165772 = CARTESIAN_POINT('Ctrl Pts',(-5.80595263122263,-5.52411754710037,
-24.4560398908365)) ;
#165773 = CARTESIAN_POINT('Ctrl Pts',(-5.83498671397625,-5.43935352749418,
-24.4656705400343)) ;
#165774 = CARTESIAN_POINT('Ctrl Pts',(-5.8452610584572,-5.53822480044432,
-24.3802256222543)) ;
#165775 = CARTESIAN_POINT('Ctrl Pts',(-5.81370932746134,-5.52260133464154,
-24.454523679668)) ;
#165776 = CARTESIAN_POINT('Ctrl Pts',(-5.84526105243719,-5.4483032770707,
-24.4701471568229)) ;
#165777 = CARTESIAN_POINT('Ctrl Pts',(-5.86378685403706,-5.55027438933182,
-24.4043225636634)) ;
#165778 = CARTESIAN_POINT('Ctrl Pts',(-5.83531854275281,-5.52733068552588,
-24.4592530334043)) ;
#165779 = CARTESIAN_POINT('Ctrl Pts',(-5.86378684816461,-5.47240021563498,
-24.4821967439585)) ;
#165780 = CARTESIAN_POINT('Ctrl Pts',(-5.87203852631583,-5.55784608774613,
-24.4194673107067)) ;
#165781 = CARTESIAN_POINT('Ctrl Pts',(-5.84834787930681,-5.53310200486445,
-24.465024354264)) ;
#165782 = CARTESIAN_POINT('Ctrl Pts',(-5.87203852123039,-5.48754496112653,
-24.4897684417941)) ;
#165783 = CARTESIAN_POINT('Ctrl Pts',(-5.892427473048,-5.58397198950289,-24.471734382694)) ;
#165784 = CARTESIAN_POINT('Ctrl Pts',(-5.88223383300416,-5.56084219746623,
-24.4927645511521)) ;
#165785 = CARTESIAN_POINT('Ctrl Pts',(-5.892427470635,-5.53981202831264,-24.5158943433873)) ;
#165786 = CARTESIAN_POINT('Ctrl Pts',(-5.9,-5.60595824049751,-24.5157331988325)) ;
#165787 = CARTESIAN_POINT('Ctrl Pts',(-5.9,-5.59485304775425,-24.5267754043855)) ;
#165788 = CARTESIAN_POINT('Ctrl Pts',(-5.9,-5.5838108421999,-24.5378805971145)) ;
#165789 = CARTESIAN_POINT('Ctrl Pts',(-5.9,-5.62807764064044,-24.56)) ;
#165790 = CARTESIAN_POINT('Ctrl Pts',(-5.9,-5.62807764064044,-24.56)) ;
#165791 = CARTESIAN_POINT('Ctrl Pts',(-5.9,-5.62807764064044,-24.56)) ;
#165792 = CARTESIAN_POINT('Origin',(7.8,2.1,-23.26)) ;
#165793 = CARTESIAN_POINT('Origin',(7.8,2.1,-23.46)) ;
#165794 = CARTESIAN_POINT('Origin',(7.6,2.1,-23.26)) ;
#165795 = CARTESIAN_POINT('Origin',(7.6,2.1,-23.26)) ;
#165796 = CARTESIAN_POINT('Origin',(7.6,2.1,-22.46)) ;
#165797 = CARTESIAN_POINT('Origin',(7.8,2.1,-23.46)) ;
#165798 = CARTESIAN_POINT('Origin',(9.6,2.1,-23.46)) ;
#165799 = CARTESIAN_POINT('Origin',(7.8,2.1,-22.46)) ;
#165800 = CARTESIAN_POINT('Origin',(7.8,2.1,-22.26)) ;
#165801 = CARTESIAN_POINT('Origin',(9.6,2.1,-23.26)) ;
#165802 = CARTESIAN_POINT('Origin',(9.8,2.1,-23.26)) ;
#165803 = CARTESIAN_POINT('Origin',(7.8,2.1,-22.26)) ;
#165804 = CARTESIAN_POINT('Origin',(9.6,2.1,-22.26)) ;
#165805 = CARTESIAN_POINT('Origin',(9.8,2.1,-23.26)) ;
#165806 = CARTESIAN_POINT('Origin',(9.8,2.1,-22.46)) ;
#165807 = CARTESIAN_POINT('Origin',(9.6,2.1,-22.46)) ;
#165808 = CARTESIAN_POINT('Origin',(-4.15,-6.25,-22.11)) ;
#165809 = CARTESIAN_POINT('Origin',(-4.15,-6.3,-22.11)) ;
#165810 = CARTESIAN_POINT('Origin',(-4.15,-6.3,-22.86)) ;
#165811 = CARTESIAN_POINT('Origin',(-4.15,-6.3,-23.61)) ;
#165812 = CARTESIAN_POINT('Origin',(-4.15,-6.3,-22.11)) ;
#165813 = CARTESIAN_POINT('Origin',(-4.15,-6.25,-23.61)) ;
#165814 = CARTESIAN_POINT('Origin',(-4.15,-6.3,-23.61)) ;
#165815 = CARTESIAN_POINT('Origin',(-4.15,-6.3,-22.11)) ;
#165816 = CARTESIAN_POINT('Origin',(-4.15,-6.3,-22.11)) ;
#165817 = CARTESIAN_POINT('Origin',(-4.15,-6.3,-23.61)) ;
#165818 = CARTESIAN_POINT('Origin',(-4.15,-6.3,-23.61)) ;
#165819 = CARTESIAN_POINT('Origin',(-4.65,-6.25,-22.11)) ;
#165820 = CARTESIAN_POINT('Origin',(-4.65,-6.3,-22.11)) ;
#165821 = CARTESIAN_POINT('Origin',(0.,-6.3,-22.11)) ;
#165822 = CARTESIAN_POINT('Origin',(-4.65,-6.3,-22.11)) ;
#165823 = CARTESIAN_POINT('Origin',(0.,-6.3,-23.61)) ;
#165824 = CARTESIAN_POINT('Origin',(-4.65,-6.3,-23.61)) ;
#165825 = CARTESIAN_POINT('Origin',(-4.65,-6.25,-23.61)) ;
#165826 = CARTESIAN_POINT('Origin',(-4.65,-6.3,-23.61)) ;
#165827 = CARTESIAN_POINT('Origin',(-4.65,-6.3,-22.11)) ;
#165828 = CARTESIAN_POINT('Origin',(-4.65,-6.3,-22.11)) ;
#165829 = CARTESIAN_POINT('Origin',(-4.65,-6.3,-23.61)) ;
#165830 = CARTESIAN_POINT('Origin',(-4.65,-6.3,-23.61)) ;
#165831 = CARTESIAN_POINT('Origin',(-4.65,-6.3,-22.86)) ;
#165832 = CARTESIAN_POINT('Origin',(-3.,4.45,-23.96)) ;
#165833 = CARTESIAN_POINT('Origin',(-2.1,4.45,-23.96)) ;
#165834 = CARTESIAN_POINT('Origin',(-2.9,4.45,-23.96)) ;
#165835 = CARTESIAN_POINT('Origin',(-2.9,4.45,-23.76)) ;
#165836 = CARTESIAN_POINT('Origin',(-3.1,4.45,-23.76)) ;
#165837 = CARTESIAN_POINT('Origin',(-2.9,4.45,-23.76)) ;
#165838 = CARTESIAN_POINT('Origin',(-2.1,4.45,-23.76)) ;
#165839 = CARTESIAN_POINT('Origin',(-2.1,4.45,-23.76)) ;
#165840 = CARTESIAN_POINT('Origin',(-1.9,4.45,-23.76)) ;
#165841 = CARTESIAN_POINT('Origin',(-3.1,4.45,-23.86)) ;
#165842 = CARTESIAN_POINT('Origin',(-3.1,4.45,-21.96)) ;
#165843 = CARTESIAN_POINT('Origin',(-2.9,4.4,-23.76)) ;
#165844 = CARTESIAN_POINT('Origin',(-2.9,4.35,-23.76)) ;
#165845 = CARTESIAN_POINT('Origin',(-1.95156391047391E-16,4.35,-23.76)) ;
#165846 = CARTESIAN_POINT('Origin',(-2.1,4.35,-23.76)) ;
#165847 = CARTESIAN_POINT('Origin',(-2.9,4.35,-23.76)) ;
#165848 = CARTESIAN_POINT('Origin',(-2.1,4.4,-23.76)) ;
#165849 = CARTESIAN_POINT('Origin',(-2.1,4.35,-23.76)) ;
#165850 = CARTESIAN_POINT('Origin',(-1.9,4.45,-23.86)) ;
#165851 = CARTESIAN_POINT('Origin',(-1.9,4.45,-21.96)) ;
#165852 = CARTESIAN_POINT('Origin',(-3.,4.45,-21.76)) ;
#165853 = CARTESIAN_POINT('Origin',(-2.9,4.45,-21.76)) ;
#165854 = CARTESIAN_POINT('Origin',(-2.1,4.45,-21.76)) ;
#165855 = CARTESIAN_POINT('Origin',(-2.9,4.45,-21.96)) ;
#165856 = CARTESIAN_POINT('Origin',(-2.9,4.45,-21.96)) ;
#165857 = CARTESIAN_POINT('Origin',(-2.9,4.35,-23.76)) ;
#165858 = CARTESIAN_POINT('Origin',(-2.9,4.35,-23.76)) ;
#165859 = CARTESIAN_POINT('Origin',(-2.1,4.35,-23.76)) ;
#165860 = CARTESIAN_POINT('Origin',(-2.1,4.35,-23.76)) ;
#165861 = CARTESIAN_POINT('Origin',(-2.1,4.45,-21.96)) ;
#165862 = CARTESIAN_POINT('Origin',(-2.1,4.45,-21.96)) ;
#165863 = CARTESIAN_POINT('Origin',(-2.9,4.4,-21.96)) ;
#165864 = CARTESIAN_POINT('Origin',(-2.9,4.35,-21.96)) ;
#165865 = CARTESIAN_POINT('Origin',(-2.9,4.35,-22.86)) ;
#165866 = CARTESIAN_POINT('Origin',(-2.9,4.35,-21.96)) ;
#165867 = CARTESIAN_POINT('Origin',(-2.1,4.35,-22.86)) ;
#165868 = CARTESIAN_POINT('Origin',(-2.1,4.35,-21.96)) ;
#165869 = CARTESIAN_POINT('Origin',(-2.1,4.4,-21.96)) ;
#165870 = CARTESIAN_POINT('Origin',(-2.1,4.35,-21.96)) ;
#165871 = CARTESIAN_POINT('Origin',(-2.9,4.35,-21.96)) ;
#165872 = CARTESIAN_POINT('Origin',(-2.9,4.35,-21.96)) ;
#165873 = CARTESIAN_POINT('Origin',(-2.1,4.35,-21.96)) ;
#165874 = CARTESIAN_POINT('Origin',(-2.1,4.35,-21.96)) ;
#165875 = CARTESIAN_POINT('Origin',(-1.95156391047391E-16,4.35,-21.96)) ;
#165876 = CARTESIAN_POINT('Origin',(-2.25,4.25,-23.61)) ;
#165877 = CARTESIAN_POINT('Origin',(-2.25,4.3,-23.61)) ;
#165878 = CARTESIAN_POINT('Origin',(-2.25,4.3,-22.86)) ;
#165879 = CARTESIAN_POINT('Origin',(-2.25,4.3,-22.11)) ;
#165880 = CARTESIAN_POINT('Origin',(-2.25,4.3,-23.61)) ;
#165881 = CARTESIAN_POINT('Origin',(-2.25,4.25,-22.11)) ;
#165882 = CARTESIAN_POINT('Origin',(-2.25,4.3,-22.11)) ;
#165883 = CARTESIAN_POINT('Origin',(-2.25,4.3,-23.61)) ;
#165884 = CARTESIAN_POINT('Origin',(-2.25,4.3,-23.61)) ;
#165885 = CARTESIAN_POINT('Origin',(-2.25,4.3,-22.11)) ;
#165886 = CARTESIAN_POINT('Origin',(-2.25,4.3,-22.11)) ;
#165887 = CARTESIAN_POINT('Origin',(-2.75,4.25,-23.61)) ;
#165888 = CARTESIAN_POINT('Origin',(-2.75,4.3,-23.61)) ;
#165889 = CARTESIAN_POINT('Origin',(-1.97127667724637E-17,4.3,-23.61)) ;
#165890 = CARTESIAN_POINT('Origin',(-2.75,4.3,-23.61)) ;
#165891 = CARTESIAN_POINT('Origin',(-1.97127667724637E-17,4.3,-22.11)) ;
#165892 = CARTESIAN_POINT('Origin',(-2.75,4.3,-22.11)) ;
#165893 = CARTESIAN_POINT('Origin',(-2.75,4.25,-22.11)) ;
#165894 = CARTESIAN_POINT('Origin',(-2.75,4.3,-22.11)) ;
#165895 = CARTESIAN_POINT('Origin',(-2.75,4.3,-23.61)) ;
#165896 = CARTESIAN_POINT('Origin',(-2.75,4.3,-23.61)) ;
#165897 = CARTESIAN_POINT('Origin',(-2.75,4.3,-22.11)) ;
#165898 = CARTESIAN_POINT('Origin',(-2.75,4.3,-22.11)) ;
#165899 = CARTESIAN_POINT('Origin',(-2.75,4.3,-22.86)) ;
#165900 = CARTESIAN_POINT('Origin',(7.8,2.9,-23.26)) ;
#165901 = CARTESIAN_POINT('Origin',(7.8,2.9,-23.26)) ;
#165902 = CARTESIAN_POINT('Origin',(7.8,2.9,-22.46)) ;
#165903 = CARTESIAN_POINT('Origin',(7.8,2.9,-22.46)) ;
#165904 = CARTESIAN_POINT('Origin',(7.8,2.9,-22.46)) ;
#165905 = CARTESIAN_POINT('Origin',(7.8,2.9,-23.26)) ;
#165906 = CARTESIAN_POINT('Origin',(7.8,2.9,-23.26)) ;
#165907 = CARTESIAN_POINT('Origin',(9.6,2.9,-22.46)) ;
#165908 = CARTESIAN_POINT('Origin',(9.6,2.9,-22.46)) ;
#165909 = CARTESIAN_POINT('Origin',(9.6,2.9,-23.26)) ;
#165910 = CARTESIAN_POINT('Origin',(9.6,2.9,-23.26)) ;
#165911 = CARTESIAN_POINT('Origin',(9.6,2.9,-22.46)) ;
#165912 = CARTESIAN_POINT('Origin',(9.6,2.9,-22.46)) ;
#165913 = CARTESIAN_POINT('Origin',(9.6,2.9,-23.26)) ;
#165914 = CARTESIAN_POINT('Origin',(9.6,2.9,-23.26)) ;
#165915 = CARTESIAN_POINT('Origin',(9.6,2.9,-23.26)) ;
#165916 = CARTESIAN_POINT('Origin',(-0.183301359729408,3.45,-21.342963213524)) ;
#165917 = CARTESIAN_POINT('Origin',(0.24923464143508,3.15,-22.7437799780213)) ;
#165918 = CARTESIAN_POINT('Origin',(-0.249234641435079,3.15,-22.9762200219787)) ;
#165919 = CARTESIAN_POINT('Origin',(-1.04429375741423,3.45,-21.7444505621777)) ;
#165920 = CARTESIAN_POINT('Origin',(10.1,-2.15,-25.7668804065906)) ;
#165921 = CARTESIAN_POINT('Origin',(10.1,-2.15,-25.7668804065906)) ;
#165922 = CARTESIAN_POINT('Origin',(10.1,-2.15,-25.7668804065906)) ;
#165923 = CARTESIAN_POINT('Origin',(10.1,-2.15,-25.7668804065906)) ;
#165924 = CARTESIAN_POINT('Origin',(10.1,-2.15,-26.67)) ;
#165925 = CARTESIAN_POINT('Origin',(10.1,-2.15,-25.365)) ;
#165926 = CARTESIAN_POINT('Origin',(10.2,-2.15,-25.7668804065906)) ;
#165927 = CARTESIAN_POINT('Origin',(3.7,-2.15,-25.7668804065906)) ;
#165928 = CARTESIAN_POINT('Origin',(10.1,-3.65625,-26.67)) ;
#165929 = CARTESIAN_POINT('Origin',(10.1,-2.15,-27.5731195934094)) ;
#165930 = CARTESIAN_POINT('Origin',(10.1,-3.65625,-25.365)) ;
#165931 = CARTESIAN_POINT('Origin',(10.1,1.9,-25.365)) ;
#165932 = CARTESIAN_POINT('Origin',(10.1,-2.15,-25.365)) ;
#165933 = CARTESIAN_POINT('Origin',(10.1,-2.15,-25.365)) ;
#165934 = CARTESIAN_POINT('Origin',(10.1,-2.15,-25.365)) ;
#165935 = CARTESIAN_POINT('Origin',(3.7,-2.15,-25.7668804065906)) ;
#165936 = CARTESIAN_POINT('Origin',(3.7,-2.32153024911032,-25.8697267659824)) ;
#165937 = CARTESIAN_POINT('Origin',(3.7,-2.35,-25.7668804065906)) ;
#165938 = CARTESIAN_POINT('Origin',(10.1,-2.15,-27.5731195934094)) ;
#165939 = CARTESIAN_POINT('Origin',(10.1,-2.15,-27.5731195934094)) ;
#165940 = CARTESIAN_POINT('Origin',(10.1,-2.15,-27.5731195934094)) ;
#165941 = CARTESIAN_POINT('Origin',(10.1,1.9,-26.67)) ;
#165942 = CARTESIAN_POINT('Origin',(10.1,1.9,-27.975)) ;
#165943 = CARTESIAN_POINT('Origin',(10.1,1.9,-25.365)) ;
#165944 = CARTESIAN_POINT('Origin',(10.2,-2.15,-25.365)) ;
#165945 = CARTESIAN_POINT('Origin',(3.7,-2.15,-25.365)) ;
#165946 = CARTESIAN_POINT('Origin',(3.7,-2.35,-25.265)) ;
#165947 = CARTESIAN_POINT('Origin',(3.7,-2.35,-25.365)) ;
#165948 = CARTESIAN_POINT('Origin',(3.7,-3.65625,-26.67)) ;
#165949 = CARTESIAN_POINT('Origin',(3.7,-2.32153024911032,-27.4702732340176)) ;
#165950 = CARTESIAN_POINT('Origin',(10.2,-2.15,-27.5731195934094)) ;
#165951 = CARTESIAN_POINT('Origin',(3.7,-2.15,-27.5731195934094)) ;
#165952 = CARTESIAN_POINT('Origin',(10.1,-2.15,-26.67)) ;
#165953 = CARTESIAN_POINT('Origin',(10.1,-2.15,-27.975)) ;
#165954 = CARTESIAN_POINT('Origin',(10.1,-3.65625,-27.975)) ;
#165955 = CARTESIAN_POINT('Origin',(10.1,1.9,-27.975)) ;
#165956 = CARTESIAN_POINT('Origin',(10.1,-2.15,-27.975)) ;
#165957 = CARTESIAN_POINT('Origin',(3.7,-2.35,-25.365)) ;
#165958 = CARTESIAN_POINT('Origin',(3.5,-2.35,-25.365)) ;
#165959 = CARTESIAN_POINT('Origin',(3.7,-2.15,-27.5731195934094)) ;
#165960 = CARTESIAN_POINT('Origin',(3.7,-2.35,-27.5731195934094)) ;
#165961 = CARTESIAN_POINT('Origin',(10.1,-2.15,-27.975)) ;
#165962 = CARTESIAN_POINT('Origin',(10.1,-2.15,-27.975)) ;
#165963 = CARTESIAN_POINT('Origin',(3.6,1.9,-25.165)) ;
#165964 = CARTESIAN_POINT('Origin',(3.5,1.9,-25.165)) ;
#165965 = CARTESIAN_POINT('Origin',(2.7,1.9,-25.165)) ;
#165966 = CARTESIAN_POINT('Origin',(3.5,2.3540679885722E-15,-25.365)) ;
#165967 = CARTESIAN_POINT('Origin',(3.5,-5.15,-25.365)) ;
#165968 = CARTESIAN_POINT('Origin',(3.7,-2.35,-27.545)) ;
#165969 = CARTESIAN_POINT('Origin',(3.7,-2.35,-27.975)) ;
#165970 = CARTESIAN_POINT('Origin',(3.6,-2.15,-27.975)) ;
#165971 = CARTESIAN_POINT('Origin',(3.7,-2.15,-27.975)) ;
#165972 = CARTESIAN_POINT('Origin',(2.7,1.9,-25.165)) ;
#165973 = CARTESIAN_POINT('Origin',(2.7,1.9,-25.165)) ;
#165974 = CARTESIAN_POINT('Origin',(3.5,-5.15,-25.365)) ;
#165975 = CARTESIAN_POINT('Origin',(3.5,-5.15,-25.365)) ;
#165976 = CARTESIAN_POINT('Origin',(3.5,-5.15,-25.365)) ;
#165977 = CARTESIAN_POINT('Origin',(3.7,-2.35,-27.975)) ;
#165978 = CARTESIAN_POINT('Origin',(3.5,-2.35,-27.975)) ;
#165979 = CARTESIAN_POINT('Origin',(2.7,2.,-25.165)) ;
#165980 = CARTESIAN_POINT('Origin',(2.7,-5.15,-25.165)) ;
#165981 = CARTESIAN_POINT('Origin',(3.6,-5.15,-25.365)) ;
#165982 = CARTESIAN_POINT('Origin',(2.7,-5.15,-25.365)) ;
#165983 = CARTESIAN_POINT('Origin',(3.5,-5.15,0.)) ;
#165984 = CARTESIAN_POINT('Origin',(3.5,-5.15,-27.975)) ;
#165985 = CARTESIAN_POINT('Origin',(3.5,-2.43197426359692E-15,-27.975)) ;
#165986 = CARTESIAN_POINT('Origin',(3.5,-5.15,-27.975)) ;
#165987 = CARTESIAN_POINT('Origin',(2.7,-5.15,-25.365)) ;
#165988 = CARTESIAN_POINT('Origin',(2.7,-5.35,-25.365)) ;
#165989 = CARTESIAN_POINT('Origin',(3.5,-5.15,-27.975)) ;
#165990 = CARTESIAN_POINT('Origin',(3.5,-5.15,-27.975)) ;
#165991 = CARTESIAN_POINT('Origin',(2.7,-5.35,-25.265)) ;
#165992 = CARTESIAN_POINT('Origin',(2.7,-5.35,-27.975)) ;
#165993 = CARTESIAN_POINT('Origin',(3.6,-5.15,-27.975)) ;
#165994 = CARTESIAN_POINT('Origin',(2.7,-5.15,-27.975)) ;
#165995 = CARTESIAN_POINT('Origin',(3.6,1.9,-28.175)) ;
#165996 = CARTESIAN_POINT('Origin',(3.5,1.9,-28.175)) ;
#165997 = CARTESIAN_POINT('Origin',(2.7,1.9,-28.175)) ;
#165998 = CARTESIAN_POINT('Origin',(2.7,1.9,-28.075)) ;
#165999 = CARTESIAN_POINT('Origin',(2.7,1.9,-28.975)) ;
#166000 = CARTESIAN_POINT('Origin',(2.7,1.9,-28.175)) ;
#166001 = CARTESIAN_POINT('Origin',(2.7,-5.15,-27.975)) ;
#166002 = CARTESIAN_POINT('Origin',(2.7,-5.15,-28.175)) ;
#166003 = CARTESIAN_POINT('Origin',(2.7,1.9,-28.175)) ;
#166004 = CARTESIAN_POINT('Origin',(2.7,1.9,-28.175)) ;
#166005 = CARTESIAN_POINT('Origin',(2.7,-5.25,-28.175)) ;
#166006 = CARTESIAN_POINT('Ctrl Pts',(-3.8,-6.55,-25.57)) ;
#166007 = CARTESIAN_POINT('Ctrl Pts',(-3.8,-6.55,-25.57)) ;
#166008 = CARTESIAN_POINT('Ctrl Pts',(-3.8,-6.55,-25.57)) ;
#166009 = CARTESIAN_POINT('Ctrl Pts',(-3.82625343282631,-6.55,-25.6225068656527)) ;
#166010 = CARTESIAN_POINT('Ctrl Pts',(-3.83954133268378,-6.55,-25.6095413326839)) ;
#166011 = CARTESIAN_POINT('Ctrl Pts',(-3.85250686565271,-6.55,-25.5962534328264)) ;
#166012 = CARTESIAN_POINT('Ctrl Pts',(-3.85219871729854,-6.53922263893877,
-25.6743974345971)) ;
#166013 = CARTESIAN_POINT('Ctrl Pts',(-3.87914655110981,-6.52362528614074,
-25.6491465511099)) ;
#166014 = CARTESIAN_POINT('Ctrl Pts',(-3.90439743459708,-6.53922263893874,
-25.6221987172986)) ;
#166015 = CARTESIAN_POINT('Ctrl Pts',(-3.87996665852871,-6.5114546977086,
-25.7299333170574)) ;
#166016 = CARTESIAN_POINT('Ctrl Pts',(-3.90288380314161,-6.48208554016475,
-25.6728838031416)) ;
#166017 = CARTESIAN_POINT('Ctrl Pts',(-3.95993331705742,-6.51145469770861,
-25.6499666585287)) ;
#166018 = CARTESIAN_POINT('Ctrl Pts',(-3.88737865704135,-6.5003618540841,
-25.7447573140827)) ;
#166019 = CARTESIAN_POINT('Ctrl Pts',(-3.90501307588296,-6.46792722356047,
-25.6750130758829)) ;
#166020 = CARTESIAN_POINT('Ctrl Pts',(-3.9747573140827,-6.5003618540841,-25.6573786570413)) ;
#166021 = CARTESIAN_POINT('Ctrl Pts',(-3.8973972494609,-6.47617483238892,
-25.7647944989218)) ;
#166022 = CARTESIAN_POINT('Ctrl Pts',(-3.90329674356407,-6.4509405986842,
-25.6732967435641)) ;
#166023 = CARTESIAN_POINT('Ctrl Pts',(-3.99479449892181,-6.47617483238891,
-25.6673972494609)) ;
#166024 = CARTESIAN_POINT('Ctrl Pts',(-3.9,-6.46309229646327,-25.7699999991818)) ;
#166025 = CARTESIAN_POINT('Ctrl Pts',(-3.90000730395982,-6.44945650152231,
-25.6700073039032)) ;
#166026 = CARTESIAN_POINT('Ctrl Pts',(-3.99999999918173,-6.46309229646329,
-25.67)) ;
#166027 = CARTESIAN_POINT('Ctrl Pts',(-3.9,-6.45,-25.77)) ;
#166028 = CARTESIAN_POINT('Ctrl Pts',(-3.9,-6.45,-25.67)) ;
#166029 = CARTESIAN_POINT('Ctrl Pts',(-4.,-6.45,-25.67)) ;
#166030 = CARTESIAN_POINT('Origin',(-4.,-6.45,-25.77)) ;
#166031 = CARTESIAN_POINT('Origin',(-4.,-6.4,-25.77)) ;
#166032 = CARTESIAN_POINT('Origin',(-4.,-6.35,-25.77)) ;
#166033 = CARTESIAN_POINT('Ctrl Pts',(-5.,-6.55,-25.57)) ;
#166034 = CARTESIAN_POINT('Ctrl Pts',(-5.,-6.55,-25.57)) ;
#166035 = CARTESIAN_POINT('Ctrl Pts',(-5.,-6.55,-25.57)) ;
#166036 = CARTESIAN_POINT('Ctrl Pts',(-4.94749313434733,-6.55,-25.5962534328264)) ;
#166037 = CARTESIAN_POINT('Ctrl Pts',(-4.96045866731621,-6.55,-25.609541332684)) ;
#166038 = CARTESIAN_POINT('Ctrl Pts',(-4.97374656717362,-6.55,-25.6225068656527)) ;
#166039 = CARTESIAN_POINT('Ctrl Pts',(-4.89560256540291,-6.53922263893874,
-25.6221987172986)) ;
#166040 = CARTESIAN_POINT('Ctrl Pts',(-4.92085344889017,-6.52362528614074,
-25.6491465511099)) ;
#166041 = CARTESIAN_POINT('Ctrl Pts',(-4.94780128270146,-6.53922263893877,
-25.6743974345971)) ;
#166042 = CARTESIAN_POINT('Ctrl Pts',(-4.84006668294258,-6.51145469770861,
-25.6499666585287)) ;
#166043 = CARTESIAN_POINT('Ctrl Pts',(-4.8971161968584,-6.48208554016475,
-25.6728838031416)) ;
#166044 = CARTESIAN_POINT('Ctrl Pts',(-4.92003334147129,-6.5114546977086,
-25.7299333170574)) ;
#166045 = CARTESIAN_POINT('Ctrl Pts',(-4.82524268591729,-6.5003618540841,
-25.6573786570413)) ;
#166046 = CARTESIAN_POINT('Ctrl Pts',(-4.89498692411703,-6.46792722356048,
-25.6750130758829)) ;
#166047 = CARTESIAN_POINT('Ctrl Pts',(-4.91262134295865,-6.5003618540841,
-25.7447573140827)) ;
#166048 = CARTESIAN_POINT('Ctrl Pts',(-4.80520550107819,-6.47617483238891,
-25.6673972494609)) ;
#166049 = CARTESIAN_POINT('Ctrl Pts',(-4.89670325643594,-6.45094059868419,
-25.6732967435642)) ;
#166050 = CARTESIAN_POINT('Ctrl Pts',(-4.90260275053909,-6.47617483238892,
-25.7647944989218)) ;
#166051 = CARTESIAN_POINT('Ctrl Pts',(-4.80000000081823,-6.46309229646328,
-25.67)) ;
#166052 = CARTESIAN_POINT('Ctrl Pts',(-4.89999269602123,-6.44945650153022,
-25.6700073039033)) ;
#166053 = CARTESIAN_POINT('Ctrl Pts',(-4.9,-6.46309229646329,-25.7699999991818)) ;
#166054 = CARTESIAN_POINT('Ctrl Pts',(-4.8,-6.45,-25.67)) ;
#166055 = CARTESIAN_POINT('Ctrl Pts',(-4.9,-6.45,-25.67)) ;
#166056 = CARTESIAN_POINT('Ctrl Pts',(-4.9,-6.45,-25.77)) ;
#166057 = CARTESIAN_POINT('Origin',(-4.8,-6.45,-25.77)) ;
#166058 = CARTESIAN_POINT('Origin',(-4.,-6.35,-25.77)) ;
#166059 = CARTESIAN_POINT('Origin',(-4.,-6.35,-25.77)) ;
#166060 = CARTESIAN_POINT('Origin',(-4.,-6.35,-25.77)) ;
#166061 = CARTESIAN_POINT('Ctrl Pts',(-3.8,-6.55,-27.77)) ;
#166062 = CARTESIAN_POINT('Ctrl Pts',(-3.8,-6.55,-27.77)) ;
#166063 = CARTESIAN_POINT('Ctrl Pts',(-3.8,-6.55,-27.77)) ;
#166064 = CARTESIAN_POINT('Ctrl Pts',(-3.85250686565272,-6.55,-27.7437465671736)) ;
#166065 = CARTESIAN_POINT('Ctrl Pts',(-3.83954133268385,-6.55,-27.7304586673161)) ;
#166066 = CARTESIAN_POINT('Ctrl Pts',(-3.82625343282628,-6.55,-27.7174931343473)) ;
#166067 = CARTESIAN_POINT('Ctrl Pts',(-3.90439743459706,-6.53922263893874,
-27.7178012827014)) ;
#166068 = CARTESIAN_POINT('Ctrl Pts',(-3.87914655110978,-6.52362528614071,
-27.6908534488901)) ;
#166069 = CARTESIAN_POINT('Ctrl Pts',(-3.85219871729855,-6.53922263893876,
-27.6656025654029)) ;
#166070 = CARTESIAN_POINT('Ctrl Pts',(-3.95993331705743,-6.51145469770861,
-27.6900333414713)) ;
#166071 = CARTESIAN_POINT('Ctrl Pts',(-3.90288380314162,-6.48208554016476,
-27.6671161968584)) ;
#166072 = CARTESIAN_POINT('Ctrl Pts',(-3.8799666585287,-6.5114546977086,-27.6100666829426)) ;
#166073 = CARTESIAN_POINT('Ctrl Pts',(-3.97475731408271,-6.5003618540841,
-27.6826213429587)) ;
#166074 = CARTESIAN_POINT('Ctrl Pts',(-3.90501307588297,-6.46792722356048,
-27.6649869241171)) ;
#166075 = CARTESIAN_POINT('Ctrl Pts',(-3.88737865704135,-6.5003618540841,
-27.5952426859173)) ;
#166076 = CARTESIAN_POINT('Ctrl Pts',(-3.9947944989218,-6.47617483238891,
-27.6726027505391)) ;
#166077 = CARTESIAN_POINT('Ctrl Pts',(-3.90329674356406,-6.45094059868419,
-27.6667032564358)) ;
#166078 = CARTESIAN_POINT('Ctrl Pts',(-3.89739724946091,-6.47617483238892,
-27.5752055010782)) ;
#166079 = CARTESIAN_POINT('Ctrl Pts',(-3.99999999918176,-6.46309229646328,
-27.67)) ;
#166080 = CARTESIAN_POINT('Ctrl Pts',(-3.90000730395532,-6.44945650152054,
-27.6699926960965)) ;
#166081 = CARTESIAN_POINT('Ctrl Pts',(-3.9,-6.46309229646329,-27.5700000008182)) ;
#166082 = CARTESIAN_POINT('Ctrl Pts',(-4.,-6.45,-27.67)) ;
#166083 = CARTESIAN_POINT('Ctrl Pts',(-3.9,-6.45,-27.67)) ;
#166084 = CARTESIAN_POINT('Ctrl Pts',(-3.9,-6.45,-27.57)) ;
#166085 = CARTESIAN_POINT('Origin',(-4.,-6.45,-27.57)) ;
#166086 = CARTESIAN_POINT('Origin',(-4.8,-6.4,-25.77)) ;
#166087 = CARTESIAN_POINT('Origin',(-4.8,-6.35,-25.77)) ;
#166088 = CARTESIAN_POINT('Origin',(1.9515639104739E-16,-6.35,-25.77)) ;
#166089 = CARTESIAN_POINT('Origin',(-4.8,-6.35,-25.77)) ;
#166090 = CARTESIAN_POINT('Origin',(-4.,-6.35,-26.67)) ;
#166091 = CARTESIAN_POINT('Origin',(-4.,-6.35,-27.57)) ;
#166092 = CARTESIAN_POINT('Origin',(-4.,-6.4,-27.57)) ;
#166093 = CARTESIAN_POINT('Origin',(-4.,-6.35,-27.57)) ;
#166094 = CARTESIAN_POINT('Origin',(-4.8,-6.35,-25.77)) ;
#166095 = CARTESIAN_POINT('Origin',(-4.8,-6.35,-25.77)) ;
#166096 = CARTESIAN_POINT('Origin',(-4.,-6.35,-27.57)) ;
#166097 = CARTESIAN_POINT('Origin',(-4.,-6.35,-27.57)) ;
#166098 = CARTESIAN_POINT('Origin',(-4.8,-6.35,-26.67)) ;
#166099 = CARTESIAN_POINT('Origin',(-4.8,-6.35,-27.57)) ;
#166100 = CARTESIAN_POINT('Origin',(1.95156391047391E-16,-6.35,-27.57)) ;
#166101 = CARTESIAN_POINT('Origin',(-4.8,-6.35,-27.57)) ;
#166102 = CARTESIAN_POINT('Origin',(-4.8,-6.35,-27.57)) ;
#166103 = CARTESIAN_POINT('Origin',(-4.8,-6.35,-27.57)) ;
#166104 = CARTESIAN_POINT('Origin',(-4.8,-6.4,-27.57)) ;
#166105 = CARTESIAN_POINT('Origin',(-4.8,-6.45,-27.57)) ;
#166106 = CARTESIAN_POINT('Ctrl Pts',(-5.,-6.55,-27.77)) ;
#166107 = CARTESIAN_POINT('Ctrl Pts',(-5.,-6.55,-27.77)) ;
#166108 = CARTESIAN_POINT('Ctrl Pts',(-5.,-6.55,-27.77)) ;
#166109 = CARTESIAN_POINT('Ctrl Pts',(-4.97374656717361,-6.55,-27.7174931343473)) ;
#166110 = CARTESIAN_POINT('Ctrl Pts',(-4.96045866731622,-6.55,-27.730458667316)) ;
#166111 = CARTESIAN_POINT('Ctrl Pts',(-4.94749313434733,-6.55,-27.7437465671736)) ;
#166112 = CARTESIAN_POINT('Ctrl Pts',(-4.94780128270146,-6.53922263893877,
-27.6656025654029)) ;
#166113 = CARTESIAN_POINT('Ctrl Pts',(-4.92085344889017,-6.52362528614073,
-27.6908534488901)) ;
#166114 = CARTESIAN_POINT('Ctrl Pts',(-4.89560256540291,-6.53922263893874,
-27.7178012827014)) ;
#166115 = CARTESIAN_POINT('Ctrl Pts',(-4.92003334147129,-6.5114546977086,
-27.6100666829426)) ;
#166116 = CARTESIAN_POINT('Ctrl Pts',(-4.8971161968584,-6.48208554016475,
-27.6671161968584)) ;
#166117 = CARTESIAN_POINT('Ctrl Pts',(-4.84006668294258,-6.51145469770861,
-27.6900333414713)) ;
#166118 = CARTESIAN_POINT('Ctrl Pts',(-4.91262134295865,-6.5003618540841,
-27.5952426859173)) ;
#166119 = CARTESIAN_POINT('Ctrl Pts',(-4.89498692411703,-6.46792722356048,
-27.6649869241171)) ;
#166120 = CARTESIAN_POINT('Ctrl Pts',(-4.82524268591729,-6.5003618540841,
-27.6826213429587)) ;
#166121 = CARTESIAN_POINT('Ctrl Pts',(-4.90260275053909,-6.47617483238892,
-27.5752055010782)) ;
#166122 = CARTESIAN_POINT('Ctrl Pts',(-4.89670325643594,-6.45094059868419,
-27.6667032564358)) ;
#166123 = CARTESIAN_POINT('Ctrl Pts',(-4.80520550107819,-6.47617483238891,
-27.6726027505391)) ;
#166124 = CARTESIAN_POINT('Ctrl Pts',(-4.9,-6.46309229646329,-27.5700000008182)) ;
#166125 = CARTESIAN_POINT('Ctrl Pts',(-4.89999269603999,-6.44945650152248,
-27.6699926960966)) ;
#166126 = CARTESIAN_POINT('Ctrl Pts',(-4.80000000081823,-6.46309229646328,
-27.67)) ;
#166127 = CARTESIAN_POINT('Ctrl Pts',(-4.9,-6.45,-27.57)) ;
#166128 = CARTESIAN_POINT('Ctrl Pts',(-4.9,-6.45,-27.67)) ;
#166129 = CARTESIAN_POINT('Ctrl Pts',(-4.8,-6.45,-27.67)) ;
#166130 = CARTESIAN_POINT('Ctrl Pts',(-5.82426676739349,-5.43399303700618,
-25.0670109659688)) ;
#166131 = CARTESIAN_POINT('Ctrl Pts',(-5.80266988778314,-5.5257236068294,
-25.0723540173506)) ;
#166132 = CARTESIAN_POINT('Ctrl Pts',(-5.82426676352018,-5.53106667371342,
-25.1640845871828)) ;
#166133 = CARTESIAN_POINT('Ctrl Pts',(-5.83498671931115,-5.43935351191914,
-25.0643294581962)) ;
#166134 = CARTESIAN_POINT('Ctrl Pts',(-5.80595263122267,-5.52411753147712,
-25.0739600935403)) ;
#166135 = CARTESIAN_POINT('Ctrl Pts',(-5.83498671397629,-5.53374818067469,
-25.1587241131463)) ;
#166136 = CARTESIAN_POINT('Ctrl Pts',(-5.84526105845711,-5.44830326289498,
-25.0598528401962)) ;
#166137 = CARTESIAN_POINT('Ctrl Pts',(-5.8137093274614,-5.52260132030856,
-25.0754763059991)) ;
#166138 = CARTESIAN_POINT('Ctrl Pts',(-5.84526105243723,-5.5382247974634,
-25.1497743635698)) ;
#166139 = CARTESIAN_POINT('Ctrl Pts',(-5.86378685403698,-5.47240020430406,
-25.0478032513087)) ;
#166140 = CARTESIAN_POINT('Ctrl Pts',(-5.83531854275285,-5.52733067404486,
-25.0707469551147)) ;
#166141 = CARTESIAN_POINT('Ctrl Pts',(-5.86378684816463,-5.55027438459901,
-25.1256774250056)) ;
#166142 = CARTESIAN_POINT('Ctrl Pts',(-5.87203852631574,-5.4875449513474,
-25.0402315528944)) ;
#166143 = CARTESIAN_POINT('Ctrl Pts',(-5.84834787930682,-5.53310199490455,
-25.0649756357762)) ;
#166144 = CARTESIAN_POINT('Ctrl Pts',(-5.87203852123042,-5.55784608243458,
-25.110532679514)) ;
#166145 = CARTESIAN_POINT('Ctrl Pts',(-5.89242747304799,-5.53981202333456,
-25.0141056511376)) ;
#166146 = CARTESIAN_POINT('Ctrl Pts',(-5.88223383300423,-5.56084219179271,
-25.0372354431741)) ;
#166147 = CARTESIAN_POINT('Ctrl Pts',(-5.89242747063502,-5.58397198402776,
-25.0582656123278)) ;
#166148 = CARTESIAN_POINT('Ctrl Pts',(-5.9,-5.58381083947299,-24.992119400143)) ;
#166149 = CARTESIAN_POINT('Ctrl Pts',(-5.9,-5.59485304502672,-25.0032245928865)) ;
#166150 = CARTESIAN_POINT('Ctrl Pts',(-5.9,-5.60595823775503,-25.0142667984405)) ;
#166151 = CARTESIAN_POINT('Ctrl Pts',(-5.9,-5.62807764064044,-24.97)) ;
#166152 = CARTESIAN_POINT('Ctrl Pts',(-5.9,-5.62807764064044,-24.97)) ;
#166153 = CARTESIAN_POINT('Ctrl Pts',(-5.9,-5.62807764064044,-24.97)) ;
#166154 = CARTESIAN_POINT('Origin',(-5.84850712500726,-5.43404914061138,-25.1640285000291)) ;
#166155 = CARTESIAN_POINT('Ctrl Pts',(-5.82425356250363,-5.53106339062591,
-25.1640285000291)) ;
#166156 = CARTESIAN_POINT('Ctrl Pts',(-5.80269484027818,-5.52567371006955,
-25.0724039305709)) ;
#166157 = CARTESIAN_POINT('Ctrl Pts',(-5.82425356250363,-5.43404914061138,
-25.0670142500145)) ;
#166158 = CARTESIAN_POINT('Ctrl Pts',(-5.80840777707096,-5.52710194426774,
-25.1679899459043)) ;
#166159 = CARTESIAN_POINT('Ctrl Pts',(-5.79341417645231,-5.52335354411309,
-25.0728358498184)) ;
#166160 = CARTESIAN_POINT('Ctrl Pts',(-5.81633079157288,-5.43008775511759,
-25.0689949427472)) ;
#166161 = CARTESIAN_POINT('Ctrl Pts',(-5.79207992677989,-5.52301998169497,
-25.169999999534)) ;
#166162 = CARTESIAN_POINT('Ctrl Pts',(-5.78430903206645,-5.52107725801649,
-25.0719613954329)) ;
#166163 = CARTESIAN_POINT('Ctrl Pts',(-5.80816665318299,-5.42600568595106,
-25.07)) ;
#166164 = CARTESIAN_POINT('Ctrl Pts',(-5.77574643749636,-5.51893660937409,
-25.17)) ;
#166165 = CARTESIAN_POINT('Ctrl Pts',(-5.77574643749636,-5.51893660937409,
-25.07)) ;
#166166 = CARTESIAN_POINT('Ctrl Pts',(-5.8,-5.42192235935956,-25.07)) ;
#166167 = CARTESIAN_POINT('Origin',(-5.8,-5.42192235935956,-25.17)) ;
#166168 = CARTESIAN_POINT('Origin',(-5.8066065036801,-5.42357398527959,-25.17)) ;
#166169 = CARTESIAN_POINT('Origin',(-5.17275707706437,-5.26511162862565,-25.17)) ;
#166170 = CARTESIAN_POINT('Origin',(-5.15068655017073,-5.25959399690224,-25.1805938529089)) ;
#166171 = CARTESIAN_POINT('Origin',(-5.17275707706436,-5.26511162862565,-25.17)) ;
#166172 = CARTESIAN_POINT('Origin',(-5.17275707706436,-5.26511162862565,-25.17)) ;
#166173 = CARTESIAN_POINT('Origin',(-5.17275707706436,-5.26511162862565,-25.17)) ;
#166174 = CARTESIAN_POINT('Origin',(-5.17275707706436,-5.05,-25.17)) ;
#166175 = CARTESIAN_POINT('Origin',(-5.17275707706436,-1.91866427917294,-25.17)) ;
#166176 = CARTESIAN_POINT('Origin',(-3.78014014831103,-3.31128120792626,-25.8384561258016)) ;
#166177 = CARTESIAN_POINT('Origin',(-5.17275707706436,-1.91866427917294,-25.17)) ;
#166178 = CARTESIAN_POINT('Origin',(-5.17275707706436,-1.91866427917293,-25.17)) ;
#166179 = CARTESIAN_POINT('Origin',(-5.17275707706436,-1.91866427917294,-25.17)) ;
#166180 = CARTESIAN_POINT('Origin',(-3.97071067811865,-3.12071067811865,-25.17)) ;
#166181 = CARTESIAN_POINT('Origin',(-5.8,-1.2914213562373,-25.17)) ;
#166182 = CARTESIAN_POINT('Ctrl Pts',(-5.87071067811865,-1.14999999999999,
-25.0407106781187)) ;
#166183 = CARTESIAN_POINT('Ctrl Pts',(-5.8471404520791,-1.10285954792089,
-25.0642809041582)) ;
#166184 = CARTESIAN_POINT('Ctrl Pts',(-5.87071067811865,-1.07928932188134,
-25.1114213562373)) ;
#166185 = CARTESIAN_POINT('Ctrl Pts',(-5.85217562795657,-1.18707010095451,
-25.0592457282807)) ;
#166186 = CARTESIAN_POINT('Ctrl Pts',(-5.81261165662078,-1.13738834337949,
-25.0858614719497)) ;
#166187 = CARTESIAN_POINT('Ctrl Pts',(-5.83353949671049,-1.1164605032895,
-25.1485925363811)) ;
#166188 = CARTESIAN_POINT('Ctrl Pts',(-5.82627077431945,-1.23887980759835,
-25.07)) ;
#166189 = CARTESIAN_POINT('Ctrl Pts',(-5.76566787907951,-1.18433212092046,
-25.0871489437127)) ;
#166190 = CARTESIAN_POINT('Ctrl Pts',(-5.78190678732229,-1.1680932126777,
-25.1699999994186)) ;
#166191 = CARTESIAN_POINT('Ctrl Pts',(-5.8,-1.2914213562373,-25.07)) ;
#166192 = CARTESIAN_POINT('Ctrl Pts',(-5.72928932188134,-1.22071067811865,
-25.07)) ;
#166193 = CARTESIAN_POINT('Ctrl Pts',(-5.72928932188134,-1.22071067811865,
-25.17)) ;
#166194 = CARTESIAN_POINT('Origin',(-5.94142135623731,-1.15,-25.1114213562373)) ;
#166195 = CARTESIAN_POINT('Ctrl Pts',(-5.9,-1.00857864376269,-24.97)) ;
#166196 = CARTESIAN_POINT('Ctrl Pts',(-5.9,-1.00857864376269,-24.97)) ;
#166197 = CARTESIAN_POINT('Ctrl Pts',(-5.9,-1.00857864376269,-24.97)) ;
#166198 = CARTESIAN_POINT('Ctrl Pts',(-5.9,-1.06112019240164,-24.9962707743195)) ;
#166199 = CARTESIAN_POINT('Ctrl Pts',(-5.9,-1.04860238145267,-25.0100237376901)) ;
#166200 = CARTESIAN_POINT('Ctrl Pts',(-5.9,-1.03484941808214,-25.022541548639)) ;
#166201 = CARTESIAN_POINT('Ctrl Pts',(-5.88924572828071,-1.11292989904543,
-25.0221756279566)) ;
#166202 = CARTESIAN_POINT('Ctrl Pts',(-5.87451700627693,-1.08721613123091,
-25.0486374874681)) ;
#166203 = CARTESIAN_POINT('Ctrl Pts',(-5.88924572828062,-1.06075427171937,
-25.0743512552826)) ;
#166204 = CARTESIAN_POINT('Ctrl Pts',(-5.87071067811865,-1.14999999999999,
-25.0407106781187)) ;
#166205 = CARTESIAN_POINT('Ctrl Pts',(-5.8471404520791,-1.10285954792089,
-25.0642809041582)) ;
#166206 = CARTESIAN_POINT('Ctrl Pts',(-5.87071067811865,-1.07928932188134,
-25.1114213562373)) ;
#166207 = CARTESIAN_POINT('Ctrl Pts',(-5.87071067811866,-1.14999999999999,
-28.2992893218813)) ;
#166208 = CARTESIAN_POINT('Ctrl Pts',(-5.84714045207911,-1.10285954792089,
-28.2757190958418)) ;
#166209 = CARTESIAN_POINT('Ctrl Pts',(-5.87071067811866,-1.07928932188134,
-28.2285786437627)) ;
#166210 = CARTESIAN_POINT('Ctrl Pts',(-5.8892457282807,-1.11292989904542,
-28.3178243720434)) ;
#166211 = CARTESIAN_POINT('Ctrl Pts',(-5.87451700627501,-1.08721613123182,
-28.2913625125304)) ;
#166212 = CARTESIAN_POINT('Ctrl Pts',(-5.88924572828062,-1.06075427171937,
-28.2656487447174)) ;
#166213 = CARTESIAN_POINT('Ctrl Pts',(-5.9,-1.06112019240159,-28.3437292256804)) ;
#166214 = CARTESIAN_POINT('Ctrl Pts',(-5.9,-1.0486023814516,-28.3299762623108)) ;
#166215 = CARTESIAN_POINT('Ctrl Pts',(-5.9,-1.03484941808214,-28.317458451361)) ;
#166216 = CARTESIAN_POINT('Ctrl Pts',(-5.9,-1.00857864376269,-28.37)) ;
#166217 = CARTESIAN_POINT('Ctrl Pts',(-5.9,-1.00857864376269,-28.37)) ;
#166218 = CARTESIAN_POINT('Ctrl Pts',(-5.9,-1.00857864376269,-28.37)) ;
#166219 = CARTESIAN_POINT('Origin',(-5.94142135623734,-1.14999999999996,-28.2285786437627)) ;
#166220 = CARTESIAN_POINT('Ctrl Pts',(-5.8,-1.2914213562373,-28.27)) ;
#166221 = CARTESIAN_POINT('Ctrl Pts',(-5.72928932188134,-1.22071067811865,
-28.27)) ;
#166222 = CARTESIAN_POINT('Ctrl Pts',(-5.72928932188134,-1.22071067811865,
-28.17)) ;
#166223 = CARTESIAN_POINT('Ctrl Pts',(-5.82627077431951,-1.23887980759822,
-28.27)) ;
#166224 = CARTESIAN_POINT('Ctrl Pts',(-5.76566787907979,-1.18433212092023,
-28.2528510562872)) ;
#166225 = CARTESIAN_POINT('Ctrl Pts',(-5.78190678732242,-1.16809321267757,
-28.1700000005814)) ;
#166226 = CARTESIAN_POINT('Ctrl Pts',(-5.85217562795678,-1.18707010095483,
-28.2807542717195)) ;
#166227 = CARTESIAN_POINT('Ctrl Pts',(-5.81261165662033,-1.13738834337968,
-28.2541385280508)) ;
#166228 = CARTESIAN_POINT('Ctrl Pts',(-5.83353949671033,-1.11646050328967,
-28.1914074636191)) ;
#166229 = CARTESIAN_POINT('Ctrl Pts',(-5.87071067811866,-1.14999999999999,
-28.2992893218813)) ;
#166230 = CARTESIAN_POINT('Ctrl Pts',(-5.84714045207911,-1.10285954792088,
-28.2757190958418)) ;
#166231 = CARTESIAN_POINT('Ctrl Pts',(-5.87071067811866,-1.07928932188133,
-28.2285786437627)) ;
#166232 = CARTESIAN_POINT('Origin',(-5.8,-1.29142135623731,-28.17)) ;
#166233 = CARTESIAN_POINT('Origin',(-3.59571067811865,-3.49571067811865,-28.17)) ;
#166234 = CARTESIAN_POINT('Origin',(-5.17275707706437,-1.91866427917293,-28.17)) ;
#166235 = CARTESIAN_POINT('Origin',(-3.09057773798104,-4.00084361825625,-27.17055391724)) ;
#166236 = CARTESIAN_POINT('Origin',(-5.17275707706436,-1.91866427917293,-28.17)) ;
#166237 = CARTESIAN_POINT('Origin',(-5.17275707706436,-1.91866427917293,-28.17)) ;
#166238 = CARTESIAN_POINT('Origin',(-5.17275707706436,-1.91866427917293,-28.17)) ;
#166239 = CARTESIAN_POINT('Origin',(-5.17275707706436,-5.05,-28.17)) ;
#166240 = CARTESIAN_POINT('Origin',(-5.17275707706436,-5.26511162862565,-28.17)) ;
#166241 = CARTESIAN_POINT('Origin',(-3.96111272388873,-4.96220054033175,-27.5884107104757)) ;
#166242 = CARTESIAN_POINT('Origin',(-5.17275707706436,-5.26511162862565,-28.17)) ;
#166243 = CARTESIAN_POINT('Origin',(-5.17275707706436,-5.26511162862565,-28.17)) ;
#166244 = CARTESIAN_POINT('Origin',(-5.17275707706436,-5.26511162862565,-28.17)) ;
#166245 = CARTESIAN_POINT('Origin',(-5.10072415073893,-5.24710339704429,-28.17)) ;
#166246 = CARTESIAN_POINT('Origin',(-5.8,-5.42192235935956,-28.17)) ;
#166247 = CARTESIAN_POINT('Ctrl Pts',(-5.77574643749636,-5.51893660937409,
-28.17)) ;
#166248 = CARTESIAN_POINT('Ctrl Pts',(-5.77574643749636,-5.51893660937409,
-28.27)) ;
#166249 = CARTESIAN_POINT('Ctrl Pts',(-5.8,-5.42192235935956,-28.27)) ;
#166250 = CARTESIAN_POINT('Ctrl Pts',(-5.7920799267799,-5.52301998169498,
-28.170000000466)) ;
#166251 = CARTESIAN_POINT('Ctrl Pts',(-5.78430903206646,-5.52107725801649,
-28.2680386045671)) ;
#166252 = CARTESIAN_POINT('Ctrl Pts',(-5.80816665318301,-5.42600568595105,
-28.27)) ;
#166253 = CARTESIAN_POINT('Ctrl Pts',(-5.80840777707094,-5.52710194426774,
-28.1720100540957)) ;
#166254 = CARTESIAN_POINT('Ctrl Pts',(-5.7934141764523,-5.52335354411309,
-28.2671641501816)) ;
#166255 = CARTESIAN_POINT('Ctrl Pts',(-5.81633079157287,-5.43008775511759,
-28.2710050572528)) ;
#166256 = CARTESIAN_POINT('Ctrl Pts',(-5.82425356250363,-5.53106339062591,
-28.1759714999709)) ;
#166257 = CARTESIAN_POINT('Ctrl Pts',(-5.80269484027818,-5.52567371006955,
-28.2675960694291)) ;
#166258 = CARTESIAN_POINT('Ctrl Pts',(-5.82425356250363,-5.43404914061138,
-28.2729857499855)) ;
#166259 = CARTESIAN_POINT('Origin',(-5.84850712500726,-5.43404914061138,-28.1759714999709)) ;
#166260 = CARTESIAN_POINT('Ctrl Pts',(-5.82426676739352,-5.53106667467169,
-28.1759153963656)) ;
#166261 = CARTESIAN_POINT('Ctrl Pts',(-5.80266988778309,-5.52572362328995,
-28.267645966189)) ;
#166262 = CARTESIAN_POINT('Ctrl Pts',(-5.82426676352022,-5.43399305345751,
-28.272989033073)) ;
#166263 = CARTESIAN_POINT('Ctrl Pts',(-5.83498671931118,-5.53374818244429,
-28.1812758712786)) ;
#166264 = CARTESIAN_POINT('Ctrl Pts',(-5.80595263122259,-5.52411754710017,
-28.2660398908368)) ;
#166265 = CARTESIAN_POINT('Ctrl Pts',(-5.83498671397633,-5.43935352749393,
-28.2756705400343)) ;
#166266 = CARTESIAN_POINT('Ctrl Pts',(-5.84526105845716,-5.53822480044429,
-28.1902256222544)) ;
#166267 = CARTESIAN_POINT('Ctrl Pts',(-5.81370932746132,-5.52260133464138,
-28.2645236796683)) ;
#166268 = CARTESIAN_POINT('Ctrl Pts',(-5.84526105243728,-5.44830327707048,
-28.280147156823)) ;
#166269 = CARTESIAN_POINT('Ctrl Pts',(-5.863786854037,-5.55027438933178,-28.2143225636635)) ;
#166270 = CARTESIAN_POINT('Ctrl Pts',(-5.83531854275277,-5.52733068552579,
-28.2692530334044)) ;
#166271 = CARTESIAN_POINT('Ctrl Pts',(-5.86378684816469,-5.47240021563481,
-28.2921967439586)) ;
#166272 = CARTESIAN_POINT('Ctrl Pts',(-5.87203852631579,-5.55784608774608,
-28.2294673107068)) ;
#166273 = CARTESIAN_POINT('Ctrl Pts',(-5.84834787930676,-5.53310200486437,
-28.2750243542641)) ;
#166274 = CARTESIAN_POINT('Ctrl Pts',(-5.87203852123048,-5.48754496112639,
-28.2997684417942)) ;
#166275 = CARTESIAN_POINT('Ctrl Pts',(-5.89242747304797,-5.58397198950285,
-28.2817343826941)) ;
#166276 = CARTESIAN_POINT('Ctrl Pts',(-5.8822338330042,-5.56084219746613,
-28.3027645511524)) ;
#166277 = CARTESIAN_POINT('Ctrl Pts',(-5.89242747063504,-5.53981202831257,
-28.3258943433874)) ;
#166278 = CARTESIAN_POINT('Ctrl Pts',(-5.9,-5.60595824049749,-28.3257331988326)) ;
#166279 = CARTESIAN_POINT('Ctrl Pts',(-5.9,-5.59485304775411,-28.3367754043862)) ;
#166280 = CARTESIAN_POINT('Ctrl Pts',(-5.9,-5.58381084219986,-28.3478805971146)) ;
#166281 = CARTESIAN_POINT('Ctrl Pts',(-5.9,-5.62807764064044,-28.37)) ;
#166282 = CARTESIAN_POINT('Ctrl Pts',(-5.9,-5.62807764064044,-28.37)) ;
#166283 = CARTESIAN_POINT('Ctrl Pts',(-5.9,-5.62807764064044,-28.37)) ;
#166284 = CARTESIAN_POINT('Origin',(7.8,2.1,-27.07)) ;
#166285 = CARTESIAN_POINT('Origin',(7.8,2.1,-27.27)) ;
#166286 = CARTESIAN_POINT('Origin',(7.6,2.1,-27.07)) ;
#166287 = CARTESIAN_POINT('Origin',(7.6,2.1,-27.07)) ;
#166288 = CARTESIAN_POINT('Origin',(7.6,2.1,-26.27)) ;
#166289 = CARTESIAN_POINT('Origin',(7.8,2.1,-27.27)) ;
#166290 = CARTESIAN_POINT('Origin',(9.6,2.1,-27.27)) ;
#166291 = CARTESIAN_POINT('Origin',(7.8,2.1,-26.27)) ;
#166292 = CARTESIAN_POINT('Origin',(7.8,2.1,-26.07)) ;
#166293 = CARTESIAN_POINT('Origin',(9.6,2.1,-27.07)) ;
#166294 = CARTESIAN_POINT('Origin',(9.8,2.1,-27.07)) ;
#166295 = CARTESIAN_POINT('Origin',(7.8,2.1,-26.07)) ;
#166296 = CARTESIAN_POINT('Origin',(9.6,2.1,-26.07)) ;
#166297 = CARTESIAN_POINT('Origin',(9.8,2.1,-27.07)) ;
#166298 = CARTESIAN_POINT('Origin',(9.8,2.1,-26.27)) ;
#166299 = CARTESIAN_POINT('Origin',(9.6,2.1,-26.27)) ;
#166300 = CARTESIAN_POINT('Origin',(-4.15,-6.25,-25.92)) ;
#166301 = CARTESIAN_POINT('Origin',(-4.15,-6.3,-25.92)) ;
#166302 = CARTESIAN_POINT('Origin',(-4.15,-6.3,-26.67)) ;
#166303 = CARTESIAN_POINT('Origin',(-4.15,-6.3,-27.42)) ;
#166304 = CARTESIAN_POINT('Origin',(-4.15,-6.3,-25.92)) ;
#166305 = CARTESIAN_POINT('Origin',(-4.15,-6.25,-27.42)) ;
#166306 = CARTESIAN_POINT('Origin',(-4.15,-6.3,-27.42)) ;
#166307 = CARTESIAN_POINT('Origin',(-4.15,-6.3,-25.92)) ;
#166308 = CARTESIAN_POINT('Origin',(-4.15,-6.3,-25.92)) ;
#166309 = CARTESIAN_POINT('Origin',(-4.15,-6.3,-27.42)) ;
#166310 = CARTESIAN_POINT('Origin',(-4.15,-6.3,-27.42)) ;
#166311 = CARTESIAN_POINT('Origin',(-4.65,-6.25,-25.92)) ;
#166312 = CARTESIAN_POINT('Origin',(-4.65,-6.3,-25.92)) ;
#166313 = CARTESIAN_POINT('Origin',(0.,-6.3,-25.92)) ;
#166314 = CARTESIAN_POINT('Origin',(-4.65,-6.3,-25.92)) ;
#166315 = CARTESIAN_POINT('Origin',(0.,-6.3,-27.42)) ;
#166316 = CARTESIAN_POINT('Origin',(-4.65,-6.3,-27.42)) ;
#166317 = CARTESIAN_POINT('Origin',(-4.65,-6.25,-27.42)) ;
#166318 = CARTESIAN_POINT('Origin',(-4.65,-6.3,-27.42)) ;
#166319 = CARTESIAN_POINT('Origin',(-4.65,-6.3,-25.92)) ;
#166320 = CARTESIAN_POINT('Origin',(-4.65,-6.3,-25.92)) ;
#166321 = CARTESIAN_POINT('Origin',(-4.65,-6.3,-27.42)) ;
#166322 = CARTESIAN_POINT('Origin',(-4.65,-6.3,-27.42)) ;
#166323 = CARTESIAN_POINT('Origin',(-4.65,-6.3,-26.67)) ;
#166324 = CARTESIAN_POINT('Origin',(-3.,4.45,-27.77)) ;
#166325 = CARTESIAN_POINT('Origin',(-2.1,4.45,-27.77)) ;
#166326 = CARTESIAN_POINT('Origin',(-2.9,4.45,-27.77)) ;
#166327 = CARTESIAN_POINT('Origin',(-2.9,4.45,-27.57)) ;
#166328 = CARTESIAN_POINT('Origin',(-3.1,4.45,-27.57)) ;
#166329 = CARTESIAN_POINT('Origin',(-2.9,4.45,-27.57)) ;
#166330 = CARTESIAN_POINT('Origin',(-2.1,4.45,-27.57)) ;
#166331 = CARTESIAN_POINT('Origin',(-2.1,4.45,-27.57)) ;
#166332 = CARTESIAN_POINT('Origin',(-1.9,4.45,-27.57)) ;
#166333 = CARTESIAN_POINT('Origin',(-3.1,4.45,-27.67)) ;
#166334 = CARTESIAN_POINT('Origin',(-3.1,4.45,-25.77)) ;
#166335 = CARTESIAN_POINT('Origin',(-2.9,4.4,-27.57)) ;
#166336 = CARTESIAN_POINT('Origin',(-2.9,4.35,-27.57)) ;
#166337 = CARTESIAN_POINT('Origin',(-1.95156391047391E-16,4.35,-27.57)) ;
#166338 = CARTESIAN_POINT('Origin',(-2.1,4.35,-27.57)) ;
#166339 = CARTESIAN_POINT('Origin',(-2.9,4.35,-27.57)) ;
#166340 = CARTESIAN_POINT('Origin',(-2.1,4.4,-27.57)) ;
#166341 = CARTESIAN_POINT('Origin',(-2.1,4.35,-27.57)) ;
#166342 = CARTESIAN_POINT('Origin',(-1.9,4.45,-27.67)) ;
#166343 = CARTESIAN_POINT('Origin',(-1.9,4.45,-25.77)) ;
#166344 = CARTESIAN_POINT('Origin',(-3.,4.45,-25.57)) ;
#166345 = CARTESIAN_POINT('Origin',(-2.9,4.45,-25.57)) ;
#166346 = CARTESIAN_POINT('Origin',(-2.1,4.45,-25.57)) ;
#166347 = CARTESIAN_POINT('Origin',(-2.9,4.45,-25.77)) ;
#166348 = CARTESIAN_POINT('Origin',(-2.9,4.45,-25.77)) ;
#166349 = CARTESIAN_POINT('Origin',(-2.9,4.35,-27.57)) ;
#166350 = CARTESIAN_POINT('Origin',(-2.9,4.35,-27.57)) ;
#166351 = CARTESIAN_POINT('Origin',(-2.1,4.35,-27.57)) ;
#166352 = CARTESIAN_POINT('Origin',(-2.1,4.35,-27.57)) ;
#166353 = CARTESIAN_POINT('Origin',(-2.1,4.45,-25.77)) ;
#166354 = CARTESIAN_POINT('Origin',(-2.1,4.45,-25.77)) ;
#166355 = CARTESIAN_POINT('Origin',(-2.9,4.4,-25.77)) ;
#166356 = CARTESIAN_POINT('Origin',(-2.9,4.35,-25.77)) ;
#166357 = CARTESIAN_POINT('Origin',(-2.9,4.35,-26.67)) ;
#166358 = CARTESIAN_POINT('Origin',(-2.9,4.35,-25.77)) ;
#166359 = CARTESIAN_POINT('Origin',(-2.1,4.35,-26.67)) ;
#166360 = CARTESIAN_POINT('Origin',(-2.1,4.35,-25.77)) ;
#166361 = CARTESIAN_POINT('Origin',(-2.1,4.4,-25.77)) ;
#166362 = CARTESIAN_POINT('Origin',(-2.1,4.35,-25.77)) ;
#166363 = CARTESIAN_POINT('Origin',(-2.9,4.35,-25.77)) ;
#166364 = CARTESIAN_POINT('Origin',(-2.9,4.35,-25.77)) ;
#166365 = CARTESIAN_POINT('Origin',(-2.1,4.35,-25.77)) ;
#166366 = CARTESIAN_POINT('Origin',(-2.1,4.35,-25.77)) ;
#166367 = CARTESIAN_POINT('Origin',(-1.95156391047391E-16,4.35,-25.77)) ;
#166368 = CARTESIAN_POINT('Origin',(-2.25,4.25,-27.42)) ;
#166369 = CARTESIAN_POINT('Origin',(-2.25,4.3,-27.42)) ;
#166370 = CARTESIAN_POINT('Origin',(-2.25,4.3,-26.67)) ;
#166371 = CARTESIAN_POINT('Origin',(-2.25,4.3,-25.92)) ;
#166372 = CARTESIAN_POINT('Origin',(-2.25,4.3,-27.42)) ;
#166373 = CARTESIAN_POINT('Origin',(-2.25,4.25,-25.92)) ;
#166374 = CARTESIAN_POINT('Origin',(-2.25,4.3,-25.92)) ;
#166375 = CARTESIAN_POINT('Origin',(-2.25,4.3,-27.42)) ;
#166376 = CARTESIAN_POINT('Origin',(-2.25,4.3,-27.42)) ;
#166377 = CARTESIAN_POINT('Origin',(-2.25,4.3,-25.92)) ;
#166378 = CARTESIAN_POINT('Origin',(-2.25,4.3,-25.92)) ;
#166379 = CARTESIAN_POINT('Origin',(-2.75,4.25,-27.42)) ;
#166380 = CARTESIAN_POINT('Origin',(-2.75,4.3,-27.42)) ;
#166381 = CARTESIAN_POINT('Origin',(-1.97127667724637E-17,4.3,-27.42)) ;
#166382 = CARTESIAN_POINT('Origin',(-2.75,4.3,-27.42)) ;
#166383 = CARTESIAN_POINT('Origin',(-1.97127667724637E-17,4.3,-25.92)) ;
#166384 = CARTESIAN_POINT('Origin',(-2.75,4.3,-25.92)) ;
#166385 = CARTESIAN_POINT('Origin',(-2.75,4.25,-25.92)) ;
#166386 = CARTESIAN_POINT('Origin',(-2.75,4.3,-25.92)) ;
#166387 = CARTESIAN_POINT('Origin',(-2.75,4.3,-27.42)) ;
#166388 = CARTESIAN_POINT('Origin',(-2.75,4.3,-27.42)) ;
#166389 = CARTESIAN_POINT('Origin',(-2.75,4.3,-25.92)) ;
#166390 = CARTESIAN_POINT('Origin',(-2.75,4.3,-25.92)) ;
#166391 = CARTESIAN_POINT('Origin',(-2.75,4.3,-26.67)) ;
#166392 = CARTESIAN_POINT('Origin',(7.8,2.9,-27.07)) ;
#166393 = CARTESIAN_POINT('Origin',(7.8,2.9,-27.07)) ;
#166394 = CARTESIAN_POINT('Origin',(7.8,2.9,-26.27)) ;
#166395 = CARTESIAN_POINT('Origin',(7.8,2.9,-26.27)) ;
#166396 = CARTESIAN_POINT('Origin',(7.8,2.9,-26.27)) ;
#166397 = CARTESIAN_POINT('Origin',(7.8,2.9,-27.07)) ;
#166398 = CARTESIAN_POINT('Origin',(7.8,2.9,-27.07)) ;
#166399 = CARTESIAN_POINT('Origin',(9.6,2.9,-26.27)) ;
#166400 = CARTESIAN_POINT('Origin',(9.6,2.9,-26.27)) ;
#166401 = CARTESIAN_POINT('Origin',(9.6,2.9,-27.07)) ;
#166402 = CARTESIAN_POINT('Origin',(9.6,2.9,-27.07)) ;
#166403 = CARTESIAN_POINT('Origin',(9.6,2.9,-26.27)) ;
#166404 = CARTESIAN_POINT('Origin',(9.6,2.9,-26.27)) ;
#166405 = CARTESIAN_POINT('Origin',(9.6,2.9,-27.07)) ;
#166406 = CARTESIAN_POINT('Origin',(9.6,2.9,-27.07)) ;
#166407 = CARTESIAN_POINT('Origin',(9.6,2.9,-27.07)) ;
#166408 = CARTESIAN_POINT('Origin',(-0.183301359729408,3.45,-25.152963213524)) ;
#166409 = CARTESIAN_POINT('Origin',(0.24923464143508,3.15,-26.5537799780213)) ;
#166410 = CARTESIAN_POINT('Origin',(-0.249234641435079,3.15,-26.7862200219787)) ;
#166411 = CARTESIAN_POINT('Origin',(-1.04429375741423,3.45,-25.5544505621777)) ;
#166412 = CARTESIAN_POINT('Origin',(10.1,-2.15,-29.5768804065906)) ;
#166413 = CARTESIAN_POINT('Origin',(10.1,-2.15,-29.5768804065906)) ;
#166414 = CARTESIAN_POINT('Origin',(10.1,-2.15,-29.5768804065906)) ;
#166415 = CARTESIAN_POINT('Origin',(10.1,-2.15,-29.5768804065906)) ;
#166416 = CARTESIAN_POINT('Origin',(10.1,-2.15,-30.48)) ;
#166417 = CARTESIAN_POINT('Origin',(10.1,-2.15,-29.175)) ;
#166418 = CARTESIAN_POINT('Origin',(10.2,-2.15,-29.5768804065906)) ;
#166419 = CARTESIAN_POINT('Origin',(3.7,-2.15,-29.5768804065906)) ;
#166420 = CARTESIAN_POINT('Origin',(10.1,-3.65625,-30.48)) ;
#166421 = CARTESIAN_POINT('Origin',(10.1,-2.15,-31.3831195934094)) ;
#166422 = CARTESIAN_POINT('Origin',(10.1,-3.65625,-29.175)) ;
#166423 = CARTESIAN_POINT('Origin',(10.1,1.9,-29.175)) ;
#166424 = CARTESIAN_POINT('Origin',(10.1,-2.15,-29.175)) ;
#166425 = CARTESIAN_POINT('Origin',(10.1,-2.15,-29.175)) ;
#166426 = CARTESIAN_POINT('Origin',(10.1,-2.15,-29.175)) ;
#166427 = CARTESIAN_POINT('Origin',(3.7,-2.15,-29.5768804065906)) ;
#166428 = CARTESIAN_POINT('Origin',(3.7,-2.32153024911032,-29.6797267659824)) ;
#166429 = CARTESIAN_POINT('Origin',(3.7,-2.35,-29.5768804065906)) ;
#166430 = CARTESIAN_POINT('Origin',(10.1,-2.15,-31.3831195934094)) ;
#166431 = CARTESIAN_POINT('Origin',(10.1,-2.15,-31.3831195934094)) ;
#166432 = CARTESIAN_POINT('Origin',(10.1,-2.15,-31.3831195934094)) ;
#166433 = CARTESIAN_POINT('Origin',(10.1,1.9,-30.48)) ;
#166434 = CARTESIAN_POINT('Origin',(10.1,1.9,-31.785)) ;
#166435 = CARTESIAN_POINT('Origin',(10.1,1.9,-29.175)) ;
#166436 = CARTESIAN_POINT('Origin',(10.2,-2.15,-29.175)) ;
#166437 = CARTESIAN_POINT('Origin',(3.7,-2.15,-29.175)) ;
#166438 = CARTESIAN_POINT('Origin',(3.7,-2.35,-29.075)) ;
#166439 = CARTESIAN_POINT('Origin',(3.7,-2.35,-29.175)) ;
#166440 = CARTESIAN_POINT('Origin',(3.7,-3.65625,-30.48)) ;
#166441 = CARTESIAN_POINT('Origin',(3.7,-2.32153024911032,-31.2802732340176)) ;
#166442 = CARTESIAN_POINT('Origin',(10.2,-2.15,-31.3831195934094)) ;
#166443 = CARTESIAN_POINT('Origin',(3.7,-2.15,-31.3831195934094)) ;
#166444 = CARTESIAN_POINT('Origin',(10.1,-2.15,-30.48)) ;
#166445 = CARTESIAN_POINT('Origin',(10.1,-2.15,-31.785)) ;
#166446 = CARTESIAN_POINT('Origin',(10.1,-3.65625,-31.785)) ;
#166447 = CARTESIAN_POINT('Origin',(10.1,1.9,-31.785)) ;
#166448 = CARTESIAN_POINT('Origin',(10.1,-2.15,-31.785)) ;
#166449 = CARTESIAN_POINT('Origin',(3.7,-2.35,-29.175)) ;
#166450 = CARTESIAN_POINT('Origin',(3.5,-2.35,-29.175)) ;
#166451 = CARTESIAN_POINT('Origin',(3.7,-2.15,-31.3831195934094)) ;
#166452 = CARTESIAN_POINT('Origin',(3.7,-2.35,-31.3831195934094)) ;
#166453 = CARTESIAN_POINT('Origin',(10.1,-2.15,-31.785)) ;
#166454 = CARTESIAN_POINT('Origin',(10.1,-2.15,-31.785)) ;
#166455 = CARTESIAN_POINT('Origin',(3.6,1.9,-28.975)) ;
#166456 = CARTESIAN_POINT('Origin',(3.5,1.9,-28.975)) ;
#166457 = CARTESIAN_POINT('Origin',(2.7,1.9,-28.975)) ;
#166458 = CARTESIAN_POINT('Origin',(3.5,2.69592814944142E-15,-29.175)) ;
#166459 = CARTESIAN_POINT('Origin',(3.5,-5.15,-29.175)) ;
#166460 = CARTESIAN_POINT('Origin',(3.7,-2.35,-31.355)) ;
#166461 = CARTESIAN_POINT('Origin',(3.7,-2.35,-31.785)) ;
#166462 = CARTESIAN_POINT('Origin',(3.6,-2.15,-31.785)) ;
#166463 = CARTESIAN_POINT('Origin',(3.7,-2.15,-31.785)) ;
#166464 = CARTESIAN_POINT('Origin',(2.7,1.9,-28.975)) ;
#166465 = CARTESIAN_POINT('Origin',(2.7,1.9,-28.975)) ;
#166466 = CARTESIAN_POINT('Origin',(3.5,-5.15,-29.175)) ;
#166467 = CARTESIAN_POINT('Origin',(3.5,-5.15,-29.175)) ;
#166468 = CARTESIAN_POINT('Origin',(3.5,-5.15,-29.175)) ;
#166469 = CARTESIAN_POINT('Origin',(3.7,-2.35,-31.785)) ;
#166470 = CARTESIAN_POINT('Origin',(3.5,-2.35,-31.785)) ;
#166471 = CARTESIAN_POINT('Origin',(2.7,2.,-28.975)) ;
#166472 = CARTESIAN_POINT('Origin',(2.7,-5.15,-28.975)) ;
#166473 = CARTESIAN_POINT('Origin',(3.6,-5.15,-29.175)) ;
#166474 = CARTESIAN_POINT('Origin',(2.7,-5.15,-29.175)) ;
#166475 = CARTESIAN_POINT('Origin',(3.5,-5.15,0.)) ;
#166476 = CARTESIAN_POINT('Origin',(3.5,-5.15,-31.785)) ;
#166477 = CARTESIAN_POINT('Origin',(3.5,-2.77383442446614E-15,-31.785)) ;
#166478 = CARTESIAN_POINT('Origin',(3.5,-5.15,-31.785)) ;
#166479 = CARTESIAN_POINT('Origin',(2.7,-5.15,-29.175)) ;
#166480 = CARTESIAN_POINT('Origin',(2.7,-5.35,-29.175)) ;
#166481 = CARTESIAN_POINT('Origin',(3.5,-5.15,-31.785)) ;
#166482 = CARTESIAN_POINT('Origin',(3.5,-5.15,-31.785)) ;
#166483 = CARTESIAN_POINT('Origin',(2.7,-5.35,-29.075)) ;
#166484 = CARTESIAN_POINT('Origin',(2.7,-5.35,-31.785)) ;
#166485 = CARTESIAN_POINT('Origin',(3.6,-5.15,-31.785)) ;
#166486 = CARTESIAN_POINT('Origin',(2.7,-5.15,-31.785)) ;
#166487 = CARTESIAN_POINT('Origin',(3.6,1.9,-31.985)) ;
#166488 = CARTESIAN_POINT('Origin',(3.5,1.9,-31.985)) ;
#166489 = CARTESIAN_POINT('Origin',(2.7,1.9,-31.985)) ;
#166490 = CARTESIAN_POINT('Origin',(2.7,1.9,-31.885)) ;
#166491 = CARTESIAN_POINT('Origin',(2.7,1.9,-32.785)) ;
#166492 = CARTESIAN_POINT('Origin',(2.7,1.9,-31.985)) ;
#166493 = CARTESIAN_POINT('Origin',(2.7,-5.15,-31.785)) ;
#166494 = CARTESIAN_POINT('Origin',(2.7,-5.15,-31.985)) ;
#166495 = CARTESIAN_POINT('Origin',(2.7,1.9,-31.985)) ;
#166496 = CARTESIAN_POINT('Origin',(2.7,1.9,-31.985)) ;
#166497 = CARTESIAN_POINT('Origin',(2.7,-5.25,-31.985)) ;
#166498 = CARTESIAN_POINT('Ctrl Pts',(-3.8,-6.55,-29.38)) ;
#166499 = CARTESIAN_POINT('Ctrl Pts',(-3.8,-6.55,-29.38)) ;
#166500 = CARTESIAN_POINT('Ctrl Pts',(-3.8,-6.55,-29.38)) ;
#166501 = CARTESIAN_POINT('Ctrl Pts',(-3.82625343282633,-6.55,-29.4325068656528)) ;
#166502 = CARTESIAN_POINT('Ctrl Pts',(-3.83954133268475,-6.55,-29.419541332684)) ;
#166503 = CARTESIAN_POINT('Ctrl Pts',(-3.8525068656527,-6.55,-29.4062534328264)) ;
#166504 = CARTESIAN_POINT('Ctrl Pts',(-3.85219871729854,-6.53922263893877,
-29.4843974345971)) ;
#166505 = CARTESIAN_POINT('Ctrl Pts',(-3.87914655110986,-6.52362528614073,
-29.4591465511098)) ;
#166506 = CARTESIAN_POINT('Ctrl Pts',(-3.90439743459708,-6.53922263893874,
-29.4321987172986)) ;
#166507 = CARTESIAN_POINT('Ctrl Pts',(-3.87996665852871,-6.5114546977086,
-29.5399333170574)) ;
#166508 = CARTESIAN_POINT('Ctrl Pts',(-3.90288380314158,-6.48208554016475,
-29.4828838031416)) ;
#166509 = CARTESIAN_POINT('Ctrl Pts',(-3.95993331705742,-6.51145469770861,
-29.4599666585287)) ;
#166510 = CARTESIAN_POINT('Ctrl Pts',(-3.88737865704135,-6.5003618540841,
-29.5547573140827)) ;
#166511 = CARTESIAN_POINT('Ctrl Pts',(-3.90501307588293,-6.46792722356046,
-29.4850130758829)) ;
#166512 = CARTESIAN_POINT('Ctrl Pts',(-3.9747573140827,-6.5003618540841,-29.4673786570414)) ;
#166513 = CARTESIAN_POINT('Ctrl Pts',(-3.8973972494609,-6.47617483238892,
-29.5747944989218)) ;
#166514 = CARTESIAN_POINT('Ctrl Pts',(-3.9032967435641,-6.45094059868421,
-29.4832967435641)) ;
#166515 = CARTESIAN_POINT('Ctrl Pts',(-3.99479449892181,-6.47617483238891,
-29.4773972494609)) ;
#166516 = CARTESIAN_POINT('Ctrl Pts',(-3.9,-6.46309229646327,-29.5799999991818)) ;
#166517 = CARTESIAN_POINT('Ctrl Pts',(-3.90000730388479,-6.44945650149135,
-29.4800073039037)) ;
#166518 = CARTESIAN_POINT('Ctrl Pts',(-3.99999999918173,-6.46309229646329,
-29.48)) ;
#166519 = CARTESIAN_POINT('Ctrl Pts',(-3.9,-6.45,-29.58)) ;
#166520 = CARTESIAN_POINT('Ctrl Pts',(-3.9,-6.45,-29.48)) ;
#166521 = CARTESIAN_POINT('Ctrl Pts',(-4.,-6.45,-29.48)) ;
#166522 = CARTESIAN_POINT('Origin',(-4.,-6.45,-29.58)) ;
#166523 = CARTESIAN_POINT('Origin',(-4.,-6.4,-29.58)) ;
#166524 = CARTESIAN_POINT('Origin',(-4.,-6.35,-29.58)) ;
#166525 = CARTESIAN_POINT('Ctrl Pts',(-5.,-6.55,-29.38)) ;
#166526 = CARTESIAN_POINT('Ctrl Pts',(-5.,-6.55,-29.38)) ;
#166527 = CARTESIAN_POINT('Ctrl Pts',(-5.,-6.55,-29.38)) ;
#166528 = CARTESIAN_POINT('Ctrl Pts',(-4.94749313434733,-6.55,-29.4062534328264)) ;
#166529 = CARTESIAN_POINT('Ctrl Pts',(-4.96045866731527,-6.55,-29.4195413326841)) ;
#166530 = CARTESIAN_POINT('Ctrl Pts',(-4.97374656717361,-6.55,-29.4325068656527)) ;
#166531 = CARTESIAN_POINT('Ctrl Pts',(-4.89560256540291,-6.53922263893874,
-29.4321987172986)) ;
#166532 = CARTESIAN_POINT('Ctrl Pts',(-4.92085344889015,-6.52362528614075,
-29.4591465511098)) ;
#166533 = CARTESIAN_POINT('Ctrl Pts',(-4.94780128270146,-6.53922263893877,
-29.4843974345971)) ;
#166534 = CARTESIAN_POINT('Ctrl Pts',(-4.84006668294258,-6.51145469770861,
-29.4599666585287)) ;
#166535 = CARTESIAN_POINT('Ctrl Pts',(-4.89711619685841,-6.48208554016473,
-29.4828838031416)) ;
#166536 = CARTESIAN_POINT('Ctrl Pts',(-4.92003334147129,-6.5114546977086,
-29.5399333170574)) ;
#166537 = CARTESIAN_POINT('Ctrl Pts',(-4.82524268591729,-6.5003618540841,
-29.4673786570414)) ;
#166538 = CARTESIAN_POINT('Ctrl Pts',(-4.89498692411706,-6.46792722356047,
-29.4850130758829)) ;
#166539 = CARTESIAN_POINT('Ctrl Pts',(-4.91262134295865,-6.5003618540841,
-29.5547573140827)) ;
#166540 = CARTESIAN_POINT('Ctrl Pts',(-4.80520550107819,-6.47617483238891,
-29.4773972494609)) ;
#166541 = CARTESIAN_POINT('Ctrl Pts',(-4.8967032564359,-6.4509405986842,-29.4832967435642)) ;
#166542 = CARTESIAN_POINT('Ctrl Pts',(-4.90260275053909,-6.47617483238892,
-29.5747944989218)) ;
#166543 = CARTESIAN_POINT('Ctrl Pts',(-4.80000000081823,-6.46309229646328,
-29.48)) ;
#166544 = CARTESIAN_POINT('Ctrl Pts',(-4.89999269609626,-6.44945650149925,
-29.4800073039037)) ;
#166545 = CARTESIAN_POINT('Ctrl Pts',(-4.9,-6.46309229646329,-29.5799999991818)) ;
#166546 = CARTESIAN_POINT('Ctrl Pts',(-4.8,-6.45,-29.48)) ;
#166547 = CARTESIAN_POINT('Ctrl Pts',(-4.9,-6.45,-29.48)) ;
#166548 = CARTESIAN_POINT('Ctrl Pts',(-4.9,-6.45,-29.58)) ;
#166549 = CARTESIAN_POINT('Origin',(-4.8,-6.45,-29.58)) ;
#166550 = CARTESIAN_POINT('Origin',(-4.,-6.35,-29.58)) ;
#166551 = CARTESIAN_POINT('Origin',(-4.,-6.35,-29.58)) ;
#166552 = CARTESIAN_POINT('Origin',(-4.,-6.35,-29.58)) ;
#166553 = CARTESIAN_POINT('Ctrl Pts',(-3.8,-6.55,-31.58)) ;
#166554 = CARTESIAN_POINT('Ctrl Pts',(-3.8,-6.55,-31.58)) ;
#166555 = CARTESIAN_POINT('Ctrl Pts',(-3.8,-6.55,-31.58)) ;
#166556 = CARTESIAN_POINT('Ctrl Pts',(-3.85250686565254,-6.55,-31.5537465671732)) ;
#166557 = CARTESIAN_POINT('Ctrl Pts',(-3.83954133268437,-6.55,-31.5404586673145)) ;
#166558 = CARTESIAN_POINT('Ctrl Pts',(-3.82625343282625,-6.55,-31.5274931343472)) ;
#166559 = CARTESIAN_POINT('Ctrl Pts',(-3.90439743459706,-6.53922263893883,
-31.5278012827015)) ;
#166560 = CARTESIAN_POINT('Ctrl Pts',(-3.87914655110982,-6.52362528614068,
-31.5008534488903)) ;
#166561 = CARTESIAN_POINT('Ctrl Pts',(-3.85219871729855,-6.53922263893876,
-31.475602565403)) ;
#166562 = CARTESIAN_POINT('Ctrl Pts',(-3.95993331705743,-6.51145469770856,
-31.5000333414713)) ;
#166563 = CARTESIAN_POINT('Ctrl Pts',(-3.9028838031416,-6.48208554016478,
-31.4771161968583)) ;
#166564 = CARTESIAN_POINT('Ctrl Pts',(-3.8799666585287,-6.5114546977086,-31.4200666829425)) ;
#166565 = CARTESIAN_POINT('Ctrl Pts',(-3.97475731408271,-6.5003618540841,
-31.4926213429587)) ;
#166566 = CARTESIAN_POINT('Ctrl Pts',(-3.90501307588293,-6.46792722356049,
-31.4749869241171)) ;
#166567 = CARTESIAN_POINT('Ctrl Pts',(-3.88737865704135,-6.5003618540841,
-31.4052426859173)) ;
#166568 = CARTESIAN_POINT('Ctrl Pts',(-3.9947944989218,-6.47617483238892,
-31.4826027505391)) ;
#166569 = CARTESIAN_POINT('Ctrl Pts',(-3.9032967435641,-6.45094059868419,
-31.4767032564359)) ;
#166570 = CARTESIAN_POINT('Ctrl Pts',(-3.89739724946091,-6.47617483238892,
-31.3852055010782)) ;
#166571 = CARTESIAN_POINT('Ctrl Pts',(-3.99999999918176,-6.46309229646328,
-31.48)) ;
#166572 = CARTESIAN_POINT('Ctrl Pts',(-3.90000730395432,-6.44945650161364,
-31.4799926958712)) ;
#166573 = CARTESIAN_POINT('Ctrl Pts',(-3.9,-6.46309229646328,-31.3800000008181)) ;
#166574 = CARTESIAN_POINT('Ctrl Pts',(-4.,-6.45,-31.48)) ;
#166575 = CARTESIAN_POINT('Ctrl Pts',(-3.9,-6.45,-31.48)) ;
#166576 = CARTESIAN_POINT('Ctrl Pts',(-3.9,-6.45,-31.38)) ;
#166577 = CARTESIAN_POINT('Origin',(-4.,-6.45,-31.38)) ;
#166578 = CARTESIAN_POINT('Origin',(-4.8,-6.4,-29.58)) ;
#166579 = CARTESIAN_POINT('Origin',(-4.8,-6.35,-29.58)) ;
#166580 = CARTESIAN_POINT('Origin',(1.9515639104739E-16,-6.35,-29.58)) ;
#166581 = CARTESIAN_POINT('Origin',(-4.8,-6.35,-29.58)) ;
#166582 = CARTESIAN_POINT('Origin',(-4.,-6.35,-30.48)) ;
#166583 = CARTESIAN_POINT('Origin',(-4.,-6.35,-31.38)) ;
#166584 = CARTESIAN_POINT('Origin',(-4.,-6.4,-31.38)) ;
#166585 = CARTESIAN_POINT('Origin',(-4.,-6.35,-31.38)) ;
#166586 = CARTESIAN_POINT('Origin',(-4.8,-6.35,-29.58)) ;
#166587 = CARTESIAN_POINT('Origin',(-4.8,-6.35,-29.58)) ;
#166588 = CARTESIAN_POINT('Origin',(-4.,-6.35,-31.38)) ;
#166589 = CARTESIAN_POINT('Origin',(-4.,-6.35,-31.38)) ;
#166590 = CARTESIAN_POINT('Origin',(-4.8,-6.35,-30.48)) ;
#166591 = CARTESIAN_POINT('Origin',(-4.8,-6.35,-31.38)) ;
#166592 = CARTESIAN_POINT('Origin',(1.9515639104739E-16,-6.35,-31.38)) ;
#166593 = CARTESIAN_POINT('Origin',(-4.8,-6.35,-31.38)) ;
#166594 = CARTESIAN_POINT('Origin',(-4.8,-6.35,-31.38)) ;
#166595 = CARTESIAN_POINT('Origin',(-4.8,-6.35,-31.38)) ;
#166596 = CARTESIAN_POINT('Origin',(-4.8,-6.4,-31.38)) ;
#166597 = CARTESIAN_POINT('Origin',(-4.8,-6.45,-31.38)) ;
#166598 = CARTESIAN_POINT('Ctrl Pts',(-5.,-6.55,-31.58)) ;
#166599 = CARTESIAN_POINT('Ctrl Pts',(-5.,-6.55,-31.58)) ;
#166600 = CARTESIAN_POINT('Ctrl Pts',(-5.,-6.55,-31.58)) ;
#166601 = CARTESIAN_POINT('Ctrl Pts',(-4.97374656717363,-6.55,-31.5274931343472)) ;
#166602 = CARTESIAN_POINT('Ctrl Pts',(-4.96045866731563,-6.55,-31.5404586673165)) ;
#166603 = CARTESIAN_POINT('Ctrl Pts',(-4.94749313434715,-6.55,-31.5537465671739)) ;
#166604 = CARTESIAN_POINT('Ctrl Pts',(-4.94780128270146,-6.53922263893877,
-31.475602565403)) ;
#166605 = CARTESIAN_POINT('Ctrl Pts',(-4.92085344889015,-6.52362528614069,
-31.5008534488903)) ;
#166606 = CARTESIAN_POINT('Ctrl Pts',(-4.89560256540291,-6.53922263893883,
-31.5278012827015)) ;
#166607 = CARTESIAN_POINT('Ctrl Pts',(-4.92003334147129,-6.5114546977086,
-31.4200666829425)) ;
#166608 = CARTESIAN_POINT('Ctrl Pts',(-4.89711619685841,-6.48208554016478,
-31.4771161968583)) ;
#166609 = CARTESIAN_POINT('Ctrl Pts',(-4.84006668294258,-6.51145469770856,
-31.5000333414713)) ;
#166610 = CARTESIAN_POINT('Ctrl Pts',(-4.91262134295865,-6.5003618540841,
-31.4052426859173)) ;
#166611 = CARTESIAN_POINT('Ctrl Pts',(-4.89498692411706,-6.46792722356049,
-31.4749869241171)) ;
#166612 = CARTESIAN_POINT('Ctrl Pts',(-4.82524268591729,-6.5003618540841,
-31.4926213429587)) ;
#166613 = CARTESIAN_POINT('Ctrl Pts',(-4.90260275053909,-6.47617483238892,
-31.3852055010782)) ;
#166614 = CARTESIAN_POINT('Ctrl Pts',(-4.8967032564359,-6.45094059868419,
-31.4767032564359)) ;
#166615 = CARTESIAN_POINT('Ctrl Pts',(-4.80520550107819,-6.47617483238892,
-31.4826027505391)) ;
#166616 = CARTESIAN_POINT('Ctrl Pts',(-4.9,-6.46309229646328,-31.3800000008181)) ;
#166617 = CARTESIAN_POINT('Ctrl Pts',(-4.89999269604099,-6.44945650161557,
-31.4799926958712)) ;
#166618 = CARTESIAN_POINT('Ctrl Pts',(-4.80000000081823,-6.46309229646328,
-31.48)) ;
#166619 = CARTESIAN_POINT('Ctrl Pts',(-4.9,-6.45,-31.38)) ;
#166620 = CARTESIAN_POINT('Ctrl Pts',(-4.9,-6.45,-31.48)) ;
#166621 = CARTESIAN_POINT('Ctrl Pts',(-4.8,-6.45,-31.48)) ;
#166622 = CARTESIAN_POINT('Ctrl Pts',(-5.82426676739353,-5.43399303700601,
-28.8770109659688)) ;
#166623 = CARTESIAN_POINT('Ctrl Pts',(-5.80266988778306,-5.52572360682955,
-28.8823540173505)) ;
#166624 = CARTESIAN_POINT('Ctrl Pts',(-5.82426676352022,-5.53106667371343,
-28.974084587183)) ;
#166625 = CARTESIAN_POINT('Ctrl Pts',(-5.83498671931121,-5.43935351191898,
-28.8743294581962)) ;
#166626 = CARTESIAN_POINT('Ctrl Pts',(-5.80595263122257,-5.52411753147731,
-28.8839600935403)) ;
#166627 = CARTESIAN_POINT('Ctrl Pts',(-5.83498671397634,-5.53374818067472,
-28.9687241131465)) ;
#166628 = CARTESIAN_POINT('Ctrl Pts',(-5.84526105845717,-5.44830326289483,
-28.8698528401961)) ;
#166629 = CARTESIAN_POINT('Ctrl Pts',(-5.81370932746127,-5.52260132030868,
-28.885476305999)) ;
#166630 = CARTESIAN_POINT('Ctrl Pts',(-5.8452610524373,-5.53822479746343,
-28.95977436357)) ;
#166631 = CARTESIAN_POINT('Ctrl Pts',(-5.86378685403704,-5.47240020430394,
-28.8578032513087)) ;
#166632 = CARTESIAN_POINT('Ctrl Pts',(-5.83531854275276,-5.5273306740449,
-28.8807469551146)) ;
#166633 = CARTESIAN_POINT('Ctrl Pts',(-5.8637868481647,-5.55027438459906,
-28.9356774250057)) ;
#166634 = CARTESIAN_POINT('Ctrl Pts',(-5.8720385263158,-5.48754495134729,
-28.8502315528944)) ;
#166635 = CARTESIAN_POINT('Ctrl Pts',(-5.84834787930678,-5.53310199490458,
-28.8749756357761)) ;
#166636 = CARTESIAN_POINT('Ctrl Pts',(-5.87203852123047,-5.55784608243464,
-28.9205326795141)) ;
#166637 = CARTESIAN_POINT('Ctrl Pts',(-5.89242747304802,-5.53981202333451,
-28.8241056511375)) ;
#166638 = CARTESIAN_POINT('Ctrl Pts',(-5.88223383300416,-5.56084219179273,
-28.8472354431742)) ;
#166639 = CARTESIAN_POINT('Ctrl Pts',(-5.89242747063505,-5.58397198402782,
-28.8682656123278)) ;
#166640 = CARTESIAN_POINT('Ctrl Pts',(-5.9,-5.58381083947297,-28.802119400143)) ;
#166641 = CARTESIAN_POINT('Ctrl Pts',(-5.9,-5.59485304502685,-28.813224592887)) ;
#166642 = CARTESIAN_POINT('Ctrl Pts',(-5.9,-5.60595823775506,-28.8242667984406)) ;
#166643 = CARTESIAN_POINT('Ctrl Pts',(-5.9,-5.62807764064044,-28.78)) ;
#166644 = CARTESIAN_POINT('Ctrl Pts',(-5.9,-5.62807764064044,-28.78)) ;
#166645 = CARTESIAN_POINT('Ctrl Pts',(-5.9,-5.62807764064044,-28.78)) ;
#166646 = CARTESIAN_POINT('Origin',(-5.84850712500726,-5.43404914061138,-28.9740285000291)) ;
#166647 = CARTESIAN_POINT('Ctrl Pts',(-5.82425356250363,-5.53106339062591,
-28.9740285000291)) ;
#166648 = CARTESIAN_POINT('Ctrl Pts',(-5.80269484027818,-5.52567371006954,
-28.8824039305709)) ;
#166649 = CARTESIAN_POINT('Ctrl Pts',(-5.82425356250363,-5.43404914061138,
-28.8770142500145)) ;
#166650 = CARTESIAN_POINT('Ctrl Pts',(-5.80840777707096,-5.52710194426774,
-28.9779899459043)) ;
#166651 = CARTESIAN_POINT('Ctrl Pts',(-5.79341417645228,-5.52335354411315,
-28.8828358498184)) ;
#166652 = CARTESIAN_POINT('Ctrl Pts',(-5.81633079157288,-5.43008775511759,
-28.8789949427472)) ;
#166653 = CARTESIAN_POINT('Ctrl Pts',(-5.79207992677989,-5.52301998169497,
-28.979999999534)) ;
#166654 = CARTESIAN_POINT('Ctrl Pts',(-5.78430903206646,-5.52107725801653,
-28.8819613954329)) ;
#166655 = CARTESIAN_POINT('Ctrl Pts',(-5.80816665318299,-5.42600568595106,
-28.88)) ;
#166656 = CARTESIAN_POINT('Ctrl Pts',(-5.77574643749636,-5.51893660937409,
-28.98)) ;
#166657 = CARTESIAN_POINT('Ctrl Pts',(-5.77574643749636,-5.5189366093741,
-28.88)) ;
#166658 = CARTESIAN_POINT('Ctrl Pts',(-5.8,-5.42192235935956,-28.88)) ;
#166659 = CARTESIAN_POINT('Origin',(-5.8,-5.42192235935956,-28.98)) ;
#166660 = CARTESIAN_POINT('Origin',(-5.8066065036801,-5.42357398527959,-28.98)) ;
#166661 = CARTESIAN_POINT('Origin',(-5.17275707706437,-5.26511162862565,-28.98)) ;
#166662 = CARTESIAN_POINT('Origin',(-5.15068655017073,-5.25959399690224,-28.9905938529089)) ;
#166663 = CARTESIAN_POINT('Origin',(-5.17275707706436,-5.26511162862565,-28.98)) ;
#166664 = CARTESIAN_POINT('Origin',(-5.17275707706436,-5.26511162862565,-28.98)) ;
#166665 = CARTESIAN_POINT('Origin',(-5.17275707706436,-5.26511162862565,-28.98)) ;
#166666 = CARTESIAN_POINT('Origin',(-5.17275707706436,-5.05,-28.98)) ;
#166667 = CARTESIAN_POINT('Origin',(-5.17275707706436,-1.91866427917294,-28.98)) ;
#166668 = CARTESIAN_POINT('Origin',(-3.78014014831103,-3.31128120792626,-29.6484561258016)) ;
#166669 = CARTESIAN_POINT('Origin',(-5.17275707706436,-1.91866427917294,-28.98)) ;
#166670 = CARTESIAN_POINT('Origin',(-5.17275707706436,-1.91866427917293,-28.98)) ;
#166671 = CARTESIAN_POINT('Origin',(-5.17275707706436,-1.91866427917294,-28.98)) ;
#166672 = CARTESIAN_POINT('Origin',(-3.97071067811865,-3.12071067811865,-28.98)) ;
#166673 = CARTESIAN_POINT('Origin',(-5.8,-1.2914213562373,-28.98)) ;
#166674 = CARTESIAN_POINT('Ctrl Pts',(-5.87071067811865,-1.14999999999999,
-28.8507106781187)) ;
#166675 = CARTESIAN_POINT('Ctrl Pts',(-5.8471404520791,-1.10285954792089,
-28.8742809041582)) ;
#166676 = CARTESIAN_POINT('Ctrl Pts',(-5.87071067811865,-1.07928932188134,
-28.9214213562373)) ;
#166677 = CARTESIAN_POINT('Ctrl Pts',(-5.85217562795658,-1.18707010095451,
-28.8692457282807)) ;
#166678 = CARTESIAN_POINT('Ctrl Pts',(-5.81261165662082,-1.1373883433793,
-28.8958614719498)) ;
#166679 = CARTESIAN_POINT('Ctrl Pts',(-5.8335394967105,-1.11646050328949,
-28.9585925363811)) ;
#166680 = CARTESIAN_POINT('Ctrl Pts',(-5.82627077431945,-1.23887980759835,
-28.88)) ;
#166681 = CARTESIAN_POINT('Ctrl Pts',(-5.76566787907959,-1.18433212092071,
-28.8971489437127)) ;
#166682 = CARTESIAN_POINT('Ctrl Pts',(-5.78190678732228,-1.16809321267771,
-28.9799999994186)) ;
#166683 = CARTESIAN_POINT('Ctrl Pts',(-5.8,-1.2914213562373,-28.88)) ;
#166684 = CARTESIAN_POINT('Ctrl Pts',(-5.72928932188134,-1.22071067811865,
-28.88)) ;
#166685 = CARTESIAN_POINT('Ctrl Pts',(-5.72928932188134,-1.22071067811865,
-28.98)) ;
#166686 = CARTESIAN_POINT('Origin',(-5.94142135623731,-1.15,-28.9214213562373)) ;
#166687 = CARTESIAN_POINT('Ctrl Pts',(-5.9,-1.00857864376269,-28.78)) ;
#166688 = CARTESIAN_POINT('Ctrl Pts',(-5.9,-1.00857864376269,-28.78)) ;
#166689 = CARTESIAN_POINT('Ctrl Pts',(-5.9,-1.00857864376269,-28.78)) ;
#166690 = CARTESIAN_POINT('Ctrl Pts',(-5.9,-1.06112019240163,-28.8062707743195)) ;
#166691 = CARTESIAN_POINT('Ctrl Pts',(-5.9,-1.04860238144513,-28.8200237376833)) ;
#166692 = CARTESIAN_POINT('Ctrl Pts',(-5.9,-1.03484941808214,-28.832541548639)) ;
#166693 = CARTESIAN_POINT('Ctrl Pts',(-5.8892457282807,-1.11292989904544,
-28.8321756279566)) ;
#166694 = CARTESIAN_POINT('Ctrl Pts',(-5.8745170062612,-1.08721613123966,
-28.8586374874774)) ;
#166695 = CARTESIAN_POINT('Ctrl Pts',(-5.88924572828062,-1.06075427171937,
-28.8843512552826)) ;
#166696 = CARTESIAN_POINT('Ctrl Pts',(-5.87071067811865,-1.14999999999999,
-28.8507106781187)) ;
#166697 = CARTESIAN_POINT('Ctrl Pts',(-5.8471404520791,-1.10285954792089,
-28.8742809041582)) ;
#166698 = CARTESIAN_POINT('Ctrl Pts',(-5.87071067811865,-1.07928932188134,
-28.9214213562373)) ;
#166699 = CARTESIAN_POINT('Ctrl Pts',(-5.87071067811866,-1.14999999999999,
-32.1092893218813)) ;
#166700 = CARTESIAN_POINT('Ctrl Pts',(-5.8471404520791,-1.10285954792089,
-32.0857190958418)) ;
#166701 = CARTESIAN_POINT('Ctrl Pts',(-5.87071067811866,-1.07928932188134,
-32.0385786437627)) ;
#166702 = CARTESIAN_POINT('Ctrl Pts',(-5.88924572828049,-1.11292989904507,
-32.1278243720432)) ;
#166703 = CARTESIAN_POINT('Ctrl Pts',(-5.87451700624374,-1.08721613124994,
-32.1013625125115)) ;
#166704 = CARTESIAN_POINT('Ctrl Pts',(-5.88924572828073,-1.06075427171926,
-32.0756487447172)) ;
#166705 = CARTESIAN_POINT('Ctrl Pts',(-5.9,-1.06112019240149,-32.1537292256798)) ;
#166706 = CARTESIAN_POINT('Ctrl Pts',(-5.9,-1.04860238143642,-32.1399762623248)) ;
#166707 = CARTESIAN_POINT('Ctrl Pts',(-5.9,-1.03484941808206,-32.127458451361)) ;
#166708 = CARTESIAN_POINT('Ctrl Pts',(-5.9,-1.00857864376269,-32.18)) ;
#166709 = CARTESIAN_POINT('Ctrl Pts',(-5.9,-1.00857864376269,-32.18)) ;
#166710 = CARTESIAN_POINT('Ctrl Pts',(-5.9,-1.00857864376269,-32.18)) ;
#166711 = CARTESIAN_POINT('Origin',(-5.94142135623734,-1.14999999999996,-32.0385786437627)) ;
#166712 = CARTESIAN_POINT('Ctrl Pts',(-5.8,-1.2914213562373,-32.08)) ;
#166713 = CARTESIAN_POINT('Ctrl Pts',(-5.72928932188134,-1.22071067811865,
-32.08)) ;
#166714 = CARTESIAN_POINT('Ctrl Pts',(-5.72928932188134,-1.22071067811865,
-31.98)) ;
#166715 = CARTESIAN_POINT('Ctrl Pts',(-5.82627077431952,-1.2388798075982,
-32.08)) ;
#166716 = CARTESIAN_POINT('Ctrl Pts',(-5.76566787907932,-1.18433212092069,
-32.0628510562865)) ;
#166717 = CARTESIAN_POINT('Ctrl Pts',(-5.7819067873223,-1.16809321267769,
-31.9800000005809)) ;
#166718 = CARTESIAN_POINT('Ctrl Pts',(-5.8521756279568,-1.18707010095488,
-32.0907542717195)) ;
#166719 = CARTESIAN_POINT('Ctrl Pts',(-5.81261165662085,-1.13738834337918,
-32.0641385280509)) ;
#166720 = CARTESIAN_POINT('Ctrl Pts',(-5.83353949671049,-1.11646050328951,
-32.0014074636193)) ;
#166721 = CARTESIAN_POINT('Ctrl Pts',(-5.87071067811865,-1.14999999999999,
-32.1092893218813)) ;
#166722 = CARTESIAN_POINT('Ctrl Pts',(-5.8471404520791,-1.10285954792089,
-32.0857190958418)) ;
#166723 = CARTESIAN_POINT('Ctrl Pts',(-5.87071067811866,-1.07928932188134,
-32.0385786437627)) ;
#166724 = CARTESIAN_POINT('Origin',(-5.8,-1.29142135623731,-31.98)) ;
#166725 = CARTESIAN_POINT('Origin',(-3.59571067811865,-3.49571067811865,-31.98)) ;
#166726 = CARTESIAN_POINT('Origin',(-5.17275707706436,-1.91866427917294,-31.98)) ;
#166727 = CARTESIAN_POINT('Origin',(-3.09057773798104,-4.00084361825625,-30.98055391724)) ;
#166728 = CARTESIAN_POINT('Origin',(-5.17275707706435,-1.91866427917295,-31.98)) ;
#166729 = CARTESIAN_POINT('Origin',(-5.17275707706435,-1.91866427917295,-31.98)) ;
#166730 = CARTESIAN_POINT('Origin',(-5.17275707706435,-1.91866427917295,-31.98)) ;
#166731 = CARTESIAN_POINT('Origin',(-5.17275707706435,-5.05,-31.98)) ;
#166732 = CARTESIAN_POINT('Origin',(-5.17275707706435,-5.26511162862565,-31.98)) ;
#166733 = CARTESIAN_POINT('Origin',(-3.96111272388873,-4.96220054033175,-31.3984107104757)) ;
#166734 = CARTESIAN_POINT('Origin',(-5.17275707706435,-5.26511162862565,-31.98)) ;
#166735 = CARTESIAN_POINT('Origin',(-5.17275707706435,-5.26511162862565,-31.98)) ;
#166736 = CARTESIAN_POINT('Origin',(-5.17275707706435,-5.26511162862565,-31.98)) ;
#166737 = CARTESIAN_POINT('Origin',(-5.10072415073893,-5.24710339704429,-31.98)) ;
#166738 = CARTESIAN_POINT('Origin',(-5.8,-5.42192235935956,-31.98)) ;
#166739 = CARTESIAN_POINT('Ctrl Pts',(-5.77574643749636,-5.51893660937409,
-31.98)) ;
#166740 = CARTESIAN_POINT('Ctrl Pts',(-5.77574643749636,-5.51893660937409,
-32.08)) ;
#166741 = CARTESIAN_POINT('Ctrl Pts',(-5.8,-5.42192235935956,-32.08)) ;
#166742 = CARTESIAN_POINT('Ctrl Pts',(-5.79207992677987,-5.52301998169497,
-31.980000000466)) ;
#166743 = CARTESIAN_POINT('Ctrl Pts',(-5.78430903206628,-5.52107725801656,
-32.078038604567)) ;
#166744 = CARTESIAN_POINT('Ctrl Pts',(-5.80816665318301,-5.42600568595105,
-32.08)) ;
#166745 = CARTESIAN_POINT('Ctrl Pts',(-5.80840777707098,-5.52710194426775,
-31.9820100540956)) ;
#166746 = CARTESIAN_POINT('Ctrl Pts',(-5.79341417645243,-5.52335354411312,
-32.0771641501814)) ;
#166747 = CARTESIAN_POINT('Ctrl Pts',(-5.81633079157286,-5.43008775511761,
-32.0810050572528)) ;
#166748 = CARTESIAN_POINT('Ctrl Pts',(-5.82425356250363,-5.53106339062591,
-31.9859714999709)) ;
#166749 = CARTESIAN_POINT('Ctrl Pts',(-5.80269484027818,-5.52567371006955,
-32.0775960694291)) ;
#166750 = CARTESIAN_POINT('Ctrl Pts',(-5.82425356250363,-5.43404914061138,
-32.0829857499855)) ;
#166751 = CARTESIAN_POINT('Origin',(-5.84850712500726,-5.43404914061138,-31.9859714999709)) ;
#166752 = CARTESIAN_POINT('Ctrl Pts',(-5.82426676739357,-5.5310666746717,
-31.9859153963653)) ;
#166753 = CARTESIAN_POINT('Ctrl Pts',(-5.80266988778296,-5.52572362329017,
-32.0776459661893)) ;
#166754 = CARTESIAN_POINT('Ctrl Pts',(-5.82426676352028,-5.43399305345725,
-32.0829890330731)) ;
#166755 = CARTESIAN_POINT('Ctrl Pts',(-5.83498671931132,-5.53374818244432,
-31.9912758712783)) ;
#166756 = CARTESIAN_POINT('Ctrl Pts',(-5.80595263122238,-5.5241175471004,
-32.0760398908369)) ;
#166757 = CARTESIAN_POINT('Ctrl Pts',(-5.83498671397641,-5.4393535274937,
-32.0856705400343)) ;
#166758 = CARTESIAN_POINT('Ctrl Pts',(-5.84526105845724,-5.53822480044432,
-32.0002256222542)) ;
#166759 = CARTESIAN_POINT('Ctrl Pts',(-5.81370932746113,-5.52260133464156,
-32.0745236796683)) ;
#166760 = CARTESIAN_POINT('Ctrl Pts',(-5.84526105243737,-5.44830327707024,
-32.0901471568231)) ;
#166761 = CARTESIAN_POINT('Ctrl Pts',(-5.86378685403709,-5.55027438933185,
-32.0243225636634)) ;
#166762 = CARTESIAN_POINT('Ctrl Pts',(-5.83531854275266,-5.52733068552581,
-32.0792530334047)) ;
#166763 = CARTESIAN_POINT('Ctrl Pts',(-5.86378684816477,-5.47240021563463,
-32.1021967439587)) ;
#166764 = CARTESIAN_POINT('Ctrl Pts',(-5.87203852631586,-5.55784608774616,
-32.0394673107066)) ;
#166765 = CARTESIAN_POINT('Ctrl Pts',(-5.84834787930667,-5.53310200486441,
-32.085024354264)) ;
#166766 = CARTESIAN_POINT('Ctrl Pts',(-5.8720385212305,-5.48754496112624,
-32.1097684417943)) ;
#166767 = CARTESIAN_POINT('Ctrl Pts',(-5.89242747304801,-5.58397198950293,
-32.0917343826941)) ;
#166768 = CARTESIAN_POINT('Ctrl Pts',(-5.88223383300416,-5.56084219746613,
-32.1127645511526)) ;
#166769 = CARTESIAN_POINT('Ctrl Pts',(-5.89242747063516,-5.53981202831248,
-32.1358943433876)) ;
#166770 = CARTESIAN_POINT('Ctrl Pts',(-5.9,-5.60595824049754,-32.1357331988324)) ;
#166771 = CARTESIAN_POINT('Ctrl Pts',(-5.9,-5.59485304775361,-32.1467754043864)) ;
#166772 = CARTESIAN_POINT('Ctrl Pts',(-5.9,-5.58381084219965,-32.1578805971149)) ;
#166773 = CARTESIAN_POINT('Ctrl Pts',(-5.9,-5.62807764064044,-32.18)) ;
#166774 = CARTESIAN_POINT('Ctrl Pts',(-5.9,-5.62807764064044,-32.18)) ;
#166775 = CARTESIAN_POINT('Ctrl Pts',(-5.9,-5.62807764064044,-32.18)) ;
#166776 = CARTESIAN_POINT('Origin',(7.8,2.1,-30.88)) ;
#166777 = CARTESIAN_POINT('Origin',(7.8,2.1,-31.08)) ;
#166778 = CARTESIAN_POINT('Origin',(7.6,2.1,-30.88)) ;
#166779 = CARTESIAN_POINT('Origin',(7.6,2.1,-30.88)) ;
#166780 = CARTESIAN_POINT('Origin',(7.6,2.1,-30.08)) ;
#166781 = CARTESIAN_POINT('Origin',(7.8,2.1,-31.08)) ;
#166782 = CARTESIAN_POINT('Origin',(9.6,2.1,-31.08)) ;
#166783 = CARTESIAN_POINT('Origin',(7.8,2.1,-30.08)) ;
#166784 = CARTESIAN_POINT('Origin',(7.8,2.1,-29.88)) ;
#166785 = CARTESIAN_POINT('Origin',(9.6,2.1,-30.88)) ;
#166786 = CARTESIAN_POINT('Origin',(9.8,2.1,-30.88)) ;
#166787 = CARTESIAN_POINT('Origin',(7.8,2.1,-29.88)) ;
#166788 = CARTESIAN_POINT('Origin',(9.6,2.1,-29.88)) ;
#166789 = CARTESIAN_POINT('Origin',(9.8,2.1,-30.88)) ;
#166790 = CARTESIAN_POINT('Origin',(9.8,2.1,-30.08)) ;
#166791 = CARTESIAN_POINT('Origin',(9.6,2.1,-30.08)) ;
#166792 = CARTESIAN_POINT('Origin',(-4.15,-6.25,-29.73)) ;
#166793 = CARTESIAN_POINT('Origin',(-4.15,-6.3,-29.73)) ;
#166794 = CARTESIAN_POINT('Origin',(-4.15,-6.3,-30.48)) ;
#166795 = CARTESIAN_POINT('Origin',(-4.15,-6.3,-31.23)) ;
#166796 = CARTESIAN_POINT('Origin',(-4.15,-6.3,-29.73)) ;
#166797 = CARTESIAN_POINT('Origin',(-4.15,-6.25,-31.23)) ;
#166798 = CARTESIAN_POINT('Origin',(-4.15,-6.3,-31.23)) ;
#166799 = CARTESIAN_POINT('Origin',(-4.15,-6.3,-29.73)) ;
#166800 = CARTESIAN_POINT('Origin',(-4.15,-6.3,-29.73)) ;
#166801 = CARTESIAN_POINT('Origin',(-4.15,-6.3,-31.23)) ;
#166802 = CARTESIAN_POINT('Origin',(-4.15,-6.3,-31.23)) ;
#166803 = CARTESIAN_POINT('Origin',(-4.65,-6.25,-29.73)) ;
#166804 = CARTESIAN_POINT('Origin',(-4.65,-6.3,-29.73)) ;
#166805 = CARTESIAN_POINT('Origin',(0.,-6.3,-29.73)) ;
#166806 = CARTESIAN_POINT('Origin',(-4.65,-6.3,-29.73)) ;
#166807 = CARTESIAN_POINT('Origin',(0.,-6.3,-31.23)) ;
#166808 = CARTESIAN_POINT('Origin',(-4.65,-6.3,-31.23)) ;
#166809 = CARTESIAN_POINT('Origin',(-4.65,-6.25,-31.23)) ;
#166810 = CARTESIAN_POINT('Origin',(-4.65,-6.3,-31.23)) ;
#166811 = CARTESIAN_POINT('Origin',(-4.65,-6.3,-29.73)) ;
#166812 = CARTESIAN_POINT('Origin',(-4.65,-6.3,-29.73)) ;
#166813 = CARTESIAN_POINT('Origin',(-4.65,-6.3,-31.23)) ;
#166814 = CARTESIAN_POINT('Origin',(-4.65,-6.3,-31.23)) ;
#166815 = CARTESIAN_POINT('Origin',(-4.65,-6.3,-30.48)) ;
#166816 = CARTESIAN_POINT('Origin',(-3.,4.45,-31.58)) ;
#166817 = CARTESIAN_POINT('Origin',(-2.1,4.45,-31.58)) ;
#166818 = CARTESIAN_POINT('Origin',(-2.9,4.45,-31.58)) ;
#166819 = CARTESIAN_POINT('Origin',(-2.9,4.45,-31.38)) ;
#166820 = CARTESIAN_POINT('Origin',(-3.1,4.45,-31.38)) ;
#166821 = CARTESIAN_POINT('Origin',(-2.9,4.45,-31.38)) ;
#166822 = CARTESIAN_POINT('Origin',(-2.1,4.45,-31.38)) ;
#166823 = CARTESIAN_POINT('Origin',(-2.1,4.45,-31.38)) ;
#166824 = CARTESIAN_POINT('Origin',(-1.9,4.45,-31.38)) ;
#166825 = CARTESIAN_POINT('Origin',(-3.1,4.45,-31.48)) ;
#166826 = CARTESIAN_POINT('Origin',(-3.1,4.45,-29.58)) ;
#166827 = CARTESIAN_POINT('Origin',(-2.9,4.4,-31.38)) ;
#166828 = CARTESIAN_POINT('Origin',(-2.9,4.35,-31.38)) ;
#166829 = CARTESIAN_POINT('Origin',(-1.95156391047391E-16,4.35,-31.38)) ;
#166830 = CARTESIAN_POINT('Origin',(-2.1,4.35,-31.38)) ;
#166831 = CARTESIAN_POINT('Origin',(-2.9,4.35,-31.38)) ;
#166832 = CARTESIAN_POINT('Origin',(-2.1,4.4,-31.38)) ;
#166833 = CARTESIAN_POINT('Origin',(-2.1,4.35,-31.38)) ;
#166834 = CARTESIAN_POINT('Origin',(-1.9,4.45,-31.48)) ;
#166835 = CARTESIAN_POINT('Origin',(-1.9,4.45,-29.58)) ;
#166836 = CARTESIAN_POINT('Origin',(-3.,4.45,-29.38)) ;
#166837 = CARTESIAN_POINT('Origin',(-2.9,4.45,-29.38)) ;
#166838 = CARTESIAN_POINT('Origin',(-2.1,4.45,-29.38)) ;
#166839 = CARTESIAN_POINT('Origin',(-2.9,4.45,-29.58)) ;
#166840 = CARTESIAN_POINT('Origin',(-2.9,4.45,-29.58)) ;
#166841 = CARTESIAN_POINT('Origin',(-2.9,4.35,-31.38)) ;
#166842 = CARTESIAN_POINT('Origin',(-2.9,4.35,-31.38)) ;
#166843 = CARTESIAN_POINT('Origin',(-2.1,4.35,-31.38)) ;
#166844 = CARTESIAN_POINT('Origin',(-2.1,4.35,-31.38)) ;
#166845 = CARTESIAN_POINT('Origin',(-2.1,4.45,-29.58)) ;
#166846 = CARTESIAN_POINT('Origin',(-2.1,4.45,-29.58)) ;
#166847 = CARTESIAN_POINT('Origin',(-2.9,4.4,-29.58)) ;
#166848 = CARTESIAN_POINT('Origin',(-2.9,4.35,-29.58)) ;
#166849 = CARTESIAN_POINT('Origin',(-2.9,4.35,-30.48)) ;
#166850 = CARTESIAN_POINT('Origin',(-2.9,4.35,-29.58)) ;
#166851 = CARTESIAN_POINT('Origin',(-2.1,4.35,-30.48)) ;
#166852 = CARTESIAN_POINT('Origin',(-2.1,4.35,-29.58)) ;
#166853 = CARTESIAN_POINT('Origin',(-2.1,4.4,-29.58)) ;
#166854 = CARTESIAN_POINT('Origin',(-2.1,4.35,-29.58)) ;
#166855 = CARTESIAN_POINT('Origin',(-2.9,4.35,-29.58)) ;
#166856 = CARTESIAN_POINT('Origin',(-2.9,4.35,-29.58)) ;
#166857 = CARTESIAN_POINT('Origin',(-2.1,4.35,-29.58)) ;
#166858 = CARTESIAN_POINT('Origin',(-2.1,4.35,-29.58)) ;
#166859 = CARTESIAN_POINT('Origin',(-1.95156391047391E-16,4.35,-29.58)) ;
#166860 = CARTESIAN_POINT('Origin',(-2.25,4.25,-31.23)) ;
#166861 = CARTESIAN_POINT('Origin',(-2.25,4.3,-31.23)) ;
#166862 = CARTESIAN_POINT('Origin',(-2.25,4.3,-30.48)) ;
#166863 = CARTESIAN_POINT('Origin',(-2.25,4.3,-29.73)) ;
#166864 = CARTESIAN_POINT('Origin',(-2.25,4.3,-31.23)) ;
#166865 = CARTESIAN_POINT('Origin',(-2.25,4.25,-29.73)) ;
#166866 = CARTESIAN_POINT('Origin',(-2.25,4.3,-29.73)) ;
#166867 = CARTESIAN_POINT('Origin',(-2.25,4.3,-31.23)) ;
#166868 = CARTESIAN_POINT('Origin',(-2.25,4.3,-31.23)) ;
#166869 = CARTESIAN_POINT('Origin',(-2.25,4.3,-29.73)) ;
#166870 = CARTESIAN_POINT('Origin',(-2.25,4.3,-29.73)) ;
#166871 = CARTESIAN_POINT('Origin',(-2.75,4.25,-31.23)) ;
#166872 = CARTESIAN_POINT('Origin',(-2.75,4.3,-31.23)) ;
#166873 = CARTESIAN_POINT('Origin',(-1.97127667724637E-17,4.3,-31.23)) ;
#166874 = CARTESIAN_POINT('Origin',(-2.75,4.3,-31.23)) ;
#166875 = CARTESIAN_POINT('Origin',(-1.97127667724637E-17,4.3,-29.73)) ;
#166876 = CARTESIAN_POINT('Origin',(-2.75,4.3,-29.73)) ;
#166877 = CARTESIAN_POINT('Origin',(-2.75,4.25,-29.73)) ;
#166878 = CARTESIAN_POINT('Origin',(-2.75,4.3,-29.73)) ;
#166879 = CARTESIAN_POINT('Origin',(-2.75,4.3,-31.23)) ;
#166880 = CARTESIAN_POINT('Origin',(-2.75,4.3,-31.23)) ;
#166881 = CARTESIAN_POINT('Origin',(-2.75,4.3,-29.73)) ;
#166882 = CARTESIAN_POINT('Origin',(-2.75,4.3,-29.73)) ;
#166883 = CARTESIAN_POINT('Origin',(-2.75,4.3,-30.48)) ;
#166884 = CARTESIAN_POINT('Origin',(7.8,2.9,-30.88)) ;
#166885 = CARTESIAN_POINT('Origin',(7.8,2.9,-30.88)) ;
#166886 = CARTESIAN_POINT('Origin',(7.8,2.9,-30.08)) ;
#166887 = CARTESIAN_POINT('Origin',(7.8,2.9,-30.08)) ;
#166888 = CARTESIAN_POINT('Origin',(7.8,2.9,-30.08)) ;
#166889 = CARTESIAN_POINT('Origin',(7.8,2.9,-30.88)) ;
#166890 = CARTESIAN_POINT('Origin',(7.8,2.9,-30.88)) ;
#166891 = CARTESIAN_POINT('Origin',(9.6,2.9,-30.08)) ;
#166892 = CARTESIAN_POINT('Origin',(9.6,2.9,-30.08)) ;
#166893 = CARTESIAN_POINT('Origin',(9.6,2.9,-30.88)) ;
#166894 = CARTESIAN_POINT('Origin',(9.6,2.9,-30.88)) ;
#166895 = CARTESIAN_POINT('Origin',(9.6,2.9,-30.08)) ;
#166896 = CARTESIAN_POINT('Origin',(9.6,2.9,-30.08)) ;
#166897 = CARTESIAN_POINT('Origin',(9.6,2.9,-30.88)) ;
#166898 = CARTESIAN_POINT('Origin',(9.6,2.9,-30.88)) ;
#166899 = CARTESIAN_POINT('Origin',(9.6,2.9,-30.88)) ;
#166900 = CARTESIAN_POINT('Origin',(-0.183301359729408,3.45,-28.962963213524)) ;
#166901 = CARTESIAN_POINT('Origin',(0.24923464143508,3.15,-30.3637799780213)) ;
#166902 = CARTESIAN_POINT('Origin',(-0.249234641435079,3.15,-30.5962200219787)) ;
#166903 = CARTESIAN_POINT('Origin',(-1.04429375741423,3.45,-29.3644505621777)) ;
#166904 = CARTESIAN_POINT('Origin',(10.1,-2.15,-33.3868804065906)) ;
#166905 = CARTESIAN_POINT('Origin',(10.1,-2.15,-33.3868804065906)) ;
#166906 = CARTESIAN_POINT('Origin',(10.1,-2.15,-33.3868804065906)) ;
#166907 = CARTESIAN_POINT('Origin',(10.1,-2.15,-33.3868804065906)) ;
#166908 = CARTESIAN_POINT('Origin',(10.1,-2.15,-34.29)) ;
#166909 = CARTESIAN_POINT('Origin',(10.1,-2.15,-32.985)) ;
#166910 = CARTESIAN_POINT('Origin',(10.2,-2.15,-33.3868804065906)) ;
#166911 = CARTESIAN_POINT('Origin',(3.7,-2.15,-33.3868804065906)) ;
#166912 = CARTESIAN_POINT('Origin',(10.1,-3.65625,-34.29)) ;
#166913 = CARTESIAN_POINT('Origin',(10.1,-2.15,-35.1931195934094)) ;
#166914 = CARTESIAN_POINT('Origin',(10.1,-3.65625,-32.985)) ;
#166915 = CARTESIAN_POINT('Origin',(10.1,1.9,-32.985)) ;
#166916 = CARTESIAN_POINT('Origin',(10.1,-2.15,-32.985)) ;
#166917 = CARTESIAN_POINT('Origin',(10.1,-2.15,-32.985)) ;
#166918 = CARTESIAN_POINT('Origin',(10.1,-2.15,-32.985)) ;
#166919 = CARTESIAN_POINT('Origin',(3.7,-2.15,-33.3868804065906)) ;
#166920 = CARTESIAN_POINT('Origin',(3.7,-2.32153024911032,-33.4897267659824)) ;
#166921 = CARTESIAN_POINT('Origin',(3.7,-2.35,-33.3868804065906)) ;
#166922 = CARTESIAN_POINT('Origin',(10.1,-2.15,-35.1931195934094)) ;
#166923 = CARTESIAN_POINT('Origin',(10.1,-2.15,-35.1931195934094)) ;
#166924 = CARTESIAN_POINT('Origin',(10.1,-2.15,-35.1931195934094)) ;
#166925 = CARTESIAN_POINT('Origin',(10.1,1.9,-34.29)) ;
#166926 = CARTESIAN_POINT('Origin',(10.1,1.9,-35.595)) ;
#166927 = CARTESIAN_POINT('Origin',(10.1,1.9,-32.985)) ;
#166928 = CARTESIAN_POINT('Origin',(10.2,-2.15,-32.985)) ;
#166929 = CARTESIAN_POINT('Origin',(3.7,-2.15,-32.985)) ;
#166930 = CARTESIAN_POINT('Origin',(3.7,-2.35,-32.885)) ;
#166931 = CARTESIAN_POINT('Origin',(3.7,-2.35,-32.985)) ;
#166932 = CARTESIAN_POINT('Origin',(3.7,-3.65625,-34.29)) ;
#166933 = CARTESIAN_POINT('Origin',(3.7,-2.32153024911032,-35.0902732340176)) ;
#166934 = CARTESIAN_POINT('Origin',(10.2,-2.15,-35.1931195934094)) ;
#166935 = CARTESIAN_POINT('Origin',(3.7,-2.15,-35.1931195934094)) ;
#166936 = CARTESIAN_POINT('Origin',(10.1,-2.15,-34.29)) ;
#166937 = CARTESIAN_POINT('Origin',(10.1,-2.15,-35.595)) ;
#166938 = CARTESIAN_POINT('Origin',(10.1,-3.65625,-35.595)) ;
#166939 = CARTESIAN_POINT('Origin',(10.1,1.9,-35.595)) ;
#166940 = CARTESIAN_POINT('Origin',(10.1,-2.15,-35.595)) ;
#166941 = CARTESIAN_POINT('Origin',(3.7,-2.35,-32.985)) ;
#166942 = CARTESIAN_POINT('Origin',(3.5,-2.35,-32.985)) ;
#166943 = CARTESIAN_POINT('Origin',(3.7,-2.15,-35.1931195934094)) ;
#166944 = CARTESIAN_POINT('Origin',(3.7,-2.35,-35.1931195934094)) ;
#166945 = CARTESIAN_POINT('Origin',(10.1,-2.15,-35.595)) ;
#166946 = CARTESIAN_POINT('Origin',(10.1,-2.15,-35.595)) ;
#166947 = CARTESIAN_POINT('Origin',(3.6,1.9,-32.785)) ;
#166948 = CARTESIAN_POINT('Origin',(3.5,1.9,-32.785)) ;
#166949 = CARTESIAN_POINT('Origin',(2.7,1.9,-32.785)) ;
#166950 = CARTESIAN_POINT('Origin',(3.5,3.03778831031064E-15,-32.985)) ;
#166951 = CARTESIAN_POINT('Origin',(3.5,-5.15,-32.985)) ;
#166952 = CARTESIAN_POINT('Origin',(3.7,-2.35,-35.165)) ;
#166953 = CARTESIAN_POINT('Origin',(3.7,-2.35,-35.595)) ;
#166954 = CARTESIAN_POINT('Origin',(3.6,-2.15,-35.595)) ;
#166955 = CARTESIAN_POINT('Origin',(3.7,-2.15,-35.595)) ;
#166956 = CARTESIAN_POINT('Origin',(2.7,1.9,-32.785)) ;
#166957 = CARTESIAN_POINT('Origin',(2.7,1.9,-32.785)) ;
#166958 = CARTESIAN_POINT('Origin',(3.5,-5.15,-32.985)) ;
#166959 = CARTESIAN_POINT('Origin',(3.5,-5.15,-32.985)) ;
#166960 = CARTESIAN_POINT('Origin',(3.5,-5.15,-32.985)) ;
#166961 = CARTESIAN_POINT('Origin',(3.7,-2.35,-35.595)) ;
#166962 = CARTESIAN_POINT('Origin',(3.5,-2.35,-35.595)) ;
#166963 = CARTESIAN_POINT('Origin',(2.7,2.,-32.785)) ;
#166964 = CARTESIAN_POINT('Origin',(2.7,-5.15,-32.785)) ;
#166965 = CARTESIAN_POINT('Origin',(3.6,-5.15,-32.985)) ;
#166966 = CARTESIAN_POINT('Origin',(2.7,-5.15,-32.985)) ;
#166967 = CARTESIAN_POINT('Origin',(3.5,-5.15,0.)) ;
#166968 = CARTESIAN_POINT('Origin',(3.5,-5.15,-35.595)) ;
#166969 = CARTESIAN_POINT('Origin',(3.5,-3.11569458533536E-15,-35.595)) ;
#166970 = CARTESIAN_POINT('Origin',(3.5,-5.15,-35.595)) ;
#166971 = CARTESIAN_POINT('Origin',(2.7,-5.15,-32.985)) ;
#166972 = CARTESIAN_POINT('Origin',(2.7,-5.35,-32.985)) ;
#166973 = CARTESIAN_POINT('Origin',(3.5,-5.15,-35.595)) ;
#166974 = CARTESIAN_POINT('Origin',(3.5,-5.15,-35.595)) ;
#166975 = CARTESIAN_POINT('Origin',(2.7,-5.35,-32.885)) ;
#166976 = CARTESIAN_POINT('Origin',(2.7,-5.35,-35.595)) ;
#166977 = CARTESIAN_POINT('Origin',(3.6,-5.15,-35.595)) ;
#166978 = CARTESIAN_POINT('Origin',(2.7,-5.15,-35.595)) ;
#166979 = CARTESIAN_POINT('Origin',(3.6,1.9,-35.795)) ;
#166980 = CARTESIAN_POINT('Origin',(3.5,1.9,-35.795)) ;
#166981 = CARTESIAN_POINT('Origin',(2.7,1.9,-35.795)) ;
#166982 = CARTESIAN_POINT('Origin',(2.7,1.9,-35.695)) ;
#166983 = CARTESIAN_POINT('Origin',(2.7,1.9,-36.49)) ;
#166984 = CARTESIAN_POINT('Origin',(2.7,1.9,-35.795)) ;
#166985 = CARTESIAN_POINT('Origin',(2.7,-5.15,-35.595)) ;
#166986 = CARTESIAN_POINT('Origin',(2.7,-5.15,-35.795)) ;
#166987 = CARTESIAN_POINT('Origin',(2.7,1.9,-35.795)) ;
#166988 = CARTESIAN_POINT('Origin',(2.7,1.9,-35.795)) ;
#166989 = CARTESIAN_POINT('Origin',(2.7,-5.25,-35.795)) ;
#166990 = CARTESIAN_POINT('Ctrl Pts',(-3.8,-6.55,-33.19)) ;
#166991 = CARTESIAN_POINT('Ctrl Pts',(-3.8,-6.55,-33.19)) ;
#166992 = CARTESIAN_POINT('Ctrl Pts',(-3.8,-6.55,-33.19)) ;
#166993 = CARTESIAN_POINT('Ctrl Pts',(-3.8262534328263,-6.55,-33.2425068656528)) ;
#166994 = CARTESIAN_POINT('Ctrl Pts',(-3.83954133268437,-6.55,-33.2295413326857)) ;
#166995 = CARTESIAN_POINT('Ctrl Pts',(-3.85250686565253,-6.55,-33.2162534328268)) ;
#166996 = CARTESIAN_POINT('Ctrl Pts',(-3.85219871729854,-6.53922263893877,
-33.294397434597)) ;
#166997 = CARTESIAN_POINT('Ctrl Pts',(-3.87914655110985,-6.52362528614074,
-33.2691465511097)) ;
#166998 = CARTESIAN_POINT('Ctrl Pts',(-3.90439743459708,-6.53922263893883,
-33.2421987172985)) ;
#166999 = CARTESIAN_POINT('Ctrl Pts',(-3.87996665852871,-6.5114546977086,
-33.3499333170575)) ;
#167000 = CARTESIAN_POINT('Ctrl Pts',(-3.90288380314158,-6.48208554016475,
-33.2928838031417)) ;
#167001 = CARTESIAN_POINT('Ctrl Pts',(-3.95993331705742,-6.51145469770856,
-33.2699666585287)) ;
#167002 = CARTESIAN_POINT('Ctrl Pts',(-3.88737865704135,-6.5003618540841,
-33.3647573140827)) ;
#167003 = CARTESIAN_POINT('Ctrl Pts',(-3.90501307588292,-6.46792722356047,
-33.295013075883)) ;
#167004 = CARTESIAN_POINT('Ctrl Pts',(-3.9747573140827,-6.5003618540841,-33.2773786570414)) ;
#167005 = CARTESIAN_POINT('Ctrl Pts',(-3.8973972494609,-6.47617483238892,
-33.3847944989218)) ;
#167006 = CARTESIAN_POINT('Ctrl Pts',(-3.90329674356411,-6.4509405986842,
-33.2932967435641)) ;
#167007 = CARTESIAN_POINT('Ctrl Pts',(-3.99479449892181,-6.47617483238892,
-33.2873972494609)) ;
#167008 = CARTESIAN_POINT('Ctrl Pts',(-3.9,-6.46309229646328,-33.3899999991819)) ;
#167009 = CARTESIAN_POINT('Ctrl Pts',(-3.90000730394006,-6.44945650160767,
-33.2900073041287)) ;
#167010 = CARTESIAN_POINT('Ctrl Pts',(-3.99999999918173,-6.46309229646328,
-33.29)) ;
#167011 = CARTESIAN_POINT('Ctrl Pts',(-3.9,-6.45,-33.39)) ;
#167012 = CARTESIAN_POINT('Ctrl Pts',(-3.9,-6.45,-33.29)) ;
#167013 = CARTESIAN_POINT('Ctrl Pts',(-4.,-6.45,-33.29)) ;
#167014 = CARTESIAN_POINT('Origin',(-4.,-6.45,-33.39)) ;
#167015 = CARTESIAN_POINT('Origin',(-4.,-6.4,-33.39)) ;
#167016 = CARTESIAN_POINT('Origin',(-4.,-6.35,-33.39)) ;
#167017 = CARTESIAN_POINT('Ctrl Pts',(-5.,-6.55,-33.19)) ;
#167018 = CARTESIAN_POINT('Ctrl Pts',(-5.,-6.55,-33.19)) ;
#167019 = CARTESIAN_POINT('Ctrl Pts',(-5.,-6.55,-33.19)) ;
#167020 = CARTESIAN_POINT('Ctrl Pts',(-4.94749313434715,-6.55,-33.2162534328261)) ;
#167021 = CARTESIAN_POINT('Ctrl Pts',(-4.96045866731563,-6.55,-33.2295413326835)) ;
#167022 = CARTESIAN_POINT('Ctrl Pts',(-4.97374656717363,-6.55,-33.2425068656528)) ;
#167023 = CARTESIAN_POINT('Ctrl Pts',(-4.89560256540291,-6.53922263893883,
-33.2421987172985)) ;
#167024 = CARTESIAN_POINT('Ctrl Pts',(-4.92085344889015,-6.52362528614069,
-33.2691465511097)) ;
#167025 = CARTESIAN_POINT('Ctrl Pts',(-4.94780128270146,-6.53922263893877,
-33.294397434597)) ;
#167026 = CARTESIAN_POINT('Ctrl Pts',(-4.84006668294258,-6.51145469770856,
-33.2699666585287)) ;
#167027 = CARTESIAN_POINT('Ctrl Pts',(-4.89711619685841,-6.48208554016478,
-33.2928838031417)) ;
#167028 = CARTESIAN_POINT('Ctrl Pts',(-4.92003334147129,-6.5114546977086,
-33.3499333170575)) ;
#167029 = CARTESIAN_POINT('Ctrl Pts',(-4.82524268591729,-6.5003618540841,
-33.2773786570414)) ;
#167030 = CARTESIAN_POINT('Ctrl Pts',(-4.89498692411706,-6.46792722356049,
-33.2950130758829)) ;
#167031 = CARTESIAN_POINT('Ctrl Pts',(-4.91262134295865,-6.5003618540841,
-33.3647573140827)) ;
#167032 = CARTESIAN_POINT('Ctrl Pts',(-4.80520550107819,-6.47617483238892,
-33.2873972494609)) ;
#167033 = CARTESIAN_POINT('Ctrl Pts',(-4.8967032564359,-6.45094059868419,
-33.2932967435641)) ;
#167034 = CARTESIAN_POINT('Ctrl Pts',(-4.90260275053909,-6.47617483238892,
-33.3847944989218)) ;
#167035 = CARTESIAN_POINT('Ctrl Pts',(-4.80000000081823,-6.46309229646328,
-33.29)) ;
#167036 = CARTESIAN_POINT('Ctrl Pts',(-4.89999269604099,-6.44945650161557,
-33.2900073041287)) ;
#167037 = CARTESIAN_POINT('Ctrl Pts',(-4.9,-6.46309229646328,-33.3899999991819)) ;
#167038 = CARTESIAN_POINT('Ctrl Pts',(-4.8,-6.45,-33.29)) ;
#167039 = CARTESIAN_POINT('Ctrl Pts',(-4.9,-6.45,-33.29)) ;
#167040 = CARTESIAN_POINT('Ctrl Pts',(-4.9,-6.45,-33.39)) ;
#167041 = CARTESIAN_POINT('Origin',(-4.8,-6.45,-33.39)) ;
#167042 = CARTESIAN_POINT('Origin',(-4.,-6.35,-33.39)) ;
#167043 = CARTESIAN_POINT('Origin',(-4.,-6.35,-33.39)) ;
#167044 = CARTESIAN_POINT('Origin',(-4.,-6.35,-33.39)) ;
#167045 = CARTESIAN_POINT('Ctrl Pts',(-3.8,-6.55,-35.39)) ;
#167046 = CARTESIAN_POINT('Ctrl Pts',(-3.8,-6.55,-35.39)) ;
#167047 = CARTESIAN_POINT('Ctrl Pts',(-3.8,-6.55,-35.39)) ;
#167048 = CARTESIAN_POINT('Ctrl Pts',(-3.85250686565255,-6.55,-35.3637465671732)) ;
#167049 = CARTESIAN_POINT('Ctrl Pts',(-3.83954133268437,-6.55,-35.3504586673145)) ;
#167050 = CARTESIAN_POINT('Ctrl Pts',(-3.82625343282626,-6.55,-35.3374931343472)) ;
#167051 = CARTESIAN_POINT('Ctrl Pts',(-3.90439743459706,-6.53922263893883,
-35.3378012827015)) ;
#167052 = CARTESIAN_POINT('Ctrl Pts',(-3.87914655110982,-6.52362528614068,
-35.3108534488903)) ;
#167053 = CARTESIAN_POINT('Ctrl Pts',(-3.85219871729855,-6.53922263893876,
-35.285602565403)) ;
#167054 = CARTESIAN_POINT('Ctrl Pts',(-3.95993331705743,-6.51145469770856,
-35.3100333414713)) ;
#167055 = CARTESIAN_POINT('Ctrl Pts',(-3.9028838031416,-6.48208554016478,
-35.2871161968583)) ;
#167056 = CARTESIAN_POINT('Ctrl Pts',(-3.8799666585287,-6.5114546977086,-35.2300666829425)) ;
#167057 = CARTESIAN_POINT('Ctrl Pts',(-3.97475731408271,-6.5003618540841,
-35.3026213429587)) ;
#167058 = CARTESIAN_POINT('Ctrl Pts',(-3.90501307588293,-6.46792722356049,
-35.284986924117)) ;
#167059 = CARTESIAN_POINT('Ctrl Pts',(-3.88737865704135,-6.5003618540841,
-35.2152426859173)) ;
#167060 = CARTESIAN_POINT('Ctrl Pts',(-3.9947944989218,-6.47617483238892,
-35.2926027505391)) ;
#167061 = CARTESIAN_POINT('Ctrl Pts',(-3.9032967435641,-6.45094059868419,
-35.2867032564359)) ;
#167062 = CARTESIAN_POINT('Ctrl Pts',(-3.89739724946091,-6.47617483238892,
-35.1952055010782)) ;
#167063 = CARTESIAN_POINT('Ctrl Pts',(-3.99999999918176,-6.46309229646328,
-35.29)) ;
#167064 = CARTESIAN_POINT('Ctrl Pts',(-3.90000730395432,-6.44945650161364,
-35.2899926958712)) ;
#167065 = CARTESIAN_POINT('Ctrl Pts',(-3.9,-6.46309229646328,-35.1900000008181)) ;
#167066 = CARTESIAN_POINT('Ctrl Pts',(-4.,-6.45,-35.29)) ;
#167067 = CARTESIAN_POINT('Ctrl Pts',(-3.9,-6.45,-35.29)) ;
#167068 = CARTESIAN_POINT('Ctrl Pts',(-3.9,-6.45,-35.19)) ;
#167069 = CARTESIAN_POINT('Origin',(-4.,-6.45,-35.19)) ;
#167070 = CARTESIAN_POINT('Origin',(-4.8,-6.4,-33.39)) ;
#167071 = CARTESIAN_POINT('Origin',(-4.8,-6.35,-33.39)) ;
#167072 = CARTESIAN_POINT('Origin',(1.9515639104739E-16,-6.35,-33.39)) ;
#167073 = CARTESIAN_POINT('Origin',(-4.8,-6.35,-33.39)) ;
#167074 = CARTESIAN_POINT('Origin',(-4.,-6.35,-34.29)) ;
#167075 = CARTESIAN_POINT('Origin',(-4.,-6.35,-35.19)) ;
#167076 = CARTESIAN_POINT('Origin',(-4.,-6.4,-35.19)) ;
#167077 = CARTESIAN_POINT('Origin',(-4.,-6.35,-35.19)) ;
#167078 = CARTESIAN_POINT('Origin',(-4.8,-6.35,-33.39)) ;
#167079 = CARTESIAN_POINT('Origin',(-4.8,-6.35,-33.39)) ;
#167080 = CARTESIAN_POINT('Origin',(-4.,-6.35,-35.19)) ;
#167081 = CARTESIAN_POINT('Origin',(-4.,-6.35,-35.19)) ;
#167082 = CARTESIAN_POINT('Origin',(-4.8,-6.35,-34.29)) ;
#167083 = CARTESIAN_POINT('Origin',(-4.8,-6.35,-35.19)) ;
#167084 = CARTESIAN_POINT('Origin',(1.9515639104739E-16,-6.35,-35.19)) ;
#167085 = CARTESIAN_POINT('Origin',(-4.8,-6.35,-35.19)) ;
#167086 = CARTESIAN_POINT('Origin',(-4.8,-6.35,-35.19)) ;
#167087 = CARTESIAN_POINT('Origin',(-4.8,-6.35,-35.19)) ;
#167088 = CARTESIAN_POINT('Origin',(-4.8,-6.4,-35.19)) ;
#167089 = CARTESIAN_POINT('Origin',(-4.8,-6.45,-35.19)) ;
#167090 = CARTESIAN_POINT('Ctrl Pts',(-5.,-6.55,-35.39)) ;
#167091 = CARTESIAN_POINT('Ctrl Pts',(-5.,-6.55,-35.39)) ;
#167092 = CARTESIAN_POINT('Ctrl Pts',(-5.,-6.55,-35.39)) ;
#167093 = CARTESIAN_POINT('Ctrl Pts',(-4.97374656717363,-6.55,-35.3374931343472)) ;
#167094 = CARTESIAN_POINT('Ctrl Pts',(-4.96045866731564,-6.55,-35.3504586673165)) ;
#167095 = CARTESIAN_POINT('Ctrl Pts',(-4.94749313434714,-6.55,-35.3637465671739)) ;
#167096 = CARTESIAN_POINT('Ctrl Pts',(-4.94780128270146,-6.53922263893877,
-35.285602565403)) ;
#167097 = CARTESIAN_POINT('Ctrl Pts',(-4.92085344889015,-6.52362528614069,
-35.3108534488903)) ;
#167098 = CARTESIAN_POINT('Ctrl Pts',(-4.89560256540291,-6.53922263893883,
-35.3378012827015)) ;
#167099 = CARTESIAN_POINT('Ctrl Pts',(-4.92003334147129,-6.5114546977086,
-35.2300666829425)) ;
#167100 = CARTESIAN_POINT('Ctrl Pts',(-4.89711619685841,-6.48208554016478,
-35.2871161968583)) ;
#167101 = CARTESIAN_POINT('Ctrl Pts',(-4.84006668294258,-6.51145469770856,
-35.3100333414713)) ;
#167102 = CARTESIAN_POINT('Ctrl Pts',(-4.91262134295865,-6.5003618540841,
-35.2152426859173)) ;
#167103 = CARTESIAN_POINT('Ctrl Pts',(-4.89498692411706,-6.46792722356049,
-35.284986924117)) ;
#167104 = CARTESIAN_POINT('Ctrl Pts',(-4.82524268591729,-6.5003618540841,
-35.3026213429587)) ;
#167105 = CARTESIAN_POINT('Ctrl Pts',(-4.90260275053909,-6.47617483238892,
-35.1952055010782)) ;
#167106 = CARTESIAN_POINT('Ctrl Pts',(-4.8967032564359,-6.45094059868419,
-35.2867032564359)) ;
#167107 = CARTESIAN_POINT('Ctrl Pts',(-4.80520550107819,-6.47617483238892,
-35.2926027505391)) ;
#167108 = CARTESIAN_POINT('Ctrl Pts',(-4.9,-6.46309229646328,-35.1900000008181)) ;
#167109 = CARTESIAN_POINT('Ctrl Pts',(-4.89999269604099,-6.44945650161557,
-35.2899926958712)) ;
#167110 = CARTESIAN_POINT('Ctrl Pts',(-4.80000000081823,-6.46309229646328,
-35.29)) ;
#167111 = CARTESIAN_POINT('Ctrl Pts',(-4.9,-6.45,-35.19)) ;
#167112 = CARTESIAN_POINT('Ctrl Pts',(-4.9,-6.45,-35.29)) ;
#167113 = CARTESIAN_POINT('Ctrl Pts',(-4.8,-6.45,-35.29)) ;
#167114 = CARTESIAN_POINT('Ctrl Pts',(-5.82426676739305,-5.43399303700803,
-32.6870109659689)) ;
#167115 = CARTESIAN_POINT('Ctrl Pts',(-5.80266988778346,-5.5257236068299,
-32.6923540173524)) ;
#167116 = CARTESIAN_POINT('Ctrl Pts',(-5.82426676352028,-5.53106667371345,
-32.7840845871832)) ;
#167117 = CARTESIAN_POINT('Ctrl Pts',(-5.83498671931055,-5.43935351192089,
-32.6843294581964)) ;
#167118 = CARTESIAN_POINT('Ctrl Pts',(-5.80595263122304,-5.52411753147769,
-32.6939600935421)) ;
#167119 = CARTESIAN_POINT('Ctrl Pts',(-5.83498671397647,-5.53374818067475,
-32.7787241131469)) ;
#167120 = CARTESIAN_POINT('Ctrl Pts',(-5.84526105845644,-5.44830326289658,
-32.6798528401965)) ;
#167121 = CARTESIAN_POINT('Ctrl Pts',(-5.81370932746181,-5.52260132030917,
-32.6954763060005)) ;
#167122 = CARTESIAN_POINT('Ctrl Pts',(-5.84526105243738,-5.53822479746348,
-32.7697743635703)) ;
#167123 = CARTESIAN_POINT('Ctrl Pts',(-5.8637868540363,-5.47240020430534,
-32.6678032513093)) ;
#167124 = CARTESIAN_POINT('Ctrl Pts',(-5.83531854275321,-5.52733067404543,
-32.6907469551157)) ;
#167125 = CARTESIAN_POINT('Ctrl Pts',(-5.86378684816478,-5.55027438459912,
-32.7456774250058)) ;
#167126 = CARTESIAN_POINT('Ctrl Pts',(-5.87203852631515,-5.48754495134849,
-32.660231552895)) ;
#167127 = CARTESIAN_POINT('Ctrl Pts',(-5.84834787930713,-5.53310199490509,
-32.6849756357771)) ;
#167128 = CARTESIAN_POINT('Ctrl Pts',(-5.87203852123054,-5.55784608243472,
-32.7305326795143)) ;
#167129 = CARTESIAN_POINT('Ctrl Pts',(-5.89242747304776,-5.53981202333512,
-32.6341056511382)) ;
#167130 = CARTESIAN_POINT('Ctrl Pts',(-5.88223383300432,-5.56084219179316,
-32.6572354431745)) ;
#167131 = CARTESIAN_POINT('Ctrl Pts',(-5.8924274706351,-5.58397198402791,
-32.6782656123278)) ;
#167132 = CARTESIAN_POINT('Ctrl Pts',(-5.9,-5.58381083947351,-32.6121194001439)) ;
#167133 = CARTESIAN_POINT('Ctrl Pts',(-5.9,-5.59485304502719,-32.6232245928871)) ;
#167134 = CARTESIAN_POINT('Ctrl Pts',(-5.9,-5.60595823775519,-32.6342667984408)) ;
#167135 = CARTESIAN_POINT('Ctrl Pts',(-5.9,-5.62807764064044,-32.59)) ;
#167136 = CARTESIAN_POINT('Ctrl Pts',(-5.9,-5.62807764064044,-32.59)) ;
#167137 = CARTESIAN_POINT('Ctrl Pts',(-5.9,-5.62807764064044,-32.59)) ;
#167138 = CARTESIAN_POINT('Origin',(-5.84850712500726,-5.43404914061138,-32.7840285000291)) ;
#167139 = CARTESIAN_POINT('Ctrl Pts',(-5.82425356250363,-5.53106339062591,
-32.7840285000291)) ;
#167140 = CARTESIAN_POINT('Ctrl Pts',(-5.80269484027818,-5.52567371006955,
-32.6924039305709)) ;
#167141 = CARTESIAN_POINT('Ctrl Pts',(-5.82425356250363,-5.43404914061138,
-32.6870142500145)) ;
#167142 = CARTESIAN_POINT('Ctrl Pts',(-5.80840777707099,-5.52710194426775,
-32.7879899459044)) ;
#167143 = CARTESIAN_POINT('Ctrl Pts',(-5.79341417645244,-5.52335354411312,
-32.6928358498186)) ;
#167144 = CARTESIAN_POINT('Ctrl Pts',(-5.81633079157287,-5.43008775511762,
-32.6889949427472)) ;
#167145 = CARTESIAN_POINT('Ctrl Pts',(-5.79207992677986,-5.52301998169497,
-32.789999999534)) ;
#167146 = CARTESIAN_POINT('Ctrl Pts',(-5.78430903206626,-5.52107725801657,
-32.691961395433)) ;
#167147 = CARTESIAN_POINT('Ctrl Pts',(-5.80816665318299,-5.42600568595105,
-32.69)) ;
#167148 = CARTESIAN_POINT('Ctrl Pts',(-5.77574643749636,-5.51893660937409,
-32.79)) ;
#167149 = CARTESIAN_POINT('Ctrl Pts',(-5.77574643749636,-5.51893660937409,
-32.69)) ;
#167150 = CARTESIAN_POINT('Ctrl Pts',(-5.8,-5.42192235935956,-32.69)) ;
#167151 = CARTESIAN_POINT('Origin',(-5.8,-5.42192235935956,-32.79)) ;
#167152 = CARTESIAN_POINT('Origin',(-5.8066065036801,-5.42357398527959,-32.79)) ;
#167153 = CARTESIAN_POINT('Origin',(-5.17275707706435,-5.26511162862565,-32.79)) ;
#167154 = CARTESIAN_POINT('Origin',(-5.15068655017073,-5.25959399690224,-32.8005938529089)) ;
#167155 = CARTESIAN_POINT('Origin',(-5.17275707706436,-5.26511162862565,-32.79)) ;
#167156 = CARTESIAN_POINT('Origin',(-5.17275707706436,-5.26511162862565,-32.79)) ;
#167157 = CARTESIAN_POINT('Origin',(-5.17275707706436,-5.26511162862565,-32.79)) ;
#167158 = CARTESIAN_POINT('Origin',(-5.17275707706436,-5.05,-32.79)) ;
#167159 = CARTESIAN_POINT('Origin',(-5.17275707706436,-1.91866427917294,-32.79)) ;
#167160 = CARTESIAN_POINT('Origin',(-3.78014014831103,-3.31128120792626,-33.4584561258016)) ;
#167161 = CARTESIAN_POINT('Origin',(-5.17275707706436,-1.91866427917294,-32.79)) ;
#167162 = CARTESIAN_POINT('Origin',(-5.17275707706436,-1.91866427917294,-32.79)) ;
#167163 = CARTESIAN_POINT('Origin',(-5.17275707706436,-1.91866427917294,-32.79)) ;
#167164 = CARTESIAN_POINT('Origin',(-3.97071067811865,-3.12071067811865,-32.79)) ;
#167165 = CARTESIAN_POINT('Origin',(-5.8,-1.2914213562373,-32.79)) ;
#167166 = CARTESIAN_POINT('Ctrl Pts',(-5.87071067811865,-1.14999999999999,
-32.6607106781187)) ;
#167167 = CARTESIAN_POINT('Ctrl Pts',(-5.8471404520791,-1.10285954792089,
-32.6842809041582)) ;
#167168 = CARTESIAN_POINT('Ctrl Pts',(-5.87071067811865,-1.07928932188134,
-32.7314213562373)) ;
#167169 = CARTESIAN_POINT('Ctrl Pts',(-5.85217562795678,-1.18707010095486,
-32.6792457282805)) ;
#167170 = CARTESIAN_POINT('Ctrl Pts',(-5.81261165662092,-1.1373883433792,
-32.7058614719491)) ;
#167171 = CARTESIAN_POINT('Ctrl Pts',(-5.83353949671048,-1.11646050328952,
-32.7685925363807)) ;
#167172 = CARTESIAN_POINT('Ctrl Pts',(-5.82627077431952,-1.2388798075982,
-32.69)) ;
#167173 = CARTESIAN_POINT('Ctrl Pts',(-5.76566787907928,-1.18433212092069,
-32.7071489437134)) ;
#167174 = CARTESIAN_POINT('Ctrl Pts',(-5.7819067873223,-1.16809321267769,
-32.7899999994191)) ;
#167175 = CARTESIAN_POINT('Ctrl Pts',(-5.8,-1.2914213562373,-32.69)) ;
#167176 = CARTESIAN_POINT('Ctrl Pts',(-5.72928932188134,-1.22071067811865,
-32.69)) ;
#167177 = CARTESIAN_POINT('Ctrl Pts',(-5.72928932188134,-1.22071067811865,
-32.79)) ;
#167178 = CARTESIAN_POINT('Origin',(-5.94142135623731,-1.14999999999999,-32.7314213562373)) ;
#167179 = CARTESIAN_POINT('Ctrl Pts',(-5.9,-1.00857864376269,-32.59)) ;
#167180 = CARTESIAN_POINT('Ctrl Pts',(-5.9,-1.00857864376269,-32.59)) ;
#167181 = CARTESIAN_POINT('Ctrl Pts',(-5.9,-1.00857864376269,-32.59)) ;
#167182 = CARTESIAN_POINT('Ctrl Pts',(-5.9,-1.06112019240157,-32.61627077432)) ;
#167183 = CARTESIAN_POINT('Ctrl Pts',(-5.9,-1.04860238143819,-32.6300237376769)) ;
#167184 = CARTESIAN_POINT('Ctrl Pts',(-5.9,-1.03484941808205,-32.642541548639)) ;
#167185 = CARTESIAN_POINT('Ctrl Pts',(-5.88924572828051,-1.11292989904511,
-32.6421756279568)) ;
#167186 = CARTESIAN_POINT('Ctrl Pts',(-5.87451700624767,-1.08721613124767,
-32.6686374874862)) ;
#167187 = CARTESIAN_POINT('Ctrl Pts',(-5.88924572828078,-1.06075427171922,
-32.6943512552828)) ;
#167188 = CARTESIAN_POINT('Ctrl Pts',(-5.87071067811865,-1.14999999999999,
-32.6607106781187)) ;
#167189 = CARTESIAN_POINT('Ctrl Pts',(-5.8471404520791,-1.10285954792089,
-32.6842809041582)) ;
#167190 = CARTESIAN_POINT('Ctrl Pts',(-5.87071067811865,-1.07928932188134,
-32.7314213562373)) ;
#167191 = CARTESIAN_POINT('Ctrl Pts',(-5.87071067811866,-1.14999999999999,
-35.9192893218814)) ;
#167192 = CARTESIAN_POINT('Ctrl Pts',(-5.8471404520791,-1.10285954792089,
-35.8957190958418)) ;
#167193 = CARTESIAN_POINT('Ctrl Pts',(-5.87071067811866,-1.07928932188134,
-35.8485786437627)) ;
#167194 = CARTESIAN_POINT('Ctrl Pts',(-5.88924572828049,-1.11292989904506,
-35.9378243720432)) ;
#167195 = CARTESIAN_POINT('Ctrl Pts',(-5.87451700624375,-1.08721613124993,
-35.9113625125116)) ;
#167196 = CARTESIAN_POINT('Ctrl Pts',(-5.88924572828075,-1.06075427171925,
-35.8856487447172)) ;
#167197 = CARTESIAN_POINT('Ctrl Pts',(-5.9,-1.0611201924015,-35.9637292256798)) ;
#167198 = CARTESIAN_POINT('Ctrl Pts',(-5.9,-1.04860238143643,-35.9499762623248)) ;
#167199 = CARTESIAN_POINT('Ctrl Pts',(-5.9,-1.03484941808207,-35.937458451361)) ;
#167200 = CARTESIAN_POINT('Ctrl Pts',(-5.9,-1.00857864376269,-35.99)) ;
#167201 = CARTESIAN_POINT('Ctrl Pts',(-5.9,-1.00857864376269,-35.99)) ;
#167202 = CARTESIAN_POINT('Ctrl Pts',(-5.9,-1.00857864376269,-35.99)) ;
#167203 = CARTESIAN_POINT('Origin',(-5.94142135623734,-1.14999999999996,-35.8485786437627)) ;
#167204 = CARTESIAN_POINT('Ctrl Pts',(-5.8,-1.2914213562373,-35.89)) ;
#167205 = CARTESIAN_POINT('Ctrl Pts',(-5.72928932188134,-1.22071067811865,
-35.89)) ;
#167206 = CARTESIAN_POINT('Ctrl Pts',(-5.72928932188134,-1.22071067811865,
-35.79)) ;
#167207 = CARTESIAN_POINT('Ctrl Pts',(-5.82627077431952,-1.2388798075982,
-35.89)) ;
#167208 = CARTESIAN_POINT('Ctrl Pts',(-5.76566787907933,-1.18433212092069,
-35.8728510562865)) ;
#167209 = CARTESIAN_POINT('Ctrl Pts',(-5.78190678732231,-1.16809321267768,
-35.7900000005809)) ;
#167210 = CARTESIAN_POINT('Ctrl Pts',(-5.8521756279568,-1.18707010095487,
-35.9007542717195)) ;
#167211 = CARTESIAN_POINT('Ctrl Pts',(-5.81261165662085,-1.13738834337918,
-35.8741385280509)) ;
#167212 = CARTESIAN_POINT('Ctrl Pts',(-5.83353949671047,-1.11646050328952,
-35.8114074636193)) ;
#167213 = CARTESIAN_POINT('Ctrl Pts',(-5.87071067811865,-1.14999999999999,
-35.9192893218814)) ;
#167214 = CARTESIAN_POINT('Ctrl Pts',(-5.8471404520791,-1.10285954792089,
-35.8957190958418)) ;
#167215 = CARTESIAN_POINT('Ctrl Pts',(-5.87071067811866,-1.07928932188134,
-35.8485786437627)) ;
#167216 = CARTESIAN_POINT('Origin',(-5.8,-1.29142135623731,-35.79)) ;
#167217 = CARTESIAN_POINT('Origin',(-3.59571067811865,-3.49571067811865,-35.79)) ;
#167218 = CARTESIAN_POINT('Origin',(-5.17275707706436,-1.91866427917294,-35.79)) ;
#167219 = CARTESIAN_POINT('Origin',(-3.09057773798104,-4.00084361825625,-34.79055391724)) ;
#167220 = CARTESIAN_POINT('Origin',(-5.17275707706435,-1.91866427917295,-35.79)) ;
#167221 = CARTESIAN_POINT('Origin',(-5.17275707706435,-1.91866427917295,-35.79)) ;
#167222 = CARTESIAN_POINT('Origin',(-5.17275707706435,-1.91866427917295,-35.79)) ;
#167223 = CARTESIAN_POINT('Origin',(-5.17275707706435,-5.05,-35.79)) ;
#167224 = CARTESIAN_POINT('Origin',(-5.17275707706435,-5.26511162862565,-35.79)) ;
#167225 = CARTESIAN_POINT('Origin',(-3.96111272388873,-4.96220054033175,-35.2084107104757)) ;
#167226 = CARTESIAN_POINT('Origin',(-5.17275707706435,-5.26511162862565,-35.79)) ;
#167227 = CARTESIAN_POINT('Origin',(-5.17275707706435,-5.26511162862565,-35.79)) ;
#167228 = CARTESIAN_POINT('Origin',(-5.17275707706435,-5.26511162862565,-35.79)) ;
#167229 = CARTESIAN_POINT('Origin',(-5.10072415073893,-5.24710339704429,-35.79)) ;
#167230 = CARTESIAN_POINT('Origin',(-5.8,-5.42192235935956,-35.79)) ;
#167231 = CARTESIAN_POINT('Ctrl Pts',(-5.77574643749636,-5.51893660937409,
-35.79)) ;
#167232 = CARTESIAN_POINT('Ctrl Pts',(-5.77574643749636,-5.51893660937409,
-35.89)) ;
#167233 = CARTESIAN_POINT('Ctrl Pts',(-5.8,-5.42192235935956,-35.89)) ;
#167234 = CARTESIAN_POINT('Ctrl Pts',(-5.79207992677986,-5.52301998169497,
-35.790000000466)) ;
#167235 = CARTESIAN_POINT('Ctrl Pts',(-5.78430903206628,-5.52107725801656,
-35.888038604567)) ;
#167236 = CARTESIAN_POINT('Ctrl Pts',(-5.808166653183,-5.42600568595104,-35.89)) ;
#167237 = CARTESIAN_POINT('Ctrl Pts',(-5.808407777071,-5.52710194426775,-35.7920100540956)) ;
#167238 = CARTESIAN_POINT('Ctrl Pts',(-5.79341417645243,-5.52335354411312,
-35.8871641501814)) ;
#167239 = CARTESIAN_POINT('Ctrl Pts',(-5.81633079157287,-5.43008775511762,
-35.8910050572528)) ;
#167240 = CARTESIAN_POINT('Ctrl Pts',(-5.82425356250363,-5.53106339062591,
-35.7959714999709)) ;
#167241 = CARTESIAN_POINT('Ctrl Pts',(-5.80269484027818,-5.52567371006955,
-35.8875960694291)) ;
#167242 = CARTESIAN_POINT('Ctrl Pts',(-5.82425356250363,-5.43404914061138,
-35.8929857499855)) ;
#167243 = CARTESIAN_POINT('Origin',(-5.84850712500726,-5.43404914061138,-35.7959714999709)) ;
#167244 = CARTESIAN_POINT('Ctrl Pts',(-5.82426676739358,-5.5310666746717,
-35.7959153963653)) ;
#167245 = CARTESIAN_POINT('Ctrl Pts',(-5.80266988778302,-5.52572362329019,
-35.8876459661891)) ;
#167246 = CARTESIAN_POINT('Ctrl Pts',(-5.82426676352022,-5.4339930534575,
-35.8929890330731)) ;
#167247 = CARTESIAN_POINT('Ctrl Pts',(-5.83498671931134,-5.53374818244432,
-35.8012758712783)) ;
#167248 = CARTESIAN_POINT('Ctrl Pts',(-5.80595263122244,-5.52411754710043,
-35.8860398908366)) ;
#167249 = CARTESIAN_POINT('Ctrl Pts',(-5.83498671397634,-5.43935352749392,
-35.8956705400343)) ;
#167250 = CARTESIAN_POINT('Ctrl Pts',(-5.84526105845725,-5.53822480044432,
-35.8102256222542)) ;
#167251 = CARTESIAN_POINT('Ctrl Pts',(-5.8137093274612,-5.5226013346416,-35.8845236796681)) ;
#167252 = CARTESIAN_POINT('Ctrl Pts',(-5.84526105243728,-5.44830327707045,
-35.900147156823)) ;
#167253 = CARTESIAN_POINT('Ctrl Pts',(-5.86378685403709,-5.55027438933186,
-35.8343225636634)) ;
#167254 = CARTESIAN_POINT('Ctrl Pts',(-5.83531854275271,-5.52733068552586,
-35.8892530334045)) ;
#167255 = CARTESIAN_POINT('Ctrl Pts',(-5.86378684816469,-5.4724002156348,
-35.9121967439586)) ;
#167256 = CARTESIAN_POINT('Ctrl Pts',(-5.87203852631588,-5.55784608774616,
-35.8494673107066)) ;
#167257 = CARTESIAN_POINT('Ctrl Pts',(-5.84834787930671,-5.53310200486446,
-35.895024354264)) ;
#167258 = CARTESIAN_POINT('Ctrl Pts',(-5.87203852123043,-5.48754496112637,
-35.9197684417942)) ;
#167259 = CARTESIAN_POINT('Ctrl Pts',(-5.89242747304801,-5.58397198950293,
-35.9017343826941)) ;
#167260 = CARTESIAN_POINT('Ctrl Pts',(-5.88223383300418,-5.56084219746617,
-35.9227645511525)) ;
#167261 = CARTESIAN_POINT('Ctrl Pts',(-5.89242747063512,-5.53981202831256,
-35.9458943433875)) ;
#167262 = CARTESIAN_POINT('Ctrl Pts',(-5.9,-5.60595824049755,-35.9457331988324)) ;
#167263 = CARTESIAN_POINT('Ctrl Pts',(-5.9,-5.59485304775362,-35.9567754043864)) ;
#167264 = CARTESIAN_POINT('Ctrl Pts',(-5.9,-5.58381084219971,-35.9678805971148)) ;
#167265 = CARTESIAN_POINT('Ctrl Pts',(-5.9,-5.62807764064044,-35.99)) ;
#167266 = CARTESIAN_POINT('Ctrl Pts',(-5.9,-5.62807764064044,-35.99)) ;
#167267 = CARTESIAN_POINT('Ctrl Pts',(-5.9,-5.62807764064044,-35.99)) ;
#167268 = CARTESIAN_POINT('Origin',(7.8,2.1,-34.69)) ;
#167269 = CARTESIAN_POINT('Origin',(7.8,2.1,-34.89)) ;
#167270 = CARTESIAN_POINT('Origin',(7.6,2.1,-34.69)) ;
#167271 = CARTESIAN_POINT('Origin',(7.6,2.1,-34.69)) ;
#167272 = CARTESIAN_POINT('Origin',(7.6,2.1,-33.89)) ;
#167273 = CARTESIAN_POINT('Origin',(7.8,2.1,-34.89)) ;
#167274 = CARTESIAN_POINT('Origin',(9.6,2.1,-34.89)) ;
#167275 = CARTESIAN_POINT('Origin',(7.8,2.1,-33.89)) ;
#167276 = CARTESIAN_POINT('Origin',(7.8,2.1,-33.69)) ;
#167277 = CARTESIAN_POINT('Origin',(9.6,2.1,-34.69)) ;
#167278 = CARTESIAN_POINT('Origin',(9.8,2.1,-34.69)) ;
#167279 = CARTESIAN_POINT('Origin',(7.8,2.1,-33.69)) ;
#167280 = CARTESIAN_POINT('Origin',(9.6,2.1,-33.69)) ;
#167281 = CARTESIAN_POINT('Origin',(9.8,2.1,-34.69)) ;
#167282 = CARTESIAN_POINT('Origin',(9.8,2.1,-33.89)) ;
#167283 = CARTESIAN_POINT('Origin',(9.6,2.1,-33.89)) ;
#167284 = CARTESIAN_POINT('Origin',(-4.15,-6.25,-33.54)) ;
#167285 = CARTESIAN_POINT('Origin',(-4.15,-6.3,-33.54)) ;
#167286 = CARTESIAN_POINT('Origin',(-4.15,-6.3,-34.29)) ;
#167287 = CARTESIAN_POINT('Origin',(-4.15,-6.3,-35.04)) ;
#167288 = CARTESIAN_POINT('Origin',(-4.15,-6.3,-33.54)) ;
#167289 = CARTESIAN_POINT('Origin',(-4.15,-6.25,-35.04)) ;
#167290 = CARTESIAN_POINT('Origin',(-4.15,-6.3,-35.04)) ;
#167291 = CARTESIAN_POINT('Origin',(-4.15,-6.3,-33.54)) ;
#167292 = CARTESIAN_POINT('Origin',(-4.15,-6.3,-33.54)) ;
#167293 = CARTESIAN_POINT('Origin',(-4.15,-6.3,-35.04)) ;
#167294 = CARTESIAN_POINT('Origin',(-4.15,-6.3,-35.04)) ;
#167295 = CARTESIAN_POINT('Origin',(-4.65,-6.25,-33.54)) ;
#167296 = CARTESIAN_POINT('Origin',(-4.65,-6.3,-33.54)) ;
#167297 = CARTESIAN_POINT('Origin',(0.,-6.3,-33.54)) ;
#167298 = CARTESIAN_POINT('Origin',(-4.65,-6.3,-33.54)) ;
#167299 = CARTESIAN_POINT('Origin',(0.,-6.3,-35.04)) ;
#167300 = CARTESIAN_POINT('Origin',(-4.65,-6.3,-35.04)) ;
#167301 = CARTESIAN_POINT('Origin',(-4.65,-6.25,-35.04)) ;
#167302 = CARTESIAN_POINT('Origin',(-4.65,-6.3,-35.04)) ;
#167303 = CARTESIAN_POINT('Origin',(-4.65,-6.3,-33.54)) ;
#167304 = CARTESIAN_POINT('Origin',(-4.65,-6.3,-33.54)) ;
#167305 = CARTESIAN_POINT('Origin',(-4.65,-6.3,-35.04)) ;
#167306 = CARTESIAN_POINT('Origin',(-4.65,-6.3,-35.04)) ;
#167307 = CARTESIAN_POINT('Origin',(-4.65,-6.3,-34.29)) ;
#167308 = CARTESIAN_POINT('Origin',(-3.,4.45,-35.39)) ;
#167309 = CARTESIAN_POINT('Origin',(-2.1,4.45,-35.39)) ;
#167310 = CARTESIAN_POINT('Origin',(-2.9,4.45,-35.39)) ;
#167311 = CARTESIAN_POINT('Origin',(-2.9,4.45,-35.19)) ;
#167312 = CARTESIAN_POINT('Origin',(-3.1,4.45,-35.19)) ;
#167313 = CARTESIAN_POINT('Origin',(-2.9,4.45,-35.19)) ;
#167314 = CARTESIAN_POINT('Origin',(-2.1,4.45,-35.19)) ;
#167315 = CARTESIAN_POINT('Origin',(-2.1,4.45,-35.19)) ;
#167316 = CARTESIAN_POINT('Origin',(-1.9,4.45,-35.19)) ;
#167317 = CARTESIAN_POINT('Origin',(-3.1,4.45,-35.29)) ;
#167318 = CARTESIAN_POINT('Origin',(-3.1,4.45,-33.39)) ;
#167319 = CARTESIAN_POINT('Origin',(-2.9,4.4,-35.19)) ;
#167320 = CARTESIAN_POINT('Origin',(-2.9,4.35,-35.19)) ;
#167321 = CARTESIAN_POINT('Origin',(-1.95156391047391E-16,4.35,-35.19)) ;
#167322 = CARTESIAN_POINT('Origin',(-2.1,4.35,-35.19)) ;
#167323 = CARTESIAN_POINT('Origin',(-2.9,4.35,-35.19)) ;
#167324 = CARTESIAN_POINT('Origin',(-2.1,4.4,-35.19)) ;
#167325 = CARTESIAN_POINT('Origin',(-2.1,4.35,-35.19)) ;
#167326 = CARTESIAN_POINT('Origin',(-1.9,4.45,-35.29)) ;
#167327 = CARTESIAN_POINT('Origin',(-1.9,4.45,-33.39)) ;
#167328 = CARTESIAN_POINT('Origin',(-3.,4.45,-33.19)) ;
#167329 = CARTESIAN_POINT('Origin',(-2.9,4.45,-33.19)) ;
#167330 = CARTESIAN_POINT('Origin',(-2.1,4.45,-33.19)) ;
#167331 = CARTESIAN_POINT('Origin',(-2.9,4.45,-33.39)) ;
#167332 = CARTESIAN_POINT('Origin',(-2.9,4.45,-33.39)) ;
#167333 = CARTESIAN_POINT('Origin',(-2.9,4.35,-35.19)) ;
#167334 = CARTESIAN_POINT('Origin',(-2.9,4.35,-35.19)) ;
#167335 = CARTESIAN_POINT('Origin',(-2.1,4.35,-35.19)) ;
#167336 = CARTESIAN_POINT('Origin',(-2.1,4.35,-35.19)) ;
#167337 = CARTESIAN_POINT('Origin',(-2.1,4.45,-33.39)) ;
#167338 = CARTESIAN_POINT('Origin',(-2.1,4.45,-33.39)) ;
#167339 = CARTESIAN_POINT('Origin',(-2.9,4.4,-33.39)) ;
#167340 = CARTESIAN_POINT('Origin',(-2.9,4.35,-33.39)) ;
#167341 = CARTESIAN_POINT('Origin',(-2.9,4.35,-34.29)) ;
#167342 = CARTESIAN_POINT('Origin',(-2.9,4.35,-33.39)) ;
#167343 = CARTESIAN_POINT('Origin',(-2.1,4.35,-34.29)) ;
#167344 = CARTESIAN_POINT('Origin',(-2.1,4.35,-33.39)) ;
#167345 = CARTESIAN_POINT('Origin',(-2.1,4.4,-33.39)) ;
#167346 = CARTESIAN_POINT('Origin',(-2.1,4.35,-33.39)) ;
#167347 = CARTESIAN_POINT('Origin',(-2.9,4.35,-33.39)) ;
#167348 = CARTESIAN_POINT('Origin',(-2.9,4.35,-33.39)) ;
#167349 = CARTESIAN_POINT('Origin',(-2.1,4.35,-33.39)) ;
#167350 = CARTESIAN_POINT('Origin',(-2.1,4.35,-33.39)) ;
#167351 = CARTESIAN_POINT('Origin',(-1.95156391047391E-16,4.35,-33.39)) ;
#167352 = CARTESIAN_POINT('Origin',(-2.25,4.25,-35.04)) ;
#167353 = CARTESIAN_POINT('Origin',(-2.25,4.3,-35.04)) ;
#167354 = CARTESIAN_POINT('Origin',(-2.25,4.3,-34.29)) ;
#167355 = CARTESIAN_POINT('Origin',(-2.25,4.3,-33.54)) ;
#167356 = CARTESIAN_POINT('Origin',(-2.25,4.3,-35.04)) ;
#167357 = CARTESIAN_POINT('Origin',(-2.25,4.25,-33.54)) ;
#167358 = CARTESIAN_POINT('Origin',(-2.25,4.3,-33.54)) ;
#167359 = CARTESIAN_POINT('Origin',(-2.25,4.3,-35.04)) ;
#167360 = CARTESIAN_POINT('Origin',(-2.25,4.3,-35.04)) ;
#167361 = CARTESIAN_POINT('Origin',(-2.25,4.3,-33.54)) ;
#167362 = CARTESIAN_POINT('Origin',(-2.25,4.3,-33.54)) ;
#167363 = CARTESIAN_POINT('Origin',(-2.75,4.25,-35.04)) ;
#167364 = CARTESIAN_POINT('Origin',(-2.75,4.3,-35.04)) ;
#167365 = CARTESIAN_POINT('Origin',(-1.97127667724637E-17,4.3,-35.04)) ;
#167366 = CARTESIAN_POINT('Origin',(-2.75,4.3,-35.04)) ;
#167367 = CARTESIAN_POINT('Origin',(-1.97127667724637E-17,4.3,-33.54)) ;
#167368 = CARTESIAN_POINT('Origin',(-2.75,4.3,-33.54)) ;
#167369 = CARTESIAN_POINT('Origin',(-2.75,4.25,-33.54)) ;
#167370 = CARTESIAN_POINT('Origin',(-2.75,4.3,-33.54)) ;
#167371 = CARTESIAN_POINT('Origin',(-2.75,4.3,-35.04)) ;
#167372 = CARTESIAN_POINT('Origin',(-2.75,4.3,-35.04)) ;
#167373 = CARTESIAN_POINT('Origin',(-2.75,4.3,-33.54)) ;
#167374 = CARTESIAN_POINT('Origin',(-2.75,4.3,-33.54)) ;
#167375 = CARTESIAN_POINT('Origin',(-2.75,4.3,-34.29)) ;
#167376 = CARTESIAN_POINT('Origin',(7.8,2.9,-34.69)) ;
#167377 = CARTESIAN_POINT('Origin',(7.8,2.9,-34.69)) ;
#167378 = CARTESIAN_POINT('Origin',(7.8,2.9,-33.89)) ;
#167379 = CARTESIAN_POINT('Origin',(7.8,2.9,-33.89)) ;
#167380 = CARTESIAN_POINT('Origin',(7.8,2.9,-33.89)) ;
#167381 = CARTESIAN_POINT('Origin',(7.8,2.9,-34.69)) ;
#167382 = CARTESIAN_POINT('Origin',(7.8,2.9,-34.69)) ;
#167383 = CARTESIAN_POINT('Origin',(9.6,2.9,-33.89)) ;
#167384 = CARTESIAN_POINT('Origin',(9.6,2.9,-33.89)) ;
#167385 = CARTESIAN_POINT('Origin',(9.6,2.9,-34.69)) ;
#167386 = CARTESIAN_POINT('Origin',(9.6,2.9,-34.69)) ;
#167387 = CARTESIAN_POINT('Origin',(9.6,2.9,-33.89)) ;
#167388 = CARTESIAN_POINT('Origin',(9.6,2.9,-33.89)) ;
#167389 = CARTESIAN_POINT('Origin',(9.6,2.9,-34.69)) ;
#167390 = CARTESIAN_POINT('Origin',(9.6,2.9,-34.69)) ;
#167391 = CARTESIAN_POINT('Origin',(9.6,2.9,-34.69)) ;
#167392 = CARTESIAN_POINT('Origin',(-0.183301359729408,3.45,-32.772963213524)) ;
#167393 = CARTESIAN_POINT('Origin',(0.24923464143508,3.15,-34.1737799780213)) ;
#167394 = CARTESIAN_POINT('Origin',(-0.249234641435079,3.15,-34.4062200219787)) ;
#167395 = CARTESIAN_POINT('Origin',(-1.04429375741423,3.45,-33.1744505621777)) ;
#167396 = CARTESIAN_POINT('Origin',(3.7,2.1,-2.405)) ;
#167397 = CARTESIAN_POINT('Origin',(3.7,2.1,-5.115)) ;
#167398 = CARTESIAN_POINT('Origin',(3.7,2.1,-2.505)) ;
#167399 = CARTESIAN_POINT('Origin',(3.7,2.1,-6.215)) ;
#167400 = CARTESIAN_POINT('Origin',(3.7,2.1,-8.925)) ;
#167401 = CARTESIAN_POINT('Origin',(3.7,2.1,-6.315)) ;
#167402 = CARTESIAN_POINT('Origin',(3.7,2.1,-10.025)) ;
#167403 = CARTESIAN_POINT('Origin',(3.7,2.1,-12.735)) ;
#167404 = CARTESIAN_POINT('Origin',(3.7,2.1,-10.125)) ;
#167405 = CARTESIAN_POINT('Origin',(3.7,2.1,-13.835)) ;
#167406 = CARTESIAN_POINT('Origin',(3.7,2.1,-16.545)) ;
#167407 = CARTESIAN_POINT('Origin',(3.7,2.1,-13.935)) ;
#167408 = CARTESIAN_POINT('Origin',(3.7,2.1,-17.645)) ;
#167409 = CARTESIAN_POINT('Origin',(3.7,2.1,-20.355)) ;
#167410 = CARTESIAN_POINT('Origin',(3.7,2.1,-17.745)) ;
#167411 = CARTESIAN_POINT('Origin',(3.7,2.1,-21.455)) ;
#167412 = CARTESIAN_POINT('Origin',(3.7,2.1,-24.165)) ;
#167413 = CARTESIAN_POINT('Origin',(3.7,2.1,-21.555)) ;
#167414 = CARTESIAN_POINT('Origin',(3.7,2.1,-25.265)) ;
#167415 = CARTESIAN_POINT('Origin',(3.7,2.1,-27.975)) ;
#167416 = CARTESIAN_POINT('Origin',(3.7,2.1,-25.365)) ;
#167417 = CARTESIAN_POINT('Origin',(3.7,2.1,-29.075)) ;
#167418 = CARTESIAN_POINT('Origin',(3.7,2.1,-31.785)) ;
#167419 = CARTESIAN_POINT('Origin',(3.7,2.1,-29.175)) ;
#167420 = CARTESIAN_POINT('Origin',(3.7,2.1,-32.885)) ;
#167421 = CARTESIAN_POINT('Origin',(3.7,2.1,-35.595)) ;
#167422 = CARTESIAN_POINT('Origin',(3.7,2.1,-32.985)) ;
#167423 = CARTESIAN_POINT('Origin',(3.5,1.9,-6.115)) ;
#167424 = CARTESIAN_POINT('',(3.55,2.01339745962156,-6.115)) ;
#167425 = CARTESIAN_POINT('Origin',(3.5,2.1,-6.115)) ;
#167426 = CARTESIAN_POINT('Ctrl Pts',(3.55,2.01339745962156,-6.115)) ;
#167427 = CARTESIAN_POINT('Ctrl Pts',(3.55164546205118,2.01434746757975,-6.115)) ;
#167428 = CARTESIAN_POINT('Ctrl Pts',(3.55326668047441,2.01534654795451,-6.1153329780303)) ;
#167429 = CARTESIAN_POINT('Ctrl Pts',(3.55550702654634,2.01680421826673,-6.11609826168305)) ;
#167430 = CARTESIAN_POINT('Ctrl Pts',(3.55618577699068,2.01725684095079,-6.11637359606383)) ;
#167431 = CARTESIAN_POINT('Ctrl Pts',(3.55727967686454,2.01800266699454,-6.1168678300958)) ;
#167432 = CARTESIAN_POINT('Ctrl Pts',(3.55771141786834,2.01830156212325,-6.11707831894258)) ;
#167433 = CARTESIAN_POINT('Ctrl Pts',(3.56202821818157,2.02133211263481,-6.1191706910972)) ;
#167434 = CARTESIAN_POINT('Ctrl Pts',(3.56570108751477,2.02427663140637,-6.12224393162826)) ;
#167435 = CARTESIAN_POINT('Ctrl Pts',(3.5699034772656,2.02797441535145,-6.12640200473845)) ;
#167436 = CARTESIAN_POINT('Ctrl Pts',(3.57072473561126,2.02871480216321,-6.12724959773093)) ;
#167437 = CARTESIAN_POINT('Ctrl Pts',(3.5738286330762,2.03157464832067,-6.13054171893286)) ;
#167438 = CARTESIAN_POINT('Ctrl Pts',(3.5759706937612,2.03369481096682,-6.13313773435733)) ;
#167439 = CARTESIAN_POINT('Ctrl Pts',(3.58156103639368,2.03956384830232,-6.14075811677975)) ;
#167440 = CARTESIAN_POINT('Ctrl Pts',(3.58475859790495,2.04336775308648,-6.14615483852158)) ;
#167441 = CARTESIAN_POINT('Ctrl Pts',(3.58897725231935,2.0490105592432,-6.15495483430059)) ;
#167442 = CARTESIAN_POINT('Ctrl Pts',(3.59034871903171,2.05099358132072,-6.15822253384318)) ;
#167443 = CARTESIAN_POINT('Ctrl Pts',(3.59365488292729,2.05613355260445,-6.16724922860835)) ;
#167444 = CARTESIAN_POINT('Ctrl Pts',(3.59534780095525,2.05919518104045,-6.17324371161029)) ;
#167445 = CARTESIAN_POINT('Ctrl Pts',(3.59674625886212,2.06216860863464,-6.17996044662966)) ;
#167446 = CARTESIAN_POINT('Ctrl Pts',(3.59685725281059,2.06240883133061,-6.18051031510962)) ;
#167447 = CARTESIAN_POINT('Ctrl Pts',(3.59768573690243,2.06423460359408,-6.18474653762001)) ;
#167448 = CARTESIAN_POINT('Ctrl Pts',(3.59826864191792,2.06571343564803,-6.18852399715655)) ;
#167449 = CARTESIAN_POINT('Ctrl Pts',(3.59959273712775,2.06963221119414,-6.19968301436906)) ;
#167450 = CARTESIAN_POINT('Ctrl Pts',(3.6,2.07172309150643,-6.2072993579658)) ;
#167451 = CARTESIAN_POINT('Ctrl Pts',(3.6,2.07320508075689,-6.215)) ;
#167452 = CARTESIAN_POINT('Origin',(3.5,2.1,-1.01757522333835E-15)) ;
#167453 = CARTESIAN_POINT('Origin',(3.5,2.1,-6.115)) ;
#167454 = CARTESIAN_POINT('',(3.55,2.01339745962156,-5.315)) ;
#167455 = CARTESIAN_POINT('Origin',(3.5,2.1,-5.315)) ;
#167456 = CARTESIAN_POINT('Origin',(3.5,2.1,-5.315)) ;
#167457 = CARTESIAN_POINT('Origin',(3.5,1.9,-5.315)) ;
#167458 = CARTESIAN_POINT('Ctrl Pts',(3.6,2.07320508075689,-5.215)) ;
#167459 = CARTESIAN_POINT('Ctrl Pts',(3.6,2.07265589924994,-5.21785357667012)) ;
#167460 = CARTESIAN_POINT('Ctrl Pts',(3.59994554076638,2.07202433860048,-5.22069358004935)) ;
#167461 = CARTESIAN_POINT('Ctrl Pts',(3.59971739924421,2.07059366100571,-5.22637921497773)) ;
#167462 = CARTESIAN_POINT('Ctrl Pts',(3.59954156373427,2.06979274847054,-5.22921873634714)) ;
#167463 = CARTESIAN_POINT('Ctrl Pts',(3.59880783141185,2.06712577191658,-5.23778089072537)) ;
#167464 = CARTESIAN_POINT('Ctrl Pts',(3.59804129495587,2.0650190276639,-5.24341713644386)) ;
#167465 = CARTESIAN_POINT('Ctrl Pts',(3.59624340061598,2.06105248659392,-5.25263353946359)) ;
#167466 = CARTESIAN_POINT('Ctrl Pts',(3.59536494855695,2.05931170891995,-5.25632347138735)) ;
#167467 = CARTESIAN_POINT('Ctrl Pts',(3.5928372720244,2.05479606436794,-5.26519943205902)) ;
#167468 = CARTESIAN_POINT('Ctrl Pts',(3.59099650883092,2.05188276467123,-5.27034424200709)) ;
#167469 = CARTESIAN_POINT('Ctrl Pts',(3.58838944624308,2.04823719194672,-5.27622737667942)) ;
#167470 = CARTESIAN_POINT('Ctrl Pts',(3.58794537962075,2.04762948672743,-5.27719091385135)) ;
#167471 = CARTESIAN_POINT('Ctrl Pts',(3.58597371492279,2.04498948329048,-5.28130665172963)) ;
#167472 = CARTESIAN_POINT('Ctrl Pts',(3.58430396743904,2.04289920268562,-5.28439316248021)) ;
#167473 = CARTESIAN_POINT('Ctrl Pts',(3.58008903321353,2.03798436571141,-5.29128092067904)) ;
#167474 = CARTESIAN_POINT('Ctrl Pts',(3.57743593401578,2.0351394536771,-5.29500157292073)) ;
#167475 = CARTESIAN_POINT('Ctrl Pts',(3.57357563759658,2.03136250950841,-5.29958640159694)) ;
#167476 = CARTESIAN_POINT('Ctrl Pts',(3.57257888733672,2.03041544381399,-5.30070656893144)) ;
#167477 = CARTESIAN_POINT('Ctrl Pts',(3.56956839719841,2.02764175140691,-5.30390390778882)) ;
#167478 = CARTESIAN_POINT('Ctrl Pts',(3.56746189551952,2.02581554544786,-5.30598430067898)) ;
#167479 = CARTESIAN_POINT('Ctrl Pts',(3.56503628433188,2.02384076964147,-5.30802226003855)) ;
#167480 = CARTESIAN_POINT('Ctrl Pts',(3.56481411023493,2.02366103014357,-5.30820583968785)) ;
#167481 = CARTESIAN_POINT('Ctrl Pts',(3.56285239425759,2.02208416924062,-5.30979838212049)) ;
#167482 = CARTESIAN_POINT('Ctrl Pts',(3.56093641846881,2.02061618613973,-5.31118717775178)) ;
#167483 = CARTESIAN_POINT('Ctrl Pts',(3.5587973662077,2.01908299720839,-5.31237714025465)) ;
#167484 = CARTESIAN_POINT('Ctrl Pts',(3.55867935922409,2.01899873301461,-5.31244171035243)) ;
#167485 = CARTESIAN_POINT('Ctrl Pts',(3.5578895339955,2.01843691186419,-5.31286648337378)) ;
#167486 = CARTESIAN_POINT('Ctrl Pts',(3.55720723474254,2.01796200020269,-5.313197549106)) ;
#167487 = CARTESIAN_POINT('Ctrl Pts',(3.55509125643152,2.01652382826846,-5.31409794445157)) ;
#167488 = CARTESIAN_POINT('Ctrl Pts',(3.55356547969792,2.01553571874065,-5.31460356135168)) ;
#167489 = CARTESIAN_POINT('Ctrl Pts',(3.55133342567605,2.01417771500982,-5.31494476439962)) ;
#167490 = CARTESIAN_POINT('Ctrl Pts',(3.55066861961529,2.01378348733643,-5.31499963178873)) ;
#167491 = CARTESIAN_POINT('Ctrl Pts',(3.55,2.01339745962156,-5.315)) ;
#167492 = CARTESIAN_POINT('Origin',(3.5,1.9,-2.305)) ;
#167493 = CARTESIAN_POINT('Ctrl Pts',(3.55000000000001,2.01339745962156,-2.305)) ;
#167494 = CARTESIAN_POINT('Ctrl Pts',(3.55164546205119,2.01434746757975,-2.305)) ;
#167495 = CARTESIAN_POINT('Ctrl Pts',(3.55326668047441,2.01534654795451,-2.30533297803029)) ;
#167496 = CARTESIAN_POINT('Ctrl Pts',(3.55550702654634,2.01680421826673,-2.30609826168304)) ;
#167497 = CARTESIAN_POINT('Ctrl Pts',(3.55618577699068,2.01725684095079,-2.30637359606382)) ;
#167498 = CARTESIAN_POINT('Ctrl Pts',(3.55727967686454,2.01800266699453,-2.3068678300958)) ;
#167499 = CARTESIAN_POINT('Ctrl Pts',(3.55771141786834,2.01830156212325,-2.30707831894258)) ;
#167500 = CARTESIAN_POINT('Ctrl Pts',(3.56202821818163,2.02133211263485,-2.30917069109723)) ;
#167501 = CARTESIAN_POINT('Ctrl Pts',(3.56570108751487,2.02427663140646,-2.31224393162834)) ;
#167502 = CARTESIAN_POINT('Ctrl Pts',(3.5699034772657,2.02797441535154,-2.31640200473853)) ;
#167503 = CARTESIAN_POINT('Ctrl Pts',(3.5707247356113,2.02871480216325,-2.31724959773097)) ;
#167504 = CARTESIAN_POINT('Ctrl Pts',(3.5738286330762,2.03157464832067,-2.32054171893286)) ;
#167505 = CARTESIAN_POINT('Ctrl Pts',(3.5759706937612,2.03369481096682,-2.32313773435733)) ;
#167506 = CARTESIAN_POINT('Ctrl Pts',(3.58156103639367,2.03956384830232,-2.33075811677975)) ;
#167507 = CARTESIAN_POINT('Ctrl Pts',(3.58475859790494,2.04336775308648,-2.33615483852158)) ;
#167508 = CARTESIAN_POINT('Ctrl Pts',(3.58897725231935,2.04901055924319,-2.34495483430059)) ;
#167509 = CARTESIAN_POINT('Ctrl Pts',(3.59034871903171,2.05099358132072,-2.34822253384318)) ;
#167510 = CARTESIAN_POINT('Ctrl Pts',(3.59365488292729,2.05613355260444,-2.35724922860834)) ;
#167511 = CARTESIAN_POINT('Ctrl Pts',(3.59534780095525,2.05919518104044,-2.36324371161028)) ;
#167512 = CARTESIAN_POINT('Ctrl Pts',(3.59674625886211,2.06216860863463,-2.36996044662965)) ;
#167513 = CARTESIAN_POINT('Ctrl Pts',(3.59685725281059,2.0624088313306,-2.37051031510962)) ;
#167514 = CARTESIAN_POINT('Ctrl Pts',(3.59768573690243,2.06423460359408,-2.37474653762001)) ;
#167515 = CARTESIAN_POINT('Ctrl Pts',(3.59826864191792,2.06571343564803,-2.37852399715655)) ;
#167516 = CARTESIAN_POINT('Ctrl Pts',(3.59959273712775,2.06963221119414,-2.38968301436905)) ;
#167517 = CARTESIAN_POINT('Ctrl Pts',(3.6,2.07172309150643,-2.3972993579658)) ;
#167518 = CARTESIAN_POINT('Ctrl Pts',(3.6,2.07320508075689,-2.405)) ;
#167519 = CARTESIAN_POINT('Origin',(3.5,1.9,-9.925)) ;
#167520 = CARTESIAN_POINT('',(3.55,2.01339745962156,-9.925)) ;
#167521 = CARTESIAN_POINT('Origin',(3.5,2.1,-9.925)) ;
#167522 = CARTESIAN_POINT('Ctrl Pts',(3.55,2.01339745962156,-9.925)) ;
#167523 = CARTESIAN_POINT('Ctrl Pts',(3.55164546205119,2.01434746757975,-9.925)) ;
#167524 = CARTESIAN_POINT('Ctrl Pts',(3.55326668047443,2.01534654795452,-9.92533297803029)) ;
#167525 = CARTESIAN_POINT('Ctrl Pts',(3.55550702654635,2.01680421826674,-9.92609826168304)) ;
#167526 = CARTESIAN_POINT('Ctrl Pts',(3.55618577699069,2.0172568409508,-9.92637359606382)) ;
#167527 = CARTESIAN_POINT('Ctrl Pts',(3.55727967686454,2.01800266699454,-9.92686783009579)) ;
#167528 = CARTESIAN_POINT('Ctrl Pts',(3.55771141786834,2.01830156212325,-9.92707831894258)) ;
#167529 = CARTESIAN_POINT('Ctrl Pts',(3.56202821818162,2.02133211263484,-9.92917069109722)) ;
#167530 = CARTESIAN_POINT('Ctrl Pts',(3.56570108751486,2.02427663140645,-9.93224393162833)) ;
#167531 = CARTESIAN_POINT('Ctrl Pts',(3.56990347726569,2.02797441535153,-9.93640200473853)) ;
#167532 = CARTESIAN_POINT('Ctrl Pts',(3.5707247356113,2.02871480216325,-9.93724959773096)) ;
#167533 = CARTESIAN_POINT('Ctrl Pts',(3.57382863307621,2.03157464832067,-9.94054171893286)) ;
#167534 = CARTESIAN_POINT('Ctrl Pts',(3.5759706937612,2.03369481096682,-9.94313773435733)) ;
#167535 = CARTESIAN_POINT('Ctrl Pts',(3.58156103639368,2.03956384830232,-9.95075811677975)) ;
#167536 = CARTESIAN_POINT('Ctrl Pts',(3.58475859790494,2.04336775308648,-9.95615483852156)) ;
#167537 = CARTESIAN_POINT('Ctrl Pts',(3.58897725231935,2.0490105592432,-9.96495483430059)) ;
#167538 = CARTESIAN_POINT('Ctrl Pts',(3.59034871903171,2.05099358132072,-9.96822253384318)) ;
#167539 = CARTESIAN_POINT('Ctrl Pts',(3.59365488292729,2.05613355260445,-9.97724922860834)) ;
#167540 = CARTESIAN_POINT('Ctrl Pts',(3.59534780095525,2.05919518104045,-9.98324371161027)) ;
#167541 = CARTESIAN_POINT('Ctrl Pts',(3.59674625886211,2.06216860863464,-9.98996044662965)) ;
#167542 = CARTESIAN_POINT('Ctrl Pts',(3.59685725281059,2.06240883133061,-9.99051031510962)) ;
#167543 = CARTESIAN_POINT('Ctrl Pts',(3.59768573690243,2.06423460359409,-9.99474653762001)) ;
#167544 = CARTESIAN_POINT('Ctrl Pts',(3.59826864191792,2.06571343564803,-9.99852399715655)) ;
#167545 = CARTESIAN_POINT('Ctrl Pts',(3.59959273712775,2.06963221119414,-10.0096830143691)) ;
#167546 = CARTESIAN_POINT('Ctrl Pts',(3.6,2.07172309150643,-10.0172993579658)) ;
#167547 = CARTESIAN_POINT('Ctrl Pts',(3.6,2.07320508075689,-10.025)) ;
#167548 = CARTESIAN_POINT('Origin',(3.5,2.1,-1.01757522333835E-15)) ;
#167549 = CARTESIAN_POINT('Origin',(3.5,2.1,-9.925)) ;
#167550 = CARTESIAN_POINT('',(3.55,2.01339745962156,-9.125)) ;
#167551 = CARTESIAN_POINT('Origin',(3.5,2.1,-9.125)) ;
#167552 = CARTESIAN_POINT('Origin',(3.5,2.1,-9.125)) ;
#167553 = CARTESIAN_POINT('Origin',(3.5,1.9,-9.125)) ;
#167554 = CARTESIAN_POINT('Ctrl Pts',(3.6,2.07320508075689,-9.025)) ;
#167555 = CARTESIAN_POINT('Ctrl Pts',(3.6,2.07265589924992,-9.02785357667023)) ;
#167556 = CARTESIAN_POINT('Ctrl Pts',(3.59994554076637,2.07202433860043,-9.03069358004957)) ;
#167557 = CARTESIAN_POINT('Ctrl Pts',(3.59971739924419,2.0705936610056,-9.03637921497813)) ;
#167558 = CARTESIAN_POINT('Ctrl Pts',(3.59954156373424,2.06979274847041,-9.03921873634762)) ;
#167559 = CARTESIAN_POINT('Ctrl Pts',(3.5988078314118,2.06712577191644,-9.04778089072574)) ;
#167560 = CARTESIAN_POINT('Ctrl Pts',(3.59804129495583,2.06501902766383,-9.05341713644404)) ;
#167561 = CARTESIAN_POINT('Ctrl Pts',(3.59624340061598,2.06105248659392,-9.06263353946358)) ;
#167562 = CARTESIAN_POINT('Ctrl Pts',(3.59536494855695,2.05931170891995,-9.06632347138735)) ;
#167563 = CARTESIAN_POINT('Ctrl Pts',(3.5928372720244,2.05479606436796,-9.075199432059)) ;
#167564 = CARTESIAN_POINT('Ctrl Pts',(3.59099650883094,2.05188276467126,-9.08034424200704)) ;
#167565 = CARTESIAN_POINT('Ctrl Pts',(3.58838944624311,2.04823719194676,-9.08622737667937)) ;
#167566 = CARTESIAN_POINT('Ctrl Pts',(3.58794537962076,2.04762948672745,-9.08719091385132)) ;
#167567 = CARTESIAN_POINT('Ctrl Pts',(3.58597371492279,2.04498948329048,-9.09130665172963)) ;
#167568 = CARTESIAN_POINT('Ctrl Pts',(3.58430396743904,2.04289920268562,-9.09439316248022)) ;
#167569 = CARTESIAN_POINT('Ctrl Pts',(3.58008903321355,2.03798436571145,-9.10128092067901)) ;
#167570 = CARTESIAN_POINT('Ctrl Pts',(3.57743593401584,2.03513945367717,-9.10500157292067)) ;
#167571 = CARTESIAN_POINT('Ctrl Pts',(3.57357563759665,2.03136250950848,-9.1095864015969)) ;
#167572 = CARTESIAN_POINT('Ctrl Pts',(3.57257888733676,2.03041544381403,-9.11070656893144)) ;
#167573 = CARTESIAN_POINT('Ctrl Pts',(3.56956839719839,2.0276417514069,-9.11390390778888)) ;
#167574 = CARTESIAN_POINT('Ctrl Pts',(3.56746189551947,2.02581554544782,-9.11598430067906)) ;
#167575 = CARTESIAN_POINT('Ctrl Pts',(3.56503628433183,2.02384076964143,-9.11802226003861)) ;
#167576 = CARTESIAN_POINT('Ctrl Pts',(3.56481411023491,2.02366103014355,-9.11820583968789)) ;
#167577 = CARTESIAN_POINT('Ctrl Pts',(3.56285239425755,2.02208416924059,-9.11979838212054)) ;
#167578 = CARTESIAN_POINT('Ctrl Pts',(3.56093641846873,2.02061618613967,-9.12118717775184)) ;
#167579 = CARTESIAN_POINT('Ctrl Pts',(3.55879736620764,2.01908299720835,-9.12237714025469)) ;
#167580 = CARTESIAN_POINT('Ctrl Pts',(3.5586793592241,2.01899873301461,-9.12244171035242)) ;
#167581 = CARTESIAN_POINT('Ctrl Pts',(3.55788953399554,2.01843691186422,-9.12286648337376)) ;
#167582 = CARTESIAN_POINT('Ctrl Pts',(3.55720723474255,2.0179620002027,-9.123197549106)) ;
#167583 = CARTESIAN_POINT('Ctrl Pts',(3.55509125643146,2.01652382826842,-9.12409794445161)) ;
#167584 = CARTESIAN_POINT('Ctrl Pts',(3.5535654796978,2.01553571874058,-9.12460356135171)) ;
#167585 = CARTESIAN_POINT('Ctrl Pts',(3.55133342567592,2.01417771500975,-9.12494476439961)) ;
#167586 = CARTESIAN_POINT('Ctrl Pts',(3.55066861961523,2.01378348733639,-9.12499963178872)) ;
#167587 = CARTESIAN_POINT('Ctrl Pts',(3.55,2.01339745962156,-9.125)) ;
#167588 = CARTESIAN_POINT('Origin',(3.5,1.9,-13.735)) ;
#167589 = CARTESIAN_POINT('',(3.55,2.01339745962156,-13.735)) ;
#167590 = CARTESIAN_POINT('Origin',(3.5,2.1,-13.735)) ;
#167591 = CARTESIAN_POINT('Ctrl Pts',(3.55,2.01339745962156,-13.735)) ;
#167592 = CARTESIAN_POINT('Ctrl Pts',(3.55164546205119,2.01434746757975,-13.735)) ;
#167593 = CARTESIAN_POINT('Ctrl Pts',(3.55326668047442,2.01534654795452,-13.7353329780303)) ;
#167594 = CARTESIAN_POINT('Ctrl Pts',(3.55550702654635,2.01680421826673,-13.736098261683)) ;
#167595 = CARTESIAN_POINT('Ctrl Pts',(3.55618577699069,2.0172568409508,-13.7363735960638)) ;
#167596 = CARTESIAN_POINT('Ctrl Pts',(3.55727967686454,2.01800266699454,-13.7368678300958)) ;
#167597 = CARTESIAN_POINT('Ctrl Pts',(3.55771141786834,2.01830156212325,-13.7370783189426)) ;
#167598 = CARTESIAN_POINT('Ctrl Pts',(3.56202821818163,2.02133211263485,-13.7391706910972)) ;
#167599 = CARTESIAN_POINT('Ctrl Pts',(3.56570108751487,2.02427663140646,-13.7422439316283)) ;
#167600 = CARTESIAN_POINT('Ctrl Pts',(3.5699034772657,2.02797441535153,-13.7464020047385)) ;
#167601 = CARTESIAN_POINT('Ctrl Pts',(3.57072473561131,2.02871480216325,-13.747249597731)) ;
#167602 = CARTESIAN_POINT('Ctrl Pts',(3.57382863307621,2.03157464832067,-13.7505417189329)) ;
#167603 = CARTESIAN_POINT('Ctrl Pts',(3.57597069376121,2.03369481096682,-13.7531377343573)) ;
#167604 = CARTESIAN_POINT('Ctrl Pts',(3.58156103639367,2.03956384830232,-13.7607581167797)) ;
#167605 = CARTESIAN_POINT('Ctrl Pts',(3.58475859790494,2.04336775308648,-13.7661548385216)) ;
#167606 = CARTESIAN_POINT('Ctrl Pts',(3.58897725231935,2.0490105592432,-13.7749548343006)) ;
#167607 = CARTESIAN_POINT('Ctrl Pts',(3.59034871903171,2.05099358132072,-13.7782225338432)) ;
#167608 = CARTESIAN_POINT('Ctrl Pts',(3.5936548829273,2.05613355260447,-13.7872492286084)) ;
#167609 = CARTESIAN_POINT('Ctrl Pts',(3.59534780095527,2.05919518104048,-13.7932437116103)) ;
#167610 = CARTESIAN_POINT('Ctrl Pts',(3.59674625886213,2.06216860863467,-13.7999604466297)) ;
#167611 = CARTESIAN_POINT('Ctrl Pts',(3.5968572528106,2.06240883133063,-13.8005103151097)) ;
#167612 = CARTESIAN_POINT('Ctrl Pts',(3.59768573690243,2.06423460359409,-13.80474653762)) ;
#167613 = CARTESIAN_POINT('Ctrl Pts',(3.59826864191792,2.06571343564803,-13.8085239971566)) ;
#167614 = CARTESIAN_POINT('Ctrl Pts',(3.59959273712776,2.06963221119414,-13.8196830143691)) ;
#167615 = CARTESIAN_POINT('Ctrl Pts',(3.6,2.07172309150643,-13.8272993579658)) ;
#167616 = CARTESIAN_POINT('Ctrl Pts',(3.6,2.07320508075689,-13.835)) ;
#167617 = CARTESIAN_POINT('Origin',(3.5,2.10000000000001,-1.01757522333835E-15)) ;
#167618 = CARTESIAN_POINT('Origin',(3.5,2.1,-13.735)) ;
#167619 = CARTESIAN_POINT('',(3.55,2.01339745962156,-12.935)) ;
#167620 = CARTESIAN_POINT('Origin',(3.5,2.1,-12.935)) ;
#167621 = CARTESIAN_POINT('Origin',(3.5,2.1,-12.935)) ;
#167622 = CARTESIAN_POINT('Origin',(3.5,1.9,-12.935)) ;
#167623 = CARTESIAN_POINT('Ctrl Pts',(3.6,2.07320508075689,-12.835)) ;
#167624 = CARTESIAN_POINT('Ctrl Pts',(3.6,2.07265589924993,-12.8378535766702)) ;
#167625 = CARTESIAN_POINT('Ctrl Pts',(3.59994554076638,2.07202433860046,-12.8406935800495)) ;
#167626 = CARTESIAN_POINT('Ctrl Pts',(3.59971739924421,2.07059366100576,-12.8463792149776)) ;
#167627 = CARTESIAN_POINT('Ctrl Pts',(3.5995415637343,2.0697927484707,-12.8492187363466)) ;
#167628 = CARTESIAN_POINT('Ctrl Pts',(3.59880783141193,2.06712577191679,-12.8577808907248)) ;
#167629 = CARTESIAN_POINT('Ctrl Pts',(3.59804129495592,2.06501902766401,-12.8634171364436)) ;
#167630 = CARTESIAN_POINT('Ctrl Pts',(3.59624340061598,2.06105248659392,-12.8726335394636)) ;
#167631 = CARTESIAN_POINT('Ctrl Pts',(3.59536494855695,2.05931170891995,-12.8763234713874)) ;
#167632 = CARTESIAN_POINT('Ctrl Pts',(3.59283727202456,2.05479606436822,-12.8851994320584)) ;
#167633 = CARTESIAN_POINT('Ctrl Pts',(3.5909965088313,2.05188276467182,-12.890344242006)) ;
#167634 = CARTESIAN_POINT('Ctrl Pts',(3.58838944624354,2.04823719194735,-12.8962273766784)) ;
#167635 = CARTESIAN_POINT('Ctrl Pts',(3.58794537962099,2.04762948672774,-12.8971909138509)) ;
#167636 = CARTESIAN_POINT('Ctrl Pts',(3.58597371492279,2.04498948329048,-12.9013066517297)) ;
#167637 = CARTESIAN_POINT('Ctrl Pts',(3.58430396743904,2.04289920268562,-12.9043931624803)) ;
#167638 = CARTESIAN_POINT('Ctrl Pts',(3.58008903321359,2.03798436571149,-12.9112809206789)) ;
#167639 = CARTESIAN_POINT('Ctrl Pts',(3.57743593401593,2.03513945367727,-12.9150015729205)) ;
#167640 = CARTESIAN_POINT('Ctrl Pts',(3.57357563759675,2.03136250950857,-12.9195864015968)) ;
#167641 = CARTESIAN_POINT('Ctrl Pts',(3.57257888733681,2.03041544381408,-12.9207065689314)) ;
#167642 = CARTESIAN_POINT('Ctrl Pts',(3.56956839719853,2.02764175140703,-12.9239039077887)) ;
#167643 = CARTESIAN_POINT('Ctrl Pts',(3.56746189551978,2.02581554544809,-12.9259843006788)) ;
#167644 = CARTESIAN_POINT('Ctrl Pts',(3.56503628433215,2.02384076964169,-12.9280222600383)) ;
#167645 = CARTESIAN_POINT('Ctrl Pts',(3.56481411023507,2.02366103014368,-12.9282058396877)) ;
#167646 = CARTESIAN_POINT('Ctrl Pts',(3.56285239425758,2.02208416924061,-12.9297983821205)) ;
#167647 = CARTESIAN_POINT('Ctrl Pts',(3.56093641846878,2.02061618613971,-12.9311871777518)) ;
#167648 = CARTESIAN_POINT('Ctrl Pts',(3.55879736620769,2.01908299720838,-12.9323771402546)) ;
#167649 = CARTESIAN_POINT('Ctrl Pts',(3.55867935922412,2.01899873301463,-12.9324417103524)) ;
#167650 = CARTESIAN_POINT('Ctrl Pts',(3.55788953399555,2.01843691186422,-12.9328664833737)) ;
#167651 = CARTESIAN_POINT('Ctrl Pts',(3.55720723474256,2.0179620002027,-12.933197549106)) ;
#167652 = CARTESIAN_POINT('Ctrl Pts',(3.55509125643146,2.01652382826842,-12.9340979444515)) ;
#167653 = CARTESIAN_POINT('Ctrl Pts',(3.55356547969779,2.01553571874057,-12.9346035613517)) ;
#167654 = CARTESIAN_POINT('Ctrl Pts',(3.55133342567592,2.01417771500975,-12.9349447643996)) ;
#167655 = CARTESIAN_POINT('Ctrl Pts',(3.55066861961523,2.01378348733639,-12.9349996317887)) ;
#167656 = CARTESIAN_POINT('Ctrl Pts',(3.55,2.01339745962156,-12.935)) ;
#167657 = CARTESIAN_POINT('Origin',(3.5,1.9,-17.545)) ;
#167658 = CARTESIAN_POINT('',(3.55,2.01339745962156,-17.545)) ;
#167659 = CARTESIAN_POINT('Origin',(3.5,2.1,-17.545)) ;
#167660 = CARTESIAN_POINT('Ctrl Pts',(3.55,2.01339745962156,-17.545)) ;
#167661 = CARTESIAN_POINT('Ctrl Pts',(3.55164546205118,2.01434746757975,-17.545)) ;
#167662 = CARTESIAN_POINT('Ctrl Pts',(3.55326668047441,2.01534654795451,-17.5453329780303)) ;
#167663 = CARTESIAN_POINT('Ctrl Pts',(3.55550702654633,2.01680421826672,-17.546098261683)) ;
#167664 = CARTESIAN_POINT('Ctrl Pts',(3.55618577699068,2.01725684095079,-17.5463735960638)) ;
#167665 = CARTESIAN_POINT('Ctrl Pts',(3.55727967686454,2.01800266699453,-17.5468678300958)) ;
#167666 = CARTESIAN_POINT('Ctrl Pts',(3.55771141786834,2.01830156212325,-17.5470783189426)) ;
#167667 = CARTESIAN_POINT('Ctrl Pts',(3.56202821818158,2.02133211263482,-17.5491706910972)) ;
#167668 = CARTESIAN_POINT('Ctrl Pts',(3.56570108751479,2.02427663140639,-17.5522439316283)) ;
#167669 = CARTESIAN_POINT('Ctrl Pts',(3.56990347726563,2.02797441535147,-17.5564020047385)) ;
#167670 = CARTESIAN_POINT('Ctrl Pts',(3.57072473561127,2.02871480216322,-17.5572495977309)) ;
#167671 = CARTESIAN_POINT('Ctrl Pts',(3.5738286330762,2.03157464832067,-17.5605417189329)) ;
#167672 = CARTESIAN_POINT('Ctrl Pts',(3.5759706937612,2.03369481096682,-17.5631377343573)) ;
#167673 = CARTESIAN_POINT('Ctrl Pts',(3.58156103639368,2.03956384830232,-17.5707581167797)) ;
#167674 = CARTESIAN_POINT('Ctrl Pts',(3.58475859790495,2.04336775308648,-17.5761548385216)) ;
#167675 = CARTESIAN_POINT('Ctrl Pts',(3.58897725231935,2.0490105592432,-17.5849548343006)) ;
#167676 = CARTESIAN_POINT('Ctrl Pts',(3.59034871903171,2.05099358132072,-17.5882225338432)) ;
#167677 = CARTESIAN_POINT('Ctrl Pts',(3.59365488292715,2.05613355260423,-17.597249228608)) ;
#167678 = CARTESIAN_POINT('Ctrl Pts',(3.59534780095503,2.05919518104004,-17.6032437116095)) ;
#167679 = CARTESIAN_POINT('Ctrl Pts',(3.59674625886195,2.06216860863428,-17.6099604466289)) ;
#167680 = CARTESIAN_POINT('Ctrl Pts',(3.59685725281051,2.06240883133043,-17.6105103151092)) ;
#167681 = CARTESIAN_POINT('Ctrl Pts',(3.59768573690243,2.06423460359408,-17.61474653762)) ;
#167682 = CARTESIAN_POINT('Ctrl Pts',(3.59826864191792,2.06571343564803,-17.6185239971566)) ;
#167683 = CARTESIAN_POINT('Ctrl Pts',(3.59959273712775,2.06963221119414,-17.6296830143691)) ;
#167684 = CARTESIAN_POINT('Ctrl Pts',(3.6,2.07172309150643,-17.6372993579658)) ;
#167685 = CARTESIAN_POINT('Ctrl Pts',(3.6,2.07320508075689,-17.645)) ;
#167686 = CARTESIAN_POINT('Origin',(3.5,2.10000000000001,-1.01757522333836E-15)) ;
#167687 = CARTESIAN_POINT('Origin',(3.5,2.1,-17.545)) ;
#167688 = CARTESIAN_POINT('',(3.55,2.01339745962156,-16.745)) ;
#167689 = CARTESIAN_POINT('Origin',(3.5,2.1,-16.745)) ;
#167690 = CARTESIAN_POINT('Origin',(3.5,2.1,-16.745)) ;
#167691 = CARTESIAN_POINT('Origin',(3.5,1.9,-16.745)) ;
#167692 = CARTESIAN_POINT('Ctrl Pts',(3.6,2.07320508075689,-16.645)) ;
#167693 = CARTESIAN_POINT('Ctrl Pts',(3.6,2.0724036454051,-16.6491643012255)) ;
#167694 = CARTESIAN_POINT('Ctrl Pts',(3.59988358031788,2.07142604615684,-16.6532993264777)) ;
#167695 = CARTESIAN_POINT('Ctrl Pts',(3.5992764543265,2.06860573724892,-16.6634232053159)) ;
#167696 = CARTESIAN_POINT('Ctrl Pts',(3.59862250828209,2.06654864780065,-16.6694017962796)) ;
#167697 = CARTESIAN_POINT('Ctrl Pts',(3.5974369582727,2.06370626825461,-16.6764308805049)) ;
#167698 = CARTESIAN_POINT('Ctrl Pts',(3.59721441711742,2.06319475755342,-16.6776558946613)) ;
#167699 = CARTESIAN_POINT('Ctrl Pts',(3.59624340061598,2.06105248659392,-16.6826335394636)) ;
#167700 = CARTESIAN_POINT('Ctrl Pts',(3.59536494855695,2.05931170891994,-16.6863234713874)) ;
#167701 = CARTESIAN_POINT('Ctrl Pts',(3.59283727202454,2.05479606436819,-16.6951994320585)) ;
#167702 = CARTESIAN_POINT('Ctrl Pts',(3.59099650883127,2.05188276467178,-16.7003442420061)) ;
#167703 = CARTESIAN_POINT('Ctrl Pts',(3.58838944624351,2.0482371919473,-16.7062273766785)) ;
#167704 = CARTESIAN_POINT('Ctrl Pts',(3.58794537962097,2.04762948672772,-16.7071909138509)) ;
#167705 = CARTESIAN_POINT('Ctrl Pts',(3.58597371492279,2.04498948329048,-16.7113066517297)) ;
#167706 = CARTESIAN_POINT('Ctrl Pts',(3.58430396743904,2.04289920268562,-16.7143931624803)) ;
#167707 = CARTESIAN_POINT('Ctrl Pts',(3.58008903321369,2.0379843657116,-16.7212809206788)) ;
#167708 = CARTESIAN_POINT('Ctrl Pts',(3.57743593401614,2.03513945367749,-16.7250015729202)) ;
#167709 = CARTESIAN_POINT('Ctrl Pts',(3.57357563759699,2.03136250950879,-16.7295864015965)) ;
#167710 = CARTESIAN_POINT('Ctrl Pts',(3.57257888733693,2.03041544381418,-16.7307065689312)) ;
#167711 = CARTESIAN_POINT('Ctrl Pts',(3.56956839719843,2.02764175140693,-16.7339039077887)) ;
#167712 = CARTESIAN_POINT('Ctrl Pts',(3.56746189551956,2.0258155454479,-16.7359843006789)) ;
#167713 = CARTESIAN_POINT('Ctrl Pts',(3.56503628433193,2.02384076964151,-16.7380222600385)) ;
#167714 = CARTESIAN_POINT('Ctrl Pts',(3.56481411023496,2.02366103014359,-16.7382058396878)) ;
#167715 = CARTESIAN_POINT('Ctrl Pts',(3.56285239425741,2.02208416924048,-16.7397983821207)) ;
#167716 = CARTESIAN_POINT('Ctrl Pts',(3.56093641846842,2.02061618613943,-16.7411871777521)) ;
#167717 = CARTESIAN_POINT('Ctrl Pts',(3.55879736620727,2.01908299720808,-16.7423771402549)) ;
#167718 = CARTESIAN_POINT('Ctrl Pts',(3.55867935922384,2.01899873301443,-16.7424417103526)) ;
#167719 = CARTESIAN_POINT('Ctrl Pts',(3.55788953399545,2.01843691186415,-16.7428664833738)) ;
#167720 = CARTESIAN_POINT('Ctrl Pts',(3.55720723474251,2.01796200020267,-16.743197549106)) ;
#167721 = CARTESIAN_POINT('Ctrl Pts',(3.55509125643154,2.01652382826847,-16.7440979444515)) ;
#167722 = CARTESIAN_POINT('Ctrl Pts',(3.55356547969798,2.01553571874069,-16.7446035613516)) ;
#167723 = CARTESIAN_POINT('Ctrl Pts',(3.55133342567611,2.01417771500986,-16.7449447643996)) ;
#167724 = CARTESIAN_POINT('Ctrl Pts',(3.55066861961532,2.01378348733645,-16.7449996317888)) ;
#167725 = CARTESIAN_POINT('Ctrl Pts',(3.55,2.01339745962156,-16.745)) ;
#167726 = CARTESIAN_POINT('Origin',(3.5,1.9,-21.355)) ;
#167727 = CARTESIAN_POINT('',(3.55,2.01339745962156,-21.355)) ;
#167728 = CARTESIAN_POINT('Origin',(3.5,2.1,-21.355)) ;
#167729 = CARTESIAN_POINT('Ctrl Pts',(3.55,2.01339745962156,-21.355)) ;
#167730 = CARTESIAN_POINT('Ctrl Pts',(3.55164546205118,2.01434746757974,-21.355)) ;
#167731 = CARTESIAN_POINT('Ctrl Pts',(3.5532666804744,2.01534654795451,-21.3553329780303)) ;
#167732 = CARTESIAN_POINT('Ctrl Pts',(3.55550702654633,2.01680421826672,-21.356098261683)) ;
#167733 = CARTESIAN_POINT('Ctrl Pts',(3.55618577699068,2.01725684095079,-21.3563735960638)) ;
#167734 = CARTESIAN_POINT('Ctrl Pts',(3.55727967686454,2.01800266699453,-21.3568678300958)) ;
#167735 = CARTESIAN_POINT('Ctrl Pts',(3.55771141786834,2.01830156212325,-21.3570783189426)) ;
#167736 = CARTESIAN_POINT('Ctrl Pts',(3.56202821818158,2.02133211263481,-21.3591706910972)) ;
#167737 = CARTESIAN_POINT('Ctrl Pts',(3.56570108751478,2.02427663140639,-21.3622439316283)) ;
#167738 = CARTESIAN_POINT('Ctrl Pts',(3.56990347726562,2.02797441535147,-21.3664020047385)) ;
#167739 = CARTESIAN_POINT('Ctrl Pts',(3.57072473561127,2.02871480216322,-21.3672495977309)) ;
#167740 = CARTESIAN_POINT('Ctrl Pts',(3.5738286330762,2.03157464832067,-21.3705417189329)) ;
#167741 = CARTESIAN_POINT('Ctrl Pts',(3.5759706937612,2.03369481096682,-21.3731377343573)) ;
#167742 = CARTESIAN_POINT('Ctrl Pts',(3.58156103639368,2.03956384830231,-21.3807581167797)) ;
#167743 = CARTESIAN_POINT('Ctrl Pts',(3.58475859790495,2.04336775308647,-21.3861548385216)) ;
#167744 = CARTESIAN_POINT('Ctrl Pts',(3.58897725231935,2.04901055924319,-21.3949548343006)) ;
#167745 = CARTESIAN_POINT('Ctrl Pts',(3.59034871903171,2.05099358132072,-21.3982225338432)) ;
#167746 = CARTESIAN_POINT('Ctrl Pts',(3.59365488292718,2.05613355260427,-21.407249228608)) ;
#167747 = CARTESIAN_POINT('Ctrl Pts',(3.59534780095507,2.05919518104011,-21.4132437116097)) ;
#167748 = CARTESIAN_POINT('Ctrl Pts',(3.59674625886198,2.06216860863434,-21.419960446629)) ;
#167749 = CARTESIAN_POINT('Ctrl Pts',(3.59685725281052,2.06240883133046,-21.4205103151093)) ;
#167750 = CARTESIAN_POINT('Ctrl Pts',(3.59768573690243,2.06423460359408,-21.42474653762)) ;
#167751 = CARTESIAN_POINT('Ctrl Pts',(3.59826864191791,2.06571343564803,-21.4285239971566)) ;
#167752 = CARTESIAN_POINT('Ctrl Pts',(3.59959273712775,2.06963221119414,-21.4396830143691)) ;
#167753 = CARTESIAN_POINT('Ctrl Pts',(3.6,2.07172309150643,-21.4472993579658)) ;
#167754 = CARTESIAN_POINT('Ctrl Pts',(3.6,2.07320508075689,-21.455)) ;
#167755 = CARTESIAN_POINT('Origin',(3.5,2.10000000000001,-1.01757522333836E-15)) ;
#167756 = CARTESIAN_POINT('Origin',(3.5,2.1,-21.355)) ;
#167757 = CARTESIAN_POINT('',(3.55,2.01339745962156,-20.555)) ;
#167758 = CARTESIAN_POINT('Origin',(3.5,2.1,-20.555)) ;
#167759 = CARTESIAN_POINT('Origin',(3.5,2.1,-20.555)) ;
#167760 = CARTESIAN_POINT('Origin',(3.5,1.9,-20.555)) ;
#167761 = CARTESIAN_POINT('Ctrl Pts',(3.6,2.07320508075689,-20.455)) ;
#167762 = CARTESIAN_POINT('Ctrl Pts',(3.6,2.07265589924995,-20.45785357667)) ;
#167763 = CARTESIAN_POINT('Ctrl Pts',(3.59994554076638,2.07202433860051,-20.4606935800491)) ;
#167764 = CARTESIAN_POINT('Ctrl Pts',(3.59971739924421,2.07059366100571,-20.4663792149777)) ;
#167765 = CARTESIAN_POINT('Ctrl Pts',(3.59954156373426,2.06979274847046,-20.4692187363474)) ;
#167766 = CARTESIAN_POINT('Ctrl Pts',(3.5988078314118,2.06712577191645,-20.4777808907258)) ;
#167767 = CARTESIAN_POINT('Ctrl Pts',(3.59804129495583,2.06501902766384,-20.4834171364441)) ;
#167768 = CARTESIAN_POINT('Ctrl Pts',(3.59624340061598,2.06105248659392,-20.4926335394636)) ;
#167769 = CARTESIAN_POINT('Ctrl Pts',(3.59536494855695,2.05931170891995,-20.4963234713874)) ;
#167770 = CARTESIAN_POINT('Ctrl Pts',(3.59283727202454,2.05479606436819,-20.5051994320585)) ;
#167771 = CARTESIAN_POINT('Ctrl Pts',(3.59099650883126,2.05188276467176,-20.5103442420061)) ;
#167772 = CARTESIAN_POINT('Ctrl Pts',(3.58838944624349,2.04823719194729,-20.5162273766785)) ;
#167773 = CARTESIAN_POINT('Ctrl Pts',(3.58794537962096,2.04762948672771,-20.5171909138509)) ;
#167774 = CARTESIAN_POINT('Ctrl Pts',(3.58597371492279,2.04498948329048,-20.5213066517297)) ;
#167775 = CARTESIAN_POINT('Ctrl Pts',(3.58430396743904,2.04289920268562,-20.5243931624803)) ;
#167776 = CARTESIAN_POINT('Ctrl Pts',(3.58008903321371,2.03798436571163,-20.5312809206787)) ;
#167777 = CARTESIAN_POINT('Ctrl Pts',(3.5774359340162,2.03513945367755,-20.5350015729202)) ;
#167778 = CARTESIAN_POINT('Ctrl Pts',(3.57357563759705,2.03136250950885,-20.5395864015964)) ;
#167779 = CARTESIAN_POINT('Ctrl Pts',(3.57257888733696,2.03041544381421,-20.5407065689312)) ;
#167780 = CARTESIAN_POINT('Ctrl Pts',(3.56956839719839,2.0276417514069,-20.5439039077888)) ;
#167781 = CARTESIAN_POINT('Ctrl Pts',(3.56746189551949,2.02581554544783,-20.545984300679)) ;
#167782 = CARTESIAN_POINT('Ctrl Pts',(3.56503628433185,2.02384076964144,-20.5480222600386)) ;
#167783 = CARTESIAN_POINT('Ctrl Pts',(3.56481411023492,2.02366103014355,-20.5482058396879)) ;
#167784 = CARTESIAN_POINT('Ctrl Pts',(3.56285239425741,2.02208416924048,-20.5497983821207)) ;
#167785 = CARTESIAN_POINT('Ctrl Pts',(3.56093641846842,2.02061618613943,-20.5511871777521)) ;
#167786 = CARTESIAN_POINT('Ctrl Pts',(3.55879736620726,2.01908299720807,-20.5523771402549)) ;
#167787 = CARTESIAN_POINT('Ctrl Pts',(3.55867935922383,2.01899873301443,-20.5524417103526)) ;
#167788 = CARTESIAN_POINT('Ctrl Pts',(3.55788953399544,2.01843691186415,-20.5528664833738)) ;
#167789 = CARTESIAN_POINT('Ctrl Pts',(3.55720723474251,2.01796200020267,-20.553197549106)) ;
#167790 = CARTESIAN_POINT('Ctrl Pts',(3.55509125643154,2.01652382826847,-20.5540979444516)) ;
#167791 = CARTESIAN_POINT('Ctrl Pts',(3.55356547969797,2.01553571874069,-20.5546035613518)) ;
#167792 = CARTESIAN_POINT('Ctrl Pts',(3.55133342567611,2.01417771500986,-20.5549447643997)) ;
#167793 = CARTESIAN_POINT('Ctrl Pts',(3.55066861961532,2.01378348733645,-20.5549996317888)) ;
#167794 = CARTESIAN_POINT('Ctrl Pts',(3.55,2.01339745962156,-20.555)) ;
#167795 = CARTESIAN_POINT('Origin',(3.5,1.9,-25.165)) ;
#167796 = CARTESIAN_POINT('',(3.55,2.01339745962156,-25.165)) ;
#167797 = CARTESIAN_POINT('Origin',(3.5,2.1,-25.165)) ;
#167798 = CARTESIAN_POINT('Ctrl Pts',(3.55,2.01339745962156,-25.165)) ;
#167799 = CARTESIAN_POINT('Ctrl Pts',(3.55164546205118,2.01434746757975,-25.165)) ;
#167800 = CARTESIAN_POINT('Ctrl Pts',(3.55326668047441,2.01534654795451,-25.1653329780303)) ;
#167801 = CARTESIAN_POINT('Ctrl Pts',(3.55550702654633,2.01680421826672,-25.166098261683)) ;
#167802 = CARTESIAN_POINT('Ctrl Pts',(3.55618577699068,2.01725684095079,-25.1663735960638)) ;
#167803 = CARTESIAN_POINT('Ctrl Pts',(3.55727967686454,2.01800266699453,-25.1668678300958)) ;
#167804 = CARTESIAN_POINT('Ctrl Pts',(3.55771141786834,2.01830156212325,-25.1670783189426)) ;
#167805 = CARTESIAN_POINT('Ctrl Pts',(3.56202821818159,2.02133211263482,-25.1691706910972)) ;
#167806 = CARTESIAN_POINT('Ctrl Pts',(3.56570108751481,2.02427663140641,-25.1722439316283)) ;
#167807 = CARTESIAN_POINT('Ctrl Pts',(3.56990347726564,2.02797441535149,-25.1764020047385)) ;
#167808 = CARTESIAN_POINT('Ctrl Pts',(3.57072473561128,2.02871480216323,-25.1772495977309)) ;
#167809 = CARTESIAN_POINT('Ctrl Pts',(3.57382863307621,2.03157464832067,-25.1805417189329)) ;
#167810 = CARTESIAN_POINT('Ctrl Pts',(3.5759706937612,2.03369481096682,-25.1831377343573)) ;
#167811 = CARTESIAN_POINT('Ctrl Pts',(3.58156103639368,2.03956384830231,-25.1907581167797)) ;
#167812 = CARTESIAN_POINT('Ctrl Pts',(3.58475859790494,2.04336775308647,-25.1961548385216)) ;
#167813 = CARTESIAN_POINT('Ctrl Pts',(3.58897725231935,2.04901055924319,-25.2049548343006)) ;
#167814 = CARTESIAN_POINT('Ctrl Pts',(3.59034871903171,2.05099358132072,-25.2082225338432)) ;
#167815 = CARTESIAN_POINT('Ctrl Pts',(3.5936548829272,2.0561335526043,-25.2172492286081)) ;
#167816 = CARTESIAN_POINT('Ctrl Pts',(3.5953478009551,2.05919518104017,-25.2232437116098)) ;
#167817 = CARTESIAN_POINT('Ctrl Pts',(3.596746258862,2.06216860863439,-25.2299604466291)) ;
#167818 = CARTESIAN_POINT('Ctrl Pts',(3.59685725281053,2.06240883133048,-25.2305103151093)) ;
#167819 = CARTESIAN_POINT('Ctrl Pts',(3.59768573690243,2.06423460359408,-25.23474653762)) ;
#167820 = CARTESIAN_POINT('Ctrl Pts',(3.59826864191792,2.06571343564803,-25.2385239971565)) ;
#167821 = CARTESIAN_POINT('Ctrl Pts',(3.59959273712775,2.06963221119414,-25.2496830143691)) ;
#167822 = CARTESIAN_POINT('Ctrl Pts',(3.6,2.07172309150643,-25.2572993579658)) ;
#167823 = CARTESIAN_POINT('Ctrl Pts',(3.6,2.07320508075689,-25.265)) ;
#167824 = CARTESIAN_POINT('Origin',(3.5,2.10000000000001,-1.01757522333836E-15)) ;
#167825 = CARTESIAN_POINT('Origin',(3.5,2.1,-25.165)) ;
#167826 = CARTESIAN_POINT('',(3.55,2.01339745962156,-24.365)) ;
#167827 = CARTESIAN_POINT('Origin',(3.5,2.1,-24.365)) ;
#167828 = CARTESIAN_POINT('Origin',(3.5,2.1,-24.365)) ;
#167829 = CARTESIAN_POINT('Origin',(3.5,1.9,-24.365)) ;
#167830 = CARTESIAN_POINT('Ctrl Pts',(3.6,2.07320508075689,-24.265)) ;
#167831 = CARTESIAN_POINT('Ctrl Pts',(3.6,2.07265589924987,-24.2678535766704)) ;
#167832 = CARTESIAN_POINT('Ctrl Pts',(3.59994554076637,2.07202433860034,-24.27069358005)) ;
#167833 = CARTESIAN_POINT('Ctrl Pts',(3.59971739924417,2.0705936610055,-24.2763792149785)) ;
#167834 = CARTESIAN_POINT('Ctrl Pts',(3.59954156373423,2.06979274847036,-24.2792187363477)) ;
#167835 = CARTESIAN_POINT('Ctrl Pts',(3.59880783141181,2.06712577191647,-24.2877808907257)) ;
#167836 = CARTESIAN_POINT('Ctrl Pts',(3.59804129495584,2.06501902766384,-24.293417136444)) ;
#167837 = CARTESIAN_POINT('Ctrl Pts',(3.59624340061598,2.06105248659392,-24.3026335394636)) ;
#167838 = CARTESIAN_POINT('Ctrl Pts',(3.59536494855695,2.05931170891994,-24.3063234713874)) ;
#167839 = CARTESIAN_POINT('Ctrl Pts',(3.59283727202457,2.05479606436824,-24.3151994320584)) ;
#167840 = CARTESIAN_POINT('Ctrl Pts',(3.59099650883134,2.05188276467188,-24.3203442420059)) ;
#167841 = CARTESIAN_POINT('Ctrl Pts',(3.58838944624358,2.04823719194741,-24.3262273766783)) ;
#167842 = CARTESIAN_POINT('Ctrl Pts',(3.58794537962101,2.04762948672777,-24.3271909138508)) ;
#167843 = CARTESIAN_POINT('Ctrl Pts',(3.58597371492279,2.04498948329048,-24.3313066517297)) ;
#167844 = CARTESIAN_POINT('Ctrl Pts',(3.58430396743904,2.04289920268562,-24.3343931624803)) ;
#167845 = CARTESIAN_POINT('Ctrl Pts',(3.58008903321372,2.03798436571164,-24.3412809206787)) ;
#167846 = CARTESIAN_POINT('Ctrl Pts',(3.57743593401622,2.03513945367757,-24.3450015729201)) ;
#167847 = CARTESIAN_POINT('Ctrl Pts',(3.57357563759708,2.03136250950888,-24.3495864015964)) ;
#167848 = CARTESIAN_POINT('Ctrl Pts',(3.57257888733697,2.03041544381422,-24.3507065689311)) ;
#167849 = CARTESIAN_POINT('Ctrl Pts',(3.56956839719845,2.02764175140695,-24.3539039077887)) ;
#167850 = CARTESIAN_POINT('Ctrl Pts',(3.5674618955196,2.02581554544793,-24.3559843006788)) ;
#167851 = CARTESIAN_POINT('Ctrl Pts',(3.56503628433197,2.02384076964154,-24.3580222600385)) ;
#167852 = CARTESIAN_POINT('Ctrl Pts',(3.56481411023498,2.0236610301436,-24.3582058396878)) ;
#167853 = CARTESIAN_POINT('Ctrl Pts',(3.5628523942574,2.02208416924047,-24.3597983821207)) ;
#167854 = CARTESIAN_POINT('Ctrl Pts',(3.56093641846841,2.02061618613942,-24.3611871777521)) ;
#167855 = CARTESIAN_POINT('Ctrl Pts',(3.55879736620725,2.01908299720807,-24.3623771402549)) ;
#167856 = CARTESIAN_POINT('Ctrl Pts',(3.55867935922383,2.01899873301442,-24.3624417103526)) ;
#167857 = CARTESIAN_POINT('Ctrl Pts',(3.55788953399544,2.01843691186415,-24.3628664833738)) ;
#167858 = CARTESIAN_POINT('Ctrl Pts',(3.55720723474251,2.01796200020267,-24.363197549106)) ;
#167859 = CARTESIAN_POINT('Ctrl Pts',(3.55509125643155,2.01652382826848,-24.3640979444516)) ;
#167860 = CARTESIAN_POINT('Ctrl Pts',(3.55356547969799,2.0155357187407,-24.3646035613517)) ;
#167861 = CARTESIAN_POINT('Ctrl Pts',(3.55133342567613,2.01417771500987,-24.3649447643996)) ;
#167862 = CARTESIAN_POINT('Ctrl Pts',(3.55066861961533,2.01378348733645,-24.3649996317888)) ;
#167863 = CARTESIAN_POINT('Ctrl Pts',(3.55,2.01339745962156,-24.365)) ;
#167864 = CARTESIAN_POINT('Origin',(3.5,1.9,-28.975)) ;
#167865 = CARTESIAN_POINT('',(3.55,2.01339745962156,-28.975)) ;
#167866 = CARTESIAN_POINT('Origin',(3.5,2.1,-28.975)) ;
#167867 = CARTESIAN_POINT('Ctrl Pts',(3.55,2.01339745962156,-28.975)) ;
#167868 = CARTESIAN_POINT('Ctrl Pts',(3.55164546205118,2.01434746757975,-28.975)) ;
#167869 = CARTESIAN_POINT('Ctrl Pts',(3.55326668047441,2.01534654795451,-28.9753329780303)) ;
#167870 = CARTESIAN_POINT('Ctrl Pts',(3.55550702654633,2.01680421826672,-28.976098261683)) ;
#167871 = CARTESIAN_POINT('Ctrl Pts',(3.55618577699068,2.01725684095079,-28.9763735960638)) ;
#167872 = CARTESIAN_POINT('Ctrl Pts',(3.55727967686454,2.01800266699453,-28.9768678300958)) ;
#167873 = CARTESIAN_POINT('Ctrl Pts',(3.55771141786834,2.01830156212325,-28.9770783189426)) ;
#167874 = CARTESIAN_POINT('Ctrl Pts',(3.56202821818157,2.02133211263481,-28.9791706910972)) ;
#167875 = CARTESIAN_POINT('Ctrl Pts',(3.56570108751476,2.02427663140637,-28.9822439316283)) ;
#167876 = CARTESIAN_POINT('Ctrl Pts',(3.5699034772656,2.02797441535145,-28.9864020047384)) ;
#167877 = CARTESIAN_POINT('Ctrl Pts',(3.57072473561126,2.02871480216321,-28.9872495977309)) ;
#167878 = CARTESIAN_POINT('Ctrl Pts',(3.5738286330762,2.03157464832067,-28.9905417189329)) ;
#167879 = CARTESIAN_POINT('Ctrl Pts',(3.5759706937612,2.03369481096682,-28.9931377343573)) ;
#167880 = CARTESIAN_POINT('Ctrl Pts',(3.58156103639367,2.03956384830231,-29.0007581167797)) ;
#167881 = CARTESIAN_POINT('Ctrl Pts',(3.58475859790494,2.04336775308647,-29.0061548385216)) ;
#167882 = CARTESIAN_POINT('Ctrl Pts',(3.58897725231935,2.04901055924319,-29.0149548343006)) ;
#167883 = CARTESIAN_POINT('Ctrl Pts',(3.59034871903171,2.05099358132072,-29.0182225338432)) ;
#167884 = CARTESIAN_POINT('Ctrl Pts',(3.59365488292715,2.05613355260422,-29.0272492286079)) ;
#167885 = CARTESIAN_POINT('Ctrl Pts',(3.59534780095502,2.05919518104002,-29.0332437116095)) ;
#167886 = CARTESIAN_POINT('Ctrl Pts',(3.59674625886194,2.06216860863426,-29.0399604466288)) ;
#167887 = CARTESIAN_POINT('Ctrl Pts',(3.5968572528105,2.06240883133042,-29.0405103151092)) ;
#167888 = CARTESIAN_POINT('Ctrl Pts',(3.59768573690243,2.06423460359408,-29.04474653762)) ;
#167889 = CARTESIAN_POINT('Ctrl Pts',(3.59826864191791,2.06571343564803,-29.0485239971566)) ;
#167890 = CARTESIAN_POINT('Ctrl Pts',(3.59959273712775,2.06963221119414,-29.0596830143691)) ;
#167891 = CARTESIAN_POINT('Ctrl Pts',(3.6,2.07172309150643,-29.0672993579658)) ;
#167892 = CARTESIAN_POINT('Ctrl Pts',(3.6,2.07320508075689,-29.075)) ;
#167893 = CARTESIAN_POINT('Origin',(3.5,2.10000000000001,-1.01757522333836E-15)) ;
#167894 = CARTESIAN_POINT('Origin',(3.5,2.1,-28.975)) ;
#167895 = CARTESIAN_POINT('',(3.55,2.01339745962156,-28.175)) ;
#167896 = CARTESIAN_POINT('Origin',(3.5,2.1,-28.175)) ;
#167897 = CARTESIAN_POINT('Origin',(3.5,2.1,-28.175)) ;
#167898 = CARTESIAN_POINT('Origin',(3.5,1.9,-28.175)) ;
#167899 = CARTESIAN_POINT('Ctrl Pts',(3.6,2.07320508075689,-28.075)) ;
#167900 = CARTESIAN_POINT('Ctrl Pts',(3.6,2.0724036454051,-28.0791643012255)) ;
#167901 = CARTESIAN_POINT('Ctrl Pts',(3.59988358031788,2.07142604615684,-28.0832993264777)) ;
#167902 = CARTESIAN_POINT('Ctrl Pts',(3.5992764543265,2.06860573724893,-28.0934232053159)) ;
#167903 = CARTESIAN_POINT('Ctrl Pts',(3.59862250828209,2.06654864780066,-28.0994017962796)) ;
#167904 = CARTESIAN_POINT('Ctrl Pts',(3.5974369582727,2.06370626825463,-28.1064308805049)) ;
#167905 = CARTESIAN_POINT('Ctrl Pts',(3.59721441711742,2.06319475755343,-28.1076558946613)) ;
#167906 = CARTESIAN_POINT('Ctrl Pts',(3.59624340061598,2.06105248659392,-28.1126335394636)) ;
#167907 = CARTESIAN_POINT('Ctrl Pts',(3.59536494855695,2.05931170891995,-28.1163234713874)) ;
#167908 = CARTESIAN_POINT('Ctrl Pts',(3.59283727202455,2.0547960643682,-28.1251994320585)) ;
#167909 = CARTESIAN_POINT('Ctrl Pts',(3.59099650883128,2.05188276467179,-28.1303442420061)) ;
#167910 = CARTESIAN_POINT('Ctrl Pts',(3.58838944624352,2.04823719194732,-28.1362273766785)) ;
#167911 = CARTESIAN_POINT('Ctrl Pts',(3.58794537962097,2.04762948672773,-28.1371909138509)) ;
#167912 = CARTESIAN_POINT('Ctrl Pts',(3.58597371492279,2.04498948329048,-28.1413066517297)) ;
#167913 = CARTESIAN_POINT('Ctrl Pts',(3.58430396743904,2.04289920268562,-28.1443931624803)) ;
#167914 = CARTESIAN_POINT('Ctrl Pts',(3.58008903321371,2.03798436571163,-28.1512809206787)) ;
#167915 = CARTESIAN_POINT('Ctrl Pts',(3.5774359340162,2.03513945367755,-28.1550015729202)) ;
#167916 = CARTESIAN_POINT('Ctrl Pts',(3.57357563759705,2.03136250950885,-28.1595864015964)) ;
#167917 = CARTESIAN_POINT('Ctrl Pts',(3.57257888733696,2.03041544381421,-28.1607065689312)) ;
#167918 = CARTESIAN_POINT('Ctrl Pts',(3.5695683971984,2.0276417514069,-28.1639039077888)) ;
#167919 = CARTESIAN_POINT('Ctrl Pts',(3.5674618955195,2.02581554544784,-28.1659843006789)) ;
#167920 = CARTESIAN_POINT('Ctrl Pts',(3.56503628433186,2.02384076964145,-28.1680222600386)) ;
#167921 = CARTESIAN_POINT('Ctrl Pts',(3.56481411023493,2.02366103014356,-28.1682058396879)) ;
#167922 = CARTESIAN_POINT('Ctrl Pts',(3.56285239425745,2.02208416924051,-28.1697983821206)) ;
#167923 = CARTESIAN_POINT('Ctrl Pts',(3.5609364184685,2.02061618613949,-28.171187177752)) ;
#167924 = CARTESIAN_POINT('Ctrl Pts',(3.55879736620735,2.01908299720814,-28.1723771402548)) ;
#167925 = CARTESIAN_POINT('Ctrl Pts',(3.55867935922389,2.01899873301446,-28.1724417103525)) ;
#167926 = CARTESIAN_POINT('Ctrl Pts',(3.55788953399546,2.01843691186416,-28.1728664833738)) ;
#167927 = CARTESIAN_POINT('Ctrl Pts',(3.55720723474251,2.01796200020267,-28.173197549106)) ;
#167928 = CARTESIAN_POINT('Ctrl Pts',(3.55509125643154,2.01652382826847,-28.1740979444515)) ;
#167929 = CARTESIAN_POINT('Ctrl Pts',(3.55356547969798,2.01553571874069,-28.1746035613518)) ;
#167930 = CARTESIAN_POINT('Ctrl Pts',(3.55133342567612,2.01417771500986,-28.1749447643997)) ;
#167931 = CARTESIAN_POINT('Ctrl Pts',(3.55066861961533,2.01378348733645,-28.1749996317888)) ;
#167932 = CARTESIAN_POINT('Ctrl Pts',(3.55,2.01339745962156,-28.175)) ;
#167933 = CARTESIAN_POINT('Origin',(3.5,1.9,-32.785)) ;
#167934 = CARTESIAN_POINT('',(3.55,2.01339745962156,-32.785)) ;
#167935 = CARTESIAN_POINT('Origin',(3.5,2.1,-32.785)) ;
#167936 = CARTESIAN_POINT('Ctrl Pts',(3.55,2.01339745962156,-32.785)) ;
#167937 = CARTESIAN_POINT('Ctrl Pts',(3.5516454620512,2.01434746757976,-32.7850000000001)) ;
#167938 = CARTESIAN_POINT('Ctrl Pts',(3.55326668047444,2.01534654795453,-32.7853329780303)) ;
#167939 = CARTESIAN_POINT('Ctrl Pts',(3.55550702654636,2.01680421826674,-32.7860982616831)) ;
#167940 = CARTESIAN_POINT('Ctrl Pts',(3.55618577699069,2.0172568409508,-32.7863735960638)) ;
#167941 = CARTESIAN_POINT('Ctrl Pts',(3.55727967686453,2.01800266699453,-32.7868678300958)) ;
#167942 = CARTESIAN_POINT('Ctrl Pts',(3.55771141786833,2.01830156212324,-32.7870783189426)) ;
#167943 = CARTESIAN_POINT('Ctrl Pts',(3.56202821818145,2.02133211263472,-32.7891706910972)) ;
#167944 = CARTESIAN_POINT('Ctrl Pts',(3.56570108751455,2.02427663140619,-32.7922439316281)) ;
#167945 = CARTESIAN_POINT('Ctrl Pts',(3.56990347726541,2.02797441535127,-32.7964020047383)) ;
#167946 = CARTESIAN_POINT('Ctrl Pts',(3.57072473561116,2.02871480216311,-32.7972495977309)) ;
#167947 = CARTESIAN_POINT('Ctrl Pts',(3.5738286330762,2.03157464832066,-32.8005417189329)) ;
#167948 = CARTESIAN_POINT('Ctrl Pts',(3.5759706937612,2.03369481096681,-32.8031377343573)) ;
#167949 = CARTESIAN_POINT('Ctrl Pts',(3.58156103639367,2.03956384830231,-32.8107581167798)) ;
#167950 = CARTESIAN_POINT('Ctrl Pts',(3.58475859790494,2.04336775308647,-32.8161548385216)) ;
#167951 = CARTESIAN_POINT('Ctrl Pts',(3.58897725231935,2.04901055924319,-32.8249548343006)) ;
#167952 = CARTESIAN_POINT('Ctrl Pts',(3.59034871903171,2.05099358132071,-32.8282225338432)) ;
#167953 = CARTESIAN_POINT('Ctrl Pts',(3.59365488292739,2.0561335526046,-32.8372492286086)) ;
#167954 = CARTESIAN_POINT('Ctrl Pts',(3.59534780095541,2.05919518104073,-32.8432437116108)) ;
#167955 = CARTESIAN_POINT('Ctrl Pts',(3.59674625886223,2.06216860863489,-32.8499604466302)) ;
#167956 = CARTESIAN_POINT('Ctrl Pts',(3.59685725281065,2.06240883133073,-32.8505103151099)) ;
#167957 = CARTESIAN_POINT('Ctrl Pts',(3.59768573690243,2.06423460359408,-32.85474653762)) ;
#167958 = CARTESIAN_POINT('Ctrl Pts',(3.59826864191792,2.06571343564803,-32.8585239971566)) ;
#167959 = CARTESIAN_POINT('Ctrl Pts',(3.59959273712776,2.06963221119414,-32.8696830143691)) ;
#167960 = CARTESIAN_POINT('Ctrl Pts',(3.6,2.07172309150643,-32.8772993579658)) ;
#167961 = CARTESIAN_POINT('Ctrl Pts',(3.6,2.07320508075689,-32.885)) ;
#167962 = CARTESIAN_POINT('Origin',(3.5,2.10000000000002,-1.01757522333836E-15)) ;
#167963 = CARTESIAN_POINT('Origin',(3.5,2.1,-32.785)) ;
#167964 = CARTESIAN_POINT('',(3.55,2.01339745962156,-31.985)) ;
#167965 = CARTESIAN_POINT('Origin',(3.5,2.1,-31.985)) ;
#167966 = CARTESIAN_POINT('Origin',(3.5,2.1,-31.985)) ;
#167967 = CARTESIAN_POINT('Origin',(3.5,1.9,-31.985)) ;
#167968 = CARTESIAN_POINT('Ctrl Pts',(3.6,2.07320508075689,-31.885)) ;
#167969 = CARTESIAN_POINT('Ctrl Pts',(3.6,2.07240364540511,-31.8891643012255)) ;
#167970 = CARTESIAN_POINT('Ctrl Pts',(3.59988358031788,2.07142604615685,-31.8932993264777)) ;
#167971 = CARTESIAN_POINT('Ctrl Pts',(3.59927645432651,2.06860573724896,-31.9034232053158)) ;
#167972 = CARTESIAN_POINT('Ctrl Pts',(3.59862250828212,2.06654864780071,-31.9094017962794)) ;
#167973 = CARTESIAN_POINT('Ctrl Pts',(3.59743695827272,2.06370626825467,-31.9164308805048)) ;
#167974 = CARTESIAN_POINT('Ctrl Pts',(3.59721441711744,2.06319475755345,-31.9176558946612)) ;
#167975 = CARTESIAN_POINT('Ctrl Pts',(3.59624340061598,2.06105248659392,-31.9226335394636)) ;
#167976 = CARTESIAN_POINT('Ctrl Pts',(3.59536494855695,2.05931170891994,-31.9263234713874)) ;
#167977 = CARTESIAN_POINT('Ctrl Pts',(3.59283727202455,2.0547960643682,-31.9351994320585)) ;
#167978 = CARTESIAN_POINT('Ctrl Pts',(3.59099650883129,2.0518827646718,-31.940344242006)) ;
#167979 = CARTESIAN_POINT('Ctrl Pts',(3.58838944624353,2.04823719194733,-31.9462273766785)) ;
#167980 = CARTESIAN_POINT('Ctrl Pts',(3.58794537962098,2.04762948672773,-31.9471909138509)) ;
#167981 = CARTESIAN_POINT('Ctrl Pts',(3.58597371492279,2.04498948329048,-31.9513066517297)) ;
#167982 = CARTESIAN_POINT('Ctrl Pts',(3.58430396743904,2.04289920268562,-31.9543931624802)) ;
#167983 = CARTESIAN_POINT('Ctrl Pts',(3.58008903321372,2.03798436571164,-31.9612809206787)) ;
#167984 = CARTESIAN_POINT('Ctrl Pts',(3.57743593401621,2.03513945367757,-31.9650015729201)) ;
#167985 = CARTESIAN_POINT('Ctrl Pts',(3.57357563759707,2.03136250950887,-31.9695864015964)) ;
#167986 = CARTESIAN_POINT('Ctrl Pts',(3.57257888733696,2.03041544381421,-31.9707065689311)) ;
#167987 = CARTESIAN_POINT('Ctrl Pts',(3.56956839719855,2.02764175140704,-31.9739039077886)) ;
#167988 = CARTESIAN_POINT('Ctrl Pts',(3.56746189551982,2.02581554544812,-31.9759843006786)) ;
#167989 = CARTESIAN_POINT('Ctrl Pts',(3.5650362843322,2.02384076964172,-31.9780222600382)) ;
#167990 = CARTESIAN_POINT('Ctrl Pts',(3.5648141102351,2.02366103014369,-31.9782058396877)) ;
#167991 = CARTESIAN_POINT('Ctrl Pts',(3.56285239425763,2.02208416924065,-31.9797983821204)) ;
#167992 = CARTESIAN_POINT('Ctrl Pts',(3.56093641846891,2.0206161861398,-31.9811871777517)) ;
#167993 = CARTESIAN_POINT('Ctrl Pts',(3.55879736620774,2.01908299720842,-31.9823771402546)) ;
#167994 = CARTESIAN_POINT('Ctrl Pts',(3.55867935922403,2.01899873301456,-31.9824417103524)) ;
#167995 = CARTESIAN_POINT('Ctrl Pts',(3.55788953399539,2.01843691186411,-31.9828664833738)) ;
#167996 = CARTESIAN_POINT('Ctrl Pts',(3.55720723474248,2.01796200020265,-31.983197549106)) ;
#167997 = CARTESIAN_POINT('Ctrl Pts',(3.55509125643159,2.01652382826851,-31.9840979444515)) ;
#167998 = CARTESIAN_POINT('Ctrl Pts',(3.55356547969806,2.01553571874074,-31.9846035613517)) ;
#167999 = CARTESIAN_POINT('Ctrl Pts',(3.55133342567619,2.01417771500991,-31.9849447643996)) ;
#168000 = CARTESIAN_POINT('Ctrl Pts',(3.55066861961536,2.01378348733647,-31.9849996317887)) ;
#168001 = CARTESIAN_POINT('Ctrl Pts',(3.55,2.01339745962156,-31.985)) ;
#168002 = CARTESIAN_POINT('Origin',(3.5,2.10000000000002,-1.01757522333836E-15)) ;
#168003 = CARTESIAN_POINT('Origin',(3.5,2.1,-36.49)) ;
#168004 = CARTESIAN_POINT('',(3.55,2.01339745962156,-35.795)) ;
#168005 = CARTESIAN_POINT('Origin',(3.5,2.1,-35.795)) ;
#168006 = CARTESIAN_POINT('Origin',(3.5,2.1,-35.795)) ;
#168007 = CARTESIAN_POINT('Origin',(3.5,1.9,-35.795)) ;
#168008 = CARTESIAN_POINT('Ctrl Pts',(3.6,2.07320508075689,-35.695)) ;
#168009 = CARTESIAN_POINT('Ctrl Pts',(3.6,2.07240364540511,-35.6991643012256)) ;
#168010 = CARTESIAN_POINT('Ctrl Pts',(3.59988358031788,2.07142604615685,-35.7032993264777)) ;
#168011 = CARTESIAN_POINT('Ctrl Pts',(3.59927645432651,2.06860573724896,-35.7134232053158)) ;
#168012 = CARTESIAN_POINT('Ctrl Pts',(3.59862250828211,2.0665486478007,-35.7194017962795)) ;
#168013 = CARTESIAN_POINT('Ctrl Pts',(3.59743695827272,2.06370626825466,-35.7264308805048)) ;
#168014 = CARTESIAN_POINT('Ctrl Pts',(3.59721441711743,2.06319475755345,-35.7276558946612)) ;
#168015 = CARTESIAN_POINT('Ctrl Pts',(3.59624340061598,2.06105248659392,-35.7326335394636)) ;
#168016 = CARTESIAN_POINT('Ctrl Pts',(3.59536494855695,2.05931170891994,-35.7363234713874)) ;
#168017 = CARTESIAN_POINT('Ctrl Pts',(3.59283727202456,2.05479606436823,-35.7451994320584)) ;
#168018 = CARTESIAN_POINT('Ctrl Pts',(3.59099650883132,2.05188276467186,-35.7503442420059)) ;
#168019 = CARTESIAN_POINT('Ctrl Pts',(3.58838944624357,2.04823719194739,-35.7562273766784)) ;
#168020 = CARTESIAN_POINT('Ctrl Pts',(3.587945379621,2.04762948672776,-35.7571909138508)) ;
#168021 = CARTESIAN_POINT('Ctrl Pts',(3.58597371492279,2.04498948329048,-35.7613066517297)) ;
#168022 = CARTESIAN_POINT('Ctrl Pts',(3.58430396743904,2.04289920268562,-35.7643931624803)) ;
#168023 = CARTESIAN_POINT('Ctrl Pts',(3.58008903321367,2.03798436571158,-35.7712809206788)) ;
#168024 = CARTESIAN_POINT('Ctrl Pts',(3.57743593401611,2.03513945367745,-35.7750015729203)) ;
#168025 = CARTESIAN_POINT('Ctrl Pts',(3.57357563759695,2.03136250950875,-35.7795864015965)) ;
#168026 = CARTESIAN_POINT('Ctrl Pts',(3.5725788873369,2.03041544381416,-35.7807065689312)) ;
#168027 = CARTESIAN_POINT('Ctrl Pts',(3.56956839719846,2.02764175140696,-35.7839039077887)) ;
#168028 = CARTESIAN_POINT('Ctrl Pts',(3.56746189551964,2.02581554544796,-35.7859843006788)) ;
#168029 = CARTESIAN_POINT('Ctrl Pts',(3.565036284332,2.02384076964157,-35.7880222600384)) ;
#168030 = CARTESIAN_POINT('Ctrl Pts',(3.564814110235,2.02366103014362,-35.7882058396878)) ;
#168031 = CARTESIAN_POINT('Ctrl Pts',(3.56285239425736,2.02208416924043,-35.7897983821207)) ;
#168032 = CARTESIAN_POINT('Ctrl Pts',(3.5609364184683,2.02061618613934,-35.7911871777521)) ;
#168033 = CARTESIAN_POINT('Ctrl Pts',(3.55879736620711,2.01908299720796,-35.7923771402549)) ;
#168034 = CARTESIAN_POINT('Ctrl Pts',(3.55867935922371,2.01899873301434,-35.7924417103526)) ;
#168035 = CARTESIAN_POINT('Ctrl Pts',(3.55788953399539,2.01843691186411,-35.7928664833738)) ;
#168036 = CARTESIAN_POINT('Ctrl Pts',(3.55720723474248,2.01796200020265,-35.793197549106)) ;
#168037 = CARTESIAN_POINT('Ctrl Pts',(3.55509125643159,2.01652382826851,-35.7940979444515)) ;
#168038 = CARTESIAN_POINT('Ctrl Pts',(3.55356547969807,2.01553571874075,-35.7946035613517)) ;
#168039 = CARTESIAN_POINT('Ctrl Pts',(3.55133342567621,2.01417771500992,-35.7949447643996)) ;
#168040 = CARTESIAN_POINT('Ctrl Pts',(3.55066861961537,2.01378348733647,-35.7949996317887)) ;
#168041 = CARTESIAN_POINT('Ctrl Pts',(3.55,2.01339745962156,-35.795)) ;
#168042 = CARTESIAN_POINT('Origin',(3.7,2.1,-5.115)) ;
#168043 = CARTESIAN_POINT('',(3.7,1.98660254037844,-5.165)) ;
#168044 = CARTESIAN_POINT('Ctrl Pts',(3.60000000000001,1.92679491924311,-5.215)) ;
#168045 = CARTESIAN_POINT('Ctrl Pts',(3.60642117639485,1.92803067521647,-5.215)) ;
#168046 = CARTESIAN_POINT('Ctrl Pts',(3.61278477806504,1.92968896670924,-5.21472281361407)) ;
#168047 = CARTESIAN_POINT('Ctrl Pts',(3.61897283239529,1.93170032347262,-5.21412352491366)) ;
#168048 = CARTESIAN_POINT('Ctrl Pts',(3.62020584678442,1.93210110079269,-5.21400411232427)) ;
#168049 = CARTESIAN_POINT('Ctrl Pts',(3.62143195421093,1.93251577262755,-5.21387200280826)) ;
#168050 = CARTESIAN_POINT('Ctrl Pts',(3.62265032708637,1.93294361409314,-5.21372698243403)) ;
#168051 = CARTESIAN_POINT('Ctrl Pts',(3.62647624625549,1.9342871164786,-5.21327159128008)) ;
#168052 = CARTESIAN_POINT('Ctrl Pts',(3.63025346237246,1.93576539638805,-5.21268573681767)) ;
#168053 = CARTESIAN_POINT('Ctrl Pts',(3.6339385638818,1.93735364065939,-5.21196503626974)) ;
#168054 = CARTESIAN_POINT('Ctrl Pts',(3.63907793749079,1.93956866259898,-5.21095992165713)) ;
#168055 = CARTESIAN_POINT('Ctrl Pts',(3.64410916187594,1.9420207691991,-5.20967872244963)) ;
#168056 = CARTESIAN_POINT('Ctrl Pts',(3.64894317395081,1.94461872744766,-5.20812217773586)) ;
#168057 = CARTESIAN_POINT('Ctrl Pts',(3.64993855309172,1.94515367717669,-5.20780166712976)) ;
#168058 = CARTESIAN_POINT('Ctrl Pts',(3.65092568100078,1.94569474416707,-5.20746960315685)) ;
#168059 = CARTESIAN_POINT('Ctrl Pts',(3.65190395907094,1.94624104404949,-5.20712618093672)) ;
#168060 = CARTESIAN_POINT('Ctrl Pts',(3.6524134286835,1.94652554719632,-5.20694733282516)) ;
#168061 = CARTESIAN_POINT('Ctrl Pts',(3.65292046817499,1.94681147780209,-5.20676540574)) ;
#168062 = CARTESIAN_POINT('Ctrl Pts',(3.65342498214111,1.94709871486665,-5.20658043363331)) ;
#168063 = CARTESIAN_POINT('Ctrl Pts',(3.65677402871197,1.94900544167845,-5.20535255840841)) ;
#168064 = CARTESIAN_POINT('Ctrl Pts',(3.66003813592315,1.95098496635821,-5.20398063668092)) ;
#168065 = CARTESIAN_POINT('Ctrl Pts',(3.66320312645638,1.95301617633166,-5.20246240139399)) ;
#168066 = CARTESIAN_POINT('Ctrl Pts',(3.66757373088823,1.95582111846932,-5.20036583718505)) ;
#168067 = CARTESIAN_POINT('Ctrl Pts',(3.67181875309394,1.95875330073085,-5.19796612617077)) ;
#168068 = CARTESIAN_POINT('Ctrl Pts',(3.67584388612554,1.96174615985082,-5.19526003578551)) ;
#168069 = CARTESIAN_POINT('Ctrl Pts',(3.67661208162804,1.96231734616877,-5.1947435791996)) ;
#168070 = CARTESIAN_POINT('Ctrl Pts',(3.6773723784937,1.96289065080929,-5.19421601587661)) ;
#168071 = CARTESIAN_POINT('Ctrl Pts',(3.67812428214755,1.96346549105991,-5.1936773988359)) ;
#168072 = CARTESIAN_POINT('Ctrl Pts',(3.6785349394885,1.96377944400799,-5.19338322944252)) ;
#168073 = CARTESIAN_POINT('Ctrl Pts',(3.67894301851534,1.96409388168819,-5.19308575174331)) ;
#168074 = CARTESIAN_POINT('Ctrl Pts',(3.67934840022277,1.96440871854257,-5.19278496939811)) ;
#168075 = CARTESIAN_POINT('Ctrl Pts',(3.68198440184427,1.96645595067818,-5.19082912695353)) ;
#168076 = CARTESIAN_POINT('Ctrl Pts',(3.68449751351864,1.96851545671307,-5.18873828347164)) ;
#168077 = CARTESIAN_POINT('Ctrl Pts',(3.68685379133723,1.97055696562013,-5.18652085039877)) ;
#168078 = CARTESIAN_POINT('Ctrl Pts',(3.68896164651385,1.97238323800785,-5.18453720155032)) ;
#168079 = CARTESIAN_POINT('Ctrl Pts',(3.69104797813205,1.97419718002547,-5.18244243877983)) ;
#168080 = CARTESIAN_POINT('Ctrl Pts',(3.69290978292493,1.97598569412168,-5.18024500103231)) ;
#168081 = CARTESIAN_POINT('Ctrl Pts',(3.69362192319645,1.97666980070416,-5.17940448116676)) ;
#168082 = CARTESIAN_POINT('Ctrl Pts',(3.69430163271861,1.97734979318971,-5.17854897561523)) ;
#168083 = CARTESIAN_POINT('Ctrl Pts',(3.69493905694205,1.97802369895108,-5.17767908836304)) ;
#168084 = CARTESIAN_POINT('Ctrl Pts',(3.69605143900785,1.9791997456958,-5.17616103030527)) ;
#168085 = CARTESIAN_POINT('Ctrl Pts',(3.69703421735413,1.98035885502255,-5.1745986233173)) ;
#168086 = CARTESIAN_POINT('Ctrl Pts',(3.6978475066491,1.98151165953424,-5.17295719153115)) ;
#168087 = CARTESIAN_POINT('Ctrl Pts',(3.69841279947843,1.98231293913807,-5.17181628186435)) ;
#168088 = CARTESIAN_POINT('Ctrl Pts',(3.69890310384953,1.98311438470598,-5.17063324801215)) ;
#168089 = CARTESIAN_POINT('Ctrl Pts',(3.69929098301994,1.98393783265455,-5.1693581070746)) ;
#168090 = CARTESIAN_POINT('Ctrl Pts',(3.69936193271525,1.98408845528529,-5.16912486211612)) ;
#168091 = CARTESIAN_POINT('Ctrl Pts',(3.69942931950317,1.98423979370566,-5.16888851468591)) ;
#168092 = CARTESIAN_POINT('Ctrl Pts',(3.69949277412724,1.98439195189924,-5.16864873028523)) ;
#168093 = CARTESIAN_POINT('Ctrl Pts',(3.69967702385849,1.98483376534755,-5.16795248139832)) ;
#168094 = CARTESIAN_POINT('Ctrl Pts',(3.69981936684305,1.98527475083258,-5.16723933425853)) ;
#168095 = CARTESIAN_POINT('Ctrl Pts',(3.69990669142684,1.98570953653121,-5.16651584102814)) ;
#168096 = CARTESIAN_POINT('Ctrl Pts',(3.69996666908332,1.98600816294479,-5.16601891992581)) ;
#168097 = CARTESIAN_POINT('Ctrl Pts',(3.7,1.98630780592128,-5.16551049505454)) ;
#168098 = CARTESIAN_POINT('Ctrl Pts',(3.7,1.98660254037844,-5.165)) ;
#168099 = CARTESIAN_POINT('Origin',(3.7,1.9,-5.115)) ;
#168100 = CARTESIAN_POINT('Origin',(10.2,1.9,-5.115)) ;
#168101 = CARTESIAN_POINT('Origin',(3.7,1.9,-5.115)) ;
#168102 = CARTESIAN_POINT('Origin',(10.1,1.9,-5.115)) ;
#168103 = CARTESIAN_POINT('Origin',(10.1,1.9,-5.115)) ;
#168104 = CARTESIAN_POINT('Origin',(3.7,2.1,-2.505)) ;
#168105 = CARTESIAN_POINT('',(3.7,1.98660254037844,-2.455)) ;
#168106 = CARTESIAN_POINT('Origin',(3.7,1.9,-2.505)) ;
#168107 = CARTESIAN_POINT('Ctrl Pts',(3.7,1.98660254037844,-2.455)) ;
#168108 = CARTESIAN_POINT('Ctrl Pts',(3.69999911718144,1.98567700534182,-2.45339692629239)) ;
#168109 = CARTESIAN_POINT('Ctrl Pts',(3.69968163901485,1.984703699336,-2.45181800228455)) ;
#168110 = CARTESIAN_POINT('Ctrl Pts',(3.69895427931585,1.98325895404995,-2.44959445604081)) ;
#168111 = CARTESIAN_POINT('Ctrl Pts',(3.69867650892745,1.98278649590681,-2.44888609842392)) ;
#168112 = CARTESIAN_POINT('Ctrl Pts',(3.69717970712967,1.9804354328423,-2.44544091878433)) ;
#168113 = CARTESIAN_POINT('Ctrl Pts',(3.69541014605544,1.97847095301992,-2.44282412084427)) ;
#168114 = CARTESIAN_POINT('Ctrl Pts',(3.69146029518774,1.97457001268155,-2.43797344350903)) ;
#168115 = CARTESIAN_POINT('Ctrl Pts',(3.68915436790411,1.97254004967205,-2.43563220687652)) ;
#168116 = CARTESIAN_POINT('Ctrl Pts',(3.68263623161792,1.9668885044718,-2.42949991845677)) ;
#168117 = CARTESIAN_POINT('Ctrl Pts',(3.67796661383159,1.96321337091313,-2.42597925228307)) ;
#168118 = CARTESIAN_POINT('Ctrl Pts',(3.67279117399678,1.95950210067477,-2.42276234339455)) ;
#168119 = CARTESIAN_POINT('Ctrl Pts',(3.67252519027994,1.95931231248683,-2.42259880905816)) ;
#168120 = CARTESIAN_POINT('Ctrl Pts',(3.6693311210617,1.95704457126181,-2.42065620430678)) ;
#168121 = CARTESIAN_POINT('Ctrl Pts',(3.66628216680076,1.95498580453519,-2.41900961223909)) ;
#168122 = CARTESIAN_POINT('Ctrl Pts',(3.65739884032377,1.94929644648107,-2.41475902421228)) ;
#168123 = CARTESIAN_POINT('Ctrl Pts',(3.65126071410426,1.94574201114262,-2.41247113326881)) ;
#168124 = CARTESIAN_POINT('Ctrl Pts',(3.64132315686417,1.94068746317945,-2.40963796590125)) ;
#168125 = CARTESIAN_POINT('Ctrl Pts',(3.63763353946351,1.93894751340588,-2.40875659938477)) ;
#168126 = CARTESIAN_POINT('Ctrl Pts',(3.62813871250319,1.93486114467728,-2.40690439135811)) ;
#168127 = CARTESIAN_POINT('Ctrl Pts',(3.62220485293009,1.93266004719381,-2.40611534404151)) ;
#168128 = CARTESIAN_POINT('Ctrl Pts',(3.6135954374234,1.9300316723429,-2.40542021745114)) ;
#168129 = CARTESIAN_POINT('Ctrl Pts',(3.61101642177029,1.92931331154719,-2.40526698255319)) ;
#168130 = CARTESIAN_POINT('Ctrl Pts',(3.60562851963663,1.92796119665949,-2.40505325677268)) ;
#168131 = CARTESIAN_POINT('Ctrl Pts',(3.60282089026148,1.92733781012842,-2.405)) ;
#168132 = CARTESIAN_POINT('Ctrl Pts',(3.6,1.92679491924311,-2.405)) ;
#168133 = CARTESIAN_POINT('Origin',(3.6,1.9,-2.505)) ;
#168134 = CARTESIAN_POINT('Origin',(3.7,1.9,-2.505)) ;
#168135 = CARTESIAN_POINT('Origin',(10.1,1.9,-2.505)) ;
#168136 = CARTESIAN_POINT('Origin',(10.1,1.9,-2.505)) ;
#168137 = CARTESIAN_POINT('Origin',(3.7,2.1,-8.925)) ;
#168138 = CARTESIAN_POINT('',(3.7,1.98660254037844,-8.975)) ;
#168139 = CARTESIAN_POINT('Ctrl Pts',(3.60000000000001,1.92679491924311,-9.025)) ;
#168140 = CARTESIAN_POINT('Ctrl Pts',(3.60642117639486,1.92803067521647,-9.025)) ;
#168141 = CARTESIAN_POINT('Ctrl Pts',(3.61278477806504,1.92968896670924,-9.02472281361407)) ;
#168142 = CARTESIAN_POINT('Ctrl Pts',(3.6189728323953,1.93170032347262,-9.02412352491366)) ;
#168143 = CARTESIAN_POINT('Ctrl Pts',(3.62020584678443,1.93210110079269,-9.02400411232427)) ;
#168144 = CARTESIAN_POINT('Ctrl Pts',(3.62143195421094,1.93251577262755,-9.02387200280826)) ;
#168145 = CARTESIAN_POINT('Ctrl Pts',(3.62265032708637,1.93294361409314,-9.02372698243403)) ;
#168146 = CARTESIAN_POINT('Ctrl Pts',(3.62647624625549,1.9342871164786,-9.02327159128008)) ;
#168147 = CARTESIAN_POINT('Ctrl Pts',(3.63025346237246,1.93576539638805,-9.02268573681767)) ;
#168148 = CARTESIAN_POINT('Ctrl Pts',(3.6339385638818,1.9373536406594,-9.02196503626974)) ;
#168149 = CARTESIAN_POINT('Ctrl Pts',(3.63907793749079,1.93956866259898,-9.02095992165713)) ;
#168150 = CARTESIAN_POINT('Ctrl Pts',(3.64410916187594,1.9420207691991,-9.01967872244964)) ;
#168151 = CARTESIAN_POINT('Ctrl Pts',(3.6489431739508,1.94461872744765,-9.01812217773586)) ;
#168152 = CARTESIAN_POINT('Ctrl Pts',(3.64993855309173,1.94515367717669,-9.01780166712976)) ;
#168153 = CARTESIAN_POINT('Ctrl Pts',(3.65092568100081,1.94569474416709,-9.01746960315684)) ;
#168154 = CARTESIAN_POINT('Ctrl Pts',(3.65190395907098,1.94624104404951,-9.01712618093671)) ;
#168155 = CARTESIAN_POINT('Ctrl Pts',(3.65241342868353,1.94652554719634,-9.01694733282515)) ;
#168156 = CARTESIAN_POINT('Ctrl Pts',(3.652920468175,1.94681147780209,-9.01676540573999)) ;
#168157 = CARTESIAN_POINT('Ctrl Pts',(3.6534249821411,1.94709871486665,-9.01658043363331)) ;
#168158 = CARTESIAN_POINT('Ctrl Pts',(3.65677402871197,1.94900544167845,-9.01535255840841)) ;
#168159 = CARTESIAN_POINT('Ctrl Pts',(3.66003813592315,1.95098496635821,-9.01398063668092)) ;
#168160 = CARTESIAN_POINT('Ctrl Pts',(3.66320312645637,1.95301617633166,-9.01246240139399)) ;
#168161 = CARTESIAN_POINT('Ctrl Pts',(3.66757373088828,1.95582111846936,-9.01036583718502)) ;
#168162 = CARTESIAN_POINT('Ctrl Pts',(3.67181875309405,1.95875330073093,-9.0079661261707)) ;
#168163 = CARTESIAN_POINT('Ctrl Pts',(3.6758438861257,1.96174615985095,-9.00526003578539)) ;
#168164 = CARTESIAN_POINT('Ctrl Pts',(3.67661208162813,1.96231734616885,-9.00474357919953)) ;
#168165 = CARTESIAN_POINT('Ctrl Pts',(3.67737237849372,1.96289065080932,-9.00421601587659)) ;
#168166 = CARTESIAN_POINT('Ctrl Pts',(3.6781242821475,1.96346549105988,-9.00367739883592)) ;
#168167 = CARTESIAN_POINT('Ctrl Pts',(3.67853493948847,1.96377944400797,-9.00338322944253)) ;
#168168 = CARTESIAN_POINT('Ctrl Pts',(3.67894301851532,1.96409388168817,-9.00308575174333)) ;
#168169 = CARTESIAN_POINT('Ctrl Pts',(3.67934840022276,1.96440871854256,-9.00278496939812)) ;
#168170 = CARTESIAN_POINT('Ctrl Pts',(3.68198440184425,1.96645595067819,-9.00082912695352)) ;
#168171 = CARTESIAN_POINT('Ctrl Pts',(3.68449751351864,1.96851545671307,-8.99873828347164)) ;
#168172 = CARTESIAN_POINT('Ctrl Pts',(3.68685379133723,1.97055696562013,-8.99652085039877)) ;
#168173 = CARTESIAN_POINT('Ctrl Pts',(3.68896164651385,1.97238323800784,-8.99453720155032)) ;
#168174 = CARTESIAN_POINT('Ctrl Pts',(3.69104797813205,1.97419718002547,-8.99244243877983)) ;
#168175 = CARTESIAN_POINT('Ctrl Pts',(3.69290978292493,1.97598569412168,-8.9902450010323)) ;
#168176 = CARTESIAN_POINT('Ctrl Pts',(3.69362192319645,1.97666980070416,-8.98940448116676)) ;
#168177 = CARTESIAN_POINT('Ctrl Pts',(3.69430163271861,1.97734979318971,-8.98854897561523)) ;
#168178 = CARTESIAN_POINT('Ctrl Pts',(3.69493905694205,1.97802369895108,-8.98767908836304)) ;
#168179 = CARTESIAN_POINT('Ctrl Pts',(3.69605143900784,1.9791997456958,-8.98616103030527)) ;
#168180 = CARTESIAN_POINT('Ctrl Pts',(3.69703421735413,1.98035885502255,-8.9845986233173)) ;
#168181 = CARTESIAN_POINT('Ctrl Pts',(3.6978475066491,1.98151165953424,-8.98295719153115)) ;
#168182 = CARTESIAN_POINT('Ctrl Pts',(3.69841279947843,1.98231293913807,-8.98181628186435)) ;
#168183 = CARTESIAN_POINT('Ctrl Pts',(3.69890310384954,1.98311438470598,-8.98063324801215)) ;
#168184 = CARTESIAN_POINT('Ctrl Pts',(3.69929098301995,1.98393783265455,-8.97935810707461)) ;
#168185 = CARTESIAN_POINT('Ctrl Pts',(3.69936193271525,1.98408845528529,-8.97912486211613)) ;
#168186 = CARTESIAN_POINT('Ctrl Pts',(3.69942931950317,1.98423979370565,-8.97888851468592)) ;
#168187 = CARTESIAN_POINT('Ctrl Pts',(3.69949277412724,1.98439195189923,-8.97864873028525)) ;
#168188 = CARTESIAN_POINT('Ctrl Pts',(3.69967702385849,1.98483376534754,-8.97795248139834)) ;
#168189 = CARTESIAN_POINT('Ctrl Pts',(3.69981936684304,1.98527475083258,-8.97723933425854)) ;
#168190 = CARTESIAN_POINT('Ctrl Pts',(3.69990669142683,1.98570953653121,-8.97651584102814)) ;
#168191 = CARTESIAN_POINT('Ctrl Pts',(3.69996666908332,1.98600816294479,-8.97601891992581)) ;
#168192 = CARTESIAN_POINT('Ctrl Pts',(3.7,1.98630780592129,-8.97551049505454)) ;
#168193 = CARTESIAN_POINT('Ctrl Pts',(3.7,1.98660254037844,-8.975)) ;
#168194 = CARTESIAN_POINT('Origin',(3.7,1.9,-8.925)) ;
#168195 = CARTESIAN_POINT('Origin',(10.2,1.9,-8.925)) ;
#168196 = CARTESIAN_POINT('Origin',(3.7,1.9,-8.925)) ;
#168197 = CARTESIAN_POINT('Origin',(10.1,1.9,-8.925)) ;
#168198 = CARTESIAN_POINT('Origin',(10.1,1.9,-8.925)) ;
#168199 = CARTESIAN_POINT('Origin',(3.7,2.1,-6.315)) ;
#168200 = CARTESIAN_POINT('',(3.7,1.98660254037844,-6.265)) ;
#168201 = CARTESIAN_POINT('Origin',(3.7,1.9,-6.315)) ;
#168202 = CARTESIAN_POINT('Ctrl Pts',(3.7,1.98660254037844,-6.265)) ;
#168203 = CARTESIAN_POINT('Ctrl Pts',(3.69999911718144,1.98567700534183,-6.26339692629239)) ;
#168204 = CARTESIAN_POINT('Ctrl Pts',(3.69968163901485,1.984703699336,-6.26181800228456)) ;
#168205 = CARTESIAN_POINT('Ctrl Pts',(3.69895427931586,1.98325895404995,-6.25959445604082)) ;
#168206 = CARTESIAN_POINT('Ctrl Pts',(3.69867650892745,1.98278649590681,-6.25888609842392)) ;
#168207 = CARTESIAN_POINT('Ctrl Pts',(3.69717970712967,1.9804354328423,-6.25544091878433)) ;
#168208 = CARTESIAN_POINT('Ctrl Pts',(3.69541014605544,1.97847095301992,-6.25282412084426)) ;
#168209 = CARTESIAN_POINT('Ctrl Pts',(3.69146029518774,1.97457001268155,-6.24797344350903)) ;
#168210 = CARTESIAN_POINT('Ctrl Pts',(3.68915436790411,1.97254004967205,-6.24563220687652)) ;
#168211 = CARTESIAN_POINT('Ctrl Pts',(3.6826362316179,1.96688850447178,-6.23949991845675)) ;
#168212 = CARTESIAN_POINT('Ctrl Pts',(3.67796661383154,1.96321337091309,-6.23597925228304)) ;
#168213 = CARTESIAN_POINT('Ctrl Pts',(3.67279117399673,1.95950210067473,-6.23276234339452)) ;
#168214 = CARTESIAN_POINT('Ctrl Pts',(3.67252519027992,1.95931231248681,-6.23259880905815)) ;
#168215 = CARTESIAN_POINT('Ctrl Pts',(3.6693311210617,1.95704457126181,-6.23065620430679)) ;
#168216 = CARTESIAN_POINT('Ctrl Pts',(3.66628216680076,1.95498580453519,-6.22900961223909)) ;
#168217 = CARTESIAN_POINT('Ctrl Pts',(3.65739884032377,1.94929644648107,-6.22475902421228)) ;
#168218 = CARTESIAN_POINT('Ctrl Pts',(3.65126071410426,1.94574201114262,-6.22247113326881)) ;
#168219 = CARTESIAN_POINT('Ctrl Pts',(3.64132315686417,1.94068746317945,-6.21963796590125)) ;
#168220 = CARTESIAN_POINT('Ctrl Pts',(3.63763353946351,1.93894751340588,-6.21875659938478)) ;
#168221 = CARTESIAN_POINT('Ctrl Pts',(3.62813871250319,1.93486114467728,-6.21690439135811)) ;
#168222 = CARTESIAN_POINT('Ctrl Pts',(3.62220485293009,1.93266004719381,-6.21611534404151)) ;
#168223 = CARTESIAN_POINT('Ctrl Pts',(3.61359543742331,1.93003167234287,-6.21542021745113)) ;
#168224 = CARTESIAN_POINT('Ctrl Pts',(3.61101642177012,1.92931331154715,-6.21526698255318)) ;
#168225 = CARTESIAN_POINT('Ctrl Pts',(3.60562851963646,1.92796119665945,-6.21505325677268)) ;
#168226 = CARTESIAN_POINT('Ctrl Pts',(3.60282089026139,1.92733781012841,-6.215)) ;
#168227 = CARTESIAN_POINT('Ctrl Pts',(3.6,1.92679491924311,-6.215)) ;
#168228 = CARTESIAN_POINT('Origin',(3.6,1.9,-6.315)) ;
#168229 = CARTESIAN_POINT('Origin',(3.7,1.9,-6.315)) ;
#168230 = CARTESIAN_POINT('Origin',(10.1,1.9,-6.315)) ;
#168231 = CARTESIAN_POINT('Origin',(10.1,1.9,-6.315)) ;
#168232 = CARTESIAN_POINT('Origin',(3.7,2.1,-12.735)) ;
#168233 = CARTESIAN_POINT('',(3.7,1.98660254037844,-12.785)) ;
#168234 = CARTESIAN_POINT('Ctrl Pts',(3.60000000000001,1.92679491924311,-12.835)) ;
#168235 = CARTESIAN_POINT('Ctrl Pts',(3.60642117639459,1.92803067521642,-12.835)) ;
#168236 = CARTESIAN_POINT('Ctrl Pts',(3.61278477806451,1.92968896670911,-12.8347228136141)) ;
#168237 = CARTESIAN_POINT('Ctrl Pts',(3.61897283239452,1.93170032347238,-12.8341235249137)) ;
#168238 = CARTESIAN_POINT('Ctrl Pts',(3.62020584678391,1.93210110079252,-12.8340041123243)) ;
#168239 = CARTESIAN_POINT('Ctrl Pts',(3.62143195421068,1.93251577262747,-12.8338720028083)) ;
#168240 = CARTESIAN_POINT('Ctrl Pts',(3.62265032708637,1.93294361409315,-12.833726982434)) ;
#168241 = CARTESIAN_POINT('Ctrl Pts',(3.62647624625549,1.9342871164786,-12.8332715912801)) ;
#168242 = CARTESIAN_POINT('Ctrl Pts',(3.63025346237246,1.93576539638805,-12.8326857368177)) ;
#168243 = CARTESIAN_POINT('Ctrl Pts',(3.6339385638818,1.93735364065939,-12.8319650362697)) ;
#168244 = CARTESIAN_POINT('Ctrl Pts',(3.63907793749009,1.93956866259867,-12.8309599216573)) ;
#168245 = CARTESIAN_POINT('Ctrl Pts',(3.64410916187458,1.94202076919845,-12.82967872245)) ;
#168246 = CARTESIAN_POINT('Ctrl Pts',(3.64894317394883,1.94461872744659,-12.8281221777365)) ;
#168247 = CARTESIAN_POINT('Ctrl Pts',(3.64993855309046,1.94515367717599,-12.8278016671302)) ;
#168248 = CARTESIAN_POINT('Ctrl Pts',(3.65092568100022,1.94569474416675,-12.8274696031571)) ;
#168249 = CARTESIAN_POINT('Ctrl Pts',(3.65190395907107,1.94624104404954,-12.8271261809367)) ;
#168250 = CARTESIAN_POINT('Ctrl Pts',(3.65241342868358,1.94652554719635,-12.8269473328251)) ;
#168251 = CARTESIAN_POINT('Ctrl Pts',(3.65292046817503,1.94681147780212,-12.82676540574)) ;
#168252 = CARTESIAN_POINT('Ctrl Pts',(3.65342498214111,1.94709871486667,-12.8265804336333)) ;
#168253 = CARTESIAN_POINT('Ctrl Pts',(3.65677402871197,1.94900544167846,-12.8253525584084)) ;
#168254 = CARTESIAN_POINT('Ctrl Pts',(3.66003813592314,1.95098496635819,-12.8239806366809)) ;
#168255 = CARTESIAN_POINT('Ctrl Pts',(3.66320312645637,1.95301617633164,-12.822462401394)) ;
#168256 = CARTESIAN_POINT('Ctrl Pts',(3.6675737308879,1.9558211184691,-12.8203658371852)) ;
#168257 = CARTESIAN_POINT('Ctrl Pts',(3.67181875309331,1.95875330073043,-12.8179661261711)) ;
#168258 = CARTESIAN_POINT('Ctrl Pts',(3.67584388612464,1.96174615985015,-12.8152600357861)) ;
#168259 = CARTESIAN_POINT('Ctrl Pts',(3.67661208162745,1.96231734616832,-12.8147435792)) ;
#168260 = CARTESIAN_POINT('Ctrl Pts',(3.67737237849342,1.96289065080907,-12.8142160158768)) ;
#168261 = CARTESIAN_POINT('Ctrl Pts',(3.67812428214757,1.96346549105991,-12.8136773988359)) ;
#168262 = CARTESIAN_POINT('Ctrl Pts',(3.67853493948852,1.96377944400797,-12.8133832294425)) ;
#168263 = CARTESIAN_POINT('Ctrl Pts',(3.67894301851535,1.96409388168821,-12.8130857517433)) ;
#168264 = CARTESIAN_POINT('Ctrl Pts',(3.67934840022277,1.96440871854258,-12.8127849693981)) ;
#168265 = CARTESIAN_POINT('Ctrl Pts',(3.68198440184426,1.96645595067818,-12.8108291269535)) ;
#168266 = CARTESIAN_POINT('Ctrl Pts',(3.68449751351864,1.96851545671311,-12.8087382834716)) ;
#168267 = CARTESIAN_POINT('Ctrl Pts',(3.68685379133723,1.97055696562016,-12.8065208503987)) ;
#168268 = CARTESIAN_POINT('Ctrl Pts',(3.68896164651378,1.97238323800782,-12.8045372015504)) ;
#168269 = CARTESIAN_POINT('Ctrl Pts',(3.69104797813192,1.97419718002535,-12.80244243878)) ;
#168270 = CARTESIAN_POINT('Ctrl Pts',(3.69290978292475,1.9759856941215,-12.8002450010325)) ;
#168271 = CARTESIAN_POINT('Ctrl Pts',(3.69362192319634,1.97666980070403,-12.7994044811669)) ;
#168272 = CARTESIAN_POINT('Ctrl Pts',(3.69430163271856,1.97734979318964,-12.7985489756153)) ;
#168273 = CARTESIAN_POINT('Ctrl Pts',(3.69493905694205,1.97802369895107,-12.797679088363)) ;
#168274 = CARTESIAN_POINT('Ctrl Pts',(3.69605143900784,1.9791997456958,-12.7961610303053)) ;
#168275 = CARTESIAN_POINT('Ctrl Pts',(3.69703421735413,1.98035885502254,-12.7945986233173)) ;
#168276 = CARTESIAN_POINT('Ctrl Pts',(3.6978475066491,1.98151165953422,-12.7929571915312)) ;
#168277 = CARTESIAN_POINT('Ctrl Pts',(3.69841279947841,1.98231293913801,-12.7918162818644)) ;
#168278 = CARTESIAN_POINT('Ctrl Pts',(3.69890310384951,1.98311438470592,-12.7906332480122)) ;
#168279 = CARTESIAN_POINT('Ctrl Pts',(3.6992909830199,1.98393783265445,-12.7893581070748)) ;
#168280 = CARTESIAN_POINT('Ctrl Pts',(3.69936193271523,1.98408845528522,-12.7891248621162)) ;
#168281 = CARTESIAN_POINT('Ctrl Pts',(3.69942931950317,1.98423979370565,-12.7888885146859)) ;
#168282 = CARTESIAN_POINT('Ctrl Pts',(3.69949277412725,1.98439195189925,-12.7886487302852)) ;
#168283 = CARTESIAN_POINT('Ctrl Pts',(3.69967702385849,1.98483376534754,-12.7879524813983)) ;
#168284 = CARTESIAN_POINT('Ctrl Pts',(3.69981936684304,1.98527475083261,-12.7872393342585)) ;
#168285 = CARTESIAN_POINT('Ctrl Pts',(3.69990669142683,1.98570953653124,-12.7865158410281)) ;
#168286 = CARTESIAN_POINT('Ctrl Pts',(3.69996666908332,1.98600816294482,-12.7860189199258)) ;
#168287 = CARTESIAN_POINT('Ctrl Pts',(3.7,1.9863078059213,-12.7855104950545)) ;
#168288 = CARTESIAN_POINT('Ctrl Pts',(3.7,1.98660254037844,-12.785)) ;
#168289 = CARTESIAN_POINT('Origin',(3.7,1.9,-12.735)) ;
#168290 = CARTESIAN_POINT('Origin',(10.2,1.9,-12.735)) ;
#168291 = CARTESIAN_POINT('Origin',(3.7,1.9,-12.735)) ;
#168292 = CARTESIAN_POINT('Origin',(10.1,1.9,-12.735)) ;
#168293 = CARTESIAN_POINT('Origin',(10.1,1.9,-12.735)) ;
#168294 = CARTESIAN_POINT('Origin',(3.7,2.1,-10.125)) ;
#168295 = CARTESIAN_POINT('',(3.7,1.98660254037844,-10.075)) ;
#168296 = CARTESIAN_POINT('Origin',(3.7,1.9,-10.125)) ;
#168297 = CARTESIAN_POINT('Ctrl Pts',(3.7,1.98660254037844,-10.075)) ;
#168298 = CARTESIAN_POINT('Ctrl Pts',(3.69999911718144,1.98567700534183,-10.0733969262924)) ;
#168299 = CARTESIAN_POINT('Ctrl Pts',(3.69968163901485,1.98470369933601,-10.0718180022846)) ;
#168300 = CARTESIAN_POINT('Ctrl Pts',(3.69895427931586,1.98325895404995,-10.0695944560408)) ;
#168301 = CARTESIAN_POINT('Ctrl Pts',(3.69867650892745,1.98278649590681,-10.0688860984239)) ;
#168302 = CARTESIAN_POINT('Ctrl Pts',(3.69717970712967,1.9804354328423,-10.0654409187843)) ;
#168303 = CARTESIAN_POINT('Ctrl Pts',(3.69541014605544,1.97847095301992,-10.0628241208443)) ;
#168304 = CARTESIAN_POINT('Ctrl Pts',(3.69146029518774,1.97457001268155,-10.057973443509)) ;
#168305 = CARTESIAN_POINT('Ctrl Pts',(3.68915436790411,1.97254004967205,-10.0556322068765)) ;
#168306 = CARTESIAN_POINT('Ctrl Pts',(3.68263623161784,1.96688850447173,-10.0494999184567)) ;
#168307 = CARTESIAN_POINT('Ctrl Pts',(3.67796661383141,1.96321337091298,-10.0459792522829)) ;
#168308 = CARTESIAN_POINT('Ctrl Pts',(3.67279117399659,1.95950210067463,-10.0427623433944)) ;
#168309 = CARTESIAN_POINT('Ctrl Pts',(3.67252519027985,1.95931231248676,-10.0425988090581)) ;
#168310 = CARTESIAN_POINT('Ctrl Pts',(3.6693311210617,1.95704457126181,-10.0406562043068)) ;
#168311 = CARTESIAN_POINT('Ctrl Pts',(3.66628216680076,1.95498580453519,-10.0390096122391)) ;
#168312 = CARTESIAN_POINT('Ctrl Pts',(3.65739884032376,1.94929644648107,-10.0347590242123)) ;
#168313 = CARTESIAN_POINT('Ctrl Pts',(3.65126071410427,1.94574201114262,-10.0324711332688)) ;
#168314 = CARTESIAN_POINT('Ctrl Pts',(3.64132315686418,1.94068746317945,-10.0296379659012)) ;
#168315 = CARTESIAN_POINT('Ctrl Pts',(3.63763353946351,1.93894751340588,-10.0287565993848)) ;
#168316 = CARTESIAN_POINT('Ctrl Pts',(3.62813871250319,1.93486114467728,-10.0269043913581)) ;
#168317 = CARTESIAN_POINT('Ctrl Pts',(3.62220485293008,1.9326600471938,-10.0261153440415)) ;
#168318 = CARTESIAN_POINT('Ctrl Pts',(3.61359543742328,1.93003167234287,-10.0254202174511)) ;
#168319 = CARTESIAN_POINT('Ctrl Pts',(3.61101642177007,1.92931331154713,-10.0252669825532)) ;
#168320 = CARTESIAN_POINT('Ctrl Pts',(3.60562851963641,1.92796119665944,-10.0250532567727)) ;
#168321 = CARTESIAN_POINT('Ctrl Pts',(3.60282089026137,1.92733781012841,-10.025)) ;
#168322 = CARTESIAN_POINT('Ctrl Pts',(3.6,1.92679491924311,-10.025)) ;
#168323 = CARTESIAN_POINT('Origin',(3.6,1.9,-10.125)) ;
#168324 = CARTESIAN_POINT('Origin',(3.7,1.9,-10.125)) ;
#168325 = CARTESIAN_POINT('Origin',(10.1,1.9,-10.125)) ;
#168326 = CARTESIAN_POINT('Origin',(10.1,1.9,-10.125)) ;
#168327 = CARTESIAN_POINT('Origin',(3.7,2.1,-16.545)) ;
#168328 = CARTESIAN_POINT('',(3.7,1.98660254037845,-16.595)) ;
#168329 = CARTESIAN_POINT('Ctrl Pts',(3.60000000000001,1.92679491924311,-16.645)) ;
#168330 = CARTESIAN_POINT('Ctrl Pts',(3.60642117639496,1.92803067521649,-16.645)) ;
#168331 = CARTESIAN_POINT('Ctrl Pts',(3.61278477806524,1.92968896670929,-16.6447228136141)) ;
#168332 = CARTESIAN_POINT('Ctrl Pts',(3.61897283239559,1.93170032347272,-16.6441235249136)) ;
#168333 = CARTESIAN_POINT('Ctrl Pts',(3.62020584678462,1.93210110079276,-16.6440041123243)) ;
#168334 = CARTESIAN_POINT('Ctrl Pts',(3.62143195421103,1.93251577262759,-16.6438720028083)) ;
#168335 = CARTESIAN_POINT('Ctrl Pts',(3.62265032708637,1.93294361409314,-16.643726982434)) ;
#168336 = CARTESIAN_POINT('Ctrl Pts',(3.62647624625549,1.9342871164786,-16.6432715912801)) ;
#168337 = CARTESIAN_POINT('Ctrl Pts',(3.63025346237246,1.93576539638807,-16.6426857368177)) ;
#168338 = CARTESIAN_POINT('Ctrl Pts',(3.6339385638818,1.9373536406594,-16.6419650362697)) ;
#168339 = CARTESIAN_POINT('Ctrl Pts',(3.6390779374911,1.93956866259911,-16.6409599216571)) ;
#168340 = CARTESIAN_POINT('Ctrl Pts',(3.64410916187654,1.94202076919938,-16.6396787224495)) ;
#168341 = CARTESIAN_POINT('Ctrl Pts',(3.64894317395167,1.94461872744812,-16.6381221777356)) ;
#168342 = CARTESIAN_POINT('Ctrl Pts',(3.64993855309228,1.945153677177,-16.6378016671296)) ;
#168343 = CARTESIAN_POINT('Ctrl Pts',(3.65092568100105,1.94569474416723,-16.6374696031568)) ;
#168344 = CARTESIAN_POINT('Ctrl Pts',(3.65190395907092,1.94624104404949,-16.6371261809367)) ;
#168345 = CARTESIAN_POINT('Ctrl Pts',(3.65241342868349,1.94652554719633,-16.6369473328252)) ;
#168346 = CARTESIAN_POINT('Ctrl Pts',(3.65292046817498,1.94681147780208,-16.63676540574)) ;
#168347 = CARTESIAN_POINT('Ctrl Pts',(3.6534249821411,1.94709871486665,-16.6365804336333)) ;
#168348 = CARTESIAN_POINT('Ctrl Pts',(3.65677402871197,1.94900544167846,-16.6353525584084)) ;
#168349 = CARTESIAN_POINT('Ctrl Pts',(3.66003813592314,1.95098496635819,-16.6339806366809)) ;
#168350 = CARTESIAN_POINT('Ctrl Pts',(3.66320312645638,1.95301617633166,-16.632462401394)) ;
#168351 = CARTESIAN_POINT('Ctrl Pts',(3.66757373088829,1.95582111846938,-16.630365837185)) ;
#168352 = CARTESIAN_POINT('Ctrl Pts',(3.67181875309404,1.95875330073095,-16.6279661261707)) ;
#168353 = CARTESIAN_POINT('Ctrl Pts',(3.67584388612568,1.96174615985092,-16.6252600357854)) ;
#168354 = CARTESIAN_POINT('Ctrl Pts',(3.67661208162821,1.96231734616889,-16.6247435791995)) ;
#168355 = CARTESIAN_POINT('Ctrl Pts',(3.6773723784939,1.96289065080943,-16.6242160158765)) ;
#168356 = CARTESIAN_POINT('Ctrl Pts',(3.67812428214779,1.96346549106007,-16.6236773988357)) ;
#168357 = CARTESIAN_POINT('Ctrl Pts',(3.67853493948866,1.96377944400807,-16.6233832294424)) ;
#168358 = CARTESIAN_POINT('Ctrl Pts',(3.67894301851542,1.96409388168823,-16.6230857517433)) ;
#168359 = CARTESIAN_POINT('Ctrl Pts',(3.67934840022277,1.96440871854255,-16.6227849693981)) ;
#168360 = CARTESIAN_POINT('Ctrl Pts',(3.68198440184425,1.96645595067818,-16.6208291269535)) ;
#168361 = CARTESIAN_POINT('Ctrl Pts',(3.68449751351864,1.96851545671311,-16.6187382834716)) ;
#168362 = CARTESIAN_POINT('Ctrl Pts',(3.68685379133723,1.97055696562017,-16.6165208503987)) ;
#168363 = CARTESIAN_POINT('Ctrl Pts',(3.68896164651388,1.9723832380079,-16.6145372015503)) ;
#168364 = CARTESIAN_POINT('Ctrl Pts',(3.6910479781321,1.97419718002554,-16.6124424387798)) ;
#168365 = CARTESIAN_POINT('Ctrl Pts',(3.69290978292499,1.97598569412176,-16.6102450010322)) ;
#168366 = CARTESIAN_POINT('Ctrl Pts',(3.6936219231965,1.97666980070422,-16.6094044811667)) ;
#168367 = CARTESIAN_POINT('Ctrl Pts',(3.69430163271864,1.97734979318976,-16.6085489756152)) ;
#168368 = CARTESIAN_POINT('Ctrl Pts',(3.69493905694207,1.9780236989511,-16.607679088363)) ;
#168369 = CARTESIAN_POINT('Ctrl Pts',(3.69605143900786,1.9791997456958,-16.6061610303053)) ;
#168370 = CARTESIAN_POINT('Ctrl Pts',(3.69703421735413,1.98035885502256,-16.6045986233173)) ;
#168371 = CARTESIAN_POINT('Ctrl Pts',(3.6978475066491,1.98151165953425,-16.6029571915311)) ;
#168372 = CARTESIAN_POINT('Ctrl Pts',(3.69841279947847,1.98231293913814,-16.6018162818643)) ;
#168373 = CARTESIAN_POINT('Ctrl Pts',(3.6989031038496,1.98311438470612,-16.6006332480119)) ;
#168374 = CARTESIAN_POINT('Ctrl Pts',(3.69929098302002,1.98393783265472,-16.5993581070744)) ;
#168375 = CARTESIAN_POINT('Ctrl Pts',(3.6993619327153,1.98408845528541,-16.5991248621159)) ;
#168376 = CARTESIAN_POINT('Ctrl Pts',(3.69942931950321,1.98423979370578,-16.5988885146857)) ;
#168377 = CARTESIAN_POINT('Ctrl Pts',(3.69949277412727,1.98439195189931,-16.5986487302851)) ;
#168378 = CARTESIAN_POINT('Ctrl Pts',(3.6996770238585,1.98483376534759,-16.5979524813983)) ;
#168379 = CARTESIAN_POINT('Ctrl Pts',(3.69981936684305,1.98527475083261,-16.5972393342585)) ;
#168380 = CARTESIAN_POINT('Ctrl Pts',(3.69990669142684,1.9857095365312,-16.5965158410282)) ;
#168381 = CARTESIAN_POINT('Ctrl Pts',(3.69996666908332,1.98600816294476,-16.5960189199259)) ;
#168382 = CARTESIAN_POINT('Ctrl Pts',(3.7,1.9863078059213,-16.5955104950545)) ;
#168383 = CARTESIAN_POINT('Ctrl Pts',(3.7,1.98660254037844,-16.595)) ;
#168384 = CARTESIAN_POINT('Origin',(3.7,1.9,-16.545)) ;
#168385 = CARTESIAN_POINT('Origin',(10.2,1.9,-16.545)) ;
#168386 = CARTESIAN_POINT('Origin',(3.7,1.9,-16.545)) ;
#168387 = CARTESIAN_POINT('Origin',(10.1,1.9,-16.545)) ;
#168388 = CARTESIAN_POINT('Origin',(10.1,1.9,-16.545)) ;
#168389 = CARTESIAN_POINT('Origin',(3.7,2.1,-13.935)) ;
#168390 = CARTESIAN_POINT('',(3.7,1.98660254037844,-13.885)) ;
#168391 = CARTESIAN_POINT('Origin',(3.7,1.9,-13.935)) ;
#168392 = CARTESIAN_POINT('Ctrl Pts',(3.7,1.98660254037844,-13.885)) ;
#168393 = CARTESIAN_POINT('Ctrl Pts',(3.69999911718144,1.98567700534183,-13.8833969262924)) ;
#168394 = CARTESIAN_POINT('Ctrl Pts',(3.69968163901485,1.984703699336,-13.8818180022846)) ;
#168395 = CARTESIAN_POINT('Ctrl Pts',(3.69895427931585,1.98325895404995,-13.8795944560408)) ;
#168396 = CARTESIAN_POINT('Ctrl Pts',(3.69867650892745,1.98278649590681,-13.8788860984239)) ;
#168397 = CARTESIAN_POINT('Ctrl Pts',(3.69717970712967,1.9804354328423,-13.8754409187843)) ;
#168398 = CARTESIAN_POINT('Ctrl Pts',(3.69541014605544,1.97847095301992,-13.8728241208443)) ;
#168399 = CARTESIAN_POINT('Ctrl Pts',(3.69146029518774,1.97457001268155,-13.867973443509)) ;
#168400 = CARTESIAN_POINT('Ctrl Pts',(3.68915436790411,1.97254004967205,-13.8656322068765)) ;
#168401 = CARTESIAN_POINT('Ctrl Pts',(3.68263623161783,1.96688850447172,-13.8594999184567)) ;
#168402 = CARTESIAN_POINT('Ctrl Pts',(3.67796661383139,1.96321337091296,-13.8559792522829)) ;
#168403 = CARTESIAN_POINT('Ctrl Pts',(3.67279117399656,1.95950210067461,-13.8527623433944)) ;
#168404 = CARTESIAN_POINT('Ctrl Pts',(3.67252519027983,1.95931231248676,-13.8525988090581)) ;
#168405 = CARTESIAN_POINT('Ctrl Pts',(3.6693311210617,1.95704457126181,-13.8506562043068)) ;
#168406 = CARTESIAN_POINT('Ctrl Pts',(3.66628216680076,1.95498580453519,-13.8490096122391)) ;
#168407 = CARTESIAN_POINT('Ctrl Pts',(3.65739884032376,1.94929644648107,-13.8447590242123)) ;
#168408 = CARTESIAN_POINT('Ctrl Pts',(3.65126071410427,1.94574201114262,-13.8424711332688)) ;
#168409 = CARTESIAN_POINT('Ctrl Pts',(3.64132315686417,1.94068746317945,-13.8396379659013)) ;
#168410 = CARTESIAN_POINT('Ctrl Pts',(3.63763353946351,1.93894751340588,-13.8387565993848)) ;
#168411 = CARTESIAN_POINT('Ctrl Pts',(3.62813871250318,1.93486114467727,-13.8369043913581)) ;
#168412 = CARTESIAN_POINT('Ctrl Pts',(3.62220485293007,1.9326600471938,-13.8361153440415)) ;
#168413 = CARTESIAN_POINT('Ctrl Pts',(3.61359543742316,1.93003167234283,-13.8354202174511)) ;
#168414 = CARTESIAN_POINT('Ctrl Pts',(3.61101642176982,1.92931331154706,-13.8352669825532)) ;
#168415 = CARTESIAN_POINT('Ctrl Pts',(3.60562851963616,1.92796119665938,-13.8350532567727)) ;
#168416 = CARTESIAN_POINT('Ctrl Pts',(3.60282089026124,1.92733781012838,-13.835)) ;
#168417 = CARTESIAN_POINT('Ctrl Pts',(3.6,1.92679491924311,-13.835)) ;
#168418 = CARTESIAN_POINT('Origin',(3.6,1.9,-13.935)) ;
#168419 = CARTESIAN_POINT('Origin',(3.7,1.9,-13.935)) ;
#168420 = CARTESIAN_POINT('Origin',(10.1,1.9,-13.935)) ;
#168421 = CARTESIAN_POINT('Origin',(10.1,1.9,-13.935)) ;
#168422 = CARTESIAN_POINT('Origin',(3.7,2.1,-20.355)) ;
#168423 = CARTESIAN_POINT('',(3.7,1.98660254037845,-20.405)) ;
#168424 = CARTESIAN_POINT('Ctrl Pts',(3.60000000000001,1.92679491924311,-20.455)) ;
#168425 = CARTESIAN_POINT('Ctrl Pts',(3.60642117639513,1.92803067521652,-20.455)) ;
#168426 = CARTESIAN_POINT('Ctrl Pts',(3.61278477806557,1.92968896670937,-20.4547228136141)) ;
#168427 = CARTESIAN_POINT('Ctrl Pts',(3.61897283239609,1.93170032347287,-20.4541235249136)) ;
#168428 = CARTESIAN_POINT('Ctrl Pts',(3.62020584678495,1.93210110079286,-20.4540041123242)) ;
#168429 = CARTESIAN_POINT('Ctrl Pts',(3.62143195421119,1.93251577262764,-20.4538720028082)) ;
#168430 = CARTESIAN_POINT('Ctrl Pts',(3.62265032708637,1.93294361409314,-20.453726982434)) ;
#168431 = CARTESIAN_POINT('Ctrl Pts',(3.62647624625549,1.9342871164786,-20.4532715912801)) ;
#168432 = CARTESIAN_POINT('Ctrl Pts',(3.63025346237246,1.93576539638807,-20.4526857368177)) ;
#168433 = CARTESIAN_POINT('Ctrl Pts',(3.6339385638818,1.9373536406594,-20.4519650362697)) ;
#168434 = CARTESIAN_POINT('Ctrl Pts',(3.63907793749117,1.93956866259914,-20.4509599216571)) ;
#168435 = CARTESIAN_POINT('Ctrl Pts',(3.64410916187667,1.94202076919945,-20.4496787224495)) ;
#168436 = CARTESIAN_POINT('Ctrl Pts',(3.64894317395187,1.94461872744823,-20.4481221777355)) ;
#168437 = CARTESIAN_POINT('Ctrl Pts',(3.64993855309242,1.94515367717707,-20.4478016671295)) ;
#168438 = CARTESIAN_POINT('Ctrl Pts',(3.65092568100113,1.94569474416727,-20.4474696031567)) ;
#168439 = CARTESIAN_POINT('Ctrl Pts',(3.65190395907093,1.94624104404949,-20.4471261809367)) ;
#168440 = CARTESIAN_POINT('Ctrl Pts',(3.6524134286835,1.94652554719633,-20.4469473328252)) ;
#168441 = CARTESIAN_POINT('Ctrl Pts',(3.65292046817498,1.94681147780208,-20.44676540574)) ;
#168442 = CARTESIAN_POINT('Ctrl Pts',(3.6534249821411,1.94709871486665,-20.4465804336333)) ;
#168443 = CARTESIAN_POINT('Ctrl Pts',(3.65677402871197,1.94900544167847,-20.4453525584084)) ;
#168444 = CARTESIAN_POINT('Ctrl Pts',(3.66003813592314,1.9509849663582,-20.4439806366809)) ;
#168445 = CARTESIAN_POINT('Ctrl Pts',(3.66320312645638,1.95301617633166,-20.442462401394)) ;
#168446 = CARTESIAN_POINT('Ctrl Pts',(3.66757373088817,1.9558211184693,-20.4403658371851)) ;
#168447 = CARTESIAN_POINT('Ctrl Pts',(3.67181875309382,1.9587533007308,-20.4379661261708)) ;
#168448 = CARTESIAN_POINT('Ctrl Pts',(3.67584388612536,1.96174615985069,-20.4352600357856)) ;
#168449 = CARTESIAN_POINT('Ctrl Pts',(3.676612081628,1.96231734616874,-20.4347435791996)) ;
#168450 = CARTESIAN_POINT('Ctrl Pts',(3.67737237849379,1.96289065080935,-20.4342160158766)) ;
#168451 = CARTESIAN_POINT('Ctrl Pts',(3.67812428214777,1.96346549106006,-20.4336773988358)) ;
#168452 = CARTESIAN_POINT('Ctrl Pts',(3.67853493948865,1.96377944400807,-20.4333832294424)) ;
#168453 = CARTESIAN_POINT('Ctrl Pts',(3.67894301851541,1.96409388168823,-20.4330857517433)) ;
#168454 = CARTESIAN_POINT('Ctrl Pts',(3.67934840022277,1.96440871854255,-20.4327849693981)) ;
#168455 = CARTESIAN_POINT('Ctrl Pts',(3.68198440184425,1.96645595067818,-20.4308291269535)) ;
#168456 = CARTESIAN_POINT('Ctrl Pts',(3.68449751351864,1.96851545671311,-20.4287382834716)) ;
#168457 = CARTESIAN_POINT('Ctrl Pts',(3.68685379133723,1.97055696562016,-20.4265208503987)) ;
#168458 = CARTESIAN_POINT('Ctrl Pts',(3.68896164651387,1.97238323800789,-20.4245372015503)) ;
#168459 = CARTESIAN_POINT('Ctrl Pts',(3.69104797813208,1.97419718002552,-20.4224424387798)) ;
#168460 = CARTESIAN_POINT('Ctrl Pts',(3.69290978292497,1.97598569412173,-20.4202450010322)) ;
#168461 = CARTESIAN_POINT('Ctrl Pts',(3.69362192319649,1.97666980070421,-20.4194044811667)) ;
#168462 = CARTESIAN_POINT('Ctrl Pts',(3.69430163271864,1.97734979318975,-20.4185489756152)) ;
#168463 = CARTESIAN_POINT('Ctrl Pts',(3.69493905694207,1.9780236989511,-20.417679088363)) ;
#168464 = CARTESIAN_POINT('Ctrl Pts',(3.69605143900786,1.9791997456958,-20.4161610303053)) ;
#168465 = CARTESIAN_POINT('Ctrl Pts',(3.69703421735413,1.98035885502256,-20.4145986233173)) ;
#168466 = CARTESIAN_POINT('Ctrl Pts',(3.69784750664911,1.98151165953425,-20.4129571915311)) ;
#168467 = CARTESIAN_POINT('Ctrl Pts',(3.69841279947848,1.98231293913814,-20.4118162818643)) ;
#168468 = CARTESIAN_POINT('Ctrl Pts',(3.69890310384961,1.98311438470612,-20.4106332480119)) ;
#168469 = CARTESIAN_POINT('Ctrl Pts',(3.69929098302003,1.98393783265478,-20.4093581070743)) ;
#168470 = CARTESIAN_POINT('Ctrl Pts',(3.69936193271531,1.98408845528547,-20.4091248621159)) ;
#168471 = CARTESIAN_POINT('Ctrl Pts',(3.69942931950321,1.98423979370578,-20.4088885146857)) ;
#168472 = CARTESIAN_POINT('Ctrl Pts',(3.69949277412726,1.9843919518993,-20.4086487302851)) ;
#168473 = CARTESIAN_POINT('Ctrl Pts',(3.6996770238585,1.98483376534759,-20.4079524813983)) ;
#168474 = CARTESIAN_POINT('Ctrl Pts',(3.69981936684305,1.98527475083261,-20.4072393342585)) ;
#168475 = CARTESIAN_POINT('Ctrl Pts',(3.69990669142684,1.9857095365312,-20.4065158410282)) ;
#168476 = CARTESIAN_POINT('Ctrl Pts',(3.69996666908332,1.98600816294476,-20.4060189199259)) ;
#168477 = CARTESIAN_POINT('Ctrl Pts',(3.7,1.98630780592131,-20.4055104950545)) ;
#168478 = CARTESIAN_POINT('Ctrl Pts',(3.7,1.98660254037844,-20.405)) ;
#168479 = CARTESIAN_POINT('Origin',(3.7,1.9,-20.355)) ;
#168480 = CARTESIAN_POINT('Origin',(10.2,1.9,-20.355)) ;
#168481 = CARTESIAN_POINT('Origin',(3.7,1.9,-20.355)) ;
#168482 = CARTESIAN_POINT('Origin',(10.1,1.9,-20.355)) ;
#168483 = CARTESIAN_POINT('Origin',(10.1,1.9,-20.355)) ;
#168484 = CARTESIAN_POINT('Origin',(3.7,2.1,-17.745)) ;
#168485 = CARTESIAN_POINT('',(3.7,1.98660254037844,-17.695)) ;
#168486 = CARTESIAN_POINT('Origin',(3.7,1.9,-17.745)) ;
#168487 = CARTESIAN_POINT('Ctrl Pts',(3.7,1.98660254037844,-17.695)) ;
#168488 = CARTESIAN_POINT('Ctrl Pts',(3.69999911718144,1.98567700534182,-17.6933969262924)) ;
#168489 = CARTESIAN_POINT('Ctrl Pts',(3.69968163901485,1.98470369933599,-17.6918180022845)) ;
#168490 = CARTESIAN_POINT('Ctrl Pts',(3.69895427931585,1.98325895404994,-17.6895944560408)) ;
#168491 = CARTESIAN_POINT('Ctrl Pts',(3.69867650892745,1.9827864959068,-17.6888860984239)) ;
#168492 = CARTESIAN_POINT('Ctrl Pts',(3.69717970712967,1.9804354328423,-17.6854409187843)) ;
#168493 = CARTESIAN_POINT('Ctrl Pts',(3.69541014605544,1.97847095301992,-17.6828241208443)) ;
#168494 = CARTESIAN_POINT('Ctrl Pts',(3.69146029518774,1.97457001268155,-17.677973443509)) ;
#168495 = CARTESIAN_POINT('Ctrl Pts',(3.68915436790411,1.97254004967205,-17.6756322068765)) ;
#168496 = CARTESIAN_POINT('Ctrl Pts',(3.68263623161792,1.9668885044718,-17.6694999184568)) ;
#168497 = CARTESIAN_POINT('Ctrl Pts',(3.67796661383158,1.96321337091312,-17.6659792522831)) ;
#168498 = CARTESIAN_POINT('Ctrl Pts',(3.67279117399677,1.95950210067476,-17.6627623433945)) ;
#168499 = CARTESIAN_POINT('Ctrl Pts',(3.67252519027994,1.95931231248683,-17.6625988090582)) ;
#168500 = CARTESIAN_POINT('Ctrl Pts',(3.6693311210617,1.95704457126181,-17.6606562043068)) ;
#168501 = CARTESIAN_POINT('Ctrl Pts',(3.66628216680076,1.95498580453519,-17.6590096122391)) ;
#168502 = CARTESIAN_POINT('Ctrl Pts',(3.65739884032376,1.94929644648107,-17.6547590242123)) ;
#168503 = CARTESIAN_POINT('Ctrl Pts',(3.65126071410426,1.94574201114262,-17.6524711332688)) ;
#168504 = CARTESIAN_POINT('Ctrl Pts',(3.64132315686417,1.94068746317945,-17.6496379659013)) ;
#168505 = CARTESIAN_POINT('Ctrl Pts',(3.63763353946351,1.93894751340588,-17.6487565993848)) ;
#168506 = CARTESIAN_POINT('Ctrl Pts',(3.62813871250313,1.93486114467725,-17.6469043913581)) ;
#168507 = CARTESIAN_POINT('Ctrl Pts',(3.62220485292998,1.93266004719376,-17.6461153440415)) ;
#168508 = CARTESIAN_POINT('Ctrl Pts',(3.61359543742287,1.93003167234274,-17.6454202174511)) ;
#168509 = CARTESIAN_POINT('Ctrl Pts',(3.61101642176938,1.92931331154694,-17.6452669825531)) ;
#168510 = CARTESIAN_POINT('Ctrl Pts',(3.60562851963576,1.92796119665929,-17.6450532567727)) ;
#168511 = CARTESIAN_POINT('Ctrl Pts',(3.60282089026104,1.92733781012834,-17.645)) ;
#168512 = CARTESIAN_POINT('Ctrl Pts',(3.6,1.92679491924311,-17.645)) ;
#168513 = CARTESIAN_POINT('Origin',(3.6,1.9,-17.745)) ;
#168514 = CARTESIAN_POINT('Origin',(3.7,1.9,-17.745)) ;
#168515 = CARTESIAN_POINT('Origin',(10.1,1.9,-17.745)) ;
#168516 = CARTESIAN_POINT('Origin',(10.1,1.9,-17.745)) ;
#168517 = CARTESIAN_POINT('Origin',(3.7,2.1,-24.165)) ;
#168518 = CARTESIAN_POINT('',(3.7,1.98660254037845,-24.215)) ;
#168519 = CARTESIAN_POINT('Ctrl Pts',(3.60000000000001,1.92679491924311,-24.265)) ;
#168520 = CARTESIAN_POINT('Ctrl Pts',(3.60642117639458,1.92803067521642,-24.265)) ;
#168521 = CARTESIAN_POINT('Ctrl Pts',(3.61278477806449,1.9296889667091,-24.2647228136141)) ;
#168522 = CARTESIAN_POINT('Ctrl Pts',(3.6189728323945,1.93170032347237,-24.2641235249137)) ;
#168523 = CARTESIAN_POINT('Ctrl Pts',(3.62020584678389,1.93210110079252,-24.2640041123243)) ;
#168524 = CARTESIAN_POINT('Ctrl Pts',(3.62143195421067,1.93251577262747,-24.2638720028083)) ;
#168525 = CARTESIAN_POINT('Ctrl Pts',(3.62265032708637,1.93294361409315,-24.263726982434)) ;
#168526 = CARTESIAN_POINT('Ctrl Pts',(3.62647624625549,1.9342871164786,-24.2632715912801)) ;
#168527 = CARTESIAN_POINT('Ctrl Pts',(3.63025346237246,1.93576539638805,-24.2626857368177)) ;
#168528 = CARTESIAN_POINT('Ctrl Pts',(3.6339385638818,1.9373536406594,-24.2619650362697)) ;
#168529 = CARTESIAN_POINT('Ctrl Pts',(3.63907793749079,1.93956866259898,-24.2609599216571)) ;
#168530 = CARTESIAN_POINT('Ctrl Pts',(3.64410916187594,1.94202076919911,-24.2596787224496)) ;
#168531 = CARTESIAN_POINT('Ctrl Pts',(3.64894317395081,1.94461872744766,-24.2581221777359)) ;
#168532 = CARTESIAN_POINT('Ctrl Pts',(3.64993855309173,1.94515367717669,-24.2578016671298)) ;
#168533 = CARTESIAN_POINT('Ctrl Pts',(3.65092568100079,1.94569474416708,-24.2574696031568)) ;
#168534 = CARTESIAN_POINT('Ctrl Pts',(3.65190395907095,1.9462410440495,-24.2571261809367)) ;
#168535 = CARTESIAN_POINT('Ctrl Pts',(3.65241342868351,1.94652554719632,-24.2569473328252)) ;
#168536 = CARTESIAN_POINT('Ctrl Pts',(3.65292046817499,1.9468114778021,-24.25676540574)) ;
#168537 = CARTESIAN_POINT('Ctrl Pts',(3.65342498214111,1.94709871486667,-24.2565804336333)) ;
#168538 = CARTESIAN_POINT('Ctrl Pts',(3.65677402871197,1.94900544167846,-24.2553525584084)) ;
#168539 = CARTESIAN_POINT('Ctrl Pts',(3.66003813592314,1.95098496635819,-24.2539806366809)) ;
#168540 = CARTESIAN_POINT('Ctrl Pts',(3.66320312645637,1.95301617633163,-24.252462401394)) ;
#168541 = CARTESIAN_POINT('Ctrl Pts',(3.66757373088834,1.95582111846937,-24.250365837185)) ;
#168542 = CARTESIAN_POINT('Ctrl Pts',(3.67181875309416,1.95875330073098,-24.2479661261707)) ;
#168543 = CARTESIAN_POINT('Ctrl Pts',(3.67584388612586,1.96174615985107,-24.2452600357853)) ;
#168544 = CARTESIAN_POINT('Ctrl Pts',(3.67661208162847,1.96231734616911,-24.2447435791993)) ;
#168545 = CARTESIAN_POINT('Ctrl Pts',(3.67737237849424,1.96289065080973,-24.2442160158762)) ;
#168546 = CARTESIAN_POINT('Ctrl Pts',(3.6781242821482,1.96346549106044,-24.2436773988354)) ;
#168547 = CARTESIAN_POINT('Ctrl Pts',(3.67853493948893,1.96377944400835,-24.2433832294422)) ;
#168548 = CARTESIAN_POINT('Ctrl Pts',(3.67894301851555,1.96409388168833,-24.2430857517432)) ;
#168549 = CARTESIAN_POINT('Ctrl Pts',(3.67934840022277,1.96440871854255,-24.2427849693981)) ;
#168550 = CARTESIAN_POINT('Ctrl Pts',(3.68198440184425,1.96645595067817,-24.2408291269535)) ;
#168551 = CARTESIAN_POINT('Ctrl Pts',(3.68449751351863,1.96851545671311,-24.2387382834716)) ;
#168552 = CARTESIAN_POINT('Ctrl Pts',(3.68685379133722,1.97055696562016,-24.2365208503987)) ;
#168553 = CARTESIAN_POINT('Ctrl Pts',(3.68896164651379,1.97238323800783,-24.2345372015503)) ;
#168554 = CARTESIAN_POINT('Ctrl Pts',(3.69104797813193,1.97419718002536,-24.23244243878)) ;
#168555 = CARTESIAN_POINT('Ctrl Pts',(3.69290978292477,1.97598569412151,-24.2302450010325)) ;
#168556 = CARTESIAN_POINT('Ctrl Pts',(3.69362192319636,1.97666980070404,-24.2294044811669)) ;
#168557 = CARTESIAN_POINT('Ctrl Pts',(3.69430163271857,1.97734979318965,-24.2285489756153)) ;
#168558 = CARTESIAN_POINT('Ctrl Pts',(3.69493905694206,1.97802369895107,-24.227679088363)) ;
#168559 = CARTESIAN_POINT('Ctrl Pts',(3.69605143900786,1.9791997456958,-24.2261610303053)) ;
#168560 = CARTESIAN_POINT('Ctrl Pts',(3.69703421735413,1.98035885502255,-24.2245986233173)) ;
#168561 = CARTESIAN_POINT('Ctrl Pts',(3.69784750664911,1.98151165953424,-24.2229571915312)) ;
#168562 = CARTESIAN_POINT('Ctrl Pts',(3.69841279947844,1.98231293913807,-24.2218162818643)) ;
#168563 = CARTESIAN_POINT('Ctrl Pts',(3.69890310384955,1.98311438470599,-24.2206332480121)) ;
#168564 = CARTESIAN_POINT('Ctrl Pts',(3.69929098301996,1.98393783265456,-24.2193581070746)) ;
#168565 = CARTESIAN_POINT('Ctrl Pts',(3.69936193271526,1.98408845528528,-24.2191248621161)) ;
#168566 = CARTESIAN_POINT('Ctrl Pts',(3.69942931950317,1.98423979370565,-24.2188885146859)) ;
#168567 = CARTESIAN_POINT('Ctrl Pts',(3.69949277412723,1.98439195189921,-24.2186487302853)) ;
#168568 = CARTESIAN_POINT('Ctrl Pts',(3.69967702385848,1.98483376534753,-24.2179524813984)) ;
#168569 = CARTESIAN_POINT('Ctrl Pts',(3.69981936684304,1.98527475083255,-24.2172393342586)) ;
#168570 = CARTESIAN_POINT('Ctrl Pts',(3.69990669142684,1.98570953653118,-24.2165158410282)) ;
#168571 = CARTESIAN_POINT('Ctrl Pts',(3.69996666908332,1.98600816294476,-24.2160189199259)) ;
#168572 = CARTESIAN_POINT('Ctrl Pts',(3.7,1.98630780592131,-24.2155104950545)) ;
#168573 = CARTESIAN_POINT('Ctrl Pts',(3.7,1.98660254037844,-24.215)) ;
#168574 = CARTESIAN_POINT('Origin',(3.7,1.9,-24.165)) ;
#168575 = CARTESIAN_POINT('Origin',(10.2,1.9,-24.165)) ;
#168576 = CARTESIAN_POINT('Origin',(3.7,1.9,-24.165)) ;
#168577 = CARTESIAN_POINT('Origin',(10.1,1.9,-24.165)) ;
#168578 = CARTESIAN_POINT('Origin',(10.1,1.9,-24.165)) ;
#168579 = CARTESIAN_POINT('Origin',(3.7,2.1,-21.555)) ;
#168580 = CARTESIAN_POINT('',(3.7,1.98660254037844,-21.505)) ;
#168581 = CARTESIAN_POINT('Origin',(3.7,1.9,-21.555)) ;
#168582 = CARTESIAN_POINT('Ctrl Pts',(3.7,1.98660254037844,-21.505)) ;
#168583 = CARTESIAN_POINT('Ctrl Pts',(3.69999911718144,1.98567700534182,-21.5033969262924)) ;
#168584 = CARTESIAN_POINT('Ctrl Pts',(3.69968163901484,1.98470369933599,-21.5018180022845)) ;
#168585 = CARTESIAN_POINT('Ctrl Pts',(3.69895427931585,1.98325895404993,-21.4995944560408)) ;
#168586 = CARTESIAN_POINT('Ctrl Pts',(3.69867650892744,1.9827864959068,-21.4988860984239)) ;
#168587 = CARTESIAN_POINT('Ctrl Pts',(3.69717970712967,1.98043543284229,-21.4954409187843)) ;
#168588 = CARTESIAN_POINT('Ctrl Pts',(3.69541014605544,1.97847095301991,-21.4928241208443)) ;
#168589 = CARTESIAN_POINT('Ctrl Pts',(3.69146029518774,1.97457001268155,-21.487973443509)) ;
#168590 = CARTESIAN_POINT('Ctrl Pts',(3.68915436790411,1.97254004967205,-21.4856322068765)) ;
#168591 = CARTESIAN_POINT('Ctrl Pts',(3.68263623161789,1.96688850447178,-21.4794999184567)) ;
#168592 = CARTESIAN_POINT('Ctrl Pts',(3.67796661383153,1.96321337091308,-21.475979252283)) ;
#168593 = CARTESIAN_POINT('Ctrl Pts',(3.67279117399672,1.95950210067472,-21.4727623433945)) ;
#168594 = CARTESIAN_POINT('Ctrl Pts',(3.67252519027991,1.95931231248681,-21.4725988090581)) ;
#168595 = CARTESIAN_POINT('Ctrl Pts',(3.6693311210617,1.95704457126181,-21.4706562043068)) ;
#168596 = CARTESIAN_POINT('Ctrl Pts',(3.66628216680076,1.95498580453519,-21.4690096122391)) ;
#168597 = CARTESIAN_POINT('Ctrl Pts',(3.65739884032377,1.94929644648107,-21.4647590242123)) ;
#168598 = CARTESIAN_POINT('Ctrl Pts',(3.65126071410427,1.94574201114262,-21.4624711332688)) ;
#168599 = CARTESIAN_POINT('Ctrl Pts',(3.64132315686418,1.94068746317945,-21.4596379659013)) ;
#168600 = CARTESIAN_POINT('Ctrl Pts',(3.63763353946351,1.93894751340588,-21.4587565993848)) ;
#168601 = CARTESIAN_POINT('Ctrl Pts',(3.62813871250314,1.93486114467726,-21.4569043913581)) ;
#168602 = CARTESIAN_POINT('Ctrl Pts',(3.62220485292999,1.93266004719377,-21.4561153440415)) ;
#168603 = CARTESIAN_POINT('Ctrl Pts',(3.61359543742306,1.9300316723428,-21.4554202174511)) ;
#168604 = CARTESIAN_POINT('Ctrl Pts',(3.61101642176975,1.92931331154704,-21.4552669825532)) ;
#168605 = CARTESIAN_POINT('Ctrl Pts',(3.60562851963613,1.92796119665937,-21.4550532567727)) ;
#168606 = CARTESIAN_POINT('Ctrl Pts',(3.60282089026123,1.92733781012838,-21.455)) ;
#168607 = CARTESIAN_POINT('Ctrl Pts',(3.6,1.92679491924311,-21.455)) ;
#168608 = CARTESIAN_POINT('Origin',(3.6,1.9,-21.555)) ;
#168609 = CARTESIAN_POINT('Origin',(3.7,1.9,-21.555)) ;
#168610 = CARTESIAN_POINT('Origin',(10.1,1.9,-21.555)) ;
#168611 = CARTESIAN_POINT('Origin',(10.1,1.9,-21.555)) ;
#168612 = CARTESIAN_POINT('Origin',(3.7,2.1,-27.975)) ;
#168613 = CARTESIAN_POINT('',(3.7,1.98660254037845,-28.025)) ;
#168614 = CARTESIAN_POINT('Ctrl Pts',(3.60000000000001,1.92679491924311,-28.075)) ;
#168615 = CARTESIAN_POINT('Ctrl Pts',(3.60642117639513,1.92803067521652,-28.075)) ;
#168616 = CARTESIAN_POINT('Ctrl Pts',(3.61278477806557,1.92968896670937,-28.074722813614)) ;
#168617 = CARTESIAN_POINT('Ctrl Pts',(3.61897283239608,1.93170032347287,-28.0741235249136)) ;
#168618 = CARTESIAN_POINT('Ctrl Pts',(3.62020584678494,1.93210110079286,-28.0740041123242)) ;
#168619 = CARTESIAN_POINT('Ctrl Pts',(3.62143195421119,1.93251577262764,-28.0738720028082)) ;
#168620 = CARTESIAN_POINT('Ctrl Pts',(3.62265032708637,1.93294361409314,-28.073726982434)) ;
#168621 = CARTESIAN_POINT('Ctrl Pts',(3.62647624625549,1.9342871164786,-28.0732715912801)) ;
#168622 = CARTESIAN_POINT('Ctrl Pts',(3.63025346237246,1.93576539638806,-28.0726857368177)) ;
#168623 = CARTESIAN_POINT('Ctrl Pts',(3.6339385638818,1.9373536406594,-28.0719650362697)) ;
#168624 = CARTESIAN_POINT('Ctrl Pts',(3.63907793749119,1.93956866259915,-28.0709599216571)) ;
#168625 = CARTESIAN_POINT('Ctrl Pts',(3.64410916187671,1.94202076919947,-28.0696787224494)) ;
#168626 = CARTESIAN_POINT('Ctrl Pts',(3.64894317395192,1.94461872744825,-28.0681221777355)) ;
#168627 = CARTESIAN_POINT('Ctrl Pts',(3.64993855309245,1.94515367717709,-28.0678016671295)) ;
#168628 = CARTESIAN_POINT('Ctrl Pts',(3.65092568100114,1.94569474416728,-28.0674696031567)) ;
#168629 = CARTESIAN_POINT('Ctrl Pts',(3.65190395907093,1.94624104404949,-28.0671261809367)) ;
#168630 = CARTESIAN_POINT('Ctrl Pts',(3.6524134286835,1.94652554719633,-28.0669473328252)) ;
#168631 = CARTESIAN_POINT('Ctrl Pts',(3.65292046817498,1.94681147780211,-28.06676540574)) ;
#168632 = CARTESIAN_POINT('Ctrl Pts',(3.6534249821411,1.94709871486668,-28.0665804336333)) ;
#168633 = CARTESIAN_POINT('Ctrl Pts',(3.65677402871197,1.94900544167846,-28.0653525584084)) ;
#168634 = CARTESIAN_POINT('Ctrl Pts',(3.66003813592314,1.95098496635819,-28.0639806366809)) ;
#168635 = CARTESIAN_POINT('Ctrl Pts',(3.66320312645637,1.95301617633164,-28.062462401394)) ;
#168636 = CARTESIAN_POINT('Ctrl Pts',(3.66757373088807,1.95582111846921,-28.0603658371851)) ;
#168637 = CARTESIAN_POINT('Ctrl Pts',(3.67181875309364,1.95875330073064,-28.0579661261709)) ;
#168638 = CARTESIAN_POINT('Ctrl Pts',(3.67584388612511,1.96174615985051,-28.0552600357858)) ;
#168639 = CARTESIAN_POINT('Ctrl Pts',(3.67661208162794,1.9623173461687,-28.0547435791997)) ;
#168640 = CARTESIAN_POINT('Ctrl Pts',(3.67737237849392,1.96289065080947,-28.0542160158765)) ;
#168641 = CARTESIAN_POINT('Ctrl Pts',(3.67812428214809,1.96346549106034,-28.0536773988355)) ;
#168642 = CARTESIAN_POINT('Ctrl Pts',(3.67853493948886,1.96377944400827,-28.0533832294423)) ;
#168643 = CARTESIAN_POINT('Ctrl Pts',(3.67894301851552,1.96409388168833,-28.0530857517432)) ;
#168644 = CARTESIAN_POINT('Ctrl Pts',(3.67934840022277,1.96440871854257,-28.0527849693981)) ;
#168645 = CARTESIAN_POINT('Ctrl Pts',(3.68198440184425,1.96645595067818,-28.0508291269535)) ;
#168646 = CARTESIAN_POINT('Ctrl Pts',(3.68449751351863,1.96851545671303,-28.0487382834717)) ;
#168647 = CARTESIAN_POINT('Ctrl Pts',(3.68685379133722,1.97055696562012,-28.0465208503988)) ;
#168648 = CARTESIAN_POINT('Ctrl Pts',(3.68896164651378,1.97238323800781,-28.0445372015504)) ;
#168649 = CARTESIAN_POINT('Ctrl Pts',(3.69104797813191,1.97419718002534,-28.04244243878)) ;
#168650 = CARTESIAN_POINT('Ctrl Pts',(3.69290978292473,1.97598569412148,-28.0402450010326)) ;
#168651 = CARTESIAN_POINT('Ctrl Pts',(3.69362192319633,1.97666980070402,-28.0394044811669)) ;
#168652 = CARTESIAN_POINT('Ctrl Pts',(3.69430163271855,1.97734979318964,-28.0385489756153)) ;
#168653 = CARTESIAN_POINT('Ctrl Pts',(3.69493905694205,1.97802369895107,-28.037679088363)) ;
#168654 = CARTESIAN_POINT('Ctrl Pts',(3.69605143900785,1.9791997456958,-28.0361610303053)) ;
#168655 = CARTESIAN_POINT('Ctrl Pts',(3.69703421735413,1.98035885502255,-28.0345986233173)) ;
#168656 = CARTESIAN_POINT('Ctrl Pts',(3.69784750664911,1.98151165953425,-28.0329571915311)) ;
#168657 = CARTESIAN_POINT('Ctrl Pts',(3.69841279947842,1.98231293913806,-28.0318162818644)) ;
#168658 = CARTESIAN_POINT('Ctrl Pts',(3.69890310384951,1.98311438470593,-28.0306332480122)) ;
#168659 = CARTESIAN_POINT('Ctrl Pts',(3.69929098301991,1.98393783265451,-28.0293581070747)) ;
#168660 = CARTESIAN_POINT('Ctrl Pts',(3.69936193271523,1.98408845528527,-28.0291248621162)) ;
#168661 = CARTESIAN_POINT('Ctrl Pts',(3.69942931950316,1.98423979370561,-28.028888514686)) ;
#168662 = CARTESIAN_POINT('Ctrl Pts',(3.69949277412724,1.9843919518992,-28.0286487302853)) ;
#168663 = CARTESIAN_POINT('Ctrl Pts',(3.69967702385849,1.98483376534753,-28.0279524813983)) ;
#168664 = CARTESIAN_POINT('Ctrl Pts',(3.69981936684304,1.98527475083255,-28.0272393342586)) ;
#168665 = CARTESIAN_POINT('Ctrl Pts',(3.69990669142683,1.98570953653118,-28.0265158410282)) ;
#168666 = CARTESIAN_POINT('Ctrl Pts',(3.69996666908332,1.98600816294476,-28.0260189199259)) ;
#168667 = CARTESIAN_POINT('Ctrl Pts',(3.7,1.98630780592131,-28.0255104950545)) ;
#168668 = CARTESIAN_POINT('Ctrl Pts',(3.7,1.98660254037844,-28.025)) ;
#168669 = CARTESIAN_POINT('Origin',(3.7,1.9,-27.975)) ;
#168670 = CARTESIAN_POINT('Origin',(10.2,1.9,-27.975)) ;
#168671 = CARTESIAN_POINT('Origin',(3.7,1.9,-27.975)) ;
#168672 = CARTESIAN_POINT('Origin',(10.1,1.9,-27.975)) ;
#168673 = CARTESIAN_POINT('Origin',(10.1,1.9,-27.975)) ;
#168674 = CARTESIAN_POINT('Origin',(3.7,2.1,-25.365)) ;
#168675 = CARTESIAN_POINT('',(3.7,1.98660254037844,-25.315)) ;
#168676 = CARTESIAN_POINT('Origin',(3.7,1.9,-25.365)) ;
#168677 = CARTESIAN_POINT('Ctrl Pts',(3.7,1.98660254037844,-25.315)) ;
#168678 = CARTESIAN_POINT('Ctrl Pts',(3.69999911718144,1.98567700534182,-25.3133969262924)) ;
#168679 = CARTESIAN_POINT('Ctrl Pts',(3.69968163901484,1.98470369933599,-25.3118180022845)) ;
#168680 = CARTESIAN_POINT('Ctrl Pts',(3.69895427931585,1.98325895404993,-25.3095944560408)) ;
#168681 = CARTESIAN_POINT('Ctrl Pts',(3.69867650892744,1.9827864959068,-25.3088860984239)) ;
#168682 = CARTESIAN_POINT('Ctrl Pts',(3.69717970712967,1.98043543284229,-25.3054409187843)) ;
#168683 = CARTESIAN_POINT('Ctrl Pts',(3.69541014605544,1.97847095301992,-25.3028241208443)) ;
#168684 = CARTESIAN_POINT('Ctrl Pts',(3.69146029518774,1.97457001268155,-25.297973443509)) ;
#168685 = CARTESIAN_POINT('Ctrl Pts',(3.68915436790411,1.97254004967205,-25.2956322068765)) ;
#168686 = CARTESIAN_POINT('Ctrl Pts',(3.68263623161792,1.96688850447181,-25.2894999184568)) ;
#168687 = CARTESIAN_POINT('Ctrl Pts',(3.6779666138316,1.96321337091313,-25.2859792522831)) ;
#168688 = CARTESIAN_POINT('Ctrl Pts',(3.67279117399679,1.95950210067478,-25.2827623433946)) ;
#168689 = CARTESIAN_POINT('Ctrl Pts',(3.67252519027995,1.95931231248684,-25.2825988090582)) ;
#168690 = CARTESIAN_POINT('Ctrl Pts',(3.6693311210617,1.95704457126181,-25.2806562043068)) ;
#168691 = CARTESIAN_POINT('Ctrl Pts',(3.66628216680076,1.95498580453519,-25.2790096122391)) ;
#168692 = CARTESIAN_POINT('Ctrl Pts',(3.65739884032376,1.94929644648107,-25.2747590242123)) ;
#168693 = CARTESIAN_POINT('Ctrl Pts',(3.65126071410426,1.94574201114262,-25.2724711332688)) ;
#168694 = CARTESIAN_POINT('Ctrl Pts',(3.64132315686417,1.94068746317945,-25.2696379659012)) ;
#168695 = CARTESIAN_POINT('Ctrl Pts',(3.63763353946351,1.93894751340588,-25.2687565993848)) ;
#168696 = CARTESIAN_POINT('Ctrl Pts',(3.62813871250315,1.93486114467726,-25.2669043913581)) ;
#168697 = CARTESIAN_POINT('Ctrl Pts',(3.62220485293001,1.93266004719377,-25.2661153440415)) ;
#168698 = CARTESIAN_POINT('Ctrl Pts',(3.61359543742302,1.93003167234278,-25.2654202174511)) ;
#168699 = CARTESIAN_POINT('Ctrl Pts',(3.61101642176965,1.92931331154701,-25.2652669825532)) ;
#168700 = CARTESIAN_POINT('Ctrl Pts',(3.60562851963602,1.92796119665935,-25.2650532567727)) ;
#168701 = CARTESIAN_POINT('Ctrl Pts',(3.60282089026117,1.92733781012837,-25.265)) ;
#168702 = CARTESIAN_POINT('Ctrl Pts',(3.6,1.92679491924311,-25.265)) ;
#168703 = CARTESIAN_POINT('Origin',(3.6,1.9,-25.365)) ;
#168704 = CARTESIAN_POINT('Origin',(3.7,1.9,-25.365)) ;
#168705 = CARTESIAN_POINT('Origin',(10.1,1.9,-25.365)) ;
#168706 = CARTESIAN_POINT('Origin',(10.1,1.9,-25.365)) ;
#168707 = CARTESIAN_POINT('Origin',(3.7,2.1,-31.785)) ;
#168708 = CARTESIAN_POINT('',(3.7,1.98660254037844,-31.835)) ;
#168709 = CARTESIAN_POINT('Ctrl Pts',(3.6,1.92679491924311,-31.885)) ;
#168710 = CARTESIAN_POINT('Ctrl Pts',(3.6064211763948,1.92803067521646,-31.885)) ;
#168711 = CARTESIAN_POINT('Ctrl Pts',(3.61278477806494,1.92968896670921,-31.8847228136141)) ;
#168712 = CARTESIAN_POINT('Ctrl Pts',(3.61897283239515,1.93170032347258,-31.8841235249137)) ;
#168713 = CARTESIAN_POINT('Ctrl Pts',(3.62020584678433,1.93210110079266,-31.8840041123243)) ;
#168714 = CARTESIAN_POINT('Ctrl Pts',(3.62143195421089,1.93251577262754,-31.8838720028083)) ;
#168715 = CARTESIAN_POINT('Ctrl Pts',(3.62265032708637,1.93294361409314,-31.883726982434)) ;
#168716 = CARTESIAN_POINT('Ctrl Pts',(3.62647624625549,1.9342871164786,-31.8832715912801)) ;
#168717 = CARTESIAN_POINT('Ctrl Pts',(3.63025346237246,1.93576539638805,-31.8826857368177)) ;
#168718 = CARTESIAN_POINT('Ctrl Pts',(3.6339385638818,1.9373536406594,-31.8819650362697)) ;
#168719 = CARTESIAN_POINT('Ctrl Pts',(3.6390779374906,1.9395686625989,-31.8809599216572)) ;
#168720 = CARTESIAN_POINT('Ctrl Pts',(3.64410916187556,1.94202076919892,-31.8796787224497)) ;
#168721 = CARTESIAN_POINT('Ctrl Pts',(3.64894317395025,1.94461872744736,-31.878122177736)) ;
#168722 = CARTESIAN_POINT('Ctrl Pts',(3.6499385530912,1.94515367717641,-31.8778016671299)) ;
#168723 = CARTESIAN_POINT('Ctrl Pts',(3.6509256810003,1.9456947441668,-31.877469603157)) ;
#168724 = CARTESIAN_POINT('Ctrl Pts',(3.65190395907048,1.94624104404923,-31.8771261809369)) ;
#168725 = CARTESIAN_POINT('Ctrl Pts',(3.6524134286832,1.94652554719615,-31.8769473328253)) ;
#168726 = CARTESIAN_POINT('Ctrl Pts',(3.65292046817483,1.94681147780198,-31.8767654057401)) ;
#168727 = CARTESIAN_POINT('Ctrl Pts',(3.6534249821411,1.94709871486664,-31.8765804336333)) ;
#168728 = CARTESIAN_POINT('Ctrl Pts',(3.65677402871197,1.94900544167845,-31.8753525584084)) ;
#168729 = CARTESIAN_POINT('Ctrl Pts',(3.66003813592314,1.95098496635819,-31.8739806366809)) ;
#168730 = CARTESIAN_POINT('Ctrl Pts',(3.66320312645637,1.95301617633165,-31.872462401394)) ;
#168731 = CARTESIAN_POINT('Ctrl Pts',(3.66757373088845,1.95582111846949,-31.8703658371849)) ;
#168732 = CARTESIAN_POINT('Ctrl Pts',(3.67181875309438,1.95875330073117,-31.8679661261705)) ;
#168733 = CARTESIAN_POINT('Ctrl Pts',(3.67584388612618,1.96174615985132,-31.8652600357851)) ;
#168734 = CARTESIAN_POINT('Ctrl Pts',(3.6766120816284,1.96231734616908,-31.8647435791993)) ;
#168735 = CARTESIAN_POINT('Ctrl Pts',(3.67737237849379,1.9628906508094,-31.8642160158765)) ;
#168736 = CARTESIAN_POINT('Ctrl Pts',(3.67812428214738,1.96346549105982,-31.863677398836)) ;
#168737 = CARTESIAN_POINT('Ctrl Pts',(3.67853493948839,1.96377944400794,-31.8633832294426)) ;
#168738 = CARTESIAN_POINT('Ctrl Pts',(3.67894301851528,1.96409388168812,-31.8630857517434)) ;
#168739 = CARTESIAN_POINT('Ctrl Pts',(3.67934840022277,1.96440871854255,-31.8627849693981)) ;
#168740 = CARTESIAN_POINT('Ctrl Pts',(3.68198440184425,1.96645595067817,-31.8608291269535)) ;
#168741 = CARTESIAN_POINT('Ctrl Pts',(3.68449751351863,1.96851545671311,-31.8587382834716)) ;
#168742 = CARTESIAN_POINT('Ctrl Pts',(3.68685379133723,1.97055696562017,-31.8565208503987)) ;
#168743 = CARTESIAN_POINT('Ctrl Pts',(3.68896164651388,1.9723832380079,-31.8545372015503)) ;
#168744 = CARTESIAN_POINT('Ctrl Pts',(3.69104797813211,1.97419718002555,-31.8524424387797)) ;
#168745 = CARTESIAN_POINT('Ctrl Pts',(3.692909782925,1.97598569412177,-31.8502450010322)) ;
#168746 = CARTESIAN_POINT('Ctrl Pts',(3.6936219231965,1.97666980070423,-31.8494044811667)) ;
#168747 = CARTESIAN_POINT('Ctrl Pts',(3.69430163271863,1.97734979318975,-31.8485489756152)) ;
#168748 = CARTESIAN_POINT('Ctrl Pts',(3.69493905694205,1.97802369895109,-31.847679088363)) ;
#168749 = CARTESIAN_POINT('Ctrl Pts',(3.69605143900784,1.9791997456958,-31.8461610303053)) ;
#168750 = CARTESIAN_POINT('Ctrl Pts',(3.69703421735413,1.98035885502255,-31.8445986233173)) ;
#168751 = CARTESIAN_POINT('Ctrl Pts',(3.6978475066491,1.98151165953424,-31.8429571915312)) ;
#168752 = CARTESIAN_POINT('Ctrl Pts',(3.69841279947843,1.98231293913806,-31.8418162818644)) ;
#168753 = CARTESIAN_POINT('Ctrl Pts',(3.69890310384954,1.98311438470598,-31.8406332480121)) ;
#168754 = CARTESIAN_POINT('Ctrl Pts',(3.69929098301994,1.98393783265454,-31.8393581070746)) ;
#168755 = CARTESIAN_POINT('Ctrl Pts',(3.69936193271525,1.98408845528528,-31.8391248621161)) ;
#168756 = CARTESIAN_POINT('Ctrl Pts',(3.69942931950318,1.98423979370566,-31.8388885146859)) ;
#168757 = CARTESIAN_POINT('Ctrl Pts',(3.69949277412726,1.98439195189924,-31.8386487302852)) ;
#168758 = CARTESIAN_POINT('Ctrl Pts',(3.6996770238585,1.98483376534753,-31.8379524813983)) ;
#168759 = CARTESIAN_POINT('Ctrl Pts',(3.69981936684305,1.98527475083261,-31.8372393342585)) ;
#168760 = CARTESIAN_POINT('Ctrl Pts',(3.69990669142684,1.98570953653123,-31.8365158410281)) ;
#168761 = CARTESIAN_POINT('Ctrl Pts',(3.69996666908332,1.98600816294481,-31.8360189199258)) ;
#168762 = CARTESIAN_POINT('Ctrl Pts',(3.7,1.98630780592131,-31.8355104950545)) ;
#168763 = CARTESIAN_POINT('Ctrl Pts',(3.7,1.98660254037844,-31.835)) ;
#168764 = CARTESIAN_POINT('Origin',(3.7,1.9,-31.785)) ;
#168765 = CARTESIAN_POINT('Origin',(10.2,1.9,-31.785)) ;
#168766 = CARTESIAN_POINT('Origin',(3.7,1.9,-31.785)) ;
#168767 = CARTESIAN_POINT('Origin',(10.1,1.9,-31.785)) ;
#168768 = CARTESIAN_POINT('Origin',(10.1,1.9,-31.785)) ;
#168769 = CARTESIAN_POINT('Origin',(3.7,2.1,-29.175)) ;
#168770 = CARTESIAN_POINT('',(3.7,1.98660254037844,-29.125)) ;
#168771 = CARTESIAN_POINT('Origin',(3.7,1.9,-29.175)) ;
#168772 = CARTESIAN_POINT('Ctrl Pts',(3.7,1.98660254037844,-29.125)) ;
#168773 = CARTESIAN_POINT('Ctrl Pts',(3.69999911718144,1.98567700534183,-29.1233969262924)) ;
#168774 = CARTESIAN_POINT('Ctrl Pts',(3.69968163901485,1.984703699336,-29.1218180022846)) ;
#168775 = CARTESIAN_POINT('Ctrl Pts',(3.69895427931585,1.98325895404995,-29.1195944560408)) ;
#168776 = CARTESIAN_POINT('Ctrl Pts',(3.69867650892745,1.98278649590681,-29.1188860984239)) ;
#168777 = CARTESIAN_POINT('Ctrl Pts',(3.69717970712967,1.9804354328423,-29.1154409187843)) ;
#168778 = CARTESIAN_POINT('Ctrl Pts',(3.69541014605544,1.97847095301992,-29.1128241208443)) ;
#168779 = CARTESIAN_POINT('Ctrl Pts',(3.69146029518774,1.97457001268155,-29.107973443509)) ;
#168780 = CARTESIAN_POINT('Ctrl Pts',(3.68915436790411,1.97254004967204,-29.1056322068765)) ;
#168781 = CARTESIAN_POINT('Ctrl Pts',(3.68263623161792,1.9668885044718,-29.0994999184568)) ;
#168782 = CARTESIAN_POINT('Ctrl Pts',(3.67796661383159,1.96321337091313,-29.0959792522831)) ;
#168783 = CARTESIAN_POINT('Ctrl Pts',(3.67279117399678,1.95950210067477,-29.0927623433945)) ;
#168784 = CARTESIAN_POINT('Ctrl Pts',(3.67252519027994,1.95931231248683,-29.0925988090582)) ;
#168785 = CARTESIAN_POINT('Ctrl Pts',(3.6693311210617,1.95704457126181,-29.0906562043068)) ;
#168786 = CARTESIAN_POINT('Ctrl Pts',(3.66628216680077,1.95498580453519,-29.0890096122391)) ;
#168787 = CARTESIAN_POINT('Ctrl Pts',(3.65739884032376,1.94929644648107,-29.0847590242123)) ;
#168788 = CARTESIAN_POINT('Ctrl Pts',(3.65126071410426,1.94574201114262,-29.0824711332688)) ;
#168789 = CARTESIAN_POINT('Ctrl Pts',(3.64132315686417,1.94068746317945,-29.0796379659012)) ;
#168790 = CARTESIAN_POINT('Ctrl Pts',(3.63763353946351,1.93894751340588,-29.0787565993848)) ;
#168791 = CARTESIAN_POINT('Ctrl Pts',(3.62813871250316,1.93486114467726,-29.0769043913581)) ;
#168792 = CARTESIAN_POINT('Ctrl Pts',(3.62220485293003,1.93266004719378,-29.0761153440415)) ;
#168793 = CARTESIAN_POINT('Ctrl Pts',(3.61359543742317,1.93003167234283,-29.0754202174511)) ;
#168794 = CARTESIAN_POINT('Ctrl Pts',(3.61101642176993,1.92931331154709,-29.0752669825532)) ;
#168795 = CARTESIAN_POINT('Ctrl Pts',(3.60562851963629,1.92796119665941,-29.0750532567727)) ;
#168796 = CARTESIAN_POINT('Ctrl Pts',(3.60282089026131,1.92733781012839,-29.075)) ;
#168797 = CARTESIAN_POINT('Ctrl Pts',(3.6,1.92679491924311,-29.075)) ;
#168798 = CARTESIAN_POINT('Origin',(3.6,1.9,-29.175)) ;
#168799 = CARTESIAN_POINT('Origin',(3.7,1.9,-29.175)) ;
#168800 = CARTESIAN_POINT('Origin',(10.1,1.9,-29.175)) ;
#168801 = CARTESIAN_POINT('Origin',(10.1,1.9,-29.175)) ;
#168802 = CARTESIAN_POINT('Origin',(3.7,2.1,-35.595)) ;
#168803 = CARTESIAN_POINT('',(3.7,1.98660254037844,-35.645)) ;
#168804 = CARTESIAN_POINT('Ctrl Pts',(3.6,1.92679491924311,-35.695)) ;
#168805 = CARTESIAN_POINT('Ctrl Pts',(3.60642117639484,1.92803067521647,-35.695)) ;
#168806 = CARTESIAN_POINT('Ctrl Pts',(3.61278477806502,1.92968896670923,-35.6947228136141)) ;
#168807 = CARTESIAN_POINT('Ctrl Pts',(3.61897283239527,1.93170032347261,-35.6941235249137)) ;
#168808 = CARTESIAN_POINT('Ctrl Pts',(3.6202058467844,1.93210110079268,-35.6940041123243)) ;
#168809 = CARTESIAN_POINT('Ctrl Pts',(3.62143195421092,1.93251577262755,-35.6938720028083)) ;
#168810 = CARTESIAN_POINT('Ctrl Pts',(3.62265032708637,1.93294361409314,-35.693726982434)) ;
#168811 = CARTESIAN_POINT('Ctrl Pts',(3.62647624625549,1.9342871164786,-35.6932715912801)) ;
#168812 = CARTESIAN_POINT('Ctrl Pts',(3.63025346237246,1.93576539638806,-35.6926857368177)) ;
#168813 = CARTESIAN_POINT('Ctrl Pts',(3.6339385638818,1.9373536406594,-35.6919650362697)) ;
#168814 = CARTESIAN_POINT('Ctrl Pts',(3.63907793749101,1.93956866259907,-35.6909599216571)) ;
#168815 = CARTESIAN_POINT('Ctrl Pts',(3.64410916187638,1.94202076919931,-35.6896787224495)) ;
#168816 = CARTESIAN_POINT('Ctrl Pts',(3.64894317395146,1.94461872744801,-35.6881221777356)) ;
#168817 = CARTESIAN_POINT('Ctrl Pts',(3.64993855309196,1.94515367717683,-35.6878016671297)) ;
#168818 = CARTESIAN_POINT('Ctrl Pts',(3.65092568100061,1.945694744167,-35.6874696031569)) ;
#168819 = CARTESIAN_POINT('Ctrl Pts',(3.65190395907037,1.94624104404919,-35.6871261809369)) ;
#168820 = CARTESIAN_POINT('Ctrl Pts',(3.65241342868313,1.94652554719613,-35.6869473328253)) ;
#168821 = CARTESIAN_POINT('Ctrl Pts',(3.65292046817479,1.94681147780199,-35.6867654057401)) ;
#168822 = CARTESIAN_POINT('Ctrl Pts',(3.6534249821411,1.94709871486666,-35.6865804336333)) ;
#168823 = CARTESIAN_POINT('Ctrl Pts',(3.65677402871197,1.94900544167846,-35.6853525584084)) ;
#168824 = CARTESIAN_POINT('Ctrl Pts',(3.66003813592314,1.95098496635819,-35.6839806366809)) ;
#168825 = CARTESIAN_POINT('Ctrl Pts',(3.66320312645637,1.95301617633165,-35.682462401394)) ;
#168826 = CARTESIAN_POINT('Ctrl Pts',(3.66757373088831,1.95582111846939,-35.680365837185)) ;
#168827 = CARTESIAN_POINT('Ctrl Pts',(3.6718187530941,1.95875330073099,-35.6779661261707)) ;
#168828 = CARTESIAN_POINT('Ctrl Pts',(3.67584388612577,1.961746159851,-35.6752600357853)) ;
#168829 = CARTESIAN_POINT('Ctrl Pts',(3.67661208162811,1.96231734616883,-35.6747435791995)) ;
#168830 = CARTESIAN_POINT('Ctrl Pts',(3.67737237849361,1.96289065080923,-35.6742160158767)) ;
#168831 = CARTESIAN_POINT('Ctrl Pts',(3.6781242821473,1.96346549105972,-35.6736773988361)) ;
#168832 = CARTESIAN_POINT('Ctrl Pts',(3.67853493948834,1.96377944400785,-35.6733832294426)) ;
#168833 = CARTESIAN_POINT('Ctrl Pts',(3.67894301851526,1.96409388168811,-35.6730857517434)) ;
#168834 = CARTESIAN_POINT('Ctrl Pts',(3.67934840022277,1.96440871854255,-35.6727849693981)) ;
#168835 = CARTESIAN_POINT('Ctrl Pts',(3.68198440184426,1.96645595067816,-35.6708291269535)) ;
#168836 = CARTESIAN_POINT('Ctrl Pts',(3.68449751351862,1.96851545671303,-35.6687382834717)) ;
#168837 = CARTESIAN_POINT('Ctrl Pts',(3.68685379133722,1.97055696562012,-35.6665208503988)) ;
#168838 = CARTESIAN_POINT('Ctrl Pts',(3.6889616465138,1.97238323800782,-35.6645372015503)) ;
#168839 = CARTESIAN_POINT('Ctrl Pts',(3.69104797813196,1.97419718002538,-35.6624424387799)) ;
#168840 = CARTESIAN_POINT('Ctrl Pts',(3.6929097829248,1.97598569412155,-35.6602450010325)) ;
#168841 = CARTESIAN_POINT('Ctrl Pts',(3.69362192319637,1.97666980070406,-35.6594044811669)) ;
#168842 = CARTESIAN_POINT('Ctrl Pts',(3.69430163271857,1.97734979318965,-35.6585489756153)) ;
#168843 = CARTESIAN_POINT('Ctrl Pts',(3.69493905694204,1.97802369895106,-35.6576790883631)) ;
#168844 = CARTESIAN_POINT('Ctrl Pts',(3.69605143900785,1.9791997456958,-35.6561610303053)) ;
#168845 = CARTESIAN_POINT('Ctrl Pts',(3.69703421735413,1.98035885502254,-35.6545986233173)) ;
#168846 = CARTESIAN_POINT('Ctrl Pts',(3.6978475066491,1.98151165953423,-35.6529571915312)) ;
#168847 = CARTESIAN_POINT('Ctrl Pts',(3.69841279947843,1.98231293913806,-35.6518162818644)) ;
#168848 = CARTESIAN_POINT('Ctrl Pts',(3.69890310384954,1.98311438470598,-35.6506332480122)) ;
#168849 = CARTESIAN_POINT('Ctrl Pts',(3.69929098301995,1.98393783265456,-35.6493581070746)) ;
#168850 = CARTESIAN_POINT('Ctrl Pts',(3.69936193271525,1.98408845528527,-35.6491248621162)) ;
#168851 = CARTESIAN_POINT('Ctrl Pts',(3.69942931950315,1.98423979370559,-35.648888514686)) ;
#168852 = CARTESIAN_POINT('Ctrl Pts',(3.69949277412721,1.98439195189914,-35.6486487302854)) ;
#168853 = CARTESIAN_POINT('Ctrl Pts',(3.69967702385847,1.98483376534747,-35.6479524813984)) ;
#168854 = CARTESIAN_POINT('Ctrl Pts',(3.69981936684304,1.98527475083255,-35.6472393342586)) ;
#168855 = CARTESIAN_POINT('Ctrl Pts',(3.69990669142684,1.98570953653122,-35.6465158410281)) ;
#168856 = CARTESIAN_POINT('Ctrl Pts',(3.69996666908332,1.98600816294481,-35.6460189199258)) ;
#168857 = CARTESIAN_POINT('Ctrl Pts',(3.7,1.9863078059213,-35.6455104950545)) ;
#168858 = CARTESIAN_POINT('Ctrl Pts',(3.7,1.98660254037844,-35.645)) ;
#168859 = CARTESIAN_POINT('Origin',(3.7,1.9,-35.595)) ;
#168860 = CARTESIAN_POINT('Origin',(10.2,1.9,-35.595)) ;
#168861 = CARTESIAN_POINT('Origin',(3.7,1.9,-35.595)) ;
#168862 = CARTESIAN_POINT('Origin',(10.1,1.9,-35.595)) ;
#168863 = CARTESIAN_POINT('Origin',(10.1,1.9,-35.595)) ;
#168864 = CARTESIAN_POINT('Origin',(3.7,2.1,-32.985)) ;
#168865 = CARTESIAN_POINT('',(3.7,1.98660254037844,-32.935)) ;
#168866 = CARTESIAN_POINT('Origin',(3.7,1.9,-32.985)) ;
#168867 = CARTESIAN_POINT('Ctrl Pts',(3.7,1.98660254037844,-32.935)) ;
#168868 = CARTESIAN_POINT('Ctrl Pts',(3.69999911718144,1.98567700534184,-32.9333969262924)) ;
#168869 = CARTESIAN_POINT('Ctrl Pts',(3.69968163901486,1.98470369933604,-32.9318180022846)) ;
#168870 = CARTESIAN_POINT('Ctrl Pts',(3.69895427931588,1.98325895404998,-32.9295944560409)) ;
#168871 = CARTESIAN_POINT('Ctrl Pts',(3.69867650892746,1.98278649590682,-32.9288860984239)) ;
#168872 = CARTESIAN_POINT('Ctrl Pts',(3.69717970712967,1.9804354328423,-32.9254409187843)) ;
#168873 = CARTESIAN_POINT('Ctrl Pts',(3.69541014605544,1.97847095301992,-32.9228241208443)) ;
#168874 = CARTESIAN_POINT('Ctrl Pts',(3.69146029518774,1.97457001268156,-32.917973443509)) ;
#168875 = CARTESIAN_POINT('Ctrl Pts',(3.6891543679041,1.97254004967205,-32.9156322068765)) ;
#168876 = CARTESIAN_POINT('Ctrl Pts',(3.68263623161782,1.96688850447172,-32.9094999184567)) ;
#168877 = CARTESIAN_POINT('Ctrl Pts',(3.6779666138314,1.96321337091297,-32.9059792522829)) ;
#168878 = CARTESIAN_POINT('Ctrl Pts',(3.67279117399658,1.95950210067462,-32.9027623433944)) ;
#168879 = CARTESIAN_POINT('Ctrl Pts',(3.67252519027984,1.95931231248676,-32.9025988090581)) ;
#168880 = CARTESIAN_POINT('Ctrl Pts',(3.6693311210617,1.95704457126181,-32.9006562043068)) ;
#168881 = CARTESIAN_POINT('Ctrl Pts',(3.66628216680076,1.95498580453518,-32.8990096122391)) ;
#168882 = CARTESIAN_POINT('Ctrl Pts',(3.65739884032377,1.94929644648108,-32.8947590242123)) ;
#168883 = CARTESIAN_POINT('Ctrl Pts',(3.65126071410426,1.94574201114262,-32.8924711332688)) ;
#168884 = CARTESIAN_POINT('Ctrl Pts',(3.64132315686417,1.94068746317946,-32.8896379659013)) ;
#168885 = CARTESIAN_POINT('Ctrl Pts',(3.63763353946351,1.93894751340588,-32.8887565993848)) ;
#168886 = CARTESIAN_POINT('Ctrl Pts',(3.62813871250328,1.93486114467731,-32.8869043913581)) ;
#168887 = CARTESIAN_POINT('Ctrl Pts',(3.62220485293027,1.93266004719387,-32.8861153440415)) ;
#168888 = CARTESIAN_POINT('Ctrl Pts',(3.61359543742306,1.93003167234279,-32.8854202174511)) ;
#168889 = CARTESIAN_POINT('Ctrl Pts',(3.61101642176932,1.92931331154692,-32.8852669825531)) ;
#168890 = CARTESIAN_POINT('Ctrl Pts',(3.60562851963555,1.92796119665925,-32.8850532567727)) ;
#168891 = CARTESIAN_POINT('Ctrl Pts',(3.60282089026094,1.92733781012832,-32.885)) ;
#168892 = CARTESIAN_POINT('Ctrl Pts',(3.6,1.92679491924311,-32.885)) ;
#168893 = CARTESIAN_POINT('Origin',(3.6,1.9,-32.985)) ;
#168894 = CARTESIAN_POINT('Origin',(3.7,1.9,-32.985)) ;
#168895 = CARTESIAN_POINT('Origin',(10.1,1.9,-32.985)) ;
#168896 = CARTESIAN_POINT('Origin',(10.1,1.9,-32.985)) ;
#168897 = CARTESIAN_POINT('Origin',(3.7,1.9,-5.115)) ;
#168898 = CARTESIAN_POINT('Origin',(3.7,2.07320508075689,-5.215)) ;
#168899 = CARTESIAN_POINT('Ctrl Pts',(3.60000659411846,1.92678349789492,-5.21500000086965)) ;
#168900 = CARTESIAN_POINT('Ctrl Pts',(3.55,2.01339745962155,-5.21498681089333)) ;
#168901 = CARTESIAN_POINT('Ctrl Pts',(3.55,2.01339745962156,-5.315)) ;
#168902 = CARTESIAN_POINT('Ctrl Pts',(3.61192169694494,1.92907674455598,-5.2150005173338)) ;
#168903 = CARTESIAN_POINT('Ctrl Pts',(3.55199190475225,2.01454315814794,-5.21100027733256)) ;
#168904 = CARTESIAN_POINT('Ctrl Pts',(3.55795064586848,2.01798776715396,-5.31499562155023)) ;
#168905 = CARTESIAN_POINT('Ctrl Pts',(3.62341406508538,1.93280912529606,-5.2140249033077)) ;
#168906 = CARTESIAN_POINT('Ctrl Pts',(3.55602946562208,2.0107204129829,-5.20668983076589)) ;
#168907 = CARTESIAN_POINT('Ctrl Pts',(3.56528619664567,2.02370799306987,-5.30863885617463)) ;
#168908 = CARTESIAN_POINT('Ctrl Pts',(3.64447698054259,1.94188479470202,-5.20990697186185)) ;
#168909 = CARTESIAN_POINT('Ctrl Pts',(3.56481337003729,2.00521659408681,-5.19818874066451)) ;
#168910 = CARTESIAN_POINT('Ctrl Pts',(3.5778513142626,2.03528605841761,-5.29516115437405)) ;
#168911 = CARTESIAN_POINT('Ctrl Pts',(3.65434383600069,1.94732274903781,-5.20671544038559)) ;
#168912 = CARTESIAN_POINT('Ctrl Pts',(3.56964037752544,2.00254785926568,-5.19373800427673)) ;
#168913 = CARTESIAN_POINT('Ctrl Pts',(3.58324299321411,2.04133793352501,-5.2870289695647)) ;
#168914 = CARTESIAN_POINT('Ctrl Pts',(3.67209270719133,1.95869361548257,-5.1982138841634)) ;
#168915 = CARTESIAN_POINT('Ctrl Pts',(3.57877657372946,1.99742369139614,-5.18460192490956)) ;
#168916 = CARTESIAN_POINT('Ctrl Pts',(3.59173571364126,2.05270412132581,-5.26927384501021)) ;
#168917 = CARTESIAN_POINT('Ctrl Pts',(3.68022412057907,1.96474917806412,-5.19281520426601)) ;
#168918 = CARTESIAN_POINT('Ctrl Pts',(3.58322866085249,1.9947527117803,-5.17977362629675)) ;
#168919 = CARTESIAN_POINT('Ctrl Pts',(3.59492343714209,2.05814036366738,-5.259399963424)) ;
#168920 = CARTESIAN_POINT('Ctrl Pts',(3.693683649568,1.97632149420531,-5.18024886281709)) ;
#168921 = CARTESIAN_POINT('Ctrl Pts',(3.59172551342568,1.98925228662578,-5.17099928071624)) ;
#168922 = CARTESIAN_POINT('Ctrl Pts',(3.59903094645825,2.06720241143976,-5.23834396451164)) ;
#168923 = CARTESIAN_POINT('Ctrl Pts',(3.70000914724963,1.98195813651218,-5.17304434431451)) ;
#168924 = CARTESIAN_POINT('Ctrl Pts',(3.59596384548937,1.98543049140365,-5.16700954448628)) ;
#168925 = CARTESIAN_POINT('Ctrl Pts',(3.6,2.07088547209221,-5.22705281147587)) ;
#168926 = CARTESIAN_POINT('Ctrl Pts',(3.70001318823691,1.98660254113158,-5.16500000043482)) ;
#168927 = CARTESIAN_POINT('Ctrl Pts',(3.6,1.98659111827701,-5.16499340544667)) ;
#168928 = CARTESIAN_POINT('Ctrl Pts',(3.6,2.07320508075689,-5.215)) ;
#168929 = CARTESIAN_POINT('Origin',(3.6,1.92679491924311,-5.315)) ;
#168930 = CARTESIAN_POINT('Origin',(3.5,2.1,-5.315)) ;
#168931 = CARTESIAN_POINT('Origin',(3.7,1.9,-2.505)) ;
#168932 = CARTESIAN_POINT('Origin',(3.7,2.07320508075689,-2.405)) ;
#168933 = CARTESIAN_POINT('Ctrl Pts',(3.70000000000001,1.98660254037844,-2.455)) ;
#168934 = CARTESIAN_POINT('Ctrl Pts',(3.59998681089333,1.98660254037844,-2.455)) ;
#168935 = CARTESIAN_POINT('Ctrl Pts',(3.60000000086965,2.07321650210508,-2.40499340588155)) ;
#168936 = CARTESIAN_POINT('Ctrl Pts',(3.69999562155021,1.98201223284605,-2.44704935413152)) ;
#168937 = CARTESIAN_POINT('Ctrl Pts',(3.59600027733255,1.98545684185207,-2.45300809524776)) ;
#168938 = CARTESIAN_POINT('Ctrl Pts',(3.60000051733381,2.07092325544402,-2.39307830305507)) ;
#168939 = CARTESIAN_POINT('Ctrl Pts',(3.69363885617462,1.97629200693012,-2.43971380335433)) ;
#168940 = CARTESIAN_POINT('Ctrl Pts',(3.59168983076591,1.98927958701711,-2.44897053437792)) ;
#168941 = CARTESIAN_POINT('Ctrl Pts',(3.5990249033077,2.06719087470394,-2.38158593491462)) ;
#168942 = CARTESIAN_POINT('Ctrl Pts',(3.68016115437407,1.9647139415824,-2.42714868573741)) ;
#168943 = CARTESIAN_POINT('Ctrl Pts',(3.58318874066451,1.99478340591318,-2.44018662996272)) ;
#168944 = CARTESIAN_POINT('Ctrl Pts',(3.59490697186185,2.05811520529797,-2.36052301945742)) ;
#168945 = CARTESIAN_POINT('Ctrl Pts',(3.6720289695647,1.95866206647499,-2.42175700678589)) ;
#168946 = CARTESIAN_POINT('Ctrl Pts',(3.57873800427671,1.99745214073432,-2.43535962247455)) ;
#168947 = CARTESIAN_POINT('Ctrl Pts',(3.59171544038559,2.05267725096218,-2.35065616399931)) ;
#168948 = CARTESIAN_POINT('Ctrl Pts',(3.6542738450102,1.94729587867419,-2.41326428635874)) ;
#168949 = CARTESIAN_POINT('Ctrl Pts',(3.56960192490958,2.00257630860386,-2.42622342627056)) ;
#168950 = CARTESIAN_POINT('Ctrl Pts',(3.5832138841634,2.04130638451743,-2.33290729280868)) ;
#168951 = CARTESIAN_POINT('Ctrl Pts',(3.644399963424,1.94185963633262,-2.41007656285791)) ;
#168952 = CARTESIAN_POINT('Ctrl Pts',(3.56477362629675,2.0052472882197,-2.42177133914751)) ;
#168953 = CARTESIAN_POINT('Ctrl Pts',(3.57781520426602,2.03525082193588,-2.32477587942094)) ;
#168954 = CARTESIAN_POINT('Ctrl Pts',(3.62334396451165,1.93279758856024,-2.40596905354176)) ;
#168955 = CARTESIAN_POINT('Ctrl Pts',(3.55599928071625,2.01074771337423,-2.41327448657433)) ;
#168956 = CARTESIAN_POINT('Ctrl Pts',(3.5652488628171,2.02367850579469,-2.311316350432)) ;
#168957 = CARTESIAN_POINT('Ctrl Pts',(3.61205281147587,1.9291145279078,-2.405)) ;
#168958 = CARTESIAN_POINT('Ctrl Pts',(3.55200954448627,2.01456950859635,-2.40903615451063)) ;
#168959 = CARTESIAN_POINT('Ctrl Pts',(3.55804434431452,2.01804186348783,-2.30499085275037)) ;
#168960 = CARTESIAN_POINT('Ctrl Pts',(3.6,1.92679491924311,-2.405)) ;
#168961 = CARTESIAN_POINT('Ctrl Pts',(3.54999340544667,2.01340888172299,-2.405)) ;
#168962 = CARTESIAN_POINT('Ctrl Pts',(3.55000000043483,2.01339745886842,-2.30498681176309)) ;
#168963 = CARTESIAN_POINT('Origin',(3.6,1.92679491924311,-2.305)) ;
#168964 = CARTESIAN_POINT('Origin',(3.5,2.1,-2.305)) ;
#168965 = CARTESIAN_POINT('Origin',(3.7,1.9,-8.925)) ;
#168966 = CARTESIAN_POINT('Origin',(3.7,2.07320508075689,-9.025)) ;
#168967 = CARTESIAN_POINT('Ctrl Pts',(3.60000659411846,1.92678349789492,-9.02500000086965)) ;
#168968 = CARTESIAN_POINT('Ctrl Pts',(3.55,2.01339745962157,-9.02498681089333)) ;
#168969 = CARTESIAN_POINT('Ctrl Pts',(3.55,2.01339745962156,-9.12500000000001)) ;
#168970 = CARTESIAN_POINT('Ctrl Pts',(3.61192169694494,1.92907674455598,-9.02500051733381)) ;
#168971 = CARTESIAN_POINT('Ctrl Pts',(3.5519919047523,2.0145431581478,-9.02100027733252)) ;
#168972 = CARTESIAN_POINT('Ctrl Pts',(3.55795064586849,2.01798776715396,-9.12499562155005)) ;
#168973 = CARTESIAN_POINT('Ctrl Pts',(3.62341406508537,1.93280912529606,-9.0240249033077)) ;
#168974 = CARTESIAN_POINT('Ctrl Pts',(3.55602946562208,2.0107204129829,-9.01668983076591)) ;
#168975 = CARTESIAN_POINT('Ctrl Pts',(3.56528619664567,2.02370799306987,-9.11863885617463)) ;
#168976 = CARTESIAN_POINT('Ctrl Pts',(3.64447698054259,1.94188479470202,-9.01990697186185)) ;
#168977 = CARTESIAN_POINT('Ctrl Pts',(3.56481337003728,2.00521659408682,-9.00818874066449)) ;
#168978 = CARTESIAN_POINT('Ctrl Pts',(3.5778513142626,2.03528605841761,-9.10516115437406)) ;
#168979 = CARTESIAN_POINT('Ctrl Pts',(3.65434383600069,1.94732274903781,-9.01671544038559)) ;
#168980 = CARTESIAN_POINT('Ctrl Pts',(3.56964037752546,2.00254785926568,-9.00373800427673)) ;
#168981 = CARTESIAN_POINT('Ctrl Pts',(3.58324299321411,2.041337933525,-9.0970289695647)) ;
#168982 = CARTESIAN_POINT('Ctrl Pts',(3.67209270719133,1.95869361548257,-9.0082138841634)) ;
#168983 = CARTESIAN_POINT('Ctrl Pts',(3.57877657372944,1.99742369139614,-8.99460192490956)) ;
#168984 = CARTESIAN_POINT('Ctrl Pts',(3.59173571364126,2.05270412132582,-9.07927384501021)) ;
#168985 = CARTESIAN_POINT('Ctrl Pts',(3.68022412057907,1.96474917806412,-9.00281520426602)) ;
#168986 = CARTESIAN_POINT('Ctrl Pts',(3.58322866085248,1.9947527117803,-8.98977362629674)) ;
#168987 = CARTESIAN_POINT('Ctrl Pts',(3.59492343714209,2.05814036366738,-9.069399963424)) ;
#168988 = CARTESIAN_POINT('Ctrl Pts',(3.693683649568,1.97632149420531,-8.9902488628171)) ;
#168989 = CARTESIAN_POINT('Ctrl Pts',(3.59172551342568,1.98925228662577,-8.98099928071626)) ;
#168990 = CARTESIAN_POINT('Ctrl Pts',(3.59903094645824,2.06720241143976,-9.04834396451164)) ;
#168991 = CARTESIAN_POINT('Ctrl Pts',(3.70000914724963,1.98195813651218,-8.98304434431452)) ;
#168992 = CARTESIAN_POINT('Ctrl Pts',(3.59596384548939,1.98543049140367,-8.97700954448631)) ;
#168993 = CARTESIAN_POINT('Ctrl Pts',(3.6,2.07088547209221,-9.03705281147587)) ;
#168994 = CARTESIAN_POINT('Ctrl Pts',(3.70001318823691,1.98660254113158,-8.97500000043482)) ;
#168995 = CARTESIAN_POINT('Ctrl Pts',(3.6,1.98659111827701,-8.97499340544666)) ;
#168996 = CARTESIAN_POINT('Ctrl Pts',(3.6,2.07320508075689,-9.025)) ;
#168997 = CARTESIAN_POINT('Origin',(3.6,1.92679491924311,-9.125)) ;
#168998 = CARTESIAN_POINT('Origin',(3.5,2.1,-9.125)) ;
#168999 = CARTESIAN_POINT('Origin',(3.7,1.9,-6.315)) ;
#169000 = CARTESIAN_POINT('Origin',(3.7,2.07320508075689,-6.215)) ;
#169001 = CARTESIAN_POINT('Ctrl Pts',(3.70000000000001,1.98660254037844,-6.265)) ;
#169002 = CARTESIAN_POINT('Ctrl Pts',(3.59998681089333,1.98660254037844,-6.265)) ;
#169003 = CARTESIAN_POINT('Ctrl Pts',(3.60000000086965,2.07321650210508,-6.21499340588155)) ;
#169004 = CARTESIAN_POINT('Ctrl Pts',(3.69999562155021,1.98201223284604,-6.25704935413151)) ;
#169005 = CARTESIAN_POINT('Ctrl Pts',(3.59600027733256,1.98545684185207,-6.26300809524773)) ;
#169006 = CARTESIAN_POINT('Ctrl Pts',(3.60000051733381,2.07092325544402,-6.20307830305506)) ;
#169007 = CARTESIAN_POINT('Ctrl Pts',(3.69363885617462,1.97629200693013,-6.24971380335433)) ;
#169008 = CARTESIAN_POINT('Ctrl Pts',(3.59168983076591,1.98927958701711,-6.25897053437793)) ;
#169009 = CARTESIAN_POINT('Ctrl Pts',(3.5990249033077,2.06719087470393,-6.19158593491463)) ;
#169010 = CARTESIAN_POINT('Ctrl Pts',(3.68016115437407,1.96471394158239,-6.2371486857374)) ;
#169011 = CARTESIAN_POINT('Ctrl Pts',(3.58318874066451,1.99478340591318,-6.25018662996271)) ;
#169012 = CARTESIAN_POINT('Ctrl Pts',(3.59490697186185,2.05811520529798,-6.17052301945741)) ;
#169013 = CARTESIAN_POINT('Ctrl Pts',(3.67202896956471,1.95866206647499,-6.23175700678589)) ;
#169014 = CARTESIAN_POINT('Ctrl Pts',(3.57873800427672,1.99745214073432,-6.24535962247454)) ;
#169015 = CARTESIAN_POINT('Ctrl Pts',(3.59171544038559,2.05267725096218,-6.16065616399931)) ;
#169016 = CARTESIAN_POINT('Ctrl Pts',(3.6542738450102,1.94729587867419,-6.22326428635874)) ;
#169017 = CARTESIAN_POINT('Ctrl Pts',(3.56960192490958,2.00257630860386,-6.23622342627057)) ;
#169018 = CARTESIAN_POINT('Ctrl Pts',(3.5832138841634,2.04130638451743,-6.14290729280868)) ;
#169019 = CARTESIAN_POINT('Ctrl Pts',(3.644399963424,1.94185963633262,-6.22007656285791)) ;
#169020 = CARTESIAN_POINT('Ctrl Pts',(3.56477362629674,2.0052472882197,-6.23177133914752)) ;
#169021 = CARTESIAN_POINT('Ctrl Pts',(3.57781520426601,2.03525082193588,-6.13477587942094)) ;
#169022 = CARTESIAN_POINT('Ctrl Pts',(3.62334396451165,1.93279758856024,-6.21596905354176)) ;
#169023 = CARTESIAN_POINT('Ctrl Pts',(3.55599928071626,2.01074771337422,-6.22327448657432)) ;
#169024 = CARTESIAN_POINT('Ctrl Pts',(3.5652488628171,2.02367850579469,-6.121316350432)) ;
#169025 = CARTESIAN_POINT('Ctrl Pts',(3.61205281147587,1.9291145279078,-6.215)) ;
#169026 = CARTESIAN_POINT('Ctrl Pts',(3.55200954448627,2.01456950859637,-6.21903615451063)) ;
#169027 = CARTESIAN_POINT('Ctrl Pts',(3.55804434431452,2.01804186348782,-6.11499085275031)) ;
#169028 = CARTESIAN_POINT('Ctrl Pts',(3.6,1.92679491924311,-6.215)) ;
#169029 = CARTESIAN_POINT('Ctrl Pts',(3.54999340544667,2.01340888172298,-6.215)) ;
#169030 = CARTESIAN_POINT('Ctrl Pts',(3.55000000043483,2.01339745886842,-6.1149868117631)) ;
#169031 = CARTESIAN_POINT('Origin',(3.6,1.92679491924311,-6.115)) ;
#169032 = CARTESIAN_POINT('Origin',(3.5,2.1,-6.115)) ;
#169033 = CARTESIAN_POINT('Origin',(3.7,1.9,-12.735)) ;
#169034 = CARTESIAN_POINT('Origin',(3.7,2.07320508075689,-12.835)) ;
#169035 = CARTESIAN_POINT('Ctrl Pts',(3.60000659411846,1.92678349789492,-12.8350000008696)) ;
#169036 = CARTESIAN_POINT('Ctrl Pts',(3.55,2.01339745962156,-12.8349868108933)) ;
#169037 = CARTESIAN_POINT('Ctrl Pts',(3.55,2.01339745962156,-12.935)) ;
#169038 = CARTESIAN_POINT('Ctrl Pts',(3.61192169694494,1.92907674455598,-12.8350005173338)) ;
#169039 = CARTESIAN_POINT('Ctrl Pts',(3.55199190475231,2.01454315814779,-12.8310002773325)) ;
#169040 = CARTESIAN_POINT('Ctrl Pts',(3.55795064586849,2.01798776715396,-12.93499562155)) ;
#169041 = CARTESIAN_POINT('Ctrl Pts',(3.62341406508537,1.93280912529606,-12.8340249033077)) ;
#169042 = CARTESIAN_POINT('Ctrl Pts',(3.55602946562208,2.01072041298289,-12.8266898307659)) ;
#169043 = CARTESIAN_POINT('Ctrl Pts',(3.56528619664567,2.02370799306987,-12.9286388561746)) ;
#169044 = CARTESIAN_POINT('Ctrl Pts',(3.64447698054259,1.94188479470202,-12.8299069718618)) ;
#169045 = CARTESIAN_POINT('Ctrl Pts',(3.56481337003728,2.00521659408682,-12.8181887406645)) ;
#169046 = CARTESIAN_POINT('Ctrl Pts',(3.5778513142626,2.03528605841761,-12.9151611543741)) ;
#169047 = CARTESIAN_POINT('Ctrl Pts',(3.6543438360007,1.94732274903782,-12.8267154403856)) ;
#169048 = CARTESIAN_POINT('Ctrl Pts',(3.56964037752546,2.00254785926569,-12.8137380042767)) ;
#169049 = CARTESIAN_POINT('Ctrl Pts',(3.58324299321411,2.04133793352501,-12.9070289695647)) ;
#169050 = CARTESIAN_POINT('Ctrl Pts',(3.67209270719132,1.95869361548257,-12.8182138841634)) ;
#169051 = CARTESIAN_POINT('Ctrl Pts',(3.57877657372944,1.99742369139614,-12.8046019249096)) ;
#169052 = CARTESIAN_POINT('Ctrl Pts',(3.59173571364126,2.05270412132581,-12.8892738450102)) ;
#169053 = CARTESIAN_POINT('Ctrl Pts',(3.68022412057907,1.96474917806412,-12.812815204266)) ;
#169054 = CARTESIAN_POINT('Ctrl Pts',(3.58322866085248,1.9947527117803,-12.7997736262967)) ;
#169055 = CARTESIAN_POINT('Ctrl Pts',(3.59492343714209,2.05814036366738,-12.879399963424)) ;
#169056 = CARTESIAN_POINT('Ctrl Pts',(3.693683649568,1.97632149420531,-12.8002488628171)) ;
#169057 = CARTESIAN_POINT('Ctrl Pts',(3.59172551342568,1.98925228662577,-12.7909992807163)) ;
#169058 = CARTESIAN_POINT('Ctrl Pts',(3.59903094645824,2.06720241143976,-12.8583439645117)) ;
#169059 = CARTESIAN_POINT('Ctrl Pts',(3.70000914724963,1.98195813651218,-12.7930443443145)) ;
#169060 = CARTESIAN_POINT('Ctrl Pts',(3.59596384548936,1.98543049140367,-12.7870095444862)) ;
#169061 = CARTESIAN_POINT('Ctrl Pts',(3.6,2.07088547209221,-12.8470528114759)) ;
#169062 = CARTESIAN_POINT('Ctrl Pts',(3.70001318823691,1.98660254113158,-12.7850000004348)) ;
#169063 = CARTESIAN_POINT('Ctrl Pts',(3.6,1.98659111827701,-12.7849934054467)) ;
#169064 = CARTESIAN_POINT('Ctrl Pts',(3.6,2.07320508075689,-12.835)) ;
#169065 = CARTESIAN_POINT('Origin',(3.6,1.92679491924311,-12.935)) ;
#169066 = CARTESIAN_POINT('Origin',(3.5,2.1,-12.935)) ;
#169067 = CARTESIAN_POINT('Origin',(3.7,1.9,-10.125)) ;
#169068 = CARTESIAN_POINT('Origin',(3.7,2.07320508075689,-10.025)) ;
#169069 = CARTESIAN_POINT('Ctrl Pts',(3.70000000000001,1.98660254037844,-10.075)) ;
#169070 = CARTESIAN_POINT('Ctrl Pts',(3.59998681089332,1.98660254037844,-10.075)) ;
#169071 = CARTESIAN_POINT('Ctrl Pts',(3.60000000086965,2.07321650210509,-10.0249934058815)) ;
#169072 = CARTESIAN_POINT('Ctrl Pts',(3.69999562155021,1.98201223284604,-10.0670493541315)) ;
#169073 = CARTESIAN_POINT('Ctrl Pts',(3.59600027733253,1.98545684185205,-10.0730080952478)) ;
#169074 = CARTESIAN_POINT('Ctrl Pts',(3.60000051733381,2.07092325544401,-10.0130783030551)) ;
#169075 = CARTESIAN_POINT('Ctrl Pts',(3.69363885617462,1.97629200693013,-10.0597138033543)) ;
#169076 = CARTESIAN_POINT('Ctrl Pts',(3.5916898307659,1.98927958701711,-10.0689705343779)) ;
#169077 = CARTESIAN_POINT('Ctrl Pts',(3.59902490330771,2.06719087470394,-10.0015859349146)) ;
#169078 = CARTESIAN_POINT('Ctrl Pts',(3.68016115437407,1.96471394158239,-10.0471486857374)) ;
#169079 = CARTESIAN_POINT('Ctrl Pts',(3.58318874066448,1.99478340591319,-10.0601866299627)) ;
#169080 = CARTESIAN_POINT('Ctrl Pts',(3.59490697186185,2.05811520529799,-9.98052301945739)) ;
#169081 = CARTESIAN_POINT('Ctrl Pts',(3.67202896956471,1.958662066475,-10.0417570067859)) ;
#169082 = CARTESIAN_POINT('Ctrl Pts',(3.57873800427672,1.99745214073432,-10.0553596224746)) ;
#169083 = CARTESIAN_POINT('Ctrl Pts',(3.5917154403856,2.05267725096219,-9.97065616399932)) ;
#169084 = CARTESIAN_POINT('Ctrl Pts',(3.6542738450102,1.94729587867418,-10.0332642863587)) ;
#169085 = CARTESIAN_POINT('Ctrl Pts',(3.56960192490955,2.00257630860387,-10.0462234262705)) ;
#169086 = CARTESIAN_POINT('Ctrl Pts',(3.5832138841634,2.04130638451744,-9.95290729280864)) ;
#169087 = CARTESIAN_POINT('Ctrl Pts',(3.644399963424,1.94185963633262,-10.0300765628579)) ;
#169088 = CARTESIAN_POINT('Ctrl Pts',(3.56477362629674,2.00524728821971,-10.0417713391475)) ;
#169089 = CARTESIAN_POINT('Ctrl Pts',(3.57781520426602,2.03525082193588,-9.94477587942092)) ;
#169090 = CARTESIAN_POINT('Ctrl Pts',(3.62334396451165,1.93279758856024,-10.0259690535418)) ;
#169091 = CARTESIAN_POINT('Ctrl Pts',(3.55599928071624,2.01074771337424,-10.0332744865743)) ;
#169092 = CARTESIAN_POINT('Ctrl Pts',(3.5652488628171,2.0236785057947,-9.93131635043199)) ;
#169093 = CARTESIAN_POINT('Ctrl Pts',(3.61205281147587,1.9291145279078,-10.025)) ;
#169094 = CARTESIAN_POINT('Ctrl Pts',(3.55200954448624,2.01456950859637,-10.0290361545106)) ;
#169095 = CARTESIAN_POINT('Ctrl Pts',(3.55804434431452,2.01804186348782,-9.92499085275035)) ;
#169096 = CARTESIAN_POINT('Ctrl Pts',(3.6,1.92679491924311,-10.025)) ;
#169097 = CARTESIAN_POINT('Ctrl Pts',(3.54999340544666,2.013408881723,-10.025)) ;
#169098 = CARTESIAN_POINT('Ctrl Pts',(3.55000000043483,2.01339745886842,-9.92498681176308)) ;
#169099 = CARTESIAN_POINT('Origin',(3.6,1.92679491924311,-9.925)) ;
#169100 = CARTESIAN_POINT('Origin',(3.5,2.1,-9.925)) ;
#169101 = CARTESIAN_POINT('Origin',(3.7,1.9,-16.545)) ;
#169102 = CARTESIAN_POINT('Origin',(3.7,2.07320508075689,-16.645)) ;
#169103 = CARTESIAN_POINT('Ctrl Pts',(3.60000659411846,1.92678349789492,-16.6450000008696)) ;
#169104 = CARTESIAN_POINT('Ctrl Pts',(3.55,2.01339745962156,-16.6449868108933)) ;
#169105 = CARTESIAN_POINT('Ctrl Pts',(3.55,2.01339745962156,-16.745)) ;
#169106 = CARTESIAN_POINT('Ctrl Pts',(3.61192169694494,1.92907674455598,-16.6450005173338)) ;
#169107 = CARTESIAN_POINT('Ctrl Pts',(3.55199190475217,2.0145431581481,-16.6410002773326)) ;
#169108 = CARTESIAN_POINT('Ctrl Pts',(3.55795064586847,2.01798776715395,-16.7449956215505)) ;
#169109 = CARTESIAN_POINT('Ctrl Pts',(3.62341406508538,1.93280912529606,-16.6440249033077)) ;
#169110 = CARTESIAN_POINT('Ctrl Pts',(3.55602946562207,2.0107204129829,-16.6366898307659)) ;
#169111 = CARTESIAN_POINT('Ctrl Pts',(3.56528619664567,2.02370799306988,-16.7386388561746)) ;
#169112 = CARTESIAN_POINT('Ctrl Pts',(3.64447698054259,1.94188479470202,-16.6399069718619)) ;
#169113 = CARTESIAN_POINT('Ctrl Pts',(3.56481337003729,2.00521659408681,-16.6281887406645)) ;
#169114 = CARTESIAN_POINT('Ctrl Pts',(3.5778513142626,2.0352860584176,-16.725161154374)) ;
#169115 = CARTESIAN_POINT('Ctrl Pts',(3.65434383600069,1.94732274903783,-16.6367154403856)) ;
#169116 = CARTESIAN_POINT('Ctrl Pts',(3.56964037752545,2.00254785926569,-16.6237380042767)) ;
#169117 = CARTESIAN_POINT('Ctrl Pts',(3.58324299321411,2.04133793352501,-16.7170289695647)) ;
#169118 = CARTESIAN_POINT('Ctrl Pts',(3.67209270719133,1.95869361548256,-16.6282138841634)) ;
#169119 = CARTESIAN_POINT('Ctrl Pts',(3.57877657372945,1.99742369139614,-16.6146019249096)) ;
#169120 = CARTESIAN_POINT('Ctrl Pts',(3.59173571364127,2.05270412132582,-16.6992738450102)) ;
#169121 = CARTESIAN_POINT('Ctrl Pts',(3.68022412057906,1.96474917806413,-16.622815204266)) ;
#169122 = CARTESIAN_POINT('Ctrl Pts',(3.58322866085249,1.99475271178031,-16.6097736262967)) ;
#169123 = CARTESIAN_POINT('Ctrl Pts',(3.59492343714209,2.05814036366738,-16.689399963424)) ;
#169124 = CARTESIAN_POINT('Ctrl Pts',(3.69368364956801,1.9763214942053,-16.6102488628171)) ;
#169125 = CARTESIAN_POINT('Ctrl Pts',(3.59172551342567,1.98925228662577,-16.6009992807163)) ;
#169126 = CARTESIAN_POINT('Ctrl Pts',(3.59903094645825,2.06720241143977,-16.6683439645117)) ;
#169127 = CARTESIAN_POINT('Ctrl Pts',(3.70000914724963,1.98195813651218,-16.6030443443145)) ;
#169128 = CARTESIAN_POINT('Ctrl Pts',(3.59596384548934,1.9854304914036,-16.5970095444861)) ;
#169129 = CARTESIAN_POINT('Ctrl Pts',(3.6,2.07088547209219,-16.6570528114759)) ;
#169130 = CARTESIAN_POINT('Ctrl Pts',(3.70001318823691,1.98660254113158,-16.5950000004348)) ;
#169131 = CARTESIAN_POINT('Ctrl Pts',(3.6,1.98659111827702,-16.5949934054467)) ;
#169132 = CARTESIAN_POINT('Ctrl Pts',(3.6,2.07320508075689,-16.645)) ;
#169133 = CARTESIAN_POINT('Origin',(3.6,1.92679491924311,-16.745)) ;
#169134 = CARTESIAN_POINT('Origin',(3.5,2.1,-16.745)) ;
#169135 = CARTESIAN_POINT('Origin',(3.7,1.9,-13.935)) ;
#169136 = CARTESIAN_POINT('Origin',(3.7,2.07320508075689,-13.835)) ;
#169137 = CARTESIAN_POINT('Ctrl Pts',(3.70000000000001,1.98660254037844,-13.885)) ;
#169138 = CARTESIAN_POINT('Ctrl Pts',(3.59998681089332,1.98660254037844,-13.885)) ;
#169139 = CARTESIAN_POINT('Ctrl Pts',(3.60000000086965,2.07321650210509,-13.8349934058815)) ;
#169140 = CARTESIAN_POINT('Ctrl Pts',(3.69999562155021,1.98201223284604,-13.8770493541315)) ;
#169141 = CARTESIAN_POINT('Ctrl Pts',(3.59600027733253,1.98545684185205,-13.8830080952478)) ;
#169142 = CARTESIAN_POINT('Ctrl Pts',(3.60000051733381,2.07092325544401,-13.823078303055)) ;
#169143 = CARTESIAN_POINT('Ctrl Pts',(3.69363885617462,1.97629200693013,-13.8697138033543)) ;
#169144 = CARTESIAN_POINT('Ctrl Pts',(3.5916898307659,1.98927958701711,-13.8789705343779)) ;
#169145 = CARTESIAN_POINT('Ctrl Pts',(3.59902490330771,2.06719087470394,-13.8115859349146)) ;
#169146 = CARTESIAN_POINT('Ctrl Pts',(3.68016115437407,1.96471394158239,-13.8571486857374)) ;
#169147 = CARTESIAN_POINT('Ctrl Pts',(3.58318874066448,1.99478340591319,-13.8701866299627)) ;
#169148 = CARTESIAN_POINT('Ctrl Pts',(3.59490697186185,2.05811520529799,-13.7905230194574)) ;
#169149 = CARTESIAN_POINT('Ctrl Pts',(3.67202896956471,1.958662066475,-13.8517570067859)) ;
#169150 = CARTESIAN_POINT('Ctrl Pts',(3.57873800427673,1.99745214073432,-13.8653596224746)) ;
#169151 = CARTESIAN_POINT('Ctrl Pts',(3.5917154403856,2.05267725096219,-13.7806561639993)) ;
#169152 = CARTESIAN_POINT('Ctrl Pts',(3.6542738450102,1.94729587867418,-13.8432642863587)) ;
#169153 = CARTESIAN_POINT('Ctrl Pts',(3.56960192490954,2.00257630860387,-13.8562234262705)) ;
#169154 = CARTESIAN_POINT('Ctrl Pts',(3.5832138841634,2.04130638451744,-13.7629072928086)) ;
#169155 = CARTESIAN_POINT('Ctrl Pts',(3.644399963424,1.94185963633262,-13.8400765628579)) ;
#169156 = CARTESIAN_POINT('Ctrl Pts',(3.56477362629673,2.00524728821971,-13.8517713391475)) ;
#169157 = CARTESIAN_POINT('Ctrl Pts',(3.57781520426602,2.03525082193588,-13.7547758794209)) ;
#169158 = CARTESIAN_POINT('Ctrl Pts',(3.62334396451165,1.93279758856024,-13.8359690535418)) ;
#169159 = CARTESIAN_POINT('Ctrl Pts',(3.55599928071625,2.01074771337423,-13.8432744865743)) ;
#169160 = CARTESIAN_POINT('Ctrl Pts',(3.5652488628171,2.0236785057947,-13.741316350432)) ;
#169161 = CARTESIAN_POINT('Ctrl Pts',(3.61205281147587,1.9291145279078,-13.835)) ;
#169162 = CARTESIAN_POINT('Ctrl Pts',(3.55200954448628,2.01456950859631,-13.8390361545106)) ;
#169163 = CARTESIAN_POINT('Ctrl Pts',(3.55804434431452,2.01804186348783,-13.7349908527504)) ;
#169164 = CARTESIAN_POINT('Ctrl Pts',(3.6,1.92679491924311,-13.835)) ;
#169165 = CARTESIAN_POINT('Ctrl Pts',(3.54999340544666,2.013408881723,-13.835)) ;
#169166 = CARTESIAN_POINT('Ctrl Pts',(3.55000000043483,2.01339745886842,-13.7349868117631)) ;
#169167 = CARTESIAN_POINT('Origin',(3.6,1.92679491924311,-13.735)) ;
#169168 = CARTESIAN_POINT('Origin',(3.5,2.1,-13.735)) ;
#169169 = CARTESIAN_POINT('Origin',(3.7,1.9,-20.355)) ;
#169170 = CARTESIAN_POINT('Origin',(3.7,2.07320508075689,-20.455)) ;
#169171 = CARTESIAN_POINT('Ctrl Pts',(3.60000659411846,1.92678349789492,-20.4550000008697)) ;
#169172 = CARTESIAN_POINT('Ctrl Pts',(3.55,2.01339745962156,-20.4549868108933)) ;
#169173 = CARTESIAN_POINT('Ctrl Pts',(3.55,2.01339745962156,-20.555)) ;
#169174 = CARTESIAN_POINT('Ctrl Pts',(3.61192169694493,1.92907674455598,-20.4550005173338)) ;
#169175 = CARTESIAN_POINT('Ctrl Pts',(3.55199190475217,2.0145431581481,-20.4510002773326)) ;
#169176 = CARTESIAN_POINT('Ctrl Pts',(3.55795064586847,2.01798776715395,-20.5549956215505)) ;
#169177 = CARTESIAN_POINT('Ctrl Pts',(3.62341406508538,1.93280912529606,-20.4540249033077)) ;
#169178 = CARTESIAN_POINT('Ctrl Pts',(3.55602946562207,2.0107204129829,-20.4466898307659)) ;
#169179 = CARTESIAN_POINT('Ctrl Pts',(3.56528619664567,2.02370799306988,-20.5486388561746)) ;
#169180 = CARTESIAN_POINT('Ctrl Pts',(3.64447698054259,1.94188479470202,-20.4499069718619)) ;
#169181 = CARTESIAN_POINT('Ctrl Pts',(3.56481337003729,2.00521659408681,-20.4381887406645)) ;
#169182 = CARTESIAN_POINT('Ctrl Pts',(3.5778513142626,2.0352860584176,-20.5351611543741)) ;
#169183 = CARTESIAN_POINT('Ctrl Pts',(3.65434383600069,1.94732274903783,-20.4467154403856)) ;
#169184 = CARTESIAN_POINT('Ctrl Pts',(3.56964037752545,2.00254785926569,-20.4337380042767)) ;
#169185 = CARTESIAN_POINT('Ctrl Pts',(3.58324299321411,2.04133793352501,-20.5270289695647)) ;
#169186 = CARTESIAN_POINT('Ctrl Pts',(3.67209270719133,1.95869361548256,-20.4382138841634)) ;
#169187 = CARTESIAN_POINT('Ctrl Pts',(3.57877657372945,1.99742369139614,-20.4246019249096)) ;
#169188 = CARTESIAN_POINT('Ctrl Pts',(3.59173571364127,2.05270412132582,-20.5092738450102)) ;
#169189 = CARTESIAN_POINT('Ctrl Pts',(3.68022412057906,1.96474917806413,-20.432815204266)) ;
#169190 = CARTESIAN_POINT('Ctrl Pts',(3.58322866085249,1.99475271178031,-20.4197736262967)) ;
#169191 = CARTESIAN_POINT('Ctrl Pts',(3.59492343714209,2.05814036366738,-20.499399963424)) ;
#169192 = CARTESIAN_POINT('Ctrl Pts',(3.69368364956801,1.9763214942053,-20.4202488628171)) ;
#169193 = CARTESIAN_POINT('Ctrl Pts',(3.59172551342567,1.98925228662577,-20.4109992807163)) ;
#169194 = CARTESIAN_POINT('Ctrl Pts',(3.59903094645825,2.06720241143977,-20.4783439645117)) ;
#169195 = CARTESIAN_POINT('Ctrl Pts',(3.70000914724963,1.98195813651218,-20.4130443443145)) ;
#169196 = CARTESIAN_POINT('Ctrl Pts',(3.59596384548934,1.9854304914036,-20.4070095444861)) ;
#169197 = CARTESIAN_POINT('Ctrl Pts',(3.6,2.07088547209219,-20.4670528114759)) ;
#169198 = CARTESIAN_POINT('Ctrl Pts',(3.70001318823691,1.98660254113158,-20.4050000004348)) ;
#169199 = CARTESIAN_POINT('Ctrl Pts',(3.6,1.98659111827701,-20.4049934054467)) ;
#169200 = CARTESIAN_POINT('Ctrl Pts',(3.6,2.07320508075689,-20.455)) ;
#169201 = CARTESIAN_POINT('Origin',(3.6,1.92679491924311,-20.555)) ;
#169202 = CARTESIAN_POINT('Origin',(3.5,2.1,-20.555)) ;
#169203 = CARTESIAN_POINT('Origin',(3.7,1.9,-17.745)) ;
#169204 = CARTESIAN_POINT('Origin',(3.7,2.07320508075689,-17.645)) ;
#169205 = CARTESIAN_POINT('Ctrl Pts',(3.70000000000001,1.98660254037844,-17.695)) ;
#169206 = CARTESIAN_POINT('Ctrl Pts',(3.59998681089334,1.98660254037844,-17.695)) ;
#169207 = CARTESIAN_POINT('Ctrl Pts',(3.60000000086965,2.07321650210508,-17.6449934058816)) ;
#169208 = CARTESIAN_POINT('Ctrl Pts',(3.69999562155021,1.98201223284605,-17.6870493541315)) ;
#169209 = CARTESIAN_POINT('Ctrl Pts',(3.59600027733259,1.9854568418521,-17.6930080952477)) ;
#169210 = CARTESIAN_POINT('Ctrl Pts',(3.60000051733381,2.07092325544402,-17.6330783030551)) ;
#169211 = CARTESIAN_POINT('Ctrl Pts',(3.69363885617462,1.97629200693012,-17.6797138033543)) ;
#169212 = CARTESIAN_POINT('Ctrl Pts',(3.59168983076589,1.98927958701711,-17.6889705343779)) ;
#169213 = CARTESIAN_POINT('Ctrl Pts',(3.5990249033077,2.06719087470394,-17.6215859349146)) ;
#169214 = CARTESIAN_POINT('Ctrl Pts',(3.68016115437406,1.9647139415824,-17.6671486857374)) ;
#169215 = CARTESIAN_POINT('Ctrl Pts',(3.58318874066453,1.99478340591318,-17.6801866299628)) ;
#169216 = CARTESIAN_POINT('Ctrl Pts',(3.59490697186185,2.05811520529797,-17.6005230194575)) ;
#169217 = CARTESIAN_POINT('Ctrl Pts',(3.6720289695647,1.958662066475,-17.6617570067859)) ;
#169218 = CARTESIAN_POINT('Ctrl Pts',(3.57873800427671,1.99745214073432,-17.6753596224745)) ;
#169219 = CARTESIAN_POINT('Ctrl Pts',(3.59171544038559,2.05267725096218,-17.5906561639993)) ;
#169220 = CARTESIAN_POINT('Ctrl Pts',(3.6542738450102,1.94729587867418,-17.6532642863587)) ;
#169221 = CARTESIAN_POINT('Ctrl Pts',(3.5696019249096,2.00257630860386,-17.6662234262706)) ;
#169222 = CARTESIAN_POINT('Ctrl Pts',(3.5832138841634,2.04130638451742,-17.5729072928087)) ;
#169223 = CARTESIAN_POINT('Ctrl Pts',(3.64439996342401,1.94185963633263,-17.6500765628579)) ;
#169224 = CARTESIAN_POINT('Ctrl Pts',(3.56477362629676,2.0052472882197,-17.6617713391475)) ;
#169225 = CARTESIAN_POINT('Ctrl Pts',(3.57781520426602,2.03525082193588,-17.5647758794209)) ;
#169226 = CARTESIAN_POINT('Ctrl Pts',(3.62334396451164,1.93279758856024,-17.6459690535418)) ;
#169227 = CARTESIAN_POINT('Ctrl Pts',(3.55599928071625,2.01074771337422,-17.6532744865743)) ;
#169228 = CARTESIAN_POINT('Ctrl Pts',(3.56524886281709,2.02367850579469,-17.551316350432)) ;
#169229 = CARTESIAN_POINT('Ctrl Pts',(3.61205281147588,1.9291145279078,-17.645)) ;
#169230 = CARTESIAN_POINT('Ctrl Pts',(3.55200954448629,2.01456950859638,-17.6490361545106)) ;
#169231 = CARTESIAN_POINT('Ctrl Pts',(3.55804434431452,2.01804186348782,-17.5449908527503)) ;
#169232 = CARTESIAN_POINT('Ctrl Pts',(3.6,1.92679491924311,-17.645)) ;
#169233 = CARTESIAN_POINT('Ctrl Pts',(3.54999340544667,2.01340888172298,-17.645)) ;
#169234 = CARTESIAN_POINT('Ctrl Pts',(3.55000000043483,2.01339745886842,-17.5449868117631)) ;
#169235 = CARTESIAN_POINT('Origin',(3.6,1.92679491924311,-17.545)) ;
#169236 = CARTESIAN_POINT('Origin',(3.5,2.1,-17.545)) ;
#169237 = CARTESIAN_POINT('Origin',(3.7,1.9,-24.165)) ;
#169238 = CARTESIAN_POINT('Origin',(3.7,2.07320508075689,-24.265)) ;
#169239 = CARTESIAN_POINT('Ctrl Pts',(3.60000659411846,1.92678349789492,-24.2650000008696)) ;
#169240 = CARTESIAN_POINT('Ctrl Pts',(3.55,2.01339745962156,-24.2649868108933)) ;
#169241 = CARTESIAN_POINT('Ctrl Pts',(3.55,2.01339745962156,-24.365)) ;
#169242 = CARTESIAN_POINT('Ctrl Pts',(3.61192169694494,1.92907674455598,-24.2650005173338)) ;
#169243 = CARTESIAN_POINT('Ctrl Pts',(3.55199190475211,2.01454315814821,-24.2610002773326)) ;
#169244 = CARTESIAN_POINT('Ctrl Pts',(3.55795064586847,2.01798776715395,-24.3649956215505)) ;
#169245 = CARTESIAN_POINT('Ctrl Pts',(3.62341406508538,1.93280912529606,-24.2640249033077)) ;
#169246 = CARTESIAN_POINT('Ctrl Pts',(3.55602946562207,2.0107204129829,-24.2566898307659)) ;
#169247 = CARTESIAN_POINT('Ctrl Pts',(3.56528619664567,2.02370799306988,-24.3586388561746)) ;
#169248 = CARTESIAN_POINT('Ctrl Pts',(3.64447698054259,1.94188479470202,-24.2599069718618)) ;
#169249 = CARTESIAN_POINT('Ctrl Pts',(3.56481337003729,2.00521659408681,-24.2481887406645)) ;
#169250 = CARTESIAN_POINT('Ctrl Pts',(3.5778513142626,2.0352860584176,-24.3451611543741)) ;
#169251 = CARTESIAN_POINT('Ctrl Pts',(3.65434383600069,1.94732274903783,-24.2567154403856)) ;
#169252 = CARTESIAN_POINT('Ctrl Pts',(3.56964037752544,2.00254785926569,-24.2437380042767)) ;
#169253 = CARTESIAN_POINT('Ctrl Pts',(3.58324299321411,2.04133793352501,-24.3370289695647)) ;
#169254 = CARTESIAN_POINT('Ctrl Pts',(3.67209270719133,1.95869361548256,-24.2482138841634)) ;
#169255 = CARTESIAN_POINT('Ctrl Pts',(3.57877657372945,1.99742369139614,-24.2346019249096)) ;
#169256 = CARTESIAN_POINT('Ctrl Pts',(3.59173571364127,2.05270412132582,-24.3192738450102)) ;
#169257 = CARTESIAN_POINT('Ctrl Pts',(3.68022412057906,1.96474917806411,-24.242815204266)) ;
#169258 = CARTESIAN_POINT('Ctrl Pts',(3.58322866085247,1.99475271178029,-24.2297736262968)) ;
#169259 = CARTESIAN_POINT('Ctrl Pts',(3.59492343714209,2.05814036366738,-24.309399963424)) ;
#169260 = CARTESIAN_POINT('Ctrl Pts',(3.69368364956801,1.97632149420531,-24.2302488628171)) ;
#169261 = CARTESIAN_POINT('Ctrl Pts',(3.59172551342569,1.98925228662579,-24.2209992807162)) ;
#169262 = CARTESIAN_POINT('Ctrl Pts',(3.59903094645825,2.06720241143977,-24.2883439645117)) ;
#169263 = CARTESIAN_POINT('Ctrl Pts',(3.70000914724963,1.98195813651217,-24.2230443443145)) ;
#169264 = CARTESIAN_POINT('Ctrl Pts',(3.59596384548931,1.98543049140359,-24.2170095444862)) ;
#169265 = CARTESIAN_POINT('Ctrl Pts',(3.6,2.07088547209219,-24.2770528114759)) ;
#169266 = CARTESIAN_POINT('Ctrl Pts',(3.70001318823691,1.98660254113158,-24.2150000004348)) ;
#169267 = CARTESIAN_POINT('Ctrl Pts',(3.6,1.98659111827701,-24.2149934054467)) ;
#169268 = CARTESIAN_POINT('Ctrl Pts',(3.6,2.07320508075689,-24.265)) ;
#169269 = CARTESIAN_POINT('Origin',(3.6,1.92679491924311,-24.365)) ;
#169270 = CARTESIAN_POINT('Origin',(3.5,2.1,-24.365)) ;
#169271 = CARTESIAN_POINT('Origin',(3.7,1.9,-21.555)) ;
#169272 = CARTESIAN_POINT('Origin',(3.7,2.07320508075689,-21.455)) ;
#169273 = CARTESIAN_POINT('Ctrl Pts',(3.70000000000001,1.98660254037844,-21.505)) ;
#169274 = CARTESIAN_POINT('Ctrl Pts',(3.59998681089334,1.98660254037844,-21.505)) ;
#169275 = CARTESIAN_POINT('Ctrl Pts',(3.60000000086965,2.07321650210507,-21.4549934058816)) ;
#169276 = CARTESIAN_POINT('Ctrl Pts',(3.69999562155021,1.98201223284605,-21.4970493541315)) ;
#169277 = CARTESIAN_POINT('Ctrl Pts',(3.59600027733255,1.98545684185209,-21.5030080952477)) ;
#169278 = CARTESIAN_POINT('Ctrl Pts',(3.60000051733381,2.07092325544402,-21.4430783030551)) ;
#169279 = CARTESIAN_POINT('Ctrl Pts',(3.69363885617462,1.97629200693012,-21.4897138033543)) ;
#169280 = CARTESIAN_POINT('Ctrl Pts',(3.59168983076595,1.98927958701713,-21.4989705343779)) ;
#169281 = CARTESIAN_POINT('Ctrl Pts',(3.5990249033077,2.06719087470394,-21.4315859349146)) ;
#169282 = CARTESIAN_POINT('Ctrl Pts',(3.68016115437406,1.9647139415824,-21.4771486857374)) ;
#169283 = CARTESIAN_POINT('Ctrl Pts',(3.58318874066447,1.99478340591315,-21.4901866299627)) ;
#169284 = CARTESIAN_POINT('Ctrl Pts',(3.59490697186185,2.05811520529797,-21.4105230194575)) ;
#169285 = CARTESIAN_POINT('Ctrl Pts',(3.6720289695647,1.958662066475,-21.4717570067859)) ;
#169286 = CARTESIAN_POINT('Ctrl Pts',(3.57873800427674,1.99745214073432,-21.4853596224745)) ;
#169287 = CARTESIAN_POINT('Ctrl Pts',(3.59171544038559,2.05267725096218,-21.4006561639993)) ;
#169288 = CARTESIAN_POINT('Ctrl Pts',(3.6542738450102,1.94729587867418,-21.4632642863587)) ;
#169289 = CARTESIAN_POINT('Ctrl Pts',(3.56960192490957,2.00257630860385,-21.4762234262706)) ;
#169290 = CARTESIAN_POINT('Ctrl Pts',(3.5832138841634,2.04130638451742,-21.3829072928087)) ;
#169291 = CARTESIAN_POINT('Ctrl Pts',(3.64439996342401,1.94185963633263,-21.4600765628579)) ;
#169292 = CARTESIAN_POINT('Ctrl Pts',(3.56477362629673,2.00524728821971,-21.4717713391475)) ;
#169293 = CARTESIAN_POINT('Ctrl Pts',(3.57781520426602,2.03525082193588,-21.3747758794209)) ;
#169294 = CARTESIAN_POINT('Ctrl Pts',(3.62334396451164,1.93279758856024,-21.4559690535418)) ;
#169295 = CARTESIAN_POINT('Ctrl Pts',(3.55599928071628,2.0107477133742,-21.4632744865743)) ;
#169296 = CARTESIAN_POINT('Ctrl Pts',(3.56524886281709,2.02367850579469,-21.361316350432)) ;
#169297 = CARTESIAN_POINT('Ctrl Pts',(3.61205281147588,1.9291145279078,-21.455)) ;
#169298 = CARTESIAN_POINT('Ctrl Pts',(3.55200954448635,2.01456950859626,-21.4590361545106)) ;
#169299 = CARTESIAN_POINT('Ctrl Pts',(3.55804434431452,2.01804186348782,-21.3549908527503)) ;
#169300 = CARTESIAN_POINT('Ctrl Pts',(3.6,1.92679491924311,-21.455)) ;
#169301 = CARTESIAN_POINT('Ctrl Pts',(3.54999340544667,2.01340888172298,-21.455)) ;
#169302 = CARTESIAN_POINT('Ctrl Pts',(3.55000000043483,2.01339745886842,-21.3549868117631)) ;
#169303 = CARTESIAN_POINT('Origin',(3.6,1.92679491924311,-21.355)) ;
#169304 = CARTESIAN_POINT('Origin',(3.5,2.1,-21.355)) ;
#169305 = CARTESIAN_POINT('Origin',(3.7,1.9,-27.975)) ;
#169306 = CARTESIAN_POINT('Origin',(3.7,2.07320508075689,-28.075)) ;
#169307 = CARTESIAN_POINT('Ctrl Pts',(3.60000659411846,1.92678349789492,-28.0750000008697)) ;
#169308 = CARTESIAN_POINT('Ctrl Pts',(3.55,2.01339745962156,-28.0749868108933)) ;
#169309 = CARTESIAN_POINT('Ctrl Pts',(3.55,2.01339745962156,-28.175)) ;
#169310 = CARTESIAN_POINT('Ctrl Pts',(3.61192169694494,1.92907674455598,-28.0750005173338)) ;
#169311 = CARTESIAN_POINT('Ctrl Pts',(3.55199190475223,2.01454315814803,-28.0710002773326)) ;
#169312 = CARTESIAN_POINT('Ctrl Pts',(3.55795064586847,2.01798776715395,-28.1749956215505)) ;
#169313 = CARTESIAN_POINT('Ctrl Pts',(3.62341406508537,1.93280912529606,-28.0740249033077)) ;
#169314 = CARTESIAN_POINT('Ctrl Pts',(3.55602946562204,2.01072041298292,-28.0666898307659)) ;
#169315 = CARTESIAN_POINT('Ctrl Pts',(3.56528619664567,2.02370799306988,-28.1686388561746)) ;
#169316 = CARTESIAN_POINT('Ctrl Pts',(3.64447698054259,1.94188479470202,-28.0699069718619)) ;
#169317 = CARTESIAN_POINT('Ctrl Pts',(3.56481337003732,2.0052165940868,-28.0581887406645)) ;
#169318 = CARTESIAN_POINT('Ctrl Pts',(3.5778513142626,2.0352860584176,-28.155161154374)) ;
#169319 = CARTESIAN_POINT('Ctrl Pts',(3.65434383600069,1.94732274903782,-28.0667154403856)) ;
#169320 = CARTESIAN_POINT('Ctrl Pts',(3.56964037752548,2.00254785926568,-28.0537380042767)) ;
#169321 = CARTESIAN_POINT('Ctrl Pts',(3.58324299321411,2.04133793352501,-28.1470289695647)) ;
#169322 = CARTESIAN_POINT('Ctrl Pts',(3.67209270719133,1.95869361548256,-28.0582138841634)) ;
#169323 = CARTESIAN_POINT('Ctrl Pts',(3.57877657372942,1.99742369139614,-28.0446019249096)) ;
#169324 = CARTESIAN_POINT('Ctrl Pts',(3.59173571364127,2.05270412132582,-28.1292738450102)) ;
#169325 = CARTESIAN_POINT('Ctrl Pts',(3.68022412057906,1.96474917806411,-28.052815204266)) ;
#169326 = CARTESIAN_POINT('Ctrl Pts',(3.5832286608525,1.99475271178031,-28.0397736262968)) ;
#169327 = CARTESIAN_POINT('Ctrl Pts',(3.59492343714209,2.05814036366738,-28.119399963424)) ;
#169328 = CARTESIAN_POINT('Ctrl Pts',(3.69368364956801,1.97632149420531,-28.0402488628171)) ;
#169329 = CARTESIAN_POINT('Ctrl Pts',(3.59172551342567,1.98925228662577,-28.0309992807162)) ;
#169330 = CARTESIAN_POINT('Ctrl Pts',(3.59903094645825,2.06720241143977,-28.0983439645117)) ;
#169331 = CARTESIAN_POINT('Ctrl Pts',(3.70000914724963,1.98195813651217,-28.0330443443145)) ;
#169332 = CARTESIAN_POINT('Ctrl Pts',(3.59596384548938,1.98543049140356,-28.0270095444862)) ;
#169333 = CARTESIAN_POINT('Ctrl Pts',(3.6,2.07088547209218,-28.0870528114759)) ;
#169334 = CARTESIAN_POINT('Ctrl Pts',(3.70001318823691,1.98660254113158,-28.0250000004348)) ;
#169335 = CARTESIAN_POINT('Ctrl Pts',(3.6,1.98659111827701,-28.0249934054467)) ;
#169336 = CARTESIAN_POINT('Ctrl Pts',(3.6,2.07320508075689,-28.075)) ;
#169337 = CARTESIAN_POINT('Origin',(3.6,1.92679491924311,-28.175)) ;
#169338 = CARTESIAN_POINT('Origin',(3.5,2.1,-28.175)) ;
#169339 = CARTESIAN_POINT('Origin',(3.7,1.9,-25.365)) ;
#169340 = CARTESIAN_POINT('Origin',(3.7,2.07320508075689,-25.265)) ;
#169341 = CARTESIAN_POINT('Ctrl Pts',(3.70000000000001,1.98660254037844,-25.315)) ;
#169342 = CARTESIAN_POINT('Ctrl Pts',(3.59998681089334,1.98660254037844,-25.315)) ;
#169343 = CARTESIAN_POINT('Ctrl Pts',(3.60000000086965,2.07321650210507,-25.2649934058815)) ;
#169344 = CARTESIAN_POINT('Ctrl Pts',(3.69999562155021,1.98201223284605,-25.3070493541315)) ;
#169345 = CARTESIAN_POINT('Ctrl Pts',(3.5960002773326,1.9854568418521,-25.3130080952477)) ;
#169346 = CARTESIAN_POINT('Ctrl Pts',(3.60000051733381,2.07092325544402,-25.2530783030551)) ;
#169347 = CARTESIAN_POINT('Ctrl Pts',(3.69363885617462,1.97629200693012,-25.2997138033543)) ;
#169348 = CARTESIAN_POINT('Ctrl Pts',(3.59168983076589,1.98927958701711,-25.3089705343779)) ;
#169349 = CARTESIAN_POINT('Ctrl Pts',(3.5990249033077,2.06719087470394,-25.2415859349146)) ;
#169350 = CARTESIAN_POINT('Ctrl Pts',(3.68016115437406,1.9647139415824,-25.2871486857374)) ;
#169351 = CARTESIAN_POINT('Ctrl Pts',(3.58318874066453,1.99478340591318,-25.3001866299628)) ;
#169352 = CARTESIAN_POINT('Ctrl Pts',(3.59490697186185,2.05811520529797,-25.2205230194575)) ;
#169353 = CARTESIAN_POINT('Ctrl Pts',(3.6720289695647,1.958662066475,-25.2817570067859)) ;
#169354 = CARTESIAN_POINT('Ctrl Pts',(3.57873800427668,1.99745214073432,-25.2953596224745)) ;
#169355 = CARTESIAN_POINT('Ctrl Pts',(3.59171544038559,2.05267725096218,-25.2106561639993)) ;
#169356 = CARTESIAN_POINT('Ctrl Pts',(3.6542738450102,1.94729587867418,-25.2732642863587)) ;
#169357 = CARTESIAN_POINT('Ctrl Pts',(3.56960192490964,2.00257630860385,-25.2862234262706)) ;
#169358 = CARTESIAN_POINT('Ctrl Pts',(3.5832138841634,2.04130638451742,-25.1929072928087)) ;
#169359 = CARTESIAN_POINT('Ctrl Pts',(3.64439996342401,1.94185963633263,-25.2700765628579)) ;
#169360 = CARTESIAN_POINT('Ctrl Pts',(3.56477362629676,2.0052472882197,-25.2817713391475)) ;
#169361 = CARTESIAN_POINT('Ctrl Pts',(3.57781520426602,2.03525082193588,-25.1847758794209)) ;
#169362 = CARTESIAN_POINT('Ctrl Pts',(3.62334396451164,1.93279758856024,-25.2659690535418)) ;
#169363 = CARTESIAN_POINT('Ctrl Pts',(3.55599928071625,2.01074771337422,-25.2732744865743)) ;
#169364 = CARTESIAN_POINT('Ctrl Pts',(3.56524886281709,2.02367850579469,-25.171316350432)) ;
#169365 = CARTESIAN_POINT('Ctrl Pts',(3.61205281147588,1.9291145279078,-25.265)) ;
#169366 = CARTESIAN_POINT('Ctrl Pts',(3.55200954448633,2.01456950859634,-25.2690361545106)) ;
#169367 = CARTESIAN_POINT('Ctrl Pts',(3.55804434431452,2.01804186348782,-25.1649908527503)) ;
#169368 = CARTESIAN_POINT('Ctrl Pts',(3.6,1.92679491924311,-25.265)) ;
#169369 = CARTESIAN_POINT('Ctrl Pts',(3.54999340544667,2.01340888172298,-25.265)) ;
#169370 = CARTESIAN_POINT('Ctrl Pts',(3.55000000043483,2.01339745886842,-25.1649868117631)) ;
#169371 = CARTESIAN_POINT('Origin',(3.6,1.92679491924311,-25.165)) ;
#169372 = CARTESIAN_POINT('Origin',(3.5,2.1,-25.165)) ;
#169373 = CARTESIAN_POINT('Origin',(3.7,1.9,-31.785)) ;
#169374 = CARTESIAN_POINT('Origin',(3.7,2.07320508075689,-31.885)) ;
#169375 = CARTESIAN_POINT('Ctrl Pts',(3.60000659411846,1.92678349789491,-31.8850000008696)) ;
#169376 = CARTESIAN_POINT('Ctrl Pts',(3.55000000000001,2.01339745962154,-31.8849868108933)) ;
#169377 = CARTESIAN_POINT('Ctrl Pts',(3.55,2.01339745962156,-31.985)) ;
#169378 = CARTESIAN_POINT('Ctrl Pts',(3.61192169694494,1.92907674455598,-31.8850005173338)) ;
#169379 = CARTESIAN_POINT('Ctrl Pts',(3.55199190475219,2.01454315814809,-31.8810002773326)) ;
#169380 = CARTESIAN_POINT('Ctrl Pts',(3.55795064586847,2.01798776715395,-31.9849956215505)) ;
#169381 = CARTESIAN_POINT('Ctrl Pts',(3.62341406508538,1.93280912529607,-31.8840249033077)) ;
#169382 = CARTESIAN_POINT('Ctrl Pts',(3.55602946562211,2.01072041298287,-31.8766898307658)) ;
#169383 = CARTESIAN_POINT('Ctrl Pts',(3.56528619664567,2.02370799306987,-31.9786388561746)) ;
#169384 = CARTESIAN_POINT('Ctrl Pts',(3.64447698054259,1.941884794702,-31.8799069718618)) ;
#169385 = CARTESIAN_POINT('Ctrl Pts',(3.56481337003728,2.00521659408683,-31.8681887406646)) ;
#169386 = CARTESIAN_POINT('Ctrl Pts',(3.5778513142626,2.0352860584176,-31.9651611543741)) ;
#169387 = CARTESIAN_POINT('Ctrl Pts',(3.65434383600069,1.94732274903778,-31.8767154403856)) ;
#169388 = CARTESIAN_POINT('Ctrl Pts',(3.56964037752544,2.00254785926569,-31.8637380042767)) ;
#169389 = CARTESIAN_POINT('Ctrl Pts',(3.58324299321411,2.04133793352501,-31.9570289695647)) ;
#169390 = CARTESIAN_POINT('Ctrl Pts',(3.67209270719134,1.95869361548259,-31.8682138841634)) ;
#169391 = CARTESIAN_POINT('Ctrl Pts',(3.57877657372946,1.99742369139612,-31.8546019249095)) ;
#169392 = CARTESIAN_POINT('Ctrl Pts',(3.59173571364126,2.0527041213258,-31.9392738450101)) ;
#169393 = CARTESIAN_POINT('Ctrl Pts',(3.68022412057906,1.9647491780641,-31.862815204266)) ;
#169394 = CARTESIAN_POINT('Ctrl Pts',(3.58322866085252,1.99475271178032,-31.8497736262967)) ;
#169395 = CARTESIAN_POINT('Ctrl Pts',(3.59492343714209,2.05814036366737,-31.929399963424)) ;
#169396 = CARTESIAN_POINT('Ctrl Pts',(3.69368364956802,1.97632149420531,-31.8502488628171)) ;
#169397 = CARTESIAN_POINT('Ctrl Pts',(3.59172551342565,1.98925228662574,-31.8409992807163)) ;
#169398 = CARTESIAN_POINT('Ctrl Pts',(3.59903094645825,2.06720241143977,-31.9083439645117)) ;
#169399 = CARTESIAN_POINT('Ctrl Pts',(3.70000914724964,1.98195813651217,-31.8430443443145)) ;
#169400 = CARTESIAN_POINT('Ctrl Pts',(3.59596384548948,1.98543049140366,-31.8370095444864)) ;
#169401 = CARTESIAN_POINT('Ctrl Pts',(3.6,2.07088547209221,-31.8970528114759)) ;
#169402 = CARTESIAN_POINT('Ctrl Pts',(3.70001318823692,1.98660254113158,-31.8350000004348)) ;
#169403 = CARTESIAN_POINT('Ctrl Pts',(3.6,1.98659111827701,-31.8349934054467)) ;
#169404 = CARTESIAN_POINT('Ctrl Pts',(3.6,2.07320508075689,-31.885)) ;
#169405 = CARTESIAN_POINT('Origin',(3.6,1.92679491924311,-31.985)) ;
#169406 = CARTESIAN_POINT('Origin',(3.5,2.1,-31.985)) ;
#169407 = CARTESIAN_POINT('Origin',(3.7,1.9,-29.175)) ;
#169408 = CARTESIAN_POINT('Origin',(3.7,2.07320508075689,-29.075)) ;
#169409 = CARTESIAN_POINT('Ctrl Pts',(3.70000000000001,1.98660254037844,-29.125)) ;
#169410 = CARTESIAN_POINT('Ctrl Pts',(3.59998681089334,1.98660254037844,-29.125)) ;
#169411 = CARTESIAN_POINT('Ctrl Pts',(3.60000000086965,2.07321650210507,-29.0749934058815)) ;
#169412 = CARTESIAN_POINT('Ctrl Pts',(3.69999562155021,1.98201223284605,-29.1170493541315)) ;
#169413 = CARTESIAN_POINT('Ctrl Pts',(3.59600027733264,1.98545684185212,-29.1230080952477)) ;
#169414 = CARTESIAN_POINT('Ctrl Pts',(3.60000051733381,2.07092325544403,-29.0630783030551)) ;
#169415 = CARTESIAN_POINT('Ctrl Pts',(3.69363885617462,1.97629200693012,-29.1097138033543)) ;
#169416 = CARTESIAN_POINT('Ctrl Pts',(3.59168983076584,1.98927958701707,-29.1189705343779)) ;
#169417 = CARTESIAN_POINT('Ctrl Pts',(3.5990249033077,2.06719087470394,-29.0515859349146)) ;
#169418 = CARTESIAN_POINT('Ctrl Pts',(3.68016115437406,1.9647139415824,-29.0971486857374)) ;
#169419 = CARTESIAN_POINT('Ctrl Pts',(3.58318874066458,1.99478340591321,-29.1101866299628)) ;
#169420 = CARTESIAN_POINT('Ctrl Pts',(3.59490697186185,2.05811520529797,-29.0305230194575)) ;
#169421 = CARTESIAN_POINT('Ctrl Pts',(3.6720289695647,1.958662066475,-29.0917570067859)) ;
#169422 = CARTESIAN_POINT('Ctrl Pts',(3.57873800427668,1.99745214073431,-29.1053596224745)) ;
#169423 = CARTESIAN_POINT('Ctrl Pts',(3.59171544038559,2.05267725096218,-29.0206561639993)) ;
#169424 = CARTESIAN_POINT('Ctrl Pts',(3.6542738450102,1.94729587867418,-29.0832642863587)) ;
#169425 = CARTESIAN_POINT('Ctrl Pts',(3.56960192490963,2.00257630860385,-29.0962234262706)) ;
#169426 = CARTESIAN_POINT('Ctrl Pts',(3.5832138841634,2.04130638451742,-29.0029072928087)) ;
#169427 = CARTESIAN_POINT('Ctrl Pts',(3.64439996342401,1.94185963633263,-29.0800765628579)) ;
#169428 = CARTESIAN_POINT('Ctrl Pts',(3.56477362629679,2.00524728821968,-29.0917713391475)) ;
#169429 = CARTESIAN_POINT('Ctrl Pts',(3.57781520426602,2.03525082193588,-28.9947758794209)) ;
#169430 = CARTESIAN_POINT('Ctrl Pts',(3.62334396451164,1.93279758856024,-29.0759690535418)) ;
#169431 = CARTESIAN_POINT('Ctrl Pts',(3.55599928071622,2.01074771337424,-29.0832744865743)) ;
#169432 = CARTESIAN_POINT('Ctrl Pts',(3.56524886281709,2.02367850579469,-28.981316350432)) ;
#169433 = CARTESIAN_POINT('Ctrl Pts',(3.61205281147588,1.9291145279078,-29.075)) ;
#169434 = CARTESIAN_POINT('Ctrl Pts',(3.55200954448622,2.01456950859647,-29.0790361545106)) ;
#169435 = CARTESIAN_POINT('Ctrl Pts',(3.55804434431452,2.01804186348782,-28.9749908527503)) ;
#169436 = CARTESIAN_POINT('Ctrl Pts',(3.6,1.92679491924311,-29.075)) ;
#169437 = CARTESIAN_POINT('Ctrl Pts',(3.54999340544667,2.01340888172298,-29.075)) ;
#169438 = CARTESIAN_POINT('Ctrl Pts',(3.55000000043483,2.01339745886842,-28.9749868117631)) ;
#169439 = CARTESIAN_POINT('Origin',(3.6,1.92679491924311,-28.975)) ;
#169440 = CARTESIAN_POINT('Origin',(3.5,2.1,-28.975)) ;
#169441 = CARTESIAN_POINT('Origin',(3.7,1.9,-35.595)) ;
#169442 = CARTESIAN_POINT('Origin',(3.7,2.07320508075689,-35.695)) ;
#169443 = CARTESIAN_POINT('Ctrl Pts',(3.60000659411846,1.92678349789491,-35.6950000008697)) ;
#169444 = CARTESIAN_POINT('Ctrl Pts',(3.55000000000001,2.01339745962154,-35.6949868108933)) ;
#169445 = CARTESIAN_POINT('Ctrl Pts',(3.55,2.01339745962156,-35.795)) ;
#169446 = CARTESIAN_POINT('Ctrl Pts',(3.61192169694494,1.92907674455598,-35.6950005173338)) ;
#169447 = CARTESIAN_POINT('Ctrl Pts',(3.55199190475219,2.01454315814809,-35.6910002773326)) ;
#169448 = CARTESIAN_POINT('Ctrl Pts',(3.55795064586847,2.01798776715395,-35.7949956215505)) ;
#169449 = CARTESIAN_POINT('Ctrl Pts',(3.62341406508538,1.93280912529607,-35.6940249033077)) ;
#169450 = CARTESIAN_POINT('Ctrl Pts',(3.55602946562211,2.01072041298287,-35.6866898307658)) ;
#169451 = CARTESIAN_POINT('Ctrl Pts',(3.56528619664567,2.02370799306987,-35.7886388561746)) ;
#169452 = CARTESIAN_POINT('Ctrl Pts',(3.64447698054259,1.941884794702,-35.6899069718619)) ;
#169453 = CARTESIAN_POINT('Ctrl Pts',(3.56481337003728,2.00521659408683,-35.6781887406645)) ;
#169454 = CARTESIAN_POINT('Ctrl Pts',(3.5778513142626,2.0352860584176,-35.7751611543741)) ;
#169455 = CARTESIAN_POINT('Ctrl Pts',(3.65434383600069,1.94732274903778,-35.6867154403856)) ;
#169456 = CARTESIAN_POINT('Ctrl Pts',(3.56964037752544,2.00254785926569,-35.6737380042767)) ;
#169457 = CARTESIAN_POINT('Ctrl Pts',(3.58324299321411,2.04133793352501,-35.7670289695647)) ;
#169458 = CARTESIAN_POINT('Ctrl Pts',(3.67209270719134,1.95869361548259,-35.6782138841634)) ;
#169459 = CARTESIAN_POINT('Ctrl Pts',(3.57877657372946,1.99742369139612,-35.6646019249095)) ;
#169460 = CARTESIAN_POINT('Ctrl Pts',(3.59173571364126,2.0527041213258,-35.7492738450102)) ;
#169461 = CARTESIAN_POINT('Ctrl Pts',(3.68022412057906,1.9647491780641,-35.672815204266)) ;
#169462 = CARTESIAN_POINT('Ctrl Pts',(3.58322866085252,1.99475271178032,-35.6597736262967)) ;
#169463 = CARTESIAN_POINT('Ctrl Pts',(3.59492343714209,2.05814036366737,-35.739399963424)) ;
#169464 = CARTESIAN_POINT('Ctrl Pts',(3.69368364956802,1.97632149420531,-35.6602488628171)) ;
#169465 = CARTESIAN_POINT('Ctrl Pts',(3.59172551342565,1.98925228662574,-35.6509992807163)) ;
#169466 = CARTESIAN_POINT('Ctrl Pts',(3.59903094645825,2.06720241143977,-35.7183439645117)) ;
#169467 = CARTESIAN_POINT('Ctrl Pts',(3.70000914724964,1.98195813651217,-35.6530443443145)) ;
#169468 = CARTESIAN_POINT('Ctrl Pts',(3.59596384548948,1.98543049140366,-35.6470095444864)) ;
#169469 = CARTESIAN_POINT('Ctrl Pts',(3.6,2.07088547209221,-35.7070528114759)) ;
#169470 = CARTESIAN_POINT('Ctrl Pts',(3.70001318823692,1.98660254113158,-35.6450000004348)) ;
#169471 = CARTESIAN_POINT('Ctrl Pts',(3.6,1.98659111827701,-35.6449934054467)) ;
#169472 = CARTESIAN_POINT('Ctrl Pts',(3.6,2.07320508075689,-35.695)) ;
#169473 = CARTESIAN_POINT('Origin',(3.6,1.92679491924311,-35.795)) ;
#169474 = CARTESIAN_POINT('Origin',(3.5,2.1,-35.795)) ;
#169475 = CARTESIAN_POINT('Origin',(3.7,1.9,-32.985)) ;
#169476 = CARTESIAN_POINT('Origin',(3.7,2.07320508075689,-32.885)) ;
#169477 = CARTESIAN_POINT('Ctrl Pts',(3.70000000000001,1.98660254037844,-32.935)) ;
#169478 = CARTESIAN_POINT('Ctrl Pts',(3.59998681089332,1.98660254037844,-32.935)) ;
#169479 = CARTESIAN_POINT('Ctrl Pts',(3.60000000086965,2.07321650210509,-32.8849934058815)) ;
#169480 = CARTESIAN_POINT('Ctrl Pts',(3.69999562155021,1.98201223284604,-32.9270493541315)) ;
#169481 = CARTESIAN_POINT('Ctrl Pts',(3.59600027733252,1.98545684185201,-32.9330080952478)) ;
#169482 = CARTESIAN_POINT('Ctrl Pts',(3.60000051733381,2.07092325544402,-32.873078303055)) ;
#169483 = CARTESIAN_POINT('Ctrl Pts',(3.69363885617463,1.97629200693015,-32.9197138033543)) ;
#169484 = CARTESIAN_POINT('Ctrl Pts',(3.59168983076591,1.98927958701709,-32.9289705343779)) ;
#169485 = CARTESIAN_POINT('Ctrl Pts',(3.59902490330771,2.06719087470393,-32.8615859349147)) ;
#169486 = CARTESIAN_POINT('Ctrl Pts',(3.68016115437406,1.96471394158237,-32.9071486857374)) ;
#169487 = CARTESIAN_POINT('Ctrl Pts',(3.58318874066448,1.99478340591319,-32.9201866299627)) ;
#169488 = CARTESIAN_POINT('Ctrl Pts',(3.59490697186185,2.05811520529799,-32.8405230194574)) ;
#169489 = CARTESIAN_POINT('Ctrl Pts',(3.6720289695647,1.95866206647497,-32.9017570067859)) ;
#169490 = CARTESIAN_POINT('Ctrl Pts',(3.57873800427671,1.99745214073432,-32.9153596224745)) ;
#169491 = CARTESIAN_POINT('Ctrl Pts',(3.59171544038559,2.05267725096218,-32.8306561639993)) ;
#169492 = CARTESIAN_POINT('Ctrl Pts',(3.65427384501021,1.9472958786742,-32.8932642863588)) ;
#169493 = CARTESIAN_POINT('Ctrl Pts',(3.56960192490956,2.00257630860387,-32.9062234262707)) ;
#169494 = CARTESIAN_POINT('Ctrl Pts',(3.5832138841634,2.04130638451744,-32.8129072928087)) ;
#169495 = CARTESIAN_POINT('Ctrl Pts',(3.64439996342399,1.94185963633262,-32.8900765628579)) ;
#169496 = CARTESIAN_POINT('Ctrl Pts',(3.5647736262967,2.00524728821974,-32.9017713391475)) ;
#169497 = CARTESIAN_POINT('Ctrl Pts',(3.57781520426601,2.03525082193589,-32.8047758794209)) ;
#169498 = CARTESIAN_POINT('Ctrl Pts',(3.62334396451166,1.93279758856024,-32.8859690535418)) ;
#169499 = CARTESIAN_POINT('Ctrl Pts',(3.55599928071631,2.01074771337418,-32.8932744865743)) ;
#169500 = CARTESIAN_POINT('Ctrl Pts',(3.5652488628171,2.02367850579469,-32.7913163504321)) ;
#169501 = CARTESIAN_POINT('Ctrl Pts',(3.61205281147586,1.9291145279078,-32.885)) ;
#169502 = CARTESIAN_POINT('Ctrl Pts',(3.55200954448637,2.01456950859641,-32.8890361545106)) ;
#169503 = CARTESIAN_POINT('Ctrl Pts',(3.55804434431452,2.01804186348783,-32.7849908527503)) ;
#169504 = CARTESIAN_POINT('Ctrl Pts',(3.6,1.92679491924311,-32.885)) ;
#169505 = CARTESIAN_POINT('Ctrl Pts',(3.54999340544667,2.01340888172297,-32.885)) ;
#169506 = CARTESIAN_POINT('Ctrl Pts',(3.55000000043483,2.01339745886842,-32.7849868117631)) ;
#169507 = CARTESIAN_POINT('Origin',(3.6,1.92679491924311,-32.785)) ;
#169508 = CARTESIAN_POINT('Origin',(3.5,2.1,-32.785)) ;
#169509 = CARTESIAN_POINT('Origin',(-1.39554230456301E-15,-1.51907484122731,
-7.62)) ;
#169510 = CARTESIAN_POINT('Origin',(-6.11095769946375E-16,4.45,-7.62)) ;
#169511 = CARTESIAN_POINT('Origin',(-1.39554230456301E-15,-1.51907484122731,
-11.43)) ;
#169512 = CARTESIAN_POINT('Origin',(-6.11095769946375E-16,4.45,-11.43)) ;
#169513 = CARTESIAN_POINT('Origin',(-1.39554230456301E-15,-1.51907484122731,
-15.24)) ;
#169514 = CARTESIAN_POINT('Origin',(-6.11095769946375E-16,4.45,-15.24)) ;
#169515 = CARTESIAN_POINT('Origin',(-1.39554230456301E-15,-1.51907484122731,
-19.05)) ;
#169516 = CARTESIAN_POINT('Origin',(-6.11095769946375E-16,4.45,-19.05)) ;
#169517 = CARTESIAN_POINT('Origin',(-1.39554230456301E-15,-1.51907484122731,
-22.86)) ;
#169518 = CARTESIAN_POINT('Origin',(-6.11095769946375E-16,4.45,-22.86)) ;
#169519 = CARTESIAN_POINT('Origin',(-1.39554230456301E-15,-1.51907484122731,
-26.67)) ;
#169520 = CARTESIAN_POINT('Origin',(-6.11095769946375E-16,4.45,-26.67)) ;
#169521 = CARTESIAN_POINT('Origin',(2.5,-6.45,-36.49)) ;
#169522 = CARTESIAN_POINT('Origin',(2.5,-6.45,-36.49)) ;
#169523 = CARTESIAN_POINT('Origin',(2.5,4.55,-36.49)) ;
#169524 = CARTESIAN_POINT('Origin',(2.5,1.9,-36.49)) ;
#169525 = CARTESIAN_POINT('Origin',(2.7,1.9,-36.49)) ;
#169526 = CARTESIAN_POINT('Origin',(2.7,2.1,-36.49)) ;
#169527 = CARTESIAN_POINT('Origin',(-1.64095463943752E-16,2.1,-36.49)) ;
#169528 = CARTESIAN_POINT('Origin',(3.5,2.1,-36.49)) ;
#169529 = CARTESIAN_POINT('Origin',(3.5,2.1,-36.49)) ;
#169530 = CARTESIAN_POINT('Origin',(3.5,2.1,-36.49)) ;
#169531 = CARTESIAN_POINT('Origin',(3.5,7.81406971160724E-17,-36.49)) ;
#169532 = CARTESIAN_POINT('Origin',(3.5,2.65,-36.49)) ;
#169533 = CARTESIAN_POINT('Origin',(3.5,2.65,-36.49)) ;
#169534 = CARTESIAN_POINT('Origin',(3.5,2.65,-36.49)) ;
#169535 = CARTESIAN_POINT('Origin',(3.6,2.65,-36.49)) ;
#169536 = CARTESIAN_POINT('Origin',(2.7,2.65,-36.49)) ;
#169537 = CARTESIAN_POINT('Origin',(-3.9,4.45,-36.49)) ;
#169538 = CARTESIAN_POINT('Origin',(-3.9,4.45,-36.49)) ;
#169539 = CARTESIAN_POINT('Origin',(2.7,2.85,-36.49)) ;
#169540 = CARTESIAN_POINT('Origin',(2.5,2.85,-36.49)) ;
#169541 = CARTESIAN_POINT('Origin',(2.7,2.85,-36.49)) ;
#169542 = CARTESIAN_POINT('Origin',(-4.,4.45,-36.49)) ;
#169543 = CARTESIAN_POINT('Origin',(2.5,4.45,-36.49)) ;
#169544 = CARTESIAN_POINT('Origin',(2.5,4.55,-36.49)) ;
#169545 = CARTESIAN_POINT('Origin',(2.5,4.45,-36.49)) ;
#169546 = CARTESIAN_POINT('Origin',(2.7,2.85,-2.3)) ;
#169547 = CARTESIAN_POINT('Origin',(2.7,2.85,-35.94)) ;
#169548 = CARTESIAN_POINT('Origin',(2.5,4.45,-36.49)) ;
#169549 = CARTESIAN_POINT('Origin',(2.5,4.45,-36.49)) ;
#169550 = CARTESIAN_POINT('Origin',(2.5,2.85,-35.94)) ;
#169551 = CARTESIAN_POINT('Origin',(2.5,2.85,-35.94)) ;
#169552 = CARTESIAN_POINT('Origin',(2.5,2.85,-35.74)) ;
#169553 = CARTESIAN_POINT('Origin',(2.5,4.45,-36.59)) ;
#169554 = CARTESIAN_POINT('Origin',(2.5,4.45,-35.94)) ;
#169555 = CARTESIAN_POINT('Origin',(2.5,-1.51907484122731,-35.94)) ;
#169556 = CARTESIAN_POINT('Origin',(2.5,4.45,-35.94)) ;
#169557 = CARTESIAN_POINT('Origin',(3.6,2.85,-35.74)) ;
#169558 = CARTESIAN_POINT('Ctrl Pts',(1.8493242008907,2.75,-35.74)) ;
#169559 = CARTESIAN_POINT('Ctrl Pts',(1.8489155297075,2.75,-35.7405602528665)) ;
#169560 = CARTESIAN_POINT('Ctrl Pts',(1.84850693760105,2.75000414964412,-35.7411205835206)) ;
#169561 = CARTESIAN_POINT('Ctrl Pts',(1.84774402267852,2.75001978545986,-35.7421661733315)) ;
#169562 = CARTESIAN_POINT('Ctrl Pts',(1.84738978525535,2.75003021925998,-35.742651541288)) ;
#169563 = CARTESIAN_POINT('Ctrl Pts',(1.84658906145061,2.75006109115737,-35.74374842884)) ;
#169564 = CARTESIAN_POINT('Ctrl Pts',(1.84614254888567,2.75008342791642,-35.744359920497)) ;
#169565 = CARTESIAN_POINT('Ctrl Pts',(1.84498586912391,2.75015481704799,-35.7459435779958)) ;
#169566 = CARTESIAN_POINT('Ctrl Pts',(1.84427568281904,2.75021186472549,-35.746915537535)) ;
#169567 = CARTESIAN_POINT('Ctrl Pts',(1.84242877605317,2.75039562881422,-35.7494423274962)) ;
#169568 = CARTESIAN_POINT('Ctrl Pts',(1.84129221873232,2.75054367055059,-35.7509964126165)) ;
#169569 = CARTESIAN_POINT('Ctrl Pts',(1.83830538692966,2.75102873153648,-35.7550782232159)) ;
#169570 = CARTESIAN_POINT('Ctrl Pts',(1.83645654188481,2.75142684996804,-35.7576027100469)) ;
#169571 = CARTESIAN_POINT('Ctrl Pts',(1.83146008674514,2.75278026662635,-35.7644125156423)) ;
#169572 = CARTESIAN_POINT('Ctrl Pts',(1.8283159214327,2.75393867343662,-35.7686876979924)) ;
#169573 = CARTESIAN_POINT('Ctrl Pts',(1.82163255793241,2.7571078032997,-35.7777453775413)) ;
#169574 = CARTESIAN_POINT('Ctrl Pts',(1.81811360872654,2.75921511002117,-35.7824849484117)) ;
#169575 = CARTESIAN_POINT('Ctrl Pts',(1.81342675453064,2.76262639234437,-35.7887744415142)) ;
#169576 = CARTESIAN_POINT('Ctrl Pts',(1.81216355883267,2.76360925975736,-35.7904674024384)) ;
#169577 = CARTESIAN_POINT('Ctrl Pts',(1.80949588405405,2.76581971270449,-35.7940412672837)) ;
#169578 = CARTESIAN_POINT('Ctrl Pts',(1.80809008635136,2.76706812937485,-35.7959240633996)) ;
#169579 = CARTESIAN_POINT('Ctrl Pts',(1.80622180825287,2.76884047115884,-35.7984273163076)) ;
#169580 = CARTESIAN_POINT('Ctrl Pts',(1.80574460306297,2.76930303796754,-35.7990667849892)) ;
#169581 = CARTESIAN_POINT('Ctrl Pts',(1.8020072303246,2.77301004154989,-35.8040760810937)) ;
#169582 = CARTESIAN_POINT('Ctrl Pts',(1.79893605118154,2.77655328823594,-35.8081869819183)) ;
#169583 = CARTESIAN_POINT('Ctrl Pts',(1.79553848385938,2.78126766498699,-35.8127195282098)) ;
#169584 = CARTESIAN_POINT('Ctrl Pts',(1.79508624826463,2.78191247648142,-35.813322487166)) ;
#169585 = CARTESIAN_POINT('Ctrl Pts',(1.79248502865789,2.78572620110035,-35.8167883578142)) ;
#169586 = CARTESIAN_POINT('Ctrl Pts',(1.79047061583886,2.7890829265238,-35.8194451149791)) ;
#169587 = CARTESIAN_POINT('Ctrl Pts',(1.78802866333258,2.79371407639528,-35.8226702366014)) ;
#169588 = CARTESIAN_POINT('Ctrl Pts',(1.78745102314761,2.7948573048606,-35.8234336014307)) ;
#169589 = CARTESIAN_POINT('Ctrl Pts',(1.78677268033909,2.79625836238382,-35.8243322112889)) ;
#169590 = CARTESIAN_POINT('Ctrl Pts',(1.78665445068052,2.79650484960405,-35.8244889072897)) ;
#169591 = CARTESIAN_POINT('Ctrl Pts',(1.78451055395601,2.80101773866204,-35.8273319791621)) ;
#169592 = CARTESIAN_POINT('Ctrl Pts',(1.78263897914008,2.80562493737592,-35.8298097275576)) ;
#169593 = CARTESIAN_POINT('Ctrl Pts',(1.78021555250218,2.8131601371182,-35.8330108372395)) ;
#169594 = CARTESIAN_POINT('Ctrl Pts',(1.77953359820565,2.81552321764106,-35.8339042399272)) ;
#169595 = CARTESIAN_POINT('Ctrl Pts',(1.77885922502008,2.81814935429725,-35.8347924283505)) ;
#169596 = CARTESIAN_POINT('Ctrl Pts',(1.77880145893001,2.81837682960042,-35.8348685024872)) ;
#169597 = CARTESIAN_POINT('Ctrl Pts',(1.77779807199381,2.8223725993423,-35.8361897865139)) ;
#169598 = CARTESIAN_POINT('Ctrl Pts',(1.77701280317414,2.82627116869043,-35.837221156511)) ;
#169599 = CARTESIAN_POINT('Ctrl Pts',(1.77629130352191,2.83098366045554,-35.83816931204)) ;
#169600 = CARTESIAN_POINT('Ctrl Pts',(1.77618324871506,2.83173306513677,-35.8383113339465)) ;
#169601 = CARTESIAN_POINT('Ctrl Pts',(1.77598237323328,2.83321827741191,-35.838575453052)) ;
#169602 = CARTESIAN_POINT('Ctrl Pts',(1.77588933458808,2.83395373307725,-35.8386979039347)) ;
#169603 = CARTESIAN_POINT('Ctrl Pts',(1.77526822780854,2.83923120109982,-35.839516785743)) ;
#169604 = CARTESIAN_POINT('Ctrl Pts',(1.77496841680888,2.84387001846842,-35.8399177608516)) ;
#169605 = CARTESIAN_POINT('Ctrl Pts',(1.77490988945624,2.84900075666618,-35.8399961754232)) ;
#169606 = CARTESIAN_POINT('Ctrl Pts',(1.77490703981929,2.8495004656413,-35.84)) ;
#169607 = CARTESIAN_POINT('Ctrl Pts',(1.77490703981929,2.85,-35.84)) ;
#169608 = CARTESIAN_POINT('Origin',(2.5,4.45,-35.94)) ;
#169609 = CARTESIAN_POINT('Origin',(2.5,4.45,-35.94)) ;
#169610 = CARTESIAN_POINT('Ctrl Pts',(1.77500103713014,2.85,-35.839999931521)) ;
#169611 = CARTESIAN_POINT('Ctrl Pts',(1.63636532444071,2.84999999999999,-35.8402019295526)) ;
#169612 = CARTESIAN_POINT('Ctrl Pts',(1.72549327481619,2.85,-35.7340128995261)) ;
#169613 = CARTESIAN_POINT('Ctrl Pts',(1.775003672721,2.83840140237647,-35.83999996665)) ;
#169614 = CARTESIAN_POINT('Ctrl Pts',(1.63647653558524,2.80016011611086,-35.8401502081412)) ;
#169615 = CARTESIAN_POINT('Ctrl Pts',(1.72549488713563,2.8384005084226,-35.7340109198666)) ;
#169616 = CARTESIAN_POINT('Ctrl Pts',(1.77656595559297,2.82767268181592,-35.837937333125)) ;
#169617 = CARTESIAN_POINT('Ctrl Pts',(1.66487156423554,2.77372961894301,-35.8269406617147)) ;
#169618 = CARTESIAN_POINT('Ctrl Pts',(1.72805121738616,2.82767128774606,-35.7341715076455)) ;
#169619 = CARTESIAN_POINT('Ctrl Pts',(1.78107127365223,2.80963025017428,-35.8319811709515)) ;
#169620 = CARTESIAN_POINT('Ctrl Pts',(1.7078319145322,2.75028955033669,-35.8069390197619)) ;
#169621 = CARTESIAN_POINT('Ctrl Pts',(1.73543500606493,2.80962842221856,-35.7346185213022)) ;
#169622 = CARTESIAN_POINT('Ctrl Pts',(1.78389779708652,2.80236854329887,-35.8282458892004)) ;
#169623 = CARTESIAN_POINT('Ctrl Pts',(1.72405887077374,2.74863416898561,-35.7993766027639)) ;
#169624 = CARTESIAN_POINT('Ctrl Pts',(1.7400684743322,2.80236673746756,-35.7348898223597)) ;
#169625 = CARTESIAN_POINT('Ctrl Pts',(1.79303410435281,2.78344495542395,-35.8161243202616)) ;
#169626 = CARTESIAN_POINT('Ctrl Pts',(1.75831223057316,2.7462997480749,-35.7833824330224)) ;
#169627 = CARTESIAN_POINT('Ctrl Pts',(1.75509542206186,2.7834434444138,-35.7357496723872)) ;
#169628 = CARTESIAN_POINT('Ctrl Pts',(1.79978086064413,2.77501182458606,-35.8071352730534)) ;
#169629 = CARTESIAN_POINT('Ctrl Pts',(1.77349404839604,2.74800701225899,-35.7762550668971)) ;
#169630 = CARTESIAN_POINT('Ctrl Pts',(1.7662373444394,2.775010621185,-35.7363505791766)) ;
#169631 = CARTESIAN_POINT('Ctrl Pts',(1.82062092254039,2.75520283445682,-35.7791823423359)) ;
#169632 = CARTESIAN_POINT('Ctrl Pts',(1.80915747696825,2.74970830577378,-35.7594018394234)) ;
#169633 = CARTESIAN_POINT('Ctrl Pts',(1.80086136857318,2.75520254410104,-35.7380912776554)) ;
#169634 = CARTESIAN_POINT('Ctrl Pts',(1.83487464178854,2.75,-35.759840908673)) ;
#169635 = CARTESIAN_POINT('Ctrl Pts',(1.82921773450097,2.75,-35.7497824526971)) ;
#169636 = CARTESIAN_POINT('Ctrl Pts',(1.82479494488362,2.75,-35.739125428875)) ;
#169637 = CARTESIAN_POINT('Ctrl Pts',(1.8493242008907,2.75,-35.74)) ;
#169638 = CARTESIAN_POINT('Ctrl Pts',(1.8493242008907,2.75,-35.74)) ;
#169639 = CARTESIAN_POINT('Ctrl Pts',(1.8493242008907,2.75,-35.74)) ;
#169640 = CARTESIAN_POINT('Origin',(2.6,4.45,-35.94)) ;
#169641 = CARTESIAN_POINT('Ctrl Pts',(1.27790541830591,2.85,-32.4381204689935)) ;
#169642 = CARTESIAN_POINT('Ctrl Pts',(1.20082240333961,2.85,-32.3849999999998)) ;
#169643 = CARTESIAN_POINT('Ctrl Pts',(1.27790541830602,2.85,-32.3318795310064)) ;
#169644 = CARTESIAN_POINT('Ctrl Pts',(1.27790638186138,2.84083632349969,-32.4381211409614)) ;
#169645 = CARTESIAN_POINT('Ctrl Pts',(1.20084678242026,2.82796155786835,-32.3849999999998)) ;
#169646 = CARTESIAN_POINT('Ctrl Pts',(1.27790638186151,2.84083632349971,-32.3318788590386)) ;
#169647 = CARTESIAN_POINT('Ctrl Pts',(1.27916908278627,2.83184203564912,-32.4374245856051)) ;
#169648 = CARTESIAN_POINT('Ctrl Pts',(1.20941464972047,2.80875345001339,-32.3849999999999)) ;
#169649 = CARTESIAN_POINT('Ctrl Pts',(1.27916908278638,2.83184203564916,-32.3325754143948)) ;
#169650 = CARTESIAN_POINT('Ctrl Pts',(1.28359729368254,2.81532455354034,-32.4349858093441)) ;
#169651 = CARTESIAN_POINT('Ctrl Pts',(1.23205483118169,2.78149692488717,-32.3849999999998)) ;
#169652 = CARTESIAN_POINT('Ctrl Pts',(1.28359729368263,2.8153245535404,-32.3350141906558)) ;
#169653 = CARTESIAN_POINT('Ctrl Pts',(1.28669991111207,2.80791239452539,-32.4332816433158)) ;
#169654 = CARTESIAN_POINT('Ctrl Pts',(1.24464080060876,2.7734468891291,-32.385)) ;
#169655 = CARTESIAN_POINT('Ctrl Pts',(1.28669991111214,2.80791239452546,-32.3367183566841)) ;
#169656 = CARTESIAN_POINT('Ctrl Pts',(1.29736892768575,2.78833251591434,-32.4274284096738)) ;
#169657 = CARTESIAN_POINT('Ctrl Pts',(1.27602012126336,2.75841927526786,-32.385)) ;
#169658 = CARTESIAN_POINT('Ctrl Pts',(1.29736892768578,2.78833251591441,-32.3425715903261)) ;
#169659 = CARTESIAN_POINT('Ctrl Pts',(1.30626047349815,2.77861339289525,-32.4225706455934)) ;
#169660 = CARTESIAN_POINT('Ctrl Pts',(1.29330467011166,2.75582184841473,-32.385)) ;
#169661 = CARTESIAN_POINT('Ctrl Pts',(1.30626047349817,2.77861339289531,-32.3474293544066)) ;
#169662 = CARTESIAN_POINT('Ctrl Pts',(1.3341796818893,2.75637252911125,-32.4073970793052)) ;
#169663 = CARTESIAN_POINT('Ctrl Pts',(1.33261582998958,2.75058962148775,-32.3849999999999)) ;
#169664 = CARTESIAN_POINT('Ctrl Pts',(1.3341796818893,2.75637252911127,-32.3626029206948)) ;
#169665 = CARTESIAN_POINT('Ctrl Pts',(1.35520432073838,2.75,-32.3960818608403)) ;
#169666 = CARTESIAN_POINT('Ctrl Pts',(1.35468704305008,2.75,-32.385)) ;
#169667 = CARTESIAN_POINT('Ctrl Pts',(1.35520432073834,2.75,-32.3739181391598)) ;
#169668 = CARTESIAN_POINT('Ctrl Pts',(1.37603597336698,2.75,-32.385)) ;
#169669 = CARTESIAN_POINT('Ctrl Pts',(1.37603597336698,2.75,-32.385)) ;
#169670 = CARTESIAN_POINT('Ctrl Pts',(1.37603597336698,2.75,-32.385)) ;
#169671 = CARTESIAN_POINT('Origin',(-5.84812080916424E-16,4.45,-34.29)) ;
#169672 = CARTESIAN_POINT('Ctrl Pts',(1.27790541830602,2.85,-28.6281204689936)) ;
#169673 = CARTESIAN_POINT('Ctrl Pts',(1.20082240333942,2.85,-28.575)) ;
#169674 = CARTESIAN_POINT('Ctrl Pts',(1.27790541830602,2.85,-28.5218795310064)) ;
#169675 = CARTESIAN_POINT('Ctrl Pts',(1.2779063818615,2.8408363234997,-28.6281211409615)) ;
#169676 = CARTESIAN_POINT('Ctrl Pts',(1.20084678242003,2.82796155786832,-28.575)) ;
#169677 = CARTESIAN_POINT('Ctrl Pts',(1.2779063818615,2.84083632349971,-28.5218788590386)) ;
#169678 = CARTESIAN_POINT('Ctrl Pts',(1.27916908278636,2.83184203564916,-28.6274245856052)) ;
#169679 = CARTESIAN_POINT('Ctrl Pts',(1.2094146497203,2.80875345001334,-28.575)) ;
#169680 = CARTESIAN_POINT('Ctrl Pts',(1.27916908278637,2.83184203564916,-28.5225754143948)) ;
#169681 = CARTESIAN_POINT('Ctrl Pts',(1.28359729368261,2.81532455354039,-28.6249858093442)) ;
#169682 = CARTESIAN_POINT('Ctrl Pts',(1.23205483118158,2.78149692488709,-28.575)) ;
#169683 = CARTESIAN_POINT('Ctrl Pts',(1.28359729368262,2.81532455354039,-28.5250141906558)) ;
#169684 = CARTESIAN_POINT('Ctrl Pts',(1.28669991111214,2.80791239452546,-28.6232816433159)) ;
#169685 = CARTESIAN_POINT('Ctrl Pts',(1.24464080060866,2.77344688912903,-28.575)) ;
#169686 = CARTESIAN_POINT('Ctrl Pts',(1.28669991111214,2.80791239452546,-28.5267183566841)) ;
#169687 = CARTESIAN_POINT('Ctrl Pts',(1.29736892768578,2.7883325159144,-28.6174284096739)) ;
#169688 = CARTESIAN_POINT('Ctrl Pts',(1.27602012126333,2.75841927526782,-28.575)) ;
#169689 = CARTESIAN_POINT('Ctrl Pts',(1.29736892768579,2.7883325159144,-28.5325715903261)) ;
#169690 = CARTESIAN_POINT('Ctrl Pts',(1.30626047349817,2.7786133928953,-28.6125706455934)) ;
#169691 = CARTESIAN_POINT('Ctrl Pts',(1.29330467011163,2.75582184841469,-28.575)) ;
#169692 = CARTESIAN_POINT('Ctrl Pts',(1.30626047349816,2.7786133928953,-28.5374293544066)) ;
#169693 = CARTESIAN_POINT('Ctrl Pts',(1.33417968188929,2.75637252911127,-28.5973970793052)) ;
#169694 = CARTESIAN_POINT('Ctrl Pts',(1.33261582998957,2.75058962148775,-28.575)) ;
#169695 = CARTESIAN_POINT('Ctrl Pts',(1.3341796818893,2.75637252911127,-28.5526029206948)) ;
#169696 = CARTESIAN_POINT('Ctrl Pts',(1.35520432073835,2.75,-28.5860818608403)) ;
#169697 = CARTESIAN_POINT('Ctrl Pts',(1.35468704305008,2.75,-28.575)) ;
#169698 = CARTESIAN_POINT('Ctrl Pts',(1.35520432073834,2.75,-28.5639181391598)) ;
#169699 = CARTESIAN_POINT('Ctrl Pts',(1.37603597336697,2.75,-28.575)) ;
#169700 = CARTESIAN_POINT('Ctrl Pts',(1.37603597336697,2.75,-28.575)) ;
#169701 = CARTESIAN_POINT('Ctrl Pts',(1.37603597336697,2.75,-28.575)) ;
#169702 = CARTESIAN_POINT('Origin',(-5.84812080916424E-16,4.45,-30.48)) ;
#169703 = CARTESIAN_POINT('Ctrl Pts',(1.27790541830606,2.85,-24.8181204689937)) ;
#169704 = CARTESIAN_POINT('Ctrl Pts',(1.20082240333964,2.85,-24.7650000000002)) ;
#169705 = CARTESIAN_POINT('Ctrl Pts',(1.27790541830584,2.85,-24.7118795310066)) ;
#169706 = CARTESIAN_POINT('Ctrl Pts',(1.27790638186154,2.84083632349972,-24.8181211409614)) ;
#169707 = CARTESIAN_POINT('Ctrl Pts',(1.20084678242024,2.82796155786836,-24.7650000000002)) ;
#169708 = CARTESIAN_POINT('Ctrl Pts',(1.27790638186134,2.84083632349968,-24.7118788590387)) ;
#169709 = CARTESIAN_POINT('Ctrl Pts',(1.27916908278641,2.83184203564917,-24.8174245856052)) ;
#169710 = CARTESIAN_POINT('Ctrl Pts',(1.20941464972049,2.8087534500134,-24.7650000000002)) ;
#169711 = CARTESIAN_POINT('Ctrl Pts',(1.27916908278621,2.8318420356491,-24.7125754143949)) ;
#169712 = CARTESIAN_POINT('Ctrl Pts',(1.28359729368265,2.81532455354041,-24.8149858093442)) ;
#169713 = CARTESIAN_POINT('Ctrl Pts',(1.2320548311817,2.78149692488718,-24.7650000000002)) ;
#169714 = CARTESIAN_POINT('Ctrl Pts',(1.28359729368249,2.8153245535403,-24.715014190656)) ;
#169715 = CARTESIAN_POINT('Ctrl Pts',(1.28669991111217,2.80791239452549,-24.8132816433159)) ;
#169716 = CARTESIAN_POINT('Ctrl Pts',(1.24464080060876,2.77344688912911,-24.7650000000002)) ;
#169717 = CARTESIAN_POINT('Ctrl Pts',(1.28669991111203,2.80791239452536,-24.7167183566842)) ;
#169718 = CARTESIAN_POINT('Ctrl Pts',(1.2973689276858,2.78833251591442,-24.807428409674)) ;
#169719 = CARTESIAN_POINT('Ctrl Pts',(1.27602012126337,2.75841927526789,-24.7650000000001)) ;
#169720 = CARTESIAN_POINT('Ctrl Pts',(1.29736892768571,2.78833251591431,-24.7225715903263)) ;
#169721 = CARTESIAN_POINT('Ctrl Pts',(1.30626047349817,2.77861339289533,-24.8025706455935)) ;
#169722 = CARTESIAN_POINT('Ctrl Pts',(1.29330467011166,2.75582184841473,-24.7650000000001)) ;
#169723 = CARTESIAN_POINT('Ctrl Pts',(1.30626047349813,2.77861339289522,-24.7274293544067)) ;
#169724 = CARTESIAN_POINT('Ctrl Pts',(1.3341796818893,2.75637252911125,-24.7873970793052)) ;
#169725 = CARTESIAN_POINT('Ctrl Pts',(1.33261582998957,2.75058962148776,-24.765)) ;
#169726 = CARTESIAN_POINT('Ctrl Pts',(1.33417968188928,2.75637252911127,-24.7426029206948)) ;
#169727 = CARTESIAN_POINT('Ctrl Pts',(1.35520432073831,2.75,-24.7760818608402)) ;
#169728 = CARTESIAN_POINT('Ctrl Pts',(1.35468704305007,2.75,-24.7649999999999)) ;
#169729 = CARTESIAN_POINT('Ctrl Pts',(1.3552043207384,2.75,-24.7539181391597)) ;
#169730 = CARTESIAN_POINT('Ctrl Pts',(1.37603597336698,2.75,-24.765)) ;
#169731 = CARTESIAN_POINT('Ctrl Pts',(1.37603597336698,2.75,-24.765)) ;
#169732 = CARTESIAN_POINT('Ctrl Pts',(1.37603597336698,2.75,-24.765)) ;
#169733 = CARTESIAN_POINT('Origin',(-6.11095769946375E-16,4.45,-26.67)) ;
#169734 = CARTESIAN_POINT('Ctrl Pts',(1.27790541830603,2.85,-21.0081204689936)) ;
#169735 = CARTESIAN_POINT('Ctrl Pts',(1.20082240333942,2.85,-20.955)) ;
#169736 = CARTESIAN_POINT('Ctrl Pts',(1.27790541830601,2.85,-20.9018795310064)) ;
#169737 = CARTESIAN_POINT('Ctrl Pts',(1.27790638186151,2.84083632349971,-21.0081211409614)) ;
#169738 = CARTESIAN_POINT('Ctrl Pts',(1.20084678242002,2.82796155786833,-20.955)) ;
#169739 = CARTESIAN_POINT('Ctrl Pts',(1.2779063818615,2.84083632349971,-20.9018788590386)) ;
#169740 = CARTESIAN_POINT('Ctrl Pts',(1.27916908278638,2.83184203564916,-21.0074245856052)) ;
#169741 = CARTESIAN_POINT('Ctrl Pts',(1.2094146497203,2.80875345001334,-20.955)) ;
#169742 = CARTESIAN_POINT('Ctrl Pts',(1.27916908278637,2.83184203564916,-20.9025754143948)) ;
#169743 = CARTESIAN_POINT('Ctrl Pts',(1.28359729368262,2.8153245535404,-21.0049858093442)) ;
#169744 = CARTESIAN_POINT('Ctrl Pts',(1.23205483118157,2.7814969248871,-20.955)) ;
#169745 = CARTESIAN_POINT('Ctrl Pts',(1.2835972936826,2.81532455354039,-20.9050141906558)) ;
#169746 = CARTESIAN_POINT('Ctrl Pts',(1.28669991111215,2.80791239452546,-21.0032816433159)) ;
#169747 = CARTESIAN_POINT('Ctrl Pts',(1.24464080060865,2.77344688912904,-20.955)) ;
#169748 = CARTESIAN_POINT('Ctrl Pts',(1.28669991111213,2.80791239452546,-20.9067183566841)) ;
#169749 = CARTESIAN_POINT('Ctrl Pts',(1.29736892768578,2.7883325159144,-20.9974284096739)) ;
#169750 = CARTESIAN_POINT('Ctrl Pts',(1.27602012126334,2.75841927526782,-20.955)) ;
#169751 = CARTESIAN_POINT('Ctrl Pts',(1.29736892768577,2.7883325159144,-20.9125715903261)) ;
#169752 = CARTESIAN_POINT('Ctrl Pts',(1.30626047349816,2.77861339289531,-20.9925706455934)) ;
#169753 = CARTESIAN_POINT('Ctrl Pts',(1.29330467011164,2.75582184841469,-20.955)) ;
#169754 = CARTESIAN_POINT('Ctrl Pts',(1.30626047349816,2.7786133928953,-20.9174293544066)) ;
#169755 = CARTESIAN_POINT('Ctrl Pts',(1.33417968188929,2.75637252911127,-20.9773970793052)) ;
#169756 = CARTESIAN_POINT('Ctrl Pts',(1.33261582998957,2.75058962148775,-20.955)) ;
#169757 = CARTESIAN_POINT('Ctrl Pts',(1.33417968188929,2.75637252911127,-20.9326029206948)) ;
#169758 = CARTESIAN_POINT('Ctrl Pts',(1.35520432073833,2.75,-20.9660818608402)) ;
#169759 = CARTESIAN_POINT('Ctrl Pts',(1.35468704305007,2.75,-20.955)) ;
#169760 = CARTESIAN_POINT('Ctrl Pts',(1.35520432073833,2.75,-20.9439181391598)) ;
#169761 = CARTESIAN_POINT('Ctrl Pts',(1.37603597336697,2.75,-20.955)) ;
#169762 = CARTESIAN_POINT('Ctrl Pts',(1.37603597336697,2.75,-20.955)) ;
#169763 = CARTESIAN_POINT('Ctrl Pts',(1.37603597336697,2.75,-20.955)) ;
#169764 = CARTESIAN_POINT('Origin',(-6.11095769946375E-16,4.45,-22.86)) ;
#169765 = CARTESIAN_POINT('Ctrl Pts',(1.27790541830603,2.85,-17.1981204689936)) ;
#169766 = CARTESIAN_POINT('Ctrl Pts',(1.20082240333937,2.85,-17.145)) ;
#169767 = CARTESIAN_POINT('Ctrl Pts',(1.27790541830605,2.85,-17.0918795310064)) ;
#169768 = CARTESIAN_POINT('Ctrl Pts',(1.2779063818615,2.84083632349971,-17.1981211409614)) ;
#169769 = CARTESIAN_POINT('Ctrl Pts',(1.20084678241998,2.82796155786832,-17.145)) ;
#169770 = CARTESIAN_POINT('Ctrl Pts',(1.27790638186153,2.84083632349972,-17.0918788590386)) ;
#169771 = CARTESIAN_POINT('Ctrl Pts',(1.27916908278638,2.83184203564916,-17.1974245856052)) ;
#169772 = CARTESIAN_POINT('Ctrl Pts',(1.20941464972025,2.80875345001333,-17.145)) ;
#169773 = CARTESIAN_POINT('Ctrl Pts',(1.27916908278639,2.83184203564917,-17.0925754143947)) ;
#169774 = CARTESIAN_POINT('Ctrl Pts',(1.28359729368262,2.8153245535404,-17.1949858093442)) ;
#169775 = CARTESIAN_POINT('Ctrl Pts',(1.23205483118153,2.78149692488708,-17.145)) ;
#169776 = CARTESIAN_POINT('Ctrl Pts',(1.28359729368264,2.81532455354041,-17.0950141906558)) ;
#169777 = CARTESIAN_POINT('Ctrl Pts',(1.28669991111215,2.80791239452546,-17.1932816433159)) ;
#169778 = CARTESIAN_POINT('Ctrl Pts',(1.24464080060863,2.77344688912901,-17.145)) ;
#169779 = CARTESIAN_POINT('Ctrl Pts',(1.28669991111216,2.80791239452547,-17.096718356684)) ;
#169780 = CARTESIAN_POINT('Ctrl Pts',(1.29736892768579,2.7883325159144,-17.1874284096739)) ;
#169781 = CARTESIAN_POINT('Ctrl Pts',(1.27602012126332,2.75841927526781,-17.145)) ;
#169782 = CARTESIAN_POINT('Ctrl Pts',(1.29736892768579,2.78833251591441,-17.1025715903261)) ;
#169783 = CARTESIAN_POINT('Ctrl Pts',(1.30626047349816,2.7786133928953,-17.1825706455934)) ;
#169784 = CARTESIAN_POINT('Ctrl Pts',(1.29330467011163,2.75582184841467,-17.145)) ;
#169785 = CARTESIAN_POINT('Ctrl Pts',(1.30626047349817,2.77861339289531,-17.1074293544065)) ;
#169786 = CARTESIAN_POINT('Ctrl Pts',(1.33417968188929,2.75637252911127,-17.1673970793052)) ;
#169787 = CARTESIAN_POINT('Ctrl Pts',(1.33261582998957,2.75058962148775,-17.145)) ;
#169788 = CARTESIAN_POINT('Ctrl Pts',(1.33417968188929,2.75637252911127,-17.1226029206948)) ;
#169789 = CARTESIAN_POINT('Ctrl Pts',(1.35520432073833,2.75,-17.1560818608402)) ;
#169790 = CARTESIAN_POINT('Ctrl Pts',(1.35468704305007,2.75,-17.145)) ;
#169791 = CARTESIAN_POINT('Ctrl Pts',(1.35520432073832,2.75,-17.1339181391597)) ;
#169792 = CARTESIAN_POINT('Ctrl Pts',(1.37603597336697,2.75,-17.145)) ;
#169793 = CARTESIAN_POINT('Ctrl Pts',(1.37603597336697,2.75,-17.145)) ;
#169794 = CARTESIAN_POINT('Ctrl Pts',(1.37603597336697,2.75,-17.145)) ;
#169795 = CARTESIAN_POINT('Origin',(-6.11095769946375E-16,4.45,-19.05)) ;
#169796 = CARTESIAN_POINT('Ctrl Pts',(1.27790541830539,2.85,-13.3881204689932)) ;
#169797 = CARTESIAN_POINT('Ctrl Pts',(1.20082240333945,2.85,-13.3349999999987)) ;
#169798 = CARTESIAN_POINT('Ctrl Pts',(1.27790541830662,2.85,-13.281879531006)) ;
#169799 = CARTESIAN_POINT('Ctrl Pts',(1.27790638186088,2.84083632349961,-13.388121140961)) ;
#169800 = CARTESIAN_POINT('Ctrl Pts',(1.20084678242006,2.82796155786833,-13.3349999999987)) ;
#169801 = CARTESIAN_POINT('Ctrl Pts',(1.27790638186211,2.84083632349981,-13.2818788590381)) ;
#169802 = CARTESIAN_POINT('Ctrl Pts',(1.27916908278578,2.83184203564898,-13.3874245856048)) ;
#169803 = CARTESIAN_POINT('Ctrl Pts',(1.20941464972031,2.80875345001336,-13.3349999999987)) ;
#169804 = CARTESIAN_POINT('Ctrl Pts',(1.27916908278694,2.83184203564935,-13.2825754143944)) ;
#169805 = CARTESIAN_POINT('Ctrl Pts',(1.28359729368214,2.81532455354009,-13.3849858093437)) ;
#169806 = CARTESIAN_POINT('Ctrl Pts',(1.23205483118158,2.7814969248871,-13.3349999999989)) ;
#169807 = CARTESIAN_POINT('Ctrl Pts',(1.28359729368306,2.81532455354069,-13.2850141906554)) ;
#169808 = CARTESIAN_POINT('Ctrl Pts',(1.28669991111174,2.80791239452513,-13.3832816433155)) ;
#169809 = CARTESIAN_POINT('Ctrl Pts',(1.24464080060867,2.77344688912904,-13.334999999999)) ;
#169810 = CARTESIAN_POINT('Ctrl Pts',(1.28669991111253,2.80791239452578,-13.2867183566837)) ;
#169811 = CARTESIAN_POINT('Ctrl Pts',(1.29736892768555,2.78833251591408,-13.3774284096734)) ;
#169812 = CARTESIAN_POINT('Ctrl Pts',(1.27602012126334,2.75841927526783,-13.3349999999992)) ;
#169813 = CARTESIAN_POINT('Ctrl Pts',(1.297368927686,2.78833251591472,-13.2925715903257)) ;
#169814 = CARTESIAN_POINT('Ctrl Pts',(1.30626047349801,2.77861339289504,-13.372570645593)) ;
#169815 = CARTESIAN_POINT('Ctrl Pts',(1.29330467011163,2.75582184841469,-13.3349999999994)) ;
#169816 = CARTESIAN_POINT('Ctrl Pts',(1.30626047349831,2.77861339289556,-13.2974293544061)) ;
#169817 = CARTESIAN_POINT('Ctrl Pts',(1.33417968188927,2.75637252911119,-13.3573970793049)) ;
#169818 = CARTESIAN_POINT('Ctrl Pts',(1.33261582998957,2.75058962148775,-13.3349999999997)) ;
#169819 = CARTESIAN_POINT('Ctrl Pts',(1.33417968188932,2.75637252911135,-13.3126029206945)) ;
#169820 = CARTESIAN_POINT('Ctrl Pts',(1.35520432073863,2.75,-13.3460818608407)) ;
#169821 = CARTESIAN_POINT('Ctrl Pts',(1.35468704305008,2.75,-13.3350000000009)) ;
#169822 = CARTESIAN_POINT('Ctrl Pts',(1.35520432073804,2.75,-13.3239181391602)) ;
#169823 = CARTESIAN_POINT('Ctrl Pts',(1.37603597336697,2.75,-13.335)) ;
#169824 = CARTESIAN_POINT('Ctrl Pts',(1.37603597336697,2.75,-13.335)) ;
#169825 = CARTESIAN_POINT('Ctrl Pts',(1.37603597336697,2.75,-13.335)) ;
#169826 = CARTESIAN_POINT('Origin',(-6.11095769946375E-16,4.45,-15.24)) ;
#169827 = CARTESIAN_POINT('Ctrl Pts',(1.27790541830668,2.85,-9.57812046899406)) ;
#169828 = CARTESIAN_POINT('Ctrl Pts',(1.20082240333937,2.85,-9.52500000000137)) ;
#169829 = CARTESIAN_POINT('Ctrl Pts',(1.27790541830539,2.85,-9.47187953100683)) ;
#169830 = CARTESIAN_POINT('Ctrl Pts',(1.27790638186216,2.84083632349982,-9.57812114096188)) ;
#169831 = CARTESIAN_POINT('Ctrl Pts',(1.20084678241997,2.82796155786831,-9.52500000000138)) ;
#169832 = CARTESIAN_POINT('Ctrl Pts',(1.27790638186088,2.8408363234996,-9.47187885903899)) ;
#169833 = CARTESIAN_POINT('Ctrl Pts',(1.27916908278698,2.83184203564936,-9.57742458560567)) ;
#169834 = CARTESIAN_POINT('Ctrl Pts',(1.20941464972025,2.80875345001332,-9.52500000000131)) ;
#169835 = CARTESIAN_POINT('Ctrl Pts',(1.27916908278579,2.83184203564897,-9.47257541439522)) ;
#169836 = CARTESIAN_POINT('Ctrl Pts',(1.2835972936831,2.81532455354072,-9.57498580934463)) ;
#169837 = CARTESIAN_POINT('Ctrl Pts',(1.23205483118154,2.78149692488707,-9.52500000000116)) ;
#169838 = CARTESIAN_POINT('Ctrl Pts',(1.28359729368215,2.81532455354009,-9.4750141906563)) ;
#169839 = CARTESIAN_POINT('Ctrl Pts',(1.28669991111256,2.8079123945258,-9.5732816433164)) ;
#169840 = CARTESIAN_POINT('Ctrl Pts',(1.24464080060864,2.77344688912901,-9.52500000000106)) ;
#169841 = CARTESIAN_POINT('Ctrl Pts',(1.28669991111174,2.80791239452513,-9.47671835668456)) ;
#169842 = CARTESIAN_POINT('Ctrl Pts',(1.29736892768603,2.78833251591475,-9.56742840967436)) ;
#169843 = CARTESIAN_POINT('Ctrl Pts',(1.27602012126331,2.7584192752678,-9.52500000000082)) ;
#169844 = CARTESIAN_POINT('Ctrl Pts',(1.29736892768555,2.78833251591409,-9.48257159032659)) ;
#169845 = CARTESIAN_POINT('Ctrl Pts',(1.30626047349833,2.77861339289558,-9.56257064559391)) ;
#169846 = CARTESIAN_POINT('Ctrl Pts',(1.29330467011162,2.75582184841468,-9.52500000000068)) ;
#169847 = CARTESIAN_POINT('Ctrl Pts',(1.30626047349802,2.77861339289504,-9.48742935440699)) ;
#169848 = CARTESIAN_POINT('Ctrl Pts',(1.33417968188932,2.75637252911135,-9.54739707930555)) ;
#169849 = CARTESIAN_POINT('Ctrl Pts',(1.33261582998957,2.75058962148774,-9.52500000000034)) ;
#169850 = CARTESIAN_POINT('Ctrl Pts',(1.33417968188927,2.75637252911119,-9.50260292069508)) ;
#169851 = CARTESIAN_POINT('Ctrl Pts',(1.35520432073802,2.75,-9.53608186083978)) ;
#169852 = CARTESIAN_POINT('Ctrl Pts',(1.35468704305008,2.75,-9.52499999999888)) ;
#169853 = CARTESIAN_POINT('Ctrl Pts',(1.35520432073864,2.75,-9.51391813915931)) ;
#169854 = CARTESIAN_POINT('Ctrl Pts',(1.37603597336697,2.75,-9.525)) ;
#169855 = CARTESIAN_POINT('Ctrl Pts',(1.37603597336697,2.75,-9.525)) ;
#169856 = CARTESIAN_POINT('Ctrl Pts',(1.37603597336697,2.75,-9.525)) ;
#169857 = CARTESIAN_POINT('Origin',(-6.11095769946375E-16,4.45,-11.43)) ;
#169858 = CARTESIAN_POINT('Ctrl Pts',(1.27790541830604,2.85,-5.76812046899362)) ;
#169859 = CARTESIAN_POINT('Ctrl Pts',(1.2008224033394,2.85,-5.71500000000003)) ;
#169860 = CARTESIAN_POINT('Ctrl Pts',(1.27790541830601,2.85,-5.6618795310064)) ;
#169861 = CARTESIAN_POINT('Ctrl Pts',(1.27790638186153,2.84083632349971,-5.76812114096144)) ;
#169862 = CARTESIAN_POINT('Ctrl Pts',(1.20084678242,2.82796155786832,-5.71500000000003)) ;
#169863 = CARTESIAN_POINT('Ctrl Pts',(1.27790638186149,2.84083632349971,-5.66187885903858)) ;
#169864 = CARTESIAN_POINT('Ctrl Pts',(1.2791690827864,2.83184203564917,-5.76742458560523)) ;
#169865 = CARTESIAN_POINT('Ctrl Pts',(1.20941464972028,2.80875345001333,-5.71500000000003)) ;
#169866 = CARTESIAN_POINT('Ctrl Pts',(1.27916908278636,2.83184203564915,-5.66257541439479)) ;
#169867 = CARTESIAN_POINT('Ctrl Pts',(1.28359729368263,2.81532455354041,-5.76498580934417)) ;
#169868 = CARTESIAN_POINT('Ctrl Pts',(1.23205483118156,2.78149692488708,-5.71500000000002)) ;
#169869 = CARTESIAN_POINT('Ctrl Pts',(1.28359729368261,2.81532455354039,-5.66501419065585)) ;
#169870 = CARTESIAN_POINT('Ctrl Pts',(1.28669991111216,2.80791239452547,-5.76328164331592)) ;
#169871 = CARTESIAN_POINT('Ctrl Pts',(1.24464080060865,2.77344688912903,-5.71500000000002)) ;
#169872 = CARTESIAN_POINT('Ctrl Pts',(1.28669991111214,2.80791239452545,-5.66671835668411)) ;
#169873 = CARTESIAN_POINT('Ctrl Pts',(1.29736892768579,2.78833251591442,-5.7574284096739)) ;
#169874 = CARTESIAN_POINT('Ctrl Pts',(1.27602012126332,2.75841927526781,-5.71500000000003)) ;
#169875 = CARTESIAN_POINT('Ctrl Pts',(1.29736892768578,2.7883325159144,-5.67257159032613)) ;
#169876 = CARTESIAN_POINT('Ctrl Pts',(1.30626047349817,2.77861339289532,-5.75257064559348)) ;
#169877 = CARTESIAN_POINT('Ctrl Pts',(1.29330467011163,2.75582184841469,-5.71500000000003)) ;
#169878 = CARTESIAN_POINT('Ctrl Pts',(1.30626047349816,2.77861339289529,-5.67742935440656)) ;
#169879 = CARTESIAN_POINT('Ctrl Pts',(1.3341796818893,2.75637252911126,-5.73739707930523)) ;
#169880 = CARTESIAN_POINT('Ctrl Pts',(1.33261582998957,2.75058962148774,-5.71499999999999)) ;
#169881 = CARTESIAN_POINT('Ctrl Pts',(1.33417968188929,2.75637252911128,-5.69260292069477)) ;
#169882 = CARTESIAN_POINT('Ctrl Pts',(1.35520432073832,2.75,-5.72608186084025)) ;
#169883 = CARTESIAN_POINT('Ctrl Pts',(1.35468704305008,2.75,-5.715)) ;
#169884 = CARTESIAN_POINT('Ctrl Pts',(1.35520432073834,2.75,-5.70391813915977)) ;
#169885 = CARTESIAN_POINT('Ctrl Pts',(1.37603597336697,2.75,-5.715)) ;
#169886 = CARTESIAN_POINT('Ctrl Pts',(1.37603597336697,2.75,-5.715)) ;
#169887 = CARTESIAN_POINT('Ctrl Pts',(1.37603597336697,2.75,-5.715)) ;
#169888 = CARTESIAN_POINT('Origin',(2.5,-6.45,2.2)) ;
#169889 = CARTESIAN_POINT('Origin',(2.5,-6.45,2.2)) ;
#169890 = CARTESIAN_POINT('Origin',(-6.11095769946375E-16,4.45,-7.62)) ;
#169891 = CARTESIAN_POINT('Origin',(2.5,1.95351742790181E-16,2.2)) ;
#169892 = CARTESIAN_POINT('Origin',(2.5,1.9,2.2)) ;
#169893 = CARTESIAN_POINT('Ctrl Pts',(1.27790541830603,2.85,-1.95812046899361)) ;
#169894 = CARTESIAN_POINT('Ctrl Pts',(1.20082240333946,2.85,-1.90500000000004)) ;
#169895 = CARTESIAN_POINT('Ctrl Pts',(1.27790541830599,2.85,-1.85187953100641)) ;
#169896 = CARTESIAN_POINT('Ctrl Pts',(1.27790638186151,2.84083632349971,-1.95812114096143)) ;
#169897 = CARTESIAN_POINT('Ctrl Pts',(1.20084678242005,2.82796155786833,-1.90500000000004)) ;
#169898 = CARTESIAN_POINT('Ctrl Pts',(1.27790638186147,2.8408363234997,-1.85187885903859)) ;
#169899 = CARTESIAN_POINT('Ctrl Pts',(1.27916908278637,2.83184203564916,-1.95742458560522)) ;
#169900 = CARTESIAN_POINT('Ctrl Pts',(1.20941464972033,2.80875345001335,-1.90500000000003)) ;
#169901 = CARTESIAN_POINT('Ctrl Pts',(1.27916908278634,2.83184203564916,-1.8525754143948)) ;
#169902 = CARTESIAN_POINT('Ctrl Pts',(1.28359729368262,2.8153245535404,-1.95498580934416)) ;
#169903 = CARTESIAN_POINT('Ctrl Pts',(1.23205483118159,2.78149692488712,-1.90500000000003)) ;
#169904 = CARTESIAN_POINT('Ctrl Pts',(1.2835972936826,2.81532455354038,-1.85501419065586)) ;
#169905 = CARTESIAN_POINT('Ctrl Pts',(1.28669991111215,2.80791239452546,-1.95328164331591)) ;
#169906 = CARTESIAN_POINT('Ctrl Pts',(1.24464080060867,2.77344688912904,-1.90500000000002)) ;
#169907 = CARTESIAN_POINT('Ctrl Pts',(1.28669991111213,2.80791239452544,-1.85671835668411)) ;
#169908 = CARTESIAN_POINT('Ctrl Pts',(1.29736892768578,2.78833251591441,-1.94742840967388)) ;
#169909 = CARTESIAN_POINT('Ctrl Pts',(1.27602012126333,2.75841927526783,-1.90500000000002)) ;
#169910 = CARTESIAN_POINT('Ctrl Pts',(1.29736892768578,2.78833251591439,-1.86257159032615)) ;
#169911 = CARTESIAN_POINT('Ctrl Pts',(1.30626047349816,2.7786133928953,-1.94257064559346)) ;
#169912 = CARTESIAN_POINT('Ctrl Pts',(1.29330467011164,2.7558218484147,-1.90500000000002)) ;
#169913 = CARTESIAN_POINT('Ctrl Pts',(1.30626047349816,2.77861339289529,-1.86742935440657)) ;
#169914 = CARTESIAN_POINT('Ctrl Pts',(1.3341796818893,2.75637252911127,-1.92739707930523)) ;
#169915 = CARTESIAN_POINT('Ctrl Pts',(1.33261582998958,2.75058962148774,-1.90500000000001)) ;
#169916 = CARTESIAN_POINT('Ctrl Pts',(1.3341796818893,2.75637252911127,-1.88260292069479)) ;
#169917 = CARTESIAN_POINT('Ctrl Pts',(1.35520432073833,2.75,-1.91608186084024)) ;
#169918 = CARTESIAN_POINT('Ctrl Pts',(1.35468704305007,2.75,-1.90499999999995)) ;
#169919 = CARTESIAN_POINT('Ctrl Pts',(1.35520432073834,2.75,-1.89391813915974)) ;
#169920 = CARTESIAN_POINT('Ctrl Pts',(1.37603597336697,2.75,-1.905)) ;
#169921 = CARTESIAN_POINT('Ctrl Pts',(1.37603597336697,2.75,-1.905)) ;
#169922 = CARTESIAN_POINT('Ctrl Pts',(1.37603597336697,2.75,-1.905)) ;
#169923 = CARTESIAN_POINT('Origin',(2.7,1.9,2.2)) ;
#169924 = CARTESIAN_POINT('Origin',(2.7,2.1,2.2)) ;
#169925 = CARTESIAN_POINT('Origin',(-6.11095769946375E-16,4.45,-3.81)) ;
#169926 = CARTESIAN_POINT('Origin',(3.6,2.1,2.2)) ;
#169927 = CARTESIAN_POINT('Origin',(3.5,2.1,2.2)) ;
#169928 = CARTESIAN_POINT('Ctrl Pts',(1.72549266760237,2.85,1.44401362298495)) ;
#169929 = CARTESIAN_POINT('Ctrl Pts',(1.63635891322671,2.84999999999999,1.55021272547567)) ;
#169930 = CARTESIAN_POINT('Ctrl Pts',(1.77500605619934,2.85,1.54999992401279)) ;
#169931 = CARTESIAN_POINT('Ctrl Pts',(1.72549428095344,2.83840024801823,1.44401164264682)) ;
#169932 = CARTESIAN_POINT('Ctrl Pts',(1.63647013043005,2.80015695736268,1.55016100506938)) ;
#169933 = CARTESIAN_POINT('Ctrl Pts',(1.77500868550276,2.83840278621153,1.54999996101813)) ;
#169934 = CARTESIAN_POINT('Ctrl Pts',(1.72805074460438,2.82767088409066,1.44417220186092)) ;
#169935 = CARTESIAN_POINT('Ctrl Pts',(1.66486766052525,2.77372556429602,1.53694944305648)) ;
#169936 = CARTESIAN_POINT('Ctrl Pts',(1.7765703971759,2.82767482693174,1.54793777023085)) ;
#169937 = CARTESIAN_POINT('Ctrl Pts',(1.73543475859394,2.80962789021929,1.44461916969382)) ;
#169938 = CARTESIAN_POINT('Ctrl Pts',(1.70783084644936,2.75028582747794,1.5169449731166)) ;
#169939 = CARTESIAN_POINT('Ctrl Pts',(1.78107476297284,2.80963307739335,1.54198236387663)) ;
#169940 = CARTESIAN_POINT('Ctrl Pts',(1.74006831828865,2.80236621373356,1.44489045092167)) ;
#169941 = CARTESIAN_POINT('Ctrl Pts',(1.72405853320849,2.74863106820581,1.50938157302589)) ;
#169942 = CARTESIAN_POINT('Ctrl Pts',(1.78390089653206,2.80237132662259,1.53824738439477)) ;
#169943 = CARTESIAN_POINT('Ctrl Pts',(1.75509546017965,2.7834430043054,1.44575023678366)) ;
#169944 = CARTESIAN_POINT('Ctrl Pts',(1.75831280076438,2.74629798483364,1.493385578669)) ;
#169945 = CARTESIAN_POINT('Ctrl Pts',(1.79303629065941,2.78344729439355,1.52612638181377)) ;
#169946 = CARTESIAN_POINT('Ctrl Pts',(1.76623743827936,2.77501027199624,1.44635109519364)) ;
#169947 = CARTESIAN_POINT('Ctrl Pts',(1.77349470226536,2.74800583767983,1.48625751636957)) ;
#169948 = CARTESIAN_POINT('Ctrl Pts',(1.79978266704186,2.77501368038732,1.5171373950458)) ;
#169949 = CARTESIAN_POINT('Ctrl Pts',(1.80086149668306,2.75520245925894,1.44809160673599)) ;
#169950 = CARTESIAN_POINT('Ctrl Pts',(1.80915794598981,2.74970810565007,1.46940296260367)) ;
#169951 = CARTESIAN_POINT('Ctrl Pts',(1.82062186326967,2.75520328537396,1.48918396557833)) ;
#169952 = CARTESIAN_POINT('Ctrl Pts',(1.82479501616833,2.75,1.4491256009755)) ;
#169953 = CARTESIAN_POINT('Ctrl Pts',(1.82921797033105,2.75,1.45978299211575)) ;
#169954 = CARTESIAN_POINT('Ctrl Pts',(1.83487512614628,2.75,1.46984177015833)) ;
#169955 = CARTESIAN_POINT('Ctrl Pts',(1.84932420089069,2.75,1.45)) ;
#169956 = CARTESIAN_POINT('Ctrl Pts',(1.84932420089069,2.75,1.45)) ;
#169957 = CARTESIAN_POINT('Ctrl Pts',(1.84932420089069,2.75,1.45)) ;
#169958 = CARTESIAN_POINT('Ctrl Pts',(1.84932420089069,2.75,1.45)) ;
#169959 = CARTESIAN_POINT('Ctrl Pts',(1.84891552970751,2.75,1.45056025286656)) ;
#169960 = CARTESIAN_POINT('Ctrl Pts',(1.84850693760102,2.7500041496442,1.45112058352057)) ;
#169961 = CARTESIAN_POINT('Ctrl Pts',(1.8477440226785,2.75001978546022,1.45216617333146)) ;
#169962 = CARTESIAN_POINT('Ctrl Pts',(1.84738978525535,2.75003021926051,1.45265154128796)) ;
#169963 = CARTESIAN_POINT('Ctrl Pts',(1.84658906145061,2.75006109115841,1.45374842884002)) ;
#169964 = CARTESIAN_POINT('Ctrl Pts',(1.84614254888567,2.75008342791781,1.45435992049693)) ;
#169965 = CARTESIAN_POINT('Ctrl Pts',(1.84498586912392,2.75015481705042,1.45594357799571)) ;
#169966 = CARTESIAN_POINT('Ctrl Pts',(1.84427568281905,2.7502118647287,1.45691553753491)) ;
#169967 = CARTESIAN_POINT('Ctrl Pts',(1.84242877605322,2.75039562881963,1.45944232749581)) ;
#169968 = CARTESIAN_POINT('Ctrl Pts',(1.84129221873239,2.75054367055756,1.46099641261588)) ;
#169969 = CARTESIAN_POINT('Ctrl Pts',(1.83830538692981,2.7510287315475,1.46507822321451)) ;
#169970 = CARTESIAN_POINT('Ctrl Pts',(1.83645654188491,2.75142684998139,1.46760271004466)) ;
#169971 = CARTESIAN_POINT('Ctrl Pts',(1.83146008674453,2.7527802666469,1.47441251564823)) ;
#169972 = CARTESIAN_POINT('Ctrl Pts',(1.82831592143432,2.75393867345932,1.47868769799754)) ;
#169973 = CARTESIAN_POINT('Ctrl Pts',(1.82163255789315,2.75710780333614,1.48774537759201)) ;
#169974 = CARTESIAN_POINT('Ctrl Pts',(1.81811360864768,2.75921511008005,1.49248494851376)) ;
#169975 = CARTESIAN_POINT('Ctrl Pts',(1.81342675445606,2.76262639240882,1.49877444161403)) ;
#169976 = CARTESIAN_POINT('Ctrl Pts',(1.81216355879702,2.76360925979239,1.50046740248774)) ;
#169977 = CARTESIAN_POINT('Ctrl Pts',(1.80949588405725,2.76581971270697,1.50404126728569)) ;
#169978 = CARTESIAN_POINT('Ctrl Pts',(1.80809008635459,2.76706812937679,1.50592406340246)) ;
#169979 = CARTESIAN_POINT('Ctrl Pts',(1.80622180825451,2.76884047116021,1.50842731630949)) ;
#169980 = CARTESIAN_POINT('Ctrl Pts',(1.80574460306458,2.76930303796854,1.50906678499061)) ;
#169981 = CARTESIAN_POINT('Ctrl Pts',(1.80200723031206,2.77301004156286,1.51407608111113)) ;
#169982 = CARTESIAN_POINT('Ctrl Pts',(1.79893605115733,2.77655328826388,1.51818698195081)) ;
#169983 = CARTESIAN_POINT('Ctrl Pts',(1.7955384838363,2.78126766501987,1.52271952824054)) ;
#169984 = CARTESIAN_POINT('Ctrl Pts',(1.79508624825315,2.78191247649822,1.5233224871813)) ;
#169985 = CARTESIAN_POINT('Ctrl Pts',(1.79248502865803,2.7857262011001,1.52678835781394)) ;
#169986 = CARTESIAN_POINT('Ctrl Pts',(1.79047061583915,2.78908292652327,1.52944511497864)) ;
#169987 = CARTESIAN_POINT('Ctrl Pts',(1.78802866333285,2.79371407639472,1.53267023660098)) ;
#169988 = CARTESIAN_POINT('Ctrl Pts',(1.78745102314773,2.79485730486032,1.53343360143046)) ;
#169989 = CARTESIAN_POINT('Ctrl Pts',(1.78677268033907,2.79625836238383,1.53433221128893)) ;
#169990 = CARTESIAN_POINT('Ctrl Pts',(1.7866544506805,2.79650484960406,1.53448890728973)) ;
#169991 = CARTESIAN_POINT('Ctrl Pts',(1.78451055395599,2.80101773866206,1.53733197916208)) ;
#169992 = CARTESIAN_POINT('Ctrl Pts',(1.78263897914004,2.80562493737595,1.53980972755757)) ;
#169993 = CARTESIAN_POINT('Ctrl Pts',(1.78021555250215,2.81316013711825,1.54301083723955)) ;
#169994 = CARTESIAN_POINT('Ctrl Pts',(1.77953359820562,2.81552321764108,1.54390423992715)) ;
#169995 = CARTESIAN_POINT('Ctrl Pts',(1.77885922502006,2.81814935429725,1.54479242835053)) ;
#169996 = CARTESIAN_POINT('Ctrl Pts',(1.77880145892999,2.81837682960042,1.54486850248715)) ;
#169997 = CARTESIAN_POINT('Ctrl Pts',(1.77779807199376,2.82237259934244,1.54618978651394)) ;
#169998 = CARTESIAN_POINT('Ctrl Pts',(1.77701280317407,2.82627116869071,1.54722115651107)) ;
#169999 = CARTESIAN_POINT('Ctrl Pts',(1.77629130352184,2.83098366045584,1.54816931204003)) ;
#170000 = CARTESIAN_POINT('Ctrl Pts',(1.77618324871501,2.83173306513696,1.54831133394653)) ;
#170001 = CARTESIAN_POINT('Ctrl Pts',(1.77598237323325,2.83321827741197,1.54857545305202)) ;
#170002 = CARTESIAN_POINT('Ctrl Pts',(1.77588933458805,2.83395373307728,1.54869790393466)) ;
#170003 = CARTESIAN_POINT('Ctrl Pts',(1.77526822780851,2.83923120109988,1.549516785743)) ;
#170004 = CARTESIAN_POINT('Ctrl Pts',(1.77496841680885,2.84387001846854,1.54991776085168)) ;
#170005 = CARTESIAN_POINT('Ctrl Pts',(1.77490988945622,2.8490007566663,1.54999617542323)) ;
#170006 = CARTESIAN_POINT('Ctrl Pts',(1.77490703981927,2.84950046564136,1.55)) ;
#170007 = CARTESIAN_POINT('Ctrl Pts',(1.77490703981927,2.85,1.55)) ;
#170008 = CARTESIAN_POINT('Origin',(3.5,2.1,2.2)) ;
#170009 = CARTESIAN_POINT('Origin',(3.5,2.1,2.2)) ;
#170010 = CARTESIAN_POINT('Origin',(-6.11095769946375E-16,4.45,0.)) ;
#170011 = CARTESIAN_POINT('Origin',(3.6,2.85,1.45)) ;
#170012 = CARTESIAN_POINT('Origin',(2.5,2.85,1.45)) ;
#170013 = CARTESIAN_POINT('Origin',(3.5,7.81406971160724E-17,2.2)) ;
#170014 = CARTESIAN_POINT('Origin',(3.5,2.65,2.2)) ;
#170015 = CARTESIAN_POINT('Origin',(2.5,2.85,1.65)) ;
#170016 = CARTESIAN_POINT('Origin',(2.5,2.85,1.65)) ;
#170017 = CARTESIAN_POINT('Origin',(2.7,2.85,1.65)) ;
#170018 = CARTESIAN_POINT('Origin',(3.5,2.65,2.2)) ;
#170019 = CARTESIAN_POINT('Origin',(3.5,2.65,2.2)) ;
#170020 = CARTESIAN_POINT('Origin',(2.6,4.45,1.65)) ;
#170021 = CARTESIAN_POINT('Origin',(2.5,4.45,1.65)) ;
#170022 = CARTESIAN_POINT('Origin',(2.5,4.55,1.65)) ;
#170023 = CARTESIAN_POINT('Origin',(2.5,4.45,1.65)) ;
#170024 = CARTESIAN_POINT('Origin',(2.7,2.85,-2.3)) ;
#170025 = CARTESIAN_POINT('Origin',(2.7,2.85,2.2)) ;
#170026 = CARTESIAN_POINT('Origin',(-2.07072847357592E-16,2.65,2.2)) ;
#170027 = CARTESIAN_POINT('Origin',(2.7,2.65,2.2)) ;
#170028 = CARTESIAN_POINT('Origin',(2.5,4.45,1.65)) ;
#170029 = CARTESIAN_POINT('Origin',(2.5,4.45,1.65)) ;
#170030 = CARTESIAN_POINT('Origin',(2.7,2.85,2.2)) ;
#170031 = CARTESIAN_POINT('Origin',(2.5,2.85,2.2)) ;
#170032 = CARTESIAN_POINT('Origin',(2.5,4.45,-36.59)) ;
#170033 = CARTESIAN_POINT('Origin',(2.5,4.45,2.2)) ;
#170034 = CARTESIAN_POINT('Origin',(2.5,1.95351742790181E-16,2.2)) ;
#170035 = CARTESIAN_POINT('Origin',(2.5,4.45,2.2)) ;
#170036 = CARTESIAN_POINT('Origin',(2.5,4.45,2.2)) ;
#170037 = CARTESIAN_POINT('Origin',(2.5,4.45,2.2)) ;
#170038 = CARTESIAN_POINT('Origin',(-5.84812080916424E-16,4.45,2.2)) ;
#170039 = CARTESIAN_POINT('Origin',(-3.9,4.45,2.2)) ;
#170040 = CARTESIAN_POINT('Origin',(-3.9,4.45,2.2)) ;
#170041 = CARTESIAN_POINT('Ctrl Pts',(-3.90000000000414,3.80333655664123,
2.22561598559544)) ;
#170042 = CARTESIAN_POINT('Ctrl Pts',(-3.76707268212211,3.78931743308928,
2.17271399006788)) ;
#170043 = CARTESIAN_POINT('Ctrl Pts',(-3.81330307515288,3.66391136972353,
2.22563750872074)) ;
#170044 = CARTESIAN_POINT('Ctrl Pts',(-3.89100560487485,3.80613461936468,
2.23617464150095)) ;
#170045 = CARTESIAN_POINT('Ctrl Pts',(-3.77789360990371,3.78258994157146,
2.17083996288935)) ;
#170046 = CARTESIAN_POINT('Ctrl Pts',(-3.80681245874446,3.67074660187605,
2.23620282118099)) ;
#170047 = CARTESIAN_POINT('Ctrl Pts',(-3.87638074624213,3.81068426137503,
2.24628380179591)) ;
#170048 = CARTESIAN_POINT('Ctrl Pts',(-3.78564407609263,3.77777446969616,
2.18265796775152)) ;
#170049 = CARTESIAN_POINT('Ctrl Pts',(-3.79626152405898,3.68185957735116,
2.24631352465829)) ;
#170050 = CARTESIAN_POINT('Ctrl Pts',(-3.83745765067443,3.82279283247717,
2.26448677971421)) ;
#170051 = CARTESIAN_POINT('Ctrl Pts',(-3.77926302941741,3.78175688793386,
2.2150310810483)) ;
#170052 = CARTESIAN_POINT('Ctrl Pts',(-3.768189957662,3.71143369374476,2.2645135067643)) ;
#170053 = CARTESIAN_POINT('Ctrl Pts',(-3.81315995987735,3.83035159193202,
2.27258505978673)) ;
#170054 = CARTESIAN_POINT('Ctrl Pts',(-3.76758783470957,3.78902661367653,
2.23385461685646)) ;
#170055 = CARTESIAN_POINT('Ctrl Pts',(-3.75066936002647,3.72989489134432,
2.27260743591321)) ;
#170056 = CARTESIAN_POINT('Ctrl Pts',(-3.72961659401614,3.8563410660704,2.29258436202037)) ;
#170057 = CARTESIAN_POINT('Ctrl Pts',(-3.71415009152798,3.82228860055657,
2.27828021342228)) ;
#170058 = CARTESIAN_POINT('Ctrl Pts',(-3.69043468851351,3.79337198420934,
2.29259398868402)) ;
#170059 = CARTESIAN_POINT('Ctrl Pts',(-3.65964870102201,3.87810735148093,
2.3)) ;
#170060 = CARTESIAN_POINT('Ctrl Pts',(-3.6494577226055,3.86254752980597,2.3)) ;
#170061 = CARTESIAN_POINT('Ctrl Pts',(-3.64000230097343,3.84653001401765,
2.3)) ;
#170062 = CARTESIAN_POINT('Ctrl Pts',(-3.58927461283679,3.9,2.3)) ;
#170063 = CARTESIAN_POINT('Ctrl Pts',(-3.58927461283679,3.9,2.3)) ;
#170064 = CARTESIAN_POINT('Ctrl Pts',(-3.58927461283679,3.9,2.3)) ;
#170065 = CARTESIAN_POINT('Origin',(-3.90000000000414,3.70667311328246,2.25123197119087)) ;
#170066 = CARTESIAN_POINT('Ctrl Pts',(-3.81328428501083,3.66396238798774,
2.22561598559596)) ;
#170067 = CARTESIAN_POINT('Ctrl Pts',(-3.7671555501966,3.78932617273336,2.17274696964475)) ;
#170068 = CARTESIAN_POINT('Ctrl Pts',(-3.90000000000184,3.80333655664137,
2.22561598559596)) ;
#170069 = CARTESIAN_POINT('Ctrl Pts',(-3.81816564857387,3.65881896296046,
2.21766737408028)) ;
#170070 = CARTESIAN_POINT('Ctrl Pts',(-3.75960462691777,3.79067973806019,
2.17785299283591)) ;
#170071 = CARTESIAN_POINT('Ctrl Pts',(-3.90338239924599,3.80123212475718,
2.21767478686741)) ;
#170072 = CARTESIAN_POINT('Ctrl Pts',(-3.82087839357381,3.65609538274431,
2.20891956015985)) ;
#170073 = CARTESIAN_POINT('Ctrl Pts',(-3.75388413987046,3.79211390479363,
2.1881053469697)) ;
#170074 = CARTESIAN_POINT('Ctrl Pts',(-3.90529366494794,3.80014021273157,
2.20891399277153)) ;
#170075 = CARTESIAN_POINT('Ctrl Pts',(-3.8208783653849,3.65609543997632,2.1999999999998)) ;
#170076 = CARTESIAN_POINT('Ctrl Pts',(-3.75388420072551,3.79211389549688,
2.20000000000026)) ;
#170077 = CARTESIAN_POINT('Ctrl Pts',(-3.9052936343757,3.80014021111094,2.1999999999998)) ;
#170078 = CARTESIAN_POINT('Ctrl Pts',(-3.8133030794565,3.6639113580445,-36.5156375136556)) ;
#170079 = CARTESIAN_POINT('Ctrl Pts',(-3.76704381845056,3.78939567609376,
-36.4626809617641)) ;
#170080 = CARTESIAN_POINT('Ctrl Pts',(-3.90005407034603,3.80334224262328,
-36.5156375087256)) ;
#170081 = CARTESIAN_POINT('Ctrl Pts',(-3.80681246159642,3.67074659083504,
-36.5262028276402)) ;
#170082 = CARTESIAN_POINT('Ctrl Pts',(-3.77787657524,3.78265576081669,-36.4608014865139)) ;
#170083 = CARTESIAN_POINT('Ctrl Pts',(-3.89105438082976,3.80614475731173,
-36.5262028211853)) ;
#170084 = CARTESIAN_POINT('Ctrl Pts',(-3.79626152519014,3.68185956709673,
-36.5363135314706)) ;
#170085 = CARTESIAN_POINT('Ctrl Pts',(-3.78563829581487,3.77782658090845,
-36.4726233726224)) ;
#170086 = CARTESIAN_POINT('Ctrl Pts',(-3.8764231237804,3.81069961887151,-36.5363135246619)) ;
#170087 = CARTESIAN_POINT('Ctrl Pts',(-3.76818995628674,3.71143368504836,
-36.5545135128898)) ;
#170088 = CARTESIAN_POINT('Ctrl Pts',(-3.77926822356639,3.78178991045914,
-36.5050078365579)) ;
#170089 = CARTESIAN_POINT('Ctrl Pts',(-3.83748909165157,3.82281499516366,
-36.554513506767)) ;
#170090 = CARTESIAN_POINT('Ctrl Pts',(-3.75066935778344,3.7298948835274,-36.5626074410416)) ;
#170091 = CARTESIAN_POINT('Ctrl Pts',(-3.76759526236367,3.78905258594164,
-36.5238375889442)) ;
#170092 = CARTESIAN_POINT('Ctrl Pts',(-3.81318628078068,3.83037545428224,
-36.5626074359153)) ;
#170093 = CARTESIAN_POINT('Ctrl Pts',(-3.69043468485542,3.79337197975756,
-36.5825939908902)) ;
#170094 = CARTESIAN_POINT('Ctrl Pts',(-3.71415903313997,3.82229950192055,
-36.5682748145391)) ;
#170095 = CARTESIAN_POINT('Ctrl Pts',(-3.7296269979651,3.85636397532361,-36.5825939886845)) ;
#170096 = CARTESIAN_POINT('Ctrl Pts',(-3.64000229942656,3.8465300114026,-36.59)) ;
#170097 = CARTESIAN_POINT('Ctrl Pts',(-3.64946108437951,3.86255322480651,
-36.59)) ;
#170098 = CARTESIAN_POINT('Ctrl Pts',(-3.6596559708903,3.87811845108851,-36.59)) ;
#170099 = CARTESIAN_POINT('Ctrl Pts',(-3.58927461283679,3.9,-36.59)) ;
#170100 = CARTESIAN_POINT('Ctrl Pts',(-3.58927461283679,3.9,-36.59)) ;
#170101 = CARTESIAN_POINT('Ctrl Pts',(-3.58927461283679,3.9,-36.59)) ;
#170102 = CARTESIAN_POINT('Origin',(-3.90000000000003,3.70667311328501,-36.5412319712005)) ;
#170103 = CARTESIAN_POINT('Ctrl Pts',(-3.90000000000002,3.80333655664251,
-36.5156159856002)) ;
#170104 = CARTESIAN_POINT('Ctrl Pts',(-3.76714499853489,3.78932505990569,
-36.4627427703234)) ;
#170105 = CARTESIAN_POINT('Ctrl Pts',(-3.81328667680337,3.66395588859535,
-36.5156187266773)) ;
#170106 = CARTESIAN_POINT('Ctrl Pts',(-3.90338239924531,3.80123212475759,
-36.5076747868706)) ;
#170107 = CARTESIAN_POINT('Ctrl Pts',(-3.75959294286619,3.79067888052345,
-36.4678497567271)) ;
#170108 = CARTESIAN_POINT('Ctrl Pts',(-3.81816861634426,3.65881228117352,
-36.5076693916882)) ;
#170109 = CARTESIAN_POINT('Ctrl Pts',(-3.90529366494794,3.80014021273158,
-36.4989139927731)) ;
#170110 = CARTESIAN_POINT('Ctrl Pts',(-3.75387165938121,3.79211324319556,
-36.478103631738)) ;
#170111 = CARTESIAN_POINT('Ctrl Pts',(-3.82088174075948,3.65608858759825,
-36.498920600033)) ;
#170112 = CARTESIAN_POINT('Ctrl Pts',(-3.9052936343757,3.80014021111094,-36.4899999999998)) ;
#170113 = CARTESIAN_POINT('Ctrl Pts',(-3.75387172171403,3.79211323397611,
-36.4900000000003)) ;
#170114 = CARTESIAN_POINT('Ctrl Pts',(-3.82088171296044,3.65608864403298,
-36.4899999999998)) ;
#170115 = CARTESIAN_POINT('',(59.8300351322441,10.15,9.89)) ;
#170116 = CARTESIAN_POINT('',(47.5,9.35,4.75)) ;
#170117 = CARTESIAN_POINT('',(59.1,9.35,-29.54)) ;
#170118 = UNCERTAINTY_MEASURE_WITH_UNIT(LENGTH_MEASURE(0.01),#170128,
'DISTANCE_ACCURACY_VALUE',
'Maximum model space distance between geometric entities at asserted c
onnectivities') ;
#170119 = UNCERTAINTY_MEASURE_WITH_UNIT(LENGTH_MEASURE(0.01),#170128,
'DISTANCE_ACCURACY_VALUE',
'Maximum model space distance between geometric entities at asserted c
onnectivities') ;
#170120 = UNCERTAINTY_MEASURE_WITH_UNIT(LENGTH_MEASURE(0.01),#170128,
'DISTANCE_ACCURACY_VALUE',
'Maximum model space distance between geometric entities at asserted c
onnectivities') ;
#170121 = UNCERTAINTY_MEASURE_WITH_UNIT(LENGTH_MEASURE(0.01),#170128,
'DISTANCE_ACCURACY_VALUE',
'Maximum model space distance between geometric entities at asserted c
onnectivities') ;
#170122 = UNCERTAINTY_MEASURE_WITH_UNIT(LENGTH_MEASURE(0.01),#170128,
'DISTANCE_ACCURACY_VALUE',
'Maximum model space distance between geometric entities at asserted c
onnectivities') ;
#170123 = (
GEOMETRIC_REPRESENTATION_CONTEXT(3)
GLOBAL_UNCERTAINTY_ASSIGNED_CONTEXT((#170118))
GLOBAL_UNIT_ASSIGNED_CONTEXT((#170128,#170130,#170131))
REPRESENTATION_CONTEXT('','3D')
) ;
#170124 = (
GEOMETRIC_REPRESENTATION_CONTEXT(3)
GLOBAL_UNCERTAINTY_ASSIGNED_CONTEXT((#170119))
GLOBAL_UNIT_ASSIGNED_CONTEXT((#170128,#170130,#170131))
REPRESENTATION_CONTEXT('','3D')
) ;
#170125 = (
GEOMETRIC_REPRESENTATION_CONTEXT(3)
GLOBAL_UNCERTAINTY_ASSIGNED_CONTEXT((#170120))
GLOBAL_UNIT_ASSIGNED_CONTEXT((#170128,#170130,#170131))
REPRESENTATION_CONTEXT('','3D')
) ;
#170126 = (
GEOMETRIC_REPRESENTATION_CONTEXT(3)
GLOBAL_UNCERTAINTY_ASSIGNED_CONTEXT((#170121))
GLOBAL_UNIT_ASSIGNED_CONTEXT((#170128,#170130,#170131))
REPRESENTATION_CONTEXT('','3D')
) ;
#170127 = (
GEOMETRIC_REPRESENTATION_CONTEXT(3)
GLOBAL_UNCERTAINTY_ASSIGNED_CONTEXT((#170122))
GLOBAL_UNIT_ASSIGNED_CONTEXT((#170128,#170130,#170131))
REPRESENTATION_CONTEXT('','3D')
) ;
#170128 = (
LENGTH_UNIT()
NAMED_UNIT(*)
SI_UNIT(.MILLI.,.METRE.)
) ;
#170129 = (
LENGTH_UNIT()
NAMED_UNIT(*)
SI_UNIT($,.METRE.)
) ;
#170130 = (
NAMED_UNIT(*)
PLANE_ANGLE_UNIT()
SI_UNIT($,.RADIAN.)
) ;
#170131 = (
NAMED_UNIT(*)
SI_UNIT($,.STERADIAN.)
SOLID_ANGLE_UNIT()
) ;
#170132 = SHAPE_DEFINITION_REPRESENTATION(#170136,#170143) ;
#170133 = SHAPE_DEFINITION_REPRESENTATION(#170137,#170144) ;
#170134 = SHAPE_DEFINITION_REPRESENTATION(#170138,#170145) ;
#170135 = SHAPE_DEFINITION_REPRESENTATION(#170139,#170146) ;
#170136 = PRODUCT_DEFINITION_SHAPE('',$,#170148) ;
#170137 = PRODUCT_DEFINITION_SHAPE('',$,#170149) ;
#170138 = PRODUCT_DEFINITION_SHAPE('',$,#170150) ;
#170139 = PRODUCT_DEFINITION_SHAPE('',$,#170151) ;
#170140 = PRODUCT_DEFINITION_SHAPE($,$,#20) ;
#170141 = PRODUCT_DEFINITION_SHAPE($,$,#21) ;
#170142 = PRODUCT_DEFINITION_SHAPE($,$,#22) ;
#170143 = SHAPE_REPRESENTATION('',(#91122,#103077,#103078,#103079),#170123) ;
#170144 = SHAPE_REPRESENTATION('',(#91123),#170124) ;
#170145 = SHAPE_REPRESENTATION('',(#93348),#170125) ;
#170146 = SHAPE_REPRESENTATION('',(#98151),#170126) ;
#170147 = PRODUCT_DEFINITION_CONTEXT('part definition',#170161,'design') ;
#170148 = PRODUCT_DEFINITION('MAS-641',
'MAS-641',#170152,#170147) ;
#170149 = PRODUCT_DEFINITION('Pin_Header_Plug','Pin_Header_Plug',#170153,
#170147) ;
#170150 = PRODUCT_DEFINITION('Terminal_Block_Header',
'Terminal_Block_Header',#170154,#170147) ;
#170151 = PRODUCT_DEFINITION('Terminal_Block_Plug','Terminal_Block_Plug',
#170155,#170147) ;
#170152 = PRODUCT_DEFINITION_FORMATION('',$,#170163) ;
#170153 = PRODUCT_DEFINITION_FORMATION('',$,#170164) ;
#170154 = PRODUCT_DEFINITION_FORMATION('',$,#170165) ;
#170155 = PRODUCT_DEFINITION_FORMATION('',$,#170166) ;
#170156 = PRODUCT_RELATED_PRODUCT_CATEGORY(
'MAS-641',
'MAS-641',(#170163)) ;
#170157 = PRODUCT_RELATED_PRODUCT_CATEGORY('Pin_Header_Plug',
'Pin_Header_Plug',(#170164)) ;
#170158 = PRODUCT_RELATED_PRODUCT_CATEGORY('Terminal_Block_Header',
'Terminal_Block_Header',(#170165)) ;
#170159 = PRODUCT_RELATED_PRODUCT_CATEGORY('Terminal_Block_Plug',
'Terminal_Block_Plug',(#170166)) ;
#170160 = APPLICATION_PROTOCOL_DEFINITION('international standard',
'automotive_design',2009,#170161) ;
#170161 = APPLICATION_CONTEXT(
'Core Data for Automotive Mechanical Design Process') ;
#170162 = PRODUCT_CONTEXT('part definition',#170161,'mechanical') ;
#170163 = PRODUCT('MAS-641',
'MAS-641',$,(#170162)) ;
#170164 = PRODUCT('Pin_Header_Plug','Pin_Header_Plug',$,(#170162)) ;
#170165 = PRODUCT('Terminal_Block_Header','Terminal_Block_Header',$,(#170162)) ;
#170166 = PRODUCT('Terminal_Block_Plug','Terminal_Block_Plug',$,(#170162)) ;
#170167 = PRESENTATION_STYLE_ASSIGNMENT((#170173)) ;
#170168 = PRESENTATION_STYLE_ASSIGNMENT((#170174)) ;
#170169 = PRESENTATION_STYLE_ASSIGNMENT((#170175)) ;
#170170 = PRESENTATION_STYLE_ASSIGNMENT((#170176)) ;
#170171 = PRESENTATION_STYLE_ASSIGNMENT((#170177)) ;
#170172 = PRESENTATION_STYLE_ASSIGNMENT((#170178)) ;
#170173 = SURFACE_STYLE_USAGE(.BOTH.,#170179) ;
#170174 = SURFACE_STYLE_USAGE(.BOTH.,#170180) ;
#170175 = SURFACE_STYLE_USAGE(.BOTH.,#170181) ;
#170176 = SURFACE_STYLE_USAGE(.BOTH.,#170182) ;
#170177 = SURFACE_STYLE_USAGE(.BOTH.,#170183) ;
#170178 = SURFACE_STYLE_USAGE(.BOTH.,#170184) ;
#170179 = SURFACE_SIDE_STYLE('',(#170185)) ;
#170180 = SURFACE_SIDE_STYLE('',(#170186)) ;
#170181 = SURFACE_SIDE_STYLE('',(#170187)) ;
#170182 = SURFACE_SIDE_STYLE('',(#170188)) ;
#170183 = SURFACE_SIDE_STYLE('',(#170189)) ;
#170184 = SURFACE_SIDE_STYLE('',(#170190)) ;
#170185 = SURFACE_STYLE_FILL_AREA(#170191) ;
#170186 = SURFACE_STYLE_FILL_AREA(#170192) ;
#170187 = SURFACE_STYLE_FILL_AREA(#170193) ;
#170188 = SURFACE_STYLE_FILL_AREA(#170194) ;
#170189 = SURFACE_STYLE_FILL_AREA(#170195) ;
#170190 = SURFACE_STYLE_FILL_AREA(#170196) ;
#170191 = FILL_AREA_STYLE('Steel - Satin',(#170197)) ;
#170192 = FILL_AREA_STYLE('Opaque(202,209,238)',(#170198)) ;
#170193 = FILL_AREA_STYLE('Opaque(128,255,128)',(#170199)) ;
#170194 = FILL_AREA_STYLE('Opaque(189,191,0)',(#170200)) ;
#170195 = FILL_AREA_STYLE('Opaque(204,207,204)',(#170201)) ;
#170196 = FILL_AREA_STYLE('Opaque(255,251,103)',(#170202)) ;
#170197 = FILL_AREA_STYLE_COLOUR('Steel - Satin',#170203) ;
#170198 = FILL_AREA_STYLE_COLOUR('Opaque(202,209,238)',#170204) ;
#170199 = FILL_AREA_STYLE_COLOUR('Opaque(128,255,128)',#170205) ;
#170200 = FILL_AREA_STYLE_COLOUR('Opaque(189,191,0)',#170206) ;
#170201 = FILL_AREA_STYLE_COLOUR('Opaque(204,207,204)',#170207) ;
#170202 = FILL_AREA_STYLE_COLOUR('Opaque(255,251,103)',#170208) ;
#170203 = COLOUR_RGB('Steel - Satin', 0.09019608, 0.27058824, 0.51372549) ;
#170204 = COLOUR_RGB('Opaque(202,209,238)', 0.09019608, 0.27058824, 0.51372549) ;
#170205 = COLOUR_RGB('Opaque(128,255,128)', 0.09019608, 0.27058824, 0.51372549) ;
#170206 = COLOUR_RGB('Opaque(189,191,0)', 0.72549020, 0.75294118, 0.79215686) ;
#170207 = COLOUR_RGB('Opaque(204,207,204)', 0.09019608, 0.27058824, 0.51372549) ;
#170208 = COLOUR_RGB('Opaque(255,251,103)', 0.40784314, 0.44705882, 0.49803922) ;
ENDSEC;
END-ISO-10303-21;
